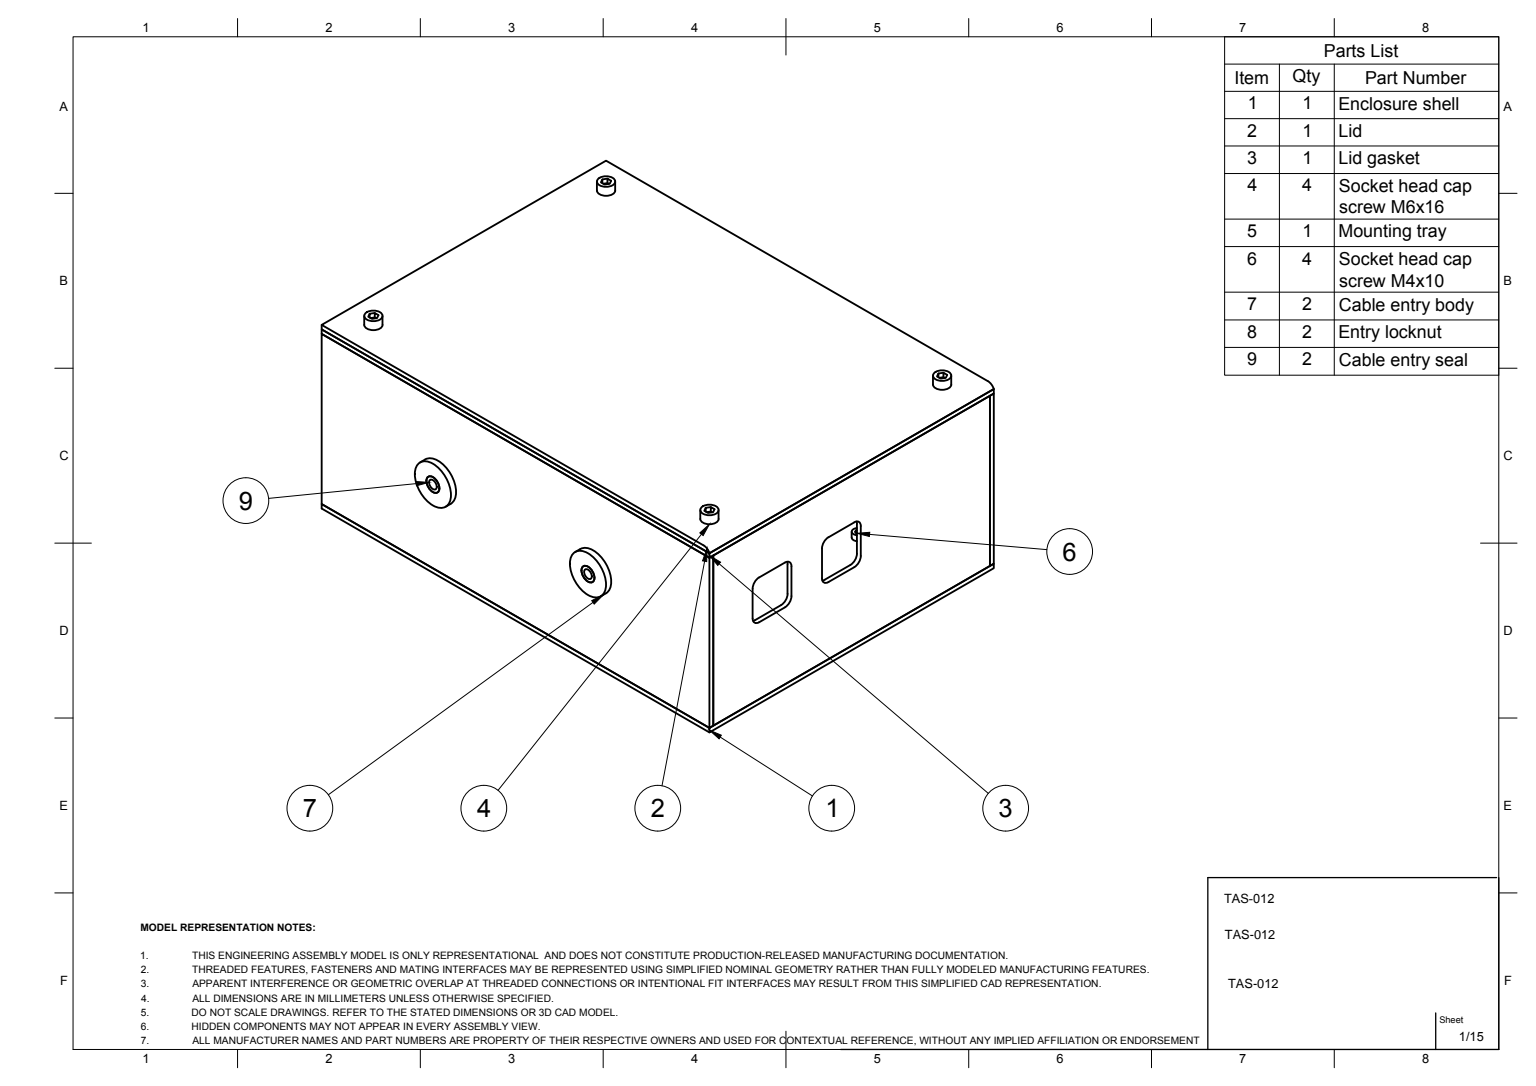
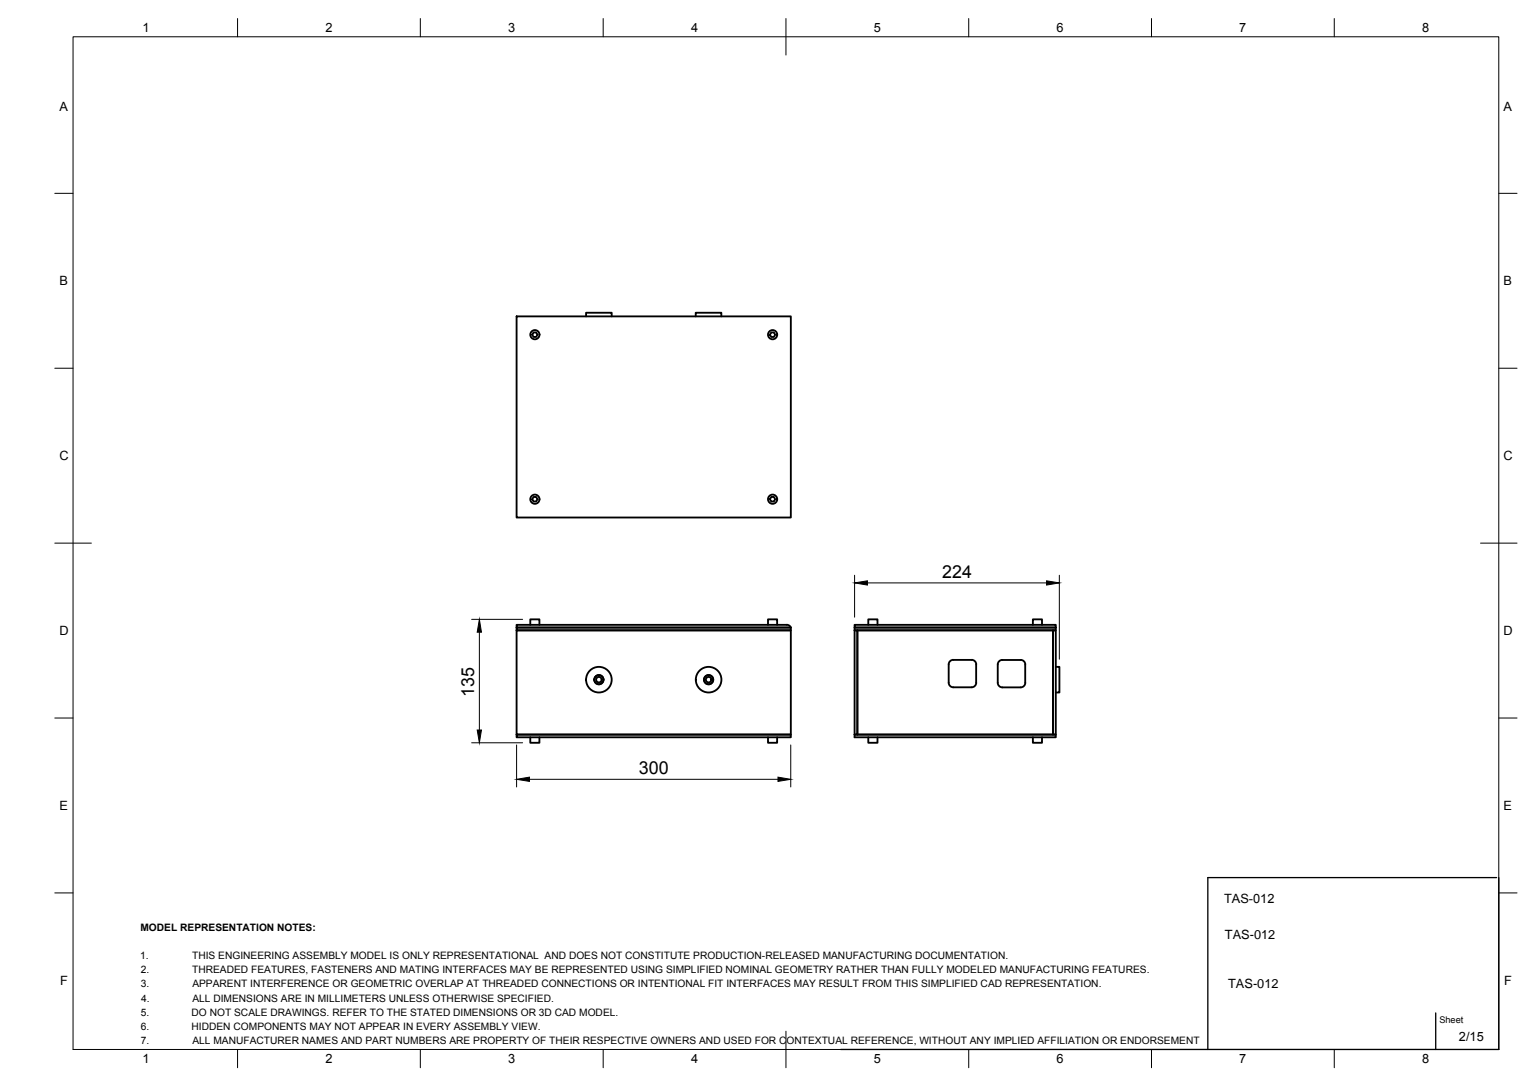
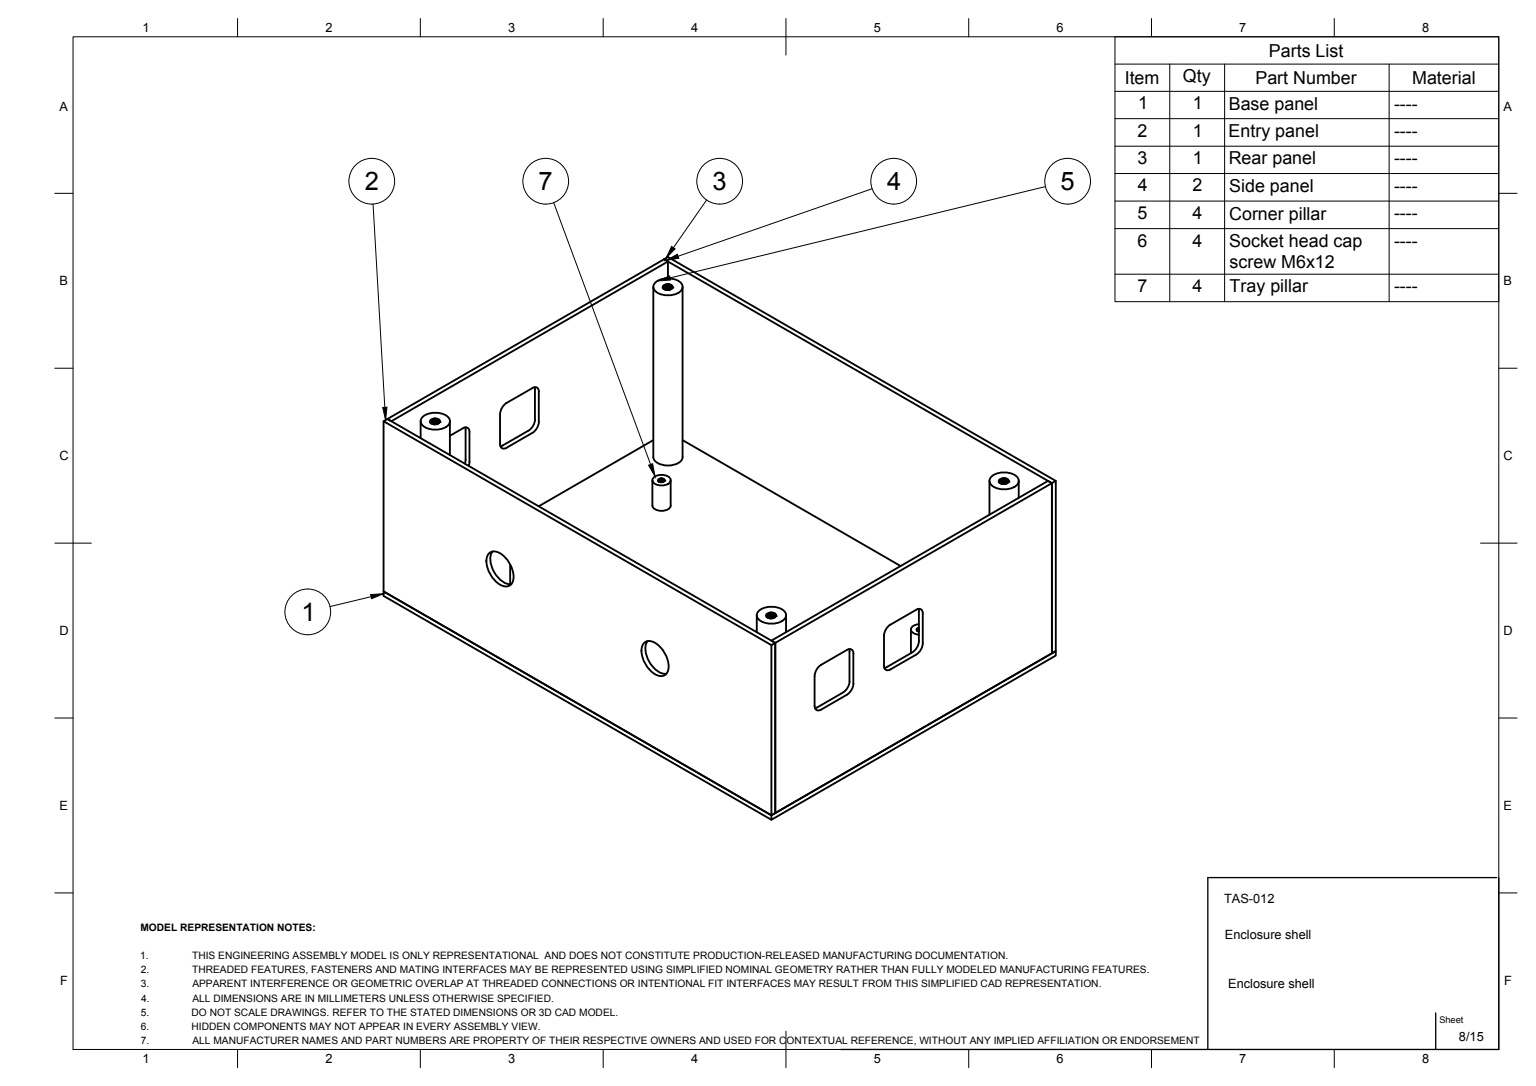
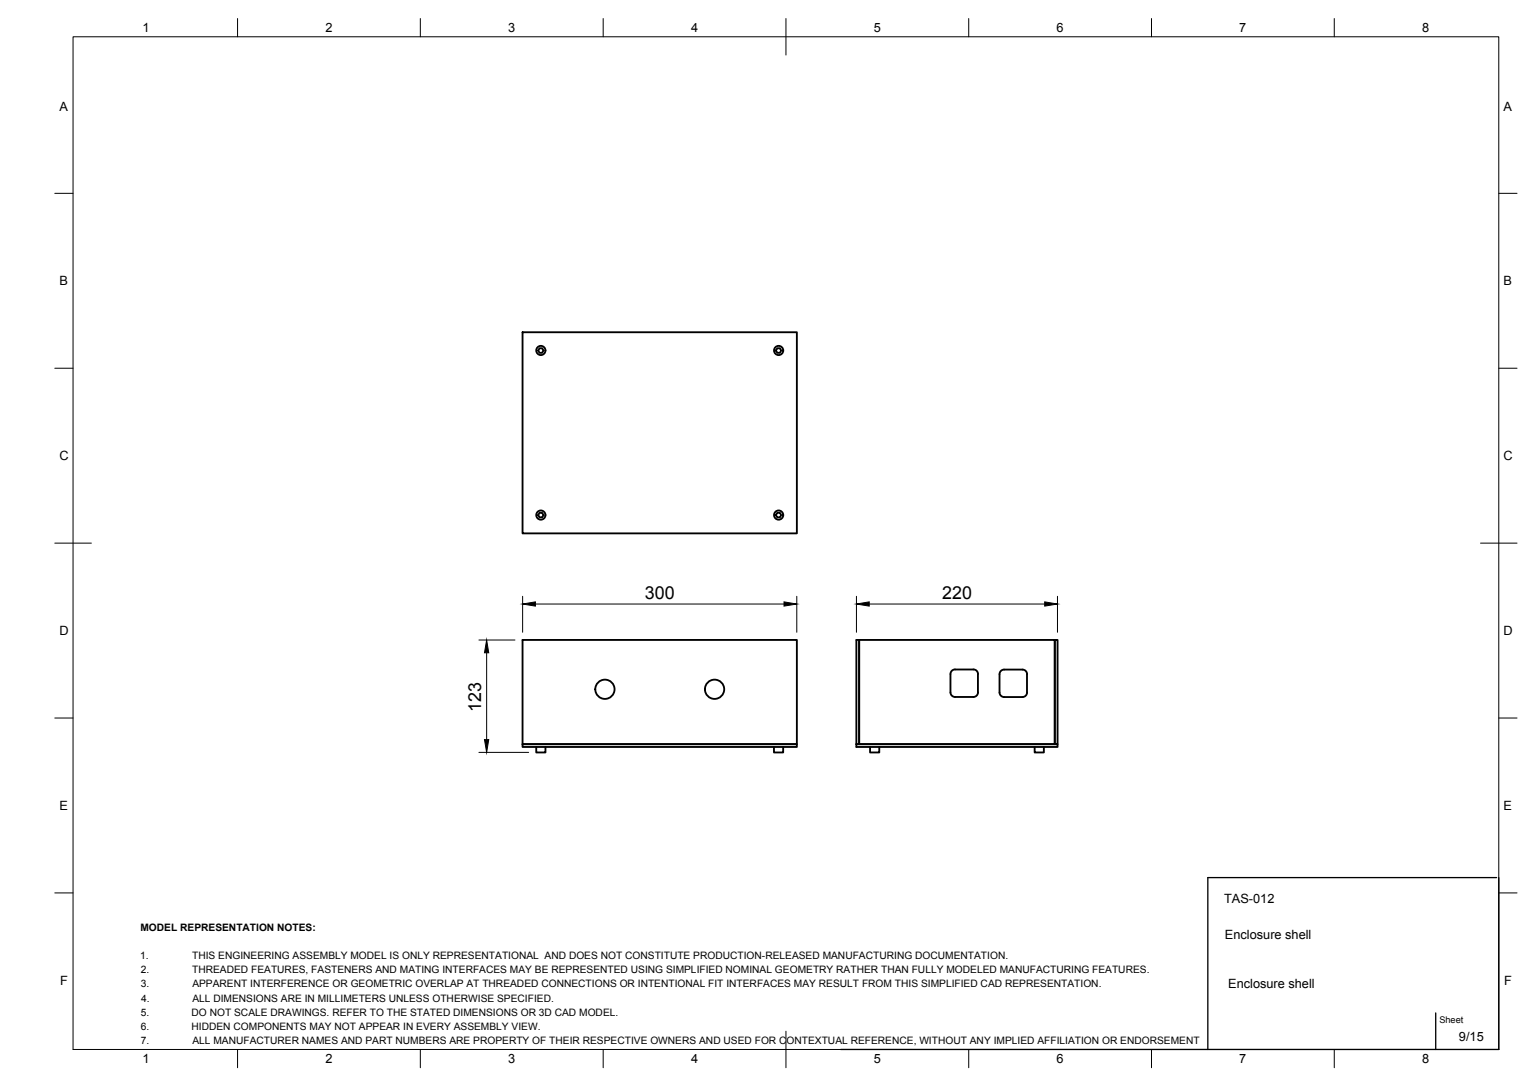
ISO-10303-21;
HEADER;
/* Generated by software containing ST-Developer
 * from STEP Tools, Inc. (www.steptools.com) 
 */

FILE_DESCRIPTION(
/* description */ (
'Independent welded steel electronics enclosure with removable sealed 
lid, internal mounting tray and two threaded cable entries. 300 x 220 
mm body. No ingress or electrical safety rating assigned.'),
/* implementation_level */ '2;1');

FILE_NAME(
/* name */ 'TAS-012.step',
/* time_stamp */ '2026-11-14T09:13:27-08:00',
/* author */ (''),
/* organization */ (''),
/* preprocessor_version */ 'ST-DEVELOPER v20.2',
/* originating_system */ 'Autodesk Translation Framework v15.17.0.0',
/* authorisation */ '');

FILE_SCHEMA (('AUTOMOTIVE_DESIGN { 1 0 10303 214 3 1 1 }'));
ENDSEC;

DATA;
#10=MECHANICAL_DESIGN_GEOMETRIC_PRESENTATION_REPRESENTATION('',(#966,#967,
#968,#969,#970,#971,#972,#973,#974,#975,#976,#977,#978,#979,#980),#94412);
#11=ITEM_DEFINED_TRANSFORMATION($,$,#8434,#8693);
#12=ITEM_DEFINED_TRANSFORMATION($,$,#8453,#8694);
#13=ITEM_DEFINED_TRANSFORMATION($,$,#8466,#8695);
#14=ITEM_DEFINED_TRANSFORMATION($,$,#8473,#8696);
#15=ITEM_DEFINED_TRANSFORMATION($,$,#8512,#8697);
#16=ITEM_DEFINED_TRANSFORMATION($,$,#8614,#8698);
#17=ITEM_DEFINED_TRANSFORMATION($,$,#8647,#8699);
#18=ITEM_DEFINED_TRANSFORMATION($,$,#8473,#8700);
#19=ITEM_DEFINED_TRANSFORMATION($,$,#8512,#8701);
#20=ITEM_DEFINED_TRANSFORMATION($,$,#8512,#8702);
#21=ITEM_DEFINED_TRANSFORMATION($,$,#8512,#8703);
#22=ITEM_DEFINED_TRANSFORMATION($,$,#8614,#8704);
#23=ITEM_DEFINED_TRANSFORMATION($,$,#8614,#8705);
#24=ITEM_DEFINED_TRANSFORMATION($,$,#8614,#8706);
#25=ITEM_DEFINED_TRANSFORMATION($,$,#8647,#8707);
#26=ITEM_DEFINED_TRANSFORMATION($,$,#8647,#8708);
#27=ITEM_DEFINED_TRANSFORMATION($,$,#8647,#8709);
#28=ITEM_DEFINED_TRANSFORMATION($,$,#8433,#8924);
#29=ITEM_DEFINED_TRANSFORMATION($,$,#8710,#8925);
#30=ITEM_DEFINED_TRANSFORMATION($,$,#8731,#8926);
#31=ITEM_DEFINED_TRANSFORMATION($,$,#8773,#8927);
#32=ITEM_DEFINED_TRANSFORMATION($,$,#8754,#8928);
#33=ITEM_DEFINED_TRANSFORMATION($,$,#8810,#8929);
#34=ITEM_DEFINED_TRANSFORMATION($,$,#8845,#8930);
#35=ITEM_DEFINED_TRANSFORMATION($,$,#8889,#8931);
#36=ITEM_DEFINED_TRANSFORMATION($,$,#8915,#8932);
#37=ITEM_DEFINED_TRANSFORMATION($,$,#8773,#8933);
#38=ITEM_DEFINED_TRANSFORMATION($,$,#8773,#8934);
#39=ITEM_DEFINED_TRANSFORMATION($,$,#8773,#8935);
#40=ITEM_DEFINED_TRANSFORMATION($,$,#8810,#8936);
#41=ITEM_DEFINED_TRANSFORMATION($,$,#8810,#8937);
#42=ITEM_DEFINED_TRANSFORMATION($,$,#8810,#8938);
#43=ITEM_DEFINED_TRANSFORMATION($,$,#8845,#8939);
#44=ITEM_DEFINED_TRANSFORMATION($,$,#8889,#8940);
#45=ITEM_DEFINED_TRANSFORMATION($,$,#8915,#8941);
#46=(
REPRESENTATION_RELATIONSHIP($,$,#94488,#94487)
REPRESENTATION_RELATIONSHIP_WITH_TRANSFORMATION(#11)
SHAPE_REPRESENTATION_RELATIONSHIP()
);
#47=(
REPRESENTATION_RELATIONSHIP($,$,#94489,#94487)
REPRESENTATION_RELATIONSHIP_WITH_TRANSFORMATION(#12)
SHAPE_REPRESENTATION_RELATIONSHIP()
);
#48=(
REPRESENTATION_RELATIONSHIP($,$,#94490,#94487)
REPRESENTATION_RELATIONSHIP_WITH_TRANSFORMATION(#13)
SHAPE_REPRESENTATION_RELATIONSHIP()
);
#49=(
REPRESENTATION_RELATIONSHIP($,$,#94491,#94487)
REPRESENTATION_RELATIONSHIP_WITH_TRANSFORMATION(#14)
SHAPE_REPRESENTATION_RELATIONSHIP()
);
#50=(
REPRESENTATION_RELATIONSHIP($,$,#94492,#94487)
REPRESENTATION_RELATIONSHIP_WITH_TRANSFORMATION(#15)
SHAPE_REPRESENTATION_RELATIONSHIP()
);
#51=(
REPRESENTATION_RELATIONSHIP($,$,#94493,#94487)
REPRESENTATION_RELATIONSHIP_WITH_TRANSFORMATION(#16)
SHAPE_REPRESENTATION_RELATIONSHIP()
);
#52=(
REPRESENTATION_RELATIONSHIP($,$,#94494,#94487)
REPRESENTATION_RELATIONSHIP_WITH_TRANSFORMATION(#17)
SHAPE_REPRESENTATION_RELATIONSHIP()
);
#53=(
REPRESENTATION_RELATIONSHIP($,$,#94491,#94487)
REPRESENTATION_RELATIONSHIP_WITH_TRANSFORMATION(#18)
SHAPE_REPRESENTATION_RELATIONSHIP()
);
#54=(
REPRESENTATION_RELATIONSHIP($,$,#94492,#94487)
REPRESENTATION_RELATIONSHIP_WITH_TRANSFORMATION(#19)
SHAPE_REPRESENTATION_RELATIONSHIP()
);
#55=(
REPRESENTATION_RELATIONSHIP($,$,#94492,#94487)
REPRESENTATION_RELATIONSHIP_WITH_TRANSFORMATION(#20)
SHAPE_REPRESENTATION_RELATIONSHIP()
);
#56=(
REPRESENTATION_RELATIONSHIP($,$,#94492,#94487)
REPRESENTATION_RELATIONSHIP_WITH_TRANSFORMATION(#21)
SHAPE_REPRESENTATION_RELATIONSHIP()
);
#57=(
REPRESENTATION_RELATIONSHIP($,$,#94493,#94487)
REPRESENTATION_RELATIONSHIP_WITH_TRANSFORMATION(#22)
SHAPE_REPRESENTATION_RELATIONSHIP()
);
#58=(
REPRESENTATION_RELATIONSHIP($,$,#94493,#94487)
REPRESENTATION_RELATIONSHIP_WITH_TRANSFORMATION(#23)
SHAPE_REPRESENTATION_RELATIONSHIP()
);
#59=(
REPRESENTATION_RELATIONSHIP($,$,#94493,#94487)
REPRESENTATION_RELATIONSHIP_WITH_TRANSFORMATION(#24)
SHAPE_REPRESENTATION_RELATIONSHIP()
);
#60=(
REPRESENTATION_RELATIONSHIP($,$,#94494,#94487)
REPRESENTATION_RELATIONSHIP_WITH_TRANSFORMATION(#25)
SHAPE_REPRESENTATION_RELATIONSHIP()
);
#61=(
REPRESENTATION_RELATIONSHIP($,$,#94494,#94487)
REPRESENTATION_RELATIONSHIP_WITH_TRANSFORMATION(#26)
SHAPE_REPRESENTATION_RELATIONSHIP()
);
#62=(
REPRESENTATION_RELATIONSHIP($,$,#94494,#94487)
REPRESENTATION_RELATIONSHIP_WITH_TRANSFORMATION(#27)
SHAPE_REPRESENTATION_RELATIONSHIP()
);
#63=(
REPRESENTATION_RELATIONSHIP($,$,#94487,#94486)
REPRESENTATION_RELATIONSHIP_WITH_TRANSFORMATION(#28)
SHAPE_REPRESENTATION_RELATIONSHIP()
);
#64=(
REPRESENTATION_RELATIONSHIP($,$,#94495,#94486)
REPRESENTATION_RELATIONSHIP_WITH_TRANSFORMATION(#29)
SHAPE_REPRESENTATION_RELATIONSHIP()
);
#65=(
REPRESENTATION_RELATIONSHIP($,$,#94496,#94486)
REPRESENTATION_RELATIONSHIP_WITH_TRANSFORMATION(#30)
SHAPE_REPRESENTATION_RELATIONSHIP()
);
#66=(
REPRESENTATION_RELATIONSHIP($,$,#94498,#94486)
REPRESENTATION_RELATIONSHIP_WITH_TRANSFORMATION(#31)
SHAPE_REPRESENTATION_RELATIONSHIP()
);
#67=(
REPRESENTATION_RELATIONSHIP($,$,#94497,#94486)
REPRESENTATION_RELATIONSHIP_WITH_TRANSFORMATION(#32)
SHAPE_REPRESENTATION_RELATIONSHIP()
);
#68=(
REPRESENTATION_RELATIONSHIP($,$,#94499,#94486)
REPRESENTATION_RELATIONSHIP_WITH_TRANSFORMATION(#33)
SHAPE_REPRESENTATION_RELATIONSHIP()
);
#69=(
REPRESENTATION_RELATIONSHIP($,$,#94500,#94486)
REPRESENTATION_RELATIONSHIP_WITH_TRANSFORMATION(#34)
SHAPE_REPRESENTATION_RELATIONSHIP()
);
#70=(
REPRESENTATION_RELATIONSHIP($,$,#94501,#94486)
REPRESENTATION_RELATIONSHIP_WITH_TRANSFORMATION(#35)
SHAPE_REPRESENTATION_RELATIONSHIP()
);
#71=(
REPRESENTATION_RELATIONSHIP($,$,#94502,#94486)
REPRESENTATION_RELATIONSHIP_WITH_TRANSFORMATION(#36)
SHAPE_REPRESENTATION_RELATIONSHIP()
);
#72=(
REPRESENTATION_RELATIONSHIP($,$,#94498,#94486)
REPRESENTATION_RELATIONSHIP_WITH_TRANSFORMATION(#37)
SHAPE_REPRESENTATION_RELATIONSHIP()
);
#73=(
REPRESENTATION_RELATIONSHIP($,$,#94498,#94486)
REPRESENTATION_RELATIONSHIP_WITH_TRANSFORMATION(#38)
SHAPE_REPRESENTATION_RELATIONSHIP()
);
#74=(
REPRESENTATION_RELATIONSHIP($,$,#94498,#94486)
REPRESENTATION_RELATIONSHIP_WITH_TRANSFORMATION(#39)
SHAPE_REPRESENTATION_RELATIONSHIP()
);
#75=(
REPRESENTATION_RELATIONSHIP($,$,#94499,#94486)
REPRESENTATION_RELATIONSHIP_WITH_TRANSFORMATION(#40)
SHAPE_REPRESENTATION_RELATIONSHIP()
);
#76=(
REPRESENTATION_RELATIONSHIP($,$,#94499,#94486)
REPRESENTATION_RELATIONSHIP_WITH_TRANSFORMATION(#41)
SHAPE_REPRESENTATION_RELATIONSHIP()
);
#77=(
REPRESENTATION_RELATIONSHIP($,$,#94499,#94486)
REPRESENTATION_RELATIONSHIP_WITH_TRANSFORMATION(#42)
SHAPE_REPRESENTATION_RELATIONSHIP()
);
#78=(
REPRESENTATION_RELATIONSHIP($,$,#94500,#94486)
REPRESENTATION_RELATIONSHIP_WITH_TRANSFORMATION(#43)
SHAPE_REPRESENTATION_RELATIONSHIP()
);
#79=(
REPRESENTATION_RELATIONSHIP($,$,#94501,#94486)
REPRESENTATION_RELATIONSHIP_WITH_TRANSFORMATION(#44)
SHAPE_REPRESENTATION_RELATIONSHIP()
);
#80=(
REPRESENTATION_RELATIONSHIP($,$,#94502,#94486)
REPRESENTATION_RELATIONSHIP_WITH_TRANSFORMATION(#45)
SHAPE_REPRESENTATION_RELATIONSHIP()
);
#81=CONTEXT_DEPENDENT_SHAPE_REPRESENTATION(#46,#94443);
#82=CONTEXT_DEPENDENT_SHAPE_REPRESENTATION(#47,#94444);
#83=CONTEXT_DEPENDENT_SHAPE_REPRESENTATION(#48,#94445);
#84=CONTEXT_DEPENDENT_SHAPE_REPRESENTATION(#49,#94446);
#85=CONTEXT_DEPENDENT_SHAPE_REPRESENTATION(#50,#94447);
#86=CONTEXT_DEPENDENT_SHAPE_REPRESENTATION(#51,#94448);
#87=CONTEXT_DEPENDENT_SHAPE_REPRESENTATION(#52,#94449);
#88=CONTEXT_DEPENDENT_SHAPE_REPRESENTATION(#53,#94450);
#89=CONTEXT_DEPENDENT_SHAPE_REPRESENTATION(#54,#94451);
#90=CONTEXT_DEPENDENT_SHAPE_REPRESENTATION(#55,#94452);
#91=CONTEXT_DEPENDENT_SHAPE_REPRESENTATION(#56,#94453);
#92=CONTEXT_DEPENDENT_SHAPE_REPRESENTATION(#57,#94454);
#93=CONTEXT_DEPENDENT_SHAPE_REPRESENTATION(#58,#94455);
#94=CONTEXT_DEPENDENT_SHAPE_REPRESENTATION(#59,#94456);
#95=CONTEXT_DEPENDENT_SHAPE_REPRESENTATION(#60,#94457);
#96=CONTEXT_DEPENDENT_SHAPE_REPRESENTATION(#61,#94458);
#97=CONTEXT_DEPENDENT_SHAPE_REPRESENTATION(#62,#94459);
#98=CONTEXT_DEPENDENT_SHAPE_REPRESENTATION(#63,#94468);
#99=CONTEXT_DEPENDENT_SHAPE_REPRESENTATION(#64,#94469);
#100=CONTEXT_DEPENDENT_SHAPE_REPRESENTATION(#65,#94470);
#101=CONTEXT_DEPENDENT_SHAPE_REPRESENTATION(#66,#94471);
#102=CONTEXT_DEPENDENT_SHAPE_REPRESENTATION(#67,#94472);
#103=CONTEXT_DEPENDENT_SHAPE_REPRESENTATION(#68,#94473);
#104=CONTEXT_DEPENDENT_SHAPE_REPRESENTATION(#69,#94474);
#105=CONTEXT_DEPENDENT_SHAPE_REPRESENTATION(#70,#94475);
#106=CONTEXT_DEPENDENT_SHAPE_REPRESENTATION(#71,#94476);
#107=CONTEXT_DEPENDENT_SHAPE_REPRESENTATION(#72,#94477);
#108=CONTEXT_DEPENDENT_SHAPE_REPRESENTATION(#73,#94478);
#109=CONTEXT_DEPENDENT_SHAPE_REPRESENTATION(#74,#94479);
#110=CONTEXT_DEPENDENT_SHAPE_REPRESENTATION(#75,#94480);
#111=CONTEXT_DEPENDENT_SHAPE_REPRESENTATION(#76,#94481);
#112=CONTEXT_DEPENDENT_SHAPE_REPRESENTATION(#77,#94482);
#113=CONTEXT_DEPENDENT_SHAPE_REPRESENTATION(#78,#94483);
#114=CONTEXT_DEPENDENT_SHAPE_REPRESENTATION(#79,#94484);
#115=CONTEXT_DEPENDENT_SHAPE_REPRESENTATION(#80,#94485);
#116=NEXT_ASSEMBLY_USAGE_OCCURRENCE('Base panel:1','Base panel:1',
'Base panel:1',#94505,#94506,'Base panel:1');
#117=NEXT_ASSEMBLY_USAGE_OCCURRENCE('Entry panel:1','Entry panel:1',
'Entry panel:1',#94505,#94507,'Entry panel:1');
#118=NEXT_ASSEMBLY_USAGE_OCCURRENCE('Rear panel:1','Rear panel:1',
'Rear panel:1',#94505,#94508,'Rear panel:1');
#119=NEXT_ASSEMBLY_USAGE_OCCURRENCE('Side panel:1','Side panel:1',
'Side panel:1',#94505,#94509,'Side panel:1');
#120=NEXT_ASSEMBLY_USAGE_OCCURRENCE('Corner pillar:1','Corner pillar:1',
'Corner pillar:1',#94505,#94510,'Corner pillar:1');
#121=NEXT_ASSEMBLY_USAGE_OCCURRENCE('Socket head cap screw M6x12:1',
'Socket head cap screw M6x12:1','Socket head cap screw M6x12:1',#94505,
#94511,'Socket head cap screw M6x12:1');
#122=NEXT_ASSEMBLY_USAGE_OCCURRENCE('Tray pillar:1','Tray pillar:1',
'Tray pillar:1',#94505,#94512,'Tray pillar:1');
#123=NEXT_ASSEMBLY_USAGE_OCCURRENCE('Side panel:2','Side panel:2',
'Side panel:2',#94505,#94509,'Side panel:2');
#124=NEXT_ASSEMBLY_USAGE_OCCURRENCE('Corner pillar:2','Corner pillar:2',
'Corner pillar:2',#94505,#94510,'Corner pillar:2');
#125=NEXT_ASSEMBLY_USAGE_OCCURRENCE('Corner pillar:3','Corner pillar:3',
'Corner pillar:3',#94505,#94510,'Corner pillar:3');
#126=NEXT_ASSEMBLY_USAGE_OCCURRENCE('Corner pillar:4','Corner pillar:4',
'Corner pillar:4',#94505,#94510,'Corner pillar:4');
#127=NEXT_ASSEMBLY_USAGE_OCCURRENCE('Socket head cap screw M6x12:2',
'Socket head cap screw M6x12:2','Socket head cap screw M6x12:2',#94505,
#94511,'Socket head cap screw M6x12:2');
#128=NEXT_ASSEMBLY_USAGE_OCCURRENCE('Socket head cap screw M6x12:3',
'Socket head cap screw M6x12:3','Socket head cap screw M6x12:3',#94505,
#94511,'Socket head cap screw M6x12:3');
#129=NEXT_ASSEMBLY_USAGE_OCCURRENCE('Socket head cap screw M6x12:4',
'Socket head cap screw M6x12:4','Socket head cap screw M6x12:4',#94505,
#94511,'Socket head cap screw M6x12:4');
#130=NEXT_ASSEMBLY_USAGE_OCCURRENCE('Tray pillar:2','Tray pillar:2',
'Tray pillar:2',#94505,#94512,'Tray pillar:2');
#131=NEXT_ASSEMBLY_USAGE_OCCURRENCE('Tray pillar:3','Tray pillar:3',
'Tray pillar:3',#94505,#94512,'Tray pillar:3');
#132=NEXT_ASSEMBLY_USAGE_OCCURRENCE('Tray pillar:4','Tray pillar:4',
'Tray pillar:4',#94505,#94512,'Tray pillar:4');
#133=NEXT_ASSEMBLY_USAGE_OCCURRENCE('Enclosure shell:1',
'Enclosure shell:1','Enclosure shell:1',#94504,#94505,
'Enclosure shell:1');
#134=NEXT_ASSEMBLY_USAGE_OCCURRENCE('Lid:1','Lid:1','Lid:1',#94504,#94513,
'Lid:1');
#135=NEXT_ASSEMBLY_USAGE_OCCURRENCE('Lid gasket:1','Lid gasket:1',
'Lid gasket:1',#94504,#94514,'Lid gasket:1');
#136=NEXT_ASSEMBLY_USAGE_OCCURRENCE('Socket head cap screw M6x16:1',
'Socket head cap screw M6x16:1','Socket head cap screw M6x16:1',#94504,
#94516,'Socket head cap screw M6x16:1');
#137=NEXT_ASSEMBLY_USAGE_OCCURRENCE('Mounting tray:1','Mounting tray:1',
'Mounting tray:1',#94504,#94515,'Mounting tray:1');
#138=NEXT_ASSEMBLY_USAGE_OCCURRENCE('Socket head cap screw M4x10:1',
'Socket head cap screw M4x10:1','Socket head cap screw M4x10:1',#94504,
#94517,'Socket head cap screw M4x10:1');
#139=NEXT_ASSEMBLY_USAGE_OCCURRENCE('Cable entry body:1',
'Cable entry body:1','Cable entry body:1',#94504,#94518,
'Cable entry body:1');
#140=NEXT_ASSEMBLY_USAGE_OCCURRENCE('Entry locknut:1','Entry locknut:1',
'Entry locknut:1',#94504,#94519,'Entry locknut:1');
#141=NEXT_ASSEMBLY_USAGE_OCCURRENCE('Cable entry seal:1',
'Cable entry seal:1','Cable entry seal:1',#94504,#94520,
'Cable entry seal:1');
#142=NEXT_ASSEMBLY_USAGE_OCCURRENCE('Socket head cap screw M6x16:2',
'Socket head cap screw M6x16:2','Socket head cap screw M6x16:2',#94504,
#94516,'Socket head cap screw M6x16:2');
#143=NEXT_ASSEMBLY_USAGE_OCCURRENCE('Socket head cap screw M6x16:3',
'Socket head cap screw M6x16:3','Socket head cap screw M6x16:3',#94504,
#94516,'Socket head cap screw M6x16:3');
#144=NEXT_ASSEMBLY_USAGE_OCCURRENCE('Socket head cap screw M6x16:4',
'Socket head cap screw M6x16:4','Socket head cap screw M6x16:4',#94504,
#94516,'Socket head cap screw M6x16:4');
#145=NEXT_ASSEMBLY_USAGE_OCCURRENCE('Socket head cap screw M4x10:2',
'Socket head cap screw M4x10:2','Socket head cap screw M4x10:2',#94504,
#94517,'Socket head cap screw M4x10:2');
#146=NEXT_ASSEMBLY_USAGE_OCCURRENCE('Socket head cap screw M4x10:3',
'Socket head cap screw M4x10:3','Socket head cap screw M4x10:3',#94504,
#94517,'Socket head cap screw M4x10:3');
#147=NEXT_ASSEMBLY_USAGE_OCCURRENCE('Socket head cap screw M4x10:4',
'Socket head cap screw M4x10:4','Socket head cap screw M4x10:4',#94504,
#94517,'Socket head cap screw M4x10:4');
#148=NEXT_ASSEMBLY_USAGE_OCCURRENCE('Cable entry body:2',
'Cable entry body:2','Cable entry body:2',#94504,#94518,
'Cable entry body:2');
#149=NEXT_ASSEMBLY_USAGE_OCCURRENCE('Entry locknut:2','Entry locknut:2',
'Entry locknut:2',#94504,#94519,'Entry locknut:2');
#150=NEXT_ASSEMBLY_USAGE_OCCURRENCE('Cable entry seal:2',
'Cable entry seal:2','Cable entry seal:2',#94504,#94520,
'Cable entry seal:2');
#151=CONICAL_SURFACE('',#8632,2.5,0.785398163397449);
#152=CONICAL_SURFACE('',#8795,2.5,0.785398163397448);
#153=CONICAL_SURFACE('',#8830,1.5,0.785398163397449);
#154=B_SPLINE_SURFACE_WITH_KNOTS('',3,3,((#38427,#38428,#38429,#38430,#38431,
#38432,#38433,#38434,#38435,#38436,#38437,#38438,#38439,#38440,#38441,#38442,
#38443,#38444,#38445,#38446,#38447,#38448,#38449,#38450,#38451,#38452,#38453,
#38454,#38455,#38456,#38457,#38458,#38459,#38460,#38461,#38462,#38463,#38464,
#38465,#38466,#38467,#38468,#38469,#38470,#38471,#38472,#38473,#38474,#38475,
#38476,#38477,#38478,#38479,#38480,#38481,#38482,#38483,#38484,#38485,#38486,
#38487,#38488,#38489,#38490,#38491,#38492,#38493,#38494,#38495,#38496,#38497,
#38498,#38499,#38500,#38501,#38502,#38503,#38504,#38505,#38506,#38507,#38508,
#38509,#38510,#38511,#38512,#38513,#38514,#38515,#38516,#38517,#38518,#38519,
#38520,#38521,#38522,#38523,#38524,#38525,#38526,#38527,#38528,#38529,#38530,
#38531,#38532,#38533,#38534,#38535,#38536,#38537,#38538,#38539,#38540,#38541,
#38542,#38543,#38544,#38545,#38546,#38547,#38548,#38549,#38550,#38551),
(#38552,#38553,#38554,#38555,#38556,#38557,#38558,#38559,#38560,#38561,
#38562,#38563,#38564,#38565,#38566,#38567,#38568,#38569,#38570,#38571,#38572,
#38573,#38574,#38575,#38576,#38577,#38578,#38579,#38580,#38581,#38582,#38583,
#38584,#38585,#38586,#38587,#38588,#38589,#38590,#38591,#38592,#38593,#38594,
#38595,#38596,#38597,#38598,#38599,#38600,#38601,#38602,#38603,#38604,#38605,
#38606,#38607,#38608,#38609,#38610,#38611,#38612,#38613,#38614,#38615,#38616,
#38617,#38618,#38619,#38620,#38621,#38622,#38623,#38624,#38625,#38626,#38627,
#38628,#38629,#38630,#38631,#38632,#38633,#38634,#38635,#38636,#38637,#38638,
#38639,#38640,#38641,#38642,#38643,#38644,#38645,#38646,#38647,#38648,#38649,
#38650,#38651,#38652,#38653,#38654,#38655,#38656,#38657,#38658,#38659,#38660,
#38661,#38662,#38663,#38664,#38665,#38666,#38667,#38668,#38669,#38670,#38671,
#38672,#38673,#38674,#38675,#38676),(#38677,#38678,#38679,#38680,#38681,
#38682,#38683,#38684,#38685,#38686,#38687,#38688,#38689,#38690,#38691,#38692,
#38693,#38694,#38695,#38696,#38697,#38698,#38699,#38700,#38701,#38702,#38703,
#38704,#38705,#38706,#38707,#38708,#38709,#38710,#38711,#38712,#38713,#38714,
#38715,#38716,#38717,#38718,#38719,#38720,#38721,#38722,#38723,#38724,#38725,
#38726,#38727,#38728,#38729,#38730,#38731,#38732,#38733,#38734,#38735,#38736,
#38737,#38738,#38739,#38740,#38741,#38742,#38743,#38744,#38745,#38746,#38747,
#38748,#38749,#38750,#38751,#38752,#38753,#38754,#38755,#38756,#38757,#38758,
#38759,#38760,#38761,#38762,#38763,#38764,#38765,#38766,#38767,#38768,#38769,
#38770,#38771,#38772,#38773,#38774,#38775,#38776,#38777,#38778,#38779,#38780,
#38781,#38782,#38783,#38784,#38785,#38786,#38787,#38788,#38789,#38790,#38791,
#38792,#38793,#38794,#38795,#38796,#38797,#38798,#38799,#38800,#38801),
(#38802,#38803,#38804,#38805,#38806,#38807,#38808,#38809,#38810,#38811,
#38812,#38813,#38814,#38815,#38816,#38817,#38818,#38819,#38820,#38821,#38822,
#38823,#38824,#38825,#38826,#38827,#38828,#38829,#38830,#38831,#38832,#38833,
#38834,#38835,#38836,#38837,#38838,#38839,#38840,#38841,#38842,#38843,#38844,
#38845,#38846,#38847,#38848,#38849,#38850,#38851,#38852,#38853,#38854,#38855,
#38856,#38857,#38858,#38859,#38860,#38861,#38862,#38863,#38864,#38865,#38866,
#38867,#38868,#38869,#38870,#38871,#38872,#38873,#38874,#38875,#38876,#38877,
#38878,#38879,#38880,#38881,#38882,#38883,#38884,#38885,#38886,#38887,#38888,
#38889,#38890,#38891,#38892,#38893,#38894,#38895,#38896,#38897,#38898,#38899,
#38900,#38901,#38902,#38903,#38904,#38905,#38906,#38907,#38908,#38909,#38910,
#38911,#38912,#38913,#38914,#38915,#38916,#38917,#38918,#38919,#38920,#38921,
#38922,#38923,#38924,#38925,#38926)),.UNSPECIFIED.,.F.,.F.,.F.,(4,4),(4,
1,1,1,1,1,1,1,1,1,1,1,1,1,1,1,1,1,1,1,1,1,1,1,1,1,1,1,1,1,1,1,1,1,1,1,1,
1,1,1,1,1,1,1,1,1,1,1,1,1,1,1,1,1,1,1,1,1,1,1,1,1,1,1,1,1,1,1,1,1,1,1,1,
1,1,1,1,1,1,1,1,1,1,1,1,1,1,1,1,1,1,1,1,1,1,1,1,1,1,1,1,1,1,1,1,1,1,1,1,
1,1,1,1,1,1,1,1,1,1,1,1,1,4),(-0.000512721802289974,0.0646569623865103),
(11.8584761405054,12.8540500568113,13.849111251315,14.8441724458186,15.8392336403222,
16.8342948348258,17.8293560293294,18.824417223833,19.8194784183366,20.8145396128402,
21.8096008073438,22.8046620018475,23.7997231963511,24.7947843908547,25.7898455853583,
26.7849067798619,27.7799679743655,28.7750291688691,29.7700903633727,30.7651515578764,
31.76021275238,32.7552739468836,33.7503351413872,34.7453963358908,35.7404575303944,
36.735518724898,37.7305799194016,38.7256411139052,39.7207023084089,40.7157635029125,
41.7108246974161,42.7058858919197,43.7009470864233,44.6960082809269,45.6910694754305,
46.6861306699341,47.6811918644377,48.6762530589414,49.671314253445,50.6663754479486,
51.6614366424522,52.6564978369558,53.6515590314594,54.646620225963,55.6416814204666,
56.6367426149702,57.6318038094739,58.6268650039775,59.6219261984811,60.6169873929847,
61.6120485874883,62.6071097819919,63.6021709764955,64.5972321709991,65.5922933655027,
66.5873545600064,67.58241575451,68.5774769490136,69.5725381435172,70.5675993380208,
71.5626605325244,72.557721727028,73.5527829215316,74.5478441160353,75.5429053105389,
76.5379665050425,77.5330276995461,78.5280888940497,79.5231500885533,80.5182112830569,
81.5132724775605,82.5083336720641,83.5033948665678,84.4984560610714,85.493517255575,
86.4885784500786,87.4836396445822,88.4787008390858,89.4737620335894,90.468823228093,
91.4638844225966,92.4589456171003,93.4540068116039,94.4490680061075,95.4441292006111,
96.4391903951147,97.4342515896183,98.4293127841219,99.4243739786255,100.419435173129,
101.414496367633,102.409557562136,103.40461875664,104.399679951144,105.394741145647,
106.389802340151,107.384863534654,108.379924729158,109.374985923662,110.370047118165,
111.365108312669,112.360169507172,113.355230701676,114.35029189618,115.345353090683,
116.340414285187,117.335475479691,118.330536674194,119.325597868698,120.320659063201,
121.315720257705,122.310781452209,123.305842646712,124.300903841216,125.295965035719,
126.291026230223,127.286087424727,128.28114861923,129.276209813734,130.271271008237,
131.266332202741,132.261393397245,133.256910204201),.UNSPECIFIED.);
#155=B_SPLINE_SURFACE_WITH_KNOTS('',3,3,((#39015,#39016,#39017,#39018,#39019,
#39020,#39021,#39022,#39023,#39024,#39025,#39026,#39027,#39028,#39029,#39030,
#39031,#39032,#39033,#39034,#39035,#39036,#39037,#39038,#39039,#39040,#39041,
#39042,#39043,#39044,#39045,#39046,#39047,#39048,#39049,#39050,#39051,#39052,
#39053,#39054,#39055,#39056,#39057,#39058,#39059,#39060,#39061,#39062,#39063,
#39064,#39065,#39066,#39067,#39068,#39069,#39070,#39071,#39072,#39073,#39074,
#39075,#39076,#39077,#39078,#39079,#39080,#39081,#39082,#39083,#39084,#39085,
#39086,#39087,#39088,#39089,#39090,#39091,#39092,#39093,#39094,#39095,#39096,
#39097,#39098,#39099,#39100,#39101,#39102,#39103,#39104,#39105,#39106,#39107,
#39108,#39109,#39110,#39111,#39112,#39113,#39114,#39115,#39116,#39117,#39118,
#39119,#39120,#39121,#39122,#39123,#39124,#39125,#39126,#39127,#39128,#39129,
#39130,#39131,#39132,#39133,#39134,#39135,#39136,#39137,#39138,#39139),
(#39140,#39141,#39142,#39143,#39144,#39145,#39146,#39147,#39148,#39149,
#39150,#39151,#39152,#39153,#39154,#39155,#39156,#39157,#39158,#39159,#39160,
#39161,#39162,#39163,#39164,#39165,#39166,#39167,#39168,#39169,#39170,#39171,
#39172,#39173,#39174,#39175,#39176,#39177,#39178,#39179,#39180,#39181,#39182,
#39183,#39184,#39185,#39186,#39187,#39188,#39189,#39190,#39191,#39192,#39193,
#39194,#39195,#39196,#39197,#39198,#39199,#39200,#39201,#39202,#39203,#39204,
#39205,#39206,#39207,#39208,#39209,#39210,#39211,#39212,#39213,#39214,#39215,
#39216,#39217,#39218,#39219,#39220,#39221,#39222,#39223,#39224,#39225,#39226,
#39227,#39228,#39229,#39230,#39231,#39232,#39233,#39234,#39235,#39236,#39237,
#39238,#39239,#39240,#39241,#39242,#39243,#39244,#39245,#39246,#39247,#39248,
#39249,#39250,#39251,#39252,#39253,#39254,#39255,#39256,#39257,#39258,#39259,
#39260,#39261,#39262,#39263,#39264),(#39265,#39266,#39267,#39268,#39269,
#39270,#39271,#39272,#39273,#39274,#39275,#39276,#39277,#39278,#39279,#39280,
#39281,#39282,#39283,#39284,#39285,#39286,#39287,#39288,#39289,#39290,#39291,
#39292,#39293,#39294,#39295,#39296,#39297,#39298,#39299,#39300,#39301,#39302,
#39303,#39304,#39305,#39306,#39307,#39308,#39309,#39310,#39311,#39312,#39313,
#39314,#39315,#39316,#39317,#39318,#39319,#39320,#39321,#39322,#39323,#39324,
#39325,#39326,#39327,#39328,#39329,#39330,#39331,#39332,#39333,#39334,#39335,
#39336,#39337,#39338,#39339,#39340,#39341,#39342,#39343,#39344,#39345,#39346,
#39347,#39348,#39349,#39350,#39351,#39352,#39353,#39354,#39355,#39356,#39357,
#39358,#39359,#39360,#39361,#39362,#39363,#39364,#39365,#39366,#39367,#39368,
#39369,#39370,#39371,#39372,#39373,#39374,#39375,#39376,#39377,#39378,#39379,
#39380,#39381,#39382,#39383,#39384,#39385,#39386,#39387,#39388,#39389),
(#39390,#39391,#39392,#39393,#39394,#39395,#39396,#39397,#39398,#39399,
#39400,#39401,#39402,#39403,#39404,#39405,#39406,#39407,#39408,#39409,#39410,
#39411,#39412,#39413,#39414,#39415,#39416,#39417,#39418,#39419,#39420,#39421,
#39422,#39423,#39424,#39425,#39426,#39427,#39428,#39429,#39430,#39431,#39432,
#39433,#39434,#39435,#39436,#39437,#39438,#39439,#39440,#39441,#39442,#39443,
#39444,#39445,#39446,#39447,#39448,#39449,#39450,#39451,#39452,#39453,#39454,
#39455,#39456,#39457,#39458,#39459,#39460,#39461,#39462,#39463,#39464,#39465,
#39466,#39467,#39468,#39469,#39470,#39471,#39472,#39473,#39474,#39475,#39476,
#39477,#39478,#39479,#39480,#39481,#39482,#39483,#39484,#39485,#39486,#39487,
#39488,#39489,#39490,#39491,#39492,#39493,#39494,#39495,#39496,#39497,#39498,
#39499,#39500,#39501,#39502,#39503,#39504,#39505,#39506,#39507,#39508,#39509,
#39510,#39511,#39512,#39513,#39514)),.UNSPECIFIED.,.F.,.F.,.F.,(4,4),(4,
1,1,1,1,1,1,1,1,1,1,1,1,1,1,1,1,1,1,1,1,1,1,1,1,1,1,1,1,1,1,1,1,1,1,1,1,
1,1,1,1,1,1,1,1,1,1,1,1,1,1,1,1,1,1,1,1,1,1,1,1,1,1,1,1,1,1,1,1,1,1,1,1,
1,1,1,1,1,1,1,1,1,1,1,1,1,1,1,1,1,1,1,1,1,1,1,1,1,1,1,1,1,1,1,1,1,1,1,1,
1,1,1,1,1,1,1,1,1,1,1,1,1,4),(-0.000455618124563469,0.0646112265793122),
(14.3984001269718,15.3934613214754,16.388522515979,17.3835837104826,18.3786449049862,
19.3737060994898,20.3687672939934,21.3638284884971,22.3588896830007,23.3539508775043,
24.3490120720079,25.3440732665115,26.3391344610151,27.3341956555187,28.3292568500223,
29.3243180445259,30.3193792390296,31.3144404335332,32.3095016280368,33.3045628225404,
34.299624017044,35.2946852115476,36.2897464060512,37.2848076005548,38.2798687950584,
39.2749299895621,40.2699911840657,41.2650523785693,42.2601135730729,43.2551747675765,
44.2502359620801,45.2452971565837,46.2403583510873,47.235419545591,48.2304807400946,
49.2255419345982,50.2206031291018,51.2156643236054,52.210725518109,53.2057867126126,
54.2008479071162,55.1959091016198,56.1909702961235,57.1860314906271,58.1810926851307,
59.1761538796343,60.1712150741379,61.1662762686415,62.1613374631451,63.1563986576487,
64.1514598521523,65.1465210466559,66.1415822411596,67.1366434356632,68.1317046301668,
69.1267658246704,70.121827019174,71.1168882136776,72.1119494081812,73.1070106026849,
74.1020717971885,75.0971329916921,76.0921941861957,77.0872553806993,78.0823165752029,
79.0773777697065,80.0724389642101,81.0675001587137,82.0625613532173,83.057622547721,
84.0526837422246,85.0477449367282,86.0428061312318,87.0378673257354,88.032928520239,
89.0279897147426,90.0230509092463,91.0181121037498,92.0131732982535,93.0082344927571,
94.0032956872607,94.9983568817643,95.9934180762679,96.9884792707715,97.9835404652751,
98.9786016597787,99.9736628542824,100.968724048786,101.96378524329,102.958846437793,
103.953907632297,104.9489688268,105.944030021304,106.939091215808,107.934152410311,
108.929213604815,109.924274799318,110.919335993822,111.914397188326,112.909458382829,
113.904519577333,114.899580771837,115.89464196634,116.889703160844,117.884764355347,
118.879825549851,119.874886744355,120.869947938858,121.865009133362,122.860070327865,
123.855131522369,124.850192716873,125.845253911376,126.84031510588,127.835376300383,
128.830437494887,129.825498689391,130.820559883894,131.815621078398,132.810682272902,
133.805743467405,134.800804661909,135.795865856412),.UNSPECIFIED.);
#156=B_SPLINE_SURFACE_WITH_KNOTS('',3,3,((#39790,#39791,#39792,#39793,#39794,
#39795,#39796,#39797,#39798,#39799,#39800,#39801,#39802,#39803,#39804,#39805,
#39806,#39807,#39808,#39809,#39810,#39811,#39812,#39813,#39814,#39815,#39816,
#39817,#39818,#39819,#39820,#39821,#39822,#39823,#39824,#39825,#39826,#39827,
#39828,#39829,#39830,#39831,#39832,#39833,#39834,#39835,#39836,#39837,#39838,
#39839,#39840,#39841,#39842,#39843,#39844,#39845,#39846,#39847,#39848,#39849,
#39850,#39851,#39852,#39853,#39854,#39855,#39856,#39857,#39858,#39859,#39860,
#39861,#39862,#39863,#39864,#39865,#39866,#39867,#39868,#39869,#39870,#39871,
#39872,#39873,#39874,#39875,#39876,#39877,#39878,#39879,#39880,#39881,#39882,
#39883,#39884,#39885,#39886,#39887,#39888,#39889,#39890,#39891,#39892,#39893,
#39894,#39895,#39896,#39897,#39898,#39899,#39900,#39901,#39902,#39903,#39904,
#39905,#39906,#39907,#39908,#39909,#39910,#39911,#39912,#39913,#39914),
(#39915,#39916,#39917,#39918,#39919,#39920,#39921,#39922,#39923,#39924,
#39925,#39926,#39927,#39928,#39929,#39930,#39931,#39932,#39933,#39934,#39935,
#39936,#39937,#39938,#39939,#39940,#39941,#39942,#39943,#39944,#39945,#39946,
#39947,#39948,#39949,#39950,#39951,#39952,#39953,#39954,#39955,#39956,#39957,
#39958,#39959,#39960,#39961,#39962,#39963,#39964,#39965,#39966,#39967,#39968,
#39969,#39970,#39971,#39972,#39973,#39974,#39975,#39976,#39977,#39978,#39979,
#39980,#39981,#39982,#39983,#39984,#39985,#39986,#39987,#39988,#39989,#39990,
#39991,#39992,#39993,#39994,#39995,#39996,#39997,#39998,#39999,#40000,#40001,
#40002,#40003,#40004,#40005,#40006,#40007,#40008,#40009,#40010,#40011,#40012,
#40013,#40014,#40015,#40016,#40017,#40018,#40019,#40020,#40021,#40022,#40023,
#40024,#40025,#40026,#40027,#40028,#40029,#40030,#40031,#40032,#40033,#40034,
#40035,#40036,#40037,#40038,#40039),(#40040,#40041,#40042,#40043,#40044,
#40045,#40046,#40047,#40048,#40049,#40050,#40051,#40052,#40053,#40054,#40055,
#40056,#40057,#40058,#40059,#40060,#40061,#40062,#40063,#40064,#40065,#40066,
#40067,#40068,#40069,#40070,#40071,#40072,#40073,#40074,#40075,#40076,#40077,
#40078,#40079,#40080,#40081,#40082,#40083,#40084,#40085,#40086,#40087,#40088,
#40089,#40090,#40091,#40092,#40093,#40094,#40095,#40096,#40097,#40098,#40099,
#40100,#40101,#40102,#40103,#40104,#40105,#40106,#40107,#40108,#40109,#40110,
#40111,#40112,#40113,#40114,#40115,#40116,#40117,#40118,#40119,#40120,#40121,
#40122,#40123,#40124,#40125,#40126,#40127,#40128,#40129,#40130,#40131,#40132,
#40133,#40134,#40135,#40136,#40137,#40138,#40139,#40140,#40141,#40142,#40143,
#40144,#40145,#40146,#40147,#40148,#40149,#40150,#40151,#40152,#40153,#40154,
#40155,#40156,#40157,#40158,#40159,#40160,#40161,#40162,#40163,#40164),
(#40165,#40166,#40167,#40168,#40169,#40170,#40171,#40172,#40173,#40174,
#40175,#40176,#40177,#40178,#40179,#40180,#40181,#40182,#40183,#40184,#40185,
#40186,#40187,#40188,#40189,#40190,#40191,#40192,#40193,#40194,#40195,#40196,
#40197,#40198,#40199,#40200,#40201,#40202,#40203,#40204,#40205,#40206,#40207,
#40208,#40209,#40210,#40211,#40212,#40213,#40214,#40215,#40216,#40217,#40218,
#40219,#40220,#40221,#40222,#40223,#40224,#40225,#40226,#40227,#40228,#40229,
#40230,#40231,#40232,#40233,#40234,#40235,#40236,#40237,#40238,#40239,#40240,
#40241,#40242,#40243,#40244,#40245,#40246,#40247,#40248,#40249,#40250,#40251,
#40252,#40253,#40254,#40255,#40256,#40257,#40258,#40259,#40260,#40261,#40262,
#40263,#40264,#40265,#40266,#40267,#40268,#40269,#40270,#40271,#40272,#40273,
#40274,#40275,#40276,#40277,#40278,#40279,#40280,#40281,#40282,#40283,#40284,
#40285,#40286,#40287,#40288,#40289)),.UNSPECIFIED.,.F.,.F.,.F.,(4,4),(4,
1,1,1,1,1,1,1,1,1,1,1,1,1,1,1,1,1,1,1,1,1,1,1,1,1,1,1,1,1,1,1,1,1,1,1,1,
1,1,1,1,1,1,1,1,1,1,1,1,1,1,1,1,1,1,1,1,1,1,1,1,1,1,1,1,1,1,1,1,1,1,1,1,
1,1,1,1,1,1,1,1,1,1,1,1,1,1,1,1,1,1,1,1,1,1,1,1,1,1,1,1,1,1,1,1,1,1,1,1,
1,1,1,1,1,1,1,1,1,1,1,1,1,4),(-0.000520200608884411,0.0646393933935523),
(11.8584686616988,12.8540500568113,13.8491112513149,14.8441724458185,15.8392336403222,
16.8342948348258,17.8293560293294,18.824417223833,19.8194784183366,20.8145396128402,
21.8096008073438,22.8046620018474,23.799723196351,24.7947843908547,25.7898455853583,
26.7849067798619,27.7799679743655,28.7750291688691,29.7700903633727,30.7651515578763,
31.7602127523799,32.7552739468835,33.7503351413872,34.7453963358908,35.7404575303944,
36.735518724898,37.7305799194016,38.7256411139052,39.7207023084088,40.7157635029124,
41.7108246974161,42.7058858919197,43.7009470864233,44.6960082809269,45.6910694754305,
46.6861306699341,47.6811918644377,48.6762530589413,49.6713142534449,50.6663754479486,
51.6614366424522,52.6564978369558,53.6515590314594,54.646620225963,55.6416814204666,
56.6367426149702,57.6318038094738,58.6268650039775,59.6219261984811,60.6169873929847,
61.6120485874883,62.6071097819919,63.6021709764955,64.5972321709991,65.5922933655027,
66.5873545600063,67.58241575451,68.5774769490136,69.5725381435172,70.5675993380208,
71.5626605325244,72.557721727028,73.5527829215316,74.5478441160352,75.5429053105389,
76.5379665050425,77.5330276995461,78.5280888940497,79.5231500885533,80.5182112830569,
81.5132724775605,82.5083336720641,83.5033948665677,84.4984560610714,85.493517255575,
86.4885784500786,87.4836396445822,88.4787008390858,89.4737620335894,90.468823228093,
91.4638844225966,92.4589456171003,93.4540068116039,94.4490680061075,95.4441292006111,
96.4391903951147,97.4342515896183,98.4293127841219,99.4243739786255,100.419435173129,
101.414496367633,102.409557562136,103.40461875664,104.399679951144,105.394741145647,
106.389802340151,107.384863534654,108.379924729158,109.374985923662,110.370047118165,
111.365108312669,112.360169507172,113.355230701676,114.35029189618,115.345353090683,
116.340414285187,117.335475479691,118.330536674194,119.325597868698,120.320659063201,
121.315720257705,122.310781452209,123.305842646712,124.300903841216,125.295965035719,
126.291026230223,127.286087424727,128.28114861923,129.276209813734,130.271271008237,
131.266332202741,132.261393397245,133.256454591748),.UNSPECIFIED.);
#157=B_SPLINE_SURFACE_WITH_KNOTS('',3,3,((#40378,#40379,#40380,#40381,#40382,
#40383,#40384,#40385,#40386,#40387,#40388,#40389,#40390,#40391,#40392,#40393,
#40394,#40395,#40396,#40397,#40398,#40399,#40400,#40401,#40402,#40403,#40404,
#40405,#40406,#40407,#40408,#40409,#40410,#40411,#40412,#40413,#40414,#40415,
#40416,#40417,#40418,#40419,#40420,#40421,#40422,#40423,#40424,#40425,#40426,
#40427,#40428,#40429,#40430,#40431,#40432,#40433,#40434,#40435,#40436,#40437,
#40438,#40439,#40440,#40441,#40442,#40443,#40444,#40445,#40446,#40447,#40448,
#40449,#40450,#40451,#40452,#40453,#40454,#40455,#40456,#40457,#40458,#40459,
#40460,#40461,#40462,#40463,#40464,#40465,#40466,#40467,#40468,#40469,#40470,
#40471,#40472,#40473,#40474,#40475,#40476,#40477,#40478,#40479,#40480,#40481,
#40482,#40483,#40484,#40485,#40486,#40487,#40488,#40489,#40490,#40491,#40492,
#40493,#40494,#40495,#40496,#40497,#40498,#40499,#40500,#40501,#40502),
(#40503,#40504,#40505,#40506,#40507,#40508,#40509,#40510,#40511,#40512,
#40513,#40514,#40515,#40516,#40517,#40518,#40519,#40520,#40521,#40522,#40523,
#40524,#40525,#40526,#40527,#40528,#40529,#40530,#40531,#40532,#40533,#40534,
#40535,#40536,#40537,#40538,#40539,#40540,#40541,#40542,#40543,#40544,#40545,
#40546,#40547,#40548,#40549,#40550,#40551,#40552,#40553,#40554,#40555,#40556,
#40557,#40558,#40559,#40560,#40561,#40562,#40563,#40564,#40565,#40566,#40567,
#40568,#40569,#40570,#40571,#40572,#40573,#40574,#40575,#40576,#40577,#40578,
#40579,#40580,#40581,#40582,#40583,#40584,#40585,#40586,#40587,#40588,#40589,
#40590,#40591,#40592,#40593,#40594,#40595,#40596,#40597,#40598,#40599,#40600,
#40601,#40602,#40603,#40604,#40605,#40606,#40607,#40608,#40609,#40610,#40611,
#40612,#40613,#40614,#40615,#40616,#40617,#40618,#40619,#40620,#40621,#40622,
#40623,#40624,#40625,#40626,#40627),(#40628,#40629,#40630,#40631,#40632,
#40633,#40634,#40635,#40636,#40637,#40638,#40639,#40640,#40641,#40642,#40643,
#40644,#40645,#40646,#40647,#40648,#40649,#40650,#40651,#40652,#40653,#40654,
#40655,#40656,#40657,#40658,#40659,#40660,#40661,#40662,#40663,#40664,#40665,
#40666,#40667,#40668,#40669,#40670,#40671,#40672,#40673,#40674,#40675,#40676,
#40677,#40678,#40679,#40680,#40681,#40682,#40683,#40684,#40685,#40686,#40687,
#40688,#40689,#40690,#40691,#40692,#40693,#40694,#40695,#40696,#40697,#40698,
#40699,#40700,#40701,#40702,#40703,#40704,#40705,#40706,#40707,#40708,#40709,
#40710,#40711,#40712,#40713,#40714,#40715,#40716,#40717,#40718,#40719,#40720,
#40721,#40722,#40723,#40724,#40725,#40726,#40727,#40728,#40729,#40730,#40731,
#40732,#40733,#40734,#40735,#40736,#40737,#40738,#40739,#40740,#40741,#40742,
#40743,#40744,#40745,#40746,#40747,#40748,#40749,#40750,#40751,#40752),
(#40753,#40754,#40755,#40756,#40757,#40758,#40759,#40760,#40761,#40762,
#40763,#40764,#40765,#40766,#40767,#40768,#40769,#40770,#40771,#40772,#40773,
#40774,#40775,#40776,#40777,#40778,#40779,#40780,#40781,#40782,#40783,#40784,
#40785,#40786,#40787,#40788,#40789,#40790,#40791,#40792,#40793,#40794,#40795,
#40796,#40797,#40798,#40799,#40800,#40801,#40802,#40803,#40804,#40805,#40806,
#40807,#40808,#40809,#40810,#40811,#40812,#40813,#40814,#40815,#40816,#40817,
#40818,#40819,#40820,#40821,#40822,#40823,#40824,#40825,#40826,#40827,#40828,
#40829,#40830,#40831,#40832,#40833,#40834,#40835,#40836,#40837,#40838,#40839,
#40840,#40841,#40842,#40843,#40844,#40845,#40846,#40847,#40848,#40849,#40850,
#40851,#40852,#40853,#40854,#40855,#40856,#40857,#40858,#40859,#40860,#40861,
#40862,#40863,#40864,#40865,#40866,#40867,#40868,#40869,#40870,#40871,#40872,
#40873,#40874,#40875,#40876,#40877)),.UNSPECIFIED.,.F.,.F.,.F.,(4,4),(4,
1,1,1,1,1,1,1,1,1,1,1,1,1,1,1,1,1,1,1,1,1,1,1,1,1,1,1,1,1,1,1,1,1,1,1,1,
1,1,1,1,1,1,1,1,1,1,1,1,1,1,1,1,1,1,1,1,1,1,1,1,1,1,1,1,1,1,1,1,1,1,1,1,
1,1,1,1,1,1,1,1,1,1,1,1,1,1,1,1,1,1,1,1,1,1,1,1,1,1,1,1,1,1,1,1,1,1,1,1,
1,1,1,1,1,1,1,1,1,1,1,1,1,4),(-0.000457317293645526,0.064610822672929),
(14.3984001269718,15.3934613214754,16.388522515979,17.3835837104827,18.3786449049863,
19.3737060994899,20.3687672939935,21.3638284884971,22.3588896830007,23.3539508775043,
24.3490120720079,25.3440732665115,26.3391344610152,27.3341956555188,28.3292568500224,
29.324318044526,30.3193792390296,31.3144404335332,32.3095016280368,33.3045628225404,
34.299624017044,35.2946852115477,36.2897464060513,37.2848076005549,38.2798687950585,
39.2749299895621,40.2699911840657,41.2650523785693,42.2601135730729,43.2551747675765,
44.2502359620802,45.2452971565838,46.2403583510874,47.235419545591,48.2304807400946,
49.2255419345982,50.2206031291018,51.2156643236054,52.2107255181091,53.2057867126127,
54.2008479071163,55.1959091016199,56.1909702961235,57.1860314906271,58.1810926851307,
59.1761538796343,60.1712150741379,61.1662762686416,62.1613374631452,63.1563986576488,
64.1514598521524,65.146521046656,66.1415822411596,67.1366434356632,68.1317046301668,
69.1267658246704,70.121827019174,71.1168882136777,72.1119494081813,73.1070106026849,
74.1020717971885,75.0971329916921,76.0921941861957,77.0872553806993,78.082316575203,
79.0773777697065,80.0724389642102,81.0675001587138,82.0625613532174,83.057622547721,
84.0526837422246,85.0477449367282,86.0428061312318,87.0378673257354,88.0329285202391,
89.0279897147427,90.0230509092463,91.0181121037499,92.0131732982535,93.0082344927571,
94.0032956872607,94.9983568817644,95.9934180762679,96.9884792707716,97.9835404652752,
98.9786016597788,99.9736628542824,100.968724048786,101.96378524329,102.958846437793,
103.953907632297,104.9489688268,105.944030021304,106.939091215808,107.934152410311,
108.929213604815,109.924274799319,110.919335993822,111.914397188326,112.909458382829,
113.904519577333,114.899580771837,115.89464196634,116.889703160844,117.884764355347,
118.879825549851,119.874886744355,120.869947938858,121.865009133362,122.860070327865,
123.855131522369,124.850192716873,125.845253911376,126.84031510588,127.835376300384,
128.830437494887,129.825498689391,130.820559883894,131.815621078398,132.810682272902,
133.805743467405,134.800804661909,135.795865856412),.UNSPECIFIED.);
#158=B_SPLINE_SURFACE_WITH_KNOTS('',3,3,((#47555,#47556,#47557,#47558,#47559,
#47560,#47561,#47562,#47563,#47564,#47565,#47566,#47567,#47568,#47569,#47570,
#47571,#47572,#47573,#47574,#47575,#47576,#47577,#47578,#47579,#47580,#47581,
#47582,#47583,#47584,#47585,#47586,#47587,#47588,#47589,#47590,#47591,#47592,
#47593,#47594,#47595,#47596,#47597,#47598,#47599,#47600,#47601,#47602,#47603,
#47604,#47605,#47606,#47607,#47608,#47609,#47610,#47611,#47612,#47613,#47614,
#47615,#47616,#47617,#47618,#47619,#47620,#47621,#47622,#47623,#47624,#47625,
#47626,#47627,#47628,#47629,#47630,#47631),(#47632,#47633,#47634,#47635,
#47636,#47637,#47638,#47639,#47640,#47641,#47642,#47643,#47644,#47645,#47646,
#47647,#47648,#47649,#47650,#47651,#47652,#47653,#47654,#47655,#47656,#47657,
#47658,#47659,#47660,#47661,#47662,#47663,#47664,#47665,#47666,#47667,#47668,
#47669,#47670,#47671,#47672,#47673,#47674,#47675,#47676,#47677,#47678,#47679,
#47680,#47681,#47682,#47683,#47684,#47685,#47686,#47687,#47688,#47689,#47690,
#47691,#47692,#47693,#47694,#47695,#47696,#47697,#47698,#47699,#47700,#47701,
#47702,#47703,#47704,#47705,#47706,#47707,#47708),(#47709,#47710,#47711,
#47712,#47713,#47714,#47715,#47716,#47717,#47718,#47719,#47720,#47721,#47722,
#47723,#47724,#47725,#47726,#47727,#47728,#47729,#47730,#47731,#47732,#47733,
#47734,#47735,#47736,#47737,#47738,#47739,#47740,#47741,#47742,#47743,#47744,
#47745,#47746,#47747,#47748,#47749,#47750,#47751,#47752,#47753,#47754,#47755,
#47756,#47757,#47758,#47759,#47760,#47761,#47762,#47763,#47764,#47765,#47766,
#47767,#47768,#47769,#47770,#47771,#47772,#47773,#47774,#47775,#47776,#47777,
#47778,#47779,#47780,#47781,#47782,#47783,#47784,#47785),(#47786,#47787,
#47788,#47789,#47790,#47791,#47792,#47793,#47794,#47795,#47796,#47797,#47798,
#47799,#47800,#47801,#47802,#47803,#47804,#47805,#47806,#47807,#47808,#47809,
#47810,#47811,#47812,#47813,#47814,#47815,#47816,#47817,#47818,#47819,#47820,
#47821,#47822,#47823,#47824,#47825,#47826,#47827,#47828,#47829,#47830,#47831,
#47832,#47833,#47834,#47835,#47836,#47837,#47838,#47839,#47840,#47841,#47842,
#47843,#47844,#47845,#47846,#47847,#47848,#47849,#47850,#47851,#47852,#47853,
#47854,#47855,#47856,#47857,#47858,#47859,#47860,#47861,#47862)),
 .UNSPECIFIED.,.F.,.F.,.F.,(4,4),(4,1,1,1,1,1,1,1,1,1,1,1,1,1,1,1,1,1,1,
1,1,1,1,1,1,1,1,1,1,1,1,1,1,1,1,1,1,1,1,1,1,1,1,1,1,1,1,1,1,1,1,1,1,1,1,
1,1,1,1,1,1,1,1,1,1,1,1,1,1,1,1,1,1,1,4),(-0.000421138100199735,0.0663160893162111),
(11.6145651291772,12.6023632471184,13.5896936464185,14.5770240457187,15.5643544450188,
16.551684844319,17.5390152436191,18.5263456429193,19.5136760422194,20.5010064415196,
21.4883368408197,22.4756672401199,23.46299763942,24.4503280387202,25.4376584380203,
26.4249888373205,27.4123192366206,28.3996496359208,29.3869800352209,30.3743104345211,
31.3616408338212,32.3489712331214,33.3363016324215,34.3236320317217,35.3109624310218,
36.298292830322,37.2856232296221,38.2729536289223,39.2602840282224,40.2476144275226,
41.2349448268227,42.2222752261229,43.209605625423,44.1969360247232,45.1842664240233,
46.1715968233235,47.1589272226236,48.1462576219238,49.1335880212239,50.1209184205241,
51.1082488198242,52.0955792191244,53.0829096184245,54.0702400177247,55.0575704170248,
56.0449008163249,57.0322312156251,58.0195616149252,59.0068920142254,59.9942224135255,
60.9815528128257,61.9688832121258,62.956213611426,63.9435440107261,64.9308744100263,
65.9182048093264,66.9055352086266,67.8928656079267,68.8801960072269,69.867526406527,
70.8548568058272,71.8421872051273,72.8295176044275,73.8168480037276,74.8041784030278,
75.7915088023279,76.7788392016281,77.7661696009282,78.7535000002284,79.7408303995285,
80.7281607988287,81.7154911981288,82.702821597429,83.6901519967291,84.6779516871444),
 .UNSPECIFIED.);
#159=B_SPLINE_SURFACE_WITH_KNOTS('',3,3,((#47951,#47952,#47953,#47954,#47955,
#47956,#47957,#47958,#47959,#47960,#47961,#47962,#47963,#47964,#47965,#47966,
#47967,#47968,#47969,#47970,#47971,#47972,#47973,#47974,#47975,#47976,#47977,
#47978,#47979,#47980,#47981,#47982,#47983,#47984,#47985,#47986,#47987,#47988,
#47989,#47990,#47991,#47992,#47993,#47994,#47995,#47996,#47997,#47998,#47999,
#48000,#48001,#48002,#48003,#48004,#48005,#48006,#48007,#48008,#48009,#48010,
#48011,#48012,#48013,#48014,#48015,#48016,#48017,#48018,#48019,#48020,#48021,
#48022,#48023,#48024,#48025,#48026,#48027,#48028,#48029),(#48030,#48031,
#48032,#48033,#48034,#48035,#48036,#48037,#48038,#48039,#48040,#48041,#48042,
#48043,#48044,#48045,#48046,#48047,#48048,#48049,#48050,#48051,#48052,#48053,
#48054,#48055,#48056,#48057,#48058,#48059,#48060,#48061,#48062,#48063,#48064,
#48065,#48066,#48067,#48068,#48069,#48070,#48071,#48072,#48073,#48074,#48075,
#48076,#48077,#48078,#48079,#48080,#48081,#48082,#48083,#48084,#48085,#48086,
#48087,#48088,#48089,#48090,#48091,#48092,#48093,#48094,#48095,#48096,#48097,
#48098,#48099,#48100,#48101,#48102,#48103,#48104,#48105,#48106,#48107,#48108),
(#48109,#48110,#48111,#48112,#48113,#48114,#48115,#48116,#48117,#48118,
#48119,#48120,#48121,#48122,#48123,#48124,#48125,#48126,#48127,#48128,#48129,
#48130,#48131,#48132,#48133,#48134,#48135,#48136,#48137,#48138,#48139,#48140,
#48141,#48142,#48143,#48144,#48145,#48146,#48147,#48148,#48149,#48150,#48151,
#48152,#48153,#48154,#48155,#48156,#48157,#48158,#48159,#48160,#48161,#48162,
#48163,#48164,#48165,#48166,#48167,#48168,#48169,#48170,#48171,#48172,#48173,
#48174,#48175,#48176,#48177,#48178,#48179,#48180,#48181,#48182,#48183,#48184,
#48185,#48186,#48187),(#48188,#48189,#48190,#48191,#48192,#48193,#48194,
#48195,#48196,#48197,#48198,#48199,#48200,#48201,#48202,#48203,#48204,#48205,
#48206,#48207,#48208,#48209,#48210,#48211,#48212,#48213,#48214,#48215,#48216,
#48217,#48218,#48219,#48220,#48221,#48222,#48223,#48224,#48225,#48226,#48227,
#48228,#48229,#48230,#48231,#48232,#48233,#48234,#48235,#48236,#48237,#48238,
#48239,#48240,#48241,#48242,#48243,#48244,#48245,#48246,#48247,#48248,#48249,
#48250,#48251,#48252,#48253,#48254,#48255,#48256,#48257,#48258,#48259,#48260,
#48261,#48262,#48263,#48264,#48265,#48266)),.UNSPECIFIED.,.F.,.F.,.F.,(4,
4),(4,1,1,1,1,1,1,1,1,1,1,1,1,1,1,1,1,1,1,1,1,1,1,1,1,1,1,1,1,1,1,1,1,1,
1,1,1,1,1,1,1,1,1,1,1,1,1,1,1,1,1,1,1,1,1,1,1,1,1,1,1,1,1,1,1,1,1,1,1,1,
1,1,1,1,1,1,4),(-0.000470199680981362,0.066270318112471),(8.30747755240104,
9.2960444961263,10.2846114398516,11.2731783835768,12.2617453273021,13.2503122710274,
14.2388792147526,15.2274461584779,16.2160131022032,17.2045800459284,18.1931469896537,
19.181713933379,20.1702808771042,21.1588478208295,22.1474147645547,23.13598170828,
24.1245486520053,25.1131155957305,26.1016825394558,27.0902494831811,28.0788164269063,
29.0673833706316,30.0559503143569,31.0445172580821,32.0330842018074,33.0216511455327,
34.0102180892579,34.9987850329832,35.9873519767085,36.9759189204337,37.964485864159,
38.9530528078842,39.9416197516095,40.9301866953348,41.91875363906,42.9073205827853,
43.8958875265106,44.8844544702358,45.8730214139611,46.8615883576864,47.8501553014116,
48.8387222451369,49.8272891888622,50.8158561325874,51.8044230763127,52.792990020038,
53.7815569637632,54.7701239074885,55.7586908512138,56.747257794939,57.7358247386643,
58.7243916823895,59.7129586261148,60.7015255698401,61.6900925135653,62.6786594572906,
63.6672264010159,64.6557933447411,65.6443602884664,66.6329272321917,67.6214941759169,
68.6100611196422,69.5986280633675,70.5871950070927,71.575761950818,72.5643288945433,
73.5528958382685,74.5414627819938,75.530029725719,76.5185966694443,77.5071636131696,
78.4957305568948,79.4842975006201,80.4728644443454,81.4614313880706,82.4499983317959,
83.4390354752022),.UNSPECIFIED.);
#160=B_SPLINE_SURFACE_WITH_KNOTS('',3,3,((#58672,#58673,#58674,#58675,#58676,
#58677,#58678,#58679,#58680,#58681,#58682,#58683,#58684,#58685,#58686,#58687,
#58688,#58689,#58690,#58691,#58692,#58693,#58694,#58695,#58696,#58697,#58698,
#58699,#58700,#58701,#58702,#58703,#58704,#58705,#58706,#58707,#58708,#58709,
#58710,#58711,#58712,#58713,#58714,#58715,#58716,#58717,#58718,#58719,#58720,
#58721,#58722,#58723,#58724,#58725,#58726,#58727,#58728,#58729,#58730,#58731,
#58732,#58733,#58734,#58735,#58736,#58737,#58738,#58739,#58740,#58741,#58742,
#58743,#58744,#58745,#58746,#58747,#58748,#58749,#58750,#58751,#58752,#58753,
#58754,#58755,#58756,#58757,#58758,#58759,#58760,#58761,#58762,#58763,#58764,
#58765,#58766,#58767,#58768,#58769,#58770,#58771,#58772,#58773,#58774,#58775),
(#58776,#58777,#58778,#58779,#58780,#58781,#58782,#58783,#58784,#58785,
#58786,#58787,#58788,#58789,#58790,#58791,#58792,#58793,#58794,#58795,#58796,
#58797,#58798,#58799,#58800,#58801,#58802,#58803,#58804,#58805,#58806,#58807,
#58808,#58809,#58810,#58811,#58812,#58813,#58814,#58815,#58816,#58817,#58818,
#58819,#58820,#58821,#58822,#58823,#58824,#58825,#58826,#58827,#58828,#58829,
#58830,#58831,#58832,#58833,#58834,#58835,#58836,#58837,#58838,#58839,#58840,
#58841,#58842,#58843,#58844,#58845,#58846,#58847,#58848,#58849,#58850,#58851,
#58852,#58853,#58854,#58855,#58856,#58857,#58858,#58859,#58860,#58861,#58862,
#58863,#58864,#58865,#58866,#58867,#58868,#58869,#58870,#58871,#58872,#58873,
#58874,#58875,#58876,#58877,#58878,#58879),(#58880,#58881,#58882,#58883,
#58884,#58885,#58886,#58887,#58888,#58889,#58890,#58891,#58892,#58893,#58894,
#58895,#58896,#58897,#58898,#58899,#58900,#58901,#58902,#58903,#58904,#58905,
#58906,#58907,#58908,#58909,#58910,#58911,#58912,#58913,#58914,#58915,#58916,
#58917,#58918,#58919,#58920,#58921,#58922,#58923,#58924,#58925,#58926,#58927,
#58928,#58929,#58930,#58931,#58932,#58933,#58934,#58935,#58936,#58937,#58938,
#58939,#58940,#58941,#58942,#58943,#58944,#58945,#58946,#58947,#58948,#58949,
#58950,#58951,#58952,#58953,#58954,#58955,#58956,#58957,#58958,#58959,#58960,
#58961,#58962,#58963,#58964,#58965,#58966,#58967,#58968,#58969,#58970,#58971,
#58972,#58973,#58974,#58975,#58976,#58977,#58978,#58979,#58980,#58981,#58982,
#58983),(#58984,#58985,#58986,#58987,#58988,#58989,#58990,#58991,#58992,
#58993,#58994,#58995,#58996,#58997,#58998,#58999,#59000,#59001,#59002,#59003,
#59004,#59005,#59006,#59007,#59008,#59009,#59010,#59011,#59012,#59013,#59014,
#59015,#59016,#59017,#59018,#59019,#59020,#59021,#59022,#59023,#59024,#59025,
#59026,#59027,#59028,#59029,#59030,#59031,#59032,#59033,#59034,#59035,#59036,
#59037,#59038,#59039,#59040,#59041,#59042,#59043,#59044,#59045,#59046,#59047,
#59048,#59049,#59050,#59051,#59052,#59053,#59054,#59055,#59056,#59057,#59058,
#59059,#59060,#59061,#59062,#59063,#59064,#59065,#59066,#59067,#59068,#59069,
#59070,#59071,#59072,#59073,#59074,#59075,#59076,#59077,#59078,#59079,#59080,
#59081,#59082,#59083,#59084,#59085,#59086,#59087)),.UNSPECIFIED.,.F.,.F.,
 .F.,(4,4),(4,1,1,1,1,1,1,1,1,1,1,1,1,1,1,1,1,1,1,1,1,1,1,1,1,1,1,1,1,1,
1,1,1,1,1,1,1,1,1,1,1,1,1,1,1,1,1,1,1,1,1,1,1,1,1,1,1,1,1,1,1,1,1,1,1,1,
1,1,1,1,1,1,1,1,1,1,1,1,1,1,1,1,1,1,1,1,1,1,1,1,1,1,1,1,1,1,1,1,1,1,1,4),
(-0.000342905668100493,0.0451832374712266),(11.8612370985886,12.8591085386933,
13.8566370731299,14.8541656075665,15.8516941420031,16.8492226764397,17.8467512108763,
18.8442797453129,19.8418082797495,20.8393368141861,21.8368653486227,22.8343938830593,
23.8319224174959,24.8294509519325,25.8269794863691,26.8245080208057,27.8220365552423,
28.8195650896789,29.8170936241155,30.8146221585521,31.8121506929887,32.8096792274253,
33.8072077618619,34.8047362962985,35.8022648307351,36.7997933651717,37.7973218996083,
38.7948504340449,39.7923789684815,40.7899075029181,41.7874360373547,42.7849645717913,
43.7824931062279,44.7800216406645,45.7775501751011,46.7750787095377,47.7726072439743,
48.7701357784109,49.7676643128475,50.7651928472841,51.7627213817207,52.7602499161573,
53.7577784505939,54.7553069850305,55.7528355194671,56.7503640539037,57.7478925883403,
58.7454211227769,59.7429496572135,60.7404781916501,61.7380067260867,62.7355352605233,
63.7330637949599,64.7305923293965,65.7281208638331,66.7256493982697,67.7231779327063,
68.7207064671429,69.7182350015795,70.7157635360161,71.7132920704527,72.7108206048892,
73.7083491393258,74.7058776737625,75.7034062081991,76.7009347426357,77.6984632770722,
78.6959918115088,79.6935203459455,80.6910488803821,81.6885774148187,82.6861059492552,
83.6836344836918,84.6811630181284,85.678691552565,86.6762200870017,87.6737486214382,
88.6712771558748,89.6688056903114,90.666334224748,91.6638627591846,92.6613912936212,
93.6589198280578,94.6564483624944,95.653976896931,96.6515054313676,97.6490339658042,
98.6465625002408,99.6440910346774,100.641619569114,101.639148103551,102.636676637987,
103.634205172424,104.63173370686,105.629262241297,106.626790775734,107.62431931017,
108.621847844607,109.619376379043,110.61690491348,111.614433447917,112.611961982353),
 .UNSPECIFIED.);
#161=B_SPLINE_SURFACE_WITH_KNOTS('',3,3,((#59170,#59171,#59172,#59173,#59174,
#59175,#59176,#59177,#59178,#59179,#59180,#59181,#59182,#59183,#59184,#59185,
#59186,#59187,#59188,#59189,#59190,#59191,#59192,#59193,#59194,#59195,#59196,
#59197,#59198,#59199,#59200,#59201,#59202,#59203,#59204,#59205,#59206,#59207,
#59208,#59209,#59210,#59211,#59212,#59213,#59214,#59215,#59216,#59217,#59218,
#59219,#59220,#59221,#59222,#59223,#59224,#59225,#59226,#59227,#59228,#59229,
#59230,#59231,#59232,#59233,#59234,#59235,#59236,#59237,#59238,#59239,#59240,
#59241,#59242,#59243,#59244,#59245,#59246,#59247,#59248,#59249,#59250,#59251,
#59252,#59253,#59254,#59255,#59256,#59257,#59258,#59259,#59260,#59261,#59262,
#59263,#59264,#59265,#59266,#59267,#59268,#59269,#59270,#59271,#59272,#59273),
(#59274,#59275,#59276,#59277,#59278,#59279,#59280,#59281,#59282,#59283,
#59284,#59285,#59286,#59287,#59288,#59289,#59290,#59291,#59292,#59293,#59294,
#59295,#59296,#59297,#59298,#59299,#59300,#59301,#59302,#59303,#59304,#59305,
#59306,#59307,#59308,#59309,#59310,#59311,#59312,#59313,#59314,#59315,#59316,
#59317,#59318,#59319,#59320,#59321,#59322,#59323,#59324,#59325,#59326,#59327,
#59328,#59329,#59330,#59331,#59332,#59333,#59334,#59335,#59336,#59337,#59338,
#59339,#59340,#59341,#59342,#59343,#59344,#59345,#59346,#59347,#59348,#59349,
#59350,#59351,#59352,#59353,#59354,#59355,#59356,#59357,#59358,#59359,#59360,
#59361,#59362,#59363,#59364,#59365,#59366,#59367,#59368,#59369,#59370,#59371,
#59372,#59373,#59374,#59375,#59376,#59377),(#59378,#59379,#59380,#59381,
#59382,#59383,#59384,#59385,#59386,#59387,#59388,#59389,#59390,#59391,#59392,
#59393,#59394,#59395,#59396,#59397,#59398,#59399,#59400,#59401,#59402,#59403,
#59404,#59405,#59406,#59407,#59408,#59409,#59410,#59411,#59412,#59413,#59414,
#59415,#59416,#59417,#59418,#59419,#59420,#59421,#59422,#59423,#59424,#59425,
#59426,#59427,#59428,#59429,#59430,#59431,#59432,#59433,#59434,#59435,#59436,
#59437,#59438,#59439,#59440,#59441,#59442,#59443,#59444,#59445,#59446,#59447,
#59448,#59449,#59450,#59451,#59452,#59453,#59454,#59455,#59456,#59457,#59458,
#59459,#59460,#59461,#59462,#59463,#59464,#59465,#59466,#59467,#59468,#59469,
#59470,#59471,#59472,#59473,#59474,#59475,#59476,#59477,#59478,#59479,#59480,
#59481),(#59482,#59483,#59484,#59485,#59486,#59487,#59488,#59489,#59490,
#59491,#59492,#59493,#59494,#59495,#59496,#59497,#59498,#59499,#59500,#59501,
#59502,#59503,#59504,#59505,#59506,#59507,#59508,#59509,#59510,#59511,#59512,
#59513,#59514,#59515,#59516,#59517,#59518,#59519,#59520,#59521,#59522,#59523,
#59524,#59525,#59526,#59527,#59528,#59529,#59530,#59531,#59532,#59533,#59534,
#59535,#59536,#59537,#59538,#59539,#59540,#59541,#59542,#59543,#59544,#59545,
#59546,#59547,#59548,#59549,#59550,#59551,#59552,#59553,#59554,#59555,#59556,
#59557,#59558,#59559,#59560,#59561,#59562,#59563,#59564,#59565,#59566,#59567,
#59568,#59569,#59570,#59571,#59572,#59573,#59574,#59575,#59576,#59577,#59578,
#59579,#59580,#59581,#59582,#59583,#59584,#59585)),.UNSPECIFIED.,.F.,.F.,
 .F.,(4,4),(4,1,1,1,1,1,1,1,1,1,1,1,1,1,1,1,1,1,1,1,1,1,1,1,1,1,1,1,1,1,
1,1,1,1,1,1,1,1,1,1,1,1,1,1,1,1,1,1,1,1,1,1,1,1,1,1,1,1,1,1,1,1,1,1,1,1,
1,1,1,1,1,1,1,1,1,1,1,1,1,1,1,1,1,1,1,1,1,1,1,1,1,1,1,1,1,1,1,1,1,1,1,4),
(-0.000291827121531397,0.0452318691957662),(14.3981410127769,15.3956695472135,
16.3931980816501,17.3907266160867,18.3882551505233,19.3857836849599,20.3833122193965,
21.3808407538331,22.3783692882697,23.3758978227063,24.3734263571429,25.3709548915795,
26.3684834260161,27.3660119604527,28.3635404948893,29.3610690293259,30.3585975637625,
31.3561260981991,32.3536546326357,33.3511831670723,34.3487117015089,35.3462402359455,
36.3437687703821,37.3412973048187,38.3388258392553,39.3363543736919,40.3338829081285,
41.3314114425651,42.3289399770017,43.3264685114383,44.3239970458749,45.3215255803115,
46.3190541147481,47.3165826491847,48.3141111836213,49.3116397180579,50.3091682524945,
51.3066967869311,52.3042253213677,53.3017538558043,54.2992823902409,55.2968109246775,
56.2943394591141,57.2918679935507,58.2893965279873,59.2869250624239,60.2844535968605,
61.2819821312971,62.2795106657337,63.2770392001703,64.2745677346069,65.2720962690435,
66.2696248034801,67.2671533379167,68.2646818723533,69.2622104067899,70.2597389412265,
71.2572674756631,72.2547960100997,73.2523245445363,74.2498530789729,75.2473816134095,
76.2449101478461,77.2424386822827,78.2399672167193,79.2374957511559,80.2350242855925,
81.2325528200291,82.2300813544657,83.2276098889023,84.2251384233389,85.2226669577755,
86.2201954922121,87.2177240266487,88.2152525610853,89.2127810955219,90.2103096299585,
91.2078381643951,92.2053666988317,93.2028952332683,94.2004237677049,95.1979523021415,
96.1954808365781,97.1930093710147,98.1905379054513,99.1880664398879,100.185594974324,
101.183123508761,102.180652043198,103.178180577634,104.175709112071,105.173237646507,
106.170766180944,107.168294715381,108.165823249817,109.163351784254,110.16088031869,
111.158408853127,112.155937387564,113.153465922,114.150994456437,115.148865876639),
 .UNSPECIFIED.);
#162=B_SPLINE_SURFACE_WITH_KNOTS('',3,3,((#69341,#69342,#69343,#69344,#69345,
#69346,#69347,#69348,#69349,#69350,#69351,#69352,#69353,#69354,#69355,#69356,
#69357,#69358,#69359,#69360,#69361,#69362,#69363,#69364,#69365,#69366,#69367,
#69368,#69369,#69370,#69371,#69372,#69373,#69374,#69375,#69376,#69377,#69378,
#69379,#69380,#69381,#69382,#69383,#69384,#69385,#69386,#69387,#69388,#69389,
#69390,#69391,#69392,#69393,#69394,#69395,#69396,#69397,#69398,#69399,#69400,
#69401,#69402,#69403,#69404,#69405,#69406,#69407,#69408,#69409,#69410,#69411,
#69412,#69413,#69414,#69415,#69416,#69417,#69418,#69419,#69420,#69421,#69422,
#69423,#69424,#69425,#69426,#69427,#69428,#69429,#69430,#69431,#69432,#69433,
#69434,#69435,#69436,#69437,#69438,#69439,#69440,#69441,#69442),(#69443,
#69444,#69445,#69446,#69447,#69448,#69449,#69450,#69451,#69452,#69453,#69454,
#69455,#69456,#69457,#69458,#69459,#69460,#69461,#69462,#69463,#69464,#69465,
#69466,#69467,#69468,#69469,#69470,#69471,#69472,#69473,#69474,#69475,#69476,
#69477,#69478,#69479,#69480,#69481,#69482,#69483,#69484,#69485,#69486,#69487,
#69488,#69489,#69490,#69491,#69492,#69493,#69494,#69495,#69496,#69497,#69498,
#69499,#69500,#69501,#69502,#69503,#69504,#69505,#69506,#69507,#69508,#69509,
#69510,#69511,#69512,#69513,#69514,#69515,#69516,#69517,#69518,#69519,#69520,
#69521,#69522,#69523,#69524,#69525,#69526,#69527,#69528,#69529,#69530,#69531,
#69532,#69533,#69534,#69535,#69536,#69537,#69538,#69539,#69540,#69541,#69542,
#69543,#69544),(#69545,#69546,#69547,#69548,#69549,#69550,#69551,#69552,
#69553,#69554,#69555,#69556,#69557,#69558,#69559,#69560,#69561,#69562,#69563,
#69564,#69565,#69566,#69567,#69568,#69569,#69570,#69571,#69572,#69573,#69574,
#69575,#69576,#69577,#69578,#69579,#69580,#69581,#69582,#69583,#69584,#69585,
#69586,#69587,#69588,#69589,#69590,#69591,#69592,#69593,#69594,#69595,#69596,
#69597,#69598,#69599,#69600,#69601,#69602,#69603,#69604,#69605,#69606,#69607,
#69608,#69609,#69610,#69611,#69612,#69613,#69614,#69615,#69616,#69617,#69618,
#69619,#69620,#69621,#69622,#69623,#69624,#69625,#69626,#69627,#69628,#69629,
#69630,#69631,#69632,#69633,#69634,#69635,#69636,#69637,#69638,#69639,#69640,
#69641,#69642,#69643,#69644,#69645,#69646),(#69647,#69648,#69649,#69650,
#69651,#69652,#69653,#69654,#69655,#69656,#69657,#69658,#69659,#69660,#69661,
#69662,#69663,#69664,#69665,#69666,#69667,#69668,#69669,#69670,#69671,#69672,
#69673,#69674,#69675,#69676,#69677,#69678,#69679,#69680,#69681,#69682,#69683,
#69684,#69685,#69686,#69687,#69688,#69689,#69690,#69691,#69692,#69693,#69694,
#69695,#69696,#69697,#69698,#69699,#69700,#69701,#69702,#69703,#69704,#69705,
#69706,#69707,#69708,#69709,#69710,#69711,#69712,#69713,#69714,#69715,#69716,
#69717,#69718,#69719,#69720,#69721,#69722,#69723,#69724,#69725,#69726,#69727,
#69728,#69729,#69730,#69731,#69732,#69733,#69734,#69735,#69736,#69737,#69738,
#69739,#69740,#69741,#69742,#69743,#69744,#69745,#69746,#69747,#69748)),
 .UNSPECIFIED.,.F.,.F.,.F.,(4,4),(4,1,1,1,1,1,1,1,1,1,1,1,1,1,1,1,1,1,1,
1,1,1,1,1,1,1,1,1,1,1,1,1,1,1,1,1,1,1,1,1,1,1,1,1,1,1,1,1,1,1,1,1,1,1,1,
1,1,1,1,1,1,1,1,1,1,1,1,1,1,1,1,1,1,1,1,1,1,1,1,1,1,1,1,1,1,1,1,1,1,1,1,
1,1,1,1,1,1,1,1,4),(-0.000429898909490116,0.0663250612852997),(11.6145561949038,
12.6069034617266,13.598774075635,14.5906446895433,15.5825153034517,16.5743859173601,
17.5662565312685,18.5581271451769,19.5499977590852,20.5418683729936,21.533738986902,
22.5256096008104,23.5174802147187,24.5093508286271,25.5012214425355,26.4930920564439,
27.4849626703523,28.4768332842606,29.468703898169,30.4605745120774,31.4524451259858,
32.4443157398941,33.4361863538025,34.4280569677109,35.4199275816193,36.4117981955277,
37.403668809436,38.3955394233444,39.3874100372528,40.3792806511612,41.3711512650695,
42.3630218789779,43.3548924928863,44.3467631067947,45.3386337207031,46.3305043346114,
47.3223749485198,48.3142455624282,49.3061161763366,50.2979867902449,51.2898574041533,
52.2817280180617,53.2735986319701,54.2654692458785,55.2573398597868,56.2492104736952,
57.2410810876036,58.232951701512,59.2248223154203,60.2166929293287,61.2085635432371,
62.2004341571455,63.1923047710539,64.1841753849622,65.1760459988706,66.167916612779,
67.1597872266874,68.1516578405957,69.1435284545041,70.1353990684125,71.1272696823209,
72.1191402962293,73.1110109101376,74.102881524046,75.0947521379544,76.0866227518628,
77.0784933657711,78.0703639796795,79.0622345935879,80.0541052074963,81.0459758214047,
82.037846435313,83.0297170492214,84.0215876631298,85.0134582770382,86.0053288909465,
86.9971995048549,87.9890701187633,88.9809407326717,89.9728113465801,90.9646819604884,
91.9565525743968,92.9484231883052,93.9402938022136,94.9321644161219,95.9240350300303,
96.9159056439387,97.9077762578471,98.8996468717555,99.8915174856638,100.883388099572,
101.875258713481,102.867129327389,103.858999941297,104.850870555206,105.842741169114,
106.834611783022,107.826482396931,108.818353010839,109.810701887832),
 .UNSPECIFIED.);
#163=B_SPLINE_SURFACE_WITH_KNOTS('',3,3,((#69837,#69838,#69839,#69840,#69841,
#69842,#69843,#69844,#69845,#69846,#69847,#69848,#69849,#69850,#69851,#69852,
#69853,#69854,#69855,#69856,#69857,#69858,#69859,#69860,#69861,#69862,#69863,
#69864,#69865,#69866,#69867,#69868,#69869,#69870,#69871,#69872,#69873,#69874,
#69875,#69876,#69877,#69878,#69879,#69880,#69881,#69882,#69883,#69884,#69885,
#69886,#69887,#69888,#69889,#69890,#69891,#69892,#69893,#69894,#69895,#69896,
#69897,#69898,#69899,#69900,#69901,#69902,#69903,#69904,#69905,#69906,#69907,
#69908,#69909,#69910,#69911,#69912,#69913,#69914,#69915,#69916,#69917,#69918,
#69919,#69920,#69921,#69922,#69923,#69924,#69925,#69926,#69927,#69928,#69929,
#69930,#69931,#69932,#69933,#69934,#69935,#69936,#69937,#69938,#69939,#69940),
(#69941,#69942,#69943,#69944,#69945,#69946,#69947,#69948,#69949,#69950,
#69951,#69952,#69953,#69954,#69955,#69956,#69957,#69958,#69959,#69960,#69961,
#69962,#69963,#69964,#69965,#69966,#69967,#69968,#69969,#69970,#69971,#69972,
#69973,#69974,#69975,#69976,#69977,#69978,#69979,#69980,#69981,#69982,#69983,
#69984,#69985,#69986,#69987,#69988,#69989,#69990,#69991,#69992,#69993,#69994,
#69995,#69996,#69997,#69998,#69999,#70000,#70001,#70002,#70003,#70004,#70005,
#70006,#70007,#70008,#70009,#70010,#70011,#70012,#70013,#70014,#70015,#70016,
#70017,#70018,#70019,#70020,#70021,#70022,#70023,#70024,#70025,#70026,#70027,
#70028,#70029,#70030,#70031,#70032,#70033,#70034,#70035,#70036,#70037,#70038,
#70039,#70040,#70041,#70042,#70043,#70044),(#70045,#70046,#70047,#70048,
#70049,#70050,#70051,#70052,#70053,#70054,#70055,#70056,#70057,#70058,#70059,
#70060,#70061,#70062,#70063,#70064,#70065,#70066,#70067,#70068,#70069,#70070,
#70071,#70072,#70073,#70074,#70075,#70076,#70077,#70078,#70079,#70080,#70081,
#70082,#70083,#70084,#70085,#70086,#70087,#70088,#70089,#70090,#70091,#70092,
#70093,#70094,#70095,#70096,#70097,#70098,#70099,#70100,#70101,#70102,#70103,
#70104,#70105,#70106,#70107,#70108,#70109,#70110,#70111,#70112,#70113,#70114,
#70115,#70116,#70117,#70118,#70119,#70120,#70121,#70122,#70123,#70124,#70125,
#70126,#70127,#70128,#70129,#70130,#70131,#70132,#70133,#70134,#70135,#70136,
#70137,#70138,#70139,#70140,#70141,#70142,#70143,#70144,#70145,#70146,#70147,
#70148),(#70149,#70150,#70151,#70152,#70153,#70154,#70155,#70156,#70157,
#70158,#70159,#70160,#70161,#70162,#70163,#70164,#70165,#70166,#70167,#70168,
#70169,#70170,#70171,#70172,#70173,#70174,#70175,#70176,#70177,#70178,#70179,
#70180,#70181,#70182,#70183,#70184,#70185,#70186,#70187,#70188,#70189,#70190,
#70191,#70192,#70193,#70194,#70195,#70196,#70197,#70198,#70199,#70200,#70201,
#70202,#70203,#70204,#70205,#70206,#70207,#70208,#70209,#70210,#70211,#70212,
#70213,#70214,#70215,#70216,#70217,#70218,#70219,#70220,#70221,#70222,#70223,
#70224,#70225,#70226,#70227,#70228,#70229,#70230,#70231,#70232,#70233,#70234,
#70235,#70236,#70237,#70238,#70239,#70240,#70241,#70242,#70243,#70244,#70245,
#70246,#70247,#70248,#70249,#70250,#70251,#70252)),.UNSPECIFIED.,.F.,.F.,
 .F.,(4,4),(4,1,1,1,1,1,1,1,1,1,1,1,1,1,1,1,1,1,1,1,1,1,1,1,1,1,1,1,1,1,
1,1,1,1,1,1,1,1,1,1,1,1,1,1,1,1,1,1,1,1,1,1,1,1,1,1,1,1,1,1,1,1,1,1,1,1,
1,1,1,1,1,1,1,1,1,1,1,1,1,1,1,1,1,1,1,1,1,1,1,1,1,1,1,1,1,1,1,1,1,1,1,4),
(-0.000478368004393251,0.0662783428032473),(8.30747755240101,9.30018873014199,
10.292899907883,11.2856110856239,12.2783222633649,13.2710334411059,14.2637446188469,
15.2564557965878,16.2491669743288,17.2418781520698,18.2345893298108,19.2273005075518,
20.2200116852927,21.2127228630337,22.2054340407747,23.1981452185157,24.1908563962566,
25.1835675739976,26.1762787517386,27.1689899294796,28.1617011072206,29.1544122849615,
30.1471234627025,31.1398346404435,32.1325458181845,33.1252569959254,34.1179681736664,
35.1106793514074,36.1033905291484,37.0961017068893,38.0888128846303,39.0815240623713,
40.0742352401123,41.0669464178533,42.0596575955942,43.0523687733352,44.0450799510762,
45.0377911288172,46.0305023065581,47.0232134842991,48.0159246620401,49.0086358397811,
50.001347017522,50.994058195263,51.986769373004,52.979480550745,53.972191728486,
54.9649029062269,55.9576140839679,56.9503252617089,57.9430364394499,58.9357476171908,
59.9284587949318,60.9211699726728,61.9138811504138,62.9065923281547,63.8993035058957,
64.8920146836367,65.8847258613777,66.8774370391187,67.8701482168596,68.8628593946006,
69.8555705723416,70.8482817500825,71.8409929278235,72.8337041055645,73.8264152833055,
74.8191264610465,75.8118376387874,76.8045488165284,77.7972599942694,78.7899711720104,
79.7826823497514,80.7753935274923,81.7681047052333,82.7608158829743,83.7535270607153,
84.7462382384562,85.7389494161972,86.7316605939382,87.7243717716792,88.7170829494201,
89.7097941271611,90.7025053049021,91.6952164826431,92.687927660384,93.680638838125,
94.673350015866,95.666061193607,96.658772371348,97.6514835490889,98.6441947268299,
99.6369059045709,100.629617082312,101.622328260053,102.615039437794,103.607750615535,
104.600461793276,105.593172971017,106.585884148758,107.578595326499,108.571784872244),
 .UNSPECIFIED.);
#164=B_SPLINE_SURFACE_WITH_KNOTS('',3,3,((#78223,#78224,#78225,#78226,#78227,
#78228,#78229,#78230,#78231,#78232,#78233,#78234,#78235,#78236,#78237,#78238,
#78239,#78240,#78241,#78242,#78243,#78244,#78245,#78246,#78247,#78248,#78249,
#78250,#78251,#78252,#78253,#78254,#78255,#78256,#78257,#78258,#78259,#78260,
#78261,#78262,#78263,#78264,#78265,#78266,#78267,#78268,#78269,#78270,#78271,
#78272,#78273,#78274,#78275,#78276,#78277,#78278,#78279,#78280,#78281,#78282,
#78283,#78284,#78285,#78286,#78287,#78288,#78289,#78290,#78291,#78292,#78293,
#78294,#78295,#78296,#78297,#78298,#78299,#78300,#78301,#78302,#78303,#78304,
#78305,#78306,#78307,#78308,#78309,#78310),(#78311,#78312,#78313,#78314,
#78315,#78316,#78317,#78318,#78319,#78320,#78321,#78322,#78323,#78324,#78325,
#78326,#78327,#78328,#78329,#78330,#78331,#78332,#78333,#78334,#78335,#78336,
#78337,#78338,#78339,#78340,#78341,#78342,#78343,#78344,#78345,#78346,#78347,
#78348,#78349,#78350,#78351,#78352,#78353,#78354,#78355,#78356,#78357,#78358,
#78359,#78360,#78361,#78362,#78363,#78364,#78365,#78366,#78367,#78368,#78369,
#78370,#78371,#78372,#78373,#78374,#78375,#78376,#78377,#78378,#78379,#78380,
#78381,#78382,#78383,#78384,#78385,#78386,#78387,#78388,#78389,#78390,#78391,
#78392,#78393,#78394,#78395,#78396,#78397,#78398),(#78399,#78400,#78401,
#78402,#78403,#78404,#78405,#78406,#78407,#78408,#78409,#78410,#78411,#78412,
#78413,#78414,#78415,#78416,#78417,#78418,#78419,#78420,#78421,#78422,#78423,
#78424,#78425,#78426,#78427,#78428,#78429,#78430,#78431,#78432,#78433,#78434,
#78435,#78436,#78437,#78438,#78439,#78440,#78441,#78442,#78443,#78444,#78445,
#78446,#78447,#78448,#78449,#78450,#78451,#78452,#78453,#78454,#78455,#78456,
#78457,#78458,#78459,#78460,#78461,#78462,#78463,#78464,#78465,#78466,#78467,
#78468,#78469,#78470,#78471,#78472,#78473,#78474,#78475,#78476,#78477,#78478,
#78479,#78480,#78481,#78482,#78483,#78484,#78485,#78486),(#78487,#78488,
#78489,#78490,#78491,#78492,#78493,#78494,#78495,#78496,#78497,#78498,#78499,
#78500,#78501,#78502,#78503,#78504,#78505,#78506,#78507,#78508,#78509,#78510,
#78511,#78512,#78513,#78514,#78515,#78516,#78517,#78518,#78519,#78520,#78521,
#78522,#78523,#78524,#78525,#78526,#78527,#78528,#78529,#78530,#78531,#78532,
#78533,#78534,#78535,#78536,#78537,#78538,#78539,#78540,#78541,#78542,#78543,
#78544,#78545,#78546,#78547,#78548,#78549,#78550,#78551,#78552,#78553,#78554,
#78555,#78556,#78557,#78558,#78559,#78560,#78561,#78562,#78563,#78564,#78565,
#78566,#78567,#78568,#78569,#78570,#78571,#78572,#78573,#78574)),
 .UNSPECIFIED.,.F.,.F.,.F.,(4,4),(4,1,1,1,1,1,1,1,1,1,1,1,1,1,1,1,1,1,1,
1,1,1,1,1,1,1,1,1,1,1,1,1,1,1,1,1,1,1,1,1,1,1,1,1,1,1,1,1,1,1,1,1,1,1,1,
1,1,1,1,1,1,1,1,1,1,1,1,1,1,1,1,1,1,1,1,1,1,1,1,1,1,1,1,1,1,4),(-0.000292644816034893,
0.0463354841736447),(11.6151020157967,12.6127583869031,13.6100952546957,
14.6074321224883,15.6047689902808,16.6021058580734,17.599442725866,18.5967795936585,
19.5941164614511,20.5914533292437,21.5887901970362,22.5861270648288,23.5834639326213,
24.5808008004139,25.5781376682065,26.575474535999,27.5728114037916,28.5701482715842,
29.5674851393767,30.5648220071693,31.5621588749619,32.5594957427544,33.556832610547,
34.5541694783396,35.5515063461321,36.5488432139247,37.5461800817173,38.5435169495098,
39.5408538173024,40.538190685095,41.5355275528875,42.5328644206801,43.5302012884726,
44.5275381562652,45.5248750240578,46.5222118918503,47.5195487596429,48.5168856274355,
49.514222495228,50.5115593630206,51.5088962308132,52.5062330986057,53.5035699663983,
54.5009068341909,55.4982437019834,56.495580569776,57.4929174375686,58.4902543053611,
59.4875911731537,60.4849280409463,61.4822649087388,62.4796017765314,63.4769386443239,
64.4742755121165,65.4716123799091,66.4689492477016,67.4662861154942,68.4636229832868,
69.4609598510793,70.4582967188719,71.4556335866645,72.452970454457,73.4503073222496,
74.4476441900422,75.4449810578347,76.4423179256273,77.4396547934198,78.4369916612124,
79.434328529005,80.4316653967976,81.4290022645901,82.4263391323827,83.4236760001752,
84.4210128679678,85.4183497357604,86.4156866035529,87.4130234713455,88.4103603391381,
89.4076972069306,90.4050340747232,91.4023709425158,92.3997078103083,93.3970446781009,
94.3943815458935,95.391718413686,96.3893759491978),.UNSPECIFIED.);
#165=B_SPLINE_SURFACE_WITH_KNOTS('',3,3,((#78660,#78661,#78662,#78663,#78664,
#78665,#78666,#78667,#78668,#78669,#78670,#78671,#78672,#78673,#78674,#78675,
#78676,#78677,#78678,#78679,#78680,#78681,#78682,#78683,#78684,#78685,#78686,
#78687,#78688,#78689,#78690,#78691,#78692,#78693,#78694,#78695,#78696,#78697,
#78698,#78699,#78700,#78701,#78702,#78703,#78704,#78705,#78706,#78707,#78708,
#78709,#78710,#78711,#78712,#78713,#78714,#78715,#78716,#78717,#78718,#78719,
#78720,#78721,#78722,#78723,#78724,#78725,#78726,#78727,#78728,#78729,#78730,
#78731,#78732,#78733,#78734,#78735,#78736,#78737,#78738,#78739,#78740,#78741,
#78742,#78743,#78744,#78745,#78746,#78747,#78748,#78749),(#78750,#78751,
#78752,#78753,#78754,#78755,#78756,#78757,#78758,#78759,#78760,#78761,#78762,
#78763,#78764,#78765,#78766,#78767,#78768,#78769,#78770,#78771,#78772,#78773,
#78774,#78775,#78776,#78777,#78778,#78779,#78780,#78781,#78782,#78783,#78784,
#78785,#78786,#78787,#78788,#78789,#78790,#78791,#78792,#78793,#78794,#78795,
#78796,#78797,#78798,#78799,#78800,#78801,#78802,#78803,#78804,#78805,#78806,
#78807,#78808,#78809,#78810,#78811,#78812,#78813,#78814,#78815,#78816,#78817,
#78818,#78819,#78820,#78821,#78822,#78823,#78824,#78825,#78826,#78827,#78828,
#78829,#78830,#78831,#78832,#78833,#78834,#78835,#78836,#78837,#78838,#78839),
(#78840,#78841,#78842,#78843,#78844,#78845,#78846,#78847,#78848,#78849,
#78850,#78851,#78852,#78853,#78854,#78855,#78856,#78857,#78858,#78859,#78860,
#78861,#78862,#78863,#78864,#78865,#78866,#78867,#78868,#78869,#78870,#78871,
#78872,#78873,#78874,#78875,#78876,#78877,#78878,#78879,#78880,#78881,#78882,
#78883,#78884,#78885,#78886,#78887,#78888,#78889,#78890,#78891,#78892,#78893,
#78894,#78895,#78896,#78897,#78898,#78899,#78900,#78901,#78902,#78903,#78904,
#78905,#78906,#78907,#78908,#78909,#78910,#78911,#78912,#78913,#78914,#78915,
#78916,#78917,#78918,#78919,#78920,#78921,#78922,#78923,#78924,#78925,#78926,
#78927,#78928,#78929),(#78930,#78931,#78932,#78933,#78934,#78935,#78936,
#78937,#78938,#78939,#78940,#78941,#78942,#78943,#78944,#78945,#78946,#78947,
#78948,#78949,#78950,#78951,#78952,#78953,#78954,#78955,#78956,#78957,#78958,
#78959,#78960,#78961,#78962,#78963,#78964,#78965,#78966,#78967,#78968,#78969,
#78970,#78971,#78972,#78973,#78974,#78975,#78976,#78977,#78978,#78979,#78980,
#78981,#78982,#78983,#78984,#78985,#78986,#78987,#78988,#78989,#78990,#78991,
#78992,#78993,#78994,#78995,#78996,#78997,#78998,#78999,#79000,#79001,#79002,
#79003,#79004,#79005,#79006,#79007,#79008,#79009,#79010,#79011,#79012,#79013,
#79014,#79015,#79016,#79017,#79018,#79019)),.UNSPECIFIED.,.F.,.F.,.F.,(4,
4),(4,1,1,1,1,1,1,1,1,1,1,1,1,1,1,1,1,1,1,1,1,1,1,1,1,1,1,1,1,1,1,1,1,1,
1,1,1,1,1,1,1,1,1,1,1,1,1,1,1,1,1,1,1,1,1,1,1,1,1,1,1,1,1,1,1,1,1,1,1,1,
1,1,1,1,1,1,1,1,1,1,1,1,1,1,1,1,1,4),(-0.00032060916664835,0.0463085361130159),
(8.3104412613233,9.30873374912645,10.3068805755132,11.3050274018999,12.3031742282867,
13.3013210546734,14.2994678810601,15.2976147074469,16.2957615338336,17.2939083602203,
18.2920551866071,19.2902020129938,20.2883488393806,21.2864956657673,22.284642492154,
23.2827893185408,24.2809361449275,25.2790829713142,26.277229797701,27.2753766240877,
28.2735234504744,29.2716702768612,30.2698171032479,31.2679639296347,32.2661107560214,
33.2642575824081,34.2624044087949,35.2605512351816,36.2586980615683,37.2568448879551,
38.2549917143418,39.2531385407286,40.2512853671153,41.249432193502,42.2475790198888,
43.2457258462755,44.2438726726622,45.242019499049,46.2401663254357,47.2383131518225,
48.2364599782092,49.2346068045959,50.2327536309827,51.2309004573694,52.2290472837561,
53.2271941101429,54.2253409365296,55.2234877629163,56.2216345893031,57.2197814156898,
58.2179282420766,59.2160750684633,60.21422189485,61.2123687212368,62.2105155476235,
63.2086623740102,64.206809200397,65.2049560267837,66.2031028531704,67.2012496795572,
68.1993965059439,69.1975433323307,70.1956901587174,71.1938369851041,72.1919838114909,
73.1901306378776,74.1882774642643,75.1864242906511,76.1845711170378,77.1827179434245,
78.1808647698113,79.179011596198,80.1771584225848,81.1753052489715,82.1734520753582,
83.171598901745,84.1697457281317,85.1678925545184,86.1660393809052,87.1641862072919,
88.1623330336787,89.1604798600654,90.1586266864521,91.1567735128389,92.1549203392256,
93.1530671656123,94.1512139919991,95.1496814275525),.UNSPECIFIED.);
#166=B_SPLINE_SURFACE_WITH_KNOTS('',3,3,((#89566,#89567,#89568,#89569,#89570,
#89571,#89572,#89573,#89574,#89575,#89576,#89577,#89578,#89579,#89580,#89581,
#89582,#89583,#89584,#89585,#89586,#89587,#89588,#89589,#89590,#89591,#89592,
#89593,#89594,#89595,#89596,#89597,#89598,#89599,#89600,#89601,#89602,#89603,
#89604,#89605,#89606,#89607,#89608,#89609,#89610,#89611,#89612,#89613,#89614,
#89615,#89616,#89617,#89618,#89619,#89620,#89621,#89622,#89623,#89624,#89625,
#89626,#89627,#89628,#89629,#89630,#89631,#89632,#89633,#89634,#89635,#89636,
#89637,#89638,#89639,#89640,#89641,#89642,#89643,#89644,#89645,#89646,#89647,
#89648,#89649,#89650,#89651,#89652,#89653,#89654,#89655,#89656,#89657,#89658,
#89659,#89660,#89661,#89662,#89663,#89664,#89665,#89666,#89667,#89668,#89669,
#89670,#89671,#89672,#89673,#89674,#89675,#89676,#89677,#89678,#89679,#89680,
#89681,#89682,#89683,#89684,#89685,#89686,#89687,#89688,#89689,#89690,#89691,
#89692,#89693,#89694,#89695,#89696,#89697,#89698,#89699,#89700,#89701,#89702,
#89703,#89704,#89705,#89706,#89707,#89708,#89709,#89710,#89711,#89712,#89713,
#89714,#89715,#89716,#89717,#89718,#89719,#89720,#89721,#89722,#89723,#89724,
#89725,#89726,#89727,#89728,#89729,#89730,#89731,#89732,#89733,#89734,#89735,
#89736,#89737,#89738,#89739,#89740,#89741,#89742,#89743,#89744,#89745,#89746,
#89747,#89748,#89749,#89750),(#89751,#89752,#89753,#89754,#89755,#89756,
#89757,#89758,#89759,#89760,#89761,#89762,#89763,#89764,#89765,#89766,#89767,
#89768,#89769,#89770,#89771,#89772,#89773,#89774,#89775,#89776,#89777,#89778,
#89779,#89780,#89781,#89782,#89783,#89784,#89785,#89786,#89787,#89788,#89789,
#89790,#89791,#89792,#89793,#89794,#89795,#89796,#89797,#89798,#89799,#89800,
#89801,#89802,#89803,#89804,#89805,#89806,#89807,#89808,#89809,#89810,#89811,
#89812,#89813,#89814,#89815,#89816,#89817,#89818,#89819,#89820,#89821,#89822,
#89823,#89824,#89825,#89826,#89827,#89828,#89829,#89830,#89831,#89832,#89833,
#89834,#89835,#89836,#89837,#89838,#89839,#89840,#89841,#89842,#89843,#89844,
#89845,#89846,#89847,#89848,#89849,#89850,#89851,#89852,#89853,#89854,#89855,
#89856,#89857,#89858,#89859,#89860,#89861,#89862,#89863,#89864,#89865,#89866,
#89867,#89868,#89869,#89870,#89871,#89872,#89873,#89874,#89875,#89876,#89877,
#89878,#89879,#89880,#89881,#89882,#89883,#89884,#89885,#89886,#89887,#89888,
#89889,#89890,#89891,#89892,#89893,#89894,#89895,#89896,#89897,#89898,#89899,
#89900,#89901,#89902,#89903,#89904,#89905,#89906,#89907,#89908,#89909,#89910,
#89911,#89912,#89913,#89914,#89915,#89916,#89917,#89918,#89919,#89920,#89921,
#89922,#89923,#89924,#89925,#89926,#89927,#89928,#89929,#89930,#89931,#89932,
#89933,#89934,#89935),(#89936,#89937,#89938,#89939,#89940,#89941,#89942,
#89943,#89944,#89945,#89946,#89947,#89948,#89949,#89950,#89951,#89952,#89953,
#89954,#89955,#89956,#89957,#89958,#89959,#89960,#89961,#89962,#89963,#89964,
#89965,#89966,#89967,#89968,#89969,#89970,#89971,#89972,#89973,#89974,#89975,
#89976,#89977,#89978,#89979,#89980,#89981,#89982,#89983,#89984,#89985,#89986,
#89987,#89988,#89989,#89990,#89991,#89992,#89993,#89994,#89995,#89996,#89997,
#89998,#89999,#90000,#90001,#90002,#90003,#90004,#90005,#90006,#90007,#90008,
#90009,#90010,#90011,#90012,#90013,#90014,#90015,#90016,#90017,#90018,#90019,
#90020,#90021,#90022,#90023,#90024,#90025,#90026,#90027,#90028,#90029,#90030,
#90031,#90032,#90033,#90034,#90035,#90036,#90037,#90038,#90039,#90040,#90041,
#90042,#90043,#90044,#90045,#90046,#90047,#90048,#90049,#90050,#90051,#90052,
#90053,#90054,#90055,#90056,#90057,#90058,#90059,#90060,#90061,#90062,#90063,
#90064,#90065,#90066,#90067,#90068,#90069,#90070,#90071,#90072,#90073,#90074,
#90075,#90076,#90077,#90078,#90079,#90080,#90081,#90082,#90083,#90084,#90085,
#90086,#90087,#90088,#90089,#90090,#90091,#90092,#90093,#90094,#90095,#90096,
#90097,#90098,#90099,#90100,#90101,#90102,#90103,#90104,#90105,#90106,#90107,
#90108,#90109,#90110,#90111,#90112,#90113,#90114,#90115,#90116,#90117,#90118,
#90119,#90120),(#90121,#90122,#90123,#90124,#90125,#90126,#90127,#90128,
#90129,#90130,#90131,#90132,#90133,#90134,#90135,#90136,#90137,#90138,#90139,
#90140,#90141,#90142,#90143,#90144,#90145,#90146,#90147,#90148,#90149,#90150,
#90151,#90152,#90153,#90154,#90155,#90156,#90157,#90158,#90159,#90160,#90161,
#90162,#90163,#90164,#90165,#90166,#90167,#90168,#90169,#90170,#90171,#90172,
#90173,#90174,#90175,#90176,#90177,#90178,#90179,#90180,#90181,#90182,#90183,
#90184,#90185,#90186,#90187,#90188,#90189,#90190,#90191,#90192,#90193,#90194,
#90195,#90196,#90197,#90198,#90199,#90200,#90201,#90202,#90203,#90204,#90205,
#90206,#90207,#90208,#90209,#90210,#90211,#90212,#90213,#90214,#90215,#90216,
#90217,#90218,#90219,#90220,#90221,#90222,#90223,#90224,#90225,#90226,#90227,
#90228,#90229,#90230,#90231,#90232,#90233,#90234,#90235,#90236,#90237,#90238,
#90239,#90240,#90241,#90242,#90243,#90244,#90245,#90246,#90247,#90248,#90249,
#90250,#90251,#90252,#90253,#90254,#90255,#90256,#90257,#90258,#90259,#90260,
#90261,#90262,#90263,#90264,#90265,#90266,#90267,#90268,#90269,#90270,#90271,
#90272,#90273,#90274,#90275,#90276,#90277,#90278,#90279,#90280,#90281,#90282,
#90283,#90284,#90285,#90286,#90287,#90288,#90289,#90290,#90291,#90292,#90293,
#90294,#90295,#90296,#90297,#90298,#90299,#90300,#90301,#90302,#90303,#90304,
#90305)),.UNSPECIFIED.,.F.,.F.,.F.,(4,4),(4,1,1,1,1,1,1,1,1,1,1,1,1,1,1,
1,1,1,1,1,1,1,1,1,1,1,1,1,1,1,1,1,1,1,1,1,1,1,1,1,1,1,1,1,1,1,1,1,1,1,1,
1,1,1,1,1,1,1,1,1,1,1,1,1,1,1,1,1,1,1,1,1,1,1,1,1,1,1,1,1,1,1,1,1,1,1,1,
1,1,1,1,1,1,1,1,1,1,1,1,1,1,1,1,1,1,1,1,1,1,1,1,1,1,1,1,1,1,1,1,1,1,1,1,
1,1,1,1,1,1,1,1,1,1,1,1,1,1,1,1,1,1,1,1,1,1,1,1,1,1,1,1,1,1,1,1,1,1,1,1,
1,1,1,1,1,1,1,1,1,1,1,1,1,1,1,1,1,1,1,1,1,1,1,4),(-0.000109569828534403,
0.0660914630517642),(8.30203615430833,8.79675414262435,9.29147213094037,
9.78619011925639,10.2809081075724,10.7756260958884,11.2703440842045,11.7650620725205,
12.2597800608365,12.7544980491525,13.2492160374685,13.7439340257846,14.2386520141006,
14.7333700024166,15.2280879907326,15.7228059790487,16.2175239673647,16.7122419556807,
17.2069599439967,17.7016779323128,18.1963959206288,18.6911139089448,19.1858318972608,
19.6805498855768,20.1752678738929,20.6699858622089,21.1647038505249,21.6594218388409,
22.1541398271569,22.648857815473,23.143575803789,23.638293792105,24.133011780421,
24.6277297687371,25.1224477570531,25.6171657453691,26.1118837336851,26.6066017220011,
27.1013197103172,27.5960376986332,28.0907556869492,28.5854736752652,29.0801916635813,
29.5749096518973,30.0696276402133,30.5643456285293,31.0590636168453,31.5537816051614,
32.0484995934774,32.5432175817934,33.0379355701094,33.5326535584255,34.0273715467415,
34.5220895350575,35.0168075233735,35.5115255116895,36.0062435000056,36.5009614883216,
36.9956794766376,37.4903974649536,37.9851154532697,38.4798334415857,38.9745514299017,
39.4692694182177,39.9639874065337,40.4587053948498,40.9534233831658,41.4481413714818,
41.9428593597978,42.4375773481139,42.9322953364299,43.4270133247459,43.9217313130619,
44.416449301378,44.911167289694,45.40588527801,45.900603266326,46.395321254642,
46.8900392429581,47.3847572312741,47.8794752195901,48.3741932079061,48.8689111962221,
49.3636291845382,49.8583471728542,50.3530651611702,50.8477831494862,51.3425011378023,
51.8372191261183,52.3319371144343,52.8266551027503,53.3213730910663,53.8160910793824,
54.3108090676984,54.8055270560144,55.3002450443304,55.7949630326465,56.2896810209625,
56.7843990092785,57.2791169975945,57.7738349859105,58.2685529742266,58.7632709625426,
59.2579889508586,59.7527069391746,60.2474249274907,60.7421429158067,61.2368609041227,
61.7315788924387,62.2262968807547,62.7210148690708,63.2157328573868,63.7104508457028,
64.2051688340188,64.6998868223349,65.1946048106509,65.6893227989669,66.1840407872829,
66.678758775599,67.173476763915,67.668194752231,68.162912740547,68.657630728863,
69.1523487171791,69.6470667054951,70.1417846938111,70.6365026821271,71.1312206704432,
71.6259386587592,72.1206566470752,72.6153746353912,73.1100926237072,73.6048106120233,
74.0995286003393,74.5942465886553,75.0889645769713,75.5836825652873,76.0784005536034,
76.5731185419194,77.0678365302354,77.5625545185514,78.0572725068675,78.5519904951835,
79.0467084834995,79.5414264718155,80.0361444601315,80.5308624484476,81.0255804367636,
81.5202984250796,82.0150164133956,82.5097344017117,83.0044523900277,83.4991703783437,
83.9938883666597,84.4886063549757,84.9833243432918,85.4780423316078,85.9727603199238,
86.4674783082398,86.9621962965559,87.4569142848719,87.9516322731879,88.4463502615039,
88.9410682498199,89.435786238136,89.930504226452,90.425222214768,90.919940203084,
91.4146581914001,91.9093761797161,92.4040941680321,92.8988121563481,93.3935301446641,
93.8882481329802,94.3829661212962,94.8776841096122,95.3724020979282,95.8671200862443,
96.3618380745603,96.8565560628763,97.3512740511923,97.8459920395083,98.3408195976529),
 .UNSPECIFIED.);
#167=B_SPLINE_SURFACE_WITH_KNOTS('',3,3,((#90545,#90546,#90547,#90548,#90549,
#90550,#90551,#90552,#90553,#90554,#90555,#90556,#90557,#90558,#90559,#90560,
#90561,#90562,#90563,#90564,#90565,#90566,#90567,#90568,#90569,#90570,#90571,
#90572,#90573,#90574,#90575,#90576,#90577,#90578,#90579,#90580,#90581,#90582,
#90583,#90584,#90585,#90586,#90587,#90588,#90589,#90590,#90591,#90592,#90593,
#90594,#90595,#90596,#90597,#90598,#90599,#90600,#90601,#90602,#90603,#90604,
#90605,#90606,#90607,#90608,#90609,#90610,#90611,#90612,#90613,#90614,#90615,
#90616,#90617,#90618,#90619,#90620,#90621,#90622,#90623,#90624,#90625,#90626,
#90627,#90628,#90629,#90630,#90631,#90632,#90633,#90634,#90635,#90636,#90637,
#90638,#90639,#90640,#90641,#90642,#90643,#90644,#90645,#90646,#90647,#90648,
#90649,#90650,#90651,#90652,#90653,#90654,#90655,#90656,#90657,#90658,#90659,
#90660,#90661,#90662,#90663,#90664,#90665,#90666,#90667,#90668,#90669,#90670,
#90671,#90672,#90673,#90674,#90675,#90676,#90677,#90678,#90679,#90680,#90681,
#90682,#90683,#90684,#90685,#90686,#90687,#90688,#90689,#90690,#90691,#90692,
#90693,#90694,#90695,#90696,#90697,#90698,#90699,#90700,#90701,#90702,#90703,
#90704,#90705,#90706,#90707,#90708,#90709,#90710,#90711,#90712,#90713,#90714,
#90715,#90716,#90717,#90718,#90719,#90720,#90721,#90722,#90723,#90724,#90725,
#90726,#90727,#90728,#90729),(#90730,#90731,#90732,#90733,#90734,#90735,
#90736,#90737,#90738,#90739,#90740,#90741,#90742,#90743,#90744,#90745,#90746,
#90747,#90748,#90749,#90750,#90751,#90752,#90753,#90754,#90755,#90756,#90757,
#90758,#90759,#90760,#90761,#90762,#90763,#90764,#90765,#90766,#90767,#90768,
#90769,#90770,#90771,#90772,#90773,#90774,#90775,#90776,#90777,#90778,#90779,
#90780,#90781,#90782,#90783,#90784,#90785,#90786,#90787,#90788,#90789,#90790,
#90791,#90792,#90793,#90794,#90795,#90796,#90797,#90798,#90799,#90800,#90801,
#90802,#90803,#90804,#90805,#90806,#90807,#90808,#90809,#90810,#90811,#90812,
#90813,#90814,#90815,#90816,#90817,#90818,#90819,#90820,#90821,#90822,#90823,
#90824,#90825,#90826,#90827,#90828,#90829,#90830,#90831,#90832,#90833,#90834,
#90835,#90836,#90837,#90838,#90839,#90840,#90841,#90842,#90843,#90844,#90845,
#90846,#90847,#90848,#90849,#90850,#90851,#90852,#90853,#90854,#90855,#90856,
#90857,#90858,#90859,#90860,#90861,#90862,#90863,#90864,#90865,#90866,#90867,
#90868,#90869,#90870,#90871,#90872,#90873,#90874,#90875,#90876,#90877,#90878,
#90879,#90880,#90881,#90882,#90883,#90884,#90885,#90886,#90887,#90888,#90889,
#90890,#90891,#90892,#90893,#90894,#90895,#90896,#90897,#90898,#90899,#90900,
#90901,#90902,#90903,#90904,#90905,#90906,#90907,#90908,#90909,#90910,#90911,
#90912,#90913,#90914),(#90915,#90916,#90917,#90918,#90919,#90920,#90921,
#90922,#90923,#90924,#90925,#90926,#90927,#90928,#90929,#90930,#90931,#90932,
#90933,#90934,#90935,#90936,#90937,#90938,#90939,#90940,#90941,#90942,#90943,
#90944,#90945,#90946,#90947,#90948,#90949,#90950,#90951,#90952,#90953,#90954,
#90955,#90956,#90957,#90958,#90959,#90960,#90961,#90962,#90963,#90964,#90965,
#90966,#90967,#90968,#90969,#90970,#90971,#90972,#90973,#90974,#90975,#90976,
#90977,#90978,#90979,#90980,#90981,#90982,#90983,#90984,#90985,#90986,#90987,
#90988,#90989,#90990,#90991,#90992,#90993,#90994,#90995,#90996,#90997,#90998,
#90999,#91000,#91001,#91002,#91003,#91004,#91005,#91006,#91007,#91008,#91009,
#91010,#91011,#91012,#91013,#91014,#91015,#91016,#91017,#91018,#91019,#91020,
#91021,#91022,#91023,#91024,#91025,#91026,#91027,#91028,#91029,#91030,#91031,
#91032,#91033,#91034,#91035,#91036,#91037,#91038,#91039,#91040,#91041,#91042,
#91043,#91044,#91045,#91046,#91047,#91048,#91049,#91050,#91051,#91052,#91053,
#91054,#91055,#91056,#91057,#91058,#91059,#91060,#91061,#91062,#91063,#91064,
#91065,#91066,#91067,#91068,#91069,#91070,#91071,#91072,#91073,#91074,#91075,
#91076,#91077,#91078,#91079,#91080,#91081,#91082,#91083,#91084,#91085,#91086,
#91087,#91088,#91089,#91090,#91091,#91092,#91093,#91094,#91095,#91096,#91097,
#91098,#91099),(#91100,#91101,#91102,#91103,#91104,#91105,#91106,#91107,
#91108,#91109,#91110,#91111,#91112,#91113,#91114,#91115,#91116,#91117,#91118,
#91119,#91120,#91121,#91122,#91123,#91124,#91125,#91126,#91127,#91128,#91129,
#91130,#91131,#91132,#91133,#91134,#91135,#91136,#91137,#91138,#91139,#91140,
#91141,#91142,#91143,#91144,#91145,#91146,#91147,#91148,#91149,#91150,#91151,
#91152,#91153,#91154,#91155,#91156,#91157,#91158,#91159,#91160,#91161,#91162,
#91163,#91164,#91165,#91166,#91167,#91168,#91169,#91170,#91171,#91172,#91173,
#91174,#91175,#91176,#91177,#91178,#91179,#91180,#91181,#91182,#91183,#91184,
#91185,#91186,#91187,#91188,#91189,#91190,#91191,#91192,#91193,#91194,#91195,
#91196,#91197,#91198,#91199,#91200,#91201,#91202,#91203,#91204,#91205,#91206,
#91207,#91208,#91209,#91210,#91211,#91212,#91213,#91214,#91215,#91216,#91217,
#91218,#91219,#91220,#91221,#91222,#91223,#91224,#91225,#91226,#91227,#91228,
#91229,#91230,#91231,#91232,#91233,#91234,#91235,#91236,#91237,#91238,#91239,
#91240,#91241,#91242,#91243,#91244,#91245,#91246,#91247,#91248,#91249,#91250,
#91251,#91252,#91253,#91254,#91255,#91256,#91257,#91258,#91259,#91260,#91261,
#91262,#91263,#91264,#91265,#91266,#91267,#91268,#91269,#91270,#91271,#91272,
#91273,#91274,#91275,#91276,#91277,#91278,#91279,#91280,#91281,#91282,#91283,
#91284)),.UNSPECIFIED.,.F.,.F.,.F.,(4,4),(4,1,1,1,1,1,1,1,1,1,1,1,1,1,1,
1,1,1,1,1,1,1,1,1,1,1,1,1,1,1,1,1,1,1,1,1,1,1,1,1,1,1,1,1,1,1,1,1,1,1,1,
1,1,1,1,1,1,1,1,1,1,1,1,1,1,1,1,1,1,1,1,1,1,1,1,1,1,1,1,1,1,1,1,1,1,1,1,
1,1,1,1,1,1,1,1,1,1,1,1,1,1,1,1,1,1,1,1,1,1,1,1,1,1,1,1,1,1,1,1,1,1,1,1,
1,1,1,1,1,1,1,1,1,1,1,1,1,1,1,1,1,1,1,1,1,1,1,1,1,1,1,1,1,1,1,1,1,1,1,1,
1,1,1,1,1,1,1,1,1,1,1,1,1,1,1,1,1,1,1,1,1,1,1,4),(-7.16819172715052E-5,
0.0661295621106345),(11.6149232889894,12.1097508361343,12.6044688244503,
13.0991868127663,13.5939048010823,14.0886227893984,14.5833407777144,15.0780587660304,
15.5727767543464,16.0674947426624,16.5622127309785,17.0569307192945,17.5516487076105,
18.0463666959265,18.5410846842426,19.0358026725586,19.5305206608746,20.0252386491906,
20.5199566375066,21.0146746258227,21.5093926141387,22.0041106024547,22.4988285907707,
22.9935465790868,23.4882645674028,23.9829825557188,24.4777005440348,24.9724185323508,
25.4671365206669,25.9618545089829,26.4565724972989,26.9512904856149,27.446008473931,
27.940726462247,28.435444450563,28.930162438879,29.424880427195,29.9195984155111,
30.4143164038271,30.9090343921431,31.4037523804591,31.8984703687752,32.3931883570912,
32.8879063454072,33.3826243337232,33.8773423220393,34.3720603103553,34.8667782986713,
35.3614962869873,35.8562142753033,36.3509322636194,36.8456502519354,37.3403682402514,
37.8350862285674,38.3298042168834,38.8245222051995,39.3192401935155,39.8139581818315,
40.3086761701475,40.8033941584636,41.2981121467796,41.7928301350956,42.2875481234116,
42.7822661117277,43.2769841000437,43.7717020883597,44.2664200766757,44.7611380649917,
45.2558560533078,45.7505740416238,46.2452920299398,46.7400100182558,47.2347280065719,
47.7294459948879,48.2241639832039,48.7188819715199,49.2135999598359,49.708317948152,
50.203035936468,50.697753924784,51.1924719131,51.6871899014161,52.1819078897321,
52.6766258780481,53.1713438663641,53.6660618546801,54.1607798429962,54.6554978313122,
55.1502158196282,55.6449338079442,56.1396517962603,56.6343697845763,57.1290877728923,
57.6238057612083,58.1185237495243,58.6132417378404,59.1079597261564,59.6026777144724,
60.0973957027884,60.5921136911045,61.0868316794205,61.5815496677365,62.0762676560525,
62.5709856443685,63.0657036326846,63.5604216210006,64.0551396093166,64.5498575976326,
65.0445755859486,65.5392935742647,66.0340115625807,66.5287295508967,67.0234475392127,
67.5181655275288,68.0128835158448,68.5076015041608,69.0023194924768,69.4970374807929,
69.9917554691089,70.4864734574249,70.9811914457409,71.4759094340569,71.970627422373,
72.465345410689,72.960063399005,73.454781387321,73.9494993756371,74.4442173639531,
74.9389353522691,75.4336533405851,75.9283713289011,76.4230893172172,76.9178073055332,
77.4125252938492,77.9072432821652,78.4019612704813,78.8966792587973,79.3913972471133,
79.8861152354293,80.3808332237453,80.8755512120614,81.3702692003774,81.8649871886934,
82.3597051770094,82.8544231653255,83.3491411536415,83.8438591419575,84.3385771302735,
84.8332951185895,85.3280131069056,85.8227310952216,86.3174490835376,86.8121670718536,
87.3068850601697,87.8016030484857,88.2963210368017,88.7910390251177,89.2857570134337,
89.7804750017498,90.2751929900658,90.7699109783818,91.2646289666978,91.7593469550139,
92.2540649433299,92.7487829316459,93.2435009199619,93.7382189082779,94.232936896594,
94.72765488491,95.222372873226,95.717090861542,96.2118088498581,96.7065268381741,
97.2012448264901,97.6959628148061,98.1906808031221,98.6853987914382,99.1801167797542,
99.6748347680702,100.169552756386,100.664270744702,101.158988733018,101.653706721334),
 .UNSPECIFIED.);
#168=B_SPLINE_SURFACE_WITH_KNOTS('',3,3,((#93399,#93400,#93401,#93402,#93403,
#93404,#93405,#93406,#93407,#93408,#93409,#93410,#93411,#93412,#93413,#93414,
#93415,#93416,#93417,#93418,#93419,#93420,#93421,#93422,#93423,#93424,#93425,
#93426,#93427,#93428,#93429,#93430,#93431,#93432,#93433,#93434,#93435,#93436,
#93437,#93438,#93439,#93440,#93441,#93442,#93443,#93444,#93445,#93446,#93447,
#93448,#93449,#93450,#93451,#93452,#93453,#93454,#93455,#93456,#93457),
(#93458,#93459,#93460,#93461,#93462,#93463,#93464,#93465,#93466,#93467,
#93468,#93469,#93470,#93471,#93472,#93473,#93474,#93475,#93476,#93477,#93478,
#93479,#93480,#93481,#93482,#93483,#93484,#93485,#93486,#93487,#93488,#93489,
#93490,#93491,#93492,#93493,#93494,#93495,#93496,#93497,#93498,#93499,#93500,
#93501,#93502,#93503,#93504,#93505,#93506,#93507,#93508,#93509,#93510,#93511,
#93512,#93513,#93514,#93515,#93516),(#93517,#93518,#93519,#93520,#93521,
#93522,#93523,#93524,#93525,#93526,#93527,#93528,#93529,#93530,#93531,#93532,
#93533,#93534,#93535,#93536,#93537,#93538,#93539,#93540,#93541,#93542,#93543,
#93544,#93545,#93546,#93547,#93548,#93549,#93550,#93551,#93552,#93553,#93554,
#93555,#93556,#93557,#93558,#93559,#93560,#93561,#93562,#93563,#93564,#93565,
#93566,#93567,#93568,#93569,#93570,#93571,#93572,#93573,#93574,#93575),
(#93576,#93577,#93578,#93579,#93580,#93581,#93582,#93583,#93584,#93585,
#93586,#93587,#93588,#93589,#93590,#93591,#93592,#93593,#93594,#93595,#93596,
#93597,#93598,#93599,#93600,#93601,#93602,#93603,#93604,#93605,#93606,#93607,
#93608,#93609,#93610,#93611,#93612,#93613,#93614,#93615,#93616,#93617,#93618,
#93619,#93620,#93621,#93622,#93623,#93624,#93625,#93626,#93627,#93628,#93629,
#93630,#93631,#93632,#93633,#93634)),.UNSPECIFIED.,.F.,.F.,.F.,(4,4),(4,
1,1,1,1,1,1,1,1,1,1,1,1,1,1,1,1,1,1,1,1,1,1,1,1,1,1,1,1,1,1,1,1,1,1,1,1,
1,1,1,1,1,1,1,1,1,1,1,1,1,1,1,1,1,1,1,4),(-0.000103475830100935,0.0645568430532792),
(11.8498163896566,12.3348976354611,12.8198754054355,13.3048531754099,13.7898309453844,
14.2748087153588,14.7597864853332,15.2447642553077,15.7297420252821,16.2147197952565,
16.6996975652309,17.1846753352054,17.6696531051798,18.1546308751542,18.6396086451287,
19.1245864151031,19.6095641850775,20.0945419550519,20.5795197250264,21.0644974950008,
21.5494752649752,22.0344530349496,22.5194308049241,23.0044085748985,23.4893863448729,
23.9743641148474,24.4593418848218,24.9443196547962,25.4292974247706,25.9142751947451,
26.3992529647195,26.8842307346939,27.3692085046684,27.8541862746428,28.3391640446172,
28.8241418145916,29.3091195845661,29.7940973545405,30.2790751245149,30.7640528944893,
31.2490306644638,31.7340084344382,32.2189862044126,32.7039639743871,33.1889417443615,
33.6739195143359,34.1588972843103,34.6438750542848,35.1288528242592,35.6138305942336,
36.0988083642081,36.5837861341825,37.0687639041569,37.5537416741313,38.0387194441058,
38.5236972140802,39.0086749840546),.UNSPECIFIED.);
#169=B_SPLINE_SURFACE_WITH_KNOTS('',3,3,((#93865,#93866,#93867,#93868,#93869,
#93870,#93871,#93872,#93873,#93874,#93875,#93876,#93877,#93878,#93879,#93880,
#93881,#93882,#93883,#93884,#93885,#93886,#93887,#93888,#93889,#93890,#93891,
#93892,#93893,#93894,#93895,#93896,#93897,#93898,#93899,#93900,#93901,#93902,
#93903,#93904,#93905,#93906,#93907,#93908,#93909,#93910,#93911,#93912,#93913,
#93914,#93915,#93916,#93917,#93918,#93919,#93920,#93921,#93922,#93923),
(#93924,#93925,#93926,#93927,#93928,#93929,#93930,#93931,#93932,#93933,
#93934,#93935,#93936,#93937,#93938,#93939,#93940,#93941,#93942,#93943,#93944,
#93945,#93946,#93947,#93948,#93949,#93950,#93951,#93952,#93953,#93954,#93955,
#93956,#93957,#93958,#93959,#93960,#93961,#93962,#93963,#93964,#93965,#93966,
#93967,#93968,#93969,#93970,#93971,#93972,#93973,#93974,#93975,#93976,#93977,
#93978,#93979,#93980,#93981,#93982),(#93983,#93984,#93985,#93986,#93987,
#93988,#93989,#93990,#93991,#93992,#93993,#93994,#93995,#93996,#93997,#93998,
#93999,#94000,#94001,#94002,#94003,#94004,#94005,#94006,#94007,#94008,#94009,
#94010,#94011,#94012,#94013,#94014,#94015,#94016,#94017,#94018,#94019,#94020,
#94021,#94022,#94023,#94024,#94025,#94026,#94027,#94028,#94029,#94030,#94031,
#94032,#94033,#94034,#94035,#94036,#94037,#94038,#94039,#94040,#94041),
(#94042,#94043,#94044,#94045,#94046,#94047,#94048,#94049,#94050,#94051,
#94052,#94053,#94054,#94055,#94056,#94057,#94058,#94059,#94060,#94061,#94062,
#94063,#94064,#94065,#94066,#94067,#94068,#94069,#94070,#94071,#94072,#94073,
#94074,#94075,#94076,#94077,#94078,#94079,#94080,#94081,#94082,#94083,#94084,
#94085,#94086,#94087,#94088,#94089,#94090,#94091,#94092,#94093,#94094,#94095,
#94096,#94097,#94098,#94099,#94100)),.UNSPECIFIED.,.F.,.F.,.F.,(4,4),(4,
1,1,1,1,1,1,1,1,1,1,1,1,1,1,1,1,1,1,1,1,1,1,1,1,1,1,1,1,1,1,1,1,1,1,1,1,
1,1,1,1,1,1,1,1,1,1,1,1,1,1,1,1,1,1,1,4),(-6.74208202416338E-5,0.0645935329637062),
(14.3984001269719,14.8833778969463,15.3683556669207,15.8533334368951,16.3383112068696,
16.823288976844,17.3082667468184,17.7932445167929,18.2782222867673,18.7632000567417,
19.2481778267161,19.7331555966906,20.218133366665,20.7031111366394,21.1880889066139,
21.6730666765883,22.1580444465627,22.6430222165371,23.1279999865116,23.612977756486,
24.0979555264604,24.5829332964348,25.0679110664093,25.5528888363837,26.0378666063581,
26.5228443763326,27.007822146307,27.4927999162814,27.9777776862558,28.4627554562303,
28.9477332262047,29.4327109961791,29.9176887661536,30.402666536128,30.8876443061024,
31.3726220760768,31.8575998460513,32.3425776160257,32.8275553860001,33.3125331559745,
33.797510925949,34.2824886959234,34.7674664658978,35.2524442358723,35.7374220058467,
36.2223997758211,36.7073775457955,37.19235531577,37.6773330857444,38.1623108557188,
38.6472886256933,39.1322663956677,39.6172441656421,40.1022219356165,40.587199705591,
41.0721774755654,41.557258753435),.UNSPECIFIED.);
#170=B_SPLINE_CURVE_WITH_KNOTS('',3,(#10608,#10609,#10610,#10611,#10612,
#10613,#10614,#10615,#10616,#10617,#10618,#10619,#10620,#10621,#10622,#10623,
#10624,#10625,#10626,#10627,#10628,#10629,#10630,#10631,#10632,#10633,#10634,
#10635,#10636,#10637,#10638,#10639,#10640,#10641,#10642,#10643,#10644,#10645,
#10646,#10647,#10648,#10649,#10650,#10651,#10652,#10653,#10654,#10655,#10656,
#10657,#10658,#10659,#10660,#10661,#10662,#10663,#10664,#10665,#10666,#10667,
#10668,#10669,#10670,#10671,#10672,#10673,#10674,#10675,#10676,#10677,#10678,
#10679,#10680,#10681,#10682,#10683),.UNSPECIFIED.,.F.,.F.,(4,3,3,3,3,3,
3,3,3,3,3,3,3,3,3,3,3,3,3,3,3,3,3,3,3,4),(131.030639485952,131.124862922685,
131.219235943061,131.266332202741,131.359553276607,131.452645853409,131.54563967122,
131.638570862278,131.731470852847,131.82436633402,131.917283987168,132.01031659896,
132.103410766158,132.196676516921,132.261393397245,132.358253800053,132.454968934237,
132.555154641426,132.651629546133,132.748037988853,132.844400764937,132.940738621606,
133.037097136043,133.133466654998,133.229897556966,133.256454591748),
 .UNSPECIFIED.);
#171=B_SPLINE_CURVE_WITH_KNOTS('',3,(#10686,#10687,#10688,#10689,#10690,
#10691,#10692,#10693,#10694,#10695,#10696,#10697,#10698,#10699,#10700,#10701,
#10702,#10703,#10704,#10705,#10706,#10707,#10708,#10709,#10710,#10711,#10712,
#10713,#10714,#10715,#10716,#10717,#10718,#10719,#10720,#10721,#10722,#10723,
#10724,#10725,#10726,#10727,#10728,#10729,#10730,#10731,#10732,#10733,#10734,
#10735,#10736,#10737,#10738,#10739,#10740,#10741,#10742,#10743,#10744,#10745,
#10746,#10747,#10748,#10749,#10750,#10751,#10752,#10753,#10754,#10755,#10756,
#10757,#10758,#10759,#10760,#10761,#10762,#10763,#10764,#10765,#10766,#10767,
#10768,#10769,#10770,#10771,#10772,#10773,#10774,#10775,#10776,#10777,#10778,
#10779),.UNSPECIFIED.,.F.,.F.,(4,3,3,3,3,3,3,3,3,3,3,3,3,3,3,3,3,3,3,3,
3,3,3,3,3,3,3,3,3,3,3,4),(131.031745185056,131.129729671724,131.223528237148,
131.317300342785,131.41107178814,131.504868364938,131.598771830413,131.692738307433,
131.78685139804,131.815621078398,131.910038792203,132.004328170091,132.098517526913,
132.192637791453,132.286722645945,132.380797529135,132.474887864195,132.569075924233,
132.663317785296,132.757707314553,132.810682272902,132.904609653633,132.998411531174,
133.095962894,133.189603092652,133.283213322859,133.376819590518,133.470447891049,
133.564178560621,133.657969940107,133.751903898015,133.778822433787),
 .UNSPECIFIED.);
#172=B_SPLINE_CURVE_WITH_KNOTS('',3,(#10785,#10786,#10787,#10788,#10789,
#10790,#10791,#10792,#10793,#10794,#10795,#10796,#10797,#10798,#10799,#10800,
#10801,#10802,#10803,#10804,#10805,#10806,#10807,#10808,#10809,#10810,#10811,
#10812,#10813,#10814,#10815,#10816,#10817,#10818,#10819,#10820,#10821,#10822,
#10823,#10824,#10825,#10826,#10827,#10828,#10829,#10830,#10831,#10832,#10833,
#10834,#10835,#10836,#10837,#10838,#10839,#10840,#10841,#10842,#10843,#10844,
#10845,#10846,#10847,#10848,#10849,#10850,#10851,#10852,#10853,#10854,#10855,
#10856,#10857,#10858,#10859,#10860,#10861,#10862,#10863,#10864,#10865,#10866,
#10867,#10868,#10869,#10870,#10871,#10872,#10873,#10874,#10875,#10876,#10877,
#10878,#10879,#10880,#10881,#10882,#10883,#10884,#10885,#10886,#10887,#10888,
#10889,#10890,#10891,#10892,#10893,#10894,#10895,#10896,#10897,#10898,#10899,
#10900,#10901,#10902,#10903,#10904,#10905,#10906,#10907,#10908,#10909,#10910,
#10911,#10912,#10913,#10914,#10915,#10916,#10917,#10918,#10919,#10920),
 .UNSPECIFIED.,.F.,.F.,(4,3,3,3,3,3,3,3,3,3,3,3,3,3,3,3,3,3,3,3,3,3,3,3,
3,3,3,3,3,3,3,3,3,3,3,3,3,3,3,3,3,3,3,3,3,4),(124.748128028511,124.842034576069,
124.935951918733,125.0299669327,125.124031831941,125.218255583323,125.295965035719,
125.390184105335,125.484275308534,125.578267220964,125.672191936185,125.766082489566,
125.859964553955,125.953863787903,126.047864515545,126.141920902379,126.236129692714,
126.291026230223,126.385285904234,126.479417652453,126.573449997981,126.667414816189,
126.761345254291,126.855266938143,126.949205479067,127.043244801221,127.137339437753,
127.231585558755,127.286087424727,127.380353085992,127.474491224045,127.568530347491,
127.662502487566,127.756440580176,127.850370239497,127.944317065442,128.038365089124,
128.132468674872,128.226724042984,128.28114861923,128.378996644742,128.476673059547,
128.574146032619,128.671497438999,128.768713686957,128.805298797182),
 .UNSPECIFIED.);
#173=B_SPLINE_CURVE_WITH_KNOTS('',3,(#10921,#10922,#10923,#10924,#10925,
#10926,#10927,#10928,#10929,#10930,#10931,#10932,#10933,#10934,#10935,#10936,
#10937,#10938,#10939,#10940,#10941,#10942,#10943,#10944,#10945,#10946,#10947,
#10948,#10949,#10950,#10951,#10952,#10953,#10954,#10955,#10956,#10957,#10958,
#10959,#10960,#10961,#10962,#10963,#10964,#10965,#10966,#10967,#10968,#10969,
#10970,#10971,#10972,#10973,#10974,#10975,#10976,#10977,#10978,#10979,#10980,
#10981,#10982,#10983,#10984,#10985,#10986,#10987,#10988,#10989,#10990,#10991,
#10992,#10993),.UNSPECIFIED.,.F.,.F.,(4,3,3,3,3,3,3,3,3,3,3,3,3,3,3,3,3,
3,3,3,3,3,3,3,4),(128.805298797455,128.904575923864,129.004169174393,129.103925506044,
129.203971261245,129.276209813734,129.370627582079,129.464917013993,129.559106424263,
129.653226741186,129.747311647382,129.84138658154,129.935476966773,130.029665075484,
130.123906984442,130.218296559918,130.271271008237,130.366192067951,130.460422790932,
130.554564192512,130.648641837038,130.744141249266,130.838189532557,130.934414509254,
131.030639485952),.UNSPECIFIED.);
#174=B_SPLINE_CURVE_WITH_KNOTS('',3,(#10995,#10996,#10997,#10998,#10999,
#11000,#11001,#11002,#11003,#11004,#11005,#11006,#11007,#11008,#11009,#11010,
#11011,#11012,#11013,#11014,#11015,#11016,#11017,#11018,#11019,#11020,#11021,
#11022,#11023,#11024,#11025,#11026,#11027,#11028,#11029,#11030,#11031,#11032,
#11033,#11034,#11035,#11036,#11037,#11038,#11039,#11040,#11041,#11042,#11043,
#11044,#11045,#11046,#11047,#11048,#11049,#11050,#11051,#11052,#11053,#11054,
#11055,#11056,#11057,#11058,#11059,#11060,#11061,#11062,#11063,#11064,#11065,
#11066,#11067,#11068,#11069,#11070,#11071,#11072,#11073),.UNSPECIFIED.,
 .F.,.F.,(4,3,3,3,3,3,3,3,3,3,3,3,3,3,3,3,3,3,3,3,3,3,3,3,3,3,4),(128.805298797182,
128.830437494887,128.924697154801,129.018828889054,129.112861220763,129.206826025422,
129.300756450148,129.394678120809,129.488616648745,129.582655958293,129.676750582416,
129.770996691439,129.825498689391,129.919764295011,130.01390237706,130.107941444223,
130.201913527833,130.295851563885,130.389781166627,130.483727936041,130.577775903607,
130.671879433392,130.766134746334,130.820559883894,130.914675364851,131.0086511327,
131.031745185056),.UNSPECIFIED.);
#175=B_SPLINE_CURVE_WITH_KNOTS('',3,(#11074,#11075,#11076,#11077,#11078,
#11079,#11080,#11081),.UNSPECIFIED.,.F.,.F.,(4,1,1,1,1,4),(124.74739205894,
124.850192716873,125.845253911376,126.84031510588,127.835376300383,128.805295331209),
 .UNSPECIFIED.);
#176=B_SPLINE_CURVE_WITH_KNOTS('',3,(#11087,#11088,#11089,#11090,#11091,
#11092,#11093,#11094,#11095,#11096,#11097,#11098,#11099,#11100,#11101,#11102,
#11103,#11104,#11105,#11106,#11107,#11108,#11109,#11110,#11111,#11112,#11113,
#11114,#11115,#11116,#11117,#11118,#11119,#11120,#11121,#11122,#11123,#11124,
#11125,#11126,#11127,#11128,#11129,#11130,#11131,#11132,#11133,#11134,#11135,
#11136,#11137,#11138,#11139,#11140,#11141,#11142,#11143,#11144,#11145,#11146,
#11147,#11148,#11149,#11150,#11151,#11152,#11153,#11154,#11155,#11156,#11157,
#11158,#11159,#11160,#11161,#11162,#11163,#11164,#11165,#11166,#11167,#11168,
#11169,#11170,#11171,#11172,#11173,#11174,#11175,#11176,#11177,#11178,#11179,
#11180,#11181,#11182,#11183,#11184,#11185,#11186,#11187,#11188,#11189,#11190,
#11191,#11192,#11193,#11194,#11195,#11196,#11197,#11198,#11199,#11200,#11201,
#11202,#11203,#11204,#11205,#11206,#11207,#11208,#11209,#11210,#11211,#11212,
#11213,#11214,#11215,#11216,#11217,#11218,#11219),.UNSPECIFIED.,.F.,.F.,
(4,3,3,3,3,3,3,3,3,3,3,3,3,3,3,3,3,3,3,3,3,3,3,3,3,3,3,3,3,3,3,3,3,3,3,
3,3,3,3,3,3,3,3,3,4),(118.465309189798,118.559373810011,118.655151817347,
118.749077565128,118.842980638927,118.936886679199,119.034064476574,119.128108308656,
119.226853088677,119.325597868698,119.419836017092,119.513946331371,119.607957361602,
119.701901126583,119.795810680877,119.889711674647,119.983629743695,120.077649048852,
120.171723895481,120.26595077801,120.320659063201,120.414897817102,120.509008734383,
120.603020364354,120.696964721818,120.790874863903,120.884776440091,120.978695085495,
121.072714954328,121.166790358315,121.261017782786,121.315720257705,121.409959739289,
121.504071392924,121.598083766821,121.69202887633,121.78593977519,121.879842111928,
121.973761520711,122.067782152519,122.16185832038,122.256086502537,122.310781452209,
122.4414864556,122.522113490002),.UNSPECIFIED.);
#177=B_SPLINE_CURVE_WITH_KNOTS('',3,(#11220,#11221,#11222,#11223,#11224,
#11225,#11226,#11227,#11228,#11229,#11230,#11231,#11232,#11233,#11234,#11235,
#11236,#11237,#11238,#11239,#11240,#11241,#11242,#11243,#11244,#11245,#11246,
#11247,#11248,#11249,#11250,#11251,#11252,#11253,#11254,#11255,#11256,#11257,
#11258,#11259,#11260,#11261,#11262,#11263,#11264,#11265,#11266,#11267,#11268,
#11269,#11270,#11271,#11272,#11273,#11274,#11275,#11276,#11277,#11278,#11279,
#11280,#11281,#11282,#11283,#11284,#11285,#11286,#11287,#11288,#11289,#11290,
#11291,#11292,#11293,#11294,#11295),.UNSPECIFIED.,.F.,.F.,(4,3,3,3,3,3,
3,3,3,3,3,3,3,3,3,3,3,3,3,3,3,3,3,3,3,4),(122.522113490206,122.614859586664,
122.707525591219,122.800150201744,122.892760399084,122.985383144327,123.078100878442,
123.170872581003,123.263789214971,123.305842646712,123.400083492223,123.494196487762,
123.588210180099,123.682156568083,123.776068720305,123.869972283944,123.96389289179,
124.057914673282,124.151991964677,124.246221218337,124.300903841216,124.395154214485,
124.489253372224,124.583264788189,124.677212213272,124.748128028511),
 .UNSPECIFIED.);
#178=B_SPLINE_CURVE_WITH_KNOTS('',3,(#11297,#11298,#11299,#11300,#11301,
#11302),.UNSPECIFIED.,.F.,.F.,(4,1,1,4),(122.522113490002,122.860070327865,
123.855131522369,124.74739205894),.UNSPECIFIED.);
#179=B_SPLINE_CURVE_WITH_KNOTS('',3,(#11303,#11304,#11305,#11306,#11307,
#11308,#11309,#11310),.UNSPECIFIED.,.F.,.F.,(4,1,1,1,1,4),(118.464366347269,
118.879825549851,119.874886744355,120.869947938858,121.865009133362,122.522113490002),
 .UNSPECIFIED.);
#180=B_SPLINE_CURVE_WITH_KNOTS('',3,(#11316,#11317,#11318,#11319,#11320,
#11321,#11322,#11323,#11324,#11325,#11326,#11327,#11328,#11329,#11330,#11331,
#11332,#11333,#11334,#11335,#11336,#11337,#11338,#11339,#11340,#11341,#11342,
#11343,#11344,#11345,#11346,#11347,#11348,#11349,#11350,#11351,#11352,#11353,
#11354,#11355,#11356,#11357,#11358,#11359,#11360,#11361,#11362,#11363,#11364,
#11365,#11366,#11367,#11368,#11369,#11370,#11371,#11372,#11373,#11374,#11375,
#11376,#11377,#11378,#11379,#11380,#11381,#11382,#11383,#11384,#11385,#11386,
#11387,#11388,#11389,#11390,#11391,#11392,#11393,#11394,#11395,#11396,#11397,
#11398,#11399,#11400,#11401,#11402,#11403,#11404,#11405,#11406,#11407,#11408,
#11409,#11410,#11411,#11412,#11413,#11414,#11415,#11416,#11417,#11418,#11419,
#11420,#11421,#11422,#11423,#11424,#11425,#11426,#11427,#11428,#11429,#11430,
#11431,#11432,#11433,#11434,#11435,#11436,#11437,#11438,#11439,#11440,#11441,
#11442,#11443,#11444,#11445,#11446,#11447,#11448,#11449,#11450,#11451),
 .UNSPECIFIED.,.F.,.F.,(4,3,3,3,3,3,3,3,3,3,3,3,3,3,3,3,3,3,3,3,3,3,3,3,
3,3,3,3,3,3,3,3,3,3,3,3,3,3,3,3,3,3,3,3,3,4),(112.181027744827,112.275243743586,
112.360169507172,112.454408044935,112.548518748739,112.642530168135,112.736474320159,
112.830384260048,112.924285637504,113.018204087869,113.112223768433,113.20629898769,
113.3005262348,113.355230701676,113.449469228602,113.543579921563,113.637591330125,
113.731535471375,113.825445400529,113.919346767303,114.013265207052,114.107284877163,
114.201360086044,114.295587323002,114.35029189618,114.444530429606,114.538641128994,
114.632652543903,114.726596691355,114.820506626619,114.914407999406,115.008326445062,
115.102346120886,115.196421335378,115.290648577732,115.345353090683,115.438408490029,
115.531337087903,115.624161186544,115.716928481106,115.809665873421,115.90240022995,
115.995209800998,116.088059601802,116.181043570387,116.238928182603),
 .UNSPECIFIED.);
#181=B_SPLINE_CURVE_WITH_KNOTS('',3,(#11452,#11453,#11454,#11455,#11456,
#11457,#11458,#11459,#11460,#11461,#11462,#11463,#11464,#11465,#11466,#11467,
#11468,#11469,#11470,#11471,#11472,#11473,#11474,#11475,#11476,#11477,#11478,
#11479,#11480,#11481,#11482,#11483,#11484,#11485,#11486,#11487,#11488,#11489,
#11490,#11491,#11492,#11493,#11494,#11495,#11496,#11497,#11498,#11499,#11500,
#11501,#11502,#11503,#11504,#11505,#11506,#11507,#11508,#11509,#11510,#11511,
#11512,#11513,#11514,#11515,#11516,#11517,#11518,#11519,#11520,#11521,#11522,
#11523,#11524,#11525,#11526,#11527),.UNSPECIFIED.,.F.,.F.,(4,3,3,3,3,3,
3,3,3,3,3,3,3,3,3,3,3,3,3,3,3,3,3,3,3,4),(116.238928182822,116.340414285187,
116.434652766824,116.528763414508,116.622774777863,116.716718874193,116.810628758621,
116.904530080917,116.998448476488,117.092468103145,117.186543268915,117.280770463729,
117.335475479691,117.429714028249,117.523824742414,117.617836171729,117.711780332983,
117.805690281671,117.899591667489,117.993510125772,118.087529813532,118.18160503959,
118.275832292814,118.330536674194,118.424770353341,118.465309189798),
 .UNSPECIFIED.);
#182=B_SPLINE_CURVE_WITH_KNOTS('',3,(#11529,#11530,#11531,#11532,#11533,
#11534),.UNSPECIFIED.,.F.,.F.,(4,1,1,4),(116.238928182822,116.889703160844,
117.884764355347,118.464366347269),.UNSPECIFIED.);
#183=B_SPLINE_CURVE_WITH_KNOTS('',3,(#11535,#11536,#11537,#11538,#11539,
#11540,#11541,#11542),.UNSPECIFIED.,.F.,.F.,(4,1,1,1,1,4),(112.182488223733,
112.909458382829,113.904519577333,114.899580771837,115.89464196634,116.238928182822),
 .UNSPECIFIED.);
#184=B_SPLINE_CURVE_WITH_KNOTS('',3,(#11548,#11549,#11550,#11551,#11552,
#11553,#11554,#11555,#11556,#11557,#11558,#11559,#11560,#11561,#11562,#11563,
#11564,#11565,#11566,#11567,#11568,#11569,#11570,#11571,#11572,#11573,#11574,
#11575,#11576,#11577,#11578,#11579,#11580,#11581,#11582,#11583,#11584,#11585,
#11586,#11587,#11588,#11589,#11590,#11591,#11592,#11593,#11594,#11595,#11596,
#11597,#11598,#11599,#11600,#11601,#11602,#11603,#11604,#11605,#11606,#11607,
#11608,#11609,#11610,#11611,#11612,#11613,#11614,#11615,#11616,#11617,#11618,
#11619,#11620,#11621,#11622,#11623,#11624,#11625,#11626,#11627,#11628,#11629,
#11630,#11631,#11632,#11633,#11634,#11635,#11636,#11637,#11638,#11639,#11640,
#11641,#11642,#11643,#11644,#11645,#11646,#11647,#11648,#11649,#11650,#11651,
#11652,#11653,#11654,#11655,#11656,#11657,#11658,#11659,#11660,#11661,#11662,
#11663,#11664,#11665,#11666,#11667,#11668,#11669,#11670,#11671,#11672,#11673,
#11674,#11675,#11676,#11677,#11678,#11679,#11680,#11681,#11682,#11683),
 .UNSPECIFIED.,.F.,.F.,(4,3,3,3,3,3,3,3,3,3,3,3,3,3,3,3,3,3,3,3,3,3,3,3,
3,3,3,3,3,3,3,3,3,3,3,3,3,3,3,3,3,3,3,3,3,4),(105.898399443487,105.992303958498,
106.08623467724,106.180271478522,106.274372028075,106.368615159332,106.389802340151,
106.484040874008,106.578151573893,106.672162989362,106.766107137465,106.860017073436,
106.953918446983,107.047836893455,107.141856570169,107.235931785597,107.330159028946,
107.384863534654,107.479102068317,107.573212768008,107.667224183284,107.761168331195,
107.855078266976,107.948979640334,108.042898086619,108.136917763148,108.230992978392,
108.325220221563,108.379924729158,108.474163262819,108.568273962506,108.662285377776,
108.756229525679,108.850139461449,108.944040834797,109.037959281067,109.131978957582,
109.226054172809,109.320281415961,109.374985923662,109.471046274508,109.566961713017,
109.664157003673,109.759830056109,109.857786465876,109.955742875643),
 .UNSPECIFIED.);
#185=B_SPLINE_CURVE_WITH_KNOTS('',3,(#11684,#11685,#11686,#11687,#11688,
#11689,#11690,#11691,#11692,#11693,#11694,#11695,#11696,#11697,#11698,#11699,
#11700,#11701,#11702,#11703,#11704,#11705,#11706,#11707,#11708,#11709,#11710,
#11711,#11712,#11713,#11714,#11715,#11716,#11717,#11718,#11719,#11720,#11721,
#11722,#11723,#11724,#11725,#11726,#11727,#11728,#11729,#11730,#11731,#11732,
#11733,#11734,#11735,#11736,#11737,#11738,#11739,#11740,#11741,#11742,#11743,
#11744,#11745,#11746,#11747,#11748,#11749,#11750,#11751,#11752,#11753,#11754,
#11755,#11756),.UNSPECIFIED.,.F.,.F.,(4,3,3,3,3,3,3,3,3,3,3,3,3,3,3,3,3,
3,3,3,3,3,3,3,4),(109.955742875829,110.059318936413,110.162337101908,110.266192110037,
110.370047118165,110.464285651067,110.558396349998,110.652407764516,110.746351911677,
110.840261846711,110.934163219329,111.028081664878,111.122101340687,111.216176555218,
111.310403797692,111.365108312669,111.459358827616,111.55345200354,111.647455302587,
111.741394476697,111.835295216048,111.929214837184,112.023142266139,112.117153308002,
112.181027744827),.UNSPECIFIED.);
#186=B_SPLINE_CURVE_WITH_KNOTS('',3,(#11758,#11759,#11760,#11761,#11762,
#11763),.UNSPECIFIED.,.F.,.F.,(4,1,1,4),(109.955742875643,110.919335993822,
111.914397188326,112.182488223733),.UNSPECIFIED.);
#187=B_SPLINE_CURVE_WITH_KNOTS('',3,(#11764,#11765,#11766,#11767,#11768,
#11769,#11770,#11771,#11772),.UNSPECIFIED.,.F.,.F.,(4,1,1,1,1,1,4),(105.898136542595,
105.944030021304,106.939091215808,107.934152410311,108.929213604815,109.924274799318,
109.955742875643),.UNSPECIFIED.);
#188=B_SPLINE_CURVE_WITH_KNOTS('',3,(#11778,#11779,#11780,#11781,#11782,
#11783,#11784,#11785,#11786,#11787,#11788,#11789,#11790,#11791,#11792,#11793,
#11794,#11795,#11796,#11797,#11798,#11799,#11800,#11801,#11802,#11803,#11804,
#11805,#11806,#11807,#11808,#11809,#11810,#11811,#11812,#11813,#11814,#11815,
#11816,#11817,#11818,#11819,#11820,#11821,#11822,#11823,#11824,#11825,#11826,
#11827,#11828,#11829,#11830,#11831,#11832,#11833,#11834,#11835,#11836,#11837,
#11838,#11839,#11840,#11841,#11842,#11843,#11844,#11845,#11846,#11847,#11848,
#11849,#11850,#11851,#11852,#11853,#11854,#11855,#11856,#11857,#11858,#11859,
#11860,#11861,#11862,#11863,#11864,#11865,#11866,#11867,#11868,#11869,#11870,
#11871,#11872,#11873,#11874,#11875,#11876,#11877,#11878,#11879,#11880,#11881,
#11882,#11883,#11884,#11885,#11886,#11887,#11888,#11889,#11890,#11891,#11892,
#11893,#11894,#11895,#11896,#11897,#11898,#11899,#11900,#11901,#11902,#11903,
#11904,#11905,#11906,#11907,#11908,#11909,#11910,#11911,#11912,#11913),
 .UNSPECIFIED.,.F.,.F.,(4,3,3,3,3,3,3,3,3,3,3,3,3,3,3,3,3,3,3,3,3,3,3,3,
3,3,3,3,3,3,3,3,3,3,3,3,3,3,3,3,3,3,3,3,3,4),(99.6158155142023,99.7098241487408,
99.8037667638163,99.8976760105222,99.9915775377616,100.085496980766,100.179518115865,
100.273595547336,100.36782410646,100.419435173129,100.513673706899,100.607784406696,
100.701795822077,100.795739970093,100.889649905977,100.983551279438,101.077469725824,
101.171489402453,101.265564617795,101.359791861062,101.414496367633,101.5087349014,
101.602845601194,101.696857016572,101.790801164585,101.884711100466,101.978612473925,
102.072530920308,102.166550596934,102.260625812274,102.354853055537,102.409557562136,
102.5037960959,102.597906795691,102.691918211066,102.785862359076,102.879772294954,
102.97367366841,103.067592114789,103.161611791412,103.255687006749,103.34991425001,
103.40461875664,103.524030082473,103.64134504394,103.672557568263),
 .UNSPECIFIED.);
#189=B_SPLINE_CURVE_WITH_KNOTS('',3,(#11914,#11915,#11916,#11917,#11918,
#11919,#11920,#11921,#11922,#11923,#11924,#11925,#11926,#11927,#11928,#11929,
#11930,#11931,#11932,#11933,#11934,#11935,#11936,#11937,#11938,#11939,#11940,
#11941,#11942,#11943,#11944,#11945,#11946,#11947,#11948,#11949,#11950,#11951,
#11952,#11953,#11954,#11955,#11956,#11957,#11958,#11959,#11960,#11961,#11962,
#11963,#11964,#11965,#11966,#11967,#11968,#11969,#11970,#11971,#11972,#11973,
#11974,#11975,#11976,#11977,#11978,#11979,#11980,#11981,#11982,#11983,#11984,
#11985,#11986,#11987,#11988,#11989),.UNSPECIFIED.,.F.,.F.,(4,3,3,3,3,3,
3,3,3,3,3,3,3,3,3,3,3,3,3,3,3,3,3,3,3,4),(103.672557568463,103.765628528253,
103.858652863662,103.951657206799,104.04466816524,104.137772858376,104.230925480976,
104.324235541602,104.399679951144,104.4939184849,104.588029184684,104.682040600052,
104.775984748054,104.869894683925,104.963796057374,105.057714503746,105.151734180363,
105.245809395693,105.340036638947,105.394741145647,105.488978918377,105.583093547084,
105.677096798483,105.771035902528,105.864939461167,105.898399443487),
 .UNSPECIFIED.);
#190=B_SPLINE_CURVE_WITH_KNOTS('',3,(#11991,#11992,#11993,#11994,#11995,
#11996),.UNSPECIFIED.,.F.,.F.,(4,1,1,4),(103.672557568463,103.953907632297,
104.9489688268,105.898136542595),.UNSPECIFIED.);
#191=B_SPLINE_CURVE_WITH_KNOTS('',3,(#11997,#11998,#11999,#12000,#12001,
#12002,#12003,#12004),.UNSPECIFIED.,.F.,.F.,(4,1,1,1,1,4),(99.6145705654374,
99.9736628542824,100.968724048786,101.96378524329,102.958846437793,103.672557568463),
 .UNSPECIFIED.);
#192=B_SPLINE_CURVE_WITH_KNOTS('',3,(#12010,#12011,#12012,#12013,#12014,
#12015,#12016,#12017,#12018,#12019,#12020,#12021,#12022,#12023,#12024,#12025,
#12026,#12027,#12028,#12029,#12030,#12031,#12032,#12033,#12034,#12035,#12036,
#12037,#12038,#12039,#12040,#12041,#12042,#12043,#12044,#12045,#12046,#12047,
#12048,#12049,#12050,#12051,#12052,#12053,#12054,#12055,#12056,#12057,#12058,
#12059,#12060,#12061,#12062,#12063,#12064,#12065,#12066,#12067,#12068,#12069,
#12070,#12071,#12072,#12073,#12074,#12075,#12076,#12077,#12078,#12079,#12080,
#12081,#12082,#12083,#12084,#12085,#12086,#12087,#12088,#12089,#12090,#12091,
#12092,#12093,#12094,#12095,#12096,#12097,#12098,#12099,#12100,#12101,#12102,
#12103,#12104,#12105,#12106,#12107,#12108,#12109,#12110,#12111,#12112,#12113,
#12114,#12115,#12116,#12117,#12118,#12119,#12120,#12121,#12122,#12123,#12124,
#12125,#12126,#12127,#12128,#12129,#12130,#12131,#12132,#12133,#12134,#12135,
#12136,#12137,#12138,#12139,#12140,#12141,#12142,#12143,#12144,#12145,#12146,
#12147,#12148),.UNSPECIFIED.,.F.,.F.,(4,3,3,3,3,3,3,3,3,3,3,3,3,3,3,3,3,
3,3,3,3,3,3,3,3,3,3,3,3,3,3,3,3,3,3,3,3,3,3,3,3,3,3,3,3,3,4),(93.3315517313818,
93.4257912333858,93.4540068116039,93.548245345372,93.6423560451674,93.7363674605468,
93.8303116085609,93.9242215444431,94.0181229179026,94.1120413642863,94.2060610409137,
94.3001362562545,94.394363499519,94.4490680061075,94.5433065398756,94.6374172396711,
94.7314286550505,94.8253728030646,94.9192827389468,95.0131841124064,95.1071025587901,
95.2011222354176,95.2951974507585,95.389424694023,95.4441292006111,95.5383677343792,
95.6324784341746,95.7264898495538,95.820433997568,95.9143439334501,96.0082453069096,
96.1021637532933,96.1961834299208,96.2902586452616,96.3844858885261,96.4391903951147,
96.5327727036347,96.6262277012863,96.7216207712496,96.8149119236731,96.9081721054003,
97.0014277028664,97.0984138423979,97.1917929587829,97.2852342917175,97.3788110498964,
97.3893722609925),.UNSPECIFIED.);
#193=B_SPLINE_CURVE_WITH_KNOTS('',3,(#12149,#12150,#12151,#12152,#12153,
#12154,#12155,#12156,#12157,#12158,#12159,#12160,#12161,#12162,#12163,#12164,
#12165,#12166,#12167,#12168,#12169,#12170,#12171,#12172,#12173,#12174,#12175,
#12176,#12177,#12178,#12179,#12180,#12181,#12182,#12183,#12184,#12185,#12186,
#12187,#12188,#12189,#12190,#12191,#12192,#12193,#12194,#12195,#12196,#12197,
#12198,#12199,#12200,#12201,#12202,#12203,#12204,#12205,#12206,#12207,#12208,
#12209,#12210,#12211,#12212,#12213,#12214,#12215,#12216,#12217,#12218,#12219,
#12220,#12221,#12222,#12223,#12224),.UNSPECIFIED.,.F.,.F.,(4,3,3,3,3,3,
3,3,3,3,3,3,3,3,3,3,3,3,3,3,3,3,3,3,3,4),(97.3893722612835,97.4342515896183,
97.5284901233866,97.6226008231821,97.7166122385618,97.8105563865762,97.9044663224586,
97.9983676959184,98.0922861423024,98.18630581893,98.280381034271,98.3746082775358,
98.4293127841219,98.5235513178899,98.6176620176852,98.7116734330645,98.8056175810786,
98.8995275169606,98.99342889042,99.0873473368037,99.181367013431,99.2754422287717,
99.3696694720362,99.4243739786255,99.5200947464139,99.6158155142023),
 .UNSPECIFIED.);
#194=B_SPLINE_CURVE_WITH_KNOTS('',3,(#12226,#12227,#12228,#12229,#12230,
#12231),.UNSPECIFIED.,.F.,.F.,(4,1,1,4),(97.3893722612835,97.9835404652751,
98.9786016597787,99.6145705654374),.UNSPECIFIED.);
#195=B_SPLINE_CURVE_WITH_KNOTS('',3,(#12232,#12233,#12234,#12235,#12236,
#12237,#12238,#12239),.UNSPECIFIED.,.F.,.F.,(4,1,1,1,1,4),(93.3328220857922,
94.0032956872607,94.9983568817643,95.9934180762679,96.9884792707715,97.3893722612835),
 .UNSPECIFIED.);
#196=B_SPLINE_CURVE_WITH_KNOTS('',3,(#12245,#12246,#12247,#12248,#12249,
#12250,#12251,#12252,#12253,#12254,#12255,#12256,#12257,#12258,#12259,#12260,
#12261,#12262,#12263,#12264,#12265,#12266,#12267,#12268,#12269,#12270,#12271,
#12272,#12273,#12274,#12275,#12276,#12277,#12278,#12279,#12280,#12281,#12282,
#12283,#12284,#12285,#12286,#12287,#12288,#12289,#12290,#12291,#12292,#12293,
#12294,#12295,#12296,#12297,#12298,#12299,#12300,#12301,#12302,#12303,#12304,
#12305,#12306,#12307,#12308,#12309,#12310,#12311,#12312,#12313,#12314,#12315,
#12316,#12317,#12318,#12319,#12320,#12321,#12322,#12323,#12324,#12325,#12326,
#12327,#12328,#12329,#12330,#12331,#12332,#12333,#12334,#12335,#12336,#12337,
#12338,#12339,#12340,#12341,#12342,#12343,#12344,#12345,#12346,#12347,#12348,
#12349,#12350,#12351,#12352,#12353,#12354,#12355,#12356,#12357,#12358,#12359,
#12360,#12361,#12362,#12363,#12364,#12365,#12366,#12367,#12368,#12369,#12370,
#12371,#12372,#12373,#12374,#12375,#12376,#12377,#12378,#12379,#12380),
 .UNSPECIFIED.,.F.,.F.,(4,3,3,3,3,3,3,3,3,3,3,3,3,3,3,3,3,3,3,3,3,3,3,3,
3,3,3,3,3,3,3,3,3,3,3,3,3,3,3,3,3,3,3,3,3,4),(87.0486737068653,87.1425908968732,
87.2366087113943,87.3306810779644,87.424906653528,87.4836396445822,87.5778781783503,
87.6719888781456,87.7660002935252,87.8599444415393,87.9538543774215,88.0477557508808,
88.1416741972643,88.2356938738917,88.3297690892326,88.4239963324971,88.4787008390858,
88.5729393728539,88.6670500726492,88.7610614880287,88.8550056360428,88.9489155719249,
89.0428169453844,89.1367353917684,89.2307550683958,89.3248302837367,89.4190575270012,
89.4737620335894,89.5680005673576,89.6621112671529,89.7561226825329,89.8500668305469,
89.9439767664291,90.0378781398886,90.1317965862726,90.2258162628999,90.3198914782409,
90.4141187215054,90.468823228093,90.5634949768986,90.6580371372986,90.7524748824258,
90.8468296227406,90.9411345169126,91.0354333352937,91.106186954104),
 .UNSPECIFIED.);
#197=B_SPLINE_CURVE_WITH_KNOTS('',3,(#12381,#12382,#12383,#12384,#12385,
#12386,#12387,#12388,#12389,#12390,#12391,#12392,#12393,#12394,#12395,#12396,
#12397,#12398,#12399,#12400,#12401,#12402,#12403,#12404,#12405,#12406,#12407,
#12408,#12409,#12410,#12411,#12412,#12413,#12414,#12415,#12416,#12417,#12418,
#12419,#12420,#12421,#12422,#12423,#12424,#12425,#12426,#12427,#12428,#12429,
#12430,#12431,#12432,#12433,#12434,#12435,#12436,#12437,#12438,#12439,#12440,
#12441,#12442,#12443,#12444,#12445,#12446,#12447,#12448,#12449,#12450,#12451,
#12452,#12453,#12454,#12455,#12456),.UNSPECIFIED.,.F.,.F.,(4,3,3,3,3,3,
3,3,3,3,3,3,3,3,3,3,3,3,3,3,3,3,3,3,3,4),(91.1061869543323,91.213064427723,
91.3204667481002,91.4284945161649,91.4638844225966,91.5581229563647,91.65223365616,
91.7462450715394,91.8401892195535,91.9340991554356,92.0280005288953,92.121918975279,
92.2159386519064,92.3100138672473,92.4042411105118,92.4589456171003,92.5531921674731,
92.6504871129617,92.7444873978673,92.8384257693604,92.9323279140037,93.0262194804531,
93.1201637235949,93.2141400856374,93.3082154234006,93.3315517313818),
 .UNSPECIFIED.);
#198=B_SPLINE_CURVE_WITH_KNOTS('',3,(#12458,#12459,#12460,#12461,#12462,
#12463),.UNSPECIFIED.,.F.,.F.,(4,1,1,4),(91.106186954104,92.0131732982535,
93.0082344927571,93.3328220857922),.UNSPECIFIED.);
#199=B_SPLINE_CURVE_WITH_KNOTS('',3,(#12464,#12465,#12466,#12467,#12468,
#12469,#12470,#12471),.UNSPECIFIED.,.F.,.F.,(4,1,1,1,1,4),(87.0489316649163,
88.032928520239,89.0279897147426,90.0230509092463,91.0181121037498,91.106186954104),
 .UNSPECIFIED.);
#200=B_SPLINE_CURVE_WITH_KNOTS('',3,(#12477,#12478,#12479,#12480,#12481,
#12482,#12483,#12484,#12485,#12486,#12487,#12488,#12489,#12490,#12491,#12492,
#12493,#12494,#12495,#12496,#12497,#12498,#12499,#12500,#12501,#12502,#12503,
#12504,#12505,#12506,#12507,#12508,#12509,#12510,#12511,#12512,#12513,#12514,
#12515,#12516,#12517,#12518,#12519,#12520,#12521,#12522,#12523,#12524,#12525,
#12526,#12527,#12528,#12529,#12530,#12531,#12532,#12533,#12534,#12535,#12536,
#12537,#12538,#12539,#12540,#12541,#12542,#12543,#12544,#12545,#12546,#12547,
#12548,#12549,#12550,#12551,#12552,#12553,#12554,#12555,#12556,#12557,#12558,
#12559,#12560,#12561,#12562,#12563,#12564,#12565,#12566,#12567,#12568,#12569,
#12570,#12571,#12572,#12573,#12574,#12575,#12576,#12577,#12578,#12579,#12580,
#12581,#12582,#12583,#12584,#12585,#12586,#12587,#12588,#12589,#12590,#12591,
#12592,#12593,#12594,#12595,#12596,#12597,#12598,#12599,#12600,#12601,#12602,
#12603,#12604,#12605,#12606,#12607,#12608,#12609),.UNSPECIFIED.,.F.,.F.,
(4,3,3,3,3,3,3,3,3,3,3,3,3,3,3,3,3,3,3,3,3,3,3,3,3,3,3,3,3,3,3,3,3,3,3,
3,3,3,3,3,3,3,3,3,4),(80.7662489266783,80.8602119699798,80.9541314258835,
81.0480329545828,81.1419421942353,81.2359473431976,81.3299996171077,81.4242143061157,
81.5132724775605,81.6075110113286,81.7016217111242,81.7956331265037,81.8895772745178,
81.9834872103999,82.0773885838594,82.1713070302434,82.2653267068708,82.3594019222119,
82.4536291654764,82.5083336720641,82.6025722058322,82.6966829056277,82.7906943210076,
82.8846384690218,82.9785484049039,83.0724497783636,83.1663682247472,83.2603879013746,
83.3544631167155,83.44869035998,83.5033948665678,83.5976334003359,83.6917441001315,
83.7857555155109,83.879699663525,83.9736095994071,84.0675109728665,84.1614294192497,
84.2554490958772,84.3495243112182,84.4437515544827,84.4984560610714,84.6098153997727,
84.7200586670623,84.8230016467187),.UNSPECIFIED.);
#201=B_SPLINE_CURVE_WITH_KNOTS('',3,(#12610,#12611,#12612,#12613,#12614,
#12615,#12616,#12617,#12618,#12619,#12620,#12621,#12622,#12623,#12624,#12625,
#12626,#12627,#12628,#12629,#12630,#12631,#12632,#12633,#12634,#12635,#12636,
#12637,#12638,#12639,#12640,#12641,#12642,#12643,#12644,#12645,#12646,#12647,
#12648,#12649,#12650,#12651,#12652,#12653,#12654,#12655,#12656,#12657,#12658,
#12659,#12660,#12661,#12662,#12663,#12664,#12665,#12666,#12667,#12668,#12669,
#12670,#12671,#12672,#12673,#12674,#12675,#12676,#12677,#12678,#12679,#12680,
#12681,#12682,#12683,#12684,#12685),.UNSPECIFIED.,.F.,.F.,(4,3,3,3,3,3,
3,3,3,3,3,3,3,3,3,3,3,3,3,3,3,3,3,3,3,4),(84.8230016469244,84.9167396222475,
85.0104582715235,85.1041833778222,85.2015168472604,85.2953896866708,85.3893326790534,
85.4834206132757,85.493517255575,85.5877557893431,85.6818664891383,85.7758779045175,
85.8698220525316,85.9637319884137,86.0576333618732,86.1515518082569,86.2455714848842,
86.3396467002252,86.4338739434898,86.4885784500786,86.5828095671125,86.6769188826881,
86.7709219388292,86.864861379201,86.9587807538247,87.0486737068653),
 .UNSPECIFIED.);
#202=B_SPLINE_CURVE_WITH_KNOTS('',3,(#12687,#12688,#12689,#12690,#12691,
#12692,#12693),.UNSPECIFIED.,.F.,.F.,(4,1,1,1,4),(84.8230016469244,85.0477449367282,
86.0428061312318,87.0378673257354,87.0489316649163),.UNSPECIFIED.);
#203=B_SPLINE_CURVE_WITH_KNOTS('',3,(#12694,#12695,#12696,#12697,#12698,
#12699,#12700,#12701),.UNSPECIFIED.,.F.,.F.,(4,1,1,1,1,4),(80.7648480623333,
81.0675001587137,82.0625613532173,83.057622547721,84.0526837422246,84.8230016469244),
 .UNSPECIFIED.);
#204=B_SPLINE_CURVE_WITH_KNOTS('',3,(#12707,#12708,#12709,#12710,#12711,
#12712,#12713,#12714,#12715),.UNSPECIFIED.,.F.,.F.,(4,1,1,1,1,1,4),(74.4820968515054,
74.5478441160353,75.5429053105389,76.5379665050425,77.5330276995461,78.5280888940497,
78.5398163397448),.UNSPECIFIED.);
#205=B_SPLINE_CURVE_WITH_KNOTS('',3,(#12716,#12717,#12718,#12719,#12720,
#12721,#12722,#12723,#12724,#12725,#12726,#12727,#12728,#12729,#12730,#12731,
#12732,#12733,#12734,#12735,#12736,#12737,#12738,#12739,#12740,#12741,#12742,
#12743,#12744,#12745,#12746,#12747,#12748,#12749,#12750,#12751,#12752,#12753,
#12754,#12755,#12756,#12757,#12758,#12759,#12760,#12761,#12762,#12763,#12764,
#12765,#12766,#12767,#12768,#12769,#12770,#12771,#12772,#12773,#12774,#12775,
#12776,#12777,#12778,#12779,#12780,#12781,#12782,#12783,#12784,#12785,#12786,
#12787,#12788,#12789,#12790,#12791),.UNSPECIFIED.,.F.,.F.,(4,3,3,3,3,3,
3,3,3,3,3,3,3,3,3,3,3,3,3,3,3,3,3,3,3,4),(78.5398163397448,78.6338611328131,
78.7277784183953,78.8215970084241,78.9153494264419,79.0090686503385,79.1027805638895,
79.1965110375713,79.290343065833,79.3842324145137,79.4782706042544,79.5231500885533,
79.6173886223214,79.7114993221167,79.8055107374961,79.8994548855102,79.9933648213923,
80.087266194852,80.1811846412356,80.275204317863,80.3692795332038,80.4635067764684,
80.5182112830569,80.6124499986686,80.7065483033557,80.7662489266783),
 .UNSPECIFIED.);
#206=B_SPLINE_CURVE_WITH_KNOTS('',3,(#12793,#12794,#12795,#12796,#12797,
#12798),.UNSPECIFIED.,.F.,.F.,(4,1,1,4),(78.5398163397448,79.0773777697065,
80.0724389642101,80.7648480623333),.UNSPECIFIED.);
#207=B_SPLINE_CURVE_WITH_KNOTS('',3,(#12799,#12800,#12801,#12802,#12803,
#12804,#12805,#12806),.UNSPECIFIED.,.F.,.F.,(4,1,1,1,1,4),(74.483068094227,
75.0971329916921,76.0921941861957,77.0872553806993,78.0823165752029,78.5398163397448),
 .UNSPECIFIED.);
#208=B_SPLINE_CURVE_WITH_KNOTS('',3,(#12812,#12813,#12814,#12815,#12816,
#12817,#12818,#12819),.UNSPECIFIED.,.F.,.F.,(4,1,1,1,1,4),(68.1987206882195,
68.5774769490136,69.5725381435172,70.5675993380208,71.5626605325244,72.2566310325652),
 .UNSPECIFIED.);
#209=B_SPLINE_CURVE_WITH_KNOTS('',3,(#12820,#12821,#12822,#12823,#12824,
#12825),.UNSPECIFIED.,.F.,.F.,(4,1,1,4),(72.2566310325652,72.557721727028,
73.5527829215316,74.4820968515054),.UNSPECIFIED.);
#210=B_SPLINE_CURVE_WITH_KNOTS('',3,(#12827,#12828,#12829,#12830,#12831,
#12832),.UNSPECIFIED.,.F.,.F.,(4,1,1,4),(72.2566310325652,73.1070106026849,
74.1020717971885,74.483068094227),.UNSPECIFIED.);
#211=B_SPLINE_CURVE_WITH_KNOTS('',3,(#12833,#12834,#12835,#12836,#12837,
#12838,#12839,#12840),.UNSPECIFIED.,.F.,.F.,(4,1,1,1,1,4),(68.1997135830677,
69.1267658246704,70.121827019174,71.1168882136776,72.1119494081812,72.2566310325652),
 .UNSPECIFIED.);
#212=B_SPLINE_CURVE_WITH_KNOTS('',3,(#12846,#12847,#12848,#12849,#12850,
#12851,#12852,#12853),.UNSPECIFIED.,.F.,.F.,(4,1,1,1,1,4),(61.9169450544327,
62.6071097819919,63.6021709764955,64.5972321709991,65.5922933655027,65.9734457253856),
 .UNSPECIFIED.);
#213=B_SPLINE_CURVE_WITH_KNOTS('',3,(#12854,#12855,#12856,#12857,#12858,
#12859),.UNSPECIFIED.,.F.,.F.,(4,1,1,4),(65.9734457253856,66.5873545600064,
67.58241575451,68.1987206882195),.UNSPECIFIED.);
#214=B_SPLINE_CURVE_WITH_KNOTS('',3,(#12861,#12862,#12863,#12864,#12865,
#12866,#12867),.UNSPECIFIED.,.F.,.F.,(4,1,1,1,4),(65.9734457253856,66.1415822411596,
67.1366434356632,68.1317046301668,68.1997135830677),.UNSPECIFIED.);
#215=B_SPLINE_CURVE_WITH_KNOTS('',3,(#12868,#12869,#12870,#12871,#12872,
#12873,#12874,#12875,#12876,#12877,#12878,#12879,#12880,#12881,#12882,#12883,
#12884,#12885,#12886,#12887,#12888,#12889,#12890,#12891,#12892,#12893,#12894,
#12895,#12896,#12897,#12898,#12899,#12900,#12901,#12902,#12903,#12904,#12905,
#12906,#12907,#12908,#12909,#12910,#12911,#12912,#12913,#12914,#12915,#12916,
#12917,#12918,#12919,#12920,#12921,#12922,#12923,#12924,#12925,#12926,#12927,
#12928,#12929,#12930,#12931,#12932,#12933,#12934,#12935,#12936,#12937,#12938,
#12939,#12940,#12941,#12942,#12943,#12944,#12945,#12946,#12947,#12948,#12949,
#12950,#12951,#12952,#12953,#12954,#12955,#12956,#12957,#12958,#12959,#12960,
#12961,#12962,#12963,#12964,#12965,#12966,#12967,#12968,#12969,#12970,#12971,
#12972,#12973,#12974,#12975,#12976,#12977,#12978,#12979,#12980,#12981,#12982,
#12983,#12984,#12985,#12986,#12987,#12988,#12989,#12990,#12991,#12992,#12993,
#12994,#12995,#12996,#12997,#12998,#12999,#13000,#13001,#13002,#13003),
 .UNSPECIFIED.,.F.,.F.,(4,3,3,3,3,3,3,3,3,3,3,3,3,3,3,3,3,3,3,3,3,3,3,3,
3,3,3,3,3,3,3,3,3,3,3,3,3,3,3,3,3,3,3,3,3,4),(61.9155474649507,62.0096207055437,
62.1038467898607,62.1613374631451,62.2555759969132,62.3496866967087,62.443698112088,
62.5376422601021,62.6315521959843,62.7254535694438,62.8193720158276,62.913391692455,
63.0074669077958,63.1016941510604,63.1563986576487,63.2506371914168,63.3447478912122,
63.4387593065916,63.5327034546057,63.6266133904879,63.7205147639474,63.8144332103311,
63.9084528869585,64.0025281022993,64.0967553455639,64.1514598521523,64.2456983859204,
64.3398090857158,64.4338205010951,64.5277646491093,64.6216745849914,64.715575958451,
64.8094944048347,64.903514081462,64.9975892968029,65.0918165400675,65.1465210466559,
65.2393639284444,65.3320574568455,65.4246665115195,65.5172182347161,65.6097397018219,
65.7023016612752,65.7948804375009,65.887574788458,65.9734457253856),
 .UNSPECIFIED.);
#216=B_SPLINE_CURVE_WITH_KNOTS('',3,(#13009,#13010,#13011,#13012,#13013,
#13014,#13015,#13016,#13017),.UNSPECIFIED.,.F.,.F.,(4,1,1,1,1,1,4),(55.63288052974,
55.6416814204666,56.6367426149702,57.6318038094739,58.6268650039775,59.6219261984811,
59.690260418206),.UNSPECIFIED.);
#217=B_SPLINE_CURVE_WITH_KNOTS('',3,(#13018,#13019,#13020,#13021,#13022,
#13023),.UNSPECIFIED.,.F.,.F.,(4,1,1,4),(59.690260418206,60.6169873929847,
61.6120485874883,61.9169450544327),.UNSPECIFIED.);
#218=B_SPLINE_CURVE_WITH_KNOTS('',3,(#13025,#13026,#13027,#13028,#13029,
#13030,#13031,#13032,#13033,#13034,#13035,#13036,#13037,#13038,#13039,#13040,
#13041,#13042,#13043,#13044,#13045,#13046,#13047,#13048,#13049,#13050,#13051,
#13052,#13053,#13054,#13055,#13056,#13057,#13058,#13059,#13060,#13061,#13062,
#13063,#13064,#13065,#13066,#13067,#13068,#13069,#13070,#13071,#13072,#13073,
#13074,#13075,#13076,#13077,#13078,#13079,#13080,#13081,#13082,#13083,#13084,
#13085,#13086,#13087,#13088,#13089,#13090,#13091,#13092,#13093,#13094,#13095,
#13096,#13097),.UNSPECIFIED.,.F.,.F.,(4,3,3,3,3,3,3,3,3,3,3,3,3,3,3,3,3,
3,3,3,3,3,3,3,4),(59.69026041838,59.7892918179424,59.8886169604212,59.9880911992762,
60.0878449487758,60.1712150741379,60.265453607906,60.3595643077015,60.453575723081,
60.5475198710951,60.6414298069773,60.7353311804368,60.8292496268206,60.9232693034479,
61.0173445187888,61.1115717620534,61.1662762686415,61.2604897277826,61.3545858806246,
61.4485905700231,61.5425295525125,61.636449941463,61.7303545167224,61.8243186129422,
61.9155474649507),.UNSPECIFIED.);
#219=B_SPLINE_CURVE_WITH_KNOTS('',3,(#13098,#13099,#13100,#13101,#13102,
#13103,#13104,#13105,#13106,#13107,#13108,#13109,#13110,#13111,#13112,#13113,
#13114,#13115,#13116,#13117,#13118,#13119,#13120,#13121,#13122,#13123,#13124,
#13125,#13126,#13127,#13128,#13129,#13130,#13131,#13132,#13133,#13134,#13135,
#13136,#13137,#13138,#13139,#13140,#13141,#13142,#13143,#13144,#13145,#13146,
#13147,#13148,#13149,#13150,#13151,#13152,#13153,#13154,#13155,#13156,#13157,
#13158,#13159,#13160,#13161,#13162,#13163,#13164,#13165,#13166,#13167,#13168,
#13169,#13170,#13171,#13172,#13173,#13174,#13175,#13176,#13177,#13178,#13179,
#13180,#13181,#13182,#13183,#13184,#13185,#13186,#13187,#13188,#13189,#13190,
#13191,#13192,#13193,#13194,#13195,#13196,#13197,#13198,#13199,#13200,#13201,
#13202,#13203,#13204,#13205,#13206,#13207,#13208,#13209,#13210,#13211,#13212,
#13213,#13214,#13215,#13216,#13217,#13218,#13219,#13220,#13221,#13222,#13223,
#13224,#13225,#13226,#13227,#13228,#13229,#13230,#13231,#13232,#13233),
 .UNSPECIFIED.,.F.,.F.,(4,3,3,3,3,3,3,3,3,3,3,3,3,3,3,3,3,3,3,3,3,3,3,3,
3,3,3,3,3,3,3,3,3,3,3,3,3,3,3,3,3,3,3,3,3,4),(55.6331177742522,55.7270192353002,
55.8209287590395,55.9149343983334,56.0089874786209,56.1032025709014,56.1909702961235,
56.2852088298917,56.3793195296874,56.4733309450668,56.5672750930809,56.661185028963,
56.7550864024225,56.8490048488062,56.9430245254336,57.0370997407745,57.1313269840391,
57.1860314906271,57.2802700243952,57.3743807241905,57.4683921395699,57.562336287584,
57.656246223466,57.7501475969256,57.8440660433095,57.9380857199369,58.0321609352777,
58.1263881785422,58.1810926851307,58.2753312188987,58.3694419186941,58.463453334074,
58.557397482088,58.6513074179702,58.7452087914297,58.8391272378137,58.933146914441,
59.0272221297817,59.1214493730463,59.1761538796343,59.274502750808,59.3726743921946,
59.4706312790708,59.568458264237,59.6661366206854,59.690260418206),
 .UNSPECIFIED.);
#220=B_SPLINE_CURVE_WITH_KNOTS('',3,(#13239,#13240,#13241,#13242,#13243,
#13244,#13245,#13246),.UNSPECIFIED.,.F.,.F.,(4,1,1,1,1,4),(49.3489697493475,
49.671314253445,50.6663754479486,51.6614366424522,52.6564978369558,53.4070751110264),
 .UNSPECIFIED.);
#221=B_SPLINE_CURVE_WITH_KNOTS('',3,(#13247,#13248,#13249,#13250,#13251,
#13252),.UNSPECIFIED.,.F.,.F.,(4,1,1,4),(53.4070751110264,53.6515590314594,
54.646620225963,55.63288052974),.UNSPECIFIED.);
#222=B_SPLINE_CURVE_WITH_KNOTS('',3,(#13254,#13255,#13256,#13257,#13258,
#13259,#13260,#13261,#13262,#13263,#13264,#13265,#13266,#13267,#13268,#13269,
#13270,#13271,#13272,#13273,#13274,#13275,#13276,#13277,#13278,#13279,#13280,
#13281,#13282,#13283,#13284,#13285,#13286,#13287,#13288,#13289,#13290,#13291,
#13292,#13293,#13294,#13295,#13296,#13297,#13298,#13299,#13300,#13301,#13302,
#13303,#13304,#13305,#13306,#13307,#13308,#13309,#13310,#13311,#13312,#13313,
#13314,#13315,#13316,#13317,#13318,#13319,#13320,#13321,#13322,#13323,#13324,
#13325,#13326,#13327,#13328,#13329),.UNSPECIFIED.,.F.,.F.,(4,3,3,3,3,3,
3,3,3,3,3,3,3,3,3,3,3,3,3,3,3,3,3,3,3,4),(53.4070751113289,53.4997993899176,
53.5924384457477,53.685032722364,53.777609233099,53.8701949680628,53.9628735164002,
54.0556031024292,54.1484802212983,54.2008479071162,54.2950864408842,54.3891971406796,
54.483208556059,54.5771527040731,54.6710626399553,54.7649640134149,54.8588824597985,
54.9529021364258,55.0469773517667,55.1412045950313,55.1959091016198,55.2901555279544,
55.3842501725594,55.4782569490822,55.5721977073362,55.6331177742522),
 .UNSPECIFIED.);
#223=B_SPLINE_CURVE_WITH_KNOTS('',3,(#13330,#13331,#13332,#13333,#13334,
#13335,#13336,#13337,#13338,#13339,#13340,#13341,#13342,#13343,#13344,#13345,
#13346,#13347,#13348,#13349,#13350,#13351,#13352,#13353,#13354,#13355,#13356,
#13357,#13358,#13359,#13360,#13361,#13362,#13363,#13364,#13365,#13366,#13367,
#13368,#13369,#13370,#13371,#13372,#13373,#13374,#13375,#13376,#13377,#13378,
#13379,#13380,#13381,#13382,#13383,#13384,#13385,#13386,#13387,#13388,#13389,
#13390,#13391,#13392,#13393,#13394,#13395,#13396,#13397,#13398,#13399,#13400,
#13401,#13402,#13403,#13404,#13405,#13406,#13407,#13408,#13409,#13410,#13411,
#13412,#13413,#13414,#13415,#13416,#13417,#13418,#13419,#13420,#13421,#13422,
#13423,#13424,#13425,#13426,#13427,#13428,#13429,#13430,#13431,#13432,#13433,
#13434,#13435,#13436,#13437,#13438,#13439,#13440,#13441,#13442,#13443,#13444,
#13445,#13446,#13447,#13448,#13449,#13450,#13451,#13452,#13453,#13454,#13455,
#13456,#13457,#13458,#13459,#13460,#13461,#13462,#13463,#13464,#13465),
 .UNSPECIFIED.,.F.,.F.,(4,3,3,3,3,3,3,3,3,3,3,3,3,3,3,3,3,3,3,3,3,3,3,3,
3,3,3,3,3,3,3,3,3,3,3,3,3,3,3,3,3,3,3,3,3,4),(49.3502511000592,49.4443265486276,
49.5413611211869,49.6352901440451,49.7291940914598,49.8230986056186,49.9170293218311,
50.0110661197233,50.1051666643787,50.1994097924107,50.2206031291018,50.3148416628698,
50.4089523626651,50.5029637780443,50.5969079260583,50.6908178619404,50.7847192353998,
50.8786376817835,50.9726573584107,51.0667325737515,51.1609598170159,51.2156643236054,
51.3099028573735,51.4040135571689,51.4980249725482,51.5919691205624,51.6858790564445,
51.779780429904,51.8736988762878,51.9677185529151,52.061793768256,52.1560210115205,
52.210725518109,52.3049640518771,52.3990747516726,52.493086167052,52.5870303150662,
52.6809402509483,52.7748416244079,52.8687600707917,52.9627797474192,53.05685496276,
53.1510822060246,53.2057867126126,53.3395856335401,53.4070751110264),
 .UNSPECIFIED.);
#224=B_SPLINE_CURVE_WITH_KNOTS('',3,(#13471,#13472,#13473,#13474,#13475,
#13476,#13477,#13478),.UNSPECIFIED.,.F.,.F.,(4,1,1,1,1,4),(43.0672191665734,
43.7009470864233,44.6960082809269,45.6910694754305,46.6861306699341,47.1238898038468),
 .UNSPECIFIED.);
#225=B_SPLINE_CURVE_WITH_KNOTS('',3,(#13479,#13480,#13481,#13482,#13483,
#13484),.UNSPECIFIED.,.F.,.F.,(4,1,1,4),(47.1238898038468,47.6811918644377,
48.6762530589414,49.3489697493475),.UNSPECIFIED.);
#226=B_SPLINE_CURVE_WITH_KNOTS('',3,(#13486,#13487,#13488,#13489,#13490,
#13491,#13492,#13493,#13494,#13495,#13496,#13497,#13498,#13499,#13500,#13501,
#13502,#13503,#13504,#13505,#13506,#13507,#13508,#13509,#13510,#13511,#13512,
#13513,#13514,#13515,#13516,#13517,#13518,#13519,#13520,#13521,#13522,#13523,
#13524,#13525,#13526,#13527,#13528,#13529,#13530,#13531,#13532,#13533,#13534,
#13535,#13536,#13537,#13538,#13539,#13540,#13541,#13542,#13543,#13544,#13545,
#13546,#13547,#13548,#13549,#13550,#13551,#13552,#13553,#13554,#13555,#13556,
#13557,#13558,#13559,#13560,#13561),.UNSPECIFIED.,.F.,.F.,(4,3,3,3,3,3,
3,3,3,3,3,3,3,3,3,3,3,3,3,3,3,3,3,3,3,4),(47.1238898038468,47.235419545591,
47.3296580793584,47.4237687791533,47.5177801945321,47.6117243425455,47.7056342784269,
47.7995356518858,47.8934540982688,47.9874737748954,48.0815489902356,48.1757762334995,
48.2304807400946,48.3247192738626,48.418829973658,48.5128413890372,48.6067855370512,
48.7006954729333,48.7945968463928,48.8885152927764,48.9825349694037,49.0766101847445,
49.1708374280089,49.2255419345982,49.3197803055326,49.3502511000592),
 .UNSPECIFIED.);
#227=B_SPLINE_CURVE_WITH_KNOTS('',3,(#13562,#13563,#13564,#13565,#13566,
#13567,#13568,#13569,#13570,#13571,#13572,#13573,#13574,#13575,#13576,#13577,
#13578,#13579,#13580,#13581,#13582,#13583,#13584,#13585,#13586,#13587,#13588,
#13589,#13590,#13591,#13592,#13593,#13594,#13595,#13596,#13597,#13598,#13599,
#13600,#13601,#13602,#13603,#13604,#13605,#13606,#13607,#13608,#13609,#13610,
#13611,#13612,#13613,#13614,#13615,#13616,#13617,#13618,#13619,#13620,#13621,
#13622,#13623,#13624,#13625,#13626,#13627,#13628,#13629,#13630,#13631,#13632,
#13633,#13634,#13635,#13636,#13637,#13638,#13639,#13640,#13641,#13642,#13643,
#13644,#13645,#13646,#13647,#13648,#13649,#13650,#13651,#13652,#13653,#13654,
#13655,#13656,#13657,#13658,#13659,#13660,#13661,#13662,#13663,#13664,#13665,
#13666,#13667,#13668,#13669,#13670,#13671,#13672,#13673,#13674,#13675,#13676,
#13677,#13678,#13679,#13680,#13681,#13682,#13683,#13684,#13685,#13686,#13687,
#13688,#13689,#13690,#13691,#13692,#13693,#13694,#13695,#13696,#13697),
 .UNSPECIFIED.,.F.,.F.,(4,3,3,3,3,3,3,3,3,3,3,3,3,3,3,3,3,3,3,3,3,3,3,3,
3,3,3,3,3,3,3,3,3,3,3,3,3,3,3,3,3,3,3,3,3,4),(43.0659835124591,43.1605791400178,
43.2551747675765,43.3494133013565,43.4435240011641,43.5375354165557,43.6314795645823,
43.725389500477,43.8192908739492,43.9132093203457,44.0072289969859,44.1013042123396,
44.1955314556169,44.2502359620801,44.3444744958442,44.4385851956356,44.5325966110109,
44.6265407590209,44.720450694899,44.8143520683544,44.908270514734,45.0022901913573,
45.0963654066941,45.1905926499546,45.2452971565837,45.3395356903508,45.4336463901451,
45.5276578055234,45.6216019535364,45.7155118894175,45.8094132628759,45.9033317092585,
45.9973513858848,46.0914266012245,46.1856538444878,46.2403583510873,46.333353832454,
46.4262225404454,46.5189866105434,46.6116939361539,46.7043714684796,46.7970461230593,
46.8897940511829,46.9825825279247,47.0754997300084,47.1238898036263),
 .UNSPECIFIED.);
#228=B_SPLINE_CURVE_WITH_KNOTS('',3,(#13703,#13704,#13705,#13706,#13707,
#13708,#13709,#13710),.UNSPECIFIED.,.F.,.F.,(4,1,1,1,1,4),(36.7836747455901,
37.7305799194016,38.7256411139052,39.7207023084089,40.7157635029125,40.8407044966672),
 .UNSPECIFIED.);
#229=B_SPLINE_CURVE_WITH_KNOTS('',3,(#13711,#13712,#13713,#13714,#13715,
#13716),.UNSPECIFIED.,.F.,.F.,(4,1,1,4),(40.8407044966672,41.7108246974161,
42.7058858919197,43.0672191665734),.UNSPECIFIED.);
#230=B_SPLINE_CURVE_WITH_KNOTS('',3,(#13718,#13719,#13720,#13721,#13722,
#13723,#13724,#13725,#13726,#13727,#13728,#13729,#13730,#13731,#13732,#13733,
#13734,#13735,#13736,#13737,#13738,#13739,#13740,#13741,#13742,#13743,#13744,
#13745,#13746,#13747,#13748,#13749,#13750,#13751,#13752,#13753,#13754,#13755,
#13756,#13757,#13758,#13759,#13760,#13761,#13762,#13763,#13764,#13765,#13766,
#13767,#13768,#13769,#13770,#13771,#13772,#13773,#13774,#13775,#13776,#13777,
#13778,#13779,#13780,#13781,#13782,#13783,#13784,#13785,#13786,#13787,#13788,
#13789,#13790),.UNSPECIFIED.,.F.,.F.,(4,3,3,3,3,3,3,3,3,3,3,3,3,3,3,3,3,
3,3,3,3,3,3,3,4),(40.8407044968377,40.9467914672706,41.0491746663428,41.1571135224561,
41.2650523785693,41.3592909123152,41.4534016120883,41.5474130274451,41.6413571754367,
41.7352671112963,41.8291684847333,41.9230869310945,42.0171066076995,42.111181823018,
42.2054090662605,42.2601135730729,42.3543648080943,42.4484583692329,42.5424618160507,
42.6364009011465,42.7303013150761,42.8242184397312,42.9181432776328,43.0121464883181,
43.0659835124591),.UNSPECIFIED.);
#231=B_SPLINE_CURVE_WITH_KNOTS('',3,(#13791,#13792,#13793,#13794,#13795,
#13796,#13797,#13798,#13799,#13800,#13801,#13802,#13803,#13804,#13805,#13806,
#13807,#13808,#13809,#13810,#13811,#13812,#13813,#13814,#13815,#13816,#13817,
#13818,#13819,#13820,#13821,#13822,#13823,#13824,#13825,#13826,#13827,#13828,
#13829,#13830,#13831,#13832,#13833,#13834,#13835,#13836,#13837,#13838,#13839,
#13840,#13841,#13842,#13843,#13844,#13845,#13846,#13847,#13848,#13849,#13850,
#13851,#13852,#13853,#13854,#13855,#13856,#13857,#13858,#13859,#13860,#13861,
#13862,#13863,#13864,#13865,#13866,#13867,#13868,#13869,#13870,#13871,#13872,
#13873,#13874,#13875,#13876,#13877,#13878,#13879,#13880,#13881,#13882,#13883,
#13884,#13885,#13886,#13887,#13888,#13889,#13890,#13891,#13892,#13893,#13894,
#13895,#13896,#13897,#13898,#13899,#13900,#13901,#13902,#13903,#13904,#13905,
#13906,#13907,#13908,#13909,#13910,#13911,#13912,#13913,#13914,#13915,#13916,
#13917,#13918,#13919,#13920,#13921,#13922,#13923,#13924,#13925,#13926),
 .UNSPECIFIED.,.F.,.F.,(4,3,3,3,3,3,3,3,3,3,3,3,3,3,3,3,3,3,3,3,3,3,3,3,
3,3,3,3,3,3,3,3,3,3,3,3,3,3,3,3,3,3,3,3,3,4),(36.7833917266701,36.8772949592417,
36.971221661623,37.0652530285966,37.1593456853982,37.2535836813732,37.2848076005548,
37.3790461348947,37.4731568352694,37.5671682512346,37.6611123998426,37.755022336323,
37.8489237103847,37.9428421573735,38.036861834607,38.1309370505553,38.2251642944236,
38.2798687950584,38.3741073287149,38.4682180283984,38.5622294436654,38.6561735915675,
38.750083527338,38.843984900686,38.9379033469586,39.0319230234764,39.1259982387085,
39.2202254818661,39.2749299895621,39.3691685232372,39.4632792229378,39.5572906382204,
39.6512347861354,39.7451447219173,39.8390460952754,39.932964541557,40.0269842180808,
40.1210594333172,40.2152866764772,40.2699911840657,40.3663474040655,40.4625550535571,
40.5586031869615,40.6545575386078,40.7504306626063,40.8407044966672),
 .UNSPECIFIED.);
#232=B_SPLINE_CURVE_WITH_KNOTS('',3,(#13932,#13933,#13934,#13935,#13936,
#13937,#13938,#13939),.UNSPECIFIED.,.F.,.F.,(4,1,1,1,1,4),(30.4993075292779,
30.7651515578764,31.76021275238,32.7552739468836,33.7503351413872,34.5575191894876),
 .UNSPECIFIED.);
#233=B_SPLINE_CURVE_WITH_KNOTS('',3,(#13940,#13941,#13942,#13943,#13944,
#13945,#13946),.UNSPECIFIED.,.F.,.F.,(4,1,1,1,4),(34.5575191894876,34.7453963358908,
35.7404575303944,36.735518724898,36.7836747455901),.UNSPECIFIED.);
#234=B_SPLINE_CURVE_WITH_KNOTS('',3,(#13948,#13949,#13950,#13951,#13952,
#13953,#13954,#13955,#13956,#13957,#13958,#13959,#13960,#13961,#13962,#13963,
#13964,#13965,#13966,#13967,#13968,#13969,#13970,#13971,#13972,#13973,#13974,
#13975,#13976,#13977,#13978,#13979,#13980,#13981,#13982,#13983,#13984,#13985,
#13986,#13987,#13988,#13989,#13990,#13991,#13992,#13993,#13994,#13995,#13996,
#13997,#13998,#13999,#14000,#14001,#14002,#14003,#14004,#14005,#14006,#14007,
#14008,#14009,#14010,#14011,#14012,#14013,#14014,#14015,#14016,#14017,#14018,
#14019,#14020,#14021,#14022,#14023),.UNSPECIFIED.,.F.,.F.,(4,3,3,3,3,3,
3,3,3,3,3,3,3,3,3,3,3,3,3,3,3,3,3,3,3,4),(34.5575191894876,34.650507384765,
34.7434447378057,34.8363579762665,34.9292737992236,35.0222802874223,35.1153312645007,
35.208542165953,35.2946852115476,35.3889237448561,35.4830344441946,35.5770458591202,
35.6709900066873,35.7648999421268,35.8588013151486,35.9527197611,36.0467394373063,
36.1408146522315,36.2350418950937,36.2897464060512,36.3839854254529,36.4781010625499,
36.572104614555,36.6660439246588,36.7599457437182,36.7833917266701),
 .UNSPECIFIED.);
#235=B_SPLINE_CURVE_WITH_KNOTS('',3,(#14024,#14025,#14026,#14027,#14028,
#14029,#14030,#14031,#14032,#14033,#14034,#14035,#14036,#14037,#14038,#14039,
#14040,#14041,#14042,#14043,#14044,#14045,#14046,#14047,#14048,#14049,#14050,
#14051,#14052,#14053,#14054,#14055,#14056,#14057,#14058,#14059,#14060,#14061,
#14062,#14063,#14064,#14065,#14066,#14067,#14068,#14069,#14070,#14071,#14072,
#14073,#14074,#14075,#14076,#14077,#14078,#14079,#14080,#14081,#14082,#14083,
#14084,#14085,#14086,#14087,#14088,#14089,#14090,#14091,#14092,#14093,#14094,
#14095,#14096,#14097,#14098,#14099,#14100,#14101,#14102,#14103,#14104,#14105,
#14106,#14107,#14108,#14109,#14110,#14111,#14112,#14113,#14114,#14115,#14116,
#14117,#14118,#14119,#14120,#14121,#14122,#14123,#14124,#14125,#14126,#14127,
#14128,#14129,#14130,#14131,#14132,#14133,#14134,#14135,#14136,#14137,#14138,
#14139,#14140,#14141,#14142,#14143,#14144,#14145,#14146,#14147,#14148,#14149,
#14150,#14151,#14152,#14153,#14154,#14155,#14156,#14157,#14158,#14159),
 .UNSPECIFIED.,.F.,.F.,(4,3,3,3,3,3,3,3,3,3,3,3,3,3,3,3,3,3,3,3,3,3,3,3,
3,3,3,3,3,3,3,3,3,3,3,3,3,3,3,3,3,3,3,3,3,4),(30.5007718328711,30.5947895666449,
30.6887372141556,30.7826487508107,30.8765498282776,30.9704660823069,31.0644825169794,
31.1585527858859,31.2527771290475,31.3144404335332,31.408678991978,31.5027897167387,
31.5968011573355,31.6907453308385,31.7846552923679,31.8785566916019,31.9724751638558,
32.0664948663422,32.1605701075741,32.2547973765244,32.3095016280368,32.4037401608989,
32.4978508598401,32.591862274418,32.6858064217136,32.7797163569288,32.8736177297741,
32.9675361755972,33.0615558517501,33.1556310666643,33.2498583095829,33.3045628225404,
33.3988013500615,33.4929120435014,33.5869234524259,33.6808675938635,33.7747775230965,
33.868678889842,33.9625973294547,34.0566169992651,34.1506922077529,34.2449194441747,
34.299624017044,34.4208944647328,34.5397648462028,34.5575191891919),
 .UNSPECIFIED.);
#236=B_SPLINE_CURVE_WITH_KNOTS('',3,(#14165,#14166,#14167,#14168,#14169,
#14170,#14171,#14172),.UNSPECIFIED.,.F.,.F.,(4,1,1,1,1,4),(24.2174208605652,
24.7947843908547,25.7898455853583,26.7849067798619,27.7799679743655,28.274333882308),
 .UNSPECIFIED.);
#237=B_SPLINE_CURVE_WITH_KNOTS('',3,(#14173,#14174,#14175,#14176,#14177,
#14178),.UNSPECIFIED.,.F.,.F.,(4,1,1,4),(28.274333882308,28.7750291688691,
29.7700903633727,30.4993075292779),.UNSPECIFIED.);
#238=B_SPLINE_CURVE_WITH_KNOTS('',3,(#14180,#14181,#14182,#14183,#14184,
#14185,#14186,#14187,#14188,#14189,#14190,#14191,#14192,#14193,#14194,#14195,
#14196,#14197,#14198,#14199,#14200,#14201,#14202,#14203,#14204,#14205,#14206,
#14207,#14208,#14209,#14210,#14211,#14212,#14213,#14214,#14215,#14216,#14217,
#14218,#14219,#14220,#14221,#14222,#14223,#14224,#14225,#14226,#14227,#14228,
#14229,#14230,#14231,#14232,#14233,#14234,#14235,#14236,#14237,#14238,#14239,
#14240,#14241,#14242,#14243,#14244,#14245,#14246,#14247,#14248,#14249,#14250,
#14251,#14252,#14253,#14254,#14255),.UNSPECIFIED.,.F.,.F.,(4,3,3,3,3,3,
3,3,3,3,3,3,3,3,3,3,3,3,3,3,3,3,3,3,3,4),(28.274333882308,28.3292568500223,
28.4234955385194,28.5176063946983,28.6116179678894,28.7055622751876,28.7994723712053,
28.8933739054553,28.9872925130887,29.0813123506841,29.1753877270723,29.2696151299171,
29.3243180445259,29.4185565881387,29.5126672983678,29.6066787247526,29.7006228845845,
29.7945328327832,29.8884342190449,29.9823526787031,30.0763723692509,30.1704475988978,
30.2646748569405,30.3193792390296,30.4135944693525,30.5007718328711),
 .UNSPECIFIED.);
#239=B_SPLINE_CURVE_WITH_KNOTS('',3,(#14256,#14257,#14258,#14259,#14260,
#14261,#14262,#14263,#14264,#14265,#14266,#14267,#14268,#14269,#14270,#14271,
#14272,#14273,#14274,#14275,#14276,#14277,#14278,#14279,#14280,#14281,#14282,
#14283,#14284,#14285,#14286,#14287,#14288,#14289,#14290,#14291,#14292,#14293,
#14294,#14295,#14296,#14297,#14298,#14299,#14300,#14301,#14302,#14303,#14304,
#14305,#14306,#14307,#14308,#14309,#14310,#14311,#14312,#14313,#14314,#14315,
#14316,#14317,#14318,#14319,#14320,#14321,#14322,#14323,#14324,#14325,#14326,
#14327,#14328,#14329,#14330,#14331,#14332,#14333,#14334,#14335,#14336,#14337,
#14338,#14339,#14340,#14341,#14342,#14343,#14344,#14345,#14346,#14347,#14348,
#14349,#14350,#14351,#14352,#14353,#14354,#14355,#14356,#14357,#14358,#14359,
#14360,#14361,#14362,#14363,#14364,#14365,#14366,#14367,#14368,#14369,#14370,
#14371,#14372,#14373,#14374,#14375,#14376,#14377,#14378,#14379,#14380,#14381,
#14382,#14383,#14384,#14385,#14386,#14387,#14388,#14389,#14390,#14391),
 .UNSPECIFIED.,.F.,.F.,(4,3,3,3,3,3,3,3,3,3,3,3,3,3,3,3,3,3,3,3,3,3,3,3,
3,3,3,3,3,3,3,3,3,3,3,3,3,3,3,3,3,3,3,3,3,4),(24.2164936820193,24.3107305689308,
24.3490120720079,24.4432480127433,24.53735608089,24.6313648298541,24.7253062705863,
24.8192134748993,24.9131120958114,25.0070277719615,25.1010446681085,25.1951170930602,
25.2893415577707,25.3440732665115,25.4383127320977,25.5324243724796,25.6264367358588,
25.720381838964,25.8142927339653,25.908195069392,26.0021144794129,26.0961351163385,
26.1902112915144,26.2844394843798,26.3391344610151,26.4333731743329,26.5274840592679,
26.6214956650936,26.7154400107166,26.8093501485702,26.903251728129,26.9971703845084,
27.0911902758432,27.185265708871,27.2794931724116,27.3341956555187,27.4276602318839,
27.5209976121009,27.6151646458553,27.7083392261065,27.8014829430723,27.8946222986052,
27.9895501944879,28.0828111807321,28.1785725314341,28.2743338821362),
 .UNSPECIFIED.);
#240=B_SPLINE_CURVE_WITH_KNOTS('',3,(#14397,#14398,#14399,#14400,#14401,
#14402,#14403,#14404,#14405,#14406,#14407,#14408,#14409,#14410,#14411,#14412,
#14413,#14414,#14415,#14416,#14417,#14418,#14419,#14420,#14421,#14422,#14423,
#14424,#14425,#14426,#14427,#14428,#14429,#14430,#14431,#14432,#14433,#14434,
#14435,#14436,#14437,#14438,#14439,#14440,#14441,#14442,#14443,#14444,#14445,
#14446,#14447,#14448,#14449,#14450,#14451,#14452,#14453,#14454,#14455,#14456,
#14457,#14458,#14459,#14460,#14461,#14462,#14463,#14464,#14465,#14466,#14467,
#14468,#14469,#14470,#14471,#14472),.UNSPECIFIED.,.F.,.F.,(4,3,3,3,3,3,
3,3,3,3,3,3,3,3,3,3,3,3,3,3,3,3,3,3,3,4),(15.7079632679489,15.8007859309492,
15.8935795723414,15.9863709089602,16.0791866498076,16.1721111225518,16.2650994944724,
16.3582389121077,16.388522515979,16.4829033285741,16.5771564891806,16.6713103389117,
16.7653962546427,16.8594474840588,16.9534894914163,17.0475477260245,17.141705019005,
17.2359168213297,17.3302776617067,17.3835837104826,17.4779774291156,17.5722520765761,
17.6664233060793,17.7605330002792,17.854621932,17.9336209525117),
 .UNSPECIFIED.);
#241=B_SPLINE_CURVE_WITH_KNOTS('',3,(#14474,#14475,#14476,#14477,#14478),
 .UNSPECIFIED.,.F.,.F.,(4,1,4),(14.3984001269718,15.3934613214754,15.7079548348344),
 .UNSPECIFIED.);
#242=B_SPLINE_CURVE_WITH_KNOTS('',3,(#14482,#14483,#14484,#14485,#14486,
#14487,#14488,#14489,#14490,#14491,#14492,#14493,#14494,#14495,#14496,#14497,
#14498,#14499,#14500,#14501,#14502,#14503,#14504,#14505,#14506,#14507,#14508,
#14509,#14510,#14511,#14512,#14513,#14514,#14515,#14516,#14517,#14518,#14519,
#14520,#14521,#14522,#14523,#14524,#14525,#14526,#14527,#14528,#14529,#14530,
#14531,#14532,#14533,#14534,#14535,#14536,#14537,#14538,#14539,#14540,#14541,
#14542,#14543,#14544,#14545),.UNSPECIFIED.,.F.,.F.,(4,3,3,3,3,3,3,3,3,3,
3,3,3,3,3,3,3,3,3,3,3,4),(13.8759338288966,13.9698681094706,14.063675502176,
14.1612376201314,14.2548798577636,14.3484908494825,14.4420966018558,14.5357231098688,
14.6294501266586,14.7232367530041,14.8171644342521,14.8441724458186,14.9372022831589,
15.0335474062577,15.1263493200002,15.2190977781909,15.3118197005127,15.4045419742366,
15.4973366037527,15.590174778641,15.6831317332385,15.7079632679489),
 .UNSPECIFIED.);
#243=B_SPLINE_CURVE_WITH_KNOTS('',3,(#14546,#14547,#14548,#14549,#14550,
#14551,#14552),.UNSPECIFIED.,.F.,.F.,(4,1,1,1,4),(15.7079632679489,15.8392336403222,
16.8342948348258,17.8293560293294,17.9344061060102),.UNSPECIFIED.);
#244=B_SPLINE_CURVE_WITH_KNOTS('',3,(#14558,#14559,#14560,#14561,#14562,
#14563,#14564,#14565,#14566,#14567,#14568,#14569),.UNSPECIFIED.,.F.,.F.,
(4,2,2,2,2,4),(-0.0891720069757108,-0.0494869050463887,-0.0101787320937009,
-0.00433426661833915,-0.00195064461630957,0.),.UNSPECIFIED.);
#245=B_SPLINE_CURVE_WITH_KNOTS('',3,(#14577,#14578,#14579,#14580,#14581,
#14582,#14583,#14584,#14585,#14586,#14587,#14588,#14589,#14590,#14591,#14592,
#14593,#14594,#14595,#14596,#14597,#14598,#14599,#14600,#14601,#14602,#14603,
#14604,#14605,#14606,#14607,#14608,#14609,#14610,#14611,#14612,#14613,#14614,
#14615,#14616,#14617,#14618,#14619,#14620,#14621,#14622,#14623,#14624,#14625,
#14626,#14627,#14628,#14629,#14630,#14631,#14632,#14633,#14634,#14635,#14636,
#14637,#14638,#14639,#14640,#14641,#14642,#14643),.UNSPECIFIED.,.F.,.F.,
(4,3,3,3,3,3,3,3,3,3,3,3,3,3,3,3,3,3,3,3,3,3,4),(-119.380510462334,-119.281771177695,
-119.183171276094,-119.084683219952,-118.98625595986,-118.88785925611,-118.789462906781,
-118.690971819416,-118.592433148612,-118.493725456286,-118.41228214593,
-118.313053489152,-118.213961788152,-118.114369183561,-118.015446937852,
-117.916554860053,-117.817663412407,-117.717552797162,-117.618516407178,
-117.517868679302,-117.417220951426,-117.311998815212,-117.299669606592),
 .UNSPECIFIED.);
#246=B_SPLINE_CURVE_WITH_KNOTS('',3,(#14649,#14650,#14651,#14652,#14653,
#14654,#14655,#14656,#14657,#14658,#14659,#14660,#14661,#14662,#14663,#14664,
#14665,#14666,#14667,#14668,#14669,#14670,#14671,#14672,#14673,#14674,#14675,
#14676,#14677,#14678,#14679,#14680,#14681,#14682,#14683,#14684,#14685,#14686,
#14687,#14688,#14689,#14690,#14691,#14692,#14693,#14694,#14695,#14696,#14697,
#14698,#14699,#14700,#14701,#14702,#14703,#14704,#14705,#14706,#14707,#14708,
#14709,#14710,#14711,#14712,#14713,#14714,#14715,#14716,#14717,#14718,#14719,
#14720,#14721,#14722,#14723,#14724,#14725,#14726,#14727,#14728,#14729,#14730,
#14731,#14732,#14733,#14734,#14735,#14736,#14737,#14738,#14739,#14740,#14741,
#14742,#14743,#14744,#14745,#14746,#14747,#14748,#14749,#14750,#14751,#14752,
#14753,#14754,#14755,#14756,#14757,#14758,#14759,#14760,#14761,#14762,#14763,
#14764,#14765,#14766,#14767,#14768,#14769,#14770,#14771,#14772,#14773,#14774,
#14775,#14776,#14777,#14778,#14779,#14780,#14781,#14782,#14783,#14784,#14785,
#14786,#14787,#14788,#14789,#14790,#14791,#14792,#14793,#14794,#14795,#14796,
#14797,#14798,#14799,#14800,#14801,#14802,#14803,#14804,#14805,#14806,#14807,
#14808,#14809,#14810,#14811,#14812,#14813,#14814,#14815,#14816,#14817,#14818,
#14819,#14820,#14821,#14822,#14823,#14824,#14825,#14826,#14827,#14828,#14829,
#14830,#14831,#14832),.UNSPECIFIED.,.F.,.F.,(4,3,3,3,3,3,3,3,3,3,3,3,3,
3,3,3,3,3,3,3,3,3,3,3,3,3,3,3,3,3,3,3,3,3,3,3,3,3,3,3,3,3,3,3,3,3,3,3,3,
3,3,3,3,3,3,3,3,3,3,3,3,4),(114.761330096248,114.860080090372,114.958806946108,
115.057540414678,115.156375577384,115.255263663134,115.354321468029,115.427098562419,
115.526186136662,115.625133609413,115.724761877852,115.823533291856,115.922272394729,
116.021008931117,116.121296637569,116.220174922379,116.321167339651,116.422159756923,
116.521079048506,116.619857573038,116.719527995337,116.818130058757,116.916700027885,
117.015267869772,117.115756140185,117.214468515351,117.315844733388,117.417220951426,
117.516468414644,117.615574873252,117.715163282337,117.814090335468,117.91298347636,
118.011872245612,118.111974720691,118.210999270349,118.311640708139,118.41228214593,
118.51148086908,118.610541479571,118.710141712178,118.809030190265,118.907887549976,
119.006743360195,119.106893355254,119.205892130244,119.306617735339,119.407343340433,
119.505333524646,119.60318256861,119.703085314401,119.800762950198,119.89841208206,
119.996063705263,120.097648912682,120.195465284113,120.293361575936,120.391426373293,
120.402404534937,120.534601350672,120.663480247902,120.690073491388),
 .UNSPECIFIED.);
#247=B_SPLINE_CURVE_WITH_KNOTS('',3,(#14833,#14834,#14835,#14836,#14837,
#14838,#14839,#14840,#14841,#14842,#14843,#14844,#14845,#14846,#14847,#14848,
#14849,#14850,#14851,#14852),.UNSPECIFIED.,.F.,.F.,(4,2,2,2,2,2,2,2,2,4),
(-0.178823947996459,-0.142362827283928,-0.126740729259348,-0.12110726670276,
-0.117062474690017,-0.113022490578283,-0.109070108678785,-0.103377303050124,
-0.0894510093045505,-0.0891720069757108),.UNSPECIFIED.);
#248=B_SPLINE_CURVE_WITH_KNOTS('',3,(#14854,#14855,#14856,#14857,#14858,
#14859,#14860,#14861,#14862,#14863,#14864,#14865,#14866),.UNSPECIFIED.,
 .F.,.F.,(4,3,3,3,4),(-117.299669606592,-117.194805922057,-117.090145972068,
-116.985755035457,-116.946309935109),.UNSPECIFIED.);
#249=B_SPLINE_CURVE_WITH_KNOTS('',3,(#14867,#14868,#14869,#14870,#14871,
#14872,#14873,#14874,#14875,#14876,#14877,#14878,#14879,#14880,#14881,#14882,
#14883,#14884,#14885,#14886,#14887,#14888,#14889,#14890,#14891,#14892,#14893,
#14894,#14895,#14896,#14897,#14898,#14899,#14900,#14901,#14902,#14903,#14904,
#14905,#14906,#14907,#14908,#14909,#14910,#14911,#14912,#14913,#14914,#14915,
#14916,#14917,#14918,#14919,#14920,#14921,#14922,#14923,#14924,#14925,#14926,
#14927,#14928,#14929,#14930,#14931,#14932,#14933,#14934,#14935,#14936,#14937,
#14938,#14939,#14940,#14941,#14942,#14943,#14944,#14945,#14946,#14947,#14948,
#14949,#14950,#14951,#14952,#14953,#14954,#14955,#14956,#14957,#14958,#14959,
#14960,#14961,#14962,#14963,#14964,#14965,#14966,#14967,#14968,#14969,#14970,
#14971,#14972,#14973,#14974,#14975,#14976,#14977,#14978,#14979,#14980,#14981,
#14982,#14983,#14984,#14985,#14986,#14987,#14988,#14989,#14990,#14991,#14992,
#14993,#14994,#14995,#14996,#14997,#14998,#14999,#15000,#15001,#15002,#15003,
#15004,#15005,#15006,#15007,#15008,#15009,#15010,#15011,#15012,#15013,#15014,
#15015,#15016,#15017,#15018,#15019,#15020,#15021,#15022,#15023,#15024,#15025,
#15026,#15027,#15028,#15029,#15030,#15031,#15032,#15033,#15034,#15035,#15036,
#15037,#15038,#15039,#15040,#15041,#15042,#15043,#15044,#15045,#15046,#15047,
#15048,#15049,#15050,#15051,#15052,#15053,#15054,#15055,#15056,#15057,#15058,
#15059,#15060,#15061,#15062,#15063,#15064,#15065,#15066),.UNSPECIFIED.,
 .F.,.F.,(4,2,2,2,2,2,2,2,2,2,2,2,2,2,2,2,2,2,2,2,2,2,2,2,2,2,2,2,2,2,2,
2,2,2,2,2,2,2,2,2,2,2,2,2,2,2,2,2,2,2,2,2,2,2,2,2,2,2,2,2,2,2,2,2,2,2,2,
2,2,2,2,2,2,2,2,2,2,2,2,2,2,2,2,2,2,2,2,2,2,2,2,2,2,2,2,2,2,2,2,4),(-3.17306480281887,
-3.17031484000139,-3.16702949099971,-3.16357845900456,-3.15898974631456,
-3.14908917358974,-3.13871904583365,-3.09338330631132,-3.0497559080526,
-3.04427467983949,-3.04173163639629,-3.03977609528626,-3.03749715605209,
-3.03349583520392,-3.01607623423926,-2.97206449120236,-2.92764725149413,
-2.92031574423137,-2.91629008485033,-2.91286552807971,-2.90879756401509,
-2.9015209743123,-2.85317700352524,-2.81612752193056,-2.80290955054846,
-2.79449102094127,-2.79145426303676,-2.78940447377351,-2.78756203924621,
-2.78502055221003,-2.77854920780034,-2.73999230460291,-2.69688096552749,
-2.67476879138662,-2.66859810618169,-2.66476788008122,-2.6612413129484,
-2.6566883864451,-2.64673342784875,-2.59498225700094,-2.56534414342733,
-2.55179741996168,-2.54323388281634,-2.54018590528232,-2.53814045860138,
-2.53630787075916,-2.53330764179099,-2.52568548954152,-2.47396426601489,
-2.42723505989897,-2.41889428352826,-2.41460669782412,-2.41112133712132,
-2.4070986672778,-2.40021003083625,-2.37040805697371,-2.31979073887641,
-2.30251506025713,-2.29567342382265,-2.29054405344137,-2.28805763546822,
-2.28628746235987,-2.28403114102655,-2.28012678810709,-2.26409276851681,
-2.19920558313719,-2.18168302415323,-2.16947559351126,-2.16448973953458,
-2.16090520542717,-2.15763752132235,-2.15324369428735,-2.14465257285608,
-2.08549010643853,-2.04487905252895,-2.03946046521272,-2.0369158830879,
-2.03495208127562,-2.03265822773036,-2.02858893341875,-2.01006858852172,
-1.95649051486607,-1.9223662483841,-1.91540697721669,-1.91140662811411,
-1.90791571821389,-1.90358913525673,-1.89690266429737,-1.84827039965294,
-1.81100662114177,-1.79781730636118,-1.78941752718114,-1.78639195533164,
-1.78435109299796,-1.78251336957195,-1.77998086993912,-1.77354403440157,
-1.73236136865648,-1.69256242796197,-1.67593543967424),.UNSPECIFIED.);
#250=B_SPLINE_CURVE_WITH_KNOTS('',3,(#15072,#15073,#15074,#15075,#15076,
#15077,#15078,#15079,#15080,#15081,#15082,#15083,#15084,#15085,#15086,#15087,
#15088,#15089,#15090,#15091,#15092,#15093,#15094,#15095,#15096,#15097,#15098,
#15099,#15100,#15101,#15102,#15103,#15104,#15105,#15106,#15107,#15108,#15109,
#15110,#15111,#15112,#15113,#15114,#15115,#15116,#15117,#15118,#15119,#15120,
#15121,#15122,#15123,#15124,#15125,#15126,#15127,#15128,#15129,#15130,#15131,
#15132,#15133,#15134,#15135,#15136,#15137,#15138,#15139,#15140,#15141,#15142,
#15143,#15144,#15145,#15146,#15147,#15148,#15149,#15150,#15151,#15152,#15153,
#15154,#15155,#15156,#15157,#15158,#15159,#15160,#15161,#15162,#15163,#15164,
#15165,#15166,#15167,#15168,#15169,#15170,#15171,#15172,#15173,#15174,#15175,
#15176,#15177,#15178,#15179,#15180,#15181,#15182,#15183,#15184,#15185,#15186,
#15187,#15188,#15189,#15190,#15191,#15192,#15193,#15194,#15195,#15196,#15197,
#15198,#15199,#15200,#15201,#15202,#15203,#15204,#15205,#15206,#15207,#15208,
#15209,#15210,#15211,#15212,#15213,#15214,#15215,#15216,#15217,#15218,#15219,
#15220,#15221,#15222,#15223,#15224,#15225,#15226,#15227,#15228,#15229,#15230,
#15231,#15232,#15233,#15234,#15235,#15236,#15237,#15238,#15239,#15240,#15241,
#15242,#15243,#15244,#15245,#15246,#15247,#15248,#15249,#15250,#15251,#15252),
 .UNSPECIFIED.,.F.,.F.,(4,3,3,3,3,3,3,3,3,3,3,3,3,3,3,3,3,3,3,3,3,3,3,3,
3,3,3,3,3,3,3,3,3,3,3,3,3,3,3,3,3,3,3,3,3,3,3,3,3,3,3,3,3,3,3,3,3,3,3,3,
4),(108.477780689588,108.5768149494,108.675714162024,108.774507135944,108.873242407719,
108.971949794152,109.070659077164,109.169467502809,109.268324650162,109.367357262576,
109.456731395397,109.555791506682,109.654711181245,109.754346357327,109.853089367671,
109.951799904424,110.050507752022,110.150828961492,110.249678553296,110.350735571598,
110.451792589901,110.550848797479,110.649764558671,110.749400711888,110.848139813769,
110.946846452491,111.045550417668,111.145876259352,111.244722046462,111.345787915433,
111.446853784404,111.545915329689,111.644836413925,111.744471234548,111.84321558588,
111.941927435112,112.040636565101,112.140956168553,112.239806956383,112.340860967646,
112.441914978908,112.540979666107,112.639903958053,112.739537984973,112.838285679204,
112.937000914266,113.035713468157,113.136029144471,113.234883413822,113.335929793617,
113.436976173412,113.535600535162,113.634084744862,113.732456535692,113.830767187538,
113.929047085794,114.027326577713,114.125701961597,114.224125092387,114.322720068555,
114.406898669989),.UNSPECIFIED.);
#251=B_SPLINE_CURVE_WITH_KNOTS('',3,(#15253,#15254,#15255,#15256,#15257,
#15258,#15259,#15260,#15261,#15262,#15263,#15264,#15265,#15266,#15267,#15268),
 .UNSPECIFIED.,.F.,.F.,(4,3,3,3,3,4),(114.40689867021,114.432037367915,
114.531100262932,114.630039899472,114.728867567748,114.761330096248),
 .UNSPECIFIED.);
#252=B_SPLINE_CURVE_WITH_KNOTS('',3,(#15269,#15270,#15271,#15272,#15273,
#15274,#15275,#15276,#15277,#15278,#15279,#15280,#15281,#15282,#15283,#15284,
#15285,#15286,#15287,#15288,#15289,#15290,#15291,#15292,#15293,#15294,#15295,
#15296,#15297,#15298,#15299,#15300,#15301,#15302,#15303,#15304,#15305,#15306,
#15307,#15308,#15309,#15310,#15311,#15312,#15313,#15314,#15315,#15316,#15317,
#15318,#15319,#15320,#15321,#15322,#15323,#15324,#15325,#15326,#15327,#15328,
#15329,#15330,#15331,#15332,#15333,#15334,#15335,#15336,#15337,#15338,#15339,
#15340,#15341,#15342,#15343,#15344,#15345,#15346,#15347,#15348,#15349,#15350,
#15351,#15352,#15353,#15354,#15355,#15356,#15357,#15358,#15359,#15360,#15361,
#15362,#15363,#15364,#15365,#15366,#15367,#15368,#15369,#15370,#15371,#15372,
#15373,#15374,#15375,#15376,#15377,#15378,#15379,#15380,#15381,#15382,#15383,
#15384,#15385,#15386,#15387,#15388,#15389,#15390,#15391,#15392,#15393,#15394,
#15395,#15396,#15397,#15398,#15399,#15400,#15401,#15402,#15403,#15404,#15405,
#15406,#15407,#15408,#15409,#15410,#15411,#15412,#15413,#15414,#15415,#15416,
#15417,#15418,#15419,#15420,#15421,#15422,#15423,#15424,#15425,#15426,#15427,
#15428,#15429,#15430,#15431,#15432,#15433,#15434,#15435,#15436,#15437,#15438,
#15439,#15440,#15441,#15442,#15443,#15444,#15445,#15446,#15447,#15448,#15449,
#15450,#15451,#15452,#15453,#15454,#15455,#15456,#15457,#15458,#15459,#15460,
#15461,#15462,#15463,#15464,#15465,#15466,#15467,#15468,#15469,#15470,#15471,
#15472,#15473,#15474,#15475,#15476,#15477,#15478,#15479,#15480,#15481,#15482,
#15483,#15484,#15485,#15486,#15487,#15488,#15489,#15490,#15491,#15492,#15493,
#15494,#15495,#15496,#15497,#15498,#15499,#15500,#15501,#15502,#15503,#15504,
#15505,#15506,#15507,#15508,#15509,#15510,#15511,#15512,#15513,#15514,#15515,
#15516,#15517,#15518,#15519,#15520,#15521,#15522,#15523,#15524,#15525,#15526,
#15527,#15528,#15529,#15530,#15531,#15532,#15533,#15534),.UNSPECIFIED.,
 .F.,.F.,(4,2,2,2,2,2,2,2,2,2,2,2,2,2,2,2,2,2,2,2,2,2,2,2,2,2,2,2,2,2,2,
2,2,2,2,2,2,2,2,2,2,2,2,2,2,2,2,2,2,2,2,2,2,2,2,2,2,2,2,2,2,2,2,2,2,2,2,
2,2,2,2,2,2,2,2,2,2,2,2,2,2,2,2,2,2,2,2,2,2,2,2,2,2,2,2,2,2,2,2,2,2,2,2,
2,2,2,2,2,2,2,2,2,2,2,2,2,2,2,2,2,2,2,2,2,2,2,2,2,2,2,2,2,4),(-1.67593543967424,
-1.66977071673315,-1.66354338195487,-1.65970269687102,-1.6561828918038,
-1.65166153531714,-1.64186898951177,-1.58634824894007,-1.54408962606901,
-1.53768435112349,-1.53515704690784,-1.53332059773318,-1.53127792378963,
-1.52824448468582,-1.51978946372215,-1.5064782730895,-1.46932156034882,
-1.42074022860206,-1.4140535538658,-1.40972678469582,-1.40623565313944,
-1.40223496659467,-1.39527486134847,-1.36113297586233,-1.33008289262082,
-1.311897933727,-1.28951619754529,-1.28561070249212,-1.28314763875336,-1.28119020106764,
-1.27883569814171,-1.274365456639,-1.24122551170778,-1.18894101047551,-1.16756528212953,
-1.16123706487441,-1.15737414235223,-1.15385999665028,-1.14930622145439,
-1.13960488170706,-1.10006900335747,-1.05784774183277,-1.03808274275315,
-1.03394194019783,-1.03163233178748,-1.02986816179068,-1.02745127240965,
-1.02267768203832,-0.980115772537609,-0.921927856483065,-0.912301497716021,
-0.907810551833117,-0.904294918827611,-0.900438921298833,-0.894141611983562,
-0.870516464371559,-0.828011912858863,-0.810533582686724,-0.803829989198249,
-0.786620077210319,-0.782634748517623,-0.780360453081858,-0.778592386597329,
-0.776130388602689,-0.771131501835579,-0.730658552018725,-0.670477574292303,
-0.661027362715015,-0.656520968644825,-0.653013057915604,-0.649126210953403,
-0.642687022142984,-0.617248156183727,-0.587319819794684,-0.538998674496578,
-0.532837592146501,-0.530351753654805,-0.528344334310793,-0.526245201980107,
-0.522947702781798,-0.512354900195278,-0.493979030775597,-0.437748537043523,
-0.414389473105762,-0.407868567874907,-0.403964070590822,-0.400460178951072,
-0.395986550410335,-0.386707768108472,-0.350631073872998,-0.322597152601837,
-0.285219816526485,-0.281097498216689,-0.278570049382816,-0.27660911752628,
-0.276597237604701,-0.276585878671202,-0.276575017380847,-0.276562679594506,
-0.276550465228692,-0.276538372722027,-0.276526400552761,-0.276514547213202,
-0.276502811223774,-0.276491191118132,-0.27647968545302,-0.276468292803317,
-0.276457011765121,-0.276445840955162,-0.276434779009765,-0.276423824572702,
-0.276412976324931,-0.276402232954849,-0.276391593166715,-0.276381055688099,
-0.276370619265946,-0.276360282659443,-0.276350044652056,-0.276339904043702,
-0.276329859643788,-0.276319910288696,-0.276310054812429,-0.273939459509603,
-0.269266499659848,-0.263130102235049,-0.200228930266931,-0.164576114030874,
-0.157409452806997,-0.153322721388574,-0.149872398915665,-0.145672531750551,
-0.137766863027111,-0.0898945060156978),.UNSPECIFIED.);
#253=B_SPLINE_CURVE_WITH_KNOTS('',3,(#15540,#15541,#15542,#15543,#15544,
#15545,#15546,#15547,#15548,#15549,#15550,#15551,#15552,#15553,#15554,#15555,
#15556,#15557,#15558,#15559,#15560,#15561,#15562,#15563,#15564,#15565,#15566,
#15567,#15568,#15569,#15570,#15571,#15572,#15573,#15574,#15575,#15576,#15577,
#15578,#15579,#15580,#15581,#15582,#15583,#15584,#15585,#15586,#15587,#15588,
#15589,#15590,#15591,#15592,#15593,#15594,#15595,#15596,#15597,#15598,#15599,
#15600,#15601,#15602,#15603,#15604,#15605,#15606,#15607,#15608,#15609,#15610,
#15611,#15612,#15613,#15614,#15615,#15616,#15617,#15618,#15619,#15620,#15621,
#15622,#15623,#15624,#15625,#15626,#15627,#15628,#15629,#15630,#15631,#15632,
#15633,#15634,#15635,#15636,#15637,#15638,#15639,#15640,#15641,#15642,#15643,
#15644,#15645,#15646,#15647,#15648,#15649,#15650,#15651,#15652,#15653,#15654,
#15655,#15656,#15657,#15658,#15659,#15660,#15661,#15662,#15663,#15664,#15665,
#15666,#15667,#15668,#15669,#15670,#15671,#15672,#15673,#15674,#15675,#15676,
#15677,#15678,#15679,#15680,#15681,#15682,#15683,#15684,#15685,#15686,#15687,
#15688,#15689,#15690,#15691,#15692,#15693,#15694,#15695,#15696,#15697,#15698,
#15699,#15700,#15701,#15702,#15703,#15704,#15705,#15706,#15707,#15708,#15709,
#15710,#15711,#15712,#15713,#15714,#15715,#15716,#15717,#15718,#15719,#15720),
 .UNSPECIFIED.,.F.,.F.,(4,3,3,3,3,3,3,3,3,3,3,3,3,3,3,3,3,3,3,3,3,3,3,3,
3,3,3,3,3,3,3,3,3,3,3,3,3,3,3,3,3,3,3,3,3,3,3,3,3,3,3,3,3,3,3,3,3,3,3,3,
4),(102.194035073172,102.293066856479,102.392288804316,102.491303033872,
102.590362151105,102.689280824941,102.788916250371,102.88765825113,102.986367777226,
103.085074614465,103.185397017943,103.28424561045,103.385304919413,103.486364228376,
103.585423372849,103.68434207411,103.783977492706,103.88271952114,103.981429074944,
104.080135939883,104.180458310632,104.279306930543,104.380366176711,104.481425422879,
104.580484485822,104.679403105462,104.779038544452,104.877780491632,104.976489964496,
105.075196748918,105.175519216035,105.274367757282,105.375427187332,105.476486617383,
105.575545750516,105.67446443986,105.774099861363,105.872841876573,105.971551416695,
106.070258267518,106.17058065361,106.26942925849,106.370488535188,106.471547811886,
106.570607096495,106.669525938662,106.769161322128,106.867903492302,106.966613187844,
107.06532019433,107.165642397345,107.264491156885,107.365550081638,107.46660900639,
107.565720969537,107.664694591166,107.763559737028,107.862348777346,107.96109209191,
108.059845284113,108.12371336303),.UNSPECIFIED.);
#254=B_SPLINE_CURVE_WITH_KNOTS('',3,(#15721,#15722,#15723,#15724,#15725,
#15726,#15727,#15728,#15729,#15730,#15731,#15732,#15733),.UNSPECIFIED.,
 .F.,.F.,(4,3,3,3,4),(108.123713363395,108.237935126024,108.353261782782,
108.461670200894,108.477780689588),.UNSPECIFIED.);
#255=B_SPLINE_CURVE_WITH_KNOTS('',3,(#15735,#15736,#15737,#15738,#15739,
#15740,#15741,#15742,#15743,#15744,#15745,#15746,#15747,#15748,#15749,#15750,
#15751,#15752,#15753,#15754,#15755,#15756,#15757,#15758),.UNSPECIFIED.,
 .F.,.F.,(4,2,2,2,2,2,2,2,2,2,2,4),(-0.0898945060156978,-0.0877788736441257,
-0.0584159942359854,-0.0420681203200915,-0.0318936166568689,-0.0285276046855637,
-0.0264136235710413,-0.0245613831015139,-0.02256053581784,-0.0198266182957172,
-0.0129848053672012,-0.00073538908808835),.UNSPECIFIED.);
#256=B_SPLINE_CURVE_WITH_KNOTS('',3,(#15759,#15760,#15761,#15762,#15763,
#15764,#15765,#15766,#15767,#15768,#15769,#15770,#15771,#15772,#15773,#15774,
#15775,#15776,#15777,#15778,#15779,#15780,#15781,#15782,#15783,#15784,#15785,
#15786,#15787,#15788,#15789,#15790,#15791,#15792,#15793,#15794,#15795,#15796,
#15797,#15798,#15799,#15800,#15801,#15802,#15803,#15804,#15805,#15806,#15807,
#15808,#15809,#15810,#15811,#15812,#15813,#15814,#15815,#15816,#15817,#15818,
#15819,#15820,#15821,#15822,#15823,#15824,#15825,#15826,#15827,#15828,#15829,
#15830,#15831,#15832,#15833,#15834,#15835,#15836,#15837,#15838,#15839,#15840,
#15841,#15842,#15843,#15844,#15845,#15846,#15847,#15848,#15849,#15850,#15851,
#15852,#15853,#15854,#15855,#15856,#15857,#15858,#15859,#15860,#15861,#15862,
#15863,#15864,#15865,#15866,#15867,#15868,#15869,#15870,#15871,#15872,#15873,
#15874,#15875,#15876,#15877,#15878,#15879,#15880,#15881,#15882,#15883,#15884,
#15885,#15886,#15887,#15888,#15889,#15890,#15891,#15892,#15893,#15894,#15895,
#15896,#15897,#15898,#15899,#15900,#15901,#15902,#15903,#15904,#15905,#15906,
#15907,#15908,#15909,#15910,#15911,#15912,#15913,#15914,#15915,#15916,#15917,
#15918,#15919,#15920,#15921,#15922,#15923,#15924,#15925,#15926,#15927,#15928,
#15929,#15930,#15931,#15932,#15933,#15934,#15935,#15936,#15937,#15938,#15939,
#15940,#15941,#15942,#15943,#15944,#15945,#15946,#15947,#15948,#15949,#15950,
#15951,#15952,#15953,#15954),.UNSPECIFIED.,.F.,.F.,(4,2,2,2,2,2,2,2,2,2,
2,2,2,2,2,2,2,2,2,2,2,2,2,2,2,2,2,2,2,2,2,2,2,2,2,2,2,2,2,2,2,2,2,2,2,2,
2,2,2,2,2,2,2,2,2,2,2,2,2,2,2,2,2,2,2,2,2,2,2,2,2,2,2,2,2,2,2,2,2,2,2,2,
2,2,2,2,2,2,2,2,2,2,2,2,2,2,2,4),(-3.17299869679545,-3.11930868620718,-3.08516340173328,
-3.0782033673962,-3.07420299319222,-3.07071230450638,-3.06638630930797,
-3.05970133226788,-3.01057690666402,-2.97143166652684,-2.95971840779162,
-2.95446075643838,-2.95144690533868,-2.94885196127524,-2.94691465319532,
-2.94475488930145,-2.94118378964679,-2.92926687777781,-2.8733577666771,
-2.83772729522022,-2.82850472930221,-2.82404147000846,-2.82053831344959,
-2.8166269896721,-2.8100763476369,-2.78639181069776,-2.7362217952012,-2.70523489407633,
-2.69984428601455,-2.69730626778358,-2.69534415057137,-2.69304812126027,
-2.68896725915922,-2.67026600134761,-2.61687386102311,-2.58276964344561,
-2.57581212225449,-2.57181256763865,-2.56832222822974,-2.56399619202329,
-2.55731024136613,-2.51013164139134,-2.47613848394035,-2.45215196593302,
-2.44794263153176,-2.44564353797843,-2.44368189528988,-2.44114847131218,
-2.43700648764584,-2.40258751709594,-2.33574739643697,-2.32625748155609,
-2.32174374069557,-2.31823510386827,-2.31435253101593,-2.3079323237752,
-2.28557987932447,-2.22837541068936,-2.20112534521756,-2.19680174369964,
-2.19447838274541,-2.1925193399347,-2.19001909025172,-2.18598847928527,
-2.16008795613757,-2.11364937095877,-2.08032853919854,-2.07340879037839,
-2.06941753445167,-2.06592654366318,-2.06158943649462,-2.05486657409817,
-2.00789996740124,-1.97417154799861,-1.95772113977322,-1.95109781991293,
-1.94609540520812,-1.94363284327397,-1.94186483412151,-1.93959127415406,
-1.93560872631805,-1.91843957669912,-1.87431182369492,-1.8314436777169,
-1.82321565830487,-1.81894926166893,-1.81546293016809,-1.81141865724694,
-1.80444174463076,-1.77305818201536,-1.72333265178782,-1.69868871668601,
-1.69445431188591,-1.69214996679527,-1.69018910419601,-1.68766348217317,
-1.68354749361738,-1.67617331063835),.UNSPECIFIED.);
#257=B_SPLINE_CURVE_WITH_KNOTS('',3,(#15960,#15961,#15962,#15963,#15964,
#15965,#15966,#15967,#15968,#15969,#15970,#15971,#15972,#15973,#15974,#15975,
#15976,#15977,#15978,#15979,#15980,#15981,#15982,#15983,#15984,#15985,#15986,
#15987,#15988,#15989,#15990,#15991,#15992,#15993,#15994,#15995,#15996,#15997,
#15998,#15999,#16000,#16001,#16002,#16003,#16004,#16005,#16006,#16007,#16008,
#16009,#16010,#16011,#16012,#16013,#16014,#16015,#16016,#16017,#16018,#16019,
#16020,#16021,#16022,#16023,#16024,#16025,#16026,#16027,#16028,#16029,#16030,
#16031,#16032,#16033,#16034,#16035,#16036,#16037,#16038,#16039,#16040,#16041,
#16042,#16043,#16044,#16045,#16046,#16047,#16048,#16049,#16050,#16051,#16052,
#16053,#16054,#16055,#16056,#16057,#16058,#16059,#16060,#16061,#16062,#16063,
#16064,#16065,#16066,#16067,#16068,#16069,#16070,#16071,#16072,#16073,#16074,
#16075,#16076,#16077,#16078,#16079,#16080,#16081,#16082,#16083,#16084,#16085,
#16086,#16087,#16088,#16089,#16090,#16091,#16092,#16093,#16094,#16095,#16096,
#16097,#16098,#16099,#16100,#16101,#16102,#16103,#16104,#16105,#16106,#16107,
#16108,#16109,#16110,#16111,#16112,#16113,#16114,#16115,#16116,#16117,#16118,
#16119,#16120,#16121,#16122,#16123,#16124,#16125,#16126,#16127,#16128,#16129,
#16130,#16131,#16132,#16133,#16134,#16135,#16136,#16137,#16138,#16139,#16140),
 .UNSPECIFIED.,.F.,.F.,(4,3,3,3,3,3,3,3,3,3,3,3,3,3,3,3,3,3,3,3,3,3,3,3,
3,3,3,3,3,3,3,3,3,3,3,3,3,3,3,3,3,3,3,3,3,3,3,3,3,3,3,3,3,3,3,3,3,3,3,3,
4),(95.9117879380488,96.0100034795647,96.1082084022929,96.2113902684322,
96.3097261601217,96.4081294765302,96.5066850939811,96.5209358668503,96.6199949843232,
96.7189136584695,96.81854908383,96.9172910850647,97.0160006116976,97.1147074495317,
97.2150298524872,97.3138784457295,97.4149377535417,97.5159970613539,97.6150561795708,
97.7139748544642,97.8136102796383,97.9123522816226,98.0110618090045,98.1097686475857,
98.2100910496536,98.3089396436311,98.4099989497443,98.5110582558575,98.6101173725349,
98.7090360458894,98.8086714714483,98.9074134719061,99.006122997769,99.1048298348414,
99.2051522387213,99.3040008312296,99.4050601407953,99.5061194503611,99.6051785675261,
99.7040972413552,99.8037326667939,99.9024746676917,100.001184193981,100.099891031466,
100.200213434816,100.299062027698,100.400121336281,100.501180644865,100.600239766633,
100.69915844509,100.798793869374,100.897535874927,100.99624540587,101.094952248002,
101.195274645844,101.294123243309,101.395182541339,101.496241839368,101.611067070977,
101.725797563226,101.840528055476),.UNSPECIFIED.);
#258=B_SPLINE_CURVE_WITH_KNOTS('',3,(#16141,#16142,#16143,#16144,#16145,
#16146,#16147,#16148,#16149,#16150,#16151,#16152,#16153),.UNSPECIFIED.,
 .F.,.F.,(4,3,3,3,4),(101.84052805585,101.939398954914,102.038252712471,
102.13715687785,102.194035073172),.UNSPECIFIED.);
#259=B_SPLINE_CURVE_WITH_KNOTS('',3,(#16154,#16155,#16156,#16157,#16158,
#16159,#16160,#16161,#16162,#16163,#16164,#16165,#16166,#16167,#16168,#16169,
#16170,#16171,#16172,#16173,#16174,#16175,#16176,#16177,#16178,#16179,#16180,
#16181,#16182,#16183,#16184,#16185,#16186,#16187,#16188,#16189,#16190,#16191,
#16192,#16193,#16194,#16195,#16196,#16197,#16198,#16199,#16200,#16201,#16202,
#16203,#16204,#16205,#16206,#16207,#16208,#16209,#16210,#16211,#16212,#16213,
#16214,#16215,#16216,#16217,#16218,#16219,#16220,#16221,#16222,#16223,#16224,
#16225,#16226,#16227,#16228,#16229,#16230,#16231,#16232,#16233,#16234,#16235,
#16236,#16237,#16238,#16239,#16240,#16241,#16242,#16243,#16244,#16245,#16246,
#16247,#16248,#16249,#16250,#16251,#16252,#16253,#16254,#16255,#16256,#16257,
#16258,#16259,#16260,#16261,#16262,#16263,#16264,#16265,#16266,#16267,#16268,
#16269,#16270,#16271,#16272,#16273,#16274,#16275,#16276,#16277,#16278,#16279,
#16280,#16281,#16282,#16283,#16284,#16285,#16286,#16287,#16288,#16289,#16290,
#16291,#16292,#16293,#16294,#16295,#16296,#16297,#16298,#16299,#16300,#16301,
#16302,#16303,#16304,#16305,#16306,#16307,#16308,#16309,#16310,#16311,#16312,
#16313,#16314,#16315,#16316,#16317,#16318,#16319,#16320,#16321,#16322,#16323,
#16324,#16325,#16326,#16327,#16328,#16329,#16330,#16331,#16332,#16333,#16334,
#16335,#16336,#16337,#16338,#16339,#16340,#16341,#16342,#16343,#16344,#16345,
#16346,#16347,#16348,#16349,#16350,#16351,#16352,#16353,#16354,#16355),
 .UNSPECIFIED.,.F.,.F.,(4,2,2,2,2,2,2,2,2,2,2,2,2,2,2,2,2,2,2,2,2,2,2,2,
2,2,2,2,2,2,2,2,2,2,2,2,2,2,2,2,2,2,2,2,2,2,2,2,2,2,2,2,2,2,2,2,2,2,2,2,
2,2,2,2,2,2,2,2,2,2,2,2,2,2,2,2,2,2,2,2,2,2,2,2,2,2,2,2,2,2,2,2,2,2,2,2,
2,2,2,2,4),(-1.67617331063835,-1.65240527865461,-1.58687592034162,-1.57442556265288,
-1.56926424535368,-1.56601000523216,-1.56241757877178,-1.55737807047799,
-1.54481344327795,-1.4793696505965,-1.44802118236873,-1.44390266605422,
-1.44137630223774,-1.43941540291114,-1.43711166835483,-1.43287998920887,
-1.40831238849089,-1.37469787011544,-1.3277573326033,-1.32105082638772,
-1.31671879965861,-1.31322833391444,-1.3092337844796,-1.30229826622656,
-1.26864079726897,-1.21935167748512,-1.19652066960891,-1.19259819116766,
-1.19013042844333,-1.18817331943532,-1.18582407860207,-1.181377308325,-1.14936068376642,
-1.14561538752557,-1.08666483299086,-1.07265258302901,-1.06724130086439,
-1.06394192907254,-1.06038726053178,-1.05555970995575,-1.04430782832272,
-1.00383906640406,-0.955902843636391,-0.943964555576926,-0.940391730966087,
-0.938231909977202,-0.936235182236847,-0.933439536542829,-0.926578127566507,
-0.916560121925209,-0.884645511785449,-0.829239768756867,-0.819441950638088,
-0.814920026342847,-0.811400557812437,-0.807561016390277,-0.801337251876116,
-0.778577818170857,-0.738872834052586,-0.697644244322333,-0.691211055000536,
-0.688679419105671,-0.68684210805264,-0.684801515971349,-0.681775846915014,
-0.673372644654906,-0.660172853642147,-0.622915133599126,-0.57429251824916,
-0.567608153363514,-0.563282978348824,-0.559793201584947,-0.555794147350037,
-0.54883710564091,-0.51471845981321,-0.461086219597697,-0.442677525577018,
-0.438616544874642,-0.436325255813899,-0.434362943197346,-0.431819124933974,
-0.426396509729469,-0.381917409217466,-0.327018231694746,-0.317305841914941,
-0.31273167827336,-0.309204618487064,-0.305389709784263,-0.29963636586302,
-0.280325453086069,-0.246025036075861,-0.194715530598949,-0.18918085810934,
-0.186259915204884,-0.1842603314317,-0.182150006312332,-0.178800731731504,
-0.167954900504291,-0.136827243060613,-0.104566733046293,-0.0902712750032826),
 .UNSPECIFIED.);
#260=B_SPLINE_CURVE_WITH_KNOTS('',3,(#16361,#16362,#16363,#16364,#16365,
#16366,#16367,#16368,#16369,#16370,#16371,#16372,#16373,#16374,#16375,#16376,
#16377,#16378,#16379,#16380,#16381,#16382,#16383,#16384,#16385,#16386,#16387,
#16388,#16389,#16390,#16391,#16392,#16393,#16394,#16395,#16396,#16397,#16398,
#16399,#16400,#16401,#16402,#16403,#16404,#16405,#16406,#16407,#16408,#16409,
#16410,#16411,#16412,#16413,#16414,#16415,#16416,#16417,#16418,#16419,#16420,
#16421,#16422,#16423,#16424,#16425,#16426,#16427,#16428,#16429,#16430,#16431,
#16432,#16433,#16434,#16435,#16436,#16437,#16438,#16439,#16440,#16441,#16442,
#16443,#16444,#16445,#16446,#16447,#16448,#16449,#16450,#16451,#16452,#16453,
#16454,#16455,#16456,#16457,#16458,#16459,#16460,#16461,#16462,#16463,#16464,
#16465,#16466,#16467,#16468,#16469,#16470,#16471,#16472,#16473,#16474,#16475,
#16476,#16477,#16478,#16479,#16480,#16481,#16482,#16483,#16484,#16485,#16486,
#16487,#16488,#16489,#16490,#16491,#16492,#16493,#16494,#16495,#16496,#16497,
#16498,#16499,#16500,#16501,#16502,#16503,#16504,#16505,#16506,#16507,#16508,
#16509,#16510,#16511,#16512,#16513,#16514,#16515,#16516,#16517,#16518,#16519,
#16520,#16521,#16522,#16523,#16524,#16525,#16526,#16527,#16528,#16529,#16530,
#16531,#16532,#16533,#16534,#16535,#16536,#16537,#16538,#16539,#16540,#16541,
#16542,#16543,#16544),.UNSPECIFIED.,.F.,.F.,(4,3,3,3,3,3,3,3,3,3,3,3,3,
3,3,3,3,3,3,3,3,3,3,3,3,3,3,3,3,3,3,3,3,3,3,3,3,3,3,3,3,3,3,3,3,3,3,3,3,
3,3,3,3,3,3,3,3,3,3,3,3,4),(89.6284844345084,89.7274368855644,89.8303283623474,
89.929082090238,90.02779646593,90.1265012818364,90.2252263120905,90.3240613148707,
90.4229615017662,90.5220189447325,90.5505686998286,90.6496278174091,90.7485464916642,
90.8481819169977,90.9469239183443,91.04563344509,91.1443402830374,91.2446626858612,
91.3435112792174,91.4445705867748,91.5456298943323,91.6446890119303,91.7436076862031,
91.8432431115322,91.9419851128963,92.0406946396595,92.1394014776244,92.2397238804273,
92.3385724738006,92.4396317813182,92.5406910888358,92.6397502064081,92.7386688806553,
92.8383043059908,92.9370463073297,93.0357558340677,93.1344626720077,93.2347850748407,
93.3336336681899,93.4346929757647,93.5357522833395,93.6348114009011,93.7337300751373,
93.8333655004755,93.9321075018028,94.030817028529,94.129523866457,94.2298462693035,
94.3286948626404,94.4297541702417,94.5308134778431,94.6298725955208,94.7287912698735,
94.8284266951827,94.9271686966265,95.0258782234692,95.1245850615132,95.2249074642216,
95.3237560576724,95.4248153650096,95.5258746723467,95.5573427486709),
 .UNSPECIFIED.);
#261=B_SPLINE_CURVE_WITH_KNOTS('',3,(#16545,#16546,#16547,#16548,#16549,
#16550,#16551,#16552,#16553,#16554,#16555,#16556,#16557),.UNSPECIFIED.,
 .F.,.F.,(4,3,3,3,4),(95.5573427489394,95.6558631085308,95.7542623752097,
95.8525566826487,95.9117879380488),.UNSPECIFIED.);
#262=B_SPLINE_CURVE_WITH_KNOTS('',3,(#16559,#16560,#16561,#16562,#16563,
#16564,#16565,#16566,#16567,#16568,#16569,#16570,#16571,#16572,#16573,#16574,
#16575,#16576),.UNSPECIFIED.,.F.,.F.,(4,2,2,2,2,2,2,2,4),(-0.0902712750032826,
-0.0715222222732456,-0.0644702729272379,-0.0604092697845244,-0.0569242638253706,
-0.0535880866901934,-0.0494330478813112,-0.0431186936204873,-0.000735300760668054),
 .UNSPECIFIED.);
#263=B_SPLINE_CURVE_WITH_KNOTS('',3,(#16577,#16578,#16579,#16580,#16581,
#16582,#16583,#16584,#16585,#16586,#16587,#16588,#16589,#16590,#16591,#16592,
#16593,#16594,#16595,#16596,#16597,#16598,#16599,#16600,#16601,#16602,#16603,
#16604,#16605,#16606,#16607,#16608,#16609,#16610,#16611,#16612,#16613,#16614,
#16615,#16616,#16617,#16618,#16619,#16620,#16621,#16622,#16623,#16624,#16625,
#16626,#16627,#16628,#16629,#16630,#16631,#16632,#16633,#16634,#16635,#16636,
#16637,#16638,#16639,#16640,#16641,#16642,#16643,#16644,#16645,#16646,#16647,
#16648,#16649,#16650,#16651,#16652,#16653,#16654,#16655,#16656,#16657,#16658,
#16659,#16660,#16661,#16662,#16663,#16664,#16665,#16666,#16667,#16668,#16669,
#16670,#16671,#16672,#16673,#16674,#16675,#16676,#16677,#16678,#16679,#16680,
#16681,#16682,#16683,#16684,#16685,#16686,#16687,#16688,#16689,#16690,#16691,
#16692,#16693,#16694,#16695,#16696,#16697,#16698,#16699,#16700,#16701,#16702,
#16703,#16704,#16705,#16706,#16707,#16708,#16709,#16710,#16711,#16712,#16713,
#16714,#16715,#16716,#16717,#16718,#16719,#16720,#16721,#16722,#16723,#16724,
#16725,#16726,#16727,#16728,#16729,#16730,#16731,#16732,#16733,#16734,#16735,
#16736,#16737,#16738,#16739,#16740,#16741,#16742,#16743,#16744,#16745,#16746,
#16747,#16748,#16749,#16750,#16751,#16752,#16753,#16754,#16755,#16756,#16757,
#16758,#16759,#16760,#16761,#16762,#16763,#16764,#16765,#16766,#16767,#16768,
#16769,#16770,#16771,#16772),.UNSPECIFIED.,.F.,.F.,(4,2,2,2,2,2,2,2,2,2,
2,2,2,2,2,2,2,2,2,2,2,2,2,2,2,2,2,2,2,2,2,2,2,2,2,2,2,2,2,2,2,2,2,2,2,2,
2,2,2,2,2,2,2,2,2,2,2,2,2,2,2,2,2,2,2,2,2,2,2,2,2,2,2,2,2,2,2,2,2,2,2,2,
2,2,2,2,2,2,2,2,2,2,2,2,2,2,2,4),(-3.17301486575304,-3.1206283445989,-3.11407337427932,
-3.11056394982659,-3.10753018932838,-3.10548730126036,-3.10365040474306,
-3.10112245888732,-3.0947153741012,-3.05241203064243,-3.01284825003375,
-2.99079619169157,-2.98488514110301,-2.98099007817135,-2.97748268291822,
-2.97298798518856,-2.96360368478635,-2.90144618614788,-2.86327364670942,
-2.85800863157681,-2.85549422419458,-2.85353353619308,-2.85121937078231,
-2.84705977303144,-2.82696252670283,-2.7602873464793,-2.74632465560078,
-2.7360404617071,-2.73137994349378,-2.7278506959479,-2.724036688092,-2.71793424587706,
-2.69861344667929,-2.63812877933858,-2.61935040144618,-2.61212096353624,
-2.60676698599902,-2.60423563489,-2.60227373439065,-2.59997218175929,-2.59586810912478,
-2.57677422610921,-2.51485685331853,-2.48879305540503,-2.48230695477302,
-2.47840940274739,-2.47490297859551,-2.47041398216779,-2.46105822842412,
-2.39996331632049,-2.3609309519789,-2.35551534083815,-2.35297233482591,
-2.35100949683694,-2.34871627676867,-2.34464880324007,-2.3261520343103,
-2.27254313667151,-2.23841063472823,-2.23145093024342,-2.22745050336487,
-2.22395962693813,-2.21963321554159,-2.21294724305685,-2.16432918558983,
-2.12707837980584,-2.11388481409811,-2.10548300889584,-2.10245696381255,
-2.10041584346821,-2.0985778517584,-2.09604499381951,-2.0896072678779,-2.04840130561755,
-2.00862123847753,-1.98583514559368,-1.97960772459686,-1.97576665709208,
-1.97224627618495,-1.96772385759357,-1.95792764197776,-1.90247498967226,
-1.88839175429163,-1.85846943078831,-1.85307884475064,-1.850540663228,-1.8485783394236,
-1.84628197463637,-1.84220029875838,-1.82349073063694,-1.77009891745668,
-1.73599163242005,-1.72903337740783,-1.7250333892754,-1.72154266468868,
-1.71721614218406,-1.7105294228205,-1.67610690530384),.UNSPECIFIED.);
#264=B_SPLINE_CURVE_WITH_KNOTS('',3,(#16778,#16779,#16780,#16781,#16782,
#16783,#16784,#16785,#16786,#16787,#16788,#16789,#16790,#16791,#16792,#16793,
#16794,#16795,#16796,#16797,#16798,#16799,#16800,#16801,#16802,#16803,#16804,
#16805,#16806,#16807,#16808,#16809,#16810,#16811,#16812,#16813,#16814,#16815,
#16816,#16817,#16818,#16819,#16820,#16821,#16822,#16823,#16824,#16825,#16826,
#16827,#16828,#16829,#16830,#16831,#16832,#16833,#16834,#16835,#16836,#16837,
#16838,#16839,#16840,#16841,#16842,#16843,#16844,#16845,#16846,#16847,#16848,
#16849,#16850,#16851,#16852,#16853,#16854,#16855,#16856,#16857,#16858,#16859,
#16860,#16861,#16862,#16863,#16864,#16865,#16866,#16867,#16868,#16869,#16870,
#16871,#16872,#16873,#16874,#16875,#16876,#16877,#16878,#16879,#16880,#16881,
#16882,#16883,#16884,#16885,#16886,#16887,#16888,#16889,#16890,#16891,#16892,
#16893,#16894,#16895,#16896,#16897,#16898,#16899,#16900,#16901,#16902,#16903,
#16904,#16905,#16906,#16907,#16908,#16909,#16910,#16911,#16912,#16913,#16914,
#16915,#16916,#16917,#16918,#16919,#16920,#16921,#16922,#16923,#16924,#16925,
#16926,#16927,#16928,#16929,#16930,#16931,#16932,#16933,#16934,#16935,#16936,
#16937,#16938,#16939,#16940,#16941,#16942,#16943,#16944,#16945,#16946,#16947,
#16948,#16949,#16950,#16951,#16952,#16953,#16954,#16955,#16956,#16957,#16958,
#16959,#16960,#16961),.UNSPECIFIED.,.F.,.F.,(4,3,3,3,3,3,3,3,3,3,3,3,3,
3,3,3,3,3,3,3,3,3,3,3,3,3,3,3,3,3,3,3,3,3,3,3,3,3,3,3,3,3,3,3,3,3,3,3,3,
3,3,3,3,3,3,3,3,3,3,3,3,4),(83.3443379263979,83.4447395826579,83.5453289227515,
83.5851403383034,83.684199455888,83.7831181301475,83.8827535554799,83.9814955568308,
84.0802050835807,84.1789119215326,84.2792343243512,84.3780829177116,84.4791422252593,
84.580201532807,84.6792606503917,84.7781793246507,84.8778147499832,84.9765567513339,
85.0752662780837,85.1739731160353,85.2742955188541,85.3731441122144,85.4742034197625,
85.5752627273106,85.6743218448955,85.7732405191552,85.8728759444876,85.9716179458387,
86.0703274725889,86.1690343105409,86.2693567133593,86.3682053067201,86.4692646142671,
86.5703239218142,86.6693830393988,86.7683017136583,86.8679371389907,86.9666791403415,
87.0653886670914,87.1640955050432,87.2644179078619,87.3632665012222,87.46432580877,
87.5653851163178,87.6644442339017,87.7633629081602,87.8629983334929,87.9617403348428,
88.060449861592,88.159156699543,88.2594791023626,88.3583276957222,88.4593870032718,
88.5604463108214,88.6586782050391,88.7567801508798,88.8547831364389,88.9527180356713,
89.0506354266417,89.1485438993684,89.2465050935619,89.2741574414913),
 .UNSPECIFIED.);
#265=B_SPLINE_CURVE_WITH_KNOTS('',3,(#16962,#16963,#16964,#16965,#16966,
#16967,#16968,#16969,#16970,#16971,#16972,#16973,#16974),.UNSPECIFIED.,
 .F.,.F.,(4,3,3,3,4),(89.2741574417129,89.3952590898568,89.5183032212418,
89.555507505325,89.6284844345084),.UNSPECIFIED.);
#266=B_SPLINE_CURVE_WITH_KNOTS('',3,(#16975,#16976,#16977,#16978,#16979,
#16980,#16981,#16982,#16983,#16984,#16985,#16986,#16987,#16988,#16989,#16990,
#16991,#16992,#16993,#16994,#16995,#16996,#16997,#16998,#16999,#17000,#17001,
#17002,#17003,#17004,#17005,#17006,#17007,#17008,#17009,#17010,#17011,#17012,
#17013,#17014,#17015,#17016,#17017,#17018,#17019,#17020,#17021,#17022,#17023,
#17024,#17025,#17026,#17027,#17028,#17029,#17030,#17031,#17032,#17033,#17034,
#17035,#17036,#17037,#17038,#17039,#17040,#17041,#17042,#17043,#17044,#17045,
#17046,#17047,#17048,#17049,#17050,#17051,#17052,#17053,#17054,#17055,#17056,
#17057,#17058,#17059,#17060,#17061,#17062,#17063,#17064,#17065,#17066,#17067,
#17068,#17069,#17070,#17071,#17072,#17073,#17074,#17075,#17076,#17077,#17078,
#17079,#17080,#17081,#17082,#17083,#17084,#17085,#17086,#17087,#17088,#17089,
#17090,#17091,#17092,#17093,#17094,#17095,#17096,#17097,#17098,#17099,#17100,
#17101,#17102,#17103,#17104,#17105,#17106,#17107,#17108,#17109,#17110,#17111,
#17112,#17113,#17114,#17115,#17116,#17117,#17118,#17119,#17120,#17121,#17122,
#17123,#17124,#17125,#17126,#17127,#17128,#17129,#17130,#17131,#17132,#17133,
#17134,#17135,#17136,#17137,#17138,#17139,#17140,#17141,#17142,#17143,#17144,
#17145,#17146,#17147,#17148,#17149,#17150,#17151,#17152,#17153,#17154,#17155,
#17156,#17157,#17158,#17159,#17160,#17161,#17162,#17163,#17164,#17165,#17166,
#17167,#17168,#17169,#17170,#17171,#17172,#17173,#17174,#17175,#17176,#17177,
#17178,#17179,#17180,#17181,#17182,#17183,#17184,#17185,#17186,#17187,#17188,
#17189,#17190,#17191,#17192,#17193,#17194,#17195,#17196,#17197,#17198,#17199,
#17200,#17201,#17202,#17203,#17204),.UNSPECIFIED.,.F.,.F.,(4,2,2,2,2,2,
2,2,2,2,2,2,2,2,2,2,2,2,2,2,2,2,2,2,2,2,2,2,2,2,2,2,2,2,2,2,2,2,2,2,2,2,
2,2,2,2,2,2,2,2,2,2,2,2,2,2,2,2,2,2,2,2,2,2,2,2,2,2,2,2,2,2,2,2,2,2,2,2,
2,2,2,2,2,2,2,2,2,2,2,2,2,2,2,2,2,2,2,2,2,2,2,2,2,2,2,2,2,2,2,2,2,2,2,2,
4),(-1.67610690530384,-1.6616369887965,-1.62333502436374,-1.61096724728315,
-1.60294978026278,-1.59997780896286,-1.59794773242811,-1.5960994502116,
-1.59352637505502,-1.58683233751666,-1.5768486480398,-1.54513187295802,
-1.48942278688358,-1.47963748100296,-1.47511721859763,-1.47159733351867,
-1.46775561050102,-1.461524424053,-1.43868987089723,-1.39875742273635,-1.3578246093106,
-1.35138663769448,-1.34885387598515,-1.34701600803389,-1.34497511122133,
-1.34194952498888,-1.33355000241599,-1.3203593926047,-1.28308031174571,
-1.23444010741391,-1.22775420407525,-1.22342804097365,-1.21993747175966,
-1.21593751468033,-1.2089789159288,-1.1748529936249,-1.12121280191642,-1.10279567750514,
-1.0987335162647,-1.09644164856244,-1.09447889831456,-1.09193458805955,
-1.08651119289879,-1.04129543346864,-0.987136726983808,-0.978257759967374,
-0.973793857064194,-0.970510122579206,-0.966942804391354,-0.962044746684032,
-0.950371840794784,-0.912877498172957,-0.869045980907529,-0.851501911813965,
-0.847494624944847,-0.845215276346162,-0.843269559894183,-0.840717627740071,
-0.835253506745143,-0.796548696827613,-0.735116849406508,-0.725795186697969,
-0.721313136481602,-0.717808029656794,-0.713907718925966,-0.707406984130386,
-0.681125986141361,-0.617641911449229,-0.600240180318242,-0.59624212837838,
-0.593964878170609,-0.592018837985877,-0.589463724190013,-0.583982715851276,
-0.543041178005608,-0.484272344219113,-0.474814472468086,-0.470289464739249,
-0.466769131731241,-0.462930195873847,-0.456710891376531,-0.434010493816948,
-0.394493357917899,-0.352996728369668,-0.346559228090515,-0.344026660515154,
-0.342188936429314,-0.34014820298669,-0.337122865100116,-0.32872407166341,
-0.315534646011128,-0.259359438239033,-0.22887831113395,-0.221951293100366,
-0.217918225180366,-0.214436322317702,-0.214354968226818,-0.214282117819541,
-0.214216647499058,-0.214157620443795,-0.214104249088067,-0.21405586634476,
-0.214011903269021,-0.213971871545232,-0.213935349618804,-0.21385359452961,
-0.209447266042847,-0.200158986039909,-0.187794132821037,-0.155762060016917,
-0.105580955608446,-0.0963519117470314,-0.0931109279364058,-0.0912314720885978,
-0.0899840747648518),.UNSPECIFIED.);
#267=B_SPLINE_CURVE_WITH_KNOTS('',3,(#17210,#17211,#17212,#17213,#17214,
#17215,#17216,#17217,#17218,#17219,#17220,#17221,#17222,#17223,#17224,#17225,
#17226,#17227,#17228,#17229,#17230,#17231,#17232,#17233,#17234,#17235,#17236,
#17237,#17238,#17239,#17240,#17241,#17242,#17243,#17244,#17245,#17246,#17247,
#17248,#17249,#17250,#17251,#17252,#17253,#17254,#17255,#17256,#17257,#17258,
#17259,#17260,#17261,#17262,#17263,#17264,#17265,#17266,#17267,#17268,#17269,
#17270,#17271,#17272,#17273,#17274,#17275,#17276,#17277,#17278,#17279,#17280,
#17281,#17282,#17283,#17284,#17285,#17286,#17287,#17288,#17289,#17290,#17291,
#17292,#17293,#17294,#17295,#17296,#17297,#17298,#17299,#17300,#17301,#17302,
#17303,#17304,#17305,#17306,#17307,#17308,#17309,#17310,#17311,#17312,#17313,
#17314,#17315,#17316,#17317,#17318,#17319,#17320,#17321,#17322,#17323,#17324,
#17325,#17326,#17327,#17328,#17329,#17330,#17331,#17332,#17333,#17334,#17335,
#17336,#17337,#17338,#17339,#17340,#17341,#17342,#17343,#17344,#17345,#17346,
#17347,#17348,#17349,#17350,#17351,#17352,#17353,#17354,#17355,#17356,#17357,
#17358,#17359,#17360,#17361,#17362,#17363,#17364,#17365,#17366,#17367,#17368,
#17369,#17370,#17371,#17372,#17373,#17374,#17375,#17376,#17377,#17378,#17379,
#17380,#17381,#17382,#17383,#17384,#17385,#17386,#17387,#17388,#17389,#17390),
 .UNSPECIFIED.,.F.,.F.,(4,3,3,3,3,3,3,3,3,3,3,3,3,3,3,3,3,3,3,3,3,3,3,3,
3,3,3,3,3,3,3,3,3,3,3,3,3,3,3,3,3,3,3,3,3,3,3,3,3,3,3,3,3,3,3,3,3,3,3,3,
4),(77.0622289400388,77.1598104900222,77.2573935220109,77.3550721489496,
77.4528016237076,77.5506953978965,77.6147731712817,77.7138322888664,77.8127509631259,
77.9123863884583,78.0111283898092,78.1098379165591,78.2085447545109,78.3088671573295,
78.4077157506899,78.5087750582376,78.6098343657853,78.7088934833699,78.8078121576294,
78.9074475829619,79.0061895843128,79.1048991110627,79.2036059490145,79.3039283518331,
79.4027769451936,79.5038362527413,79.6048955602889,79.7039546778735,79.802873352133,
79.9025087774654,80.0012507788162,80.0999603055661,80.1986671435179,80.2989895463366,
80.397838139697,80.4988974472448,80.5999567547925,80.6990158723771,80.7979345466367,
80.8975699719691,80.99631197332,81.0950215000699,81.1937283380216,81.2940507408402,
81.3928993342007,81.4939586417484,81.5950179492961,81.6940770668806,81.7929957411399,
81.8926311664724,81.9913731678233,82.0900826945732,82.1887895325249,82.2891119353436,
82.3879605287041,82.4890198362519,82.5900791437997,82.699827112012,82.8092455102988,
82.9180995588103,82.990972133969),.UNSPECIFIED.);
#268=B_SPLINE_CURVE_WITH_KNOTS('',3,(#17391,#17392,#17393,#17394,#17395,
#17396,#17397,#17398,#17399,#17400,#17401,#17402,#17403),.UNSPECIFIED.,
 .F.,.F.,(4,3,3,3,4),(82.9909721343117,83.0910899879919,83.1912299242207,
83.2914717628289,83.3443379263979),.UNSPECIFIED.);
#269=B_SPLINE_CURVE_WITH_KNOTS('',3,(#17405,#17406,#17407,#17408,#17409,
#17410,#17411,#17412,#17413,#17414,#17415,#17416),.UNSPECIFIED.,.F.,.F.,
(4,2,2,2,2,4),(-0.0899840747648518,-0.0892272765238516,-0.086389960181531,
-0.0792681453191874,-0.0687374840803309,-0.000736241093440834),
 .UNSPECIFIED.);
#270=B_SPLINE_CURVE_WITH_KNOTS('',3,(#17417,#17418,#17419,#17420,#17421,
#17422,#17423,#17424,#17425,#17426,#17427,#17428,#17429,#17430,#17431,#17432,
#17433,#17434,#17435,#17436,#17437,#17438,#17439,#17440,#17441,#17442,#17443,
#17444,#17445,#17446,#17447,#17448,#17449,#17450,#17451,#17452,#17453,#17454,
#17455,#17456,#17457,#17458,#17459,#17460,#17461,#17462,#17463,#17464,#17465,
#17466,#17467,#17468,#17469,#17470,#17471,#17472,#17473,#17474,#17475,#17476,
#17477,#17478,#17479,#17480,#17481,#17482,#17483,#17484,#17485,#17486,#17487,
#17488,#17489,#17490,#17491,#17492,#17493,#17494,#17495,#17496,#17497,#17498,
#17499,#17500,#17501,#17502,#17503,#17504,#17505,#17506,#17507,#17508,#17509,
#17510,#17511,#17512,#17513,#17514,#17515,#17516,#17517,#17518,#17519,#17520,
#17521,#17522,#17523,#17524,#17525,#17526,#17527,#17528,#17529,#17530,#17531,
#17532,#17533,#17534,#17535,#17536,#17537,#17538,#17539,#17540,#17541,#17542,
#17543,#17544,#17545,#17546,#17547,#17548,#17549,#17550,#17551,#17552,#17553,
#17554,#17555,#17556,#17557,#17558,#17559,#17560,#17561,#17562,#17563,#17564,
#17565,#17566,#17567,#17568,#17569,#17570,#17571,#17572,#17573,#17574,#17575,
#17576,#17577,#17578,#17579,#17580,#17581,#17582,#17583,#17584,#17585,#17586,
#17587,#17588,#17589,#17590,#17591,#17592,#17593,#17594,#17595,#17596,#17597,
#17598,#17599,#17600,#17601,#17602,#17603,#17604,#17605,#17606,#17607,#17608,
#17609,#17610,#17611,#17612,#17613,#17614,#17615,#17616,#17617,#17618,#17619,
#17620,#17621,#17622,#17623,#17624,#17625,#17626,#17627,#17628,#17629,#17630,
#17631,#17632,#17633,#17634,#17635,#17636,#17637,#17638,#17639,#17640,#17641,
#17642,#17643,#17644,#17645,#17646,#17647,#17648,#17649,#17650,#17651,#17652,
#17653,#17654,#17655,#17656),.UNSPECIFIED.,.F.,.F.,(4,2,2,2,2,2,2,2,2,2,
2,2,2,2,2,2,2,2,2,2,2,2,2,2,2,2,2,2,2,2,2,2,2,2,2,2,2,2,2,2,2,2,2,2,2,2,
2,2,2,2,2,2,2,2,2,2,2,2,2,2,2,2,2,2,2,2,2,2,2,2,2,2,2,2,2,2,2,2,2,2,2,2,
2,2,2,2,2,2,2,2,2,2,2,2,2,2,2,2,2,2,2,2,2,2,2,2,2,2,2,2,2,2,2,2,2,2,2,2,
2,4),(-3.17255739968768,-3.1576069634066,-3.14810732836851,-3.1434954008955,
-3.14001384955691,-3.1366931493451,-3.13341536905306,-3.12897456274974,
-3.11789721165226,-3.09383691093029,-3.05431535560038,-3.02234715151782,
-3.01585248463183,-3.0131172296154,-3.0111303830683,-3.00894508086758,-3.00525735952246,
-2.99217804282792,-2.93735433907239,-2.91155966332515,-2.90077694145438,
-2.89242416032427,-2.888175408801,-2.88813682609947,-2.88809592484398,-2.88805255764975,
-2.88800656701802,-2.88795778460018,-2.88790603041391,-2.88785111200833,
-2.8877928235698,-2.88773094498928,-2.88766524088317,-2.88759545956919,
-2.88752133201663,-2.88744257077892,-2.8873916312179,-2.88732376443447,
-2.88383385795497,-2.87950808817963,-2.87282203001381,-2.82425470811119,
-2.78707875500556,-2.77382862793589,-2.76540157604663,-2.76237260180553,
-2.76033129012896,-2.75849452277717,-2.75596512238182,-2.7495456510586,
-2.70805249457556,-2.66848411540881,-2.65343162211825,-2.64254216049128,
-2.63777630490657,-2.63423179872332,-2.6304619102664,-2.62455886316772,
-2.60692581809593,-2.54452914118,-2.52565285485955,-2.51839967740849,-2.51303255352772,
-2.51049922246228,-2.50853776331244,-2.50623903802823,-2.50214536434144,
-2.48321505155067,-2.41545795016458,-2.40141088354109,-2.39108020280365,
-2.38641256868019,-2.38288347968782,-2.37954029889709,-2.37389537766366,
-2.35826974519288,-2.29366213650761,-2.27455594012858,-2.26368070816965,
-2.26035230955456,-2.25824652364475,-2.25624393067389,-2.25377574107253,
-2.24771576250172,-2.19730867504513,-2.15167721387559,-2.14035302513635,
-2.13551344101775,-2.13195685753111,-2.12866062188454,-2.12326571199652,
-2.10935786499212,-2.05034045231045,-2.01466594914582,-2.01015434745451,
-2.00779164049775,-2.00583529778113,-2.00338352628568,-1.99951373709683,
-1.97798602112789,-1.92961929266239,-1.90580901282673,-1.89557754644634,
-1.88750095468426,-1.88326570157758,-1.88011904533669,-1.87617276256836,
-1.86945916271794,-1.84363199615531,-1.78972878497356,-1.77173815772437,
-1.7647101512041,-1.75947235049566,-1.75696389032812,-1.7551908631053,-1.75294907964165,
-1.74910487000024,-1.73376493847121,-1.68831539067684,-1.67587718660285),
 .UNSPECIFIED.);
#271=B_SPLINE_CURVE_WITH_KNOTS('',3,(#17662,#17663,#17664,#17665,#17666,
#17667,#17668,#17669,#17670,#17671,#17672,#17673,#17674,#17675,#17676,#17677,
#17678,#17679,#17680,#17681,#17682,#17683,#17684,#17685,#17686,#17687,#17688,
#17689,#17690,#17691,#17692,#17693,#17694,#17695,#17696,#17697,#17698,#17699,
#17700,#17701,#17702,#17703,#17704,#17705,#17706,#17707,#17708,#17709,#17710,
#17711,#17712,#17713,#17714,#17715,#17716,#17717,#17718,#17719,#17720,#17721,
#17722,#17723,#17724,#17725,#17726,#17727,#17728,#17729,#17730,#17731,#17732,
#17733,#17734,#17735,#17736,#17737,#17738,#17739,#17740,#17741,#17742,#17743,
#17744,#17745,#17746,#17747,#17748,#17749,#17750,#17751,#17752,#17753,#17754,
#17755,#17756,#17757,#17758,#17759,#17760,#17761,#17762,#17763,#17764,#17765,
#17766,#17767,#17768,#17769,#17770,#17771,#17772,#17773,#17774,#17775,#17776,
#17777,#17778,#17779,#17780,#17781,#17782,#17783,#17784,#17785,#17786,#17787,
#17788,#17789,#17790,#17791,#17792,#17793,#17794,#17795,#17796,#17797,#17798,
#17799,#17800,#17801,#17802,#17803,#17804,#17805,#17806,#17807,#17808,#17809,
#17810,#17811,#17812,#17813,#17814,#17815,#17816,#17817,#17818,#17819,#17820,
#17821,#17822,#17823,#17824,#17825,#17826,#17827,#17828,#17829,#17830,#17831,
#17832,#17833,#17834,#17835,#17836,#17837,#17838,#17839,#17840,#17841,#17842),
 .UNSPECIFIED.,.F.,.F.,(4,3,3,3,3,3,3,3,3,3,3,3,3,3,3,3,3,3,3,3,3,3,3,3,
3,3,3,3,3,3,3,3,3,3,3,3,3,3,3,3,3,3,3,3,3,3,3,3,3,3,3,3,3,3,3,3,3,3,3,3,
4),(70.7790859150367,70.8779677866101,70.976750148986,71.0754792147284,
71.1741847940566,71.272896666296,71.3717103894916,71.4705767843822,71.5696140703515,
71.64440600426,71.7434651218447,71.8423837961042,71.9420192214366,72.0407612227875,
72.1394707495375,72.2381775874893,72.3384999903079,72.4373485836684,72.5384078912161,
72.6394671987637,72.7385263163483,72.8374449906077,72.9370804159401,73.0358224172909,
73.1345319440408,73.2332387819926,73.3335611848112,73.4324097781717,73.5334690857194,
73.6345283932672,73.7335875108519,73.8325061851113,73.9321416104438,74.0308836117947,
74.1295931385446,74.2282999764964,74.328622379315,74.4274709726755,74.5285302802232,
74.6295895877709,74.7286487053556,74.827567379615,74.9272028049475,75.0259448062983,
75.1246543330483,75.223361171,75.3236835738186,75.4225321671791,75.5235914747268,
75.6246507822745,75.7237098998592,75.8226285741186,75.9222639994511,76.0210060008019,
76.1197155275518,76.2184223655036,76.3187447683222,76.4175933616826,76.5186526692304,
76.6197119767781,76.7077868271321),.UNSPECIFIED.);
#272=B_SPLINE_CURVE_WITH_KNOTS('',3,(#17843,#17844,#17845,#17846,#17847,
#17848,#17849,#17850,#17851,#17852,#17853,#17854,#17855),.UNSPECIFIED.,
 .F.,.F.,(4,3,3,3,4),(76.7077868273919,76.80563266964,76.9033659598873,
77.0010095015004,77.0622289400388),.UNSPECIFIED.);
#273=B_SPLINE_CURVE_WITH_KNOTS('',3,(#17856,#17857,#17858,#17859,#17860,
#17861,#17862,#17863,#17864,#17865,#17866,#17867,#17868,#17869,#17870,#17871,
#17872,#17873,#17874,#17875,#17876,#17877,#17878,#17879,#17880,#17881,#17882,
#17883,#17884,#17885,#17886,#17887,#17888,#17889,#17890,#17891,#17892,#17893,
#17894,#17895,#17896,#17897,#17898,#17899,#17900,#17901,#17902,#17903,#17904,
#17905,#17906,#17907,#17908,#17909,#17910,#17911,#17912,#17913,#17914,#17915,
#17916,#17917,#17918,#17919,#17920,#17921,#17922,#17923,#17924,#17925,#17926,
#17927,#17928,#17929,#17930,#17931,#17932,#17933,#17934,#17935,#17936,#17937,
#17938,#17939,#17940,#17941,#17942,#17943,#17944,#17945,#17946,#17947,#17948,
#17949,#17950,#17951,#17952,#17953,#17954,#17955,#17956,#17957,#17958,#17959,
#17960,#17961,#17962,#17963,#17964,#17965,#17966,#17967,#17968,#17969,#17970,
#17971,#17972,#17973,#17974,#17975,#17976,#17977,#17978,#17979,#17980,#17981,
#17982,#17983,#17984,#17985,#17986,#17987,#17988,#17989,#17990,#17991,#17992,
#17993,#17994,#17995,#17996,#17997,#17998,#17999,#18000,#18001,#18002,#18003,
#18004,#18005,#18006,#18007,#18008,#18009,#18010,#18011,#18012,#18013,#18014,
#18015,#18016,#18017,#18018,#18019,#18020,#18021,#18022,#18023,#18024,#18025,
#18026,#18027,#18028,#18029,#18030,#18031,#18032,#18033,#18034,#18035,#18036,
#18037,#18038,#18039,#18040,#18041,#18042,#18043,#18044,#18045,#18046,#18047,
#18048,#18049,#18050,#18051,#18052,#18053,#18054,#18055,#18056,#18057,#18058,
#18059,#18060,#18061,#18062,#18063,#18064,#18065,#18066,#18067,#18068,#18069,
#18070,#18071,#18072,#18073,#18074,#18075,#18076,#18077,#18078,#18079,#18080,
#18081,#18082,#18083,#18084,#18085,#18086,#18087,#18088,#18089,#18090,#18091,
#18092,#18093,#18094,#18095,#18096,#18097,#18098,#18099,#18100,#18101,#18102,
#18103,#18104,#18105,#18106,#18107,#18108,#18109,#18110,#18111,#18112,#18113,
#18114,#18115,#18116,#18117,#18118,#18119),.UNSPECIFIED.,.F.,.F.,(4,2,2,
2,2,2,2,2,2,2,2,2,2,2,2,2,2,2,2,2,2,2,2,2,2,2,2,2,2,2,2,2,2,2,2,2,2,2,2,
2,2,2,2,2,2,2,2,2,2,2,2,2,2,2,2,2,2,2,2,2,2,2,2,2,2,2,2,2,2,2,2,2,2,2,2,
2,2,2,2,2,2,2,2,2,2,2,2,2,2,2,2,2,2,2,2,2,2,2,2,2,2,2,2,2,2,2,2,2,2,2,2,
2,2,2,2,2,2,2,2,2,2,2,2,2,2,2,2,2,2,2,2,4),(-1.67587718660285,-1.64470114731754,
-1.63647046963179,-1.63220378597921,-1.62871775902039,-1.62467444600192,
-1.6177007090087,-1.58636809487528,-1.55382222748207,-1.51560561651707,
-1.50915676664446,-1.50662260068978,-1.50478470099826,-1.50274495878806,
-1.4997231097777,-1.49134699995697,-1.47820598339102,-1.44088827611686,
-1.39223653872546,-1.38555236722436,-1.38122735493086,-1.37773773384927,
-1.37373888475572,-1.36678226923295,-1.33266754457923,-1.27905923984327,
-1.26062970521329,-1.25656758957397,-1.25427610557754,-1.25231392102026,
-1.24977065231729,-1.24435057700418,-1.20064947555576,-1.14488351546687,
-1.1351050407246,-1.13058685891227,-1.1270681467531,-1.12322725200407,-1.11699639170761,
-1.09415043676683,-1.05417258885683,-1.01333443966294,-1.0068962700886,
-1.00436392221548,-1.00252652364608,-1.00048635198209,-0.997462188138732,
-0.989068854014529,-0.975890169613667,-0.938614078903735,-0.889984451129513,
-0.883300572107022,-0.878975723789251,-0.875486218612126,-0.871487484358028,
-0.864531022016475,-0.830415817385973,-0.776794804848949,-0.758380451001099,
-0.754319355211467,-0.752028147121937,-0.75006600050795,-0.747522523119937,
-0.742101083048869,-0.697144193570694,-0.64273914651985,-0.633021504888423,
-0.628446534665607,-0.624919573066694,-0.621105483888715,-0.614997317620162,
-0.593529695061223,-0.523171917700296,-0.506923580403083,-0.50300514422664,
-0.500746351216423,-0.498976348647329,-0.496493494002344,-0.491387295857933,
-0.484585700126944,-0.467463706225077,-0.416972038713945,-0.386891587004229,
-0.379985316746016,-0.375957271575916,-0.372470138009076,-0.368183977833826,
-0.359857332809512,-0.308097725810674,-0.259426865680415,-0.253290154277052,
-0.250589983140797,-0.248631522338408,-0.248546394839057,-0.248480095286316,
-0.248434302691515,-0.248401216776203,-0.248356785540407,-0.248314849649355,
-0.248275051527834,-0.24823709904409,-0.248200750116737,-0.248165801610515,
-0.24813208113155,-0.248099440884787,-0.248067752982383,-0.2480369058037,
-0.248006801144657,-0.247977351956688,-0.247948480520079,-0.247920116975015,
-0.247892198115205,-0.247864666392897,-0.247837469092272,-0.247810557626377,
-0.247783886950667,-0.247757415076964,-0.247731102636315,-0.247704912507719,
-0.247678809502094,-0.247652760086345,-0.245124567611522,-0.239610186869502,
-0.194140884841972,-0.140430070911066,-0.131537338139361,-0.127070658394206,
-0.123786806840283,-0.120221209184394,-0.115328872331299,-0.103686018322656,
-0.0900938466068125),.UNSPECIFIED.);
#274=B_SPLINE_CURVE_WITH_KNOTS('',3,(#18125,#18126,#18127,#18128,#18129,
#18130,#18131,#18132,#18133,#18134,#18135,#18136,#18137,#18138,#18139,#18140,
#18141,#18142,#18143,#18144,#18145,#18146,#18147,#18148,#18149,#18150,#18151,
#18152,#18153,#18154,#18155,#18156,#18157,#18158,#18159,#18160,#18161,#18162,
#18163,#18164,#18165,#18166,#18167,#18168,#18169,#18170,#18171,#18172,#18173,
#18174,#18175,#18176,#18177,#18178,#18179,#18180,#18181,#18182,#18183,#18184,
#18185,#18186,#18187,#18188,#18189,#18190,#18191,#18192,#18193,#18194,#18195,
#18196,#18197,#18198,#18199,#18200,#18201,#18202,#18203,#18204,#18205,#18206,
#18207,#18208,#18209,#18210,#18211,#18212,#18213,#18214,#18215,#18216,#18217,
#18218,#18219,#18220,#18221,#18222,#18223,#18224,#18225,#18226,#18227,#18228,
#18229,#18230,#18231,#18232,#18233,#18234,#18235,#18236,#18237,#18238,#18239,
#18240,#18241,#18242,#18243,#18244,#18245,#18246,#18247,#18248,#18249,#18250,
#18251,#18252,#18253,#18254,#18255,#18256,#18257,#18258,#18259,#18260,#18261,
#18262,#18263,#18264,#18265,#18266,#18267,#18268,#18269,#18270,#18271,#18272,
#18273,#18274,#18275,#18276,#18277,#18278,#18279,#18280,#18281,#18282,#18283,
#18284,#18285,#18286,#18287,#18288,#18289,#18290,#18291,#18292,#18293,#18294,
#18295,#18296,#18297,#18298,#18299,#18300,#18301,#18302,#18303,#18304,#18305),
 .UNSPECIFIED.,.F.,.F.,(4,3,3,3,3,3,3,3,3,3,3,3,3,3,3,3,3,3,3,3,3,3,3,3,
3,3,3,3,3,3,3,3,3,3,3,3,3,3,3,3,3,3,3,3,3,3,3,3,3,3,3,3,3,3,3,3,3,3,3,3,
4),(64.494741390819,64.5971431881403,64.6789776427348,64.7780367603194,
64.8769554345788,64.9765908599113,65.0753328612621,65.1740423880121,65.2727492259639,
65.3730716287825,65.471920222143,65.5729795296907,65.6740388372384,65.7730979548231,
65.8720166290825,65.9716520544149,66.0703940557658,66.1691035825159,66.2678104204676,
66.3681328232862,66.4669814166466,66.5680407241943,66.669100031742,66.7681591493267,
66.8670778235862,66.9667132489186,67.0654552502695,67.1641647770195,67.2628716149714,
67.36319401779,67.4620426111503,67.563101918698,67.6641612262456,67.7632203438303,
67.8621390180899,67.9617744434223,68.0605164447731,68.1592259715231,68.257932809475,
68.3582552122935,68.457103805654,68.5581631132016,68.6592224207492,68.7582815383338,
68.8572002125931,68.9568356379256,69.0555776392764,69.1542871660265,69.252994003978,
69.3533164067967,69.4521650001572,69.553224307705,69.6542836152528,69.7520048359883,
69.8496009043765,69.9471033152915,70.0445434457333,70.1419872142467,70.239427096225,
70.3369604616554,70.4246015196188),.UNSPECIFIED.);
#275=B_SPLINE_CURVE_WITH_KNOTS('',3,(#18306,#18307,#18308,#18309,#18310,
#18311,#18312,#18313,#18314,#18315,#18316,#18317,#18318),.UNSPECIFIED.,
 .F.,.F.,(4,3,3,3,4),(70.4246015199525,70.558216925384,70.6493448097564,
70.7484011637564,70.7790859150367),.UNSPECIFIED.);
#276=B_SPLINE_CURVE_WITH_KNOTS('',3,(#18320,#18321,#18322,#18323,#18324,
#18325,#18326,#18327,#18328,#18329,#18330,#18331),.UNSPECIFIED.,.F.,.F.,
(4,2,2,2,2,4),(-0.0900938466068125,-0.0674452343315531,-0.0150635790955834,
-0.00474487467251724,-0.00202527891974473,-0.000735711368292737),
 .UNSPECIFIED.);
#277=B_SPLINE_CURVE_WITH_KNOTS('',3,(#18332,#18333,#18334,#18335,#18336,
#18337,#18338,#18339,#18340,#18341,#18342,#18343,#18344,#18345,#18346,#18347,
#18348,#18349,#18350,#18351,#18352,#18353,#18354,#18355,#18356,#18357,#18358,
#18359,#18360,#18361,#18362,#18363,#18364,#18365,#18366,#18367,#18368,#18369,
#18370,#18371,#18372,#18373,#18374,#18375,#18376,#18377,#18378,#18379,#18380,
#18381,#18382,#18383,#18384,#18385,#18386,#18387,#18388,#18389,#18390,#18391,
#18392,#18393,#18394,#18395,#18396,#18397,#18398,#18399,#18400,#18401,#18402,
#18403,#18404,#18405,#18406,#18407,#18408,#18409,#18410,#18411,#18412,#18413,
#18414,#18415,#18416,#18417,#18418,#18419,#18420,#18421,#18422,#18423,#18424,
#18425,#18426,#18427,#18428,#18429,#18430,#18431,#18432,#18433,#18434,#18435,
#18436,#18437,#18438,#18439,#18440,#18441,#18442,#18443,#18444,#18445,#18446,
#18447,#18448,#18449,#18450,#18451,#18452,#18453,#18454,#18455,#18456,#18457,
#18458,#18459,#18460,#18461,#18462,#18463,#18464,#18465,#18466,#18467,#18468,
#18469,#18470,#18471,#18472,#18473,#18474,#18475,#18476,#18477,#18478,#18479,
#18480,#18481,#18482,#18483,#18484,#18485,#18486,#18487,#18488,#18489,#18490,
#18491,#18492,#18493,#18494,#18495,#18496,#18497,#18498,#18499,#18500,#18501,
#18502,#18503,#18504,#18505,#18506,#18507,#18508,#18509,#18510,#18511,#18512,
#18513,#18514,#18515,#18516,#18517,#18518,#18519,#18520,#18521,#18522,#18523,
#18524,#18525,#18526,#18527,#18528,#18529),.UNSPECIFIED.,.F.,.F.,(4,2,2,
2,2,2,2,2,2,2,2,2,2,2,2,2,2,2,2,2,2,2,2,2,2,2,2,2,2,2,2,2,2,2,2,2,2,2,2,
2,2,2,2,2,2,2,2,2,2,2,2,2,2,2,2,2,2,2,2,2,2,2,2,2,2,2,2,2,2,2,2,2,2,2,2,
2,2,2,2,2,2,2,2,2,2,2,2,2,2,2,2,2,2,2,2,2,2,2,4),(-3.17281145082706,-3.17188027035177,
-3.17011455900862,-3.16814177566368,-3.16536628592734,-3.15874480285747,
-3.15220734656136,-3.10107551468508,-3.06396462670712,-3.05229874038881,
-3.04740198696655,-3.04383505388989,-3.04055129370548,-3.03608676995585,
-3.02720478086407,-2.97321112537944,-2.9403159161049,-2.92508434746351,
-2.9223517896374,-2.91989294767224,-2.91796885123375,-2.91567095303065,
-2.91165945767271,-2.89355018091552,-2.82498478813721,-2.8108738051289,
-2.80050696065795,-2.79583260004176,-2.7923022345682,-2.78849601899172,
-2.78242566322933,-2.76338309446505,-2.69540674641322,-2.68133621198321,
-2.67253820728772,-2.66945904008345,-2.66740713480705,-2.66557876538935,
-2.66308337399262,-2.65686647058534,-2.60936117063643,-2.57254067602311,
-2.55910703345573,-2.54912373534732,-2.54451843205932,-2.54099786332001,
-2.53716081099802,-2.53094935906433,-2.5106642423816,-2.45128072817204,
-2.43258150088448,-2.42186218796596,-2.41855062813285,-2.41644837588608,
-2.41444303680745,-2.41196504279072,-2.40584956329628,-2.35672826458412,
-2.30473691496518,-2.29676401322865,-2.29254987678195,-2.28940496931344,
-2.28544258395633,-2.27865582592454,-2.2517194580498,-2.19877863104351,
-2.18097230430283,-2.17399163084602,-2.16878106314646,-2.16627774498469,
-2.16450522136393,-2.16225978498189,-2.15840015819994,-2.1429358618492,
-2.0975776506416,-2.05401530361326,-2.04578419546068,-2.04151720767012,
-2.03803089221701,-2.03398719957246,-2.02701269506793,-1.99567387081475,
-1.94591795336698,-1.92125799155268,-1.91702303195283,-1.91471858844261,
-1.91275776866927,-1.91023236524179,-1.90611705058611,-1.87501721898451,
-1.82536639610872,-1.79974373585842,-1.79329110579242,-1.78940152535256,
-1.78589457133846,-1.78139417962398,-1.7719744872921,-1.71154169179078,
-1.67612525783103),.UNSPECIFIED.);
#278=B_SPLINE_CURVE_WITH_KNOTS('',3,(#18535,#18536,#18537,#18538,#18539,
#18540,#18541,#18542,#18543,#18544,#18545,#18546,#18547,#18548,#18549,#18550,
#18551,#18552,#18553,#18554,#18555,#18556,#18557,#18558,#18559,#18560,#18561,
#18562,#18563,#18564,#18565,#18566,#18567,#18568,#18569,#18570,#18571,#18572,
#18573,#18574,#18575,#18576,#18577,#18578,#18579,#18580,#18581,#18582,#18583,
#18584,#18585,#18586,#18587,#18588,#18589,#18590,#18591,#18592,#18593,#18594,
#18595,#18596,#18597,#18598,#18599,#18600,#18601,#18602,#18603,#18604,#18605,
#18606,#18607,#18608,#18609,#18610,#18611,#18612,#18613,#18614,#18615,#18616,
#18617,#18618,#18619,#18620,#18621,#18622,#18623,#18624,#18625,#18626,#18627,
#18628,#18629,#18630,#18631,#18632,#18633,#18634,#18635,#18636,#18637,#18638,
#18639,#18640,#18641,#18642,#18643,#18644,#18645,#18646,#18647,#18648,#18649,
#18650,#18651,#18652,#18653,#18654,#18655,#18656,#18657,#18658,#18659,#18660,
#18661,#18662,#18663,#18664,#18665,#18666,#18667,#18668,#18669,#18670,#18671,
#18672,#18673,#18674,#18675,#18676,#18677,#18678,#18679,#18680,#18681,#18682,
#18683,#18684,#18685,#18686,#18687,#18688,#18689,#18690,#18691,#18692,#18693,
#18694,#18695,#18696,#18697,#18698,#18699,#18700,#18701,#18702,#18703,#18704,
#18705,#18706,#18707,#18708,#18709,#18710,#18711,#18712,#18713,#18714,#18715),
 .UNSPECIFIED.,.F.,.F.,(4,3,3,3,3,3,3,3,3,3,3,3,3,3,3,3,3,3,3,3,3,3,3,3,
3,3,3,3,3,3,3,3,3,3,3,3,3,3,3,3,3,3,3,3,3,3,3,3,3,3,3,3,3,3,3,3,3,3,3,3,
4),(58.2125415401659,58.3098255944961,58.4095218148003,58.506928276048,
58.6077693758806,58.7086104757131,58.8076695932977,58.9065882675571,59.0062236928895,
59.1049656942404,59.2036752209903,59.302382058942,59.4027044617607,59.5015530551212,
59.602612362669,59.7036716702167,59.8027307878014,59.901649462061,60.0012848873934,
60.1000268887443,60.1987364154943,60.297443253446,60.3977656562646,60.4966142496251,
60.5976735571727,60.6987328647203,60.7977919823049,60.8967106565642,60.9963460818967,
61.0950880832477,61.1937976099976,61.2925044479492,61.3928268507679,61.4916754441283,
61.5927347516761,61.6937940592239,61.7928531768085,61.891771851068,61.9914072764005,
62.0901492777514,62.1888588045013,62.287565642453,62.3878880452717,62.4867366386322,
62.5877959461799,62.6888552537275,62.787914371312,62.886833045571,62.9864684709035,
63.0852104722542,63.1839199990042,63.2826268369558,63.3829492397746,63.4817978331351,
63.5828571406831,63.6839164482311,63.790091202586,63.8959105065078,64.0015055025796,
64.1067929756919,64.1414162124289),.UNSPECIFIED.);
#279=B_SPLINE_CURVE_WITH_KNOTS('',3,(#18716,#18717,#18718,#18719,#18720,
#18721,#18722,#18723,#18724,#18725,#18726,#18727,#18728),.UNSPECIFIED.,
 .F.,.F.,(4,3,3,3,4),(64.1414162127729,64.2432632342092,64.3451869563365,
64.4472800563271,64.494741390819),.UNSPECIFIED.);
#280=B_SPLINE_CURVE_WITH_KNOTS('',3,(#18729,#18730,#18731,#18732,#18733,
#18734,#18735,#18736,#18737,#18738,#18739,#18740,#18741,#18742,#18743,#18744,
#18745,#18746,#18747,#18748,#18749,#18750,#18751,#18752,#18753,#18754,#18755,
#18756,#18757,#18758,#18759,#18760,#18761,#18762,#18763,#18764,#18765,#18766,
#18767,#18768,#18769,#18770,#18771,#18772,#18773,#18774,#18775,#18776,#18777,
#18778,#18779,#18780,#18781,#18782,#18783,#18784,#18785,#18786,#18787,#18788,
#18789,#18790,#18791,#18792,#18793,#18794,#18795,#18796,#18797,#18798,#18799,
#18800,#18801,#18802,#18803,#18804,#18805,#18806,#18807,#18808,#18809,#18810,
#18811,#18812,#18813,#18814,#18815,#18816,#18817,#18818,#18819,#18820,#18821,
#18822,#18823,#18824,#18825,#18826,#18827,#18828,#18829,#18830,#18831,#18832,
#18833,#18834,#18835,#18836,#18837,#18838,#18839,#18840,#18841,#18842,#18843,
#18844,#18845,#18846,#18847,#18848,#18849,#18850,#18851,#18852,#18853,#18854,
#18855,#18856,#18857,#18858,#18859,#18860,#18861,#18862,#18863,#18864,#18865,
#18866,#18867,#18868,#18869,#18870,#18871,#18872,#18873,#18874,#18875,#18876,
#18877,#18878,#18879,#18880,#18881,#18882,#18883,#18884,#18885,#18886,#18887,
#18888,#18889,#18890,#18891,#18892,#18893,#18894,#18895,#18896,#18897,#18898,
#18899,#18900,#18901,#18902,#18903,#18904,#18905,#18906,#18907,#18908,#18909,
#18910,#18911,#18912,#18913,#18914,#18915,#18916,#18917,#18918,#18919,#18920,
#18921,#18922,#18923,#18924,#18925,#18926,#18927,#18928,#18929,#18930,#18931,
#18932,#18933,#18934,#18935,#18936,#18937,#18938,#18939,#18940,#18941,#18942,
#18943,#18944,#18945,#18946,#18947,#18948,#18949,#18950,#18951,#18952,#18953,
#18954,#18955,#18956,#18957,#18958,#18959,#18960,#18961,#18962),
 .UNSPECIFIED.,.F.,.F.,(4,2,2,2,2,2,2,2,2,2,2,2,2,2,2,2,2,2,2,2,2,2,2,2,
2,2,2,2,2,2,2,2,2,2,2,2,2,2,2,2,2,2,2,2,2,2,2,2,2,2,2,2,2,2,2,2,2,2,2,2,
2,2,2,2,2,2,2,2,2,2,2,2,2,2,2,2,2,2,2,2,2,2,2,2,2,2,2,2,2,2,2,2,2,2,2,2,
2,2,2,2,2,2,2,2,2,2,2,2,2,2,2,2,2,2,2,2,4),(-1.67612525783103,-1.67174155907941,
-1.66648156089626,-1.66396868833182,-1.66200878639615,-1.65969506490472,
-1.65553511836417,-1.63540930721214,-1.62791510237671,-1.58699491302144,
-1.55012914773024,-1.54355213901721,-1.53925941060774,-1.53577151944839,
-1.53174770444095,-1.52467686017826,-1.4879475655404,-1.43011326387354,
-1.41778899611528,-1.41417614708776,-1.41200731945494,-1.41001406766565,
-1.4072399095018,-1.40051159009237,-1.39075243572799,-1.36026795863329,
-1.30278664947792,-1.29310955289729,-1.28860944621497,-1.28509274360082,
-1.28124178547242,-1.27496683694818,-1.25160834000514,-1.20998964578862,
-1.17140470168752,-1.16494154608508,-1.16240479488504,-1.1605660603719,
-1.15852664402118,-1.15550740738203,-1.14715219810917,-1.13405737329597,
-1.09653663451939,-1.04799751253387,-1.04131266115002,-1.03698710189031,
-1.03349697003164,-1.02949745947286,-1.02253949583949,-0.988412944134841,
-0.934735496039016,-0.916364898014789,-0.91230593754306,-0.910014964838313,
-0.908052377271597,-0.905507492527266,-0.900080067987926,-0.892720579479789,
-0.873418276659511,-0.808250294851859,-0.793223255264992,-0.787662671944456,
-0.784335242298483,-0.780797485085342,-0.776074978341524,-0.765435754157361,
-0.750838630810988,-0.708071731289013,-0.669041224697704,-0.662597791203747,
-0.660064384195309,-0.658226564648076,-0.65618634450042,-0.653162822247264,
-0.644775864418675,-0.631611716705835,-0.594313695712995,-0.545669150698194,
-0.538984390849457,-0.534658983050692,-0.531169033245429,-0.527169796921197,
-0.520212480438021,-0.486093596738575,-0.432471748943184,-0.41404901850279,
-0.409987038857585,-0.407695456099797,-0.405733070753092,-0.403189390685247,
-0.397767899600971,-0.353325302359996,-0.298385286632885,-0.288670657109038,
-0.284095927751782,-0.280568643134865,-0.280263529789934,-0.280127193369226,
-0.280024732261122,-0.279947873131842,-0.279890296579403,-0.27981037236961,
-0.279735201254423,-0.275740057189021,-0.27146445934223,-0.264857510107381,
-0.252288982215485,-0.219383292098332,-0.165732596392655,-0.15990316160231,
-0.157505808860149,-0.155521027524159,-0.153383949837367,-0.149913837214301,
-0.137656752234916,-0.114724389595725,-0.0901916154543634),
 .UNSPECIFIED.);
#281=B_SPLINE_CURVE_WITH_KNOTS('',3,(#18968,#18969,#18970,#18971,#18972,
#18973,#18974,#18975,#18976,#18977,#18978,#18979,#18980,#18981,#18982,#18983,
#18984,#18985,#18986,#18987,#18988,#18989,#18990,#18991,#18992,#18993,#18994,
#18995,#18996,#18997,#18998,#18999,#19000,#19001,#19002,#19003,#19004,#19005,
#19006,#19007,#19008,#19009,#19010,#19011,#19012,#19013,#19014,#19015,#19016,
#19017,#19018,#19019,#19020,#19021,#19022,#19023,#19024,#19025,#19026,#19027,
#19028,#19029,#19030,#19031,#19032,#19033,#19034,#19035,#19036,#19037,#19038,
#19039,#19040,#19041,#19042,#19043,#19044,#19045,#19046,#19047,#19048,#19049,
#19050,#19051,#19052,#19053,#19054,#19055,#19056,#19057,#19058,#19059,#19060,
#19061,#19062,#19063,#19064,#19065,#19066,#19067,#19068,#19069,#19070,#19071,
#19072,#19073,#19074,#19075,#19076,#19077,#19078,#19079,#19080,#19081,#19082,
#19083,#19084,#19085,#19086,#19087,#19088,#19089,#19090,#19091,#19092,#19093,
#19094,#19095,#19096,#19097,#19098,#19099,#19100,#19101,#19102,#19103,#19104,
#19105,#19106,#19107,#19108,#19109,#19110,#19111,#19112,#19113,#19114,#19115,
#19116,#19117,#19118,#19119,#19120,#19121,#19122,#19123,#19124,#19125,#19126,
#19127,#19128,#19129,#19130,#19131,#19132,#19133,#19134,#19135,#19136,#19137,
#19138,#19139,#19140,#19141,#19142,#19143,#19144,#19145,#19146,#19147,#19148),
 .UNSPECIFIED.,.F.,.F.,(4,3,3,3,3,3,3,3,3,3,3,3,3,3,3,3,3,3,3,3,3,3,3,3,
3,3,3,3,3,3,3,3,3,3,3,3,3,3,3,3,3,3,3,3,3,3,3,3,3,3,3,3,3,3,3,3,3,3,3,3,
4),(51.9295993767367,52.030679868231,52.1294268781299,52.2281383612316,
52.3268441060956,52.4296939067445,52.5285380981942,52.6274520266398,52.7265185872557,
52.7382433086914,52.8373024262761,52.9362211005355,53.0358565258679,53.1345985272188,
53.2333080539687,53.3320148919204,53.4323372947391,53.5311858880996,53.6322451956473,
53.733304503195,53.8323636207796,53.9312822950391,54.0309177203715,54.1296597217224,
54.2283692484723,54.327076086424,54.4273984892427,54.5262470826031,54.6273063901509,
54.7283656976986,54.8274248152833,54.9263434895427,55.0259789148752,55.1247209162261,
55.223430442976,55.3221372809278,55.4224596837464,55.5213082771069,55.6223675846546,
55.7234268922023,55.822486009787,55.9214046840465,56.0210401093789,56.1197821107298,
56.2184916374798,56.3171984754316,56.4175208782501,56.5163694716106,56.6174287791582,
56.7184880867059,56.8175472042906,56.9164658785501,57.0161013038825,57.1148433052334,
57.2135528319833,57.3122596699351,57.4125820727537,57.5114306661142,57.6124899736618,
57.7135492812095,57.8582309055933),.UNSPECIFIED.);
#282=B_SPLINE_CURVE_WITH_KNOTS('',3,(#19149,#19150,#19151,#19152,#19153,
#19154,#19155,#19156,#19157,#19158,#19159,#19160,#19161),.UNSPECIFIED.,
 .F.,.F.,(4,3,3,3,4),(57.8582309058197,57.9557212700061,58.0531125158964,
58.1504356450135,58.2125415401659),.UNSPECIFIED.);
#283=B_SPLINE_CURVE_WITH_KNOTS('',3,(#19163,#19164,#19165,#19166,#19167,
#19168,#19169,#19170,#19171,#19172,#19173,#19174,#19175,#19176,#19177,#19178,
#19179,#19180,#19181,#19182),.UNSPECIFIED.,.F.,.F.,(4,2,2,2,2,2,2,2,2,4),
(-0.0901916154543634,-0.0674014413990488,-0.0431045913887549,-0.0359174086979867,
-0.031825889082996,-0.0286630733899206,-0.0253644269643822,-0.0213655915020832,
-0.0130902425129321,-0.000734942023342333),.UNSPECIFIED.);
#284=B_SPLINE_CURVE_WITH_KNOTS('',3,(#19183,#19184,#19185,#19186,#19187,
#19188,#19189,#19190,#19191,#19192,#19193,#19194,#19195,#19196,#19197,#19198,
#19199,#19200,#19201,#19202,#19203,#19204,#19205,#19206,#19207,#19208,#19209,
#19210,#19211,#19212,#19213,#19214,#19215,#19216,#19217,#19218,#19219,#19220,
#19221,#19222,#19223,#19224,#19225,#19226,#19227,#19228,#19229,#19230,#19231,
#19232,#19233,#19234,#19235,#19236,#19237,#19238,#19239,#19240,#19241,#19242,
#19243,#19244,#19245,#19246,#19247,#19248,#19249,#19250,#19251,#19252,#19253,
#19254,#19255,#19256,#19257,#19258,#19259,#19260,#19261,#19262,#19263,#19264,
#19265,#19266,#19267,#19268,#19269,#19270,#19271,#19272,#19273,#19274,#19275,
#19276,#19277,#19278,#19279,#19280,#19281,#19282,#19283,#19284,#19285,#19286,
#19287,#19288,#19289,#19290,#19291,#19292,#19293,#19294,#19295,#19296,#19297,
#19298,#19299,#19300,#19301,#19302,#19303,#19304,#19305,#19306,#19307,#19308,
#19309,#19310,#19311,#19312,#19313,#19314,#19315,#19316,#19317,#19318,#19319,
#19320,#19321,#19322,#19323,#19324,#19325,#19326,#19327,#19328,#19329,#19330,
#19331,#19332,#19333,#19334,#19335,#19336,#19337,#19338,#19339,#19340,#19341,
#19342,#19343,#19344,#19345,#19346,#19347,#19348,#19349,#19350,#19351,#19352,
#19353,#19354,#19355,#19356,#19357,#19358,#19359,#19360,#19361,#19362,#19363,
#19364,#19365,#19366,#19367,#19368,#19369,#19370,#19371,#19372,#19373,#19374,
#19375,#19376,#19377,#19378,#19379,#19380,#19381,#19382,#19383,#19384,#19385,
#19386,#19387,#19388),.UNSPECIFIED.,.F.,.F.,(4,2,2,2,2,2,2,2,2,2,2,2,2,
2,2,2,2,2,2,2,2,2,2,2,2,2,2,2,2,2,2,2,2,2,2,2,2,2,2,2,2,2,2,2,2,2,2,2,2,
2,2,2,2,2,2,2,2,2,2,2,2,2,2,2,2,2,2,2,2,2,2,2,2,2,2,2,2,2,2,2,2,2,2,2,2,
2,2,2,2,2,2,2,2,2,2,2,2,2,2,2,2,2,4),(-3.17197906884703,-3.10233466004078,
-3.089202820326,-3.08083016006895,-3.0778087659958,-3.07576908159546,-3.07393104859413,
-3.07139643924237,-3.06494515748726,-3.0250064008028,-2.98434155349365,
-2.969062282852,-2.96149583078054,-2.95522557350808,-2.95145121181416,-2.94795203707633,
-2.94351945030074,-2.93445282117953,-2.87091017572828,-2.83390571702822,
-2.82849433722826,-2.82595265796583,-2.8239905392314,-2.82169780433466,
-2.81763037603098,-2.79911749706469,-2.74554947518647,-2.71143124425603,
-2.70447406319494,-2.70047504552521,-2.69698537465109,-2.69266042605793,
-2.68597665402958,-2.63734724162226,-2.60005378034847,-2.58691715724735,
-2.5785423167163,-2.57552063662163,-2.5734809049158,-2.57164294363849,-2.56910857842963,
-2.56265869954775,-2.52377639203534,-2.48087102576355,-2.45881671916317,
-2.45265493229194,-2.44882903076144,-2.44530566693922,-2.4407557949069,
-2.43080303020682,-2.37959668304745,-2.34968991379883,-2.33608719051898,
-2.32749975612256,-2.32444905958529,-2.32240334456791,-2.32057057596628,
-2.3180567157288,-2.31172952406076,-2.26675882142933,-2.22823420224264,
-2.21444975133346,-2.20426730008706,-2.19962628629593,-2.19610111206187,
-2.19228113815883,-2.18614633315895,-2.16651063085258,-2.10641258449006,
-2.0876653494613,-2.07692801989668,-2.07361479158612,-2.07151237925171,
-2.06950765985588,-2.06703124301668,-2.06092364659599,-2.01164170773385,
-1.98226238920811,-1.95708012101653,-1.95066083152453,-1.94677874952197,
-1.94327051996894,-1.93875725086566,-1.92926807521707,-1.86956606516565,
-1.84058779339195,-1.83111315372105,-1.82453252462884,-1.8217830304196,
-1.81979405219135,-1.81761531280894,-1.81395671970291,-1.8011863593112,
-1.78980566277747,-1.77194431229076,-1.72787970199721,-1.70550815978039,
-1.69931810463794,-1.69548595781237,-1.69196437054264,-1.68742732020908,
-1.67754594539564,-1.67566955000462),.UNSPECIFIED.);
#285=B_SPLINE_CURVE_WITH_KNOTS('',3,(#19394,#19395,#19396,#19397,#19398,
#19399,#19400,#19401,#19402,#19403,#19404,#19405,#19406,#19407,#19408,#19409,
#19410,#19411,#19412,#19413,#19414,#19415,#19416,#19417,#19418,#19419,#19420,
#19421,#19422,#19423,#19424,#19425,#19426,#19427,#19428,#19429,#19430,#19431,
#19432,#19433,#19434,#19435,#19436,#19437,#19438,#19439,#19440,#19441,#19442,
#19443,#19444,#19445,#19446,#19447,#19448,#19449,#19450,#19451,#19452,#19453,
#19454,#19455,#19456,#19457,#19458,#19459,#19460,#19461,#19462,#19463,#19464,
#19465,#19466,#19467,#19468,#19469,#19470,#19471,#19472,#19473,#19474,#19475,
#19476,#19477,#19478,#19479,#19480,#19481,#19482,#19483,#19484,#19485,#19486,
#19487,#19488,#19489,#19490,#19491,#19492,#19493,#19494,#19495,#19496,#19497,
#19498,#19499,#19500,#19501,#19502,#19503,#19504,#19505,#19506,#19507,#19508,
#19509,#19510,#19511,#19512,#19513,#19514,#19515,#19516,#19517,#19518,#19519,
#19520,#19521,#19522,#19523,#19524,#19525,#19526,#19527,#19528,#19529,#19530,
#19531,#19532,#19533,#19534,#19535,#19536,#19537,#19538,#19539,#19540,#19541,
#19542,#19543,#19544,#19545,#19546,#19547,#19548,#19549,#19550,#19551,#19552,
#19553,#19554,#19555,#19556,#19557,#19558,#19559,#19560,#19561,#19562,#19563,
#19564,#19565,#19566,#19567,#19568,#19569,#19570,#19571,#19572,#19573,#19574,
#19575,#19576,#19577),.UNSPECIFIED.,.F.,.F.,(4,3,3,3,3,3,3,3,3,3,3,3,3,
3,3,3,3,3,3,3,3,3,3,3,3,3,3,3,3,3,3,3,3,3,3,3,3,3,3,3,3,3,3,3,3,3,3,3,3,
3,3,3,3,3,3,3,3,3,3,3,3,4),(45.6452617210371,45.7501727111588,45.7728149471661,
45.8718740647507,45.9707927390101,46.0704281643426,46.1691701656934,46.2678796924433,
46.3665865303951,46.4669089332138,46.5657575265742,46.666816834122,46.7678761416697,
46.8669352592544,46.9658539335139,47.0654893588463,47.1642313601972,47.2629408869472,
47.361647724899,47.4619701277176,47.5608187210781,47.6618780286258,47.7629373361734,
47.8619964537581,47.9609151280175,48.0605505533499,48.1592925547008,48.2580020814507,
48.3567089194025,48.4570313222211,48.5558799155816,48.6569392231293,48.757998530677,
48.8570576482616,48.955976322521,49.0556117478535,49.1543537492043,49.2530632759542,
49.351770113906,49.4520925167247,49.5509411100851,49.6520004176329,49.7530597251806,
49.8521188427653,49.9510375170247,50.0506729423571,50.149414943708,50.2481244704579,
50.3468313084097,50.4471537112284,50.5460023045888,50.6470616121365,50.7481209196842,
50.8457129935021,50.9431428324126,51.0404816382021,51.1377609277277,51.2350121400979,
51.3323110164863,51.4296360130142,51.5270774501447,51.5750455980568),
 .UNSPECIFIED.);
#286=B_SPLINE_CURVE_WITH_KNOTS('',3,(#19578,#19579,#19580,#19581,#19582,
#19583,#19584,#19585,#19586,#19587,#19588,#19589,#19590),.UNSPECIFIED.,
 .F.,.F.,(4,3,3,3,4),(51.5750455984137,51.7300295918744,51.7431821141878,
51.842215157546,51.9295993767367),.UNSPECIFIED.);
#287=B_SPLINE_CURVE_WITH_KNOTS('',3,(#19591,#19592,#19593,#19594,#19595,
#19596,#19597,#19598,#19599,#19600,#19601,#19602,#19603,#19604,#19605,#19606,
#19607,#19608,#19609,#19610,#19611,#19612,#19613,#19614,#19615,#19616,#19617,
#19618,#19619,#19620,#19621,#19622,#19623,#19624,#19625,#19626,#19627,#19628,
#19629,#19630,#19631,#19632,#19633,#19634,#19635,#19636,#19637,#19638,#19639,
#19640,#19641,#19642,#19643,#19644,#19645,#19646,#19647,#19648,#19649,#19650,
#19651,#19652,#19653,#19654,#19655,#19656,#19657,#19658,#19659,#19660,#19661,
#19662,#19663,#19664,#19665,#19666,#19667,#19668,#19669,#19670,#19671,#19672,
#19673,#19674,#19675,#19676,#19677,#19678,#19679,#19680,#19681,#19682,#19683,
#19684,#19685,#19686,#19687,#19688,#19689,#19690,#19691,#19692,#19693,#19694,
#19695,#19696,#19697,#19698,#19699,#19700,#19701,#19702,#19703,#19704,#19705,
#19706,#19707,#19708,#19709,#19710,#19711,#19712,#19713,#19714,#19715,#19716,
#19717,#19718,#19719,#19720,#19721,#19722,#19723,#19724,#19725,#19726,#19727,
#19728,#19729,#19730,#19731,#19732,#19733,#19734,#19735,#19736,#19737,#19738,
#19739,#19740,#19741,#19742,#19743,#19744,#19745,#19746,#19747,#19748,#19749,
#19750,#19751,#19752,#19753,#19754,#19755,#19756,#19757,#19758,#19759,#19760,
#19761,#19762,#19763,#19764,#19765,#19766,#19767,#19768,#19769,#19770,#19771,
#19772,#19773,#19774,#19775,#19776,#19777,#19778,#19779,#19780,#19781,#19782,
#19783,#19784,#19785,#19786,#19787,#19788,#19789,#19790,#19791,#19792,#19793,
#19794,#19795,#19796,#19797,#19798,#19799,#19800),.UNSPECIFIED.,.F.,.F.,
(4,2,2,2,2,2,2,2,2,2,2,2,2,2,2,2,2,2,2,2,2,2,2,2,2,2,2,2,2,2,2,2,2,2,2,
2,2,2,2,2,2,2,2,2,2,2,2,2,2,2,2,2,2,2,2,2,2,2,2,2,2,2,2,2,2,2,2,2,2,2,2,
2,2,2,2,2,2,2,2,2,2,2,2,2,2,2,2,2,2,2,2,2,2,2,2,2,2,2,2,2,2,2,2,2,4),(-1.67566955000462,
-1.62411491162083,-1.60674415883351,-1.58623055946249,-1.57503720608005,
-1.57154768364484,-1.56940633036676,-1.56740097292286,-1.56455629235962,
-1.55738628313311,-1.54675921648381,-1.5112589881279,-1.46074593018652,
-1.4507750026778,-1.44622171730574,-1.44269772364112,-1.43887314646134,
-1.43271793382074,-1.41073790447629,-1.3681008033436,-1.3288992828815,-1.32245896173317,
-1.31992615367768,-1.31808855393356,-1.3160483189293,-1.3130243337789,-1.30463325217463,
-1.29145983491177,-1.25417454372432,-1.20553814664101,-1.19885378435457,
-1.19452862728413,-1.19103887555055,-1.18703986156701,-1.18008291986628,
-1.14596555666727,-1.09234301715617,-1.07392508799704,-1.0698635670663,
-1.06757216588501,-1.06560988488886,-1.06306627358454,-1.05764469179629,
-1.01288069432577,-0.958261093183116,-0.948551928914253,-0.943978409472746,
-0.9404514681725,-0.936636312780529,-0.930524050795131,-0.909015149970924,
-0.838288406454097,-0.822399702657275,-0.818507573102457,-0.816254703494791,
-0.814483558449131,-0.811991575260142,-0.806839205561288,-0.79995834299321,
-0.782534985482966,-0.73147080004639,-0.702309511062795,-0.695455624195293,
-0.691439289955971,-0.687950927486531,-0.683648711071536,-0.675243445917033,
-0.62915881384798,-0.578652117622415,-0.569791322604171,-0.566602315316714,
-0.564733098986074,-0.562721715518813,-0.559844891891954,-0.55246797125806,
-0.541425267082822,-0.503271993686869,-0.456142650631887,-0.446146552816527,
-0.441588513029076,-0.438063587498571,-0.43424073841388,-0.428094367904544,
-0.4062162620152,-0.363944647654126,-0.324250480498227,-0.317808583247715,
-0.315275397716622,-0.31343760739642,-0.311397261223514,-0.30837328233016,
-0.299983319833441,-0.286812744540177,-0.230838151453552,-0.21565229953022,
-0.19802124651622,-0.192118292723605,-0.188348355919944,-0.184803732176448,
-0.181320715284496,-0.17349963142948,-0.140472726878903,-0.10990709668926,
-0.0921187839005196,-0.0898458279024645),.UNSPECIFIED.);
#288=B_SPLINE_CURVE_WITH_KNOTS('',3,(#19806,#19807,#19808,#19809,#19810,
#19811,#19812,#19813,#19814,#19815,#19816,#19817,#19818,#19819,#19820,#19821,
#19822,#19823,#19824,#19825,#19826,#19827,#19828,#19829,#19830,#19831,#19832,
#19833,#19834,#19835,#19836,#19837,#19838,#19839,#19840,#19841,#19842,#19843,
#19844,#19845,#19846,#19847,#19848,#19849,#19850,#19851,#19852,#19853,#19854,
#19855,#19856,#19857,#19858,#19859,#19860,#19861,#19862,#19863,#19864,#19865,
#19866,#19867,#19868,#19869,#19870,#19871,#19872,#19873,#19874,#19875,#19876,
#19877,#19878,#19879,#19880,#19881,#19882,#19883,#19884,#19885,#19886,#19887,
#19888,#19889,#19890,#19891,#19892,#19893,#19894,#19895,#19896,#19897,#19898,
#19899,#19900,#19901,#19902,#19903,#19904,#19905,#19906,#19907,#19908,#19909,
#19910,#19911,#19912,#19913,#19914,#19915,#19916,#19917,#19918,#19919,#19920,
#19921,#19922,#19923,#19924,#19925,#19926,#19927,#19928,#19929,#19930,#19931,
#19932,#19933,#19934,#19935,#19936,#19937,#19938,#19939,#19940,#19941,#19942,
#19943,#19944,#19945,#19946,#19947,#19948,#19949,#19950,#19951,#19952,#19953,
#19954,#19955,#19956,#19957,#19958,#19959,#19960,#19961,#19962,#19963,#19964,
#19965,#19966,#19967,#19968,#19969,#19970,#19971,#19972,#19973,#19974,#19975,
#19976,#19977,#19978,#19979,#19980,#19981,#19982,#19983,#19984,#19985,#19986),
 .UNSPECIFIED.,.F.,.F.,(4,3,3,3,3,3,3,3,3,3,3,3,3,3,3,3,3,3,3,3,3,3,3,3,
3,3,3,3,3,3,3,3,3,3,3,3,3,3,3,3,3,3,3,3,3,3,3,3,3,3,3,3,3,3,3,3,3,3,3,3,
4),(39.3627720041259,39.4600899844457,39.5575043562114,39.6549724183856,
39.752599552229,39.8024477801445,39.9015068977291,40.0004255719885,40.1000609973209,
40.1988029986718,40.2975125254217,40.3962193633734,40.4965417661921,40.5953903595525,
40.6964496671003,40.7975089746481,40.8965680922327,40.995486766492,41.0951221918245,
41.1938641931753,41.2925737199253,41.3912805578772,41.4916029606958,41.5904515540563,
41.691510861604,41.7925701691517,41.8916292867364,41.990547960996,42.0901833863284,
42.1889253876793,42.2876349144293,42.3863417523808,42.4866641551994,42.58551274856,
42.6865720561076,42.7876313636553,42.8866904812401,42.9856091554995,43.0852445808319,
43.1839865821829,43.2826961089329,43.3814029468845,43.4817253497031,43.5805739430635,
43.6816332506112,43.7826925581589,43.8817516757435,43.9806703500029,44.0803057753354,
44.1790477766862,44.2777573034362,44.376464141388,44.4767865442066,44.5756351375672,
44.6766944451148,44.7777537526625,44.8811334637464,44.9842446946408,45.0871977961317,
45.1899571772782,45.2918602912341),.UNSPECIFIED.);
#289=B_SPLINE_CURVE_WITH_KNOTS('',3,(#19987,#19988,#19989,#19990,#19991,
#19992,#19993,#19994,#19995,#19996,#19997,#19998,#19999),.UNSPECIFIED.,
 .F.,.F.,(4,3,3,3,4),(45.2918602914992,45.3960300356268,45.5003580442835,
45.6049490187659,45.6452617210371),.UNSPECIFIED.);
#290=B_SPLINE_CURVE_WITH_KNOTS('',3,(#20001,#20002,#20003,#20004,#20005,
#20006,#20007,#20008,#20009,#20010,#20011,#20012,#20013,#20014,#20015,#20016,
#20017,#20018,#20019,#20020),.UNSPECIFIED.,.F.,.F.,(4,2,2,2,2,2,2,2,2,4),
(-0.0898458279024645,-0.0696861600915073,-0.0657796954558397,-0.0633168309216045,
-0.0613600445003724,-0.0590069121563804,-0.0564756214434564,-0.0524233687460561,
-0.044365270485274,-0.000735688467659968),.UNSPECIFIED.);
#291=B_SPLINE_CURVE_WITH_KNOTS('',3,(#20021,#20022,#20023,#20024,#20025,
#20026,#20027,#20028,#20029,#20030,#20031,#20032,#20033,#20034,#20035,#20036,
#20037,#20038,#20039,#20040,#20041,#20042,#20043,#20044,#20045,#20046,#20047,
#20048,#20049,#20050,#20051,#20052,#20053,#20054,#20055,#20056,#20057,#20058,
#20059,#20060,#20061,#20062,#20063,#20064,#20065,#20066,#20067,#20068,#20069,
#20070,#20071,#20072,#20073,#20074,#20075,#20076,#20077,#20078,#20079,#20080,
#20081,#20082,#20083,#20084,#20085,#20086,#20087,#20088,#20089,#20090,#20091,
#20092,#20093,#20094,#20095,#20096,#20097,#20098,#20099,#20100,#20101,#20102,
#20103,#20104,#20105,#20106,#20107,#20108,#20109,#20110,#20111,#20112,#20113,
#20114,#20115,#20116,#20117,#20118,#20119,#20120,#20121,#20122,#20123,#20124,
#20125,#20126,#20127,#20128,#20129,#20130,#20131,#20132,#20133,#20134,#20135,
#20136,#20137,#20138,#20139,#20140,#20141,#20142,#20143,#20144,#20145,#20146,
#20147,#20148,#20149,#20150,#20151,#20152,#20153,#20154,#20155,#20156,#20157,
#20158,#20159,#20160,#20161,#20162,#20163,#20164,#20165,#20166,#20167,#20168,
#20169,#20170,#20171,#20172,#20173,#20174,#20175,#20176,#20177,#20178,#20179,
#20180,#20181,#20182,#20183,#20184,#20185,#20186,#20187,#20188,#20189,#20190,
#20191,#20192,#20193,#20194,#20195,#20196,#20197,#20198,#20199,#20200,#20201,
#20202,#20203,#20204,#20205,#20206,#20207,#20208,#20209,#20210,#20211,#20212,
#20213,#20214,#20215,#20216,#20217,#20218,#20219,#20220,#20221,#20222,#20223,
#20224,#20225,#20226,#20227,#20228,#20229,#20230),.UNSPECIFIED.,.F.,.F.,
(4,2,2,2,2,2,2,2,2,2,2,2,2,2,2,2,2,2,2,2,2,2,2,2,2,2,2,2,2,2,2,2,2,2,2,
2,2,2,2,2,2,2,2,2,2,2,2,2,2,2,2,2,2,2,2,2,2,2,2,2,2,2,2,2,2,2,2,2,2,2,2,
2,2,2,2,2,2,2,2,2,2,2,2,2,2,2,2,2,2,2,2,2,2,2,2,2,2,2,2,2,2,2,2,2,4),(-3.17259999392289,
-3.12496881097331,-3.11836850531031,-3.11409579174395,-3.11002953984388,
-3.10689426367969,-3.10280406102069,-3.09562214452332,-3.05960615618452,
-3.02877649122314,-3.00059430551812,-2.98882473813139,-2.98538225075395,
-2.98325139063015,-2.98126368167241,-2.97885376594607,-2.97270862514894,
-2.92190725684228,-2.88722496237993,-2.87425465035336,-2.86453796234612,
-2.85998224423964,-2.85646882497619,-2.85260892897295,-2.84629076818517,
-2.82498876061778,-2.75953341354037,-2.74562383800142,-2.73689813799119,
-2.73382884353142,-2.73177921139855,-2.7299495445617,-2.72744822390498,
-2.7211251809285,-2.67558398587311,-2.65399673618474,-2.6305432910418,-2.62041360092054,
-2.61240032196748,-2.608178148527,-2.60503280917959,-2.60107718417831,-2.59432029185784,
-2.56783148277945,-2.51451017236128,-2.49663007165224,-2.48963060511916,
-2.48440930915592,-2.48190407937595,-2.47994493067311,-2.47762594694345,
-2.47344187708961,-2.45284748328633,-2.38668621375722,-2.3727707006047,
-2.36251429884992,-2.35786014461553,-2.35433322507059,-2.35051932673315,
-2.34441178492399,-2.32502587302667,-2.26465423624521,-2.24589026394476,
-2.23514667285458,-2.23183287369807,-2.22973041292791,-2.2277259167726,
-2.22525005872627,-2.2191452309043,-2.16980389027994,-2.13419142953018,
-2.12101714495601,-2.11118291204162,-2.1066054820195,-2.10308924688258,
-2.09924010951645,-2.09297109912761,-2.07210282520022,-2.01943346272415,
-1.98615278737952,-1.98168173241009,-1.97932761105158,-1.97737106295488,
-1.97490982246655,-1.97100831342367,-1.94869780021006,-1.93049401466996,
-1.89957831685155,-1.86523602564397,-1.8582685817792,-1.85426741581928,
-1.85077806427195,-1.84645635066849,-1.83978302805478,-1.79122605800795,
-1.75368854772611,-1.74064835924039,-1.73231798451588,-1.72930250868749,
-1.72726408851753,-1.72542504877492,-1.72288632131961,-1.71641036265964,
-1.67799079970043,-1.67605418873215),.UNSPECIFIED.);
#292=B_SPLINE_CURVE_WITH_KNOTS('',3,(#20236,#20237,#20238,#20239,#20240,
#20241,#20242,#20243,#20244,#20245,#20246,#20247,#20248,#20249,#20250,#20251,
#20252,#20253,#20254,#20255,#20256,#20257,#20258,#20259,#20260,#20261,#20262,
#20263,#20264,#20265,#20266,#20267,#20268,#20269,#20270,#20271,#20272,#20273,
#20274,#20275,#20276,#20277,#20278,#20279,#20280,#20281,#20282,#20283,#20284,
#20285,#20286,#20287,#20288,#20289,#20290,#20291,#20292,#20293,#20294,#20295,
#20296,#20297,#20298,#20299,#20300,#20301,#20302,#20303,#20304,#20305,#20306,
#20307,#20308,#20309,#20310,#20311,#20312,#20313,#20314,#20315,#20316,#20317,
#20318,#20319,#20320,#20321,#20322,#20323,#20324,#20325,#20326,#20327,#20328,
#20329,#20330,#20331,#20332,#20333,#20334,#20335,#20336,#20337,#20338,#20339,
#20340,#20341,#20342,#20343,#20344,#20345,#20346,#20347,#20348,#20349,#20350,
#20351,#20352,#20353,#20354,#20355,#20356,#20357,#20358,#20359,#20360,#20361,
#20362,#20363,#20364,#20365,#20366,#20367,#20368,#20369,#20370,#20371,#20372,
#20373,#20374,#20375,#20376,#20377,#20378,#20379,#20380,#20381,#20382,#20383,
#20384,#20385,#20386,#20387,#20388,#20389,#20390,#20391,#20392,#20393,#20394,
#20395,#20396,#20397,#20398,#20399,#20400,#20401,#20402,#20403,#20404,#20405,
#20406,#20407,#20408,#20409,#20410,#20411,#20412,#20413,#20414,#20415,#20416),
 .UNSPECIFIED.,.F.,.F.,(4,3,3,3,3,3,3,3,3,3,3,3,3,3,3,3,3,3,3,3,3,3,3,3,
3,3,3,3,3,3,3,3,3,3,3,3,3,3,3,3,3,3,3,3,3,3,3,3,3,3,3,3,3,3,3,3,3,3,3,3,
4),(33.0800387021028,33.1788114424491,33.2775352322483,33.3762398755367,
33.4749551493895,33.5737748761942,33.672651172472,33.7716939664021,33.8320806131228,
33.9311397307074,34.0300584049669,34.1296938302993,34.2284358316502,34.3271453584,
34.4258521963517,34.5261745991704,34.6250231925307,34.7260825000786,34.8271418076264,
34.9262009252113,35.025119599471,35.1247550248034,35.2234970261545,35.3222065529047,
35.4209133908568,35.5212357936751,35.6200843870359,35.7211436945829,35.82220300213,
35.9212621197145,36.0201807939738,36.1198162193063,36.218558220657,36.3172677474068,
36.4159745853584,36.5162969881772,36.6151455815376,36.7162048890856,36.8172641966336,
36.9163233142183,37.0152419884777,37.1148774138102,37.213619415161,37.312328941911,
37.4110357798628,37.5113581826814,37.6102067760418,37.7112660835895,37.8123253911372,
37.9113845087219,38.0103031829812,38.1099386083137,38.2086806096646,38.3073901364146,
38.4060969743664,38.506419377185,38.6052679705455,38.7063272780932,38.8073865856408,
38.9480297229087,39.0086749840545),.UNSPECIFIED.);
#293=B_SPLINE_CURVE_WITH_KNOTS('',3,(#20417,#20418,#20419,#20420,#20421,
#20422,#20423,#20424,#20425,#20426,#20427,#20428,#20429),.UNSPECIFIED.,
 .F.,.F.,(4,3,3,3,4),(39.0086749844145,39.1061283325211,39.2034999693848,
39.3008301805805,39.3627720041259),.UNSPECIFIED.);
#294=B_SPLINE_CURVE_WITH_KNOTS('',3,(#20430,#20431,#20432,#20433,#20434,
#20435,#20436,#20437,#20438,#20439,#20440,#20441,#20442,#20443,#20444,#20445,
#20446,#20447,#20448,#20449,#20450,#20451,#20452,#20453,#20454,#20455,#20456,
#20457,#20458,#20459,#20460,#20461,#20462,#20463,#20464,#20465,#20466,#20467,
#20468,#20469,#20470,#20471,#20472,#20473,#20474,#20475,#20476,#20477,#20478,
#20479,#20480,#20481,#20482,#20483,#20484,#20485,#20486,#20487,#20488,#20489,
#20490,#20491,#20492,#20493,#20494,#20495,#20496,#20497,#20498,#20499,#20500,
#20501,#20502,#20503,#20504,#20505,#20506,#20507,#20508,#20509,#20510,#20511,
#20512,#20513,#20514,#20515,#20516,#20517,#20518,#20519,#20520,#20521,#20522,
#20523,#20524,#20525,#20526,#20527,#20528,#20529,#20530,#20531,#20532,#20533,
#20534,#20535,#20536,#20537,#20538,#20539,#20540,#20541,#20542,#20543,#20544,
#20545,#20546,#20547,#20548,#20549,#20550,#20551,#20552,#20553,#20554,#20555,
#20556,#20557,#20558,#20559,#20560,#20561,#20562,#20563,#20564,#20565,#20566,
#20567,#20568,#20569,#20570,#20571,#20572,#20573,#20574,#20575,#20576,#20577,
#20578,#20579,#20580,#20581,#20582,#20583,#20584,#20585,#20586,#20587,#20588,
#20589,#20590,#20591,#20592,#20593,#20594,#20595,#20596,#20597,#20598,#20599,
#20600,#20601,#20602,#20603,#20604,#20605,#20606,#20607,#20608,#20609,#20610,
#20611,#20612,#20613,#20614,#20615,#20616,#20617,#20618,#20619,#20620,#20621,
#20622,#20623,#20624,#20625,#20626,#20627,#20628,#20629,#20630,#20631,#20632,
#20633,#20634,#20635,#20636,#20637,#20638,#20639,#20640,#20641,#20642,#20643,
#20644,#20645,#20646,#20647,#20648,#20649,#20650,#20651,#20652,#20653,#20654,
#20655,#20656,#20657,#20658,#20659,#20660,#20661,#20662,#20663,#20664,#20665,
#20666,#20667,#20668,#20669,#20670,#20671,#20672,#20673,#20674,#20675,#20676,
#20677,#20678,#20679,#20680,#20681,#20682,#20683,#20684,#20685,#20686,#20687,
#20688,#20689,#20690,#20691,#20692,#20693,#20694,#20695,#20696,#20697,#20698,
#20699,#20700,#20701,#20702,#20703,#20704,#20705,#20706,#20707,#20708,#20709,
#20710,#20711),.UNSPECIFIED.,.F.,.F.,(4,2,2,2,2,2,2,2,2,2,2,2,2,2,2,2,2,
2,2,2,2,2,2,2,2,2,2,2,2,2,2,2,2,2,2,2,2,2,2,2,2,2,2,2,2,2,2,2,2,2,2,2,2,
2,2,2,2,2,2,2,2,2,2,2,2,2,2,2,2,2,2,2,2,2,2,2,2,2,2,2,2,2,2,2,2,2,2,2,2,
2,2,2,2,2,2,2,2,2,2,2,2,2,2,2,2,2,2,2,2,2,2,2,2,2,2,2,2,2,2,2,2,2,2,2,2,
2,2,2,2,2,2,2,2,2,2,2,2,2,2,2,4),(-1.67605418873215,-1.64446552570341,-1.61379541775656,
-1.60701601277305,-1.60305556305347,-1.59956146742909,-1.59518083036428,
-1.5866652416678,-1.55554836586235,-1.5033602837115,-1.48349741059974,-1.47935214976674,
-1.47704191306747,-1.47508196051158,-1.47256513654394,-1.46728355612929,
-1.46017877962238,-1.44188723341273,-1.38622875021952,-1.36227578346616,
-1.35570970119145,-1.35179569110038,-1.34829420571763,-1.34383866044754,
-1.3346523968148,-1.29929990316282,-1.24450322155425,-1.23144841080082,
-1.22776336141326,-1.22557881180475,-1.22359203767492,-1.22085601540368,
-1.21435562866304,-1.18232067991372,-1.12494103461589,-1.10929772679816,
-1.10365023977041,-1.10030660719022,-1.0967778391588,-1.09211195806968,
-1.0817906749433,-1.06776180082129,-1.00019830630836,-0.981109862488433,
-0.977007476205776,-0.974706853092972,-0.972745751438243,-0.970215414628244,
-0.964863569053112,-0.95763633031546,-0.938861914522575,-0.878450212878529,
-0.85905961949471,-0.8529511941131,-0.849136922517839,-0.845609782394701,
-0.840955519171999,-0.83069956500679,-0.816786713232761,-0.750636562863323,
-0.730066131986696,-0.725883341835163,-0.723564581856462,-0.721605327615493,
-0.719099565054224,-0.713875843771598,-0.706871626704422,-0.688972709089678,
-0.635575059923181,-0.609127613602163,-0.602373012061714,-0.59841781204071,
-0.595272308838384,-0.591049287001067,-0.583032205895378,-0.572897405359785,
-0.549427761675534,-0.502070482124086,-0.4908011501141,-0.477937518753328,
-0.474270282965583,-0.472089614076389,-0.470101324319369,-0.467356181427008,
-0.460801770271742,-0.451376249849108,-0.422654098414317,-0.362494730231977,
-0.35304486090271,-0.348538984343869,-0.345031630484092,-0.341145558191662,
-0.334708025063276,-0.309281319965056,-0.251283129256886,-0.228028623128943,
-0.224087392688026,-0.221614070539676,-0.219656813946372,-0.219638336092407,
-0.219620301519892,-0.219602694229522,-0.219585498971227,-0.219568701210277,
-0.219552287083677,-0.219536243368154,-0.219520557435778,-0.219505217218149,
-0.219490211197498,-0.219475528353639,-0.219461158145889,-0.219447090482153,
-0.219433315699463,-0.219419824552559,-0.219406608180464,-0.219393658073746,
-0.21938096608702,-0.219368524395416,-0.219356325492313,-0.219344362172756,
-0.219332627505137,-0.219321114832145,-0.219309817756675,-0.21929873012358,
-0.21928784600388,-0.219277159697579,-0.219266665729188,-0.219256358809398,
-0.21924623383803,-0.219236285913427,-0.219226510299542,-0.216726955493797,
-0.211587091030562,-0.20456762403992,-0.186609213777033,-0.132898376147193,
-0.10681202752676,-0.100081213120034,-0.0961312667424419,-0.0929852106039781,
-0.0902181295836139),.UNSPECIFIED.);
#295=B_SPLINE_CURVE_WITH_KNOTS('',3,(#20717,#20718,#20719,#20720,#20721,
#20722,#20723,#20724,#20725,#20726,#20727,#20728,#20729,#20730,#20731,#20732,
#20733,#20734,#20735,#20736,#20737,#20738,#20739,#20740,#20741,#20742,#20743,
#20744,#20745,#20746,#20747,#20748,#20749,#20750,#20751,#20752,#20753,#20754,
#20755,#20756,#20757,#20758,#20759,#20760,#20761,#20762,#20763,#20764,#20765,
#20766,#20767,#20768,#20769,#20770,#20771,#20772,#20773,#20774,#20775,#20776,
#20777,#20778,#20779,#20780,#20781,#20782,#20783,#20784,#20785,#20786,#20787,
#20788,#20789,#20790,#20791,#20792,#20793,#20794,#20795,#20796,#20797,#20798,
#20799,#20800,#20801,#20802,#20803,#20804,#20805,#20806,#20807,#20808,#20809,
#20810,#20811,#20812,#20813,#20814,#20815,#20816,#20817,#20818,#20819,#20820,
#20821,#20822,#20823,#20824,#20825,#20826,#20827,#20828,#20829,#20830,#20831,
#20832,#20833,#20834,#20835,#20836,#20837,#20838,#20839,#20840,#20841,#20842,
#20843,#20844,#20845,#20846,#20847,#20848,#20849,#20850,#20851,#20852,#20853,
#20854,#20855,#20856,#20857,#20858,#20859,#20860,#20861,#20862,#20863,#20864,
#20865,#20866,#20867,#20868,#20869,#20870,#20871,#20872,#20873,#20874,#20875,
#20876,#20877,#20878,#20879,#20880,#20881,#20882,#20883,#20884,#20885,#20886,
#20887,#20888,#20889,#20890,#20891,#20892,#20893,#20894,#20895,#20896,#20897),
 .UNSPECIFIED.,.F.,.F.,(4,3,3,3,3,3,3,3,3,3,3,3,3,3,3,3,3,3,3,3,3,3,3,3,
3,3,3,3,3,3,3,3,3,3,3,3,3,3,3,3,3,3,3,3,3,3,3,3,3,3,3,3,3,3,3,3,3,3,3,3,
4),(26.7958998905728,26.8666522515975,26.9657113691588,27.0646300433946,
27.1642654687329,27.2630074700601,27.3617169967863,27.4604238347143,27.560746237561,
27.6595948308979,27.7606541384995,27.8617134461011,27.9607725636749,28.0596912379233,
28.1593266632585,28.2580686645977,28.3567781913358,28.4554850292756,28.5558074321079,
28.654656025456,28.7557153330304,28.8567746406047,28.9558337582019,29.0547524324741,
29.1543878578034,29.2531298591674,29.3518393859305,29.4505462238956,29.5508686266988,
29.6497172200727,29.7507765275905,29.8518358351083,29.9508949526888,30.049813626944,
30.1494490522775,30.2481910536241,30.3469005803698,30.4456074183172,30.5459298211409,
30.6447784144971,30.7458377220545,30.846897029612,30.9459561471956,31.044874821454,
31.1445102467867,31.2432522481365,31.3419617748852,31.4406686128358,31.5409910156558,
31.639839609015,31.7408989165653,31.8419582241156,31.9397107034381,32.037933075085,
32.1354344299592,32.2328770951257,32.3302923655568,32.429091693321,32.5265951482302,
32.6260424124219,32.7254896766136),.UNSPECIFIED.);
#296=B_SPLINE_CURVE_WITH_KNOTS('',3,(#20898,#20899,#20900,#20901,#20902,
#20903,#20904,#20905,#20906,#20907,#20908,#20909,#20910),.UNSPECIFIED.,
 .F.,.F.,(4,3,3,3,4),(32.7254896768749,32.8370194186192,32.936080057733,
33.0349883528382,33.0800387021028),.UNSPECIFIED.);
#297=B_SPLINE_CURVE_WITH_KNOTS('',3,(#20912,#20913,#20914,#20915,#20916,
#20917,#20918,#20919,#20920,#20921,#20922,#20923),.UNSPECIFIED.,.F.,.F.,
(4,2,2,2,2,4),(-0.0902181295836139,-0.0887553371504392,-0.0807045076511089,
-0.0705153572373448,-0.0468548506221579,-0.000736301001977398),
 .UNSPECIFIED.);
#298=B_SPLINE_CURVE_WITH_KNOTS('',3,(#20924,#20925,#20926,#20927,#20928,
#20929,#20930,#20931,#20932,#20933,#20934,#20935,#20936,#20937,#20938,#20939,
#20940,#20941,#20942,#20943,#20944,#20945,#20946,#20947,#20948,#20949,#20950,
#20951,#20952,#20953,#20954,#20955,#20956,#20957,#20958,#20959,#20960,#20961,
#20962,#20963,#20964,#20965,#20966,#20967,#20968,#20969,#20970,#20971,#20972,
#20973,#20974,#20975,#20976,#20977,#20978,#20979,#20980,#20981,#20982,#20983,
#20984,#20985,#20986,#20987,#20988,#20989,#20990,#20991,#20992,#20993,#20994,
#20995,#20996,#20997,#20998,#20999,#21000,#21001,#21002,#21003,#21004,#21005,
#21006,#21007,#21008,#21009,#21010,#21011,#21012,#21013,#21014,#21015,#21016,
#21017,#21018,#21019,#21020,#21021,#21022,#21023,#21024,#21025,#21026,#21027,
#21028,#21029,#21030,#21031,#21032,#21033,#21034,#21035,#21036,#21037,#21038,
#21039,#21040,#21041,#21042,#21043,#21044,#21045,#21046,#21047,#21048,#21049,
#21050,#21051,#21052,#21053,#21054,#21055,#21056,#21057,#21058,#21059,#21060,
#21061,#21062,#21063,#21064,#21065,#21066,#21067,#21068,#21069,#21070,#21071,
#21072,#21073,#21074,#21075,#21076,#21077,#21078,#21079,#21080,#21081,#21082,
#21083,#21084,#21085,#21086,#21087,#21088,#21089,#21090,#21091,#21092,#21093,
#21094,#21095,#21096,#21097,#21098,#21099,#21100,#21101,#21102,#21103,#21104,
#21105,#21106,#21107,#21108,#21109,#21110,#21111,#21112,#21113,#21114,#21115,
#21116,#21117,#21118,#21119,#21120,#21121,#21122,#21123,#21124,#21125),
 .UNSPECIFIED.,.F.,.F.,(4,2,2,2,2,2,2,2,2,2,2,2,2,2,2,2,2,2,2,2,2,2,2,2,
2,2,2,2,2,2,2,2,2,2,2,2,2,2,2,2,2,2,2,2,2,2,2,2,2,2,2,2,2,2,2,2,2,2,2,2,
2,2,2,2,2,2,2,2,2,2,2,2,2,2,2,2,2,2,2,2,2,2,2,2,2,2,2,2,2,2,2,2,2,2,2,2,
2,2,2,2,4),(-3.17338897415504,-3.15145317667747,-3.14756194944923,-3.14509576002276,
-3.14318825463869,-3.14141535638956,-3.13916544226158,-3.13528952983564,
-3.11963491996032,-3.10145196086512,-3.04897341387108,-3.0344935147722,
-3.02391898825236,-3.01920624991346,-3.01566846281435,-3.01187475928096,
-3.00586853141856,-2.98739721949976,-2.93257978086865,-2.90911608726844,
-2.90077838506334,-2.89484499951574,-2.89223441317387,-2.89028827015876,
-2.88809411425886,-2.88436962501802,-2.87091237686426,-2.81629739892998,
-2.78108350996001,-2.77191243662363,-2.76745810105447,-2.76395483749657,
-2.76003600221971,-2.7534549666887,-2.72934498263058,-2.67938776270491,
-2.64990438696998,-2.64365174469296,-2.64095697210415,-2.63897553599654,
-2.63676972479563,-2.63299197959258,-2.61895275076301,-2.55203199647492,
-2.52530058844043,-2.51876657121876,-2.51485828579963,-2.51135354158148,
-2.50688233168194,-2.49762149406868,-2.43563900632499,-2.39733040241475,
-2.39191501264215,-2.38937187009492,-2.38740881571431,-2.3851152135072,
-2.381046765334,-2.3625396277497,-2.30893254648497,-2.27479692368528,-2.26783644213133,
-2.26383555357514,-2.26034426548011,-2.25601733248866,-2.24933053204391,
-2.2006961827,-2.16342015612807,-2.15024469047998,-2.14185091834582,-2.13882576047495,
-2.13678465577309,-2.13494622137547,-2.13241217364397,-2.1259683135347,
-2.08665031358038,-2.04402966533529,-2.02205008673329,-2.01589305528209,
-2.01206703761017,-2.00854151307228,-2.00398596608263,-1.99400882575514,
-1.94371019187171,-1.90805558163563,-1.89740222508034,-1.89021768609199,
-1.88737003247275,-1.88536351595007,-1.88322192583434,-1.879733861959,-1.86856123299659,
-1.81098941514518,-1.78546219930833,-1.77475114567881,-1.76637809000447,
-1.7620815756749,-1.75859260958355,-1.75456977841347,-1.74769053193514,
-1.71811416048442,-1.67634727028989),.UNSPECIFIED.);
#299=B_SPLINE_CURVE_WITH_KNOTS('',3,(#21131,#21132,#21133,#21134,#21135,
#21136,#21137,#21138,#21139,#21140,#21141,#21142,#21143,#21144,#21145,#21146,
#21147,#21148,#21149,#21150,#21151,#21152,#21153,#21154,#21155,#21156,#21157,
#21158,#21159,#21160,#21161,#21162,#21163,#21164,#21165,#21166,#21167,#21168,
#21169,#21170,#21171,#21172,#21173,#21174,#21175,#21176,#21177,#21178,#21179,
#21180,#21181,#21182,#21183,#21184,#21185,#21186,#21187,#21188,#21189,#21190,
#21191,#21192,#21193,#21194,#21195,#21196,#21197,#21198,#21199,#21200,#21201,
#21202,#21203,#21204,#21205,#21206,#21207,#21208,#21209,#21210,#21211,#21212,
#21213,#21214,#21215,#21216,#21217,#21218,#21219,#21220,#21221,#21222,#21223,
#21224,#21225,#21226,#21227,#21228,#21229,#21230,#21231,#21232,#21233,#21234,
#21235,#21236,#21237,#21238,#21239,#21240,#21241,#21242,#21243,#21244,#21245,
#21246,#21247,#21248,#21249,#21250,#21251,#21252,#21253,#21254,#21255,#21256,
#21257,#21258,#21259,#21260,#21261,#21262,#21263,#21264,#21265,#21266,#21267,
#21268,#21269,#21270,#21271,#21272,#21273,#21274,#21275,#21276,#21277,#21278,
#21279,#21280,#21281,#21282,#21283,#21284,#21285,#21286,#21287,#21288,#21289,
#21290,#21291,#21292,#21293,#21294,#21295,#21296,#21297,#21298,#21299,#21300,
#21301,#21302,#21303,#21304,#21305,#21306,#21307,#21308,#21309,#21310,#21311),
 .UNSPECIFIED.,.F.,.F.,(4,3,3,3,3,3,3,3,3,3,3,3,3,3,3,3,3,3,3,3,3,3,3,3,
3,3,3,3,3,3,3,3,3,3,3,3,3,3,3,3,3,3,3,3,3,3,3,3,3,3,3,3,3,3,3,3,3,3,3,3,
4),(20.5129680002155,20.6107259391232,20.7085286089183,20.8065050140131,
20.8962850845758,20.9953442016773,21.0942628754568,21.1938983009096,21.292640301791,
21.3913498280767,21.4900566655699,21.5903790689473,21.6892276618682,21.7902869704738,
21.8913462790794,21.9904053958419,22.0893240692632,22.1889594948032,22.2877014952828,
22.386411021151,22.4851178582115,22.5854402620544,22.6842888545097,22.7853481640464,
22.8864074735831,22.9854665917689,23.0843852666377,23.1840206918188,23.282762693795,
23.3814722211749,23.4801790597604,23.580501461842,23.6793500558389,23.7804093619628,
23.8814686680867,23.9805277855541,24.0794464596959,24.1790818850577,24.2778238862909,
24.3765334129235,24.4752402507583,24.5755626537163,24.6744112469619,24.7754705547761,
24.8765298625903,24.975588980077,25.0745076542362,25.1741430795934,25.27288508084,
25.3715946074844,25.4703014453291,25.5706238482703,25.6694724415217,25.7705317493078,
25.8715910570939,25.9728761869164,26.0739977696392,26.1749480073185,26.2757973957606,
26.3765610499166,26.4423043696953),.UNSPECIFIED.);
#300=B_SPLINE_CURVE_WITH_KNOTS('',3,(#21312,#21313,#21314,#21315,#21316,
#21317,#21318,#21319,#21320,#21321,#21322,#21323,#21324),.UNSPECIFIED.,
 .F.,.F.,(4,3,3,3,4),(26.4423043699728,26.5495705796222,26.6571264780996,
26.765082346119,26.7958998905728),.UNSPECIFIED.);
#301=B_SPLINE_CURVE_WITH_KNOTS('',3,(#21325,#21326,#21327,#21328,#21329,
#21330,#21331,#21332,#21333,#21334,#21335,#21336,#21337,#21338,#21339,#21340,
#21341,#21342,#21343,#21344,#21345,#21346,#21347,#21348,#21349,#21350,#21351,
#21352,#21353,#21354,#21355,#21356,#21357,#21358,#21359,#21360,#21361,#21362,
#21363,#21364,#21365,#21366,#21367,#21368,#21369,#21370,#21371,#21372,#21373,
#21374,#21375,#21376,#21377,#21378,#21379,#21380,#21381,#21382,#21383,#21384,
#21385,#21386,#21387,#21388,#21389,#21390,#21391,#21392,#21393,#21394,#21395,
#21396,#21397,#21398,#21399,#21400,#21401,#21402,#21403,#21404,#21405,#21406,
#21407,#21408,#21409,#21410,#21411,#21412,#21413,#21414,#21415,#21416,#21417,
#21418,#21419,#21420,#21421,#21422,#21423,#21424,#21425,#21426,#21427,#21428,
#21429,#21430,#21431,#21432,#21433,#21434,#21435,#21436,#21437,#21438,#21439,
#21440,#21441,#21442,#21443,#21444,#21445,#21446,#21447,#21448,#21449,#21450,
#21451,#21452,#21453,#21454,#21455,#21456,#21457,#21458,#21459,#21460,#21461,
#21462,#21463,#21464,#21465,#21466,#21467,#21468,#21469,#21470,#21471,#21472,
#21473,#21474,#21475,#21476,#21477,#21478,#21479,#21480,#21481,#21482,#21483,
#21484,#21485,#21486,#21487,#21488,#21489,#21490,#21491,#21492,#21493,#21494,
#21495,#21496,#21497,#21498,#21499,#21500,#21501,#21502,#21503,#21504,#21505,
#21506,#21507,#21508,#21509,#21510,#21511,#21512,#21513,#21514,#21515,#21516,
#21517,#21518,#21519,#21520,#21521,#21522,#21523,#21524,#21525,#21526,#21527,
#21528,#21529,#21530,#21531,#21532,#21533,#21534,#21535,#21536,#21537,#21538,
#21539,#21540,#21541,#21542,#21543,#21544,#21545,#21546,#21547,#21548,#21549,
#21550,#21551,#21552,#21553,#21554,#21555,#21556),.UNSPECIFIED.,.F.,.F.,
(4,2,2,2,2,2,2,2,2,2,2,2,2,2,2,2,2,2,2,2,2,2,2,2,2,2,2,2,2,2,2,2,2,2,2,
2,2,2,2,2,2,2,2,2,2,2,2,2,2,2,2,2,2,2,2,2,2,2,2,2,2,2,2,2,2,2,2,2,2,2,2,
2,2,2,2,2,2,2,2,2,2,2,2,2,2,2,2,2,2,2,2,2,2,2,2,2,2,2,2,2,2,2,2,2,2,2,2,
2,2,2,2,2,2,2,2,4),(-1.67634727028989,-1.66741515781725,-1.65007009753052,
-1.64320884805284,-1.63806717820834,-1.63557685571605,-1.63380546311439,
-1.63155034778241,-1.62765009107774,-1.61166443286676,-1.60273261522532,
-1.58721972708483,-1.52486415310859,-1.51564296736236,-1.51117969066712,
-1.50767621711202,-1.50376422498485,-1.49721170849928,-1.47020172013932,
-1.40068169303466,-1.38914158875836,-1.38561174988993,-1.3834609372194,
-1.38145901503103,-1.3786367864817,-1.37161344401501,-1.36127887301356,
-1.32755292182266,-1.27462480242134,-1.26471717194173,-1.26017426015671,
-1.25665068583042,-1.2528189443509,-1.24663525729233,-1.22435372328808,
-1.18063693076381,-1.16673827571981,-1.15823326743009,-1.13908221184482,
-1.1349751377007,-1.13267294041826,-1.13071118576053,-1.12818089747551,
-1.12283227601954,-1.1156114729253,-1.09686633357667,-1.03698458136081,
-1.01708923153163,-1.01092464452101,-1.00709720834416,-1.00357256756493,
-0.998943121216566,-0.98883068662824,-0.975172844065648,-0.937279909720506,
-0.891402723743196,-0.885089300562871,-0.882588766966048,-0.880758870749702,
-0.878708017677102,-0.875635203490524,-0.866888202350397,-0.852931320846599,
-0.786872125674087,-0.766053683765324,-0.759788706660085,-0.755939624042054,
-0.752421854319723,-0.747840148259659,-0.737987620695772,-0.724784247100402,
-0.68904544589373,-0.639916004034322,-0.633801977568994,-0.631324110062701,
-0.629318670685728,-0.627216094946634,-0.623903612812235,-0.613178048028686,
-0.594461268734392,-0.534944580871909,-0.514733791760564,-0.508533247839354,
-0.504698380367309,-0.501176798729665,-0.496565786413771,-0.486552301820809,
-0.473067577684551,-0.436005111597049,-0.432337303794875,-0.389149229170169,
-0.382756589481615,-0.380231480904177,-0.378395641265319,-0.376352730259696,
-0.37331687277746,-0.364841502733728,-0.35148476677032,-0.322641606957777,
-0.269891760856808,-0.260149903565411,-0.255567057890482,-0.25217184455642,
-0.248905096645079,-0.243525283894319,-0.228601392735488,-0.205469003111721,
-0.174869595024417,-0.157070991986575,-0.134640831473529,-0.130734154595829,
-0.128271092978842,-0.126314108723162,-0.123960689724939,-0.119494270154341,
-0.0901440899991799),.UNSPECIFIED.);
#302=B_SPLINE_CURVE_WITH_KNOTS('',3,(#21562,#21563,#21564,#21565,#21566,
#21567,#21568,#21569,#21570,#21571,#21572,#21573,#21574,#21575,#21576,#21577,
#21578,#21579,#21580,#21581,#21582,#21583,#21584,#21585,#21586,#21587,#21588,
#21589,#21590,#21591,#21592,#21593,#21594,#21595,#21596,#21597,#21598,#21599,
#21600,#21601,#21602,#21603,#21604,#21605,#21606,#21607,#21608,#21609,#21610,
#21611,#21612,#21613,#21614,#21615,#21616,#21617,#21618,#21619,#21620,#21621,
#21622,#21623,#21624,#21625,#21626,#21627,#21628,#21629,#21630,#21631,#21632,
#21633,#21634,#21635,#21636,#21637,#21638,#21639,#21640,#21641,#21642,#21643,
#21644,#21645,#21646,#21647,#21648,#21649,#21650,#21651,#21652,#21653,#21654,
#21655,#21656,#21657,#21658,#21659,#21660,#21661,#21662,#21663,#21664,#21665,
#21666,#21667,#21668,#21669,#21670,#21671,#21672,#21673,#21674,#21675,#21676,
#21677,#21678,#21679,#21680,#21681,#21682,#21683,#21684,#21685,#21686,#21687,
#21688,#21689,#21690,#21691,#21692,#21693,#21694,#21695,#21696,#21697,#21698,
#21699,#21700,#21701,#21702,#21703,#21704,#21705,#21706,#21707,#21708,#21709,
#21710,#21711,#21712,#21713,#21714,#21715,#21716,#21717,#21718,#21719,#21720,
#21721,#21722,#21723,#21724,#21725,#21726,#21727,#21728,#21729,#21730,#21731,
#21732,#21733,#21734,#21735,#21736,#21737,#21738,#21739),.UNSPECIFIED.,
 .F.,.F.,(4,3,3,3,3,3,3,3,3,3,3,3,3,3,3,3,3,3,3,3,3,3,3,3,3,3,3,3,3,3,3,
3,3,3,3,3,3,3,3,3,3,3,3,3,3,3,3,3,3,3,3,3,3,3,3,3,3,3,3,4),(14.2304175189723,
14.3291587597253,14.4278681142516,14.5265753676279,14.6264110051095,14.7252606329009,
14.8255892752276,14.9259179175542,15.0249770454872,15.1238957307452,15.2235311534093,
15.3222731672754,15.4209827070846,15.5196895586242,15.6200119469826,15.7188605551067,
15.8199198335823,15.9209791120578,16.0200381791658,16.1189568020786,16.218592240139,
16.3173341883945,16.4160436615095,16.5147504453582,16.615072910659,16.7139214493074,
16.8149808779344,16.9160403065614,17.0150994500851,17.1140181506013,17.2136535694092,
17.3123955975981,17.4111051513445,17.5098120164147,17.6101343875773,17.7089830080811,
17.8100422545731,17.911101501065,18.0101606176973,18.1090792910617,18.2087147166251,
18.3074567172289,18.4061662432893,18.5048730806102,18.6051954843498,18.7040440772322,
18.8051033864004,18.9061626955686,19.0052218065867,19.1041404741599,19.2037759011489,
19.3025178955699,19.4012274153137,19.4999342461923,19.6002566571623,19.6991052433558,
19.800164566714,19.9012238900722,20.0301714761699,20.1591190622677),
 .UNSPECIFIED.);
#303=B_SPLINE_CURVE_WITH_KNOTS('',3,(#21740,#21741,#21742,#21743,#21744,
#21745,#21746,#21747,#21748,#21749,#21750,#21751,#21752),.UNSPECIFIED.,
 .F.,.F.,(4,3,3,3,4),(20.1591190625158,20.2568630563804,20.3545467790412,
20.4522206776011,20.5129680002155),.UNSPECIFIED.);
#304=B_SPLINE_CURVE_WITH_KNOTS('',3,(#21754,#21755,#21756,#21757,#21758,
#21759,#21760,#21761,#21762,#21763,#21764,#21765,#21766,#21767),
 .UNSPECIFIED.,.F.,.F.,(4,2,2,2,2,2,4),(-0.0901440899991799,-0.0865142020355592,
-0.0179497024792971,-0.00869120363488619,-0.00427521847958375,-0.00207284054739809,
-0.000735550131679377),.UNSPECIFIED.);
#305=B_SPLINE_CURVE_WITH_KNOTS('',3,(#21768,#21769,#21770,#21771,#21772,
#21773,#21774,#21775,#21776,#21777,#21778,#21779,#21780,#21781,#21782,#21783,
#21784,#21785,#21786,#21787,#21788,#21789,#21790,#21791,#21792,#21793,#21794,
#21795,#21796,#21797,#21798,#21799,#21800,#21801,#21802,#21803,#21804,#21805,
#21806,#21807,#21808,#21809,#21810,#21811,#21812,#21813,#21814,#21815,#21816,
#21817,#21818,#21819,#21820,#21821,#21822,#21823,#21824,#21825,#21826,#21827,
#21828,#21829,#21830,#21831,#21832,#21833,#21834,#21835,#21836,#21837,#21838,
#21839,#21840,#21841,#21842,#21843,#21844,#21845,#21846,#21847,#21848,#21849,
#21850,#21851,#21852,#21853,#21854,#21855,#21856,#21857,#21858,#21859,#21860,
#21861,#21862,#21863,#21864,#21865,#21866,#21867,#21868,#21869,#21870,#21871,
#21872,#21873,#21874,#21875,#21876,#21877,#21878,#21879,#21880,#21881,#21882,
#21883,#21884,#21885,#21886,#21887,#21888,#21889,#21890,#21891,#21892,#21893,
#21894,#21895,#21896,#21897,#21898,#21899,#21900,#21901,#21902,#21903,#21904,
#21905,#21906,#21907,#21908,#21909,#21910,#21911,#21912,#21913,#21914,#21915,
#21916,#21917,#21918,#21919,#21920,#21921,#21922,#21923,#21924,#21925,#21926,
#21927,#21928,#21929,#21930,#21931,#21932,#21933,#21934,#21935,#21936,#21937,
#21938,#21939,#21940,#21941,#21942,#21943,#21944,#21945,#21946,#21947,#21948,
#21949,#21950,#21951,#21952,#21953,#21954,#21955,#21956,#21957,#21958,#21959,
#21960,#21961,#21962,#21963,#21964,#21965,#21966,#21967,#21968,#21969,#21970,
#21971),.UNSPECIFIED.,.F.,.F.,(4,2,2,2,2,2,2,2,2,2,2,2,2,2,2,2,2,2,2,2,
2,2,2,2,2,2,2,2,2,2,2,2,2,2,2,2,2,2,2,2,2,2,2,2,2,2,2,2,2,2,2,2,2,2,2,2,
2,2,2,2,2,2,2,2,2,2,2,2,2,2,2,2,2,2,2,2,2,2,2,2,2,2,2,2,2,2,2,2,2,2,2,2,
2,2,2,2,2,2,2,2,2,4),(-3.1722509398096,-3.17060364178562,-3.16756475987777,
-3.16076857491728,-3.13202985013187,-3.08130818076906,-3.06339374770734,
-3.05638483235411,-3.05115778742784,-3.04865107524353,-3.04687793928561,
-3.04463418047412,-3.0407826670575,-3.02542533057891,-3.01857113997389,
-2.95893977948005,-2.9332330746546,-2.92677375012245,-2.92346955050727,
-2.9203213030464,-2.91636991923783,-2.90957452080238,-2.88068670174827,
-2.83632851963011,-2.80674846121586,-2.80048740143094,-2.79779183442152,
-2.79581092189301,-2.79360690004671,-2.78983481507202,-2.77584730469061,
-2.76578292607347,-2.74800166937713,-2.70395026721197,-2.68158065245759,
-2.67539006103701,-2.67155737864756,-2.66803516305312,-2.66349711221027,
-2.65361276970661,-2.600208147281,-2.58280452884286,-2.55529296747341,-2.54924577813284,
-2.54658754310513,-2.54461192544506,-2.54238909799065,-2.538531275098,-2.52355856240514,
-2.5145469624538,-2.46830336670483,-2.43430116973454,-2.42592508108142,
-2.42162858020279,-2.41814038861373,-2.41411929948595,-2.40724512539072,
-2.37773552562209,-2.32699665401711,-2.3096447536604,-2.3027822612045,-2.29764014561524,
-2.29515009680769,-2.29337909812818,-2.29112476577515,-2.28722647397197,
-2.27125846537618,-2.20056490119876,-2.17905603290402,-2.17294358245344,
-2.16912833361109,-2.16560132708545,-2.16102775594893,-2.15131857266118,
-2.09676063498915,-2.05199131310598,-2.04656643728882,-2.04402217086125,
-2.0420597212145,-2.03976847212473,-2.03570822808801,-2.0173176594134,-1.96363422800829,
-1.92950574779454,-1.92254781741689,-1.91854846217572,-1.91505854555955,
-1.91073335040183,-1.90404929937544,-1.85543194457712,-1.81816313581032,
-1.80500257106894,-1.79661667137624,-1.79359340868247,-1.791553324392,-1.78971587244261,
-1.7871829365979,-1.78074074700496,-1.74158616324513,-1.70684684234202,
-1.67788094058519,-1.67566337115906),.UNSPECIFIED.);
#306=B_SPLINE_CURVE_WITH_KNOTS('',3,(#21977,#21978,#21979,#21980,#21981,
#21982,#21983,#21984,#21985,#21986,#21987,#21988,#21989,#21990,#21991,#21992,
#21993,#21994,#21995,#21996,#21997,#21998),.UNSPECIFIED.,.F.,.F.,(4,2,2,
2,2,2,2,2,2,2,4),(-0.0899054331255484,-0.076554022126443,-0.0575923344739192,
-0.0404520211695611,-0.0364869914952116,-0.0342258185213306,-0.0324608490723674,
-0.0305641377237055,-0.0281332474336483,-0.0243291396135012,-0.00076704490792084),
 .UNSPECIFIED.);
#307=B_SPLINE_CURVE_WITH_KNOTS('',3,(#22000,#22001,#22002,#22003,#22004,
#22005,#22006,#22007,#22008,#22009,#22010,#22011,#22012,#22013,#22014,#22015,
#22016,#22017,#22018,#22019,#22020,#22021,#22022,#22023,#22024,#22025,#22026,
#22027,#22028,#22029,#22030,#22031,#22032,#22033,#22034,#22035,#22036,#22037,
#22038,#22039,#22040,#22041,#22042,#22043,#22044,#22045,#22046,#22047,#22048,
#22049,#22050,#22051,#22052,#22053,#22054,#22055,#22056,#22057,#22058,#22059,
#22060,#22061,#22062,#22063,#22064,#22065,#22066,#22067,#22068,#22069,#22070,
#22071,#22072,#22073,#22074,#22075,#22076,#22077,#22078,#22079,#22080,#22081,
#22082,#22083,#22084,#22085,#22086,#22087,#22088,#22089,#22090,#22091,#22092,
#22093,#22094,#22095,#22096,#22097,#22098,#22099,#22100,#22101,#22102,#22103,
#22104,#22105,#22106,#22107,#22108,#22109,#22110,#22111,#22112,#22113,#22114,
#22115,#22116,#22117,#22118,#22119,#22120),.UNSPECIFIED.,.F.,.F.,(4,3,3,
3,3,3,3,3,3,3,3,3,3,3,3,3,3,3,3,3,3,3,3,3,3,3,3,3,3,3,3,3,3,3,3,3,3,3,3,
3,4),(-3.84897440539517,-3.75125824246988,-3.65367165958683,-3.55615640926645,
-3.45868120095872,-3.36121479544941,-3.26366285251732,-3.16606894445241,
-3.06831010828305,-2.98518358351084,-2.88598456951401,-2.78692366642958,
-2.68732350675178,-2.58843473405244,-2.48957707964969,-2.39072097507435,
-2.29057132855757,-2.19157226309705,-2.09084732605214,-1.99012238900722,
-1.89213277745176,-1.7942843081741,-1.69438141896529,-1.59670435988929,
-1.49905580466275,-1.40140475752039,-1.29981886676619,-1.20200306502378,
-1.10410734082398,-1.00604310459973,-0.995061194503613,-0.893246091409371,
-0.791590847240874,-0.690095795641479,-0.588695144143975,-0.487364670179868,
-0.386080230764985,-0.284788586297225,-0.183499496794958,-0.0821381948532282,
-1.10844070079203E-14),.UNSPECIFIED.);
#308=B_SPLINE_CURVE_WITH_KNOTS('',3,(#22124,#22125,#22126,#22127,#22128,
#22129,#22130,#22131,#22132,#22133,#22134,#22135,#22136,#22137,#22138,#22139,
#22140,#22141,#22142,#22143,#22144,#22145,#22146,#22147,#22148,#22149,#22150,
#22151,#22152,#22153,#22154,#22155,#22156,#22157,#22158,#22159,#22160,#22161,
#22162,#22163,#22164,#22165,#22166,#22167,#22168,#22169,#22170,#22171,#22172,
#22173,#22174,#22175,#22176,#22177,#22178,#22179,#22180,#22181,#22182,#22183,
#22184,#22185,#22186,#22187,#22188,#22189,#22190,#22191,#22192,#22193,#22194,
#22195,#22196,#22197,#22198,#22199,#22200,#22201,#22202,#22203,#22204,#22205,
#22206,#22207,#22208,#22209,#22210,#22211,#22212,#22213,#22214,#22215,#22216,
#22217,#22218,#22219,#22220,#22221,#22222,#22223,#22224,#22225,#22226,#22227,
#22228,#22229,#22230,#22231,#22232,#22233,#22234,#22235,#22236,#22237,#22238,
#22239,#22240,#22241,#22242,#22243,#22244,#22245,#22246,#22247,#22248,#22249,
#22250,#22251,#22252,#22253,#22254,#22255,#22256,#22257,#22258,#22259,#22260,
#22261,#22262,#22263,#22264,#22265,#22266,#22267,#22268,#22269,#22270,#22271,
#22272,#22273,#22274,#22275,#22276,#22277,#22278,#22279,#22280,#22281,#22282,
#22283,#22284,#22285,#22286,#22287,#22288,#22289,#22290,#22291,#22292,#22293,
#22294,#22295),.UNSPECIFIED.,.F.,.F.,(4,3,3,3,3,3,3,3,3,3,3,3,3,3,3,3,3,
3,3,3,3,3,3,3,3,3,3,3,3,3,3,3,3,3,3,3,3,3,3,3,3,3,3,3,3,3,3,3,3,3,3,3,3,
3,3,3,3,4),(2.01695526861829,2.11569428289456,2.21429391180832,2.31278169291955,
2.41120867663817,2.50960510300603,2.60800117427649,2.70649198428098,2.80503037766619,
2.90373779545109,2.98518358351083,3.08441219206656,3.18350384345799,3.28309646027754,
3.38201865334366,3.4809106774714,3.57980207048774,3.67991274736941,3.77894908090012,
3.87959692945728,3.98024477801444,4.07917123083895,4.17795538394911,4.27762420752023,
4.37622812463871,4.4747985304458,4.57336539305711,4.67385053792235,4.77255845171639,
4.87393221211723,4.97530597251806,5.0743944712415,5.17334267030362,5.27297073239337,
5.37174238517647,5.47048154357541,5.56921795237523,5.66950525603684,5.76838296393618,
5.86937506547893,5.97036716702167,6.06944598088698,6.16838478747198,6.26801523422864,
6.3667782867615,6.46550916360479,6.56423762247439,6.66453530723711,6.76340597267392,
6.8644171670996,6.96542836152528,7.06514551960968,7.1647175303196,7.2641732783273,
7.36353573611598,7.46284448248297,7.5621384291416,7.59274844815658),
 .UNSPECIFIED.);
#309=B_SPLINE_CURVE_WITH_KNOTS('',3,(#22296,#22297,#22298,#22299,#22300,
#22301,#22302,#22303,#22304,#22305,#22306,#22307,#22308),.UNSPECIFIED.,
 .F.,.F.,(4,3,3,3,4),(7.59274844853383,7.7041721787488,7.81611578899353,
7.92866788548955,7.94663621176237),.UNSPECIFIED.);
#310=B_SPLINE_CURVE_WITH_KNOTS('',3,(#22314,#22315,#22316,#22317,#22318,
#22319),.UNSPECIFIED.,.F.,.F.,(4,1,1,4),(131.030246900353,131.266332202741,
132.261393397245,133.256454591748),.UNSPECIFIED.);
#311=B_SPLINE_CURVE_WITH_KNOTS('',3,(#22322,#22323,#22324,#22325,#22326,
#22327,#22328,#22329,#22330,#22331,#22332,#22333,#22334,#22335,#22336,#22337,
#22338,#22339,#22340,#22341,#22342,#22343,#22344,#22345,#22346,#22347,#22348,
#22349,#22350,#22351,#22352,#22353,#22354,#22355,#22356,#22357,#22358,#22359,
#22360,#22361,#22362,#22363,#22364,#22365,#22366,#22367,#22368,#22369,#22370,
#22371,#22372,#22373,#22374,#22375,#22376,#22377,#22378,#22379,#22380,#22381,
#22382,#22383,#22384,#22385,#22386,#22387,#22388,#22389,#22390,#22391,#22392,
#22393,#22394,#22395,#22396,#22397,#22398,#22399,#22400,#22401,#22402,#22403,
#22404,#22405,#22406,#22407,#22408,#22409,#22410,#22411,#22412,#22413,#22414,
#22415),.UNSPECIFIED.,.F.,.F.,(4,3,3,3,3,3,3,3,3,3,3,3,3,3,3,3,3,3,3,3,
3,3,3,3,3,3,3,3,3,3,3,4),(131.031732990453,131.129719001446,131.223540756003,
131.317335965402,131.411130403081,131.504949834588,131.598875844033,131.69286470379,
131.786999793311,131.815621078398,131.910029099741,132.004308879585,132.098488743851,
132.192599708902,132.286675386837,132.38074122658,132.474822661588,132.569002090768,
132.663235460962,132.757616799081,132.810682272902,132.90455843657,132.998308854135,
133.095869530573,133.189457985588,133.283016460457,133.376571017001,133.470147706645,
133.563827171698,133.657567522566,133.751451095249,133.778794265637),
 .UNSPECIFIED.);
#312=B_SPLINE_CURVE_WITH_KNOTS('',3,(#22421,#22422,#22423,#22424,#22425,
#22426,#22427,#22428,#22429,#22430,#22431,#22432,#22433,#22434,#22435,#22436,
#22437,#22438,#22439,#22440,#22441,#22442,#22443,#22444,#22445,#22446,#22447,
#22448,#22449,#22450,#22451,#22452,#22453,#22454,#22455,#22456,#22457,#22458,
#22459,#22460,#22461,#22462,#22463,#22464,#22465,#22466,#22467,#22468,#22469,
#22470,#22471,#22472,#22473,#22474,#22475,#22476,#22477,#22478,#22479,#22480,
#22481,#22482,#22483,#22484,#22485,#22486,#22487,#22488,#22489,#22490,#22491,
#22492,#22493,#22494,#22495,#22496,#22497,#22498,#22499,#22500,#22501,#22502,
#22503,#22504,#22505,#22506,#22507,#22508,#22509,#22510,#22511,#22512,#22513,
#22514,#22515,#22516,#22517,#22518,#22519,#22520,#22521,#22522,#22523,#22524,
#22525,#22526,#22527,#22528,#22529,#22530,#22531,#22532,#22533,#22534,#22535,
#22536,#22537,#22538,#22539,#22540,#22541,#22542,#22543,#22544,#22545,#22546,
#22547,#22548,#22549,#22550,#22551,#22552,#22553,#22554,#22555,#22556),
 .UNSPECIFIED.,.F.,.F.,(4,3,3,3,3,3,3,3,3,3,3,3,3,3,3,3,3,3,3,3,3,3,3,3,
3,3,3,3,3,3,3,3,3,3,3,3,3,3,3,3,3,3,3,3,3,4),(124.748116942751,124.842021477706,
124.935936809012,125.029949826741,125.124012734743,125.21823452561,125.295965035719,
125.390188901834,125.484284908524,125.578281625117,125.672211126157,125.766106452365,
125.859993270984,125.953897234944,126.047902627316,126.14196364901,126.236176981576,
126.291026230223,126.385283355284,126.479412577247,126.573442422118,126.667404787361,
126.761332802783,126.8552520969,126.949188283725,127.043225319743,127.13731770511,
127.231561651695,127.286087424727,127.380343323035,127.474471636526,127.568500887675,
127.662463125408,127.756391300844,127.85031104033,127.944247955951,128.038286144246,
128.132379922439,128.226625623753,128.28114861923,128.379025264194,128.47673030057,
128.574231689995,128.671611327341,128.768855381404,128.805298797182),
 .UNSPECIFIED.);
#313=B_SPLINE_CURVE_WITH_KNOTS('',3,(#22557,#22558,#22559,#22560,#22561,
#22562),.UNSPECIFIED.,.F.,.F.,(4,1,1,4),(128.80530075582,129.276209813734,
130.271271008237,131.030246900353),.UNSPECIFIED.);
#314=B_SPLINE_CURVE_WITH_KNOTS('',3,(#22564,#22565,#22566,#22567,#22568,
#22569,#22570,#22571,#22572,#22573,#22574,#22575,#22576,#22577,#22578,#22579,
#22580,#22581,#22582,#22583,#22584,#22585,#22586,#22587,#22588,#22589,#22590,
#22591,#22592,#22593,#22594,#22595,#22596,#22597,#22598,#22599,#22600,#22601,
#22602,#22603,#22604,#22605,#22606,#22607,#22608,#22609,#22610,#22611,#22612,
#22613,#22614,#22615,#22616,#22617,#22618,#22619,#22620,#22621,#22622,#22623,
#22624,#22625,#22626,#22627,#22628,#22629,#22630,#22631,#22632,#22633,#22634,
#22635,#22636,#22637,#22638,#22639,#22640,#22641,#22642),.UNSPECIFIED.,
 .F.,.F.,(4,3,3,3,3,3,3,3,3,3,3,3,3,3,3,3,3,3,3,3,3,3,3,3,3,3,4),(128.805298797182,
128.830437494887,128.924694627589,129.018823857126,129.1128537095,129.206816082106,
129.300744104803,129.394663406099,129.488599599999,129.582636642893,129.676729035032,
129.770972988163,129.825498689391,129.919754615869,130.013882957705,130.107912237332,
130.201874503625,130.29580270766,130.389722475749,130.483659419942,130.577697636588,
130.671791443048,130.766037172219,130.820559883894,130.914698557345,131.008697567804,
131.031732990453),.UNSPECIFIED.);
#315=B_SPLINE_CURVE_WITH_KNOTS('',3,(#22643,#22644,#22645,#22646,#22647,
#22648,#22649,#22650),.UNSPECIFIED.,.F.,.F.,(4,1,1,1,1,4),(124.747381147578,
124.850192716873,125.845253911376,126.84031510588,127.835376300384,128.805295307034),
 .UNSPECIFIED.);
#316=B_SPLINE_CURVE_WITH_KNOTS('',3,(#22656,#22657,#22658,#22659,#22660,
#22661,#22662,#22663,#22664,#22665,#22666,#22667,#22668,#22669,#22670,#22671,
#22672,#22673,#22674,#22675,#22676,#22677,#22678,#22679,#22680,#22681,#22682,
#22683,#22684,#22685,#22686,#22687,#22688,#22689,#22690,#22691,#22692,#22693,
#22694,#22695,#22696,#22697,#22698,#22699,#22700,#22701,#22702,#22703,#22704,
#22705,#22706,#22707,#22708,#22709,#22710,#22711,#22712,#22713,#22714,#22715,
#22716,#22717,#22718,#22719,#22720,#22721,#22722,#22723,#22724,#22725,#22726,
#22727,#22728,#22729,#22730,#22731,#22732,#22733,#22734,#22735,#22736,#22737,
#22738,#22739,#22740,#22741,#22742,#22743,#22744,#22745,#22746,#22747,#22748,
#22749,#22750,#22751,#22752,#22753,#22754,#22755,#22756,#22757,#22758,#22759,
#22760,#22761,#22762,#22763,#22764,#22765,#22766,#22767,#22768,#22769,#22770,
#22771,#22772,#22773,#22774,#22775,#22776,#22777,#22778,#22779,#22780,#22781,
#22782,#22783,#22784,#22785,#22786,#22787,#22788),.UNSPECIFIED.,.F.,.F.,
(4,3,3,3,3,3,3,3,3,3,3,3,3,3,3,3,3,3,3,3,3,3,3,3,3,3,3,3,3,3,3,3,3,3,3,
3,3,3,3,3,3,3,3,3,4),(118.465298607546,118.559363166675,118.655142504428,
118.749068183104,118.842971185363,118.936877151751,119.034057330988,119.12810108778,
119.226849478239,119.325597868698,119.419836160087,119.513946617396,119.607957790504,
119.701901697558,119.795811393377,119.889712527958,119.983630736934,120.077650179834,
120.171725163178,120.265952179458,120.320659063201,120.414897776923,120.50900865503,
120.603020246869,120.696964567888,120.790874674582,120.884776216466,120.978694828691,
121.072714666242,121.166790039971,121.261017436083,121.315720257705,121.40995935154,
121.504070615355,121.598082597901,121.692027315394,121.785937821971,121.879839766635,
121.97375878403,122.067779027872,122.161854809123,122.256082610628,122.310781452209,
122.44149000973,122.522113490002),.UNSPECIFIED.);
#317=B_SPLINE_CURVE_WITH_KNOTS('',3,(#22789,#22790,#22791,#22792,#22793,
#22794,#22795,#22796,#22797,#22798,#22799,#22800,#22801,#22802,#22803,#22804,
#22805,#22806,#22807,#22808,#22809,#22810,#22811,#22812,#22813,#22814,#22815,
#22816,#22817,#22818,#22819,#22820,#22821,#22822,#22823,#22824,#22825,#22826,
#22827,#22828,#22829,#22830,#22831,#22832,#22833,#22834,#22835,#22836,#22837,
#22838,#22839,#22840,#22841,#22842,#22843,#22844,#22845,#22846,#22847,#22848,
#22849,#22850,#22851,#22852,#22853,#22854,#22855,#22856,#22857,#22858,#22859,
#22860,#22861,#22862,#22863,#22864),.UNSPECIFIED.,.F.,.F.,(4,3,3,3,3,3,
3,3,3,3,3,3,3,3,3,3,3,3,3,3,3,3,3,3,3,4),(122.522113490219,122.614860375032,
122.707527160722,122.800152547904,122.892763516874,122.98538702816,123.078105516595,
123.170877967855,123.26379533639,123.305842646712,123.400083101606,123.494195711582,
123.58820902383,123.682155041317,123.776066829089,123.869970034715,123.963890291383,
124.057911734141,124.15198869332,124.246217628225,124.300903841216,124.395152233769,
124.489249395523,124.583258807334,124.677204221474,124.748116942751),
 .UNSPECIFIED.);
#318=B_SPLINE_CURVE_WITH_KNOTS('',3,(#22866,#22867,#22868,#22869,#22870,
#22871),.UNSPECIFIED.,.F.,.F.,(4,1,1,4),(122.522120559769,122.860070327865,
123.855131522369,124.747381147578),.UNSPECIFIED.);
#319=B_SPLINE_CURVE_WITH_KNOTS('',3,(#22872,#22873,#22874,#22875,#22876,
#22877,#22878,#22879,#22880,#22881,#22882,#22883,#22884,#22885,#22886,#22887,
#22888,#22889,#22890,#22891,#22892,#22893,#22894,#22895,#22896,#22897,#22898,
#22899,#22900,#22901,#22902,#22903,#22904,#22905,#22906,#22907,#22908,#22909,
#22910,#22911,#22912,#22913,#22914,#22915,#22916,#22917,#22918,#22919,#22920,
#22921,#22922,#22923,#22924,#22925,#22926,#22927,#22928,#22929,#22930,#22931,
#22932,#22933,#22934,#22935,#22936,#22937,#22938,#22939,#22940,#22941,#22942,
#22943,#22944,#22945,#22946,#22947,#22948,#22949,#22950,#22951,#22952,#22953,
#22954,#22955,#22956,#22957,#22958,#22959,#22960,#22961,#22962,#22963,#22964,
#22965,#22966,#22967,#22968,#22969,#22970,#22971,#22972,#22973,#22974,#22975,
#22976,#22977,#22978,#22979,#22980,#22981,#22982,#22983,#22984,#22985,#22986,
#22987,#22988,#22989,#22990,#22991,#22992,#22993,#22994,#22995,#22996,#22997,
#22998,#22999,#23000,#23001,#23002,#23003,#23004,#23005,#23006,#23007),
 .UNSPECIFIED.,.F.,.F.,(4,3,3,3,3,3,3,3,3,3,3,3,3,3,3,3,3,3,3,3,3,3,3,3,
3,3,3,3,3,3,3,3,3,3,3,3,3,3,3,3,3,3,3,3,3,4),(118.464533283335,118.558457081294,
118.652484421599,118.74657114206,118.840805385433,118.879825549851,118.974064053571,
119.068174723327,119.162186108714,119.256130226928,119.35004013314,119.443941477094,
119.537859894174,119.631879541979,119.725954728729,119.820181944045,119.874886744355,
119.969125291968,120.063236005371,120.157247434107,120.251191595053,120.3451015436,
120.439002929444,120.532921387917,120.626941076116,120.721016302753,120.81524355677,
120.869947938858,120.964186560255,121.05829734816,121.152308852005,121.246253088645,
121.340163113221,121.434064575333,121.527983110218,121.622002874577,121.716078177344,
121.810305506689,121.865009133362,121.959298109332,122.053461225864,122.147524199852,
122.24151443669,122.335459191593,122.429414396328,122.522113490002),
 .UNSPECIFIED.);
#320=B_SPLINE_CURVE_WITH_KNOTS('',3,(#23013,#23014,#23015,#23016,#23017,
#23018,#23019,#23020,#23021,#23022,#23023,#23024,#23025,#23026,#23027,#23028,
#23029,#23030,#23031,#23032,#23033,#23034,#23035,#23036,#23037,#23038,#23039,
#23040,#23041,#23042,#23043,#23044,#23045,#23046,#23047,#23048,#23049,#23050,
#23051,#23052,#23053,#23054,#23055,#23056,#23057,#23058,#23059,#23060,#23061,
#23062,#23063,#23064,#23065,#23066,#23067,#23068,#23069,#23070,#23071,#23072,
#23073,#23074,#23075,#23076,#23077,#23078,#23079,#23080,#23081,#23082,#23083,
#23084,#23085,#23086,#23087,#23088,#23089,#23090,#23091,#23092,#23093,#23094,
#23095,#23096,#23097,#23098,#23099,#23100,#23101,#23102,#23103,#23104,#23105,
#23106,#23107,#23108,#23109,#23110,#23111,#23112,#23113,#23114,#23115,#23116,
#23117,#23118,#23119,#23120,#23121,#23122,#23123,#23124,#23125,#23126,#23127,
#23128,#23129,#23130,#23131,#23132,#23133,#23134,#23135,#23136,#23137,#23138,
#23139,#23140,#23141,#23142,#23143,#23144,#23145,#23146,#23147,#23148),
 .UNSPECIFIED.,.F.,.F.,(4,3,3,3,3,3,3,3,3,3,3,3,3,3,3,3,3,3,3,3,3,3,3,3,
3,3,3,3,3,3,3,3,3,3,3,3,3,3,3,3,3,3,3,3,3,4),(112.181017173795,112.275233169463,
112.360169507172,112.454408042794,112.548518744449,112.642530161692,112.736474311568,
112.83038424931,112.924285624625,113.018204072858,113.112223751313,113.206298968473,
113.300526213524,113.355230701676,113.449469231835,113.543579928025,113.637591339807,
113.731535484251,113.825445416582,113.919346786512,114.013265229393,114.107284902579,
114.201360114508,114.295587354442,114.35029189618,114.444530430473,114.53864113076,
114.632652546598,114.72659669502,114.820506631279,114.914408005084,115.008326451781,
115.102346128671,115.196421344247,115.290648587701,115.345353090683,115.438408479076,
115.531337065953,115.624161153566,115.71692843708,115.809665818337,115.902400163806,
115.995209723843,116.088059513646,116.181043471339,116.238928182601),
 .UNSPECIFIED.);
#321=B_SPLINE_CURVE_WITH_KNOTS('',3,(#23149,#23150,#23151,#23152,#23153,
#23154,#23155,#23156,#23157,#23158,#23159,#23160,#23161,#23162,#23163,#23164,
#23165,#23166,#23167,#23168,#23169,#23170,#23171,#23172,#23173,#23174,#23175,
#23176,#23177,#23178,#23179,#23180,#23181,#23182,#23183,#23184,#23185,#23186,
#23187,#23188,#23189,#23190,#23191,#23192,#23193,#23194,#23195,#23196,#23197,
#23198,#23199,#23200,#23201,#23202,#23203,#23204,#23205,#23206,#23207,#23208,
#23209,#23210,#23211,#23212,#23213,#23214,#23215,#23216,#23217,#23218,#23219,
#23220,#23221,#23222,#23223,#23224),.UNSPECIFIED.,.F.,.F.,(4,3,3,3,3,3,
3,3,3,3,3,3,3,3,3,3,3,3,3,3,3,3,3,3,3,4),(116.238928182822,116.340414285187,
116.434652788961,116.528763458769,116.622774844209,116.716718962476,116.810628868741,
116.904530212748,116.998448629879,117.092468277736,117.186543464536,117.280770679902,
117.335475479691,117.429714027298,117.523824740696,117.617836169426,117.711780330368,
117.80569027891,117.899591664751,117.993510123221,118.087529811417,118.181605038051,
118.275832292067,118.330536674194,118.424770286337,118.465298607546),
 .UNSPECIFIED.);
#322=B_SPLINE_CURVE_WITH_KNOTS('',3,(#23226,#23227,#23228,#23229,#23230,
#23231,#23232,#23233,#23234,#23235,#23236,#23237,#23238,#23239,#23240,#23241,
#23242,#23243,#23244,#23245,#23246,#23247,#23248,#23249,#23250,#23251,#23252,
#23253,#23254,#23255,#23256,#23257,#23258,#23259,#23260,#23261,#23262,#23263,
#23264,#23265,#23266,#23267,#23268,#23269,#23270,#23271,#23272,#23273,#23274,
#23275,#23276,#23277,#23278,#23279,#23280,#23281,#23282,#23283,#23284,#23285,
#23286,#23287,#23288,#23289,#23290,#23291,#23292,#23293,#23294,#23295,#23296,
#23297,#23298,#23299,#23300,#23301),.UNSPECIFIED.,.F.,.F.,(4,3,3,3,3,3,
3,3,3,3,3,3,3,3,3,3,3,3,3,3,3,3,3,3,3,4),(116.238928182822,116.332983170984,
116.427030095315,116.521094265264,116.615267370442,116.709495278438,116.803894854092,
116.889703160844,116.983941695136,117.078052395421,117.172063811258,117.266007959679,
117.359917895936,117.453819269739,117.547737716434,117.641757393322,117.735832608897,
117.830059852349,117.884764355347,117.978993315107,118.073100941312,118.170959026818,
118.264897087566,118.358795692125,118.452689035773,118.464533283335),
 .UNSPECIFIED.);
#323=B_SPLINE_CURVE_WITH_KNOTS('',3,(#23302,#23303,#23304,#23305,#23306,
#23307,#23308,#23309,#23310,#23311,#23312,#23313,#23314,#23315,#23316,#23317,
#23318,#23319,#23320,#23321,#23322,#23323,#23324,#23325,#23326,#23327,#23328,
#23329,#23330,#23331,#23332,#23333,#23334,#23335,#23336,#23337,#23338,#23339,
#23340,#23341,#23342,#23343,#23344,#23345,#23346,#23347,#23348,#23349,#23350,
#23351,#23352,#23353,#23354,#23355,#23356,#23357,#23358,#23359,#23360,#23361,
#23362,#23363,#23364,#23365,#23366,#23367,#23368,#23369,#23370,#23371,#23372,
#23373,#23374,#23375,#23376,#23377,#23378,#23379,#23380,#23381,#23382,#23383,
#23384,#23385,#23386,#23387,#23388,#23389,#23390,#23391,#23392,#23393,#23394,
#23395,#23396,#23397,#23398,#23399,#23400,#23401,#23402,#23403,#23404,#23405,
#23406,#23407,#23408,#23409,#23410,#23411,#23412,#23413,#23414,#23415,#23416,
#23417,#23418,#23419,#23420,#23421,#23422,#23423,#23424,#23425,#23426,#23427,
#23428,#23429,#23430,#23431,#23432,#23433,#23434,#23435,#23436,#23437),
 .UNSPECIFIED.,.F.,.F.,(4,3,3,3,3,3,3,3,3,3,3,3,3,3,3,3,3,3,3,3,3,3,3,3,
3,3,3,3,3,3,3,3,3,3,3,3,3,3,3,3,3,3,3,3,3,4),(112.182146568534,112.276098342198,
112.370011913038,112.463912934884,112.557827043936,112.651840160733,112.745905233754,
112.840126670004,112.909458382829,113.003696916176,113.09780761555,113.19181903051,
113.285763178109,113.379673113578,113.473574486628,113.567492932605,113.661512608834,
113.755587823779,113.849815066659,113.904519577333,113.998758111003,114.092868810696,
114.186880225968,114.28082437387,114.374734309636,114.468635682976,114.562554129237,
114.656573805737,114.750649020949,114.844876264081,114.899580771837,114.993819307463,
115.087930009123,115.181941426371,115.275885576251,115.369795513998,115.463696889318,
115.557615337555,115.651635016015,115.745710233179,115.839937478235,115.89464196634,
116.00387938609,116.112620366374,116.220504130663,116.238928182603),
 .UNSPECIFIED.);
#324=B_SPLINE_CURVE_WITH_KNOTS('',3,(#23443,#23444,#23445,#23446,#23447,
#23448,#23449,#23450,#23451,#23452,#23453,#23454,#23455,#23456,#23457,#23458,
#23459,#23460,#23461,#23462,#23463,#23464,#23465,#23466,#23467,#23468,#23469,
#23470,#23471,#23472,#23473,#23474,#23475,#23476,#23477,#23478,#23479,#23480,
#23481,#23482,#23483,#23484,#23485,#23486,#23487,#23488,#23489,#23490,#23491,
#23492,#23493,#23494,#23495,#23496,#23497,#23498,#23499,#23500,#23501,#23502,
#23503,#23504,#23505,#23506,#23507,#23508,#23509,#23510,#23511,#23512,#23513,
#23514,#23515,#23516,#23517,#23518,#23519,#23520,#23521,#23522,#23523,#23524,
#23525,#23526,#23527,#23528,#23529,#23530,#23531,#23532,#23533,#23534,#23535,
#23536,#23537,#23538,#23539,#23540,#23541,#23542,#23543,#23544,#23545,#23546,
#23547,#23548,#23549,#23550,#23551,#23552,#23553,#23554,#23555,#23556,#23557,
#23558,#23559,#23560,#23561,#23562,#23563,#23564,#23565,#23566,#23567,#23568,
#23569,#23570,#23571,#23572,#23573,#23574,#23575,#23576,#23577,#23578),
 .UNSPECIFIED.,.F.,.F.,(4,3,3,3,3,3,3,3,3,3,3,3,3,3,3,3,3,3,3,3,3,3,3,3,
3,3,3,3,3,3,3,3,3,3,3,3,3,3,3,3,3,3,3,3,3,4),(105.898388911918,105.992293425444,
106.086224139824,106.180260935269,106.274361476398,106.368604602101,106.389802340151,
106.484040873954,106.578151573784,106.672162989198,106.766107137247,106.860017073163,
106.953918446657,107.047836893075,107.141856569736,107.235931785111,107.330159028408,
107.384863534654,107.479102068375,107.573212768123,107.667224183456,107.761168331424,
107.85507826726,107.948979640674,108.042898087013,108.136917763597,108.230992978894,
108.325220222116,108.379924729158,108.474163262893,108.568273962654,108.662285377998,
108.756229525977,108.850139461823,108.944040835246,109.037959281593,109.131978958184,
109.226054173488,109.320281416716,109.374985923662,109.471046274231,109.566961712461,
109.664157003256,109.759830055412,109.857786465528,109.955742875643),
 .UNSPECIFIED.);
#325=B_SPLINE_CURVE_WITH_KNOTS('',3,(#23579,#23580,#23581,#23582,#23583,
#23584,#23585,#23586,#23587,#23588,#23589,#23590,#23591,#23592,#23593,#23594,
#23595,#23596,#23597,#23598,#23599,#23600,#23601,#23602,#23603,#23604,#23605,
#23606,#23607,#23608,#23609,#23610,#23611,#23612,#23613,#23614,#23615,#23616,
#23617,#23618,#23619,#23620,#23621,#23622,#23623,#23624,#23625,#23626,#23627,
#23628,#23629,#23630,#23631,#23632,#23633,#23634,#23635,#23636,#23637,#23638,
#23639,#23640,#23641,#23642,#23643,#23644,#23645,#23646,#23647,#23648,#23649,
#23650,#23651),.UNSPECIFIED.,.F.,.F.,(4,3,3,3,3,3,3,3,3,3,3,3,3,3,3,3,3,
3,3,3,3,3,3,3,4),(109.955742875827,110.059318936412,110.162337101285,110.266192109725,
110.370047118165,110.464285651513,110.558396350888,110.652407765849,110.746351913449,
110.840261848919,110.934163221969,111.028081667947,111.122101344177,111.216176559123,
111.310403802003,111.365108312669,111.459358828674,111.553452005303,111.64745530481,
111.741394479135,111.835295218455,111.929214837249,112.023142263765,112.11715329755,
112.181017173795),.UNSPECIFIED.);
#326=B_SPLINE_CURVE_WITH_KNOTS('',3,(#23653,#23654,#23655,#23656,#23657,
#23658,#23659,#23660,#23661,#23662,#23663,#23664,#23665,#23666,#23667,#23668,
#23669,#23670,#23671,#23672,#23673,#23674,#23675,#23676,#23677,#23678,#23679,
#23680,#23681,#23682,#23683,#23684,#23685,#23686,#23687,#23688,#23689,#23690,
#23691,#23692,#23693,#23694,#23695,#23696,#23697,#23698,#23699,#23700,#23701,
#23702,#23703,#23704,#23705,#23706,#23707,#23708,#23709,#23710,#23711,#23712,
#23713,#23714,#23715,#23716,#23717,#23718,#23719,#23720,#23721,#23722,#23723,
#23724,#23725,#23726,#23727,#23728),.UNSPECIFIED.,.F.,.F.,(4,3,3,3,3,3,
3,3,3,3,3,3,3,3,3,3,3,3,3,3,3,3,3,3,3,4),(109.955742875862,110.04949173415,
110.143114524302,110.240142207992,110.333603103301,110.427034076366,110.520461333779,
110.613911072019,110.707463740762,110.801077867967,110.894834565712,110.919335993822,
111.013574527556,111.107685227317,111.201696642662,111.29564079064,111.389550726486,
111.483452099909,111.577370546256,111.671390222847,111.765465438151,111.859692681378,
111.914397188326,112.008631127952,112.102725431347,112.182146568534),
 .UNSPECIFIED.);
#327=B_SPLINE_CURVE_WITH_KNOTS('',3,(#23729,#23730,#23731,#23732,#23733,
#23734,#23735,#23736,#23737,#23738,#23739,#23740,#23741,#23742,#23743,#23744,
#23745,#23746,#23747,#23748,#23749,#23750,#23751,#23752,#23753,#23754,#23755,
#23756,#23757,#23758,#23759,#23760,#23761,#23762,#23763,#23764,#23765,#23766,
#23767,#23768,#23769,#23770,#23771,#23772,#23773,#23774,#23775,#23776,#23777,
#23778,#23779,#23780,#23781,#23782,#23783,#23784,#23785,#23786,#23787,#23788,
#23789,#23790,#23791,#23792,#23793,#23794,#23795,#23796,#23797,#23798,#23799,
#23800,#23801,#23802,#23803,#23804,#23805,#23806,#23807,#23808,#23809,#23810,
#23811,#23812,#23813,#23814,#23815,#23816,#23817,#23818,#23819,#23820,#23821,
#23822,#23823,#23824,#23825,#23826,#23827,#23828,#23829,#23830,#23831,#23832,
#23833,#23834,#23835,#23836,#23837,#23838,#23839,#23840,#23841,#23842,#23843,
#23844,#23845,#23846,#23847,#23848,#23849,#23850,#23851,#23852,#23853,#23854,
#23855,#23856,#23857,#23858,#23859,#23860,#23861,#23862,#23863,#23864,#23865,
#23866,#23867),.UNSPECIFIED.,.F.,.F.,(4,3,3,3,3,3,3,3,3,3,3,3,3,3,3,3,3,
3,3,3,3,3,3,3,3,3,3,3,3,3,3,3,3,3,3,3,3,3,3,3,3,3,3,3,3,3,4),(105.898164363444,
105.944030021304,106.038268555077,106.132379254877,106.226390670261,106.320334818279,
106.414244754166,106.50814612763,106.602064574018,106.69608425065,106.790159465995,
106.884386709264,106.939091215808,107.033329749571,107.127440449361,107.221451864736,
107.315396012745,107.409305948622,107.503207322077,107.597125768456,107.691145445079,
107.785220660415,107.879447903675,107.934152410311,108.028390944072,108.12250164386,
108.216513059233,108.31045720724,108.404367143114,108.498268516567,108.592186962943,
108.686206639563,108.780281854897,108.874509098154,108.929213604815,109.023452138618,
109.117562838448,109.211574253862,109.305518401911,109.399428337828,109.493329711322,
109.58724815774,109.681267834401,109.775343049776,109.869570293073,109.924274799319,
109.955742875643),.UNSPECIFIED.);
#328=B_SPLINE_CURVE_WITH_KNOTS('',3,(#23873,#23874,#23875,#23876,#23877,
#23878,#23879,#23880,#23881,#23882,#23883,#23884,#23885,#23886,#23887,#23888,
#23889,#23890,#23891,#23892,#23893,#23894,#23895,#23896,#23897,#23898,#23899,
#23900,#23901,#23902,#23903,#23904,#23905,#23906,#23907,#23908,#23909,#23910,
#23911,#23912,#23913,#23914,#23915,#23916,#23917,#23918,#23919,#23920,#23921,
#23922,#23923,#23924,#23925,#23926,#23927,#23928,#23929,#23930,#23931,#23932,
#23933,#23934,#23935,#23936,#23937,#23938,#23939,#23940,#23941,#23942,#23943,
#23944,#23945,#23946,#23947,#23948,#23949,#23950,#23951,#23952,#23953,#23954,
#23955,#23956,#23957,#23958,#23959,#23960,#23961,#23962,#23963,#23964,#23965,
#23966,#23967,#23968,#23969,#23970,#23971,#23972,#23973,#23974,#23975,#23976,
#23977,#23978,#23979,#23980,#23981,#23982,#23983,#23984,#23985,#23986,#23987,
#23988,#23989,#23990,#23991,#23992,#23993,#23994,#23995,#23996,#23997,#23998,
#23999,#24000,#24001,#24002,#24003,#24004,#24005,#24006,#24007,#24008),
 .UNSPECIFIED.,.F.,.F.,(4,3,3,3,3,3,3,3,3,3,3,3,3,3,3,3,3,3,3,3,3,3,3,3,
3,3,3,3,3,3,3,3,3,3,3,3,3,3,3,3,3,3,3,3,3,4),(99.6158049460037,99.7098135899942,
99.803756210262,99.8976654592765,99.9915669859436,100.085486425495,100.179507555568,
100.273584979423,100.367813533998,100.419435173129,100.513673706898,100.607784406694,
100.701795822074,100.795739970088,100.889649905971,100.983551279431,101.077469725815,
101.171489402443,101.265564617785,101.35979186105,101.414496367633,101.508734901401,
101.602845601196,101.696857016574,101.790801164588,101.88471110047,101.978612473929,
102.072530920312,102.166550596939,102.260625812279,102.354853055544,102.409557562136,
102.503796095903,102.597906795697,102.691918211075,102.785862359088,102.879772294969,
102.973673668427,103.067592114809,103.161611791436,103.255687006775,103.349914250038,
103.40461875664,103.524030082458,103.641345043911,103.67255756827),
 .UNSPECIFIED.);
#329=B_SPLINE_CURVE_WITH_KNOTS('',3,(#24009,#24010,#24011,#24012,#24013,
#24014,#24015,#24016,#24017,#24018,#24019,#24020,#24021,#24022,#24023,#24024,
#24025,#24026,#24027,#24028,#24029,#24030,#24031,#24032,#24033,#24034,#24035,
#24036,#24037,#24038,#24039,#24040,#24041,#24042,#24043,#24044,#24045,#24046,
#24047,#24048,#24049,#24050,#24051,#24052,#24053,#24054,#24055,#24056,#24057,
#24058,#24059,#24060,#24061,#24062,#24063,#24064,#24065,#24066,#24067,#24068,
#24069,#24070,#24071,#24072,#24073,#24074,#24075,#24076,#24077,#24078,#24079,
#24080,#24081,#24082,#24083,#24084),.UNSPECIFIED.,.F.,.F.,(4,3,3,3,3,3,
3,3,3,3,3,3,3,3,3,3,3,3,3,3,3,3,3,3,3,4),(103.672557568463,103.765628528244,
103.858652863645,103.951657206775,104.044668165207,104.137772858336,104.230925480928,
104.324235541546,104.399679951144,104.493918484907,104.588029184698,104.682040600072,
104.775984748081,104.869894683959,104.963796057413,105.057714503792,105.151734180415,
105.245809395752,105.340036639012,105.394741145647,105.488978919694,105.583093549466,
105.677096801156,105.771035905391,105.864939462047,105.898388911918),
 .UNSPECIFIED.);
#330=B_SPLINE_CURVE_WITH_KNOTS('',3,(#24086,#24087,#24088,#24089,#24090,
#24091,#24092,#24093,#24094,#24095,#24096,#24097,#24098,#24099,#24100,#24101,
#24102,#24103,#24104,#24105,#24106,#24107,#24108,#24109,#24110,#24111,#24112,
#24113,#24114,#24115,#24116,#24117,#24118,#24119,#24120,#24121,#24122,#24123,
#24124,#24125,#24126,#24127,#24128,#24129,#24130,#24131,#24132,#24133,#24134,
#24135,#24136,#24137,#24138,#24139,#24140,#24141,#24142,#24143,#24144,#24145,
#24146,#24147,#24148,#24149,#24150,#24151,#24152,#24153,#24154,#24155,#24156,
#24157,#24158),.UNSPECIFIED.,.F.,.F.,(4,3,3,3,3,3,3,3,3,3,3,3,3,3,3,3,3,
3,3,3,3,3,3,3,4),(103.67255756872,103.787765961805,103.90478701078,103.953907632297,
104.048146166065,104.14225686586,104.236268281238,104.330212429252,104.424122365134,
104.518023738593,104.611942184976,104.705961861603,104.800037076944,104.894264320208,
104.9489688268,105.043210275337,105.137323127687,105.232428282157,105.326369980879,
105.420276687691,105.514174051776,105.610171629693,105.704174610095,105.801169486769,
105.898164363444),.UNSPECIFIED.);
#331=B_SPLINE_CURVE_WITH_KNOTS('',3,(#24159,#24160,#24161,#24162,#24163,
#24164,#24165,#24166,#24167,#24168,#24169,#24170,#24171,#24172,#24173,#24174,
#24175,#24176,#24177,#24178,#24179,#24180,#24181,#24182,#24183,#24184,#24185,
#24186,#24187,#24188,#24189,#24190,#24191,#24192,#24193,#24194,#24195,#24196,
#24197,#24198,#24199,#24200,#24201,#24202,#24203,#24204,#24205,#24206,#24207,
#24208,#24209,#24210,#24211,#24212,#24213,#24214,#24215,#24216,#24217,#24218,
#24219,#24220,#24221,#24222,#24223,#24224,#24225,#24226,#24227,#24228,#24229,
#24230,#24231,#24232,#24233,#24234,#24235,#24236,#24237,#24238,#24239,#24240,
#24241,#24242,#24243,#24244,#24245,#24246,#24247,#24248,#24249,#24250,#24251,
#24252,#24253,#24254,#24255,#24256,#24257,#24258,#24259,#24260,#24261,#24262,
#24263,#24264,#24265,#24266,#24267,#24268,#24269,#24270,#24271,#24272,#24273,
#24274,#24275,#24276,#24277,#24278,#24279,#24280,#24281,#24282,#24283,#24284,
#24285,#24286,#24287,#24288,#24289,#24290,#24291,#24292,#24293,#24294),
 .UNSPECIFIED.,.F.,.F.,(4,3,3,3,3,3,3,3,3,3,3,3,3,3,3,3,3,3,3,3,3,3,3,3,
3,3,3,3,3,3,3,3,3,3,3,3,3,3,3,3,3,3,3,3,3,4),(99.614830573868,99.7088406605666,
99.802900937315,99.8971197623276,99.9736628542824,100.067901388051,100.162012087846,
100.256023503225,100.34996765124,100.443877587122,100.537778960582,100.631697406966,
100.725717083593,100.819792298935,100.914019542199,100.968724048786,101.062962582554,
101.157073282349,101.251084697729,101.345028845743,101.438938781625,101.532840155084,
101.626758601468,101.720778278096,101.814853493436,101.909080736701,101.96378524329,
102.058023777058,102.152134476853,102.246145892232,102.340090040246,102.433999976128,
102.527901349588,102.621819795971,102.715839472598,102.809914687939,102.904141931203,
102.958846437793,103.052298003948,103.145631281771,103.238872954843,103.332049611754,
103.425206679406,103.51835021553,103.611545131343,103.672557568463),
 .UNSPECIFIED.);
#332=B_SPLINE_CURVE_WITH_KNOTS('',3,(#24300,#24301,#24302,#24303,#24304,
#24305,#24306,#24307,#24308,#24309,#24310,#24311,#24312,#24313,#24314,#24315,
#24316,#24317,#24318,#24319,#24320,#24321,#24322,#24323,#24324,#24325,#24326,
#24327,#24328,#24329,#24330,#24331,#24332,#24333,#24334,#24335,#24336,#24337,
#24338,#24339,#24340,#24341,#24342,#24343,#24344,#24345,#24346,#24347,#24348,
#24349,#24350,#24351,#24352,#24353,#24354,#24355,#24356,#24357,#24358,#24359,
#24360,#24361,#24362,#24363,#24364,#24365,#24366,#24367,#24368,#24369,#24370,
#24371,#24372,#24373,#24374,#24375,#24376,#24377,#24378,#24379,#24380,#24381,
#24382,#24383,#24384,#24385,#24386,#24387,#24388,#24389,#24390,#24391,#24392,
#24393,#24394,#24395,#24396,#24397,#24398,#24399,#24400,#24401,#24402,#24403,
#24404,#24405,#24406,#24407,#24408,#24409,#24410,#24411,#24412,#24413,#24414,
#24415,#24416,#24417,#24418,#24419,#24420,#24421,#24422,#24423,#24424,#24425,
#24426,#24427,#24428,#24429,#24430,#24431,#24432,#24433,#24434,#24435,#24436,
#24437,#24438),.UNSPECIFIED.,.F.,.F.,(4,3,3,3,3,3,3,3,3,3,3,3,3,3,3,3,3,
3,3,3,3,3,3,3,3,3,3,3,3,3,3,3,3,3,3,3,3,3,3,3,3,3,3,3,3,3,4),(93.3315411447136,
93.4257806413673,93.4540068116039,93.548245345372,93.6423560451674,93.7363674605467,
93.8303116085608,93.924221544443,94.0181229179025,94.1120413642862,94.2060610409136,
94.3001362562545,94.394363499519,94.4490680061075,94.5433065398756,94.637417239671,
94.7314286550504,94.8253728030645,94.9192827389467,95.0131841124063,95.10710255879,
95.2011222354174,95.2951974507582,95.3894246940228,95.4441292006111,95.5383677343792,
95.6324784341746,95.726489849554,95.8204339975681,95.9143439334503,96.0082453069098,
96.1021637532934,96.1961834299208,96.2902586452616,96.3844858885262,96.4391903951147,
96.5327727036348,96.6262277012867,96.7216207712496,96.8149119236732,96.9081721054004,
97.0014277028667,97.0984138423976,97.1917929587827,97.2852342917173,97.3788110498964,
97.3893722609902),.UNSPECIFIED.);
#333=B_SPLINE_CURVE_WITH_KNOTS('',3,(#24439,#24440,#24441,#24442,#24443,
#24444,#24445,#24446,#24447,#24448,#24449,#24450,#24451,#24452,#24453,#24454,
#24455,#24456,#24457,#24458,#24459,#24460,#24461,#24462,#24463,#24464,#24465,
#24466,#24467,#24468,#24469,#24470,#24471,#24472,#24473,#24474,#24475,#24476,
#24477,#24478,#24479,#24480,#24481,#24482,#24483,#24484,#24485,#24486,#24487,
#24488,#24489,#24490,#24491,#24492,#24493,#24494,#24495,#24496,#24497,#24498,
#24499,#24500,#24501,#24502,#24503,#24504,#24505,#24506,#24507,#24508,#24509,
#24510,#24511,#24512,#24513,#24514),.UNSPECIFIED.,.F.,.F.,(4,3,3,3,3,3,
3,3,3,3,3,3,3,3,3,3,3,3,3,3,3,3,3,3,3,4),(97.3893722612835,97.4342515896183,
97.5284901233865,97.6226008231819,97.7166122385613,97.8105563865755,97.9044663224577,
97.9983676959173,98.0922861423011,98.1863058189285,98.2803810342694,98.3746082775341,
98.4293127841219,98.5235513178899,98.6176620176852,98.7116734330645,98.8056175810786,
98.8995275169606,98.9934288904202,99.0873473368038,99.1813670134312,99.275442228772,
99.3696694720365,99.4243739786255,99.5200894623146,99.6158049460037),
 .UNSPECIFIED.);
#334=B_SPLINE_CURVE_WITH_KNOTS('',3,(#24516,#24517,#24518,#24519,#24520,
#24521,#24522,#24523,#24524,#24525,#24526,#24527,#24528,#24529,#24530,#24531,
#24532,#24533,#24534,#24535,#24536,#24537,#24538,#24539,#24540,#24541,#24542,
#24543,#24544,#24545,#24546,#24547,#24548,#24549,#24550,#24551,#24552,#24553,
#24554,#24555,#24556,#24557,#24558,#24559,#24560,#24561,#24562,#24563,#24564,
#24565,#24566,#24567,#24568,#24569,#24570,#24571,#24572,#24573,#24574,#24575,
#24576,#24577,#24578,#24579,#24580,#24581,#24582,#24583,#24584,#24585,#24586,
#24587,#24588,#24589,#24590,#24591),.UNSPECIFIED.,.F.,.F.,(4,3,3,3,3,3,
3,3,3,3,3,3,3,3,3,3,3,3,3,3,3,3,3,3,3,4),(97.3893722612835,97.4846035291451,
97.5798662932485,97.6751835878792,97.7706423523568,97.8661846756541,97.961893063649,
97.9835404652752,98.0777789990433,98.1718896988386,98.2659011142179,98.359845262232,
98.4537551981142,98.5476565715738,98.6415750179575,98.7355946945849,98.8296699099256,
98.9238971531902,98.9786016597788,99.0728248085171,99.1669279658269,99.2609369867913,
99.3548809239173,99.4487849917754,99.5427012429723,99.614830573868),
 .UNSPECIFIED.);
#335=B_SPLINE_CURVE_WITH_KNOTS('',3,(#24592,#24593,#24594,#24595,#24596,
#24597,#24598,#24599,#24600,#24601,#24602,#24603,#24604,#24605,#24606,#24607,
#24608,#24609,#24610,#24611,#24612,#24613,#24614,#24615,#24616,#24617,#24618,
#24619,#24620,#24621,#24622,#24623,#24624,#24625,#24626,#24627,#24628,#24629,
#24630,#24631,#24632,#24633,#24634,#24635,#24636,#24637,#24638,#24639,#24640,
#24641,#24642,#24643,#24644,#24645,#24646,#24647,#24648,#24649,#24650,#24651,
#24652,#24653,#24654,#24655,#24656,#24657,#24658,#24659,#24660,#24661,#24662,
#24663,#24664,#24665,#24666,#24667,#24668,#24669,#24670,#24671,#24672,#24673,
#24674,#24675,#24676,#24677,#24678,#24679,#24680,#24681,#24682,#24683,#24684,
#24685,#24686,#24687,#24688,#24689,#24690,#24691,#24692,#24693,#24694,#24695,
#24696,#24697,#24698,#24699,#24700,#24701,#24702,#24703,#24704,#24705,#24706,
#24707,#24708,#24709,#24710,#24711,#24712,#24713,#24714,#24715,#24716,#24717,
#24718,#24719,#24720,#24721,#24722,#24723,#24724),.UNSPECIFIED.,.F.,.F.,
(4,3,3,3,3,3,3,3,3,3,3,3,3,3,3,3,3,3,3,3,3,3,3,3,3,3,3,3,3,3,3,3,3,3,3,
3,3,3,3,3,3,3,3,3,4),(93.3325033045339,93.4264290221299,93.520331971357,
93.6142377929244,93.7115022665084,93.8055457879678,93.9044207376143,94.0032956872607,
94.0975342210288,94.191644920824,94.2856563362031,94.3796004842171,94.4735104200992,
94.5674117935589,94.6613302399424,94.7553499165697,94.8494251319105,94.9436523751751,
94.9983568817644,95.0925954155325,95.1867061153279,95.280717530707,95.374661678721,
95.4685716146033,95.5624729880632,95.6563914344467,95.750411111074,95.8444863264147,
95.9387135696792,95.9934180762679,96.0876566100358,96.1817673098313,96.2757787252102,
96.3697228732243,96.4636328091064,96.5575341825662,96.6514526289502,96.7454723055776,
96.8395475209183,96.9337747641829,96.9884792707716,97.0928864960786,97.1969961549413,
97.3005780262804,97.3893722610814),.UNSPECIFIED.);
#336=B_SPLINE_CURVE_WITH_KNOTS('',3,(#24730,#24731,#24732,#24733,#24734,
#24735,#24736,#24737,#24738,#24739,#24740,#24741,#24742,#24743,#24744,#24745,
#24746,#24747,#24748,#24749,#24750,#24751,#24752,#24753,#24754,#24755,#24756,
#24757,#24758,#24759,#24760,#24761,#24762,#24763,#24764,#24765,#24766,#24767,
#24768,#24769,#24770,#24771,#24772,#24773,#24774,#24775,#24776,#24777,#24778,
#24779,#24780,#24781,#24782,#24783,#24784,#24785,#24786,#24787,#24788,#24789,
#24790,#24791,#24792,#24793,#24794,#24795,#24796,#24797,#24798,#24799,#24800,
#24801,#24802,#24803,#24804,#24805,#24806,#24807,#24808,#24809,#24810,#24811,
#24812,#24813,#24814,#24815,#24816,#24817,#24818,#24819,#24820,#24821,#24822,
#24823,#24824,#24825,#24826,#24827,#24828,#24829,#24830,#24831,#24832,#24833,
#24834,#24835,#24836,#24837,#24838,#24839,#24840,#24841,#24842,#24843,#24844,
#24845,#24846,#24847,#24848,#24849,#24850,#24851,#24852,#24853,#24854,#24855,
#24856,#24857,#24858,#24859,#24860,#24861,#24862,#24863,#24864,#24865),
 .UNSPECIFIED.,.F.,.F.,(4,3,3,3,3,3,3,3,3,3,3,3,3,3,3,3,3,3,3,3,3,3,3,3,
3,3,3,3,3,3,3,3,3,3,3,3,3,3,3,3,3,3,3,3,3,4),(87.0486631737809,87.1425803605593,
87.2365981702577,87.3306705294207,87.424896100684,87.4836396445822,87.5778781783503,
87.6719888781456,87.7660002935253,87.8599444415394,87.9538543774217,88.0477557508812,
88.1416741972647,88.2356938738921,88.3297690892331,88.4239963324976,88.4787008390858,
88.5729393728539,88.6670500726492,88.7610614880286,88.8550056360427,88.9489155719248,
89.0428169453843,89.1367353917682,89.2307550683955,89.3248302837365,89.4190575270009,
89.4737620335894,89.5680005673576,89.6621112671533,89.7561226825328,89.8500668305468,
89.9439767664289,90.0378781398886,90.1317965862717,90.2258162628992,90.3198914782399,
90.4141187215044,90.468823228093,90.5634949768987,90.6580371372988,90.7524748824259,
90.8468296227406,90.9411345169124,91.0354333352935,91.106186954104),
 .UNSPECIFIED.);
#337=B_SPLINE_CURVE_WITH_KNOTS('',3,(#24866,#24867,#24868,#24869,#24870,
#24871,#24872,#24873,#24874,#24875,#24876,#24877,#24878,#24879,#24880,#24881,
#24882,#24883,#24884,#24885,#24886,#24887,#24888,#24889,#24890,#24891,#24892,
#24893,#24894,#24895,#24896,#24897,#24898,#24899,#24900,#24901,#24902,#24903,
#24904,#24905,#24906,#24907,#24908,#24909,#24910,#24911,#24912,#24913,#24914,
#24915,#24916,#24917,#24918,#24919,#24920,#24921,#24922,#24923,#24924,#24925,
#24926,#24927,#24928,#24929,#24930,#24931,#24932,#24933,#24934,#24935,#24936,
#24937,#24938,#24939,#24940,#24941),.UNSPECIFIED.,.F.,.F.,(4,3,3,3,3,3,
3,3,3,3,3,3,3,3,3,3,3,3,3,3,3,3,3,3,3,4),(91.1061869543297,91.2130644277206,
91.3204667480979,91.4284945161628,91.4638844225966,91.5581229563647,91.6522336561603,
91.7462450715397,91.8401892195538,91.9340991554359,92.0280005288955,92.1219189752793,
92.2159386519067,92.3100138672475,92.404241110512,92.4589456171003,92.5531921681985,
92.6504857902629,92.744486076237,92.8384244481871,92.9323265926773,93.0262181583636,
93.1201623979588,93.21413875603,93.3082140844942,93.3315411447136),
 .UNSPECIFIED.);
#338=B_SPLINE_CURVE_WITH_KNOTS('',3,(#24943,#24944,#24945,#24946,#24947,
#24948,#24949,#24950,#24951,#24952,#24953,#24954,#24955,#24956,#24957,#24958,
#24959,#24960,#24961,#24962,#24963,#24964,#24965,#24966,#24967,#24968,#24969,
#24970,#24971,#24972,#24973,#24974,#24975,#24976,#24977,#24978,#24979,#24980,
#24981,#24982,#24983,#24984,#24985,#24986,#24987,#24988,#24989,#24990,#24991,
#24992,#24993,#24994,#24995,#24996,#24997,#24998,#24999,#25000,#25001,#25002,
#25003,#25004,#25005,#25006,#25007,#25008,#25009,#25010,#25011,#25012,#25013,
#25014,#25015,#25016,#25017,#25018),.UNSPECIFIED.,.F.,.F.,(4,3,3,3,3,3,
3,3,3,3,3,3,3,3,3,3,3,3,3,3,3,3,3,3,3,4),(91.10618695432,91.1992936832594,
91.29228331494,91.3851832836713,91.4780353414083,91.5708662949906,91.6637029252771,
91.7566310763317,91.8496066804956,91.9427360265074,92.0131732982535,92.1074118320216,
92.2015225318168,92.2955339471963,92.3894780952104,92.4833880310926,92.5772894045521,
92.6712078509361,92.7652275275635,92.8593027429045,92.9535299861691,93.0082344927571,
93.102456462241,93.1965663039992,93.2905714705558,93.3325033045339),
 .UNSPECIFIED.);
#339=B_SPLINE_CURVE_WITH_KNOTS('',3,(#25019,#25020,#25021,#25022,#25023,
#25024,#25025,#25026,#25027,#25028,#25029,#25030,#25031,#25032,#25033,#25034,
#25035,#25036,#25037,#25038,#25039,#25040,#25041,#25042,#25043,#25044,#25045,
#25046,#25047,#25048,#25049,#25050,#25051,#25052,#25053,#25054,#25055,#25056,
#25057,#25058,#25059,#25060,#25061,#25062,#25063,#25064,#25065,#25066,#25067,
#25068,#25069,#25070,#25071,#25072,#25073,#25074,#25075,#25076,#25077,#25078,
#25079,#25080,#25081,#25082,#25083,#25084,#25085,#25086,#25087,#25088,#25089,
#25090,#25091,#25092,#25093,#25094,#25095,#25096,#25097,#25098,#25099,#25100,
#25101,#25102,#25103,#25104,#25105,#25106,#25107,#25108,#25109,#25110,#25111,
#25112,#25113,#25114,#25115,#25116,#25117,#25118,#25119,#25120,#25121,#25122,
#25123,#25124,#25125,#25126,#25127,#25128,#25129,#25130,#25131,#25132,#25133,
#25134,#25135,#25136,#25137,#25138,#25139,#25140,#25141,#25142,#25143,#25144,
#25145,#25146,#25147,#25148,#25149,#25150,#25151,#25152,#25153,#25154),
 .UNSPECIFIED.,.F.,.F.,(4,3,3,3,3,3,3,3,3,3,3,3,3,3,3,3,3,3,3,3,3,3,3,3,
3,3,3,3,3,3,3,3,3,3,3,3,3,3,3,3,3,3,3,3,3,4),(87.0489171655824,87.1431392396,
87.2372368316046,87.3312384766754,87.425177288261,87.5190848946421,87.6129869427592,
87.7069090676515,87.8009340558435,87.8950172831459,87.9892493561579,88.0329285202391,
88.1271670540072,88.2212777538026,88.315289169182,88.4092333171961,88.5031432530783,
88.5970446265378,88.6909630729216,88.784982749549,88.8790579648898,88.9732852081544,
89.0279897147427,89.1222282485108,89.2163389483061,89.3103503636855,89.4042945116996,
89.4982044475817,89.5921058210413,89.6860242674251,89.7800439440525,89.8741191593933,
89.9683464026579,90.0230509092463,90.1172894430144,90.2114001428099,90.3054115581892,
90.3993557062033,90.4932656420854,90.587167015545,90.6810854619286,90.775105138556,
90.8691803538968,90.9634075971614,91.0181121037499,91.106186954104),
 .UNSPECIFIED.);
#340=B_SPLINE_CURVE_WITH_KNOTS('',3,(#25160,#25161,#25162,#25163,#25164,
#25165,#25166,#25167,#25168,#25169,#25170,#25171,#25172,#25173,#25174,#25175,
#25176,#25177,#25178,#25179,#25180,#25181,#25182,#25183,#25184,#25185,#25186,
#25187,#25188,#25189,#25190,#25191,#25192,#25193,#25194,#25195,#25196,#25197,
#25198,#25199,#25200,#25201,#25202,#25203,#25204,#25205,#25206,#25207,#25208,
#25209,#25210,#25211,#25212,#25213,#25214,#25215,#25216,#25217,#25218,#25219,
#25220,#25221,#25222,#25223,#25224,#25225,#25226,#25227,#25228,#25229,#25230,
#25231,#25232,#25233,#25234,#25235,#25236,#25237,#25238,#25239,#25240,#25241,
#25242,#25243,#25244,#25245,#25246,#25247,#25248,#25249,#25250,#25251,#25252,
#25253,#25254,#25255,#25256,#25257,#25258,#25259,#25260,#25261,#25262,#25263,
#25264,#25265,#25266,#25267,#25268,#25269,#25270,#25271,#25272,#25273,#25274,
#25275,#25276,#25277,#25278,#25279,#25280,#25281,#25282,#25283,#25284,#25285,
#25286,#25287,#25288,#25289,#25290,#25291,#25292),.UNSPECIFIED.,.F.,.F.,
(4,3,3,3,3,3,3,3,3,3,3,3,3,3,3,3,3,3,3,3,3,3,3,3,3,3,3,3,3,3,3,3,3,3,3,
3,3,3,3,3,3,3,3,3,4),(80.7662383708046,80.8602014204436,80.954120879801,
81.0480224090736,81.1419316464207,81.2359367913877,81.329989058716,81.4242037444454,
81.5132724775605,81.6075110113286,81.701621711124,81.795633126503,81.8895772745172,
81.9834872103992,82.0773885838586,82.1713070302423,82.2653267068696,82.3594019222105,
82.4536291654751,82.5083336720641,82.6025722058321,82.6966829056277,82.7906943210076,
82.8846384690217,82.9785484049038,83.0724497783633,83.1663682247469,83.2603879013744,
83.3544631167152,83.4486903599797,83.5033948665677,83.5976334003357,83.6917441001312,
83.7857555155109,83.879699663525,83.9736095994071,84.0675109728667,84.1614294192501,
84.2554490958774,84.3495243112181,84.4437515544826,84.4984560610714,84.6098153997746,
84.7200586670639,84.8230016467217),.UNSPECIFIED.);
#341=B_SPLINE_CURVE_WITH_KNOTS('',3,(#25293,#25294,#25295,#25296,#25297,
#25298,#25299,#25300,#25301,#25302,#25303,#25304,#25305,#25306,#25307,#25308,
#25309,#25310,#25311,#25312,#25313,#25314,#25315,#25316,#25317,#25318,#25319,
#25320,#25321,#25322,#25323,#25324,#25325,#25326,#25327,#25328,#25329,#25330,
#25331,#25332,#25333,#25334,#25335,#25336,#25337,#25338,#25339,#25340,#25341,
#25342,#25343,#25344,#25345,#25346,#25347,#25348,#25349,#25350,#25351,#25352,
#25353,#25354,#25355,#25356,#25357,#25358,#25359,#25360,#25361,#25362,#25363,
#25364,#25365,#25366,#25367,#25368),.UNSPECIFIED.,.F.,.F.,(4,3,3,3,3,3,
3,3,3,3,3,3,3,3,3,3,3,3,3,3,3,3,3,3,3,4),(84.8230016469244,84.9167396222475,
85.0104582715234,85.1041833778223,85.2015168472605,85.2953896866708,85.3893326790537,
85.4834206132759,85.493517255575,85.5877557893431,85.6818664891387,85.775877904518,
85.8698220525321,85.9637319884143,86.0576333618738,86.1515518082575,86.2455714848849,
86.3396467002259,86.4338739434905,86.4885784500786,86.5828095682953,86.6769188848032,
86.7709219407424,86.8648613808132,86.9587807515315,87.0486631737809),
 .UNSPECIFIED.);
#342=B_SPLINE_CURVE_WITH_KNOTS('',3,(#25370,#25371,#25372,#25373,#25374,
#25375,#25376,#25377,#25378,#25379,#25380,#25381,#25382,#25383,#25384,#25385,
#25386,#25387,#25388,#25389,#25390,#25391,#25392,#25393,#25394,#25395,#25396,
#25397,#25398,#25399,#25400,#25401,#25402,#25403,#25404,#25405,#25406,#25407,
#25408,#25409,#25410,#25411,#25412,#25413,#25414,#25415,#25416,#25417,#25418,
#25419,#25420,#25421,#25422,#25423,#25424,#25425,#25426,#25427,#25428,#25429,
#25430,#25431,#25432,#25433,#25434,#25435,#25436,#25437,#25438,#25439,#25440,
#25441,#25442,#25443,#25444,#25445),.UNSPECIFIED.,.F.,.F.,(4,3,3,3,3,3,
3,3,3,3,3,3,3,3,3,3,3,3,3,3,3,3,3,3,3,4),(84.8230016469244,84.9501148314948,
85.0477449367282,85.1419834704963,85.2360941702917,85.330105585671,85.4240497336852,
85.5179596695673,85.6118610430269,85.7057794894107,85.7997991660381,85.893874381379,
85.9881016246435,86.0428061312318,86.1370446649999,86.2311553647953,86.3251667801747,
86.4191109281888,86.5130208640709,86.6069222375305,86.7008406839142,86.7948603605416,
86.8889355758824,86.983162819147,87.0378673257354,87.0489171655824),
 .UNSPECIFIED.);
#343=B_SPLINE_CURVE_WITH_KNOTS('',3,(#25446,#25447,#25448,#25449,#25450,
#25451,#25452,#25453,#25454,#25455,#25456,#25457,#25458,#25459,#25460,#25461,
#25462,#25463,#25464,#25465,#25466,#25467,#25468,#25469,#25470,#25471,#25472,
#25473,#25474,#25475,#25476,#25477,#25478,#25479,#25480,#25481,#25482,#25483,
#25484,#25485,#25486,#25487,#25488,#25489,#25490,#25491,#25492,#25493,#25494,
#25495,#25496,#25497,#25498,#25499,#25500,#25501,#25502,#25503,#25504,#25505,
#25506,#25507,#25508,#25509,#25510,#25511,#25512,#25513,#25514,#25515,#25516,
#25517,#25518,#25519,#25520,#25521,#25522,#25523,#25524,#25525,#25526,#25527,
#25528,#25529,#25530,#25531,#25532,#25533,#25534,#25535,#25536,#25537,#25538,
#25539,#25540,#25541,#25542,#25543,#25544,#25545,#25546,#25547,#25548,#25549,
#25550,#25551,#25552,#25553,#25554,#25555,#25556,#25557,#25558,#25559,#25560,
#25561,#25562,#25563,#25564,#25565,#25566,#25567,#25568,#25569,#25570,#25571,
#25572,#25573,#25574,#25575,#25576,#25577,#25578,#25579,#25580,#25581,#25582,
#25583,#25584),.UNSPECIFIED.,.F.,.F.,(4,3,3,3,3,3,3,3,3,3,3,3,3,3,3,3,3,
3,3,3,3,3,3,3,3,3,3,3,3,3,3,3,3,3,3,3,3,3,3,3,3,3,3,3,3,3,4),(80.7651606363239,
80.8591981217149,80.9532996567776,81.047543439675,81.0675001587138,81.161738692482,
81.2558493922774,81.3498608076566,81.4438049556707,81.5377148915528,81.6316162650124,
81.7255347113963,81.8195543880237,81.9136296033645,82.007856846629,82.0625613532174,
82.1567998869855,82.2509105867808,82.34492200216,82.4388661501741,82.5327760860562,
82.6266774595158,82.7205959058996,82.8146155825271,82.908690797868,83.0029180411326,
83.057622547721,83.151861081489,83.2459717812843,83.3399831966636,83.4339273446778,
83.52783728056,83.6217386540197,83.7156571004035,83.8096767770308,83.9037519923715,
83.997979235636,84.0526837422246,84.1489734802914,84.241821690845,84.3345840307345,
84.4272875189037,84.5199591070544,84.6126557703783,84.7053683378321,84.7981603124173,
84.8230016467593),.UNSPECIFIED.);
#344=B_SPLINE_CURVE_WITH_KNOTS('',3,(#25590,#25591,#25592,#25593,#25594,
#25595,#25596,#25597,#25598,#25599,#25600,#25601,#25602,#25603,#25604,#25605,
#25606,#25607,#25608,#25609,#25610,#25611,#25612,#25613,#25614,#25615,#25616,
#25617,#25618,#25619,#25620,#25621,#25622,#25623,#25624,#25625,#25626,#25627,
#25628,#25629,#25630,#25631,#25632,#25633,#25634,#25635,#25636,#25637,#25638,
#25639,#25640,#25641,#25642,#25643,#25644,#25645,#25646,#25647,#25648,#25649,
#25650,#25651,#25652,#25653,#25654,#25655,#25656,#25657,#25658,#25659,#25660,
#25661,#25662,#25663,#25664,#25665,#25666,#25667,#25668,#25669,#25670,#25671,
#25672,#25673,#25674,#25675,#25676,#25677,#25678,#25679,#25680,#25681,#25682,
#25683,#25684,#25685,#25686,#25687,#25688,#25689,#25690,#25691,#25692,#25693,
#25694,#25695,#25696,#25697,#25698,#25699,#25700,#25701,#25702,#25703,#25704,
#25705,#25706,#25707,#25708,#25709,#25710,#25711,#25712,#25713,#25714,#25715,
#25716,#25717,#25718,#25719,#25720,#25721,#25722,#25723,#25724,#25725,#25726,
#25727,#25728),.UNSPECIFIED.,.F.,.F.,(4,3,3,3,3,3,3,3,3,3,3,3,3,3,3,3,3,
3,3,3,3,3,3,3,3,3,3,3,3,3,3,3,3,3,3,3,3,3,3,3,3,3,3,3,3,3,4),(74.4821549297256,
74.5478441160352,74.6420826498033,74.7361933495987,74.8302047649781,74.9241489129923,
75.0180588488744,75.111960222334,75.2058786687177,75.2998983453451,75.393973560686,
75.4882008039505,75.5429053105389,75.637143844307,75.7312545441024,75.8252659594818,
75.9192101074959,76.0131200433781,76.1070214168377,76.2009398632214,76.2949595398488,
76.3890347551896,76.4832619984542,76.5379665050425,76.6322050388106,76.726315738606,
76.8203271539855,76.9142713019996,77.0081812378817,77.1020826113412,77.1960010577249,
77.2900207343523,77.3840959496932,77.4783231929578,77.5330276995461,77.6272662333142,
77.7213769331097,77.815388348489,77.9093324965031,78.0032424323852,78.0971438058448,
78.1910622522284,78.2850819288558,78.3791571441966,78.4733843874612,78.5280888940497,
78.5398163397448),.UNSPECIFIED.);
#345=B_SPLINE_CURVE_WITH_KNOTS('',3,(#25729,#25730,#25731,#25732,#25733,
#25734,#25735,#25736,#25737,#25738,#25739,#25740,#25741,#25742,#25743,#25744,
#25745,#25746,#25747,#25748,#25749,#25750,#25751,#25752,#25753,#25754,#25755,
#25756,#25757,#25758,#25759,#25760,#25761,#25762,#25763,#25764,#25765,#25766,
#25767,#25768,#25769,#25770,#25771,#25772,#25773,#25774,#25775,#25776,#25777,
#25778,#25779,#25780,#25781,#25782,#25783,#25784,#25785,#25786,#25787,#25788,
#25789,#25790,#25791,#25792,#25793,#25794,#25795,#25796,#25797,#25798,#25799,
#25800,#25801,#25802,#25803,#25804),.UNSPECIFIED.,.F.,.F.,(4,3,3,3,3,3,
3,3,3,3,3,3,3,3,3,3,3,3,3,3,3,3,3,3,3,4),(78.5398163399313,78.6338611329994,
78.7277784185812,78.8215970086099,78.9153494266275,79.0090686505241,79.1027805640751,
79.1965110377571,79.2903430660188,79.3842324146997,79.4782706044405,79.5231500885533,
79.6173886223214,79.7114993221168,79.8055107374961,79.8994548855102,79.9933648213924,
80.0872661948518,80.1811846412358,80.2752043178631,80.3692795332041,80.4635067764686,
80.5182112830569,80.6124500013097,80.7065483084735,80.7662383708046),
 .UNSPECIFIED.);
#346=B_SPLINE_CURVE_WITH_KNOTS('',3,(#25806,#25807,#25808,#25809,#25810,
#25811,#25812,#25813,#25814,#25815,#25816,#25817,#25818,#25819,#25820,#25821,
#25822,#25823,#25824,#25825,#25826,#25827,#25828,#25829,#25830,#25831,#25832,
#25833,#25834,#25835,#25836,#25837,#25838,#25839,#25840,#25841,#25842,#25843,
#25844,#25845,#25846,#25847,#25848,#25849,#25850,#25851,#25852,#25853,#25854,
#25855,#25856,#25857,#25858,#25859,#25860,#25861,#25862,#25863,#25864,#25865,
#25866,#25867,#25868,#25869,#25870,#25871,#25872,#25873,#25874,#25875,#25876,
#25877,#25878,#25879,#25880,#25881),.UNSPECIFIED.,.F.,.F.,(4,3,3,3,3,3,
3,3,3,3,3,3,3,3,3,3,3,3,3,3,3,3,3,3,3,4),(78.5398163397448,78.6366735783784,
78.7336184927698,78.8307516518218,78.9279875108045,79.0254289346791,79.0773777697065,
79.1716163034746,79.26572700327,79.3597384186493,79.4536825666634,79.5475925025456,
79.6414938760053,79.7354123223889,79.8294319990163,79.9235072143572,80.0177344576217,
80.0724389642102,80.1666569505644,80.2607562877407,80.3547628245391,80.4487023217272,
80.5426132656405,80.6365078669387,80.7304367289939,80.7651606363239),
 .UNSPECIFIED.);
#347=B_SPLINE_CURVE_WITH_KNOTS('',3,(#25882,#25883,#25884,#25885,#25886,
#25887,#25888,#25889,#25890,#25891,#25892,#25893,#25894,#25895,#25896,#25897,
#25898,#25899,#25900,#25901,#25902,#25903,#25904,#25905,#25906,#25907,#25908,
#25909,#25910,#25911,#25912,#25913,#25914,#25915,#25916,#25917,#25918,#25919,
#25920,#25921,#25922,#25923,#25924,#25925,#25926,#25927,#25928,#25929,#25930,
#25931,#25932,#25933,#25934,#25935,#25936,#25937,#25938,#25939,#25940,#25941,
#25942,#25943,#25944,#25945,#25946,#25947,#25948,#25949,#25950,#25951,#25952,
#25953,#25954,#25955,#25956,#25957,#25958,#25959,#25960,#25961,#25962,#25963,
#25964,#25965,#25966,#25967,#25968,#25969,#25970,#25971,#25972,#25973,#25974,
#25975,#25976,#25977,#25978,#25979,#25980,#25981,#25982,#25983,#25984,#25985,
#25986,#25987,#25988,#25989,#25990,#25991,#25992,#25993,#25994,#25995,#25996,
#25997,#25998,#25999,#26000,#26001,#26002,#26003,#26004,#26005,#26006,#26007,
#26008,#26009,#26010,#26011,#26012,#26013,#26014,#26015,#26016,#26017),
 .UNSPECIFIED.,.F.,.F.,(4,3,3,3,3,3,3,3,3,3,3,3,3,3,3,3,3,3,3,3,3,3,3,3,
3,3,3,3,3,3,3,3,3,3,3,3,3,3,3,3,3,3,3,3,3,4),(74.4828190591072,74.5767280122671,
74.6706296157027,74.7645495046023,74.8585712872853,74.952649698683,75.0468788446621,
75.0971329916921,75.1913715254602,75.2854822252557,75.3794936406352,75.4734377886494,
75.5673477245314,75.6612490979911,75.755167544375,75.8491872210025,75.9432624363433,
76.0374896796078,76.0921941861957,76.1864327199638,76.2805434197591,76.3745548351389,
76.468498983153,76.5624089190352,76.6563102924947,76.7502287388782,76.8442484155056,
76.9383236308464,77.0325508741109,77.0872553806993,77.1814939144675,77.2756046142628,
77.3696160296426,77.4635601776567,77.5574701135388,77.6513714869983,77.7452899333823,
77.8393096100098,77.9333848253505,78.0276120686152,78.082316575203,78.1833244724824,
78.2840046924094,78.3844817302127,78.4846682932388,78.5398163395429),
 .UNSPECIFIED.);
#348=B_SPLINE_CURVE_WITH_KNOTS('',3,(#26023,#26024,#26025,#26026,#26027,
#26028,#26029,#26030,#26031,#26032,#26033,#26034,#26035,#26036,#26037,#26038,
#26039,#26040,#26041,#26042,#26043,#26044,#26045,#26046,#26047,#26048,#26049,
#26050,#26051,#26052,#26053,#26054,#26055,#26056,#26057,#26058,#26059,#26060,
#26061,#26062,#26063,#26064,#26065,#26066,#26067,#26068,#26069,#26070,#26071,
#26072,#26073,#26074,#26075,#26076,#26077,#26078,#26079,#26080,#26081,#26082,
#26083,#26084,#26085,#26086,#26087,#26088,#26089,#26090,#26091,#26092,#26093,
#26094,#26095,#26096,#26097,#26098,#26099,#26100,#26101,#26102,#26103,#26104,
#26105,#26106,#26107,#26108,#26109,#26110,#26111,#26112,#26113,#26114,#26115,
#26116,#26117,#26118,#26119,#26120,#26121,#26122,#26123,#26124,#26125,#26126,
#26127,#26128,#26129,#26130,#26131,#26132,#26133,#26134,#26135,#26136,#26137,
#26138,#26139,#26140,#26141,#26142,#26143,#26144,#26145,#26146,#26147,#26148,
#26149,#26150,#26151,#26152,#26153,#26154,#26155,#26156,#26157,#26158),
 .UNSPECIFIED.,.F.,.F.,(4,3,3,3,3,3,3,3,3,3,3,3,3,3,3,3,3,3,3,3,3,3,3,3,
3,3,3,3,3,3,3,3,3,3,3,3,3,3,3,3,3,3,3,3,3,4),(68.1989521886483,68.2935833787396,
68.3876316115364,68.482554280275,68.5774769490136,68.6717154827817,68.7658261825771,
68.8598375979564,68.9537817459705,69.0476916818527,69.1415930553122,69.2355115016959,
69.3295311783233,69.4236063936641,69.5178336369287,69.5725381435172,69.6667766772854,
69.7608873770811,69.8548987924605,69.9488429404746,70.0427528763567,70.136654249816,
70.2305726961998,70.3245923728273,70.418667588168,70.5128948314325,70.5675993380208,
70.6618378717889,70.7559485715847,70.849959986964,70.943904134978,71.0378140708604,
71.1317154443199,71.2256338907041,71.3196535673314,71.4137287826723,71.5079560259368,
71.5626605325244,71.6563624008107,71.7499437866432,71.8434311143557,71.9368507142558,
72.0302428754377,72.1236189950162,72.2170329468858,72.2566310325651),
 .UNSPECIFIED.);
#349=B_SPLINE_CURVE_WITH_KNOTS('',3,(#26159,#26160,#26161,#26162,#26163,
#26164,#26165,#26166,#26167,#26168,#26169,#26170,#26171,#26172,#26173,#26174,
#26175,#26176,#26177,#26178,#26179,#26180,#26181,#26182,#26183,#26184,#26185,
#26186,#26187,#26188,#26189,#26190,#26191,#26192,#26193,#26194,#26195,#26196,
#26197,#26198,#26199,#26200,#26201,#26202,#26203,#26204,#26205,#26206,#26207,
#26208,#26209,#26210,#26211,#26212,#26213,#26214,#26215,#26216,#26217,#26218,
#26219,#26220,#26221,#26222,#26223,#26224,#26225,#26226,#26227,#26228,#26229,
#26230,#26231),.UNSPECIFIED.,.F.,.F.,(4,3,3,3,3,3,3,3,3,3,3,3,3,3,3,3,3,
3,3,3,3,3,3,3,4),(72.2566310327337,72.3692721053914,72.4833775848208,72.557721727028,
72.6519602607961,72.7460709605916,72.8400823759709,72.934026523985,73.0279364598672,
73.1218378333268,73.2157562797105,73.3097759563379,73.4038511716787,73.4980784149432,
73.5527829215316,73.6470256624285,73.7411394776692,73.8351424981322,73.9290840728993,
74.022989888567,74.1168855945947,74.2108478893634,74.3048420661471,74.3989695987264,
74.4821549297256),.UNSPECIFIED.);
#350=B_SPLINE_CURVE_WITH_KNOTS('',3,(#26233,#26234,#26235,#26236,#26237,
#26238,#26239,#26240,#26241,#26242,#26243,#26244,#26245,#26246,#26247,#26248,
#26249,#26250,#26251,#26252,#26253,#26254,#26255,#26256,#26257,#26258,#26259,
#26260,#26261,#26262,#26263,#26264,#26265,#26266,#26267,#26268,#26269,#26270,
#26271,#26272,#26273,#26274,#26275,#26276,#26277,#26278,#26279,#26280,#26281,
#26282,#26283,#26284,#26285,#26286,#26287,#26288,#26289,#26290,#26291,#26292,
#26293,#26294,#26295,#26296,#26297,#26298,#26299,#26300,#26301,#26302,#26303,
#26304,#26305,#26306,#26307,#26308),.UNSPECIFIED.,.F.,.F.,(4,3,3,3,3,3,
3,3,3,3,3,3,3,3,3,3,3,3,3,3,3,3,3,3,3,4),(72.2566310327574,72.3493964521512,
72.4440982209679,72.5366897572247,72.6292473245243,72.7217979449971,72.8181011094191,
72.9107727200092,73.0035061356872,73.0963757548764,73.1070106026849,73.2012491364529,
73.2953598362483,73.3893712516278,73.4833153996419,73.577225335524,73.6711267089834,
73.7650451553672,73.8590648319946,73.9531400473355,74.0473672906001,74.1020717971885,
74.1972586126682,74.2913585663729,74.3870888127401,74.4828190591072),
 .UNSPECIFIED.);
#351=B_SPLINE_CURVE_WITH_KNOTS('',3,(#26309,#26310,#26311,#26312,#26313,
#26314,#26315,#26316,#26317,#26318,#26319,#26320,#26321,#26322,#26323,#26324,
#26325,#26326,#26327,#26328,#26329,#26330,#26331,#26332,#26333,#26334,#26335,
#26336,#26337,#26338,#26339,#26340,#26341,#26342,#26343,#26344,#26345,#26346,
#26347,#26348,#26349,#26350,#26351,#26352,#26353,#26354,#26355,#26356,#26357,
#26358,#26359,#26360,#26361,#26362,#26363,#26364,#26365,#26366,#26367,#26368,
#26369,#26370,#26371,#26372,#26373,#26374,#26375,#26376,#26377,#26378,#26379,
#26380,#26381,#26382,#26383,#26384,#26385,#26386,#26387,#26388,#26389,#26390,
#26391,#26392,#26393,#26394,#26395,#26396,#26397,#26398,#26399,#26400,#26401,
#26402,#26403,#26404,#26405,#26406,#26407,#26408,#26409,#26410,#26411,#26412,
#26413,#26414,#26415,#26416,#26417,#26418,#26419,#26420,#26421,#26422,#26423,
#26424,#26425,#26426,#26427,#26428,#26429,#26430,#26431,#26432,#26433,#26434,
#26435,#26436,#26437,#26438,#26439,#26440,#26441),.UNSPECIFIED.,.F.,.F.,
(4,3,3,3,3,3,3,3,3,3,3,3,3,3,3,3,3,3,3,3,3,3,3,3,3,3,3,3,3,3,3,3,3,3,3,
3,3,3,3,3,3,3,3,3,4),(68.1996305298463,68.293774062422,68.3878103472842,
68.4817686413498,68.5756855520616,68.6695867368963,68.7634978330989,68.8575061207158,
68.9515635104959,69.0457808101111,69.1267658246704,69.2210043584385,69.3151150582339,
69.4091264736133,69.5030706216274,69.5969805575096,69.6908819309691,69.7848003773529,
69.8788200539803,69.9728952693211,70.0671225125857,70.121827019174,70.2160655529421,
70.3101762527375,70.4041876681169,70.498131816131,70.5920417520132,70.6859431254727,
70.7798615718566,70.8738812484839,70.9679564638248,71.0621837070894,71.1168882136777,
71.2111267474458,71.3052374472412,71.3992488626206,71.4931930106347,71.5871029465169,
71.6810043199765,71.7749227663603,71.8689424429877,71.9630176583286,72.0572449015932,
72.1119494081813,72.2566310325651),.UNSPECIFIED.);
#352=B_SPLINE_CURVE_WITH_KNOTS('',3,(#26447,#26448,#26449,#26450,#26451,
#26452,#26453,#26454,#26455,#26456,#26457,#26458,#26459,#26460,#26461,#26462,
#26463,#26464,#26465,#26466,#26467,#26468,#26469,#26470,#26471,#26472,#26473,
#26474,#26475,#26476,#26477,#26478,#26479,#26480,#26481,#26482,#26483,#26484,
#26485,#26486,#26487,#26488,#26489,#26490,#26491,#26492,#26493,#26494,#26495,
#26496,#26497,#26498,#26499,#26500,#26501,#26502,#26503,#26504,#26505,#26506,
#26507,#26508,#26509,#26510,#26511,#26512,#26513,#26514,#26515,#26516,#26517,
#26518,#26519,#26520,#26521,#26522,#26523,#26524,#26525,#26526,#26527,#26528,
#26529,#26530,#26531,#26532,#26533,#26534,#26535,#26536,#26537,#26538,#26539,
#26540,#26541,#26542,#26543,#26544,#26545,#26546,#26547,#26548,#26549,#26550,
#26551,#26552,#26553,#26554,#26555,#26556,#26557,#26558,#26559,#26560,#26561,
#26562,#26563,#26564,#26565,#26566,#26567,#26568,#26569,#26570,#26571,#26572,
#26573,#26574,#26575,#26576,#26577,#26578,#26579,#26580,#26581,#26582),
 .UNSPECIFIED.,.F.,.F.,(4,3,3,3,3,3,3,3,3,3,3,3,3,3,3,3,3,3,3,3,3,3,3,3,
3,3,3,3,3,3,3,3,3,3,3,3,3,3,3,3,3,3,3,3,3,4),(61.9166125687905,62.0105463165949,
62.1044519156713,62.1983550104404,62.292281235926,62.3863119480559,62.480403645108,
62.5746410275793,62.6071097819919,62.7013483157599,62.7954590155553,62.8894704309345,
62.9834145789486,63.0773245148308,63.1712258882903,63.2651443346738,63.3591640113012,
63.4532392266421,63.5474664699067,63.6021709764955,63.6964095102636,63.7905202100592,
63.8845316254386,63.9784757734527,64.072385709335,64.1662870827944,64.2602055291778,
64.3542252058052,64.4483004211459,64.5425276644105,64.5972321709991,64.6914707047674,
64.7855814045625,64.8795928199422,64.9735369679563,65.0674469038384,65.1613482772981,
65.2552667236817,65.3492864003091,65.44336161565,65.5375888589146,65.5922933655027,
65.6982067190135,65.803770718088,65.9087146730012,65.9734457251659),
 .UNSPECIFIED.);
#353=B_SPLINE_CURVE_WITH_KNOTS('',3,(#26583,#26584,#26585,#26586,#26587,
#26588,#26589,#26590,#26591,#26592,#26593,#26594,#26595,#26596,#26597,#26598,
#26599,#26600,#26601,#26602,#26603,#26604,#26605,#26606,#26607,#26608,#26609,
#26610,#26611,#26612,#26613,#26614,#26615,#26616,#26617,#26618,#26619,#26620,
#26621,#26622,#26623,#26624,#26625,#26626,#26627,#26628,#26629,#26630,#26631,
#26632,#26633,#26634,#26635,#26636,#26637,#26638,#26639,#26640,#26641,#26642,
#26643,#26644,#26645,#26646,#26647,#26648,#26649,#26650,#26651,#26652,#26653,
#26654,#26655,#26656,#26657,#26658),.UNSPECIFIED.,.F.,.F.,(4,3,3,3,3,3,
3,3,3,3,3,3,3,3,3,3,3,3,3,3,3,3,3,3,3,4),(65.9734457253856,66.0682195696543,
66.1630096695599,66.2578400499857,66.3527995240518,66.447831815984,66.5430314924363,
66.5873545600063,66.6815930937744,66.77570379357,66.8697152089495,66.9636593569636,
67.0575692928457,67.1514706663053,67.2453891126893,67.3394087893166,67.4334840046574,
67.527711247922,67.58241575451,67.6766408530215,67.7707454920501,67.8647555289504,
67.9586978558374,68.0526001292267,68.1465074888003,68.1989521886483),
 .UNSPECIFIED.);
#354=B_SPLINE_CURVE_WITH_KNOTS('',3,(#26660,#26661,#26662,#26663,#26664,
#26665,#26666,#26667,#26668,#26669,#26670,#26671,#26672,#26673,#26674,#26675,
#26676,#26677,#26678,#26679,#26680,#26681,#26682,#26683,#26684,#26685,#26686,
#26687,#26688,#26689,#26690,#26691,#26692,#26693,#26694,#26695,#26696,#26697,
#26698,#26699,#26700,#26701,#26702,#26703,#26704,#26705,#26706,#26707,#26708,
#26709,#26710,#26711,#26712,#26713,#26714,#26715,#26716,#26717,#26718,#26719,
#26720,#26721,#26722,#26723,#26724,#26725,#26726,#26727,#26728,#26729,#26730,
#26731,#26732,#26733,#26734,#26735),.UNSPECIFIED.,.F.,.F.,(4,3,3,3,3,3,
3,3,3,3,3,3,3,3,3,3,3,3,3,3,3,3,3,3,3,4),(65.9734457253856,66.1208876232955,
66.1415822411596,66.2358207749277,66.3299314747231,66.4239428901025,66.5178870381166,
66.6117969739988,66.7056983474584,66.7996167938421,66.8936364704694,66.9877116858102,
67.0819389290748,67.1366434356632,67.2308819694313,67.3249926692268,67.4190040846061,
67.5129482326202,67.6068581685024,67.700759541962,67.7946779883457,67.8886976649731,
67.982772880314,68.0770001235786,68.1317046301668,68.1996305298463),
 .UNSPECIFIED.);
#355=B_SPLINE_CURVE_WITH_KNOTS('',3,(#26736,#26737,#26738,#26739,#26740,
#26741,#26742,#26743,#26744,#26745,#26746,#26747,#26748,#26749,#26750,#26751,
#26752,#26753,#26754,#26755,#26756,#26757,#26758,#26759,#26760,#26761,#26762,
#26763,#26764,#26765,#26766,#26767,#26768,#26769,#26770,#26771,#26772,#26773,
#26774,#26775,#26776,#26777,#26778,#26779,#26780,#26781,#26782,#26783,#26784,
#26785,#26786,#26787,#26788,#26789,#26790,#26791,#26792,#26793,#26794,#26795,
#26796,#26797,#26798,#26799,#26800,#26801,#26802,#26803,#26804,#26805,#26806,
#26807,#26808,#26809,#26810,#26811,#26812,#26813,#26814,#26815,#26816,#26817,
#26818,#26819,#26820,#26821,#26822,#26823,#26824,#26825,#26826,#26827,#26828,
#26829,#26830,#26831,#26832,#26833,#26834,#26835,#26836,#26837,#26838,#26839,
#26840,#26841,#26842,#26843,#26844,#26845,#26846,#26847,#26848,#26849,#26850,
#26851,#26852,#26853,#26854,#26855,#26856,#26857,#26858,#26859,#26860,#26861,
#26862,#26863,#26864,#26865,#26866,#26867,#26868,#26869,#26870,#26871),
 .UNSPECIFIED.,.F.,.F.,(4,3,3,3,3,3,3,3,3,3,3,3,3,3,3,3,3,3,3,3,3,3,3,3,
3,3,3,3,3,3,3,3,3,3,3,3,3,3,3,3,3,3,3,3,3,4),(61.915536908638,62.009610141779,
62.1038362217474,62.1613374631452,62.2555759969133,62.3496866967087,62.4436981120881,
62.5376422601022,62.6315521959843,62.7254535694439,62.8193720158276,62.913391692455,
63.0074669077959,63.1016941510604,63.1563986576488,63.2506371914169,63.3447478912123,
63.4387593065916,63.5327034546057,63.6266133904879,63.7205147639474,63.8144332103312,
63.9084528869586,64.0025281022995,64.096755345564,64.1514598521524,64.2456983859205,
64.339809085716,64.4338205010953,64.5277646491094,64.6216745849916,64.7155759584511,
64.8094944048348,64.9035140814622,64.997589296803,65.0918165400676,65.146521046656,
65.2393639284447,65.3320574568457,65.4246665115197,65.5172182347163,65.6097397018221,
65.7023016612755,65.794880437501,65.8875747884578,65.9734457250788),
 .UNSPECIFIED.);
#356=B_SPLINE_CURVE_WITH_KNOTS('',3,(#26877,#26878,#26879,#26880,#26881,
#26882,#26883,#26884,#26885,#26886,#26887,#26888,#26889,#26890,#26891,#26892,
#26893,#26894,#26895,#26896,#26897,#26898,#26899,#26900,#26901,#26902,#26903,
#26904,#26905,#26906,#26907,#26908,#26909,#26910,#26911,#26912,#26913,#26914,
#26915,#26916,#26917,#26918,#26919,#26920,#26921,#26922,#26923,#26924,#26925,
#26926,#26927,#26928,#26929,#26930,#26931,#26932,#26933,#26934,#26935,#26936,
#26937,#26938,#26939,#26940,#26941,#26942,#26943,#26944,#26945,#26946,#26947,
#26948,#26949,#26950,#26951,#26952,#26953,#26954,#26955,#26956,#26957,#26958,
#26959,#26960,#26961,#26962,#26963,#26964,#26965,#26966,#26967,#26968,#26969,
#26970,#26971,#26972,#26973,#26974,#26975,#26976,#26977,#26978,#26979,#26980,
#26981,#26982,#26983,#26984,#26985,#26986,#26987,#26988,#26989,#26990,#26991,
#26992,#26993,#26994,#26995,#26996,#26997,#26998,#26999,#27000,#27001,#27002,
#27003,#27004,#27005,#27006,#27007,#27008,#27009,#27010,#27011,#27012,#27013,
#27014,#27015),.UNSPECIFIED.,.F.,.F.,(4,3,3,3,3,3,3,3,3,3,3,3,3,3,3,3,3,
3,3,3,3,3,3,3,3,3,3,3,3,3,3,3,3,3,3,3,3,3,3,3,3,3,3,3,3,3,4),(55.6328726554313,
55.6416814204666,55.7359199542347,55.8300306540301,55.9240420694095,56.0179862174236,
56.1118961533058,56.2057975267653,56.2997159731491,56.3937356497765,56.4878108651173,
56.5820381083819,56.6367426149702,56.7309811487383,56.8250918485337,56.9191032639131,
57.0130474119272,57.1069573478094,57.200858721269,57.2947771676527,57.3887968442801,
57.482872059621,57.5770993028855,57.6318038094738,57.7260423432419,57.8201530430373,
57.9141644584167,58.0081086064308,58.1020185423129,58.1959199157725,58.2898383621563,
58.3838580387837,58.4779332541246,58.5721604973891,58.6268650039775,58.7211035377456,
58.8152142375411,58.9092256529204,59.0031698009346,59.0970797368167,59.1909811102763,
59.28489955666,59.3789192332874,59.4729944486282,59.5672216918928,59.6219261984811,
59.690260418206),.UNSPECIFIED.);
#357=B_SPLINE_CURVE_WITH_KNOTS('',3,(#27016,#27017,#27018,#27019,#27020,
#27021,#27022,#27023,#27024,#27025,#27026,#27027,#27028,#27029,#27030,#27031,
#27032,#27033,#27034,#27035,#27036,#27037,#27038,#27039,#27040,#27041,#27042,
#27043,#27044,#27045,#27046,#27047,#27048,#27049,#27050,#27051,#27052,#27053,
#27054,#27055,#27056,#27057,#27058,#27059,#27060,#27061,#27062,#27063,#27064,
#27065,#27066,#27067,#27068,#27069,#27070,#27071,#27072,#27073,#27074,#27075,
#27076,#27077,#27078,#27079,#27080,#27081,#27082,#27083,#27084,#27085,#27086,
#27087,#27088,#27089,#27090,#27091),.UNSPECIFIED.,.F.,.F.,(4,3,3,3,3,3,
3,3,3,3,3,3,3,3,3,3,3,3,3,3,3,3,3,3,3,4),(59.6902604184034,59.7835566480732,
59.8767319494283,59.9698120649093,60.0628405197121,60.1558439723099,60.2488490519494,
60.3419437097565,60.4350818947519,60.5283799236479,60.6169873929847,60.7112259267528,
60.8053366265483,60.8993480419277,60.9932921899417,61.0872021258239,61.1811034992834,
61.275021945667,61.3690416222944,61.4631168376352,61.5573440808998,61.6120485874883,
61.7062744396242,61.8003879713356,61.8943961635387,61.9166125687905),
 .UNSPECIFIED.);
#358=B_SPLINE_CURVE_WITH_KNOTS('',3,(#27093,#27094,#27095,#27096,#27097,
#27098,#27099,#27100,#27101,#27102,#27103,#27104,#27105,#27106,#27107,#27108,
#27109,#27110,#27111,#27112,#27113,#27114,#27115,#27116,#27117,#27118,#27119,
#27120,#27121,#27122,#27123,#27124,#27125,#27126,#27127,#27128,#27129,#27130,
#27131,#27132,#27133,#27134,#27135,#27136,#27137,#27138,#27139,#27140,#27141,
#27142,#27143,#27144,#27145,#27146,#27147,#27148,#27149,#27150,#27151,#27152,
#27153,#27154,#27155,#27156,#27157,#27158,#27159,#27160,#27161,#27162,#27163,
#27164,#27165),.UNSPECIFIED.,.F.,.F.,(4,3,3,3,3,3,3,3,3,3,3,3,3,3,3,3,3,
3,3,3,3,3,3,3,4),(59.6902604183787,59.7892918179411,59.8886169604199,59.988091199275,
60.0878449487747,60.1712150741379,60.265453607906,60.3595643077015,60.4535757230808,
60.547519871095,60.6414298069772,60.7353311804367,60.8292496268203,60.9232693034477,
61.0173445187886,61.1115717620532,61.1662762686416,61.260489728568,61.3545858819447,
61.4485905716283,61.5425295541541,61.6364499411022,61.7303545142604,61.8243186029466,
61.915536908638),.UNSPECIFIED.);
#359=B_SPLINE_CURVE_WITH_KNOTS('',3,(#27166,#27167,#27168,#27169,#27170,
#27171,#27172,#27173,#27174,#27175,#27176,#27177,#27178,#27179,#27180,#27181,
#27182,#27183,#27184,#27185,#27186,#27187,#27188,#27189,#27190,#27191,#27192,
#27193,#27194,#27195,#27196,#27197,#27198,#27199,#27200,#27201,#27202,#27203,
#27204,#27205,#27206,#27207,#27208,#27209,#27210,#27211,#27212,#27213,#27214,
#27215,#27216,#27217,#27218,#27219,#27220,#27221,#27222,#27223,#27224,#27225,
#27226,#27227,#27228,#27229,#27230,#27231,#27232,#27233,#27234,#27235,#27236,
#27237,#27238,#27239,#27240,#27241,#27242,#27243,#27244,#27245,#27246,#27247,
#27248,#27249,#27250,#27251,#27252,#27253,#27254,#27255,#27256,#27257,#27258,
#27259,#27260,#27261,#27262,#27263,#27264,#27265,#27266,#27267,#27268,#27269,
#27270,#27271,#27272,#27273,#27274,#27275,#27276,#27277,#27278,#27279,#27280,
#27281,#27282,#27283,#27284,#27285,#27286,#27287,#27288,#27289,#27290,#27291,
#27292,#27293,#27294,#27295,#27296,#27297,#27298,#27299,#27300,#27301),
 .UNSPECIFIED.,.F.,.F.,(4,3,3,3,3,3,3,3,3,3,3,3,3,3,3,3,3,3,3,3,3,3,3,3,
3,3,3,3,3,3,3,3,3,3,3,3,3,3,3,3,3,3,3,3,3,4),(55.6331072412748,55.7270087028561,
55.8209182242538,55.9149238595219,56.0089769332002,56.1031920221626,56.1909702961235,
56.2852088298915,56.3793195296868,56.4733309450663,56.5672750930804,56.6611850289626,
56.7550864024222,56.849004848806,56.9430245254334,57.0370997407743,57.1313269840389,
57.1860314906271,57.2802700243952,57.3743807241906,57.46839213957,57.5623362875841,
57.6562462234663,57.7501475969257,57.8440660433094,57.9380857199368,58.0321609352776,
58.1263881785422,58.1810926851307,58.2753312188987,58.3694419186943,58.4634533340735,
58.5573974820876,58.6513074179696,58.7452087914292,58.8391272378128,58.9331469144401,
59.0272221297808,59.1214493730453,59.1761538796343,59.2745027508079,59.3726743921948,
59.4706312790709,59.5684582642373,59.6661366206867,59.690260418206),
 .UNSPECIFIED.);
#360=B_SPLINE_CURVE_WITH_KNOTS('',3,(#27307,#27308,#27309,#27310,#27311,
#27312,#27313,#27314,#27315,#27316,#27317,#27318,#27319,#27320,#27321,#27322,
#27323,#27324,#27325,#27326,#27327,#27328,#27329,#27330,#27331,#27332,#27333,
#27334,#27335,#27336,#27337,#27338,#27339,#27340,#27341,#27342,#27343,#27344,
#27345,#27346,#27347,#27348,#27349,#27350,#27351,#27352,#27353,#27354,#27355,
#27356,#27357,#27358,#27359,#27360,#27361,#27362,#27363,#27364,#27365,#27366,
#27367,#27368,#27369,#27370,#27371,#27372,#27373,#27374,#27375,#27376,#27377,
#27378,#27379,#27380,#27381,#27382,#27383,#27384,#27385,#27386,#27387,#27388,
#27389,#27390,#27391,#27392,#27393,#27394,#27395,#27396,#27397,#27398,#27399,
#27400,#27401,#27402,#27403,#27404,#27405,#27406,#27407,#27408,#27409,#27410,
#27411,#27412,#27413,#27414,#27415,#27416,#27417,#27418,#27419,#27420,#27421,
#27422,#27423,#27424,#27425,#27426,#27427,#27428,#27429,#27430,#27431,#27432,
#27433,#27434,#27435,#27436,#27437,#27438,#27439,#27440,#27441,#27442),
 .UNSPECIFIED.,.F.,.F.,(4,3,3,3,3,3,3,3,3,3,3,3,3,3,3,3,3,3,3,3,3,3,3,3,
3,3,3,3,3,3,3,3,3,3,3,3,3,3,3,3,3,3,3,3,3,4),(49.3492693022874,49.4432962859874,
49.5373824839442,49.6316163965574,49.6713142534449,49.765552787213,49.8596634870087,
49.9536749023884,50.0476190504025,50.1415289862847,50.2354303597442,50.3293488061279,
50.4233684827553,50.5174436980961,50.6116709413607,50.6663754479486,50.7606139817167,
50.8547246815122,50.9487360968916,51.0426802449057,51.1365901807879,51.2304915542473,
51.3244100006314,51.4184296772588,51.5125048925997,51.6067321358643,51.6614366424522,
51.7556751762202,51.8497858760156,51.9437972913951,52.0377414394091,52.1316513752914,
52.2255527487512,52.3194711951354,52.4134908717627,52.5075660871034,52.601793330368,
52.6564978369558,52.7503199962146,52.8433012289229,52.9361944978272,53.0290267156312,
53.12353881448,53.2163550637721,53.3117150873993,53.4070751110265),
 .UNSPECIFIED.);
#361=B_SPLINE_CURVE_WITH_KNOTS('',3,(#27443,#27444,#27445,#27446,#27447,
#27448,#27449,#27450,#27451,#27452,#27453,#27454,#27455,#27456,#27457,#27458,
#27459,#27460,#27461,#27462,#27463,#27464,#27465,#27466,#27467,#27468,#27469,
#27470,#27471,#27472,#27473,#27474,#27475,#27476,#27477,#27478,#27479,#27480,
#27481,#27482,#27483,#27484,#27485,#27486,#27487,#27488,#27489,#27490,#27491,
#27492,#27493,#27494,#27495,#27496,#27497,#27498,#27499,#27500,#27501,#27502,
#27503,#27504,#27505,#27506,#27507,#27508,#27509,#27510,#27511,#27512,#27513,
#27514,#27515),.UNSPECIFIED.,.F.,.F.,(4,3,3,3,3,3,3,3,3,3,3,3,3,3,3,3,3,
3,3,3,3,3,3,3,4),(53.4070751112921,53.5297330757898,53.6515590314594,53.7457975652275,
53.839908265023,53.9339196804023,54.0278638284164,54.1217737642986,54.2156751377582,
54.309593584142,54.4036132607693,54.4976884761102,54.5919157193747,54.646620225963,
54.7408593113648,54.8349704164143,54.9289820913343,55.0229258433417,55.1168351761681,
55.2107357394637,55.3046531682905,55.3986692222742,55.4927407296692,55.5869583613849,
55.6328726554313),.UNSPECIFIED.);
#362=B_SPLINE_CURVE_WITH_KNOTS('',3,(#27517,#27518,#27519,#27520,#27521,
#27522,#27523,#27524,#27525,#27526,#27527,#27528,#27529,#27530,#27531,#27532,
#27533,#27534,#27535,#27536,#27537,#27538,#27539,#27540,#27541,#27542,#27543,
#27544,#27545,#27546,#27547,#27548,#27549,#27550,#27551,#27552,#27553,#27554,
#27555,#27556,#27557,#27558,#27559,#27560,#27561,#27562,#27563,#27564,#27565,
#27566,#27567,#27568,#27569,#27570,#27571,#27572,#27573,#27574,#27575,#27576,
#27577,#27578,#27579,#27580,#27581,#27582,#27583,#27584,#27585,#27586,#27587,
#27588,#27589,#27590,#27591,#27592),.UNSPECIFIED.,.F.,.F.,(4,3,3,3,3,3,
3,3,3,3,3,3,3,3,3,3,3,3,3,3,3,3,3,3,3,4),(53.407075111341,53.4997993899299,
53.59243844576,53.6850327223763,53.7776092331113,53.8701949680753,53.9628735164128,
54.0556031024416,54.1484802213107,54.2008479071163,54.2950864408844,54.3891971406799,
54.4832085560591,54.5771527040732,54.6710626399553,54.7649640134149,54.8588824597986,
54.9529021364259,55.0469773517668,55.1412045950314,55.1959091016199,55.2901555293964,
55.3842501749379,55.4782569522969,55.5721977094091,55.6331072412748),
 .UNSPECIFIED.);
#363=B_SPLINE_CURVE_WITH_KNOTS('',3,(#27593,#27594,#27595,#27596,#27597,
#27598,#27599,#27600,#27601,#27602,#27603,#27604,#27605,#27606,#27607,#27608,
#27609,#27610,#27611,#27612,#27613,#27614,#27615,#27616,#27617,#27618,#27619,
#27620,#27621,#27622,#27623,#27624,#27625,#27626,#27627,#27628,#27629,#27630,
#27631,#27632,#27633,#27634,#27635,#27636,#27637,#27638,#27639,#27640,#27641,
#27642,#27643,#27644,#27645,#27646,#27647,#27648,#27649,#27650,#27651,#27652,
#27653,#27654,#27655,#27656,#27657,#27658,#27659,#27660,#27661,#27662,#27663,
#27664,#27665,#27666,#27667,#27668,#27669,#27670,#27671,#27672,#27673,#27674,
#27675,#27676,#27677,#27678,#27679,#27680,#27681,#27682,#27683,#27684,#27685,
#27686,#27687,#27688,#27689,#27690,#27691,#27692,#27693,#27694,#27695,#27696,
#27697,#27698,#27699,#27700,#27701,#27702,#27703,#27704,#27705,#27706,#27707,
#27708,#27709,#27710,#27711,#27712,#27713,#27714,#27715,#27716,#27717,#27718,
#27719,#27720,#27721,#27722,#27723,#27724,#27725,#27726,#27727,#27728),
 .UNSPECIFIED.,.F.,.F.,(4,3,3,3,3,3,3,3,3,3,3,3,3,3,3,3,3,3,3,3,3,3,3,3,
3,3,3,3,3,3,3,3,3,3,3,3,3,3,3,3,3,3,3,3,3,4),(49.3502405140517,49.4443159743505,
49.5413518686944,49.6352808952855,49.7291848439067,49.8230893567473,49.9170200691168,
50.0110568618701,50.1051573991158,50.1994005222569,50.2206031291018,50.3148416628699,
50.4089523626653,50.5029637780446,50.5969079260587,50.6908178619408,50.7847192354003,
50.878637681784,50.9726573584114,51.0667325737522,51.1609598170167,51.2156643236054,
51.3099028573735,51.404013557169,51.4980249725484,51.5919691205625,51.6858790564447,
51.7797804299042,51.873698876288,51.9677185529154,52.0617937682562,52.1560210115208,
52.2107255181091,52.3049640518772,52.3990747516726,52.493086167052,52.5870303150661,
52.6809402509483,52.7748416244078,52.8687600707916,52.962779747419,53.0568549627599,
53.1510822060245,53.2057867126127,53.3395856335398,53.4070751110265),
 .UNSPECIFIED.);
#364=B_SPLINE_CURVE_WITH_KNOTS('',3,(#27734,#27735,#27736,#27737,#27738,
#27739,#27740,#27741,#27742,#27743,#27744,#27745,#27746,#27747,#27748,#27749,
#27750,#27751,#27752,#27753,#27754,#27755,#27756,#27757,#27758,#27759,#27760,
#27761,#27762,#27763,#27764,#27765,#27766,#27767,#27768,#27769,#27770,#27771,
#27772,#27773,#27774,#27775,#27776,#27777,#27778,#27779,#27780,#27781,#27782,
#27783,#27784,#27785,#27786,#27787,#27788,#27789,#27790,#27791,#27792,#27793,
#27794,#27795,#27796,#27797,#27798,#27799,#27800,#27801,#27802,#27803,#27804,
#27805,#27806,#27807,#27808,#27809,#27810,#27811,#27812,#27813,#27814,#27815,
#27816,#27817,#27818,#27819,#27820,#27821,#27822,#27823,#27824,#27825,#27826,
#27827,#27828,#27829,#27830,#27831,#27832,#27833,#27834,#27835,#27836,#27837,
#27838,#27839,#27840,#27841,#27842,#27843,#27844,#27845,#27846,#27847,#27848,
#27849,#27850,#27851,#27852,#27853,#27854,#27855,#27856,#27857,#27858,#27859,
#27860,#27861,#27862,#27863,#27864,#27865,#27866,#27867,#27868,#27869),
 .UNSPECIFIED.,.F.,.F.,(4,3,3,3,3,3,3,3,3,3,3,3,3,3,3,3,3,3,3,3,3,3,3,3,
3,3,3,3,3,3,3,3,3,3,3,3,3,3,3,3,3,3,3,3,3,4),(43.0669410879269,43.1608548335968,
43.254755853933,43.3486697851862,43.442682624419,43.5367472614373,43.6309684564177,
43.7009470864233,43.7951856201919,43.889296319988,43.9833077353676,44.0772518833823,
44.1711618192651,44.2650631927253,44.3589816391098,44.4530013157377,44.5470765310791,
44.6413037743443,44.6960082809269,44.7902468146948,44.8843575144902,44.9783689298692,
45.0723130778831,45.1662230137652,45.2601243872245,45.3540428336081,45.4480625102353,
45.5421377255761,45.6363649688403,45.6910694754305,45.7853080091985,45.8794187089939,
45.9734301243732,46.0673742723873,46.1612842082693,46.2551855817288,46.3491040281125,
46.4431237047399,46.5371989200807,46.6314261633452,46.6861306699341,46.7882622974101,
46.890027682399,46.9915575618476,47.0927492023486,47.1238898035594),
 .UNSPECIFIED.);
#365=B_SPLINE_CURVE_WITH_KNOTS('',3,(#27870,#27871,#27872,#27873,#27874,
#27875,#27876,#27877,#27878,#27879,#27880,#27881,#27882,#27883,#27884,#27885,
#27886,#27887,#27888,#27889,#27890,#27891,#27892,#27893,#27894,#27895,#27896,
#27897,#27898,#27899,#27900,#27901,#27902,#27903,#27904,#27905,#27906,#27907,
#27908,#27909,#27910,#27911,#27912,#27913,#27914,#27915,#27916,#27917,#27918,
#27919,#27920,#27921,#27922,#27923,#27924,#27925,#27926,#27927,#27928,#27929,
#27930,#27931,#27932,#27933,#27934,#27935,#27936,#27937,#27938,#27939,#27940,
#27941,#27942,#27943,#27944,#27945),.UNSPECIFIED.,.F.,.F.,(4,3,3,3,3,3,
3,3,3,3,3,3,3,3,3,3,3,3,3,3,3,3,3,3,3,4),(47.1238898038468,47.2201237011967,
47.3164231550396,47.4128894374831,47.5094431103066,47.606199734555,47.6811918644377,
47.7754303982057,47.8695410980011,47.9635525133803,48.0574966613944,48.1514065972766,
48.245307970736,48.3392264171196,48.433246093747,48.5273213090879,48.6215485523525,
48.6762530589413,48.7704727733985,48.864573370564,48.95858070139,49.0562528516144,
49.1501600113785,49.2440515574863,49.3379704500663,49.3492693022874),
 .UNSPECIFIED.);
#366=B_SPLINE_CURVE_WITH_KNOTS('',3,(#27947,#27948,#27949,#27950,#27951,
#27952,#27953,#27954,#27955,#27956,#27957,#27958,#27959,#27960,#27961,#27962,
#27963,#27964,#27965,#27966,#27967,#27968,#27969,#27970,#27971,#27972,#27973,
#27974,#27975,#27976,#27977,#27978,#27979,#27980,#27981,#27982,#27983,#27984,
#27985,#27986,#27987,#27988,#27989,#27990,#27991,#27992,#27993,#27994,#27995,
#27996,#27997,#27998,#27999,#28000,#28001,#28002,#28003,#28004,#28005,#28006,
#28007,#28008,#28009,#28010,#28011,#28012,#28013,#28014,#28015,#28016,#28017,
#28018,#28019,#28020,#28021,#28022),.UNSPECIFIED.,.F.,.F.,(4,3,3,3,3,3,
3,3,3,3,3,3,3,3,3,3,3,3,3,3,3,3,3,3,3,4),(47.1238898038468,47.235419545591,
47.3296580793589,47.4237687791541,47.5177801945334,47.6117243425473,47.7056342784293,
47.7995356518887,47.8934540982721,47.9874737748993,48.08154899024,48.1757762335043,
48.2304807400946,48.3247192738627,48.4188299736581,48.5128413890375,48.6067855370516,
48.7006954729337,48.7945968463932,48.8885152927769,48.9825349694042,49.076610184745,
49.1708374280095,49.2255419345982,49.3197803108064,49.3502405140517),
 .UNSPECIFIED.);
#367=B_SPLINE_CURVE_WITH_KNOTS('',3,(#28023,#28024,#28025,#28026,#28027,
#28028,#28029,#28030,#28031,#28032,#28033,#28034,#28035,#28036,#28037,#28038,
#28039,#28040,#28041,#28042,#28043,#28044,#28045,#28046,#28047,#28048,#28049,
#28050,#28051,#28052,#28053,#28054,#28055,#28056,#28057,#28058,#28059,#28060,
#28061,#28062,#28063,#28064,#28065,#28066,#28067,#28068,#28069,#28070,#28071,
#28072,#28073,#28074,#28075,#28076,#28077,#28078,#28079,#28080,#28081,#28082,
#28083,#28084,#28085,#28086,#28087,#28088,#28089,#28090,#28091,#28092,#28093,
#28094,#28095,#28096,#28097,#28098,#28099,#28100,#28101,#28102,#28103,#28104,
#28105,#28106,#28107,#28108,#28109,#28110,#28111,#28112,#28113,#28114,#28115,
#28116,#28117,#28118,#28119,#28120,#28121,#28122,#28123,#28124,#28125,#28126,
#28127,#28128,#28129,#28130,#28131,#28132,#28133,#28134,#28135,#28136,#28137,
#28138,#28139,#28140,#28141,#28142,#28143,#28144,#28145,#28146,#28147,#28148,
#28149,#28150,#28151,#28152,#28153,#28154,#28155,#28156,#28157,#28158),
 .UNSPECIFIED.,.F.,.F.,(4,3,3,3,3,3,3,3,3,3,3,3,3,3,3,3,3,3,3,3,3,3,3,3,
3,3,3,3,3,3,3,3,3,3,3,3,3,3,3,3,3,3,3,3,3,4),(43.0659729437217,43.1605738556491,
43.2551747675765,43.3494133013489,43.4435240011486,43.5375354165324,43.631479564551,
43.7253895004376,43.8192908739017,43.91320932029,44.007228996922,44.1013042122674,
44.1955314555366,44.2502359620802,44.3444744958471,44.4385851956413,44.5325966110194,
44.6265407590322,44.7204506949132,44.8143520683715,44.9082705147539,45.0022901913801,
45.0963654067197,45.1905926499831,45.2452971565838,45.3395356903515,45.4336463901465,
45.5276578055255,45.6216019535392,45.7155118894209,45.8094132628799,45.9033317092632,
45.9973513858901,46.0914266012305,46.1856538444945,46.2403583510874,46.333353832453,
46.4262225404432,46.51898661054,46.6116939361495,46.7043714684739,46.7970461230525,
46.8897940511749,46.9825825279157,47.0754997299982,47.1238898036239),
 .UNSPECIFIED.);
#368=B_SPLINE_CURVE_WITH_KNOTS('',3,(#28164,#28165,#28166,#28167,#28168,
#28169,#28170,#28171,#28172,#28173,#28174,#28175,#28176,#28177,#28178,#28179,
#28180,#28181,#28182,#28183,#28184,#28185,#28186,#28187,#28188,#28189,#28190,
#28191,#28192,#28193,#28194,#28195,#28196,#28197,#28198,#28199,#28200,#28201,
#28202,#28203,#28204,#28205,#28206,#28207,#28208,#28209,#28210,#28211,#28212,
#28213,#28214,#28215,#28216,#28217,#28218,#28219,#28220,#28221,#28222,#28223,
#28224,#28225,#28226,#28227,#28228,#28229,#28230,#28231,#28232,#28233,#28234,
#28235,#28236,#28237,#28238,#28239,#28240,#28241,#28242,#28243,#28244,#28245,
#28246,#28247,#28248,#28249,#28250,#28251,#28252,#28253,#28254,#28255,#28256,
#28257,#28258,#28259,#28260,#28261,#28262,#28263,#28264,#28265,#28266,#28267,
#28268,#28269,#28270,#28271,#28272,#28273,#28274,#28275,#28276,#28277,#28278,
#28279,#28280,#28281,#28282,#28283,#28284,#28285,#28286,#28287,#28288,#28289,
#28290,#28291,#28292,#28293,#28294,#28295,#28296),.UNSPECIFIED.,.F.,.F.,
(4,3,3,3,3,3,3,3,3,3,3,3,3,3,3,3,3,3,3,3,3,3,3,3,3,3,3,3,3,3,3,3,3,3,3,
3,3,3,3,3,3,3,3,3,4),(36.7836225529413,36.8777922829933,36.9718487623956,
37.0666901570213,37.1606133284242,37.2545156160629,37.3484226595646,37.4439619745238,
37.5380085641333,37.6342942417675,37.7305799194016,37.8248184532023,37.9189291530308,
38.0129405684437,38.1068847164918,38.2007946524082,38.2946960259022,38.3886144723206,
38.4826341489828,38.5767093643585,38.6709366076577,38.7256411139052,38.8198796476661,
38.9139903474544,39.0080017628264,39.1019459108333,39.1958558467081,39.2897572201605,
39.3836756665371,39.4776953431573,39.571770558491,39.6659978017485,39.7207023084088,
39.8149408421724,39.9090515419633,40.0030629573379,40.0970071053473,40.1909170412247,
40.2848184146794,40.3787368610583,40.4727565376808,40.5668317530167,40.6610589962762,
40.7157635029124,40.8407044966672),.UNSPECIFIED.);
#369=B_SPLINE_CURVE_WITH_KNOTS('',3,(#28297,#28298,#28299,#28300,#28301,
#28302,#28303,#28304,#28305,#28306,#28307,#28308,#28309,#28310,#28311,#28312,
#28313,#28314,#28315,#28316,#28317,#28318,#28319,#28320,#28321,#28322,#28323,
#28324,#28325,#28326,#28327,#28328,#28329,#28330,#28331,#28332,#28333,#28334,
#28335,#28336,#28337,#28338,#28339,#28340,#28341,#28342,#28343,#28344,#28345,
#28346,#28347,#28348,#28349,#28350,#28351,#28352,#28353,#28354,#28355,#28356,
#28357,#28358,#28359,#28360,#28361,#28362,#28363,#28364,#28365,#28366,#28367,
#28368,#28369,#28370,#28371,#28372),.UNSPECIFIED.,.F.,.F.,(4,3,3,3,3,3,
3,3,3,3,3,3,3,3,3,3,3,3,3,3,3,3,3,3,3,4),(40.8407044968828,40.9335549962785,
41.0307137089207,41.1233759605245,41.2159998721551,41.3086124205635,41.4012405658138,
41.4939653595684,41.5867468664922,41.6796701952324,41.7108246974161,41.8050632311829,
41.8991739309771,41.993185346355,42.0871294943679,42.1810394302488,42.2749408037072,
42.3688592500896,42.4628789267157,42.5569541420554,42.6511813853187,42.7058858919197,
42.8001014455114,42.894205230012,42.9882080806231,43.0669410879269),
 .UNSPECIFIED.);
#370=B_SPLINE_CURVE_WITH_KNOTS('',3,(#28374,#28375,#28376,#28377,#28378,
#28379,#28380,#28381,#28382,#28383,#28384,#28385,#28386,#28387,#28388,#28389,
#28390,#28391,#28392,#28393,#28394,#28395,#28396,#28397,#28398,#28399,#28400,
#28401,#28402,#28403,#28404,#28405,#28406,#28407,#28408,#28409,#28410,#28411,
#28412,#28413,#28414,#28415,#28416,#28417,#28418,#28419,#28420,#28421,#28422,
#28423,#28424,#28425,#28426,#28427,#28428,#28429,#28430,#28431,#28432,#28433,
#28434,#28435,#28436,#28437,#28438,#28439,#28440,#28441,#28442,#28443,#28444,
#28445,#28446),.UNSPECIFIED.,.F.,.F.,(4,3,3,3,3,3,3,3,3,3,3,3,3,3,3,3,3,
3,3,3,3,3,3,3,4),(40.8407044968363,40.9467914672695,41.0491746662872,41.1571135224282,
41.2650523785693,41.3592909123302,41.4534016121184,41.5474130274904,41.6413571754972,
41.7352671113721,41.8291684848244,41.9230869312007,42.0171066078209,42.1111818231546,
42.205409066412,42.2601135730729,42.3543648088597,42.4484583704197,42.5424618174093,
42.636400902428,42.7303013160319,42.8242184381103,42.9181432733357,43.0121464759615,
43.0659729437217),.UNSPECIFIED.);
#371=B_SPLINE_CURVE_WITH_KNOTS('',3,(#28447,#28448,#28449,#28450,#28451,
#28452,#28453,#28454,#28455,#28456,#28457,#28458,#28459,#28460,#28461,#28462,
#28463,#28464,#28465,#28466,#28467,#28468,#28469,#28470,#28471,#28472,#28473,
#28474,#28475,#28476,#28477,#28478,#28479,#28480,#28481,#28482,#28483,#28484,
#28485,#28486,#28487,#28488,#28489,#28490,#28491,#28492,#28493,#28494,#28495,
#28496,#28497,#28498,#28499,#28500,#28501,#28502,#28503,#28504,#28505,#28506,
#28507,#28508,#28509,#28510,#28511,#28512,#28513,#28514,#28515,#28516,#28517,
#28518,#28519,#28520,#28521,#28522,#28523,#28524,#28525,#28526,#28527,#28528,
#28529,#28530,#28531,#28532,#28533,#28534,#28535,#28536,#28537,#28538,#28539,
#28540,#28541,#28542,#28543,#28544,#28545,#28546,#28547,#28548,#28549,#28550,
#28551,#28552,#28553,#28554,#28555,#28556,#28557,#28558,#28559,#28560,#28561,
#28562,#28563,#28564,#28565,#28566,#28567,#28568,#28569,#28570,#28571,#28572,
#28573,#28574,#28575,#28576,#28577,#28578,#28579,#28580,#28581,#28582),
 .UNSPECIFIED.,.F.,.F.,(4,3,3,3,3,3,3,3,3,3,3,3,3,3,3,3,3,3,3,3,3,3,3,3,
3,3,3,3,3,3,3,3,3,3,3,3,3,3,3,3,3,3,3,3,3,4),(36.7833811949732,36.8772844267835,
36.9712111255313,37.0652424873676,37.1593351364484,37.2535731276351,37.2848076005549,
37.3790461345677,37.473156834611,37.5671682502409,37.6611123985091,37.7550223346473,
37.8489237083645,37.942842155007,38.0368618318937,38.1309370474943,38.2251642910171,
38.2798687950585,38.3741073287897,38.4682180285484,38.562229443891,38.6561735918686,
38.7500835277143,38.8439849011377,38.9379033474859,39.0319230240781,39.1259982393842,
39.2202254826146,39.2749299895621,39.3691685232879,39.46327922304,39.5572906383755,
39.6512347863447,39.7451447221812,39.8390460955947,39.9329645419325,40.0269842185129,
40.1210594338062,40.2152866770234,40.2699911840657,40.3663474040034,40.4625550534326,
40.5586031867734,40.6545575383556,40.7504306622901,40.8407044966672),
 .UNSPECIFIED.);
#372=B_SPLINE_CURVE_WITH_KNOTS('',3,(#28588,#28589,#28590,#28591,#28592,
#28593,#28594,#28595,#28596,#28597,#28598,#28599,#28600,#28601,#28602,#28603,
#28604,#28605,#28606,#28607,#28608,#28609,#28610,#28611,#28612,#28613,#28614,
#28615,#28616,#28617,#28618,#28619,#28620,#28621,#28622,#28623,#28624,#28625,
#28626,#28627,#28628,#28629,#28630,#28631,#28632,#28633,#28634,#28635,#28636,
#28637,#28638,#28639,#28640,#28641,#28642,#28643,#28644,#28645,#28646,#28647,
#28648,#28649,#28650,#28651,#28652,#28653,#28654,#28655,#28656,#28657,#28658,
#28659,#28660,#28661,#28662,#28663,#28664,#28665,#28666,#28667,#28668,#28669,
#28670,#28671,#28672,#28673,#28674,#28675,#28676,#28677,#28678,#28679,#28680,
#28681,#28682,#28683,#28684,#28685,#28686,#28687,#28688,#28689,#28690,#28691,
#28692,#28693,#28694,#28695,#28696,#28697,#28698,#28699,#28700,#28701,#28702,
#28703,#28704,#28705,#28706,#28707,#28708,#28709,#28710,#28711,#28712,#28713,
#28714,#28715,#28716,#28717,#28718,#28719,#28720,#28721,#28722,#28723),
 .UNSPECIFIED.,.F.,.F.,(4,3,3,3,3,3,3,3,3,3,3,3,3,3,3,3,3,3,3,3,3,3,3,3,
3,3,3,3,3,3,3,3,3,3,3,3,3,3,3,3,3,3,3,3,3,4),(30.4996279272502,30.5936877447165,
30.6879063249188,30.7651515578763,30.8593900883337,30.9535007847613,31.0475121967206,
31.141456341251,31.2353662736114,31.3292676435152,31.4231860863138,31.5172057593323,
31.6112809710456,31.7055082106889,31.7602127523799,31.8544512879246,31.9485619895187,
32.0425734067164,32.13651755657,32.2304274943042,32.3243288696259,32.4182473178801,
32.5122669963787,32.606342213594,32.7005694587196,32.7552739468835,32.84951248052,
32.9436231801865,33.0376345954395,33.1315787433317,33.2254886790948,33.3193900524384,
33.4133084987091,33.5073281752292,33.6014033904657,33.6956306336318,33.7503351413872,
33.843198509978,33.9359114578974,34.0285393283358,34.1211092506416,34.2136482865597,
34.3062224486771,34.3988130903768,34.4915064402966,34.5575191892671),
 .UNSPECIFIED.);
#373=B_SPLINE_CURVE_WITH_KNOTS('',3,(#28724,#28725,#28726,#28727,#28728,
#28729,#28730,#28731,#28732,#28733,#28734,#28735,#28736,#28737,#28738,#28739,
#28740,#28741,#28742,#28743,#28744,#28745,#28746,#28747,#28748,#28749,#28750,
#28751,#28752,#28753,#28754,#28755,#28756,#28757,#28758,#28759,#28760,#28761,
#28762,#28763,#28764,#28765,#28766,#28767,#28768,#28769,#28770,#28771,#28772,
#28773,#28774,#28775,#28776,#28777,#28778,#28779,#28780,#28781,#28782,#28783,
#28784,#28785,#28786,#28787,#28788,#28789,#28790,#28791,#28792,#28793,#28794,
#28795,#28796,#28797,#28798,#28799),.UNSPECIFIED.,.F.,.F.,(4,3,3,3,3,3,
3,3,3,3,3,3,3,3,3,3,3,3,3,3,3,3,3,3,3,4),(34.5575191894877,34.6960958089033,
34.7453963358908,34.8396348699029,34.9337455699456,35.0277569855753,35.1217011338427,
35.2156110699801,35.3095124436966,35.4034308903384,35.4974505672243,35.5915257828243,
35.6857530263464,35.7404575303944,35.8346960641258,35.9288067638846,36.0228181792274,
36.1167623272052,36.2106722630512,36.3045736364748,36.3984920828229,36.4925117594152,
36.5865869747213,36.6808142179519,36.735518724898,36.7836225529413),
 .UNSPECIFIED.);
#374=B_SPLINE_CURVE_WITH_KNOTS('',3,(#28801,#28802,#28803,#28804,#28805,
#28806,#28807,#28808,#28809,#28810,#28811,#28812,#28813,#28814,#28815,#28816,
#28817,#28818,#28819,#28820,#28821,#28822,#28823,#28824,#28825,#28826,#28827,
#28828,#28829,#28830,#28831,#28832,#28833,#28834,#28835,#28836,#28837,#28838,
#28839,#28840,#28841,#28842,#28843,#28844,#28845,#28846,#28847,#28848,#28849,
#28850,#28851,#28852,#28853,#28854,#28855,#28856,#28857,#28858,#28859,#28860,
#28861,#28862,#28863,#28864,#28865,#28866,#28867,#28868,#28869,#28870,#28871,
#28872,#28873,#28874,#28875,#28876),.UNSPECIFIED.,.F.,.F.,(4,3,3,3,3,3,
3,3,3,3,3,3,3,3,3,3,3,3,3,3,3,3,3,3,3,4),(34.5575191894877,34.6505073831219,
34.7434447345139,34.8363579713218,34.9292737926231,35.0222802791695,35.1153312545951,
35.2085421544079,35.2946852115477,35.3889237451837,35.4830344448493,35.5770458601016,
35.6709900079932,35.7648999437556,35.8588013170986,35.9527197633688,36.0467394398882,
36.1408146551243,36.2350418982897,36.2897464060513,36.3839854271749,36.4781010657501,
36.57210461853,36.666043929314,36.7599457471408,36.7833811949732),
 .UNSPECIFIED.);
#375=B_SPLINE_CURVE_WITH_KNOTS('',3,(#28877,#28878,#28879,#28880,#28881,
#28882,#28883,#28884,#28885,#28886,#28887,#28888,#28889,#28890,#28891,#28892,
#28893,#28894,#28895,#28896,#28897,#28898,#28899,#28900,#28901,#28902,#28903,
#28904,#28905,#28906,#28907,#28908,#28909,#28910,#28911,#28912,#28913,#28914,
#28915,#28916,#28917,#28918,#28919,#28920,#28921,#28922,#28923,#28924,#28925,
#28926,#28927,#28928,#28929,#28930,#28931,#28932,#28933,#28934,#28935,#28936,
#28937,#28938,#28939,#28940,#28941,#28942,#28943,#28944,#28945,#28946,#28947,
#28948,#28949,#28950,#28951,#28952,#28953,#28954,#28955,#28956,#28957,#28958,
#28959,#28960,#28961,#28962,#28963,#28964,#28965,#28966,#28967,#28968,#28969,
#28970,#28971,#28972,#28973,#28974,#28975,#28976,#28977,#28978,#28979,#28980,
#28981,#28982,#28983,#28984,#28985,#28986,#28987,#28988,#28989,#28990,#28991,
#28992,#28993,#28994,#28995,#28996,#28997,#28998,#28999,#29000,#29001,#29002,
#29003,#29004,#29005,#29006,#29007,#29008,#29009,#29010,#29011,#29012),
 .UNSPECIFIED.,.F.,.F.,(4,3,3,3,3,3,3,3,3,3,3,3,3,3,3,3,3,3,3,3,3,3,3,3,
3,3,3,3,3,3,3,3,3,3,3,3,3,3,3,3,3,3,3,3,3,4),(30.5007612509717,30.5947790154448,
30.6887266897135,30.7826382504506,30.8765393493006,30.9704556219893,31.0644720738379,
31.1585423574244,31.25276671836,31.3144404335332,31.4086789798773,31.5027896923931,
31.5968011206189,31.6907452816136,31.7846552305545,31.8785566171349,31.9724750766856,
32.06649476647,32.1605699949819,32.254797251309,32.3095016280368,32.4037401619858,
32.497850861999,32.5918622776326,32.6858064259543,32.7797163621772,32.8736177360103,
32.9675361827999,33.0615558598808,33.1556310757027,33.2498583194874,33.3045628225404,
33.398801352991,33.4929120494117,33.586923461364,33.6808676058873,33.7747775382403,
33.8686789081369,33.9625973509281,34.0566170239391,34.1506922356449,34.2449194752806,
34.299624017044,34.4208944554796,34.5397648284115,34.557519189206),
 .UNSPECIFIED.);
#376=B_SPLINE_CURVE_WITH_KNOTS('',3,(#29018,#29019,#29020,#29021,#29022,
#29023,#29024,#29025),.UNSPECIFIED.,.F.,.F.,(4,1,1,1,1,4),(24.2174104409543,
24.7947843908547,25.7898455853583,26.7849067798619,27.7799679743655,28.2743336440772),
 .UNSPECIFIED.);
#377=B_SPLINE_CURVE_WITH_KNOTS('',3,(#29026,#29027,#29028,#29029,#29030,
#29031,#29032,#29033,#29034,#29035,#29036,#29037,#29038,#29039,#29040,#29041,
#29042,#29043,#29044,#29045,#29046,#29047,#29048,#29049,#29050,#29051,#29052,
#29053,#29054,#29055,#29056,#29057,#29058,#29059,#29060,#29061,#29062,#29063,
#29064,#29065,#29066,#29067,#29068,#29069,#29070,#29071,#29072,#29073,#29074,
#29075,#29076,#29077,#29078,#29079,#29080,#29081,#29082,#29083,#29084,#29085,
#29086,#29087,#29088,#29089,#29090,#29091,#29092,#29093,#29094,#29095,#29096,
#29097,#29098),.UNSPECIFIED.,.F.,.F.,(4,3,3,3,3,3,3,3,3,3,3,3,3,3,3,3,3,
3,3,3,3,3,3,3,4),(28.2743338823081,28.3725366417317,28.473159773516,28.5717415465316,
28.6733853577003,28.7750291688691,28.8692677151853,28.963378427673,29.0573898558701,
29.151334016836,29.2452439657479,29.3391453522992,29.4330638118205,29.5270835015756,
29.6211587300581,29.7153859863561,29.7700903633727,29.8643053297425,29.9584025213165,
30.0524077829851,30.1463468727215,30.2402636747242,30.3341644786122,30.4281151158429,
30.4996279272502),.UNSPECIFIED.);
#378=B_SPLINE_CURVE_WITH_KNOTS('',3,(#29100,#29101,#29102,#29103,#29104,
#29105,#29106,#29107,#29108,#29109,#29110,#29111,#29112,#29113,#29114,#29115,
#29116,#29117,#29118,#29119,#29120,#29121,#29122,#29123,#29124,#29125,#29126,
#29127,#29128,#29129,#29130,#29131,#29132,#29133,#29134,#29135,#29136,#29137,
#29138,#29139,#29140,#29141,#29142,#29143,#29144,#29145,#29146,#29147,#29148,
#29149,#29150,#29151,#29152,#29153,#29154,#29155,#29156,#29157,#29158,#29159,
#29160,#29161,#29162,#29163,#29164,#29165,#29166,#29167,#29168,#29169,#29170,
#29171,#29172,#29173,#29174,#29175),.UNSPECIFIED.,.F.,.F.,(4,3,3,3,3,3,
3,3,3,3,3,3,3,3,3,3,3,3,3,3,3,3,3,3,3,4),(28.2743338823081,28.3292568500224,
28.423495469431,28.5176062557521,28.6116177584166,28.7055619944834,28.7994720188599,
28.8933734811464,28.9872920165809,29.0813117820562,29.1753870862621,29.2696144175385,
29.324318044526,29.4185565889438,29.5126672998036,29.6066787266445,29.7006228866682,
29.7945328348948,29.8884342210195,29.9823526803752,30.0763723703673,30.1704475993146,
30.2646748564353,30.3193792390296,30.4135944930383,30.5007612509717),
 .UNSPECIFIED.);
#379=B_SPLINE_CURVE_WITH_KNOTS('',3,(#29176,#29177,#29178,#29179,#29180,
#29181,#29182,#29183,#29184,#29185,#29186,#29187,#29188,#29189,#29190,#29191,
#29192,#29193,#29194,#29195,#29196,#29197,#29198,#29199,#29200,#29201,#29202,
#29203,#29204,#29205,#29206,#29207,#29208,#29209,#29210,#29211,#29212,#29213,
#29214,#29215,#29216,#29217,#29218,#29219,#29220,#29221,#29222,#29223,#29224,
#29225,#29226,#29227,#29228,#29229,#29230,#29231,#29232,#29233,#29234,#29235,
#29236,#29237,#29238,#29239,#29240,#29241,#29242,#29243,#29244,#29245,#29246,
#29247,#29248,#29249,#29250,#29251,#29252,#29253,#29254,#29255,#29256,#29257,
#29258,#29259,#29260,#29261,#29262,#29263,#29264,#29265,#29266,#29267,#29268,
#29269,#29270,#29271,#29272,#29273,#29274,#29275,#29276,#29277,#29278,#29279,
#29280,#29281,#29282,#29283,#29284,#29285,#29286,#29287,#29288,#29289,#29290,
#29291,#29292,#29293,#29294,#29295,#29296,#29297,#29298,#29299,#29300,#29301,
#29302,#29303,#29304,#29305,#29306,#29307,#29308,#29309,#29310,#29311),
 .UNSPECIFIED.,.F.,.F.,(4,3,3,3,3,3,3,3,3,3,3,3,3,3,3,3,3,3,3,3,3,3,3,3,
3,3,3,3,3,3,3,3,3,3,3,3,3,3,3,3,3,3,3,3,3,4),(24.216482857356,24.3107193521127,
24.3490120720079,24.4432488148445,24.5373576970504,24.6313672708521,24.72530954913,
24.8192175985477,24.91311707111,25.0070336044477,25.1010513610802,25.1951246496571,
25.2893499744683,25.3440732665115,25.4383123567688,25.5324236179415,25.6264355987757,
25.7203803159484,25.8142908230647,25.9081927691272,26.0021117887765,26.0961320361662,
26.1902078217006,26.2844356286052,26.3391344610152,26.4333731465367,26.5274840022162,
26.6214955773734,26.7154398903322,26.809349994297,26.903251538779,26.9971701589291,
27.0911900124797,27.185265406789,27.2794928305046,27.3341956555188,27.4276603575711,
27.5209978653467,27.6151648674452,27.7083395791818,27.8014834289019,27.894622918338,
27.9895506592872,28.0828117812111,28.178572831673,28.2743338821349),
 .UNSPECIFIED.);
#380=B_SPLINE_CURVE_WITH_KNOTS('',3,(#29317,#29318,#29319,#29320,#29321,
#29322,#29323,#29324,#29325,#29326,#29327,#29328,#29329,#29330,#29331,#29332,
#29333,#29334,#29335,#29336,#29337,#29338,#29339,#29340,#29341,#29342,#29343,
#29344,#29345,#29346,#29347,#29348,#29349,#29350,#29351,#29352,#29353,#29354,
#29355,#29356,#29357,#29358,#29359,#29360,#29361,#29362,#29363,#29364,#29365,
#29366,#29367,#29368,#29369,#29370,#29371,#29372,#29373,#29374,#29375,#29376,
#29377,#29378,#29379,#29380,#29381,#29382,#29383,#29384,#29385,#29386,#29387,
#29388,#29389,#29390,#29391,#29392),.UNSPECIFIED.,.F.,.F.,(4,3,3,3,3,3,
3,3,3,3,3,3,3,3,3,3,3,3,3,3,3,3,3,3,3,4),(15.7079632679489,15.8009022570379,
15.8938127630074,15.9867214110195,16.0796548185911,16.1726969971519,16.2658032398934,
16.3590599897109,16.388522515979,16.482850675556,16.577050577067,16.6711506419944,
16.7651822193176,16.8591787913051,16.9531658921126,17.0471690407496,17.1412713132475,
17.235428054019,17.329734309839,17.3835837104827,17.4779692848255,17.5722355767653,
17.6663981576832,17.7604990407976,17.8545789396576,17.9336096034474),
 .UNSPECIFIED.);
#381=B_SPLINE_CURVE_WITH_KNOTS('',3,(#29394,#29395,#29396,#29397,#29398),
 .UNSPECIFIED.,.F.,.F.,(4,1,4),(14.3984001269718,15.3934613214754,15.7079548718395),
 .UNSPECIFIED.);
#382=B_SPLINE_CURVE_WITH_KNOTS('',3,(#29402,#29403,#29404,#29405,#29406,
#29407,#29408,#29409,#29410,#29411,#29412,#29413,#29414,#29415,#29416,#29417,
#29418,#29419,#29420,#29421,#29422,#29423,#29424,#29425,#29426,#29427,#29428,
#29429,#29430,#29431,#29432,#29433,#29434,#29435,#29436,#29437,#29438,#29439,
#29440,#29441,#29442,#29443,#29444,#29445,#29446,#29447,#29448,#29449,#29450,
#29451,#29452,#29453,#29454,#29455,#29456,#29457,#29458,#29459,#29460,#29461,
#29462,#29463,#29464,#29465),.UNSPECIFIED.,.F.,.F.,(4,3,3,3,3,3,3,3,3,3,
3,3,3,3,3,3,3,3,3,3,3,4),(13.875933913584,13.9698176198018,14.0635739700505,
14.1611487795215,14.2547391272248,14.3482980121981,14.4418514975605,14.5354256347481,
14.6291003941672,14.7228347639158,14.8167105981944,14.8441724458185,14.9372024528207,
15.0335475547118,15.1263491052847,15.2190970034976,15.3118181687131,15.4045394876794,
15.4973328718652,15.5901696304292,15.6831249272467,15.7079632679489),
 .UNSPECIFIED.);
#383=B_SPLINE_CURVE_WITH_KNOTS('',3,(#29466,#29467,#29468,#29469,#29470,
#29471,#29472),.UNSPECIFIED.,.F.,.F.,(4,1,1,1,4),(15.7079632679489,15.8392336403222,
16.8342948348258,17.8293560293294,17.9343967671566),.UNSPECIFIED.);
#384=B_SPLINE_CURVE_WITH_KNOTS('',3,(#29478,#29479,#29480,#29481,#29482,
#29483,#29484,#29485,#29486,#29487,#29488,#29489),.UNSPECIFIED.,.F.,.F.,
(4,2,2,2,2,4),(-0.0891744238985337,-0.0496035464748441,-0.0101627518981445,
-0.0043205186654138,-0.00194322075801571,0.),.UNSPECIFIED.);
#385=B_SPLINE_CURVE_WITH_KNOTS('',3,(#29497,#29498,#29499,#29500,#29501,
#29502,#29503,#29504,#29505,#29506,#29507,#29508,#29509,#29510,#29511,#29512,
#29513,#29514,#29515,#29516,#29517,#29518,#29519,#29520,#29521,#29522,#29523,
#29524,#29525,#29526,#29527,#29528,#29529,#29530,#29531,#29532,#29533,#29534,
#29535,#29536,#29537,#29538,#29539,#29540,#29541,#29542,#29543,#29544,#29545,
#29546,#29547,#29548,#29549,#29550,#29551,#29552,#29553,#29554,#29555,#29556,
#29557,#29558,#29559,#29560,#29561,#29562,#29563),.UNSPECIFIED.,.F.,.F.,
(4,3,3,3,3,3,3,3,3,3,3,3,3,3,3,3,3,3,3,3,3,3,4),(-119.380510126605,-119.281824003816,
-119.183277779352,-119.08484394797,-118.986471229893,-118.88812931942,-118.789787948957,
-118.691351781982,-118.592868088032,-118.494214874655,-118.41228214593,
-118.313062108565,-118.213979277463,-118.114384486708,-118.015471660298,
-117.916589188221,-117.817707520535,-117.717585878258,-117.618559601633,
-117.517890276529,-117.417220951426,-117.311975507606,-117.299671991106),
 .UNSPECIFIED.);
#386=B_SPLINE_CURVE_WITH_KNOTS('',3,(#29569,#29570,#29571,#29572,#29573,
#29574,#29575,#29576,#29577,#29578,#29579,#29580,#29581,#29582,#29583,#29584,
#29585,#29586,#29587,#29588,#29589,#29590,#29591,#29592,#29593,#29594,#29595,
#29596,#29597,#29598,#29599,#29600,#29601,#29602,#29603,#29604,#29605,#29606,
#29607,#29608,#29609,#29610,#29611,#29612,#29613,#29614,#29615,#29616,#29617,
#29618,#29619,#29620,#29621,#29622,#29623,#29624,#29625,#29626,#29627,#29628,
#29629,#29630,#29631,#29632,#29633,#29634,#29635,#29636,#29637,#29638,#29639,
#29640,#29641,#29642,#29643,#29644,#29645,#29646,#29647,#29648,#29649,#29650,
#29651,#29652,#29653,#29654,#29655,#29656,#29657,#29658,#29659,#29660,#29661,
#29662,#29663,#29664,#29665,#29666,#29667,#29668,#29669,#29670,#29671,#29672,
#29673,#29674,#29675,#29676,#29677,#29678,#29679,#29680,#29681,#29682,#29683,
#29684,#29685,#29686,#29687,#29688,#29689,#29690,#29691,#29692,#29693,#29694,
#29695,#29696,#29697,#29698,#29699,#29700,#29701,#29702,#29703,#29704,#29705,
#29706,#29707,#29708,#29709,#29710,#29711,#29712,#29713,#29714,#29715,#29716,
#29717,#29718,#29719,#29720,#29721,#29722,#29723,#29724,#29725,#29726,#29727,
#29728,#29729,#29730,#29731,#29732,#29733,#29734,#29735,#29736,#29737,#29738,
#29739,#29740,#29741,#29742,#29743,#29744,#29745,#29746,#29747,#29748,#29749,
#29750,#29751,#29752),.UNSPECIFIED.,.F.,.F.,(4,3,3,3,3,3,3,3,3,3,3,3,3,
3,3,3,3,3,3,3,3,3,3,3,3,3,3,3,3,3,3,3,3,3,3,3,3,3,3,3,3,3,3,3,3,3,3,3,3,
3,3,3,3,3,3,3,3,3,3,3,3,4),(114.761320057655,114.860067511219,114.958791860699,
115.057522860401,115.156355627907,115.25524135556,115.354296888589,115.427098562419,
115.526175962403,115.625113193801,115.724744014191,115.82350509915,115.922233863131,
116.020960064793,116.121259987825,116.220128053757,116.32114390534,116.422159756923,
116.521103426722,116.619906372427,116.719570694802,116.818197115993,116.916791368532,
117.015383389193,117.115842779751,117.214578838161,117.315899894793,117.417220951426,
117.516458226383,117.615554601375,117.715145544445,117.814062836174,117.912946357322,
118.011825660325,118.111939781727,118.21095533248,118.311618739205,118.41228214593,
118.511423730653,118.610426918485,118.710041471229,118.808872273556,118.907671994955,
119.006470285157,119.106688548976,119.205630694478,119.306487017455,119.407343340433,
119.505449657559,119.603415177681,119.703288847338,119.801083195662,119.898848954802,
119.99661701861,120.098063897692,120.195995241008,120.294006021494,120.392183906562,
120.402404534937,120.533901068514,120.662199975167,120.69007258227),
 .UNSPECIFIED.);
#387=B_SPLINE_CURVE_WITH_KNOTS('',3,(#29753,#29754,#29755,#29756,#29757,
#29758,#29759,#29760,#29761,#29762,#29763,#29764,#29765,#29766,#29767,#29768,
#29769,#29770,#29771,#29772),.UNSPECIFIED.,.F.,.F.,(4,2,2,2,2,2,2,2,2,4),
(-0.178840503134635,-0.141813169590022,-0.126245575166451,-0.120975056350671,
-0.117078626547339,-0.11313785577946,-0.109546939480627,-0.103794973539924,
-0.0894553738401638,-0.0891744238985337),.UNSPECIFIED.);
#388=B_SPLINE_CURVE_WITH_KNOTS('',3,(#29774,#29775,#29776,#29777,#29778,
#29779,#29780,#29781,#29782,#29783,#29784,#29785,#29786),.UNSPECIFIED.,
 .F.,.F.,(4,3,3,3,4),(-117.299671991106,-117.194784025774,-117.090099445131,
-116.985683593692,-116.946309934874),.UNSPECIFIED.);
#389=B_SPLINE_CURVE_WITH_KNOTS('',3,(#29787,#29788,#29789,#29790,#29791,
#29792,#29793,#29794,#29795,#29796),.UNSPECIFIED.,.F.,.F.,(4,1,1,1,1,1,
1,4),(-116.946309934874,-116.422159756923,-115.427098562419,-114.432037367915,
-113.436976173412,-112.441914978908,-111.446853784405,-111.016736858085),
 .UNSPECIFIED.);
#390=B_SPLINE_CURVE_WITH_KNOTS('',3,(#29802,#29803,#29804,#29805,#29806,
#29807,#29808,#29809,#29810,#29811,#29812,#29813,#29814,#29815,#29816,#29817,
#29818,#29819,#29820,#29821,#29822,#29823,#29824,#29825,#29826,#29827,#29828,
#29829,#29830,#29831,#29832,#29833,#29834,#29835,#29836,#29837,#29838,#29839,
#29840,#29841,#29842,#29843,#29844,#29845,#29846,#29847,#29848,#29849,#29850,
#29851,#29852,#29853,#29854,#29855,#29856,#29857,#29858,#29859,#29860,#29861,
#29862,#29863,#29864,#29865,#29866,#29867,#29868,#29869,#29870,#29871,#29872,
#29873,#29874,#29875,#29876,#29877,#29878,#29879,#29880,#29881,#29882,#29883,
#29884,#29885,#29886,#29887,#29888,#29889,#29890,#29891,#29892,#29893,#29894,
#29895,#29896,#29897,#29898,#29899,#29900,#29901,#29902,#29903,#29904,#29905,
#29906,#29907,#29908,#29909,#29910,#29911,#29912,#29913,#29914,#29915,#29916,
#29917,#29918,#29919,#29920,#29921,#29922,#29923,#29924,#29925,#29926,#29927,
#29928,#29929,#29930,#29931,#29932,#29933,#29934,#29935,#29936,#29937,#29938,
#29939,#29940,#29941,#29942,#29943,#29944,#29945,#29946,#29947,#29948,#29949,
#29950,#29951,#29952,#29953,#29954,#29955,#29956,#29957,#29958,#29959,#29960,
#29961,#29962,#29963,#29964,#29965,#29966,#29967,#29968,#29969,#29970,#29971,
#29972,#29973,#29974,#29975,#29976,#29977,#29978,#29979,#29980,#29981,#29982),
 .UNSPECIFIED.,.F.,.F.,(4,3,3,3,3,3,3,3,3,3,3,3,3,3,3,3,3,3,3,3,3,3,3,3,
3,3,3,3,3,3,3,3,3,3,3,3,3,3,3,3,3,3,3,3,3,3,3,3,3,3,3,3,3,3,3,3,3,3,3,3,
4),(108.477770244024,108.576804478106,108.675703662613,108.774496605418,
108.873231844062,108.971939195394,109.070648441376,109.169456830148,109.268313938915,
109.367346518269,109.456731395397,109.555791102734,109.654710371096,109.754345648446,
109.853088250073,109.951798378069,110.050505817417,110.150827510538,110.249676699491,
110.350734644696,110.451792589901,110.550849698287,110.649766361109,110.74940228902,
110.84814228808,110.946849820364,111.045554674319,111.14587945184,111.244726107047,
111.345789945725,111.446853784404,111.545914922601,111.644835605295,111.744470526997,
111.843214492961,111.941925963677,112.040634722456,112.140954786569,112.239805224716,
112.340860101812,112.441914978908,112.540977599963,112.639899812681,112.739534357772,
112.838279956175,112.936993093827,113.035703551551,113.136021707016,113.234873904593,
113.335925039003,113.436976173412,113.535605508397,113.634094697856,113.732471458206,
113.830787072003,113.929071919081,114.027356341127,114.125736595437,114.224164571909,
114.322764300366,114.406898669987),.UNSPECIFIED.);
#391=B_SPLINE_CURVE_WITH_KNOTS('',3,(#29983,#29984,#29985,#29986,#29987,
#29988,#29989,#29990,#29991,#29992,#29993,#29994,#29995,#29996,#29997,#29998),
 .UNSPECIFIED.,.F.,.F.,(4,3,3,3,3,4),(114.40689867021,114.432037367915,
114.531097614611,114.63003462159,114.72885969336,114.761320057655),
 .UNSPECIFIED.);
#392=B_SPLINE_CURVE_WITH_KNOTS('',3,(#30000,#30001,#30002,#30003),
 .UNSPECIFIED.,.F.,.F.,(4,4),(-111.016736858085,-110.663126671174),
 .UNSPECIFIED.);
#393=B_SPLINE_CURVE_WITH_KNOTS('',3,(#30004,#30005,#30006,#30007,#30008,
#30009,#30010,#30011,#30012,#30013,#30014,#30015,#30016,#30017,#30018,#30019,
#30020,#30021,#30022,#30023,#30024,#30025,#30026,#30027,#30028,#30029,#30030,
#30031,#30032,#30033,#30034,#30035,#30036,#30037,#30038,#30039,#30040,#30041,
#30042,#30043,#30044,#30045,#30046,#30047,#30048,#30049,#30050,#30051,#30052,
#30053,#30054,#30055,#30056,#30057,#30058,#30059,#30060,#30061,#30062,#30063,
#30064,#30065,#30066,#30067,#30068,#30069,#30070,#30071,#30072,#30073,#30074,
#30075,#30076,#30077,#30078,#30079,#30080,#30081,#30082,#30083,#30084,#30085,
#30086,#30087,#30088,#30089,#30090,#30091,#30092,#30093,#30094,#30095,#30096,
#30097,#30098,#30099,#30100,#30101,#30102,#30103,#30104,#30105,#30106,#30107,
#30108,#30109,#30110,#30111,#30112,#30113,#30114,#30115,#30116,#30117,#30118,
#30119,#30120,#30121,#30122,#30123,#30124,#30125,#30126,#30127,#30128,#30129,
#30130,#30131,#30132,#30133,#30134,#30135,#30136,#30137,#30138,#30139,#30140,
#30141,#30142,#30143,#30144,#30145,#30146,#30147,#30148,#30149,#30150,#30151,
#30152,#30153,#30154,#30155,#30156,#30157,#30158,#30159,#30160,#30161,#30162,
#30163,#30164,#30165,#30166,#30167,#30168,#30169,#30170,#30171,#30172,#30173,
#30174,#30175,#30176,#30177,#30178,#30179,#30180,#30181,#30182,#30183,#30184,
#30185,#30186,#30187,#30188,#30189,#30190,#30191,#30192,#30193,#30194,#30195,
#30196,#30197,#30198,#30199),.UNSPECIFIED.,.F.,.F.,(4,2,2,2,2,2,2,2,2,2,
2,2,2,2,2,2,2,2,2,2,2,2,2,2,2,2,2,2,2,2,2,2,2,2,2,2,2,2,2,2,2,2,2,2,2,2,
2,2,2,2,2,2,2,2,2,2,2,2,2,2,2,2,2,2,2,2,2,2,2,2,2,2,2,2,2,2,2,2,2,2,2,2,
2,2,2,2,2,2,2,2,2,2,2,2,2,2,2,4),(-3.17357790823559,-3.12979346273682,-3.12593076395734,
-3.12347643776689,-3.1211769410646,-3.119214678798,-3.11668020948361,-3.11253627497692,
-3.07720090000462,-3.04609543198994,-3.00836826368396,-3.00093513976047,
-2.9967042786001,-2.9935565107799,-2.98960312508386,-2.98286326098669,-2.9566808240345,
-2.89669536297659,-2.87623910016699,-2.87228075136747,-2.86995070680013,
-2.86799119315247,-2.86549692111373,-2.86148827761377,-2.83625400853403,
-2.78992482397229,-2.75579095842182,-2.7488298752571,-2.74482858885487,
-2.7413369307013,-2.73700951754869,-2.73032195565072,-2.68310823494367,
-2.64908548782712,-2.62510115459664,-2.62089062446662,-2.61859075072306,
-2.61662837427167,-2.61409394361257,-2.60995021278302,-2.57555402720399,
-2.50879733975849,-2.49919798758817,-2.49466266245402,-2.4911502642112,
-2.48727669215012,-2.48090199051045,-2.45904305875434,-2.40129094881048,
-2.38272990119718,-2.37206266247051,-2.36875609378411,-2.3666544435217,
-2.36464745659887,-2.3621651327232,-2.35602764800739,-2.30725456870824,
-2.27752702082482,-2.25217547315175,-2.24574098049604,-2.2418542696633,
-2.23834477455688,-2.23383396642056,-2.22436550020225,-2.16434426128313,
-2.12446738983707,-2.11899333033687,-2.11643903370558,-2.11449253073795,
-2.11221351407662,-2.10820956447202,-2.09073378455542,-2.02149873611586,
-2.00733261126076,-1.99693387191696,-1.99225281717305,-1.98872044498262,
-1.98491499560063,-1.97885224162176,-1.95988848354198,-1.94872277603346,
-1.89713060891502,-1.87959725169687,-1.87268661520277,-1.86751620560193,
-1.86502022242423,-1.86324811851203,-1.86099667659176,-1.85711269440354,
-1.84134505355604,-1.77041524509253,-1.74887593022735,-1.74275954437367,
-1.73894278031217,-1.73541501400231,-1.73084137269319,-1.72113555474525,
-1.67627843319428),.UNSPECIFIED.);
#394=B_SPLINE_CURVE_WITH_KNOTS('',3,(#30205,#30206,#30207,#30208,#30209,
#30210,#30211,#30212,#30213,#30214,#30215,#30216,#30217,#30218,#30219,#30220,
#30221,#30222,#30223,#30224,#30225,#30226,#30227,#30228,#30229,#30230,#30231,
#30232,#30233,#30234,#30235,#30236,#30237,#30238,#30239,#30240,#30241,#30242,
#30243,#30244,#30245,#30246,#30247,#30248,#30249,#30250,#30251,#30252,#30253,
#30254,#30255,#30256,#30257,#30258,#30259,#30260,#30261,#30262,#30263,#30264,
#30265,#30266,#30267,#30268,#30269,#30270,#30271,#30272,#30273,#30274,#30275,
#30276,#30277,#30278,#30279,#30280,#30281,#30282,#30283,#30284,#30285,#30286,
#30287,#30288,#30289,#30290,#30291,#30292,#30293,#30294,#30295,#30296,#30297,
#30298,#30299,#30300,#30301,#30302,#30303,#30304,#30305,#30306,#30307,#30308,
#30309,#30310,#30311,#30312,#30313,#30314,#30315,#30316,#30317,#30318,#30319,
#30320,#30321,#30322,#30323,#30324,#30325,#30326,#30327,#30328,#30329,#30330,
#30331,#30332,#30333,#30334,#30335,#30336,#30337,#30338,#30339,#30340,#30341,
#30342,#30343,#30344,#30345,#30346,#30347,#30348,#30349,#30350,#30351,#30352,
#30353,#30354,#30355,#30356,#30357,#30358,#30359,#30360,#30361,#30362,#30363,
#30364,#30365,#30366,#30367,#30368,#30369,#30370,#30371,#30372,#30373,#30374,
#30375,#30376,#30377,#30378,#30379,#30380,#30381,#30382,#30383,#30384,#30385),
 .UNSPECIFIED.,.F.,.F.,(4,3,3,3,3,3,3,3,3,3,3,3,3,3,3,3,3,3,3,3,3,3,3,3,
3,3,3,3,3,3,3,3,3,3,3,3,3,3,3,3,3,3,3,3,3,3,3,3,3,3,3,3,3,3,3,3,3,3,3,3,
4),(102.19402465094,102.293056429024,102.392278375189,102.491303033872,
102.590362152007,102.68928082678,102.78891625198,102.887658253753,102.98636778089,
103.085074619194,103.18539702149,103.284245615113,103.385304921744,103.486364228376,
103.585423359634,103.684342047628,103.783977469535,103.88271948467,103.981429025192,
104.080135876886,104.180458263384,104.27930687027,104.380366146575,104.481425422879,
104.580484508879,104.679403151563,104.779038584791,104.877780554818,104.976490050407,
105.075196857402,105.175519297397,105.274367860614,105.375427238998,105.476486617383,
105.575545749521,105.674464438071,105.774099859798,105.872841874706,105.97155141471,
106.070258265596,106.170580652169,106.269429257555,106.370488534721,106.471547811886,
106.570607021582,106.66952578848,106.769161190719,106.867903285305,106.966612905307,
107.065319836401,107.165642128898,107.264490814177,107.365549910283,107.46660900639,
107.565721146446,107.664694944783,107.763560266908,107.86234948203,107.961092970623,
108.059846334627,108.12371336303),.UNSPECIFIED.);
#395=B_SPLINE_CURVE_WITH_KNOTS('',3,(#30386,#30387,#30388,#30389,#30390,
#30391,#30392,#30393,#30394,#30395,#30396,#30397,#30398),.UNSPECIFIED.,
 .F.,.F.,(4,3,3,3,4),(108.12371336339,108.237935255045,108.353262022111,
108.461670200894,108.477770244024),.UNSPECIFIED.);
#396=B_SPLINE_CURVE_WITH_KNOTS('',3,(#30399,#30400,#30401,#30402,#30403,
#30404,#30405,#30406,#30407,#30408,#30409,#30410,#30411,#30412,#30413,#30414,
#30415,#30416,#30417,#30418,#30419,#30420,#30421,#30422,#30423,#30424,#30425,
#30426,#30427,#30428,#30429,#30430,#30431,#30432,#30433,#30434,#30435,#30436,
#30437,#30438,#30439,#30440,#30441,#30442,#30443,#30444,#30445,#30446,#30447,
#30448,#30449,#30450,#30451,#30452,#30453,#30454,#30455,#30456,#30457,#30458,
#30459,#30460,#30461,#30462,#30463,#30464,#30465,#30466,#30467,#30468,#30469,
#30470,#30471,#30472,#30473,#30474,#30475,#30476,#30477,#30478,#30479,#30480,
#30481,#30482,#30483,#30484,#30485,#30486,#30487,#30488,#30489,#30490,#30491,
#30492,#30493,#30494,#30495,#30496,#30497,#30498,#30499,#30500,#30501,#30502,
#30503,#30504,#30505,#30506,#30507,#30508,#30509,#30510,#30511,#30512,#30513,
#30514,#30515,#30516,#30517,#30518,#30519,#30520,#30521,#30522,#30523,#30524,
#30525,#30526,#30527,#30528,#30529,#30530,#30531,#30532,#30533,#30534,#30535,
#30536,#30537,#30538,#30539,#30540,#30541,#30542,#30543,#30544,#30545,#30546,
#30547,#30548,#30549,#30550,#30551,#30552,#30553,#30554,#30555,#30556,#30557,
#30558,#30559,#30560,#30561,#30562,#30563,#30564,#30565,#30566,#30567,#30568,
#30569,#30570,#30571,#30572,#30573,#30574,#30575,#30576,#30577,#30578,#30579,
#30580,#30581,#30582,#30583,#30584,#30585,#30586,#30587,#30588,#30589,#30590,
#30591,#30592,#30593,#30594,#30595,#30596,#30597,#30598,#30599,#30600,#30601,
#30602,#30603,#30604,#30605,#30606,#30607,#30608,#30609,#30610,#30611,#30612,
#30613,#30614,#30615,#30616,#30617,#30618,#30619,#30620,#30621,#30622,#30623,
#30624),.UNSPECIFIED.,.F.,.F.,(4,2,2,2,2,2,2,2,2,2,2,2,2,2,2,2,2,2,2,2,
2,2,2,2,2,2,2,2,2,2,2,2,2,2,2,2,2,2,2,2,2,2,2,2,2,2,2,2,2,2,2,2,2,2,2,2,
2,2,2,2,2,2,2,2,2,2,2,2,2,2,2,2,2,2,2,2,2,2,2,2,2,2,2,2,2,2,2,2,2,2,2,2,
2,2,2,2,2,2,2,2,2,2,2,2,2,2,2,2,2,2,2,2,4),(-1.67627843319428,-1.66639710885997,
-1.62175007372191,-1.61632633228209,-1.61378191144318,-1.61181909335474,
-1.60952721381829,-1.60546516618932,-1.5870545286888,-1.5488705408948,-1.50004385234283,
-1.49335660614414,-1.48902994844544,-1.4855392313552,-1.48153938705054,
-1.47458173804716,-1.44048275966846,-1.38713403887994,-1.36841168351906,
-1.36432944439178,-1.36203298095122,-1.36007074387167,-1.35753289569351,
-1.35214386950049,-1.30767616711323,-1.25263791439702,-1.24281819148523,
-1.23829164261158,-1.23477085926177,-1.23093219358501,-1.22471505248399,
-1.20204426838429,-1.15686220004863,-1.14448152278534,-1.11781581791389,
-1.11375476189054,-1.11124527065836,-1.10928538903317,-1.10696862856517,
-1.10267684680963,-1.07643690716525,-1.02366380264669,-0.996477277876009,
-0.989746221280685,-0.985757497749172,-0.982299187811502,-0.97797384203867,
-0.969455117625521,-0.95850625782231,-0.932100235446576,-0.895789011145295,
-0.86667208461556,-0.862589377129645,-0.86007352901182,-0.858113299618529,
-0.855801561005835,-0.851532940145751,-0.825961943601439,-0.775419296037052,
-0.745604062262852,-0.738711876987958,-0.73468666865785,-0.731198768333297,
-0.726907565002085,-0.718557857908503,-0.667291122726274,-0.618093004951914,
-0.611981572897479,-0.609504260270671,-0.607499069966088,-0.605396527039538,
-0.602083723675056,-0.591353893081907,-0.57262586593982,-0.51296750366228,
-0.492876941554744,-0.486691526098369,-0.482860144684468,-0.479337865418448,
-0.474720272561702,-0.464669518094046,-0.451119228271358,-0.413742392379747,
-0.367121008886682,-0.360855969057173,-0.358352433549508,-0.356522081176278,
-0.354472859369076,-0.351406222596919,-0.342702196891811,-0.328840114076413,
-0.264182848743525,-0.242089245399464,-0.235689991207248,-0.231812179741444,
-0.228450119783473,-0.228393888750984,-0.228342085052784,-0.228294229412539,
-0.228249910148991,-0.228208771500177,-0.223847818883286,-0.218968131988291,
-0.210884133534484,-0.194071607632333,-0.164215288729475,-0.11576510171549,
-0.109613820321097,-0.107129860694167,-0.105123125874876,-0.103023683126422,
-0.0997239845329725,-0.0900473953080078),.UNSPECIFIED.);
#397=B_SPLINE_CURVE_WITH_KNOTS('',3,(#30630,#30631,#30632,#30633,#30634,
#30635,#30636,#30637,#30638,#30639,#30640,#30641,#30642,#30643,#30644,#30645,
#30646,#30647,#30648,#30649,#30650,#30651,#30652,#30653,#30654,#30655,#30656,
#30657,#30658,#30659,#30660,#30661,#30662,#30663,#30664,#30665,#30666,#30667,
#30668,#30669,#30670,#30671,#30672,#30673,#30674,#30675,#30676,#30677,#30678,
#30679,#30680,#30681,#30682,#30683,#30684,#30685,#30686,#30687,#30688,#30689,
#30690,#30691,#30692,#30693,#30694,#30695,#30696,#30697,#30698,#30699,#30700,
#30701,#30702,#30703,#30704,#30705,#30706,#30707,#30708,#30709,#30710,#30711,
#30712,#30713,#30714,#30715,#30716,#30717,#30718,#30719,#30720,#30721,#30722,
#30723,#30724,#30725,#30726,#30727,#30728,#30729,#30730,#30731,#30732,#30733,
#30734,#30735,#30736,#30737,#30738,#30739,#30740,#30741,#30742,#30743,#30744,
#30745,#30746,#30747,#30748,#30749,#30750,#30751,#30752,#30753,#30754,#30755,
#30756,#30757,#30758,#30759,#30760,#30761,#30762,#30763,#30764,#30765,#30766,
#30767,#30768,#30769,#30770,#30771,#30772,#30773,#30774,#30775,#30776,#30777,
#30778,#30779,#30780,#30781,#30782,#30783,#30784,#30785,#30786,#30787,#30788,
#30789,#30790,#30791,#30792,#30793,#30794,#30795,#30796,#30797,#30798,#30799,
#30800,#30801,#30802,#30803,#30804,#30805,#30806,#30807,#30808,#30809,#30810),
 .UNSPECIFIED.,.F.,.F.,(4,3,3,3,3,3,3,3,3,3,3,3,3,3,3,3,3,3,3,3,3,3,3,3,
3,3,3,3,3,3,3,3,3,3,3,3,3,3,3,3,3,3,3,3,3,3,3,3,3,3,3,3,3,3,3,3,3,3,3,3,
4),(95.9117775219804,96.0099930662897,96.1081979885838,96.2113824581504,
96.309718345621,96.4081216556358,96.5066772687822,96.5209358668503,96.6199949843994,
96.7189136586225,96.8185490839639,96.9172910852772,97.0160006119892,97.1147074499024,
97.2150298527653,97.313878446087,97.4149377537205,97.5159970613539,97.615056179209,
97.7139748537395,97.8136102790043,97.9123522806262,98.0110618076464,98.1097686458675,
98.210091048365,98.3089396419895,98.4099989489235,98.5110582558575,98.6101173729991,
98.7090360468166,98.8086714722597,98.9074134731739,99.0061229994903,99.104829837012,
99.2051522403493,99.3040008332928,99.405060141827,99.5061194503612,99.6051785678429,
99.7040972419944,99.8037326673532,99.902474668585,100.001184195212,100.099891033037,
100.200213435994,100.299062029221,100.400121337043,100.501180644865,100.600239764403,
100.699158440622,100.798793865465,100.897535868779,100.996245397488,101.094952237394,
101.195274637887,101.294123233167,101.395182536267,101.496241839368,101.611067080966,
101.725797568223,101.84052805548),.UNSPECIFIED.);
#398=B_SPLINE_CURVE_WITH_KNOTS('',3,(#30811,#30812,#30813,#30814,#30815,
#30816,#30817,#30818,#30819,#30820,#30821,#30822,#30823),.UNSPECIFIED.,
 .F.,.F.,(4,3,3,3,4),(101.84052805585,101.939398955072,102.038252712645,
102.137156873093,102.19402465094),.UNSPECIFIED.);
#399=B_SPLINE_CURVE_WITH_KNOTS('',3,(#30825,#30826,#30827,#30828,#30829,
#30830,#30831,#30832),.UNSPECIFIED.,.F.,.F.,(4,2,2,4),(-0.0900473953080078,
-0.0891091977982808,-0.0706763169128908,-0.000735701929119057),
 .UNSPECIFIED.);
#400=B_SPLINE_CURVE_WITH_KNOTS('',3,(#30833,#30834,#30835,#30836,#30837,
#30838,#30839,#30840,#30841,#30842,#30843,#30844,#30845,#30846,#30847,#30848,
#30849,#30850,#30851,#30852,#30853,#30854,#30855,#30856,#30857,#30858,#30859,
#30860,#30861,#30862,#30863,#30864,#30865,#30866,#30867,#30868,#30869,#30870,
#30871,#30872,#30873,#30874,#30875,#30876,#30877,#30878,#30879,#30880,#30881,
#30882,#30883,#30884,#30885,#30886,#30887,#30888,#30889,#30890,#30891,#30892,
#30893,#30894,#30895,#30896,#30897,#30898,#30899,#30900,#30901,#30902,#30903,
#30904,#30905,#30906,#30907,#30908,#30909,#30910,#30911,#30912,#30913,#30914,
#30915,#30916,#30917,#30918,#30919,#30920,#30921,#30922,#30923,#30924,#30925,
#30926,#30927,#30928,#30929,#30930,#30931,#30932,#30933,#30934,#30935,#30936,
#30937,#30938,#30939,#30940,#30941,#30942,#30943,#30944,#30945,#30946,#30947,
#30948,#30949,#30950,#30951,#30952,#30953,#30954,#30955,#30956,#30957,#30958,
#30959,#30960,#30961,#30962,#30963,#30964,#30965,#30966,#30967,#30968,#30969,
#30970,#30971,#30972,#30973,#30974,#30975,#30976,#30977,#30978,#30979,#30980,
#30981,#30982,#30983,#30984,#30985,#30986,#30987,#30988,#30989,#30990,#30991,
#30992,#30993,#30994,#30995,#30996,#30997,#30998,#30999,#31000,#31001,#31002,
#31003,#31004,#31005,#31006,#31007,#31008,#31009,#31010,#31011,#31012,#31013,
#31014,#31015,#31016,#31017,#31018,#31019,#31020,#31021,#31022,#31023,#31024,
#31025,#31026,#31027,#31028,#31029,#31030,#31031,#31032,#31033,#31034,#31035,
#31036,#31037,#31038,#31039,#31040,#31041,#31042),.UNSPECIFIED.,.F.,.F.,
(4,2,2,2,2,2,2,2,2,2,2,2,2,2,2,2,2,2,2,2,2,2,2,2,2,2,2,2,2,2,2,2,2,2,2,
2,2,2,2,2,2,2,2,2,2,2,2,2,2,2,2,2,2,2,2,2,2,2,2,2,2,2,2,2,2,2,2,2,2,2,2,
2,2,2,2,2,2,2,2,2,2,2,2,2,2,2,2,2,2,2,2,2,2,2,2,2,2,2,2,2,2,2,2,2,4),(-3.17216731230386,
-3.16150091109955,-3.15706135222654,-3.15363950664677,-3.1502747241594,
-3.14646252263513,-3.14036139560858,-3.12101710243409,-3.05783810323741,
-3.04091305881212,-3.0341636521033,-3.02908772453886,-3.02661108861964,
-3.02484204505949,-3.02257972701094,-3.01864471304799,-3.00215905357304,
-2.99408950606481,-2.953475865593,-2.92627126967372,-2.9151120828329,-2.90902930873973,
-2.90496975873134,-2.90112262783562,-2.89780194758751,-2.89347770156811,
-2.88679502367664,-2.83824735383611,-2.80111658919068,-2.78782751153759,
-2.77938305099513,-2.77635209006198,-2.77431067792622,-2.77247480173877,
-2.76945821243725,-2.76173768551373,-2.7101503769379,-2.66333258814837,
-2.65508823582814,-2.65081934424015,-2.64733392916629,-2.64329404828012,
-2.63633306320586,-2.60522340607424,-2.5553195740956,-2.53860089344422,
-2.53190645453539,-2.52686271279235,-2.52439248683972,-2.52262420595838,
-2.52035757281562,-2.51640335833064,-2.49963996646639,-2.43551997335584,
-2.41807375326111,-2.40590910910997,-2.40093334314769,-2.39735360228157,
-2.39408864104896,-2.38969603515127,-2.38110010028033,-2.32202946415757,
-2.28071453761144,-2.2756957484835,-2.27323053107066,-2.27146285698618,
-2.26919286460552,-2.26522358835,-2.24823657897472,-2.19463172011816,-2.17096427140933,
-2.16077442882095,-2.15272423985745,-2.14849527527369,-2.14535015460792,
-2.14140171060477,-2.13467430370914,-2.10861404513114,-2.0549295124778,
-2.02844890262111,-2.02415126045534,-2.02183401788994,-2.0198753759667,
-2.01736956368279,-2.01331842440849,-1.98685232221298,-1.97235854549532,
-1.93550011379477,-1.90722258753614,-1.90058851049009,-1.89666025441831,
-1.89316225987929,-1.8887332258888,-1.87968128872629,-1.81601967290809,
-1.7789972838733,-1.77367015581183,-1.77114491115142,-1.7691846565658,-1.76688144080074,
-1.76276604492914,-1.74343783266141,-1.73496306212675,-1.68973337728938,
-1.67575143484598),.UNSPECIFIED.);
#401=B_SPLINE_CURVE_WITH_KNOTS('',3,(#31048,#31049,#31050,#31051,#31052,
#31053,#31054,#31055,#31056,#31057,#31058,#31059,#31060,#31061,#31062,#31063,
#31064,#31065,#31066,#31067,#31068,#31069,#31070,#31071,#31072,#31073,#31074,
#31075,#31076,#31077,#31078,#31079,#31080,#31081,#31082,#31083,#31084,#31085,
#31086,#31087,#31088,#31089,#31090,#31091,#31092,#31093,#31094,#31095,#31096,
#31097,#31098,#31099,#31100,#31101,#31102,#31103,#31104,#31105,#31106,#31107,
#31108,#31109,#31110,#31111,#31112,#31113,#31114,#31115,#31116,#31117,#31118,
#31119,#31120,#31121,#31122,#31123,#31124,#31125,#31126,#31127,#31128,#31129,
#31130,#31131,#31132,#31133,#31134,#31135,#31136,#31137,#31138,#31139,#31140,
#31141,#31142,#31143,#31144,#31145,#31146,#31147,#31148,#31149,#31150,#31151,
#31152,#31153,#31154,#31155,#31156,#31157,#31158,#31159,#31160,#31161,#31162,
#31163,#31164,#31165,#31166,#31167,#31168,#31169,#31170,#31171,#31172,#31173,
#31174,#31175,#31176,#31177,#31178,#31179,#31180,#31181,#31182,#31183,#31184,
#31185,#31186,#31187,#31188,#31189,#31190,#31191,#31192,#31193,#31194,#31195,
#31196,#31197,#31198,#31199,#31200,#31201,#31202,#31203,#31204,#31205,#31206,
#31207,#31208,#31209,#31210,#31211,#31212,#31213,#31214,#31215,#31216,#31217,
#31218,#31219,#31220,#31221,#31222,#31223,#31224,#31225,#31226,#31227,#31228,
#31229,#31230,#31231),.UNSPECIFIED.,.F.,.F.,(4,3,3,3,3,3,3,3,3,3,3,3,3,
3,3,3,3,3,3,3,3,3,3,3,3,3,3,3,3,3,3,3,3,3,3,3,3,3,3,3,3,3,3,3,3,3,3,3,3,
3,3,3,3,3,3,3,3,3,3,3,3,4),(89.6284739524251,89.7274264175165,89.8303192028056,
89.9290729357282,90.0277873136882,90.1264921291014,90.2252171561015,90.3240521540832,
90.422952333698,90.5220097719534,90.5505686998287,90.649627817412,90.7485464916702,
90.8481819170029,90.9469239183524,91.045633445101,91.1443402830514,91.2446626858716,
91.3435112792307,91.4445705867815,91.5456298943322,91.6446890119216,91.7436076861859,
91.8432431115171,91.9419851128728,92.0406946396275,92.139401477584,92.239723880397,
92.3385724737621,92.439631781299,92.5406910888359,92.6397502064153,92.7386688806695,
92.8383043060033,92.937046307349,93.0357558340939,93.1344626720407,93.2347850748654,
93.3336336682211,93.4346929757803,93.5357522833395,93.6348114009167,93.7337300751687,
93.833365500503,93.9321075018462,94.0308170285885,94.1295238665326,94.2298462693603,
94.3286948627131,94.4297541702781,94.5308134778431,94.6298725954642,94.7287912697602,
94.8284266950835,94.9271686964708,95.025878223257,95.1245850612449,95.2249074640203,
95.3237560574162,95.4248153648815,95.5258746723467,95.5573427486708),
 .UNSPECIFIED.);
#402=B_SPLINE_CURVE_WITH_KNOTS('',3,(#31232,#31233,#31234,#31235,#31236,
#31237,#31238,#31239,#31240,#31241,#31242,#31243,#31244),.UNSPECIFIED.,
 .F.,.F.,(4,3,3,3,4),(95.5573427489414,95.6558631102801,95.7542623785887,
95.8525566861535,95.9117775219804),.UNSPECIFIED.);
#403=B_SPLINE_CURVE_WITH_KNOTS('',3,(#31245,#31246,#31247,#31248,#31249,
#31250,#31251,#31252,#31253,#31254,#31255,#31256,#31257,#31258,#31259,#31260,
#31261,#31262,#31263,#31264,#31265,#31266,#31267,#31268,#31269,#31270,#31271,
#31272,#31273,#31274,#31275,#31276,#31277,#31278,#31279,#31280,#31281,#31282,
#31283,#31284,#31285,#31286,#31287,#31288,#31289,#31290,#31291,#31292,#31293,
#31294,#31295,#31296,#31297,#31298,#31299,#31300,#31301,#31302,#31303,#31304,
#31305,#31306,#31307,#31308,#31309,#31310,#31311,#31312,#31313,#31314,#31315,
#31316,#31317,#31318,#31319,#31320,#31321,#31322,#31323,#31324,#31325,#31326,
#31327,#31328,#31329,#31330,#31331,#31332,#31333,#31334,#31335,#31336,#31337,
#31338,#31339,#31340,#31341,#31342,#31343,#31344,#31345,#31346,#31347,#31348,
#31349,#31350,#31351,#31352,#31353,#31354,#31355,#31356,#31357,#31358,#31359,
#31360,#31361,#31362,#31363,#31364,#31365,#31366,#31367,#31368,#31369,#31370,
#31371,#31372,#31373,#31374,#31375,#31376,#31377,#31378,#31379,#31380,#31381,
#31382,#31383,#31384,#31385,#31386,#31387,#31388,#31389,#31390,#31391,#31392,
#31393,#31394,#31395,#31396,#31397,#31398,#31399,#31400,#31401,#31402,#31403,
#31404,#31405,#31406,#31407,#31408,#31409,#31410,#31411,#31412,#31413,#31414,
#31415,#31416,#31417,#31418,#31419,#31420,#31421,#31422,#31423,#31424,#31425,
#31426,#31427,#31428,#31429,#31430,#31431,#31432,#31433,#31434,#31435,#31436,
#31437,#31438,#31439,#31440,#31441,#31442,#31443,#31444,#31445,#31446,#31447,
#31448,#31449,#31450,#31451,#31452,#31453,#31454,#31455,#31456,#31457,#31458,
#31459,#31460,#31461,#31462,#31463,#31464,#31465,#31466,#31467,#31468),
 .UNSPECIFIED.,.F.,.F.,(4,2,2,2,2,2,2,2,2,2,2,2,2,2,2,2,2,2,2,2,2,2,2,2,
2,2,2,2,2,2,2,2,2,2,2,2,2,2,2,2,2,2,2,2,2,2,2,2,2,2,2,2,2,2,2,2,2,2,2,2,
2,2,2,2,2,2,2,2,2,2,2,2,2,2,2,2,2,2,2,2,2,2,2,2,2,2,2,2,2,2,2,2,2,2,2,2,
2,2,2,2,2,2,2,2,2,2,2,2,2,2,2,4),(-1.67575143484598,-1.65659760087301,-1.64968873704058,
-1.64570073195418,-1.64221080669793,-1.63787271447791,-1.63114388060775,
-1.58622326395788,-1.54071426114126,-1.52550359318917,-1.5216265495086,
-1.51940001325016,-1.51742632422234,-1.51477769681934,-1.50878127891758,
-1.48173292771081,-1.47983099492858,-1.46488570894065,-1.41028476343868,
-1.400576122209,-1.39600327537135,-1.3924770473776,-1.38866286298393,-1.38255261067803,
-1.3610563928036,-1.29043405636996,-1.27444728676971,-1.27054837538144,
-1.26829424495471,-1.2665237858399,-1.26403497073859,-1.25889721131732,
-1.25204112447926,-1.23471087891285,-1.18408446699519,-1.15440822229045,
-1.14752545855638,-1.14350309474887,-1.14001606076846,-1.1357238828875,
-1.12736564754565,-1.11667832001598,-1.09123282933259,-1.03282421715994,
-1.02230211225346,-1.01889285046758,-1.01676943157181,-1.01475474381244,
-1.01185869077247,-1.00435281590645,-0.993047045034347,-0.921226724243941,
-0.901629043921063,-0.895498994096946,-0.891680537389021,-0.88815580386089,
-0.883513966692085,-0.873323885144974,-0.85952679965963,-0.820934356568901,
-0.77612425276344,-0.769792771707386,-0.767278517724604,-0.765445912756933,
-0.763400964174954,-0.760352419423677,-0.751777995489701,-0.738201410154419,
-0.708411151081063,-0.656992866968003,-0.647044412847752,-0.642495912023615,
-0.638973390578904,-0.635148189088157,-0.628987059927146,-0.606928996177307,
-0.564005236263803,-0.525209872388838,-0.518760239326155,-0.516226278789947,
-0.514388705649824,-0.51234955444375,-0.509328995058965,-0.500959168860953,
-0.487830863114414,-0.450355188759478,-0.401848694733782,-0.395166042683844,
-0.390842015027932,-0.387353197742139,-0.383355286908634,-0.376400370451799,
-0.342298167552213,-0.28878119060417,-0.270267835775364,-0.266199440051551,
-0.263906847897739,-0.261983190249551,-0.259522377970279,-0.25678391564395,
-0.252219111522213,-0.242660989339562,-0.213242927003015,-0.154177680014348,
-0.145576792461579,-0.14118282947613,-0.137917405760792,-0.134337693350936,
-0.129362939181372,-0.117205649688445,-0.0997761726508418,-0.0900570484866832),
 .UNSPECIFIED.);
#404=B_SPLINE_CURVE_WITH_KNOTS('',3,(#31474,#31475,#31476,#31477,#31478,
#31479,#31480,#31481,#31482,#31483,#31484,#31485,#31486,#31487,#31488,#31489,
#31490,#31491,#31492,#31493,#31494,#31495,#31496,#31497,#31498,#31499,#31500,
#31501,#31502,#31503,#31504,#31505,#31506,#31507,#31508,#31509,#31510,#31511,
#31512,#31513,#31514,#31515,#31516,#31517,#31518,#31519,#31520,#31521,#31522,
#31523,#31524,#31525,#31526,#31527,#31528,#31529,#31530,#31531,#31532,#31533,
#31534,#31535,#31536,#31537,#31538,#31539,#31540,#31541,#31542,#31543,#31544,
#31545,#31546,#31547,#31548,#31549,#31550,#31551,#31552,#31553,#31554,#31555,
#31556,#31557,#31558,#31559,#31560,#31561,#31562,#31563,#31564,#31565,#31566,
#31567,#31568,#31569,#31570,#31571,#31572,#31573,#31574,#31575,#31576,#31577,
#31578,#31579,#31580,#31581,#31582,#31583,#31584,#31585,#31586,#31587,#31588,
#31589,#31590,#31591,#31592,#31593,#31594,#31595,#31596,#31597,#31598,#31599,
#31600,#31601,#31602,#31603,#31604,#31605,#31606,#31607,#31608,#31609,#31610,
#31611,#31612,#31613,#31614,#31615,#31616,#31617,#31618,#31619,#31620,#31621,
#31622,#31623,#31624,#31625,#31626,#31627,#31628,#31629,#31630,#31631,#31632,
#31633,#31634,#31635,#31636,#31637,#31638,#31639,#31640,#31641,#31642,#31643,
#31644,#31645,#31646,#31647,#31648,#31649,#31650,#31651,#31652,#31653,#31654,
#31655,#31656,#31657),.UNSPECIFIED.,.F.,.F.,(4,3,3,3,3,3,3,3,3,3,3,3,3,
3,3,3,3,3,3,3,3,3,3,3,3,3,3,3,3,3,3,3,3,3,3,3,3,3,3,3,3,3,3,3,3,3,3,3,3,
3,3,3,3,3,3,3,3,3,3,3,3,4),(83.3443274880435,83.4447291342008,83.5453184679384,
83.5851403383034,83.6841994558881,83.7831181301476,83.88275355548,83.9814955568309,
84.0802050835808,84.1789119215326,84.2792343243512,84.3780829177117,84.4791422252593,
84.580201532807,84.6792606503917,84.7781793246512,84.8778147499837,84.9765567513346,
85.0752662780845,85.1739731160364,85.2742955188549,85.3731441122155,85.474203419763,
85.5752627273106,85.6743218448953,85.7732405191548,85.8728759444872,85.9716179458382,
86.0703274725881,86.1690343105399,86.2693567133585,86.3682053067192,86.4692646142667,
86.5703239218142,86.6693830393988,86.7683017136584,86.8679371389908,86.9666791403416,
87.0653886670914,87.1640955050431,87.2644179078617,87.3632665012221,87.4643258087699,
87.5653851163178,87.6644442339022,87.7633629081615,87.862998333494,87.9617403348446,
88.0604498615943,88.1591566995457,88.2594791023646,88.3583276957249,88.4593870032732,
88.5604463108214,88.6586782050377,88.7567801508771,88.8547831364347,88.952718035666,
89.0506354266354,89.1485438993612,89.2465050935532,89.2741574414912),
 .UNSPECIFIED.);
#405=B_SPLINE_CURVE_WITH_KNOTS('',3,(#31658,#31659,#31660,#31661,#31662,
#31663,#31664,#31665,#31666,#31667,#31668,#31669,#31670),.UNSPECIFIED.,
 .F.,.F.,(4,3,3,3,4),(89.2741574417072,89.3952590898502,89.5183032212342,
89.555507505325,89.6284739524251),.UNSPECIFIED.);
#406=B_SPLINE_CURVE_WITH_KNOTS('',3,(#31672,#31673,#31674,#31675,#31676,
#31677,#31678,#31679,#31680,#31681,#31682,#31683,#31684,#31685,#31686,#31687,
#31688,#31689),.UNSPECIFIED.,.F.,.F.,(4,2,2,2,2,2,2,2,4),(-0.0900570484866832,
-0.0300743745962655,-0.0180942513927445,-0.0145216738161618,-0.0123622070809486,
-0.0104875353781127,-0.0085158896592708,-0.00500391853466027,-0.00073464173219576),
 .UNSPECIFIED.);
#407=B_SPLINE_CURVE_WITH_KNOTS('',3,(#31690,#31691,#31692,#31693,#31694,
#31695,#31696,#31697,#31698,#31699,#31700,#31701,#31702,#31703,#31704,#31705,
#31706,#31707,#31708,#31709,#31710,#31711,#31712,#31713,#31714,#31715,#31716,
#31717,#31718,#31719,#31720,#31721,#31722,#31723,#31724,#31725,#31726,#31727,
#31728,#31729,#31730,#31731,#31732,#31733,#31734,#31735,#31736,#31737,#31738,
#31739,#31740,#31741,#31742,#31743,#31744,#31745,#31746,#31747,#31748,#31749,
#31750,#31751,#31752,#31753,#31754,#31755,#31756,#31757,#31758,#31759,#31760,
#31761,#31762,#31763,#31764,#31765,#31766,#31767,#31768,#31769,#31770,#31771,
#31772,#31773,#31774,#31775,#31776,#31777,#31778,#31779,#31780,#31781,#31782,
#31783,#31784,#31785,#31786,#31787,#31788,#31789,#31790,#31791,#31792,#31793,
#31794,#31795,#31796,#31797,#31798,#31799,#31800,#31801,#31802,#31803,#31804,
#31805,#31806,#31807,#31808,#31809,#31810,#31811,#31812,#31813,#31814,#31815,
#31816,#31817,#31818,#31819,#31820,#31821,#31822,#31823,#31824,#31825,#31826,
#31827,#31828,#31829,#31830,#31831,#31832,#31833,#31834,#31835,#31836,#31837,
#31838,#31839,#31840,#31841,#31842,#31843,#31844,#31845,#31846,#31847,#31848,
#31849,#31850,#31851,#31852,#31853,#31854,#31855,#31856,#31857,#31858,#31859,
#31860,#31861,#31862,#31863,#31864,#31865,#31866,#31867,#31868,#31869,#31870,
#31871,#31872,#31873,#31874,#31875,#31876,#31877,#31878,#31879,#31880,#31881,
#31882,#31883,#31884,#31885,#31886,#31887,#31888,#31889,#31890,#31891,#31892,
#31893,#31894,#31895,#31896,#31897,#31898,#31899,#31900,#31901,#31902,#31903,
#31904,#31905,#31906,#31907,#31908,#31909),.UNSPECIFIED.,.F.,.F.,(4,2,2,
2,2,2,2,2,2,2,2,2,2,2,2,2,2,2,2,2,2,2,2,2,2,2,2,2,2,2,2,2,2,2,2,2,2,2,2,
2,2,2,2,2,2,2,2,2,2,2,2,2,2,2,2,2,2,2,2,2,2,2,2,2,2,2,2,2,2,2,2,2,2,2,2,
2,2,2,2,2,2,2,2,2,2,2,2,2,2,2,2,2,2,2,2,2,2,2,2,2,2,2,2,2,2,2,2,2,2,4),
(-3.17296637197709,-3.13078746919988,-3.0925286644018,-3.0695906434777,
-3.06335111484647,-3.0595079607854,-3.05598922374801,-3.05147385451278,
-3.0417129483066,-2.98561694806597,-2.95420895217546,-2.94428148541909,
-2.93959386722636,-2.93680582930531,-2.93435532750786,-2.93434349414453,
-2.93433151630648,-2.93431938943293,-2.93430710881415,-2.93429466956216,
-2.93428206659688,-2.9342692946296,-2.93425634818182,-2.93424322154498,
-2.93422990875741,-2.93421640363605,-2.93420269972696,-2.93418879031003,
-2.93228208241657,-2.92997144626731,-2.92582524274472,-2.90605137058816,
-2.85385911403481,-2.81974157680881,-2.81278384511443,-2.80878448979208,
-2.80529451940085,-2.80096920112055,-2.79428488068219,-2.74575956037338,
-2.70825470123193,-2.6951685751157,-2.68681667134174,-2.68379799411075,
-2.68175875606987,-2.67992004905516,-2.67738315897735,-2.67091881198376,
-2.6322882637127,-2.59602562765379,-2.56796164317022,-2.56133965675876,
-2.55741315550891,-2.55391338865715,-2.54947758509592,-2.54039555090182,
-2.47692937905085,-2.43981823134715,-2.43442438368728,-2.43188589670098,
-2.42992391273856,-2.42762864129485,-2.42355053547913,-2.40489238177681,
-2.35145350166597,-2.31734295794089,-2.31038555351585,-2.30638626893895,
-2.30289629153778,-2.29857087551525,-2.29188623289546,-2.24325844439625,
-2.20598393968121,-2.19281836607498,-2.18442992384185,-2.18140619833199,
-2.17936592317891,-2.17752814189548,-2.17499489180802,-2.16855252078573,
-2.12928902664488,-2.07311645703369,-2.06174160674081,-2.05689341140303,
-2.05333524928393,-2.04959430980873,-2.04382580005754,-2.02725785281374,
-1.97075000790547,-1.93599678355961,-1.93149930624142,-1.92913949463042,
-1.9271829674771,-1.92472774704299,-1.92084669559392,-1.89904951802421,
-1.85287952211509,-1.82784062804831,-1.81726477658645,-1.80897527249778,
-1.80469648362572,-1.80120960724638,-1.79717544842081,-1.79024279660622,
-1.75968796282355,-1.70942068280025,-1.68441845478752,-1.68017082479052,
-1.67786370871181,-1.67616180579166),.UNSPECIFIED.);
#408=B_SPLINE_CURVE_WITH_KNOTS('',3,(#31915,#31916,#31917,#31918,#31919,
#31920,#31921,#31922,#31923,#31924,#31925,#31926,#31927,#31928,#31929,#31930,
#31931,#31932,#31933,#31934,#31935,#31936,#31937,#31938,#31939,#31940,#31941,
#31942,#31943,#31944,#31945,#31946,#31947,#31948,#31949,#31950,#31951,#31952,
#31953,#31954,#31955,#31956,#31957,#31958,#31959,#31960,#31961,#31962,#31963,
#31964,#31965,#31966,#31967,#31968,#31969,#31970,#31971,#31972,#31973,#31974,
#31975,#31976,#31977,#31978,#31979,#31980,#31981,#31982,#31983,#31984,#31985,
#31986,#31987,#31988,#31989,#31990,#31991,#31992,#31993,#31994,#31995,#31996,
#31997,#31998,#31999,#32000,#32001,#32002,#32003,#32004,#32005,#32006,#32007,
#32008,#32009,#32010,#32011,#32012,#32013,#32014,#32015,#32016,#32017,#32018,
#32019,#32020,#32021,#32022,#32023,#32024,#32025,#32026,#32027,#32028,#32029,
#32030,#32031,#32032,#32033,#32034,#32035,#32036,#32037,#32038,#32039,#32040,
#32041,#32042,#32043,#32044,#32045,#32046,#32047,#32048,#32049,#32050,#32051,
#32052,#32053,#32054,#32055,#32056,#32057,#32058,#32059,#32060,#32061,#32062,
#32063,#32064,#32065,#32066,#32067,#32068,#32069,#32070,#32071,#32072,#32073,
#32074,#32075,#32076,#32077,#32078,#32079,#32080,#32081,#32082,#32083,#32084,
#32085,#32086,#32087,#32088,#32089,#32090,#32091,#32092,#32093,#32094,#32095),
 .UNSPECIFIED.,.F.,.F.,(4,3,3,3,3,3,3,3,3,3,3,3,3,3,3,3,3,3,3,3,3,3,3,3,
3,3,3,3,3,3,3,3,3,3,3,3,3,3,3,3,3,3,3,3,3,3,3,3,3,3,3,3,3,3,3,3,3,3,3,3,
4),(77.0622185302826,77.159800081767,77.2573831119389,77.3550617349471,
77.4527912027954,77.5506849731481,77.6147731712817,77.7138322888664,77.8127509631257,
77.9123863884582,78.0111283898091,78.109837916559,78.2085447545109,78.3088671573295,
78.4077157506899,78.5087750582376,78.6098343657853,78.7088934833699,78.8078121576293,
78.9074475829618,79.0061895843126,79.1048991110625,79.2036059490143,79.3039283518329,
79.4027769451934,79.5038362527411,79.6048955602889,79.7039546778735,79.8028733521328,
79.9025087774653,80.0012507788162,80.0999603055662,80.1986671435177,80.2989895463364,
80.3978381396968,80.4988974472446,80.5999567547925,80.6990158723772,80.7979345466366,
80.8975699719691,80.9963119733199,81.0950215000699,81.1937283380219,81.2940507408404,
81.3928993342009,81.4939586417485,81.5950179492961,81.6940770668809,81.79299574114,
81.8926311664725,81.9913731678234,82.0900826945733,82.1887895325252,82.2891119353438,
82.3879605287044,82.4890198362521,82.5900791437998,82.6998271120124,82.8092455102998,
82.9180995588121,82.990972133972),.UNSPECIFIED.);
#409=B_SPLINE_CURVE_WITH_KNOTS('',3,(#32096,#32097,#32098,#32099,#32100,
#32101,#32102,#32103,#32104,#32105,#32106,#32107,#32108),.UNSPECIFIED.,
 .F.,.F.,(4,3,3,3,4),(82.9909721343116,83.0910899849471,83.1912299180565,
83.2914717478673,83.3443274880435),.UNSPECIFIED.);
#410=B_SPLINE_CURVE_WITH_KNOTS('',3,(#32109,#32110,#32111,#32112,#32113,
#32114,#32115,#32116,#32117,#32118,#32119,#32120,#32121,#32122,#32123,#32124,
#32125,#32126,#32127,#32128,#32129,#32130,#32131,#32132,#32133,#32134,#32135,
#32136,#32137,#32138,#32139,#32140,#32141,#32142,#32143,#32144,#32145,#32146,
#32147,#32148,#32149,#32150,#32151,#32152,#32153,#32154,#32155,#32156,#32157,
#32158,#32159,#32160,#32161,#32162,#32163,#32164,#32165,#32166,#32167,#32168,
#32169,#32170,#32171,#32172,#32173,#32174,#32175,#32176,#32177,#32178,#32179,
#32180,#32181,#32182,#32183,#32184,#32185,#32186,#32187,#32188,#32189,#32190,
#32191,#32192,#32193,#32194,#32195,#32196,#32197,#32198,#32199,#32200,#32201,
#32202,#32203,#32204,#32205,#32206,#32207,#32208,#32209,#32210,#32211,#32212,
#32213,#32214,#32215,#32216,#32217,#32218,#32219,#32220,#32221,#32222,#32223,
#32224,#32225,#32226,#32227,#32228,#32229,#32230,#32231,#32232,#32233,#32234,
#32235,#32236,#32237,#32238,#32239,#32240,#32241,#32242,#32243,#32244,#32245,
#32246,#32247,#32248,#32249,#32250,#32251,#32252,#32253,#32254,#32255,#32256,
#32257,#32258,#32259,#32260,#32261,#32262,#32263,#32264,#32265,#32266,#32267,
#32268,#32269,#32270,#32271,#32272,#32273,#32274,#32275,#32276,#32277,#32278,
#32279,#32280,#32281,#32282,#32283,#32284,#32285,#32286,#32287,#32288,#32289,
#32290,#32291,#32292,#32293,#32294,#32295,#32296,#32297,#32298,#32299,#32300,
#32301,#32302,#32303,#32304,#32305,#32306,#32307,#32308,#32309,#32310,#32311,
#32312,#32313,#32314,#32315,#32316,#32317,#32318,#32319,#32320,#32321,#32322,
#32323,#32324,#32325,#32326,#32327,#32328,#32329,#32330,#32331,#32332,#32333,
#32334,#32335,#32336,#32337,#32338,#32339,#32340,#32341,#32342),
 .UNSPECIFIED.,.F.,.F.,(4,2,2,2,2,2,2,2,2,2,2,2,2,2,2,2,2,2,2,2,2,2,2,2,
2,2,2,2,2,2,2,2,2,2,2,2,2,2,2,2,2,2,2,2,2,2,2,2,2,2,2,2,2,2,2,2,2,2,2,2,
2,2,2,2,2,2,2,2,2,2,2,2,2,2,2,2,2,2,2,2,2,2,2,2,2,2,2,2,2,2,2,2,2,2,2,2,
2,2,2,2,2,2,2,2,2,2,2,2,2,2,2,2,2,2,2,2,4),(-1.67616180579166,-1.67590324059147,
-1.67338170220638,-1.66927931773268,-1.63900712545492,-1.58695747241575,
-1.5630710905474,-1.55650970438415,-1.55259648265019,-1.54909445605647,
-1.54463652286485,-1.5354391752262,-1.50000443508411,-1.4450906792585,-1.43219539103183,
-1.42852504090574,-1.42634360912866,-1.42435545860539,-1.42161169852704,
-1.41506611382747,-1.40565769974616,-1.37702624774906,-1.31670134210244,
-1.30726514297897,-1.30276169796662,-1.29925447831602,-1.29536676792491,
-1.28892233960465,-1.26340720815674,-1.20490588541381,-1.18218710761623,
-1.17826903002877,-1.17580260541207,-1.17384558215083,-1.17149529857281,
-1.16704348282125,-1.1347874113362,-1.08477727224885,-1.06070206024459,
-1.05412593336901,-1.05020949460017,-1.0467080581074,-1.04225562170707,
-1.03308691244677,-0.997876251810065,-0.942777711211275,-0.929810669456865,
-0.926133595562848,-0.923950674736683,-0.921963058706431,-0.919222669962956,
-0.912697241400724,-0.880402724237487,-0.82225357056646,-0.807401858428773,
-0.801866291913438,-0.798543681397679,-0.795003477859689,-0.790264614188273,
-0.779531050021669,-0.764763543817644,-0.721045767084842,-0.706929024066574,
-0.680115484606524,-0.676048880761138,-0.673538033476851,-0.671578459373667,
-0.669263673327676,-0.664979672206178,-0.638947608603592,-0.586888922367753,
-0.558886681525968,-0.552107329240199,-0.548108164150461,-0.544618561544081,
-0.540293960443175,-0.531775997788042,-0.520827702395861,-0.494420521592979,
-0.457967415154464,-0.429013006457582,-0.424933936310385,-0.422419463944681,
-0.420459738043952,-0.418147924234948,-0.413877461091165,-0.388232119442468,
-0.337345190076549,-0.307934774758003,-0.301067016493568,-0.297047910273152,
-0.293560378716109,-0.293517093482187,-0.293476237509801,-0.293437665027781,
-0.29340123983713,-0.293366834616729,-0.293334330293681,-0.29330361545272,
-0.293274585787413,-0.293247143603894,-0.29322119736386,-0.29319666124197,
-0.288971835318852,-0.280285996621542,-0.26895192213428,-0.241080750136327,
-0.206362284970749,-0.177891574683012,-0.173820872606083,-0.171308973212394,
-0.169349551514988,-0.167036092461159,-0.162757477725552,-0.136870408833084,
-0.0972604102131988,-0.0902219335216519),.UNSPECIFIED.);
#411=B_SPLINE_CURVE_WITH_KNOTS('',3,(#32348,#32349,#32350,#32351,#32352,
#32353,#32354,#32355,#32356,#32357,#32358,#32359,#32360,#32361,#32362,#32363,
#32364,#32365,#32366,#32367,#32368,#32369,#32370,#32371,#32372,#32373,#32374,
#32375,#32376,#32377,#32378,#32379,#32380,#32381,#32382,#32383,#32384,#32385,
#32386,#32387,#32388,#32389,#32390,#32391,#32392,#32393,#32394,#32395,#32396,
#32397,#32398,#32399,#32400,#32401,#32402,#32403,#32404,#32405,#32406,#32407,
#32408,#32409,#32410,#32411,#32412,#32413,#32414,#32415,#32416,#32417,#32418,
#32419,#32420,#32421,#32422,#32423,#32424,#32425,#32426,#32427,#32428,#32429,
#32430,#32431,#32432,#32433,#32434,#32435,#32436,#32437,#32438,#32439,#32440,
#32441,#32442,#32443,#32444,#32445,#32446,#32447,#32448,#32449,#32450,#32451,
#32452,#32453,#32454,#32455,#32456,#32457,#32458,#32459,#32460,#32461,#32462,
#32463,#32464,#32465,#32466,#32467,#32468,#32469,#32470,#32471,#32472,#32473,
#32474,#32475,#32476,#32477,#32478,#32479,#32480,#32481,#32482,#32483,#32484,
#32485,#32486,#32487,#32488,#32489,#32490,#32491,#32492,#32493,#32494,#32495,
#32496,#32497,#32498,#32499,#32500,#32501,#32502,#32503,#32504,#32505,#32506,
#32507,#32508,#32509,#32510,#32511,#32512,#32513,#32514,#32515,#32516,#32517,
#32518,#32519,#32520,#32521,#32522,#32523,#32524,#32525,#32526,#32527,#32528),
 .UNSPECIFIED.,.F.,.F.,(4,3,3,3,3,3,3,3,3,3,3,3,3,3,3,3,3,3,3,3,3,3,3,3,
3,3,3,3,3,3,3,3,3,3,3,3,3,3,3,3,3,3,3,3,3,3,3,3,3,3,3,3,3,3,3,3,3,3,3,3,
4),(70.779075450487,70.8779573340721,70.976739703664,71.0754687734666,71.174174353704,
71.2728862237033,71.3716999427462,71.4705663306546,71.5696036128791,71.64440600426,
71.7434651218446,71.842383796104,71.9420192214365,72.0407612227874,72.1394707495373,
72.238177587489,72.3384999903077,72.4373485836681,72.5384078912159,72.6394671987636,
72.7385263163483,72.8374449906077,72.9370804159402,73.035822417291,73.134531944041,
73.2332387819928,73.3335611848114,73.4324097781719,73.5334690857196,73.6345283932673,
73.7335875108519,73.8325061851114,73.9321416104438,74.0308836117947,74.1295931385446,
74.2282999764964,74.328622379315,74.4274709726755,74.5285302802232,74.6295895877709,
74.7286487053555,74.827567379615,74.9272028049474,75.0259448062983,75.1246543330482,
75.223361171,75.3236835738186,75.4225321671791,75.5235914747268,75.6246507822745,
75.7237098998592,75.8226285741186,75.9222639994511,76.0210060008019,76.1197155275519,
76.2184223655036,76.3187447683222,76.4175933616827,76.5186526692304,76.6197119767781,
76.707786827132),.UNSPECIFIED.);
#412=B_SPLINE_CURVE_WITH_KNOTS('',3,(#32529,#32530,#32531,#32532,#32533,
#32534,#32535,#32536,#32537,#32538,#32539,#32540,#32541),.UNSPECIFIED.,
 .F.,.F.,(4,3,3,3,4),(76.7077868273942,76.8056326709673,76.9033659624181,
77.0010095032294,77.0622185302826),.UNSPECIFIED.);
#413=B_SPLINE_CURVE_WITH_KNOTS('',3,(#32543,#32544,#32545,#32546,#32547,
#32548,#32549,#32550,#32551,#32552,#32553,#32554,#32555,#32556,#32557,#32558,
#32559,#32560,#32561,#32562),.UNSPECIFIED.,.F.,.F.,(4,2,2,2,2,2,2,2,2,4),
(-0.0902219335216519,-0.0726583194898945,-0.0548807383335625,-0.0489604234752576,
-0.0451871616823215,-0.0416448559837934,-0.0381656831375037,-0.0335591450836605,
-0.0219875622138333,-0.000734571677354467),.UNSPECIFIED.);
#414=B_SPLINE_CURVE_WITH_KNOTS('',3,(#32563,#32564,#32565,#32566,#32567,
#32568,#32569,#32570,#32571,#32572,#32573,#32574,#32575,#32576,#32577,#32578,
#32579,#32580,#32581,#32582,#32583,#32584,#32585,#32586,#32587,#32588,#32589,
#32590,#32591,#32592,#32593,#32594,#32595,#32596,#32597,#32598,#32599,#32600,
#32601,#32602,#32603,#32604,#32605,#32606,#32607,#32608,#32609,#32610,#32611,
#32612,#32613,#32614,#32615,#32616,#32617,#32618,#32619,#32620,#32621,#32622,
#32623,#32624,#32625,#32626,#32627,#32628,#32629,#32630,#32631,#32632,#32633,
#32634,#32635,#32636,#32637,#32638,#32639,#32640,#32641,#32642,#32643,#32644,
#32645,#32646,#32647,#32648,#32649,#32650,#32651,#32652,#32653,#32654,#32655,
#32656,#32657,#32658,#32659,#32660,#32661,#32662,#32663,#32664,#32665,#32666,
#32667,#32668,#32669,#32670,#32671,#32672,#32673,#32674,#32675,#32676,#32677,
#32678,#32679,#32680,#32681,#32682,#32683,#32684,#32685,#32686,#32687,#32688,
#32689,#32690,#32691,#32692,#32693,#32694,#32695,#32696,#32697,#32698,#32699,
#32700,#32701,#32702,#32703,#32704,#32705,#32706,#32707,#32708,#32709,#32710,
#32711,#32712,#32713,#32714,#32715,#32716,#32717,#32718,#32719,#32720,#32721,
#32722,#32723,#32724,#32725,#32726,#32727,#32728,#32729,#32730,#32731,#32732,
#32733,#32734,#32735,#32736,#32737,#32738,#32739,#32740,#32741,#32742,#32743,
#32744,#32745,#32746,#32747,#32748,#32749,#32750,#32751,#32752,#32753,#32754,
#32755,#32756,#32757,#32758,#32759,#32760,#32761,#32762,#32763,#32764,#32765,
#32766,#32767,#32768,#32769,#32770),.UNSPECIFIED.,.F.,.F.,(4,2,2,2,2,2,
2,2,2,2,2,2,2,2,2,2,2,2,2,2,2,2,2,2,2,2,2,2,2,2,2,2,2,2,2,2,2,2,2,2,2,2,
2,2,2,2,2,2,2,2,2,2,2,2,2,2,2,2,2,2,2,2,2,2,2,2,2,2,2,2,2,2,2,2,2,2,2,2,
2,2,2,2,2,2,2,2,2,2,2,2,2,2,2,2,2,2,2,2,2,2,2,2,2,4),(-3.17255687017752,
-3.12637703617202,-3.10731238378642,-3.09645286141489,-3.09312618082806,
-3.09102078364667,-3.08901797848521,-3.08654893600502,-3.08048399926583,
-3.03015395700328,-2.99518292861147,-2.98214811192475,-2.9724776644585,
-2.9680745089668,-2.9647436284611,-2.96100286704291,-2.95523478465193,-2.93866917271469,
-2.87509434693847,-2.85609132604166,-2.84880636641023,-2.84342110699485,
-2.84088437453105,-2.83892268500488,-2.8366265188053,-2.83254396436203,
-2.8138052891689,-2.77081297205662,-2.73093660955173,-2.72119675699531,
-2.71663647969869,-2.71312220255679,-2.70926402702509,-2.7029547969899,
-2.68173202399022,-2.62335191115039,-2.59593027505255,-2.59160157084977,
-2.58927722486086,-2.58731842144972,-2.58481987107659,-2.5807946572808,
-2.55503861369596,-2.54153489467532,-2.49643847865547,-2.4737917097306,
-2.46757733058487,-2.46373972940524,-2.46021950234468,-2.45569308688616,
-2.44587120514403,-2.39099050241885,-2.34647231815942,-2.34106477153636,
-2.33852372765471,-2.33656156666864,-2.33426818511227,-2.33019826053288,
-2.31164778324914,-2.30244987001193,-2.29051103749268,-2.26115855679399,
-2.23661142484505,-2.22617192208892,-2.21796631126521,-2.2137043849023,
-2.21055472614897,-2.20662640323419,-2.19999664637356,-2.17520900703381,
-2.12033477075688,-2.10217056605457,-2.09509763809575,-2.08983378484832,
-2.08732012688649,-2.08536012178259,-2.08304690234235,-2.07888935945493,
-2.05881144511315,-1.99213472436227,-1.97817395567435,-1.9678916226495,
-1.96323242059507,-1.95970436939832,-1.95635822076576,-1.95069862832457,
-1.93496910985383,-1.87042844786639,-1.85135140988253,-1.84404783533786,
-1.83865190141036,-1.8361130709971,-1.83415111741865,-1.83185622657302,
-1.82777959190046,-1.80914482675449,-1.75568531757039,-1.72157350370027,
-1.71461622657685,-1.71061705644185,-1.70712720307786,-1.70280197209477,
-1.6961176756079,-1.67598768218192),.UNSPECIFIED.);
#415=B_SPLINE_CURVE_WITH_KNOTS('',3,(#32776,#32777,#32778,#32779,#32780,
#32781,#32782,#32783,#32784,#32785,#32786,#32787,#32788,#32789,#32790,#32791,
#32792,#32793,#32794,#32795,#32796,#32797,#32798,#32799,#32800,#32801,#32802,
#32803,#32804,#32805,#32806,#32807,#32808,#32809,#32810,#32811,#32812,#32813,
#32814,#32815,#32816,#32817,#32818,#32819,#32820,#32821,#32822,#32823,#32824,
#32825,#32826,#32827,#32828,#32829,#32830,#32831,#32832,#32833,#32834,#32835,
#32836,#32837,#32838,#32839,#32840,#32841,#32842,#32843,#32844,#32845,#32846,
#32847,#32848,#32849,#32850,#32851,#32852,#32853,#32854,#32855,#32856,#32857,
#32858,#32859,#32860,#32861,#32862,#32863,#32864,#32865,#32866,#32867,#32868,
#32869,#32870,#32871,#32872,#32873,#32874,#32875,#32876,#32877,#32878,#32879,
#32880,#32881,#32882,#32883,#32884,#32885,#32886,#32887,#32888,#32889,#32890,
#32891,#32892,#32893,#32894,#32895,#32896,#32897,#32898,#32899,#32900,#32901,
#32902,#32903,#32904,#32905,#32906,#32907,#32908,#32909,#32910,#32911,#32912,
#32913,#32914,#32915,#32916,#32917,#32918,#32919,#32920,#32921,#32922,#32923,
#32924,#32925,#32926,#32927,#32928,#32929,#32930,#32931,#32932,#32933,#32934,
#32935,#32936,#32937,#32938,#32939,#32940,#32941,#32942,#32943,#32944,#32945,
#32946,#32947,#32948,#32949,#32950,#32951,#32952,#32953,#32954,#32955,#32956),
 .UNSPECIFIED.,.F.,.F.,(4,3,3,3,3,3,3,3,3,3,3,3,3,3,3,3,3,3,3,3,3,3,3,3,
3,3,3,3,3,3,3,3,3,3,3,3,3,3,3,3,3,3,3,3,3,3,3,3,3,3,3,3,3,3,3,3,3,3,3,3,
4),(64.4947309352028,64.5971327257698,64.6789776427347,64.7780367603194,
64.8769554345788,64.9765908599112,65.0753328612621,65.1740423880121,65.2727492259639,
65.3730716287825,65.4719202221431,65.5729795296907,65.6740388372384,65.7730979548231,
65.8720166290824,65.9716520544149,66.0703940557658,66.1691035825158,66.2678104204676,
66.3681328232862,66.4669814166466,66.5680407241943,66.669100031742,66.7681591493266,
66.8670778235863,66.9667132489188,67.0654552502696,67.1641647770196,67.2628716149713,
67.3631940177899,67.4620426111503,67.563101918698,67.6641612262456,67.7632203438303,
67.8621390180898,67.9617744434222,68.0605164447731,68.1592259715233,68.2579328094751,
68.3582552122936,68.4571038056543,68.5581631132017,68.6592224207492,68.7582815383338,
68.8572002125931,68.9568356379256,69.0555776392765,69.1542871660265,69.2529940039784,
69.353316406797,69.4521650001575,69.5532243077052,69.6542836152528,69.7520048359883,
69.8496009043764,69.9471033152912,70.0445434457332,70.1419872142465,70.2394270962248,
70.3369604616551,70.4246015195609),.UNSPECIFIED.);
#416=B_SPLINE_CURVE_WITH_KNOTS('',3,(#32957,#32958,#32959,#32960,#32961,
#32962,#32963,#32964,#32965,#32966,#32967,#32968,#32969),.UNSPECIFIED.,
 .F.,.F.,(4,3,3,3,4),(70.4246015199524,70.5582169253846,70.6493448097564,
70.7484011690592,70.779075450487),.UNSPECIFIED.);
#417=B_SPLINE_CURVE_WITH_KNOTS('',3,(#32970,#32971,#32972,#32973,#32974,
#32975,#32976,#32977,#32978,#32979,#32980,#32981,#32982,#32983,#32984,#32985,
#32986,#32987,#32988,#32989,#32990,#32991,#32992,#32993,#32994,#32995,#32996,
#32997,#32998,#32999,#33000,#33001,#33002,#33003,#33004,#33005,#33006,#33007,
#33008,#33009,#33010,#33011,#33012,#33013,#33014,#33015,#33016,#33017,#33018,
#33019,#33020,#33021,#33022,#33023,#33024,#33025,#33026,#33027,#33028,#33029,
#33030,#33031,#33032,#33033,#33034,#33035,#33036,#33037,#33038,#33039,#33040,
#33041,#33042,#33043,#33044,#33045,#33046,#33047,#33048,#33049,#33050,#33051,
#33052,#33053,#33054,#33055,#33056,#33057,#33058,#33059,#33060,#33061,#33062,
#33063,#33064,#33065,#33066,#33067,#33068,#33069,#33070,#33071,#33072,#33073,
#33074,#33075,#33076,#33077,#33078,#33079,#33080,#33081,#33082,#33083,#33084,
#33085,#33086,#33087,#33088,#33089,#33090,#33091,#33092,#33093,#33094,#33095,
#33096,#33097,#33098,#33099,#33100,#33101,#33102,#33103,#33104,#33105,#33106,
#33107,#33108,#33109,#33110,#33111,#33112,#33113,#33114,#33115,#33116,#33117,
#33118,#33119,#33120,#33121,#33122,#33123,#33124,#33125,#33126,#33127,#33128,
#33129,#33130,#33131,#33132,#33133,#33134,#33135,#33136,#33137,#33138,#33139,
#33140,#33141,#33142,#33143,#33144,#33145,#33146,#33147,#33148,#33149,#33150,
#33151,#33152,#33153,#33154,#33155,#33156,#33157,#33158,#33159,#33160,#33161,
#33162,#33163,#33164,#33165,#33166,#33167,#33168,#33169,#33170,#33171,#33172,
#33173,#33174,#33175,#33176,#33177,#33178,#33179,#33180,#33181,#33182,#33183,
#33184,#33185,#33186,#33187,#33188,#33189,#33190,#33191),.UNSPECIFIED.,
 .F.,.F.,(4,2,2,2,2,2,2,2,2,2,2,2,2,2,2,2,2,2,2,2,2,2,2,2,2,2,2,2,2,2,2,
2,2,2,2,2,2,2,2,2,2,2,2,2,2,2,2,2,2,2,2,2,2,2,2,2,2,2,2,2,2,2,2,2,2,2,2,
2,2,2,2,2,2,2,2,2,2,2,2,2,2,2,2,2,2,2,2,2,2,2,2,2,2,2,2,2,2,2,2,2,2,2,2,
2,2,2,2,2,2,2,4),(-1.67598768218192,-1.64781802973257,-1.61129200490768,
-1.59068631767884,-1.58662859151187,-1.58436231468612,-1.58259340344101,
-1.58012109046356,-1.57506885255693,-1.56835983506212,-1.55158797940551,
-1.50156219162751,-1.49928274739267,-1.47034641909263,-1.46350659234859,
-1.45949352857199,-1.4560050068863,-1.45169875058855,-1.44327302165624,
-1.3950818856265,-1.34262895883037,-1.33667164920921,-1.33425237643543,
-1.33226221628564,-1.33013538111098,-1.32671169469097,-1.31492668526521,
-1.293349568365,-1.28016256034407,-1.22378661028309,-1.21403922495425,-1.20952648862046,
-1.20600830713213,-1.20216424306298,-1.19591980341672,-1.17291949412122,
-1.1324594421586,-1.09230875019351,-1.08583460035202,-1.08329609004918,
-1.08145702347058,-1.07941838777931,-1.07640228371058,-1.06806842766069,
-1.05501966955518,-1.01745094942914,-0.968879935990084,-0.962195341532359,
-0.957870079997983,-0.954380282063035,-0.950381263816085,-0.943424463195269,
-0.909314139420925,-0.855795355488474,-0.83726055985558,-0.833191864005302,
-0.830898819053043,-0.828936728818177,-0.82639546768346,-0.820986409217987,
-0.813659033888703,-0.7944853757041,-0.729658190600643,-0.714221158355355,
-0.70860348948435,-0.705265450932967,-0.701733752306944,-0.697048982826981,
-0.686622315631573,-0.672406078420063,-0.602405137493447,-0.58578216499317,
-0.581836951263677,-0.579571959272974,-0.57780281332374,-0.575328571867578,
-0.570266685426739,-0.563541200546925,-0.546707599066957,-0.496554966091625,
-0.484131392750421,-0.464145258862735,-0.457971797803325,-0.454143137060589,
-0.450620235454031,-0.44599726963226,-0.435916220811467,-0.422312523715144,
-0.384676579876693,-0.338425674441042,-0.332156138326956,-0.329651907815647,
-0.327821439567445,-0.32577256727383,-0.322707282051559,-0.314012696228027,
-0.300171376462531,-0.235809667458605,-0.213437476766805,-0.207015727125252,
-0.203133119718856,-0.19962503682749,-0.199583845669812,-0.19954628633179,
-0.199511981429396,-0.195123927313244,-0.18594143980428,-0.173719309919359,
-0.142286043005557,-0.0938487373820991,-0.0899211228894936),
 .UNSPECIFIED.);
#418=B_SPLINE_CURVE_WITH_KNOTS('',3,(#33197,#33198,#33199,#33200,#33201,
#33202,#33203,#33204,#33205,#33206,#33207,#33208,#33209,#33210,#33211,#33212,
#33213,#33214,#33215,#33216,#33217,#33218,#33219,#33220,#33221,#33222,#33223,
#33224,#33225,#33226,#33227,#33228,#33229,#33230,#33231,#33232,#33233,#33234,
#33235,#33236,#33237,#33238,#33239,#33240,#33241,#33242,#33243,#33244,#33245,
#33246,#33247,#33248,#33249,#33250,#33251,#33252,#33253,#33254,#33255,#33256,
#33257,#33258,#33259,#33260,#33261,#33262,#33263,#33264,#33265,#33266,#33267,
#33268,#33269,#33270,#33271,#33272,#33273,#33274,#33275,#33276,#33277,#33278,
#33279,#33280,#33281,#33282,#33283,#33284,#33285,#33286,#33287,#33288,#33289,
#33290,#33291,#33292,#33293,#33294,#33295,#33296,#33297,#33298,#33299,#33300,
#33301,#33302,#33303,#33304,#33305,#33306,#33307,#33308,#33309,#33310,#33311,
#33312,#33313,#33314,#33315,#33316,#33317,#33318,#33319,#33320,#33321,#33322,
#33323,#33324,#33325,#33326,#33327,#33328,#33329,#33330,#33331,#33332,#33333,
#33334,#33335,#33336,#33337,#33338,#33339,#33340,#33341,#33342,#33343,#33344,
#33345,#33346,#33347,#33348,#33349,#33350,#33351,#33352,#33353,#33354,#33355,
#33356,#33357,#33358,#33359,#33360,#33361,#33362,#33363,#33364,#33365,#33366,
#33367,#33368,#33369,#33370,#33371,#33372,#33373,#33374,#33375,#33376,#33377),
 .UNSPECIFIED.,.F.,.F.,(4,3,3,3,3,3,3,3,3,3,3,3,3,3,3,3,3,3,3,3,3,3,3,3,
3,3,3,3,3,3,3,3,3,3,3,3,3,3,3,3,3,3,3,3,3,3,3,3,3,3,3,3,3,3,3,3,3,3,3,3,
4),(58.21253113431,58.3098151884965,58.4095140103006,58.5069204673879,58.6077654715505,
58.7086104757131,58.8076695932978,58.9065882675572,59.0062236928896,59.1049656942405,
59.2036752209904,59.3023820589422,59.4027044617608,59.5015530551214,59.602612362669,
59.7036716702167,59.8027307878014,59.9016494620607,60.0012848873931,60.1000268887439,
60.1987364154939,60.2974432534456,60.3977656562643,60.4966142496248,60.5976735571725,
60.6987328647203,60.7977919823049,60.8967106565645,60.9963460818969,61.0950880832477,
61.1937976099976,61.2925044479495,61.3928268507681,61.4916754441286,61.5927347516762,
61.6937940592239,61.7928531768085,61.8917718510678,61.9914072764003,62.0901492777511,
62.188858804501,62.2875656424526,62.3878880452713,62.4867366386318,62.5877959461796,
62.6888552537275,62.787914371312,62.8868330455714,62.9864684709039,63.0852104722547,
63.1839199990046,63.2826268369563,63.382949239775,63.4817978331354,63.5828571406832,
63.6839164482311,63.7900912025854,63.8959105065072,64.0015055025791,64.1067929756915,
64.1414162124316),.UNSPECIFIED.);
#419=B_SPLINE_CURVE_WITH_KNOTS('',3,(#33378,#33379,#33380,#33381,#33382,
#33383,#33384,#33385,#33386,#33387,#33388,#33389,#33390),.UNSPECIFIED.,
 .F.,.F.,(4,3,3,3,4),(64.1414162127729,64.2432632295712,64.3451869470676,
64.4472800358431,64.4947309352028),.UNSPECIFIED.);
#420=B_SPLINE_CURVE_WITH_KNOTS('',3,(#33392,#33393,#33394,#33395,#33396,
#33397,#33398,#33399,#33400,#33401,#33402,#33403,#33404,#33405,#33406,#33407),
 .UNSPECIFIED.,.F.,.F.,(4,2,2,2,2,2,2,4),(-0.0899211228894936,-0.0825382572484242,
-0.0790353552956432,-0.0768911011408069,-0.0748873442578905,-0.0720511616616847,
-0.0649348746284129,-0.00073565181987095),.UNSPECIFIED.);
#421=B_SPLINE_CURVE_WITH_KNOTS('',3,(#33408,#33409,#33410,#33411,#33412,
#33413,#33414,#33415,#33416,#33417,#33418,#33419,#33420,#33421,#33422,#33423,
#33424,#33425,#33426,#33427,#33428,#33429,#33430,#33431,#33432,#33433,#33434,
#33435,#33436,#33437,#33438,#33439,#33440,#33441,#33442,#33443,#33444,#33445,
#33446,#33447,#33448,#33449,#33450,#33451,#33452,#33453,#33454,#33455,#33456,
#33457,#33458,#33459,#33460,#33461,#33462,#33463,#33464,#33465,#33466,#33467,
#33468,#33469,#33470,#33471,#33472,#33473,#33474,#33475,#33476,#33477,#33478,
#33479,#33480,#33481,#33482,#33483,#33484,#33485,#33486,#33487,#33488,#33489,
#33490,#33491,#33492,#33493,#33494,#33495,#33496,#33497,#33498,#33499,#33500,
#33501,#33502,#33503,#33504,#33505,#33506,#33507,#33508,#33509,#33510,#33511,
#33512,#33513,#33514,#33515,#33516,#33517,#33518,#33519,#33520,#33521,#33522,
#33523,#33524,#33525,#33526,#33527,#33528,#33529,#33530,#33531,#33532,#33533,
#33534,#33535,#33536,#33537,#33538,#33539,#33540,#33541,#33542,#33543,#33544,
#33545,#33546,#33547,#33548,#33549,#33550,#33551,#33552,#33553,#33554,#33555,
#33556,#33557,#33558,#33559,#33560,#33561,#33562,#33563,#33564,#33565,#33566,
#33567,#33568,#33569,#33570,#33571,#33572,#33573,#33574,#33575,#33576,#33577,
#33578,#33579,#33580,#33581,#33582,#33583,#33584,#33585,#33586,#33587,#33588,
#33589,#33590,#33591,#33592,#33593,#33594,#33595,#33596,#33597,#33598,#33599,
#33600,#33601,#33602,#33603,#33604,#33605,#33606,#33607,#33608,#33609,#33610,
#33611,#33612,#33613,#33614,#33615,#33616,#33617,#33618,#33619,#33620,#33621,
#33622,#33623,#33624,#33625,#33626,#33627,#33628,#33629,#33630,#33631,#33632,
#33633,#33634,#33635,#33636,#33637,#33638,#33639,#33640,#33641,#33642,#33643,
#33644,#33645,#33646,#33647,#33648,#33649,#33650,#33651,#33652,#33653,#33654,
#33655,#33656,#33657,#33658,#33659,#33660,#33661),.UNSPECIFIED.,.F.,.F.,
(4,2,2,2,2,2,2,2,2,2,2,2,2,2,2,2,2,2,2,2,2,2,2,2,2,2,2,2,2,2,2,2,2,2,2,
2,2,2,2,2,2,2,2,2,2,2,2,2,2,2,2,2,2,2,2,2,2,2,2,2,2,2,2,2,2,2,2,2,2,2,2,
2,2,2,2,2,2,2,2,2,2,2,2,2,2,2,2,2,2,2,2,2,2,2,2,2,2,2,2,2,2,2,2,2,2,2,2,
2,2,2,2,2,2,2,2,2,2,2,2,2,2,2,2,2,2,2,4),(-3.17295317748813,-3.13881949854016,
-3.13254270590914,-3.12840291351881,-3.12507038797027,-3.12192404985369,
-3.11797162534583,-3.11123133273975,-3.08501080934386,-3.05522340437467,
-3.03074665335081,-3.00497439810983,-3.0006991674959,-2.99838609230363,
-2.99642612004274,-2.99391236753246,-2.9898364238491,-2.9611176016517,-2.92662814993266,
-2.89871982649288,-2.88737551382644,-2.87868711235728,-2.8744600006815,
-2.8744364134477,-2.87441147941909,-2.87438511682015,-2.8743572384032,-2.87432775102356,
-2.87429655520012,-2.8742635446276,-2.87422860563979,-2.87419161662758,
-2.87415244742281,-2.8741109586162,-2.87406700082171,-2.87402041387674,
-2.87397102598451,-2.87391865277373,-2.87386309629366,-2.87380414393727,
-2.87374156727799,-2.87367512083198,-2.87360454074046,-2.87352954338432,
-2.87344982393563,-2.8733929887828,-2.87331706586271,-2.87321562690077,
-2.87308008082605,-2.86957491218778,-2.86509160468945,-2.85576294460097,
-2.79450934558193,-2.75558287221551,-2.75017890530165,-2.74763840595148,
-2.74567613933805,-2.74338202098676,-2.73930937866326,-2.7207181388602,
-2.66720596802176,-2.63308569150018,-2.62612750684263,-2.62212790243688,
-2.61863772129548,-2.61431215038077,-2.60762745597193,-2.55911536298477,
-2.52163446164379,-2.50852108535286,-2.50015649708243,-2.49713595237334,
-2.49509624506778,-2.49325773677067,-2.49072191109271,-2.48426452412769,
-2.44550110633697,-2.40249047862435,-2.38040457173732,-2.37423929543012,
-2.37041226741027,-2.36688856816085,-2.3623392562156,-2.3523918819042,-2.30086983474745,
-2.27116430152585,-2.25760646902335,-2.24903891214524,-2.24599061920154,
-2.24394519611649,-2.24211167596562,-2.23959552548921,-2.23325599985454,
-2.18850062422496,-2.13301145627603,-2.12470306567651,-2.12042041084192,
-2.11693326434142,-2.1129020124388,-2.10598235030052,-2.07566510148396,
-2.02527526430655,-2.00827971161612,-2.00151107708111,-1.99642364881248,
-1.9939443902317,-1.99217469169529,-1.98991322019257,-1.98598337853484,
-1.96958029229012,-1.90508280392682,-1.88759985645926,-1.87541527587832,
-1.87043544890947,-1.86685418031766,-1.86358877407033,-1.85919699769326,
-1.8506070444512,-1.79142675495546,-1.75017420819679,-1.7451558612457,-1.74269029675122,
-1.74092214038338,-1.73865120440277,-1.7346795553971,-1.71766968926413,
-1.67592320998144),.UNSPECIFIED.);
#422=B_SPLINE_CURVE_WITH_KNOTS('',3,(#33667,#33668,#33669,#33670,#33671,
#33672,#33673,#33674,#33675,#33676,#33677,#33678,#33679,#33680,#33681,#33682,
#33683,#33684,#33685,#33686,#33687,#33688,#33689,#33690,#33691,#33692,#33693,
#33694,#33695,#33696,#33697,#33698,#33699,#33700,#33701,#33702,#33703,#33704,
#33705,#33706,#33707,#33708,#33709,#33710,#33711,#33712,#33713,#33714,#33715,
#33716,#33717,#33718,#33719,#33720,#33721,#33722,#33723,#33724,#33725,#33726,
#33727,#33728,#33729,#33730,#33731,#33732,#33733,#33734,#33735,#33736,#33737,
#33738,#33739,#33740,#33741,#33742,#33743,#33744,#33745,#33746,#33747,#33748,
#33749,#33750,#33751,#33752,#33753,#33754,#33755,#33756,#33757,#33758,#33759,
#33760,#33761,#33762,#33763,#33764,#33765,#33766,#33767,#33768,#33769,#33770,
#33771,#33772,#33773,#33774,#33775,#33776,#33777,#33778,#33779,#33780,#33781,
#33782,#33783,#33784,#33785,#33786,#33787,#33788,#33789,#33790,#33791,#33792,
#33793,#33794,#33795,#33796,#33797,#33798,#33799,#33800,#33801,#33802,#33803,
#33804,#33805,#33806,#33807,#33808,#33809,#33810,#33811,#33812,#33813,#33814,
#33815,#33816,#33817,#33818,#33819,#33820,#33821,#33822,#33823,#33824,#33825,
#33826,#33827,#33828,#33829,#33830,#33831,#33832,#33833,#33834,#33835,#33836,
#33837,#33838,#33839,#33840,#33841,#33842,#33843,#33844,#33845,#33846,#33847),
 .UNSPECIFIED.,.F.,.F.,(4,3,3,3,3,3,3,3,3,3,3,3,3,3,3,3,3,3,3,3,3,3,3,3,
3,3,3,3,3,3,3,3,3,3,3,3,3,3,3,3,3,3,3,3,3,3,3,3,3,3,3,3,3,3,3,3,3,3,3,3,
4),(51.9295889271401,52.030670724834,52.1294177394015,52.2281292244128,
52.3268349684299,52.4296870534953,52.5285312410374,52.6274451637171,52.7265117204176,
52.7382433086914,52.8373024262761,52.9362211005355,53.035856525868,53.1345985272188,
53.2333080539688,53.3320148919206,53.4323372947392,53.5311858880997,53.6322451956473,
53.733304503195,53.8323636207797,53.9312822950391,54.0309177203715,54.1296597217224,
54.2283692484724,54.3270760864241,54.4273984892428,54.5262470826032,54.6273063901509,
54.7283656976986,54.8274248152832,54.9263434895427,55.0259789148751,55.124720916226,
55.2234304429759,55.3221372809276,55.4224596837463,55.5213082771068,55.6223675846545,
55.7234268922022,55.8224860097869,55.9214046840463,56.0210401093787,56.1197821107296,
56.2184916374796,56.3171984754314,56.41752087825,56.5163694716105,56.6174287791582,
56.7184880867059,56.8175472042906,56.91646587855,57.0161013038825,57.1148433052334,
57.2135528319833,57.3122596699352,57.4125820727538,57.5114306661142,57.6124899736619,
57.7135492812095,57.8582309055932),.UNSPECIFIED.);
#423=B_SPLINE_CURVE_WITH_KNOTS('',3,(#33848,#33849,#33850,#33851,#33852,
#33853,#33854,#33855,#33856,#33857,#33858,#33859,#33860),.UNSPECIFIED.,
 .F.,.F.,(4,3,3,3,4),(57.8582309058229,57.9557212708262,58.053112517412,
58.150435644654,58.21253113431),.UNSPECIFIED.);
#424=B_SPLINE_CURVE_WITH_KNOTS('',3,(#33861,#33862,#33863,#33864,#33865,
#33866,#33867,#33868,#33869,#33870,#33871,#33872,#33873,#33874,#33875,#33876,
#33877,#33878,#33879,#33880,#33881,#33882,#33883,#33884,#33885,#33886,#33887,
#33888,#33889,#33890,#33891,#33892,#33893,#33894,#33895,#33896,#33897,#33898,
#33899,#33900,#33901,#33902,#33903,#33904,#33905,#33906,#33907,#33908,#33909,
#33910,#33911,#33912,#33913,#33914,#33915,#33916,#33917,#33918,#33919,#33920,
#33921,#33922,#33923,#33924,#33925,#33926,#33927,#33928,#33929,#33930,#33931,
#33932,#33933,#33934,#33935,#33936,#33937,#33938,#33939,#33940,#33941,#33942,
#33943,#33944,#33945,#33946,#33947,#33948,#33949,#33950,#33951,#33952,#33953,
#33954,#33955,#33956,#33957,#33958,#33959,#33960,#33961,#33962,#33963,#33964,
#33965,#33966,#33967,#33968,#33969,#33970,#33971,#33972,#33973,#33974,#33975,
#33976,#33977,#33978,#33979,#33980,#33981,#33982,#33983,#33984,#33985,#33986,
#33987,#33988,#33989,#33990,#33991,#33992,#33993,#33994,#33995,#33996,#33997,
#33998,#33999,#34000,#34001,#34002,#34003,#34004,#34005,#34006,#34007,#34008,
#34009,#34010,#34011,#34012,#34013,#34014,#34015,#34016,#34017,#34018,#34019,
#34020,#34021,#34022,#34023,#34024,#34025,#34026,#34027,#34028,#34029,#34030,
#34031,#34032,#34033,#34034,#34035,#34036,#34037,#34038,#34039,#34040,#34041,
#34042,#34043,#34044,#34045,#34046,#34047,#34048,#34049,#34050,#34051,#34052,
#34053,#34054,#34055,#34056,#34057,#34058,#34059,#34060,#34061,#34062,#34063,
#34064,#34065,#34066,#34067,#34068,#34069,#34070,#34071,#34072,#34073,#34074,
#34075,#34076,#34077,#34078,#34079,#34080,#34081,#34082,#34083,#34084,#34085,
#34086,#34087,#34088,#34089,#34090,#34091,#34092,#34093,#34094,#34095,#34096,
#34097,#34098,#34099,#34100,#34101,#34102,#34103,#34104,#34105,#34106,#34107,
#34108,#34109,#34110,#34111,#34112,#34113,#34114,#34115,#34116,#34117,#34118,
#34119,#34120,#34121,#34122,#34123,#34124,#34125,#34126,#34127,#34128,#34129,
#34130,#34131,#34132,#34133,#34134,#34135,#34136,#34137,#34138,#34139,#34140,
#34141,#34142,#34143,#34144),.UNSPECIFIED.,.F.,.F.,(4,2,2,2,2,2,2,2,2,2,
2,2,2,2,2,2,2,2,2,2,2,2,2,2,2,2,2,2,2,2,2,2,2,2,2,2,2,2,2,2,2,2,2,2,2,2,
2,2,2,2,2,2,2,2,2,2,2,2,2,2,2,2,2,2,2,2,2,2,2,2,2,2,2,2,2,2,2,2,2,2,2,2,
2,2,2,2,2,2,2,2,2,2,2,2,2,2,2,2,2,2,2,2,2,2,2,2,2,2,2,2,2,2,2,2,2,2,2,2,
2,2,2,2,2,2,2,2,2,2,2,2,2,2,2,2,2,2,2,2,2,2,2,4),(-1.67592320998144,-1.64801987356236,
-1.63382763456696,-1.62341555588315,-1.61873363522818,-1.61520263671616,
-1.61140060802024,-1.60534751231179,-1.58644977368995,-1.55255126979351,
-1.50058225176569,-1.49450383036933,-1.49210459370419,-1.49011959022917,
-1.48798398052661,-1.48451948762301,-1.47231678925401,-1.44954183418719,
-1.39715730539802,-1.37591560258209,-1.36960485512921,-1.36574678339733,
-1.36223327665017,-1.35767496110344,-1.34794300656535,-1.30812976654373,
-1.26525775355338,-1.24641153155549,-1.24232347314032,-1.24002631665237,
-1.23806518190785,-1.235530956359,-1.2301573812203,-1.22289180980846,-1.20396354763412,
-1.14057172608681,-1.12375311573915,-1.11795315223345,-1.11420606475655,
-1.11065229109488,-1.10582614633735,-1.09457850972797,-1.05189306089402,
-0.999138571291884,-0.992634191801533,-0.990090867899693,-0.988250830218791,
-0.986214138505041,-0.983206029528501,-0.974926774739709,-0.918371911446345,
-0.875678779087676,-0.868990641786553,-0.864664937209232,-0.861175981087088,
-0.857179241571935,-0.85022980876337,-0.816245099449129,-0.763823548761383,
-0.744201390372336,-0.740069840368587,-0.737762978002056,-0.735803135369725,
-0.733282929926665,-0.727982113991956,-0.697844496036856,-0.684698883442765,
-0.628300630357481,-0.618558241503323,-0.614047196493481,-0.610530073999733,
-0.606686904126458,-0.600443323483241,-0.577438742636601,-0.536955774331928,
-0.496827218990667,-0.490379968424935,-0.487846408578358,-0.486008942353855,
-0.483969688502199,-0.480948600462394,-0.472574889440919,-0.459438111384135,
-0.422120589282921,-0.373470484552808,-0.366787522559929,-0.362463410562818,
-0.358974600626299,-0.354976780873375,-0.348022237096805,-0.313927516957458,
-0.26393248475239,-0.242215310075114,-0.238339088188428,-0.235885712801448,
-0.233993280108135,-0.233974273408042,-0.233955712653511,-0.233937580843393,
-0.233919861832381,-0.233902540274617,-0.23388560157789,-0.233869031867375,
-0.233852817934698,-0.233836947198216,-0.233821407641112,-0.233806187816045,
-0.233791276823863,-0.233776664239748,-0.233762340095032,-0.233748294873074,
-0.233734519460936,-0.233721005171065,-0.233707743668982,-0.233694726943997,
-0.233681947358699,-0.233669397574497,-0.233657070550256,-0.233644959535232,
-0.23363305807667,-0.23362135993261,-0.233609859115898,-0.23359854988632,
-0.233587426734408,-0.233576484351445,-0.233565717605655,-0.233555121573784,
-0.233544691527589,-0.233534422903674,-0.233524311295459,-0.231035451518287,
-0.22823743117379,-0.223523867326237,-0.213515204647212,-0.181647151558495,
-0.126191035270392,-0.116398316434333,-0.11187816708323,-0.108359849878644,
-0.104521338766822,-0.0982987539848973,-0.0902547838960883),
 .UNSPECIFIED.);
#425=B_SPLINE_CURVE_WITH_KNOTS('',3,(#34150,#34151,#34152,#34153,#34154,
#34155,#34156,#34157,#34158,#34159,#34160,#34161,#34162,#34163,#34164,#34165,
#34166,#34167,#34168,#34169,#34170,#34171,#34172,#34173,#34174,#34175,#34176,
#34177,#34178,#34179,#34180,#34181,#34182,#34183,#34184,#34185,#34186,#34187,
#34188,#34189,#34190,#34191,#34192,#34193,#34194,#34195,#34196,#34197,#34198,
#34199,#34200,#34201,#34202,#34203,#34204,#34205,#34206,#34207,#34208,#34209,
#34210,#34211,#34212,#34213,#34214,#34215,#34216,#34217,#34218,#34219,#34220,
#34221,#34222,#34223,#34224,#34225,#34226,#34227,#34228,#34229,#34230,#34231,
#34232,#34233,#34234,#34235,#34236,#34237,#34238,#34239,#34240,#34241,#34242,
#34243,#34244,#34245,#34246,#34247,#34248,#34249,#34250,#34251,#34252,#34253,
#34254,#34255,#34256,#34257,#34258,#34259,#34260,#34261,#34262,#34263,#34264,
#34265,#34266,#34267,#34268,#34269,#34270,#34271,#34272,#34273,#34274,#34275,
#34276,#34277,#34278,#34279,#34280,#34281,#34282,#34283,#34284,#34285,#34286,
#34287,#34288,#34289,#34290,#34291,#34292,#34293,#34294,#34295,#34296,#34297,
#34298,#34299,#34300,#34301,#34302,#34303,#34304,#34305,#34306,#34307,#34308,
#34309,#34310,#34311,#34312,#34313,#34314,#34315,#34316,#34317,#34318,#34319,
#34320,#34321,#34322,#34323,#34324,#34325,#34326,#34327,#34328,#34329,#34330,
#34331,#34332,#34333),.UNSPECIFIED.,.F.,.F.,(4,3,3,3,3,3,3,3,3,3,3,3,3,
3,3,3,3,3,3,3,3,3,3,3,3,3,3,3,3,3,3,3,3,3,3,3,3,3,3,3,3,3,3,3,3,3,3,3,3,
3,3,3,3,3,3,3,3,3,3,3,3,4),(45.6452512469328,45.7501622262758,45.7728149471661,
45.8718740647508,45.9707927390103,46.0704281643427,46.1691701656936,46.2678796924436,
46.3665865303954,46.466908933214,46.5657575265745,46.6668168341221,46.7678761416697,
46.8669352592544,46.9658539335138,47.0654893588463,47.1642313601972,47.2629408869471,
47.3616477248989,47.4619701277175,47.560818721078,47.6618780286257,47.7629373361734,
47.861996453758,47.9609151280175,48.0605505533499,48.1592925547008,48.2580020814507,
48.3567089194025,48.4570313222211,48.5558799155816,48.6569392231293,48.757998530677,
48.8570576482617,48.955976322521,49.0556117478535,49.1543537492043,49.2530632759543,
49.351770113906,49.4520925167247,49.5509411100851,49.6520004176329,49.7530597251806,
49.8521188427653,49.9510375170247,50.0506729423571,50.149414943708,50.248124470458,
50.3468313084098,50.4471537112284,50.5460023045889,50.6470616121365,50.7481209196842,
50.8457129935022,50.9431428324126,51.0404816382021,51.1377609277275,51.2350121400975,
51.3323110164859,51.4296360130139,51.5270774501444,51.5750455980497),
 .UNSPECIFIED.);
#426=B_SPLINE_CURVE_WITH_KNOTS('',3,(#34334,#34335,#34336,#34337,#34338,
#34339,#34340,#34341,#34342,#34343,#34344,#34345,#34346),.UNSPECIFIED.,
 .F.,.F.,(4,3,3,3,4),(51.5750455984136,51.7300295918754,51.7431821141878,
51.8422151608463,51.9295889271401),.UNSPECIFIED.);
#427=B_SPLINE_CURVE_WITH_KNOTS('',3,(#34348,#34349,#34350,#34351,#34352,
#34353),.UNSPECIFIED.,.F.,.F.,(4,2,4),(-0.0902547838960883,-0.0755381864946324,
-0.000735838667914899),.UNSPECIFIED.);
#428=B_SPLINE_CURVE_WITH_KNOTS('',3,(#34354,#34355,#34356,#34357,#34358,
#34359,#34360,#34361,#34362,#34363,#34364,#34365,#34366,#34367,#34368,#34369,
#34370,#34371,#34372,#34373,#34374,#34375,#34376,#34377,#34378,#34379,#34380,
#34381,#34382,#34383,#34384,#34385,#34386,#34387,#34388,#34389,#34390,#34391,
#34392,#34393,#34394,#34395,#34396,#34397,#34398,#34399,#34400,#34401,#34402,
#34403,#34404,#34405,#34406,#34407,#34408,#34409,#34410,#34411,#34412,#34413,
#34414,#34415,#34416,#34417,#34418,#34419,#34420,#34421,#34422,#34423,#34424,
#34425,#34426,#34427,#34428,#34429,#34430,#34431,#34432,#34433,#34434,#34435,
#34436,#34437,#34438,#34439,#34440,#34441,#34442,#34443,#34444,#34445,#34446,
#34447,#34448,#34449,#34450,#34451,#34452,#34453,#34454,#34455,#34456,#34457,
#34458,#34459,#34460,#34461,#34462,#34463,#34464,#34465,#34466,#34467,#34468,
#34469,#34470,#34471,#34472,#34473,#34474,#34475,#34476,#34477,#34478,#34479,
#34480,#34481,#34482,#34483,#34484,#34485,#34486,#34487,#34488,#34489,#34490,
#34491,#34492,#34493,#34494,#34495,#34496,#34497,#34498,#34499,#34500,#34501,
#34502,#34503,#34504,#34505,#34506,#34507,#34508,#34509,#34510,#34511,#34512,
#34513,#34514,#34515,#34516,#34517,#34518,#34519,#34520,#34521,#34522,#34523,
#34524,#34525,#34526,#34527,#34528,#34529,#34530,#34531,#34532,#34533,#34534,
#34535,#34536,#34537,#34538,#34539,#34540,#34541,#34542,#34543,#34544,#34545,
#34546,#34547,#34548,#34549,#34550,#34551,#34552,#34553,#34554,#34555,#34556,
#34557),.UNSPECIFIED.,.F.,.F.,(4,2,2,2,2,2,2,2,2,2,2,2,2,2,2,2,2,2,2,2,
2,2,2,2,2,2,2,2,2,2,2,2,2,2,2,2,2,2,2,2,2,2,2,2,2,2,2,2,2,2,2,2,2,2,2,2,
2,2,2,2,2,2,2,2,2,2,2,2,2,2,2,2,2,2,2,2,2,2,2,2,2,2,2,2,2,2,2,2,2,2,2,2,
2,2,2,2,2,2,2,2,2,4),(-3.17298666581179,-3.16563141916398,-3.16059756997835,
-3.15835235769896,-3.15650595198463,-3.15462878690909,-3.15209114925753,
-3.1479350984291,-3.13236830659073,-3.06800305622745,-3.04166816243616,
-3.03516350889059,-3.03126242370672,-3.02775762557886,-3.02327736620085,
-3.01396460456103,-2.95248174887367,-2.92459997801962,-2.91533808156676,
-2.91087169695868,-2.90817241857315,-2.90574168526152,-2.90381935963668,
-2.90150573483734,-2.8973465919083,-2.87726454855109,-2.81059087786807,
-2.79663008411779,-2.78634765729626,-2.78168834538372,-2.77816018411837,
-2.77481391115882,-2.76915405957496,-2.75342346764264,-2.69613911881825,
-2.6610955226833,-2.65659319807143,-2.65423231370343,-2.65227574303146,
-2.64982153022093,-2.64594399790897,-2.62423560721442,-2.57802327778507,
-2.55294696862275,-2.54236062444264,-2.53406458939325,-2.52978436337409,
-2.526297263886,-2.52226390750591,-2.51533527089136,-2.48485795017648,-2.43454581906813,
-2.41761362011077,-2.41086169515979,-2.40578398538528,-2.40330659278867,
-2.40153705482741,-2.39927416826418,-2.39533830573911,-2.37885141408669,
-2.3086733539788,-2.29444180510874,-2.28400750064803,-2.2793214002882,-2.27578953883554,
-2.27245197735828,-2.26683659806314,-2.2514154710157,-2.18662120967513,
-2.16744718799289,-2.15654586787731,-2.15321460908982,-2.15110818648012,
-2.14910600115559,-2.14663939466139,-2.14058855242489,-2.08999986217308,
-2.0444108637344,-2.0331619659822,-2.0283350017407,-2.02478053842007,-2.021032646738,
-2.01523127308426,-1.99840699957501,-1.94213711660028,-1.91048059898588,
-1.90401588276398,-1.90128582086879,-1.89929993583942,-1.89711264558408,
-1.89341535429896,-1.88023206284989,-1.82539214966138,-1.79014171544812,
-1.78096875465978,-1.77651574521964,-1.77301453179121,-1.76909904415105,
-1.76252619374566,-1.73848491173098,-1.6885199140946,-1.67620980708928),
 .UNSPECIFIED.);
#429=B_SPLINE_CURVE_WITH_KNOTS('',3,(#34563,#34564,#34565,#34566,#34567,
#34568,#34569,#34570,#34571,#34572,#34573,#34574,#34575,#34576,#34577,#34578,
#34579,#34580,#34581,#34582,#34583,#34584,#34585,#34586,#34587,#34588,#34589,
#34590,#34591,#34592,#34593,#34594,#34595,#34596,#34597,#34598,#34599,#34600,
#34601,#34602,#34603,#34604,#34605,#34606,#34607,#34608,#34609,#34610,#34611,
#34612,#34613,#34614,#34615,#34616,#34617,#34618,#34619,#34620,#34621,#34622,
#34623,#34624,#34625,#34626,#34627,#34628,#34629,#34630,#34631,#34632,#34633,
#34634,#34635,#34636,#34637,#34638,#34639,#34640,#34641,#34642,#34643,#34644,
#34645,#34646,#34647,#34648,#34649,#34650,#34651,#34652,#34653,#34654,#34655,
#34656,#34657,#34658,#34659,#34660,#34661,#34662,#34663,#34664,#34665,#34666,
#34667,#34668,#34669,#34670,#34671,#34672,#34673,#34674,#34675,#34676,#34677,
#34678,#34679,#34680,#34681,#34682,#34683,#34684,#34685,#34686,#34687,#34688,
#34689,#34690,#34691,#34692,#34693,#34694,#34695,#34696,#34697,#34698,#34699,
#34700,#34701,#34702,#34703,#34704,#34705,#34706,#34707,#34708,#34709,#34710,
#34711,#34712,#34713,#34714,#34715,#34716,#34717,#34718,#34719,#34720,#34721,
#34722,#34723,#34724,#34725,#34726,#34727,#34728,#34729,#34730,#34731,#34732,
#34733,#34734,#34735,#34736,#34737,#34738,#34739,#34740,#34741,#34742,#34743),
 .UNSPECIFIED.,.F.,.F.,(4,3,3,3,3,3,3,3,3,3,3,3,3,3,3,3,3,3,3,3,3,3,3,3,
3,3,3,3,3,3,3,3,3,3,3,3,3,3,3,3,3,3,3,3,3,3,3,3,3,3,3,3,3,3,3,3,3,3,3,3,
4),(39.3627615986102,39.4600795768122,39.5574939443465,39.6549619992771,
39.7525891288265,39.8024477801445,39.9015068977292,40.0004255719887,40.1000609973211,
40.198802998672,40.2975125254219,40.3962193633735,40.4965417661922,40.5953903595526,
40.6964496671004,40.7975089746481,40.8965680922328,40.9954867664921,41.0951221918246,
41.1938641931755,41.2925737199253,41.391280557877,41.4916029606957,41.5904515540561,
41.6915108616039,41.7925701691517,41.8916292867363,41.9905479609956,42.0901833863281,
42.1889253876789,42.2876349144288,42.3863417523807,42.4866641551993,42.5855127485597,
42.6865720561075,42.7876313636553,42.88669048124,42.9856091554994,43.0852445808319,
43.1839865821828,43.2826961089327,43.3814029468844,43.481725349703,43.5805739430635,
43.6816332506112,43.7826925581589,43.8817516757436,43.9806703500033,44.0803057753357,
44.1790477766866,44.2777573034363,44.3764641413878,44.4767865442065,44.575635137567,
44.6766944451147,44.7777537526625,44.8811334637461,44.9842446946404,45.0871977961312,
45.1899571772778,45.2918602912341),.UNSPECIFIED.);
#430=B_SPLINE_CURVE_WITH_KNOTS('',3,(#34744,#34745,#34746,#34747,#34748,
#34749,#34750,#34751,#34752,#34753,#34754,#34755,#34756),.UNSPECIFIED.,
 .F.,.F.,(4,3,3,3,4),(45.2918602914973,45.3960300286389,45.5003580305241,
45.6049489906218,45.6452512469328),.UNSPECIFIED.);
#431=B_SPLINE_CURVE_WITH_KNOTS('',3,(#34757,#34758,#34759,#34760,#34761,
#34762,#34763,#34764,#34765,#34766,#34767,#34768,#34769,#34770,#34771,#34772,
#34773,#34774,#34775,#34776,#34777,#34778,#34779,#34780,#34781,#34782,#34783,
#34784,#34785,#34786,#34787,#34788,#34789,#34790,#34791,#34792,#34793,#34794,
#34795,#34796,#34797,#34798,#34799,#34800,#34801,#34802,#34803,#34804,#34805,
#34806,#34807,#34808,#34809,#34810,#34811,#34812,#34813,#34814,#34815,#34816,
#34817,#34818,#34819,#34820,#34821,#34822,#34823,#34824,#34825,#34826,#34827,
#34828,#34829,#34830,#34831,#34832,#34833,#34834,#34835,#34836,#34837,#34838,
#34839,#34840,#34841,#34842,#34843,#34844,#34845,#34846,#34847,#34848,#34849,
#34850,#34851,#34852,#34853,#34854,#34855,#34856,#34857,#34858,#34859,#34860,
#34861,#34862,#34863,#34864,#34865,#34866,#34867,#34868,#34869,#34870,#34871,
#34872,#34873,#34874,#34875,#34876,#34877,#34878,#34879,#34880,#34881,#34882,
#34883,#34884,#34885,#34886,#34887,#34888,#34889,#34890,#34891,#34892,#34893,
#34894,#34895,#34896,#34897,#34898,#34899,#34900,#34901,#34902,#34903,#34904,
#34905,#34906,#34907,#34908,#34909,#34910,#34911,#34912,#34913,#34914,#34915,
#34916,#34917,#34918,#34919,#34920,#34921,#34922,#34923,#34924,#34925,#34926,
#34927,#34928,#34929,#34930,#34931,#34932,#34933,#34934,#34935,#34936,#34937,
#34938,#34939,#34940,#34941,#34942,#34943,#34944,#34945,#34946,#34947,#34948,
#34949,#34950,#34951,#34952,#34953,#34954,#34955,#34956,#34957,#34958,#34959,
#34960,#34961,#34962,#34963,#34964,#34965,#34966,#34967,#34968,#34969,#34970,
#34971,#34972,#34973,#34974,#34975,#34976),.UNSPECIFIED.,.F.,.F.,(4,2,2,
2,2,2,2,2,2,2,2,2,2,2,2,2,2,2,2,2,2,2,2,2,2,2,2,2,2,2,2,2,2,2,2,2,2,2,2,
2,2,2,2,2,2,2,2,2,2,2,2,2,2,2,2,2,2,2,2,2,2,2,2,2,2,2,2,2,2,2,2,2,2,2,2,
2,2,2,2,2,2,2,2,2,2,2,2,2,2,2,2,2,2,2,2,2,2,2,2,2,2,2,2,2,2,2,2,2,2,4),
(-1.67620980708928,-1.66640396248898,-1.65442852491712,-1.65098613315536,
-1.64885529433634,-1.64686758732065,-1.64445767447368,-1.63831256449055,
-1.58708365957732,-1.54037389911875,-1.53029087362987,-1.52571772696811,
-1.52219105788161,-1.51837618836454,-1.51226438188968,-1.49075755169447,
-1.42005532763171,-1.40413557489153,-1.40024128409183,-1.39798802132766,
-1.39621711346142,-1.39372619749178,-1.38857873613451,-1.38170622448344,
-1.36431448504218,-1.31340038515004,-1.28405334736977,-1.27718886084294,
-1.2731703025766,-1.26968242211879,-1.26538389909587,-1.25699601434651,
-1.21275366991191,-1.16582932985959,-1.15254605342861,-1.14883941199621,
-1.14665003850391,-1.14466484676266,-1.1419393032769,-1.1355014577652,-1.10412259193519,
-1.04868002323832,-1.03090739425258,-1.02498730949448,-1.02121384829015,
-1.01767111313951,-1.01291550301722,-1.00208462613817,-0.987140444444101,
-0.94240665056427,-0.925877880191999,-0.919080720755033,-0.901983154629366,
-0.898005848074418,-0.895733662995074,-0.893965765407025,-0.891502116813433,
-0.886493201876764,-0.845610100424215,-0.785938569314373,-0.776441463805464,
-0.77192684995559,-0.768418640465444,-0.764537670644353,-0.758122775715849,
-0.732993785994031,-0.703728287952091,-0.654306317631853,-0.648205655514477,
-0.645730575823987,-0.643726325894904,-0.641623699313264,-0.638308892099879,
-0.627555868853611,-0.60876537285979,-0.548097229529708,-0.528933710734291,
-0.52285039706297,-0.519041897927518,-0.515513389284958,-0.510847394425225,
-0.500523998685228,-0.486491083448626,-0.418878452089067,-0.399835748695025,
-0.395736202912422,-0.393436352806003,-0.391475382090186,-0.388944557094879,
-0.383589399826682,-0.376356216443083,-0.357557645879962,-0.296761032303342,
-0.277709131803074,-0.271638333137631,-0.267832487266175,-0.264373154669794,
-0.259895189605234,-0.254907261259269,-0.246554379639805,-0.228921935900892,
-0.162569436010408,-0.148050774553925,-0.144232290987578,-0.142018380918343,
-0.140040963712573,-0.137367023269518,-0.131228439263144,-0.102837806382509,
-0.0901712924560195),.UNSPECIFIED.);
#432=B_SPLINE_CURVE_WITH_KNOTS('',3,(#34982,#34983,#34984,#34985,#34986,
#34987,#34988,#34989,#34990,#34991,#34992,#34993,#34994,#34995,#34996,#34997,
#34998,#34999,#35000,#35001,#35002,#35003,#35004,#35005,#35006,#35007,#35008,
#35009,#35010,#35011,#35012,#35013,#35014,#35015,#35016,#35017,#35018,#35019,
#35020,#35021,#35022,#35023,#35024,#35025,#35026,#35027,#35028,#35029,#35030,
#35031,#35032,#35033,#35034,#35035,#35036,#35037,#35038,#35039,#35040,#35041,
#35042,#35043,#35044,#35045,#35046,#35047,#35048,#35049,#35050,#35051,#35052,
#35053,#35054,#35055,#35056,#35057,#35058,#35059,#35060,#35061,#35062,#35063,
#35064,#35065,#35066,#35067,#35068,#35069,#35070,#35071,#35072,#35073,#35074,
#35075,#35076,#35077,#35078,#35079,#35080,#35081,#35082,#35083,#35084,#35085,
#35086,#35087,#35088,#35089,#35090,#35091,#35092,#35093,#35094,#35095,#35096,
#35097,#35098,#35099,#35100,#35101,#35102,#35103,#35104,#35105,#35106,#35107,
#35108,#35109,#35110,#35111,#35112,#35113,#35114,#35115,#35116,#35117,#35118,
#35119,#35120,#35121,#35122,#35123,#35124,#35125,#35126,#35127,#35128,#35129,
#35130,#35131,#35132,#35133,#35134,#35135,#35136,#35137,#35138,#35139,#35140,
#35141,#35142,#35143,#35144,#35145,#35146,#35147,#35148,#35149,#35150,#35151,
#35152,#35153,#35154,#35155,#35156,#35157,#35158,#35159,#35160,#35161,#35162),
 .UNSPECIFIED.,.F.,.F.,(4,3,3,3,3,3,3,3,3,3,3,3,3,3,3,3,3,3,3,3,3,3,3,3,
3,3,3,3,3,3,3,3,3,3,3,3,3,3,3,3,3,3,3,3,3,3,3,3,3,3,3,3,3,3,3,3,3,3,3,3,
4),(33.0800282649154,33.1788010120089,33.2775248054047,33.3762294491433,
33.4749447203013,33.5737644425482,33.672640731442,33.7716835211257,33.8320806131228,
33.9311397307074,34.0300584049668,34.1296938302993,34.2284358316501,34.3271453584001,
34.4258521963519,34.5261745991705,34.6250231925309,34.7260825000787,34.8271418076264,
34.9262009252112,35.0251195994707,35.1247550248031,35.2234970261541,35.3222065529041,
35.420913390856,35.5212357936745,35.6200843870351,35.7211436945826,35.82220300213,
35.9212621197146,36.020180793974,36.1198162193064,36.2185582206573,36.3172677474071,
36.4159745853588,36.5162969881775,36.615145581538,36.7162048890858,36.8172641966336,
36.9163233142182,37.0152419884777,37.1148774138101,37.213619415161,37.3123289419109,
37.4110357798627,37.5113581826814,37.6102067760418,37.7112660835895,37.8123253911372,
37.9113845087219,38.0103031829814,38.1099386083138,38.2086806096647,38.3073901364147,
38.4060969743665,38.5064193771851,38.6052679705456,38.7063272780932,38.8073865856408,
38.9480297229085,39.0086749840545),.UNSPECIFIED.);
#433=B_SPLINE_CURVE_WITH_KNOTS('',3,(#35163,#35164,#35165,#35166,#35167,
#35168,#35169,#35170,#35171,#35172,#35173,#35174,#35175),.UNSPECIFIED.,
 .F.,.F.,(4,3,3,3,4),(39.0086749844289,39.1061283327374,39.2034999696831,
39.3008301777854,39.3627615986102),.UNSPECIFIED.);
#434=B_SPLINE_CURVE_WITH_KNOTS('',3,(#35177,#35178,#35179,#35180,#35181,
#35182,#35183,#35184,#35185,#35186,#35187,#35188,#35189,#35190,#35191,#35192,
#35193,#35194),.UNSPECIFIED.,.F.,.F.,(4,2,2,2,2,2,2,2,4),(-0.0901712924560195,
-0.0419045892551838,-0.0257637905534428,-0.0200541212030024,-0.0163260946354891,
-0.0130012968151968,-0.00952881353369847,-0.00531895993925087,-0.000734738427498389),
 .UNSPECIFIED.);
#435=B_SPLINE_CURVE_WITH_KNOTS('',3,(#35195,#35196,#35197,#35198,#35199,
#35200,#35201,#35202,#35203,#35204,#35205,#35206,#35207,#35208,#35209,#35210,
#35211,#35212,#35213,#35214,#35215,#35216,#35217,#35218,#35219,#35220,#35221,
#35222,#35223,#35224,#35225,#35226,#35227,#35228,#35229,#35230,#35231,#35232,
#35233,#35234,#35235,#35236,#35237,#35238,#35239,#35240,#35241,#35242,#35243,
#35244,#35245,#35246,#35247,#35248,#35249,#35250,#35251,#35252,#35253,#35254,
#35255,#35256,#35257,#35258,#35259,#35260,#35261,#35262,#35263,#35264,#35265,
#35266,#35267,#35268,#35269,#35270,#35271,#35272,#35273,#35274,#35275,#35276,
#35277,#35278,#35279,#35280,#35281,#35282,#35283,#35284,#35285,#35286,#35287,
#35288,#35289,#35290,#35291,#35292,#35293,#35294,#35295,#35296,#35297,#35298,
#35299,#35300,#35301,#35302,#35303,#35304,#35305,#35306,#35307,#35308,#35309,
#35310,#35311,#35312,#35313,#35314,#35315,#35316,#35317,#35318,#35319,#35320,
#35321,#35322,#35323,#35324,#35325,#35326,#35327,#35328,#35329,#35330,#35331,
#35332,#35333,#35334,#35335,#35336,#35337,#35338,#35339,#35340,#35341,#35342,
#35343,#35344,#35345,#35346,#35347,#35348,#35349,#35350,#35351,#35352,#35353,
#35354,#35355,#35356,#35357,#35358,#35359,#35360,#35361,#35362,#35363,#35364,
#35365,#35366,#35367,#35368,#35369,#35370,#35371,#35372,#35373,#35374,#35375,
#35376,#35377,#35378,#35379,#35380,#35381,#35382,#35383,#35384,#35385,#35386,
#35387,#35388,#35389,#35390,#35391,#35392,#35393,#35394,#35395,#35396,#35397,
#35398,#35399,#35400,#35401,#35402,#35403,#35404,#35405,#35406,#35407,#35408,
#35409,#35410,#35411,#35412,#35413,#35414),.UNSPECIFIED.,.F.,.F.,(4,2,2,
2,2,2,2,2,2,2,2,2,2,2,2,2,2,2,2,2,2,2,2,2,2,2,2,2,2,2,2,2,2,2,2,2,2,2,2,
2,2,2,2,2,2,2,2,2,2,2,2,2,2,2,2,2,2,2,2,2,2,2,2,2,2,2,2,2,2,2,2,2,2,2,2,
2,2,2,2,2,2,2,2,2,2,2,2,2,2,2,2,2,2,2,2,2,2,2,2,2,2,2,2,2,2,2,2,2,2,4),
(-3.17213860495443,-3.1305769562313,-3.1011543313151,-3.07940569487357,
-3.06755913278467,-3.06412937072432,-3.06200121614224,-3.06001183753837,
-3.05759557415168,-3.05141079880141,-3.00074436630835,-2.95610171727953,
-2.94799787544405,-2.94311028336209,-2.9388423190976,-2.93878581376589,
-2.93872617091512,-2.93866302170105,-2.93859593747089,-2.93852441661367,
-2.93844786771765,-2.93836558771644,-2.93827673316758,-2.93818028195483,
-2.93807498135861,-2.93795927634505,-2.93463290382022,-2.93058354075275,
-2.92358311452377,-2.89261504641914,-2.85020348039682,-2.8283124036129,
-2.81641575970837,-2.81298110322945,-2.8108519274099,-2.80886323377176,
-2.80644949850555,-2.80028041505933,-2.74937910858284,-2.69963783857535,
-2.69130680027413,-2.68701988286206,-2.68353288471406,-2.67950584130784,
-2.67260340068405,-2.64258311380944,-2.59209004602213,-2.56675694200023,
-2.56249770513191,-2.56018826617702,-2.55822828324274,-2.55571053571208,
-2.55162043853799,-2.52205241740852,-2.48615474983624,-2.450024113373,-2.44073933772684,
-2.43626485570551,-2.43276121089515,-2.42885794036158,-2.42234136089115,
-2.39902370075791,-2.34278808641017,-2.32441657854521,-2.31382489314394,
-2.31052782164752,-2.30842895870605,-2.30642185025093,-2.30393641996668,
-2.29777657575977,-2.24939876308865,-2.2131415114354,-2.19982771577643,
-2.18991321886205,-2.18532086469977,-2.18180245458665,-2.17796012698621,
-2.17172298777249,-2.15115357121809,-2.09207049766749,-2.07339437663057,
-2.06268427389943,-2.05937400263014,-2.05727221534484,-2.05526703028496,
-2.05278894115209,-2.04667183055632,-1.99759164633159,-1.94556170241649,
-1.93758819768458,-1.93337427330436,-1.93022975370303,-1.92626816563616,
-1.91948356943942,-1.89257179180857,-1.83960741097014,-1.82179683775734,
-1.81481528442673,-1.80960433593195,-1.80710113985355,-1.80514217479726,
-1.80282176944635,-1.79863123416595,-1.77791047766794,-1.72651371559181,
-1.69262381260827,-1.68567753170966,-1.68168099400651,-1.67819127484788,
-1.67563146043802),.UNSPECIFIED.);
#436=B_SPLINE_CURVE_WITH_KNOTS('',3,(#35420,#35421,#35422,#35423,#35424,
#35425,#35426,#35427,#35428,#35429,#35430,#35431,#35432,#35433,#35434,#35435,
#35436,#35437,#35438,#35439,#35440,#35441,#35442,#35443,#35444,#35445,#35446,
#35447,#35448,#35449,#35450,#35451,#35452,#35453,#35454,#35455,#35456,#35457,
#35458,#35459,#35460,#35461,#35462,#35463,#35464,#35465,#35466,#35467,#35468,
#35469,#35470,#35471,#35472,#35473,#35474,#35475,#35476,#35477,#35478,#35479,
#35480,#35481,#35482,#35483,#35484,#35485,#35486,#35487,#35488,#35489,#35490,
#35491,#35492,#35493,#35494,#35495,#35496,#35497,#35498,#35499,#35500,#35501,
#35502,#35503,#35504,#35505,#35506,#35507,#35508,#35509,#35510,#35511,#35512,
#35513,#35514,#35515,#35516,#35517,#35518,#35519,#35520,#35521,#35522,#35523,
#35524,#35525,#35526,#35527,#35528,#35529,#35530,#35531,#35532,#35533,#35534,
#35535,#35536,#35537,#35538,#35539,#35540,#35541,#35542,#35543,#35544,#35545,
#35546,#35547,#35548,#35549,#35550,#35551,#35552,#35553,#35554,#35555,#35556,
#35557,#35558,#35559,#35560,#35561,#35562,#35563,#35564,#35565,#35566,#35567,
#35568,#35569,#35570,#35571,#35572,#35573,#35574,#35575,#35576,#35577,#35578,
#35579,#35580,#35581,#35582,#35583,#35584,#35585,#35586,#35587,#35588,#35589,
#35590,#35591,#35592,#35593,#35594,#35595,#35596,#35597,#35598,#35599,#35600),
 .UNSPECIFIED.,.F.,.F.,(4,3,3,3,3,3,3,3,3,3,3,3,3,3,3,3,3,3,3,3,3,3,3,3,
3,3,3,3,3,3,3,3,3,3,3,3,3,3,3,3,3,3,3,3,3,3,3,3,3,3,3,3,3,3,3,3,3,3,3,3,
4),(26.7958893988467,26.8666522515975,26.9657113691745,27.0646300434264,
27.1642654687607,27.2630074701039,27.3617169968462,27.4604238347903,27.560746237618,
27.659594830971,27.760654138536,27.8617134461011,27.9607725636811,28.0596912379358,
28.1593266632694,28.2580686646153,28.3567781913602,28.4554850293069,28.5558074321313,
28.6546560254866,28.7557153330456,28.8567746406047,28.9558337581938,29.0547524324578,
29.1543878577891,29.2531298591447,29.3518393858993,29.4505462238559,29.550868626669,
29.6497172200342,29.7507765275713,29.8518358351083,29.9508949526917,30.0498136269499,
30.1494490522826,30.2481910536322,30.3469005803809,30.4456074183313,30.5459298211515,
30.6447784145107,30.7458377220613,30.846897029612,30.9459561471962,31.0448748214552,
31.1445102467877,31.2432522481381,31.3419617748876,31.440668612839,31.5409910156581,
31.6398396090181,31.7408989165668,31.8419582241156,31.9397107034369,32.0379330750836,
32.1354344299566,32.2328770951219,32.3302923655519,32.4290916933166,32.5265951482246,
32.6260424124176,32.7254896766106),.UNSPECIFIED.);
#437=B_SPLINE_CURVE_WITH_KNOTS('',3,(#35601,#35602,#35603,#35604,#35605,
#35606,#35607,#35608,#35609,#35610,#35611,#35612,#35613),.UNSPECIFIED.,
 .F.,.F.,(4,3,3,3,4),(32.7254896768748,32.8370194186192,32.9360800605226,
33.034988358453,33.0800282649154),.UNSPECIFIED.);
#438=B_SPLINE_CURVE_WITH_KNOTS('',3,(#35614,#35615,#35616,#35617,#35618,
#35619,#35620,#35621,#35622,#35623,#35624,#35625,#35626,#35627,#35628,#35629,
#35630,#35631,#35632,#35633,#35634,#35635,#35636,#35637,#35638,#35639,#35640,
#35641,#35642,#35643,#35644,#35645,#35646,#35647,#35648,#35649,#35650,#35651,
#35652,#35653,#35654,#35655,#35656,#35657,#35658,#35659,#35660,#35661,#35662,
#35663,#35664,#35665,#35666,#35667,#35668,#35669,#35670,#35671,#35672,#35673,
#35674,#35675,#35676,#35677,#35678,#35679,#35680,#35681,#35682,#35683,#35684,
#35685,#35686,#35687,#35688,#35689,#35690,#35691,#35692,#35693,#35694,#35695,
#35696,#35697,#35698,#35699,#35700,#35701,#35702,#35703,#35704,#35705,#35706,
#35707,#35708,#35709,#35710,#35711,#35712,#35713,#35714,#35715,#35716,#35717,
#35718,#35719,#35720,#35721,#35722,#35723,#35724,#35725,#35726,#35727,#35728,
#35729,#35730,#35731,#35732,#35733,#35734,#35735,#35736,#35737,#35738,#35739,
#35740,#35741,#35742,#35743,#35744,#35745,#35746,#35747,#35748,#35749,#35750,
#35751,#35752,#35753,#35754,#35755,#35756,#35757,#35758,#35759,#35760,#35761,
#35762,#35763,#35764,#35765,#35766,#35767,#35768,#35769,#35770,#35771,#35772,
#35773,#35774,#35775,#35776,#35777,#35778,#35779,#35780,#35781,#35782,#35783,
#35784,#35785,#35786,#35787,#35788,#35789,#35790,#35791,#35792,#35793,#35794,
#35795,#35796,#35797,#35798,#35799,#35800,#35801,#35802,#35803,#35804,#35805,
#35806,#35807,#35808,#35809,#35810,#35811,#35812,#35813,#35814,#35815,#35816,
#35817,#35818,#35819,#35820,#35821,#35822,#35823,#35824,#35825,#35826,#35827),
 .UNSPECIFIED.,.F.,.F.,(4,2,2,2,2,2,2,2,2,2,2,2,2,2,2,2,2,2,2,2,2,2,2,2,
2,2,2,2,2,2,2,2,2,2,2,2,2,2,2,2,2,2,2,2,2,2,2,2,2,2,2,2,2,2,2,2,2,2,2,2,
2,2,2,2,2,2,2,2,2,2,2,2,2,2,2,2,2,2,2,2,2,2,2,2,2,2,2,2,2,2,2,2,2,2,2,2,
2,2,2,2,2,2,2,2,2,2,4),(-1.67563146043802,-1.67386340543512,-1.66716963604788,
-1.62004883247232,-1.58613256227116,-1.57812154314721,-1.56164137422588,
-1.55770653562442,-1.55544409047493,-1.55367482768604,-1.55119769607692,
-1.54612013620645,-1.53936756252354,-1.52243077556491,-1.47211079425904,
-1.44161344681044,-1.43468430113439,-1.43065124715619,-1.4271647674396,
-1.42288575641767,-1.41459350625165,-1.40401381610217,-1.37896072319609,
-1.35009178044402,-1.34249707529684,-1.31153884432721,-1.30742659067437,
-1.30490234200958,-1.30294196663873,-1.30063756072213,-1.29640143650009,
-1.27169965427544,-1.22186607519781,-1.19059645293358,-1.18362628927154,
-1.17958411893583,-1.17609853363485,-1.17183171184376,-1.16359860289831,
-1.11906762448112,-1.07207694077685,-1.05889386108005,-1.05519697111931,
-1.05300993992704,-1.05102431851501,-1.04829464233656,-1.04183100449143,
-1.01017901911471,-0.953933685971024,-0.937056764507021,-0.931249132624984,
-0.927500254438264,-0.923947048010284,-0.91912522029482,-0.90790420809942,
-0.853500325655078,-0.812323806393507,-0.805882857328167,-0.803350148009882,
-0.801512740246387,-0.799472878164731,-0.796449742909075,-0.788062982445321,
-0.774898473240685,-0.737603586528475,-0.688961050274329,-0.682277256365227,
-0.677952588488077,-0.674463318632621,-0.670464959340183,-0.663509444542555,
-0.629409107630959,-0.575942090823529,-0.557366179423912,-0.553295455319311,
-0.551002160769359,-0.549040447091492,-0.546500440077176,-0.541096774914267,
-0.533778536942428,-0.514639994577777,-0.449906076524378,-0.434379647271338,
-0.428744882578528,-0.425403933652341,-0.421874459938085,-0.417201654005583,
-0.406839825564649,-0.392738490504648,-0.324253248694902,-0.3061122984198,
-0.302065712893207,-0.299777868167652,-0.297834089769661,-0.295347737666655,
-0.290212683319745,-0.2832643398259,-0.265580625678848,-0.212103045580461,
-0.185437985291434,-0.178669690013046,-0.174711832992602,-0.171567133299975,
-0.167348948614878,-0.15935377467112,-0.130573393771694,-0.0898485202972664),
 .UNSPECIFIED.);
#439=B_SPLINE_CURVE_WITH_KNOTS('',3,(#35833,#35834,#35835,#35836,#35837,
#35838,#35839,#35840,#35841,#35842,#35843,#35844,#35845,#35846,#35847,#35848,
#35849,#35850,#35851,#35852,#35853,#35854,#35855,#35856,#35857,#35858,#35859,
#35860,#35861,#35862,#35863,#35864,#35865,#35866,#35867,#35868,#35869,#35870,
#35871,#35872,#35873,#35874,#35875,#35876,#35877,#35878,#35879,#35880,#35881,
#35882,#35883,#35884,#35885,#35886,#35887,#35888,#35889,#35890,#35891,#35892,
#35893,#35894,#35895,#35896,#35897,#35898,#35899,#35900,#35901,#35902,#35903,
#35904,#35905,#35906,#35907,#35908,#35909,#35910,#35911,#35912,#35913,#35914,
#35915,#35916,#35917,#35918,#35919,#35920,#35921,#35922,#35923,#35924,#35925,
#35926,#35927,#35928,#35929,#35930,#35931,#35932,#35933,#35934,#35935,#35936,
#35937,#35938,#35939,#35940,#35941,#35942,#35943,#35944,#35945,#35946,#35947,
#35948,#35949,#35950,#35951,#35952,#35953,#35954,#35955,#35956,#35957,#35958,
#35959,#35960,#35961,#35962,#35963,#35964,#35965,#35966,#35967,#35968,#35969,
#35970,#35971,#35972,#35973,#35974,#35975,#35976,#35977,#35978,#35979,#35980,
#35981,#35982,#35983,#35984,#35985,#35986,#35987,#35988,#35989,#35990,#35991,
#35992,#35993,#35994,#35995,#35996,#35997,#35998,#35999,#36000,#36001,#36002,
#36003,#36004,#36005,#36006,#36007,#36008,#36009,#36010,#36011,#36012,#36013),
 .UNSPECIFIED.,.F.,.F.,(4,3,3,3,3,3,3,3,3,3,3,3,3,3,3,3,3,3,3,3,3,3,3,3,
3,3,3,3,3,3,3,3,3,3,3,3,3,3,3,3,3,3,3,3,3,3,3,3,3,3,3,3,3,3,3,3,3,3,3,3,
4),(20.512957591123,20.6107155250157,20.7085181868304,20.8064945872437,
20.8962850845758,20.9953442020216,21.0942628761449,21.1938983015117,21.2926403027342,
21.3913498293589,21.4900566671889,21.5903790701615,21.68922766341,21.7902869712447,
21.8913462790794,21.9904053962616,22.0893240701107,22.1889594955448,22.2877014964694,
22.3864110227881,22.4851178603042,22.5854402636239,22.6842888565421,22.7853481650626,
22.8864074735831,22.985466591425,23.0843852659453,23.1840206912129,23.2827626928314,
23.3814722198508,23.4801790580737,23.580501460577,23.6793500542096,23.7804093611482,
23.8814686680867,23.9805277856326,24.0794464598534,24.1790818851955,24.277823886508,
24.37653341322,24.4752402511339,24.575562653998,24.6744112473215,24.7754705549559,
24.8765298625903,24.9755889801305,25.0745076543444,25.1741430796881,25.2728850809916,
25.3715946076934,25.4703014455965,25.5706238484709,25.669472441782,25.7705317494379,
25.8715910570939,25.9728761868512,26.0739977695077,26.1749480071203,26.2757973954954,
26.376561049584,26.4423043696953),.UNSPECIFIED.);
#440=B_SPLINE_CURVE_WITH_KNOTS('',3,(#36014,#36015,#36016,#36017,#36018,
#36019,#36020,#36021,#36022,#36023,#36024,#36025,#36026),.UNSPECIFIED.,
 .F.,.F.,(4,3,3,3,4),(26.4423043699706,26.5495705688098,26.6571264572063,
26.7650823065106,26.7958893988467),.UNSPECIFIED.);
#441=B_SPLINE_CURVE_WITH_KNOTS('',3,(#36028,#36029,#36030,#36031,#36032,
#36033,#36034,#36035,#36036,#36037,#36038,#36039,#36040,#36041,#36042,#36043,
#36044,#36045,#36046,#36047),.UNSPECIFIED.,.F.,.F.,(4,2,2,2,2,2,2,2,2,4),
(-0.0898485202972664,-0.088519391729811,-0.055828355046822,-0.0516951276582153,
-0.0491646822441494,-0.047203825256235,-0.0449039201267464,-0.0424484392440899,
-0.0385816794505213,-0.000734785208168012),.UNSPECIFIED.);
#442=B_SPLINE_CURVE_WITH_KNOTS('',3,(#36048,#36049,#36050,#36051,#36052,
#36053,#36054,#36055,#36056,#36057,#36058,#36059,#36060,#36061,#36062,#36063,
#36064,#36065,#36066,#36067,#36068,#36069,#36070,#36071,#36072,#36073,#36074,
#36075,#36076,#36077,#36078,#36079,#36080,#36081,#36082,#36083,#36084,#36085,
#36086,#36087,#36088,#36089,#36090,#36091,#36092,#36093,#36094,#36095,#36096,
#36097,#36098,#36099,#36100,#36101,#36102,#36103,#36104,#36105,#36106,#36107,
#36108,#36109,#36110,#36111,#36112,#36113,#36114,#36115,#36116,#36117,#36118,
#36119,#36120,#36121,#36122,#36123,#36124,#36125,#36126,#36127,#36128,#36129,
#36130,#36131,#36132,#36133,#36134,#36135,#36136,#36137,#36138,#36139,#36140,
#36141,#36142,#36143,#36144,#36145,#36146,#36147,#36148,#36149,#36150,#36151,
#36152,#36153,#36154,#36155,#36156,#36157,#36158,#36159,#36160,#36161,#36162,
#36163,#36164,#36165,#36166,#36167,#36168,#36169,#36170,#36171,#36172,#36173,
#36174,#36175,#36176,#36177,#36178,#36179,#36180,#36181,#36182,#36183,#36184,
#36185,#36186,#36187,#36188,#36189,#36190,#36191,#36192,#36193,#36194,#36195,
#36196,#36197,#36198,#36199,#36200,#36201,#36202,#36203,#36204,#36205,#36206,
#36207,#36208,#36209,#36210,#36211,#36212,#36213,#36214,#36215,#36216,#36217,
#36218,#36219,#36220,#36221,#36222,#36223,#36224,#36225,#36226,#36227,#36228,
#36229,#36230,#36231,#36232,#36233,#36234,#36235,#36236,#36237,#36238,#36239),
 .UNSPECIFIED.,.F.,.F.,(4,2,2,2,2,2,2,2,2,2,2,2,2,2,2,2,2,2,2,2,2,2,2,2,
2,2,2,2,2,2,2,2,2,2,2,2,2,2,2,2,2,2,2,2,2,2,2,2,2,2,2,2,2,2,2,2,2,2,2,2,
2,2,2,2,2,2,2,2,2,2,2,2,2,2,2,2,2,2,2,2,2,2,2,2,2,2,2,2,2,2,2,2,2,2,2,4),
(-3.17305528611881,-3.12119598485782,-3.10694997652477,-3.09999708888609,
-3.09599853846014,-3.09250811032236,-3.08818072111211,-3.081490309315,-3.03342159340058,
-2.99274582943489,-2.98132422407236,-2.97385514052582,-2.97101260883616,
-2.96897096893944,-2.96713402424151,-2.96411408264857,-2.95637669928287,
-2.8832775912868,-2.85508809567373,-2.84845826867864,-2.84453020763418,
-2.84103095571322,-2.83659838943983,-2.82753227050961,-2.76396187037434,
-2.72693156883095,-2.72154125280845,-2.71900352543636,-2.71704170994051,
-2.71474614698292,-2.71066639720707,-2.69197707082225,-2.63857324484164,
-2.60446818881316,-2.59751135516865,-2.59351234002292,-2.59002256336977,
-2.58569735161569,-2.57901293907899,-2.53684202504075,-2.47981143701736,
-2.47150581351878,-2.46849361347391,-2.46645574528543,-2.46461590921309,
-2.46157953045154,-2.45373928276605,-2.37990453612947,-2.35250493155654,
-2.34592780132056,-2.34201155910593,-2.33851079216589,-2.33405988214605,
-2.3248967722079,-2.26213151552723,-2.2244837019353,-2.21908248588282,-2.21654290289892,
-2.21458116984241,-2.2122874722992,-2.20821510969055,-2.18961572829298,
-2.13613031711779,-2.10202031010675,-2.09506400109957,-2.09106545166044,
-2.08757617756413,-2.08325171325803,-2.0765686952944,-2.0280387753872,-1.99051817903146,
-1.97745807415392,-1.96911862154623,-1.96610204001727,-1.96406351487456,
-1.96222489682589,-1.95968742708636,-1.95321809107746,-1.91469568611194,
-1.87153696877301,-1.84941278137741,-1.84324518000014,-1.83941828947981,
-1.83589577240727,-1.83134946655419,-1.82141478159157,-1.76954856914802,
-1.74010019936102,-1.72660385128643,-1.71806482397902,-1.71502088900458,
-1.71297673750873,-1.71114307354735,-1.70862510368386,-1.7022724913293,
-1.67601819536357),.UNSPECIFIED.);
#443=B_SPLINE_CURVE_WITH_KNOTS('',3,(#36245,#36246,#36247,#36248,#36249,
#36250,#36251,#36252,#36253,#36254,#36255,#36256,#36257,#36258,#36259,#36260,
#36261,#36262,#36263,#36264,#36265,#36266,#36267,#36268,#36269,#36270,#36271,
#36272,#36273,#36274,#36275,#36276,#36277,#36278,#36279,#36280,#36281,#36282,
#36283,#36284,#36285,#36286,#36287,#36288,#36289,#36290,#36291,#36292,#36293,
#36294,#36295,#36296,#36297,#36298,#36299,#36300,#36301,#36302,#36303,#36304,
#36305,#36306,#36307,#36308,#36309,#36310,#36311,#36312,#36313,#36314,#36315,
#36316,#36317,#36318,#36319,#36320,#36321,#36322,#36323,#36324,#36325,#36326,
#36327,#36328,#36329,#36330,#36331,#36332,#36333,#36334,#36335,#36336,#36337,
#36338,#36339,#36340,#36341,#36342,#36343,#36344,#36345,#36346,#36347,#36348,
#36349,#36350,#36351,#36352,#36353,#36354,#36355,#36356,#36357,#36358,#36359,
#36360,#36361,#36362,#36363,#36364,#36365,#36366,#36367,#36368,#36369,#36370,
#36371,#36372,#36373,#36374,#36375,#36376,#36377,#36378,#36379,#36380,#36381,
#36382,#36383,#36384,#36385,#36386,#36387,#36388,#36389,#36390,#36391,#36392,
#36393,#36394,#36395,#36396,#36397,#36398,#36399,#36400,#36401,#36402,#36403,
#36404,#36405,#36406,#36407,#36408,#36409,#36410,#36411,#36412,#36413,#36414,
#36415,#36416,#36417,#36418,#36419,#36420,#36421,#36422),.UNSPECIFIED.,
 .F.,.F.,(4,3,3,3,3,3,3,3,3,3,3,3,3,3,3,3,3,3,3,3,3,3,3,3,3,3,3,3,3,3,3,
3,3,3,3,3,3,3,3,3,3,3,3,3,3,3,3,3,3,3,3,3,3,3,3,3,3,3,3,4),(14.2304071265534,
14.3291482971637,14.4278575780463,14.5265647543816,14.6264030451747,14.7252525926983,
14.8255852551262,14.9259179175542,15.0249770463333,15.1238957322449,15.2235311547215,
15.3222731687617,15.4209827085634,15.5196895599131,15.6200119479492,15.718860555431,
15.8199198337444,15.9209791120578,16.0200382004424,16.1189568450004,16.2185922776956,
16.3173342483389,16.4160437440714,16.5147505507373,16.6150729896934,16.7139215514226,
16.814980928992,16.9160403065614,17.0150994373653,17.1140181250032,17.2136535470109,
17.312395562029,17.411105102524,17.5098119542802,17.6101343409764,17.7089829481464,
17.8100422246057,17.911101501065,18.0101606188399,18.1090792933301,18.2087147186099,
18.30745672029,18.4061662474056,18.504873085759,18.6051954882114,18.704044082059,
18.8051033888138,18.9061626955686,19.005221809666,19.1041404803751,19.2037759065872,
19.3025179042597,19.4012274272912,19.4999342614895,19.6002566686351,19.6991052581938,
19.800164574133,19.9012238900722,20.0301714761758,20.1591190622793),
 .UNSPECIFIED.);
#444=B_SPLINE_CURVE_WITH_KNOTS('',3,(#36423,#36424,#36425,#36426,#36427,
#36428,#36429,#36430,#36431,#36432,#36433,#36434,#36435),.UNSPECIFIED.,
 .F.,.F.,(4,3,3,3,4),(20.1591190625157,20.2568630541379,20.3545467744327,
20.4522206668084,20.512957591123),.UNSPECIFIED.);
#445=B_SPLINE_CURVE_WITH_KNOTS('',3,(#36436,#36437,#36438,#36439,#36440,
#36441,#36442,#36443,#36444,#36445,#36446,#36447,#36448,#36449,#36450,#36451,
#36452,#36453,#36454,#36455,#36456,#36457,#36458,#36459,#36460,#36461,#36462,
#36463,#36464,#36465,#36466,#36467,#36468,#36469,#36470,#36471,#36472,#36473,
#36474,#36475,#36476,#36477,#36478,#36479,#36480,#36481,#36482,#36483,#36484,
#36485,#36486,#36487,#36488,#36489,#36490,#36491,#36492,#36493,#36494,#36495,
#36496,#36497,#36498,#36499,#36500,#36501,#36502,#36503,#36504,#36505,#36506,
#36507,#36508,#36509,#36510,#36511,#36512,#36513,#36514,#36515,#36516,#36517,
#36518,#36519,#36520,#36521,#36522,#36523,#36524,#36525,#36526,#36527,#36528,
#36529,#36530,#36531,#36532,#36533,#36534,#36535,#36536,#36537,#36538,#36539,
#36540,#36541,#36542,#36543,#36544,#36545,#36546,#36547,#36548,#36549,#36550,
#36551,#36552,#36553,#36554,#36555,#36556,#36557,#36558,#36559,#36560,#36561,
#36562,#36563,#36564,#36565,#36566,#36567,#36568,#36569,#36570,#36571,#36572,
#36573,#36574,#36575,#36576,#36577,#36578,#36579,#36580,#36581,#36582,#36583,
#36584,#36585,#36586,#36587,#36588,#36589,#36590,#36591,#36592,#36593,#36594,
#36595,#36596,#36597,#36598,#36599,#36600,#36601,#36602,#36603,#36604,#36605,
#36606,#36607,#36608,#36609,#36610,#36611,#36612,#36613,#36614,#36615,#36616,
#36617,#36618,#36619,#36620,#36621,#36622,#36623,#36624,#36625,#36626,#36627,
#36628,#36629,#36630,#36631,#36632,#36633,#36634,#36635,#36636,#36637,#36638,
#36639,#36640,#36641,#36642,#36643,#36644,#36645),.UNSPECIFIED.,.F.,.F.,
(4,2,2,2,2,2,2,2,2,2,2,2,2,2,2,2,2,2,2,2,2,2,2,2,2,2,2,2,2,2,2,2,2,2,2,
2,2,2,2,2,2,2,2,2,2,2,2,2,2,2,2,2,2,2,2,2,2,2,2,2,2,2,2,2,2,2,2,2,2,2,2,
2,2,2,2,2,2,2,2,2,2,2,2,2,2,2,2,2,2,2,2,2,2,2,2,2,2,2,2,2,2,2,2,2,4),(-1.67601819536357,
-1.65790025499768,-1.61896284412362,-1.60509562768696,-1.59486655864749,
-1.59021745821083,-1.58669143392088,-1.58287567134888,-1.57675893988783,
-1.55519531241609,-1.48395421543031,-1.46857009413773,-1.4647172953657,
-1.46247364218787,-1.46070116686806,-1.45819612567498,-1.4529754007906,
-1.44597622680274,-1.42809635724663,-1.37479644466355,-1.34823059336616,
-1.34146861434871,-1.33751204574301,-1.33436706400397,-1.33014682113187,
-1.32214207392476,-1.31202687293987,-1.28862509419608,-1.25835229108425,
-1.24086345010961,-1.21824854332673,-1.2143351572252,-1.21187038725554,
-1.20991377772064,-1.20756290828643,-1.20310707712571,-1.17062074321288,
-1.12038416497146,-1.09670656245716,-1.09017793969407,-1.08627230939772,
-1.08276959461745,-1.07830049764668,-1.06904232599539,-1.03312176721833,
-1.00178015394779,-0.967567612180327,-0.963427606838462,-0.960895207831793,
-0.958934267849848,-0.956635946957671,-0.952427836578429,-0.928448821204537,
-0.894431230410167,-0.847246193343973,-0.840556552502571,-0.836230258557596,
-0.832741076230961,-0.828744351174761,-0.821795653901332,-0.787833356059805,
-0.735643723495315,-0.715781079097813,-0.711636231704487,-0.709326296461956,
-0.707366653453092,-0.704850326843802,-0.699570167470669,-0.692467608790283,
-0.674183788867987,-0.618574581215839,-0.594565641896955,-0.587995754370924,
-0.584081261981406,-0.580580464692471,-0.57612733547081,-0.566951714772156,
-0.531678367384627,-0.476953464893904,-0.463757039289214,-0.460058964574486,
-0.457871710637919,-0.455886158413932,-0.453157021728804,-0.446696800430247,
-0.415080292744081,-0.358932806466596,-0.341955533618985,-0.336135123207361,
-0.332383491413861,-0.328831597930515,-0.324017674883814,-0.312843500835583,
-0.258969096150844,-0.217169344008483,-0.210749869566655,-0.208220789721541,
-0.206384342851417,-0.204343743325026,-0.201503213626732,-0.194026652308553,
-0.182594928304509,-0.14240303572949,-0.0938347109390278,-0.0902767619888763),
 .UNSPECIFIED.);
#446=B_SPLINE_CURVE_WITH_KNOTS('',3,(#36651,#36652,#36653,#36654,#36655,
#36656,#36657,#36658,#36659,#36660,#36661,#36662,#36663),.UNSPECIFIED.,
 .F.,.F.,(4,3,3,3,4),(-4.20357826990315,-4.10478695491414,-4.00583745897424,
-3.98024477801445,-3.84897440564112),.UNSPECIFIED.);
#447=B_SPLINE_CURVE_WITH_KNOTS('',3,(#36665,#36666,#36667,#36668,#36669,
#36670,#36671,#36672,#36673,#36674,#36675,#36676,#36677,#36678,#36679,#36680,
#36681,#36682,#36683,#36684,#36685,#36686,#36687,#36688,#36689,#36690,#36691,
#36692,#36693,#36694,#36695,#36696,#36697,#36698,#36699,#36700,#36701,#36702,
#36703,#36704,#36705,#36706,#36707,#36708,#36709,#36710,#36711,#36712,#36713,
#36714,#36715,#36716,#36717,#36718,#36719,#36720,#36721,#36722,#36723,#36724,
#36725,#36726,#36727,#36728,#36729,#36730,#36731,#36732,#36733,#36734,#36735,
#36736,#36737,#36738,#36739,#36740,#36741,#36742,#36743,#36744,#36745,#36746,
#36747,#36748,#36749,#36750,#36751,#36752,#36753,#36754,#36755,#36756,#36757,
#36758,#36759,#36760,#36761,#36762,#36763,#36764,#36765,#36766,#36767,#36768,
#36769,#36770,#36771,#36772,#36773,#36774,#36775,#36776,#36777,#36778,#36779,
#36780,#36781,#36782,#36783,#36784,#36785),.UNSPECIFIED.,.F.,.F.,(4,3,3,
3,3,3,3,3,3,3,3,3,3,3,3,3,3,3,3,3,3,3,3,3,3,3,3,3,3,3,3,3,3,3,3,3,3,3,3,
3,4),(-3.84897440539329,-3.75125999555739,-3.65367480658484,-3.55616073132701,
-3.45868648046565,-3.36122081576358,-3.26366927760976,-3.16607558945825,
-3.06831667010992,-2.98518358351084,-2.88604218773156,-2.78703918957161,
-2.68742458950106,-2.58859397716361,-2.48979444543964,-2.39099634432946,
-2.2907778554989,-2.19183589568085,-2.09097914234403,-1.99012238900722,
-1.89201567343051,-1.79404975393482,-1.69417618400592,-1.59638143615237,
-1.49861527802913,-1.40084681613672,-1.29940041072845,-1.2014686750187,
-1.10345750403516,-1.00527923358739,-0.99506119450361,-0.893332626667933,
-0.791764351772391,-0.690356289583907,-0.58904245229151,-0.487798384630709,
-0.386599710304198,-0.28539210708937,-0.184186082512049,-0.0829053445198521,
-3.08113896577085E-14),.UNSPECIFIED.);
#448=B_SPLINE_CURVE_WITH_KNOTS('',3,(#36789,#36790,#36791,#36792,#36793,
#36794,#36795,#36796,#36797,#36798,#36799,#36800,#36801,#36802,#36803,#36804,
#36805,#36806,#36807,#36808,#36809,#36810,#36811,#36812,#36813,#36814,#36815,
#36816,#36817,#36818,#36819,#36820,#36821,#36822,#36823,#36824,#36825,#36826,
#36827,#36828,#36829,#36830,#36831,#36832,#36833,#36834,#36835,#36836,#36837,
#36838,#36839,#36840,#36841,#36842,#36843,#36844,#36845,#36846,#36847,#36848,
#36849,#36850,#36851,#36852,#36853,#36854,#36855,#36856,#36857,#36858,#36859,
#36860,#36861,#36862,#36863,#36864,#36865,#36866,#36867,#36868,#36869,#36870,
#36871,#36872,#36873,#36874,#36875,#36876,#36877,#36878,#36879,#36880,#36881,
#36882,#36883,#36884,#36885,#36886,#36887,#36888,#36889,#36890,#36891,#36892,
#36893,#36894,#36895,#36896,#36897,#36898,#36899,#36900,#36901,#36902,#36903,
#36904,#36905,#36906,#36907,#36908,#36909,#36910,#36911,#36912,#36913,#36914,
#36915,#36916,#36917,#36918,#36919,#36920,#36921,#36922,#36923,#36924,#36925,
#36926,#36927,#36928,#36929,#36930,#36931,#36932,#36933,#36934,#36935,#36936,
#36937,#36938,#36939,#36940,#36941,#36942,#36943,#36944,#36945,#36946,#36947,
#36948,#36949,#36950,#36951,#36952,#36953,#36954,#36955,#36956,#36957,#36958,
#36959,#36960),.UNSPECIFIED.,.F.,.F.,(4,3,3,3,3,3,3,3,3,3,3,3,3,3,3,3,3,
3,3,3,3,3,3,3,3,3,3,3,3,3,3,3,3,3,3,3,3,3,3,3,3,3,3,3,3,3,3,3,3,3,3,3,3,
3,3,3,3,4),(2.01695560162626,2.11564189726858,2.21418829647648,2.31262230469899,
2.41099520084271,2.50933729039148,2.60767884072445,2.70611518766494,2.80459906192678,
2.9032524542413,2.98518358351084,3.08440364663108,3.18348650423872,3.28308128846069,
3.3819941430274,3.48087664382076,3.57975834074699,3.67987995006385,3.77890625693714,
3.87957551747579,3.98024477801444,4.07919428955199,4.1780018264564,4.27766484471411,
4.37629277757328,4.47488738556402,4.57347860632559,4.67393544787371,4.77266786606485,
4.87398691929145,4.97530597251806,5.07438444725685,5.17332252305007,5.27295310354652,
5.37171446613478,5.47044329472867,5.56916934814539,5.66946880286446,5.76833619817666,
5.86935168259916,5.97036716702167,6.06944373196721,6.16838022720496,6.268011243995,
6.36677184867722,6.46550023158715,6.56422615356924,6.66452670555825,6.76339475286863,
6.86441155719695,6.96542836152528,7.06514996643927,7.16472649372704,7.26418682012562,
7.36355392634545,7.46286736071847,7.56216603022671,7.59274844815647),
 .UNSPECIFIED.);
#449=B_SPLINE_CURVE_WITH_KNOTS('',3,(#36961,#36962,#36963,#36964,#36965,
#36966,#36967,#36968,#36969,#36970,#36971,#36972,#36973),.UNSPECIFIED.,
 .F.,.F.,(4,3,3,3,4),(7.59274844852976,7.7041800085765,7.8161317130083,
7.928691988329,7.9466267193592),.UNSPECIFIED.);
#450=B_SPLINE_CURVE_WITH_KNOTS('',3,(#36976,#36977,#36978,#36979,#36980,
#36981,#36982,#36983,#36984,#36985,#36986,#36987,#36988,#36989,#36990,#36991,
#36992,#36993,#36994,#36995,#36996,#36997,#36998,#36999,#37000,#37001,#37002,
#37003,#37004,#37005,#37006,#37007,#37008,#37009,#37010,#37011,#37012,#37013,
#37014,#37015,#37016,#37017,#37018,#37019,#37020,#37021,#37022,#37023,#37024,
#37025,#37026,#37027,#37028,#37029,#37030,#37031,#37032,#37033,#37034,#37035,
#37036,#37037,#37038,#37039,#37040,#37041,#37042,#37043,#37044,#37045,#37046,
#37047,#37048,#37049,#37050,#37051,#37052,#37053,#37054,#37055,#37056,#37057,
#37058,#37059,#37060,#37061,#37062,#37063,#37064,#37065,#37066,#37067,#37068,
#37069,#37070,#37071,#37072,#37073,#37074,#37075,#37076,#37077,#37078,#37079,
#37080,#37081,#37082,#37083,#37084,#37085,#37086,#37087,#37088,#37089,#37090,
#37091,#37092,#37093,#37094,#37095,#37096,#37097,#37098,#37099,#37100,#37101,
#37102,#37103,#37104,#37105,#37106,#37107,#37108,#37109,#37110,#37111,#37112,
#37113,#37114,#37115,#37116,#37117,#37118,#37119,#37120,#37121,#37122,#37123,
#37124,#37125,#37126,#37127,#37128,#37129,#37130,#37131,#37132,#37133,#37134,
#37135,#37136,#37137,#37138,#37139,#37140,#37141,#37142,#37143,#37144,#37145,
#37146,#37147,#37148,#37149,#37150,#37151,#37152,#37153,#37154,#37155,#37156,
#37157,#37158,#37159),.UNSPECIFIED.,.F.,.F.,(4,3,3,3,3,3,3,3,3,3,3,3,3,
3,3,3,3,3,3,3,3,3,3,3,3,3,3,3,3,3,3,3,3,3,3,3,3,3,3,3,3,3,3,3,3,3,3,3,3,
3,3,3,3,3,3,3,3,3,3,3,3,4),(7.9466267193592,7.96048955602889,8.05955222869409,
8.15847448196122,8.25810901553263,8.35685462726907,8.45556776802807,8.55427821863936,
8.65459635161265,8.75344851699117,8.85449963376183,8.9555507505325,9.05461163472714,
9.15353211785238,9.25316709625034,9.35191099658619,9.450622452008,9.54933124579016,
9.64965142060165,9.74850201721232,9.84955698112422,9.95061194503612,10.0496691800778,
10.148585942413,10.2482218420539,10.3469618738397,10.4456694137526,10.544374250258,
10.6446989725784,10.7435455487723,10.844609344156,10.9456731395397,11.0447328420797,
11.1436521066727,11.243287385094,11.3420299854808,11.4407401131877,11.5394475531969,
11.6397692484085,11.738618440354,11.8396763871987,11.9407343340433,12.039793611144,
12.1387124494771,12.2383478343608,12.3370900097446,12.4357997138898,12.5345067323694,
12.6348289314138,12.7336777112374,12.8347366198922,12.9357955285469,13.0340412306013,
13.1321472235822,13.2301416920862,13.3280762000881,13.4259815616605,13.5238885532223,
13.6218885616932,13.7199390884583,13.8181477780583,13.875933755129),
 .UNSPECIFIED.);
#451=B_SPLINE_CURVE_WITH_KNOTS('',3,(#37160,#37161,#37162,#37163,#37164,
#37165,#37166,#37167,#37168,#37169,#37170,#37171,#37172),.UNSPECIFIED.,
 .F.,.F.,(4,3,3,3,4),(13.8759337553361,13.9308567230506,14.0299036910203,
14.1301554087868,14.2304071265534),.UNSPECIFIED.);
#452=B_SPLINE_CURVE_WITH_KNOTS('',3,(#37174,#37175,#37176,#37177,#37178,
#37179,#37180,#37181,#37182,#37183,#37184,#37185,#37186,#37187,#37188,#37189),
 .UNSPECIFIED.,.F.,.F.,(4,2,2,2,2,2,2,4),(-0.0902767619888763,-0.0871517738827283,
-0.0828276961846434,-0.0793389329993606,-0.0753411934293112,-0.0683868759572198,
-0.0544509421788097,-0.000738945914559194),.UNSPECIFIED.);
#453=B_SPLINE_CURVE_WITH_KNOTS('',3,(#37190,#37191,#37192,#37193,#37194,
#37195,#37196,#37197,#37198,#37199,#37200,#37201,#37202,#37203,#37204,#37205,
#37206,#37207,#37208,#37209,#37210,#37211,#37212,#37213,#37214,#37215,#37216,
#37217,#37218,#37219,#37220,#37221,#37222,#37223,#37224,#37225,#37226,#37227,
#37228,#37229,#37230,#37231,#37232,#37233,#37234,#37235,#37236,#37237,#37238,
#37239,#37240,#37241,#37242,#37243,#37244,#37245,#37246,#37247,#37248,#37249,
#37250,#37251,#37252,#37253,#37254,#37255,#37256,#37257,#37258,#37259,#37260,
#37261,#37262,#37263,#37264,#37265,#37266,#37267,#37268,#37269,#37270,#37271,
#37272,#37273,#37274,#37275,#37276,#37277,#37278,#37279,#37280,#37281,#37282,
#37283,#37284,#37285,#37286,#37287,#37288,#37289,#37290,#37291,#37292,#37293,
#37294,#37295,#37296,#37297,#37298,#37299,#37300,#37301,#37302,#37303,#37304,
#37305,#37306,#37307,#37308,#37309,#37310,#37311,#37312,#37313,#37314,#37315,
#37316,#37317,#37318,#37319,#37320,#37321,#37322,#37323,#37324,#37325,#37326,
#37327,#37328,#37329,#37330,#37331,#37332,#37333,#37334,#37335,#37336,#37337,
#37338,#37339,#37340,#37341,#37342,#37343,#37344,#37345,#37346,#37347,#37348,
#37349,#37350,#37351,#37352,#37353,#37354,#37355,#37356,#37357,#37358,#37359,
#37360,#37361,#37362,#37363,#37364,#37365,#37366,#37367,#37368,#37369,#37370),
 .UNSPECIFIED.,.F.,.F.,(4,3,3,3,3,3,3,3,3,3,3,3,3,3,3,3,3,3,3,3,3,3,3,3,
3,3,3,3,3,3,3,3,3,3,3,3,3,3,3,3,3,3,3,3,3,3,3,3,3,3,3,3,3,3,3,3,3,3,3,3,
4),(-10.1321597128208,-9.98380287347192,-9.95061194503611,-9.85155080805362,
-9.75263012655875,-9.65299520455547,-9.55425123974632,-9.45553977016634,
-9.3568310125024,-9.25651094700993,-9.15766050991737,-9.05660563022494,
-8.95555075053251,-8.85648813509386,-8.75756592802855,-8.6579313815286,
-8.55918578882376,-8.46047265687315,-8.36176220484683,-8.26144404264234,
-8.1625918506966,-8.06154070336275,-7.96048955602889,-7.86144585639168,
-7.76254262764497,-7.66290334438001,-7.56417674344362,-7.46548256638777,
-7.3667910070416,-7.26645034566252,-7.16761670121533,-7.06652253137031,
-6.96542836152528,-6.8663497016468,-6.76741156214399,-6.6677810127537,-6.56901987256432,
-6.47029137085155,-6.37156574645098,-6.27126610159365,-6.1723993736445,
-6.07138327033308,-5.97036716702167,-5.87128979664853,-5.77235259505363,
-5.67272176723669,-5.57396071232545,-5.47523197841698,-5.37650580681207,
-5.27620584823857,-5.17733781201762,-5.07632189226784,-4.97530597251806,
-4.87639029978064,-4.7776031596478,-4.67891439036993,-4.58029393416826,
-4.4816847956452,-4.38308674516142,-4.28441542602605,-4.20357826990315),
 .UNSPECIFIED.);
#454=B_SPLINE_CURVE_WITH_KNOTS('',3,(#37373,#37374,#37375,#37376,#37377,
#37378,#37379,#37380),.UNSPECIFIED.,.F.,.F.,(4,1,1,1,1,4),(17.9343967671566,
18.824417223833,19.8194784183366,20.8145396128402,21.8096008073438,21.9911485751284),
 .UNSPECIFIED.);
#455=B_SPLINE_CURVE_WITH_KNOTS('',3,(#37381,#37382,#37383,#37384,#37385,
#37386),.UNSPECIFIED.,.F.,.F.,(4,1,1,4),(21.9911485751284,22.8046620018474,
23.799723196351,24.2174104409543),.UNSPECIFIED.);
#456=B_SPLINE_CURVE_WITH_KNOTS('',3,(#37388,#37389,#37390,#37391,#37392,
#37393,#37394,#37395,#37396,#37397,#37398,#37399,#37400,#37401,#37402,#37403,
#37404,#37405,#37406,#37407,#37408,#37409,#37410,#37411,#37412,#37413,#37414,
#37415,#37416,#37417,#37418,#37419,#37420,#37421,#37422,#37423,#37424,#37425,
#37426,#37427,#37428,#37429,#37430,#37431,#37432,#37433,#37434,#37435,#37436,
#37437,#37438,#37439,#37440,#37441,#37442,#37443,#37444,#37445,#37446,#37447,
#37448,#37449,#37450,#37451,#37452,#37453,#37454,#37455,#37456,#37457,#37458,
#37459,#37460,#37461,#37462,#37463),.UNSPECIFIED.,.F.,.F.,(4,3,3,3,3,3,
3,3,3,3,3,3,3,3,3,3,3,3,3,3,3,3,3,3,3,4),(21.9911485753542,22.0971791978026,
22.2036796189916,22.3107685681831,22.3588896830007,22.453131598846,22.5472457024974,
22.6412605386286,22.7352081181162,22.8291214907904,22.9230263020776,23.0169481830416,
23.110971268134,23.2050498822345,23.2992804751442,23.3539508775043,23.4481997979404,
23.5442351803674,23.638238265709,23.7321788858051,23.8260827259759,23.9236827588209,
24.0176263675221,24.1116026174092,24.2056723410817,24.216482857356),
 .UNSPECIFIED.);
#457=B_SPLINE_CURVE_WITH_KNOTS('',3,(#37464,#37465,#37466,#37467,#37468,
#37469,#37470,#37471,#37472,#37473,#37474,#37475,#37476,#37477,#37478,#37479,
#37480,#37481,#37482,#37483,#37484,#37485,#37486,#37487,#37488,#37489,#37490,
#37491,#37492,#37493,#37494,#37495,#37496,#37497,#37498,#37499,#37500,#37501,
#37502,#37503,#37504,#37505,#37506,#37507,#37508,#37509,#37510,#37511,#37512,
#37513,#37514,#37515,#37516,#37517,#37518,#37519,#37520,#37521,#37522,#37523,
#37524,#37525,#37526,#37527,#37528,#37529,#37530,#37531,#37532,#37533,#37534,
#37535,#37536,#37537,#37538,#37539,#37540,#37541,#37542,#37543,#37544,#37545,
#37546,#37547,#37548,#37549,#37550,#37551,#37552,#37553,#37554,#37555,#37556,
#37557,#37558,#37559,#37560,#37561,#37562,#37563,#37564,#37565,#37566,#37567,
#37568,#37569,#37570,#37571,#37572,#37573,#37574,#37575,#37576,#37577,#37578,
#37579,#37580,#37581,#37582,#37583,#37584,#37585,#37586,#37587,#37588,#37589,
#37590,#37591,#37592,#37593,#37594,#37595,#37596,#37597,#37598,#37599),
 .UNSPECIFIED.,.F.,.F.,(4,3,3,3,3,3,3,3,3,3,3,3,3,3,3,3,3,3,3,3,3,3,3,3,
3,3,3,3,3,3,3,3,3,3,3,3,3,3,3,3,3,3,3,3,3,4),(17.9336096034474,18.0276908933547,
18.1218726198763,18.2161072832475,18.3104984450518,18.3786449049863,18.4727791665438,
18.566784204418,18.6606887201774,18.7545245606333,18.8483253559992,18.9421168868663,
19.0359249189042,19.1298339751119,19.2237982875258,19.3179152766156,19.3737060994899,
19.4679630484211,19.5620922042144,19.6561220902177,19.7500846514864,19.8440129578934,
19.9379326359175,20.0318692976143,20.1259069400813,20.2200000068637,20.3142447427367,
20.3687672939935,20.4630224260692,20.5571500629404,20.6511787288197,20.7451405242449,
20.8390683466272,20.9329878241461,21.0269245707971,21.1209627371732,21.2150565766248,
21.3093024733283,21.3638284884971,21.4586972705057,21.5534341189419,21.6480638995539,
21.7426049418883,21.8370934443179,21.9315675426925,21.9911485751284),
 .UNSPECIFIED.);
#458=B_SPLINE_CURVE_WITH_KNOTS('',3,(#37602,#37603,#37604,#37605,#37606,
#37607,#37608,#37609,#37610,#37611,#37612,#37613,#37614,#37615,#37616,#37617,
#37618,#37619,#37620,#37621,#37622,#37623,#37624,#37625,#37626,#37627,#37628,
#37629,#37630,#37631,#37632,#37633,#37634,#37635,#37636,#37637,#37638,#37639,
#37640,#37641,#37642,#37643,#37644,#37645,#37646,#37647,#37648,#37649,#37650,
#37651,#37652,#37653,#37654,#37655,#37656,#37657,#37658,#37659,#37660,#37661,
#37662,#37663,#37664,#37665,#37666,#37667,#37668,#37669,#37670,#37671,#37672,
#37673,#37674,#37675,#37676,#37677,#37678,#37679,#37680,#37681,#37682,#37683,
#37684,#37685,#37686,#37687,#37688,#37689,#37690,#37691,#37692,#37693,#37694,
#37695,#37696,#37697,#37698,#37699,#37700,#37701,#37702,#37703,#37704,#37705,
#37706,#37707,#37708,#37709,#37710,#37711,#37712,#37713,#37714,#37715,#37716,
#37717,#37718,#37719,#37720,#37721,#37722,#37723,#37724,#37725,#37726,#37727,
#37728,#37729,#37730,#37731,#37732,#37733,#37734,#37735,#37736,#37737,#37738,
#37739,#37740,#37741,#37742,#37743,#37744,#37745,#37746,#37747,#37748,#37749,
#37750,#37751,#37752,#37753,#37754,#37755,#37756,#37757,#37758,#37759,#37760,
#37761,#37762,#37763,#37764,#37765,#37766,#37767,#37768,#37769,#37770,#37771,
#37772,#37773,#37774,#37775,#37776,#37777,#37778,#37779,#37780,#37781,#37782,
#37783,#37784,#37785),.UNSPECIFIED.,.F.,.F.,(4,3,3,3,3,3,3,3,3,3,3,3,3,
3,3,3,3,3,3,3,3,3,3,3,3,3,3,3,3,3,3,3,3,3,3,3,3,3,3,3,3,3,3,3,3,3,3,3,3,
3,3,3,3,3,3,3,3,3,3,3,3,4),(7.94663621176237,7.96048955602889,8.05955426029293,
8.15847856564649,8.25811258875724,8.35686028739783,8.45557552348595,8.5542880750255,
8.65460374390225,8.75345800260633,8.85450437656942,8.9555507505325,9.05461196409969,
9.15353278770629,9.25316768237252,9.35191194799743,9.45062377725602,9.54933295295884,
9.64965270097816,9.74850369575663,9.84955782039637,9.95061194503612,10.0496683369466,
10.1485842429707,10.2482203550418,10.3469595045535,10.4456661543797,10.5443700941613,
10.6446958555059,10.7435415276227,10.8446073335812,10.9456731395397,11.0447332366077,
11.1436529000012,11.2432880792565,11.3420310859267,11.4407416218237,11.5394494713804,
11.6397706870461,11.738620287719,11.8396773108812,11.9407343340433,12.0397936403621,
12.1387125095246,12.2383478869024,12.3370900968523,12.4357998368967,12.5345068925667,
12.6348290515617,12.7336778714118,12.8347366999794,12.9357955285469,13.0340410984849,
13.1321469572857,13.2301412890246,13.32807565869,13.4259808804952,13.5238877309982,
13.6218875972222,13.7199379808394,13.8181465272218,13.8759337551308),
 .UNSPECIFIED.);
#459=B_SPLINE_CURVE_WITH_KNOTS('',3,(#37786,#37787,#37788,#37789,#37790,
#37791,#37792,#37793,#37794,#37795,#37796,#37797,#37798),.UNSPECIFIED.,
 .F.,.F.,(4,3,3,3,4),(13.8759337553362,13.9308567230506,14.0299037614613,
14.1301606402168,14.2304175189723),.UNSPECIFIED.);
#460=B_SPLINE_CURVE_WITH_KNOTS('',3,(#37799,#37800,#37801,#37802,#37803,
#37804,#37805,#37806,#37807,#37808,#37809,#37810,#37811,#37812,#37813,#37814,
#37815,#37816,#37817,#37818,#37819,#37820,#37821,#37822,#37823,#37824,#37825,
#37826,#37827,#37828,#37829,#37830,#37831,#37832,#37833,#37834,#37835,#37836,
#37837,#37838,#37839,#37840,#37841,#37842,#37843,#37844,#37845,#37846,#37847,
#37848,#37849,#37850,#37851,#37852,#37853,#37854,#37855,#37856,#37857,#37858,
#37859,#37860,#37861,#37862,#37863,#37864,#37865,#37866,#37867,#37868,#37869,
#37870,#37871,#37872,#37873,#37874,#37875,#37876,#37877,#37878,#37879,#37880,
#37881,#37882,#37883,#37884,#37885,#37886,#37887,#37888,#37889,#37890,#37891,
#37892,#37893,#37894,#37895,#37896,#37897,#37898,#37899,#37900,#37901,#37902,
#37903,#37904,#37905,#37906,#37907,#37908,#37909,#37910,#37911,#37912,#37913,
#37914,#37915,#37916,#37917,#37918,#37919,#37920,#37921,#37922,#37923,#37924,
#37925,#37926,#37927,#37928,#37929,#37930,#37931,#37932,#37933,#37934,#37935,
#37936,#37937,#37938,#37939,#37940,#37941,#37942,#37943,#37944,#37945,#37946,
#37947,#37948,#37949,#37950,#37951,#37952,#37953,#37954,#37955,#37956,#37957,
#37958,#37959,#37960,#37961,#37962,#37963,#37964,#37965,#37966,#37967,#37968,
#37969,#37970,#37971,#37972,#37973,#37974,#37975,#37976,#37977,#37978,#37979,
#37980,#37981,#37982,#37983,#37984,#37985,#37986,#37987,#37988,#37989,#37990,
#37991,#37992,#37993,#37994,#37995,#37996,#37997,#37998,#37999,#38000,#38001,
#38002,#38003,#38004,#38005,#38006,#38007,#38008,#38009,#38010,#38011,#38012,
#38013,#38014),.UNSPECIFIED.,.F.,.F.,(4,2,2,2,2,2,2,2,2,2,2,2,2,2,2,2,2,
2,2,2,2,2,2,2,2,2,2,2,2,2,2,2,2,2,2,2,2,2,2,2,2,2,2,2,2,2,2,2,2,2,2,2,2,
2,2,2,2,2,2,2,2,2,2,2,2,2,2,2,2,2,2,2,2,2,2,2,2,2,2,2,2,2,2,2,2,2,2,2,2,
2,2,2,2,2,2,2,2,2,2,2,2,2,2,2,2,2,2,4),(-1.67566337115906,-1.67120280065352,
-1.66726462128888,-1.66376769450309,-1.6593533715074,-1.65037907026849,
-1.58608340457434,-1.54833271630198,-1.54422098019783,-1.54169685999936,
-1.53973643199843,-1.53743177573583,-1.53319487640862,-1.50847890562579,
-1.45861073239527,-1.42736542077124,-1.42039558024787,-1.41635304716419,
-1.41286681818005,-1.4085987839144,-1.40036193884745,-1.35513827352513,
-1.30690664318352,-1.29535139711433,-1.29182033823835,-1.28966953119213,
-1.28766728590246,-1.28484499900533,-1.27782445047594,-1.26749550757044,
-1.2337952532973,-1.18093350517499,-1.17103122946286,-1.16648914127488,
-1.16296548088014,-1.15913288833492,-1.15294607384776,-1.13063081054186,
-1.08678693108625,-1.07049635409441,-1.0596647395255,-1.0448694921111,-1.0410267620009,
-1.0388072323975,-1.03683256472885,-1.03417153449766,-1.02809754080505,
-1.00030329743465,-0.980650030647354,-0.92985854140192,-0.919893440014821,
-0.915343865946071,-0.911823267533509,-0.908002954572419,-0.901856027950359,
-0.87992633456036,-0.837456771983163,-0.79801271437362,-0.791575854261773,
-0.789044804597,-0.787208692572457,-0.785169324595953,-0.782147444534211,
-0.773768467704869,-0.760621899397138,-0.723106531134634,-0.67453467344312,
-0.667845909333403,-0.663518345032452,-0.660026956015257,-0.656026387260442,
-0.649067493270492,-0.614943041357905,-0.583937145289183,-0.565893892558729,
-0.543422439879807,-0.539511130531841,-0.537045046536865,-0.535082597996337,
-0.532717497650554,-0.528224751178082,-0.494449832370743,-0.440408974454265,
-0.421425209527758,-0.415353353066085,-0.411540367366554,-0.407999540220032,
-0.403304853582722,-0.392864074507233,-0.378634910208049,-0.308664620705708,
-0.291943317772405,-0.287990326349166,-0.285723052767593,-0.283785578936228,
-0.281289562982911,-0.276005321504606,-0.268808352370668,-0.250107053490611,
-0.191316020790503,-0.170087279042834,-0.163801700873181,-0.159966627906554,
-0.156479460721741,-0.151963516330361,-0.142356961979044,-0.10337591065964,
-0.0899054331255484),.UNSPECIFIED.);
#461=B_SPLINE_CURVE_WITH_KNOTS('',3,(#38017,#38018,#38019,#38020,#38021,
#38022,#38023,#38024),.UNSPECIFIED.,.F.,.F.,(4,1,1,1,1,4),(17.9344061060102,
18.824417223833,19.8194784183366,20.8145396128402,21.8096008073438,21.9911485751285),
 .UNSPECIFIED.);
#462=B_SPLINE_CURVE_WITH_KNOTS('',3,(#38025,#38026,#38027,#38028,#38029,
#38030),.UNSPECIFIED.,.F.,.F.,(4,1,1,4),(21.9911485751285,22.8046620018475,
23.7997231963511,24.2174208605652),.UNSPECIFIED.);
#463=B_SPLINE_CURVE_WITH_KNOTS('',3,(#38032,#38033,#38034,#38035,#38036,
#38037,#38038,#38039,#38040,#38041,#38042,#38043,#38044,#38045,#38046,#38047,
#38048,#38049,#38050,#38051,#38052,#38053,#38054,#38055,#38056,#38057,#38058,
#38059,#38060,#38061,#38062,#38063,#38064,#38065,#38066,#38067,#38068,#38069,
#38070,#38071,#38072,#38073,#38074,#38075,#38076,#38077,#38078,#38079,#38080,
#38081,#38082,#38083,#38084,#38085,#38086,#38087,#38088,#38089,#38090,#38091,
#38092,#38093,#38094,#38095,#38096,#38097,#38098,#38099,#38100,#38101,#38102,
#38103,#38104,#38105,#38106,#38107),.UNSPECIFIED.,.F.,.F.,(4,3,3,3,3,3,
3,3,3,3,3,3,3,3,3,3,3,3,3,3,3,3,3,3,3,4),(21.9911485753567,22.0971717254703,
22.2036644377552,22.3107455936571,22.3588896830007,22.4531335315797,22.5472495865776,
22.6412663898706,22.7352159519276,22.8291313159636,22.9230381249701,23.0169620075806,
23.1109870881314,23.2050676971499,23.2993002644203,23.3539508775043,23.448200109615,
23.5442368061655,23.6382402270581,23.73218119163,23.8260853847912,23.9236874590982,
24.0176314416696,24.1116080720406,24.2056781869892,24.2164936820193),
 .UNSPECIFIED.);
#464=B_SPLINE_CURVE_WITH_KNOTS('',3,(#38108,#38109,#38110,#38111,#38112,
#38113,#38114,#38115,#38116,#38117,#38118,#38119,#38120,#38121,#38122,#38123,
#38124,#38125,#38126,#38127,#38128,#38129,#38130,#38131,#38132,#38133,#38134,
#38135,#38136,#38137,#38138,#38139,#38140,#38141,#38142,#38143,#38144,#38145,
#38146,#38147,#38148,#38149,#38150,#38151,#38152,#38153,#38154,#38155,#38156,
#38157,#38158,#38159,#38160,#38161,#38162,#38163,#38164,#38165,#38166,#38167,
#38168,#38169,#38170,#38171,#38172,#38173,#38174,#38175,#38176,#38177,#38178,
#38179,#38180,#38181,#38182,#38183,#38184,#38185,#38186,#38187,#38188,#38189,
#38190,#38191,#38192,#38193,#38194,#38195,#38196,#38197,#38198,#38199,#38200,
#38201,#38202,#38203,#38204,#38205,#38206,#38207,#38208,#38209,#38210,#38211,
#38212,#38213,#38214,#38215,#38216,#38217,#38218,#38219,#38220,#38221,#38222,
#38223,#38224,#38225,#38226,#38227,#38228,#38229,#38230,#38231,#38232,#38233,
#38234,#38235,#38236,#38237,#38238,#38239,#38240,#38241,#38242,#38243),
 .UNSPECIFIED.,.F.,.F.,(4,3,3,3,3,3,3,3,3,3,3,3,3,3,3,3,3,3,3,3,3,3,3,3,
3,3,3,3,3,3,3,3,3,3,3,3,3,3,3,3,3,3,3,3,3,4),(17.9336209525117,18.0277115439587,
18.1219027474085,18.2161469932096,18.3105478396887,18.3786449049862,18.4727572299532,
18.5667400362569,18.6606220561052,18.7544350950428,18.8482129069823,18.9419812987881,
19.0357660622794,19.12965178978,19.223592703853,19.3176864139379,19.3737060994898,
19.4679725846016,19.5621113667816,19.6561509555016,19.7501232927928,19.8440614168356,
19.9379909420193,20.0319374683321,20.1259849418975,20.2200878353086,20.3143422937485,
20.3687672939934,20.4630245655481,20.5571543984776,20.6511853137657,20.7451494294165,
20.8390796150494,20.9330014961429,21.0269406840253,21.1209813348621,21.2150776868747,
21.309326116205,21.3638284884971,21.4586930400753,21.5534255947856,21.6480510252089,
21.7425876513507,21.8370717007576,21.9315413125657,21.9911485751285),
 .UNSPECIFIED.);
#465=B_SPLINE_CURVE_WITH_KNOTS('',3,(#38245,#38246,#38247,#38248,#38249,
#38250,#38251,#38252,#38253,#38254,#38255,#38256,#38257,#38258,#38259,#38260,
#38261,#38262,#38263,#38264,#38265,#38266,#38267,#38268,#38269,#38270,#38271,
#38272,#38273,#38274,#38275,#38276,#38277,#38278,#38279,#38280,#38281,#38282,
#38283,#38284,#38285,#38286,#38287,#38288,#38289,#38290,#38291,#38292,#38293,
#38294,#38295,#38296,#38297,#38298,#38299,#38300,#38301,#38302,#38303,#38304,
#38305,#38306,#38307,#38308,#38309,#38310,#38311,#38312,#38313,#38314,#38315,
#38316,#38317,#38318,#38319,#38320,#38321,#38322,#38323,#38324,#38325,#38326,
#38327,#38328,#38329,#38330,#38331,#38332),.UNSPECIFIED.,.F.,.F.,(4,3,3,
3,3,3,3,3,3,3,3,3,3,3,3,3,3,3,3,3,3,3,3,3,3,3,3,3,3,4),(-0.569248610399504,
-0.543620267538966,-0.517275308318863,-0.510365772288032,-0.504797425837249,
-0.476915498166719,-0.449033570496189,-0.44252399619976,-0.414641409554834,
-0.386493730355128,-0.358554115912246,-0.344587775116203,-0.340093641025723,
-0.311161006381323,-0.302297526319618,-0.274516016182276,-0.24600118036232,
-0.234427379674768,-0.228081846962352,-0.199138916344677,-0.169673832321506,
-0.139875499189353,-0.12331359040414,-0.118150586823425,-0.113404796669263,
-0.082855962759546,-0.0522791701779296,-0.0223319110835381,-0.00827276376604753,
-4.5575133329622E-5),.UNSPECIFIED.);
#466=B_SPLINE_CURVE_WITH_KNOTS('',3,(#38333,#38334,#38335,#38336,#38337,
#38338,#38339,#38340,#38341,#38342,#38343,#38344,#38345,#38346,#38347,#38348,
#38349,#38350,#38351,#38352,#38353,#38354,#38355,#38356,#38357,#38358,#38359,
#38360,#38361,#38362,#38363,#38364,#38365,#38366,#38367,#38368,#38369,#38370,
#38371,#38372,#38373,#38374,#38375,#38376,#38377,#38378,#38379,#38380,#38381,
#38382,#38383,#38384,#38385,#38386,#38387,#38388,#38389,#38390,#38391,#38392,
#38393,#38394,#38395,#38396,#38397,#38398,#38399,#38400,#38401,#38402,#38403,
#38404,#38405,#38406,#38407,#38408,#38409,#38410,#38411,#38412,#38413,#38414,
#38415,#38416,#38417,#38418,#38419,#38420,#38421,#38422,#38423,#38424,#38425,
#38426),.UNSPECIFIED.,.F.,.F.,(4,3,3,3,3,3,3,3,3,3,3,3,3,3,3,3,3,3,3,3,
3,3,3,3,3,3,3,3,3,3,3,4),(-0.566847306048012,-0.536671615274114,-0.508620133545833,
-0.497368804130827,-0.489151108516999,-0.459017262376303,-0.429054732234886,
-0.424465688360989,-0.419732324172897,-0.390343746603834,-0.361246162165409,
-0.332930307421861,-0.318054544345632,-0.31168393575571,-0.307251657998185,
-0.279282126811528,-0.273681209148948,-0.244539503877978,-0.215397798607007,
-0.20526406080706,-0.200835933876738,-0.173001262381593,-0.145191835190121,
-0.117980004611901,-0.104040576094789,-0.0999820633207585,-0.0958220791342219,
-0.0691487206705904,-0.0429261084718551,-0.0175178608047413,-0.00680668378120295,
0.),.UNSPECIFIED.);
#467=B_SPLINE_CURVE_WITH_KNOTS('',3,(#38927,#38928,#38929,#38930,#38931,
#38932,#38933,#38934,#38935,#38936,#38937,#38938,#38939,#38940,#38941,#38942,
#38943,#38944,#38945,#38946,#38947,#38948,#38949,#38950,#38951,#38952,#38953,
#38954,#38955,#38956,#38957,#38958,#38959,#38960,#38961,#38962,#38963,#38964,
#38965,#38966,#38967,#38968,#38969,#38970,#38971,#38972,#38973,#38974,#38975,
#38976,#38977,#38978,#38979,#38980,#38981,#38982,#38983,#38984,#38985,#38986,
#38987,#38988,#38989,#38990,#38991,#38992,#38993,#38994,#38995,#38996,#38997,
#38998,#38999,#39000,#39001,#39002,#39003,#39004,#39005,#39006,#39007,#39008,
#39009,#39010,#39011,#39012,#39013,#39014),.UNSPECIFIED.,.F.,.F.,(4,3,3,
3,3,3,3,3,3,3,3,3,3,3,3,3,3,3,3,3,3,3,3,3,3,3,3,3,3,4),(2.82480432200989E-15,
0.0255907113803957,0.0517115692667785,0.0784881552197149,0.0965722362830325,
0.102694013405744,0.130071949357647,0.157822871079344,0.185608274535105,
0.195879267308504,0.202565921639154,0.206307055202583,0.236218131652208,
0.266129208101832,0.294041562878489,0.304150158806137,0.310346957232328,
0.314587143109714,0.342995349661446,0.371961471638149,0.401417288131293,
0.421839549604331,0.426720525203164,0.456769376649525,0.482228947818515,
0.491806157628287,0.499594300990965,0.530091426825922,0.558607661325485,
0.566782725939973),.UNSPECIFIED.);
#468=B_SPLINE_CURVE_WITH_KNOTS('',3,(#39515,#39516,#39517,#39518,#39519,
#39520,#39521,#39522,#39523,#39524,#39525,#39526,#39527,#39528,#39529,#39530,
#39531,#39532,#39533,#39534,#39535,#39536,#39537,#39538,#39539,#39540,#39541,
#39542,#39543,#39544,#39545,#39546,#39547,#39548,#39549,#39550,#39551,#39552,
#39553,#39554,#39555,#39556,#39557,#39558,#39559,#39560,#39561,#39562,#39563,
#39564,#39565,#39566,#39567,#39568,#39569,#39570,#39571,#39572,#39573,#39574,
#39575,#39576,#39577,#39578,#39579,#39580,#39581,#39582,#39583,#39584,#39585,
#39586,#39587,#39588,#39589,#39590,#39591,#39592,#39593,#39594,#39595,#39596,
#39597,#39598,#39599,#39600,#39601,#39602,#39603,#39604,#39605),
 .UNSPECIFIED.,.F.,.F.,(4,3,3,3,3,3,3,3,3,3,3,3,3,3,3,3,3,3,3,3,3,3,3,3,
3,3,3,3,3,3,4),(0.,0.0300171424118715,0.0604767221703259,0.0909614341218146,
0.115102967540566,0.120639952334797,0.150400143466383,0.179964556841017,
0.208757681432093,0.230868013600899,0.235298565007282,0.264095539603867,
0.292892514200451,0.294713444433599,0.323669923579346,0.332474977672906,
0.339298452935022,0.344533949196672,0.37258896016374,0.400766388632645,
0.428518995586946,0.4381296236022,0.44395402827716,0.448920751577058,0.475994417150381,
0.498576104022106,0.507824680125155,0.516910851418298,0.542764323146054,
0.562418700022881,0.569248610399432),.UNSPECIFIED.);
#469=B_SPLINE_CURVE_WITH_KNOTS('',3,(#39608,#39609,#39610,#39611,#39612,
#39613,#39614,#39615,#39616,#39617,#39618,#39619,#39620,#39621,#39622,#39623,
#39624,#39625,#39626,#39627,#39628,#39629,#39630,#39631,#39632,#39633,#39634,
#39635,#39636,#39637,#39638,#39639,#39640,#39641,#39642,#39643,#39644,#39645,
#39646,#39647,#39648,#39649,#39650,#39651,#39652,#39653,#39654,#39655,#39656,
#39657,#39658,#39659,#39660,#39661,#39662,#39663,#39664,#39665,#39666,#39667,
#39668,#39669,#39670,#39671,#39672,#39673,#39674,#39675,#39676,#39677,#39678,
#39679,#39680,#39681,#39682,#39683,#39684,#39685,#39686,#39687,#39688,#39689,
#39690,#39691,#39692,#39693,#39694,#39695),.UNSPECIFIED.,.F.,.F.,(4,3,3,
3,3,3,3,3,3,3,3,3,3,3,3,3,3,3,3,3,3,3,3,3,3,3,3,3,3,4),(-0.569248610399404,
-0.543256008460987,-0.51726340652257,-0.510386891772649,-0.504799190792994,
-0.477751536649517,-0.455804039579998,-0.449084589588299,-0.442520438246206,
-0.414640209544556,-0.386493193867354,-0.358551902567642,-0.344585820477761,
-0.340095051696883,-0.311162205934168,-0.302297526319553,-0.274512659934108,
-0.245995923672874,-0.234411538368291,-0.228082474140717,-0.199101564186637,
-0.169609516621985,-0.139817484612857,-0.118141598597594,-0.113403755408093,
-0.0828544964287721,-0.0522777598708405,-0.0223298996975752,-0.00827276376605614,
-3.66886802170398E-5),.UNSPECIFIED.);
#470=B_SPLINE_CURVE_WITH_KNOTS('',3,(#39696,#39697,#39698,#39699,#39700,
#39701,#39702,#39703,#39704,#39705,#39706,#39707,#39708,#39709,#39710,#39711,
#39712,#39713,#39714,#39715,#39716,#39717,#39718,#39719,#39720,#39721,#39722,
#39723,#39724,#39725,#39726,#39727,#39728,#39729,#39730,#39731,#39732,#39733,
#39734,#39735,#39736,#39737,#39738,#39739,#39740,#39741,#39742,#39743,#39744,
#39745,#39746,#39747,#39748,#39749,#39750,#39751,#39752,#39753,#39754,#39755,
#39756,#39757,#39758,#39759,#39760,#39761,#39762,#39763,#39764,#39765,#39766,
#39767,#39768,#39769,#39770,#39771,#39772,#39773,#39774,#39775,#39776,#39777,
#39778,#39779,#39780,#39781,#39782,#39783,#39784,#39785,#39786,#39787,#39788,
#39789),.UNSPECIFIED.,.F.,.F.,(4,3,3,3,3,3,3,3,3,3,3,3,3,3,3,3,3,3,3,3,
3,3,3,3,3,3,3,3,3,3,3,4),(-0.566847306048046,-0.536423709701718,-0.50605441769512,
-0.496627814140597,-0.490481618468529,-0.460353524838767,-0.430379918137283,
-0.424467116489513,-0.418175703681424,-0.38879497848851,-0.359717952452969,
-0.331422325041021,-0.31805487155635,-0.311685352544617,-0.307252153320408,
-0.279281311857458,-0.273681209148987,-0.244539457621602,-0.215397706094217,
-0.205263802913415,-0.200835700491466,-0.173001176808448,-0.145191581540721,
-0.11797816426377,-0.104038996818512,-0.0999813512410115,-0.0958216236861764,
-0.069100446739826,-0.0431518956349564,-0.0175111779746322,-0.00680668378123909,
0.),.UNSPECIFIED.);
#471=B_SPLINE_CURVE_WITH_KNOTS('',3,(#40290,#40291,#40292,#40293,#40294,
#40295,#40296,#40297,#40298,#40299,#40300,#40301,#40302,#40303,#40304,#40305,
#40306,#40307,#40308,#40309,#40310,#40311,#40312,#40313,#40314,#40315,#40316,
#40317,#40318,#40319,#40320,#40321,#40322,#40323,#40324,#40325,#40326,#40327,
#40328,#40329,#40330,#40331,#40332,#40333,#40334,#40335,#40336,#40337,#40338,
#40339,#40340,#40341,#40342,#40343,#40344,#40345,#40346,#40347,#40348,#40349,
#40350,#40351,#40352,#40353,#40354,#40355,#40356,#40357,#40358,#40359,#40360,
#40361,#40362,#40363,#40364,#40365,#40366,#40367,#40368,#40369,#40370,#40371,
#40372,#40373,#40374,#40375,#40376,#40377),.UNSPECIFIED.,.F.,.F.,(4,3,3,
3,3,3,3,3,3,3,3,3,3,3,3,3,3,3,3,3,3,3,3,3,3,3,3,3,3,4),(7.74627845254649E-15,
0.0255384719591611,0.0516106888482134,0.0783325514691107,0.0899901572052831,
0.0973264106699432,0.102694480428545,0.130069272970533,0.157818590910839,
0.185604967740116,0.195878534404192,0.202565264334309,0.206306310167482,
0.236217759134657,0.266129208101832,0.294113525899595,0.310415969469161,
0.314649901542024,0.34306364441444,0.372033774758409,0.401490366934477,
0.422001683954396,0.426785325677536,0.456835670166022,0.482278667955884,
0.491831076392005,0.499580324142813,0.530077574030736,0.55860766132547,
0.566782993632779),.UNSPECIFIED.);
#472=B_SPLINE_CURVE_WITH_KNOTS('',3,(#40878,#40879,#40880,#40881,#40882,
#40883,#40884,#40885,#40886,#40887,#40888,#40889,#40890,#40891,#40892,#40893,
#40894,#40895,#40896,#40897,#40898,#40899,#40900,#40901,#40902,#40903,#40904,
#40905,#40906,#40907,#40908,#40909,#40910,#40911,#40912,#40913,#40914,#40915,
#40916,#40917,#40918,#40919,#40920,#40921,#40922,#40923,#40924,#40925,#40926,
#40927,#40928,#40929,#40930,#40931,#40932,#40933,#40934,#40935,#40936,#40937,
#40938,#40939,#40940,#40941,#40942,#40943,#40944,#40945,#40946,#40947,#40948,
#40949,#40950,#40951,#40952,#40953,#40954,#40955,#40956,#40957,#40958,#40959,
#40960,#40961,#40962,#40963,#40964,#40965,#40966,#40967,#40968,#40969,#40970,
#40971),.UNSPECIFIED.,.F.,.F.,(4,3,3,3,3,3,3,3,3,3,3,3,3,3,3,3,3,3,3,3,
3,3,3,3,3,3,3,3,3,3,3,4),(5.65216427767104E-15,0.0300138468892199,0.0604718986070861,
0.090957520735419,0.115098416893496,0.120639356618796,0.150402829187302,
0.180004389620233,0.208931385640857,0.22092145313717,0.230873872217119,
0.235299701846774,0.264096922839113,0.292894143831452,0.294713444433604,
0.323669767997715,0.332475376686475,0.339302265504674,0.343483980235969,
0.371527376856032,0.399706760133745,0.427472592753052,0.438139069525203,
0.443961451456035,0.449567836675998,0.476635483291862,0.498576344057142,
0.50782599044979,0.516923305096603,0.54277922365799,0.562418700022943,0.569248610399501),
 .UNSPECIFIED.);
#473=B_SPLINE_CURVE_WITH_KNOTS('',3,(#40987,#40988,#40989,#40990,#40991,
#40992,#40993,#40994,#40995,#40996,#40997,#40998,#40999,#41000,#41001,#41002,
#41003,#41004,#41005,#41006,#41007,#41008,#41009,#41010,#41011,#41012,#41013,
#41014,#41015,#41016,#41017,#41018,#41019,#41020,#41021,#41022,#41023,#41024,
#41025,#41026,#41027,#41028,#41029,#41030,#41031,#41032,#41033,#41034,#41035,
#41036,#41037,#41038,#41039,#41040,#41041,#41042,#41043,#41044,#41045,#41046,
#41047,#41048,#41049,#41050,#41051,#41052,#41053,#41054,#41055,#41056,#41057,
#41058,#41059,#41060,#41061,#41062,#41063,#41064,#41065,#41066,#41067,#41068,
#41069,#41070,#41071,#41072,#41073,#41074,#41075,#41076,#41077,#41078,#41079,
#41080,#41081,#41082,#41083,#41084,#41085,#41086,#41087,#41088,#41089,#41090,
#41091,#41092,#41093,#41094,#41095,#41096,#41097,#41098,#41099,#41100,#41101,
#41102,#41103,#41104,#41105,#41106,#41107,#41108,#41109,#41110,#41111,#41112,
#41113,#41114,#41115,#41116,#41117,#41118,#41119,#41120,#41121,#41122,#41123,
#41124,#41125,#41126,#41127,#41128,#41129,#41130,#41131,#41132,#41133,#41134,
#41135,#41136,#41137,#41138,#41139,#41140,#41141,#41142,#41143,#41144,#41145,
#41146),.UNSPECIFIED.,.F.,.F.,(4,3,3,3,3,3,3,3,3,3,3,3,3,3,3,3,3,3,3,3,
3,3,3,3,3,3,3,3,3,3,3,3,3,3,3,3,3,3,3,3,3,3,3,3,3,3,3,3,3,3,3,3,3,4),(10.3765884621259,
10.476062504193,10.575701989116,10.6749488225681,10.7741470583041,10.8733291136227,
10.9732914311112,11.0725937393473,11.1728860614621,11.2731783835768,11.3739734315995,
11.4746293425727,11.5751758025763,11.675662893882,11.7761214170926,11.8765821358525,
11.9771435293855,12.0777554996725,12.1785433307966,12.2617453273021,12.3622418849439,
12.4625938656695,12.5628296768858,12.6630021764353,12.7631426194066,12.8632822204417,
12.963519970855,13.0638064174393,13.1642692822289,13.2503122710274,13.3509733722753,
13.4514920114239,13.5518968662201,13.6522397819783,13.7525517715489,13.8528638085318,
13.9532741952591,14.0537336534519,14.1543681892404,14.2388792147526,14.3395272139403,
14.4400329912056,14.5404254117544,14.6407561617772,14.7410562727562,14.8413567371902,
14.94175611485,15.0422048581083,15.1428292957157,15.2274461584779,15.3337058424558,
15.4397656277915,15.5455522467424,15.6354744060799),.UNSPECIFIED.);
#474=B_SPLINE_CURVE_WITH_KNOTS('',3,(#41149,#41150,#41151,#41152,#41153,
#41154,#41155,#41156,#41157,#41158,#41159,#41160,#41161,#41162,#41163,#41164,
#41165,#41166,#41167,#41168,#41169,#41170,#41171,#41172,#41173,#41174,#41175,
#41176,#41177,#41178,#41179,#41180,#41181,#41182,#41183,#41184,#41185,#41186,
#41187,#41188,#41189,#41190,#41191,#41192,#41193,#41194,#41195,#41196,#41197,
#41198,#41199,#41200,#41201,#41202,#41203,#41204,#41205,#41206,#41207,#41208,
#41209,#41210,#41211,#41212,#41213,#41214,#41215,#41216,#41217,#41218,#41219,
#41220,#41221,#41222,#41223,#41224,#41225,#41226,#41227,#41228,#41229,#41230,
#41231,#41232,#41233,#41234,#41235,#41236,#41237,#41238,#41239,#41240,#41241,
#41242,#41243,#41244,#41245,#41246,#41247,#41248,#41249,#41250,#41251,#41252,
#41253,#41254,#41255,#41256,#41257,#41258,#41259,#41260,#41261,#41262,#41263,
#41264,#41265,#41266,#41267,#41268,#41269,#41270,#41271,#41272),
 .UNSPECIFIED.,.F.,.F.,(4,3,3,3,3,3,3,3,3,3,3,3,3,3,3,3,3,3,3,3,3,3,3,3,
3,3,3,3,3,3,3,3,3,3,3,3,3,3,3,3,3,4),(11.6150328478182,11.7179803808624,
11.8208668123936,11.923743825148,12.0266196557919,12.1295192791407,12.2324676902163,
12.3355662546403,12.4387454167019,12.542116677988,12.6023632471184,12.7020014773053,
12.8014824096587,12.9008317510654,13.000108664494,13.099345507238,13.1985745856525,
13.2978965799461,13.3972630234654,13.4968082248626,13.5896936464185,13.6904969772465,
13.7911583780746,13.8917060070265,13.9921916408381,14.0926460713056,14.1931000507582,
14.2936502312469,14.394248707087,14.4950184335624,14.5770240457187,14.6778335761568,
14.7785042978673,14.8790659281952,14.979568424407,15.0800425628274,15.1805190830172,
15.2810961053189,15.3817238399707,15.4825265426885,15.5643544450188,15.6355313030285),
 .UNSPECIFIED.);
#475=B_SPLINE_CURVE_WITH_KNOTS('',3,(#41278,#41279,#41280,#41281,#41282,
#41283,#41284,#41285,#41286,#41287,#41288,#41289,#41290,#41291,#41292,#41293,
#41294,#41295,#41296,#41297,#41298,#41299,#41300,#41301,#41302,#41303,#41304,
#41305,#41306,#41307,#41308,#41309,#41310,#41311,#41312,#41313,#41314,#41315,
#41316,#41317,#41318,#41319,#41320,#41321,#41322,#41323,#41324,#41325,#41326,
#41327,#41328,#41329,#41330,#41331,#41332,#41333,#41334,#41335,#41336,#41337,
#41338,#41339,#41340,#41341,#41342,#41343,#41344,#41345,#41346,#41347,#41348,
#41349,#41350,#41351,#41352,#41353,#41354,#41355,#41356,#41357,#41358,#41359,
#41360,#41361,#41362,#41363,#41364,#41365,#41366,#41367,#41368,#41369,#41370,
#41371,#41372,#41373,#41374,#41375,#41376,#41377,#41378,#41379,#41380,#41381,
#41382,#41383,#41384,#41385,#41386,#41387,#41388,#41389,#41390,#41391,#41392,
#41393,#41394,#41395,#41396,#41397,#41398,#41399,#41400,#41401,#41402,#41403,
#41404,#41405,#41406,#41407,#41408,#41409,#41410,#41411,#41412,#41413,#41414,
#41415,#41416,#41417,#41418,#41419,#41420,#41421,#41422,#41423,#41424,#41425,
#41426,#41427,#41428,#41429,#41430,#41431,#41432,#41433,#41434,#41435,#41436,
#41437,#41438,#41439,#41440,#41441,#41442,#41443,#41444,#41445,#41446,#41447,
#41448,#41449,#41450,#41451,#41452,#41453,#41454,#41455,#41456,#41457,#41458,
#41459,#41460,#41461),.UNSPECIFIED.,.F.,.F.,(4,2,2,2,2,2,2,2,2,2,2,2,2,
2,2,2,2,2,2,2,2,2,2,2,2,2,2,2,2,2,2,2,2,2,2,2,2,2,2,2,2,2,2,2,2,2,2,2,2,
2,2,2,2,2,2,2,2,2,2,2,2,2,2,2,2,2,2,2,2,2,2,2,2,2,2,2,2,2,2,2,2,2,2,2,2,
2,2,2,2,2,2,4),(-1.47798032885567,-1.43330105002829,-1.42266852888909,-1.41621704688726,
-1.41027667209523,-1.40235146932106,-1.38344869116994,-1.35396756134988,
-1.3091633574122,-1.30211462050817,-1.29824709869633,-1.29489743491915,
-1.29022623422255,-1.27832883877505,-1.25912318836693,-1.19890762103143,
-1.18784880209941,-1.1813102518222,-1.17539478173152,-1.16765724412668,
-1.14999889591902,-1.1235476371968,-1.08192378164802,-1.06959618943341,
-1.06474023502206,-1.06136355574123,-1.05758671301682,-1.05077554176365,
-1.01806758726353,-0.962977770637023,-0.952336094674094,-0.945882670659189,
-0.939942764890604,-0.93202156547281,-0.9131465496835,-0.88373568893161,
-0.838807211319577,-0.831771220103658,-0.827906481021687,-0.82455656142266,
-0.819881135432661,-0.807951240464271,-0.788664305236778,-0.728660656187504,
-0.717559851953047,-0.711013527078348,-0.705101348091632,-0.697383101725452,
-0.679842868340105,-0.653664381381004,-0.612777103535746,-0.599561789074333,
-0.594580702093023,-0.591217259868671,-0.587506562220662,-0.581007157752874,
-0.572743609204568,-0.553375085000751,-0.493566314178682,-0.482423023175997,
-0.475867857016003,-0.469957418340135,-0.462255416920299,-0.444819551716769,
-0.418879940450158,-0.378623921495441,-0.36464191210661,-0.359556448377355,
-0.356173850391463,-0.352497902133166,-0.346169854884155,-0.338192522185705,
-0.31989959428381,-0.257381885070499,-0.246832400336662,-0.2403970147588,
-0.234449302618064,-0.226480297593191,-0.207281769146584,-0.177040028124113,
-0.133597692724678,-0.126444614393014,-0.122554866839668,-0.119213442765481,
-0.114589088484696,-0.102989423542528,-0.0845016583938039,-0.0329586557572508,
-0.0160821659939653,-0.00847164830242694,-0.00409788643911735,-0.000676582743011211),
 .UNSPECIFIED.);
#476=B_SPLINE_CURVE_WITH_KNOTS('',3,(#41462,#41463,#41464,#41465),
 .UNSPECIFIED.,.F.,.F.,(4,4),(15.6354744060799,15.7079632677027),
 .UNSPECIFIED.);
#477=B_SPLINE_CURVE_WITH_KNOTS('',3,(#41467,#41468,#41469,#41470),
 .UNSPECIFIED.,.F.,.F.,(4,4),(15.6355313030285,15.7079632679489),
 .UNSPECIFIED.);
#478=B_SPLINE_CURVE_WITH_KNOTS('',3,(#41471,#41472,#41473,#41474,#41475,
#41476,#41477,#41478,#41479,#41480,#41481,#41482,#41483,#41484,#41485,#41486,
#41487,#41488,#41489,#41490,#41491,#41492,#41493,#41494,#41495,#41496,#41497,
#41498,#41499,#41500,#41501,#41502,#41503,#41504,#41505,#41506,#41507,#41508,
#41509,#41510,#41511,#41512,#41513,#41514,#41515,#41516,#41517,#41518,#41519,
#41520,#41521,#41522,#41523,#41524,#41525,#41526,#41527,#41528,#41529,#41530,
#41531,#41532,#41533,#41534,#41535,#41536,#41537,#41538,#41539,#41540,#41541,
#41542,#41543,#41544,#41545,#41546,#41547,#41548,#41549,#41550,#41551,#41552,
#41553,#41554,#41555,#41556,#41557,#41558,#41559,#41560,#41561,#41562,#41563,
#41564,#41565,#41566,#41567,#41568,#41569,#41570,#41571,#41572,#41573,#41574,
#41575,#41576,#41577,#41578,#41579,#41580,#41581,#41582,#41583,#41584,#41585,
#41586,#41587,#41588,#41589,#41590,#41591,#41592,#41593,#41594,#41595,#41596,
#41597,#41598,#41599,#41600,#41601,#41602,#41603,#41604,#41605,#41606,#41607,
#41608,#41609,#41610,#41611,#41612,#41613,#41614,#41615,#41616,#41617,#41618,
#41619,#41620,#41621,#41622,#41623,#41624,#41625,#41626,#41627,#41628,#41629,
#41630,#41631,#41632,#41633,#41634,#41635,#41636,#41637,#41638,#41639,#41640,
#41641,#41642,#41643,#41644,#41645,#41646),.UNSPECIFIED.,.F.,.F.,(4,2,2,
2,2,2,2,2,2,2,2,2,2,2,2,2,2,2,2,2,2,2,2,2,2,2,2,2,2,2,2,2,2,2,2,2,2,2,2,
2,2,2,2,2,2,2,2,2,2,2,2,2,2,2,2,2,2,2,2,2,2,2,2,2,2,2,2,2,2,2,2,2,2,2,2,
2,2,2,2,2,2,2,2,2,2,2,2,4),(-2.98914895289037,-2.92873298419057,-2.91557163843783,
-2.90851700668525,-2.90251005083803,-2.89513756844254,-2.88357783616708,
-2.82436448753581,-2.80641267797751,-2.79499011906609,-2.79032938790222,
-2.78690735675631,-2.78283376851302,-2.77514768041812,-2.74274361420564,
-2.712729735914,-2.68565752927767,-2.67659514414619,-2.6703109293323,-2.66390874398197,
-2.65422566793543,-2.62169798390984,-2.58559988663249,-2.56308780984347,
-2.55724497620969,-2.55359428444409,-2.55037600554499,-2.54488793851854,
-2.52828106190174,-2.47617012571485,-2.45094016063448,-2.44207653621755,
-2.43583961700925,-2.42941077081661,-2.41953799437294,-2.38097245010046,
-2.35217056537171,-2.32842811017426,-2.32252209973905,-2.31886943808619,
-2.31567471695582,-2.31028656663783,-2.29455324852778,-2.25152087325597,
-2.22467561339994,-2.21131814894629,-2.20419919317128,-2.19815544289559,
-2.19075783572952,-2.17590297969063,-2.12392107427581,-2.1036799968007,
-2.09131052756701,-2.08649194610422,-2.08304040155196,-2.07903831159411,
-2.07168601841267,-2.0302764061936,-1.9991916879254,-1.9857341978946,-1.97473076940944,
-1.96807318546886,-1.96194506926809,-1.95390177747934,-1.93962735355907,
-1.88876658204379,-1.86882473320778,-1.85657172497545,-1.8517651228926,
-1.8483119790225,-1.84429763895165,-1.83688783626045,-1.78557122892761,
-1.76081295925951,-1.74382015979252,-1.73605165035796,-1.72997662243179,
-1.72311212880431,-1.71138977724004,-1.64550743179752,-1.62384772720852,
-1.61807613133524,-1.61445116995907,-1.61123326167678,-1.6057250927514,
-1.5888725507394,-1.52239112292902,-1.5122482337056),.UNSPECIFIED.);
#479=B_SPLINE_CURVE_WITH_KNOTS('',3,(#41651,#41652,#41653,#41654,#41655,
#41656,#41657,#41658,#41659,#41660,#41661,#41662,#41663,#41664,#41665,#41666,
#41667,#41668,#41669,#41670,#41671,#41672,#41673,#41674,#41675,#41676,#41677,
#41678,#41679,#41680,#41681,#41682,#41683,#41684,#41685,#41686,#41687,#41688,
#41689,#41690,#41691,#41692,#41693,#41694,#41695,#41696,#41697,#41698,#41699,
#41700,#41701,#41702,#41703,#41704,#41705,#41706,#41707,#41708,#41709,#41710,
#41711,#41712,#41713,#41714,#41715,#41716,#41717,#41718,#41719,#41720,#41721,
#41722,#41723,#41724,#41725,#41726,#41727,#41728,#41729,#41730,#41731,#41732,
#41733,#41734,#41735,#41736,#41737,#41738,#41739,#41740,#41741,#41742,#41743,
#41744,#41745,#41746,#41747,#41748,#41749,#41750,#41751,#41752,#41753,#41754,
#41755,#41756,#41757,#41758,#41759,#41760,#41761,#41762,#41763,#41764,#41765,
#41766,#41767,#41768,#41769,#41770,#41771,#41772,#41773,#41774,#41775,#41776,
#41777,#41778,#41779,#41780,#41781,#41782,#41783,#41784,#41785,#41786,#41787,
#41788,#41789,#41790,#41791,#41792,#41793,#41794,#41795,#41796,#41797,#41798,
#41799,#41800,#41801,#41802,#41803,#41804,#41805,#41806,#41807,#41808,#41809,
#41810,#41811,#41812,#41813,#41814,#41815,#41816,#41817,#41818,#41819,#41820,
#41821,#41822,#41823,#41824,#41825,#41826,#41827,#41828,#41829,#41830,#41831,
#41832,#41833,#41834,#41835,#41836,#41837,#41838,#41839,#41840,#41841,#41842,
#41843,#41844),.UNSPECIFIED.,.F.,.F.,(4,2,2,2,2,2,2,2,2,2,2,2,2,2,2,2,2,
2,2,2,2,2,2,2,2,2,2,2,2,2,2,2,2,2,2,2,2,2,2,2,2,2,2,2,2,2,2,2,2,2,2,2,2,
2,2,2,2,2,2,2,2,2,2,2,2,2,2,2,2,2,2,2,2,2,2,2,2,2,2,2,2,2,2,2,2,2,2,2,2,
2,2,2,2,2,2,2,4),(-2.97274808995521,-2.9640236472047,-2.95348427225043,
-2.94901602775192,-2.94571010502777,-2.9423799428634,-2.93840614716746,
-2.93085861552232,-2.90087241224702,-2.86180870102341,-2.84018005884101,
-2.83159264178222,-2.82554402332727,-2.8193129722081,-2.80977031046813,
-2.77679441215418,-2.74252183651167,-2.7258834978171,-2.71507553790633,
-2.71056794796063,-2.70723687863763,-2.70326996368559,-2.69552335076595,
-2.66352120051562,-2.62676763795099,-2.61165712902711,-2.59972363568552,
-2.59300760017189,-2.58712348657146,-2.57969079658784,-2.5675960404565,
-2.51387425148791,-2.49304943582902,-2.48441129141955,-2.4776896882762,
-2.47393129906078,-2.47054696725103,-2.46564674441967,-2.45304579248103,
-2.4066702531642,-2.38334206226959,-2.36708320757952,-2.35957023449622,
-2.35367846775746,-2.34701275133626,-2.33563756635945,-2.29396326529225,
-2.26232848687584,-2.24627499211812,-2.24108783663789,-2.23765216846806,
-2.23399976311814,-2.22777900848114,-2.19251209728969,-2.15620489824737,
-2.13409952585812,-2.12574258082685,-2.11973381380674,-2.11343723379616,
-2.10356944174534,-2.06337947624062,-2.02930305555997,-2.01146750304277,
-2.0061040285687,-2.00263368022068,-1.9994783002486,-1.99396391983363,-1.97599426442391,
-1.91006906850456,-1.89568388821476,-1.88849842755302,-1.88319914011093,
-1.8765164238814,-1.86505879860271,-1.82657694156904,-1.79264819722716,
-1.77599453154855,-1.77074576917699,-1.76729847897115,-1.76366583687039,
-1.75753641811003,-1.72775772653704,-1.68662224085544,-1.66388369827819,
-1.65545058559946,-1.64942935756776,-1.64315651564052,-1.63340388715119,
-1.59433835042962,-1.55815798263997,-1.54095617863748,-1.53565317271213,
-1.53219522158039,-1.52857876487849,-1.52252452838479,-1.49551164359983,
-1.47798032885567),.UNSPECIFIED.);
#480=B_SPLINE_CURVE_WITH_KNOTS('',3,(#41845,#41846,#41847,#41848,#41849,
#41850,#41851,#41852,#41853,#41854,#41855,#41856,#41857,#41858,#41859,#41860,
#41861,#41862,#41863,#41864,#41865,#41866,#41867,#41868,#41869,#41870,#41871,
#41872,#41873,#41874,#41875,#41876,#41877,#41878,#41879,#41880,#41881,#41882,
#41883,#41884,#41885,#41886,#41887,#41888,#41889,#41890,#41891,#41892,#41893,
#41894,#41895,#41896,#41897,#41898,#41899,#41900,#41901,#41902,#41903,#41904,
#41905,#41906,#41907,#41908,#41909,#41910,#41911,#41912,#41913,#41914,#41915,
#41916,#41917,#41918,#41919,#41920,#41921,#41922,#41923,#41924,#41925,#41926,
#41927,#41928,#41929,#41930,#41931,#41932,#41933,#41934,#41935,#41936,#41937,
#41938,#41939,#41940,#41941,#41942,#41943,#41944,#41945,#41946,#41947,#41948,
#41949,#41950,#41951,#41952,#41953,#41954,#41955,#41956,#41957,#41958,#41959,
#41960,#41961,#41962,#41963,#41964,#41965,#41966,#41967,#41968,#41969,#41970,
#41971,#41972,#41973,#41974,#41975,#41976,#41977,#41978,#41979,#41980,#41981,
#41982,#41983,#41984,#41985,#41986,#41987,#41988,#41989,#41990,#41991,#41992,
#41993,#41994,#41995,#41996,#41997,#41998,#41999,#42000,#42001,#42002,#42003,
#42004,#42005,#42006,#42007,#42008,#42009,#42010,#42011,#42012,#42013,#42014,
#42015,#42016,#42017,#42018,#42019,#42020,#42021,#42022,#42023,#42024,#42025,
#42026),.UNSPECIFIED.,.F.,.F.,(4,2,2,2,2,2,2,2,2,2,2,2,2,2,2,2,2,2,2,2,
2,2,2,2,2,2,2,2,2,2,2,2,2,2,2,2,2,2,2,2,2,2,2,2,2,2,2,2,2,2,2,2,2,2,2,2,
2,2,2,2,2,2,2,2,2,2,2,2,2,2,2,2,2,2,2,2,2,2,2,2,2,2,2,2,2,2,2,2,2,2,4),
(-1.5122482337056,-1.50772542513188,-1.50035846230784,-1.49489987394033,
-1.48797405338146,-1.47562536103928,-1.45991055432274,-1.41752610048913,
-1.38983746359247,-1.38365368734325,-1.37994094669798,-1.37635789481356,
-1.37078982936435,-1.35173470670003,-1.3067976258637,-1.27831789422885,
-1.26884624678052,-1.26313112407836,-1.25693462816383,-1.24829850699851,
-1.22510288341081,-1.18252099732315,-1.15508616577586,-1.14891064752082,
-1.14519909407883,-1.14161431561776,-1.13603811019637,-1.11688852049896,
-1.07140854713519,-1.04346491180145,-1.03404764333776,-1.02834218426725,
-1.02213864785108,-1.01345943662038,-0.989893809829303,-0.945832431633345,
-0.9201913339134,-0.914091173173159,-0.910395957622099,-0.906798821014502,
-0.901161874026297,-0.88128153350777,-0.831217203568471,-0.807539369798536,
-0.798640523854862,-0.792460683310774,-0.786057130955777,-0.776305747126482,
-0.739022113301222,-0.687985932876878,-0.680518493001488,-0.676492020185392,
-0.67304305770072,-0.668261655524246,-0.656173077550299,-0.636642848035639,
-0.577749184812847,-0.566384531927911,-0.559655172273088,-0.553550988884097,
-0.545530950763918,-0.526938396743792,-0.498439726677072,-0.452308710537718,
-0.44526763531528,-0.441373227883966,-0.437886630791347,-0.432842424602708,
-0.41880488843608,-0.394015180370477,-0.342646677984083,-0.331454568756659,
-0.324760053346076,-0.318646059672227,-0.31055172393684,-0.29146048132108,
-0.261706745715902,-0.217916538552625,-0.210730749320117,-0.206764377280321,
-0.20330067367785,-0.198408320850292,-0.185532114874522,-0.163984773395862,
-0.106200338112068,-0.0958600959611263,-0.0893383548318248,-0.083157605038447,
-0.0746178047795694,-0.0522232617175424,-0.0181623686306291),
 .UNSPECIFIED.);
#481=B_SPLINE_CURVE_WITH_KNOTS('',3,(#42032,#42033,#42034,#42035,#42036,
#42037,#42038,#42039,#42040,#42041,#42042,#42043,#42044,#42045,#42046,#42047,
#42048,#42049,#42050,#42051,#42052,#42053,#42054,#42055,#42056,#42057,#42058,
#42059,#42060,#42061,#42062,#42063,#42064,#42065,#42066,#42067,#42068,#42069,
#42070,#42071,#42072,#42073,#42074,#42075,#42076,#42077,#42078,#42079,#42080,
#42081,#42082,#42083,#42084,#42085,#42086,#42087,#42088,#42089,#42090,#42091,
#42092,#42093,#42094,#42095,#42096,#42097,#42098,#42099,#42100,#42101,#42102,
#42103,#42104,#42105,#42106,#42107,#42108,#42109,#42110,#42111,#42112,#42113,
#42114,#42115,#42116,#42117,#42118,#42119,#42120,#42121,#42122,#42123,#42124,
#42125,#42126,#42127,#42128,#42129,#42130,#42131,#42132,#42133,#42134,#42135,
#42136,#42137,#42138,#42139,#42140,#42141,#42142,#42143,#42144,#42145,#42146,
#42147,#42148,#42149,#42150,#42151,#42152,#42153,#42154,#42155,#42156,#42157,
#42158,#42159,#42160,#42161,#42162,#42163,#42164,#42165,#42166,#42167,#42168,
#42169,#42170,#42171,#42172,#42173,#42174,#42175,#42176,#42177,#42178,#42179,
#42180,#42181,#42182,#42183,#42184,#42185,#42186,#42187,#42188,#42189,#42190,
#42191,#42192,#42193,#42194,#42195,#42196,#42197,#42198,#42199,#42200,#42201,
#42202,#42203,#42204,#42205,#42206,#42207,#42208,#42209),.UNSPECIFIED.,
 .F.,.F.,(4,2,2,2,2,2,2,2,2,2,2,2,2,2,2,2,2,2,2,2,2,2,2,2,2,2,2,2,2,2,2,
2,2,2,2,2,2,2,2,2,2,2,2,2,2,2,2,2,2,2,2,2,2,2,2,2,2,2,2,2,2,2,2,2,2,2,2,
2,2,2,2,2,2,2,2,2,2,2,2,2,2,2,2,2,2,2,2,2,4),(-1.4777460824475,-1.47573978689171,
-1.46618077890607,-1.42946098154568,-1.37702591149363,-1.36982749058004,
-1.36592864696727,-1.36258738617596,-1.35797547138166,-1.34647594486204,
-1.32823061002263,-1.26670142863415,-1.25556300132005,-1.24900975001786,
-1.24310044149456,-1.23539904509031,-1.21796048791087,-1.19201282697499,
-1.1517362206291,-1.13778908053883,-1.13270933081852,-1.12932894721775,
-1.12565532017276,-1.11932860968657,-1.08139798378654,-1.03185411698654,
-1.0205978945993,-1.0140209026593,-1.00811727050498,-1.00046196495041,-0.983312743943603,
-0.958022872794609,-0.907373812178612,-0.899863490423314,-0.895898763938141,
-0.892569323425368,-0.88806376458844,-0.877259378847734,-0.86062674071379,
-0.826350549151681,-0.793464788560218,-0.7839315132419,-0.777704518404759,
-0.771658292452442,-0.763071631932232,-0.738978265771288,-0.692305104954863,
-0.669320532771877,-0.663427440968239,-0.659846413083829,-0.656364513410194,
-0.650938634201847,-0.632386345995213,-0.589795975442162,-0.558250512578107,
-0.548786776467311,-0.542573453910063,-0.536517178466571,-0.527875507423322,
-0.503280280406226,-0.454232936447933,-0.433908046004194,-0.428186881703376,
-0.424642617772866,-0.421128728299778,-0.415550004391565,-0.395128302092214,
-0.340541670586779,-0.320493766122117,-0.312207870985494,-0.306213243181289,
-0.299898698101786,-0.28993175752408,-0.243536204030134,-0.201674328221789,
-0.194434036500395,-0.190526073901684,-0.187522265175158,-0.183144207166153,
-0.173130113941981,-0.158231371441998,-0.102854711434871,-0.0847466893602929,
-0.0775112901881956,-0.0715235085403913,-0.06531131571646,-0.0558539703595871,
-0.041686806976749,-0.000673344736818981),.UNSPECIFIED.);
#482=B_SPLINE_CURVE_WITH_KNOTS('',3,(#42210,#42211,#42212,#42213),
 .UNSPECIFIED.,.F.,.F.,(4,4),(-2.98989863407752,-2.97274808995521),
 .UNSPECIFIED.);
#483=B_SPLINE_CURVE_WITH_KNOTS('',3,(#42215,#42216,#42217,#42218),
 .UNSPECIFIED.,.F.,.F.,(4,4),(-0.0181623686306291,-0.000670468894133524),
 .UNSPECIFIED.);
#484=B_SPLINE_CURVE_WITH_KNOTS('',3,(#42219,#42220,#42221,#42222,#42223,
#42224,#42225,#42226,#42227,#42228,#42229,#42230,#42231,#42232,#42233,#42234,
#42235,#42236,#42237,#42238,#42239,#42240,#42241,#42242,#42243,#42244,#42245,
#42246,#42247,#42248,#42249,#42250,#42251,#42252,#42253,#42254,#42255,#42256,
#42257,#42258,#42259,#42260,#42261,#42262,#42263,#42264,#42265,#42266,#42267,
#42268,#42269,#42270,#42271,#42272,#42273,#42274,#42275,#42276,#42277,#42278,
#42279,#42280,#42281,#42282,#42283,#42284,#42285,#42286,#42287,#42288,#42289,
#42290,#42291,#42292,#42293,#42294,#42295,#42296,#42297,#42298,#42299,#42300,
#42301,#42302,#42303,#42304,#42305,#42306,#42307,#42308,#42309,#42310,#42311,
#42312,#42313,#42314,#42315,#42316,#42317,#42318,#42319,#42320,#42321,#42322,
#42323,#42324,#42325,#42326,#42327,#42328,#42329,#42330,#42331,#42332,#42333,
#42334,#42335,#42336,#42337,#42338,#42339,#42340,#42341,#42342,#42343,#42344,
#42345,#42346,#42347,#42348,#42349,#42350,#42351,#42352,#42353,#42354,#42355,
#42356,#42357,#42358,#42359,#42360,#42361,#42362,#42363,#42364,#42365,#42366,
#42367,#42368,#42369,#42370,#42371,#42372,#42373,#42374,#42375,#42376,#42377,
#42378,#42379,#42380,#42381,#42382,#42383,#42384,#42385,#42386,#42387,#42388,
#42389,#42390,#42391,#42392,#42393,#42394,#42395,#42396,#42397,#42398,#42399,
#42400,#42401,#42402,#42403,#42404),.UNSPECIFIED.,.F.,.F.,(4,2,2,2,2,2,
2,2,2,2,2,2,2,2,2,2,2,2,2,2,2,2,2,2,2,2,2,2,2,2,2,2,2,2,2,2,2,2,2,2,2,2,
2,2,2,2,2,2,2,2,2,2,2,2,2,2,2,2,2,2,2,2,2,2,2,2,2,2,2,2,2,2,2,2,2,2,2,2,
2,2,2,2,2,2,2,2,2,2,2,2,2,2,4),(-2.98908487091722,-2.96886855829473,-2.96450205707518,
-2.96117612391201,-2.95775733401322,-2.95342242295158,-2.94410224265239,
-2.90147405121839,-2.86461822457242,-2.85165208120246,-2.84460439146685,
-2.83855011127857,-2.83104843045247,-2.81912520641453,-2.76073307004609,
-2.74293070077161,-2.73156074721739,-2.72688652967381,-2.72348020146249,
-2.71940239891614,-2.71169066217723,-2.68008656356456,-2.64341671589513,
-2.62111565549577,-2.61258814368928,-2.60640976797286,-2.59988468845634,
-2.58952636135325,-2.53182902609499,-2.51021838400767,-2.50132651405739,
-2.49441955208431,-2.49055312559073,-2.48709534551545,-2.48201703008245,
-2.46872894727117,-2.41305544126296,-2.38723337185768,-2.37830875503061,
-2.37206189959498,-2.36565047559016,-2.35586078008269,-2.31992548948552,
-2.27044235473586,-2.26109308774307,-2.25675260348975,-2.25333336365217,
-2.24896794365217,-2.23947783105127,-2.19528354486361,-2.1680635499048,
-2.15557724201101,-2.14517925025786,-2.13864572125017,-2.13247051390237,
-2.12396557467725,-2.10341298706472,-2.04979098138973,-2.02941193917131,
-2.0237344600582,-2.02012859466126,-2.01689392977582,-2.01129707047237,
-1.99348520446533,-1.92698093979589,-1.91303898508549,-1.90580451154975,
-1.89975675013751,-1.8924688277342,-1.87868572678518,-1.82567481587226,
-1.80518343015311,-1.79657086485733,-1.78982837142721,-1.78599635911805,
-1.78252406094718,-1.77819267307977,-1.76701723046152,-1.72460308979061,
-1.69802649616672,-1.68023268405016,-1.67233507652708,-1.66624522771497,
-1.65945214727735,-1.64777405605952,-1.59192109787737,-1.57073892565109,
-1.55800167319201,-1.55312817927367,-1.54966703105588,-1.54569058373772,
-1.53845859496727,-1.51233049812282),.UNSPECIFIED.);
#485=B_SPLINE_CURVE_WITH_KNOTS('',3,(#42409,#42410,#42411,#42412,#42413,
#42414,#42415,#42416,#42417,#42418,#42419,#42420,#42421,#42422,#42423,#42424,
#42425,#42426,#42427,#42428,#42429,#42430,#42431,#42432,#42433,#42434,#42435,
#42436,#42437,#42438,#42439,#42440,#42441,#42442,#42443,#42444,#42445,#42446,
#42447,#42448,#42449,#42450,#42451,#42452,#42453,#42454,#42455,#42456,#42457,
#42458,#42459,#42460,#42461,#42462,#42463,#42464,#42465,#42466,#42467,#42468,
#42469,#42470,#42471,#42472,#42473,#42474,#42475,#42476,#42477,#42478,#42479,
#42480,#42481,#42482,#42483,#42484,#42485,#42486,#42487,#42488,#42489,#42490,
#42491,#42492,#42493,#42494,#42495,#42496,#42497,#42498,#42499,#42500,#42501,
#42502,#42503,#42504,#42505,#42506,#42507,#42508,#42509,#42510,#42511,#42512,
#42513,#42514,#42515,#42516,#42517,#42518,#42519,#42520,#42521,#42522,#42523,
#42524,#42525,#42526,#42527,#42528,#42529,#42530,#42531,#42532,#42533,#42534,
#42535,#42536,#42537,#42538,#42539,#42540,#42541,#42542,#42543,#42544,#42545,
#42546,#42547,#42548,#42549,#42550,#42551,#42552,#42553,#42554,#42555,#42556,
#42557,#42558,#42559,#42560,#42561,#42562,#42563,#42564,#42565,#42566,#42567,
#42568,#42569,#42570,#42571,#42572,#42573,#42574,#42575,#42576,#42577,#42578,
#42579,#42580,#42581,#42582,#42583,#42584,#42585,#42586,#42587,#42588,#42589,
#42590),.UNSPECIFIED.,.F.,.F.,(4,2,2,2,2,2,2,2,2,2,2,2,2,2,2,2,2,2,2,2,
2,2,2,2,2,2,2,2,2,2,2,2,2,2,2,2,2,2,2,2,2,2,2,2,2,2,2,2,2,2,2,2,2,2,2,2,
2,2,2,2,2,2,2,2,2,2,2,2,2,2,2,2,2,2,2,2,2,2,2,2,2,2,2,2,2,2,2,2,2,2,4),
(-2.97165059380248,-2.92985561646699,-2.90664980664673,-2.89816571205665,
-2.89213883549381,-2.88662716188596,-2.87761848441644,-2.85112920410734,
-2.79237798509216,-2.7817480326958,-2.77727045252068,-2.7739441805029,-2.76996172162346,
-2.76236468760279,-2.72985809350361,-2.69271539810152,-2.67113811733543,
-2.66285133733886,-2.65685765252881,-2.65130315593011,-2.64205070898714,
-2.61330081692205,-2.56801167805497,-2.54896851637548,-2.5435009653401,
-2.54001099237372,-2.53644152592569,-2.53060022117996,-2.50845534342929,
-2.46109680664917,-2.436860401744,-2.42825947219759,-2.42221157573852,-2.41598988703573,
-2.40647909790062,-2.37406135408483,-2.33942454343257,-2.3226741719821,
-2.31181911125481,-2.30730609971663,-2.3040060171452,-2.30006118022646,
-2.29264344181399,-2.24150833419156,-2.21646408953766,-2.1994241218767,
-2.19178718319025,-2.18588642470474,-2.17930113546562,-2.16800095288249,
-2.11902482674775,-2.08046920919528,-2.07419846877499,-2.07053710606172,
-2.06715096370826,-2.06203779157594,-2.04782997660692,-2.00779869866169,
-1.98194956430747,-1.96455377186536,-1.95685984188138,-1.950952030794,-1.94439617581489,
-1.93324256581522,-1.8735005604764,-1.85410511947647,-1.8421333884692,-1.83745275452307,
-1.8341031134667,-1.83024354880006,-1.82322685980951,-1.77819742072212,
-1.74889265130891,-1.73006196307184,-1.72214971052551,-1.71621323791485,
-1.70976041457717,-1.69911243766783,-1.63698185553424,-1.61850874363784,
-1.60691494836906,-1.60228920226273,-1.5989464888609,-1.59505609596995,
-1.58789650402166,-1.54467737183832,-1.51435025689767,-1.49512204388784,
-1.48794496120307,-1.48197166787465,-1.4777460824475),.UNSPECIFIED.);
#486=B_SPLINE_CURVE_WITH_KNOTS('',3,(#42591,#42592,#42593,#42594,#42595,
#42596,#42597,#42598,#42599,#42600,#42601,#42602,#42603,#42604,#42605,#42606,
#42607,#42608,#42609,#42610,#42611,#42612,#42613,#42614,#42615,#42616,#42617,
#42618,#42619,#42620,#42621,#42622,#42623,#42624,#42625,#42626,#42627,#42628,
#42629,#42630,#42631,#42632,#42633,#42634,#42635,#42636,#42637,#42638,#42639,
#42640,#42641,#42642,#42643,#42644,#42645,#42646,#42647,#42648,#42649,#42650,
#42651,#42652,#42653,#42654,#42655,#42656,#42657,#42658,#42659,#42660,#42661,
#42662,#42663,#42664,#42665,#42666,#42667,#42668,#42669,#42670,#42671,#42672,
#42673,#42674,#42675,#42676,#42677,#42678,#42679,#42680,#42681,#42682,#42683,
#42684,#42685,#42686,#42687,#42688,#42689,#42690,#42691,#42692,#42693,#42694,
#42695,#42696,#42697,#42698,#42699,#42700,#42701,#42702,#42703,#42704,#42705,
#42706,#42707,#42708,#42709,#42710,#42711,#42712,#42713,#42714,#42715,#42716,
#42717,#42718,#42719,#42720,#42721,#42722,#42723,#42724,#42725,#42726,#42727,
#42728,#42729,#42730,#42731,#42732,#42733,#42734,#42735,#42736,#42737,#42738,
#42739,#42740,#42741,#42742,#42743,#42744,#42745,#42746,#42747,#42748,#42749,
#42750,#42751,#42752,#42753,#42754,#42755,#42756,#42757,#42758,#42759,#42760,
#42761,#42762,#42763,#42764,#42765,#42766,#42767,#42768,#42769,#42770,#42771,
#42772,#42773,#42774,#42775,#42776),.UNSPECIFIED.,.F.,.F.,(4,2,2,2,2,2,
2,2,2,2,2,2,2,2,2,2,2,2,2,2,2,2,2,2,2,2,2,2,2,2,2,2,2,2,2,2,2,2,2,2,2,2,
2,2,2,2,2,2,2,2,2,2,2,2,2,2,2,2,2,2,2,2,2,2,2,2,2,2,2,2,2,2,2,2,2,2,2,2,
2,2,2,2,2,2,2,2,2,2,2,2,2,2,4),(-1.51233049812282,-1.49520335693357,-1.45341890982416,
-1.44179633687685,-1.43501448275276,-1.42892221739244,-1.42100365384326,
-1.40307666162952,-1.37618571162187,-1.33293026571111,-1.32266149263571,
-1.31847012783979,-1.31499447906295,-1.31106794433204,-1.30387191976979,
-1.29448320663815,-1.27077863110474,-1.21738804641697,-1.20643332393897,
-1.19978697260604,-1.19365780029338,-1.18545370203068,-1.16560011804255,
-1.13382929713325,-1.09370820494154,-1.08617021238293,-1.08212869115169,
-1.07902932792658,-1.07450155365158,-1.06405705714836,-1.04834628073441,
-1.01910222836283,-0.980492342424274,-0.970617949033637,-0.964189423944362,
-0.957953738999441,-0.949093672426513,-0.923901845062781,-0.872103253505443,
-0.855076986265714,-0.849550864306135,-0.846329101973191,-0.842706965479036,
-0.836951945327968,-0.81553272571764,-0.752350025092124,-0.740119777069768,
-0.732532379017395,-0.726471826127508,-0.71948612745093,-0.706840689927197,
-0.690611628062002,-0.644933748027284,-0.621247171007705,-0.615217829002575,
-0.611537412443848,-0.607927010256222,-0.602227544307099,-0.581557178844596,
-0.525543692297731,-0.507085354766102,-0.4996709517369,-0.493507919090064,
-0.487077773354796,-0.477194564606135,-0.436497505104086,-0.392439880641663,
-0.382774944748766,-0.378378828239623,-0.374959158200164,-0.370647958429207,
-0.361462417670658,-0.348373069524263,-0.30220794346562,-0.274713640483251,
-0.265459003477948,-0.259780921655329,-0.253552134851733,-0.244730887352929,
-0.219902010546971,-0.170050912909116,-0.151014058248076,-0.145300861927663,
-0.142044477138465,-0.138462511690016,-0.132902130437931,-0.113944075677719,
-0.0723202506959316,-0.0405572695984405,-0.0310096331612037,-0.0252806452145648,
-0.0195007169690655,-0.0181291440337079),.UNSPECIFIED.);
#487=B_SPLINE_CURVE_WITH_KNOTS('',3,(#42782,#42783,#42784,#42785,#42786,
#42787,#42788,#42789,#42790,#42791,#42792,#42793,#42794,#42795,#42796,#42797,
#42798,#42799,#42800,#42801,#42802,#42803,#42804,#42805,#42806,#42807,#42808,
#42809,#42810,#42811,#42812,#42813,#42814,#42815,#42816,#42817,#42818,#42819,
#42820,#42821,#42822,#42823,#42824,#42825,#42826,#42827,#42828,#42829,#42830,
#42831,#42832,#42833,#42834,#42835,#42836,#42837,#42838,#42839,#42840,#42841,
#42842,#42843,#42844,#42845,#42846,#42847,#42848,#42849,#42850,#42851,#42852,
#42853,#42854,#42855,#42856,#42857,#42858,#42859,#42860,#42861,#42862,#42863,
#42864,#42865,#42866,#42867,#42868,#42869,#42870,#42871,#42872,#42873,#42874,
#42875,#42876,#42877,#42878,#42879,#42880,#42881,#42882,#42883,#42884,#42885,
#42886,#42887,#42888,#42889,#42890,#42891,#42892,#42893,#42894,#42895,#42896,
#42897,#42898,#42899,#42900,#42901,#42902,#42903,#42904,#42905,#42906,#42907,
#42908,#42909,#42910,#42911,#42912,#42913,#42914,#42915,#42916,#42917,#42918,
#42919,#42920,#42921,#42922,#42923,#42924,#42925,#42926,#42927,#42928,#42929,
#42930,#42931,#42932,#42933,#42934,#42935,#42936,#42937,#42938,#42939,#42940,
#42941,#42942,#42943,#42944,#42945,#42946,#42947,#42948,#42949,#42950,#42951,
#42952,#42953,#42954,#42955,#42956,#42957,#42958,#42959,#42960,#42961,#42962,
#42963,#42964,#42965,#42966,#42967,#42968,#42969,#42970,#42971,#42972,#42973,
#42974,#42975),.UNSPECIFIED.,.F.,.F.,(4,2,2,2,2,2,2,2,2,2,2,2,2,2,2,2,2,
2,2,2,2,2,2,2,2,2,2,2,2,2,2,2,2,2,2,2,2,2,2,2,2,2,2,2,2,2,2,2,2,2,2,2,2,
2,2,2,2,2,2,2,2,2,2,2,2,2,2,2,2,2,2,2,2,2,2,2,2,2,2,2,2,2,2,2,2,2,2,2,2,
2,2,2,2,2,2,2,4),(-1.47740198524613,-1.45419209782398,-1.44032045971751,
-1.4352501292993,-1.43187101371906,-1.42819313379095,-1.42184832287723,
-1.41384206164589,-1.39543862935915,-1.33316152820262,-1.32255035193238,
-1.31610438786692,-1.31016435928457,-1.30223242871395,-1.28327390158397,
-1.25364515757429,-1.20914089113941,-1.20206732243934,-1.19819508434785,
-1.19484766352072,-1.19018811197207,-1.17836578113044,-1.15934145208305,
-1.09869918621491,-1.08773733534814,-1.0812197654682,-1.0753010762563,-1.06752689704047,
-1.04962249895316,-1.02258882149787,-0.979381500558301,-0.968901700613474,
-0.964786742597108,-0.961405132962325,-0.957646011017135,-0.950915371829222,
-0.942261411252994,-0.921365445595675,-0.867317357953329,-0.855520581228181,
-0.848172429018052,-0.8422975477032,-0.835529214059519,-0.823322601153206,
-0.80773920255148,-0.765666384383375,-0.737085149840926,-0.730980303476517,
-0.72735393822743,-0.723904999743672,-0.718642814307026,-0.701838814172476,
-0.66728983497446,-0.626452321077116,-0.616581878607501,-0.61028699035061,
-0.604282158373453,-0.595934562392113,-0.573883613892663,-0.537732734324123,
-0.502256062008874,-0.496026961049312,-0.492373954403145,-0.488941422419189,
-0.483764444369893,-0.4677889554156,-0.436423670465519,-0.394476418726455,
-0.383111768498982,-0.376450408138287,-0.370561372713379,-0.363050357603699,
-0.346789737931292,-0.323449907419803,-0.277011149509601,-0.264466005738296,
-0.259575807388622,-0.256194349316924,-0.252434396578643,-0.245700175762511,
-0.237040224633817,-0.216120757830807,-0.161978125765649,-0.150250295558495,
-0.14292122163854,-0.137047484638825,-0.130264958745839,-0.117987470160476,
-0.102281713933086,-0.060379973287392,-0.0319124698728966,-0.0257839457279635,
-0.0221524351675295,-0.0190288398810346,-0.0155703878589853,-0.00939615265272851,
-0.000672416806236772),.UNSPECIFIED.);
#488=B_SPLINE_CURVE_WITH_KNOTS('',3,(#42976,#42977,#42978,#42979),
 .UNSPECIFIED.,.F.,.F.,(4,4),(-2.9891163108282,-2.97165059380248),
 .UNSPECIFIED.);
#489=B_SPLINE_CURVE_WITH_KNOTS('',3,(#42981,#42982,#42983,#42984,#42985,
#42986),.UNSPECIFIED.,.F.,.F.,(4,2,4),(-0.0181291440337079,-0.0134571638401088,
-0.000668810733621533),.UNSPECIFIED.);
#490=B_SPLINE_CURVE_WITH_KNOTS('',3,(#42987,#42988,#42989,#42990,#42991,
#42992,#42993,#42994,#42995,#42996,#42997,#42998,#42999,#43000,#43001,#43002,
#43003,#43004,#43005,#43006,#43007,#43008,#43009,#43010,#43011,#43012,#43013,
#43014,#43015,#43016,#43017,#43018,#43019,#43020,#43021,#43022,#43023,#43024,
#43025,#43026,#43027,#43028,#43029,#43030,#43031,#43032,#43033,#43034,#43035,
#43036,#43037,#43038,#43039,#43040,#43041,#43042,#43043,#43044,#43045,#43046,
#43047,#43048,#43049,#43050,#43051,#43052,#43053,#43054,#43055,#43056,#43057,
#43058,#43059,#43060,#43061,#43062,#43063,#43064,#43065,#43066,#43067,#43068,
#43069,#43070,#43071,#43072,#43073,#43074,#43075,#43076,#43077,#43078,#43079,
#43080,#43081,#43082,#43083,#43084,#43085,#43086,#43087,#43088,#43089,#43090,
#43091,#43092,#43093,#43094,#43095,#43096,#43097,#43098,#43099,#43100,#43101,
#43102,#43103,#43104,#43105,#43106,#43107,#43108,#43109,#43110,#43111,#43112,
#43113,#43114,#43115,#43116,#43117,#43118,#43119,#43120,#43121,#43122,#43123,
#43124,#43125,#43126,#43127,#43128,#43129,#43130,#43131,#43132,#43133,#43134,
#43135,#43136,#43137,#43138,#43139,#43140,#43141,#43142,#43143,#43144,#43145,
#43146,#43147,#43148,#43149,#43150,#43151,#43152,#43153,#43154,#43155,#43156,
#43157,#43158,#43159,#43160,#43161,#43162,#43163,#43164,#43165,#43166),
 .UNSPECIFIED.,.F.,.F.,(4,2,2,2,2,2,2,2,2,2,2,2,2,2,2,2,2,2,2,2,2,2,2,2,
2,2,2,2,2,2,2,2,2,2,2,2,2,2,2,2,2,2,2,2,2,2,2,2,2,2,2,2,2,2,2,2,2,2,2,2,
2,2,2,2,2,2,2,2,2,2,2,2,2,2,2,2,2,2,2,2,2,2,2,2,2,2,2,2,2,4),(-2.98881938810218,
-2.93439497537859,-2.9145800492518,-2.90614190069954,-2.89950338942194,
-2.89569383111583,-2.89221221432576,-2.88783944062521,-2.87612034321371,
-2.829062810777,-2.80109454743576,-2.7876893881572,-2.78055730618365,-2.77450814625825,
-2.76711070710711,-2.75276469706528,-2.70042708522535,-2.68010482159931,
-2.66770201444379,-2.66287603700549,-2.65942194876788,-2.65542164570109,
-2.64807553758926,-2.60663019871394,-2.57557111169767,-2.56212174080765,
-2.55112457018215,-2.54447037600708,-2.53834529042842,-2.53030610745481,
-2.51247271231874,-2.45761655136665,-2.44235650375148,-2.43212163562672,
-2.42762893439963,-2.42453390605158,-2.42046934605467,-2.41282017713579,
-2.38239946644278,-2.35661588930368,-2.33497759196849,-2.31945630389264,
-2.31193610815551,-2.30588072152425,-2.29884717652222,-2.28631763288667,
-2.23177054917505,-2.21090286647497,-2.19828719256164,-2.19343107434001,
-2.18997276002405,-2.18598823095726,-2.17871673527048,-2.13635825847007,
-2.0909895213314,-2.0808190560409,-2.07433209400389,-2.06820373419418,-2.05960656820613,
-2.03842930636657,-1.97311389950393,-1.96265062722635,-1.95811981327767,
-1.95502021377962,-1.95098091708932,-1.94345322408305,-1.9035001161836,
-1.8716435726131,-1.85175855894381,-1.84355026667493,-1.83742052797324,
-1.83077598431345,-1.81983017266896,-1.76632252253541,-1.74265006321361,
-1.73326821121888,-1.72607672236816,-1.72215114226118,-1.71867513948953,
-1.71448236264089,-1.70420485872274,-1.66098552097911,-1.63411434959317,
-1.61619483341578,-1.60827748096783,-1.60218525173031,-1.59540251917259,
-1.58377621770273,-1.54207743820327,-1.51221321296554),.UNSPECIFIED.);
#491=B_SPLINE_CURVE_WITH_KNOTS('',3,(#43171,#43172,#43173,#43174,#43175,
#43176,#43177,#43178,#43179,#43180,#43181,#43182,#43183,#43184,#43185,#43186,
#43187,#43188,#43189,#43190,#43191,#43192,#43193,#43194,#43195,#43196,#43197,
#43198,#43199,#43200,#43201,#43202,#43203,#43204,#43205,#43206,#43207,#43208,
#43209,#43210,#43211,#43212,#43213,#43214,#43215,#43216,#43217,#43218,#43219,
#43220,#43221,#43222,#43223,#43224,#43225,#43226,#43227,#43228,#43229,#43230,
#43231,#43232,#43233,#43234,#43235,#43236,#43237,#43238,#43239,#43240,#43241,
#43242,#43243,#43244,#43245,#43246,#43247,#43248,#43249,#43250,#43251,#43252,
#43253,#43254,#43255,#43256,#43257,#43258,#43259,#43260,#43261,#43262,#43263,
#43264,#43265,#43266,#43267,#43268,#43269,#43270,#43271,#43272,#43273,#43274,
#43275,#43276,#43277,#43278,#43279,#43280,#43281,#43282,#43283,#43284,#43285,
#43286,#43287,#43288,#43289,#43290,#43291,#43292,#43293,#43294,#43295,#43296,
#43297,#43298,#43299,#43300,#43301,#43302,#43303,#43304,#43305,#43306,#43307,
#43308,#43309,#43310,#43311,#43312,#43313,#43314,#43315,#43316,#43317,#43318,
#43319,#43320,#43321,#43322,#43323,#43324,#43325,#43326,#43327,#43328,#43329,
#43330,#43331,#43332,#43333,#43334,#43335,#43336,#43337,#43338,#43339,#43340,
#43341,#43342,#43343,#43344,#43345,#43346,#43347,#43348,#43349,#43350,#43351,
#43352,#43353,#43354,#43355,#43356),.UNSPECIFIED.,.F.,.F.,(4,2,2,2,2,2,
2,2,2,2,2,2,2,2,2,2,2,2,2,2,2,2,2,2,2,2,2,2,2,2,2,2,2,2,2,2,2,2,2,2,2,2,
2,2,2,2,2,2,2,2,2,2,2,2,2,2,2,2,2,2,2,2,2,2,2,2,2,2,2,2,2,2,2,2,2,2,2,2,
2,2,2,2,2,2,2,2,2,2,2,2,2,2,4),(-2.9716555919461,-2.97154817145025,-2.96562500995768,
-2.96005983868355,-2.95383901635577,-2.94433737881855,-2.91042200232887,
-2.86852541548387,-2.8513991194649,-2.84610485960585,-2.84264957015553,
-2.8390325070509,-2.83297145461849,-2.80573416970697,-2.76262311128696,
-2.73937387006405,-2.73088303932833,-2.72485365470322,-2.71934120629572,
-2.71033477040861,-2.68389380009236,-2.62507751112293,-2.61443080687828,
-2.60994974676855,-2.60662230104157,-2.60264016113958,-2.59504803234435,
-2.56061750264067,-2.52552509769381,-2.51076101299859,-2.49903285782614,
-2.49235964550477,-2.4864721512604,-2.47897955202297,-2.46283025579605,
-2.40289420833313,-2.38185584238939,-2.37623055989595,-2.37270655457017,
-2.36917208392626,-2.36349800441212,-2.34383769818164,-2.29421154679409,
-2.26950356352012,-2.26084938984811,-2.25479028582538,-2.24857898769667,
-2.2391283201122,-2.20782648423084,-2.16496056829367,-2.14635185798616,
-2.14092024430943,-2.13743685635153,-2.13385655909084,-2.12796856647655,
-2.10509538831603,-2.05835465463885,-2.03424771442571,-2.02565895080156,
-2.01961163613887,-2.013383827537,-2.00385000383816,-1.97100922053,-1.9366573715958,
-1.91999726119949,-1.90918084326314,-1.90467288741157,-1.90134276866777,
-1.89737847087723,-1.88964090997174,-1.85773347962173,-1.82092565319927,
-1.79866573414472,-1.79029205047388,-1.78428228818944,-1.77799434293165,
-1.76816076292468,-1.7268722606643,-1.69256122991686,-1.67581401960605,
-1.67055687743046,-1.66710865618302,-1.6634801096047,-1.65736654063487,
-1.62841318210618,-1.58666063730659,-1.56376059691621,-1.55531002587557,
-1.54928716040567,-1.54302197764727,-1.53330094026359,-1.49453840988134,
-1.47740198524613),.UNSPECIFIED.);
#492=B_SPLINE_CURVE_WITH_KNOTS('',3,(#43357,#43358,#43359,#43360,#43361,
#43362,#43363,#43364,#43365,#43366,#43367,#43368,#43369,#43370,#43371,#43372,
#43373,#43374,#43375,#43376,#43377,#43378,#43379,#43380,#43381,#43382,#43383,
#43384,#43385,#43386,#43387,#43388,#43389,#43390,#43391,#43392,#43393,#43394,
#43395,#43396,#43397,#43398,#43399,#43400,#43401,#43402,#43403,#43404,#43405,
#43406,#43407,#43408,#43409,#43410,#43411,#43412,#43413,#43414,#43415,#43416,
#43417,#43418,#43419,#43420,#43421,#43422,#43423,#43424,#43425,#43426,#43427,
#43428,#43429,#43430,#43431,#43432,#43433,#43434,#43435,#43436,#43437,#43438,
#43439,#43440,#43441,#43442,#43443,#43444,#43445,#43446,#43447,#43448,#43449,
#43450,#43451,#43452,#43453,#43454,#43455,#43456,#43457,#43458,#43459,#43460,
#43461,#43462,#43463,#43464,#43465,#43466,#43467,#43468,#43469,#43470,#43471,
#43472,#43473,#43474,#43475,#43476,#43477,#43478,#43479,#43480,#43481,#43482,
#43483,#43484,#43485,#43486,#43487,#43488,#43489,#43490,#43491,#43492,#43493,
#43494,#43495,#43496,#43497,#43498,#43499,#43500,#43501,#43502,#43503,#43504,
#43505,#43506,#43507,#43508,#43509,#43510,#43511,#43512,#43513,#43514,#43515,
#43516,#43517,#43518,#43519,#43520,#43521,#43522,#43523,#43524,#43525,#43526,
#43527,#43528,#43529,#43530,#43531,#43532,#43533,#43534,#43535,#43536,#43537,
#43538,#43539,#43540,#43541,#43542),.UNSPECIFIED.,.F.,.F.,(4,2,2,2,2,2,
2,2,2,2,2,2,2,2,2,2,2,2,2,2,2,2,2,2,2,2,2,2,2,2,2,2,2,2,2,2,2,2,2,2,2,2,
2,2,2,2,2,2,2,2,2,2,2,2,2,2,2,2,2,2,2,2,2,2,2,2,2,2,2,2,2,2,2,2,2,2,2,2,
2,2,2,2,2,2,2,2,2,2,2,2,2,2,4),(-1.51221321296554,-1.51085484546286,-1.49484427234498,
-1.48956990796848,-1.48607821760021,-1.4822859170049,-1.4757319796956,-1.46743687932551,
-1.44817086842178,-1.38861439066354,-1.37738351716336,-1.37068117478839,
-1.3645694920746,-1.35649227251671,-1.3375169891521,-1.30805928939344,-1.26376081573809,
-1.25660526368414,-1.25264542141063,-1.24917991699939,-1.24427476966737,
-1.23130443964399,-1.2095066873353,-1.15225764308533,-1.14183767370461,
-1.13529983490702,-1.12912697543539,-1.12063568008592,-1.09862995947849,
-1.06288856704313,-1.02736365562602,-1.02102341321342,-1.01727665699929,
-1.01371634365497,-1.00826393385117,-0.9904932218741,-0.952110080253169,
-0.916210482773215,-0.906422808865517,-0.900011525037985,-0.893763900962858,
-0.88483664013308,-0.858996623044593,-0.803251455004088,-0.789990848365579,
-0.78491523699523,-0.781423330324444,-0.777541968066019,-0.770564575860217,
-0.761553469633356,-0.739452753531308,-0.682838850924898,-0.672325065863944,
-0.665768099625375,-0.659603789833833,-0.65116703023199,-0.629590554626786,
-0.592731122358163,-0.560392452056923,-0.552624309903082,-0.548534467194944,
-0.545129568803643,-0.540472601588181,-0.529216700190913,-0.511682420954267,
-0.455263475391965,-0.440581766892907,-0.433210612644359,-0.427161116294937,
-0.420003326845187,-0.406468599704118,-0.33913585792777,-0.321417424973873,
-0.315828066139664,-0.312594631019935,-0.3089867166535,-0.303300383466177,
-0.282806771731894,-0.228252557069223,-0.208469866538841,-0.200931991000315,
-0.19473877762972,-0.188350386942891,-0.178680975267564,-0.143101944131677,
-0.0935604393360744,-0.0847617326463241,-0.0804581162290219,-0.0769919585924988,
-0.0731442758265341,-0.066328792090819,-0.0575939795842131,-0.0178393446226998),
 .UNSPECIFIED.);
#493=B_SPLINE_CURVE_WITH_KNOTS('',3,(#43548,#43549,#43550,#43551,#43552,
#43553,#43554,#43555,#43556,#43557,#43558,#43559,#43560,#43561,#43562,#43563,
#43564,#43565,#43566,#43567,#43568,#43569,#43570,#43571,#43572,#43573,#43574,
#43575,#43576,#43577,#43578,#43579,#43580,#43581,#43582,#43583,#43584,#43585,
#43586,#43587,#43588,#43589,#43590,#43591,#43592,#43593,#43594,#43595,#43596,
#43597,#43598,#43599,#43600,#43601,#43602,#43603,#43604,#43605,#43606,#43607,
#43608,#43609,#43610,#43611,#43612,#43613,#43614,#43615,#43616,#43617,#43618,
#43619,#43620,#43621,#43622,#43623,#43624,#43625,#43626,#43627,#43628,#43629,
#43630,#43631,#43632,#43633,#43634,#43635,#43636,#43637,#43638,#43639,#43640,
#43641,#43642,#43643,#43644,#43645,#43646,#43647,#43648,#43649,#43650,#43651,
#43652,#43653,#43654,#43655,#43656,#43657,#43658,#43659,#43660,#43661,#43662,
#43663,#43664,#43665,#43666,#43667,#43668,#43669,#43670,#43671,#43672,#43673,
#43674,#43675,#43676,#43677,#43678,#43679,#43680,#43681,#43682,#43683,#43684,
#43685,#43686,#43687,#43688,#43689,#43690,#43691,#43692,#43693,#43694,#43695,
#43696,#43697,#43698,#43699,#43700,#43701,#43702,#43703,#43704,#43705,#43706,
#43707,#43708,#43709,#43710,#43711,#43712,#43713,#43714,#43715,#43716,#43717,
#43718,#43719,#43720,#43721,#43722,#43723,#43724,#43725),.UNSPECIFIED.,
 .F.,.F.,(4,2,2,2,2,2,2,2,2,2,2,2,2,2,2,2,2,2,2,2,2,2,2,2,2,2,2,2,2,2,2,
2,2,2,2,2,2,2,2,2,2,2,2,2,2,2,2,2,2,2,2,2,2,2,2,2,2,2,2,2,2,2,2,2,2,2,2,
2,2,2,2,2,2,2,2,2,2,2,2,2,2,2,2,2,2,2,2,2,4),(-1.47759266585272,-1.47583902726231,
-1.44357763760892,-1.40282698793516,-1.39145610972514,-1.38479306930802,
-1.37890371782198,-1.37139390483523,-1.35514289943167,-1.33182451894543,
-1.28552002324551,-1.27284185197666,-1.26793124540071,-1.26454620903653,
-1.26079442794825,-1.25410014054262,-1.24550819972451,-1.22486098243887,
-1.17181956373618,-1.15804517865605,-1.15088889585203,-1.14502343023918,
-1.1381019052825,-1.12511555701983,-1.08529653068715,-1.04219353760626,
-1.03502442930169,-1.03113152417172,-1.02778843535297,-1.02316470249161,
-1.01158823444863,-0.99316018795545,-0.930943083829598,-0.920317454469369,
-0.913868291989847,-0.90792886474967,-0.900003118701505,-0.881089033406792,
-0.851574886104677,-0.806854911075443,-0.799800666323608,-0.795932451125106,
-0.792583827677378,-0.787916278389732,-0.776039923746547,-0.756883711320975,
-0.696571545983134,-0.685538991332259,-0.679006748262875,-0.673091380849142,
-0.665345827782787,-0.647628761643719,-0.621037215485704,-0.579029457168609,
-0.567160937681541,-0.562379668855682,-0.559015233292986,-0.555205671877932,
-0.548233251102993,-0.509439276894764,-0.462137164521418,-0.450743910226097,
-0.444138518098801,-0.438239683105726,-0.430633358617338,-0.413792904738116,
-0.389194087090511,-0.336916459752479,-0.329687883995292,-0.325782357178985,
-0.322778032310721,-0.318396075404208,-0.308358989994193,-0.293411418199345,
-0.257639984165958,-0.223524409444837,-0.213959562965366,-0.207725653791638,
-0.201682678058227,-0.19311786264907,-0.16922825281877,-0.123469658836699,
-0.0993831546337505,-0.0934465306990903,-0.0898558423729977,-0.0863806053261936,
-0.080988929077923,-0.0628273352297112,-0.000673664115542865),
 .UNSPECIFIED.);
#494=B_SPLINE_CURVE_WITH_KNOTS('',3,(#43726,#43727,#43728,#43729,#43730,
#43731),.UNSPECIFIED.,.F.,.F.,(4,2,4),(-2.98910690514882,-2.9794000728681,
-2.9716555919461),.UNSPECIFIED.);
#495=B_SPLINE_CURVE_WITH_KNOTS('',3,(#43733,#43734,#43735,#43736),
 .UNSPECIFIED.,.F.,.F.,(4,4),(-0.0178393446226998,-0.000669879165383271),
 .UNSPECIFIED.);
#496=B_SPLINE_CURVE_WITH_KNOTS('',3,(#43737,#43738,#43739,#43740,#43741,
#43742,#43743,#43744,#43745,#43746,#43747,#43748,#43749,#43750,#43751,#43752,
#43753,#43754,#43755,#43756,#43757,#43758,#43759,#43760,#43761,#43762,#43763,
#43764,#43765,#43766,#43767,#43768,#43769,#43770,#43771,#43772,#43773,#43774,
#43775,#43776,#43777,#43778,#43779,#43780,#43781,#43782,#43783,#43784,#43785,
#43786,#43787,#43788,#43789,#43790,#43791,#43792,#43793,#43794,#43795,#43796,
#43797,#43798,#43799,#43800,#43801,#43802,#43803,#43804,#43805,#43806,#43807,
#43808,#43809,#43810,#43811,#43812,#43813,#43814,#43815,#43816,#43817,#43818,
#43819,#43820,#43821,#43822,#43823,#43824,#43825,#43826,#43827,#43828,#43829,
#43830,#43831,#43832,#43833,#43834,#43835,#43836,#43837,#43838,#43839,#43840,
#43841,#43842,#43843,#43844,#43845,#43846,#43847,#43848,#43849,#43850,#43851,
#43852,#43853,#43854,#43855,#43856,#43857,#43858,#43859,#43860,#43861,#43862,
#43863,#43864,#43865,#43866,#43867,#43868,#43869,#43870,#43871,#43872,#43873,
#43874,#43875,#43876,#43877,#43878,#43879,#43880,#43881,#43882,#43883,#43884,
#43885,#43886,#43887,#43888,#43889,#43890,#43891,#43892,#43893,#43894,#43895,
#43896,#43897,#43898,#43899,#43900,#43901,#43902,#43903,#43904,#43905,#43906,
#43907,#43908,#43909,#43910,#43911,#43912,#43913,#43914,#43915,#43916,#43917,
#43918),.UNSPECIFIED.,.F.,.F.,(4,2,2,2,2,2,2,2,2,2,2,2,2,2,2,2,2,2,2,2,
2,2,2,2,2,2,2,2,2,2,2,2,2,2,2,2,2,2,2,2,2,2,2,2,2,2,2,2,2,2,2,2,2,2,2,2,
2,2,2,2,2,2,2,2,2,2,2,2,2,2,2,2,2,2,2,2,2,2,2,2,2,2,2,2,2,2,2,2,2,2,4),
(-2.98894532842057,-2.96679766759181,-2.95895194939698,-2.95299040461239,
-2.94688554234206,-2.94015963035491,-2.92881155233073,-2.88051159025543,
-2.84886443595245,-2.83784551973106,-2.8332256742013,-2.82979396244754,
-2.82566495177523,-2.81745385019771,-2.77198792205609,-2.74433561670034,
-2.72608918694708,-2.71812198458179,-2.71202447485776,-2.70526903091423,
-2.69377513069564,-2.64604539526109,-2.60816966081843,-2.60102031220554,
-2.5971035383971,-2.59362484956453,-2.58863072902918,-2.57593175789617,
-2.51959588682296,-2.49367578698727,-2.48474120277274,-2.47849255209288,
-2.47208360061814,-2.46230643032818,-2.42691896305785,-2.38807462163282,
-2.37020233164769,-2.3647402752484,-2.36117821981831,-2.35743456252897,
-2.35110844570821,-2.31584339009273,-2.27994130921511,-2.26492263576045,
-2.25297939586326,-2.24613340943604,-2.24005431974874,-2.23225222737033,
-2.21572099481243,-2.15832914657657,-2.14326678316657,-2.13312386458711,
-2.12864610895088,-2.12522384127365,-2.12098533011795,-2.11219699852639,
-2.05080030250098,-2.02422687262648,-2.01522738099746,-2.00896703140146,
-2.00257390830332,-1.99287680613008,-1.95992483733062,-1.91899502335571,
-1.90068912626002,-1.89518693704619,-1.89161696413409,-1.88834931939354,
-1.88257538865616,-1.86290446052514,-1.81370721255665,-1.78901287109256,
-1.78020720307339,-1.77398163990907,-1.76830129606733,-1.7590311582901,
-1.73138176545606,-1.68534114535974,-1.66609182213885,-1.66050670321025,
-1.65692009052091,-1.65321108586562,-1.64704707731286,-1.61990304476685,
-1.57711487869409,-1.55386793511717,-1.54522603008742,-1.53902861293514,
-1.53331479880452,-1.52385069073556,-1.51202351089742),.UNSPECIFIED.);
#497=B_SPLINE_CURVE_WITH_KNOTS('',3,(#43923,#43924,#43925,#43926,#43927,
#43928,#43929,#43930,#43931,#43932,#43933,#43934,#43935,#43936,#43937,#43938,
#43939,#43940,#43941,#43942,#43943,#43944,#43945,#43946,#43947,#43948,#43949,
#43950,#43951,#43952,#43953,#43954,#43955,#43956,#43957,#43958,#43959,#43960,
#43961,#43962,#43963,#43964,#43965,#43966,#43967,#43968,#43969,#43970,#43971,
#43972,#43973,#43974,#43975,#43976,#43977,#43978,#43979,#43980,#43981,#43982,
#43983,#43984,#43985,#43986,#43987,#43988,#43989,#43990,#43991,#43992,#43993,
#43994,#43995,#43996,#43997,#43998,#43999,#44000,#44001,#44002,#44003,#44004,
#44005,#44006,#44007,#44008,#44009,#44010,#44011,#44012,#44013,#44014,#44015,
#44016,#44017,#44018,#44019,#44020,#44021,#44022,#44023,#44024,#44025,#44026,
#44027,#44028,#44029,#44030,#44031,#44032,#44033,#44034,#44035,#44036,#44037,
#44038,#44039,#44040,#44041,#44042,#44043,#44044,#44045,#44046,#44047,#44048,
#44049,#44050,#44051,#44052,#44053,#44054,#44055,#44056,#44057,#44058,#44059,
#44060,#44061,#44062,#44063,#44064,#44065,#44066,#44067,#44068,#44069,#44070,
#44071,#44072,#44073,#44074,#44075,#44076,#44077,#44078,#44079,#44080,#44081,
#44082,#44083,#44084,#44085,#44086,#44087,#44088,#44089,#44090,#44091,#44092,
#44093,#44094,#44095,#44096,#44097,#44098,#44099,#44100,#44101,#44102,#44103,
#44104,#44105,#44106,#44107,#44108),.UNSPECIFIED.,.F.,.F.,(4,2,2,2,2,2,
2,2,2,2,2,2,2,2,2,2,2,2,2,2,2,2,2,2,2,2,2,2,2,2,2,2,2,2,2,2,2,2,2,2,2,2,
2,2,2,2,2,2,2,2,2,2,2,2,2,2,2,2,2,2,2,2,2,2,2,2,2,2,2,2,2,2,2,2,2,2,2,2,
2,2,2,2,2,2,2,2,2,2,2,2,2,2,4),(-2.9718798661411,-2.92833422092586,-2.91754480451469,
-2.91304124566946,-2.90974131486556,-2.90578828592925,-2.89833497354585,
-2.84737885793396,-2.82224322820136,-2.80516076667878,-2.79751556758755,
-2.79161238385916,-2.78502841449271,-2.77374097876193,-2.72442391911659,
-2.6863392061329,-2.67996517302808,-2.67628113578022,-2.67290516971136,
-2.66785240361569,-2.65411145792008,-2.60891342949597,-2.58579311774677,
-2.56963426639711,-2.56214003685471,-2.55625224218432,-2.54957971525801,
-2.53816407024515,-2.49932129767375,-2.46563387246433,-2.44904378045224,
-2.44380253340108,-2.44035744773731,-2.43672415821915,-2.43058829529567,
-2.39964548903531,-2.35940066815492,-2.33690977930333,-2.3285081480383,
-2.32249373740921,-2.31621437322995,-2.30642278092401,-2.26575853088833,
-2.23090366431735,-2.2140222697628,-2.2087518173252,-2.20530103728228,-2.20167657954524,
-2.19558186336725,-2.16736205417542,-2.12503467590148,-2.10198455319833,
-2.09351645960803,-2.08749066622084,-2.08197310437768,-2.07293886603976,
-2.04618825963088,-1.9876284293558,-1.97705680568901,-1.97258748370793,
-1.96926086364871,-1.96527005268775,-1.95763720337968,-1.9259235242493,
-1.8889589752926,-1.8666494532543,-1.85826947025256,-1.85225844538663,-1.845972030648,
-1.83614692345946,-1.79663369523838,-1.76150029995517,-1.74394531245887,
-1.73860938034474,-1.73514542677704,-1.7315394766195,-1.7255318735531,-1.69960685868486,
-1.65540848140326,-1.63188891567363,-1.62336613668799,-1.61733049215749,
-1.6110851140738,-1.60146353288126,-1.56605727446876,-1.53231996876569,
-1.51696069078904,-1.50673255100101,-1.5023189224699,-1.49899692535738,
-1.49496616648127,-1.48688770425023,-1.47759266585272),.UNSPECIFIED.);
#498=B_SPLINE_CURVE_WITH_KNOTS('',3,(#44109,#44110,#44111,#44112,#44113,
#44114,#44115,#44116,#44117,#44118,#44119,#44120,#44121,#44122,#44123,#44124,
#44125,#44126,#44127,#44128,#44129,#44130,#44131,#44132,#44133,#44134,#44135,
#44136,#44137,#44138,#44139,#44140,#44141,#44142,#44143,#44144,#44145,#44146,
#44147,#44148,#44149,#44150,#44151,#44152,#44153,#44154,#44155,#44156,#44157,
#44158,#44159,#44160,#44161,#44162,#44163,#44164,#44165,#44166,#44167,#44168,
#44169,#44170,#44171,#44172,#44173,#44174,#44175,#44176,#44177,#44178,#44179,
#44180,#44181,#44182,#44183,#44184,#44185,#44186,#44187,#44188,#44189,#44190,
#44191,#44192,#44193,#44194,#44195,#44196,#44197,#44198,#44199,#44200,#44201,
#44202,#44203,#44204,#44205,#44206,#44207,#44208,#44209,#44210,#44211,#44212,
#44213,#44214,#44215,#44216,#44217,#44218,#44219,#44220,#44221,#44222,#44223,
#44224,#44225,#44226,#44227,#44228,#44229,#44230,#44231,#44232,#44233,#44234,
#44235,#44236,#44237,#44238,#44239,#44240,#44241,#44242,#44243,#44244,#44245,
#44246,#44247,#44248,#44249,#44250,#44251,#44252,#44253,#44254,#44255,#44256,
#44257,#44258,#44259,#44260,#44261,#44262,#44263,#44264,#44265,#44266,#44267,
#44268,#44269,#44270,#44271,#44272,#44273,#44274,#44275,#44276,#44277,#44278,
#44279,#44280,#44281,#44282,#44283,#44284,#44285,#44286,#44287,#44288,#44289,
#44290),.UNSPECIFIED.,.F.,.F.,(4,2,2,2,2,2,2,2,2,2,2,2,2,2,2,2,2,2,2,2,
2,2,2,2,2,2,2,2,2,2,2,2,2,2,2,2,2,2,2,2,2,2,2,2,2,2,2,2,2,2,2,2,2,2,2,2,
2,2,2,2,2,2,2,2,2,2,2,2,2,2,2,2,2,2,2,2,2,2,2,2,2,2,2,2,2,2,2,2,2,2,4),
(-1.51202351089742,-1.49449240811967,-1.45667173300721,-1.43227678108567,
-1.42622370023567,-1.42253844292242,-1.41893281371061,-1.41325518393757,
-1.39286349735994,-1.33909010650591,-1.31869231935832,-1.31021804321852,
-1.30404827134258,-1.29750531163309,-1.28705854709645,-1.27449300749082,
-1.24697289772713,-1.20192620313761,-1.19328075226823,-1.1890690690116,
-1.18598862455779,-1.18167885613466,-1.17249990441517,-1.15942318858956,
-1.11336386847791,-1.08577253446091,-1.07650881157454,-1.07082955720942,
-1.0646029030008,-1.0557913515612,-1.03104693085066,-0.981620263707763,
-0.962138817641369,-0.956388603537074,-0.953125416503227,-0.949550912447172,
-0.944026524766034,-0.925473119625564,-0.883272275422081,-0.851776518799035,
-0.842154500198513,-0.835775928968778,-0.829503648362441,-0.820440033989039,
-0.79320445428282,-0.763440710119895,-0.731148219548661,-0.723384167091417,
-0.719295260506067,-0.715890353808088,-0.711232334437589,-0.699968969113581,
-0.682417090596136,-0.625865676701502,-0.611465296223883,-0.604056643041399,
-0.59800613102232,-0.590881443815959,-0.577519130217075,-0.55077469138695,
-0.50809783953738,-0.491949968254766,-0.486512761700874,-0.483307183798012,
-0.479663483642516,-0.473805488927917,-0.450855961060644,-0.421495425269382,
-0.382785434418195,-0.372902320473972,-0.366472266931216,-0.360238101984609,
-0.351385408219891,-0.326260518998026,-0.27482914644042,-0.257429685626527,
-0.251869123788893,-0.248641189206723,-0.245027282671453,-0.23931102011774,
-0.218418076884369,-0.160464312214743,-0.143113177841032,-0.135285917195027,
-0.129204015954906,-0.122372217698661,-0.110500714053059,-0.0956018553195042,
-0.0455136996519052,-0.0233411546340862,-0.0179078448206664),
 .UNSPECIFIED.);
#499=B_SPLINE_CURVE_WITH_KNOTS('',3,(#44296,#44297,#44298,#44299,#44300,
#44301,#44302,#44303,#44304,#44305,#44306,#44307,#44308,#44309,#44310,#44311,
#44312,#44313,#44314,#44315,#44316,#44317,#44318,#44319,#44320,#44321,#44322,
#44323,#44324,#44325,#44326,#44327,#44328,#44329,#44330,#44331,#44332,#44333,
#44334,#44335,#44336,#44337,#44338,#44339,#44340,#44341,#44342,#44343,#44344,
#44345,#44346,#44347,#44348,#44349,#44350,#44351,#44352,#44353,#44354,#44355,
#44356,#44357,#44358,#44359,#44360,#44361,#44362,#44363,#44364,#44365,#44366,
#44367,#44368,#44369,#44370,#44371,#44372,#44373,#44374,#44375,#44376,#44377,
#44378,#44379,#44380,#44381,#44382,#44383,#44384,#44385,#44386,#44387,#44388,
#44389,#44390,#44391,#44392,#44393,#44394,#44395,#44396,#44397,#44398,#44399,
#44400,#44401,#44402,#44403,#44404,#44405,#44406,#44407,#44408,#44409,#44410,
#44411,#44412,#44413,#44414,#44415,#44416,#44417,#44418,#44419,#44420,#44421,
#44422,#44423,#44424,#44425,#44426,#44427,#44428,#44429,#44430,#44431,#44432,
#44433,#44434,#44435,#44436,#44437,#44438,#44439,#44440,#44441,#44442,#44443,
#44444,#44445,#44446,#44447,#44448,#44449,#44450,#44451,#44452,#44453,#44454,
#44455,#44456,#44457,#44458,#44459,#44460,#44461,#44462,#44463,#44464,#44465,
#44466,#44467,#44468,#44469,#44470,#44471,#44472,#44473,#44474,#44475,#44476,
#44477,#44478,#44479,#44480,#44481,#44482,#44483),.UNSPECIFIED.,.F.,.F.,
(4,2,2,2,2,2,2,2,2,2,2,2,2,2,2,2,2,2,2,2,2,2,2,2,2,2,2,2,2,2,2,2,2,2,2,
2,2,2,2,2,2,2,2,2,2,2,2,2,2,2,2,2,2,2,2,2,2,2,2,2,2,2,2,2,2,2,2,2,2,2,2,
2,2,2,2,2,2,2,2,2,2,2,2,2,2,2,2,2,2,2,2,2,2,4),(-1.47753946869224,-1.46618248352132,
-1.45691851919379,-1.45136133851937,-1.44536781524085,-1.4370870041636,
-1.41556570221468,-1.37860916525036,-1.34325380867798,-1.33703153954625,
-1.3333800194858,-1.32994688395311,-1.3247657300231,-1.30874770913032,-1.2772238021133,
-1.23550219801313,-1.22413729202231,-1.21747637383588,-1.21158808214697,
-1.20407850559651,-1.18782320912539,-1.16449365988635,-1.11810927644965,
-1.10551704404071,-1.10061988830811,-1.09723763413345,-1.09348144488119,
-1.08676374894339,-1.07813152235602,-1.05732120876362,-1.00361841829855,
-0.991564649268644,-0.984145642407389,-0.978265757513395,-0.971547452429796,
-0.959590138548559,-0.944434200786007,-0.907441973027564,-0.875735155161742,
-0.868104334406487,-0.864114602826274,-0.860788807267809,-0.85632061096433,
-0.845751433122958,-0.787224528868138,-0.760505684120399,-0.751476240724885,
-0.74596035248848,-0.73993534232369,-0.731466440891137,-0.708401842201584,
-0.666017075838354,-0.637839663340758,-0.63174657323786,-0.628122923275746,
-0.624672724341686,-0.619402944062406,-0.60251908955384,-0.567641895910534,
-0.527026487599689,-0.517261790184601,-0.510988704370244,-0.504972526134255,
-0.496555407958669,-0.473929093663006,-0.433192562673141,-0.402875551349121,
-0.39674253876911,-0.393110306139631,-0.38966557533869,-0.384424058309238,
-0.367823156862109,-0.334083134923481,-0.295387092282997,-0.283968265791485,
-0.277295805630139,-0.271998076212244,-0.264806017603035,-0.250373220942863,
-0.184319218400211,-0.166526503446687,-0.161028660228815,-0.157877333845171,
-0.154405702471056,-0.149030907458394,-0.131052134028601,-0.103753202124731,
-0.0587944974736545,-0.0480352831879279,-0.0415587955374134,-0.0358769710594849,
-0.0301150406546835,-0.0225717469071839,-0.000673031561821805),
 .UNSPECIFIED.);
#500=B_SPLINE_CURVE_WITH_KNOTS('',3,(#44484,#44485,#44486,#44487),
 .UNSPECIFIED.,.F.,.F.,(4,4),(-2.98904500870718,-2.9718798661411),
 .UNSPECIFIED.);
#501=B_SPLINE_CURVE_WITH_KNOTS('',3,(#44489,#44490,#44491,#44492,#44493,
#44494,#44495,#44496,#44497,#44498,#44499,#44500),.UNSPECIFIED.,.F.,.F.,
(4,2,2,2,2,4),(-0.0179078448206664,-0.0174171828290496,-0.0137593046355443,
-0.0105814554284645,-0.00598018056482628,-0.000668823528435467),
 .UNSPECIFIED.);
#502=B_SPLINE_CURVE_WITH_KNOTS('',3,(#44501,#44502,#44503,#44504,#44505,
#44506,#44507,#44508,#44509,#44510,#44511,#44512,#44513,#44514,#44515,#44516,
#44517,#44518,#44519,#44520,#44521,#44522,#44523,#44524,#44525,#44526,#44527,
#44528,#44529,#44530,#44531,#44532,#44533,#44534,#44535,#44536,#44537,#44538,
#44539,#44540,#44541,#44542,#44543,#44544,#44545,#44546,#44547,#44548,#44549,
#44550,#44551,#44552,#44553,#44554,#44555,#44556,#44557,#44558,#44559,#44560,
#44561,#44562,#44563,#44564,#44565,#44566,#44567,#44568,#44569,#44570,#44571,
#44572,#44573,#44574,#44575,#44576,#44577,#44578,#44579,#44580,#44581,#44582,
#44583,#44584,#44585,#44586,#44587,#44588,#44589,#44590,#44591,#44592,#44593,
#44594,#44595,#44596,#44597,#44598,#44599,#44600,#44601,#44602,#44603,#44604,
#44605,#44606,#44607,#44608,#44609,#44610,#44611,#44612,#44613,#44614,#44615,
#44616,#44617,#44618,#44619,#44620,#44621,#44622,#44623,#44624,#44625,#44626,
#44627,#44628,#44629,#44630,#44631,#44632,#44633,#44634,#44635,#44636,#44637,
#44638,#44639,#44640,#44641,#44642,#44643,#44644,#44645,#44646,#44647,#44648,
#44649,#44650,#44651,#44652,#44653,#44654,#44655,#44656,#44657,#44658,#44659,
#44660,#44661,#44662,#44663,#44664,#44665,#44666,#44667,#44668,#44669,#44670,
#44671,#44672,#44673,#44674,#44675,#44676),.UNSPECIFIED.,.F.,.F.,(4,2,2,
2,2,2,2,2,2,2,2,2,2,2,2,2,2,2,2,2,2,2,2,2,2,2,2,2,2,2,2,2,2,2,2,2,2,2,2,
2,2,2,2,2,2,2,2,2,2,2,2,2,2,2,2,2,2,2,2,2,2,2,2,2,2,2,2,2,2,2,2,2,2,2,2,
2,2,2,2,2,2,2,2,2,2,2,2,4),(-2.9893589500714,-2.95396180238871,-2.92167880417226,
-2.89897537225032,-2.89039827744236,-2.88421156194824,-2.87848314243502,
-2.86893603254614,-2.83859933256492,-2.79528018187012,-2.77651284475504,
-2.77096928492961,-2.76739100976997,-2.76367060426163,-2.75745352729353,
-2.72868485465799,-2.6871891202505,-2.66427774458408,-2.65567556146713,
-2.64948467221613,-2.64376190246831,-2.63424709836998,-2.60415218206783,
-2.56057742482876,-2.54176287545832,-2.5362151629149,-2.53263605008132,
-2.52891679696925,-2.52270508527172,-2.49408539926091,-2.45247093231994,
-2.4295280563586,-2.42092211318199,-2.41473061158603,-2.40900870563828,
-2.39949877201175,-2.36954676781733,-2.32584577114125,-2.30700805930769,
-2.30145832699222,-2.29787881513964,-2.29416013608815,-2.28795107984734,
-2.25943620007469,-2.21773930442969,-2.19477457467764,-2.18616601086925,
-2.17997407065333,-2.17425274676923,-2.16474614980756,-2.13488939141179,
-2.09110428883567,-2.07829060284367,-2.06924513546892,-2.06495945484263,
-2.061880061416,-2.05764571318632,-2.04887942275539,-2.00398066299054,-1.9765176231576,
-1.95834963862161,-1.95039421647341,-1.94429786304221,-1.93753582274803,
-1.92601041527089,-1.87893304191309,-1.8400010618519,-1.83311412112586,
-1.829251753799,-1.82579217605242,-1.82070344413138,-1.8073378147123,-1.76197160465683,
-1.73437690700031,-1.72103900827823,-1.71391878422196,-1.70786769452151,
-1.70045285734424,-1.68884209475638,-1.63453186031581,-1.61372033428905,
-1.60112564720196,-1.59627199375223,-1.59281360746012,-1.58882685126493,
-1.58154657646952,-1.53933447853739,-1.51257715954122),.UNSPECIFIED.);
#503=B_SPLINE_CURVE_WITH_KNOTS('',3,(#44681,#44682,#44683,#44684,#44685,
#44686,#44687,#44688,#44689,#44690,#44691,#44692,#44693,#44694,#44695,#44696,
#44697,#44698,#44699,#44700,#44701,#44702,#44703,#44704,#44705,#44706,#44707,
#44708,#44709,#44710,#44711,#44712,#44713,#44714,#44715,#44716,#44717,#44718,
#44719,#44720,#44721,#44722,#44723,#44724,#44725,#44726,#44727,#44728,#44729,
#44730,#44731,#44732,#44733,#44734,#44735,#44736,#44737,#44738,#44739,#44740,
#44741,#44742,#44743,#44744,#44745,#44746,#44747,#44748,#44749,#44750,#44751,
#44752,#44753,#44754,#44755,#44756,#44757,#44758,#44759,#44760,#44761,#44762,
#44763,#44764,#44765,#44766,#44767,#44768,#44769,#44770,#44771,#44772,#44773,
#44774,#44775,#44776,#44777,#44778,#44779,#44780,#44781,#44782,#44783,#44784,
#44785,#44786,#44787,#44788,#44789,#44790,#44791,#44792,#44793,#44794,#44795,
#44796,#44797,#44798,#44799,#44800,#44801,#44802,#44803,#44804,#44805,#44806,
#44807,#44808,#44809,#44810,#44811,#44812,#44813,#44814,#44815,#44816,#44817,
#44818,#44819,#44820,#44821,#44822,#44823,#44824,#44825,#44826,#44827,#44828,
#44829,#44830,#44831,#44832,#44833,#44834,#44835,#44836,#44837,#44838,#44839,
#44840,#44841,#44842,#44843,#44844,#44845,#44846,#44847,#44848,#44849,#44850,
#44851,#44852,#44853,#44854,#44855,#44856,#44857,#44858,#44859,#44860,#44861,
#44862),.UNSPECIFIED.,.F.,.F.,(4,2,2,2,2,2,2,2,2,2,2,2,2,2,2,2,2,2,2,2,
2,2,2,2,2,2,2,2,2,2,2,2,2,2,2,2,2,2,2,2,2,2,2,2,2,2,2,2,2,2,2,2,2,2,2,2,
2,2,2,2,2,2,2,2,2,2,2,2,2,2,2,2,2,2,2,2,2,2,2,2,2,2,2,2,2,2,2,2,2,2,4),
(-2.97128357771462,-2.96865392351007,-2.94839507124107,-2.89743779778867,
-2.87424675097357,-2.86575034232415,-2.85970887341184,-2.85343553355014,
-2.84372254817052,-2.80512921397255,-2.76888139095612,-2.75167646141285,
-2.74636299393873,-2.74289482553345,-2.73927080171485,-2.73318777092222,
-2.70540183360721,-2.66280405476377,-2.6396957081517,-2.63122186480837,
-2.62519536408187,-2.61967937212161,-2.61065280919548,-2.58399436181157,
-2.52532943588081,-2.51470033019289,-2.51022382573427,-2.50689960110064,
-2.50292240379257,-2.49533992985453,-2.46439673151686,-2.43759652774324,
-2.41661326589724,-2.40149715217623,-2.39418792858843,-2.38832206388745,
-2.38154008369257,-2.36958025763954,-2.31427702486669,-2.29306261007733,
-2.28433149290656,-2.27755752343797,-2.27379214458389,-2.27041571944382,
-2.26555014922623,-2.25315685078844,-2.20659774123285,-2.18324631269954,
-2.16697842734428,-2.15946529237677,-2.15357477231354,-2.14691174631869,
-2.13554374860428,-2.09444098992591,-2.06246445164476,-2.04632417711657,
-2.04112840198186,-2.03769134119473,-2.03404332448252,-2.02783718033924,
-1.99280148943343,-1.95636639207222,-1.93422852071963,-1.92587155874946,
-1.9198660034611,-1.91357562420648,-1.90372367178009,-1.86304824391755,
-1.82830275820345,-1.81144989803916,-1.80618357332534,-1.80273456002231,
-1.79911110429465,-1.79301662424825,-1.76473876971035,-1.72247310490631,
-1.69944253718217,-1.69097893907457,-1.68495576169298,-1.67944023333038,
-1.67040855311391,-1.64365922914048,-1.58512035514045,-1.57455119987541,
-1.57008335592917,-1.56675784628897,-1.56276826608674,-1.55513850805868,
-1.52344861547318,-1.49504695531263,-1.47753946869224),.UNSPECIFIED.);
#504=B_SPLINE_CURVE_WITH_KNOTS('',3,(#44863,#44864,#44865,#44866,#44867,
#44868,#44869,#44870,#44871,#44872,#44873,#44874,#44875,#44876,#44877,#44878,
#44879,#44880,#44881,#44882,#44883,#44884,#44885,#44886,#44887,#44888,#44889,
#44890,#44891,#44892,#44893,#44894,#44895,#44896,#44897,#44898,#44899,#44900,
#44901,#44902,#44903,#44904,#44905,#44906,#44907,#44908,#44909,#44910,#44911,
#44912,#44913,#44914,#44915,#44916,#44917,#44918,#44919,#44920,#44921,#44922,
#44923,#44924,#44925,#44926,#44927,#44928,#44929,#44930,#44931,#44932,#44933,
#44934,#44935,#44936,#44937,#44938,#44939,#44940,#44941,#44942,#44943,#44944,
#44945,#44946,#44947,#44948,#44949,#44950,#44951,#44952,#44953,#44954,#44955,
#44956,#44957,#44958,#44959,#44960,#44961,#44962,#44963,#44964,#44965,#44966,
#44967,#44968,#44969,#44970,#44971,#44972,#44973,#44974,#44975,#44976,#44977,
#44978,#44979,#44980,#44981,#44982,#44983,#44984,#44985,#44986,#44987,#44988,
#44989,#44990,#44991,#44992,#44993,#44994,#44995,#44996,#44997,#44998,#44999,
#45000,#45001,#45002,#45003,#45004,#45005,#45006,#45007,#45008,#45009,#45010,
#45011,#45012,#45013,#45014,#45015,#45016,#45017,#45018,#45019,#45020,#45021,
#45022,#45023,#45024,#45025,#45026,#45027,#45028,#45029,#45030,#45031,#45032,
#45033,#45034,#45035,#45036,#45037,#45038,#45039,#45040,#45041,#45042,#45043,
#45044,#45045,#45046,#45047,#45048,#45049,#45050,#45051,#45052),
 .UNSPECIFIED.,.F.,.F.,(4,2,2,2,2,2,2,2,2,2,2,2,2,2,2,2,2,2,2,2,2,2,2,2,
2,2,2,2,2,2,2,2,2,2,2,2,2,2,2,2,2,2,2,2,2,2,2,2,2,2,2,2,2,2,2,2,2,2,2,2,
2,2,2,2,2,2,2,2,2,2,2,2,2,2,2,2,2,2,2,2,2,2,2,2,2,2,2,2,2,2,2,2,2,2,4),
(-1.51257715954122,-1.50868742133966,-1.49533487415107,-1.48439664682859,
-1.47775337250042,-1.47162264174556,-1.4634097442554,-1.44349605745563,
-1.41156197950073,-1.37163042281252,-1.36412190088113,-1.36008640345056,
-1.35698548095647,-1.35244730746324,-1.34194205458545,-1.27645812943356,
-1.25548021491546,-1.24691136569469,-1.24072542154754,-1.23421220372519,
-1.22391623137693,-1.17835395477159,-1.13641975126835,-1.12911786017158,
-1.12512635660953,-1.12166924981505,-1.11682456796411,-1.10429140385316,
-1.0836392559053,-1.02996126523853,-1.01790672689637,-1.01036825263347,
-1.00431147151791,-0.997291145783022,-0.984467134770748,-0.935729749958118,
-0.9022517156857,-0.894560149693531,-0.890486462769247,-0.88707925026059,
-0.882398395641776,-0.870986077329699,-0.853087660077437,-0.793935948229813,
-0.781406214468887,-0.77437186552303,-0.768315389399056,-0.760793346275567,
-0.745266769469627,-0.723616522503956,-0.697810717945532,-0.667369937506699,
-0.659717484936392,-0.655651421174981,-0.652554121265546,-0.648056854209032,
-0.637807989600492,-0.622522149567441,-0.586094067756851,-0.553599773624756,
-0.543922700212964,-0.537530990548716,-0.531263006261938,-0.522236189919012,
-0.495419122025837,-0.438774520429816,-0.427067279172335,-0.422693862835207,
-0.419211562122838,-0.415404105964945,-0.408768356524173,-0.400334784303282,
-0.380534455343681,-0.322242811813613,-0.310751272000897,-0.303999848558903,
-0.297907870823549,-0.289951107422307,-0.271749399225708,-0.244199026294971,
-0.19902214586421,-0.190474022986768,-0.186282516667828,-0.182891977094015,
-0.178383628957853,-0.168052989178377,-0.152591079151827,-0.0961144860805975,
-0.079151616139969,-0.0713849303718217,-0.065307044284041,-0.0584348018970584,
-0.0512357942656692,-0.0366507069838287,-0.0182409621825525),
 .UNSPECIFIED.);
#505=B_SPLINE_CURVE_WITH_KNOTS('',3,(#45056,#45057,#45058,#45059,#45060,
#45061),.UNSPECIFIED.,.F.,.F.,(4,1,1,4),(-4.09293042013066,-3.9493215972006,
-2.96199119790045,-2.06910254442638),.UNSPECIFIED.);
#506=B_SPLINE_CURVE_WITH_KNOTS('',3,(#45065,#45066,#45067,#45068,#45069),
 .UNSPECIFIED.,.F.,.F.,(4,1,4),(0.,0.988566943725272,1.11730040836823),
 .UNSPECIFIED.);
#507=B_SPLINE_CURVE_WITH_KNOTS('',3,(#45071,#45072,#45073,#45074,#45075,
#45076,#45077,#45078,#45079,#45080,#45081,#45082,#45083,#45084,#45085,#45086,
#45087,#45088,#45089,#45090,#45091,#45092,#45093,#45094,#45095,#45096,#45097,
#45098,#45099,#45100,#45101,#45102,#45103,#45104,#45105,#45106,#45107,#45108,
#45109,#45110,#45111,#45112,#45113,#45114,#45115,#45116,#45117,#45118,#45119,
#45120,#45121,#45122,#45123,#45124,#45125,#45126,#45127,#45128,#45129,#45130,
#45131,#45132,#45133,#45134,#45135,#45136,#45137,#45138,#45139,#45140,#45141,
#45142,#45143,#45144,#45145,#45146,#45147,#45148,#45149,#45150,#45151,#45152,
#45153,#45154,#45155,#45156,#45157,#45158,#45159,#45160,#45161,#45162,#45163,
#45164,#45165,#45166,#45167,#45168,#45169,#45170,#45171,#45172,#45173,#45174,
#45175,#45176,#45177,#45178,#45179,#45180,#45181,#45182,#45183,#45184,#45185,
#45186,#45187,#45188,#45189,#45190,#45191,#45192,#45193,#45194,#45195,#45196,
#45197,#45198,#45199,#45200,#45201,#45202,#45203,#45204,#45205,#45206,#45207,
#45208,#45209,#45210,#45211,#45212,#45213,#45214,#45215,#45216,#45217,#45218,
#45219,#45220,#45221,#45222,#45223,#45224,#45225,#45226,#45227,#45228,#45229,
#45230,#45231,#45232,#45233,#45234,#45235,#45236,#45237,#45238,#45239,#45240,
#45241,#45242,#45243,#45244,#45245,#45246,#45247,#45248,#45249,#45250,#45251,
#45252,#45253,#45254,#45255,#45256,#45257,#45258,#45259,#45260,#45261,#45262,
#45263,#45264,#45265,#45266,#45267,#45268,#45269,#45270,#45271,#45272,#45273,
#45274,#45275,#45276,#45277,#45278,#45279,#45280,#45281),.UNSPECIFIED.,
 .F.,.F.,(4,3,3,3,3,3,3,3,3,3,3,3,3,3,3,3,3,3,3,3,3,3,3,3,3,3,3,3,3,3,3,
3,3,3,3,3,3,3,3,3,3,3,3,3,3,3,3,3,3,3,3,3,3,3,3,3,3,3,3,3,3,3,3,3,3,3,3,
3,3,3,4),(1.11730040836823,1.21037388007188,1.30621888099421,1.39909202481253,
1.49192328569137,1.58474107162718,1.67757377046851,1.77050322392294,1.86349120514412,
1.95661989431377,1.97713388745054,2.07263487628453,2.16800729129127,2.26771898377683,
2.36292314190516,2.45809521423212,2.55326139142238,2.64844785131489,2.74373567178762,
2.83908288421244,2.9345736252384,2.9657008311758,3.0612101519017,3.15659374321842,
3.25630299717875,3.35152542041667,3.44671833584018,3.54190791950783,3.63712033682998,
3.7324378035997,3.82781683687417,3.92334239041227,3.95426777490106,4.04949425818523,
4.14459011568218,4.2443706910502,4.33929523863208,4.43418719540974,4.52907312140792,
4.62397956378642,4.71898930590132,4.81405924567905,4.90927623089053,4.94283471862632,
5.03821711679297,5.13347079444595,5.23321215293416,5.32829814620465,5.42335253563372,
5.51840167611464,5.61347191028934,5.70864539355769,5.80387923767303,5.89925900834736,
5.93140166235159,6.02677164553458,6.12201312336192,6.22175755870129,6.31683198767932,
6.41187507260355,6.50691318440943,6.60197268202006,6.6971359286251,6.79235981409918,
6.88773012583267,6.91996860607685,7.02073121797426,7.12120864243437,7.22151462151028,
7.32158735870522,7.40048571527184),.UNSPECIFIED.);
#508=B_SPLINE_CURVE_WITH_KNOTS('',3,(#45283,#45284,#45285,#45286,#45287,
#45288,#45289,#45290,#45291,#45292,#45293,#45294,#45295,#45296,#45297,#45298,
#45299,#45300,#45301,#45302,#45303,#45304,#45305,#45306,#45307,#45308,#45309,
#45310,#45311,#45312,#45313,#45314,#45315,#45316,#45317,#45318,#45319,#45320,
#45321,#45322,#45323,#45324,#45325,#45326,#45327,#45328,#45329,#45330,#45331,
#45332,#45333,#45334,#45335,#45336,#45337,#45338,#45339,#45340,#45341,#45342,
#45343,#45344,#45345,#45346,#45347,#45348,#45349,#45350,#45351,#45352,#45353,
#45354,#45355,#45356,#45357,#45358,#45359,#45360,#45361,#45362,#45363,#45364,
#45365,#45366,#45367,#45368,#45369,#45370,#45371,#45372,#45373,#45374,#45375,
#45376,#45377,#45378,#45379,#45380,#45381,#45382,#45383,#45384,#45385,#45386,
#45387,#45388,#45389,#45390,#45391,#45392,#45393,#45394,#45395,#45396,#45397,
#45398,#45399,#45400,#45401,#45402,#45403,#45404,#45405,#45406,#45407,#45408,
#45409,#45410,#45411,#45412,#45413,#45414,#45415,#45416,#45417,#45418,#45419,
#45420,#45421,#45422,#45423,#45424,#45425,#45426,#45427,#45428,#45429,#45430,
#45431,#45432,#45433,#45434,#45435,#45436,#45437,#45438,#45439,#45440,#45441,
#45442,#45443,#45444,#45445,#45446,#45447,#45448,#45449,#45450,#45451,#45452,
#45453,#45454,#45455,#45456,#45457,#45458,#45459,#45460,#45461,#45462,#45463,
#45464,#45465,#45466,#45467,#45468,#45469,#45470,#45471,#45472,#45473,#45474,
#45475,#45476,#45477,#45478,#45479,#45480,#45481,#45482,#45483,#45484,#45485,
#45486,#45487,#45488,#45489,#45490),.UNSPECIFIED.,.F.,.F.,(4,3,3,3,3,3,
3,3,3,3,3,3,3,3,3,3,3,3,3,3,3,3,3,3,3,3,3,3,3,3,3,3,3,3,3,3,3,3,3,3,3,3,
3,3,3,3,3,3,3,3,3,3,3,3,3,3,3,3,3,3,3,3,3,3,3,3,3,3,3,4),(7.40048571554782,
7.49937034306215,7.60166164474714,7.70089351874772,7.80471453427491,7.90853554980211,
8.00389380426277,8.09912321670652,8.19887062630912,8.29393223320934,8.38896224533412,
8.48398704975616,8.57903302133985,8.67418248971306,8.76939243491052,8.86474867946115,
8.89710249352738,8.99245676209535,9.08768218520464,9.18743059171064,9.28248823090432,
9.3775142919929,9.47253516730274,9.56757723697213,9.66272286636021,9.75792900460433,
9.85328152193589,9.88566943725264,9.98101947654195,10.0762405859611,10.1759900603382,
10.2710432057759,10.3660647165878,10.4610809908222,10.5561184142973,10.651259355886,
10.7464607767975,10.841808571773,10.8742363809779,10.9695899428316,11.064814624289,
11.1645632118408,11.2596200269402,11.3546452353564,11.4496652304129,11.5447063932207,
11.6398510808652,11.735056256063,11.8304077864152,11.8628033247032,11.9581560172067,
12.0533798239388,12.1531286295,12.2481845629618,12.3432088891243,12.4382280024644,
12.5332682852472,12.6284121003789,12.7236164064074,12.8189670798418,12.8513702684284,
12.9453321463137,13.039144360993,13.1328721337901,13.2265434258128,13.3201861320926,
13.4138735216964,13.5075805203644,13.60140729215,13.6836710227274),
 .UNSPECIFIED.);
#509=B_SPLINE_CURVE_WITH_KNOTS('',3,(#45492,#45493,#45494,#45495,#45496,
#45497,#45498,#45499,#45500,#45501,#45502),.UNSPECIFIED.,.F.,.F.,(4,1,1,
1,1,1,1,1,4),(13.6836710227274,13.8399372121537,14.828504155879,15.8170710996042,
16.8056380433295,17.7942049870548,18.78277193078,19.7713388745053,19.966856329907),
 .UNSPECIFIED.);
#510=B_SPLINE_CURVE_WITH_KNOTS('',3,(#45504,#45505,#45506,#45507,#45508,
#45509,#45510,#45511,#45512,#45513,#45514,#45515,#45516,#45517,#45518,#45519,
#45520,#45521,#45522,#45523,#45524,#45525,#45526,#45527,#45528,#45529,#45530,
#45531,#45532,#45533,#45534,#45535,#45536,#45537,#45538,#45539,#45540,#45541,
#45542,#45543,#45544,#45545,#45546,#45547,#45548,#45549,#45550,#45551,#45552,
#45553,#45554,#45555,#45556,#45557,#45558,#45559,#45560,#45561,#45562,#45563,
#45564,#45565,#45566,#45567,#45568,#45569,#45570,#45571,#45572,#45573,#45574,
#45575,#45576,#45577,#45578,#45579,#45580,#45581,#45582,#45583,#45584,#45585,
#45586,#45587,#45588,#45589,#45590,#45591,#45592,#45593,#45594,#45595,#45596,
#45597,#45598,#45599,#45600,#45601,#45602,#45603,#45604,#45605,#45606,#45607,
#45608,#45609,#45610,#45611,#45612,#45613,#45614,#45615,#45616,#45617,#45618,
#45619,#45620,#45621,#45622,#45623,#45624,#45625,#45626,#45627,#45628,#45629,
#45630,#45631,#45632,#45633,#45634,#45635,#45636,#45637,#45638,#45639,#45640,
#45641,#45642,#45643,#45644,#45645,#45646,#45647,#45648,#45649,#45650,#45651,
#45652,#45653,#45654,#45655,#45656,#45657,#45658,#45659,#45660,#45661,#45662,
#45663,#45664,#45665,#45666,#45667,#45668,#45669,#45670,#45671,#45672,#45673,
#45674,#45675,#45676,#45677,#45678,#45679,#45680,#45681,#45682,#45683,#45684,
#45685,#45686,#45687,#45688,#45689,#45690,#45691,#45692,#45693,#45694,#45695,
#45696,#45697,#45698,#45699,#45700,#45701,#45702,#45703,#45704,#45705,#45706,
#45707,#45708,#45709,#45710,#45711,#45712,#45713,#45714),.UNSPECIFIED.,
 .F.,.F.,(4,3,3,3,3,3,3,3,3,3,3,3,3,3,3,3,3,3,3,3,3,3,3,3,3,3,3,3,3,3,3,
3,3,3,3,3,3,3,3,3,3,3,3,3,3,3,3,3,3,3,3,3,3,3,3,3,3,3,3,3,3,3,3,3,3,3,3,
3,3,3,4),(19.966856329907,20.0606883778646,20.1544324765222,20.2481305658949,
20.3418104960079,20.4355000925652,20.5292828743492,20.6231185270144,20.7170997179296,
20.7599058182306,20.8552583879036,20.9504820669485,21.0502309038244,21.145286698325,
21.2403108816755,21.3353298485237,21.4303699813028,21.5255136419971,21.6207177908408,
21.7160683042774,21.7484727619558,21.8438253317088,21.9390490108222,22.0387978476796,
22.1338536422197,22.2288778255989,22.3238967924648,22.4189369252509,22.5140805859356,
22.60928473476,22.7046352481631,22.7370397056811,22.8323922766482,22.9276159569972,
23.0273647935483,23.1224205893681,23.2174447740405,23.3124637422117,23.4075038763132,
23.5026475383213,23.5978516884751,23.6932022032059,23.7256066494064,23.8209592196533,
23.9161828992727,24.0159317360051,24.110987531078,24.2060117149986,24.3010306824142,
24.3960708157573,24.4912144770068,24.5864186264011,24.6817691403775,24.7141735931316,
24.8095261634606,24.9047498431618,25.0044986798737,25.0995544750262,25.1945786590253,
25.2895976265183,25.3846377599378,25.4797814212618,25.5749855707292,25.6703360847763,
25.7027405368569,25.8008404154051,25.8987825103485,25.9965488931931,26.0942114708792,
26.1917715987827,26.2500416370866),.UNSPECIFIED.);
#511=B_SPLINE_CURVE_WITH_KNOTS('',3,(#45716,#45717,#45718,#45719,#45720,
#45721,#45722,#45723,#45724,#45725,#45726,#45727,#45728,#45729,#45730,#45731,
#45732,#45733,#45734,#45735,#45736,#45737,#45738,#45739,#45740,#45741,#45742,
#45743,#45744,#45745,#45746,#45747,#45748,#45749,#45750,#45751,#45752,#45753,
#45754,#45755,#45756,#45757,#45758,#45759,#45760,#45761,#45762,#45763,#45764,
#45765,#45766,#45767,#45768,#45769,#45770,#45771,#45772,#45773,#45774,#45775,
#45776,#45777,#45778,#45779,#45780,#45781,#45782,#45783,#45784,#45785,#45786,
#45787,#45788,#45789,#45790,#45791,#45792,#45793,#45794,#45795,#45796,#45797,
#45798,#45799,#45800,#45801,#45802,#45803,#45804,#45805,#45806,#45807,#45808,
#45809,#45810,#45811,#45812,#45813,#45814,#45815,#45816,#45817,#45818,#45819,
#45820,#45821,#45822,#45823,#45824,#45825,#45826,#45827,#45828,#45829,#45830,
#45831,#45832,#45833,#45834,#45835,#45836,#45837,#45838,#45839,#45840,#45841,
#45842,#45843,#45844,#45845,#45846,#45847,#45848,#45849,#45850,#45851,#45852,
#45853,#45854,#45855,#45856,#45857,#45858,#45859,#45860,#45861,#45862,#45863,
#45864,#45865,#45866,#45867,#45868,#45869,#45870,#45871,#45872,#45873,#45874,
#45875,#45876,#45877,#45878,#45879,#45880,#45881,#45882,#45883,#45884,#45885,
#45886,#45887,#45888,#45889,#45890,#45891,#45892,#45893,#45894,#45895,#45896,
#45897,#45898,#45899,#45900,#45901,#45902,#45903,#45904,#45905,#45906,#45907,
#45908,#45909,#45910,#45911,#45912,#45913,#45914,#45915,#45916,#45917,#45918,
#45919,#45920,#45921,#45922,#45923,#45924,#45925,#45926),.UNSPECIFIED.,
 .F.,.F.,(4,3,3,3,3,3,3,3,3,3,3,3,3,3,3,3,3,3,3,3,3,3,3,3,3,3,3,3,3,3,3,
3,3,3,3,3,3,3,3,3,3,3,3,3,3,3,3,3,3,3,3,3,3,3,3,3,3,3,3,3,3,3,3,3,3,3,3,
3,3,3,4),(26.2500416373359,26.3519613122933,26.4542712901962,26.5567882928527,
26.6596074482971,26.6913074805822,26.7866600509523,26.8818837306959,26.9816325673974,
27.0766883625954,27.1717125466414,27.2667315141822,27.3617716476502,27.4569153090236,
27.5521194585415,27.6474699726396,27.6798744243074,27.7752269946991,27.8704506744644,
27.9701995111604,28.0652553063801,28.1602794904476,28.25529845801,28.3503385914995,
28.4454822528942,28.5406864024331,28.6360369165519,28.6684413680327,28.7637939384417,
28.8590176182246,28.9587664549163,29.0538222501544,29.1488464342407,29.2438654018219,
29.3389055353305,29.4340491967444,29.5292533463028,29.624603860441,29.6570083117579,
29.752360882151,29.8475845619179,29.9473333986136,30.0423891938351,30.1374133779048,
30.2324323454692,30.3274724789609,30.422616140358,30.5178202898994,30.6131708040208,
30.6455752554832,30.7409278258807,30.8361515056521,30.9359003423466,31.0309561375726,
31.1259803216467,31.2209992892157,31.3160394227119,31.4111830841135,31.5063872336593,
31.6017377477851,31.6341421992085,31.7283920093595,31.822513801464,31.9165313934101,
32.0104926734926,32.1044252862533,32.1983568418308,32.2923673015784,32.386420948748,
32.4806113479254,32.5332269440593),.UNSPECIFIED.);
#512=B_SPLINE_CURVE_WITH_KNOTS('',3,(#45928,#45929,#45930,#45931,#45932,
#45933,#45934,#45935,#45936,#45937,#45938,#45939,#45940,#45941,#45942,#45943,
#45944,#45945,#45946,#45947,#45948,#45949,#45950,#45951,#45952,#45953,#45954,
#45955,#45956,#45957,#45958,#45959,#45960,#45961,#45962,#45963,#45964,#45965,
#45966,#45967,#45968,#45969,#45970,#45971,#45972,#45973,#45974,#45975,#45976,
#45977,#45978,#45979,#45980,#45981,#45982,#45983,#45984,#45985,#45986,#45987,
#45988,#45989,#45990,#45991,#45992,#45993,#45994,#45995,#45996,#45997,#45998,
#45999,#46000,#46001,#46002,#46003,#46004,#46005,#46006,#46007,#46008,#46009,
#46010,#46011,#46012,#46013,#46014,#46015,#46016,#46017,#46018,#46019,#46020,
#46021,#46022,#46023,#46024,#46025,#46026,#46027,#46028,#46029,#46030,#46031,
#46032,#46033,#46034,#46035,#46036,#46037,#46038,#46039,#46040,#46041,#46042,
#46043,#46044,#46045,#46046,#46047,#46048,#46049,#46050,#46051,#46052,#46053,
#46054,#46055,#46056,#46057,#46058,#46059,#46060,#46061,#46062,#46063,#46064,
#46065,#46066,#46067,#46068,#46069,#46070,#46071,#46072,#46073,#46074,#46075,
#46076,#46077,#46078,#46079,#46080,#46081,#46082,#46083,#46084,#46085,#46086,
#46087,#46088,#46089,#46090,#46091,#46092,#46093,#46094,#46095,#46096,#46097,
#46098,#46099,#46100,#46101,#46102,#46103,#46104,#46105,#46106,#46107,#46108,
#46109,#46110,#46111,#46112,#46113,#46114,#46115,#46116,#46117,#46118,#46119,
#46120,#46121,#46122,#46123,#46124,#46125,#46126,#46127,#46128,#46129,#46130,
#46131,#46132,#46133,#46134,#46135,#46136,#46137,#46138),.UNSPECIFIED.,
 .F.,.F.,(4,3,3,3,3,3,3,3,3,3,3,3,3,3,3,3,3,3,3,3,3,3,3,3,3,3,3,3,3,3,3,
3,3,3,3,3,3,3,3,3,3,3,3,3,3,3,3,3,3,3,3,3,3,3,3,3,3,3,3,3,3,3,3,3,3,3,3,
3,3,3,4),(32.5332269442662,32.6227091429337,32.7180617133311,32.8132853931022,
32.9130342297968,33.0080900250228,33.1031142090968,33.1981331766657,33.2931733101617,
33.3883169715633,33.4835211211092,33.578871635235,33.611276086659,33.7066286570568,
33.8018523368284,33.9016011735229,33.9966569687493,34.0916811528238,34.1867001203931,
34.2817402538897,34.3768839152916,34.4720880648378,34.567438578964,34.5998430303843,
34.6951956007822,34.790419280554,34.8901681172485,34.985223912475,35.0802480965497,
35.1752670641192,35.270307197616,35.3654508590182,35.4606550085646,35.556005522691,
35.5884099741095,35.6837625445072,35.7789862242788,35.8787350609733,35.9737908561996,
36.068815040274,36.1638340078432,36.2588741413398,36.3540178027417,36.4492219522878,
36.544572466414,36.5769769178348,36.6723294882327,36.7675531680045,36.8673020046989,
36.9623577999254,37.057381984,37.1524009515694,37.247441085066,37.3425847464681,
37.4377888960145,37.5331394101408,37.5655438615601,37.660896431958,37.7561201117295,
37.855868948424,37.9509247436504,38.0459489277249,38.1409678952943,38.2360080287909,
38.3311516901928,38.4263558397392,38.5217063538654,38.5541108052853,38.6750958169878,
38.7939679214662,38.8164120719258),.UNSPECIFIED.);
#513=B_SPLINE_CURVE_WITH_KNOTS('',3,(#46140,#46141,#46142,#46143,#46144,
#46145,#46146,#46147,#46148,#46149),.UNSPECIFIED.,.F.,.F.,(4,1,1,1,1,1,
1,4),(38.8164122514458,39.5426777490106,40.5312446927359,41.5198116364611,
42.5083785801864,43.4969455239117,44.4855124676369,45.0995975586253),
 .UNSPECIFIED.);
#514=B_SPLINE_CURVE_WITH_KNOTS('',3,(#46151,#46152,#46153,#46154,#46155,
#46156,#46157,#46158,#46159,#46160),.UNSPECIFIED.,.F.,.F.,(4,1,1,1,1,1,
1,4),(45.0995975586253,45.4740794113622,46.4626463550875,47.4512132988127,
48.439780242538,49.4283471862633,50.4169141299885,51.3827800491886),
 .UNSPECIFIED.);
#515=B_SPLINE_CURVE_WITH_KNOTS('',3,(#46162,#46163,#46164,#46165,#46166,
#46167,#46168,#46169,#46170,#46171,#46172,#46173,#46174,#46175,#46176,#46177,
#46178,#46179,#46180,#46181,#46182,#46183,#46184,#46185,#46186,#46187,#46188,
#46189,#46190,#46191,#46192,#46193,#46194,#46195,#46196,#46197,#46198,#46199,
#46200,#46201,#46202,#46203,#46204,#46205,#46206,#46207,#46208,#46209,#46210,
#46211,#46212,#46213,#46214,#46215,#46216,#46217,#46218,#46219,#46220,#46221,
#46222,#46223,#46224,#46225,#46226,#46227,#46228,#46229,#46230,#46231,#46232,
#46233,#46234,#46235,#46236,#46237,#46238,#46239,#46240,#46241,#46242,#46243,
#46244,#46245,#46246,#46247,#46248,#46249,#46250,#46251,#46252,#46253,#46254,
#46255,#46256,#46257,#46258,#46259,#46260,#46261,#46262,#46263,#46264,#46265,
#46266,#46267,#46268,#46269,#46270,#46271,#46272,#46273,#46274,#46275,#46276,
#46277,#46278,#46279,#46280,#46281,#46282,#46283,#46284,#46285,#46286,#46287,
#46288,#46289,#46290,#46291,#46292,#46293,#46294,#46295,#46296,#46297,#46298,
#46299,#46300,#46301,#46302,#46303,#46304,#46305,#46306,#46307,#46308,#46309,
#46310,#46311,#46312,#46313,#46314,#46315,#46316,#46317,#46318,#46319,#46320,
#46321,#46322,#46323,#46324,#46325,#46326,#46327,#46328,#46329,#46330,#46331,
#46332,#46333,#46334,#46335,#46336,#46337,#46338,#46339,#46340,#46341,#46342,
#46343,#46344,#46345,#46346,#46347,#46348,#46349,#46350,#46351,#46352,#46353,
#46354,#46355,#46356,#46357,#46358,#46359,#46360,#46361,#46362,#46363,#46364,
#46365,#46366,#46367,#46368,#46369,#46370,#46371,#46372),.UNSPECIFIED.,
 .F.,.F.,(4,3,3,3,3,3,3,3,3,3,3,3,3,3,3,3,3,3,3,3,3,3,3,3,3,3,3,3,3,3,3,
3,3,3,3,3,3,3,3,3,3,3,3,3,3,3,3,3,3,3,3,3,3,3,3,3,3,3,3,3,3,3,3,3,3,3,3,
3,3,3,4),(51.3827828658049,51.4054810737138,51.5008336447139,51.5960573250891,
51.6958061616329,51.7908619574615,51.8858861421364,51.9809051103038,52.075945244395,
52.1710889063835,52.2662930565123,52.36164357121,52.394048017439,52.4894005871162,
52.5846242661698,52.6843731030441,52.7794288975638,52.8744530809372,52.969472047812,
53.0645121806213,53.1596558413507,53.2548599902323,53.3502105037107,53.3826149611643,
53.4779675308754,53.5731912099506,53.672940046818,53.7679958413289,53.8630200246824,
53.9580389915263,54.053079124294,54.148222784966,54.2434269337809,54.3387774471797,
54.3711819048896,54.4665344793659,54.5617581632274,54.6615069989008,54.7565627982158,
54.8515869863696,54.946605958004,55.0416460955462,55.136789760942,55.2319939144568,
55.327344432481,55.3597488486148,55.4551014129466,55.5503250866643,55.6500739248737,
55.7451297141187,55.8401538922509,55.9351728539245,56.0302129815792,56.1253566372516,
56.2205607811269,56.3159112897158,56.3483157923401,56.4436683605826,56.5388920381325,
56.6386408753741,56.7336966682308,56.828720849887,56.9237398149926,57.0187799459837,
57.1139236048325,57.2091277517951,57.3044782633144,57.3368827360654,57.4485132464071,
57.5591246734767,57.6659679604612),.UNSPECIFIED.);
#516=B_SPLINE_CURVE_WITH_KNOTS('',3,(#46374,#46375,#46376,#46377,#46378,
#46379,#46380,#46381,#46382,#46383),.UNSPECIFIED.,.F.,.F.,(4,1,1,1,1,1,
1,4),(57.6659681729845,58.3254496797906,59.3140166235159,60.3025835672412,
61.2911505109664,62.2797174546917,63.268284398417,63.9491534801641),
 .UNSPECIFIED.);
#517=B_SPLINE_CURVE_WITH_KNOTS('',3,(#46385,#46386,#46387,#46388,#46389,
#46390,#46391,#46392,#46393,#46394),.UNSPECIFIED.,.F.,.F.,(4,1,1,1,1,1,
1,4),(63.9491534801641,64.2568513421422,65.2454182858675,66.2339852295928,
67.222552173318,68.2111191170433,69.1996860607685,69.4794631267919),
 .UNSPECIFIED.);
#518=B_SPLINE_CURVE_WITH_KNOTS('',3,(#46398,#46399,#46400,#46401,#46402,
#46403,#46404,#46405,#46406,#46407,#46408,#46409,#46410,#46411,#46412,#46413,
#46414,#46415,#46416,#46417,#46418,#46419,#46420,#46421,#46422,#46423,#46424,
#46425,#46426,#46427,#46428,#46429,#46430,#46431,#46432,#46433,#46434,#46435,
#46436,#46437,#46438,#46439,#46440,#46441,#46442,#46443,#46444,#46445,#46446,
#46447,#46448,#46449,#46450,#46451,#46452,#46453,#46454,#46455,#46456,#46457,
#46458,#46459,#46460,#46461,#46462,#46463,#46464,#46465,#46466,#46467,#46468,
#46469,#46470,#46471,#46472,#46473,#46474,#46475,#46476,#46477,#46478,#46479,
#46480,#46481,#46482,#46483,#46484,#46485,#46486,#46487,#46488,#46489,#46490,
#46491,#46492,#46493,#46494,#46495,#46496,#46497,#46498,#46499,#46500,#46501,
#46502,#46503,#46504,#46505,#46506,#46507,#46508,#46509,#46510,#46511,#46512,
#46513,#46514,#46515,#46516,#46517,#46518,#46519,#46520,#46521,#46522,#46523,
#46524,#46525,#46526,#46527,#46528,#46529,#46530,#46531,#46532,#46533,#46534,
#46535,#46536,#46537,#46538,#46539,#46540,#46541,#46542,#46543,#46544,#46545,
#46546,#46547,#46548,#46549,#46550,#46551),.UNSPECIFIED.,.F.,.F.,(4,3,3,
3,3,3,3,3,3,3,3,3,3,3,3,3,3,3,3,3,3,3,3,3,3,3,3,3,3,3,3,3,3,3,3,3,3,3,3,
3,3,3,3,3,3,3,3,3,3,3,3,4),(-71.5480958397728,-71.4478687915014,-71.3473161830486,
-71.2465915735931,-71.1455739445365,-71.0877887496107,-70.9922715804326,
-70.8968826481691,-70.7973296109368,-70.702108211632,-70.6069187283835,
-70.5117349944208,-70.4165308556829,-70.3212255530631,-70.2258607810251,
-70.1303531882947,-70.1004583503106,-70.004935306632,-69.9095376969293,
-69.8099864786894,-69.7147494053626,-69.6195416955273,-69.5243371935969,
-69.4291097545351,-69.3337774799512,-69.2383835718144,-69.142843853146,
-69.1131279510104,-69.0178865528629,-68.922775479434,-68.8231532384685,
-68.7282128188874,-68.633304840629,-68.5384027636419,-68.4434800606417,
-68.3484542673785,-68.2533682026849,-68.1581358107866,-68.1257975517103,
-68.0303999276791,-67.9351307097886,-67.8355477651162,-67.7404455532529,
-67.6453747884525,-67.5503091374064,-67.4552222789518,-67.360032376824,
-67.2647820395354,-67.1693864892511,-67.1384671524101,-67.0084331297282,
-66.9247834919266),.UNSPECIFIED.);
#519=B_SPLINE_CURVE_WITH_KNOTS('',3,(#46553,#46554,#46555,#46556,#46557,
#46558,#46559,#46560,#46561,#46562),.UNSPECIFIED.,.F.,.F.,(4,1,1,1,1,1,
1,4),(-66.9247821671427,-66.15113675311,-65.1638063538098,-64.1764759545097,
-63.1891455552095,-62.2018151559094,-61.2144847566092,-60.641598184747),
 .UNSPECIFIED.);
#520=B_SPLINE_CURVE_WITH_KNOTS('',3,(#46564,#46565,#46566,#46567,#46568,
#46569,#46570,#46571,#46572,#46573),.UNSPECIFIED.,.F.,.F.,(4,1,1,1,1,1,
1,4),(-60.641598184747,-60.2271543573091,-59.2398239580089,-58.2524935587088,
-57.2651631594086,-56.2778327601085,-55.2905023608083,-54.3584128775674),
 .UNSPECIFIED.);
#521=B_SPLINE_CURVE_WITH_KNOTS('',3,(#46575,#46576,#46577,#46578,#46579,
#46580,#46581,#46582,#46583,#46584,#46585),.UNSPECIFIED.,.F.,.F.,(4,1,1,
1,1,1,1,1,4),(-54.3584128775674,-54.3031719615082,-53.315841562208,-52.3285111629079,
-51.3411807636077,-50.3538503643076,-49.3665199650074,-48.3791895657073,
-48.0752275703878),.UNSPECIFIED.);
#522=B_SPLINE_CURVE_WITH_KNOTS('',3,(#46587,#46588,#46589,#46590,#46591,
#46592,#46593,#46594,#46595,#46596),.UNSPECIFIED.,.F.,.F.,(4,1,1,1,1,1,
1,4),(-48.0752275703878,-47.3918591664071,-46.404528767107,-45.4171983678069,
-44.4298679685067,-43.4425375692066,-42.4552071699064,-41.7920422632082),
 .UNSPECIFIED.);
#523=B_SPLINE_CURVE_WITH_KNOTS('',3,(#46598,#46599,#46600,#46601,#46602,
#46603,#46604,#46605,#46606,#46607,#46608),.UNSPECIFIED.,.F.,.F.,(4,1,1,
1,1,1,1,1,4),(-41.7920422632082,-41.4678767706063,-40.4805463713061,-39.4932159720059,
-38.5058855727058,-37.5185551734057,-36.5312247741055,-35.5438943748054,
-35.5088569560286),.UNSPECIFIED.);
#524=B_SPLINE_CURVE_WITH_KNOTS('',3,(#46610,#46611,#46612,#46613,#46614,
#46615,#46616,#46617,#46618,#46619),.UNSPECIFIED.,.F.,.F.,(4,1,1,1,1,1,
1,4),(-35.5088569560286,-34.5565639755052,-33.5692335762051,-32.5819031769049,
-31.5945727776048,-30.6072423783046,-29.6199119790045,-29.225671648849),
 .UNSPECIFIED.);
#525=B_SPLINE_CURVE_WITH_KNOTS('',3,(#46621,#46622,#46623,#46624,#46625,
#46626,#46627,#46628,#46629,#46630),.UNSPECIFIED.,.F.,.F.,(4,1,1,1,1,1,
1,4),(-29.225671648849,-28.6325815797043,-27.6452511804042,-26.657920781104,
-25.6705903818039,-24.6832599825037,-23.6959295832036,-22.9424863416694),
 .UNSPECIFIED.);
#526=B_SPLINE_CURVE_WITH_KNOTS('',3,(#46632,#46633,#46634,#46635,#46636,
#46637,#46638,#46639,#46640,#46641,#46642),.UNSPECIFIED.,.F.,.F.,(4,1,1,
1,1,1,1,1,4),(-22.9424863416694,-22.7085991839034,-21.7212687846033,-20.7339383853031,
-19.746607986003,-18.7592775867028,-17.7719471874027,-16.7846167881025,
-16.6593010344898),.UNSPECIFIED.);
#527=B_SPLINE_CURVE_WITH_KNOTS('',3,(#46644,#46645,#46646,#46647,#46648,
#46649,#46650,#46651,#46652,#46653,#46654,#46655,#46656,#46657,#46658,#46659,
#46660,#46661,#46662,#46663,#46664,#46665,#46666,#46667,#46668,#46669,#46670,
#46671,#46672,#46673,#46674,#46675,#46676,#46677,#46678,#46679,#46680,#46681,
#46682,#46683,#46684,#46685,#46686,#46687,#46688,#46689,#46690,#46691,#46692,
#46693,#46694,#46695,#46696,#46697,#46698,#46699,#46700,#46701,#46702,#46703,
#46704,#46705,#46706,#46707,#46708,#46709,#46710,#46711,#46712,#46713,#46714,
#46715,#46716,#46717,#46718,#46719,#46720,#46721,#46722,#46723,#46724,#46725,
#46726,#46727,#46728,#46729,#46730,#46731,#46732,#46733,#46734,#46735,#46736,
#46737,#46738,#46739,#46740,#46741,#46742,#46743,#46744,#46745,#46746,#46747,
#46748,#46749,#46750,#46751,#46752,#46753,#46754,#46755,#46756,#46757,#46758,
#46759,#46760,#46761,#46762,#46763,#46764,#46765,#46766,#46767,#46768,#46769,
#46770,#46771,#46772,#46773,#46774,#46775,#46776,#46777,#46778,#46779,#46780,
#46781,#46782,#46783,#46784,#46785,#46786,#46787,#46788,#46789,#46790,#46791,
#46792,#46793,#46794,#46795,#46796,#46797,#46798,#46799,#46800,#46801,#46802,
#46803,#46804,#46805,#46806,#46807,#46808,#46809,#46810,#46811,#46812,#46813,
#46814,#46815,#46816,#46817,#46818,#46819,#46820,#46821,#46822,#46823,#46824,
#46825,#46826,#46827,#46828,#46829,#46830,#46831,#46832,#46833,#46834,#46835,
#46836,#46837,#46838,#46839,#46840,#46841,#46842,#46843,#46844,#46845,#46846,
#46847,#46848,#46849,#46850,#46851,#46852,#46853,#46854),.UNSPECIFIED.,
 .F.,.F.,(4,3,3,3,3,3,3,3,3,3,3,3,3,3,3,3,3,3,3,3,3,3,3,3,3,3,3,3,3,3,3,
3,3,3,3,3,3,3,3,3,3,3,3,3,3,3,3,3,3,3,3,3,3,3,3,3,3,3,3,3,3,3,3,3,3,3,3,
3,3,3,4),(-16.6593010344898,-16.5653248924565,-16.4693200794998,-16.3755301668361,
-16.281777908926,-16.1880355175729,-16.0903482353803,-15.9964879999612,
-15.9025665271193,-15.8085079323049,-15.7972863888024,-15.7019189811482,
-15.6066801580444,-15.5070896369767,-15.4120180367218,-15.316977895839,
-15.2219428405017,-15.1268865089978,-15.0317268581315,-14.9365066464886,
-14.8411407847332,-14.8099559895022,-14.7145884131069,-14.6193494200575,
-14.5197589413256,-14.4246871693757,-14.3296468565278,-14.2346116291798,
-14.1395551258434,-14.0443953043764,-13.9491749226522,-13.8538088929973,
-13.8226255902021,-13.727258549964,-13.6320200938329,-13.5324294809666,
-13.4373582439689,-13.3423184642153,-13.2472837674279,-13.1522277914397,
-13.0570684896125,-12.9618486236562,-12.8664830997774,-12.8352951909019,
-12.7399276379914,-12.6446886719872,-12.5450981869391,-12.4500264506047,
-12.3549861764143,-12.2599509906954,-12.1648945318917,-12.0697347589848,
-11.9745144282059,-11.8791484525789,-11.8479647916018,-11.7525963589307,
-11.6573565044856,-11.5577662404626,-11.4626936006782,-11.3676524195072,
-11.2726163244718,-11.1775589552082,-11.0823982752983,-10.9871770384881,
-10.8918101658113,-10.8606343923016,-10.7600650610283,-10.6597728389421,
-10.5596465466219,-10.4597437159183,-10.3761157274923),.UNSPECIFIED.);
#528=B_SPLINE_CURVE_WITH_KNOTS('',3,(#46855,#46856,#46857,#46858,#46859,
#46860,#46861,#46862,#46863,#46864,#46865,#46866,#46867,#46868,#46869,#46870,
#46871,#46872,#46873,#46874,#46875,#46876,#46877,#46878,#46879,#46880,#46881,
#46882,#46883,#46884,#46885,#46886,#46887,#46888,#46889,#46890,#46891,#46892,
#46893,#46894,#46895,#46896,#46897,#46898,#46899,#46900,#46901,#46902,#46903,
#46904,#46905,#46906,#46907,#46908,#46909,#46910,#46911,#46912,#46913,#46914,
#46915,#46916,#46917,#46918,#46919,#46920,#46921,#46922,#46923,#46924,#46925,
#46926,#46927,#46928,#46929,#46930,#46931,#46932,#46933,#46934,#46935,#46936,
#46937,#46938,#46939,#46940,#46941,#46942,#46943,#46944,#46945,#46946,#46947,
#46948,#46949,#46950,#46951,#46952,#46953,#46954,#46955,#46956,#46957,#46958,
#46959,#46960,#46961,#46962,#46963,#46964,#46965,#46966,#46967,#46968,#46969,
#46970,#46971,#46972,#46973,#46974,#46975,#46976,#46977,#46978,#46979,#46980,
#46981,#46982,#46983,#46984,#46985,#46986,#46987,#46988,#46989,#46990,#46991,
#46992,#46993,#46994,#46995,#46996,#46997,#46998,#46999,#47000,#47001,#47002,
#47003,#47004,#47005,#47006,#47007,#47008,#47009,#47010,#47011,#47012,#47013,
#47014,#47015,#47016,#47017,#47018,#47019,#47020,#47021,#47022,#47023,#47024,
#47025,#47026,#47027,#47028,#47029,#47030,#47031,#47032,#47033,#47034,#47035,
#47036,#47037,#47038,#47039,#47040,#47041,#47042,#47043,#47044,#47045,#47046,
#47047,#47048,#47049,#47050,#47051,#47052,#47053,#47054,#47055,#47056,#47057,
#47058,#47059,#47060,#47061,#47062),.UNSPECIFIED.,.F.,.F.,(4,3,3,3,3,3,
3,3,3,3,3,3,3,3,3,3,3,3,3,3,3,3,3,3,3,3,3,3,3,3,3,3,3,3,3,3,3,3,3,3,3,3,
3,3,3,3,3,3,3,3,3,3,3,3,3,3,3,3,3,3,3,3,3,3,3,3,3,3,3,4),(-10.3761157273102,
-10.277030159422,-10.1760986178168,-10.0766550971632,-9.97497954508236,
-9.87330399300149,-9.77793465170269,-9.68269391144577,-9.58310387172771,
-9.48803040862856,-9.39298842864118,-9.29795156015412,-9.20289344369246,
-9.10773205948534,-9.01251014240612,-8.91714263045597,-8.88597359370134,
-8.7906003941096,-8.69535573499435,-8.5957666674202,-8.50068916445218,-8.40564310920763,
-8.31060213558218,-8.21553988958314,-8.12037436320737,-8.02514829195954,
-7.92977664283056,-7.89864319440119,-7.80329505616397,-7.70807553182495,
-7.60848018973446,-7.51342782279223,-7.41840685045479,-7.32339087466709,
-7.22835350940553,-7.13321255084905,-7.03801089429927,-6.94266323112823,
-6.91131279510104,-6.81592594731719,-6.7206677800099,-6.62108210698378,
-6.52599153730943,-6.43093260402686,-6.33587895645016,-6.24080425618366,
-6.14562666958989,-6.05038875257428,-5.9550056715846,-5.92398239580089,
-5.82858542316081,-5.73331672119191,-5.63373363060551,-5.5386315937293,
-5.44356087860388,-5.34849515201683,-5.25340809279504,-5.15821780479437,
-5.06296697390101,-4.96757077445709,-4.93665199650074,-4.84277093189022,
-4.7490388889567,-4.65539094679393,-4.56179908829439,-4.46823536276442,
-4.37440912710598,-4.28077696275078,-4.18685369144072,-4.09293042013066),
 .UNSPECIFIED.);
#529=B_SPLINE_CURVE_WITH_KNOTS('',3,(#47065,#47066,#47067,#47068),
 .UNSPECIFIED.,.F.,.F.,(4,4),(-0.0182409621825525,-0.000698701667614549),
 .UNSPECIFIED.);
#530=B_SPLINE_CURVE_WITH_KNOTS('',3,(#47070,#47071,#47072,#47073,#47074,
#47075,#47076,#47077,#47078,#47079,#47080,#47081,#47082,#47083,#47084,#47085,
#47086,#47087,#47088,#47089,#47090,#47091,#47092,#47093,#47094,#47095,#47096,
#47097,#47098,#47099,#47100,#47101,#47102,#47103,#47104,#47105,#47106,#47107,
#47108,#47109,#47110,#47111,#47112,#47113,#47114,#47115,#47116,#47117,#47118,
#47119,#47120,#47121,#47122,#47123,#47124,#47125,#47126,#47127,#47128,#47129,
#47130,#47131,#47132,#47133,#47134,#47135,#47136,#47137,#47138,#47139,#47140,
#47141,#47142,#47143,#47144,#47145,#47146,#47147,#47148,#47149,#47150,#47151,
#47152,#47153,#47154,#47155,#47156,#47157,#47158,#47159,#47160,#47161,#47162,
#47163,#47164,#47165,#47166,#47167,#47168,#47169,#47170,#47171,#47172,#47173,
#47174,#47175,#47176,#47177,#47178,#47179,#47180,#47181,#47182,#47183,#47184,
#47185,#47186,#47187,#47188,#47189,#47190,#47191,#47192,#47193,#47194,#47195,
#47196,#47197,#47198,#47199,#47200,#47201,#47202,#47203,#47204,#47205,#47206,
#47207,#47208,#47209,#47210,#47211,#47212,#47213,#47214,#47215,#47216,#47217,
#47218,#47219,#47220,#47221,#47222,#47223,#47224,#47225,#47226,#47227,#47228,
#47229,#47230,#47231,#47232,#47233,#47234,#47235,#47236,#47237,#47238,#47239,
#47240,#47241,#47242,#47243,#47244,#47245,#47246,#47247,#47248,#47249,#47250,
#47251,#47252,#47253,#47254,#47255,#47256),.UNSPECIFIED.,.F.,.F.,(4,3,3,
3,3,3,3,3,3,3,3,3,3,3,3,3,3,3,3,3,3,3,3,3,3,3,3,3,3,3,3,3,3,3,3,3,3,3,3,
3,3,3,3,3,3,3,3,3,3,3,3,3,3,3,3,3,3,3,3,3,3,3,4),(78.5398163397448,78.677046774016,
78.7535000002284,78.8541764825381,78.9547110029923,79.0551323551228,79.1554921585444,
79.2558214002717,79.3561510284159,79.4565790619252,79.5570564320356,79.6577081753727,
79.7408303995285,79.8413353461935,79.9416976613493,80.0419466171441,80.1421339931493,
80.2422910182837,80.342448882667,80.4427070395265,80.5430153144406,80.6435011743321,
80.7281607988287,80.8289888931789,80.9296740991317,81.0302440428158,81.1307510764058,
81.2312259823438,81.3316995027274,81.4322676917544,81.5328833565173,81.6336687762747,
81.7154911981288,81.8162854342717,81.9169397387056,82.0174832941154,82.1179667039081,
82.2184207568815,82.318876204121,82.4194307102225,82.5200350970089,82.6208132889057,
82.702821597429,82.8023943022322,82.9018239519552,83.0011436471454,83.1004040721794,
83.1996375603753,83.2988764084443,83.3982287259881,83.4976367746819,83.5972422198623,
83.6901519967291,83.7935465522308,83.8967794207781,83.9998522816575,84.1028308874541,
84.2057403662952,84.3086057649522,84.4114805456595,84.5143560839271,84.6173011712591,
84.6774823960293),.UNSPECIFIED.);
#531=B_SPLINE_CURVE_WITH_KNOTS('',3,(#47260,#47261,#47262,#47263,#47264,
#47265,#47266,#47267,#47268,#47269,#47270,#47271,#47272,#47273,#47274,#47275,
#47276,#47277,#47278,#47279,#47280,#47281,#47282,#47283,#47284,#47285,#47286,
#47287,#47288,#47289,#47290,#47291,#47292,#47293,#47294,#47295,#47296,#47297,
#47298,#47299,#47300,#47301,#47302,#47303,#47304,#47305,#47306,#47307,#47308,
#47309,#47310,#47311,#47312,#47313,#47314,#47315,#47316,#47317,#47318,#47319,
#47320,#47321,#47322,#47323,#47324,#47325,#47326,#47327,#47328,#47329,#47330,
#47331,#47332,#47333,#47334,#47335,#47336,#47337,#47338,#47339,#47340,#47341,
#47342,#47343,#47344,#47345,#47346,#47347,#47348,#47349,#47350,#47351,#47352,
#47353,#47354,#47355,#47356,#47357,#47358,#47359,#47360,#47361,#47362,#47363,
#47364,#47365,#47366,#47367,#47368,#47369,#47370,#47371,#47372,#47373,#47374,
#47375,#47376,#47377,#47378,#47379,#47380,#47381,#47382,#47383,#47384,#47385,
#47386,#47387,#47388,#47389,#47390,#47391,#47392,#47393,#47394,#47395,#47396,
#47397,#47398,#47399,#47400,#47401,#47402,#47403,#47404,#47405,#47406,#47407,
#47408,#47409,#47410),.UNSPECIFIED.,.F.,.F.,(4,3,3,3,3,3,3,3,3,3,3,3,3,
3,3,3,3,3,3,3,3,3,3,3,3,3,3,3,3,3,3,3,3,3,3,3,3,3,3,3,3,3,3,3,3,3,3,3,3,
3,4),(78.5398163400955,78.6396051546265,78.7392548410145,78.8387975186506,
78.9382836159524,79.0377452469571,79.1372144915425,79.2367866223946,79.3364166299699,
79.4362117134907,79.4842975006201,79.5851111912929,79.6857816535804,79.7863364727349,
79.8868281365189,79.9872874516924,80.0877451844647,80.1882977346122,80.2888976157929,
80.3896681150517,80.4728644443454,80.5736414351339,80.6742781542139,80.7748037594743,
80.8752689834692,80.9757046432654,81.0761415180248,81.1766776525678,81.277263544666,
81.3780241833049,81.4614313880706,81.5609873162485,81.6603998580491,81.7597020774321,
81.8589447763137,81.9581603063024,82.0573809821283,82.1567152897885,82.2561051556921,
82.3556933778849,82.4499983317959,82.5533841966888,82.6566079229631,82.7596710669683,
82.8626396280425,82.9655387682385,83.0683935679595,83.1712576539379,83.2741223179695,
83.3770569248603,83.4385652755212),.UNSPECIFIED.);
#532=B_SPLINE_CURVE_WITH_KNOTS('',3,(#47411,#47412,#47413,#47414,#47415,
#47416,#47417,#47418,#47419,#47420,#47421,#47422),.UNSPECIFIED.,.F.,.F.,
(4,2,2,2,2,4),(-2.98855656026776,-2.98466939185962,-2.98096825215168,-2.9778891399808,
-2.97434988120648,-2.97128357771462),.UNSPECIFIED.);
#533=B_SPLINE_CURVE_WITH_KNOTS('',3,(#47425,#47426,#47427,#47428,#47429,
#47430,#47431,#47432,#47433,#47434,#47435,#47436,#47437,#47438,#47439,#47440,
#47441,#47442,#47443,#47444,#47445,#47446,#47447,#47448,#47449,#47450,#47451,
#47452,#47453,#47454,#47455,#47456),.UNSPECIFIED.,.F.,.F.,(4,2,2,2,2,2,
2,2,2,2,2,2,2,2,2,4),(-2.19429233995567,-2.08491574472027,-1.96884002433686,
-1.79513299643777,-1.58607354155283,-1.34152662368927,-1.12750671314745,
-1.05017184774955,-0.892675460524429,-0.709583783276434,-0.553226716657333,
-0.367073680837577,-0.242877737203899,-0.136980729082507,-0.0715905781283026,
-7.46082012014841E-5),.UNSPECIFIED.);
#534=B_SPLINE_CURVE_WITH_KNOTS('',3,(#47457,#47458,#47459,#47460,#47461,
#47462,#47463,#47464,#47465,#47466,#47467,#47468,#47469,#47470,#47471,#47472,
#47473,#47474,#47475,#47476,#47477,#47478,#47479,#47480,#47481,#47482,#47483,
#47484,#47485,#47486,#47487,#47488,#47489,#47490,#47491,#47492,#47493,#47494,
#47495,#47496,#47497,#47498,#47499,#47500,#47501,#47502,#47503,#47504,#47505,
#47506,#47507,#47508,#47509,#47510,#47511,#47512,#47513,#47514,#47515,#47516,
#47517),.UNSPECIFIED.,.F.,.F.,(4,3,3,3,3,3,3,3,3,3,3,3,3,3,3,3,3,3,3,3,
4),(-0.410648750432938,-0.381294613665594,-0.352267124576947,-0.328792823836752,
-0.311187098281605,-0.306018425011984,-0.301691296836585,-0.274143229574461,
-0.258369921616165,-0.230117472373342,-0.201352788326674,-0.195525900786732,
-0.16833922287309,-0.141249160586392,-0.114615533759621,-0.100282139063474,
-0.0960342097686789,-0.0702554174629941,-0.0448546715641945,-0.0201984500449382,
0.),.UNSPECIFIED.);
#535=B_SPLINE_CURVE_WITH_KNOTS('',3,(#47518,#47519,#47520,#47521,#47522,
#47523,#47524,#47525,#47526,#47527,#47528,#47529,#47530,#47531,#47532,#47533,
#47534,#47535,#47536,#47537,#47538,#47539,#47540,#47541,#47542,#47543,#47544,
#47545,#47546,#47547,#47548,#47549,#47550,#47551),.UNSPECIFIED.,.F.,.F.,
(4,3,3,3,3,3,3,3,3,3,3,4),(-0.219677966288006,-0.206985183547511,-0.179985476037348,
-0.178213580556878,-0.148819200354015,-0.130216800309763,-0.118450459252591,
-0.113866160083042,-0.0841488051349767,-0.0540951018364117,-0.0242019686830237,
0.),.UNSPECIFIED.);
#536=B_SPLINE_CURVE_WITH_KNOTS('',3,(#47863,#47864,#47865,#47866,#47867,
#47868,#47869,#47870,#47871,#47872,#47873,#47874,#47875,#47876,#47877,#47878,
#47879,#47880,#47881,#47882,#47883,#47884,#47885,#47886,#47887,#47888,#47889,
#47890,#47891,#47892,#47893,#47894,#47895,#47896,#47897,#47898,#47899,#47900,
#47901,#47902,#47903,#47904,#47905,#47906,#47907,#47908,#47909,#47910,#47911,
#47912,#47913,#47914,#47915,#47916,#47917,#47918,#47919,#47920,#47921,#47922,
#47923,#47924,#47925,#47926,#47927,#47928,#47929,#47930,#47931,#47932,#47933,
#47934,#47935,#47936,#47937,#47938,#47939,#47940,#47941,#47942,#47943,#47944,
#47945,#47946,#47947,#47948,#47949,#47950),.UNSPECIFIED.,.F.,.F.,(4,3,3,
3,3,3,3,3,3,3,3,3,3,3,3,3,3,3,3,3,3,3,3,3,3,3,3,3,3,4),(-0.55274537837504,
-0.525174630400016,-0.495956305234574,-0.483208430614118,-0.476222765985277,
-0.469631349081844,-0.440661555816212,-0.411705679997849,-0.408301329738247,
-0.401969450637142,-0.397429868442983,-0.369148459214845,-0.341142139849232,
-0.313940382864803,-0.29772704364586,-0.291366968188088,-0.26455959815265,
-0.249599392264211,-0.222018910858968,-0.194438429453726,-0.189292991414398,
-0.162671573252089,-0.136033750846249,-0.109916719326503,-0.0950850259724172,
-0.09115324392662,-0.0655931049064447,-0.0404250325731723,-0.0160423336426468,
0.),.UNSPECIFIED.);
#537=B_SPLINE_CURVE_WITH_KNOTS('',3,(#48267,#48268,#48269,#48270,#48271,
#48272,#48273,#48274,#48275,#48276,#48277,#48278,#48279,#48280,#48281,#48282,
#48283,#48284,#48285,#48286,#48287,#48288,#48289,#48290,#48291,#48292,#48293,
#48294,#48295,#48296,#48297,#48298,#48299,#48300,#48301,#48302,#48303,#48304,
#48305,#48306,#48307,#48308,#48309,#48310,#48311,#48312,#48313,#48314,#48315,
#48316,#48317,#48318,#48319,#48320,#48321,#48322,#48323,#48324,#48325,#48326,
#48327,#48328,#48329,#48330,#48331,#48332,#48333,#48334,#48335,#48336,#48337,
#48338,#48339,#48340,#48341,#48342,#48343,#48344,#48345,#48346,#48347,#48348,
#48349,#48350,#48351),.UNSPECIFIED.,.F.,.F.,(4,3,3,3,3,3,3,3,3,3,3,3,3,
3,3,3,3,3,3,3,3,3,3,3,3,3,3,3,4),(-0.555272788399385,-0.533197712400843,
-0.50828572908666,-0.492097097422296,-0.487698425831477,-0.462241873724153,
-0.43610473287827,-0.427671428401512,-0.42202191869945,-0.395298681472729,
-0.368236505229611,-0.341280288641109,-0.32517826205158,-0.321068892319616,
-0.293156561265571,-0.279892116585652,-0.252647806442289,-0.225403496298925,
-0.220542492202756,-0.216708298034074,-0.188804183704433,-0.160414457473374,
-0.131690244065431,-0.114355289595352,-0.109564750157472,-0.0800994390250807,
-0.0505572378463981,-0.021577624140468,-4.47678306657353E-15),
 .UNSPECIFIED.);
#538=B_SPLINE_CURVE_WITH_KNOTS('',3,(#48404,#48405,#48406,#48407),
 .UNSPECIFIED.,.F.,.F.,(4,4),(112.182457130247,112.611961982353),
 .UNSPECIFIED.);
#539=B_SPLINE_CURVE_WITH_KNOTS('',3,(#48410,#48411,#48412,#48413,#48414,
#48415,#48416,#48417,#48418,#48419,#48420,#48421,#48422,#48423,#48424,#48425,
#48426,#48427,#48428,#48429,#48430,#48431,#48432,#48433,#48434,#48435,#48436,
#48437,#48438,#48439,#48440),.UNSPECIFIED.,.F.,.F.,(4,3,3,3,3,3,3,3,3,3,
4),(112.181990371131,112.285911257127,112.391911114027,112.495583234741,
112.599202596607,112.702804270412,112.81058073089,112.914317775615,113.018127482769,
113.122103490096,113.133910112327),.UNSPECIFIED.);
#540=B_SPLINE_CURVE_WITH_KNOTS('',3,(#48446,#48447,#48448,#48449,#48450,
#48451,#48452,#48453,#48454,#48455,#48456,#48457,#48458,#48459,#48460,#48461,
#48462,#48463,#48464,#48465,#48466,#48467,#48468,#48469,#48470,#48471,#48472,
#48473,#48474,#48475,#48476,#48477,#48478,#48479,#48480,#48481,#48482,#48483,
#48484,#48485,#48486,#48487,#48488,#48489,#48490,#48491,#48492,#48493,#48494,
#48495,#48496,#48497,#48498,#48499,#48500,#48501,#48502,#48503,#48504,#48505,
#48506,#48507,#48508,#48509,#48510,#48511,#48512,#48513,#48514,#48515,#48516,
#48517,#48518,#48519,#48520,#48521,#48522,#48523,#48524,#48525,#48526,#48527,
#48528,#48529,#48530,#48531,#48532,#48533,#48534,#48535,#48536,#48537,#48538,
#48539,#48540,#48541,#48542,#48543,#48544,#48545,#48546,#48547,#48548,#48549,
#48550,#48551,#48552,#48553,#48554,#48555,#48556,#48557,#48558,#48559,#48560,
#48561,#48562,#48563,#48564,#48565,#48566),.UNSPECIFIED.,.F.,.F.,(4,3,3,
3,3,3,3,3,3,3,3,3,3,3,3,3,3,3,3,3,3,3,3,3,3,3,3,3,3,3,3,3,3,3,3,3,3,3,3,
3,4),(105.899155442176,106.00304508501,106.1068896956,106.210723989893,
106.314740686353,106.41871988312,106.522893881941,106.626790775734,106.731006157979,
106.835066684879,106.939005596441,107.042879290909,107.146722500751,107.250569915224,
107.354526007897,107.45854099524,107.562737655316,107.62431931017,107.728358547242,
107.832242196635,107.936003986749,108.03970049976,108.143366723004,108.247037600669,
108.350819047469,108.454660186161,108.558686145832,108.621847844607,108.726235019868,
108.830466334637,108.934573735116,109.038614403188,109.14262283246,109.246633471616,
109.350748646957,109.45492061008,109.559269251373,109.619376379043,109.74022388422,
109.860008885434,109.955742675385),.UNSPECIFIED.);
#541=B_SPLINE_CURVE_WITH_KNOTS('',3,(#48567,#48568,#48569,#48570,#48571,
#48572),.UNSPECIFIED.,.F.,.F.,(4,1,1,4),(109.955742875643,110.61690491348,
111.614433447917,112.182457130247),.UNSPECIFIED.);
#542=B_SPLINE_CURVE_WITH_KNOTS('',3,(#48574,#48575,#48576,#48577,#48578,
#48579,#48580,#48581,#48582,#48583,#48584,#48585,#48586,#48587,#48588,#48589,
#48590,#48591,#48592,#48593,#48594,#48595,#48596,#48597,#48598,#48599,#48600,
#48601,#48602,#48603,#48604,#48605,#48606,#48607,#48608,#48609,#48610,#48611,
#48612,#48613,#48614,#48615,#48616,#48617,#48618,#48619,#48620,#48621,#48622,
#48623,#48624,#48625,#48626,#48627,#48628,#48629,#48630,#48631,#48632,#48633,
#48634,#48635,#48636,#48637,#48638,#48639,#48640,#48641,#48642,#48643),
 .UNSPECIFIED.,.F.,.F.,(4,3,3,3,3,3,3,3,3,3,3,3,3,3,3,3,3,3,3,3,3,3,3,4),
(109.955742875643,110.103561930893,110.16088031869,110.264919435449,110.368802964289,
110.472564634045,110.576261026872,110.679927130268,110.783597888585,110.887379217594,
110.991220239184,111.095246084109,111.158408853127,111.262796080625,111.367027447102,
111.471134898278,111.575175616393,111.679184094987,111.783194782677,111.887310005039,
111.991482014394,112.0958307002,112.155937387564,112.181990371131),
 .UNSPECIFIED.);
#543=B_SPLINE_CURVE_WITH_KNOTS('',3,(#48644,#48645,#48646,#48647,#48648,
#48649,#48650,#48651),.UNSPECIFIED.,.F.,.F.,(4,1,1,1,1,4),(105.897706904075,
106.170766180944,107.168294715381,108.165823249817,109.163351784254,109.955739920457),
 .UNSPECIFIED.);
#544=B_SPLINE_CURVE_WITH_KNOTS('',3,(#48657,#48658,#48659,#48660,#48661,
#48662,#48663,#48664,#48665,#48666,#48667,#48668,#48669,#48670,#48671,#48672,
#48673,#48674,#48675,#48676,#48677,#48678,#48679,#48680,#48681,#48682,#48683,
#48684,#48685,#48686,#48687,#48688,#48689,#48690,#48691,#48692,#48693,#48694,
#48695,#48696,#48697,#48698,#48699,#48700,#48701,#48702,#48703,#48704,#48705,
#48706,#48707,#48708,#48709,#48710,#48711,#48712,#48713,#48714,#48715,#48716,
#48717,#48718,#48719,#48720,#48721,#48722,#48723,#48724,#48725,#48726,#48727,
#48728,#48729,#48730,#48731,#48732,#48733,#48734,#48735,#48736,#48737,#48738,
#48739,#48740,#48741,#48742,#48743,#48744,#48745,#48746,#48747,#48748,#48749,
#48750,#48751,#48752,#48753,#48754,#48755,#48756,#48757,#48758,#48759,#48760,
#48761,#48762,#48763,#48764,#48765,#48766,#48767,#48768,#48769,#48770,#48771,
#48772,#48773,#48774,#48775,#48776,#48777,#48778,#48779,#48780,#48781,#48782,
#48783),.UNSPECIFIED.,.F.,.F.,(4,3,3,3,3,3,3,3,3,3,3,3,3,3,3,3,3,3,3,3,
3,3,3,3,3,3,3,3,3,3,3,3,3,3,3,3,3,3,3,3,3,3,4),(99.6152477845043,99.6440910346774,
99.7482777229514,99.8523091754732,99.9562185935285,100.060062552649,100.163875831174,
100.267693164011,100.371619156583,100.475603988335,100.57977073543,100.641619569114,
100.745806998585,100.849839202802,100.95374938437,101.057594113864,101.161408168437,
101.265226281812,101.369153056302,101.473138671925,101.577306197386,101.639148103551,
101.743331447498,101.847359555346,101.951265644064,102.055106285069,102.158916261446,
102.262730312857,102.366653077886,102.470634707604,102.574798327491,102.636676637987,
102.740865744067,102.844899598207,102.94881138278,103.052657685547,103.156473281631,
103.260292902696,103.364221123497,103.468208153012,103.572377026272,103.634205172424,
103.672557568463),.UNSPECIFIED.);
#545=B_SPLINE_CURVE_WITH_KNOTS('',3,(#48784,#48785,#48786,#48787,#48788,
#48789,#48790,#48791,#48792,#48793,#48794,#48795,#48796,#48797,#48798,#48799,
#48800,#48801,#48802,#48803,#48804,#48805,#48806,#48807,#48808,#48809,#48810,
#48811,#48812,#48813,#48814,#48815,#48816,#48817,#48818,#48819,#48820,#48821,
#48822,#48823,#48824,#48825,#48826,#48827,#48828,#48829,#48830,#48831,#48832,
#48833,#48834,#48835,#48836,#48837,#48838,#48839,#48840,#48841,#48842,#48843,
#48844,#48845,#48846,#48847,#48848,#48849,#48850,#48851,#48852,#48853),
 .UNSPECIFIED.,.F.,.F.,(4,3,3,3,3,3,3,3,3,3,3,3,3,3,3,3,3,3,3,3,3,3,3,4),
(103.672557568731,103.776102954499,103.883056798544,103.98633119127,104.089546016561,
104.192736914806,104.295939489046,104.399253774652,104.502635390832,104.606186629628,
104.63173370686,104.735898602296,104.839908226138,104.943795866233,105.047618090183,
105.151409707593,105.255205484688,105.359110229006,105.463073953701,105.567220044936,
105.629262241297,105.733467137487,105.837506123452,105.899155442176),
 .UNSPECIFIED.);
#546=B_SPLINE_CURVE_WITH_KNOTS('',3,(#48855,#48856,#48857,#48858,#48859,
#48860),.UNSPECIFIED.,.F.,.F.,(4,1,1,4),(103.672557568463,104.175709112071,
105.173237646507,105.897706904075),.UNSPECIFIED.);
#547=B_SPLINE_CURVE_WITH_KNOTS('',3,(#48861,#48862,#48863,#48864,#48865,
#48866,#48867,#48868),.UNSPECIFIED.,.F.,.F.,(4,1,1,1,1,4),(99.6157845049343,
100.185594974324,101.183123508761,102.180652043198,103.178180577634,103.672557568463),
 .UNSPECIFIED.);
#548=B_SPLINE_CURVE_WITH_KNOTS('',3,(#48874,#48875,#48876,#48877,#48878,
#48879,#48880,#48881,#48882,#48883,#48884,#48885,#48886,#48887,#48888,#48889,
#48890,#48891,#48892,#48893,#48894,#48895,#48896,#48897,#48898,#48899,#48900,
#48901,#48902,#48903,#48904,#48905,#48906,#48907,#48908,#48909,#48910,#48911,
#48912,#48913,#48914,#48915,#48916,#48917,#48918,#48919,#48920,#48921,#48922,
#48923,#48924,#48925,#48926,#48927,#48928,#48929,#48930,#48931,#48932,#48933,
#48934,#48935,#48936,#48937,#48938,#48939,#48940,#48941,#48942,#48943,#48944,
#48945,#48946,#48947,#48948,#48949,#48950,#48951,#48952,#48953,#48954,#48955,
#48956,#48957,#48958,#48959,#48960,#48961,#48962,#48963,#48964,#48965,#48966,
#48967,#48968,#48969,#48970,#48971,#48972,#48973,#48974,#48975,#48976,#48977,
#48978,#48979,#48980,#48981,#48982,#48983,#48984,#48985,#48986,#48987,#48988,
#48989,#48990,#48991,#48992,#48993,#48994,#48995,#48996,#48997,#48998,#48999,
#49000),.UNSPECIFIED.,.F.,.F.,(4,3,3,3,3,3,3,3,3,3,3,3,3,3,3,3,3,3,3,3,
3,3,3,3,3,3,3,3,3,3,3,3,3,3,3,3,3,3,3,3,3,3,4),(93.3317577724807,93.4357061372678,
93.5397274007927,93.6439169172147,93.6589198280578,93.7631062477657,93.8671374348272,
93.9710465932312,94.0748902964138,94.178703323056,94.2825204084065,94.3864461618292,
94.4904307587697,94.5945972803976,94.6564483624944,94.7606348092475,94.8646660235604,
94.9685752093887,95.0724189400873,95.1762319942962,95.2800491072232,95.3839748880465,
95.4879595123299,95.5921260609117,95.653976896931,95.7581632576346,95.862194385787,
95.9661034856999,96.0699471306798,96.1737600994903,96.2775771274626,96.3815028245876,
96.4854873657548,96.5896538330368,96.6515054313676,96.7545601552911,96.8574737962598,
96.9602827783287,97.0675551490674,97.1702895580433,97.2730250439425,97.3758312784415,
97.3893722612836),.UNSPECIFIED.);
#549=B_SPLINE_CURVE_WITH_KNOTS('',3,(#49001,#49002,#49003,#49004,#49005,
#49006,#49007,#49008,#49009,#49010,#49011,#49012,#49013,#49014,#49015,#49016,
#49017,#49018,#49019,#49020,#49021,#49022,#49023,#49024,#49025,#49026,#49027,
#49028,#49029,#49030,#49031,#49032,#49033,#49034,#49035,#49036,#49037,#49038,
#49039,#49040,#49041,#49042,#49043,#49044,#49045,#49046,#49047,#49048,#49049,
#49050,#49051,#49052,#49053,#49054,#49055,#49056,#49057,#49058,#49059,#49060,
#49061,#49062,#49063,#49064,#49065,#49066,#49067),.UNSPECIFIED.,.F.,.F.,
(4,3,3,3,3,3,3,3,3,3,3,3,3,3,3,3,3,3,3,3,3,3,4),(97.3893722615972,97.522113023048,
97.6490339658042,97.753220555222,97.8572519130545,97.9611612429749,98.0650051180403,
98.1688183166771,98.2726355738801,98.3765614977545,98.4805462646138,98.5847129534722,
98.6465625002408,98.7507505133837,98.8588126722738,98.9627174078728,99.0665572074508,
99.1703668484503,99.274181065115,99.3780952818548,99.482069213541,99.5862024944616,
99.6152477845043),.UNSPECIFIED.);
#550=B_SPLINE_CURVE_WITH_KNOTS('',3,(#49069,#49070,#49071,#49072,#49073,
#49074),.UNSPECIFIED.,.F.,.F.,(4,1,1,4),(97.3893756995033,98.1905379054513,
99.1880664398879,99.6157845049343),.UNSPECIFIED.);
#551=B_SPLINE_CURVE_WITH_KNOTS('',3,(#49075,#49076,#49077,#49078,#49079,
#49080,#49081,#49082,#49083,#49084,#49085,#49086,#49087,#49088,#49089,#49090,
#49091,#49092,#49093,#49094,#49095,#49096,#49097,#49098,#49099,#49100,#49101,
#49102,#49103,#49104,#49105,#49106,#49107,#49108,#49109,#49110,#49111,#49112,
#49113,#49114,#49115,#49116,#49117,#49118,#49119,#49120,#49121,#49122,#49123,
#49124,#49125,#49126,#49127,#49128,#49129,#49130,#49131,#49132,#49133,#49134,
#49135,#49136,#49137,#49138,#49139,#49140,#49141,#49142,#49143,#49144,#49145,
#49146,#49147,#49148,#49149,#49150,#49151,#49152,#49153,#49154,#49155,#49156,
#49157,#49158,#49159,#49160,#49161,#49162,#49163,#49164,#49165,#49166,#49167,
#49168,#49169,#49170,#49171,#49172,#49173,#49174,#49175,#49176,#49177,#49178,
#49179,#49180,#49181,#49182,#49183,#49184,#49185,#49186,#49187,#49188,#49189,
#49190,#49191,#49192,#49193,#49194,#49195,#49196,#49197,#49198),
 .UNSPECIFIED.,.F.,.F.,(4,3,3,3,3,3,3,3,3,3,3,3,3,3,3,3,3,3,3,3,3,3,3,3,
3,3,3,3,3,3,3,3,3,3,3,3,3,3,3,3,3,4),(93.3327430891432,93.4412031739634,
93.5450898018628,93.6489210495062,93.7527316794015,93.856556420739,93.9604959875624,
94.0645034316264,94.1686838441858,94.2004237677049,94.304610191284,94.4086413823106,
94.5125505447987,94.6163942521362,94.7202072829974,94.8240243726246,94.9279501303813,
95.0319347316947,95.1361012577082,95.1979523021415,95.3021387136097,95.4061698925181,
95.5100790429346,95.6139227382356,95.7177357571129,95.8215528348257,95.9254785808556,
96.02946317053,96.1336296851692,96.1954808365781,96.2996672562813,96.403698443338,
96.507607601737,96.6114513049142,96.7152643315507,96.8190814168954,96.9230071703122,
97.0269917672468,97.1311582888685,97.1930093710147,97.3433995313053,97.3893722612836),
 .UNSPECIFIED.);
#552=B_SPLINE_CURVE_WITH_KNOTS('',3,(#49204,#49205,#49206,#49207,#49208,
#49209,#49210,#49211),.UNSPECIFIED.,.F.,.F.,(4,1,1,1,1,4),(87.0496595016183,
87.6737486214382,88.6712771558748,89.6688056903114,90.666334224748,91.1061824133145),
 .UNSPECIFIED.);
#553=B_SPLINE_CURVE_WITH_KNOTS('',3,(#49212,#49213,#49214,#49215,#49216,
#49217,#49218,#49219,#49220,#49221,#49222,#49223,#49224,#49225,#49226,#49227,
#49228,#49229,#49230,#49231,#49232,#49233,#49234,#49235,#49236,#49237,#49238,
#49239,#49240,#49241,#49242,#49243,#49244,#49245,#49246,#49247,#49248,#49249,
#49250,#49251,#49252,#49253,#49254,#49255,#49256,#49257,#49258,#49259,#49260,
#49261,#49262,#49263,#49264,#49265,#49266,#49267,#49268,#49269,#49270,#49271,
#49272,#49273,#49274,#49275,#49276,#49277,#49278,#49279,#49280,#49281),
 .UNSPECIFIED.,.F.,.F.,(4,3,3,3,3,3,3,3,3,3,3,3,3,3,3,3,3,3,3,3,3,3,3,4),
(91.106186954104,91.2126211244869,91.3191385189971,91.4258526613343,91.5326811144277,
91.6397297919096,91.6638627591846,91.7680491827495,91.872080373762,91.9759895362358,
92.0798332435591,92.1836462744062,92.2874633640191,92.3913891217618,92.4953737230612,
92.5995402490611,92.6613912936212,92.7655571697299,92.8695782280914,92.9734894823971,
93.0773351303294,93.1811423577143,93.2849756902826,93.3317577724807),
 .UNSPECIFIED.);
#554=B_SPLINE_CURVE_WITH_KNOTS('',3,(#49283,#49284,#49285,#49286,#49287,
#49288,#49289,#49290,#49291,#49292,#49293,#49294,#49295,#49296,#49297,#49298,
#49299,#49300,#49301,#49302,#49303,#49304,#49305,#49306,#49307,#49308,#49309,
#49310,#49311,#49312,#49313,#49314,#49315,#49316,#49317,#49318,#49319,#49320,
#49321,#49322,#49323,#49324,#49325,#49326,#49327,#49328,#49329,#49330,#49331,
#49332,#49333,#49334,#49335,#49336,#49337,#49338,#49339,#49340,#49341,#49342,
#49343,#49344,#49345,#49346,#49347,#49348,#49349,#49350,#49351,#49352),
 .UNSPECIFIED.,.F.,.F.,(4,3,3,3,3,3,3,3,3,3,3,3,3,3,3,3,3,3,3,3,3,3,3,4),
(91.106186954104,91.2078381643951,91.3120245843195,91.4160557716771,91.5199649304926,
91.6238086341573,91.7276216613509,91.8314387473207,91.9353645014613,92.0393490991763,
92.1435156216584,92.2053666988317,92.3095531170952,92.4135843027923,92.5174934599552,
92.6213371619734,92.7251501875286,92.8289672718709,92.9328930244111,93.0368776205386,
93.1410441414708,93.2028952332683,93.3070788384004,93.3327430891432),
 .UNSPECIFIED.);
#555=B_SPLINE_CURVE_WITH_KNOTS('',3,(#49353,#49354,#49355,#49356,#49357,
#49358,#49359,#49360,#49361,#49362,#49363,#49364,#49365,#49366,#49367,#49368,
#49369,#49370,#49371,#49372,#49373,#49374,#49375,#49376,#49377,#49378,#49379,
#49380,#49381,#49382,#49383,#49384,#49385,#49386,#49387,#49388,#49389,#49390,
#49391,#49392,#49393,#49394,#49395,#49396,#49397,#49398,#49399,#49400,#49401,
#49402,#49403,#49404,#49405,#49406,#49407,#49408,#49409,#49410,#49411,#49412,
#49413,#49414,#49415,#49416,#49417,#49418,#49419,#49420,#49421,#49422,#49423,
#49424,#49425,#49426,#49427,#49428,#49429,#49430,#49431,#49432,#49433,#49434,
#49435,#49436,#49437,#49438,#49439,#49440,#49441,#49442,#49443,#49444,#49445,
#49446,#49447,#49448,#49449,#49450,#49451,#49452,#49453,#49454,#49455,#49456,
#49457,#49458,#49459,#49460,#49461,#49462,#49463,#49464,#49465,#49466,#49467,
#49468,#49469,#49470,#49471,#49472,#49473,#49474,#49475,#49476),
 .UNSPECIFIED.,.F.,.F.,(4,3,3,3,3,3,3,3,3,3,3,3,3,3,3,3,3,3,3,3,3,3,3,3,
3,3,3,3,3,3,3,3,3,3,3,3,3,3,3,3,3,4),(87.0484659949012,87.1526312129392,
87.2177240266487,87.3219104458962,87.4259416325748,87.5298507907112,87.6336944936971,
87.7375075202133,87.8413246055082,87.9452503589819,88.0492349560335,88.1534014778652,
88.2152525610853,88.3194389804513,88.4234701672489,88.5273793255043,88.6312230286093,
88.7350360552444,88.8388531406578,88.9427788942487,89.0467634914171,89.1509300133632,
89.2127810955219,89.3169675146659,89.4209987012417,89.5249078592767,89.6287515621622,
89.7325645885791,89.8363816737758,89.940307427154,90.0442920241114,90.1484585458519,
90.2103096299585,90.3131827202774,90.4158805806228,90.5184806859093,90.6210195308692,
90.7235335246182,90.8261208446082,90.9287446851267,91.0315305432363,91.1061869536522),
 .UNSPECIFIED.);
#556=B_SPLINE_CURVE_WITH_KNOTS('',3,(#49482,#49483,#49484,#49485,#49486,
#49487,#49488,#49489,#49490,#49491,#49492,#49493,#49494,#49495,#49496,#49497,
#49498,#49499,#49500,#49501,#49502,#49503,#49504,#49505,#49506,#49507,#49508,
#49509,#49510,#49511,#49512,#49513,#49514,#49515,#49516,#49517,#49518,#49519,
#49520,#49521,#49522,#49523,#49524,#49525,#49526,#49527,#49528,#49529,#49530,
#49531,#49532,#49533,#49534,#49535,#49536,#49537,#49538,#49539,#49540,#49541,
#49542,#49543,#49544,#49545,#49546,#49547,#49548,#49549,#49550,#49551,#49552,
#49553,#49554,#49555,#49556,#49557,#49558,#49559,#49560,#49561,#49562,#49563,
#49564,#49565,#49566,#49567,#49568,#49569,#49570,#49571,#49572,#49573,#49574,
#49575,#49576,#49577,#49578,#49579,#49580,#49581,#49582,#49583,#49584,#49585,
#49586,#49587,#49588,#49589,#49590,#49591,#49592,#49593,#49594,#49595,#49596,
#49597,#49598,#49599,#49600,#49601,#49602),.UNSPECIFIED.,.F.,.F.,(4,3,3,
3,3,3,3,3,3,3,3,3,3,3,3,3,3,3,3,3,3,3,3,3,3,3,3,3,3,3,3,3,3,3,3,3,3,3,3,
3,4),(80.7662207640143,80.8702913123123,80.9742249190925,81.0780833656369,
81.1819014489876,81.2857139129852,81.3896288357873,81.4935939089057,81.5977500997127,
81.6885774148187,81.7927638340834,81.8967950207793,82.0007041789332,82.1045478819369,
82.2083609084708,82.3121779937836,82.4161037472752,82.5200883443447,82.6242548661941,
82.6861059492552,82.7902923685379,82.8943235552519,82.9982327134239,83.1020764164457,
83.2058894429977,83.3097065283284,83.4136322818377,83.517616878925,83.6217834007917,
83.6836344836918,83.7878209029459,83.8918520896312,83.9957612477749,84.0996049507683,
84.2034179772922,84.3072350625951,84.4111608160771,84.5151454131373,84.6193119349777,
84.6811630181284,84.8230016469244),.UNSPECIFIED.);
#557=B_SPLINE_CURVE_WITH_KNOTS('',3,(#49603,#49604,#49605,#49606,#49607,
#49608),.UNSPECIFIED.,.F.,.F.,(4,1,1,4),(84.8230094328245,85.678691552565,
86.6762200870017,87.0496595016183),.UNSPECIFIED.);
#558=B_SPLINE_CURVE_WITH_KNOTS('',3,(#49610,#49611,#49612,#49613,#49614,
#49615,#49616,#49617,#49618,#49619,#49620,#49621,#49622,#49623,#49624,#49625,
#49626,#49627,#49628,#49629,#49630,#49631,#49632,#49633,#49634,#49635,#49636,
#49637,#49638,#49639,#49640,#49641,#49642,#49643,#49644,#49645,#49646,#49647,
#49648,#49649,#49650,#49651,#49652,#49653,#49654,#49655,#49656,#49657,#49658,
#49659,#49660,#49661,#49662,#49663,#49664,#49665,#49666,#49667,#49668,#49669,
#49670,#49671,#49672,#49673,#49674,#49675,#49676),.UNSPECIFIED.,.F.,.F.,
(4,3,3,3,3,3,3,3,3,3,3,3,3,3,3,3,3,3,3,3,3,3,4),(84.8230020854923,84.9377584637952,
85.0529305011137,85.1686597771981,85.2226669577755,85.3268533770583,85.4308845637724,
85.5347937219446,85.6386374249663,85.7424504515183,85.8462675368491,85.9501932903585,
86.0541778874458,86.1583444093125,86.2201954922121,86.3243482544069,86.4283607931299,
86.5322681004129,86.6361050454483,86.7399459750719,86.843781441697,86.947723926167,
87.0484659949012),.UNSPECIFIED.);
#559=B_SPLINE_CURVE_WITH_KNOTS('',3,(#49677,#49678,#49679,#49680,#49681,
#49682,#49683,#49684),.UNSPECIFIED.,.F.,.F.,(4,1,1,1,1,4),(80.7656839778309,
81.2325528200291,82.2300813544657,83.2276098889023,84.2251384233389,84.8230016469244),
 .UNSPECIFIED.);
#560=B_SPLINE_CURVE_WITH_KNOTS('',3,(#49690,#49691,#49692,#49693,#49694,
#49695,#49696,#49697,#49698,#49699,#49700,#49701,#49702,#49703,#49704,#49705,
#49706,#49707,#49708,#49709,#49710,#49711,#49712,#49713,#49714,#49715,#49716,
#49717,#49718,#49719,#49720,#49721,#49722,#49723,#49724,#49725,#49726,#49727,
#49728,#49729,#49730,#49731,#49732,#49733,#49734,#49735,#49736,#49737,#49738,
#49739,#49740,#49741,#49742,#49743,#49744,#49745,#49746,#49747,#49748,#49749,
#49750,#49751,#49752,#49753,#49754,#49755,#49756,#49757,#49758,#49759,#49760,
#49761,#49762,#49763,#49764,#49765,#49766,#49767,#49768,#49769,#49770,#49771,
#49772,#49773,#49774,#49775,#49776,#49777,#49778,#49779,#49780,#49781,#49782,
#49783,#49784,#49785,#49786,#49787,#49788,#49789,#49790,#49791,#49792,#49793,
#49794,#49795,#49796,#49797,#49798,#49799,#49800,#49801,#49802,#49803,#49804,
#49805,#49806,#49807,#49808,#49809,#49810,#49811,#49812,#49813,#49814,#49815,
#49816),.UNSPECIFIED.,.F.,.F.,(4,3,3,3,3,3,3,3,3,3,3,3,3,3,3,3,3,3,3,3,
3,3,3,3,3,3,3,3,3,3,3,3,3,3,3,3,3,3,3,3,3,3,4),(74.4820777272201,74.5860984994285,
74.6902876866266,74.7058776737625,74.8100640930311,74.9140952797311,75.0180044378891,
75.1218481408968,75.2256611674348,75.3294782527517,75.4334040062473,75.5373886033209,
75.6415551251743,75.7034062081991,75.8075926274676,75.9116238141675,76.0155329723254,
76.1193766753329,76.2231897018708,76.3270067871875,76.430932540683,76.5349171377565,
76.6390836596097,76.7009347426357,76.8051211619046,76.9091523486048,77.0130615067631,
77.1169052097711,77.2207182363094,77.3245353216266,77.4284610751225,77.5324456721964,
77.63661219405,77.6984632770722,77.8036324098624,77.9060965907556,78.0084634414074,
78.1107696824831,78.2180313467107,78.3203753326952,78.4227592903825,78.5252692707006,
78.5398163393936),.UNSPECIFIED.);
#561=B_SPLINE_CURVE_WITH_KNOTS('',3,(#49817,#49818,#49819,#49820,#49821,
#49822,#49823,#49824,#49825,#49826,#49827,#49828,#49829,#49830,#49831,#49832,
#49833,#49834,#49835,#49836,#49837,#49838,#49839,#49840,#49841,#49842,#49843,
#49844,#49845,#49846,#49847,#49848,#49849,#49850,#49851,#49852,#49853,#49854,
#49855,#49856,#49857,#49858,#49859,#49860,#49861,#49862,#49863,#49864,#49865,
#49866,#49867,#49868,#49869,#49870,#49871,#49872,#49873,#49874,#49875,#49876,
#49877,#49878,#49879,#49880,#49881,#49882,#49883),.UNSPECIFIED.,.F.,.F.,
(4,3,3,3,3,3,3,3,3,3,3,3,3,3,3,3,3,3,3,3,3,3,4),(78.5398163397448,78.6959918115088,
78.8001782307767,78.904209417476,79.0081185756333,79.1119622786403,79.2157753051776,
79.3195923904937,79.4235181439887,79.5275027410616,79.6316692629143,79.6935203459455,
79.7977067652162,79.9017379519181,80.0056471100781,80.1094908130878,80.2133038396278,
80.3171209249467,80.4210466784442,80.5250312755198,80.629197797375,80.6910488803821,
80.7662207640143),.UNSPECIFIED.);
#562=B_SPLINE_CURVE_WITH_KNOTS('',3,(#49885,#49886,#49887,#49888,#49889,
#49890),.UNSPECIFIED.,.F.,.F.,(4,1,1,4),(78.5398163397448,79.2374957511559,
80.2350242855925,80.7656839778309),.UNSPECIFIED.);
#563=B_SPLINE_CURVE_WITH_KNOTS('',3,(#49891,#49892,#49893,#49894,#49895,
#49896,#49897,#49898,#49899,#49900,#49901,#49902,#49903,#49904,#49905,#49906,
#49907,#49908,#49909,#49910,#49911,#49912,#49913,#49914,#49915,#49916,#49917,
#49918,#49919,#49920,#49921,#49922,#49923,#49924,#49925,#49926,#49927,#49928,
#49929,#49930,#49931,#49932,#49933,#49934,#49935,#49936,#49937,#49938,#49939,
#49940,#49941,#49942,#49943,#49944,#49945,#49946,#49947,#49948,#49949,#49950,
#49951,#49952,#49953,#49954,#49955,#49956,#49957,#49958,#49959,#49960,#49961,
#49962,#49963,#49964,#49965,#49966,#49967,#49968,#49969,#49970,#49971,#49972,
#49973,#49974,#49975,#49976,#49977,#49978,#49979,#49980,#49981,#49982,#49983,
#49984,#49985,#49986,#49987,#49988,#49989,#49990,#49991,#49992,#49993,#49994,
#49995,#49996,#49997,#49998,#49999,#50000,#50001,#50002,#50003,#50004,#50005,
#50006,#50007,#50008,#50009,#50010,#50011,#50012,#50013,#50014),
 .UNSPECIFIED.,.F.,.F.,(4,3,3,3,3,3,3,3,3,3,3,3,3,3,3,3,3,3,3,3,3,3,3,3,
3,3,3,3,3,3,3,3,3,3,3,3,3,3,3,3,3,4),(74.483258856194,74.58714895619,74.6909820348205,
74.7947928570274,74.8986161527883,75.0025532911364,75.1065568345892,75.2107347646363,
75.2473816134095,75.3515680326781,75.4555992193779,75.5595083775358,75.6633520805436,
75.7671651070816,75.8709821923984,75.974907945894,76.0788925429675,76.1830590648209,
76.2449101478461,76.3490965671147,76.4531277538146,76.5570369119727,76.6608806149803,
76.7646936415184,76.8685107268353,76.9724364803309,77.0764210774048,77.1805875992581,
77.2424386822827,77.3466251015512,77.4506562882509,77.5545654464089,77.6584091494165,
77.7622221759546,77.8660392612716,77.9699650147671,78.0739496118409,78.1781161336942,
78.2399672167193,78.3667743019381,78.4918646593798,78.5398161595682),
 .UNSPECIFIED.);
#564=B_SPLINE_CURVE_WITH_KNOTS('',3,(#50020,#50021,#50022,#50023,#50024,
#50025,#50026,#50027),.UNSPECIFIED.,.F.,.F.,(4,1,1,1,1,4),(68.1996051490179,
68.7207064671429,69.7182350015795,70.7157635360161,71.7132920704527,72.2566310325652),
 .UNSPECIFIED.);
#565=B_SPLINE_CURVE_WITH_KNOTS('',3,(#50028,#50029,#50030,#50031,#50032,
#50033,#50034,#50035,#50036,#50037,#50038,#50039,#50040,#50041,#50042,#50043,
#50044,#50045,#50046,#50047,#50048,#50049,#50050,#50051,#50052,#50053,#50054,
#50055,#50056,#50057,#50058,#50059,#50060,#50061,#50062,#50063,#50064,#50065,
#50066,#50067,#50068,#50069,#50070,#50071,#50072,#50073,#50074,#50075,#50076,
#50077,#50078,#50079,#50080,#50081,#50082,#50083,#50084,#50085,#50086,#50087,
#50088,#50089,#50090,#50091,#50092,#50093,#50094),.UNSPECIFIED.,.F.,.F.,
(4,3,3,3,3,3,3,3,3,3,3,3,3,3,3,3,3,3,3,3,3,3,4),(72.2566312677228,72.3701786020144,
72.4815875706104,72.5962040877498,72.7108206048892,72.8150070241578,72.9190382108577,
73.0229473690157,73.1267910720234,73.2306040985615,73.3344211838783,73.438346937374,
73.5423315344476,73.646498056301,73.7083491393258,73.8125058078903,73.9165206668431,
74.0204287152825,74.1242648270253,74.228091613986,74.3319123109939,74.4358068237418,
74.4820777272201),.UNSPECIFIED.);
#566=B_SPLINE_CURVE_WITH_KNOTS('',3,(#50096,#50097,#50098,#50099,#50100,
#50101,#50102,#50103,#50104,#50105,#50106,#50107,#50108,#50109,#50110,#50111,
#50112,#50113,#50114,#50115,#50116,#50117,#50118,#50119,#50120,#50121,#50122,
#50123,#50124,#50125,#50126,#50127,#50128,#50129,#50130,#50131,#50132,#50133,
#50134,#50135,#50136,#50137,#50138,#50139,#50140,#50141,#50142,#50143,#50144,
#50145,#50146,#50147,#50148,#50149,#50150,#50151,#50152,#50153,#50154,#50155,
#50156,#50157,#50158,#50159,#50160,#50161,#50162,#50163,#50164,#50165),
 .UNSPECIFIED.,.F.,.F.,(4,3,3,3,3,3,3,3,3,3,3,3,3,3,3,3,3,3,3,3,3,3,3,4),
(72.2566310325652,72.3607828828408,72.4647795326403,72.5686542861374,72.6724637223968,
72.7762426721719,72.8800259229371,72.983917905017,73.0878690474533,73.1920015684938,
73.2523245445363,73.356510963805,73.4605421505049,73.564451308663,73.6682950116707,
73.7721080382088,73.8759251235256,73.9798508770212,74.0838354740948,74.1880019959481,
74.2498530789729,74.3540440432939,74.4580688811934,74.483258856194),
 .UNSPECIFIED.);
#567=B_SPLINE_CURVE_WITH_KNOTS('',3,(#50166,#50167,#50168,#50169,#50170,
#50171,#50172,#50173,#50174,#50175,#50176,#50177,#50178,#50179,#50180,#50181,
#50182,#50183,#50184,#50185,#50186,#50187,#50188,#50189,#50190,#50191,#50192,
#50193,#50194,#50195,#50196,#50197,#50198,#50199,#50200,#50201,#50202,#50203,
#50204,#50205,#50206,#50207,#50208,#50209,#50210,#50211,#50212,#50213,#50214,
#50215,#50216,#50217,#50218,#50219,#50220,#50221,#50222,#50223,#50224,#50225,
#50226,#50227,#50228,#50229,#50230,#50231,#50232,#50233,#50234,#50235,#50236,
#50237,#50238,#50239,#50240,#50241,#50242,#50243,#50244,#50245,#50246,#50247,
#50248,#50249,#50250,#50251,#50252,#50253,#50254,#50255,#50256,#50257,#50258,
#50259,#50260,#50261,#50262,#50263,#50264,#50265,#50266,#50267,#50268,#50269,
#50270,#50271,#50272,#50273,#50274,#50275,#50276,#50277,#50278,#50279,#50280,
#50281,#50282,#50283,#50284,#50285,#50286,#50287,#50288,#50289,#50290,#50291,
#50292),.UNSPECIFIED.,.F.,.F.,(4,3,3,3,3,3,3,3,3,3,3,3,3,3,3,3,3,3,3,3,
3,3,3,3,3,3,3,3,3,3,3,3,3,3,3,3,3,3,3,3,3,3,4),(68.1991556033306,68.2646818723533,
68.3688682916219,68.4728994783219,68.5768086364799,68.6806523394876,68.7844653660256,
68.8882824513425,68.9922082048381,69.0961928019117,69.2003593237651,69.2622104067899,
69.3663968260585,69.4704280127585,69.5743371709165,69.6781808739242,69.7819939004622,
69.885810985779,69.9897367392747,70.0937213363483,70.1978878582017,70.2597389412265,
70.3639253604952,70.4679565471951,70.5718657053531,70.6757094083608,70.7795224348989,
70.8833395202158,70.9872652737114,71.091249870785,71.1954163926384,71.2572674756631,
71.3614538949318,71.4654850816318,71.5693942397898,71.6732379427974,71.7770509693354,
71.8808680546522,71.9847938081478,72.0887784052214,72.1929449270748,72.2547960100997,
72.2566310321323),.UNSPECIFIED.);
#568=B_SPLINE_CURVE_WITH_KNOTS('',3,(#50298,#50299,#50300,#50301,#50302,
#50303,#50304,#50305,#50306,#50307,#50308,#50309,#50310,#50311,#50312,#50313,
#50314,#50315,#50316,#50317,#50318,#50319,#50320,#50321,#50322,#50323,#50324,
#50325,#50326,#50327,#50328,#50329,#50330,#50331,#50332,#50333,#50334,#50335,
#50336,#50337,#50338,#50339,#50340,#50341,#50342,#50343,#50344,#50345,#50346,
#50347,#50348,#50349,#50350,#50351,#50352,#50353,#50354,#50355,#50356,#50357,
#50358,#50359,#50360,#50361,#50362,#50363,#50364,#50365,#50366,#50367,#50368,
#50369,#50370,#50371,#50372,#50373,#50374,#50375,#50376,#50377,#50378,#50379,
#50380,#50381,#50382,#50383,#50384,#50385,#50386,#50387,#50388,#50389,#50390,
#50391,#50392,#50393,#50394,#50395,#50396,#50397,#50398,#50399,#50400,#50401,
#50402,#50403,#50404,#50405,#50406,#50407,#50408,#50409,#50410,#50411,#50412,
#50413,#50414,#50415,#50416,#50417,#50418),.UNSPECIFIED.,.F.,.F.,(4,3,3,
3,3,3,3,3,3,3,3,3,3,3,3,3,3,3,3,3,3,3,3,3,3,3,3,3,3,3,3,3,3,3,3,3,3,3,3,
3,4),(61.9168822289229,62.0208161626315,62.1246748131786,62.2284929778564,
62.3323054006316,62.4362202018145,62.5401850432597,62.6443411223858,62.7355352605233,
62.8397216797919,62.9437528664919,63.0476620246499,63.1515057276576,63.2553187541956,
63.3591358395125,63.4630615930081,63.5670461900817,63.6712127119351,63.7330637949599,
63.8372502142285,63.9412814009285,64.0451905590865,64.1490342620942,64.2528472886323,
64.356664373949,64.4605901274447,64.5645747245183,64.6687412463717,64.7305923293965,
64.8347787486652,64.9388099353651,65.0427190935231,65.1465627965308,65.2503758230688,
65.3541929083857,65.4581186618813,65.5621032589549,65.6662697808083,65.7281208638331,
65.8639211032556,65.9734456460794),.UNSPECIFIED.);
#569=B_SPLINE_CURVE_WITH_KNOTS('',3,(#50419,#50420,#50421,#50422,#50423,
#50424),.UNSPECIFIED.,.F.,.F.,(4,1,1,4),(65.9734457253856,66.7256493982697,
67.7231779327063,68.1996051490179),.UNSPECIFIED.);
#570=B_SPLINE_CURVE_WITH_KNOTS('',3,(#50426,#50427,#50428,#50429,#50430,
#50431,#50432,#50433,#50434,#50435,#50436,#50437,#50438,#50439,#50440,#50441,
#50442,#50443,#50444,#50445,#50446,#50447,#50448,#50449,#50450,#50451,#50452,
#50453,#50454,#50455,#50456,#50457,#50458,#50459,#50460,#50461,#50462,#50463,
#50464,#50465,#50466,#50467,#50468,#50469,#50470,#50471,#50472,#50473,#50474,
#50475,#50476,#50477,#50478,#50479,#50480,#50481,#50482,#50483,#50484,#50485,
#50486,#50487,#50488,#50489,#50490,#50491,#50492),.UNSPECIFIED.,.F.,.F.,
(4,3,3,3,3,3,3,3,3,3,3,3,3,3,3,3,3,3,3,3,3,3,4),(65.973445898234,66.098877789982,
66.2261301221736,66.2696248034801,66.3738112227488,66.4778424094487,66.5817515676067,
66.6855952706144,66.7894082971524,66.8932253824693,66.9971511359649,67.1011357330385,
67.2053022548919,67.2671533379167,67.371344420459,67.4753543177416,67.5792620003784,
67.6831023298771,67.7869100863057,67.8907809338262,67.9946786755476,68.0987368797689,
68.1991556033306),.UNSPECIFIED.);
#571=B_SPLINE_CURVE_WITH_KNOTS('',3,(#50493,#50494,#50495,#50496,#50497,
#50498,#50499,#50500),.UNSPECIFIED.,.F.,.F.,(4,1,1,1,1,4),(61.91564316731,
62.2795106657337,63.2770392001703,64.2745677346069,65.2720962690435,65.9734457253856),
 .UNSPECIFIED.);
#572=B_SPLINE_CURVE_WITH_KNOTS('',3,(#50506,#50507,#50508,#50509,#50510,
#50511,#50512,#50513,#50514,#50515,#50516,#50517,#50518,#50519,#50520,#50521,
#50522,#50523,#50524,#50525,#50526,#50527,#50528,#50529,#50530,#50531,#50532,
#50533,#50534,#50535,#50536,#50537,#50538,#50539,#50540,#50541,#50542,#50543,
#50544,#50545,#50546,#50547,#50548,#50549,#50550,#50551,#50552,#50553,#50554,
#50555,#50556,#50557,#50558,#50559,#50560,#50561,#50562,#50563,#50564,#50565,
#50566,#50567,#50568,#50569,#50570,#50571,#50572,#50573,#50574,#50575,#50576,
#50577,#50578,#50579,#50580,#50581,#50582,#50583,#50584,#50585,#50586,#50587,
#50588,#50589,#50590,#50591,#50592,#50593,#50594,#50595,#50596,#50597,#50598,
#50599,#50600,#50601,#50602,#50603,#50604,#50605,#50606,#50607,#50608,#50609,
#50610,#50611,#50612,#50613,#50614,#50615,#50616,#50617,#50618,#50619,#50620,
#50621,#50622,#50623,#50624,#50625,#50626,#50627,#50628,#50629,#50630,#50631,
#50632),.UNSPECIFIED.,.F.,.F.,(4,3,3,3,3,3,3,3,3,3,3,3,3,3,3,3,3,3,3,3,
3,3,3,3,3,3,3,3,3,3,3,3,3,3,3,3,3,3,3,3,3,3,4),(55.6326174533268,55.73680638972,
55.7528355194671,55.8570219387357,55.9610531254357,56.0649622835937,56.1688059866014,
56.2726190131394,56.3764360984563,56.4803618519519,56.5843464490255,56.6885129708789,
56.7503640539037,56.8545504731723,56.9585816598723,57.0624908180303,57.166334521038,
57.270147547576,57.3739646328929,57.4778903863885,57.5818749834621,57.6860415053155,
57.7478925883403,57.8520790076089,57.9561101943089,58.0600193524669,58.1638630554746,
58.2676760820126,58.3714931673294,58.475418920825,58.5794035178986,58.683570039752,
58.7454211227769,58.8487780338705,58.9539633318708,59.0570447634811,59.1600643665938,
59.2630580262842,59.3698586241814,59.4729706208906,59.5761501528133,59.6794897442538,
59.690260417873),.UNSPECIFIED.);
#573=B_SPLINE_CURVE_WITH_KNOTS('',3,(#50633,#50634,#50635,#50636,#50637,
#50638,#50639,#50640,#50641,#50642,#50643,#50644,#50645,#50646,#50647,#50648,
#50649,#50650,#50651,#50652,#50653,#50654,#50655,#50656,#50657,#50658,#50659,
#50660,#50661,#50662,#50663,#50664,#50665,#50666,#50667,#50668,#50669,#50670,
#50671,#50672,#50673,#50674,#50675,#50676,#50677,#50678,#50679,#50680,#50681,
#50682,#50683,#50684,#50685,#50686,#50687,#50688,#50689,#50690,#50691,#50692,
#50693,#50694,#50695,#50696,#50697,#50698,#50699,#50700,#50701,#50702),
 .UNSPECIFIED.,.F.,.F.,(4,3,3,3,3,3,3,3,3,3,3,3,3,3,3,3,3,3,3,3,3,3,3,4),
(59.690260418206,59.7429496572135,59.8471360764821,59.9511672631822,60.0550764213402,
60.1589201243479,60.2627331508859,60.3665502362027,60.4704759896983,60.574460586772,
60.6786271086253,60.7404781916501,60.8446646109187,60.9486957976187,61.0526049557767,
61.1564486587844,61.2602616853224,61.3640787706392,61.4680045241349,61.5719891212085,
61.6761556430618,61.7380067260867,61.842168294112,61.9168822289229),
 .UNSPECIFIED.);
#574=B_SPLINE_CURVE_WITH_KNOTS('',3,(#50704,#50705,#50706,#50707,#50708,
#50709),.UNSPECIFIED.,.F.,.F.,(4,1,1,4),(59.690260418206,60.2844535968605,
61.2819821312971,61.91564316731),.UNSPECIFIED.);
#575=B_SPLINE_CURVE_WITH_KNOTS('',3,(#50710,#50711,#50712,#50713,#50714,
#50715,#50716,#50717,#50718,#50719,#50720,#50721,#50722,#50723,#50724,#50725,
#50726,#50727,#50728,#50729,#50730,#50731,#50732,#50733,#50734,#50735,#50736,
#50737,#50738,#50739,#50740,#50741,#50742,#50743,#50744,#50745,#50746,#50747,
#50748,#50749,#50750,#50751,#50752,#50753,#50754,#50755,#50756,#50757,#50758,
#50759,#50760,#50761,#50762,#50763,#50764,#50765,#50766,#50767,#50768,#50769,
#50770,#50771,#50772,#50773,#50774,#50775,#50776,#50777,#50778,#50779,#50780,
#50781,#50782,#50783,#50784,#50785,#50786,#50787,#50788,#50789,#50790,#50791,
#50792,#50793,#50794,#50795,#50796,#50797,#50798,#50799,#50800,#50801,#50802,
#50803,#50804,#50805,#50806,#50807,#50808,#50809,#50810,#50811,#50812,#50813,
#50814,#50815,#50816,#50817,#50818,#50819,#50820,#50821,#50822,#50823,#50824,
#50825,#50826,#50827,#50828,#50829,#50830,#50831,#50832,#50833),
 .UNSPECIFIED.,.F.,.F.,(4,3,3,3,3,3,3,3,3,3,3,3,3,3,3,3,3,3,3,3,3,3,3,3,
3,3,3,3,3,3,3,3,3,3,3,3,3,3,3,3,3,4),(55.6335626494765,55.7373959362262,
55.8412067845232,55.9450299244374,56.0489667972699,56.1529699116885,56.2571475712116,
56.2943394591141,56.3985258783827,56.5025570650826,56.6064662232406,56.7103099262482,
56.8141229527862,56.9179400381028,57.0218657915985,57.1258503886722,57.2300169105256,
57.2918679935507,57.3960544128194,57.5000855995192,57.6039947576773,57.7078384606848,
57.8116514872228,57.9154685725394,58.019394326035,58.1233789231088,58.2275454449622,
58.2893965279873,58.3935829472557,58.4976141339561,58.6015232921141,58.7053669951219,
58.8091800216598,58.9129971069768,59.0169228604724,59.120907457546,59.2250739793994,
59.2869250624239,59.4023023751458,59.5173142795046,59.631721429585,59.6902599887701),
 .UNSPECIFIED.);
#576=B_SPLINE_CURVE_WITH_KNOTS('',3,(#50839,#50840,#50841,#50842,#50843,
#50844,#50845,#50846),.UNSPECIFIED.,.F.,.F.,(4,1,1,1,1,4),(49.3495089121257,
49.7676643128475,50.7651928472841,51.7627213817207,52.7602499161573,53.4070751110264),
 .UNSPECIFIED.);
#577=B_SPLINE_CURVE_WITH_KNOTS('',3,(#50847,#50848,#50849,#50850,#50851,
#50852,#50853,#50854,#50855,#50856,#50857,#50858,#50859,#50860,#50861,#50862,
#50863,#50864,#50865,#50866,#50867,#50868,#50869,#50870,#50871,#50872,#50873,
#50874,#50875,#50876,#50877,#50878,#50879,#50880,#50881,#50882,#50883,#50884,
#50885,#50886,#50887,#50888,#50889,#50890,#50891,#50892,#50893,#50894,#50895,
#50896,#50897,#50898,#50899,#50900,#50901,#50902,#50903,#50904,#50905,#50906,
#50907,#50908,#50909,#50910,#50911,#50912,#50913),.UNSPECIFIED.,.F.,.F.,
(4,3,3,3,3,3,3,3,3,3,3,3,3,3,3,3,3,3,3,3,3,3,4),(53.4070753517635,53.5260748736241,
53.6461598280863,53.7577784505939,53.8619648698625,53.9659960565623,54.0699052147203,
54.173748917728,54.277561944266,54.3813790295829,54.4853047830786,54.5892893801522,
54.6934559020056,54.7553069850305,54.8649707935675,54.9689754329642,55.0728781103241,
55.1767136856929,55.2805169373318,55.3843685433793,55.4882480448386,55.5922481426596,
55.6326174533268),.UNSPECIFIED.);
#578=B_SPLINE_CURVE_WITH_KNOTS('',3,(#50915,#50916,#50917,#50918,#50919,
#50920,#50921,#50922,#50923,#50924,#50925,#50926,#50927,#50928,#50929,#50930,
#50931,#50932,#50933,#50934,#50935,#50936,#50937,#50938,#50939,#50940,#50941,
#50942,#50943,#50944,#50945,#50946,#50947,#50948,#50949,#50950,#50951,#50952,
#50953,#50954,#50955,#50956,#50957,#50958,#50959,#50960,#50961,#50962,#50963,
#50964,#50965,#50966,#50967,#50968,#50969,#50970,#50971,#50972,#50973,#50974,
#50975,#50976,#50977,#50978,#50979,#50980,#50981,#50982,#50983,#50984),
 .UNSPECIFIED.,.F.,.F.,(4,3,3,3,3,3,3,3,3,3,3,3,3,3,3,3,3,3,3,3,3,3,3,4),
(53.4070751114733,53.5098558320602,53.612486311178,53.7150344153122,53.8175366234368,
53.920029348614,54.0226180274639,54.1252565130453,54.2280753277646,54.2992823902409,
54.4034688095096,54.5074999962095,54.6114091543675,54.7152528573752,54.8190658839133,
54.9228829692301,55.0268087227257,55.1307933197992,55.2349598416526,55.2968109246775,
55.4009764939796,55.505005930678,55.6089152639628,55.6335626494765),
 .UNSPECIFIED.);
#579=B_SPLINE_CURVE_WITH_KNOTS('',3,(#50985,#50986,#50987,#50988,#50989,
#50990,#50991,#50992,#50993,#50994,#50995,#50996,#50997,#50998,#50999,#51000,
#51001,#51002,#51003,#51004,#51005,#51006,#51007,#51008,#51009,#51010,#51011,
#51012,#51013,#51014,#51015,#51016,#51017,#51018,#51019,#51020,#51021,#51022,
#51023,#51024,#51025,#51026,#51027,#51028,#51029,#51030,#51031,#51032,#51033,
#51034,#51035,#51036,#51037,#51038,#51039,#51040,#51041,#51042,#51043,#51044,
#51045,#51046,#51047,#51048,#51049,#51050,#51051,#51052,#51053,#51054,#51055,
#51056,#51057,#51058,#51059,#51060,#51061,#51062,#51063,#51064,#51065,#51066,
#51067,#51068,#51069,#51070,#51071,#51072,#51073,#51074,#51075,#51076,#51077,
#51078,#51079,#51080,#51081,#51082,#51083,#51084,#51085,#51086,#51087,#51088,
#51089,#51090,#51091,#51092,#51093,#51094,#51095,#51096,#51097,#51098,#51099,
#51100,#51101,#51102,#51103,#51104,#51105,#51106,#51107,#51108),
 .UNSPECIFIED.,.F.,.F.,(4,3,3,3,3,3,3,3,3,3,3,3,3,3,3,3,3,3,3,3,3,3,3,3,
3,3,3,3,3,3,3,3,3,3,3,3,3,3,3,3,3,4),(49.3501402663156,49.4542648365893,
49.5611277635774,49.6650067633435,49.7688341253606,49.8726446068756,49.9817755182803,
50.0857237633826,50.1897448377912,50.2939342287898,50.3091682524945,50.413354671763,
50.5173858584629,50.6212950166208,50.7251387196283,50.8289517461662,50.932768831483,
51.0366945849785,51.140679182052,51.2448457039053,51.3066967869311,51.4108832061997,
51.5149143928997,51.6188235510577,51.7226672540654,51.8264802806034,51.9302973659203,
52.0342231194159,52.1382077164896,52.2423742383429,52.3042253213677,52.4084117406364,
52.5124429273364,52.6163520854945,52.7201957885022,52.8240088150403,52.9278259003571,
53.0317516538528,53.1357362509265,53.2399027727799,53.3017538558043,53.4070751110264),
 .UNSPECIFIED.);
#580=B_SPLINE_CURVE_WITH_KNOTS('',3,(#51114,#51115,#51116,#51117,#51118,
#51119,#51120,#51121,#51122,#51123,#51124,#51125,#51126,#51127,#51128,#51129,
#51130,#51131,#51132,#51133,#51134,#51135,#51136,#51137,#51138,#51139,#51140,
#51141,#51142,#51143,#51144,#51145,#51146,#51147,#51148,#51149,#51150,#51151,
#51152,#51153,#51154,#51155,#51156,#51157,#51158,#51159,#51160,#51161,#51162,
#51163,#51164,#51165,#51166,#51167,#51168,#51169,#51170,#51171,#51172,#51173,
#51174,#51175,#51176,#51177,#51178,#51179,#51180,#51181,#51182,#51183,#51184,
#51185,#51186,#51187,#51188,#51189,#51190,#51191,#51192,#51193,#51194,#51195,
#51196,#51197,#51198,#51199,#51200,#51201,#51202,#51203,#51204,#51205,#51206,
#51207,#51208,#51209,#51210,#51211,#51212,#51213,#51214,#51215,#51216,#51217,
#51218,#51219,#51220,#51221,#51222,#51223,#51224,#51225,#51226,#51227,#51228,
#51229,#51230,#51231,#51232,#51233,#51234),.UNSPECIFIED.,.F.,.F.,(4,3,3,
3,3,3,3,3,3,3,3,3,3,3,3,3,3,3,3,3,3,3,3,3,3,3,3,3,3,3,3,3,3,3,3,3,3,3,3,
3,4),(43.0672872443465,43.1711461664278,43.274964439754,43.3787768084601,
43.4826914487572,43.5866559831908,43.690811914766,43.7824931062279,43.8866795254984,
43.9907107122005,44.0946198703604,44.1984635733701,44.3022765999102,44.4060936852289,
44.5100194387266,44.6140040358023,44.7181705576576,44.7800216406645,44.8842080599324,
44.9882392466315,45.0921484047887,45.1959921077957,45.2998051343331,45.4036222196496,
45.5075479731445,45.6115325702172,45.7156990920699,45.7775501751011,45.8817365943696,
45.9857677810689,46.0896769392268,46.1935206422343,46.2973336687722,46.4011507540888,
46.5050765075843,46.6090611046576,46.7132276265108,46.7750787095377,46.8955468169138,
47.0149579018511,47.1238895638475),.UNSPECIFIED.);
#581=B_SPLINE_CURVE_WITH_KNOTS('',3,(#51235,#51236,#51237,#51238,#51239,
#51240),.UNSPECIFIED.,.F.,.F.,(4,1,1,4),(47.1238898038468,47.7726072439743,
48.7701357784109,49.3495089121257),.UNSPECIFIED.);
#582=B_SPLINE_CURVE_WITH_KNOTS('',3,(#51242,#51243,#51244,#51245,#51246,
#51247,#51248,#51249,#51250,#51251,#51252,#51253,#51254,#51255,#51256,#51257,
#51258,#51259,#51260,#51261,#51262,#51263,#51264,#51265,#51266,#51267,#51268,
#51269,#51270,#51271,#51272,#51273,#51274,#51275,#51276,#51277,#51278,#51279,
#51280,#51281,#51282,#51283,#51284,#51285,#51286,#51287,#51288,#51289,#51290,
#51291,#51292,#51293,#51294,#51295,#51296,#51297,#51298,#51299,#51300,#51301,
#51302,#51303,#51304,#51305,#51306,#51307,#51308,#51309,#51310,#51311),
 .UNSPECIFIED.,.F.,.F.,(4,3,3,3,3,3,3,3,3,3,3,3,3,3,3,3,3,3,3,3,3,3,3,4),
(47.1238898038468,47.2757519674286,47.3165826491847,47.4207690684526,47.524800255152,
47.6287094133093,47.7325531163163,47.8363661428537,47.9401832281699,48.0441089816649,
48.1480935787378,48.2522601005905,48.3141111836213,48.4182976028898,48.5223287895896,
48.6262379477475,48.7300816507551,48.8338946772929,48.9377117626097,49.0416375161052,
49.1456221131786,49.2497886350318,49.3116397180579,49.3501402663156),
 .UNSPECIFIED.);
#583=B_SPLINE_CURVE_WITH_KNOTS('',3,(#51312,#51313,#51314,#51315,#51316,
#51317,#51318,#51319),.UNSPECIFIED.,.F.,.F.,(4,1,1,1,1,4),(43.0658398005562,
43.3264685114383,44.3239970458749,45.3215255803115,46.3190541147481,47.1238860295235),
 .UNSPECIFIED.);
#584=B_SPLINE_CURVE_WITH_KNOTS('',3,(#51325,#51326,#51327,#51328,#51329,
#51330,#51331,#51332,#51333,#51334,#51335,#51336,#51337,#51338,#51339,#51340,
#51341,#51342,#51343,#51344,#51345,#51346,#51347,#51348,#51349,#51350,#51351,
#51352,#51353,#51354,#51355,#51356,#51357,#51358,#51359,#51360,#51361,#51362,
#51363,#51364,#51365,#51366,#51367,#51368,#51369,#51370,#51371,#51372,#51373,
#51374,#51375,#51376,#51377,#51378,#51379,#51380,#51381,#51382,#51383,#51384,
#51385,#51386,#51387,#51388,#51389,#51390,#51391,#51392,#51393,#51394,#51395,
#51396,#51397,#51398,#51399,#51400,#51401,#51402,#51403,#51404,#51405,#51406,
#51407,#51408,#51409,#51410,#51411,#51412,#51413,#51414,#51415,#51416,#51417,
#51418,#51419,#51420,#51421,#51422,#51423,#51424,#51425,#51426,#51427,#51428,
#51429,#51430,#51431,#51432,#51433,#51434,#51435,#51436,#51437,#51438,#51439,
#51440,#51441,#51442,#51443,#51444,#51445,#51446,#51447,#51448,#51449,#51450,
#51451),.UNSPECIFIED.,.F.,.F.,(4,3,3,3,3,3,3,3,3,3,3,3,3,3,3,3,3,3,3,3,
3,3,3,3,3,3,3,3,3,3,3,3,3,3,3,3,3,3,3,3,3,3,4),(36.7834620528982,36.7997933651717,
36.9039797843287,37.0080109709146,37.1119201289555,37.2157638318444,37.3195768582619,
37.4233939434569,37.5273196968292,37.6313042937785,37.7354708155074,37.7973218996083,
37.9015083189688,38.0055395057619,38.1094486640147,38.2132923671181,38.3171053937527,
38.4209224791667,38.5248482327598,38.6288328299312,38.7329993518819,38.7948504340449,
38.899036853292,39.0030680399703,39.1069771981065,39.2108209010924,39.3146339276087,
39.4184510129037,39.5223767663778,39.6263613634299,39.7305278852622,39.7923789684815,
39.8965653877372,40.0005965744239,40.1045057325683,40.2083494355621,40.3121624620861,
40.4159795473886,40.5199053008698,40.6238898979288,40.7280564197675,40.7899075029181,
40.8407044966672),.UNSPECIFIED.);
#585=B_SPLINE_CURVE_WITH_KNOTS('',3,(#51452,#51453,#51454,#51455,#51456,
#51457,#51458,#51459,#51460,#51461,#51462,#51463,#51464,#51465,#51466,#51467,
#51468,#51469,#51470,#51471,#51472,#51473,#51474,#51475,#51476,#51477,#51478,
#51479,#51480,#51481,#51482,#51483,#51484,#51485,#51486,#51487,#51488,#51489,
#51490,#51491,#51492,#51493,#51494,#51495,#51496,#51497,#51498,#51499,#51500,
#51501,#51502,#51503,#51504,#51505,#51506,#51507,#51508,#51509,#51510,#51511,
#51512,#51513,#51514,#51515,#51516,#51517,#51518,#51519,#51520,#51521),
 .UNSPECIFIED.,.F.,.F.,(4,3,3,3,3,3,3,3,3,3,3,3,3,3,3,3,3,3,3,3,3,3,3,4),
(40.8407044969988,40.9440672893101,41.0494883828156,41.1525861150597,41.2556259852456,
41.3586438439961,41.4658418923358,41.5689883265775,41.6722057013573,41.7755885097806,
41.7874360373547,41.8916224566194,41.9956536433155,42.0995628014695,42.2034065044732,
42.3072195310072,42.4110366163199,42.5149623698115,42.6189469668809,42.7231134887303,
42.7849645717913,42.8891423345831,42.9931552794839,43.0672872443465),
 .UNSPECIFIED.);
#586=B_SPLINE_CURVE_WITH_KNOTS('',3,(#51523,#51524,#51525,#51526,#51527,
#51528),.UNSPECIFIED.,.F.,.F.,(4,1,1,4),(40.8407051184979,41.3314114425651,
42.3289399770017,43.0658398005562),.UNSPECIFIED.);
#587=B_SPLINE_CURVE_WITH_KNOTS('',3,(#51529,#51530,#51531,#51532,#51533,
#51534,#51535,#51536,#51537,#51538,#51539,#51540,#51541,#51542,#51543,#51544,
#51545,#51546,#51547,#51548,#51549,#51550,#51551,#51552,#51553,#51554,#51555,
#51556,#51557,#51558,#51559,#51560,#51561,#51562,#51563,#51564,#51565,#51566,
#51567,#51568,#51569,#51570,#51571,#51572,#51573,#51574,#51575,#51576,#51577,
#51578,#51579,#51580,#51581,#51582,#51583,#51584,#51585,#51586,#51587,#51588,
#51589,#51590,#51591,#51592,#51593,#51594,#51595,#51596,#51597,#51598,#51599,
#51600,#51601,#51602,#51603,#51604,#51605,#51606,#51607,#51608,#51609,#51610,
#51611,#51612,#51613,#51614,#51615,#51616,#51617,#51618,#51619,#51620,#51621,
#51622,#51623,#51624,#51625,#51626,#51627,#51628,#51629,#51630,#51631,#51632,
#51633,#51634,#51635,#51636,#51637,#51638,#51639,#51640,#51641,#51642,#51643,
#51644,#51645,#51646,#51647,#51648,#51649,#51650,#51651,#51652),
 .UNSPECIFIED.,.F.,.F.,(4,3,3,3,3,3,3,3,3,3,3,3,3,3,3,3,3,3,3,3,3,3,3,3,
3,3,3,3,3,3,3,3,3,3,3,3,3,3,3,3,3,4),(36.7837376627694,36.887548540786,
36.9913715043335,37.0953080764532,37.1993107049402,37.303488058312,37.3412973048187,
37.4454837247122,37.5495149120458,37.6534240708478,37.7572677745056,37.8610808016985,
37.9648978876741,38.0688236418301,38.172808239566,38.2769747620775,38.3388258392553,
38.4430122584196,38.547043445015,38.6509526030691,38.7547963059732,38.8586093324081,
38.9624264176225,39.0663521710174,39.1703367679912,39.2745032897469,39.3363543736919,
39.4405407928485,39.544571979434,39.6484811374745,39.7523248403629,39.85613786678,
39.9599549519746,40.0638807053465,40.1678653022953,40.2720318240237,40.3338829081285,
40.4430298278223,40.5518710897036,40.6605292202185,40.7689635853024,40.8407044966672),
 .UNSPECIFIED.);
#588=B_SPLINE_CURVE_WITH_KNOTS('',3,(#51658,#51659,#51660,#51661,#51662,
#51663,#51664,#51665),.UNSPECIFIED.,.F.,.F.,(4,1,1,1,1,4),(30.4995607225879,
30.8146221585521,31.8121506929887,32.8096792274253,33.8072077618619,34.5575191894876),
 .UNSPECIFIED.);
#589=B_SPLINE_CURVE_WITH_KNOTS('',3,(#51666,#51667,#51668,#51669,#51670,
#51671,#51672,#51673,#51674,#51675,#51676,#51677,#51678,#51679,#51680,#51681,
#51682,#51683,#51684,#51685,#51686,#51687,#51688,#51689,#51690,#51691,#51692,
#51693,#51694,#51695,#51696,#51697,#51698,#51699,#51700,#51701,#51702,#51703,
#51704,#51705,#51706,#51707,#51708,#51709,#51710,#51711,#51712,#51713,#51714,
#51715,#51716,#51717,#51718,#51719,#51720,#51721,#51722,#51723,#51724,#51725,
#51726,#51727,#51728,#51729,#51730,#51731,#51732),.UNSPECIFIED.,.F.,.F.,
(4,3,3,3,3,3,3,3,3,3,3,3,3,3,3,3,3,3,3,3,3,3,4),(34.5575192801504,34.6928923433788,
34.8047362962985,34.9089227161898,35.0129539035213,35.116863062321,35.2207067659762,
35.3245197931666,35.4283368791399,35.5322626332934,35.6362472310269,35.7404137535359,
35.8022648307351,35.9064523898748,36.0104843838919,36.1143930799466,36.2182358499137,
36.3220474727609,36.4258626833867,36.5297810949895,36.6337581570599,36.7379046758095,
36.7834620528982),.UNSPECIFIED.);
#590=B_SPLINE_CURVE_WITH_KNOTS('',3,(#51734,#51735,#51736,#51737,#51738,
#51739,#51740,#51741,#51742,#51743,#51744,#51745,#51746,#51747,#51748,#51749,
#51750,#51751,#51752,#51753,#51754,#51755,#51756,#51757,#51758,#51759,#51760,
#51761,#51762,#51763,#51764,#51765,#51766,#51767,#51768,#51769,#51770,#51771,
#51772,#51773,#51774,#51775,#51776,#51777,#51778,#51779,#51780,#51781,#51782,
#51783,#51784,#51785,#51786,#51787,#51788,#51789,#51790,#51791,#51792,#51793,
#51794,#51795,#51796,#51797,#51798,#51799,#51800,#51801,#51802,#51803),
 .UNSPECIFIED.,.F.,.F.,(4,3,3,3,3,3,3,3,3,3,3,3,3,3,3,3,3,3,3,3,3,3,3,4),
(34.5575191899647,34.6600276259523,34.7624524502431,34.8648302680991,34.9671976162021,
35.0696598730461,35.1721712758146,35.2748625475711,35.3462402359455,35.4504266548286,
35.5544578411485,35.658366998936,35.7622107015796,35.8660237277603,35.9698408127272,
36.0737665658867,36.1777511626315,36.2819176841713,36.3437687703821,36.4479637269223,
36.5519784416308,36.6558896246249,36.75972644537,36.7837376627694),
 .UNSPECIFIED.);
#591=B_SPLINE_CURVE_WITH_KNOTS('',3,(#51804,#51805,#51806,#51807,#51808,
#51809,#51810,#51811,#51812,#51813,#51814,#51815,#51816,#51817,#51818,#51819,
#51820,#51821,#51822,#51823,#51824,#51825,#51826,#51827,#51828,#51829,#51830,
#51831,#51832,#51833,#51834,#51835,#51836,#51837,#51838,#51839,#51840,#51841,
#51842,#51843,#51844,#51845,#51846,#51847,#51848,#51849,#51850,#51851,#51852,
#51853,#51854,#51855,#51856,#51857,#51858,#51859,#51860,#51861,#51862,#51863,
#51864,#51865,#51866,#51867,#51868,#51869,#51870,#51871,#51872,#51873,#51874,
#51875,#51876,#51877,#51878,#51879,#51880,#51881,#51882,#51883,#51884,#51885,
#51886,#51887,#51888,#51889,#51890,#51891,#51892,#51893,#51894,#51895,#51896,
#51897,#51898,#51899,#51900,#51901,#51902,#51903,#51904,#51905,#51906,#51907,
#51908,#51909,#51910,#51911,#51912,#51913,#51914,#51915,#51916,#51917,#51918,
#51919,#51920,#51921,#51922,#51923,#51924,#51925,#51926,#51927),
 .UNSPECIFIED.,.F.,.F.,(4,3,3,3,3,3,3,3,3,3,3,3,3,3,3,3,3,3,3,3,3,3,3,3,
3,3,3,3,3,3,3,3,3,3,3,3,3,3,3,3,3,4),(30.5009126726331,30.6078143508288,
30.7116934740814,30.815520868173,30.9193312905574,31.0285299924679,31.1324780670269,
31.2364989095826,31.3406881250854,31.3561260981991,31.4603125441236,31.5643437578127,
31.6682529433233,31.7720966738931,31.8759097281617,31.9797268413366,32.0836526226934,
32.1876372476719,32.2918037971965,32.3536546326357,32.4578410516562,32.5618722381836,
32.6657813962831,32.769625099303,32.8734381259239,32.9772552113946,33.0811809651525,
33.1851655625499,33.2893320848217,33.3511831670723,33.4553695791772,33.5594007585792,
33.6633099092749,33.7671536047227,33.8709666236145,33.9747837012098,34.0787094469216,
34.1826940361645,34.2868605501974,34.3487117015089,34.4945927786811,34.5575191894876),
 .UNSPECIFIED.);
#592=B_SPLINE_CURVE_WITH_KNOTS('',3,(#51933,#51934,#51935,#51936,#51937,
#51938,#51939,#51940),.UNSPECIFIED.,.F.,.F.,(4,1,1,1,1,4),(24.2177548267501,
24.8294509519325,25.8269794863691,26.8245080208057,27.8220365552423,28.274333882308),
 .UNSPECIFIED.);
#593=B_SPLINE_CURVE_WITH_KNOTS('',3,(#51941,#51942,#51943,#51944,#51945,
#51946),.UNSPECIFIED.,.F.,.F.,(4,1,1,4),(28.274333882308,28.8195650896789,
29.8170936241155,30.4995607225879),.UNSPECIFIED.);
#594=B_SPLINE_CURVE_WITH_KNOTS('',3,(#51948,#51949,#51950,#51951,#51952,
#51953,#51954,#51955,#51956,#51957,#51958,#51959,#51960,#51961,#51962,#51963,
#51964,#51965,#51966,#51967,#51968,#51969,#51970,#51971,#51972,#51973,#51974,
#51975,#51976,#51977,#51978,#51979,#51980,#51981,#51982,#51983,#51984,#51985,
#51986,#51987,#51988,#51989,#51990,#51991,#51992,#51993,#51994,#51995,#51996,
#51997,#51998,#51999,#52000,#52001,#52002,#52003,#52004,#52005,#52006,#52007,
#52008,#52009,#52010,#52011,#52012,#52013,#52014,#52015,#52016,#52017),
 .UNSPECIFIED.,.F.,.F.,(4,3,3,3,3,3,3,3,3,3,3,3,3,3,3,3,3,3,3,3,3,3,3,4),
(28.2743338823081,28.3635404948893,28.4677270806907,28.5717584358195,28.6756677644013,
28.779511638971,28.883324837953,28.9871420963408,29.0910680226713,29.1950527927073,
29.2992194858461,29.3610690293259,29.4652554639064,29.569286666705,29.6731958420586,
29.777039562931,29.8808526079774,29.984669712422,30.0885954858662,30.1925801033819,
30.2967466462425,30.3585975637625,30.4627747018241,30.5009126726331),
 .UNSPECIFIED.);
#595=B_SPLINE_CURVE_WITH_KNOTS('',3,(#52018,#52019,#52020,#52021,#52022,
#52023,#52024,#52025),.UNSPECIFIED.,.F.,.F.,(4,1,1,1,1,4),(24.2163931842857,
24.3734263571429,25.3709548915795,26.3684834260161,27.3660119604527,28.2743252313376),
 .UNSPECIFIED.);
#596=B_SPLINE_CURVE_WITH_KNOTS('',3,(#52031,#52032,#52033,#52034,#52035,
#52036),.UNSPECIFIED.,.F.,.F.,(4,1,1,4),(15.7079632679489,16.3931980816501,
17.3907266160867,17.9337012577548),.UNSPECIFIED.);
#597=B_SPLINE_CURVE_WITH_KNOTS('',3,(#52038,#52039,#52040,#52041,#52042),
 .UNSPECIFIED.,.F.,.F.,(4,1,4),(14.3981410127769,15.3956695472135,15.7079632679489),
 .UNSPECIFIED.);
#598=B_SPLINE_CURVE_WITH_KNOTS('',3,(#52046,#52047,#52048,#52049,#52050,
#52051,#52052,#52053,#52054,#52055,#52056,#52057,#52058,#52059,#52060,#52061,
#52062,#52063,#52064,#52065,#52066,#52067,#52068,#52069,#52070,#52071,#52072,
#52073,#52074,#52075,#52076,#52077,#52078,#52079,#52080,#52081,#52082,#52083,
#52084,#52085,#52086,#52087,#52088,#52089,#52090,#52091,#52092,#52093,#52094,
#52095,#52096,#52097,#52098,#52099,#52100,#52101,#52102,#52103),
 .UNSPECIFIED.,.F.,.F.,(4,3,3,3,3,3,3,3,3,3,3,3,3,3,3,3,3,3,3,4),(13.8761928828999,
13.9801649720632,14.0894150515011,14.1931072386484,14.296736927948,14.4003392051333,
14.5039491154842,14.6076671378982,14.7114479052023,14.8153999666522,14.8541656075665,
14.9608903151143,15.0635176111712,15.1660512775799,15.2685278719585,15.3709838699761,
15.4735074808561,15.5760720021476,15.6787728795733,15.7079632679489),
 .UNSPECIFIED.);
#599=B_SPLINE_CURVE_WITH_KNOTS('',3,(#52104,#52105,#52106,#52107,#52108,
#52109,#52110),.UNSPECIFIED.,.F.,.F.,(4,1,1,1,4),(15.7079632679489,15.8516941420031,
16.8492226764397,17.8467512108763,17.9345079337947),.UNSPECIFIED.);
#600=B_SPLINE_CURVE_WITH_KNOTS('',3,(#52116,#52117,#52118,#52119,#52120,
#52121,#52122,#52123,#52124,#52125,#52126,#52127,#52128,#52129,#52130,#52131,
#52132,#52133,#52134,#52135,#52136,#52137,#52138,#52139,#52140,#52141,#52142,
#52143,#52144,#52145,#52146,#52147,#52148,#52149,#52150,#52151,#52152,#52153,
#52154,#52155,#52156,#52157,#52158,#52159,#52160,#52161,#52162,#52163,#52164,
#52165,#52166,#52167,#52168,#52169,#52170,#52171,#52172,#52173,#52174,#52175,
#52176,#52177,#52178,#52179,#52180,#52181,#52182,#52183,#52184,#52185,#52186,
#52187,#52188,#52189,#52190,#52191,#52192,#52193,#52194,#52195,#52196,#52197,
#52198,#52199,#52200,#52201,#52202,#52203,#52204,#52205,#52206,#52207,#52208,
#52209,#52210,#52211,#52212,#52213,#52214,#52215,#52216,#52217,#52218,#52219,
#52220,#52221,#52222,#52223,#52224,#52225,#52226,#52227,#52228,#52229,#52230,
#52231,#52232,#52233,#52234,#52235,#52236,#52237,#52238,#52239,#52240,#52241,
#52242,#52243,#52244,#52245,#52246,#52247,#52248,#52249,#52250,#52251),
 .UNSPECIFIED.,.F.,.F.,(4,3,3,3,3,3,3,3,3,3,3,3,3,3,3,3,3,3,3,3,3,3,3,3,
3,3,3,3,3,3,3,3,3,3,3,3,3,3,3,3,3,3,3,3,3,4),(95.9108836822778,96.0202873100601,
96.1295970836597,96.2388539961436,96.3480989644021,96.4574524049631,96.5668605200234,
96.6764760888946,96.7602678403501,96.870274343827,96.981214597697,97.0909160403511,
97.2005489408146,97.3101536583972,97.4220643374946,97.5318017309419,97.6447990528643,
97.7577963747867,97.8677427759327,97.978690542594,98.088340801476,98.1979259593122,
98.3074864207066,98.4194460428358,98.529148157587,98.6422365334051,98.7553249092233,
98.863931659696,98.9750468826915,99.0833537633358,99.1915974508863,99.2998202680834,
99.4130785619775,99.5214671674737,99.6299441469002,99.7386243094718,99.7528534436599,
99.8657192639262,99.9783447484258,100.090828298591,100.203203130945,100.315502311895,
100.42779296924,100.54006917202,100.652430269464,100.750381978097),
 .UNSPECIFIED.);
#601=B_SPLINE_CURVE_WITH_KNOTS('',3,(#52255,#52256,#52257,#52258,#52259,
#52260,#52261,#52262,#52263,#52264),.UNSPECIFIED.,.F.,.F.,(4,3,3,4),(-98.7357640758916,
-98.6263458761001,-98.5171144442792,-98.4464074264151),.UNSPECIFIED.);
#602=B_SPLINE_CURVE_WITH_KNOTS('',3,(#52269,#52270,#52271,#52272,#52273,
#52274,#52275,#52276,#52277,#52278,#52279,#52280,#52281),.UNSPECIFIED.,
 .F.,.F.,(4,3,3,3,4),(-98.4464074264151,-98.3373449196508,-98.228335758133,
-98.1193172715618,-98.094162871386),.UNSPECIFIED.);
#603=B_SPLINE_CURVE_WITH_KNOTS('',3,(#52282,#52283,#52284,#52285,#52286,
#52287,#52288,#52289,#52290,#52291,#52292,#52293,#52294,#52295,#52296,#52297,
#52298,#52299,#52300,#52301,#52302,#52303,#52304,#52305,#52306,#52307,#52308,
#52309,#52310,#52311,#52312,#52313,#52314,#52315,#52316,#52317,#52318,#52319,
#52320,#52321,#52322,#52323,#52324,#52325,#52326,#52327,#52328,#52329,#52330,
#52331,#52332,#52333,#52334,#52335,#52336,#52337,#52338,#52339,#52340,#52341,
#52342,#52343,#52344,#52345,#52346,#52347,#52348,#52349,#52350,#52351,#52352,
#52353,#52354,#52355,#52356,#52357,#52358,#52359,#52360,#52361,#52362,#52363,
#52364,#52365,#52366,#52367,#52368,#52369,#52370,#52371,#52372,#52373,#52374,
#52375,#52376,#52377,#52378,#52379,#52380,#52381,#52382,#52383,#52384,#52385,
#52386,#52387,#52388,#52389,#52390,#52391,#52392,#52393,#52394,#52395,#52396,
#52397,#52398,#52399,#52400,#52401,#52402,#52403,#52404,#52405,#52406,#52407,
#52408,#52409,#52410,#52411,#52412,#52413,#52414,#52415,#52416,#52417,#52418,
#52419,#52420,#52421,#52422,#52423,#52424,#52425,#52426,#52427,#52428,#52429,
#52430,#52431,#52432,#52433,#52434,#52435,#52436,#52437,#52438,#52439,#52440,
#52441,#52442,#52443,#52444),.UNSPECIFIED.,.F.,.F.,(4,3,3,3,3,3,3,3,3,3,
3,3,3,3,3,3,3,3,3,3,3,3,3,3,3,3,3,3,3,3,3,3,3,3,3,3,3,3,3,3,3,3,3,3,3,3,
3,3,3,3,3,3,3,3,4),(-98.0941628710682,-97.96814081787,-97.8409325597495,
-97.7577963747867,-97.6478110000828,-97.5368681051162,-97.4271754338014,
-97.3175466708406,-97.2079414641239,-97.0960230581805,-96.9862737960981,
-96.8732708182241,-96.7602678403501,-96.6506201762776,-96.5396350674821,
-96.4302948044108,-96.3210229586511,-96.2117785902267,-96.0995187691484,
-95.9901358924464,-95.8764375991799,-95.7627393059135,-95.6529127814426,
-95.5419500301969,-95.4324257238689,-95.3229684069732,-95.2135374400353,
-95.1014557728957,-94.991885638747,-94.8785482051119,-94.7652107714769,
-94.6553934240873,-94.5444295257064,-94.4349133954284,-94.3254638552065,
-94.2160402511401,-94.1039507476152,-93.9943868569596,-93.881034547,-93.7676822370403,
-93.6579087468788,-93.5469393663444,-93.4374690990798,-93.3280660442032,
-93.2186894719818,-93.1065555296373,-92.9970394857318,-92.8835965941678,
-92.7701537026037,-92.6610396721199,-92.5520859975439,-92.4432521481903,
-92.3344888111749,-92.2257252315868,-92.1641970933112),.UNSPECIFIED.);
#604=B_SPLINE_CURVE_WITH_KNOTS('',3,(#52450,#52451,#52452,#52453,#52454,
#52455,#52456,#52457,#52458,#52459,#52460,#52461,#52462,#52463,#52464,#52465,
#52466,#52467,#52468,#52469,#52470,#52471,#52472,#52473,#52474,#52475,#52476,
#52477,#52478,#52479,#52480,#52481,#52482,#52483,#52484,#52485,#52486,#52487,
#52488,#52489,#52490,#52491,#52492,#52493,#52494,#52495,#52496,#52497,#52498,
#52499,#52500,#52501,#52502,#52503,#52504,#52505,#52506,#52507,#52508,#52509,
#52510,#52511,#52512,#52513,#52514,#52515,#52516,#52517,#52518,#52519,#52520,
#52521,#52522,#52523,#52524,#52525,#52526,#52527,#52528,#52529,#52530,#52531,
#52532,#52533,#52534,#52535,#52536,#52537,#52538,#52539,#52540,#52541,#52542,
#52543,#52544,#52545,#52546,#52547,#52548,#52549,#52550,#52551,#52552,#52553,
#52554,#52555,#52556,#52557,#52558,#52559,#52560,#52561,#52562,#52563,#52564,
#52565,#52566,#52567,#52568,#52569,#52570,#52571,#52572,#52573,#52574,#52575,
#52576,#52577,#52578,#52579,#52580,#52581,#52582,#52583,#52584,#52585,#52586,
#52587,#52588,#52589,#52590,#52591,#52592,#52593,#52594,#52595,#52596,#52597,
#52598,#52599,#52600,#52601,#52602,#52603,#52604,#52605,#52606,#52607,#52608,
#52609,#52610,#52611,#52612,#52613,#52614,#52615),.UNSPECIFIED.,.F.,.F.,
(4,3,3,3,3,3,3,3,3,3,3,3,3,3,3,3,3,3,3,3,3,3,3,3,3,3,3,3,3,3,3,3,3,3,3,
3,3,3,3,3,3,3,3,3,3,3,3,3,3,3,3,3,3,3,3,4),(89.6265168405702,89.7416999786078,
89.7775680992939,89.8873597387442,89.9983268506175,90.1078160365984,90.2172382449346,
90.326634173892,90.4387497888516,90.5482854700897,90.6616910519101,90.7750966337305,
90.8848943530555,90.9958607049444,91.1053559024537,91.2147840805338,91.3241859281211,
91.4362957381326,91.5458371451358,91.6592311566515,91.7726251681671,91.8824260289159,
91.9933919881269,92.1028905104742,92.2123220720462,92.3217273557269,92.4338339424461,
92.5433788739247,92.6567662882642,92.7701537026037,92.8799258782005,92.9908954230555,
93.1003651299235,93.2097679068537,93.3191444831736,93.4312789216403,93.5407956652934,
93.6542389511669,93.7676822370403,93.8775024156856,93.9884659601595,94.0979832706209,
94.2074333726056,94.3168569209728,94.4289453835988,94.538507696895,94.651859234186,
94.7652107714769,94.8734085310505,94.9814556744687,95.089395275171,95.1972702333879,
95.305166435024,95.4130758431646,95.5210990899593,95.5576018624958),
 .UNSPECIFIED.);
#605=B_SPLINE_CURVE_WITH_KNOTS('',3,(#52616,#52617,#52618,#52619,#52620,
#52621,#52622,#52623,#52624,#52625,#52626,#52627,#52628),.UNSPECIFIED.,
 .F.,.F.,(4,3,3,3,4),(95.5576018628657,95.7133781757262,95.7627393059135,
95.8723662565049,95.9108836822778),.UNSPECIFIED.);
#606=B_SPLINE_CURVE_WITH_KNOTS('',3,(#52630,#52631,#52632,#52633,#52634,
#52635,#52636,#52637,#52638,#52639,#52640,#52641,#52642),.UNSPECIFIED.,
 .F.,.F.,(4,3,3,3,4),(-92.1641970933112,-92.0553357947036,-91.9464069945238,
-91.8372961626777,-91.8109778956704),.UNSPECIFIED.);
#607=B_SPLINE_CURVE_WITH_KNOTS('',3,(#52643,#52644,#52645,#52646,#52647,
#52648,#52649,#52650,#52651,#52652),.UNSPECIFIED.,.F.,.F.,(4,1,1,1,1,1,
1,4),(-91.8109775642065,-91.7726251681671,-90.7750966337305,-89.7775680992939,
-88.7800395648573,-87.7825110304207,-86.7849824959841,-85.8810642303289),
 .UNSPECIFIED.);
#608=B_SPLINE_CURVE_WITH_KNOTS('',3,(#52658,#52659,#52660,#52661,#52662,
#52663,#52664,#52665,#52666,#52667,#52668,#52669,#52670,#52671,#52672,#52673,
#52674,#52675,#52676,#52677,#52678,#52679,#52680,#52681,#52682,#52683,#52684,
#52685,#52686,#52687,#52688,#52689,#52690,#52691,#52692,#52693,#52694,#52695,
#52696,#52697,#52698,#52699,#52700,#52701,#52702,#52703,#52704,#52705,#52706,
#52707,#52708,#52709,#52710,#52711,#52712,#52713,#52714,#52715,#52716,#52717,
#52718,#52719,#52720,#52721,#52722,#52723,#52724,#52725,#52726,#52727,#52728,
#52729,#52730,#52731,#52732,#52733,#52734,#52735,#52736,#52737,#52738,#52739,
#52740,#52741,#52742,#52743,#52744,#52745,#52746,#52747,#52748,#52749,#52750,
#52751,#52752,#52753,#52754,#52755,#52756,#52757,#52758,#52759,#52760,#52761,
#52762,#52763,#52764,#52765,#52766,#52767,#52768,#52769,#52770,#52771,#52772,
#52773,#52774,#52775,#52776,#52777,#52778,#52779,#52780,#52781,#52782,#52783,
#52784,#52785,#52786,#52787,#52788,#52789,#52790,#52791,#52792,#52793,#52794,
#52795,#52796,#52797,#52798,#52799,#52800,#52801,#52802,#52803,#52804,#52805,
#52806,#52807,#52808,#52809,#52810,#52811,#52812,#52813,#52814,#52815,#52816,
#52817,#52818,#52819,#52820,#52821,#52822,#52823,#52824,#52825,#52826,#52827,
#52828,#52829,#52830,#52831,#52832,#52833,#52834,#52835,#52836,#52837,#52838,
#52839,#52840,#52841,#52842,#52843,#52844,#52845,#52846,#52847,#52848,#52849,
#52850,#52851,#52852,#52853),.UNSPECIFIED.,.F.,.F.,(4,2,2,2,2,2,2,2,2,2,
2,2,2,2,2,2,2,2,2,2,2,2,2,2,2,2,2,2,2,2,2,2,2,2,2,2,2,2,2,2,2,2,2,2,2,2,
2,2,2,2,2,2,2,2,2,2,2,2,2,2,2,2,2,2,2,2,2,2,2,2,2,2,2,2,2,2,2,2,2,2,2,2,
2,2,2,2,2,2,2,2,2,2,2,2,2,2,2,4),(-0.991236153398999,-0.990017865976998,
-0.964607879434727,-0.943939536477733,-0.922340595067815,-0.91885741669439,
-0.916924820957,-0.915292113581256,-0.913130929280484,-0.908382445715242,
-0.886866887530864,-0.847302037237583,-0.838963004043493,-0.835172705929818,
-0.83222782939185,-0.829008582358732,-0.823744300259359,-0.802366888533965,
-0.781707146913141,-0.775200231778021,-0.755609484870657,-0.752164588709421,
-0.750240610566901,-0.748606734880102,-0.746432954453861,-0.741614150301461,
-0.734848095536509,-0.714847540287023,-0.678606366608066,-0.672285034585661,
-0.668505018026553,-0.665561651923485,-0.662337497142246,-0.657050020559074,
-0.635291539871278,-0.604902387260126,-0.588774647522847,-0.585428344628336,
-0.583526493905173,-0.582038967196741,-0.579918876560076,-0.575393286400109,
-0.556033025010661,-0.522722974749949,-0.508051222584194,-0.503202641130385,
-0.500072158908907,-0.497092601997238,-0.493012007878406,-0.483182245670826,
-0.468851008500812,-0.448369897731706,-0.442067401786093,-0.42232462769962,
-0.418875902185947,-0.41695111693077,-0.41531747189453,-0.413145182831603,
-0.408334228069118,-0.401582738643682,-0.381657016717515,-0.345307233686974,
-0.338992396615969,-0.335214346322189,-0.332271413861628,-0.329046622193269,
-0.323755526239595,-0.301932589169151,-0.271249539362225,-0.255458224900243,
-0.252129948707979,-0.25023224562982,-0.248744110519532,-0.246618113211251,
-0.242060270886421,-0.222397340509815,-0.188245937030999,-0.174547669159655,
-0.169803535366404,-0.166695138592338,-0.163918924956194,-0.160999925688576,
-0.153812070139955,-0.144424563473928,-0.119742431598706,-0.0909134879582886,
-0.0862462850030538,-0.0841228543318537,-0.0824756176659709,-0.0805358393016943,
-0.0769189482045256,-0.0722721498534541,-0.0613630431171712,-0.0268129717864068,
-0.00882475856751817,-0.00411511755648563,-0.00192617516552268,-0.000492596523146994),
 .UNSPECIFIED.);
#609=B_SPLINE_CURVE_WITH_KNOTS('',3,(#52854,#52855,#52856,#52857,#52858,
#52859,#52860,#52861,#52862,#52863),.UNSPECIFIED.,.F.,.F.,(4,3,3,4),(89.2744165556861,
89.3888571977691,89.5076870191697,89.6265168405702),.UNSPECIFIED.);
#610=B_SPLINE_CURVE_WITH_KNOTS('',3,(#52865,#52866,#52867,#52868,#52869),
 .UNSPECIFIED.,.F.,.F.,(4,1,4),(-85.8810642303289,-85.7874539615475,-85.5277947543664),
 .UNSPECIFIED.);
#611=B_SPLINE_CURVE_WITH_KNOTS('',3,(#52870,#52871,#52872,#52873,#52874,
#52875,#52876,#52877,#52878,#52879,#52880,#52881,#52882,#52883,#52884,#52885,
#52886,#52887,#52888,#52889,#52890,#52891,#52892,#52893,#52894,#52895,#52896,
#52897,#52898,#52899,#52900,#52901,#52902,#52903,#52904,#52905,#52906,#52907,
#52908,#52909,#52910,#52911,#52912,#52913,#52914,#52915,#52916,#52917,#52918,
#52919,#52920,#52921,#52922,#52923,#52924,#52925,#52926,#52927,#52928,#52929,
#52930,#52931,#52932,#52933,#52934,#52935,#52936,#52937,#52938,#52939,#52940,
#52941,#52942,#52943,#52944,#52945,#52946,#52947,#52948,#52949,#52950,#52951,
#52952,#52953,#52954,#52955,#52956,#52957,#52958,#52959,#52960,#52961,#52962,
#52963,#52964,#52965,#52966,#52967,#52968,#52969,#52970,#52971,#52972,#52973,
#52974,#52975,#52976,#52977,#52978,#52979,#52980,#52981,#52982,#52983,#52984,
#52985,#52986,#52987,#52988,#52989,#52990,#52991,#52992,#52993,#52994,#52995,
#52996,#52997,#52998,#52999,#53000,#53001,#53002,#53003,#53004,#53005,#53006,
#53007,#53008,#53009,#53010,#53011,#53012,#53013,#53014,#53015,#53016,#53017,
#53018,#53019,#53020,#53021,#53022,#53023,#53024,#53025,#53026,#53027,#53028,
#53029,#53030,#53031,#53032,#53033,#53034,#53035,#53036,#53037,#53038,#53039,
#53040,#53041,#53042,#53043,#53044,#53045,#53046,#53047,#53048,#53049,#53050,
#53051,#53052,#53053,#53054,#53055,#53056,#53057,#53058,#53059,#53060,#53061,
#53062,#53063,#53064,#53065,#53066,#53067),.UNSPECIFIED.,.F.,.F.,(4,2,2,
2,2,2,2,2,2,2,2,2,2,2,2,2,2,2,2,2,2,2,2,2,2,2,2,2,2,2,2,2,2,2,2,2,2,2,2,
2,2,2,2,2,2,2,2,2,2,2,2,2,2,2,2,2,2,2,2,2,2,2,2,2,2,2,2,2,2,2,2,2,2,2,2,
2,2,2,2,2,2,2,2,2,2,2,2,2,2,2,2,2,2,2,2,2,2,2,4),(-2.10007152061629,-2.0785364363192,
-2.06876879443929,-2.06502723271782,-2.06215732255702,-2.05921404607757,
-2.05598824670138,-2.05069402147021,-2.03118054673824,-2.00235696093729,
-1.98395474968524,-1.97974526720886,-1.97762987828826,-1.97614281246107,
-1.97423760999817,-1.97087673633506,-1.95440479701274,-1.92475158618459,
-1.91005468091917,-1.90004862616664,-1.89594033809507,-1.89295588930762,
-1.88983397620689,-1.88502666320277,-1.87074353320602,-1.83712252901638,
-1.81765266149352,-1.81311512035469,-1.81099274588001,-1.80950487068175,
-1.80760434937467,-1.80426421072928,-1.78830678225958,-1.75774075509178,
-1.73594359349288,-1.73065335347535,-1.7274285024067,-1.72448514336714,
-1.72070602457934,-1.71438825398602,-1.67812384382059,-1.65816570442503,
-1.65140813162939,-1.64659340759779,-1.64442030513839,-1.64278642186039,
-1.64086183814362,-1.63741442463673,-1.61774086211831,-1.61091935796612,
-1.58934289314332,-1.57589480595146,-1.56650337691086,-1.56249273044517,
-1.55952460204975,-1.55636969220717,-1.55140653185989,-1.53567471638681,
-1.50330150153963,-1.48428216903819,-1.47979338804293,-1.47768013943784,
-1.47619333302005,-1.47428671986486,-1.47091952137281,-1.45431269890522,
-1.42472988080548,-1.40267757024358,-1.39737216894697,-1.39414406265657,
-1.3912015888965,-1.38742894494581,-1.38113410054262,-1.34447867491172,
-1.32477939660341,-1.31807187240799,-1.3132839097142,-1.31111561939044,
-1.30946745101539,-1.30753341744949,-1.30404363491216,-1.28090286767243,
-1.26369671357128,-1.23877829312778,-1.23190785859255,-1.22835316959585,
-1.22571934640295,-1.22241412492548,-1.21674873049364,-1.18586948899327,
-1.16100699126578,-1.15264414030638,-1.14700762821841,-1.14469491349508,
-1.14302837901843,-1.14117530047933,-1.13796378017104,-1.12482076840509,
-1.10917023491673),.UNSPECIFIED.);
#612=B_SPLINE_CURVE_WITH_KNOTS('',3,(#53072,#53073,#53074,#53075,#53076,
#53077,#53078,#53079,#53080,#53081,#53082,#53083,#53084,#53085,#53086,#53087,
#53088,#53089,#53090,#53091,#53092,#53093,#53094,#53095,#53096,#53097,#53098,
#53099,#53100,#53101,#53102,#53103,#53104,#53105,#53106,#53107,#53108,#53109,
#53110,#53111,#53112,#53113,#53114,#53115,#53116,#53117,#53118,#53119,#53120,
#53121,#53122,#53123,#53124,#53125,#53126,#53127,#53128,#53129,#53130,#53131,
#53132,#53133,#53134,#53135,#53136,#53137,#53138,#53139,#53140,#53141,#53142,
#53143,#53144,#53145,#53146,#53147,#53148,#53149,#53150,#53151,#53152,#53153,
#53154,#53155,#53156,#53157,#53158,#53159,#53160,#53161,#53162,#53163,#53164,
#53165,#53166,#53167,#53168,#53169,#53170,#53171,#53172,#53173,#53174,#53175,
#53176,#53177,#53178,#53179,#53180,#53181,#53182,#53183,#53184,#53185,#53186,
#53187,#53188,#53189,#53190,#53191,#53192,#53193,#53194,#53195,#53196,#53197,
#53198,#53199,#53200,#53201,#53202,#53203,#53204,#53205,#53206,#53207,#53208,
#53209,#53210,#53211,#53212,#53213,#53214,#53215,#53216,#53217,#53218,#53219,
#53220,#53221,#53222,#53223,#53224,#53225,#53226,#53227,#53228,#53229,#53230,
#53231,#53232,#53233,#53234,#53235,#53236,#53237,#53238,#53239,#53240,#53241,
#53242,#53243,#53244,#53245,#53246,#53247,#53248,#53249,#53250,#53251,#53252,
#53253,#53254,#53255,#53256,#53257,#53258,#53259,#53260,#53261,#53262,#53263,
#53264,#53265,#53266,#53267,#53268,#53269,#53270,#53271,#53272,#53273,#53274,
#53275,#53276,#53277),.UNSPECIFIED.,.F.,.F.,(4,2,2,2,2,2,2,2,2,2,2,2,2,
2,2,2,2,2,2,2,2,2,2,2,2,2,2,2,2,2,2,2,2,2,2,2,2,2,2,2,2,2,2,2,2,2,2,2,2,
2,2,2,2,2,2,2,2,2,2,2,2,2,2,2,2,2,2,2,2,2,2,2,2,2,2,2,2,2,2,2,2,2,2,2,2,
2,2,2,2,2,2,2,2,2,2,2,2,2,2,2,2,2,4),(-2.04110855067476,-2.03076381586652,
-2.0089897584076,-2.00370085006763,-2.00047627473838,-1.99753282492654,
-1.99375311899073,-1.98743331218493,-1.95119882772989,-1.9227955618766,
-1.91903491361895,-1.91706514786033,-1.91542090533246,-1.91330183013505,
-1.9087821044297,-1.87733516721823,-1.84328564492068,-1.8374611115415,-1.83412207505555,
-1.83120008618467,-1.82755386181497,-1.82045488802992,-1.79003848636111,
-1.76583945065451,-1.75833314785634,-1.75312652038043,-1.75088491962852,
-1.74922852743731,-1.74733944422112,-1.74404971753485,-1.72886487565409,
-1.69991045873406,-1.68066422640008,-1.67235630589557,-1.66853045390329,
-1.66558949205946,-1.66235617697529,-1.65702615309848,-1.63683232564857,
-1.59348012562206,-1.58694185735254,-1.5844926639368,-1.58280268163173,
-1.5810039402212,-1.57804075298967,-1.56789594052795,-1.5614471595886,-1.53077701651864,
-1.50895423388436,-1.50366243583937,-1.50043725944239,-1.49749401035757,
-1.49371560151973,-1.48740032500443,-1.45108553155655,-1.43115839232335,
-1.42440671967328,-1.41959513566273,-1.41742260217782,-1.41578878496851,
-1.41386385492518,-1.41041487609998,-1.39068210556499,-1.3843349556325,
-1.36377373663007,-1.34226063994424,-1.33698756646965,-1.33376636446422,
-1.33082192576004,-1.32703529271342,-1.31871741782793,-1.27915109257104,
-1.25763989993403,-1.25289175908312,-1.25073061963213,-1.24909788341911,
-1.24716521061065,-1.24368172671001,-1.22210948972152,-1.21796305475088,
-1.19793272430067,-1.18314095768735,-1.1730891574056,-1.16897367766887,
-1.16598788307167,-1.16323883382283,-1.15948784036015,-1.15190960686635,
-1.1124401334353,-1.09095944765144,-1.08621421578381,-1.08405354553322,
-1.0824207897418,-1.08048764160776,-1.07700226613155,-1.05522095651838,
-1.05034361097503,-1.01159072374133,-1.00545858411251,-1.00169182335993,
-0.998757891544168,-0.99549323853491,-0.991236153398999),.UNSPECIFIED.);
#613=B_SPLINE_CURVE_WITH_KNOTS('',3,(#53278,#53279,#53280,#53281,#53282,
#53283,#53284,#53285,#53286,#53287,#53288,#53289,#53290,#53291,#53292,#53293,
#53294,#53295,#53296,#53297,#53298,#53299,#53300,#53301,#53302,#53303,#53304,
#53305,#53306,#53307,#53308,#53309,#53310,#53311,#53312,#53313,#53314,#53315,
#53316,#53317,#53318,#53319,#53320,#53321,#53322,#53323,#53324,#53325,#53326,
#53327,#53328,#53329,#53330,#53331,#53332,#53333,#53334,#53335,#53336,#53337,
#53338,#53339,#53340,#53341,#53342,#53343,#53344,#53345,#53346,#53347,#53348,
#53349,#53350,#53351,#53352,#53353,#53354,#53355,#53356,#53357,#53358,#53359,
#53360,#53361,#53362,#53363,#53364,#53365,#53366,#53367,#53368,#53369,#53370,
#53371,#53372,#53373,#53374,#53375,#53376,#53377,#53378,#53379,#53380,#53381,
#53382,#53383,#53384,#53385,#53386,#53387,#53388,#53389,#53390,#53391,#53392,
#53393,#53394,#53395,#53396,#53397,#53398,#53399,#53400,#53401,#53402,#53403,
#53404,#53405,#53406,#53407,#53408,#53409,#53410,#53411,#53412,#53413,#53414,
#53415,#53416,#53417,#53418,#53419,#53420,#53421,#53422,#53423,#53424,#53425,
#53426,#53427,#53428,#53429,#53430,#53431,#53432,#53433,#53434,#53435,#53436,
#53437,#53438,#53439,#53440,#53441,#53442,#53443,#53444,#53445,#53446,#53447,
#53448,#53449,#53450,#53451,#53452,#53453,#53454,#53455,#53456,#53457,#53458,
#53459,#53460,#53461,#53462,#53463,#53464,#53465,#53466,#53467,#53468,#53469,
#53470,#53471,#53472,#53473,#53474,#53475,#53476,#53477,#53478,#53479,#53480,
#53481,#53482,#53483,#53484,#53485),.UNSPECIFIED.,.F.,.F.,(4,2,2,2,2,2,
2,2,2,2,2,2,2,2,2,2,2,2,2,2,2,2,2,2,2,2,2,2,2,2,2,2,2,2,2,2,2,2,2,2,2,2,
2,2,2,2,2,2,2,2,2,2,2,2,2,2,2,2,2,2,2,2,2,2,2,2,2,2,2,2,2,2,2,2,2,2,2,2,
2,2,2,2,2,2,2,2,2,2,2,2,2,2,2,2,2,2,2,2,2,2,2,2,2,4),(-1.10917023491673,
-1.09780314118422,-1.07225908258597,-1.06530958502227,-1.06173924456896,
-1.05910391043913,-1.05580982384355,-1.05019632888415,-1.02079744724882,
-0.991284433603716,-0.981650882393839,-0.978739801476121,-0.976952504346429,
-0.975255931018385,-0.972771926128064,-0.965985524808992,-0.955132329620842,
-0.933346313864944,-0.903406464592416,-0.89773614042774,-0.89442984961194,
-0.891796144927973,-0.888242899319584,-0.881379711288852,-0.856519376055898,
-0.839293624574117,-0.816141745348745,-0.812652454382971,-0.810718532503337,
-0.809070373076671,-0.806901949031408,-0.80211321737921,-0.795403477182408,
-0.775694480284611,-0.739015888895629,-0.73272011790953,-0.728947250626557,
-0.726004774124995,-0.722776837720733,-0.717472097304373,-0.695425227256277,
-0.66590515143579,-0.656794159610615,-0.648140599938779,-0.645338199308374,
-0.643574731727522,-0.641861932312708,-0.63929625790687,-0.631894661130396,
-0.619577769341614,-0.582592117112216,-0.568401254974707,-0.56360377197765,
-0.560484046483025,-0.557498655147684,-0.553384158147427,-0.543336734996394,
-0.528555263686441,-0.508544994584828,-0.504278305999244,-0.482840000822797,
-0.479358804460191,-0.477426768689665,-0.475794169803756,-0.47363264486231,
-0.46888156102796,-0.447336716776784,-0.407675194317095,-0.399431332731411,
-0.395658018203836,-0.392715731836914,-0.38948855191263,-0.3841863293089,
-0.36217520988874,-0.332095131052859,-0.315950488554445,-0.312603752403881,
-0.310701885660114,-0.309214500928508,-0.307094799918483,-0.302570723735803,
-0.283222458346412,-0.249943173278937,-0.235241836313093,-0.230390355519392,
-0.227259427235587,-0.22428046285279,-0.220202299774329,-0.210386694139145,
-0.19608391261695,-0.175665101246482,-0.151511714522243,-0.146768846520951,
-0.144631870956978,-0.142983443199958,-0.141215798394648,-0.138114853869353,
-0.134124858945641,-0.12544065447551,-0.0954286080090174,-0.0700939486962987,
-0.064493435702309,-0.0612024694929878,-0.0595374781479462),
 .UNSPECIFIED.);
#614=B_SPLINE_CURVE_WITH_KNOTS('',3,(#53491,#53492,#53493,#53494,#53495,
#53496,#53497,#53498,#53499,#53500,#53501,#53502,#53503,#53504,#53505,#53506,
#53507,#53508,#53509,#53510,#53511,#53512,#53513,#53514,#53515,#53516,#53517,
#53518,#53519,#53520,#53521,#53522,#53523,#53524,#53525,#53526,#53527,#53528,
#53529,#53530,#53531,#53532,#53533,#53534,#53535,#53536,#53537,#53538,#53539,
#53540,#53541,#53542,#53543,#53544,#53545,#53546,#53547,#53548,#53549,#53550,
#53551,#53552,#53553,#53554,#53555,#53556,#53557,#53558,#53559,#53560,#53561,
#53562,#53563,#53564,#53565,#53566,#53567,#53568,#53569,#53570,#53571,#53572,
#53573,#53574,#53575,#53576,#53577,#53578,#53579,#53580,#53581,#53582,#53583,
#53584,#53585,#53586,#53587,#53588,#53589,#53590,#53591,#53592,#53593,#53594,
#53595,#53596,#53597,#53598,#53599,#53600,#53601,#53602,#53603,#53604,#53605,
#53606,#53607,#53608,#53609,#53610,#53611,#53612,#53613,#53614,#53615,#53616,
#53617,#53618,#53619,#53620,#53621,#53622,#53623,#53624,#53625,#53626,#53627,
#53628,#53629,#53630,#53631,#53632,#53633,#53634,#53635,#53636,#53637,#53638,
#53639,#53640,#53641,#53642,#53643,#53644,#53645,#53646,#53647,#53648,#53649,
#53650,#53651,#53652,#53653,#53654,#53655,#53656,#53657,#53658,#53659,#53660,
#53661,#53662,#53663,#53664,#53665,#53666,#53667,#53668,#53669,#53670,#53671,
#53672,#53673,#53674,#53675,#53676,#53677,#53678,#53679,#53680,#53681,#53682,
#53683,#53684,#53685,#53686,#53687,#53688,#53689,#53690,#53691,#53692,#53693,
#53694,#53695,#53696,#53697,#53698,#53699,#53700),.UNSPECIFIED.,.F.,.F.,
(4,2,2,2,2,2,2,2,2,2,2,2,2,2,2,2,2,2,2,2,2,2,2,2,2,2,2,2,2,2,2,2,2,2,2,
2,2,2,2,2,2,2,2,2,2,2,2,2,2,2,2,2,2,2,2,2,2,2,2,2,2,2,2,2,2,2,2,2,2,2,2,
2,2,2,2,2,2,2,2,2,2,2,2,2,2,2,2,2,2,2,2,2,2,2,2,2,2,2,2,2,2,2,2,2,4),(-0.991340061094534,
-0.98920246580239,-0.985892070943082,-0.983998417543123,-0.9823432842587,
-0.980110386246792,-0.974953970657174,-0.967544151433446,-0.943937354432828,
-0.912714269366428,-0.905623704154458,-0.90197943989973,-0.899057888336441,
-0.895718120940077,-0.889889042822999,-0.855667907249648,-0.824460926690277,
-0.819932370416947,-0.817811816006102,-0.816167668474606,-0.814199530731012,
-0.81044599135912,-0.782161991903423,-0.745755684101324,-0.739444483520501,
-0.735667531524847,-0.732724835093212,-0.729499672142621,-0.724206501792553,
-0.702346267814432,-0.671566076484301,-0.655890806045303,-0.652577464861746,
-0.650683172186911,-0.649028228394813,-0.646796586869404,-0.641647315516918,
-0.634251286145616,-0.61072709880859,-0.579397105721552,-0.572307765744901,
-0.568663805211868,-0.565742339225463,-0.562402497996578,-0.55657283896063,
-0.522141438871249,-0.491184089837036,-0.486631504524908,-0.48450650002899,
-0.482862087066209,-0.480897454163308,-0.477160737336082,-0.472314058866212,
-0.460681236454466,-0.439388367291313,-0.410256793518379,-0.404609510813054,
-0.401276691124032,-0.398382162433067,-0.394741678270005,-0.387432190858959,
-0.377835793013308,-0.352143498200701,-0.324794333482777,-0.320082217557296,
-0.31795072339367,-0.316302806272113,-0.314369013785592,-0.31078001980745,
-0.282230708124701,-0.245814300630239,-0.239504047872713,-0.23572745066662,
-0.232784908843778,-0.229559791713426,-0.224266409621652,-0.202399707202107,
-0.171610172324106,-0.155971765936306,-0.152648983812978,-0.150752608621542,
-0.149153715295316,-0.149134145752116,-0.149114703943759,-0.149095383505877,
-0.149076178237325,-0.149057082091785,-0.149038089174465,-0.149019193737152,
-0.14900039015904,-0.148981672947616,-0.148963036725475,-0.146845365989864,
-0.144331827442144,-0.139921370409683,-0.1298384769529,-0.0943091076171302,
-0.0760052498260046,-0.0708057193007756,-0.0676007636255934,-0.0646523535893921,
-0.060768233202206,-0.0521261683564409,-0.0242665367690054,-0.000492710661275274),
 .UNSPECIFIED.);
#615=B_SPLINE_CURVE_WITH_KNOTS('',3,(#53701,#53702,#53703,#53704,#53705,
#53706,#53707,#53708,#53709,#53710,#53711,#53712,#53713,#53714,#53715,#53716,
#53717,#53718,#53719,#53720),.UNSPECIFIED.,.F.,.F.,(4,2,2,2,2,2,2,2,2,4),
(-2.09993882802925,-2.08869886965324,-2.08628696029132,-2.08456699226199,
-2.083031835045,-2.08149453819177,-2.07937193789139,-2.07393091411062,-2.05926295066118,
-2.04110855067476),.UNSPECIFIED.);
#616=B_SPLINE_CURVE_WITH_KNOTS('',3,(#53722,#53723,#53724,#53725,#53726,
#53727,#53728,#53729,#53730,#53731,#53732,#53733),.UNSPECIFIED.,.F.,.F.,
(4,2,2,2,2,4),(-0.0595374781479462,-0.0582743076702352,-0.0545553048994626,
-0.0468312306777383,-0.0365100484917665,-0.000492659668756888),
 .UNSPECIFIED.);
#617=B_SPLINE_CURVE_WITH_KNOTS('',3,(#53734,#53735,#53736,#53737,#53738,
#53739,#53740,#53741,#53742,#53743,#53744,#53745,#53746,#53747,#53748,#53749,
#53750,#53751,#53752,#53753,#53754,#53755,#53756,#53757,#53758,#53759,#53760,
#53761,#53762,#53763,#53764,#53765,#53766,#53767,#53768,#53769,#53770,#53771,
#53772,#53773,#53774,#53775,#53776,#53777,#53778,#53779,#53780,#53781,#53782,
#53783,#53784,#53785,#53786,#53787,#53788,#53789,#53790,#53791,#53792,#53793,
#53794,#53795,#53796,#53797,#53798,#53799,#53800,#53801,#53802,#53803,#53804,
#53805,#53806,#53807,#53808,#53809,#53810,#53811,#53812,#53813,#53814,#53815,
#53816,#53817,#53818,#53819,#53820,#53821,#53822,#53823,#53824,#53825,#53826,
#53827,#53828,#53829,#53830,#53831,#53832,#53833,#53834,#53835,#53836,#53837,
#53838,#53839,#53840,#53841,#53842,#53843,#53844,#53845,#53846,#53847,#53848,
#53849,#53850,#53851,#53852,#53853,#53854,#53855,#53856,#53857,#53858,#53859,
#53860,#53861,#53862,#53863,#53864,#53865,#53866,#53867,#53868,#53869,#53870,
#53871,#53872,#53873,#53874,#53875,#53876,#53877,#53878,#53879,#53880,#53881,
#53882,#53883,#53884,#53885,#53886,#53887,#53888,#53889,#53890,#53891,#53892,
#53893,#53894,#53895,#53896,#53897,#53898,#53899,#53900,#53901,#53902,#53903,
#53904,#53905,#53906,#53907,#53908,#53909,#53910,#53911,#53912,#53913,#53914,
#53915,#53916,#53917,#53918,#53919,#53920,#53921,#53922,#53923,#53924,#53925,
#53926,#53927),.UNSPECIFIED.,.F.,.F.,(4,2,2,2,2,2,2,2,2,2,2,2,2,2,2,2,2,
2,2,2,2,2,2,2,2,2,2,2,2,2,2,2,2,2,2,2,2,2,2,2,2,2,2,2,2,2,2,2,2,2,2,2,2,
2,2,2,2,2,2,2,2,2,2,2,2,2,2,2,2,2,2,2,2,2,2,2,2,2,2,2,2,2,2,2,2,2,2,2,2,
2,2,2,2,2,2,2,4),(-2.10000173286267,-2.08784529945252,-2.0818241350934,
-2.07949850599191,-2.0778111684359,-2.07613401143259,-2.07430816150208,
-2.07122208891968,-2.05973632205585,-2.0406965402433,-2.02426558874489,
-2.00238112718897,-1.99708503033397,-1.99385859131561,-1.99091506206345,
-1.98713749800015,-1.98082635373945,-1.94442082373072,-1.91584332378824,
-1.91227305338482,-1.91034281151202,-1.90869375455209,-1.90655549055158,
-1.90180801965512,-1.87801516213019,-1.85810522698771,-1.84324566348585,
-1.83316100065038,-1.82904006134694,-1.82605296058888,-1.82293408717729,
-1.81814324970362,-1.8040214362917,-1.77025181881292,-1.75072729195109,
-1.74618340308607,-1.74405958903847,-1.74257129557485,-1.74067106548965,
-1.73733322421561,-1.72144948256797,-1.69101286710652,-1.66901622816419,
-1.66371331839731,-1.66048533576287,-1.65754207797673,-1.65376718790769,
-1.64746578413458,-1.61088989558763,-1.58249500163516,-1.57890531012757,
-1.57697093211146,-1.57532239559003,-1.57318990373664,-1.56847489950099,
-1.54107916896174,-1.51538017288048,-1.50578041664814,-1.49846906384927,
-1.49482743453616,-1.49193191133557,-1.48859784864288,-1.48294820288119,
-1.45382101360991,-1.43252740890118,-1.42090686924639,-1.4160628922804,
-1.41232721597242,-1.41036238500471,-1.40871736604499,-1.40659097788066,
-1.40203333348044,-1.37106994167086,-1.33659729825625,-1.33076479108221,
-1.3274236643598,-1.32450128086828,-1.32085644192214,-1.31376619512649,
-1.28248779203966,-1.25894019818624,-1.25154000611395,-1.2463877398711,
-1.2441551699199,-1.24249966160833,-1.24060489505375,-1.23729101618844,
-1.22162033473911,-1.19087605209644,-1.16892862033792,-1.16362881542626,
-1.16040159976283,-1.15745831756361,-1.15368239412195,-1.14737699328768,
-1.11087458577517,-1.10913982844865),.UNSPECIFIED.);
#618=B_SPLINE_CURVE_WITH_KNOTS('',3,(#53932,#53933,#53934,#53935,#53936,
#53937,#53938,#53939,#53940,#53941,#53942,#53943,#53944,#53945,#53946,#53947,
#53948,#53949,#53950,#53951,#53952,#53953,#53954,#53955,#53956,#53957,#53958,
#53959,#53960,#53961,#53962,#53963,#53964,#53965,#53966,#53967,#53968,#53969,
#53970,#53971,#53972,#53973,#53974,#53975,#53976,#53977,#53978,#53979,#53980,
#53981,#53982,#53983,#53984,#53985,#53986,#53987,#53988,#53989,#53990,#53991,
#53992,#53993,#53994,#53995,#53996,#53997,#53998,#53999,#54000,#54001,#54002,
#54003,#54004,#54005,#54006,#54007,#54008,#54009,#54010,#54011,#54012,#54013,
#54014,#54015,#54016,#54017,#54018,#54019,#54020,#54021,#54022,#54023,#54024,
#54025,#54026,#54027,#54028,#54029,#54030,#54031,#54032,#54033,#54034,#54035,
#54036,#54037,#54038,#54039,#54040,#54041,#54042,#54043,#54044,#54045,#54046,
#54047,#54048,#54049,#54050,#54051,#54052,#54053,#54054,#54055,#54056,#54057,
#54058,#54059,#54060,#54061,#54062,#54063,#54064,#54065,#54066,#54067,#54068,
#54069,#54070,#54071,#54072,#54073,#54074,#54075,#54076,#54077,#54078,#54079,
#54080,#54081,#54082,#54083,#54084,#54085,#54086,#54087,#54088,#54089,#54090,
#54091,#54092,#54093,#54094,#54095,#54096,#54097,#54098,#54099,#54100,#54101,
#54102,#54103,#54104,#54105,#54106,#54107,#54108,#54109,#54110,#54111,#54112,
#54113,#54114,#54115,#54116,#54117,#54118,#54119,#54120,#54121,#54122,#54123,
#54124,#54125,#54126,#54127,#54128,#54129,#54130,#54131),.UNSPECIFIED.,
 .F.,.F.,(4,2,2,2,2,2,2,2,2,2,2,2,2,2,2,2,2,2,2,2,2,2,2,2,2,2,2,2,2,2,2,
2,2,2,2,2,2,2,2,2,2,2,2,2,2,2,2,2,2,2,2,2,2,2,2,2,2,2,2,2,2,2,2,2,2,2,2,
2,2,2,2,2,2,2,2,2,2,2,2,2,2,2,2,2,2,2,2,2,2,2,2,2,2,2,2,2,2,2,2,4),(-2.04097989592064,
-2.01643454881326,-1.99867457066985,-1.98823495665113,-1.98533631711536,
-1.98355188807003,-1.98187373456921,-1.97979424848172,-1.97461318682226,
-1.93094583053922,-1.90926005730472,-1.90397737789773,-1.90075461085136,
-1.89781152551908,-1.89403050179105,-1.88574139544896,-1.84615706595855,
-1.82463996225972,-1.81989185650961,-1.81773103186237,-1.81609866344362,
-1.81416658211516,-1.81068452397676,-1.78917818454528,-1.78496385128544,
-1.76502065433151,-1.75018716651009,-1.7401160856542,-1.73599824120865,
-1.73301257318057,-1.72989447874049,-1.72510339229687,-1.71096730234241,
-1.67395778297624,-1.66164165710378,-1.65661185068838,-1.65276631331365,
-1.65077934945949,-1.64913666607856,-1.64703984197957,-1.64263691113105,
-1.60940824133699,-1.58149842274345,-1.57286227549758,-1.56897911009622,
-1.56603078727429,-1.56282530839965,-1.55762350900728,-1.53928147727738,
-1.5039076559364,-1.49377807312749,-1.48731153633058,-1.48487291656532,
-1.48318514643127,-1.48160694366644,-1.47885640457167,-1.47063158883834,
-1.46097793927844,-1.43144234155053,-1.4093908147684,-1.40408622499255,
-1.40085871152601,-1.39791684553085,-1.39414507832638,-1.38785193178936,
-1.35119126814421,-1.33150154608391,-1.32479638229279,-1.3200099074253,
-1.31784214574603,-1.31619431841227,-1.31426062354715,-1.3107713203957,
-1.28759459939239,-1.27033585626588,-1.24787614812831,-1.23948837808926,
-1.23564870486035,-1.23270630613491,-1.22948053264786,-1.22418418485653,
-1.20461265651106,-1.16085419733883,-1.1562515897723,-1.15266118188117,
-1.15072706590745,-1.14907916860977,-1.14694803739181,-1.14223810389979,
-1.11470911711937,-1.08911525072692,-1.07480794059978,-1.07013750571097,
-1.06704446230174,-1.06407714097964,-1.05989566405639,-1.05017299558284,
-1.03563134770873,-1.00482702409126,-0.991340061094534),.UNSPECIFIED.);
#619=B_SPLINE_CURVE_WITH_KNOTS('',3,(#54132,#54133,#54134,#54135,#54136,
#54137,#54138,#54139,#54140,#54141,#54142,#54143,#54144,#54145,#54146,#54147,
#54148,#54149,#54150,#54151,#54152,#54153,#54154,#54155,#54156,#54157,#54158,
#54159,#54160,#54161,#54162,#54163,#54164,#54165,#54166,#54167,#54168,#54169,
#54170,#54171,#54172,#54173,#54174,#54175,#54176,#54177,#54178,#54179,#54180,
#54181,#54182,#54183,#54184,#54185,#54186,#54187,#54188,#54189,#54190,#54191,
#54192,#54193,#54194,#54195,#54196,#54197,#54198,#54199,#54200,#54201,#54202,
#54203,#54204,#54205,#54206,#54207,#54208,#54209,#54210,#54211,#54212,#54213,
#54214,#54215,#54216,#54217,#54218,#54219,#54220,#54221,#54222,#54223,#54224,
#54225,#54226,#54227,#54228,#54229,#54230,#54231,#54232,#54233,#54234,#54235,
#54236,#54237,#54238,#54239,#54240,#54241,#54242,#54243,#54244,#54245,#54246,
#54247,#54248,#54249,#54250,#54251,#54252,#54253,#54254,#54255,#54256,#54257,
#54258,#54259,#54260,#54261,#54262,#54263,#54264,#54265,#54266,#54267,#54268,
#54269,#54270,#54271,#54272,#54273,#54274,#54275,#54276,#54277,#54278,#54279,
#54280,#54281,#54282,#54283,#54284,#54285,#54286,#54287,#54288,#54289,#54290,
#54291,#54292,#54293,#54294,#54295,#54296,#54297,#54298,#54299,#54300,#54301,
#54302,#54303,#54304,#54305,#54306,#54307,#54308,#54309,#54310,#54311,#54312,
#54313,#54314,#54315,#54316,#54317,#54318,#54319,#54320,#54321,#54322,#54323,
#54324,#54325,#54326,#54327,#54328,#54329,#54330,#54331,#54332,#54333,#54334,
#54335,#54336,#54337,#54338,#54339,#54340,#54341,#54342,#54343,#54344,#54345,
#54346,#54347,#54348,#54349,#54350,#54351,#54352,#54353,#54354,#54355,#54356,
#54357),.UNSPECIFIED.,.F.,.F.,(4,2,2,2,2,2,2,2,2,2,2,2,2,2,2,2,2,2,2,2,
2,2,2,2,2,2,2,2,2,2,2,2,2,2,2,2,2,2,2,2,2,2,2,2,2,2,2,2,2,2,2,2,2,2,2,2,
2,2,2,2,2,2,2,2,2,2,2,2,2,2,2,2,2,2,2,2,2,2,2,2,2,2,2,2,2,2,2,2,2,2,2,2,
2,2,2,2,2,2,2,2,2,2,2,2,2,2,2,2,2,2,2,2,4),(-1.10913982844865,-1.09106795055996,
-1.084339173503,-1.07953965907219,-1.0773690951644,-1.075735260039,-1.07380849983863,
-1.07035212401128,-1.05034070711872,-1.00500181410813,-0.998796004615634,
-0.995048507963371,-0.992109253737245,-0.988867863748533,-0.983501070336844,
-0.960350817368616,-0.930304611090647,-0.915259285440901,-0.911976323597886,
-0.910088670522428,-0.90843177836852,-0.906187085717017,-0.900962974022094,
-0.893421857911931,-0.869012640474297,-0.838843482889157,-0.831733018178526,
-0.828084257752818,-0.825161867104849,-0.821824138487046,-0.816006486673927,
-0.779593122733005,-0.750755265648821,-0.746087432986437,-0.743963636303344,
-0.742316129337228,-0.740376097056809,-0.736758660438702,-0.70720974270184,
-0.671929604503066,-0.665562772728414,-0.6617697733166,-0.65882439883221,
-0.655606218072681,-0.650347376521122,-0.629059517547184,-0.608319980153307,
-0.601733200781957,-0.582200106433717,-0.578756636158879,-0.576832920459043,
-0.575198902864116,-0.573024444829927,-0.568202222356984,-0.561429840172035,
-0.541396630496964,-0.50520549265272,-0.49888142881401,-0.495100549399652,
-0.492156947280929,-0.488932972074349,-0.483646795348441,-0.461912400671883,
-0.431660848866696,-0.415380230393842,-0.412027905528294,-0.41012464830468,
-0.408637300633719,-0.406519119590564,-0.40200395121782,-0.38274076947758,
-0.34969940393548,-0.334719566271866,-0.329835559107048,-0.326697510677828,
-0.323721627064164,-0.319663319304236,-0.309975102200079,-0.295932772271624,
-0.27521813333345,-0.268188939960367,-0.248899798409811,-0.245463052959539,
-0.243540896974316,-0.242056603922087,-0.239965790128632,-0.235595186403043,
-0.217633463249286,-0.185672870046334,-0.168553711526254,-0.163442706653727,
-0.160256378829578,-0.157506521636873,-0.157347050096386,-0.1571997612204,
-0.157060874279407,-0.156927548981441,-0.156797526364973,-0.156668907090355,
-0.156540004483214,-0.156409239524296,-0.153312770234407,-0.148952569479307,
-0.141429206504758,-0.124370185405663,-0.105014574945038,-0.0823638306380467,
-0.0788764371682638,-0.0769430257481847,-0.0753106291282405,-0.0731511473577938,
-0.0684113095755912,-0.0594010420905767),.UNSPECIFIED.);
#620=B_SPLINE_CURVE_WITH_KNOTS('',3,(#54363,#54364,#54365,#54366,#54367,
#54368,#54369,#54370,#54371,#54372,#54373,#54374,#54375,#54376,#54377,#54378,
#54379,#54380,#54381,#54382,#54383,#54384,#54385,#54386,#54387,#54388,#54389,
#54390,#54391,#54392,#54393,#54394,#54395,#54396,#54397,#54398,#54399,#54400,
#54401,#54402,#54403,#54404,#54405,#54406,#54407,#54408,#54409,#54410,#54411,
#54412,#54413,#54414,#54415,#54416,#54417,#54418,#54419,#54420,#54421,#54422,
#54423,#54424,#54425,#54426,#54427,#54428,#54429,#54430,#54431,#54432,#54433,
#54434,#54435,#54436,#54437,#54438,#54439,#54440,#54441,#54442,#54443,#54444,
#54445,#54446,#54447,#54448,#54449,#54450,#54451,#54452,#54453,#54454,#54455,
#54456,#54457,#54458,#54459,#54460,#54461,#54462,#54463,#54464,#54465,#54466,
#54467,#54468,#54469,#54470,#54471,#54472,#54473,#54474,#54475,#54476,#54477,
#54478,#54479,#54480,#54481,#54482,#54483,#54484,#54485,#54486,#54487,#54488,
#54489,#54490,#54491,#54492,#54493,#54494,#54495,#54496,#54497,#54498,#54499,
#54500,#54501,#54502,#54503,#54504,#54505,#54506,#54507,#54508,#54509,#54510,
#54511,#54512,#54513,#54514,#54515,#54516,#54517,#54518,#54519,#54520,#54521,
#54522,#54523,#54524,#54525,#54526,#54527,#54528,#54529,#54530,#54531,#54532,
#54533,#54534,#54535,#54536,#54537,#54538,#54539,#54540,#54541,#54542,#54543,
#54544,#54545,#54546,#54547,#54548,#54549,#54550,#54551,#54552,#54553,#54554,
#54555,#54556,#54557,#54558,#54559,#54560),.UNSPECIFIED.,.F.,.F.,(4,2,2,
2,2,2,2,2,2,2,2,2,2,2,2,2,2,2,2,2,2,2,2,2,2,2,2,2,2,2,2,2,2,2,2,2,2,2,2,
2,2,2,2,2,2,2,2,2,2,2,2,2,2,2,2,2,2,2,2,2,2,2,2,2,2,2,2,2,2,2,2,2,2,2,2,
2,2,2,2,2,2,2,2,2,2,2,2,2,2,2,2,2,2,2,2,2,2,2,4),(-0.991324874888266,-0.976739863257293,
-0.97132404534437,-0.9680718997956,-0.965134788555649,-0.961343670438805,
-0.953231687803036,-0.925996969295892,-0.892901263883769,-0.88755141755747,
-0.885443544004503,-0.883757626556907,-0.881984258502916,-0.879137521470844,
-0.869182132443042,-0.84949895295485,-0.812767132215365,-0.806473074275067,
-0.802700394931127,-0.799757587866313,-0.796528806945328,-0.791221566304062,
-0.769142814089731,-0.740242030405451,-0.723060592501381,-0.719663886134979,
-0.717750497905008,-0.716264597104834,-0.714160638432258,-0.709721983734,
-0.691159604463721,-0.645942161180393,-0.639709908564875,-0.635954908158763,
-0.633014682940957,-0.629777267565902,-0.624428950938107,-0.601620481290346,
-0.570022012622387,-0.556046124880154,-0.552779930235178,-0.55091489918402,
-0.549251997097842,-0.546963887581918,-0.541479622435086,-0.533423736025437,
-0.505566285595962,-0.477117657240083,-0.471450133161718,-0.468144343035572,
-0.465510431747339,-0.46195612249418,-0.455088109869861,-0.430191779750625,
-0.41298779477031,-0.389850134986449,-0.38636068152024,-0.384426670059028,
-0.382778438811334,-0.3806099374494,-0.375821114883758,-0.369111337072889,
-0.349403208019381,-0.312716183273986,-0.306420196159932,-0.302647173907626,
-0.299704566828113,-0.296476480729612,-0.291171488673828,-0.269124112555203,
-0.239561566097529,-0.229557653630966,-0.22164623104683,-0.21893474500181,
-0.217363954288633,-0.215669937024994,-0.213199481235841,-0.206511008517992,
-0.162846542597495,-0.143110644288626,-0.137789571447329,-0.134558234162309,
-0.131616865973127,-0.131487372485602,-0.131362803029669,-0.131242428153373,
-0.131125605603381,-0.131011764075998,-0.127489392331951,-0.118715462853635,
-0.106353615936504,-0.0804420554854634,-0.0565122364423548,-0.0530177863972708,
-0.0510828083351631,-0.0494349514420726,-0.0472685080778907,-0.0424901910055939,
-0.000492539812704547),.UNSPECIFIED.);
#621=B_SPLINE_CURVE_WITH_KNOTS('',3,(#54561,#54562,#54563,#54564,#54565,
#54566,#54567,#54568,#54569,#54570,#54571,#54572,#54573,#54574,#54575,#54576,
#54577,#54578,#54579,#54580),.UNSPECIFIED.,.F.,.F.,(4,2,2,2,2,2,2,2,2,4),
(-2.10003377121719,-2.08459930780237,-2.0760706583423,-2.07213879347443,
-2.06920340574752,-2.06622732444713,-2.0630905739407,-2.05821171241528,
-2.04326789181161,-2.04097989592064),.UNSPECIFIED.);
#622=B_SPLINE_CURVE_WITH_KNOTS('',3,(#54582,#54583,#54584,#54585,#54586,
#54587,#54588,#54589),.UNSPECIFIED.,.F.,.F.,(4,2,2,4),(-0.0594010420905767,
-0.0469797452701944,-0.00923093699204744,-0.000492411924495984),
 .UNSPECIFIED.);
#623=B_SPLINE_CURVE_WITH_KNOTS('',3,(#54590,#54591,#54592,#54593,#54594,
#54595,#54596,#54597,#54598,#54599,#54600,#54601,#54602,#54603,#54604,#54605,
#54606,#54607,#54608,#54609,#54610,#54611,#54612,#54613,#54614,#54615,#54616,
#54617,#54618,#54619,#54620,#54621,#54622,#54623,#54624,#54625,#54626,#54627,
#54628,#54629,#54630,#54631,#54632,#54633,#54634,#54635,#54636,#54637,#54638,
#54639,#54640,#54641,#54642,#54643,#54644,#54645,#54646,#54647,#54648,#54649,
#54650,#54651,#54652,#54653,#54654,#54655,#54656,#54657,#54658,#54659,#54660,
#54661,#54662,#54663,#54664,#54665,#54666,#54667,#54668,#54669,#54670,#54671,
#54672,#54673,#54674,#54675,#54676,#54677,#54678,#54679,#54680,#54681,#54682,
#54683,#54684,#54685,#54686,#54687,#54688,#54689,#54690,#54691,#54692,#54693,
#54694,#54695,#54696,#54697,#54698,#54699,#54700,#54701,#54702,#54703,#54704,
#54705,#54706,#54707,#54708,#54709,#54710,#54711,#54712,#54713,#54714,#54715,
#54716,#54717,#54718,#54719,#54720,#54721,#54722,#54723,#54724,#54725,#54726,
#54727,#54728,#54729,#54730,#54731,#54732,#54733,#54734,#54735,#54736,#54737,
#54738,#54739,#54740,#54741,#54742,#54743,#54744,#54745,#54746,#54747,#54748,
#54749,#54750,#54751,#54752,#54753,#54754,#54755,#54756,#54757,#54758,#54759,
#54760,#54761,#54762,#54763,#54764,#54765,#54766,#54767,#54768,#54769,#54770,
#54771,#54772,#54773,#54774,#54775,#54776,#54777,#54778,#54779,#54780,#54781,
#54782,#54783,#54784,#54785),.UNSPECIFIED.,.F.,.F.,(4,2,2,2,2,2,2,2,2,2,
2,2,2,2,2,2,2,2,2,2,2,2,2,2,2,2,2,2,2,2,2,2,2,2,2,2,2,2,2,2,2,2,2,2,2,2,
2,2,2,2,2,2,2,2,2,2,2,2,2,2,2,2,2,2,2,2,2,2,2,2,2,2,2,2,2,2,2,2,2,2,2,2,
2,2,2,2,2,2,2,2,2,2,2,2,2,2,2,4),(-2.09968458105429,-2.09731412985729,-2.09467903382393,
-2.0919058211916,-2.08880466245833,-2.0840951227781,-2.07059180368999,-2.02615847253882,
-2.01796616203498,-2.01241383089942,-2.0101148004495,-2.0084504287947,-2.0065910758917,
-2.00335035789764,-1.98977461733642,-1.96306696649972,-1.93767331476089,
-1.93074293448994,-1.92717651869468,-1.92454172588388,-1.92124527557621,
-1.91562011309231,-1.88635358662017,-1.8651031661546,-1.85345166798431,
-1.84632420712183,-1.84379431072544,-1.842088833935,-1.8403156444537,-1.83746834126897,
-1.82842234805155,-1.82065795448036,-1.78998778027071,-1.76816706326629,
-1.76287584474351,-1.75965101225839,-1.75670806738825,-1.75293003141391,
-1.74661532366266,-1.71031196095746,-1.69038451391682,-1.6836331638887,
-1.67882189485682,-1.67664955647517,-1.67501590571389,-1.6730911851793,
-1.6696426018293,-1.64991166355826,-1.64356689621778,-1.62300825172028,
-1.60871963610255,-1.59891174835192,-1.59483466261056,-1.59185578800477,
-1.58872432854165,-1.5838707204169,-1.56914958775325,-1.53591074285196,
-1.51657963151166,-1.51205726580885,-1.50993785558262,-1.50845045998029,
-1.50654832081517,-1.50320046929565,-1.48703645491905,-1.45694693675365,
-1.43492761107478,-1.42962457074456,-1.42639719018042,-1.42345492024717,
-1.41968190443652,-1.41338500525859,-1.37677741883421,-1.34843042423717,
-1.3448410194355,-1.34290705708564,-1.34125904080504,-1.33912743065624,
-1.3344151773375,-1.30704854662197,-1.28134086087788,-1.27174066592667,
-1.26442958450656,-1.26078867996609,-1.25789399819178,-1.25456119740361,
-1.24891440363802,-1.21980895362846,-1.19855495402512,-1.18690664084724,
-1.18205561883779,-1.17831599836515,-1.17635071084594,-1.17470628252862,
-1.1725819091216,-1.16803301826951,-1.13701033063592,-1.10891213746094),
 .UNSPECIFIED.);
#624=B_SPLINE_CURVE_WITH_KNOTS('',3,(#54790,#54791,#54792,#54793,#54794,
#54795,#54796,#54797,#54798,#54799,#54800,#54801,#54802,#54803,#54804,#54805,
#54806,#54807,#54808,#54809,#54810,#54811,#54812,#54813,#54814,#54815,#54816,
#54817,#54818,#54819,#54820,#54821,#54822,#54823,#54824,#54825,#54826,#54827,
#54828,#54829,#54830,#54831,#54832,#54833,#54834,#54835,#54836,#54837,#54838,
#54839,#54840,#54841,#54842,#54843,#54844,#54845,#54846,#54847,#54848,#54849,
#54850,#54851,#54852,#54853,#54854,#54855,#54856,#54857,#54858,#54859,#54860,
#54861,#54862,#54863,#54864,#54865,#54866,#54867,#54868,#54869,#54870,#54871,
#54872,#54873,#54874,#54875,#54876,#54877,#54878,#54879,#54880,#54881,#54882,
#54883,#54884,#54885,#54886,#54887,#54888,#54889,#54890,#54891,#54892,#54893,
#54894,#54895,#54896,#54897,#54898,#54899,#54900,#54901,#54902,#54903,#54904,
#54905,#54906,#54907,#54908,#54909,#54910,#54911,#54912,#54913,#54914,#54915,
#54916,#54917,#54918,#54919,#54920,#54921,#54922,#54923,#54924,#54925,#54926,
#54927,#54928,#54929,#54930,#54931,#54932,#54933,#54934,#54935,#54936,#54937,
#54938,#54939,#54940,#54941,#54942,#54943,#54944,#54945,#54946,#54947,#54948,
#54949,#54950,#54951,#54952,#54953,#54954,#54955,#54956,#54957,#54958,#54959,
#54960,#54961,#54962,#54963,#54964,#54965,#54966,#54967,#54968,#54969,#54970,
#54971,#54972,#54973,#54974,#54975,#54976,#54977,#54978,#54979,#54980,#54981,
#54982,#54983,#54984,#54985,#54986,#54987,#54988,#54989,#54990,#54991),
 .UNSPECIFIED.,.F.,.F.,(4,2,2,2,2,2,2,2,2,2,2,2,2,2,2,2,2,2,2,2,2,2,2,2,
2,2,2,2,2,2,2,2,2,2,2,2,2,2,2,2,2,2,2,2,2,2,2,2,2,2,2,2,2,2,2,2,2,2,2,2,
2,2,2,2,2,2,2,2,2,2,2,2,2,2,2,2,2,2,2,2,2,2,2,2,2,2,2,2,2,2,2,2,2,2,2,2,
2,2,2,2,4),(-2.04133053968484,-2.00942223267799,-1.98795143919906,-1.97509604920505,
-1.97112329979462,-1.96807677610341,-1.96512522884565,-1.96129213452401,
-1.95303791682513,-1.91351867964898,-1.89201084448789,-1.8872625944005,
-1.88510121523301,-1.88346821490706,-1.88153512918655,-1.8780506710343,
-1.85643322193555,-1.85233311422696,-1.83213734321064,-1.81743756213607,
-1.80742944091667,-1.8033202825645,-1.80033520078978,-1.79721262807208,
-1.79240431156436,-1.77811853012929,-1.74448730218503,-1.72501198332002,
-1.72047330597303,-1.71835044768818,-1.7168622551832,-1.71496137023007,
-1.71162068632634,-1.69566475339045,-1.66508540409417,-1.64328136065559,
-1.63798983732462,-1.63476427433656,-1.63182031474892,-1.62804049768809,
-1.62172174024913,-1.58543742188698,-1.56548051770844,-1.55872249340508,
-1.55390725974498,-1.55173379183105,-1.5500995775605,-1.5481745458862,-1.54472621542136,
-1.52504269730513,-1.5182229436901,-1.49663901712644,-1.48318900479111,
-1.4737960033512,-1.46978457248824,-1.46681582961828,-1.46366023857543,
-1.45869595479566,-1.44296031706477,-1.4105781386192,-1.39155354968455,
-1.3870636548549,-1.38494992787545,-1.38346280514221,-1.38155582439192,
-1.37818807047584,-1.36158153196709,-1.33198545659644,-1.30992730332048,
-1.30462067555095,-1.30139186559733,-1.29844878149714,-1.29467540227027,
-1.28837945222244,-1.25170717386403,-1.23200708220547,-1.2252987191653,
-1.22051003932177,-1.21834134355003,-1.21669283455972,-1.2147583733192,
-1.21126776474198,-1.18811478769983,-1.17089578437679,-1.14598239922988,
-1.13911178210425,-1.13555659528586,-1.13292224432861,-1.12961615727611,
-1.12394877422018,-1.09320784447763,-1.06947528105522,-1.06034051730432,
-1.05433192601215,-1.05196062056218,-1.05028432022268,-1.04845608644409,
-1.04535946854249,-1.0322681027794,-0.998255818184011,-0.991324874888266),
 .UNSPECIFIED.);
#625=B_SPLINE_CURVE_WITH_KNOTS('',3,(#54992,#54993,#54994,#54995,#54996,
#54997,#54998,#54999,#55000,#55001,#55002,#55003,#55004,#55005,#55006,#55007,
#55008,#55009,#55010,#55011,#55012,#55013,#55014,#55015,#55016,#55017,#55018,
#55019,#55020,#55021,#55022,#55023,#55024,#55025,#55026,#55027,#55028,#55029,
#55030,#55031,#55032,#55033,#55034,#55035,#55036,#55037,#55038,#55039,#55040,
#55041,#55042,#55043,#55044,#55045,#55046,#55047,#55048,#55049,#55050,#55051,
#55052,#55053,#55054,#55055,#55056,#55057,#55058,#55059,#55060,#55061,#55062,
#55063,#55064,#55065,#55066,#55067,#55068,#55069,#55070,#55071,#55072,#55073,
#55074,#55075,#55076,#55077,#55078,#55079,#55080,#55081,#55082,#55083,#55084,
#55085,#55086,#55087,#55088,#55089,#55090,#55091,#55092,#55093,#55094,#55095,
#55096,#55097,#55098,#55099,#55100,#55101,#55102,#55103,#55104,#55105,#55106,
#55107,#55108,#55109,#55110,#55111,#55112,#55113,#55114,#55115,#55116,#55117,
#55118,#55119,#55120,#55121,#55122,#55123,#55124,#55125,#55126,#55127,#55128,
#55129,#55130,#55131,#55132,#55133,#55134,#55135,#55136,#55137,#55138,#55139,
#55140,#55141,#55142,#55143,#55144,#55145,#55146,#55147,#55148,#55149,#55150,
#55151,#55152,#55153,#55154,#55155,#55156,#55157,#55158,#55159,#55160,#55161,
#55162,#55163,#55164,#55165,#55166,#55167,#55168,#55169,#55170,#55171,#55172,
#55173,#55174,#55175,#55176,#55177,#55178,#55179,#55180,#55181,#55182,#55183,
#55184,#55185,#55186,#55187,#55188,#55189,#55190,#55191,#55192,#55193,#55194,
#55195,#55196,#55197,#55198,#55199,#55200,#55201),.UNSPECIFIED.,.F.,.F.,
(4,2,2,2,2,2,2,2,2,2,2,2,2,2,2,2,2,2,2,2,2,2,2,2,2,2,2,2,2,2,2,2,2,2,2,
2,2,2,2,2,2,2,2,2,2,2,2,2,2,2,2,2,2,2,2,2,2,2,2,2,2,2,2,2,2,2,2,2,2,2,2,
2,2,2,2,2,2,2,2,2,2,2,2,2,2,2,2,2,2,2,2,2,2,2,2,2,2,2,2,2,2,2,2,2,4),(-1.10891213746094,
-1.1025633642418,-1.09675596498821,-1.09342079918388,-1.09049873079705,
-1.08684784268661,-1.07972500987875,-1.04984946772662,-1.01641280378912,
-1.01203215014507,-1.00993950979549,-1.00829694968953,-1.00630630431078,
-1.00244296863831,-0.997382484187126,-0.984949815622372,-0.947137552229913,
-0.933764272117823,-0.92905725596907,-0.925956683426332,-0.922960333752754,
-0.918782528297241,-0.908315985064879,-0.892645539132459,-0.863007997155038,
-0.848033052976157,-0.844754056027536,-0.842867547764913,-0.841210837261998,
-0.838965284184677,-0.833734379988036,-0.826179421124063,-0.801678757061201,
-0.77165171134716,-0.764535389508557,-0.76088589450098,-0.757964011777495,
-0.754628051859136,-0.748816601694433,-0.741684943745739,-0.725990412548922,
-0.696612974909208,-0.68143520548209,-0.678146421345032,-0.676257694871797,
-0.67460150521706,-0.672359971784562,-0.667152730616636,-0.659643961682607,
-0.635430963657303,-0.605008980703444,-0.597909140214804,-0.594263036266875,
-0.591341421426077,-0.588003111309202,-0.582180588827743,-0.547717074415929,
-0.516788018608673,-0.512232779815384,-0.510107292827893,-0.508462856755302,
-0.506498606252927,-0.502763688836621,-0.497920003563948,-0.486298037287833,
-0.464995829294303,-0.435862159743072,-0.430214682084528,-0.426881836216722,
-0.423987334639317,-0.420346945837214,-0.413037846239776,-0.403442054520717,
-0.377751919203769,-0.350404162156482,-0.345692216817802,-0.343560764867445,
-0.341912862038218,-0.339979054060065,-0.33638993902098,-0.307783451178721,
-0.271435876720952,-0.265122102020854,-0.261344529032147,-0.25840187089686,
-0.255177276220613,-0.249886250283688,-0.228057817584104,-0.197351102087575,
-0.181589326238876,-0.178268193931256,-0.176372201113465,-0.174717731899929,
-0.172489337486825,-0.167358551905306,-0.159998141976578,-0.136685618662079,
-0.105083823888635,-0.0979982857234888,-0.0943552260900261,-0.0914339671919788,
-0.0880937989132507,-0.0822620718678626,-0.0750984618859152,-0.0593641111093442),
 .UNSPECIFIED.);
#626=B_SPLINE_CURVE_WITH_KNOTS('',3,(#55207,#55208,#55209,#55210,#55211,
#55212,#55213,#55214,#55215,#55216,#55217,#55218,#55219,#55220,#55221,#55222,
#55223,#55224,#55225,#55226,#55227,#55228,#55229,#55230,#55231,#55232,#55233,
#55234,#55235,#55236,#55237,#55238,#55239,#55240,#55241,#55242,#55243,#55244,
#55245,#55246,#55247,#55248,#55249,#55250,#55251,#55252,#55253,#55254,#55255,
#55256,#55257,#55258,#55259,#55260,#55261,#55262,#55263,#55264,#55265,#55266,
#55267,#55268,#55269,#55270,#55271,#55272,#55273,#55274,#55275,#55276,#55277,
#55278,#55279,#55280,#55281,#55282,#55283,#55284,#55285,#55286,#55287,#55288,
#55289,#55290,#55291,#55292,#55293,#55294,#55295,#55296,#55297,#55298,#55299,
#55300,#55301,#55302,#55303,#55304,#55305,#55306,#55307,#55308,#55309,#55310,
#55311,#55312,#55313,#55314,#55315,#55316,#55317,#55318,#55319,#55320,#55321,
#55322,#55323,#55324,#55325,#55326,#55327,#55328,#55329,#55330,#55331,#55332,
#55333,#55334,#55335,#55336,#55337,#55338,#55339,#55340,#55341,#55342,#55343,
#55344,#55345,#55346,#55347,#55348,#55349,#55350,#55351,#55352,#55353,#55354,
#55355,#55356,#55357,#55358,#55359,#55360,#55361,#55362,#55363,#55364,#55365,
#55366,#55367,#55368,#55369,#55370,#55371,#55372),.UNSPECIFIED.,.F.,.F.,
(4,3,3,3,3,3,3,3,3,3,3,3,3,3,3,3,3,3,3,3,3,3,3,3,3,3,3,3,3,3,3,3,3,3,3,
3,3,3,3,3,3,3,3,3,3,3,3,3,3,3,3,3,3,3,3,4),(45.6442294067315,45.755562043948,
45.8671127049469,45.8863125840836,45.9961074696102,46.107074175724,46.2165666038188,
46.3259920438982,46.4353911890671,46.5475036714304,46.6570424939021,46.7704418062112,
46.8838411185202,46.9936360040466,47.1046027101604,47.2140951382552,47.3235205783346,
47.4329197235036,47.5450322058669,47.6545710283387,47.7679703406478,47.8813696529568,
47.9911645384834,48.1021312445971,48.211623672692,48.3210491127715,48.4304482579405,
48.5425607403037,48.6520995627755,48.7654988750845,48.8788981873934,48.9886930729199,
49.0996597790337,49.2091522071285,49.3185776472081,49.4279767923771,49.5400892747403,
49.649628097212,49.763027409521,49.87642672183,49.9862216073565,50.0971883134703,
50.2066807415652,50.3161061816448,50.4255053268137,50.5376178091769,50.6471566316488,
50.7605559439577,50.8739552562666,50.9830326905725,51.0919496345074,51.2007480886016,
51.3094873290939,51.418191872754,51.5269441665217,51.5753047126086),
 .UNSPECIFIED.);
#627=B_SPLINE_CURVE_WITH_KNOTS('',3,(#55373,#55374,#55375,#55376,#55377,
#55378,#55379,#55380,#55381,#55382,#55383,#55384,#55385,#55386,#55387,#55388,
#55389,#55390),.UNSPECIFIED.,.F.,.F.,(4,2,2,2,2,2,2,2,4),(-2.10014213462196,
-2.06257558601288,-2.05743286849352,-2.05352065982169,-2.05151969222044,
-2.04987707829303,-2.04779506593583,-2.04347211109637,-2.04133053968484),
 .UNSPECIFIED.);
#628=B_SPLINE_CURVE_WITH_KNOTS('',3,(#55392,#55393,#55394,#55395,#55396,
#55397,#55398,#55399,#55400,#55401,#55402,#55403,#55404,#55405,#55406,#55407,
#55408,#55409,#55410,#55411),.UNSPECIFIED.,.F.,.F.,(4,2,2,2,2,2,2,2,2,4),
(-0.0593641111093442,-0.0592945763534438,-0.0244898707930381,-0.014250358420362,
-0.0112791011793178,-0.00947879736946485,-0.00791757388433898,-0.00623963099242318,
-0.00362518939908151,-0.000491822792723786),.UNSPECIFIED.);
#629=B_SPLINE_CURVE_WITH_KNOTS('',3,(#55412,#55413,#55414,#55415,#55416,
#55417,#55418,#55419,#55420,#55421,#55422,#55423,#55424,#55425,#55426,#55427,
#55428,#55429,#55430,#55431,#55432,#55433,#55434,#55435,#55436,#55437,#55438,
#55439,#55440,#55441,#55442,#55443,#55444,#55445,#55446,#55447,#55448,#55449,
#55450,#55451,#55452,#55453,#55454,#55455,#55456,#55457,#55458,#55459,#55460,
#55461,#55462,#55463,#55464,#55465,#55466,#55467,#55468,#55469,#55470,#55471,
#55472,#55473,#55474,#55475,#55476,#55477,#55478,#55479,#55480,#55481,#55482,
#55483,#55484,#55485,#55486,#55487,#55488,#55489,#55490,#55491,#55492,#55493,
#55494,#55495,#55496,#55497,#55498,#55499,#55500,#55501,#55502,#55503,#55504,
#55505,#55506,#55507,#55508,#55509,#55510,#55511,#55512,#55513,#55514,#55515,
#55516,#55517,#55518,#55519,#55520,#55521,#55522,#55523,#55524,#55525,#55526,
#55527,#55528,#55529,#55530,#55531,#55532,#55533,#55534,#55535,#55536,#55537,
#55538,#55539,#55540,#55541,#55542,#55543,#55544,#55545,#55546,#55547,#55548,
#55549,#55550,#55551,#55552,#55553,#55554,#55555,#55556,#55557,#55558,#55559,
#55560,#55561,#55562,#55563,#55564,#55565,#55566,#55567,#55568,#55569,#55570,
#55571,#55572,#55573,#55574,#55575,#55576,#55577,#55578,#55579,#55580,#55581,
#55582,#55583,#55584,#55585,#55586,#55587,#55588,#55589,#55590,#55591,#55592,
#55593,#55594,#55595,#55596,#55597,#55598,#55599,#55600,#55601,#55602,#55603,
#55604,#55605,#55606,#55607,#55608,#55609,#55610,#55611,#55612,#55613,#55614,
#55615,#55616,#55617,#55618,#55619,#55620,#55621,#55622,#55623,#55624,#55625,
#55626,#55627,#55628,#55629,#55630,#55631,#55632,#55633,#55634,#55635,#55636,
#55637,#55638,#55639,#55640,#55641,#55642,#55643,#55644,#55645,#55646,#55647,
#55648,#55649,#55650,#55651,#55652,#55653,#55654,#55655,#55656,#55657,#55658,
#55659,#55660,#55661,#55662,#55663,#55664,#55665,#55666,#55667,#55668,#55669,
#55670,#55671),.UNSPECIFIED.,.F.,.F.,(4,2,2,2,2,2,2,2,2,2,2,2,2,2,2,2,2,
2,2,2,2,2,2,2,2,2,2,2,2,2,2,2,2,2,2,2,2,2,2,2,2,2,2,2,2,2,2,2,2,2,2,2,2,
2,2,2,2,2,2,2,2,2,2,2,2,2,2,2,2,2,2,2,2,2,2,2,2,2,2,2,2,2,2,2,2,2,2,2,2,
2,2,2,2,2,2,2,2,2,2,2,2,2,2,2,2,2,2,2,2,2,2,2,2,2,2,2,2,2,2,2,2,2,2,2,2,
2,2,2,2,4),(-2.10006909147699,-2.06042698248811,-2.03980647629323,-2.03146648594754,
-2.02763510315893,-2.02469359950251,-2.02146337858658,-2.01614706804224,
-1.9962000499577,-1.95269366760667,-1.94816988454401,-1.9456127155445,-1.94345601991161,
-1.94343583567694,-1.94341562285936,-1.94339537552586,-1.94337508765153,
-1.94335475310606,-1.94333436565094,-1.94332346393289,-1.94331229026595,
-1.94330083104297,-1.94328907174349,-1.94327699684956,-1.94326458976273,
-1.94325183269404,-1.94323870656951,-1.94322519089653,-1.94321126362617,
-1.94319690099945,-1.94318207737893,-1.94316676504375,-1.94315093398021,
-1.94313455162251,-1.94311758257521,-1.94309998828557,-1.94308172667756,
-1.94306275172435,-1.94304301296563,-1.94302245494273,-1.94300101655145,
-1.94297863027483,-1.94295522130587,-1.94293070650797,-1.9429049931827,
-1.94287797761661,-1.94284954334717,-1.94281955908304,-1.94278787619298,
-1.94275432565812,-1.94271871433806,-1.94268082036658,-1.9426509704841,
-1.94106261086972,-1.93892177710552,-1.93415824915268,-1.90981690568386,
-1.88889157001418,-1.86796294276235,-1.86272692591118,-1.85951375564633,
-1.85656712836847,-1.85276434150927,-1.8443535857145,-1.80489322408999,
-1.7834167699023,-1.7786722163301,-1.77651177960524,-1.77487916580743,-1.77294613552,
-1.76946084057255,-1.74764142224433,-1.72666562914355,-1.70171666859176,
-1.69626138724263,-1.69300111494656,-1.69006638979896,-1.68629198979989,
-1.68013322697073,-1.64170984436539,-1.61505485131496,-1.61138390437407,
-1.60943272697357,-1.60778665110324,-1.6056782471193,-1.60109476798526,
-1.57036777474382,-1.53571154464025,-1.52987941141069,-1.52653873141973,
-1.52361687344045,-1.5199728666579,-1.51288480756635,-1.48151926610307,
-1.45804627885887,-1.45065909735514,-1.44551377912789,-1.4432826365378,
-1.44162754666876,-1.4397325201904,-1.43641660695055,-1.42071035358183,
-1.38992362895068,-1.36806146041605,-1.36276742635263,-1.35954181364691,
-1.35659876059069,-1.35282142280912,-1.34650978290014,-1.31013975697264,
-1.2815396563814,-1.27797123007123,-1.27604159322631,-1.27439280202657,
-1.27225456611438,-1.26750592928128,-1.24199245658235,-1.21960968147045,
-1.20721341351749,-1.19836180926394,-1.19444110580818,-1.19148686272814,
-1.18829666656338,-1.18316827059753,-1.16617833419779,-1.13421088682827,
-1.11620325570252,-1.11182720358427,-1.10973528143656,-1.10915292416611),
 .UNSPECIFIED.);
#630=B_SPLINE_CURVE_WITH_KNOTS('',3,(#55677,#55678,#55679,#55680,#55681,
#55682,#55683,#55684,#55685,#55686,#55687,#55688,#55689,#55690,#55691,#55692,
#55693,#55694,#55695,#55696,#55697,#55698,#55699,#55700,#55701,#55702,#55703,
#55704,#55705,#55706,#55707,#55708,#55709,#55710,#55711,#55712,#55713,#55714,
#55715,#55716,#55717,#55718,#55719,#55720,#55721,#55722,#55723,#55724,#55725,
#55726,#55727,#55728,#55729,#55730,#55731,#55732,#55733,#55734,#55735,#55736,
#55737,#55738,#55739,#55740,#55741,#55742,#55743,#55744,#55745,#55746,#55747,
#55748,#55749,#55750,#55751,#55752,#55753,#55754,#55755,#55756,#55757,#55758,
#55759,#55760,#55761,#55762,#55763,#55764,#55765,#55766,#55767,#55768,#55769,
#55770,#55771,#55772,#55773,#55774,#55775,#55776,#55777,#55778,#55779,#55780,
#55781,#55782,#55783,#55784,#55785,#55786,#55787,#55788,#55789,#55790,#55791,
#55792,#55793,#55794,#55795,#55796,#55797,#55798,#55799,#55800,#55801,#55802,
#55803,#55804,#55805,#55806,#55807,#55808,#55809,#55810,#55811,#55812,#55813,
#55814,#55815,#55816,#55817,#55818,#55819,#55820,#55821,#55822,#55823,#55824,
#55825,#55826,#55827,#55828,#55829,#55830,#55831,#55832,#55833,#55834,#55835,
#55836,#55837,#55838,#55839,#55840,#55841,#55842,#55843,#55844,#55845,#55846,
#55847,#55848,#55849,#55850,#55851,#55852,#55853,#55854,#55855,#55856,#55857,
#55858,#55859,#55860,#55861,#55862,#55863,#55864,#55865,#55866,#55867,#55868,
#55869,#55870,#55871,#55872,#55873,#55874),.UNSPECIFIED.,.F.,.F.,(4,2,2,
2,2,2,2,2,2,2,2,2,2,2,2,2,2,2,2,2,2,2,2,2,2,2,2,2,2,2,2,2,2,2,2,2,2,2,2,
2,2,2,2,2,2,2,2,2,2,2,2,2,2,2,2,2,2,2,2,2,2,2,2,2,2,2,2,2,2,2,2,2,2,2,2,
2,2,2,2,2,2,2,2,2,2,2,2,2,2,2,2,2,2,2,2,2,2,2,4),(-0.991222341842758,-0.988736115830365,
-0.985429716872542,-0.982795938841155,-0.979242614379858,-0.97237936274641,
-0.947519773672175,-0.930290479672997,-0.907134999625649,-0.903645530734768,
-0.901711534824292,-0.900063332870706,-0.897894891023519,-0.893106279894226,
-0.886396860354405,-0.866690331178903,-0.830001964819376,-0.823706201888839,
-0.819933275710456,-0.816990721566128,-0.813762671172812,-0.808457685745978,
-0.786409302719088,-0.756874383810196,-0.747473952614986,-0.739061707527578,
-0.736287968513925,-0.734704989278039,-0.733019983597198,-0.730597830420924,
-0.724247191690939,-0.714373236978621,-0.692675034975813,-0.661142621969833,
-0.655506115389764,-0.652175401548015,-0.649280127069679,-0.645635326646925,
-0.638305155457721,-0.62867351816379,-0.602809969022405,-0.57570419916963,
-0.570981310248147,-0.568847690715342,-0.567199351129337,-0.565266535647471,
-0.561683013099233,-0.55709150769755,-0.513350292512699,-0.493703961778137,
-0.488402931426541,-0.485175984463718,-0.482233604856421,-0.478395525181586,
-0.47001767855272,-0.447878611317424,-0.40878714859733,-0.404208972333476,
-0.402079171605349,-0.400434372151114,-0.398473261013458,-0.394753734461102,
-0.389935915374499,-0.378409162882555,-0.357003699504285,-0.327747189498164,
-0.322071754712161,-0.318764586794498,-0.316131316457517,-0.31258013407555,
-0.305726186973548,-0.280935442020369,-0.263662120324144,-0.240476898439039,
-0.236987752763299,-0.235053980647722,-0.233405999141088,-0.231237886185148,
-0.226450149586381,-0.219742070273756,-0.200040491879911,-0.163350076492882,
-0.15705717722147,-0.153285322170092,-0.150426831357105,-0.147370968562231,
-0.143046309003511,-0.137612748193346,-0.127188487944933,-0.10056308469208,
-0.0980535496024327,-0.0738493315394838,-0.0703514591928269,-0.0684157770337268,
-0.0667681107699831,-0.0646029501361435,-0.0598313828507849,-0.0380777263262519,
-0.000492602108507802),.UNSPECIFIED.);
#631=B_SPLINE_CURVE_WITH_KNOTS('',3,(#55875,#55876,#55877,#55878,#55879,
#55880,#55881,#55882,#55883,#55884,#55885,#55886,#55887),.UNSPECIFIED.,
 .F.,.F.,(4,3,3,3,4),(45.292119405429,45.4031325580051,45.5141760165917,
45.6253344673629,45.6442294067315),.UNSPECIFIED.);
#632=B_SPLINE_CURVE_WITH_KNOTS('',3,(#55888,#55889,#55890,#55891,#55892,
#55893,#55894,#55895,#55896,#55897,#55898,#55899,#55900,#55901,#55902,#55903,
#55904,#55905,#55906,#55907,#55908,#55909,#55910,#55911,#55912,#55913,#55914,
#55915,#55916,#55917,#55918,#55919,#55920,#55921,#55922,#55923,#55924,#55925,
#55926,#55927,#55928,#55929,#55930,#55931,#55932,#55933,#55934,#55935,#55936,
#55937,#55938,#55939,#55940,#55941,#55942,#55943,#55944,#55945,#55946,#55947,
#55948,#55949,#55950,#55951,#55952,#55953,#55954,#55955,#55956,#55957,#55958,
#55959,#55960,#55961,#55962,#55963,#55964,#55965,#55966,#55967,#55968,#55969,
#55970,#55971,#55972,#55973,#55974,#55975,#55976,#55977,#55978,#55979,#55980,
#55981,#55982,#55983,#55984,#55985,#55986,#55987,#55988,#55989,#55990,#55991,
#55992,#55993,#55994,#55995,#55996,#55997,#55998,#55999,#56000,#56001,#56002,
#56003,#56004,#56005,#56006,#56007,#56008,#56009,#56010,#56011,#56012,#56013,
#56014,#56015,#56016,#56017,#56018,#56019,#56020,#56021,#56022,#56023,#56024,
#56025,#56026,#56027,#56028,#56029,#56030,#56031,#56032,#56033,#56034,#56035,
#56036,#56037,#56038,#56039,#56040,#56041,#56042,#56043,#56044,#56045,#56046,
#56047,#56048,#56049,#56050,#56051,#56052,#56053,#56054,#56055,#56056,#56057,
#56058,#56059,#56060,#56061,#56062,#56063,#56064,#56065,#56066,#56067,#56068,
#56069,#56070,#56071,#56072,#56073,#56074,#56075,#56076,#56077,#56078,#56079,
#56080,#56081,#56082,#56083,#56084,#56085,#56086,#56087,#56088,#56089,#56090,
#56091,#56092,#56093),.UNSPECIFIED.,.F.,.F.,(4,2,2,2,2,2,2,2,2,2,2,2,2,
2,2,2,2,2,2,2,2,2,2,2,2,2,2,2,2,2,2,2,2,2,2,2,2,2,2,2,2,2,2,2,2,2,2,2,2,
2,2,2,2,2,2,2,2,2,2,2,2,2,2,2,2,2,2,2,2,2,2,2,2,2,2,2,2,2,2,2,2,2,2,2,2,
2,2,2,2,2,2,2,2,2,2,2,2,2,2,2,2,2,4),(-1.10915292416611,-1.10825079081598,
-1.1063292457688,-1.10289549192893,-1.08373122537149,-1.05032496968337,
-1.034182926507,-1.02917413652272,-1.02600957642963,-1.02304572664456,-1.0190614413913,
-1.00983003115074,-0.996699510755589,-0.974812585359114,-0.969892933399924,
-0.948188552366218,-0.944704778830646,-0.942772132535236,-0.941139560443809,
-0.938978777311095,-0.934232014918134,-0.912731628609526,-0.873210557968264,
-0.86494358154075,-0.861108709719495,-0.85815753172259,-0.854959575707928,
-0.849793919947537,-0.8299010179121,-0.808108115825579,-0.80243886498364,
-0.781526984439174,-0.778053098808981,-0.776122729579546,-0.77448995192073,
-0.772326122139348,-0.767562066886004,-0.745884970981147,-0.705803009331144,
-0.697938340202351,-0.694193146788012,-0.691262126798466,-0.687986381573837,
-0.682457315225892,-0.655683597708827,-0.616535719565333,-0.611970389837679,
-0.609843019397428,-0.608198443177589,-0.606235604667619,-0.602507540321231,
-0.597675354062329,-0.586095646882868,-0.564748692695435,-0.53552226810327,
-0.529847010859261,-0.526539953097078,-0.523906770614772,-0.52035570345531,
-0.513501949899647,-0.488711339626953,-0.471441110104947,-0.448259215918448,
-0.444770263564931,-0.442836574476547,-0.441188643516863,-0.43902055935761,
-0.434232728108947,-0.427524365655815,-0.407820441283542,-0.371143199941577,
-0.364848511758308,-0.361076221795289,-0.358134154423512,-0.354906625022364,
-0.34960245615806,-0.327556027713085,-0.29809201700578,-0.290151711519928,
-0.280500342728967,-0.277587680632365,-0.275800206820813,-0.274104153945243,
-0.27162191162735,-0.264846607656808,-0.254018215977439,-0.232211835145648,
-0.204762088487403,-0.197717886763157,-0.194083215877829,-0.191162420136257,
-0.187815947342846,-0.181955129649531,-0.148651351729641,-0.116513062467537,
-0.112089796990142,-0.109981402893426,-0.108335548915263,-0.106384922637174,
-0.102715710338574,-0.0979818938659247,-0.086760354592038,-0.0595119917279155),
 .UNSPECIFIED.);
#633=B_SPLINE_CURVE_WITH_KNOTS('',3,(#56098,#56099,#56100,#56101,#56102,
#56103,#56104,#56105,#56106,#56107,#56108,#56109,#56110,#56111,#56112,#56113,
#56114,#56115,#56116,#56117,#56118,#56119,#56120,#56121,#56122,#56123,#56124,
#56125,#56126,#56127,#56128,#56129,#56130,#56131,#56132,#56133,#56134,#56135,
#56136,#56137,#56138,#56139,#56140,#56141,#56142,#56143,#56144,#56145,#56146,
#56147,#56148,#56149,#56150,#56151,#56152,#56153,#56154,#56155,#56156,#56157,
#56158,#56159,#56160,#56161,#56162,#56163,#56164,#56165,#56166,#56167,#56168,
#56169,#56170,#56171,#56172,#56173,#56174,#56175,#56176,#56177,#56178,#56179,
#56180,#56181,#56182,#56183,#56184,#56185,#56186,#56187,#56188,#56189,#56190,
#56191,#56192,#56193,#56194,#56195,#56196,#56197,#56198,#56199,#56200,#56201,
#56202,#56203,#56204,#56205,#56206,#56207,#56208,#56209,#56210,#56211,#56212,
#56213,#56214,#56215,#56216,#56217,#56218,#56219,#56220,#56221,#56222,#56223,
#56224,#56225,#56226,#56227,#56228,#56229,#56230,#56231,#56232,#56233,#56234,
#56235,#56236,#56237,#56238,#56239,#56240,#56241,#56242,#56243,#56244,#56245,
#56246,#56247,#56248,#56249,#56250,#56251,#56252,#56253,#56254,#56255,#56256,
#56257,#56258,#56259,#56260,#56261,#56262,#56263,#56264,#56265,#56266,#56267,
#56268,#56269,#56270,#56271,#56272,#56273,#56274,#56275,#56276,#56277,#56278,
#56279,#56280,#56281,#56282,#56283,#56284,#56285,#56286,#56287,#56288,#56289,
#56290,#56291,#56292,#56293,#56294,#56295),.UNSPECIFIED.,.F.,.F.,(4,2,2,
2,2,2,2,2,2,2,2,2,2,2,2,2,2,2,2,2,2,2,2,2,2,2,2,2,2,2,2,2,2,2,2,2,2,2,2,
2,2,2,2,2,2,2,2,2,2,2,2,2,2,2,2,2,2,2,2,2,2,2,2,2,2,2,2,2,2,2,2,2,2,2,2,
2,2,2,2,2,2,2,2,2,2,2,2,2,2,2,2,2,2,2,2,2,2,2,4),(-2.04125292518874,-2.03894385906771,
-2.0086167602156,-1.9987512842822,-1.99063901794145,-1.98680858232649,-1.98386672724615,
-1.98063505013605,-1.97531385257718,-1.95529170396841,-1.91182131686073,
-1.90522195471023,-1.90276389947667,-1.90107210296551,-1.89949808281679,
-1.89677059908336,-1.88873496970261,-1.87884691711931,-1.84929135617849,
-1.82723320617522,-1.82192692860413,-1.81869837618869,-1.8157555554526,
-1.81198255346591,-1.805687322463,-1.76901551993487,-1.74931893601361,-1.7426115061407,
-1.73782343040583,-1.735654957439,-1.73400659546301,-1.73207228034356,-1.72858187445159,
-1.70540462604948,-1.68815013902088,-1.66329142738332,-1.65642812632849,
-1.65287458858188,-1.6502405978268,-1.64693384168821,-1.64126246351765,
-1.61146634867061,-1.58996633424274,-1.57885772947006,-1.57415475056505,
-1.57050358363136,-1.56855643539007,-1.56690974422363,-1.56479554535921,
-1.56018091462033,-1.5212275442612,-1.49428882348829,-1.48875217555391,
-1.48547435892506,-1.48254298373868,-1.47879940539059,-1.47094602709401,
-1.43086114350963,-1.40918592963673,-1.40442145407425,-1.40225729315876,
-1.4006241911428,-1.39869339030437,-1.39521856928128,-1.37431388654119,
-1.3693983096508,-1.35200433253846,-1.32741732477023,-1.32197815909426,
-1.31872113395761,-1.3157853426765,-1.31200397973758,-1.30582179682574,
-1.2603921976727,-1.24195914797297,-1.23753472188651,-1.23543340192903,
-1.23394771856894,-1.23203233495851,-1.22862692917518,-1.2105229577108,
-1.16505843700595,-1.15697142647289,-1.15318503265454,-1.15024872501543,
-1.14699457244317,-1.14156845026328,-1.11988391122826,-1.08606896867069,
-1.07728730461913,-1.07144720620063,-1.0691021411999,-1.0674303954053,-1.06559159566497,
-1.06244592629941,-1.05027315976444,-1.0243561927847,-0.994406655279623,
-0.991222341842758),.UNSPECIFIED.);
#634=B_SPLINE_CURVE_WITH_KNOTS('',3,(#56297,#56298,#56299,#56300,#56301,
#56302,#56303,#56304,#56305,#56306,#56307,#56308,#56309,#56310,#56311,#56312,
#56313,#56314,#56315,#56316),.UNSPECIFIED.,.F.,.F.,(4,2,2,2,2,2,2,2,2,4),
(-0.0595119917279155,-0.0586930344537183,-0.0373482121527803,-0.0313487865350335,
-0.0276208962624948,-0.0246916304183028,-0.0219520084146087,-0.0187213524838508,
-0.0116698606299128,-0.000491772399311334),.UNSPECIFIED.);
#635=B_SPLINE_CURVE_WITH_KNOTS('',3,(#56317,#56318,#56319,#56320,#56321,
#56322,#56323,#56324,#56325,#56326,#56327,#56328,#56329,#56330,#56331,#56332,
#56333,#56334,#56335,#56336,#56337,#56338,#56339,#56340,#56341,#56342,#56343,
#56344,#56345,#56346,#56347,#56348,#56349,#56350,#56351,#56352,#56353,#56354,
#56355,#56356,#56357,#56358,#56359,#56360,#56361,#56362,#56363,#56364,#56365,
#56366,#56367,#56368,#56369,#56370,#56371,#56372,#56373,#56374,#56375,#56376,
#56377,#56378,#56379,#56380,#56381,#56382,#56383,#56384,#56385,#56386,#56387,
#56388,#56389,#56390,#56391,#56392,#56393,#56394,#56395,#56396,#56397,#56398,
#56399,#56400,#56401,#56402,#56403,#56404,#56405,#56406,#56407,#56408,#56409,
#56410,#56411,#56412,#56413,#56414,#56415,#56416,#56417,#56418,#56419,#56420,
#56421,#56422,#56423,#56424,#56425,#56426,#56427,#56428,#56429,#56430,#56431,
#56432,#56433,#56434,#56435,#56436,#56437,#56438,#56439,#56440,#56441,#56442,
#56443,#56444,#56445,#56446,#56447,#56448,#56449,#56450,#56451,#56452,#56453,
#56454,#56455,#56456,#56457,#56458,#56459,#56460,#56461,#56462,#56463,#56464,
#56465,#56466,#56467,#56468,#56469,#56470,#56471,#56472,#56473,#56474,#56475,
#56476,#56477,#56478,#56479,#56480,#56481,#56482,#56483,#56484,#56485,#56486,
#56487,#56488,#56489,#56490,#56491,#56492,#56493,#56494,#56495,#56496,#56497,
#56498,#56499,#56500,#56501,#56502,#56503,#56504,#56505,#56506,#56507,#56508),
 .UNSPECIFIED.,.F.,.F.,(4,2,2,2,2,2,2,2,2,2,2,2,2,2,2,2,2,2,2,2,2,2,2,2,
2,2,2,2,2,2,2,2,2,2,2,2,2,2,2,2,2,2,2,2,2,2,2,2,2,2,2,2,2,2,2,2,2,2,2,2,
2,2,2,2,2,2,2,2,2,2,2,2,2,2,2,2,2,2,2,2,2,2,2,2,2,2,2,2,2,2,2,2,2,2,2,4),
(-2.09985264300038,-2.07634126040968,-2.0477689920784,-2.04419976479163,
-2.04226962137628,-2.04062035027246,-2.03848143268273,-2.03390404652844,
-2.00367752407994,-1.97990014181989,-1.97070510626822,-1.96369652470103,
-1.96018700760897,-1.95731214266405,-1.95400536132066,-1.94833536546717,
-1.91899508832036,-1.89188103455156,-1.88393026275446,-1.87849779140609,
-1.87621791806677,-1.87455590342492,-1.87268611498573,-1.86939907698012,
-1.8550482065297,-1.82377445548619,-1.80100035802833,-1.79565283567918,
-1.79241516797978,-1.78947425041419,-1.78571772784181,-1.77948155930131,
-1.7419519284354,-1.71468113426106,-1.71091699538094,-1.70894621044565,
-1.70730159572318,-1.70518264378745,-1.70066528096452,-1.66924956737454,
-1.63516145693111,-1.62932990872132,-1.62598885726903,-1.62306626476174,
-1.61942080460461,-1.61232818849689,-1.58125977909918,-1.55754893325383,
-1.55012152043423,-1.54495513727622,-1.54272006680958,-1.54106416116889,
-1.53917061969497,-1.53586246591984,-1.52030333385083,-1.491369123967,-1.47561549844014,
-1.46846572503323,-1.46264273169486,-1.45930353940011,-1.45638080715795,
-1.45273285379155,-1.44562790888823,-1.41536663362571,-1.39104426208925,
-1.38351736472024,-1.37829988427577,-1.37605612779594,-1.37439914198933,
-1.37251052066494,-1.36922399137595,-1.35411744860148,-1.32460582471591,
-1.30890549408723,-1.30177142889655,-1.29595846626567,-1.29262145640245,
-1.2896985584405,-1.28604766821214,-1.27892817879026,-1.24896296684978,
-1.22442902039424,-1.21318670327752,-1.21022695482445,-1.20842874223766,
-1.20675744247451,-1.20470659342738,-1.20067066639486,-1.16834932325329,
-1.13513191413727,-1.12928549372802,-1.12594145994443,-1.12301946258418,
-1.11937894018971,-1.11230940815688,-1.10892217029559),.UNSPECIFIED.);
#636=B_SPLINE_CURVE_WITH_KNOTS('',3,(#56514,#56515,#56516,#56517,#56518,
#56519,#56520,#56521,#56522,#56523,#56524,#56525,#56526,#56527,#56528,#56529,
#56530,#56531,#56532,#56533,#56534,#56535,#56536,#56537,#56538,#56539,#56540,
#56541,#56542,#56543,#56544,#56545,#56546,#56547,#56548,#56549,#56550,#56551,
#56552,#56553,#56554,#56555,#56556,#56557,#56558,#56559,#56560,#56561,#56562,
#56563,#56564,#56565,#56566,#56567,#56568,#56569,#56570,#56571,#56572,#56573,
#56574,#56575,#56576,#56577,#56578,#56579,#56580,#56581,#56582,#56583,#56584,
#56585,#56586,#56587,#56588,#56589,#56590,#56591,#56592,#56593,#56594,#56595,
#56596,#56597,#56598,#56599,#56600,#56601,#56602,#56603,#56604,#56605,#56606,
#56607,#56608,#56609,#56610,#56611,#56612,#56613,#56614,#56615,#56616,#56617,
#56618,#56619,#56620,#56621,#56622,#56623,#56624,#56625,#56626,#56627,#56628,
#56629,#56630,#56631,#56632,#56633,#56634,#56635,#56636,#56637,#56638,#56639,
#56640,#56641,#56642,#56643,#56644,#56645,#56646,#56647,#56648,#56649,#56650,
#56651,#56652,#56653,#56654,#56655,#56656,#56657,#56658,#56659,#56660,#56661,
#56662,#56663,#56664,#56665,#56666,#56667,#56668,#56669,#56670,#56671,#56672,
#56673,#56674,#56675,#56676,#56677,#56678,#56679,#56680,#56681,#56682,#56683,
#56684,#56685,#56686,#56687,#56688,#56689,#56690,#56691,#56692,#56693,#56694,
#56695,#56696,#56697,#56698,#56699,#56700,#56701,#56702,#56703,#56704,#56705,
#56706,#56707,#56708,#56709,#56710,#56711),.UNSPECIFIED.,.F.,.F.,(4,2,2,
2,2,2,2,2,2,2,2,2,2,2,2,2,2,2,2,2,2,2,2,2,2,2,2,2,2,2,2,2,2,2,2,2,2,2,2,
2,2,2,2,2,2,2,2,2,2,2,2,2,2,2,2,2,2,2,2,2,2,2,2,2,2,2,2,2,2,2,2,2,2,2,2,
2,2,2,2,2,2,2,2,2,2,2,2,2,2,2,2,2,2,2,2,2,2,2,4),(-0.991342359623623,-0.975835741061672,
-0.971794971303946,-0.969743212814923,-0.968072009170711,-0.966275028603975,
-0.963319374625724,-0.952121241183367,-0.927768063492579,-0.897528344122859,
-0.890422007491915,-0.88677445412746,-0.883852594659744,-0.880515003648459,
-0.874696371383313,-0.841004067262,-0.809194504970679,-0.80475635347989,
-0.802644998649867,-0.800998853951234,-0.799050350652882,-0.795391476131473,
-0.790674925746254,-0.779515916321856,-0.758056026301051,-0.728274550313147,
-0.722603026298116,-0.71929668125776,-0.716663283719795,-0.713110911863436,
-0.706251058904969,-0.681414394153353,-0.664173309890699,-0.641010840331872,
-0.637521770485119,-0.635588009058922,-0.633940015803678,-0.631771860119216,
-0.626983925141381,-0.620275487243704,-0.600572143853975,-0.563887321355189,
-0.557592417685907,-0.553819985285405,-0.550877804085015,-0.547650150454212,
-0.542345788290194,-0.52029942361843,-0.490783397563295,-0.481730749060472,
-0.473028532839146,-0.470220605273364,-0.468456040720251,-0.466744374073428,
-0.464183686712158,-0.456819858487764,-0.444595292746979,-0.408196906789883,
-0.393413768926188,-0.388553455325311,-0.385420683702292,-0.382442721578806,
-0.378370326822386,-0.368591201930815,-0.354363130366284,-0.333746464794258,
-0.327283429937007,-0.307663483050674,-0.304218190638545,-0.302294269442552,
-0.300660627497915,-0.298487399945628,-0.293670763739243,-0.286908483169456,
-0.266925607332375,-0.230666924039089,-0.224347649236332,-0.22056846853901,
-0.217625527026843,-0.214401607785031,-0.209113985222482,-0.187344644158807,
-0.167058649673325,-0.143036928693502,-0.138294097017229,-0.136157184391538,
-0.134508828517522,-0.132953913036267,-0.130112873812364,-0.118903817561915,
-0.0944770245339817,-0.0643468468871919,-0.057236613713599,-0.0535885291722072,
-0.0506669537412706,-0.0473304568577627,-0.0415157530421755,-0.0343788544218471,
-0.00049243862796517),.UNSPECIFIED.);
#637=B_SPLINE_CURVE_WITH_KNOTS('',3,(#56712,#56713,#56714,#56715,#56716,
#56717,#56718,#56719,#56720,#56721,#56722,#56723,#56724,#56725,#56726,#56727,
#56728,#56729),.UNSPECIFIED.,.F.,.F.,(4,2,2,2,2,2,2,2,4),(-2.10003863830129,
-2.07623146422239,-2.07278785006591,-2.07065464050834,-2.0690363565175,
-2.0674037107728,-2.06546955883118,-2.06197975505772,-2.04125292518874),
 .UNSPECIFIED.);
#638=B_SPLINE_CURVE_WITH_KNOTS('',3,(#56730,#56731,#56732,#56733,#56734,
#56735,#56736,#56737,#56738,#56739,#56740,#56741,#56742,#56743,#56744,#56745,
#56746,#56747,#56748,#56749,#56750,#56751,#56752,#56753,#56754,#56755,#56756,
#56757,#56758,#56759,#56760,#56761,#56762,#56763,#56764,#56765,#56766,#56767,
#56768,#56769,#56770,#56771,#56772,#56773,#56774,#56775,#56776,#56777,#56778,
#56779,#56780,#56781,#56782,#56783,#56784,#56785,#56786,#56787,#56788,#56789,
#56790,#56791,#56792,#56793,#56794,#56795,#56796,#56797,#56798,#56799,#56800,
#56801,#56802,#56803,#56804,#56805,#56806,#56807,#56808,#56809,#56810,#56811,
#56812,#56813,#56814,#56815,#56816,#56817,#56818,#56819,#56820,#56821,#56822,
#56823,#56824,#56825,#56826,#56827,#56828,#56829,#56830,#56831,#56832,#56833,
#56834,#56835,#56836,#56837,#56838,#56839,#56840,#56841,#56842,#56843,#56844,
#56845,#56846,#56847,#56848,#56849,#56850,#56851,#56852,#56853,#56854,#56855,
#56856,#56857,#56858,#56859,#56860,#56861,#56862,#56863,#56864,#56865,#56866,
#56867,#56868,#56869,#56870,#56871,#56872,#56873,#56874,#56875,#56876,#56877,
#56878,#56879,#56880,#56881,#56882,#56883,#56884,#56885,#56886,#56887,#56888,
#56889,#56890,#56891,#56892,#56893,#56894,#56895,#56896,#56897,#56898,#56899,
#56900,#56901,#56902,#56903,#56904,#56905,#56906,#56907,#56908,#56909,#56910,
#56911,#56912,#56913,#56914,#56915,#56916,#56917,#56918,#56919,#56920,#56921,
#56922,#56923,#56924,#56925,#56926,#56927,#56928,#56929,#56930,#56931),
 .UNSPECIFIED.,.F.,.F.,(4,2,2,2,2,2,2,2,2,2,2,2,2,2,2,2,2,2,2,2,2,2,2,2,
2,2,2,2,2,2,2,2,2,2,2,2,2,2,2,2,2,2,2,2,2,2,2,2,2,2,2,2,2,2,2,2,2,2,2,2,
2,2,2,2,2,2,2,2,2,2,2,2,2,2,2,2,2,2,2,2,2,2,2,2,2,2,2,2,2,2,2,2,2,2,2,2,
2,2,2,2,4),(-1.10892217029559,-1.07977061052498,-1.05716920039812,-1.04992924047292,
-1.04486002851235,-1.04266549991244,-1.04100992873101,-1.03911560203961,
-1.03571400353351,-1.01627636280745,-0.984411849646787,-0.967153296080242,
-0.961999934824887,-0.958804169550778,-0.955851415031561,-0.951942584082718,
-0.943161785897095,-0.930902592489248,-0.909029488294242,-0.882809097489435,
-0.878053163624821,-0.875913518789525,-0.87426444993826,-0.87233549498649,
-0.868770758403794,-0.864210344046972,-0.820568312949517,-0.800799331652675,
-0.795476441022647,-0.792244627651719,-0.789303225026949,-0.785474199084657,
-0.777148459163312,-0.757063927222483,-0.736613062583773,-0.714189528100988,
-0.710702658399633,-0.70876932791681,-0.70713686119596,-0.704977106573372,
-0.700235985337598,-0.678792316347286,-0.63944817301007,-0.630911625566706,
-0.627087149890059,-0.624137522882779,-0.620934841114427,-0.61574710587523,
-0.595536204111023,-0.573963587623792,-0.567249067055552,-0.547481566526644,
-0.544032326559917,-0.542107459018176,-0.540473853577796,-0.538301761381941,
-0.533491848869111,-0.526742255744353,-0.50682574584309,-0.470468009964309,
-0.464154122883258,-0.460376354461172,-0.457433470609105,-0.454208554046077,
-0.448916827016657,-0.427082142033797,-0.396359823121102,-0.380611628413457,
-0.377291981024385,-0.375396229468092,-0.373741538414354,-0.371512267349576,
-0.366377026296749,-0.35900820694939,-0.335647175203267,-0.304104335968121,
-0.297017436280988,-0.293373916451746,-0.290452404761072,-0.287112073825418,
-0.281280395793052,-0.274117027901466,-0.258314683090749,-0.229447591516495,
-0.213959816265293,-0.210656215495483,-0.20876409421353,-0.207108606424764,
-0.204872950091473,-0.199700445513516,-0.19225937055201,-0.16846260644167,
-0.137546108323334,-0.130419868389251,-0.126768253711598,-0.123846104205907,
-0.12051138894092,-0.114927369485567,-0.0925606574938055,-0.0692245969056221,
-0.0592684060220813),.UNSPECIFIED.);
#639=B_SPLINE_CURVE_WITH_KNOTS('',3,(#56936,#56937,#56938,#56939,#56940,
#56941,#56942,#56943,#56944,#56945,#56946,#56947,#56948,#56949,#56950,#56951,
#56952,#56953,#56954,#56955,#56956,#56957,#56958,#56959,#56960,#56961,#56962,
#56963,#56964,#56965,#56966,#56967,#56968,#56969,#56970,#56971,#56972,#56973,
#56974,#56975,#56976,#56977,#56978,#56979,#56980,#56981,#56982,#56983,#56984,
#56985,#56986,#56987,#56988,#56989,#56990,#56991,#56992,#56993,#56994,#56995,
#56996,#56997,#56998,#56999,#57000,#57001,#57002,#57003,#57004,#57005,#57006,
#57007,#57008,#57009,#57010,#57011,#57012,#57013,#57014,#57015,#57016,#57017,
#57018,#57019,#57020,#57021,#57022,#57023,#57024,#57025,#57026,#57027,#57028,
#57029,#57030,#57031,#57032,#57033,#57034,#57035,#57036,#57037,#57038,#57039,
#57040,#57041,#57042,#57043,#57044,#57045,#57046,#57047,#57048,#57049,#57050,
#57051,#57052,#57053,#57054,#57055,#57056,#57057,#57058,#57059,#57060,#57061,
#57062,#57063,#57064,#57065,#57066,#57067,#57068,#57069,#57070,#57071,#57072,
#57073,#57074,#57075,#57076,#57077,#57078,#57079,#57080,#57081,#57082,#57083,
#57084,#57085,#57086,#57087,#57088,#57089,#57090,#57091,#57092,#57093,#57094,
#57095,#57096,#57097,#57098,#57099,#57100,#57101,#57102,#57103,#57104,#57105,
#57106,#57107,#57108,#57109,#57110,#57111,#57112,#57113,#57114,#57115,#57116,
#57117,#57118,#57119,#57120,#57121,#57122,#57123,#57124,#57125,#57126,#57127,
#57128,#57129,#57130,#57131,#57132,#57133,#57134,#57135,#57136,#57137,#57138,
#57139,#57140,#57141,#57142,#57143,#57144,#57145,#57146,#57147,#57148,#57149,
#57150,#57151,#57152,#57153,#57154,#57155),.UNSPECIFIED.,.F.,.F.,(4,2,2,
2,2,2,2,2,2,2,2,2,2,2,2,2,2,2,2,2,2,2,2,2,2,2,2,2,2,2,2,2,2,2,2,2,2,2,2,
2,2,2,2,2,2,2,2,2,2,2,2,2,2,2,2,2,2,2,2,2,2,2,2,2,2,2,2,2,2,2,2,2,2,2,2,
2,2,2,2,2,2,2,2,2,2,2,2,2,2,2,2,2,2,2,2,2,2,2,2,2,2,2,2,2,2,2,2,2,2,4),
(-2.04107968292539,-2.03912981917729,-2.0048225815275,-1.98351435642058,
-1.97650461157569,-1.97166709581427,-1.96954725840733,-1.9695285662276,
-1.96950978091368,-1.96949089720669,-1.9694719097205,-1.96945281294638,
-1.96943360124378,-1.96941426883361,-1.96939480978555,-1.96937521801775,
-1.96935548728387,-1.96933561116716,-1.96931558306975,-1.96768229331185,
-1.96575619541819,-1.9623010616684,-1.94230173381455,-1.9363019019545,-1.91613618146969,
-1.89421833913387,-1.88892149847947,-1.88569557019274,-1.88275313205163,
-1.87897783864951,-1.87267247716432,-1.83620825638503,-1.81638736440693,
-1.80965665605659,-1.80485646689005,-1.80268618791043,-1.80105282377578,
-1.79912693680099,-1.79567286095932,-1.77571946601929,-1.76913999928947,
-1.74748708344607,-1.72736324038356,-1.72218144260936,-1.71898014772262,
-1.71603030302744,-1.71220343282242,-1.70365209525522,-1.66434714192865,
-1.64292097543161,-1.63818169056154,-1.63602236387148,-1.63439002904643,
-1.63245666470425,-1.62896924848144,-1.6064982183182,-1.58606343303989,
-1.56597522035059,-1.55764800827625,-1.55381889592321,-1.55087769236065,
-1.54764636768968,-1.54232490151658,-1.52256891253161,-1.47895025392957,
-1.47439047428474,-1.47082595849344,-1.46889720594573,-1.46724838536718,
-1.46510913243169,-1.46035444640193,-1.43408802627636,-1.39878650370007,
-1.39078641298447,-1.38701616642852,-1.38408211823684,-1.38081999444658,
-1.37535530481451,-1.35304886052624,-1.3198322720283,-1.31111597266874,
-1.30530757804627,-1.30296768369608,-1.30129696484661,-1.2994563381938,
-1.29630154351432,-1.28399906419146,-1.25639063979944,-1.22812636576549,
-1.22254554291355,-1.21925860776149,-1.21632945573473,-1.21260294499472,
-1.20660840436975,-1.16655994392253,-1.14140035187514,-1.13762737104125,
-1.13565516393516,-1.134011272871,-1.13189571311841,-1.12739418954014,-1.09573079631599,
-1.0624488105668,-1.05630214962849,-1.05289547679305,-1.05027172928781,
-1.04684103859437,-1.0405789325978,-1.00799398371958,-0.991342359623623),
 .UNSPECIFIED.);
#640=B_SPLINE_CURVE_WITH_KNOTS('',3,(#57157,#57158,#57159,#57160,#57161,
#57162,#57163,#57164,#57165,#57166,#57167,#57168,#57169,#57170,#57171,#57172,
#57173,#57174),.UNSPECIFIED.,.F.,.F.,(4,2,2,2,2,2,2,2,4),(-0.0592684060220813,
-0.0476535235343102,-0.0441711697069289,-0.0422389384242401,-0.0406064702951486,
-0.0384455037053382,-0.0360426986767971,-0.0291414406123908,-0.000492293290300633),
 .UNSPECIFIED.);
#641=B_SPLINE_CURVE_WITH_KNOTS('',3,(#57175,#57176,#57177,#57178,#57179,
#57180,#57181,#57182,#57183,#57184,#57185,#57186,#57187,#57188,#57189,#57190,
#57191,#57192,#57193,#57194,#57195,#57196,#57197,#57198,#57199,#57200,#57201,
#57202,#57203,#57204,#57205,#57206,#57207,#57208,#57209,#57210,#57211,#57212,
#57213,#57214,#57215,#57216,#57217,#57218,#57219,#57220,#57221,#57222,#57223,
#57224,#57225,#57226,#57227,#57228,#57229,#57230,#57231,#57232,#57233,#57234,
#57235,#57236,#57237,#57238,#57239,#57240,#57241,#57242,#57243,#57244,#57245,
#57246,#57247,#57248,#57249,#57250,#57251,#57252,#57253,#57254,#57255,#57256,
#57257,#57258,#57259,#57260,#57261,#57262,#57263,#57264,#57265,#57266,#57267,
#57268,#57269,#57270,#57271,#57272,#57273,#57274,#57275,#57276,#57277,#57278,
#57279,#57280,#57281,#57282,#57283,#57284,#57285,#57286,#57287,#57288,#57289,
#57290,#57291,#57292,#57293,#57294,#57295,#57296,#57297,#57298,#57299,#57300,
#57301,#57302,#57303,#57304,#57305,#57306,#57307,#57308,#57309,#57310,#57311,
#57312,#57313,#57314,#57315,#57316,#57317,#57318,#57319,#57320,#57321,#57322,
#57323,#57324,#57325,#57326,#57327,#57328,#57329,#57330,#57331,#57332,#57333,
#57334,#57335,#57336,#57337,#57338,#57339,#57340,#57341,#57342,#57343,#57344,
#57345,#57346,#57347,#57348,#57349,#57350,#57351,#57352,#57353,#57354,#57355,
#57356,#57357,#57358,#57359,#57360,#57361,#57362,#57363,#57364,#57365,#57366),
 .UNSPECIFIED.,.F.,.F.,(4,2,2,2,2,2,2,2,2,2,2,2,2,2,2,2,2,2,2,2,2,2,2,2,
2,2,2,2,2,2,2,2,2,2,2,2,2,2,2,2,2,2,2,2,2,2,2,2,2,2,2,2,2,2,2,2,2,2,2,2,
2,2,2,2,2,2,2,2,2,2,2,2,2,2,2,2,2,2,2,2,2,2,2,2,2,2,2,2,2,2,2,2,2,2,2,4),
(-2.10024321870136,-2.07707792275481,-2.06711782544992,-2.06329783132158,
-2.05972750725702,-2.05709217806112,-2.05379808839827,-2.04818456503473,
-2.02230314793019,-1.99230694904503,-1.98355151667432,-1.97831015024971,
-1.97601402809443,-1.97435004430234,-1.97248918633476,-1.96924172354253,
-1.95559655504945,-1.92250708278932,-1.90068718550792,-1.89539582732966,
-1.89217086591551,-1.88922777510974,-1.88544951258308,-1.87913433710995,
-1.84270016161805,-1.81418127696254,-1.81060830863966,-1.80867775764828,
-1.80702917180144,-1.80489244488389,-1.80015197634527,-1.77433796645994,
-1.75215349924101,-1.73980992255565,-1.73098599752092,-1.7270701043728,
-1.72411665625155,-1.72092460280781,-1.71578717108399,-1.69869766620876,
-1.66678662080639,-1.64883354501731,-1.64446379018397,-1.64237311605805,
-1.64088880077462,-1.63896648074959,-1.6355290666056,-1.61622713407328,
-1.60917179549341,-1.59223406547781,-1.56767410822126,-1.56223672969039,
-1.55898031957867,-1.55604479404011,-1.55226336367259,-1.54608017128318,
-1.50066732507311,-1.48223264758986,-1.47780833117923,-1.47570717308704,
-1.47422164579736,-1.47230651246261,-1.46890164978239,-1.4510590234456,
-1.40576998535077,-1.3974001136669,-1.39356326812386,-1.39062088277286,
-1.38739298356253,-1.38208815819019,-1.3623654816402,-1.31870481884646,
-1.31413282570107,-1.31056085255604,-1.30863044521136,-1.30698172807918,
-1.30484451165599,-1.30010172423279,-1.27420809119123,-1.25207771052209,
-1.23974817930593,-1.23093148578801,-1.22701669035783,-1.22406326691605,
-1.22087046843874,-1.21573011602368,-1.1986107891338,-1.16671382283516,
-1.14877524470587,-1.1444070115815,-1.14231655680953,-1.14083219336127,
-1.13890952443559,-1.1354708287498,-1.11612762531855,-1.10923588654368),
 .UNSPECIFIED.);
#642=B_SPLINE_CURVE_WITH_KNOTS('',3,(#57372,#57373,#57374,#57375,#57376,
#57377,#57378,#57379,#57380,#57381,#57382,#57383,#57384,#57385,#57386,#57387,
#57388,#57389,#57390,#57391,#57392,#57393,#57394,#57395,#57396,#57397,#57398,
#57399,#57400,#57401,#57402,#57403,#57404,#57405,#57406,#57407,#57408,#57409,
#57410,#57411,#57412,#57413,#57414,#57415,#57416,#57417,#57418,#57419,#57420,
#57421,#57422,#57423,#57424,#57425,#57426,#57427,#57428,#57429,#57430,#57431,
#57432,#57433,#57434,#57435,#57436,#57437,#57438,#57439,#57440,#57441,#57442,
#57443,#57444,#57445,#57446,#57447,#57448,#57449,#57450,#57451,#57452,#57453,
#57454,#57455,#57456,#57457,#57458,#57459,#57460,#57461,#57462,#57463,#57464,
#57465,#57466,#57467,#57468,#57469,#57470,#57471,#57472,#57473,#57474,#57475,
#57476,#57477,#57478,#57479,#57480,#57481,#57482,#57483,#57484,#57485,#57486,
#57487,#57488,#57489,#57490,#57491,#57492,#57493,#57494,#57495,#57496,#57497,
#57498,#57499,#57500,#57501,#57502,#57503,#57504,#57505,#57506,#57507,#57508,
#57509,#57510,#57511,#57512,#57513,#57514,#57515,#57516,#57517,#57518,#57519,
#57520,#57521,#57522,#57523,#57524,#57525,#57526,#57527,#57528,#57529,#57530,
#57531,#57532,#57533,#57534,#57535,#57536,#57537,#57538,#57539,#57540,#57541,
#57542,#57543,#57544,#57545,#57546,#57547,#57548,#57549,#57550,#57551,#57552,
#57553,#57554,#57555,#57556,#57557,#57558,#57559,#57560,#57561),
 .UNSPECIFIED.,.F.,.F.,(4,2,2,2,2,2,2,2,2,2,2,2,2,2,2,2,2,2,2,2,2,2,2,2,
2,2,2,2,2,2,2,2,2,2,2,2,2,2,2,2,2,2,2,2,2,2,2,2,2,2,2,2,2,2,2,2,2,2,2,2,
2,2,2,2,2,2,2,2,2,2,2,2,2,2,2,2,2,2,2,2,2,2,2,2,2,2,2,2,2,2,2,2,2,2,4),
(-0.991267371540882,-0.981097406136092,-0.961289637880318,-0.955963818240538,
-0.952730934488633,-0.949789014332813,-0.945959973544135,-0.937636954346978,
-0.917741432724483,-0.899079532049941,-0.874679746066063,-0.871177710298744,
-0.869240758346818,-0.86759270846697,-0.865427943897829,-0.860660623001553,
-0.838957771522791,-0.79880290397272,-0.790989179326245,-0.787252812944483,
-0.784322095269493,-0.781039835244787,-0.775482867469908,-0.747961936710415,
-0.721701316292262,-0.707512672722365,-0.704234828931467,-0.702367217000256,
-0.700704961506073,-0.698421757030807,-0.692967771532784,-0.68497266253003,
-0.657551018852252,-0.628614552485425,-0.622983204284046,-0.619653476414371,
-0.616757809401868,-0.613110873353384,-0.605770555596228,-0.596121644487729,
-0.570173960882816,-0.543192066135581,-0.538460341580936,-0.536325031335904,
-0.534676403898006,-0.532744477392873,-0.529165651271156,-0.524582011701536,
-0.480864614772306,-0.461176484442266,-0.455872907032115,-0.452645234750042,
-0.449702725036517,-0.445865241338196,-0.437491895333081,-0.415543915585245,
-0.376154006902127,-0.371637296527056,-0.369518833154948,-0.367874677932461,
-0.365904570733226,-0.362142035717488,-0.335352594349984,-0.297235673647581,
-0.291046981012426,-0.287264091086249,-0.284328531102157,-0.281073205365896,
-0.275640321869276,-0.251163953398819,-0.235940471739304,-0.209866033016854,
-0.205097771000572,-0.202956161961828,-0.201307155286976,-0.199380178941985,
-0.195823792956285,-0.167698745841791,-0.130677556443954,-0.124434073669649,
-0.120676282483605,-0.117736173207668,-0.114501241627693,-0.110357857457294,
-0.0954997269774895,-0.0680120021072093,-0.0665756166986164,-0.0431806880535247,
-0.0384358331732864,-0.0362985123773095,-0.0346500636920598,-0.0327204332147608,
-0.0306502677252412,-0.027362718736346,-0.000492130215965281),
 .UNSPECIFIED.);
#643=B_SPLINE_CURVE_WITH_KNOTS('',3,(#57562,#57563,#57564,#57565,#57566,
#57567,#57568,#57569,#57570,#57571,#57572,#57573,#57574,#57575,#57576,#57577),
 .UNSPECIFIED.,.F.,.F.,(4,2,2,2,2,2,2,4),(-2.10016741640826,-2.06493740655749,
-2.05955177493146,-2.05604419942285,-2.05269364711443,-2.04977344098074,
-2.04614491118763,-2.04107968292539),.UNSPECIFIED.);
#644=B_SPLINE_CURVE_WITH_KNOTS('',3,(#57578,#57579,#57580,#57581,#57582,
#57583,#57584,#57585,#57586,#57587,#57588,#57589,#57590,#57591,#57592,#57593,
#57594,#57595,#57596,#57597,#57598,#57599,#57600,#57601,#57602,#57603,#57604,
#57605,#57606,#57607,#57608,#57609,#57610,#57611,#57612,#57613,#57614,#57615,
#57616,#57617,#57618,#57619,#57620,#57621,#57622,#57623,#57624,#57625,#57626,
#57627,#57628,#57629,#57630,#57631,#57632,#57633,#57634,#57635,#57636,#57637,
#57638,#57639,#57640,#57641,#57642,#57643,#57644,#57645,#57646,#57647,#57648,
#57649,#57650,#57651,#57652,#57653,#57654,#57655,#57656,#57657,#57658,#57659,
#57660,#57661,#57662,#57663,#57664,#57665,#57666,#57667,#57668,#57669,#57670,
#57671,#57672,#57673,#57674,#57675,#57676,#57677,#57678,#57679,#57680,#57681,
#57682,#57683,#57684,#57685,#57686,#57687,#57688,#57689,#57690,#57691,#57692,
#57693,#57694,#57695,#57696,#57697,#57698,#57699,#57700,#57701,#57702,#57703,
#57704,#57705,#57706,#57707,#57708,#57709,#57710,#57711,#57712,#57713,#57714,
#57715,#57716,#57717,#57718,#57719,#57720,#57721,#57722,#57723,#57724,#57725,
#57726,#57727,#57728,#57729,#57730,#57731,#57732,#57733,#57734,#57735,#57736,
#57737,#57738,#57739,#57740,#57741,#57742,#57743,#57744,#57745,#57746,#57747,
#57748,#57749,#57750,#57751,#57752,#57753,#57754,#57755,#57756,#57757,#57758,
#57759,#57760,#57761,#57762,#57763,#57764,#57765,#57766,#57767,#57768,#57769,
#57770,#57771,#57772,#57773,#57774,#57775,#57776,#57777,#57778,#57779,#57780,
#57781,#57782,#57783,#57784,#57785,#57786,#57787,#57788,#57789,#57790,#57791),
 .UNSPECIFIED.,.F.,.F.,(4,2,2,2,2,2,2,2,2,2,2,2,2,2,2,2,2,2,2,2,2,2,2,2,
2,2,2,2,2,2,2,2,2,2,2,2,2,2,2,2,2,2,2,2,2,2,2,2,2,2,2,2,2,2,2,2,2,2,2,2,
2,2,2,2,2,2,2,2,2,2,2,2,2,2,2,2,2,2,2,2,2,2,2,2,2,2,2,2,2,2,2,2,2,2,2,2,
2,2,2,2,2,2,2,2,2,2,4),(-1.10923588654368,-1.10907489650741,-1.08811016372412,
-1.0742351092368,-1.064630297109,-1.06058510884969,-1.05761126720607,-1.05484576592113,
-1.05027687983568,-1.0368672406629,-1.0139618145347,-0.982338813730652,
-0.977836583040976,-0.975720782895241,-0.974076736880993,-0.97210439253702,
-0.968331230092938,-0.943182445645729,-0.903080754354083,-0.897088202095896,
-0.893362148587139,-0.890432858589156,-0.887145247687724,-0.881561944909125,
-0.853209100684674,-0.825443254516931,-0.813394637755911,-0.810258547377462,
-0.80842192441521,-0.806749511416559,-0.804399805379745,-0.798529409980879,
-0.789683242550104,-0.755268601597045,-0.734188241135488,-0.728801347940153,
-0.725555796140642,-0.722617826945827,-0.718815949577427,-0.710641946634318,
-0.68706843989935,-0.660144754735399,-0.646899933302174,-0.643683003100304,
-0.641828772518293,-0.640162724308558,-0.63785269387803,-0.632232526221822,
-0.623901805757191,-0.597859235588111,-0.568080476315045,-0.562408813783103,
-0.559102368203098,-0.55646887779565,-0.552916361888428,-0.546056153431242,
-0.521217451267762,-0.503977855429484,-0.480816552076902,-0.477327416086255,
-0.475393603404864,-0.473745555206681,-0.471577308491671,-0.466789096983762,
-0.460080209879909,-0.440374969823515,-0.403691347393369,-0.397396071909866,
-0.393623437094854,-0.390681107057097,-0.387453296630241,-0.38214868304125,
-0.360100628016921,-0.330638238472297,-0.322750972856152,-0.313051057321137,
-0.310133127459941,-0.308344368223593,-0.306648647781612,-0.304169277322039,
-0.297416795480203,-0.253609349296573,-0.234068468048544,-0.228773062820673,
-0.225547285533778,-0.222604507906213,-0.218763783217159,-0.210371186849552,
-0.187685857503641,-0.161867181656076,-0.147127221360853,-0.14385974154063,
-0.141975822633647,-0.140318648031415,-0.140299661724828,-0.140280785134233,
-0.140262012701252,-0.14024333899365,-0.140224758702261,-0.138112029931578,
-0.133231174375814,-0.12618494866544,-0.10467721515721,-0.0706109688986338,
-0.0635859596188316,-0.0599556336597502,-0.059542488620295),
 .UNSPECIFIED.);
#645=B_SPLINE_CURVE_WITH_KNOTS('',3,(#57797,#57798,#57799,#57800,#57801,
#57802,#57803,#57804,#57805,#57806),.UNSPECIFIED.,.F.,.F.,(4,3,3,4),(-4.19977379117109,
-4.09016305838479,-3.9901141377464,-3.84638326369218),.UNSPECIFIED.);
#646=B_SPLINE_CURVE_WITH_KNOTS('',3,(#57808,#57809,#57810,#57811,#57812,
#57813,#57814,#57815,#57816,#57817,#57818,#57819,#57820,#57821,#57822,#57823,
#57824,#57825,#57826,#57827,#57828,#57829,#57830,#57831,#57832,#57833,#57834,
#57835,#57836,#57837,#57838,#57839,#57840,#57841,#57842,#57843,#57844,#57845,
#57846,#57847,#57848,#57849,#57850,#57851,#57852,#57853,#57854,#57855,#57856,
#57857,#57858,#57859,#57860,#57861,#57862,#57863,#57864,#57865,#57866,#57867,
#57868,#57869,#57870,#57871,#57872,#57873,#57874,#57875,#57876,#57877,#57878,
#57879,#57880,#57881,#57882,#57883,#57884,#57885,#57886,#57887,#57888,#57889,
#57890,#57891,#57892,#57893,#57894,#57895,#57896,#57897,#57898,#57899,#57900,
#57901,#57902,#57903,#57904,#57905,#57906,#57907,#57908,#57909,#57910,#57911,
#57912,#57913,#57914,#57915,#57916),.UNSPECIFIED.,.F.,.F.,(4,3,3,3,3,3,
3,3,3,3,3,3,3,3,3,3,3,3,3,3,3,3,3,3,3,3,3,3,3,3,3,3,3,3,3,3,4),(-3.84638326322552,
-3.73817105610137,-3.63007941822935,-3.52206551072006,-3.41408661602619,
-3.30602494476234,-3.19792576134903,-3.08962895712806,-2.9925856033098,
-2.88263947138076,-2.77169167106731,-2.66204168456622,-2.55245679950798,
-2.44289661082298,-2.33093672533553,-2.22123487990582,-2.10814597438951,
-1.9950570688732,-1.88644978490181,-1.77533462859366,-1.66702721094067,
-1.55878298609703,-1.45055963187852,-1.33730185751804,-1.22891272071361,
-1.12043521194772,-1.0117545264651,-0.997528534436599,-0.884663102669983,
-0.77203800889968,-0.659554849770297,-0.547180407463164,-0.434881614271142,
-0.322591337129412,-0.210315510204404,-0.0979547765619886,0.),
 .UNSPECIFIED.);
#647=B_SPLINE_CURVE_WITH_KNOTS('',3,(#57920,#57921,#57922,#57923,#57924,
#57925,#57926,#57927,#57928,#57929,#57930,#57931,#57932,#57933,#57934,#57935,
#57936,#57937,#57938,#57939,#57940,#57941,#57942,#57943,#57944,#57945,#57946,
#57947,#57948,#57949,#57950,#57951,#57952,#57953,#57954,#57955,#57956,#57957,
#57958,#57959,#57960,#57961,#57962,#57963,#57964,#57965,#57966,#57967,#57968,
#57969,#57970,#57971,#57972,#57973,#57974,#57975,#57976,#57977,#57978,#57979,
#57980,#57981,#57982,#57983,#57984,#57985,#57986,#57987,#57988,#57989,#57990,
#57991,#57992,#57993,#57994,#57995,#57996,#57997,#57998,#57999,#58000,#58001,
#58002,#58003,#58004,#58005,#58006,#58007,#58008,#58009,#58010,#58011,#58012,
#58013,#58014,#58015,#58016,#58017,#58018,#58019,#58020,#58021,#58022,#58023,
#58024,#58025,#58026,#58027,#58028,#58029,#58030,#58031,#58032,#58033,#58034,
#58035,#58036,#58037,#58038,#58039,#58040,#58041,#58042,#58043,#58044,#58045,
#58046,#58047,#58048,#58049,#58050,#58051,#58052,#58053,#58054,#58055,#58056,
#58057,#58058,#58059,#58060,#58061,#58062,#58063,#58064,#58065,#58066,#58067,
#58068,#58069,#58070,#58071,#58072,#58073),.UNSPECIFIED.,.F.,.F.,(4,3,3,
3,3,3,3,3,3,3,3,3,3,3,3,3,3,3,3,3,3,3,3,3,3,3,3,3,3,3,3,3,3,3,3,3,3,3,3,
3,3,3,3,3,3,3,3,3,3,3,3,4),(2.01461790129682,2.12418716397154,2.23356422085981,
2.34283392492382,2.4520374248202,2.56121577723765,2.67048870477471,2.77980488942863,
2.889327464259,2.9925856033098,3.10257102449589,3.2135139136522,3.3232066348227,
3.43283544876539,3.54244070750851,3.65435906506798,3.76410838117625,3.87711125946132,
3.9901141377464,4.09976168164098,4.21074680545873,4.32008694433128,4.42935866471988,
4.53860290679355,4.65086284814091,4.76024559746015,4.87394413482158,4.987642672183,
5.09746924953473,5.20843199417034,5.31795635452642,5.42741372572691,5.53684474715618,
5.64892636202204,5.75849655049291,5.87183387855625,5.9851712066196,6.09498856633222,
6.20595246317272,6.31546860664133,6.42491816034262,6.53434177815616,6.64643126888117,
6.75599517379492,6.86934745742556,6.98269974105619,7.09372976479652,7.20457605112106,
7.31525682042945,7.42584067486135,7.5363740838632,7.59300756235147),
 .UNSPECIFIED.);
#648=B_SPLINE_CURVE_WITH_KNOTS('',3,(#58074,#58075,#58076,#58077,#58078,
#58079,#58080,#58081,#58082,#58083),.UNSPECIFIED.,.F.,.F.,(4,2,2,2,4),(-2.10021521608555,
-2.08977397566189,-2.04619577452829,-2.04163297633637,-2.04133728664231),
 .UNSPECIFIED.);
#649=B_SPLINE_CURVE_WITH_KNOTS('',3,(#58085,#58086,#58087,#58088,#58089,
#58090,#58091,#58092,#58093,#58094,#58095,#58096,#58097,#58098,#58099,#58100,
#58101,#58102,#58103,#58104,#58105,#58106,#58107,#58108,#58109,#58110,#58111,
#58112,#58113,#58114,#58115,#58116,#58117,#58118,#58119,#58120,#58121,#58122,
#58123,#58124,#58125,#58126,#58127,#58128,#58129,#58130,#58131,#58132,#58133,
#58134,#58135,#58136,#58137,#58138,#58139,#58140,#58141,#58142,#58143,#58144,
#58145,#58146,#58147,#58148,#58149,#58150,#58151,#58152,#58153,#58154,#58155,
#58156,#58157,#58158,#58159,#58160,#58161,#58162,#58163,#58164,#58165,#58166,
#58167,#58168,#58169,#58170,#58171,#58172,#58173,#58174,#58175,#58176,#58177,
#58178,#58179,#58180,#58181,#58182,#58183,#58184,#58185,#58186,#58187,#58188,
#58189,#58190,#58191,#58192,#58193,#58194,#58195,#58196,#58197,#58198,#58199,
#58200,#58201,#58202,#58203,#58204,#58205,#58206,#58207,#58208,#58209,#58210,
#58211,#58212,#58213,#58214,#58215,#58216,#58217,#58218,#58219,#58220,#58221,
#58222,#58223,#58224,#58225,#58226,#58227,#58228,#58229,#58230,#58231,#58232,
#58233,#58234,#58235,#58236,#58237,#58238,#58239,#58240,#58241,#58242,#58243,
#58244,#58245,#58246,#58247,#58248,#58249,#58250,#58251,#58252,#58253,#58254,
#58255,#58256,#58257,#58258,#58259,#58260,#58261,#58262,#58263,#58264,#58265,
#58266,#58267,#58268,#58269,#58270,#58271,#58272,#58273,#58274,#58275,#58276,
#58277,#58278,#58279,#58280,#58281,#58282,#58283,#58284,#58285,#58286,#58287,
#58288,#58289,#58290),.UNSPECIFIED.,.F.,.F.,(4,2,2,2,2,2,2,2,2,2,2,2,2,
2,2,2,2,2,2,2,2,2,2,2,2,2,2,2,2,2,2,2,2,2,2,2,2,2,2,2,2,2,2,2,2,2,2,2,2,
2,2,2,2,2,2,2,2,2,2,2,2,2,2,2,2,2,2,2,2,2,2,2,2,2,2,2,2,2,2,2,2,2,2,2,2,
2,2,2,2,2,2,2,2,2,2,2,2,2,2,2,2,2,4),(-2.04133728664231,-2.03806711232071,
-2.03613907650113,-2.03449055238448,-2.03235217524117,-2.02760496330045,
-2.00202283253427,-1.97591246252407,-1.96559219509398,-1.96019425817351,
-1.95593710094107,-1.95287443123683,-1.94992358151013,-1.94610252245451,
-1.93759501511552,-1.89825821024276,-1.87681852679445,-1.87207606932991,
-1.8699148703817,-1.8682811787169,-1.86634641277876,-1.8628553805761,-1.83968413016769,
-1.82243749714789,-1.79756842834387,-1.79070352001133,-1.78714940531321,
-1.78451508752835,-1.78120805003946,-1.77553653065459,-1.74564750693976,
-1.72396566567071,-1.71301873243646,-1.70619061438184,-1.70370068664817,
-1.70200282576786,-1.70043652798863,-1.69774825086984,-1.69001707168038,
-1.68012220978552,-1.64983524325786,-1.62808615729811,-1.62279842835429,
-1.61957399019187,-1.61663030034402,-1.61284979232203,-1.60456738736788,
-1.56495150346657,-1.54342226860357,-1.53867210557083,-1.53651054213067,
-1.53487761097175,-1.53294478498958,-1.52946168918287,-1.50799234015133,
-1.48675521374221,-1.46170057201891,-1.45623931075393,-1.45297715685123,
-1.4500417908405,-1.44626803601958,-1.43825317764822,-1.39834539656004,
-1.37672504194426,-1.37196540548511,-1.36980178070214,-1.36816840109125,
-1.36623647588984,-1.36275755849242,-1.34162583446689,-1.33696943245491,
-1.316926136774,-1.30217031603712,-1.29213517037851,-1.28802172545601,-1.28503580743141,
-1.2819143899054,-1.27711198179445,-1.26288326346744,-1.22919925276079,
-1.20970439702231,-1.20516353826991,-1.20304024190205,-1.20155196837831,
-1.19965130151577,-1.19631170686557,-1.18038607711524,-1.14977864296839,
-1.12796756740681,-1.12267550373085,-1.11944977035899,-1.1165057593254,
-1.11272602219167,-1.10640773541409,-1.07010882937329,-1.05015950680568,
-1.04028702126582,-1.03735074321361,-1.03555761652194,-1.03386376621982,
-1.03139575260707,-1.02472742835449,-0.991267371540882),.UNSPECIFIED.);
#650=B_SPLINE_CURVE_WITH_KNOTS('',3,(#58292,#58293,#58294,#58295,#58296,
#58297,#58298,#58299,#58300,#58301,#58302,#58303),.UNSPECIFIED.,.F.,.F.,
(4,2,2,2,2,4),(-0.059542488620295,-0.0570356295461016,-0.0536871209915682,
-0.0478149555195779,-0.0135375548234137,-0.000495262918588897),
 .UNSPECIFIED.);
#651=B_SPLINE_CURVE_WITH_KNOTS('',3,(#58304,#58305,#58306,#58307,#58308,
#58309,#58310,#58311,#58312,#58313,#58314,#58315,#58316,#58317,#58318,#58319,
#58320,#58321,#58322,#58323,#58324,#58325,#58326,#58327,#58328,#58329,#58330,
#58331,#58332,#58333,#58334,#58335,#58336,#58337,#58338,#58339,#58340,#58341,
#58342,#58343,#58344,#58345,#58346,#58347,#58348,#58349,#58350,#58351,#58352,
#58353,#58354,#58355,#58356,#58357,#58358,#58359,#58360,#58361,#58362,#58363,
#58364,#58365,#58366,#58367,#58368,#58369,#58370,#58371,#58372,#58373,#58374,
#58375,#58376,#58377,#58378,#58379,#58380,#58381,#58382,#58383,#58384,#58385,
#58386,#58387,#58388,#58389,#58390,#58391,#58392,#58393,#58394,#58395,#58396,
#58397,#58398,#58399,#58400,#58401,#58402,#58403,#58404,#58405,#58406,#58407,
#58408,#58409,#58410,#58411,#58412,#58413,#58414,#58415,#58416,#58417,#58418,
#58419,#58420,#58421,#58422,#58423,#58424,#58425,#58426,#58427,#58428,#58429,
#58430,#58431,#58432,#58433,#58434,#58435,#58436,#58437,#58438,#58439,#58440,
#58441,#58442,#58443,#58444,#58445,#58446,#58447,#58448,#58449,#58450,#58451,
#58452,#58453,#58454,#58455,#58456,#58457,#58458,#58459,#58460,#58461,#58462,
#58463,#58464,#58465,#58466),.UNSPECIFIED.,.F.,.F.,(4,3,3,3,3,3,3,3,3,3,
3,3,3,3,3,3,3,3,3,3,3,3,3,3,3,3,3,3,3,3,3,3,3,3,3,3,3,3,3,3,3,3,3,3,3,3,
3,3,3,3,3,3,3,3,4),(-10.1295685708718,-9.97528534436599,-9.86548762739471,
-9.75452127521155,-9.64502607996208,-9.53559790410113,-9.42619605868901,
-9.31408624649911,-9.20454484153936,-9.09115082573437,-8.97775680992939,
-8.86795596066623,-8.75699000001955,-8.64749148931064,-8.53805993940168,
-8.42865466738962,-8.31654806941542,-8.2070031494851,-8.09361571248895,
-7.9802282754928,-7.87045607245003,-7.7594865310258,-7.65001679670524,-7.54061399239432,
-7.43123738880844,-7.31910297687038,-7.20958620654151,-7.09614297379885,
-6.9826997410562,-6.87287957692727,-6.76191603063881,-6.65239873427587,
-6.54294864619697,-6.43352511152299,-6.32143663529715,-6.21187433502042,
-6.09852277082001,-5.9851712066196,-5.87534579900835,-5.76438290815518,
-5.65485906417595,-5.54540196447979,-5.43597096998016,-5.32388889553087,
-5.21431813074235,-5.10098040146268,-4.987642672183,-4.87803538336313,-4.76858440184659,
-4.65924852673594,-4.54437984284473,-4.43511949060869,-4.32585491445155,
-4.21650483607428,-4.19977379117109),.UNSPECIFIED.);
#652=B_SPLINE_CURVE_WITH_KNOTS('',3,(#58469,#58470,#58471,#58472,#58473,
#58474,#58475,#58476),.UNSPECIFIED.,.F.,.F.,(4,1,1,1,1,4),(17.9345079337947,
18.8442797453129,19.8418082797495,20.8393368141861,21.8368653486227,21.9911485751285),
 .UNSPECIFIED.);
#653=B_SPLINE_CURVE_WITH_KNOTS('',3,(#58477,#58478,#58479,#58480,#58481,
#58482),.UNSPECIFIED.,.F.,.F.,(4,1,1,4),(21.9911485751285,22.8343938830593,
23.8319224174959,24.2177548267501),.UNSPECIFIED.);
#654=B_SPLINE_CURVE_WITH_KNOTS('',3,(#58484,#58485,#58486,#58487,#58488,
#58489),.UNSPECIFIED.,.F.,.F.,(4,1,1,4),(21.9911485751285,22.3783692882697,
23.3758978227063,24.2163931842857),.UNSPECIFIED.);
#655=B_SPLINE_CURVE_WITH_KNOTS('',3,(#58490,#58491,#58492,#58493,#58494,
#58495,#58496,#58497),.UNSPECIFIED.,.F.,.F.,(4,1,1,1,1,4),(17.9337012577548,
18.3882551505233,19.3857836849599,20.3833122193965,21.3808407538331,21.9911485751285),
 .UNSPECIFIED.);
#656=B_SPLINE_CURVE_WITH_KNOTS('',3,(#58499,#58500,#58501,#58502,#58503,
#58504,#58505,#58506,#58507,#58508,#58509,#58510,#58511,#58512,#58513,#58514,
#58515,#58516,#58517,#58518,#58519,#58520,#58521,#58522,#58523,#58524,#58525,
#58526,#58527,#58528,#58529,#58530,#58531,#58532,#58533,#58534,#58535,#58536,
#58537,#58538,#58539,#58540,#58541,#58542,#58543,#58544,#58545,#58546,#58547,
#58548,#58549,#58550,#58551,#58552,#58553,#58554,#58555,#58556,#58557,#58558,
#58559,#58560,#58561,#58562,#58563,#58564,#58565,#58566,#58567,#58568,#58569,
#58570,#58571,#58572,#58573,#58574,#58575,#58576,#58577,#58578,#58579,#58580,
#58581,#58582,#58583,#58584,#58585,#58586),.UNSPECIFIED.,.F.,.F.,(4,3,3,
3,3,3,3,3,3,3,3,3,3,3,3,3,3,3,3,3,3,3,3,3,3,3,3,3,3,4),(-0.378621596831436,
-0.359663577262707,-0.347848706298584,-0.340612126761629,-0.335326919244971,
-0.315444091624407,-0.301124382400315,-0.297137489673917,-0.293208696506955,
-0.272699616571317,-0.251996264868775,-0.231506732846842,-0.228782241774587,
-0.224183786203168,-0.203193217736025,-0.200837552551342,-0.180373385774626,
-0.159349797507194,-0.154347721681245,-0.15081253799708,-0.12949386489982,
-0.107562916419308,-0.085631967938795,-0.0802146534577825,-0.0759481457753231,
-0.0534010597619021,-0.0308288102439276,-0.00877074246183405,-0.00403427920390156,
-4.65348914561155E-5),.UNSPECIFIED.);
#657=B_SPLINE_CURVE_WITH_KNOTS('',3,(#58587,#58588,#58589,#58590,#58591,
#58592,#58593,#58594,#58595,#58596,#58597,#58598,#58599,#58600,#58601,#58602,
#58603,#58604,#58605,#58606,#58607,#58608,#58609,#58610,#58611,#58612,#58613,
#58614,#58615,#58616,#58617,#58618,#58619,#58620,#58621,#58622,#58623,#58624,
#58625,#58626,#58627,#58628,#58629,#58630,#58631,#58632,#58633,#58634,#58635,
#58636,#58637,#58638,#58639,#58640,#58641,#58642,#58643,#58644,#58645,#58646,
#58647,#58648,#58649,#58650,#58651,#58652,#58653,#58654,#58655,#58656,#58657,
#58658,#58659,#58660,#58661,#58662,#58663,#58664,#58665,#58666,#58667,#58668,
#58669,#58670,#58671),.UNSPECIFIED.,.F.,.F.,(4,3,3,3,3,3,3,3,3,3,3,3,3,
3,3,3,3,3,3,3,3,3,3,3,3,3,3,3,4),(-0.376940817211628,-0.354431931598271,
-0.33291050214917,-0.328061832757599,-0.305813770680128,-0.290194499089435,
-0.284255854807366,-0.277973785325902,-0.256315628127061,-0.235159936382763,
-0.214950283336026,-0.208195454784792,-0.204402290359773,-0.183827312742316,
-0.180862865680239,-0.159776092357818,-0.140305803166316,-0.136023358723937,
-0.132589553322146,-0.112137183595652,-0.0919021865118393,-0.0718392599446326,
-0.0676313463151555,-0.0636633141776788,-0.044090905576146,-0.0251703687379681,
-0.00636244806541706,-0.00328482218945705,0.),.UNSPECIFIED.);
#658=B_SPLINE_CURVE_WITH_KNOTS('',3,(#59088,#59089,#59090,#59091,#59092,
#59093,#59094,#59095,#59096,#59097,#59098,#59099,#59100,#59101,#59102,#59103,
#59104,#59105,#59106,#59107,#59108,#59109,#59110,#59111,#59112,#59113,#59114,
#59115,#59116,#59117,#59118,#59119,#59120,#59121,#59122,#59123,#59124,#59125,
#59126,#59127,#59128,#59129,#59130,#59131,#59132,#59133,#59134,#59135,#59136,
#59137,#59138,#59139,#59140,#59141,#59142,#59143,#59144,#59145,#59146,#59147,
#59148,#59149,#59150,#59151,#59152,#59153,#59154,#59155,#59156,#59157,#59158,
#59159,#59160,#59161,#59162,#59163,#59164,#59165,#59166,#59167,#59168,#59169),
 .UNSPECIFIED.,.F.,.F.,(4,3,3,3,3,3,3,3,3,3,3,3,3,3,3,3,3,3,3,3,3,3,3,3,
3,3,3,4),(0.,0.0186931777979472,0.038069582663444,0.0557727123654966,0.0644773333531983,
0.0684521454610112,0.0885308791156241,0.108995971082426,0.125989856347167,
0.133855323484509,0.137288340283486,0.158362746619097,0.177197233492055,
0.197771878148169,0.205648382326712,0.209124428921397,0.22992781965306,
0.251270152758872,0.269193970891297,0.278737264184526,0.284782300229465,
0.307041766598089,0.322965425288574,0.328171269586608,0.333183333893234,
0.355704745759864,0.37292316965919,0.376894465478604),.UNSPECIFIED.);
#659=B_SPLINE_CURVE_WITH_KNOTS('',3,(#59586,#59587,#59588,#59589,#59590,
#59591,#59592,#59593,#59594,#59595,#59596,#59597,#59598,#59599,#59600,#59601,
#59602,#59603,#59604,#59605,#59606,#59607,#59608,#59609,#59610,#59611,#59612,
#59613,#59614,#59615,#59616,#59617,#59618,#59619,#59620,#59621,#59622,#59623,
#59624,#59625,#59626,#59627,#59628,#59629,#59630,#59631,#59632,#59633,#59634,
#59635,#59636,#59637,#59638,#59639,#59640,#59641,#59642,#59643,#59644,#59645,
#59646,#59647,#59648,#59649,#59650,#59651,#59652,#59653,#59654,#59655,#59656,
#59657,#59658,#59659,#59660,#59661,#59662,#59663,#59664,#59665,#59666,#59667,
#59668,#59669,#59670),.UNSPECIFIED.,.F.,.F.,(4,3,3,3,3,3,3,3,3,3,3,3,3,
3,3,3,3,3,3,3,3,3,3,3,3,3,3,3,4),(1.30794053536005E-15,0.0222065049803711,
0.0447372655622252,0.062893202204516,0.0719711705256613,0.0777843945802568,
0.0810491388468067,0.102995977799722,0.124600763208028,0.142866962546818,
0.150422887918052,0.153918794618638,0.157566976032779,0.17833659004605,
0.197155519647457,0.218478442759019,0.224327897336195,0.229401225301518,
0.250048769456985,0.270748189563912,0.291016884823382,0.296885783013855,
0.300621344353643,0.320441444472329,0.334296858333292,0.338763771301729,
0.357786582134865,0.375324744080583,0.378621596831427),.UNSPECIFIED.);
#660=B_SPLINE_CURVE_WITH_KNOTS('',3,(#59880,#59881,#59882,#59883,#59884,
#59885,#59886,#59887,#59888,#59889,#59890,#59891,#59892,#59893,#59894,#59895,
#59896,#59897,#59898,#59899,#59900,#59901,#59902,#59903,#59904,#59905,#59906,
#59907,#59908,#59909,#59910,#59911,#59912,#59913,#59914,#59915,#59916,#59917,
#59918,#59919,#59920,#59921,#59922,#59923,#59924,#59925,#59926,#59927,#59928,
#59929,#59930,#59931,#59932,#59933,#59934,#59935,#59936,#59937,#59938,#59939,
#59940,#59941,#59942,#59943,#59944,#59945,#59946,#59947,#59948,#59949,#59950,
#59951,#59952,#59953,#59954,#59955,#59956,#59957,#59958,#59959,#59960,#59961,
#59962,#59963,#59964,#59965,#59966,#59967,#59968,#59969,#59970,#59971,#59972,
#59973,#59974,#59975,#59976,#59977,#59978,#59979,#59980,#59981,#59982,#59983,
#59984,#59985,#59986,#59987,#59988,#59989,#59990,#59991,#59992,#59993,#59994,
#59995,#59996,#59997,#59998,#59999,#60000,#60001,#60002,#60003,#60004,#60005,
#60006,#60007,#60008,#60009,#60010,#60011,#60012,#60013,#60014,#60015,#60016,
#60017,#60018,#60019,#60020,#60021,#60022,#60023,#60024,#60025,#60026,#60027,
#60028,#60029,#60030,#60031,#60032,#60033,#60034,#60035,#60036,#60037,#60038,
#60039,#60040,#60041,#60042,#60043,#60044,#60045,#60046,#60047,#60048,#60049,
#60050,#60051,#60052,#60053,#60054,#60055,#60056,#60057,#60058,#60059,#60060,
#60061,#60062,#60063,#60064,#60065,#60066,#60067,#60068,#60069,#60070,#60071,
#60072,#60073,#60074,#60075,#60076,#60077,#60078,#60079,#60080,#60081,#60082,
#60083,#60084,#60085,#60086,#60087,#60088,#60089,#60090,#60091,#60092,#60093,
#60094,#60095,#60096,#60097,#60098,#60099),.UNSPECIFIED.,.F.,.F.,(4,2,2,
2,2,2,2,2,2,2,2,2,2,2,2,2,2,2,2,2,2,2,2,2,2,2,2,2,2,2,2,2,2,2,2,2,2,2,2,
2,2,2,2,2,2,2,2,2,2,2,2,2,2,2,2,2,2,2,2,2,2,2,2,2,2,2,2,2,2,2,2,2,2,2,2,
2,2,2,2,2,2,2,2,2,2,2,2,2,2,2,2,2,2,2,2,2,2,2,2,2,2,2,2,2,2,2,2,2,2,4),
(-1.25131977917524,-1.23656241881066,-1.20701295486785,-1.19935871676255,
-1.16998794161902,-1.16491791364363,-1.16206861960701,-1.15985345132094,
-1.15669994958711,-1.14996749086125,-1.12074390449838,-1.0680149534151,
-1.05340619187006,-1.04716889055948,-1.04274260344209,-1.03812375910127,
-1.03112895839771,-1.00928158984193,-0.968195495489653,-0.933932853647884,
-0.92881700987865,-0.925953556630634,-0.923730250269325,-0.920569233340291,
-0.913843744006523,-0.884771920553245,-0.832301822404733,-0.817786153245362,
-0.811551968163211,-0.807118490998376,-0.802483582653689,-0.795446646811962,
-0.773291417064023,-0.731159554570256,-0.698108987017462,-0.693006864744909,
-0.690148059879696,-0.687721451057466,-0.684473160784883,-0.677133693698043,
-0.666683646671541,-0.634103674058093,-0.589030563247094,-0.579716218945477,
-0.574137223679013,-0.569781993080877,-0.564995877635212,-0.557099295630797,
-0.522644451837198,-0.498367101298772,-0.491757393674209,-0.461620048853493,
-0.45655361502068,-0.453713766588345,-0.451501624306616,-0.448354019829487,
-0.441665163028119,-0.412925065500677,-0.361710023544992,-0.345200197292985,
-0.338660560506218,-0.334572225302417,-0.330068155759284,-0.323731329808694,
-0.307418910181425,-0.282201113022025,-0.22776757811646,-0.221258922839231,
-0.218103105280213,-0.215673498636336,-0.215595324444493,-0.215532309095076,
-0.215481049666447,-0.215439050839442,-0.215404439133561,-0.215346195470749,
-0.215290095264256,-0.215235966328501,-0.215183653324741,-0.215133015668737,
-0.215083925738375,-0.215036267342248,-0.214989934391034,-0.214944829751753,
-0.214900864254929,-0.214857955826897,-0.214816028731415,-0.214775012905456,
-0.214734843373777,-0.21469545973249,-0.214656805689996,-0.214618828661828,
-0.214581479411155,-0.214544711722475,-0.214508482116246,-0.214472749586117,
-0.214437475364664,-0.214402622713177,-0.211017314188223,-0.202128083903168,
-0.188616362646853,-0.128692901795126,-0.112341255688242,-0.105779734258138,
-0.10123828105323,-0.0965920861369307,-0.0897300410221464,-0.0697341073430826,
-0.0351736997662141,-0.00354544123312327),.UNSPECIFIED.);
#661=B_SPLINE_CURVE_WITH_KNOTS('',3,(#60102,#60103,#60104,#60105,#60106,
#60107,#60108,#60109,#60110,#60111,#60112,#60113,#60114,#60115,#60116,#60117,
#60118,#60119,#60120,#60121,#60122,#60123,#60124,#60125,#60126,#60127,#60128,
#60129,#60130,#60131,#60132,#60133,#60134,#60135,#60136,#60137,#60138,#60139,
#60140,#60141,#60142,#60143,#60144,#60145,#60146,#60147,#60148,#60149,#60150,
#60151,#60152,#60153,#60154,#60155,#60156,#60157,#60158,#60159,#60160,#60161,
#60162,#60163,#60164,#60165,#60166,#60167,#60168,#60169,#60170,#60171,#60172,
#60173,#60174,#60175,#60176,#60177,#60178,#60179,#60180,#60181,#60182,#60183,
#60184,#60185,#60186,#60187,#60188,#60189,#60190,#60191,#60192,#60193,#60194,
#60195,#60196,#60197,#60198,#60199,#60200,#60201,#60202,#60203,#60204,#60205,
#60206,#60207,#60208,#60209,#60210,#60211,#60212,#60213,#60214,#60215,#60216,
#60217,#60218,#60219,#60220,#60221,#60222,#60223,#60224,#60225),
 .UNSPECIFIED.,.F.,.F.,(4,3,3,3,3,3,3,3,3,3,3,3,3,3,3,3,3,3,3,3,3,3,3,3,
3,3,3,3,3,3,3,3,3,3,3,3,3,3,3,3,3,4),(11.6150328478182,11.7179446012586,
11.8207946212876,11.923634938576,12.0264737944964,12.1293362764885,12.2322474918762,
12.335310488753,12.4384541798223,12.5417938440493,12.6069034617266,12.706476373012,
12.8058907630902,12.9051721677229,13.0043802300127,13.103547378039,13.2027059877237,
13.3019580568064,13.4012539542961,13.5007320275801,13.598774075635,13.6995165720154,
13.8001157862556,13.9005997135967,14.0010206760435,14.1014095657536,14.2017972346013,
14.3022816451625,14.4028137969415,14.5035204650583,14.5906446895433,14.691401271234,
14.7920178477645,14.8925240235074,14.9929702101377,15.0933872721949,15.1938060367443,
15.2943259460171,15.3948960718821,15.4956444670245,15.5825153034517,15.63538085578),
 .UNSPECIFIED.);
#662=B_SPLINE_CURVE_WITH_KNOTS('',3,(#60230,#60231,#60232,#60233,#60234,
#60235,#60236,#60237,#60238,#60239,#60240,#60241,#60242,#60243,#60244,#60245,
#60246,#60247,#60248,#60249,#60250,#60251,#60252,#60253,#60254,#60255,#60256,
#60257,#60258,#60259,#60260,#60261,#60262,#60263,#60264,#60265,#60266,#60267,
#60268,#60269,#60270,#60271,#60272,#60273,#60274,#60275,#60276,#60277,#60278,
#60279,#60280,#60281,#60282,#60283,#60284,#60285,#60286,#60287,#60288,#60289,
#60290,#60291,#60292,#60293,#60294,#60295,#60296,#60297,#60298,#60299,#60300,
#60301,#60302,#60303,#60304,#60305,#60306,#60307,#60308,#60309,#60310,#60311,
#60312,#60313,#60314,#60315,#60316,#60317,#60318,#60319,#60320,#60321,#60322,
#60323,#60324,#60325,#60326,#60327,#60328,#60329,#60330,#60331,#60332,#60333,
#60334,#60335,#60336,#60337,#60338,#60339,#60340,#60341,#60342,#60343,#60344,
#60345,#60346,#60347,#60348,#60349,#60350,#60351,#60352,#60353,#60354,#60355,
#60356,#60357,#60358,#60359,#60360,#60361,#60362,#60363,#60364,#60365,#60366,
#60367,#60368,#60369,#60370,#60371,#60372,#60373,#60374,#60375,#60376,#60377,
#60378,#60379,#60380,#60381,#60382,#60383,#60384,#60385,#60386,#60387,#60388,
#60389,#60390,#60391,#60392,#60393,#60394,#60395,#60396,#60397,#60398,#60399,
#60400,#60401,#60402,#60403,#60404,#60405,#60406,#60407,#60408,#60409,#60410,
#60411,#60412,#60413,#60414,#60415,#60416,#60417,#60418,#60419,#60420,#60421,
#60422,#60423,#60424,#60425,#60426,#60427,#60428,#60429,#60430,#60431,#60432,
#60433,#60434,#60435,#60436,#60437),.UNSPECIFIED.,.F.,.F.,(4,2,2,2,2,2,
2,2,2,2,2,2,2,2,2,2,2,2,2,2,2,2,2,2,2,2,2,2,2,2,2,2,2,2,2,2,2,2,2,2,2,2,
2,2,2,2,2,2,2,2,2,2,2,2,2,2,2,2,2,2,2,2,2,2,2,2,2,2,2,2,2,2,2,2,2,2,2,2,
2,2,2,2,2,2,2,2,2,2,2,2,2,2,2,2,2,2,2,2,2,2,2,2,2,4),(-2.74540210132995,
-2.71148878064438,-2.70502039877798,-2.69915538242511,-2.69474829232318,
-2.68999575073976,-2.68235751778743,-2.65577199448838,-2.61843778059984,
-2.58646854578538,-2.58146128272585,-2.57906790744654,-2.57685167660375,
-2.5740019528062,-2.56893555598404,-2.53982230770332,-2.53176532679166,
-2.50196619744075,-2.48265943784217,-2.46910514556952,-2.46320930388327,
-2.45879747327701,-2.45405728408279,-2.44647752147774,-2.42140337771276,
-2.37665569015157,-2.35859977029646,-2.35122810245577,-2.3455848945712,
-2.34264415389782,-2.34019248203058,-2.33702027417077,-2.33042982937092,
-2.288215565947,-2.27425605039392,-2.24993867509917,-2.23401637799999,-2.22775355936165,
-2.22327975268266,-2.21920417986974,-2.21265335612755,-2.19593832494037,
-2.14529820496415,-2.11679946167232,-2.11014329207341,-2.10700360387211,
-2.1047891237258,-2.10192724727491,-2.09680631926088,-2.0620156496777,-2.03518318405526,
-2.01273978387739,-2.00245242345074,-1.99402362209504,-1.98910255041698,
-1.98473739185936,-1.97920515005959,-1.97033142881071,-1.91601554106387,
-1.87897954341978,-1.87342601186145,-1.87050375095237,-1.86805047724644,
-1.86490727860569,-1.85805079628739,-1.82035089359626,-1.78375010644519,
-1.76321164751351,-1.75635960175413,-1.7517712136186,-1.74732686040429,
-1.74098224081769,-1.72559708094449,-1.6736629840931,-1.64471559334932,
-1.63801146479455,-1.63486230392345,-1.63264573452409,-1.62978691323599,
-1.62468688200851,-1.59180961546464,-1.56425704241657,-1.52943407360889,
-1.52148361789708,-1.51666231162885,-1.51227240238779,-1.50664404484596,
-1.49723139443558,-1.45555750097605,-1.42076350483367,-1.40468769956954,
-1.40034876208145,-1.39768636854869,-1.39518354337576,-1.39147126710944,
-1.38196612464931,-1.31695904095716,-1.29241366120115,-1.28488616538071,
-1.28015964555661,-1.27574774387445,-1.26983247445604,-1.25614345626771,
-1.25131977917524),.UNSPECIFIED.);
#663=B_SPLINE_CURVE_WITH_KNOTS('',3,(#60439,#60440,#60441,#60442),
 .UNSPECIFIED.,.F.,.F.,(4,4),(15.63538085578,15.7079632679489),
 .UNSPECIFIED.);
#664=B_SPLINE_CURVE_WITH_KNOTS('',3,(#60443,#60444,#60445,#60446,#60447,
#60448,#60449,#60450,#60451,#60452,#60453,#60454,#60455,#60456,#60457,#60458,
#60459,#60460,#60461,#60462,#60463,#60464,#60465,#60466,#60467,#60468,#60469,
#60470,#60471,#60472,#60473,#60474,#60475,#60476,#60477,#60478,#60479,#60480,
#60481,#60482,#60483,#60484,#60485,#60486,#60487,#60488,#60489,#60490,#60491,
#60492,#60493,#60494,#60495,#60496,#60497,#60498,#60499,#60500,#60501,#60502,
#60503,#60504,#60505,#60506,#60507,#60508,#60509,#60510,#60511,#60512,#60513,
#60514,#60515,#60516,#60517,#60518,#60519,#60520,#60521,#60522,#60523,#60524,
#60525,#60526,#60527,#60528,#60529,#60530,#60531,#60532,#60533,#60534,#60535,
#60536,#60537,#60538,#60539,#60540,#60541,#60542,#60543,#60544,#60545,#60546,
#60547,#60548,#60549,#60550,#60551,#60552,#60553,#60554,#60555,#60556,#60557,
#60558,#60559,#60560,#60561,#60562,#60563,#60564,#60565,#60566,#60567,#60568,
#60569,#60570,#60571,#60572,#60573,#60574,#60575,#60576,#60577,#60578,#60579,
#60580,#60581,#60582,#60583,#60584,#60585,#60586,#60587,#60588,#60589,#60590,
#60591,#60592,#60593,#60594,#60595,#60596,#60597,#60598,#60599,#60600,#60601,
#60602,#60603,#60604,#60605,#60606,#60607,#60608,#60609,#60610,#60611,#60612,
#60613,#60614,#60615,#60616,#60617,#60618,#60619,#60620,#60621,#60622,#60623,
#60624,#60625,#60626,#60627,#60628,#60629,#60630,#60631,#60632,#60633,#60634,
#60635,#60636,#60637,#60638,#60639,#60640,#60641,#60642,#60643,#60644),
 .UNSPECIFIED.,.F.,.F.,(4,2,2,2,2,2,2,2,2,2,2,2,2,2,2,2,2,2,2,2,2,2,2,2,
2,2,2,2,2,2,2,2,2,2,2,2,2,2,2,2,2,2,2,2,2,2,2,2,2,2,2,2,2,2,2,2,2,2,2,2,
2,2,2,2,2,2,2,2,2,2,2,2,2,2,2,2,2,2,2,2,2,2,2,2,2,2,2,2,2,2,2,2,2,2,2,2,
2,2,2,2,4),(-2.98988513948328,-2.9890416521686,-2.92263169910402,-2.91052211338097,
-2.9048225881356,-2.90037948007852,-2.89542472032189,-2.88706812245068,
-2.84498674133361,-2.81330044732805,-2.79856800781766,-2.79208647956025,
-2.78714431285256,-2.78427320418269,-2.78176278084892,-2.77848125081889,
-2.77109437620559,-2.71703359952672,-2.69214521419253,-2.68109477778924,
-2.67214054105368,-2.66702812690655,-2.66255677049176,-2.65697043445206,
-2.64565031060122,-2.5895185263064,-2.56698077938366,-2.55846505756579,
-2.55213377816661,-2.54900629168709,-2.54649376766983,-2.54335120435105,
-2.53691296744397,-2.49073918797809,-2.44466978940957,-2.43626015740604,
-2.43127026806654,-2.42679216377246,-2.42104160876643,-2.40879222669042,
-2.3407514312561,-2.32660208625429,-2.31740882957647,-2.31379753759757,
-2.31124456163607,-2.30844073832737,-2.30362363718131,-2.28399700056034,
-2.24687156102182,-2.21489833999116,-2.20269571671468,-2.19695802201051,
-2.19248628526751,-2.18749989640427,-2.1790879421364,-2.13842309363864,
-2.1083431943885,-2.09199254371572,-2.08182672658222,-2.07807663020203,
-2.07549982550455,-2.07308939971531,-2.06886808333821,-2.05594812003229,
-2.00914412269069,-1.98453734522703,-1.97357278556821,-1.96467723026801,
-1.95958411605605,-1.95512177504329,-1.94953678494926,-1.94071360967437,
-1.87646035777905,-1.85749363828203,-1.84984564474205,-1.84401589113536,
-1.84099521807015,-1.83848503844687,-1.83523888030372,-1.82848788858546,
-1.78966867805449,-1.76999982516351,-1.74742136431683,-1.73703879719564,
-1.7285131056941,-1.72349915266241,-1.71902672977988,-1.71332117265768,
-1.70408025654224,-1.65409075944999,-1.62557319984512,-1.61580239479506,
-1.60878389507161,-1.60553432523165,-1.60326403243555,-1.60035323528149,
-1.59518844543772,-1.56351406666289,-1.55856664877721,-1.52619751615928,
-1.51264578802335),.UNSPECIFIED.);
#665=B_SPLINE_CURVE_WITH_KNOTS('',3,(#60650,#60651,#60652,#60653,#60654,
#60655,#60656,#60657,#60658,#60659,#60660),.UNSPECIFIED.,.F.,.F.,(4,1,1,
1,1,1,1,1,4),(21.9911485751285,22.2054340407747,23.1981452185157,24.1908563962566,
25.1835675739976,26.1762787517386,27.1689899294796,28.1617011072206,28.2016224877447),
 .UNSPECIFIED.);
#666=B_SPLINE_CURVE_WITH_KNOTS('',3,(#60661,#60662,#60663,#60664),
 .UNSPECIFIED.,.F.,.F.,(4,4),(-2.762961044583,-2.74540210132995),
 .UNSPECIFIED.);
#667=B_SPLINE_CURVE_WITH_KNOTS('',3,(#60665,#60666,#60667,#60668,#60669,
#60670,#60671,#60672,#60673,#60674,#60675,#60676,#60677,#60678,#60679,#60680,
#60681,#60682,#60683,#60684,#60685,#60686,#60687,#60688,#60689,#60690,#60691,
#60692,#60693,#60694,#60695,#60696,#60697,#60698,#60699,#60700,#60701,#60702,
#60703,#60704,#60705,#60706,#60707,#60708,#60709,#60710,#60711,#60712,#60713,
#60714,#60715,#60716,#60717,#60718,#60719,#60720,#60721,#60722,#60723,#60724,
#60725,#60726,#60727,#60728,#60729,#60730,#60731,#60732,#60733,#60734,#60735,
#60736,#60737,#60738,#60739,#60740,#60741,#60742,#60743,#60744,#60745,#60746,
#60747,#60748,#60749,#60750,#60751,#60752,#60753,#60754,#60755,#60756,#60757,
#60758,#60759,#60760,#60761,#60762,#60763,#60764,#60765,#60766,#60767,#60768,
#60769,#60770,#60771,#60772,#60773,#60774,#60775,#60776,#60777,#60778,#60779,
#60780,#60781,#60782,#60783,#60784,#60785,#60786,#60787,#60788,#60789,#60790,
#60791,#60792,#60793,#60794,#60795,#60796,#60797,#60798,#60799,#60800,#60801,
#60802,#60803,#60804,#60805,#60806,#60807,#60808,#60809,#60810,#60811,#60812,
#60813,#60814,#60815,#60816,#60817,#60818,#60819,#60820,#60821,#60822,#60823,
#60824,#60825,#60826,#60827,#60828,#60829,#60830,#60831,#60832,#60833,#60834,
#60835,#60836,#60837,#60838,#60839,#60840,#60841,#60842,#60843,#60844,#60845,
#60846,#60847,#60848,#60849,#60850,#60851,#60852,#60853,#60854,#60855,#60856,
#60857,#60858,#60859,#60860,#60861,#60862,#60863,#60864,#60865,#60866,#60867,
#60868,#60869,#60870,#60871,#60872,#60873,#60874,#60875,#60876,#60877,#60878,
#60879,#60880),.UNSPECIFIED.,.F.,.F.,(4,2,2,2,2,2,2,2,2,2,2,2,2,2,2,2,2,
2,2,2,2,2,2,2,2,2,2,2,2,2,2,2,2,2,2,2,2,2,2,2,2,2,2,2,2,2,2,2,2,2,2,2,2,
2,2,2,2,2,2,2,2,2,2,2,2,2,2,2,2,2,2,2,2,2,2,2,2,2,2,2,2,2,2,2,2,2,2,2,2,
2,2,2,2,2,2,2,2,2,2,2,2,2,2,2,2,2,2,4),(-1.51264578802335,-1.50824742685751,
-1.49533761970036,-1.48953443554317,-1.48503835802918,-1.48012834175573,
-1.47208960266296,-1.43768348666959,-1.41207448473708,-1.37709072636435,
-1.3718917214899,-1.36897323675787,-1.36670395455006,-1.36346509250798,
-1.35650637519991,-1.32565656373753,-1.26655813435419,-1.25736763246281,
-1.25215959838171,-1.24775061296511,-1.24234006042237,-1.2318878269114,
-1.21836221161977,-1.18325177190705,-1.1436904093263,-1.13694585630377,
-1.13370104690605,-1.13119171527509,-1.12817229721059,-1.12234305813237,
-1.09805717878198,-1.04539492736767,-1.02620490939015,-1.0192124889966,
-1.01499050691231,-1.01045185975469,-1.00426957108446,-0.989441746128937,
-0.967641506053302,-0.924403025948637,-0.904505636141447,-0.899659065410351,
-0.896847146869314,-0.894294815974935,-0.890693927051407,-0.881574126068692,
-0.867585440150397,-0.802323655848105,-0.78841984888466,-0.782832153608177,
-0.778671699346145,-0.774083128238035,-0.767614388424231,-0.750847631532854,
-0.724715793534429,-0.686591942583678,-0.668354451969255,-0.663623739851483,
-0.660837131401936,-0.658274547699032,-0.654612485700317,-0.645081672151302,
-0.580326066405161,-0.555678940085506,-0.548037582743291,-0.543212133210271,
-0.538686221769879,-0.532580758242613,-0.51823649151297,-0.497442371630394,
-0.469183815947758,-0.436055784894154,-0.429142947436221,-0.425912986079974,
-0.423405037435553,-0.420375001722253,-0.414491988616732,-0.374626674798603,
-0.324495723259461,-0.315268308078574,-0.309567249806176,-0.305096086043443,
-0.300081178282735,-0.29154798623774,-0.281152175522218,-0.258526113875507,
-0.218170322377199,-0.196907800629956,-0.191989462241814,-0.189162234580494,
-0.186615972927455,-0.186594270579785,-0.18657307999466,-0.186552377311534,
-0.186532140083982,-0.186512347162349,-0.183227486755542,-0.175322346189646,
-0.163544859603235,-0.122545419456931,-0.0852549480989891,-0.0769461251879338,
-0.0719788213987705,-0.0674979115811748,-0.0617113107814555,-0.0553956176738501,
-0.0447410390484928,-0.0182464691462297),.UNSPECIFIED.);
#668=B_SPLINE_CURVE_WITH_KNOTS('',3,(#60886,#60887,#60888,#60889,#60890,
#60891,#60892,#60893,#60894,#60895,#60896,#60897,#60898,#60899,#60900,#60901,
#60902,#60903,#60904,#60905,#60906,#60907,#60908,#60909,#60910,#60911,#60912,
#60913,#60914,#60915,#60916,#60917,#60918,#60919,#60920,#60921,#60922,#60923,
#60924,#60925,#60926,#60927,#60928,#60929,#60930,#60931,#60932,#60933,#60934,
#60935,#60936,#60937,#60938,#60939,#60940,#60941,#60942,#60943,#60944,#60945,
#60946,#60947,#60948,#60949,#60950,#60951,#60952,#60953,#60954,#60955,#60956,
#60957,#60958,#60959,#60960,#60961,#60962,#60963,#60964,#60965,#60966,#60967,
#60968,#60969,#60970,#60971,#60972,#60973,#60974,#60975,#60976,#60977,#60978,
#60979,#60980,#60981,#60982,#60983,#60984,#60985,#60986,#60987,#60988,#60989,
#60990,#60991,#60992,#60993,#60994,#60995,#60996,#60997,#60998,#60999,#61000,
#61001,#61002,#61003,#61004,#61005,#61006,#61007,#61008,#61009,#61010,#61011,
#61012,#61013,#61014,#61015,#61016,#61017,#61018,#61019,#61020,#61021,#61022,
#61023,#61024,#61025,#61026,#61027,#61028,#61029,#61030,#61031,#61032,#61033,
#61034,#61035,#61036,#61037,#61038,#61039,#61040,#61041,#61042,#61043,#61044,
#61045,#61046,#61047,#61048,#61049,#61050,#61051,#61052,#61053,#61054,#61055,
#61056,#61057,#61058,#61059,#61060,#61061,#61062,#61063,#61064,#61065,#61066,
#61067,#61068,#61069,#61070,#61071,#61072,#61073,#61074,#61075),
 .UNSPECIFIED.,.F.,.F.,(4,3,3,3,3,3,3,3,3,3,3,3,3,3,3,3,3,3,3,3,3,3,3,3,
3,3,3,3,3,3,3,3,3,3,3,3,3,3,3,3,3,3,3,3,3,3,3,3,3,3,3,3,3,3,3,3,3,3,3,3,
3,3,3,4),(28.2743341515405,28.373510423933,28.4725496186461,28.5715132139937,
28.6704339425324,28.7693444802945,28.8683439593539,28.9673864432613,29.0666027207686,
29.1544122849615,29.2549893084417,29.3554225402566,29.4557405947623,29.555995827914,
29.6562193813565,29.7564423567437,29.8567645084394,29.9571353509374,30.0576848454224,
30.1471234627025,30.2477004859965,30.348133717608,30.4484517718857,30.5487070047943,
30.6489305579792,30.7491535330941,30.8494756844967,30.9498465266896,31.0503960208528,
31.1398346404435,31.240411665129,31.3408448981566,31.441162953881,31.5414181882544,
31.6416417429197,31.741864719529,31.8421868724372,31.9425577161444,32.0431072118187,
32.1325458181845,32.2331228421251,32.3335560743984,32.4338741293577,32.5341293629598,
32.6343529168488,32.7345758926779,32.8348980448052,32.9352688877297,33.0358183826278,
33.1252569959254,33.2258340199109,33.3262672522277,33.4265853072283,33.5268405408702,
33.6270640947977,33.7272870706639,33.8276092228255,33.9279800657829,34.028529560711,
34.1179681736664,34.2266510107969,34.3350816319526,34.4431465276488,34.4851594650687),
 .UNSPECIFIED.);
#669=B_SPLINE_CURVE_WITH_KNOTS('',3,(#61076,#61077,#61078,#61079),
 .UNSPECIFIED.,.F.,.F.,(4,4),(28.2016224877447,28.2743338823081),
 .UNSPECIFIED.);
#670=B_SPLINE_CURVE_WITH_KNOTS('',3,(#61081,#61082,#61083,#61084),
 .UNSPECIFIED.,.F.,.F.,(4,4),(-0.0182464691462297,-0.000683907669467373),
 .UNSPECIFIED.);
#671=B_SPLINE_CURVE_WITH_KNOTS('',3,(#61085,#61086,#61087,#61088,#61089,
#61090,#61091,#61092,#61093,#61094,#61095,#61096,#61097,#61098,#61099,#61100,
#61101,#61102,#61103,#61104,#61105,#61106,#61107,#61108,#61109,#61110,#61111,
#61112,#61113,#61114,#61115,#61116,#61117,#61118,#61119,#61120,#61121,#61122,
#61123,#61124,#61125,#61126,#61127,#61128,#61129,#61130,#61131,#61132,#61133,
#61134,#61135,#61136,#61137,#61138,#61139,#61140,#61141,#61142,#61143,#61144,
#61145,#61146,#61147,#61148,#61149,#61150,#61151,#61152,#61153,#61154,#61155,
#61156,#61157,#61158,#61159,#61160,#61161,#61162,#61163,#61164,#61165,#61166,
#61167,#61168,#61169,#61170,#61171,#61172,#61173,#61174,#61175,#61176,#61177,
#61178,#61179,#61180,#61181,#61182,#61183,#61184,#61185,#61186,#61187,#61188,
#61189,#61190,#61191,#61192,#61193,#61194,#61195,#61196,#61197,#61198,#61199,
#61200,#61201,#61202,#61203,#61204,#61205,#61206,#61207,#61208,#61209,#61210,
#61211,#61212,#61213,#61214,#61215,#61216,#61217,#61218,#61219,#61220,#61221,
#61222,#61223,#61224,#61225,#61226,#61227,#61228,#61229,#61230,#61231,#61232,
#61233,#61234,#61235,#61236,#61237,#61238,#61239,#61240,#61241,#61242,#61243,
#61244,#61245,#61246,#61247,#61248,#61249,#61250,#61251,#61252,#61253,#61254,
#61255,#61256,#61257,#61258,#61259,#61260,#61261,#61262,#61263,#61264,#61265,
#61266,#61267,#61268,#61269,#61270,#61271,#61272,#61273,#61274,#61275,#61276),
 .UNSPECIFIED.,.F.,.F.,(4,2,2,2,2,2,2,2,2,2,2,2,2,2,2,2,2,2,2,2,2,2,2,2,
2,2,2,2,2,2,2,2,2,2,2,2,2,2,2,2,2,2,2,2,2,2,2,2,2,2,2,2,2,2,2,2,2,2,2,2,
2,2,2,2,2,2,2,2,2,2,2,2,2,2,2,2,2,2,2,2,2,2,2,2,2,2,2,2,2,2,2,2,2,2,2,4),
(-2.98929371686741,-2.95942260090057,-2.94908673202952,-2.94568016859995,
-2.94316029079119,-2.94062978415982,-2.93775045959017,-2.93272485907433,
-2.90843250200678,-2.87437961387487,-2.83806022771823,-2.82988827047787,
-2.82487872151955,-2.82040690508782,-2.81469754036461,-2.80544058838125,
-2.75593338036318,-2.7158543386228,-2.70972363013292,-2.70664396034991,
-2.70413863945052,-2.70096718609043,-2.69436491288393,-2.65053170443754,
-2.60255764740952,-2.59401548864488,-2.58899881337042,-2.58452817192148,
-2.5788306642466,-2.56961506201767,-2.51918854198363,-2.47993569648334,
-2.47381344470312,-2.47073541619546,-2.46822998609407,-2.46505657156555,
-2.45844424087166,-2.41492993222893,-2.36663326561542,-2.35809988403435,
-2.35308499392165,-2.34861390609176,-2.34291303084164,-2.33368600588134,
-2.28348667391634,-2.24385299524389,-2.23783757590937,-2.23478083512784,
-2.2322744837398,-2.22907669904788,-2.22233593505826,-2.17997121825981,
-2.13055414439691,-2.12210950622387,-2.11711337269429,-2.11263862408216,
-2.1069048595422,-2.09756380269823,-2.05062964505076,-2.00816461292868,
-2.0020088171623,-1.99892404087715,-1.99641868753577,-1.99325238957545,
-1.98667783099717,-1.94278275659959,-1.89622751751532,-1.88690136356124,
-1.88171981654142,-1.87726777759646,-1.87180809826288,-1.86340471640823,
-1.80448355847513,-1.77349374584792,-1.76652174530783,-1.76328075195105,
-1.7610114383161,-1.7580947528467,-1.75290379581136,-1.71823848535071,-1.6913656798286,
-1.66908442485546,-1.6540291179165,-1.64781178677845,-1.64326744954752,
-1.63848103257163,-1.63102546613321,-1.60757504267856,-1.55338306018242,
-1.54017386336012,-1.53141974456107,-1.52787527070329,-1.52533191440914,
-1.52249470265252,-1.51753139877423,-1.51249653208003),.UNSPECIFIED.);
#672=B_SPLINE_CURVE_WITH_KNOTS('',3,(#61282,#61283,#61284,#61285,#61286,
#61287,#61288,#61289,#61290,#61291,#61292,#61293,#61294,#61295,#61296,#61297,
#61298,#61299,#61300,#61301,#61302,#61303,#61304,#61305,#61306,#61307,#61308,
#61309,#61310,#61311,#61312,#61313,#61314,#61315,#61316,#61317,#61318,#61319,
#61320,#61321,#61322,#61323,#61324,#61325,#61326,#61327,#61328,#61329,#61330,
#61331,#61332,#61333,#61334,#61335,#61336,#61337,#61338,#61339,#61340,#61341,
#61342,#61343,#61344,#61345,#61346,#61347,#61348,#61349,#61350,#61351,#61352,
#61353,#61354,#61355,#61356,#61357,#61358,#61359,#61360,#61361,#61362,#61363,
#61364,#61365,#61366,#61367,#61368,#61369,#61370,#61371,#61372,#61373,#61374,
#61375,#61376,#61377,#61378,#61379,#61380,#61381,#61382,#61383,#61384,#61385,
#61386,#61387,#61388,#61389,#61390,#61391,#61392,#61393,#61394,#61395,#61396,
#61397,#61398,#61399,#61400,#61401,#61402,#61403,#61404,#61405,#61406,#61407,
#61408,#61409,#61410,#61411,#61412,#61413,#61414,#61415,#61416,#61417,#61418,
#61419,#61420,#61421,#61422,#61423,#61424,#61425,#61426,#61427,#61428,#61429,
#61430,#61431,#61432,#61433,#61434,#61435,#61436,#61437,#61438,#61439,#61440,
#61441,#61442,#61443,#61444,#61445,#61446,#61447,#61448,#61449,#61450,#61451,
#61452,#61453,#61454,#61455,#61456,#61457,#61458,#61459,#61460,#61461,#61462,
#61463,#61464,#61465,#61466,#61467,#61468,#61469,#61470,#61471,#61472,#61473,
#61474,#61475,#61476,#61477,#61478,#61479,#61480,#61481,#61482,#61483,#61484,
#61485,#61486,#61487,#61488,#61489,#61490,#61491,#61492,#61493),
 .UNSPECIFIED.,.F.,.F.,(4,2,2,2,2,2,2,2,2,2,2,2,2,2,2,2,2,2,2,2,2,2,2,2,
2,2,2,2,2,2,2,2,2,2,2,2,2,2,2,2,2,2,2,2,2,2,2,2,2,2,2,2,2,2,2,2,2,2,2,2,
2,2,2,2,2,2,2,2,2,2,2,2,2,2,2,2,2,2,2,2,2,2,2,2,2,2,2,2,2,2,2,2,2,2,2,2,
2,2,2,2,2,2,2,2,2,4),(-1.47764986309498,-1.44881698295396,-1.43952935990818,
-1.43393724919047,-1.42955351574726,-1.42471638787349,-1.41668651112816,
-1.38010143774755,-1.36673596052301,-1.3238902221451,-1.3173053247027,-1.31413388159894,
-1.31168179412128,-1.30873929395105,-1.30308979745928,-1.29570878360394,
-1.27762005080888,-1.23287911256112,-1.20786267104714,-1.20028680944599,
-1.19554653131156,-1.19113289607351,-1.18523203237493,-1.17165416714221,
-1.15230025713113,-1.12244653776663,-1.11456732622048,-1.0853317294815,
-1.08026094845732,-1.07740969601219,-1.07519282195167,-1.0720358270436,
-1.06528879051481,-1.03592788138144,-0.982763616052192,-0.96867115490706,
-0.963124607704263,-0.959037394949743,-0.954572856963394,-0.948364471522385,
-0.932819019168934,-0.909343910254935,-0.88178178658113,-0.849287754897747,
-0.844189428715838,-0.841332067872399,-0.839116256016836,-0.835968326961959,
-0.829269658035917,-0.80037308628289,-0.748574614133139,-0.73307883344986,
-0.72671348772298,-0.722265155154821,-0.717681504132227,-0.710853651652471,
-0.690533097450211,-0.654617291282131,-0.615826663941689,-0.609030837664496,
-0.605864859041756,-0.603413243436209,-0.600466773694076,-0.594797424277209,
-0.587382541278495,-0.569163338586325,-0.524253167997968,-0.499551149716652,
-0.492004393270059,-0.487270472516489,-0.482854716063843,-0.476938764594269,
-0.463268157125065,-0.443729201528938,-0.41412128665872,-0.406489302572081,
-0.377089580736931,-0.372015853250601,-0.369164033033085,-0.366947395512771,
-0.36379162035778,-0.357050598854746,-0.327745978010035,-0.27474717456546,
-0.260494257252249,-0.254924401431048,-0.250831639655306,-0.246372204598149,
-0.240191700280601,-0.224832490828784,-0.201766456536337,-0.175008249335334,
-0.141068520831317,-0.135961156695513,-0.13310186622085,-0.13088649291921,
-0.127741700869035,-0.121059297816463,-0.0923160942520134,-0.0460591495953894,
-0.0261999556201138,-0.0192392761083748,-0.0150892407283716,-0.0109091130635428,
-0.0059084454421249,-0.00068537780707878),.UNSPECIFIED.);
#673=B_SPLINE_CURVE_WITH_KNOTS('',3,(#61494,#61495,#61496,#61497),
 .UNSPECIFIED.,.F.,.F.,(4,4),(34.4851594650687,34.557519189258),
 .UNSPECIFIED.);
#674=B_SPLINE_CURVE_WITH_KNOTS('',3,(#61498,#61499,#61500,#61501,#61502,
#61503,#61504,#61505,#61506,#61507,#61508,#61509,#61510,#61511,#61512,#61513,
#61514,#61515,#61516,#61517,#61518,#61519,#61520,#61521,#61522,#61523,#61524,
#61525,#61526,#61527,#61528,#61529,#61530,#61531,#61532,#61533,#61534,#61535,
#61536,#61537,#61538,#61539,#61540,#61541,#61542,#61543,#61544,#61545,#61546,
#61547,#61548,#61549,#61550,#61551,#61552,#61553,#61554,#61555,#61556,#61557,
#61558,#61559,#61560,#61561,#61562,#61563,#61564,#61565,#61566,#61567,#61568,
#61569,#61570,#61571,#61572,#61573,#61574,#61575,#61576,#61577,#61578,#61579,
#61580,#61581,#61582,#61583,#61584,#61585,#61586,#61587,#61588,#61589,#61590,
#61591,#61592,#61593,#61594,#61595,#61596,#61597,#61598,#61599,#61600,#61601,
#61602,#61603,#61604,#61605,#61606,#61607,#61608,#61609,#61610,#61611,#61612,
#61613,#61614,#61615,#61616,#61617,#61618,#61619,#61620,#61621,#61622,#61623,
#61624,#61625,#61626,#61627,#61628,#61629,#61630,#61631,#61632,#61633,#61634,
#61635,#61636,#61637,#61638,#61639,#61640,#61641,#61642,#61643,#61644,#61645,
#61646,#61647,#61648,#61649,#61650,#61651,#61652,#61653,#61654,#61655,#61656,
#61657,#61658,#61659,#61660,#61661,#61662,#61663,#61664,#61665,#61666,#61667,
#61668,#61669,#61670,#61671,#61672,#61673,#61674,#61675,#61676,#61677,#61678,
#61679,#61680,#61681,#61682,#61683,#61684,#61685),.UNSPECIFIED.,.F.,.F.,
(4,2,2,2,2,2,2,2,2,2,2,2,2,2,2,2,2,2,2,2,2,2,2,2,2,2,2,2,2,2,2,2,2,2,2,
2,2,2,2,2,2,2,2,2,2,2,2,2,2,2,2,2,2,2,2,2,2,2,2,2,2,2,2,2,2,2,2,2,2,2,2,
2,2,2,2,2,2,2,2,2,2,2,2,2,2,2,2,2,2,2,2,2,2,4),(-1.51249653208003,-1.49532235228339,
-1.46458408338178,-1.42271694013379,-1.41433716581086,-1.4093543853258,
-1.40487617875404,-1.39911645151077,-1.38681096003889,-1.35206241795467,
-1.31023612226106,-1.29707975235174,-1.29283106324752,-1.2901496382989,
-1.28752206697662,-1.2835244523702,-1.27144029660535,-1.25023835607663,
-1.19930033730217,-1.18307841925596,-1.17650573344924,-1.17194350696784,
-1.16726573912676,-1.16033721323982,-1.13994895294347,-1.10402802489318,
-1.06568240683567,-1.05880163461925,-1.05557740777576,-1.05306950387456,
-1.05003415764808,-1.04412606768488,-1.01231876880348,-0.956134751789516,
-0.944651118225109,-0.93904235943167,-0.93457966203583,-0.92950623864646,
-0.920698109854971,-0.875213513816718,-0.829062597455482,-0.822617541309217,
-0.819475930441066,-0.816970753190448,-0.813862126005212,-0.807586417741081,
-0.799163071815572,-0.777007837465092,-0.722531516718579,-0.709667997760202,
-0.703783173293315,-0.699274966223604,-0.694402196525816,-0.686539012550412,
-0.655275588327369,-0.627014132778495,-0.593882809767509,-0.586969370135155,
-0.583739154616511,-0.581231009634986,-0.578200736404825,-0.572317327458206,
-0.532551298529391,-0.48230275119364,-0.473079938289183,-0.467379937167282,
-0.46290854034125,-0.457892265062286,-0.449353968788562,-0.401310764105049,
-0.357438847579887,-0.350857567516843,-0.347689830387979,-0.345184251086645,
-0.342100310645394,-0.335949489212392,-0.293906824364619,-0.246666962872415,
-0.23728011121668,-0.231532871480163,-0.227232089831868,-0.22247592499597,
-0.217439405894266,-0.199883383200268,-0.171834221934627,-0.128940005275336,
-0.117149301677165,-0.113066575360789,-0.110683308995864,-0.108081841643167,
-0.104212107675829,-0.0931671729726866,-0.0746899741359773,-0.0180297629229655),
 .UNSPECIFIED.);
#675=B_SPLINE_CURVE_WITH_KNOTS('',3,(#61690,#61691,#61692,#61693,#61694,
#61695,#61696,#61697,#61698,#61699,#61700,#61701,#61702,#61703,#61704,#61705,
#61706,#61707,#61708,#61709,#61710,#61711,#61712,#61713,#61714,#61715,#61716,
#61717,#61718,#61719,#61720,#61721,#61722,#61723,#61724,#61725,#61726,#61727,
#61728,#61729,#61730,#61731,#61732,#61733,#61734,#61735,#61736,#61737,#61738,
#61739,#61740,#61741,#61742,#61743,#61744,#61745,#61746,#61747,#61748,#61749,
#61750,#61751,#61752,#61753,#61754,#61755,#61756,#61757,#61758,#61759,#61760,
#61761,#61762,#61763,#61764,#61765,#61766,#61767,#61768,#61769,#61770,#61771,
#61772,#61773,#61774,#61775,#61776,#61777,#61778,#61779,#61780,#61781,#61782,
#61783,#61784,#61785,#61786,#61787,#61788,#61789,#61790,#61791,#61792,#61793,
#61794,#61795,#61796,#61797,#61798,#61799,#61800,#61801,#61802,#61803,#61804,
#61805,#61806,#61807,#61808,#61809,#61810,#61811,#61812,#61813,#61814,#61815,
#61816,#61817,#61818,#61819,#61820,#61821,#61822,#61823,#61824,#61825,#61826,
#61827,#61828,#61829,#61830,#61831,#61832,#61833,#61834,#61835,#61836,#61837,
#61838,#61839,#61840,#61841,#61842,#61843,#61844,#61845,#61846,#61847,#61848,
#61849,#61850,#61851,#61852,#61853,#61854,#61855,#61856,#61857,#61858,#61859,
#61860,#61861,#61862,#61863,#61864,#61865,#61866,#61867,#61868,#61869,#61870,
#61871,#61872,#61873,#61874,#61875,#61876,#61877,#61878,#61879,#61880,#61881,
#61882,#61883,#61884,#61885,#61886,#61887,#61888,#61889,#61890,#61891),
 .UNSPECIFIED.,.F.,.F.,(4,2,2,2,2,2,2,2,2,2,2,2,2,2,2,2,2,2,2,2,2,2,2,2,
2,2,2,2,2,2,2,2,2,2,2,2,2,2,2,2,2,2,2,2,2,2,2,2,2,2,2,2,2,2,2,2,2,2,2,2,
2,2,2,2,2,2,2,2,2,2,2,2,2,2,2,2,2,2,2,2,2,2,2,2,2,2,2,2,2,2,2,2,2,2,2,2,
2,2,2,2,4),(-2.97190100113565,-2.97131175839763,-2.96845623843134,-2.96614107326616,
-2.96368022360977,-2.96045676381779,-2.95314821990278,-2.9310116849298,
-2.8994834220475,-2.8741892507486,-2.85784077341721,-2.8515174500756,-2.84703296917863,
-2.84296937776516,-2.83648537192792,-2.82021859310396,-2.7691538133824,
-2.74783173551207,-2.73964661187022,-2.73353245624978,-2.73049709068879,
-2.72804986538015,-2.72498731645274,-2.71873425796821,-2.67134910166512,
-2.62584286662948,-2.61755510053169,-2.61266388972297,-2.60829333690894,
-2.60271046178093,-2.59366244347109,-2.53047808995372,-2.51090300052764,
-2.50314293653978,-2.4972728276138,-2.49428592775775,-2.4918372626154,-2.4887214702138,
-2.48219178918329,-2.43821677823288,-2.39005253042042,-2.38158662294442,
-2.37665736844077,-2.372292967894,-2.36677250990311,-2.35794023223671,-2.30319488462053,
-2.26702351366726,-2.26116128265609,-2.25817590582041,-2.2557270818585,
-2.25260930181604,-2.24606947775557,-2.20219743268914,-2.15388707018597,
-2.14545093407467,-2.14052788955146,-2.13616234341669,-2.13063143780608,
-2.12176362860523,-2.06738242309581,-2.03039970235347,-2.02484735762898,
-2.02192509490361,-2.01947146370955,-2.01632727476398,-2.00946641205748,
-1.97242088651315,-1.95327364695403,-1.92913718080272,-1.9132943332153,
-1.90704270160636,-1.90257066044696,-1.89849250452637,-1.89192825028888,
-1.87512632282246,-1.82456092977286,-1.79608646698237,-1.78943242359899,
-1.78629291450267,-1.78407810670438,-1.78121503164371,-1.77609084830558,
-1.74120126708856,-1.71422341379356,-1.69192515350075,-1.68167972891799,
-1.67327725702302,-1.66836091218807,-1.66399354090812,-1.65844976348067,
-1.6495391375974,-1.59560011757762,-1.55825787324151,-1.55269382525663,
-1.54976889499946,-1.54731514883066,-1.54417345713816,-1.53756924516136,
-1.49521188663987,-1.47764986309498),.UNSPECIFIED.);
#676=B_SPLINE_CURVE_WITH_KNOTS('',3,(#61893,#61894,#61895,#61896,#61897,
#61898,#61899,#61900),.UNSPECIFIED.,.F.,.F.,(4,2,2,4),(-0.0180297629229655,
-0.0117363126142654,-0.00498186049605689,-0.000717196793377947),
 .UNSPECIFIED.);
#677=B_SPLINE_CURVE_WITH_KNOTS('',3,(#61901,#61902,#61903,#61904,#61905,
#61906,#61907,#61908,#61909,#61910),.UNSPECIFIED.,.F.,.F.,(4,1,1,1,1,1,
1,4),(40.8407044966673,41.3711512650695,42.3630218789779,43.3548924928863,
44.3467631067947,45.3386337207031,46.3305043346114,47.0500693632372),
 .UNSPECIFIED.);
#678=B_SPLINE_CURVE_WITH_KNOTS('',3,(#61916,#61917,#61918,#61919,#61920,
#61921,#61922,#61923,#61924,#61925),.UNSPECIFIED.,.F.,.F.,(4,1,1,1,1,1,
1,4),(47.1238982701508,48.0159246620401,49.0086358397811,50.001347017522,
50.994058195263,51.986769373004,52.979480550745,53.334785281413),
 .UNSPECIFIED.);
#679=B_SPLINE_CURVE_WITH_KNOTS('',3,(#61926,#61927,#61928,#61929,#61930,
#61931),.UNSPECIFIED.,.F.,.F.,(4,2,4),(-2.98912319920029,-2.97800245941442,
-2.97190100113565),.UNSPECIFIED.);
#680=B_SPLINE_CURVE_WITH_KNOTS('',3,(#61933,#61934,#61935,#61936),
 .UNSPECIFIED.,.F.,.F.,(4,4),(47.0500693632372,47.1238868231314),
 .UNSPECIFIED.);
#681=B_SPLINE_CURVE_WITH_KNOTS('',3,(#61937,#61938,#61939,#61940,#61941,
#61942,#61943,#61944,#61945,#61946,#61947,#61948,#61949,#61950,#61951,#61952,
#61953,#61954,#61955,#61956,#61957,#61958,#61959,#61960,#61961,#61962,#61963,
#61964,#61965,#61966,#61967,#61968,#61969,#61970,#61971,#61972,#61973,#61974,
#61975,#61976,#61977,#61978,#61979,#61980,#61981,#61982,#61983,#61984,#61985,
#61986,#61987,#61988,#61989,#61990,#61991,#61992,#61993,#61994,#61995,#61996,
#61997,#61998,#61999,#62000,#62001,#62002,#62003,#62004,#62005,#62006,#62007,
#62008,#62009,#62010,#62011,#62012,#62013,#62014,#62015,#62016,#62017,#62018,
#62019,#62020,#62021,#62022,#62023,#62024,#62025,#62026,#62027,#62028,#62029,
#62030,#62031,#62032,#62033,#62034,#62035,#62036,#62037,#62038,#62039,#62040,
#62041,#62042,#62043,#62044,#62045,#62046,#62047,#62048,#62049,#62050,#62051,
#62052,#62053,#62054,#62055,#62056,#62057,#62058,#62059,#62060,#62061,#62062,
#62063,#62064,#62065,#62066,#62067,#62068,#62069,#62070,#62071,#62072,#62073,
#62074,#62075,#62076,#62077,#62078,#62079,#62080,#62081,#62082,#62083,#62084,
#62085,#62086,#62087,#62088,#62089,#62090,#62091,#62092,#62093,#62094,#62095,
#62096,#62097,#62098,#62099,#62100,#62101,#62102,#62103,#62104,#62105,#62106,
#62107,#62108,#62109,#62110,#62111,#62112,#62113,#62114,#62115,#62116,#62117,
#62118,#62119,#62120,#62121,#62122,#62123,#62124,#62125,#62126,#62127,#62128,
#62129,#62130,#62131,#62132),.UNSPECIFIED.,.F.,.F.,(4,2,2,2,2,2,2,2,2,2,
2,2,2,2,2,2,2,2,2,2,2,2,2,2,2,2,2,2,2,2,2,2,2,2,2,2,2,2,2,2,2,2,2,2,2,2,
2,2,2,2,2,2,2,2,2,2,2,2,2,2,2,2,2,2,2,2,2,2,2,2,2,2,2,2,2,2,2,2,2,2,2,2,
2,2,2,2,2,2,2,2,2,2,2,2,2,2,2,4),(-2.98909564641531,-2.96016523086049,-2.94987452961653,
-2.94645872464972,-2.94393562506273,-2.94140386423417,-2.93853047506777,
-2.93353056391019,-2.9097072416286,-2.87574585450262,-2.83957868726566,
-2.83099748365331,-2.82590079067047,-2.82144224541615,-2.81587122359658,
-2.80708918644641,-2.75168571123234,-2.71653949738635,-2.71046049087622,
-2.70739124745004,-2.70488575083645,-2.70170311196662,-2.69504130183218,
-2.65219393568004,-2.60317763100082,-2.59471946091289,-2.58972083401277,
-2.58524722022996,-2.57951958099087,-2.5701985894611,-2.5225942068571,-2.48058541046492,
-2.47454829458135,-2.47148738179386,-2.46898147804595,-2.46578917294243,
-2.45907649892798,-2.4163849241686,-2.36743409430002,-2.35889744843827,
-2.35388208983118,-2.34941146072798,-2.3437123742855,-2.33449081491071,
-2.28419526214826,-2.25591530249727,-2.2461917115635,-2.23919903320737,
-2.23595455218833,-2.23368514586778,-2.23077164283522,-2.22559364226457,
-2.19158596652003,-2.18795264412711,-2.14966417018502,-2.12854639265802,
-2.12153709128879,-2.11684371734355,-2.11229536734441,-2.10579395675903,
-2.08996220026183,-2.03860744878683,-2.01728738733133,-2.00906080850749,
-2.00289778220183,-1.9998117494116,-1.99730667387238,-1.99414236314651,
-1.9875772571877,-1.94357760116908,-1.89584018740329,-1.88723032427049,
-1.88219937517131,-1.87773130277114,-1.87205793923073,-1.86292562612946,
-1.80012982619518,-1.7736545022907,-1.76715992439133,-1.76400902932515,
-1.76150407853096,-1.75840518126524,-1.7521776128705,-1.70393705597441,
-1.66620796990811,-1.65375655302756,-1.64797126848625,-1.64349058091613,
-1.63852271118832,-1.63021101707353,-1.59282358972378,-1.54079007272048,
-1.53221975494757,-1.52870455191223,-1.52616578910238,-1.52331499820292,
-1.51828796833696,-1.51241459518593),.UNSPECIFIED.);
#682=B_SPLINE_CURVE_WITH_KNOTS('',3,(#62138,#62139,#62140,#62141,#62142,
#62143,#62144,#62145,#62146,#62147,#62148,#62149,#62150,#62151,#62152,#62153,
#62154,#62155,#62156,#62157,#62158,#62159,#62160,#62161,#62162,#62163,#62164,
#62165,#62166,#62167,#62168,#62169,#62170,#62171,#62172,#62173,#62174,#62175,
#62176,#62177,#62178,#62179,#62180,#62181,#62182,#62183,#62184,#62185,#62186,
#62187,#62188,#62189,#62190,#62191,#62192,#62193,#62194,#62195,#62196,#62197,
#62198,#62199,#62200,#62201,#62202,#62203,#62204,#62205,#62206,#62207,#62208,
#62209,#62210,#62211,#62212,#62213,#62214,#62215,#62216,#62217,#62218,#62219,
#62220,#62221,#62222,#62223,#62224,#62225,#62226,#62227,#62228,#62229,#62230,
#62231,#62232,#62233,#62234,#62235,#62236,#62237,#62238,#62239,#62240,#62241,
#62242,#62243,#62244,#62245,#62246,#62247,#62248,#62249,#62250,#62251,#62252,
#62253,#62254,#62255,#62256,#62257,#62258,#62259,#62260,#62261,#62262,#62263,
#62264,#62265,#62266,#62267,#62268,#62269,#62270,#62271,#62272,#62273,#62274,
#62275,#62276,#62277,#62278,#62279,#62280,#62281,#62282,#62283,#62284,#62285,
#62286,#62287,#62288,#62289,#62290,#62291,#62292,#62293,#62294,#62295,#62296,
#62297,#62298,#62299,#62300,#62301,#62302,#62303,#62304,#62305,#62306,#62307,
#62308,#62309,#62310,#62311,#62312,#62313,#62314,#62315,#62316,#62317,#62318,
#62319,#62320,#62321,#62322,#62323,#62324,#62325,#62326,#62327),
 .UNSPECIFIED.,.F.,.F.,(4,3,3,3,3,3,3,3,3,3,3,3,3,3,3,3,3,3,3,3,3,3,3,3,
3,3,3,3,3,3,3,3,3,3,3,3,3,3,3,3,3,3,3,3,3,3,3,3,3,3,3,3,3,3,3,3,3,3,3,3,
3,3,3,4),(53.4070751110264,53.5094895370782,53.611968539674,53.7146203178466,
53.8173674042498,53.9203240275781,53.972191728486,54.0727687525615,54.1732019849704,
54.2735200400656,54.3737752738037,54.4739988278287,54.5742218037934,54.6745439560551,
54.7749147991135,54.8754642941431,54.9649029062269,55.0654799303024,55.165913162711,
55.2662312178063,55.3664864515444,55.4667100055694,55.5669329815341,55.6672551337958,
55.7676259768542,55.8681754718837,55.9576140839679,56.0581911080434,56.1586243404524,
56.2589423955477,56.3591976292858,56.4594211833108,56.5596441592756,56.6599663115373,
56.7603371545958,56.8608866496254,56.9503252617089,57.0509022857844,57.1513355181932,
57.2516535732885,57.3519088070266,57.4521323610516,57.5523553370163,57.6526774892779,
57.7530483323363,57.8535978273659,57.9430364394499,58.0436134635254,58.1440466959342,
58.2443647510295,58.3446199847677,58.4448435387926,58.5450665147576,58.6453886670194,
58.7457595100778,58.8463090051074,58.9357476171908,59.0350728526044,59.1342668431611,
59.2333624091373,59.3324091722181,59.4314232994544,59.5304864406886,59.6164740057542),
 .UNSPECIFIED.);
#683=B_SPLINE_CURVE_WITH_KNOTS('',3,(#62328,#62329,#62330,#62331),
 .UNSPECIFIED.,.F.,.F.,(4,4),(53.334785281413,53.4070701237542),
 .UNSPECIFIED.);
#684=B_SPLINE_CURVE_WITH_KNOTS('',3,(#62332,#62333,#62334,#62335,#62336,
#62337,#62338,#62339,#62340,#62341,#62342,#62343,#62344,#62345,#62346,#62347,
#62348,#62349,#62350,#62351,#62352,#62353,#62354,#62355,#62356,#62357,#62358,
#62359,#62360,#62361,#62362,#62363,#62364,#62365,#62366,#62367,#62368,#62369,
#62370,#62371,#62372,#62373,#62374,#62375,#62376,#62377,#62378,#62379,#62380,
#62381,#62382,#62383,#62384,#62385,#62386,#62387,#62388,#62389,#62390,#62391,
#62392,#62393,#62394,#62395,#62396,#62397,#62398,#62399,#62400,#62401,#62402,
#62403,#62404,#62405,#62406,#62407,#62408,#62409,#62410,#62411,#62412,#62413,
#62414,#62415,#62416,#62417,#62418,#62419,#62420,#62421,#62422,#62423,#62424,
#62425,#62426,#62427,#62428,#62429,#62430,#62431,#62432,#62433,#62434,#62435,
#62436,#62437,#62438,#62439,#62440,#62441,#62442,#62443,#62444,#62445,#62446,
#62447,#62448,#62449,#62450,#62451,#62452,#62453,#62454,#62455,#62456,#62457,
#62458,#62459,#62460,#62461,#62462,#62463,#62464,#62465,#62466,#62467,#62468,
#62469,#62470,#62471,#62472,#62473,#62474,#62475,#62476,#62477,#62478,#62479,
#62480,#62481,#62482,#62483,#62484,#62485,#62486,#62487,#62488,#62489,#62490,
#62491,#62492,#62493,#62494,#62495,#62496,#62497,#62498,#62499,#62500,#62501,
#62502,#62503,#62504,#62505,#62506,#62507,#62508,#62509,#62510,#62511,#62512,
#62513,#62514,#62515,#62516,#62517),.UNSPECIFIED.,.F.,.F.,(4,2,2,2,2,2,
2,2,2,2,2,2,2,2,2,2,2,2,2,2,2,2,2,2,2,2,2,2,2,2,2,2,2,2,2,2,2,2,2,2,2,2,
2,2,2,2,2,2,2,2,2,2,2,2,2,2,2,2,2,2,2,2,2,2,2,2,2,2,2,2,2,2,2,2,2,2,2,2,
2,2,2,2,2,2,2,2,2,2,2,2,2,2,4),(-1.51241459518593,-1.49524509246308,-1.46505511337229,
-1.42360606407568,-1.41522311013593,-1.41023995122281,-1.40576233768265,
-1.40000467888127,-1.38770887107532,-1.35318820490325,-1.3117549439869,
-1.29808955902646,-1.29378382502586,-1.29109013811061,-1.28847284228217,
-1.28452410408607,-1.27284615938273,-1.25273662743795,-1.20569110063573,
-1.18525163153861,-1.17811502024508,-1.17339514153084,-1.16881191855104,
-1.16237214340507,-1.14581063957843,-1.12016133266688,-1.09611557475652,
-1.06394850766189,-1.05878169525847,-1.05587045934723,-1.05360024374072,
-1.05035130867201,-1.04333585878254,-1.03357148537055,-1.00508041225542,
-0.955137735674959,-0.945900910309668,-0.940196955583426,-0.935725252867187,
-0.930711542384892,-0.922184902475477,-0.873835482265823,-0.830306263634118,
-0.823689576972656,-0.820515143933244,-0.818009453206771,-0.81493175935616,
-0.808812116937569,-0.769760127189184,-0.719147160121579,-0.709943008732649,
-0.704248427502345,-0.699777641969742,-0.694758257362915,-0.686205127832704,
-0.637702076993659,-0.594420233382172,-0.58777320939651,-0.584592975690829,
-0.582087066564602,-0.579014465404662,-0.572920562333852,-0.536349612376319,
-0.48282439921669,-0.473828365994832,-0.468194089672247,-0.463729205340216,
-0.458672599772318,-0.449943755976233,-0.401925510290071,-0.35844253953196,
-0.351820136631256,-0.348644566767666,-0.346138781236953,-0.343061958930788,
-0.336946936495131,-0.298352707192188,-0.24724089508629,-0.238053169451893,
-0.232363258103448,-0.228092179612958,-0.223252127632017,-0.218161637497641,
-0.199900841164055,-0.170049856811425,-0.121938455918974,-0.115690262250876,
-0.112587085718642,-0.110081899281292,-0.106934758984033,-0.100460824792478,
-0.0741727939511685,-0.0180007184006807),.UNSPECIFIED.);
#685=B_SPLINE_CURVE_WITH_KNOTS('',3,(#62523,#62524,#62525,#62526,#62527,
#62528,#62529,#62530,#62531,#62532,#62533,#62534,#62535,#62536,#62537,#62538,
#62539,#62540,#62541,#62542,#62543,#62544,#62545,#62546,#62547,#62548,#62549,
#62550,#62551,#62552,#62553,#62554,#62555,#62556,#62557,#62558,#62559,#62560,
#62561,#62562,#62563,#62564,#62565,#62566,#62567,#62568,#62569,#62570,#62571,
#62572,#62573,#62574,#62575,#62576,#62577,#62578,#62579,#62580,#62581,#62582,
#62583,#62584,#62585,#62586,#62587,#62588,#62589,#62590,#62591,#62592,#62593,
#62594,#62595,#62596,#62597,#62598,#62599,#62600,#62601,#62602,#62603,#62604,
#62605,#62606,#62607,#62608,#62609,#62610,#62611,#62612,#62613,#62614,#62615,
#62616,#62617,#62618,#62619,#62620,#62621,#62622,#62623,#62624,#62625,#62626,
#62627,#62628,#62629,#62630,#62631,#62632,#62633,#62634,#62635,#62636,#62637,
#62638,#62639,#62640,#62641,#62642,#62643,#62644,#62645,#62646,#62647,#62648,
#62649,#62650,#62651,#62652,#62653,#62654,#62655,#62656,#62657,#62658,#62659,
#62660,#62661,#62662,#62663,#62664,#62665,#62666,#62667,#62668,#62669,#62670,
#62671,#62672,#62673,#62674,#62675,#62676,#62677,#62678,#62679,#62680,#62681,
#62682,#62683,#62684,#62685,#62686,#62687,#62688,#62689,#62690,#62691,#62692,
#62693,#62694,#62695,#62696,#62697,#62698,#62699,#62700,#62701,#62702,#62703,
#62704,#62705,#62706,#62707,#62708,#62709,#62710,#62711,#62712,#62713,#62714,
#62715,#62716,#62717,#62718,#62719,#62720,#62721,#62722,#62723,#62724,#62725,
#62726,#62727,#62728),.UNSPECIFIED.,.F.,.F.,(4,2,2,2,2,2,2,2,2,2,2,2,2,
2,2,2,2,2,2,2,2,2,2,2,2,2,2,2,2,2,2,2,2,2,2,2,2,2,2,2,2,2,2,2,2,2,2,2,2,
2,2,2,2,2,2,2,2,2,2,2,2,2,2,2,2,2,2,2,2,2,2,2,2,2,2,2,2,2,2,2,2,2,2,2,2,
2,2,2,2,2,2,2,2,2,2,2,2,2,2,2,2,2,4),(-1.47756856596777,-1.47667518010056,
-1.47402767376772,-1.47148251209158,-1.46769128329404,-1.4568569678724,
-1.43879538213463,-1.39408829884182,-1.36900200688479,-1.36141950416248,
-1.35667758649383,-1.35226412399069,-1.34636607086331,-1.3328068075458,
-1.31349037355033,-1.28358727468684,-1.27565553739564,-1.24644897713212,
-1.24137845605213,-1.23852713753658,-1.23631007987131,-1.23315265124239,
-1.22640402224165,-1.19703029445297,-1.14383034860837,-1.1297679363977,
-1.12422576203256,-1.1201394154692,-1.11567355010628,-1.10945906303664,
-1.09387420491701,-1.07031265089973,-1.04315932934328,-1.01039061091018,
-1.00529095439064,-1.00243317233192,-1.00021723432547,-0.997069386712347,
-0.990371887374177,-0.961489030219941,-0.909732843962621,-0.894191467386958,
-0.88781729693775,-0.883367104204696,-0.878785147064071,-0.871966779059083,
-0.851732597209932,-0.816087272756875,-0.776882310149309,-0.770104851823568,
-0.76694213732142,-0.764490561249494,-0.761541129569988,-0.755857930867351,
-0.748419638422406,-0.730111089011565,-0.670366855268694,-0.657149882358595,
-0.651745696304398,-0.647287261691925,-0.64271634239969,-0.635951725103874,
-0.616181514229606,-0.581942003030305,-0.540629896265991,-0.533934140365763,
-0.530786727433254,-0.52833615314165,-0.525374738656974,-0.519632322484477,
-0.512092865096358,-0.493391591500168,-0.429962513770676,-0.419414811119862,
-0.413991023162881,-0.409634379042546,-0.404639474259673,-0.395864875451135,
-0.348284159340901,-0.304211584097677,-0.297685142273985,-0.294569675055742,
-0.292120673318311,-0.289132619720033,-0.283258159864416,-0.275491752606876,
-0.255893014993365,-0.19283578273377,-0.183755819193247,-0.178163213947666,
-0.173790991041131,-0.168904058046772,-0.160966872435302,-0.128065793818931,
-0.0940482035040311,-0.0657814238749686,-0.0607335324943708,-0.0578875980400268,
-0.0556701326240175,-0.0525061282772593,-0.0490024008786595,-0.0389255836744063,
-0.000685810379229455),.UNSPECIFIED.);
#686=B_SPLINE_CURVE_WITH_KNOTS('',3,(#62729,#62730,#62731,#62732),
 .UNSPECIFIED.,.F.,.F.,(4,4),(59.6164740057542,59.690260418206),
 .UNSPECIFIED.);
#687=B_SPLINE_CURVE_WITH_KNOTS('',3,(#62734,#62735,#62736,#62737,#62738,
#62739,#62740,#62741),.UNSPECIFIED.,.F.,.F.,(4,2,2,4),(-0.0180007184006807,
-0.0122274356288746,-0.00513494177923378,-0.000683356472381724),
 .UNSPECIFIED.);
#688=B_SPLINE_CURVE_WITH_KNOTS('',3,(#62742,#62743,#62744,#62745,#62746,
#62747,#62748,#62749,#62750,#62751,#62752,#62753,#62754,#62755,#62756,#62757,
#62758,#62759,#62760,#62761,#62762,#62763,#62764,#62765,#62766,#62767,#62768,
#62769,#62770,#62771,#62772,#62773,#62774,#62775,#62776,#62777,#62778,#62779,
#62780,#62781,#62782,#62783,#62784,#62785,#62786,#62787,#62788,#62789,#62790,
#62791,#62792,#62793,#62794,#62795,#62796,#62797,#62798,#62799,#62800,#62801,
#62802,#62803,#62804,#62805,#62806,#62807,#62808,#62809,#62810,#62811,#62812,
#62813,#62814,#62815,#62816,#62817,#62818,#62819,#62820,#62821,#62822,#62823,
#62824,#62825,#62826,#62827,#62828,#62829,#62830,#62831,#62832,#62833,#62834,
#62835,#62836,#62837,#62838,#62839,#62840,#62841,#62842,#62843,#62844,#62845,
#62846,#62847,#62848,#62849,#62850,#62851,#62852,#62853,#62854,#62855,#62856,
#62857,#62858,#62859,#62860,#62861,#62862,#62863,#62864,#62865,#62866,#62867,
#62868,#62869,#62870,#62871,#62872,#62873,#62874,#62875,#62876,#62877,#62878,
#62879,#62880,#62881,#62882,#62883,#62884,#62885,#62886,#62887,#62888,#62889,
#62890,#62891,#62892,#62893,#62894,#62895,#62896,#62897,#62898,#62899,#62900,
#62901,#62902,#62903,#62904,#62905,#62906,#62907,#62908,#62909,#62910,#62911,
#62912,#62913,#62914,#62915,#62916,#62917,#62918,#62919,#62920,#62921,#62922,
#62923,#62924,#62925,#62926,#62927,#62928,#62929,#62930,#62931,#62932,#62933,
#62934,#62935,#62936,#62937,#62938,#62939,#62940,#62941,#62942,#62943,#62944,
#62945,#62946,#62947),.UNSPECIFIED.,.F.,.F.,(4,2,2,2,2,2,2,2,2,2,2,2,2,
2,2,2,2,2,2,2,2,2,2,2,2,2,2,2,2,2,2,2,2,2,2,2,2,2,2,2,2,2,2,2,2,2,2,2,2,
2,2,2,2,2,2,2,2,2,2,2,2,2,2,2,2,2,2,2,2,2,2,2,2,2,2,2,2,2,2,2,2,2,2,2,2,
2,2,2,2,2,2,2,2,2,2,2,2,2,2,2,2,2,4),(-2.98838788646982,-2.98528829418108,
-2.98146659002245,-2.97698691775857,-2.97081660209869,-2.95622861621512,
-2.94199447241219,-2.90215992325245,-2.88154888698576,-2.8734939388036,
-2.86742976418027,-2.86436410567773,-2.86185935104928,-2.85867488688888,
-2.8520000353513,-2.80903100507921,-2.7602925067911,-2.7517825329484,-2.74677398413034,
-2.74230405660114,-2.73659847599713,-2.7273506004005,-2.67725560329362,
-2.64889106712198,-2.63915262817281,-2.63215259343949,-2.62890746399829,
-2.62663866234702,-2.62372742221094,-2.61855671960823,-2.5850262691835,
-2.55849687775771,-2.53532586746911,-2.51986167747301,-2.5135841501213,
-2.50903140221415,-2.50483499055254,-2.49797458944606,-2.47973438304461,
-2.42604023861142,-2.40847775111068,-2.39780500766514,-2.39398502459098,
-2.39139427283262,-2.38866508409898,-2.38419332343814,-2.36890733353992,
-2.32348241613457,-2.29984068542966,-2.28416264700806,-2.27785303069014,
-2.27329462940184,-2.26910511197311,-2.26228360239454,-2.24431833420245,
-2.19031822096395,-2.17271683158259,-2.16202805560938,-2.15820588586896,
-2.15561466131597,-2.15288605412615,-2.14841716375823,-2.1331631205036,
-2.08771965115224,-2.06406438951804,-2.05337176105262,-2.04464970313674,
-2.03959597537389,-2.03513299238843,-2.02950025852013,-2.02050481739934,
-1.95707037668424,-1.93776486726977,-1.93003288892616,-1.92415534085002,
-1.92112698118282,-1.91861975919638,-1.91538991616257,-1.90847433297581,
-1.87503247989781,-1.84639674010233,-1.81583133899907,-1.80801480599274,
-1.8031531778308,-1.79864340372126,-1.79273940388295,-1.77922388291805,
-1.72525466950789,-1.70322992144778,-1.69483799623768,-1.68858116350246,
-1.68547694434599,-1.68297266310022,-1.67982885004434,-1.67336872111006,
-1.62750489725578,-1.58185642475913,-1.5730452000715,-1.56797224927187,
-1.56351126538561,-1.55790639166416,-1.54900779818947,-1.5120028941296),
 .UNSPECIFIED.);
#689=B_SPLINE_CURVE_WITH_KNOTS('',3,(#62952,#62953,#62954,#62955,#62956,
#62957,#62958,#62959,#62960,#62961,#62962,#62963,#62964,#62965,#62966,#62967,
#62968,#62969,#62970,#62971,#62972,#62973,#62974,#62975,#62976,#62977,#62978,
#62979,#62980,#62981,#62982,#62983,#62984,#62985,#62986,#62987,#62988,#62989,
#62990,#62991,#62992,#62993,#62994,#62995,#62996,#62997,#62998,#62999,#63000,
#63001,#63002,#63003,#63004,#63005,#63006,#63007,#63008,#63009,#63010,#63011,
#63012,#63013,#63014,#63015,#63016,#63017,#63018,#63019,#63020,#63021,#63022,
#63023,#63024,#63025,#63026,#63027,#63028,#63029,#63030,#63031,#63032,#63033,
#63034,#63035,#63036,#63037,#63038,#63039,#63040,#63041,#63042,#63043,#63044,
#63045,#63046,#63047,#63048,#63049,#63050,#63051,#63052,#63053,#63054,#63055,
#63056,#63057,#63058,#63059,#63060,#63061,#63062,#63063,#63064,#63065,#63066,
#63067,#63068,#63069,#63070,#63071,#63072,#63073,#63074,#63075,#63076,#63077,
#63078,#63079,#63080,#63081,#63082,#63083,#63084,#63085,#63086,#63087,#63088,
#63089,#63090,#63091,#63092,#63093,#63094,#63095,#63096,#63097,#63098,#63099,
#63100,#63101,#63102,#63103,#63104,#63105,#63106,#63107,#63108,#63109,#63110,
#63111,#63112,#63113,#63114,#63115,#63116,#63117,#63118,#63119,#63120,#63121,
#63122,#63123,#63124,#63125,#63126,#63127,#63128,#63129,#63130,#63131,#63132,
#63133,#63134,#63135,#63136,#63137,#63138,#63139,#63140,#63141,#63142,#63143,
#63144,#63145,#63146,#63147,#63148,#63149,#63150,#63151,#63152,#63153,#63154,
#63155,#63156,#63157,#63158,#63159,#63160,#63161,#63162,#63163,#63164,#63165,
#63166,#63167,#63168,#63169,#63170,#63171,#63172,#63173,#63174,#63175),
 .UNSPECIFIED.,.F.,.F.,(4,2,2,2,2,2,2,2,2,2,2,2,2,2,2,2,2,2,2,2,2,2,2,2,
2,2,2,2,2,2,2,2,2,2,2,2,2,2,2,2,2,2,2,2,2,2,2,2,2,2,2,2,2,2,2,2,2,2,2,2,
2,2,2,2,2,2,2,2,2,2,2,2,2,2,2,2,2,2,2,2,2,2,2,2,2,2,2,2,2,2,2,2,2,2,2,2,
2,2,2,2,2,2,2,2,2,2,2,2,2,2,2,4),(-2.97196931891727,-2.91428574589538,-2.89770718111958,
-2.89332752620021,-2.89065668856314,-2.8881571917411,-2.88506034809745,
-2.87733615891202,-2.83080695999882,-2.80140723545357,-2.78924401518633,
-2.78239363240096,-2.77683289895904,-2.77675093910441,-2.77666503218692,
-2.77657439665546,-2.77647809242424,-2.77637497071679,-2.77626360401267,
-2.77614218585477,-2.77600838367988,-2.77585911584778,-2.77569020139731,
-2.77151261174643,-2.76677917299566,-2.75923275586235,-2.73403288392933,
-2.68930540982225,-2.67126639267519,-2.66389889500036,-2.65825802425226,
-2.65531760896332,-2.65286580560208,-2.64969289432205,-2.64309896224071,
-2.60041906988531,-2.58694267669041,-2.56260522765195,-2.54667350710196,
-2.54040916226628,-2.53593496955431,-2.53131623922925,-2.52431587657374,
-2.50426004130823,-2.45668716948417,-2.43634704095623,-2.42839779910167,
-2.42241840095309,-2.41940947627274,-2.41696141396609,-2.4138698835983,
-2.40746814786311,-2.36129838918073,-2.35101771342128,-2.32659359258713,
-2.31062344486255,-2.3043534254354,-2.29987810058965,-2.29580359007659,
-2.28925989618402,-2.27259386323244,-2.22189897772901,-2.19337950611251,
-2.18672074475212,-2.18358037378002,-2.18136549643623,-2.1785030912631,
-2.17338182004744,-2.13861537134678,-2.11263585630217,-2.089649271752,-2.07432504692235,
-2.0681497711038,-2.06369119347227,-2.05959719771755,-2.05402254107939,
-2.04276512924811,-1.98170695539743,-1.96324744653309,-1.9557701536014,
-1.95006453590518,-1.94711055600451,-1.94465935321661,-1.94150247240344,
-1.93475626206012,-1.89437742870489,-1.85957041175885,-1.83960993084124,
-1.83282307632219,-1.82824748064158,-1.82379229001105,-1.81739122276488,
-1.80170578259206,-1.75006355372384,-1.72857959653916,-1.72035516172327,
-1.7142181717278,-1.71117772595403,-1.7087297468675,-1.70567042821201,-1.69943700442974,
-1.65149482931027,-1.60646578565236,-1.59818389317943,-1.59329293009228,
-1.588920634794,-1.58333282259018,-1.57427100609585,-1.5222212838022,-1.49481084704842,
-1.48094622016344,-1.47756856596777),.UNSPECIFIED.);
#690=B_SPLINE_CURVE_WITH_KNOTS('',3,(#63176,#63177,#63178,#63179,#63180,
#63181,#63182,#63183,#63184,#63185,#63186,#63187,#63188,#63189,#63190,#63191,
#63192,#63193,#63194,#63195,#63196,#63197,#63198,#63199,#63200,#63201,#63202,
#63203,#63204,#63205,#63206,#63207,#63208,#63209,#63210,#63211,#63212,#63213,
#63214,#63215,#63216,#63217,#63218,#63219,#63220,#63221,#63222,#63223,#63224,
#63225,#63226,#63227,#63228,#63229,#63230,#63231,#63232,#63233,#63234,#63235,
#63236,#63237,#63238,#63239,#63240,#63241,#63242,#63243,#63244,#63245,#63246,
#63247,#63248,#63249,#63250,#63251,#63252,#63253,#63254,#63255,#63256,#63257,
#63258,#63259,#63260,#63261,#63262,#63263,#63264,#63265,#63266,#63267,#63268,
#63269,#63270,#63271,#63272,#63273,#63274,#63275,#63276,#63277,#63278,#63279,
#63280,#63281,#63282,#63283,#63284,#63285,#63286,#63287,#63288,#63289,#63290,
#63291,#63292,#63293,#63294,#63295,#63296,#63297,#63298,#63299,#63300,#63301,
#63302,#63303,#63304,#63305,#63306,#63307,#63308,#63309,#63310,#63311,#63312,
#63313,#63314,#63315,#63316,#63317,#63318,#63319,#63320,#63321,#63322,#63323,
#63324,#63325,#63326,#63327,#63328,#63329,#63330,#63331,#63332,#63333,#63334,
#63335,#63336,#63337,#63338,#63339,#63340,#63341,#63342,#63343,#63344,#63345,
#63346,#63347,#63348,#63349,#63350,#63351,#63352,#63353,#63354,#63355,#63356,
#63357,#63358,#63359,#63360,#63361,#63362,#63363,#63364,#63365,#63366,#63367,
#63368,#63369,#63370,#63371,#63372,#63373,#63374,#63375,#63376,#63377,#63378,
#63379),.UNSPECIFIED.,.F.,.F.,(4,2,2,2,2,2,2,2,2,2,2,2,2,2,2,2,2,2,2,2,
2,2,2,2,2,2,2,2,2,2,2,2,2,2,2,2,2,2,2,2,2,2,2,2,2,2,2,2,2,2,2,2,2,2,2,2,
2,2,2,2,2,2,2,2,2,2,2,2,2,2,2,2,2,2,2,2,2,2,2,2,2,2,2,2,2,2,2,2,2,2,2,2,
2,2,2,2,2,2,2,2,2,4),(-1.5120028941296,-1.49444504748298,-1.48728459445354,
-1.45724761769968,-1.45209467100208,-1.4491869789942,-1.44691683246572,
-1.44366447210436,-1.43662765579084,-1.42682267054302,-1.39811444349937,
-1.34851334425224,-1.33926454099114,-1.33355789785115,-1.32908688024209,
-1.32407683922482,-1.31556370112943,-1.26712239155253,-1.22370563941062,
-1.21707857541056,-1.21390264893852,-1.21139751980532,-1.20832265762709,
-1.20221489895544,-1.16416629342023,-1.1124282396071,-1.10329512972379,
-1.09762185695204,-1.0931542402523,-1.08812420456324,-1.07951697127604,
-1.03267877083928,-0.987655116524005,-0.981141842507781,-0.977987636574164,
-0.975482995647184,-0.972388122203787,-0.966179543090284,-0.957873677743406,
-0.936216969035032,-0.883605726750471,-0.869115066171862,-0.863435418991197,
-0.859253556753791,-0.854686904773009,-0.848334975518078,-0.832377054725447,
-0.808109829651744,-0.761758703975713,-0.748010228477541,-0.743695910328262,
-0.741000695311787,-0.738385488167906,-0.734445219280618,-0.722832593392474,
-0.70289333577784,-0.656441201509723,-0.63532751128321,-0.628121469429759,
-0.6233878902741,-0.618815212573951,-0.612430104171281,-0.596245082914192,
-0.571463117374698,-0.517978298974142,-0.510303021561183,-0.507174599073968,
-0.50462776690422,-0.50187130991816,-0.497277351391218,-0.478702815592633,
-0.431620935217259,-0.401101540546551,-0.393087553320132,-0.388183410694565,
-0.383686678799748,-0.377774027577873,-0.364590799483157,-0.298543914095754,
-0.277389452300924,-0.272476340623328,-0.269650200824313,-0.267103474300365,
-0.263536057283984,-0.254632889000594,-0.241108764369719,-0.182931385201981,
-0.163200816634732,-0.156143039607164,-0.151909514214553,-0.147379338457002,
-0.141245807342578,-0.126724135291483,-0.0825275835693964,-0.0545755851130164,
-0.0404434800717171,-0.036087373177055,-0.0333827955054112,-0.0310247821076836,
-0.0284248721535145,-0.0248021682944244,-0.0178498417920879),
 .UNSPECIFIED.);
#691=B_SPLINE_CURVE_WITH_KNOTS('',3,(#63385,#63386,#63387,#63388,#63389,
#63390,#63391,#63392,#63393,#63394),.UNSPECIFIED.,.F.,.F.,(4,1,1,1,1,1,
1,4),(72.2566310325652,72.8337041055645,73.8264152833055,74.8191264610465,
75.8118376387874,76.8045488165284,77.7972599942694,78.4660953116528),
 .UNSPECIFIED.);
#692=B_SPLINE_CURVE_WITH_KNOTS('',3,(#63395,#63396,#63397,#63398),
 .UNSPECIFIED.,.F.,.F.,(4,4),(-2.98921828163543,-2.97196931891727),
 .UNSPECIFIED.);
#693=B_SPLINE_CURVE_WITH_KNOTS('',3,(#63400,#63401,#63402,#63403),
 .UNSPECIFIED.,.F.,.F.,(4,4),(-0.0178498417920879,-0.000682550733952316),
 .UNSPECIFIED.);
#694=B_SPLINE_CURVE_WITH_KNOTS('',3,(#63404,#63405,#63406,#63407,#63408,
#63409,#63410,#63411,#63412,#63413,#63414,#63415,#63416,#63417,#63418,#63419,
#63420,#63421,#63422,#63423,#63424,#63425,#63426,#63427,#63428,#63429,#63430,
#63431,#63432,#63433,#63434,#63435,#63436,#63437,#63438,#63439,#63440,#63441,
#63442,#63443,#63444,#63445,#63446,#63447,#63448,#63449,#63450,#63451,#63452,
#63453,#63454,#63455,#63456,#63457,#63458,#63459,#63460,#63461,#63462,#63463,
#63464,#63465,#63466,#63467,#63468,#63469,#63470,#63471,#63472,#63473,#63474,
#63475,#63476,#63477,#63478,#63479,#63480,#63481,#63482,#63483,#63484,#63485,
#63486,#63487,#63488,#63489,#63490,#63491,#63492,#63493,#63494,#63495,#63496,
#63497,#63498,#63499,#63500,#63501,#63502,#63503,#63504,#63505,#63506,#63507,
#63508,#63509,#63510,#63511,#63512,#63513,#63514,#63515,#63516,#63517,#63518,
#63519,#63520,#63521,#63522,#63523,#63524,#63525,#63526,#63527,#63528,#63529,
#63530,#63531,#63532,#63533,#63534,#63535,#63536,#63537,#63538,#63539,#63540,
#63541,#63542,#63543,#63544,#63545,#63546,#63547,#63548,#63549,#63550,#63551,
#63552,#63553,#63554,#63555,#63556,#63557,#63558,#63559,#63560,#63561,#63562,
#63563,#63564,#63565,#63566,#63567,#63568,#63569,#63570,#63571,#63572,#63573,
#63574,#63575,#63576,#63577,#63578,#63579,#63580,#63581,#63582,#63583,#63584,
#63585,#63586,#63587,#63588,#63589,#63590,#63591,#63592,#63593,#63594,#63595),
 .UNSPECIFIED.,.F.,.F.,(4,2,2,2,2,2,2,2,2,2,2,2,2,2,2,2,2,2,2,2,2,2,2,2,
2,2,2,2,2,2,2,2,2,2,2,2,2,2,2,2,2,2,2,2,2,2,2,2,2,2,2,2,2,2,2,2,2,2,2,2,
2,2,2,2,2,2,2,2,2,2,2,2,2,2,2,2,2,2,2,2,2,2,2,2,2,2,2,2,2,2,2,2,2,2,2,4),
(-2.98961608686735,-2.92955913902989,-2.91434706881341,-2.90810641341164,
-2.90355878245489,-2.89878126957801,-2.89136529818291,-2.86828728786766,
-2.81952199490476,-2.80265574864177,-2.79556266327165,-2.7902365920153,
-2.78738327906901,-2.78487795006288,-2.78170355459493,-2.77508552931107,
-2.73176464316543,-2.68325779438362,-2.67474161328496,-2.66973054623383,
-2.6652590592707,-2.65955243548637,-2.65030489731358,-2.60057345985161,
-2.57191013064851,-2.56211255982198,-2.55508008937664,-2.55182827136203,
-2.54955797523332,-2.54664928170565,-2.54149290374496,-2.51116381551174,
-2.50419149324638,-2.46562836721085,-2.44442895495745,-2.43741060940826,
-2.4327153431829,-2.42816825824175,-2.42167408142716,-2.40588093378539,
-2.35448508388209,-2.33315361186218,-2.32492426680635,-2.31875963743648,
-2.31567325629579,-2.31316814710835,-2.31000410779275,-2.30344058556475,
-2.25941788879275,-2.21217626815809,-2.20330445866743,-2.19821813770763,
-2.19375787644256,-2.18817045447724,-2.17933346841292,-2.12413724305368,
-2.08887880164089,-2.08279807846928,-2.07972831250716,-2.07722258152124,
-2.07403988823319,-2.06737877282502,-2.02426117147748,-1.97561129597601,
-1.96709475401779,-1.96208342366462,-1.95761167086137,-1.95190466527456,
-1.94265641734554,-1.89292608283016,-1.86425834913199,-1.85445968316169,
-1.847426521533,-1.84417446243856,-1.8419040278866,-1.8389951989531,-1.83383867288096,
-1.80352186809264,-1.79692428835465,-1.76704386674269,-1.74784768075342,
-1.73429599963488,-1.72832061537338,-1.72381459720499,-1.71893741187965,
-1.71105181699964,-1.68269328521487,-1.6335070501788,-1.61459848585955,
-1.60998049580903,-1.60721855136846,-1.60467387721262,-1.60096911118102,
-1.59390153680279,-1.54740719322482,-1.51254166440623),.UNSPECIFIED.);
#695=B_SPLINE_CURVE_WITH_KNOTS('',3,(#63601,#63602,#63603,#63604,#63605,
#63606,#63607,#63608,#63609,#63610,#63611,#63612,#63613,#63614,#63615,#63616,
#63617,#63618,#63619,#63620,#63621,#63622,#63623,#63624,#63625,#63626,#63627,
#63628,#63629,#63630,#63631,#63632,#63633,#63634,#63635,#63636,#63637,#63638,
#63639,#63640,#63641,#63642,#63643,#63644,#63645,#63646,#63647,#63648,#63649,
#63650,#63651,#63652,#63653,#63654,#63655,#63656,#63657,#63658,#63659,#63660,
#63661,#63662,#63663,#63664,#63665,#63666,#63667,#63668,#63669,#63670,#63671,
#63672,#63673,#63674,#63675,#63676,#63677,#63678,#63679,#63680,#63681,#63682,
#63683,#63684,#63685,#63686,#63687,#63688,#63689,#63690,#63691,#63692,#63693,
#63694,#63695,#63696,#63697,#63698,#63699,#63700,#63701,#63702,#63703,#63704,
#63705,#63706,#63707,#63708,#63709,#63710,#63711,#63712,#63713,#63714,#63715,
#63716,#63717,#63718,#63719,#63720,#63721,#63722,#63723,#63724,#63725,#63726,
#63727,#63728,#63729,#63730,#63731,#63732,#63733,#63734,#63735,#63736,#63737,
#63738,#63739,#63740,#63741,#63742,#63743,#63744,#63745,#63746,#63747,#63748,
#63749,#63750,#63751,#63752,#63753,#63754,#63755,#63756,#63757,#63758,#63759,
#63760,#63761,#63762,#63763,#63764,#63765,#63766,#63767,#63768,#63769,#63770,
#63771,#63772,#63773,#63774,#63775,#63776,#63777,#63778,#63779,#63780,#63781,
#63782,#63783,#63784,#63785,#63786,#63787,#63788,#63789,#63790),
 .UNSPECIFIED.,.F.,.F.,(4,3,3,3,3,3,3,3,3,3,3,3,3,3,3,3,3,3,3,3,3,3,3,3,
3,3,3,3,3,3,3,3,3,3,3,3,3,3,3,3,3,3,3,3,3,3,3,3,3,3,3,3,3,3,3,3,3,3,3,3,
3,3,3,4),(78.5398163397448,78.669184564488,78.7899711720104,78.8905481960992,
78.9909814285215,79.09129948363,79.1915547173813,79.2917782714196,79.3920012473976,
79.4923233996722,79.5926942427436,79.6932437377857,79.7826823497514,79.8832593738159,
79.9836926062141,80.0840106612987,80.1842658950263,80.2844894490409,80.3847124249955,
80.4850345772472,80.5854054202958,80.6859549153159,80.7753935274923,80.8759705515419,
80.9764037839248,81.0767218389937,81.1769770727055,81.277200626704,81.3774236026423,
81.4777457548775,81.5781165979097,81.6786660929132,81.7681047052333,81.8686817294026,
81.9691149619056,82.0694330170946,82.1696882509264,82.2699118050448,82.3701347811025,
82.4704569334559,82.5708277766054,82.6713772717241,82.7608158829743,82.8613929069483,
82.9618261392563,83.0621441942518,83.1623994278909,83.2626229818178,83.3628459576855,
83.4631681098523,83.563538952817,83.6640884477557,83.7535270607153,83.8541040846601,
83.9545373169367,84.0548553718979,84.1551106055011,84.2553341593904,84.3555571352188,
84.4558792873442,84.5562501302661,84.6567996251603,84.7462382384562,84.7500696323053),
 .UNSPECIFIED.);
#696=B_SPLINE_CURVE_WITH_KNOTS('',3,(#63791,#63792,#63793,#63794),
 .UNSPECIFIED.,.F.,.F.,(4,4),(78.4660953116528,78.5398163397448),
 .UNSPECIFIED.);
#697=B_SPLINE_CURVE_WITH_KNOTS('',3,(#63795,#63796,#63797,#63798,#63799,
#63800,#63801,#63802,#63803,#63804,#63805,#63806,#63807,#63808,#63809,#63810,
#63811,#63812,#63813,#63814,#63815,#63816,#63817,#63818,#63819,#63820,#63821,
#63822,#63823,#63824,#63825,#63826,#63827,#63828,#63829,#63830,#63831,#63832,
#63833,#63834,#63835,#63836,#63837,#63838,#63839,#63840,#63841,#63842,#63843,
#63844,#63845,#63846,#63847,#63848,#63849,#63850,#63851,#63852,#63853,#63854,
#63855,#63856,#63857,#63858,#63859,#63860,#63861,#63862,#63863,#63864,#63865,
#63866,#63867,#63868,#63869,#63870,#63871,#63872,#63873,#63874,#63875,#63876,
#63877,#63878,#63879,#63880,#63881,#63882,#63883,#63884,#63885,#63886,#63887,
#63888,#63889,#63890,#63891,#63892,#63893,#63894,#63895,#63896,#63897,#63898,
#63899,#63900,#63901,#63902,#63903,#63904,#63905,#63906,#63907,#63908,#63909,
#63910,#63911,#63912,#63913,#63914,#63915,#63916,#63917,#63918,#63919,#63920,
#63921,#63922,#63923,#63924,#63925,#63926,#63927,#63928,#63929,#63930,#63931,
#63932,#63933,#63934,#63935,#63936,#63937,#63938,#63939,#63940,#63941,#63942,
#63943,#63944,#63945,#63946,#63947,#63948,#63949,#63950,#63951,#63952,#63953,
#63954,#63955,#63956,#63957,#63958,#63959,#63960,#63961,#63962,#63963,#63964,
#63965,#63966,#63967,#63968,#63969,#63970,#63971,#63972,#63973,#63974,#63975,
#63976,#63977,#63978,#63979,#63980,#63981,#63982,#63983,#63984,#63985,#63986,
#63987,#63988,#63989,#63990,#63991,#63992,#63993,#63994,#63995,#63996,#63997,
#63998,#63999,#64000,#64001,#64002,#64003,#64004,#64005,#64006,#64007,#64008,
#64009,#64010,#64011,#64012,#64013,#64014,#64015,#64016,#64017,#64018,#64019,
#64020,#64021,#64022,#64023,#64024,#64025,#64026,#64027,#64028,#64029,#64030,
#64031,#64032,#64033,#64034,#64035,#64036,#64037,#64038,#64039,#64040,#64041,
#64042,#64043,#64044,#64045,#64046,#64047,#64048,#64049,#64050,#64051,#64052,
#64053,#64054,#64055,#64056,#64057,#64058,#64059,#64060),.UNSPECIFIED.,
 .F.,.F.,(4,2,2,2,2,2,2,2,2,2,2,2,2,2,2,2,2,2,2,2,2,2,2,2,2,2,2,2,2,2,2,
2,2,2,2,2,2,2,2,2,2,2,2,2,2,2,2,2,2,2,2,2,2,2,2,2,2,2,2,2,2,2,2,2,2,2,2,
2,2,2,2,2,2,2,2,2,2,2,2,2,2,2,2,2,2,2,2,2,2,2,2,2,2,2,2,2,2,2,2,2,2,2,2,
2,2,2,2,2,2,2,2,2,2,2,2,2,2,2,2,2,2,2,2,2,2,2,2,2,2,2,2,2,4),(-1.51254166440623,
-1.50358687733872,-1.49521768662821,-1.49023743753114,-1.48575918136067,
-1.47999613363582,-1.46767039141004,-1.43238520659278,-1.38960746151934,
-1.37767405555367,-1.3735732534584,-1.37118657045784,-1.36858843453146,
-1.36473510723931,-1.35381633081085,-1.33565393081433,-1.27696212473058,
-1.26307088832274,-1.25748537385371,-1.25332555565174,-1.24873671272699,
-1.24226571564178,-1.22548154805426,-1.19930777629856,-1.16107507700933,
-1.14299695310182,-1.1382776414061,-1.13549359618687,-1.13293007873679,
-1.12926199883559,-1.11968899045097,-1.05483920518293,-1.03021664517121,
-1.02264111850684,-1.01782981551288,-1.01329818103851,-1.0071553853881,
-0.992574997544352,-0.971291801131024,-0.928899172051115,-0.907462969713808,
-0.902536198441425,-0.899707147346546,-0.897161522018309,-0.893600777255911,
-0.884740280170151,-0.871306797053486,-0.81431481812923,-0.793507373232208,
-0.786332615335024,-0.78160518115067,-0.777027760574175,-0.77061818250404,
-0.754265956675427,-0.729101403556005,-0.674411365757629,-0.667761866795157,
-0.664581318302855,-0.662075593307231,-0.659003749268963,-0.652912891037507,
-0.616590240131492,-0.562768921474694,-0.553800789239317,-0.548174885242987,
-0.543711091212179,-0.538649814232322,-0.529897606858921,-0.481156763813978,
-0.438618535914785,-0.431885478227617,-0.428689115376463,-0.426182796879897,
-0.423124751072955,-0.417102966785914,-0.409123661148039,-0.388828131798958,
-0.341126501054896,-0.321439833701956,-0.314386989202548,-0.310154259528849,
-0.30562332056504,-0.299485886361556,-0.284940522597808,-0.263730620661781,
-0.236097740513245,-0.203010952122292,-0.196119542944986,-0.192893608593384,
-0.190385934214598,-0.190331662082248,-0.190279979933743,-0.190230688356025,
-0.190183607911403,-0.190138576699426,-0.190095448269347,-0.190054089815314,
-0.190014380625071,-0.189976210726914,-0.18993947971519,-0.189904095729544,
-0.189869974564239,-0.189837038875559,-0.189805217494056,-0.189774444819543,
-0.189744660278097,-0.189715807843964,-0.189687835624076,-0.189660695471361,
-0.189634342651879,-0.189608735545615,-0.189583835371524,-0.189559605951785,
-0.189536013493062,-0.189513026385609,-0.189490615029967,-0.189468751676441,
-0.189447410277488,-0.189426566364043,-0.189406196915075,-0.189386280251627,
-0.186109378997095,-0.178221264837677,-0.16649512808658,-0.125880405963827,
-0.0881332296270172,-0.0798166726120481,-0.0748477520311481,-0.0703672557747848,
-0.0645838298938687,-0.0582726373553926,-0.0476295332544095,-0.018241527118741),
 .UNSPECIFIED.);
#698=B_SPLINE_CURVE_WITH_KNOTS('',3,(#64066,#64067,#64068,#64069,#64070,
#64071,#64072,#64073,#64074,#64075,#64076,#64077,#64078,#64079,#64080,#64081,
#64082,#64083,#64084,#64085,#64086,#64087,#64088,#64089,#64090,#64091,#64092,
#64093,#64094,#64095,#64096,#64097,#64098,#64099,#64100,#64101,#64102,#64103,
#64104,#64105,#64106,#64107,#64108,#64109,#64110,#64111,#64112,#64113,#64114,
#64115,#64116,#64117,#64118,#64119,#64120,#64121,#64122,#64123,#64124,#64125,
#64126,#64127,#64128,#64129,#64130,#64131,#64132,#64133,#64134,#64135,#64136,
#64137,#64138,#64139,#64140,#64141,#64142,#64143,#64144,#64145,#64146,#64147,
#64148,#64149,#64150,#64151,#64152,#64153,#64154,#64155,#64156,#64157,#64158,
#64159,#64160,#64161,#64162,#64163,#64164,#64165,#64166,#64167,#64168,#64169,
#64170,#64171,#64172,#64173,#64174,#64175,#64176,#64177,#64178,#64179,#64180,
#64181,#64182,#64183,#64184,#64185,#64186,#64187,#64188,#64189,#64190,#64191,
#64192,#64193,#64194,#64195,#64196,#64197,#64198,#64199,#64200,#64201,#64202,
#64203,#64204,#64205,#64206,#64207,#64208,#64209,#64210,#64211,#64212,#64213,
#64214,#64215,#64216,#64217,#64218,#64219,#64220,#64221,#64222,#64223,#64224,
#64225,#64226,#64227,#64228,#64229,#64230,#64231,#64232,#64233,#64234,#64235,
#64236,#64237,#64238,#64239,#64240,#64241,#64242,#64243,#64244,#64245,#64246,
#64247,#64248,#64249,#64250,#64251,#64252,#64253,#64254,#64255,#64256,#64257,
#64258,#64259,#64260,#64261,#64262,#64263,#64264,#64265,#64266,#64267,#64268,
#64269,#64270,#64271,#64272,#64273,#64274,#64275,#64276,#64277,#64278,#64279,
#64280,#64281,#64282,#64283,#64284,#64285,#64286,#64287,#64288,#64289,#64290,
#64291,#64292,#64293,#64294,#64295,#64296,#64297,#64298,#64299,#64300,#64301,
#64302,#64303,#64304,#64305,#64306,#64307,#64308,#64309,#64310,#64311,#64312,
#64313,#64314,#64315,#64316,#64317,#64318,#64319,#64320,#64321,#64322,#64323,
#64324,#64325,#64326,#64327,#64328,#64329,#64330,#64331,#64332,#64333,#64334,
#64335,#64336,#64337,#64338,#64339),.UNSPECIFIED.,.F.,.F.,(4,2,2,2,2,2,
2,2,2,2,2,2,2,2,2,2,2,2,2,2,2,2,2,2,2,2,2,2,2,2,2,2,2,2,2,2,2,2,2,2,2,2,
2,2,2,2,2,2,2,2,2,2,2,2,2,2,2,2,2,2,2,2,2,2,2,2,2,2,2,2,2,2,2,2,2,2,2,2,
2,2,2,2,2,2,2,2,2,2,2,2,2,2,2,2,2,2,2,2,2,2,2,2,2,2,2,2,2,2,2,2,2,2,2,2,
2,2,2,2,2,2,2,2,2,2,2,2,2,2,2,2,2,2,2,2,2,2,4),(-1.47758203553868,-1.42899975050051,
-1.40713396065841,-1.40225440817748,-1.39947453781305,-1.3969931931183,
-1.39355802552855,-1.38519875808859,-1.37273993155273,-1.32570381463777,
-1.29475606810944,-1.28681911537627,-1.28200235399692,-1.27761433094251,
-1.27188949146447,-1.2593428096774,-1.2227452640396,-1.17694041345732,-1.16840489189888,
-1.16484135947674,-1.16236394737657,-1.15964851340514,-1.15506554840041,
-1.13569936181252,-1.08283230436195,-1.05794342324226,-1.05038012635333,
-1.04564311339815,-1.04122940714009,-1.03532371679027,-1.02171241288969,
-1.00229058451556,-0.972532735680228,-0.964753332609068,-0.93546001536075,
-0.930388941922798,-0.927537948770019,-0.925321539766668,-0.922165550488369,
-0.915421990420157,-0.886087943674784,-0.832997115617142,-0.818845009136248,
-0.813290140658679,-0.809201415034091,-0.804739670631151,-0.798543469926555,
-0.783075299601176,-0.759768673717856,-0.731919319327381,-0.699458372272132,
-0.694361092433451,-0.691504288722078,-0.689288891172297,-0.686141527371202,
-0.67944397083235,-0.650551410103965,-0.598758518977501,-0.583269703219454,
-0.576906316715529,-0.57245896232353,-0.567875990948625,-0.561048516978307,
-0.540723772421731,-0.504789693549326,-0.466042391789734,-0.459247212219221,
-0.456081713271364,-0.453630552682631,-0.450684730797207,-0.445016901202972,
-0.437604183251857,-0.419391363518556,-0.374493515410956,-0.349789149628837,
-0.342243162330127,-0.337509995168157,-0.333095125730737,-0.327180643448004,
-0.313514765506184,-0.293983788171101,-0.26437545984912,-0.230141940365606,
-0.223269271662711,-0.220123160218621,-0.217765263502421,-0.217724439695203,
-0.217668032038743,-0.217614643452261,-0.217564008431681,-0.21751589221921,
-0.217470086422374,-0.217426405360392,-0.217384683009115,-0.217344770432778,
-0.217306533610085,-0.217269851581783,-0.217234614873007,-0.217200724139939,
-0.217168089011508,-0.217136627076906,-0.217106263010309,-0.217076927817307,
-0.217048558167393,-0.217021095815192,-0.21699448709232,-0.216968682453933,
-0.216943636077767,-0.216919305522286,-0.216895651408788,-0.216872637143664,
-0.216850228665975,-0.216828394236927,-0.216807104224317,-0.216786330941784,
-0.216766048473687,-0.216746232539398,-0.216726860360167,-0.216707910535952,
-0.21668936293948,-0.216671198627902,-0.216653399739507,-0.216635949424207,
-0.21661883176486,-0.213409431385154,-0.209564823591307,-0.202719038906595,
-0.186615837149335,-0.156725257244662,-0.115182717864199,-0.106906053210041,
-0.102017091908541,-0.0976459234138118,-0.0920586358523389,-0.0802794519782047,
-0.0133182801247358,-0.000686390217275949),.UNSPECIFIED.);
#699=B_SPLINE_CURVE_WITH_KNOTS('',3,(#64340,#64341,#64342,#64343),
 .UNSPECIFIED.,.F.,.F.,(4,4),(84.7500696323053,84.8230016469244),
 .UNSPECIFIED.);
#700=B_SPLINE_CURVE_WITH_KNOTS('',3,(#64345,#64346,#64347,#64348),
 .UNSPECIFIED.,.F.,.F.,(4,4),(-0.018241527118741,-0.00068348472876189),
 .UNSPECIFIED.);
#701=B_SPLINE_CURVE_WITH_KNOTS('',3,(#64349,#64350,#64351,#64352,#64353,
#64354,#64355,#64356,#64357,#64358,#64359,#64360,#64361,#64362,#64363,#64364,
#64365,#64366,#64367,#64368,#64369,#64370,#64371,#64372,#64373,#64374,#64375,
#64376,#64377,#64378,#64379,#64380,#64381,#64382,#64383,#64384,#64385,#64386,
#64387,#64388,#64389,#64390,#64391,#64392,#64393,#64394,#64395,#64396,#64397,
#64398,#64399,#64400,#64401,#64402,#64403,#64404,#64405,#64406,#64407,#64408,
#64409,#64410,#64411,#64412,#64413,#64414,#64415,#64416,#64417,#64418,#64419,
#64420,#64421,#64422,#64423,#64424,#64425,#64426,#64427,#64428,#64429,#64430,
#64431,#64432,#64433,#64434,#64435,#64436,#64437,#64438,#64439,#64440,#64441,
#64442,#64443,#64444,#64445,#64446,#64447,#64448,#64449,#64450,#64451,#64452,
#64453,#64454,#64455,#64456,#64457,#64458,#64459,#64460,#64461,#64462,#64463,
#64464,#64465,#64466,#64467,#64468,#64469,#64470,#64471,#64472,#64473,#64474,
#64475,#64476,#64477,#64478,#64479,#64480,#64481,#64482,#64483,#64484,#64485,
#64486,#64487,#64488,#64489,#64490,#64491,#64492,#64493,#64494,#64495,#64496,
#64497,#64498,#64499,#64500,#64501,#64502,#64503,#64504,#64505,#64506,#64507,
#64508,#64509,#64510,#64511,#64512,#64513,#64514,#64515,#64516,#64517,#64518,
#64519,#64520,#64521,#64522,#64523,#64524,#64525,#64526,#64527,#64528,#64529,
#64530,#64531,#64532,#64533,#64534,#64535,#64536,#64537,#64538,#64539,#64540,
#64541,#64542,#64543,#64544,#64545,#64546,#64547,#64548,#64549,#64550,#64551,
#64552,#64553,#64554),.UNSPECIFIED.,.F.,.F.,(4,2,2,2,2,2,2,2,2,2,2,2,2,
2,2,2,2,2,2,2,2,2,2,2,2,2,2,2,2,2,2,2,2,2,2,2,2,2,2,2,2,2,2,2,2,2,2,2,2,
2,2,2,2,2,2,2,2,2,2,2,2,2,2,2,2,2,2,2,2,2,2,2,2,2,2,2,2,2,2,2,2,2,2,2,2,
2,2,2,2,2,2,2,2,2,2,2,2,2,2,2,2,2,4),(-2.98941746380008,-2.96248487704949,
-2.95231218207499,-2.94882509966526,-2.94627588425307,-2.94373207430651,
-2.94089801440436,-2.93594791514604,-2.91432438045648,-2.8836342351491,
-2.85719872258917,-2.85385350591768,-2.84108214507179,-2.83289489716619,
-2.82788178193595,-2.82341030018426,-2.81770620487656,-2.80846815849808,
-2.75850278040354,-2.7299945269286,-2.72022646336742,-2.71320971940145,
-2.70996065224898,-2.70769055209363,-2.70477968793288,-2.69961414476861,
-2.66748843187319,-2.62506845358489,-2.60279592023616,-2.59566308670309,
-2.59094421025465,-2.58641306322525,-2.58000852807909,-2.56478878050303,
-2.5128242690168,-2.49133668963146,-2.48307011798251,-2.47688417195004,
-2.47379346268617,-2.47128830746959,-2.46812857314816,-2.4615881171433,
-2.41718024451569,-2.3710766057594,-2.3617565374957,-2.35657631550999,-2.35212428603858,
-2.34666319032082,-2.33825485350738,-2.2793750251368,-2.24835956015106,
-2.24138509149896,-2.2381436810177,-2.23587435621901,-2.2329580516155,-2.22776864658227,
-2.19316842332354,-2.16639978102874,-2.1440154174088,-2.13369023897457,
-2.12520137845459,-2.12019559056495,-2.11572225121708,-2.11000420519358,
-2.10071871235496,-2.05192667878566,-2.01107833642564,-2.00500291545911,
-2.00193397183937,-1.99942787532982,-1.99624340477556,-1.98957420302857,
-1.94650761390652,-1.89783660757977,-1.88930258607995,-1.88428713949085,
-1.87981544634602,-1.87411364917727,-1.86488481127286,-1.81469155770055,
-1.78633021881076,-1.77659001368226,-1.76958804112824,-1.7663414572083,
-1.76407142606589,-1.76115830980542,-1.75598361612362,-1.72232344586827,
-1.68106494468326,-1.65910026878054,-1.65199894354638,-1.64728615091001,
-1.6427500366689,-1.63631989534542,-1.6209137889279,-1.55749218930709,-1.54360611773456,
-1.53453442609139,-1.53094071300473,-1.52838945582394,-1.52557417449396,
-1.52071262104022,-1.5126288124337),.UNSPECIFIED.);
#702=B_SPLINE_CURVE_WITH_KNOTS('',3,(#64559,#64560,#64561,#64562,#64563,
#64564,#64565,#64566,#64567,#64568,#64569,#64570,#64571,#64572,#64573,#64574,
#64575,#64576,#64577,#64578,#64579,#64580,#64581,#64582,#64583,#64584,#64585,
#64586,#64587,#64588,#64589,#64590,#64591,#64592,#64593,#64594,#64595,#64596,
#64597,#64598,#64599,#64600,#64601,#64602,#64603,#64604,#64605,#64606,#64607,
#64608,#64609,#64610,#64611,#64612,#64613,#64614,#64615,#64616,#64617,#64618,
#64619,#64620,#64621,#64622,#64623,#64624,#64625,#64626,#64627,#64628,#64629,
#64630,#64631,#64632,#64633,#64634,#64635,#64636,#64637,#64638,#64639,#64640,
#64641,#64642,#64643,#64644,#64645,#64646,#64647,#64648,#64649,#64650,#64651,
#64652,#64653,#64654,#64655,#64656,#64657,#64658,#64659,#64660,#64661,#64662,
#64663,#64664,#64665,#64666,#64667,#64668,#64669,#64670,#64671,#64672,#64673,
#64674,#64675,#64676,#64677,#64678,#64679,#64680,#64681,#64682,#64683,#64684,
#64685,#64686,#64687,#64688,#64689,#64690,#64691,#64692,#64693,#64694,#64695,
#64696,#64697,#64698,#64699,#64700,#64701,#64702,#64703,#64704,#64705,#64706,
#64707,#64708,#64709,#64710,#64711,#64712,#64713,#64714,#64715,#64716,#64717,
#64718,#64719,#64720,#64721,#64722,#64723,#64724,#64725,#64726,#64727,#64728,
#64729,#64730,#64731,#64732,#64733,#64734,#64735,#64736,#64737,#64738,#64739,
#64740,#64741,#64742,#64743,#64744,#64745,#64746,#64747,#64748,#64749,#64750,
#64751,#64752,#64753,#64754,#64755,#64756,#64757,#64758,#64759,#64760,#64761,
#64762,#64763,#64764,#64765,#64766,#64767,#64768,#64769,#64770),
 .UNSPECIFIED.,.F.,.F.,(4,2,2,2,2,2,2,2,2,2,2,2,2,2,2,2,2,2,2,2,2,2,2,2,
2,2,2,2,2,2,2,2,2,2,2,2,2,2,2,2,2,2,2,2,2,2,2,2,2,2,2,2,2,2,2,2,2,2,2,2,
2,2,2,2,2,2,2,2,2,2,2,2,2,2,2,2,2,2,2,2,2,2,2,2,2,2,2,2,2,2,2,2,2,2,2,2,
2,2,2,2,2,2,2,2,2,4),(-2.97123293200389,-2.96018209535889,-2.94653467953259,
-2.94079549607278,-2.93646395987323,-2.93205085822967,-2.92731797038154,
-2.91976888812843,-2.89452044756518,-2.85305399826597,-2.83095702050522,
-2.82093864347159,-2.81719917840001,-2.81466532553443,-2.81200479945457,
-2.80766912760509,-2.79316376233238,-2.74654337121384,-2.72285941677932,
-2.70722156330017,-2.70100199176108,-2.6965374885075,-2.69245577118526,
-2.68692507089546,-2.6729220767887,-2.61967055034795,-2.59028083733551,
-2.58353308211964,-2.58037710025521,-2.57816148795362,-2.57531257791512,
-2.57024769457214,-2.54114604092698,-2.53307565643954,-2.50305994527748,
-2.47424683310716,-2.46665470925122,-2.46191282517589,-2.45750347458752,
-2.45171891303322,-2.43844732353472,-2.37841434063925,-2.36007289003813,
-2.35262755738223,-2.34694137947838,-2.34399231281459,-2.34154212281015,
-2.33838262903737,-2.33161714927247,-2.29182937796836,-2.27299017606512,
-2.25029265179837,-2.23993149663796,-2.23145590628294,-2.22652531930293,
-2.22216229783813,-2.21664703612831,-2.20783025530979,-2.15296321683991,
-2.11638120526222,-2.11084257064889,-2.10792360009756,-2.10547035317752,
-2.1023236770765,-2.09544626523312,-2.05969758416929,-2.02174087186709,
-2.00078955048243,-1.99389317820185,-1.98929664490684,-1.98486034402827,
-1.97855490257305,-1.96340147311525,-1.9112460583597,-1.88222542586457,
-1.87551505987632,-1.87236556510723,-1.87015021318367,-1.86729558461131,
-1.86220703159483,-1.83158661124563,-1.82167068961519,-1.7851724584713,
-1.76466958750591,-1.7578226795325,-1.75323610498249,-1.74879229022575,
-1.74244630831792,-1.72704898276516,-1.67513483577027,-1.646196369831,-1.63949441442758,
-1.63634640075441,-1.63413112420566,-1.63127522924421,-1.62618137293291,
-1.59446744729977,-1.5896706765963,-1.56069768784271,-1.53039679859945,
-1.52270284543596,-1.51793834871118,-1.5135352569642,-1.50779809362037,
-1.49481626177982,-1.47758203553868),.UNSPECIFIED.);
#703=B_SPLINE_CURVE_WITH_KNOTS('',3,(#64771,#64772,#64773,#64774,#64775,
#64776,#64777,#64778,#64779,#64780,#64781,#64782,#64783,#64784,#64785,#64786,
#64787,#64788,#64789,#64790,#64791,#64792,#64793,#64794,#64795,#64796,#64797,
#64798,#64799,#64800,#64801,#64802,#64803,#64804,#64805,#64806,#64807,#64808,
#64809,#64810,#64811,#64812,#64813,#64814,#64815,#64816,#64817,#64818,#64819,
#64820,#64821,#64822,#64823,#64824,#64825,#64826,#64827,#64828,#64829,#64830,
#64831,#64832,#64833,#64834,#64835,#64836,#64837,#64838,#64839,#64840,#64841,
#64842,#64843,#64844,#64845,#64846,#64847,#64848,#64849,#64850,#64851,#64852,
#64853,#64854,#64855,#64856,#64857,#64858,#64859,#64860,#64861,#64862,#64863,
#64864,#64865,#64866,#64867,#64868,#64869,#64870,#64871,#64872,#64873,#64874,
#64875,#64876,#64877,#64878,#64879,#64880,#64881,#64882,#64883,#64884,#64885,
#64886,#64887,#64888,#64889,#64890,#64891,#64892,#64893,#64894,#64895,#64896,
#64897,#64898,#64899,#64900,#64901,#64902,#64903,#64904,#64905,#64906,#64907,
#64908,#64909,#64910,#64911,#64912,#64913,#64914,#64915,#64916,#64917,#64918,
#64919,#64920,#64921,#64922,#64923,#64924,#64925,#64926,#64927,#64928,#64929,
#64930,#64931,#64932,#64933,#64934,#64935,#64936,#64937,#64938,#64939,#64940,
#64941,#64942,#64943,#64944,#64945,#64946,#64947,#64948,#64949,#64950,#64951,
#64952,#64953,#64954,#64955,#64956,#64957,#64958,#64959,#64960,#64961,#64962,
#64963,#64964,#64965,#64966,#64967,#64968),.UNSPECIFIED.,.F.,.F.,(4,2,2,
2,2,2,2,2,2,2,2,2,2,2,2,2,2,2,2,2,2,2,2,2,2,2,2,2,2,2,2,2,2,2,2,2,2,2,2,
2,2,2,2,2,2,2,2,2,2,2,2,2,2,2,2,2,2,2,2,2,2,2,2,2,2,2,2,2,2,2,2,2,2,2,2,
2,2,2,2,2,2,2,2,2,2,2,2,2,2,2,2,2,2,2,2,2,2,2,4),(-1.5126288124337,-1.50038114054109,
-1.49546479199589,-1.44606412386808,-1.42366624092399,-1.41631822307126,
-1.4115541165769,-1.40699740606741,-1.40070895674774,-1.38518831930661,
-1.36189724087179,-1.33558914890058,-1.30191823245816,-1.2967426740572,
-1.29382928014378,-1.29155911992285,-1.28831253492428,-1.28131112506051,
-1.27157323930674,-1.24322194045223,-1.19306223892939,-1.18383415560942,
-1.17813236805072,-1.17366044373705,-1.16864448607963,-1.16010901161033,
-1.11197953383842,-1.06819237216739,-1.06160211412162,-1.05843249665659,
-1.05592666101242,-1.05284392336975,-1.046699957856,-1.00536760922362,-0.957249337814812,
-0.947943166028995,-0.942218832374047,-0.937744412304101,-0.93274138091446,
-0.924267106080874,-0.875232155528154,-0.832413316551177,-0.825706622371078,
-0.82251486321443,-0.820008271450277,-0.816945132400755,-0.810899680953753,
-0.802879772017047,-0.782420659953794,-0.734145338154514,-0.71508205717588,
-0.708106128584507,-0.703886922727287,-0.699345825018686,-0.693150408393322,
-0.678240186779483,-0.656266216843191,-0.612830331704289,-0.593349426309233,
-0.588537752568741,-0.585733238735222,-0.583177617711738,-0.579558131695105,
-0.570316762160553,-0.556064258954025,-0.485626409173881,-0.476148484033475,
-0.470375057600833,-0.465895201878667,-0.460919756707715,-0.452574728771954,
-0.409888181588814,-0.365730445953171,-0.355471964610801,-0.351597197392485,
-0.349252732260916,-0.346607310085745,-0.342525237517454,-0.329701962106306,
-0.306408896864487,-0.247724994857589,-0.239296265007748,-0.233828769446615,
-0.229375971070713,-0.227916074284677,-0.227172544964561,-0.22641533902017,
-0.219485513050008,-0.199084759498255,-0.163124337587808,-0.124902246056914,
-0.117977158098232,-0.11474477389471,-0.112236499212788,-0.109207970221842,
-0.103333172622581,-0.0956076681871372,-0.0763324108419592,-0.0180105444581843),
 .UNSPECIFIED.);
#704=B_SPLINE_CURVE_WITH_KNOTS('',3,(#64974,#64975,#64976,#64977,#64978,
#64979,#64980,#64981,#64982,#64983),.UNSPECIFIED.,.F.,.F.,(4,1,1,1,1,1,
1,4),(97.3893749664237,97.6514835490889,98.6441947268299,99.6369059045709,
100.629617082312,101.622328260053,102.615039437794,103.599566372989),
 .UNSPECIFIED.);
#705=B_SPLINE_CURVE_WITH_KNOTS('',3,(#64984,#64985,#64986,#64987),
 .UNSPECIFIED.,.F.,.F.,(4,4),(-2.98877382828685,-2.97123293200389),
 .UNSPECIFIED.);
#706=B_SPLINE_CURVE_WITH_KNOTS('',3,(#64989,#64990,#64991,#64992,#64993,
#64994,#64995,#64996),.UNSPECIFIED.,.F.,.F.,(4,2,2,4),(-0.0180105444581843,
-0.0141561210882267,-0.00572761886439141,-0.000683821560827492),
 .UNSPECIFIED.);
#707=B_SPLINE_CURVE_WITH_KNOTS('',3,(#64997,#64998,#64999,#65000,#65001,
#65002,#65003,#65004,#65005,#65006,#65007,#65008,#65009,#65010,#65011,#65012,
#65013,#65014,#65015,#65016,#65017,#65018,#65019,#65020,#65021,#65022,#65023,
#65024,#65025,#65026,#65027,#65028,#65029,#65030,#65031,#65032,#65033,#65034,
#65035,#65036,#65037,#65038,#65039,#65040,#65041,#65042,#65043,#65044,#65045,
#65046,#65047,#65048,#65049,#65050,#65051,#65052,#65053,#65054,#65055,#65056,
#65057,#65058,#65059,#65060,#65061,#65062,#65063,#65064,#65065,#65066,#65067,
#65068,#65069,#65070,#65071,#65072,#65073,#65074,#65075,#65076,#65077,#65078,
#65079,#65080,#65081,#65082,#65083,#65084,#65085,#65086,#65087,#65088,#65089,
#65090,#65091,#65092,#65093,#65094,#65095,#65096,#65097,#65098,#65099,#65100,
#65101,#65102,#65103,#65104,#65105,#65106,#65107,#65108,#65109,#65110,#65111,
#65112,#65113,#65114,#65115,#65116,#65117,#65118,#65119,#65120,#65121,#65122,
#65123,#65124,#65125,#65126,#65127,#65128,#65129,#65130,#65131,#65132,#65133,
#65134,#65135,#65136,#65137,#65138,#65139,#65140,#65141,#65142,#65143,#65144,
#65145,#65146,#65147,#65148,#65149,#65150,#65151,#65152,#65153,#65154,#65155,
#65156,#65157,#65158,#65159,#65160,#65161,#65162,#65163,#65164,#65165,#65166,
#65167,#65168,#65169,#65170,#65171,#65172,#65173,#65174,#65175,#65176,#65177,
#65178,#65179,#65180,#65181,#65182,#65183,#65184,#65185,#65186),
 .UNSPECIFIED.,.F.,.F.,(4,3,3,3,3,3,3,3,3,3,3,3,3,3,3,3,3,3,3,3,3,3,3,3,
3,3,3,3,3,3,3,3,3,3,3,3,3,3,3,3,3,3,3,3,3,3,3,3,3,3,3,3,3,3,3,3,3,3,3,3,
3,3,3,4),(97.3893722612836,97.493384673513,97.5976334276354,97.7019998579112,
97.8066354474768,97.9077762578471,98.0083650106068,98.1088102098943,98.2091404938834,
98.3094081259277,98.4096442296323,98.5098798887576,98.6102146041844,98.7105981065155,
98.8111596237581,98.8996468717555,99.000231660288,99.1006728858691,99.2009992006014,
99.301262868009,99.4014950171848,99.5017267373846,99.6020575655355,99.7024372028987,
99.8029949370643,99.8915174856638,99.9921074860471,100.092553907656,100.192885370718,
100.293154154975,100.393391382668,100.493628136167,100.593963892524,100.694348408067,
100.794910880808,100.883388099572,100.983981673788,101.08443173694,101.184766925044,
101.285039483294,101.385280528212,101.485521136495,101.585860778769,101.686249203348,
101.786815578012,101.875258713481,101.975825805746,102.076249303367,102.176557925544,
102.27680393036,102.377018471189,102.477232661605,102.57754620383,102.677908662145,
102.778449594122,102.867129327389,102.96625050879,103.065243338486,103.164140823337,
103.262975843551,103.361809067418,103.4606412558,103.559547384382,103.598719667128),
 .UNSPECIFIED.);
#708=B_SPLINE_CURVE_WITH_KNOTS('',3,(#65190,#65191,#65192,#65193,#65194,
#65195),.UNSPECIFIED.,.F.,.F.,(4,1,1,4),(-4.09293042013066,-3.96748245563351,
-2.97561184172513,-2.06906822660971),.UNSPECIFIED.);
#709=B_SPLINE_CURVE_WITH_KNOTS('',3,(#65199,#65200,#65201,#65202,#65203),
 .UNSPECIFIED.,.F.,.F.,(4,1,4),(0.,0.992711177740983,1.1173004083682),
 .UNSPECIFIED.);
#710=B_SPLINE_CURVE_WITH_KNOTS('',3,(#65205,#65206,#65207,#65208,#65209,
#65210,#65211,#65212,#65213,#65214,#65215,#65216,#65217,#65218,#65219,#65220,
#65221,#65222,#65223,#65224,#65225,#65226,#65227,#65228,#65229,#65230,#65231,
#65232,#65233,#65234,#65235,#65236,#65237,#65238,#65239,#65240,#65241,#65242,
#65243,#65244,#65245,#65246,#65247,#65248,#65249,#65250,#65251,#65252,#65253,
#65254,#65255,#65256,#65257,#65258,#65259,#65260,#65261,#65262,#65263,#65264,
#65265,#65266,#65267,#65268,#65269,#65270,#65271,#65272,#65273,#65274,#65275,
#65276,#65277,#65278,#65279,#65280,#65281,#65282,#65283,#65284,#65285,#65286,
#65287,#65288,#65289,#65290,#65291,#65292,#65293,#65294,#65295,#65296,#65297,
#65298,#65299,#65300,#65301,#65302,#65303,#65304,#65305,#65306,#65307,#65308,
#65309,#65310,#65311,#65312,#65313,#65314,#65315,#65316,#65317,#65318,#65319,
#65320,#65321,#65322,#65323,#65324,#65325,#65326,#65327,#65328,#65329,#65330,
#65331,#65332,#65333,#65334,#65335,#65336,#65337,#65338,#65339,#65340,#65341,
#65342,#65343,#65344,#65345,#65346,#65347,#65348,#65349,#65350,#65351,#65352,
#65353,#65354,#65355,#65356,#65357,#65358,#65359,#65360,#65361,#65362,#65363,
#65364,#65365,#65366,#65367,#65368,#65369,#65370,#65371,#65372,#65373,#65374,
#65375,#65376,#65377,#65378,#65379,#65380,#65381,#65382,#65383,#65384,#65385,
#65386,#65387,#65388,#65389,#65390,#65391,#65392,#65393,#65394,#65395,#65396,
#65397,#65398,#65399,#65400,#65401,#65402,#65403,#65404,#65405,#65406,#65407,
#65408,#65409,#65410,#65411,#65412,#65413,#65414,#65415),.UNSPECIFIED.,
 .F.,.F.,(4,3,3,3,3,3,3,3,3,3,3,3,3,3,3,3,3,3,3,3,3,3,3,3,3,3,3,3,3,3,3,
3,3,3,3,3,3,3,3,3,3,3,3,3,3,3,3,3,3,3,3,3,3,3,3,3,3,3,3,3,3,3,3,3,3,3,3,
3,3,3,4),(1.1173004083682,1.21032980834395,1.3072163767362,1.4000398708129,
1.49281995955612,1.58558508021891,1.6783636479266,1.77123897043941,1.8641715077765,
1.95724799133377,1.98542235548196,2.08087078878419,2.17618953906202,2.27140784073711,
2.3665583879355,2.46167490015914,2.55678364613916,2.65191088024338,2.74713937184165,
2.84242574410779,2.93785940901966,2.97813353322293,3.07359703316209,3.16893382142426,
3.26917268261672,3.36434619530356,3.45948972117081,3.55462950391444,3.64979177626171,
3.74505982279029,3.84038921166125,3.93586752489477,3.97084471096391,4.06602029899652,
4.16106424190066,4.25600618469319,4.35087925914523,4.44571772712217,4.54054821730625,
4.63539734391196,4.73034964786798,4.82536054310032,4.92052244082011,4.96355588870488,
5.05888749329321,5.15408932749402,5.24919080357482,5.3442251834698,5.43922599598654,
5.53421966847994,5.62923261450247,5.72434871738995,5.81952363603612,5.91484834628159,
5.95626706644586,6.05158819173318,6.14677979675512,6.24187130762467,6.33689615981954,
6.43188772174665,6.52687243390915,6.62187672325866,6.71698468340639,6.81215174233597,
6.90746910348022,6.94897824418683,7.05133621204183,7.1533540140597,7.25515818809801,
7.35665992559863,7.40048571532638),.UNSPECIFIED.);
#711=B_SPLINE_CURVE_WITH_KNOTS('',3,(#65417,#65418,#65419,#65420,#65421,
#65422,#65423,#65424,#65425,#65426,#65427,#65428,#65429,#65430,#65431,#65432,
#65433,#65434,#65435,#65436,#65437,#65438,#65439,#65440,#65441,#65442,#65443,
#65444,#65445,#65446,#65447,#65448,#65449,#65450,#65451,#65452,#65453,#65454,
#65455,#65456,#65457,#65458,#65459,#65460,#65461,#65462,#65463,#65464,#65465,
#65466,#65467,#65468,#65469,#65470,#65471,#65472,#65473,#65474,#65475,#65476,
#65477,#65478,#65479,#65480,#65481,#65482,#65483,#65484,#65485,#65486,#65487,
#65488,#65489,#65490,#65491,#65492,#65493,#65494,#65495,#65496,#65497,#65498,
#65499,#65500,#65501,#65502,#65503,#65504,#65505,#65506,#65507,#65508,#65509,
#65510,#65511,#65512,#65513,#65514,#65515,#65516,#65517,#65518,#65519,#65520,
#65521,#65522,#65523,#65524,#65525,#65526,#65527,#65528,#65529,#65530,#65531,
#65532,#65533,#65534,#65535,#65536,#65537,#65538,#65539,#65540,#65541,#65542,
#65543,#65544,#65545,#65546,#65547,#65548,#65549,#65550,#65551,#65552,#65553,
#65554,#65555,#65556,#65557,#65558,#65559,#65560,#65561,#65562,#65563,#65564,
#65565,#65566,#65567,#65568,#65569,#65570,#65571,#65572,#65573,#65574,#65575,
#65576,#65577,#65578,#65579,#65580,#65581,#65582,#65583,#65584,#65585,#65586,
#65587,#65588,#65589,#65590,#65591,#65592,#65593,#65594,#65595,#65596,#65597,
#65598,#65599,#65600,#65601,#65602,#65603,#65604,#65605,#65606,#65607,#65608,
#65609,#65610,#65611,#65612,#65613,#65614,#65615,#65616,#65617,#65618,#65619,
#65620,#65621,#65622,#65623,#65624,#65625,#65626,#65627),.UNSPECIFIED.,
 .F.,.F.,(4,3,3,3,3,3,3,3,3,3,3,3,3,3,3,3,3,3,3,3,3,3,3,3,3,3,3,3,3,3,3,
3,3,3,3,3,3,3,3,3,3,3,3,3,3,3,3,3,3,3,3,3,3,3,3,3,3,3,3,3,3,3,3,3,3,3,3,
3,3,3,4),(7.40048571554779,7.49824612985645,7.59608965728392,7.69411743523722,
7.79224606749592,7.89057934795509,7.94168942192781,8.03699764920788,8.13217600279553,
8.22725392955767,8.32226475962273,8.41724203232331,8.51221220555734,8.60720172346273,
8.7022946487693,8.79744650061537,8.89274853363321,8.93440059966879,9.02970523102217,
9.12487999259607,9.21995433644279,9.31496161266825,9.40993535119827,9.50490201456794,
9.59988805157463,9.69497756112813,9.79012602969033,9.8854247615887,9.92711177740977,
10.0224119143356,10.1175820941002,10.212651775755,10.3076542898582,10.4026232059893,
10.4975849926482,10.5925661045524,10.6876506453834,10.7827941131637,10.8780878423386,
10.9198229551507,11.015126647672,11.1103004319231,11.2053737615344,11.3003799727728,
11.3953526151215,11.4903181524017,11.5853030346704,11.680391352975,11.7755386076768,
11.870836102385,11.9125341328917,12.0078370228027,12.1030100004079,12.1980825205225,
12.2930879215015,12.3880597534642,12.4830244812746,12.5780085560348,12.6730960747126,
12.7682425331656,12.8635392443914,12.9052453106327,13.0025485246029,13.0963989586797,
13.1901630945498,13.2838688632371,13.3775441272426,13.4712489108769,13.5649722634797,
13.6587806403493,13.6836710223941),.UNSPECIFIED.);
#712=B_SPLINE_CURVE_WITH_KNOTS('',3,(#65629,#65630,#65631,#65632,#65633,
#65634,#65635,#65636,#65637,#65638,#65639,#65640,#65641,#65642,#65643,#65644,
#65645,#65646,#65647,#65648,#65649,#65650,#65651,#65652,#65653,#65654,#65655,
#65656,#65657,#65658,#65659,#65660,#65661,#65662,#65663,#65664,#65665,#65666,
#65667,#65668,#65669,#65670,#65671,#65672,#65673,#65674,#65675,#65676,#65677,
#65678,#65679,#65680,#65681,#65682,#65683,#65684,#65685,#65686,#65687,#65688,
#65689,#65690,#65691,#65692,#65693,#65694,#65695,#65696,#65697,#65698,#65699,
#65700,#65701,#65702,#65703,#65704,#65705,#65706,#65707,#65708,#65709,#65710,
#65711,#65712,#65713,#65714,#65715,#65716,#65717,#65718,#65719,#65720,#65721,
#65722,#65723,#65724,#65725,#65726,#65727,#65728,#65729,#65730,#65731,#65732,
#65733,#65734,#65735,#65736,#65737,#65738,#65739,#65740,#65741,#65742,#65743,
#65744,#65745,#65746,#65747,#65748,#65749,#65750,#65751,#65752,#65753,#65754,
#65755,#65756,#65757,#65758,#65759,#65760,#65761,#65762,#65763,#65764,#65765,
#65766,#65767,#65768,#65769,#65770,#65771,#65772,#65773,#65774,#65775,#65776,
#65777,#65778,#65779,#65780,#65781,#65782,#65783,#65784,#65785,#65786,#65787,
#65788,#65789,#65790,#65791,#65792,#65793,#65794,#65795,#65796,#65797,#65798,
#65799,#65800,#65801,#65802,#65803,#65804,#65805,#65806,#65807,#65808,#65809,
#65810,#65811,#65812,#65813,#65814,#65815,#65816,#65817,#65818,#65819,#65820,
#65821,#65822,#65823,#65824,#65825,#65826,#65827,#65828,#65829,#65830,#65831,
#65832,#65833,#65834,#65835,#65836),.UNSPECIFIED.,.F.,.F.,(4,3,3,3,3,3,
3,3,3,3,3,3,3,3,3,3,3,3,3,3,3,3,3,3,3,3,3,3,3,3,3,3,3,3,3,3,3,3,3,3,3,3,
3,3,3,3,3,3,3,3,3,3,3,3,3,3,3,3,3,3,3,3,3,3,3,3,3,3,3,4),(13.6836710227274,
13.8145638300528,13.8979564883737,13.9932593777273,14.0884323511339,14.1835048634302,
14.2785102512182,14.3734820666447,14.4684467745816,14.5634308261355,14.6585183166849,
14.7536647441496,14.8489614202729,14.8906676661147,14.9859704022949,15.0811432213058,
15.1762155782123,15.2712208097971,15.3661924685803,15.4611570196336,15.5561409142636,
15.6512282487803,15.7463745205009,15.8416710428038,15.8833788438556,15.9786815267226,
16.0738542910791,16.1689265920748,16.2639317661137,16.3589033663558,16.4538678579444,
16.5488516922565,16.6439389655255,16.7390851753785,16.8343816354455,16.8760900215966,
16.971392776919,17.0665656148329,17.1616379903769,17.2566432401223,17.3516149167606,
17.4465794853395,17.5415633971411,17.6366507481872,17.7317970360928,17.8270935738962,
17.8688011993376,17.9641039278211,18.0592767386331,18.1543490868526,18.249354309059,
18.3443259580365,18.4392904988676,18.5342743828697,18.6293617062065,18.7245079664151,
18.8198044768031,18.8615123770786,18.9568151010649,19.0519879072284,19.1470602506551,
19.2420654678741,19.337037111745,19.4320016473566,19.5269855260317,19.6220728439113,
19.7172190985804,19.8125156033542,19.8542235548195,19.966856329907),
 .UNSPECIFIED.);
#713=B_SPLINE_CURVE_WITH_KNOTS('',3,(#65838,#65839,#65840,#65841,#65842,
#65843,#65844,#65845,#65846,#65847),.UNSPECIFIED.,.F.,.F.,(4,1,1,1,1,1,
1,4),(19.9668647663903,20.8469347325605,21.8396459103015,22.8323570880425,
23.8250682657834,24.8177794435244,25.8104906212654,26.2500416370865),
 .UNSPECIFIED.);
#714=B_SPLINE_CURVE_WITH_KNOTS('',3,(#65849,#65850,#65851,#65852,#65853,
#65854,#65855,#65856,#65857,#65858),.UNSPECIFIED.,.F.,.F.,(4,1,1,1,1,1,
1,4),(26.2500416370865,26.8032017990064,27.7959129767474,28.7886241544883,
29.7813353322293,30.7740465099703,31.7667576877113,32.5332265095628),
 .UNSPECIFIED.);
#715=B_SPLINE_CURVE_WITH_KNOTS('',3,(#65860,#65861,#65862,#65863,#65864,
#65865,#65866,#65867,#65868,#65869,#65870,#65871,#65872,#65873,#65874,#65875,
#65876,#65877,#65878,#65879,#65880,#65881,#65882,#65883,#65884,#65885,#65886,
#65887,#65888,#65889,#65890,#65891,#65892,#65893,#65894,#65895,#65896,#65897,
#65898,#65899,#65900,#65901,#65902,#65903,#65904,#65905,#65906,#65907,#65908,
#65909,#65910,#65911,#65912,#65913,#65914,#65915,#65916,#65917,#65918,#65919,
#65920,#65921,#65922,#65923,#65924,#65925,#65926,#65927,#65928,#65929,#65930,
#65931,#65932,#65933,#65934,#65935,#65936,#65937,#65938,#65939,#65940,#65941,
#65942,#65943,#65944,#65945,#65946,#65947,#65948,#65949,#65950,#65951,#65952,
#65953,#65954,#65955,#65956,#65957,#65958,#65959,#65960,#65961,#65962,#65963,
#65964,#65965,#65966,#65967,#65968,#65969,#65970,#65971,#65972,#65973,#65974,
#65975,#65976,#65977,#65978,#65979,#65980,#65981,#65982,#65983,#65984,#65985,
#65986,#65987,#65988,#65989,#65990,#65991,#65992,#65993,#65994,#65995,#65996,
#65997,#65998,#65999,#66000,#66001,#66002,#66003,#66004,#66005,#66006,#66007,
#66008,#66009,#66010,#66011,#66012,#66013,#66014,#66015,#66016,#66017,#66018,
#66019,#66020,#66021,#66022,#66023,#66024,#66025,#66026,#66027,#66028,#66029,
#66030,#66031,#66032,#66033,#66034,#66035,#66036,#66037,#66038,#66039,#66040,
#66041,#66042,#66043,#66044,#66045,#66046,#66047,#66048,#66049,#66050,#66051,
#66052,#66053,#66054,#66055,#66056,#66057,#66058,#66059,#66060,#66061,#66062,
#66063,#66064,#66065,#66066,#66067),.UNSPECIFIED.,.F.,.F.,(4,3,3,3,3,3,
3,3,3,3,3,3,3,3,3,3,3,3,3,3,3,3,3,3,3,3,3,3,3,3,3,3,3,3,3,3,3,3,3,3,3,3,
3,3,3,3,3,3,3,3,3,3,3,3,3,3,3,3,3,3,3,3,3,3,3,3,3,3,3,4),(32.5332269442661,
32.6610063604515,32.7594688654522,32.8547715954818,32.9499444077968,33.0450167574743,
33.140021981065,33.2349936313803,33.329958173501,33.4249420587423,33.5200293832342,
33.6151756445514,33.7104721559659,33.7521800431932,33.8474827732234,33.9426555855391,
34.0377279352173,34.1327331588088,34.2277048091247,34.3226693512461,34.417653236488,
34.5127405609806,34.6078868222985,34.7031833337137,34.7448912209342,34.8401939509647,
34.9353667632806,35.030439112959,35.1254443365508,35.220415986867,35.3153805289887,
35.4103644142309,35.5054517387237,35.6005980000419,35.6958945114574,35.7376023986752,
35.8329051287053,35.9280779410209,36.0231502906989,36.1181555142903,36.2131271646062,
36.3080917067275,36.4030755919693,36.4981629164617,36.5933091777795,36.6886056891946,
36.7303135764161,36.8256163064463,36.920789118762,37.0158614684403,37.1108666920318,
37.2058383423478,37.3008028844693,37.3957867697112,37.4908740942038,37.5860203555218,
37.681316866937,37.7230247541571,37.8183274841874,37.9135002965031,38.0085726461813,
38.1035778697729,38.198549520089,38.2935140622104,38.3884979474524,38.483585271945,
38.5787315332631,38.6740280446784,38.7157359318981,38.8164122514457),
 .UNSPECIFIED.);
#716=B_SPLINE_CURVE_WITH_KNOTS('',3,(#66069,#66070,#66071,#66072,#66073,
#66074,#66075,#66076,#66077,#66078,#66079,#66080,#66081,#66082,#66083,#66084,
#66085,#66086,#66087,#66088,#66089,#66090,#66091,#66092,#66093,#66094,#66095,
#66096,#66097,#66098,#66099,#66100,#66101,#66102,#66103,#66104,#66105,#66106,
#66107,#66108,#66109,#66110,#66111,#66112,#66113,#66114,#66115,#66116,#66117,
#66118,#66119,#66120,#66121,#66122,#66123,#66124,#66125,#66126,#66127,#66128,
#66129,#66130,#66131,#66132,#66133,#66134,#66135,#66136,#66137,#66138,#66139,
#66140,#66141,#66142,#66143,#66144,#66145,#66146,#66147,#66148,#66149,#66150,
#66151,#66152,#66153,#66154,#66155,#66156,#66157,#66158,#66159,#66160,#66161,
#66162,#66163,#66164,#66165,#66166,#66167,#66168,#66169,#66170,#66171,#66172,
#66173,#66174,#66175,#66176,#66177,#66178,#66179,#66180,#66181,#66182,#66183,
#66184,#66185,#66186,#66187,#66188,#66189,#66190,#66191,#66192,#66193,#66194,
#66195,#66196,#66197,#66198,#66199,#66200,#66201,#66202,#66203,#66204,#66205,
#66206,#66207,#66208,#66209,#66210,#66211,#66212,#66213,#66214,#66215,#66216,
#66217,#66218,#66219,#66220,#66221,#66222,#66223,#66224,#66225,#66226,#66227,
#66228,#66229,#66230,#66231,#66232,#66233,#66234,#66235,#66236,#66237,#66238,
#66239,#66240,#66241,#66242,#66243,#66244,#66245,#66246,#66247,#66248,#66249,
#66250,#66251,#66252,#66253,#66254,#66255,#66256,#66257,#66258,#66259,#66260,
#66261,#66262,#66263,#66264,#66265,#66266,#66267,#66268,#66269,#66270,#66271,
#66272,#66273,#66274,#66275,#66276,#66277,#66278,#66279),.UNSPECIFIED.,
 .F.,.F.,(4,3,3,3,3,3,3,3,3,3,3,3,3,3,3,3,3,3,3,3,3,3,3,3,3,3,3,3,3,3,3,
3,3,3,3,3,3,3,3,3,3,3,3,3,3,3,3,3,3,3,3,3,3,3,3,3,3,3,3,3,3,3,3,3,3,3,3,
3,3,3,4),(38.8164122516606,38.9104710740768,39.0044137650042,39.0982701591792,
39.1920814649995,39.2858754296552,39.3796797770884,39.4735791389773,39.5675317808481,
39.6616329706406,39.7084471096391,39.8037498396694,39.8989226519849,39.993995001663,
40.0890002252545,40.1839718755706,40.2789364176921,40.3739203029341,40.4690076274267,
40.5641538887446,40.6594504001598,40.7011582873801,40.7964610174103,40.8916338297258,
40.9867061794043,41.0817114029959,41.1766830533118,41.2716475954333,41.3666314806755,
41.4617188051681,41.5568650664861,41.6521615779013,41.693869465121,41.7891721951512,
41.8843450074669,41.9794173571453,42.0744225807369,42.1693942310528,42.2643587731741,
42.3593426584158,42.4544299829083,42.5495762442263,42.6448727556416,42.686580642862,
42.7818833728922,42.8770561852078,42.972128534886,43.0671337584776,43.1621054087936,
43.2570699509149,43.3520538361566,43.4471411606493,43.542287421967,43.6375839333822,
43.679291820603,43.7745945506333,43.8697673629495,43.9648397126277,44.0598449362192,
44.1548165865352,44.2497811286566,44.3447650138982,44.4398523383908,44.5349985997084,
44.6302951111235,44.672002998344,44.778901555894,44.8823115123222,44.985464121309,
45.0882552304087,45.099597228544),.UNSPECIFIED.);
#717=B_SPLINE_CURVE_WITH_KNOTS('',3,(#66281,#66282,#66283,#66284,#66285,
#66286,#66287,#66288,#66289,#66290),.UNSPECIFIED.,.F.,.F.,(4,1,1,1,1,1,
1,4),(45.0995975586253,45.6647141760849,46.6574253538259,47.6501365315669,
48.6428477093079,49.6355588870488,50.6282700647898,51.3827828658049),
 .UNSPECIFIED.);
#718=B_SPLINE_CURVE_WITH_KNOTS('',3,(#66292,#66293,#66294,#66295,#66296,
#66297,#66298,#66299,#66300,#66301,#66302),.UNSPECIFIED.,.F.,.F.,(4,1,1,
1,1,1,1,1,4),(51.3827828658049,51.6209812425308,52.6136924202718,53.6064035980127,
54.5991147757537,55.5918259534947,56.5845371312357,57.5772483089767,57.6659681729845),
 .UNSPECIFIED.);
#719=B_SPLINE_CURVE_WITH_KNOTS('',3,(#66304,#66305,#66306,#66307,#66308,
#66309,#66310,#66311,#66312,#66313,#66314,#66315,#66316,#66317,#66318,#66319,
#66320,#66321,#66322,#66323,#66324,#66325,#66326,#66327,#66328,#66329,#66330,
#66331,#66332,#66333,#66334,#66335,#66336,#66337,#66338,#66339,#66340,#66341,
#66342,#66343,#66344,#66345,#66346,#66347,#66348,#66349,#66350,#66351,#66352,
#66353,#66354,#66355,#66356,#66357,#66358,#66359,#66360,#66361,#66362,#66363,
#66364,#66365,#66366,#66367,#66368,#66369,#66370,#66371,#66372,#66373,#66374,
#66375,#66376,#66377,#66378,#66379,#66380,#66381,#66382,#66383,#66384,#66385,
#66386,#66387,#66388,#66389,#66390,#66391,#66392,#66393,#66394,#66395,#66396,
#66397,#66398,#66399,#66400,#66401,#66402,#66403,#66404,#66405,#66406,#66407,
#66408,#66409,#66410,#66411,#66412,#66413,#66414,#66415,#66416,#66417,#66418,
#66419,#66420,#66421,#66422,#66423,#66424,#66425,#66426,#66427,#66428,#66429,
#66430,#66431,#66432,#66433,#66434,#66435,#66436,#66437,#66438,#66439,#66440,
#66441,#66442,#66443,#66444,#66445,#66446,#66447,#66448,#66449,#66450,#66451,
#66452,#66453,#66454,#66455,#66456,#66457,#66458,#66459,#66460,#66461,#66462,
#66463,#66464,#66465,#66466,#66467,#66468,#66469,#66470,#66471,#66472,#66473,
#66474,#66475,#66476,#66477,#66478,#66479,#66480,#66481,#66482,#66483,#66484,
#66485,#66486,#66487,#66488,#66489,#66490,#66491,#66492,#66493,#66494,#66495,
#66496,#66497,#66498,#66499,#66500,#66501,#66502,#66503,#66504,#66505,#66506,
#66507,#66508,#66509,#66510,#66511),.UNSPECIFIED.,.F.,.F.,(4,3,3,3,3,3,
3,3,3,3,3,3,3,3,3,3,3,3,3,3,3,3,3,3,3,3,3,3,3,3,3,3,3,3,3,3,3,3,3,3,3,3,
3,3,3,3,3,3,3,3,3,3,3,3,3,3,3,3,3,3,3,3,3,3,3,3,3,3,3,4),(57.6659681729845,
57.7601239022619,57.8541607955583,57.9481076140006,58.0420067651304,58.1358859245011,
58.229772741962,58.3237532139684,58.4177843761107,58.5119675653933,58.5699594867177,
58.665262216748,58.7604350290637,58.8555073787417,58.9505126023331,59.0454842526491,
59.1404487947705,59.2354326800123,59.330520004505,59.425666265823,59.5209627772383,
59.5626706644586,59.6579733944888,59.7531462068047,59.8482185564831,59.9432237800747,
60.0381954303908,60.133159972512,60.2281438577538,60.3232311822464,60.4183774435642,
60.5136739549794,60.5553818421996,60.6506845722298,60.7458573845455,60.8409297342235,
60.935934957815,61.0309066081311,61.1258711502524,61.2208550354948,61.3159423599874,
61.4110886213055,61.5063851327206,61.5480930199406,61.6433957499709,61.7385685622864,
61.833640911965,61.9286461355565,62.0236177858725,62.118582327994,62.2135662132359,
62.3086535377286,62.4037997990464,62.4990963104617,62.5408041976816,62.6361069277118,
62.7312797400277,62.826352089706,62.9213573132975,63.0163289636135,63.111293505735,
63.206277390977,63.3013647154696,63.3965109767875,63.4918074882025,63.5335153754225,
63.6379533631389,63.7421227640998,63.8458245660772,63.9491534799855),
 .UNSPECIFIED.);
#720=B_SPLINE_CURVE_WITH_KNOTS('',3,(#66513,#66514,#66515,#66516,#66517,
#66518,#66519,#66520,#66521,#66522,#66523,#66524,#66525,#66526,#66527,#66528,
#66529,#66530,#66531,#66532,#66533,#66534,#66535,#66536,#66537,#66538,#66539,
#66540,#66541,#66542,#66543,#66544,#66545,#66546,#66547,#66548,#66549,#66550,
#66551,#66552,#66553,#66554,#66555,#66556,#66557,#66558,#66559,#66560,#66561,
#66562,#66563,#66564,#66565,#66566,#66567,#66568,#66569,#66570,#66571,#66572,
#66573,#66574,#66575,#66576,#66577,#66578,#66579,#66580,#66581,#66582,#66583,
#66584,#66585,#66586,#66587,#66588,#66589,#66590,#66591,#66592,#66593,#66594,
#66595,#66596,#66597,#66598,#66599,#66600,#66601,#66602,#66603,#66604,#66605,
#66606,#66607,#66608,#66609,#66610,#66611,#66612,#66613,#66614,#66615,#66616,
#66617,#66618,#66619,#66620,#66621,#66622,#66623,#66624,#66625,#66626,#66627,
#66628,#66629,#66630,#66631,#66632,#66633,#66634,#66635,#66636,#66637,#66638,
#66639,#66640,#66641,#66642,#66643,#66644,#66645,#66646,#66647,#66648,#66649,
#66650,#66651,#66652,#66653,#66654,#66655,#66656,#66657,#66658,#66659,#66660,
#66661,#66662,#66663,#66664,#66665,#66666,#66667,#66668,#66669,#66670,#66671,
#66672,#66673,#66674,#66675,#66676,#66677,#66678,#66679,#66680,#66681,#66682,
#66683,#66684,#66685,#66686,#66687,#66688,#66689,#66690,#66691,#66692,#66693,
#66694,#66695,#66696,#66697,#66698,#66699,#66700,#66701,#66702,#66703,#66704,
#66705,#66706,#66707,#66708,#66709,#66710,#66711,#66712,#66713,#66714,#66715,
#66716,#66717,#66718,#66719,#66720),.UNSPECIFIED.,.F.,.F.,(4,3,3,3,3,3,
3,3,3,3,3,3,3,3,3,3,3,3,3,3,3,3,3,3,3,3,3,3,3,3,3,3,3,3,3,3,3,3,3,3,3,3,
3,3,3,3,3,3,3,3,3,3,3,3,3,3,3,3,3,3,3,3,3,3,3,3,3,3,3,4),(63.9491534801641,
64.0458634592205,64.1426193688178,64.2395234686266,64.3365021408146,64.4336819362929,
64.5262265531635,64.6215292831939,64.7167020955097,64.811774445188,64.9067796687797,
65.0017513190958,65.0967158612177,65.1916997464599,65.2867870709527,65.3819333322708,
65.4772298436862,65.5189377309045,65.6142404609347,65.7094132732503,65.8044856229284,
65.8994908465199,65.9944624968358,66.0894270389571,66.1844109241988,66.2794982486914,
66.3746445100095,66.4699410214246,66.5116489086455,66.6069516386749,66.70212445099,
66.797196800667,66.8922020242578,66.987173674573,67.0821382166934,67.1771221019346,
67.2722094264265,67.3673556877436,67.4626521991581,67.5043600863864,67.5996628164186,
67.694835628736,67.789907978416,67.8849132020092,67.979884852327,68.07484939445,
68.1698332796939,68.2649206041882,68.3600668655079,68.4553633769248,68.4970712641274,
68.5923739941569,68.6875468064717,68.7826191561489,68.8776243797395,68.9725960300548,
69.0675605721757,69.1625444574167,69.2576317819083,69.3527780432254,69.4480745546398,
69.4897824418684,69.5839866200001,69.6780732484959,69.7720701604336,69.8660050891807,
69.9599324042788,70.0538503457583,70.1478411652905,70.2323387873437),
 .UNSPECIFIED.);
#721=B_SPLINE_CURVE_WITH_KNOTS('',3,(#66722,#66723,#66724,#66725,#66726,
#66727,#66728,#66729,#66730,#66731,#66732),.UNSPECIFIED.,.F.,.F.,(4,1,1,
1,1,1,1,1,4),(70.2323404852416,70.4824936196094,71.4752047973503,72.4679159750913,
73.4606271528323,74.4533383305733,75.4460495083142,76.4387606860552,76.5155240945233),
 .UNSPECIFIED.);
#722=B_SPLINE_CURVE_WITH_KNOTS('',3,(#66734,#66735,#66736,#66737,#66738,
#66739,#66740,#66741,#66742,#66743),.UNSPECIFIED.,.F.,.F.,(4,1,1,1,1,1,
1,4),(76.5155240945233,77.4314718637962,78.4241830415372,79.4168942192782,
80.4096053970191,81.4023165747601,82.3950277525011,82.7987030501078),
 .UNSPECIFIED.);
#723=B_SPLINE_CURVE_WITH_KNOTS('',3,(#66745,#66746,#66747,#66748,#66749,
#66750,#66751,#66752,#66753,#66754,#66755,#66756,#66757,#66758,#66759,#66760,
#66761,#66762,#66763,#66764,#66765,#66766,#66767,#66768,#66769,#66770,#66771,
#66772,#66773,#66774,#66775,#66776,#66777,#66778,#66779,#66780,#66781,#66782,
#66783,#66784,#66785,#66786,#66787,#66788,#66789,#66790,#66791,#66792,#66793,
#66794,#66795,#66796,#66797,#66798,#66799,#66800,#66801,#66802,#66803,#66804,
#66805,#66806,#66807,#66808,#66809,#66810,#66811,#66812,#66813,#66814,#66815,
#66816,#66817,#66818,#66819,#66820,#66821,#66822,#66823,#66824,#66825,#66826,
#66827,#66828,#66829,#66830,#66831,#66832,#66833,#66834,#66835,#66836,#66837,
#66838,#66839,#66840,#66841,#66842,#66843,#66844,#66845,#66846,#66847,#66848,
#66849,#66850,#66851,#66852,#66853,#66854,#66855,#66856,#66857,#66858,#66859,
#66860,#66861,#66862,#66863,#66864,#66865,#66866,#66867,#66868,#66869,#66870,
#66871,#66872,#66873,#66874,#66875,#66876,#66877,#66878,#66879,#66880,#66881,
#66882,#66883,#66884,#66885,#66886,#66887,#66888,#66889,#66890,#66891,#66892,
#66893,#66894,#66895,#66896,#66897,#66898,#66899,#66900,#66901,#66902,#66903,
#66904,#66905,#66906,#66907,#66908,#66909,#66910,#66911,#66912,#66913,#66914,
#66915,#66916,#66917,#66918,#66919,#66920,#66921,#66922,#66923,#66924,#66925,
#66926,#66927,#66928,#66929,#66930,#66931,#66932,#66933,#66934,#66935,#66936,
#66937,#66938,#66939,#66940,#66941,#66942,#66943,#66944,#66945,#66946,#66947,
#66948,#66949,#66950,#66951,#66952),.UNSPECIFIED.,.F.,.F.,(4,3,3,3,3,3,
3,3,3,3,3,3,3,3,3,3,3,3,3,3,3,3,3,3,3,3,3,3,3,3,3,3,3,3,3,3,3,3,3,3,3,3,
3,3,3,3,3,3,3,3,3,3,3,3,3,3,3,3,3,3,3,3,3,3,3,3,3,3,3,4),(82.7987094017029,
82.895106815508,82.9915395652103,83.0905894064683,83.1872287620549,83.2874838461485,
83.3877389302421,83.4830416091242,83.5782143703192,83.6732866689735,83.7682918418933,
83.863263441777,83.9582279337673,84.0532117692414,84.148299044809,84.2434452576144,
84.338741721605,84.380450107983,84.4757528488978,84.5709256716648,84.6659980313535,
84.7610032642682,84.8559749234772,84.9509394740533,85.0459233673026,85.1410106990881,
85.2361569673007,85.3314534849416,85.373161285724,85.468464179738,85.5636371568421,
85.6587096718769,85.7537150609738,85.8486868768196,85.9436515842866,86.0386356344819,
86.1337231223428,86.2288695463545,86.324166217889,86.365872463465,86.4611748113714,
86.5563472414657,86.6514192093459,86.7464240533369,86.841395325572,86.9363594915972,
87.031343003194,87.126429959959,87.2215758564116,87.3168720107783,87.358583641206,
87.4538865705107,87.5490595793686,87.6441321226302,87.7391375346734,87.8341093701794,
87.9290740940189,88.0240581572941,88.1191456532476,88.2142920825123,88.3095887549497,
88.351294818947,88.4456074585947,88.5398015981657,88.6339049701896,88.7279452082351,
88.8219735339946,88.9159914878525,89.0100736649993,89.0818947088825),
 .UNSPECIFIED.);
#724=B_SPLINE_CURVE_WITH_KNOTS('',3,(#66954,#66955,#66956,#66957,#66958,
#66959,#66960,#66961,#66962,#66963,#66964,#66965,#66966,#66967,#66968,#66969,
#66970,#66971,#66972,#66973,#66974,#66975,#66976,#66977,#66978,#66979,#66980,
#66981,#66982,#66983,#66984,#66985,#66986,#66987,#66988,#66989,#66990,#66991,
#66992,#66993,#66994,#66995,#66996,#66997,#66998,#66999,#67000,#67001,#67002,
#67003,#67004,#67005,#67006,#67007,#67008,#67009,#67010,#67011,#67012,#67013,
#67014,#67015,#67016,#67017,#67018,#67019,#67020,#67021,#67022,#67023,#67024,
#67025,#67026,#67027,#67028,#67029,#67030,#67031,#67032,#67033,#67034,#67035,
#67036,#67037,#67038,#67039,#67040,#67041,#67042,#67043,#67044,#67045,#67046,
#67047,#67048,#67049,#67050,#67051,#67052,#67053,#67054,#67055,#67056,#67057,
#67058,#67059,#67060,#67061,#67062,#67063,#67064,#67065,#67066,#67067,#67068,
#67069,#67070,#67071,#67072,#67073,#67074,#67075,#67076,#67077,#67078,#67079,
#67080,#67081,#67082,#67083,#67084,#67085,#67086,#67087,#67088,#67089,#67090,
#67091,#67092,#67093,#67094,#67095,#67096,#67097,#67098,#67099,#67100,#67101,
#67102,#67103,#67104,#67105,#67106,#67107,#67108,#67109,#67110,#67111,#67112,
#67113,#67114,#67115,#67116,#67117,#67118,#67119,#67120,#67121,#67122,#67123,
#67124,#67125,#67126,#67127,#67128,#67129,#67130,#67131,#67132,#67133,#67134,
#67135,#67136,#67137),.UNSPECIFIED.,.F.,.F.,(4,3,3,3,3,3,3,3,3,3,3,3,3,
3,3,3,3,3,3,3,3,3,3,3,3,3,3,3,3,3,3,3,3,3,3,3,3,3,3,3,3,3,3,3,3,3,3,3,3,
3,3,3,3,3,3,3,3,3,3,3,3,4),(89.0818947090523,89.2010772987298,89.3225086931315,
89.3440059966879,89.4393059557034,89.5344759943235,89.6295455714376,89.72454803557,
89.819516935694,89.9144787402817,90.0094599040507,90.1045445475032,90.1996881470965,
90.2949820514435,90.3367171744289,90.4320221177038,90.5271971267366,90.622271653863,
90.7172790176911,90.8122527842734,90.9072194161947,91.0022053622507,91.0972946918649,
91.1924429293055,91.287741354068,91.3294283521699,91.4247365779264,91.5199149303054,
91.6149928561725,91.7100036858097,91.8049809583734,91.899951131761,91.9949406501105,
92.0900335762961,92.1851854292711,92.2804874637891,92.3221395299109,92.4174227169089,
92.5125759541894,92.607628723862,92.702614440878,92.7975666381309,92.8925118047009,
92.9874764159754,93.0825447346589,93.1776721164449,93.2729501198545,93.3148507076518,
93.4101742137088,93.505367707397,93.6004606169913,93.6954861375727,93.7904779132753,
93.8854623849804,93.9804659796295,94.0755725658572,94.1707378601395,94.266052876599,
94.3075618853928,94.4222874520932,94.5356827162139,94.6122043555102),
 .UNSPECIFIED.);
#725=B_SPLINE_CURVE_WITH_KNOTS('',3,(#67141,#67142,#67143,#67144,#67145,
#67146,#67147,#67148,#67149,#67150,#67151,#67152,#67153,#67154,#67155,#67156,
#67157,#67158,#67159,#67160,#67161,#67162,#67163,#67164,#67165,#67166,#67167,
#67168,#67169,#67170,#67171,#67172,#67173,#67174,#67175,#67176,#67177,#67178,
#67179,#67180,#67181,#67182,#67183,#67184,#67185,#67186,#67187,#67188,#67189,
#67190,#67191,#67192,#67193,#67194,#67195,#67196,#67197,#67198,#67199,#67200,
#67201,#67202,#67203,#67204,#67205,#67206,#67207,#67208,#67209,#67210,#67211,
#67212,#67213,#67214,#67215,#67216,#67217,#67218,#67219,#67220,#67221,#67222,
#67223,#67224,#67225,#67226,#67227,#67228,#67229,#67230,#67231,#67232,#67233,
#67234,#67235,#67236,#67237,#67238,#67239,#67240,#67241,#67242,#67243,#67244,
#67245,#67246,#67247,#67248,#67249,#67250,#67251,#67252,#67253,#67254,#67255,
#67256,#67257,#67258,#67259,#67260,#67261,#67262,#67263,#67264,#67265,#67266,
#67267,#67268,#67269,#67270,#67271,#67272,#67273,#67274,#67275,#67276,#67277,
#67278,#67279,#67280,#67281,#67282,#67283,#67284,#67285,#67286,#67287,#67288,
#67289,#67290,#67291,#67292,#67293,#67294),.UNSPECIFIED.,.F.,.F.,(4,3,3,
3,3,3,3,3,3,3,3,3,3,3,3,3,3,3,3,3,3,3,3,3,3,3,3,3,3,3,3,3,3,3,3,3,3,3,3,
3,3,3,3,3,3,3,3,3,3,3,3,4),(-96.6808311787084,-96.5809449266008,-96.480745285623,
-96.3803817017057,-96.2797248066616,-96.2114495491126,-96.1159900242025,
-96.0206599529141,-95.9205248257004,-95.8253649156292,-95.730237536908,
-95.6351164381511,-95.5399753811037,-95.4447324428179,-95.3494303233826,
-95.2539827866144,-95.2195789352043,-95.1241060636225,-95.0287597025951,
-94.9286282799327,-94.8334447617397,-94.7382911316415,-94.6431411596734,
-94.5479686267728,-94.452690465454,-94.357350914987,-94.2618629298127,-94.2277083212959,
-94.1325225818946,-94.03746828344,-93.9425157966575,-93.8476319848257,-93.7527826436286,
-93.6579411577424,-93.5630809262139,-93.4681176414075,-93.3730956835252,
-93.2779232583095,-93.2358377073875,-93.140495698385,-93.0452832460174,
-92.9501709549859,-92.8551255574552,-92.7601135863588,-92.665108628832,
-92.5700842857123,-92.4749569070836,-92.3797706305332,-92.2844350940134,
-92.2439670934791,-92.1042237372444,-92.0575247206449),.UNSPECIFIED.);
#726=B_SPLINE_CURVE_WITH_KNOTS('',3,(#67296,#67297,#67298,#67299,#67300,
#67301,#67302,#67303,#67304,#67305),.UNSPECIFIED.,.F.,.F.,(4,1,1,1,1,1,
1,4),(-92.0575206890591,-91.2520964795708,-90.2602258656624,-89.268355251754,
-88.2764846378456,-87.2846140239373,-86.2927434100289,-85.7743394134653),
 .UNSPECIFIED.);
#727=B_SPLINE_CURVE_WITH_KNOTS('',3,(#67307,#67308,#67309,#67310,#67311,
#67312,#67313,#67314,#67315,#67316,#67317,#67318,#67319,#67320,#67321,#67322,
#67323,#67324,#67325,#67326,#67327,#67328,#67329,#67330,#67331,#67332,#67333,
#67334,#67335,#67336,#67337,#67338,#67339,#67340,#67341,#67342,#67343,#67344,
#67345,#67346,#67347,#67348,#67349,#67350,#67351,#67352,#67353,#67354,#67355,
#67356,#67357,#67358,#67359,#67360,#67361,#67362,#67363,#67364,#67365,#67366,
#67367,#67368,#67369,#67370,#67371,#67372,#67373,#67374,#67375,#67376,#67377,
#67378,#67379,#67380,#67381,#67382,#67383,#67384,#67385,#67386,#67387,#67388,
#67389,#67390,#67391,#67392,#67393,#67394,#67395,#67396,#67397,#67398,#67399,
#67400,#67401,#67402,#67403,#67404,#67405,#67406,#67407,#67408,#67409,#67410,
#67411,#67412,#67413,#67414,#67415,#67416,#67417,#67418,#67419,#67420,#67421,
#67422,#67423,#67424,#67425,#67426,#67427,#67428,#67429,#67430,#67431,#67432,
#67433,#67434,#67435,#67436,#67437,#67438,#67439,#67440,#67441,#67442,#67443,
#67444,#67445,#67446,#67447,#67448,#67449,#67450,#67451,#67452,#67453,#67454,
#67455,#67456,#67457,#67458,#67459,#67460,#67461,#67462,#67463,#67464,#67465,
#67466,#67467,#67468,#67469,#67470,#67471,#67472,#67473,#67474,#67475,#67476,
#67477,#67478,#67479,#67480,#67481,#67482,#67483,#67484,#67485,#67486,#67487,
#67488,#67489,#67490,#67491,#67492,#67493,#67494,#67495,#67496,#67497,#67498,
#67499,#67500,#67501,#67502,#67503,#67504,#67505,#67506,#67507,#67508,#67509,
#67510,#67511,#67512,#67513,#67514),.UNSPECIFIED.,.F.,.F.,(4,3,3,3,3,3,
3,3,3,3,3,3,3,3,3,3,3,3,3,3,3,3,3,3,3,3,3,3,3,3,3,3,3,3,3,3,3,3,3,3,3,3,
3,3,3,3,3,3,3,3,3,3,3,3,3,3,3,3,3,3,3,3,3,3,3,3,3,3,3,4),(-85.7743392960028,
-85.6739374733394,-85.5732262312564,-85.472355561626,-85.371202429377,-85.3008727961205,
-85.2055602958256,-85.1103775106317,-85.0152950012911,-84.9202794272017,
-84.8252972923522,-84.7303221451598,-84.635327547713,-84.5402296359904,
-84.4450727078759,-84.3497660603351,-84.3090021822121,-84.2136891674468,
-84.1185058602982,-84.023422822308,-83.9284067118599,-83.8334240360757,
-83.7384483440533,-83.6434531985585,-83.5483547372275,-83.4531972578332,
-83.3578900616534,-83.3171315683037,-83.2218187096071,-83.1266355598024,
-83.0315526801975,-82.9365367290044,-82.8415542129483,-82.7465786809226,
-82.6515836954888,-82.5564853933454,-82.4613280728628,-82.3660210336682,
-82.3252609543953,-82.2299481472722,-82.1347650503614,-82.0396822248883,
-81.9446663294413,-81.8496838701141,-81.754708395731,-81.6597134687846,
-81.5646152260565,-81.4694579656052,-81.3741509868217,-81.333390340487,
-81.2380774610597,-81.1428942907392,-81.0478113908618,-80.9527954198476,
-80.8578128842607,-80.7628373330209,-80.6678423287162,-80.5727440083377,
-80.4775866699588,-80.382279613558,-80.3415197265786,-80.2475783950597,
-80.1530253589629,-80.0593194743372,-79.9656701712186,-79.8720495386157,
-79.7768256805332,-79.6831364418205,-79.5871452740531,-79.4911541062857),
 .UNSPECIFIED.);
#728=B_SPLINE_CURVE_WITH_KNOTS('',3,(#67516,#67517,#67518,#67519,#67520,
#67521,#67522,#67523,#67524,#67525,#67526),.UNSPECIFIED.,.F.,.F.,(4,1,1,
1,1,1,1,1,4),(-79.4911541062857,-79.3496491126702,-78.3577784987618,-77.3659078848535,
-76.3740372709451,-75.3821666570367,-74.3902960431283,-73.3984254292199,
-73.2079687991062),.UNSPECIFIED.);
#729=B_SPLINE_CURVE_WITH_KNOTS('',3,(#67528,#67529,#67530,#67531,#67532,
#67533,#67534,#67535,#67536,#67537,#67538,#67539,#67540,#67541,#67542,#67543,
#67544,#67545,#67546,#67547,#67548,#67549,#67550,#67551,#67552,#67553,#67554,
#67555,#67556,#67557,#67558,#67559,#67560,#67561,#67562,#67563,#67564,#67565,
#67566,#67567,#67568,#67569,#67570,#67571,#67572,#67573,#67574,#67575,#67576,
#67577,#67578,#67579,#67580,#67581,#67582,#67583,#67584,#67585,#67586,#67587,
#67588,#67589,#67590,#67591,#67592,#67593,#67594,#67595,#67596,#67597,#67598,
#67599,#67600,#67601,#67602,#67603,#67604,#67605,#67606,#67607,#67608,#67609,
#67610,#67611,#67612,#67613,#67614,#67615,#67616,#67617,#67618,#67619,#67620,
#67621,#67622,#67623,#67624,#67625,#67626,#67627,#67628,#67629,#67630,#67631,
#67632,#67633,#67634,#67635,#67636,#67637,#67638,#67639,#67640,#67641,#67642,
#67643,#67644,#67645,#67646,#67647,#67648,#67649,#67650,#67651,#67652,#67653,
#67654,#67655,#67656,#67657,#67658,#67659,#67660,#67661,#67662,#67663,#67664,
#67665,#67666,#67667,#67668,#67669,#67670,#67671,#67672,#67673,#67674,#67675,
#67676,#67677,#67678,#67679,#67680,#67681,#67682,#67683,#67684,#67685,#67686,
#67687,#67688,#67689,#67690,#67691,#67692,#67693,#67694,#67695,#67696,#67697,
#67698,#67699,#67700,#67701,#67702,#67703,#67704,#67705,#67706,#67707,#67708,
#67709,#67710,#67711,#67712,#67713,#67714,#67715,#67716,#67717,#67718,#67719,
#67720,#67721,#67722,#67723,#67724,#67725,#67726,#67727,#67728,#67729,#67730,
#67731,#67732,#67733,#67734,#67735,#67736,#67737,#67738),.UNSPECIFIED.,
 .F.,.F.,(4,3,3,3,3,3,3,3,3,3,3,3,3,3,3,3,3,3,3,3,3,3,3,3,3,3,3,3,3,3,3,
3,3,3,3,3,3,3,3,3,3,3,3,3,3,3,3,3,3,3,3,3,3,3,3,3,3,3,3,3,3,3,3,3,3,3,3,
3,3,3,4),(-73.2079687991062,-73.1141930383266,-73.0205086469885,-72.9268725476114,
-72.8332568363415,-72.7396336360451,-72.6459179993694,-72.5521513863378,
-72.4582359235161,-72.4065548153116,-72.3112419613016,-72.2160588167084,
-72.1209759428295,-72.0259599981062,-71.9309774889811,-71.8360019643406,
-71.7410069867394,-71.6459086930605,-71.5507513814166,-71.4554443515525,
-71.4146842014032,-71.3193713475026,-71.2241882030198,-71.1291053292529,
-71.0340893846429,-70.9391068756322,-70.8441313511065,-70.7491363736211,
-70.6540380800576,-70.5588807685294,-70.4635737387803,-70.4228135874948,
-70.3275007335772,-70.2323175890775,-70.1372347152933,-70.0422187706665,
-69.9472362616387,-69.8522607370961,-69.7572657595937,-69.662167466014,
-69.5670101544696,-69.4717031247048,-69.4309429735864,-69.3356301196485,
-69.2404469751282,-69.145364101323,-69.0503481566748,-68.9553656476253,
-68.8603901230612,-68.7653951455369,-68.670296851935,-68.5751395403683,
-68.4798325105811,-68.4390723596781,-68.3437595057564,-68.2485763612523,
-68.1534934874637,-68.0584775428324,-67.9634950338001,-67.8685195092529,
-67.7735245317458,-67.678426238161,-67.5832689266113,-67.4879618968412,
-67.4472017457697,-67.3481553896538,-67.249282246638,-67.1506135548848,
-67.0520677119532,-66.9536573933733,-66.9247834919266),.UNSPECIFIED.);
#730=B_SPLINE_CURVE_WITH_KNOTS('',3,(#67740,#67741,#67742,#67743,#67744,
#67745,#67746,#67747,#67748,#67749,#67750,#67751,#67752,#67753,#67754,#67755,
#67756,#67757,#67758,#67759,#67760,#67761,#67762,#67763,#67764,#67765,#67766,
#67767,#67768,#67769,#67770,#67771,#67772,#67773,#67774,#67775,#67776,#67777,
#67778,#67779,#67780,#67781,#67782,#67783,#67784,#67785,#67786,#67787,#67788,
#67789,#67790,#67791,#67792,#67793,#67794,#67795,#67796,#67797,#67798,#67799,
#67800,#67801,#67802,#67803,#67804,#67805,#67806,#67807,#67808,#67809,#67810,
#67811,#67812,#67813,#67814,#67815,#67816,#67817,#67818,#67819,#67820,#67821,
#67822,#67823,#67824,#67825,#67826,#67827,#67828,#67829,#67830,#67831,#67832,
#67833,#67834,#67835,#67836,#67837,#67838,#67839,#67840,#67841,#67842,#67843,
#67844,#67845,#67846,#67847,#67848,#67849,#67850,#67851,#67852,#67853,#67854,
#67855,#67856,#67857,#67858,#67859,#67860,#67861,#67862,#67863,#67864,#67865,
#67866,#67867,#67868,#67869,#67870,#67871,#67872,#67873,#67874,#67875,#67876,
#67877,#67878,#67879,#67880,#67881,#67882,#67883,#67884,#67885,#67886,#67887,
#67888,#67889,#67890,#67891,#67892,#67893,#67894,#67895,#67896,#67897,#67898,
#67899,#67900,#67901,#67902,#67903,#67904,#67905,#67906,#67907,#67908,#67909,
#67910,#67911,#67912,#67913,#67914,#67915,#67916,#67917,#67918,#67919,#67920,
#67921,#67922,#67923,#67924,#67925,#67926,#67927,#67928,#67929,#67930,#67931,
#67932,#67933,#67934,#67935,#67936,#67937,#67938,#67939,#67940,#67941,#67942,
#67943,#67944,#67945,#67946,#67947),.UNSPECIFIED.,.F.,.F.,(4,3,3,3,3,3,
3,3,3,3,3,3,3,3,3,3,3,3,3,3,3,3,3,3,3,3,3,3,3,3,3,3,3,3,3,3,3,3,3,3,3,3,
3,3,3,3,3,3,3,3,3,3,3,3,3,3,3,3,3,3,3,3,3,3,3,3,3,3,3,4),(-66.9247834916582,
-66.8241972479502,-66.7232917051859,-66.6222208880497,-66.5208647849073,
-66.4553311318613,-66.3600182779336,-66.2648351334237,-66.1697522596294,
-66.0747363149919,-65.9797538059533,-65.8847782813999,-65.7897833038863,
-65.6946850102952,-65.5995276987392,-65.5042206689629,-65.4634605179529,
-65.3681476640275,-65.2729645195198,-65.1778816457278,-65.0828657010926,
-64.9878831920564,-64.8929076675055,-64.7979126899944,-64.7028143964057,
-64.6076570848523,-64.5123500550785,-64.4715899040445,-64.3762770501184,
-64.2810939056101,-64.1860110318173,-64.0909950871814,-63.9960125781445,
-63.9010370535929,-63.8060420760811,-63.7109437824917,-63.6157864709376,
-63.5204794411631,-63.4797192901362,-63.3844064362099,-63.2892232917013,
-63.1941404179083,-63.0991244732721,-63.004141964235,-62.9091664396831,
-62.8141714621711,-62.7190731685814,-62.623915857027,-62.5286088272522,
-62.4878486762278,-62.3925358223018,-62.2973526777935,-62.2022698040008,
-62.107253859365,-62.0122713503281,-61.9172958257766,-61.8223008482649,
-61.7272025546755,-61.6320452431215,-61.5367382133469,-61.4959780623194,
-61.4020258640311,-61.3069724041206,-61.2132558463476,-61.1195956834216,
-61.0259640136845,-60.9298725564501,-60.8361708089317,-60.7388844968393,
-60.641598184747),.UNSPECIFIED.);
#731=B_SPLINE_CURVE_WITH_KNOTS('',3,(#67949,#67950,#67951,#67952,#67953,
#67954,#67955,#67956,#67957,#67958,#67959),.UNSPECIFIED.,.F.,.F.,(4,1,1,
1,1,1,1,1,4),(-60.641598184747,-60.5041074484111,-59.5122368345027,-58.5203662205943,
-57.5284956066859,-56.5366249927775,-55.5447543788692,-54.5528837649608,
-54.3584128775674),.UNSPECIFIED.);
#732=B_SPLINE_CURVE_WITH_KNOTS('',3,(#67961,#67962,#67963,#67964,#67965,
#67966,#67967,#67968,#67969,#67970,#67971,#67972,#67973,#67974,#67975,#67976,
#67977,#67978,#67979,#67980,#67981,#67982,#67983,#67984,#67985,#67986,#67987,
#67988,#67989,#67990,#67991,#67992,#67993,#67994,#67995,#67996,#67997,#67998,
#67999,#68000,#68001,#68002,#68003,#68004,#68005,#68006,#68007,#68008,#68009,
#68010,#68011,#68012,#68013,#68014,#68015,#68016,#68017,#68018,#68019,#68020,
#68021,#68022,#68023,#68024,#68025,#68026,#68027,#68028,#68029,#68030,#68031,
#68032,#68033,#68034,#68035,#68036,#68037,#68038,#68039,#68040,#68041,#68042,
#68043,#68044,#68045,#68046,#68047,#68048,#68049,#68050,#68051,#68052,#68053,
#68054,#68055,#68056,#68057,#68058,#68059,#68060,#68061,#68062,#68063,#68064,
#68065,#68066,#68067,#68068,#68069,#68070,#68071,#68072,#68073,#68074,#68075,
#68076,#68077,#68078,#68079,#68080,#68081,#68082,#68083,#68084,#68085,#68086,
#68087,#68088,#68089,#68090,#68091,#68092,#68093,#68094,#68095,#68096,#68097,
#68098,#68099,#68100,#68101,#68102,#68103,#68104,#68105,#68106,#68107,#68108,
#68109,#68110,#68111,#68112,#68113,#68114,#68115,#68116,#68117,#68118,#68119,
#68120,#68121,#68122,#68123,#68124,#68125,#68126,#68127,#68128,#68129,#68130,
#68131,#68132,#68133,#68134,#68135,#68136,#68137,#68138,#68139,#68140,#68141,
#68142,#68143,#68144,#68145,#68146,#68147,#68148,#68149,#68150,#68151,#68152,
#68153,#68154,#68155,#68156,#68157,#68158,#68159,#68160,#68161,#68162,#68163,
#68164,#68165,#68166,#68167,#68168,#68169,#68170,#68171),.UNSPECIFIED.,
 .F.,.F.,(4,3,3,3,3,3,3,3,3,3,3,3,3,3,3,3,3,3,3,3,3,3,3,3,3,3,3,3,3,3,3,
3,3,3,3,3,3,3,3,3,3,3,3,3,3,3,3,3,3,3,3,3,3,3,3,3,3,3,3,3,3,3,3,3,3,3,3,
3,3,3,4),(-54.3584128775674,-54.2646323366795,-54.1709411722708,-54.0772969876914,
-53.9836718890636,-53.8900380078539,-53.7963108600296,-53.7025315890191,
-53.6086045466861,-53.5610131510524,-53.4657002971262,-53.3705171526179,
-53.2754342788251,-53.1804183341892,-53.0854358251522,-52.9904603006004,
-52.8954653230883,-52.8003670294989,-52.7052097179446,-52.60990268817,-52.569142537144,
-52.4738296832179,-52.3786465387095,-52.2835636649166,-52.1885477202807,
-52.0935652112438,-51.9985896866921,-51.9035947091802,-51.8084964155908,
-51.7133391040365,-51.6180320742619,-51.5772719232356,-51.4819590693095,
-51.3867759248012,-51.2916930510088,-51.1966771063729,-51.101694597336,
-51.0067190727841,-50.9117240952724,-50.8166258016831,-50.7214684901288,
-50.6261614603543,-50.5854013093273,-50.4900884554012,-50.394905310893,
-50.2998224371,-50.2048064924641,-50.1098239834272,-50.0148484588757,-49.9198534813636,
-49.8247551877742,-49.7295978762199,-49.6342908464453,-49.5935306954189,
-49.4982178414929,-49.4030346969844,-49.3079518231912,-49.2129358785552,
-49.1179533695183,-49.0229778449664,-48.9279828674541,-48.8328845738646,
-48.7377272623104,-48.6424202325358,-48.6016600815105,-48.5027680424292,
-48.4040468426938,-48.3055256886538,-48.2071242950924,-48.1088534778964,
-48.0752275703878),.UNSPECIFIED.);
#733=B_SPLINE_CURVE_WITH_KNOTS('',3,(#68173,#68174,#68175,#68176,#68177,
#68178,#68179,#68180,#68181,#68182,#68183,#68184,#68185,#68186,#68187,#68188,
#68189,#68190,#68191,#68192,#68193,#68194,#68195,#68196,#68197,#68198,#68199,
#68200,#68201,#68202,#68203,#68204,#68205,#68206,#68207,#68208,#68209,#68210,
#68211,#68212,#68213,#68214,#68215,#68216,#68217,#68218,#68219,#68220,#68221,
#68222,#68223,#68224,#68225,#68226,#68227,#68228,#68229,#68230,#68231,#68232,
#68233,#68234,#68235,#68236,#68237,#68238,#68239,#68240,#68241,#68242,#68243,
#68244,#68245,#68246,#68247,#68248,#68249,#68250,#68251,#68252,#68253,#68254,
#68255,#68256,#68257,#68258,#68259,#68260,#68261,#68262,#68263,#68264,#68265,
#68266,#68267,#68268,#68269,#68270,#68271,#68272,#68273,#68274,#68275,#68276,
#68277,#68278,#68279,#68280,#68281,#68282,#68283,#68284,#68285,#68286,#68287,
#68288,#68289,#68290,#68291,#68292,#68293,#68294,#68295,#68296,#68297,#68298,
#68299,#68300,#68301,#68302,#68303,#68304,#68305,#68306,#68307,#68308,#68309,
#68310,#68311,#68312,#68313,#68314,#68315,#68316,#68317,#68318,#68319,#68320,
#68321,#68322,#68323,#68324,#68325,#68326,#68327,#68328,#68329,#68330,#68331,
#68332,#68333,#68334,#68335,#68336,#68337,#68338,#68339,#68340,#68341,#68342,
#68343,#68344,#68345,#68346,#68347,#68348,#68349,#68350,#68351,#68352,#68353,
#68354,#68355,#68356,#68357,#68358,#68359,#68360,#68361,#68362,#68363,#68364,
#68365,#68366,#68367,#68368,#68369,#68370,#68371,#68372,#68373,#68374,#68375,
#68376,#68377,#68378,#68379,#68380),.UNSPECIFIED.,.F.,.F.,(4,3,3,3,3,3,
3,3,3,3,3,3,3,3,3,3,3,3,3,3,3,3,3,3,3,3,3,3,3,3,3,3,3,3,3,3,3,3,3,3,3,3,
3,3,3,3,3,3,3,3,3,3,3,3,3,3,3,3,3,3,3,3,3,3,3,3,3,3,3,4),(-48.0752275700803,
-47.9744522344853,-47.8733473108059,-47.772071053497,-47.6705065609339,
-47.6097894676021,-47.5144766136761,-47.4192934691677,-47.3242105953751,
-47.2291946507392,-47.1342121417024,-47.0392366171508,-46.944241639639,
-46.8491433460497,-46.7539860344955,-46.6586790047209,-46.6179188536938,
-46.5226059997677,-46.4274228552593,-46.3323399814666,-46.2373240368307,
-46.1423415277937,-46.0473660032421,-45.9523710257302,-45.8572727321408,
-45.7621154205866,-45.666808390812,-45.6260482397854,-45.5307353858593,
-45.4355522413509,-45.3404693675581,-45.2454534229221,-45.1504709138852,
-45.0554953893335,-44.9605004118216,-44.8654021182322,-44.770244806678,
-44.6749377769034,-44.634177625877,-44.5388647719509,-44.4436816274425,
-44.3485987536498,-44.2535828090139,-44.1586002999769,-44.0636247754252,
-43.9686297979134,-43.873531504324,-43.7783741927699,-43.6830671629953,
-43.6423070119686,-43.5469941580425,-43.4518110135341,-43.3567281397412,
-43.2617121951052,-43.1667296860683,-43.0717541615167,-42.9767591840048,
-42.8816608904153,-42.7865035788611,-42.6911965490865,-42.6504363980602,
-42.5564717447825,-42.4609180595857,-42.3671892541391,-42.2735166658413,
-42.1798724036703,-42.0829148685548,-41.9891990816263,-41.8906206724173,
-41.7920422632082),.UNSPECIFIED.);
#734=B_SPLINE_CURVE_WITH_KNOTS('',3,(#68382,#68383,#68384,#68385,#68386,
#68387,#68388,#68389,#68390,#68391,#68392),.UNSPECIFIED.,.F.,.F.,(4,1,1,
1,1,1,1,1,4),(-41.7920422632082,-41.6585657841519,-40.6666951702435,-39.6748245563351,
-38.6829539424267,-37.6910833285184,-36.69921271461,-35.7073421007016,-35.5088569560286),
 .UNSPECIFIED.);
#735=B_SPLINE_CURVE_WITH_KNOTS('',3,(#68394,#68395,#68396,#68397,#68398,
#68399,#68400,#68401,#68402,#68403,#68404,#68405,#68406,#68407,#68408,#68409,
#68410,#68411,#68412,#68413,#68414,#68415,#68416,#68417,#68418,#68419,#68420,
#68421,#68422,#68423,#68424,#68425,#68426,#68427,#68428,#68429,#68430,#68431,
#68432,#68433,#68434,#68435,#68436,#68437,#68438,#68439,#68440,#68441,#68442,
#68443,#68444,#68445,#68446,#68447,#68448,#68449,#68450,#68451,#68452,#68453,
#68454,#68455,#68456,#68457,#68458,#68459,#68460,#68461,#68462,#68463,#68464,
#68465,#68466,#68467,#68468,#68469,#68470,#68471,#68472,#68473,#68474,#68475,
#68476,#68477,#68478,#68479,#68480,#68481,#68482,#68483,#68484,#68485,#68486,
#68487,#68488,#68489,#68490,#68491,#68492,#68493,#68494,#68495,#68496,#68497,
#68498,#68499,#68500,#68501,#68502,#68503,#68504,#68505,#68506,#68507,#68508,
#68509,#68510,#68511,#68512,#68513,#68514,#68515,#68516,#68517,#68518,#68519,
#68520,#68521,#68522,#68523,#68524,#68525,#68526,#68527,#68528,#68529,#68530,
#68531,#68532,#68533,#68534,#68535,#68536,#68537,#68538,#68539,#68540,#68541,
#68542,#68543,#68544,#68545,#68546,#68547,#68548,#68549,#68550,#68551,#68552,
#68553,#68554,#68555,#68556,#68557,#68558,#68559,#68560,#68561,#68562,#68563,
#68564,#68565,#68566,#68567,#68568,#68569,#68570,#68571,#68572,#68573,#68574,
#68575,#68576,#68577,#68578,#68579,#68580,#68581,#68582,#68583,#68584,#68585,
#68586,#68587,#68588,#68589,#68590,#68591,#68592,#68593,#68594,#68595,#68596,
#68597,#68598,#68599,#68600,#68601,#68602,#68603,#68604),.UNSPECIFIED.,
 .F.,.F.,(4,3,3,3,3,3,3,3,3,3,3,3,3,3,3,3,3,3,3,3,3,3,3,3,3,3,3,3,3,3,3,
3,3,3,3,3,3,3,3,3,3,3,3,3,3,3,3,3,3,3,3,3,3,3,3,3,3,3,3,3,3,3,3,3,3,3,3,
3,3,3,4),(-35.5088569560286,-35.4150700759351,-35.321370554688,-35.2277166821189,
-35.1340805756398,-35.0404343766173,-34.9466940692927,-34.8529004798333,
-34.758960180959,-34.7154714867932,-34.6201586328671,-34.5249754883587,
-34.429892614566,-34.3348766699301,-34.2398941608932,-34.1449186363415,
-34.0499236588296,-33.9548253652401,-33.859668053686,-33.7643610239114,
-33.7236008728848,-33.6282880189595,-33.5331048744518,-33.4380220006598,
-33.3430060560246,-33.2480235469885,-33.1530480224376,-33.0580530449264,
-32.9629547513378,-32.8677974397844,-32.7724904100105,-32.7317302589765,
-32.6364174050486,-32.5412342605387,-32.4461513867441,-32.3511354421064,
-32.2561529330677,-32.1611774085145,-32.0661824310004,-31.9710841374094,
-31.8759268258537,-31.7806197960775,-31.7398596450681,-31.6445467911428,
-31.5493636466353,-31.4542807728439,-31.3592648282087,-31.2642823191725,
-31.1693067946216,-31.0743118171102,-30.9792135235215,-30.8840562119678,
-30.7887491821939,-30.7479890311597,-30.6526761772381,-30.5574930327345,
-30.4624101589461,-30.3673942143148,-30.2724117052827,-30.1774361807356,
-30.0824412032285,-29.9873429096436,-29.8921855980939,-29.7968785683237,
-29.7561184172513,-29.6573775631943,-29.5588052664884,-29.4604287441025,
-29.3621690345465,-29.2640350167219,-29.225671648849),.UNSPECIFIED.);
#736=B_SPLINE_CURVE_WITH_KNOTS('',3,(#68606,#68607,#68608,#68609,#68610,
#68611,#68612,#68613,#68614,#68615),.UNSPECIFIED.,.F.,.F.,(4,1,1,1,1,1,
1,4),(-29.2256689641518,-28.764247803343,-27.7723771894346,-26.7805065755262,
-25.7886359616178,-24.7967653477094,-23.8048947338011,-22.9424863416694),
 .UNSPECIFIED.);
#737=B_SPLINE_CURVE_WITH_KNOTS('',3,(#68617,#68618,#68619,#68620,#68621,
#68622,#68623,#68624,#68625,#68626,#68627),.UNSPECIFIED.,.F.,.F.,(4,1,1,
1,1,1,1,1,4),(-22.9424863416694,-22.8130241198927,-21.8211535059843,-20.8292828920759,
-19.8374122781676,-18.8455416642592,-17.8536710503508,-16.8618004364424,
-16.6593010344898),.UNSPECIFIED.);
#738=B_SPLINE_CURVE_WITH_KNOTS('',3,(#68629,#68630,#68631,#68632,#68633,
#68634,#68635,#68636,#68637,#68638,#68639,#68640,#68641,#68642,#68643,#68644,
#68645,#68646,#68647,#68648,#68649,#68650,#68651,#68652,#68653,#68654,#68655,
#68656,#68657,#68658,#68659,#68660,#68661,#68662,#68663,#68664,#68665,#68666,
#68667,#68668,#68669,#68670,#68671,#68672,#68673,#68674,#68675,#68676,#68677,
#68678,#68679,#68680,#68681,#68682,#68683,#68684,#68685,#68686,#68687,#68688,
#68689,#68690,#68691,#68692,#68693,#68694,#68695,#68696,#68697,#68698,#68699,
#68700,#68701,#68702,#68703,#68704,#68705,#68706,#68707,#68708,#68709,#68710,
#68711,#68712,#68713,#68714,#68715,#68716,#68717,#68718,#68719,#68720,#68721,
#68722,#68723,#68724,#68725,#68726,#68727,#68728,#68729,#68730,#68731,#68732,
#68733,#68734,#68735,#68736,#68737,#68738,#68739,#68740,#68741,#68742,#68743,
#68744,#68745,#68746,#68747,#68748,#68749,#68750,#68751,#68752,#68753,#68754,
#68755,#68756,#68757,#68758,#68759,#68760,#68761,#68762,#68763,#68764,#68765,
#68766,#68767,#68768,#68769,#68770,#68771,#68772,#68773,#68774,#68775,#68776,
#68777,#68778,#68779,#68780,#68781,#68782,#68783,#68784,#68785,#68786,#68787,
#68788,#68789,#68790,#68791,#68792,#68793,#68794,#68795,#68796,#68797,#68798,
#68799,#68800,#68801,#68802,#68803,#68804,#68805,#68806,#68807,#68808,#68809,
#68810,#68811,#68812,#68813,#68814,#68815,#68816,#68817,#68818,#68819,#68820,
#68821,#68822,#68823,#68824,#68825,#68826,#68827,#68828,#68829,#68830,#68831,
#68832,#68833,#68834,#68835,#68836,#68837,#68838,#68839),.UNSPECIFIED.,
 .F.,.F.,(4,3,3,3,3,3,3,3,3,3,3,3,3,3,3,3,3,3,3,3,3,3,3,3,3,3,3,3,3,3,3,
3,3,3,3,3,3,3,3,3,3,3,3,3,3,3,3,3,3,3,3,3,3,3,3,3,3,3,3,3,3,3,3,3,3,3,3,
3,3,3,4),(-16.6593010344898,-16.5606296329953,-16.4669232014932,-16.3732596170644,
-16.2796110115953,-16.1859495380336,-16.0921922443136,-15.9983791947975,
-15.9044217971492,-15.869929822534,-15.774616959187,-15.6794338056938,-15.5843509233581,
-15.4893349708615,-15.3943524543906,-15.2993769228379,-15.2043819387649,
-15.1092836393092,-15.0141263222782,-14.9188192876671,-14.8780592086257,
-14.7827461890252,-14.6875628780416,-14.592479837212,-14.4974637254086,
-14.402481049193,-14.3075053576623,-14.2125102135824,-14.1174117550459,
-14.0222542792401,-13.9269470878258,-13.8861885947173,-13.7908761215009,
-13.6956933577844,-13.6006108643442,-13.5055952978454,-13.4106131654119,
-13.3156380154653,-13.2206434100938,-13.1255454827213,-13.0303885345095,
-12.9350818602807,-12.8943179808089,-12.7990049356622,-12.7038216026842,
-12.6087385433885,-12.5137224183594,-12.4187397321764,-12.3237640339271,
-12.2287688863699,-12.1336704292036,-12.0385129575439,-11.9432057744304,
-11.9024473669005,-11.8071335232423,-11.7119493829509,-11.6168655087749,
-11.5218485611603,-11.4268650479544,-11.3318885193192,-11.2368925390841,
-11.1417932508704,-11.046634947928,-10.9513269410766,-10.9105767529922,
-10.8119870552616,-10.7135637207956,-10.6153319956712,-10.5172142509035,
-10.4192173278538,-10.3761157273102),.UNSPECIFIED.);
#739=B_SPLINE_CURVE_WITH_KNOTS('',3,(#68840,#68841,#68842,#68843,#68844,
#68845,#68846,#68847,#68848,#68849),.UNSPECIFIED.,.F.,.F.,(4,1,1,1,1,1,
1,4),(-10.3761127482158,-9.91870613908378,-8.9268355251754,-7.93496491126702,
-6.94309429735864,-5.95122368345026,-4.95935306954189,-4.09293042013066),
 .UNSPECIFIED.);
#740=B_SPLINE_CURVE_WITH_KNOTS('',3,(#68852,#68853,#68854,#68855),
 .UNSPECIFIED.,.F.,.F.,(4,4),(103.598719667128,103.672557568218),
 .UNSPECIFIED.);
#741=B_SPLINE_CURVE_WITH_KNOTS('',3,(#68857,#68858,#68859,#68860,#68861,
#68862,#68863,#68864,#68865,#68866,#68867,#68868,#68869,#68870,#68871,#68872,
#68873,#68874,#68875,#68876,#68877,#68878,#68879,#68880,#68881,#68882,#68883,
#68884,#68885,#68886,#68887,#68888,#68889,#68890,#68891,#68892,#68893,#68894,
#68895,#68896,#68897,#68898,#68899,#68900,#68901,#68902,#68903,#68904,#68905,
#68906,#68907,#68908,#68909,#68910,#68911,#68912,#68913,#68914,#68915,#68916,
#68917,#68918,#68919,#68920,#68921,#68922,#68923,#68924,#68925,#68926,#68927,
#68928,#68929,#68930,#68931,#68932,#68933,#68934,#68935,#68936,#68937,#68938,
#68939,#68940,#68941,#68942,#68943,#68944,#68945,#68946,#68947,#68948,#68949,
#68950,#68951,#68952,#68953,#68954,#68955,#68956,#68957,#68958,#68959,#68960,
#68961,#68962,#68963,#68964,#68965,#68966,#68967,#68968,#68969,#68970,#68971,
#68972,#68973,#68974,#68975,#68976,#68977,#68978,#68979,#68980,#68981,#68982,
#68983,#68984,#68985,#68986,#68987,#68988,#68989,#68990,#68991,#68992,#68993,
#68994,#68995,#68996,#68997,#68998,#68999,#69000,#69001,#69002,#69003,#69004,
#69005,#69006,#69007,#69008,#69009,#69010,#69011,#69012,#69013,#69014,#69015,
#69016,#69017,#69018,#69019,#69020,#69021,#69022,#69023,#69024,#69025,#69026,
#69027,#69028,#69029,#69030,#69031,#69032,#69033,#69034,#69035,#69036,#69037,
#69038,#69039,#69040,#69041,#69042,#69043),.UNSPECIFIED.,.F.,.F.,(4,3,3,
3,3,3,3,3,3,3,3,3,3,3,3,3,3,3,3,3,3,3,3,3,3,3,3,3,3,3,3,3,3,3,3,3,3,3,3,
3,3,3,3,3,3,3,3,3,3,3,3,3,3,3,3,3,3,3,3,3,3,3,4),(103.672557568463,103.820034675392,
103.858999941297,103.959617585576,104.060092020312,104.160451913393,104.260749367129,
104.361015461365,104.461281236281,104.561646050319,104.662059688377,104.762651052579,
104.850870555206,104.951316799698,105.051619155889,105.151806756723,105.251931866953,
105.352025803237,105.452119842625,105.552314769,105.652559264494,105.752984690398,
105.842741169114,105.943516664012,106.044148018232,106.144662702836,106.245113571047,
106.34553149369,106.44594730048,106.546458311783,106.647016259314,106.747747136848,
106.834611783022,106.935344605953,107.035936261338,107.136415835605,107.236834401933,
107.337222849264,107.437612028115,107.538100986795,107.638639364,107.739354989191,
107.826482396931,107.925989483572,108.025352284445,108.124603771469,108.223795063832,
108.322958565098,108.422126641208,108.521408812288,108.620746084475,108.720284355729,
108.818353010839,108.921718483103,109.024920625112,109.127960648325,109.230905205988,
109.333779542361,109.436608819253,109.539447067769,109.642285379207,109.745194616777,
109.810223624748),.UNSPECIFIED.);
#742=B_SPLINE_CURVE_WITH_KNOTS('',3,(#69047,#69048,#69049,#69050,#69051,
#69052,#69053,#69054,#69055,#69056,#69057,#69058,#69059,#69060,#69061,#69062,
#69063,#69064,#69065,#69066,#69067,#69068,#69069,#69070,#69071,#69072,#69073,
#69074,#69075,#69076,#69077,#69078,#69079,#69080,#69081,#69082,#69083,#69084,
#69085,#69086,#69087,#69088,#69089,#69090,#69091,#69092,#69093,#69094,#69095,
#69096,#69097,#69098,#69099,#69100,#69101,#69102,#69103,#69104,#69105,#69106,
#69107,#69108,#69109,#69110,#69111,#69112,#69113,#69114,#69115,#69116,#69117,
#69118,#69119,#69120,#69121,#69122,#69123,#69124,#69125,#69126,#69127,#69128,
#69129,#69130,#69131,#69132,#69133,#69134,#69135,#69136,#69137,#69138,#69139,
#69140,#69141,#69142,#69143,#69144,#69145,#69146,#69147,#69148,#69149,#69150,
#69151,#69152,#69153,#69154,#69155,#69156,#69157,#69158,#69159,#69160,#69161,
#69162,#69163,#69164,#69165,#69166,#69167,#69168,#69169,#69170,#69171,#69172,
#69173,#69174,#69175,#69176,#69177,#69178,#69179,#69180,#69181,#69182,#69183,
#69184,#69185,#69186,#69187,#69188,#69189,#69190,#69191,#69192,#69193,#69194,
#69195,#69196,#69197),.UNSPECIFIED.,.F.,.F.,(4,3,3,3,3,3,3,3,3,3,3,3,3,
3,3,3,3,3,3,3,3,3,3,3,3,3,3,3,3,3,3,3,3,3,3,3,3,3,3,3,3,3,3,3,3,3,3,3,3,
3,4),(103.67255780872,103.772028396805,103.875582571364,103.974810689988,
104.073986558126,104.173142610607,104.272311252423,104.371585990288,104.47092364339,
104.570421796513,104.600461793276,104.701227449666,104.8018487344,104.902353090162,
105.002793462484,105.103200738506,105.203605764118,105.304106096047,105.404653264734,
105.50537395965,105.593172971017,105.693893970835,105.794473571861,105.894940843091,
105.995346945599,106.095722787311,106.196099237591,106.296575605139,106.397101306063,
106.497804905763,106.585884148758,106.685379877789,106.784731096122,106.883970749977,
106.98315003858,107.082301377603,107.181457144904,107.280741690303,107.380066654784,
107.47959327395,107.578595326499,107.681954817579,107.785150670333,107.888184011499,
107.991121663445,108.093988893523,108.196810886437,108.299641785865,108.402472625654,
108.505374666306,108.57130650424),.UNSPECIFIED.);
#743=B_SPLINE_CURVE_WITH_KNOTS('',3,(#69198,#69199,#69200,#69201,#69202),
 .UNSPECIFIED.,.F.,.F.,(4,1,4),(103.599566372989,103.607750615535,103.672557568463),
 .UNSPECIFIED.);
#744=B_SPLINE_CURVE_WITH_KNOTS('',3,(#69205,#69206,#69207,#69208,#69209,
#69210,#69211,#69212,#69213,#69214,#69215,#69216,#69217,#69218,#69219,#69220,
#69221,#69222,#69223,#69224,#69225,#69226,#69227,#69228,#69229,#69230,#69231,
#69232,#69233,#69234),.UNSPECIFIED.,.F.,.F.,(4,2,2,2,2,2,2,2,2,2,2,2,2,
2,4),(-2.23305280487553,-1.97896579953537,-1.73577232135028,-1.53430986639811,
-1.37974696990534,-1.21783860833472,-1.04897899044366,-0.891695760805949,
-0.708676356012324,-0.554482474707368,-0.368500908541818,-0.241956806614549,
-0.138087935175818,-0.0732023944895521,-0.00018678784649391),
 .UNSPECIFIED.);
#745=B_SPLINE_CURVE_WITH_KNOTS('',3,(#69235,#69236,#69237,#69238,#69239,
#69240,#69241,#69242,#69243,#69244,#69245,#69246,#69247,#69248,#69249,#69250,
#69251,#69252,#69253,#69254,#69255,#69256,#69257,#69258,#69259,#69260,#69261,
#69262,#69263,#69264,#69265,#69266,#69267,#69268,#69269,#69270,#69271,#69272,
#69273,#69274,#69275,#69276,#69277,#69278,#69279,#69280,#69281,#69282,#69283,
#69284,#69285,#69286,#69287,#69288,#69289,#69290,#69291,#69292,#69293,#69294,
#69295,#69296,#69297,#69298),.UNSPECIFIED.,.F.,.F.,(4,3,3,3,3,3,3,3,3,3,
3,3,3,3,3,3,3,3,3,3,3,4),(-0.410648750433038,-0.381296088292737,-0.350882391849445,
-0.328072119516976,-0.310964415267624,-0.305842993500878,-0.301661871504881,
-0.274116258800685,-0.259641302519569,-0.231392457082299,-0.202468399947011,
-0.198019208917011,-0.170841895434807,-0.143725312403613,-0.117042212888725,
-0.102411936277635,-0.097195049751494,-0.0935363835720784,-0.0677899334604712,
-0.0424347820407558,-0.0178142542830924,0.),.UNSPECIFIED.);
#746=B_SPLINE_CURVE_WITH_KNOTS('',3,(#69300,#69301,#69302,#69303,#69304,
#69305,#69306,#69307,#69308,#69309,#69310,#69311,#69312,#69313,#69314,#69315,
#69316,#69317,#69318,#69319,#69320,#69321,#69322,#69323,#69324,#69325,#69326,
#69327,#69328,#69329,#69330,#69331,#69332,#69333),.UNSPECIFIED.,.F.,.F.,
(4,3,3,3,3,3,3,3,3,3,3,4),(-0.219677966288016,-0.201006229477425,-0.173906949584204,
-0.172158028090248,-0.142713390739092,-0.124874216896705,-0.114789665948937,
-0.110082687886506,-0.0803547102951982,-0.0502957032480209,-0.0203907630638487,
0.),.UNSPECIFIED.);
#747=B_SPLINE_CURVE_WITH_KNOTS('',3,(#69334,#69335,#69336,#69337),
 .UNSPECIFIED.,.F.,.F.,(4,4),(-0.00018678784649391,-7.03322184060005E-5),
 .UNSPECIFIED.);
#748=B_SPLINE_CURVE_WITH_KNOTS('',3,(#69749,#69750,#69751,#69752,#69753,
#69754,#69755,#69756,#69757,#69758,#69759,#69760,#69761,#69762,#69763,#69764,
#69765,#69766,#69767,#69768,#69769,#69770,#69771,#69772,#69773,#69774,#69775,
#69776,#69777,#69778,#69779,#69780,#69781,#69782,#69783,#69784,#69785,#69786,
#69787,#69788,#69789,#69790,#69791,#69792,#69793,#69794,#69795,#69796,#69797,
#69798,#69799,#69800,#69801,#69802,#69803,#69804,#69805,#69806,#69807,#69808,
#69809,#69810,#69811,#69812,#69813,#69814,#69815,#69816,#69817,#69818,#69819,
#69820,#69821,#69822,#69823,#69824,#69825,#69826,#69827,#69828,#69829,#69830,
#69831,#69832,#69833,#69834,#69835,#69836),.UNSPECIFIED.,.F.,.F.,(4,3,3,
3,3,3,3,3,3,3,3,3,3,3,3,3,3,3,3,3,3,3,3,3,3,3,3,3,3,4),(-0.552745378375041,
-0.527830263536694,-0.499859837592608,-0.485874624620565,-0.477192997531472,
-0.471889411648522,-0.442927810370459,-0.413963015571315,-0.408336266644177,
-0.40114435110069,-0.397446251891128,-0.369166582261538,-0.341169387622816,
-0.31397908943666,-0.298150853306366,-0.293754274173184,-0.266922432865955,
-0.250809444272419,-0.223156811908825,-0.19550417954523,-0.19139998392206,
-0.16479071965233,-0.138164593557966,-0.111921701546741,-0.097931488853398,
-0.091170251499608,-0.0656115897288642,-0.0404467470576775,-0.0160684028764294,
0.),.UNSPECIFIED.);
#749=B_SPLINE_CURVE_WITH_KNOTS('',3,(#70254,#70255,#70256,#70257,#70258,
#70259,#70260,#70261,#70262,#70263,#70264,#70265,#70266,#70267,#70268,#70269,
#70270,#70271,#70272,#70273,#70274,#70275,#70276,#70277,#70278,#70279,#70280,
#70281,#70282,#70283,#70284,#70285,#70286,#70287,#70288,#70289,#70290,#70291,
#70292,#70293,#70294,#70295,#70296,#70297,#70298,#70299,#70300,#70301,#70302,
#70303,#70304,#70305,#70306,#70307,#70308,#70309,#70310,#70311,#70312,#70313,
#70314,#70315,#70316,#70317,#70318,#70319,#70320,#70321,#70322,#70323,#70324,
#70325,#70326,#70327,#70328,#70329,#70330,#70331,#70332,#70333,#70334,#70335,
#70336,#70337,#70338,#70339,#70340,#70341,#70342,#70343,#70344),
 .UNSPECIFIED.,.F.,.F.,(4,3,3,3,3,3,3,3,3,3,3,3,3,3,3,3,3,3,3,3,3,3,3,3,
3,3,3,3,3,3,4),(-0.555272788399392,-0.535208229286056,-0.510357943747353,
-0.495927663091087,-0.490771565699598,-0.465394215383921,-0.439311463621092,
-0.431518091480653,-0.425427657470475,-0.415445052851753,-0.3887274389215,
-0.361614454556187,-0.341463747205989,-0.332379220304646,-0.326285899706679,
-0.321326754662703,-0.293412801441296,-0.281011625155395,-0.25378286604002,
-0.226554106924644,-0.220947145848259,-0.216688100237889,-0.188776530116757,
-0.160380134586806,-0.131653127387196,-0.114279480489655,-0.109581292141837,
-0.0801117384511105,-0.0505679692699675,-0.0215915474950309,-5.6663350074274E-15),
 .UNSPECIFIED.);
#750=B_SPLINE_CURVE_WITH_KNOTS('',3,(#70345,#70346,#70347,#70348),
 .UNSPECIFIED.,.F.,.F.,(4,4),(-0.0122626075766948,0.),.UNSPECIFIED.);
#751=B_SPLINE_CURVE_WITH_KNOTS('',3,(#70401,#70402,#70403,#70404,#70405,
#70406,#70407,#70408,#70409,#70410,#70411,#70412,#70413,#70414,#70415,#70416,
#70417,#70418,#70419,#70420,#70421,#70422,#70423,#70424,#70425,#70426,#70427,
#70428,#70429,#70430,#70431,#70432,#70433,#70434,#70435,#70436,#70437,#70438,
#70439,#70440,#70441,#70442,#70443,#70444,#70445,#70446,#70447,#70448,#70449,
#70450,#70451,#70452,#70453,#70454,#70455,#70456,#70457,#70458,#70459,#70460,
#70461,#70462,#70463,#70464,#70465,#70466,#70467,#70468,#70469,#70470,#70471,
#70472,#70473,#70474,#70475,#70476,#70477,#70478,#70479,#70480,#70481,#70482,
#70483,#70484,#70485,#70486,#70487,#70488,#70489,#70490,#70491,#70492,#70493,
#70494,#70495,#70496,#70497,#70498,#70499,#70500,#70501,#70502,#70503,#70504,
#70505,#70506,#70507,#70508,#70509,#70510,#70511,#70512,#70513,#70514,#70515,
#70516,#70517,#70518,#70519,#70520,#70521,#70522,#70523,#70524,#70525,#70526,
#70527,#70528,#70529,#70530,#70531,#70532,#70533,#70534,#70535,#70536,#70537,
#70538,#70539,#70540,#70541,#70542,#70543,#70544,#70545,#70546,#70547,#70548,
#70549,#70550,#70551,#70552),.UNSPECIFIED.,.F.,.F.,(4,2,2,2,2,2,2,2,2,2,
2,2,2,2,2,2,2,2,2,2,2,2,2,2,2,2,2,2,2,2,2,2,2,2,2,2,2,2,2,2,2,2,2,2,2,2,
2,2,2,2,2,2,2,2,2,2,2,2,2,2,2,2,2,2,2,2,2,2,2,2,2,2,2,2,2,4),(-0.832439720450299,
-0.826869617590163,-0.808861481405132,-0.780833499987269,-0.773067704421429,
-0.770108009538214,-0.768116382574119,-0.765959909741239,-0.762312705606626,
-0.745384908804739,-0.710099303019498,-0.698437745806221,-0.693536562115759,
-0.690028044113998,-0.686321672851416,-0.680574311193837,-0.659513503810848,
-0.641702968844016,-0.619034945456304,-0.615199849331523,-0.613000754903716,
-0.610993910382176,-0.608099115151558,-0.600283250865247,-0.587338578003027,
-0.547496595729687,-0.540453152200995,-0.53643269261139,-0.532958434968226,
-0.528651633463663,-0.519936259154898,-0.496482419123063,-0.466547506714132,
-0.460791187104995,-0.458246606971097,-0.456292094196737,-0.453959155317699,
-0.449413634630061,-0.432138088304667,-0.391101350064625,-0.384215720243609,
-0.380253477545728,-0.376813274772498,-0.372529386569256,-0.363797509627219,
-0.340555173373787,-0.310851867363394,-0.304874719620947,-0.302302699397911,
-0.300345282932302,-0.298021463020673,-0.293587363299895,-0.266670733512251,
-0.235518952311434,-0.228315190518444,-0.224253817045827,-0.220772909219321,
-0.216494292647445,-0.207963661830024,-0.187274992636306,-0.162167397931397,
-0.150746811951765,-0.147346959752381,-0.145436952164745,-0.143356908199464,
-0.140258588566548,-0.131161889402246,-0.114680445555956,-0.0814104958311417,
-0.0745199702012672,-0.0704979001465721,-0.0673189880139064,-0.0630357511075485,
-0.054645733886394,-0.0361759680233267,-0.0023879060453043),
 .UNSPECIFIED.);
#752=B_SPLINE_CURVE_WITH_KNOTS('',3,(#70555,#70556,#70557,#70558,#70559,
#70560,#70561,#70562,#70563,#70564,#70565,#70566,#70567,#70568,#70569,#70570,
#70571,#70572,#70573,#70574,#70575,#70576,#70577,#70578,#70579,#70580,#70581,
#70582,#70583,#70584,#70585,#70586,#70587,#70588,#70589,#70590,#70591,#70592,
#70593,#70594,#70595,#70596,#70597,#70598,#70599,#70600,#70601,#70602,#70603,
#70604,#70605,#70606,#70607,#70608,#70609,#70610,#70611,#70612,#70613,#70614,
#70615,#70616,#70617,#70618,#70619,#70620,#70621,#70622,#70623,#70624,#70625,
#70626,#70627,#70628,#70629,#70630,#70631,#70632,#70633,#70634,#70635,#70636,
#70637,#70638,#70639,#70640,#70641,#70642,#70643,#70644,#70645,#70646,#70647,
#70648,#70649,#70650,#70651,#70652,#70653,#70654,#70655,#70656,#70657,#70658,
#70659,#70660,#70661,#70662,#70663,#70664,#70665,#70666),.UNSPECIFIED.,
 .F.,.F.,(4,3,3,3,3,3,3,3,3,3,3,3,3,3,3,3,3,3,3,3,3,3,3,3,3,3,3,3,3,3,3,
3,3,3,3,3,3,4),(11.6154215191106,11.7297367073171,11.8439967914085,11.9582288133417,
12.0724673659051,12.1867470405937,12.3011995048193,12.4157406678187,12.530525337464,
12.6127583869031,12.7233097241135,12.8341579154363,12.9443596551425,13.0544807973123,
13.1645659360347,13.2759482656999,13.3861659307822,13.4981305927389,13.6100952546957,
13.7219645675355,13.833635115484,13.9451945236061,14.0566854135963,14.1681503097769,
14.2797130483556,14.3913205741359,14.5031410552373,14.6074321224883,14.7193243877964,
14.8310242929563,14.9426169352525,15.0541448818272,15.165650607069,15.2772598312806,
15.3889170097142,15.5007919240759,15.6047689902808,15.7079632679489),
 .UNSPECIFIED.);
#753=B_SPLINE_CURVE_WITH_KNOTS('',3,(#70671,#70672,#70673,#70674,#70675,
#70676,#70677,#70678,#70679,#70680,#70681,#70682,#70683,#70684,#70685,#70686,
#70687,#70688,#70689,#70690,#70691,#70692,#70693,#70694,#70695,#70696,#70697,
#70698,#70699,#70700,#70701,#70702,#70703,#70704,#70705,#70706,#70707,#70708,
#70709,#70710,#70711,#70712,#70713,#70714,#70715,#70716,#70717,#70718,#70719,
#70720,#70721,#70722,#70723,#70724,#70725,#70726,#70727,#70728,#70729,#70730,
#70731,#70732,#70733,#70734,#70735,#70736,#70737,#70738,#70739,#70740,#70741,
#70742,#70743,#70744,#70745,#70746,#70747,#70748,#70749,#70750,#70751,#70752,
#70753,#70754,#70755,#70756,#70757,#70758,#70759,#70760,#70761,#70762,#70763,
#70764,#70765,#70766,#70767,#70768,#70769,#70770,#70771,#70772,#70773,#70774,
#70775,#70776,#70777,#70778,#70779,#70780,#70781,#70782,#70783,#70784,#70785,
#70786,#70787,#70788,#70789,#70790,#70791,#70792,#70793,#70794,#70795,#70796,
#70797,#70798,#70799,#70800,#70801,#70802,#70803,#70804,#70805,#70806,#70807,
#70808,#70809,#70810,#70811,#70812,#70813,#70814,#70815,#70816,#70817,#70818,
#70819,#70820,#70821,#70822,#70823,#70824,#70825,#70826,#70827,#70828,#70829,
#70830,#70831,#70832,#70833,#70834,#70835,#70836,#70837,#70838,#70839,#70840,
#70841,#70842,#70843,#70844,#70845,#70846,#70847,#70848,#70849,#70850,#70851,
#70852,#70853,#70854,#70855,#70856,#70857,#70858,#70859,#70860,#70861,#70862,
#70863,#70864,#70865,#70866),.UNSPECIFIED.,.F.,.F.,(4,2,2,2,2,2,2,2,2,2,
2,2,2,2,2,2,2,2,2,2,2,2,2,2,2,2,2,2,2,2,2,2,2,2,2,2,2,2,2,2,2,2,2,2,2,2,
2,2,2,2,2,2,2,2,2,2,2,2,2,2,2,2,2,2,2,2,2,2,2,2,2,2,2,2,2,2,2,2,2,2,2,2,
2,2,2,2,2,2,2,2,2,2,2,2,2,2,2,4),(-1.81266124409322,-1.79276733540908,-1.78774245874958,
-1.78413545154694,-1.78088602738699,-1.77736034007158,-1.77313278625767,
-1.7628751938338,-1.7323430897624,-1.71481907485556,-1.70722121063355,-1.70434762990126,
-1.7023504852535,-1.70015348315893,-1.69631767835098,-1.67351815566529,
-1.65541173314562,-1.64160753480484,-1.63183242889914,-1.62734498751931,
-1.62386335554168,-1.61997943666278,-1.61337001706326,-1.57553292977467,
-1.55521461552979,-1.55031952255415,-1.5479061712476,-1.54614597725326,
-1.54373626788022,-1.53886064333773,-1.51624503464281,-1.49171518082637,
-1.48221880177508,-1.47477499011064,-1.47072014374758,-1.46725832855774,
-1.46302087718533,-1.45646202949209,-1.42673369885665,-1.40664731369372,
-1.39972586861402,-1.39469439482473,-1.39225491704881,-1.39049374067723,
-1.38810922361249,-1.38350809718788,-1.35550847596574,-1.33447172786105,
-1.32160487271448,-1.31664992147481,-1.31309896675601,-1.30940398565582,
-1.30370368758022,-1.28496422757591,-1.25377074519704,-1.2452465080184,
-1.23938766061273,-1.23679901624852,-1.23483900918868,-1.23248535635403,
-1.22803136628759,-1.19791152225578,-1.17811930534118,-1.16966889416318,
-1.16285427057515,-1.1589275445767,-1.1554530653352,-1.15103746979047,-1.14167963972413,
-1.10345299130861,-1.08597266242713,-1.08230006165834,-1.08013759385632,
-1.07814544078735,-1.07519412185959,-1.0675132415997,-1.03577012209783,
-1.01674010447895,-1.00827217657733,-1.00401716030596,-1.00055292200238,
-0.996508697051606,-0.989330113494435,-0.958829720251869,-0.939285289971974,
-0.929240270944908,-0.926087449720401,-0.924036862450091,-0.921932934084776,
-0.918522952283085,-0.906720319599159,-0.879123388800726,-0.856559613760745,
-0.850608065480583,-0.846863204477219,-0.843342368646973,-0.838554784676353,
-0.832439720450299),.UNSPECIFIED.);
#754=B_SPLINE_CURVE_WITH_KNOTS('',3,(#70867,#70868,#70869,#70870,#70871,
#70872,#70873,#70874,#70875,#70876,#70877,#70878,#70879,#70880,#70881,#70882,
#70883,#70884,#70885,#70886,#70887,#70888,#70889,#70890,#70891,#70892,#70893,
#70894,#70895,#70896,#70897,#70898,#70899,#70900,#70901,#70902,#70903,#70904,
#70905,#70906,#70907,#70908,#70909,#70910,#70911,#70912,#70913,#70914,#70915,
#70916,#70917,#70918,#70919,#70920,#70921,#70922,#70923,#70924,#70925,#70926,
#70927,#70928,#70929,#70930,#70931,#70932,#70933,#70934,#70935,#70936,#70937,
#70938,#70939,#70940,#70941,#70942,#70943,#70944,#70945,#70946,#70947,#70948,
#70949,#70950,#70951,#70952,#70953,#70954,#70955,#70956,#70957,#70958,#70959,
#70960,#70961,#70962,#70963,#70964,#70965,#70966,#70967,#70968,#70969,#70970,
#70971,#70972,#70973,#70974,#70975,#70976,#70977,#70978,#70979,#70980,#70981,
#70982,#70983,#70984,#70985,#70986,#70987,#70988,#70989,#70990,#70991,#70992,
#70993,#70994,#70995,#70996,#70997,#70998,#70999,#71000,#71001,#71002,#71003,
#71004,#71005,#71006,#71007,#71008,#71009,#71010,#71011,#71012,#71013,#71014,
#71015,#71016,#71017,#71018,#71019,#71020,#71021,#71022,#71023,#71024,#71025,
#71026,#71027,#71028,#71029,#71030,#71031,#71032,#71033,#71034,#71035,#71036,
#71037,#71038,#71039,#71040,#71041,#71042,#71043,#71044,#71045,#71046,#71047,
#71048),.UNSPECIFIED.,.F.,.F.,(4,2,2,2,2,2,2,2,2,2,2,2,2,2,2,2,2,2,2,2,
2,2,2,2,2,2,2,2,2,2,2,2,2,2,2,2,2,2,2,2,2,2,2,2,2,2,2,2,2,2,2,2,2,2,2,2,
2,2,2,2,2,2,2,2,2,2,2,2,2,2,2,2,2,2,2,2,2,2,2,2,2,2,2,2,2,2,2,2,2,2,4),
(-1.96102087353794,-1.9210778220991,-1.90768908845313,-1.90261212238301,
-1.89899015149673,-1.89523318959838,-1.88945687161051,-1.87049428660702,
-1.83951008342334,-1.83097501089664,-1.82509143330846,-1.82247247770524,
-1.82048980956498,-1.81806425199519,-1.81343965417973,-1.78516880189389,
-1.76443962673408,-1.75162769858289,-1.74659723188267,-1.74295525739004,
-1.73912896791266,-1.73313981744852,-1.71180491373212,-1.68359856445809,
-1.67539295566126,-1.66966423271282,-1.66705279884891,-1.66523129778753,
-1.66284792368806,-1.65842885407551,-1.62771414722485,-1.61961046122069,
-1.60534611178343,-1.59530372652048,-1.59070105366264,-1.58712704584553,
-1.58313340890746,-1.57630917514173,-1.5346589707257,-1.51655478492516,
-1.51279866884452,-1.51058411870794,-1.50853877336182,-1.50548920668655,
-1.4973716571128,-1.46972231222516,-1.44787597417284,-1.43901825751871,
-1.43462845050102,-1.43107726977685,-1.42695364633554,-1.41968164444321,
-1.39470015102531,-1.37120756793841,-1.36008734388033,-1.35678146074471,
-1.35466499630122,-1.35251672689708,-1.34907010977359,-1.33745151397172,
-1.29225652359672,-1.28337842663391,-1.27898131374437,-1.27542515951872,
-1.27129654480343,-1.26401681150532,-1.23627793034829,-1.21497380005684,
-1.20779765089936,-1.20260594018093,-1.20009827410376,-1.19828959709471,
-1.19583459759449,-1.19091409455555,-1.16913219523892,-1.14959138748375,
-1.1371471825431,-1.12802558112617,-1.12358507365322,-1.12002743601037,
-1.11593420152398,-1.10881552061661,-1.07570747800498,-1.05034180750753,
-1.04630214323217,-1.0440267864096,-1.04198301226627,-1.0390664807431,-1.03185902089032,
-1.00344831019565,-0.980904423115737),.UNSPECIFIED.);
#755=B_SPLINE_CURVE_WITH_KNOTS('',3,(#71054,#71055,#71056,#71057,#71058,
#71059,#71060,#71061,#71062,#71063,#71064,#71065,#71066,#71067,#71068,#71069,
#71070,#71071,#71072,#71073,#71074,#71075,#71076,#71077,#71078,#71079,#71080,
#71081,#71082,#71083,#71084,#71085,#71086,#71087,#71088,#71089,#71090,#71091,
#71092,#71093,#71094,#71095,#71096,#71097,#71098,#71099,#71100,#71101,#71102,
#71103,#71104,#71105,#71106,#71107,#71108,#71109,#71110,#71111,#71112,#71113,
#71114,#71115,#71116,#71117,#71118,#71119,#71120,#71121,#71122,#71123,#71124,
#71125,#71126,#71127,#71128,#71129,#71130,#71131,#71132,#71133,#71134,#71135,
#71136,#71137,#71138,#71139,#71140,#71141,#71142,#71143,#71144,#71145,#71146,
#71147,#71148,#71149,#71150,#71151,#71152,#71153,#71154,#71155,#71156,#71157,
#71158,#71159,#71160,#71161,#71162,#71163,#71164,#71165,#71166,#71167,#71168,
#71169,#71170,#71171,#71172,#71173,#71174,#71175,#71176,#71177,#71178,#71179,
#71180,#71181,#71182,#71183,#71184,#71185,#71186,#71187,#71188,#71189,#71190,
#71191,#71192,#71193,#71194,#71195,#71196,#71197,#71198,#71199,#71200,#71201,
#71202,#71203,#71204,#71205,#71206,#71207,#71208,#71209,#71210,#71211,#71212,
#71213,#71214,#71215,#71216,#71217,#71218,#71219,#71220,#71221,#71222,#71223,
#71224,#71225,#71226,#71227,#71228,#71229,#71230,#71231,#71232,#71233,#71234,
#71235,#71236,#71237,#71238,#71239,#71240,#71241,#71242,#71243,#71244,#71245,
#71246,#71247,#71248,#71249,#71250,#71251,#71252,#71253,#71254,#71255),
 .UNSPECIFIED.,.F.,.F.,(4,2,2,2,2,2,2,2,2,2,2,2,2,2,2,2,2,2,2,2,2,2,2,2,
2,2,2,2,2,2,2,2,2,2,2,2,2,2,2,2,2,2,2,2,2,2,2,2,2,2,2,2,2,2,2,2,2,2,2,2,
2,2,2,2,2,2,2,2,2,2,2,2,2,2,2,2,2,2,2,2,2,2,2,2,2,2,2,2,2,2,2,2,2,2,2,2,
2,2,2,2,4),(-0.980716191876809,-0.978672414235096,-0.975552940822149,-0.9658198544226,
-0.947332372975558,-0.915346301054667,-0.908220296565291,-0.904188294608421,
-0.900724825447165,-0.896458506346105,-0.887925166365051,-0.867229831789358,
-0.851433104800938,-0.831211436196844,-0.827406101660201,-0.825215264582828,
-0.823214725473008,-0.820323686055612,-0.812482189011151,-0.799467606998332,
-0.759486841028773,-0.752420392631451,-0.748401240518977,-0.744937024328307,
-0.740654684353247,-0.732034741535917,-0.709515640088466,-0.681414125596727,
-0.673741943135579,-0.670792836053422,-0.668801940592265,-0.666639961731244,
-0.662968627902431,-0.645501182592887,-0.607320550303155,-0.597940841755656,
-0.593521418931444,-0.590046548917378,-0.586122134330912,-0.579318836840885,
-0.570885681008858,-0.551164226425078,-0.520884723318463,-0.516443766903541,
-0.514092675065296,-0.512131947584437,-0.50953863252289,-0.50365430091602,
-0.495080015106225,-0.46340479176953,-0.445223537395943,-0.439544557874311,
-0.435853383142865,-0.432298818044017,-0.427326658916701,-0.414336065217353,
-0.392957897996095,-0.365563030778318,-0.360817628661323,-0.358433238305253,
-0.356671732192621,-0.354231240731384,-0.349195017611983,-0.342265819072556,
-0.322135019265096,-0.292499944231819,-0.285940715682199,-0.281703032443595,
-0.278241069661093,-0.274186109587776,-0.266742437072289,-0.25724536044257,
-0.232720451109095,-0.210047820755655,-0.205170490036375,-0.202760397462087,
-0.201000066178924,-0.198586752943693,-0.19369283147691,-0.173388659758249,
-0.135538027557963,-0.128941334878982,-0.125059671368355,-0.121576885851969,
-0.121418326610126,-0.121105132131795,-0.120818138703037,-0.120549361318739,
-0.120292763115349,-0.12004352354332,-0.114702401092651,-0.10833759547208,
-0.095859929684811,-0.0672894665218258,-0.0521997457773358,-0.048558064801975,
-0.0464025343649477,-0.0443849164773167,-0.0413984264305185,-0.0379008712970157,
-0.000461226072117141),.UNSPECIFIED.);
#756=B_SPLINE_CURVE_WITH_KNOTS('',3,(#71256,#71257,#71258,#71259),
 .UNSPECIFIED.,.F.,.F.,(4,4),(-1.81279307941281,-1.81266124409322),
 .UNSPECIFIED.);
#757=B_SPLINE_CURVE_WITH_KNOTS('',3,(#71260,#71261,#71262,#71263,#71264,
#71265,#71266,#71267,#71268,#71269,#71270,#71271,#71272,#71273,#71274,#71275,
#71276,#71277,#71278,#71279,#71280,#71281,#71282,#71283,#71284,#71285,#71286,
#71287,#71288,#71289,#71290,#71291,#71292,#71293,#71294,#71295,#71296,#71297,
#71298,#71299,#71300,#71301,#71302,#71303,#71304,#71305,#71306,#71307,#71308,
#71309,#71310,#71311,#71312,#71313,#71314,#71315,#71316,#71317,#71318,#71319,
#71320,#71321,#71322,#71323,#71324,#71325,#71326,#71327,#71328,#71329,#71330,
#71331,#71332,#71333,#71334,#71335,#71336,#71337,#71338,#71339,#71340,#71341,
#71342,#71343,#71344,#71345,#71346,#71347,#71348,#71349,#71350,#71351,#71352,
#71353,#71354,#71355,#71356,#71357,#71358,#71359,#71360,#71361,#71362,#71363,
#71364,#71365,#71366,#71367,#71368,#71369,#71370,#71371,#71372,#71373,#71374,
#71375,#71376,#71377,#71378,#71379,#71380,#71381,#71382,#71383,#71384,#71385,
#71386,#71387,#71388,#71389,#71390,#71391,#71392,#71393,#71394,#71395,#71396,
#71397,#71398,#71399,#71400,#71401,#71402,#71403,#71404,#71405,#71406,#71407,
#71408,#71409,#71410,#71411,#71412,#71413,#71414,#71415,#71416,#71417,#71418,
#71419,#71420,#71421,#71422,#71423,#71424,#71425,#71426,#71427,#71428,#71429,
#71430,#71431,#71432,#71433,#71434,#71435,#71436,#71437,#71438,#71439,#71440,
#71441,#71442,#71443,#71444,#71445,#71446,#71447,#71448,#71449,#71450,#71451),
 .UNSPECIFIED.,.F.,.F.,(4,2,2,2,2,2,2,2,2,2,2,2,2,2,2,2,2,2,2,2,2,2,2,2,
2,2,2,2,2,2,2,2,2,2,2,2,2,2,2,2,2,2,2,2,2,2,2,2,2,2,2,2,2,2,2,2,2,2,2,2,
2,2,2,2,2,2,2,2,2,2,2,2,2,2,2,2,2,2,2,2,2,2,2,2,2,2,2,2,2,2,2,2,2,2,2,4),
(-0.980904423115737,-0.972309092665265,-0.967911239980157,-0.964356670061167,
-0.96023244197007,-0.952761930816234,-0.943276463222857,-0.90475584504256,
-0.893569305804469,-0.890160546322017,-0.888020726753385,-0.885894250088703,
-0.882548861917824,-0.871021927181748,-0.845746410962784,-0.820760652838631,
-0.814660219619431,-0.810817202357983,-0.807197220895649,-0.802258543788371,
-0.790053692382802,-0.770883527908946,-0.739872021250145,-0.735481255138904,
-0.733105515086185,-0.731289433760281,-0.728684994697651,-0.722959927762331,
-0.714757572972524,-0.686593909683455,-0.664982129833851,-0.658982708344533,
-0.655160576120025,-0.651530644986104,-0.646530683504691,-0.633888634654308,
-0.613587865561554,-0.584603538494515,-0.580024773159365,-0.577609051934373,
-0.575595831675303,-0.572925510782955,-0.566819246973655,-0.557846581828862,
-0.522421297807217,-0.508032661170162,-0.502665909260056,-0.499339314808945,
-0.495678356795963,-0.490499572828544,-0.476486923011896,-0.439072799233891,
-0.42696797794444,-0.423469899586423,-0.421310447275918,-0.419200546260371,
-0.41593476390406,-0.405257096551555,-0.383548484379536,-0.35632540096174,
-0.349042137014981,-0.344912979061732,-0.341357276543842,-0.336961999290346,
-0.328092887858217,-0.30640436039894,-0.279004868602742,-0.270548502866671,
-0.267450027899942,-0.265394080363657,-0.263193208916502,-0.259503681376291,
-0.242900379794272,-0.20897487711414,-0.196292724032656,-0.191152695594487,
-0.18753475804462,-0.183762378235801,-0.178007648640162,-0.15806775532313,
-0.139471274744065,-0.116531584014577,-0.112631590709609,-0.110385528703995,
-0.108328879096892,-0.105338770352972,-0.0971946734452351,-0.0803228132367113,
-0.0490461816621293,-0.0392202172345926,-0.0346546877443938,-0.0310851311254527,
-0.0277462493411522,-0.0237922304117463,-0.0153089648461796,-0.000597831378872224),
 .UNSPECIFIED.);
#758=B_SPLINE_CURVE_WITH_KNOTS('',3,(#71456,#71457,#71458,#71459,#71460,
#71461,#71462,#71463,#71464,#71465,#71466,#71467,#71468,#71469,#71470,#71471,
#71472,#71473,#71474,#71475,#71476,#71477,#71478,#71479,#71480,#71481,#71482,
#71483,#71484,#71485,#71486,#71487,#71488,#71489,#71490,#71491,#71492,#71493,
#71494,#71495,#71496,#71497,#71498,#71499,#71500,#71501,#71502,#71503,#71504,
#71505,#71506,#71507,#71508,#71509,#71510,#71511,#71512,#71513,#71514,#71515,
#71516,#71517,#71518,#71519,#71520,#71521,#71522,#71523,#71524,#71525,#71526,
#71527,#71528,#71529,#71530,#71531,#71532,#71533,#71534,#71535,#71536,#71537,
#71538,#71539,#71540,#71541,#71542,#71543,#71544,#71545,#71546,#71547,#71548,
#71549,#71550,#71551,#71552,#71553,#71554,#71555,#71556,#71557,#71558,#71559,
#71560,#71561,#71562,#71563,#71564,#71565,#71566,#71567,#71568,#71569,#71570,
#71571,#71572,#71573,#71574,#71575,#71576,#71577,#71578,#71579,#71580,#71581,
#71582,#71583,#71584,#71585,#71586,#71587,#71588,#71589,#71590,#71591,#71592,
#71593,#71594,#71595,#71596,#71597,#71598,#71599,#71600,#71601,#71602,#71603,
#71604,#71605,#71606,#71607,#71608,#71609,#71610,#71611,#71612,#71613,#71614,
#71615,#71616,#71617,#71618,#71619,#71620,#71621,#71622,#71623,#71624,#71625,
#71626,#71627,#71628,#71629,#71630,#71631,#71632,#71633,#71634,#71635,#71636,
#71637,#71638,#71639,#71640,#71641,#71642,#71643,#71644,#71645,#71646,#71647,
#71648,#71649),.UNSPECIFIED.,.F.,.F.,(4,2,2,2,2,2,2,2,2,2,2,2,2,2,2,2,2,
2,2,2,2,2,2,2,2,2,2,2,2,2,2,2,2,2,2,2,2,2,2,2,2,2,2,2,2,2,2,2,2,2,2,2,2,
2,2,2,2,2,2,2,2,2,2,2,2,2,2,2,2,2,2,2,2,2,2,2,2,2,2,2,2,2,2,2,2,2,2,2,2,
2,2,2,2,2,2,2,4),(-1.96077830518356,-1.92303894553549,-1.9195585575685,
-1.91658380744085,-1.9145687419356,-1.91240997604103,-1.90875175203967,
-1.89321851940835,-1.86415749453336,-1.8522439460463,-1.84606658036546,
-1.84085238143544,-1.84059957515371,-1.8403367951535,-1.836767361395,-1.83353101195692,
-1.82916628937187,-1.81800094255874,-1.78514103559423,-1.76697589556691,
-1.76231414430016,-1.75994658742278,-1.75798800408095,-1.75546118351887,
-1.74980269346822,-1.71982555162952,-1.69641729695568,-1.68769612473125,
-1.683395728164,-1.6799311672285,-1.67592743936131,-1.66893016253422,-1.63503008075999,
-1.61774316276034,-1.60838458051561,-1.60530687648307,-1.60327189209518,
-1.6014080574858,-1.5981679426452,-1.58817764278762,-1.56193844426803,-1.54462594126031,
-1.53323266176232,-1.52848627646465,-1.52496963953694,-1.52120487833068,
-1.51516720654675,-1.48955336042955,-1.46455211737487,-1.45681757544216,
-1.4513574615147,-1.44883891487086,-1.44688311432965,-1.4444736878445,-1.4395981081522,
-1.41745863509723,-1.39735585152558,-1.3852885529307,-1.37640520956997,
-1.37207497037054,-1.36860820717853,-1.36462587699,-1.3577284847528,-1.31693071867146,
-1.30423768142103,-1.29652465936375,-1.29365133925854,-1.2916540969872,
-1.28945666156045,-1.28561942663399,-1.2627869355318,-1.24465266536888,
-1.23088331404665,-1.22112532142519,-1.21664059111359,-1.21315904218343,
-1.20927314628933,-1.20265510938848,-1.16487163089148,-1.14451539340036,
-1.13961622560703,-1.13720201432049,-1.13544178047744,-1.13303291572945,
-1.1281614471451,-1.1065266821292,-1.08766959324548,-1.06813449892399,-1.06249601517894,
-1.05881313566057,-1.05529383379258,-1.05032143653054,-1.03824005750755,
-0.999864443733036,-0.986286956218584,-0.982831507346819,-0.980716191876809),
 .UNSPECIFIED.);
#759=B_SPLINE_CURVE_WITH_KNOTS('',3,(#71651,#71652,#71653,#71654),
 .UNSPECIFIED.,.F.,.F.,(4,4),(-0.000597831378872224,-0.000459283554306568),
 .UNSPECIFIED.);
#760=B_SPLINE_CURVE_WITH_KNOTS('',3,(#71655,#71656,#71657,#71658,#71659,
#71660,#71661,#71662,#71663,#71664,#71665,#71666,#71667,#71668,#71669,#71670,
#71671,#71672,#71673,#71674,#71675,#71676,#71677,#71678,#71679,#71680,#71681,
#71682,#71683,#71684,#71685,#71686,#71687,#71688,#71689,#71690,#71691,#71692,
#71693,#71694,#71695,#71696,#71697,#71698,#71699,#71700,#71701,#71702,#71703,
#71704,#71705,#71706,#71707,#71708,#71709,#71710,#71711,#71712,#71713,#71714,
#71715,#71716,#71717,#71718,#71719,#71720,#71721,#71722,#71723,#71724,#71725,
#71726,#71727,#71728,#71729,#71730,#71731,#71732,#71733,#71734,#71735,#71736,
#71737,#71738,#71739,#71740,#71741,#71742,#71743,#71744,#71745,#71746,#71747,
#71748,#71749,#71750,#71751,#71752,#71753,#71754,#71755,#71756,#71757,#71758,
#71759,#71760,#71761,#71762,#71763,#71764,#71765,#71766,#71767,#71768,#71769,
#71770,#71771,#71772,#71773,#71774,#71775,#71776,#71777,#71778,#71779,#71780,
#71781,#71782,#71783,#71784,#71785,#71786,#71787,#71788,#71789,#71790,#71791,
#71792,#71793,#71794,#71795,#71796,#71797,#71798,#71799,#71800,#71801,#71802,
#71803,#71804,#71805,#71806,#71807,#71808,#71809,#71810,#71811,#71812,#71813,
#71814,#71815,#71816,#71817,#71818,#71819,#71820,#71821,#71822,#71823,#71824,
#71825,#71826,#71827,#71828,#71829,#71830,#71831,#71832,#71833,#71834,#71835,
#71836,#71837,#71838,#71839,#71840,#71841,#71842),.UNSPECIFIED.,.F.,.F.,
(4,2,2,2,2,2,2,2,2,2,2,2,2,2,2,2,2,2,2,2,2,2,2,2,2,2,2,2,2,2,2,2,2,2,2,
2,2,2,2,2,2,2,2,2,2,2,2,2,2,2,2,2,2,2,2,2,2,2,2,2,2,2,2,2,2,2,2,2,2,2,2,
2,2,2,2,2,2,2,2,2,2,2,2,2,2,2,2,2,2,2,2,2,2,4),(-1.96074712009502,-1.92330424369733,
-1.91964900608186,-1.9165439369243,-1.91446667464182,-1.91226232233701,
-1.90855451791569,-1.89319835882291,-1.86270909330847,-1.85157888718564,
-1.84325044659449,-1.83909365930445,-1.83553748075556,-1.83143088685372,
-1.82424920041514,-1.79201810489301,-1.7660358722662,-1.76192199699911,
-1.75963086648069,-1.75759221883059,-1.75470944996851,-1.74774631995332,
-1.71913240192821,-1.70099305695676,-1.692916777697,-1.68630278654894,-1.68235370328846,
-1.67877137455857,-1.67416767598951,-1.66381511017221,-1.62321974667725,
-1.61385009927947,-1.60755407687908,-1.60485220579725,-1.60283635909023,
-1.60044296819685,-1.59596875323513,-1.56575238006591,-1.54618049028869,
-1.53381754508987,-1.52885686033675,-1.52523362303198,-1.5213988312098,
-1.51533697940125,-1.49203488962347,-1.45787684641395,-1.45184851036184,
-1.44919146734801,-1.44717937984815,-1.44475410711998,-1.44012978729441,
-1.40504022982573,-1.38246919686681,-1.37544078819509,-1.37140591104813,
-1.36784042477756,-1.36331120523256,-1.35369281373714,-1.31590449233759,
-1.30413128628005,-1.29905106068833,-1.29504853712373,-1.29278070371425,
-1.2907332666829,-1.28779703409595,-1.28047076918301,-1.2521577912366,-1.23412924260284,
-1.22238684520311,-1.2175154038011,-1.21390593321297,-1.21003814889031,
-1.20381827504736,-1.17635519627127,-1.1531758249164,-1.14568426713791,
-1.14032563253653,-1.13778740111077,-1.13578019987408,-1.13325293777625,
-1.12795342809861,-1.09766149812672,-1.07893185758297,-1.07070186369002,
-1.06399169130368,-1.06002215112043,-1.05644384244576,-1.05187637399718,
-1.04174797824096,-1.00458373023303,-0.992891559070608,-0.985555656151887,
-0.982692227419022,-0.98065608999199),.UNSPECIFIED.);
#761=B_SPLINE_CURVE_WITH_KNOTS('',3,(#71847,#71848,#71849,#71850,#71851,
#71852,#71853,#71854,#71855,#71856,#71857,#71858,#71859,#71860,#71861,#71862,
#71863,#71864,#71865,#71866,#71867,#71868,#71869,#71870,#71871,#71872,#71873,
#71874,#71875,#71876,#71877,#71878,#71879,#71880,#71881,#71882,#71883,#71884,
#71885,#71886,#71887,#71888,#71889,#71890,#71891,#71892,#71893,#71894,#71895,
#71896,#71897,#71898,#71899,#71900,#71901,#71902,#71903,#71904,#71905,#71906,
#71907,#71908,#71909,#71910,#71911,#71912,#71913,#71914,#71915,#71916,#71917,
#71918,#71919,#71920,#71921,#71922,#71923,#71924,#71925,#71926,#71927,#71928,
#71929,#71930,#71931,#71932,#71933,#71934,#71935,#71936,#71937,#71938,#71939,
#71940,#71941,#71942,#71943,#71944,#71945,#71946,#71947,#71948,#71949,#71950,
#71951,#71952,#71953,#71954,#71955,#71956,#71957,#71958,#71959,#71960,#71961,
#71962,#71963,#71964,#71965,#71966,#71967,#71968,#71969,#71970,#71971,#71972,
#71973,#71974,#71975,#71976,#71977,#71978,#71979,#71980,#71981,#71982,#71983,
#71984,#71985,#71986,#71987,#71988,#71989,#71990,#71991,#71992,#71993,#71994,
#71995,#71996,#71997,#71998,#71999,#72000,#72001,#72002,#72003,#72004,#72005,
#72006,#72007,#72008,#72009,#72010,#72011,#72012,#72013,#72014,#72015,#72016,
#72017,#72018,#72019,#72020,#72021),.UNSPECIFIED.,.F.,.F.,(4,3,3,3,3,3,
3,3,3,3,3,3,3,3,3,3,3,3,3,3,3,3,3,3,3,3,3,3,3,3,3,3,3,3,3,3,3,3,3,3,3,3,
3,3,3,3,3,3,3,3,3,3,3,3,3,3,3,3,4),(34.5575191894876,34.6681294449895,34.7786939471955,
34.8892566164147,34.9999369681898,35.1106862346866,35.2216338987612,35.2605512351816,
35.37223736211,35.4837245346131,35.59510057765,35.7064084453262,35.8176909943029,
35.9290742355253,36.0405033729067,36.1521504834875,36.2586980615683,36.370384188506,
36.4818713610179,36.5932474040636,36.7045552717483,36.8158378207331,36.9272210619631,
37.0386501993518,37.1502973099394,37.2568448879551,37.3685310149238,37.4800181874678,
37.591394230546,37.7027020982637,37.8139846472819,37.9253678885457,38.0367970259687,
38.1484441365904,38.2549917143418,38.3666778412903,38.4781650138137,38.5895410568709,
38.7008489245676,38.8121314735645,38.923514714807,39.0349438522084,39.1465909628088,
39.2531385407286,39.3648246676801,39.4763118402064,39.5876878832665,39.6989957509661,
39.810278299966,39.9216615412113,40.0330906786155,40.1447377892186,40.2512853671153,
40.3649135742225,40.4838613048337,40.5970963231696,40.7102234970804,40.8232764462415,
40.8407044966673),.UNSPECIFIED.);
#762=B_SPLINE_CURVE_WITH_KNOTS('',3,(#72023,#72024,#72025,#72026,#72027,
#72028,#72029,#72030,#72031,#72032,#72033,#72034,#72035,#72036,#72037,#72038,
#72039,#72040,#72041,#72042,#72043,#72044,#72045,#72046,#72047,#72048,#72049,
#72050,#72051,#72052,#72053,#72054,#72055,#72056,#72057,#72058,#72059,#72060,
#72061,#72062,#72063,#72064,#72065,#72066,#72067,#72068,#72069,#72070,#72071,
#72072,#72073,#72074,#72075,#72076,#72077,#72078,#72079,#72080,#72081,#72082,
#72083,#72084,#72085,#72086,#72087,#72088,#72089,#72090,#72091,#72092,#72093,
#72094,#72095,#72096,#72097,#72098,#72099,#72100,#72101,#72102,#72103,#72104,
#72105,#72106,#72107,#72108,#72109,#72110,#72111,#72112,#72113,#72114,#72115,
#72116,#72117,#72118,#72119,#72120,#72121,#72122,#72123,#72124,#72125,#72126,
#72127,#72128,#72129,#72130,#72131,#72132,#72133,#72134,#72135,#72136,#72137,
#72138,#72139,#72140,#72141,#72142,#72143,#72144,#72145,#72146,#72147,#72148,
#72149,#72150,#72151,#72152,#72153,#72154,#72155,#72156,#72157,#72158,#72159,
#72160,#72161,#72162,#72163,#72164,#72165,#72166,#72167,#72168,#72169,#72170,
#72171,#72172,#72173,#72174,#72175,#72176,#72177,#72178,#72179,#72180,#72181,
#72182,#72183,#72184,#72185,#72186,#72187,#72188,#72189,#72190,#72191,#72192,
#72193,#72194,#72195,#72196,#72197,#72198,#72199,#72200,#72201,#72202,#72203,
#72204,#72205,#72206,#72207,#72208,#72209,#72210),.UNSPECIFIED.,.F.,.F.,
(4,2,2,2,2,2,2,2,2,2,2,2,2,2,2,2,2,2,2,2,2,2,2,2,2,2,2,2,2,2,2,2,2,2,2,
2,2,2,2,2,2,2,2,2,2,2,2,2,2,2,2,2,2,2,2,2,2,2,2,2,2,2,2,2,2,2,2,2,2,2,2,
2,2,2,2,2,2,2,2,2,2,2,2,2,2,2,2,2,2,2,2,2,2,4),(-0.98065608999199,-0.978354702906265,
-0.974193919631416,-0.949387547585181,-0.915908231415091,-0.908821162648226,
-0.904734130968147,-0.901174921302342,-0.896723296316679,-0.887544075129815,
-0.874989860281017,-0.855663936812527,-0.833802167380706,-0.828878787362181,
-0.826423081130071,-0.82461481632714,-0.822109099220653,-0.816924570097771,
-0.809762571184661,-0.788538410753232,-0.76067583807875,-0.75339538298205,
-0.74926700149047,-0.745711510526034,-0.741315910330264,-0.732444019185328,
-0.710902281581362,-0.683737513180867,-0.674991815107569,-0.671854897333428,
-0.669977362296841,-0.667842635552226,-0.664459261541117,-0.652499968117858,
-0.625142869306548,-0.602615314358564,-0.596577586739665,-0.592747420525063,
-0.589121192518809,-0.584144603645494,-0.571672275053566,-0.551817993592194,
-0.522063864325581,-0.517540737473104,-0.51513669383677,-0.513121874948797,
-0.510434546710223,-0.504227734429962,-0.49504679898894,-0.457076872418203,
-0.444858001434442,-0.439797534295136,-0.436193291229638,-0.432398455631287,
-0.426533013505774,-0.40497061089671,-0.396478025091819,-0.366393612079883,
-0.361901695905956,-0.359504295286125,-0.357488593866831,-0.354791605270093,
-0.348526688220211,-0.339224200642259,-0.299582270111105,-0.28869705123921,
-0.284334487053402,-0.2807101963141,-0.276947551747818,-0.271240817672782,
-0.251930638356581,-0.222204132934795,-0.209058317342049,-0.20547891517917,
-0.20330189090496,-0.201205602423778,-0.198006186347572,-0.187976053693093,
-0.168623959617772,-0.138280502160977,-0.130982680625002,-0.126850506466004,
-0.123295148575431,-0.119161910226838,-0.110979038605763,-0.100108977707732,
-0.0691474134185848,-0.0537121579076861,-0.0499997589962834,-0.0477939540241356,
-0.0457163929279189,-0.0426124913361034,-0.0389597549555495,-0.000459537643221521),
 .UNSPECIFIED.);
#763=B_SPLINE_CURVE_WITH_KNOTS('',3,(#72211,#72212,#72213,#72214),
 .UNSPECIFIED.,.F.,.F.,(4,4),(-1.96107617980448,-1.96094824870565),
 .UNSPECIFIED.);
#764=B_SPLINE_CURVE_WITH_KNOTS('',3,(#72219,#72220,#72221,#72222,#72223,
#72224,#72225,#72226,#72227,#72228,#72229,#72230,#72231,#72232,#72233,#72234,
#72235,#72236,#72237,#72238,#72239,#72240,#72241,#72242,#72243,#72244,#72245,
#72246,#72247,#72248,#72249,#72250,#72251,#72252,#72253,#72254,#72255,#72256,
#72257,#72258,#72259,#72260,#72261,#72262,#72263,#72264,#72265,#72266,#72267,
#72268,#72269,#72270,#72271,#72272,#72273,#72274,#72275,#72276,#72277,#72278,
#72279,#72280,#72281,#72282,#72283,#72284,#72285,#72286,#72287,#72288,#72289,
#72290,#72291,#72292,#72293,#72294,#72295,#72296,#72297,#72298,#72299,#72300,
#72301,#72302,#72303,#72304,#72305,#72306,#72307,#72308,#72309,#72310,#72311,
#72312,#72313,#72314,#72315,#72316,#72317,#72318,#72319,#72320,#72321,#72322,
#72323,#72324,#72325,#72326,#72327,#72328,#72329,#72330,#72331,#72332,#72333,
#72334,#72335,#72336,#72337,#72338,#72339,#72340,#72341,#72342,#72343,#72344,
#72345,#72346,#72347,#72348,#72349,#72350,#72351,#72352,#72353,#72354,#72355,
#72356,#72357,#72358,#72359,#72360,#72361,#72362,#72363,#72364,#72365,#72366,
#72367,#72368,#72369,#72370,#72371,#72372,#72373,#72374,#72375,#72376,#72377,
#72378,#72379,#72380,#72381,#72382,#72383,#72384,#72385,#72386,#72387,#72388,
#72389,#72390,#72391,#72392,#72393,#72394,#72395,#72396,#72397,#72398,#72399,
#72400),.UNSPECIFIED.,.F.,.F.,(4,2,2,2,2,2,2,2,2,2,2,2,2,2,2,2,2,2,2,2,
2,2,2,2,2,2,2,2,2,2,2,2,2,2,2,2,2,2,2,2,2,2,2,2,2,2,2,2,2,2,2,2,2,2,2,2,
2,2,2,2,2,2,2,2,2,2,2,2,2,2,2,2,2,2,2,2,2,2,2,2,2,2,2,2,2,2,2,2,2,2,4),
(-0.980843112000428,-0.951920574072764,-0.93097803249815,-0.925099911148539,
-0.921367497327225,-0.91783491128297,-0.912993712403994,-0.900959549939245,
-0.882102504874166,-0.851692751608264,-0.846500859890778,-0.843996323995269,
-0.842040399321844,-0.839617112311938,-0.834672024400599,-0.82791130780217,
-0.808676648352998,-0.777776377591259,-0.770611187344655,-0.766570667561399,
-0.763107510018653,-0.758851260513236,-0.750372561968623,-0.7311477990017,
-0.698670106784975,-0.691619400082618,-0.688768213516583,-0.686774255122743,
-0.684566624811173,-0.680683350602813,-0.654745732793106,-0.621847824984893,
-0.614772571925623,-0.610751308994798,-0.607286912467112,-0.603006452561707,
-0.594397921901346,-0.572089128443636,-0.544372433545687,-0.536220949894704,
-0.533208722537171,-0.531206090741462,-0.529065140719352,-0.525491672187407,
-0.510019644546239,-0.490440197595961,-0.464169367786274,-0.458064434101782,
-0.454284899439612,-0.450772458330907,-0.446059429260661,-0.434893145343032,
-0.418105823058623,-0.40231999448564,-0.382063445330295,-0.378257749039759,
-0.376066771552237,-0.374066157652966,-0.371175085181421,-0.363333968365896,
-0.350320666080443,-0.31033364904223,-0.303267813120982,-0.299248678097146,
-0.295784288883258,-0.29150149383613,-0.282879758802574,-0.26033630380799,
-0.232190580316864,-0.224570131660876,-0.221628142527779,-0.219638453710298,
-0.2174737853687,-0.213790256587188,-0.196037542778051,-0.15627237749183,
-0.148909068258633,-0.144442515297959,-0.140962687612453,-0.137065955198825,
-0.130396844528511,-0.122181170805865,-0.1033298746528,-0.0729347737568217,
-0.0677325559330417,-0.0652261680387528,-0.0632703974100668,-0.060849291775129,
-0.0559147129440345,-0.0352129286778182,-0.000461241006961862),
 .UNSPECIFIED.);
#765=B_SPLINE_CURVE_WITH_KNOTS('',3,(#72401,#72402,#72403,#72404,#72405,
#72406,#72407,#72408,#72409,#72410,#72411,#72412,#72413,#72414,#72415,#72416,
#72417,#72418,#72419,#72420,#72421,#72422,#72423,#72424,#72425,#72426,#72427,
#72428,#72429,#72430,#72431,#72432,#72433,#72434,#72435,#72436,#72437,#72438,
#72439,#72440,#72441,#72442,#72443,#72444,#72445,#72446,#72447,#72448,#72449,
#72450,#72451,#72452,#72453,#72454,#72455,#72456,#72457,#72458,#72459,#72460,
#72461,#72462,#72463,#72464,#72465,#72466,#72467,#72468,#72469,#72470,#72471,
#72472,#72473,#72474,#72475,#72476,#72477,#72478,#72479,#72480,#72481,#72482,
#72483,#72484,#72485,#72486,#72487,#72488,#72489,#72490,#72491,#72492,#72493,
#72494,#72495,#72496,#72497,#72498,#72499,#72500,#72501,#72502,#72503,#72504,
#72505,#72506,#72507,#72508,#72509,#72510,#72511,#72512,#72513,#72514,#72515,
#72516,#72517,#72518,#72519,#72520,#72521,#72522,#72523,#72524,#72525,#72526,
#72527,#72528,#72529,#72530,#72531,#72532,#72533,#72534,#72535,#72536,#72537,
#72538,#72539,#72540,#72541,#72542,#72543,#72544,#72545,#72546,#72547,#72548,
#72549,#72550,#72551,#72552,#72553,#72554,#72555,#72556,#72557,#72558,#72559,
#72560,#72561,#72562,#72563,#72564,#72565,#72566,#72567,#72568,#72569,#72570,
#72571,#72572,#72573,#72574,#72575,#72576,#72577,#72578,#72579,#72580,#72581,
#72582,#72583,#72584,#72585,#72586,#72587,#72588,#72589,#72590,#72591,#72592,
#72593,#72594,#72595,#72596),.UNSPECIFIED.,.F.,.F.,(4,2,2,2,2,2,2,2,2,2,
2,2,2,2,2,2,2,2,2,2,2,2,2,2,2,2,2,2,2,2,2,2,2,2,2,2,2,2,2,2,2,2,2,2,2,2,
2,2,2,2,2,2,2,2,2,2,2,2,2,2,2,2,2,2,2,2,2,2,2,2,2,2,2,2,2,2,2,2,2,2,2,2,
2,2,2,2,2,2,2,2,2,2,2,2,2,2,2,4),(-1.96094824870565,-1.94267634822966,-1.93757453855741,
-1.93389463107528,-1.93055551091535,-1.9269214938182,-1.92251663056985,
-1.91154006639502,-1.87350459780632,-1.85864331623043,-1.85496703801708,
-1.85276935269738,-1.85071229151882,-1.84760615733215,-1.83908925293603,
-1.81176687156231,-1.79012862831546,-1.78126315531497,-1.77686916771891,
-1.77331423489394,-1.76918566440406,-1.76190268610234,-1.7343598368956,
-1.71287409363393,-1.70566593266085,-1.70045741216294,-1.69794737952514,
-1.69613912756977,-1.69368799836249,-1.6887871031636,-1.66477914100608,
-1.64186978462822,-1.62779393690583,-1.62260782452132,-1.61894576998243,
-1.61562084588853,-1.6111258986462,-1.59938454147771,-1.56082000852686,
-1.55159161358485,-1.54536280668352,-1.54267198467194,-1.54065707216635,
-1.53825592832371,-1.53374570314146,-1.50389074900865,-1.48411910081444,
-1.47167854009571,-1.46670677666156,-1.46308157573251,-1.45925023965997,
-1.45320583801524,-1.43049911488401,-1.40327188396087,-1.39133703508837,
-1.38795574999922,-1.38582158762654,-1.38394390962964,-1.38080570146556,
-1.37204859339793,-1.34491635319189,-1.32339648253723,-1.31452753071019,
-1.31013264948267,-1.30657736343626,-1.3024487962458,-1.29516694059518,
-1.26727687454462,-1.2460478462039,-1.23888422228237,-1.23369935126642,
-1.23119363198083,-1.22938545045483,-1.22692995124973,-1.22200731257903,
-1.20005947164307,-1.18040185363748,-1.16810231749209,-1.15905619361396,
-1.15462879402588,-1.15107139437516,-1.14696713959246,-1.13979947207659,
-1.10741709051519,-1.08935693558775,-1.07971427928637,-1.07655697035418,
-1.07446917337377,-1.07255135964997,-1.06919749202155,-1.05860448862994,
-1.03288755325588,-1.00939408982909,-1.00224172321199,-0.998181261802422,
-0.994619040136678,-0.990128788067818,-0.980733160320695),.UNSPECIFIED.);
#766=B_SPLINE_CURVE_WITH_KNOTS('',3,(#72602,#72603,#72604,#72605),
 .UNSPECIFIED.,.F.,.F.,(4,4),(-0.00059011187237714,-0.000461155693138806),
 .UNSPECIFIED.);
#767=B_SPLINE_CURVE_WITH_KNOTS('',3,(#72606,#72607,#72608,#72609,#72610,
#72611,#72612,#72613,#72614,#72615,#72616,#72617,#72618,#72619,#72620,#72621,
#72622,#72623,#72624,#72625,#72626,#72627,#72628,#72629,#72630,#72631,#72632,
#72633,#72634,#72635,#72636,#72637,#72638,#72639,#72640,#72641,#72642,#72643,
#72644,#72645,#72646,#72647,#72648,#72649,#72650,#72651,#72652,#72653,#72654,
#72655,#72656,#72657,#72658,#72659,#72660,#72661,#72662,#72663,#72664,#72665,
#72666,#72667,#72668,#72669,#72670,#72671,#72672,#72673,#72674,#72675,#72676,
#72677,#72678,#72679,#72680,#72681,#72682,#72683,#72684,#72685,#72686,#72687,
#72688,#72689,#72690,#72691,#72692,#72693,#72694,#72695,#72696,#72697,#72698,
#72699,#72700,#72701,#72702,#72703,#72704,#72705,#72706,#72707,#72708,#72709,
#72710,#72711,#72712,#72713,#72714,#72715,#72716,#72717,#72718,#72719,#72720,
#72721,#72722,#72723,#72724,#72725,#72726,#72727,#72728,#72729,#72730,#72731,
#72732,#72733,#72734,#72735,#72736,#72737,#72738,#72739,#72740,#72741,#72742,
#72743,#72744,#72745,#72746,#72747,#72748,#72749,#72750,#72751,#72752,#72753,
#72754,#72755,#72756,#72757,#72758,#72759,#72760,#72761,#72762,#72763,#72764,
#72765,#72766,#72767,#72768,#72769,#72770,#72771,#72772,#72773,#72774,#72775,
#72776,#72777,#72778,#72779,#72780,#72781,#72782,#72783,#72784,#72785,#72786,
#72787,#72788,#72789,#72790,#72791,#72792,#72793,#72794,#72795,#72796,#72797,
#72798,#72799,#72800,#72801),.UNSPECIFIED.,.F.,.F.,(4,2,2,2,2,2,2,2,2,2,
2,2,2,2,2,2,2,2,2,2,2,2,2,2,2,2,2,2,2,2,2,2,2,2,2,2,2,2,2,2,2,2,2,2,2,2,
2,2,2,2,2,2,2,2,2,2,2,2,2,2,2,2,2,2,2,2,2,2,2,2,2,2,2,2,2,2,2,2,2,2,2,2,
2,2,2,2,2,2,2,2,2,2,2,2,2,2,2,4),(-1.96127857229901,-1.93985522552035,-1.93700892692586,
-1.93497772268674,-1.93297545631679,-1.9307879581078,-1.92699884857685,
-1.90790234968511,-1.87940921983079,-1.87195841343185,-1.86239540273868,
-1.85790757498593,-1.85442493793339,-1.85053917484657,-1.84392478290888,
-1.80609446922914,-1.78575694549569,-1.78085901044206,-1.77844467143018,
-1.77668401697316,-1.77427409324974,-1.76939903078909,-1.74652197923517,
-1.72215977722551,-1.71269518625917,-1.70526957307602,-1.70121772876528,
-1.69775484887694,-1.69351154078721,-1.68693455370028,-1.65825100925579,
-1.63739223770426,-1.62698053371964,-1.6237901417199,-1.62173153125583,
-1.61963407206586,-1.61626223470719,-1.60492755997675,-1.57965943749913,
-1.55876354021825,-1.55022265238004,-1.54595450920383,-1.54249039986191,
-1.53845859622391,-1.5313355561556,-1.49920527951765,-1.48078140345377,
-1.47106678260229,-1.46794885087909,-1.46590515583363,-1.46404846154953,
-1.46084862882604,-1.45121968388429,-1.42140637127894,-1.40285859854245,
-1.39440415322682,-1.39015220588884,-1.38668890395976,-1.38264408512937,
-1.37546006126579,-1.34522146269267,-1.32548750285831,-1.31863081097612,
-1.31363393132335,-1.31120058178205,-1.30943908130048,-1.30704709829179,
-1.30226459374186,-1.26775643081585,-1.24719481008332,-1.23866762891304,
-1.23440207498481,-1.23093813475068,-1.22690435255795,-1.21977193102939,
-1.18784730529338,-1.16928634353494,-1.15953032900894,-1.15640795109055,
-1.15436336841416,-1.15224834363795,-1.14879534229973,-1.1366500323816,
-1.09134295434657,-1.08283722572539,-1.07857598041775,-1.07511261894959,
-1.07107621795231,-1.06393023611763,-1.03236525183324,-1.01356487762936,
-1.00373761011916,-1.00060782109162,-0.998561885635286,-0.996449192684477,
-0.993006259241398,-0.980949239411572,-0.980843112000428),.UNSPECIFIED.);
#768=B_SPLINE_CURVE_WITH_KNOTS('',3,(#72802,#72803,#72804,#72805,#72806,
#72807,#72808,#72809,#72810,#72811,#72812,#72813,#72814,#72815,#72816,#72817,
#72818,#72819,#72820,#72821,#72822,#72823,#72824,#72825,#72826,#72827,#72828,
#72829,#72830,#72831,#72832,#72833,#72834,#72835,#72836,#72837,#72838,#72839,
#72840,#72841,#72842,#72843,#72844,#72845,#72846,#72847,#72848,#72849,#72850,
#72851,#72852,#72853,#72854,#72855,#72856,#72857,#72858,#72859,#72860,#72861,
#72862,#72863,#72864,#72865,#72866,#72867,#72868,#72869,#72870,#72871,#72872,
#72873,#72874,#72875,#72876,#72877,#72878,#72879,#72880,#72881,#72882,#72883,
#72884,#72885,#72886,#72887,#72888,#72889,#72890,#72891,#72892,#72893,#72894,
#72895,#72896,#72897,#72898,#72899,#72900,#72901,#72902,#72903,#72904,#72905,
#72906,#72907,#72908,#72909,#72910,#72911,#72912,#72913,#72914,#72915,#72916,
#72917,#72918,#72919,#72920,#72921,#72922,#72923,#72924,#72925,#72926,#72927,
#72928,#72929,#72930,#72931,#72932,#72933,#72934,#72935,#72936,#72937,#72938,
#72939,#72940,#72941,#72942,#72943,#72944,#72945,#72946,#72947,#72948,#72949,
#72950,#72951,#72952,#72953,#72954,#72955,#72956,#72957,#72958,#72959,#72960,
#72961,#72962,#72963,#72964,#72965,#72966,#72967,#72968,#72969,#72970,#72971,
#72972,#72973,#72974,#72975,#72976,#72977,#72978,#72979,#72980,#72981,#72982,
#72983,#72984,#72985,#72986,#72987),.UNSPECIFIED.,.F.,.F.,(4,2,2,2,2,2,
2,2,2,2,2,2,2,2,2,2,2,2,2,2,2,2,2,2,2,2,2,2,2,2,2,2,2,2,2,2,2,2,2,2,2,2,
2,2,2,2,2,2,2,2,2,2,2,2,2,2,2,2,2,2,2,2,2,2,2,2,2,2,2,2,2,2,2,2,2,2,2,2,
2,2,2,2,2,2,2,2,2,2,2,2,2,2,4),(-0.980733160320695,-0.967761504262221,-0.948816939040578,
-0.925615934930639,-0.921704656449749,-0.919456247566718,-0.917400783658444,
-0.914417073381265,-0.906210218868975,-0.892340202238349,-0.857447780109865,
-0.84805983114872,-0.84357098931083,-0.84000888947004,-0.83594749315517,
-0.828790636149438,-0.805263320242643,-0.779487937654314,-0.768944693925615,
-0.765595495593097,-0.763678570539921,-0.761589899403417,-0.758428350507042,
-0.748746862897344,-0.730560785329596,-0.69840951887371,-0.691231455176459,
-0.68712493722333,-0.683567663126316,-0.679143139684937,-0.670113361242895,
-0.657843241635455,-0.638007028562777,-0.616141147498622,-0.611217759662292,
-0.608762059977652,-0.606953805240607,-0.604448108809262,-0.599263646035777,
-0.592101757689801,-0.570878122232942,-0.543015147146856,-0.535734734621049,
-0.531606375940406,-0.528050903872007,-0.523655326072108,-0.514783476570161,
-0.493242124790231,-0.466077933963418,-0.457331743442727,-0.454194771661292,
-0.452317234082736,-0.450182537319255,-0.446799267891242,-0.434841052809533,
-0.407489250081597,-0.384955897295301,-0.378917993806803,-0.375087805123129,
-0.371461617414524,-0.366485182889639,-0.354013835852142,-0.334162041423826,
-0.304403816341197,-0.299881093357489,-0.297477143201675,-0.295462324625449,
-0.292774894446566,-0.286567418615831,-0.277385079455814,-0.239396270312896,
-0.227191933947655,-0.222134383304945,-0.218530646968789,-0.214734972591239,
-0.208865350260263,-0.187235817964272,-0.178898893781169,-0.148678529994814,
-0.144220005801542,-0.141829740753544,-0.139813034845904,-0.137105467137435,
-0.130776404475948,-0.121338809078955,-0.079629984705879,-0.070119736786701,
-0.0656092752384031,-0.0620452669038608,-0.0579979519653199,-0.050910013176525,
-0.0279014211884546,-0.000459681452164959),.UNSPECIFIED.);
#769=B_SPLINE_CURVE_WITH_KNOTS('',3,(#72992,#72993,#72994,#72995,#72996,
#72997,#72998,#72999,#73000,#73001,#73002,#73003,#73004,#73005,#73006,#73007,
#73008,#73009,#73010,#73011,#73012,#73013,#73014,#73015,#73016,#73017,#73018,
#73019,#73020,#73021,#73022,#73023,#73024,#73025,#73026,#73027,#73028,#73029,
#73030,#73031,#73032,#73033,#73034,#73035,#73036,#73037,#73038,#73039,#73040,
#73041,#73042,#73043,#73044,#73045,#73046,#73047,#73048,#73049,#73050,#73051,
#73052,#73053,#73054,#73055,#73056,#73057,#73058,#73059,#73060,#73061,#73062,
#73063,#73064,#73065,#73066,#73067,#73068,#73069,#73070,#73071,#73072,#73073,
#73074,#73075,#73076,#73077,#73078,#73079,#73080,#73081,#73082,#73083,#73084,
#73085,#73086,#73087,#73088,#73089,#73090,#73091,#73092,#73093,#73094,#73095,
#73096,#73097,#73098,#73099,#73100,#73101,#73102,#73103,#73104,#73105,#73106,
#73107,#73108,#73109,#73110,#73111,#73112,#73113,#73114,#73115,#73116,#73117,
#73118,#73119,#73120,#73121,#73122,#73123,#73124,#73125,#73126,#73127,#73128,
#73129,#73130,#73131,#73132,#73133,#73134,#73135,#73136,#73137,#73138,#73139,
#73140,#73141,#73142,#73143,#73144,#73145,#73146,#73147,#73148,#73149,#73150,
#73151,#73152,#73153,#73154,#73155,#73156,#73157,#73158,#73159,#73160,#73161,
#73162,#73163,#73164,#73165,#73166,#73167,#73168,#73169,#73170,#73171,#73172,
#73173,#73174,#73175,#73176,#73177,#73178,#73179,#73180,#73181,#73182,#73183,
#73184,#73185,#73186,#73187,#73188,#73189,#73190,#73191,#73192,#73193),
 .UNSPECIFIED.,.F.,.F.,(4,2,2,2,2,2,2,2,2,2,2,2,2,2,2,2,2,2,2,2,2,2,2,2,
2,2,2,2,2,2,2,2,2,2,2,2,2,2,2,2,2,2,2,2,2,2,2,2,2,2,2,2,2,2,2,2,2,2,2,2,
2,2,2,2,2,2,2,2,2,2,2,2,2,2,2,2,2,2,2,2,2,2,2,2,2,2,2,2,2,2,2,2,2,2,2,2,
2,2,2,2,4),(-0.980958235625572,-0.975406899605016,-0.956980154301351,-0.937231546846887,
-0.915150637366387,-0.910272526204308,-0.907862091967822,-0.906101545886403,
-0.903687986300938,-0.898793683562232,-0.878489188932872,-0.840649420634971,
-0.834041349898184,-0.830157017775664,-0.82667426539394,-0.822184329765441,
-0.812399541060252,-0.79857560561528,-0.780471253032548,-0.757646123466051,
-0.753808693670861,-0.751610917625146,-0.749613154731316,-0.746738837912992,
-0.739021188337069,-0.726319242544386,-0.685568997510446,-0.678664072793847,
-0.67467954056057,-0.67121208938256,-0.666882607455337,-0.658007148872636,
-0.645954181051805,-0.625705485140268,-0.603629163034814,-0.598751555046212,
-0.596341365080416,-0.594580995264852,-0.592167674597972,-0.587273847306234,
-0.566971242905889,-0.529135492171083,-0.52252805126537,-0.518644101583167,
-0.515161699457701,-0.510672225720102,-0.500888488324427,-0.487066081313597,
-0.468963384765506,-0.446140456083161,-0.442303407652579,-0.440105851115569,
-0.438108288613477,-0.435234261312038,-0.427517396431934,-0.414816752040312,
-0.374070516828562,-0.367166299282084,-0.363182169535609,-0.359715065365717,
-0.355386012453588,-0.346511417249682,-0.334459608486693,-0.314212928270044,
-0.292138917556691,-0.287261798795247,-0.284851850388718,-0.283091656914107,
-0.280678577880857,-0.275785240201533,-0.255484663542433,-0.217652712589653,
-0.211045932227278,-0.207162371337938,-0.203680318120044,-0.199191294627028,
-0.189408540320903,-0.175587524035446,-0.157482387143983,-0.134673379179808,
-0.130832621134821,-0.128634409119919,-0.126637404924991,-0.126596649745598,
-0.126556227922343,-0.126516094302381,-0.126476205440239,-0.12643651938905,
-0.126396995504326,-0.126357594267301,-0.12367729715794,-0.115989709383476,
-0.10318508505241,-0.0716022958255544,-0.0588240534330478,-0.0537446451827897,
-0.0502066078269937,-0.0465521100214381,-0.0410533708285637,-0.0321694988875906,
-0.00059011187237714),.UNSPECIFIED.);
#770=B_SPLINE_CURVE_WITH_KNOTS('',3,(#73194,#73195,#73196,#73197,#73198,
#73199,#73200,#73201,#73202,#73203,#73204),.UNSPECIFIED.,.F.,.F.,(4,1,1,
1,1,1,1,1,4),(53.4070751110265,53.5035699663983,54.5009068341909,55.4982437019834,
56.495580569776,57.4929174375686,58.4902543053611,59.4875911731537,59.690260418206),
 .UNSPECIFIED.);
#771=B_SPLINE_CURVE_WITH_KNOTS('',3,(#73209,#73210,#73211,#73212,#73213,
#73214,#73215,#73216,#73217,#73218,#73219,#73220,#73221,#73222,#73223,#73224,
#73225,#73226,#73227,#73228,#73229,#73230,#73231,#73232,#73233,#73234,#73235,
#73236,#73237,#73238,#73239,#73240,#73241,#73242,#73243,#73244,#73245,#73246,
#73247,#73248,#73249,#73250,#73251,#73252,#73253,#73254,#73255,#73256,#73257,
#73258,#73259,#73260,#73261,#73262,#73263,#73264,#73265,#73266,#73267,#73268,
#73269,#73270,#73271,#73272,#73273,#73274,#73275,#73276,#73277,#73278,#73279,
#73280,#73281,#73282,#73283,#73284,#73285,#73286,#73287,#73288,#73289,#73290,
#73291,#73292,#73293,#73294,#73295,#73296,#73297,#73298,#73299,#73300,#73301,
#73302,#73303,#73304,#73305,#73306,#73307,#73308,#73309,#73310,#73311,#73312,
#73313,#73314,#73315,#73316,#73317,#73318,#73319,#73320,#73321,#73322,#73323,
#73324,#73325,#73326,#73327,#73328,#73329,#73330,#73331,#73332,#73333,#73334,
#73335,#73336,#73337,#73338,#73339,#73340,#73341,#73342,#73343,#73344,#73345,
#73346,#73347,#73348,#73349,#73350,#73351,#73352,#73353,#73354,#73355,#73356,
#73357,#73358,#73359,#73360,#73361,#73362,#73363,#73364,#73365,#73366,#73367,
#73368,#73369,#73370,#73371,#73372,#73373,#73374,#73375,#73376,#73377,#73378,
#73379,#73380,#73381,#73382,#73383,#73384,#73385,#73386,#73387,#73388,#73389,
#73390,#73391,#73392,#73393,#73394,#73395,#73396,#73397,#73398,#73399,#73400,
#73401,#73402,#73403,#73404,#73405,#73406,#73407,#73408,#73409,#73410,#73411,
#73412,#73413,#73414),.UNSPECIFIED.,.F.,.F.,(4,2,2,2,2,2,2,2,2,2,2,2,2,
2,2,2,2,2,2,2,2,2,2,2,2,2,2,2,2,2,2,2,2,2,2,2,2,2,2,2,2,2,2,2,2,2,2,2,2,
2,2,2,2,2,2,2,2,2,2,2,2,2,2,2,2,2,2,2,2,2,2,2,2,2,2,2,2,2,2,2,2,2,2,2,2,
2,2,2,2,2,2,2,2,2,2,2,2,2,2,2,2,2,4),(-1.96126727528156,-1.93105273007122,
-1.92614954479132,-1.9225878868318,-1.9190141682557,-1.91578186639374,-1.91060622751215,
-1.8971310223569,-1.86633677311141,-1.85360048447955,-1.84595726088857,
-1.84327343451982,-1.84323393550042,-1.84319431115929,-1.84315452198443,
-1.84311452734102,-1.84307428529263,-1.84303375240652,-1.84299288354599,
-1.84099577856314,-1.83879891828285,-1.83496354364745,-1.81217175410611,
-1.7940741447777,-1.78026355404499,-1.77048549291687,-1.76599770443607,
-1.76251619351848,-1.75863280749374,-1.75202530252767,-1.714178197679,-1.69386802818047,
-1.68897397016179,-1.68656093249807,-1.6848009550598,-1.68239155645483,
-1.67751634973343,-1.65547438286872,-1.6352431033575,-1.62319130938956,
-1.61431613734523,-1.60998730604795,-1.60652055169849,-1.60253700940801,
-1.59563434610147,-1.55485900302106,-1.5421561108588,-1.53443907116245,
-1.53156514719995,-1.52956775785536,-1.52737046975683,-1.52353411615729,
-1.50072836385892,-1.48264311429537,-1.46882789384559,-1.45904707339614,
-1.45455836707444,-1.45107628042242,-1.44719239157592,-1.44058438424282,
-1.40272741777444,-1.38241646894521,-1.37752188648585,-1.37510851450253,
-1.37334825943277,-1.37093843086255,-1.36606220420035,-1.34397497225194,
-1.32386963099932,-1.31176816100545,-1.30286619566858,-1.2985320530226,
-1.29506440608076,-1.29108350664864,-1.28419492750851,-1.24334228229088,
-1.23066571853421,-1.22295878625003,-1.22008595558023,-1.21808850931274,
-1.21589023180595,-1.2120502790455,-1.18916021826107,-1.17093210297243,
-1.15724498181596,-1.14752731350888,-1.14304894156047,-1.13956753873734,
-1.13567689041728,-1.12903824464905,-1.09138538062198,-1.07093762712603,
-1.06602852102047,-1.06361211869405,-1.06185149136653,-1.05944386438801,
-1.05458021903962,-1.03062461239784,-1.00701771470968,-0.993266430473634,
-0.988196433148869,-0.984623917390367,-0.980958235625572),.UNSPECIFIED.);
#772=B_SPLINE_CURVE_WITH_KNOTS('',3,(#73415,#73416,#73417,#73418,#73419,
#73420,#73421,#73422,#73423,#73424,#73425,#73426,#73427,#73428,#73429,#73430,
#73431,#73432,#73433,#73434,#73435,#73436,#73437,#73438,#73439,#73440,#73441,
#73442,#73443,#73444,#73445,#73446,#73447,#73448,#73449,#73450,#73451,#73452,
#73453,#73454,#73455,#73456,#73457,#73458,#73459,#73460,#73461,#73462,#73463,
#73464,#73465,#73466,#73467,#73468,#73469,#73470,#73471,#73472,#73473,#73474,
#73475,#73476,#73477,#73478,#73479,#73480,#73481,#73482,#73483,#73484,#73485,
#73486,#73487,#73488,#73489,#73490,#73491,#73492,#73493,#73494,#73495,#73496,
#73497,#73498,#73499,#73500,#73501,#73502,#73503,#73504,#73505,#73506,#73507,
#73508,#73509,#73510,#73511,#73512,#73513,#73514,#73515,#73516,#73517,#73518,
#73519,#73520,#73521,#73522,#73523,#73524,#73525,#73526,#73527,#73528,#73529,
#73530,#73531,#73532,#73533,#73534,#73535,#73536,#73537,#73538,#73539,#73540,
#73541,#73542,#73543,#73544,#73545,#73546,#73547,#73548,#73549,#73550,#73551,
#73552,#73553,#73554,#73555,#73556,#73557,#73558,#73559,#73560,#73561,#73562,
#73563,#73564,#73565,#73566,#73567,#73568,#73569,#73570,#73571,#73572,#73573,
#73574,#73575,#73576,#73577,#73578,#73579,#73580,#73581,#73582,#73583,#73584,
#73585,#73586,#73587,#73588,#73589,#73590,#73591,#73592,#73593,#73594,#73595,
#73596,#73597,#73598,#73599,#73600,#73601,#73602,#73603,#73604,#73605,#73606,
#73607,#73608,#73609,#73610,#73611,#73612,#73613,#73614,#73615,#73616,#73617,
#73618,#73619,#73620,#73621,#73622,#73623,#73624,#73625,#73626,#73627,#73628,
#73629,#73630,#73631,#73632,#73633,#73634,#73635,#73636,#73637,#73638,#73639,
#73640,#73641,#73642),.UNSPECIFIED.,.F.,.F.,(4,2,2,2,2,2,2,2,2,2,2,2,2,
2,2,2,2,2,2,2,2,2,2,2,2,2,2,2,2,2,2,2,2,2,2,2,2,2,2,2,2,2,2,2,2,2,2,2,2,
2,2,2,2,2,2,2,2,2,2,2,2,2,2,2,2,2,2,2,2,2,2,2,2,2,2,2,2,2,2,2,2,2,2,2,2,
2,2,2,2,2,2,2,2,2,2,2,2,2,2,2,2,2,2,2,2,2,2,2,2,2,2,2,2,4),(-1.96131520446786,
-1.92943788095853,-1.92355672830733,-1.91837460556017,-1.91471296339964,
-1.91138682424772,-1.90688779805298,-1.89510294268181,-1.86372161370852,
-1.84999153718589,-1.84190809620745,-1.83915186119982,-1.83910758411492,
-1.83906325091772,-1.83901881608251,-1.83897423305584,-1.83892945405349,
-1.83888442984455,-1.83883910951657,-1.83879344021992,-1.83874736689821,
-1.83870083198413,-1.83865377506573,-1.83860613252695,-1.83855783714504,
-1.83853547678861,-1.8385110017733,-1.83848414646628,-1.83845459947384,
-1.83842199313684,-1.83838588992743,-1.83834576463254,-1.83635435198796,
-1.83391150945114,-1.82905403662827,-1.80453896845411,-1.78146948874141,
-1.76784738566127,-1.76271755252238,-1.75906519874492,-1.75528189243785,
-1.74947292118165,-1.73076361478782,-1.69983068591383,-1.69129819113837,
-1.68540827473551,-1.68277488549388,-1.68078271735008,-1.67834796852817,
-1.6735319106261,-1.64664242592921,-1.62516055964462,-1.61208483775083,
-1.60702606446256,-1.6033860227435,-1.59958199752634,-1.59367168168661,
-1.5735367041001,-1.54396919897841,-1.53559271686923,-1.52978051426087,
-1.52716063798383,-1.525342894526,-1.52297802099035,-1.51863753168265,-1.48721048630946,
-1.46827175016755,-1.4561578629458,-1.45123214649465,-1.44761411998053,
-1.44376628162906,-1.43764310130131,-1.41208793139349,-1.38726369023038,
-1.37583450283323,-1.3724975502077,-1.37037274843329,-1.36848817139706,
-1.36531206127979,-1.3562621341192,-1.32936021908511,-1.30803579769229,
-1.29912998301075,-1.29472808674067,-1.29117211718057,-1.28704832559484,
-1.27978989045142,-1.25015983649447,-1.23019949219605,-1.22326526031531,
-1.21820366844893,-1.21572123541111,-1.21371292489881,-1.21112617790703,
-1.20550117193668,-1.15935381865111,-1.14548612303428,-1.14032552970299,
-1.13666786901576,-1.13333789054813,-1.12795141043088,-1.11338299794338,
-1.0781257168,-1.06916468951207,-1.06306458668341,-1.06039527187634,-1.05838212573782,
-1.05596560285485,-1.05138316117734,-1.02250725217986,-1.00216615844222,
-0.989508566415736,-0.984506513065352,-0.980876168428268),.UNSPECIFIED.);
#773=B_SPLINE_CURVE_WITH_KNOTS('',3,(#73648,#73649,#73650,#73651,#73652,
#73653,#73654,#73655,#73656,#73657,#73658,#73659,#73660,#73661,#73662,#73663,
#73664,#73665,#73666,#73667,#73668,#73669,#73670,#73671,#73672,#73673,#73674,
#73675,#73676,#73677,#73678,#73679,#73680,#73681,#73682,#73683,#73684,#73685,
#73686,#73687,#73688,#73689,#73690,#73691,#73692,#73693,#73694,#73695,#73696,
#73697,#73698,#73699,#73700,#73701,#73702,#73703,#73704,#73705,#73706,#73707,
#73708,#73709,#73710,#73711,#73712,#73713,#73714,#73715,#73716,#73717,#73718,
#73719,#73720,#73721,#73722,#73723,#73724,#73725,#73726,#73727,#73728,#73729,
#73730,#73731,#73732,#73733,#73734,#73735,#73736,#73737,#73738,#73739,#73740,
#73741,#73742,#73743,#73744,#73745,#73746,#73747,#73748,#73749,#73750,#73751,
#73752,#73753,#73754,#73755,#73756,#73757,#73758,#73759,#73760,#73761,#73762,
#73763,#73764,#73765,#73766,#73767,#73768,#73769,#73770,#73771,#73772,#73773,
#73774,#73775,#73776,#73777,#73778,#73779,#73780,#73781,#73782,#73783,#73784,
#73785,#73786,#73787,#73788,#73789,#73790,#73791,#73792,#73793,#73794,#73795,
#73796,#73797,#73798,#73799,#73800,#73801,#73802,#73803,#73804,#73805,#73806,
#73807,#73808,#73809,#73810,#73811,#73812,#73813,#73814,#73815,#73816,#73817,
#73818,#73819,#73820,#73821,#73822,#73823,#73824,#73825,#73826,#73827,#73828,
#73829,#73830,#73831,#73832,#73833,#73834,#73835,#73836,#73837,#73838,#73839,
#73840,#73841,#73842,#73843),.UNSPECIFIED.,.F.,.F.,(4,2,2,2,2,2,2,2,2,2,
2,2,2,2,2,2,2,2,2,2,2,2,2,2,2,2,2,2,2,2,2,2,2,2,2,2,2,2,2,2,2,2,2,2,2,2,
2,2,2,2,2,2,2,2,2,2,2,2,2,2,2,2,2,2,2,2,2,2,2,2,2,2,2,2,2,2,2,2,2,2,2,2,
2,2,2,2,2,2,2,2,2,2,2,2,2,2,2,4),(-0.980645665338926,-0.974666323535037,
-0.97223769601446,-0.970257683639558,-0.968071541575421,-0.964288528935635,
-0.943592129360979,-0.908089213287009,-0.899205389329285,-0.894874388002916,
-0.891406785570255,-0.887423241042882,-0.880333304964163,-0.85676840480011,
-0.831089529238214,-0.820300547249837,-0.816977775915276,-0.814891115931844,
-0.812823437358398,-0.809589205111678,-0.798722729599752,-0.776101980797758,
-0.74984617806715,-0.743234039859205,-0.738980812807193,-0.735517896332518,
-0.73147514494383,-0.724093278070161,-0.714701125806817,-0.690700662497402,
-0.66726349693708,-0.662401068154134,-0.659993746122316,-0.658233185691063,
-0.655816696659856,-0.650906776451215,-0.630449032200712,-0.592853965402241,
-0.586212115740881,-0.58232090418751,-0.578839760015425,-0.574362793964848,
-0.564653076170167,-0.550979972651322,-0.532716106511657,-0.509798427376246,
-0.505957740907556,-0.50375933952987,-0.501761982408931,-0.498889608050369,
-0.491185464030826,-0.478516946050841,-0.437686937697177,-0.430799919361101,
-0.42681938163587,-0.423351716855175,-0.419017117386274,-0.410112784871566,
-0.39800523574692,-0.377884853016302,-0.35578324384419,-0.350905737624942,
-0.348495644493398,-0.34673536829787,-0.3443222050675,-0.339428793451435,
-0.319128790248061,-0.281292609047425,-0.274685858405628,-0.270802184187558,
-0.267319950605578,-0.262830583825892,-0.253046602453103,-0.239223390495474,
-0.221123327188658,-0.19830251176959,-0.194465697669086,-0.192268263689428,
-0.190270803426278,-0.187396910440489,-0.17968032809377,-0.166980042977409,
-0.126237977392895,-0.119333261613625,-0.115349155606177,-0.111882252861876,
-0.107553688668094,-0.0989119825103673,-0.0871418306658754,-0.0577696942921653,
-0.0422319173104418,-0.0385724939397159,-0.0364132232087641,-0.0343978211934399,
-0.0323424207994555,-0.0294317383989918,-0.0243303419455859,-0.000460869334322469),
 .UNSPECIFIED.);
#774=B_SPLINE_CURVE_WITH_KNOTS('',3,(#73844,#73845,#73846,#73847),
 .UNSPECIFIED.,.F.,.F.,(4,4),(-1.96141007892017,-1.96126727528156),
 .UNSPECIFIED.);
#775=B_SPLINE_CURVE_WITH_KNOTS('',3,(#73848,#73849,#73850,#73851,#73852,
#73853,#73854,#73855,#73856,#73857,#73858,#73859,#73860,#73861,#73862,#73863,
#73864,#73865,#73866,#73867,#73868,#73869,#73870,#73871,#73872,#73873,#73874,
#73875,#73876,#73877,#73878,#73879,#73880,#73881,#73882,#73883,#73884,#73885,
#73886,#73887,#73888,#73889,#73890,#73891,#73892,#73893,#73894,#73895,#73896,
#73897,#73898,#73899,#73900,#73901,#73902,#73903,#73904,#73905,#73906,#73907,
#73908,#73909,#73910,#73911,#73912,#73913,#73914,#73915,#73916,#73917,#73918,
#73919,#73920,#73921,#73922,#73923,#73924,#73925,#73926,#73927,#73928,#73929,
#73930,#73931,#73932,#73933,#73934,#73935,#73936,#73937,#73938,#73939,#73940,
#73941,#73942,#73943,#73944,#73945,#73946,#73947,#73948,#73949,#73950,#73951,
#73952,#73953,#73954,#73955,#73956,#73957,#73958,#73959,#73960,#73961,#73962,
#73963,#73964,#73965,#73966,#73967,#73968,#73969,#73970,#73971,#73972,#73973,
#73974,#73975,#73976,#73977,#73978,#73979,#73980,#73981,#73982,#73983,#73984,
#73985,#73986,#73987,#73988,#73989,#73990,#73991,#73992,#73993,#73994,#73995,
#73996,#73997,#73998,#73999,#74000,#74001,#74002,#74003,#74004,#74005,#74006,
#74007,#74008,#74009,#74010,#74011,#74012,#74013,#74014,#74015,#74016,#74017,
#74018,#74019,#74020,#74021,#74022,#74023,#74024,#74025,#74026,#74027,#74028,
#74029,#74030,#74031,#74032,#74033,#74034,#74035),.UNSPECIFIED.,.F.,.F.,
(4,2,2,2,2,2,2,2,2,2,2,2,2,2,2,2,2,2,2,2,2,2,2,2,2,2,2,2,2,2,2,2,2,2,2,
2,2,2,2,2,2,2,2,2,2,2,2,2,2,2,2,2,2,2,2,2,2,2,2,2,2,2,2,2,2,2,2,2,2,2,2,
2,2,2,2,2,2,2,2,2,2,2,2,2,2,2,2,2,2,2,2,2,2,4),(-0.980876168428268,-0.977054577333388,
-0.971058136352527,-0.947128510180332,-0.913627961840072,-0.907482535791466,
-0.904833905222632,-0.902818455338693,-0.900419719119447,-0.895784983276597,
-0.878273227041829,-0.83826909371721,-0.831190969785972,-0.827105983365669,
-0.823580675930354,-0.819143780139889,-0.81004528608956,-0.797644721499304,
-0.778040914206429,-0.756182211256192,-0.751259083678782,-0.748803498409371,
-0.746995320137182,-0.744489719700661,-0.739305420901276,-0.732143731276741,
-0.710920394724917,-0.683059416039829,-0.675779308071825,-0.671651124032574,
-0.668095803463219,-0.663700414361992,-0.654828950867061,-0.633288137205705,
-0.606124496814735,-0.597379435812432,-0.594242696942268,-0.592365256933383,
-0.59023062496181,-0.586847378039513,-0.574888246676247,-0.547530371600936,
-0.525006295033887,-0.51896894127087,-0.515138976049794,-0.511512913338456,
-0.506536511101398,-0.494064408776799,-0.474210112073718,-0.44445913581959,
-0.439936071794941,-0.43753211068626,-0.435517392602543,-0.432830240312782,
-0.426624007951772,-0.417444101433213,-0.379483725265717,-0.367259580537071,
-0.362198184110808,-0.358593915911576,-0.354799609725716,-0.348936152852545,
-0.327401860553773,-0.318880499806321,-0.288795859276366,-0.284304324023758,
-0.281907073605292,-0.279891463930923,-0.277194552678228,-0.270929622593811,
-0.261626923386461,-0.221977407363355,-0.211100078830289,-0.206738840858881,
-0.20311499433603,-0.199352136194739,-0.193643715993576,-0.174309406808942,
-0.144190326869769,-0.131417655661919,-0.127864249414894,-0.125692908616759,
-0.123592591542536,-0.120838162179996,-0.112761670237951,-0.0990543182056354,
-0.0674553159482955,-0.0558526492312413,-0.0513687559118857,-0.0480461738853702,
-0.044381004067567,-0.0391794224292523,-0.0332689907290768,-0.000593869235482755),
 .UNSPECIFIED.);
#776=B_SPLINE_CURVE_WITH_KNOTS('',3,(#74041,#74042,#74043,#74044),
 .UNSPECIFIED.,.F.,.F.,(4,4),(-0.000575552145866446,-0.000460828836829869),
 .UNSPECIFIED.);
#777=B_SPLINE_CURVE_WITH_KNOTS('',3,(#74045,#74046,#74047,#74048,#74049,
#74050,#74051,#74052,#74053,#74054,#74055,#74056,#74057,#74058,#74059,#74060,
#74061,#74062,#74063,#74064,#74065,#74066,#74067,#74068,#74069,#74070,#74071,
#74072,#74073,#74074,#74075,#74076,#74077,#74078,#74079,#74080,#74081,#74082,
#74083,#74084,#74085,#74086,#74087,#74088,#74089,#74090,#74091,#74092,#74093,
#74094,#74095,#74096,#74097,#74098,#74099,#74100,#74101,#74102,#74103,#74104,
#74105,#74106,#74107,#74108,#74109,#74110,#74111,#74112,#74113,#74114,#74115,
#74116,#74117,#74118,#74119,#74120,#74121,#74122,#74123,#74124,#74125,#74126,
#74127,#74128,#74129,#74130,#74131,#74132,#74133,#74134,#74135,#74136,#74137,
#74138,#74139,#74140,#74141,#74142,#74143,#74144,#74145,#74146,#74147,#74148,
#74149,#74150,#74151,#74152,#74153,#74154,#74155,#74156,#74157,#74158,#74159,
#74160,#74161,#74162,#74163,#74164,#74165,#74166,#74167,#74168,#74169,#74170,
#74171,#74172,#74173,#74174,#74175,#74176,#74177,#74178,#74179,#74180,#74181,
#74182,#74183,#74184,#74185,#74186,#74187,#74188,#74189,#74190,#74191,#74192,
#74193,#74194,#74195,#74196,#74197,#74198,#74199,#74200,#74201,#74202,#74203,
#74204,#74205,#74206,#74207,#74208,#74209,#74210,#74211,#74212,#74213,#74214,
#74215,#74216,#74217,#74218,#74219,#74220,#74221,#74222,#74223,#74224,#74225,
#74226,#74227,#74228,#74229,#74230,#74231,#74232,#74233,#74234,#74235,#74236,
#74237,#74238,#74239,#74240,#74241,#74242,#74243,#74244,#74245,#74246),
 .UNSPECIFIED.,.F.,.F.,(4,2,2,2,2,2,2,2,2,2,2,2,2,2,2,2,2,2,2,2,2,2,2,2,
2,2,2,2,2,2,2,2,2,2,2,2,2,2,2,2,2,2,2,2,2,2,2,2,2,2,2,2,2,2,2,2,2,2,2,2,
2,2,2,2,2,2,2,2,2,2,2,2,2,2,2,2,2,2,2,2,2,2,2,2,2,2,2,2,2,2,2,2,2,2,2,2,
2,2,2,2,4),(-1.961075810873,-1.91899853770295,-1.90998182103901,-1.90694299155077,
-1.90491534220976,-1.90304236077713,-1.8997563454517,-1.8893489139275,-1.86341553042212,
-1.84622210656141,-1.83844349395447,-1.83215983190748,-1.83188418037971,
-1.83161731506151,-1.83135527090537,-1.83109406229579,-1.8308294449826,
-1.83055660950542,-1.83026974685407,-1.82996137869829,-1.82986837677026,
-1.82968979753097,-1.82929230164806,-1.82582900399034,-1.82179662391704,
-1.81466844992312,-1.78236237688157,-1.76408344162407,-1.75441378202244,
-1.75130115434868,-1.7492588257632,-1.7471417152126,-1.74367783445721,-1.73139069868062,
-1.68623717362766,-1.67774757120391,-1.67348987226925,-1.67002732821849,
-1.6659895482079,-1.65883478865551,-1.62757226213126,-1.60857171259333,
-1.59868595244813,-1.59555035007265,-1.59350350518122,-1.59165102702241,
-1.58847137800807,-1.57900844240478,-1.55236121576361,-1.5283076110314,
-1.5211548559745,-1.51715893867982,-1.51369317433401,-1.50938093191052,
-1.50256268998503,-1.46193662360606,-1.44402953233452,-1.44033945560061,
-1.43817346777158,-1.4361845989699,-1.43324681038929,-1.42565416635324,
-1.39750794326695,-1.37496776301316,-1.36634819298059,-1.36206593053318,
-1.35860168529218,-1.35458239461893,-1.34751548241122,-1.30750617965681,
-1.29448563991458,-1.28664220003162,-1.28375081202092,-1.28175019362452,
-1.27955941510628,-1.27575453902151,-1.25548477657915,-1.23972014239311,
-1.22295403440966,-1.21179633566403,-1.20708473601124,-1.20357254405719,
-1.19979250101891,-1.1936850302796,-1.1673764481476,-1.14772300672639,-1.13232057046893,
-1.12875071981942,-1.12661057406961,-1.12460748037476,-1.12159283019553,
-1.11342327548466,-1.07482374194821,-1.05772822712093,-1.05229567064237,
-1.04865398905507,-1.04510515845138,-1.0399686208525,-1.02678462238953,
-0.989724130567848,-0.980645665338926),.UNSPECIFIED.);
#778=B_SPLINE_CURVE_WITH_KNOTS('',3,(#74248,#74249,#74250,#74251),
 .UNSPECIFIED.,.F.,.F.,(4,4),(-0.000593869235482755,-0.000459408681297817),
 .UNSPECIFIED.);
#779=B_SPLINE_CURVE_WITH_KNOTS('',3,(#74252,#74253,#74254,#74255,#74256,
#74257,#74258,#74259,#74260,#74261,#74262,#74263,#74264,#74265,#74266,#74267,
#74268,#74269,#74270,#74271,#74272,#74273,#74274,#74275,#74276,#74277,#74278,
#74279,#74280,#74281,#74282,#74283,#74284,#74285,#74286,#74287,#74288,#74289,
#74290,#74291,#74292,#74293,#74294,#74295,#74296,#74297,#74298,#74299,#74300,
#74301,#74302,#74303,#74304,#74305,#74306,#74307,#74308,#74309,#74310,#74311,
#74312,#74313,#74314,#74315,#74316,#74317,#74318,#74319,#74320,#74321,#74322,
#74323,#74324,#74325,#74326,#74327,#74328,#74329,#74330,#74331,#74332,#74333,
#74334,#74335,#74336,#74337,#74338,#74339,#74340,#74341,#74342,#74343,#74344,
#74345,#74346,#74347,#74348,#74349,#74350,#74351,#74352,#74353,#74354,#74355,
#74356,#74357,#74358,#74359,#74360,#74361,#74362,#74363,#74364,#74365,#74366,
#74367,#74368,#74369,#74370,#74371,#74372,#74373,#74374,#74375,#74376,#74377,
#74378,#74379,#74380,#74381,#74382,#74383,#74384,#74385,#74386,#74387,#74388,
#74389,#74390,#74391,#74392,#74393,#74394,#74395,#74396,#74397,#74398,#74399,
#74400,#74401,#74402,#74403,#74404,#74405,#74406,#74407,#74408,#74409,#74410,
#74411,#74412,#74413,#74414,#74415,#74416,#74417,#74418,#74419,#74420,#74421,
#74422,#74423,#74424,#74425,#74426,#74427,#74428,#74429,#74430,#74431,#74432,
#74433,#74434,#74435,#74436,#74437,#74438,#74439,#74440,#74441,#74442,#74443,
#74444,#74445,#74446,#74447),.UNSPECIFIED.,.F.,.F.,(4,2,2,2,2,2,2,2,2,2,
2,2,2,2,2,2,2,2,2,2,2,2,2,2,2,2,2,2,2,2,2,2,2,2,2,2,2,2,2,2,2,2,2,2,2,2,
2,2,2,2,2,2,2,2,2,2,2,2,2,2,2,2,2,2,2,2,2,2,2,2,2,2,2,2,2,2,2,2,2,2,2,2,
2,2,2,2,2,2,2,2,2,2,2,2,2,2,2,4),(-1.96095646099311,-1.93797621015352,-1.9347460978949,
-1.93254341532058,-1.93041904654259,-1.92827638974903,-1.92485595093305,
-1.91354033516731,-1.88921053153627,-1.86780065348812,-1.8591642713876,
-1.85476922440857,-1.85121379045361,-1.84708503604146,-1.83980280839497,
-1.81192126711676,-1.79068411128328,-1.78351891530459,-1.77833314729868,
-1.77582719487037,-1.77401893116401,-1.77156344685772,-1.76664120722514,
-1.74478166349544,-1.72518210094038,-1.71279999533315,-1.70371020745299,
-1.69927475738958,-1.69571666817842,-1.69161797086906,-1.68447675942516,
-1.65166771350105,-1.62594442589702,-1.62195617052201,-1.61969121517274,
-1.61764235909756,-1.61469844374575,-1.60732581056317,-1.57534812098983,
-1.55177478391219,-1.5457960189052,-1.54197781464795,-1.53834516078742,
-1.53333095064799,-1.52138774635452,-1.4830397119817,-1.4738260797527,-1.46760396261687,
-1.46491391257529,-1.46289870369644,-1.46049614633478,-1.45598067874288,
-1.42616602642821,-1.40636450065013,-1.39391143065581,-1.38893724766454,
-1.38531106842197,-1.38147940727529,-1.37543602554564,-1.35279227623871,
-1.325500776513,-1.3135518393757,-1.31016886069965,-1.30803404276792,-1.30615612044012,
-1.30301807546051,-1.29426535540527,-1.26712253259344,-1.24559510288315,
-1.23672438290905,-1.2323286050034,-1.22877258450223,-1.22464315431967,
-1.21735974942338,-1.18946990832735,-1.16823199635046,-1.16106610088098,
-1.15587973537714,-1.15337341850365,-1.15156485961709,-1.14910892750324,
-1.1441856525028,-1.12229264185881,-1.10245524418662,-1.09021670995437,
-1.08120233489742,-1.07678014582888,-1.07322241907951,-1.06911280232661,
-1.06192255250942,-1.02993008681522,-1.01160663459219,-1.00188219983893,
-0.998715416197789,-0.996625442669738,-0.994709137080463,-0.991364475530684,
-0.980870200702631),.UNSPECIFIED.);
#780=B_SPLINE_CURVE_WITH_KNOTS('',3,(#74452,#74453,#74454,#74455,#74456,
#74457,#74458,#74459,#74460,#74461,#74462,#74463,#74464,#74465,#74466,#74467,
#74468,#74469,#74470,#74471,#74472,#74473,#74474,#74475,#74476,#74477,#74478,
#74479,#74480,#74481,#74482,#74483,#74484,#74485,#74486,#74487,#74488,#74489,
#74490,#74491,#74492,#74493,#74494,#74495,#74496,#74497,#74498,#74499,#74500,
#74501,#74502,#74503,#74504,#74505,#74506,#74507,#74508,#74509,#74510,#74511,
#74512,#74513,#74514,#74515,#74516,#74517,#74518,#74519,#74520,#74521,#74522,
#74523,#74524,#74525,#74526,#74527,#74528,#74529,#74530,#74531,#74532,#74533,
#74534,#74535,#74536,#74537,#74538,#74539,#74540,#74541,#74542,#74543,#74544,
#74545,#74546,#74547,#74548,#74549,#74550,#74551,#74552,#74553,#74554,#74555,
#74556,#74557,#74558,#74559,#74560,#74561,#74562,#74563,#74564,#74565,#74566,
#74567,#74568,#74569,#74570,#74571,#74572,#74573,#74574,#74575,#74576,#74577,
#74578,#74579,#74580,#74581,#74582,#74583,#74584,#74585,#74586,#74587,#74588,
#74589,#74590,#74591,#74592,#74593,#74594,#74595,#74596,#74597,#74598,#74599,
#74600,#74601,#74602,#74603,#74604,#74605,#74606,#74607,#74608,#74609,#74610,
#74611,#74612,#74613,#74614,#74615,#74616,#74617,#74618,#74619,#74620,#74621,
#74622,#74623,#74624,#74625,#74626,#74627,#74628,#74629,#74630,#74631,#74632,
#74633,#74634,#74635,#74636,#74637,#74638,#74639,#74640,#74641,#74642,#74643,
#74644,#74645,#74646,#74647,#74648,#74649),.UNSPECIFIED.,.F.,.F.,(4,2,2,
2,2,2,2,2,2,2,2,2,2,2,2,2,2,2,2,2,2,2,2,2,2,2,2,2,2,2,2,2,2,2,2,2,2,2,2,
2,2,2,2,2,2,2,2,2,2,2,2,2,2,2,2,2,2,2,2,2,2,2,2,2,2,2,2,2,2,2,2,2,2,2,2,
2,2,2,2,2,2,2,2,2,2,2,2,2,2,2,2,2,2,2,2,2,2,2,4),(-0.980863317691536,-0.965867117327354,
-0.960509977420319,-0.957246005987621,-0.953700602037113,-0.948778820150156,
-0.936160706365215,-0.915796960466177,-0.886633299232025,-0.882101790965228,
-0.879731730871915,-0.877791687500907,-0.875235281143686,-0.869564325728112,
-0.861418051207541,-0.833411462878822,-0.811346039029316,-0.805410731783076,
-0.801666513767412,-0.798139560333822,-0.793332781792027,-0.781537061532407,
-0.763266075494988,-0.734529140602185,-0.727602164655597,-0.724769359783965,
-0.722778449107396,-0.720563024669574,-0.716642471906693,-0.711668238966146,
-0.700170469933032,-0.664625105612122,-0.653268497146771,-0.648885013568821,
-0.64564373405902,-0.642077590800852,-0.637040066926753,-0.623543900163697,
-0.600708867265467,-0.575511695663898,-0.570716949960351,-0.568322971638379,
-0.566562074793609,-0.564132239351519,-0.559151679267259,-0.552325315706278,
-0.53274413159117,-0.502342724765227,-0.495166210540832,-0.491123668033165,
-0.487661210975058,-0.483408908339107,-0.474949025075862,-0.456241589004391,
-0.425830697244409,-0.416794217648005,-0.413666201389874,-0.411823256843222,
-0.409765135979663,-0.406575817981292,-0.39616940360447,-0.375325037058781,
-0.346670459095679,-0.340096333282019,-0.335854279904117,-0.332392069852111,
-0.328340602631258,-0.3209145732756,-0.311447462031061,-0.287073273178223,
-0.264187156199857,-0.259311646353736,-0.256901878484548,-0.25514152450932,
-0.252727849594165,-0.247832003799856,-0.227509167754953,-0.189707310226555,
-0.183095414116581,-0.179210607710657,-0.175728497822314,-0.171240891875978,
-0.161467671206921,-0.147666351322913,-0.129541294107978,-0.106706335594181,
-0.10286893895474,-0.100671349009583,-0.0986738861195674,-0.0958001874210858,
-0.0880853442082756,-0.0557117277541239,-0.0327323384169256,-0.0267749109151,
-0.0230263763554905,-0.0197066597234133,-0.0162728494754162,-0.00976563376091629,
-0.000575552145866446),.UNSPECIFIED.);
#781=B_SPLINE_CURVE_WITH_KNOTS('',3,(#74650,#74651,#74652,#74653,#74654,
#74655,#74656,#74657,#74658,#74659,#74660,#74661,#74662,#74663,#74664,#74665,
#74666,#74667,#74668,#74669,#74670,#74671,#74672,#74673,#74674,#74675,#74676,
#74677,#74678,#74679,#74680,#74681,#74682,#74683,#74684,#74685,#74686,#74687,
#74688,#74689,#74690,#74691,#74692,#74693,#74694,#74695,#74696,#74697,#74698,
#74699,#74700,#74701,#74702,#74703,#74704,#74705,#74706,#74707,#74708,#74709,
#74710,#74711,#74712,#74713,#74714,#74715,#74716,#74717,#74718,#74719,#74720,
#74721,#74722,#74723,#74724,#74725,#74726,#74727,#74728,#74729,#74730,#74731,
#74732,#74733,#74734,#74735,#74736,#74737,#74738,#74739,#74740,#74741,#74742,
#74743,#74744,#74745,#74746,#74747,#74748,#74749,#74750,#74751,#74752,#74753,
#74754,#74755,#74756,#74757,#74758,#74759,#74760,#74761,#74762,#74763,#74764,
#74765,#74766,#74767,#74768,#74769,#74770,#74771,#74772,#74773,#74774,#74775,
#74776,#74777,#74778,#74779,#74780,#74781,#74782,#74783,#74784,#74785,#74786,
#74787,#74788,#74789,#74790,#74791,#74792,#74793,#74794,#74795,#74796,#74797,
#74798,#74799,#74800,#74801,#74802,#74803,#74804,#74805,#74806,#74807,#74808,
#74809,#74810,#74811,#74812,#74813,#74814,#74815,#74816,#74817,#74818,#74819,
#74820,#74821,#74822,#74823,#74824,#74825,#74826,#74827,#74828,#74829,#74830,
#74831,#74832,#74833),.UNSPECIFIED.,.F.,.F.,(4,2,2,2,2,2,2,2,2,2,2,2,2,
2,2,2,2,2,2,2,2,2,2,2,2,2,2,2,2,2,2,2,2,2,2,2,2,2,2,2,2,2,2,2,2,2,2,2,2,
2,2,2,2,2,2,2,2,2,2,2,2,2,2,2,2,2,2,2,2,2,2,2,2,2,2,2,2,2,2,2,2,2,2,2,2,
2,2,2,2,2,2,4),(-0.980870200702631,-0.959233141018411,-0.93190896443026,
-0.924624978851224,-0.920495370274395,-0.916939257898618,-0.91254344802788,
-0.903673180419709,-0.881982256206798,-0.854580117112285,-0.846121338780522,
-0.843022317621479,-0.840966102919178,-0.838765037533061,-0.835075393420603,
-0.818476808473076,-0.784580675202224,-0.771866281982843,-0.766721228358717,
-0.763102076304601,-0.759330410068892,-0.753580809435499,-0.733717236154346,
-0.715126304519363,-0.692092080343054,-0.688187746217947,-0.685940577943202,
-0.683884040587284,-0.680895671239572,-0.672655764602268,-0.658699668096323,
-0.623474250443168,-0.61437873329379,-0.609941876992769,-0.606383262467072,
-0.602284622260668,-0.594946843738724,-0.570014243225577,-0.54140189445304,
-0.534395639274989,-0.531506733698327,-0.529466550543011,-0.52717683878325,
-0.523072437473335,-0.517823279884699,-0.505421432498898,-0.46416692731791,
-0.457272884855933,-0.453265143176066,-0.449694296194633,-0.445117747607311,
-0.435228549961263,-0.42127824178971,-0.403401120909165,-0.380802589911048,
-0.376914723694649,-0.374671180476488,-0.372613267552639,-0.369616253580438,
-0.361308613811237,-0.347171414597535,-0.311227236971825,-0.302865741900337,
-0.298513455877025,-0.294959963192897,-0.290796418098491,-0.283134262465949,
-0.273323743896622,-0.247400704669714,-0.226926391642494,-0.222011856884129,
-0.219557785889306,-0.217749322902074,-0.215241546837998,-0.210046558937141,
-0.202865165695763,-0.181531973896022,-0.1538286593312,-0.146535290734253,
-0.142403965070233,-0.13884840128958,-0.134455871016647,-0.125601745092855,
-0.103360060575001,-0.0750737990044077,-0.0676887033980364,-0.0647427232674537,
-0.0626934621791439,-0.0604290573631328,-0.0564441447427007,-0.0309181846902309,
-0.000459946153919901),.UNSPECIFIED.);
#782=B_SPLINE_CURVE_WITH_KNOTS('',3,(#74838,#74839,#74840,#74841,#74842,
#74843,#74844,#74845,#74846,#74847,#74848,#74849,#74850,#74851,#74852,#74853,
#74854,#74855,#74856,#74857,#74858,#74859,#74860,#74861,#74862,#74863,#74864,
#74865,#74866,#74867,#74868,#74869,#74870,#74871,#74872,#74873,#74874,#74875,
#74876,#74877,#74878,#74879,#74880,#74881,#74882,#74883,#74884,#74885,#74886,
#74887,#74888,#74889,#74890,#74891,#74892,#74893,#74894,#74895,#74896,#74897,
#74898,#74899,#74900,#74901,#74902,#74903,#74904,#74905,#74906,#74907,#74908,
#74909,#74910,#74911,#74912,#74913,#74914,#74915,#74916,#74917,#74918,#74919,
#74920,#74921,#74922,#74923,#74924,#74925,#74926,#74927,#74928,#74929,#74930,
#74931,#74932,#74933,#74934,#74935,#74936,#74937,#74938,#74939,#74940,#74941,
#74942,#74943,#74944,#74945,#74946,#74947,#74948,#74949,#74950,#74951,#74952,
#74953,#74954,#74955,#74956,#74957,#74958,#74959,#74960,#74961,#74962,#74963,
#74964,#74965,#74966,#74967,#74968,#74969,#74970,#74971,#74972,#74973,#74974,
#74975,#74976,#74977,#74978,#74979,#74980,#74981,#74982,#74983,#74984,#74985,
#74986,#74987,#74988,#74989,#74990,#74991,#74992,#74993,#74994,#74995,#74996,
#74997,#74998,#74999,#75000,#75001,#75002,#75003,#75004,#75005,#75006,#75007,
#75008,#75009,#75010,#75011,#75012,#75013,#75014,#75015,#75016,#75017,#75018,
#75019,#75020,#75021,#75022,#75023),.UNSPECIFIED.,.F.,.F.,(4,2,2,2,2,2,
2,2,2,2,2,2,2,2,2,2,2,2,2,2,2,2,2,2,2,2,2,2,2,2,2,2,2,2,2,2,2,2,2,2,2,2,
2,2,2,2,2,2,2,2,2,2,2,2,2,2,2,2,2,2,2,2,2,2,2,2,2,2,2,2,2,2,2,2,2,2,2,2,
2,2,2,2,2,2,2,2,2,2,2,2,2,2,4),(-1.96110176712048,-1.93829452872204,-1.9186414530334,
-1.9006083574055,-1.89511660925849,-1.89148282314228,-1.8879775752466,-1.88296957684836,
-1.8705452485945,-1.83871994755745,-1.82085867669616,-1.81624560361653,
-1.8138996090342,-1.81194724276637,-1.80942122989633,-1.8037698646084,-1.77377296835817,
-1.75031288736422,-1.74158015519043,-1.73727086618697,-1.73379725776558,
-1.72978049298282,-1.72275139326327,-1.68282918403212,-1.66990776228069,
-1.66210217842162,-1.65920917062187,-1.65720301166931,-1.65500399323105,
-1.65116775426461,-1.62844641714766,-1.61049576819412,-1.5965862356164,
-1.5867598494002,-1.5822626255474,-1.57877859390135,-1.57489724205419,-1.5683054359448,
-1.53026405657233,-1.51002820173751,-1.50514152785202,-1.5027302127129,
-1.50097133141034,-1.49856354659451,-1.49368966976771,-1.47157101569616,
-1.45146416591831,-1.43938269548927,-1.43049338145184,-1.42616464337538,
-1.42273291481658,-1.41876854997284,-1.41194303965079,-1.37078896027392,
-1.35822156490455,-1.3505599610277,-1.3476955096223,-1.34570092152039,-1.34350102237631,
-1.33965322447287,-1.31655626217935,-1.29810095462964,-1.28467235989981,
-1.27508348352818,-1.27062655032077,-1.26714662126167,-1.26324183739805,
-1.25653819528689,-1.21940199925403,-1.19865761267728,-1.19371779055523,
-1.19129475812602,-1.18953338640535,-1.18713056761634,-1.18229177995356,
-1.15869262558282,-1.13481850835135,-1.12098292052455,-1.11590301804018,
-1.1123290773621,-1.10909528462873,-1.10474409925921,-1.09369781525337,
-1.06070327618473,-1.04725096680036,-1.03923958507351,-1.0363260922519,
-1.03432190919966,-1.03214053542194,-1.02837803395873,-1.0101859617264,
-0.980971677752746,-0.980863317691536),.UNSPECIFIED.);
#783=B_SPLINE_CURVE_WITH_KNOTS('',3,(#75024,#75025,#75026,#75027,#75028,
#75029,#75030,#75031,#75032,#75033,#75034,#75035,#75036,#75037,#75038,#75039,
#75040,#75041,#75042,#75043,#75044,#75045,#75046,#75047,#75048,#75049,#75050,
#75051,#75052,#75053,#75054,#75055,#75056,#75057,#75058,#75059,#75060,#75061,
#75062,#75063,#75064,#75065,#75066,#75067,#75068,#75069,#75070,#75071,#75072,
#75073,#75074,#75075,#75076,#75077,#75078,#75079,#75080,#75081,#75082,#75083,
#75084,#75085,#75086,#75087,#75088,#75089,#75090,#75091,#75092,#75093,#75094,
#75095,#75096,#75097,#75098,#75099,#75100,#75101,#75102,#75103,#75104,#75105,
#75106,#75107,#75108,#75109,#75110,#75111,#75112,#75113,#75114,#75115,#75116,
#75117,#75118,#75119,#75120,#75121,#75122,#75123,#75124,#75125,#75126,#75127,
#75128,#75129,#75130,#75131,#75132,#75133,#75134,#75135,#75136,#75137,#75138,
#75139,#75140,#75141,#75142,#75143,#75144,#75145,#75146,#75147,#75148,#75149,
#75150,#75151,#75152,#75153,#75154,#75155,#75156,#75157,#75158,#75159,#75160,
#75161,#75162,#75163,#75164,#75165,#75166,#75167,#75168,#75169,#75170,#75171,
#75172,#75173,#75174,#75175,#75176,#75177,#75178,#75179,#75180,#75181,#75182,
#75183,#75184,#75185,#75186,#75187,#75188,#75189,#75190,#75191,#75192,#75193,
#75194,#75195,#75196,#75197,#75198),.UNSPECIFIED.,.F.,.F.,(4,3,3,3,3,3,
3,3,3,3,3,3,3,3,3,3,3,3,3,3,3,3,3,3,3,3,3,3,3,3,3,3,3,3,3,3,3,3,3,3,3,3,
3,3,3,3,3,3,3,3,3,3,3,3,3,3,3,3,4),(84.8230016469244,84.9358865834066,85.0488192149489,
85.161925902012,85.2751347285546,85.3885713550513,85.4183497357604,85.5300439425675,
85.6415395478339,85.7529242433787,85.8642409672866,85.9755325604619,86.0869248023224,
86.198363088933,86.3100187360176,86.4156866035529,86.5273871490937,86.638889046833,
86.7502800027488,86.8616029448844,86.9729007040699,87.0842989814853,87.1957432424682,
87.307404682471,87.4130234713455,87.5247274427104,87.636232886227,87.7476274581574,
87.8589540796684,87.9702555748027,88.0816576457093,88.1931057379006,88.3047710215193,
88.4103603391381,88.5220342594052,88.6335095720259,88.7448739843744,88.856170468079,
88.9674418975776,89.0788142562456,89.1902327795706,89.3018691256319,89.4076972069306,
89.5194208240826,89.6309455635425,89.7423592069936,89.8537046463937,89.9650246763212,
90.0764446943708,90.187910442542,90.2995926613635,90.4050340747232,90.5159923259385,
90.6267854997885,90.7374578203841,90.8480714967823,90.9586521781964,91.0692819971788,
91.106186954104),.UNSPECIFIED.);
#784=B_SPLINE_CURVE_WITH_KNOTS('',3,(#75202,#75203,#75204,#75205,#75206,
#75207,#75208,#75209,#75210,#75211,#75212,#75213,#75214,#75215,#75216,#75217,
#75218,#75219,#75220,#75221,#75222,#75223,#75224,#75225,#75226,#75227,#75228,
#75229,#75230,#75231,#75232,#75233,#75234,#75235,#75236,#75237,#75238,#75239,
#75240,#75241,#75242,#75243,#75244,#75245,#75246,#75247,#75248,#75249,#75250,
#75251,#75252,#75253,#75254,#75255,#75256,#75257,#75258,#75259,#75260,#75261,
#75262),.UNSPECIFIED.,.F.,.F.,(4,3,3,3,3,3,3,3,3,3,3,3,3,3,3,3,3,3,3,3,
4),(-4.09254174883832,-3.98934747117026,-3.88363643282297,-3.77808492915444,
-3.6726592602599,-3.56730087600952,-3.46197396509548,-3.35664276205073,
-3.25120381048226,-3.14570400968359,-3.04002763980351,-2.99201060337769,
-2.88747517765022,-2.78311496418647,-2.67885241980798,-2.57465006492938,
-2.47047050196767,-2.36620671122195,-2.26190327247319,-2.15741710786687,
-2.06549325648379),.UNSPECIFIED.);
#785=B_SPLINE_CURVE_WITH_KNOTS('',3,(#75266,#75267,#75268,#75269,#75270,
#75271,#75272,#75273,#75274,#75275,#75276,#75277,#75278,#75279,#75280,#75281,
#75282,#75283,#75284,#75285,#75286,#75287,#75288,#75289,#75290,#75291,#75292,
#75293,#75294,#75295,#75296,#75297,#75298,#75299),.UNSPECIFIED.,.F.,.F.,
(4,3,3,3,3,3,3,3,3,3,3,4),(0.,0.107971890026954,0.219243757071925,0.327137813760554,
0.435034263883378,0.542962282944035,0.650951076303133,0.759107773599422,
0.867362596774567,0.975816836522539,0.998146826386724,1.11419103802952),
 .UNSPECIFIED.);
#786=B_SPLINE_CURVE_WITH_KNOTS('',3,(#75301,#75302,#75303,#75304,#75305,
#75306,#75307,#75308,#75309,#75310,#75311,#75312,#75313,#75314,#75315,#75316,
#75317,#75318,#75319,#75320,#75321,#75322,#75323,#75324,#75325,#75326,#75327,
#75328,#75329,#75330,#75331,#75332,#75333,#75334,#75335,#75336,#75337,#75338,
#75339,#75340,#75341,#75342,#75343,#75344,#75345,#75346,#75347,#75348,#75349,
#75350,#75351,#75352,#75353,#75354,#75355,#75356,#75357,#75358,#75359,#75360,
#75361,#75362,#75363,#75364,#75365,#75366,#75367,#75368,#75369,#75370,#75371,
#75372,#75373,#75374,#75375,#75376,#75377,#75378,#75379,#75380,#75381,#75382,
#75383,#75384,#75385,#75386,#75387,#75388,#75389,#75390,#75391,#75392,#75393,
#75394,#75395,#75396,#75397,#75398,#75399,#75400,#75401,#75402,#75403,#75404,
#75405,#75406,#75407,#75408,#75409,#75410,#75411,#75412,#75413,#75414,#75415,
#75416,#75417,#75418,#75419,#75420,#75421,#75422,#75423,#75424,#75425,#75426,
#75427,#75428,#75429,#75430,#75431,#75432,#75433,#75434,#75435,#75436,#75437,
#75438,#75439,#75440,#75441,#75442,#75443,#75444,#75445,#75446,#75447,#75448,
#75449,#75450,#75451,#75452,#75453,#75454,#75455,#75456,#75457,#75458,#75459,
#75460,#75461,#75462,#75463,#75464,#75465,#75466,#75467,#75468,#75469,#75470,
#75471,#75472,#75473,#75474,#75475,#75476,#75477,#75478,#75479,#75480,#75481,
#75482,#75483,#75484,#75485,#75486,#75487,#75488,#75489,#75490),
 .UNSPECIFIED.,.F.,.F.,(4,3,3,3,3,3,3,3,3,3,3,3,3,3,3,3,3,3,3,3,3,3,3,3,
3,3,3,3,3,3,3,3,3,3,3,3,3,3,3,3,3,3,3,3,3,3,3,3,3,3,3,3,3,3,3,3,3,3,3,3,
3,3,3,4),(1.11419103844362,1.21719178712621,1.32003180936696,1.42278371743724,
1.52548628532692,1.62817819909424,1.7309676550256,1.83380962645345,1.93683300941319,
1.99629365277347,2.10195062249824,2.20744865406854,2.31282196833917,2.41812869905107,
2.52340471398939,2.62868583588416,2.73407645641426,2.83952870871035,2.94515978418996,
2.9944404791602,3.10012104081475,3.20564648920596,3.31105278134987,3.41639592985287,
3.52171175683583,3.62703604294105,3.7324746359267,3.83797767810928,3.94366338405182,
3.99258730554694,4.09793916383869,4.20312978186129,4.30819381927125,4.41319030347723,
4.51815558391299,4.62312596419388,4.72820798570695,4.83335241117602,4.93868011359328,
4.99073413193368,5.09626132963981,5.20162955424616,5.30687369011875,5.4120517192167,
5.51719971962021,5.62235372499639,5.72761949265099,5.83294800853446,5.93845839412689,
5.98888095832042,6.09439886020279,6.19975815061375,6.30499393635141,6.41016398359831,
6.51530438389174,6.62045118475443,6.72571040049498,6.83103272751,6.93653755417126,
6.98702778470716,7.10330090801871,7.21921658035719,7.33454806250759,7.39737593147595),
 .UNSPECIFIED.);
#787=B_SPLINE_CURVE_WITH_KNOTS('',3,(#75492,#75493,#75494,#75495,#75496,
#75497,#75498,#75499,#75500,#75501),.UNSPECIFIED.,.F.,.F.,(4,1,1,1,1,1,
1,4),(7.39737634520911,7.9851746110939,8.98332143748063,9.98146826386737,
10.9796150902541,11.9777619166408,12.9759087430276,13.6805616523887),
 .UNSPECIFIED.);
#788=B_SPLINE_CURVE_WITH_KNOTS('',3,(#75503,#75504,#75505,#75506,#75507,
#75508,#75509,#75510,#75511,#75512,#75513,#75514,#75515,#75516,#75517,#75518,
#75519,#75520,#75521,#75522,#75523,#75524,#75525,#75526,#75527,#75528,#75529,
#75530,#75531,#75532,#75533,#75534,#75535,#75536,#75537,#75538,#75539,#75540,
#75541,#75542,#75543,#75544,#75545,#75546,#75547,#75548,#75549,#75550,#75551,
#75552,#75553,#75554,#75555,#75556,#75557,#75558,#75559,#75560,#75561,#75562,
#75563,#75564,#75565,#75566,#75567,#75568,#75569,#75570,#75571,#75572,#75573,
#75574,#75575,#75576,#75577,#75578,#75579,#75580,#75581,#75582,#75583,#75584,
#75585,#75586,#75587,#75588,#75589,#75590,#75591,#75592,#75593,#75594,#75595,
#75596,#75597,#75598,#75599,#75600,#75601,#75602,#75603,#75604,#75605,#75606,
#75607,#75608,#75609,#75610,#75611,#75612,#75613,#75614,#75615,#75616,#75617,
#75618,#75619,#75620,#75621,#75622,#75623,#75624,#75625,#75626,#75627,#75628,
#75629,#75630,#75631,#75632,#75633,#75634,#75635,#75636,#75637,#75638,#75639,
#75640,#75641,#75642,#75643,#75644,#75645,#75646,#75647,#75648,#75649,#75650,
#75651,#75652,#75653,#75654,#75655,#75656,#75657,#75658,#75659,#75660,#75661,
#75662,#75663,#75664,#75665,#75666,#75667,#75668,#75669,#75670,#75671,#75672,
#75673,#75674,#75675,#75676,#75677,#75678,#75679,#75680,#75681,#75682,#75683,
#75684,#75685,#75686,#75687,#75688,#75689,#75690,#75691,#75692),
 .UNSPECIFIED.,.F.,.F.,(4,3,3,3,3,3,3,3,3,3,3,3,3,3,3,3,3,3,3,3,3,3,3,3,
3,3,3,3,3,3,3,3,3,3,3,3,3,3,3,3,3,3,3,3,3,3,3,3,3,3,3,3,3,3,3,3,3,3,3,3,
3,3,3,4),(13.6805618202843,13.8080138554844,13.9373859483242,13.9740555694143,
14.0795516490623,14.1848886090792,14.2901014205325,14.3952481069312,14.5003647949379,
14.6054875668125,14.7107224370753,14.8160202021566,14.9215003896649,14.972202395801,
15.0776983156651,15.1830351147283,15.2882477642988,15.3933942883333,15.4985108137438,
15.6036334230391,15.7088681318705,15.8141657359377,15.9196457647817,15.9703492221878,
16.0758450672949,16.181181789708,16.2863943601952,16.3915408036808,16.4966572471969,
16.6017797733711,16.707014397786,16.8123119165726,16.9177918596926,16.9684960485745,
17.0739919802754,17.179328790682,17.2845414508035,17.38968798489,17.4948045198368,
17.5999271381349,17.7051618550945,17.8104594668023,17.915939502448,17.9666428749613,
18.0721387779979,18.1774755594657,18.2826881903856,18.3878346951245,18.4929512006224,
18.5980737894155,18.7033084769877,18.8086060593322,18.9140860659618,18.964789701348,
19.0703011871416,19.1756535393357,19.2808816837827,19.3860436404998,19.4911755122156,
19.596313357183,19.7015632702855,19.8068759332889,19.9123712558797,19.9637469595683),
 .UNSPECIFIED.);
#789=B_SPLINE_CURVE_WITH_KNOTS('',3,(#75694,#75695,#75696,#75697,#75698,
#75699,#75700,#75701,#75702,#75703,#75704,#75705,#75706,#75707,#75708,#75709,
#75710,#75711,#75712,#75713,#75714,#75715,#75716,#75717,#75718,#75719,#75720,
#75721,#75722,#75723,#75724,#75725,#75726,#75727,#75728,#75729,#75730,#75731,
#75732,#75733,#75734,#75735,#75736,#75737,#75738,#75739,#75740,#75741,#75742,
#75743,#75744,#75745,#75746,#75747,#75748,#75749,#75750,#75751,#75752,#75753,
#75754,#75755,#75756,#75757,#75758,#75759,#75760,#75761,#75762,#75763,#75764,
#75765,#75766,#75767,#75768,#75769,#75770,#75771,#75772,#75773,#75774,#75775,
#75776,#75777,#75778,#75779,#75780,#75781,#75782,#75783,#75784,#75785,#75786,
#75787,#75788,#75789,#75790,#75791,#75792,#75793,#75794,#75795,#75796,#75797,
#75798,#75799,#75800,#75801,#75802,#75803,#75804,#75805,#75806,#75807,#75808,
#75809,#75810,#75811,#75812,#75813,#75814,#75815,#75816,#75817,#75818,#75819,
#75820,#75821,#75822,#75823,#75824,#75825,#75826,#75827,#75828,#75829,#75830,
#75831,#75832,#75833,#75834,#75835,#75836,#75837,#75838,#75839,#75840,#75841,
#75842,#75843,#75844,#75845,#75846,#75847,#75848,#75849,#75850,#75851,#75852,
#75853,#75854,#75855,#75856,#75857,#75858,#75859,#75860,#75861,#75862,#75863,
#75864,#75865,#75866,#75867,#75868,#75869,#75870,#75871,#75872,#75873,#75874,
#75875,#75876,#75877,#75878,#75879,#75880,#75881,#75882,#75883),
 .UNSPECIFIED.,.F.,.F.,(4,3,3,3,3,3,3,3,3,3,3,3,3,3,3,3,3,3,3,3,3,3,3,3,
3,3,3,3,3,3,3,3,3,3,3,3,3,3,3,3,3,3,3,3,3,3,3,3,3,3,3,3,3,3,3,3,3,3,3,3,
3,3,3,4),(19.9637469598682,20.0692273547104,20.1745486411723,20.279745835274,
20.3848769652241,20.4899781819352,20.5950855919875,20.7003051304565,20.8055877081546,
20.911052473179,20.9610833541215,21.0665792569406,21.1719160381134,21.2771286686244,
21.382275172884,21.4873916778326,21.5925142660069,21.6977489528586,21.8030465344233,
21.9085265401897,21.9592301805082,22.0647260827278,22.170062863275,22.2752754931247,
22.3804219967011,22.4855385009456,22.5906610883958,22.6958957744983,22.8011933552983,
22.9066733602838,22.9573770068949,23.0628729107958,23.1682096930542,23.2734223246508,
23.3785688299953,23.4836853360264,23.5888079252789,23.6940426131956,23.7993401958192,
23.9048202026235,23.9555238332817,24.0610197363911,24.1663565178484,24.2715691486333,
24.3767156531599,24.4818321583686,24.5869547467952,24.6921894338859,24.7974870156826,
24.9029670216672,24.9536706596684,25.0591665627647,25.1645033442062,25.2697159749714,
25.374862479476,25.4799789846599,25.5851015730596,25.6903362601201,25.7956338418846,
25.9011138478342,25.9518174860552,26.0810388351796,26.2084013336569,26.2469320954389),
 .UNSPECIFIED.);
#790=B_SPLINE_CURVE_WITH_KNOTS('',3,(#75885,#75886,#75887,#75888,#75889,
#75890,#75891,#75892,#75893,#75894),.UNSPECIFIED.,.F.,.F.,(4,1,1,1,1,1,
1,4),(26.2469322667479,26.9499643124419,27.9481111388286,28.9462579652154,
29.9444047916021,30.9425516179888,31.9406984443756,32.5301175739274),
 .UNSPECIFIED.);
#791=B_SPLINE_CURVE_WITH_KNOTS('',3,(#75896,#75897,#75898,#75899,#75900,
#75901,#75902,#75903,#75904,#75905,#75906,#75907,#75908,#75909,#75910,#75911,
#75912,#75913,#75914,#75915,#75916,#75917,#75918,#75919,#75920,#75921,#75922,
#75923,#75924,#75925,#75926,#75927,#75928,#75929,#75930,#75931,#75932,#75933,
#75934,#75935,#75936,#75937,#75938,#75939,#75940,#75941,#75942,#75943,#75944,
#75945,#75946,#75947,#75948,#75949,#75950,#75951,#75952,#75953,#75954,#75955,
#75956,#75957,#75958,#75959,#75960,#75961,#75962,#75963,#75964,#75965,#75966,
#75967,#75968,#75969,#75970,#75971,#75972,#75973,#75974,#75975,#75976,#75977,
#75978,#75979,#75980,#75981,#75982,#75983,#75984,#75985,#75986,#75987,#75988,
#75989,#75990,#75991,#75992,#75993,#75994,#75995,#75996,#75997,#75998,#75999,
#76000,#76001,#76002,#76003,#76004,#76005,#76006,#76007,#76008,#76009,#76010,
#76011,#76012,#76013,#76014,#76015,#76016,#76017,#76018,#76019,#76020,#76021,
#76022,#76023,#76024,#76025,#76026,#76027,#76028,#76029,#76030,#76031,#76032,
#76033,#76034,#76035,#76036,#76037,#76038,#76039,#76040,#76041,#76042,#76043,
#76044,#76045,#76046,#76047,#76048,#76049,#76050,#76051,#76052,#76053,#76054,
#76055,#76056,#76057,#76058,#76059,#76060,#76061,#76062,#76063,#76064,#76065,
#76066,#76067,#76068,#76069,#76070,#76071,#76072,#76073,#76074,#76075,#76076,
#76077,#76078,#76079,#76080,#76081,#76082,#76083,#76084,#76085),
 .UNSPECIFIED.,.F.,.F.,(4,3,3,3,3,3,3,3,3,3,3,3,3,3,3,3,3,3,3,3,3,3,3,3,
3,3,3,3,3,3,3,3,3,3,3,3,3,3,3,3,3,3,3,3,3,3,3,3,3,3,3,3,3,3,3,3,3,3,3,3,
3,3,3,4),(32.5301179915019,32.6456707590869,32.7616131287804,32.8780966879654,
32.9388452707623,33.0443411739821,33.1496779555496,33.2548905864443,33.3600370910804,
33.4651535963978,33.5702761849327,33.6755108721297,33.7808084540318,33.8862884601192,
33.9369920971491,34.0424880003695,34.1478247819377,34.253037412833,34.3581839174697,
34.4633004227878,34.5684230113232,34.6736576985209,34.7789552804236,34.8844352865115,
34.9351389235358,35.0406348267566,35.1459716083252,35.251184239221,35.3563307438581,
35.4614472491767,35.5665698377125,35.6718045249107,35.7771021068139,35.8825821129023,
35.9332857499225,36.038781653143,36.1441184347112,36.2493310656066,36.3544775702434,
36.4595940755615,36.564716664097,36.6699513512947,36.7752489331975,36.8807289392856,
36.9314325763093,37.0369284795299,37.1422652610982,37.2474778919937,37.3526243966306,
37.4577409019488,37.5628634904844,37.6680981776822,37.7733957595852,37.8788757656733,
37.929579402696,38.0336606369063,38.1375625429156,38.2413648015755,38.3451054038156,
38.4488222501643,38.552612207333,38.6564423147378,38.7604271016251,38.813302881107),
 .UNSPECIFIED.);
#792=B_SPLINE_CURVE_WITH_KNOTS('',3,(#76087,#76088,#76089,#76090,#76091,
#76092,#76093,#76094,#76095,#76096,#76097),.UNSPECIFIED.,.F.,.F.,(4,1,1,
1,1,1,1,1,4),(38.813302881107,38.9277262290827,39.9258730554695,40.9240198818562,
41.9221667082429,42.9203135346297,43.9184603610164,44.9166071874032,45.0964881882866),
 .UNSPECIFIED.);
#793=B_SPLINE_CURVE_WITH_KNOTS('',3,(#76099,#76100,#76101,#76102,#76103,
#76104,#76105,#76106,#76107,#76108),.UNSPECIFIED.,.F.,.F.,(4,1,1,1,1,1,
1,4),(45.0964881882866,45.9147540137899,46.9129008401766,47.9110476665634,
48.9091944929501,49.9073413193368,50.9054881457236,51.3796715846493),
 .UNSPECIFIED.);
#794=B_SPLINE_CURVE_WITH_KNOTS('',3,(#76110,#76111,#76112,#76113,#76114,
#76115,#76116,#76117,#76118,#76119,#76120,#76121,#76122,#76123,#76124,#76125,
#76126,#76127,#76128,#76129,#76130,#76131,#76132,#76133,#76134,#76135,#76136,
#76137,#76138,#76139,#76140,#76141,#76142,#76143,#76144,#76145,#76146,#76147,
#76148,#76149,#76150,#76151,#76152,#76153,#76154,#76155,#76156,#76157,#76158,
#76159,#76160,#76161,#76162,#76163,#76164,#76165,#76166,#76167,#76168,#76169,
#76170,#76171,#76172,#76173,#76174,#76175,#76176,#76177,#76178,#76179,#76180,
#76181,#76182,#76183,#76184,#76185,#76186,#76187,#76188,#76189,#76190,#76191,
#76192,#76193,#76194,#76195,#76196,#76197,#76198,#76199,#76200,#76201,#76202,
#76203,#76204,#76205,#76206,#76207,#76208,#76209,#76210,#76211,#76212,#76213,
#76214,#76215,#76216,#76217,#76218,#76219,#76220,#76221,#76222,#76223,#76224,
#76225,#76226,#76227,#76228,#76229,#76230,#76231,#76232,#76233,#76234,#76235,
#76236,#76237,#76238,#76239,#76240,#76241,#76242,#76243,#76244,#76245,#76246,
#76247,#76248,#76249,#76250,#76251,#76252,#76253,#76254,#76255,#76256,#76257,
#76258,#76259,#76260,#76261,#76262,#76263,#76264,#76265,#76266,#76267,#76268,
#76269,#76270,#76271,#76272,#76273,#76274,#76275,#76276,#76277,#76278,#76279,
#76280,#76281,#76282,#76283,#76284,#76285,#76286,#76287,#76288,#76289,#76290,
#76291,#76292,#76293,#76294,#76295,#76296,#76297,#76298,#76299),
 .UNSPECIFIED.,.F.,.F.,(4,3,3,3,3,3,3,3,3,3,3,3,3,3,3,3,3,3,3,3,3,3,3,3,
3,3,3,3,3,3,3,3,3,3,3,3,3,3,3,3,3,3,3,3,3,3,3,3,3,3,3,3,3,3,3,3,3,3,3,3,
3,3,3,4),(51.3796734954662,51.4887071556465,51.5979949885878,51.7074131825927,
51.8171173718269,51.9036349721103,52.0091308753307,52.1144676568988,52.2196802877941,
52.3248267924308,52.4299432977489,52.5350658862844,52.640300573482,52.7455981553849,
52.8510781614729,52.901781798497,53.0072777017168,53.1126144832843,53.217827114179,
53.3229736188151,53.4280901241326,53.5332127126676,53.6384473998648,53.743744981767,
53.8492249878544,53.8999286248838,54.0054245281066,54.1107613096772,54.2159739405749,
54.3211204452141,54.4262369505345,54.5313595390723,54.6365942262723,54.7418918081774,
54.8473718142677,54.8980754512705,55.0035713544892,55.1089081360556,55.2141207669493,
55.3192672715845,55.4243837769011,55.529506365435,55.6347410526312,55.7400386345324,
55.8455186406191,55.8962222776573,56.0017181808736,56.1070549624377,56.2122675933288,
56.3174140979613,56.422530603275,56.5276531918063,56.6328878789998,56.7381854608983,
56.843665466982,56.894369104044,56.9984595657844,57.1024080693009,57.2062527224879,
57.3100314827545,57.413817463461,57.5176075792081,57.6214910298516,57.6628588026458),
 .UNSPECIFIED.);
#795=B_SPLINE_CURVE_WITH_KNOTS('',3,(#76301,#76302,#76303,#76304,#76305,
#76306,#76307,#76308,#76309,#76310,#76311),.UNSPECIFIED.,.F.,.F.,(4,1,1,
1,1,1,1,1,4),(57.6628588026458,57.8925159304307,58.8906627568175,59.8888095832042,
60.8869564095909,61.8851032359777,62.8832500623644,63.8813968887512,63.9460441098254),
 .UNSPECIFIED.);
#796=B_SPLINE_CURVE_WITH_KNOTS('',3,(#76313,#76314,#76315,#76316,#76317,
#76318,#76319,#76320,#76321,#76322,#76323,#76324,#76325,#76326,#76327,#76328,
#76329,#76330,#76331,#76332,#76333,#76334,#76335,#76336,#76337,#76338,#76339,
#76340,#76341,#76342,#76343,#76344,#76345,#76346,#76347,#76348,#76349,#76350,
#76351,#76352,#76353,#76354,#76355,#76356,#76357,#76358,#76359,#76360,#76361,
#76362,#76363,#76364,#76365,#76366,#76367,#76368,#76369,#76370,#76371,#76372,
#76373,#76374,#76375,#76376,#76377,#76378,#76379,#76380,#76381,#76382,#76383,
#76384,#76385,#76386,#76387,#76388,#76389,#76390,#76391,#76392,#76393,#76394,
#76395,#76396,#76397,#76398,#76399,#76400,#76401,#76402,#76403,#76404,#76405,
#76406,#76407,#76408,#76409,#76410,#76411,#76412,#76413,#76414,#76415,#76416,
#76417,#76418,#76419,#76420,#76421,#76422,#76423,#76424,#76425,#76426,#76427,
#76428,#76429,#76430,#76431,#76432,#76433,#76434,#76435,#76436,#76437,#76438,
#76439,#76440,#76441,#76442,#76443,#76444,#76445,#76446,#76447,#76448,#76449,
#76450,#76451,#76452,#76453,#76454,#76455,#76456,#76457,#76458,#76459,#76460,
#76461,#76462,#76463,#76464,#76465,#76466,#76467,#76468,#76469,#76470,#76471,
#76472,#76473,#76474,#76475,#76476,#76477,#76478,#76479,#76480,#76481,#76482,
#76483,#76484,#76485,#76486,#76487,#76488,#76489,#76490,#76491,#76492,#76493,
#76494,#76495,#76496,#76497,#76498,#76499),.UNSPECIFIED.,.F.,.F.,(4,3,3,
3,3,3,3,3,3,3,3,3,3,3,3,3,3,3,3,3,3,3,3,3,3,3,3,3,3,3,3,3,3,3,3,3,3,3,3,
3,3,3,3,3,3,3,3,3,3,3,3,3,3,3,3,3,3,3,3,3,3,3,4),(63.9460441098254,64.050525963831,
64.1548391807715,64.2590586452409,64.3632218680578,64.4673662827088,64.5716035009599,
64.6758837527691,64.7803585946505,64.8795437151379,64.9850396180399,65.0903763992768,
65.1955890298238,65.3007355341018,65.4058520390515,65.5109746272094,65.6162093140186,
65.721506895526,65.8269869012125,65.8776905415246,65.9831864493903,66.0885232356215,
66.1937358711839,66.2988823804876,66.4039988904652,66.509121483646,66.6143561754361,
66.7196537619078,66.8251337724805,66.8758373679114,66.9813332627005,67.0866700358464,
67.1918826583736,67.2970291546803,67.4021456517187,67.507268232037,67.6125029111667,
67.7178004850744,67.823280483364,67.8739841942981,67.979480098073,68.0848168801108,
68.1900295113507,68.2951760162542,68.4002925217617,68.5054151104092,68.610649797603,
68.7159473794359,68.8214273853541,68.8721310206848,68.9776269533426,69.0829637644887,
69.1881764250249,69.2933229593248,69.398439494284,69.5035621123933,69.6087968288627,
69.7140944399076,69.8195744746314,69.8702778470716,69.9912176372233,70.1111669584549,
70.2292291731328),.UNSPECIFIED.);
#797=B_SPLINE_CURVE_WITH_KNOTS('',3,(#76501,#76502,#76503,#76504,#76505,
#76506,#76507,#76508,#76509,#76510),.UNSPECIFIED.,.F.,.F.,(4,1,1,1,1,1,
1,4),(70.229229417005,70.8684246734583,71.8665714998451,72.8647183262318,
73.8628651526185,74.8610119790053,75.859158805392,76.5124147241846),
 .UNSPECIFIED.);
#798=B_SPLINE_CURVE_WITH_KNOTS('',3,(#76512,#76513,#76514,#76515,#76516,
#76517,#76518,#76519,#76520,#76521,#76522,#76523,#76524,#76525,#76526,#76527,
#76528,#76529,#76530,#76531,#76532,#76533,#76534,#76535,#76536,#76537,#76538,
#76539,#76540,#76541,#76542,#76543,#76544,#76545,#76546,#76547,#76548,#76549,
#76550,#76551,#76552,#76553,#76554,#76555,#76556,#76557,#76558,#76559,#76560,
#76561,#76562,#76563,#76564,#76565,#76566,#76567,#76568,#76569,#76570,#76571,
#76572,#76573,#76574,#76575,#76576,#76577,#76578,#76579,#76580,#76581,#76582,
#76583,#76584,#76585,#76586,#76587,#76588,#76589,#76590,#76591,#76592,#76593,
#76594,#76595,#76596,#76597,#76598,#76599,#76600,#76601,#76602,#76603,#76604,
#76605,#76606,#76607,#76608,#76609,#76610,#76611,#76612,#76613,#76614,#76615,
#76616,#76617,#76618,#76619,#76620,#76621,#76622,#76623,#76624,#76625,#76626,
#76627,#76628,#76629,#76630,#76631,#76632,#76633,#76634,#76635,#76636,#76637,
#76638,#76639,#76640,#76641,#76642,#76643,#76644,#76645,#76646,#76647,#76648,
#76649,#76650),.UNSPECIFIED.,.F.,.F.,(4,3,3,3,3,3,3,3,3,3,3,3,3,3,3,3,3,
3,3,3,3,3,3,3,3,3,3,3,3,3,3,3,3,3,3,3,3,3,3,3,3,3,3,3,3,3,4),(76.5124149635497,
76.6335427431329,76.755837417112,76.8573056317787,76.9628043403963,77.0681439068555,
77.1733592794405,77.2785084974948,77.3836276841624,77.488752918151,77.5939901791019,
77.6992902976895,77.8047727570283,77.8554524581655,77.9609542845702,78.0662970454053,
78.17151570875,78.276668275278,78.3817908625963,78.4869195439332,78.5921602982041,
78.6974639414213,78.8029499357427,78.8535992845522,78.9590728007151,79.0643871541541,
79.1695774039509,79.2747015691714,79.3797958096304,79.4848962408019,79.5901090829246,
79.6953849654392,79.8008437246019,79.8517461109389,79.9572667741261,80.0626281974763,
80.1678651799042,80.2730358426097,80.3781762780868,80.4833225342001,80.5885803347549,
80.6939007480483,80.7994029135444,80.8498929373257,80.972024192404,81.0930688950015,
81.1967061267808),.UNSPECIFIED.);
#799=B_SPLINE_CURVE_WITH_KNOTS('',3,(#76654,#76655,#76656,#76657,#76658,
#76659,#76660,#76661,#76662,#76663,#76664,#76665,#76666,#76667,#76668,#76669,
#76670,#76671,#76672,#76673,#76674,#76675,#76676,#76677,#76678,#76679,#76680,
#76681,#76682,#76683,#76684,#76685,#76686,#76687,#76688,#76689,#76690,#76691,
#76692,#76693,#76694,#76695,#76696,#76697,#76698,#76699,#76700,#76701,#76702,
#76703,#76704,#76705,#76706,#76707,#76708,#76709,#76710,#76711,#76712,#76713,
#76714,#76715,#76716,#76717,#76718,#76719,#76720,#76721,#76722,#76723,#76724,
#76725,#76726,#76727,#76728,#76729,#76730,#76731,#76732,#76733,#76734,#76735,
#76736,#76737,#76738,#76739,#76740,#76741,#76742,#76743,#76744,#76745,#76746,
#76747,#76748,#76749,#76750,#76751,#76752,#76753,#76754,#76755,#76756,#76757,
#76758,#76759,#76760,#76761,#76762,#76763,#76764,#76765,#76766,#76767,#76768),
 .UNSPECIFIED.,.F.,.F.,(4,3,3,3,3,3,3,3,3,3,3,3,3,3,3,3,3,3,3,3,3,3,3,3,
3,3,3,3,3,3,3,3,3,3,3,3,3,3,4),(-83.261823785886,-83.1517588372496,-83.0413517915619,
-82.930757367669,-82.8198433883014,-82.7789600267829,-82.6732910907865,
-82.5677808221992,-82.4623949729488,-82.3570755146399,-82.2517866003674,
-82.1464924281016,-82.0410888596141,-81.9356235523786,-81.8299800036617,
-81.7816231589903,-81.6759325426703,-81.5703968024453,-81.4649799626522,
-81.3596260975942,-81.2542994029756,-81.1489641158244,-81.0435146406177,
-80.938000619518,-80.8323045173012,-80.7842862911978,-80.6789235796683,
-80.5737218686868,-80.4686464770282,-80.3636384661016,-80.2586615036662,
-80.1536793031293,-80.0485855762287,-79.9434293428101,-79.8380904225242,
-79.7869494234052,-79.6576514134494,-79.5302108335803,-79.4907655987199),
 .UNSPECIFIED.);
#800=B_SPLINE_CURVE_WITH_KNOTS('',3,(#76770,#76771,#76772,#76773,#76774,
#76775,#76776,#76777,#76778,#76779),.UNSPECIFIED.,.F.,.F.,(4,1,1,1,1,1,
1,4),(-79.4907654349934,-78.7896125556126,-77.7922756878201,-76.7949388200275,
-75.7976019522349,-74.8002650844424,-73.8029282166498,-73.2075801278138),
 .UNSPECIFIED.);
#801=B_SPLINE_CURVE_WITH_KNOTS('',3,(#76781,#76782,#76783,#76784,#76785,
#76786,#76787,#76788,#76789,#76790,#76791,#76792,#76793,#76794,#76795,#76796,
#76797,#76798,#76799,#76800,#76801,#76802,#76803,#76804,#76805,#76806,#76807,
#76808,#76809,#76810,#76811,#76812,#76813,#76814,#76815,#76816,#76817,#76818,
#76819,#76820,#76821,#76822,#76823,#76824,#76825,#76826,#76827,#76828,#76829,
#76830,#76831,#76832,#76833,#76834,#76835,#76836,#76837,#76838,#76839,#76840,
#76841,#76842,#76843,#76844,#76845,#76846,#76847,#76848,#76849,#76850,#76851,
#76852,#76853,#76854,#76855,#76856,#76857,#76858,#76859,#76860,#76861,#76862,
#76863,#76864,#76865,#76866,#76867,#76868,#76869,#76870,#76871,#76872,#76873,
#76874,#76875,#76876,#76877,#76878,#76879,#76880,#76881,#76882,#76883,#76884,
#76885,#76886,#76887,#76888,#76889,#76890,#76891,#76892,#76893,#76894,#76895,
#76896,#76897,#76898,#76899,#76900,#76901,#76902,#76903,#76904,#76905,#76906,
#76907,#76908,#76909,#76910,#76911,#76912,#76913,#76914,#76915,#76916,#76917,
#76918,#76919,#76920,#76921,#76922,#76923,#76924,#76925,#76926,#76927,#76928,
#76929,#76930,#76931,#76932,#76933,#76934,#76935,#76936,#76937,#76938,#76939,
#76940,#76941,#76942,#76943,#76944,#76945,#76946,#76947,#76948,#76949,#76950,
#76951,#76952,#76953,#76954,#76955,#76956,#76957,#76958,#76959,#76960,#76961,
#76962,#76963,#76964,#76965,#76966,#76967,#76968,#76969,#76970),
 .UNSPECIFIED.,.F.,.F.,(4,3,3,3,3,3,3,3,3,3,3,3,3,3,3,3,3,3,3,3,3,3,3,3,
3,3,3,3,3,3,3,3,3,3,3,3,3,3,3,3,3,3,3,3,3,3,3,3,3,3,3,3,3,3,3,3,3,3,3,3,
3,3,3,4),(-73.2075796958808,-73.091556451448,-72.9751182134163,-72.8581229582674,
-72.8055913488572,-72.7000843592375,-72.594736238552,-72.4895119913637,
-72.38435368872,-72.2792252221004,-72.1740905272145,-72.0688438405957,-71.963534153129,
-71.8580426246082,-71.8082544810647,-71.7027481426044,-71.5974006878884,
-71.4921771253551,-71.3870195185762,-71.2818917579841,-71.1767577782527,
-71.071511815753,-70.9662028585869,-70.8607120622803,-70.8109176132721,
-70.7054106731065,-70.6000626073486,-70.4948384229603,-70.3896801879757,
-70.284551793783,-70.1794171760054,-70.0741705730911,-69.9688609732197,
-69.8633695374144,-69.8135807454795,-69.7080739686073,-69.602726067379,
-69.4975020485289,-69.39234397961,-69.2872157517546,-69.1820813003305,-69.076834862647,
-68.971525427607,-68.8660341542782,-68.816243877687,-68.7107371737072,-68.605389347242,
-68.5001654055624,-68.3950074152649,-68.289879267364,-68.1847448971112,
-68.079498541892,-67.9741891901756,-67.868698000628,-67.8189070098944,-67.7147383019953,
-67.6107484692928,-67.506858120488,-67.4030293549668,-67.2992243609191,
-67.1953437258928,-67.0914232330471,-66.9873412561956,-66.9243948210849),
 .UNSPECIFIED.);
#802=B_SPLINE_CURVE_WITH_KNOTS('',3,(#76972,#76973,#76974,#76975,#76976,
#76977,#76978,#76979,#76980,#76981,#76982,#76983,#76984,#76985,#76986,#76987,
#76988,#76989,#76990,#76991,#76992,#76993,#76994,#76995,#76996,#76997,#76998,
#76999,#77000,#77001,#77002,#77003,#77004,#77005,#77006,#77007,#77008,#77009,
#77010,#77011,#77012,#77013,#77014,#77015,#77016,#77017,#77018,#77019,#77020,
#77021,#77022,#77023,#77024,#77025,#77026,#77027,#77028,#77029,#77030,#77031,
#77032,#77033,#77034,#77035,#77036,#77037,#77038,#77039,#77040,#77041,#77042,
#77043,#77044,#77045,#77046,#77047,#77048,#77049,#77050,#77051,#77052,#77053,
#77054,#77055,#77056,#77057,#77058,#77059,#77060,#77061,#77062,#77063,#77064,
#77065,#77066,#77067,#77068,#77069,#77070,#77071,#77072,#77073,#77074,#77075,
#77076,#77077,#77078,#77079,#77080,#77081,#77082,#77083,#77084,#77085,#77086,
#77087,#77088,#77089,#77090,#77091,#77092,#77093,#77094,#77095,#77096,#77097,
#77098,#77099,#77100,#77101,#77102,#77103,#77104,#77105,#77106,#77107,#77108,
#77109,#77110,#77111,#77112,#77113,#77114,#77115,#77116,#77117,#77118,#77119,
#77120,#77121,#77122,#77123,#77124,#77125,#77126,#77127,#77128,#77129,#77130,
#77131,#77132,#77133,#77134,#77135,#77136,#77137,#77138,#77139,#77140,#77141,
#77142,#77143,#77144,#77145,#77146,#77147,#77148,#77149,#77150,#77151,#77152,
#77153,#77154,#77155,#77156,#77157,#77158,#77159,#77160,#77161),
 .UNSPECIFIED.,.F.,.F.,(4,3,3,3,3,3,3,3,3,3,3,3,3,3,3,3,3,3,3,3,3,3,3,3,
3,3,3,3,3,3,3,3,3,3,3,3,3,3,3,3,3,3,3,3,3,3,3,3,3,3,3,3,3,3,3,3,3,3,3,3,
3,3,3,4),(-66.9243948206342,-66.8215701421018,-66.7160633807799,-66.6107154958515,
-66.505491494335,-66.4003334433823,-66.2952052340995,-66.1900708018291,
-66.084824384052,-65.9795149693774,-65.8740237169125,-65.8242332743093,
-65.7187265202069,-65.6133786427231,-65.5081546489489,-65.4029966059188,
-65.2978684047274,-65.1927339807054,-65.0874875713589,-64.9821781652316,
-64.8766869214049,-64.8268964065167,-64.7213896402397,-64.6160417503741,
-64.5108177439724,-64.4056596881695,-64.3005314740794,-64.1953970370521,
-64.0901506146277,-63.9848411953617,-63.8793499384404,-63.8295595387242,
-63.7240527773937,-63.6187048925305,-63.5134808911892,-63.4083228404798,
-63.3031946315083,-63.1980601996171,-63.0928137823199,-62.9875043681835,
-62.8820131163417,-62.8322226709316,-62.72671591014,-62.621368025841,-62.5161440250985,
-62.4109859750092,-62.3058577666781,-62.2007233354468,-62.0954769188346,
-61.9901675053986,-61.8846762542736,-61.834885803139,-61.7293790406761,
-61.624031154676,-61.5188071521967,-61.4136491003493,-61.3085208902418,
-61.203386457218,-61.0981400388015,-60.9928306235517,-60.8873393706174,
-60.8375489353465,-60.6852937514664,-60.6412095134546),.UNSPECIFIED.);
#803=B_SPLINE_CURVE_WITH_KNOTS('',3,(#77163,#77164,#77165,#77166,#77167,
#77168,#77169,#77170,#77171,#77172),.UNSPECIFIED.,.F.,.F.,(4,1,1,1,1,1,
1,4),(-60.6412060917588,-59.8402120675539,-58.8428751997613,-57.8455383319688,
-56.8482014641762,-55.8508645963836,-54.8535277285911,-54.358024206275),
 .UNSPECIFIED.);
#804=B_SPLINE_CURVE_WITH_KNOTS('',3,(#77174,#77175,#77176,#77177,#77178,
#77179,#77180,#77181,#77182,#77183),.UNSPECIFIED.,.F.,.F.,(4,1,1,1,1,1,
1,4),(-54.358024206275,-53.8561908607985,-52.8588539930059,-51.8615171252134,
-50.8641802574208,-49.8668433896283,-48.8695065218357,-48.0748417313677),
 .UNSPECIFIED.);
#805=B_SPLINE_CURVE_WITH_KNOTS('',3,(#77185,#77186,#77187,#77188,#77189,
#77190,#77191,#77192,#77193,#77194,#77195,#77196,#77197,#77198,#77199,#77200,
#77201,#77202,#77203,#77204,#77205,#77206,#77207,#77208,#77209,#77210,#77211,
#77212,#77213,#77214,#77215,#77216,#77217,#77218,#77219,#77220,#77221,#77222,
#77223,#77224,#77225,#77226,#77227,#77228,#77229,#77230,#77231,#77232,#77233,
#77234,#77235,#77236,#77237,#77238,#77239,#77240,#77241,#77242,#77243,#77244,
#77245,#77246,#77247,#77248,#77249,#77250,#77251,#77252,#77253,#77254,#77255,
#77256,#77257,#77258,#77259,#77260,#77261,#77262,#77263,#77264,#77265,#77266,
#77267,#77268,#77269,#77270,#77271,#77272,#77273,#77274,#77275,#77276,#77277,
#77278,#77279,#77280,#77281,#77282,#77283,#77284,#77285,#77286,#77287,#77288,
#77289,#77290,#77291,#77292,#77293,#77294,#77295,#77296,#77297,#77298,#77299,
#77300,#77301,#77302,#77303,#77304,#77305,#77306,#77307,#77308,#77309,#77310,
#77311,#77312,#77313,#77314,#77315,#77316,#77317,#77318,#77319,#77320,#77321,
#77322,#77323,#77324,#77325,#77326,#77327,#77328,#77329,#77330,#77331,#77332,
#77333,#77334,#77335,#77336,#77337,#77338,#77339,#77340,#77341,#77342,#77343,
#77344,#77345,#77346,#77347,#77348,#77349,#77350,#77351,#77352,#77353,#77354,
#77355,#77356,#77357,#77358,#77359,#77360,#77361,#77362,#77363,#77364,#77365,
#77366,#77367,#77368,#77369,#77370,#77371,#77372,#77373,#77374),
 .UNSPECIFIED.,.F.,.F.,(4,3,3,3,3,3,3,3,3,3,3,3,3,3,3,3,3,3,3,3,3,3,3,3,
3,3,3,3,3,3,3,3,3,3,3,3,3,3,3,3,3,3,3,3,3,3,3,3,3,3,3,3,3,3,3,3,3,3,3,3,
3,3,3,4),(-48.0748388990954,-47.9249917028415,-47.8721696540431,-47.7666628922655,
-47.6613150069605,-47.5560910051876,-47.4509329540531,-47.3458047446638,
-47.2406703123627,-47.1354238946705,-47.0301144801472,-46.9246232279348,
-46.8748327862506,-46.7693260244729,-46.6639781391679,-46.5587541373949,
-46.4535960862603,-46.3484678768709,-46.2433334445698,-46.1380870268776,
-46.0327776123541,-45.9272863601416,-45.877495918458,-45.7719891566803,
-45.6666412713754,-45.5614172696023,-45.4562592184678,-45.3511310090785,
-45.2459965767774,-45.1407501590852,-45.0354407445618,-44.9299494923494,
-44.8801590506654,-44.7746522888878,-44.6693044035828,-44.5640804018098,
-44.4589223506753,-44.353794141286,-44.248659708985,-44.1434132912928,-44.0381038767694,
-43.932612624557,-43.8828221828729,-43.7773154210952,-43.6719675357902,
-43.5667435340172,-43.4615854828827,-43.3564572734934,-43.2513228411923,
-43.1460764235,-43.0407670089766,-42.9352757567642,-42.8854853150803,-42.7799785533026,
-42.6746306679976,-42.5694066662245,-42.46424861509,-42.3591204057007,-42.2539859733997,
-42.1487395557075,-42.043430141184,-41.9379388889716,-41.8881484472877,
-41.7916535919158),.UNSPECIFIED.);
#806=B_SPLINE_CURVE_WITH_KNOTS('',3,(#77376,#77377,#77378,#77379,#77380,
#77381,#77382,#77383,#77384,#77385),.UNSPECIFIED.,.F.,.F.,(4,1,1,1,1,1,
1,4),(-41.7916448301768,-40.8908115794952,-39.8934747117026,-38.89613784391,
-37.8988009761175,-36.9014641083249,-35.9041272405323,-35.5084682847363),
 .UNSPECIFIED.);
#807=B_SPLINE_CURVE_WITH_KNOTS('',3,(#77387,#77388,#77389,#77390,#77391,
#77392,#77393,#77394,#77395,#77396),.UNSPECIFIED.,.F.,.F.,(4,1,1,1,1,1,
1,4),(-35.5084682847363,-34.9067903727398,-33.9094535049472,-32.9121166371546,
-31.9147797693621,-30.9174429015695,-29.9201060337769,-29.2252829775567),
 .UNSPECIFIED.);
#808=B_SPLINE_CURVE_WITH_KNOTS('',3,(#77398,#77399,#77400,#77401,#77402,
#77403,#77404,#77405,#77406,#77407,#77408,#77409,#77410,#77411,#77412,#77413,
#77414,#77415,#77416,#77417,#77418,#77419,#77420,#77421,#77422,#77423,#77424,
#77425,#77426,#77427,#77428,#77429,#77430,#77431,#77432,#77433,#77434,#77435,
#77436,#77437,#77438,#77439,#77440,#77441,#77442,#77443,#77444,#77445,#77446,
#77447,#77448,#77449,#77450,#77451,#77452,#77453,#77454,#77455,#77456,#77457,
#77458,#77459,#77460,#77461,#77462,#77463,#77464,#77465,#77466,#77467,#77468,
#77469,#77470,#77471,#77472,#77473,#77474,#77475,#77476,#77477,#77478,#77479,
#77480,#77481,#77482,#77483,#77484,#77485,#77486,#77487,#77488,#77489,#77490,
#77491,#77492,#77493,#77494,#77495,#77496,#77497,#77498,#77499,#77500,#77501,
#77502,#77503,#77504,#77505,#77506,#77507,#77508,#77509,#77510,#77511,#77512,
#77513,#77514,#77515,#77516,#77517,#77518,#77519,#77520,#77521,#77522,#77523,
#77524,#77525,#77526,#77527,#77528,#77529,#77530,#77531,#77532,#77533,#77534,
#77535,#77536,#77537,#77538,#77539,#77540,#77541,#77542,#77543,#77544,#77545,
#77546,#77547,#77548,#77549,#77550,#77551,#77552,#77553,#77554,#77555,#77556,
#77557,#77558,#77559,#77560,#77561,#77562,#77563,#77564,#77565,#77566,#77567,
#77568,#77569,#77570,#77571,#77572,#77573,#77574,#77575,#77576,#77577,#77578,
#77579,#77580,#77581,#77582,#77583,#77584,#77585,#77586,#77587),
 .UNSPECIFIED.,.F.,.F.,(4,3,3,3,3,3,3,3,3,3,3,3,3,3,3,3,3,3,3,3,3,3,3,3,
3,3,3,3,3,3,3,3,3,3,3,3,3,3,3,3,3,3,3,3,3,3,3,3,3,3,3,3,3,3,3,3,3,3,3,3,
3,3,3,4),(-29.2252827922655,-29.0991589622948,-28.9713058339057,-28.9227691659844,
-28.8172624042227,-28.7119145189336,-28.6066905171762,-28.5015324660573,
-28.3964042566833,-28.2912698243975,-28.1860234067202,-28.0807139922114,
-27.9752227400132,-27.9254322981918,-27.8199255364382,-27.7145776511576,
-27.6093536494092,-27.5041955982994,-27.399067388935,-27.2939329566588,
-27.1886865389915,-27.083377124493,-26.9778858723053,-26.9280954303993,
-26.822588668514,-26.7172407831012,-26.6120167812205,-26.5068587299785,
-26.4017305204819,-26.2965960880741,-26.1913496702766,-26.0860402556486,
-25.9805490033337,-25.9307585626067,-25.8252518009642,-25.7199039157939,
-25.6146799141543,-25.5095218631522,-25.4043936538942,-25.2992592217232,
-25.1940128041582,-25.0887033897605,-24.9832121376703,-24.9334216948141,
-24.8279149331472,-24.7225670479549,-24.6173430462968,-24.5121849952785,
-24.4070567860065,-24.3019223538238,-24.1966759362505,-24.0913665218466,
-23.985875269753,-23.9360848270216,-23.8306415847865,-23.7253571698249,
-23.6201964101123,-23.5151013526131,-23.4100357905481,-23.3049635610877,
-23.1997792451331,-23.0945313462189,-22.989102608445,-22.9420976708651),
 .UNSPECIFIED.);
#809=B_SPLINE_CURVE_WITH_KNOTS('',3,(#77589,#77590,#77591,#77592,#77593,
#77594,#77595,#77596,#77597,#77598,#77599,#77600,#77601,#77602,#77603,#77604,
#77605,#77606,#77607,#77608,#77609,#77610,#77611,#77612,#77613,#77614,#77615,
#77616,#77617,#77618,#77619,#77620,#77621,#77622,#77623,#77624,#77625,#77626,
#77627,#77628,#77629,#77630,#77631,#77632,#77633,#77634,#77635,#77636,#77637,
#77638,#77639,#77640,#77641,#77642,#77643,#77644,#77645,#77646,#77647,#77648,
#77649,#77650,#77651,#77652,#77653,#77654,#77655,#77656,#77657,#77658,#77659,
#77660,#77661,#77662,#77663,#77664,#77665,#77666,#77667,#77668,#77669,#77670,
#77671,#77672,#77673,#77674,#77675,#77676,#77677,#77678,#77679,#77680,#77681,
#77682,#77683,#77684,#77685,#77686,#77687,#77688,#77689,#77690,#77691,#77692,
#77693,#77694,#77695,#77696,#77697,#77698,#77699,#77700,#77701,#77702,#77703,
#77704,#77705,#77706,#77707,#77708,#77709,#77710,#77711,#77712,#77713,#77714,
#77715,#77716,#77717,#77718,#77719,#77720,#77721,#77722,#77723,#77724,#77725,
#77726,#77727,#77728,#77729,#77730,#77731,#77732,#77733,#77734,#77735,#77736,
#77737,#77738,#77739,#77740,#77741,#77742,#77743,#77744,#77745,#77746,#77747,
#77748,#77749,#77750,#77751,#77752,#77753,#77754,#77755,#77756,#77757,#77758,
#77759,#77760,#77761,#77762,#77763,#77764,#77765,#77766,#77767,#77768,#77769,
#77770,#77771,#77772,#77773,#77774,#77775,#77776,#77777,#77778,#77779,#77780,
#77781),.UNSPECIFIED.,.F.,.F.,(4,3,3,3,3,3,3,3,3,3,3,3,3,3,3,3,3,3,3,3,
3,3,3,3,3,3,3,3,3,3,3,3,3,3,3,3,3,3,3,3,3,3,3,3,3,3,3,3,3,3,3,3,3,3,3,3,
3,3,3,3,3,3,3,3,4),(-22.9420976703771,-22.938747959229,-22.8332411985356,
-22.7278933143125,-22.6226693136126,-22.5175112635451,-22.4123830552153,
-22.3072486239646,-22.202002207302,-22.0966927937979,-21.9912015425781,
-21.9414110914364,-21.8359043300259,-21.7305564451011,-21.6253324437251,
-21.5201743929979,-21.4150461840255,-21.3099117521501,-21.2046653348939,
-21.099355920813,-20.9938646690483,-20.9440742236439,-20.8385674571758,
-20.7332195671627,-20.6279955606782,-20.5228375048328,-20.4177092907404,
-20.312574853751,-20.2073284314246,-20.1020190122912,-19.9965277555541,
-19.9467373558513,-19.8412306024336,-19.7358827254785,-19.6306587320008,
-19.5255006891231,-19.42037248794,-19.3152380637825,-19.2099916540847,-19.1046822474822,
-18.9991910029953,-18.9494004880587,-18.843893726015,-18.738545840529,-18.6333218386999,
-18.5281637875865,-18.4230355782947,-18.3179011461671,-18.2126547287602,
-18.1073453145864,-18.0018540628175,-17.9520636202662,-17.8465568287251,
-17.7412089135173,-17.6359848817813,-17.5308268006639,-17.425698561317,
-17.3205640991286,-17.2153176518591,-17.1100082078919,-17.0045169267502,
-16.9547267524736,-16.8256995639624,-16.6984996556285,-16.6589125353624),
 .UNSPECIFIED.);
#810=B_SPLINE_CURVE_WITH_KNOTS('',3,(#77783,#77784,#77785,#77786,#77787,
#77788,#77789,#77790,#77791,#77792),.UNSPECIFIED.,.F.,.F.,(4,1,1,1,1,1,
1,4),(-16.6589123631975,-15.957389884681,-14.9600530168885,-13.9627161490959,
-12.9653792813033,-11.9680424135108,-10.9707055457182,-10.3757270560179),
 .UNSPECIFIED.);
#811=B_SPLINE_CURVE_WITH_KNOTS('',3,(#77793,#77794,#77795,#77796,#77797,
#77798,#77799,#77800,#77801,#77802),.UNSPECIFIED.,.F.,.F.,(4,1,1,1,1,1,
1,4),(-10.3757270560179,-9.97336867792565,-8.97603181013308,-7.97869494234052,
-6.98135807454796,-5.98402120675539,-4.98668433896283,-4.09255056086263),
 .UNSPECIFIED.);
#812=B_SPLINE_CURVE_WITH_KNOTS('',3,(#77805,#77806,#77807,#77808,#77809,
#77810,#77811,#77812,#77813,#77814,#77815,#77816,#77817,#77818,#77819,#77820,
#77821,#77822,#77823,#77824,#77825,#77826,#77827,#77828,#77829,#77830,#77831,
#77832,#77833,#77834,#77835,#77836,#77837,#77838,#77839,#77840,#77841,#77842,
#77843,#77844,#77845,#77846,#77847,#77848,#77849,#77850,#77851,#77852,#77853,
#77854,#77855,#77856,#77857,#77858,#77859,#77860,#77861,#77862,#77863,#77864,
#77865,#77866,#77867,#77868,#77869,#77870,#77871,#77872,#77873,#77874,#77875,
#77876,#77877,#77878,#77879,#77880,#77881,#77882,#77883,#77884,#77885,#77886,
#77887,#77888,#77889,#77890,#77891,#77892,#77893,#77894,#77895,#77896,#77897,
#77898,#77899,#77900,#77901,#77902,#77903,#77904,#77905,#77906,#77907,#77908,
#77909,#77910,#77911,#77912,#77913,#77914,#77915,#77916,#77917,#77918,#77919,
#77920,#77921,#77922,#77923,#77924,#77925,#77926,#77927,#77928,#77929,#77930,
#77931,#77932,#77933,#77934,#77935,#77936,#77937,#77938,#77939,#77940,#77941,
#77942,#77943,#77944,#77945,#77946,#77947,#77948,#77949),.UNSPECIFIED.,
 .F.,.F.,(4,3,3,3,3,3,3,3,3,3,3,3,3,3,3,3,3,3,3,3,3,3,3,3,3,3,3,3,3,3,3,
3,3,3,3,3,3,3,3,3,3,3,3,3,3,3,3,3,4),(91.1061869546275,91.240949975046,
91.377756011333,91.4023709425158,91.5139078873181,91.6252460499158,91.736473290312,
91.8476328030592,91.9587676852827,92.0700052418336,92.1812896847161,92.2927949344866,
92.3997078103083,92.5116216959549,92.6233352578315,92.7349367134751,92.8464686433293,
92.9579735293104,93.0695743704088,93.1812190271,93.2930745898801,93.3970446781009,
93.508902541041,93.6205658556783,93.7321205945633,93.8436093723387,93.9550747093353,
94.0666418835812,94.1782560360033,94.2900867617897,94.3943815458935,94.5048591627506,
94.6157165691175,94.7258879039597,94.8359949135827,94.9460821633185,95.0574912259104,
95.167750747137,95.2797345804115,95.391718413686,95.5065472606386,95.6211289936563,
95.7355648062727,95.849889628328,95.9641382305635,96.0783796323015,96.1926089700896,
96.3069226046808,96.3890552814785),.UNSPECIFIED.);
#813=B_SPLINE_CURVE_WITH_KNOTS('',3,(#77952,#77953,#77954,#77955,#77956,
#77957,#77958,#77959,#77960,#77961,#77962,#77963,#77964,#77965,#77966,#77967,
#77968,#77969,#77970,#77971,#77972,#77973,#77974,#77975,#77976,#77977,#77978,
#77979,#77980,#77981,#77982,#77983,#77984,#77985,#77986,#77987,#77988,#77989,
#77990,#77991,#77992,#77993,#77994,#77995,#77996,#77997,#77998,#77999,#78000,
#78001,#78002,#78003,#78004,#78005,#78006,#78007,#78008,#78009,#78010,#78011,
#78012,#78013,#78014,#78015,#78016,#78017,#78018,#78019,#78020,#78021,#78022,
#78023,#78024,#78025,#78026,#78027,#78028,#78029,#78030,#78031,#78032,#78033,
#78034,#78035,#78036,#78037,#78038,#78039,#78040,#78041,#78042,#78043,#78044,
#78045,#78046,#78047,#78048,#78049,#78050,#78051,#78052,#78053,#78054,#78055,
#78056,#78057,#78058,#78059,#78060,#78061,#78062,#78063),.UNSPECIFIED.,
 .F.,.F.,(4,3,3,3,3,3,3,3,3,3,3,3,3,3,3,3,3,3,3,3,3,3,3,3,3,3,3,3,3,3,3,
3,3,3,3,3,3,4),(91.106186954104,91.1567735128389,91.2686768073151,91.380379426595,
91.4919697243224,91.603490302343,91.7149836637296,91.8265730643033,91.938206154167,
92.0500508175322,92.1549203392256,92.2667654043467,92.3784155768566,92.4899569626954,
92.6014322014353,92.712883838097,92.824437435839,92.9360379010216,93.0478556711412,
93.1530671656123,93.2635326749248,93.3744928395591,93.4846514236711,93.5947455296085,
93.7048197379926,93.8164183014942,93.9266649332374,94.0389394626183,94.1512139919991,
94.2660363471297,94.3806110684729,94.4950395788434,94.6093568388985,94.7235976498901,
94.8378311521221,94.9520524352461,95.066358323657,95.1493608183857),
 .UNSPECIFIED.);
#814=B_SPLINE_CURVE_WITH_KNOTS('',3,(#78066,#78067,#78068,#78069,#78070,
#78071,#78072,#78073,#78074,#78075,#78076,#78077,#78078,#78079,#78080,#78081,
#78082,#78083,#78084,#78085,#78086,#78087,#78088,#78089,#78090,#78091),
 .UNSPECIFIED.,.F.,.F.,(4,2,2,2,2,2,2,2,2,2,2,2,4),(-0.913628530073302,
-0.835954964095443,-0.751212961809997,-0.639956110136178,-0.529437845948086,
-0.428568674976155,-0.345923223199362,-0.279967532511881,-0.210201642795373,
-0.152537234598984,-0.0832286370344242,-0.0398354201531648,-4.96018234762577E-5),
 .UNSPECIFIED.);
#815=B_SPLINE_CURVE_WITH_KNOTS('',3,(#78092,#78093,#78094,#78095,#78096,
#78097,#78098,#78099,#78100,#78101,#78102,#78103,#78104,#78105,#78106,#78107,
#78108,#78109,#78110,#78111,#78112,#78113,#78114,#78115,#78116,#78117,#78118,
#78119,#78120,#78121,#78122,#78123,#78124,#78125,#78126,#78127,#78128,#78129,
#78130,#78131,#78132,#78133,#78134,#78135,#78136,#78137,#78138,#78139,#78140,
#78141,#78142,#78143,#78144,#78145,#78146,#78147,#78148,#78149,#78150,#78151,
#78152),.UNSPECIFIED.,.F.,.F.,(4,3,3,3,3,3,3,3,3,3,3,3,3,3,3,3,3,3,3,3,
4),(-0.271362855059931,-0.249815153611103,-0.228817936840513,-0.21475709335129,
-0.20269615019584,-0.199258579296682,-0.179079219908023,-0.172574562883619,
-0.151002742523167,-0.132127399707771,-0.128545224966699,-0.108660381316369,
-0.088904641890274,-0.0695673848931777,-0.0643977176859483,-0.0611873514593056,
-0.0424333152675423,-0.0240015440670001,-0.00742689876696626,-0.00610711498195276,
-1.33929388601358E-14),.UNSPECIFIED.);
#816=B_SPLINE_CURVE_WITH_KNOTS('',3,(#78153,#78154,#78155,#78156,#78157,
#78158,#78159,#78160,#78161,#78162,#78163,#78164,#78165,#78166,#78167,#78168,
#78169,#78170,#78171,#78172,#78173,#78174,#78175,#78176,#78177,#78178,#78179,
#78180,#78181,#78182,#78183,#78184,#78185,#78186,#78187,#78188,#78189,#78190,
#78191,#78192,#78193,#78194,#78195,#78196,#78197,#78198,#78199,#78200,#78201,
#78202,#78203,#78204,#78205,#78206,#78207,#78208,#78209,#78210,#78211,#78212,
#78213,#78214,#78215,#78216,#78217,#78218,#78219),.UNSPECIFIED.,.F.,.F.,
(4,3,3,3,3,3,3,3,3,3,3,3,3,3,3,3,3,3,3,3,3,3,4),(-0.304888653691309,-0.297138437894475,
-0.27579526247451,-0.25452115728438,-0.238505141940676,-0.229387728747905,
-0.225368790891129,-0.221917825979367,-0.200380627888395,-0.178797401191701,
-0.157590348312134,-0.15077543359462,-0.1472283770012,-0.12639303453475,
-0.106224887749054,-0.105100297430208,-0.083375892217648,-0.0782531846850942,
-0.0733795998480499,-0.0515968866484263,-0.0295071888683422,-0.00749310652115608,
-5.77388764150222E-6),.UNSPECIFIED.);
#817=B_SPLINE_CURVE_WITH_KNOTS('',3,(#78575,#78576,#78577,#78578,#78579,
#78580,#78581,#78582,#78583,#78584,#78585,#78586,#78587,#78588,#78589,#78590,
#78591,#78592,#78593,#78594,#78595,#78596,#78597,#78598,#78599,#78600,#78601,
#78602,#78603,#78604,#78605,#78606,#78607,#78608,#78609,#78610,#78611,#78612,
#78613,#78614,#78615,#78616,#78617,#78618,#78619,#78620,#78621,#78622,#78623,
#78624,#78625,#78626,#78627,#78628,#78629,#78630,#78631,#78632,#78633,#78634,
#78635,#78636,#78637,#78638,#78639,#78640,#78641,#78642,#78643,#78644,#78645,
#78646,#78647,#78648,#78649,#78650,#78651,#78652,#78653,#78654,#78655,#78656,
#78657,#78658,#78659),.UNSPECIFIED.,.F.,.F.,(4,3,3,3,3,3,3,3,3,3,3,3,3,
3,3,3,3,3,3,3,3,3,3,3,3,3,3,3,4),(-0.364629307890664,-0.350886157932352,
-0.32922367190401,-0.318978960138819,-0.313744359949613,-0.309365983727222,
-0.288066930719578,-0.266904292681073,-0.264007580396482,-0.260298494201204,
-0.239603026511185,-0.219189259610856,-0.199417582510638,-0.194877404256716,
-0.191399198693004,-0.171813503246808,-0.166173778995206,-0.146078326122423,
-0.126707179806039,-0.123380359543154,-0.103933540649634,-0.0846710840002831,
-0.0655680939453014,-0.062174737667072,-0.0589393440631834,-0.0403289038697169,
-0.0223014018348129,-0.00442011167346308,0.),.UNSPECIFIED.);
#818=B_SPLINE_CURVE_WITH_KNOTS('',3,(#79021,#79022,#79023,#79024,#79025,
#79026,#79027,#79028,#79029,#79030,#79031,#79032,#79033,#79034,#79035,#79036,
#79037,#79038,#79039,#79040,#79041,#79042,#79043,#79044,#79045,#79046,#79047,
#79048,#79049,#79050,#79051,#79052,#79053,#79054,#79055,#79056,#79057,#79058,
#79059,#79060,#79061,#79062,#79063,#79064,#79065,#79066,#79067,#79068,#79069,
#79070,#79071,#79072,#79073,#79074,#79075,#79076,#79077,#79078,#79079,#79080,
#79081,#79082,#79083,#79084,#79085,#79086,#79087,#79088,#79089,#79090,#79091,
#79092,#79093,#79094,#79095,#79096,#79097,#79098,#79099,#79100,#79101,#79102),
 .UNSPECIFIED.,.F.,.F.,(4,3,3,3,3,3,3,3,3,3,3,3,3,3,3,3,3,3,3,3,3,3,3,3,
3,3,3,4),(-0.366397579005846,-0.355505695503922,-0.337427534487906,-0.327287439123245,
-0.321639660907082,-0.302932980904847,-0.290487499977824,-0.283637563200549,
-0.278450433971176,-0.258630766453179,-0.238832793368305,-0.226847110991912,
-0.218285448981465,-0.214861428615519,-0.194431505887542,-0.187234374154516,
-0.16731282220457,-0.147391270254625,-0.143955108128756,-0.123548173224516,
-0.102525007863438,-0.0815018425023604,-0.0762248591763458,-0.071232862628432,
-0.0495803100067464,-0.0278917785029102,-0.0066769277724615,-3.86019020422907E-15),
 .UNSPECIFIED.);
#819=B_SPLINE_CURVE_WITH_KNOTS('',3,(#79103,#79104,#79105,#79106),
 .UNSPECIFIED.,.F.,.F.,(4,4),(-0.0125583369336329,0.),.UNSPECIFIED.);
#820=B_SPLINE_CURVE_WITH_KNOTS('',3,(#79159,#79160,#79161,#79162,#79163,
#79164,#79165,#79166,#79167,#79168,#79169,#79170,#79171,#79172,#79173,#79174,
#79175,#79176,#79177,#79178,#79179,#79180,#79181,#79182,#79183,#79184,#79185,
#79186,#79187,#79188,#79189,#79190,#79191,#79192,#79193,#79194,#79195,#79196,
#79197,#79198,#79199,#79200,#79201,#79202,#79203,#79204,#79205,#79206,#79207,
#79208,#79209,#79210,#79211,#79212,#79213,#79214,#79215,#79216,#79217,#79218,
#79219,#79220,#79221,#79222,#79223,#79224,#79225,#79226,#79227,#79228,#79229,
#79230,#79231,#79232,#79233,#79234,#79235,#79236,#79237,#79238,#79239,#79240,
#79241,#79242,#79243,#79244,#79245,#79246,#79247,#79248,#79249,#79250,#79251,
#79252,#79253,#79254,#79255,#79256,#79257,#79258,#79259,#79260,#79261,#79262,
#79263,#79264,#79265,#79266,#79267,#79268,#79269,#79270,#79271,#79272,#79273,
#79274,#79275,#79276,#79277,#79278,#79279,#79280,#79281,#79282,#79283,#79284,
#79285,#79286,#79287,#79288,#79289,#79290,#79291,#79292,#79293,#79294,#79295,
#79296,#79297,#79298,#79299,#79300),.UNSPECIFIED.,.F.,.F.,(4,3,3,3,3,3,
3,3,3,3,3,3,3,3,3,3,3,3,3,3,3,3,3,3,3,3,3,3,3,3,3,3,3,3,3,3,3,3,3,3,3,3,
3,3,3,3,3,4),(10.3761157660455,10.4506267934108,10.5251285903801,10.5996351081557,
10.6741416414348,10.7486637991409,10.7756260958884,10.8504232250368,10.9252072529087,
10.9999831359438,11.074764867993,11.1495458255052,11.224342920955,11.2703440842045,
11.345139615213,11.4199219903501,11.494696171193,11.5694761383234,11.6442552982486,
11.719050557087,11.7650620725205,11.8398643668488,11.9146536010829,11.9894347157191,
12.064221679377,12.1390078597512,12.2138101295199,12.2597800608365,12.3345766451278,
12.409360096945,12.4841353745425,12.5589164609149,12.6336967509814,12.7084931494411,
12.7544980491525,12.8292980165575,12.9040848916852,12.9788636222862,13.0536481814959,
13.1284319498564,13.2032318119081,13.2492160374685,13.3240137948197,13.3987981794526,
13.4735800434188,13.5483567240136,13.6231416482335,13.6614849715988),
 .UNSPECIFIED.);
#821=B_SPLINE_CURVE_WITH_KNOTS('',3,(#79303,#79304,#79305,#79306,#79307,
#79308,#79309,#79310,#79311,#79312,#79313,#79314,#79315,#79316,#79317,#79318,
#79319,#79320,#79321,#79322,#79323,#79324,#79325,#79326,#79327,#79328,#79329,
#79330,#79331,#79332,#79333,#79334,#79335,#79336,#79337,#79338,#79339,#79340,
#79341,#79342,#79343,#79344,#79345,#79346,#79347,#79348,#79349,#79350,#79351,
#79352,#79353,#79354,#79355,#79356,#79357,#79358,#79359,#79360,#79361,#79362,
#79363,#79364,#79365,#79366,#79367,#79368,#79369,#79370,#79371,#79372,#79373,
#79374,#79375,#79376,#79377,#79378,#79379,#79380,#79381,#79382,#79383,#79384,
#79385,#79386,#79387,#79388,#79389,#79390),.UNSPECIFIED.,.F.,.F.,(4,3,3,
3,3,3,3,3,3,3,3,3,3,3,3,3,3,3,3,3,3,3,3,3,3,3,3,3,3,4),(11.6150328478182,
11.6902644851111,11.765490800086,11.8407152603781,11.915951572411,11.9911896602386,
12.0664446325848,12.1097508361343,12.1843206348914,12.2588742437492,12.3334173056347,
12.4079642286108,12.4825096216488,12.5570715231469,12.6044688244503,12.6793948372725,
12.7543093202956,12.8292168206913,12.9041309543681,12.9790445298975,13.0539736854477,
13.0991868127663,13.1739291377348,13.2486577313256,13.3233777185475,13.3981032598866,
13.4728279518355,13.5475690389764,13.5939048010823,13.6615138258512),
 .UNSPECIFIED.);
#822=B_SPLINE_CURVE_WITH_KNOTS('',3,(#79396,#79397,#79398,#79399,#79400,
#79401,#79402,#79403,#79404,#79405,#79406,#79407,#79408,#79409,#79410,#79411,
#79412,#79413,#79414,#79415,#79416,#79417,#79418,#79419,#79420,#79421,#79422,
#79423,#79424,#79425,#79426,#79427,#79428,#79429,#79430,#79431,#79432,#79433,
#79434,#79435,#79436,#79437,#79438,#79439,#79440,#79441,#79442,#79443,#79444,
#79445,#79446,#79447,#79448,#79449,#79450,#79451,#79452,#79453,#79454,#79455,
#79456,#79457,#79458,#79459,#79460,#79461,#79462,#79463,#79464,#79465,#79466,
#79467,#79468,#79469,#79470,#79471,#79472,#79473,#79474,#79475,#79476,#79477,
#79478,#79479,#79480,#79481,#79482,#79483,#79484,#79485,#79486,#79487,#79488,
#79489,#79490,#79491,#79492,#79493,#79494,#79495,#79496,#79497,#79498,#79499,
#79500,#79501,#79502,#79503,#79504,#79505,#79506,#79507,#79508,#79509,#79510,
#79511,#79512,#79513,#79514,#79515,#79516,#79517,#79518,#79519,#79520,#79521,
#79522,#79523,#79524,#79525,#79526,#79527,#79528,#79529,#79530,#79531,#79532,
#79533,#79534,#79535,#79536,#79537,#79538,#79539,#79540,#79541,#79542,#79543,
#79544,#79545,#79546,#79547,#79548,#79549,#79550,#79551,#79552,#79553,#79554,
#79555,#79556,#79557,#79558,#79559,#79560,#79561,#79562,#79563,#79564,#79565,
#79566,#79567,#79568,#79569,#79570,#79571,#79572,#79573,#79574,#79575,#79576,
#79577,#79578,#79579,#79580,#79581,#79582,#79583,#79584,#79585,#79586,#79587,
#79588,#79589,#79590,#79591,#79592,#79593,#79594,#79595,#79596,#79597),
 .UNSPECIFIED.,.F.,.F.,(4,2,2,2,2,2,2,2,2,2,2,2,2,2,2,2,2,2,2,2,2,2,2,2,
2,2,2,2,2,2,2,2,2,2,2,2,2,2,2,2,2,2,2,2,2,2,2,2,2,2,2,2,2,2,2,2,2,2,2,2,
2,2,2,2,2,2,2,2,2,2,2,2,2,2,2,2,2,2,2,2,2,2,2,2,2,2,2,2,2,2,2,2,2,2,2,2,
2,2,2,2,4),(-3.97109063192392,-3.9649584214025,-3.94125537962466,-3.91058322495257,
-3.89203316749827,-3.84035677009342,-3.74824131557227,-3.73197860427002,
-3.71922584434786,-3.7030726518714,-3.65804376908474,-3.52982073441756,
-3.50151446932462,-3.47782076935689,-3.4473215548278,-3.41239070554766,
-3.33572477575311,-3.28181642319089,-3.26520322651505,-3.25253604022651,
-3.23404990159059,-3.16534005368315,-3.07245755536263,-3.04222784660332,
-3.01852003999537,-2.99040223435899,-2.92206615278128,-2.82216886043237,
-2.80355774413339,-2.79088364704611,-2.77406349559966,-2.71944855650011,
-2.60247397040471,-2.57415598977363,-2.55046311454246,-2.51997956828078,
-2.4850754427358,-2.40855380420268,-2.35454076431744,-2.33788289742667,
-2.3252186833505,-2.30679093405412,-2.23683808586572,-2.14563298851787,
-2.11519033019849,-2.09146875015941,-2.0635047653402,-1.99725335964054,
-1.92544579474782,-1.88783821260595,-1.87222481097903,-1.85935818272856,
-1.83875150547172,-1.81194280557731,-1.73607218751607,-1.67481226399478,
-1.64659832981041,-1.62289804626951,-1.5922742192944,-1.57376850668018,
-1.52228771650205,-1.42937494715888,-1.41329236281721,-1.40056336817996,
-1.38425485370735,-1.33736129887648,-1.23960749036547,-1.19865388794307,
-1.17365645574888,-1.14883914487401,-1.10910255959279,-1.05646920957979,
-0.965000054988304,-0.949200763425442,-0.936504180056433,-0.919932085860634,
-0.869443816545504,-0.752738157034909,-0.722675470641795,-0.699000369934617,
-0.673666991491305,-0.664833626055923,-0.649423893463878,-0.601283018334735,
-0.502106716811277,-0.484581341103242,-0.47641641941256,-0.464785993756397,
-0.449891830642469,-0.436902619345004,-0.358101489383389,-0.286795121484024,
-0.257554411525978,-0.233892389125443,-0.211223048857578,-0.156660280482908,
-0.0839224513368464,-0.0354159956040736,-0.0191828792016435,-0.00973861638456724,
-0.000140069715062154),.UNSPECIFIED.);
#823=B_SPLINE_CURVE_WITH_KNOTS('',3,(#79598,#79599,#79600,#79601,#79602,
#79603,#79604,#79605,#79606,#79607,#79608,#79609,#79610,#79611,#79612,#79613,
#79614,#79615,#79616,#79617,#79618,#79619,#79620,#79621,#79622,#79623,#79624,
#79625,#79626,#79627,#79628,#79629,#79630,#79631,#79632,#79633,#79634,#79635,
#79636,#79637,#79638,#79639,#79640,#79641,#79642,#79643,#79644,#79645,#79646,
#79647,#79648,#79649,#79650,#79651,#79652,#79653,#79654,#79655,#79656,#79657,
#79658,#79659,#79660,#79661,#79662,#79663,#79664,#79665,#79666,#79667,#79668,
#79669,#79670,#79671,#79672,#79673,#79674,#79675,#79676,#79677,#79678,#79679,
#79680,#79681,#79682,#79683,#79684,#79685,#79686,#79687,#79688),
 .UNSPECIFIED.,.F.,.F.,(4,3,3,3,3,3,3,3,3,3,3,3,3,3,3,3,3,3,3,3,3,3,3,3,
3,3,3,3,3,3,4),(13.6614849715988,13.7362826754358,13.7439340257846,13.8187329504215,
13.8935187704987,13.9682964370049,14.0430799261714,14.1178626229009,14.1926614179982,
14.2386520141006,14.3134508885949,14.3882366586011,14.4630142752602,14.5377977152858,
14.6125803633574,14.6873791108762,14.7333700024166,14.8081687869976,14.882954465705,
14.9577319899606,15.0325153365808,15.1072978908342,15.1820965445166,15.2280879907326,
15.302789587196,15.3774777760568,15.4521578013161,15.5268433257792,15.6015287495532,
15.6762295160124,15.7079632678645),.UNSPECIFIED.);
#824=B_SPLINE_CURVE_WITH_KNOTS('',3,(#79690,#79691,#79692,#79693,#79694,
#79695,#79696,#79697,#79698,#79699,#79700,#79701,#79702,#79703,#79704,#79705,
#79706,#79707,#79708,#79709,#79710,#79711,#79712,#79713,#79714,#79715,#79716,
#79717,#79718,#79719,#79720,#79721,#79722,#79723,#79724,#79725,#79726,#79727,
#79728,#79729,#79730,#79731,#79732,#79733,#79734,#79735,#79736,#79737,#79738,
#79739,#79740,#79741,#79742,#79743,#79744,#79745,#79746,#79747,#79748,#79749,
#79750,#79751,#79752,#79753,#79754,#79755,#79756,#79757,#79758,#79759,#79760,
#79761,#79762,#79763,#79764,#79765,#79766,#79767,#79768,#79769,#79770,#79771,
#79772,#79773,#79774,#79775,#79776,#79777),.UNSPECIFIED.,.F.,.F.,(4,3,3,
3,3,3,3,3,3,3,3,3,3,3,3,3,3,3,3,3,3,3,3,3,3,3,3,3,3,4),(13.6615138258512,
13.7363191624509,13.8111159963363,13.8859184780869,13.9607196890201,14.0355373534483,
14.0886227893984,14.1634199053517,14.2382039199167,14.3129797895736,14.3877615082347,
14.4625424523753,14.5373395345686,14.5833407777144,14.6581363061753,14.7329186787134,
14.8076928569137,14.8824728213545,14.9572519785678,15.0320472346775,15.0780587660304,
15.1528610671284,15.2276503082195,15.302431429779,15.3772184004102,15.4520045877747,
15.5268068645131,15.5727767543464,15.650970727164,15.7079632679489),
 .UNSPECIFIED.);
#825=B_SPLINE_CURVE_WITH_KNOTS('',3,(#79778,#79779,#79780,#79781,#79782,
#79783,#79784,#79785,#79786,#79787,#79788,#79789),.UNSPECIFIED.,.F.,.F.,
(4,1,1,1,1,1,1,1,1,4),(15.7079632679489,16.0674947426624,16.5622127309785,
17.0569307192945,17.5516487076105,18.0463666959265,18.5410846842426,19.0358026725586,
19.5305206608746,19.9446639604968),.UNSPECIFIED.);
#826=B_SPLINE_CURVE_WITH_KNOTS('',3,(#79794,#79795,#79796,#79797,#79798,
#79799,#79800,#79801,#79802,#79803,#79804,#79805,#79806,#79807,#79808,#79809,
#79810,#79811,#79812,#79813,#79814,#79815,#79816,#79817,#79818,#79819,#79820,
#79821,#79822,#79823,#79824,#79825,#79826,#79827,#79828,#79829,#79830,#79831,
#79832,#79833,#79834,#79835,#79836,#79837,#79838,#79839,#79840,#79841,#79842,
#79843,#79844,#79845,#79846,#79847,#79848,#79849,#79850,#79851,#79852,#79853,
#79854,#79855,#79856,#79857,#79858,#79859,#79860,#79861,#79862,#79863,#79864,
#79865,#79866,#79867,#79868,#79869,#79870,#79871,#79872,#79873,#79874,#79875,
#79876,#79877,#79878,#79879,#79880,#79881,#79882,#79883,#79884,#79885,#79886,
#79887,#79888,#79889,#79890,#79891,#79892,#79893,#79894,#79895,#79896,#79897,
#79898,#79899,#79900,#79901,#79902,#79903,#79904,#79905,#79906,#79907,#79908,
#79909,#79910,#79911,#79912,#79913,#79914,#79915,#79916,#79917,#79918,#79919,
#79920,#79921,#79922,#79923,#79924,#79925,#79926,#79927,#79928,#79929,#79930,
#79931,#79932,#79933,#79934,#79935,#79936,#79937,#79938,#79939,#79940,#79941,
#79942,#79943,#79944,#79945,#79946,#79947,#79948,#79949,#79950,#79951,#79952,
#79953,#79954,#79955,#79956,#79957,#79958,#79959,#79960,#79961,#79962,#79963,
#79964,#79965,#79966,#79967,#79968,#79969,#79970,#79971,#79972,#79973,#79974,
#79975,#79976,#79977,#79978,#79979,#79980,#79981,#79982,#79983,#79984,#79985,
#79986,#79987,#79988,#79989,#79990,#79991,#79992,#79993,#79994,#79995,#79996,
#79997,#79998,#79999,#80000,#80001,#80002,#80003,#80004,#80005,#80006,#80007,
#80008,#80009,#80010,#80011,#80012,#80013,#80014,#80015,#80016,#80017,#80018,
#80019,#80020,#80021,#80022,#80023,#80024,#80025,#80026,#80027,#80028,#80029,
#80030,#80031,#80032,#80033,#80034,#80035,#80036,#80037,#80038,#80039,#80040,
#80041,#80042,#80043,#80044,#80045,#80046,#80047,#80048,#80049,#80050,#80051,
#80052,#80053,#80054,#80055,#80056,#80057,#80058,#80059,#80060,#80061,#80062,
#80063,#80064,#80065,#80066,#80067,#80068,#80069,#80070,#80071,#80072,#80073,
#80074,#80075,#80076,#80077,#80078,#80079,#80080,#80081,#80082,#80083,#80084,
#80085,#80086,#80087,#80088,#80089,#80090,#80091,#80092,#80093,#80094,#80095,
#80096,#80097,#80098,#80099,#80100,#80101),.UNSPECIFIED.,.F.,.F.,(4,2,2,
2,2,2,2,2,2,2,2,2,2,2,2,2,2,2,2,2,2,2,2,2,2,2,2,2,2,2,2,2,2,2,2,2,2,2,2,
2,2,2,2,2,2,2,2,2,2,2,2,2,2,2,2,2,2,2,2,2,2,2,2,2,2,2,2,2,2,2,2,2,2,2,2,
2,2,2,2,2,2,2,2,2,2,2,2,2,2,2,2,2,2,2,2,2,2,2,2,2,2,2,2,2,2,2,2,2,2,2,2,
2,2,2,2,2,2,2,2,2,2,2,2,2,2,2,2,2,2,2,2,2,2,2,2,2,2,2,2,2,2,2,2,2,2,2,2,
2,2,2,2,2,2,4),(-9.86013605182866,-9.85775592310744,-9.80120571927038,-9.78509274360098,
-9.76249470244743,-9.74934425532136,-9.73451575923864,-9.70134415794215,
-9.62845209064997,-9.55767673893976,-9.52939672097626,-9.50570105156311,
-9.47568485969833,-9.38097537979839,-9.33321054321053,-9.31169702354504,
-9.29405595272518,-9.28265001569269,-9.26623359882227,-9.21661344277033,
-9.13666290115609,-9.10114259414212,-9.07029916734766,-9.04658601691335,
-9.01852858927522,-8.89654998353862,-8.84560378324243,-8.8290011938466,
-8.81630761709997,-8.8005391354648,-8.70955394869662,-8.65661582770117,
-8.61674042232065,-8.59190236775481,-8.56692658301866,-8.52612083856455,
-8.42830549826841,-8.38123731803778,-8.3649147337912,-8.35218752366493,
-8.33612032199704,-8.24313778883039,-8.16742303449248,-8.13887189008925,
-8.11519192950506,-8.08500583940029,-7.98521965495371,-7.92449884912506,
-7.90501076512387,-7.8922684876077,-7.87604877900771,-7.83693885180086,
-7.7655751863258,-7.72118503160559,-7.68545871628982,-7.6612173431972,-7.63535576288555,
-7.58841906612945,-7.49441766873105,-7.47359980156074,-7.44683028829438,
-7.43298830831523,-7.41914254335625,-7.39235073028266,-7.28964779422958,
-7.25087949922825,-7.21818171589099,-7.19431121702325,-7.16732570321357,
-7.11144587243985,-7.02819044901947,-6.98844486983763,-6.97280647748618,
-6.95994613294143,-6.93939078254868,-6.88412961052176,-6.85306375000533,
-6.77649597594078,-6.74790554766224,-6.72422736167339,-6.69408941231124,
-6.59384716829753,-6.54927633205444,-6.52053385070342,-6.50636651372026,
-6.49448858324354,-6.47179765676272,-6.36363430158537,-6.32427069852211,
-6.29124106043262,-6.26733515011524,-6.24050357706787,-6.18597660025094,
-6.16949424205874,-6.09754507421765,-6.07916661576279,-6.06729844499258,
-6.0490075016292,-6.03634929855385,-6.01958334460289,-5.96547711678565,
-5.88919331281921,-5.84055104036619,-5.81445688424311,-5.79031754994828,
-5.75535671470574,-5.71242984849447,-5.64152711550889,-5.59920056388999,
-5.58285392158756,-5.5701300056767,-5.55084368472898,-5.53804144574276,
-5.45977517752814,-5.38672804378348,-5.35770365462632,-5.33403881488783,
-5.30440026965166,-5.27092874007404,-5.2016691711656,-5.19262313337488,
-5.13721349899873,-5.12033590631651,-5.10768281194952,-5.08952855945553,
-5.07778672957253,-5.05969028240922,-4.98987066092593,-4.96996673442988,
-4.91648815815063,-4.88953017159539,-4.86565349808146,-4.83289749484037,
-4.75387142711427,-4.67736449371335,-4.65855758971717,-4.64587098151835,
-4.62919627952934,-4.57711505794881,-4.45671660136064,-4.4285728621856,
-4.4048668683294,-4.37414531940268,-4.35554992977496,-4.30367308439143,
-4.28314416449104,-4.26293236475343,-4.21358916027192,-4.19482286021633,
-4.18213903445771,-4.16543487941048,-4.1128678875124,-3.99313738636478,
-3.97109063192392),.UNSPECIFIED.);
#827=B_SPLINE_CURVE_WITH_KNOTS('',3,(#80103,#80104,#80105,#80106,#80107,
#80108,#80109,#80110),.UNSPECIFIED.,.F.,.F.,(4,1,1,1,1,4),(19.9446639604968,
20.0252386491906,20.5199566375066,21.0146746258227,21.5093926141387,21.9911485575199),
 .UNSPECIFIED.);
#828=B_SPLINE_CURVE_WITH_KNOTS('',3,(#80111,#80112,#80113,#80114,#80115,
#80116,#80117,#80118,#80119,#80120,#80121,#80122,#80123,#80124,#80125,#80126,
#80127,#80128,#80129,#80130,#80131,#80132,#80133,#80134,#80135,#80136,#80137,
#80138,#80139,#80140,#80141,#80142,#80143,#80144,#80145,#80146,#80147,#80148,
#80149,#80150,#80151,#80152,#80153,#80154,#80155,#80156,#80157,#80158,#80159,
#80160,#80161,#80162,#80163,#80164,#80165,#80166,#80167,#80168,#80169,#80170,
#80171,#80172,#80173,#80174,#80175,#80176,#80177,#80178,#80179,#80180,#80181,
#80182,#80183,#80184,#80185,#80186,#80187,#80188,#80189,#80190,#80191,#80192,
#80193,#80194,#80195,#80196,#80197,#80198,#80199,#80200,#80201,#80202,#80203,
#80204,#80205,#80206,#80207,#80208,#80209,#80210,#80211,#80212,#80213,#80214,
#80215,#80216,#80217,#80218,#80219,#80220,#80221,#80222,#80223,#80224,#80225,
#80226,#80227,#80228,#80229,#80230,#80231,#80232,#80233,#80234,#80235,#80236,
#80237,#80238,#80239,#80240,#80241,#80242,#80243,#80244,#80245,#80246,#80247,
#80248,#80249,#80250,#80251,#80252,#80253,#80254,#80255,#80256,#80257,#80258,
#80259,#80260,#80261,#80262,#80263,#80264,#80265,#80266,#80267,#80268,#80269,
#80270,#80271,#80272,#80273,#80274,#80275,#80276,#80277,#80278,#80279,#80280,
#80281,#80282,#80283,#80284,#80285,#80286,#80287,#80288,#80289,#80290,#80291,
#80292,#80293,#80294,#80295,#80296,#80297,#80298,#80299,#80300,#80301,#80302,
#80303,#80304,#80305,#80306,#80307,#80308,#80309,#80310),.UNSPECIFIED.,
 .F.,.F.,(4,2,2,2,2,2,2,2,2,2,2,2,2,2,2,2,2,2,2,2,2,2,2,2,2,2,2,2,2,2,2,
2,2,2,2,2,2,2,2,2,2,2,2,2,2,2,2,2,2,2,2,2,2,2,2,2,2,2,2,2,2,2,2,2,2,2,2,
2,2,2,2,2,2,2,2,2,2,2,2,2,2,2,2,2,2,2,2,2,2,2,2,2,2,2,2,2,2,2,2,4),(-11.7781659429298,
-11.7695015011355,-11.7608648717293,-11.7446191234857,-11.6961485739992,
-11.6253310868354,-11.5693010683801,-11.546580909873,-11.5229169989328,
-11.4938896650299,-11.4207905883937,-11.3425572214838,-11.3297661630289,
-11.3149993089201,-11.3033988389499,-11.2945967762062,-11.27631395539,-11.1983463453215,
-11.13949459,-11.1168460665849,-11.1068983920934,-11.0813894076414,-11.0577201330965,
-11.0278361945305,-10.9092863261089,-10.8599661768067,-10.8434748824404,
-10.830769568392,-10.8117030092558,-10.757330661835,-10.6843363809635,-10.6501063763627,
-10.6200191075797,-10.5965648779771,-10.5680452639929,-10.4555779698413,
-10.3974659494186,-10.3804778821854,-10.3678152467337,-10.3494180968824,
-10.2636130824389,-10.1884160541029,-10.1575629366113,-10.1338495789973,
-10.1057997660604,-9.98369695884995,-9.93284204766808,-9.91624569593284,
-9.90355173584416,-9.88463638359643,-9.81037554518269,-9.7497025044728,
-9.7292453368533,-9.6965321207523,-9.6726603626042,-9.64568293025807,-9.58987219510691,
-9.50654307814477,-9.47869354785551,-9.45753575641754,-9.44459690261661,
-9.42923247726541,-9.39657756671605,-9.3238580101053,-9.2537602354624,-9.22552374854818,
-9.20182540347174,-9.17175387252392,-9.07754270399396,-9.00960384726125,
-8.99118342280821,-8.97851965180629,-8.96185630990279,-8.90783600130185,
-8.83133154849194,-8.79643098946603,-8.76594954274167,-8.74225692517295,
-8.71393769160619,-8.59699032178751,-8.54235438486408,-8.52553317220681,
-8.51285924140121,-8.49424976045908,-8.39900512355604,-8.3496835568728,
-8.31149720599506,-8.28690780339787,-8.26465669098099,-8.22564678861382,
-8.12025152888348,-8.07671557608262,-8.06069651088904,-8.04792037962756,
-8.03149393709917,-7.92656790738476,-7.86153813609482,-7.83367099818519,
-7.80993962364222,-7.80726529325742),.UNSPECIFIED.);
#829=B_SPLINE_CURVE_WITH_KNOTS('',3,(#80316,#80317,#80318,#80319,#80320,
#80321,#80322,#80323,#80324,#80325,#80326,#80327),.UNSPECIFIED.,.F.,.F.,
(4,1,1,1,1,1,1,1,1,4),(28.2743338823081,28.5854736752652,29.0801916635813,
29.5749096518973,30.0696276402133,30.5643456285293,31.0590636168453,31.5537816051614,
32.0484995934774,32.5110459440461),.UNSPECIFIED.);
#830=B_SPLINE_CURVE_WITH_KNOTS('',3,(#80328,#80329,#80330,#80331,#80332,
#80333,#80334,#80335,#80336,#80337,#80338,#80339,#80340,#80341,#80342,#80343,
#80344,#80345,#80346,#80347,#80348,#80349,#80350,#80351,#80352,#80353,#80354,
#80355,#80356,#80357,#80358,#80359,#80360,#80361,#80362,#80363,#80364,#80365,
#80366,#80367,#80368,#80369,#80370,#80371,#80372,#80373,#80374,#80375,#80376,
#80377,#80378,#80379,#80380,#80381,#80382,#80383,#80384,#80385,#80386,#80387,
#80388,#80389,#80390,#80391,#80392,#80393,#80394,#80395,#80396,#80397,#80398,
#80399,#80400,#80401,#80402,#80403,#80404,#80405,#80406,#80407,#80408,#80409,
#80410,#80411,#80412,#80413,#80414,#80415,#80416,#80417,#80418,#80419,#80420,
#80421,#80422,#80423,#80424,#80425,#80426,#80427,#80428,#80429,#80430,#80431,
#80432,#80433,#80434,#80435),.UNSPECIFIED.,.F.,.F.,(4,2,2,2,2,2,2,2,2,2,
2,2,2,2,2,2,2,2,2,2,2,2,2,2,2,2,2,2,2,2,2,2,2,2,2,2,2,2,2,2,2,2,2,2,2,2,
2,2,2,2,2,2,2,4),(-11.778252564853,-11.6406709475873,-11.6235349277419,
-11.6112523485181,-11.598568535928,-11.5798024599838,-11.5304636051125,
-11.5206877207964,-11.5075055668975,-11.445472516879,-11.4136118290732,
-11.3858150712362,-11.3629328315184,-11.3338397533264,-11.2579743756513,
-11.1949532381769,-11.1702611569884,-11.152796955343,-11.152515566578,-11.1520536549756,
-11.1513315226703,-11.150268370153,-11.1496141462943,-11.1369542046494,
-11.1202217431636,-11.0691368366197,-10.9907289590674,-10.9554812177169,
-10.924796590793,-10.9010927554962,-10.8729225884066,-10.7530181607851,
-10.7005758873345,-10.6838791394854,-10.6711945775082,-10.6555200921164,
-10.5636129805667,-10.4860973636492,-10.4574659762096,-10.4361630462076,
-10.4073916427012,-10.3366881833582,-10.2569399767523,-10.2293878667224,
-10.2154146117674,-10.2034293258265,-10.1800043676687,-10.0728753989478,
-10.0336200014843,-10.0006505217454,-9.97675121384317,-9.94989254594728,
-9.89513072885096,-9.86013605182866),.UNSPECIFIED.);
#831=B_SPLINE_CURVE_WITH_KNOTS('',3,(#80436,#80437,#80438,#80439,#80440,
#80441,#80442,#80443,#80444,#80445,#80446,#80447,#80448,#80449,#80450,#80451,
#80452,#80453,#80454,#80455,#80456,#80457,#80458,#80459,#80460,#80461,#80462,
#80463,#80464,#80465,#80466,#80467,#80468,#80469,#80470,#80471,#80472,#80473,
#80474,#80475,#80476,#80477,#80478,#80479,#80480,#80481,#80482,#80483,#80484,
#80485,#80486,#80487,#80488,#80489,#80490,#80491,#80492,#80493,#80494,#80495,
#80496,#80497,#80498,#80499,#80500,#80501,#80502,#80503,#80504,#80505,#80506,
#80507,#80508,#80509,#80510,#80511,#80512,#80513,#80514,#80515,#80516,#80517,
#80518,#80519,#80520,#80521,#80522,#80523,#80524,#80525,#80526,#80527,#80528,
#80529,#80530,#80531,#80532,#80533,#80534,#80535,#80536,#80537,#80538,#80539,
#80540,#80541,#80542,#80543,#80544,#80545,#80546,#80547,#80548,#80549,#80550,
#80551,#80552,#80553,#80554,#80555,#80556,#80557,#80558,#80559,#80560,#80561,
#80562,#80563,#80564,#80565,#80566,#80567,#80568,#80569,#80570,#80571,#80572,
#80573,#80574,#80575,#80576,#80577,#80578,#80579,#80580,#80581,#80582,#80583,
#80584,#80585,#80586,#80587,#80588,#80589,#80590,#80591,#80592,#80593,#80594,
#80595,#80596,#80597,#80598,#80599,#80600,#80601,#80602,#80603,#80604,#80605,
#80606,#80607,#80608,#80609,#80610,#80611,#80612,#80613,#80614,#80615,#80616,
#80617,#80618,#80619,#80620,#80621,#80622,#80623,#80624,#80625,#80626,#80627,
#80628,#80629,#80630,#80631,#80632,#80633,#80634,#80635,#80636,#80637,#80638,
#80639,#80640,#80641,#80642,#80643,#80644,#80645,#80646,#80647,#80648,#80649,
#80650,#80651,#80652,#80653,#80654,#80655,#80656,#80657,#80658,#80659,#80660,
#80661,#80662,#80663,#80664,#80665,#80666,#80667,#80668,#80669,#80670,#80671,
#80672,#80673,#80674,#80675,#80676,#80677,#80678,#80679,#80680,#80681,#80682,
#80683,#80684,#80685,#80686,#80687,#80688,#80689,#80690,#80691,#80692,#80693,
#80694,#80695,#80696,#80697,#80698,#80699,#80700,#80701,#80702,#80703,#80704,
#80705,#80706,#80707,#80708,#80709,#80710,#80711,#80712,#80713,#80714,#80715,
#80716,#80717,#80718,#80719,#80720,#80721,#80722,#80723,#80724,#80725,#80726,
#80727,#80728,#80729,#80730,#80731,#80732,#80733,#80734,#80735),
 .UNSPECIFIED.,.F.,.F.,(4,2,2,2,2,2,2,2,2,2,2,2,2,2,2,2,2,2,2,2,2,2,2,2,
2,2,2,2,2,2,2,2,2,2,2,2,2,2,2,2,2,2,2,2,2,2,2,2,2,2,2,2,2,2,2,2,2,2,2,2,
2,2,2,2,2,2,2,2,2,2,2,2,2,2,2,2,2,2,2,2,2,2,2,2,2,2,2,2,2,2,2,2,2,2,2,2,
2,2,2,2,2,2,2,2,2,2,2,2,2,2,2,2,2,2,2,2,2,2,2,2,2,2,2,2,2,2,2,2,2,2,2,2,
2,2,2,2,2,2,2,2,2,2,2,2,2,2,2,2,2,4),(-7.80726529325742,-7.77935749609294,
-7.67305087886337,-7.61532396084259,-7.59835246544215,-7.58568871944003,
-7.56727066738562,-7.47118503282339,-7.42209034280295,-7.38401311193093,
-7.35943952478874,-7.33717305143281,-7.29804852312495,-7.19964982003832,
-7.15047690409958,-7.13399591078041,-7.12128917107599,-7.10220677162885,
-7.04762646706141,-7.01303062849308,-6.96101782570722,-6.94239188993943,
-6.91163719378434,-6.88792947523917,-6.85980982007647,-6.73896706821418,
-6.68720740777731,-6.67055278508652,-6.65786440302101,-6.63903011343649,
-6.56284146877764,-6.48357197730743,-6.45081089598387,-6.42693388028032,
-6.39997866352125,-6.34652087598751,-6.32989519195407,-6.25758324449705,
-6.23131673594426,-6.21100128453345,-6.19817022235686,-6.18241309711473,
-6.14686954960281,-6.11611080039932,-6.04600090885001,-6.02380754583908,
-5.98930233089118,-5.96522178535301,-5.93897523237577,-5.88918110525131,
-5.80898148854834,-5.75967792345171,-5.74327726051686,-5.73187018921226,
-5.71420974715616,-5.6926632020871,-5.64475803048892,-5.55036136288458,
-5.52031075793103,-5.49661326915974,-5.46835998403671,-5.39800749783332,
-5.32522198340407,-5.29281571825591,-5.27749425283985,-5.26454117835684,
-5.24328084015127,-5.21523579186608,-5.13040125871549,-5.0759326908419,
-5.0491080994601,-5.02520070541903,-4.99215618326773,-4.95276549104083,
-4.84434110764955,-4.82183199912996,-4.80998016703858,-4.79576089979521,
-4.76669207336761,-4.6887629815646,-4.65102056503018,-4.60678762499012,
-4.58130911634682,-4.55685806621619,-4.51963156128297,-4.49466563782946,
-4.40554657926642,-4.36686138093599,-4.3510076779813,-4.33949694543313,
-4.32066136354435,-4.29707312666952,-4.23980418042955,-4.1963896853928,
-4.14646511054971,-4.12020136732982,-4.09612672528735,-4.06166971512036,
-4.0395240005844,-3.9696941780766,-3.92927284834963,-3.89911281573639,-3.8847234296745,
-3.87132508166856,-3.84718798128298,-3.723868174573,-3.67950966880563,-3.65401301968522,
-3.62957324258816,-3.59242578765454,-3.56754300871115,-3.47909488615639,
-3.44000695207153,-3.42395354489741,-3.41130481685074,-3.39166051011915,
-3.3295062352493,-3.23111223937331,-3.20106004713098,-3.17738496280548,
-3.14872381429807,-3.07048034386312,-2.97957200166355,-2.96382341457031,
-2.95113180129177,-2.93450944732577,-2.88325837040146,-2.76170931335911,
-2.73362826711275,-2.70991711376523,-2.67910727891974,-2.64364459968794,
-2.56402503823103,-2.51397747236937,-2.49754039088955,-2.48613588695837,
-2.46852001598447,-2.44704958953221,-2.3994666130595,-2.30436443440703,
-2.27439122337597,-2.2506977762483,-2.22238404925131,-2.15106455046269,
-2.05533442705832,-2.03644540328393,-2.02375314844008,-2.00713760892109,
-1.95599150686342,-1.91824501396425),.UNSPECIFIED.);
#832=B_SPLINE_CURVE_WITH_KNOTS('',3,(#80741,#80742,#80743,#80744,#80745,
#80746,#80747,#80748,#80749,#80750,#80751,#80752,#80753,#80754,#80755,#80756,
#80757,#80758,#80759,#80760,#80761,#80762,#80763,#80764,#80765,#80766,#80767,
#80768,#80769,#80770,#80771,#80772,#80773,#80774,#80775,#80776,#80777,#80778,
#80779,#80780,#80781,#80782,#80783,#80784,#80785,#80786,#80787,#80788,#80789,
#80790,#80791,#80792,#80793,#80794,#80795,#80796,#80797,#80798,#80799,#80800,
#80801,#80802,#80803,#80804,#80805,#80806,#80807,#80808,#80809,#80810,#80811,
#80812,#80813,#80814,#80815,#80816,#80817,#80818,#80819,#80820,#80821,#80822,
#80823,#80824,#80825,#80826,#80827,#80828,#80829,#80830,#80831,#80832,#80833,
#80834,#80835,#80836,#80837,#80838,#80839,#80840,#80841,#80842,#80843,#80844,
#80845,#80846,#80847,#80848,#80849,#80850,#80851,#80852,#80853,#80854,#80855,
#80856,#80857,#80858,#80859,#80860,#80861,#80862,#80863,#80864,#80865,#80866,
#80867,#80868,#80869,#80870,#80871,#80872,#80873,#80874,#80875,#80876,#80877,
#80878,#80879,#80880,#80881,#80882,#80883,#80884,#80885,#80886,#80887,#80888,
#80889,#80890,#80891,#80892,#80893,#80894,#80895,#80896,#80897,#80898,#80899,
#80900,#80901,#80902,#80903,#80904,#80905,#80906,#80907,#80908,#80909,#80910,
#80911,#80912,#80913,#80914,#80915,#80916,#80917,#80918,#80919,#80920,#80921,
#80922,#80923,#80924,#80925,#80926,#80927,#80928,#80929,#80930,#80931,#80932,
#80933,#80934),.UNSPECIFIED.,.F.,.F.,(4,2,2,2,2,2,2,2,2,2,2,2,2,2,2,2,2,
2,2,2,2,2,2,2,2,2,2,2,2,2,2,2,2,2,2,2,2,2,2,2,2,2,2,2,2,2,2,2,2,2,2,2,2,
2,2,2,2,2,2,2,2,2,2,2,2,2,2,2,2,2,2,2,2,2,2,2,2,2,2,2,2,2,2,2,2,2,2,2,2,
2,2,2,2,2,2,2,4),(-3.97117590885512,-3.94669210599682,-3.91832163603527,
-3.89463165039578,-3.86421585636958,-3.8294276465923,-3.7535305641743,-3.70095786973156,
-3.68480102203414,-3.67206237742609,-3.65581860712673,-3.60972342272422,
-3.48546404062927,-3.45625278551107,-3.43259021326658,-3.40314936400795,
-3.37001008928841,-3.30231304465889,-3.25471306968969,-3.22710654390848,
-3.21312430909366,-3.19941166328336,-3.17340453068049,-3.09590210320283,
-3.02140843908474,-2.99233187439596,-2.96866796824151,-2.93908586509719,
-2.85571691487168,-2.77465612436432,-2.75627897603085,-2.74361703761271,
-2.72661210030565,-2.66810690159166,-2.55612981204258,-2.52758977816173,
-2.50413606401613,-2.47407252071042,-2.38836528380176,-2.3118553058605,
-2.29304889556372,-2.28036241622853,-2.26368760924573,-2.21160285508002,
-2.09121087589847,-2.06306707946917,-2.03936130748535,-2.00864042433467,
-1.99004556608244,-1.93817082040966,-1.91785217331093,-1.89587697902556,
-1.84473820161903,-1.82916976320421,-1.81649459529526,-1.7996884101607,
-1.74533279986831,-1.62801440519616,-1.59971318465083,-1.576019203503,-1.54551343126094,
-1.45913347520987,-1.38469760991913,-1.365779818563,-1.35308564020557,-1.33649089694924,
-1.28566093199827,-1.16352397162026,-1.13547607916695,-1.11176242983227,
-1.08090624861425,-1.00568594923737,-0.919885438748811,-0.901498384786369,
-0.888836175204954,-0.871839799565827,-0.8135330797845,-0.701310851708188,
-0.672781243510081,-0.649327404532392,-0.62189163869072,-0.589287260920047,
-0.524022535056337,-0.457700442076925,-0.438593440647315,-0.426817530209833,
-0.411870657074917,-0.393914572892701,-0.375874474294829,-0.306470523602214,
-0.286747545038346,-0.232123890928064,-0.205281683836191,-0.182245325000184,
-0.158840728001359,-0.126585532836681,-0.000142354813690746),
 .UNSPECIFIED.);
#833=B_SPLINE_CURVE_WITH_KNOTS('',3,(#80935,#80936,#80937,#80938,#80939,
#80940,#80941,#80942,#80943),.UNSPECIFIED.,.F.,.F.,(4,1,1,1,1,1,4),(32.5110459440461,
32.5432175817934,33.0379355701094,33.5326535584255,34.0273715467415,34.5220895350575,
34.5575191894876),.UNSPECIFIED.);
#834=B_SPLINE_CURVE_WITH_KNOTS('',3,(#80945,#80946,#80947,#80948,#80949,
#80950,#80951,#80952,#80953,#80954,#80955,#80956,#80957,#80958,#80959,#80960,
#80961,#80962,#80963,#80964,#80965,#80966,#80967,#80968,#80969,#80970,#80971,
#80972,#80973,#80974,#80975,#80976,#80977,#80978,#80979,#80980,#80981,#80982,
#80983,#80984,#80985,#80986,#80987,#80988,#80989,#80990,#80991,#80992,#80993,
#80994,#80995,#80996,#80997,#80998,#80999,#81000,#81001,#81002,#81003,#81004,
#81005,#81006,#81007,#81008,#81009,#81010,#81011,#81012,#81013,#81014,#81015,
#81016,#81017,#81018,#81019,#81020,#81021,#81022,#81023,#81024,#81025,#81026,
#81027,#81028,#81029,#81030,#81031,#81032,#81033,#81034,#81035,#81036,#81037,
#81038,#81039,#81040,#81041,#81042,#81043,#81044,#81045,#81046,#81047,#81048,
#81049,#81050,#81051,#81052,#81053,#81054),.UNSPECIFIED.,.F.,.F.,(4,2,2,
2,2,2,2,2,2,2,2,2,2,2,2,2,2,2,2,2,2,2,2,2,2,2,2,2,2,2,2,2,2,2,2,2,2,2,2,
2,2,2,2,2,2,2,2,2,2,2,2,2,2,2,4),(-1.91824501396425,-1.8342962072515,-1.8062233370852,
-1.78251154726549,-1.75169024170491,-1.64528869417893,-1.59185174083218,
-1.572850276496,-1.5601497685894,-1.5436131796231,-1.49364886915071,-1.39509152131626,
-1.35654326121122,-1.33435343049951,-1.3096967027995,-1.27105115822649,
-1.24456381956939,-1.14148313179044,-1.11499221548568,-1.1011975431422,
-1.0873036587019,-1.06022641471589,-0.98116527554644,-0.909790542086502,
-0.88076198567875,-0.857097422887064,-0.827463893622975,-0.794000655713836,
-0.724779681140215,-0.716059543688041,-0.660156861263222,-0.64332592836881,
-0.630670960003319,-0.629780525361832,-0.628733844006517,-0.62803050250851,
-0.627587692028264,-0.627323204165017,-0.609917659297998,-0.585254988701595,
-0.522393448448096,-0.446313546842396,-0.417219738677862,-0.394335955943159,
-0.36653663262421,-0.334674406927403,-0.272634956591863,-0.259378025635748,
-0.23422814172291,-0.196144838492948,-0.179462759142269,-0.166799940165386,
-0.153984094128512,-0.135253108926845,-0.000139984804832171),
 .UNSPECIFIED.);
#835=B_SPLINE_CURVE_WITH_KNOTS('',3,(#81055,#81056,#81057,#81058,#81059,
#81060,#81061,#81062,#81063,#81064,#81065,#81066),.UNSPECIFIED.,.F.,.F.,
(4,1,1,1,1,1,1,1,1,4),(34.5575191894876,34.8667782986713,35.3614962869873,
35.8562142753033,36.3509322636194,36.8456502519354,37.3403682402514,37.8350862285674,
38.3298042168834,38.7942318298859),.UNSPECIFIED.);
#836=B_SPLINE_CURVE_WITH_KNOTS('',3,(#81071,#81072,#81073,#81074,#81075,
#81076,#81077,#81078,#81079,#81080,#81081,#81082,#81083,#81084,#81085,#81086,
#81087,#81088,#81089,#81090,#81091,#81092,#81093,#81094,#81095,#81096,#81097,
#81098,#81099,#81100,#81101,#81102,#81103,#81104,#81105,#81106,#81107,#81108,
#81109,#81110,#81111,#81112,#81113,#81114,#81115,#81116,#81117,#81118,#81119,
#81120,#81121,#81122,#81123,#81124,#81125,#81126,#81127,#81128,#81129,#81130,
#81131,#81132,#81133,#81134,#81135,#81136,#81137,#81138,#81139,#81140,#81141,
#81142,#81143,#81144,#81145,#81146,#81147,#81148,#81149,#81150,#81151,#81152,
#81153,#81154,#81155,#81156,#81157,#81158,#81159,#81160,#81161,#81162,#81163,
#81164,#81165,#81166,#81167,#81168,#81169,#81170,#81171,#81172,#81173,#81174,
#81175,#81176,#81177,#81178,#81179,#81180,#81181,#81182,#81183,#81184,#81185,
#81186,#81187,#81188,#81189,#81190,#81191,#81192,#81193,#81194,#81195,#81196,
#81197,#81198,#81199,#81200,#81201,#81202,#81203,#81204,#81205,#81206,#81207,
#81208,#81209,#81210,#81211,#81212,#81213,#81214,#81215,#81216,#81217,#81218,
#81219,#81220,#81221,#81222,#81223,#81224,#81225,#81226,#81227,#81228,#81229,
#81230,#81231,#81232,#81233,#81234,#81235,#81236,#81237,#81238,#81239,#81240,
#81241,#81242,#81243,#81244,#81245,#81246,#81247,#81248,#81249,#81250,#81251,
#81252,#81253,#81254,#81255,#81256,#81257,#81258,#81259,#81260,#81261,#81262,
#81263,#81264,#81265,#81266,#81267,#81268,#81269,#81270,#81271,#81272,#81273,
#81274,#81275,#81276,#81277,#81278,#81279,#81280,#81281,#81282,#81283,#81284,
#81285,#81286,#81287,#81288,#81289,#81290,#81291,#81292,#81293,#81294,#81295,
#81296,#81297,#81298,#81299,#81300,#81301,#81302,#81303,#81304,#81305,#81306,
#81307,#81308,#81309,#81310,#81311,#81312,#81313,#81314,#81315,#81316,#81317,
#81318,#81319,#81320,#81321,#81322,#81323,#81324,#81325,#81326,#81327,#81328,
#81329,#81330,#81331,#81332,#81333,#81334,#81335,#81336,#81337,#81338,#81339,
#81340,#81341,#81342,#81343,#81344,#81345,#81346,#81347,#81348,#81349,#81350,
#81351,#81352,#81353,#81354,#81355,#81356,#81357,#81358,#81359,#81360,#81361,
#81362,#81363,#81364,#81365,#81366,#81367,#81368),.UNSPECIFIED.,.F.,.F.,
(4,2,2,2,2,2,2,2,2,2,2,2,2,2,2,2,2,2,2,2,2,2,2,2,2,2,2,2,2,2,2,2,2,2,2,
2,2,2,2,2,2,2,2,2,2,2,2,2,2,2,2,2,2,2,2,2,2,2,2,2,2,2,2,2,2,2,2,2,2,2,2,
2,2,2,2,2,2,2,2,2,2,2,2,2,2,2,2,2,2,2,2,2,2,2,2,2,2,2,2,2,2,2,2,2,2,2,2,
2,2,2,2,2,2,2,2,2,2,2,2,2,2,2,2,2,2,2,2,2,2,2,2,2,2,2,2,2,2,2,2,2,2,2,2,
2,2,2,2,2,4),(-9.86033244913055,-9.77739253699707,-9.72608805652884,-9.70946221456373,
-9.69677094322151,-9.67789630566169,-9.58370404394948,-9.53411900141677,
-9.4958060569039,-9.47119783710931,-9.44896361531342,-9.41008279524055,
-9.31161175459176,-9.26210699274753,-9.24560223454247,-9.2328980318875,
-9.21384994916835,-9.15973800623508,-9.0865412548556,-9.05227082661466,
-9.02215941597697,-8.99870349725517,-8.97020186124062,-8.91993015267223,
-8.83613964537186,-8.80822929074451,-8.78703944730677,-8.77409598781925,
-8.75874466618789,-8.72616719264965,-8.71460591101003,-8.64361178224165,
-8.58131395590594,-8.55368052872497,-8.52992100104272,-8.49898199278193,
-8.41371278870625,-8.36129776720617,-8.33872740203133,-8.32047261013326,
-8.30781587696831,-8.29102083704401,-8.23690113026724,-8.22576947493894,
-8.15689905032915,-8.12350961599345,-8.09391980192682,-8.07025570510155,
-8.04118613511597,-7.96727658597128,-7.91431314121214,-7.87005969786478,
-7.85397490925657,-7.84121039815357,-7.82486478496651,-7.73961184116769,
-7.66314229947051,-7.63230474640208,-7.60859179350799,-7.58052989993121,
-7.45862679723594,-7.40762576420864,-7.39101949292255,-7.37832618291459,
-7.36256119343595,-7.27146810243856,-7.21858318283746,-7.17873180614436,
-7.15389716371441,-7.12891735908514,-7.08808541847225,-6.99027954696925,
-6.94324135847825,-6.92692105665543,-6.91419341668011,-6.89812340003582,
-6.80515230070911,-6.75368581940515,-6.73518324516962,-6.70456260377428,
-6.6808620763586,-6.65264484757364,-6.53363498250119,-6.48053465728852,
-6.463798708702,-6.45111745010716,-6.4354809092715,-6.34385213485923,-6.27122998973946,
-6.2407010657508,-6.21700532389978,-6.1887201022444,-6.07105406488286,-6.01695397039558,
-6.00016133534451,-5.98748472432999,-5.96883638058315,-5.88932349350522,
-5.85688907718263,-5.7996625413613,-5.77186850167902,-5.74835431386524,
-5.71726481319648,-5.64013499651377,-5.5561899478352,-5.53983783589433,
-5.52707224812301,-5.51099234058698,-5.46679473976078,-5.40816786213515,
-5.39720969879808,-5.33637019363306,-5.30845410012555,-5.28472697569694,
-5.25367452506697,-5.23477430860724,-5.18153367420624,-5.09224079483206,
-5.07600190110426,-5.06325217333186,-5.04707826682177,-5.00181284160679,
-4.87419332313879,-4.84578181499333,-4.82209415948423,-4.79173118246769,
-4.7570330918028,-4.68161596568595,-4.62656862638144,-4.6096571361798,-4.59700524646752,
-4.57889121193606,-4.56718649646222,-4.54917257720713,-4.47996380352212,
-4.46032468063247,-4.40545256047621,-4.37858099181817,-4.35468437146394,
-4.3217420755776,-4.30106674047401,-4.23928386116105,-4.22927950101439,
-4.16785287070975,-4.14845555875556,-4.13572163212356,-4.11944533935889,
-4.07295488621113,-3.97117590885512),.UNSPECIFIED.);
#837=B_SPLINE_CURVE_WITH_KNOTS('',3,(#81370,#81371,#81372,#81373,#81374,
#81375,#81376,#81377,#81378),.UNSPECIFIED.,.F.,.F.,(4,1,1,1,1,1,4),(38.7942318298859,
38.8245222051995,39.3192401935155,39.8139581818315,40.3086761701475,40.8033941584636,
40.8407044966672),.UNSPECIFIED.);
#838=B_SPLINE_CURVE_WITH_KNOTS('',3,(#81379,#81380,#81381,#81382,#81383,
#81384,#81385,#81386,#81387,#81388,#81389,#81390,#81391,#81392,#81393,#81394,
#81395,#81396,#81397,#81398,#81399,#81400,#81401,#81402,#81403,#81404,#81405,
#81406,#81407,#81408,#81409,#81410,#81411,#81412,#81413,#81414,#81415,#81416,
#81417,#81418,#81419,#81420,#81421,#81422,#81423,#81424,#81425,#81426,#81427,
#81428,#81429,#81430,#81431,#81432,#81433,#81434,#81435,#81436,#81437,#81438,
#81439,#81440,#81441,#81442,#81443,#81444,#81445,#81446,#81447,#81448,#81449,
#81450,#81451,#81452,#81453,#81454,#81455,#81456,#81457,#81458,#81459,#81460,
#81461,#81462,#81463,#81464,#81465,#81466,#81467,#81468,#81469,#81470,#81471,
#81472,#81473,#81474,#81475,#81476,#81477,#81478,#81479,#81480,#81481,#81482,
#81483,#81484,#81485,#81486,#81487,#81488,#81489,#81490,#81491,#81492,#81493,
#81494,#81495,#81496,#81497,#81498,#81499,#81500,#81501,#81502,#81503,#81504,
#81505,#81506,#81507,#81508,#81509,#81510,#81511,#81512,#81513,#81514,#81515,
#81516,#81517,#81518,#81519,#81520,#81521,#81522,#81523,#81524,#81525,#81526,
#81527,#81528,#81529,#81530,#81531,#81532,#81533,#81534,#81535,#81536,#81537,
#81538,#81539,#81540,#81541,#81542,#81543,#81544,#81545,#81546,#81547,#81548,
#81549,#81550,#81551,#81552,#81553,#81554,#81555,#81556,#81557,#81558,#81559,
#81560,#81561,#81562,#81563,#81564,#81565,#81566,#81567,#81568,#81569,#81570,
#81571,#81572,#81573,#81574,#81575,#81576,#81577,#81578,#81579,#81580,#81581,
#81582,#81583,#81584),.UNSPECIFIED.,.F.,.F.,(4,2,2,2,2,2,2,2,2,2,2,2,2,
2,2,2,2,2,2,2,2,2,2,2,2,2,2,2,2,2,2,2,2,2,2,2,2,2,2,2,2,2,2,2,2,2,2,2,2,
2,2,2,2,2,2,2,2,2,2,2,2,2,2,2,2,2,2,2,2,2,2,2,2,2,2,2,2,2,2,2,2,2,2,2,2,
2,2,2,2,2,2,2,2,2,2,2,2,2,2,2,2,2,4),(-11.7781831743828,-11.6260661591714,
-11.6017687512626,-11.5793373662868,-11.5539682497423,-11.5104874491002,
-11.4117913943339,-11.3821460219622,-11.365635591246,-11.3568105796511,
-11.3448291022619,-11.3284934608432,-11.2832616135781,-11.2097913377315,
-11.1693775682343,-11.1378568324822,-11.1343972580855,-11.1114130120227,
-11.0846875885037,-11.0310599347158,-11.0142787233368,-10.9415863014961,
-10.9152604997613,-10.8949131518813,-10.8820784311998,-10.8663378351426,
-10.8303263626715,-10.7390074721489,-10.7137762171665,-10.6762987149449,
-10.6518120688465,-10.6294573281325,-10.5896720157373,-10.4914848761713,
-10.4431744763155,-10.4267566561111,-10.4140423728019,-10.3948660301994,
-10.3303755979629,-10.2640571819278,-10.2312187377213,-10.2019574387005,
-10.1782955211556,-10.1489069072841,-10.025056066204,-9.97904025569186,
-9.96280326709271,-9.9500638566959,-9.93389977234738,-9.84134158836594,
-9.78977879127754,-9.77125454352334,-9.74061054432852,-9.71690924558964,
-9.68871022344481,-9.56202468271073,-9.51544944811176,-9.49916648734847,
-9.48643380623231,-9.47032222349466,-9.37754625099469,-9.32603165477186,
-9.30751829735652,-9.27688610265486,-9.25318533589026,-9.22497743715288,
-9.16377067687952,-9.08784253829277,-9.06102515672551,-9.04041388539968,
-9.02754667261904,-9.0119354141544,-8.97443421784928,-8.90261099926778,
-8.83628479849076,-8.80831510907377,-8.78459403637256,-8.75415933515382,
-8.66289066274043,-8.59341019005958,-8.57477704409865,-8.56328836775181,
-8.54730785134841,-8.5062499668104,-8.43507091744583,-8.39124270955568,
-8.35580860507305,-8.33160692971632,-8.30566037143869,-8.25810507985645,
-8.21190747541639,-8.15402958371029,-8.13031948200305,-8.11141517262278,
-8.09989680431939,-8.08408519176954,-8.04553184658872,-7.97394355569426,
-7.90868877073898,-7.88080345692803,-7.85707400606071,-7.8265184254936,
-7.80724139219308),.UNSPECIFIED.);
#839=B_SPLINE_CURVE_WITH_KNOTS('',3,(#81590,#81591,#81592,#81593,#81594,
#81595,#81596,#81597,#81598,#81599,#81600,#81601,#81602),.UNSPECIFIED.,
 .F.,.F.,(4,1,1,1,1,1,1,1,1,1,4),(47.1238898038468,47.3847572312741,47.8794752195901,
48.3741932079061,48.8689111962221,49.3636291845382,49.8583471728542,50.3530651611702,
50.8477831494862,51.3425011378023,51.3606186663471),.UNSPECIFIED.);
#840=B_SPLINE_CURVE_WITH_KNOTS('',3,(#81603,#81604,#81605,#81606,#81607,
#81608,#81609,#81610,#81611,#81612,#81613,#81614,#81615,#81616,#81617,#81618,
#81619,#81620,#81621,#81622,#81623,#81624,#81625,#81626,#81627,#81628,#81629,
#81630,#81631,#81632,#81633,#81634,#81635,#81636,#81637,#81638,#81639,#81640,
#81641,#81642,#81643,#81644,#81645,#81646,#81647,#81648,#81649,#81650,#81651,
#81652,#81653,#81654,#81655,#81656,#81657,#81658,#81659,#81660,#81661,#81662,
#81663,#81664,#81665,#81666,#81667,#81668,#81669,#81670,#81671,#81672,#81673,
#81674,#81675,#81676,#81677,#81678,#81679,#81680,#81681,#81682,#81683,#81684,
#81685,#81686,#81687,#81688,#81689,#81690,#81691,#81692,#81693,#81694,#81695,
#81696,#81697,#81698,#81699,#81700,#81701,#81702),.UNSPECIFIED.,.F.,.F.,
(4,2,2,2,2,2,2,2,2,2,2,2,2,2,2,2,2,2,2,2,2,2,2,2,2,2,2,2,2,2,2,2,2,2,2,
2,2,2,2,2,2,2,2,2,2,2,2,2,2,4),(-11.7784366611071,-11.7628329720818,-11.7438991398111,
-11.6731931297632,-11.5857198879355,-11.5712330140719,-11.5596933549217,
-11.5477413454121,-11.5245409275816,-11.429055081479,-11.3974403810343,
-11.3770429577357,-11.3465365156196,-11.3239349171576,-11.2987398156749,
-11.2552837584844,-11.157740113712,-11.1282150063576,-11.1117428477294,
-11.0996706976597,-11.0868939480905,-11.0704638980195,-10.9731801343212,
-10.9019065435147,-10.8735957935129,-10.8499022671194,-10.8199255897818,
-10.724853489267,-10.6772553015051,-10.6557812424994,-10.6381633068063,
-10.6267587391384,-10.6103235151704,-10.5603129861121,-10.4806667080049,
-10.4451996306652,-10.4143872066649,-10.3906759963909,-10.362597003124,
-10.2410084683321,-10.1897840972919,-10.1731634678615,-10.1604717404985,
-10.1415899762254,-10.0660389719386,-9.98146986987404,-9.95066607423389,
-9.92695529116087,-9.89887002508965,-9.86033244913055),.UNSPECIFIED.);
#841=B_SPLINE_CURVE_WITH_KNOTS('',3,(#81703,#81704,#81705,#81706,#81707,
#81708,#81709,#81710,#81711,#81712,#81713,#81714,#81715,#81716,#81717,#81718,
#81719,#81720,#81721,#81722,#81723,#81724,#81725,#81726,#81727,#81728,#81729,
#81730,#81731,#81732,#81733,#81734,#81735,#81736,#81737,#81738,#81739,#81740,
#81741,#81742,#81743,#81744,#81745,#81746,#81747,#81748,#81749,#81750,#81751,
#81752,#81753,#81754,#81755,#81756,#81757,#81758,#81759,#81760,#81761,#81762,
#81763,#81764,#81765,#81766,#81767,#81768,#81769,#81770,#81771,#81772,#81773,
#81774,#81775,#81776,#81777,#81778,#81779,#81780,#81781,#81782,#81783,#81784,
#81785,#81786,#81787,#81788,#81789,#81790,#81791,#81792,#81793,#81794,#81795,
#81796,#81797,#81798,#81799,#81800,#81801,#81802,#81803,#81804,#81805,#81806,
#81807,#81808,#81809,#81810,#81811,#81812,#81813,#81814,#81815,#81816,#81817,
#81818,#81819,#81820,#81821,#81822,#81823,#81824,#81825,#81826,#81827,#81828,
#81829,#81830,#81831,#81832,#81833,#81834,#81835,#81836,#81837,#81838,#81839,
#81840,#81841,#81842,#81843,#81844,#81845,#81846,#81847,#81848,#81849,#81850,
#81851,#81852,#81853,#81854,#81855,#81856,#81857,#81858,#81859,#81860,#81861,
#81862,#81863,#81864,#81865,#81866,#81867,#81868,#81869,#81870,#81871,#81872,
#81873,#81874,#81875,#81876,#81877,#81878,#81879,#81880,#81881,#81882,#81883,
#81884,#81885,#81886,#81887,#81888,#81889,#81890,#81891,#81892,#81893,#81894,
#81895,#81896,#81897,#81898,#81899,#81900,#81901,#81902,#81903,#81904,#81905,
#81906,#81907,#81908,#81909,#81910,#81911,#81912,#81913,#81914,#81915,#81916,
#81917,#81918,#81919,#81920,#81921,#81922,#81923,#81924,#81925,#81926,#81927,
#81928,#81929,#81930,#81931,#81932,#81933,#81934,#81935,#81936,#81937,#81938,
#81939,#81940,#81941,#81942,#81943,#81944,#81945,#81946,#81947,#81948,#81949,
#81950,#81951,#81952,#81953,#81954,#81955,#81956,#81957,#81958,#81959,#81960,
#81961,#81962,#81963,#81964,#81965,#81966,#81967,#81968,#81969,#81970,#81971,
#81972,#81973,#81974,#81975,#81976,#81977,#81978,#81979,#81980,#81981,#81982,
#81983,#81984,#81985,#81986,#81987,#81988,#81989,#81990,#81991,#81992,#81993,
#81994),.UNSPECIFIED.,.F.,.F.,(4,2,2,2,2,2,2,2,2,2,2,2,2,2,2,2,2,2,2,2,
2,2,2,2,2,2,2,2,2,2,2,2,2,2,2,2,2,2,2,2,2,2,2,2,2,2,2,2,2,2,2,2,2,2,2,2,
2,2,2,2,2,2,2,2,2,2,2,2,2,2,2,2,2,2,2,2,2,2,2,2,2,2,2,2,2,2,2,2,2,2,2,2,
2,2,2,2,2,2,2,2,2,2,2,2,2,2,2,2,2,2,2,2,2,2,2,2,2,2,2,2,2,2,2,2,2,2,2,2,
2,2,2,2,2,2,2,2,2,2,2,2,2,2,2,2,2,4),(-7.80724139219308,-7.71981411584434,
-7.66238540670509,-7.64542715140195,-7.63276260216355,-7.61432806879973,
-7.51902370635884,-7.46954082116731,-7.43127702730007,-7.40667626901852,
-7.38443574036619,-7.34550564743403,-7.24705048558355,-7.19761483203255,
-7.18111515690178,-7.16841058865532,-7.14935567740324,-7.09514549910357,
-7.06013174301192,-7.00811444826017,-6.98948750202281,-6.95873170878801,
-6.93502392881301,-6.90690505996573,-6.78604788650302,-6.73429865586456,
-6.71764468902357,-6.7049562462725,-6.68612105310803,-6.60994322166724,
-6.52663647899754,-6.49554504837585,-6.4718157252893,-6.44392648958552,
-6.38310357438839,-6.30610461156731,-6.28709356693267,-6.26185675755588,
-6.248274504511,-6.23413839171721,-6.20558963652288,-6.08739629825127,-6.06691649875384,
-6.03417942648747,-6.01030504049926,-5.9833386803844,-5.92762805862817,
-5.9085270784957,-5.88912162087633,-5.8114649031761,-5.79277306680576,-5.78009411540398,
-5.76333503166283,-5.70982622853529,-5.59289502256792,-5.56414726593092,
-5.54284402610689,-5.51418991434288,-5.43611253566099,-5.34507201881703,
-5.32930315830641,-5.31660970274705,-5.30000788713656,-5.24906994341387,
-5.12708537128809,-5.09902902657562,-5.07531612920752,-5.04447208400203,
-5.02576378834927,-4.97338409018216,-4.88079830608383,-4.86525974655114,
-4.85258707442919,-4.83574942302132,-4.78080134286866,-4.66426854438349,
-4.63592963200015,-4.61223831586623,-4.58178290849773,-4.54692666753449,
-4.47066198081675,-4.41655177900153,-4.39977664938611,-4.38711922061191,
-4.36884058323063,-4.34622863933131,-4.29362138147143,-4.20868051162857,
-4.17772831554607,-4.153968166327,-4.12634409390635,-4.06414485520939,-3.99316939908279,
-3.9512880072954,-3.9350046218929,-3.9222721619858,-3.90288743283804,-3.82514334413091,
-3.79455919053801,-3.73524112807164,-3.70744511817718,-3.68393208073028,
-3.65284815981533,-3.57575833230207,-3.49175970537597,-3.47541175515693,
-3.46264712666091,-3.44656482193475,-3.40233582021728,-3.34944051758646,
-3.27544666702614,-3.24637554499574,-3.22271196292625,-3.1931250345579,
-3.0666442707149,-3.02358198437376,-3.00743616719612,-2.99468229505708,
-2.97507273668637,-2.9619614306192,-2.92136634805748,-2.81027466971957,
-2.7817001388985,-2.75824833629441,-2.7282273842617,-2.64473239184088,-2.56664748201972,
-2.54747680819553,-2.53476292974152,-2.51834114956905,-2.46997835697277,
-2.37177799286476,-2.33203424036561,-2.30968496589827,-2.28519289835624,
-2.24767871416892,-2.22240866395265,-2.13076386697722,-2.09522623310789,
-2.07946916398594,-2.06663819593896,-2.0463229812227,-2.0200569220251,-1.94774618660062,
-1.93112068746492,-1.91819499630147),.UNSPECIFIED.);
#842=B_SPLINE_CURVE_WITH_KNOTS('',3,(#82000,#82001,#82002,#82003,#82004,
#82005,#82006,#82007,#82008,#82009,#82010,#82011,#82012,#82013,#82014,#82015,
#82016,#82017,#82018,#82019,#82020,#82021,#82022,#82023,#82024,#82025,#82026,
#82027,#82028,#82029,#82030,#82031,#82032,#82033,#82034,#82035,#82036,#82037,
#82038,#82039,#82040,#82041,#82042,#82043,#82044,#82045,#82046,#82047,#82048,
#82049,#82050,#82051,#82052,#82053,#82054,#82055,#82056,#82057,#82058,#82059,
#82060,#82061,#82062,#82063,#82064,#82065,#82066,#82067,#82068,#82069,#82070,
#82071,#82072,#82073,#82074,#82075,#82076,#82077,#82078,#82079,#82080,#82081,
#82082,#82083,#82084,#82085,#82086,#82087,#82088,#82089,#82090,#82091,#82092,
#82093,#82094,#82095,#82096,#82097,#82098,#82099,#82100,#82101,#82102,#82103,
#82104,#82105,#82106,#82107,#82108,#82109,#82110,#82111,#82112,#82113,#82114,
#82115,#82116,#82117,#82118,#82119,#82120,#82121,#82122,#82123,#82124,#82125,
#82126,#82127,#82128,#82129,#82130,#82131,#82132,#82133,#82134,#82135,#82136,
#82137,#82138,#82139,#82140,#82141,#82142,#82143,#82144,#82145,#82146,#82147,
#82148,#82149,#82150,#82151,#82152,#82153,#82154,#82155,#82156,#82157,#82158,
#82159,#82160,#82161,#82162,#82163,#82164,#82165,#82166,#82167,#82168,#82169,
#82170,#82171,#82172,#82173,#82174,#82175,#82176,#82177,#82178,#82179,#82180,
#82181,#82182,#82183,#82184,#82185,#82186,#82187,#82188,#82189,#82190,#82191,
#82192,#82193,#82194,#82195,#82196,#82197,#82198,#82199,#82200,#82201,#82202,
#82203,#82204,#82205,#82206,#82207,#82208,#82209,#82210,#82211,#82212,#82213,
#82214,#82215,#82216,#82217,#82218,#82219,#82220,#82221,#82222,#82223,#82224,
#82225,#82226,#82227,#82228,#82229,#82230,#82231,#82232,#82233,#82234,#82235,
#82236,#82237,#82238,#82239,#82240,#82241,#82242,#82243,#82244,#82245,#82246,
#82247,#82248,#82249,#82250,#82251,#82252,#82253,#82254,#82255,#82256,#82257,
#82258,#82259,#82260,#82261),.UNSPECIFIED.,.F.,.F.,(4,2,2,2,2,2,2,2,2,2,
2,2,2,2,2,2,2,2,2,2,2,2,2,2,2,2,2,2,2,2,2,2,2,2,2,2,2,2,2,2,2,2,2,2,2,2,
2,2,2,2,2,2,2,2,2,2,2,2,2,2,2,2,2,2,2,2,2,2,2,2,2,2,2,2,2,2,2,2,2,2,2,2,
2,2,2,2,2,2,2,2,2,2,2,2,2,2,2,2,2,2,2,2,2,2,2,2,2,2,2,2,2,2,2,2,2,2,2,2,
2,2,2,2,2,2,2,2,2,2,2,2,4),(-3.97106902784548,-3.92763702759207,-3.88658726948169,
-3.86157564296453,-3.83677143377912,-3.79712325142066,-3.74468343813467,
-3.71930870986453,-3.67855003444377,-3.64596163986994,-3.63121485673307,
-3.61802438814193,-3.59516984522404,-3.57878598034135,-3.52057697670576,
-3.47447712698077,-3.42716169972195,-3.40124808422559,-3.3770314632448,
-3.34148628585702,-3.29655584204512,-3.22516500407385,-3.18603234543882,
-3.16989907684228,-3.15714308560228,-3.13751237530974,-3.07548303671522,
-2.97699289886706,-2.94692082160117,-2.92324532436927,-2.89460137822684,
-2.81677771574109,-2.72646537129329,-2.71028098076275,-2.69753885782243,
-2.68131928490212,-2.63551235245105,-2.51274633614994,-2.48287398686597,
-2.45920466084796,-2.43039101748281,-2.34751381213038,-2.26309873669759,
-2.2467721866917,-2.23401058227639,-2.21791067086075,-2.17348570310189,
-2.1200220147858,-2.04674442946513,-2.0177048269426,-1.99404069618889,-1.96441975132728,
-1.93097753686296,-1.86185582314895,-1.85352372285057,-1.79693737035706,
-1.78016703054182,-1.76750929180927,-1.74922452449514,-1.68025602220506,
-1.58712567071024,-1.55692645471647,-1.53322060704891,-1.50508041606367,
-1.4364223163488,-1.36405595990008,-1.32992978739223,-1.31433086946165,
-1.3014604671143,-1.28082355616448,-1.2539582281551,-1.17770366320611,-1.11698099230666,
-1.08875463234774,-1.06505534980239,-1.03444869698213,-1.01595871852822,
-0.964547150835598,-0.871350335210757,-0.855331785850333,-0.842610685524731,
-0.841971808595246,-0.841598533267113,-0.841016873017116,-0.840476030622721,
-0.839967576677204,-0.839484904299374,-0.839022702077622,-0.838576597640662,
-0.838142908864513,-0.837718465167538,-0.837300475579303,-0.836886428710489,
-0.83647401478626,-0.83606106307723,-0.835645490086229,-0.835225255142268,
-0.8347983209602,-0.834362617250619,-0.833916005886004,-0.83345624637869,
-0.83298096054626,-0.832487595370593,-0.831973383073842,-0.831435297421812,
-0.830870005246937,-0.830273812123175,-0.829642601008122,-0.828971762612169,
-0.811325756352297,-0.778014452110565,-0.656225603591129,-0.627005057000953,
-0.60526296837011,-0.578223232538482,-0.513942971878402,-0.408329105522501,
-0.392024514695536,-0.37945768711879,-0.372205583438089,-0.368508017567174,
-0.364538771885888,-0.35870535677802,-0.336516659750203,-0.28582242840502,
-0.19456591449315,-0.164613128014372,-0.140941586881161,-0.118416890036587,
-0.0893764328265369,-0.000139981276188635),.UNSPECIFIED.);
#843=B_SPLINE_CURVE_WITH_KNOTS('',3,(#82262,#82263,#82264,#82265,#82266,
#82267,#82268,#82269),.UNSPECIFIED.,.F.,.F.,(4,1,1,1,1,4),(51.3606186663471,
51.8372191261183,52.3319371144343,52.8266551027503,53.3213730910663,53.4070751110264),
 .UNSPECIFIED.);
#844=B_SPLINE_CURVE_WITH_KNOTS('',3,(#82271,#82272,#82273,#82274,#82275,
#82276,#82277,#82278,#82279,#82280,#82281,#82282,#82283,#82284,#82285,#82286,
#82287,#82288,#82289,#82290,#82291,#82292,#82293,#82294,#82295,#82296,#82297,
#82298,#82299,#82300,#82301,#82302,#82303,#82304,#82305,#82306,#82307,#82308,
#82309,#82310,#82311,#82312,#82313,#82314,#82315,#82316,#82317,#82318,#82319,
#82320,#82321,#82322,#82323,#82324,#82325,#82326,#82327,#82328,#82329,#82330,
#82331,#82332,#82333,#82334,#82335,#82336,#82337,#82338,#82339,#82340,#82341,
#82342,#82343,#82344,#82345,#82346,#82347,#82348,#82349,#82350,#82351,#82352,
#82353,#82354,#82355,#82356,#82357,#82358,#82359,#82360,#82361,#82362,#82363,
#82364,#82365,#82366,#82367,#82368,#82369,#82370,#82371,#82372,#82373,#82374,
#82375,#82376),.UNSPECIFIED.,.F.,.F.,(4,2,2,2,2,2,2,2,2,2,2,2,2,2,2,2,2,
2,2,2,2,2,2,2,2,2,2,2,2,2,2,2,2,2,2,2,2,2,2,2,2,2,2,2,2,2,2,2,2,2,2,2,4),
(-1.91819499630147,-1.87766457283462,-1.85070973980333,-1.82683283538219,
-1.79407155318896,-1.71482950507396,-1.63860667925558,-1.61977518415059,
-1.6070870775522,-1.59043063343498,-1.53863980797281,-1.41784389016388,
-1.38972214811814,-1.36601476848303,-1.33526346641363,-1.31664055887158,
-1.26464110781738,-1.23166413753118,-1.22234416155914,-1.17083002724642,
-1.15404420940821,-1.1413872571699,-1.12312171934314,-1.10053258824019,
-1.0480302443296,-0.96291390268036,-0.931969030139395,-0.908209396563523,
-0.880580497888131,-0.818328981072665,-0.747343504341567,-0.740218637105036,
-0.70416063323493,-0.688422966350614,-0.675998044370477,-0.662701351071325,
-0.642577968887252,-0.600420092881105,-0.493624541301765,-0.464976406255507,
-0.443133510839089,-0.420702987473508,-0.368555841706777,-0.279372293480822,
-0.24073541960509,-0.224897825626572,-0.212422821125956,-0.199161181862277,
-0.179138713400343,-0.100949134524616,-0.0341860253130483,-0.0155898498183682,
-0.000147296708047949),.UNSPECIFIED.);
#845=B_SPLINE_CURVE_WITH_KNOTS('',3,(#82377,#82378,#82379,#82380,#82381,
#82382,#82383,#82384,#82385,#82386,#82387,#82388,#82389),.UNSPECIFIED.,
 .F.,.F.,(4,1,1,1,1,1,1,1,1,1,4),(53.4070751110264,53.6660618546801,54.1607798429962,
54.6554978313122,55.1502158196282,55.6449338079442,56.1396517962603,56.6343697845763,
57.1290877728923,57.6238057612083,57.6438045939519),.UNSPECIFIED.);
#846=B_SPLINE_CURVE_WITH_KNOTS('',3,(#82394,#82395,#82396,#82397,#82398,
#82399,#82400,#82401,#82402,#82403,#82404,#82405,#82406,#82407,#82408,#82409,
#82410,#82411,#82412,#82413,#82414,#82415,#82416,#82417,#82418,#82419,#82420,
#82421,#82422,#82423,#82424,#82425,#82426,#82427,#82428,#82429,#82430,#82431,
#82432,#82433,#82434,#82435,#82436,#82437,#82438,#82439,#82440,#82441,#82442,
#82443,#82444,#82445,#82446,#82447,#82448,#82449,#82450,#82451,#82452,#82453,
#82454,#82455,#82456,#82457,#82458,#82459,#82460,#82461,#82462,#82463,#82464,
#82465,#82466,#82467,#82468,#82469,#82470,#82471,#82472,#82473,#82474,#82475,
#82476,#82477,#82478,#82479,#82480,#82481,#82482,#82483,#82484,#82485,#82486,
#82487,#82488,#82489,#82490,#82491,#82492,#82493,#82494,#82495,#82496,#82497,
#82498,#82499,#82500,#82501,#82502,#82503,#82504,#82505,#82506,#82507,#82508,
#82509,#82510,#82511,#82512,#82513,#82514,#82515,#82516,#82517,#82518,#82519,
#82520,#82521,#82522,#82523,#82524,#82525,#82526,#82527,#82528,#82529,#82530,
#82531,#82532,#82533,#82534,#82535,#82536,#82537,#82538,#82539,#82540,#82541,
#82542,#82543,#82544,#82545,#82546,#82547,#82548,#82549,#82550,#82551,#82552,
#82553,#82554,#82555,#82556,#82557,#82558,#82559,#82560,#82561,#82562,#82563,
#82564,#82565,#82566,#82567,#82568,#82569,#82570,#82571,#82572,#82573,#82574,
#82575,#82576,#82577,#82578,#82579,#82580,#82581,#82582,#82583,#82584,#82585,
#82586,#82587,#82588,#82589,#82590,#82591,#82592,#82593,#82594,#82595,#82596,
#82597,#82598,#82599,#82600,#82601,#82602,#82603,#82604,#82605,#82606,#82607,
#82608,#82609,#82610,#82611,#82612,#82613,#82614,#82615,#82616,#82617,#82618,
#82619,#82620,#82621,#82622,#82623,#82624,#82625,#82626,#82627,#82628,#82629,
#82630,#82631,#82632,#82633,#82634,#82635,#82636,#82637,#82638,#82639,#82640,
#82641,#82642,#82643,#82644,#82645,#82646,#82647,#82648,#82649,#82650,#82651,
#82652,#82653,#82654,#82655,#82656,#82657,#82658,#82659,#82660,#82661,#82662,
#82663,#82664,#82665,#82666,#82667,#82668,#82669,#82670,#82671,#82672,#82673,
#82674,#82675,#82676,#82677,#82678,#82679,#82680,#82681,#82682,#82683,#82684,
#82685),.UNSPECIFIED.,.F.,.F.,(4,2,2,2,2,2,2,2,2,2,2,2,2,2,2,2,2,2,2,2,
2,2,2,2,2,2,2,2,2,2,2,2,2,2,2,2,2,2,2,2,2,2,2,2,2,2,2,2,2,2,2,2,2,2,2,2,
2,2,2,2,2,2,2,2,2,2,2,2,2,2,2,2,2,2,2,2,2,2,2,2,2,2,2,2,2,2,2,2,2,2,2,2,
2,2,2,2,2,2,2,2,2,2,2,2,2,2,2,2,2,2,2,2,2,2,2,2,2,2,2,2,2,2,2,2,2,2,2,2,
2,2,2,2,2,2,2,2,2,2,2,2,2,2,2,2,2,4),(-9.86015336115856,-9.85112107665557,
-9.73234097774461,-9.67907491002362,-9.66232973585665,-9.64964966553001,
-9.63093939286098,-9.55346161428105,-9.46848977915582,-9.43844076773081,
-9.41498789206796,-9.38643655715724,-9.2747466562768,-9.21601068168618,
-9.19899630765461,-9.18633504712259,-9.16796991697759,-9.11662958873329,
-9.04061738726003,-9.00580818792979,-8.97538018470112,-8.95168998360197,
-8.92332970768221,-8.80723506060394,-8.75194962552062,-8.73509428103419,
-8.7224227714209,-8.70385735242706,-8.62502559433194,-8.54105198095022,
-8.51102185785259,-8.48756957904827,-8.45900234775354,-8.3477111488377,
-8.3072202899935,-8.28012563495795,-8.26622884022644,-8.25243701797931,
-8.22596286234655,-8.12286278334457,-8.09637382329746,-8.05772678593365,
-8.03306987492616,-8.01088026991953,-7.97233364650726,-7.87377414164528,
-7.82380622701391,-7.80726935678347,-7.79456889389346,-7.77556793543447,
-7.72280811588031,-7.6863040883554,-7.63424773593838,-7.59477525556185,
-7.56999679569308,-7.54790772441784,-7.51012282186554,-7.40273633132772,
-7.35891725706706,-7.34287192003409,-7.33010040689837,-7.31370626843554,
-7.2282247323264,-7.22215939427984,-7.170348323014,-7.13098885485114,-7.10622698907692,
-7.0811671137208,-7.03979329316824,-7.00574600627153,-6.93141886167929,
-6.90484124158917,-6.88435831391051,-6.87150695686912,-6.85583337717617,
-6.82117650596712,-6.72870682155704,-6.70334030097632,-6.66573504471784,
-6.64122963123573,-6.61889390092359,-6.57925290940474,-6.48101497679801,
-6.43251820348115,-6.41608627558843,-6.40337347458836,-6.38421758849865,
-6.31915745810591,-6.25316707945606,-6.23169953994733,-6.19793527587825,
-6.17394561104494,-6.147424039819,-6.0954754239936,-6.0546002044583,-5.99766332840923,
-5.97414202140216,-5.9553443672419,-5.9438378775019,-5.92796091797475,-5.88921018058492,
-5.80738331403327,-5.751789343871,-5.72419275012434,-5.702808400446,-5.67277371661147,
-5.58763036529654,-5.5103155132909,-5.49158776523044,-5.47890645502993,
-5.46217389855026,-5.409127062288,-5.29005024509407,-5.26183725705596,-5.23813683574541,
-5.20751153712327,-5.18900449860782,-5.13751794380597,-5.04462723108378,
-5.02853972464975,-5.01581007563393,-4.99950581333244,-4.95266601441447,
-4.85493067453439,-4.81393048047088,-4.78892608679856,-4.76411500771177,
-4.72442103281901,-4.67188119314957,-4.57984323469745,-4.56420311164501,
-4.55152179124098,-4.53479024155588,-4.48175935887976,-4.36266193486768,
-4.33445019780762,-4.31074982326731,-4.28012318965012,-4.26161487334029,
-4.21012252237014,-4.1172562378652,-4.10116362116595,-4.0884333873929,-4.0721338186792,
-4.02535174248445,-3.97106902784548),.UNSPECIFIED.);
#847=B_SPLINE_CURVE_WITH_KNOTS('',3,(#82687,#82688,#82689,#82690,#82691,
#82692,#82693,#82694),.UNSPECIFIED.,.F.,.F.,(4,1,1,1,1,4),(57.6438045939519,
58.1185237495243,58.6132417378404,59.1079597261564,59.6026777144724,59.690260418206),
 .UNSPECIFIED.);
#848=B_SPLINE_CURVE_WITH_KNOTS('',3,(#82695,#82696,#82697,#82698,#82699,
#82700,#82701,#82702,#82703,#82704,#82705,#82706,#82707,#82708,#82709,#82710,
#82711,#82712,#82713,#82714,#82715,#82716,#82717,#82718,#82719,#82720,#82721,
#82722,#82723,#82724,#82725,#82726,#82727,#82728,#82729,#82730,#82731,#82732,
#82733,#82734,#82735,#82736,#82737,#82738,#82739,#82740,#82741,#82742,#82743,
#82744,#82745,#82746,#82747,#82748,#82749,#82750,#82751,#82752,#82753,#82754,
#82755,#82756,#82757,#82758,#82759,#82760,#82761,#82762,#82763,#82764,#82765,
#82766,#82767,#82768,#82769,#82770,#82771,#82772,#82773,#82774,#82775,#82776,
#82777,#82778,#82779,#82780,#82781,#82782,#82783,#82784,#82785,#82786,#82787,
#82788,#82789,#82790,#82791,#82792,#82793,#82794,#82795,#82796,#82797,#82798,
#82799,#82800,#82801,#82802,#82803,#82804,#82805,#82806,#82807,#82808,#82809,
#82810,#82811,#82812,#82813,#82814,#82815,#82816,#82817,#82818,#82819,#82820,
#82821,#82822,#82823,#82824,#82825,#82826,#82827,#82828,#82829,#82830,#82831,
#82832,#82833,#82834,#82835,#82836,#82837,#82838,#82839,#82840,#82841,#82842,
#82843,#82844,#82845,#82846,#82847,#82848,#82849,#82850,#82851,#82852,#82853,
#82854,#82855,#82856,#82857,#82858,#82859,#82860,#82861,#82862,#82863,#82864,
#82865,#82866,#82867,#82868,#82869,#82870,#82871,#82872,#82873,#82874,#82875,
#82876,#82877,#82878,#82879,#82880,#82881,#82882,#82883,#82884,#82885,#82886,
#82887,#82888,#82889,#82890,#82891,#82892,#82893,#82894,#82895,#82896,#82897,
#82898,#82899,#82900,#82901,#82902,#82903,#82904,#82905,#82906,#82907,#82908,
#82909,#82910,#82911,#82912,#82913,#82914,#82915,#82916,#82917,#82918,#82919,
#82920,#82921,#82922,#82923,#82924,#82925,#82926,#82927,#82928,#82929,#82930,
#82931,#82932,#82933,#82934,#82935,#82936,#82937,#82938),.UNSPECIFIED.,
 .F.,.F.,(4,2,2,2,2,2,2,2,2,2,2,2,2,2,2,2,2,2,2,2,2,2,2,2,2,2,2,2,2,2,2,
2,2,2,2,2,2,2,2,2,2,2,2,2,2,2,2,2,2,2,2,2,2,2,2,2,2,2,2,2,2,2,2,2,2,2,2,
2,2,2,2,2,2,2,2,2,2,2,2,2,2,2,2,2,2,2,2,2,2,2,2,2,2,2,2,2,2,2,2,2,2,2,2,
2,2,2,2,2,2,2,2,2,2,2,2,2,2,2,2,2,2,4),(-11.7782433813122,-11.671195119626,
-11.6473056010272,-11.6246665597352,-11.598752315003,-11.5514323970964,
-11.5051023112653,-11.4470576971769,-11.4233144249748,-11.4167649936174,
-11.412514330664,-11.408934675872,-11.4013304508867,-11.3888355709107,-11.3698816668961,
-11.2712794337868,-11.2029058896194,-11.1753604768282,-11.1537618919276,
-11.1248693547153,-11.0009641587299,-10.9682950672716,-10.9508432664319,
-10.9501945134906,-10.9495829148123,-10.9490041309768,-10.9484542778668,
-10.9479298614948,-10.9474277204746,-10.946944974927,-10.9464789807197,
-10.9460272879692,-10.9455876028475,-10.9451577517098,-10.9447356465859,
-10.9443192509673,-10.9439065447685,-10.9434954871308,-10.9430839754008,
-10.9426697982165,-10.942250579915,-10.9293947922388,-10.9137394347937,
-10.876819551278,-10.8455121371138,-10.7764745552988,-10.7430501617321,
-10.7134397120378,-10.6897756517681,-10.6607260850306,-10.550848274455,
-10.5103612654862,-10.4972729434807,-10.4776873479655,-10.4649358198072,
-10.4487756267148,-10.4096435430698,-10.3214283543408,-10.2965750221025,
-10.2594557512361,-10.2350202376197,-10.2126083449402,-10.1723981475647,
-10.0688810548932,-10.0256192830561,-10.0096257475398,-9.99684474971968,
-9.98038599542834,-9.8835911299728,-9.82680570880455,-9.79262003133798,
-9.76857950739939,-9.7422188362255,-9.69154298124339,-9.60225585210072,
-9.56134555490115,-9.54558388244023,-9.53275390079849,-9.5124474570374,
-9.45661100564261,-9.38619139679131,-9.36394538057102,-9.329386850422,-9.30529951752727,
-9.27907138823502,-9.22941808939449,-9.18566307231222,-9.12834348619326,
-9.10474506181329,-9.08590380981178,-9.07439252219019,-9.05854250537307,
-9.01986837505997,-8.94831148201065,-8.88320511691128,-8.85533163827514,
-8.83160077915512,-8.80102750444044,-8.69458410696588,-8.63695913221868,
-8.61999204731709,-8.60732795400351,-8.5889041838377,-8.49284378594965,
-8.44374158551736,-8.40566064934577,-8.38108641082387,-8.35579106529998,
-8.31281680921966,-8.21339842953975,-8.17076238758113,-8.15482828655533,
-8.1420355796061,-8.12550048789552,-8.04370013019104,-7.96980156264351,
-7.936648225396,-7.91272887766949,-7.88595269996078,-7.83189839505448,-7.81526137055862,
-7.8073037175468),.UNSPECIFIED.);
#849=B_SPLINE_CURVE_WITH_KNOTS('',3,(#82944,#82945,#82946,#82947,#82948,
#82949,#82950,#82951,#82952,#82953,#82954,#82955,#82956,#82957,#82958,#82959,
#82960,#82961,#82962,#82963,#82964,#82965,#82966,#82967,#82968,#82969,#82970,
#82971,#82972,#82973,#82974,#82975,#82976,#82977,#82978,#82979,#82980,#82981,
#82982,#82983,#82984,#82985,#82986,#82987,#82988,#82989,#82990,#82991,#82992,
#82993,#82994,#82995,#82996,#82997,#82998,#82999,#83000,#83001,#83002,#83003,
#83004,#83005,#83006,#83007,#83008,#83009,#83010,#83011,#83012,#83013,#83014,
#83015,#83016,#83017,#83018,#83019,#83020,#83021,#83022,#83023,#83024,#83025,
#83026,#83027,#83028,#83029,#83030,#83031,#83032,#83033,#83034,#83035,#83036,
#83037,#83038,#83039,#83040,#83041,#83042,#83043,#83044,#83045,#83046,#83047,
#83048,#83049,#83050,#83051,#83052,#83053,#83054,#83055,#83056,#83057,#83058,
#83059,#83060,#83061,#83062,#83063,#83064,#83065,#83066,#83067,#83068,#83069,
#83070,#83071,#83072,#83073,#83074,#83075,#83076,#83077,#83078,#83079,#83080,
#83081,#83082,#83083,#83084,#83085,#83086,#83087,#83088,#83089,#83090,#83091,
#83092,#83093,#83094,#83095,#83096,#83097,#83098,#83099,#83100,#83101,#83102,
#83103,#83104,#83105,#83106,#83107,#83108,#83109,#83110,#83111,#83112,#83113,
#83114,#83115,#83116,#83117,#83118,#83119,#83120,#83121,#83122,#83123,#83124,
#83125,#83126,#83127,#83128,#83129,#83130,#83131,#83132,#83133,#83134,#83135,
#83136,#83137,#83138,#83139,#83140,#83141,#83142,#83143,#83144,#83145,#83146,
#83147,#83148,#83149),.UNSPECIFIED.,.F.,.F.,(4,2,2,2,2,2,2,2,2,2,2,2,2,
2,2,2,2,2,2,2,2,2,2,2,2,2,2,2,2,2,2,2,2,2,2,2,2,2,2,2,2,2,2,2,2,2,2,2,2,
2,2,2,2,2,2,2,2,2,2,2,2,2,2,2,2,2,2,2,2,2,2,2,2,2,2,2,2,2,2,2,2,2,2,2,2,
2,2,2,2,2,2,2,2,2,2,2,2,2,2,2,2,2,4),(-3.97106360210015,-3.93154941246759,
-3.91534326741906,-3.90259826317977,-3.88639738128753,-3.84081185867932,
-3.71951182690687,-3.68931028839893,-3.66560431106409,-3.63746587323261,
-3.56883288056332,-3.49647260530372,-3.46232003672252,-3.44671727956274,
-3.4338479046664,-3.41321909845903,-3.38636894111882,-3.31021733843855,
-3.24969937392289,-3.22136309713559,-3.19767141447138,-3.16721203280993,
-3.13234915561305,-3.05604983167387,-3.00194770542473,-2.98518978414246,
-2.97253136466594,-2.95423098475025,-2.93158130477272,-2.87880094740292,
-2.7941439040794,-2.76318007271603,-2.73941878842122,-2.71180168845739,
-2.6496813948042,-2.57872010813792,-2.53681247685938,-2.52049133638009,
-2.50776412338351,-2.48843866028749,-2.47559908004031,-2.39722618196737,
-2.3243639623351,-2.29535416049886,-2.27168940342283,-2.24203587860026,
-2.22441494897889,-2.19927707050256,-2.1087441126888,-2.07134810063568,
-2.05573238847377,-2.04286631347507,-2.02226430252417,-1.99546437139115,
-1.9196533220304,-1.85833069935911,-1.83011171892852,-1.80641172640206,
-1.77579456936414,-1.7572950110357,-1.70584144049654,-1.6128177573806,-1.59675964194115,
-1.58403364622509,-1.56770317870616,-1.52053350097482,-1.42268634605136,
-1.38196842104908,-1.35700580281315,-1.33215568560653,-1.29219779257155,
-1.23907726405921,-1.14832949305187,-1.13259936320152,-1.11990966706137,
-1.10326930029612,-1.05173452906981,-0.936637390580611,-0.906425310718271,
-0.882744613850218,-0.854215098157555,-0.778946988843379,-0.684767816069046,
-0.668980502577175,-0.656285143818308,-0.644039947635034,-0.627019610541083,
-0.59575401550241,-0.479312122330603,-0.447076554926775,-0.423615884180066,
-0.399483243967795,-0.372125365902695,-0.34827155072839,-0.267531186387864,
-0.218913608109173,-0.202548666952636,-0.191138962330041,-0.178542598726127,
-0.160457842190778,-0.125671030034368,-0.025411561791965,-0.000144225401985139),
 .UNSPECIFIED.);
#850=B_SPLINE_CURVE_WITH_KNOTS('',3,(#83150,#83151,#83152,#83153,#83154,
#83155,#83156,#83157,#83158,#83159,#83160,#83161,#83162,#83163,#83164,#83165,
#83166,#83167,#83168,#83169,#83170,#83171,#83172,#83173,#83174,#83175,#83176,
#83177,#83178,#83179,#83180,#83181,#83182,#83183,#83184,#83185,#83186,#83187,
#83188,#83189,#83190,#83191,#83192,#83193,#83194,#83195,#83196,#83197,#83198,
#83199,#83200,#83201,#83202,#83203,#83204,#83205,#83206,#83207,#83208,#83209,
#83210,#83211,#83212,#83213,#83214,#83215,#83216,#83217,#83218,#83219,#83220,
#83221,#83222,#83223,#83224,#83225,#83226,#83227,#83228,#83229,#83230,#83231,
#83232,#83233,#83234,#83235,#83236,#83237,#83238,#83239,#83240,#83241,#83242,
#83243,#83244,#83245,#83246,#83247,#83248,#83249,#83250,#83251,#83252,#83253,
#83254,#83255,#83256,#83257,#83258,#83259,#83260,#83261,#83262,#83263,#83264,
#83265,#83266,#83267,#83268,#83269,#83270,#83271,#83272,#83273,#83274,#83275,
#83276,#83277,#83278,#83279,#83280,#83281,#83282,#83283),.UNSPECIFIED.,
 .F.,.F.,(4,2,2,2,2,2,2,2,2,2,2,2,2,2,2,2,2,2,2,2,2,2,2,2,2,2,2,2,2,2,2,
2,2,2,2,2,2,2,2,2,2,2,2,2,2,2,2,2,2,2,2,2,2,2,2,2,2,2,2,2,2,2,2,2,2,2,4),
(-11.7782575909705,-11.7575540749702,-11.7369611070762,-11.7099771235911,
-11.6568567564943,-11.5552551067953,-11.5282812880275,-11.516182296382,
-11.5034219449728,-11.4871032548703,-11.4023154228092,-11.3197716048351,
-11.2964182480323,-11.2787602779056,-11.2535336455908,-11.212763532941,
-11.1112177793469,-11.0812833824136,-11.0776916759057,-11.0756434608909,
-11.073407044803,-11.071605746434,-11.0701524098604,-11.0689762136385,-11.0680206179461,
-11.0672409400877,-11.0666020329901,-11.0660762717131,-11.0656419014181,
-11.0652817257151,-11.0649820852044,-11.0647320703852,-11.0645229180375,
-11.0637768884411,-11.0630779539183,-11.0624209159605,-11.0618010465555,
-11.0533233711773,-11.0406372792275,-11.0249428765762,-10.9303725641988,
-10.8792717018237,-10.8608525571439,-10.8303232403025,-10.8066283466347,
-10.7783454237913,-10.6606599979269,-10.6065800181202,-10.5897890331692,
-10.5771128407755,-10.5584639193114,-10.4804095028337,-10.3930812579989,
-10.3640423659618,-10.3403784154605,-10.3107571883045,-10.1896140519374,
-10.1418789080586,-10.1255045955927,-10.1127846910637,-10.0967756194634,
-10.0035404674789,-9.95213954384135,-9.93365204672542,-9.90304812855436,
-9.87934913223944,-9.86015336115856),.UNSPECIFIED.);
#851=B_SPLINE_CURVE_WITH_KNOTS('',3,(#83284,#83285,#83286,#83287,#83288,
#83289,#83290,#83291,#83292,#83293,#83294,#83295,#83296,#83297,#83298,#83299,
#83300,#83301,#83302,#83303,#83304,#83305,#83306,#83307,#83308,#83309,#83310,
#83311,#83312,#83313,#83314,#83315,#83316,#83317,#83318,#83319,#83320,#83321,
#83322,#83323,#83324,#83325,#83326,#83327,#83328,#83329,#83330,#83331,#83332,
#83333,#83334,#83335,#83336,#83337,#83338,#83339,#83340,#83341,#83342,#83343,
#83344,#83345,#83346,#83347,#83348,#83349,#83350,#83351,#83352,#83353,#83354,
#83355,#83356,#83357,#83358,#83359,#83360,#83361,#83362,#83363,#83364,#83365,
#83366,#83367,#83368,#83369,#83370,#83371,#83372,#83373,#83374,#83375,#83376,
#83377,#83378,#83379,#83380,#83381,#83382,#83383,#83384,#83385,#83386,#83387,
#83388,#83389,#83390,#83391,#83392,#83393,#83394,#83395,#83396,#83397,#83398,
#83399,#83400,#83401,#83402,#83403,#83404,#83405,#83406,#83407,#83408,#83409,
#83410,#83411,#83412,#83413,#83414,#83415,#83416,#83417,#83418,#83419,#83420,
#83421,#83422,#83423,#83424,#83425,#83426,#83427,#83428,#83429,#83430,#83431,
#83432,#83433,#83434,#83435,#83436,#83437,#83438,#83439,#83440,#83441,#83442,
#83443,#83444,#83445,#83446,#83447,#83448,#83449,#83450,#83451,#83452,#83453,
#83454,#83455,#83456,#83457,#83458,#83459,#83460,#83461,#83462,#83463,#83464,
#83465,#83466,#83467,#83468,#83469,#83470,#83471,#83472,#83473,#83474,#83475,
#83476,#83477,#83478,#83479,#83480,#83481,#83482,#83483,#83484,#83485,#83486,
#83487,#83488,#83489,#83490,#83491,#83492,#83493,#83494,#83495,#83496,#83497,
#83498,#83499,#83500,#83501,#83502,#83503,#83504,#83505,#83506,#83507,#83508,
#83509,#83510,#83511,#83512,#83513,#83514,#83515,#83516,#83517,#83518,#83519,
#83520,#83521,#83522,#83523,#83524,#83525,#83526,#83527,#83528,#83529,#83530,
#83531,#83532,#83533,#83534,#83535,#83536,#83537,#83538,#83539,#83540,#83541,
#83542,#83543,#83544,#83545,#83546,#83547,#83548,#83549,#83550,#83551,#83552,
#83553,#83554,#83555,#83556,#83557,#83558,#83559,#83560,#83561,#83562,#83563,
#83564,#83565,#83566,#83567,#83568,#83569,#83570,#83571,#83572,#83573,#83574,
#83575),.UNSPECIFIED.,.F.,.F.,(4,2,2,2,2,2,2,2,2,2,2,2,2,2,2,2,2,2,2,2,
2,2,2,2,2,2,2,2,2,2,2,2,2,2,2,2,2,2,2,2,2,2,2,2,2,2,2,2,2,2,2,2,2,2,2,2,
2,2,2,2,2,2,2,2,2,2,2,2,2,2,2,2,2,2,2,2,2,2,2,2,2,2,2,2,2,2,2,2,2,2,2,2,
2,2,2,2,2,2,2,2,2,2,2,2,2,2,2,2,2,2,2,2,2,2,2,2,2,2,2,2,2,2,2,2,2,2,2,2,
2,2,2,2,2,2,2,2,2,2,2,2,2,2,2,2,2,4),(-7.8073037175468,-7.74292118198365,
-7.72449205042442,-7.71260130911684,-7.69428604059757,-7.68162690632006,
-7.66488060267763,-7.61367995023372,-7.59095399533706,-7.52745080722082,
-7.50644536633783,-7.47315903063662,-7.44922483001077,-7.42250653484181,
-7.36894106007636,-7.34884172523891,-7.27858411274764,-7.26042892551343,
-7.24866073428695,-7.23047799738935,-7.21782404205162,-7.20097033190753,
-7.14531212426787,-7.07022069676661,-7.03558484160617,-7.00525851864319,
-6.98157288953722,-6.95313368063236,-6.82423245389675,-6.7800873275622,
-6.76401234746762,-6.75124615385068,-6.73488860646261,-6.64579612220412,
-6.59260484784879,-6.55261484140024,-6.52775983008803,-6.50280191517561,
-6.4621168874173,-6.36425471880772,-6.31704451025778,-6.30071072326953,
-6.28798505209198,-6.27193033623732,-6.17889231185864,-6.12744299971697,
-6.10894438036917,-6.07832812733441,-6.0546279934244,-6.02640789041755,
-5.9648222721677,-5.88921276289147,-5.85155812821751,-5.83593747359763,
-5.82307248216422,-5.80248010435335,-5.7756983179467,-5.70001064467656,
-5.63853809686397,-5.61031499222469,-5.58661499050462,-5.55600259843744,
-5.53750752466101,-5.48607402915805,-5.39296460190005,-5.37692548423314,
-5.36420168938903,-5.34785376741974,-5.30046325973471,-5.20254393802874,
-5.16201099553745,-5.13707554200837,-5.11219868402656,-5.0720616089203,
-5.01854408903397,-4.93091528972588,-4.91241031564853,-4.89974197024353,
-4.88283908428359,-4.82660225763457,-4.71828360346469,-4.68784014166486,
-4.66411818976943,-4.63615403090008,-4.56990446544818,-4.49809651958925,
-4.46048584326041,-4.44487184088536,-4.43200512455116,-4.411398905625,-4.38459121790057,
-4.30872876916115,-4.24745901609728,-4.21924384248143,-4.19554328001026,
-4.16492013479057,-4.14641518012815,-4.09493811802865,-4.00200708452449,
-3.9859280708723,-3.97319935991522,-3.95688717489712,-3.90994985184454,
-3.81218014182191,-3.77126329230043,-3.74627101771131,-3.72144820066655,
-3.68167629419756,-3.62896589164102,-3.53876932865768,-3.52250366458213,
-3.5097504086274,-3.49359941899154,-3.44859693966417,-3.32031140685774,
-3.29201449886223,-3.26831995178768,-3.23780768369129,-3.16531250903986,
-3.07345863005895,-3.05784470727535,-3.04516560990965,-3.02840673795051,
-2.97490384846812,-2.85796307568887,-2.82921547333254,-2.80791202717228,
-2.77925723658052,-2.70116875374401,-2.61014015700233,-2.5943707035695,
-2.58167708720648,-2.56507556253835,-2.51414391047934,-2.39214873923174,
-2.36409266784384,-2.34037950757043,-2.30953442163685,-2.23440519405854,
-2.14857693793214,-2.13014579159411,-2.1174813608415,-2.10052024235325,
-2.04302775384782,-1.9364103796757,-1.91819812389623),.UNSPECIFIED.);
#852=B_SPLINE_CURVE_WITH_KNOTS('',3,(#83580,#83581,#83582,#83583,#83584,
#83585,#83586,#83587,#83588,#83589,#83590,#83591,#83592,#83593,#83594,#83595,
#83596,#83597,#83598,#83599,#83600,#83601,#83602,#83603,#83604,#83605,#83606,
#83607,#83608,#83609,#83610,#83611,#83612,#83613,#83614,#83615,#83616,#83617,
#83618,#83619,#83620,#83621,#83622,#83623,#83624,#83625,#83626,#83627,#83628,
#83629,#83630,#83631,#83632,#83633,#83634,#83635,#83636,#83637,#83638,#83639,
#83640,#83641,#83642,#83643,#83644,#83645,#83646,#83647,#83648,#83649,#83650,
#83651,#83652,#83653,#83654,#83655,#83656,#83657,#83658,#83659,#83660,#83661,
#83662,#83663,#83664,#83665,#83666,#83667,#83668,#83669,#83670,#83671,#83672,
#83673,#83674,#83675,#83676,#83677,#83678,#83679,#83680,#83681,#83682,#83683,
#83684,#83685,#83686,#83687,#83688,#83689,#83690,#83691,#83692,#83693,#83694,
#83695,#83696,#83697,#83698,#83699,#83700,#83701,#83702,#83703,#83704,#83705,
#83706,#83707,#83708,#83709,#83710,#83711,#83712,#83713,#83714,#83715,#83716,
#83717,#83718,#83719,#83720,#83721,#83722,#83723,#83724,#83725,#83726,#83727,
#83728,#83729,#83730,#83731,#83732,#83733,#83734,#83735,#83736,#83737,#83738,
#83739,#83740,#83741,#83742,#83743,#83744,#83745,#83746,#83747,#83748,#83749,
#83750,#83751,#83752,#83753,#83754,#83755,#83756,#83757,#83758,#83759,#83760,
#83761,#83762,#83763,#83764,#83765,#83766,#83767,#83768,#83769,#83770,#83771,
#83772,#83773,#83774,#83775,#83776,#83777,#83778,#83779,#83780,#83781,#83782,
#83783,#83784,#83785,#83786,#83787,#83788,#83789,#83790,#83791,#83792,#83793,
#83794,#83795,#83796,#83797,#83798,#83799,#83800,#83801,#83802,#83803,#83804,
#83805,#83806,#83807,#83808,#83809,#83810,#83811,#83812,#83813,#83814,#83815,
#83816,#83817,#83818,#83819,#83820,#83821,#83822,#83823,#83824,#83825,#83826,
#83827,#83828,#83829,#83830,#83831,#83832,#83833,#83834,#83835,#83836,#83837,
#83838,#83839,#83840,#83841,#83842,#83843,#83844,#83845,#83846,#83847,#83848,
#83849,#83850,#83851,#83852,#83853,#83854,#83855,#83856,#83857,#83858,#83859,
#83860,#83861,#83862,#83863,#83864,#83865,#83866,#83867,#83868,#83869,#83870,
#83871),.UNSPECIFIED.,.F.,.F.,(4,2,2,2,2,2,2,2,2,2,2,2,2,2,2,2,2,2,2,2,
2,2,2,2,2,2,2,2,2,2,2,2,2,2,2,2,2,2,2,2,2,2,2,2,2,2,2,2,2,2,2,2,2,2,2,2,
2,2,2,2,2,2,2,2,2,2,2,2,2,2,2,2,2,2,2,2,2,2,2,2,2,2,2,2,2,2,2,2,2,2,2,2,
2,2,2,2,2,2,2,2,2,2,2,2,2,2,2,2,2,2,2,2,2,2,2,2,2,2,2,2,2,2,2,2,2,2,2,2,
2,2,2,2,2,2,2,2,2,2,2,2,2,2,2,2,2,4),(-9.86012475374465,-9.81805694591507,
-9.76638317281649,-9.7478337986043,-9.71716245642267,-9.69345967754844,
-9.66528061631865,-9.54555410367724,-9.49298378056098,-9.47627951278026,
-9.46359582714404,-9.44792917678455,-9.35599498939593,-9.27848877374205,
-9.2498581365546,-9.22618212653158,-9.19609412078237,-9.09756635372558,
-9.03560090988958,-9.01597708359595,-9.00333063785702,-8.98726567364478,
-8.94583519820819,-8.85912738720152,-8.83446527295588,-8.797528558207,-8.77311903712428,
-8.74757353706966,-8.70287391096224,-8.60587561757498,-8.56362781215548,
-8.54773149448201,-8.5349311880803,-8.51488175645492,-8.41798442006454,
-8.34957371320675,-8.32145076090209,-8.29774339591059,-8.26752068805409,
-8.17457810077457,-8.10400393729673,-8.08639603827367,-8.07499209212843,
-8.05854877960523,-8.00836498502534,-7.92885360126043,-7.89341029095786,
-7.86261175139507,-7.83890147756646,-7.81081295402954,-7.6894002479943,
-7.63805055333626,-7.62142192899553,-7.6087310591234,-7.58986068890172,
-7.49565365602257,-7.43545002996782,-7.40226368727481,-7.3783407408959,
-7.35157920361877,-7.29764869517202,-7.28097034323694,-7.2085273413631,
-7.18224031306595,-7.1619138010534,-7.14908145427972,-7.13333004864614,
-7.09800147018681,-7.00618995472378,-6.98090040037943,-6.94336774212854,
-6.9188729496194,-6.89652639576043,-6.85680356230483,-6.75859380374859,
-6.71020258763505,-6.69377859603814,-6.68106493058263,-6.66189746374913,
-6.59716168654103,-6.53098402851683,-6.49817641346088,-6.46893341864697,
-6.44527117415028,-6.41586328678028,-6.31097887003897,-6.26806098370764,
-6.23997186839252,-6.22591030662268,-6.21397617601239,-6.19089758677078,
-6.08328545867654,-6.04397954033149,-6.01098207459441,-5.98707990649186,
-5.96023430116837,-5.90558409960236,-5.88914154606991,-5.81713829752032,
-5.78112854424425,-5.76538747743229,-5.75255264710922,-5.73220558493534,
-5.70588056727411,-5.63319361589111,-5.61641489390075,-5.56278034871493,
-5.53605385922234,-5.51212180327659,-5.47885455286815,-5.41720906178363,
-5.32477741280231,-5.30583278021585,-5.29313653306905,-5.27656039918392,
-5.22601295040308,-5.10939772673686,-5.07932617848319,-5.05565063942082,
-5.02700611151578,-4.94916988681424,-4.85843366697098,-4.84243004761189,
-4.82971068321558,-4.81333104316248,-4.76552781880852,-4.64449837592189,
-4.61486517093543,-4.59120076920861,-4.56217230790328,-4.54511589829703,
-4.52119248885457,-4.43996218829928,-4.39195915984871,-4.37562787348718,
-4.3642154411799,-4.34646832220976,-4.3350999553969,-4.30221744949254,-4.20427050082486,
-4.16381437130908,-4.13889058125131,-4.1140030748158,-4.07379210163428,
-4.02010945622261,-3.97106360210015),.UNSPECIFIED.);
#853=B_SPLINE_CURVE_WITH_KNOTS('',3,(#83873,#83874,#83875,#83876,#83877,
#83878,#83879,#83880,#83881,#83882,#83883,#83884,#83885,#83886,#83887,#83888,
#83889,#83890,#83891,#83892,#83893,#83894,#83895,#83896,#83897,#83898,#83899,
#83900,#83901,#83902,#83903,#83904,#83905,#83906,#83907,#83908,#83909,#83910,
#83911,#83912,#83913,#83914,#83915,#83916,#83917,#83918,#83919,#83920,#83921,
#83922,#83923,#83924,#83925,#83926,#83927,#83928,#83929,#83930,#83931,#83932,
#83933,#83934,#83935,#83936,#83937,#83938,#83939,#83940,#83941,#83942,#83943,
#83944,#83945,#83946,#83947,#83948,#83949,#83950,#83951,#83952,#83953,#83954,
#83955,#83956,#83957,#83958,#83959,#83960,#83961,#83962,#83963,#83964,#83965,
#83966,#83967,#83968,#83969,#83970,#83971,#83972,#83973,#83974,#83975,#83976,
#83977,#83978,#83979,#83980,#83981,#83982,#83983,#83984,#83985,#83986,#83987,
#83988,#83989,#83990,#83991,#83992,#83993,#83994,#83995,#83996,#83997,#83998,
#83999,#84000,#84001,#84002,#84003,#84004,#84005,#84006,#84007,#84008,#84009,
#84010,#84011,#84012,#84013,#84014,#84015,#84016,#84017,#84018),
 .UNSPECIFIED.,.F.,.F.,(4,2,2,2,2,2,2,2,2,2,2,2,2,2,2,2,2,2,2,2,2,2,2,2,
2,2,2,2,2,2,2,2,2,2,2,2,2,2,2,2,2,2,2,2,2,2,2,2,2,2,2,2,2,2,2,2,2,2,2,2,
2,2,2,2,2,2,2,2,2,2,2,2,4),(-1.91819812389623,-1.9058490804987,-1.88211911746911,
-1.8542374965745,-1.78903080278789,-1.71745145019472,-1.67885684990661,
-1.66303268597609,-1.65151661409857,-1.632632900303,-1.60895940878541,-1.55126479817968,
-1.50557186200159,-1.45752823120374,-1.43151501950158,-1.40734235008991,
-1.37212664127907,-1.32871571446535,-1.22425509209492,-1.20433294426275,
-1.19154660427064,-1.17558047072642,-1.13260917932051,-1.03102427025317,
-0.989537169418201,-0.964460755422503,-0.939713715787689,-0.900453552421356,
-0.848856656785603,-0.756458768016186,-0.740252681795145,-0.727507654282451,
-0.719301269264677,-0.71873817849579,-0.718145823758188,-0.717520203283071,
-0.716856944383347,-0.716151248054843,-0.715397830381653,-0.7151825000816,
-0.714925079174424,-0.714616512330017,-0.714245513008139,-0.713797931162959,
-0.713255927242603,-0.712596898445036,-0.711792097955374,-0.710804894237682,
-0.709588649502659,-0.708084278206175,-0.706217712918539,-0.705744296785534,
-0.704892428077784,-0.703365751696435,-0.70065560504686,-0.672629558219046,
-0.587941888667891,-0.534793224722198,-0.507542293239183,-0.489843497568673,
-0.4673732733938,-0.438828689271821,-0.389528553450192,-0.294195689020745,
-0.275606447982955,-0.262933621783939,-0.250609911718129,-0.218573040534112,
-0.146182347082779,-0.0746323275261985,-0.0468036259155507,-0.0233663524740781,
-0.000143848792500651),.UNSPECIFIED.);
#854=B_SPLINE_CURVE_WITH_KNOTS('',3,(#84019,#84020,#84021,#84022,#84023,
#84024,#84025,#84026,#84027,#84028,#84029,#84030,#84031,#84032,#84033,#84034,
#84035,#84036,#84037,#84038,#84039,#84040,#84041,#84042,#84043,#84044,#84045,
#84046,#84047,#84048,#84049,#84050,#84051,#84052,#84053,#84054,#84055,#84056,
#84057,#84058,#84059,#84060,#84061,#84062,#84063,#84064,#84065,#84066,#84067,
#84068,#84069,#84070,#84071,#84072,#84073,#84074,#84075,#84076,#84077,#84078,
#84079,#84080,#84081,#84082,#84083,#84084,#84085,#84086,#84087,#84088,#84089,
#84090,#84091,#84092,#84093,#84094,#84095,#84096,#84097,#84098,#84099,#84100,
#84101,#84102,#84103,#84104,#84105,#84106,#84107,#84108,#84109,#84110,#84111,
#84112,#84113,#84114,#84115,#84116,#84117,#84118,#84119,#84120,#84121,#84122,
#84123,#84124,#84125,#84126,#84127,#84128,#84129,#84130,#84131,#84132,#84133,
#84134,#84135,#84136,#84137,#84138,#84139,#84140,#84141,#84142,#84143,#84144,
#84145,#84146,#84147,#84148,#84149,#84150,#84151,#84152,#84153,#84154,#84155,
#84156,#84157,#84158,#84159,#84160,#84161,#84162,#84163,#84164,#84165,#84166,
#84167,#84168,#84169,#84170,#84171,#84172,#84173,#84174,#84175,#84176,#84177,
#84178,#84179,#84180,#84181,#84182,#84183,#84184,#84185,#84186,#84187,#84188,
#84189,#84190,#84191,#84192,#84193,#84194,#84195,#84196,#84197,#84198,#84199,
#84200,#84201,#84202,#84203,#84204,#84205,#84206,#84207,#84208,#84209,#84210,
#84211,#84212,#84213,#84214,#84215,#84216,#84217,#84218,#84219,#84220,#84221,
#84222),.UNSPECIFIED.,.F.,.F.,(4,2,2,2,2,2,2,2,2,2,2,2,2,2,2,2,2,2,2,2,
2,2,2,2,2,2,2,2,2,2,2,2,2,2,2,2,2,2,2,2,2,2,2,2,2,2,2,2,2,2,2,2,2,2,2,2,
2,2,2,2,2,2,2,2,2,2,2,2,2,2,2,2,2,2,2,2,2,2,2,2,2,2,2,2,2,2,2,2,2,2,2,2,
2,2,2,2,2,2,2,2,2,4),(-11.7783190292283,-11.7492162270637,-11.6675692593062,
-11.6250943656212,-11.6048886037439,-11.5915631425151,-11.5791772908065,
-11.5635179196079,-11.525627476028,-11.4538809289882,-11.3879040295678,
-11.3609520810337,-11.3392014628929,-11.3107537491765,-11.2008946537563,
-11.1602437590013,-11.14051677233,-11.1273575764358,-11.1232389866094,-11.1104767599408,
-11.0941474555619,-11.0097935177337,-10.9268645008013,-10.8980490731557,
-10.8743792632854,-10.8445075675873,-10.7258181191681,-10.6765803703627,
-10.660094455377,-10.6473879660322,-10.6283118597966,-10.5738190323731,
-10.5009125332178,-10.4666990779374,-10.4366211984448,-10.4131665256044,
-10.3846372850365,-10.2723753449478,-10.2140939986964,-10.1970981782366,
-10.1844354813104,-10.1660464241347,-10.0850851367844,-10.0039359258322,
-9.97350105142926,-9.94980993292345,-9.92145352610052,-9.80525892818735,
-9.75004641150789,-9.73319446332854,-9.72052233655845,-9.70195142450754,
-9.62316445555718,-9.53811863693912,-9.50846790629941,-9.48480253204695,
-9.45578853103084,-9.38288293308005,-9.30453061291114,-9.29169887196127,
-9.27238150622478,-9.25965469807577,-9.24332753729619,-9.19800023294773,
-9.11456874202166,-9.06388283604925,-9.03752038408268,-9.01347958822037,
-8.98482051548703,-8.93972627840673,-8.93224317711163,-8.85712997391759,
-8.83043356948044,-8.80988686941316,-8.79702747752518,-8.7813845630056,
-8.74433414612589,-8.65359593667067,-8.62843334346072,-8.61080096401444,
-8.581134549036,-8.5574690611916,-8.52846982546471,-8.41722914928883,-8.3592803577413,
-8.34229878682887,-8.32963526726845,-8.31122863279196,-8.2233421871445,
-8.16985239876153,-8.1508972069372,-8.11978528243707,-8.09605412315632,
-8.06817744717281,-8.00405001307945,-7.9295594695943,-7.90295688921793,
-7.88246048809213,-7.86960732914023,-7.85393996722258,-7.81713156719808,
-7.80730129127322),.UNSPECIFIED.);
#855=B_SPLINE_CURVE_WITH_KNOTS('',3,(#84228,#84229,#84230,#84231,#84232,
#84233,#84234,#84235,#84236,#84237,#84238,#84239,#84240,#84241,#84242,#84243,
#84244,#84245,#84246,#84247,#84248,#84249,#84250,#84251,#84252,#84253,#84254,
#84255,#84256,#84257,#84258,#84259,#84260,#84261,#84262,#84263,#84264,#84265,
#84266,#84267,#84268,#84269,#84270,#84271,#84272,#84273,#84274,#84275,#84276,
#84277,#84278,#84279,#84280,#84281,#84282,#84283,#84284,#84285,#84286,#84287,
#84288,#84289,#84290,#84291,#84292,#84293,#84294,#84295,#84296,#84297,#84298,
#84299,#84300,#84301,#84302,#84303,#84304,#84305,#84306,#84307,#84308,#84309,
#84310,#84311,#84312,#84313,#84314,#84315,#84316,#84317,#84318,#84319,#84320,
#84321,#84322,#84323,#84324,#84325,#84326,#84327,#84328,#84329,#84330,#84331,
#84332,#84333,#84334,#84335,#84336,#84337,#84338,#84339,#84340,#84341,#84342,
#84343,#84344,#84345,#84346,#84347,#84348,#84349,#84350,#84351,#84352,#84353,
#84354,#84355,#84356,#84357,#84358,#84359,#84360,#84361,#84362,#84363,#84364,
#84365,#84366,#84367,#84368,#84369,#84370,#84371,#84372,#84373,#84374,#84375,
#84376,#84377,#84378,#84379,#84380,#84381,#84382,#84383,#84384,#84385,#84386,
#84387,#84388,#84389,#84390,#84391,#84392,#84393,#84394,#84395,#84396,#84397,
#84398,#84399,#84400,#84401,#84402,#84403,#84404,#84405,#84406,#84407,#84408,
#84409,#84410,#84411,#84412,#84413,#84414,#84415,#84416,#84417,#84418,#84419,
#84420,#84421,#84422,#84423,#84424,#84425,#84426,#84427,#84428,#84429,#84430,
#84431,#84432,#84433,#84434,#84435),.UNSPECIFIED.,.F.,.F.,(4,2,2,2,2,2,
2,2,2,2,2,2,2,2,2,2,2,2,2,2,2,2,2,2,2,2,2,2,2,2,2,2,2,2,2,2,2,2,2,2,2,2,
2,2,2,2,2,2,2,2,2,2,2,2,2,2,2,2,2,2,2,2,2,2,2,2,2,2,2,2,2,2,2,2,2,2,2,2,
2,2,2,2,2,2,2,2,2,2,2,2,2,2,2,2,2,2,2,2,2,2,2,2,2,4),(-3.97107570014323,
-3.95473179825932,-3.93020570680576,-3.89245600578724,-3.86693551442944,
-3.77312373637299,-3.73891431794088,-3.72373572613475,-3.71073286783546,
-3.68911897534789,-3.66039358571638,-3.5700233681002,-3.5202329848614,-3.49398699035555,
-3.46990632381394,-3.435399829625,-3.41320515749296,-3.34308808260247,-3.31458177455716,
-3.27658819463,-3.26091007323842,-3.24805997714065,-3.22758670622655,-3.20102707365061,
-3.12681642009985,-3.11318670439561,-3.05874838764347,-3.0319273757567,
-3.00801922012637,-2.97496708060967,-2.93556261129145,-2.82700389684559,
-2.80458806588298,-2.79274951820068,-2.77850296973325,-2.74926141772127,
-2.6715669437198,-2.6012429510694,-2.57252089631481,-2.55121669997346,-2.52253624128907,
-2.4437933480278,-2.35348830357128,-2.33772156953117,-2.32502823325172,
-2.30842407283542,-2.25745220623051,-2.13551300270738,-2.10745377660231,
-2.08374091170392,-2.05290041843001,-1.97974715544867,-1.89197199852887,
-1.87352118462463,-1.86085578434366,-1.8439104376255,-1.78676740370546,
-1.67968103479866,-1.64915145851153,-1.62542377696657,-1.59752035123772,
-1.53204166259927,-1.46040373978181,-1.4220408298139,-1.40628173318693,
-1.39345118573078,-1.3731398189934,-1.34688094275814,-1.27461648875262,
-1.25800982781872,-1.20449761438769,-1.17753565025881,-1.15366022090385,
-1.12091370672339,-1.10042492291373,-1.03959272848015,-0.965578501506255,
-0.94667038583358,-0.933976851013923,-0.917375117779512,-0.866439678260105,
-0.744449990918004,-0.716393696059684,-0.692680660979183,-0.665114002403756,
-0.652555049898491,-0.609840083087632,-0.538690221656287,-0.495670496848202,
-0.479810627250529,-0.471533796712322,-0.459537431588819,-0.429186928283623,
-0.40372805506196,-0.305148315625417,-0.266691316274866,-0.244513739481454,
-0.222150760767069,-0.197667044314299,-0.108830485409659,-0.0392328373056414,
-0.0201720577622807,-0.00991112195934663,-0.000147043797163775),
 .UNSPECIFIED.);
#856=B_SPLINE_CURVE_WITH_KNOTS('',3,(#84436,#84437,#84438,#84439,#84440,
#84441,#84442,#84443,#84444,#84445,#84446,#84447,#84448,#84449,#84450,#84451,
#84452,#84453,#84454,#84455,#84456,#84457,#84458,#84459,#84460,#84461,#84462,
#84463,#84464,#84465,#84466,#84467,#84468,#84469,#84470,#84471,#84472,#84473,
#84474,#84475,#84476,#84477,#84478,#84479,#84480,#84481,#84482,#84483,#84484,
#84485,#84486,#84487,#84488,#84489,#84490,#84491,#84492,#84493,#84494,#84495,
#84496,#84497,#84498,#84499,#84500,#84501,#84502,#84503,#84504,#84505,#84506,
#84507,#84508,#84509,#84510,#84511,#84512,#84513,#84514,#84515,#84516,#84517,
#84518,#84519,#84520,#84521,#84522,#84523,#84524,#84525,#84526,#84527,#84528,
#84529,#84530,#84531,#84532,#84533,#84534,#84535,#84536,#84537,#84538,#84539,
#84540,#84541,#84542,#84543,#84544,#84545),.UNSPECIFIED.,.F.,.F.,(4,2,2,
2,2,2,2,2,2,2,2,2,2,2,2,2,2,2,2,2,2,2,2,2,2,2,2,2,2,2,2,2,2,2,2,2,2,2,2,
2,2,2,2,2,2,2,2,2,2,2,2,2,2,2,4),(-11.7781571887288,-11.7684257903246,-11.7554890562485,
-11.6940865751676,-11.6184770809455,-11.5900780734401,-11.567636756316,
-11.5439447904632,-11.5139922544665,-11.4186973918007,-11.3712036358175,
-11.349754490077,-11.3335855379709,-11.3300998060477,-11.3175519573378,
-11.2987524687992,-11.2329152060424,-11.1673992444472,-11.1347387363269,
-11.1112175349723,-11.0882967914464,-11.0617153499735,-11.0092792105663,
-10.9690171151081,-10.9121529858805,-10.8886466206752,-10.869857523657,
-10.8583521437458,-10.8424703702003,-10.8037065509359,-10.7749688230159,
-10.7058418005106,-10.6723987048533,-10.6427772116743,-10.6191131712757,
-10.5900743152024,-10.5145386260965,-10.5015478941132,-10.4473075308457,
-10.4243447954512,-10.4058650551817,-10.3931983270468,-10.3765805758244,
-10.3226581850168,-10.2460126486708,-10.2110859833837,-10.1805892538587,
-10.1568959033466,-10.128588281631,-10.0003736155827,-9.95534136766762,
-9.93918797693893,-9.92643540149527,-9.91017329198182,-9.86012475374465),
 .UNSPECIFIED.);
#857=B_SPLINE_CURVE_WITH_KNOTS('',3,(#84546,#84547,#84548,#84549,#84550,
#84551,#84552,#84553,#84554,#84555,#84556,#84557,#84558,#84559,#84560,#84561,
#84562,#84563,#84564,#84565,#84566,#84567,#84568,#84569,#84570,#84571,#84572,
#84573,#84574,#84575,#84576,#84577,#84578,#84579,#84580,#84581,#84582,#84583,
#84584,#84585,#84586,#84587,#84588,#84589,#84590,#84591,#84592,#84593,#84594,
#84595,#84596,#84597,#84598,#84599,#84600,#84601,#84602,#84603,#84604,#84605,
#84606,#84607,#84608,#84609,#84610,#84611,#84612,#84613,#84614,#84615,#84616,
#84617,#84618,#84619,#84620,#84621,#84622,#84623,#84624,#84625,#84626,#84627,
#84628,#84629,#84630,#84631,#84632,#84633,#84634,#84635,#84636,#84637,#84638,
#84639,#84640,#84641,#84642,#84643,#84644,#84645,#84646,#84647,#84648,#84649,
#84650,#84651,#84652,#84653,#84654,#84655,#84656,#84657,#84658,#84659,#84660,
#84661,#84662,#84663,#84664,#84665,#84666,#84667,#84668,#84669,#84670,#84671,
#84672,#84673,#84674,#84675,#84676,#84677,#84678,#84679,#84680,#84681,#84682,
#84683,#84684,#84685,#84686,#84687,#84688,#84689,#84690,#84691,#84692,#84693,
#84694,#84695,#84696,#84697,#84698,#84699,#84700,#84701,#84702,#84703,#84704,
#84705,#84706,#84707,#84708,#84709,#84710,#84711,#84712,#84713,#84714,#84715,
#84716,#84717,#84718,#84719,#84720,#84721,#84722,#84723,#84724,#84725,#84726,
#84727,#84728,#84729,#84730,#84731,#84732,#84733,#84734,#84735,#84736,#84737,
#84738,#84739,#84740,#84741,#84742,#84743,#84744,#84745,#84746,#84747,#84748,
#84749,#84750,#84751,#84752,#84753,#84754,#84755,#84756,#84757,#84758,#84759,
#84760,#84761,#84762,#84763,#84764,#84765,#84766,#84767,#84768,#84769,#84770,
#84771,#84772,#84773,#84774,#84775,#84776,#84777,#84778,#84779,#84780,#84781,
#84782,#84783,#84784,#84785,#84786,#84787,#84788,#84789,#84790,#84791,#84792,
#84793,#84794,#84795,#84796,#84797,#84798,#84799,#84800,#84801,#84802,#84803,
#84804,#84805,#84806,#84807,#84808,#84809,#84810,#84811,#84812,#84813,#84814,
#84815,#84816,#84817,#84818,#84819,#84820,#84821,#84822,#84823,#84824,#84825,
#84826,#84827,#84828,#84829,#84830,#84831,#84832,#84833,#84834,#84835,#84836,
#84837,#84838,#84839,#84840,#84841),.UNSPECIFIED.,.F.,.F.,(4,2,2,2,2,2,
2,2,2,2,2,2,2,2,2,2,2,2,2,2,2,2,2,2,2,2,2,2,2,2,2,2,2,2,2,2,2,2,2,2,2,2,
2,2,2,2,2,2,2,2,2,2,2,2,2,2,2,2,2,2,2,2,2,2,2,2,2,2,2,2,2,2,2,2,2,2,2,2,
2,2,2,2,2,2,2,2,2,2,2,2,2,2,2,2,2,2,2,2,2,2,2,2,2,2,2,2,2,2,2,2,2,2,2,2,
2,2,2,2,2,2,2,2,2,2,2,2,2,2,2,2,2,2,2,2,2,2,2,2,2,2,2,2,2,2,2,2,2,4),(-7.80730129127322,
-7.72626070803151,-7.7010822693862,-7.68344262614194,-7.65376820880232,
-7.63010261009414,-7.60111076828799,-7.48968140974421,-7.43188466833877,
-7.41490973134245,-7.40224583193526,-7.38383101509938,-7.28772569745943,
-7.23863452479943,-7.20055861038576,-7.17598471389478,-7.15371732777224,
-7.1145893216891,-7.01618875752558,-6.98220030310816,-6.95799161114217,
-6.94458131688635,-6.93020955348779,-6.90016498701403,-6.78420541842453,
-6.76372608325726,-6.73098929393947,-6.70711456424249,-6.68014729356618,
-6.6244319247151,-6.54099330071706,-6.51312896722129,-6.49196324499553,
-6.47902305637814,-6.46366139852171,-6.43102404018116,-6.3921140042867,
-6.3828728016361,-6.30179277408867,-6.26829252794629,-6.24433370615216,
-6.21770519992345,-6.16488740897721,-6.14781873464011,-6.07445189168421,
-6.04802116493502,-6.02761715835029,-6.01477537602664,-5.99906261136243,
-5.96089838110735,-5.88921372726034,-5.87222516816054,-5.82413357039492,
-5.79601889169422,-5.77231047110769,-5.74154799098932,-5.72291497052435,
-5.67087114022673,-5.63446608085268,-5.58157199415807,-5.56257499411121,
-5.54987477891329,-5.533334978487,-5.48332472992724,-5.38475873854658,-5.34624272353777,
-5.32405710250212,-5.29939539128026,-5.26071639208904,-5.23419256346272,
-5.13073009081111,-5.10454072761013,-5.09079717233722,-5.0768488704392,
-5.0494467043246,-5.00821659146785,-4.8983025910283,-4.86968351672077,-4.84623348659058,
-4.81626545227133,-4.7355749325088,-4.65241000009572,-4.63600142053206,
-4.6232278169302,-4.60719412831721,-4.56350114418109,-4.45700660607494,
-4.41867979288013,-4.39651931476581,-4.37182872781416,-4.33295255148146,
-4.28217884332469,-4.19043276846567,-4.17146627557357,-4.15876841884557,
-4.14220758361283,-4.0918874399943,-3.99326890603292,-3.95497042562246,
-3.93281373032131,-3.90811878823828,-3.86921273373862,-3.81837530397846,
-3.72385475547863,-3.70793706089702,-3.69522766568379,-3.67876860681528,
-3.62990008463346,-3.53157225065714,-3.49221893819145,-3.46992183369893,
-3.44537909090425,-3.40751491414312,-3.38187216716478,-3.28697109242537,
-3.25457842163597,-3.23925935398732,-3.22630551638532,-3.20503953442129,
-3.17698367024549,-3.09206456882485,-3.03767070147343,-3.01085483748964,
-2.98694536507005,-2.95388153121467,-2.91445600178413,-2.80569186649304,
-2.78341806290467,-2.7715995416598,-2.75731036407457,-2.72779742144896,
-2.68121261314395,-2.58403220313755,-2.55393779383181,-2.53026137975239,
-2.501635595418,-2.42425151436333,-2.33196494646441,-2.31638248565394,-2.3037060794182,
-2.28691440657283,-2.23282568172364,-2.11515125868408,-2.08686739980335,
-2.06317206648552,-2.03264264600147,-1.96001370979526,-1.91821254494555),
 .UNSPECIFIED.);
#858=B_SPLINE_CURVE_WITH_KNOTS('',3,(#84846,#84847,#84848,#84849,#84850,
#84851,#84852,#84853,#84854,#84855,#84856,#84857,#84858,#84859,#84860,#84861,
#84862,#84863,#84864,#84865,#84866,#84867,#84868,#84869,#84870,#84871,#84872,
#84873,#84874,#84875,#84876,#84877,#84878,#84879,#84880,#84881,#84882,#84883,
#84884,#84885,#84886,#84887,#84888,#84889,#84890,#84891,#84892,#84893,#84894,
#84895,#84896,#84897,#84898,#84899,#84900,#84901,#84902,#84903,#84904,#84905,
#84906,#84907,#84908,#84909,#84910,#84911,#84912,#84913,#84914,#84915,#84916,
#84917,#84918,#84919,#84920,#84921,#84922,#84923,#84924,#84925,#84926,#84927,
#84928,#84929,#84930,#84931,#84932,#84933,#84934,#84935,#84936,#84937,#84938,
#84939,#84940,#84941,#84942,#84943,#84944,#84945,#84946,#84947,#84948,#84949,
#84950,#84951,#84952,#84953,#84954,#84955,#84956,#84957,#84958,#84959,#84960,
#84961,#84962,#84963,#84964,#84965,#84966,#84967,#84968,#84969,#84970,#84971,
#84972,#84973,#84974,#84975,#84976,#84977,#84978,#84979,#84980,#84981,#84982,
#84983,#84984,#84985,#84986,#84987,#84988,#84989,#84990,#84991,#84992,#84993,
#84994,#84995,#84996,#84997,#84998,#84999,#85000,#85001,#85002,#85003,#85004,
#85005,#85006,#85007,#85008,#85009,#85010,#85011,#85012,#85013,#85014,#85015,
#85016,#85017,#85018,#85019,#85020,#85021,#85022,#85023,#85024,#85025,#85026,
#85027,#85028,#85029,#85030,#85031,#85032,#85033,#85034,#85035,#85036,#85037,
#85038,#85039,#85040,#85041,#85042,#85043,#85044,#85045,#85046,#85047,#85048,
#85049,#85050,#85051,#85052,#85053,#85054,#85055,#85056,#85057,#85058,#85059,
#85060,#85061,#85062,#85063,#85064,#85065,#85066,#85067,#85068,#85069,#85070,
#85071,#85072,#85073,#85074,#85075,#85076,#85077,#85078,#85079,#85080,#85081,
#85082,#85083,#85084,#85085,#85086,#85087,#85088,#85089,#85090,#85091,#85092,
#85093,#85094,#85095,#85096,#85097,#85098,#85099,#85100,#85101,#85102,#85103,
#85104,#85105,#85106,#85107,#85108,#85109,#85110,#85111,#85112,#85113,#85114,
#85115,#85116,#85117,#85118,#85119,#85120,#85121,#85122,#85123,#85124,#85125,
#85126,#85127,#85128,#85129,#85130,#85131,#85132,#85133,#85134,#85135,#85136,
#85137,#85138,#85139,#85140,#85141,#85142,#85143,#85144,#85145),
 .UNSPECIFIED.,.F.,.F.,(4,2,2,2,2,2,2,2,2,2,2,2,2,2,2,2,2,2,2,2,2,2,2,2,
2,2,2,2,2,2,2,2,2,2,2,2,2,2,2,2,2,2,2,2,2,2,2,2,2,2,2,2,2,2,2,2,2,2,2,2,
2,2,2,2,2,2,2,2,2,2,2,2,2,2,2,2,2,2,2,2,2,2,2,2,2,2,2,2,2,2,2,2,2,2,2,2,
2,2,2,2,2,2,2,2,2,2,2,2,2,2,2,2,2,2,2,2,2,2,2,2,2,2,2,2,2,2,2,2,2,2,2,2,
2,2,2,2,2,2,2,2,2,2,2,2,2,2,2,2,2,4),(-9.8600466769179,-9.84206584295104,
-9.79430053056243,-9.77278706780202,-9.75514611306556,-9.74374035233858,
-9.72732434117913,-9.67770771118887,-9.59775640398324,-9.5622363248628,
-9.53139320116547,-9.50768043446348,-9.47962362525768,-9.35764431995831,
-9.30670089523282,-9.29009870977196,-9.27740533364911,-9.26163699141251,
-9.1706516862146,-9.09252639283127,-9.06387052371785,-9.04019569192078,
-9.01013840244186,-8.91243686329657,-8.84726702784952,-8.82876592470117,
-8.81609803268091,-8.79949637671837,-8.74632813309397,-8.73373247455104,
-8.66489886320464,-8.63151756204156,-8.60193276709316,-8.57826917693296,
-8.54919598653495,-8.47445370961755,-8.382795493253,-8.36466988482914,-8.35201795540257,
-8.33511703818709,-8.28095016071714,-8.20492567263585,-8.1701142663127,
-8.13968501214976,-8.1159948466224,-8.08763574886608,-7.95968375768151,
-7.91456398152732,-7.89840293084959,-7.88565151964558,-7.86939832085296,
-7.77721892949442,-7.72556684497607,-7.70702233864676,-7.67635623416614,
-7.65265361993511,-7.62447047066011,-7.56248924296279,-7.48709766992981,
-7.46035999964738,-7.43979135923156,-7.42692949892786,-7.4112978538634,
-7.37357186022674,-7.2833181460758,-7.25821413681925,-7.24060880799932,
-7.21097249982408,-7.1873080957152,-7.15828261302411,-7.08521608330629,
-7.03157243862825,-6.98708575100017,-6.97098029202599,-6.95821961452808,
-6.94189975247792,-6.85702473987766,-6.85210149800976,-6.799249349395,-6.75941316163392,
-6.73458112984575,-6.70959952742261,-6.66875298260193,-6.57095507150738,
-6.52393579735874,-6.50761723821256,-6.49488964383261,-6.47556007015856,
-6.4185636006122,-6.34764494607684,-6.32531467145704,-6.29067099213656,
-6.26657284584925,-6.24037397369317,-6.19094286150453,-6.14691162042031,
-6.089548533163,-6.06594136975729,-6.04709518216505,-6.03451899219249,-6.01824476240093,
-5.97111573519495,-5.88917195261918,-5.83889056476543,-5.81258073154367,
-5.78852284640933,-5.75419725231639,-5.73218081449458,-5.66310093541642,
-5.65472823129876,-5.59811080858734,-5.58134289117328,-5.56868497150465,
-5.55039702061101,-5.48146309781162,-5.38829079710632,-5.35809650215912,
-5.334390859045,-5.30624678933474,-5.2375340976441,-5.16515432719394,-5.13108510646865,
-5.11549448602193,-5.1026217984588,-5.081967154605,-5.05506865657269,-4.97858870805779,
-4.91773408247829,-4.88964365055376,-4.86593346613737,-4.83513744712718,
-4.76040354563755,-4.67441673901827,-4.65581324173366,-4.64313956778014,
-4.62631353331931,-4.57158857672458,-4.454759122508,-4.42643406752544,-4.40274161142435,
-4.37226730420765,-4.27753378678927,-4.21180739773302,-4.19267462735229,
-4.17996384509378,-4.16351678919367,-4.11481223648704,-4.01652416287867,
-3.97704559273293,-3.97107570014323),.UNSPECIFIED.);
#859=B_SPLINE_CURVE_WITH_KNOTS('',3,(#85147,#85148,#85149,#85150,#85151,
#85152,#85153,#85154,#85155,#85156,#85157,#85158,#85159,#85160,#85161,#85162,
#85163,#85164,#85165,#85166,#85167,#85168,#85169,#85170,#85171,#85172,#85173,
#85174,#85175,#85176,#85177,#85178,#85179,#85180,#85181,#85182,#85183,#85184,
#85185,#85186,#85187,#85188,#85189,#85190,#85191,#85192,#85193,#85194,#85195,
#85196,#85197,#85198,#85199,#85200,#85201,#85202,#85203,#85204,#85205,#85206,
#85207,#85208,#85209,#85210,#85211,#85212,#85213,#85214,#85215,#85216,#85217,
#85218,#85219,#85220,#85221,#85222,#85223,#85224,#85225,#85226,#85227,#85228,
#85229,#85230,#85231,#85232,#85233,#85234,#85235,#85236,#85237,#85238,#85239,
#85240,#85241,#85242,#85243,#85244,#85245,#85246,#85247,#85248),
 .UNSPECIFIED.,.F.,.F.,(4,2,2,2,2,2,2,2,2,2,2,2,2,2,2,2,2,2,2,2,2,2,2,2,
2,2,2,2,2,2,2,2,2,2,2,2,2,2,2,2,2,2,2,2,2,2,2,2,2,2,4),(-1.91821254494555,
-1.86839903619994,-1.85276133308806,-1.84008019964067,-1.82334605577424,
-1.77027108258705,-1.6512336036067,-1.62301874449097,-1.59931853966615,
-1.56869598641094,-1.55019143328576,-1.49871569663207,-1.40578377547403,
-1.389705496664,-1.37697703585121,-1.36066464945206,-1.3137224669229,-1.21595229946101,
-1.17504082588153,-1.15004962676499,-1.12522652147238,-1.08545077294208,
-1.03273142049454,-0.941827689680017,-0.925862908919356,-0.913148172761548,
-0.89673304559461,-0.848459661708831,-0.75028302974387,-0.710468741360725,
-0.688109987795645,-0.665657646085728,-0.641409806040928,-0.606317324509801,
-0.5287690856591,-0.476739578401613,-0.460004654608429,-0.448135954610373,
-0.437461668385129,-0.40482392682485,-0.349255322368366,-0.322063337722082,
-0.260137630910478,-0.231948035731113,-0.208246000535885,-0.185278800870477,
-0.154617101514796,-0.0828852558936575,-0.0228474886777043,-0.00990135018824966,
-0.000147253532549841),.UNSPECIFIED.);
#860=B_SPLINE_CURVE_WITH_KNOTS('',3,(#85249,#85250,#85251,#85252,#85253,
#85254,#85255,#85256,#85257,#85258,#85259,#85260,#85261,#85262,#85263,#85264,
#85265,#85266,#85267,#85268,#85269,#85270,#85271,#85272,#85273,#85274,#85275,
#85276,#85277,#85278,#85279,#85280,#85281,#85282,#85283,#85284,#85285,#85286,
#85287,#85288,#85289,#85290,#85291,#85292,#85293,#85294,#85295,#85296,#85297,
#85298,#85299,#85300,#85301,#85302,#85303,#85304,#85305,#85306,#85307,#85308,
#85309,#85310,#85311,#85312,#85313,#85314,#85315,#85316,#85317,#85318,#85319,
#85320,#85321,#85322,#85323,#85324,#85325,#85326,#85327,#85328,#85329,#85330,
#85331,#85332,#85333,#85334,#85335,#85336,#85337,#85338,#85339,#85340,#85341,
#85342,#85343,#85344,#85345,#85346,#85347,#85348,#85349,#85350,#85351,#85352,
#85353,#85354,#85355,#85356,#85357,#85358,#85359,#85360,#85361,#85362,#85363,
#85364,#85365,#85366,#85367,#85368,#85369,#85370,#85371,#85372,#85373,#85374,
#85375,#85376,#85377,#85378,#85379,#85380,#85381,#85382,#85383,#85384,#85385,
#85386,#85387,#85388,#85389,#85390,#85391,#85392,#85393,#85394,#85395,#85396,
#85397,#85398,#85399,#85400,#85401,#85402,#85403,#85404,#85405,#85406,#85407,
#85408,#85409,#85410,#85411,#85412,#85413,#85414,#85415,#85416,#85417,#85418,
#85419,#85420,#85421,#85422,#85423,#85424,#85425,#85426,#85427,#85428,#85429,
#85430,#85431,#85432),.UNSPECIFIED.,.F.,.F.,(4,3,3,3,3,3,3,3,3,3,3,3,3,
3,3,3,3,3,3,3,3,3,3,3,3,3,3,3,3,3,3,3,3,3,3,3,3,3,3,3,3,3,3,3,3,3,3,3,3,
3,3,3,3,3,3,3,3,3,3,3,3,4),(84.8230016469244,84.8332951185895,84.9080939578295,
84.9828796919349,85.0576572721575,85.1324406751991,85.2072232860376,85.2820219961831,
85.3280131069056,85.4028119461453,85.4775976802505,85.5523752604729,85.6271586635142,
85.7019412743525,85.7767399844978,85.8227310952216,85.8975299344615,85.972315668567,
86.0470932487896,86.1218766518312,86.1966592626696,86.271457972815,86.3174490835376,
86.3922479227778,86.4670336568836,86.5418112371066,86.6165946401485,86.6913772509873,
86.766175961133,86.8121670718536,86.886965911092,86.9617516451959,87.036529225417,
87.111312628457,87.186095239294,87.2608939494379,87.3068850601697,87.3816838994136,
87.4564696335229,87.5312472137495,87.606030616795,87.6808132276374,87.7556119377866,
87.8016030484857,87.8764018877177,87.9511876218152,88.0259652020298,88.1007486050634,
88.1755312158941,88.2503299260317,88.2963210368017,88.3711198760534,88.4459056101707,
88.5206831904052,88.5954665934584,88.6702492043086,88.7450479144654,88.7910390251177,
88.8658384445578,88.9406237466334,89.0154044721172,89.0597207272658),
 .UNSPECIFIED.);
#861=B_SPLINE_CURVE_WITH_KNOTS('',3,(#85438,#85439,#85440,#85441,#85442,
#85443,#85444,#85445,#85446,#85447,#85448,#85449),.UNSPECIFIED.,.F.,.F.,
(4,1,1,1,1,1,1,1,1,4),(91.106186954104,91.4146581914001,91.9093761797161,
92.4040941680321,92.8988121563481,93.3935301446641,93.8882481329802,94.3829661212962,
94.8776841096122,95.3428995923426),.UNSPECIFIED.);
#862=B_SPLINE_CURVE_WITH_KNOTS('',3,(#85450,#85451,#85452,#85453,#85454,
#85455,#85456,#85457,#85458,#85459,#85460,#85461,#85462,#85463,#85464,#85465,
#85466,#85467,#85468,#85469,#85470,#85471,#85472,#85473,#85474,#85475,#85476,
#85477,#85478,#85479,#85480,#85481,#85482,#85483,#85484,#85485,#85486,#85487,
#85488,#85489,#85490,#85491,#85492,#85493,#85494,#85495,#85496,#85497,#85498,
#85499,#85500,#85501,#85502,#85503,#85504,#85505,#85506,#85507,#85508,#85509,
#85510,#85511,#85512,#85513,#85514,#85515,#85516,#85517,#85518,#85519,#85520,
#85521,#85522,#85523,#85524,#85525,#85526,#85527,#85528,#85529,#85530,#85531,
#85532,#85533,#85534,#85535,#85536,#85537,#85538,#85539,#85540,#85541,#85542,
#85543,#85544,#85545,#85546,#85547,#85548,#85549,#85550,#85551),
 .UNSPECIFIED.,.F.,.F.,(4,2,2,2,2,2,2,2,2,2,2,2,2,2,2,2,2,2,2,2,2,2,2,2,
2,2,2,2,2,2,2,2,2,2,2,2,2,2,2,2,2,2,2,2,2,2,2,2,2,2,4),(-11.7781008861112,
-11.6373344995044,-11.6204440228226,-11.6082405011693,-11.5955300900881,
-11.5764003055972,-11.521236726541,-11.448850777203,-11.4147410879726,-11.3853834696144,
-11.3650025297003,-11.3380786473167,-11.2870480504116,-11.1997437417241,
-11.1713879083436,-11.1552922460493,-11.1423547247261,-11.1294614398261,
-11.1077194521551,-10.9981785551021,-10.9586748743302,-10.9255678000331,
-10.901653876741,-10.8748578918298,-10.8226435275272,-10.7359207671394,
-10.6954923810874,-10.679781165207,-10.6669393575842,-10.6465333506768,
-10.5875984842728,-10.5771417319825,-10.5153295996795,-10.4946488797552,
-10.4617012485059,-10.4378046521462,-10.4109367477416,-10.356091672179,
-10.3188209767005,-10.2622824118571,-10.2461714752425,-10.223575498489,
-10.2104255409795,-10.1955967608558,-10.1624218729707,-10.0895319682909,
-10.0187614880707,-9.99048216776105,-9.96678687148919,-9.93677087038606,
-9.8600466769179),.UNSPECIFIED.);
#863=B_SPLINE_CURVE_WITH_KNOTS('',3,(#85553,#85554,#85555,#85556,#85557,
#85558,#85559,#85560,#85561,#85562,#85563,#85564,#85565,#85566,#85567,#85568,
#85569,#85570,#85571,#85572,#85573,#85574,#85575,#85576,#85577,#85578,#85579,
#85580,#85581,#85582,#85583,#85584,#85585,#85586,#85587,#85588,#85589,#85590,
#85591,#85592,#85593,#85594,#85595,#85596,#85597,#85598,#85599,#85600,#85601,
#85602,#85603,#85604,#85605,#85606,#85607,#85608,#85609,#85610,#85611,#85612,
#85613,#85614,#85615,#85616,#85617,#85618,#85619,#85620,#85621,#85622,#85623,
#85624,#85625,#85626,#85627,#85628,#85629,#85630,#85631,#85632,#85633,#85634,
#85635,#85636,#85637,#85638,#85639,#85640),.UNSPECIFIED.,.F.,.F.,(4,3,3,
3,3,3,3,3,3,3,3,3,3,3,3,3,3,3,3,3,3,3,3,3,3,3,3,3,3,4),(89.0597207272658,
89.1345030603627,89.2101300368982,89.2857570134337,89.3605558526666,89.4353415867648,
89.51011916698,89.5849025700143,89.6596851808455,89.7344838909835,89.7804750017498,
89.8552738410552,89.9300595752263,90.0048371555148,90.0796205586221,90.1544031695262,
90.2292018797362,90.2751929900658,90.3499918291084,90.4247775630155,90.4995551430398,
90.574338545884,90.6491211565263,90.7239198664782,90.7699109783818,90.844662845243,
90.9194034691721,90.9941340614828,91.0688657268607,91.106186954104),
 .UNSPECIFIED.);
#864=B_SPLINE_CURVE_WITH_KNOTS('',3,(#85641,#85642,#85643,#85644,#85645,
#85646,#85647,#85648,#85649,#85650,#85651,#85652,#85653,#85654,#85655,#85656,
#85657,#85658,#85659,#85660,#85661,#85662,#85663,#85664,#85665,#85666,#85667,
#85668,#85669,#85670,#85671,#85672,#85673,#85674,#85675,#85676,#85677,#85678,
#85679,#85680,#85681,#85682,#85683,#85684,#85685,#85686,#85687,#85688,#85689,
#85690,#85691,#85692,#85693,#85694,#85695,#85696,#85697,#85698,#85699,#85700,
#85701,#85702,#85703,#85704,#85705,#85706,#85707,#85708,#85709,#85710,#85711,
#85712,#85713,#85714,#85715,#85716,#85717,#85718,#85719,#85720,#85721,#85722,
#85723,#85724,#85725,#85726,#85727,#85728,#85729,#85730,#85731,#85732,#85733,
#85734,#85735,#85736,#85737,#85738,#85739,#85740,#85741,#85742,#85743,#85744,
#85745,#85746,#85747,#85748,#85749,#85750,#85751,#85752,#85753,#85754,#85755,
#85756,#85757,#85758,#85759,#85760,#85761,#85762,#85763,#85764,#85765,#85766,
#85767,#85768,#85769,#85770,#85771,#85772,#85773,#85774,#85775,#85776,#85777,
#85778,#85779,#85780,#85781,#85782,#85783,#85784,#85785,#85786,#85787,#85788,
#85789,#85790,#85791,#85792,#85793,#85794,#85795,#85796,#85797,#85798,#85799,
#85800,#85801,#85802,#85803,#85804,#85805,#85806,#85807,#85808,#85809,#85810,
#85811,#85812,#85813,#85814,#85815,#85816,#85817,#85818,#85819,#85820,#85821,
#85822,#85823,#85824,#85825,#85826,#85827,#85828,#85829,#85830,#85831,#85832,
#85833,#85834,#85835,#85836,#85837,#85838,#85839,#85840,#85841,#85842,#85843,
#85844,#85845,#85846),.UNSPECIFIED.,.F.,.F.,(4,2,2,2,2,2,2,2,2,2,2,2,2,
2,2,2,2,2,2,2,2,2,2,2,2,2,2,2,2,2,2,2,2,2,2,2,2,2,2,2,2,2,2,2,2,2,2,2,2,
2,2,2,2,2,2,2,2,2,2,2,2,2,2,2,2,2,2,2,2,2,2,2,2,2,2,2,2,2,2,2,2,2,2,2,2,
2,2,2,2,2,2,2,2,2,2,2,2,2,2,2,2,2,4),(3.97111550692216,3.97113291895875,
4.05886938220161,4.0753469959609,4.08813073331088,4.10410901890245,4.14720834959645,
4.24963595295934,4.29056238122401,4.31555593643396,4.34037718712831,4.38013965713478,
4.43282973021619,4.52464759682786,4.54026339947647,4.55294268108289,4.56969968345249,
4.62316945547823,4.74015577297554,4.76890125462364,4.7902047242648,4.8188615406612,
4.89700492592713,4.98797494789984,5.00374183230533,5.01643515394136,5.03303905472039,
5.08400744818666,5.20595262076944,5.2340115200502,5.25772426301847,5.28856482758201,
5.36213873326477,5.45026796838605,5.4666165203696,5.47938127320626,5.49546317426482,
5.53968671564407,5.59825383041793,5.60908745337636,5.66994420194613,5.69790110751523,
5.72162340382834,5.75261292456542,5.82892088851126,5.91398669658113,5.93031406258297,
5.94307581000045,5.9591751323507,6.00359319168067,6.0570361280124,6.13034059755623,
6.15938195459454,6.18304606453259,6.21266514967658,6.31223090855942,6.35175081649339,
6.38420996516903,6.39954059264249,6.41249050247763,6.4337284912338,6.46173099130339,
6.54623412483111,6.60099653493925,6.62785504108533,6.6517540685518,6.68472296091405,
6.72397753991101,6.83110222091231,6.85452882225789,6.86651426093276,6.88048691393189,
6.90803603368656,6.9877793691155,7.05848750832287,7.08725928390142,7.10856196329304,
7.11361305138611,7.11757744323573,7.12180840095472,7.12584174217891,7.13010887615431,
7.15838277076461,7.20673642095831,7.27959302486014,7.31290626717513,7.3277542678025,
7.33388097037029,7.34868294758195,7.36666252185189,7.40109222177752,7.52017794390152,
7.54964610547424,7.57248418053326,7.5997657930554,7.63094270208009,7.69014620826772,
7.76724077614046,7.78599033757201,7.79867295753841,7.81095914821328,7.82810653147107,
7.94206718808575),.UNSPECIFIED.);
#865=B_SPLINE_CURVE_WITH_KNOTS('',3,(#85852,#85853,#85854,#85855,#85856,
#85857,#85858,#85859,#85860,#85861,#85862,#85863,#85864,#85865,#85866,#85867,
#85868,#85869,#85870,#85871,#85872,#85873,#85874,#85875,#85876,#85877,#85878,
#85879,#85880,#85881,#85882,#85883,#85884,#85885,#85886,#85887,#85888,#85889,
#85890,#85891,#85892,#85893,#85894,#85895,#85896,#85897,#85898,#85899,#85900,
#85901,#85902,#85903,#85904,#85905,#85906,#85907,#85908,#85909,#85910,#85911,
#85912,#85913,#85914,#85915,#85916,#85917,#85918,#85919,#85920,#85921,#85922,
#85923,#85924,#85925,#85926,#85927,#85928,#85929,#85930,#85931,#85932,#85933,
#85934,#85935,#85936,#85937,#85938,#85939),.UNSPECIFIED.,.F.,.F.,(4,3,3,
3,3,3,3,3,3,3,3,3,3,3,3,3,3,3,3,3,3,3,3,3,3,3,3,3,3,4),(-4.09293042005646,
-4.0158857439365,-3.95774390652818,-3.88404094726653,-3.81035073834264,
-3.7366685538583,-3.66298068070267,-3.58929384691513,-3.51559086689293,
-3.46302591821216,-3.38932987780264,-3.3156465955138,-3.24197132533718,
-3.16829029817759,-3.09461026130577,-3.02091395433786,-2.96830792989613,
-2.89461009057983,-2.82092503805656,-2.74724803112181,-2.67356533033049,
-2.59988365776423,-2.52618578604003,-2.47358994158011,-2.4001630892653,
-2.326749936501,-2.25333914533707,-2.17993256163102,-2.10651636312689,-2.07410208625457),
 .UNSPECIFIED.);
#866=B_SPLINE_CURVE_WITH_KNOTS('',3,(#85942,#85943,#85944,#85945,#85946,
#85947),.UNSPECIFIED.,.F.,.F.,(4,1,1,4),(0.,0.494717988316024,0.989435976632052,
1.12274180646091),.UNSPECIFIED.);
#867=B_SPLINE_CURVE_WITH_KNOTS('',3,(#85952,#85953,#85954,#85955,#85956,
#85957,#85958,#85959,#85960,#85961,#85962,#85963,#85964,#85965,#85966,#85967,
#85968,#85969,#85970,#85971,#85972,#85973,#85974,#85975,#85976,#85977,#85978,
#85979,#85980,#85981,#85982,#85983,#85984,#85985,#85986,#85987,#85988,#85989,
#85990,#85991,#85992,#85993,#85994,#85995,#85996,#85997,#85998,#85999,#86000,
#86001,#86002,#86003,#86004,#86005,#86006,#86007,#86008,#86009,#86010,#86011,
#86012,#86013,#86014,#86015,#86016,#86017,#86018,#86019,#86020,#86021,#86022,
#86023,#86024,#86025,#86026,#86027,#86028,#86029,#86030,#86031,#86032,#86033,
#86034,#86035,#86036,#86037,#86038,#86039,#86040,#86041,#86042,#86043,#86044,
#86045,#86046,#86047,#86048,#86049,#86050,#86051,#86052,#86053,#86054,#86055,
#86056,#86057,#86058,#86059,#86060,#86061,#86062,#86063,#86064,#86065,#86066,
#86067,#86068,#86069,#86070,#86071,#86072,#86073,#86074,#86075,#86076,#86077,
#86078,#86079,#86080,#86081,#86082,#86083,#86084,#86085,#86086,#86087,#86088,
#86089,#86090,#86091,#86092,#86093,#86094,#86095,#86096,#86097,#86098,#86099,
#86100,#86101,#86102,#86103,#86104,#86105,#86106,#86107,#86108,#86109,#86110,
#86111,#86112,#86113,#86114,#86115,#86116,#86117,#86118,#86119,#86120,#86121,
#86122,#86123,#86124,#86125,#86126,#86127,#86128,#86129,#86130,#86131,#86132,
#86133,#86134,#86135,#86136,#86137,#86138,#86139,#86140,#86141,#86142,#86143,
#86144,#86145,#86146,#86147,#86148,#86149,#86150,#86151,#86152,#86153,#86154,
#86155,#86156,#86157,#86158,#86159,#86160,#86161,#86162,#86163,#86164,#86165,
#86166,#86167,#86168,#86169,#86170,#86171,#86172,#86173,#86174,#86175,#86176,
#86177,#86178,#86179,#86180,#86181,#86182,#86183,#86184,#86185,#86186,#86187,
#86188,#86189,#86190,#86191,#86192,#86193,#86194,#86195,#86196,#86197,#86198,
#86199,#86200,#86201,#86202,#86203,#86204,#86205,#86206,#86207,#86208,#86209,
#86210,#86211,#86212,#86213,#86214,#86215,#86216,#86217,#86218,#86219),
 .UNSPECIFIED.,.F.,.F.,(4,3,3,3,3,3,3,3,3,3,3,3,3,3,3,3,3,3,3,3,3,3,3,3,
3,3,3,3,3,3,3,3,3,3,3,3,3,3,3,3,3,3,3,3,3,3,3,3,3,3,3,3,3,3,3,3,3,3,3,3,
3,3,3,3,3,3,3,3,3,3,3,3,3,3,3,3,3,3,3,3,3,3,3,3,3,3,3,3,3,4),(-10.3761157273102,
-10.3025013652053,-10.2288999145983,-10.1553063912111,-10.0817072749245,
-10.0081084996647,-9.93449407177046,-9.89435976632045,-9.82066032120756,
-9.7469736341422,-9.67329496895587,-9.59961058593755,-9.52592722042616,
-9.45222765048504,-9.39964177800442,-9.32594233388247,-9.25225564780493,
-9.17857698360052,-9.10489260154891,-9.03120923699388,-8.95750966798643,
-8.9049237896884,-8.83122434794995,-8.75753766427595,-8.6838590024869,-8.61017462285223,
-8.53649126071152,-8.46279169409683,-8.41020580137238,-8.33650634776591,
-8.26281965216746,-8.18914097843315,-8.11545658690664,-8.04177321292283,
-7.96807363462363,-7.91548781305636,-7.8417883910061,-7.76810172708217,
-7.69442308504722,-7.62073872503153,-7.54705538240238,-7.4733558349973,
-7.42076982474033,-7.34707033959855,-7.27338361239049,-7.1997049070654,
-7.12602048420316,-7.05233707907581,-6.97863747014909,-6.92605183642431,
-6.85235244796297,-6.77866581764632,-6.70498720914059,-6.63130288229327,
-6.55761957257925,-6.48392005746314,-6.43133384810829,-6.35763436695287,
-6.28394764394594,-6.21026894302116,-6.13658452482969,-6.06290112451683,
-5.98920152059817,-5.93661585979227,-5.8629163313047,-5.7892295601607,-5.71555081044249,
-5.6418663428139,-5.56818289278328,-5.49448323904549,-5.44189787147625,
-5.36819885346765,-5.29451259553663,-5.22083436025188,-5.14715040521026,
-5.07346746591818,-4.99976831650723,-4.94717988316022,-4.87347930006267,
-4.79979147073412,-4.72611166235466,-4.65242614294801,-4.57874164666216,
-4.50504096253567,-4.4524618948442,-4.37893940144604,-4.30542631917865,
-4.23192289045638,-4.15841395294959,-4.09293042013065),.UNSPECIFIED.);
#868=B_SPLINE_CURVE_WITH_KNOTS('',3,(#86220,#86221,#86222,#86223,#86224,
#86225,#86226,#86227,#86228,#86229,#86230,#86231,#86232,#86233,#86234,#86235),
 .UNSPECIFIED.,.F.,.F.,(4,1,1,1,1,1,1,1,1,1,1,1,1,4),(1.12274180646091,
1.48415396494807,1.97887195326409,2.47358994158012,2.96830792989614,3.46302591821216,
3.95774390652818,4.4524618948442,4.94717988316022,5.44189787147624,5.93661585979226,
6.43133384810828,6.9260518364243,7.4059271136405),.UNSPECIFIED.);
#869=B_SPLINE_CURVE_WITH_KNOTS('',3,(#86240,#86241,#86242,#86243,#86244,
#86245,#86246,#86247,#86248,#86249,#86250,#86251,#86252,#86253,#86254,#86255,
#86256),.UNSPECIFIED.,.F.,.F.,(4,1,1,1,1,1,1,1,1,1,1,1,1,1,4),(-16.6593010344898,
-16.3256936144287,-15.8309756261127,-15.3362576377967,-14.8415396494807,
-14.3468216611646,-13.8521036728486,-13.3573856845326,-12.8626676962166,
-12.3679497079006,-11.8732317195845,-11.3785137312685,-10.8837957429525,
-10.3890777546365,-10.3761157273102),.UNSPECIFIED.);
#870=B_SPLINE_CURVE_WITH_KNOTS('',3,(#86257,#86258,#86259,#86260,#86261,
#86262,#86263,#86264,#86265,#86266,#86267,#86268,#86269,#86270,#86271,#86272,
#86273),.UNSPECIFIED.,.F.,.F.,(4,1,1,1,1,1,1,1,1,1,1,1,1,1,4),(7.4059271136405,
7.42076982474033,7.91548781305635,8.41020580137237,8.90492378968839,9.39964177800441,
9.89435976632044,10.3890777546365,10.8837957429525,11.3785137312685,11.8732317195845,
12.3679497079006,12.8626676962166,13.3573856845326,13.6891124208201),
 .UNSPECIFIED.);
#871=B_SPLINE_CURVE_WITH_KNOTS('',3,(#86278,#86279,#86280,#86281,#86282,
#86283,#86284,#86285,#86286,#86287,#86288,#86289,#86290,#86291,#86292,#86293,
#86294),.UNSPECIFIED.,.F.,.F.,(4,1,1,1,1,1,1,1,1,1,1,1,1,1,4),(-22.9424863074193,
-22.757027462537,-22.262309474221,-21.767591485905,-21.272873497589,-20.7781555092729,
-20.2834375209569,-19.7887195326409,-19.2940015443249,-18.7992835560088,
-18.3045655676928,-17.8098475793768,-17.3151295910608,-16.8204116027448,
-16.6593010344898),.UNSPECIFIED.);
#872=B_SPLINE_CURVE_WITH_KNOTS('',3,(#86295,#86296,#86297,#86298,#86299,
#86300,#86301,#86302,#86303,#86304,#86305,#86306,#86307,#86308,#86309,#86310,
#86311),.UNSPECIFIED.,.F.,.F.,(4,1,1,1,1,1,1,1,1,1,1,1,1,1,4),(13.6891124208201,
13.8521036728486,14.3468216611646,14.8415396494807,15.3362576377967,15.8309756261127,
16.3256936144287,16.8204116027448,17.3151295910608,17.8098475793768,18.3045655676928,
18.7992835560088,19.2940015443249,19.7887195326409,19.9722976935382),
 .UNSPECIFIED.);
#873=B_SPLINE_CURVE_WITH_KNOTS('',3,(#86316,#86317,#86318,#86319,#86320,
#86321,#86322,#86323,#86324,#86325,#86326,#86327,#86328,#86329,#86330,#86331,
#86332,#86333,#86334,#86335,#86336,#86337,#86338,#86339,#86340,#86341,#86342,
#86343,#86344,#86345,#86346,#86347,#86348,#86349,#86350,#86351,#86352,#86353,
#86354,#86355,#86356,#86357,#86358,#86359,#86360,#86361,#86362,#86363,#86364,
#86365,#86366,#86367,#86368,#86369,#86370,#86371,#86372,#86373,#86374,#86375,
#86376,#86377,#86378,#86379,#86380,#86381,#86382,#86383,#86384,#86385,#86386,
#86387,#86388,#86389,#86390,#86391,#86392,#86393,#86394,#86395,#86396,#86397,
#86398,#86399,#86400,#86401,#86402,#86403,#86404,#86405,#86406,#86407,#86408,
#86409,#86410,#86411,#86412,#86413,#86414,#86415,#86416,#86417,#86418,#86419,
#86420,#86421,#86422,#86423,#86424,#86425,#86426,#86427,#86428,#86429,#86430,
#86431,#86432,#86433,#86434,#86435,#86436,#86437,#86438,#86439,#86440,#86441,
#86442,#86443,#86444,#86445,#86446,#86447,#86448,#86449,#86450,#86451,#86452,
#86453,#86454,#86455,#86456,#86457,#86458,#86459,#86460,#86461,#86462,#86463,
#86464,#86465,#86466,#86467,#86468,#86469,#86470,#86471,#86472,#86473,#86474,
#86475,#86476,#86477,#86478,#86479,#86480,#86481,#86482,#86483,#86484,#86485,
#86486,#86487,#86488,#86489,#86490,#86491,#86492,#86493,#86494,#86495,#86496,
#86497,#86498,#86499,#86500,#86501,#86502,#86503,#86504,#86505,#86506,#86507,
#86508,#86509,#86510,#86511,#86512,#86513,#86514,#86515,#86516,#86517,#86518,
#86519,#86520,#86521,#86522,#86523,#86524,#86525,#86526,#86527,#86528,#86529,
#86530,#86531,#86532,#86533,#86534,#86535,#86536,#86537,#86538,#86539,#86540,
#86541,#86542,#86543,#86544,#86545,#86546,#86547,#86548,#86549,#86550,#86551,
#86552,#86553,#86554,#86555,#86556,#86557,#86558,#86559,#86560,#86561,#86562,
#86563,#86564,#86565,#86566,#86567,#86568,#86569,#86570,#86571,#86572,#86573,
#86574,#86575,#86576,#86577,#86578,#86579,#86580,#86581,#86582,#86583,#86584,
#86585,#86586),.UNSPECIFIED.,.F.,.F.,(4,3,3,3,3,3,3,3,3,3,3,3,3,3,3,3,3,
3,3,3,3,3,3,3,3,3,3,3,3,3,3,3,3,3,3,3,3,3,3,3,3,3,3,3,3,3,3,3,3,3,3,3,3,
3,3,3,3,3,3,3,3,3,3,3,3,3,3,3,3,3,3,3,3,3,3,3,3,3,3,3,3,3,3,3,3,3,3,3,3,
3,4),(-29.225671648849,-29.1883613106453,-29.1146618663602,-29.0409751801236,
-28.9672965157639,-28.8936121335643,-28.8199287688656,-28.7462291997225,
-28.6936433223293,-28.6199438780423,-28.5462571918037,-28.4725785274421,
-28.3988941452407,-28.3252107805401,-28.2515112113951,-28.1989253340133,
-28.125225889727,-28.051539203489,-27.9778605391277,-27.9041761569269,-27.830492792227,
-27.7567932230827,-27.7042073456973,-27.6305079014107,-27.5568212151724,
-27.4831425508109,-27.4094581686098,-27.3357748039096,-27.262075234765,
-27.2094893573812,-27.1357899130947,-27.0621032268566,-26.9884245624954,
-26.9147401802944,-26.8410568155944,-26.7673572464499,-26.7147713690652,
-26.6410719247788,-26.5673852385407,-26.4937065741796,-26.4200221919787,
-26.3463388272787,-26.2726392581342,-26.2200533807492,-26.1463539364628,
-26.0726672502246,-25.9989885858634,-25.9253042036624,-25.8516208389624,
-25.7779212698179,-25.7253353924332,-25.6516359481466,-25.5779492619084,
-25.5042705975471,-25.430586215346,-25.3569028506459,-25.2832032815013,
-25.2306174041171,-25.1569179598307,-25.0832312735925,-25.0095526092314,
-24.9358682270305,-24.8621848623305,-24.788485293186,-24.7358994158011,
-24.6621999715146,-24.5885132852765,-24.5148346209152,-24.4411502387143,
-24.3674668740142,-24.2937673048697,-24.2411814274851,-24.1674819831987,
-24.0937952969606,-24.0201166325994,-23.9464322503984,-23.8727488856986,
-23.7990493165541,-23.7464634391691,-23.6727639948825,-23.5990773086443,
-23.525398644283,-23.4517142620819,-23.3780308973818,-23.3043313282371,
-23.251745450853,-23.1744306735571,-23.1005806216386,-23.0267406498906,
-22.9529038759223,-22.9424863416694),.UNSPECIFIED.);
#874=B_SPLINE_CURVE_WITH_KNOTS('',3,(#86587,#86588,#86589,#86590,#86591,
#86592,#86593,#86594,#86595,#86596,#86597,#86598,#86599,#86600,#86601,#86602,
#86603,#86604,#86605,#86606,#86607,#86608,#86609,#86610,#86611,#86612,#86613,
#86614,#86615,#86616,#86617,#86618,#86619,#86620,#86621,#86622,#86623,#86624,
#86625,#86626,#86627,#86628,#86629,#86630,#86631,#86632,#86633,#86634,#86635,
#86636,#86637,#86638,#86639,#86640,#86641,#86642,#86643,#86644,#86645,#86646,
#86647,#86648,#86649,#86650,#86651,#86652,#86653,#86654,#86655,#86656,#86657,
#86658,#86659,#86660,#86661,#86662,#86663,#86664,#86665,#86666,#86667,#86668,
#86669,#86670,#86671,#86672,#86673,#86674,#86675,#86676,#86677,#86678,#86679,
#86680,#86681,#86682,#86683,#86684,#86685,#86686,#86687,#86688,#86689,#86690,
#86691,#86692,#86693,#86694,#86695,#86696,#86697,#86698,#86699,#86700,#86701,
#86702,#86703,#86704,#86705,#86706,#86707,#86708,#86709,#86710,#86711,#86712,
#86713,#86714,#86715,#86716,#86717,#86718,#86719,#86720,#86721,#86722,#86723,
#86724,#86725,#86726,#86727,#86728,#86729,#86730,#86731,#86732,#86733,#86734,
#86735,#86736,#86737,#86738,#86739,#86740,#86741,#86742,#86743,#86744,#86745,
#86746,#86747,#86748,#86749,#86750,#86751,#86752,#86753,#86754,#86755,#86756,
#86757,#86758,#86759,#86760,#86761,#86762,#86763,#86764,#86765,#86766,#86767,
#86768,#86769,#86770,#86771,#86772,#86773,#86774,#86775,#86776,#86777,#86778,
#86779,#86780,#86781,#86782,#86783,#86784,#86785,#86786,#86787,#86788,#86789,
#86790,#86791,#86792,#86793,#86794,#86795,#86796,#86797,#86798,#86799,#86800,
#86801,#86802,#86803,#86804,#86805,#86806,#86807,#86808,#86809,#86810,#86811,
#86812,#86813,#86814,#86815,#86816,#86817,#86818,#86819,#86820,#86821,#86822,
#86823,#86824,#86825,#86826,#86827,#86828,#86829,#86830,#86831,#86832,#86833,
#86834,#86835,#86836,#86837,#86838,#86839,#86840,#86841,#86842,#86843,#86844,
#86845,#86846,#86847,#86848,#86849,#86850,#86851,#86852,#86853,#86854,#86855,
#86856,#86857),.UNSPECIFIED.,.F.,.F.,(4,3,3,3,3,3,3,3,3,3,3,3,3,3,3,3,3,
3,3,3,3,3,3,3,3,3,3,3,3,3,3,3,3,3,3,3,3,3,3,3,3,3,3,3,3,3,3,3,3,3,3,3,3,
3,3,3,3,3,3,3,3,3,3,3,3,3,3,3,3,3,3,3,3,3,3,3,3,3,3,3,3,3,3,3,3,3,3,3,3,
3,4),(19.9722977279997,20.0461173438319,20.1199461706305,20.1937774306606,
20.2676235799437,20.2834375209569,20.3571369652434,20.4308236514814,20.5045023158425,
20.5781866980435,20.6518700627436,20.7255696318881,20.7781555092729,20.8518549535596,
20.925541639798,20.9992203041592,21.0729046863603,21.1465880510605,21.2202876202051,
21.272873497589,21.3465729418755,21.4202596281136,21.4939382924747,21.5676226746756,
21.6413060393754,21.7150056085199,21.767591485905,21.8412909301915,21.9149776164295,
21.9886562807907,22.0623406629917,22.1360240276917,22.2097235968362,22.262309474221,
22.3360089185075,22.4096956047458,22.4833742691071,22.557058651308,22.6307420160076,
22.7044415851521,22.757027462537,22.8307269068236,22.9044135930619,22.9780922574236,
23.0517766396246,23.1254600043248,23.1991595734695,23.2517454508531,23.3254448951396,
23.3991315813778,23.4728102457384,23.5464946279395,23.6201779926391,23.6938775617836,
23.7464634391691,23.8201628834554,23.8938495696935,23.9675282340557,24.0412126162567,
24.1148959809567,24.188595550101,24.2411814274851,24.3148808717717,24.3885675580098,
24.4622462223718,24.5359306045729,24.609613969273,24.6833135384175,24.7358994158011,
24.8095988600875,24.8832855463251,24.9569642106865,25.0306485928871,25.1043319575873,
25.1780315267316,25.2306174041171,25.3043168484037,25.3780035346426,25.4516821990037,
25.5253665812046,25.5990499459048,25.6727495150494,25.7253353924332,25.7990348367194,
25.8727215229571,25.9464001873184,26.0200845695193,26.09376793422,26.1674675033644,
26.2200533807492,26.2554830351793),.UNSPECIFIED.);
#875=B_SPLINE_CURVE_WITH_KNOTS('',3,(#86862,#86863,#86864,#86865,#86866,
#86867,#86868,#86869,#86870,#86871,#86872,#86873,#86874,#86875,#86876,#86877),
 .UNSPECIFIED.,.F.,.F.,(4,1,1,1,1,1,1,1,1,1,1,1,1,4),(-35.5088569560286,
-35.1249771704376,-34.6302591821216,-34.1355411938056,-33.6408232054895,
-33.1461052171735,-32.6513872288575,-32.1566692405415,-31.6619512522254,
-31.1672332639094,-30.6725152755934,-30.1777972872774,-29.6830792989613,
-29.2256716823632),.UNSPECIFIED.);
#876=B_SPLINE_CURVE_WITH_KNOTS('',3,(#86878,#86879,#86880,#86881,#86882,
#86883,#86884,#86885,#86886,#86887,#86888,#86889,#86890,#86891,#86892,#86893),
 .UNSPECIFIED.,.F.,.F.,(4,1,1,1,1,1,1,1,1,1,1,1,1,4),(26.2554830679407,
26.7147713690652,27.2094893573812,27.7042073456972,28.1989253340133,28.6936433223293,
29.1883613106453,29.6830792989613,30.1777972872774,30.6725152755934,31.1672332639094,
31.6619512522254,32.1566692405414,32.5386683423589),.UNSPECIFIED.);
#877=B_SPLINE_CURVE_WITH_KNOTS('',3,(#86898,#86899,#86900,#86901,#86902,
#86903,#86904,#86905,#86906,#86907,#86908,#86909,#86910,#86911,#86912,#86913,
#86914),.UNSPECIFIED.,.F.,.F.,(4,1,1,1,1,1,1,1,1,1,1,1,1,1,4),(-41.7920422544505,
-41.5563110185459,-41.0615930302299,-40.5668750419138,-40.0721570535978,
-39.5774390652818,-39.0827210769658,-38.5880030886497,-38.0932851003337,
-37.5985671120177,-37.1038491237017,-36.6091311353857,-36.1144131470696,
-35.6196951587536,-35.5088569560286),.UNSPECIFIED.);
#878=B_SPLINE_CURVE_WITH_KNOTS('',3,(#86915,#86916,#86917,#86918,#86919,
#86920,#86921,#86922,#86923,#86924,#86925,#86926,#86927,#86928,#86929,#86930,
#86931),.UNSPECIFIED.,.F.,.F.,(4,1,1,1,1,1,1,1,1,1,1,1,1,1,4),(32.5386683423589,
32.6513872288575,33.1461052171735,33.6408232054895,34.1355411938055,34.6302591821215,
35.1249771704376,35.6196951587536,36.1144131470696,36.6091311353856,37.1038491237017,
37.5985671120177,38.0932851003337,38.5880030886497,38.8218536394787),
 .UNSPECIFIED.);
#879=B_SPLINE_CURVE_WITH_KNOTS('',3,(#86936,#86937,#86938,#86939,#86940,
#86941,#86942,#86943,#86944,#86945,#86946,#86947,#86948,#86949,#86950,#86951,
#86952,#86953,#86954,#86955,#86956,#86957,#86958,#86959,#86960,#86961,#86962,
#86963,#86964,#86965,#86966,#86967,#86968,#86969,#86970,#86971,#86972,#86973,
#86974,#86975,#86976,#86977,#86978,#86979,#86980,#86981,#86982,#86983,#86984,
#86985,#86986,#86987,#86988,#86989,#86990,#86991,#86992,#86993,#86994,#86995,
#86996,#86997,#86998,#86999,#87000,#87001,#87002,#87003,#87004,#87005,#87006,
#87007,#87008,#87009,#87010,#87011,#87012,#87013,#87014,#87015,#87016,#87017,
#87018,#87019,#87020,#87021,#87022,#87023,#87024,#87025,#87026,#87027,#87028,
#87029,#87030,#87031,#87032,#87033,#87034,#87035,#87036,#87037,#87038,#87039,
#87040,#87041,#87042,#87043,#87044,#87045,#87046,#87047,#87048,#87049,#87050,
#87051,#87052,#87053,#87054,#87055,#87056,#87057,#87058,#87059,#87060,#87061,
#87062,#87063,#87064,#87065,#87066,#87067,#87068,#87069,#87070,#87071,#87072,
#87073,#87074,#87075,#87076,#87077,#87078,#87079,#87080,#87081,#87082,#87083,
#87084,#87085,#87086,#87087,#87088,#87089,#87090,#87091,#87092,#87093,#87094,
#87095,#87096,#87097,#87098,#87099,#87100,#87101,#87102,#87103,#87104,#87105,
#87106,#87107,#87108,#87109,#87110,#87111,#87112,#87113,#87114,#87115,#87116,
#87117,#87118,#87119,#87120,#87121,#87122,#87123,#87124,#87125,#87126,#87127,
#87128,#87129,#87130,#87131,#87132,#87133,#87134,#87135,#87136,#87137,#87138,
#87139,#87140,#87141,#87142,#87143,#87144,#87145,#87146,#87147,#87148,#87149,
#87150,#87151,#87152,#87153,#87154,#87155,#87156,#87157,#87158,#87159,#87160,
#87161,#87162,#87163,#87164,#87165,#87166,#87167,#87168,#87169,#87170,#87171,
#87172,#87173,#87174,#87175,#87176,#87177,#87178,#87179,#87180,#87181,#87182,
#87183,#87184,#87185,#87186,#87187,#87188,#87189,#87190,#87191,#87192,#87193,
#87194,#87195,#87196,#87197,#87198,#87199,#87200,#87201,#87202,#87203,#87204,
#87205,#87206),.UNSPECIFIED.,.F.,.F.,(4,3,3,3,3,3,3,3,3,3,3,3,3,3,3,3,3,
3,3,3,3,3,3,3,3,3,3,3,3,3,3,3,3,3,3,3,3,3,3,3,3,3,3,3,3,3,3,3,3,3,3,3,3,
3,3,3,3,3,3,3,3,3,3,3,3,3,3,3,3,3,3,3,3,3,3,3,3,3,3,3,3,3,3,3,3,3,3,3,3,
3,4),(-48.0752275703878,-47.9965820207153,-47.9876448666542,-47.9139454223674,
-47.840258736129,-47.7665800717675,-47.6928956895662,-47.6192123248658,
-47.545512755721,-47.4929268783381,-47.4192274340518,-47.3455407478136,
-47.2718620834526,-47.1981777012517,-47.1244943365519,-47.0507947674075,
-46.9982088900221,-46.9245094457356,-46.8508227594974,-46.7771440951362,
-46.7034597129352,-46.6297763482352,-46.5560767790907,-46.5034909017061,
-46.4297914574196,-46.3561047711814,-46.2824261068201,-46.2087417246192,
-46.1350583599191,-46.0613587907746,-46.0087729133901,-45.9350734691036,
-45.8613867828655,-45.7877081185043,-45.7140237363033,-45.6403403716033,
-45.5666408024589,-45.5140549250741,-45.4403554807875,-45.3666687945493,
-45.292990130188,-45.2193057479869,-45.1456223832868,-45.0719228141422,
-45.019336936758,-44.9456374924716,-44.8719508062334,-44.7982721418722,
-44.7245877596713,-44.6509043949712,-44.5772048258267,-44.524618948442,
-44.4509195041556,-44.3772328179174,-44.3035541535563,-44.2298697713553,
-44.1561864066553,-44.0824868375109,-44.029900960126,-43.9562015158396,
-43.8825148296014,-43.8088361652403,-43.7351517830394,-43.6614684183394,
-43.5877688491949,-43.53518297181,-43.4614835275234,-43.3877968412851,-43.3141181769239,
-43.2404337947228,-43.1667504300226,-43.093050860878,-43.0404649834939,
-42.9667655392075,-42.8930788529692,-42.819400188608,-42.7457158064071,
-42.6720324417071,-42.5983328725626,-42.5457469951779,-42.4720475508914,
-42.3983608646531,-42.3246822002922,-42.2509978180912,-42.177314453391,
-42.1036148842465,-42.0510290068619,-41.9765921073299,-41.9021699654454,
-41.8277591073817,-41.7920422632082),.UNSPECIFIED.);
#880=B_SPLINE_CURVE_WITH_KNOTS('',3,(#87207,#87208,#87209,#87210,#87211,
#87212,#87213,#87214,#87215,#87216,#87217,#87218,#87219,#87220,#87221,#87222,
#87223,#87224,#87225,#87226,#87227,#87228,#87229,#87230,#87231,#87232,#87233,
#87234,#87235,#87236,#87237,#87238,#87239,#87240,#87241,#87242,#87243,#87244,
#87245,#87246,#87247,#87248,#87249,#87250,#87251,#87252,#87253,#87254,#87255,
#87256,#87257,#87258,#87259,#87260,#87261,#87262,#87263,#87264,#87265,#87266,
#87267,#87268,#87269,#87270,#87271,#87272,#87273,#87274,#87275,#87276,#87277,
#87278,#87279,#87280,#87281,#87282,#87283,#87284,#87285,#87286,#87287,#87288,
#87289,#87290,#87291,#87292,#87293,#87294,#87295,#87296,#87297,#87298,#87299,
#87300,#87301,#87302,#87303,#87304,#87305,#87306,#87307,#87308,#87309,#87310,
#87311,#87312,#87313,#87314,#87315,#87316,#87317,#87318,#87319,#87320,#87321,
#87322,#87323,#87324,#87325,#87326,#87327,#87328,#87329,#87330,#87331,#87332,
#87333,#87334,#87335,#87336,#87337,#87338,#87339,#87340,#87341,#87342,#87343,
#87344,#87345,#87346,#87347,#87348,#87349,#87350,#87351,#87352,#87353,#87354,
#87355,#87356,#87357,#87358,#87359,#87360,#87361,#87362,#87363,#87364,#87365,
#87366,#87367,#87368,#87369,#87370,#87371,#87372,#87373,#87374,#87375,#87376,
#87377,#87378,#87379,#87380,#87381,#87382,#87383,#87384,#87385,#87386,#87387,
#87388,#87389,#87390,#87391,#87392,#87393,#87394,#87395,#87396,#87397,#87398,
#87399,#87400,#87401,#87402,#87403,#87404,#87405,#87406,#87407,#87408,#87409,
#87410,#87411,#87412,#87413,#87414,#87415,#87416,#87417,#87418,#87419,#87420,
#87421,#87422,#87423,#87424,#87425,#87426,#87427,#87428,#87429,#87430,#87431,
#87432,#87433,#87434,#87435,#87436,#87437,#87438,#87439,#87440,#87441,#87442,
#87443,#87444,#87445,#87446,#87447,#87448,#87449,#87450,#87451,#87452,#87453,
#87454,#87455,#87456,#87457,#87458,#87459,#87460,#87461,#87462,#87463,#87464,
#87465,#87466,#87467,#87468,#87469,#87470,#87471,#87472,#87473,#87474,#87475,
#87476,#87477),.UNSPECIFIED.,.F.,.F.,(4,3,3,3,3,3,3,3,3,3,3,3,3,3,3,3,3,
3,3,3,3,3,3,3,3,3,3,3,3,3,3,3,3,3,3,3,3,3,3,3,3,3,3,3,3,3,3,3,3,3,3,3,3,
3,3,3,3,3,3,3,3,3,3,3,3,3,3,3,3,3,3,3,3,3,3,3,3,3,3,3,3,3,3,3,3,3,3,3,3,
3,4),(38.8218536495384,38.8962424641098,38.9706355075857,39.0450460704514,
39.0827210769657,39.1564205212523,39.2301072074908,39.3037858718524,39.3774702540536,
39.4511536187539,39.5248531878985,39.5774390652818,39.6511385095681,39.7248251958061,
39.7985038601673,39.8721882423682,39.9458716070683,40.0195711762127,40.0721570535978,
40.1458564978843,40.2195431841225,40.2932218484837,40.3669062306847,40.4405895953846,
40.5142891645291,40.5668750419138,40.6405744862003,40.7142611724381,40.7879398367993,
40.8616242190003,40.9353075837005,41.009007152845,41.0615930302298,41.1352924745163,
41.2089791607543,41.2826578251155,41.3563422073166,41.4300255720167,41.5037251411614,
41.5563110185459,41.6300104628323,41.7036971490704,41.7773758134322,41.8510601956332,
41.924743560333,41.9984431294775,42.0510290068619,42.1247284511482,42.1984151373863,
42.2720938017479,42.3457781839489,42.419461548649,42.4931611177934,42.5457469951779,
42.6194464394643,42.6931331257019,42.7668117900624,42.8404961722633,42.9141795369633,
42.9878791061077,43.0404649834939,43.1141644277804,43.1878511140188,43.2615297783803,
43.3352141605814,43.4088975252817,43.4825970944261,43.53518297181,43.6088824160963,
43.6825691023342,43.7562477666954,43.8299321488965,43.9036155135963,43.9773150827406,
44.029900960126,44.1036004044123,44.1772870906506,44.2509657550119,44.3246501372129,
44.3983335019129,44.4720330710574,44.524618948442,44.5983183927284,44.6720050789663,
44.7456837433274,44.8193681255284,44.8930514902286,44.9667510593729,45.019336936758,
45.0980543814215,45.105038956718),.UNSPECIFIED.);
#881=B_SPLINE_CURVE_WITH_KNOTS('',3,(#87482,#87483,#87484,#87485,#87486,
#87487,#87488,#87489,#87490,#87491,#87492,#87493,#87494,#87495,#87496,#87497,
#87498,#87499,#87500,#87501,#87502,#87503,#87504,#87505,#87506,#87507,#87508,
#87509,#87510,#87511,#87512,#87513,#87514,#87515,#87516,#87517,#87518,#87519,
#87520,#87521,#87522,#87523,#87524,#87525,#87526,#87527,#87528,#87529,#87530,
#87531,#87532,#87533,#87534,#87535,#87536,#87537,#87538,#87539,#87540,#87541,
#87542,#87543,#87544,#87545,#87546,#87547,#87548,#87549,#87550,#87551,#87552,
#87553,#87554,#87555,#87556,#87557,#87558,#87559,#87560,#87561,#87562,#87563,
#87564,#87565,#87566,#87567,#87568,#87569,#87570,#87571,#87572,#87573,#87574,
#87575,#87576,#87577,#87578,#87579,#87580,#87581,#87582,#87583,#87584,#87585,
#87586,#87587,#87588,#87589,#87590,#87591,#87592,#87593,#87594,#87595,#87596,
#87597,#87598,#87599,#87600,#87601,#87602,#87603,#87604,#87605,#87606,#87607,
#87608,#87609,#87610,#87611,#87612,#87613,#87614,#87615,#87616,#87617,#87618,
#87619,#87620,#87621,#87622,#87623,#87624,#87625,#87626,#87627,#87628,#87629,
#87630,#87631,#87632,#87633,#87634,#87635,#87636,#87637,#87638,#87639,#87640,
#87641,#87642,#87643,#87644,#87645,#87646,#87647,#87648,#87649,#87650,#87651,
#87652,#87653,#87654,#87655,#87656,#87657,#87658,#87659,#87660,#87661,#87662,
#87663,#87664,#87665,#87666,#87667,#87668,#87669,#87670,#87671,#87672,#87673,
#87674,#87675,#87676,#87677,#87678,#87679,#87680,#87681,#87682,#87683,#87684,
#87685,#87686,#87687,#87688,#87689,#87690,#87691,#87692,#87693,#87694,#87695,
#87696,#87697,#87698,#87699,#87700,#87701,#87702,#87703,#87704,#87705,#87706,
#87707,#87708,#87709,#87710,#87711,#87712,#87713,#87714,#87715,#87716,#87717,
#87718,#87719,#87720,#87721,#87722,#87723,#87724,#87725,#87726,#87727,#87728,
#87729,#87730,#87731,#87732,#87733,#87734,#87735,#87736,#87737,#87738,#87739,
#87740,#87741,#87742,#87743,#87744,#87745,#87746,#87747,#87748,#87749),
 .UNSPECIFIED.,.F.,.F.,(4,3,3,3,3,3,3,3,3,3,3,3,3,3,3,3,3,3,3,3,3,3,3,3,
3,3,3,3,3,3,3,3,3,3,3,3,3,3,3,3,3,3,3,3,3,3,3,3,3,3,3,3,3,3,3,3,3,3,3,3,
3,3,3,3,3,3,3,3,3,3,3,3,3,3,3,3,3,3,3,3,3,3,3,3,3,3,3,3,3,4),(-54.3584128775674,
-54.2849899685177,-54.2115785832115,-54.1381640530566,-54.0647521810993,
-53.9913225211834,-53.9242607264464,-53.85056128216,-53.7768745959221,-53.703195931561,
-53.62951154936,-53.5558281846599,-53.4821286155154,-53.4295427381304,-53.355843293844,
-53.282156607606,-53.2084779432451,-53.1347935610442,-53.0611101963441,
-52.9874106271997,-52.9348247498144,-52.8611253055281,-52.7874386192901,
-52.7137599549282,-52.6400755727273,-52.5663922080273,-52.4926926388828,
-52.4401067614984,-52.3664073172119,-52.2927206309733,-52.2190419666122,
-52.1453575844111,-52.0716742197112,-51.9979746505666,-51.9453887731823,
-51.871689328896,-51.7980026426579,-51.7243239782976,-51.6506395960966,
-51.5769562313966,-51.5032566622521,-51.4506707848663,-51.3769713405799,
-51.3032846543415,-51.2296059899809,-51.1559216077799,-51.0822382430798,
-51.0085386739351,-50.9559527965503,-50.882253352264,-50.8085666660261,
-50.7348880016648,-50.6612036194638,-50.587520254764,-50.5138206856195,
-50.4612348082343,-50.3875353639481,-50.3138486777102,-50.2401700133499,
-50.1664856311489,-50.092802266449,-50.0191026973044,-49.9665168199183,
-49.8928173756317,-49.8191306893936,-49.7454520250325,-49.6717676428314,
-49.5980842781316,-49.5243847089868,-49.4717988316022,-49.3980993873157,
-49.3244127010775,-49.2507340367163,-49.1770496545154,-49.1033662898151,
-49.0296667206704,-48.9770808432862,-48.9033813989998,-48.8296947127613,
-48.7560160484013,-48.6823316662005,-48.6086483015005,-48.5349487323562,
-48.4823628549702,-48.4089545042359,-48.3355599148838,-48.262167220395,
-48.1887787589612,-48.115379492763,-48.0752275704749),.UNSPECIFIED.);
#882=B_SPLINE_CURVE_WITH_KNOTS('',3,(#87750,#87751,#87752,#87753,#87754,
#87755,#87756,#87757,#87758,#87759,#87760,#87761,#87762,#87763,#87764,#87765,
#87766,#87767,#87768,#87769,#87770,#87771,#87772,#87773,#87774,#87775,#87776,
#87777,#87778,#87779,#87780,#87781,#87782,#87783,#87784,#87785,#87786,#87787,
#87788,#87789,#87790,#87791,#87792,#87793,#87794,#87795,#87796,#87797,#87798,
#87799,#87800,#87801,#87802,#87803,#87804,#87805,#87806,#87807,#87808,#87809,
#87810,#87811,#87812,#87813,#87814,#87815,#87816,#87817,#87818,#87819,#87820,
#87821,#87822,#87823,#87824,#87825,#87826,#87827,#87828,#87829,#87830,#87831,
#87832,#87833,#87834,#87835,#87836,#87837,#87838,#87839,#87840,#87841,#87842,
#87843,#87844,#87845,#87846,#87847,#87848,#87849,#87850,#87851,#87852,#87853,
#87854,#87855,#87856,#87857,#87858,#87859,#87860,#87861,#87862,#87863,#87864,
#87865,#87866,#87867,#87868,#87869,#87870,#87871,#87872,#87873,#87874,#87875,
#87876,#87877,#87878,#87879,#87880,#87881,#87882,#87883,#87884,#87885,#87886,
#87887,#87888,#87889,#87890,#87891,#87892,#87893,#87894,#87895,#87896,#87897,
#87898,#87899,#87900,#87901,#87902,#87903,#87904,#87905,#87906,#87907,#87908,
#87909,#87910,#87911,#87912,#87913,#87914,#87915,#87916,#87917,#87918,#87919,
#87920,#87921,#87922,#87923,#87924,#87925,#87926,#87927,#87928,#87929,#87930,
#87931,#87932,#87933,#87934,#87935,#87936,#87937,#87938,#87939,#87940,#87941,
#87942,#87943,#87944,#87945,#87946,#87947,#87948,#87949,#87950,#87951,#87952,
#87953,#87954,#87955,#87956,#87957,#87958,#87959,#87960,#87961,#87962,#87963,
#87964,#87965,#87966,#87967,#87968,#87969,#87970,#87971,#87972,#87973,#87974,
#87975,#87976,#87977,#87978,#87979,#87980,#87981,#87982,#87983,#87984,#87985,
#87986,#87987,#87988,#87989,#87990,#87991,#87992,#87993,#87994,#87995,#87996,
#87997,#87998,#87999,#88000,#88001,#88002,#88003,#88004,#88005,#88006,#88007,
#88008,#88009,#88010,#88011,#88012,#88013,#88014,#88015,#88016,#88017),
 .UNSPECIFIED.,.F.,.F.,(4,3,3,3,3,3,3,3,3,3,3,3,3,3,3,3,3,3,3,3,3,3,3,3,
3,3,3,3,3,3,3,3,3,3,3,3,3,3,3,3,3,3,3,3,3,3,3,3,3,3,3,3,3,3,3,3,3,3,3,3,
3,3,3,3,3,3,3,3,3,3,3,3,3,3,3,3,3,3,3,3,3,3,3,3,3,3,3,3,3,4),(45.1050389568105,
45.1784373110113,45.2518258373623,45.3252185210999,45.3986103264318,45.4720183448909,
45.514054925074,45.5877543693606,45.661441055599,45.7351197199599,45.808804102161,
45.8824874668611,45.9561870360059,46.0087729133901,46.0824723576764,46.1561590439145,
46.2298377082755,46.3035220904764,46.3772054551767,46.4509050243212,46.5034909017061,
46.5771903459926,46.6508770322308,46.7245556965918,46.7982400787927,46.8719234434926,
46.9456230126372,46.9982088900221,47.0719083343085,47.1455950205465,47.2192736849076,
47.2929580671085,47.3666414318084,47.4403410009529,47.4929268783381,47.5666263226245,
47.6403130088627,47.7139916732241,47.7876760554253,47.8613594201254,47.9350589892702,
47.9876448666542,48.0613443109406,48.1350309971786,48.2087096615394,48.2823940437402,
48.3560774084403,48.4297769775848,48.4823628549702,48.5560622992565,48.6297489854944,
48.703427649855,48.7771120320559,48.8507953967557,48.9244949659001,48.9770808432862,
49.0507802875726,49.1244669738108,49.1981456381717,49.2718300203727,49.3455133850727,
49.4192129542173,49.4717988316022,49.5454982758885,49.6191849621266,49.6928636264875,
49.7665480086884,49.8402313733884,49.9139309425329,49.9665168199182,50.0402162642048,
50.1139029504433,50.1875816148053,50.2612659970064,50.334949361707,50.4086489308515,
50.4612348082343,50.5349342525207,50.6086209387594,50.6822996031205,50.7559839853216,
50.8296673500208,50.9033669191653,50.9559527965503,51.0293775994402,51.1027887792278,
51.1761997331969,51.2496062660259,51.3230273800014,51.3882242638976),
 .UNSPECIFIED.);
#883=B_SPLINE_CURVE_WITH_KNOTS('',3,(#88022,#88023,#88024,#88025,#88026,
#88027,#88028,#88029,#88030,#88031,#88032,#88033,#88034,#88035,#88036,#88037,
#88038),.UNSPECIFIED.,.F.,.F.,(4,1,1,1,1,1,1,1,1,1,1,1,1,1,4),(-60.641598184747,
-60.3555945745547,-59.8608765862387,-59.3661585979227,-58.8714406096067,
-58.3767226212906,-57.8820046329746,-57.3872866446586,-56.8925686563426,
-56.3978506680265,-55.9031326797105,-55.4084146913945,-54.9136967030785,
-54.4189787147625,-54.3584128775674),.UNSPECIFIED.);
#884=B_SPLINE_CURVE_WITH_KNOTS('',3,(#88039,#88040,#88041,#88042,#88043,
#88044,#88045,#88046,#88047,#88048,#88049,#88050,#88051,#88052,#88053,#88054,
#88055),.UNSPECIFIED.,.F.,.F.,(4,1,1,1,1,1,1,1,1,1,1,1,1,1,4),(51.3882242638976,
51.4506707848663,51.9453887731823,52.4401067614984,52.9348247498144,53.4295427381304,
53.9242607264464,54.4189787147624,54.9136967030785,55.4084146913945,55.9031326797105,
56.3978506680265,56.8925686563425,57.3872866446586,57.6714095710772),
 .UNSPECIFIED.);
#885=B_SPLINE_CURVE_WITH_KNOTS('',3,(#88060,#88061,#88062,#88063,#88064,
#88065,#88066,#88067,#88068,#88069,#88070,#88071,#88072,#88073,#88074,#88075,
#88076,#88077,#88078,#88079,#88080,#88081,#88082,#88083,#88084,#88085,#88086,
#88087,#88088,#88089,#88090,#88091,#88092,#88093,#88094,#88095,#88096,#88097,
#88098,#88099,#88100,#88101,#88102,#88103,#88104,#88105,#88106,#88107,#88108,
#88109,#88110,#88111,#88112,#88113,#88114,#88115,#88116,#88117,#88118,#88119,
#88120,#88121,#88122,#88123,#88124,#88125,#88126,#88127,#88128,#88129,#88130,
#88131,#88132,#88133,#88134,#88135,#88136,#88137,#88138,#88139,#88140,#88141,
#88142,#88143,#88144,#88145,#88146,#88147,#88148,#88149,#88150,#88151,#88152,
#88153,#88154,#88155,#88156,#88157,#88158,#88159,#88160,#88161,#88162,#88163,
#88164,#88165,#88166,#88167,#88168,#88169,#88170,#88171,#88172,#88173,#88174,
#88175,#88176,#88177,#88178,#88179,#88180,#88181,#88182,#88183,#88184,#88185,
#88186,#88187,#88188,#88189,#88190,#88191,#88192,#88193,#88194,#88195,#88196,
#88197,#88198,#88199,#88200,#88201,#88202,#88203,#88204,#88205,#88206,#88207,
#88208,#88209,#88210,#88211,#88212,#88213,#88214,#88215,#88216,#88217,#88218,
#88219,#88220,#88221,#88222,#88223,#88224,#88225,#88226,#88227,#88228,#88229,
#88230,#88231,#88232,#88233,#88234,#88235,#88236,#88237,#88238,#88239,#88240,
#88241,#88242,#88243,#88244,#88245,#88246,#88247,#88248,#88249,#88250,#88251,
#88252,#88253,#88254,#88255,#88256,#88257,#88258,#88259,#88260,#88261,#88262,
#88263,#88264,#88265,#88266,#88267,#88268,#88269,#88270,#88271,#88272,#88273,
#88274,#88275,#88276,#88277,#88278,#88279,#88280,#88281,#88282,#88283,#88284,
#88285,#88286,#88287,#88288,#88289,#88290,#88291,#88292,#88293,#88294,#88295,
#88296,#88297,#88298,#88299,#88300,#88301,#88302,#88303,#88304,#88305,#88306,
#88307,#88308,#88309,#88310,#88311,#88312,#88313,#88314,#88315,#88316,#88317,
#88318,#88319,#88320,#88321,#88322,#88323,#88324,#88325,#88326,#88327),
 .UNSPECIFIED.,.F.,.F.,(4,3,3,3,3,3,3,3,3,3,3,3,3,3,3,3,3,3,3,3,3,3,3,3,
3,3,3,3,3,3,3,3,3,3,3,3,3,3,3,3,3,3,3,3,3,3,3,3,3,3,3,3,3,3,3,3,3,3,3,3,
3,3,3,3,3,3,3,3,3,3,3,3,3,3,3,3,3,3,3,3,3,3,3,3,3,3,3,3,3,4),(-66.9247834918443,
-66.8478145143248,-66.786928422663,-66.7132289783763,-66.639542292138,-66.5658636277763,
-66.4921792455751,-66.4184958808748,-66.3447963117301,-66.292210434347,
-66.2185109900607,-66.1448243038226,-66.0711456394617,-65.9974612572609,
-65.923777892561,-65.8500783234165,-65.797492446031,-65.7237930017444,-65.650106315506,
-65.5764276511447,-65.5027432689435,-65.4290599042433,-65.3553603350986,
-65.3027744577149,-65.2290750134285,-65.1553883271904,-65.0817096628292,
-65.0080252806283,-64.9343419159282,-64.8606423467837,-64.8080564693989,
-64.7343570251125,-64.6606703388743,-64.5869916745131,-64.5133072923122,
-64.4396239276122,-64.3659243584678,-64.3133384810829,-64.2396390367964,
-64.1659523505581,-64.0922736861969,-64.0185893039959,-63.9449059392958,
-63.8712063701512,-63.8186204927669,-63.7449210484805,-63.6712343622425,
-63.5975556978814,-63.5238713156805,-63.4501879509805,-63.3764883818361,
-63.3239025044509,-63.2502030601643,-63.176516373926,-63.1028377095646,
-63.0291533273635,-62.9554699626634,-62.8817703935188,-62.8291845161348,
-62.7554850718484,-62.6817983856102,-62.608119721249,-62.5344353390481,
-62.4607519743481,-62.3870524052036,-62.3344665278188,-62.2607670835324,
-62.1870803972943,-62.1134017329332,-62.0397173507323,-61.9660339860323,
-61.8923344168878,-61.8397485395028,-61.7660490952164,-61.6923624089782,
-61.6186837446169,-61.5449993624159,-61.4713159977159,-61.3976164285713,
-61.3450305511868,-61.2713311069004,-61.1976444206621,-61.1239657563008,
-61.0502813740998,-60.9765980093998,-60.9028984402553,-60.8503125628708,
-60.7750416493584,-60.6997883345464,-60.6415981883296),.UNSPECIFIED.);
#886=B_SPLINE_CURVE_WITH_KNOTS('',3,(#88328,#88329,#88330,#88331,#88332,
#88333,#88334,#88335,#88336,#88337,#88338,#88339,#88340,#88341,#88342,#88343,
#88344,#88345,#88346,#88347,#88348,#88349,#88350,#88351,#88352,#88353,#88354,
#88355,#88356,#88357,#88358,#88359,#88360,#88361,#88362,#88363,#88364,#88365,
#88366,#88367,#88368,#88369,#88370,#88371,#88372,#88373,#88374,#88375,#88376,
#88377,#88378,#88379,#88380,#88381,#88382,#88383,#88384,#88385,#88386,#88387,
#88388,#88389,#88390,#88391,#88392,#88393,#88394,#88395,#88396,#88397,#88398,
#88399,#88400,#88401,#88402,#88403,#88404,#88405,#88406,#88407,#88408,#88409,
#88410,#88411,#88412,#88413,#88414,#88415,#88416,#88417,#88418,#88419,#88420,
#88421,#88422,#88423,#88424,#88425,#88426,#88427,#88428,#88429,#88430,#88431,
#88432,#88433,#88434,#88435,#88436,#88437,#88438,#88439,#88440,#88441,#88442,
#88443,#88444,#88445,#88446,#88447,#88448,#88449,#88450,#88451,#88452,#88453,
#88454,#88455,#88456,#88457,#88458,#88459,#88460,#88461,#88462,#88463,#88464,
#88465,#88466,#88467,#88468,#88469,#88470,#88471,#88472,#88473,#88474,#88475,
#88476,#88477,#88478,#88479,#88480,#88481,#88482,#88483,#88484,#88485,#88486,
#88487,#88488,#88489,#88490,#88491,#88492,#88493,#88494,#88495,#88496,#88497,
#88498,#88499,#88500,#88501,#88502,#88503,#88504,#88505,#88506,#88507,#88508,
#88509,#88510,#88511,#88512,#88513,#88514,#88515,#88516,#88517,#88518,#88519,
#88520,#88521,#88522,#88523,#88524,#88525,#88526,#88527,#88528,#88529,#88530,
#88531,#88532,#88533,#88534,#88535,#88536,#88537,#88538,#88539,#88540,#88541,
#88542,#88543,#88544,#88545,#88546,#88547,#88548,#88549,#88550,#88551,#88552,
#88553,#88554,#88555,#88556,#88557,#88558,#88559,#88560,#88561,#88562,#88563,
#88564,#88565,#88566,#88567,#88568,#88569,#88570,#88571,#88572,#88573,#88574,
#88575,#88576,#88577,#88578,#88579,#88580,#88581,#88582,#88583,#88584,#88585,
#88586,#88587,#88588,#88589,#88590,#88591,#88592,#88593,#88594,#88595),
 .UNSPECIFIED.,.F.,.F.,(4,3,3,3,3,3,3,3,3,3,3,3,3,3,3,3,3,3,3,3,3,3,3,3,
3,3,3,3,3,3,3,3,3,3,3,3,3,3,3,3,3,3,3,3,3,3,3,3,3,3,3,3,3,3,3,3,3,3,3,3,
3,3,3,3,3,3,3,3,3,3,3,3,3,3,3,3,3,3,3,3,3,3,3,3,3,3,3,3,3,4),(57.6714095742863,
57.7466199377083,57.8218544415793,57.8820046329746,57.9557040772608,58.0293907634987,
58.1030694278597,58.1767538100604,58.2504371747602,58.3241367439045,58.3767226212906,
58.4504220655772,58.5241087518157,58.5977874161769,58.671471798378,58.7451551630782,
58.8188547322229,58.8714406096067,58.9451400538932,59.0188267401314,59.0925054044924,
59.1661897866933,59.2398731513933,59.3135727205378,59.3661585979227,59.4398580422092,
59.5135447284473,59.5872233928085,59.6609077750095,59.7345911397095,59.808290708854,
59.8608765862387,59.9345760305252,60.0082627167634,60.0819413811247,60.1556257633256,
60.2293091280257,60.3030086971702,60.3555945745547,60.4292940188412,60.5029807050793,
60.5766593694405,60.6503437516414,60.7240271163415,60.797726685486,60.8503125628707,
60.9240120071571,60.9976986933953,61.0713773577564,61.1450617399574,61.2187451046574,
61.2924446738019,61.3450305511867,61.4187299954732,61.4924166817115,61.5660953460727,
61.6397797282737,61.7134630929739,61.7871626621185,61.8397485395028,61.9134479837892,
61.9871346700274,62.0608133343884,62.1344977165894,62.2081810812892,62.2818806504337,
62.3344665278188,62.4081659721052,62.4818526583434,62.5555313227047,62.6292157049056,
62.7028990696057,62.7765986387502,62.8291845161348,62.9028839604212,62.9765706466592,
63.0502493110202,63.1239336932211,63.1976170579211,63.2713166270657,63.3239025044508,
63.3976019487374,63.4712886349756,63.5449672993371,63.6186516815382,63.6923350462384,
63.7660346153831,63.8186204927669,63.8956443550278,63.9545948781802),
 .UNSPECIFIED.);
#887=B_SPLINE_CURVE_WITH_KNOTS('',3,(#88600,#88601,#88602,#88603,#88604,
#88605,#88606,#88607,#88608,#88609,#88610,#88611,#88612,#88613,#88614,#88615,
#88616,#88617,#88618,#88619,#88620,#88621,#88622,#88623,#88624,#88625,#88626,
#88627,#88628,#88629,#88630,#88631,#88632,#88633,#88634,#88635,#88636,#88637,
#88638,#88639,#88640,#88641,#88642,#88643,#88644,#88645,#88646,#88647,#88648,
#88649,#88650,#88651,#88652,#88653,#88654,#88655,#88656,#88657,#88658,#88659,
#88660,#88661,#88662,#88663,#88664,#88665,#88666,#88667,#88668,#88669,#88670,
#88671,#88672,#88673,#88674,#88675,#88676,#88677,#88678,#88679,#88680,#88681,
#88682,#88683,#88684,#88685,#88686,#88687,#88688,#88689,#88690,#88691,#88692,
#88693,#88694,#88695,#88696,#88697,#88698,#88699,#88700,#88701,#88702,#88703,
#88704,#88705,#88706,#88707,#88708,#88709,#88710,#88711,#88712,#88713,#88714,
#88715,#88716,#88717,#88718,#88719,#88720,#88721,#88722,#88723,#88724,#88725,
#88726,#88727,#88728,#88729,#88730,#88731,#88732,#88733,#88734,#88735,#88736,
#88737,#88738,#88739,#88740,#88741,#88742,#88743,#88744,#88745,#88746,#88747,
#88748,#88749,#88750,#88751,#88752,#88753,#88754,#88755,#88756,#88757,#88758,
#88759,#88760,#88761,#88762,#88763,#88764,#88765,#88766,#88767,#88768,#88769,
#88770,#88771,#88772,#88773,#88774,#88775,#88776,#88777,#88778,#88779,#88780,
#88781,#88782,#88783,#88784,#88785,#88786,#88787,#88788,#88789,#88790,#88791,
#88792,#88793,#88794,#88795,#88796,#88797,#88798,#88799,#88800,#88801,#88802,
#88803,#88804,#88805,#88806,#88807,#88808,#88809,#88810,#88811,#88812,#88813,
#88814,#88815,#88816,#88817,#88818,#88819,#88820,#88821,#88822,#88823,#88824,
#88825,#88826,#88827,#88828,#88829,#88830,#88831,#88832,#88833,#88834,#88835,
#88836,#88837,#88838,#88839,#88840,#88841,#88842,#88843,#88844,#88845,#88846,
#88847,#88848,#88849,#88850,#88851,#88852,#88853,#88854,#88855,#88856,#88857,
#88858,#88859,#88860,#88861,#88862,#88863,#88864,#88865,#88866,#88867),
 .UNSPECIFIED.,.F.,.F.,(4,3,3,3,3,3,3,3,3,3,3,3,3,3,3,3,3,3,3,3,3,3,3,3,
3,3,3,3,3,3,3,3,3,3,3,3,3,3,3,3,3,3,3,3,3,3,3,3,3,3,3,3,3,3,3,3,3,3,3,3,
3,3,3,3,3,3,3,3,3,3,3,3,3,3,3,3,3,3,3,3,3,3,3,3,3,3,3,3,3,4),(-73.2079687991061,
-73.1343380786446,-73.0607202596719,-72.9871104049237,-72.9134949479314,
-72.8398799780221,-72.7662492451856,-72.7235442824553,-72.6498448381687,
-72.5761581519305,-72.502479487569,-72.4287951053677,-72.3551117406675,
-72.2814121715227,-72.2288262941392,-72.1551268498529,-72.081440163615,
-72.0077614992544,-71.9340771170534,-71.8603937523532,-71.7866941832088,
-71.7341083058232,-71.6604088615369,-71.5867221752989,-71.5130435109382,
-71.4393591287373,-71.3656757640373,-71.2919761948928,-71.2393903175072,
-71.1656908732209,-71.0920041869828,-71.0183255226214,-70.9446411404204,
-70.8709577757201,-70.7972582065759,-70.7446723291912,-70.6709728849046,
-70.5972861986664,-70.5236075343048,-70.4499231521037,-70.3762397874038,
-70.3025402182592,-70.2499543408751,-70.1762548965886,-70.1025682103503,
-70.028889545989,-69.9552051637882,-69.8815217990882,-69.8078222299438,
-69.7552363525591,-69.6815369082727,-69.6078502220346,-69.534171557674,
-69.4604871754731,-69.3868038107734,-69.3131042416287,-69.2605183642431,
-69.1868189199567,-69.1131322337188,-69.039453569357,-68.9657691871559,
-68.8920858224556,-68.8183862533109,-68.7658003759271,-68.6921009316406,
-68.6184142454021,-68.544735581041,-68.4710511988402,-68.3973678341401,
-68.3236682649954,-68.2710823876111,-68.1973829433246,-68.1236962570865,
-68.0500175927256,-67.9763332105245,-67.9026498458241,-67.8289502766797,
-67.7763643992951,-67.7026649550085,-67.62897826877,-67.5552996044088,-67.4816152222079,
-67.4079318575082,-67.3342322883634,-67.281646410979,-67.2081092887614,
-67.134581747801,-67.0610638753131,-66.987541017849,-66.9247834919265),
 .UNSPECIFIED.);
#888=B_SPLINE_CURVE_WITH_KNOTS('',3,(#88868,#88869,#88870,#88871,#88872,
#88873,#88874,#88875,#88876,#88877,#88878,#88879,#88880,#88881,#88882,#88883,
#88884,#88885,#88886,#88887,#88888,#88889,#88890,#88891,#88892,#88893,#88894,
#88895,#88896,#88897,#88898,#88899,#88900,#88901,#88902,#88903,#88904,#88905,
#88906,#88907,#88908,#88909,#88910,#88911,#88912,#88913,#88914,#88915,#88916,
#88917,#88918,#88919,#88920,#88921,#88922,#88923,#88924,#88925,#88926,#88927,
#88928,#88929,#88930,#88931,#88932,#88933,#88934,#88935,#88936,#88937,#88938,
#88939,#88940,#88941,#88942,#88943,#88944,#88945,#88946,#88947,#88948,#88949,
#88950,#88951,#88952,#88953,#88954,#88955,#88956,#88957,#88958,#88959,#88960,
#88961,#88962,#88963,#88964,#88965,#88966,#88967,#88968,#88969,#88970,#88971,
#88972,#88973,#88974,#88975,#88976,#88977,#88978,#88979,#88980,#88981,#88982,
#88983,#88984,#88985,#88986,#88987,#88988,#88989,#88990,#88991,#88992,#88993,
#88994,#88995,#88996,#88997,#88998,#88999,#89000,#89001,#89002,#89003,#89004,
#89005,#89006,#89007,#89008,#89009,#89010,#89011,#89012,#89013,#89014,#89015,
#89016,#89017,#89018,#89019,#89020,#89021,#89022,#89023,#89024,#89025,#89026,
#89027,#89028,#89029,#89030,#89031,#89032,#89033,#89034,#89035,#89036,#89037,
#89038,#89039,#89040,#89041,#89042,#89043,#89044,#89045,#89046,#89047,#89048,
#89049,#89050,#89051,#89052,#89053,#89054,#89055,#89056,#89057,#89058,#89059,
#89060,#89061,#89062,#89063,#89064,#89065,#89066,#89067,#89068,#89069,#89070,
#89071,#89072,#89073,#89074,#89075,#89076,#89077,#89078,#89079,#89080,#89081,
#89082,#89083,#89084,#89085,#89086,#89087,#89088,#89089,#89090,#89091,#89092,
#89093,#89094,#89095,#89096,#89097,#89098,#89099,#89100,#89101,#89102,#89103,
#89104,#89105,#89106,#89107,#89108,#89109,#89110,#89111,#89112,#89113,#89114,
#89115,#89116,#89117,#89118,#89119,#89120,#89121,#89122,#89123,#89124,#89125,
#89126,#89127,#89128,#89129,#89130,#89131,#89132,#89133,#89134,#89135),
 .UNSPECIFIED.,.F.,.F.,(4,3,3,3,3,3,3,3,3,3,3,3,3,3,3,3,3,3,3,3,3,3,3,3,
3,3,3,3,3,3,3,3,3,3,3,3,3,3,3,3,3,3,3,3,3,3,3,3,3,3,3,3,3,3,3,3,3,3,3,3,
3,3,3,3,3,3,3,3,3,3,3,3,3,3,3,3,3,3,3,3,3,3,3,3,3,3,3,3,3,4),(63.9545948782568,
64.0281047268907,64.1016188939417,64.1751309958523,64.2486607942513,64.3133384810829,
64.3870379253694,64.4607246116078,64.5344032759691,64.6080876581701,64.6817710228699,
64.7554705920144,64.8080564693989,64.8817559136852,64.9554425999232,65.0291212642843,
65.1028056464851,65.176489011185,65.2501885803294,65.3027744577149,65.3764739020017,
65.4501605882402,65.5238392526012,65.5975236348023,65.6712069995025,65.7449065686472,
65.797492446031,65.8711918903174,65.9448785765557,66.0185572409169,66.0922416231179,
66.165924987818,66.2396245569625,66.292210434347,66.3659098786334,66.4395965648714,
66.5132752292325,66.5869596114334,66.6606429761336,66.7343425452781,66.786928422663,
66.8606278669494,66.9343145531879,67.0079932175491,67.08167759975,67.15536096445,
67.2290605335945,67.281646410979,67.3553458552654,67.4290325415035,67.5027112058644,
67.5763955880654,67.6500789527652,67.7237785219097,67.776364399295,67.8500638435817,
67.9237505298202,67.9974291941811,68.0711135763821,68.1447969410826,68.2184965102273,
68.2710823876111,68.3447818318976,68.4184685181356,68.492147182497,68.565831564698,
68.6395149293978,68.7132144985424,68.7658003759271,68.8394998202134,68.9131865064515,
68.9868651708136,69.0605495530148,69.1342329177144,69.2079324868591,69.2605183642431,
69.3342178085296,69.4079044947675,69.4815831591289,69.5552675413299,69.6289509060304,
69.7026504751748,69.7552363525591,69.828855753,69.902462147405,69.9760605064764,
70.0496643152218,70.1232676569756,70.1968865583481,70.2377801854364),
 .UNSPECIFIED.);
#889=B_SPLINE_CURVE_WITH_KNOTS('',3,(#89140,#89141,#89142,#89143,#89144,
#89145,#89146,#89147,#89148,#89149,#89150,#89151,#89152,#89153,#89154,#89155,
#89156),.UNSPECIFIED.,.F.,.F.,(4,1,1,1,1,1,1,1,1,1,1,1,1,1,4),(-79.4911541062857,
-79.1548781305636,-78.6601601422475,-78.1654421539315,-77.6707241656155,
-77.1760061772995,-76.6812881889835,-76.1865702006674,-75.6918522123514,
-75.1971342240354,-74.7024162357194,-74.2076982474033,-73.7129802590873,
-73.2182622707713,-73.2079687991061),.UNSPECIFIED.);
#890=B_SPLINE_CURVE_WITH_KNOTS('',3,(#89157,#89158,#89159,#89160,#89161,
#89162,#89163,#89164,#89165,#89166,#89167,#89168,#89169,#89170,#89171,#89172,
#89173,#89174),.UNSPECIFIED.,.F.,.F.,(4,2,1,1,1,1,1,1,1,1,1,1,1,1,4),(70.2377801854364,
70.2499543408751,70.7446723291912,71.2393903175072,71.7341083058232,72.2288262941392,
72.7235442824553,73.2182622707713,73.7129802590873,74.2076982474033,74.7024162357194,
75.1971342240354,75.6918522123514,76.1865702006674,76.520965492616),
 .UNSPECIFIED.);
#891=B_SPLINE_CURVE_WITH_KNOTS('',3,(#89179,#89180,#89181,#89182,#89183,
#89184,#89185,#89186,#89187,#89188,#89189,#89190,#89191,#89192,#89193,#89194,
#89195),.UNSPECIFIED.,.F.,.F.,(4,1,1,1,1,1,1,1,1,1,1,1,1,1,4),(-85.7743394134653,
-85.5862119786719,-85.0914939903558,-84.5967760020398,-84.1020580137238,
-83.6073400254078,-83.1126220370918,-82.6179040487757,-82.1231860604597,
-81.6284680721437,-81.1337500838277,-80.6390320955116,-80.1443141071956,
-79.6495961188796,-79.4911541062857),.UNSPECIFIED.);
#892=B_SPLINE_CURVE_WITH_KNOTS('',3,(#89196,#89197,#89198,#89199,#89200,
#89201,#89202,#89203,#89204,#89205,#89206,#89207,#89208,#89209,#89210,#89211,
#89212),.UNSPECIFIED.,.F.,.F.,(4,1,1,1,1,1,1,1,1,1,1,1,1,1,4),(76.520965492616,
76.6812881889834,77.1760061772995,77.6707241656155,78.1654421539315,78.6601601422475,
79.1548781305636,79.6495961188796,80.1443141071956,80.6390320955116,81.1337500838276,
81.6284680721437,82.1231860604597,82.6179040487757,82.8041507997956),
 .UNSPECIFIED.);
#893=B_SPLINE_CURVE_WITH_KNOTS('',3,(#89215,#89216,#89217,#89218,#89219,
#89220,#89221,#89222,#89223,#89224,#89225,#89226,#89227,#89228),
 .UNSPECIFIED.,.F.,.F.,(4,1,1,1,1,1,1,1,1,1,1,4),(82.8041507997956,83.1126220370917,
83.6073400254078,84.1020580137238,84.5967760020398,85.0914939903558,85.5862119786719,
86.0809299669879,86.5756479553039,87.0703659436199,87.5650839319359,87.9645943005142),
 .UNSPECIFIED.);
#894=B_SPLINE_CURVE_WITH_KNOTS('',3,(#89231,#89232,#89233,#89234,#89235,
#89236,#89237,#89238,#89239,#89240,#89241,#89242),.UNSPECIFIED.,.F.,.F.,
(4,1,1,1,1,1,1,1,1,4),(-90.0386738735161,-89.5439558852,-89.049237896884,
-88.554519908568,-88.059801920252,-87.565083931936,-87.0703659436199,-86.5756479553039,
-86.0809299669879,-85.7743394134653),.UNSPECIFIED.);
#895=B_SPLINE_CURVE_WITH_KNOTS('',3,(#89245,#89246,#89247,#89248,#89249,
#89250,#89251,#89252,#89253,#89254,#89255,#89256,#89257,#89258,#89259,#89260,
#89261,#89262,#89263,#89264,#89265,#89266,#89267,#89268,#89269,#89270,#89271,
#89272,#89273,#89274,#89275,#89276,#89277,#89278,#89279,#89280,#89281,#89282,
#89283,#89284,#89285,#89286,#89287,#89288,#89289,#89290,#89291,#89292,#89293,
#89294,#89295,#89296,#89297,#89298,#89299,#89300,#89301,#89302,#89303,#89304,
#89305,#89306,#89307,#89308,#89309,#89310,#89311,#89312,#89313,#89314,#89315,
#89316,#89317,#89318,#89319,#89320,#89321,#89322,#89323,#89324,#89325,#89326,
#89327,#89328,#89329,#89330,#89331,#89332,#89333,#89334,#89335,#89336,#89337,
#89338,#89339,#89340,#89341,#89342,#89343,#89344,#89345,#89346,#89347,#89348,
#89349,#89350,#89351,#89352,#89353,#89354,#89355,#89356,#89357,#89358,#89359,
#89360,#89361,#89362,#89363,#89364,#89365,#89366,#89367,#89368,#89369,#89370,
#89371,#89372,#89373,#89374,#89375,#89376,#89377,#89378,#89379,#89380,#89381,
#89382,#89383,#89384,#89385,#89386,#89387,#89388,#89389,#89390,#89391,#89392,
#89393,#89394,#89395,#89396,#89397,#89398,#89399,#89400,#89401,#89402,#89403,
#89404,#89405,#89406,#89407,#89408,#89409,#89410,#89411,#89412,#89413,#89414,
#89415,#89416,#89417,#89418,#89419,#89420,#89421,#89422,#89423,#89424,#89425,
#89426,#89427,#89428,#89429,#89430,#89431,#89432,#89433,#89434,#89435,#89436,
#89437,#89438,#89439,#89440,#89441,#89442,#89443,#89444,#89445,#89446,#89447,
#89448,#89449,#89450,#89451,#89452,#89453,#89454,#89455,#89456,#89457,#89458,
#89459,#89460,#89461,#89462,#89463,#89464,#89465,#89466,#89467,#89468,#89469,
#89470,#89471,#89472,#89473,#89474,#89475,#89476,#89477,#89478,#89479,#89480,
#89481,#89482,#89483,#89484,#89485,#89486,#89487,#89488,#89489,#89490,#89491,
#89492,#89493,#89494,#89495,#89496,#89497,#89498,#89499,#89500,#89501,#89502,
#89503,#89504,#89505,#89506,#89507,#89508,#89509,#89510),.UNSPECIFIED.,
 .F.,.F.,(4,2,2,2,2,2,2,2,2,2,2,2,2,2,2,2,2,2,2,2,2,2,2,2,2,2,2,2,2,2,2,
2,2,2,2,2,2,2,2,2,2,2,2,2,2,2,2,2,2,2,2,2,2,2,2,2,2,2,2,2,2,2,2,2,2,2,2,
2,2,2,2,2,2,2,2,2,2,2,2,2,2,2,2,2,2,2,2,2,2,2,2,2,2,2,2,2,2,2,2,2,2,2,2,
2,2,2,2,2,2,2,2,2,2,2,2,2,2,2,2,2,2,2,2,2,2,2,2,2,2,2,2,2,4),(0.000806536570366526,
0.0978003361637292,0.122342092926343,0.144799418030591,0.170108313118547,
0.212755320991058,0.311961287499786,0.341649545444072,0.350237546985673,
0.352689178741491,0.357656528872034,0.361646872304124,0.369787679675562,
0.382333782200091,0.401478017557775,0.456766923535376,0.507133058620796,
0.550622939497385,0.584005853074657,0.602887593835211,0.615707664529721,
0.64389890831545,0.768159170579458,0.802030575372541,0.819832498734995,
0.820510466711981,0.821147232581718,0.821747546569198,0.822315640753646,
0.822855301407632,0.823369932496131,0.823862611612536,0.824336139550256,
0.824793084584511,0.825235822466177,0.82566657306378,0.826087434577109,
0.826500416210535,0.826907470256461,0.827310524617655,0.827711516934067,
0.828112431733179,0.828515342373826,0.828922460087897,0.82933619324368,
0.829759221158954,0.830194588654903,0.830645830450056,0.831117139099606,
0.831613597758712,0.832141511881989,0.832708896547149,0.832988407388964,
0.833454442338801,0.834298637669974,0.834887291990056,0.837917198917195,
0.849841924882182,0.872904700728933,0.980586037635136,1.01991034241355,
1.05292365511241,1.07683603606502,1.1036947511368,1.15842606998003,1.17857090524075,
1.23687903608412,1.2815776031101,1.2977091084122,1.31047768007438,1.32680346737593,
1.41501023402502,1.46871813436071,1.508939195608,1.53382891132972,1.55875272082743,
1.59920151456328,1.69718527454096,1.7446997449492,1.76105644238005,1.77377592145688,
1.7897964777256,1.88298181221335,1.9343978888977,1.95288847865006,1.98349465481415,
2.00719076852861,2.03540940789467,2.09694696682855,2.17258861480466,2.19936264635097,
2.21995029942446,2.23281393268813,2.24843594844663,2.28271950079373,2.35505383464592,
2.42356416928124,2.45169641598032,2.47540641013983,2.5056264398898,2.59858526291233,
2.66907531156463,2.68671086066504,2.69811732658436,2.71454126798159,2.76432041916046,
2.84414567412818,2.87964328691644,2.91047271917343,2.93418332506308,2.96224620540681,
3.0841214683408,3.13514871107225,3.15175565772508,3.16444780888165,3.18334490460585,
3.27745398936972,3.32706045035602,3.36538391255637,3.38999416386613,3.41222778470923,
3.45110120676371,3.55670717924409,3.6002730318699,3.616295430426,3.62907171901554,
3.64549628961051,3.75045023678176,3.81546463042191,3.84333064507004,3.8670621649,
3.89764589794579,3.97111550692216),.UNSPECIFIED.);
#896=B_SPLINE_CURVE_WITH_KNOTS('',3,(#89514,#89515,#89516,#89517,#89518,
#89519,#89520,#89521,#89522,#89523,#89524,#89525,#89526,#89527,#89528,#89529,
#89530,#89531,#89532,#89533,#89534,#89535,#89536,#89537,#89538,#89539,#89540,
#89541,#89542,#89543,#89544,#89545,#89546,#89547,#89548,#89549,#89550,#89551,
#89552,#89553,#89554,#89555,#89556),.UNSPECIFIED.,.F.,.F.,(4,3,3,3,3,3,
3,3,3,3,3,3,3,3,4),(97.3893722664106,97.463731471798,97.5380780115012,97.615056518503,
97.6894051268309,97.76375727863,97.8381276809787,97.8459920395083,97.9212470945102,
97.9964884789106,98.0717196667722,98.1469501062026,98.2221751739854,98.2974062174588,
98.3407100278244),.UNSPECIFIED.);
#897=B_SPLINE_CURVE_WITH_KNOTS('',3,(#89557,#89558,#89559,#89560,#89561,
#89562,#89563,#89564,#89565),.UNSPECIFIED.,.F.,.F.,(4,1,1,1,1,1,4),(95.3428995923426,
95.3724020979282,95.8671200862443,96.3618380745603,96.8565560628763,97.3512740511923,
97.3893722612836),.UNSPECIFIED.);
#898=B_SPLINE_CURVE_WITH_KNOTS('',3,(#90306,#90307,#90308,#90309,#90310,
#90311,#90312,#90313,#90314,#90315,#90316,#90317,#90318,#90319,#90320,#90321,
#90322,#90323,#90324,#90325,#90326,#90327,#90328,#90329,#90330,#90331,#90332,
#90333,#90334,#90335,#90336,#90337,#90338,#90339,#90340,#90341,#90342,#90343,
#90344,#90345,#90346,#90347,#90348,#90349,#90350,#90351,#90352,#90353,#90354,
#90355,#90356,#90357,#90358,#90359,#90360,#90361,#90362,#90363,#90364,#90365,
#90366,#90367,#90368,#90369,#90370,#90371,#90372,#90373,#90374,#90375,#90376,
#90377,#90378,#90379,#90380,#90381,#90382,#90383,#90384,#90385,#90386,#90387,
#90388,#90389,#90390,#90391,#90392,#90393,#90394,#90395,#90396,#90397,#90398,
#90399,#90400,#90401,#90402,#90403,#90404,#90405,#90406,#90407,#90408,#90409,
#90410,#90411,#90412,#90413,#90414,#90415,#90416,#90417,#90418,#90419,#90420,
#90421,#90422,#90423),.UNSPECIFIED.,.F.,.F.,(4,3,3,3,3,3,3,3,3,3,3,3,3,
3,3,3,3,3,3,3,3,3,3,3,3,3,3,3,3,3,3,3,3,3,3,3,3,3,3,4),(3.9627874635238E-7,
0.0743187604012306,0.0947553987316233,0.168865895081324,0.24331753745554,
0.317543543810035,0.384132560472308,0.394183661157522,0.467915452531873,
0.541515418454756,0.583899610459125,0.657733552016035,0.731321143746018,
0.752263425776805,0.765228983131914,0.775235303088961,0.848353720857463,
0.921585303941482,0.99412411295158,1.06639765623861,1.12291086999283,1.13978254049866,
1.15333692391085,1.22526683640984,1.29857596887547,1.37106752217119,1.44478544422177,
1.51850336627235,1.52634774495678,1.54198813411966,1.6136839676136,1.68574649957796,
1.72631299944046,1.74783827110233,1.76349445406413,1.77572612606673,1.84737189178447,
1.91878510437671,1.9892523021272,2.01027849847794),.UNSPECIFIED.);
#899=B_SPLINE_CURVE_WITH_KNOTS('',3,(#90424,#90425,#90426,#90427,#90428,
#90429,#90430,#90431,#90432,#90433,#90434,#90435,#90436,#90437,#90438,#90439,
#90440,#90441,#90442,#90443,#90444,#90445,#90446,#90447,#90448,#90449,#90450,
#90451,#90452,#90453,#90454,#90455,#90456,#90457,#90458,#90459,#90460,#90461,
#90462,#90463,#90464,#90465,#90466,#90467,#90468,#90469,#90470,#90471,#90472,
#90473,#90474,#90475,#90476,#90477,#90478,#90479,#90480,#90481,#90482,#90483,
#90484,#90485,#90486,#90487,#90488,#90489,#90490,#90491,#90492,#90493,#90494,
#90495,#90496,#90497,#90498,#90499,#90500,#90501,#90502,#90503,#90504,#90505,
#90506,#90507,#90508,#90509,#90510,#90511,#90512,#90513,#90514,#90515,#90516,
#90517,#90518,#90519,#90520,#90521,#90522,#90523,#90524,#90525,#90526,#90527,
#90528,#90529,#90530,#90531,#90532,#90533,#90534,#90535,#90536,#90537,#90538,
#90539,#90540,#90541,#90542,#90543,#90544),.UNSPECIFIED.,.F.,.F.,(4,3,3,
3,3,3,3,3,3,3,3,3,3,3,3,3,3,3,3,3,3,3,3,3,3,3,3,3,3,3,3,3,3,3,3,3,3,3,3,
3,4),(-2.01027849847796,-1.93864883240901,-1.92070302042893,-1.84940600763368,
-1.79961994695732,-1.77688322270267,-1.7655613495308,-1.73844370067774,
-1.66642770916695,-1.59440274213944,-1.55318604449898,-1.52608655166908,
-1.51248154317586,-1.4511175222228,-1.37975752627662,-1.30728555503059,
-1.23463428834696,-1.16242067546908,-1.1463119704265,-1.09560707621285,
-1.02237008042034,-0.973988125444813,-0.901002560842819,-0.82780347338264,
-0.785600895008091,-0.772328125694967,-0.76155408296478,-0.688117520641271,
-0.614297719065266,-0.540711111505799,-0.490182846386249,-0.430056172450728,
-0.403750752603938,-0.389451921142354,-0.379313437087383,-0.306096966484562,
-0.231747457148313,-0.157301211215449,-0.0832353330587671,-0.00916945490208512,
-5.46117353640499E-15),.UNSPECIFIED.);
#900=B_SPLINE_CURVE_WITH_KNOTS('',3,(#91286,#91287,#91288,#91289,#91290,
#91291,#91292,#91293,#91294,#91295,#91296,#91297,#91298,#91299,#91300,#91301,
#91302,#91303,#91304,#91305,#91306,#91307,#91308,#91309,#91310,#91311,#91312,
#91313,#91314,#91315,#91316,#91317,#91318,#91319,#91320,#91321,#91322,#91323,
#91324,#91325,#91326,#91327,#91328,#91329,#91330,#91331,#91332,#91333,#91334,
#91335,#91336,#91337,#91338,#91339,#91340,#91341,#91342,#91343,#91344,#91345,
#91346,#91347,#91348,#91349,#91350,#91351,#91352,#91353,#91354,#91355,#91356,
#91357,#91358,#91359,#91360,#91361,#91362,#91363,#91364,#91365,#91366,#91367,
#91368,#91369,#91370,#91371,#91372,#91373,#91374,#91375,#91376,#91377,#91378,
#91379,#91380,#91381,#91382,#91383,#91384,#91385,#91386,#91387,#91388,#91389,
#91390,#91391,#91392,#91393,#91394,#91395,#91396,#91397,#91398,#91399,#91400,
#91401,#91402,#91403,#91404,#91405,#91406),.UNSPECIFIED.,.F.,.F.,(4,3,3,
3,3,3,3,3,3,3,3,3,3,3,3,3,3,3,3,3,3,3,3,3,3,3,3,3,3,3,3,3,3,3,3,3,3,3,3,
3,4),(0.,0.0716146571298102,0.0895455174761734,0.161056667463161,0.232704853117562,
0.304147485270842,0.339868801347482,0.357918124505382,0.366825163752922,
0.375590117424122,0.447629242845613,0.519979645211168,0.559487114576289,
0.63157350721065,0.703843799735493,0.73770758688256,0.745512094209105,0.818142982850016,
0.8910726172438,0.96376737166813,1.03603564877275,1.10887280851242,1.11368092827931,
1.12160931061262,1.19382320400099,1.26874221162545,1.34231143819719,1.41790533634802,
1.49349923449884,1.50227960552724,1.51891527711939,1.59200292456703,1.66575726114028,
1.70851112764835,1.73020926256932,1.74764381613927,1.76035480684199,1.78416451981067,
1.85850190150601,1.93314504735542,2.00778819320483),.UNSPECIFIED.);
#901=B_SPLINE_CURVE_WITH_KNOTS('',3,(#91407,#91408,#91409,#91410),
 .UNSPECIFIED.,.F.,.F.,(4,4),(0.,0.000711284740995393),.UNSPECIFIED.);
#902=B_SPLINE_CURVE_WITH_KNOTS('',3,(#91411,#91412,#91413,#91414,#91415,
#91416,#91417,#91418,#91419,#91420,#91421,#91422,#91423,#91424,#91425,#91426,
#91427,#91428,#91429,#91430,#91431,#91432,#91433,#91434,#91435,#91436,#91437,
#91438,#91439,#91440,#91441,#91442,#91443,#91444,#91445,#91446,#91447,#91448,
#91449,#91450,#91451,#91452,#91453,#91454,#91455,#91456,#91457,#91458,#91459,
#91460,#91461,#91462,#91463,#91464,#91465,#91466,#91467,#91468,#91469,#91470,
#91471,#91472,#91473,#91474,#91475,#91476,#91477,#91478,#91479,#91480,#91481,
#91482,#91483,#91484,#91485,#91486,#91487,#91488,#91489,#91490,#91491,#91492,
#91493,#91494,#91495,#91496,#91497,#91498,#91499,#91500,#91501,#91502,#91503,
#91504,#91505,#91506,#91507,#91508,#91509,#91510,#91511,#91512,#91513,#91514,
#91515,#91516,#91517,#91518,#91519,#91520,#91521,#91522,#91523,#91524,#91525,
#91526,#91527,#91528,#91529,#91530,#91531),.UNSPECIFIED.,.F.,.F.,(4,3,3,
3,3,3,3,3,3,3,3,3,3,3,3,3,3,3,3,3,3,3,3,3,3,3,3,3,3,3,3,3,3,3,3,3,3,3,3,
3,4),(-2.00778819320479,-1.93363330609131,-1.91321255832737,-1.83897355307137,
-1.76467605789325,-1.75162085734409,-1.74164675852145,-1.67739297918314,
-1.60348492023008,-1.53028776793595,-1.49971429773937,-1.49060173162983,
-1.42561568789313,-1.35278602352358,-1.27922221004438,-1.20576872343774,
-1.13312878374067,-1.11692732896057,-1.10856339625353,-1.03571490313795,
-0.96298798677832,-0.943739908687974,-0.870803091850739,-0.797994780817984,
-0.756800525433452,-0.743508832763832,-0.732449565606889,-0.660202669875926,
-0.58787384738682,-0.516205504225887,-0.468440737741721,-0.410352915438056,
-0.384939493180202,-0.37128601545293,-0.360693101664746,-0.28954884186388,
-0.217764646472875,-0.146189250061888,-0.0749637046871438,-0.00373815931239996,
0.),.UNSPECIFIED.);
#903=B_SPLINE_CURVE_WITH_KNOTS('',3,(#91553,#91554,#91555,#91556,#91557,
#91558,#91559,#91560),.UNSPECIFIED.,.F.,.F.,(4,1,1,1,1,4),(36.7831101328767,
37.0687639041569,37.5537416741313,38.0387194441058,38.5236972140802,39.0086749840546),
 .UNSPECIFIED.);
#904=B_SPLINE_CURVE_WITH_KNOTS('',3,(#91563,#91564,#91565,#91566,#91567,
#91568,#91569,#91570,#91571),.UNSPECIFIED.,.F.,.F.,(4,1,1,1,1,1,4),(36.7831178657995,
37.19235531577,37.6773330857444,38.1623108557188,38.6472886256933,39.1322663956677,
39.5311215742981),.UNSPECIFIED.);
#905=B_SPLINE_CURVE_WITH_KNOTS('',3,(#91577,#91578,#91579,#91580,#91581,
#91582,#91583,#91584,#91585,#91586,#91587,#91588,#91589,#91590,#91591,#91592,
#91593,#91594,#91595,#91596,#91597,#91598,#91599,#91600,#91601,#91602,#91603,
#91604,#91605,#91606,#91607,#91608,#91609,#91610,#91611,#91612,#91613,#91614,
#91615,#91616,#91617,#91618,#91619,#91620,#91621,#91622,#91623,#91624,#91625,
#91626,#91627,#91628,#91629,#91630,#91631,#91632,#91633,#91634,#91635,#91636,
#91637,#91638,#91639,#91640,#91641,#91642,#91643,#91644,#91645,#91646,#91647,
#91648,#91649,#91650,#91651,#91652,#91653,#91654,#91655,#91656,#91657,#91658,
#91659,#91660,#91661,#91662,#91663,#91664,#91665,#91666,#91667,#91668,#91669,
#91670,#91671,#91672,#91673,#91674,#91675,#91676,#91677,#91678,#91679,#91680,
#91681,#91682,#91683,#91684,#91685,#91686,#91687,#91688,#91689,#91690,#91691,
#91692,#91693,#91694,#91695,#91696,#91697,#91698,#91699,#91700,#91701,#91702,
#91703,#91704,#91705,#91706,#91707,#91708,#91709,#91710,#91711,#91712,#91713,
#91714,#91715,#91716,#91717,#91718,#91719,#91720,#91721,#91722,#91723,#91724,
#91725,#91726,#91727,#91728,#91729,#91730,#91731,#91732,#91733,#91734,#91735,
#91736,#91737,#91738,#91739,#91740,#91741,#91742,#91743,#91744,#91745,#91746,
#91747,#91748,#91749,#91750,#91751,#91752,#91753,#91754),.UNSPECIFIED.,
 .F.,.F.,(4,3,3,3,3,3,3,3,3,3,3,3,3,3,3,3,3,3,3,3,3,3,3,3,3,3,3,3,3,3,3,
3,3,3,3,3,3,3,3,3,3,3,3,3,3,3,3,3,3,3,3,3,3,3,3,3,3,3,3,4),(30.4999165270005,
30.5734012599987,30.6468852042545,30.7203838367086,30.7640528944893,30.8375517166681,
30.9110384964528,30.9845177829552,31.0580025409672,31.1314864866202,31.2049851437445,
31.2490306644638,31.3225294639419,31.3960162209481,31.4694954846612,31.5429802200288,
31.6164641431568,31.6899627780857,31.7340084344382,31.8075072776668,31.8809940785443,
31.9544733861202,32.0279581650285,32.1014421314428,32.1749408089864,32.2189862044126,
32.2924849833025,32.3659717197231,32.4394509629135,32.5129356779971,32.5864195810097,
32.6599181962126,32.7039639743871,32.7774628074511,32.8509495979873,32.9244288950775,
32.9979136633574,33.0713976190805,33.1448962859055,33.1889417443615,33.2624406390856,
33.3359274919474,33.4094068518393,33.4828916831912,33.5563757020343,33.6298744316436,
33.6739195143359,33.7474179822581,33.8209044062208,33.8943833363914,33.9678677398215,
34.04135133247,34.1148496413041,34.1588972843103,34.2321178175882,34.3053253639141,
34.3785312054903,34.4517331639191,34.5249449085031,34.5575191894877),
 .UNSPECIFIED.);
#906=B_SPLINE_CURVE_WITH_KNOTS('',3,(#91755,#91756,#91757,#91758,#91759,
#91760,#91761,#91762,#91763),.UNSPECIFIED.,.F.,.F.,(4,1,1,1,1,1,4),(34.5575191894877,
34.6438750542848,35.1288528242592,35.6138305942336,36.0988083642081,36.5837861341825,
36.7831101328767),.UNSPECIFIED.);
#907=B_SPLINE_CURVE_WITH_KNOTS('',3,(#91765,#91766,#91767,#91768,#91769,
#91770,#91771,#91772,#91773),.UNSPECIFIED.,.F.,.F.,(4,1,1,1,1,1,4),(34.5575191894877,
34.7674664658978,35.2524442358723,35.7374220058467,36.2223997758211,36.7073775457955,
36.7831178657995),.UNSPECIFIED.);
#908=B_SPLINE_CURVE_WITH_KNOTS('',3,(#91774,#91775,#91776,#91777,#91778,
#91779,#91780,#91781,#91782,#91783,#91784,#91785),.UNSPECIFIED.,.F.,.F.,
(4,1,1,1,1,1,1,1,1,4),(30.4999349764196,30.8876443061024,31.3726220760768,
31.8575998460513,32.3425776160257,32.8275553860001,33.3125331559745,33.797510925949,
34.2824886959234,34.5575191894877),.UNSPECIFIED.);
#909=B_SPLINE_CURVE_WITH_KNOTS('',3,(#91791,#91792,#91793,#91794,#91795,
#91796,#91797,#91798,#91799,#91800,#91801,#91802),.UNSPECIFIED.,.F.,.F.,
(4,1,1,1,1,1,1,1,1,4),(24.2167278608201,24.4593418848218,24.9443196547962,
25.4292974247706,25.9142751947451,26.3992529647195,26.8842307346939,27.3692085046684,
27.8541862746428,28.2743338538108),.UNSPECIFIED.);
#910=B_SPLINE_CURVE_WITH_KNOTS('',3,(#91803,#91804,#91805,#91806,#91807,
#91808,#91809,#91810,#91811,#91812,#91813,#91814,#91815,#91816,#91817,#91818,
#91819,#91820,#91821,#91822,#91823,#91824,#91825,#91826,#91827,#91828,#91829,
#91830,#91831,#91832,#91833,#91834,#91835,#91836,#91837,#91838,#91839,#91840,
#91841,#91842,#91843,#91844,#91845,#91846,#91847,#91848,#91849,#91850,#91851,
#91852,#91853,#91854,#91855,#91856,#91857,#91858,#91859,#91860,#91861,#91862,
#91863,#91864,#91865,#91866,#91867,#91868,#91869,#91870,#91871,#91872,#91873,
#91874,#91875,#91876,#91877,#91878,#91879,#91880,#91881,#91882,#91883,#91884,
#91885,#91886,#91887,#91888,#91889,#91890,#91891,#91892,#91893,#91894,#91895,
#91896,#91897,#91898,#91899),.UNSPECIFIED.,.F.,.F.,(4,3,3,3,3,3,3,3,3,3,
3,3,3,3,3,3,3,3,3,3,3,3,3,3,3,3,3,3,3,3,3,3,4),(28.2743338823081,28.3391640446172,
28.4126628601145,28.4861496331911,28.5596289129786,28.6331136643131,28.7065976033206,
28.780096253892,28.8241418145916,28.8976406294224,28.9711274018309,29.0446066809508,
29.118091431623,29.1915753699723,29.2650740198958,29.3091195845661,29.382618400207,
29.4561051734266,29.5295844533558,29.6030692048292,29.6765531439741,29.7500517946789,
29.7940973545405,29.86759616995,29.9410829429414,30.0145622226464,30.0880469739032,
30.1615309128359,30.2350295633372,30.2790751245149,30.3525735089709,30.4262450179857,
30.4999165270005),.UNSPECIFIED.);
#911=B_SPLINE_CURVE_WITH_KNOTS('',3,(#91901,#91902,#91903,#91904,#91905,
#91906,#91907,#91908,#91909),.UNSPECIFIED.,.F.,.F.,(4,1,1,1,1,1,4),(28.2743338823081,
28.4627554562303,28.9477332262047,29.4327109961791,29.9176887661536,30.402666536128,
30.4999349764196),.UNSPECIFIED.);
#912=B_SPLINE_CURVE_WITH_KNOTS('',3,(#91910,#91911,#91912,#91913,#91914,
#91915,#91916,#91917,#91918,#91919,#91920,#91921),.UNSPECIFIED.,.F.,.F.,
(4,1,1,1,1,1,1,1,1,4),(24.2167503458098,24.5829332964348,25.0679110664093,
25.5528888363837,26.0378666063581,26.5228443763326,27.007822146307,27.4927999162814,
27.9777776862558,28.2743338823081),.UNSPECIFIED.);
#913=B_SPLINE_CURVE_WITH_KNOTS('',3,(#91927,#91928,#91929,#91930,#91931,
#91932,#91933,#91934,#91935,#91936,#91937,#91938,#91939,#91940,#91941,#91942,
#91943,#91944,#91945,#91946,#91947,#91948,#91949,#91950,#91951,#91952,#91953,
#91954,#91955,#91956,#91957,#91958,#91959,#91960,#91961,#91962,#91963,#91964,
#91965,#91966,#91967,#91968,#91969,#91970,#91971,#91972,#91973,#91974,#91975,
#91976,#91977,#91978,#91979,#91980,#91981,#91982,#91983,#91984,#91985,#91986,
#91987,#91988,#91989,#91990,#91991,#91992,#91993,#91994,#91995,#91996,#91997,
#91998,#91999,#92000,#92001,#92002,#92003,#92004,#92005,#92006,#92007,#92008,
#92009,#92010,#92011,#92012,#92013,#92014,#92015,#92016,#92017,#92018,#92019,
#92020,#92021,#92022,#92023),.UNSPECIFIED.,.F.,.F.,(4,3,3,3,3,3,3,3,3,3,
3,3,3,3,3,3,3,3,3,3,3,3,3,3,3,3,3,3,3,3,3,3,4),(15.707963270772,15.7844208965149,
15.8533334368951,15.926784338244,16.0002226755263,16.0736531423664,16.1470888545948,
16.2205237063183,16.2939735101588,16.3383112068696,16.4118254124913,16.4853277239607,
16.5588226436237,16.6323230769943,16.7058226958758,16.7793369216993,16.823288976844,
16.8967862501396,16.9702714821782,17.0437492266874,17.1172324624461,17.1907148995946,
17.2642120793322,17.3082667468184,17.3817630095345,17.455247191035,17.5287238482588,
17.6022059487071,17.6756872251217,17.7491832120583,17.7932445167929,17.8667471690964,
17.9335555972082),.UNSPECIFIED.);
#914=B_SPLINE_CURVE_WITH_KNOTS('',3,(#92025,#92026,#92027,#92028,#92029,
#92030),.UNSPECIFIED.,.F.,.F.,(4,1,1,4),(14.3984001269719,14.8833778969463,
15.3683556669207,15.707963267949),.UNSPECIFIED.);
#915=B_SPLINE_CURVE_WITH_KNOTS('',3,(#92034,#92035,#92036,#92037,#92038,
#92039,#92040),.UNSPECIFIED.,.F.,.F.,(4,1,1,1,4),(13.8759337553363,14.2748087153588,
14.7597864853332,15.2447642553077,15.707963267949),.UNSPECIFIED.);
#916=B_SPLINE_CURVE_WITH_KNOTS('',3,(#92041,#92042,#92043,#92044,#92045,
#92046,#92047,#92048,#92049),.UNSPECIFIED.,.F.,.F.,(4,1,1,1,1,1,4),(15.707963267949,
15.7297420252821,16.2147197952565,16.6996975652309,17.1846753352054,17.6696531051798,
17.9335366650258),.UNSPECIFIED.);
#917=B_SPLINE_CURVE_WITH_KNOTS('',3,(#92055,#92056,#92057,#92058,#92059,
#92060,#92061,#92062,#92063,#92064,#92065,#92066,#92067,#92068,#92069,#92070,
#92071,#92072,#92073,#92074,#92075,#92076,#92077,#92078,#92079,#92080,#92081,
#92082,#92083,#92084,#92085),.UNSPECIFIED.,.F.,.F.,(4,3,3,3,3,3,3,3,3,3,
4),(26.4423043696954,26.5177281543605,26.595752751477,26.6737773485935,
26.7487609216721,26.8237315844015,26.8986926879938,26.9736532318385,27.0486088408042,
27.1235698163438,27.158755118568),.UNSPECIFIED.);
#918=B_SPLINE_CURVE_WITH_KNOTS('',3,(#92088,#92089,#92090,#92091,#92092,
#92093,#92094,#92095,#92096,#92097,#92098,#92099,#92100,#92101,#92102,#92103,
#92104,#92105,#92106,#92107,#92108,#92109,#92110,#92111,#92112,#92113,#92114,
#92115,#92116,#92117,#92118,#92119,#92120,#92121,#92122,#92123,#92124,#92125,
#92126,#92127,#92128,#92129,#92130,#92131,#92132,#92133,#92134,#92135,#92136,
#92137,#92138,#92139,#92140,#92141,#92142,#92143,#92144,#92145,#92146,#92147,
#92148,#92149,#92150,#92151,#92152,#92153,#92154,#92155,#92156,#92157,#92158,
#92159,#92160,#92161,#92162,#92163,#92164,#92165,#92166,#92167,#92168,#92169,
#92170,#92171,#92172,#92173,#92174,#92175,#92176,#92177,#92178,#92179,#92180,
#92181,#92182,#92183,#92184,#92185,#92186,#92187,#92188,#92189,#92190,#92191,
#92192,#92193,#92194,#92195,#92196),.UNSPECIFIED.,.F.,.F.,(4,3,3,3,3,3,
3,3,3,3,3,3,3,3,3,3,3,3,3,3,3,3,3,3,3,3,3,3,3,3,3,3,3,3,3,3,4),(-25.1327214822589,
-25.0584480753609,-24.9841839577683,-24.9099156896555,-24.8356478285455,
-24.7613652784986,-24.7338662686958,-24.6593137477544,-24.584773583022,
-24.5102410217215,-24.4357028715999,-24.3611653050792,-24.2866130834149,
-24.2488884987214,-24.1743369699811,-24.0997978383104,-24.0252663476834,
-23.9507293171368,-23.8761928963057,-23.8016418528938,-23.763910728747,
-23.6893538742066,-23.6148093411984,-23.5402723904301,-23.4657298505343,
-23.3911879016937,-23.3166313367843,-23.2789329587725,-23.2043806207413,
-23.1298406614389,-23.055308327415,-22.9807704358101,-22.9062331452823,
-22.8316812245033,-22.7939551887981,-22.7146359699226,-22.7075993240011),
 .UNSPECIFIED.);
#919=B_SPLINE_CURVE_WITH_KNOTS('',3,(#92201,#92202,#92203,#92204,#92205,
#92206,#92207,#92208,#92209,#92210,#92211,#92212,#92213,#92214,#92215,#92216,
#92217),.UNSPECIFIED.,.F.,.F.,(4,1,1,1,1,1,1,1,1,1,1,1,1,1,4),(20.1591190804798,
20.369066338926,20.8540441089004,21.3390218788748,21.8239996488493,22.3089774188237,
22.7939551887981,23.2789329587725,23.763910728747,24.2488884987214,24.7338662686958,
25.2188440386703,25.7038218086447,26.1887995786191,26.4423043696954),
 .UNSPECIFIED.);
#920=B_SPLINE_CURVE_WITH_KNOTS('',3,(#92218,#92219,#92220,#92221,#92222,
#92223,#92224,#92225,#92226,#92227,#92228,#92229,#92230,#92231,#92232,#92233,
#92234),.UNSPECIFIED.,.F.,.F.,(4,1,1,1,1,1,1,1,1,1,1,1,1,1,4),(-22.7075993038896,
-22.3089774188237,-21.8239996488493,-21.3390218788748,-20.8540441089004,
-20.369066338926,-19.8840885689515,-19.3991107989771,-18.9141330290027,
-18.4291552590283,-17.9441774890538,-17.4591997190794,-16.974221949105,
-16.4892441791305,-16.4244140168215),.UNSPECIFIED.);
#921=B_SPLINE_CURVE_WITH_KNOTS('',3,(#92239,#92240,#92241,#92242,#92243,
#92244,#92245,#92246,#92247,#92248,#92249,#92250,#92251,#92252,#92253,#92254,
#92255,#92256,#92257,#92258,#92259,#92260,#92261,#92262,#92263,#92264,#92265,
#92266,#92267,#92268,#92269,#92270,#92271,#92272,#92273,#92274,#92275,#92276,
#92277,#92278,#92279,#92280,#92281,#92282,#92283,#92284,#92285,#92286,#92287,
#92288,#92289,#92290,#92291,#92292,#92293,#92294,#92295,#92296,#92297,#92298,
#92299,#92300,#92301,#92302,#92303,#92304,#92305,#92306,#92307,#92308,#92309,
#92310,#92311,#92312,#92313,#92314,#92315,#92316,#92317,#92318,#92319,#92320,
#92321,#92322,#92323,#92324,#92325,#92326,#92327,#92328,#92329,#92330,#92331,
#92332,#92333,#92334,#92335,#92336,#92337,#92338,#92339,#92340,#92341,#92342,
#92343,#92344,#92345,#92346,#92347,#92348,#92349,#92350,#92351,#92352,#92353,
#92354,#92355,#92356,#92357,#92358,#92359,#92360,#92361,#92362,#92363,#92364,
#92365,#92366,#92367,#92368,#92369,#92370,#92371,#92372,#92373,#92374,#92375,
#92376,#92377,#92378,#92379,#92380,#92381,#92382,#92383,#92384,#92385,#92386,
#92387,#92388,#92389,#92390,#92391,#92392,#92393,#92394,#92395,#92396,#92397,
#92398,#92399,#92400,#92401,#92402,#92403,#92404,#92405,#92406,#92407,#92408,
#92409,#92410,#92411,#92412,#92413,#92414,#92415,#92416,#92417,#92418,#92419,
#92420,#92421,#92422,#92423,#92424,#92425,#92426,#92427,#92428,#92429,#92430,
#92431,#92432,#92433,#92434,#92435,#92436,#92437,#92438,#92439,#92440,#92441,
#92442,#92443,#92444,#92445,#92446,#92447,#92448,#92449,#92450,#92451,#92452,
#92453,#92454,#92455,#92456,#92457,#92458,#92459,#92460,#92461,#92462,#92463,
#92464,#92465,#92466,#92467,#92468,#92469,#92470,#92471,#92472,#92473,#92474,
#92475,#92476,#92477,#92478,#92479,#92480,#92481,#92482,#92483,#92484,#92485,
#92486,#92487,#92488,#92489,#92490,#92491,#92492,#92493,#92494,#92495,#92496,
#92497,#92498,#92499,#92500,#92501,#92502,#92503,#92504,#92505,#92506,#92507,
#92508,#92509,#92510,#92511,#92512),.UNSPECIFIED.,.F.,.F.,(4,3,3,3,3,3,
3,3,3,3,3,3,3,3,3,3,3,3,3,3,3,3,3,3,3,3,3,3,3,3,3,3,3,3,3,3,3,3,3,3,3,3,
3,3,3,3,3,3,3,3,3,3,3,3,3,3,3,3,3,3,3,3,3,3,3,3,3,3,3,3,3,3,3,3,3,3,3,3,
3,3,3,3,3,3,3,3,3,3,3,3,3,4),(13.875933755441,13.9523182994839,14.0287249568119,
14.0643553292584,14.1389094507212,14.2134512150667,14.2879853701618,14.3625250938589,
14.4370642196202,14.5116179688183,14.5493330992328,14.6238872206886,14.6984289850271,
14.7729631401157,14.847502863806,14.9220419895609,14.9965957387525,15.0343108692073,
15.1088649906549,15.1834067549852,15.2579409100652,15.3324806337471,15.4070197594934,
15.4815735086768,15.5192886391817,15.5938427606885,15.6683845250781,15.7429186802175,
15.8174584039587,15.8919975297641,15.9665512790057,16.0042664091561,16.0788205304861,
16.1533622946982,16.2278964496601,16.3024361732247,16.3769752988544,16.4515290479228,
16.4892441791306,16.5637983008486,16.63834006545,16.7128742208012,16.7874139447523,
16.8619530707664,16.9365068202134,16.974221949105,17.0487760701572,17.1233178340913,
17.1978519887755,17.2723917120651,17.3469308374218,17.421484586222,17.4591997190794,
17.5337538409431,17.6082956056894,17.6828297611844,17.7573694852764,17.8319086114295,
17.9064623610119,17.9441774890538,18.0187316106808,18.0932733751937,18.1678075304591,
18.2423472543295,18.3168863802656,18.3914401296395,18.4291552590283,18.5037093783136,
18.5782511404699,18.652785293371,18.7273250148823,18.8018641384667,18.8764178855145,
18.9141330290027,18.9886871574017,19.0632289287109,19.1377630907763,19.2123028214034,
19.2868419540601,19.361395710057,19.3991107989771,19.4736649046515,19.5482066531576,
19.6227407924106,19.6972805003736,19.7718196104903,19.8463733442772,19.8840885689515,
19.9590919762986,20.0340811182084,20.1090627868793,20.1591190625159),
 .UNSPECIFIED.);
#922=B_SPLINE_CURVE_WITH_KNOTS('',3,(#92513,#92514,#92515,#92516,#92517,
#92518,#92519,#92520,#92521,#92522,#92523,#92524,#92525,#92526,#92527,#92528,
#92529,#92530,#92531,#92532,#92533,#92534,#92535,#92536,#92537,#92538,#92539,
#92540,#92541,#92542,#92543,#92544,#92545,#92546,#92547,#92548,#92549,#92550,
#92551,#92552,#92553,#92554,#92555,#92556,#92557,#92558,#92559,#92560,#92561,
#92562,#92563,#92564,#92565,#92566,#92567,#92568,#92569,#92570,#92571,#92572,
#92573,#92574,#92575,#92576,#92577,#92578,#92579,#92580,#92581,#92582,#92583,
#92584,#92585,#92586,#92587,#92588,#92589,#92590,#92591,#92592,#92593,#92594,
#92595,#92596,#92597,#92598,#92599,#92600,#92601,#92602,#92603,#92604,#92605,
#92606,#92607,#92608,#92609,#92610,#92611,#92612,#92613,#92614,#92615,#92616,
#92617,#92618,#92619,#92620,#92621,#92622,#92623,#92624,#92625,#92626,#92627,
#92628,#92629,#92630,#92631,#92632,#92633,#92634,#92635,#92636,#92637,#92638,
#92639,#92640,#92641,#92642,#92643,#92644,#92645,#92646),.UNSPECIFIED.,
 .F.,.F.,(4,2,2,2,2,2,2,2,2,2,2,2,2,2,2,2,2,2,2,2,2,2,2,2,2,2,2,2,2,2,2,
2,2,2,2,2,2,2,2,2,2,2,2,2,2,2,2,2,2,2,2,2,2,2,2,2,2,2,2,2,2,2,2,2,2,2,4),
(-11.9638822364953,-11.8246083790295,-11.7850044251456,-11.6666270333911,
-11.5743370158719,-11.5215522030845,-11.4158180763237,-11.3232843333124,
-11.2057648180386,-11.1128389478311,-11.0601758544271,-10.9543628118302,
-10.8617403001231,-10.7431358111963,-10.6510075779731,-10.5981889032602,
-10.4924721527717,-10.3999587256611,-10.2827338271333,-10.1895841942765,
-10.1369613809018,-10.0311187869314,-9.93846355365529,-9.81949932331109,
-9.72762965184425,-9.67475748844462,-9.56907034488649,-9.47659094888344,
-9.35985373725229,-9.26633560082532,-9.21377938322884,-9.10789030268266,
-9.01518304757671,-8.89564575967799,-8.80418932594369,-8.75123141475238,
-8.64559381869177,-8.553170722345,-8.43726518248948,-8.34311795190573,-8.29067395121869,
-8.18470869086248,-8.09191538508498,-7.97144842696542,-7.88066151373026,
-7.82756201475512,-7.72200805187734,-7.62967907343574,-7.51531308141315,
-7.4216169743245,-7.37052605180074,-7.26053897090964,-7.16810461835174,
-7.05208466657828,-6.95801620826587,-6.90555528047204,-6.79959525914511,
-6.70680909004534,-6.58645618078307,-6.49557951578119,-6.44249606341095,
-6.33692658741559,-6.24458135416368,-6.12999569275972,-6.03483388751013,
-5.98256195553799,-5.98255038595961),.UNSPECIFIED.);
#923=B_SPLINE_CURVE_WITH_KNOTS('',3,(#92652,#92653,#92654,#92655,#92656,
#92657,#92658,#92659,#92660,#92661,#92662,#92663,#92664,#92665,#92666,#92667,
#92668,#92669,#92670,#92671,#92672,#92673,#92674,#92675,#92676,#92677,#92678,
#92679,#92680,#92681,#92682,#92683,#92684,#92685,#92686,#92687,#92688,#92689,
#92690,#92691,#92692,#92693,#92694,#92695,#92696,#92697,#92698,#92699,#92700,
#92701,#92702,#92703,#92704,#92705,#92706,#92707,#92708,#92709,#92710,#92711,
#92712,#92713,#92714,#92715,#92716,#92717,#92718,#92719,#92720,#92721,#92722,
#92723,#92724,#92725,#92726,#92727,#92728,#92729,#92730,#92731,#92732,#92733,
#92734,#92735,#92736,#92737,#92738,#92739,#92740,#92741,#92742,#92743,#92744,
#92745,#92746,#92747,#92748,#92749,#92750,#92751,#92752,#92753,#92754,#92755,
#92756,#92757,#92758,#92759,#92760,#92761,#92762,#92763,#92764,#92765,#92766,
#92767,#92768,#92769,#92770,#92771,#92772,#92773,#92774,#92775,#92776,#92777,
#92778,#92779,#92780,#92781,#92782,#92783,#92784,#92785,#92786,#92787,#92788,
#92789,#92790,#92791,#92792,#92793,#92794,#92795,#92796,#92797,#92798,#92799,
#92800,#92801,#92802,#92803,#92804,#92805,#92806,#92807,#92808,#92809,#92810,
#92811,#92812,#92813,#92814,#92815,#92816,#92817,#92818,#92819,#92820),
 .UNSPECIFIED.,.F.,.F.,(4,3,3,3,3,3,3,3,3,3,3,3,3,3,3,3,3,3,3,3,3,3,3,3,
3,3,3,3,3,3,3,3,3,3,3,3,3,3,3,3,3,3,3,3,3,3,3,3,3,3,3,3,3,3,3,3,4),(-3.85804340235828,
-3.78362003001371,-3.70920911636523,-3.63480552147699,-3.56039643756462,
-3.48598674990222,-3.41156317849099,-3.394844389821,-3.32029297434401,-3.24575391528527,
-3.17122245665661,-3.09668539716685,-3.02214891259346,-2.94759775312034,
-2.90986661984657,-2.83531402775715,-2.76077381741281,-2.68624123601308,
-2.61170310407322,-2.53716557759435,-2.46261342883627,-2.42488884987214,
-2.35031879820004,-2.27576102010989,-2.2012108168873,-2.12665510830727,
-2.05210006164846,-1.97753058928639,-1.93991107989771,-1.86540678926133,
-1.79091504818262,-1.71643095751296,-1.64194100546716,-1.56745139902857,
-1.49294647488379,-1.45493330992328,-1.38026437631378,-1.30560745184444,
-1.23095814532789,-1.15630411372744,-1.08165136647512,-1.00698575704174,
-0.969955539948856,-0.895616091376641,-0.821289274965453,-0.746969710952536,
-0.672642549632695,-0.598314479491087,-0.523968178294443,-0.484977769974428,
-0.409993929498993,-0.335022998273941,-0.260061626001027,-0.185100815258932,
-0.110144940981982,-0.0351837042315546,-1.28400083291566E-15),
 .UNSPECIFIED.);
#924=B_SPLINE_CURVE_WITH_KNOTS('',3,(#92823,#92824,#92825,#92826,#92827,
#92828,#92829,#92830,#92831,#92832,#92833,#92834,#92835,#92836,#92837,#92838,
#92839,#92840,#92841,#92842,#92843,#92844,#92845,#92846,#92847,#92848,#92849,
#92850,#92851,#92852,#92853,#92854,#92855,#92856,#92857,#92858,#92859,#92860,
#92861,#92862,#92863,#92864,#92865,#92866,#92867,#92868,#92869,#92870,#92871,
#92872,#92873,#92874,#92875,#92876,#92877,#92878,#92879,#92880,#92881,#92882,
#92883,#92884,#92885,#92886,#92887,#92888,#92889,#92890,#92891,#92892,#92893,
#92894,#92895,#92896,#92897,#92898,#92899,#92900,#92901,#92902,#92903,#92904,
#92905,#92906,#92907,#92908,#92909,#92910,#92911,#92912,#92913,#92914,#92915,
#92916,#92917,#92918,#92919,#92920,#92921,#92922,#92923,#92924,#92925,#92926,
#92927,#92928,#92929,#92930,#92931,#92932,#92933,#92934,#92935,#92936),
 .UNSPECIFIED.,.F.,.F.,(4,2,2,2,2,2,2,2,2,2,2,2,2,2,2,2,2,2,2,2,2,2,2,2,
2,2,2,2,2,2,2,2,2,2,2,2,2,2,2,2,2,2,2,2,2,2,2,2,2,2,2,2,2,2,2,2,4),(-11.2826168307778,
-11.1762469541903,-11.125251757876,-11.0024781283703,-10.913262956463,-10.8603484703286,
-10.7551997075349,-10.6630450538886,-10.5459538031153,-10.4526792588227,
-10.4002938827596,-10.2941831409333,-10.2013817166273,-10.0822414864162,
-9.99048362981615,-9.93747996123894,-9.83187816625984,-9.73943941398009,
-9.6233884934606,-9.52931042843913,-9.4768674967077,-9.37088092946969,-9.2780814777363,
-9.15745351747334,-9.06676588322009,-9.01363578521839,-8.90807491228135,
-8.86523714088575,-8.7827607709068,-8.65107318309677,-8.59051603867521,
-8.49516414937743,-8.3776343569781,-8.28788852307351,-8.18483687985127,
-8.12709756418481,-8.01873894340126,-7.9048736756614,-7.738383419085,-7.68875444778559,
-7.63979152259541,-7.5167676520058,-7.47512511439043,-7.39235876813903,
-7.26177739136488,-7.20372069393057,-7.09423898142508,-6.98111650500347,
-6.81154393892334,-6.74566579468266,-6.64203139701929,-6.52111251348614,
-6.34946821939356,-6.28376743197177,-6.18037248448461,-6.05975907348889,
-5.98309645076391),.UNSPECIFIED.);
#925=B_SPLINE_CURVE_WITH_KNOTS('',3,(#92938,#92939,#92940,#92941,#92942,
#92943,#92944,#92945,#92946,#92947,#92948,#92949,#92950,#92951,#92952,#92953,
#92954,#92955,#92956,#92957,#92958,#92959,#92960,#92961,#92962,#92963,#92964,
#92965,#92966,#92967,#92968,#92969,#92970,#92971,#92972,#92973,#92974,#92975,
#92976,#92977,#92978,#92979,#92980,#92981,#92982,#92983,#92984,#92985,#92986,
#92987,#92988,#92989,#92990,#92991,#92992,#92993,#92994,#92995,#92996,#92997,
#92998,#92999,#93000,#93001,#93002,#93003,#93004,#93005,#93006,#93007,#93008,
#93009,#93010,#93011,#93012,#93013,#93014,#93015,#93016,#93017,#93018,#93019,
#93020,#93021,#93022,#93023,#93024,#93025,#93026,#93027,#93028,#93029,#93030,
#93031,#93032,#93033,#93034,#93035,#93036,#93037,#93038,#93039,#93040,#93041,
#93042,#93043,#93044,#93045,#93046,#93047,#93048,#93049,#93050,#93051,#93052,
#93053),.UNSPECIFIED.,.F.,.F.,(4,2,2,2,2,2,2,2,2,2,2,2,2,2,2,2,2,2,2,2,
2,2,2,2,2,2,2,2,2,2,2,2,2,2,2,2,2,2,2,2,2,2,2,2,2,2,2,2,2,2,2,2,2,2,2,2,
2,4),(-5.98309645076391,-5.96179369819221,-5.87096264149203,-5.8159836647812,
-5.7322865699612,-5.64206252030099,-5.55924398589808,-5.51771648526159,
-5.39571852179474,-5.34633766037634,-5.22017712755589,-5.12476205799574,
-5.00448193589412,-4.90358088052579,-4.83962638261926,-4.66429586956545,
-4.54360496937077,-4.44139652900391,-4.37654387058763,-4.20314070678402,
-4.08320416938816,-3.97905656025761,-3.9127972674704,-3.74229346245245,
-3.62029939866371,-3.51762452494512,-3.45244184022386,-3.27973147588721,
-3.15905809947262,-3.05558871364941,-2.98983174029597,-2.81830834359997,
-2.69742813409663,-2.59369687418265,-2.52774726666072,-2.35661682998401,
-2.23138451959968,-2.13347087231659,-2.07142227037775,-1.89177931761666,
-1.77501663505352,-1.67613549123449,-1.62112530578369,-1.53015943268023,
-1.43230303448501,-1.31210058664763,-1.20826608339593,-1.14224024437481,
-0.97125966403786,-0.847074837591189,-0.747627482567506,-0.684625096025565,
-0.507174670272276,-0.387108301925727,-0.285075944693684,-0.220346759625927,
-0.0744964973377189,-0.0001310575238002),.UNSPECIFIED.);
#926=B_SPLINE_CURVE_WITH_KNOTS('',3,(#93054,#93055,#93056,#93057,#93058,
#93059,#93060,#93061,#93062,#93063,#93064,#93065,#93066,#93067,#93068,#93069,
#93070,#93071,#93072,#93073,#93074,#93075,#93076,#93077,#93078,#93079,#93080,
#93081,#93082,#93083,#93084,#93085,#93086,#93087,#93088,#93089,#93090,#93091,
#93092,#93093,#93094,#93095,#93096,#93097,#93098,#93099,#93100,#93101,#93102,
#93103,#93104,#93105,#93106,#93107,#93108,#93109,#93110,#93111,#93112,#93113,
#93114,#93115,#93116,#93117,#93118,#93119,#93120,#93121,#93122,#93123,#93124,
#93125,#93126,#93127,#93128,#93129,#93130,#93131,#93132,#93133,#93134,#93135,
#93136,#93137,#93138,#93139,#93140,#93141,#93142,#93143,#93144,#93145,#93146,
#93147,#93148,#93149,#93150,#93151,#93152,#93153,#93154,#93155,#93156,#93157,
#93158,#93159,#93160,#93161,#93162,#93163,#93164,#93165,#93166,#93167,#93168,
#93169,#93170,#93171,#93172,#93173,#93174,#93175),.UNSPECIFIED.,.F.,.F.,
(4,2,2,2,2,2,2,2,2,2,2,2,2,2,2,2,2,2,2,2,2,2,2,2,2,2,2,2,2,2,2,2,2,2,2,
2,2,2,2,2,2,2,2,2,2,2,2,2,2,2,2,2,2,2,2,2,2,2,2,2,4),(-5.98255038595961,
-5.90311477667104,-5.80173701362555,-5.70830267876734,-5.60178531374225,
-5.55015212437345,-5.41169735934466,-5.32015103300485,-5.20817938309062,
-5.10826992870272,-5.05297087285603,-4.96075345802036,-4.86390438307122,
-4.74332112600621,-4.64111274998532,-4.5762623599312,-4.40286879072047,
-4.28277227534319,-4.17885092835326,-4.11276209785121,-3.94192825741033,
-3.81850957491799,-3.71795461265881,-3.65423326151255,-3.47840649608167,
-3.35992304227894,-3.26149860727525,-3.20661906968306,-3.11620539458233,
-3.01790489144965,-2.89723410425966,-2.79358318138824,-2.72769335289786,
-2.55815918652112,-2.4450887916942,-2.33554639484681,-2.27747578243195,
-2.14689175849319,-2.06413358293121,-2.02248679724396,-1.89940786726995,
-1.85047156732237,-1.71740925151478,-1.62591851574838,-1.51377348428522,
-1.41419276829883,-1.35899612404205,-1.26721981099963,-1.17002106870236,
-1.05004144920438,-0.94659983994607,-0.880841108726548,-0.709318050707547,
-0.580922441173507,-0.490518786270498,-0.435174627672907,-0.342764808991137,
-0.246067136066954,-0.170663750263522,-0.032663736953733,-0.000134629797728273),
 .UNSPECIFIED.);
#927=B_SPLINE_CURVE_WITH_KNOTS('',3,(#93178,#93179,#93180,#93181,#93182,
#93183,#93184,#93185,#93186,#93187,#93188,#93189),.UNSPECIFIED.,.F.,.F.,
(4,1,1,1,1,1,1,1,1,4),(17.9335366650258,18.1546308751542,18.6396086451287,
19.1245864151031,19.6095641850775,20.0945419550519,20.5795197250264,21.0644974950008,
21.5494752649752,21.9911485751285),.UNSPECIFIED.);
#928=B_SPLINE_CURVE_WITH_KNOTS('',3,(#93190,#93191,#93192,#93193,#93194,
#93195,#93196,#93197,#93198),.UNSPECIFIED.,.F.,.F.,(4,1,1,1,1,1,4),(21.9911485751285,
22.0344530349496,22.5194308049241,23.0044085748985,23.4893863448729,23.9743641148474,
24.2167278608201),.UNSPECIFIED.);
#929=B_SPLINE_CURVE_WITH_KNOTS('',3,(#93200,#93201,#93202,#93203,#93204,
#93205,#93206,#93207,#93208),.UNSPECIFIED.,.F.,.F.,(4,1,1,1,1,1,4),(21.9911486045731,
22.1580444465627,22.6430222165371,23.1279999865116,23.612977756486,24.0979555264604,
24.2167503458098),.UNSPECIFIED.);
#930=B_SPLINE_CURVE_WITH_KNOTS('',3,(#93209,#93210,#93211,#93212,#93213,
#93214,#93215,#93216,#93217,#93218,#93219,#93220,#93221,#93222,#93223,#93224,
#93225,#93226,#93227,#93228,#93229,#93230,#93231,#93232,#93233,#93234,#93235,
#93236,#93237,#93238,#93239,#93240,#93241,#93242,#93243,#93244,#93245,#93246,
#93247,#93248,#93249,#93250,#93251,#93252,#93253,#93254,#93255,#93256,#93257,
#93258,#93259,#93260,#93261,#93262,#93263,#93264,#93265,#93266,#93267,#93268,
#93269,#93270,#93271,#93272,#93273,#93274,#93275,#93276,#93277,#93278,#93279,
#93280,#93281,#93282,#93283,#93284,#93285,#93286,#93287,#93288,#93289,#93290,
#93291,#93292,#93293,#93294,#93295,#93296,#93297,#93298,#93299,#93300,#93301,
#93302,#93303,#93304,#93305,#93306,#93307,#93308,#93309,#93310,#93311,#93312,
#93313,#93314,#93315,#93316,#93317,#93318,#93319,#93320,#93321,#93322,#93323,
#93324,#93325,#93326,#93327,#93328,#93329,#93330,#93331,#93332,#93333,#93334,
#93335,#93336,#93337,#93338,#93339,#93340,#93341,#93342,#93343,#93344,#93345,
#93346,#93347,#93348,#93349,#93350,#93351,#93352,#93353,#93354,#93355,#93356,
#93357,#93358,#93359,#93360,#93361,#93362,#93363,#93364,#93365,#93366,#93367,
#93368,#93369,#93370,#93371,#93372,#93373,#93374,#93375,#93376,#93377,#93378,
#93379,#93380,#93381,#93382,#93383,#93384,#93385,#93386),.UNSPECIFIED.,
 .F.,.F.,(4,3,3,3,3,3,3,3,3,3,3,3,3,3,3,3,3,3,3,3,3,3,3,3,3,3,3,3,3,3,3,
3,3,3,3,3,3,3,3,3,3,3,3,3,3,3,3,3,3,3,3,3,3,3,3,3,3,3,3,4),(17.9335555972082,
18.007038108634,18.0805259216794,18.1540125117814,18.2275142346009,18.2782222867673,
18.3517193566403,18.4252043632004,18.498681860891,18.5721648191973,18.6456469619359,
18.7191438227812,18.7632000567417,18.836699748599,18.9101874079279,18.9836675811948,
19.0571532306,19.1306380687981,19.2041376145015,19.2481778267161,19.3216763040303,
19.395162735418,19.4686416710373,19.5421260768971,19.6156096702605,19.6891079771531,
19.7331555966906,19.8066544900448,19.8801413415835,19.9536207002029,20.0271055303679,
20.1005895480742,20.1740882766318,20.218133366665,20.291632198477,20.3651189882224,
20.4385982849825,20.5120830536293,20.5855670101137,20.659065678305,20.7031111366394,
20.7766099170402,20.8500966545468,20.9235758983977,20.9970606134957,21.0705445161567,
21.1440431304441,21.1880889066139,21.2615877487943,21.3350745488855,21.4085538559384,
21.4820386347234,21.5555226012415,21.629021279239,21.6730666765883,21.7466012061225,
21.8201249209659,21.893639208639,21.9671526510914,21.9911485751285),
 .UNSPECIFIED.);
#931=B_SPLINE_CURVE_WITH_KNOTS('',3,(#93635,#93636,#93637,#93638,#93639,
#93640,#93641,#93642,#93643,#93644,#93645,#93646,#93647,#93648,#93649,#93650,
#93651,#93652,#93653,#93654,#93655,#93656,#93657,#93658,#93659,#93660,#93661,
#93662,#93663,#93664,#93665,#93666,#93667,#93668,#93669,#93670,#93671,#93672,
#93673,#93674,#93675,#93676,#93677,#93678,#93679,#93680,#93681,#93682,#93683,
#93684,#93685,#93686,#93687,#93688,#93689,#93690,#93691,#93692,#93693,#93694,
#93695,#93696,#93697,#93698,#93699,#93700,#93701,#93702,#93703,#93704,#93705,
#93706,#93707,#93708,#93709,#93710,#93711,#93712,#93713,#93714,#93715,#93716,
#93717,#93718,#93719,#93720,#93721,#93722,#93723,#93724,#93725,#93726,#93727,
#93728,#93729,#93730,#93731,#93732,#93733,#93734,#93735,#93736,#93737,#93738,
#93739,#93740,#93741,#93742,#93743,#93744,#93745,#93746,#93747,#93748,#93749),
 .UNSPECIFIED.,.F.,.F.,(4,3,3,3,3,3,3,3,3,3,3,3,3,3,3,3,3,3,3,3,3,3,3,3,
3,3,3,3,3,3,3,3,3,3,3,3,3,3,4),(0.,0.0739126635462495,0.150740513686272,
0.225935951919889,0.303580008013115,0.381224064106341,0.389885207948467,
0.400073548669132,0.474555444274402,0.487104039232364,0.561377161816764,
0.635987840137627,0.710367183555496,0.774793244282009,0.786415201228137,
0.860297905292171,0.934077532582566,0.968071426461548,1.04206547690771,
1.1158601918424,1.15671189269083,1.16870781265367,1.24198330165962,1.31537204770392,
1.38812719592645,1.4426737986298,1.50108005437742,1.52663279126701,1.54012983179738,
1.55002299318499,1.57202511761386,1.6448077654029,1.71108678520487,1.76079605005635,
1.77610764545378,1.84829504017901,1.9099238446108,1.98235653582154,1.99217144768675),
 .UNSPECIFIED.);
#932=B_SPLINE_CURVE_WITH_KNOTS('',3,(#93750,#93751,#93752,#93753,#93754,
#93755,#93756,#93757,#93758,#93759,#93760,#93761,#93762,#93763,#93764,#93765,
#93766,#93767,#93768,#93769,#93770,#93771,#93772,#93773,#93774,#93775,#93776,
#93777,#93778,#93779,#93780,#93781,#93782,#93783,#93784,#93785,#93786,#93787,
#93788,#93789,#93790,#93791,#93792,#93793,#93794,#93795,#93796,#93797,#93798,
#93799,#93800,#93801,#93802,#93803,#93804,#93805,#93806,#93807,#93808,#93809,
#93810,#93811,#93812,#93813,#93814,#93815,#93816,#93817,#93818,#93819,#93820,
#93821,#93822,#93823,#93824,#93825,#93826,#93827,#93828,#93829,#93830,#93831,
#93832,#93833,#93834,#93835,#93836,#93837,#93838,#93839,#93840,#93841,#93842,
#93843,#93844,#93845,#93846,#93847,#93848,#93849,#93850,#93851,#93852,#93853,
#93854,#93855,#93856,#93857,#93858,#93859,#93860,#93861,#93862,#93863,#93864),
 .UNSPECIFIED.,.F.,.F.,(4,3,3,3,3,3,3,3,3,3,3,3,3,3,3,3,3,3,3,3,3,3,3,3,
3,3,3,3,3,3,3,3,3,3,3,3,3,3,4),(0.,0.0709761209897443,0.142931446040141,
0.21545925542993,0.287856627714121,0.332469159572249,0.365928558465845,
0.375861814980538,0.448916300094163,0.466306755146632,0.538880173574122,
0.611947284117477,0.684979149532332,0.748511465508852,0.756781309220838,
0.830210843243463,0.903989318076003,0.939195971997139,1.01278289101164,
1.08650672760772,1.12800034646411,1.14013519160853,1.21408946536429,1.28844299347222,
1.36258786411151,1.41845567845884,1.47903742889201,1.50554194470653,1.51621439279437,
1.52551173241115,1.59979138412183,1.67562095857243,1.73249313941038,1.74983333918112,
1.76344979329115,1.83852338945091,1.90310968192423,1.97800052830964,1.98979055697635),
 .UNSPECIFIED.);
#933=B_SPLINE_CURVE_WITH_KNOTS('',3,(#94101,#94102,#94103,#94104,#94105,
#94106,#94107,#94108,#94109,#94110,#94111,#94112,#94113,#94114,#94115,#94116,
#94117,#94118,#94119,#94120,#94121,#94122,#94123,#94124,#94125,#94126,#94127,
#94128,#94129,#94130,#94131,#94132,#94133,#94134,#94135,#94136,#94137,#94138,
#94139,#94140,#94141,#94142,#94143,#94144,#94145,#94146,#94147,#94148,#94149,
#94150,#94151,#94152,#94153,#94154,#94155,#94156,#94157,#94158,#94159,#94160,
#94161,#94162,#94163,#94164,#94165,#94166,#94167,#94168,#94169,#94170,#94171,
#94172,#94173,#94174,#94175,#94176,#94177,#94178,#94179,#94180,#94181,#94182,
#94183,#94184,#94185,#94186,#94187,#94188,#94189,#94190,#94191,#94192,#94193,
#94194,#94195,#94196,#94197,#94198,#94199,#94200,#94201,#94202,#94203,#94204,
#94205,#94206,#94207,#94208,#94209,#94210,#94211,#94212),.UNSPECIFIED.,
 .F.,.F.,(4,3,3,3,3,3,3,3,3,3,3,3,3,3,3,3,3,3,3,3,3,3,3,3,3,3,3,3,3,3,3,
3,3,3,3,3,3,4),(0.,0.0707412612887614,0.144538066072586,0.217130768668796,
0.291529624546427,0.365928480424058,0.374378535179976,0.447428921852669,
0.466306755146633,0.538735411390327,0.611788295327192,0.684950044616232,
0.748511526461462,0.757906047956915,0.831343763816251,0.905121500651129,
0.939195971997151,1.01278287709315,1.08650671046459,1.12800033146387,1.14013518859003,
1.21408944402746,1.28844296470764,1.36258783663024,1.41845567845885,1.47903742889203,
1.50554194470654,1.51621439199532,1.52551173161284,1.5997913820326,1.67562095700551,
1.7324931382352,1.74983333999573,1.76344979518143,1.83852339153841,1.90310968192426,
1.97800053497444,1.98979104577926),.UNSPECIFIED.);
#934=B_SPLINE_CURVE_WITH_KNOTS('',3,(#94214,#94215,#94216,#94217),
 .UNSPECIFIED.,.F.,.F.,(4,4),(0.,0.000891519205898623),.UNSPECIFIED.);
#935=B_SPLINE_CURVE_WITH_KNOTS('',3,(#94218,#94219,#94220,#94221,#94222,
#94223,#94224,#94225,#94226,#94227,#94228,#94229,#94230,#94231,#94232,#94233,
#94234,#94235,#94236,#94237,#94238,#94239,#94240,#94241,#94242,#94243,#94244,
#94245,#94246,#94247,#94248,#94249,#94250,#94251,#94252,#94253,#94254,#94255,
#94256,#94257,#94258,#94259,#94260,#94261,#94262,#94263,#94264,#94265,#94266,
#94267,#94268,#94269,#94270,#94271,#94272,#94273,#94274,#94275,#94276,#94277,
#94278,#94279,#94280,#94281,#94282,#94283,#94284,#94285,#94286,#94287,#94288,
#94289,#94290,#94291,#94292,#94293,#94294,#94295,#94296,#94297,#94298,#94299,
#94300,#94301,#94302,#94303,#94304,#94305,#94306,#94307,#94308,#94309,#94310,
#94311,#94312,#94313,#94314,#94315,#94316,#94317,#94318,#94319,#94320,#94321,
#94322,#94323,#94324,#94325,#94326,#94327,#94328,#94329,#94330,#94331,#94332,
#94333,#94334,#94335),.UNSPECIFIED.,.F.,.F.,(4,3,3,3,3,3,3,3,3,3,3,3,3,
3,3,3,3,3,3,3,3,3,3,3,3,3,3,3,3,3,3,3,3,3,3,3,3,3,3,4),(0.,0.0741261668227613,
0.149049466564394,0.224263098602536,0.298872907613775,0.34593069051842,
0.381224027696904,0.391900396664017,0.403121243662082,0.477602560183117,
0.487104039232354,0.561377195983551,0.635987882023318,0.710367213466364,
0.774793266715159,0.786415222382851,0.860297938446043,0.934077552859576,
0.968071426461543,1.04206547223162,1.11586018693168,1.15671188839394,1.16870781125156,
1.2419832929878,1.31537203776292,1.38812718419361,1.4426737986298,1.50108005437742,
1.52663279126701,1.54012983204117,1.55002299328553,1.57202512135779,1.64480776723829,
1.71108678658141,1.76079605108876,1.77610764643868,1.84829504471514,1.90992384461079,
1.98235653831781,1.99217144768673),.UNSPECIFIED.);
#936=SHAPE_REPRESENTATION_RELATIONSHIP('SRR','None',#94488,#951);
#937=SHAPE_REPRESENTATION_RELATIONSHIP('SRR','None',#94489,#952);
#938=SHAPE_REPRESENTATION_RELATIONSHIP('SRR','None',#94490,#953);
#939=SHAPE_REPRESENTATION_RELATIONSHIP('SRR','None',#94491,#954);
#940=SHAPE_REPRESENTATION_RELATIONSHIP('SRR','None',#94492,#955);
#941=SHAPE_REPRESENTATION_RELATIONSHIP('SRR','None',#94493,#956);
#942=SHAPE_REPRESENTATION_RELATIONSHIP('SRR','None',#94494,#957);
#943=SHAPE_REPRESENTATION_RELATIONSHIP('SRR','None',#94495,#958);
#944=SHAPE_REPRESENTATION_RELATIONSHIP('SRR','None',#94496,#959);
#945=SHAPE_REPRESENTATION_RELATIONSHIP('SRR','None',#94497,#960);
#946=SHAPE_REPRESENTATION_RELATIONSHIP('SRR','None',#94498,#961);
#947=SHAPE_REPRESENTATION_RELATIONSHIP('SRR','None',#94499,#962);
#948=SHAPE_REPRESENTATION_RELATIONSHIP('SRR','None',#94500,#963);
#949=SHAPE_REPRESENTATION_RELATIONSHIP('SRR','None',#94501,#964);
#950=SHAPE_REPRESENTATION_RELATIONSHIP('SRR','None',#94502,#965);
#951=ADVANCED_BREP_SHAPE_REPRESENTATION('',(#981),#94397);
#952=ADVANCED_BREP_SHAPE_REPRESENTATION('',(#982),#94398);
#953=ADVANCED_BREP_SHAPE_REPRESENTATION('',(#983),#94399);
#954=ADVANCED_BREP_SHAPE_REPRESENTATION('',(#984),#94400);
#955=ADVANCED_BREP_SHAPE_REPRESENTATION('',(#985),#94401);
#956=ADVANCED_BREP_SHAPE_REPRESENTATION('',(#986),#94402);
#957=ADVANCED_BREP_SHAPE_REPRESENTATION('',(#987),#94403);
#958=ADVANCED_BREP_SHAPE_REPRESENTATION('',(#988),#94404);
#959=ADVANCED_BREP_SHAPE_REPRESENTATION('',(#989),#94405);
#960=ADVANCED_BREP_SHAPE_REPRESENTATION('',(#990),#94406);
#961=ADVANCED_BREP_SHAPE_REPRESENTATION('',(#991),#94407);
#962=ADVANCED_BREP_SHAPE_REPRESENTATION('',(#992),#94408);
#963=ADVANCED_BREP_SHAPE_REPRESENTATION('',(#993),#94409);
#964=ADVANCED_BREP_SHAPE_REPRESENTATION('',(#994),#94410);
#965=ADVANCED_BREP_SHAPE_REPRESENTATION('',(#995),#94411);
#966=STYLED_ITEM('',(#94576),#981);
#967=STYLED_ITEM('',(#94576),#982);
#968=STYLED_ITEM('',(#94576),#983);
#969=STYLED_ITEM('',(#94576),#984);
#970=STYLED_ITEM('',(#94577),#985);
#971=STYLED_ITEM('',(#94578),#986);
#972=STYLED_ITEM('',(#94577),#987);
#973=STYLED_ITEM('',(#94579),#988);
#974=STYLED_ITEM('',(#94578),#989);
#975=STYLED_ITEM('',(#94580),#990);
#976=STYLED_ITEM('',(#94578),#991);
#977=STYLED_ITEM('',(#94578),#992);
#978=STYLED_ITEM('',(#94577),#993);
#979=STYLED_ITEM('',(#94581),#994);
#980=STYLED_ITEM('',(#94578),#995);
#981=MANIFOLD_SOLID_BREP('Body1',#8251);
#982=MANIFOLD_SOLID_BREP('Body1',#8252);
#983=MANIFOLD_SOLID_BREP('Body1',#8253);
#984=MANIFOLD_SOLID_BREP('Body1',#8254);
#985=MANIFOLD_SOLID_BREP('Body1',#8255);
#986=MANIFOLD_SOLID_BREP('Body1',#8256);
#987=MANIFOLD_SOLID_BREP('Body1',#8257);
#988=MANIFOLD_SOLID_BREP('Body1',#8258);
#989=MANIFOLD_SOLID_BREP('Body1',#8259);
#990=MANIFOLD_SOLID_BREP('Body1',#8260);
#991=MANIFOLD_SOLID_BREP('Body1',#8261);
#992=MANIFOLD_SOLID_BREP('Body1',#8262);
#993=MANIFOLD_SOLID_BREP('Body1',#8263);
#994=MANIFOLD_SOLID_BREP('Body1',#8264);
#995=MANIFOLD_SOLID_BREP('Body1',#8265);
#996=FACE_BOUND('',#1523,.T.);
#997=FACE_BOUND('',#1524,.T.);
#998=FACE_BOUND('',#1525,.T.);
#999=FACE_BOUND('',#1526,.T.);
#1000=FACE_BOUND('',#1528,.T.);
#1001=FACE_BOUND('',#1529,.T.);
#1002=FACE_BOUND('',#1530,.T.);
#1003=FACE_BOUND('',#1531,.T.);
#1004=FACE_BOUND('',#1535,.T.);
#1005=FACE_BOUND('',#1536,.T.);
#1006=FACE_BOUND('',#1539,.T.);
#1007=FACE_BOUND('',#1540,.T.);
#1008=FACE_BOUND('',#1568,.T.);
#1009=FACE_BOUND('',#1569,.T.);
#1010=FACE_BOUND('',#1572,.T.);
#1011=FACE_BOUND('',#1573,.T.);
#1012=FACE_BOUND('',#1666,.T.);
#1013=FACE_BOUND('',#1668,.T.);
#1014=FACE_BOUND('',#1693,.T.);
#1015=FACE_BOUND('',#1696,.T.);
#1016=FACE_BOUND('',#1737,.T.);
#1017=FACE_BOUND('',#1741,.T.);
#1018=FACE_BOUND('',#1742,.T.);
#1019=FACE_BOUND('',#1743,.T.);
#1020=FACE_BOUND('',#1744,.T.);
#1021=FACE_BOUND('',#1753,.T.);
#1022=FACE_BOUND('',#1754,.T.);
#1023=FACE_BOUND('',#1755,.T.);
#1024=FACE_BOUND('',#1756,.T.);
#1025=FACE_BOUND('',#1770,.T.);
#1026=FACE_BOUND('',#1771,.T.);
#1027=FACE_BOUND('',#1772,.T.);
#1028=FACE_BOUND('',#1773,.T.);
#1029=FACE_BOUND('',#1774,.T.);
#1030=FACE_BOUND('',#1776,.T.);
#1031=FACE_BOUND('',#1777,.T.);
#1032=FACE_BOUND('',#1778,.T.);
#1033=FACE_BOUND('',#1779,.T.);
#1034=FACE_BOUND('',#1780,.T.);
#1035=FACE_BOUND('',#1790,.T.);
#1036=FACE_BOUND('',#1791,.T.);
#1037=FACE_BOUND('',#1792,.T.);
#1038=FACE_BOUND('',#1793,.T.);
#1039=FACE_BOUND('',#1795,.T.);
#1040=FACE_BOUND('',#1796,.T.);
#1041=FACE_BOUND('',#1797,.T.);
#1042=FACE_BOUND('',#1798,.T.);
#1043=FACE_BOUND('',#1827,.T.);
#1044=FACE_BOUND('',#1830,.T.);
#1045=FACE_BOUND('',#1858,.T.);
#1046=FACE_BOUND('',#1861,.T.);
#1047=FACE_BOUND('',#1896,.T.);
#1048=FACE_BOUND('',#1900,.T.);
#1049=FACE_BOUND('',#1902,.T.);
#1050=FACE_BOUND('',#1918,.T.);
#1051=FACE_BOUND('',#1919,.T.);
#1052=FACE_BOUND('',#1920,.T.);
#1053=FACE_BOUND('',#1923,.T.);
#1054=FACE_BOUND('',#1924,.T.);
#1055=FACE_BOUND('',#1925,.T.);
#1056=FACE_BOUND('',#1929,.T.);
#1057=FACE_BOUND('',#1931,.T.);
#1058=PLANE('',#8447);
#1059=PLANE('',#8448);
#1060=PLANE('',#8449);
#1061=PLANE('',#8450);
#1062=PLANE('',#8451);
#1063=PLANE('',#8452);
#1064=PLANE('',#8460);
#1065=PLANE('',#8461);
#1066=PLANE('',#8462);
#1067=PLANE('',#8463);
#1068=PLANE('',#8464);
#1069=PLANE('',#8465);
#1070=PLANE('',#8467);
#1071=PLANE('',#8468);
#1072=PLANE('',#8469);
#1073=PLANE('',#8470);
#1074=PLANE('',#8471);
#1075=PLANE('',#8472);
#1076=PLANE('',#8477);
#1077=PLANE('',#8481);
#1078=PLANE('',#8485);
#1079=PLANE('',#8489);
#1080=PLANE('',#8493);
#1081=PLANE('',#8497);
#1082=PLANE('',#8501);
#1083=PLANE('',#8505);
#1084=PLANE('',#8506);
#1085=PLANE('',#8507);
#1086=PLANE('',#8508);
#1087=PLANE('',#8509);
#1088=PLANE('',#8510);
#1089=PLANE('',#8511);
#1090=PLANE('',#8605);
#1091=PLANE('',#8606);
#1092=PLANE('',#8607);
#1093=PLANE('',#8608);
#1094=PLANE('',#8612);
#1095=PLANE('',#8613);
#1096=PLANE('',#8634);
#1097=PLANE('',#8635);
#1098=PLANE('',#8636);
#1099=PLANE('',#8637);
#1100=PLANE('',#8638);
#1101=PLANE('',#8639);
#1102=PLANE('',#8640);
#1103=PLANE('',#8641);
#1104=PLANE('',#8645);
#1105=PLANE('',#8646);
#1106=PLANE('',#8686);
#1107=PLANE('',#8687);
#1108=PLANE('',#8691);
#1109=PLANE('',#8692);
#1110=PLANE('',#8714);
#1111=PLANE('',#8719);
#1112=PLANE('',#8728);
#1113=PLANE('',#8729);
#1114=PLANE('',#8730);
#1115=PLANE('',#8744);
#1116=PLANE('',#8745);
#1117=PLANE('',#8746);
#1118=PLANE('',#8747);
#1119=PLANE('',#8748);
#1120=PLANE('',#8749);
#1121=PLANE('',#8750);
#1122=PLANE('',#8751);
#1123=PLANE('',#8752);
#1124=PLANE('',#8753);
#1125=PLANE('',#8767);
#1126=PLANE('',#8768);
#1127=PLANE('',#8769);
#1128=PLANE('',#8770);
#1129=PLANE('',#8771);
#1130=PLANE('',#8772);
#1131=PLANE('',#8797);
#1132=PLANE('',#8798);
#1133=PLANE('',#8799);
#1134=PLANE('',#8800);
#1135=PLANE('',#8801);
#1136=PLANE('',#8802);
#1137=PLANE('',#8803);
#1138=PLANE('',#8804);
#1139=PLANE('',#8808);
#1140=PLANE('',#8809);
#1141=PLANE('',#8832);
#1142=PLANE('',#8833);
#1143=PLANE('',#8834);
#1144=PLANE('',#8835);
#1145=PLANE('',#8836);
#1146=PLANE('',#8837);
#1147=PLANE('',#8838);
#1148=PLANE('',#8839);
#1149=PLANE('',#8843);
#1150=PLANE('',#8844);
#1151=PLANE('',#8880);
#1152=PLANE('',#8887);
#1153=PLANE('',#8888);
#1154=PLANE('',#8910);
#1155=PLANE('',#8914);
#1156=PLANE('',#8922);
#1157=PLANE('',#8923);
#1158=FACE_OUTER_BOUND('',#1514,.T.);
#1159=FACE_OUTER_BOUND('',#1515,.T.);
#1160=FACE_OUTER_BOUND('',#1516,.T.);
#1161=FACE_OUTER_BOUND('',#1517,.T.);
#1162=FACE_OUTER_BOUND('',#1518,.T.);
#1163=FACE_OUTER_BOUND('',#1519,.T.);
#1164=FACE_OUTER_BOUND('',#1520,.T.);
#1165=FACE_OUTER_BOUND('',#1521,.T.);
#1166=FACE_OUTER_BOUND('',#1522,.T.);
#1167=FACE_OUTER_BOUND('',#1527,.T.);
#1168=FACE_OUTER_BOUND('',#1532,.T.);
#1169=FACE_OUTER_BOUND('',#1533,.T.);
#1170=FACE_OUTER_BOUND('',#1534,.T.);
#1171=FACE_OUTER_BOUND('',#1537,.T.);
#1172=FACE_OUTER_BOUND('',#1538,.T.);
#1173=FACE_OUTER_BOUND('',#1541,.T.);
#1174=FACE_OUTER_BOUND('',#1542,.T.);
#1175=FACE_OUTER_BOUND('',#1543,.T.);
#1176=FACE_OUTER_BOUND('',#1544,.T.);
#1177=FACE_OUTER_BOUND('',#1545,.T.);
#1178=FACE_OUTER_BOUND('',#1546,.T.);
#1179=FACE_OUTER_BOUND('',#1547,.T.);
#1180=FACE_OUTER_BOUND('',#1548,.T.);
#1181=FACE_OUTER_BOUND('',#1549,.T.);
#1182=FACE_OUTER_BOUND('',#1550,.T.);
#1183=FACE_OUTER_BOUND('',#1551,.T.);
#1184=FACE_OUTER_BOUND('',#1552,.T.);
#1185=FACE_OUTER_BOUND('',#1553,.T.);
#1186=FACE_OUTER_BOUND('',#1554,.T.);
#1187=FACE_OUTER_BOUND('',#1555,.T.);
#1188=FACE_OUTER_BOUND('',#1556,.T.);
#1189=FACE_OUTER_BOUND('',#1557,.T.);
#1190=FACE_OUTER_BOUND('',#1558,.T.);
#1191=FACE_OUTER_BOUND('',#1559,.T.);
#1192=FACE_OUTER_BOUND('',#1560,.T.);
#1193=FACE_OUTER_BOUND('',#1561,.T.);
#1194=FACE_OUTER_BOUND('',#1562,.T.);
#1195=FACE_OUTER_BOUND('',#1563,.T.);
#1196=FACE_OUTER_BOUND('',#1564,.T.);
#1197=FACE_OUTER_BOUND('',#1565,.T.);
#1198=FACE_OUTER_BOUND('',#1566,.T.);
#1199=FACE_OUTER_BOUND('',#1567,.T.);
#1200=FACE_OUTER_BOUND('',#1570,.T.);
#1201=FACE_OUTER_BOUND('',#1571,.T.);
#1202=FACE_OUTER_BOUND('',#1574,.T.);
#1203=FACE_OUTER_BOUND('',#1575,.T.);
#1204=FACE_OUTER_BOUND('',#1576,.T.);
#1205=FACE_OUTER_BOUND('',#1577,.T.);
#1206=FACE_OUTER_BOUND('',#1578,.T.);
#1207=FACE_OUTER_BOUND('',#1579,.T.);
#1208=FACE_OUTER_BOUND('',#1580,.T.);
#1209=FACE_OUTER_BOUND('',#1581,.T.);
#1210=FACE_OUTER_BOUND('',#1582,.T.);
#1211=FACE_OUTER_BOUND('',#1583,.T.);
#1212=FACE_OUTER_BOUND('',#1584,.T.);
#1213=FACE_OUTER_BOUND('',#1585,.T.);
#1214=FACE_OUTER_BOUND('',#1586,.T.);
#1215=FACE_OUTER_BOUND('',#1587,.T.);
#1216=FACE_OUTER_BOUND('',#1588,.T.);
#1217=FACE_OUTER_BOUND('',#1589,.T.);
#1218=FACE_OUTER_BOUND('',#1590,.T.);
#1219=FACE_OUTER_BOUND('',#1591,.T.);
#1220=FACE_OUTER_BOUND('',#1592,.T.);
#1221=FACE_OUTER_BOUND('',#1593,.T.);
#1222=FACE_OUTER_BOUND('',#1594,.T.);
#1223=FACE_OUTER_BOUND('',#1595,.T.);
#1224=FACE_OUTER_BOUND('',#1596,.T.);
#1225=FACE_OUTER_BOUND('',#1597,.T.);
#1226=FACE_OUTER_BOUND('',#1598,.T.);
#1227=FACE_OUTER_BOUND('',#1599,.T.);
#1228=FACE_OUTER_BOUND('',#1600,.T.);
#1229=FACE_OUTER_BOUND('',#1601,.T.);
#1230=FACE_OUTER_BOUND('',#1602,.T.);
#1231=FACE_OUTER_BOUND('',#1603,.T.);
#1232=FACE_OUTER_BOUND('',#1604,.T.);
#1233=FACE_OUTER_BOUND('',#1605,.T.);
#1234=FACE_OUTER_BOUND('',#1606,.T.);
#1235=FACE_OUTER_BOUND('',#1607,.T.);
#1236=FACE_OUTER_BOUND('',#1608,.T.);
#1237=FACE_OUTER_BOUND('',#1609,.T.);
#1238=FACE_OUTER_BOUND('',#1610,.T.);
#1239=FACE_OUTER_BOUND('',#1611,.T.);
#1240=FACE_OUTER_BOUND('',#1612,.T.);
#1241=FACE_OUTER_BOUND('',#1613,.T.);
#1242=FACE_OUTER_BOUND('',#1614,.T.);
#1243=FACE_OUTER_BOUND('',#1615,.T.);
#1244=FACE_OUTER_BOUND('',#1616,.T.);
#1245=FACE_OUTER_BOUND('',#1617,.T.);
#1246=FACE_OUTER_BOUND('',#1618,.T.);
#1247=FACE_OUTER_BOUND('',#1619,.T.);
#1248=FACE_OUTER_BOUND('',#1620,.T.);
#1249=FACE_OUTER_BOUND('',#1621,.T.);
#1250=FACE_OUTER_BOUND('',#1622,.T.);
#1251=FACE_OUTER_BOUND('',#1623,.T.);
#1252=FACE_OUTER_BOUND('',#1624,.T.);
#1253=FACE_OUTER_BOUND('',#1625,.T.);
#1254=FACE_OUTER_BOUND('',#1626,.T.);
#1255=FACE_OUTER_BOUND('',#1627,.T.);
#1256=FACE_OUTER_BOUND('',#1628,.T.);
#1257=FACE_OUTER_BOUND('',#1629,.T.);
#1258=FACE_OUTER_BOUND('',#1630,.T.);
#1259=FACE_OUTER_BOUND('',#1631,.T.);
#1260=FACE_OUTER_BOUND('',#1632,.T.);
#1261=FACE_OUTER_BOUND('',#1633,.T.);
#1262=FACE_OUTER_BOUND('',#1634,.T.);
#1263=FACE_OUTER_BOUND('',#1635,.T.);
#1264=FACE_OUTER_BOUND('',#1636,.T.);
#1265=FACE_OUTER_BOUND('',#1637,.T.);
#1266=FACE_OUTER_BOUND('',#1638,.T.);
#1267=FACE_OUTER_BOUND('',#1639,.T.);
#1268=FACE_OUTER_BOUND('',#1640,.T.);
#1269=FACE_OUTER_BOUND('',#1641,.T.);
#1270=FACE_OUTER_BOUND('',#1642,.T.);
#1271=FACE_OUTER_BOUND('',#1643,.T.);
#1272=FACE_OUTER_BOUND('',#1644,.T.);
#1273=FACE_OUTER_BOUND('',#1645,.T.);
#1274=FACE_OUTER_BOUND('',#1646,.T.);
#1275=FACE_OUTER_BOUND('',#1647,.T.);
#1276=FACE_OUTER_BOUND('',#1648,.T.);
#1277=FACE_OUTER_BOUND('',#1649,.T.);
#1278=FACE_OUTER_BOUND('',#1650,.T.);
#1279=FACE_OUTER_BOUND('',#1651,.T.);
#1280=FACE_OUTER_BOUND('',#1652,.T.);
#1281=FACE_OUTER_BOUND('',#1653,.T.);
#1282=FACE_OUTER_BOUND('',#1654,.T.);
#1283=FACE_OUTER_BOUND('',#1655,.T.);
#1284=FACE_OUTER_BOUND('',#1656,.T.);
#1285=FACE_OUTER_BOUND('',#1657,.T.);
#1286=FACE_OUTER_BOUND('',#1658,.T.);
#1287=FACE_OUTER_BOUND('',#1659,.T.);
#1288=FACE_OUTER_BOUND('',#1660,.T.);
#1289=FACE_OUTER_BOUND('',#1661,.T.);
#1290=FACE_OUTER_BOUND('',#1662,.T.);
#1291=FACE_OUTER_BOUND('',#1663,.T.);
#1292=FACE_OUTER_BOUND('',#1664,.T.);
#1293=FACE_OUTER_BOUND('',#1665,.T.);
#1294=FACE_OUTER_BOUND('',#1667,.T.);
#1295=FACE_OUTER_BOUND('',#1669,.T.);
#1296=FACE_OUTER_BOUND('',#1670,.T.);
#1297=FACE_OUTER_BOUND('',#1671,.T.);
#1298=FACE_OUTER_BOUND('',#1672,.T.);
#1299=FACE_OUTER_BOUND('',#1673,.T.);
#1300=FACE_OUTER_BOUND('',#1674,.T.);
#1301=FACE_OUTER_BOUND('',#1675,.T.);
#1302=FACE_OUTER_BOUND('',#1676,.T.);
#1303=FACE_OUTER_BOUND('',#1677,.T.);
#1304=FACE_OUTER_BOUND('',#1678,.T.);
#1305=FACE_OUTER_BOUND('',#1679,.T.);
#1306=FACE_OUTER_BOUND('',#1680,.T.);
#1307=FACE_OUTER_BOUND('',#1681,.T.);
#1308=FACE_OUTER_BOUND('',#1682,.T.);
#1309=FACE_OUTER_BOUND('',#1683,.T.);
#1310=FACE_OUTER_BOUND('',#1684,.T.);
#1311=FACE_OUTER_BOUND('',#1685,.T.);
#1312=FACE_OUTER_BOUND('',#1686,.T.);
#1313=FACE_OUTER_BOUND('',#1687,.T.);
#1314=FACE_OUTER_BOUND('',#1688,.T.);
#1315=FACE_OUTER_BOUND('',#1689,.T.);
#1316=FACE_OUTER_BOUND('',#1690,.T.);
#1317=FACE_OUTER_BOUND('',#1691,.T.);
#1318=FACE_OUTER_BOUND('',#1692,.T.);
#1319=FACE_OUTER_BOUND('',#1694,.T.);
#1320=FACE_OUTER_BOUND('',#1695,.T.);
#1321=FACE_OUTER_BOUND('',#1697,.T.);
#1322=FACE_OUTER_BOUND('',#1698,.T.);
#1323=FACE_OUTER_BOUND('',#1699,.T.);
#1324=FACE_OUTER_BOUND('',#1700,.T.);
#1325=FACE_OUTER_BOUND('',#1701,.T.);
#1326=FACE_OUTER_BOUND('',#1702,.T.);
#1327=FACE_OUTER_BOUND('',#1703,.T.);
#1328=FACE_OUTER_BOUND('',#1704,.T.);
#1329=FACE_OUTER_BOUND('',#1705,.T.);
#1330=FACE_OUTER_BOUND('',#1706,.T.);
#1331=FACE_OUTER_BOUND('',#1707,.T.);
#1332=FACE_OUTER_BOUND('',#1708,.T.);
#1333=FACE_OUTER_BOUND('',#1709,.T.);
#1334=FACE_OUTER_BOUND('',#1710,.T.);
#1335=FACE_OUTER_BOUND('',#1711,.T.);
#1336=FACE_OUTER_BOUND('',#1712,.T.);
#1337=FACE_OUTER_BOUND('',#1713,.T.);
#1338=FACE_OUTER_BOUND('',#1714,.T.);
#1339=FACE_OUTER_BOUND('',#1715,.T.);
#1340=FACE_OUTER_BOUND('',#1716,.T.);
#1341=FACE_OUTER_BOUND('',#1717,.T.);
#1342=FACE_OUTER_BOUND('',#1718,.T.);
#1343=FACE_OUTER_BOUND('',#1719,.T.);
#1344=FACE_OUTER_BOUND('',#1720,.T.);
#1345=FACE_OUTER_BOUND('',#1721,.T.);
#1346=FACE_OUTER_BOUND('',#1722,.T.);
#1347=FACE_OUTER_BOUND('',#1723,.T.);
#1348=FACE_OUTER_BOUND('',#1724,.T.);
#1349=FACE_OUTER_BOUND('',#1725,.T.);
#1350=FACE_OUTER_BOUND('',#1726,.T.);
#1351=FACE_OUTER_BOUND('',#1727,.T.);
#1352=FACE_OUTER_BOUND('',#1728,.T.);
#1353=FACE_OUTER_BOUND('',#1729,.T.);
#1354=FACE_OUTER_BOUND('',#1730,.T.);
#1355=FACE_OUTER_BOUND('',#1731,.T.);
#1356=FACE_OUTER_BOUND('',#1732,.T.);
#1357=FACE_OUTER_BOUND('',#1733,.T.);
#1358=FACE_OUTER_BOUND('',#1734,.T.);
#1359=FACE_OUTER_BOUND('',#1735,.T.);
#1360=FACE_OUTER_BOUND('',#1736,.T.);
#1361=FACE_OUTER_BOUND('',#1738,.T.);
#1362=FACE_OUTER_BOUND('',#1739,.T.);
#1363=FACE_OUTER_BOUND('',#1740,.T.);
#1364=FACE_OUTER_BOUND('',#1745,.T.);
#1365=FACE_OUTER_BOUND('',#1746,.T.);
#1366=FACE_OUTER_BOUND('',#1747,.T.);
#1367=FACE_OUTER_BOUND('',#1748,.T.);
#1368=FACE_OUTER_BOUND('',#1749,.T.);
#1369=FACE_OUTER_BOUND('',#1750,.T.);
#1370=FACE_OUTER_BOUND('',#1751,.T.);
#1371=FACE_OUTER_BOUND('',#1752,.T.);
#1372=FACE_OUTER_BOUND('',#1757,.T.);
#1373=FACE_OUTER_BOUND('',#1758,.T.);
#1374=FACE_OUTER_BOUND('',#1759,.T.);
#1375=FACE_OUTER_BOUND('',#1760,.T.);
#1376=FACE_OUTER_BOUND('',#1761,.T.);
#1377=FACE_OUTER_BOUND('',#1762,.T.);
#1378=FACE_OUTER_BOUND('',#1763,.T.);
#1379=FACE_OUTER_BOUND('',#1764,.T.);
#1380=FACE_OUTER_BOUND('',#1765,.T.);
#1381=FACE_OUTER_BOUND('',#1766,.T.);
#1382=FACE_OUTER_BOUND('',#1767,.T.);
#1383=FACE_OUTER_BOUND('',#1768,.T.);
#1384=FACE_OUTER_BOUND('',#1769,.T.);
#1385=FACE_OUTER_BOUND('',#1775,.T.);
#1386=FACE_OUTER_BOUND('',#1781,.T.);
#1387=FACE_OUTER_BOUND('',#1782,.T.);
#1388=FACE_OUTER_BOUND('',#1783,.T.);
#1389=FACE_OUTER_BOUND('',#1784,.T.);
#1390=FACE_OUTER_BOUND('',#1785,.T.);
#1391=FACE_OUTER_BOUND('',#1786,.T.);
#1392=FACE_OUTER_BOUND('',#1787,.T.);
#1393=FACE_OUTER_BOUND('',#1788,.T.);
#1394=FACE_OUTER_BOUND('',#1789,.T.);
#1395=FACE_OUTER_BOUND('',#1794,.T.);
#1396=FACE_OUTER_BOUND('',#1799,.T.);
#1397=FACE_OUTER_BOUND('',#1800,.T.);
#1398=FACE_OUTER_BOUND('',#1801,.T.);
#1399=FACE_OUTER_BOUND('',#1802,.T.);
#1400=FACE_OUTER_BOUND('',#1803,.T.);
#1401=FACE_OUTER_BOUND('',#1804,.T.);
#1402=FACE_OUTER_BOUND('',#1805,.T.);
#1403=FACE_OUTER_BOUND('',#1806,.T.);
#1404=FACE_OUTER_BOUND('',#1807,.T.);
#1405=FACE_OUTER_BOUND('',#1808,.T.);
#1406=FACE_OUTER_BOUND('',#1809,.T.);
#1407=FACE_OUTER_BOUND('',#1810,.T.);
#1408=FACE_OUTER_BOUND('',#1811,.T.);
#1409=FACE_OUTER_BOUND('',#1812,.T.);
#1410=FACE_OUTER_BOUND('',#1813,.T.);
#1411=FACE_OUTER_BOUND('',#1814,.T.);
#1412=FACE_OUTER_BOUND('',#1815,.T.);
#1413=FACE_OUTER_BOUND('',#1816,.T.);
#1414=FACE_OUTER_BOUND('',#1817,.T.);
#1415=FACE_OUTER_BOUND('',#1818,.T.);
#1416=FACE_OUTER_BOUND('',#1819,.T.);
#1417=FACE_OUTER_BOUND('',#1820,.T.);
#1418=FACE_OUTER_BOUND('',#1821,.T.);
#1419=FACE_OUTER_BOUND('',#1822,.T.);
#1420=FACE_OUTER_BOUND('',#1823,.T.);
#1421=FACE_OUTER_BOUND('',#1824,.T.);
#1422=FACE_OUTER_BOUND('',#1825,.T.);
#1423=FACE_OUTER_BOUND('',#1826,.T.);
#1424=FACE_OUTER_BOUND('',#1828,.T.);
#1425=FACE_OUTER_BOUND('',#1829,.T.);
#1426=FACE_OUTER_BOUND('',#1831,.T.);
#1427=FACE_OUTER_BOUND('',#1832,.T.);
#1428=FACE_OUTER_BOUND('',#1833,.T.);
#1429=FACE_OUTER_BOUND('',#1834,.T.);
#1430=FACE_OUTER_BOUND('',#1835,.T.);
#1431=FACE_OUTER_BOUND('',#1836,.T.);
#1432=FACE_OUTER_BOUND('',#1837,.T.);
#1433=FACE_OUTER_BOUND('',#1838,.T.);
#1434=FACE_OUTER_BOUND('',#1839,.T.);
#1435=FACE_OUTER_BOUND('',#1840,.T.);
#1436=FACE_OUTER_BOUND('',#1841,.T.);
#1437=FACE_OUTER_BOUND('',#1842,.T.);
#1438=FACE_OUTER_BOUND('',#1843,.T.);
#1439=FACE_OUTER_BOUND('',#1844,.T.);
#1440=FACE_OUTER_BOUND('',#1845,.T.);
#1441=FACE_OUTER_BOUND('',#1846,.T.);
#1442=FACE_OUTER_BOUND('',#1847,.T.);
#1443=FACE_OUTER_BOUND('',#1848,.T.);
#1444=FACE_OUTER_BOUND('',#1849,.T.);
#1445=FACE_OUTER_BOUND('',#1850,.T.);
#1446=FACE_OUTER_BOUND('',#1851,.T.);
#1447=FACE_OUTER_BOUND('',#1852,.T.);
#1448=FACE_OUTER_BOUND('',#1853,.T.);
#1449=FACE_OUTER_BOUND('',#1854,.T.);
#1450=FACE_OUTER_BOUND('',#1855,.T.);
#1451=FACE_OUTER_BOUND('',#1856,.T.);
#1452=FACE_OUTER_BOUND('',#1857,.T.);
#1453=FACE_OUTER_BOUND('',#1859,.T.);
#1454=FACE_OUTER_BOUND('',#1860,.T.);
#1455=FACE_OUTER_BOUND('',#1862,.T.);
#1456=FACE_OUTER_BOUND('',#1863,.T.);
#1457=FACE_OUTER_BOUND('',#1864,.T.);
#1458=FACE_OUTER_BOUND('',#1865,.T.);
#1459=FACE_OUTER_BOUND('',#1866,.T.);
#1460=FACE_OUTER_BOUND('',#1867,.T.);
#1461=FACE_OUTER_BOUND('',#1868,.T.);
#1462=FACE_OUTER_BOUND('',#1869,.T.);
#1463=FACE_OUTER_BOUND('',#1870,.T.);
#1464=FACE_OUTER_BOUND('',#1871,.T.);
#1465=FACE_OUTER_BOUND('',#1872,.T.);
#1466=FACE_OUTER_BOUND('',#1873,.T.);
#1467=FACE_OUTER_BOUND('',#1874,.T.);
#1468=FACE_OUTER_BOUND('',#1875,.T.);
#1469=FACE_OUTER_BOUND('',#1876,.T.);
#1470=FACE_OUTER_BOUND('',#1877,.T.);
#1471=FACE_OUTER_BOUND('',#1878,.T.);
#1472=FACE_OUTER_BOUND('',#1879,.T.);
#1473=FACE_OUTER_BOUND('',#1880,.T.);
#1474=FACE_OUTER_BOUND('',#1881,.T.);
#1475=FACE_OUTER_BOUND('',#1882,.T.);
#1476=FACE_OUTER_BOUND('',#1883,.T.);
#1477=FACE_OUTER_BOUND('',#1884,.T.);
#1478=FACE_OUTER_BOUND('',#1885,.T.);
#1479=FACE_OUTER_BOUND('',#1886,.T.);
#1480=FACE_OUTER_BOUND('',#1887,.T.);
#1481=FACE_OUTER_BOUND('',#1888,.T.);
#1482=FACE_OUTER_BOUND('',#1889,.T.);
#1483=FACE_OUTER_BOUND('',#1890,.T.);
#1484=FACE_OUTER_BOUND('',#1891,.T.);
#1485=FACE_OUTER_BOUND('',#1892,.T.);
#1486=FACE_OUTER_BOUND('',#1893,.T.);
#1487=FACE_OUTER_BOUND('',#1894,.T.);
#1488=FACE_OUTER_BOUND('',#1895,.T.);
#1489=FACE_OUTER_BOUND('',#1897,.T.);
#1490=FACE_OUTER_BOUND('',#1898,.T.);
#1491=FACE_OUTER_BOUND('',#1899,.T.);
#1492=FACE_OUTER_BOUND('',#1901,.T.);
#1493=FACE_OUTER_BOUND('',#1903,.T.);
#1494=FACE_OUTER_BOUND('',#1904,.T.);
#1495=FACE_OUTER_BOUND('',#1905,.T.);
#1496=FACE_OUTER_BOUND('',#1906,.T.);
#1497=FACE_OUTER_BOUND('',#1907,.T.);
#1498=FACE_OUTER_BOUND('',#1908,.T.);
#1499=FACE_OUTER_BOUND('',#1909,.T.);
#1500=FACE_OUTER_BOUND('',#1910,.T.);
#1501=FACE_OUTER_BOUND('',#1911,.T.);
#1502=FACE_OUTER_BOUND('',#1912,.T.);
#1503=FACE_OUTER_BOUND('',#1913,.T.);
#1504=FACE_OUTER_BOUND('',#1914,.T.);
#1505=FACE_OUTER_BOUND('',#1915,.T.);
#1506=FACE_OUTER_BOUND('',#1916,.T.);
#1507=FACE_OUTER_BOUND('',#1917,.T.);
#1508=FACE_OUTER_BOUND('',#1921,.T.);
#1509=FACE_OUTER_BOUND('',#1922,.T.);
#1510=FACE_OUTER_BOUND('',#1926,.T.);
#1511=FACE_OUTER_BOUND('',#1927,.T.);
#1512=FACE_OUTER_BOUND('',#1928,.T.);
#1513=FACE_OUTER_BOUND('',#1930,.T.);
#1514=EDGE_LOOP('',(#5094,#5095,#5096,#5097));
#1515=EDGE_LOOP('',(#5098,#5099,#5100,#5101));
#1516=EDGE_LOOP('',(#5102,#5103,#5104,#5105));
#1517=EDGE_LOOP('',(#5106,#5107,#5108,#5109));
#1518=EDGE_LOOP('',(#5110,#5111,#5112,#5113));
#1519=EDGE_LOOP('',(#5114,#5115,#5116,#5117));
#1520=EDGE_LOOP('',(#5118,#5119,#5120,#5121));
#1521=EDGE_LOOP('',(#5122,#5123,#5124,#5125));
#1522=EDGE_LOOP('',(#5126,#5127,#5128,#5129));
#1523=EDGE_LOOP('',(#5130));
#1524=EDGE_LOOP('',(#5131));
#1525=EDGE_LOOP('',(#5132));
#1526=EDGE_LOOP('',(#5133));
#1527=EDGE_LOOP('',(#5134,#5135,#5136,#5137));
#1528=EDGE_LOOP('',(#5138));
#1529=EDGE_LOOP('',(#5139));
#1530=EDGE_LOOP('',(#5140));
#1531=EDGE_LOOP('',(#5141));
#1532=EDGE_LOOP('',(#5142,#5143,#5144,#5145));
#1533=EDGE_LOOP('',(#5146,#5147,#5148,#5149));
#1534=EDGE_LOOP('',(#5150,#5151,#5152,#5153));
#1535=EDGE_LOOP('',(#5154));
#1536=EDGE_LOOP('',(#5155));
#1537=EDGE_LOOP('',(#5156,#5157,#5158,#5159));
#1538=EDGE_LOOP('',(#5160,#5161,#5162,#5163));
#1539=EDGE_LOOP('',(#5164));
#1540=EDGE_LOOP('',(#5165));
#1541=EDGE_LOOP('',(#5166,#5167,#5168,#5169));
#1542=EDGE_LOOP('',(#5170,#5171,#5172,#5173));
#1543=EDGE_LOOP('',(#5174,#5175,#5176,#5177));
#1544=EDGE_LOOP('',(#5178,#5179,#5180,#5181));
#1545=EDGE_LOOP('',(#5182,#5183,#5184,#5185));
#1546=EDGE_LOOP('',(#5186,#5187,#5188,#5189));
#1547=EDGE_LOOP('',(#5190,#5191,#5192,#5193));
#1548=EDGE_LOOP('',(#5194,#5195,#5196,#5197));
#1549=EDGE_LOOP('',(#5198,#5199,#5200,#5201));
#1550=EDGE_LOOP('',(#5202,#5203,#5204,#5205));
#1551=EDGE_LOOP('',(#5206,#5207,#5208,#5209));
#1552=EDGE_LOOP('',(#5210,#5211,#5212,#5213));
#1553=EDGE_LOOP('',(#5214,#5215,#5216,#5217));
#1554=EDGE_LOOP('',(#5218,#5219,#5220,#5221));
#1555=EDGE_LOOP('',(#5222,#5223,#5224,#5225));
#1556=EDGE_LOOP('',(#5226,#5227,#5228,#5229));
#1557=EDGE_LOOP('',(#5230,#5231,#5232,#5233));
#1558=EDGE_LOOP('',(#5234,#5235,#5236,#5237));
#1559=EDGE_LOOP('',(#5238,#5239,#5240,#5241));
#1560=EDGE_LOOP('',(#5242,#5243,#5244,#5245));
#1561=EDGE_LOOP('',(#5246,#5247,#5248,#5249));
#1562=EDGE_LOOP('',(#5250,#5251,#5252,#5253));
#1563=EDGE_LOOP('',(#5254,#5255,#5256,#5257));
#1564=EDGE_LOOP('',(#5258,#5259,#5260,#5261));
#1565=EDGE_LOOP('',(#5262,#5263,#5264,#5265));
#1566=EDGE_LOOP('',(#5266,#5267,#5268,#5269));
#1567=EDGE_LOOP('',(#5270,#5271,#5272,#5273));
#1568=EDGE_LOOP('',(#5274,#5275,#5276,#5277,#5278,#5279,#5280,#5281));
#1569=EDGE_LOOP('',(#5282,#5283,#5284,#5285,#5286,#5287,#5288,#5289));
#1570=EDGE_LOOP('',(#5290,#5291,#5292,#5293));
#1571=EDGE_LOOP('',(#5294,#5295,#5296,#5297));
#1572=EDGE_LOOP('',(#5298,#5299,#5300,#5301,#5302,#5303,#5304,#5305));
#1573=EDGE_LOOP('',(#5306,#5307,#5308,#5309,#5310,#5311,#5312,#5313));
#1574=EDGE_LOOP('',(#5314,#5315,#5316,#5317));
#1575=EDGE_LOOP('',(#5318,#5319,#5320,#5321));
#1576=EDGE_LOOP('',(#5322,#5323,#5324,#5325));
#1577=EDGE_LOOP('',(#5326,#5327,#5328,#5329,#5330,#5331));
#1578=EDGE_LOOP('',(#5332,#5333,#5334,#5335,#5336,#5337));
#1579=EDGE_LOOP('',(#5338,#5339,#5340,#5341,#5342,#5343));
#1580=EDGE_LOOP('',(#5344,#5345,#5346,#5347,#5348,#5349));
#1581=EDGE_LOOP('',(#5350,#5351,#5352,#5353,#5354,#5355));
#1582=EDGE_LOOP('',(#5356,#5357,#5358,#5359,#5360,#5361));
#1583=EDGE_LOOP('',(#5362,#5363,#5364,#5365,#5366,#5367));
#1584=EDGE_LOOP('',(#5368,#5369,#5370,#5371,#5372,#5373));
#1585=EDGE_LOOP('',(#5374,#5375,#5376,#5377,#5378,#5379));
#1586=EDGE_LOOP('',(#5380,#5381,#5382,#5383,#5384,#5385));
#1587=EDGE_LOOP('',(#5386,#5387,#5388,#5389,#5390,#5391));
#1588=EDGE_LOOP('',(#5392,#5393,#5394,#5395,#5396,#5397));
#1589=EDGE_LOOP('',(#5398,#5399,#5400,#5401,#5402,#5403));
#1590=EDGE_LOOP('',(#5404,#5405,#5406,#5407,#5408,#5409));
#1591=EDGE_LOOP('',(#5410,#5411,#5412,#5413,#5414,#5415));
#1592=EDGE_LOOP('',(#5416,#5417,#5418,#5419,#5420,#5421));
#1593=EDGE_LOOP('',(#5422,#5423,#5424,#5425,#5426,#5427));
#1594=EDGE_LOOP('',(#5428,#5429,#5430,#5431,#5432,#5433));
#1595=EDGE_LOOP('',(#5434,#5435,#5436,#5437,#5438,#5439,#5440,#5441));
#1596=EDGE_LOOP('',(#5442,#5443,#5444,#5445,#5446,#5447));
#1597=EDGE_LOOP('',(#5448,#5449,#5450,#5451,#5452));
#1598=EDGE_LOOP('',(#5453,#5454,#5455,#5456,#5457,#5458));
#1599=EDGE_LOOP('',(#5459,#5460,#5461,#5462,#5463));
#1600=EDGE_LOOP('',(#5464,#5465,#5466,#5467,#5468,#5469));
#1601=EDGE_LOOP('',(#5470,#5471,#5472,#5473,#5474));
#1602=EDGE_LOOP('',(#5475,#5476,#5477,#5478,#5479,#5480));
#1603=EDGE_LOOP('',(#5481,#5482,#5483,#5484,#5485));
#1604=EDGE_LOOP('',(#5486,#5487,#5488,#5489,#5490,#5491));
#1605=EDGE_LOOP('',(#5492,#5493,#5494,#5495,#5496));
#1606=EDGE_LOOP('',(#5497,#5498,#5499,#5500,#5501,#5502));
#1607=EDGE_LOOP('',(#5503,#5504,#5505,#5506,#5507));
#1608=EDGE_LOOP('',(#5508,#5509,#5510,#5511,#5512,#5513));
#1609=EDGE_LOOP('',(#5514,#5515,#5516,#5517,#5518));
#1610=EDGE_LOOP('',(#5519,#5520,#5521,#5522,#5523,#5524));
#1611=EDGE_LOOP('',(#5525,#5526,#5527,#5528,#5529));
#1612=EDGE_LOOP('',(#5530,#5531,#5532,#5533,#5534,#5535));
#1613=EDGE_LOOP('',(#5536,#5537,#5538,#5539,#5540,#5541));
#1614=EDGE_LOOP('',(#5542,#5543,#5544,#5545));
#1615=EDGE_LOOP('',(#5546,#5547,#5548,#5549,#5550,#5551));
#1616=EDGE_LOOP('',(#5552,#5553,#5554,#5555,#5556,#5557));
#1617=EDGE_LOOP('',(#5558,#5559,#5560,#5561,#5562,#5563));
#1618=EDGE_LOOP('',(#5564,#5565,#5566,#5567,#5568,#5569));
#1619=EDGE_LOOP('',(#5570,#5571,#5572,#5573,#5574,#5575));
#1620=EDGE_LOOP('',(#5576,#5577,#5578,#5579,#5580,#5581));
#1621=EDGE_LOOP('',(#5582,#5583,#5584,#5585,#5586,#5587));
#1622=EDGE_LOOP('',(#5588,#5589,#5590,#5591,#5592,#5593));
#1623=EDGE_LOOP('',(#5594,#5595,#5596,#5597,#5598,#5599));
#1624=EDGE_LOOP('',(#5600,#5601,#5602,#5603,#5604,#5605));
#1625=EDGE_LOOP('',(#5606,#5607,#5608,#5609,#5610,#5611));
#1626=EDGE_LOOP('',(#5612,#5613,#5614,#5615,#5616,#5617));
#1627=EDGE_LOOP('',(#5618,#5619,#5620,#5621,#5622,#5623));
#1628=EDGE_LOOP('',(#5624,#5625,#5626,#5627,#5628,#5629));
#1629=EDGE_LOOP('',(#5630,#5631,#5632,#5633,#5634,#5635));
#1630=EDGE_LOOP('',(#5636,#5637,#5638,#5639,#5640,#5641));
#1631=EDGE_LOOP('',(#5642,#5643,#5644,#5645,#5646,#5647));
#1632=EDGE_LOOP('',(#5648,#5649,#5650,#5651,#5652,#5653));
#1633=EDGE_LOOP('',(#5654,#5655,#5656,#5657,#5658,#5659,#5660,#5661));
#1634=EDGE_LOOP('',(#5662,#5663,#5664,#5665,#5666,#5667));
#1635=EDGE_LOOP('',(#5668,#5669,#5670,#5671,#5672,#5673));
#1636=EDGE_LOOP('',(#5674,#5675,#5676,#5677,#5678));
#1637=EDGE_LOOP('',(#5679,#5680,#5681,#5682,#5683,#5684));
#1638=EDGE_LOOP('',(#5685,#5686,#5687,#5688,#5689));
#1639=EDGE_LOOP('',(#5690,#5691,#5692,#5693,#5694,#5695));
#1640=EDGE_LOOP('',(#5696,#5697,#5698,#5699,#5700));
#1641=EDGE_LOOP('',(#5701,#5702,#5703,#5704,#5705,#5706));
#1642=EDGE_LOOP('',(#5707,#5708,#5709,#5710,#5711));
#1643=EDGE_LOOP('',(#5712,#5713,#5714,#5715,#5716,#5717));
#1644=EDGE_LOOP('',(#5718,#5719,#5720,#5721,#5722));
#1645=EDGE_LOOP('',(#5723,#5724,#5725,#5726,#5727,#5728));
#1646=EDGE_LOOP('',(#5729,#5730,#5731,#5732,#5733));
#1647=EDGE_LOOP('',(#5734,#5735,#5736,#5737,#5738,#5739));
#1648=EDGE_LOOP('',(#5740,#5741,#5742,#5743,#5744));
#1649=EDGE_LOOP('',(#5745,#5746,#5747,#5748,#5749,#5750));
#1650=EDGE_LOOP('',(#5751,#5752,#5753,#5754,#5755));
#1651=EDGE_LOOP('',(#5756,#5757,#5758,#5759,#5760,#5761));
#1652=EDGE_LOOP('',(#5762,#5763,#5764,#5765,#5766,#5767));
#1653=EDGE_LOOP('',(#5768,#5769,#5770,#5771,#5772,#5773));
#1654=EDGE_LOOP('',(#5774,#5775,#5776,#5777,#5778));
#1655=EDGE_LOOP('',(#5779,#5780,#5781,#5782,#5783,#5784));
#1656=EDGE_LOOP('',(#5785,#5786,#5787,#5788,#5789));
#1657=EDGE_LOOP('',(#5790,#5791,#5792,#5793,#5794,#5795,#5796,#5797,#5798,
#5799,#5800,#5801,#5802,#5803,#5804,#5805,#5806,#5807,#5808,#5809,#5810,
#5811,#5812,#5813,#5814,#5815,#5816,#5817,#5818,#5819,#5820,#5821,#5822,
#5823,#5824,#5825,#5826,#5827,#5828,#5829,#5830,#5831,#5832,#5833,#5834,
#5835,#5836,#5837,#5838,#5839,#5840,#5841,#5842,#5843,#5844,#5845,#5846,
#5847,#5848,#5849,#5850,#5851,#5852,#5853,#5854,#5855,#5856,#5857,#5858,
#5859,#5860));
#1658=EDGE_LOOP('',(#5861,#5862,#5863,#5864,#5865,#5866,#5867,#5868,#5869,
#5870,#5871,#5872,#5873,#5874,#5875,#5876,#5877,#5878,#5879,#5880,#5881,
#5882,#5883,#5884,#5885,#5886,#5887,#5888,#5889,#5890,#5891,#5892,#5893,
#5894,#5895,#5896,#5897,#5898,#5899,#5900,#5901,#5902,#5903,#5904,#5905,
#5906,#5907,#5908,#5909,#5910,#5911,#5912,#5913,#5914,#5915,#5916,#5917,
#5918,#5919,#5920,#5921,#5922,#5923,#5924,#5925,#5926,#5927,#5928,#5929,
#5930,#5931,#5932,#5933,#5934,#5935,#5936,#5937,#5938,#5939,#5940));
#1659=EDGE_LOOP('',(#5941));
#1660=EDGE_LOOP('',(#5942,#5943,#5944,#5945,#5946));
#1661=EDGE_LOOP('',(#5947,#5948,#5949,#5950,#5951,#5952,#5953,#5954,#5955,
#5956,#5957,#5958,#5959,#5960,#5961,#5962,#5963,#5964,#5965,#5966,#5967,
#5968,#5969,#5970,#5971,#5972,#5973,#5974,#5975,#5976,#5977,#5978,#5979,
#5980,#5981,#5982,#5983,#5984,#5985,#5986,#5987,#5988,#5989,#5990,#5991,
#5992,#5993,#5994,#5995,#5996,#5997,#5998,#5999,#6000,#6001,#6002,#6003,
#6004,#6005,#6006,#6007,#6008,#6009,#6010,#6011,#6012,#6013,#6014,#6015,
#6016,#6017,#6018));
#1662=EDGE_LOOP('',(#6019,#6020,#6021,#6022,#6023,#6024,#6025,#6026,#6027,
#6028,#6029,#6030,#6031,#6032,#6033,#6034,#6035,#6036,#6037,#6038,#6039,
#6040,#6041,#6042,#6043,#6044,#6045,#6046,#6047,#6048,#6049,#6050,#6051,
#6052,#6053,#6054,#6055,#6056,#6057,#6058,#6059,#6060,#6061,#6062,#6063,
#6064,#6065,#6066,#6067,#6068,#6069,#6070,#6071,#6072,#6073,#6074,#6075,
#6076,#6077,#6078,#6079,#6080,#6081,#6082,#6083,#6084,#6085,#6086,#6087,
#6088,#6089,#6090,#6091,#6092,#6093,#6094,#6095,#6096,#6097,#6098));
#1663=EDGE_LOOP('',(#6099));
#1664=EDGE_LOOP('',(#6100,#6101,#6102,#6103));
#1665=EDGE_LOOP('',(#6104));
#1666=EDGE_LOOP('',(#6105,#6106,#6107,#6108));
#1667=EDGE_LOOP('',(#6109));
#1668=EDGE_LOOP('',(#6110,#6111,#6112,#6113));
#1669=EDGE_LOOP('',(#6114,#6115,#6116,#6117));
#1670=EDGE_LOOP('',(#6118,#6119,#6120,#6121,#6122,#6123));
#1671=EDGE_LOOP('',(#6124,#6125,#6126,#6127));
#1672=EDGE_LOOP('',(#6128,#6129,#6130,#6131,#6132,#6133));
#1673=EDGE_LOOP('',(#6134,#6135,#6136,#6137));
#1674=EDGE_LOOP('',(#6138,#6139,#6140,#6141,#6142,#6143));
#1675=EDGE_LOOP('',(#6144,#6145,#6146,#6147));
#1676=EDGE_LOOP('',(#6148,#6149,#6150,#6151,#6152,#6153));
#1677=EDGE_LOOP('',(#6154,#6155,#6156,#6157));
#1678=EDGE_LOOP('',(#6158,#6159,#6160,#6161,#6162,#6163));
#1679=EDGE_LOOP('',(#6164,#6165,#6166,#6167));
#1680=EDGE_LOOP('',(#6168,#6169,#6170,#6171,#6172,#6173,#6174,#6175,#6176,
#6177,#6178,#6179,#6180,#6181,#6182,#6183,#6184,#6185,#6186,#6187,#6188,
#6189,#6190,#6191,#6192,#6193));
#1681=EDGE_LOOP('',(#6194,#6195,#6196,#6197,#6198,#6199));
#1682=EDGE_LOOP('',(#6200,#6201,#6202,#6203,#6204,#6205,#6206,#6207));
#1683=EDGE_LOOP('',(#6208,#6209,#6210,#6211,#6212,#6213,#6214,#6215,#6216,
#6217,#6218,#6219,#6220,#6221,#6222,#6223,#6224,#6225,#6226,#6227,#6228,
#6229,#6230,#6231,#6232,#6233,#6234,#6235,#6236,#6237,#6238,#6239));
#1684=EDGE_LOOP('',(#6240,#6241,#6242,#6243,#6244,#6245,#6246,#6247,#6248,
#6249,#6250,#6251,#6252,#6253,#6254,#6255,#6256,#6257,#6258,#6259,#6260,
#6261,#6262,#6263,#6264,#6265,#6266,#6267,#6268,#6269,#6270,#6271,#6272));
#1685=EDGE_LOOP('',(#6273,#6274,#6275,#6276));
#1686=EDGE_LOOP('',(#6277,#6278,#6279,#6280));
#1687=EDGE_LOOP('',(#6281,#6282,#6283,#6284));
#1688=EDGE_LOOP('',(#6285,#6286,#6287,#6288));
#1689=EDGE_LOOP('',(#6289,#6290,#6291,#6292));
#1690=EDGE_LOOP('',(#6293,#6294,#6295,#6296));
#1691=EDGE_LOOP('',(#6297,#6298,#6299,#6300,#6301,#6302));
#1692=EDGE_LOOP('',(#6303));
#1693=EDGE_LOOP('',(#6304,#6305,#6306,#6307));
#1694=EDGE_LOOP('',(#6308,#6309,#6310,#6311));
#1695=EDGE_LOOP('',(#6312));
#1696=EDGE_LOOP('',(#6313,#6314,#6315,#6316,#6317,#6318));
#1697=EDGE_LOOP('',(#6319));
#1698=EDGE_LOOP('',(#6320,#6321,#6322,#6323));
#1699=EDGE_LOOP('',(#6324,#6325,#6326,#6327,#6328,#6329));
#1700=EDGE_LOOP('',(#6330,#6331,#6332,#6333,#6334,#6335));
#1701=EDGE_LOOP('',(#6336,#6337,#6338,#6339,#6340,#6341));
#1702=EDGE_LOOP('',(#6342,#6343,#6344,#6345,#6346,#6347));
#1703=EDGE_LOOP('',(#6348,#6349,#6350,#6351,#6352,#6353));
#1704=EDGE_LOOP('',(#6354,#6355,#6356,#6357,#6358,#6359));
#1705=EDGE_LOOP('',(#6360,#6361,#6362,#6363,#6364,#6365));
#1706=EDGE_LOOP('',(#6366,#6367,#6368,#6369,#6370,#6371));
#1707=EDGE_LOOP('',(#6372,#6373,#6374,#6375,#6376,#6377));
#1708=EDGE_LOOP('',(#6378,#6379,#6380,#6381,#6382,#6383));
#1709=EDGE_LOOP('',(#6384,#6385,#6386,#6387,#6388,#6389));
#1710=EDGE_LOOP('',(#6390,#6391,#6392,#6393,#6394,#6395));
#1711=EDGE_LOOP('',(#6396,#6397,#6398,#6399,#6400,#6401));
#1712=EDGE_LOOP('',(#6402,#6403,#6404,#6405,#6406,#6407));
#1713=EDGE_LOOP('',(#6408,#6409,#6410,#6411,#6412,#6413));
#1714=EDGE_LOOP('',(#6414,#6415,#6416,#6417,#6418,#6419,#6420,#6421,#6422));
#1715=EDGE_LOOP('',(#6423,#6424,#6425,#6426,#6427,#6428));
#1716=EDGE_LOOP('',(#6429,#6430,#6431,#6432,#6433,#6434));
#1717=EDGE_LOOP('',(#6435,#6436,#6437,#6438));
#1718=EDGE_LOOP('',(#6439,#6440,#6441,#6442,#6443,#6444));
#1719=EDGE_LOOP('',(#6445,#6446,#6447,#6448));
#1720=EDGE_LOOP('',(#6449,#6450,#6451,#6452,#6453,#6454));
#1721=EDGE_LOOP('',(#6455,#6456,#6457,#6458));
#1722=EDGE_LOOP('',(#6459,#6460,#6461,#6462,#6463,#6464));
#1723=EDGE_LOOP('',(#6465,#6466,#6467,#6468,#6469));
#1724=EDGE_LOOP('',(#6470,#6471,#6472,#6473,#6474));
#1725=EDGE_LOOP('',(#6475,#6476,#6477,#6478,#6479));
#1726=EDGE_LOOP('',(#6480,#6481,#6482,#6483,#6484));
#1727=EDGE_LOOP('',(#6485,#6486,#6487,#6488,#6489));
#1728=EDGE_LOOP('',(#6490,#6491,#6492,#6493,#6494,#6495));
#1729=EDGE_LOOP('',(#6496,#6497,#6498,#6499,#6500));
#1730=EDGE_LOOP('',(#6501,#6502,#6503,#6504,#6505,#6506));
#1731=EDGE_LOOP('',(#6507,#6508,#6509,#6510));
#1732=EDGE_LOOP('',(#6511,#6512,#6513,#6514,#6515,#6516,#6517,#6518,#6519,
#6520,#6521,#6522,#6523,#6524,#6525,#6526,#6527,#6528,#6529,#6530,#6531,
#6532,#6533,#6534,#6535,#6536,#6537,#6538,#6539,#6540,#6541,#6542,#6543,
#6544,#6545,#6546,#6547,#6548,#6549,#6550,#6551,#6552,#6553,#6554,#6555,
#6556,#6557,#6558,#6559,#6560,#6561,#6562,#6563,#6564,#6565,#6566,#6567,
#6568,#6569,#6570,#6571,#6572));
#1733=EDGE_LOOP('',(#6573,#6574,#6575,#6576,#6577,#6578,#6579,#6580,#6581,
#6582,#6583,#6584,#6585,#6586,#6587,#6588,#6589,#6590,#6591,#6592,#6593,
#6594,#6595,#6596,#6597,#6598,#6599,#6600,#6601,#6602,#6603,#6604,#6605,
#6606,#6607,#6608,#6609,#6610,#6611,#6612,#6613,#6614,#6615,#6616,#6617,
#6618,#6619,#6620,#6621,#6622,#6623,#6624,#6625,#6626,#6627,#6628,#6629,
#6630,#6631,#6632));
#1734=EDGE_LOOP('',(#6633));
#1735=EDGE_LOOP('',(#6634,#6635,#6636,#6637));
#1736=EDGE_LOOP('',(#6638));
#1737=EDGE_LOOP('',(#6639,#6640,#6641,#6642));
#1738=EDGE_LOOP('',(#6643));
#1739=EDGE_LOOP('',(#6644,#6645,#6646,#6647));
#1740=EDGE_LOOP('',(#6648,#6649,#6650,#6651));
#1741=EDGE_LOOP('',(#6652));
#1742=EDGE_LOOP('',(#6653));
#1743=EDGE_LOOP('',(#6654));
#1744=EDGE_LOOP('',(#6655));
#1745=EDGE_LOOP('',(#6656,#6657,#6658,#6659));
#1746=EDGE_LOOP('',(#6660,#6661,#6662,#6663));
#1747=EDGE_LOOP('',(#6664,#6665,#6666,#6667));
#1748=EDGE_LOOP('',(#6668,#6669,#6670,#6671));
#1749=EDGE_LOOP('',(#6672,#6673,#6674,#6675));
#1750=EDGE_LOOP('',(#6676,#6677,#6678,#6679));
#1751=EDGE_LOOP('',(#6680,#6681,#6682,#6683));
#1752=EDGE_LOOP('',(#6684,#6685,#6686,#6687));
#1753=EDGE_LOOP('',(#6688));
#1754=EDGE_LOOP('',(#6689));
#1755=EDGE_LOOP('',(#6690));
#1756=EDGE_LOOP('',(#6691));
#1757=EDGE_LOOP('',(#6692,#6693,#6694,#6695));
#1758=EDGE_LOOP('',(#6696,#6697,#6698,#6699));
#1759=EDGE_LOOP('',(#6700,#6701,#6702,#6703));
#1760=EDGE_LOOP('',(#6704,#6705,#6706,#6707));
#1761=EDGE_LOOP('',(#6708,#6709,#6710,#6711));
#1762=EDGE_LOOP('',(#6712,#6713,#6714,#6715));
#1763=EDGE_LOOP('',(#6716,#6717,#6718,#6719));
#1764=EDGE_LOOP('',(#6720,#6721,#6722,#6723));
#1765=EDGE_LOOP('',(#6724,#6725,#6726,#6727));
#1766=EDGE_LOOP('',(#6728,#6729,#6730,#6731));
#1767=EDGE_LOOP('',(#6732,#6733,#6734,#6735));
#1768=EDGE_LOOP('',(#6736,#6737,#6738,#6739));
#1769=EDGE_LOOP('',(#6740,#6741,#6742,#6743));
#1770=EDGE_LOOP('',(#6744,#6745,#6746,#6747));
#1771=EDGE_LOOP('',(#6748));
#1772=EDGE_LOOP('',(#6749));
#1773=EDGE_LOOP('',(#6750));
#1774=EDGE_LOOP('',(#6751));
#1775=EDGE_LOOP('',(#6752,#6753,#6754,#6755));
#1776=EDGE_LOOP('',(#6756,#6757,#6758,#6759));
#1777=EDGE_LOOP('',(#6760));
#1778=EDGE_LOOP('',(#6761));
#1779=EDGE_LOOP('',(#6762));
#1780=EDGE_LOOP('',(#6763));
#1781=EDGE_LOOP('',(#6764,#6765,#6766,#6767));
#1782=EDGE_LOOP('',(#6768,#6769,#6770,#6771));
#1783=EDGE_LOOP('',(#6772,#6773,#6774,#6775));
#1784=EDGE_LOOP('',(#6776,#6777,#6778,#6779));
#1785=EDGE_LOOP('',(#6780,#6781,#6782,#6783));
#1786=EDGE_LOOP('',(#6784,#6785,#6786,#6787));
#1787=EDGE_LOOP('',(#6788,#6789,#6790,#6791));
#1788=EDGE_LOOP('',(#6792,#6793,#6794,#6795));
#1789=EDGE_LOOP('',(#6796,#6797,#6798,#6799));
#1790=EDGE_LOOP('',(#6800));
#1791=EDGE_LOOP('',(#6801));
#1792=EDGE_LOOP('',(#6802));
#1793=EDGE_LOOP('',(#6803));
#1794=EDGE_LOOP('',(#6804,#6805,#6806,#6807));
#1795=EDGE_LOOP('',(#6808));
#1796=EDGE_LOOP('',(#6809));
#1797=EDGE_LOOP('',(#6810));
#1798=EDGE_LOOP('',(#6811));
#1799=EDGE_LOOP('',(#6812,#6813,#6814,#6815));
#1800=EDGE_LOOP('',(#6816,#6817,#6818,#6819,#6820));
#1801=EDGE_LOOP('',(#6821,#6822,#6823,#6824,#6825));
#1802=EDGE_LOOP('',(#6826,#6827,#6828,#6829,#6830,#6831));
#1803=EDGE_LOOP('',(#6832,#6833,#6834,#6835,#6836));
#1804=EDGE_LOOP('',(#6837,#6838,#6839,#6840,#6841));
#1805=EDGE_LOOP('',(#6842,#6843,#6844,#6845,#6846,#6847));
#1806=EDGE_LOOP('',(#6848,#6849,#6850,#6851,#6852));
#1807=EDGE_LOOP('',(#6853,#6854,#6855,#6856,#6857,#6858));
#1808=EDGE_LOOP('',(#6859,#6860,#6861,#6862));
#1809=EDGE_LOOP('',(#6863,#6864,#6865,#6866,#6867,#6868));
#1810=EDGE_LOOP('',(#6869,#6870,#6871,#6872,#6873));
#1811=EDGE_LOOP('',(#6874,#6875,#6876,#6877,#6878,#6879));
#1812=EDGE_LOOP('',(#6880,#6881,#6882,#6883));
#1813=EDGE_LOOP('',(#6884,#6885,#6886,#6887,#6888,#6889));
#1814=EDGE_LOOP('',(#6890,#6891,#6892,#6893,#6894,#6895,#6896,#6897,#6898,
#6899,#6900,#6901,#6902,#6903,#6904,#6905,#6906,#6907,#6908,#6909,#6910,
#6911,#6912,#6913,#6914,#6915,#6916,#6917,#6918,#6919,#6920,#6921,#6922,
#6923));
#1815=EDGE_LOOP('',(#6924,#6925,#6926,#6927,#6928,#6929));
#1816=EDGE_LOOP('',(#6930,#6931,#6932,#6933,#6934,#6935,#6936,#6937,#6938));
#1817=EDGE_LOOP('',(#6939,#6940,#6941,#6942,#6943,#6944,#6945,#6946,#6947,
#6948,#6949,#6950,#6951,#6952,#6953,#6954,#6955,#6956,#6957,#6958,#6959,
#6960,#6961,#6962,#6963,#6964,#6965,#6966,#6967,#6968,#6969,#6970,#6971,
#6972,#6973,#6974,#6975,#6976,#6977,#6978,#6979,#6980,#6981));
#1818=EDGE_LOOP('',(#6982,#6983,#6984,#6985,#6986,#6987,#6988,#6989,#6990,
#6991,#6992,#6993,#6994,#6995,#6996,#6997,#6998,#6999,#7000,#7001,#7002,
#7003,#7004,#7005,#7006,#7007,#7008,#7009,#7010,#7011,#7012,#7013,#7014,
#7015,#7016,#7017,#7018,#7019,#7020,#7021,#7022,#7023,#7024,#7025,#7026,
#7027,#7028,#7029));
#1819=EDGE_LOOP('',(#7030,#7031,#7032,#7033));
#1820=EDGE_LOOP('',(#7034,#7035,#7036,#7037));
#1821=EDGE_LOOP('',(#7038,#7039,#7040,#7041));
#1822=EDGE_LOOP('',(#7042,#7043,#7044,#7045));
#1823=EDGE_LOOP('',(#7046,#7047,#7048,#7049));
#1824=EDGE_LOOP('',(#7050,#7051,#7052,#7053));
#1825=EDGE_LOOP('',(#7054,#7055,#7056,#7057,#7058,#7059));
#1826=EDGE_LOOP('',(#7060));
#1827=EDGE_LOOP('',(#7061,#7062,#7063,#7064,#7065));
#1828=EDGE_LOOP('',(#7066,#7067,#7068,#7069));
#1829=EDGE_LOOP('',(#7070));
#1830=EDGE_LOOP('',(#7071,#7072,#7073,#7074,#7075,#7076));
#1831=EDGE_LOOP('',(#7077));
#1832=EDGE_LOOP('',(#7078,#7079,#7080,#7081));
#1833=EDGE_LOOP('',(#7082,#7083,#7084,#7085));
#1834=EDGE_LOOP('',(#7086,#7087,#7088,#7089,#7090));
#1835=EDGE_LOOP('',(#7091,#7092,#7093,#7094,#7095));
#1836=EDGE_LOOP('',(#7096,#7097,#7098,#7099,#7100));
#1837=EDGE_LOOP('',(#7101,#7102,#7103,#7104));
#1838=EDGE_LOOP('',(#7105,#7106,#7107,#7108,#7109));
#1839=EDGE_LOOP('',(#7110,#7111,#7112,#7113));
#1840=EDGE_LOOP('',(#7114,#7115,#7116,#7117));
#1841=EDGE_LOOP('',(#7118,#7119,#7120,#7121,#7122));
#1842=EDGE_LOOP('',(#7123,#7124,#7125,#7126,#7127,#7128));
#1843=EDGE_LOOP('',(#7129,#7130,#7131,#7132));
#1844=EDGE_LOOP('',(#7133,#7134,#7135,#7136));
#1845=EDGE_LOOP('',(#7137,#7138,#7139,#7140,#7141,#7142,#7143,#7144,#7145,
#7146,#7147,#7148,#7149,#7150,#7151,#7152,#7153,#7154,#7155,#7156,#7157,
#7158,#7159,#7160,#7161,#7162,#7163,#7164,#7165,#7166));
#1846=EDGE_LOOP('',(#7167,#7168,#7169,#7170));
#1847=EDGE_LOOP('',(#7171,#7172,#7173,#7174,#7175,#7176,#7177,#7178));
#1848=EDGE_LOOP('',(#7179,#7180,#7181,#7182,#7183,#7184,#7185,#7186,#7187,
#7188,#7189,#7190,#7191,#7192,#7193,#7194,#7195,#7196,#7197,#7198,#7199,
#7200,#7201,#7202,#7203,#7204,#7205,#7206,#7207,#7208,#7209,#7210,#7211));
#1849=EDGE_LOOP('',(#7212,#7213,#7214,#7215,#7216,#7217,#7218,#7219,#7220,
#7221,#7222,#7223,#7224,#7225,#7226,#7227,#7228,#7229,#7230,#7231,#7232,
#7233,#7234,#7235,#7236,#7237,#7238,#7239,#7240,#7241,#7242,#7243,#7244,
#7245,#7246,#7247));
#1850=EDGE_LOOP('',(#7248,#7249,#7250,#7251));
#1851=EDGE_LOOP('',(#7252,#7253,#7254,#7255));
#1852=EDGE_LOOP('',(#7256,#7257,#7258,#7259));
#1853=EDGE_LOOP('',(#7260,#7261,#7262,#7263));
#1854=EDGE_LOOP('',(#7264,#7265,#7266,#7267));
#1855=EDGE_LOOP('',(#7268,#7269,#7270,#7271));
#1856=EDGE_LOOP('',(#7272,#7273,#7274,#7275,#7276,#7277));
#1857=EDGE_LOOP('',(#7278));
#1858=EDGE_LOOP('',(#7279,#7280,#7281,#7282,#7283));
#1859=EDGE_LOOP('',(#7284,#7285,#7286,#7287));
#1860=EDGE_LOOP('',(#7288));
#1861=EDGE_LOOP('',(#7289,#7290,#7291,#7292,#7293,#7294));
#1862=EDGE_LOOP('',(#7295));
#1863=EDGE_LOOP('',(#7296,#7297,#7298,#7299));
#1864=EDGE_LOOP('',(#7300,#7301,#7302,#7303,#7304,#7305));
#1865=EDGE_LOOP('',(#7306,#7307,#7308,#7309,#7310));
#1866=EDGE_LOOP('',(#7311,#7312,#7313,#7314,#7315));
#1867=EDGE_LOOP('',(#7316,#7317,#7318,#7319,#7320,#7321));
#1868=EDGE_LOOP('',(#7322,#7323,#7324,#7325,#7326));
#1869=EDGE_LOOP('',(#7327,#7328,#7329,#7330,#7331));
#1870=EDGE_LOOP('',(#7332,#7333,#7334,#7335,#7336,#7337));
#1871=EDGE_LOOP('',(#7338,#7339,#7340,#7341,#7342));
#1872=EDGE_LOOP('',(#7343,#7344,#7345,#7346,#7347));
#1873=EDGE_LOOP('',(#7348,#7349,#7350,#7351,#7352));
#1874=EDGE_LOOP('',(#7353,#7354,#7355,#7356,#7357));
#1875=EDGE_LOOP('',(#7358,#7359,#7360,#7361,#7362));
#1876=EDGE_LOOP('',(#7363,#7364,#7365,#7366,#7367,#7368));
#1877=EDGE_LOOP('',(#7369,#7370,#7371,#7372));
#1878=EDGE_LOOP('',(#7373,#7374,#7375,#7376));
#1879=EDGE_LOOP('',(#7377,#7378,#7379,#7380));
#1880=EDGE_LOOP('',(#7381,#7382,#7383,#7384));
#1881=EDGE_LOOP('',(#7385,#7386,#7387,#7388));
#1882=EDGE_LOOP('',(#7389,#7390,#7391,#7392));
#1883=EDGE_LOOP('',(#7393,#7394,#7395,#7396));
#1884=EDGE_LOOP('',(#7397,#7398,#7399,#7400));
#1885=EDGE_LOOP('',(#7401,#7402,#7403,#7404));
#1886=EDGE_LOOP('',(#7405,#7406,#7407,#7408));
#1887=EDGE_LOOP('',(#7409,#7410,#7411,#7412));
#1888=EDGE_LOOP('',(#7413,#7414,#7415,#7416));
#1889=EDGE_LOOP('',(#7417,#7418,#7419,#7420));
#1890=EDGE_LOOP('',(#7421,#7422,#7423,#7424));
#1891=EDGE_LOOP('',(#7425,#7426,#7427,#7428));
#1892=EDGE_LOOP('',(#7429,#7430,#7431,#7432,#7433));
#1893=EDGE_LOOP('',(#7434,#7435,#7436,#7437,#7438,#7439,#7440,#7441,#7442,
#7443,#7444,#7445,#7446,#7447,#7448,#7449,#7450,#7451,#7452,#7453,#7454,
#7455,#7456,#7457,#7458,#7459,#7460,#7461,#7462,#7463,#7464,#7465,#7466,
#7467,#7468,#7469,#7470,#7471,#7472,#7473,#7474));
#1894=EDGE_LOOP('',(#7475,#7476,#7477,#7478,#7479,#7480,#7481,#7482,#7483,
#7484,#7485,#7486,#7487,#7488,#7489,#7490,#7491,#7492,#7493,#7494,#7495,
#7496,#7497,#7498,#7499,#7500,#7501,#7502,#7503,#7504,#7505,#7506,#7507,
#7508,#7509,#7510,#7511,#7512,#7513,#7514,#7515,#7516));
#1895=EDGE_LOOP('',(#7517));
#1896=EDGE_LOOP('',(#7518,#7519,#7520,#7521));
#1897=EDGE_LOOP('',(#7522,#7523,#7524,#7525));
#1898=EDGE_LOOP('',(#7526,#7527,#7528,#7529));
#1899=EDGE_LOOP('',(#7530,#7531,#7532,#7533,#7534));
#1900=EDGE_LOOP('',(#7535));
#1901=EDGE_LOOP('',(#7536));
#1902=EDGE_LOOP('',(#7537));
#1903=EDGE_LOOP('',(#7538,#7539,#7540,#7541));
#1904=EDGE_LOOP('',(#7542,#7543,#7544,#7545,#7546,#7547));
#1905=EDGE_LOOP('',(#7548,#7549,#7550,#7551,#7552,#7553));
#1906=EDGE_LOOP('',(#7554,#7555,#7556,#7557,#7558,#7559));
#1907=EDGE_LOOP('',(#7560,#7561,#7562,#7563));
#1908=EDGE_LOOP('',(#7564,#7565,#7566,#7567));
#1909=EDGE_LOOP('',(#7568,#7569,#7570,#7571));
#1910=EDGE_LOOP('',(#7572,#7573,#7574,#7575));
#1911=EDGE_LOOP('',(#7576,#7577,#7578,#7579));
#1912=EDGE_LOOP('',(#7580,#7581,#7582,#7583,#7584,#7585));
#1913=EDGE_LOOP('',(#7586,#7587,#7588,#7589));
#1914=EDGE_LOOP('',(#7590,#7591,#7592,#7593));
#1915=EDGE_LOOP('',(#7594,#7595,#7596,#7597,#7598,#7599,#7600,#7601,#7602,
#7603,#7604,#7605,#7606,#7607,#7608,#7609));
#1916=EDGE_LOOP('',(#7610,#7611,#7612,#7613,#7614,#7615,#7616,#7617,#7618,
#7619,#7620,#7621,#7622,#7623,#7624,#7625,#7626));
#1917=EDGE_LOOP('',(#7627));
#1918=EDGE_LOOP('',(#7628));
#1919=EDGE_LOOP('',(#7629));
#1920=EDGE_LOOP('',(#7630,#7631,#7632,#7633));
#1921=EDGE_LOOP('',(#7634,#7635,#7636,#7637));
#1922=EDGE_LOOP('',(#7638));
#1923=EDGE_LOOP('',(#7639));
#1924=EDGE_LOOP('',(#7640));
#1925=EDGE_LOOP('',(#7641,#7642,#7643,#7644,#7645));
#1926=EDGE_LOOP('',(#7646,#7647,#7648,#7649));
#1927=EDGE_LOOP('',(#7650,#7651,#7652,#7653));
#1928=EDGE_LOOP('',(#7654));
#1929=EDGE_LOOP('',(#7655));
#1930=EDGE_LOOP('',(#7656));
#1931=EDGE_LOOP('',(#7657));
#1932=LINE('',#10367,#2330);
#1933=LINE('',#10373,#2331);
#1934=LINE('',#10379,#2332);
#1935=LINE('',#10385,#2333);
#1936=LINE('',#10390,#2334);
#1937=LINE('',#10392,#2335);
#1938=LINE('',#10394,#2336);
#1939=LINE('',#10395,#2337);
#1940=LINE('',#10398,#2338);
#1941=LINE('',#10400,#2339);
#1942=LINE('',#10401,#2340);
#1943=LINE('',#10404,#2341);
#1944=LINE('',#10406,#2342);
#1945=LINE('',#10407,#2343);
#1946=LINE('',#10409,#2344);
#1947=LINE('',#10410,#2345);
#1948=LINE('',#10418,#2346);
#1949=LINE('',#10424,#2347);
#1950=LINE('',#10429,#2348);
#1951=LINE('',#10431,#2349);
#1952=LINE('',#10433,#2350);
#1953=LINE('',#10434,#2351);
#1954=LINE('',#10437,#2352);
#1955=LINE('',#10439,#2353);
#1956=LINE('',#10440,#2354);
#1957=LINE('',#10443,#2355);
#1958=LINE('',#10445,#2356);
#1959=LINE('',#10446,#2357);
#1960=LINE('',#10448,#2358);
#1961=LINE('',#10449,#2359);
#1962=LINE('',#10456,#2360);
#1963=LINE('',#10458,#2361);
#1964=LINE('',#10460,#2362);
#1965=LINE('',#10461,#2363);
#1966=LINE('',#10464,#2364);
#1967=LINE('',#10466,#2365);
#1968=LINE('',#10467,#2366);
#1969=LINE('',#10470,#2367);
#1970=LINE('',#10472,#2368);
#1971=LINE('',#10473,#2369);
#1972=LINE('',#10475,#2370);
#1973=LINE('',#10476,#2371);
#1974=LINE('',#10485,#2372);
#1975=LINE('',#10488,#2373);
#1976=LINE('',#10491,#2374);
#1977=LINE('',#10493,#2375);
#1978=LINE('',#10494,#2376);
#1979=LINE('',#10499,#2377);
#1980=LINE('',#10503,#2378);
#1981=LINE('',#10505,#2379);
#1982=LINE('',#10506,#2380);
#1983=LINE('',#10512,#2381);
#1984=LINE('',#10515,#2382);
#1985=LINE('',#10517,#2383);
#1986=LINE('',#10518,#2384);
#1987=LINE('',#10523,#2385);
#1988=LINE('',#10526,#2386);
#1989=LINE('',#10527,#2387);
#1990=LINE('',#10533,#2388);
#1991=LINE('',#10536,#2389);
#1992=LINE('',#10539,#2390);
#1993=LINE('',#10541,#2391);
#1994=LINE('',#10542,#2392);
#1995=LINE('',#10548,#2393);
#1996=LINE('',#10551,#2394);
#1997=LINE('',#10553,#2395);
#1998=LINE('',#10554,#2396);
#1999=LINE('',#10559,#2397);
#2000=LINE('',#10563,#2398);
#2001=LINE('',#10565,#2399);
#2002=LINE('',#10566,#2400);
#2003=LINE('',#10571,#2401);
#2004=LINE('',#10574,#2402);
#2005=LINE('',#10575,#2403);
#2006=LINE('',#10579,#2404);
#2007=LINE('',#10581,#2405);
#2008=LINE('',#10583,#2406);
#2009=LINE('',#10584,#2407);
#2010=LINE('',#10587,#2408);
#2011=LINE('',#10589,#2409);
#2012=LINE('',#10590,#2410);
#2013=LINE('',#10593,#2411);
#2014=LINE('',#10595,#2412);
#2015=LINE('',#10596,#2413);
#2016=LINE('',#10598,#2414);
#2017=LINE('',#10599,#2415);
#2018=LINE('',#10606,#2416);
#2019=LINE('',#10783,#2417);
#2020=LINE('',#11085,#2418);
#2021=LINE('',#11314,#2419);
#2022=LINE('',#11546,#2420);
#2023=LINE('',#11776,#2421);
#2024=LINE('',#12008,#2422);
#2025=LINE('',#12243,#2423);
#2026=LINE('',#12475,#2424);
#2027=LINE('',#12705,#2425);
#2028=LINE('',#12810,#2426);
#2029=LINE('',#12844,#2427);
#2030=LINE('',#13007,#2428);
#2031=LINE('',#13237,#2429);
#2032=LINE('',#13469,#2430);
#2033=LINE('',#13701,#2431);
#2034=LINE('',#13930,#2432);
#2035=LINE('',#14163,#2433);
#2036=LINE('',#14395,#2434);
#2037=LINE('',#14556,#2435);
#2038=LINE('',#14573,#2436);
#2039=LINE('',#14647,#2437);
#2040=LINE('',#15070,#2438);
#2041=LINE('',#15538,#2439);
#2042=LINE('',#15958,#2440);
#2043=LINE('',#16359,#2441);
#2044=LINE('',#16776,#2442);
#2045=LINE('',#17208,#2443);
#2046=LINE('',#17660,#2444);
#2047=LINE('',#18123,#2445);
#2048=LINE('',#18533,#2446);
#2049=LINE('',#18966,#2447);
#2050=LINE('',#19392,#2448);
#2051=LINE('',#19804,#2449);
#2052=LINE('',#20234,#2450);
#2053=LINE('',#20715,#2451);
#2054=LINE('',#21129,#2452);
#2055=LINE('',#21560,#2453);
#2056=LINE('',#21975,#2454);
#2057=LINE('',#22312,#2455);
#2058=LINE('',#22419,#2456);
#2059=LINE('',#22654,#2457);
#2060=LINE('',#23011,#2458);
#2061=LINE('',#23441,#2459);
#2062=LINE('',#23871,#2460);
#2063=LINE('',#24298,#2461);
#2064=LINE('',#24728,#2462);
#2065=LINE('',#25158,#2463);
#2066=LINE('',#25588,#2464);
#2067=LINE('',#26021,#2465);
#2068=LINE('',#26445,#2466);
#2069=LINE('',#26875,#2467);
#2070=LINE('',#27305,#2468);
#2071=LINE('',#27732,#2469);
#2072=LINE('',#28162,#2470);
#2073=LINE('',#28586,#2471);
#2074=LINE('',#29016,#2472);
#2075=LINE('',#29315,#2473);
#2076=LINE('',#29476,#2474);
#2077=LINE('',#29493,#2475);
#2078=LINE('',#29567,#2476);
#2079=LINE('',#29800,#2477);
#2080=LINE('',#30203,#2478);
#2081=LINE('',#30628,#2479);
#2082=LINE('',#31046,#2480);
#2083=LINE('',#31472,#2481);
#2084=LINE('',#31913,#2482);
#2085=LINE('',#32346,#2483);
#2086=LINE('',#32774,#2484);
#2087=LINE('',#33195,#2485);
#2088=LINE('',#33665,#2486);
#2089=LINE('',#34148,#2487);
#2090=LINE('',#34561,#2488);
#2091=LINE('',#34980,#2489);
#2092=LINE('',#35418,#2490);
#2093=LINE('',#35831,#2491);
#2094=LINE('',#36243,#2492);
#2095=LINE('',#36649,#2493);
#2096=LINE('',#40977,#2494);
#2097=LINE('',#40985,#2495);
#2098=LINE('',#41276,#2496);
#2099=LINE('',#41650,#2497);
#2100=LINE('',#42030,#2498);
#2101=LINE('',#42408,#2499);
#2102=LINE('',#42780,#2500);
#2103=LINE('',#43170,#2501);
#2104=LINE('',#43546,#2502);
#2105=LINE('',#43922,#2503);
#2106=LINE('',#44294,#2504);
#2107=LINE('',#44680,#2505);
#2108=LINE('',#47553,#2506);
#2109=LINE('',#48355,#2507);
#2110=LINE('',#48357,#2508);
#2111=LINE('',#48359,#2509);
#2112=LINE('',#48360,#2510);
#2113=LINE('',#48363,#2511);
#2114=LINE('',#48365,#2512);
#2115=LINE('',#48366,#2513);
#2116=LINE('',#48369,#2514);
#2117=LINE('',#48371,#2515);
#2118=LINE('',#48372,#2516);
#2119=LINE('',#48375,#2517);
#2120=LINE('',#48377,#2518);
#2121=LINE('',#48378,#2519);
#2122=LINE('',#48381,#2520);
#2123=LINE('',#48383,#2521);
#2124=LINE('',#48384,#2522);
#2125=LINE('',#48386,#2523);
#2126=LINE('',#48387,#2524);
#2127=LINE('',#48394,#2525);
#2128=LINE('',#48402,#2526);
#2129=LINE('',#48444,#2527);
#2130=LINE('',#48655,#2528);
#2131=LINE('',#48872,#2529);
#2132=LINE('',#49202,#2530);
#2133=LINE('',#49480,#2531);
#2134=LINE('',#49688,#2532);
#2135=LINE('',#50018,#2533);
#2136=LINE('',#50296,#2534);
#2137=LINE('',#50504,#2535);
#2138=LINE('',#50837,#2536);
#2139=LINE('',#51112,#2537);
#2140=LINE('',#51323,#2538);
#2141=LINE('',#51656,#2539);
#2142=LINE('',#51931,#2540);
#2143=LINE('',#52029,#2541);
#2144=LINE('',#52114,#2542);
#2145=LINE('',#52266,#2543);
#2146=LINE('',#52448,#2544);
#2147=LINE('',#52656,#2545);
#2148=LINE('',#53071,#2546);
#2149=LINE('',#53489,#2547);
#2150=LINE('',#53931,#2548);
#2151=LINE('',#54361,#2549);
#2152=LINE('',#54789,#2550);
#2153=LINE('',#55205,#2551);
#2154=LINE('',#55675,#2552);
#2155=LINE('',#56097,#2553);
#2156=LINE('',#56512,#2554);
#2157=LINE('',#56935,#2555);
#2158=LINE('',#57370,#2556);
#2159=LINE('',#57795,#2557);
#2160=LINE('',#59676,#2558);
#2161=LINE('',#59703,#2559);
#2162=LINE('',#59706,#2560);
#2163=LINE('',#59709,#2561);
#2164=LINE('',#59711,#2562);
#2165=LINE('',#59712,#2563);
#2166=LINE('',#59723,#2564);
#2167=LINE('',#59724,#2565);
#2168=LINE('',#59727,#2566);
#2169=LINE('',#59731,#2567);
#2170=LINE('',#59735,#2568);
#2171=LINE('',#59739,#2569);
#2172=LINE('',#59743,#2570);
#2173=LINE('',#59744,#2571);
#2174=LINE('',#59746,#2572);
#2175=LINE('',#59753,#2573);
#2176=LINE('',#59759,#2574);
#2177=LINE('',#59765,#2575);
#2178=LINE('',#59771,#2576);
#2179=LINE('',#59776,#2577);
#2180=LINE('',#59778,#2578);
#2181=LINE('',#59780,#2579);
#2182=LINE('',#59781,#2580);
#2183=LINE('',#59784,#2581);
#2184=LINE('',#59786,#2582);
#2185=LINE('',#59787,#2583);
#2186=LINE('',#59790,#2584);
#2187=LINE('',#59792,#2585);
#2188=LINE('',#59793,#2586);
#2189=LINE('',#59795,#2587);
#2190=LINE('',#59796,#2588);
#2191=LINE('',#59800,#2589);
#2192=LINE('',#59802,#2590);
#2193=LINE('',#59804,#2591);
#2194=LINE('',#59805,#2592);
#2195=LINE('',#59808,#2593);
#2196=LINE('',#59810,#2594);
#2197=LINE('',#59811,#2595);
#2198=LINE('',#59814,#2596);
#2199=LINE('',#59816,#2597);
#2200=LINE('',#59817,#2598);
#2201=LINE('',#59819,#2599);
#2202=LINE('',#59820,#2600);
#2203=LINE('',#59828,#2601);
#2204=LINE('',#59834,#2602);
#2205=LINE('',#59840,#2603);
#2206=LINE('',#59846,#2604);
#2207=LINE('',#59851,#2605);
#2208=LINE('',#59853,#2606);
#2209=LINE('',#59855,#2607);
#2210=LINE('',#59856,#2608);
#2211=LINE('',#59859,#2609);
#2212=LINE('',#59861,#2610);
#2213=LINE('',#59862,#2611);
#2214=LINE('',#59865,#2612);
#2215=LINE('',#59867,#2613);
#2216=LINE('',#59868,#2614);
#2217=LINE('',#59870,#2615);
#2218=LINE('',#59871,#2616);
#2219=LINE('',#59878,#2617);
#2220=LINE('',#60229,#2618);
#2221=LINE('',#60648,#2619);
#2222=LINE('',#60884,#2620);
#2223=LINE('',#61280,#2621);
#2224=LINE('',#61689,#2622);
#2225=LINE('',#61914,#2623);
#2226=LINE('',#62136,#2624);
#2227=LINE('',#62521,#2625);
#2228=LINE('',#62951,#2626);
#2229=LINE('',#63383,#2627);
#2230=LINE('',#63599,#2628);
#2231=LINE('',#64064,#2629);
#2232=LINE('',#64558,#2630);
#2233=LINE('',#64972,#2631);
#2234=LINE('',#69339,#2632);
#2235=LINE('',#70352,#2633);
#2236=LINE('',#70354,#2634);
#2237=LINE('',#70356,#2635);
#2238=LINE('',#70357,#2636);
#2239=LINE('',#70360,#2637);
#2240=LINE('',#70362,#2638);
#2241=LINE('',#70363,#2639);
#2242=LINE('',#70366,#2640);
#2243=LINE('',#70368,#2641);
#2244=LINE('',#70369,#2642);
#2245=LINE('',#70372,#2643);
#2246=LINE('',#70374,#2644);
#2247=LINE('',#70375,#2645);
#2248=LINE('',#70378,#2646);
#2249=LINE('',#70380,#2647);
#2250=LINE('',#70381,#2648);
#2251=LINE('',#70383,#2649);
#2252=LINE('',#70384,#2650);
#2253=LINE('',#70391,#2651);
#2254=LINE('',#70399,#2652);
#2255=LINE('',#70670,#2653);
#2256=LINE('',#71052,#2654);
#2257=LINE('',#71455,#2655);
#2258=LINE('',#71846,#2656);
#2259=LINE('',#72218,#2657);
#2260=LINE('',#72600,#2658);
#2261=LINE('',#72991,#2659);
#2262=LINE('',#73208,#2660);
#2263=LINE('',#73646,#2661);
#2264=LINE('',#74039,#2662);
#2265=LINE('',#74451,#2663);
#2266=LINE('',#74837,#2664);
#2267=LINE('',#78221,#2665);
#2268=LINE('',#79110,#2666);
#2269=LINE('',#79112,#2667);
#2270=LINE('',#79114,#2668);
#2271=LINE('',#79115,#2669);
#2272=LINE('',#79118,#2670);
#2273=LINE('',#79120,#2671);
#2274=LINE('',#79121,#2672);
#2275=LINE('',#79124,#2673);
#2276=LINE('',#79126,#2674);
#2277=LINE('',#79127,#2675);
#2278=LINE('',#79130,#2676);
#2279=LINE('',#79132,#2677);
#2280=LINE('',#79133,#2678);
#2281=LINE('',#79136,#2679);
#2282=LINE('',#79138,#2680);
#2283=LINE('',#79139,#2681);
#2284=LINE('',#79141,#2682);
#2285=LINE('',#79142,#2683);
#2286=LINE('',#79149,#2684);
#2287=LINE('',#79157,#2685);
#2288=LINE('',#79394,#2686);
#2289=LINE('',#79793,#2687);
#2290=LINE('',#80314,#2688);
#2291=LINE('',#80739,#2689);
#2292=LINE('',#81070,#2690);
#2293=LINE('',#81588,#2691);
#2294=LINE('',#81998,#2692);
#2295=LINE('',#82393,#2693);
#2296=LINE('',#82942,#2694);
#2297=LINE('',#83579,#2695);
#2298=LINE('',#84226,#2696);
#2299=LINE('',#84845,#2697);
#2300=LINE('',#85436,#2698);
#2301=LINE('',#85850,#2699);
#2302=LINE('',#85951,#2700);
#2303=LINE('',#86239,#2701);
#2304=LINE('',#86277,#2702);
#2305=LINE('',#86315,#2703);
#2306=LINE('',#86861,#2704);
#2307=LINE('',#86897,#2705);
#2308=LINE('',#86935,#2706);
#2309=LINE('',#87481,#2707);
#2310=LINE('',#88021,#2708);
#2311=LINE('',#88059,#2709);
#2312=LINE('',#88599,#2710);
#2313=LINE('',#89139,#2711);
#2314=LINE('',#89178,#2712);
#2315=LINE('',#91537,#2713);
#2316=LINE('',#91543,#2714);
#2317=LINE('',#91551,#2715);
#2318=LINE('',#91575,#2716);
#2319=LINE('',#91789,#2717);
#2320=LINE('',#91925,#2718);
#2321=LINE('',#92053,#2719);
#2322=LINE('',#92200,#2720);
#2323=LINE('',#92238,#2721);
#2324=LINE('',#92650,#2722);
#2325=LINE('',#93391,#2723);
#2326=LINE('',#93397,#2724);
#2327=LINE('',#94341,#2725);
#2328=LINE('',#94349,#2726);
#2329=LINE('',#94355,#2727);
#2330=VECTOR('',#8952,3.5);
#2331=VECTOR('',#8959,3.5);
#2332=VECTOR('',#8966,3.5);
#2333=VECTOR('',#8973,3.5);
#2334=VECTOR('',#8978,10.);
#2335=VECTOR('',#8979,10.);
#2336=VECTOR('',#8980,10.);
#2337=VECTOR('',#8981,10.);
#2338=VECTOR('',#8984,10.);
#2339=VECTOR('',#8985,10.);
#2340=VECTOR('',#8986,10.);
#2341=VECTOR('',#8989,10.);
#2342=VECTOR('',#8990,10.);
#2343=VECTOR('',#8991,10.);
#2344=VECTOR('',#8994,10.);
#2345=VECTOR('',#8995,10.);
#2346=VECTOR('',#9006,10.5);
#2347=VECTOR('',#9013,10.5);
#2348=VECTOR('',#9018,10.);
#2349=VECTOR('',#9019,10.);
#2350=VECTOR('',#9020,10.);
#2351=VECTOR('',#9021,10.);
#2352=VECTOR('',#9024,10.);
#2353=VECTOR('',#9025,10.);
#2354=VECTOR('',#9026,10.);
#2355=VECTOR('',#9029,10.);
#2356=VECTOR('',#9030,10.);
#2357=VECTOR('',#9031,10.);
#2358=VECTOR('',#9034,10.);
#2359=VECTOR('',#9035,10.);
#2360=VECTOR('',#9044,10.);
#2361=VECTOR('',#9045,10.);
#2362=VECTOR('',#9046,10.);
#2363=VECTOR('',#9047,10.);
#2364=VECTOR('',#9050,10.);
#2365=VECTOR('',#9051,10.);
#2366=VECTOR('',#9052,10.);
#2367=VECTOR('',#9055,10.);
#2368=VECTOR('',#9056,10.);
#2369=VECTOR('',#9057,10.);
#2370=VECTOR('',#9060,10.);
#2371=VECTOR('',#9061,10.);
#2372=VECTOR('',#9072,10.);
#2373=VECTOR('',#9075,10.);
#2374=VECTOR('',#9078,10.);
#2375=VECTOR('',#9079,10.);
#2376=VECTOR('',#9080,10.);
#2377=VECTOR('',#9085,10.);
#2378=VECTOR('',#9090,10.);
#2379=VECTOR('',#9091,10.);
#2380=VECTOR('',#9092,10.);
#2381=VECTOR('',#9097,10.);
#2382=VECTOR('',#9100,10.);
#2383=VECTOR('',#9103,10.);
#2384=VECTOR('',#9104,10.);
#2385=VECTOR('',#9109,10.);
#2386=VECTOR('',#9114,10.);
#2387=VECTOR('',#9115,10.);
#2388=VECTOR('',#9120,10.);
#2389=VECTOR('',#9123,10.);
#2390=VECTOR('',#9126,10.);
#2391=VECTOR('',#9127,10.);
#2392=VECTOR('',#9128,10.);
#2393=VECTOR('',#9133,10.);
#2394=VECTOR('',#9136,10.);
#2395=VECTOR('',#9139,10.);
#2396=VECTOR('',#9140,10.);
#2397=VECTOR('',#9145,10.);
#2398=VECTOR('',#9150,10.);
#2399=VECTOR('',#9151,10.);
#2400=VECTOR('',#9152,10.);
#2401=VECTOR('',#9157,10.);
#2402=VECTOR('',#9162,10.);
#2403=VECTOR('',#9163,10.);
#2404=VECTOR('',#9166,10.);
#2405=VECTOR('',#9167,10.);
#2406=VECTOR('',#9168,10.);
#2407=VECTOR('',#9169,10.);
#2408=VECTOR('',#9172,10.);
#2409=VECTOR('',#9173,10.);
#2410=VECTOR('',#9174,10.);
#2411=VECTOR('',#9177,10.);
#2412=VECTOR('',#9178,10.);
#2413=VECTOR('',#9179,10.);
#2414=VECTOR('',#9182,10.);
#2415=VECTOR('',#9183,10.);
#2416=VECTOR('',#9192,3.0735);
#2417=VECTOR('',#9197,3.0735);
#2418=VECTOR('',#9200,3.0735);
#2419=VECTOR('',#9203,3.0735);
#2420=VECTOR('',#9206,3.0735);
#2421=VECTOR('',#9209,3.0735);
#2422=VECTOR('',#9212,3.0735);
#2423=VECTOR('',#9215,3.0735);
#2424=VECTOR('',#9218,3.0735);
#2425=VECTOR('',#9221,3.0735);
#2426=VECTOR('',#9224,3.0735);
#2427=VECTOR('',#9227,3.0735);
#2428=VECTOR('',#9230,3.0735);
#2429=VECTOR('',#9233,3.0735);
#2430=VECTOR('',#9236,3.0735);
#2431=VECTOR('',#9239,3.0735);
#2432=VECTOR('',#9242,3.0735);
#2433=VECTOR('',#9245,3.0735);
#2434=VECTOR('',#9248,3.0735);
#2435=VECTOR('',#9253,2.5175);
#2436=VECTOR('',#9256,2.5175);
#2437=VECTOR('',#9263,2.5175);
#2438=VECTOR('',#9266,2.5175);
#2439=VECTOR('',#9269,2.5175);
#2440=VECTOR('',#9272,2.5175);
#2441=VECTOR('',#9275,2.5175);
#2442=VECTOR('',#9278,2.5175);
#2443=VECTOR('',#9281,2.5175);
#2444=VECTOR('',#9284,2.5175);
#2445=VECTOR('',#9287,2.5175);
#2446=VECTOR('',#9290,2.5175);
#2447=VECTOR('',#9293,2.5175);
#2448=VECTOR('',#9296,2.5175);
#2449=VECTOR('',#9299,2.5175);
#2450=VECTOR('',#9302,2.5175);
#2451=VECTOR('',#9305,2.5175);
#2452=VECTOR('',#9308,2.5175);
#2453=VECTOR('',#9311,2.5175);
#2454=VECTOR('',#9314,2.5175);
#2455=VECTOR('',#9319,3.0735);
#2456=VECTOR('',#9324,3.0735);
#2457=VECTOR('',#9327,3.0735);
#2458=VECTOR('',#9330,3.0735);
#2459=VECTOR('',#9333,3.0735);
#2460=VECTOR('',#9336,3.0735);
#2461=VECTOR('',#9339,3.0735);
#2462=VECTOR('',#9342,3.0735);
#2463=VECTOR('',#9345,3.0735);
#2464=VECTOR('',#9348,3.0735);
#2465=VECTOR('',#9351,3.0735);
#2466=VECTOR('',#9354,3.0735);
#2467=VECTOR('',#9357,3.0735);
#2468=VECTOR('',#9360,3.0735);
#2469=VECTOR('',#9363,3.0735);
#2470=VECTOR('',#9366,3.0735);
#2471=VECTOR('',#9369,3.0735);
#2472=VECTOR('',#9372,3.0735);
#2473=VECTOR('',#9375,3.0735);
#2474=VECTOR('',#9380,2.5175);
#2475=VECTOR('',#9383,2.5175);
#2476=VECTOR('',#9390,2.5175);
#2477=VECTOR('',#9393,2.5175);
#2478=VECTOR('',#9396,2.5175);
#2479=VECTOR('',#9399,2.5175);
#2480=VECTOR('',#9402,2.5175);
#2481=VECTOR('',#9405,2.5175);
#2482=VECTOR('',#9408,2.5175);
#2483=VECTOR('',#9411,2.5175);
#2484=VECTOR('',#9414,2.5175);
#2485=VECTOR('',#9417,2.5175);
#2486=VECTOR('',#9420,2.5175);
#2487=VECTOR('',#9423,2.5175);
#2488=VECTOR('',#9426,2.5175);
#2489=VECTOR('',#9429,2.5175);
#2490=VECTOR('',#9432,2.5175);
#2491=VECTOR('',#9435,2.5175);
#2492=VECTOR('',#9438,2.5175);
#2493=VECTOR('',#9441,2.5175);
#2494=VECTOR('',#9464,8.);
#2495=VECTOR('',#9475,2.37175);
#2496=VECTOR('',#9480,2.37175);
#2497=VECTOR('',#9483,2.37175);
#2498=VECTOR('',#9486,2.37175);
#2499=VECTOR('',#9489,2.37175);
#2500=VECTOR('',#9492,2.37175);
#2501=VECTOR('',#9495,2.37175);
#2502=VECTOR('',#9498,2.37175);
#2503=VECTOR('',#9501,2.37175);
#2504=VECTOR('',#9504,2.37175);
#2505=VECTOR('',#9507,2.37175);
#2506=VECTOR('',#9520,2.5);
#2507=VECTOR('',#9525,10.);
#2508=VECTOR('',#9526,10.);
#2509=VECTOR('',#9527,10.);
#2510=VECTOR('',#9528,10.);
#2511=VECTOR('',#9531,10.);
#2512=VECTOR('',#9532,10.);
#2513=VECTOR('',#9533,10.);
#2514=VECTOR('',#9536,9.99999999999999);
#2515=VECTOR('',#9537,10.);
#2516=VECTOR('',#9538,10.);
#2517=VECTOR('',#9541,10.);
#2518=VECTOR('',#9542,10.);
#2519=VECTOR('',#9543,10.);
#2520=VECTOR('',#9546,10.);
#2521=VECTOR('',#9547,10.);
#2522=VECTOR('',#9548,10.);
#2523=VECTOR('',#9551,10.);
#2524=VECTOR('',#9552,10.);
#2525=VECTOR('',#9561,5.);
#2526=VECTOR('',#9572,2.05475);
#2527=VECTOR('',#9577,2.05475);
#2528=VECTOR('',#9580,2.05475);
#2529=VECTOR('',#9583,2.05475);
#2530=VECTOR('',#9586,2.05475);
#2531=VECTOR('',#9589,2.05475);
#2532=VECTOR('',#9592,2.05475);
#2533=VECTOR('',#9595,2.05475);
#2534=VECTOR('',#9598,2.05475);
#2535=VECTOR('',#9601,2.05475);
#2536=VECTOR('',#9604,2.05475);
#2537=VECTOR('',#9607,2.05475);
#2538=VECTOR('',#9610,2.05475);
#2539=VECTOR('',#9613,2.05475);
#2540=VECTOR('',#9616,2.05475);
#2541=VECTOR('',#9619,2.05475);
#2542=VECTOR('',#9624,1.666);
#2543=VECTOR('',#9627,1.666);
#2544=VECTOR('',#9632,1.666);
#2545=VECTOR('',#9635,1.666);
#2546=VECTOR('',#9638,1.666);
#2547=VECTOR('',#9641,1.666);
#2548=VECTOR('',#9644,1.666);
#2549=VECTOR('',#9647,1.666);
#2550=VECTOR('',#9650,1.666);
#2551=VECTOR('',#9653,1.666);
#2552=VECTOR('',#9656,1.666);
#2553=VECTOR('',#9659,1.666);
#2554=VECTOR('',#9662,1.666);
#2555=VECTOR('',#9665,1.666);
#2556=VECTOR('',#9668,1.666);
#2557=VECTOR('',#9671,1.666);
#2558=VECTOR('',#9686,5.);
#2559=VECTOR('',#9733,5.);
#2560=VECTOR('',#9736,10.);
#2561=VECTOR('',#9739,10.);
#2562=VECTOR('',#9740,10.);
#2563=VECTOR('',#9741,10.);
#2564=VECTOR('',#9752,10.);
#2565=VECTOR('',#9753,10.);
#2566=VECTOR('',#9756,3.5);
#2567=VECTOR('',#9761,3.5);
#2568=VECTOR('',#9766,3.5);
#2569=VECTOR('',#9771,3.5);
#2570=VECTOR('',#9776,10.);
#2571=VECTOR('',#9777,10.);
#2572=VECTOR('',#9780,10.);
#2573=VECTOR('',#9789,3.5);
#2574=VECTOR('',#9796,3.5);
#2575=VECTOR('',#9803,3.5);
#2576=VECTOR('',#9810,3.5);
#2577=VECTOR('',#9815,10.);
#2578=VECTOR('',#9816,10.);
#2579=VECTOR('',#9817,10.);
#2580=VECTOR('',#9818,10.);
#2581=VECTOR('',#9821,10.);
#2582=VECTOR('',#9822,10.);
#2583=VECTOR('',#9823,10.);
#2584=VECTOR('',#9826,10.);
#2585=VECTOR('',#9827,10.);
#2586=VECTOR('',#9828,10.);
#2587=VECTOR('',#9831,10.);
#2588=VECTOR('',#9832,10.);
#2589=VECTOR('',#9835,10.);
#2590=VECTOR('',#9836,10.);
#2591=VECTOR('',#9837,10.);
#2592=VECTOR('',#9838,10.);
#2593=VECTOR('',#9841,10.);
#2594=VECTOR('',#9842,10.);
#2595=VECTOR('',#9843,10.);
#2596=VECTOR('',#9846,10.);
#2597=VECTOR('',#9847,10.);
#2598=VECTOR('',#9848,10.);
#2599=VECTOR('',#9851,10.);
#2600=VECTOR('',#9852,10.);
#2601=VECTOR('',#9863,2.5);
#2602=VECTOR('',#9870,2.5);
#2603=VECTOR('',#9877,2.5);
#2604=VECTOR('',#9884,2.5);
#2605=VECTOR('',#9889,10.);
#2606=VECTOR('',#9890,10.);
#2607=VECTOR('',#9891,10.);
#2608=VECTOR('',#9892,10.);
#2609=VECTOR('',#9895,10.);
#2610=VECTOR('',#9896,10.);
#2611=VECTOR('',#9897,10.);
#2612=VECTOR('',#9900,10.);
#2613=VECTOR('',#9901,10.);
#2614=VECTOR('',#9902,10.);
#2615=VECTOR('',#9905,10.);
#2616=VECTOR('',#9906,10.);
#2617=VECTOR('',#9915,2.37175);
#2618=VECTOR('',#9920,2.37175);
#2619=VECTOR('',#9923,2.37175);
#2620=VECTOR('',#9926,2.37175);
#2621=VECTOR('',#9929,2.37175);
#2622=VECTOR('',#9932,2.37175);
#2623=VECTOR('',#9935,2.37175);
#2624=VECTOR('',#9938,2.37175);
#2625=VECTOR('',#9941,2.37175);
#2626=VECTOR('',#9944,2.37175);
#2627=VECTOR('',#9947,2.37175);
#2628=VECTOR('',#9950,2.37175);
#2629=VECTOR('',#9953,2.37175);
#2630=VECTOR('',#9956,2.37175);
#2631=VECTOR('',#9959,2.37175);
#2632=VECTOR('',#9972,2.5);
#2633=VECTOR('',#9977,10.);
#2634=VECTOR('',#9978,10.);
#2635=VECTOR('',#9979,10.);
#2636=VECTOR('',#9980,10.);
#2637=VECTOR('',#9983,10.);
#2638=VECTOR('',#9984,10.);
#2639=VECTOR('',#9985,10.);
#2640=VECTOR('',#9988,9.99999999999999);
#2641=VECTOR('',#9989,10.);
#2642=VECTOR('',#9990,10.);
#2643=VECTOR('',#9993,10.);
#2644=VECTOR('',#9994,10.);
#2645=VECTOR('',#9995,10.);
#2646=VECTOR('',#9998,10.);
#2647=VECTOR('',#9999,10.);
#2648=VECTOR('',#10000,10.);
#2649=VECTOR('',#10003,10.);
#2650=VECTOR('',#10004,10.);
#2651=VECTOR('',#10013,5.);
#2652=VECTOR('',#10024,1.5555);
#2653=VECTOR('',#10029,1.5555);
#2654=VECTOR('',#10032,1.5555);
#2655=VECTOR('',#10035,1.5555);
#2656=VECTOR('',#10038,1.5555);
#2657=VECTOR('',#10041,1.5555);
#2658=VECTOR('',#10044,1.5555);
#2659=VECTOR('',#10047,1.5555);
#2660=VECTOR('',#10050,1.5555);
#2661=VECTOR('',#10053,1.5555);
#2662=VECTOR('',#10056,1.5555);
#2663=VECTOR('',#10059,1.5555);
#2664=VECTOR('',#10062,1.5555);
#2665=VECTOR('',#10075,1.5);
#2666=VECTOR('',#10080,10.);
#2667=VECTOR('',#10081,10.);
#2668=VECTOR('',#10082,10.);
#2669=VECTOR('',#10083,10.);
#2670=VECTOR('',#10086,10.);
#2671=VECTOR('',#10087,10.);
#2672=VECTOR('',#10088,10.);
#2673=VECTOR('',#10091,10.);
#2674=VECTOR('',#10092,10.);
#2675=VECTOR('',#10093,10.);
#2676=VECTOR('',#10096,10.);
#2677=VECTOR('',#10097,10.);
#2678=VECTOR('',#10098,10.);
#2679=VECTOR('',#10101,10.);
#2680=VECTOR('',#10102,10.);
#2681=VECTOR('',#10103,10.);
#2682=VECTOR('',#10106,10.);
#2683=VECTOR('',#10107,10.);
#2684=VECTOR('',#10116,3.5);
#2685=VECTOR('',#10127,9.37025);
#2686=VECTOR('',#10132,9.37025);
#2687=VECTOR('',#10135,9.37025);
#2688=VECTOR('',#10138,9.37025);
#2689=VECTOR('',#10141,9.37025);
#2690=VECTOR('',#10144,9.37025);
#2691=VECTOR('',#10147,9.37025);
#2692=VECTOR('',#10150,9.37025);
#2693=VECTOR('',#10153,9.37025);
#2694=VECTOR('',#10156,9.37025);
#2695=VECTOR('',#10159,9.37025);
#2696=VECTOR('',#10162,9.37025);
#2697=VECTOR('',#10165,9.37025);
#2698=VECTOR('',#10168,9.37025);
#2699=VECTOR('',#10171,9.942);
#2700=VECTOR('',#10176,9.942);
#2701=VECTOR('',#10179,9.942);
#2702=VECTOR('',#10182,9.942);
#2703=VECTOR('',#10185,9.942);
#2704=VECTOR('',#10188,9.942);
#2705=VECTOR('',#10191,9.942);
#2706=VECTOR('',#10194,9.942);
#2707=VECTOR('',#10197,9.942);
#2708=VECTOR('',#10200,9.942);
#2709=VECTOR('',#10203,9.942);
#2710=VECTOR('',#10206,9.942);
#2711=VECTOR('',#10209,9.942);
#2712=VECTOR('',#10212,9.942);
#2713=VECTOR('',#10227,14.);
#2714=VECTOR('',#10234,5.);
#2715=VECTOR('',#10245,10.076);
#2716=VECTOR('',#10250,10.076);
#2717=VECTOR('',#10253,10.076);
#2718=VECTOR('',#10256,10.076);
#2719=VECTOR('',#10261,9.5175);
#2720=VECTOR('',#10266,9.5175);
#2721=VECTOR('',#10269,9.5175);
#2722=VECTOR('',#10272,9.5175);
#2723=VECTOR('',#10283,1.);
#2724=VECTOR('',#10290,1.);
#2725=VECTOR('',#10299,14.);
#2726=VECTOR('',#10310,3.);
#2727=VECTOR('',#10317,5.);
#2728=CIRCLE('',#8436,3.5);
#2729=CIRCLE('',#8437,3.5);
#2730=CIRCLE('',#8439,3.5);
#2731=CIRCLE('',#8440,3.5);
#2732=CIRCLE('',#8442,3.5);
#2733=CIRCLE('',#8443,3.5);
#2734=CIRCLE('',#8445,3.5);
#2735=CIRCLE('',#8446,3.5);
#2736=CIRCLE('',#8455,10.5);
#2737=CIRCLE('',#8456,10.5);
#2738=CIRCLE('',#8458,10.5);
#2739=CIRCLE('',#8459,10.5);
#2740=CIRCLE('',#8475,5.);
#2741=CIRCLE('',#8476,5.);
#2742=CIRCLE('',#8479,5.);
#2743=CIRCLE('',#8480,5.);
#2744=CIRCLE('',#8483,5.);
#2745=CIRCLE('',#8484,5.);
#2746=CIRCLE('',#8487,5.);
#2747=CIRCLE('',#8488,5.);
#2748=CIRCLE('',#8491,5.);
#2749=CIRCLE('',#8492,5.);
#2750=CIRCLE('',#8495,5.);
#2751=CIRCLE('',#8496,5.);
#2752=CIRCLE('',#8499,5.);
#2753=CIRCLE('',#8500,5.);
#2754=CIRCLE('',#8503,5.);
#2755=CIRCLE('',#8504,5.);
#2756=CIRCLE('',#8514,3.0735);
#2757=CIRCLE('',#8533,3.0735);
#2758=CIRCLE('',#8535,2.5175);
#2759=CIRCLE('',#8536,2.5175);
#2760=CIRCLE('',#8537,2.5175);
#2761=CIRCLE('',#8556,2.5175);
#2762=CIRCLE('',#8558,3.0735);
#2763=CIRCLE('',#8577,3.0735);
#2764=CIRCLE('',#8579,2.5175);
#2765=CIRCLE('',#8580,2.5175);
#2766=CIRCLE('',#8581,2.5175);
#2767=CIRCLE('',#8600,2.5175);
#2768=CIRCLE('',#8610,8.);
#2769=CIRCLE('',#8611,8.);
#2770=CIRCLE('',#8616,2.37175);
#2771=CIRCLE('',#8628,2.942);
#2772=CIRCLE('',#8629,2.942);
#2773=CIRCLE('',#8631,2.37175);
#2774=CIRCLE('',#8633,2.);
#2775=CIRCLE('',#8642,5.);
#2776=CIRCLE('',#8644,5.);
#2777=CIRCLE('',#8649,2.05475);
#2778=CIRCLE('',#8665,2.05475);
#2779=CIRCLE('',#8667,1.666);
#2780=CIRCLE('',#8668,1.666);
#2781=CIRCLE('',#8683,1.666);
#2782=CIRCLE('',#8689,5.);
#2783=CIRCLE('',#8690,5.);
#2784=CIRCLE('',#8712,5.00000000000001);
#2785=CIRCLE('',#8713,5.00000000000001);
#2786=CIRCLE('',#8715,3.5);
#2787=CIRCLE('',#8716,3.5);
#2788=CIRCLE('',#8717,3.5);
#2789=CIRCLE('',#8718,3.5);
#2790=CIRCLE('',#8721,3.5);
#2791=CIRCLE('',#8723,3.5);
#2792=CIRCLE('',#8725,3.5);
#2793=CIRCLE('',#8727,3.5);
#2794=CIRCLE('',#8733,3.5);
#2795=CIRCLE('',#8734,3.5);
#2796=CIRCLE('',#8736,3.5);
#2797=CIRCLE('',#8737,3.5);
#2798=CIRCLE('',#8739,3.5);
#2799=CIRCLE('',#8740,3.5);
#2800=CIRCLE('',#8742,3.5);
#2801=CIRCLE('',#8743,3.5);
#2802=CIRCLE('',#8756,2.5);
#2803=CIRCLE('',#8757,2.5);
#2804=CIRCLE('',#8759,2.5);
#2805=CIRCLE('',#8760,2.5);
#2806=CIRCLE('',#8762,2.5);
#2807=CIRCLE('',#8763,2.5);
#2808=CIRCLE('',#8765,2.5);
#2809=CIRCLE('',#8766,2.5);
#2810=CIRCLE('',#8775,2.37175);
#2811=CIRCLE('',#8791,2.942);
#2812=CIRCLE('',#8792,2.942);
#2813=CIRCLE('',#8794,2.37175);
#2814=CIRCLE('',#8796,2.);
#2815=CIRCLE('',#8805,5.);
#2816=CIRCLE('',#8807,5.);
#2817=CIRCLE('',#8812,1.5555);
#2818=CIRCLE('',#8826,1.954);
#2819=CIRCLE('',#8827,1.954);
#2820=CIRCLE('',#8829,1.5555);
#2821=CIRCLE('',#8831,1.);
#2822=CIRCLE('',#8840,3.5);
#2823=CIRCLE('',#8842,3.5);
#2824=CIRCLE('',#8847,9.37025);
#2825=CIRCLE('',#8862,9.942);
#2826=CIRCLE('',#8877,9.942);
#2827=CIRCLE('',#8879,9.37025);
#2828=CIRCLE('',#8881,14.);
#2829=CIRCLE('',#8883,14.);
#2830=CIRCLE('',#8885,5.);
#2831=CIRCLE('',#8886,5.);
#2832=CIRCLE('',#8891,10.076);
#2833=CIRCLE('',#8895,10.076);
#2834=CIRCLE('',#8897,9.5175);
#2835=CIRCLE('',#8901,9.5175);
#2836=CIRCLE('',#8905,1.);
#2837=CIRCLE('',#8906,1.);
#2838=CIRCLE('',#8908,1.);
#2839=CIRCLE('',#8909,1.);
#2840=CIRCLE('',#8911,14.);
#2841=CIRCLE('',#8913,14.);
#2842=CIRCLE('',#8917,3.);
#2843=CIRCLE('',#8918,3.);
#2844=CIRCLE('',#8920,5.);
#2845=CIRCLE('',#8921,5.);
#2846=VERTEX_POINT('',#10364);
#2847=VERTEX_POINT('',#10366);
#2848=VERTEX_POINT('',#10370);
#2849=VERTEX_POINT('',#10372);
#2850=VERTEX_POINT('',#10376);
#2851=VERTEX_POINT('',#10378);
#2852=VERTEX_POINT('',#10382);
#2853=VERTEX_POINT('',#10384);
#2854=VERTEX_POINT('',#10388);
#2855=VERTEX_POINT('',#10389);
#2856=VERTEX_POINT('',#10391);
#2857=VERTEX_POINT('',#10393);
#2858=VERTEX_POINT('',#10397);
#2859=VERTEX_POINT('',#10399);
#2860=VERTEX_POINT('',#10403);
#2861=VERTEX_POINT('',#10405);
#2862=VERTEX_POINT('',#10415);
#2863=VERTEX_POINT('',#10417);
#2864=VERTEX_POINT('',#10421);
#2865=VERTEX_POINT('',#10423);
#2866=VERTEX_POINT('',#10427);
#2867=VERTEX_POINT('',#10428);
#2868=VERTEX_POINT('',#10430);
#2869=VERTEX_POINT('',#10432);
#2870=VERTEX_POINT('',#10436);
#2871=VERTEX_POINT('',#10438);
#2872=VERTEX_POINT('',#10442);
#2873=VERTEX_POINT('',#10444);
#2874=VERTEX_POINT('',#10454);
#2875=VERTEX_POINT('',#10455);
#2876=VERTEX_POINT('',#10457);
#2877=VERTEX_POINT('',#10459);
#2878=VERTEX_POINT('',#10463);
#2879=VERTEX_POINT('',#10465);
#2880=VERTEX_POINT('',#10469);
#2881=VERTEX_POINT('',#10471);
#2882=VERTEX_POINT('',#10481);
#2883=VERTEX_POINT('',#10482);
#2884=VERTEX_POINT('',#10484);
#2885=VERTEX_POINT('',#10486);
#2886=VERTEX_POINT('',#10490);
#2887=VERTEX_POINT('',#10492);
#2888=VERTEX_POINT('',#10496);
#2889=VERTEX_POINT('',#10498);
#2890=VERTEX_POINT('',#10502);
#2891=VERTEX_POINT('',#10504);
#2892=VERTEX_POINT('',#10508);
#2893=VERTEX_POINT('',#10509);
#2894=VERTEX_POINT('',#10511);
#2895=VERTEX_POINT('',#10513);
#2896=VERTEX_POINT('',#10520);
#2897=VERTEX_POINT('',#10522);
#2898=VERTEX_POINT('',#10529);
#2899=VERTEX_POINT('',#10530);
#2900=VERTEX_POINT('',#10532);
#2901=VERTEX_POINT('',#10534);
#2902=VERTEX_POINT('',#10538);
#2903=VERTEX_POINT('',#10540);
#2904=VERTEX_POINT('',#10544);
#2905=VERTEX_POINT('',#10545);
#2906=VERTEX_POINT('',#10547);
#2907=VERTEX_POINT('',#10549);
#2908=VERTEX_POINT('',#10556);
#2909=VERTEX_POINT('',#10558);
#2910=VERTEX_POINT('',#10562);
#2911=VERTEX_POINT('',#10564);
#2912=VERTEX_POINT('',#10568);
#2913=VERTEX_POINT('',#10570);
#2914=VERTEX_POINT('',#10577);
#2915=VERTEX_POINT('',#10578);
#2916=VERTEX_POINT('',#10580);
#2917=VERTEX_POINT('',#10582);
#2918=VERTEX_POINT('',#10586);
#2919=VERTEX_POINT('',#10588);
#2920=VERTEX_POINT('',#10592);
#2921=VERTEX_POINT('',#10594);
#2922=VERTEX_POINT('',#10604);
#2923=VERTEX_POINT('',#10605);
#2924=VERTEX_POINT('',#10607);
#2925=VERTEX_POINT('',#10684);
#2926=VERTEX_POINT('',#10781);
#2927=VERTEX_POINT('',#10782);
#2928=VERTEX_POINT('',#10784);
#2929=VERTEX_POINT('',#10994);
#2930=VERTEX_POINT('',#11083);
#2931=VERTEX_POINT('',#11084);
#2932=VERTEX_POINT('',#11086);
#2933=VERTEX_POINT('',#11296);
#2934=VERTEX_POINT('',#11312);
#2935=VERTEX_POINT('',#11313);
#2936=VERTEX_POINT('',#11315);
#2937=VERTEX_POINT('',#11528);
#2938=VERTEX_POINT('',#11544);
#2939=VERTEX_POINT('',#11545);
#2940=VERTEX_POINT('',#11547);
#2941=VERTEX_POINT('',#11757);
#2942=VERTEX_POINT('',#11774);
#2943=VERTEX_POINT('',#11775);
#2944=VERTEX_POINT('',#11777);
#2945=VERTEX_POINT('',#11990);
#2946=VERTEX_POINT('',#12006);
#2947=VERTEX_POINT('',#12007);
#2948=VERTEX_POINT('',#12009);
#2949=VERTEX_POINT('',#12225);
#2950=VERTEX_POINT('',#12241);
#2951=VERTEX_POINT('',#12242);
#2952=VERTEX_POINT('',#12244);
#2953=VERTEX_POINT('',#12457);
#2954=VERTEX_POINT('',#12473);
#2955=VERTEX_POINT('',#12474);
#2956=VERTEX_POINT('',#12476);
#2957=VERTEX_POINT('',#12686);
#2958=VERTEX_POINT('',#12703);
#2959=VERTEX_POINT('',#12704);
#2960=VERTEX_POINT('',#12706);
#2961=VERTEX_POINT('',#12792);
#2962=VERTEX_POINT('',#12808);
#2963=VERTEX_POINT('',#12809);
#2964=VERTEX_POINT('',#12811);
#2965=VERTEX_POINT('',#12826);
#2966=VERTEX_POINT('',#12842);
#2967=VERTEX_POINT('',#12843);
#2968=VERTEX_POINT('',#12845);
#2969=VERTEX_POINT('',#12860);
#2970=VERTEX_POINT('',#13005);
#2971=VERTEX_POINT('',#13006);
#2972=VERTEX_POINT('',#13008);
#2973=VERTEX_POINT('',#13024);
#2974=VERTEX_POINT('',#13235);
#2975=VERTEX_POINT('',#13236);
#2976=VERTEX_POINT('',#13238);
#2977=VERTEX_POINT('',#13253);
#2978=VERTEX_POINT('',#13467);
#2979=VERTEX_POINT('',#13468);
#2980=VERTEX_POINT('',#13470);
#2981=VERTEX_POINT('',#13485);
#2982=VERTEX_POINT('',#13699);
#2983=VERTEX_POINT('',#13700);
#2984=VERTEX_POINT('',#13702);
#2985=VERTEX_POINT('',#13717);
#2986=VERTEX_POINT('',#13928);
#2987=VERTEX_POINT('',#13929);
#2988=VERTEX_POINT('',#13931);
#2989=VERTEX_POINT('',#13947);
#2990=VERTEX_POINT('',#14161);
#2991=VERTEX_POINT('',#14162);
#2992=VERTEX_POINT('',#14164);
#2993=VERTEX_POINT('',#14179);
#2994=VERTEX_POINT('',#14393);
#2995=VERTEX_POINT('',#14394);
#2996=VERTEX_POINT('',#14396);
#2997=VERTEX_POINT('',#14473);
#2998=VERTEX_POINT('',#14479);
#2999=VERTEX_POINT('',#14481);
#3000=VERTEX_POINT('',#14554);
#3001=VERTEX_POINT('',#14555);
#3002=VERTEX_POINT('',#14557);
#3003=VERTEX_POINT('',#14570);
#3004=VERTEX_POINT('',#14572);
#3005=VERTEX_POINT('',#14575);
#3006=VERTEX_POINT('',#14645);
#3007=VERTEX_POINT('',#14646);
#3008=VERTEX_POINT('',#14648);
#3009=VERTEX_POINT('',#14853);
#3010=VERTEX_POINT('',#15068);
#3011=VERTEX_POINT('',#15069);
#3012=VERTEX_POINT('',#15071);
#3013=VERTEX_POINT('',#15536);
#3014=VERTEX_POINT('',#15537);
#3015=VERTEX_POINT('',#15539);
#3016=VERTEX_POINT('',#15734);
#3017=VERTEX_POINT('',#15956);
#3018=VERTEX_POINT('',#15957);
#3019=VERTEX_POINT('',#15959);
#3020=VERTEX_POINT('',#16357);
#3021=VERTEX_POINT('',#16358);
#3022=VERTEX_POINT('',#16360);
#3023=VERTEX_POINT('',#16558);
#3024=VERTEX_POINT('',#16774);
#3025=VERTEX_POINT('',#16775);
#3026=VERTEX_POINT('',#16777);
#3027=VERTEX_POINT('',#17206);
#3028=VERTEX_POINT('',#17207);
#3029=VERTEX_POINT('',#17209);
#3030=VERTEX_POINT('',#17404);
#3031=VERTEX_POINT('',#17658);
#3032=VERTEX_POINT('',#17659);
#3033=VERTEX_POINT('',#17661);
#3034=VERTEX_POINT('',#18121);
#3035=VERTEX_POINT('',#18122);
#3036=VERTEX_POINT('',#18124);
#3037=VERTEX_POINT('',#18319);
#3038=VERTEX_POINT('',#18531);
#3039=VERTEX_POINT('',#18532);
#3040=VERTEX_POINT('',#18534);
#3041=VERTEX_POINT('',#18964);
#3042=VERTEX_POINT('',#18965);
#3043=VERTEX_POINT('',#18967);
#3044=VERTEX_POINT('',#19162);
#3045=VERTEX_POINT('',#19390);
#3046=VERTEX_POINT('',#19391);
#3047=VERTEX_POINT('',#19393);
#3048=VERTEX_POINT('',#19802);
#3049=VERTEX_POINT('',#19803);
#3050=VERTEX_POINT('',#19805);
#3051=VERTEX_POINT('',#20000);
#3052=VERTEX_POINT('',#20232);
#3053=VERTEX_POINT('',#20233);
#3054=VERTEX_POINT('',#20235);
#3055=VERTEX_POINT('',#20713);
#3056=VERTEX_POINT('',#20714);
#3057=VERTEX_POINT('',#20716);
#3058=VERTEX_POINT('',#20911);
#3059=VERTEX_POINT('',#21127);
#3060=VERTEX_POINT('',#21128);
#3061=VERTEX_POINT('',#21130);
#3062=VERTEX_POINT('',#21558);
#3063=VERTEX_POINT('',#21559);
#3064=VERTEX_POINT('',#21561);
#3065=VERTEX_POINT('',#21753);
#3066=VERTEX_POINT('',#21973);
#3067=VERTEX_POINT('',#21974);
#3068=VERTEX_POINT('',#21976);
#3069=VERTEX_POINT('',#21999);
#3070=VERTEX_POINT('',#22121);
#3071=VERTEX_POINT('',#22123);
#3072=VERTEX_POINT('',#22310);
#3073=VERTEX_POINT('',#22311);
#3074=VERTEX_POINT('',#22313);
#3075=VERTEX_POINT('',#22320);
#3076=VERTEX_POINT('',#22417);
#3077=VERTEX_POINT('',#22418);
#3078=VERTEX_POINT('',#22420);
#3079=VERTEX_POINT('',#22563);
#3080=VERTEX_POINT('',#22652);
#3081=VERTEX_POINT('',#22653);
#3082=VERTEX_POINT('',#22655);
#3083=VERTEX_POINT('',#22865);
#3084=VERTEX_POINT('',#23009);
#3085=VERTEX_POINT('',#23010);
#3086=VERTEX_POINT('',#23012);
#3087=VERTEX_POINT('',#23225);
#3088=VERTEX_POINT('',#23439);
#3089=VERTEX_POINT('',#23440);
#3090=VERTEX_POINT('',#23442);
#3091=VERTEX_POINT('',#23652);
#3092=VERTEX_POINT('',#23869);
#3093=VERTEX_POINT('',#23870);
#3094=VERTEX_POINT('',#23872);
#3095=VERTEX_POINT('',#24085);
#3096=VERTEX_POINT('',#24296);
#3097=VERTEX_POINT('',#24297);
#3098=VERTEX_POINT('',#24299);
#3099=VERTEX_POINT('',#24515);
#3100=VERTEX_POINT('',#24726);
#3101=VERTEX_POINT('',#24727);
#3102=VERTEX_POINT('',#24729);
#3103=VERTEX_POINT('',#24942);
#3104=VERTEX_POINT('',#25156);
#3105=VERTEX_POINT('',#25157);
#3106=VERTEX_POINT('',#25159);
#3107=VERTEX_POINT('',#25369);
#3108=VERTEX_POINT('',#25586);
#3109=VERTEX_POINT('',#25587);
#3110=VERTEX_POINT('',#25589);
#3111=VERTEX_POINT('',#25805);
#3112=VERTEX_POINT('',#26019);
#3113=VERTEX_POINT('',#26020);
#3114=VERTEX_POINT('',#26022);
#3115=VERTEX_POINT('',#26232);
#3116=VERTEX_POINT('',#26443);
#3117=VERTEX_POINT('',#26444);
#3118=VERTEX_POINT('',#26446);
#3119=VERTEX_POINT('',#26659);
#3120=VERTEX_POINT('',#26873);
#3121=VERTEX_POINT('',#26874);
#3122=VERTEX_POINT('',#26876);
#3123=VERTEX_POINT('',#27092);
#3124=VERTEX_POINT('',#27303);
#3125=VERTEX_POINT('',#27304);
#3126=VERTEX_POINT('',#27306);
#3127=VERTEX_POINT('',#27516);
#3128=VERTEX_POINT('',#27730);
#3129=VERTEX_POINT('',#27731);
#3130=VERTEX_POINT('',#27733);
#3131=VERTEX_POINT('',#27946);
#3132=VERTEX_POINT('',#28160);
#3133=VERTEX_POINT('',#28161);
#3134=VERTEX_POINT('',#28163);
#3135=VERTEX_POINT('',#28373);
#3136=VERTEX_POINT('',#28584);
#3137=VERTEX_POINT('',#28585);
#3138=VERTEX_POINT('',#28587);
#3139=VERTEX_POINT('',#28800);
#3140=VERTEX_POINT('',#29014);
#3141=VERTEX_POINT('',#29015);
#3142=VERTEX_POINT('',#29017);
#3143=VERTEX_POINT('',#29099);
#3144=VERTEX_POINT('',#29313);
#3145=VERTEX_POINT('',#29314);
#3146=VERTEX_POINT('',#29316);
#3147=VERTEX_POINT('',#29393);
#3148=VERTEX_POINT('',#29399);
#3149=VERTEX_POINT('',#29401);
#3150=VERTEX_POINT('',#29474);
#3151=VERTEX_POINT('',#29475);
#3152=VERTEX_POINT('',#29477);
#3153=VERTEX_POINT('',#29490);
#3154=VERTEX_POINT('',#29492);
#3155=VERTEX_POINT('',#29495);
#3156=VERTEX_POINT('',#29565);
#3157=VERTEX_POINT('',#29566);
#3158=VERTEX_POINT('',#29568);
#3159=VERTEX_POINT('',#29773);
#3160=VERTEX_POINT('',#29798);
#3161=VERTEX_POINT('',#29799);
#3162=VERTEX_POINT('',#29801);
#3163=VERTEX_POINT('',#29999);
#3164=VERTEX_POINT('',#30201);
#3165=VERTEX_POINT('',#30202);
#3166=VERTEX_POINT('',#30204);
#3167=VERTEX_POINT('',#30626);
#3168=VERTEX_POINT('',#30627);
#3169=VERTEX_POINT('',#30629);
#3170=VERTEX_POINT('',#30824);
#3171=VERTEX_POINT('',#31044);
#3172=VERTEX_POINT('',#31045);
#3173=VERTEX_POINT('',#31047);
#3174=VERTEX_POINT('',#31470);
#3175=VERTEX_POINT('',#31471);
#3176=VERTEX_POINT('',#31473);
#3177=VERTEX_POINT('',#31671);
#3178=VERTEX_POINT('',#31911);
#3179=VERTEX_POINT('',#31912);
#3180=VERTEX_POINT('',#31914);
#3181=VERTEX_POINT('',#32344);
#3182=VERTEX_POINT('',#32345);
#3183=VERTEX_POINT('',#32347);
#3184=VERTEX_POINT('',#32542);
#3185=VERTEX_POINT('',#32772);
#3186=VERTEX_POINT('',#32773);
#3187=VERTEX_POINT('',#32775);
#3188=VERTEX_POINT('',#33193);
#3189=VERTEX_POINT('',#33194);
#3190=VERTEX_POINT('',#33196);
#3191=VERTEX_POINT('',#33391);
#3192=VERTEX_POINT('',#33663);
#3193=VERTEX_POINT('',#33664);
#3194=VERTEX_POINT('',#33666);
#3195=VERTEX_POINT('',#34146);
#3196=VERTEX_POINT('',#34147);
#3197=VERTEX_POINT('',#34149);
#3198=VERTEX_POINT('',#34347);
#3199=VERTEX_POINT('',#34559);
#3200=VERTEX_POINT('',#34560);
#3201=VERTEX_POINT('',#34562);
#3202=VERTEX_POINT('',#34978);
#3203=VERTEX_POINT('',#34979);
#3204=VERTEX_POINT('',#34981);
#3205=VERTEX_POINT('',#35176);
#3206=VERTEX_POINT('',#35416);
#3207=VERTEX_POINT('',#35417);
#3208=VERTEX_POINT('',#35419);
#3209=VERTEX_POINT('',#35829);
#3210=VERTEX_POINT('',#35830);
#3211=VERTEX_POINT('',#35832);
#3212=VERTEX_POINT('',#36027);
#3213=VERTEX_POINT('',#36241);
#3214=VERTEX_POINT('',#36242);
#3215=VERTEX_POINT('',#36244);
#3216=VERTEX_POINT('',#36647);
#3217=VERTEX_POINT('',#36648);
#3218=VERTEX_POINT('',#36650);
#3219=VERTEX_POINT('',#36664);
#3220=VERTEX_POINT('',#36786);
#3221=VERTEX_POINT('',#36788);
#3222=VERTEX_POINT('',#36975);
#3223=VERTEX_POINT('',#37173);
#3224=VERTEX_POINT('',#37372);
#3225=VERTEX_POINT('',#37387);
#3226=VERTEX_POINT('',#37601);
#3227=VERTEX_POINT('',#38016);
#3228=VERTEX_POINT('',#38031);
#3229=VERTEX_POINT('',#40974);
#3230=VERTEX_POINT('',#40976);
#3231=VERTEX_POINT('',#40983);
#3232=VERTEX_POINT('',#40984);
#3233=VERTEX_POINT('',#40986);
#3234=VERTEX_POINT('',#41147);
#3235=VERTEX_POINT('',#41274);
#3236=VERTEX_POINT('',#41275);
#3237=VERTEX_POINT('',#41277);
#3238=VERTEX_POINT('',#41466);
#3239=VERTEX_POINT('',#41648);
#3240=VERTEX_POINT('',#41649);
#3241=VERTEX_POINT('',#42028);
#3242=VERTEX_POINT('',#42029);
#3243=VERTEX_POINT('',#42031);
#3244=VERTEX_POINT('',#42214);
#3245=VERTEX_POINT('',#42406);
#3246=VERTEX_POINT('',#42407);
#3247=VERTEX_POINT('',#42778);
#3248=VERTEX_POINT('',#42779);
#3249=VERTEX_POINT('',#42781);
#3250=VERTEX_POINT('',#42980);
#3251=VERTEX_POINT('',#43168);
#3252=VERTEX_POINT('',#43169);
#3253=VERTEX_POINT('',#43544);
#3254=VERTEX_POINT('',#43545);
#3255=VERTEX_POINT('',#43547);
#3256=VERTEX_POINT('',#43732);
#3257=VERTEX_POINT('',#43920);
#3258=VERTEX_POINT('',#43921);
#3259=VERTEX_POINT('',#44292);
#3260=VERTEX_POINT('',#44293);
#3261=VERTEX_POINT('',#44295);
#3262=VERTEX_POINT('',#44488);
#3263=VERTEX_POINT('',#44678);
#3264=VERTEX_POINT('',#44679);
#3265=VERTEX_POINT('',#45054);
#3266=VERTEX_POINT('',#45055);
#3267=VERTEX_POINT('',#45062);
#3268=VERTEX_POINT('',#45064);
#3269=VERTEX_POINT('',#45070);
#3270=VERTEX_POINT('',#45282);
#3271=VERTEX_POINT('',#45491);
#3272=VERTEX_POINT('',#45503);
#3273=VERTEX_POINT('',#45715);
#3274=VERTEX_POINT('',#45927);
#3275=VERTEX_POINT('',#46139);
#3276=VERTEX_POINT('',#46150);
#3277=VERTEX_POINT('',#46161);
#3278=VERTEX_POINT('',#46373);
#3279=VERTEX_POINT('',#46384);
#3280=VERTEX_POINT('',#46395);
#3281=VERTEX_POINT('',#46397);
#3282=VERTEX_POINT('',#46552);
#3283=VERTEX_POINT('',#46563);
#3284=VERTEX_POINT('',#46574);
#3285=VERTEX_POINT('',#46586);
#3286=VERTEX_POINT('',#46597);
#3287=VERTEX_POINT('',#46609);
#3288=VERTEX_POINT('',#46620);
#3289=VERTEX_POINT('',#46631);
#3290=VERTEX_POINT('',#46643);
#3291=VERTEX_POINT('',#47064);
#3292=VERTEX_POINT('',#47069);
#3293=VERTEX_POINT('',#47257);
#3294=VERTEX_POINT('',#47259);
#3295=VERTEX_POINT('',#47424);
#3296=VERTEX_POINT('',#47552);
#3297=VERTEX_POINT('',#48353);
#3298=VERTEX_POINT('',#48354);
#3299=VERTEX_POINT('',#48356);
#3300=VERTEX_POINT('',#48358);
#3301=VERTEX_POINT('',#48362);
#3302=VERTEX_POINT('',#48364);
#3303=VERTEX_POINT('',#48368);
#3304=VERTEX_POINT('',#48370);
#3305=VERTEX_POINT('',#48374);
#3306=VERTEX_POINT('',#48376);
#3307=VERTEX_POINT('',#48380);
#3308=VERTEX_POINT('',#48382);
#3309=VERTEX_POINT('',#48390);
#3310=VERTEX_POINT('',#48393);
#3311=VERTEX_POINT('',#48400);
#3312=VERTEX_POINT('',#48401);
#3313=VERTEX_POINT('',#48403);
#3314=VERTEX_POINT('',#48408);
#3315=VERTEX_POINT('',#48442);
#3316=VERTEX_POINT('',#48443);
#3317=VERTEX_POINT('',#48445);
#3318=VERTEX_POINT('',#48573);
#3319=VERTEX_POINT('',#48653);
#3320=VERTEX_POINT('',#48654);
#3321=VERTEX_POINT('',#48656);
#3322=VERTEX_POINT('',#48854);
#3323=VERTEX_POINT('',#48870);
#3324=VERTEX_POINT('',#48871);
#3325=VERTEX_POINT('',#48873);
#3326=VERTEX_POINT('',#49068);
#3327=VERTEX_POINT('',#49200);
#3328=VERTEX_POINT('',#49201);
#3329=VERTEX_POINT('',#49203);
#3330=VERTEX_POINT('',#49282);
#3331=VERTEX_POINT('',#49478);
#3332=VERTEX_POINT('',#49479);
#3333=VERTEX_POINT('',#49481);
#3334=VERTEX_POINT('',#49609);
#3335=VERTEX_POINT('',#49686);
#3336=VERTEX_POINT('',#49687);
#3337=VERTEX_POINT('',#49689);
#3338=VERTEX_POINT('',#49884);
#3339=VERTEX_POINT('',#50016);
#3340=VERTEX_POINT('',#50017);
#3341=VERTEX_POINT('',#50019);
#3342=VERTEX_POINT('',#50095);
#3343=VERTEX_POINT('',#50294);
#3344=VERTEX_POINT('',#50295);
#3345=VERTEX_POINT('',#50297);
#3346=VERTEX_POINT('',#50425);
#3347=VERTEX_POINT('',#50502);
#3348=VERTEX_POINT('',#50503);
#3349=VERTEX_POINT('',#50505);
#3350=VERTEX_POINT('',#50703);
#3351=VERTEX_POINT('',#50835);
#3352=VERTEX_POINT('',#50836);
#3353=VERTEX_POINT('',#50838);
#3354=VERTEX_POINT('',#50914);
#3355=VERTEX_POINT('',#51110);
#3356=VERTEX_POINT('',#51111);
#3357=VERTEX_POINT('',#51113);
#3358=VERTEX_POINT('',#51241);
#3359=VERTEX_POINT('',#51321);
#3360=VERTEX_POINT('',#51322);
#3361=VERTEX_POINT('',#51324);
#3362=VERTEX_POINT('',#51522);
#3363=VERTEX_POINT('',#51654);
#3364=VERTEX_POINT('',#51655);
#3365=VERTEX_POINT('',#51657);
#3366=VERTEX_POINT('',#51733);
#3367=VERTEX_POINT('',#51929);
#3368=VERTEX_POINT('',#51930);
#3369=VERTEX_POINT('',#51932);
#3370=VERTEX_POINT('',#51947);
#3371=VERTEX_POINT('',#52027);
#3372=VERTEX_POINT('',#52028);
#3373=VERTEX_POINT('',#52030);
#3374=VERTEX_POINT('',#52037);
#3375=VERTEX_POINT('',#52043);
#3376=VERTEX_POINT('',#52045);
#3377=VERTEX_POINT('',#52112);
#3378=VERTEX_POINT('',#52113);
#3379=VERTEX_POINT('',#52115);
#3380=VERTEX_POINT('',#52252);
#3381=VERTEX_POINT('',#52254);
#3382=VERTEX_POINT('',#52265);
#3383=VERTEX_POINT('',#52268);
#3384=VERTEX_POINT('',#52446);
#3385=VERTEX_POINT('',#52447);
#3386=VERTEX_POINT('',#52449);
#3387=VERTEX_POINT('',#52629);
#3388=VERTEX_POINT('',#52654);
#3389=VERTEX_POINT('',#52655);
#3390=VERTEX_POINT('',#52657);
#3391=VERTEX_POINT('',#52864);
#3392=VERTEX_POINT('',#53069);
#3393=VERTEX_POINT('',#53070);
#3394=VERTEX_POINT('',#53487);
#3395=VERTEX_POINT('',#53488);
#3396=VERTEX_POINT('',#53490);
#3397=VERTEX_POINT('',#53721);
#3398=VERTEX_POINT('',#53929);
#3399=VERTEX_POINT('',#53930);
#3400=VERTEX_POINT('',#54359);
#3401=VERTEX_POINT('',#54360);
#3402=VERTEX_POINT('',#54362);
#3403=VERTEX_POINT('',#54581);
#3404=VERTEX_POINT('',#54787);
#3405=VERTEX_POINT('',#54788);
#3406=VERTEX_POINT('',#55203);
#3407=VERTEX_POINT('',#55204);
#3408=VERTEX_POINT('',#55206);
#3409=VERTEX_POINT('',#55391);
#3410=VERTEX_POINT('',#55673);
#3411=VERTEX_POINT('',#55674);
#3412=VERTEX_POINT('',#55676);
#3413=VERTEX_POINT('',#56095);
#3414=VERTEX_POINT('',#56096);
#3415=VERTEX_POINT('',#56296);
#3416=VERTEX_POINT('',#56510);
#3417=VERTEX_POINT('',#56511);
#3418=VERTEX_POINT('',#56513);
#3419=VERTEX_POINT('',#56933);
#3420=VERTEX_POINT('',#56934);
#3421=VERTEX_POINT('',#57156);
#3422=VERTEX_POINT('',#57368);
#3423=VERTEX_POINT('',#57369);
#3424=VERTEX_POINT('',#57371);
#3425=VERTEX_POINT('',#57793);
#3426=VERTEX_POINT('',#57794);
#3427=VERTEX_POINT('',#57796);
#3428=VERTEX_POINT('',#57807);
#3429=VERTEX_POINT('',#57917);
#3430=VERTEX_POINT('',#57919);
#3431=VERTEX_POINT('',#58291);
#3432=VERTEX_POINT('',#58468);
#3433=VERTEX_POINT('',#58483);
#3434=VERTEX_POINT('',#59673);
#3435=VERTEX_POINT('',#59675);
#3436=VERTEX_POINT('',#59699);
#3437=VERTEX_POINT('',#59700);
#3438=VERTEX_POINT('',#59702);
#3439=VERTEX_POINT('',#59704);
#3440=VERTEX_POINT('',#59708);
#3441=VERTEX_POINT('',#59710);
#3442=VERTEX_POINT('',#59713);
#3443=VERTEX_POINT('',#59715);
#3444=VERTEX_POINT('',#59717);
#3445=VERTEX_POINT('',#59719);
#3446=VERTEX_POINT('',#59722);
#3447=VERTEX_POINT('',#59726);
#3448=VERTEX_POINT('',#59730);
#3449=VERTEX_POINT('',#59734);
#3450=VERTEX_POINT('',#59738);
#3451=VERTEX_POINT('',#59742);
#3452=VERTEX_POINT('',#59750);
#3453=VERTEX_POINT('',#59752);
#3454=VERTEX_POINT('',#59756);
#3455=VERTEX_POINT('',#59758);
#3456=VERTEX_POINT('',#59762);
#3457=VERTEX_POINT('',#59764);
#3458=VERTEX_POINT('',#59768);
#3459=VERTEX_POINT('',#59770);
#3460=VERTEX_POINT('',#59774);
#3461=VERTEX_POINT('',#59775);
#3462=VERTEX_POINT('',#59777);
#3463=VERTEX_POINT('',#59779);
#3464=VERTEX_POINT('',#59783);
#3465=VERTEX_POINT('',#59785);
#3466=VERTEX_POINT('',#59789);
#3467=VERTEX_POINT('',#59791);
#3468=VERTEX_POINT('',#59798);
#3469=VERTEX_POINT('',#59799);
#3470=VERTEX_POINT('',#59801);
#3471=VERTEX_POINT('',#59803);
#3472=VERTEX_POINT('',#59807);
#3473=VERTEX_POINT('',#59809);
#3474=VERTEX_POINT('',#59813);
#3475=VERTEX_POINT('',#59815);
#3476=VERTEX_POINT('',#59825);
#3477=VERTEX_POINT('',#59827);
#3478=VERTEX_POINT('',#59831);
#3479=VERTEX_POINT('',#59833);
#3480=VERTEX_POINT('',#59837);
#3481=VERTEX_POINT('',#59839);
#3482=VERTEX_POINT('',#59843);
#3483=VERTEX_POINT('',#59845);
#3484=VERTEX_POINT('',#59849);
#3485=VERTEX_POINT('',#59850);
#3486=VERTEX_POINT('',#59852);
#3487=VERTEX_POINT('',#59854);
#3488=VERTEX_POINT('',#59858);
#3489=VERTEX_POINT('',#59860);
#3490=VERTEX_POINT('',#59864);
#3491=VERTEX_POINT('',#59866);
#3492=VERTEX_POINT('',#59876);
#3493=VERTEX_POINT('',#59877);
#3494=VERTEX_POINT('',#59879);
#3495=VERTEX_POINT('',#60100);
#3496=VERTEX_POINT('',#60227);
#3497=VERTEX_POINT('',#60228);
#3498=VERTEX_POINT('',#60438);
#3499=VERTEX_POINT('',#60646);
#3500=VERTEX_POINT('',#60647);
#3501=VERTEX_POINT('',#60649);
#3502=VERTEX_POINT('',#60882);
#3503=VERTEX_POINT('',#60883);
#3504=VERTEX_POINT('',#60885);
#3505=VERTEX_POINT('',#61080);
#3506=VERTEX_POINT('',#61278);
#3507=VERTEX_POINT('',#61279);
#3508=VERTEX_POINT('',#61281);
#3509=VERTEX_POINT('',#61687);
#3510=VERTEX_POINT('',#61688);
#3511=VERTEX_POINT('',#61892);
#3512=VERTEX_POINT('',#61912);
#3513=VERTEX_POINT('',#61913);
#3514=VERTEX_POINT('',#61915);
#3515=VERTEX_POINT('',#61932);
#3516=VERTEX_POINT('',#62134);
#3517=VERTEX_POINT('',#62135);
#3518=VERTEX_POINT('',#62137);
#3519=VERTEX_POINT('',#62519);
#3520=VERTEX_POINT('',#62520);
#3521=VERTEX_POINT('',#62522);
#3522=VERTEX_POINT('',#62733);
#3523=VERTEX_POINT('',#62949);
#3524=VERTEX_POINT('',#62950);
#3525=VERTEX_POINT('',#63381);
#3526=VERTEX_POINT('',#63382);
#3527=VERTEX_POINT('',#63384);
#3528=VERTEX_POINT('',#63399);
#3529=VERTEX_POINT('',#63597);
#3530=VERTEX_POINT('',#63598);
#3531=VERTEX_POINT('',#63600);
#3532=VERTEX_POINT('',#64062);
#3533=VERTEX_POINT('',#64063);
#3534=VERTEX_POINT('',#64065);
#3535=VERTEX_POINT('',#64344);
#3536=VERTEX_POINT('',#64556);
#3537=VERTEX_POINT('',#64557);
#3538=VERTEX_POINT('',#64970);
#3539=VERTEX_POINT('',#64971);
#3540=VERTEX_POINT('',#64973);
#3541=VERTEX_POINT('',#64988);
#3542=VERTEX_POINT('',#65188);
#3543=VERTEX_POINT('',#65189);
#3544=VERTEX_POINT('',#65196);
#3545=VERTEX_POINT('',#65198);
#3546=VERTEX_POINT('',#65204);
#3547=VERTEX_POINT('',#65416);
#3548=VERTEX_POINT('',#65628);
#3549=VERTEX_POINT('',#65837);
#3550=VERTEX_POINT('',#65848);
#3551=VERTEX_POINT('',#65859);
#3552=VERTEX_POINT('',#66068);
#3553=VERTEX_POINT('',#66280);
#3554=VERTEX_POINT('',#66291);
#3555=VERTEX_POINT('',#66303);
#3556=VERTEX_POINT('',#66512);
#3557=VERTEX_POINT('',#66721);
#3558=VERTEX_POINT('',#66733);
#3559=VERTEX_POINT('',#66744);
#3560=VERTEX_POINT('',#66953);
#3561=VERTEX_POINT('',#67138);
#3562=VERTEX_POINT('',#67140);
#3563=VERTEX_POINT('',#67295);
#3564=VERTEX_POINT('',#67306);
#3565=VERTEX_POINT('',#67515);
#3566=VERTEX_POINT('',#67527);
#3567=VERTEX_POINT('',#67739);
#3568=VERTEX_POINT('',#67948);
#3569=VERTEX_POINT('',#67960);
#3570=VERTEX_POINT('',#68172);
#3571=VERTEX_POINT('',#68381);
#3572=VERTEX_POINT('',#68393);
#3573=VERTEX_POINT('',#68605);
#3574=VERTEX_POINT('',#68616);
#3575=VERTEX_POINT('',#68628);
#3576=VERTEX_POINT('',#68851);
#3577=VERTEX_POINT('',#68856);
#3578=VERTEX_POINT('',#69044);
#3579=VERTEX_POINT('',#69046);
#3580=VERTEX_POINT('',#69204);
#3581=VERTEX_POINT('',#69299);
#3582=VERTEX_POINT('',#69338);
#3583=VERTEX_POINT('',#70253);
#3584=VERTEX_POINT('',#70350);
#3585=VERTEX_POINT('',#70351);
#3586=VERTEX_POINT('',#70353);
#3587=VERTEX_POINT('',#70355);
#3588=VERTEX_POINT('',#70359);
#3589=VERTEX_POINT('',#70361);
#3590=VERTEX_POINT('',#70365);
#3591=VERTEX_POINT('',#70367);
#3592=VERTEX_POINT('',#70371);
#3593=VERTEX_POINT('',#70373);
#3594=VERTEX_POINT('',#70377);
#3595=VERTEX_POINT('',#70379);
#3596=VERTEX_POINT('',#70387);
#3597=VERTEX_POINT('',#70390);
#3598=VERTEX_POINT('',#70397);
#3599=VERTEX_POINT('',#70398);
#3600=VERTEX_POINT('',#70400);
#3601=VERTEX_POINT('',#70553);
#3602=VERTEX_POINT('',#70668);
#3603=VERTEX_POINT('',#70669);
#3604=VERTEX_POINT('',#71050);
#3605=VERTEX_POINT('',#71051);
#3606=VERTEX_POINT('',#71053);
#3607=VERTEX_POINT('',#71453);
#3608=VERTEX_POINT('',#71454);
#3609=VERTEX_POINT('',#71650);
#3610=VERTEX_POINT('',#71844);
#3611=VERTEX_POINT('',#71845);
#3612=VERTEX_POINT('',#72022);
#3613=VERTEX_POINT('',#72216);
#3614=VERTEX_POINT('',#72217);
#3615=VERTEX_POINT('',#72598);
#3616=VERTEX_POINT('',#72599);
#3617=VERTEX_POINT('',#72601);
#3618=VERTEX_POINT('',#72989);
#3619=VERTEX_POINT('',#72990);
#3620=VERTEX_POINT('',#73206);
#3621=VERTEX_POINT('',#73207);
#3622=VERTEX_POINT('',#73644);
#3623=VERTEX_POINT('',#73645);
#3624=VERTEX_POINT('',#73647);
#3625=VERTEX_POINT('',#74037);
#3626=VERTEX_POINT('',#74038);
#3627=VERTEX_POINT('',#74040);
#3628=VERTEX_POINT('',#74247);
#3629=VERTEX_POINT('',#74449);
#3630=VERTEX_POINT('',#74450);
#3631=VERTEX_POINT('',#74835);
#3632=VERTEX_POINT('',#74836);
#3633=VERTEX_POINT('',#75200);
#3634=VERTEX_POINT('',#75201);
#3635=VERTEX_POINT('',#75263);
#3636=VERTEX_POINT('',#75265);
#3637=VERTEX_POINT('',#75300);
#3638=VERTEX_POINT('',#75491);
#3639=VERTEX_POINT('',#75502);
#3640=VERTEX_POINT('',#75693);
#3641=VERTEX_POINT('',#75884);
#3642=VERTEX_POINT('',#75895);
#3643=VERTEX_POINT('',#76086);
#3644=VERTEX_POINT('',#76098);
#3645=VERTEX_POINT('',#76109);
#3646=VERTEX_POINT('',#76300);
#3647=VERTEX_POINT('',#76312);
#3648=VERTEX_POINT('',#76500);
#3649=VERTEX_POINT('',#76511);
#3650=VERTEX_POINT('',#76651);
#3651=VERTEX_POINT('',#76653);
#3652=VERTEX_POINT('',#76769);
#3653=VERTEX_POINT('',#76780);
#3654=VERTEX_POINT('',#76971);
#3655=VERTEX_POINT('',#77162);
#3656=VERTEX_POINT('',#77173);
#3657=VERTEX_POINT('',#77184);
#3658=VERTEX_POINT('',#77375);
#3659=VERTEX_POINT('',#77386);
#3660=VERTEX_POINT('',#77397);
#3661=VERTEX_POINT('',#77588);
#3662=VERTEX_POINT('',#77782);
#3663=VERTEX_POINT('',#77804);
#3664=VERTEX_POINT('',#77950);
#3665=VERTEX_POINT('',#78065);
#3666=VERTEX_POINT('',#78220);
#3667=VERTEX_POINT('',#79020);
#3668=VERTEX_POINT('',#79108);
#3669=VERTEX_POINT('',#79109);
#3670=VERTEX_POINT('',#79111);
#3671=VERTEX_POINT('',#79113);
#3672=VERTEX_POINT('',#79117);
#3673=VERTEX_POINT('',#79119);
#3674=VERTEX_POINT('',#79123);
#3675=VERTEX_POINT('',#79125);
#3676=VERTEX_POINT('',#79129);
#3677=VERTEX_POINT('',#79131);
#3678=VERTEX_POINT('',#79135);
#3679=VERTEX_POINT('',#79137);
#3680=VERTEX_POINT('',#79145);
#3681=VERTEX_POINT('',#79148);
#3682=VERTEX_POINT('',#79155);
#3683=VERTEX_POINT('',#79156);
#3684=VERTEX_POINT('',#79158);
#3685=VERTEX_POINT('',#79301);
#3686=VERTEX_POINT('',#79392);
#3687=VERTEX_POINT('',#79393);
#3688=VERTEX_POINT('',#79395);
#3689=VERTEX_POINT('',#79689);
#3690=VERTEX_POINT('',#79791);
#3691=VERTEX_POINT('',#79792);
#3692=VERTEX_POINT('',#80102);
#3693=VERTEX_POINT('',#80312);
#3694=VERTEX_POINT('',#80313);
#3695=VERTEX_POINT('',#80315);
#3696=VERTEX_POINT('',#80737);
#3697=VERTEX_POINT('',#80738);
#3698=VERTEX_POINT('',#80740);
#3699=VERTEX_POINT('',#80944);
#3700=VERTEX_POINT('',#81068);
#3701=VERTEX_POINT('',#81069);
#3702=VERTEX_POINT('',#81369);
#3703=VERTEX_POINT('',#81586);
#3704=VERTEX_POINT('',#81587);
#3705=VERTEX_POINT('',#81589);
#3706=VERTEX_POINT('',#81996);
#3707=VERTEX_POINT('',#81997);
#3708=VERTEX_POINT('',#81999);
#3709=VERTEX_POINT('',#82270);
#3710=VERTEX_POINT('',#82391);
#3711=VERTEX_POINT('',#82392);
#3712=VERTEX_POINT('',#82686);
#3713=VERTEX_POINT('',#82940);
#3714=VERTEX_POINT('',#82941);
#3715=VERTEX_POINT('',#82943);
#3716=VERTEX_POINT('',#83577);
#3717=VERTEX_POINT('',#83578);
#3718=VERTEX_POINT('',#83872);
#3719=VERTEX_POINT('',#84224);
#3720=VERTEX_POINT('',#84225);
#3721=VERTEX_POINT('',#84227);
#3722=VERTEX_POINT('',#84843);
#3723=VERTEX_POINT('',#84844);
#3724=VERTEX_POINT('',#85146);
#3725=VERTEX_POINT('',#85434);
#3726=VERTEX_POINT('',#85435);
#3727=VERTEX_POINT('',#85437);
#3728=VERTEX_POINT('',#85552);
#3729=VERTEX_POINT('',#85848);
#3730=VERTEX_POINT('',#85849);
#3731=VERTEX_POINT('',#85851);
#3732=VERTEX_POINT('',#85940);
#3733=VERTEX_POINT('',#85949);
#3734=VERTEX_POINT('',#85950);
#3735=VERTEX_POINT('',#86237);
#3736=VERTEX_POINT('',#86238);
#3737=VERTEX_POINT('',#86275);
#3738=VERTEX_POINT('',#86276);
#3739=VERTEX_POINT('',#86313);
#3740=VERTEX_POINT('',#86314);
#3741=VERTEX_POINT('',#86859);
#3742=VERTEX_POINT('',#86860);
#3743=VERTEX_POINT('',#86895);
#3744=VERTEX_POINT('',#86896);
#3745=VERTEX_POINT('',#86933);
#3746=VERTEX_POINT('',#86934);
#3747=VERTEX_POINT('',#87479);
#3748=VERTEX_POINT('',#87480);
#3749=VERTEX_POINT('',#88019);
#3750=VERTEX_POINT('',#88020);
#3751=VERTEX_POINT('',#88057);
#3752=VERTEX_POINT('',#88058);
#3753=VERTEX_POINT('',#88597);
#3754=VERTEX_POINT('',#88598);
#3755=VERTEX_POINT('',#89137);
#3756=VERTEX_POINT('',#89138);
#3757=VERTEX_POINT('',#89176);
#3758=VERTEX_POINT('',#89177);
#3759=VERTEX_POINT('',#89214);
#3760=VERTEX_POINT('',#89229);
#3761=VERTEX_POINT('',#89244);
#3762=VERTEX_POINT('',#89511);
#3763=VERTEX_POINT('',#89513);
#3764=VERTEX_POINT('',#91285);
#3765=VERTEX_POINT('',#91533);
#3766=VERTEX_POINT('',#91536);
#3767=VERTEX_POINT('',#91540);
#3768=VERTEX_POINT('',#91542);
#3769=VERTEX_POINT('',#91549);
#3770=VERTEX_POINT('',#91550);
#3771=VERTEX_POINT('',#91552);
#3772=VERTEX_POINT('',#91561);
#3773=VERTEX_POINT('',#91573);
#3774=VERTEX_POINT('',#91574);
#3775=VERTEX_POINT('',#91576);
#3776=VERTEX_POINT('',#91764);
#3777=VERTEX_POINT('',#91787);
#3778=VERTEX_POINT('',#91788);
#3779=VERTEX_POINT('',#91790);
#3780=VERTEX_POINT('',#91900);
#3781=VERTEX_POINT('',#91923);
#3782=VERTEX_POINT('',#91924);
#3783=VERTEX_POINT('',#91926);
#3784=VERTEX_POINT('',#92024);
#3785=VERTEX_POINT('',#92031);
#3786=VERTEX_POINT('',#92033);
#3787=VERTEX_POINT('',#92051);
#3788=VERTEX_POINT('',#92052);
#3789=VERTEX_POINT('',#92054);
#3790=VERTEX_POINT('',#92086);
#3791=VERTEX_POINT('',#92198);
#3792=VERTEX_POINT('',#92199);
#3793=VERTEX_POINT('',#92236);
#3794=VERTEX_POINT('',#92237);
#3795=VERTEX_POINT('',#92648);
#3796=VERTEX_POINT('',#92649);
#3797=VERTEX_POINT('',#92651);
#3798=VERTEX_POINT('',#92821);
#3799=VERTEX_POINT('',#93177);
#3800=VERTEX_POINT('',#93199);
#3801=VERTEX_POINT('',#93388);
#3802=VERTEX_POINT('',#93390);
#3803=VERTEX_POINT('',#93394);
#3804=VERTEX_POINT('',#93396);
#3805=VERTEX_POINT('',#94213);
#3806=VERTEX_POINT('',#94337);
#3807=VERTEX_POINT('',#94340);
#3808=VERTEX_POINT('',#94346);
#3809=VERTEX_POINT('',#94348);
#3810=VERTEX_POINT('',#94352);
#3811=VERTEX_POINT('',#94354);
#3812=EDGE_CURVE('',#2846,#2846,#2728,.T.);
#3813=EDGE_CURVE('',#2846,#2847,#1932,.T.);
#3814=EDGE_CURVE('',#2847,#2847,#2729,.T.);
#3815=EDGE_CURVE('',#2848,#2848,#2730,.T.);
#3816=EDGE_CURVE('',#2848,#2849,#1933,.T.);
#3817=EDGE_CURVE('',#2849,#2849,#2731,.T.);
#3818=EDGE_CURVE('',#2850,#2850,#2732,.T.);
#3819=EDGE_CURVE('',#2850,#2851,#1934,.T.);
#3820=EDGE_CURVE('',#2851,#2851,#2733,.T.);
#3821=EDGE_CURVE('',#2852,#2852,#2734,.T.);
#3822=EDGE_CURVE('',#2852,#2853,#1935,.T.);
#3823=EDGE_CURVE('',#2853,#2853,#2735,.T.);
#3824=EDGE_CURVE('',#2854,#2855,#1936,.T.);
#3825=EDGE_CURVE('',#2855,#2856,#1937,.T.);
#3826=EDGE_CURVE('',#2857,#2856,#1938,.T.);
#3827=EDGE_CURVE('',#2854,#2857,#1939,.T.);
#3828=EDGE_CURVE('',#2858,#2854,#1940,.T.);
#3829=EDGE_CURVE('',#2859,#2857,#1941,.T.);
#3830=EDGE_CURVE('',#2858,#2859,#1942,.T.);
#3831=EDGE_CURVE('',#2860,#2858,#1943,.T.);
#3832=EDGE_CURVE('',#2861,#2859,#1944,.T.);
#3833=EDGE_CURVE('',#2860,#2861,#1945,.T.);
#3834=EDGE_CURVE('',#2855,#2860,#1946,.T.);
#3835=EDGE_CURVE('',#2856,#2861,#1947,.T.);
#3836=EDGE_CURVE('',#2862,#2862,#2736,.T.);
#3837=EDGE_CURVE('',#2862,#2863,#1948,.T.);
#3838=EDGE_CURVE('',#2863,#2863,#2737,.T.);
#3839=EDGE_CURVE('',#2864,#2864,#2738,.T.);
#3840=EDGE_CURVE('',#2864,#2865,#1949,.T.);
#3841=EDGE_CURVE('',#2865,#2865,#2739,.T.);
#3842=EDGE_CURVE('',#2866,#2867,#1950,.T.);
#3843=EDGE_CURVE('',#2867,#2868,#1951,.T.);
#3844=EDGE_CURVE('',#2869,#2868,#1952,.T.);
#3845=EDGE_CURVE('',#2866,#2869,#1953,.T.);
#3846=EDGE_CURVE('',#2870,#2866,#1954,.T.);
#3847=EDGE_CURVE('',#2871,#2869,#1955,.T.);
#3848=EDGE_CURVE('',#2870,#2871,#1956,.T.);
#3849=EDGE_CURVE('',#2872,#2870,#1957,.T.);
#3850=EDGE_CURVE('',#2873,#2871,#1958,.T.);
#3851=EDGE_CURVE('',#2872,#2873,#1959,.T.);
#3852=EDGE_CURVE('',#2867,#2872,#1960,.T.);
#3853=EDGE_CURVE('',#2868,#2873,#1961,.T.);
#3854=EDGE_CURVE('',#2874,#2875,#1962,.T.);
#3855=EDGE_CURVE('',#2875,#2876,#1963,.T.);
#3856=EDGE_CURVE('',#2877,#2876,#1964,.T.);
#3857=EDGE_CURVE('',#2874,#2877,#1965,.T.);
#3858=EDGE_CURVE('',#2878,#2874,#1966,.T.);
#3859=EDGE_CURVE('',#2879,#2877,#1967,.T.);
#3860=EDGE_CURVE('',#2878,#2879,#1968,.T.);
#3861=EDGE_CURVE('',#2880,#2878,#1969,.T.);
#3862=EDGE_CURVE('',#2881,#2879,#1970,.T.);
#3863=EDGE_CURVE('',#2880,#2881,#1971,.T.);
#3864=EDGE_CURVE('',#2875,#2880,#1972,.T.);
#3865=EDGE_CURVE('',#2876,#2881,#1973,.T.);
#3866=EDGE_CURVE('',#2882,#2883,#2740,.T.);
#3867=EDGE_CURVE('',#2883,#2884,#1974,.T.);
#3868=EDGE_CURVE('',#2884,#2885,#2741,.T.);
#3869=EDGE_CURVE('',#2885,#2882,#1975,.T.);
#3870=EDGE_CURVE('',#2886,#2883,#1976,.T.);
#3871=EDGE_CURVE('',#2887,#2886,#1977,.T.);
#3872=EDGE_CURVE('',#2884,#2887,#1978,.T.);
#3873=EDGE_CURVE('',#2886,#2888,#2742,.T.);
#3874=EDGE_CURVE('',#2888,#2889,#1979,.T.);
#3875=EDGE_CURVE('',#2889,#2887,#2743,.T.);
#3876=EDGE_CURVE('',#2890,#2888,#1980,.T.);
#3877=EDGE_CURVE('',#2891,#2890,#1981,.T.);
#3878=EDGE_CURVE('',#2889,#2891,#1982,.T.);
#3879=EDGE_CURVE('',#2892,#2893,#2744,.T.);
#3880=EDGE_CURVE('',#2893,#2894,#1983,.T.);
#3881=EDGE_CURVE('',#2894,#2895,#2745,.T.);
#3882=EDGE_CURVE('',#2895,#2892,#1984,.T.);
#3883=EDGE_CURVE('',#2894,#2885,#1985,.T.);
#3884=EDGE_CURVE('',#2882,#2893,#1986,.T.);
#3885=EDGE_CURVE('',#2890,#2896,#2746,.T.);
#3886=EDGE_CURVE('',#2896,#2897,#1987,.T.);
#3887=EDGE_CURVE('',#2897,#2891,#2747,.T.);
#3888=EDGE_CURVE('',#2897,#2895,#1988,.T.);
#3889=EDGE_CURVE('',#2892,#2896,#1989,.T.);
#3890=EDGE_CURVE('',#2898,#2899,#2748,.T.);
#3891=EDGE_CURVE('',#2899,#2900,#1990,.T.);
#3892=EDGE_CURVE('',#2900,#2901,#2749,.T.);
#3893=EDGE_CURVE('',#2901,#2898,#1991,.T.);
#3894=EDGE_CURVE('',#2902,#2899,#1992,.T.);
#3895=EDGE_CURVE('',#2903,#2902,#1993,.T.);
#3896=EDGE_CURVE('',#2900,#2903,#1994,.T.);
#3897=EDGE_CURVE('',#2904,#2905,#2750,.T.);
#3898=EDGE_CURVE('',#2905,#2906,#1995,.T.);
#3899=EDGE_CURVE('',#2906,#2907,#2751,.T.);
#3900=EDGE_CURVE('',#2907,#2904,#1996,.T.);
#3901=EDGE_CURVE('',#2906,#2901,#1997,.T.);
#3902=EDGE_CURVE('',#2898,#2905,#1998,.T.);
#3903=EDGE_CURVE('',#2902,#2908,#2752,.T.);
#3904=EDGE_CURVE('',#2908,#2909,#1999,.T.);
#3905=EDGE_CURVE('',#2909,#2903,#2753,.T.);
#3906=EDGE_CURVE('',#2910,#2908,#2000,.T.);
#3907=EDGE_CURVE('',#2911,#2910,#2001,.T.);
#3908=EDGE_CURVE('',#2909,#2911,#2002,.T.);
#3909=EDGE_CURVE('',#2910,#2912,#2754,.T.);
#3910=EDGE_CURVE('',#2912,#2913,#2003,.T.);
#3911=EDGE_CURVE('',#2913,#2911,#2755,.T.);
#3912=EDGE_CURVE('',#2913,#2907,#2004,.T.);
#3913=EDGE_CURVE('',#2904,#2912,#2005,.T.);
#3914=EDGE_CURVE('',#2914,#2915,#2006,.T.);
#3915=EDGE_CURVE('',#2915,#2916,#2007,.T.);
#3916=EDGE_CURVE('',#2917,#2916,#2008,.T.);
#3917=EDGE_CURVE('',#2914,#2917,#2009,.T.);
#3918=EDGE_CURVE('',#2918,#2914,#2010,.T.);
#3919=EDGE_CURVE('',#2919,#2917,#2011,.T.);
#3920=EDGE_CURVE('',#2918,#2919,#2012,.T.);
#3921=EDGE_CURVE('',#2920,#2918,#2013,.T.);
#3922=EDGE_CURVE('',#2921,#2919,#2014,.T.);
#3923=EDGE_CURVE('',#2920,#2921,#2015,.T.);
#3924=EDGE_CURVE('',#2915,#2920,#2016,.T.);
#3925=EDGE_CURVE('',#2916,#2921,#2017,.T.);
#3926=EDGE_CURVE('',#2922,#2923,#2018,.T.);
#3927=EDGE_CURVE('',#2923,#2924,#170,.T.);
#3928=EDGE_CURVE('',#2925,#2924,#2756,.T.);
#3929=EDGE_CURVE('',#2922,#2925,#171,.T.);
#3930=EDGE_CURVE('',#2926,#2927,#2019,.T.);
#3931=EDGE_CURVE('',#2927,#2928,#172,.T.);
#3932=EDGE_CURVE('',#2928,#2923,#173,.T.);
#3933=EDGE_CURVE('',#2929,#2922,#174,.T.);
#3934=EDGE_CURVE('',#2926,#2929,#175,.T.);
#3935=EDGE_CURVE('',#2930,#2931,#2020,.T.);
#3936=EDGE_CURVE('',#2931,#2932,#176,.T.);
#3937=EDGE_CURVE('',#2932,#2927,#177,.T.);
#3938=EDGE_CURVE('',#2933,#2926,#178,.T.);
#3939=EDGE_CURVE('',#2930,#2933,#179,.T.);
#3940=EDGE_CURVE('',#2934,#2935,#2021,.T.);
#3941=EDGE_CURVE('',#2935,#2936,#180,.T.);
#3942=EDGE_CURVE('',#2936,#2931,#181,.T.);
#3943=EDGE_CURVE('',#2937,#2930,#182,.T.);
#3944=EDGE_CURVE('',#2934,#2937,#183,.T.);
#3945=EDGE_CURVE('',#2938,#2939,#2022,.T.);
#3946=EDGE_CURVE('',#2939,#2940,#184,.T.);
#3947=EDGE_CURVE('',#2940,#2935,#185,.T.);
#3948=EDGE_CURVE('',#2941,#2934,#186,.T.);
#3949=EDGE_CURVE('',#2938,#2941,#187,.T.);
#3950=EDGE_CURVE('',#2942,#2943,#2023,.T.);
#3951=EDGE_CURVE('',#2943,#2944,#188,.T.);
#3952=EDGE_CURVE('',#2944,#2939,#189,.T.);
#3953=EDGE_CURVE('',#2945,#2938,#190,.T.);
#3954=EDGE_CURVE('',#2942,#2945,#191,.T.);
#3955=EDGE_CURVE('',#2946,#2947,#2024,.T.);
#3956=EDGE_CURVE('',#2947,#2948,#192,.T.);
#3957=EDGE_CURVE('',#2948,#2943,#193,.T.);
#3958=EDGE_CURVE('',#2949,#2942,#194,.T.);
#3959=EDGE_CURVE('',#2946,#2949,#195,.T.);
#3960=EDGE_CURVE('',#2950,#2951,#2025,.T.);
#3961=EDGE_CURVE('',#2951,#2952,#196,.T.);
#3962=EDGE_CURVE('',#2952,#2947,#197,.T.);
#3963=EDGE_CURVE('',#2953,#2946,#198,.T.);
#3964=EDGE_CURVE('',#2950,#2953,#199,.T.);
#3965=EDGE_CURVE('',#2954,#2955,#2026,.T.);
#3966=EDGE_CURVE('',#2955,#2956,#200,.T.);
#3967=EDGE_CURVE('',#2956,#2951,#201,.T.);
#3968=EDGE_CURVE('',#2957,#2950,#202,.T.);
#3969=EDGE_CURVE('',#2954,#2957,#203,.T.);
#3970=EDGE_CURVE('',#2958,#2959,#2027,.T.);
#3971=EDGE_CURVE('',#2959,#2960,#204,.T.);
#3972=EDGE_CURVE('',#2960,#2955,#205,.T.);
#3973=EDGE_CURVE('',#2961,#2954,#206,.T.);
#3974=EDGE_CURVE('',#2958,#2961,#207,.T.);
#3975=EDGE_CURVE('',#2962,#2963,#2028,.T.);
#3976=EDGE_CURVE('',#2963,#2964,#208,.T.);
#3977=EDGE_CURVE('',#2964,#2959,#209,.T.);
#3978=EDGE_CURVE('',#2965,#2958,#210,.T.);
#3979=EDGE_CURVE('',#2962,#2965,#211,.T.);
#3980=EDGE_CURVE('',#2966,#2967,#2029,.T.);
#3981=EDGE_CURVE('',#2967,#2968,#212,.T.);
#3982=EDGE_CURVE('',#2968,#2963,#213,.T.);
#3983=EDGE_CURVE('',#2969,#2962,#214,.T.);
#3984=EDGE_CURVE('',#2966,#2969,#215,.T.);
#3985=EDGE_CURVE('',#2970,#2971,#2030,.T.);
#3986=EDGE_CURVE('',#2971,#2972,#216,.T.);
#3987=EDGE_CURVE('',#2972,#2967,#217,.T.);
#3988=EDGE_CURVE('',#2973,#2966,#218,.T.);
#3989=EDGE_CURVE('',#2970,#2973,#219,.T.);
#3990=EDGE_CURVE('',#2974,#2975,#2031,.T.);
#3991=EDGE_CURVE('',#2975,#2976,#220,.T.);
#3992=EDGE_CURVE('',#2976,#2971,#221,.T.);
#3993=EDGE_CURVE('',#2977,#2970,#222,.T.);
#3994=EDGE_CURVE('',#2974,#2977,#223,.T.);
#3995=EDGE_CURVE('',#2978,#2979,#2032,.T.);
#3996=EDGE_CURVE('',#2979,#2980,#224,.T.);
#3997=EDGE_CURVE('',#2980,#2975,#225,.T.);
#3998=EDGE_CURVE('',#2981,#2974,#226,.T.);
#3999=EDGE_CURVE('',#2978,#2981,#227,.T.);
#4000=EDGE_CURVE('',#2982,#2983,#2033,.T.);
#4001=EDGE_CURVE('',#2983,#2984,#228,.T.);
#4002=EDGE_CURVE('',#2984,#2979,#229,.T.);
#4003=EDGE_CURVE('',#2985,#2978,#230,.T.);
#4004=EDGE_CURVE('',#2982,#2985,#231,.T.);
#4005=EDGE_CURVE('',#2986,#2987,#2034,.T.);
#4006=EDGE_CURVE('',#2987,#2988,#232,.T.);
#4007=EDGE_CURVE('',#2988,#2983,#233,.T.);
#4008=EDGE_CURVE('',#2989,#2982,#234,.T.);
#4009=EDGE_CURVE('',#2986,#2989,#235,.T.);
#4010=EDGE_CURVE('',#2990,#2991,#2035,.T.);
#4011=EDGE_CURVE('',#2991,#2992,#236,.T.);
#4012=EDGE_CURVE('',#2992,#2987,#237,.T.);
#4013=EDGE_CURVE('',#2993,#2986,#238,.T.);
#4014=EDGE_CURVE('',#2990,#2993,#239,.T.);
#4015=EDGE_CURVE('',#2994,#2995,#2036,.T.);
#4016=EDGE_CURVE('',#2996,#2994,#240,.T.);
#4017=EDGE_CURVE('',#2997,#2996,#241,.T.);
#4018=EDGE_CURVE('',#2998,#2997,#2757,.T.);
#4019=EDGE_CURVE('',#2998,#2999,#242,.T.);
#4020=EDGE_CURVE('',#2999,#2995,#243,.T.);
#4021=EDGE_CURVE('',#3000,#3001,#2037,.T.);
#4022=EDGE_CURVE('',#3001,#3002,#244,.T.);
#4023=EDGE_CURVE('',#3002,#3003,#2758,.T.);
#4024=EDGE_CURVE('',#3003,#3004,#2038,.T.);
#4025=EDGE_CURVE('',#3004,#3004,#2759,.F.);
#4026=EDGE_CURVE('',#3003,#3005,#2760,.T.);
#4027=EDGE_CURVE('',#3005,#3000,#245,.T.);
#4028=EDGE_CURVE('',#3006,#3007,#2039,.T.);
#4029=EDGE_CURVE('',#3007,#3008,#246,.T.);
#4030=EDGE_CURVE('',#3008,#3001,#247,.T.);
#4031=EDGE_CURVE('',#3000,#3009,#248,.T.);
#4032=EDGE_CURVE('',#3009,#3006,#249,.T.);
#4033=EDGE_CURVE('',#3010,#3011,#2040,.T.);
#4034=EDGE_CURVE('',#3011,#3012,#250,.T.);
#4035=EDGE_CURVE('',#3012,#3007,#251,.T.);
#4036=EDGE_CURVE('',#3006,#3010,#252,.T.);
#4037=EDGE_CURVE('',#3013,#3014,#2041,.T.);
#4038=EDGE_CURVE('',#3014,#3015,#253,.T.);
#4039=EDGE_CURVE('',#3015,#3011,#254,.T.);
#4040=EDGE_CURVE('',#3010,#3016,#255,.T.);
#4041=EDGE_CURVE('',#3016,#3013,#256,.T.);
#4042=EDGE_CURVE('',#3017,#3018,#2042,.T.);
#4043=EDGE_CURVE('',#3018,#3019,#257,.T.);
#4044=EDGE_CURVE('',#3019,#3014,#258,.T.);
#4045=EDGE_CURVE('',#3013,#3017,#259,.T.);
#4046=EDGE_CURVE('',#3020,#3021,#2043,.T.);
#4047=EDGE_CURVE('',#3021,#3022,#260,.T.);
#4048=EDGE_CURVE('',#3022,#3018,#261,.T.);
#4049=EDGE_CURVE('',#3017,#3023,#262,.T.);
#4050=EDGE_CURVE('',#3023,#3020,#263,.T.);
#4051=EDGE_CURVE('',#3024,#3025,#2044,.T.);
#4052=EDGE_CURVE('',#3025,#3026,#264,.T.);
#4053=EDGE_CURVE('',#3026,#3021,#265,.T.);
#4054=EDGE_CURVE('',#3020,#3024,#266,.T.);
#4055=EDGE_CURVE('',#3027,#3028,#2045,.T.);
#4056=EDGE_CURVE('',#3028,#3029,#267,.T.);
#4057=EDGE_CURVE('',#3029,#3025,#268,.T.);
#4058=EDGE_CURVE('',#3024,#3030,#269,.T.);
#4059=EDGE_CURVE('',#3030,#3027,#270,.T.);
#4060=EDGE_CURVE('',#3031,#3032,#2046,.T.);
#4061=EDGE_CURVE('',#3032,#3033,#271,.T.);
#4062=EDGE_CURVE('',#3033,#3028,#272,.T.);
#4063=EDGE_CURVE('',#3027,#3031,#273,.T.);
#4064=EDGE_CURVE('',#3034,#3035,#2047,.T.);
#4065=EDGE_CURVE('',#3035,#3036,#274,.T.);
#4066=EDGE_CURVE('',#3036,#3032,#275,.T.);
#4067=EDGE_CURVE('',#3031,#3037,#276,.T.);
#4068=EDGE_CURVE('',#3037,#3034,#277,.T.);
#4069=EDGE_CURVE('',#3038,#3039,#2048,.T.);
#4070=EDGE_CURVE('',#3039,#3040,#278,.T.);
#4071=EDGE_CURVE('',#3040,#3035,#279,.T.);
#4072=EDGE_CURVE('',#3034,#3038,#280,.T.);
#4073=EDGE_CURVE('',#3041,#3042,#2049,.T.);
#4074=EDGE_CURVE('',#3042,#3043,#281,.T.);
#4075=EDGE_CURVE('',#3043,#3039,#282,.T.);
#4076=EDGE_CURVE('',#3038,#3044,#283,.T.);
#4077=EDGE_CURVE('',#3044,#3041,#284,.T.);
#4078=EDGE_CURVE('',#3045,#3046,#2050,.T.);
#4079=EDGE_CURVE('',#3046,#3047,#285,.T.);
#4080=EDGE_CURVE('',#3047,#3042,#286,.T.);
#4081=EDGE_CURVE('',#3041,#3045,#287,.T.);
#4082=EDGE_CURVE('',#3048,#3049,#2051,.T.);
#4083=EDGE_CURVE('',#3049,#3050,#288,.T.);
#4084=EDGE_CURVE('',#3050,#3046,#289,.T.);
#4085=EDGE_CURVE('',#3045,#3051,#290,.T.);
#4086=EDGE_CURVE('',#3051,#3048,#291,.T.);
#4087=EDGE_CURVE('',#3052,#3053,#2052,.T.);
#4088=EDGE_CURVE('',#3053,#3054,#292,.T.);
#4089=EDGE_CURVE('',#3054,#3049,#293,.T.);
#4090=EDGE_CURVE('',#3048,#3052,#294,.T.);
#4091=EDGE_CURVE('',#3055,#3056,#2053,.T.);
#4092=EDGE_CURVE('',#3056,#3057,#295,.T.);
#4093=EDGE_CURVE('',#3057,#3053,#296,.T.);
#4094=EDGE_CURVE('',#3052,#3058,#297,.T.);
#4095=EDGE_CURVE('',#3058,#3055,#298,.T.);
#4096=EDGE_CURVE('',#3059,#3060,#2054,.T.);
#4097=EDGE_CURVE('',#3060,#3061,#299,.T.);
#4098=EDGE_CURVE('',#3061,#3056,#300,.T.);
#4099=EDGE_CURVE('',#3055,#3059,#301,.T.);
#4100=EDGE_CURVE('',#3062,#3063,#2055,.T.);
#4101=EDGE_CURVE('',#3063,#3064,#302,.T.);
#4102=EDGE_CURVE('',#3064,#3060,#303,.T.);
#4103=EDGE_CURVE('',#3059,#3065,#304,.T.);
#4104=EDGE_CURVE('',#3065,#3062,#305,.T.);
#4105=EDGE_CURVE('',#3066,#3067,#2056,.T.);
#4106=EDGE_CURVE('',#3066,#3068,#306,.T.);
#4107=EDGE_CURVE('',#3068,#3069,#307,.T.);
#4108=EDGE_CURVE('',#3070,#3069,#2761,.F.);
#4109=EDGE_CURVE('',#3070,#3071,#308,.T.);
#4110=EDGE_CURVE('',#3071,#3067,#309,.T.);
#4111=EDGE_CURVE('',#3072,#3073,#2057,.T.);
#4112=EDGE_CURVE('',#3073,#3074,#310,.T.);
#4113=EDGE_CURVE('',#3075,#3074,#2762,.T.);
#4114=EDGE_CURVE('',#3072,#3075,#311,.T.);
#4115=EDGE_CURVE('',#3076,#3077,#2058,.T.);
#4116=EDGE_CURVE('',#3077,#3078,#312,.T.);
#4117=EDGE_CURVE('',#3078,#3073,#313,.T.);
#4118=EDGE_CURVE('',#3079,#3072,#314,.T.);
#4119=EDGE_CURVE('',#3076,#3079,#315,.T.);
#4120=EDGE_CURVE('',#3080,#3081,#2059,.T.);
#4121=EDGE_CURVE('',#3081,#3082,#316,.T.);
#4122=EDGE_CURVE('',#3082,#3077,#317,.T.);
#4123=EDGE_CURVE('',#3083,#3076,#318,.T.);
#4124=EDGE_CURVE('',#3080,#3083,#319,.T.);
#4125=EDGE_CURVE('',#3084,#3085,#2060,.T.);
#4126=EDGE_CURVE('',#3085,#3086,#320,.T.);
#4127=EDGE_CURVE('',#3086,#3081,#321,.T.);
#4128=EDGE_CURVE('',#3087,#3080,#322,.T.);
#4129=EDGE_CURVE('',#3084,#3087,#323,.T.);
#4130=EDGE_CURVE('',#3088,#3089,#2061,.T.);
#4131=EDGE_CURVE('',#3089,#3090,#324,.T.);
#4132=EDGE_CURVE('',#3090,#3085,#325,.T.);
#4133=EDGE_CURVE('',#3091,#3084,#326,.T.);
#4134=EDGE_CURVE('',#3088,#3091,#327,.T.);
#4135=EDGE_CURVE('',#3092,#3093,#2062,.T.);
#4136=EDGE_CURVE('',#3093,#3094,#328,.T.);
#4137=EDGE_CURVE('',#3094,#3089,#329,.T.);
#4138=EDGE_CURVE('',#3095,#3088,#330,.T.);
#4139=EDGE_CURVE('',#3092,#3095,#331,.T.);
#4140=EDGE_CURVE('',#3096,#3097,#2063,.T.);
#4141=EDGE_CURVE('',#3097,#3098,#332,.T.);
#4142=EDGE_CURVE('',#3098,#3093,#333,.T.);
#4143=EDGE_CURVE('',#3099,#3092,#334,.T.);
#4144=EDGE_CURVE('',#3096,#3099,#335,.T.);
#4145=EDGE_CURVE('',#3100,#3101,#2064,.T.);
#4146=EDGE_CURVE('',#3101,#3102,#336,.T.);
#4147=EDGE_CURVE('',#3102,#3097,#337,.T.);
#4148=EDGE_CURVE('',#3103,#3096,#338,.T.);
#4149=EDGE_CURVE('',#3100,#3103,#339,.T.);
#4150=EDGE_CURVE('',#3104,#3105,#2065,.T.);
#4151=EDGE_CURVE('',#3105,#3106,#340,.T.);
#4152=EDGE_CURVE('',#3106,#3101,#341,.T.);
#4153=EDGE_CURVE('',#3107,#3100,#342,.T.);
#4154=EDGE_CURVE('',#3104,#3107,#343,.T.);
#4155=EDGE_CURVE('',#3108,#3109,#2066,.T.);
#4156=EDGE_CURVE('',#3109,#3110,#344,.T.);
#4157=EDGE_CURVE('',#3110,#3105,#345,.T.);
#4158=EDGE_CURVE('',#3111,#3104,#346,.T.);
#4159=EDGE_CURVE('',#3108,#3111,#347,.T.);
#4160=EDGE_CURVE('',#3112,#3113,#2067,.T.);
#4161=EDGE_CURVE('',#3113,#3114,#348,.T.);
#4162=EDGE_CURVE('',#3114,#3109,#349,.T.);
#4163=EDGE_CURVE('',#3115,#3108,#350,.T.);
#4164=EDGE_CURVE('',#3112,#3115,#351,.T.);
#4165=EDGE_CURVE('',#3116,#3117,#2068,.T.);
#4166=EDGE_CURVE('',#3117,#3118,#352,.T.);
#4167=EDGE_CURVE('',#3118,#3113,#353,.T.);
#4168=EDGE_CURVE('',#3119,#3112,#354,.T.);
#4169=EDGE_CURVE('',#3116,#3119,#355,.T.);
#4170=EDGE_CURVE('',#3120,#3121,#2069,.T.);
#4171=EDGE_CURVE('',#3121,#3122,#356,.T.);
#4172=EDGE_CURVE('',#3122,#3117,#357,.T.);
#4173=EDGE_CURVE('',#3123,#3116,#358,.T.);
#4174=EDGE_CURVE('',#3120,#3123,#359,.T.);
#4175=EDGE_CURVE('',#3124,#3125,#2070,.T.);
#4176=EDGE_CURVE('',#3125,#3126,#360,.T.);
#4177=EDGE_CURVE('',#3126,#3121,#361,.T.);
#4178=EDGE_CURVE('',#3127,#3120,#362,.T.);
#4179=EDGE_CURVE('',#3124,#3127,#363,.T.);
#4180=EDGE_CURVE('',#3128,#3129,#2071,.T.);
#4181=EDGE_CURVE('',#3129,#3130,#364,.T.);
#4182=EDGE_CURVE('',#3130,#3125,#365,.T.);
#4183=EDGE_CURVE('',#3131,#3124,#366,.T.);
#4184=EDGE_CURVE('',#3128,#3131,#367,.T.);
#4185=EDGE_CURVE('',#3132,#3133,#2072,.T.);
#4186=EDGE_CURVE('',#3133,#3134,#368,.T.);
#4187=EDGE_CURVE('',#3134,#3129,#369,.T.);
#4188=EDGE_CURVE('',#3135,#3128,#370,.T.);
#4189=EDGE_CURVE('',#3132,#3135,#371,.T.);
#4190=EDGE_CURVE('',#3136,#3137,#2073,.T.);
#4191=EDGE_CURVE('',#3137,#3138,#372,.T.);
#4192=EDGE_CURVE('',#3138,#3133,#373,.T.);
#4193=EDGE_CURVE('',#3139,#3132,#374,.T.);
#4194=EDGE_CURVE('',#3136,#3139,#375,.T.);
#4195=EDGE_CURVE('',#3140,#3141,#2074,.T.);
#4196=EDGE_CURVE('',#3141,#3142,#376,.T.);
#4197=EDGE_CURVE('',#3142,#3137,#377,.T.);
#4198=EDGE_CURVE('',#3143,#3136,#378,.T.);
#4199=EDGE_CURVE('',#3140,#3143,#379,.T.);
#4200=EDGE_CURVE('',#3144,#3145,#2075,.T.);
#4201=EDGE_CURVE('',#3146,#3144,#380,.T.);
#4202=EDGE_CURVE('',#3147,#3146,#381,.T.);
#4203=EDGE_CURVE('',#3148,#3147,#2763,.T.);
#4204=EDGE_CURVE('',#3148,#3149,#382,.T.);
#4205=EDGE_CURVE('',#3149,#3145,#383,.T.);
#4206=EDGE_CURVE('',#3150,#3151,#2076,.T.);
#4207=EDGE_CURVE('',#3151,#3152,#384,.T.);
#4208=EDGE_CURVE('',#3152,#3153,#2764,.T.);
#4209=EDGE_CURVE('',#3153,#3154,#2077,.T.);
#4210=EDGE_CURVE('',#3154,#3154,#2765,.F.);
#4211=EDGE_CURVE('',#3153,#3155,#2766,.T.);
#4212=EDGE_CURVE('',#3155,#3150,#385,.T.);
#4213=EDGE_CURVE('',#3156,#3157,#2078,.T.);
#4214=EDGE_CURVE('',#3157,#3158,#386,.T.);
#4215=EDGE_CURVE('',#3158,#3151,#387,.T.);
#4216=EDGE_CURVE('',#3150,#3159,#388,.T.);
#4217=EDGE_CURVE('',#3159,#3156,#389,.T.);
#4218=EDGE_CURVE('',#3160,#3161,#2079,.T.);
#4219=EDGE_CURVE('',#3161,#3162,#390,.T.);
#4220=EDGE_CURVE('',#3162,#3157,#391,.T.);
#4221=EDGE_CURVE('',#3156,#3163,#392,.T.);
#4222=EDGE_CURVE('',#3163,#3160,#393,.T.);
#4223=EDGE_CURVE('',#3164,#3165,#2080,.T.);
#4224=EDGE_CURVE('',#3165,#3166,#394,.T.);
#4225=EDGE_CURVE('',#3166,#3161,#395,.T.);
#4226=EDGE_CURVE('',#3160,#3164,#396,.T.);
#4227=EDGE_CURVE('',#3167,#3168,#2081,.T.);
#4228=EDGE_CURVE('',#3168,#3169,#397,.T.);
#4229=EDGE_CURVE('',#3169,#3165,#398,.T.);
#4230=EDGE_CURVE('',#3164,#3170,#399,.T.);
#4231=EDGE_CURVE('',#3170,#3167,#400,.T.);
#4232=EDGE_CURVE('',#3171,#3172,#2082,.T.);
#4233=EDGE_CURVE('',#3172,#3173,#401,.T.);
#4234=EDGE_CURVE('',#3173,#3168,#402,.T.);
#4235=EDGE_CURVE('',#3167,#3171,#403,.T.);
#4236=EDGE_CURVE('',#3174,#3175,#2083,.T.);
#4237=EDGE_CURVE('',#3175,#3176,#404,.T.);
#4238=EDGE_CURVE('',#3176,#3172,#405,.T.);
#4239=EDGE_CURVE('',#3171,#3177,#406,.T.);
#4240=EDGE_CURVE('',#3177,#3174,#407,.T.);
#4241=EDGE_CURVE('',#3178,#3179,#2084,.T.);
#4242=EDGE_CURVE('',#3179,#3180,#408,.T.);
#4243=EDGE_CURVE('',#3180,#3175,#409,.T.);
#4244=EDGE_CURVE('',#3174,#3178,#410,.T.);
#4245=EDGE_CURVE('',#3181,#3182,#2085,.T.);
#4246=EDGE_CURVE('',#3182,#3183,#411,.T.);
#4247=EDGE_CURVE('',#3183,#3179,#412,.T.);
#4248=EDGE_CURVE('',#3178,#3184,#413,.T.);
#4249=EDGE_CURVE('',#3184,#3181,#414,.T.);
#4250=EDGE_CURVE('',#3185,#3186,#2086,.T.);
#4251=EDGE_CURVE('',#3186,#3187,#415,.T.);
#4252=EDGE_CURVE('',#3187,#3182,#416,.T.);
#4253=EDGE_CURVE('',#3181,#3185,#417,.T.);
#4254=EDGE_CURVE('',#3188,#3189,#2087,.T.);
#4255=EDGE_CURVE('',#3189,#3190,#418,.T.);
#4256=EDGE_CURVE('',#3190,#3186,#419,.T.);
#4257=EDGE_CURVE('',#3185,#3191,#420,.T.);
#4258=EDGE_CURVE('',#3191,#3188,#421,.T.);
#4259=EDGE_CURVE('',#3192,#3193,#2088,.T.);
#4260=EDGE_CURVE('',#3193,#3194,#422,.T.);
#4261=EDGE_CURVE('',#3194,#3189,#423,.T.);
#4262=EDGE_CURVE('',#3188,#3192,#424,.T.);
#4263=EDGE_CURVE('',#3195,#3196,#2089,.T.);
#4264=EDGE_CURVE('',#3196,#3197,#425,.T.);
#4265=EDGE_CURVE('',#3197,#3193,#426,.T.);
#4266=EDGE_CURVE('',#3192,#3198,#427,.T.);
#4267=EDGE_CURVE('',#3198,#3195,#428,.T.);
#4268=EDGE_CURVE('',#3199,#3200,#2090,.T.);
#4269=EDGE_CURVE('',#3200,#3201,#429,.T.);
#4270=EDGE_CURVE('',#3201,#3196,#430,.T.);
#4271=EDGE_CURVE('',#3195,#3199,#431,.T.);
#4272=EDGE_CURVE('',#3202,#3203,#2091,.T.);
#4273=EDGE_CURVE('',#3203,#3204,#432,.T.);
#4274=EDGE_CURVE('',#3204,#3200,#433,.T.);
#4275=EDGE_CURVE('',#3199,#3205,#434,.T.);
#4276=EDGE_CURVE('',#3205,#3202,#435,.T.);
#4277=EDGE_CURVE('',#3206,#3207,#2092,.T.);
#4278=EDGE_CURVE('',#3207,#3208,#436,.T.);
#4279=EDGE_CURVE('',#3208,#3203,#437,.T.);
#4280=EDGE_CURVE('',#3202,#3206,#438,.T.);
#4281=EDGE_CURVE('',#3209,#3210,#2093,.T.);
#4282=EDGE_CURVE('',#3210,#3211,#439,.T.);
#4283=EDGE_CURVE('',#3211,#3207,#440,.T.);
#4284=EDGE_CURVE('',#3206,#3212,#441,.T.);
#4285=EDGE_CURVE('',#3212,#3209,#442,.T.);
#4286=EDGE_CURVE('',#3213,#3214,#2094,.T.);
#4287=EDGE_CURVE('',#3214,#3215,#443,.T.);
#4288=EDGE_CURVE('',#3215,#3210,#444,.T.);
#4289=EDGE_CURVE('',#3209,#3213,#445,.T.);
#4290=EDGE_CURVE('',#3216,#3217,#2095,.T.);
#4291=EDGE_CURVE('',#3216,#3218,#446,.T.);
#4292=EDGE_CURVE('',#3218,#3219,#447,.T.);
#4293=EDGE_CURVE('',#3220,#3219,#2767,.T.);
#4294=EDGE_CURVE('',#3220,#3221,#448,.T.);
#4295=EDGE_CURVE('',#3221,#3217,#449,.T.);
#4296=EDGE_CURVE('',#3217,#3222,#450,.T.);
#4297=EDGE_CURVE('',#3222,#3214,#451,.T.);
#4298=EDGE_CURVE('',#3213,#3223,#452,.T.);
#4299=EDGE_CURVE('',#3223,#3216,#453,.T.);
#4300=EDGE_CURVE('',#3145,#3224,#454,.T.);
#4301=EDGE_CURVE('',#3224,#3141,#455,.T.);
#4302=EDGE_CURVE('',#3225,#3140,#456,.T.);
#4303=EDGE_CURVE('',#3144,#3225,#457,.T.);
#4304=EDGE_CURVE('',#3067,#3226,#458,.T.);
#4305=EDGE_CURVE('',#3226,#3063,#459,.T.);
#4306=EDGE_CURVE('',#3062,#3066,#460,.T.);
#4307=EDGE_CURVE('',#2995,#3227,#461,.T.);
#4308=EDGE_CURVE('',#3227,#2991,#462,.T.);
#4309=EDGE_CURVE('',#3228,#2990,#463,.T.);
#4310=EDGE_CURVE('',#2994,#3228,#464,.T.);
#4311=EDGE_CURVE('',#3002,#2925,#465,.T.);
#4312=EDGE_CURVE('',#2924,#3005,#466,.T.);
#4313=EDGE_CURVE('',#3069,#2998,#467,.T.);
#4314=EDGE_CURVE('',#2997,#3070,#468,.T.);
#4315=EDGE_CURVE('',#3152,#3075,#469,.T.);
#4316=EDGE_CURVE('',#3074,#3155,#470,.T.);
#4317=EDGE_CURVE('',#3219,#3148,#471,.T.);
#4318=EDGE_CURVE('',#3147,#3220,#472,.T.);
#4319=EDGE_CURVE('',#3229,#3229,#2768,.T.);
#4320=EDGE_CURVE('',#3229,#3230,#2096,.T.);
#4321=EDGE_CURVE('',#3230,#3230,#2769,.T.);
#4322=EDGE_CURVE('',#3231,#3232,#2097,.T.);
#4323=EDGE_CURVE('',#3233,#3231,#473,.T.);
#4324=EDGE_CURVE('',#3234,#3233,#2770,.T.);
#4325=EDGE_CURVE('',#3234,#3232,#474,.T.);
#4326=EDGE_CURVE('',#3235,#3236,#2098,.T.);
#4327=EDGE_CURVE('',#3237,#3235,#475,.F.);
#4328=EDGE_CURVE('',#3231,#3237,#476,.T.);
#4329=EDGE_CURVE('',#3232,#3238,#477,.T.);
#4330=EDGE_CURVE('',#3238,#3236,#478,.T.);
#4331=EDGE_CURVE('',#3239,#3240,#2099,.T.);
#4332=EDGE_CURVE('',#3235,#3239,#479,.F.);
#4333=EDGE_CURVE('',#3236,#3240,#480,.T.);
#4334=EDGE_CURVE('',#3241,#3242,#2100,.T.);
#4335=EDGE_CURVE('',#3243,#3241,#481,.F.);
#4336=EDGE_CURVE('',#3239,#3243,#482,.F.);
#4337=EDGE_CURVE('',#3240,#3244,#483,.T.);
#4338=EDGE_CURVE('',#3244,#3242,#484,.T.);
#4339=EDGE_CURVE('',#3245,#3246,#2101,.T.);
#4340=EDGE_CURVE('',#3241,#3245,#485,.F.);
#4341=EDGE_CURVE('',#3242,#3246,#486,.T.);
#4342=EDGE_CURVE('',#3247,#3248,#2102,.T.);
#4343=EDGE_CURVE('',#3249,#3247,#487,.F.);
#4344=EDGE_CURVE('',#3245,#3249,#488,.F.);
#4345=EDGE_CURVE('',#3246,#3250,#489,.T.);
#4346=EDGE_CURVE('',#3250,#3248,#490,.T.);
#4347=EDGE_CURVE('',#3251,#3252,#2103,.T.);
#4348=EDGE_CURVE('',#3247,#3251,#491,.F.);
#4349=EDGE_CURVE('',#3248,#3252,#492,.T.);
#4350=EDGE_CURVE('',#3253,#3254,#2104,.T.);
#4351=EDGE_CURVE('',#3255,#3253,#493,.F.);
#4352=EDGE_CURVE('',#3251,#3255,#494,.F.);
#4353=EDGE_CURVE('',#3252,#3256,#495,.T.);
#4354=EDGE_CURVE('',#3256,#3254,#496,.T.);
#4355=EDGE_CURVE('',#3257,#3258,#2105,.T.);
#4356=EDGE_CURVE('',#3253,#3257,#497,.F.);
#4357=EDGE_CURVE('',#3254,#3258,#498,.T.);
#4358=EDGE_CURVE('',#3259,#3260,#2106,.T.);
#4359=EDGE_CURVE('',#3261,#3259,#499,.F.);
#4360=EDGE_CURVE('',#3257,#3261,#500,.F.);
#4361=EDGE_CURVE('',#3258,#3262,#501,.T.);
#4362=EDGE_CURVE('',#3262,#3260,#502,.T.);
#4363=EDGE_CURVE('',#3263,#3264,#2107,.T.);
#4364=EDGE_CURVE('',#3259,#3263,#503,.F.);
#4365=EDGE_CURVE('',#3260,#3264,#504,.T.);
#4366=EDGE_CURVE('',#3265,#3266,#505,.T.);
#4367=EDGE_CURVE('',#3266,#3267,#2771,.F.);
#4368=EDGE_CURVE('',#3267,#3268,#506,.T.);
#4369=EDGE_CURVE('',#3268,#3269,#507,.T.);
#4370=EDGE_CURVE('',#3269,#3270,#508,.T.);
#4371=EDGE_CURVE('',#3270,#3271,#509,.T.);
#4372=EDGE_CURVE('',#3271,#3272,#510,.T.);
#4373=EDGE_CURVE('',#3272,#3273,#511,.T.);
#4374=EDGE_CURVE('',#3273,#3274,#512,.T.);
#4375=EDGE_CURVE('',#3274,#3275,#513,.T.);
#4376=EDGE_CURVE('',#3275,#3276,#514,.T.);
#4377=EDGE_CURVE('',#3276,#3277,#515,.T.);
#4378=EDGE_CURVE('',#3277,#3278,#516,.T.);
#4379=EDGE_CURVE('',#3278,#3279,#517,.T.);
#4380=EDGE_CURVE('',#3279,#3280,#2772,.T.);
#4381=EDGE_CURVE('',#3280,#3281,#518,.T.);
#4382=EDGE_CURVE('',#3281,#3282,#519,.T.);
#4383=EDGE_CURVE('',#3282,#3283,#520,.T.);
#4384=EDGE_CURVE('',#3283,#3284,#521,.T.);
#4385=EDGE_CURVE('',#3284,#3285,#522,.T.);
#4386=EDGE_CURVE('',#3285,#3286,#523,.T.);
#4387=EDGE_CURVE('',#3286,#3287,#524,.T.);
#4388=EDGE_CURVE('',#3287,#3288,#525,.T.);
#4389=EDGE_CURVE('',#3288,#3289,#526,.T.);
#4390=EDGE_CURVE('',#3289,#3290,#527,.T.);
#4391=EDGE_CURVE('',#3290,#3265,#528,.T.);
#4392=EDGE_CURVE('',#3264,#3291,#529,.T.);
#4393=EDGE_CURVE('',#3291,#3292,#530,.T.);
#4394=EDGE_CURVE('',#3292,#3293,#2773,.T.);
#4395=EDGE_CURVE('',#3294,#3293,#531,.T.);
#4396=EDGE_CURVE('',#3263,#3294,#532,.F.);
#4397=EDGE_CURVE('',#3293,#3295,#533,.T.);
#4398=EDGE_CURVE('',#3280,#3292,#534,.T.);
#4399=EDGE_CURVE('',#3295,#3279,#535,.T.);
#4400=EDGE_CURVE('',#3295,#3296,#2108,.T.);
#4401=EDGE_CURVE('',#3296,#3296,#2774,.T.);
#4402=EDGE_CURVE('',#3266,#3234,#536,.T.);
#4403=EDGE_CURVE('',#3233,#3267,#537,.T.);
#4404=EDGE_CURVE('',#3297,#3298,#2109,.T.);
#4405=EDGE_CURVE('',#3297,#3299,#2110,.T.);
#4406=EDGE_CURVE('',#3299,#3300,#2111,.T.);
#4407=EDGE_CURVE('',#3298,#3300,#2112,.T.);
#4408=EDGE_CURVE('',#3301,#3297,#2113,.T.);
#4409=EDGE_CURVE('',#3301,#3302,#2114,.T.);
#4410=EDGE_CURVE('',#3302,#3299,#2115,.T.);
#4411=EDGE_CURVE('',#3303,#3301,#2116,.T.);
#4412=EDGE_CURVE('',#3303,#3304,#2117,.T.);
#4413=EDGE_CURVE('',#3304,#3302,#2118,.T.);
#4414=EDGE_CURVE('',#3305,#3303,#2119,.T.);
#4415=EDGE_CURVE('',#3305,#3306,#2120,.T.);
#4416=EDGE_CURVE('',#3306,#3304,#2121,.T.);
#4417=EDGE_CURVE('',#3307,#3305,#2122,.T.);
#4418=EDGE_CURVE('',#3307,#3308,#2123,.T.);
#4419=EDGE_CURVE('',#3308,#3306,#2124,.T.);
#4420=EDGE_CURVE('',#3298,#3307,#2125,.T.);
#4421=EDGE_CURVE('',#3300,#3308,#2126,.T.);
#4422=EDGE_CURVE('',#3309,#3309,#2775,.T.);
#4423=EDGE_CURVE('',#3309,#3310,#2127,.T.);
#4424=EDGE_CURVE('',#3310,#3310,#2776,.T.);
#4425=EDGE_CURVE('',#3311,#3312,#2128,.T.);
#4426=EDGE_CURVE('',#3312,#3313,#538,.T.);
#4427=EDGE_CURVE('',#3314,#3313,#2777,.T.);
#4428=EDGE_CURVE('',#3311,#3314,#539,.T.);
#4429=EDGE_CURVE('',#3315,#3316,#2129,.T.);
#4430=EDGE_CURVE('',#3316,#3317,#540,.T.);
#4431=EDGE_CURVE('',#3317,#3312,#541,.T.);
#4432=EDGE_CURVE('',#3318,#3311,#542,.T.);
#4433=EDGE_CURVE('',#3315,#3318,#543,.T.);
#4434=EDGE_CURVE('',#3319,#3320,#2130,.T.);
#4435=EDGE_CURVE('',#3320,#3321,#544,.T.);
#4436=EDGE_CURVE('',#3321,#3316,#545,.T.);
#4437=EDGE_CURVE('',#3322,#3315,#546,.T.);
#4438=EDGE_CURVE('',#3319,#3322,#547,.T.);
#4439=EDGE_CURVE('',#3323,#3324,#2131,.T.);
#4440=EDGE_CURVE('',#3324,#3325,#548,.T.);
#4441=EDGE_CURVE('',#3325,#3320,#549,.T.);
#4442=EDGE_CURVE('',#3326,#3319,#550,.T.);
#4443=EDGE_CURVE('',#3323,#3326,#551,.T.);
#4444=EDGE_CURVE('',#3327,#3328,#2132,.T.);
#4445=EDGE_CURVE('',#3328,#3329,#552,.T.);
#4446=EDGE_CURVE('',#3329,#3324,#553,.T.);
#4447=EDGE_CURVE('',#3330,#3323,#554,.T.);
#4448=EDGE_CURVE('',#3327,#3330,#555,.T.);
#4449=EDGE_CURVE('',#3331,#3332,#2133,.T.);
#4450=EDGE_CURVE('',#3332,#3333,#556,.T.);
#4451=EDGE_CURVE('',#3333,#3328,#557,.T.);
#4452=EDGE_CURVE('',#3334,#3327,#558,.T.);
#4453=EDGE_CURVE('',#3331,#3334,#559,.T.);
#4454=EDGE_CURVE('',#3335,#3336,#2134,.T.);
#4455=EDGE_CURVE('',#3336,#3337,#560,.T.);
#4456=EDGE_CURVE('',#3337,#3332,#561,.T.);
#4457=EDGE_CURVE('',#3338,#3331,#562,.T.);
#4458=EDGE_CURVE('',#3335,#3338,#563,.T.);
#4459=EDGE_CURVE('',#3339,#3340,#2135,.T.);
#4460=EDGE_CURVE('',#3340,#3341,#564,.T.);
#4461=EDGE_CURVE('',#3341,#3336,#565,.T.);
#4462=EDGE_CURVE('',#3342,#3335,#566,.T.);
#4463=EDGE_CURVE('',#3339,#3342,#567,.T.);
#4464=EDGE_CURVE('',#3343,#3344,#2136,.T.);
#4465=EDGE_CURVE('',#3344,#3345,#568,.T.);
#4466=EDGE_CURVE('',#3345,#3340,#569,.T.);
#4467=EDGE_CURVE('',#3346,#3339,#570,.T.);
#4468=EDGE_CURVE('',#3343,#3346,#571,.T.);
#4469=EDGE_CURVE('',#3347,#3348,#2137,.T.);
#4470=EDGE_CURVE('',#3348,#3349,#572,.T.);
#4471=EDGE_CURVE('',#3349,#3344,#573,.T.);
#4472=EDGE_CURVE('',#3350,#3343,#574,.T.);
#4473=EDGE_CURVE('',#3347,#3350,#575,.T.);
#4474=EDGE_CURVE('',#3351,#3352,#2138,.T.);
#4475=EDGE_CURVE('',#3352,#3353,#576,.T.);
#4476=EDGE_CURVE('',#3353,#3348,#577,.T.);
#4477=EDGE_CURVE('',#3354,#3347,#578,.T.);
#4478=EDGE_CURVE('',#3351,#3354,#579,.T.);
#4479=EDGE_CURVE('',#3355,#3356,#2139,.T.);
#4480=EDGE_CURVE('',#3356,#3357,#580,.T.);
#4481=EDGE_CURVE('',#3357,#3352,#581,.T.);
#4482=EDGE_CURVE('',#3358,#3351,#582,.T.);
#4483=EDGE_CURVE('',#3355,#3358,#583,.T.);
#4484=EDGE_CURVE('',#3359,#3360,#2140,.T.);
#4485=EDGE_CURVE('',#3360,#3361,#584,.T.);
#4486=EDGE_CURVE('',#3361,#3356,#585,.T.);
#4487=EDGE_CURVE('',#3362,#3355,#586,.T.);
#4488=EDGE_CURVE('',#3359,#3362,#587,.T.);
#4489=EDGE_CURVE('',#3363,#3364,#2141,.T.);
#4490=EDGE_CURVE('',#3364,#3365,#588,.T.);
#4491=EDGE_CURVE('',#3365,#3360,#589,.T.);
#4492=EDGE_CURVE('',#3366,#3359,#590,.T.);
#4493=EDGE_CURVE('',#3363,#3366,#591,.T.);
#4494=EDGE_CURVE('',#3367,#3368,#2142,.T.);
#4495=EDGE_CURVE('',#3368,#3369,#592,.T.);
#4496=EDGE_CURVE('',#3369,#3364,#593,.T.);
#4497=EDGE_CURVE('',#3370,#3363,#594,.T.);
#4498=EDGE_CURVE('',#3367,#3370,#595,.T.);
#4499=EDGE_CURVE('',#3371,#3372,#2143,.T.);
#4500=EDGE_CURVE('',#3373,#3371,#596,.T.);
#4501=EDGE_CURVE('',#3374,#3373,#597,.T.);
#4502=EDGE_CURVE('',#3375,#3374,#2778,.T.);
#4503=EDGE_CURVE('',#3375,#3376,#598,.T.);
#4504=EDGE_CURVE('',#3376,#3372,#599,.T.);
#4505=EDGE_CURVE('',#3377,#3378,#2144,.T.);
#4506=EDGE_CURVE('',#3378,#3379,#600,.T.);
#4507=EDGE_CURVE('',#3379,#3380,#2779,.T.);
#4508=EDGE_CURVE('',#3380,#3381,#601,.T.);
#4509=EDGE_CURVE('',#3381,#3382,#2145,.T.);
#4510=EDGE_CURVE('',#3382,#3382,#2780,.F.);
#4511=EDGE_CURVE('',#3381,#3383,#602,.T.);
#4512=EDGE_CURVE('',#3383,#3377,#603,.T.);
#4513=EDGE_CURVE('',#3384,#3385,#2146,.T.);
#4514=EDGE_CURVE('',#3385,#3386,#604,.T.);
#4515=EDGE_CURVE('',#3386,#3378,#605,.T.);
#4516=EDGE_CURVE('',#3377,#3387,#606,.T.);
#4517=EDGE_CURVE('',#3387,#3384,#607,.T.);
#4518=EDGE_CURVE('',#3388,#3389,#2147,.T.);
#4519=EDGE_CURVE('',#3389,#3390,#608,.T.);
#4520=EDGE_CURVE('',#3390,#3385,#609,.T.);
#4521=EDGE_CURVE('',#3384,#3391,#610,.T.);
#4522=EDGE_CURVE('',#3391,#3388,#611,.T.);
#4523=EDGE_CURVE('',#3392,#3393,#2148,.T.);
#4524=EDGE_CURVE('',#3393,#3389,#612,.T.);
#4525=EDGE_CURVE('',#3388,#3392,#613,.T.);
#4526=EDGE_CURVE('',#3394,#3395,#2149,.T.);
#4527=EDGE_CURVE('',#3395,#3396,#614,.T.);
#4528=EDGE_CURVE('',#3396,#3393,#615,.T.);
#4529=EDGE_CURVE('',#3392,#3397,#616,.T.);
#4530=EDGE_CURVE('',#3397,#3394,#617,.T.);
#4531=EDGE_CURVE('',#3398,#3399,#2150,.T.);
#4532=EDGE_CURVE('',#3399,#3395,#618,.T.);
#4533=EDGE_CURVE('',#3394,#3398,#619,.T.);
#4534=EDGE_CURVE('',#3400,#3401,#2151,.T.);
#4535=EDGE_CURVE('',#3401,#3402,#620,.T.);
#4536=EDGE_CURVE('',#3402,#3399,#621,.T.);
#4537=EDGE_CURVE('',#3398,#3403,#622,.T.);
#4538=EDGE_CURVE('',#3403,#3400,#623,.T.);
#4539=EDGE_CURVE('',#3404,#3405,#2152,.T.);
#4540=EDGE_CURVE('',#3405,#3401,#624,.T.);
#4541=EDGE_CURVE('',#3400,#3404,#625,.T.);
#4542=EDGE_CURVE('',#3406,#3407,#2153,.T.);
#4543=EDGE_CURVE('',#3407,#3408,#626,.T.);
#4544=EDGE_CURVE('',#3408,#3405,#627,.T.);
#4545=EDGE_CURVE('',#3404,#3409,#628,.T.);
#4546=EDGE_CURVE('',#3409,#3406,#629,.T.);
#4547=EDGE_CURVE('',#3410,#3411,#2154,.T.);
#4548=EDGE_CURVE('',#3411,#3412,#630,.T.);
#4549=EDGE_CURVE('',#3412,#3407,#631,.T.);
#4550=EDGE_CURVE('',#3406,#3410,#632,.T.);
#4551=EDGE_CURVE('',#3413,#3414,#2155,.T.);
#4552=EDGE_CURVE('',#3414,#3411,#633,.T.);
#4553=EDGE_CURVE('',#3410,#3415,#634,.T.);
#4554=EDGE_CURVE('',#3415,#3413,#635,.T.);
#4555=EDGE_CURVE('',#3416,#3417,#2156,.T.);
#4556=EDGE_CURVE('',#3417,#3418,#636,.T.);
#4557=EDGE_CURVE('',#3418,#3414,#637,.T.);
#4558=EDGE_CURVE('',#3413,#3416,#638,.T.);
#4559=EDGE_CURVE('',#3419,#3420,#2157,.T.);
#4560=EDGE_CURVE('',#3420,#3417,#639,.T.);
#4561=EDGE_CURVE('',#3416,#3421,#640,.T.);
#4562=EDGE_CURVE('',#3421,#3419,#641,.T.);
#4563=EDGE_CURVE('',#3422,#3423,#2158,.T.);
#4564=EDGE_CURVE('',#3423,#3424,#642,.T.);
#4565=EDGE_CURVE('',#3424,#3420,#643,.T.);
#4566=EDGE_CURVE('',#3419,#3422,#644,.T.);
#4567=EDGE_CURVE('',#3425,#3426,#2159,.T.);
#4568=EDGE_CURVE('',#3425,#3427,#645,.T.);
#4569=EDGE_CURVE('',#3427,#3428,#646,.T.);
#4570=EDGE_CURVE('',#3429,#3428,#2781,.T.);
#4571=EDGE_CURVE('',#3429,#3430,#647,.T.);
#4572=EDGE_CURVE('',#3430,#3426,#648,.T.);
#4573=EDGE_CURVE('',#3426,#3423,#649,.T.);
#4574=EDGE_CURVE('',#3422,#3431,#650,.T.);
#4575=EDGE_CURVE('',#3431,#3425,#651,.T.);
#4576=EDGE_CURVE('',#3372,#3432,#652,.T.);
#4577=EDGE_CURVE('',#3432,#3368,#653,.T.);
#4578=EDGE_CURVE('',#3433,#3367,#654,.T.);
#4579=EDGE_CURVE('',#3371,#3433,#655,.T.);
#4580=EDGE_CURVE('',#3379,#3314,#656,.T.);
#4581=EDGE_CURVE('',#3313,#3380,#657,.T.);
#4582=EDGE_CURVE('',#3428,#3375,#658,.T.);
#4583=EDGE_CURVE('',#3374,#3429,#659,.T.);
#4584=EDGE_CURVE('',#3434,#3434,#2782,.T.);
#4585=EDGE_CURVE('',#3434,#3435,#2160,.T.);
#4586=EDGE_CURVE('',#3435,#3435,#2783,.T.);
#4587=EDGE_CURVE('',#3436,#3437,#2784,.T.);
#4588=EDGE_CURVE('',#3437,#3438,#2161,.T.);
#4589=EDGE_CURVE('',#3438,#3439,#2785,.T.);
#4590=EDGE_CURVE('',#3439,#3436,#2162,.T.);
#4591=EDGE_CURVE('',#3437,#3440,#2163,.T.);
#4592=EDGE_CURVE('',#3440,#3441,#2164,.T.);
#4593=EDGE_CURVE('',#3441,#3438,#2165,.T.);
#4594=EDGE_CURVE('',#3442,#3442,#2786,.T.);
#4595=EDGE_CURVE('',#3443,#3443,#2787,.T.);
#4596=EDGE_CURVE('',#3444,#3444,#2788,.T.);
#4597=EDGE_CURVE('',#3445,#3445,#2789,.T.);
#4598=EDGE_CURVE('',#3436,#3446,#2166,.T.);
#4599=EDGE_CURVE('',#3446,#3440,#2167,.T.);
#4600=EDGE_CURVE('',#3445,#3447,#2168,.T.);
#4601=EDGE_CURVE('',#3447,#3447,#2790,.T.);
#4602=EDGE_CURVE('',#3444,#3448,#2169,.T.);
#4603=EDGE_CURVE('',#3448,#3448,#2791,.T.);
#4604=EDGE_CURVE('',#3443,#3449,#2170,.T.);
#4605=EDGE_CURVE('',#3449,#3449,#2792,.T.);
#4606=EDGE_CURVE('',#3442,#3450,#2171,.T.);
#4607=EDGE_CURVE('',#3450,#3450,#2793,.T.);
#4608=EDGE_CURVE('',#3451,#3441,#2172,.T.);
#4609=EDGE_CURVE('',#3451,#3439,#2173,.T.);
#4610=EDGE_CURVE('',#3446,#3451,#2174,.T.);
#4611=EDGE_CURVE('',#3452,#3452,#2794,.T.);
#4612=EDGE_CURVE('',#3452,#3453,#2175,.T.);
#4613=EDGE_CURVE('',#3453,#3453,#2795,.T.);
#4614=EDGE_CURVE('',#3454,#3454,#2796,.T.);
#4615=EDGE_CURVE('',#3454,#3455,#2176,.T.);
#4616=EDGE_CURVE('',#3455,#3455,#2797,.T.);
#4617=EDGE_CURVE('',#3456,#3456,#2798,.T.);
#4618=EDGE_CURVE('',#3456,#3457,#2177,.T.);
#4619=EDGE_CURVE('',#3457,#3457,#2799,.T.);
#4620=EDGE_CURVE('',#3458,#3458,#2800,.T.);
#4621=EDGE_CURVE('',#3458,#3459,#2178,.T.);
#4622=EDGE_CURVE('',#3459,#3459,#2801,.T.);
#4623=EDGE_CURVE('',#3460,#3461,#2179,.T.);
#4624=EDGE_CURVE('',#3461,#3462,#2180,.T.);
#4625=EDGE_CURVE('',#3463,#3462,#2181,.T.);
#4626=EDGE_CURVE('',#3460,#3463,#2182,.T.);
#4627=EDGE_CURVE('',#3464,#3460,#2183,.T.);
#4628=EDGE_CURVE('',#3465,#3463,#2184,.T.);
#4629=EDGE_CURVE('',#3464,#3465,#2185,.T.);
#4630=EDGE_CURVE('',#3466,#3464,#2186,.T.);
#4631=EDGE_CURVE('',#3467,#3465,#2187,.T.);
#4632=EDGE_CURVE('',#3466,#3467,#2188,.T.);
#4633=EDGE_CURVE('',#3461,#3466,#2189,.T.);
#4634=EDGE_CURVE('',#3462,#3467,#2190,.T.);
#4635=EDGE_CURVE('',#3468,#3469,#2191,.T.);
#4636=EDGE_CURVE('',#3469,#3470,#2192,.T.);
#4637=EDGE_CURVE('',#3471,#3470,#2193,.T.);
#4638=EDGE_CURVE('',#3468,#3471,#2194,.T.);
#4639=EDGE_CURVE('',#3472,#3468,#2195,.T.);
#4640=EDGE_CURVE('',#3473,#3471,#2196,.T.);
#4641=EDGE_CURVE('',#3472,#3473,#2197,.T.);
#4642=EDGE_CURVE('',#3474,#3472,#2198,.T.);
#4643=EDGE_CURVE('',#3475,#3473,#2199,.T.);
#4644=EDGE_CURVE('',#3474,#3475,#2200,.T.);
#4645=EDGE_CURVE('',#3469,#3474,#2201,.T.);
#4646=EDGE_CURVE('',#3470,#3475,#2202,.T.);
#4647=EDGE_CURVE('',#3476,#3476,#2802,.T.);
#4648=EDGE_CURVE('',#3476,#3477,#2203,.T.);
#4649=EDGE_CURVE('',#3477,#3477,#2803,.T.);
#4650=EDGE_CURVE('',#3478,#3478,#2804,.T.);
#4651=EDGE_CURVE('',#3478,#3479,#2204,.T.);
#4652=EDGE_CURVE('',#3479,#3479,#2805,.T.);
#4653=EDGE_CURVE('',#3480,#3480,#2806,.T.);
#4654=EDGE_CURVE('',#3480,#3481,#2205,.T.);
#4655=EDGE_CURVE('',#3481,#3481,#2807,.T.);
#4656=EDGE_CURVE('',#3482,#3482,#2808,.T.);
#4657=EDGE_CURVE('',#3482,#3483,#2206,.T.);
#4658=EDGE_CURVE('',#3483,#3483,#2809,.T.);
#4659=EDGE_CURVE('',#3484,#3485,#2207,.T.);
#4660=EDGE_CURVE('',#3485,#3486,#2208,.T.);
#4661=EDGE_CURVE('',#3487,#3486,#2209,.T.);
#4662=EDGE_CURVE('',#3484,#3487,#2210,.T.);
#4663=EDGE_CURVE('',#3488,#3484,#2211,.T.);
#4664=EDGE_CURVE('',#3489,#3487,#2212,.T.);
#4665=EDGE_CURVE('',#3488,#3489,#2213,.T.);
#4666=EDGE_CURVE('',#3490,#3488,#2214,.T.);
#4667=EDGE_CURVE('',#3491,#3489,#2215,.T.);
#4668=EDGE_CURVE('',#3490,#3491,#2216,.T.);
#4669=EDGE_CURVE('',#3485,#3490,#2217,.T.);
#4670=EDGE_CURVE('',#3486,#3491,#2218,.T.);
#4671=EDGE_CURVE('',#3492,#3493,#2219,.T.);
#4672=EDGE_CURVE('',#3494,#3492,#660,.F.);
#4673=EDGE_CURVE('',#3495,#3494,#2810,.T.);
#4674=EDGE_CURVE('',#3495,#3493,#661,.T.);
#4675=EDGE_CURVE('',#3496,#3497,#2220,.T.);
#4676=EDGE_CURVE('',#3492,#3496,#662,.F.);
#4677=EDGE_CURVE('',#3493,#3498,#663,.T.);
#4678=EDGE_CURVE('',#3498,#3497,#664,.T.);
#4679=EDGE_CURVE('',#3499,#3500,#2221,.T.);
#4680=EDGE_CURVE('',#3501,#3499,#665,.T.);
#4681=EDGE_CURVE('',#3496,#3501,#666,.F.);
#4682=EDGE_CURVE('',#3497,#3500,#667,.T.);
#4683=EDGE_CURVE('',#3502,#3503,#2222,.T.);
#4684=EDGE_CURVE('',#3504,#3502,#668,.T.);
#4685=EDGE_CURVE('',#3499,#3504,#669,.T.);
#4686=EDGE_CURVE('',#3500,#3505,#670,.T.);
#4687=EDGE_CURVE('',#3505,#3503,#671,.T.);
#4688=EDGE_CURVE('',#3506,#3507,#2223,.T.);
#4689=EDGE_CURVE('',#3508,#3506,#672,.F.);
#4690=EDGE_CURVE('',#3502,#3508,#673,.T.);
#4691=EDGE_CURVE('',#3503,#3507,#674,.T.);
#4692=EDGE_CURVE('',#3509,#3510,#2224,.T.);
#4693=EDGE_CURVE('',#3506,#3509,#675,.F.);
#4694=EDGE_CURVE('',#3507,#3511,#676,.T.);
#4695=EDGE_CURVE('',#3511,#3510,#677,.T.);
#4696=EDGE_CURVE('',#3512,#3513,#2225,.T.);
#4697=EDGE_CURVE('',#3514,#3512,#678,.T.);
#4698=EDGE_CURVE('',#3509,#3514,#679,.F.);
#4699=EDGE_CURVE('',#3510,#3515,#680,.T.);
#4700=EDGE_CURVE('',#3515,#3513,#681,.T.);
#4701=EDGE_CURVE('',#3516,#3517,#2226,.T.);
#4702=EDGE_CURVE('',#3518,#3516,#682,.T.);
#4703=EDGE_CURVE('',#3512,#3518,#683,.T.);
#4704=EDGE_CURVE('',#3513,#3517,#684,.T.);
#4705=EDGE_CURVE('',#3519,#3520,#2227,.T.);
#4706=EDGE_CURVE('',#3521,#3519,#685,.F.);
#4707=EDGE_CURVE('',#3516,#3521,#686,.T.);
#4708=EDGE_CURVE('',#3517,#3522,#687,.T.);
#4709=EDGE_CURVE('',#3522,#3520,#688,.T.);
#4710=EDGE_CURVE('',#3523,#3524,#2228,.T.);
#4711=EDGE_CURVE('',#3519,#3523,#689,.F.);
#4712=EDGE_CURVE('',#3520,#3524,#690,.T.);
#4713=EDGE_CURVE('',#3525,#3526,#2229,.T.);
#4714=EDGE_CURVE('',#3527,#3525,#691,.T.);
#4715=EDGE_CURVE('',#3523,#3527,#692,.F.);
#4716=EDGE_CURVE('',#3524,#3528,#693,.T.);
#4717=EDGE_CURVE('',#3528,#3526,#694,.T.);
#4718=EDGE_CURVE('',#3529,#3530,#2230,.T.);
#4719=EDGE_CURVE('',#3531,#3529,#695,.T.);
#4720=EDGE_CURVE('',#3525,#3531,#696,.T.);
#4721=EDGE_CURVE('',#3526,#3530,#697,.T.);
#4722=EDGE_CURVE('',#3532,#3533,#2231,.T.);
#4723=EDGE_CURVE('',#3534,#3532,#698,.F.);
#4724=EDGE_CURVE('',#3529,#3534,#699,.T.);
#4725=EDGE_CURVE('',#3530,#3535,#700,.T.);
#4726=EDGE_CURVE('',#3535,#3533,#701,.T.);
#4727=EDGE_CURVE('',#3536,#3537,#2232,.T.);
#4728=EDGE_CURVE('',#3532,#3536,#702,.F.);
#4729=EDGE_CURVE('',#3533,#3537,#703,.T.);
#4730=EDGE_CURVE('',#3538,#3539,#2233,.T.);
#4731=EDGE_CURVE('',#3540,#3538,#704,.T.);
#4732=EDGE_CURVE('',#3536,#3540,#705,.F.);
#4733=EDGE_CURVE('',#3537,#3541,#706,.T.);
#4734=EDGE_CURVE('',#3541,#3539,#707,.T.);
#4735=EDGE_CURVE('',#3542,#3543,#708,.T.);
#4736=EDGE_CURVE('',#3543,#3544,#2811,.F.);
#4737=EDGE_CURVE('',#3544,#3545,#709,.T.);
#4738=EDGE_CURVE('',#3545,#3546,#710,.T.);
#4739=EDGE_CURVE('',#3546,#3547,#711,.T.);
#4740=EDGE_CURVE('',#3547,#3548,#712,.T.);
#4741=EDGE_CURVE('',#3548,#3549,#713,.T.);
#4742=EDGE_CURVE('',#3549,#3550,#714,.T.);
#4743=EDGE_CURVE('',#3550,#3551,#715,.T.);
#4744=EDGE_CURVE('',#3551,#3552,#716,.T.);
#4745=EDGE_CURVE('',#3552,#3553,#717,.T.);
#4746=EDGE_CURVE('',#3553,#3554,#718,.T.);
#4747=EDGE_CURVE('',#3554,#3555,#719,.T.);
#4748=EDGE_CURVE('',#3555,#3556,#720,.T.);
#4749=EDGE_CURVE('',#3556,#3557,#721,.T.);
#4750=EDGE_CURVE('',#3557,#3558,#722,.T.);
#4751=EDGE_CURVE('',#3558,#3559,#723,.T.);
#4752=EDGE_CURVE('',#3559,#3560,#724,.T.);
#4753=EDGE_CURVE('',#3560,#3561,#2812,.T.);
#4754=EDGE_CURVE('',#3561,#3562,#725,.T.);
#4755=EDGE_CURVE('',#3562,#3563,#726,.T.);
#4756=EDGE_CURVE('',#3563,#3564,#727,.T.);
#4757=EDGE_CURVE('',#3564,#3565,#728,.T.);
#4758=EDGE_CURVE('',#3565,#3566,#729,.T.);
#4759=EDGE_CURVE('',#3566,#3567,#730,.T.);
#4760=EDGE_CURVE('',#3567,#3568,#731,.T.);
#4761=EDGE_CURVE('',#3568,#3569,#732,.T.);
#4762=EDGE_CURVE('',#3569,#3570,#733,.T.);
#4763=EDGE_CURVE('',#3570,#3571,#734,.T.);
#4764=EDGE_CURVE('',#3571,#3572,#735,.T.);
#4765=EDGE_CURVE('',#3572,#3573,#736,.T.);
#4766=EDGE_CURVE('',#3573,#3574,#737,.T.);
#4767=EDGE_CURVE('',#3574,#3575,#738,.T.);
#4768=EDGE_CURVE('',#3575,#3542,#739,.T.);
#4769=EDGE_CURVE('',#3539,#3576,#740,.T.);
#4770=EDGE_CURVE('',#3576,#3577,#741,.T.);
#4771=EDGE_CURVE('',#3577,#3578,#2813,.T.);
#4772=EDGE_CURVE('',#3579,#3578,#742,.T.);
#4773=EDGE_CURVE('',#3538,#3579,#743,.T.);
#4774=EDGE_CURVE('',#3578,#3580,#744,.T.);
#4775=EDGE_CURVE('',#3561,#3577,#745,.T.);
#4776=EDGE_CURVE('',#3581,#3560,#746,.T.);
#4777=EDGE_CURVE('',#3580,#3581,#747,.T.);
#4778=EDGE_CURVE('',#3580,#3582,#2234,.T.);
#4779=EDGE_CURVE('',#3582,#3582,#2814,.T.);
#4780=EDGE_CURVE('',#3543,#3495,#748,.T.);
#4781=EDGE_CURVE('',#3583,#3544,#749,.T.);
#4782=EDGE_CURVE('',#3583,#3494,#750,.T.);
#4783=EDGE_CURVE('',#3584,#3585,#2235,.T.);
#4784=EDGE_CURVE('',#3584,#3586,#2236,.T.);
#4785=EDGE_CURVE('',#3586,#3587,#2237,.T.);
#4786=EDGE_CURVE('',#3585,#3587,#2238,.T.);
#4787=EDGE_CURVE('',#3588,#3584,#2239,.T.);
#4788=EDGE_CURVE('',#3588,#3589,#2240,.T.);
#4789=EDGE_CURVE('',#3589,#3586,#2241,.T.);
#4790=EDGE_CURVE('',#3590,#3588,#2242,.T.);
#4791=EDGE_CURVE('',#3590,#3591,#2243,.T.);
#4792=EDGE_CURVE('',#3591,#3589,#2244,.T.);
#4793=EDGE_CURVE('',#3592,#3590,#2245,.T.);
#4794=EDGE_CURVE('',#3592,#3593,#2246,.T.);
#4795=EDGE_CURVE('',#3593,#3591,#2247,.T.);
#4796=EDGE_CURVE('',#3594,#3592,#2248,.T.);
#4797=EDGE_CURVE('',#3594,#3595,#2249,.T.);
#4798=EDGE_CURVE('',#3595,#3593,#2250,.T.);
#4799=EDGE_CURVE('',#3585,#3594,#2251,.T.);
#4800=EDGE_CURVE('',#3587,#3595,#2252,.T.);
#4801=EDGE_CURVE('',#3596,#3596,#2815,.T.);
#4802=EDGE_CURVE('',#3596,#3597,#2253,.T.);
#4803=EDGE_CURVE('',#3597,#3597,#2816,.T.);
#4804=EDGE_CURVE('',#3598,#3599,#2254,.T.);
#4805=EDGE_CURVE('',#3600,#3598,#751,.F.);
#4806=EDGE_CURVE('',#3601,#3600,#2817,.T.);
#4807=EDGE_CURVE('',#3601,#3599,#752,.T.);
#4808=EDGE_CURVE('',#3602,#3603,#2255,.T.);
#4809=EDGE_CURVE('',#3598,#3602,#753,.F.);
#4810=EDGE_CURVE('',#3599,#3603,#754,.T.);
#4811=EDGE_CURVE('',#3604,#3605,#2256,.T.);
#4812=EDGE_CURVE('',#3606,#3604,#755,.F.);
#4813=EDGE_CURVE('',#3602,#3606,#756,.F.);
#4814=EDGE_CURVE('',#3603,#3605,#757,.T.);
#4815=EDGE_CURVE('',#3607,#3608,#2257,.T.);
#4816=EDGE_CURVE('',#3604,#3607,#758,.F.);
#4817=EDGE_CURVE('',#3605,#3609,#759,.T.);
#4818=EDGE_CURVE('',#3609,#3608,#760,.T.);
#4819=EDGE_CURVE('',#3610,#3611,#2258,.T.);
#4820=EDGE_CURVE('',#3607,#3610,#761,.T.);
#4821=EDGE_CURVE('',#3608,#3612,#762,.T.);
#4822=EDGE_CURVE('',#3612,#3611,#763,.T.);
#4823=EDGE_CURVE('',#3613,#3614,#2259,.T.);
#4824=EDGE_CURVE('',#3610,#3613,#764,.F.);
#4825=EDGE_CURVE('',#3611,#3614,#765,.T.);
#4826=EDGE_CURVE('',#3615,#3616,#2260,.T.);
#4827=EDGE_CURVE('',#3617,#3615,#766,.F.);
#4828=EDGE_CURVE('',#3613,#3617,#767,.F.);
#4829=EDGE_CURVE('',#3614,#3616,#768,.T.);
#4830=EDGE_CURVE('',#3618,#3619,#2261,.T.);
#4831=EDGE_CURVE('',#3615,#3618,#769,.F.);
#4832=EDGE_CURVE('',#3616,#3619,#770,.T.);
#4833=EDGE_CURVE('',#3620,#3621,#2262,.T.);
#4834=EDGE_CURVE('',#3618,#3620,#771,.F.);
#4835=EDGE_CURVE('',#3619,#3621,#772,.T.);
#4836=EDGE_CURVE('',#3622,#3623,#2263,.T.);
#4837=EDGE_CURVE('',#3624,#3622,#773,.F.);
#4838=EDGE_CURVE('',#3620,#3624,#774,.F.);
#4839=EDGE_CURVE('',#3621,#3623,#775,.T.);
#4840=EDGE_CURVE('',#3625,#3626,#2264,.T.);
#4841=EDGE_CURVE('',#3627,#3625,#776,.F.);
#4842=EDGE_CURVE('',#3622,#3627,#777,.F.);
#4843=EDGE_CURVE('',#3623,#3628,#778,.T.);
#4844=EDGE_CURVE('',#3628,#3626,#779,.T.);
#4845=EDGE_CURVE('',#3629,#3630,#2265,.T.);
#4846=EDGE_CURVE('',#3625,#3629,#780,.F.);
#4847=EDGE_CURVE('',#3626,#3630,#781,.T.);
#4848=EDGE_CURVE('',#3631,#3632,#2266,.T.);
#4849=EDGE_CURVE('',#3629,#3631,#782,.F.);
#4850=EDGE_CURVE('',#3630,#3632,#783,.T.);
#4851=EDGE_CURVE('',#3633,#3634,#784,.T.);
#4852=EDGE_CURVE('',#3634,#3635,#2818,.F.);
#4853=EDGE_CURVE('',#3635,#3636,#785,.T.);
#4854=EDGE_CURVE('',#3636,#3637,#786,.T.);
#4855=EDGE_CURVE('',#3637,#3638,#787,.T.);
#4856=EDGE_CURVE('',#3638,#3639,#788,.T.);
#4857=EDGE_CURVE('',#3639,#3640,#789,.T.);
#4858=EDGE_CURVE('',#3640,#3641,#790,.T.);
#4859=EDGE_CURVE('',#3641,#3642,#791,.T.);
#4860=EDGE_CURVE('',#3642,#3643,#792,.T.);
#4861=EDGE_CURVE('',#3643,#3644,#793,.T.);
#4862=EDGE_CURVE('',#3644,#3645,#794,.T.);
#4863=EDGE_CURVE('',#3645,#3646,#795,.T.);
#4864=EDGE_CURVE('',#3646,#3647,#796,.T.);
#4865=EDGE_CURVE('',#3647,#3648,#797,.T.);
#4866=EDGE_CURVE('',#3648,#3649,#798,.T.);
#4867=EDGE_CURVE('',#3649,#3650,#2819,.T.);
#4868=EDGE_CURVE('',#3650,#3651,#799,.T.);
#4869=EDGE_CURVE('',#3651,#3652,#800,.T.);
#4870=EDGE_CURVE('',#3652,#3653,#801,.T.);
#4871=EDGE_CURVE('',#3653,#3654,#802,.T.);
#4872=EDGE_CURVE('',#3654,#3655,#803,.T.);
#4873=EDGE_CURVE('',#3655,#3656,#804,.T.);
#4874=EDGE_CURVE('',#3656,#3657,#805,.T.);
#4875=EDGE_CURVE('',#3657,#3658,#806,.T.);
#4876=EDGE_CURVE('',#3658,#3659,#807,.T.);
#4877=EDGE_CURVE('',#3659,#3660,#808,.T.);
#4878=EDGE_CURVE('',#3660,#3661,#809,.T.);
#4879=EDGE_CURVE('',#3661,#3662,#810,.T.);
#4880=EDGE_CURVE('',#3662,#3633,#811,.T.);
#4881=EDGE_CURVE('',#3632,#3663,#812,.T.);
#4882=EDGE_CURVE('',#3663,#3664,#2820,.T.);
#4883=EDGE_CURVE('',#3631,#3664,#813,.T.);
#4884=EDGE_CURVE('',#3664,#3665,#814,.T.);
#4885=EDGE_CURVE('',#3650,#3663,#815,.T.);
#4886=EDGE_CURVE('',#3665,#3649,#816,.T.);
#4887=EDGE_CURVE('',#3665,#3666,#2267,.T.);
#4888=EDGE_CURVE('',#3666,#3666,#2821,.T.);
#4889=EDGE_CURVE('',#3634,#3601,#817,.T.);
#4890=EDGE_CURVE('',#3667,#3635,#818,.T.);
#4891=EDGE_CURVE('',#3667,#3600,#819,.T.);
#4892=EDGE_CURVE('',#3668,#3669,#2268,.T.);
#4893=EDGE_CURVE('',#3668,#3670,#2269,.T.);
#4894=EDGE_CURVE('',#3670,#3671,#2270,.T.);
#4895=EDGE_CURVE('',#3669,#3671,#2271,.T.);
#4896=EDGE_CURVE('',#3672,#3668,#2272,.T.);
#4897=EDGE_CURVE('',#3672,#3673,#2273,.T.);
#4898=EDGE_CURVE('',#3673,#3670,#2274,.T.);
#4899=EDGE_CURVE('',#3674,#3672,#2275,.T.);
#4900=EDGE_CURVE('',#3674,#3675,#2276,.T.);
#4901=EDGE_CURVE('',#3675,#3673,#2277,.T.);
#4902=EDGE_CURVE('',#3676,#3674,#2278,.T.);
#4903=EDGE_CURVE('',#3676,#3677,#2279,.T.);
#4904=EDGE_CURVE('',#3677,#3675,#2280,.T.);
#4905=EDGE_CURVE('',#3678,#3676,#2281,.T.);
#4906=EDGE_CURVE('',#3678,#3679,#2282,.T.);
#4907=EDGE_CURVE('',#3679,#3677,#2283,.T.);
#4908=EDGE_CURVE('',#3669,#3678,#2284,.T.);
#4909=EDGE_CURVE('',#3671,#3679,#2285,.T.);
#4910=EDGE_CURVE('',#3680,#3680,#2822,.T.);
#4911=EDGE_CURVE('',#3680,#3681,#2286,.T.);
#4912=EDGE_CURVE('',#3681,#3681,#2823,.T.);
#4913=EDGE_CURVE('',#3682,#3683,#2287,.T.);
#4914=EDGE_CURVE('',#3684,#3682,#820,.T.);
#4915=EDGE_CURVE('',#3685,#3684,#2824,.T.);
#4916=EDGE_CURVE('',#3685,#3683,#821,.T.);
#4917=EDGE_CURVE('',#3686,#3687,#2288,.T.);
#4918=EDGE_CURVE('',#3688,#3686,#822,.F.);
#4919=EDGE_CURVE('',#3682,#3688,#823,.T.);
#4920=EDGE_CURVE('',#3683,#3689,#824,.T.);
#4921=EDGE_CURVE('',#3689,#3687,#825,.T.);
#4922=EDGE_CURVE('',#3690,#3691,#2289,.T.);
#4923=EDGE_CURVE('',#3686,#3690,#826,.F.);
#4924=EDGE_CURVE('',#3687,#3692,#827,.T.);
#4925=EDGE_CURVE('',#3692,#3691,#828,.T.);
#4926=EDGE_CURVE('',#3693,#3694,#2290,.T.);
#4927=EDGE_CURVE('',#3695,#3693,#829,.T.);
#4928=EDGE_CURVE('',#3690,#3695,#830,.F.);
#4929=EDGE_CURVE('',#3691,#3694,#831,.T.);
#4930=EDGE_CURVE('',#3696,#3697,#2291,.T.);
#4931=EDGE_CURVE('',#3698,#3696,#832,.F.);
#4932=EDGE_CURVE('',#3693,#3698,#833,.T.);
#4933=EDGE_CURVE('',#3694,#3699,#834,.T.);
#4934=EDGE_CURVE('',#3699,#3697,#835,.T.);
#4935=EDGE_CURVE('',#3700,#3701,#2292,.T.);
#4936=EDGE_CURVE('',#3696,#3700,#836,.F.);
#4937=EDGE_CURVE('',#3697,#3702,#837,.T.);
#4938=EDGE_CURVE('',#3702,#3701,#838,.T.);
#4939=EDGE_CURVE('',#3703,#3704,#2293,.T.);
#4940=EDGE_CURVE('',#3705,#3703,#839,.T.);
#4941=EDGE_CURVE('',#3700,#3705,#840,.F.);
#4942=EDGE_CURVE('',#3701,#3704,#841,.T.);
#4943=EDGE_CURVE('',#3706,#3707,#2294,.T.);
#4944=EDGE_CURVE('',#3708,#3706,#842,.F.);
#4945=EDGE_CURVE('',#3703,#3708,#843,.T.);
#4946=EDGE_CURVE('',#3704,#3709,#844,.T.);
#4947=EDGE_CURVE('',#3709,#3707,#845,.T.);
#4948=EDGE_CURVE('',#3710,#3711,#2295,.T.);
#4949=EDGE_CURVE('',#3706,#3710,#846,.F.);
#4950=EDGE_CURVE('',#3707,#3712,#847,.T.);
#4951=EDGE_CURVE('',#3712,#3711,#848,.T.);
#4952=EDGE_CURVE('',#3713,#3714,#2296,.T.);
#4953=EDGE_CURVE('',#3715,#3713,#849,.F.);
#4954=EDGE_CURVE('',#3710,#3715,#850,.F.);
#4955=EDGE_CURVE('',#3711,#3714,#851,.T.);
#4956=EDGE_CURVE('',#3716,#3717,#2297,.T.);
#4957=EDGE_CURVE('',#3713,#3716,#852,.F.);
#4958=EDGE_CURVE('',#3714,#3718,#853,.T.);
#4959=EDGE_CURVE('',#3718,#3717,#854,.T.);
#4960=EDGE_CURVE('',#3719,#3720,#2298,.T.);
#4961=EDGE_CURVE('',#3721,#3719,#855,.F.);
#4962=EDGE_CURVE('',#3716,#3721,#856,.F.);
#4963=EDGE_CURVE('',#3717,#3720,#857,.T.);
#4964=EDGE_CURVE('',#3722,#3723,#2299,.T.);
#4965=EDGE_CURVE('',#3719,#3722,#858,.F.);
#4966=EDGE_CURVE('',#3720,#3724,#859,.T.);
#4967=EDGE_CURVE('',#3724,#3723,#860,.T.);
#4968=EDGE_CURVE('',#3725,#3726,#2300,.T.);
#4969=EDGE_CURVE('',#3727,#3725,#861,.T.);
#4970=EDGE_CURVE('',#3722,#3727,#862,.F.);
#4971=EDGE_CURVE('',#3723,#3728,#863,.T.);
#4972=EDGE_CURVE('',#3728,#3726,#864,.F.);
#4973=EDGE_CURVE('',#3729,#3730,#2301,.T.);
#4974=EDGE_CURVE('',#3729,#3731,#865,.T.);
#4975=EDGE_CURVE('',#3731,#3732,#2825,.F.);
#4976=EDGE_CURVE('',#3732,#3730,#866,.T.);
#4977=EDGE_CURVE('',#3733,#3734,#2302,.T.);
#4978=EDGE_CURVE('',#3733,#3729,#867,.T.);
#4979=EDGE_CURVE('',#3730,#3734,#868,.T.);
#4980=EDGE_CURVE('',#3735,#3736,#2303,.T.);
#4981=EDGE_CURVE('',#3735,#3733,#869,.T.);
#4982=EDGE_CURVE('',#3734,#3736,#870,.T.);
#4983=EDGE_CURVE('',#3737,#3738,#2304,.T.);
#4984=EDGE_CURVE('',#3737,#3735,#871,.T.);
#4985=EDGE_CURVE('',#3736,#3738,#872,.T.);
#4986=EDGE_CURVE('',#3739,#3740,#2305,.T.);
#4987=EDGE_CURVE('',#3739,#3737,#873,.T.);
#4988=EDGE_CURVE('',#3738,#3740,#874,.T.);
#4989=EDGE_CURVE('',#3741,#3742,#2306,.T.);
#4990=EDGE_CURVE('',#3741,#3739,#875,.T.);
#4991=EDGE_CURVE('',#3740,#3742,#876,.T.);
#4992=EDGE_CURVE('',#3743,#3744,#2307,.T.);
#4993=EDGE_CURVE('',#3743,#3741,#877,.T.);
#4994=EDGE_CURVE('',#3742,#3744,#878,.T.);
#4995=EDGE_CURVE('',#3745,#3746,#2308,.T.);
#4996=EDGE_CURVE('',#3745,#3743,#879,.T.);
#4997=EDGE_CURVE('',#3744,#3746,#880,.T.);
#4998=EDGE_CURVE('',#3747,#3748,#2309,.T.);
#4999=EDGE_CURVE('',#3747,#3745,#881,.T.);
#5000=EDGE_CURVE('',#3746,#3748,#882,.T.);
#5001=EDGE_CURVE('',#3749,#3750,#2310,.T.);
#5002=EDGE_CURVE('',#3749,#3747,#883,.T.);
#5003=EDGE_CURVE('',#3748,#3750,#884,.T.);
#5004=EDGE_CURVE('',#3751,#3752,#2311,.T.);
#5005=EDGE_CURVE('',#3751,#3749,#885,.T.);
#5006=EDGE_CURVE('',#3750,#3752,#886,.T.);
#5007=EDGE_CURVE('',#3753,#3754,#2312,.T.);
#5008=EDGE_CURVE('',#3753,#3751,#887,.T.);
#5009=EDGE_CURVE('',#3752,#3754,#888,.T.);
#5010=EDGE_CURVE('',#3755,#3756,#2313,.T.);
#5011=EDGE_CURVE('',#3755,#3753,#889,.T.);
#5012=EDGE_CURVE('',#3754,#3756,#890,.T.);
#5013=EDGE_CURVE('',#3757,#3758,#2314,.T.);
#5014=EDGE_CURVE('',#3757,#3755,#891,.T.);
#5015=EDGE_CURVE('',#3756,#3758,#892,.T.);
#5016=EDGE_CURVE('',#3758,#3759,#893,.T.);
#5017=EDGE_CURVE('',#3760,#3759,#2826,.F.);
#5018=EDGE_CURVE('',#3760,#3757,#894,.T.);
#5019=EDGE_CURVE('',#3726,#3761,#895,.F.);
#5020=EDGE_CURVE('',#3762,#3761,#2827,.T.);
#5021=EDGE_CURVE('',#3763,#3762,#896,.T.);
#5022=EDGE_CURVE('',#3725,#3763,#897,.T.);
#5023=EDGE_CURVE('',#3759,#3762,#898,.T.);
#5024=EDGE_CURVE('',#3684,#3732,#899,.T.);
#5025=EDGE_CURVE('',#3764,#3760,#900,.T.);
#5026=EDGE_CURVE('',#3761,#3764,#901,.T.);
#5027=EDGE_CURVE('',#3731,#3685,#902,.T.);
#5028=EDGE_CURVE('',#3765,#3765,#2828,.T.);
#5029=EDGE_CURVE('',#3765,#3766,#2315,.T.);
#5030=EDGE_CURVE('',#3766,#3766,#2829,.T.);
#5031=EDGE_CURVE('',#3767,#3767,#2830,.T.);
#5032=EDGE_CURVE('',#3767,#3768,#2316,.T.);
#5033=EDGE_CURVE('',#3768,#3768,#2831,.T.);
#5034=EDGE_CURVE('',#3769,#3770,#2317,.T.);
#5035=EDGE_CURVE('',#3770,#3771,#903,.T.);
#5036=EDGE_CURVE('',#3772,#3771,#2832,.T.);
#5037=EDGE_CURVE('',#3769,#3772,#904,.T.);
#5038=EDGE_CURVE('',#3773,#3774,#2318,.T.);
#5039=EDGE_CURVE('',#3774,#3775,#905,.T.);
#5040=EDGE_CURVE('',#3775,#3770,#906,.T.);
#5041=EDGE_CURVE('',#3776,#3769,#907,.T.);
#5042=EDGE_CURVE('',#3773,#3776,#908,.T.);
#5043=EDGE_CURVE('',#3777,#3778,#2319,.T.);
#5044=EDGE_CURVE('',#3778,#3779,#909,.T.);
#5045=EDGE_CURVE('',#3779,#3774,#910,.T.);
#5046=EDGE_CURVE('',#3780,#3773,#911,.T.);
#5047=EDGE_CURVE('',#3777,#3780,#912,.T.);
#5048=EDGE_CURVE('',#3781,#3782,#2320,.T.);
#5049=EDGE_CURVE('',#3783,#3781,#913,.T.);
#5050=EDGE_CURVE('',#3784,#3783,#914,.T.);
#5051=EDGE_CURVE('',#3785,#3784,#2833,.T.);
#5052=EDGE_CURVE('',#3785,#3786,#915,.T.);
#5053=EDGE_CURVE('',#3786,#3782,#916,.T.);
#5054=EDGE_CURVE('',#3787,#3788,#2321,.T.);
#5055=EDGE_CURVE('',#3788,#3789,#917,.T.);
#5056=EDGE_CURVE('',#3790,#3789,#2834,.F.);
#5057=EDGE_CURVE('',#3790,#3787,#918,.T.);
#5058=EDGE_CURVE('',#3791,#3792,#2322,.T.);
#5059=EDGE_CURVE('',#3792,#3788,#919,.T.);
#5060=EDGE_CURVE('',#3787,#3791,#920,.T.);
#5061=EDGE_CURVE('',#3793,#3794,#2323,.T.);
#5062=EDGE_CURVE('',#3794,#3792,#921,.T.);
#5063=EDGE_CURVE('',#3791,#3793,#922,.T.);
#5064=EDGE_CURVE('',#3795,#3796,#2324,.T.);
#5065=EDGE_CURVE('',#3795,#3797,#923,.T.);
#5066=EDGE_CURVE('',#3797,#3798,#2835,.F.);
#5067=EDGE_CURVE('',#3798,#3796,#924,.T.);
#5068=EDGE_CURVE('',#3796,#3794,#925,.T.);
#5069=EDGE_CURVE('',#3793,#3795,#926,.T.);
#5070=EDGE_CURVE('',#3782,#3799,#927,.T.);
#5071=EDGE_CURVE('',#3799,#3778,#928,.T.);
#5072=EDGE_CURVE('',#3800,#3777,#929,.T.);
#5073=EDGE_CURVE('',#3781,#3800,#930,.T.);
#5074=EDGE_CURVE('',#3801,#3801,#2836,.T.);
#5075=EDGE_CURVE('',#3801,#3802,#2325,.T.);
#5076=EDGE_CURVE('',#3802,#3802,#2837,.T.);
#5077=EDGE_CURVE('',#3803,#3803,#2838,.T.);
#5078=EDGE_CURVE('',#3803,#3804,#2326,.T.);
#5079=EDGE_CURVE('',#3804,#3804,#2839,.T.);
#5080=EDGE_CURVE('',#3771,#3790,#931,.T.);
#5081=EDGE_CURVE('',#3797,#3785,#932,.T.);
#5082=EDGE_CURVE('',#3789,#3772,#933,.T.);
#5083=EDGE_CURVE('',#3798,#3805,#934,.T.);
#5084=EDGE_CURVE('',#3784,#3805,#935,.T.);
#5085=EDGE_CURVE('',#3806,#3806,#2840,.T.);
#5086=EDGE_CURVE('',#3806,#3807,#2327,.T.);
#5087=EDGE_CURVE('',#3807,#3807,#2841,.T.);
#5088=EDGE_CURVE('',#3808,#3808,#2842,.T.);
#5089=EDGE_CURVE('',#3808,#3809,#2328,.T.);
#5090=EDGE_CURVE('',#3809,#3809,#2843,.T.);
#5091=EDGE_CURVE('',#3810,#3810,#2844,.T.);
#5092=EDGE_CURVE('',#3810,#3811,#2329,.T.);
#5093=EDGE_CURVE('',#3811,#3811,#2845,.T.);
#5094=ORIENTED_EDGE('',*,*,#3812,.F.);
#5095=ORIENTED_EDGE('',*,*,#3813,.T.);
#5096=ORIENTED_EDGE('',*,*,#3814,.F.);
#5097=ORIENTED_EDGE('',*,*,#3813,.F.);
#5098=ORIENTED_EDGE('',*,*,#3815,.F.);
#5099=ORIENTED_EDGE('',*,*,#3816,.T.);
#5100=ORIENTED_EDGE('',*,*,#3817,.F.);
#5101=ORIENTED_EDGE('',*,*,#3816,.F.);
#5102=ORIENTED_EDGE('',*,*,#3818,.F.);
#5103=ORIENTED_EDGE('',*,*,#3819,.T.);
#5104=ORIENTED_EDGE('',*,*,#3820,.F.);
#5105=ORIENTED_EDGE('',*,*,#3819,.F.);
#5106=ORIENTED_EDGE('',*,*,#3821,.F.);
#5107=ORIENTED_EDGE('',*,*,#3822,.T.);
#5108=ORIENTED_EDGE('',*,*,#3823,.F.);
#5109=ORIENTED_EDGE('',*,*,#3822,.F.);
#5110=ORIENTED_EDGE('',*,*,#3824,.T.);
#5111=ORIENTED_EDGE('',*,*,#3825,.T.);
#5112=ORIENTED_EDGE('',*,*,#3826,.F.);
#5113=ORIENTED_EDGE('',*,*,#3827,.F.);
#5114=ORIENTED_EDGE('',*,*,#3828,.T.);
#5115=ORIENTED_EDGE('',*,*,#3827,.T.);
#5116=ORIENTED_EDGE('',*,*,#3829,.F.);
#5117=ORIENTED_EDGE('',*,*,#3830,.F.);
#5118=ORIENTED_EDGE('',*,*,#3831,.T.);
#5119=ORIENTED_EDGE('',*,*,#3830,.T.);
#5120=ORIENTED_EDGE('',*,*,#3832,.F.);
#5121=ORIENTED_EDGE('',*,*,#3833,.F.);
#5122=ORIENTED_EDGE('',*,*,#3834,.T.);
#5123=ORIENTED_EDGE('',*,*,#3833,.T.);
#5124=ORIENTED_EDGE('',*,*,#3835,.F.);
#5125=ORIENTED_EDGE('',*,*,#3825,.F.);
#5126=ORIENTED_EDGE('',*,*,#3835,.T.);
#5127=ORIENTED_EDGE('',*,*,#3832,.T.);
#5128=ORIENTED_EDGE('',*,*,#3829,.T.);
#5129=ORIENTED_EDGE('',*,*,#3826,.T.);
#5130=ORIENTED_EDGE('',*,*,#3812,.T.);
#5131=ORIENTED_EDGE('',*,*,#3815,.T.);
#5132=ORIENTED_EDGE('',*,*,#3818,.T.);
#5133=ORIENTED_EDGE('',*,*,#3821,.T.);
#5134=ORIENTED_EDGE('',*,*,#3834,.F.);
#5135=ORIENTED_EDGE('',*,*,#3824,.F.);
#5136=ORIENTED_EDGE('',*,*,#3828,.F.);
#5137=ORIENTED_EDGE('',*,*,#3831,.F.);
#5138=ORIENTED_EDGE('',*,*,#3814,.T.);
#5139=ORIENTED_EDGE('',*,*,#3817,.T.);
#5140=ORIENTED_EDGE('',*,*,#3820,.T.);
#5141=ORIENTED_EDGE('',*,*,#3823,.T.);
#5142=ORIENTED_EDGE('',*,*,#3836,.F.);
#5143=ORIENTED_EDGE('',*,*,#3837,.T.);
#5144=ORIENTED_EDGE('',*,*,#3838,.F.);
#5145=ORIENTED_EDGE('',*,*,#3837,.F.);
#5146=ORIENTED_EDGE('',*,*,#3839,.F.);
#5147=ORIENTED_EDGE('',*,*,#3840,.T.);
#5148=ORIENTED_EDGE('',*,*,#3841,.F.);
#5149=ORIENTED_EDGE('',*,*,#3840,.F.);
#5150=ORIENTED_EDGE('',*,*,#3842,.T.);
#5151=ORIENTED_EDGE('',*,*,#3843,.T.);
#5152=ORIENTED_EDGE('',*,*,#3844,.F.);
#5153=ORIENTED_EDGE('',*,*,#3845,.F.);
#5154=ORIENTED_EDGE('',*,*,#3836,.T.);
#5155=ORIENTED_EDGE('',*,*,#3839,.T.);
#5156=ORIENTED_EDGE('',*,*,#3846,.T.);
#5157=ORIENTED_EDGE('',*,*,#3845,.T.);
#5158=ORIENTED_EDGE('',*,*,#3847,.F.);
#5159=ORIENTED_EDGE('',*,*,#3848,.F.);
#5160=ORIENTED_EDGE('',*,*,#3849,.T.);
#5161=ORIENTED_EDGE('',*,*,#3848,.T.);
#5162=ORIENTED_EDGE('',*,*,#3850,.F.);
#5163=ORIENTED_EDGE('',*,*,#3851,.F.);
#5164=ORIENTED_EDGE('',*,*,#3838,.T.);
#5165=ORIENTED_EDGE('',*,*,#3841,.T.);
#5166=ORIENTED_EDGE('',*,*,#3852,.T.);
#5167=ORIENTED_EDGE('',*,*,#3851,.T.);
#5168=ORIENTED_EDGE('',*,*,#3853,.F.);
#5169=ORIENTED_EDGE('',*,*,#3843,.F.);
#5170=ORIENTED_EDGE('',*,*,#3853,.T.);
#5171=ORIENTED_EDGE('',*,*,#3850,.T.);
#5172=ORIENTED_EDGE('',*,*,#3847,.T.);
#5173=ORIENTED_EDGE('',*,*,#3844,.T.);
#5174=ORIENTED_EDGE('',*,*,#3852,.F.);
#5175=ORIENTED_EDGE('',*,*,#3842,.F.);
#5176=ORIENTED_EDGE('',*,*,#3846,.F.);
#5177=ORIENTED_EDGE('',*,*,#3849,.F.);
#5178=ORIENTED_EDGE('',*,*,#3854,.T.);
#5179=ORIENTED_EDGE('',*,*,#3855,.T.);
#5180=ORIENTED_EDGE('',*,*,#3856,.F.);
#5181=ORIENTED_EDGE('',*,*,#3857,.F.);
#5182=ORIENTED_EDGE('',*,*,#3858,.T.);
#5183=ORIENTED_EDGE('',*,*,#3857,.T.);
#5184=ORIENTED_EDGE('',*,*,#3859,.F.);
#5185=ORIENTED_EDGE('',*,*,#3860,.F.);
#5186=ORIENTED_EDGE('',*,*,#3861,.T.);
#5187=ORIENTED_EDGE('',*,*,#3860,.T.);
#5188=ORIENTED_EDGE('',*,*,#3862,.F.);
#5189=ORIENTED_EDGE('',*,*,#3863,.F.);
#5190=ORIENTED_EDGE('',*,*,#3864,.T.);
#5191=ORIENTED_EDGE('',*,*,#3863,.T.);
#5192=ORIENTED_EDGE('',*,*,#3865,.F.);
#5193=ORIENTED_EDGE('',*,*,#3855,.F.);
#5194=ORIENTED_EDGE('',*,*,#3865,.T.);
#5195=ORIENTED_EDGE('',*,*,#3862,.T.);
#5196=ORIENTED_EDGE('',*,*,#3859,.T.);
#5197=ORIENTED_EDGE('',*,*,#3856,.T.);
#5198=ORIENTED_EDGE('',*,*,#3864,.F.);
#5199=ORIENTED_EDGE('',*,*,#3854,.F.);
#5200=ORIENTED_EDGE('',*,*,#3858,.F.);
#5201=ORIENTED_EDGE('',*,*,#3861,.F.);
#5202=ORIENTED_EDGE('',*,*,#3866,.T.);
#5203=ORIENTED_EDGE('',*,*,#3867,.T.);
#5204=ORIENTED_EDGE('',*,*,#3868,.T.);
#5205=ORIENTED_EDGE('',*,*,#3869,.T.);
#5206=ORIENTED_EDGE('',*,*,#3867,.F.);
#5207=ORIENTED_EDGE('',*,*,#3870,.F.);
#5208=ORIENTED_EDGE('',*,*,#3871,.F.);
#5209=ORIENTED_EDGE('',*,*,#3872,.F.);
#5210=ORIENTED_EDGE('',*,*,#3873,.T.);
#5211=ORIENTED_EDGE('',*,*,#3874,.T.);
#5212=ORIENTED_EDGE('',*,*,#3875,.T.);
#5213=ORIENTED_EDGE('',*,*,#3871,.T.);
#5214=ORIENTED_EDGE('',*,*,#3874,.F.);
#5215=ORIENTED_EDGE('',*,*,#3876,.F.);
#5216=ORIENTED_EDGE('',*,*,#3877,.F.);
#5217=ORIENTED_EDGE('',*,*,#3878,.F.);
#5218=ORIENTED_EDGE('',*,*,#3879,.T.);
#5219=ORIENTED_EDGE('',*,*,#3880,.T.);
#5220=ORIENTED_EDGE('',*,*,#3881,.T.);
#5221=ORIENTED_EDGE('',*,*,#3882,.T.);
#5222=ORIENTED_EDGE('',*,*,#3869,.F.);
#5223=ORIENTED_EDGE('',*,*,#3883,.F.);
#5224=ORIENTED_EDGE('',*,*,#3880,.F.);
#5225=ORIENTED_EDGE('',*,*,#3884,.F.);
#5226=ORIENTED_EDGE('',*,*,#3885,.T.);
#5227=ORIENTED_EDGE('',*,*,#3886,.T.);
#5228=ORIENTED_EDGE('',*,*,#3887,.T.);
#5229=ORIENTED_EDGE('',*,*,#3877,.T.);
#5230=ORIENTED_EDGE('',*,*,#3882,.F.);
#5231=ORIENTED_EDGE('',*,*,#3888,.F.);
#5232=ORIENTED_EDGE('',*,*,#3886,.F.);
#5233=ORIENTED_EDGE('',*,*,#3889,.F.);
#5234=ORIENTED_EDGE('',*,*,#3890,.T.);
#5235=ORIENTED_EDGE('',*,*,#3891,.T.);
#5236=ORIENTED_EDGE('',*,*,#3892,.T.);
#5237=ORIENTED_EDGE('',*,*,#3893,.T.);
#5238=ORIENTED_EDGE('',*,*,#3891,.F.);
#5239=ORIENTED_EDGE('',*,*,#3894,.F.);
#5240=ORIENTED_EDGE('',*,*,#3895,.F.);
#5241=ORIENTED_EDGE('',*,*,#3896,.F.);
#5242=ORIENTED_EDGE('',*,*,#3897,.T.);
#5243=ORIENTED_EDGE('',*,*,#3898,.T.);
#5244=ORIENTED_EDGE('',*,*,#3899,.T.);
#5245=ORIENTED_EDGE('',*,*,#3900,.T.);
#5246=ORIENTED_EDGE('',*,*,#3893,.F.);
#5247=ORIENTED_EDGE('',*,*,#3901,.F.);
#5248=ORIENTED_EDGE('',*,*,#3898,.F.);
#5249=ORIENTED_EDGE('',*,*,#3902,.F.);
#5250=ORIENTED_EDGE('',*,*,#3903,.T.);
#5251=ORIENTED_EDGE('',*,*,#3904,.T.);
#5252=ORIENTED_EDGE('',*,*,#3905,.T.);
#5253=ORIENTED_EDGE('',*,*,#3895,.T.);
#5254=ORIENTED_EDGE('',*,*,#3904,.F.);
#5255=ORIENTED_EDGE('',*,*,#3906,.F.);
#5256=ORIENTED_EDGE('',*,*,#3907,.F.);
#5257=ORIENTED_EDGE('',*,*,#3908,.F.);
#5258=ORIENTED_EDGE('',*,*,#3909,.T.);
#5259=ORIENTED_EDGE('',*,*,#3910,.T.);
#5260=ORIENTED_EDGE('',*,*,#3911,.T.);
#5261=ORIENTED_EDGE('',*,*,#3907,.T.);
#5262=ORIENTED_EDGE('',*,*,#3900,.F.);
#5263=ORIENTED_EDGE('',*,*,#3912,.F.);
#5264=ORIENTED_EDGE('',*,*,#3910,.F.);
#5265=ORIENTED_EDGE('',*,*,#3913,.F.);
#5266=ORIENTED_EDGE('',*,*,#3914,.T.);
#5267=ORIENTED_EDGE('',*,*,#3915,.T.);
#5268=ORIENTED_EDGE('',*,*,#3916,.F.);
#5269=ORIENTED_EDGE('',*,*,#3917,.F.);
#5270=ORIENTED_EDGE('',*,*,#3918,.T.);
#5271=ORIENTED_EDGE('',*,*,#3917,.T.);
#5272=ORIENTED_EDGE('',*,*,#3919,.F.);
#5273=ORIENTED_EDGE('',*,*,#3920,.F.);
#5274=ORIENTED_EDGE('',*,*,#3906,.T.);
#5275=ORIENTED_EDGE('',*,*,#3903,.F.);
#5276=ORIENTED_EDGE('',*,*,#3894,.T.);
#5277=ORIENTED_EDGE('',*,*,#3890,.F.);
#5278=ORIENTED_EDGE('',*,*,#3902,.T.);
#5279=ORIENTED_EDGE('',*,*,#3897,.F.);
#5280=ORIENTED_EDGE('',*,*,#3913,.T.);
#5281=ORIENTED_EDGE('',*,*,#3909,.F.);
#5282=ORIENTED_EDGE('',*,*,#3870,.T.);
#5283=ORIENTED_EDGE('',*,*,#3866,.F.);
#5284=ORIENTED_EDGE('',*,*,#3884,.T.);
#5285=ORIENTED_EDGE('',*,*,#3879,.F.);
#5286=ORIENTED_EDGE('',*,*,#3889,.T.);
#5287=ORIENTED_EDGE('',*,*,#3885,.F.);
#5288=ORIENTED_EDGE('',*,*,#3876,.T.);
#5289=ORIENTED_EDGE('',*,*,#3873,.F.);
#5290=ORIENTED_EDGE('',*,*,#3921,.T.);
#5291=ORIENTED_EDGE('',*,*,#3920,.T.);
#5292=ORIENTED_EDGE('',*,*,#3922,.F.);
#5293=ORIENTED_EDGE('',*,*,#3923,.F.);
#5294=ORIENTED_EDGE('',*,*,#3924,.T.);
#5295=ORIENTED_EDGE('',*,*,#3923,.T.);
#5296=ORIENTED_EDGE('',*,*,#3925,.F.);
#5297=ORIENTED_EDGE('',*,*,#3915,.F.);
#5298=ORIENTED_EDGE('',*,*,#3908,.T.);
#5299=ORIENTED_EDGE('',*,*,#3911,.F.);
#5300=ORIENTED_EDGE('',*,*,#3912,.T.);
#5301=ORIENTED_EDGE('',*,*,#3899,.F.);
#5302=ORIENTED_EDGE('',*,*,#3901,.T.);
#5303=ORIENTED_EDGE('',*,*,#3892,.F.);
#5304=ORIENTED_EDGE('',*,*,#3896,.T.);
#5305=ORIENTED_EDGE('',*,*,#3905,.F.);
#5306=ORIENTED_EDGE('',*,*,#3872,.T.);
#5307=ORIENTED_EDGE('',*,*,#3875,.F.);
#5308=ORIENTED_EDGE('',*,*,#3878,.T.);
#5309=ORIENTED_EDGE('',*,*,#3887,.F.);
#5310=ORIENTED_EDGE('',*,*,#3888,.T.);
#5311=ORIENTED_EDGE('',*,*,#3881,.F.);
#5312=ORIENTED_EDGE('',*,*,#3883,.T.);
#5313=ORIENTED_EDGE('',*,*,#3868,.F.);
#5314=ORIENTED_EDGE('',*,*,#3925,.T.);
#5315=ORIENTED_EDGE('',*,*,#3922,.T.);
#5316=ORIENTED_EDGE('',*,*,#3919,.T.);
#5317=ORIENTED_EDGE('',*,*,#3916,.T.);
#5318=ORIENTED_EDGE('',*,*,#3924,.F.);
#5319=ORIENTED_EDGE('',*,*,#3914,.F.);
#5320=ORIENTED_EDGE('',*,*,#3918,.F.);
#5321=ORIENTED_EDGE('',*,*,#3921,.F.);
#5322=ORIENTED_EDGE('',*,*,#3926,.T.);
#5323=ORIENTED_EDGE('',*,*,#3927,.T.);
#5324=ORIENTED_EDGE('',*,*,#3928,.F.);
#5325=ORIENTED_EDGE('',*,*,#3929,.F.);
#5326=ORIENTED_EDGE('',*,*,#3930,.T.);
#5327=ORIENTED_EDGE('',*,*,#3931,.T.);
#5328=ORIENTED_EDGE('',*,*,#3932,.T.);
#5329=ORIENTED_EDGE('',*,*,#3926,.F.);
#5330=ORIENTED_EDGE('',*,*,#3933,.F.);
#5331=ORIENTED_EDGE('',*,*,#3934,.F.);
#5332=ORIENTED_EDGE('',*,*,#3935,.T.);
#5333=ORIENTED_EDGE('',*,*,#3936,.T.);
#5334=ORIENTED_EDGE('',*,*,#3937,.T.);
#5335=ORIENTED_EDGE('',*,*,#3930,.F.);
#5336=ORIENTED_EDGE('',*,*,#3938,.F.);
#5337=ORIENTED_EDGE('',*,*,#3939,.F.);
#5338=ORIENTED_EDGE('',*,*,#3940,.T.);
#5339=ORIENTED_EDGE('',*,*,#3941,.T.);
#5340=ORIENTED_EDGE('',*,*,#3942,.T.);
#5341=ORIENTED_EDGE('',*,*,#3935,.F.);
#5342=ORIENTED_EDGE('',*,*,#3943,.F.);
#5343=ORIENTED_EDGE('',*,*,#3944,.F.);
#5344=ORIENTED_EDGE('',*,*,#3945,.T.);
#5345=ORIENTED_EDGE('',*,*,#3946,.T.);
#5346=ORIENTED_EDGE('',*,*,#3947,.T.);
#5347=ORIENTED_EDGE('',*,*,#3940,.F.);
#5348=ORIENTED_EDGE('',*,*,#3948,.F.);
#5349=ORIENTED_EDGE('',*,*,#3949,.F.);
#5350=ORIENTED_EDGE('',*,*,#3950,.T.);
#5351=ORIENTED_EDGE('',*,*,#3951,.T.);
#5352=ORIENTED_EDGE('',*,*,#3952,.T.);
#5353=ORIENTED_EDGE('',*,*,#3945,.F.);
#5354=ORIENTED_EDGE('',*,*,#3953,.F.);
#5355=ORIENTED_EDGE('',*,*,#3954,.F.);
#5356=ORIENTED_EDGE('',*,*,#3955,.T.);
#5357=ORIENTED_EDGE('',*,*,#3956,.T.);
#5358=ORIENTED_EDGE('',*,*,#3957,.T.);
#5359=ORIENTED_EDGE('',*,*,#3950,.F.);
#5360=ORIENTED_EDGE('',*,*,#3958,.F.);
#5361=ORIENTED_EDGE('',*,*,#3959,.F.);
#5362=ORIENTED_EDGE('',*,*,#3960,.T.);
#5363=ORIENTED_EDGE('',*,*,#3961,.T.);
#5364=ORIENTED_EDGE('',*,*,#3962,.T.);
#5365=ORIENTED_EDGE('',*,*,#3955,.F.);
#5366=ORIENTED_EDGE('',*,*,#3963,.F.);
#5367=ORIENTED_EDGE('',*,*,#3964,.F.);
#5368=ORIENTED_EDGE('',*,*,#3965,.T.);
#5369=ORIENTED_EDGE('',*,*,#3966,.T.);
#5370=ORIENTED_EDGE('',*,*,#3967,.T.);
#5371=ORIENTED_EDGE('',*,*,#3960,.F.);
#5372=ORIENTED_EDGE('',*,*,#3968,.F.);
#5373=ORIENTED_EDGE('',*,*,#3969,.F.);
#5374=ORIENTED_EDGE('',*,*,#3970,.T.);
#5375=ORIENTED_EDGE('',*,*,#3971,.T.);
#5376=ORIENTED_EDGE('',*,*,#3972,.T.);
#5377=ORIENTED_EDGE('',*,*,#3965,.F.);
#5378=ORIENTED_EDGE('',*,*,#3973,.F.);
#5379=ORIENTED_EDGE('',*,*,#3974,.F.);
#5380=ORIENTED_EDGE('',*,*,#3975,.T.);
#5381=ORIENTED_EDGE('',*,*,#3976,.T.);
#5382=ORIENTED_EDGE('',*,*,#3977,.T.);
#5383=ORIENTED_EDGE('',*,*,#3970,.F.);
#5384=ORIENTED_EDGE('',*,*,#3978,.F.);
#5385=ORIENTED_EDGE('',*,*,#3979,.F.);
#5386=ORIENTED_EDGE('',*,*,#3980,.T.);
#5387=ORIENTED_EDGE('',*,*,#3981,.T.);
#5388=ORIENTED_EDGE('',*,*,#3982,.T.);
#5389=ORIENTED_EDGE('',*,*,#3975,.F.);
#5390=ORIENTED_EDGE('',*,*,#3983,.F.);
#5391=ORIENTED_EDGE('',*,*,#3984,.F.);
#5392=ORIENTED_EDGE('',*,*,#3985,.T.);
#5393=ORIENTED_EDGE('',*,*,#3986,.T.);
#5394=ORIENTED_EDGE('',*,*,#3987,.T.);
#5395=ORIENTED_EDGE('',*,*,#3980,.F.);
#5396=ORIENTED_EDGE('',*,*,#3988,.F.);
#5397=ORIENTED_EDGE('',*,*,#3989,.F.);
#5398=ORIENTED_EDGE('',*,*,#3990,.T.);
#5399=ORIENTED_EDGE('',*,*,#3991,.T.);
#5400=ORIENTED_EDGE('',*,*,#3992,.T.);
#5401=ORIENTED_EDGE('',*,*,#3985,.F.);
#5402=ORIENTED_EDGE('',*,*,#3993,.F.);
#5403=ORIENTED_EDGE('',*,*,#3994,.F.);
#5404=ORIENTED_EDGE('',*,*,#3995,.T.);
#5405=ORIENTED_EDGE('',*,*,#3996,.T.);
#5406=ORIENTED_EDGE('',*,*,#3997,.T.);
#5407=ORIENTED_EDGE('',*,*,#3990,.F.);
#5408=ORIENTED_EDGE('',*,*,#3998,.F.);
#5409=ORIENTED_EDGE('',*,*,#3999,.F.);
#5410=ORIENTED_EDGE('',*,*,#4000,.T.);
#5411=ORIENTED_EDGE('',*,*,#4001,.T.);
#5412=ORIENTED_EDGE('',*,*,#4002,.T.);
#5413=ORIENTED_EDGE('',*,*,#3995,.F.);
#5414=ORIENTED_EDGE('',*,*,#4003,.F.);
#5415=ORIENTED_EDGE('',*,*,#4004,.F.);
#5416=ORIENTED_EDGE('',*,*,#4005,.T.);
#5417=ORIENTED_EDGE('',*,*,#4006,.T.);
#5418=ORIENTED_EDGE('',*,*,#4007,.T.);
#5419=ORIENTED_EDGE('',*,*,#4000,.F.);
#5420=ORIENTED_EDGE('',*,*,#4008,.F.);
#5421=ORIENTED_EDGE('',*,*,#4009,.F.);
#5422=ORIENTED_EDGE('',*,*,#4010,.T.);
#5423=ORIENTED_EDGE('',*,*,#4011,.T.);
#5424=ORIENTED_EDGE('',*,*,#4012,.T.);
#5425=ORIENTED_EDGE('',*,*,#4005,.F.);
#5426=ORIENTED_EDGE('',*,*,#4013,.F.);
#5427=ORIENTED_EDGE('',*,*,#4014,.F.);
#5428=ORIENTED_EDGE('',*,*,#4015,.F.);
#5429=ORIENTED_EDGE('',*,*,#4016,.F.);
#5430=ORIENTED_EDGE('',*,*,#4017,.F.);
#5431=ORIENTED_EDGE('',*,*,#4018,.F.);
#5432=ORIENTED_EDGE('',*,*,#4019,.T.);
#5433=ORIENTED_EDGE('',*,*,#4020,.T.);
#5434=ORIENTED_EDGE('',*,*,#4021,.T.);
#5435=ORIENTED_EDGE('',*,*,#4022,.T.);
#5436=ORIENTED_EDGE('',*,*,#4023,.T.);
#5437=ORIENTED_EDGE('',*,*,#4024,.T.);
#5438=ORIENTED_EDGE('',*,*,#4025,.T.);
#5439=ORIENTED_EDGE('',*,*,#4024,.F.);
#5440=ORIENTED_EDGE('',*,*,#4026,.T.);
#5441=ORIENTED_EDGE('',*,*,#4027,.T.);
#5442=ORIENTED_EDGE('',*,*,#4028,.T.);
#5443=ORIENTED_EDGE('',*,*,#4029,.T.);
#5444=ORIENTED_EDGE('',*,*,#4030,.T.);
#5445=ORIENTED_EDGE('',*,*,#4021,.F.);
#5446=ORIENTED_EDGE('',*,*,#4031,.T.);
#5447=ORIENTED_EDGE('',*,*,#4032,.T.);
#5448=ORIENTED_EDGE('',*,*,#4033,.T.);
#5449=ORIENTED_EDGE('',*,*,#4034,.T.);
#5450=ORIENTED_EDGE('',*,*,#4035,.T.);
#5451=ORIENTED_EDGE('',*,*,#4028,.F.);
#5452=ORIENTED_EDGE('',*,*,#4036,.T.);
#5453=ORIENTED_EDGE('',*,*,#4037,.T.);
#5454=ORIENTED_EDGE('',*,*,#4038,.T.);
#5455=ORIENTED_EDGE('',*,*,#4039,.T.);
#5456=ORIENTED_EDGE('',*,*,#4033,.F.);
#5457=ORIENTED_EDGE('',*,*,#4040,.T.);
#5458=ORIENTED_EDGE('',*,*,#4041,.T.);
#5459=ORIENTED_EDGE('',*,*,#4042,.T.);
#5460=ORIENTED_EDGE('',*,*,#4043,.T.);
#5461=ORIENTED_EDGE('',*,*,#4044,.T.);
#5462=ORIENTED_EDGE('',*,*,#4037,.F.);
#5463=ORIENTED_EDGE('',*,*,#4045,.T.);
#5464=ORIENTED_EDGE('',*,*,#4046,.T.);
#5465=ORIENTED_EDGE('',*,*,#4047,.T.);
#5466=ORIENTED_EDGE('',*,*,#4048,.T.);
#5467=ORIENTED_EDGE('',*,*,#4042,.F.);
#5468=ORIENTED_EDGE('',*,*,#4049,.T.);
#5469=ORIENTED_EDGE('',*,*,#4050,.T.);
#5470=ORIENTED_EDGE('',*,*,#4051,.T.);
#5471=ORIENTED_EDGE('',*,*,#4052,.T.);
#5472=ORIENTED_EDGE('',*,*,#4053,.T.);
#5473=ORIENTED_EDGE('',*,*,#4046,.F.);
#5474=ORIENTED_EDGE('',*,*,#4054,.T.);
#5475=ORIENTED_EDGE('',*,*,#4055,.T.);
#5476=ORIENTED_EDGE('',*,*,#4056,.T.);
#5477=ORIENTED_EDGE('',*,*,#4057,.T.);
#5478=ORIENTED_EDGE('',*,*,#4051,.F.);
#5479=ORIENTED_EDGE('',*,*,#4058,.T.);
#5480=ORIENTED_EDGE('',*,*,#4059,.T.);
#5481=ORIENTED_EDGE('',*,*,#4060,.T.);
#5482=ORIENTED_EDGE('',*,*,#4061,.T.);
#5483=ORIENTED_EDGE('',*,*,#4062,.T.);
#5484=ORIENTED_EDGE('',*,*,#4055,.F.);
#5485=ORIENTED_EDGE('',*,*,#4063,.T.);
#5486=ORIENTED_EDGE('',*,*,#4064,.T.);
#5487=ORIENTED_EDGE('',*,*,#4065,.T.);
#5488=ORIENTED_EDGE('',*,*,#4066,.T.);
#5489=ORIENTED_EDGE('',*,*,#4060,.F.);
#5490=ORIENTED_EDGE('',*,*,#4067,.T.);
#5491=ORIENTED_EDGE('',*,*,#4068,.T.);
#5492=ORIENTED_EDGE('',*,*,#4069,.T.);
#5493=ORIENTED_EDGE('',*,*,#4070,.T.);
#5494=ORIENTED_EDGE('',*,*,#4071,.T.);
#5495=ORIENTED_EDGE('',*,*,#4064,.F.);
#5496=ORIENTED_EDGE('',*,*,#4072,.T.);
#5497=ORIENTED_EDGE('',*,*,#4073,.T.);
#5498=ORIENTED_EDGE('',*,*,#4074,.T.);
#5499=ORIENTED_EDGE('',*,*,#4075,.T.);
#5500=ORIENTED_EDGE('',*,*,#4069,.F.);
#5501=ORIENTED_EDGE('',*,*,#4076,.T.);
#5502=ORIENTED_EDGE('',*,*,#4077,.T.);
#5503=ORIENTED_EDGE('',*,*,#4078,.T.);
#5504=ORIENTED_EDGE('',*,*,#4079,.T.);
#5505=ORIENTED_EDGE('',*,*,#4080,.T.);
#5506=ORIENTED_EDGE('',*,*,#4073,.F.);
#5507=ORIENTED_EDGE('',*,*,#4081,.T.);
#5508=ORIENTED_EDGE('',*,*,#4082,.T.);
#5509=ORIENTED_EDGE('',*,*,#4083,.T.);
#5510=ORIENTED_EDGE('',*,*,#4084,.T.);
#5511=ORIENTED_EDGE('',*,*,#4078,.F.);
#5512=ORIENTED_EDGE('',*,*,#4085,.T.);
#5513=ORIENTED_EDGE('',*,*,#4086,.T.);
#5514=ORIENTED_EDGE('',*,*,#4087,.T.);
#5515=ORIENTED_EDGE('',*,*,#4088,.T.);
#5516=ORIENTED_EDGE('',*,*,#4089,.T.);
#5517=ORIENTED_EDGE('',*,*,#4082,.F.);
#5518=ORIENTED_EDGE('',*,*,#4090,.T.);
#5519=ORIENTED_EDGE('',*,*,#4091,.T.);
#5520=ORIENTED_EDGE('',*,*,#4092,.T.);
#5521=ORIENTED_EDGE('',*,*,#4093,.T.);
#5522=ORIENTED_EDGE('',*,*,#4087,.F.);
#5523=ORIENTED_EDGE('',*,*,#4094,.T.);
#5524=ORIENTED_EDGE('',*,*,#4095,.T.);
#5525=ORIENTED_EDGE('',*,*,#4096,.T.);
#5526=ORIENTED_EDGE('',*,*,#4097,.T.);
#5527=ORIENTED_EDGE('',*,*,#4098,.T.);
#5528=ORIENTED_EDGE('',*,*,#4091,.F.);
#5529=ORIENTED_EDGE('',*,*,#4099,.T.);
#5530=ORIENTED_EDGE('',*,*,#4100,.T.);
#5531=ORIENTED_EDGE('',*,*,#4101,.T.);
#5532=ORIENTED_EDGE('',*,*,#4102,.T.);
#5533=ORIENTED_EDGE('',*,*,#4096,.F.);
#5534=ORIENTED_EDGE('',*,*,#4103,.T.);
#5535=ORIENTED_EDGE('',*,*,#4104,.T.);
#5536=ORIENTED_EDGE('',*,*,#4105,.F.);
#5537=ORIENTED_EDGE('',*,*,#4106,.T.);
#5538=ORIENTED_EDGE('',*,*,#4107,.T.);
#5539=ORIENTED_EDGE('',*,*,#4108,.F.);
#5540=ORIENTED_EDGE('',*,*,#4109,.T.);
#5541=ORIENTED_EDGE('',*,*,#4110,.T.);
#5542=ORIENTED_EDGE('',*,*,#4111,.T.);
#5543=ORIENTED_EDGE('',*,*,#4112,.T.);
#5544=ORIENTED_EDGE('',*,*,#4113,.F.);
#5545=ORIENTED_EDGE('',*,*,#4114,.F.);
#5546=ORIENTED_EDGE('',*,*,#4115,.T.);
#5547=ORIENTED_EDGE('',*,*,#4116,.T.);
#5548=ORIENTED_EDGE('',*,*,#4117,.T.);
#5549=ORIENTED_EDGE('',*,*,#4111,.F.);
#5550=ORIENTED_EDGE('',*,*,#4118,.F.);
#5551=ORIENTED_EDGE('',*,*,#4119,.F.);
#5552=ORIENTED_EDGE('',*,*,#4120,.T.);
#5553=ORIENTED_EDGE('',*,*,#4121,.T.);
#5554=ORIENTED_EDGE('',*,*,#4122,.T.);
#5555=ORIENTED_EDGE('',*,*,#4115,.F.);
#5556=ORIENTED_EDGE('',*,*,#4123,.F.);
#5557=ORIENTED_EDGE('',*,*,#4124,.F.);
#5558=ORIENTED_EDGE('',*,*,#4125,.T.);
#5559=ORIENTED_EDGE('',*,*,#4126,.T.);
#5560=ORIENTED_EDGE('',*,*,#4127,.T.);
#5561=ORIENTED_EDGE('',*,*,#4120,.F.);
#5562=ORIENTED_EDGE('',*,*,#4128,.F.);
#5563=ORIENTED_EDGE('',*,*,#4129,.F.);
#5564=ORIENTED_EDGE('',*,*,#4130,.T.);
#5565=ORIENTED_EDGE('',*,*,#4131,.T.);
#5566=ORIENTED_EDGE('',*,*,#4132,.T.);
#5567=ORIENTED_EDGE('',*,*,#4125,.F.);
#5568=ORIENTED_EDGE('',*,*,#4133,.F.);
#5569=ORIENTED_EDGE('',*,*,#4134,.F.);
#5570=ORIENTED_EDGE('',*,*,#4135,.T.);
#5571=ORIENTED_EDGE('',*,*,#4136,.T.);
#5572=ORIENTED_EDGE('',*,*,#4137,.T.);
#5573=ORIENTED_EDGE('',*,*,#4130,.F.);
#5574=ORIENTED_EDGE('',*,*,#4138,.F.);
#5575=ORIENTED_EDGE('',*,*,#4139,.F.);
#5576=ORIENTED_EDGE('',*,*,#4140,.T.);
#5577=ORIENTED_EDGE('',*,*,#4141,.T.);
#5578=ORIENTED_EDGE('',*,*,#4142,.T.);
#5579=ORIENTED_EDGE('',*,*,#4135,.F.);
#5580=ORIENTED_EDGE('',*,*,#4143,.F.);
#5581=ORIENTED_EDGE('',*,*,#4144,.F.);
#5582=ORIENTED_EDGE('',*,*,#4145,.T.);
#5583=ORIENTED_EDGE('',*,*,#4146,.T.);
#5584=ORIENTED_EDGE('',*,*,#4147,.T.);
#5585=ORIENTED_EDGE('',*,*,#4140,.F.);
#5586=ORIENTED_EDGE('',*,*,#4148,.F.);
#5587=ORIENTED_EDGE('',*,*,#4149,.F.);
#5588=ORIENTED_EDGE('',*,*,#4150,.T.);
#5589=ORIENTED_EDGE('',*,*,#4151,.T.);
#5590=ORIENTED_EDGE('',*,*,#4152,.T.);
#5591=ORIENTED_EDGE('',*,*,#4145,.F.);
#5592=ORIENTED_EDGE('',*,*,#4153,.F.);
#5593=ORIENTED_EDGE('',*,*,#4154,.F.);
#5594=ORIENTED_EDGE('',*,*,#4155,.T.);
#5595=ORIENTED_EDGE('',*,*,#4156,.T.);
#5596=ORIENTED_EDGE('',*,*,#4157,.T.);
#5597=ORIENTED_EDGE('',*,*,#4150,.F.);
#5598=ORIENTED_EDGE('',*,*,#4158,.F.);
#5599=ORIENTED_EDGE('',*,*,#4159,.F.);
#5600=ORIENTED_EDGE('',*,*,#4160,.T.);
#5601=ORIENTED_EDGE('',*,*,#4161,.T.);
#5602=ORIENTED_EDGE('',*,*,#4162,.T.);
#5603=ORIENTED_EDGE('',*,*,#4155,.F.);
#5604=ORIENTED_EDGE('',*,*,#4163,.F.);
#5605=ORIENTED_EDGE('',*,*,#4164,.F.);
#5606=ORIENTED_EDGE('',*,*,#4165,.T.);
#5607=ORIENTED_EDGE('',*,*,#4166,.T.);
#5608=ORIENTED_EDGE('',*,*,#4167,.T.);
#5609=ORIENTED_EDGE('',*,*,#4160,.F.);
#5610=ORIENTED_EDGE('',*,*,#4168,.F.);
#5611=ORIENTED_EDGE('',*,*,#4169,.F.);
#5612=ORIENTED_EDGE('',*,*,#4170,.T.);
#5613=ORIENTED_EDGE('',*,*,#4171,.T.);
#5614=ORIENTED_EDGE('',*,*,#4172,.T.);
#5615=ORIENTED_EDGE('',*,*,#4165,.F.);
#5616=ORIENTED_EDGE('',*,*,#4173,.F.);
#5617=ORIENTED_EDGE('',*,*,#4174,.F.);
#5618=ORIENTED_EDGE('',*,*,#4175,.T.);
#5619=ORIENTED_EDGE('',*,*,#4176,.T.);
#5620=ORIENTED_EDGE('',*,*,#4177,.T.);
#5621=ORIENTED_EDGE('',*,*,#4170,.F.);
#5622=ORIENTED_EDGE('',*,*,#4178,.F.);
#5623=ORIENTED_EDGE('',*,*,#4179,.F.);
#5624=ORIENTED_EDGE('',*,*,#4180,.T.);
#5625=ORIENTED_EDGE('',*,*,#4181,.T.);
#5626=ORIENTED_EDGE('',*,*,#4182,.T.);
#5627=ORIENTED_EDGE('',*,*,#4175,.F.);
#5628=ORIENTED_EDGE('',*,*,#4183,.F.);
#5629=ORIENTED_EDGE('',*,*,#4184,.F.);
#5630=ORIENTED_EDGE('',*,*,#4185,.T.);
#5631=ORIENTED_EDGE('',*,*,#4186,.T.);
#5632=ORIENTED_EDGE('',*,*,#4187,.T.);
#5633=ORIENTED_EDGE('',*,*,#4180,.F.);
#5634=ORIENTED_EDGE('',*,*,#4188,.F.);
#5635=ORIENTED_EDGE('',*,*,#4189,.F.);
#5636=ORIENTED_EDGE('',*,*,#4190,.T.);
#5637=ORIENTED_EDGE('',*,*,#4191,.T.);
#5638=ORIENTED_EDGE('',*,*,#4192,.T.);
#5639=ORIENTED_EDGE('',*,*,#4185,.F.);
#5640=ORIENTED_EDGE('',*,*,#4193,.F.);
#5641=ORIENTED_EDGE('',*,*,#4194,.F.);
#5642=ORIENTED_EDGE('',*,*,#4195,.T.);
#5643=ORIENTED_EDGE('',*,*,#4196,.T.);
#5644=ORIENTED_EDGE('',*,*,#4197,.T.);
#5645=ORIENTED_EDGE('',*,*,#4190,.F.);
#5646=ORIENTED_EDGE('',*,*,#4198,.F.);
#5647=ORIENTED_EDGE('',*,*,#4199,.F.);
#5648=ORIENTED_EDGE('',*,*,#4200,.F.);
#5649=ORIENTED_EDGE('',*,*,#4201,.F.);
#5650=ORIENTED_EDGE('',*,*,#4202,.F.);
#5651=ORIENTED_EDGE('',*,*,#4203,.F.);
#5652=ORIENTED_EDGE('',*,*,#4204,.T.);
#5653=ORIENTED_EDGE('',*,*,#4205,.T.);
#5654=ORIENTED_EDGE('',*,*,#4206,.T.);
#5655=ORIENTED_EDGE('',*,*,#4207,.T.);
#5656=ORIENTED_EDGE('',*,*,#4208,.T.);
#5657=ORIENTED_EDGE('',*,*,#4209,.T.);
#5658=ORIENTED_EDGE('',*,*,#4210,.T.);
#5659=ORIENTED_EDGE('',*,*,#4209,.F.);
#5660=ORIENTED_EDGE('',*,*,#4211,.T.);
#5661=ORIENTED_EDGE('',*,*,#4212,.T.);
#5662=ORIENTED_EDGE('',*,*,#4213,.T.);
#5663=ORIENTED_EDGE('',*,*,#4214,.T.);
#5664=ORIENTED_EDGE('',*,*,#4215,.T.);
#5665=ORIENTED_EDGE('',*,*,#4206,.F.);
#5666=ORIENTED_EDGE('',*,*,#4216,.T.);
#5667=ORIENTED_EDGE('',*,*,#4217,.T.);
#5668=ORIENTED_EDGE('',*,*,#4218,.T.);
#5669=ORIENTED_EDGE('',*,*,#4219,.T.);
#5670=ORIENTED_EDGE('',*,*,#4220,.T.);
#5671=ORIENTED_EDGE('',*,*,#4213,.F.);
#5672=ORIENTED_EDGE('',*,*,#4221,.T.);
#5673=ORIENTED_EDGE('',*,*,#4222,.T.);
#5674=ORIENTED_EDGE('',*,*,#4223,.T.);
#5675=ORIENTED_EDGE('',*,*,#4224,.T.);
#5676=ORIENTED_EDGE('',*,*,#4225,.T.);
#5677=ORIENTED_EDGE('',*,*,#4218,.F.);
#5678=ORIENTED_EDGE('',*,*,#4226,.T.);
#5679=ORIENTED_EDGE('',*,*,#4227,.T.);
#5680=ORIENTED_EDGE('',*,*,#4228,.T.);
#5681=ORIENTED_EDGE('',*,*,#4229,.T.);
#5682=ORIENTED_EDGE('',*,*,#4223,.F.);
#5683=ORIENTED_EDGE('',*,*,#4230,.T.);
#5684=ORIENTED_EDGE('',*,*,#4231,.T.);
#5685=ORIENTED_EDGE('',*,*,#4232,.T.);
#5686=ORIENTED_EDGE('',*,*,#4233,.T.);
#5687=ORIENTED_EDGE('',*,*,#4234,.T.);
#5688=ORIENTED_EDGE('',*,*,#4227,.F.);
#5689=ORIENTED_EDGE('',*,*,#4235,.T.);
#5690=ORIENTED_EDGE('',*,*,#4236,.T.);
#5691=ORIENTED_EDGE('',*,*,#4237,.T.);
#5692=ORIENTED_EDGE('',*,*,#4238,.T.);
#5693=ORIENTED_EDGE('',*,*,#4232,.F.);
#5694=ORIENTED_EDGE('',*,*,#4239,.T.);
#5695=ORIENTED_EDGE('',*,*,#4240,.T.);
#5696=ORIENTED_EDGE('',*,*,#4241,.T.);
#5697=ORIENTED_EDGE('',*,*,#4242,.T.);
#5698=ORIENTED_EDGE('',*,*,#4243,.T.);
#5699=ORIENTED_EDGE('',*,*,#4236,.F.);
#5700=ORIENTED_EDGE('',*,*,#4244,.T.);
#5701=ORIENTED_EDGE('',*,*,#4245,.T.);
#5702=ORIENTED_EDGE('',*,*,#4246,.T.);
#5703=ORIENTED_EDGE('',*,*,#4247,.T.);
#5704=ORIENTED_EDGE('',*,*,#4241,.F.);
#5705=ORIENTED_EDGE('',*,*,#4248,.T.);
#5706=ORIENTED_EDGE('',*,*,#4249,.T.);
#5707=ORIENTED_EDGE('',*,*,#4250,.T.);
#5708=ORIENTED_EDGE('',*,*,#4251,.T.);
#5709=ORIENTED_EDGE('',*,*,#4252,.T.);
#5710=ORIENTED_EDGE('',*,*,#4245,.F.);
#5711=ORIENTED_EDGE('',*,*,#4253,.T.);
#5712=ORIENTED_EDGE('',*,*,#4254,.T.);
#5713=ORIENTED_EDGE('',*,*,#4255,.T.);
#5714=ORIENTED_EDGE('',*,*,#4256,.T.);
#5715=ORIENTED_EDGE('',*,*,#4250,.F.);
#5716=ORIENTED_EDGE('',*,*,#4257,.T.);
#5717=ORIENTED_EDGE('',*,*,#4258,.T.);
#5718=ORIENTED_EDGE('',*,*,#4259,.T.);
#5719=ORIENTED_EDGE('',*,*,#4260,.T.);
#5720=ORIENTED_EDGE('',*,*,#4261,.T.);
#5721=ORIENTED_EDGE('',*,*,#4254,.F.);
#5722=ORIENTED_EDGE('',*,*,#4262,.T.);
#5723=ORIENTED_EDGE('',*,*,#4263,.T.);
#5724=ORIENTED_EDGE('',*,*,#4264,.T.);
#5725=ORIENTED_EDGE('',*,*,#4265,.T.);
#5726=ORIENTED_EDGE('',*,*,#4259,.F.);
#5727=ORIENTED_EDGE('',*,*,#4266,.T.);
#5728=ORIENTED_EDGE('',*,*,#4267,.T.);
#5729=ORIENTED_EDGE('',*,*,#4268,.T.);
#5730=ORIENTED_EDGE('',*,*,#4269,.T.);
#5731=ORIENTED_EDGE('',*,*,#4270,.T.);
#5732=ORIENTED_EDGE('',*,*,#4263,.F.);
#5733=ORIENTED_EDGE('',*,*,#4271,.T.);
#5734=ORIENTED_EDGE('',*,*,#4272,.T.);
#5735=ORIENTED_EDGE('',*,*,#4273,.T.);
#5736=ORIENTED_EDGE('',*,*,#4274,.T.);
#5737=ORIENTED_EDGE('',*,*,#4268,.F.);
#5738=ORIENTED_EDGE('',*,*,#4275,.T.);
#5739=ORIENTED_EDGE('',*,*,#4276,.T.);
#5740=ORIENTED_EDGE('',*,*,#4277,.T.);
#5741=ORIENTED_EDGE('',*,*,#4278,.T.);
#5742=ORIENTED_EDGE('',*,*,#4279,.T.);
#5743=ORIENTED_EDGE('',*,*,#4272,.F.);
#5744=ORIENTED_EDGE('',*,*,#4280,.T.);
#5745=ORIENTED_EDGE('',*,*,#4281,.T.);
#5746=ORIENTED_EDGE('',*,*,#4282,.T.);
#5747=ORIENTED_EDGE('',*,*,#4283,.T.);
#5748=ORIENTED_EDGE('',*,*,#4277,.F.);
#5749=ORIENTED_EDGE('',*,*,#4284,.T.);
#5750=ORIENTED_EDGE('',*,*,#4285,.T.);
#5751=ORIENTED_EDGE('',*,*,#4286,.T.);
#5752=ORIENTED_EDGE('',*,*,#4287,.T.);
#5753=ORIENTED_EDGE('',*,*,#4288,.T.);
#5754=ORIENTED_EDGE('',*,*,#4281,.F.);
#5755=ORIENTED_EDGE('',*,*,#4289,.T.);
#5756=ORIENTED_EDGE('',*,*,#4290,.F.);
#5757=ORIENTED_EDGE('',*,*,#4291,.T.);
#5758=ORIENTED_EDGE('',*,*,#4292,.T.);
#5759=ORIENTED_EDGE('',*,*,#4293,.F.);
#5760=ORIENTED_EDGE('',*,*,#4294,.T.);
#5761=ORIENTED_EDGE('',*,*,#4295,.T.);
#5762=ORIENTED_EDGE('',*,*,#4290,.T.);
#5763=ORIENTED_EDGE('',*,*,#4296,.T.);
#5764=ORIENTED_EDGE('',*,*,#4297,.T.);
#5765=ORIENTED_EDGE('',*,*,#4286,.F.);
#5766=ORIENTED_EDGE('',*,*,#4298,.T.);
#5767=ORIENTED_EDGE('',*,*,#4299,.T.);
#5768=ORIENTED_EDGE('',*,*,#4200,.T.);
#5769=ORIENTED_EDGE('',*,*,#4300,.T.);
#5770=ORIENTED_EDGE('',*,*,#4301,.T.);
#5771=ORIENTED_EDGE('',*,*,#4195,.F.);
#5772=ORIENTED_EDGE('',*,*,#4302,.F.);
#5773=ORIENTED_EDGE('',*,*,#4303,.F.);
#5774=ORIENTED_EDGE('',*,*,#4105,.T.);
#5775=ORIENTED_EDGE('',*,*,#4304,.T.);
#5776=ORIENTED_EDGE('',*,*,#4305,.T.);
#5777=ORIENTED_EDGE('',*,*,#4100,.F.);
#5778=ORIENTED_EDGE('',*,*,#4306,.T.);
#5779=ORIENTED_EDGE('',*,*,#4015,.T.);
#5780=ORIENTED_EDGE('',*,*,#4307,.T.);
#5781=ORIENTED_EDGE('',*,*,#4308,.T.);
#5782=ORIENTED_EDGE('',*,*,#4010,.F.);
#5783=ORIENTED_EDGE('',*,*,#4309,.F.);
#5784=ORIENTED_EDGE('',*,*,#4310,.F.);
#5785=ORIENTED_EDGE('',*,*,#4023,.F.);
#5786=ORIENTED_EDGE('',*,*,#4311,.T.);
#5787=ORIENTED_EDGE('',*,*,#3928,.T.);
#5788=ORIENTED_EDGE('',*,*,#4312,.T.);
#5789=ORIENTED_EDGE('',*,*,#4026,.F.);
#5790=ORIENTED_EDGE('',*,*,#4312,.F.);
#5791=ORIENTED_EDGE('',*,*,#3927,.F.);
#5792=ORIENTED_EDGE('',*,*,#3932,.F.);
#5793=ORIENTED_EDGE('',*,*,#3931,.F.);
#5794=ORIENTED_EDGE('',*,*,#3937,.F.);
#5795=ORIENTED_EDGE('',*,*,#3936,.F.);
#5796=ORIENTED_EDGE('',*,*,#3942,.F.);
#5797=ORIENTED_EDGE('',*,*,#3941,.F.);
#5798=ORIENTED_EDGE('',*,*,#3947,.F.);
#5799=ORIENTED_EDGE('',*,*,#3946,.F.);
#5800=ORIENTED_EDGE('',*,*,#3952,.F.);
#5801=ORIENTED_EDGE('',*,*,#3951,.F.);
#5802=ORIENTED_EDGE('',*,*,#3957,.F.);
#5803=ORIENTED_EDGE('',*,*,#3956,.F.);
#5804=ORIENTED_EDGE('',*,*,#3962,.F.);
#5805=ORIENTED_EDGE('',*,*,#3961,.F.);
#5806=ORIENTED_EDGE('',*,*,#3967,.F.);
#5807=ORIENTED_EDGE('',*,*,#3966,.F.);
#5808=ORIENTED_EDGE('',*,*,#3972,.F.);
#5809=ORIENTED_EDGE('',*,*,#3971,.F.);
#5810=ORIENTED_EDGE('',*,*,#3977,.F.);
#5811=ORIENTED_EDGE('',*,*,#3976,.F.);
#5812=ORIENTED_EDGE('',*,*,#3982,.F.);
#5813=ORIENTED_EDGE('',*,*,#3981,.F.);
#5814=ORIENTED_EDGE('',*,*,#3987,.F.);
#5815=ORIENTED_EDGE('',*,*,#3986,.F.);
#5816=ORIENTED_EDGE('',*,*,#3992,.F.);
#5817=ORIENTED_EDGE('',*,*,#3991,.F.);
#5818=ORIENTED_EDGE('',*,*,#3997,.F.);
#5819=ORIENTED_EDGE('',*,*,#3996,.F.);
#5820=ORIENTED_EDGE('',*,*,#4002,.F.);
#5821=ORIENTED_EDGE('',*,*,#4001,.F.);
#5822=ORIENTED_EDGE('',*,*,#4007,.F.);
#5823=ORIENTED_EDGE('',*,*,#4006,.F.);
#5824=ORIENTED_EDGE('',*,*,#4012,.F.);
#5825=ORIENTED_EDGE('',*,*,#4011,.F.);
#5826=ORIENTED_EDGE('',*,*,#4308,.F.);
#5827=ORIENTED_EDGE('',*,*,#4307,.F.);
#5828=ORIENTED_EDGE('',*,*,#4020,.F.);
#5829=ORIENTED_EDGE('',*,*,#4019,.F.);
#5830=ORIENTED_EDGE('',*,*,#4313,.F.);
#5831=ORIENTED_EDGE('',*,*,#4107,.F.);
#5832=ORIENTED_EDGE('',*,*,#4106,.F.);
#5833=ORIENTED_EDGE('',*,*,#4306,.F.);
#5834=ORIENTED_EDGE('',*,*,#4104,.F.);
#5835=ORIENTED_EDGE('',*,*,#4103,.F.);
#5836=ORIENTED_EDGE('',*,*,#4099,.F.);
#5837=ORIENTED_EDGE('',*,*,#4095,.F.);
#5838=ORIENTED_EDGE('',*,*,#4094,.F.);
#5839=ORIENTED_EDGE('',*,*,#4090,.F.);
#5840=ORIENTED_EDGE('',*,*,#4086,.F.);
#5841=ORIENTED_EDGE('',*,*,#4085,.F.);
#5842=ORIENTED_EDGE('',*,*,#4081,.F.);
#5843=ORIENTED_EDGE('',*,*,#4077,.F.);
#5844=ORIENTED_EDGE('',*,*,#4076,.F.);
#5845=ORIENTED_EDGE('',*,*,#4072,.F.);
#5846=ORIENTED_EDGE('',*,*,#4068,.F.);
#5847=ORIENTED_EDGE('',*,*,#4067,.F.);
#5848=ORIENTED_EDGE('',*,*,#4063,.F.);
#5849=ORIENTED_EDGE('',*,*,#4059,.F.);
#5850=ORIENTED_EDGE('',*,*,#4058,.F.);
#5851=ORIENTED_EDGE('',*,*,#4054,.F.);
#5852=ORIENTED_EDGE('',*,*,#4050,.F.);
#5853=ORIENTED_EDGE('',*,*,#4049,.F.);
#5854=ORIENTED_EDGE('',*,*,#4045,.F.);
#5855=ORIENTED_EDGE('',*,*,#4041,.F.);
#5856=ORIENTED_EDGE('',*,*,#4040,.F.);
#5857=ORIENTED_EDGE('',*,*,#4036,.F.);
#5858=ORIENTED_EDGE('',*,*,#4032,.F.);
#5859=ORIENTED_EDGE('',*,*,#4031,.F.);
#5860=ORIENTED_EDGE('',*,*,#4027,.F.);
#5861=ORIENTED_EDGE('',*,*,#4311,.F.);
#5862=ORIENTED_EDGE('',*,*,#4022,.F.);
#5863=ORIENTED_EDGE('',*,*,#4030,.F.);
#5864=ORIENTED_EDGE('',*,*,#4029,.F.);
#5865=ORIENTED_EDGE('',*,*,#4035,.F.);
#5866=ORIENTED_EDGE('',*,*,#4034,.F.);
#5867=ORIENTED_EDGE('',*,*,#4039,.F.);
#5868=ORIENTED_EDGE('',*,*,#4038,.F.);
#5869=ORIENTED_EDGE('',*,*,#4044,.F.);
#5870=ORIENTED_EDGE('',*,*,#4043,.F.);
#5871=ORIENTED_EDGE('',*,*,#4048,.F.);
#5872=ORIENTED_EDGE('',*,*,#4047,.F.);
#5873=ORIENTED_EDGE('',*,*,#4053,.F.);
#5874=ORIENTED_EDGE('',*,*,#4052,.F.);
#5875=ORIENTED_EDGE('',*,*,#4057,.F.);
#5876=ORIENTED_EDGE('',*,*,#4056,.F.);
#5877=ORIENTED_EDGE('',*,*,#4062,.F.);
#5878=ORIENTED_EDGE('',*,*,#4061,.F.);
#5879=ORIENTED_EDGE('',*,*,#4066,.F.);
#5880=ORIENTED_EDGE('',*,*,#4065,.F.);
#5881=ORIENTED_EDGE('',*,*,#4071,.F.);
#5882=ORIENTED_EDGE('',*,*,#4070,.F.);
#5883=ORIENTED_EDGE('',*,*,#4075,.F.);
#5884=ORIENTED_EDGE('',*,*,#4074,.F.);
#5885=ORIENTED_EDGE('',*,*,#4080,.F.);
#5886=ORIENTED_EDGE('',*,*,#4079,.F.);
#5887=ORIENTED_EDGE('',*,*,#4084,.F.);
#5888=ORIENTED_EDGE('',*,*,#4083,.F.);
#5889=ORIENTED_EDGE('',*,*,#4089,.F.);
#5890=ORIENTED_EDGE('',*,*,#4088,.F.);
#5891=ORIENTED_EDGE('',*,*,#4093,.F.);
#5892=ORIENTED_EDGE('',*,*,#4092,.F.);
#5893=ORIENTED_EDGE('',*,*,#4098,.F.);
#5894=ORIENTED_EDGE('',*,*,#4097,.F.);
#5895=ORIENTED_EDGE('',*,*,#4102,.F.);
#5896=ORIENTED_EDGE('',*,*,#4101,.F.);
#5897=ORIENTED_EDGE('',*,*,#4305,.F.);
#5898=ORIENTED_EDGE('',*,*,#4304,.F.);
#5899=ORIENTED_EDGE('',*,*,#4110,.F.);
#5900=ORIENTED_EDGE('',*,*,#4109,.F.);
#5901=ORIENTED_EDGE('',*,*,#4314,.F.);
#5902=ORIENTED_EDGE('',*,*,#4017,.T.);
#5903=ORIENTED_EDGE('',*,*,#4016,.T.);
#5904=ORIENTED_EDGE('',*,*,#4310,.T.);
#5905=ORIENTED_EDGE('',*,*,#4309,.T.);
#5906=ORIENTED_EDGE('',*,*,#4014,.T.);
#5907=ORIENTED_EDGE('',*,*,#4013,.T.);
#5908=ORIENTED_EDGE('',*,*,#4009,.T.);
#5909=ORIENTED_EDGE('',*,*,#4008,.T.);
#5910=ORIENTED_EDGE('',*,*,#4004,.T.);
#5911=ORIENTED_EDGE('',*,*,#4003,.T.);
#5912=ORIENTED_EDGE('',*,*,#3999,.T.);
#5913=ORIENTED_EDGE('',*,*,#3998,.T.);
#5914=ORIENTED_EDGE('',*,*,#3994,.T.);
#5915=ORIENTED_EDGE('',*,*,#3993,.T.);
#5916=ORIENTED_EDGE('',*,*,#3989,.T.);
#5917=ORIENTED_EDGE('',*,*,#3988,.T.);
#5918=ORIENTED_EDGE('',*,*,#3984,.T.);
#5919=ORIENTED_EDGE('',*,*,#3983,.T.);
#5920=ORIENTED_EDGE('',*,*,#3979,.T.);
#5921=ORIENTED_EDGE('',*,*,#3978,.T.);
#5922=ORIENTED_EDGE('',*,*,#3974,.T.);
#5923=ORIENTED_EDGE('',*,*,#3973,.T.);
#5924=ORIENTED_EDGE('',*,*,#3969,.T.);
#5925=ORIENTED_EDGE('',*,*,#3968,.T.);
#5926=ORIENTED_EDGE('',*,*,#3964,.T.);
#5927=ORIENTED_EDGE('',*,*,#3963,.T.);
#5928=ORIENTED_EDGE('',*,*,#3959,.T.);
#5929=ORIENTED_EDGE('',*,*,#3958,.T.);
#5930=ORIENTED_EDGE('',*,*,#3954,.T.);
#5931=ORIENTED_EDGE('',*,*,#3953,.T.);
#5932=ORIENTED_EDGE('',*,*,#3949,.T.);
#5933=ORIENTED_EDGE('',*,*,#3948,.T.);
#5934=ORIENTED_EDGE('',*,*,#3944,.T.);
#5935=ORIENTED_EDGE('',*,*,#3943,.T.);
#5936=ORIENTED_EDGE('',*,*,#3939,.T.);
#5937=ORIENTED_EDGE('',*,*,#3938,.T.);
#5938=ORIENTED_EDGE('',*,*,#3934,.T.);
#5939=ORIENTED_EDGE('',*,*,#3933,.T.);
#5940=ORIENTED_EDGE('',*,*,#3929,.T.);
#5941=ORIENTED_EDGE('',*,*,#4025,.F.);
#5942=ORIENTED_EDGE('',*,*,#4208,.F.);
#5943=ORIENTED_EDGE('',*,*,#4315,.T.);
#5944=ORIENTED_EDGE('',*,*,#4113,.T.);
#5945=ORIENTED_EDGE('',*,*,#4316,.T.);
#5946=ORIENTED_EDGE('',*,*,#4211,.F.);
#5947=ORIENTED_EDGE('',*,*,#4316,.F.);
#5948=ORIENTED_EDGE('',*,*,#4112,.F.);
#5949=ORIENTED_EDGE('',*,*,#4117,.F.);
#5950=ORIENTED_EDGE('',*,*,#4116,.F.);
#5951=ORIENTED_EDGE('',*,*,#4122,.F.);
#5952=ORIENTED_EDGE('',*,*,#4121,.F.);
#5953=ORIENTED_EDGE('',*,*,#4127,.F.);
#5954=ORIENTED_EDGE('',*,*,#4126,.F.);
#5955=ORIENTED_EDGE('',*,*,#4132,.F.);
#5956=ORIENTED_EDGE('',*,*,#4131,.F.);
#5957=ORIENTED_EDGE('',*,*,#4137,.F.);
#5958=ORIENTED_EDGE('',*,*,#4136,.F.);
#5959=ORIENTED_EDGE('',*,*,#4142,.F.);
#5960=ORIENTED_EDGE('',*,*,#4141,.F.);
#5961=ORIENTED_EDGE('',*,*,#4147,.F.);
#5962=ORIENTED_EDGE('',*,*,#4146,.F.);
#5963=ORIENTED_EDGE('',*,*,#4152,.F.);
#5964=ORIENTED_EDGE('',*,*,#4151,.F.);
#5965=ORIENTED_EDGE('',*,*,#4157,.F.);
#5966=ORIENTED_EDGE('',*,*,#4156,.F.);
#5967=ORIENTED_EDGE('',*,*,#4162,.F.);
#5968=ORIENTED_EDGE('',*,*,#4161,.F.);
#5969=ORIENTED_EDGE('',*,*,#4167,.F.);
#5970=ORIENTED_EDGE('',*,*,#4166,.F.);
#5971=ORIENTED_EDGE('',*,*,#4172,.F.);
#5972=ORIENTED_EDGE('',*,*,#4171,.F.);
#5973=ORIENTED_EDGE('',*,*,#4177,.F.);
#5974=ORIENTED_EDGE('',*,*,#4176,.F.);
#5975=ORIENTED_EDGE('',*,*,#4182,.F.);
#5976=ORIENTED_EDGE('',*,*,#4181,.F.);
#5977=ORIENTED_EDGE('',*,*,#4187,.F.);
#5978=ORIENTED_EDGE('',*,*,#4186,.F.);
#5979=ORIENTED_EDGE('',*,*,#4192,.F.);
#5980=ORIENTED_EDGE('',*,*,#4191,.F.);
#5981=ORIENTED_EDGE('',*,*,#4197,.F.);
#5982=ORIENTED_EDGE('',*,*,#4196,.F.);
#5983=ORIENTED_EDGE('',*,*,#4301,.F.);
#5984=ORIENTED_EDGE('',*,*,#4300,.F.);
#5985=ORIENTED_EDGE('',*,*,#4205,.F.);
#5986=ORIENTED_EDGE('',*,*,#4204,.F.);
#5987=ORIENTED_EDGE('',*,*,#4317,.F.);
#5988=ORIENTED_EDGE('',*,*,#4292,.F.);
#5989=ORIENTED_EDGE('',*,*,#4291,.F.);
#5990=ORIENTED_EDGE('',*,*,#4299,.F.);
#5991=ORIENTED_EDGE('',*,*,#4298,.F.);
#5992=ORIENTED_EDGE('',*,*,#4289,.F.);
#5993=ORIENTED_EDGE('',*,*,#4285,.F.);
#5994=ORIENTED_EDGE('',*,*,#4284,.F.);
#5995=ORIENTED_EDGE('',*,*,#4280,.F.);
#5996=ORIENTED_EDGE('',*,*,#4276,.F.);
#5997=ORIENTED_EDGE('',*,*,#4275,.F.);
#5998=ORIENTED_EDGE('',*,*,#4271,.F.);
#5999=ORIENTED_EDGE('',*,*,#4267,.F.);
#6000=ORIENTED_EDGE('',*,*,#4266,.F.);
#6001=ORIENTED_EDGE('',*,*,#4262,.F.);
#6002=ORIENTED_EDGE('',*,*,#4258,.F.);
#6003=ORIENTED_EDGE('',*,*,#4257,.F.);
#6004=ORIENTED_EDGE('',*,*,#4253,.F.);
#6005=ORIENTED_EDGE('',*,*,#4249,.F.);
#6006=ORIENTED_EDGE('',*,*,#4248,.F.);
#6007=ORIENTED_EDGE('',*,*,#4244,.F.);
#6008=ORIENTED_EDGE('',*,*,#4240,.F.);
#6009=ORIENTED_EDGE('',*,*,#4239,.F.);
#6010=ORIENTED_EDGE('',*,*,#4235,.F.);
#6011=ORIENTED_EDGE('',*,*,#4231,.F.);
#6012=ORIENTED_EDGE('',*,*,#4230,.F.);
#6013=ORIENTED_EDGE('',*,*,#4226,.F.);
#6014=ORIENTED_EDGE('',*,*,#4222,.F.);
#6015=ORIENTED_EDGE('',*,*,#4221,.F.);
#6016=ORIENTED_EDGE('',*,*,#4217,.F.);
#6017=ORIENTED_EDGE('',*,*,#4216,.F.);
#6018=ORIENTED_EDGE('',*,*,#4212,.F.);
#6019=ORIENTED_EDGE('',*,*,#4315,.F.);
#6020=ORIENTED_EDGE('',*,*,#4207,.F.);
#6021=ORIENTED_EDGE('',*,*,#4215,.F.);
#6022=ORIENTED_EDGE('',*,*,#4214,.F.);
#6023=ORIENTED_EDGE('',*,*,#4220,.F.);
#6024=ORIENTED_EDGE('',*,*,#4219,.F.);
#6025=ORIENTED_EDGE('',*,*,#4225,.F.);
#6026=ORIENTED_EDGE('',*,*,#4224,.F.);
#6027=ORIENTED_EDGE('',*,*,#4229,.F.);
#6028=ORIENTED_EDGE('',*,*,#4228,.F.);
#6029=ORIENTED_EDGE('',*,*,#4234,.F.);
#6030=ORIENTED_EDGE('',*,*,#4233,.F.);
#6031=ORIENTED_EDGE('',*,*,#4238,.F.);
#6032=ORIENTED_EDGE('',*,*,#4237,.F.);
#6033=ORIENTED_EDGE('',*,*,#4243,.F.);
#6034=ORIENTED_EDGE('',*,*,#4242,.F.);
#6035=ORIENTED_EDGE('',*,*,#4247,.F.);
#6036=ORIENTED_EDGE('',*,*,#4246,.F.);
#6037=ORIENTED_EDGE('',*,*,#4252,.F.);
#6038=ORIENTED_EDGE('',*,*,#4251,.F.);
#6039=ORIENTED_EDGE('',*,*,#4256,.F.);
#6040=ORIENTED_EDGE('',*,*,#4255,.F.);
#6041=ORIENTED_EDGE('',*,*,#4261,.F.);
#6042=ORIENTED_EDGE('',*,*,#4260,.F.);
#6043=ORIENTED_EDGE('',*,*,#4265,.F.);
#6044=ORIENTED_EDGE('',*,*,#4264,.F.);
#6045=ORIENTED_EDGE('',*,*,#4270,.F.);
#6046=ORIENTED_EDGE('',*,*,#4269,.F.);
#6047=ORIENTED_EDGE('',*,*,#4274,.F.);
#6048=ORIENTED_EDGE('',*,*,#4273,.F.);
#6049=ORIENTED_EDGE('',*,*,#4279,.F.);
#6050=ORIENTED_EDGE('',*,*,#4278,.F.);
#6051=ORIENTED_EDGE('',*,*,#4283,.F.);
#6052=ORIENTED_EDGE('',*,*,#4282,.F.);
#6053=ORIENTED_EDGE('',*,*,#4288,.F.);
#6054=ORIENTED_EDGE('',*,*,#4287,.F.);
#6055=ORIENTED_EDGE('',*,*,#4297,.F.);
#6056=ORIENTED_EDGE('',*,*,#4296,.F.);
#6057=ORIENTED_EDGE('',*,*,#4295,.F.);
#6058=ORIENTED_EDGE('',*,*,#4294,.F.);
#6059=ORIENTED_EDGE('',*,*,#4318,.F.);
#6060=ORIENTED_EDGE('',*,*,#4202,.T.);
#6061=ORIENTED_EDGE('',*,*,#4201,.T.);
#6062=ORIENTED_EDGE('',*,*,#4303,.T.);
#6063=ORIENTED_EDGE('',*,*,#4302,.T.);
#6064=ORIENTED_EDGE('',*,*,#4199,.T.);
#6065=ORIENTED_EDGE('',*,*,#4198,.T.);
#6066=ORIENTED_EDGE('',*,*,#4194,.T.);
#6067=ORIENTED_EDGE('',*,*,#4193,.T.);
#6068=ORIENTED_EDGE('',*,*,#4189,.T.);
#6069=ORIENTED_EDGE('',*,*,#4188,.T.);
#6070=ORIENTED_EDGE('',*,*,#4184,.T.);
#6071=ORIENTED_EDGE('',*,*,#4183,.T.);
#6072=ORIENTED_EDGE('',*,*,#4179,.T.);
#6073=ORIENTED_EDGE('',*,*,#4178,.T.);
#6074=ORIENTED_EDGE('',*,*,#4174,.T.);
#6075=ORIENTED_EDGE('',*,*,#4173,.T.);
#6076=ORIENTED_EDGE('',*,*,#4169,.T.);
#6077=ORIENTED_EDGE('',*,*,#4168,.T.);
#6078=ORIENTED_EDGE('',*,*,#4164,.T.);
#6079=ORIENTED_EDGE('',*,*,#4163,.T.);
#6080=ORIENTED_EDGE('',*,*,#4159,.T.);
#6081=ORIENTED_EDGE('',*,*,#4158,.T.);
#6082=ORIENTED_EDGE('',*,*,#4154,.T.);
#6083=ORIENTED_EDGE('',*,*,#4153,.T.);
#6084=ORIENTED_EDGE('',*,*,#4149,.T.);
#6085=ORIENTED_EDGE('',*,*,#4148,.T.);
#6086=ORIENTED_EDGE('',*,*,#4144,.T.);
#6087=ORIENTED_EDGE('',*,*,#4143,.T.);
#6088=ORIENTED_EDGE('',*,*,#4139,.T.);
#6089=ORIENTED_EDGE('',*,*,#4138,.T.);
#6090=ORIENTED_EDGE('',*,*,#4134,.T.);
#6091=ORIENTED_EDGE('',*,*,#4133,.T.);
#6092=ORIENTED_EDGE('',*,*,#4129,.T.);
#6093=ORIENTED_EDGE('',*,*,#4128,.T.);
#6094=ORIENTED_EDGE('',*,*,#4124,.T.);
#6095=ORIENTED_EDGE('',*,*,#4123,.T.);
#6096=ORIENTED_EDGE('',*,*,#4119,.T.);
#6097=ORIENTED_EDGE('',*,*,#4118,.T.);
#6098=ORIENTED_EDGE('',*,*,#4114,.T.);
#6099=ORIENTED_EDGE('',*,*,#4210,.F.);
#6100=ORIENTED_EDGE('',*,*,#4319,.F.);
#6101=ORIENTED_EDGE('',*,*,#4320,.T.);
#6102=ORIENTED_EDGE('',*,*,#4321,.T.);
#6103=ORIENTED_EDGE('',*,*,#4320,.F.);
#6104=ORIENTED_EDGE('',*,*,#4319,.T.);
#6105=ORIENTED_EDGE('',*,*,#4318,.T.);
#6106=ORIENTED_EDGE('',*,*,#4293,.T.);
#6107=ORIENTED_EDGE('',*,*,#4317,.T.);
#6108=ORIENTED_EDGE('',*,*,#4203,.T.);
#6109=ORIENTED_EDGE('',*,*,#4321,.F.);
#6110=ORIENTED_EDGE('',*,*,#4314,.T.);
#6111=ORIENTED_EDGE('',*,*,#4108,.T.);
#6112=ORIENTED_EDGE('',*,*,#4313,.T.);
#6113=ORIENTED_EDGE('',*,*,#4018,.T.);
#6114=ORIENTED_EDGE('',*,*,#4322,.F.);
#6115=ORIENTED_EDGE('',*,*,#4323,.F.);
#6116=ORIENTED_EDGE('',*,*,#4324,.F.);
#6117=ORIENTED_EDGE('',*,*,#4325,.T.);
#6118=ORIENTED_EDGE('',*,*,#4326,.F.);
#6119=ORIENTED_EDGE('',*,*,#4327,.F.);
#6120=ORIENTED_EDGE('',*,*,#4328,.F.);
#6121=ORIENTED_EDGE('',*,*,#4322,.T.);
#6122=ORIENTED_EDGE('',*,*,#4329,.T.);
#6123=ORIENTED_EDGE('',*,*,#4330,.T.);
#6124=ORIENTED_EDGE('',*,*,#4331,.F.);
#6125=ORIENTED_EDGE('',*,*,#4332,.F.);
#6126=ORIENTED_EDGE('',*,*,#4326,.T.);
#6127=ORIENTED_EDGE('',*,*,#4333,.T.);
#6128=ORIENTED_EDGE('',*,*,#4334,.F.);
#6129=ORIENTED_EDGE('',*,*,#4335,.F.);
#6130=ORIENTED_EDGE('',*,*,#4336,.F.);
#6131=ORIENTED_EDGE('',*,*,#4331,.T.);
#6132=ORIENTED_EDGE('',*,*,#4337,.T.);
#6133=ORIENTED_EDGE('',*,*,#4338,.T.);
#6134=ORIENTED_EDGE('',*,*,#4339,.F.);
#6135=ORIENTED_EDGE('',*,*,#4340,.F.);
#6136=ORIENTED_EDGE('',*,*,#4334,.T.);
#6137=ORIENTED_EDGE('',*,*,#4341,.T.);
#6138=ORIENTED_EDGE('',*,*,#4342,.F.);
#6139=ORIENTED_EDGE('',*,*,#4343,.F.);
#6140=ORIENTED_EDGE('',*,*,#4344,.F.);
#6141=ORIENTED_EDGE('',*,*,#4339,.T.);
#6142=ORIENTED_EDGE('',*,*,#4345,.T.);
#6143=ORIENTED_EDGE('',*,*,#4346,.T.);
#6144=ORIENTED_EDGE('',*,*,#4347,.F.);
#6145=ORIENTED_EDGE('',*,*,#4348,.F.);
#6146=ORIENTED_EDGE('',*,*,#4342,.T.);
#6147=ORIENTED_EDGE('',*,*,#4349,.T.);
#6148=ORIENTED_EDGE('',*,*,#4350,.F.);
#6149=ORIENTED_EDGE('',*,*,#4351,.F.);
#6150=ORIENTED_EDGE('',*,*,#4352,.F.);
#6151=ORIENTED_EDGE('',*,*,#4347,.T.);
#6152=ORIENTED_EDGE('',*,*,#4353,.T.);
#6153=ORIENTED_EDGE('',*,*,#4354,.T.);
#6154=ORIENTED_EDGE('',*,*,#4355,.F.);
#6155=ORIENTED_EDGE('',*,*,#4356,.F.);
#6156=ORIENTED_EDGE('',*,*,#4350,.T.);
#6157=ORIENTED_EDGE('',*,*,#4357,.T.);
#6158=ORIENTED_EDGE('',*,*,#4358,.F.);
#6159=ORIENTED_EDGE('',*,*,#4359,.F.);
#6160=ORIENTED_EDGE('',*,*,#4360,.F.);
#6161=ORIENTED_EDGE('',*,*,#4355,.T.);
#6162=ORIENTED_EDGE('',*,*,#4361,.T.);
#6163=ORIENTED_EDGE('',*,*,#4362,.T.);
#6164=ORIENTED_EDGE('',*,*,#4363,.F.);
#6165=ORIENTED_EDGE('',*,*,#4364,.F.);
#6166=ORIENTED_EDGE('',*,*,#4358,.T.);
#6167=ORIENTED_EDGE('',*,*,#4365,.T.);
#6168=ORIENTED_EDGE('',*,*,#4366,.T.);
#6169=ORIENTED_EDGE('',*,*,#4367,.T.);
#6170=ORIENTED_EDGE('',*,*,#4368,.T.);
#6171=ORIENTED_EDGE('',*,*,#4369,.T.);
#6172=ORIENTED_EDGE('',*,*,#4370,.T.);
#6173=ORIENTED_EDGE('',*,*,#4371,.T.);
#6174=ORIENTED_EDGE('',*,*,#4372,.T.);
#6175=ORIENTED_EDGE('',*,*,#4373,.T.);
#6176=ORIENTED_EDGE('',*,*,#4374,.T.);
#6177=ORIENTED_EDGE('',*,*,#4375,.T.);
#6178=ORIENTED_EDGE('',*,*,#4376,.T.);
#6179=ORIENTED_EDGE('',*,*,#4377,.T.);
#6180=ORIENTED_EDGE('',*,*,#4378,.T.);
#6181=ORIENTED_EDGE('',*,*,#4379,.T.);
#6182=ORIENTED_EDGE('',*,*,#4380,.T.);
#6183=ORIENTED_EDGE('',*,*,#4381,.T.);
#6184=ORIENTED_EDGE('',*,*,#4382,.T.);
#6185=ORIENTED_EDGE('',*,*,#4383,.T.);
#6186=ORIENTED_EDGE('',*,*,#4384,.T.);
#6187=ORIENTED_EDGE('',*,*,#4385,.T.);
#6188=ORIENTED_EDGE('',*,*,#4386,.T.);
#6189=ORIENTED_EDGE('',*,*,#4387,.T.);
#6190=ORIENTED_EDGE('',*,*,#4388,.T.);
#6191=ORIENTED_EDGE('',*,*,#4389,.T.);
#6192=ORIENTED_EDGE('',*,*,#4390,.T.);
#6193=ORIENTED_EDGE('',*,*,#4391,.T.);
#6194=ORIENTED_EDGE('',*,*,#4363,.T.);
#6195=ORIENTED_EDGE('',*,*,#4392,.T.);
#6196=ORIENTED_EDGE('',*,*,#4393,.T.);
#6197=ORIENTED_EDGE('',*,*,#4394,.T.);
#6198=ORIENTED_EDGE('',*,*,#4395,.F.);
#6199=ORIENTED_EDGE('',*,*,#4396,.F.);
#6200=ORIENTED_EDGE('',*,*,#4397,.F.);
#6201=ORIENTED_EDGE('',*,*,#4394,.F.);
#6202=ORIENTED_EDGE('',*,*,#4398,.F.);
#6203=ORIENTED_EDGE('',*,*,#4380,.F.);
#6204=ORIENTED_EDGE('',*,*,#4399,.F.);
#6205=ORIENTED_EDGE('',*,*,#4400,.T.);
#6206=ORIENTED_EDGE('',*,*,#4401,.F.);
#6207=ORIENTED_EDGE('',*,*,#4400,.F.);
#6208=ORIENTED_EDGE('',*,*,#4398,.T.);
#6209=ORIENTED_EDGE('',*,*,#4393,.F.);
#6210=ORIENTED_EDGE('',*,*,#4392,.F.);
#6211=ORIENTED_EDGE('',*,*,#4365,.F.);
#6212=ORIENTED_EDGE('',*,*,#4362,.F.);
#6213=ORIENTED_EDGE('',*,*,#4361,.F.);
#6214=ORIENTED_EDGE('',*,*,#4357,.F.);
#6215=ORIENTED_EDGE('',*,*,#4354,.F.);
#6216=ORIENTED_EDGE('',*,*,#4353,.F.);
#6217=ORIENTED_EDGE('',*,*,#4349,.F.);
#6218=ORIENTED_EDGE('',*,*,#4346,.F.);
#6219=ORIENTED_EDGE('',*,*,#4345,.F.);
#6220=ORIENTED_EDGE('',*,*,#4341,.F.);
#6221=ORIENTED_EDGE('',*,*,#4338,.F.);
#6222=ORIENTED_EDGE('',*,*,#4337,.F.);
#6223=ORIENTED_EDGE('',*,*,#4333,.F.);
#6224=ORIENTED_EDGE('',*,*,#4330,.F.);
#6225=ORIENTED_EDGE('',*,*,#4329,.F.);
#6226=ORIENTED_EDGE('',*,*,#4325,.F.);
#6227=ORIENTED_EDGE('',*,*,#4402,.F.);
#6228=ORIENTED_EDGE('',*,*,#4366,.F.);
#6229=ORIENTED_EDGE('',*,*,#4391,.F.);
#6230=ORIENTED_EDGE('',*,*,#4390,.F.);
#6231=ORIENTED_EDGE('',*,*,#4389,.F.);
#6232=ORIENTED_EDGE('',*,*,#4388,.F.);
#6233=ORIENTED_EDGE('',*,*,#4387,.F.);
#6234=ORIENTED_EDGE('',*,*,#4386,.F.);
#6235=ORIENTED_EDGE('',*,*,#4385,.F.);
#6236=ORIENTED_EDGE('',*,*,#4384,.F.);
#6237=ORIENTED_EDGE('',*,*,#4383,.F.);
#6238=ORIENTED_EDGE('',*,*,#4382,.F.);
#6239=ORIENTED_EDGE('',*,*,#4381,.F.);
#6240=ORIENTED_EDGE('',*,*,#4397,.T.);
#6241=ORIENTED_EDGE('',*,*,#4399,.T.);
#6242=ORIENTED_EDGE('',*,*,#4379,.F.);
#6243=ORIENTED_EDGE('',*,*,#4378,.F.);
#6244=ORIENTED_EDGE('',*,*,#4377,.F.);
#6245=ORIENTED_EDGE('',*,*,#4376,.F.);
#6246=ORIENTED_EDGE('',*,*,#4375,.F.);
#6247=ORIENTED_EDGE('',*,*,#4374,.F.);
#6248=ORIENTED_EDGE('',*,*,#4373,.F.);
#6249=ORIENTED_EDGE('',*,*,#4372,.F.);
#6250=ORIENTED_EDGE('',*,*,#4371,.F.);
#6251=ORIENTED_EDGE('',*,*,#4370,.F.);
#6252=ORIENTED_EDGE('',*,*,#4369,.F.);
#6253=ORIENTED_EDGE('',*,*,#4368,.F.);
#6254=ORIENTED_EDGE('',*,*,#4403,.F.);
#6255=ORIENTED_EDGE('',*,*,#4323,.T.);
#6256=ORIENTED_EDGE('',*,*,#4328,.T.);
#6257=ORIENTED_EDGE('',*,*,#4327,.T.);
#6258=ORIENTED_EDGE('',*,*,#4332,.T.);
#6259=ORIENTED_EDGE('',*,*,#4336,.T.);
#6260=ORIENTED_EDGE('',*,*,#4335,.T.);
#6261=ORIENTED_EDGE('',*,*,#4340,.T.);
#6262=ORIENTED_EDGE('',*,*,#4344,.T.);
#6263=ORIENTED_EDGE('',*,*,#4343,.T.);
#6264=ORIENTED_EDGE('',*,*,#4348,.T.);
#6265=ORIENTED_EDGE('',*,*,#4352,.T.);
#6266=ORIENTED_EDGE('',*,*,#4351,.T.);
#6267=ORIENTED_EDGE('',*,*,#4356,.T.);
#6268=ORIENTED_EDGE('',*,*,#4360,.T.);
#6269=ORIENTED_EDGE('',*,*,#4359,.T.);
#6270=ORIENTED_EDGE('',*,*,#4364,.T.);
#6271=ORIENTED_EDGE('',*,*,#4396,.T.);
#6272=ORIENTED_EDGE('',*,*,#4395,.T.);
#6273=ORIENTED_EDGE('',*,*,#4404,.F.);
#6274=ORIENTED_EDGE('',*,*,#4405,.T.);
#6275=ORIENTED_EDGE('',*,*,#4406,.T.);
#6276=ORIENTED_EDGE('',*,*,#4407,.F.);
#6277=ORIENTED_EDGE('',*,*,#4408,.F.);
#6278=ORIENTED_EDGE('',*,*,#4409,.T.);
#6279=ORIENTED_EDGE('',*,*,#4410,.T.);
#6280=ORIENTED_EDGE('',*,*,#4405,.F.);
#6281=ORIENTED_EDGE('',*,*,#4411,.F.);
#6282=ORIENTED_EDGE('',*,*,#4412,.T.);
#6283=ORIENTED_EDGE('',*,*,#4413,.T.);
#6284=ORIENTED_EDGE('',*,*,#4409,.F.);
#6285=ORIENTED_EDGE('',*,*,#4414,.F.);
#6286=ORIENTED_EDGE('',*,*,#4415,.T.);
#6287=ORIENTED_EDGE('',*,*,#4416,.T.);
#6288=ORIENTED_EDGE('',*,*,#4412,.F.);
#6289=ORIENTED_EDGE('',*,*,#4417,.F.);
#6290=ORIENTED_EDGE('',*,*,#4418,.T.);
#6291=ORIENTED_EDGE('',*,*,#4419,.T.);
#6292=ORIENTED_EDGE('',*,*,#4415,.F.);
#6293=ORIENTED_EDGE('',*,*,#4420,.F.);
#6294=ORIENTED_EDGE('',*,*,#4407,.T.);
#6295=ORIENTED_EDGE('',*,*,#4421,.T.);
#6296=ORIENTED_EDGE('',*,*,#4418,.F.);
#6297=ORIENTED_EDGE('',*,*,#4421,.F.);
#6298=ORIENTED_EDGE('',*,*,#4406,.F.);
#6299=ORIENTED_EDGE('',*,*,#4410,.F.);
#6300=ORIENTED_EDGE('',*,*,#4413,.F.);
#6301=ORIENTED_EDGE('',*,*,#4416,.F.);
#6302=ORIENTED_EDGE('',*,*,#4419,.F.);
#6303=ORIENTED_EDGE('',*,*,#4422,.T.);
#6304=ORIENTED_EDGE('',*,*,#4402,.T.);
#6305=ORIENTED_EDGE('',*,*,#4324,.T.);
#6306=ORIENTED_EDGE('',*,*,#4403,.T.);
#6307=ORIENTED_EDGE('',*,*,#4367,.F.);
#6308=ORIENTED_EDGE('',*,*,#4422,.F.);
#6309=ORIENTED_EDGE('',*,*,#4423,.T.);
#6310=ORIENTED_EDGE('',*,*,#4424,.T.);
#6311=ORIENTED_EDGE('',*,*,#4423,.F.);
#6312=ORIENTED_EDGE('',*,*,#4424,.F.);
#6313=ORIENTED_EDGE('',*,*,#4404,.T.);
#6314=ORIENTED_EDGE('',*,*,#4420,.T.);
#6315=ORIENTED_EDGE('',*,*,#4417,.T.);
#6316=ORIENTED_EDGE('',*,*,#4414,.T.);
#6317=ORIENTED_EDGE('',*,*,#4411,.T.);
#6318=ORIENTED_EDGE('',*,*,#4408,.T.);
#6319=ORIENTED_EDGE('',*,*,#4401,.T.);
#6320=ORIENTED_EDGE('',*,*,#4425,.T.);
#6321=ORIENTED_EDGE('',*,*,#4426,.T.);
#6322=ORIENTED_EDGE('',*,*,#4427,.F.);
#6323=ORIENTED_EDGE('',*,*,#4428,.F.);
#6324=ORIENTED_EDGE('',*,*,#4429,.T.);
#6325=ORIENTED_EDGE('',*,*,#4430,.T.);
#6326=ORIENTED_EDGE('',*,*,#4431,.T.);
#6327=ORIENTED_EDGE('',*,*,#4425,.F.);
#6328=ORIENTED_EDGE('',*,*,#4432,.F.);
#6329=ORIENTED_EDGE('',*,*,#4433,.F.);
#6330=ORIENTED_EDGE('',*,*,#4434,.T.);
#6331=ORIENTED_EDGE('',*,*,#4435,.T.);
#6332=ORIENTED_EDGE('',*,*,#4436,.T.);
#6333=ORIENTED_EDGE('',*,*,#4429,.F.);
#6334=ORIENTED_EDGE('',*,*,#4437,.F.);
#6335=ORIENTED_EDGE('',*,*,#4438,.F.);
#6336=ORIENTED_EDGE('',*,*,#4439,.T.);
#6337=ORIENTED_EDGE('',*,*,#4440,.T.);
#6338=ORIENTED_EDGE('',*,*,#4441,.T.);
#6339=ORIENTED_EDGE('',*,*,#4434,.F.);
#6340=ORIENTED_EDGE('',*,*,#4442,.F.);
#6341=ORIENTED_EDGE('',*,*,#4443,.F.);
#6342=ORIENTED_EDGE('',*,*,#4444,.T.);
#6343=ORIENTED_EDGE('',*,*,#4445,.T.);
#6344=ORIENTED_EDGE('',*,*,#4446,.T.);
#6345=ORIENTED_EDGE('',*,*,#4439,.F.);
#6346=ORIENTED_EDGE('',*,*,#4447,.F.);
#6347=ORIENTED_EDGE('',*,*,#4448,.F.);
#6348=ORIENTED_EDGE('',*,*,#4449,.T.);
#6349=ORIENTED_EDGE('',*,*,#4450,.T.);
#6350=ORIENTED_EDGE('',*,*,#4451,.T.);
#6351=ORIENTED_EDGE('',*,*,#4444,.F.);
#6352=ORIENTED_EDGE('',*,*,#4452,.F.);
#6353=ORIENTED_EDGE('',*,*,#4453,.F.);
#6354=ORIENTED_EDGE('',*,*,#4454,.T.);
#6355=ORIENTED_EDGE('',*,*,#4455,.T.);
#6356=ORIENTED_EDGE('',*,*,#4456,.T.);
#6357=ORIENTED_EDGE('',*,*,#4449,.F.);
#6358=ORIENTED_EDGE('',*,*,#4457,.F.);
#6359=ORIENTED_EDGE('',*,*,#4458,.F.);
#6360=ORIENTED_EDGE('',*,*,#4459,.T.);
#6361=ORIENTED_EDGE('',*,*,#4460,.T.);
#6362=ORIENTED_EDGE('',*,*,#4461,.T.);
#6363=ORIENTED_EDGE('',*,*,#4454,.F.);
#6364=ORIENTED_EDGE('',*,*,#4462,.F.);
#6365=ORIENTED_EDGE('',*,*,#4463,.F.);
#6366=ORIENTED_EDGE('',*,*,#4464,.T.);
#6367=ORIENTED_EDGE('',*,*,#4465,.T.);
#6368=ORIENTED_EDGE('',*,*,#4466,.T.);
#6369=ORIENTED_EDGE('',*,*,#4459,.F.);
#6370=ORIENTED_EDGE('',*,*,#4467,.F.);
#6371=ORIENTED_EDGE('',*,*,#4468,.F.);
#6372=ORIENTED_EDGE('',*,*,#4469,.T.);
#6373=ORIENTED_EDGE('',*,*,#4470,.T.);
#6374=ORIENTED_EDGE('',*,*,#4471,.T.);
#6375=ORIENTED_EDGE('',*,*,#4464,.F.);
#6376=ORIENTED_EDGE('',*,*,#4472,.F.);
#6377=ORIENTED_EDGE('',*,*,#4473,.F.);
#6378=ORIENTED_EDGE('',*,*,#4474,.T.);
#6379=ORIENTED_EDGE('',*,*,#4475,.T.);
#6380=ORIENTED_EDGE('',*,*,#4476,.T.);
#6381=ORIENTED_EDGE('',*,*,#4469,.F.);
#6382=ORIENTED_EDGE('',*,*,#4477,.F.);
#6383=ORIENTED_EDGE('',*,*,#4478,.F.);
#6384=ORIENTED_EDGE('',*,*,#4479,.T.);
#6385=ORIENTED_EDGE('',*,*,#4480,.T.);
#6386=ORIENTED_EDGE('',*,*,#4481,.T.);
#6387=ORIENTED_EDGE('',*,*,#4474,.F.);
#6388=ORIENTED_EDGE('',*,*,#4482,.F.);
#6389=ORIENTED_EDGE('',*,*,#4483,.F.);
#6390=ORIENTED_EDGE('',*,*,#4484,.T.);
#6391=ORIENTED_EDGE('',*,*,#4485,.T.);
#6392=ORIENTED_EDGE('',*,*,#4486,.T.);
#6393=ORIENTED_EDGE('',*,*,#4479,.F.);
#6394=ORIENTED_EDGE('',*,*,#4487,.F.);
#6395=ORIENTED_EDGE('',*,*,#4488,.F.);
#6396=ORIENTED_EDGE('',*,*,#4489,.T.);
#6397=ORIENTED_EDGE('',*,*,#4490,.T.);
#6398=ORIENTED_EDGE('',*,*,#4491,.T.);
#6399=ORIENTED_EDGE('',*,*,#4484,.F.);
#6400=ORIENTED_EDGE('',*,*,#4492,.F.);
#6401=ORIENTED_EDGE('',*,*,#4493,.F.);
#6402=ORIENTED_EDGE('',*,*,#4494,.T.);
#6403=ORIENTED_EDGE('',*,*,#4495,.T.);
#6404=ORIENTED_EDGE('',*,*,#4496,.T.);
#6405=ORIENTED_EDGE('',*,*,#4489,.F.);
#6406=ORIENTED_EDGE('',*,*,#4497,.F.);
#6407=ORIENTED_EDGE('',*,*,#4498,.F.);
#6408=ORIENTED_EDGE('',*,*,#4499,.F.);
#6409=ORIENTED_EDGE('',*,*,#4500,.F.);
#6410=ORIENTED_EDGE('',*,*,#4501,.F.);
#6411=ORIENTED_EDGE('',*,*,#4502,.F.);
#6412=ORIENTED_EDGE('',*,*,#4503,.T.);
#6413=ORIENTED_EDGE('',*,*,#4504,.T.);
#6414=ORIENTED_EDGE('',*,*,#4505,.T.);
#6415=ORIENTED_EDGE('',*,*,#4506,.T.);
#6416=ORIENTED_EDGE('',*,*,#4507,.T.);
#6417=ORIENTED_EDGE('',*,*,#4508,.T.);
#6418=ORIENTED_EDGE('',*,*,#4509,.T.);
#6419=ORIENTED_EDGE('',*,*,#4510,.T.);
#6420=ORIENTED_EDGE('',*,*,#4509,.F.);
#6421=ORIENTED_EDGE('',*,*,#4511,.T.);
#6422=ORIENTED_EDGE('',*,*,#4512,.T.);
#6423=ORIENTED_EDGE('',*,*,#4513,.T.);
#6424=ORIENTED_EDGE('',*,*,#4514,.T.);
#6425=ORIENTED_EDGE('',*,*,#4515,.T.);
#6426=ORIENTED_EDGE('',*,*,#4505,.F.);
#6427=ORIENTED_EDGE('',*,*,#4516,.T.);
#6428=ORIENTED_EDGE('',*,*,#4517,.T.);
#6429=ORIENTED_EDGE('',*,*,#4518,.T.);
#6430=ORIENTED_EDGE('',*,*,#4519,.T.);
#6431=ORIENTED_EDGE('',*,*,#4520,.T.);
#6432=ORIENTED_EDGE('',*,*,#4513,.F.);
#6433=ORIENTED_EDGE('',*,*,#4521,.T.);
#6434=ORIENTED_EDGE('',*,*,#4522,.T.);
#6435=ORIENTED_EDGE('',*,*,#4523,.T.);
#6436=ORIENTED_EDGE('',*,*,#4524,.T.);
#6437=ORIENTED_EDGE('',*,*,#4518,.F.);
#6438=ORIENTED_EDGE('',*,*,#4525,.T.);
#6439=ORIENTED_EDGE('',*,*,#4526,.T.);
#6440=ORIENTED_EDGE('',*,*,#4527,.T.);
#6441=ORIENTED_EDGE('',*,*,#4528,.T.);
#6442=ORIENTED_EDGE('',*,*,#4523,.F.);
#6443=ORIENTED_EDGE('',*,*,#4529,.T.);
#6444=ORIENTED_EDGE('',*,*,#4530,.T.);
#6445=ORIENTED_EDGE('',*,*,#4531,.T.);
#6446=ORIENTED_EDGE('',*,*,#4532,.T.);
#6447=ORIENTED_EDGE('',*,*,#4526,.F.);
#6448=ORIENTED_EDGE('',*,*,#4533,.T.);
#6449=ORIENTED_EDGE('',*,*,#4534,.T.);
#6450=ORIENTED_EDGE('',*,*,#4535,.T.);
#6451=ORIENTED_EDGE('',*,*,#4536,.T.);
#6452=ORIENTED_EDGE('',*,*,#4531,.F.);
#6453=ORIENTED_EDGE('',*,*,#4537,.T.);
#6454=ORIENTED_EDGE('',*,*,#4538,.T.);
#6455=ORIENTED_EDGE('',*,*,#4539,.T.);
#6456=ORIENTED_EDGE('',*,*,#4540,.T.);
#6457=ORIENTED_EDGE('',*,*,#4534,.F.);
#6458=ORIENTED_EDGE('',*,*,#4541,.T.);
#6459=ORIENTED_EDGE('',*,*,#4542,.T.);
#6460=ORIENTED_EDGE('',*,*,#4543,.T.);
#6461=ORIENTED_EDGE('',*,*,#4544,.T.);
#6462=ORIENTED_EDGE('',*,*,#4539,.F.);
#6463=ORIENTED_EDGE('',*,*,#4545,.T.);
#6464=ORIENTED_EDGE('',*,*,#4546,.T.);
#6465=ORIENTED_EDGE('',*,*,#4547,.T.);
#6466=ORIENTED_EDGE('',*,*,#4548,.T.);
#6467=ORIENTED_EDGE('',*,*,#4549,.T.);
#6468=ORIENTED_EDGE('',*,*,#4542,.F.);
#6469=ORIENTED_EDGE('',*,*,#4550,.T.);
#6470=ORIENTED_EDGE('',*,*,#4551,.T.);
#6471=ORIENTED_EDGE('',*,*,#4552,.T.);
#6472=ORIENTED_EDGE('',*,*,#4547,.F.);
#6473=ORIENTED_EDGE('',*,*,#4553,.T.);
#6474=ORIENTED_EDGE('',*,*,#4554,.T.);
#6475=ORIENTED_EDGE('',*,*,#4555,.T.);
#6476=ORIENTED_EDGE('',*,*,#4556,.T.);
#6477=ORIENTED_EDGE('',*,*,#4557,.T.);
#6478=ORIENTED_EDGE('',*,*,#4551,.F.);
#6479=ORIENTED_EDGE('',*,*,#4558,.T.);
#6480=ORIENTED_EDGE('',*,*,#4559,.T.);
#6481=ORIENTED_EDGE('',*,*,#4560,.T.);
#6482=ORIENTED_EDGE('',*,*,#4555,.F.);
#6483=ORIENTED_EDGE('',*,*,#4561,.T.);
#6484=ORIENTED_EDGE('',*,*,#4562,.T.);
#6485=ORIENTED_EDGE('',*,*,#4563,.T.);
#6486=ORIENTED_EDGE('',*,*,#4564,.T.);
#6487=ORIENTED_EDGE('',*,*,#4565,.T.);
#6488=ORIENTED_EDGE('',*,*,#4559,.F.);
#6489=ORIENTED_EDGE('',*,*,#4566,.T.);
#6490=ORIENTED_EDGE('',*,*,#4567,.F.);
#6491=ORIENTED_EDGE('',*,*,#4568,.T.);
#6492=ORIENTED_EDGE('',*,*,#4569,.T.);
#6493=ORIENTED_EDGE('',*,*,#4570,.F.);
#6494=ORIENTED_EDGE('',*,*,#4571,.T.);
#6495=ORIENTED_EDGE('',*,*,#4572,.T.);
#6496=ORIENTED_EDGE('',*,*,#4567,.T.);
#6497=ORIENTED_EDGE('',*,*,#4573,.T.);
#6498=ORIENTED_EDGE('',*,*,#4563,.F.);
#6499=ORIENTED_EDGE('',*,*,#4574,.T.);
#6500=ORIENTED_EDGE('',*,*,#4575,.T.);
#6501=ORIENTED_EDGE('',*,*,#4499,.T.);
#6502=ORIENTED_EDGE('',*,*,#4576,.T.);
#6503=ORIENTED_EDGE('',*,*,#4577,.T.);
#6504=ORIENTED_EDGE('',*,*,#4494,.F.);
#6505=ORIENTED_EDGE('',*,*,#4578,.F.);
#6506=ORIENTED_EDGE('',*,*,#4579,.F.);
#6507=ORIENTED_EDGE('',*,*,#4507,.F.);
#6508=ORIENTED_EDGE('',*,*,#4580,.T.);
#6509=ORIENTED_EDGE('',*,*,#4427,.T.);
#6510=ORIENTED_EDGE('',*,*,#4581,.T.);
#6511=ORIENTED_EDGE('',*,*,#4581,.F.);
#6512=ORIENTED_EDGE('',*,*,#4426,.F.);
#6513=ORIENTED_EDGE('',*,*,#4431,.F.);
#6514=ORIENTED_EDGE('',*,*,#4430,.F.);
#6515=ORIENTED_EDGE('',*,*,#4436,.F.);
#6516=ORIENTED_EDGE('',*,*,#4435,.F.);
#6517=ORIENTED_EDGE('',*,*,#4441,.F.);
#6518=ORIENTED_EDGE('',*,*,#4440,.F.);
#6519=ORIENTED_EDGE('',*,*,#4446,.F.);
#6520=ORIENTED_EDGE('',*,*,#4445,.F.);
#6521=ORIENTED_EDGE('',*,*,#4451,.F.);
#6522=ORIENTED_EDGE('',*,*,#4450,.F.);
#6523=ORIENTED_EDGE('',*,*,#4456,.F.);
#6524=ORIENTED_EDGE('',*,*,#4455,.F.);
#6525=ORIENTED_EDGE('',*,*,#4461,.F.);
#6526=ORIENTED_EDGE('',*,*,#4460,.F.);
#6527=ORIENTED_EDGE('',*,*,#4466,.F.);
#6528=ORIENTED_EDGE('',*,*,#4465,.F.);
#6529=ORIENTED_EDGE('',*,*,#4471,.F.);
#6530=ORIENTED_EDGE('',*,*,#4470,.F.);
#6531=ORIENTED_EDGE('',*,*,#4476,.F.);
#6532=ORIENTED_EDGE('',*,*,#4475,.F.);
#6533=ORIENTED_EDGE('',*,*,#4481,.F.);
#6534=ORIENTED_EDGE('',*,*,#4480,.F.);
#6535=ORIENTED_EDGE('',*,*,#4486,.F.);
#6536=ORIENTED_EDGE('',*,*,#4485,.F.);
#6537=ORIENTED_EDGE('',*,*,#4491,.F.);
#6538=ORIENTED_EDGE('',*,*,#4490,.F.);
#6539=ORIENTED_EDGE('',*,*,#4496,.F.);
#6540=ORIENTED_EDGE('',*,*,#4495,.F.);
#6541=ORIENTED_EDGE('',*,*,#4577,.F.);
#6542=ORIENTED_EDGE('',*,*,#4576,.F.);
#6543=ORIENTED_EDGE('',*,*,#4504,.F.);
#6544=ORIENTED_EDGE('',*,*,#4503,.F.);
#6545=ORIENTED_EDGE('',*,*,#4582,.F.);
#6546=ORIENTED_EDGE('',*,*,#4569,.F.);
#6547=ORIENTED_EDGE('',*,*,#4568,.F.);
#6548=ORIENTED_EDGE('',*,*,#4575,.F.);
#6549=ORIENTED_EDGE('',*,*,#4574,.F.);
#6550=ORIENTED_EDGE('',*,*,#4566,.F.);
#6551=ORIENTED_EDGE('',*,*,#4562,.F.);
#6552=ORIENTED_EDGE('',*,*,#4561,.F.);
#6553=ORIENTED_EDGE('',*,*,#4558,.F.);
#6554=ORIENTED_EDGE('',*,*,#4554,.F.);
#6555=ORIENTED_EDGE('',*,*,#4553,.F.);
#6556=ORIENTED_EDGE('',*,*,#4550,.F.);
#6557=ORIENTED_EDGE('',*,*,#4546,.F.);
#6558=ORIENTED_EDGE('',*,*,#4545,.F.);
#6559=ORIENTED_EDGE('',*,*,#4541,.F.);
#6560=ORIENTED_EDGE('',*,*,#4538,.F.);
#6561=ORIENTED_EDGE('',*,*,#4537,.F.);
#6562=ORIENTED_EDGE('',*,*,#4533,.F.);
#6563=ORIENTED_EDGE('',*,*,#4530,.F.);
#6564=ORIENTED_EDGE('',*,*,#4529,.F.);
#6565=ORIENTED_EDGE('',*,*,#4525,.F.);
#6566=ORIENTED_EDGE('',*,*,#4522,.F.);
#6567=ORIENTED_EDGE('',*,*,#4521,.F.);
#6568=ORIENTED_EDGE('',*,*,#4517,.F.);
#6569=ORIENTED_EDGE('',*,*,#4516,.F.);
#6570=ORIENTED_EDGE('',*,*,#4512,.F.);
#6571=ORIENTED_EDGE('',*,*,#4511,.F.);
#6572=ORIENTED_EDGE('',*,*,#4508,.F.);
#6573=ORIENTED_EDGE('',*,*,#4580,.F.);
#6574=ORIENTED_EDGE('',*,*,#4506,.F.);
#6575=ORIENTED_EDGE('',*,*,#4515,.F.);
#6576=ORIENTED_EDGE('',*,*,#4514,.F.);
#6577=ORIENTED_EDGE('',*,*,#4520,.F.);
#6578=ORIENTED_EDGE('',*,*,#4519,.F.);
#6579=ORIENTED_EDGE('',*,*,#4524,.F.);
#6580=ORIENTED_EDGE('',*,*,#4528,.F.);
#6581=ORIENTED_EDGE('',*,*,#4527,.F.);
#6582=ORIENTED_EDGE('',*,*,#4532,.F.);
#6583=ORIENTED_EDGE('',*,*,#4536,.F.);
#6584=ORIENTED_EDGE('',*,*,#4535,.F.);
#6585=ORIENTED_EDGE('',*,*,#4540,.F.);
#6586=ORIENTED_EDGE('',*,*,#4544,.F.);
#6587=ORIENTED_EDGE('',*,*,#4543,.F.);
#6588=ORIENTED_EDGE('',*,*,#4549,.F.);
#6589=ORIENTED_EDGE('',*,*,#4548,.F.);
#6590=ORIENTED_EDGE('',*,*,#4552,.F.);
#6591=ORIENTED_EDGE('',*,*,#4557,.F.);
#6592=ORIENTED_EDGE('',*,*,#4556,.F.);
#6593=ORIENTED_EDGE('',*,*,#4560,.F.);
#6594=ORIENTED_EDGE('',*,*,#4565,.F.);
#6595=ORIENTED_EDGE('',*,*,#4564,.F.);
#6596=ORIENTED_EDGE('',*,*,#4573,.F.);
#6597=ORIENTED_EDGE('',*,*,#4572,.F.);
#6598=ORIENTED_EDGE('',*,*,#4571,.F.);
#6599=ORIENTED_EDGE('',*,*,#4583,.F.);
#6600=ORIENTED_EDGE('',*,*,#4501,.T.);
#6601=ORIENTED_EDGE('',*,*,#4500,.T.);
#6602=ORIENTED_EDGE('',*,*,#4579,.T.);
#6603=ORIENTED_EDGE('',*,*,#4578,.T.);
#6604=ORIENTED_EDGE('',*,*,#4498,.T.);
#6605=ORIENTED_EDGE('',*,*,#4497,.T.);
#6606=ORIENTED_EDGE('',*,*,#4493,.T.);
#6607=ORIENTED_EDGE('',*,*,#4492,.T.);
#6608=ORIENTED_EDGE('',*,*,#4488,.T.);
#6609=ORIENTED_EDGE('',*,*,#4487,.T.);
#6610=ORIENTED_EDGE('',*,*,#4483,.T.);
#6611=ORIENTED_EDGE('',*,*,#4482,.T.);
#6612=ORIENTED_EDGE('',*,*,#4478,.T.);
#6613=ORIENTED_EDGE('',*,*,#4477,.T.);
#6614=ORIENTED_EDGE('',*,*,#4473,.T.);
#6615=ORIENTED_EDGE('',*,*,#4472,.T.);
#6616=ORIENTED_EDGE('',*,*,#4468,.T.);
#6617=ORIENTED_EDGE('',*,*,#4467,.T.);
#6618=ORIENTED_EDGE('',*,*,#4463,.T.);
#6619=ORIENTED_EDGE('',*,*,#4462,.T.);
#6620=ORIENTED_EDGE('',*,*,#4458,.T.);
#6621=ORIENTED_EDGE('',*,*,#4457,.T.);
#6622=ORIENTED_EDGE('',*,*,#4453,.T.);
#6623=ORIENTED_EDGE('',*,*,#4452,.T.);
#6624=ORIENTED_EDGE('',*,*,#4448,.T.);
#6625=ORIENTED_EDGE('',*,*,#4447,.T.);
#6626=ORIENTED_EDGE('',*,*,#4443,.T.);
#6627=ORIENTED_EDGE('',*,*,#4442,.T.);
#6628=ORIENTED_EDGE('',*,*,#4438,.T.);
#6629=ORIENTED_EDGE('',*,*,#4437,.T.);
#6630=ORIENTED_EDGE('',*,*,#4433,.T.);
#6631=ORIENTED_EDGE('',*,*,#4432,.T.);
#6632=ORIENTED_EDGE('',*,*,#4428,.T.);
#6633=ORIENTED_EDGE('',*,*,#4510,.F.);
#6634=ORIENTED_EDGE('',*,*,#4584,.F.);
#6635=ORIENTED_EDGE('',*,*,#4585,.T.);
#6636=ORIENTED_EDGE('',*,*,#4586,.T.);
#6637=ORIENTED_EDGE('',*,*,#4585,.F.);
#6638=ORIENTED_EDGE('',*,*,#4584,.T.);
#6639=ORIENTED_EDGE('',*,*,#4583,.T.);
#6640=ORIENTED_EDGE('',*,*,#4570,.T.);
#6641=ORIENTED_EDGE('',*,*,#4582,.T.);
#6642=ORIENTED_EDGE('',*,*,#4502,.T.);
#6643=ORIENTED_EDGE('',*,*,#4586,.F.);
#6644=ORIENTED_EDGE('',*,*,#4587,.T.);
#6645=ORIENTED_EDGE('',*,*,#4588,.T.);
#6646=ORIENTED_EDGE('',*,*,#4589,.T.);
#6647=ORIENTED_EDGE('',*,*,#4590,.T.);
#6648=ORIENTED_EDGE('',*,*,#4588,.F.);
#6649=ORIENTED_EDGE('',*,*,#4591,.T.);
#6650=ORIENTED_EDGE('',*,*,#4592,.T.);
#6651=ORIENTED_EDGE('',*,*,#4593,.T.);
#6652=ORIENTED_EDGE('',*,*,#4594,.T.);
#6653=ORIENTED_EDGE('',*,*,#4595,.T.);
#6654=ORIENTED_EDGE('',*,*,#4596,.T.);
#6655=ORIENTED_EDGE('',*,*,#4597,.T.);
#6656=ORIENTED_EDGE('',*,*,#4587,.F.);
#6657=ORIENTED_EDGE('',*,*,#4598,.T.);
#6658=ORIENTED_EDGE('',*,*,#4599,.T.);
#6659=ORIENTED_EDGE('',*,*,#4591,.F.);
#6660=ORIENTED_EDGE('',*,*,#4597,.F.);
#6661=ORIENTED_EDGE('',*,*,#4600,.T.);
#6662=ORIENTED_EDGE('',*,*,#4601,.F.);
#6663=ORIENTED_EDGE('',*,*,#4600,.F.);
#6664=ORIENTED_EDGE('',*,*,#4596,.F.);
#6665=ORIENTED_EDGE('',*,*,#4602,.T.);
#6666=ORIENTED_EDGE('',*,*,#4603,.F.);
#6667=ORIENTED_EDGE('',*,*,#4602,.F.);
#6668=ORIENTED_EDGE('',*,*,#4595,.F.);
#6669=ORIENTED_EDGE('',*,*,#4604,.T.);
#6670=ORIENTED_EDGE('',*,*,#4605,.F.);
#6671=ORIENTED_EDGE('',*,*,#4604,.F.);
#6672=ORIENTED_EDGE('',*,*,#4594,.F.);
#6673=ORIENTED_EDGE('',*,*,#4606,.T.);
#6674=ORIENTED_EDGE('',*,*,#4607,.F.);
#6675=ORIENTED_EDGE('',*,*,#4606,.F.);
#6676=ORIENTED_EDGE('',*,*,#4589,.F.);
#6677=ORIENTED_EDGE('',*,*,#4593,.F.);
#6678=ORIENTED_EDGE('',*,*,#4608,.F.);
#6679=ORIENTED_EDGE('',*,*,#4609,.T.);
#6680=ORIENTED_EDGE('',*,*,#4610,.T.);
#6681=ORIENTED_EDGE('',*,*,#4608,.T.);
#6682=ORIENTED_EDGE('',*,*,#4592,.F.);
#6683=ORIENTED_EDGE('',*,*,#4599,.F.);
#6684=ORIENTED_EDGE('',*,*,#4610,.F.);
#6685=ORIENTED_EDGE('',*,*,#4598,.F.);
#6686=ORIENTED_EDGE('',*,*,#4590,.F.);
#6687=ORIENTED_EDGE('',*,*,#4609,.F.);
#6688=ORIENTED_EDGE('',*,*,#4601,.T.);
#6689=ORIENTED_EDGE('',*,*,#4603,.T.);
#6690=ORIENTED_EDGE('',*,*,#4605,.T.);
#6691=ORIENTED_EDGE('',*,*,#4607,.T.);
#6692=ORIENTED_EDGE('',*,*,#4611,.F.);
#6693=ORIENTED_EDGE('',*,*,#4612,.T.);
#6694=ORIENTED_EDGE('',*,*,#4613,.F.);
#6695=ORIENTED_EDGE('',*,*,#4612,.F.);
#6696=ORIENTED_EDGE('',*,*,#4614,.F.);
#6697=ORIENTED_EDGE('',*,*,#4615,.T.);
#6698=ORIENTED_EDGE('',*,*,#4616,.F.);
#6699=ORIENTED_EDGE('',*,*,#4615,.F.);
#6700=ORIENTED_EDGE('',*,*,#4617,.F.);
#6701=ORIENTED_EDGE('',*,*,#4618,.T.);
#6702=ORIENTED_EDGE('',*,*,#4619,.F.);
#6703=ORIENTED_EDGE('',*,*,#4618,.F.);
#6704=ORIENTED_EDGE('',*,*,#4620,.F.);
#6705=ORIENTED_EDGE('',*,*,#4621,.T.);
#6706=ORIENTED_EDGE('',*,*,#4622,.F.);
#6707=ORIENTED_EDGE('',*,*,#4621,.F.);
#6708=ORIENTED_EDGE('',*,*,#4623,.T.);
#6709=ORIENTED_EDGE('',*,*,#4624,.T.);
#6710=ORIENTED_EDGE('',*,*,#4625,.F.);
#6711=ORIENTED_EDGE('',*,*,#4626,.F.);
#6712=ORIENTED_EDGE('',*,*,#4627,.T.);
#6713=ORIENTED_EDGE('',*,*,#4626,.T.);
#6714=ORIENTED_EDGE('',*,*,#4628,.F.);
#6715=ORIENTED_EDGE('',*,*,#4629,.F.);
#6716=ORIENTED_EDGE('',*,*,#4630,.T.);
#6717=ORIENTED_EDGE('',*,*,#4629,.T.);
#6718=ORIENTED_EDGE('',*,*,#4631,.F.);
#6719=ORIENTED_EDGE('',*,*,#4632,.F.);
#6720=ORIENTED_EDGE('',*,*,#4633,.T.);
#6721=ORIENTED_EDGE('',*,*,#4632,.T.);
#6722=ORIENTED_EDGE('',*,*,#4634,.F.);
#6723=ORIENTED_EDGE('',*,*,#4624,.F.);
#6724=ORIENTED_EDGE('',*,*,#4635,.T.);
#6725=ORIENTED_EDGE('',*,*,#4636,.T.);
#6726=ORIENTED_EDGE('',*,*,#4637,.F.);
#6727=ORIENTED_EDGE('',*,*,#4638,.F.);
#6728=ORIENTED_EDGE('',*,*,#4639,.T.);
#6729=ORIENTED_EDGE('',*,*,#4638,.T.);
#6730=ORIENTED_EDGE('',*,*,#4640,.F.);
#6731=ORIENTED_EDGE('',*,*,#4641,.F.);
#6732=ORIENTED_EDGE('',*,*,#4642,.T.);
#6733=ORIENTED_EDGE('',*,*,#4641,.T.);
#6734=ORIENTED_EDGE('',*,*,#4643,.F.);
#6735=ORIENTED_EDGE('',*,*,#4644,.F.);
#6736=ORIENTED_EDGE('',*,*,#4645,.T.);
#6737=ORIENTED_EDGE('',*,*,#4644,.T.);
#6738=ORIENTED_EDGE('',*,*,#4646,.F.);
#6739=ORIENTED_EDGE('',*,*,#4636,.F.);
#6740=ORIENTED_EDGE('',*,*,#4646,.T.);
#6741=ORIENTED_EDGE('',*,*,#4643,.T.);
#6742=ORIENTED_EDGE('',*,*,#4640,.T.);
#6743=ORIENTED_EDGE('',*,*,#4637,.T.);
#6744=ORIENTED_EDGE('',*,*,#4634,.T.);
#6745=ORIENTED_EDGE('',*,*,#4631,.T.);
#6746=ORIENTED_EDGE('',*,*,#4628,.T.);
#6747=ORIENTED_EDGE('',*,*,#4625,.T.);
#6748=ORIENTED_EDGE('',*,*,#4620,.T.);
#6749=ORIENTED_EDGE('',*,*,#4617,.T.);
#6750=ORIENTED_EDGE('',*,*,#4614,.T.);
#6751=ORIENTED_EDGE('',*,*,#4611,.T.);
#6752=ORIENTED_EDGE('',*,*,#4645,.F.);
#6753=ORIENTED_EDGE('',*,*,#4635,.F.);
#6754=ORIENTED_EDGE('',*,*,#4639,.F.);
#6755=ORIENTED_EDGE('',*,*,#4642,.F.);
#6756=ORIENTED_EDGE('',*,*,#4633,.F.);
#6757=ORIENTED_EDGE('',*,*,#4623,.F.);
#6758=ORIENTED_EDGE('',*,*,#4627,.F.);
#6759=ORIENTED_EDGE('',*,*,#4630,.F.);
#6760=ORIENTED_EDGE('',*,*,#4622,.T.);
#6761=ORIENTED_EDGE('',*,*,#4619,.T.);
#6762=ORIENTED_EDGE('',*,*,#4616,.T.);
#6763=ORIENTED_EDGE('',*,*,#4613,.T.);
#6764=ORIENTED_EDGE('',*,*,#4647,.F.);
#6765=ORIENTED_EDGE('',*,*,#4648,.T.);
#6766=ORIENTED_EDGE('',*,*,#4649,.F.);
#6767=ORIENTED_EDGE('',*,*,#4648,.F.);
#6768=ORIENTED_EDGE('',*,*,#4650,.F.);
#6769=ORIENTED_EDGE('',*,*,#4651,.T.);
#6770=ORIENTED_EDGE('',*,*,#4652,.F.);
#6771=ORIENTED_EDGE('',*,*,#4651,.F.);
#6772=ORIENTED_EDGE('',*,*,#4653,.F.);
#6773=ORIENTED_EDGE('',*,*,#4654,.T.);
#6774=ORIENTED_EDGE('',*,*,#4655,.F.);
#6775=ORIENTED_EDGE('',*,*,#4654,.F.);
#6776=ORIENTED_EDGE('',*,*,#4656,.F.);
#6777=ORIENTED_EDGE('',*,*,#4657,.T.);
#6778=ORIENTED_EDGE('',*,*,#4658,.F.);
#6779=ORIENTED_EDGE('',*,*,#4657,.F.);
#6780=ORIENTED_EDGE('',*,*,#4659,.T.);
#6781=ORIENTED_EDGE('',*,*,#4660,.T.);
#6782=ORIENTED_EDGE('',*,*,#4661,.F.);
#6783=ORIENTED_EDGE('',*,*,#4662,.F.);
#6784=ORIENTED_EDGE('',*,*,#4663,.T.);
#6785=ORIENTED_EDGE('',*,*,#4662,.T.);
#6786=ORIENTED_EDGE('',*,*,#4664,.F.);
#6787=ORIENTED_EDGE('',*,*,#4665,.F.);
#6788=ORIENTED_EDGE('',*,*,#4666,.T.);
#6789=ORIENTED_EDGE('',*,*,#4665,.T.);
#6790=ORIENTED_EDGE('',*,*,#4667,.F.);
#6791=ORIENTED_EDGE('',*,*,#4668,.F.);
#6792=ORIENTED_EDGE('',*,*,#4669,.T.);
#6793=ORIENTED_EDGE('',*,*,#4668,.T.);
#6794=ORIENTED_EDGE('',*,*,#4670,.F.);
#6795=ORIENTED_EDGE('',*,*,#4660,.F.);
#6796=ORIENTED_EDGE('',*,*,#4670,.T.);
#6797=ORIENTED_EDGE('',*,*,#4667,.T.);
#6798=ORIENTED_EDGE('',*,*,#4664,.T.);
#6799=ORIENTED_EDGE('',*,*,#4661,.T.);
#6800=ORIENTED_EDGE('',*,*,#4647,.T.);
#6801=ORIENTED_EDGE('',*,*,#4650,.T.);
#6802=ORIENTED_EDGE('',*,*,#4653,.T.);
#6803=ORIENTED_EDGE('',*,*,#4656,.T.);
#6804=ORIENTED_EDGE('',*,*,#4669,.F.);
#6805=ORIENTED_EDGE('',*,*,#4659,.F.);
#6806=ORIENTED_EDGE('',*,*,#4663,.F.);
#6807=ORIENTED_EDGE('',*,*,#4666,.F.);
#6808=ORIENTED_EDGE('',*,*,#4649,.T.);
#6809=ORIENTED_EDGE('',*,*,#4652,.T.);
#6810=ORIENTED_EDGE('',*,*,#4655,.T.);
#6811=ORIENTED_EDGE('',*,*,#4658,.T.);
#6812=ORIENTED_EDGE('',*,*,#4671,.F.);
#6813=ORIENTED_EDGE('',*,*,#4672,.F.);
#6814=ORIENTED_EDGE('',*,*,#4673,.F.);
#6815=ORIENTED_EDGE('',*,*,#4674,.T.);
#6816=ORIENTED_EDGE('',*,*,#4675,.F.);
#6817=ORIENTED_EDGE('',*,*,#4676,.F.);
#6818=ORIENTED_EDGE('',*,*,#4671,.T.);
#6819=ORIENTED_EDGE('',*,*,#4677,.T.);
#6820=ORIENTED_EDGE('',*,*,#4678,.T.);
#6821=ORIENTED_EDGE('',*,*,#4679,.F.);
#6822=ORIENTED_EDGE('',*,*,#4680,.F.);
#6823=ORIENTED_EDGE('',*,*,#4681,.F.);
#6824=ORIENTED_EDGE('',*,*,#4675,.T.);
#6825=ORIENTED_EDGE('',*,*,#4682,.T.);
#6826=ORIENTED_EDGE('',*,*,#4683,.F.);
#6827=ORIENTED_EDGE('',*,*,#4684,.F.);
#6828=ORIENTED_EDGE('',*,*,#4685,.F.);
#6829=ORIENTED_EDGE('',*,*,#4679,.T.);
#6830=ORIENTED_EDGE('',*,*,#4686,.T.);
#6831=ORIENTED_EDGE('',*,*,#4687,.T.);
#6832=ORIENTED_EDGE('',*,*,#4688,.F.);
#6833=ORIENTED_EDGE('',*,*,#4689,.F.);
#6834=ORIENTED_EDGE('',*,*,#4690,.F.);
#6835=ORIENTED_EDGE('',*,*,#4683,.T.);
#6836=ORIENTED_EDGE('',*,*,#4691,.T.);
#6837=ORIENTED_EDGE('',*,*,#4692,.F.);
#6838=ORIENTED_EDGE('',*,*,#4693,.F.);
#6839=ORIENTED_EDGE('',*,*,#4688,.T.);
#6840=ORIENTED_EDGE('',*,*,#4694,.T.);
#6841=ORIENTED_EDGE('',*,*,#4695,.T.);
#6842=ORIENTED_EDGE('',*,*,#4696,.F.);
#6843=ORIENTED_EDGE('',*,*,#4697,.F.);
#6844=ORIENTED_EDGE('',*,*,#4698,.F.);
#6845=ORIENTED_EDGE('',*,*,#4692,.T.);
#6846=ORIENTED_EDGE('',*,*,#4699,.T.);
#6847=ORIENTED_EDGE('',*,*,#4700,.T.);
#6848=ORIENTED_EDGE('',*,*,#4701,.F.);
#6849=ORIENTED_EDGE('',*,*,#4702,.F.);
#6850=ORIENTED_EDGE('',*,*,#4703,.F.);
#6851=ORIENTED_EDGE('',*,*,#4696,.T.);
#6852=ORIENTED_EDGE('',*,*,#4704,.T.);
#6853=ORIENTED_EDGE('',*,*,#4705,.F.);
#6854=ORIENTED_EDGE('',*,*,#4706,.F.);
#6855=ORIENTED_EDGE('',*,*,#4707,.F.);
#6856=ORIENTED_EDGE('',*,*,#4701,.T.);
#6857=ORIENTED_EDGE('',*,*,#4708,.T.);
#6858=ORIENTED_EDGE('',*,*,#4709,.T.);
#6859=ORIENTED_EDGE('',*,*,#4710,.F.);
#6860=ORIENTED_EDGE('',*,*,#4711,.F.);
#6861=ORIENTED_EDGE('',*,*,#4705,.T.);
#6862=ORIENTED_EDGE('',*,*,#4712,.T.);
#6863=ORIENTED_EDGE('',*,*,#4713,.F.);
#6864=ORIENTED_EDGE('',*,*,#4714,.F.);
#6865=ORIENTED_EDGE('',*,*,#4715,.F.);
#6866=ORIENTED_EDGE('',*,*,#4710,.T.);
#6867=ORIENTED_EDGE('',*,*,#4716,.T.);
#6868=ORIENTED_EDGE('',*,*,#4717,.T.);
#6869=ORIENTED_EDGE('',*,*,#4718,.F.);
#6870=ORIENTED_EDGE('',*,*,#4719,.F.);
#6871=ORIENTED_EDGE('',*,*,#4720,.F.);
#6872=ORIENTED_EDGE('',*,*,#4713,.T.);
#6873=ORIENTED_EDGE('',*,*,#4721,.T.);
#6874=ORIENTED_EDGE('',*,*,#4722,.F.);
#6875=ORIENTED_EDGE('',*,*,#4723,.F.);
#6876=ORIENTED_EDGE('',*,*,#4724,.F.);
#6877=ORIENTED_EDGE('',*,*,#4718,.T.);
#6878=ORIENTED_EDGE('',*,*,#4725,.T.);
#6879=ORIENTED_EDGE('',*,*,#4726,.T.);
#6880=ORIENTED_EDGE('',*,*,#4727,.F.);
#6881=ORIENTED_EDGE('',*,*,#4728,.F.);
#6882=ORIENTED_EDGE('',*,*,#4722,.T.);
#6883=ORIENTED_EDGE('',*,*,#4729,.T.);
#6884=ORIENTED_EDGE('',*,*,#4730,.F.);
#6885=ORIENTED_EDGE('',*,*,#4731,.F.);
#6886=ORIENTED_EDGE('',*,*,#4732,.F.);
#6887=ORIENTED_EDGE('',*,*,#4727,.T.);
#6888=ORIENTED_EDGE('',*,*,#4733,.T.);
#6889=ORIENTED_EDGE('',*,*,#4734,.T.);
#6890=ORIENTED_EDGE('',*,*,#4735,.T.);
#6891=ORIENTED_EDGE('',*,*,#4736,.T.);
#6892=ORIENTED_EDGE('',*,*,#4737,.T.);
#6893=ORIENTED_EDGE('',*,*,#4738,.T.);
#6894=ORIENTED_EDGE('',*,*,#4739,.T.);
#6895=ORIENTED_EDGE('',*,*,#4740,.T.);
#6896=ORIENTED_EDGE('',*,*,#4741,.T.);
#6897=ORIENTED_EDGE('',*,*,#4742,.T.);
#6898=ORIENTED_EDGE('',*,*,#4743,.T.);
#6899=ORIENTED_EDGE('',*,*,#4744,.T.);
#6900=ORIENTED_EDGE('',*,*,#4745,.T.);
#6901=ORIENTED_EDGE('',*,*,#4746,.T.);
#6902=ORIENTED_EDGE('',*,*,#4747,.T.);
#6903=ORIENTED_EDGE('',*,*,#4748,.T.);
#6904=ORIENTED_EDGE('',*,*,#4749,.T.);
#6905=ORIENTED_EDGE('',*,*,#4750,.T.);
#6906=ORIENTED_EDGE('',*,*,#4751,.T.);
#6907=ORIENTED_EDGE('',*,*,#4752,.T.);
#6908=ORIENTED_EDGE('',*,*,#4753,.T.);
#6909=ORIENTED_EDGE('',*,*,#4754,.T.);
#6910=ORIENTED_EDGE('',*,*,#4755,.T.);
#6911=ORIENTED_EDGE('',*,*,#4756,.T.);
#6912=ORIENTED_EDGE('',*,*,#4757,.T.);
#6913=ORIENTED_EDGE('',*,*,#4758,.T.);
#6914=ORIENTED_EDGE('',*,*,#4759,.T.);
#6915=ORIENTED_EDGE('',*,*,#4760,.T.);
#6916=ORIENTED_EDGE('',*,*,#4761,.T.);
#6917=ORIENTED_EDGE('',*,*,#4762,.T.);
#6918=ORIENTED_EDGE('',*,*,#4763,.T.);
#6919=ORIENTED_EDGE('',*,*,#4764,.T.);
#6920=ORIENTED_EDGE('',*,*,#4765,.T.);
#6921=ORIENTED_EDGE('',*,*,#4766,.T.);
#6922=ORIENTED_EDGE('',*,*,#4767,.T.);
#6923=ORIENTED_EDGE('',*,*,#4768,.T.);
#6924=ORIENTED_EDGE('',*,*,#4730,.T.);
#6925=ORIENTED_EDGE('',*,*,#4769,.T.);
#6926=ORIENTED_EDGE('',*,*,#4770,.T.);
#6927=ORIENTED_EDGE('',*,*,#4771,.T.);
#6928=ORIENTED_EDGE('',*,*,#4772,.F.);
#6929=ORIENTED_EDGE('',*,*,#4773,.F.);
#6930=ORIENTED_EDGE('',*,*,#4774,.F.);
#6931=ORIENTED_EDGE('',*,*,#4771,.F.);
#6932=ORIENTED_EDGE('',*,*,#4775,.F.);
#6933=ORIENTED_EDGE('',*,*,#4753,.F.);
#6934=ORIENTED_EDGE('',*,*,#4776,.F.);
#6935=ORIENTED_EDGE('',*,*,#4777,.F.);
#6936=ORIENTED_EDGE('',*,*,#4778,.T.);
#6937=ORIENTED_EDGE('',*,*,#4779,.F.);
#6938=ORIENTED_EDGE('',*,*,#4778,.F.);
#6939=ORIENTED_EDGE('',*,*,#4775,.T.);
#6940=ORIENTED_EDGE('',*,*,#4770,.F.);
#6941=ORIENTED_EDGE('',*,*,#4769,.F.);
#6942=ORIENTED_EDGE('',*,*,#4734,.F.);
#6943=ORIENTED_EDGE('',*,*,#4733,.F.);
#6944=ORIENTED_EDGE('',*,*,#4729,.F.);
#6945=ORIENTED_EDGE('',*,*,#4726,.F.);
#6946=ORIENTED_EDGE('',*,*,#4725,.F.);
#6947=ORIENTED_EDGE('',*,*,#4721,.F.);
#6948=ORIENTED_EDGE('',*,*,#4717,.F.);
#6949=ORIENTED_EDGE('',*,*,#4716,.F.);
#6950=ORIENTED_EDGE('',*,*,#4712,.F.);
#6951=ORIENTED_EDGE('',*,*,#4709,.F.);
#6952=ORIENTED_EDGE('',*,*,#4708,.F.);
#6953=ORIENTED_EDGE('',*,*,#4704,.F.);
#6954=ORIENTED_EDGE('',*,*,#4700,.F.);
#6955=ORIENTED_EDGE('',*,*,#4699,.F.);
#6956=ORIENTED_EDGE('',*,*,#4695,.F.);
#6957=ORIENTED_EDGE('',*,*,#4694,.F.);
#6958=ORIENTED_EDGE('',*,*,#4691,.F.);
#6959=ORIENTED_EDGE('',*,*,#4687,.F.);
#6960=ORIENTED_EDGE('',*,*,#4686,.F.);
#6961=ORIENTED_EDGE('',*,*,#4682,.F.);
#6962=ORIENTED_EDGE('',*,*,#4678,.F.);
#6963=ORIENTED_EDGE('',*,*,#4677,.F.);
#6964=ORIENTED_EDGE('',*,*,#4674,.F.);
#6965=ORIENTED_EDGE('',*,*,#4780,.F.);
#6966=ORIENTED_EDGE('',*,*,#4735,.F.);
#6967=ORIENTED_EDGE('',*,*,#4768,.F.);
#6968=ORIENTED_EDGE('',*,*,#4767,.F.);
#6969=ORIENTED_EDGE('',*,*,#4766,.F.);
#6970=ORIENTED_EDGE('',*,*,#4765,.F.);
#6971=ORIENTED_EDGE('',*,*,#4764,.F.);
#6972=ORIENTED_EDGE('',*,*,#4763,.F.);
#6973=ORIENTED_EDGE('',*,*,#4762,.F.);
#6974=ORIENTED_EDGE('',*,*,#4761,.F.);
#6975=ORIENTED_EDGE('',*,*,#4760,.F.);
#6976=ORIENTED_EDGE('',*,*,#4759,.F.);
#6977=ORIENTED_EDGE('',*,*,#4758,.F.);
#6978=ORIENTED_EDGE('',*,*,#4757,.F.);
#6979=ORIENTED_EDGE('',*,*,#4756,.F.);
#6980=ORIENTED_EDGE('',*,*,#4755,.F.);
#6981=ORIENTED_EDGE('',*,*,#4754,.F.);
#6982=ORIENTED_EDGE('',*,*,#4774,.T.);
#6983=ORIENTED_EDGE('',*,*,#4777,.T.);
#6984=ORIENTED_EDGE('',*,*,#4776,.T.);
#6985=ORIENTED_EDGE('',*,*,#4752,.F.);
#6986=ORIENTED_EDGE('',*,*,#4751,.F.);
#6987=ORIENTED_EDGE('',*,*,#4750,.F.);
#6988=ORIENTED_EDGE('',*,*,#4749,.F.);
#6989=ORIENTED_EDGE('',*,*,#4748,.F.);
#6990=ORIENTED_EDGE('',*,*,#4747,.F.);
#6991=ORIENTED_EDGE('',*,*,#4746,.F.);
#6992=ORIENTED_EDGE('',*,*,#4745,.F.);
#6993=ORIENTED_EDGE('',*,*,#4744,.F.);
#6994=ORIENTED_EDGE('',*,*,#4743,.F.);
#6995=ORIENTED_EDGE('',*,*,#4742,.F.);
#6996=ORIENTED_EDGE('',*,*,#4741,.F.);
#6997=ORIENTED_EDGE('',*,*,#4740,.F.);
#6998=ORIENTED_EDGE('',*,*,#4739,.F.);
#6999=ORIENTED_EDGE('',*,*,#4738,.F.);
#7000=ORIENTED_EDGE('',*,*,#4737,.F.);
#7001=ORIENTED_EDGE('',*,*,#4781,.F.);
#7002=ORIENTED_EDGE('',*,*,#4782,.T.);
#7003=ORIENTED_EDGE('',*,*,#4672,.T.);
#7004=ORIENTED_EDGE('',*,*,#4676,.T.);
#7005=ORIENTED_EDGE('',*,*,#4681,.T.);
#7006=ORIENTED_EDGE('',*,*,#4680,.T.);
#7007=ORIENTED_EDGE('',*,*,#4685,.T.);
#7008=ORIENTED_EDGE('',*,*,#4684,.T.);
#7009=ORIENTED_EDGE('',*,*,#4690,.T.);
#7010=ORIENTED_EDGE('',*,*,#4689,.T.);
#7011=ORIENTED_EDGE('',*,*,#4693,.T.);
#7012=ORIENTED_EDGE('',*,*,#4698,.T.);
#7013=ORIENTED_EDGE('',*,*,#4697,.T.);
#7014=ORIENTED_EDGE('',*,*,#4703,.T.);
#7015=ORIENTED_EDGE('',*,*,#4702,.T.);
#7016=ORIENTED_EDGE('',*,*,#4707,.T.);
#7017=ORIENTED_EDGE('',*,*,#4706,.T.);
#7018=ORIENTED_EDGE('',*,*,#4711,.T.);
#7019=ORIENTED_EDGE('',*,*,#4715,.T.);
#7020=ORIENTED_EDGE('',*,*,#4714,.T.);
#7021=ORIENTED_EDGE('',*,*,#4720,.T.);
#7022=ORIENTED_EDGE('',*,*,#4719,.T.);
#7023=ORIENTED_EDGE('',*,*,#4724,.T.);
#7024=ORIENTED_EDGE('',*,*,#4723,.T.);
#7025=ORIENTED_EDGE('',*,*,#4728,.T.);
#7026=ORIENTED_EDGE('',*,*,#4732,.T.);
#7027=ORIENTED_EDGE('',*,*,#4731,.T.);
#7028=ORIENTED_EDGE('',*,*,#4773,.T.);
#7029=ORIENTED_EDGE('',*,*,#4772,.T.);
#7030=ORIENTED_EDGE('',*,*,#4783,.F.);
#7031=ORIENTED_EDGE('',*,*,#4784,.T.);
#7032=ORIENTED_EDGE('',*,*,#4785,.T.);
#7033=ORIENTED_EDGE('',*,*,#4786,.F.);
#7034=ORIENTED_EDGE('',*,*,#4787,.F.);
#7035=ORIENTED_EDGE('',*,*,#4788,.T.);
#7036=ORIENTED_EDGE('',*,*,#4789,.T.);
#7037=ORIENTED_EDGE('',*,*,#4784,.F.);
#7038=ORIENTED_EDGE('',*,*,#4790,.F.);
#7039=ORIENTED_EDGE('',*,*,#4791,.T.);
#7040=ORIENTED_EDGE('',*,*,#4792,.T.);
#7041=ORIENTED_EDGE('',*,*,#4788,.F.);
#7042=ORIENTED_EDGE('',*,*,#4793,.F.);
#7043=ORIENTED_EDGE('',*,*,#4794,.T.);
#7044=ORIENTED_EDGE('',*,*,#4795,.T.);
#7045=ORIENTED_EDGE('',*,*,#4791,.F.);
#7046=ORIENTED_EDGE('',*,*,#4796,.F.);
#7047=ORIENTED_EDGE('',*,*,#4797,.T.);
#7048=ORIENTED_EDGE('',*,*,#4798,.T.);
#7049=ORIENTED_EDGE('',*,*,#4794,.F.);
#7050=ORIENTED_EDGE('',*,*,#4799,.F.);
#7051=ORIENTED_EDGE('',*,*,#4786,.T.);
#7052=ORIENTED_EDGE('',*,*,#4800,.T.);
#7053=ORIENTED_EDGE('',*,*,#4797,.F.);
#7054=ORIENTED_EDGE('',*,*,#4800,.F.);
#7055=ORIENTED_EDGE('',*,*,#4785,.F.);
#7056=ORIENTED_EDGE('',*,*,#4789,.F.);
#7057=ORIENTED_EDGE('',*,*,#4792,.F.);
#7058=ORIENTED_EDGE('',*,*,#4795,.F.);
#7059=ORIENTED_EDGE('',*,*,#4798,.F.);
#7060=ORIENTED_EDGE('',*,*,#4801,.T.);
#7061=ORIENTED_EDGE('',*,*,#4780,.T.);
#7062=ORIENTED_EDGE('',*,*,#4673,.T.);
#7063=ORIENTED_EDGE('',*,*,#4782,.F.);
#7064=ORIENTED_EDGE('',*,*,#4781,.T.);
#7065=ORIENTED_EDGE('',*,*,#4736,.F.);
#7066=ORIENTED_EDGE('',*,*,#4801,.F.);
#7067=ORIENTED_EDGE('',*,*,#4802,.T.);
#7068=ORIENTED_EDGE('',*,*,#4803,.T.);
#7069=ORIENTED_EDGE('',*,*,#4802,.F.);
#7070=ORIENTED_EDGE('',*,*,#4803,.F.);
#7071=ORIENTED_EDGE('',*,*,#4783,.T.);
#7072=ORIENTED_EDGE('',*,*,#4799,.T.);
#7073=ORIENTED_EDGE('',*,*,#4796,.T.);
#7074=ORIENTED_EDGE('',*,*,#4793,.T.);
#7075=ORIENTED_EDGE('',*,*,#4790,.T.);
#7076=ORIENTED_EDGE('',*,*,#4787,.T.);
#7077=ORIENTED_EDGE('',*,*,#4779,.T.);
#7078=ORIENTED_EDGE('',*,*,#4804,.F.);
#7079=ORIENTED_EDGE('',*,*,#4805,.F.);
#7080=ORIENTED_EDGE('',*,*,#4806,.F.);
#7081=ORIENTED_EDGE('',*,*,#4807,.T.);
#7082=ORIENTED_EDGE('',*,*,#4808,.F.);
#7083=ORIENTED_EDGE('',*,*,#4809,.F.);
#7084=ORIENTED_EDGE('',*,*,#4804,.T.);
#7085=ORIENTED_EDGE('',*,*,#4810,.T.);
#7086=ORIENTED_EDGE('',*,*,#4811,.F.);
#7087=ORIENTED_EDGE('',*,*,#4812,.F.);
#7088=ORIENTED_EDGE('',*,*,#4813,.F.);
#7089=ORIENTED_EDGE('',*,*,#4808,.T.);
#7090=ORIENTED_EDGE('',*,*,#4814,.T.);
#7091=ORIENTED_EDGE('',*,*,#4815,.F.);
#7092=ORIENTED_EDGE('',*,*,#4816,.F.);
#7093=ORIENTED_EDGE('',*,*,#4811,.T.);
#7094=ORIENTED_EDGE('',*,*,#4817,.T.);
#7095=ORIENTED_EDGE('',*,*,#4818,.T.);
#7096=ORIENTED_EDGE('',*,*,#4819,.F.);
#7097=ORIENTED_EDGE('',*,*,#4820,.F.);
#7098=ORIENTED_EDGE('',*,*,#4815,.T.);
#7099=ORIENTED_EDGE('',*,*,#4821,.T.);
#7100=ORIENTED_EDGE('',*,*,#4822,.T.);
#7101=ORIENTED_EDGE('',*,*,#4823,.F.);
#7102=ORIENTED_EDGE('',*,*,#4824,.F.);
#7103=ORIENTED_EDGE('',*,*,#4819,.T.);
#7104=ORIENTED_EDGE('',*,*,#4825,.T.);
#7105=ORIENTED_EDGE('',*,*,#4826,.F.);
#7106=ORIENTED_EDGE('',*,*,#4827,.F.);
#7107=ORIENTED_EDGE('',*,*,#4828,.F.);
#7108=ORIENTED_EDGE('',*,*,#4823,.T.);
#7109=ORIENTED_EDGE('',*,*,#4829,.T.);
#7110=ORIENTED_EDGE('',*,*,#4830,.F.);
#7111=ORIENTED_EDGE('',*,*,#4831,.F.);
#7112=ORIENTED_EDGE('',*,*,#4826,.T.);
#7113=ORIENTED_EDGE('',*,*,#4832,.T.);
#7114=ORIENTED_EDGE('',*,*,#4833,.F.);
#7115=ORIENTED_EDGE('',*,*,#4834,.F.);
#7116=ORIENTED_EDGE('',*,*,#4830,.T.);
#7117=ORIENTED_EDGE('',*,*,#4835,.T.);
#7118=ORIENTED_EDGE('',*,*,#4836,.F.);
#7119=ORIENTED_EDGE('',*,*,#4837,.F.);
#7120=ORIENTED_EDGE('',*,*,#4838,.F.);
#7121=ORIENTED_EDGE('',*,*,#4833,.T.);
#7122=ORIENTED_EDGE('',*,*,#4839,.T.);
#7123=ORIENTED_EDGE('',*,*,#4840,.F.);
#7124=ORIENTED_EDGE('',*,*,#4841,.F.);
#7125=ORIENTED_EDGE('',*,*,#4842,.F.);
#7126=ORIENTED_EDGE('',*,*,#4836,.T.);
#7127=ORIENTED_EDGE('',*,*,#4843,.T.);
#7128=ORIENTED_EDGE('',*,*,#4844,.T.);
#7129=ORIENTED_EDGE('',*,*,#4845,.F.);
#7130=ORIENTED_EDGE('',*,*,#4846,.F.);
#7131=ORIENTED_EDGE('',*,*,#4840,.T.);
#7132=ORIENTED_EDGE('',*,*,#4847,.T.);
#7133=ORIENTED_EDGE('',*,*,#4848,.F.);
#7134=ORIENTED_EDGE('',*,*,#4849,.F.);
#7135=ORIENTED_EDGE('',*,*,#4845,.T.);
#7136=ORIENTED_EDGE('',*,*,#4850,.T.);
#7137=ORIENTED_EDGE('',*,*,#4851,.T.);
#7138=ORIENTED_EDGE('',*,*,#4852,.T.);
#7139=ORIENTED_EDGE('',*,*,#4853,.T.);
#7140=ORIENTED_EDGE('',*,*,#4854,.T.);
#7141=ORIENTED_EDGE('',*,*,#4855,.T.);
#7142=ORIENTED_EDGE('',*,*,#4856,.T.);
#7143=ORIENTED_EDGE('',*,*,#4857,.T.);
#7144=ORIENTED_EDGE('',*,*,#4858,.T.);
#7145=ORIENTED_EDGE('',*,*,#4859,.T.);
#7146=ORIENTED_EDGE('',*,*,#4860,.T.);
#7147=ORIENTED_EDGE('',*,*,#4861,.T.);
#7148=ORIENTED_EDGE('',*,*,#4862,.T.);
#7149=ORIENTED_EDGE('',*,*,#4863,.T.);
#7150=ORIENTED_EDGE('',*,*,#4864,.T.);
#7151=ORIENTED_EDGE('',*,*,#4865,.T.);
#7152=ORIENTED_EDGE('',*,*,#4866,.T.);
#7153=ORIENTED_EDGE('',*,*,#4867,.T.);
#7154=ORIENTED_EDGE('',*,*,#4868,.T.);
#7155=ORIENTED_EDGE('',*,*,#4869,.T.);
#7156=ORIENTED_EDGE('',*,*,#4870,.T.);
#7157=ORIENTED_EDGE('',*,*,#4871,.T.);
#7158=ORIENTED_EDGE('',*,*,#4872,.T.);
#7159=ORIENTED_EDGE('',*,*,#4873,.T.);
#7160=ORIENTED_EDGE('',*,*,#4874,.T.);
#7161=ORIENTED_EDGE('',*,*,#4875,.T.);
#7162=ORIENTED_EDGE('',*,*,#4876,.T.);
#7163=ORIENTED_EDGE('',*,*,#4877,.T.);
#7164=ORIENTED_EDGE('',*,*,#4878,.T.);
#7165=ORIENTED_EDGE('',*,*,#4879,.T.);
#7166=ORIENTED_EDGE('',*,*,#4880,.T.);
#7167=ORIENTED_EDGE('',*,*,#4848,.T.);
#7168=ORIENTED_EDGE('',*,*,#4881,.T.);
#7169=ORIENTED_EDGE('',*,*,#4882,.T.);
#7170=ORIENTED_EDGE('',*,*,#4883,.F.);
#7171=ORIENTED_EDGE('',*,*,#4884,.F.);
#7172=ORIENTED_EDGE('',*,*,#4882,.F.);
#7173=ORIENTED_EDGE('',*,*,#4885,.F.);
#7174=ORIENTED_EDGE('',*,*,#4867,.F.);
#7175=ORIENTED_EDGE('',*,*,#4886,.F.);
#7176=ORIENTED_EDGE('',*,*,#4887,.T.);
#7177=ORIENTED_EDGE('',*,*,#4888,.F.);
#7178=ORIENTED_EDGE('',*,*,#4887,.F.);
#7179=ORIENTED_EDGE('',*,*,#4885,.T.);
#7180=ORIENTED_EDGE('',*,*,#4881,.F.);
#7181=ORIENTED_EDGE('',*,*,#4850,.F.);
#7182=ORIENTED_EDGE('',*,*,#4847,.F.);
#7183=ORIENTED_EDGE('',*,*,#4844,.F.);
#7184=ORIENTED_EDGE('',*,*,#4843,.F.);
#7185=ORIENTED_EDGE('',*,*,#4839,.F.);
#7186=ORIENTED_EDGE('',*,*,#4835,.F.);
#7187=ORIENTED_EDGE('',*,*,#4832,.F.);
#7188=ORIENTED_EDGE('',*,*,#4829,.F.);
#7189=ORIENTED_EDGE('',*,*,#4825,.F.);
#7190=ORIENTED_EDGE('',*,*,#4822,.F.);
#7191=ORIENTED_EDGE('',*,*,#4821,.F.);
#7192=ORIENTED_EDGE('',*,*,#4818,.F.);
#7193=ORIENTED_EDGE('',*,*,#4817,.F.);
#7194=ORIENTED_EDGE('',*,*,#4814,.F.);
#7195=ORIENTED_EDGE('',*,*,#4810,.F.);
#7196=ORIENTED_EDGE('',*,*,#4807,.F.);
#7197=ORIENTED_EDGE('',*,*,#4889,.F.);
#7198=ORIENTED_EDGE('',*,*,#4851,.F.);
#7199=ORIENTED_EDGE('',*,*,#4880,.F.);
#7200=ORIENTED_EDGE('',*,*,#4879,.F.);
#7201=ORIENTED_EDGE('',*,*,#4878,.F.);
#7202=ORIENTED_EDGE('',*,*,#4877,.F.);
#7203=ORIENTED_EDGE('',*,*,#4876,.F.);
#7204=ORIENTED_EDGE('',*,*,#4875,.F.);
#7205=ORIENTED_EDGE('',*,*,#4874,.F.);
#7206=ORIENTED_EDGE('',*,*,#4873,.F.);
#7207=ORIENTED_EDGE('',*,*,#4872,.F.);
#7208=ORIENTED_EDGE('',*,*,#4871,.F.);
#7209=ORIENTED_EDGE('',*,*,#4870,.F.);
#7210=ORIENTED_EDGE('',*,*,#4869,.F.);
#7211=ORIENTED_EDGE('',*,*,#4868,.F.);
#7212=ORIENTED_EDGE('',*,*,#4886,.T.);
#7213=ORIENTED_EDGE('',*,*,#4866,.F.);
#7214=ORIENTED_EDGE('',*,*,#4865,.F.);
#7215=ORIENTED_EDGE('',*,*,#4864,.F.);
#7216=ORIENTED_EDGE('',*,*,#4863,.F.);
#7217=ORIENTED_EDGE('',*,*,#4862,.F.);
#7218=ORIENTED_EDGE('',*,*,#4861,.F.);
#7219=ORIENTED_EDGE('',*,*,#4860,.F.);
#7220=ORIENTED_EDGE('',*,*,#4859,.F.);
#7221=ORIENTED_EDGE('',*,*,#4858,.F.);
#7222=ORIENTED_EDGE('',*,*,#4857,.F.);
#7223=ORIENTED_EDGE('',*,*,#4856,.F.);
#7224=ORIENTED_EDGE('',*,*,#4855,.F.);
#7225=ORIENTED_EDGE('',*,*,#4854,.F.);
#7226=ORIENTED_EDGE('',*,*,#4853,.F.);
#7227=ORIENTED_EDGE('',*,*,#4890,.F.);
#7228=ORIENTED_EDGE('',*,*,#4891,.T.);
#7229=ORIENTED_EDGE('',*,*,#4805,.T.);
#7230=ORIENTED_EDGE('',*,*,#4809,.T.);
#7231=ORIENTED_EDGE('',*,*,#4813,.T.);
#7232=ORIENTED_EDGE('',*,*,#4812,.T.);
#7233=ORIENTED_EDGE('',*,*,#4816,.T.);
#7234=ORIENTED_EDGE('',*,*,#4820,.T.);
#7235=ORIENTED_EDGE('',*,*,#4824,.T.);
#7236=ORIENTED_EDGE('',*,*,#4828,.T.);
#7237=ORIENTED_EDGE('',*,*,#4827,.T.);
#7238=ORIENTED_EDGE('',*,*,#4831,.T.);
#7239=ORIENTED_EDGE('',*,*,#4834,.T.);
#7240=ORIENTED_EDGE('',*,*,#4838,.T.);
#7241=ORIENTED_EDGE('',*,*,#4837,.T.);
#7242=ORIENTED_EDGE('',*,*,#4842,.T.);
#7243=ORIENTED_EDGE('',*,*,#4841,.T.);
#7244=ORIENTED_EDGE('',*,*,#4846,.T.);
#7245=ORIENTED_EDGE('',*,*,#4849,.T.);
#7246=ORIENTED_EDGE('',*,*,#4883,.T.);
#7247=ORIENTED_EDGE('',*,*,#4884,.T.);
#7248=ORIENTED_EDGE('',*,*,#4892,.F.);
#7249=ORIENTED_EDGE('',*,*,#4893,.T.);
#7250=ORIENTED_EDGE('',*,*,#4894,.T.);
#7251=ORIENTED_EDGE('',*,*,#4895,.F.);
#7252=ORIENTED_EDGE('',*,*,#4896,.F.);
#7253=ORIENTED_EDGE('',*,*,#4897,.T.);
#7254=ORIENTED_EDGE('',*,*,#4898,.T.);
#7255=ORIENTED_EDGE('',*,*,#4893,.F.);
#7256=ORIENTED_EDGE('',*,*,#4899,.F.);
#7257=ORIENTED_EDGE('',*,*,#4900,.T.);
#7258=ORIENTED_EDGE('',*,*,#4901,.T.);
#7259=ORIENTED_EDGE('',*,*,#4897,.F.);
#7260=ORIENTED_EDGE('',*,*,#4902,.F.);
#7261=ORIENTED_EDGE('',*,*,#4903,.T.);
#7262=ORIENTED_EDGE('',*,*,#4904,.T.);
#7263=ORIENTED_EDGE('',*,*,#4900,.F.);
#7264=ORIENTED_EDGE('',*,*,#4905,.F.);
#7265=ORIENTED_EDGE('',*,*,#4906,.T.);
#7266=ORIENTED_EDGE('',*,*,#4907,.T.);
#7267=ORIENTED_EDGE('',*,*,#4903,.F.);
#7268=ORIENTED_EDGE('',*,*,#4908,.F.);
#7269=ORIENTED_EDGE('',*,*,#4895,.T.);
#7270=ORIENTED_EDGE('',*,*,#4909,.T.);
#7271=ORIENTED_EDGE('',*,*,#4906,.F.);
#7272=ORIENTED_EDGE('',*,*,#4909,.F.);
#7273=ORIENTED_EDGE('',*,*,#4894,.F.);
#7274=ORIENTED_EDGE('',*,*,#4898,.F.);
#7275=ORIENTED_EDGE('',*,*,#4901,.F.);
#7276=ORIENTED_EDGE('',*,*,#4904,.F.);
#7277=ORIENTED_EDGE('',*,*,#4907,.F.);
#7278=ORIENTED_EDGE('',*,*,#4910,.T.);
#7279=ORIENTED_EDGE('',*,*,#4889,.T.);
#7280=ORIENTED_EDGE('',*,*,#4806,.T.);
#7281=ORIENTED_EDGE('',*,*,#4891,.F.);
#7282=ORIENTED_EDGE('',*,*,#4890,.T.);
#7283=ORIENTED_EDGE('',*,*,#4852,.F.);
#7284=ORIENTED_EDGE('',*,*,#4910,.F.);
#7285=ORIENTED_EDGE('',*,*,#4911,.T.);
#7286=ORIENTED_EDGE('',*,*,#4912,.T.);
#7287=ORIENTED_EDGE('',*,*,#4911,.F.);
#7288=ORIENTED_EDGE('',*,*,#4912,.F.);
#7289=ORIENTED_EDGE('',*,*,#4892,.T.);
#7290=ORIENTED_EDGE('',*,*,#4908,.T.);
#7291=ORIENTED_EDGE('',*,*,#4905,.T.);
#7292=ORIENTED_EDGE('',*,*,#4902,.T.);
#7293=ORIENTED_EDGE('',*,*,#4899,.T.);
#7294=ORIENTED_EDGE('',*,*,#4896,.T.);
#7295=ORIENTED_EDGE('',*,*,#4888,.T.);
#7296=ORIENTED_EDGE('',*,*,#4913,.F.);
#7297=ORIENTED_EDGE('',*,*,#4914,.F.);
#7298=ORIENTED_EDGE('',*,*,#4915,.F.);
#7299=ORIENTED_EDGE('',*,*,#4916,.T.);
#7300=ORIENTED_EDGE('',*,*,#4917,.F.);
#7301=ORIENTED_EDGE('',*,*,#4918,.F.);
#7302=ORIENTED_EDGE('',*,*,#4919,.F.);
#7303=ORIENTED_EDGE('',*,*,#4913,.T.);
#7304=ORIENTED_EDGE('',*,*,#4920,.T.);
#7305=ORIENTED_EDGE('',*,*,#4921,.T.);
#7306=ORIENTED_EDGE('',*,*,#4922,.F.);
#7307=ORIENTED_EDGE('',*,*,#4923,.F.);
#7308=ORIENTED_EDGE('',*,*,#4917,.T.);
#7309=ORIENTED_EDGE('',*,*,#4924,.T.);
#7310=ORIENTED_EDGE('',*,*,#4925,.T.);
#7311=ORIENTED_EDGE('',*,*,#4926,.F.);
#7312=ORIENTED_EDGE('',*,*,#4927,.F.);
#7313=ORIENTED_EDGE('',*,*,#4928,.F.);
#7314=ORIENTED_EDGE('',*,*,#4922,.T.);
#7315=ORIENTED_EDGE('',*,*,#4929,.T.);
#7316=ORIENTED_EDGE('',*,*,#4930,.F.);
#7317=ORIENTED_EDGE('',*,*,#4931,.F.);
#7318=ORIENTED_EDGE('',*,*,#4932,.F.);
#7319=ORIENTED_EDGE('',*,*,#4926,.T.);
#7320=ORIENTED_EDGE('',*,*,#4933,.T.);
#7321=ORIENTED_EDGE('',*,*,#4934,.T.);
#7322=ORIENTED_EDGE('',*,*,#4935,.F.);
#7323=ORIENTED_EDGE('',*,*,#4936,.F.);
#7324=ORIENTED_EDGE('',*,*,#4930,.T.);
#7325=ORIENTED_EDGE('',*,*,#4937,.T.);
#7326=ORIENTED_EDGE('',*,*,#4938,.T.);
#7327=ORIENTED_EDGE('',*,*,#4939,.F.);
#7328=ORIENTED_EDGE('',*,*,#4940,.F.);
#7329=ORIENTED_EDGE('',*,*,#4941,.F.);
#7330=ORIENTED_EDGE('',*,*,#4935,.T.);
#7331=ORIENTED_EDGE('',*,*,#4942,.T.);
#7332=ORIENTED_EDGE('',*,*,#4943,.F.);
#7333=ORIENTED_EDGE('',*,*,#4944,.F.);
#7334=ORIENTED_EDGE('',*,*,#4945,.F.);
#7335=ORIENTED_EDGE('',*,*,#4939,.T.);
#7336=ORIENTED_EDGE('',*,*,#4946,.T.);
#7337=ORIENTED_EDGE('',*,*,#4947,.T.);
#7338=ORIENTED_EDGE('',*,*,#4948,.F.);
#7339=ORIENTED_EDGE('',*,*,#4949,.F.);
#7340=ORIENTED_EDGE('',*,*,#4943,.T.);
#7341=ORIENTED_EDGE('',*,*,#4950,.T.);
#7342=ORIENTED_EDGE('',*,*,#4951,.T.);
#7343=ORIENTED_EDGE('',*,*,#4952,.F.);
#7344=ORIENTED_EDGE('',*,*,#4953,.F.);
#7345=ORIENTED_EDGE('',*,*,#4954,.F.);
#7346=ORIENTED_EDGE('',*,*,#4948,.T.);
#7347=ORIENTED_EDGE('',*,*,#4955,.T.);
#7348=ORIENTED_EDGE('',*,*,#4956,.F.);
#7349=ORIENTED_EDGE('',*,*,#4957,.F.);
#7350=ORIENTED_EDGE('',*,*,#4952,.T.);
#7351=ORIENTED_EDGE('',*,*,#4958,.T.);
#7352=ORIENTED_EDGE('',*,*,#4959,.T.);
#7353=ORIENTED_EDGE('',*,*,#4960,.F.);
#7354=ORIENTED_EDGE('',*,*,#4961,.F.);
#7355=ORIENTED_EDGE('',*,*,#4962,.F.);
#7356=ORIENTED_EDGE('',*,*,#4956,.T.);
#7357=ORIENTED_EDGE('',*,*,#4963,.T.);
#7358=ORIENTED_EDGE('',*,*,#4964,.F.);
#7359=ORIENTED_EDGE('',*,*,#4965,.F.);
#7360=ORIENTED_EDGE('',*,*,#4960,.T.);
#7361=ORIENTED_EDGE('',*,*,#4966,.T.);
#7362=ORIENTED_EDGE('',*,*,#4967,.T.);
#7363=ORIENTED_EDGE('',*,*,#4968,.F.);
#7364=ORIENTED_EDGE('',*,*,#4969,.F.);
#7365=ORIENTED_EDGE('',*,*,#4970,.F.);
#7366=ORIENTED_EDGE('',*,*,#4964,.T.);
#7367=ORIENTED_EDGE('',*,*,#4971,.T.);
#7368=ORIENTED_EDGE('',*,*,#4972,.T.);
#7369=ORIENTED_EDGE('',*,*,#4973,.F.);
#7370=ORIENTED_EDGE('',*,*,#4974,.T.);
#7371=ORIENTED_EDGE('',*,*,#4975,.T.);
#7372=ORIENTED_EDGE('',*,*,#4976,.T.);
#7373=ORIENTED_EDGE('',*,*,#4977,.F.);
#7374=ORIENTED_EDGE('',*,*,#4978,.T.);
#7375=ORIENTED_EDGE('',*,*,#4973,.T.);
#7376=ORIENTED_EDGE('',*,*,#4979,.T.);
#7377=ORIENTED_EDGE('',*,*,#4980,.F.);
#7378=ORIENTED_EDGE('',*,*,#4981,.T.);
#7379=ORIENTED_EDGE('',*,*,#4977,.T.);
#7380=ORIENTED_EDGE('',*,*,#4982,.T.);
#7381=ORIENTED_EDGE('',*,*,#4983,.F.);
#7382=ORIENTED_EDGE('',*,*,#4984,.T.);
#7383=ORIENTED_EDGE('',*,*,#4980,.T.);
#7384=ORIENTED_EDGE('',*,*,#4985,.T.);
#7385=ORIENTED_EDGE('',*,*,#4986,.F.);
#7386=ORIENTED_EDGE('',*,*,#4987,.T.);
#7387=ORIENTED_EDGE('',*,*,#4983,.T.);
#7388=ORIENTED_EDGE('',*,*,#4988,.T.);
#7389=ORIENTED_EDGE('',*,*,#4989,.F.);
#7390=ORIENTED_EDGE('',*,*,#4990,.T.);
#7391=ORIENTED_EDGE('',*,*,#4986,.T.);
#7392=ORIENTED_EDGE('',*,*,#4991,.T.);
#7393=ORIENTED_EDGE('',*,*,#4992,.F.);
#7394=ORIENTED_EDGE('',*,*,#4993,.T.);
#7395=ORIENTED_EDGE('',*,*,#4989,.T.);
#7396=ORIENTED_EDGE('',*,*,#4994,.T.);
#7397=ORIENTED_EDGE('',*,*,#4995,.F.);
#7398=ORIENTED_EDGE('',*,*,#4996,.T.);
#7399=ORIENTED_EDGE('',*,*,#4992,.T.);
#7400=ORIENTED_EDGE('',*,*,#4997,.T.);
#7401=ORIENTED_EDGE('',*,*,#4998,.F.);
#7402=ORIENTED_EDGE('',*,*,#4999,.T.);
#7403=ORIENTED_EDGE('',*,*,#4995,.T.);
#7404=ORIENTED_EDGE('',*,*,#5000,.T.);
#7405=ORIENTED_EDGE('',*,*,#5001,.F.);
#7406=ORIENTED_EDGE('',*,*,#5002,.T.);
#7407=ORIENTED_EDGE('',*,*,#4998,.T.);
#7408=ORIENTED_EDGE('',*,*,#5003,.T.);
#7409=ORIENTED_EDGE('',*,*,#5004,.F.);
#7410=ORIENTED_EDGE('',*,*,#5005,.T.);
#7411=ORIENTED_EDGE('',*,*,#5001,.T.);
#7412=ORIENTED_EDGE('',*,*,#5006,.T.);
#7413=ORIENTED_EDGE('',*,*,#5007,.F.);
#7414=ORIENTED_EDGE('',*,*,#5008,.T.);
#7415=ORIENTED_EDGE('',*,*,#5004,.T.);
#7416=ORIENTED_EDGE('',*,*,#5009,.T.);
#7417=ORIENTED_EDGE('',*,*,#5010,.F.);
#7418=ORIENTED_EDGE('',*,*,#5011,.T.);
#7419=ORIENTED_EDGE('',*,*,#5007,.T.);
#7420=ORIENTED_EDGE('',*,*,#5012,.T.);
#7421=ORIENTED_EDGE('',*,*,#5013,.F.);
#7422=ORIENTED_EDGE('',*,*,#5014,.T.);
#7423=ORIENTED_EDGE('',*,*,#5010,.T.);
#7424=ORIENTED_EDGE('',*,*,#5015,.T.);
#7425=ORIENTED_EDGE('',*,*,#5013,.T.);
#7426=ORIENTED_EDGE('',*,*,#5016,.T.);
#7427=ORIENTED_EDGE('',*,*,#5017,.F.);
#7428=ORIENTED_EDGE('',*,*,#5018,.T.);
#7429=ORIENTED_EDGE('',*,*,#4968,.T.);
#7430=ORIENTED_EDGE('',*,*,#5019,.T.);
#7431=ORIENTED_EDGE('',*,*,#5020,.F.);
#7432=ORIENTED_EDGE('',*,*,#5021,.F.);
#7433=ORIENTED_EDGE('',*,*,#5022,.F.);
#7434=ORIENTED_EDGE('',*,*,#5023,.F.);
#7435=ORIENTED_EDGE('',*,*,#5016,.F.);
#7436=ORIENTED_EDGE('',*,*,#5015,.F.);
#7437=ORIENTED_EDGE('',*,*,#5012,.F.);
#7438=ORIENTED_EDGE('',*,*,#5009,.F.);
#7439=ORIENTED_EDGE('',*,*,#5006,.F.);
#7440=ORIENTED_EDGE('',*,*,#5003,.F.);
#7441=ORIENTED_EDGE('',*,*,#5000,.F.);
#7442=ORIENTED_EDGE('',*,*,#4997,.F.);
#7443=ORIENTED_EDGE('',*,*,#4994,.F.);
#7444=ORIENTED_EDGE('',*,*,#4991,.F.);
#7445=ORIENTED_EDGE('',*,*,#4988,.F.);
#7446=ORIENTED_EDGE('',*,*,#4985,.F.);
#7447=ORIENTED_EDGE('',*,*,#4982,.F.);
#7448=ORIENTED_EDGE('',*,*,#4979,.F.);
#7449=ORIENTED_EDGE('',*,*,#4976,.F.);
#7450=ORIENTED_EDGE('',*,*,#5024,.F.);
#7451=ORIENTED_EDGE('',*,*,#4914,.T.);
#7452=ORIENTED_EDGE('',*,*,#4919,.T.);
#7453=ORIENTED_EDGE('',*,*,#4918,.T.);
#7454=ORIENTED_EDGE('',*,*,#4923,.T.);
#7455=ORIENTED_EDGE('',*,*,#4928,.T.);
#7456=ORIENTED_EDGE('',*,*,#4927,.T.);
#7457=ORIENTED_EDGE('',*,*,#4932,.T.);
#7458=ORIENTED_EDGE('',*,*,#4931,.T.);
#7459=ORIENTED_EDGE('',*,*,#4936,.T.);
#7460=ORIENTED_EDGE('',*,*,#4941,.T.);
#7461=ORIENTED_EDGE('',*,*,#4940,.T.);
#7462=ORIENTED_EDGE('',*,*,#4945,.T.);
#7463=ORIENTED_EDGE('',*,*,#4944,.T.);
#7464=ORIENTED_EDGE('',*,*,#4949,.T.);
#7465=ORIENTED_EDGE('',*,*,#4954,.T.);
#7466=ORIENTED_EDGE('',*,*,#4953,.T.);
#7467=ORIENTED_EDGE('',*,*,#4957,.T.);
#7468=ORIENTED_EDGE('',*,*,#4962,.T.);
#7469=ORIENTED_EDGE('',*,*,#4961,.T.);
#7470=ORIENTED_EDGE('',*,*,#4965,.T.);
#7471=ORIENTED_EDGE('',*,*,#4970,.T.);
#7472=ORIENTED_EDGE('',*,*,#4969,.T.);
#7473=ORIENTED_EDGE('',*,*,#5022,.T.);
#7474=ORIENTED_EDGE('',*,*,#5021,.T.);
#7475=ORIENTED_EDGE('',*,*,#5025,.F.);
#7476=ORIENTED_EDGE('',*,*,#5026,.F.);
#7477=ORIENTED_EDGE('',*,*,#5019,.F.);
#7478=ORIENTED_EDGE('',*,*,#4972,.F.);
#7479=ORIENTED_EDGE('',*,*,#4971,.F.);
#7480=ORIENTED_EDGE('',*,*,#4967,.F.);
#7481=ORIENTED_EDGE('',*,*,#4966,.F.);
#7482=ORIENTED_EDGE('',*,*,#4963,.F.);
#7483=ORIENTED_EDGE('',*,*,#4959,.F.);
#7484=ORIENTED_EDGE('',*,*,#4958,.F.);
#7485=ORIENTED_EDGE('',*,*,#4955,.F.);
#7486=ORIENTED_EDGE('',*,*,#4951,.F.);
#7487=ORIENTED_EDGE('',*,*,#4950,.F.);
#7488=ORIENTED_EDGE('',*,*,#4947,.F.);
#7489=ORIENTED_EDGE('',*,*,#4946,.F.);
#7490=ORIENTED_EDGE('',*,*,#4942,.F.);
#7491=ORIENTED_EDGE('',*,*,#4938,.F.);
#7492=ORIENTED_EDGE('',*,*,#4937,.F.);
#7493=ORIENTED_EDGE('',*,*,#4934,.F.);
#7494=ORIENTED_EDGE('',*,*,#4933,.F.);
#7495=ORIENTED_EDGE('',*,*,#4929,.F.);
#7496=ORIENTED_EDGE('',*,*,#4925,.F.);
#7497=ORIENTED_EDGE('',*,*,#4924,.F.);
#7498=ORIENTED_EDGE('',*,*,#4921,.F.);
#7499=ORIENTED_EDGE('',*,*,#4920,.F.);
#7500=ORIENTED_EDGE('',*,*,#4916,.F.);
#7501=ORIENTED_EDGE('',*,*,#5027,.F.);
#7502=ORIENTED_EDGE('',*,*,#4974,.F.);
#7503=ORIENTED_EDGE('',*,*,#4978,.F.);
#7504=ORIENTED_EDGE('',*,*,#4981,.F.);
#7505=ORIENTED_EDGE('',*,*,#4984,.F.);
#7506=ORIENTED_EDGE('',*,*,#4987,.F.);
#7507=ORIENTED_EDGE('',*,*,#4990,.F.);
#7508=ORIENTED_EDGE('',*,*,#4993,.F.);
#7509=ORIENTED_EDGE('',*,*,#4996,.F.);
#7510=ORIENTED_EDGE('',*,*,#4999,.F.);
#7511=ORIENTED_EDGE('',*,*,#5002,.F.);
#7512=ORIENTED_EDGE('',*,*,#5005,.F.);
#7513=ORIENTED_EDGE('',*,*,#5008,.F.);
#7514=ORIENTED_EDGE('',*,*,#5011,.F.);
#7515=ORIENTED_EDGE('',*,*,#5014,.F.);
#7516=ORIENTED_EDGE('',*,*,#5018,.F.);
#7517=ORIENTED_EDGE('',*,*,#5028,.T.);
#7518=ORIENTED_EDGE('',*,*,#5027,.T.);
#7519=ORIENTED_EDGE('',*,*,#4915,.T.);
#7520=ORIENTED_EDGE('',*,*,#5024,.T.);
#7521=ORIENTED_EDGE('',*,*,#4975,.F.);
#7522=ORIENTED_EDGE('',*,*,#5028,.F.);
#7523=ORIENTED_EDGE('',*,*,#5029,.T.);
#7524=ORIENTED_EDGE('',*,*,#5030,.T.);
#7525=ORIENTED_EDGE('',*,*,#5029,.F.);
#7526=ORIENTED_EDGE('',*,*,#5031,.T.);
#7527=ORIENTED_EDGE('',*,*,#5032,.T.);
#7528=ORIENTED_EDGE('',*,*,#5033,.F.);
#7529=ORIENTED_EDGE('',*,*,#5032,.F.);
#7530=ORIENTED_EDGE('',*,*,#5025,.T.);
#7531=ORIENTED_EDGE('',*,*,#5017,.T.);
#7532=ORIENTED_EDGE('',*,*,#5023,.T.);
#7533=ORIENTED_EDGE('',*,*,#5020,.T.);
#7534=ORIENTED_EDGE('',*,*,#5026,.T.);
#7535=ORIENTED_EDGE('',*,*,#5033,.T.);
#7536=ORIENTED_EDGE('',*,*,#5030,.F.);
#7537=ORIENTED_EDGE('',*,*,#5031,.F.);
#7538=ORIENTED_EDGE('',*,*,#5034,.T.);
#7539=ORIENTED_EDGE('',*,*,#5035,.T.);
#7540=ORIENTED_EDGE('',*,*,#5036,.F.);
#7541=ORIENTED_EDGE('',*,*,#5037,.F.);
#7542=ORIENTED_EDGE('',*,*,#5038,.T.);
#7543=ORIENTED_EDGE('',*,*,#5039,.T.);
#7544=ORIENTED_EDGE('',*,*,#5040,.T.);
#7545=ORIENTED_EDGE('',*,*,#5034,.F.);
#7546=ORIENTED_EDGE('',*,*,#5041,.F.);
#7547=ORIENTED_EDGE('',*,*,#5042,.F.);
#7548=ORIENTED_EDGE('',*,*,#5043,.T.);
#7549=ORIENTED_EDGE('',*,*,#5044,.T.);
#7550=ORIENTED_EDGE('',*,*,#5045,.T.);
#7551=ORIENTED_EDGE('',*,*,#5038,.F.);
#7552=ORIENTED_EDGE('',*,*,#5046,.F.);
#7553=ORIENTED_EDGE('',*,*,#5047,.F.);
#7554=ORIENTED_EDGE('',*,*,#5048,.F.);
#7555=ORIENTED_EDGE('',*,*,#5049,.F.);
#7556=ORIENTED_EDGE('',*,*,#5050,.F.);
#7557=ORIENTED_EDGE('',*,*,#5051,.F.);
#7558=ORIENTED_EDGE('',*,*,#5052,.T.);
#7559=ORIENTED_EDGE('',*,*,#5053,.T.);
#7560=ORIENTED_EDGE('',*,*,#5054,.T.);
#7561=ORIENTED_EDGE('',*,*,#5055,.T.);
#7562=ORIENTED_EDGE('',*,*,#5056,.F.);
#7563=ORIENTED_EDGE('',*,*,#5057,.T.);
#7564=ORIENTED_EDGE('',*,*,#5058,.T.);
#7565=ORIENTED_EDGE('',*,*,#5059,.T.);
#7566=ORIENTED_EDGE('',*,*,#5054,.F.);
#7567=ORIENTED_EDGE('',*,*,#5060,.T.);
#7568=ORIENTED_EDGE('',*,*,#5061,.T.);
#7569=ORIENTED_EDGE('',*,*,#5062,.T.);
#7570=ORIENTED_EDGE('',*,*,#5058,.F.);
#7571=ORIENTED_EDGE('',*,*,#5063,.T.);
#7572=ORIENTED_EDGE('',*,*,#5064,.F.);
#7573=ORIENTED_EDGE('',*,*,#5065,.T.);
#7574=ORIENTED_EDGE('',*,*,#5066,.T.);
#7575=ORIENTED_EDGE('',*,*,#5067,.T.);
#7576=ORIENTED_EDGE('',*,*,#5064,.T.);
#7577=ORIENTED_EDGE('',*,*,#5068,.T.);
#7578=ORIENTED_EDGE('',*,*,#5061,.F.);
#7579=ORIENTED_EDGE('',*,*,#5069,.T.);
#7580=ORIENTED_EDGE('',*,*,#5048,.T.);
#7581=ORIENTED_EDGE('',*,*,#5070,.T.);
#7582=ORIENTED_EDGE('',*,*,#5071,.T.);
#7583=ORIENTED_EDGE('',*,*,#5043,.F.);
#7584=ORIENTED_EDGE('',*,*,#5072,.F.);
#7585=ORIENTED_EDGE('',*,*,#5073,.F.);
#7586=ORIENTED_EDGE('',*,*,#5074,.F.);
#7587=ORIENTED_EDGE('',*,*,#5075,.T.);
#7588=ORIENTED_EDGE('',*,*,#5076,.F.);
#7589=ORIENTED_EDGE('',*,*,#5075,.F.);
#7590=ORIENTED_EDGE('',*,*,#5077,.F.);
#7591=ORIENTED_EDGE('',*,*,#5078,.T.);
#7592=ORIENTED_EDGE('',*,*,#5079,.F.);
#7593=ORIENTED_EDGE('',*,*,#5078,.F.);
#7594=ORIENTED_EDGE('',*,*,#5080,.F.);
#7595=ORIENTED_EDGE('',*,*,#5035,.F.);
#7596=ORIENTED_EDGE('',*,*,#5040,.F.);
#7597=ORIENTED_EDGE('',*,*,#5039,.F.);
#7598=ORIENTED_EDGE('',*,*,#5045,.F.);
#7599=ORIENTED_EDGE('',*,*,#5044,.F.);
#7600=ORIENTED_EDGE('',*,*,#5071,.F.);
#7601=ORIENTED_EDGE('',*,*,#5070,.F.);
#7602=ORIENTED_EDGE('',*,*,#5053,.F.);
#7603=ORIENTED_EDGE('',*,*,#5052,.F.);
#7604=ORIENTED_EDGE('',*,*,#5081,.F.);
#7605=ORIENTED_EDGE('',*,*,#5065,.F.);
#7606=ORIENTED_EDGE('',*,*,#5069,.F.);
#7607=ORIENTED_EDGE('',*,*,#5063,.F.);
#7608=ORIENTED_EDGE('',*,*,#5060,.F.);
#7609=ORIENTED_EDGE('',*,*,#5057,.F.);
#7610=ORIENTED_EDGE('',*,*,#5082,.F.);
#7611=ORIENTED_EDGE('',*,*,#5055,.F.);
#7612=ORIENTED_EDGE('',*,*,#5059,.F.);
#7613=ORIENTED_EDGE('',*,*,#5062,.F.);
#7614=ORIENTED_EDGE('',*,*,#5068,.F.);
#7615=ORIENTED_EDGE('',*,*,#5067,.F.);
#7616=ORIENTED_EDGE('',*,*,#5083,.T.);
#7617=ORIENTED_EDGE('',*,*,#5084,.F.);
#7618=ORIENTED_EDGE('',*,*,#5050,.T.);
#7619=ORIENTED_EDGE('',*,*,#5049,.T.);
#7620=ORIENTED_EDGE('',*,*,#5073,.T.);
#7621=ORIENTED_EDGE('',*,*,#5072,.T.);
#7622=ORIENTED_EDGE('',*,*,#5047,.T.);
#7623=ORIENTED_EDGE('',*,*,#5046,.T.);
#7624=ORIENTED_EDGE('',*,*,#5042,.T.);
#7625=ORIENTED_EDGE('',*,*,#5041,.T.);
#7626=ORIENTED_EDGE('',*,*,#5037,.T.);
#7627=ORIENTED_EDGE('',*,*,#5085,.T.);
#7628=ORIENTED_EDGE('',*,*,#5074,.T.);
#7629=ORIENTED_EDGE('',*,*,#5077,.T.);
#7630=ORIENTED_EDGE('',*,*,#5082,.T.);
#7631=ORIENTED_EDGE('',*,*,#5036,.T.);
#7632=ORIENTED_EDGE('',*,*,#5080,.T.);
#7633=ORIENTED_EDGE('',*,*,#5056,.T.);
#7634=ORIENTED_EDGE('',*,*,#5085,.F.);
#7635=ORIENTED_EDGE('',*,*,#5086,.T.);
#7636=ORIENTED_EDGE('',*,*,#5087,.T.);
#7637=ORIENTED_EDGE('',*,*,#5086,.F.);
#7638=ORIENTED_EDGE('',*,*,#5087,.F.);
#7639=ORIENTED_EDGE('',*,*,#5076,.T.);
#7640=ORIENTED_EDGE('',*,*,#5079,.T.);
#7641=ORIENTED_EDGE('',*,*,#5084,.T.);
#7642=ORIENTED_EDGE('',*,*,#5083,.F.);
#7643=ORIENTED_EDGE('',*,*,#5066,.F.);
#7644=ORIENTED_EDGE('',*,*,#5081,.T.);
#7645=ORIENTED_EDGE('',*,*,#5051,.T.);
#7646=ORIENTED_EDGE('',*,*,#5088,.T.);
#7647=ORIENTED_EDGE('',*,*,#5089,.T.);
#7648=ORIENTED_EDGE('',*,*,#5090,.F.);
#7649=ORIENTED_EDGE('',*,*,#5089,.F.);
#7650=ORIENTED_EDGE('',*,*,#5091,.F.);
#7651=ORIENTED_EDGE('',*,*,#5092,.T.);
#7652=ORIENTED_EDGE('',*,*,#5093,.T.);
#7653=ORIENTED_EDGE('',*,*,#5092,.F.);
#7654=ORIENTED_EDGE('',*,*,#5091,.T.);
#7655=ORIENTED_EDGE('',*,*,#5090,.T.);
#7656=ORIENTED_EDGE('',*,*,#5093,.F.);
#7657=ORIENTED_EDGE('',*,*,#5088,.F.);
#7658=CYLINDRICAL_SURFACE('',#8435,3.5);
#7659=CYLINDRICAL_SURFACE('',#8438,3.5);
#7660=CYLINDRICAL_SURFACE('',#8441,3.5);
#7661=CYLINDRICAL_SURFACE('',#8444,3.5);
#7662=CYLINDRICAL_SURFACE('',#8454,10.5);
#7663=CYLINDRICAL_SURFACE('',#8457,10.5);
#7664=CYLINDRICAL_SURFACE('',#8474,5.);
#7665=CYLINDRICAL_SURFACE('',#8478,5.);
#7666=CYLINDRICAL_SURFACE('',#8482,5.);
#7667=CYLINDRICAL_SURFACE('',#8486,5.);
#7668=CYLINDRICAL_SURFACE('',#8490,5.);
#7669=CYLINDRICAL_SURFACE('',#8494,5.);
#7670=CYLINDRICAL_SURFACE('',#8498,5.);
#7671=CYLINDRICAL_SURFACE('',#8502,5.);
#7672=CYLINDRICAL_SURFACE('',#8513,3.0735);
#7673=CYLINDRICAL_SURFACE('',#8515,3.0735);
#7674=CYLINDRICAL_SURFACE('',#8516,3.0735);
#7675=CYLINDRICAL_SURFACE('',#8517,3.0735);
#7676=CYLINDRICAL_SURFACE('',#8518,3.0735);
#7677=CYLINDRICAL_SURFACE('',#8519,3.0735);
#7678=CYLINDRICAL_SURFACE('',#8520,3.0735);
#7679=CYLINDRICAL_SURFACE('',#8521,3.0735);
#7680=CYLINDRICAL_SURFACE('',#8522,3.0735);
#7681=CYLINDRICAL_SURFACE('',#8523,3.0735);
#7682=CYLINDRICAL_SURFACE('',#8524,3.0735);
#7683=CYLINDRICAL_SURFACE('',#8525,3.0735);
#7684=CYLINDRICAL_SURFACE('',#8526,3.0735);
#7685=CYLINDRICAL_SURFACE('',#8527,3.0735);
#7686=CYLINDRICAL_SURFACE('',#8528,3.0735);
#7687=CYLINDRICAL_SURFACE('',#8529,3.0735);
#7688=CYLINDRICAL_SURFACE('',#8530,3.0735);
#7689=CYLINDRICAL_SURFACE('',#8531,3.0735);
#7690=CYLINDRICAL_SURFACE('',#8532,3.0735);
#7691=CYLINDRICAL_SURFACE('',#8534,2.5175);
#7692=CYLINDRICAL_SURFACE('',#8538,2.5175);
#7693=CYLINDRICAL_SURFACE('',#8539,2.5175);
#7694=CYLINDRICAL_SURFACE('',#8540,2.5175);
#7695=CYLINDRICAL_SURFACE('',#8541,2.5175);
#7696=CYLINDRICAL_SURFACE('',#8542,2.5175);
#7697=CYLINDRICAL_SURFACE('',#8543,2.5175);
#7698=CYLINDRICAL_SURFACE('',#8544,2.5175);
#7699=CYLINDRICAL_SURFACE('',#8545,2.5175);
#7700=CYLINDRICAL_SURFACE('',#8546,2.5175);
#7701=CYLINDRICAL_SURFACE('',#8547,2.5175);
#7702=CYLINDRICAL_SURFACE('',#8548,2.5175);
#7703=CYLINDRICAL_SURFACE('',#8549,2.5175);
#7704=CYLINDRICAL_SURFACE('',#8550,2.5175);
#7705=CYLINDRICAL_SURFACE('',#8551,2.5175);
#7706=CYLINDRICAL_SURFACE('',#8552,2.5175);
#7707=CYLINDRICAL_SURFACE('',#8553,2.5175);
#7708=CYLINDRICAL_SURFACE('',#8554,2.5175);
#7709=CYLINDRICAL_SURFACE('',#8555,2.5175);
#7710=CYLINDRICAL_SURFACE('',#8557,3.0735);
#7711=CYLINDRICAL_SURFACE('',#8559,3.0735);
#7712=CYLINDRICAL_SURFACE('',#8560,3.0735);
#7713=CYLINDRICAL_SURFACE('',#8561,3.0735);
#7714=CYLINDRICAL_SURFACE('',#8562,3.0735);
#7715=CYLINDRICAL_SURFACE('',#8563,3.0735);
#7716=CYLINDRICAL_SURFACE('',#8564,3.0735);
#7717=CYLINDRICAL_SURFACE('',#8565,3.0735);
#7718=CYLINDRICAL_SURFACE('',#8566,3.0735);
#7719=CYLINDRICAL_SURFACE('',#8567,3.0735);
#7720=CYLINDRICAL_SURFACE('',#8568,3.0735);
#7721=CYLINDRICAL_SURFACE('',#8569,3.0735);
#7722=CYLINDRICAL_SURFACE('',#8570,3.0735);
#7723=CYLINDRICAL_SURFACE('',#8571,3.0735);
#7724=CYLINDRICAL_SURFACE('',#8572,3.0735);
#7725=CYLINDRICAL_SURFACE('',#8573,3.0735);
#7726=CYLINDRICAL_SURFACE('',#8574,3.0735);
#7727=CYLINDRICAL_SURFACE('',#8575,3.0735);
#7728=CYLINDRICAL_SURFACE('',#8576,3.0735);
#7729=CYLINDRICAL_SURFACE('',#8578,2.5175);
#7730=CYLINDRICAL_SURFACE('',#8582,2.5175);
#7731=CYLINDRICAL_SURFACE('',#8583,2.5175);
#7732=CYLINDRICAL_SURFACE('',#8584,2.5175);
#7733=CYLINDRICAL_SURFACE('',#8585,2.5175);
#7734=CYLINDRICAL_SURFACE('',#8586,2.5175);
#7735=CYLINDRICAL_SURFACE('',#8587,2.5175);
#7736=CYLINDRICAL_SURFACE('',#8588,2.5175);
#7737=CYLINDRICAL_SURFACE('',#8589,2.5175);
#7738=CYLINDRICAL_SURFACE('',#8590,2.5175);
#7739=CYLINDRICAL_SURFACE('',#8591,2.5175);
#7740=CYLINDRICAL_SURFACE('',#8592,2.5175);
#7741=CYLINDRICAL_SURFACE('',#8593,2.5175);
#7742=CYLINDRICAL_SURFACE('',#8594,2.5175);
#7743=CYLINDRICAL_SURFACE('',#8595,2.5175);
#7744=CYLINDRICAL_SURFACE('',#8596,2.5175);
#7745=CYLINDRICAL_SURFACE('',#8597,2.5175);
#7746=CYLINDRICAL_SURFACE('',#8598,2.5175);
#7747=CYLINDRICAL_SURFACE('',#8599,2.5175);
#7748=CYLINDRICAL_SURFACE('',#8601,2.5175);
#7749=CYLINDRICAL_SURFACE('',#8602,3.0735);
#7750=CYLINDRICAL_SURFACE('',#8603,2.5175);
#7751=CYLINDRICAL_SURFACE('',#8604,3.0735);
#7752=CYLINDRICAL_SURFACE('',#8609,8.);
#7753=CYLINDRICAL_SURFACE('',#8615,2.37175);
#7754=CYLINDRICAL_SURFACE('',#8617,2.37175);
#7755=CYLINDRICAL_SURFACE('',#8618,2.37175);
#7756=CYLINDRICAL_SURFACE('',#8619,2.37175);
#7757=CYLINDRICAL_SURFACE('',#8620,2.37175);
#7758=CYLINDRICAL_SURFACE('',#8621,2.37175);
#7759=CYLINDRICAL_SURFACE('',#8622,2.37175);
#7760=CYLINDRICAL_SURFACE('',#8623,2.37175);
#7761=CYLINDRICAL_SURFACE('',#8624,2.37175);
#7762=CYLINDRICAL_SURFACE('',#8625,2.37175);
#7763=CYLINDRICAL_SURFACE('',#8626,2.37175);
#7764=CYLINDRICAL_SURFACE('',#8627,2.942);
#7765=CYLINDRICAL_SURFACE('',#8630,2.37175);
#7766=CYLINDRICAL_SURFACE('',#8643,5.);
#7767=CYLINDRICAL_SURFACE('',#8648,2.05475);
#7768=CYLINDRICAL_SURFACE('',#8650,2.05475);
#7769=CYLINDRICAL_SURFACE('',#8651,2.05475);
#7770=CYLINDRICAL_SURFACE('',#8652,2.05475);
#7771=CYLINDRICAL_SURFACE('',#8653,2.05475);
#7772=CYLINDRICAL_SURFACE('',#8654,2.05475);
#7773=CYLINDRICAL_SURFACE('',#8655,2.05475);
#7774=CYLINDRICAL_SURFACE('',#8656,2.05475);
#7775=CYLINDRICAL_SURFACE('',#8657,2.05475);
#7776=CYLINDRICAL_SURFACE('',#8658,2.05475);
#7777=CYLINDRICAL_SURFACE('',#8659,2.05475);
#7778=CYLINDRICAL_SURFACE('',#8660,2.05475);
#7779=CYLINDRICAL_SURFACE('',#8661,2.05475);
#7780=CYLINDRICAL_SURFACE('',#8662,2.05475);
#7781=CYLINDRICAL_SURFACE('',#8663,2.05475);
#7782=CYLINDRICAL_SURFACE('',#8664,2.05475);
#7783=CYLINDRICAL_SURFACE('',#8666,1.666);
#7784=CYLINDRICAL_SURFACE('',#8669,1.666);
#7785=CYLINDRICAL_SURFACE('',#8670,1.666);
#7786=CYLINDRICAL_SURFACE('',#8671,1.666);
#7787=CYLINDRICAL_SURFACE('',#8672,1.666);
#7788=CYLINDRICAL_SURFACE('',#8673,1.666);
#7789=CYLINDRICAL_SURFACE('',#8674,1.666);
#7790=CYLINDRICAL_SURFACE('',#8675,1.666);
#7791=CYLINDRICAL_SURFACE('',#8676,1.666);
#7792=CYLINDRICAL_SURFACE('',#8677,1.666);
#7793=CYLINDRICAL_SURFACE('',#8678,1.666);
#7794=CYLINDRICAL_SURFACE('',#8679,1.666);
#7795=CYLINDRICAL_SURFACE('',#8680,1.666);
#7796=CYLINDRICAL_SURFACE('',#8681,1.666);
#7797=CYLINDRICAL_SURFACE('',#8682,1.666);
#7798=CYLINDRICAL_SURFACE('',#8684,1.666);
#7799=CYLINDRICAL_SURFACE('',#8685,2.05475);
#7800=CYLINDRICAL_SURFACE('',#8688,5.);
#7801=CYLINDRICAL_SURFACE('',#8711,5.00000000000001);
#7802=CYLINDRICAL_SURFACE('',#8720,3.5);
#7803=CYLINDRICAL_SURFACE('',#8722,3.5);
#7804=CYLINDRICAL_SURFACE('',#8724,3.5);
#7805=CYLINDRICAL_SURFACE('',#8726,3.5);
#7806=CYLINDRICAL_SURFACE('',#8732,3.5);
#7807=CYLINDRICAL_SURFACE('',#8735,3.5);
#7808=CYLINDRICAL_SURFACE('',#8738,3.5);
#7809=CYLINDRICAL_SURFACE('',#8741,3.5);
#7810=CYLINDRICAL_SURFACE('',#8755,2.5);
#7811=CYLINDRICAL_SURFACE('',#8758,2.5);
#7812=CYLINDRICAL_SURFACE('',#8761,2.5);
#7813=CYLINDRICAL_SURFACE('',#8764,2.5);
#7814=CYLINDRICAL_SURFACE('',#8774,2.37175);
#7815=CYLINDRICAL_SURFACE('',#8776,2.37175);
#7816=CYLINDRICAL_SURFACE('',#8777,2.37175);
#7817=CYLINDRICAL_SURFACE('',#8778,2.37175);
#7818=CYLINDRICAL_SURFACE('',#8779,2.37175);
#7819=CYLINDRICAL_SURFACE('',#8780,2.37175);
#7820=CYLINDRICAL_SURFACE('',#8781,2.37175);
#7821=CYLINDRICAL_SURFACE('',#8782,2.37175);
#7822=CYLINDRICAL_SURFACE('',#8783,2.37175);
#7823=CYLINDRICAL_SURFACE('',#8784,2.37175);
#7824=CYLINDRICAL_SURFACE('',#8785,2.37175);
#7825=CYLINDRICAL_SURFACE('',#8786,2.37175);
#7826=CYLINDRICAL_SURFACE('',#8787,2.37175);
#7827=CYLINDRICAL_SURFACE('',#8788,2.37175);
#7828=CYLINDRICAL_SURFACE('',#8789,2.37175);
#7829=CYLINDRICAL_SURFACE('',#8790,2.942);
#7830=CYLINDRICAL_SURFACE('',#8793,2.37175);
#7831=CYLINDRICAL_SURFACE('',#8806,5.);
#7832=CYLINDRICAL_SURFACE('',#8811,1.5555);
#7833=CYLINDRICAL_SURFACE('',#8813,1.5555);
#7834=CYLINDRICAL_SURFACE('',#8814,1.5555);
#7835=CYLINDRICAL_SURFACE('',#8815,1.5555);
#7836=CYLINDRICAL_SURFACE('',#8816,1.5555);
#7837=CYLINDRICAL_SURFACE('',#8817,1.5555);
#7838=CYLINDRICAL_SURFACE('',#8818,1.5555);
#7839=CYLINDRICAL_SURFACE('',#8819,1.5555);
#7840=CYLINDRICAL_SURFACE('',#8820,1.5555);
#7841=CYLINDRICAL_SURFACE('',#8821,1.5555);
#7842=CYLINDRICAL_SURFACE('',#8822,1.5555);
#7843=CYLINDRICAL_SURFACE('',#8823,1.5555);
#7844=CYLINDRICAL_SURFACE('',#8824,1.5555);
#7845=CYLINDRICAL_SURFACE('',#8825,1.954);
#7846=CYLINDRICAL_SURFACE('',#8828,1.5555);
#7847=CYLINDRICAL_SURFACE('',#8841,3.5);
#7848=CYLINDRICAL_SURFACE('',#8846,9.37025);
#7849=CYLINDRICAL_SURFACE('',#8848,9.37025);
#7850=CYLINDRICAL_SURFACE('',#8849,9.37025);
#7851=CYLINDRICAL_SURFACE('',#8850,9.37025);
#7852=CYLINDRICAL_SURFACE('',#8851,9.37025);
#7853=CYLINDRICAL_SURFACE('',#8852,9.37025);
#7854=CYLINDRICAL_SURFACE('',#8853,9.37025);
#7855=CYLINDRICAL_SURFACE('',#8854,9.37025);
#7856=CYLINDRICAL_SURFACE('',#8855,9.37025);
#7857=CYLINDRICAL_SURFACE('',#8856,9.37025);
#7858=CYLINDRICAL_SURFACE('',#8857,9.37025);
#7859=CYLINDRICAL_SURFACE('',#8858,9.37025);
#7860=CYLINDRICAL_SURFACE('',#8859,9.37025);
#7861=CYLINDRICAL_SURFACE('',#8860,9.37025);
#7862=CYLINDRICAL_SURFACE('',#8861,9.942);
#7863=CYLINDRICAL_SURFACE('',#8863,9.942);
#7864=CYLINDRICAL_SURFACE('',#8864,9.942);
#7865=CYLINDRICAL_SURFACE('',#8865,9.942);
#7866=CYLINDRICAL_SURFACE('',#8866,9.942);
#7867=CYLINDRICAL_SURFACE('',#8867,9.942);
#7868=CYLINDRICAL_SURFACE('',#8868,9.942);
#7869=CYLINDRICAL_SURFACE('',#8869,9.942);
#7870=CYLINDRICAL_SURFACE('',#8870,9.942);
#7871=CYLINDRICAL_SURFACE('',#8871,9.942);
#7872=CYLINDRICAL_SURFACE('',#8872,9.942);
#7873=CYLINDRICAL_SURFACE('',#8873,9.942);
#7874=CYLINDRICAL_SURFACE('',#8874,9.942);
#7875=CYLINDRICAL_SURFACE('',#8875,9.942);
#7876=CYLINDRICAL_SURFACE('',#8876,9.942);
#7877=CYLINDRICAL_SURFACE('',#8878,9.37025);
#7878=CYLINDRICAL_SURFACE('',#8882,14.);
#7879=CYLINDRICAL_SURFACE('',#8884,5.);
#7880=CYLINDRICAL_SURFACE('',#8890,10.076);
#7881=CYLINDRICAL_SURFACE('',#8892,10.076);
#7882=CYLINDRICAL_SURFACE('',#8893,10.076);
#7883=CYLINDRICAL_SURFACE('',#8894,10.076);
#7884=CYLINDRICAL_SURFACE('',#8896,9.5175);
#7885=CYLINDRICAL_SURFACE('',#8898,9.5175);
#7886=CYLINDRICAL_SURFACE('',#8899,9.5175);
#7887=CYLINDRICAL_SURFACE('',#8900,9.5175);
#7888=CYLINDRICAL_SURFACE('',#8902,9.5175);
#7889=CYLINDRICAL_SURFACE('',#8903,10.076);
#7890=CYLINDRICAL_SURFACE('',#8904,1.);
#7891=CYLINDRICAL_SURFACE('',#8907,1.);
#7892=CYLINDRICAL_SURFACE('',#8912,14.);
#7893=CYLINDRICAL_SURFACE('',#8916,3.);
#7894=CYLINDRICAL_SURFACE('',#8919,5.);
#7895=ADVANCED_FACE('',(#1158),#7658,.F.);
#7896=ADVANCED_FACE('',(#1159),#7659,.F.);
#7897=ADVANCED_FACE('',(#1160),#7660,.F.);
#7898=ADVANCED_FACE('',(#1161),#7661,.F.);
#7899=ADVANCED_FACE('',(#1162),#1058,.T.);
#7900=ADVANCED_FACE('',(#1163),#1059,.T.);
#7901=ADVANCED_FACE('',(#1164),#1060,.T.);
#7902=ADVANCED_FACE('',(#1165),#1061,.T.);
#7903=ADVANCED_FACE('',(#1166,#996,#997,#998,#999),#1062,.T.);
#7904=ADVANCED_FACE('',(#1167,#1000,#1001,#1002,#1003),#1063,.F.);
#7905=ADVANCED_FACE('',(#1168),#7662,.F.);
#7906=ADVANCED_FACE('',(#1169),#7663,.F.);
#7907=ADVANCED_FACE('',(#1170,#1004,#1005),#1064,.T.);
#7908=ADVANCED_FACE('',(#1171),#1065,.T.);
#7909=ADVANCED_FACE('',(#1172,#1006,#1007),#1066,.T.);
#7910=ADVANCED_FACE('',(#1173),#1067,.T.);
#7911=ADVANCED_FACE('',(#1174),#1068,.T.);
#7912=ADVANCED_FACE('',(#1175),#1069,.F.);
#7913=ADVANCED_FACE('',(#1176),#1070,.T.);
#7914=ADVANCED_FACE('',(#1177),#1071,.T.);
#7915=ADVANCED_FACE('',(#1178),#1072,.T.);
#7916=ADVANCED_FACE('',(#1179),#1073,.T.);
#7917=ADVANCED_FACE('',(#1180),#1074,.T.);
#7918=ADVANCED_FACE('',(#1181),#1075,.F.);
#7919=ADVANCED_FACE('',(#1182),#7664,.F.);
#7920=ADVANCED_FACE('',(#1183),#1076,.F.);
#7921=ADVANCED_FACE('',(#1184),#7665,.F.);
#7922=ADVANCED_FACE('',(#1185),#1077,.F.);
#7923=ADVANCED_FACE('',(#1186),#7666,.F.);
#7924=ADVANCED_FACE('',(#1187),#1078,.F.);
#7925=ADVANCED_FACE('',(#1188),#7667,.F.);
#7926=ADVANCED_FACE('',(#1189),#1079,.F.);
#7927=ADVANCED_FACE('',(#1190),#7668,.F.);
#7928=ADVANCED_FACE('',(#1191),#1080,.F.);
#7929=ADVANCED_FACE('',(#1192),#7669,.F.);
#7930=ADVANCED_FACE('',(#1193),#1081,.F.);
#7931=ADVANCED_FACE('',(#1194),#7670,.F.);
#7932=ADVANCED_FACE('',(#1195),#1082,.F.);
#7933=ADVANCED_FACE('',(#1196),#7671,.F.);
#7934=ADVANCED_FACE('',(#1197),#1083,.F.);
#7935=ADVANCED_FACE('',(#1198),#1084,.T.);
#7936=ADVANCED_FACE('',(#1199,#1008,#1009),#1085,.T.);
#7937=ADVANCED_FACE('',(#1200),#1086,.T.);
#7938=ADVANCED_FACE('',(#1201,#1010,#1011),#1087,.T.);
#7939=ADVANCED_FACE('',(#1202),#1088,.T.);
#7940=ADVANCED_FACE('',(#1203),#1089,.F.);
#7941=ADVANCED_FACE('',(#1204),#7672,.F.);
#7942=ADVANCED_FACE('',(#1205),#7673,.F.);
#7943=ADVANCED_FACE('',(#1206),#7674,.F.);
#7944=ADVANCED_FACE('',(#1207),#7675,.F.);
#7945=ADVANCED_FACE('',(#1208),#7676,.F.);
#7946=ADVANCED_FACE('',(#1209),#7677,.F.);
#7947=ADVANCED_FACE('',(#1210),#7678,.F.);
#7948=ADVANCED_FACE('',(#1211),#7679,.F.);
#7949=ADVANCED_FACE('',(#1212),#7680,.F.);
#7950=ADVANCED_FACE('',(#1213),#7681,.F.);
#7951=ADVANCED_FACE('',(#1214),#7682,.F.);
#7952=ADVANCED_FACE('',(#1215),#7683,.F.);
#7953=ADVANCED_FACE('',(#1216),#7684,.F.);
#7954=ADVANCED_FACE('',(#1217),#7685,.F.);
#7955=ADVANCED_FACE('',(#1218),#7686,.F.);
#7956=ADVANCED_FACE('',(#1219),#7687,.F.);
#7957=ADVANCED_FACE('',(#1220),#7688,.F.);
#7958=ADVANCED_FACE('',(#1221),#7689,.F.);
#7959=ADVANCED_FACE('',(#1222),#7690,.F.);
#7960=ADVANCED_FACE('',(#1223),#7691,.F.);
#7961=ADVANCED_FACE('',(#1224),#7692,.F.);
#7962=ADVANCED_FACE('',(#1225),#7693,.F.);
#7963=ADVANCED_FACE('',(#1226),#7694,.F.);
#7964=ADVANCED_FACE('',(#1227),#7695,.F.);
#7965=ADVANCED_FACE('',(#1228),#7696,.F.);
#7966=ADVANCED_FACE('',(#1229),#7697,.F.);
#7967=ADVANCED_FACE('',(#1230),#7698,.F.);
#7968=ADVANCED_FACE('',(#1231),#7699,.F.);
#7969=ADVANCED_FACE('',(#1232),#7700,.F.);
#7970=ADVANCED_FACE('',(#1233),#7701,.F.);
#7971=ADVANCED_FACE('',(#1234),#7702,.F.);
#7972=ADVANCED_FACE('',(#1235),#7703,.F.);
#7973=ADVANCED_FACE('',(#1236),#7704,.F.);
#7974=ADVANCED_FACE('',(#1237),#7705,.F.);
#7975=ADVANCED_FACE('',(#1238),#7706,.F.);
#7976=ADVANCED_FACE('',(#1239),#7707,.F.);
#7977=ADVANCED_FACE('',(#1240),#7708,.F.);
#7978=ADVANCED_FACE('',(#1241),#7709,.F.);
#7979=ADVANCED_FACE('',(#1242),#7710,.F.);
#7980=ADVANCED_FACE('',(#1243),#7711,.F.);
#7981=ADVANCED_FACE('',(#1244),#7712,.F.);
#7982=ADVANCED_FACE('',(#1245),#7713,.F.);
#7983=ADVANCED_FACE('',(#1246),#7714,.F.);
#7984=ADVANCED_FACE('',(#1247),#7715,.F.);
#7985=ADVANCED_FACE('',(#1248),#7716,.F.);
#7986=ADVANCED_FACE('',(#1249),#7717,.F.);
#7987=ADVANCED_FACE('',(#1250),#7718,.F.);
#7988=ADVANCED_FACE('',(#1251),#7719,.F.);
#7989=ADVANCED_FACE('',(#1252),#7720,.F.);
#7990=ADVANCED_FACE('',(#1253),#7721,.F.);
#7991=ADVANCED_FACE('',(#1254),#7722,.F.);
#7992=ADVANCED_FACE('',(#1255),#7723,.F.);
#7993=ADVANCED_FACE('',(#1256),#7724,.F.);
#7994=ADVANCED_FACE('',(#1257),#7725,.F.);
#7995=ADVANCED_FACE('',(#1258),#7726,.F.);
#7996=ADVANCED_FACE('',(#1259),#7727,.F.);
#7997=ADVANCED_FACE('',(#1260),#7728,.F.);
#7998=ADVANCED_FACE('',(#1261),#7729,.F.);
#7999=ADVANCED_FACE('',(#1262),#7730,.F.);
#8000=ADVANCED_FACE('',(#1263),#7731,.F.);
#8001=ADVANCED_FACE('',(#1264),#7732,.F.);
#8002=ADVANCED_FACE('',(#1265),#7733,.F.);
#8003=ADVANCED_FACE('',(#1266),#7734,.F.);
#8004=ADVANCED_FACE('',(#1267),#7735,.F.);
#8005=ADVANCED_FACE('',(#1268),#7736,.F.);
#8006=ADVANCED_FACE('',(#1269),#7737,.F.);
#8007=ADVANCED_FACE('',(#1270),#7738,.F.);
#8008=ADVANCED_FACE('',(#1271),#7739,.F.);
#8009=ADVANCED_FACE('',(#1272),#7740,.F.);
#8010=ADVANCED_FACE('',(#1273),#7741,.F.);
#8011=ADVANCED_FACE('',(#1274),#7742,.F.);
#8012=ADVANCED_FACE('',(#1275),#7743,.F.);
#8013=ADVANCED_FACE('',(#1276),#7744,.F.);
#8014=ADVANCED_FACE('',(#1277),#7745,.F.);
#8015=ADVANCED_FACE('',(#1278),#7746,.F.);
#8016=ADVANCED_FACE('',(#1279),#7747,.F.);
#8017=ADVANCED_FACE('',(#1280),#7748,.F.);
#8018=ADVANCED_FACE('',(#1281),#7749,.F.);
#8019=ADVANCED_FACE('',(#1282),#7750,.F.);
#8020=ADVANCED_FACE('',(#1283),#7751,.F.);
#8021=ADVANCED_FACE('',(#1284),#1090,.F.);
#8022=ADVANCED_FACE('',(#1285),#154,.F.);
#8023=ADVANCED_FACE('',(#1286),#155,.F.);
#8024=ADVANCED_FACE('',(#1287),#1091,.F.);
#8025=ADVANCED_FACE('',(#1288),#1092,.T.);
#8026=ADVANCED_FACE('',(#1289),#156,.F.);
#8027=ADVANCED_FACE('',(#1290),#157,.F.);
#8028=ADVANCED_FACE('',(#1291),#1093,.F.);
#8029=ADVANCED_FACE('',(#1292),#7752,.T.);
#8030=ADVANCED_FACE('',(#1293,#1012),#1094,.T.);
#8031=ADVANCED_FACE('',(#1294,#1013),#1095,.F.);
#8032=ADVANCED_FACE('',(#1295),#7753,.T.);
#8033=ADVANCED_FACE('',(#1296),#7754,.T.);
#8034=ADVANCED_FACE('',(#1297),#7755,.T.);
#8035=ADVANCED_FACE('',(#1298),#7756,.T.);
#8036=ADVANCED_FACE('',(#1299),#7757,.T.);
#8037=ADVANCED_FACE('',(#1300),#7758,.T.);
#8038=ADVANCED_FACE('',(#1301),#7759,.T.);
#8039=ADVANCED_FACE('',(#1302),#7760,.T.);
#8040=ADVANCED_FACE('',(#1303),#7761,.T.);
#8041=ADVANCED_FACE('',(#1304),#7762,.T.);
#8042=ADVANCED_FACE('',(#1305),#7763,.T.);
#8043=ADVANCED_FACE('',(#1306),#7764,.T.);
#8044=ADVANCED_FACE('',(#1307),#7765,.T.);
#8045=ADVANCED_FACE('',(#1308),#151,.T.);
#8046=ADVANCED_FACE('',(#1309),#158,.F.);
#8047=ADVANCED_FACE('',(#1310),#159,.F.);
#8048=ADVANCED_FACE('',(#1311),#1096,.F.);
#8049=ADVANCED_FACE('',(#1312),#1097,.F.);
#8050=ADVANCED_FACE('',(#1313),#1098,.F.);
#8051=ADVANCED_FACE('',(#1314),#1099,.F.);
#8052=ADVANCED_FACE('',(#1315),#1100,.F.);
#8053=ADVANCED_FACE('',(#1316),#1101,.F.);
#8054=ADVANCED_FACE('',(#1317),#1102,.F.);
#8055=ADVANCED_FACE('',(#1318,#1014),#1103,.T.);
#8056=ADVANCED_FACE('',(#1319),#7766,.T.);
#8057=ADVANCED_FACE('',(#1320,#1015),#1104,.F.);
#8058=ADVANCED_FACE('',(#1321),#1105,.T.);
#8059=ADVANCED_FACE('',(#1322),#7767,.F.);
#8060=ADVANCED_FACE('',(#1323),#7768,.F.);
#8061=ADVANCED_FACE('',(#1324),#7769,.F.);
#8062=ADVANCED_FACE('',(#1325),#7770,.F.);
#8063=ADVANCED_FACE('',(#1326),#7771,.F.);
#8064=ADVANCED_FACE('',(#1327),#7772,.F.);
#8065=ADVANCED_FACE('',(#1328),#7773,.F.);
#8066=ADVANCED_FACE('',(#1329),#7774,.F.);
#8067=ADVANCED_FACE('',(#1330),#7775,.F.);
#8068=ADVANCED_FACE('',(#1331),#7776,.F.);
#8069=ADVANCED_FACE('',(#1332),#7777,.F.);
#8070=ADVANCED_FACE('',(#1333),#7778,.F.);
#8071=ADVANCED_FACE('',(#1334),#7779,.F.);
#8072=ADVANCED_FACE('',(#1335),#7780,.F.);
#8073=ADVANCED_FACE('',(#1336),#7781,.F.);
#8074=ADVANCED_FACE('',(#1337),#7782,.F.);
#8075=ADVANCED_FACE('',(#1338),#7783,.F.);
#8076=ADVANCED_FACE('',(#1339),#7784,.F.);
#8077=ADVANCED_FACE('',(#1340),#7785,.F.);
#8078=ADVANCED_FACE('',(#1341),#7786,.F.);
#8079=ADVANCED_FACE('',(#1342),#7787,.F.);
#8080=ADVANCED_FACE('',(#1343),#7788,.F.);
#8081=ADVANCED_FACE('',(#1344),#7789,.F.);
#8082=ADVANCED_FACE('',(#1345),#7790,.F.);
#8083=ADVANCED_FACE('',(#1346),#7791,.F.);
#8084=ADVANCED_FACE('',(#1347),#7792,.F.);
#8085=ADVANCED_FACE('',(#1348),#7793,.F.);
#8086=ADVANCED_FACE('',(#1349),#7794,.F.);
#8087=ADVANCED_FACE('',(#1350),#7795,.F.);
#8088=ADVANCED_FACE('',(#1351),#7796,.F.);
#8089=ADVANCED_FACE('',(#1352),#7797,.F.);
#8090=ADVANCED_FACE('',(#1353),#7798,.F.);
#8091=ADVANCED_FACE('',(#1354),#7799,.F.);
#8092=ADVANCED_FACE('',(#1355),#1106,.T.);
#8093=ADVANCED_FACE('',(#1356),#160,.F.);
#8094=ADVANCED_FACE('',(#1357),#161,.F.);
#8095=ADVANCED_FACE('',(#1358),#1107,.F.);
#8096=ADVANCED_FACE('',(#1359),#7800,.T.);
#8097=ADVANCED_FACE('',(#1360,#1016),#1108,.T.);
#8098=ADVANCED_FACE('',(#1361),#1109,.F.);
#8099=ADVANCED_FACE('',(#1362),#7801,.T.);
#8100=ADVANCED_FACE('',(#1363,#1017,#1018,#1019,#1020),#1110,.T.);
#8101=ADVANCED_FACE('',(#1364),#1111,.T.);
#8102=ADVANCED_FACE('',(#1365),#7802,.F.);
#8103=ADVANCED_FACE('',(#1366),#7803,.F.);
#8104=ADVANCED_FACE('',(#1367),#7804,.F.);
#8105=ADVANCED_FACE('',(#1368),#7805,.F.);
#8106=ADVANCED_FACE('',(#1369),#1112,.T.);
#8107=ADVANCED_FACE('',(#1370),#1113,.T.);
#8108=ADVANCED_FACE('',(#1371,#1021,#1022,#1023,#1024),#1114,.F.);
#8109=ADVANCED_FACE('',(#1372),#7806,.F.);
#8110=ADVANCED_FACE('',(#1373),#7807,.F.);
#8111=ADVANCED_FACE('',(#1374),#7808,.F.);
#8112=ADVANCED_FACE('',(#1375),#7809,.F.);
#8113=ADVANCED_FACE('',(#1376),#1115,.T.);
#8114=ADVANCED_FACE('',(#1377),#1116,.T.);
#8115=ADVANCED_FACE('',(#1378),#1117,.T.);
#8116=ADVANCED_FACE('',(#1379),#1118,.T.);
#8117=ADVANCED_FACE('',(#1380),#1119,.T.);
#8118=ADVANCED_FACE('',(#1381),#1120,.T.);
#8119=ADVANCED_FACE('',(#1382),#1121,.T.);
#8120=ADVANCED_FACE('',(#1383),#1122,.T.);
#8121=ADVANCED_FACE('',(#1384,#1025,#1026,#1027,#1028,#1029),#1123,.T.);
#8122=ADVANCED_FACE('',(#1385,#1030,#1031,#1032,#1033,#1034),#1124,.F.);
#8123=ADVANCED_FACE('',(#1386),#7810,.F.);
#8124=ADVANCED_FACE('',(#1387),#7811,.F.);
#8125=ADVANCED_FACE('',(#1388),#7812,.F.);
#8126=ADVANCED_FACE('',(#1389),#7813,.F.);
#8127=ADVANCED_FACE('',(#1390),#1125,.T.);
#8128=ADVANCED_FACE('',(#1391),#1126,.T.);
#8129=ADVANCED_FACE('',(#1392),#1127,.T.);
#8130=ADVANCED_FACE('',(#1393),#1128,.T.);
#8131=ADVANCED_FACE('',(#1394,#1035,#1036,#1037,#1038),#1129,.T.);
#8132=ADVANCED_FACE('',(#1395,#1039,#1040,#1041,#1042),#1130,.F.);
#8133=ADVANCED_FACE('',(#1396),#7814,.T.);
#8134=ADVANCED_FACE('',(#1397),#7815,.T.);
#8135=ADVANCED_FACE('',(#1398),#7816,.T.);
#8136=ADVANCED_FACE('',(#1399),#7817,.T.);
#8137=ADVANCED_FACE('',(#1400),#7818,.T.);
#8138=ADVANCED_FACE('',(#1401),#7819,.T.);
#8139=ADVANCED_FACE('',(#1402),#7820,.T.);
#8140=ADVANCED_FACE('',(#1403),#7821,.T.);
#8141=ADVANCED_FACE('',(#1404),#7822,.T.);
#8142=ADVANCED_FACE('',(#1405),#7823,.T.);
#8143=ADVANCED_FACE('',(#1406),#7824,.T.);
#8144=ADVANCED_FACE('',(#1407),#7825,.T.);
#8145=ADVANCED_FACE('',(#1408),#7826,.T.);
#8146=ADVANCED_FACE('',(#1409),#7827,.T.);
#8147=ADVANCED_FACE('',(#1410),#7828,.T.);
#8148=ADVANCED_FACE('',(#1411),#7829,.T.);
#8149=ADVANCED_FACE('',(#1412),#7830,.T.);
#8150=ADVANCED_FACE('',(#1413),#152,.T.);
#8151=ADVANCED_FACE('',(#1414),#162,.F.);
#8152=ADVANCED_FACE('',(#1415),#163,.F.);
#8153=ADVANCED_FACE('',(#1416),#1131,.F.);
#8154=ADVANCED_FACE('',(#1417),#1132,.F.);
#8155=ADVANCED_FACE('',(#1418),#1133,.F.);
#8156=ADVANCED_FACE('',(#1419),#1134,.F.);
#8157=ADVANCED_FACE('',(#1420),#1135,.F.);
#8158=ADVANCED_FACE('',(#1421),#1136,.F.);
#8159=ADVANCED_FACE('',(#1422),#1137,.F.);
#8160=ADVANCED_FACE('',(#1423,#1043),#1138,.T.);
#8161=ADVANCED_FACE('',(#1424),#7831,.T.);
#8162=ADVANCED_FACE('',(#1425,#1044),#1139,.F.);
#8163=ADVANCED_FACE('',(#1426),#1140,.T.);
#8164=ADVANCED_FACE('',(#1427),#7832,.T.);
#8165=ADVANCED_FACE('',(#1428),#7833,.T.);
#8166=ADVANCED_FACE('',(#1429),#7834,.T.);
#8167=ADVANCED_FACE('',(#1430),#7835,.T.);
#8168=ADVANCED_FACE('',(#1431),#7836,.T.);
#8169=ADVANCED_FACE('',(#1432),#7837,.T.);
#8170=ADVANCED_FACE('',(#1433),#7838,.T.);
#8171=ADVANCED_FACE('',(#1434),#7839,.T.);
#8172=ADVANCED_FACE('',(#1435),#7840,.T.);
#8173=ADVANCED_FACE('',(#1436),#7841,.T.);
#8174=ADVANCED_FACE('',(#1437),#7842,.T.);
#8175=ADVANCED_FACE('',(#1438),#7843,.T.);
#8176=ADVANCED_FACE('',(#1439),#7844,.T.);
#8177=ADVANCED_FACE('',(#1440),#7845,.T.);
#8178=ADVANCED_FACE('',(#1441),#7846,.T.);
#8179=ADVANCED_FACE('',(#1442),#153,.T.);
#8180=ADVANCED_FACE('',(#1443),#164,.F.);
#8181=ADVANCED_FACE('',(#1444),#165,.F.);
#8182=ADVANCED_FACE('',(#1445),#1141,.F.);
#8183=ADVANCED_FACE('',(#1446),#1142,.F.);
#8184=ADVANCED_FACE('',(#1447),#1143,.F.);
#8185=ADVANCED_FACE('',(#1448),#1144,.F.);
#8186=ADVANCED_FACE('',(#1449),#1145,.F.);
#8187=ADVANCED_FACE('',(#1450),#1146,.F.);
#8188=ADVANCED_FACE('',(#1451),#1147,.F.);
#8189=ADVANCED_FACE('',(#1452,#1045),#1148,.T.);
#8190=ADVANCED_FACE('',(#1453),#7847,.T.);
#8191=ADVANCED_FACE('',(#1454,#1046),#1149,.F.);
#8192=ADVANCED_FACE('',(#1455),#1150,.T.);
#8193=ADVANCED_FACE('',(#1456),#7848,.T.);
#8194=ADVANCED_FACE('',(#1457),#7849,.T.);
#8195=ADVANCED_FACE('',(#1458),#7850,.T.);
#8196=ADVANCED_FACE('',(#1459),#7851,.T.);
#8197=ADVANCED_FACE('',(#1460),#7852,.T.);
#8198=ADVANCED_FACE('',(#1461),#7853,.T.);
#8199=ADVANCED_FACE('',(#1462),#7854,.T.);
#8200=ADVANCED_FACE('',(#1463),#7855,.T.);
#8201=ADVANCED_FACE('',(#1464),#7856,.T.);
#8202=ADVANCED_FACE('',(#1465),#7857,.T.);
#8203=ADVANCED_FACE('',(#1466),#7858,.T.);
#8204=ADVANCED_FACE('',(#1467),#7859,.T.);
#8205=ADVANCED_FACE('',(#1468),#7860,.T.);
#8206=ADVANCED_FACE('',(#1469),#7861,.T.);
#8207=ADVANCED_FACE('',(#1470),#7862,.T.);
#8208=ADVANCED_FACE('',(#1471),#7863,.T.);
#8209=ADVANCED_FACE('',(#1472),#7864,.T.);
#8210=ADVANCED_FACE('',(#1473),#7865,.T.);
#8211=ADVANCED_FACE('',(#1474),#7866,.T.);
#8212=ADVANCED_FACE('',(#1475),#7867,.T.);
#8213=ADVANCED_FACE('',(#1476),#7868,.T.);
#8214=ADVANCED_FACE('',(#1477),#7869,.T.);
#8215=ADVANCED_FACE('',(#1478),#7870,.T.);
#8216=ADVANCED_FACE('',(#1479),#7871,.T.);
#8217=ADVANCED_FACE('',(#1480),#7872,.T.);
#8218=ADVANCED_FACE('',(#1481),#7873,.T.);
#8219=ADVANCED_FACE('',(#1482),#7874,.T.);
#8220=ADVANCED_FACE('',(#1483),#7875,.T.);
#8221=ADVANCED_FACE('',(#1484),#7876,.T.);
#8222=ADVANCED_FACE('',(#1485),#7877,.T.);
#8223=ADVANCED_FACE('',(#1486),#166,.F.);
#8224=ADVANCED_FACE('',(#1487),#167,.F.);
#8225=ADVANCED_FACE('',(#1488,#1047),#1151,.T.);
#8226=ADVANCED_FACE('',(#1489),#7878,.T.);
#8227=ADVANCED_FACE('',(#1490),#7879,.F.);
#8228=ADVANCED_FACE('',(#1491,#1048),#1152,.T.);
#8229=ADVANCED_FACE('',(#1492,#1049),#1153,.F.);
#8230=ADVANCED_FACE('',(#1493),#7880,.F.);
#8231=ADVANCED_FACE('',(#1494),#7881,.F.);
#8232=ADVANCED_FACE('',(#1495),#7882,.F.);
#8233=ADVANCED_FACE('',(#1496),#7883,.F.);
#8234=ADVANCED_FACE('',(#1497),#7884,.F.);
#8235=ADVANCED_FACE('',(#1498),#7885,.F.);
#8236=ADVANCED_FACE('',(#1499),#7886,.F.);
#8237=ADVANCED_FACE('',(#1500),#7887,.F.);
#8238=ADVANCED_FACE('',(#1501),#7888,.F.);
#8239=ADVANCED_FACE('',(#1502),#7889,.F.);
#8240=ADVANCED_FACE('',(#1503),#7890,.F.);
#8241=ADVANCED_FACE('',(#1504),#7891,.F.);
#8242=ADVANCED_FACE('',(#1505),#168,.F.);
#8243=ADVANCED_FACE('',(#1506),#169,.F.);
#8244=ADVANCED_FACE('',(#1507,#1050,#1051,#1052),#1154,.T.);
#8245=ADVANCED_FACE('',(#1508),#7892,.T.);
#8246=ADVANCED_FACE('',(#1509,#1053,#1054,#1055),#1155,.F.);
#8247=ADVANCED_FACE('',(#1510),#7893,.F.);
#8248=ADVANCED_FACE('',(#1511),#7894,.T.);
#8249=ADVANCED_FACE('',(#1512,#1056),#1156,.T.);
#8250=ADVANCED_FACE('',(#1513,#1057),#1157,.F.);
#8251=CLOSED_SHELL('',(#7895,#7896,#7897,#7898,#7899,#7900,#7901,#7902,
#7903,#7904));
#8252=CLOSED_SHELL('',(#7905,#7906,#7907,#7908,#7909,#7910,#7911,#7912));
#8253=CLOSED_SHELL('',(#7913,#7914,#7915,#7916,#7917,#7918));
#8254=CLOSED_SHELL('',(#7919,#7920,#7921,#7922,#7923,#7924,#7925,#7926,
#7927,#7928,#7929,#7930,#7931,#7932,#7933,#7934,#7935,#7936,#7937,#7938,
#7939,#7940));
#8255=CLOSED_SHELL('',(#7941,#7942,#7943,#7944,#7945,#7946,#7947,#7948,
#7949,#7950,#7951,#7952,#7953,#7954,#7955,#7956,#7957,#7958,#7959,#7960,
#7961,#7962,#7963,#7964,#7965,#7966,#7967,#7968,#7969,#7970,#7971,#7972,
#7973,#7974,#7975,#7976,#7977,#7978,#7979,#7980,#7981,#7982,#7983,#7984,
#7985,#7986,#7987,#7988,#7989,#7990,#7991,#7992,#7993,#7994,#7995,#7996,
#7997,#7998,#7999,#8000,#8001,#8002,#8003,#8004,#8005,#8006,#8007,#8008,
#8009,#8010,#8011,#8012,#8013,#8014,#8015,#8016,#8017,#8018,#8019,#8020,
#8021,#8022,#8023,#8024,#8025,#8026,#8027,#8028,#8029,#8030,#8031));
#8256=CLOSED_SHELL('',(#8032,#8033,#8034,#8035,#8036,#8037,#8038,#8039,
#8040,#8041,#8042,#8043,#8044,#8045,#8046,#8047,#8048,#8049,#8050,#8051,
#8052,#8053,#8054,#8055,#8056,#8057,#8058));
#8257=CLOSED_SHELL('',(#8059,#8060,#8061,#8062,#8063,#8064,#8065,#8066,
#8067,#8068,#8069,#8070,#8071,#8072,#8073,#8074,#8075,#8076,#8077,#8078,
#8079,#8080,#8081,#8082,#8083,#8084,#8085,#8086,#8087,#8088,#8089,#8090,
#8091,#8092,#8093,#8094,#8095,#8096,#8097,#8098));
#8258=CLOSED_SHELL('',(#8099,#8100,#8101,#8102,#8103,#8104,#8105,#8106,
#8107,#8108));
#8259=CLOSED_SHELL('',(#8109,#8110,#8111,#8112,#8113,#8114,#8115,#8116,
#8117,#8118,#8119,#8120,#8121,#8122));
#8260=CLOSED_SHELL('',(#8123,#8124,#8125,#8126,#8127,#8128,#8129,#8130,
#8131,#8132));
#8261=CLOSED_SHELL('',(#8133,#8134,#8135,#8136,#8137,#8138,#8139,#8140,
#8141,#8142,#8143,#8144,#8145,#8146,#8147,#8148,#8149,#8150,#8151,#8152,
#8153,#8154,#8155,#8156,#8157,#8158,#8159,#8160,#8161,#8162,#8163));
#8262=CLOSED_SHELL('',(#8164,#8165,#8166,#8167,#8168,#8169,#8170,#8171,
#8172,#8173,#8174,#8175,#8176,#8177,#8178,#8179,#8180,#8181,#8182,#8183,
#8184,#8185,#8186,#8187,#8188,#8189,#8190,#8191,#8192));
#8263=CLOSED_SHELL('',(#8193,#8194,#8195,#8196,#8197,#8198,#8199,#8200,
#8201,#8202,#8203,#8204,#8205,#8206,#8207,#8208,#8209,#8210,#8211,#8212,
#8213,#8214,#8215,#8216,#8217,#8218,#8219,#8220,#8221,#8222,#8223,#8224,
#8225,#8226,#8227,#8228,#8229));
#8264=CLOSED_SHELL('',(#8230,#8231,#8232,#8233,#8234,#8235,#8236,#8237,
#8238,#8239,#8240,#8241,#8242,#8243,#8244,#8245,#8246));
#8265=CLOSED_SHELL('',(#8247,#8248,#8249,#8250));
#8266=DERIVED_UNIT_ELEMENT(#8296,1.);
#8267=DERIVED_UNIT_ELEMENT(#94414,-3.);
#8268=DERIVED_UNIT_ELEMENT(#8296,1.);
#8269=DERIVED_UNIT_ELEMENT(#94414,-3.);
#8270=DERIVED_UNIT_ELEMENT(#8296,1.);
#8271=DERIVED_UNIT_ELEMENT(#94414,-3.);
#8272=DERIVED_UNIT_ELEMENT(#8296,1.);
#8273=DERIVED_UNIT_ELEMENT(#94414,-3.);
#8274=DERIVED_UNIT_ELEMENT(#8296,1.);
#8275=DERIVED_UNIT_ELEMENT(#94414,-3.);
#8276=DERIVED_UNIT_ELEMENT(#8296,1.);
#8277=DERIVED_UNIT_ELEMENT(#94414,-3.);
#8278=DERIVED_UNIT_ELEMENT(#8296,1.);
#8279=DERIVED_UNIT_ELEMENT(#94414,-3.);
#8280=DERIVED_UNIT_ELEMENT(#8296,1.);
#8281=DERIVED_UNIT_ELEMENT(#94414,-3.);
#8282=DERIVED_UNIT_ELEMENT(#8296,1.);
#8283=DERIVED_UNIT_ELEMENT(#94414,-3.);
#8284=DERIVED_UNIT_ELEMENT(#8296,1.);
#8285=DERIVED_UNIT_ELEMENT(#94414,-3.);
#8286=DERIVED_UNIT_ELEMENT(#8296,1.);
#8287=DERIVED_UNIT_ELEMENT(#94414,-3.);
#8288=DERIVED_UNIT_ELEMENT(#8296,1.);
#8289=DERIVED_UNIT_ELEMENT(#94414,-3.);
#8290=DERIVED_UNIT_ELEMENT(#8296,1.);
#8291=DERIVED_UNIT_ELEMENT(#94414,-3.);
#8292=DERIVED_UNIT_ELEMENT(#8296,1.);
#8293=DERIVED_UNIT_ELEMENT(#94414,-3.);
#8294=DERIVED_UNIT_ELEMENT(#8296,1.);
#8295=DERIVED_UNIT_ELEMENT(#94414,-3.);
#8296=(
MASS_UNIT()
NAMED_UNIT(*)
SI_UNIT(.KILO.,.GRAM.)
);
#8297=DERIVED_UNIT((#8266,#8267));
#8298=DERIVED_UNIT((#8268,#8269));
#8299=DERIVED_UNIT((#8270,#8271));
#8300=DERIVED_UNIT((#8272,#8273));
#8301=DERIVED_UNIT((#8274,#8275));
#8302=DERIVED_UNIT((#8276,#8277));
#8303=DERIVED_UNIT((#8278,#8279));
#8304=DERIVED_UNIT((#8280,#8281));
#8305=DERIVED_UNIT((#8282,#8283));
#8306=DERIVED_UNIT((#8284,#8285));
#8307=DERIVED_UNIT((#8286,#8287));
#8308=DERIVED_UNIT((#8288,#8289));
#8309=DERIVED_UNIT((#8290,#8291));
#8310=DERIVED_UNIT((#8292,#8293));
#8311=DERIVED_UNIT((#8294,#8295));
#8312=MEASURE_REPRESENTATION_ITEM('density measure',
POSITIVE_RATIO_MEASURE(7850.),#8297);
#8313=MEASURE_REPRESENTATION_ITEM('density measure',
POSITIVE_RATIO_MEASURE(7850.),#8298);
#8314=MEASURE_REPRESENTATION_ITEM('density measure',
POSITIVE_RATIO_MEASURE(7850.),#8299);
#8315=MEASURE_REPRESENTATION_ITEM('density measure',
POSITIVE_RATIO_MEASURE(7850.),#8300);
#8316=MEASURE_REPRESENTATION_ITEM('density measure',
POSITIVE_RATIO_MEASURE(7850.),#8301);
#8317=MEASURE_REPRESENTATION_ITEM('density measure',
POSITIVE_RATIO_MEASURE(7850.),#8302);
#8318=MEASURE_REPRESENTATION_ITEM('density measure',
POSITIVE_RATIO_MEASURE(7850.),#8303);
#8319=MEASURE_REPRESENTATION_ITEM('density measure',
POSITIVE_RATIO_MEASURE(7850.),#8304);
#8320=MEASURE_REPRESENTATION_ITEM('density measure',
POSITIVE_RATIO_MEASURE(1250.),#8305);
#8321=MEASURE_REPRESENTATION_ITEM('density measure',
POSITIVE_RATIO_MEASURE(7850.),#8306);
#8322=MEASURE_REPRESENTATION_ITEM('density measure',
POSITIVE_RATIO_MEASURE(7850.),#8307);
#8323=MEASURE_REPRESENTATION_ITEM('density measure',
POSITIVE_RATIO_MEASURE(7850.),#8308);
#8324=MEASURE_REPRESENTATION_ITEM('density measure',
POSITIVE_RATIO_MEASURE(7850.),#8309);
#8325=MEASURE_REPRESENTATION_ITEM('density measure',
POSITIVE_RATIO_MEASURE(7850.),#8310);
#8326=MEASURE_REPRESENTATION_ITEM('density measure',
POSITIVE_RATIO_MEASURE(1200.),#8311);
#8327=PROPERTY_DEFINITION_REPRESENTATION(#8402,#8357);
#8328=PROPERTY_DEFINITION_REPRESENTATION(#8403,#8358);
#8329=PROPERTY_DEFINITION_REPRESENTATION(#8404,#8359);
#8330=PROPERTY_DEFINITION_REPRESENTATION(#8405,#8360);
#8331=PROPERTY_DEFINITION_REPRESENTATION(#8406,#8361);
#8332=PROPERTY_DEFINITION_REPRESENTATION(#8407,#8362);
#8333=PROPERTY_DEFINITION_REPRESENTATION(#8408,#8363);
#8334=PROPERTY_DEFINITION_REPRESENTATION(#8409,#8364);
#8335=PROPERTY_DEFINITION_REPRESENTATION(#8410,#8365);
#8336=PROPERTY_DEFINITION_REPRESENTATION(#8411,#8366);
#8337=PROPERTY_DEFINITION_REPRESENTATION(#8412,#8367);
#8338=PROPERTY_DEFINITION_REPRESENTATION(#8413,#8368);
#8339=PROPERTY_DEFINITION_REPRESENTATION(#8414,#8369);
#8340=PROPERTY_DEFINITION_REPRESENTATION(#8415,#8370);
#8341=PROPERTY_DEFINITION_REPRESENTATION(#8416,#8371);
#8342=PROPERTY_DEFINITION_REPRESENTATION(#8417,#8372);
#8343=PROPERTY_DEFINITION_REPRESENTATION(#8418,#8373);
#8344=PROPERTY_DEFINITION_REPRESENTATION(#8419,#8374);
#8345=PROPERTY_DEFINITION_REPRESENTATION(#8420,#8375);
#8346=PROPERTY_DEFINITION_REPRESENTATION(#8421,#8376);
#8347=PROPERTY_DEFINITION_REPRESENTATION(#8422,#8377);
#8348=PROPERTY_DEFINITION_REPRESENTATION(#8423,#8378);
#8349=PROPERTY_DEFINITION_REPRESENTATION(#8424,#8379);
#8350=PROPERTY_DEFINITION_REPRESENTATION(#8425,#8380);
#8351=PROPERTY_DEFINITION_REPRESENTATION(#8426,#8381);
#8352=PROPERTY_DEFINITION_REPRESENTATION(#8427,#8382);
#8353=PROPERTY_DEFINITION_REPRESENTATION(#8428,#8383);
#8354=PROPERTY_DEFINITION_REPRESENTATION(#8429,#8384);
#8355=PROPERTY_DEFINITION_REPRESENTATION(#8430,#8385);
#8356=PROPERTY_DEFINITION_REPRESENTATION(#8431,#8386);
#8357=REPRESENTATION('material name',(#8387),#94397);
#8358=REPRESENTATION('density',(#8312),#94397);
#8359=REPRESENTATION('material name',(#8388),#94398);
#8360=REPRESENTATION('density',(#8313),#94398);
#8361=REPRESENTATION('material name',(#8389),#94399);
#8362=REPRESENTATION('density',(#8314),#94399);
#8363=REPRESENTATION('material name',(#8390),#94400);
#8364=REPRESENTATION('density',(#8315),#94400);
#8365=REPRESENTATION('material name',(#8391),#94401);
#8366=REPRESENTATION('density',(#8316),#94401);
#8367=REPRESENTATION('material name',(#8392),#94402);
#8368=REPRESENTATION('density',(#8317),#94402);
#8369=REPRESENTATION('material name',(#8393),#94403);
#8370=REPRESENTATION('density',(#8318),#94403);
#8371=REPRESENTATION('material name',(#8394),#94404);
#8372=REPRESENTATION('density',(#8319),#94404);
#8373=REPRESENTATION('material name',(#8395),#94405);
#8374=REPRESENTATION('density',(#8320),#94405);
#8375=REPRESENTATION('material name',(#8396),#94406);
#8376=REPRESENTATION('density',(#8321),#94406);
#8377=REPRESENTATION('material name',(#8397),#94407);
#8378=REPRESENTATION('density',(#8322),#94407);
#8379=REPRESENTATION('material name',(#8398),#94408);
#8380=REPRESENTATION('density',(#8323),#94408);
#8381=REPRESENTATION('material name',(#8399),#94409);
#8382=REPRESENTATION('density',(#8324),#94409);
#8383=REPRESENTATION('material name',(#8400),#94410);
#8384=REPRESENTATION('density',(#8325),#94410);
#8385=REPRESENTATION('material name',(#8401),#94411);
#8386=REPRESENTATION('density',(#8326),#94411);
#8387=DESCRIPTIVE_REPRESENTATION_ITEM('Steel','Steel');
#8388=DESCRIPTIVE_REPRESENTATION_ITEM('Steel','Steel');
#8389=DESCRIPTIVE_REPRESENTATION_ITEM('Steel','Steel');
#8390=DESCRIPTIVE_REPRESENTATION_ITEM('Steel','Steel');
#8391=DESCRIPTIVE_REPRESENTATION_ITEM('Steel','Steel');
#8392=DESCRIPTIVE_REPRESENTATION_ITEM('Steel','Steel');
#8393=DESCRIPTIVE_REPRESENTATION_ITEM('Steel','Steel');
#8394=DESCRIPTIVE_REPRESENTATION_ITEM('Steel','Steel');
#8395=DESCRIPTIVE_REPRESENTATION_ITEM('Rubber, Silicone',
'Rubber, Silicone');
#8396=DESCRIPTIVE_REPRESENTATION_ITEM('Steel','Steel');
#8397=DESCRIPTIVE_REPRESENTATION_ITEM('Steel','Steel');
#8398=DESCRIPTIVE_REPRESENTATION_ITEM('Steel','Steel');
#8399=DESCRIPTIVE_REPRESENTATION_ITEM('Steel','Steel');
#8400=DESCRIPTIVE_REPRESENTATION_ITEM('Steel','Steel');
#8401=DESCRIPTIVE_REPRESENTATION_ITEM('Rubber, Nitrile',
'Rubber, Nitrile');
#8402=PROPERTY_DEFINITION('material property','material name',#94506);
#8403=PROPERTY_DEFINITION('material property','density of part',#94506);
#8404=PROPERTY_DEFINITION('material property','material name',#94507);
#8405=PROPERTY_DEFINITION('material property','density of part',#94507);
#8406=PROPERTY_DEFINITION('material property','material name',#94508);
#8407=PROPERTY_DEFINITION('material property','density of part',#94508);
#8408=PROPERTY_DEFINITION('material property','material name',#94509);
#8409=PROPERTY_DEFINITION('material property','density of part',#94509);
#8410=PROPERTY_DEFINITION('material property','material name',#94510);
#8411=PROPERTY_DEFINITION('material property','density of part',#94510);
#8412=PROPERTY_DEFINITION('material property','material name',#94511);
#8413=PROPERTY_DEFINITION('material property','density of part',#94511);
#8414=PROPERTY_DEFINITION('material property','material name',#94512);
#8415=PROPERTY_DEFINITION('material property','density of part',#94512);
#8416=PROPERTY_DEFINITION('material property','material name',#94513);
#8417=PROPERTY_DEFINITION('material property','density of part',#94513);
#8418=PROPERTY_DEFINITION('material property','material name',#94514);
#8419=PROPERTY_DEFINITION('material property','density of part',#94514);
#8420=PROPERTY_DEFINITION('material property','material name',#94515);
#8421=PROPERTY_DEFINITION('material property','density of part',#94515);
#8422=PROPERTY_DEFINITION('material property','material name',#94516);
#8423=PROPERTY_DEFINITION('material property','density of part',#94516);
#8424=PROPERTY_DEFINITION('material property','material name',#94517);
#8425=PROPERTY_DEFINITION('material property','density of part',#94517);
#8426=PROPERTY_DEFINITION('material property','material name',#94518);
#8427=PROPERTY_DEFINITION('material property','density of part',#94518);
#8428=PROPERTY_DEFINITION('material property','material name',#94519);
#8429=PROPERTY_DEFINITION('material property','density of part',#94519);
#8430=PROPERTY_DEFINITION('material property','material name',#94520);
#8431=PROPERTY_DEFINITION('material property','density of part',#94520);
#8432=AXIS2_PLACEMENT_3D('',#10360,#8942,#8943);
#8433=AXIS2_PLACEMENT_3D('',#10361,#8944,#8945);
#8434=AXIS2_PLACEMENT_3D('',#10362,#8946,#8947);
#8435=AXIS2_PLACEMENT_3D('',#10363,#8948,#8949);
#8436=AXIS2_PLACEMENT_3D('',#10365,#8950,#8951);
#8437=AXIS2_PLACEMENT_3D('',#10368,#8953,#8954);
#8438=AXIS2_PLACEMENT_3D('',#10369,#8955,#8956);
#8439=AXIS2_PLACEMENT_3D('',#10371,#8957,#8958);
#8440=AXIS2_PLACEMENT_3D('',#10374,#8960,#8961);
#8441=AXIS2_PLACEMENT_3D('',#10375,#8962,#8963);
#8442=AXIS2_PLACEMENT_3D('',#10377,#8964,#8965);
#8443=AXIS2_PLACEMENT_3D('',#10380,#8967,#8968);
#8444=AXIS2_PLACEMENT_3D('',#10381,#8969,#8970);
#8445=AXIS2_PLACEMENT_3D('',#10383,#8971,#8972);
#8446=AXIS2_PLACEMENT_3D('',#10386,#8974,#8975);
#8447=AXIS2_PLACEMENT_3D('',#10387,#8976,#8977);
#8448=AXIS2_PLACEMENT_3D('',#10396,#8982,#8983);
#8449=AXIS2_PLACEMENT_3D('',#10402,#8987,#8988);
#8450=AXIS2_PLACEMENT_3D('',#10408,#8992,#8993);
#8451=AXIS2_PLACEMENT_3D('',#10411,#8996,#8997);
#8452=AXIS2_PLACEMENT_3D('',#10412,#8998,#8999);
#8453=AXIS2_PLACEMENT_3D('',#10413,#9000,#9001);
#8454=AXIS2_PLACEMENT_3D('',#10414,#9002,#9003);
#8455=AXIS2_PLACEMENT_3D('',#10416,#9004,#9005);
#8456=AXIS2_PLACEMENT_3D('',#10419,#9007,#9008);
#8457=AXIS2_PLACEMENT_3D('',#10420,#9009,#9010);
#8458=AXIS2_PLACEMENT_3D('',#10422,#9011,#9012);
#8459=AXIS2_PLACEMENT_3D('',#10425,#9014,#9015);
#8460=AXIS2_PLACEMENT_3D('',#10426,#9016,#9017);
#8461=AXIS2_PLACEMENT_3D('',#10435,#9022,#9023);
#8462=AXIS2_PLACEMENT_3D('',#10441,#9027,#9028);
#8463=AXIS2_PLACEMENT_3D('',#10447,#9032,#9033);
#8464=AXIS2_PLACEMENT_3D('',#10450,#9036,#9037);
#8465=AXIS2_PLACEMENT_3D('',#10451,#9038,#9039);
#8466=AXIS2_PLACEMENT_3D('',#10452,#9040,#9041);
#8467=AXIS2_PLACEMENT_3D('',#10453,#9042,#9043);
#8468=AXIS2_PLACEMENT_3D('',#10462,#9048,#9049);
#8469=AXIS2_PLACEMENT_3D('',#10468,#9053,#9054);
#8470=AXIS2_PLACEMENT_3D('',#10474,#9058,#9059);
#8471=AXIS2_PLACEMENT_3D('',#10477,#9062,#9063);
#8472=AXIS2_PLACEMENT_3D('',#10478,#9064,#9065);
#8473=AXIS2_PLACEMENT_3D('',#10479,#9066,#9067);
#8474=AXIS2_PLACEMENT_3D('',#10480,#9068,#9069);
#8475=AXIS2_PLACEMENT_3D('',#10483,#9070,#9071);
#8476=AXIS2_PLACEMENT_3D('',#10487,#9073,#9074);
#8477=AXIS2_PLACEMENT_3D('',#10489,#9076,#9077);
#8478=AXIS2_PLACEMENT_3D('',#10495,#9081,#9082);
#8479=AXIS2_PLACEMENT_3D('',#10497,#9083,#9084);
#8480=AXIS2_PLACEMENT_3D('',#10500,#9086,#9087);
#8481=AXIS2_PLACEMENT_3D('',#10501,#9088,#9089);
#8482=AXIS2_PLACEMENT_3D('',#10507,#9093,#9094);
#8483=AXIS2_PLACEMENT_3D('',#10510,#9095,#9096);
#8484=AXIS2_PLACEMENT_3D('',#10514,#9098,#9099);
#8485=AXIS2_PLACEMENT_3D('',#10516,#9101,#9102);
#8486=AXIS2_PLACEMENT_3D('',#10519,#9105,#9106);
#8487=AXIS2_PLACEMENT_3D('',#10521,#9107,#9108);
#8488=AXIS2_PLACEMENT_3D('',#10524,#9110,#9111);
#8489=AXIS2_PLACEMENT_3D('',#10525,#9112,#9113);
#8490=AXIS2_PLACEMENT_3D('',#10528,#9116,#9117);
#8491=AXIS2_PLACEMENT_3D('',#10531,#9118,#9119);
#8492=AXIS2_PLACEMENT_3D('',#10535,#9121,#9122);
#8493=AXIS2_PLACEMENT_3D('',#10537,#9124,#9125);
#8494=AXIS2_PLACEMENT_3D('',#10543,#9129,#9130);
#8495=AXIS2_PLACEMENT_3D('',#10546,#9131,#9132);
#8496=AXIS2_PLACEMENT_3D('',#10550,#9134,#9135);
#8497=AXIS2_PLACEMENT_3D('',#10552,#9137,#9138);
#8498=AXIS2_PLACEMENT_3D('',#10555,#9141,#9142);
#8499=AXIS2_PLACEMENT_3D('',#10557,#9143,#9144);
#8500=AXIS2_PLACEMENT_3D('',#10560,#9146,#9147);
#8501=AXIS2_PLACEMENT_3D('',#10561,#9148,#9149);
#8502=AXIS2_PLACEMENT_3D('',#10567,#9153,#9154);
#8503=AXIS2_PLACEMENT_3D('',#10569,#9155,#9156);
#8504=AXIS2_PLACEMENT_3D('',#10572,#9158,#9159);
#8505=AXIS2_PLACEMENT_3D('',#10573,#9160,#9161);
#8506=AXIS2_PLACEMENT_3D('',#10576,#9164,#9165);
#8507=AXIS2_PLACEMENT_3D('',#10585,#9170,#9171);
#8508=AXIS2_PLACEMENT_3D('',#10591,#9175,#9176);
#8509=AXIS2_PLACEMENT_3D('',#10597,#9180,#9181);
#8510=AXIS2_PLACEMENT_3D('',#10600,#9184,#9185);
#8511=AXIS2_PLACEMENT_3D('',#10601,#9186,#9187);
#8512=AXIS2_PLACEMENT_3D('',#10602,#9188,#9189);
#8513=AXIS2_PLACEMENT_3D('',#10603,#9190,#9191);
#8514=AXIS2_PLACEMENT_3D('',#10685,#9193,#9194);
#8515=AXIS2_PLACEMENT_3D('',#10780,#9195,#9196);
#8516=AXIS2_PLACEMENT_3D('',#11082,#9198,#9199);
#8517=AXIS2_PLACEMENT_3D('',#11311,#9201,#9202);
#8518=AXIS2_PLACEMENT_3D('',#11543,#9204,#9205);
#8519=AXIS2_PLACEMENT_3D('',#11773,#9207,#9208);
#8520=AXIS2_PLACEMENT_3D('',#12005,#9210,#9211);
#8521=AXIS2_PLACEMENT_3D('',#12240,#9213,#9214);
#8522=AXIS2_PLACEMENT_3D('',#12472,#9216,#9217);
#8523=AXIS2_PLACEMENT_3D('',#12702,#9219,#9220);
#8524=AXIS2_PLACEMENT_3D('',#12807,#9222,#9223);
#8525=AXIS2_PLACEMENT_3D('',#12841,#9225,#9226);
#8526=AXIS2_PLACEMENT_3D('',#13004,#9228,#9229);
#8527=AXIS2_PLACEMENT_3D('',#13234,#9231,#9232);
#8528=AXIS2_PLACEMENT_3D('',#13466,#9234,#9235);
#8529=AXIS2_PLACEMENT_3D('',#13698,#9237,#9238);
#8530=AXIS2_PLACEMENT_3D('',#13927,#9240,#9241);
#8531=AXIS2_PLACEMENT_3D('',#14160,#9243,#9244);
#8532=AXIS2_PLACEMENT_3D('',#14392,#9246,#9247);
#8533=AXIS2_PLACEMENT_3D('',#14480,#9249,#9250);
#8534=AXIS2_PLACEMENT_3D('',#14553,#9251,#9252);
#8535=AXIS2_PLACEMENT_3D('',#14571,#9254,#9255);
#8536=AXIS2_PLACEMENT_3D('',#14574,#9257,#9258);
#8537=AXIS2_PLACEMENT_3D('',#14576,#9259,#9260);
#8538=AXIS2_PLACEMENT_3D('',#14644,#9261,#9262);
#8539=AXIS2_PLACEMENT_3D('',#15067,#9264,#9265);
#8540=AXIS2_PLACEMENT_3D('',#15535,#9267,#9268);
#8541=AXIS2_PLACEMENT_3D('',#15955,#9270,#9271);
#8542=AXIS2_PLACEMENT_3D('',#16356,#9273,#9274);
#8543=AXIS2_PLACEMENT_3D('',#16773,#9276,#9277);
#8544=AXIS2_PLACEMENT_3D('',#17205,#9279,#9280);
#8545=AXIS2_PLACEMENT_3D('',#17657,#9282,#9283);
#8546=AXIS2_PLACEMENT_3D('',#18120,#9285,#9286);
#8547=AXIS2_PLACEMENT_3D('',#18530,#9288,#9289);
#8548=AXIS2_PLACEMENT_3D('',#18963,#9291,#9292);
#8549=AXIS2_PLACEMENT_3D('',#19389,#9294,#9295);
#8550=AXIS2_PLACEMENT_3D('',#19801,#9297,#9298);
#8551=AXIS2_PLACEMENT_3D('',#20231,#9300,#9301);
#8552=AXIS2_PLACEMENT_3D('',#20712,#9303,#9304);
#8553=AXIS2_PLACEMENT_3D('',#21126,#9306,#9307);
#8554=AXIS2_PLACEMENT_3D('',#21557,#9309,#9310);
#8555=AXIS2_PLACEMENT_3D('',#21972,#9312,#9313);
#8556=AXIS2_PLACEMENT_3D('',#22122,#9315,#9316);
#8557=AXIS2_PLACEMENT_3D('',#22309,#9317,#9318);
#8558=AXIS2_PLACEMENT_3D('',#22321,#9320,#9321);
#8559=AXIS2_PLACEMENT_3D('',#22416,#9322,#9323);
#8560=AXIS2_PLACEMENT_3D('',#22651,#9325,#9326);
#8561=AXIS2_PLACEMENT_3D('',#23008,#9328,#9329);
#8562=AXIS2_PLACEMENT_3D('',#23438,#9331,#9332);
#8563=AXIS2_PLACEMENT_3D('',#23868,#9334,#9335);
#8564=AXIS2_PLACEMENT_3D('',#24295,#9337,#9338);
#8565=AXIS2_PLACEMENT_3D('',#24725,#9340,#9341);
#8566=AXIS2_PLACEMENT_3D('',#25155,#9343,#9344);
#8567=AXIS2_PLACEMENT_3D('',#25585,#9346,#9347);
#8568=AXIS2_PLACEMENT_3D('',#26018,#9349,#9350);
#8569=AXIS2_PLACEMENT_3D('',#26442,#9352,#9353);
#8570=AXIS2_PLACEMENT_3D('',#26872,#9355,#9356);
#8571=AXIS2_PLACEMENT_3D('',#27302,#9358,#9359);
#8572=AXIS2_PLACEMENT_3D('',#27729,#9361,#9362);
#8573=AXIS2_PLACEMENT_3D('',#28159,#9364,#9365);
#8574=AXIS2_PLACEMENT_3D('',#28583,#9367,#9368);
#8575=AXIS2_PLACEMENT_3D('',#29013,#9370,#9371);
#8576=AXIS2_PLACEMENT_3D('',#29312,#9373,#9374);
#8577=AXIS2_PLACEMENT_3D('',#29400,#9376,#9377);
#8578=AXIS2_PLACEMENT_3D('',#29473,#9378,#9379);
#8579=AXIS2_PLACEMENT_3D('',#29491,#9381,#9382);
#8580=AXIS2_PLACEMENT_3D('',#29494,#9384,#9385);
#8581=AXIS2_PLACEMENT_3D('',#29496,#9386,#9387);
#8582=AXIS2_PLACEMENT_3D('',#29564,#9388,#9389);
#8583=AXIS2_PLACEMENT_3D('',#29797,#9391,#9392);
#8584=AXIS2_PLACEMENT_3D('',#30200,#9394,#9395);
#8585=AXIS2_PLACEMENT_3D('',#30625,#9397,#9398);
#8586=AXIS2_PLACEMENT_3D('',#31043,#9400,#9401);
#8587=AXIS2_PLACEMENT_3D('',#31469,#9403,#9404);
#8588=AXIS2_PLACEMENT_3D('',#31910,#9406,#9407);
#8589=AXIS2_PLACEMENT_3D('',#32343,#9409,#9410);
#8590=AXIS2_PLACEMENT_3D('',#32771,#9412,#9413);
#8591=AXIS2_PLACEMENT_3D('',#33192,#9415,#9416);
#8592=AXIS2_PLACEMENT_3D('',#33662,#9418,#9419);
#8593=AXIS2_PLACEMENT_3D('',#34145,#9421,#9422);
#8594=AXIS2_PLACEMENT_3D('',#34558,#9424,#9425);
#8595=AXIS2_PLACEMENT_3D('',#34977,#9427,#9428);
#8596=AXIS2_PLACEMENT_3D('',#35415,#9430,#9431);
#8597=AXIS2_PLACEMENT_3D('',#35828,#9433,#9434);
#8598=AXIS2_PLACEMENT_3D('',#36240,#9436,#9437);
#8599=AXIS2_PLACEMENT_3D('',#36646,#9439,#9440);
#8600=AXIS2_PLACEMENT_3D('',#36787,#9442,#9443);
#8601=AXIS2_PLACEMENT_3D('',#36974,#9444,#9445);
#8602=AXIS2_PLACEMENT_3D('',#37371,#9446,#9447);
#8603=AXIS2_PLACEMENT_3D('',#37600,#9448,#9449);
#8604=AXIS2_PLACEMENT_3D('',#38015,#9450,#9451);
#8605=AXIS2_PLACEMENT_3D('',#38244,#9452,#9453);
#8606=AXIS2_PLACEMENT_3D('',#39606,#9454,#9455);
#8607=AXIS2_PLACEMENT_3D('',#39607,#9456,#9457);
#8608=AXIS2_PLACEMENT_3D('',#40972,#9458,#9459);
#8609=AXIS2_PLACEMENT_3D('',#40973,#9460,#9461);
#8610=AXIS2_PLACEMENT_3D('',#40975,#9462,#9463);
#8611=AXIS2_PLACEMENT_3D('',#40978,#9465,#9466);
#8612=AXIS2_PLACEMENT_3D('',#40979,#9467,#9468);
#8613=AXIS2_PLACEMENT_3D('',#40980,#9469,#9470);
#8614=AXIS2_PLACEMENT_3D('',#40981,#9471,#9472);
#8615=AXIS2_PLACEMENT_3D('',#40982,#9473,#9474);
#8616=AXIS2_PLACEMENT_3D('',#41148,#9476,#9477);
#8617=AXIS2_PLACEMENT_3D('',#41273,#9478,#9479);
#8618=AXIS2_PLACEMENT_3D('',#41647,#9481,#9482);
#8619=AXIS2_PLACEMENT_3D('',#42027,#9484,#9485);
#8620=AXIS2_PLACEMENT_3D('',#42405,#9487,#9488);
#8621=AXIS2_PLACEMENT_3D('',#42777,#9490,#9491);
#8622=AXIS2_PLACEMENT_3D('',#43167,#9493,#9494);
#8623=AXIS2_PLACEMENT_3D('',#43543,#9496,#9497);
#8624=AXIS2_PLACEMENT_3D('',#43919,#9499,#9500);
#8625=AXIS2_PLACEMENT_3D('',#44291,#9502,#9503);
#8626=AXIS2_PLACEMENT_3D('',#44677,#9505,#9506);
#8627=AXIS2_PLACEMENT_3D('',#45053,#9508,#9509);
#8628=AXIS2_PLACEMENT_3D('',#45063,#9510,#9511);
#8629=AXIS2_PLACEMENT_3D('',#46396,#9512,#9513);
#8630=AXIS2_PLACEMENT_3D('',#47063,#9514,#9515);
#8631=AXIS2_PLACEMENT_3D('',#47258,#9516,#9517);
#8632=AXIS2_PLACEMENT_3D('',#47423,#9518,#9519);
#8633=AXIS2_PLACEMENT_3D('',#47554,#9521,#9522);
#8634=AXIS2_PLACEMENT_3D('',#48352,#9523,#9524);
#8635=AXIS2_PLACEMENT_3D('',#48361,#9529,#9530);
#8636=AXIS2_PLACEMENT_3D('',#48367,#9534,#9535);
#8637=AXIS2_PLACEMENT_3D('',#48373,#9539,#9540);
#8638=AXIS2_PLACEMENT_3D('',#48379,#9544,#9545);
#8639=AXIS2_PLACEMENT_3D('',#48385,#9549,#9550);
#8640=AXIS2_PLACEMENT_3D('',#48388,#9553,#9554);
#8641=AXIS2_PLACEMENT_3D('',#48389,#9555,#9556);
#8642=AXIS2_PLACEMENT_3D('',#48391,#9557,#9558);
#8643=AXIS2_PLACEMENT_3D('',#48392,#9559,#9560);
#8644=AXIS2_PLACEMENT_3D('',#48395,#9562,#9563);
#8645=AXIS2_PLACEMENT_3D('',#48396,#9564,#9565);
#8646=AXIS2_PLACEMENT_3D('',#48397,#9566,#9567);
#8647=AXIS2_PLACEMENT_3D('',#48398,#9568,#9569);
#8648=AXIS2_PLACEMENT_3D('',#48399,#9570,#9571);
#8649=AXIS2_PLACEMENT_3D('',#48409,#9573,#9574);
#8650=AXIS2_PLACEMENT_3D('',#48441,#9575,#9576);
#8651=AXIS2_PLACEMENT_3D('',#48652,#9578,#9579);
#8652=AXIS2_PLACEMENT_3D('',#48869,#9581,#9582);
#8653=AXIS2_PLACEMENT_3D('',#49199,#9584,#9585);
#8654=AXIS2_PLACEMENT_3D('',#49477,#9587,#9588);
#8655=AXIS2_PLACEMENT_3D('',#49685,#9590,#9591);
#8656=AXIS2_PLACEMENT_3D('',#50015,#9593,#9594);
#8657=AXIS2_PLACEMENT_3D('',#50293,#9596,#9597);
#8658=AXIS2_PLACEMENT_3D('',#50501,#9599,#9600);
#8659=AXIS2_PLACEMENT_3D('',#50834,#9602,#9603);
#8660=AXIS2_PLACEMENT_3D('',#51109,#9605,#9606);
#8661=AXIS2_PLACEMENT_3D('',#51320,#9608,#9609);
#8662=AXIS2_PLACEMENT_3D('',#51653,#9611,#9612);
#8663=AXIS2_PLACEMENT_3D('',#51928,#9614,#9615);
#8664=AXIS2_PLACEMENT_3D('',#52026,#9617,#9618);
#8665=AXIS2_PLACEMENT_3D('',#52044,#9620,#9621);
#8666=AXIS2_PLACEMENT_3D('',#52111,#9622,#9623);
#8667=AXIS2_PLACEMENT_3D('',#52253,#9625,#9626);
#8668=AXIS2_PLACEMENT_3D('',#52267,#9628,#9629);
#8669=AXIS2_PLACEMENT_3D('',#52445,#9630,#9631);
#8670=AXIS2_PLACEMENT_3D('',#52653,#9633,#9634);
#8671=AXIS2_PLACEMENT_3D('',#53068,#9636,#9637);
#8672=AXIS2_PLACEMENT_3D('',#53486,#9639,#9640);
#8673=AXIS2_PLACEMENT_3D('',#53928,#9642,#9643);
#8674=AXIS2_PLACEMENT_3D('',#54358,#9645,#9646);
#8675=AXIS2_PLACEMENT_3D('',#54786,#9648,#9649);
#8676=AXIS2_PLACEMENT_3D('',#55202,#9651,#9652);
#8677=AXIS2_PLACEMENT_3D('',#55672,#9654,#9655);
#8678=AXIS2_PLACEMENT_3D('',#56094,#9657,#9658);
#8679=AXIS2_PLACEMENT_3D('',#56509,#9660,#9661);
#8680=AXIS2_PLACEMENT_3D('',#56932,#9663,#9664);
#8681=AXIS2_PLACEMENT_3D('',#57367,#9666,#9667);
#8682=AXIS2_PLACEMENT_3D('',#57792,#9669,#9670);
#8683=AXIS2_PLACEMENT_3D('',#57918,#9672,#9673);
#8684=AXIS2_PLACEMENT_3D('',#58084,#9674,#9675);
#8685=AXIS2_PLACEMENT_3D('',#58467,#9676,#9677);
#8686=AXIS2_PLACEMENT_3D('',#58498,#9678,#9679);
#8687=AXIS2_PLACEMENT_3D('',#59671,#9680,#9681);
#8688=AXIS2_PLACEMENT_3D('',#59672,#9682,#9683);
#8689=AXIS2_PLACEMENT_3D('',#59674,#9684,#9685);
#8690=AXIS2_PLACEMENT_3D('',#59677,#9687,#9688);
#8691=AXIS2_PLACEMENT_3D('',#59678,#9689,#9690);
#8692=AXIS2_PLACEMENT_3D('',#59679,#9691,#9692);
#8693=AXIS2_PLACEMENT_3D('',#59680,#9693,#9694);
#8694=AXIS2_PLACEMENT_3D('',#59681,#9695,#9696);
#8695=AXIS2_PLACEMENT_3D('',#59682,#9697,#9698);
#8696=AXIS2_PLACEMENT_3D('',#59683,#9699,#9700);
#8697=AXIS2_PLACEMENT_3D('',#59684,#9701,#9702);
#8698=AXIS2_PLACEMENT_3D('',#59685,#9703,#9704);
#8699=AXIS2_PLACEMENT_3D('',#59686,#9705,#9706);
#8700=AXIS2_PLACEMENT_3D('',#59687,#9707,#9708);
#8701=AXIS2_PLACEMENT_3D('',#59688,#9709,#9710);
#8702=AXIS2_PLACEMENT_3D('',#59689,#9711,#9712);
#8703=AXIS2_PLACEMENT_3D('',#59690,#9713,#9714);
#8704=AXIS2_PLACEMENT_3D('',#59691,#9715,#9716);
#8705=AXIS2_PLACEMENT_3D('',#59692,#9717,#9718);
#8706=AXIS2_PLACEMENT_3D('',#59693,#9719,#9720);
#8707=AXIS2_PLACEMENT_3D('',#59694,#9721,#9722);
#8708=AXIS2_PLACEMENT_3D('',#59695,#9723,#9724);
#8709=AXIS2_PLACEMENT_3D('',#59696,#9725,#9726);
#8710=AXIS2_PLACEMENT_3D('',#59697,#9727,#9728);
#8711=AXIS2_PLACEMENT_3D('',#59698,#9729,#9730);
#8712=AXIS2_PLACEMENT_3D('',#59701,#9731,#9732);
#8713=AXIS2_PLACEMENT_3D('',#59705,#9734,#9735);
#8714=AXIS2_PLACEMENT_3D('',#59707,#9737,#9738);
#8715=AXIS2_PLACEMENT_3D('',#59714,#9742,#9743);
#8716=AXIS2_PLACEMENT_3D('',#59716,#9744,#9745);
#8717=AXIS2_PLACEMENT_3D('',#59718,#9746,#9747);
#8718=AXIS2_PLACEMENT_3D('',#59720,#9748,#9749);
#8719=AXIS2_PLACEMENT_3D('',#59721,#9750,#9751);
#8720=AXIS2_PLACEMENT_3D('',#59725,#9754,#9755);
#8721=AXIS2_PLACEMENT_3D('',#59728,#9757,#9758);
#8722=AXIS2_PLACEMENT_3D('',#59729,#9759,#9760);
#8723=AXIS2_PLACEMENT_3D('',#59732,#9762,#9763);
#8724=AXIS2_PLACEMENT_3D('',#59733,#9764,#9765);
#8725=AXIS2_PLACEMENT_3D('',#59736,#9767,#9768);
#8726=AXIS2_PLACEMENT_3D('',#59737,#9769,#9770);
#8727=AXIS2_PLACEMENT_3D('',#59740,#9772,#9773);
#8728=AXIS2_PLACEMENT_3D('',#59741,#9774,#9775);
#8729=AXIS2_PLACEMENT_3D('',#59745,#9778,#9779);
#8730=AXIS2_PLACEMENT_3D('',#59747,#9781,#9782);
#8731=AXIS2_PLACEMENT_3D('',#59748,#9783,#9784);
#8732=AXIS2_PLACEMENT_3D('',#59749,#9785,#9786);
#8733=AXIS2_PLACEMENT_3D('',#59751,#9787,#9788);
#8734=AXIS2_PLACEMENT_3D('',#59754,#9790,#9791);
#8735=AXIS2_PLACEMENT_3D('',#59755,#9792,#9793);
#8736=AXIS2_PLACEMENT_3D('',#59757,#9794,#9795);
#8737=AXIS2_PLACEMENT_3D('',#59760,#9797,#9798);
#8738=AXIS2_PLACEMENT_3D('',#59761,#9799,#9800);
#8739=AXIS2_PLACEMENT_3D('',#59763,#9801,#9802);
#8740=AXIS2_PLACEMENT_3D('',#59766,#9804,#9805);
#8741=AXIS2_PLACEMENT_3D('',#59767,#9806,#9807);
#8742=AXIS2_PLACEMENT_3D('',#59769,#9808,#9809);
#8743=AXIS2_PLACEMENT_3D('',#59772,#9811,#9812);
#8744=AXIS2_PLACEMENT_3D('',#59773,#9813,#9814);
#8745=AXIS2_PLACEMENT_3D('',#59782,#9819,#9820);
#8746=AXIS2_PLACEMENT_3D('',#59788,#9824,#9825);
#8747=AXIS2_PLACEMENT_3D('',#59794,#9829,#9830);
#8748=AXIS2_PLACEMENT_3D('',#59797,#9833,#9834);
#8749=AXIS2_PLACEMENT_3D('',#59806,#9839,#9840);
#8750=AXIS2_PLACEMENT_3D('',#59812,#9844,#9845);
#8751=AXIS2_PLACEMENT_3D('',#59818,#9849,#9850);
#8752=AXIS2_PLACEMENT_3D('',#59821,#9853,#9854);
#8753=AXIS2_PLACEMENT_3D('',#59822,#9855,#9856);
#8754=AXIS2_PLACEMENT_3D('',#59823,#9857,#9858);
#8755=AXIS2_PLACEMENT_3D('',#59824,#9859,#9860);
#8756=AXIS2_PLACEMENT_3D('',#59826,#9861,#9862);
#8757=AXIS2_PLACEMENT_3D('',#59829,#9864,#9865);
#8758=AXIS2_PLACEMENT_3D('',#59830,#9866,#9867);
#8759=AXIS2_PLACEMENT_3D('',#59832,#9868,#9869);
#8760=AXIS2_PLACEMENT_3D('',#59835,#9871,#9872);
#8761=AXIS2_PLACEMENT_3D('',#59836,#9873,#9874);
#8762=AXIS2_PLACEMENT_3D('',#59838,#9875,#9876);
#8763=AXIS2_PLACEMENT_3D('',#59841,#9878,#9879);
#8764=AXIS2_PLACEMENT_3D('',#59842,#9880,#9881);
#8765=AXIS2_PLACEMENT_3D('',#59844,#9882,#9883);
#8766=AXIS2_PLACEMENT_3D('',#59847,#9885,#9886);
#8767=AXIS2_PLACEMENT_3D('',#59848,#9887,#9888);
#8768=AXIS2_PLACEMENT_3D('',#59857,#9893,#9894);
#8769=AXIS2_PLACEMENT_3D('',#59863,#9898,#9899);
#8770=AXIS2_PLACEMENT_3D('',#59869,#9903,#9904);
#8771=AXIS2_PLACEMENT_3D('',#59872,#9907,#9908);
#8772=AXIS2_PLACEMENT_3D('',#59873,#9909,#9910);
#8773=AXIS2_PLACEMENT_3D('',#59874,#9911,#9912);
#8774=AXIS2_PLACEMENT_3D('',#59875,#9913,#9914);
#8775=AXIS2_PLACEMENT_3D('',#60101,#9916,#9917);
#8776=AXIS2_PLACEMENT_3D('',#60226,#9918,#9919);
#8777=AXIS2_PLACEMENT_3D('',#60645,#9921,#9922);
#8778=AXIS2_PLACEMENT_3D('',#60881,#9924,#9925);
#8779=AXIS2_PLACEMENT_3D('',#61277,#9927,#9928);
#8780=AXIS2_PLACEMENT_3D('',#61686,#9930,#9931);
#8781=AXIS2_PLACEMENT_3D('',#61911,#9933,#9934);
#8782=AXIS2_PLACEMENT_3D('',#62133,#9936,#9937);
#8783=AXIS2_PLACEMENT_3D('',#62518,#9939,#9940);
#8784=AXIS2_PLACEMENT_3D('',#62948,#9942,#9943);
#8785=AXIS2_PLACEMENT_3D('',#63380,#9945,#9946);
#8786=AXIS2_PLACEMENT_3D('',#63596,#9948,#9949);
#8787=AXIS2_PLACEMENT_3D('',#64061,#9951,#9952);
#8788=AXIS2_PLACEMENT_3D('',#64555,#9954,#9955);
#8789=AXIS2_PLACEMENT_3D('',#64969,#9957,#9958);
#8790=AXIS2_PLACEMENT_3D('',#65187,#9960,#9961);
#8791=AXIS2_PLACEMENT_3D('',#65197,#9962,#9963);
#8792=AXIS2_PLACEMENT_3D('',#67139,#9964,#9965);
#8793=AXIS2_PLACEMENT_3D('',#68850,#9966,#9967);
#8794=AXIS2_PLACEMENT_3D('',#69045,#9968,#9969);
#8795=AXIS2_PLACEMENT_3D('',#69203,#9970,#9971);
#8796=AXIS2_PLACEMENT_3D('',#69340,#9973,#9974);
#8797=AXIS2_PLACEMENT_3D('',#70349,#9975,#9976);
#8798=AXIS2_PLACEMENT_3D('',#70358,#9981,#9982);
#8799=AXIS2_PLACEMENT_3D('',#70364,#9986,#9987);
#8800=AXIS2_PLACEMENT_3D('',#70370,#9991,#9992);
#8801=AXIS2_PLACEMENT_3D('',#70376,#9996,#9997);
#8802=AXIS2_PLACEMENT_3D('',#70382,#10001,#10002);
#8803=AXIS2_PLACEMENT_3D('',#70385,#10005,#10006);
#8804=AXIS2_PLACEMENT_3D('',#70386,#10007,#10008);
#8805=AXIS2_PLACEMENT_3D('',#70388,#10009,#10010);
#8806=AXIS2_PLACEMENT_3D('',#70389,#10011,#10012);
#8807=AXIS2_PLACEMENT_3D('',#70392,#10014,#10015);
#8808=AXIS2_PLACEMENT_3D('',#70393,#10016,#10017);
#8809=AXIS2_PLACEMENT_3D('',#70394,#10018,#10019);
#8810=AXIS2_PLACEMENT_3D('',#70395,#10020,#10021);
#8811=AXIS2_PLACEMENT_3D('',#70396,#10022,#10023);
#8812=AXIS2_PLACEMENT_3D('',#70554,#10025,#10026);
#8813=AXIS2_PLACEMENT_3D('',#70667,#10027,#10028);
#8814=AXIS2_PLACEMENT_3D('',#71049,#10030,#10031);
#8815=AXIS2_PLACEMENT_3D('',#71452,#10033,#10034);
#8816=AXIS2_PLACEMENT_3D('',#71843,#10036,#10037);
#8817=AXIS2_PLACEMENT_3D('',#72215,#10039,#10040);
#8818=AXIS2_PLACEMENT_3D('',#72597,#10042,#10043);
#8819=AXIS2_PLACEMENT_3D('',#72988,#10045,#10046);
#8820=AXIS2_PLACEMENT_3D('',#73205,#10048,#10049);
#8821=AXIS2_PLACEMENT_3D('',#73643,#10051,#10052);
#8822=AXIS2_PLACEMENT_3D('',#74036,#10054,#10055);
#8823=AXIS2_PLACEMENT_3D('',#74448,#10057,#10058);
#8824=AXIS2_PLACEMENT_3D('',#74834,#10060,#10061);
#8825=AXIS2_PLACEMENT_3D('',#75199,#10063,#10064);
#8826=AXIS2_PLACEMENT_3D('',#75264,#10065,#10066);
#8827=AXIS2_PLACEMENT_3D('',#76652,#10067,#10068);
#8828=AXIS2_PLACEMENT_3D('',#77803,#10069,#10070);
#8829=AXIS2_PLACEMENT_3D('',#77951,#10071,#10072);
#8830=AXIS2_PLACEMENT_3D('',#78064,#10073,#10074);
#8831=AXIS2_PLACEMENT_3D('',#78222,#10076,#10077);
#8832=AXIS2_PLACEMENT_3D('',#79107,#10078,#10079);
#8833=AXIS2_PLACEMENT_3D('',#79116,#10084,#10085);
#8834=AXIS2_PLACEMENT_3D('',#79122,#10089,#10090);
#8835=AXIS2_PLACEMENT_3D('',#79128,#10094,#10095);
#8836=AXIS2_PLACEMENT_3D('',#79134,#10099,#10100);
#8837=AXIS2_PLACEMENT_3D('',#79140,#10104,#10105);
#8838=AXIS2_PLACEMENT_3D('',#79143,#10108,#10109);
#8839=AXIS2_PLACEMENT_3D('',#79144,#10110,#10111);
#8840=AXIS2_PLACEMENT_3D('',#79146,#10112,#10113);
#8841=AXIS2_PLACEMENT_3D('',#79147,#10114,#10115);
#8842=AXIS2_PLACEMENT_3D('',#79150,#10117,#10118);
#8843=AXIS2_PLACEMENT_3D('',#79151,#10119,#10120);
#8844=AXIS2_PLACEMENT_3D('',#79152,#10121,#10122);
#8845=AXIS2_PLACEMENT_3D('',#79153,#10123,#10124);
#8846=AXIS2_PLACEMENT_3D('',#79154,#10125,#10126);
#8847=AXIS2_PLACEMENT_3D('',#79302,#10128,#10129);
#8848=AXIS2_PLACEMENT_3D('',#79391,#10130,#10131);
#8849=AXIS2_PLACEMENT_3D('',#79790,#10133,#10134);
#8850=AXIS2_PLACEMENT_3D('',#80311,#10136,#10137);
#8851=AXIS2_PLACEMENT_3D('',#80736,#10139,#10140);
#8852=AXIS2_PLACEMENT_3D('',#81067,#10142,#10143);
#8853=AXIS2_PLACEMENT_3D('',#81585,#10145,#10146);
#8854=AXIS2_PLACEMENT_3D('',#81995,#10148,#10149);
#8855=AXIS2_PLACEMENT_3D('',#82390,#10151,#10152);
#8856=AXIS2_PLACEMENT_3D('',#82939,#10154,#10155);
#8857=AXIS2_PLACEMENT_3D('',#83576,#10157,#10158);
#8858=AXIS2_PLACEMENT_3D('',#84223,#10160,#10161);
#8859=AXIS2_PLACEMENT_3D('',#84842,#10163,#10164);
#8860=AXIS2_PLACEMENT_3D('',#85433,#10166,#10167);
#8861=AXIS2_PLACEMENT_3D('',#85847,#10169,#10170);
#8862=AXIS2_PLACEMENT_3D('',#85941,#10172,#10173);
#8863=AXIS2_PLACEMENT_3D('',#85948,#10174,#10175);
#8864=AXIS2_PLACEMENT_3D('',#86236,#10177,#10178);
#8865=AXIS2_PLACEMENT_3D('',#86274,#10180,#10181);
#8866=AXIS2_PLACEMENT_3D('',#86312,#10183,#10184);
#8867=AXIS2_PLACEMENT_3D('',#86858,#10186,#10187);
#8868=AXIS2_PLACEMENT_3D('',#86894,#10189,#10190);
#8869=AXIS2_PLACEMENT_3D('',#86932,#10192,#10193);
#8870=AXIS2_PLACEMENT_3D('',#87478,#10195,#10196);
#8871=AXIS2_PLACEMENT_3D('',#88018,#10198,#10199);
#8872=AXIS2_PLACEMENT_3D('',#88056,#10201,#10202);
#8873=AXIS2_PLACEMENT_3D('',#88596,#10204,#10205);
#8874=AXIS2_PLACEMENT_3D('',#89136,#10207,#10208);
#8875=AXIS2_PLACEMENT_3D('',#89175,#10210,#10211);
#8876=AXIS2_PLACEMENT_3D('',#89213,#10213,#10214);
#8877=AXIS2_PLACEMENT_3D('',#89230,#10215,#10216);
#8878=AXIS2_PLACEMENT_3D('',#89243,#10217,#10218);
#8879=AXIS2_PLACEMENT_3D('',#89512,#10219,#10220);
#8880=AXIS2_PLACEMENT_3D('',#91532,#10221,#10222);
#8881=AXIS2_PLACEMENT_3D('',#91534,#10223,#10224);
#8882=AXIS2_PLACEMENT_3D('',#91535,#10225,#10226);
#8883=AXIS2_PLACEMENT_3D('',#91538,#10228,#10229);
#8884=AXIS2_PLACEMENT_3D('',#91539,#10230,#10231);
#8885=AXIS2_PLACEMENT_3D('',#91541,#10232,#10233);
#8886=AXIS2_PLACEMENT_3D('',#91544,#10235,#10236);
#8887=AXIS2_PLACEMENT_3D('',#91545,#10237,#10238);
#8888=AXIS2_PLACEMENT_3D('',#91546,#10239,#10240);
#8889=AXIS2_PLACEMENT_3D('',#91547,#10241,#10242);
#8890=AXIS2_PLACEMENT_3D('',#91548,#10243,#10244);
#8891=AXIS2_PLACEMENT_3D('',#91562,#10246,#10247);
#8892=AXIS2_PLACEMENT_3D('',#91572,#10248,#10249);
#8893=AXIS2_PLACEMENT_3D('',#91786,#10251,#10252);
#8894=AXIS2_PLACEMENT_3D('',#91922,#10254,#10255);
#8895=AXIS2_PLACEMENT_3D('',#92032,#10257,#10258);
#8896=AXIS2_PLACEMENT_3D('',#92050,#10259,#10260);
#8897=AXIS2_PLACEMENT_3D('',#92087,#10262,#10263);
#8898=AXIS2_PLACEMENT_3D('',#92197,#10264,#10265);
#8899=AXIS2_PLACEMENT_3D('',#92235,#10267,#10268);
#8900=AXIS2_PLACEMENT_3D('',#92647,#10270,#10271);
#8901=AXIS2_PLACEMENT_3D('',#92822,#10273,#10274);
#8902=AXIS2_PLACEMENT_3D('',#92937,#10275,#10276);
#8903=AXIS2_PLACEMENT_3D('',#93176,#10277,#10278);
#8904=AXIS2_PLACEMENT_3D('',#93387,#10279,#10280);
#8905=AXIS2_PLACEMENT_3D('',#93389,#10281,#10282);
#8906=AXIS2_PLACEMENT_3D('',#93392,#10284,#10285);
#8907=AXIS2_PLACEMENT_3D('',#93393,#10286,#10287);
#8908=AXIS2_PLACEMENT_3D('',#93395,#10288,#10289);
#8909=AXIS2_PLACEMENT_3D('',#93398,#10291,#10292);
#8910=AXIS2_PLACEMENT_3D('',#94336,#10293,#10294);
#8911=AXIS2_PLACEMENT_3D('',#94338,#10295,#10296);
#8912=AXIS2_PLACEMENT_3D('',#94339,#10297,#10298);
#8913=AXIS2_PLACEMENT_3D('',#94342,#10300,#10301);
#8914=AXIS2_PLACEMENT_3D('',#94343,#10302,#10303);
#8915=AXIS2_PLACEMENT_3D('',#94344,#10304,#10305);
#8916=AXIS2_PLACEMENT_3D('',#94345,#10306,#10307);
#8917=AXIS2_PLACEMENT_3D('',#94347,#10308,#10309);
#8918=AXIS2_PLACEMENT_3D('',#94350,#10311,#10312);
#8919=AXIS2_PLACEMENT_3D('',#94351,#10313,#10314);
#8920=AXIS2_PLACEMENT_3D('',#94353,#10315,#10316);
#8921=AXIS2_PLACEMENT_3D('',#94356,#10318,#10319);
#8922=AXIS2_PLACEMENT_3D('',#94357,#10320,#10321);
#8923=AXIS2_PLACEMENT_3D('',#94358,#10322,#10323);
#8924=AXIS2_PLACEMENT_3D('',#94359,#10324,#10325);
#8925=AXIS2_PLACEMENT_3D('',#94360,#10326,#10327);
#8926=AXIS2_PLACEMENT_3D('',#94361,#10328,#10329);
#8927=AXIS2_PLACEMENT_3D('',#94362,#10330,#10331);
#8928=AXIS2_PLACEMENT_3D('',#94363,#10332,#10333);
#8929=AXIS2_PLACEMENT_3D('',#94364,#10334,#10335);
#8930=AXIS2_PLACEMENT_3D('',#94365,#10336,#10337);
#8931=AXIS2_PLACEMENT_3D('',#94366,#10338,#10339);
#8932=AXIS2_PLACEMENT_3D('',#94367,#10340,#10341);
#8933=AXIS2_PLACEMENT_3D('',#94368,#10342,#10343);
#8934=AXIS2_PLACEMENT_3D('',#94369,#10344,#10345);
#8935=AXIS2_PLACEMENT_3D('',#94370,#10346,#10347);
#8936=AXIS2_PLACEMENT_3D('',#94371,#10348,#10349);
#8937=AXIS2_PLACEMENT_3D('',#94372,#10350,#10351);
#8938=AXIS2_PLACEMENT_3D('',#94373,#10352,#10353);
#8939=AXIS2_PLACEMENT_3D('',#94374,#10354,#10355);
#8940=AXIS2_PLACEMENT_3D('',#94375,#10356,#10357);
#8941=AXIS2_PLACEMENT_3D('',#94376,#10358,#10359);
#8942=DIRECTION('axis',(0.,0.,1.));
#8943=DIRECTION('refdir',(1.,0.,0.));
#8944=DIRECTION('axis',(0.,0.,1.));
#8945=DIRECTION('refdir',(1.,0.,0.));
#8946=DIRECTION('axis',(0.,0.,1.));
#8947=DIRECTION('refdir',(1.,0.,0.));
#8948=DIRECTION('center_axis',(0.,0.,-1.));
#8949=DIRECTION('ref_axis',(1.,0.,0.));
#8950=DIRECTION('center_axis',(0.,0.,-1.));
#8951=DIRECTION('ref_axis',(1.,0.,0.));
#8952=DIRECTION('',(0.,0.,-1.));
#8953=DIRECTION('center_axis',(0.,0.,1.));
#8954=DIRECTION('ref_axis',(1.,0.,0.));
#8955=DIRECTION('center_axis',(0.,0.,-1.));
#8956=DIRECTION('ref_axis',(1.,0.,0.));
#8957=DIRECTION('center_axis',(0.,0.,-1.));
#8958=DIRECTION('ref_axis',(1.,0.,0.));
#8959=DIRECTION('',(0.,0.,-1.));
#8960=DIRECTION('center_axis',(0.,0.,1.));
#8961=DIRECTION('ref_axis',(1.,0.,0.));
#8962=DIRECTION('center_axis',(0.,0.,-1.));
#8963=DIRECTION('ref_axis',(1.,0.,0.));
#8964=DIRECTION('center_axis',(0.,0.,-1.));
#8965=DIRECTION('ref_axis',(1.,0.,0.));
#8966=DIRECTION('',(0.,0.,-1.));
#8967=DIRECTION('center_axis',(0.,0.,1.));
#8968=DIRECTION('ref_axis',(1.,0.,0.));
#8969=DIRECTION('center_axis',(0.,0.,-1.));
#8970=DIRECTION('ref_axis',(1.,0.,0.));
#8971=DIRECTION('center_axis',(0.,0.,-1.));
#8972=DIRECTION('ref_axis',(1.,0.,0.));
#8973=DIRECTION('',(0.,0.,-1.));
#8974=DIRECTION('center_axis',(0.,0.,1.));
#8975=DIRECTION('ref_axis',(1.,0.,0.));
#8976=DIRECTION('center_axis',(0.,1.,0.));
#8977=DIRECTION('ref_axis',(-1.,0.,0.));
#8978=DIRECTION('',(-1.,0.,0.));
#8979=DIRECTION('',(0.,0.,1.));
#8980=DIRECTION('',(-1.,0.,0.));
#8981=DIRECTION('',(0.,0.,1.));
#8982=DIRECTION('center_axis',(1.,0.,0.));
#8983=DIRECTION('ref_axis',(0.,1.,0.));
#8984=DIRECTION('',(0.,1.,0.));
#8985=DIRECTION('',(0.,1.,0.));
#8986=DIRECTION('',(0.,0.,1.));
#8987=DIRECTION('center_axis',(0.,-1.,0.));
#8988=DIRECTION('ref_axis',(1.,0.,0.));
#8989=DIRECTION('',(1.,0.,0.));
#8990=DIRECTION('',(1.,0.,0.));
#8991=DIRECTION('',(0.,0.,1.));
#8992=DIRECTION('center_axis',(-1.,0.,0.));
#8993=DIRECTION('ref_axis',(0.,-1.,0.));
#8994=DIRECTION('',(0.,-1.,0.));
#8995=DIRECTION('',(0.,-1.,0.));
#8996=DIRECTION('center_axis',(0.,0.,1.));
#8997=DIRECTION('ref_axis',(1.,0.,0.));
#8998=DIRECTION('center_axis',(0.,0.,1.));
#8999=DIRECTION('ref_axis',(1.,0.,0.));
#9000=DIRECTION('axis',(0.,0.,1.));
#9001=DIRECTION('refdir',(1.,0.,0.));
#9002=DIRECTION('center_axis',(0.,-1.,0.));
#9003=DIRECTION('ref_axis',(0.,0.,1.));
#9004=DIRECTION('center_axis',(0.,-1.,0.));
#9005=DIRECTION('ref_axis',(0.,0.,1.));
#9006=DIRECTION('',(0.,-1.,0.));
#9007=DIRECTION('center_axis',(0.,1.,0.));
#9008=DIRECTION('ref_axis',(0.,0.,1.));
#9009=DIRECTION('center_axis',(0.,-1.,0.));
#9010=DIRECTION('ref_axis',(0.,0.,1.));
#9011=DIRECTION('center_axis',(0.,-1.,0.));
#9012=DIRECTION('ref_axis',(0.,0.,1.));
#9013=DIRECTION('',(0.,-1.,0.));
#9014=DIRECTION('center_axis',(0.,1.,0.));
#9015=DIRECTION('ref_axis',(0.,0.,1.));
#9016=DIRECTION('center_axis',(0.,1.,0.));
#9017=DIRECTION('ref_axis',(-1.,0.,0.));
#9018=DIRECTION('',(-1.,0.,0.));
#9019=DIRECTION('',(0.,0.,1.));
#9020=DIRECTION('',(-1.,0.,0.));
#9021=DIRECTION('',(0.,0.,1.));
#9022=DIRECTION('center_axis',(1.,0.,0.));
#9023=DIRECTION('ref_axis',(0.,1.,0.));
#9024=DIRECTION('',(0.,1.,0.));
#9025=DIRECTION('',(0.,1.,0.));
#9026=DIRECTION('',(0.,0.,1.));
#9027=DIRECTION('center_axis',(0.,-1.,0.));
#9028=DIRECTION('ref_axis',(1.,0.,0.));
#9029=DIRECTION('',(1.,0.,0.));
#9030=DIRECTION('',(1.,0.,0.));
#9031=DIRECTION('',(0.,0.,1.));
#9032=DIRECTION('center_axis',(-1.,0.,0.));
#9033=DIRECTION('ref_axis',(0.,-1.,0.));
#9034=DIRECTION('',(0.,-1.,0.));
#9035=DIRECTION('',(0.,-1.,0.));
#9036=DIRECTION('center_axis',(0.,0.,1.));
#9037=DIRECTION('ref_axis',(1.,0.,0.));
#9038=DIRECTION('center_axis',(0.,0.,1.));
#9039=DIRECTION('ref_axis',(1.,0.,0.));
#9040=DIRECTION('axis',(0.,0.,1.));
#9041=DIRECTION('refdir',(1.,0.,0.));
#9042=DIRECTION('center_axis',(0.,1.,0.));
#9043=DIRECTION('ref_axis',(-1.,0.,0.));
#9044=DIRECTION('',(-1.,0.,0.));
#9045=DIRECTION('',(0.,0.,1.));
#9046=DIRECTION('',(-1.,0.,0.));
#9047=DIRECTION('',(0.,0.,1.));
#9048=DIRECTION('center_axis',(1.,0.,0.));
#9049=DIRECTION('ref_axis',(0.,1.,0.));
#9050=DIRECTION('',(0.,1.,0.));
#9051=DIRECTION('',(0.,1.,0.));
#9052=DIRECTION('',(0.,0.,1.));
#9053=DIRECTION('center_axis',(0.,-1.,0.));
#9054=DIRECTION('ref_axis',(1.,0.,0.));
#9055=DIRECTION('',(1.,0.,0.));
#9056=DIRECTION('',(1.,0.,0.));
#9057=DIRECTION('',(0.,0.,1.));
#9058=DIRECTION('center_axis',(-1.,0.,0.));
#9059=DIRECTION('ref_axis',(0.,-1.,0.));
#9060=DIRECTION('',(0.,-1.,0.));
#9061=DIRECTION('',(0.,-1.,0.));
#9062=DIRECTION('center_axis',(0.,0.,1.));
#9063=DIRECTION('ref_axis',(1.,0.,0.));
#9064=DIRECTION('center_axis',(0.,0.,1.));
#9065=DIRECTION('ref_axis',(1.,0.,0.));
#9066=DIRECTION('axis',(0.,0.,1.));
#9067=DIRECTION('refdir',(1.,0.,0.));
#9068=DIRECTION('center_axis',(-1.,0.,0.));
#9069=DIRECTION('ref_axis',(0.,-0.707106781186548,0.707106781186548));
#9070=DIRECTION('center_axis',(1.,0.,0.));
#9071=DIRECTION('ref_axis',(0.,-0.707106781186548,0.707106781186548));
#9072=DIRECTION('',(-1.,0.,0.));
#9073=DIRECTION('center_axis',(-1.,0.,0.));
#9074=DIRECTION('ref_axis',(0.,-0.707106781186548,0.707106781186548));
#9075=DIRECTION('',(1.,0.,0.));
#9076=DIRECTION('center_axis',(0.,-1.,0.));
#9077=DIRECTION('ref_axis',(0.,0.,1.));
#9078=DIRECTION('',(0.,0.,1.));
#9079=DIRECTION('',(1.,0.,0.));
#9080=DIRECTION('',(0.,0.,-1.));
#9081=DIRECTION('center_axis',(-1.,0.,0.));
#9082=DIRECTION('ref_axis',(0.,-0.707106781186548,-0.707106781186548));
#9083=DIRECTION('center_axis',(1.,0.,0.));
#9084=DIRECTION('ref_axis',(0.,-0.707106781186548,-0.707106781186548));
#9085=DIRECTION('',(-1.,0.,0.));
#9086=DIRECTION('center_axis',(-1.,0.,0.));
#9087=DIRECTION('ref_axis',(0.,-0.707106781186548,-0.707106781186548));
#9088=DIRECTION('center_axis',(0.,0.,-1.));
#9089=DIRECTION('ref_axis',(0.,-1.,0.));
#9090=DIRECTION('',(0.,-1.,0.));
#9091=DIRECTION('',(1.,0.,0.));
#9092=DIRECTION('',(0.,1.,0.));
#9093=DIRECTION('center_axis',(-1.,0.,0.));
#9094=DIRECTION('ref_axis',(0.,0.707106781186548,0.707106781186548));
#9095=DIRECTION('center_axis',(1.,0.,0.));
#9096=DIRECTION('ref_axis',(0.,0.707106781186548,0.707106781186548));
#9097=DIRECTION('',(-1.,0.,0.));
#9098=DIRECTION('center_axis',(-1.,0.,0.));
#9099=DIRECTION('ref_axis',(0.,0.707106781186548,0.707106781186548));
#9100=DIRECTION('',(1.,0.,0.));
#9101=DIRECTION('center_axis',(0.,0.,1.));
#9102=DIRECTION('ref_axis',(0.,1.,0.));
#9103=DIRECTION('',(0.,-1.,0.));
#9104=DIRECTION('',(0.,1.,0.));
#9105=DIRECTION('center_axis',(-1.,0.,0.));
#9106=DIRECTION('ref_axis',(0.,0.707106781186548,-0.707106781186548));
#9107=DIRECTION('center_axis',(1.,0.,0.));
#9108=DIRECTION('ref_axis',(0.,0.707106781186548,-0.707106781186548));
#9109=DIRECTION('',(-1.,0.,0.));
#9110=DIRECTION('center_axis',(-1.,0.,0.));
#9111=DIRECTION('ref_axis',(0.,0.707106781186548,-0.707106781186548));
#9112=DIRECTION('center_axis',(0.,1.,0.));
#9113=DIRECTION('ref_axis',(0.,0.,-1.));
#9114=DIRECTION('',(0.,0.,1.));
#9115=DIRECTION('',(0.,0.,-1.));
#9116=DIRECTION('center_axis',(-1.,0.,0.));
#9117=DIRECTION('ref_axis',(0.,0.707106781186548,0.707106781186548));
#9118=DIRECTION('center_axis',(1.,0.,0.));
#9119=DIRECTION('ref_axis',(0.,0.707106781186548,0.707106781186548));
#9120=DIRECTION('',(-1.,0.,0.));
#9121=DIRECTION('center_axis',(-1.,0.,0.));
#9122=DIRECTION('ref_axis',(0.,0.707106781186548,0.707106781186548));
#9123=DIRECTION('',(1.,0.,0.));
#9124=DIRECTION('center_axis',(0.,0.,1.));
#9125=DIRECTION('ref_axis',(0.,1.,0.));
#9126=DIRECTION('',(0.,1.,0.));
#9127=DIRECTION('',(1.,0.,0.));
#9128=DIRECTION('',(0.,-1.,0.));
#9129=DIRECTION('center_axis',(-1.,0.,0.));
#9130=DIRECTION('ref_axis',(0.,0.707106781186548,-0.707106781186548));
#9131=DIRECTION('center_axis',(1.,0.,0.));
#9132=DIRECTION('ref_axis',(0.,0.707106781186548,-0.707106781186548));
#9133=DIRECTION('',(-1.,0.,0.));
#9134=DIRECTION('center_axis',(-1.,0.,0.));
#9135=DIRECTION('ref_axis',(0.,0.707106781186548,-0.707106781186548));
#9136=DIRECTION('',(1.,0.,0.));
#9137=DIRECTION('center_axis',(0.,1.,0.));
#9138=DIRECTION('ref_axis',(0.,0.,-1.));
#9139=DIRECTION('',(0.,0.,1.));
#9140=DIRECTION('',(0.,0.,-1.));
#9141=DIRECTION('center_axis',(-1.,0.,0.));
#9142=DIRECTION('ref_axis',(0.,-0.707106781186548,0.707106781186548));
#9143=DIRECTION('center_axis',(1.,0.,0.));
#9144=DIRECTION('ref_axis',(0.,-0.707106781186548,0.707106781186548));
#9145=DIRECTION('',(-1.,0.,0.));
#9146=DIRECTION('center_axis',(-1.,0.,0.));
#9147=DIRECTION('ref_axis',(0.,-0.707106781186548,0.707106781186548));
#9148=DIRECTION('center_axis',(0.,-1.,0.));
#9149=DIRECTION('ref_axis',(0.,0.,1.));
#9150=DIRECTION('',(0.,0.,1.));
#9151=DIRECTION('',(1.,0.,0.));
#9152=DIRECTION('',(0.,0.,-1.));
#9153=DIRECTION('center_axis',(-1.,0.,0.));
#9154=DIRECTION('ref_axis',(0.,-0.707106781186548,-0.707106781186548));
#9155=DIRECTION('center_axis',(1.,0.,0.));
#9156=DIRECTION('ref_axis',(0.,-0.707106781186548,-0.707106781186548));
#9157=DIRECTION('',(-1.,0.,0.));
#9158=DIRECTION('center_axis',(-1.,0.,0.));
#9159=DIRECTION('ref_axis',(0.,-0.707106781186548,-0.707106781186548));
#9160=DIRECTION('center_axis',(0.,0.,-1.));
#9161=DIRECTION('ref_axis',(0.,-1.,0.));
#9162=DIRECTION('',(0.,1.,0.));
#9163=DIRECTION('',(0.,-1.,0.));
#9164=DIRECTION('center_axis',(0.,1.,0.));
#9165=DIRECTION('ref_axis',(-1.,0.,0.));
#9166=DIRECTION('',(-1.,0.,0.));
#9167=DIRECTION('',(0.,0.,1.));
#9168=DIRECTION('',(-1.,0.,0.));
#9169=DIRECTION('',(0.,0.,1.));
#9170=DIRECTION('center_axis',(1.,0.,0.));
#9171=DIRECTION('ref_axis',(0.,1.,0.));
#9172=DIRECTION('',(0.,1.,0.));
#9173=DIRECTION('',(0.,1.,0.));
#9174=DIRECTION('',(0.,0.,1.));
#9175=DIRECTION('center_axis',(0.,-1.,0.));
#9176=DIRECTION('ref_axis',(1.,0.,0.));
#9177=DIRECTION('',(1.,0.,0.));
#9178=DIRECTION('',(1.,0.,0.));
#9179=DIRECTION('',(0.,0.,1.));
#9180=DIRECTION('center_axis',(-1.,0.,0.));
#9181=DIRECTION('ref_axis',(0.,-1.,0.));
#9182=DIRECTION('',(0.,-1.,0.));
#9183=DIRECTION('',(0.,-1.,0.));
#9184=DIRECTION('center_axis',(0.,0.,1.));
#9185=DIRECTION('ref_axis',(1.,0.,0.));
#9186=DIRECTION('center_axis',(0.,0.,1.));
#9187=DIRECTION('ref_axis',(1.,0.,0.));
#9188=DIRECTION('axis',(0.,0.,1.));
#9189=DIRECTION('refdir',(1.,0.,0.));
#9190=DIRECTION('center_axis',(0.,0.,1.));
#9191=DIRECTION('ref_axis',(0.60921024449365,-0.793008750269496,0.));
#9192=DIRECTION('',(0.,0.,1.));
#9193=DIRECTION('center_axis',(0.,0.,-1.));
#9194=DIRECTION('ref_axis',(-1.,-8.91852360097567E-14,0.));
#9195=DIRECTION('center_axis',(0.,0.,1.));
#9196=DIRECTION('ref_axis',(0.60921024449365,-0.793008750269496,0.));
#9197=DIRECTION('',(0.,0.,1.));
#9198=DIRECTION('center_axis',(0.,0.,1.));
#9199=DIRECTION('ref_axis',(0.60921024449365,-0.793008750269496,0.));
#9200=DIRECTION('',(0.,0.,1.));
#9201=DIRECTION('center_axis',(0.,0.,1.));
#9202=DIRECTION('ref_axis',(0.60921024449365,-0.793008750269496,0.));
#9203=DIRECTION('',(0.,0.,1.));
#9204=DIRECTION('center_axis',(0.,0.,1.));
#9205=DIRECTION('ref_axis',(0.60921024449365,-0.793008750269496,0.));
#9206=DIRECTION('',(0.,0.,1.));
#9207=DIRECTION('center_axis',(0.,0.,1.));
#9208=DIRECTION('ref_axis',(0.60921024449365,-0.793008750269496,0.));
#9209=DIRECTION('',(0.,0.,1.));
#9210=DIRECTION('center_axis',(0.,0.,1.));
#9211=DIRECTION('ref_axis',(0.60921024449365,-0.793008750269496,0.));
#9212=DIRECTION('',(0.,0.,1.));
#9213=DIRECTION('center_axis',(0.,0.,1.));
#9214=DIRECTION('ref_axis',(0.60921024449365,-0.793008750269496,0.));
#9215=DIRECTION('',(0.,0.,1.));
#9216=DIRECTION('center_axis',(0.,0.,1.));
#9217=DIRECTION('ref_axis',(0.60921024449365,-0.793008750269496,0.));
#9218=DIRECTION('',(0.,0.,1.));
#9219=DIRECTION('center_axis',(0.,0.,1.));
#9220=DIRECTION('ref_axis',(0.60921024449365,-0.793008750269496,0.));
#9221=DIRECTION('',(0.,0.,1.));
#9222=DIRECTION('center_axis',(0.,0.,1.));
#9223=DIRECTION('ref_axis',(0.60921024449365,-0.793008750269496,0.));
#9224=DIRECTION('',(0.,0.,1.));
#9225=DIRECTION('center_axis',(0.,0.,1.));
#9226=DIRECTION('ref_axis',(0.60921024449365,-0.793008750269496,0.));
#9227=DIRECTION('',(0.,0.,1.));
#9228=DIRECTION('center_axis',(0.,0.,1.));
#9229=DIRECTION('ref_axis',(0.60921024449365,-0.793008750269496,0.));
#9230=DIRECTION('',(0.,0.,1.));
#9231=DIRECTION('center_axis',(0.,0.,1.));
#9232=DIRECTION('ref_axis',(0.60921024449365,-0.793008750269496,0.));
#9233=DIRECTION('',(0.,0.,1.));
#9234=DIRECTION('center_axis',(0.,0.,1.));
#9235=DIRECTION('ref_axis',(0.60921024449365,-0.793008750269496,0.));
#9236=DIRECTION('',(0.,0.,1.));
#9237=DIRECTION('center_axis',(0.,0.,1.));
#9238=DIRECTION('ref_axis',(0.60921024449365,-0.793008750269496,0.));
#9239=DIRECTION('',(0.,0.,1.));
#9240=DIRECTION('center_axis',(0.,0.,1.));
#9241=DIRECTION('ref_axis',(0.60921024449365,-0.793008750269496,0.));
#9242=DIRECTION('',(0.,0.,1.));
#9243=DIRECTION('center_axis',(0.,0.,1.));
#9244=DIRECTION('ref_axis',(0.60921024449365,-0.793008750269496,0.));
#9245=DIRECTION('',(0.,0.,1.));
#9246=DIRECTION('center_axis',(0.,0.,1.));
#9247=DIRECTION('ref_axis',(0.60921024449365,-0.793008750269496,0.));
#9248=DIRECTION('',(0.,0.,1.));
#9249=DIRECTION('center_axis',(0.,0.,1.));
#9250=DIRECTION('ref_axis',(-1.,-8.91852360097567E-14,0.));
#9251=DIRECTION('center_axis',(0.,0.,1.));
#9252=DIRECTION('ref_axis',(-0.938002783430529,-0.346627722890971,0.));
#9253=DIRECTION('',(0.,0.,1.));
#9254=DIRECTION('center_axis',(0.,0.,-1.));
#9255=DIRECTION('ref_axis',(-1.,0.,0.));
#9256=DIRECTION('',(0.,0.,1.));
#9257=DIRECTION('center_axis',(0.,0.,-1.));
#9258=DIRECTION('ref_axis',(-1.,0.,0.));
#9259=DIRECTION('center_axis',(0.,0.,-1.));
#9260=DIRECTION('ref_axis',(-1.,0.,0.));
#9261=DIRECTION('center_axis',(0.,0.,1.));
#9262=DIRECTION('ref_axis',(-0.938002783430529,-0.346627722890971,0.));
#9263=DIRECTION('',(0.,0.,1.));
#9264=DIRECTION('center_axis',(0.,0.,1.));
#9265=DIRECTION('ref_axis',(-0.938002783430529,-0.346627722890971,0.));
#9266=DIRECTION('',(0.,0.,1.));
#9267=DIRECTION('center_axis',(0.,0.,1.));
#9268=DIRECTION('ref_axis',(-0.938002783430529,-0.346627722890971,0.));
#9269=DIRECTION('',(0.,0.,1.));
#9270=DIRECTION('center_axis',(0.,0.,1.));
#9271=DIRECTION('ref_axis',(-0.938002783430529,-0.346627722890971,0.));
#9272=DIRECTION('',(0.,0.,1.));
#9273=DIRECTION('center_axis',(0.,0.,1.));
#9274=DIRECTION('ref_axis',(-0.938002783430529,-0.346627722890971,0.));
#9275=DIRECTION('',(0.,0.,1.));
#9276=DIRECTION('center_axis',(0.,0.,1.));
#9277=DIRECTION('ref_axis',(-0.938002783430529,-0.346627722890971,0.));
#9278=DIRECTION('',(0.,0.,1.));
#9279=DIRECTION('center_axis',(0.,0.,1.));
#9280=DIRECTION('ref_axis',(-0.938002783430529,-0.346627722890971,0.));
#9281=DIRECTION('',(0.,0.,1.));
#9282=DIRECTION('center_axis',(0.,0.,1.));
#9283=DIRECTION('ref_axis',(-0.938002783430529,-0.346627722890971,0.));
#9284=DIRECTION('',(0.,0.,1.));
#9285=DIRECTION('center_axis',(0.,0.,1.));
#9286=DIRECTION('ref_axis',(-0.938002783430529,-0.346627722890971,0.));
#9287=DIRECTION('',(0.,0.,1.));
#9288=DIRECTION('center_axis',(0.,0.,1.));
#9289=DIRECTION('ref_axis',(-0.938002783430529,-0.346627722890971,0.));
#9290=DIRECTION('',(0.,0.,1.));
#9291=DIRECTION('center_axis',(0.,0.,1.));
#9292=DIRECTION('ref_axis',(-0.938002783430529,-0.346627722890971,0.));
#9293=DIRECTION('',(0.,0.,1.));
#9294=DIRECTION('center_axis',(0.,0.,1.));
#9295=DIRECTION('ref_axis',(-0.938002783430529,-0.346627722890971,0.));
#9296=DIRECTION('',(0.,0.,1.));
#9297=DIRECTION('center_axis',(0.,0.,1.));
#9298=DIRECTION('ref_axis',(-0.938002783430529,-0.346627722890971,0.));
#9299=DIRECTION('',(0.,0.,1.));
#9300=DIRECTION('center_axis',(0.,0.,1.));
#9301=DIRECTION('ref_axis',(-0.938002783430529,-0.346627722890971,0.));
#9302=DIRECTION('',(0.,0.,1.));
#9303=DIRECTION('center_axis',(0.,0.,1.));
#9304=DIRECTION('ref_axis',(-0.938002783430529,-0.346627722890971,0.));
#9305=DIRECTION('',(0.,0.,1.));
#9306=DIRECTION('center_axis',(0.,0.,1.));
#9307=DIRECTION('ref_axis',(-0.938002783430529,-0.346627722890971,0.));
#9308=DIRECTION('',(0.,0.,1.));
#9309=DIRECTION('center_axis',(0.,0.,1.));
#9310=DIRECTION('ref_axis',(-0.938002783430529,-0.346627722890971,0.));
#9311=DIRECTION('',(0.,0.,1.));
#9312=DIRECTION('center_axis',(0.,0.,1.));
#9313=DIRECTION('ref_axis',(-0.938002783430529,-0.346627722890971,0.));
#9314=DIRECTION('',(0.,0.,1.));
#9315=DIRECTION('center_axis',(0.,0.,-1.));
#9316=DIRECTION('ref_axis',(-1.,0.,0.));
#9317=DIRECTION('center_axis',(0.,0.,-1.));
#9318=DIRECTION('ref_axis',(-0.609201867263802,-0.793015185808126,0.));
#9319=DIRECTION('',(0.,0.,-1.));
#9320=DIRECTION('center_axis',(0.,0.,1.));
#9321=DIRECTION('ref_axis',(1.,-1.05172447564359E-13,0.));
#9322=DIRECTION('center_axis',(0.,0.,-1.));
#9323=DIRECTION('ref_axis',(-0.609201867263802,-0.793015185808126,0.));
#9324=DIRECTION('',(0.,0.,-1.));
#9325=DIRECTION('center_axis',(0.,0.,-1.));
#9326=DIRECTION('ref_axis',(-0.609201867263802,-0.793015185808126,0.));
#9327=DIRECTION('',(0.,0.,-1.));
#9328=DIRECTION('center_axis',(0.,0.,-1.));
#9329=DIRECTION('ref_axis',(-0.609201867263802,-0.793015185808126,0.));
#9330=DIRECTION('',(0.,0.,-1.));
#9331=DIRECTION('center_axis',(0.,0.,-1.));
#9332=DIRECTION('ref_axis',(-0.609201867263802,-0.793015185808126,0.));
#9333=DIRECTION('',(0.,0.,-1.));
#9334=DIRECTION('center_axis',(0.,0.,-1.));
#9335=DIRECTION('ref_axis',(-0.609201867263802,-0.793015185808126,0.));
#9336=DIRECTION('',(0.,0.,-1.));
#9337=DIRECTION('center_axis',(0.,0.,-1.));
#9338=DIRECTION('ref_axis',(-0.609201867263802,-0.793015185808126,0.));
#9339=DIRECTION('',(0.,0.,-1.));
#9340=DIRECTION('center_axis',(0.,0.,-1.));
#9341=DIRECTION('ref_axis',(-0.609201867263802,-0.793015185808126,0.));
#9342=DIRECTION('',(0.,0.,-1.));
#9343=DIRECTION('center_axis',(0.,0.,-1.));
#9344=DIRECTION('ref_axis',(-0.609201867263802,-0.793015185808126,0.));
#9345=DIRECTION('',(0.,0.,-1.));
#9346=DIRECTION('center_axis',(0.,0.,-1.));
#9347=DIRECTION('ref_axis',(-0.609201867263802,-0.793015185808126,0.));
#9348=DIRECTION('',(0.,0.,-1.));
#9349=DIRECTION('center_axis',(0.,0.,-1.));
#9350=DIRECTION('ref_axis',(-0.609201867263802,-0.793015185808126,0.));
#9351=DIRECTION('',(0.,0.,-1.));
#9352=DIRECTION('center_axis',(0.,0.,-1.));
#9353=DIRECTION('ref_axis',(-0.609201867263802,-0.793015185808126,0.));
#9354=DIRECTION('',(0.,0.,-1.));
#9355=DIRECTION('center_axis',(0.,0.,-1.));
#9356=DIRECTION('ref_axis',(-0.609201867263802,-0.793015185808126,0.));
#9357=DIRECTION('',(0.,0.,-1.));
#9358=DIRECTION('center_axis',(0.,0.,-1.));
#9359=DIRECTION('ref_axis',(-0.609201867263802,-0.793015185808126,0.));
#9360=DIRECTION('',(0.,0.,-1.));
#9361=DIRECTION('center_axis',(0.,0.,-1.));
#9362=DIRECTION('ref_axis',(-0.609201867263802,-0.793015185808126,0.));
#9363=DIRECTION('',(0.,0.,-1.));
#9364=DIRECTION('center_axis',(0.,0.,-1.));
#9365=DIRECTION('ref_axis',(-0.609201867263802,-0.793015185808126,0.));
#9366=DIRECTION('',(0.,0.,-1.));
#9367=DIRECTION('center_axis',(0.,0.,-1.));
#9368=DIRECTION('ref_axis',(-0.609201867263802,-0.793015185808126,0.));
#9369=DIRECTION('',(0.,0.,-1.));
#9370=DIRECTION('center_axis',(0.,0.,-1.));
#9371=DIRECTION('ref_axis',(-0.609201867263802,-0.793015185808126,0.));
#9372=DIRECTION('',(0.,0.,-1.));
#9373=DIRECTION('center_axis',(0.,0.,-1.));
#9374=DIRECTION('ref_axis',(-0.609201867263802,-0.793015185808126,0.));
#9375=DIRECTION('',(0.,0.,-1.));
#9376=DIRECTION('center_axis',(0.,0.,-1.));
#9377=DIRECTION('ref_axis',(1.,-1.05172447564359E-13,0.));
#9378=DIRECTION('center_axis',(0.,0.,-1.));
#9379=DIRECTION('ref_axis',(0.938006403579049,-0.346617926317579,0.));
#9380=DIRECTION('',(0.,0.,-1.));
#9381=DIRECTION('center_axis',(0.,0.,1.));
#9382=DIRECTION('ref_axis',(1.,0.,0.));
#9383=DIRECTION('',(0.,0.,-1.));
#9384=DIRECTION('center_axis',(0.,0.,1.));
#9385=DIRECTION('ref_axis',(1.,0.,0.));
#9386=DIRECTION('center_axis',(0.,0.,1.));
#9387=DIRECTION('ref_axis',(1.,0.,0.));
#9388=DIRECTION('center_axis',(0.,0.,-1.));
#9389=DIRECTION('ref_axis',(0.938006403579049,-0.346617926317579,0.));
#9390=DIRECTION('',(0.,0.,-1.));
#9391=DIRECTION('center_axis',(0.,0.,-1.));
#9392=DIRECTION('ref_axis',(0.938006403579049,-0.346617926317579,0.));
#9393=DIRECTION('',(0.,0.,-1.));
#9394=DIRECTION('center_axis',(0.,0.,-1.));
#9395=DIRECTION('ref_axis',(0.938006403579049,-0.346617926317579,0.));
#9396=DIRECTION('',(0.,0.,-1.));
#9397=DIRECTION('center_axis',(0.,0.,-1.));
#9398=DIRECTION('ref_axis',(0.938006403579049,-0.346617926317579,0.));
#9399=DIRECTION('',(0.,0.,-1.));
#9400=DIRECTION('center_axis',(0.,0.,-1.));
#9401=DIRECTION('ref_axis',(0.938006403579049,-0.346617926317579,0.));
#9402=DIRECTION('',(0.,0.,-1.));
#9403=DIRECTION('center_axis',(0.,0.,-1.));
#9404=DIRECTION('ref_axis',(0.938006403579049,-0.346617926317579,0.));
#9405=DIRECTION('',(0.,0.,-1.));
#9406=DIRECTION('center_axis',(0.,0.,-1.));
#9407=DIRECTION('ref_axis',(0.938006403579049,-0.346617926317579,0.));
#9408=DIRECTION('',(0.,0.,-1.));
#9409=DIRECTION('center_axis',(0.,0.,-1.));
#9410=DIRECTION('ref_axis',(0.938006403579049,-0.346617926317579,0.));
#9411=DIRECTION('',(0.,0.,-1.));
#9412=DIRECTION('center_axis',(0.,0.,-1.));
#9413=DIRECTION('ref_axis',(0.938006403579049,-0.346617926317579,0.));
#9414=DIRECTION('',(0.,0.,-1.));
#9415=DIRECTION('center_axis',(0.,0.,-1.));
#9416=DIRECTION('ref_axis',(0.938006403579049,-0.346617926317579,0.));
#9417=DIRECTION('',(0.,0.,-1.));
#9418=DIRECTION('center_axis',(0.,0.,-1.));
#9419=DIRECTION('ref_axis',(0.938006403579049,-0.346617926317579,0.));
#9420=DIRECTION('',(0.,0.,-1.));
#9421=DIRECTION('center_axis',(0.,0.,-1.));
#9422=DIRECTION('ref_axis',(0.938006403579049,-0.346617926317579,0.));
#9423=DIRECTION('',(0.,0.,-1.));
#9424=DIRECTION('center_axis',(0.,0.,-1.));
#9425=DIRECTION('ref_axis',(0.938006403579049,-0.346617926317579,0.));
#9426=DIRECTION('',(0.,0.,-1.));
#9427=DIRECTION('center_axis',(0.,0.,-1.));
#9428=DIRECTION('ref_axis',(0.938006403579049,-0.346617926317579,0.));
#9429=DIRECTION('',(0.,0.,-1.));
#9430=DIRECTION('center_axis',(0.,0.,-1.));
#9431=DIRECTION('ref_axis',(0.938006403579049,-0.346617926317579,0.));
#9432=DIRECTION('',(0.,0.,-1.));
#9433=DIRECTION('center_axis',(0.,0.,-1.));
#9434=DIRECTION('ref_axis',(0.938006403579049,-0.346617926317579,0.));
#9435=DIRECTION('',(0.,0.,-1.));
#9436=DIRECTION('center_axis',(0.,0.,-1.));
#9437=DIRECTION('ref_axis',(0.938006403579049,-0.346617926317579,0.));
#9438=DIRECTION('',(0.,0.,-1.));
#9439=DIRECTION('center_axis',(0.,0.,-1.));
#9440=DIRECTION('ref_axis',(0.938006403579049,-0.346617926317579,0.));
#9441=DIRECTION('',(0.,0.,-1.));
#9442=DIRECTION('center_axis',(0.,0.,-1.));
#9443=DIRECTION('ref_axis',(1.,0.,0.));
#9444=DIRECTION('center_axis',(0.,0.,-1.));
#9445=DIRECTION('ref_axis',(0.938006403579049,-0.346617926317579,0.));
#9446=DIRECTION('center_axis',(0.,0.,-1.));
#9447=DIRECTION('ref_axis',(-0.609201867263802,-0.793015185808126,0.));
#9448=DIRECTION('center_axis',(0.,0.,1.));
#9449=DIRECTION('ref_axis',(-0.938002783430529,-0.346627722890971,0.));
#9450=DIRECTION('center_axis',(0.,0.,1.));
#9451=DIRECTION('ref_axis',(0.60921024449365,-0.793008750269496,0.));
#9452=DIRECTION('center_axis',(0.,0.,1.));
#9453=DIRECTION('ref_axis',(1.,0.,0.));
#9454=DIRECTION('center_axis',(0.,0.,1.));
#9455=DIRECTION('ref_axis',(-1.,0.,0.));
#9456=DIRECTION('center_axis',(0.,0.,1.));
#9457=DIRECTION('ref_axis',(1.,0.,0.));
#9458=DIRECTION('center_axis',(0.,0.,-1.));
#9459=DIRECTION('ref_axis',(1.,0.,0.));
#9460=DIRECTION('center_axis',(0.,0.,1.));
#9461=DIRECTION('ref_axis',(1.,0.,0.));
#9462=DIRECTION('center_axis',(0.,0.,1.));
#9463=DIRECTION('ref_axis',(1.,0.,0.));
#9464=DIRECTION('',(0.,0.,-1.));
#9465=DIRECTION('center_axis',(0.,0.,1.));
#9466=DIRECTION('ref_axis',(1.,0.,0.));
#9467=DIRECTION('center_axis',(0.,0.,1.));
#9468=DIRECTION('ref_axis',(1.,0.,0.));
#9469=DIRECTION('center_axis',(0.,0.,1.));
#9470=DIRECTION('ref_axis',(1.,0.,0.));
#9471=DIRECTION('axis',(0.,0.,1.));
#9472=DIRECTION('refdir',(1.,0.,0.));
#9473=DIRECTION('center_axis',(0.,0.,1.));
#9474=DIRECTION('ref_axis',(0.997344302588954,-0.0728309144069492,0.));
#9475=DIRECTION('',(0.,0.,-1.));
#9476=DIRECTION('center_axis',(0.,0.,-1.));
#9477=DIRECTION('ref_axis',(1.,7.52212518638754E-14,0.));
#9478=DIRECTION('center_axis',(0.,0.,1.));
#9479=DIRECTION('ref_axis',(0.997344302588954,-0.0728309144069492,0.));
#9480=DIRECTION('',(0.,0.,-1.));
#9481=DIRECTION('center_axis',(0.,0.,1.));
#9482=DIRECTION('ref_axis',(0.997344302588954,-0.0728309144069492,0.));
#9483=DIRECTION('',(0.,0.,-1.));
#9484=DIRECTION('center_axis',(0.,0.,1.));
#9485=DIRECTION('ref_axis',(0.997344302588954,-0.0728309144069492,0.));
#9486=DIRECTION('',(0.,0.,-1.));
#9487=DIRECTION('center_axis',(0.,0.,1.));
#9488=DIRECTION('ref_axis',(0.997344302588954,-0.0728309144069492,0.));
#9489=DIRECTION('',(0.,0.,-1.));
#9490=DIRECTION('center_axis',(0.,0.,1.));
#9491=DIRECTION('ref_axis',(0.997344302588954,-0.0728309144069492,0.));
#9492=DIRECTION('',(0.,0.,-1.));
#9493=DIRECTION('center_axis',(0.,0.,1.));
#9494=DIRECTION('ref_axis',(0.997344302588954,-0.0728309144069492,0.));
#9495=DIRECTION('',(0.,0.,-1.));
#9496=DIRECTION('center_axis',(0.,0.,1.));
#9497=DIRECTION('ref_axis',(0.997344302588954,-0.0728309144069492,0.));
#9498=DIRECTION('',(0.,0.,-1.));
#9499=DIRECTION('center_axis',(0.,0.,1.));
#9500=DIRECTION('ref_axis',(0.997344302588954,-0.0728309144069492,0.));
#9501=DIRECTION('',(0.,0.,-1.));
#9502=DIRECTION('center_axis',(0.,0.,1.));
#9503=DIRECTION('ref_axis',(0.997344302588954,-0.0728309144069492,0.));
#9504=DIRECTION('',(0.,0.,-1.));
#9505=DIRECTION('center_axis',(0.,0.,1.));
#9506=DIRECTION('ref_axis',(0.997344302588954,-0.0728309144069492,0.));
#9507=DIRECTION('',(0.,0.,-1.));
#9508=DIRECTION('center_axis',(0.,0.,1.));
#9509=DIRECTION('ref_axis',(1.,0.,0.));
#9510=DIRECTION('center_axis',(0.,0.,-1.));
#9511=DIRECTION('ref_axis',(1.,0.,0.));
#9512=DIRECTION('center_axis',(0.,0.,-1.));
#9513=DIRECTION('ref_axis',(1.,0.,0.));
#9514=DIRECTION('center_axis',(0.,0.,1.));
#9515=DIRECTION('ref_axis',(0.997344302588954,-0.0728309144069492,0.));
#9516=DIRECTION('center_axis',(0.,0.,-1.));
#9517=DIRECTION('ref_axis',(1.,7.52212518638754E-14,0.));
#9518=DIRECTION('center_axis',(0.,0.,-1.));
#9519=DIRECTION('ref_axis',(1.,0.,0.));
#9520=DIRECTION('',(0.707106781186548,-8.65956056235494E-17,0.707106781186547));
#9521=DIRECTION('center_axis',(0.,0.,1.));
#9522=DIRECTION('ref_axis',(1.,0.,0.));
#9523=DIRECTION('center_axis',(-1.92296268638356E-16,-1.,0.));
#9524=DIRECTION('ref_axis',(1.,-1.92296268638356E-16,0.));
#9525=DIRECTION('',(1.,-1.92296268638356E-16,0.));
#9526=DIRECTION('',(0.,0.,1.));
#9527=DIRECTION('',(1.,-1.92296268638356E-16,0.));
#9528=DIRECTION('',(0.,0.,1.));
#9529=DIRECTION('center_axis',(-0.866025403784439,-0.5,0.));
#9530=DIRECTION('ref_axis',(0.5,-0.866025403784439,0.));
#9531=DIRECTION('',(0.5,-0.866025403784439,0.));
#9532=DIRECTION('',(0.,0.,1.));
#9533=DIRECTION('',(0.5,-0.866025403784439,0.));
#9534=DIRECTION('center_axis',(-0.866025403784439,0.5,0.));
#9535=DIRECTION('ref_axis',(-0.5,-0.866025403784439,0.));
#9536=DIRECTION('',(-0.5,-0.866025403784439,0.));
#9537=DIRECTION('',(0.,0.,1.));
#9538=DIRECTION('',(-0.5,-0.866025403784439,0.));
#9539=DIRECTION('center_axis',(1.92296268638356E-16,1.,0.));
#9540=DIRECTION('ref_axis',(-1.,1.92296268638356E-16,0.));
#9541=DIRECTION('',(-1.,1.92296268638356E-16,0.));
#9542=DIRECTION('',(0.,0.,1.));
#9543=DIRECTION('',(-1.,1.92296268638356E-16,0.));
#9544=DIRECTION('center_axis',(0.866025403784439,0.5,0.));
#9545=DIRECTION('ref_axis',(-0.5,0.866025403784439,0.));
#9546=DIRECTION('',(-0.5,0.866025403784439,0.));
#9547=DIRECTION('',(0.,0.,1.));
#9548=DIRECTION('',(-0.5,0.866025403784439,0.));
#9549=DIRECTION('center_axis',(0.866025403784439,-0.5,0.));
#9550=DIRECTION('ref_axis',(0.5,0.866025403784439,0.));
#9551=DIRECTION('',(0.5,0.866025403784439,0.));
#9552=DIRECTION('',(0.5,0.866025403784439,0.));
#9553=DIRECTION('center_axis',(0.,0.,1.));
#9554=DIRECTION('ref_axis',(1.,0.,0.));
#9555=DIRECTION('center_axis',(0.,0.,1.));
#9556=DIRECTION('ref_axis',(1.,0.,0.));
#9557=DIRECTION('center_axis',(0.,0.,1.));
#9558=DIRECTION('ref_axis',(1.,0.,0.));
#9559=DIRECTION('center_axis',(0.,0.,1.));
#9560=DIRECTION('ref_axis',(1.,0.,0.));
#9561=DIRECTION('',(0.,0.,-1.));
#9562=DIRECTION('center_axis',(0.,0.,1.));
#9563=DIRECTION('ref_axis',(1.,0.,0.));
#9564=DIRECTION('center_axis',(0.,0.,1.));
#9565=DIRECTION('ref_axis',(1.,0.,0.));
#9566=DIRECTION('center_axis',(0.,0.,1.));
#9567=DIRECTION('ref_axis',(1.,0.,0.));
#9568=DIRECTION('axis',(0.,0.,1.));
#9569=DIRECTION('refdir',(1.,0.,0.));
#9570=DIRECTION('center_axis',(0.,0.,-1.));
#9571=DIRECTION('ref_axis',(-0.609351707504989,-0.792900054584911,0.));
#9572=DIRECTION('',(0.,0.,-1.));
#9573=DIRECTION('center_axis',(0.,0.,1.));
#9574=DIRECTION('ref_axis',(1.,-8.20798086521558E-14,0.));
#9575=DIRECTION('center_axis',(0.,0.,-1.));
#9576=DIRECTION('ref_axis',(-0.609351707504989,-0.792900054584911,0.));
#9577=DIRECTION('',(0.,0.,-1.));
#9578=DIRECTION('center_axis',(0.,0.,-1.));
#9579=DIRECTION('ref_axis',(-0.609351707504989,-0.792900054584911,0.));
#9580=DIRECTION('',(0.,0.,-1.));
#9581=DIRECTION('center_axis',(0.,0.,-1.));
#9582=DIRECTION('ref_axis',(-0.609351707504989,-0.792900054584911,0.));
#9583=DIRECTION('',(0.,0.,-1.));
#9584=DIRECTION('center_axis',(0.,0.,-1.));
#9585=DIRECTION('ref_axis',(-0.609351707504989,-0.792900054584911,0.));
#9586=DIRECTION('',(0.,0.,-1.));
#9587=DIRECTION('center_axis',(0.,0.,-1.));
#9588=DIRECTION('ref_axis',(-0.609351707504989,-0.792900054584911,0.));
#9589=DIRECTION('',(0.,0.,-1.));
#9590=DIRECTION('center_axis',(0.,0.,-1.));
#9591=DIRECTION('ref_axis',(-0.609351707504989,-0.792900054584911,0.));
#9592=DIRECTION('',(0.,0.,-1.));
#9593=DIRECTION('center_axis',(0.,0.,-1.));
#9594=DIRECTION('ref_axis',(-0.609351707504989,-0.792900054584911,0.));
#9595=DIRECTION('',(0.,0.,-1.));
#9596=DIRECTION('center_axis',(0.,0.,-1.));
#9597=DIRECTION('ref_axis',(-0.609351707504989,-0.792900054584911,0.));
#9598=DIRECTION('',(0.,0.,-1.));
#9599=DIRECTION('center_axis',(0.,0.,-1.));
#9600=DIRECTION('ref_axis',(-0.609351707504989,-0.792900054584911,0.));
#9601=DIRECTION('',(0.,0.,-1.));
#9602=DIRECTION('center_axis',(0.,0.,-1.));
#9603=DIRECTION('ref_axis',(-0.609351707504989,-0.792900054584911,0.));
#9604=DIRECTION('',(0.,0.,-1.));
#9605=DIRECTION('center_axis',(0.,0.,-1.));
#9606=DIRECTION('ref_axis',(-0.609351707504989,-0.792900054584911,0.));
#9607=DIRECTION('',(0.,0.,-1.));
#9608=DIRECTION('center_axis',(0.,0.,-1.));
#9609=DIRECTION('ref_axis',(-0.609351707504989,-0.792900054584911,0.));
#9610=DIRECTION('',(0.,0.,-1.));
#9611=DIRECTION('center_axis',(0.,0.,-1.));
#9612=DIRECTION('ref_axis',(-0.609351707504989,-0.792900054584911,0.));
#9613=DIRECTION('',(0.,0.,-1.));
#9614=DIRECTION('center_axis',(0.,0.,-1.));
#9615=DIRECTION('ref_axis',(-0.609351707504989,-0.792900054584911,0.));
#9616=DIRECTION('',(0.,0.,-1.));
#9617=DIRECTION('center_axis',(0.,0.,-1.));
#9618=DIRECTION('ref_axis',(-0.609351707504989,-0.792900054584911,0.));
#9619=DIRECTION('',(0.,0.,-1.));
#9620=DIRECTION('center_axis',(0.,0.,-1.));
#9621=DIRECTION('ref_axis',(1.,-8.20798086521558E-14,0.));
#9622=DIRECTION('center_axis',(0.,0.,-1.));
#9623=DIRECTION('ref_axis',(0.938434153860821,-0.345458157911382,0.));
#9624=DIRECTION('',(0.,0.,-1.));
#9625=DIRECTION('center_axis',(0.,0.,1.));
#9626=DIRECTION('ref_axis',(1.,0.,0.));
#9627=DIRECTION('',(0.,0.,-1.));
#9628=DIRECTION('center_axis',(0.,0.,1.));
#9629=DIRECTION('ref_axis',(1.,0.,0.));
#9630=DIRECTION('center_axis',(0.,0.,-1.));
#9631=DIRECTION('ref_axis',(0.938434153860821,-0.345458157911382,0.));
#9632=DIRECTION('',(0.,0.,-1.));
#9633=DIRECTION('center_axis',(0.,0.,-1.));
#9634=DIRECTION('ref_axis',(0.938434153860821,-0.345458157911382,0.));
#9635=DIRECTION('',(0.,0.,-1.));
#9636=DIRECTION('center_axis',(0.,0.,-1.));
#9637=DIRECTION('ref_axis',(0.938434153860821,-0.345458157911382,0.));
#9638=DIRECTION('',(0.,0.,-1.));
#9639=DIRECTION('center_axis',(0.,0.,-1.));
#9640=DIRECTION('ref_axis',(0.938434153860821,-0.345458157911382,0.));
#9641=DIRECTION('',(0.,0.,-1.));
#9642=DIRECTION('center_axis',(0.,0.,-1.));
#9643=DIRECTION('ref_axis',(0.938434153860821,-0.345458157911382,0.));
#9644=DIRECTION('',(0.,0.,-1.));
#9645=DIRECTION('center_axis',(0.,0.,-1.));
#9646=DIRECTION('ref_axis',(0.938434153860821,-0.345458157911382,0.));
#9647=DIRECTION('',(0.,0.,-1.));
#9648=DIRECTION('center_axis',(0.,0.,-1.));
#9649=DIRECTION('ref_axis',(0.938434153860821,-0.345458157911382,0.));
#9650=DIRECTION('',(0.,0.,-1.));
#9651=DIRECTION('center_axis',(0.,0.,-1.));
#9652=DIRECTION('ref_axis',(0.938434153860821,-0.345458157911382,0.));
#9653=DIRECTION('',(0.,0.,-1.));
#9654=DIRECTION('center_axis',(0.,0.,-1.));
#9655=DIRECTION('ref_axis',(0.938434153860821,-0.345458157911382,0.));
#9656=DIRECTION('',(0.,0.,-1.));
#9657=DIRECTION('center_axis',(0.,0.,-1.));
#9658=DIRECTION('ref_axis',(0.938434153860821,-0.345458157911382,0.));
#9659=DIRECTION('',(0.,0.,-1.));
#9660=DIRECTION('center_axis',(0.,0.,-1.));
#9661=DIRECTION('ref_axis',(0.938434153860821,-0.345458157911382,0.));
#9662=DIRECTION('',(0.,0.,-1.));
#9663=DIRECTION('center_axis',(0.,0.,-1.));
#9664=DIRECTION('ref_axis',(0.938434153860821,-0.345458157911382,0.));
#9665=DIRECTION('',(0.,0.,-1.));
#9666=DIRECTION('center_axis',(0.,0.,-1.));
#9667=DIRECTION('ref_axis',(0.938434153860821,-0.345458157911382,0.));
#9668=DIRECTION('',(0.,0.,-1.));
#9669=DIRECTION('center_axis',(0.,0.,-1.));
#9670=DIRECTION('ref_axis',(0.938434153860821,-0.345458157911382,0.));
#9671=DIRECTION('',(0.,0.,-1.));
#9672=DIRECTION('center_axis',(0.,0.,-1.));
#9673=DIRECTION('ref_axis',(1.,0.,0.));
#9674=DIRECTION('center_axis',(0.,0.,-1.));
#9675=DIRECTION('ref_axis',(0.938434153860821,-0.345458157911382,0.));
#9676=DIRECTION('center_axis',(0.,0.,-1.));
#9677=DIRECTION('ref_axis',(-0.609351707504989,-0.792900054584911,0.));
#9678=DIRECTION('center_axis',(0.,0.,1.));
#9679=DIRECTION('ref_axis',(1.,0.,0.));
#9680=DIRECTION('center_axis',(0.,0.,-1.));
#9681=DIRECTION('ref_axis',(1.,0.,0.));
#9682=DIRECTION('center_axis',(0.,0.,1.));
#9683=DIRECTION('ref_axis',(1.,0.,0.));
#9684=DIRECTION('center_axis',(0.,0.,1.));
#9685=DIRECTION('ref_axis',(1.,0.,0.));
#9686=DIRECTION('',(0.,0.,-1.));
#9687=DIRECTION('center_axis',(0.,0.,1.));
#9688=DIRECTION('ref_axis',(1.,0.,0.));
#9689=DIRECTION('center_axis',(0.,0.,1.));
#9690=DIRECTION('ref_axis',(1.,0.,0.));
#9691=DIRECTION('center_axis',(0.,0.,1.));
#9692=DIRECTION('ref_axis',(1.,0.,0.));
#9693=DIRECTION('',(0.,0.,1.));
#9694=DIRECTION('',(1.,0.,0.));
#9695=DIRECTION('',(0.,0.,1.));
#9696=DIRECTION('',(1.,0.,0.));
#9697=DIRECTION('',(0.,0.,1.));
#9698=DIRECTION('',(1.,0.,0.));
#9699=DIRECTION('',(0.,0.,1.));
#9700=DIRECTION('',(1.,0.,0.));
#9701=DIRECTION('',(0.,0.,1.));
#9702=DIRECTION('',(1.,0.,0.));
#9703=DIRECTION('',(0.,0.,1.));
#9704=DIRECTION('',(-1.,1.22464679914735E-16,0.));
#9705=DIRECTION('',(0.,0.,1.));
#9706=DIRECTION('',(1.,0.,0.));
#9707=DIRECTION('',(0.,0.,1.));
#9708=DIRECTION('',(1.,0.,0.));
#9709=DIRECTION('',(0.,0.,1.));
#9710=DIRECTION('',(1.,0.,0.));
#9711=DIRECTION('',(0.,0.,1.));
#9712=DIRECTION('',(1.,0.,0.));
#9713=DIRECTION('',(0.,0.,1.));
#9714=DIRECTION('',(1.,0.,0.));
#9715=DIRECTION('',(0.,0.,1.));
#9716=DIRECTION('',(-1.,1.22464679914735E-16,0.));
#9717=DIRECTION('',(0.,0.,1.));
#9718=DIRECTION('',(-1.,1.22464679914735E-16,0.));
#9719=DIRECTION('',(0.,0.,1.));
#9720=DIRECTION('',(-1.,1.22464679914735E-16,0.));
#9721=DIRECTION('',(0.,0.,1.));
#9722=DIRECTION('',(1.,0.,0.));
#9723=DIRECTION('',(0.,0.,1.));
#9724=DIRECTION('',(1.,0.,0.));
#9725=DIRECTION('',(0.,0.,1.));
#9726=DIRECTION('',(1.,0.,0.));
#9727=DIRECTION('axis',(0.,0.,1.));
#9728=DIRECTION('refdir',(1.,0.,0.));
#9729=DIRECTION('center_axis',(0.,-1.,0.));
#9730=DIRECTION('ref_axis',(0.916515138991168,0.,0.399999999999999));
#9731=DIRECTION('center_axis',(0.,-1.,0.));
#9732=DIRECTION('ref_axis',(0.916515138991168,0.,0.399999999999999));
#9733=DIRECTION('',(0.,-1.,0.));
#9734=DIRECTION('center_axis',(0.,1.,0.));
#9735=DIRECTION('ref_axis',(0.916515138991168,0.,0.399999999999999));
#9736=DIRECTION('',(0.,1.,0.));
#9737=DIRECTION('center_axis',(0.,0.,1.));
#9738=DIRECTION('ref_axis',(1.,0.,0.));
#9739=DIRECTION('',(-1.,0.,0.));
#9740=DIRECTION('',(0.,-1.,0.));
#9741=DIRECTION('',(1.,0.,0.));
#9742=DIRECTION('center_axis',(0.,0.,-1.));
#9743=DIRECTION('ref_axis',(1.,0.,0.));
#9744=DIRECTION('center_axis',(0.,0.,-1.));
#9745=DIRECTION('ref_axis',(1.,0.,0.));
#9746=DIRECTION('center_axis',(0.,0.,-1.));
#9747=DIRECTION('ref_axis',(1.,0.,0.));
#9748=DIRECTION('center_axis',(0.,0.,-1.));
#9749=DIRECTION('ref_axis',(1.,0.,0.));
#9750=DIRECTION('center_axis',(0.,1.,0.));
#9751=DIRECTION('ref_axis',(-1.,0.,0.));
#9752=DIRECTION('',(-1.,0.,0.));
#9753=DIRECTION('',(0.,0.,1.));
#9754=DIRECTION('center_axis',(0.,0.,-1.));
#9755=DIRECTION('ref_axis',(1.,0.,0.));
#9756=DIRECTION('',(0.,0.,-1.));
#9757=DIRECTION('center_axis',(0.,0.,1.));
#9758=DIRECTION('ref_axis',(1.,0.,0.));
#9759=DIRECTION('center_axis',(0.,0.,-1.));
#9760=DIRECTION('ref_axis',(1.,0.,0.));
#9761=DIRECTION('',(0.,0.,-1.));
#9762=DIRECTION('center_axis',(0.,0.,1.));
#9763=DIRECTION('ref_axis',(1.,0.,0.));
#9764=DIRECTION('center_axis',(0.,0.,-1.));
#9765=DIRECTION('ref_axis',(1.,0.,0.));
#9766=DIRECTION('',(0.,0.,-1.));
#9767=DIRECTION('center_axis',(0.,0.,1.));
#9768=DIRECTION('ref_axis',(1.,0.,0.));
#9769=DIRECTION('center_axis',(0.,0.,-1.));
#9770=DIRECTION('ref_axis',(1.,0.,0.));
#9771=DIRECTION('',(0.,0.,-1.));
#9772=DIRECTION('center_axis',(0.,0.,1.));
#9773=DIRECTION('ref_axis',(1.,0.,0.));
#9774=DIRECTION('center_axis',(0.,-1.,0.));
#9775=DIRECTION('ref_axis',(1.,0.,0.));
#9776=DIRECTION('',(0.,0.,1.));
#9777=DIRECTION('',(1.,0.,0.));
#9778=DIRECTION('center_axis',(-1.,0.,0.));
#9779=DIRECTION('ref_axis',(0.,-1.,0.));
#9780=DIRECTION('',(0.,-1.,0.));
#9781=DIRECTION('center_axis',(0.,0.,1.));
#9782=DIRECTION('ref_axis',(1.,0.,0.));
#9783=DIRECTION('axis',(0.,0.,1.));
#9784=DIRECTION('refdir',(1.,0.,0.));
#9785=DIRECTION('center_axis',(0.,0.,-1.));
#9786=DIRECTION('ref_axis',(1.,0.,0.));
#9787=DIRECTION('center_axis',(0.,0.,-1.));
#9788=DIRECTION('ref_axis',(1.,0.,0.));
#9789=DIRECTION('',(0.,0.,-1.));
#9790=DIRECTION('center_axis',(0.,0.,1.));
#9791=DIRECTION('ref_axis',(1.,0.,0.));
#9792=DIRECTION('center_axis',(0.,0.,-1.));
#9793=DIRECTION('ref_axis',(1.,0.,0.));
#9794=DIRECTION('center_axis',(0.,0.,-1.));
#9795=DIRECTION('ref_axis',(1.,0.,0.));
#9796=DIRECTION('',(0.,0.,-1.));
#9797=DIRECTION('center_axis',(0.,0.,1.));
#9798=DIRECTION('ref_axis',(1.,0.,0.));
#9799=DIRECTION('center_axis',(0.,0.,-1.));
#9800=DIRECTION('ref_axis',(1.,0.,0.));
#9801=DIRECTION('center_axis',(0.,0.,-1.));
#9802=DIRECTION('ref_axis',(1.,0.,0.));
#9803=DIRECTION('',(0.,0.,-1.));
#9804=DIRECTION('center_axis',(0.,0.,1.));
#9805=DIRECTION('ref_axis',(1.,0.,0.));
#9806=DIRECTION('center_axis',(0.,0.,-1.));
#9807=DIRECTION('ref_axis',(1.,0.,0.));
#9808=DIRECTION('center_axis',(0.,0.,-1.));
#9809=DIRECTION('ref_axis',(1.,0.,0.));
#9810=DIRECTION('',(0.,0.,-1.));
#9811=DIRECTION('center_axis',(0.,0.,1.));
#9812=DIRECTION('ref_axis',(1.,0.,0.));
#9813=DIRECTION('center_axis',(0.,1.,0.));
#9814=DIRECTION('ref_axis',(-1.,0.,0.));
#9815=DIRECTION('',(-1.,0.,0.));
#9816=DIRECTION('',(0.,0.,1.));
#9817=DIRECTION('',(-1.,0.,0.));
#9818=DIRECTION('',(0.,0.,1.));
#9819=DIRECTION('center_axis',(-1.,0.,0.));
#9820=DIRECTION('ref_axis',(0.,-1.,0.));
#9821=DIRECTION('',(0.,-1.,0.));
#9822=DIRECTION('',(0.,-1.,0.));
#9823=DIRECTION('',(0.,0.,1.));
#9824=DIRECTION('center_axis',(0.,-1.,0.));
#9825=DIRECTION('ref_axis',(1.,0.,0.));
#9826=DIRECTION('',(1.,0.,0.));
#9827=DIRECTION('',(1.,0.,0.));
#9828=DIRECTION('',(0.,0.,1.));
#9829=DIRECTION('center_axis',(1.,0.,0.));
#9830=DIRECTION('ref_axis',(0.,1.,0.));
#9831=DIRECTION('',(0.,1.,0.));
#9832=DIRECTION('',(0.,1.,0.));
#9833=DIRECTION('center_axis',(0.,1.,0.));
#9834=DIRECTION('ref_axis',(-1.,0.,0.));
#9835=DIRECTION('',(-1.,0.,0.));
#9836=DIRECTION('',(0.,0.,1.));
#9837=DIRECTION('',(-1.,0.,0.));
#9838=DIRECTION('',(0.,0.,1.));
#9839=DIRECTION('center_axis',(1.,0.,0.));
#9840=DIRECTION('ref_axis',(0.,1.,0.));
#9841=DIRECTION('',(0.,1.,0.));
#9842=DIRECTION('',(0.,1.,0.));
#9843=DIRECTION('',(0.,0.,1.));
#9844=DIRECTION('center_axis',(0.,-1.,0.));
#9845=DIRECTION('ref_axis',(1.,0.,0.));
#9846=DIRECTION('',(1.,0.,0.));
#9847=DIRECTION('',(1.,0.,0.));
#9848=DIRECTION('',(0.,0.,1.));
#9849=DIRECTION('center_axis',(-1.,0.,0.));
#9850=DIRECTION('ref_axis',(0.,-1.,0.));
#9851=DIRECTION('',(0.,-1.,0.));
#9852=DIRECTION('',(0.,-1.,0.));
#9853=DIRECTION('center_axis',(0.,0.,1.));
#9854=DIRECTION('ref_axis',(1.,0.,0.));
#9855=DIRECTION('center_axis',(0.,0.,1.));
#9856=DIRECTION('ref_axis',(1.,0.,0.));
#9857=DIRECTION('axis',(0.,0.,1.));
#9858=DIRECTION('refdir',(1.,0.,0.));
#9859=DIRECTION('center_axis',(0.,0.,-1.));
#9860=DIRECTION('ref_axis',(1.,0.,0.));
#9861=DIRECTION('center_axis',(0.,0.,-1.));
#9862=DIRECTION('ref_axis',(1.,0.,0.));
#9863=DIRECTION('',(0.,0.,-1.));
#9864=DIRECTION('center_axis',(0.,0.,1.));
#9865=DIRECTION('ref_axis',(1.,0.,0.));
#9866=DIRECTION('center_axis',(0.,0.,-1.));
#9867=DIRECTION('ref_axis',(1.,0.,0.));
#9868=DIRECTION('center_axis',(0.,0.,-1.));
#9869=DIRECTION('ref_axis',(1.,0.,0.));
#9870=DIRECTION('',(0.,0.,-1.));
#9871=DIRECTION('center_axis',(0.,0.,1.));
#9872=DIRECTION('ref_axis',(1.,0.,0.));
#9873=DIRECTION('center_axis',(0.,0.,-1.));
#9874=DIRECTION('ref_axis',(1.,0.,0.));
#9875=DIRECTION('center_axis',(0.,0.,-1.));
#9876=DIRECTION('ref_axis',(1.,0.,0.));
#9877=DIRECTION('',(0.,0.,-1.));
#9878=DIRECTION('center_axis',(0.,0.,1.));
#9879=DIRECTION('ref_axis',(1.,0.,0.));
#9880=DIRECTION('center_axis',(0.,0.,-1.));
#9881=DIRECTION('ref_axis',(1.,0.,0.));
#9882=DIRECTION('center_axis',(0.,0.,-1.));
#9883=DIRECTION('ref_axis',(1.,0.,0.));
#9884=DIRECTION('',(0.,0.,-1.));
#9885=DIRECTION('center_axis',(0.,0.,1.));
#9886=DIRECTION('ref_axis',(1.,0.,0.));
#9887=DIRECTION('center_axis',(0.,1.,0.));
#9888=DIRECTION('ref_axis',(-1.,0.,0.));
#9889=DIRECTION('',(-1.,0.,0.));
#9890=DIRECTION('',(0.,0.,1.));
#9891=DIRECTION('',(-1.,0.,0.));
#9892=DIRECTION('',(0.,0.,1.));
#9893=DIRECTION('center_axis',(1.,0.,0.));
#9894=DIRECTION('ref_axis',(0.,1.,0.));
#9895=DIRECTION('',(0.,1.,0.));
#9896=DIRECTION('',(0.,1.,0.));
#9897=DIRECTION('',(0.,0.,1.));
#9898=DIRECTION('center_axis',(0.,-1.,0.));
#9899=DIRECTION('ref_axis',(1.,0.,0.));
#9900=DIRECTION('',(1.,0.,0.));
#9901=DIRECTION('',(1.,0.,0.));
#9902=DIRECTION('',(0.,0.,1.));
#9903=DIRECTION('center_axis',(-1.,0.,0.));
#9904=DIRECTION('ref_axis',(0.,-1.,0.));
#9905=DIRECTION('',(0.,-1.,0.));
#9906=DIRECTION('',(0.,-1.,0.));
#9907=DIRECTION('center_axis',(0.,0.,1.));
#9908=DIRECTION('ref_axis',(1.,0.,0.));
#9909=DIRECTION('center_axis',(0.,0.,1.));
#9910=DIRECTION('ref_axis',(1.,0.,0.));
#9911=DIRECTION('axis',(0.,0.,1.));
#9912=DIRECTION('refdir',(1.,0.,0.));
#9913=DIRECTION('center_axis',(0.,0.,1.));
#9914=DIRECTION('ref_axis',(0.997339946684471,-0.0728905394918792,0.));
#9915=DIRECTION('',(0.,0.,-1.));
#9916=DIRECTION('center_axis',(0.,0.,-1.));
#9917=DIRECTION('ref_axis',(1.,1.10476514494527E-13,0.));
#9918=DIRECTION('center_axis',(0.,0.,1.));
#9919=DIRECTION('ref_axis',(0.997339946684471,-0.0728905394918792,0.));
#9920=DIRECTION('',(0.,0.,-1.));
#9921=DIRECTION('center_axis',(0.,0.,1.));
#9922=DIRECTION('ref_axis',(0.997339946684471,-0.0728905394918792,0.));
#9923=DIRECTION('',(0.,0.,-1.));
#9924=DIRECTION('center_axis',(0.,0.,1.));
#9925=DIRECTION('ref_axis',(0.997339946684471,-0.0728905394918792,0.));
#9926=DIRECTION('',(0.,0.,-1.));
#9927=DIRECTION('center_axis',(0.,0.,1.));
#9928=DIRECTION('ref_axis',(0.997339946684471,-0.0728905394918792,0.));
#9929=DIRECTION('',(0.,0.,-1.));
#9930=DIRECTION('center_axis',(0.,0.,1.));
#9931=DIRECTION('ref_axis',(0.997339946684471,-0.0728905394918792,0.));
#9932=DIRECTION('',(0.,0.,-1.));
#9933=DIRECTION('center_axis',(0.,0.,1.));
#9934=DIRECTION('ref_axis',(0.997339946684471,-0.0728905394918792,0.));
#9935=DIRECTION('',(0.,0.,-1.));
#9936=DIRECTION('center_axis',(0.,0.,1.));
#9937=DIRECTION('ref_axis',(0.997339946684471,-0.0728905394918792,0.));
#9938=DIRECTION('',(0.,0.,-1.));
#9939=DIRECTION('center_axis',(0.,0.,1.));
#9940=DIRECTION('ref_axis',(0.997339946684471,-0.0728905394918792,0.));
#9941=DIRECTION('',(0.,0.,-1.));
#9942=DIRECTION('center_axis',(0.,0.,1.));
#9943=DIRECTION('ref_axis',(0.997339946684471,-0.0728905394918792,0.));
#9944=DIRECTION('',(0.,0.,-1.));
#9945=DIRECTION('center_axis',(0.,0.,1.));
#9946=DIRECTION('ref_axis',(0.997339946684471,-0.0728905394918792,0.));
#9947=DIRECTION('',(0.,0.,-1.));
#9948=DIRECTION('center_axis',(0.,0.,1.));
#9949=DIRECTION('ref_axis',(0.997339946684471,-0.0728905394918792,0.));
#9950=DIRECTION('',(0.,0.,-1.));
#9951=DIRECTION('center_axis',(0.,0.,1.));
#9952=DIRECTION('ref_axis',(0.997339946684471,-0.0728905394918792,0.));
#9953=DIRECTION('',(0.,0.,-1.));
#9954=DIRECTION('center_axis',(0.,0.,1.));
#9955=DIRECTION('ref_axis',(0.997339946684471,-0.0728905394918792,0.));
#9956=DIRECTION('',(0.,0.,-1.));
#9957=DIRECTION('center_axis',(0.,0.,1.));
#9958=DIRECTION('ref_axis',(0.997339946684471,-0.0728905394918792,0.));
#9959=DIRECTION('',(0.,0.,-1.));
#9960=DIRECTION('center_axis',(0.,0.,1.));
#9961=DIRECTION('ref_axis',(1.,0.,0.));
#9962=DIRECTION('center_axis',(0.,0.,-1.));
#9963=DIRECTION('ref_axis',(1.,0.,0.));
#9964=DIRECTION('center_axis',(0.,0.,-1.));
#9965=DIRECTION('ref_axis',(1.,0.,0.));
#9966=DIRECTION('center_axis',(0.,0.,1.));
#9967=DIRECTION('ref_axis',(0.997339946684471,-0.0728905394918792,0.));
#9968=DIRECTION('center_axis',(0.,0.,-1.));
#9969=DIRECTION('ref_axis',(1.,1.10476514494527E-13,0.));
#9970=DIRECTION('center_axis',(0.,0.,-1.));
#9971=DIRECTION('ref_axis',(1.,0.,0.));
#9972=DIRECTION('',(0.707106781186547,-8.65956056235493E-17,0.707106781186548));
#9973=DIRECTION('center_axis',(0.,0.,1.));
#9974=DIRECTION('ref_axis',(1.,0.,0.));
#9975=DIRECTION('center_axis',(-1.92296268638356E-16,-1.,0.));
#9976=DIRECTION('ref_axis',(1.,-1.92296268638356E-16,0.));
#9977=DIRECTION('',(1.,-1.92296268638356E-16,0.));
#9978=DIRECTION('',(0.,0.,1.));
#9979=DIRECTION('',(1.,-1.92296268638356E-16,0.));
#9980=DIRECTION('',(0.,0.,1.));
#9981=DIRECTION('center_axis',(-0.866025403784439,-0.5,0.));
#9982=DIRECTION('ref_axis',(0.5,-0.866025403784439,0.));
#9983=DIRECTION('',(0.5,-0.866025403784439,0.));
#9984=DIRECTION('',(0.,0.,1.));
#9985=DIRECTION('',(0.5,-0.866025403784439,0.));
#9986=DIRECTION('center_axis',(-0.866025403784439,0.5,0.));
#9987=DIRECTION('ref_axis',(-0.5,-0.866025403784439,0.));
#9988=DIRECTION('',(-0.5,-0.866025403784439,0.));
#9989=DIRECTION('',(0.,0.,1.));
#9990=DIRECTION('',(-0.5,-0.866025403784439,0.));
#9991=DIRECTION('center_axis',(1.92296268638356E-16,1.,0.));
#9992=DIRECTION('ref_axis',(-1.,1.92296268638356E-16,0.));
#9993=DIRECTION('',(-1.,1.92296268638356E-16,0.));
#9994=DIRECTION('',(0.,0.,1.));
#9995=DIRECTION('',(-1.,1.92296268638356E-16,0.));
#9996=DIRECTION('center_axis',(0.866025403784439,0.5,0.));
#9997=DIRECTION('ref_axis',(-0.5,0.866025403784439,0.));
#9998=DIRECTION('',(-0.5,0.866025403784439,0.));
#9999=DIRECTION('',(0.,0.,1.));
#10000=DIRECTION('',(-0.5,0.866025403784439,0.));
#10001=DIRECTION('center_axis',(0.866025403784439,-0.5,0.));
#10002=DIRECTION('ref_axis',(0.5,0.866025403784439,0.));
#10003=DIRECTION('',(0.5,0.866025403784439,0.));
#10004=DIRECTION('',(0.5,0.866025403784439,0.));
#10005=DIRECTION('center_axis',(0.,0.,1.));
#10006=DIRECTION('ref_axis',(1.,0.,0.));
#10007=DIRECTION('center_axis',(0.,0.,1.));
#10008=DIRECTION('ref_axis',(1.,0.,0.));
#10009=DIRECTION('center_axis',(0.,0.,1.));
#10010=DIRECTION('ref_axis',(1.,0.,0.));
#10011=DIRECTION('center_axis',(0.,0.,1.));
#10012=DIRECTION('ref_axis',(1.,0.,0.));
#10013=DIRECTION('',(0.,0.,-1.));
#10014=DIRECTION('center_axis',(0.,0.,1.));
#10015=DIRECTION('ref_axis',(1.,0.,0.));
#10016=DIRECTION('center_axis',(0.,0.,1.));
#10017=DIRECTION('ref_axis',(1.,0.,0.));
#10018=DIRECTION('center_axis',(0.,0.,1.));
#10019=DIRECTION('ref_axis',(1.,0.,0.));
#10020=DIRECTION('axis',(0.,0.,1.));
#10021=DIRECTION('refdir',(1.,0.,0.));
#10022=DIRECTION('center_axis',(0.,0.,1.));
#10023=DIRECTION('ref_axis',(1.,9.40280585438808E-14,0.));
#10024=DIRECTION('',(0.,0.,-1.));
#10025=DIRECTION('center_axis',(0.,0.,-1.));
#10026=DIRECTION('ref_axis',(1.,9.40280585438808E-14,0.));
#10027=DIRECTION('center_axis',(0.,0.,1.));
#10028=DIRECTION('ref_axis',(1.,9.40280585438808E-14,0.));
#10029=DIRECTION('',(0.,0.,-1.));
#10030=DIRECTION('center_axis',(0.,0.,1.));
#10031=DIRECTION('ref_axis',(1.,9.40280585438808E-14,0.));
#10032=DIRECTION('',(0.,0.,-1.));
#10033=DIRECTION('center_axis',(0.,0.,1.));
#10034=DIRECTION('ref_axis',(1.,9.40280585438808E-14,0.));
#10035=DIRECTION('',(0.,0.,-1.));
#10036=DIRECTION('center_axis',(0.,0.,1.));
#10037=DIRECTION('ref_axis',(1.,9.40280585438808E-14,0.));
#10038=DIRECTION('',(0.,0.,-1.));
#10039=DIRECTION('center_axis',(0.,0.,1.));
#10040=DIRECTION('ref_axis',(1.,9.40280585438808E-14,0.));
#10041=DIRECTION('',(0.,0.,-1.));
#10042=DIRECTION('center_axis',(0.,0.,1.));
#10043=DIRECTION('ref_axis',(1.,9.40280585438808E-14,0.));
#10044=DIRECTION('',(0.,0.,-1.));
#10045=DIRECTION('center_axis',(0.,0.,1.));
#10046=DIRECTION('ref_axis',(1.,9.40280585438808E-14,0.));
#10047=DIRECTION('',(0.,0.,-1.));
#10048=DIRECTION('center_axis',(0.,0.,1.));
#10049=DIRECTION('ref_axis',(1.,9.40280585438808E-14,0.));
#10050=DIRECTION('',(0.,0.,-1.));
#10051=DIRECTION('center_axis',(0.,0.,1.));
#10052=DIRECTION('ref_axis',(1.,9.40280585438808E-14,0.));
#10053=DIRECTION('',(0.,0.,-1.));
#10054=DIRECTION('center_axis',(0.,0.,1.));
#10055=DIRECTION('ref_axis',(1.,9.40280585438808E-14,0.));
#10056=DIRECTION('',(0.,0.,-1.));
#10057=DIRECTION('center_axis',(0.,0.,1.));
#10058=DIRECTION('ref_axis',(1.,9.40280585438808E-14,0.));
#10059=DIRECTION('',(0.,0.,-1.));
#10060=DIRECTION('center_axis',(0.,0.,1.));
#10061=DIRECTION('ref_axis',(1.,9.40280585438808E-14,0.));
#10062=DIRECTION('',(0.,0.,-1.));
#10063=DIRECTION('center_axis',(0.,0.,1.));
#10064=DIRECTION('ref_axis',(1.,0.,0.));
#10065=DIRECTION('center_axis',(0.,0.,-1.));
#10066=DIRECTION('ref_axis',(1.,0.,0.));
#10067=DIRECTION('center_axis',(0.,0.,-1.));
#10068=DIRECTION('ref_axis',(1.,0.,0.));
#10069=DIRECTION('center_axis',(0.,0.,1.));
#10070=DIRECTION('ref_axis',(1.,9.40280585438808E-14,0.));
#10071=DIRECTION('center_axis',(0.,0.,-1.));
#10072=DIRECTION('ref_axis',(1.,9.40280585438808E-14,0.));
#10073=DIRECTION('center_axis',(0.,0.,-1.));
#10074=DIRECTION('ref_axis',(1.,0.,0.));
#10075=DIRECTION('',(0.707106781186548,-8.65956056235494E-17,0.707106781186547));
#10076=DIRECTION('center_axis',(0.,0.,1.));
#10077=DIRECTION('ref_axis',(1.,0.,0.));
#10078=DIRECTION('center_axis',(-1.60246890531964E-16,-1.,0.));
#10079=DIRECTION('ref_axis',(1.,-1.60246890531964E-16,0.));
#10080=DIRECTION('',(1.,-1.60246890531964E-16,0.));
#10081=DIRECTION('',(0.,0.,1.));
#10082=DIRECTION('',(1.,-1.60246890531964E-16,0.));
#10083=DIRECTION('',(0.,0.,1.));
#10084=DIRECTION('center_axis',(-0.866025403784439,-0.5,0.));
#10085=DIRECTION('ref_axis',(0.5,-0.866025403784439,0.));
#10086=DIRECTION('',(0.5,-0.866025403784439,0.));
#10087=DIRECTION('',(0.,0.,1.));
#10088=DIRECTION('',(0.5,-0.866025403784439,0.));
#10089=DIRECTION('center_axis',(-0.866025403784439,0.5,0.));
#10090=DIRECTION('ref_axis',(-0.5,-0.866025403784439,0.));
#10091=DIRECTION('',(-0.5,-0.866025403784439,0.));
#10092=DIRECTION('',(0.,0.,1.));
#10093=DIRECTION('',(-0.5,-0.866025403784439,0.));
#10094=DIRECTION('center_axis',(1.60246890531964E-16,1.,0.));
#10095=DIRECTION('ref_axis',(-1.,1.60246890531964E-16,0.));
#10096=DIRECTION('',(-1.,1.60246890531964E-16,0.));
#10097=DIRECTION('',(0.,0.,1.));
#10098=DIRECTION('',(-1.,1.60246890531964E-16,0.));
#10099=DIRECTION('center_axis',(0.866025403784439,0.5,0.));
#10100=DIRECTION('ref_axis',(-0.5,0.866025403784439,0.));
#10101=DIRECTION('',(-0.5,0.866025403784439,0.));
#10102=DIRECTION('',(0.,0.,1.));
#10103=DIRECTION('',(-0.5,0.866025403784439,0.));
#10104=DIRECTION('center_axis',(0.866025403784439,-0.5,0.));
#10105=DIRECTION('ref_axis',(0.5,0.866025403784439,0.));
#10106=DIRECTION('',(0.5,0.866025403784439,0.));
#10107=DIRECTION('',(0.5,0.866025403784439,0.));
#10108=DIRECTION('center_axis',(0.,0.,1.));
#10109=DIRECTION('ref_axis',(1.,0.,0.));
#10110=DIRECTION('center_axis',(0.,0.,1.));
#10111=DIRECTION('ref_axis',(1.,0.,0.));
#10112=DIRECTION('center_axis',(0.,0.,1.));
#10113=DIRECTION('ref_axis',(1.,0.,0.));
#10114=DIRECTION('center_axis',(0.,0.,1.));
#10115=DIRECTION('ref_axis',(1.,0.,0.));
#10116=DIRECTION('',(0.,0.,-1.));
#10117=DIRECTION('center_axis',(0.,0.,1.));
#10118=DIRECTION('ref_axis',(1.,0.,0.));
#10119=DIRECTION('center_axis',(0.,0.,1.));
#10120=DIRECTION('ref_axis',(1.,0.,0.));
#10121=DIRECTION('center_axis',(0.,0.,1.));
#10122=DIRECTION('ref_axis',(1.,0.,0.));
#10123=DIRECTION('axis',(0.,0.,1.));
#10124=DIRECTION('refdir',(1.,0.,0.));
#10125=DIRECTION('center_axis',(0.,0.,1.));
#10126=DIRECTION('ref_axis',(-0.457930858638424,-0.888987811337521,0.));
#10127=DIRECTION('',(0.,0.,-1.));
#10128=DIRECTION('center_axis',(0.,0.,-1.));
#10129=DIRECTION('ref_axis',(1.,7.94191995926203E-14,0.));
#10130=DIRECTION('center_axis',(0.,0.,1.));
#10131=DIRECTION('ref_axis',(-0.457930858638424,-0.888987811337521,0.));
#10132=DIRECTION('',(0.,0.,-1.));
#10133=DIRECTION('center_axis',(0.,0.,1.));
#10134=DIRECTION('ref_axis',(-0.457930858638424,-0.888987811337521,0.));
#10135=DIRECTION('',(0.,0.,-1.));
#10136=DIRECTION('center_axis',(0.,0.,1.));
#10137=DIRECTION('ref_axis',(-0.457930858638424,-0.888987811337521,0.));
#10138=DIRECTION('',(0.,0.,-1.));
#10139=DIRECTION('center_axis',(0.,0.,1.));
#10140=DIRECTION('ref_axis',(-0.457930858638424,-0.888987811337521,0.));
#10141=DIRECTION('',(0.,0.,-1.));
#10142=DIRECTION('center_axis',(0.,0.,1.));
#10143=DIRECTION('ref_axis',(-0.457930858638424,-0.888987811337521,0.));
#10144=DIRECTION('',(0.,0.,-1.));
#10145=DIRECTION('center_axis',(0.,0.,1.));
#10146=DIRECTION('ref_axis',(-0.457930858638424,-0.888987811337521,0.));
#10147=DIRECTION('',(0.,0.,-1.));
#10148=DIRECTION('center_axis',(0.,0.,1.));
#10149=DIRECTION('ref_axis',(-0.457930858638424,-0.888987811337521,0.));
#10150=DIRECTION('',(0.,0.,-1.));
#10151=DIRECTION('center_axis',(0.,0.,1.));
#10152=DIRECTION('ref_axis',(-0.457930858638424,-0.888987811337521,0.));
#10153=DIRECTION('',(0.,0.,-1.));
#10154=DIRECTION('center_axis',(0.,0.,1.));
#10155=DIRECTION('ref_axis',(-0.457930858638424,-0.888987811337521,0.));
#10156=DIRECTION('',(0.,0.,-1.));
#10157=DIRECTION('center_axis',(0.,0.,1.));
#10158=DIRECTION('ref_axis',(-0.457930858638424,-0.888987811337521,0.));
#10159=DIRECTION('',(0.,0.,-1.));
#10160=DIRECTION('center_axis',(0.,0.,1.));
#10161=DIRECTION('ref_axis',(-0.457930858638424,-0.888987811337521,0.));
#10162=DIRECTION('',(0.,0.,-1.));
#10163=DIRECTION('center_axis',(0.,0.,1.));
#10164=DIRECTION('ref_axis',(-0.457930858638424,-0.888987811337521,0.));
#10165=DIRECTION('',(0.,0.,-1.));
#10166=DIRECTION('center_axis',(0.,0.,1.));
#10167=DIRECTION('ref_axis',(-0.457930858638424,-0.888987811337521,0.));
#10168=DIRECTION('',(0.,0.,-1.));
#10169=DIRECTION('center_axis',(0.,0.,1.));
#10170=DIRECTION('ref_axis',(1.,0.,0.));
#10171=DIRECTION('',(0.,0.,-1.));
#10172=DIRECTION('center_axis',(0.,0.,-1.));
#10173=DIRECTION('ref_axis',(1.,0.,0.));
#10174=DIRECTION('center_axis',(0.,0.,1.));
#10175=DIRECTION('ref_axis',(1.,0.,0.));
#10176=DIRECTION('',(0.,0.,-1.));
#10177=DIRECTION('center_axis',(0.,0.,1.));
#10178=DIRECTION('ref_axis',(1.,0.,0.));
#10179=DIRECTION('',(0.,0.,-1.));
#10180=DIRECTION('center_axis',(0.,0.,1.));
#10181=DIRECTION('ref_axis',(1.,0.,0.));
#10182=DIRECTION('',(0.,0.,-1.));
#10183=DIRECTION('center_axis',(0.,0.,1.));
#10184=DIRECTION('ref_axis',(1.,0.,0.));
#10185=DIRECTION('',(0.,0.,-1.));
#10186=DIRECTION('center_axis',(0.,0.,1.));
#10187=DIRECTION('ref_axis',(1.,0.,0.));
#10188=DIRECTION('',(0.,0.,-1.));
#10189=DIRECTION('center_axis',(0.,0.,1.));
#10190=DIRECTION('ref_axis',(1.,0.,0.));
#10191=DIRECTION('',(0.,0.,-1.));
#10192=DIRECTION('center_axis',(0.,0.,1.));
#10193=DIRECTION('ref_axis',(1.,0.,0.));
#10194=DIRECTION('',(0.,0.,-1.));
#10195=DIRECTION('center_axis',(0.,0.,1.));
#10196=DIRECTION('ref_axis',(1.,0.,0.));
#10197=DIRECTION('',(0.,0.,-1.));
#10198=DIRECTION('center_axis',(0.,0.,1.));
#10199=DIRECTION('ref_axis',(1.,0.,0.));
#10200=DIRECTION('',(0.,0.,-1.));
#10201=DIRECTION('center_axis',(0.,0.,1.));
#10202=DIRECTION('ref_axis',(1.,0.,0.));
#10203=DIRECTION('',(0.,0.,-1.));
#10204=DIRECTION('center_axis',(0.,0.,1.));
#10205=DIRECTION('ref_axis',(1.,0.,0.));
#10206=DIRECTION('',(0.,0.,-1.));
#10207=DIRECTION('center_axis',(0.,0.,1.));
#10208=DIRECTION('ref_axis',(1.,0.,0.));
#10209=DIRECTION('',(0.,0.,-1.));
#10210=DIRECTION('center_axis',(0.,0.,1.));
#10211=DIRECTION('ref_axis',(1.,0.,0.));
#10212=DIRECTION('',(0.,0.,-1.));
#10213=DIRECTION('center_axis',(0.,0.,1.));
#10214=DIRECTION('ref_axis',(1.,0.,0.));
#10215=DIRECTION('center_axis',(0.,0.,-1.));
#10216=DIRECTION('ref_axis',(1.,0.,0.));
#10217=DIRECTION('center_axis',(0.,0.,1.));
#10218=DIRECTION('ref_axis',(-0.457930858638424,-0.888987811337521,0.));
#10219=DIRECTION('center_axis',(0.,0.,1.));
#10220=DIRECTION('ref_axis',(1.,7.94191995926203E-14,0.));
#10221=DIRECTION('center_axis',(0.,0.,1.));
#10222=DIRECTION('ref_axis',(1.,0.,0.));
#10223=DIRECTION('center_axis',(0.,0.,1.));
#10224=DIRECTION('ref_axis',(1.,0.,0.));
#10225=DIRECTION('center_axis',(0.,0.,1.));
#10226=DIRECTION('ref_axis',(1.,0.,0.));
#10227=DIRECTION('',(0.,0.,-1.));
#10228=DIRECTION('center_axis',(0.,0.,1.));
#10229=DIRECTION('ref_axis',(1.,0.,0.));
#10230=DIRECTION('center_axis',(0.,0.,1.));
#10231=DIRECTION('ref_axis',(1.,0.,0.));
#10232=DIRECTION('center_axis',(0.,0.,-1.));
#10233=DIRECTION('ref_axis',(1.,0.,0.));
#10234=DIRECTION('',(0.,0.,1.));
#10235=DIRECTION('center_axis',(0.,0.,-1.));
#10236=DIRECTION('ref_axis',(1.,0.,0.));
#10237=DIRECTION('center_axis',(0.,0.,1.));
#10238=DIRECTION('ref_axis',(1.,0.,0.));
#10239=DIRECTION('center_axis',(0.,0.,1.));
#10240=DIRECTION('ref_axis',(1.,0.,0.));
#10241=DIRECTION('axis',(0.,0.,1.));
#10242=DIRECTION('refdir',(1.,0.,0.));
#10243=DIRECTION('center_axis',(0.,0.,1.));
#10244=DIRECTION('ref_axis',(-0.608987077531584,0.793180143094581,0.));
#10245=DIRECTION('',(0.,0.,1.));
#10246=DIRECTION('center_axis',(0.,0.,-1.));
#10247=DIRECTION('ref_axis',(1.,3.67286437305492E-16,0.));
#10248=DIRECTION('center_axis',(0.,0.,1.));
#10249=DIRECTION('ref_axis',(-0.608987077531584,0.793180143094581,0.));
#10250=DIRECTION('',(0.,0.,1.));
#10251=DIRECTION('center_axis',(0.,0.,1.));
#10252=DIRECTION('ref_axis',(-0.608987077531584,0.793180143094581,0.));
#10253=DIRECTION('',(0.,0.,1.));
#10254=DIRECTION('center_axis',(0.,0.,1.));
#10255=DIRECTION('ref_axis',(-0.608987077531584,0.793180143094581,0.));
#10256=DIRECTION('',(0.,0.,1.));
#10257=DIRECTION('center_axis',(0.,0.,1.));
#10258=DIRECTION('ref_axis',(1.,3.67286437305492E-16,0.));
#10259=DIRECTION('center_axis',(0.,0.,1.));
#10260=DIRECTION('ref_axis',(1.,0.,0.));
#10261=DIRECTION('',(0.,0.,1.));
#10262=DIRECTION('center_axis',(0.,0.,1.));
#10263=DIRECTION('ref_axis',(1.,0.,0.));
#10264=DIRECTION('center_axis',(0.,0.,1.));
#10265=DIRECTION('ref_axis',(1.,0.,0.));
#10266=DIRECTION('',(0.,0.,1.));
#10267=DIRECTION('center_axis',(0.,0.,1.));
#10268=DIRECTION('ref_axis',(1.,0.,0.));
#10269=DIRECTION('',(0.,0.,1.));
#10270=DIRECTION('center_axis',(0.,0.,1.));
#10271=DIRECTION('ref_axis',(1.,0.,0.));
#10272=DIRECTION('',(0.,0.,1.));
#10273=DIRECTION('center_axis',(0.,0.,1.));
#10274=DIRECTION('ref_axis',(1.,0.,0.));
#10275=DIRECTION('center_axis',(0.,0.,1.));
#10276=DIRECTION('ref_axis',(1.,0.,0.));
#10277=DIRECTION('center_axis',(0.,0.,1.));
#10278=DIRECTION('ref_axis',(-0.608987077531584,0.793180143094581,0.));
#10279=DIRECTION('center_axis',(0.,0.,-1.));
#10280=DIRECTION('ref_axis',(1.,0.,0.));
#10281=DIRECTION('center_axis',(0.,0.,-1.));
#10282=DIRECTION('ref_axis',(1.,0.,0.));
#10283=DIRECTION('',(0.,0.,-1.));
#10284=DIRECTION('center_axis',(0.,0.,1.));
#10285=DIRECTION('ref_axis',(1.,0.,0.));
#10286=DIRECTION('center_axis',(0.,0.,-1.));
#10287=DIRECTION('ref_axis',(1.,0.,0.));
#10288=DIRECTION('center_axis',(0.,0.,-1.));
#10289=DIRECTION('ref_axis',(1.,0.,0.));
#10290=DIRECTION('',(0.,0.,-1.));
#10291=DIRECTION('center_axis',(0.,0.,1.));
#10292=DIRECTION('ref_axis',(1.,0.,0.));
#10293=DIRECTION('center_axis',(0.,0.,1.));
#10294=DIRECTION('ref_axis',(1.,0.,0.));
#10295=DIRECTION('center_axis',(0.,0.,1.));
#10296=DIRECTION('ref_axis',(1.,0.,0.));
#10297=DIRECTION('center_axis',(0.,0.,1.));
#10298=DIRECTION('ref_axis',(1.,0.,0.));
#10299=DIRECTION('',(0.,0.,-1.));
#10300=DIRECTION('center_axis',(0.,0.,1.));
#10301=DIRECTION('ref_axis',(1.,0.,0.));
#10302=DIRECTION('center_axis',(0.,0.,1.));
#10303=DIRECTION('ref_axis',(1.,0.,0.));
#10304=DIRECTION('axis',(0.,0.,1.));
#10305=DIRECTION('refdir',(1.,0.,0.));
#10306=DIRECTION('center_axis',(0.,0.,1.));
#10307=DIRECTION('ref_axis',(1.,0.,0.));
#10308=DIRECTION('center_axis',(0.,0.,-1.));
#10309=DIRECTION('ref_axis',(1.,0.,0.));
#10310=DIRECTION('',(0.,0.,1.));
#10311=DIRECTION('center_axis',(0.,0.,-1.));
#10312=DIRECTION('ref_axis',(1.,0.,0.));
#10313=DIRECTION('center_axis',(0.,0.,1.));
#10314=DIRECTION('ref_axis',(1.,0.,0.));
#10315=DIRECTION('center_axis',(0.,0.,1.));
#10316=DIRECTION('ref_axis',(1.,0.,0.));
#10317=DIRECTION('',(0.,0.,-1.));
#10318=DIRECTION('center_axis',(0.,0.,1.));
#10319=DIRECTION('ref_axis',(1.,0.,0.));
#10320=DIRECTION('center_axis',(0.,0.,1.));
#10321=DIRECTION('ref_axis',(1.,0.,0.));
#10322=DIRECTION('center_axis',(0.,0.,1.));
#10323=DIRECTION('ref_axis',(1.,0.,0.));
#10324=DIRECTION('',(0.,0.,1.));
#10325=DIRECTION('',(1.,0.,0.));
#10326=DIRECTION('',(0.,0.,1.));
#10327=DIRECTION('',(1.,0.,0.));
#10328=DIRECTION('',(0.,0.,1.));
#10329=DIRECTION('',(1.,0.,0.));
#10330=DIRECTION('',(0.,-1.22464679914735E-16,-1.));
#10331=DIRECTION('',(1.,0.,0.));
#10332=DIRECTION('',(0.,0.,1.));
#10333=DIRECTION('',(1.,0.,0.));
#10334=DIRECTION('',(-5.87255029570814E-33,-1.22464679914735E-16,-1.));
#10335=DIRECTION('',(-0.342020143325668,0.939692620785909,-1.15079156022785E-16));
#10336=DIRECTION('',(0.,1.,2.22044604925031E-16));
#10337=DIRECTION('',(1.,0.,0.));
#10338=DIRECTION('',(0.,1.,2.22044604925031E-16));
#10339=DIRECTION('',(1.,0.,0.));
#10340=DIRECTION('',(0.,1.,2.22044604925031E-16));
#10341=DIRECTION('',(1.,0.,0.));
#10342=DIRECTION('',(0.,-1.22464679914735E-16,-1.));
#10343=DIRECTION('',(1.,0.,0.));
#10344=DIRECTION('',(0.,-1.22464679914735E-16,-1.));
#10345=DIRECTION('',(1.,0.,0.));
#10346=DIRECTION('',(0.,-1.22464679914735E-16,-1.));
#10347=DIRECTION('',(1.,0.,0.));
#10348=DIRECTION('',(-1.16638531977603E-32,-1.22464679914735E-16,-1.));
#10349=DIRECTION('',(-0.342020143325668,0.939692620785909,-1.15079156022785E-16));
#10350=DIRECTION('',(-1.16638531977603E-32,-1.22464679914735E-16,-1.));
#10351=DIRECTION('',(-0.342020143325668,0.939692620785909,-1.15079156022785E-16));
#10352=DIRECTION('',(-1.16638531977603E-32,-1.22464679914735E-16,-1.));
#10353=DIRECTION('',(-0.342020143325668,0.939692620785909,-1.15079156022785E-16));
#10354=DIRECTION('',(0.,1.,2.22044604925031E-16));
#10355=DIRECTION('',(1.,0.,0.));
#10356=DIRECTION('',(0.,1.,2.22044604925031E-16));
#10357=DIRECTION('',(1.,0.,0.));
#10358=DIRECTION('',(0.,1.,2.22044604925031E-16));
#10359=DIRECTION('',(1.,0.,0.));
#10360=CARTESIAN_POINT('',(0.,0.,0.));
#10361=CARTESIAN_POINT('',(0.,0.,0.));
#10362=CARTESIAN_POINT('',(0.,0.,0.));
#10363=CARTESIAN_POINT('Origin',(130.,-90.,1.5));
#10364=CARTESIAN_POINT('',(126.5,-90.,3.));
#10365=CARTESIAN_POINT('Origin',(130.,-90.,3.));
#10366=CARTESIAN_POINT('',(126.5,-90.,0.));
#10367=CARTESIAN_POINT('',(126.5,-90.,1.5));
#10368=CARTESIAN_POINT('Origin',(130.,-90.,0.));
#10369=CARTESIAN_POINT('Origin',(-130.,-90.,1.5));
#10370=CARTESIAN_POINT('',(-133.5,-90.,3.));
#10371=CARTESIAN_POINT('Origin',(-130.,-90.,3.));
#10372=CARTESIAN_POINT('',(-133.5,-90.,0.));
#10373=CARTESIAN_POINT('',(-133.5,-90.,1.5));
#10374=CARTESIAN_POINT('Origin',(-130.,-90.,0.));
#10375=CARTESIAN_POINT('Origin',(-130.,90.,1.5));
#10376=CARTESIAN_POINT('',(-133.5,90.,3.));
#10377=CARTESIAN_POINT('Origin',(-130.,90.,3.));
#10378=CARTESIAN_POINT('',(-133.5,90.,0.));
#10379=CARTESIAN_POINT('',(-133.5,90.,1.5));
#10380=CARTESIAN_POINT('Origin',(-130.,90.,0.));
#10381=CARTESIAN_POINT('Origin',(130.,90.,1.5));
#10382=CARTESIAN_POINT('',(126.5,90.,3.));
#10383=CARTESIAN_POINT('Origin',(130.,90.,3.));
#10384=CARTESIAN_POINT('',(126.5,90.,0.));
#10385=CARTESIAN_POINT('',(126.5,90.,1.5));
#10386=CARTESIAN_POINT('Origin',(130.,90.,0.));
#10387=CARTESIAN_POINT('Origin',(150.,110.,0.));
#10388=CARTESIAN_POINT('',(150.,110.,0.));
#10389=CARTESIAN_POINT('',(-150.,110.,0.));
#10390=CARTESIAN_POINT('',(150.,110.,0.));
#10391=CARTESIAN_POINT('',(-150.,110.,3.));
#10392=CARTESIAN_POINT('',(-150.,110.,0.));
#10393=CARTESIAN_POINT('',(150.,110.,3.));
#10394=CARTESIAN_POINT('',(150.,110.,3.));
#10395=CARTESIAN_POINT('',(150.,110.,0.));
#10396=CARTESIAN_POINT('Origin',(150.,-110.,0.));
#10397=CARTESIAN_POINT('',(150.,-110.,0.));
#10398=CARTESIAN_POINT('',(150.,-110.,0.));
#10399=CARTESIAN_POINT('',(150.,-110.,3.));
#10400=CARTESIAN_POINT('',(150.,-110.,3.));
#10401=CARTESIAN_POINT('',(150.,-110.,0.));
#10402=CARTESIAN_POINT('Origin',(-150.,-110.,0.));
#10403=CARTESIAN_POINT('',(-150.,-110.,0.));
#10404=CARTESIAN_POINT('',(-150.,-110.,0.));
#10405=CARTESIAN_POINT('',(-150.,-110.,3.));
#10406=CARTESIAN_POINT('',(-150.,-110.,3.));
#10407=CARTESIAN_POINT('',(-150.,-110.,0.));
#10408=CARTESIAN_POINT('Origin',(-150.,110.,0.));
#10409=CARTESIAN_POINT('',(-150.,110.,0.));
#10410=CARTESIAN_POINT('',(-150.,110.,3.));
#10411=CARTESIAN_POINT('Origin',(0.,0.,3.));
#10412=CARTESIAN_POINT('Origin',(0.,0.,0.));
#10413=CARTESIAN_POINT('',(0.,0.,0.));
#10414=CARTESIAN_POINT('Origin',(-60.,-2.77555756156289E-16,60.));
#10415=CARTESIAN_POINT('',(-60.,1.5,49.5));
#10416=CARTESIAN_POINT('Origin',(-60.,1.5,60.));
#10417=CARTESIAN_POINT('',(-60.,-1.5,49.5));
#10418=CARTESIAN_POINT('',(-60.,-2.77555756156289E-16,49.5));
#10419=CARTESIAN_POINT('Origin',(-60.,-1.5,60.));
#10420=CARTESIAN_POINT('Origin',(60.,-2.77555756156289E-16,60.));
#10421=CARTESIAN_POINT('',(60.,1.5,49.5));
#10422=CARTESIAN_POINT('Origin',(60.,1.5,60.));
#10423=CARTESIAN_POINT('',(60.,-1.5,49.5));
#10424=CARTESIAN_POINT('',(60.,-2.77555756156289E-16,49.5));
#10425=CARTESIAN_POINT('Origin',(60.,-1.5,60.));
#10426=CARTESIAN_POINT('Origin',(150.,1.5,0.));
#10427=CARTESIAN_POINT('',(150.,1.5,0.));
#10428=CARTESIAN_POINT('',(-150.,1.5,0.));
#10429=CARTESIAN_POINT('',(150.,1.5,0.));
#10430=CARTESIAN_POINT('',(-150.,1.5,114.));
#10431=CARTESIAN_POINT('',(-150.,1.5,0.));
#10432=CARTESIAN_POINT('',(150.,1.5,114.));
#10433=CARTESIAN_POINT('',(150.,1.5,114.));
#10434=CARTESIAN_POINT('',(150.,1.5,0.));
#10435=CARTESIAN_POINT('Origin',(150.,-1.5,0.));
#10436=CARTESIAN_POINT('',(150.,-1.5,0.));
#10437=CARTESIAN_POINT('',(150.,-1.5,0.));
#10438=CARTESIAN_POINT('',(150.,-1.5,114.));
#10439=CARTESIAN_POINT('',(150.,-1.5,114.));
#10440=CARTESIAN_POINT('',(150.,-1.5,0.));
#10441=CARTESIAN_POINT('Origin',(-150.,-1.5,0.));
#10442=CARTESIAN_POINT('',(-150.,-1.5,0.));
#10443=CARTESIAN_POINT('',(-150.,-1.5,0.));
#10444=CARTESIAN_POINT('',(-150.,-1.5,114.));
#10445=CARTESIAN_POINT('',(-150.,-1.5,114.));
#10446=CARTESIAN_POINT('',(-150.,-1.5,0.));
#10447=CARTESIAN_POINT('Origin',(-150.,1.5,0.));
#10448=CARTESIAN_POINT('',(-150.,1.5,0.));
#10449=CARTESIAN_POINT('',(-150.,1.5,114.));
#10450=CARTESIAN_POINT('Origin',(0.,0.,114.));
#10451=CARTESIAN_POINT('Origin',(0.,0.,0.));
#10452=CARTESIAN_POINT('',(0.,0.,0.));
#10453=CARTESIAN_POINT('Origin',(150.,1.5,0.));
#10454=CARTESIAN_POINT('',(150.,1.5,0.));
#10455=CARTESIAN_POINT('',(-150.,1.5,0.));
#10456=CARTESIAN_POINT('',(150.,1.5,0.));
#10457=CARTESIAN_POINT('',(-150.,1.5,114.));
#10458=CARTESIAN_POINT('',(-150.,1.5,0.));
#10459=CARTESIAN_POINT('',(150.,1.5,114.));
#10460=CARTESIAN_POINT('',(150.,1.5,114.));
#10461=CARTESIAN_POINT('',(150.,1.5,0.));
#10462=CARTESIAN_POINT('Origin',(150.,-1.5,0.));
#10463=CARTESIAN_POINT('',(150.,-1.5,0.));
#10464=CARTESIAN_POINT('',(150.,-1.5,0.));
#10465=CARTESIAN_POINT('',(150.,-1.5,114.));
#10466=CARTESIAN_POINT('',(150.,-1.5,114.));
#10467=CARTESIAN_POINT('',(150.,-1.5,0.));
#10468=CARTESIAN_POINT('Origin',(-150.,-1.5,0.));
#10469=CARTESIAN_POINT('',(-150.,-1.5,0.));
#10470=CARTESIAN_POINT('',(-150.,-1.5,0.));
#10471=CARTESIAN_POINT('',(-150.,-1.5,114.));
#10472=CARTESIAN_POINT('',(-150.,-1.5,114.));
#10473=CARTESIAN_POINT('',(-150.,-1.5,0.));
#10474=CARTESIAN_POINT('Origin',(-150.,1.5,0.));
#10475=CARTESIAN_POINT('',(-150.,1.5,0.));
#10476=CARTESIAN_POINT('',(-150.,1.5,114.));
#10477=CARTESIAN_POINT('Origin',(0.,0.,114.));
#10478=CARTESIAN_POINT('Origin',(0.,0.,0.));
#10479=CARTESIAN_POINT('',(0.,0.,0.));
#10480=CARTESIAN_POINT('Origin',(298.5,-17.9108928257202,76.6590099406496));
#10481=CARTESIAN_POINT('',(1.5,-17.9108928257202,81.6590099406496));
#10482=CARTESIAN_POINT('',(1.5,-22.9108928257202,76.6590099406496));
#10483=CARTESIAN_POINT('Origin',(1.49999999999999,-17.9108928257202,76.6590099406496));
#10484=CARTESIAN_POINT('',(-1.5,-22.9108928257202,76.6590099406496));
#10485=CARTESIAN_POINT('',(298.5,-22.9108928257202,76.6590099406496));
#10486=CARTESIAN_POINT('',(-1.5,-17.9108928257202,81.6590099406496));
#10487=CARTESIAN_POINT('Origin',(-1.49999999999999,-17.9108928257202,76.6590099406496));
#10488=CARTESIAN_POINT('',(298.5,-17.9108928257202,81.6590099406496));
#10489=CARTESIAN_POINT('Origin',(298.5,-22.9108928257202,51.6590099406496));
#10490=CARTESIAN_POINT('',(1.5,-22.9108928257202,56.6590099406496));
#10491=CARTESIAN_POINT('',(1.5,-22.9108928257202,25.8295049703248));
#10492=CARTESIAN_POINT('',(-1.5,-22.9108928257202,56.6590099406496));
#10493=CARTESIAN_POINT('',(298.5,-22.9108928257202,56.6590099406496));
#10494=CARTESIAN_POINT('',(-1.5,-22.9108928257202,25.8295049703248));
#10495=CARTESIAN_POINT('Origin',(298.5,-17.9108928257202,56.6590099406496));
#10496=CARTESIAN_POINT('',(1.5,-17.9108928257202,51.6590099406496));
#10497=CARTESIAN_POINT('Origin',(1.49999999999999,-17.9108928257202,56.6590099406496));
#10498=CARTESIAN_POINT('',(-1.5,-17.9108928257202,51.6590099406496));
#10499=CARTESIAN_POINT('',(298.5,-17.9108928257202,51.6590099406496));
#10500=CARTESIAN_POINT('Origin',(-1.49999999999999,-17.9108928257202,56.6590099406496));
#10501=CARTESIAN_POINT('Origin',(298.5,7.0891071742798,51.6590099406496));
#10502=CARTESIAN_POINT('',(1.5,2.0891071742798,51.6590099406496));
#10503=CARTESIAN_POINT('',(1.5,-49.9554464128601,51.6590099406496));
#10504=CARTESIAN_POINT('',(-1.5,2.0891071742798,51.6590099406496));
#10505=CARTESIAN_POINT('',(298.5,2.0891071742798,51.6590099406496));
#10506=CARTESIAN_POINT('',(-1.5,57.0445535871399,51.6590099406496));
#10507=CARTESIAN_POINT('Origin',(298.5,2.0891071742798,76.6590099406496));
#10508=CARTESIAN_POINT('',(1.5,7.0891071742798,76.6590099406496));
#10509=CARTESIAN_POINT('',(1.5,2.0891071742798,81.6590099406496));
#10510=CARTESIAN_POINT('Origin',(1.49999999999999,2.0891071742798,76.6590099406496));
#10511=CARTESIAN_POINT('',(-1.5,2.0891071742798,81.6590099406496));
#10512=CARTESIAN_POINT('',(298.5,2.0891071742798,81.6590099406496));
#10513=CARTESIAN_POINT('',(-1.5,7.0891071742798,76.6590099406496));
#10514=CARTESIAN_POINT('Origin',(-1.49999999999999,2.0891071742798,76.6590099406496));
#10515=CARTESIAN_POINT('',(298.5,7.0891071742798,76.6590099406496));
#10516=CARTESIAN_POINT('Origin',(298.5,-22.9108928257202,81.6590099406496));
#10517=CARTESIAN_POINT('',(-1.5,42.0445535871399,81.6590099406496));
#10518=CARTESIAN_POINT('',(1.5,-64.9554464128601,81.6590099406496));
#10519=CARTESIAN_POINT('Origin',(298.5,2.0891071742798,56.6590099406496));
#10520=CARTESIAN_POINT('',(1.5,7.0891071742798,56.6590099406496));
#10521=CARTESIAN_POINT('Origin',(1.49999999999999,2.0891071742798,56.6590099406496));
#10522=CARTESIAN_POINT('',(-1.5,7.0891071742798,56.6590099406496));
#10523=CARTESIAN_POINT('',(298.5,7.0891071742798,56.6590099406496));
#10524=CARTESIAN_POINT('Origin',(-1.49999999999999,2.0891071742798,56.6590099406496));
#10525=CARTESIAN_POINT('Origin',(298.5,7.0891071742798,81.6590099406496));
#10526=CARTESIAN_POINT('',(-1.5,7.0891071742798,40.8295049703248));
#10527=CARTESIAN_POINT('',(1.5,7.0891071742798,40.8295049703248));
#10528=CARTESIAN_POINT('Origin',(298.5,-51.5734387277091,76.5706645852841));
#10529=CARTESIAN_POINT('',(1.5,-46.5734387277091,76.5706645852841));
#10530=CARTESIAN_POINT('',(1.5,-51.5734387277091,81.5706645852841));
#10531=CARTESIAN_POINT('Origin',(1.49999999999999,-51.5734387277091,76.5706645852841));
#10532=CARTESIAN_POINT('',(-1.5,-51.5734387277091,81.5706645852841));
#10533=CARTESIAN_POINT('',(298.5,-51.5734387277091,81.5706645852841));
#10534=CARTESIAN_POINT('',(-1.5,-46.5734387277091,76.5706645852841));
#10535=CARTESIAN_POINT('Origin',(-1.49999999999999,-51.5734387277091,76.5706645852841));
#10536=CARTESIAN_POINT('',(298.5,-46.5734387277091,76.5706645852841));
#10537=CARTESIAN_POINT('Origin',(298.5,-76.5734387277091,81.5706645852841));
#10538=CARTESIAN_POINT('',(1.5,-71.5734387277091,81.5706645852841));
#10539=CARTESIAN_POINT('',(1.5,-91.7867193638546,81.5706645852841));
#10540=CARTESIAN_POINT('',(-1.5,-71.5734387277091,81.5706645852841));
#10541=CARTESIAN_POINT('',(298.5,-71.5734387277091,81.5706645852841));
#10542=CARTESIAN_POINT('',(-1.5,15.2132806361454,81.5706645852841));
#10543=CARTESIAN_POINT('Origin',(298.5,-51.5734387277091,56.5706645852841));
#10544=CARTESIAN_POINT('',(1.5,-51.5734387277091,51.5706645852841));
#10545=CARTESIAN_POINT('',(1.5,-46.5734387277091,56.5706645852841));
#10546=CARTESIAN_POINT('Origin',(1.49999999999999,-51.5734387277091,56.5706645852841));
#10547=CARTESIAN_POINT('',(-1.5,-46.5734387277091,56.5706645852841));
#10548=CARTESIAN_POINT('',(298.5,-46.5734387277091,56.5706645852841));
#10549=CARTESIAN_POINT('',(-1.5,-51.5734387277091,51.5706645852841));
#10550=CARTESIAN_POINT('Origin',(-1.49999999999999,-51.5734387277091,56.5706645852841));
#10551=CARTESIAN_POINT('',(298.5,-51.5734387277091,51.5706645852841));
#10552=CARTESIAN_POINT('Origin',(298.5,-46.5734387277091,81.5706645852841));
#10553=CARTESIAN_POINT('',(-1.5,-46.5734387277091,40.785332292642));
#10554=CARTESIAN_POINT('',(1.5,-46.5734387277091,40.785332292642));
#10555=CARTESIAN_POINT('Origin',(298.5,-71.5734387277091,76.5706645852841));
#10556=CARTESIAN_POINT('',(1.5,-76.5734387277091,76.5706645852841));
#10557=CARTESIAN_POINT('Origin',(1.49999999999999,-71.5734387277091,76.5706645852841));
#10558=CARTESIAN_POINT('',(-1.5,-76.5734387277091,76.5706645852841));
#10559=CARTESIAN_POINT('',(298.5,-76.5734387277091,76.5706645852841));
#10560=CARTESIAN_POINT('Origin',(-1.49999999999999,-71.5734387277091,76.5706645852841));
#10561=CARTESIAN_POINT('Origin',(298.5,-76.5734387277091,51.5706645852841));
#10562=CARTESIAN_POINT('',(1.5,-76.5734387277091,56.5706645852841));
#10563=CARTESIAN_POINT('',(1.5,-76.5734387277091,25.785332292642));
#10564=CARTESIAN_POINT('',(-1.5,-76.5734387277091,56.5706645852841));
#10565=CARTESIAN_POINT('',(298.5,-76.5734387277091,56.5706645852841));
#10566=CARTESIAN_POINT('',(-1.5,-76.5734387277091,25.785332292642));
#10567=CARTESIAN_POINT('Origin',(298.5,-71.5734387277091,56.5706645852841));
#10568=CARTESIAN_POINT('',(1.5,-71.5734387277091,51.5706645852841));
#10569=CARTESIAN_POINT('Origin',(1.49999999999999,-71.5734387277091,56.5706645852841));
#10570=CARTESIAN_POINT('',(-1.5,-71.5734387277091,51.5706645852841));
#10571=CARTESIAN_POINT('',(298.5,-71.5734387277091,51.5706645852841));
#10572=CARTESIAN_POINT('Origin',(-1.49999999999999,-71.5734387277091,56.5706645852841));
#10573=CARTESIAN_POINT('Origin',(298.5,-46.5734387277091,51.5706645852841));
#10574=CARTESIAN_POINT('',(-1.5,30.2132806361454,51.5706645852841));
#10575=CARTESIAN_POINT('',(1.5,-76.7867193638546,51.5706645852841));
#10576=CARTESIAN_POINT('Origin',(1.5,107.,0.));
#10577=CARTESIAN_POINT('',(1.5,107.,0.));
#10578=CARTESIAN_POINT('',(-1.5,107.,0.));
#10579=CARTESIAN_POINT('',(1.5,107.,0.));
#10580=CARTESIAN_POINT('',(-1.5,107.,114.));
#10581=CARTESIAN_POINT('',(-1.5,107.,0.));
#10582=CARTESIAN_POINT('',(1.5,107.,114.));
#10583=CARTESIAN_POINT('',(1.5,107.,114.));
#10584=CARTESIAN_POINT('',(1.5,107.,0.));
#10585=CARTESIAN_POINT('Origin',(1.5,-107.,0.));
#10586=CARTESIAN_POINT('',(1.5,-107.,0.));
#10587=CARTESIAN_POINT('',(1.5,-107.,0.));
#10588=CARTESIAN_POINT('',(1.5,-107.,114.));
#10589=CARTESIAN_POINT('',(1.5,-107.,114.));
#10590=CARTESIAN_POINT('',(1.5,-107.,0.));
#10591=CARTESIAN_POINT('Origin',(-1.5,-107.,0.));
#10592=CARTESIAN_POINT('',(-1.5,-107.,0.));
#10593=CARTESIAN_POINT('',(-1.5,-107.,0.));
#10594=CARTESIAN_POINT('',(-1.5,-107.,114.));
#10595=CARTESIAN_POINT('',(-1.5,-107.,114.));
#10596=CARTESIAN_POINT('',(-1.5,-107.,0.));
#10597=CARTESIAN_POINT('Origin',(-1.5,107.,0.));
#10598=CARTESIAN_POINT('',(-1.5,107.,0.));
#10599=CARTESIAN_POINT('',(-1.5,107.,114.));
#10600=CARTESIAN_POINT('Origin',(0.,0.,114.));
#10601=CARTESIAN_POINT('Origin',(0.,0.,0.));
#10602=CARTESIAN_POINT('',(0.,0.,0.));
#10603=CARTESIAN_POINT('Origin',(0.,0.,-2.20842344717744));
#10604=CARTESIAN_POINT('',(-1.87240768645123,2.4373123939533,18.5627733953368));
#10605=CARTESIAN_POINT('',(-1.87240768645124,2.43731239395329,18.6457505235039));
#10606=CARTESIAN_POINT('',(-1.87240768645123,2.4373123939533,-2.20842344717744));
#10607=CARTESIAN_POINT('',(-0.793799282532847,-2.9692229537457,19.));
#10608=CARTESIAN_POINT('Ctrl Pts',(-1.87240768645124,2.43731239395329,18.6457505235039));
#10609=CARTESIAN_POINT('Ctrl Pts',(-1.94899259408632,2.37847784731174,18.6507492320743));
#10610=CARTESIAN_POINT('Ctrl Pts',(-2.02273224209293,2.31608369066104,18.6557479406448));
#10611=CARTESIAN_POINT('Ctrl Pts',(-2.09329518872703,2.25044828930866,18.6607466492152));
#10612=CARTESIAN_POINT('Ctrl Pts',(-2.16397015698635,2.18470868901501,18.6657532934443));
#10613=CARTESIAN_POINT('Ctrl Pts',(-2.23145804949518,2.11571788291669,18.6707599376733));
#10614=CARTESIAN_POINT('Ctrl Pts',(-2.29546581565982,2.04382947897744,18.6757665819024));
#10615=CARTESIAN_POINT('Ctrl Pts',(-2.32740848703842,2.00795402509804,18.6782651160788));
#10616=CARTESIAN_POINT('Ctrl Pts',(-2.35848510104462,1.97135743377959,18.6807636502553));
#10617=CARTESIAN_POINT('Ctrl Pts',(-2.38866325982295,1.93408636859164,18.6832621844317));
#10618=CARTESIAN_POINT('Ctrl Pts',(-2.44839709830004,1.86031302131227,18.6882077160004));
#10619=CARTESIAN_POINT('Ctrl Pts',(-2.5048278901498,1.78362392824008,18.6931532475691));
#10620=CARTESIAN_POINT('Ctrl Pts',(-2.55765354176341,1.7043504951462,18.6980987791378));
#10621=CARTESIAN_POINT('Ctrl Pts',(-2.61040637785506,1.62518633351858,18.7030374937256));
#10622=CARTESIAN_POINT('Ctrl Pts',(-2.65956369759587,1.5434452776277,18.7079762083133));
#10623=CARTESIAN_POINT('Ctrl Pts',(-2.70486310812873,1.45949231456839,18.712914922901));
#10624=CARTESIAN_POINT('Ctrl Pts',(-2.75011446193948,1.37562841457122,18.7178483981616));
#10625=CARTESIAN_POINT('Ctrl Pts',(-2.79151582599366,1.28955766248506,18.7227818734221));
#10626=CARTESIAN_POINT('Ctrl Pts',(-2.8288483148355,1.20167360861939,18.7277153486826));
#10627=CARTESIAN_POINT('Ctrl Pts',(-2.86615566208602,1.11384874033268,18.7326455014907));
#10628=CARTESIAN_POINT('Ctrl Pts',(-2.89939940145408,1.02421340789372,18.7375756542988));
#10629=CARTESIAN_POINT('Ctrl Pts',(-2.92840727959673,0.933184362709153,
18.7425058071068));
#10630=CARTESIAN_POINT('Ctrl Pts',(-2.95740541870615,0.842185879390947,
18.7474343046776));
#10631=CARTESIAN_POINT('Ctrl Pts',(-2.98217038382058,0.749795039982814,
18.7523628022484));
#10632=CARTESIAN_POINT('Ctrl Pts',(-3.00257903406844,0.656446032947613,
18.7572912998191));
#10633=CARTESIAN_POINT('Ctrl Pts',(-3.02298669367368,0.563101557104024,
18.762219558159));
#10634=CARTESIAN_POINT('Ctrl Pts',(-3.03903836267948,0.46879944501066,18.7671478164989));
#10635=CARTESIAN_POINT('Ctrl Pts',(-3.05066178046823,0.373985228572495,
18.7720760748388));
#10636=CARTESIAN_POINT('Ctrl Pts',(-3.06228797249442,0.279148382202736,
18.7770055094384));
#10637=CARTESIAN_POINT('Ctrl Pts',(-3.06948376034883,0.183799634724477,
18.7819349440381));
#10638=CARTESIAN_POINT('Ctrl Pts',(-3.07222875606254,0.0883895945368608,
18.7868643786377));
#10639=CARTESIAN_POINT('Ctrl Pts',(-3.07497714791223,-0.00713848790058853,
18.7917999119828));
#10640=CARTESIAN_POINT('Ctrl Pts',(-3.07326374320136,-0.10272756458361,
18.796735445328));
#10641=CARTESIAN_POINT('Ctrl Pts',(-3.06712031399051,-0.197927333905002,
18.8016709786731));
#10642=CARTESIAN_POINT('Ctrl Pts',(-3.06097281995468,-0.293190092541926,
18.806609777634));
#10643=CARTESIAN_POINT('Ctrl Pts',(-3.05038952050478,-0.388062585579013,
18.8115485765948));
#10644=CARTESIAN_POINT('Ctrl Pts',(-3.03545377308445,-0.482102314314468,
18.8164873755557));
#10645=CARTESIAN_POINT('Ctrl Pts',(-3.02049049731446,-0.576315369396592,
18.8214352773074));
#10646=CARTESIAN_POINT('Ctrl Pts',(-3.00115884957716,-0.669692156824441,
18.8263831790592));
#10647=CARTESIAN_POINT('Ctrl Pts',(-2.97759271814336,-0.761803028912078,
18.8313310808109));
#10648=CARTESIAN_POINT('Ctrl Pts',(-2.96124023617427,-0.825718541697934,
18.8347644179459));
#10649=CARTESIAN_POINT('Ctrl Pts',(-2.94284992820392,-0.889024842653302,
18.8381977550809));
#10650=CARTESIAN_POINT('Ctrl Pts',(-2.92248003136601,-0.95158431905266,
18.8416310922159));
#10651=CARTESIAN_POINT('Ctrl Pts',(-2.89199283230741,-1.04521578047666,
18.8467696961815));
#10652=CARTESIAN_POINT('Ctrl Pts',(-2.85695819522448,-1.13751478481036,
18.851908300147));
#10653=CARTESIAN_POINT('Ctrl Pts',(-2.8175101424337,-1.22802233175267,18.8570469041126));
#10654=CARTESIAN_POINT('Ctrl Pts',(-2.77812125277038,-1.31839413791291,
18.8621778013383));
#10655=CARTESIAN_POINT('Ctrl Pts',(-2.73433228100744,-1.40697946042347,
18.867308698564));
#10656=CARTESIAN_POINT('Ctrl Pts',(-2.68632654671846,-1.49333584112739,
18.8724395957898));
#10657=CARTESIAN_POINT('Ctrl Pts',(-2.63659815126665,-1.58279107627869,
18.8777546126318));
#10658=CARTESIAN_POINT('Ctrl Pts',(-2.5823447794107,-1.66985396060582,18.8830696294739));
#10659=CARTESIAN_POINT('Ctrl Pts',(-2.5238245897669,-1.75405578306049,18.888384646316));
#10660=CARTESIAN_POINT('Ctrl Pts',(-2.46747194348866,-1.83513883398108,
18.8935027989722));
#10661=CARTESIAN_POINT('Ctrl Pts',(-2.40716320133204,-1.91356862756652,
18.8986209516284));
#10662=CARTESIAN_POINT('Ctrl Pts',(-2.34317480499982,-1.98895301181654,
18.9037391042846));
#10663=CARTESIAN_POINT('Ctrl Pts',(-2.27923049055607,-2.06428546343174,
18.9088537310228));
#10664=CARTESIAN_POINT('Ctrl Pts',(-2.21161183051787,-2.1365763693934,18.913968357761));
#10665=CARTESIAN_POINT('Ctrl Pts',(-2.14063640845943,-2.20546548755085,
18.9190829844993));
#10666=CARTESIAN_POINT('Ctrl Pts',(-2.06969460595462,-2.27432197439262,
18.9241951885472));
#10667=CARTESIAN_POINT('Ctrl Pts',(-1.99539949979887,-2.33977959626579,
18.9293073925951));
#10668=CARTESIAN_POINT('Ctrl Pts',(-1.91810601416181,-2.40151443227732,
18.934419596643));
#10669=CARTESIAN_POINT('Ctrl Pts',(-1.84083251662006,-2.46323330366033,
18.939530478675));
#10670=CARTESIAN_POINT('Ctrl Pts',(-1.7605625036411,-2.52123105148741,18.9446413607069));
#10671=CARTESIAN_POINT('Ctrl Pts',(-1.67768396001371,-2.57522402526707,
18.9497522427389));
#10672=CARTESIAN_POINT('Ctrl Pts',(-1.59478764470598,-2.62922857678238,
18.9548642206994));
#10673=CARTESIAN_POINT('Ctrl Pts',(-1.50928202221776,-2.67922641180854,
18.9599761986599));
#10674=CARTESIAN_POINT('Ctrl Pts',(-1.4215837615457,-2.72497740521084,18.9650881766204));
#10675=CARTESIAN_POINT('Ctrl Pts',(-1.33387548538877,-2.77073362355578,
18.9702007383888));
#10676=CARTESIAN_POINT('Ctrl Pts',(-1.24397443858875,-2.81224185129505,
18.9753133001572));
#10677=CARTESIAN_POINT('Ctrl Pts',(-1.15232053332067,-2.84930862464696,
18.9804258619256));
#10678=CARTESIAN_POINT('Ctrl Pts',(-1.06060824867288,-2.88639900785194,
18.9855416801639));
#10679=CARTESIAN_POINT('Ctrl Pts',(-0.967141258677279,-2.91904214160113,
18.9906574984022));
#10680=CARTESIAN_POINT('Ctrl Pts',(-0.872377774838882,-2.94709335922145,
18.9957733166406));
#10681=CARTESIAN_POINT('Ctrl Pts',(-0.846279946393651,-2.95481865419249,
18.9971822110937));
#10682=CARTESIAN_POINT('Ctrl Pts',(-0.820083868285662,-2.96219596869362,
18.9985911055469));
#10683=CARTESIAN_POINT('Ctrl Pts',(-0.793799282532847,-2.9692229537457,
19.));
#10684=CARTESIAN_POINT('',(0.793800071764984,-2.96922274275035,18.9999843185276));
#10685=CARTESIAN_POINT('Origin',(0.,0.,19.));
#10686=CARTESIAN_POINT('Ctrl Pts',(-1.87240768645123,2.4373123939533,18.5627733953368));
#10687=CARTESIAN_POINT('Ctrl Pts',(-1.95202497174946,2.37614829478545,18.5679716338033));
#10688=CARTESIAN_POINT('Ctrl Pts',(-2.02872648937363,2.31101413800602,18.5731698722698));
#10689=CARTESIAN_POINT('Ctrl Pts',(-2.10209926441082,2.24222677991399,18.5783681107363));
#10690=CARTESIAN_POINT('Ctrl Pts',(-2.17233753654655,2.17637803458964,18.5833442791837));
#10691=CARTESIAN_POINT('Ctrl Pts',(-2.23952528158551,2.10718214798762,18.5883204476311));
#10692=CARTESIAN_POINT('Ctrl Pts',(-2.30333394996718,2.03495822191233,18.5932966160784));
#10693=CARTESIAN_POINT('Ctrl Pts',(-2.36712461846038,1.9627546695989,18.5982713807906));
#10694=CARTESIAN_POINT('Ctrl Pts',(-2.42753781287959,1.88752510479804,18.6032461455027));
#10695=CARTESIAN_POINT('Ctrl Pts',(-2.48428317614486,1.8096240909989,18.6082209102148));
#10696=CARTESIAN_POINT('Ctrl Pts',(-2.54102813984596,1.73172362572836,18.6131956398978));
#10697=CARTESIAN_POINT('Ctrl Pts',(-2.59410506502922,1.65115210523789,18.6181703695809));
#10698=CARTESIAN_POINT('Ctrl Pts',(-2.64326574704364,1.5682947556202,18.6231450992639));
#10699=CARTESIAN_POINT('Ctrl Pts',(-2.69243960448518,1.48541519961873,18.6281211622114));
#10700=CARTESIAN_POINT('Ctrl Pts',(-2.7376949094152,1.40024897630273,18.6330972251589));
#10701=CARTESIAN_POINT('Ctrl Pts',(-2.77882895177474,1.31320672659657,18.6380732881063));
#10702=CARTESIAN_POINT('Ctrl Pts',(-2.82000986965535,1.22606528530661,18.6430550216743));
#10703=CARTESIAN_POINT('Ctrl Pts',(-2.85705996437771,1.13704394986257,18.6480367552422));
#10704=CARTESIAN_POINT('Ctrl Pts',(-2.88982443219444,1.04657393484267,18.6530184888102));
#10705=CARTESIAN_POINT('Ctrl Pts',(-2.92261088577821,0.95604321220851,18.6580035652444));
#10706=CARTESIAN_POINT('Ctrl Pts',(-2.9511058585197,0.864062295027149,18.6629886416786));
#10707=CARTESIAN_POINT('Ctrl Pts',(-2.975204841963,0.771076130067551,18.6679737181128));
#10708=CARTESIAN_POINT('Ctrl Pts',(-2.99934142645839,0.677944881078109,
18.6729665726394));
#10709=CARTESIAN_POINT('Ctrl Pts',(-3.01906824474975,0.583805684132802,
18.6779594271659));
#10710=CARTESIAN_POINT('Ctrl Pts',(-3.03433217735862,0.489111937542002,
18.6829522816925));
#10711=CARTESIAN_POINT('Ctrl Pts',(-3.03899824941449,0.46016475491518,18.6844785606392));
#10712=CARTESIAN_POINT('Ctrl Pts',(-3.04324764171201,0.431165770154121,
18.686004839586));
#10713=CARTESIAN_POINT('Ctrl Pts',(-3.04707980808541,0.402127956200752,
18.6875311185327));
#10714=CARTESIAN_POINT('Ctrl Pts',(-3.05965639508212,0.30683026873236,18.6925401338219));
#10715=CARTESIAN_POINT('Ctrl Pts',(-3.06777977856026,0.210777340040537,
18.697549149111));
#10716=CARTESIAN_POINT('Ctrl Pts',(-3.07136944940218,0.114420082498388,
18.7025581644002));
#10717=CARTESIAN_POINT('Ctrl Pts',(-3.07495424103575,0.018193797169766,
18.7075603712575));
#10718=CARTESIAN_POINT('Ctrl Pts',(-3.07401755234348,-0.0783355616180718,
18.7125625781148));
#10719=CARTESIAN_POINT('Ctrl Pts',(-3.06853038122612,-0.174709900956579,
18.7175647849721));
#10720=CARTESIAN_POINT('Ctrl Pts',(-3.0630490308355,-0.270982007526868,
18.7225616855471));
#10721=CARTESIAN_POINT('Ctrl Pts',(-3.05302681956203,-0.367098987402478,
18.7275585861221));
#10722=CARTESIAN_POINT('Ctrl Pts',(-3.03848678339903,-0.462601682994587,
18.732555486697));
#10723=CARTESIAN_POINT('Ctrl Pts',(-3.02395741303011,-0.558034322909119,
18.7375487218126));
#10724=CARTESIAN_POINT('Ctrl Pts',(-3.00491687262805,-0.652853143524043,
18.7425419569282));
#10725=CARTESIAN_POINT('Ctrl Pts',(-2.98144003620813,-0.746604018536794,
18.7475351920437));
#10726=CARTESIAN_POINT('Ctrl Pts',(-2.95797203227419,-0.840319622473202,
18.7525265485979));
#10727=CARTESIAN_POINT('Ctrl Pts',(-2.93007115499145,-0.932967655586887,
18.757517905152));
#10728=CARTESIAN_POINT('Ctrl Pts',(-2.89786320815082,-1.02410501260654,
18.7625092617061));
#10729=CARTESIAN_POINT('Ctrl Pts',(-2.86565867477284,-1.11523271070675,
18.7675000892663));
#10730=CARTESIAN_POINT('Ctrl Pts',(-2.82914812531306,-1.20484963895358,
18.7724909168265));
#10731=CARTESIAN_POINT('Ctrl Pts',(-2.78850664465149,-1.29252966802874,
18.7774817443867));
#10732=CARTESIAN_POINT('Ctrl Pts',(-2.74785848859646,-1.38022409861397,
18.782473391694));
#10733=CARTESIAN_POINT('Ctrl Pts',(-2.70307823772816,-1.4659806016047,18.7874650390013));
#10734=CARTESIAN_POINT('Ctrl Pts',(-2.65438789732525,-1.54939573399866,
18.7924566863087));
#10735=CARTESIAN_POINT('Ctrl Pts',(-2.60564698570869,-1.6328975037923,18.7974535180871));
#10736=CARTESIAN_POINT('Ctrl Pts',(-2.55298809732327,-1.71405266973642,
18.8024503498655));
#10737=CARTESIAN_POINT('Ctrl Pts',(-2.49667761527606,-1.79248518414503,
18.8074471816439));
#10738=CARTESIAN_POINT('Ctrl Pts',(-2.44033496820012,-1.87096249987637,
18.8124468676554));
#10739=CARTESIAN_POINT('Ctrl Pts',(-2.38033684479047,-1.94671372420204,
18.8174465536668));
#10740=CARTESIAN_POINT('Ctrl Pts',(-2.31698981315392,-2.01939606212871,
18.8224462396782));
#10741=CARTESIAN_POINT('Ctrl Pts',(-2.25354352263576,-2.09219228648999,
18.8274537597307));
#10742=CARTESIAN_POINT('Ctrl Pts',(-2.18673814776625,-2.16190970667863,
18.8324612797831));
#10743=CARTESIAN_POINT('Ctrl Pts',(-2.11691691042164,-2.2282425910055,18.8374687998355));
#10744=CARTESIAN_POINT('Ctrl Pts',(-2.07773060268851,-2.26547110366031,
18.8402792086627));
#10745=CARTESIAN_POINT('Ctrl Pts',(-2.03759494160999,-2.30163425068253,
18.8430896174898));
#10746=CARTESIAN_POINT('Ctrl Pts',(-1.99657483514119,-2.33668379925075,
18.8459000263169));
#10747=CARTESIAN_POINT('Ctrl Pts',(-1.92384403406119,-2.39882848789992,
18.8508830286286));
#10748=CARTESIAN_POINT('Ctrl Pts',(-1.84807908471453,-2.45768521307757,
18.8558660309403));
#10749=CARTESIAN_POINT('Ctrl Pts',(-1.76961069950184,-2.51294254256013,
18.860849033252));
#10750=CARTESIAN_POINT('Ctrl Pts',(-1.69124716159385,-2.56812603871422,
18.8658253774126));
#10751=CARTESIAN_POINT('Ctrl Pts',(-1.61018772438855,-2.61971944386175,
18.8708017215732));
#10752=CARTESIAN_POINT('Ctrl Pts',(-1.52679728102083,-2.6674505267516,18.8757780657338));
#10753=CARTESIAN_POINT('Ctrl Pts',(-1.44007352228023,-2.7170895351295,18.8809533262669));
#10754=CARTESIAN_POINT('Ctrl Pts',(-1.35082886036575,-2.76255065514993,
18.8861285868));
#10755=CARTESIAN_POINT('Ctrl Pts',(-1.25950866889961,-2.80357631659399,
18.8913038473331));
#10756=CARTESIAN_POINT('Ctrl Pts',(-1.1718498128674,-2.84295712047113,18.8962716141622));
#10757=CARTESIAN_POINT('Ctrl Pts',(-1.08227910453418,-2.87825109438257,
18.9012393809914));
#10758=CARTESIAN_POINT('Ctrl Pts',(-0.991215645650244,-2.90927719439351,
18.9062071478205));
#10759=CARTESIAN_POINT('Ctrl Pts',(-0.900181330555704,-2.94029336486591,
18.9111733247743));
#10760=CARTESIAN_POINT('Ctrl Pts',(-0.807655632238675,-2.96704423262761,
18.9161395017281));
#10761=CARTESIAN_POINT('Ctrl Pts',(-0.71407584706654,-2.98939758724667,
18.9211056786819));
#10762=CARTESIAN_POINT('Ctrl Pts',(-0.620500023152401,-3.01174999564209,
18.9260716454161));
#10763=CARTESIAN_POINT('Ctrl Pts',(-0.525870631315329,-3.02970515889201,
18.9310376121502));
#10764=CARTESIAN_POINT('Ctrl Pts',(-0.43063719198603,-3.04318153564298,
18.9360035788844));
#10765=CARTESIAN_POINT('Ctrl Pts',(-0.335381336785275,-3.05666108443869,
18.9409707144986));
#10766=CARTESIAN_POINT('Ctrl Pts',(-0.239521589473096,-3.06565969150054,
18.9459378501129));
#10767=CARTESIAN_POINT('Ctrl Pts',(-0.143513543742,-3.07014757182169,18.9509049857271));
#10768=CARTESIAN_POINT('Ctrl Pts',(-0.047400527061884,-3.0746403589926,
18.9558775521877));
#10769=CARTESIAN_POINT('Ctrl Pts',(0.0488606694604206,-3.07461255735108,
18.9608501186482));
#10770=CARTESIAN_POINT('Ctrl Pts',(0.144813823536495,-3.07008651449967,
18.9658226851088));
#10771=CARTESIAN_POINT('Ctrl Pts',(0.240829127043579,-3.06555754010328,
18.9707984723303));
#10772=CARTESIAN_POINT('Ctrl Pts',(0.336535551564223,-3.05652456728976,
18.9757742595519));
#10773=CARTESIAN_POINT('Ctrl Pts',(0.431483474223454,-3.04306165916369,
18.9807500467734));
#10774=CARTESIAN_POINT('Ctrl Pts',(0.526575733441245,-3.02957828518883,
18.9857333980152));
#10775=CARTESIAN_POINT('Ctrl Pts',(0.620906757112716,-3.01165162134643,
18.9907167492569));
#10776=CARTESIAN_POINT('Ctrl Pts',(0.714038869693054,-2.9894064197709,18.9957001004986));
#10777=CARTESIAN_POINT('Ctrl Pts',(0.740727621661937,-2.98303164042897,
18.997128173175));
#10778=CARTESIAN_POINT('Ctrl Pts',(0.767318026974863,-2.97630252452361,
18.9985562458513));
#10779=CARTESIAN_POINT('Ctrl Pts',(0.793800071764984,-2.96922274275035,
18.9999843185276));
#10780=CARTESIAN_POINT('Origin',(0.,0.,-2.20842344717744));
#10781=CARTESIAN_POINT('',(-1.8746299318936,2.44024828799233,17.5625875311804));
#10782=CARTESIAN_POINT('',(-1.87240768645122,2.4373123939533,17.6458577700207));
#10783=CARTESIAN_POINT('',(-1.87240768645123,2.4373123939533,-2.20842344717744));
#10784=CARTESIAN_POINT('',(3.07349994772162,0.000566881991104972,18.2915765528661));
#10785=CARTESIAN_POINT('Ctrl Pts',(-1.87240768645122,2.4373123939533,17.6458577700207));
#10786=CARTESIAN_POINT('Ctrl Pts',(-1.94892700937515,2.37852823121723,17.6508396670982));
#10787=CARTESIAN_POINT('Ctrl Pts',(-2.0226886447178,2.31612696413998,17.6558215641758));
#10788=CARTESIAN_POINT('Ctrl Pts',(-2.09334166204538,2.25040506041581,17.6608034612533));
#10789=CARTESIAN_POINT('Ctrl Pts',(-2.16400280134918,2.18467560157567,17.665785931029));
#10790=CARTESIAN_POINT('Ctrl Pts',(-2.23155429177968,2.11562504719635,17.6707684008046));
#10791=CARTESIAN_POINT('Ctrl Pts',(-2.29568115259007,2.04358760410282,17.6757508705803));
#10792=CARTESIAN_POINT('Ctrl Pts',(-2.35987470346979,1.97147524416458,17.6807385219795));
#10793=CARTESIAN_POINT('Ctrl Pts',(-2.4206362195532,1.89637012043201,17.6857261733787));
#10794=CARTESIAN_POINT('Ctrl Pts',(-2.47769035766569,1.81864035519133,17.690713824778));
#10795=CARTESIAN_POINT('Ctrl Pts',(-2.53477476925467,1.74086934578681,17.6957041226732));
#10796=CARTESIAN_POINT('Ctrl Pts',(-2.5881476418964,1.66047128685132,17.7006944205684));
#10797=CARTESIAN_POINT('Ctrl Pts',(-2.63757762074887,1.57784236998654,17.7056847184636));
#10798=CARTESIAN_POINT('Ctrl Pts',(-2.68709107450033,1.49507391350127,17.7106834437267));
#10799=CARTESIAN_POINT('Ctrl Pts',(-2.73264812472186,1.41006746009895,17.7156821689897));
#10800=CARTESIAN_POINT('Ctrl Pts',(-2.77406388216768,1.32324292087764,17.7206808942527));
#10801=CARTESIAN_POINT('Ctrl Pts',(-2.80822083075527,1.25163584412182,17.724803508744));
#10802=CARTESIAN_POINT('Ctrl Pts',(-2.83956177706021,1.17879263909227,17.7289261232353));
#10803=CARTESIAN_POINT('Ctrl Pts',(-2.86800843670303,1.1049569480302,17.7330487377265));
#10804=CARTESIAN_POINT('Ctrl Pts',(-2.90249867852821,1.01543463250934,17.7380472146142));
#10805=CARTESIAN_POINT('Ctrl Pts',(-2.9328540880347,0.924138278697285,17.7430456915019));
#10806=CARTESIAN_POINT('Ctrl Pts',(-2.95889064443608,0.831485660891783,
17.7480441683895));
#10807=CARTESIAN_POINT('Ctrl Pts',(-2.98489186615198,0.738958783643437,
17.7530358617531));
#10808=CARTESIAN_POINT('Ctrl Pts',(-3.00658576558368,0.645079719611513,
17.7580275551166));
#10809=CARTESIAN_POINT('Ctrl Pts',(-3.02383667694098,0.550285381585332,
17.7630192484801));
#10810=CARTESIAN_POINT('Ctrl Pts',(-3.04106938408581,0.45559107631888,17.7680056743047));
#10811=CARTESIAN_POINT('Ctrl Pts',(-3.05386834532723,0.359983846857202,
17.7729921001294));
#10812=CARTESIAN_POINT('Ctrl Pts',(-3.06214821691609,0.263913901940749,
17.777978525954));
#10813=CARTESIAN_POINT('Ctrl Pts',(-3.07042216901413,0.167912639871801,
17.782961386856));
#10814=CARTESIAN_POINT('Ctrl Pts',(-3.07418341646149,0.0714497562502933,
17.7879442477579));
#10815=CARTESIAN_POINT('Ctrl Pts',(-3.07339818251466,-0.0250172283751209,
17.7929271086599));
#10816=CARTESIAN_POINT('Ctrl Pts',(-3.0726132341693,-0.121449126499266,
17.79790815722));
#10817=CARTESIAN_POINT('Ctrl Pts',(-3.0672850935275,-0.217884683964007,
17.8028892057801));
#10818=CARTESIAN_POINT('Ctrl Pts',(-3.05743207966062,-0.313865143432855,
17.8078702543401));
#10819=CARTESIAN_POINT('Ctrl Pts',(-3.04757995664121,-0.409836924952933,
17.8128508525452));
#10820=CARTESIAN_POINT('Ctrl Pts',(-3.03320381880281,-0.505353253435056,
17.8178314507502));
#10821=CARTESIAN_POINT('Ctrl Pts',(-3.01437387261111,-0.599960337121987,
17.8228120489553));
#10822=CARTESIAN_POINT('Ctrl Pts',(-2.99554048271711,-0.694584722963035,
17.8277935580337));
#10823=CARTESIAN_POINT('Ctrl Pts',(-2.97225175257638,-0.78829910306216,
17.8327750671122));
#10824=CARTESIAN_POINT('Ctrl Pts',(-2.94462881146846,-0.880660781839319,
17.8377565761907));
#10825=CARTESIAN_POINT('Ctrl Pts',(-2.91697601330841,-0.973122292399328,
17.8427434696768));
#10826=CARTESIAN_POINT('Ctrl Pts',(-2.88497977756987,-1.06422776123953,
17.847730363163));
#10827=CARTESIAN_POINT('Ctrl Pts',(-2.8488107845463,-1.15355076344854,17.8527172566491));
#10828=CARTESIAN_POINT('Ctrl Pts',(-2.81262037533797,-1.2429266551012,17.8577071029471));
#10829=CARTESIAN_POINT('Ctrl Pts',(-2.77225247299561,-1.33051757998906,
17.8626969492451));
#10830=CARTESIAN_POINT('Ctrl Pts',(-2.72792457571076,-1.41592011046997,
17.8676867955432));
#10831=CARTESIAN_POINT('Ctrl Pts',(-2.6835248520789,-1.50146102224493,17.872684727098));
#10832=CARTESIAN_POINT('Ctrl Pts',(-2.63515254142937,-1.58480607960722,
17.8776826586528));
#10833=CARTESIAN_POINT('Ctrl Pts',(-2.58306941612667,-1.66557937111116,
17.8826805902075));
#10834=CARTESIAN_POINT('Ctrl Pts',(-2.55271998449031,-1.71264689008769,
17.8855929419753));
#10835=CARTESIAN_POINT('Ctrl Pts',(-2.52111132603805,-1.75884173985027,
17.888505293743));
#10836=CARTESIAN_POINT('Ctrl Pts',(-2.48830142754434,-1.80409485772806,
17.8914176455108));
#10837=CARTESIAN_POINT('Ctrl Pts',(-2.43196544577463,-1.88179637284473,
17.8964182765285));
#10838=CARTESIAN_POINT('Ctrl Pts',(-2.37188764610327,-1.95699282588048,
17.9014189075462));
#10839=CARTESIAN_POINT('Ctrl Pts',(-2.30831858452725,-2.02930223533265,
17.9064195385639));
#10840=CARTESIAN_POINT('Ctrl Pts',(-2.24483579656334,-2.10151350909133,
17.9114133829075));
#10841=CARTESIAN_POINT('Ctrl Pts',(-2.17787145089707,-2.17084519978337,
17.9164072272512));
#10842=CARTESIAN_POINT('Ctrl Pts',(-2.10771847124951,-2.23694548345587,
17.9214010715948));
#10843=CARTESIAN_POINT('Ctrl Pts',(-2.03763957282423,-2.30297596553431,
17.9263896424619));
#10844=CARTESIAN_POINT('Ctrl Pts',(-1.96437905187812,-2.36578152492138,
17.931378213329));
#10845=CARTESIAN_POINT('Ctrl Pts',(-1.88826837164119,-2.42504532053724,
17.9363667841961));
#10846=CARTESIAN_POINT('Ctrl Pts',(-1.81221234866321,-2.4842665571244,17.9413517726276));
#10847=CARTESIAN_POINT('Ctrl Pts',(-1.73331058057633,-2.53995081750557,
17.9463367610591));
#10848=CARTESIAN_POINT('Ctrl Pts',(-1.65192872920764,-2.59182054232511,
17.9513217494906));
#10849=CARTESIAN_POINT('Ctrl Pts',(-1.57057665405401,-2.64367128890743,
17.9563049140009));
#10850=CARTESIAN_POINT('Ctrl Pts',(-1.48674666820128,-2.69171003744208,
17.9612880785111));
#10851=CARTESIAN_POINT('Ctrl Pts',(-1.40083382973748,-2.73570225563072,
17.9662712430214));
#10852=CARTESIAN_POINT('Ctrl Pts',(-1.31492899828999,-2.77969037377547,
17.9712539431042));
#10853=CARTESIAN_POINT('Ctrl Pts',(-1.22694209079712,-2.81963251158411,
17.976236643187));
#10854=CARTESIAN_POINT('Ctrl Pts',(-1.13729225024013,-2.85534036281907,
17.9812193432699));
#10855=CARTESIAN_POINT('Ctrl Pts',(-1.0476263193209,-2.8910546229027,17.9862029376482));
#10856=CARTESIAN_POINT('Ctrl Pts',(-0.956297270211579,-2.92253292479704,
17.9911865320265));
#10857=CARTESIAN_POINT('Ctrl Pts',(-0.863742668553909,-2.94963571522305,
17.9961701264049));
#10858=CARTESIAN_POINT('Ctrl Pts',(-0.771088770415735,-2.97676758266578,
18.0011590673934));
#10859=CARTESIAN_POINT('Ctrl Pts',(-0.677207116561666,-2.99951444348679,
18.006148008382));
#10860=CARTESIAN_POINT('Ctrl Pts',(-0.582548608831353,-3.01778716418979,
18.0111369493706));
#10861=CARTESIAN_POINT('Ctrl Pts',(-0.487834422514082,-3.0360706329945,
18.0161288248781));
#10862=CARTESIAN_POINT('Ctrl Pts',(-0.392342906487234,-3.0498746586468,
18.0211207003856));
#10863=CARTESIAN_POINT('Ctrl Pts',(-0.296531179966286,-3.05916189655072,
18.0261125758932));
#10864=CARTESIAN_POINT('Ctrl Pts',(-0.200565204604544,-3.06846408612843,
18.0311124879014));
#10865=CARTESIAN_POINT('Ctrl Pts',(-0.104278427312059,-3.0732349463007,
18.0361123999097));
#10866=CARTESIAN_POINT('Ctrl Pts',(-0.00812900767658515,-3.07348924989729,
18.0411123119179));
#10867=CARTESIAN_POINT('Ctrl Pts',(0.0474735224485313,-3.07363631187066,
18.0440037257103));
#10868=CARTESIAN_POINT('Ctrl Pts',(0.103030173947787,-3.07227390587906,
18.0468951395027));
#10869=CARTESIAN_POINT('Ctrl Pts',(0.158453394787989,-3.06941277310175,
18.049786553295));
#10870=CARTESIAN_POINT('Ctrl Pts',(0.254312618482903,-3.06446419806834,
18.0547875019464));
#10871=CARTESIAN_POINT('Ctrl Pts',(0.350107281262537,-3.05501208153653,
18.0597884505978));
#10872=CARTESIAN_POINT('Ctrl Pts',(0.4453804778901,-3.0410587761361,18.0647893992492));
#10873=CARTESIAN_POINT('Ctrl Pts',(0.540524788304321,-3.02712434685991,
18.0697835825841));
#10874=CARTESIAN_POINT('Ctrl Pts',(0.635148604263144,-3.00870089391408,
18.0747777659189));
#10875=CARTESIAN_POINT('Ctrl Pts',(0.728797270700946,-2.9858427266383,18.0797719492538));
#10876=CARTESIAN_POINT('Ctrl Pts',(0.822347437359301,-2.96300860161023,
18.0847608797006));
#10877=CARTESIAN_POINT('Ctrl Pts',(0.914924069585438,-2.93574913850191,
18.0897498101474));
#10878=CARTESIAN_POINT('Ctrl Pts',(1.00608089271511,-2.90417001694349,18.0947387405942));
#10879=CARTESIAN_POINT('Ctrl Pts',(1.09717278551479,-2.87261338895948,18.0997241174629));
#10880=CARTESIAN_POINT('Ctrl Pts',(1.18684646638078,-2.83674336243439,18.1047094943315));
#10881=CARTESIAN_POINT('Ctrl Pts',(1.27467000622693,-2.79671568544703,18.1096948712001));
#10882=CARTESIAN_POINT('Ctrl Pts',(1.36246172633447,-2.75670251106593,18.1146784417946));
#10883=CARTESIAN_POINT('Ctrl Pts',(1.44840423857149,-2.71253486102905,18.1196620123891));
#10884=CARTESIAN_POINT('Ctrl Pts',(1.53208571652399,-2.66441656037925,18.1246455829836));
#10885=CARTESIAN_POINT('Ctrl Pts',(1.61575968197491,-2.6163025795481,18.1296287061782));
#10886=CARTESIAN_POINT('Ctrl Pts',(1.6971726365371,-2.56423887209535,18.1346118293728));
#10887=CARTESIAN_POINT('Ctrl Pts',(1.77593842944867,-2.50847462510733,18.1395949525674));
#10888=CARTESIAN_POINT('Ctrl Pts',(1.85471861763025,-2.45270018662168,18.1445789864798));
#10889=CARTESIAN_POINT('Ctrl Pts',(1.93085032532406,-2.39322411890687,18.1495630203921));
#10890=CARTESIAN_POINT('Ctrl Pts',(2.00397827758716,-2.33033759634925,18.1545470543045));
#10891=CARTESIAN_POINT('Ctrl Pts',(2.07718500189069,-2.26738333362465,18.1595364569234));
#10892=CARTESIAN_POINT('Ctrl Pts',(2.14738117805299,-2.2010115683744,18.1645258595424));
#10893=CARTESIAN_POINT('Ctrl Pts',(2.21424657112028,-2.1315521040505,18.1695152621613));
#10894=CARTESIAN_POINT('Ctrl Pts',(2.28115146719131,-2.06205160418707,18.1745076124395));
#10895=CARTESIAN_POINT('Ctrl Pts',(2.34472137306829,-1.98946010282752,18.1794999627176));
#10896=CARTESIAN_POINT('Ctrl Pts',(2.40467611751276,-1.91414080460758,18.1844923129958));
#10897=CARTESIAN_POINT('Ctrl Pts',(2.46472756467901,-1.83870002173771,18.1894927155784));
#10898=CARTESIAN_POINT('Ctrl Pts',(2.5211519506014,-1.76052301211704,18.1944931181611));
#10899=CARTESIAN_POINT('Ctrl Pts',(2.57371225948025,-1.68000221886791,18.1994935207438));
#10900=CARTESIAN_POINT('Ctrl Pts',(2.6040614331707,-1.63350820861306,18.2023808341889));
#10901=CARTESIAN_POINT('Ctrl Pts',(2.63312313152376,-1.58623323858147,18.205268147634));
#10902=CARTESIAN_POINT('Ctrl Pts',(2.6608588761498,-1.53825625017903,18.208155461079));
#10903=CARTESIAN_POINT('Ctrl Pts',(2.71072399288484,-1.45200011537753,18.2133464600564));
#10904=CARTESIAN_POINT('Ctrl Pts',(2.75646487212837,-1.36318966043797,18.2185374590337));
#10905=CARTESIAN_POINT('Ctrl Pts',(2.79782224151893,-1.27223934653115,18.2237284580111));
#10906=CARTESIAN_POINT('Ctrl Pts',(2.83910707630913,-1.1814485457841,18.2289103527576));
#10907=CARTESIAN_POINT('Ctrl Pts',(2.87602354093142,-1.08852570938133,18.2340922475042));
#10908=CARTESIAN_POINT('Ctrl Pts',(2.90835739213462,-0.993911228237162,
18.2392741422507));
#10909=CARTESIAN_POINT('Ctrl Pts',(2.94062389796345,-0.899493811389925,
18.2444452440782));
#10910=CARTESIAN_POINT('Ctrl Pts',(2.96832668061917,-0.803392138253361,
18.2496163459056));
#10911=CARTESIAN_POINT('Ctrl Pts',(2.99129936445153,-0.706066825613475,
18.254787447733));
#10912=CARTESIAN_POINT('Ctrl Pts',(3.01424339712983,-0.608862895505413,
18.2599521002471));
#10913=CARTESIAN_POINT('Ctrl Pts',(3.0324689794172,-0.510438741737216,18.2651167527612));
#10914=CARTESIAN_POINT('Ctrl Pts',(3.0458592447649,-0.411270848809141,18.2702814052753));
#10915=CARTESIAN_POINT('Ctrl Pts',(3.05923091965564,-0.312240636232969,
18.2754388874125));
#10916=CARTESIAN_POINT('Ctrl Pts',(3.06778059797625,-0.212469128371478,
18.2805963695496));
#10917=CARTESIAN_POINT('Ctrl Pts',(3.0714424736794,-0.112442789356175,18.2857538516868));
#10918=CARTESIAN_POINT('Ctrl Pts',(3.07282053680199,-0.0748001656682735,
18.2876947520654));
#10919=CARTESIAN_POINT('Ctrl Pts',(3.07350689903397,-0.0371215440459636,
18.289635652444));
#10920=CARTESIAN_POINT('Ctrl Pts',(3.07349994772178,0.000566881145854129,
18.2915765528226));
#10921=CARTESIAN_POINT('Ctrl Pts',(3.07349994772162,0.000566881991102313,
18.2915765528661));
#10922=CARTESIAN_POINT('Ctrl Pts',(3.07348108465619,0.102837956996753,18.2968433680007));
#10923=CARTESIAN_POINT('Ctrl Pts',(3.06835333742015,0.204987653606154,18.3021101831354));
#10924=CARTESIAN_POINT('Ctrl Pts',(3.05817840423343,0.306507908348619,18.30737699827));
#10925=CARTESIAN_POINT('Ctrl Pts',(3.04797107142034,0.408351429913868,18.3126605843101));
#10926=CARTESIAN_POINT('Ctrl Pts',(3.03268444834494,0.509561143595813,18.3179441703501));
#10927=CARTESIAN_POINT('Ctrl Pts',(3.01243181314503,0.609636630421547,18.3232277563902));
#10928=CARTESIAN_POINT('Ctrl Pts',(2.99214601482956,0.709875988017733,18.3285199941525));
#10929=CARTESIAN_POINT('Ctrl Pts',(2.96687806690077,0.808977066377082,18.3338122319149));
#10930=CARTESIAN_POINT('Ctrl Pts',(2.93679113505847,0.906454675668872,18.3391044696772));
#10931=CARTESIAN_POINT('Ctrl Pts',(2.90661691184847,1.0042150972421,18.3444120618357));
#10932=CARTESIAN_POINT('Ctrl Pts',(2.87159586571238,1.10034229232758,18.3497196539942));
#10933=CARTESIAN_POINT('Ctrl Pts',(2.83193989422544,1.19436957659444,18.3550272461528));
#10934=CARTESIAN_POINT('Ctrl Pts',(2.80330609589967,1.26226246116806,18.3588596203896));
#10935=CARTESIAN_POINT('Ctrl Pts',(2.77225681532059,1.32906099180651,18.3626919946264));
#10936=CARTESIAN_POINT('Ctrl Pts',(2.73888628269538,1.3945982147067,18.3665243688633));
#10937=CARTESIAN_POINT('Ctrl Pts',(2.69527008178349,1.48025716157833,18.3715333870459));
#10938=CARTESIAN_POINT('Ctrl Pts',(2.64755618379696,1.56401602255294,18.3765424052285));
#10939=CARTESIAN_POINT('Ctrl Pts',(2.59593365674044,1.64545759586876,18.3815514234111));
#10940=CARTESIAN_POINT('Ctrl Pts',(2.54438129710067,1.72678847051985,18.3865536331346));
#10941=CARTESIAN_POINT('Ctrl Pts',(2.48893110021215,1.8058079518594,18.3915558428581));
#10942=CARTESIAN_POINT('Ctrl Pts',(2.42981864846207,1.88212209635452,18.3965580525815));
#10943=CARTESIAN_POINT('Ctrl Pts',(2.37076890283357,1.95835528727927,18.401554955992));
#10944=CARTESIAN_POINT('Ctrl Pts',(2.30806489226961,2.03188850305573,18.4065518594025));
#10945=CARTESIAN_POINT('Ctrl Pts',(2.24198568692741,2.10235639928453,18.411548762813));
#10946=CARTESIAN_POINT('Ctrl Pts',(2.17595495448098,2.17277260326051,18.4165420007075));
#10947=CARTESIAN_POINT('Ctrl Pts',(2.10655424822711,2.24012764054148,18.4215352386021));
#10948=CARTESIAN_POINT('Ctrl Pts',(2.03410250820549,2.30408967623054,18.4265284764967));
#10949=CARTESIAN_POINT('Ctrl Pts',(1.96167802657922,2.36802764759131,18.4315198357938));
#10950=CARTESIAN_POINT('Ctrl Pts',(1.88620511956672,2.42857486500866,18.4365111950909));
#10951=CARTESIAN_POINT('Ctrl Pts',(1.80803845577153,2.4854374247708,18.4415025543881));
#10952=CARTESIAN_POINT('Ctrl Pts',(1.72988007684324,2.54229395768317,18.4464933846522));
#10953=CARTESIAN_POINT('Ctrl Pts',(1.64902886245486,2.59546635246374,18.4514842149163));
#10954=CARTESIAN_POINT('Ctrl Pts',(1.56587047797939,2.64470261016104,18.4564750451804));
#10955=CARTESIAN_POINT('Ctrl Pts',(1.48269843538775,2.69394695452971,18.4614666951494));
#10956=CARTESIAN_POINT('Ctrl Pts',(1.39721884635418,2.73925365523797,18.4664583451185));
#10957=CARTESIAN_POINT('Ctrl Pts',(1.30984319299196,2.78041598682151,18.4714499950875));
#10958=CARTESIAN_POINT('Ctrl Pts',(1.22237679015729,2.82162107012973,18.4764468294482));
#10959=CARTESIAN_POINT('Ctrl Pts',(1.13301078749947,2.85867300405083,18.4814436638088));
#10960=CARTESIAN_POINT('Ctrl Pts',(1.04217772116053,2.89141277708954,18.4864404981694));
#10961=CARTESIAN_POINT('Ctrl Pts',(0.951292770975532,2.92417125108609,18.4914401867218));
#10962=CARTESIAN_POINT('Ctrl Pts',(0.858939505900463,2.95261253015875,18.4964398752741));
#10963=CARTESIAN_POINT('Ctrl Pts',(0.765564742944816,2.97662776886191,18.5014395638265));
#10964=CARTESIAN_POINT('Ctrl Pts',(0.672043672190903,3.0006806367551,18.5064470863309));
#10965=CARTESIAN_POINT('Ctrl Pts',(0.577498335266228,3.02029352699308,18.5114546088354));
#10966=CARTESIAN_POINT('Ctrl Pts',(0.482384761461372,3.03540890028178,18.5164621313399));
#10967=CARTESIAN_POINT('Ctrl Pts',(0.429003982127228,3.0438921311583,18.5192725131091));
#10968=CARTESIAN_POINT('Ctrl Pts',(0.37544430968187,3.05095966618729,18.5220828948782));
#10969=CARTESIAN_POINT('Ctrl Pts',(0.321786553589066,3.05660852317226,18.5248932766474));
#10970=CARTESIAN_POINT('Ctrl Pts',(0.225641124389739,3.0667302990133,18.5299289952664));
#10971=CARTESIAN_POINT('Ctrl Pts',(0.128852929442827,3.0723286581662,18.5349647138855));
#10972=CARTESIAN_POINT('Ctrl Pts',(0.0318828348761874,3.073334627866,18.5400004325045));
#10973=CARTESIAN_POINT('Ctrl Pts',(-0.0643820208470067,3.07433328140395,
18.5449995276223));
#10974=CARTESIAN_POINT('Ctrl Pts',(-0.16082569776443,3.07080608065001,18.5499986227401));
#10975=CARTESIAN_POINT('Ctrl Pts',(-0.256989783873565,3.06273709302392,
18.5549977178579));
#10976=CARTESIAN_POINT('Ctrl Pts',(-0.353062715945296,3.05467575399961,
18.5599920743283));
#10977=CARTESIAN_POINT('Ctrl Pts',(-0.448856150415055,3.04208121920463,
18.5649864307986));
#10978=CARTESIAN_POINT('Ctrl Pts',(-0.543911997377421,3.02498958495875,
18.569980787269));
#10979=CARTESIAN_POINT('Ctrl Pts',(-0.638903467979729,3.00790952598399,
18.5749717613226));
#10980=CARTESIAN_POINT('Ctrl Pts',(-0.733157914833171,2.98633849890491,
18.5799627353762));
#10981=CARTESIAN_POINT('Ctrl Pts',(-0.826223737422982,2.96036426571441,
18.5849537094297));
#10982=CARTESIAN_POINT('Ctrl Pts',(-0.92069603634875,2.93399749159631,18.5900201106026));
#10983=CARTESIAN_POINT('Ctrl Pts',(-1.01394303112386,2.90309338515365,18.5950865117754));
#10984=CARTESIAN_POINT('Ctrl Pts',(-1.1055050498395,2.86779720949361,18.6001529129483));
#10985=CARTESIAN_POINT('Ctrl Pts',(-1.19567576894536,2.83303736490308,18.60514232934));
#10986=CARTESIAN_POINT('Ctrl Pts',(-1.28421195811642,2.79401819649673,18.6101317457316));
#10987=CARTESIAN_POINT('Ctrl Pts',(-1.37069309330137,2.75092760609507,18.6151211621233));
#10988=CARTESIAN_POINT('Ctrl Pts',(-1.45917578460393,2.70683970877039,18.6202260556867));
#10989=CARTESIAN_POINT('Ctrl Pts',(-1.54550667851344,2.65848978448217,18.6253309492502));
#10990=CARTESIAN_POINT('Ctrl Pts',(-1.62926181217111,2.60612896791408,18.6304358428136));
#10991=CARTESIAN_POINT('Ctrl Pts',(-1.71301694582878,2.55376815134599,18.635540736377));
#10992=CARTESIAN_POINT('Ctrl Pts',(-1.79419592504642,2.49739673258324,18.6406456299405));
#10993=CARTESIAN_POINT('Ctrl Pts',(-1.87240768645124,2.43731239395329,18.6457505235039));
#10994=CARTESIAN_POINT('',(3.07396038371946,0.000496328078016796,18.2084233953208));
#10995=CARTESIAN_POINT('Ctrl Pts',(3.07349995977581,0.000497250552599549,
18.2084234471775));
#10996=CARTESIAN_POINT('Ctrl Pts',(3.07349581818499,0.0260963758433496,
18.2097570965117));
#10997=CARTESIAN_POINT('Ctrl Pts',(3.07317186094799,0.0516926665754111,
18.2110907458459));
#10998=CARTESIAN_POINT('Ctrl Pts',(3.07252826222747,0.0772808372976627,
18.2124243951801));
#10999=CARTESIAN_POINT('Ctrl Pts',(3.07011503473139,0.173225834067707,18.21742502545));
#11000=CARTESIAN_POINT('Ctrl Pts',(3.06319919775923,0.269225925428171,18.2224256557198));
#11001=CARTESIAN_POINT('Ctrl Pts',(3.05177086479431,0.364824394459287,18.2274262859897));
#11002=CARTESIAN_POINT('Ctrl Pts',(3.04035804193262,0.460293120847487,18.2324201295924));
#11003=CARTESIAN_POINT('Ctrl Pts',(3.02444494626311,0.555360876268122,18.2374139731951));
#11004=CARTESIAN_POINT('Ctrl Pts',(3.00407368908106,0.64957179785678,18.2424078167978));
#11005=CARTESIAN_POINT('Ctrl Pts',(2.9837239438239,0.743683233279711,18.2473963869318));
#11006=CARTESIAN_POINT('Ctrl Pts',(2.95892548819042,0.836939207032645,18.2523849570657));
#11007=CARTESIAN_POINT('Ctrl Pts',(2.92977200971182,0.928890855326471,18.2573735271997));
#11008=CARTESIAN_POINT('Ctrl Pts',(2.90063946710002,1.02077647076384,18.2623585149124));
#11009=CARTESIAN_POINT('Ctrl Pts',(2.86715825122914,1.11135920580007,18.2673435026252));
#11010=CARTESIAN_POINT('Ctrl Pts',(2.82947248356031,1.2002031972858,18.2723284903379));
#11011=CARTESIAN_POINT('Ctrl Pts',(2.79180050439657,1.28901468244607,18.2773116541385));
#11012=CARTESIAN_POINT('Ctrl Pts',(2.74992720120223,1.37608828457834,18.2822948179391));
#11013=CARTESIAN_POINT('Ctrl Pts',(2.70404529326473,1.46100694795502,18.2872779817398));
#11014=CARTESIAN_POINT('Ctrl Pts',(2.6581676613985,1.54591769713911,18.2922606811228));
#11015=CARTESIAN_POINT('Ctrl Pts',(2.60828237629102,1.6286735209441,18.2972433805059));
#11016=CARTESIAN_POINT('Ctrl Pts',(2.55462818999486,1.7088818159497,18.3022260798889));
#11017=CARTESIAN_POINT('Ctrl Pts',(2.50096437372331,1.78910450692254,18.3072096735782));
#11018=CARTESIAN_POINT('Ctrl Pts',(2.44353055681198,1.86677839636644,18.3121932672675));
#11019=CARTESIAN_POINT('Ctrl Pts',(2.38260828915974,1.94154062291452,18.3171768609568));
#11020=CARTESIAN_POINT('Ctrl Pts',(2.32162066127232,2.01638305784778,18.3221658012766));
#11021=CARTESIAN_POINT('Ctrl Pts',(2.25713738853279,2.08830725285345,18.3271547415964));
#11022=CARTESIAN_POINT('Ctrl Pts',(2.18947957108095,2.15698434343395,18.3321436819162));
#11023=CARTESIAN_POINT('Ctrl Pts',(2.12178195683039,2.22570183035671,18.3371355567654));
#11024=CARTESIAN_POINT('Ctrl Pts',(2.05090640186082,2.291168112132,18.3421274316146));
#11025=CARTESIAN_POINT('Ctrl Pts',(1.97720846543889,2.35309348182277,18.3471193064637));
#11026=CARTESIAN_POINT('Ctrl Pts',(1.90339188117032,2.41511854645919,18.3521192178365));
#11027=CARTESIAN_POINT('Ctrl Pts',(1.82674419102255,2.47359105018672,18.3571191292092));
#11028=CARTESIAN_POINT('Ctrl Pts',(1.74765133310118,2.52826364683545,18.362119040582));
#11029=CARTESIAN_POINT('Ctrl Pts',(1.7019123755448,2.5598805038227,18.3650104613761));
#11030=CARTESIAN_POINT('Ctrl Pts',(1.65535619738727,2.59022741164452,18.3679018821703));
#11031=CARTESIAN_POINT('Ctrl Pts',(1.60806103526927,2.61926362874162,18.3707933029644));
#11032=CARTESIAN_POINT('Ctrl Pts',(1.52626023406071,2.66948411041971,18.3757942486638));
#11033=CARTESIAN_POINT('Ctrl Pts',(1.44196164653047,2.71595665020612,18.3807951943631));
#11034=CARTESIAN_POINT('Ctrl Pts',(1.355543141196,2.75842437676955,18.3857961400624));
#11035=CARTESIAN_POINT('Ctrl Pts',(1.26924154378735,2.80083465251492,18.3907903204262));
#11036=CARTESIAN_POINT('Ctrl Pts',(1.18082611868765,2.83925069083241,18.39578450079));
#11037=CARTESIAN_POINT('Ctrl Pts',(1.09070231052193,2.87345971258031,18.4007786811537));
#11038=CARTESIAN_POINT('Ctrl Pts',(1.00067329500927,2.9076327531153,18.4057676086146));
#11039=CARTESIAN_POINT('Ctrl Pts',(0.908939876541152,2.9376074189381,18.4107565360755));
#11040=CARTESIAN_POINT('Ctrl Pts',(0.815929691739153,2.96321801225263,18.4157454635365));
#11041=CARTESIAN_POINT('Ctrl Pts',(0.722985757623182,2.98881036327058,18.4207308374095));
#11042=CARTESIAN_POINT('Ctrl Pts',(0.628767286827081,3.01004470529546,18.4257162112825));
#11043=CARTESIAN_POINT('Ctrl Pts',(0.533718454632727,3.02680472795727,18.4307015851556));
#11044=CARTESIAN_POINT('Ctrl Pts',(0.438704060118033,3.04355867820052,18.4356851527496));
#11045=CARTESIAN_POINT('Ctrl Pts',(0.342860333539901,3.05584145402598,18.4406687203437));
#11046=CARTESIAN_POINT('Ctrl Pts',(0.246642116342153,3.06358775236589,18.4456522879377));
#11047=CARTESIAN_POINT('Ctrl Pts',(0.150432537159386,3.07133335527989,18.4506354081307));
#11048=CARTESIAN_POINT('Ctrl Pts',(0.0538489714644777,3.07454325542527,
18.4556185283237));
#11049=CARTESIAN_POINT('Ctrl Pts',(-0.0426492036916367,3.07320407643626,
18.4606016485167));
#11050=CARTESIAN_POINT('Ctrl Pts',(-0.139165014954978,3.0718646526975,18.4655856794299));
#11051=CARTESIAN_POINT('Ctrl Pts',(-0.235594966070892,3.06597450475753,
18.4705697103432));
#11052=CARTESIAN_POINT('Ctrl Pts',(-0.331481341451637,3.05557234741209,
18.4755537412564));
#11053=CARTESIAN_POINT('Ctrl Pts',(-0.427471004300964,3.04515898500758,
18.4805431408984));
#11054=CARTESIAN_POINT('Ctrl Pts',(-0.522915485626964,3.03022395747985,
18.4855325405403));
#11055=CARTESIAN_POINT('Ctrl Pts',(-0.617364065253234,3.01085766201825,
18.4905219401823));
#11056=CARTESIAN_POINT('Ctrl Pts',(-0.711868443774845,2.99147992522108,
18.4955142874915));
#11057=CARTESIAN_POINT('Ctrl Pts',(-0.805375324145514,2.96766581587002,
18.5005066348007));
#11058=CARTESIAN_POINT('Ctrl Pts',(-0.89744808296427,2.93955595088506,18.50549898211));
#11059=CARTESIAN_POINT('Ctrl Pts',(-0.989669349432891,2.91140074643117,
18.5104993817658));
#11060=CARTESIAN_POINT('Ctrl Pts',(-1.08045146271283,2.87893609864151,18.5154997814216));
#11061=CARTESIAN_POINT('Ctrl Pts',(-1.16937680199829,2.84235116495978,18.5205001810775));
#11062=CARTESIAN_POINT('Ctrl Pts',(-1.2207242928934,2.82122620143178,18.5233875243012));
#11063=CARTESIAN_POINT('Ctrl Pts',(-1.27145312842869,2.79872833948767,18.5262748675248));
#11064=CARTESIAN_POINT('Ctrl Pts',(-1.32148688040794,2.77490084055443,18.5291622107485));
#11065=CARTESIAN_POINT('Ctrl Pts',(-1.40800849234638,2.7336967826013,18.5341551920871));
#11066=CARTESIAN_POINT('Ctrl Pts',(-1.49275570937198,2.68836859676869,18.5391481734257));
#11067=CARTESIAN_POINT('Ctrl Pts',(-1.5753080589408,2.63909203504466,18.5441411547643));
#11068=CARTESIAN_POINT('Ctrl Pts',(-1.65773786070718,2.5898886236838,18.5491267240923));
#11069=CARTESIAN_POINT('Ctrl Pts',(-1.73797889834575,2.53674871403438,18.5541122934203));
#11070=CARTESIAN_POINT('Ctrl Pts',(-1.81563271272675,2.47989517973573,18.5590978627483));
#11071=CARTESIAN_POINT('Ctrl Pts',(-1.83471573057289,2.465923721691,18.5603230402778));
#11072=CARTESIAN_POINT('Ctrl Pts',(-1.85364261641151,2.45172821585054,18.5615482178073));
#11073=CARTESIAN_POINT('Ctrl Pts',(-1.87240768645123,2.4373123939533,18.5627733953368));
#11074=CARTESIAN_POINT('Ctrl Pts',(-1.8746299318936,2.44024828799233,17.5625875311804));
#11075=CARTESIAN_POINT('Ctrl Pts',(-1.95834209400996,2.37692452213389,17.5680412754681));
#11076=CARTESIAN_POINT('Ctrl Pts',(-2.81517875351248,1.65341120062326,17.6262846556839));
#11077=CARTESIAN_POINT('Ctrl Pts',(-3.56999562230916,-0.655354264402703,
17.7373176718277));
#11078=CARTESIAN_POINT('Ctrl Pts',(-1.39399312869632,-3.35125860275677,
17.8956865796119));
#11079=CARTESIAN_POINT('Ctrl Pts',(2.02304254293428,-2.99694469112536,18.0527216541862));
#11080=CARTESIAN_POINT('Ctrl Pts',(3.07627241680049,-0.988770447851309,
18.1569670928325));
#11081=CARTESIAN_POINT('Ctrl Pts',(3.0783977291544,0.000487437709835295,
18.2084228955508));
#11082=CARTESIAN_POINT('Origin',(0.,0.,-2.20842344717744));
#11083=CARTESIAN_POINT('',(-1.86972588535603,2.43378780274861,16.5626129315945));
#11084=CARTESIAN_POINT('',(-1.87240768645125,2.43731239395329,16.6459160952886));
#11085=CARTESIAN_POINT('',(-1.87240768645123,2.4373123939533,-2.20842344717744));
#11086=CARTESIAN_POINT('',(3.07349878900434,-0.00272836743798955,17.2915765528552));
#11087=CARTESIAN_POINT('Ctrl Pts',(-1.87240768645125,2.43731239395329,16.6459160952886));
#11088=CARTESIAN_POINT('Ctrl Pts',(-1.94869008435301,2.3787102432702,16.650906378381));
#11089=CARTESIAN_POINT('Ctrl Pts',(-2.02231571227431,2.31644890824351,16.6558966614733));
#11090=CARTESIAN_POINT('Ctrl Pts',(-2.09291629670881,2.25080066309095,16.6608869445657));
#11091=CARTESIAN_POINT('Ctrl Pts',(-2.16480287083741,2.18395663510773,16.665968125668));
#11092=CARTESIAN_POINT('Ctrl Pts',(-2.23355271443631,2.11360133218143,16.6710493067703));
#11093=CARTESIAN_POINT('Ctrl Pts',(-2.29881105051213,2.04006617638824,16.6761304878727));
#11094=CARTESIAN_POINT('Ctrl Pts',(-2.36280734971843,1.96795312363041,16.6811134035536));
#11095=CARTESIAN_POINT('Ctrl Pts',(-2.42344567718209,1.89278245461709,16.6860963192346));
#11096=CARTESIAN_POINT('Ctrl Pts',(-2.4804285996563,1.81490391261,16.6910792349156));
#11097=CARTESIAN_POINT('Ctrl Pts',(-2.53739776626703,1.73704417073715,16.6960609477044));
#11098=CARTESIAN_POINT('Ctrl Pts',(-2.59071302240877,1.65647820902671,16.7010426604933));
#11099=CARTESIAN_POINT('Ctrl Pts',(-2.64011835287779,1.57358740869322,16.7060243732821));
#11100=CARTESIAN_POINT('Ctrl Pts',(-2.68952524410106,1.4906939897725,16.7110062434473));
#11101=CARTESIAN_POINT('Ctrl Pts',(-2.7350217401748,1.40547596383643,16.7159881136125));
#11102=CARTESIAN_POINT('Ctrl Pts',(-2.77639671341757,1.31834120762575,16.7209699837777));
#11103=CARTESIAN_POINT('Ctrl Pts',(-2.81921322186053,1.22817061094453,16.726125426048));
#11104=CARTESIAN_POINT('Ctrl Pts',(-2.8576155186533,1.13594772403954,16.7312808683183));
#11105=CARTESIAN_POINT('Ctrl Pts',(-2.8914236036249,1.04214768358462,16.7364363105887));
#11106=CARTESIAN_POINT('Ctrl Pts',(-2.92414138435231,0.951372676410906,
16.7414254908364));
#11107=CARTESIAN_POINT('Ctrl Pts',(-2.95255666769649,0.859121130163589,
16.7464146710841));
#11108=CARTESIAN_POINT('Ctrl Pts',(-2.97655742563126,0.765838195651939,
16.7514038513318));
#11109=CARTESIAN_POINT('Ctrl Pts',(-3.00175790406929,0.6678923480172,16.7566424246134));
#11110=CARTESIAN_POINT('Ctrl Pts',(-3.02209094743006,0.56880986948559,16.761880997895));
#11111=CARTESIAN_POINT('Ctrl Pts',(-3.03748798446673,0.469115118302798,
16.7671195711767));
#11112=CARTESIAN_POINT('Ctrl Pts',(-3.0528850215034,0.369420367120006,16.7723581444583));
#11113=CARTESIAN_POINT('Ctrl Pts',(-3.06334606838429,0.269113900212103,
16.7775967177399));
#11114=CARTESIAN_POINT('Ctrl Pts',(-3.0688654966124,0.168721112199794,16.7828352910216));
#11115=CARTESIAN_POINT('Ctrl Pts',(-3.07413302261529,0.0729101695618671,
16.7878347800698));
#11116=CARTESIAN_POINT('Ctrl Pts',(-3.07491862900344,-0.02331598262082,
16.7928342691181));
#11117=CARTESIAN_POINT('Ctrl Pts',(-3.07117587759827,-0.119503049578297,
16.7978337581663));
#11118=CARTESIAN_POINT('Ctrl Pts',(-3.06743820323802,-0.215559638711458,
16.8028264654041));
#11119=CARTESIAN_POINT('Ctrl Pts',(-3.05918439625417,-0.311576813109383,
16.8078191726419));
#11120=CARTESIAN_POINT('Ctrl Pts',(-3.04641991747264,-0.407096961946395,
16.8128118798798));
#11121=CARTESIAN_POINT('Ctrl Pts',(-3.03366890489975,-0.502516339394628,
16.8177993199352));
#11122=CARTESIAN_POINT('Ctrl Pts',(-3.01641673826346,-0.597439300872269,
16.8227867599907));
#11123=CARTESIAN_POINT('Ctrl Pts',(-2.99472084953958,-0.69141108129167,
16.8277742000462));
#11124=CARTESIAN_POINT('Ctrl Pts',(-2.97304048430665,-0.785315624544578,
16.8327580715693));
#11125=CARTESIAN_POINT('Ctrl Pts',(-2.9469228161462,-0.878269913198738,
16.8377419430925));
#11126=CARTESIAN_POINT('Ctrl Pts',(-2.91647659018144,-0.9698281027706,16.8427258146156));
#11127=CARTESIAN_POINT('Ctrl Pts',(-2.8860414515551,-1.06135295038955,16.8477078712054));
#11128=CARTESIAN_POINT('Ctrl Pts',(-2.85128102541957,-1.15148229295804,
16.8526899277952));
#11129=CARTESIAN_POINT('Ctrl Pts',(-2.812354003565,-1.23978514615714,16.857671984385));
#11130=CARTESIAN_POINT('Ctrl Pts',(-2.77343053018542,-1.32807994992298,
16.8626535868249));
#11131=CARTESIAN_POINT('Ctrl Pts',(-2.73034139346628,-1.41454819375258,
16.8676351892648));
#11132=CARTESIAN_POINT('Ctrl Pts',(-2.68329312531964,-1.49877958806903,
16.8726167917047));
#11133=CARTESIAN_POINT('Ctrl Pts',(-2.63623630175471,-1.58302629931083,
16.8775993000163));
#11134=CARTESIAN_POINT('Ctrl Pts',(-2.58521913104524,-1.66503497000622,
16.8825818083278));
#11135=CARTESIAN_POINT('Ctrl Pts',(-2.53049318192716,-1.74442153914131,
16.8875643166394));
#11136=CARTESIAN_POINT('Ctrl Pts',(-2.47570824264697,-1.82389368059919,
16.8925521956933));
#11137=CARTESIAN_POINT('Ctrl Pts',(-2.41720679334826,-1.90073771581067,
16.8975400747472));
#11138=CARTESIAN_POINT('Ctrl Pts',(-2.35528254233724,-1.97460031291435,
16.9025279538011));
#11139=CARTESIAN_POINT('Ctrl Pts',(-2.29332170985965,-2.04850654400765,
16.9075187794217));
#11140=CARTESIAN_POINT('Ctrl Pts',(-2.22793434694105,-2.11942750743609,
16.9125096050422));
#11141=CARTESIAN_POINT('Ctrl Pts',(-2.15945163440285,-2.18704615604584,
16.9175004306627));
#11142=CARTESIAN_POINT('Ctrl Pts',(-2.09085824583123,-2.25477408426114,
16.9224993220383));
#11143=CARTESIAN_POINT('Ctrl Pts',(-2.01915984518205,-2.31918874783033,
16.9274982134139));
#11144=CARTESIAN_POINT('Ctrl Pts',(-1.94472127489543,-2.3800129018493,16.9324971047894));
#11145=CARTESIAN_POINT('Ctrl Pts',(-1.90150211680463,-2.41532750714279,
16.9353994694615));
#11146=CARTESIAN_POINT('Ctrl Pts',(-1.857359822824,-2.44943255052934,16.9383018341336));
#11147=CARTESIAN_POINT('Ctrl Pts',(-1.81237000627372,-2.48228064697757,
16.9412041988057));
#11148=CARTESIAN_POINT('Ctrl Pts',(-1.73487197768212,-2.5388637342831,16.946203719977));
#11149=CARTESIAN_POINT('Ctrl Pts',(-1.65458546237634,-2.59191343652079,
16.9512032411484));
#11150=CARTESIAN_POINT('Ctrl Pts',(-1.57186624083407,-2.64114345898253,
16.9562027623198));
#11151=CARTESIAN_POINT('Ctrl Pts',(-1.48925922945181,-2.69030670000465,
16.9611955015478));
#11152=CARTESIAN_POINT('Ctrl Pts',(-1.40422644437154,-2.73566033649841,
16.9661882407759));
#11153=CARTESIAN_POINT('Ctrl Pts',(-1.31715470384538,-2.77695980095823,
16.971180980004));
#11154=CARTESIAN_POINT('Ctrl Pts',(-1.23017482427609,-2.8182156943547,16.9761684518766));
#11155=CARTESIAN_POINT('Ctrl Pts',(-1.14116066002593,-2.85542573134479,
16.9811559237493));
#11156=CARTESIAN_POINT('Ctrl Pts',(-1.05052493798665,-2.88839048687468,
16.986143395622));
#11157=CARTESIAN_POINT('Ctrl Pts',(-0.959954072733928,-2.92133165360244,
16.9911272985773));
#11158=CARTESIAN_POINT('Ctrl Pts',(-0.86776436775069,-2.95003342831423,
16.9961112015327));
#11159=CARTESIAN_POINT('Ctrl Pts',(-0.774389004784814,-2.97434428391677,
17.001095104488));
#11160=CARTESIAN_POINT('Ctrl Pts',(-0.681047649964934,-2.99864628528732,
17.0060771922611));
#11161=CARTESIAN_POINT('Ctrl Pts',(-0.586521919521054,-3.01856043452411,
17.0110592800342));
#11162=CARTESIAN_POINT('Ctrl Pts',(-0.491259724133798,-3.03398519005021,
17.0160413678073));
#11163=CARTESIAN_POINT('Ctrl Pts',(-0.396006217970347,-3.04940853862623,
17.0210230011454));
#11164=CARTESIAN_POINT('Ctrl Pts',(-0.300016813767278,-3.06034323766132,
17.0260046344836));
#11165=CARTESIAN_POINT('Ctrl Pts',(-0.203748110307505,-3.06673914077251,
17.0309862678217));
#11166=CARTESIAN_POINT('Ctrl Pts',(-0.107461907339179,-3.0731362065166,
17.0359688067099));
#11167=CARTESIAN_POINT('Ctrl Pts',(-0.0108967422766421,-3.07499280871843,
17.0409513455981));
#11168=CARTESIAN_POINT('Ctrl Pts',(0.0854882658993729,-3.0723108577085,
17.0459338844863));
#11169=CARTESIAN_POINT('Ctrl Pts',(0.181977155694252,-3.06962601615139,
17.0509217934442));
#11170=CARTESIAN_POINT('Ctrl Pts',(0.2782850614439,-3.06239286808041,17.0559097024021));
#11171=CARTESIAN_POINT('Ctrl Pts',(0.373955696445788,-3.05066540071109,
17.0608976113599));
#11172=CARTESIAN_POINT('Ctrl Pts',(0.469682841667079,-3.03893100622402,
17.0658884665492));
#11173=CARTESIAN_POINT('Ctrl Pts',(0.564771534129519,-3.02269708037209,
17.0708793217385));
#11174=CARTESIAN_POINT('Ctrl Pts',(0.658775520175408,-3.00206879734919,
17.0758701769277));
#11175=CARTESIAN_POINT('Ctrl Pts',(0.752931411299467,-2.98140718019785,
17.0808690970542));
#11176=CARTESIAN_POINT('Ctrl Pts',(0.845998672439075,-2.95633714078435,
17.0858680171808));
#11177=CARTESIAN_POINT('Ctrl Pts',(0.937546108359654,-2.92701375888459,
17.0908669373073));
#11178=CARTESIAN_POINT('Ctrl Pts',(0.990692751657682,-2.90999046049892,
17.0937689937348));
#11179=CARTESIAN_POINT('Ctrl Pts',(1.04332753340845,-2.89153459877591,17.0966710501624));
#11180=CARTESIAN_POINT('Ctrl Pts',(1.09536956551501,-2.87168378568105,17.0995731065899));
#11181=CARTESIAN_POINT('Ctrl Pts',(1.18502573068125,-2.83748550968229,17.1045726663661));
#11182=CARTESIAN_POINT('Ctrl Pts',(1.27323626739536,-2.79902445047461,17.1095722261422));
#11183=CARTESIAN_POINT('Ctrl Pts',(1.35956732428756,-2.75644316842005,17.1145717859184));
#11184=CARTESIAN_POINT('Ctrl Pts',(1.44578128034576,-2.71391964430129,17.1195645642113));
#11185=CARTESIAN_POINT('Ctrl Pts',(1.53012043295859,-2.66728719709655,17.1245573425042));
#11186=CARTESIAN_POINT('Ctrl Pts',(1.61216903342187,-2.61673713958349,17.129550120797));
#11187=CARTESIAN_POINT('Ctrl Pts',(1.69413107963522,-2.5662404080539,17.1345376321362));
#11188=CARTESIAN_POINT('Ctrl Pts',(1.77380700550127,-2.5118345108883,17.1395251434754));
#11189=CARTESIAN_POINT('Ctrl Pts',(1.8508048220962,-2.45375707039337,17.1445126548146));
#11190=CARTESIAN_POINT('Ctrl Pts',(1.92774754795333,-2.39572118340201,17.1494965976671));
#11191=CARTESIAN_POINT('Ctrl Pts',(2.00201562431126,-2.33401923887228,17.1544805405196));
#11192=CARTESIAN_POINT('Ctrl Pts',(2.07324610249455,-2.26893209428823,17.1594644833722));
#11193=CARTESIAN_POINT('Ctrl Pts',(2.1444506416915,-2.20386865156042,17.1644466112934));
#11194=CARTESIAN_POINT('Ctrl Pts',(2.21261945681859,-2.13542275389542,17.1694287392146));
#11195=CARTESIAN_POINT('Ctrl Pts',(2.27742350786363,-2.06391482765887,17.1744108671358));
#11196=CARTESIAN_POINT('Ctrl Pts',(2.34222165054095,-1.99241342100119,17.1793925408224));
#11197=CARTESIAN_POINT('Ctrl Pts',(2.40365534443321,-1.91785086620241,17.184374214509));
#11198=CARTESIAN_POINT('Ctrl Pts',(2.46143392943952,-1.84058285904328,17.1893558881956));
#11199=CARTESIAN_POINT('Ctrl Pts',(2.51922301896186,-1.76330080406661,17.1943384675824));
#11200=CARTESIAN_POINT('Ctrl Pts',(2.57335541701767,-1.68331267143298,17.1993210469691));
#11201=CARTESIAN_POINT('Ctrl Pts',(2.62358275631767,-1.60100461297042,17.2043036263558));
#11202=CARTESIAN_POINT('Ctrl Pts',(2.6738642288716,-1.51860784578685,17.2092915757907));
#11203=CARTESIAN_POINT('Ctrl Pts',(2.72023201128706,-1.43388653640455,17.2142795252257));
#11204=CARTESIAN_POINT('Ctrl Pts',(2.76248296010173,-1.34725281411753,17.2192674746606));
#11205=CARTESIAN_POINT('Ctrl Pts',(2.80475886568258,-1.26056791907319,17.2242583703747));
#11206=CARTESIAN_POINT('Ctrl Pts',(2.84291292215504,-1.17196876482895,17.2292492660888));
#11207=CARTESIAN_POINT('Ctrl Pts',(2.87679038382587,-1.08188693379992,17.2342401618028));
#11208=CARTESIAN_POINT('Ctrl Pts',(2.91072258686855,-0.9916595427801,17.2392391221258));
#11209=CARTESIAN_POINT('Ctrl Pts',(2.94036426167294,-0.899945108481694,
17.2442380824487));
#11210=CARTESIAN_POINT('Ctrl Pts',(2.96561072154697,-0.807189753555912,
17.2492370427717));
#11211=CARTESIAN_POINT('Ctrl Pts',(2.98026508312541,-0.753349709597235,
17.2521386999725));
#11212=CARTESIAN_POINT('Ctrl Pts',(2.99343954445976,-0.699159152140327,
17.2550403571733));
#11213=CARTESIAN_POINT('Ctrl Pts',(3.00512161925494,-0.644706369975154,
17.2579420143741));
#11214=CARTESIAN_POINT('Ctrl Pts',(3.03303837637569,-0.514580076409504,
17.2648761301663));
#11215=CARTESIAN_POINT('Ctrl Pts',(3.05251132490793,-0.382583461353266,
17.2718102459585));
#11216=CARTESIAN_POINT('Ctrl Pts',(3.06334550588529,-0.249632853551782,
17.2787443617507));
#11217=CARTESIAN_POINT('Ctrl Pts',(3.07002870744382,-0.167620589669179,
17.2830217587747));
#11218=CARTESIAN_POINT('Ctrl Pts',(3.073425537775,-0.0852456668693086,17.2872991557986));
#11219=CARTESIAN_POINT('Ctrl Pts',(3.07349878900378,-0.0027283680658539,
17.2915765528226));
#11220=CARTESIAN_POINT('Ctrl Pts',(3.07349878900434,-0.00272836743798955,
17.2915765528551));
#11221=CARTESIAN_POINT('Ctrl Pts',(3.07358305061729,0.0921921193577995,
17.2964968860897));
#11222=CARTESIAN_POINT('Ctrl Pts',(3.06926587962942,0.187247177514582,17.3014172193243));
#11223=CARTESIAN_POINT('Ctrl Pts',(3.06053658859495,0.281989432198457,17.3063375525589));
#11224=CARTESIAN_POINT('Ctrl Pts',(3.05181483583495,0.376649871174996,17.311253636786));
#11225=CARTESIAN_POINT('Ctrl Pts',(3.03868857510245,0.470997594766093,17.3161697210132));
#11226=CARTESIAN_POINT('Ctrl Pts',(3.02119917645395,0.564586385058986,17.3210858052403));
#11227=CARTESIAN_POINT('Ctrl Pts',(3.00371759034355,0.658133369112316,17.325999693446));
#11228=CARTESIAN_POINT('Ctrl Pts',(2.9818768187115,0.7509216489512,17.3309135816516));
#11229=CARTESIAN_POINT('Ctrl Pts',(2.95576980972152,0.842512363077729,17.3358274698573));
#11230=CARTESIAN_POINT('Ctrl Pts',(2.92966686320602,0.934088824903684,17.3407405934198));
#11231=CARTESIAN_POINT('Ctrl Pts',(2.89929912243473,1.02446765630521,17.3456537169823));
#11232=CARTESIAN_POINT('Ctrl Pts',(2.8648098432871,1.11322361266969,17.3505668405448));
#11233=CARTESIAN_POINT('Ctrl Pts',(2.8303158911327,1.2019915947185,17.3554806297942));
#11234=CARTESIAN_POINT('Ctrl Pts',(2.79169945727649,1.28913584410698,17.3603944190435));
#11235=CARTESIAN_POINT('Ctrl Pts',(2.74915205689293,1.37425078427534,17.3653082082929));
#11236=CARTESIAN_POINT('Ctrl Pts',(2.70656102219928,1.45945301371776,17.3702270368584));
#11237=CARTESIAN_POINT('Ctrl Pts',(2.66003117857506,1.54262137562882,17.375145865424));
#11238=CARTESIAN_POINT('Ctrl Pts',(2.60979994620126,1.62337503085637,17.3800646939895));
#11239=CARTESIAN_POINT('Ctrl Pts',(2.55953947560667,1.70417569056875,17.3849863856701));
#11240=CARTESIAN_POINT('Ctrl Pts',(2.50557358689705,1.78255847568588,17.3899080773507));
#11241=CARTESIAN_POINT('Ctrl Pts',(2.44818165604469,1.85817351961713,17.3948297690312));
#11242=CARTESIAN_POINT('Ctrl Pts',(2.39070006538224,1.93390669218384,17.3997591495617));
#11243=CARTESIAN_POINT('Ctrl Pts',(2.32978204222512,2.00686314975054,17.4046885300922));
#11244=CARTESIAN_POINT('Ctrl Pts',(2.26574540435209,2.07672819903265,17.4096179106226));
#11245=CARTESIAN_POINT('Ctrl Pts',(2.23676286091777,2.10834864152643,17.4118489144678));
#11246=CARTESIAN_POINT('Ctrl Pts',(2.20714197249847,2.13933636676563,17.414079918313));
#11247=CARTESIAN_POINT('Ctrl Pts',(2.17691441210261,2.16966492629161,17.4163109221582));
#11248=CARTESIAN_POINT('Ctrl Pts',(2.10917509258733,2.2376305827079,17.421310554293));
#11249=CARTESIAN_POINT('Ctrl Pts',(2.03813081623026,2.30254021499092,17.4263101864277));
#11250=CARTESIAN_POINT('Ctrl Pts',(1.96408843828732,2.36405559507091,17.4313098185624));
#11251=CARTESIAN_POINT('Ctrl Pts',(1.89014650846582,2.42548752153231,17.4363026680455));
#11252=CARTESIAN_POINT('Ctrl Pts',(1.81321489532017,2.48353406932517,17.4412955175286));
#11253=CARTESIAN_POINT('Ctrl Pts',(1.73363761247245,2.53789339386445,17.4462883670117));
#11254=CARTESIAN_POINT('Ctrl Pts',(1.65414429548935,2.59219536123443,17.4512759482963));
#11255=CARTESIAN_POINT('Ctrl Pts',(1.57201121881274,2.6428175933025,17.4562635295809));
#11256=CARTESIAN_POINT('Ctrl Pts',(1.48761502005967,2.68949880128117,17.4612511108654));
#11257=CARTESIAN_POINT('Ctrl Pts',(1.40327924050138,2.73614659020735,17.4662351215432));
#11258=CARTESIAN_POINT('Ctrl Pts',(1.31668394268969,2.77885875197917,17.4712191322209));
#11259=CARTESIAN_POINT('Ctrl Pts',(1.22823343028284,2.81741812493915,17.4762031428986));
#11260=CARTESIAN_POINT('Ctrl Pts',(1.13981515084028,2.85596344616718,17.4811853373129));
#11261=CARTESIAN_POINT('Ctrl Pts',(1.049543402046,2.89035881022278,17.4861675317271));
#11262=CARTESIAN_POINT('Ctrl Pts',(0.957844823162484,2.920434136347,17.4911497261413));
#11263=CARTESIAN_POINT('Ctrl Pts',(0.866154630424322,2.95050671198086,17.496131464917));
#11264=CARTESIAN_POINT('Ctrl Pts',(0.773038284169241,2.9762598985608,17.5011132036927));
#11265=CARTESIAN_POINT('Ctrl Pts',(0.678939012032467,2.99757302962586,17.5060949424683));
#11266=CARTESIAN_POINT('Ctrl Pts',(0.584822660166249,3.01889002918538,17.5110775854673));
#11267=CARTESIAN_POINT('Ctrl Pts',(0.489723456199211,3.0357652757786,17.5160602284662));
#11268=CARTESIAN_POINT('Ctrl Pts',(0.394095226857328,3.04812913147857,17.5210428714652));
#11269=CARTESIAN_POINT('Ctrl Pts',(0.298363984376298,3.06050630583554,17.5260308818927));
#11270=CARTESIAN_POINT('Ctrl Pts',(0.202103014846611,3.06836233080819,17.5310188923203));
#11271=CARTESIAN_POINT('Ctrl Pts',(0.105771460058256,3.07167945076259,17.5360069027479));
#11272=CARTESIAN_POINT('Ctrl Pts',(0.0093830316901561,3.07499852912497,
17.5409978580673));
#11273=CARTESIAN_POINT('Ctrl Pts',(-0.0870756262138116,3.07377337222112,
17.5459888133867));
#11274=CARTESIAN_POINT('Ctrl Pts',(-0.183147307629121,3.06803834945201,
17.5509797687061));
#11275=CARTESIAN_POINT('Ctrl Pts',(-0.2793741728314,3.06229406294837,17.5559787858741));
#11276=CARTESIAN_POINT('Ctrl Pts',(-0.375212377248489,3.0520254112681,17.5609778030421));
#11277=CARTESIAN_POINT('Ctrl Pts',(-0.470211814422976,3.0373184060248,17.5659768202101));
#11278=CARTESIAN_POINT('Ctrl Pts',(-0.525341386131542,3.02878371440669,
17.5688778234542));
#11279=CARTESIAN_POINT('Ctrl Pts',(-0.580188698312286,3.01875529372928,
17.5717788266983));
#11280=CARTESIAN_POINT('Ctrl Pts',(-0.63466808551724,3.00725766625108,17.5746798299425));
#11281=CARTESIAN_POINT('Ctrl Pts',(-0.72856816399157,2.98744048074548,17.5796799675404));
#11282=CARTESIAN_POINT('Ctrl Pts',(-0.821703970702003,2.96318632888084,
17.5846801051384));
#11283=CARTESIAN_POINT('Ctrl Pts',(-0.91362461730408,2.93456850467935,17.5896802427364));
#11284=CARTESIAN_POINT('Ctrl Pts',(-1.00539778619647,2.90599659498482,17.5946723581014));
#11285=CARTESIAN_POINT('Ctrl Pts',(-1.09595925769914,2.87307506905623,17.5996644734665));
#11286=CARTESIAN_POINT('Ctrl Pts',(-1.18486876550315,2.8359281123708,17.6046565888315));
#11287=CARTESIAN_POINT('Ctrl Pts',(-1.27369537056722,2.79881579297632,17.6096440493508));
#11288=CARTESIAN_POINT('Ctrl Pts',(-1.36087266910783,2.75748603727323,17.6146315098701));
#11289=CARTESIAN_POINT('Ctrl Pts',(-1.44597648784965,2.71211250625522,17.6196189703894));
#11290=CARTESIAN_POINT('Ctrl Pts',(-1.53102237885595,2.66676985970214,17.6246030360869));
#11291=CARTESIAN_POINT('Ctrl Pts',(-1.61399720877885,2.61738911376037,17.6295871017845));
#11292=CARTESIAN_POINT('Ctrl Pts',(-1.6944987107767,2.56419117250959,17.6345711674821));
#11293=CARTESIAN_POINT('Ctrl Pts',(-1.75526492802091,2.52403493225613,17.6383333683283));
#11294=CARTESIAN_POINT('Ctrl Pts',(-1.81462225713076,2.48170468535302,17.6420955691745));
#11295=CARTESIAN_POINT('Ctrl Pts',(-1.87240768645122,2.4373123939533,17.6458577700207));
#11296=CARTESIAN_POINT('',(3.07052265917054,0.00228167610776854,17.2084234471775));
#11297=CARTESIAN_POINT('Ctrl Pts',(3.07052265917054,0.00228167610776854,
17.2084234471775));
#11298=CARTESIAN_POINT('Ctrl Pts',(3.07292892970749,0.349269622054914,17.2263526142767));
#11299=CARTESIAN_POINT('Ctrl Pts',(2.85875296905493,1.71502694578071,17.297071417304));
#11300=CARTESIAN_POINT('Ctrl Pts',(0.943423291082137,3.4474838904957,17.4151261119716));
#11301=CARTESIAN_POINT('Ctrl Pts',(-1.14804840810742,2.98986828496906,17.51525163954));
#11302=CARTESIAN_POINT('Ctrl Pts',(-1.8746299318936,2.44024828799233,17.5625875311804));
#11303=CARTESIAN_POINT('Ctrl Pts',(-1.869725885356,2.43378780274863,16.5626129315945));
#11304=CARTESIAN_POINT('Ctrl Pts',(-2.20951416667467,2.1750721455896,16.5846537268424));
#11305=CARTESIAN_POINT('Ctrl Pts',(-3.18623258927536,1.06968771491757,16.6594841580185));
#11306=CARTESIAN_POINT('Ctrl Pts',(-3.19506800687155,-1.72217162700502,
16.7871042251226));
#11307=CARTESIAN_POINT('Ctrl Pts',(-0.295015685898992,-3.61763670826351,
16.9454731329068));
#11308=CARTESIAN_POINT('Ctrl Pts',(2.51507553838982,-2.37564449952294,17.0859128735917));
#11309=CARTESIAN_POINT('Ctrl Pts',(3.06584404144206,-0.672382261526633,
17.1735629783486));
#11310=CARTESIAN_POINT('Ctrl Pts',(3.07052265917054,0.00228167610776854,
17.2084234471775));
#11311=CARTESIAN_POINT('Origin',(0.,0.,-2.20842344717744));
#11312=CARTESIAN_POINT('',(-1.87172893090613,2.4364505825814,15.5628209763329));
#11313=CARTESIAN_POINT('',(-1.87240768645122,2.43731239395331,15.6457416395408));
#11314=CARTESIAN_POINT('',(-1.87240768645123,2.4373123939533,-2.20842344717744));
#11315=CARTESIAN_POINT('',(3.07349950431729,0.00174555474377873,16.2915765527877));
#11316=CARTESIAN_POINT('Ctrl Pts',(-1.87240768645122,2.4373123939533,15.6457416395408));
#11317=CARTESIAN_POINT('Ctrl Pts',(-1.94889871322255,2.37854996906821,15.6507399535145));
#11318=CARTESIAN_POINT('Ctrl Pts',(-2.02253509863369,2.31624920628633,15.6557382674881));
#11319=CARTESIAN_POINT('Ctrl Pts',(-2.09298992423544,2.25073219798557,15.6607365814617));
#11320=CARTESIAN_POINT('Ctrl Pts',(-2.15649750194303,2.19167554061267,15.6652420331519));
#11321=CARTESIAN_POINT('Ctrl Pts',(-2.21742035531678,2.13000631152701,15.6697474848421));
#11322=CARTESIAN_POINT('Ctrl Pts',(-2.27554719717683,2.06598335022833,15.6742529365322));
#11323=CARTESIAN_POINT('Ctrl Pts',(-2.3400481018543,1.9949397705025,15.6792524462372));
#11324=CARTESIAN_POINT('Ctrl Pts',(-2.40133209132135,1.92074789302041,15.6842519559421));
#11325=CARTESIAN_POINT('Ctrl Pts',(-2.45907667225312,1.84373104599899,15.689251465647));
#11326=CARTESIAN_POINT('Ctrl Pts',(-2.51674292303881,1.76681867182645,15.6942441935498));
#11327=CARTESIAN_POINT('Ctrl Pts',(-2.57087904625347,1.68708929227079,15.6992369214525));
#11328=CARTESIAN_POINT('Ctrl Pts',(-2.62120073979498,1.60490153333414,15.7042296493553));
#11329=CARTESIAN_POINT('Ctrl Pts',(-2.67146934522459,1.52280048040112,15.7092171100566));
#11330=CARTESIAN_POINT('Ctrl Pts',(-2.71793129270596,1.43824657623757,15.7142045707578));
#11331=CARTESIAN_POINT('Ctrl Pts',(-2.7603444125331,1.35162900760427,15.7191920314591));
#11332=CARTESIAN_POINT('Ctrl Pts',(-2.8027271847805,1.26507341586823,15.7241759235156));
#11333=CARTESIAN_POINT('Ctrl Pts',(-2.84106669604593,1.17645748818041,15.729159815572));
#11334=CARTESIAN_POINT('Ctrl Pts',(-2.87516622868607,1.0861958421128,15.7341437076285));
#11335=CARTESIAN_POINT('Ctrl Pts',(-2.9092533431198,0.995967067104246,15.7391257846747));
#11336=CARTESIAN_POINT('Ctrl Pts',(-2.9391033919043,0.904094174735669,15.7441078617209));
#11337=CARTESIAN_POINT('Ctrl Pts',(-2.96456779391088,0.811011741780841,
15.7490899387671));
#11338=CARTESIAN_POINT('Ctrl Pts',(-2.99002987414817,0.717937795808494,
15.7540715615622));
#11339=CARTESIAN_POINT('Ctrl Pts',(-3.0111069869707,0.623654951964332,15.7590531843573));
#11340=CARTESIAN_POINT('Ctrl Pts',(-3.0277007316326,0.528611889453358,15.7640348071524));
#11341=CARTESIAN_POINT('Ctrl Pts',(-3.04429749332698,0.433551546454296,
15.7690173356935));
#11342=CARTESIAN_POINT('Ctrl Pts',(-3.05640919250096,0.337731142704052,
15.7739998642346));
#11343=CARTESIAN_POINT('Ctrl Pts',(-3.06398892224302,0.241607397179938,
15.7789823927757));
#11344=CARTESIAN_POINT('Ctrl Pts',(-3.07157682181259,0.145380044476267,
15.7839702917455));
#11345=CARTESIAN_POINT('Ctrl Pts',(-3.0746229653488,0.0488491355876539,
15.7889581907154));
#11346=CARTESIAN_POINT('Ctrl Pts',(-3.07313252882311,-0.0475258907255083,
15.7939460896852));
#11347=CARTESIAN_POINT('Ctrl Pts',(-3.07164121187647,-0.143957847066444,
15.7989369350743));
#11348=CARTESIAN_POINT('Ctrl Pts',(-3.0656080063516,-0.240233299583437,
15.8039277804633));
#11349=CARTESIAN_POINT('Ctrl Pts',(-3.05509005170745,-0.335897344374959,
15.8089186258524));
#11350=CARTESIAN_POINT('Ctrl Pts',(-3.04455509979157,-0.431715984600633,
15.8139175365696));
#11351=CARTESIAN_POINT('Ctrl Pts',(-3.02952099559556,-0.526920810886396,
15.8189164472867));
#11352=CARTESIAN_POINT('Ctrl Pts',(-3.01009610214631,-0.621066587286403,
15.8239153580039));
#11353=CARTESIAN_POINT('Ctrl Pts',(-2.99881880738429,-0.675723755617151,
15.8268175201081));
#11354=CARTESIAN_POINT('Ctrl Pts',(-2.98606254577936,-0.730024228112748,
15.8297196822123));
#11355=CARTESIAN_POINT('Ctrl Pts',(-2.9718561208065,-0.783883567390549,
15.8326218443165));
#11356=CARTESIAN_POINT('Ctrl Pts',(-2.94738293536546,-0.876666206259633,
15.8376213534465));
#11357=CARTESIAN_POINT('Ctrl Pts',(-2.91851752846084,-0.968464617543111,
15.8426208625764));
#11358=CARTESIAN_POINT('Ctrl Pts',(-2.88535552324197,-1.05883225984905,
15.8476203717064));
#11359=CARTESIAN_POINT('Ctrl Pts',(-2.85223850207296,-1.14907731902107,
15.8526130990339));
#11360=CARTESIAN_POINT('Ctrl Pts',(-2.81483661589741,-1.23789505791854,
15.8576058263614));
#11361=CARTESIAN_POINT('Ctrl Pts',(-2.77329588864699,-1.32485175171175,
15.862598553689));
#11362=CARTESIAN_POINT('Ctrl Pts',(-2.73179898581234,-1.41171670839406,
15.8675860138155));
#11363=CARTESIAN_POINT('Ctrl Pts',(-2.68617211019909,-1.49672412902359,
15.8725734739421));
#11364=CARTESIAN_POINT('Ctrl Pts',(-2.63660985891815,-1.57945899024179,
15.8775609340687));
#11365=CARTESIAN_POINT('Ctrl Pts',(-2.58708307056109,-1.66213465277532,
15.8825448255535));
#11366=CARTESIAN_POINT('Ctrl Pts',(-2.53362672924973,-1.74254061295899,
15.8875287170383));
#11367=CARTESIAN_POINT('Ctrl Pts',(-2.47648150971177,-1.82028612642511,
15.8925126085232));
#11368=CARTESIAN_POINT('Ctrl Pts',(-2.41935710102748,-1.89800332692791,
15.8974946849999));
#11369=CARTESIAN_POINT('Ctrl Pts',(-2.35854674301075,-1.97306165241466,
15.9024767614766));
#11370=CARTESIAN_POINT('Ctrl Pts',(-2.29433406001567,-2.04509986823431,
15.9074588379533));
#11371=CARTESIAN_POINT('Ctrl Pts',(-2.2301272317088,-2.117131515861,15.9124404601817));
#11372=CARTESIAN_POINT('Ctrl Pts',(-2.16251898740404,-2.18614327373474,
15.9174220824101));
#11373=CARTESIAN_POINT('Ctrl Pts',(-2.09183210125438,-2.25180832003119,
15.9224037046385));
#11374=CARTESIAN_POINT('Ctrl Pts',(-2.02113236294399,-2.31748530542661,
15.9273862326164));
#11375=CARTESIAN_POINT('Ctrl Pts',(-1.94735319274614,-2.37981407204683,
15.9323687605942));
#11376=CARTESIAN_POINT('Ctrl Pts',(-1.87085214441084,-2.43850661343236,
15.9373512885721));
#11377=CARTESIAN_POINT('Ctrl Pts',(-1.79426863911818,-2.49726241680564,
15.9423391869874));
#11378=CARTESIAN_POINT('Ctrl Pts',(-1.71495774750215,-2.5523739027431,15.9473270854027));
#11379=CARTESIAN_POINT('Ctrl Pts',(-1.63330766125205,-2.60359527071612,
15.9523149838181));
#11380=CARTESIAN_POINT('Ctrl Pts',(-1.55160934312264,-2.65484689588729,
15.9573058286567));
#11381=CARTESIAN_POINT('Ctrl Pts',(-1.46756946122401,-2.70220361210594,
15.9622966734953));
#11382=CARTESIAN_POINT('Ctrl Pts',(-1.38160069503937,-2.74546567442879,
15.9672875183339));
#11383=CARTESIAN_POINT('Ctrl Pts',(-1.29549300100815,-2.78879764941206,
15.9722864285125));
#11384=CARTESIAN_POINT('Ctrl Pts',(-1.20745059917281,-2.82802157915426,
15.9772853386911));
#11385=CARTESIAN_POINT('Ctrl Pts',(-1.11790594835827,-2.86298594838068,
15.9822842488697));
#11386=CARTESIAN_POINT('Ctrl Pts',(-1.06591989781353,-2.88328486572901,
15.9851864166133));
#11387=CARTESIAN_POINT('Ctrl Pts',(-1.0134278131718,-2.90214902794488,15.988088584357));
#11388=CARTESIAN_POINT('Ctrl Pts',(-0.960516202473417,-2.91955662297994,
15.9909907521007));
#11389=CARTESIAN_POINT('Ctrl Pts',(-0.869366371595686,-2.94954435766598,
15.9959902615755));
#11390=CARTESIAN_POINT('Ctrl Pts',(-0.776650751275227,-2.97531206614178,
16.0009897710503));
#11391=CARTESIAN_POINT('Ctrl Pts',(-0.68279595920373,-2.99669683620066,
16.0059892805251));
#11392=CARTESIAN_POINT('Ctrl Pts',(-0.589068480626812,-3.01805259793991,
16.0109820081936));
#11393=CARTESIAN_POINT('Ctrl Pts',(-0.494205325772783,-3.03503714072928,
16.0159747358621));
#11394=CARTESIAN_POINT('Ctrl Pts',(-0.398649802683796,-3.04753680614692,
16.0209674635306));
#11395=CARTESIAN_POINT('Ctrl Pts',(-0.303195088327821,-3.06002328472414,
16.0259549239939));
#11396=CARTESIAN_POINT('Ctrl Pts',(-0.207049890730401,-3.06803423510474,
16.0309423844572));
#11397=CARTESIAN_POINT('Ctrl Pts',(-0.110668277027359,-3.07150692371998,
16.0359298449204));
#11398=CARTESIAN_POINT('Ctrl Pts',(-0.0143556267159142,-3.07497712754196,
16.0409137367343));
#11399=CARTESIAN_POINT('Ctrl Pts',(0.0821926659962651,-3.07391550919141,
16.0458976285481));
#11400=CARTESIAN_POINT('Ctrl Pts',(0.17851781197312,-3.06831120338344,16.050881520362));
#11401=CARTESIAN_POINT('Ctrl Pts',(0.274807878659714,-3.06270893852821,
16.0558635971629));
#11402=CARTESIAN_POINT('Ctrl Pts',(0.370874522301607,-3.05256729867365,
16.0608456739638));
#11403=CARTESIAN_POINT('Ctrl Pts',(0.466260322292488,-3.03792751096133,
16.0658277507647));
#11404=CARTESIAN_POINT('Ctrl Pts',(0.561637425239996,-3.02328905806896,
16.0708093733121));
#11405=CARTESIAN_POINT('Ctrl Pts',(0.656333374104444,-3.00415333950665,
16.0757909958594));
#11406=CARTESIAN_POINT('Ctrl Pts',(0.749898298321378,-2.98061315708273,
16.0807726184068));
#11407=CARTESIAN_POINT('Ctrl Pts',(0.843480234236463,-2.95706869465238,
16.0857551466981));
#11408=CARTESIAN_POINT('Ctrl Pts',(0.935930311420518,-2.9291182850923,16.0907376749893));
#11409=CARTESIAN_POINT('Ctrl Pts',(1.02681228152849,-2.89690503615535,16.0957202032806));
#11410=CARTESIAN_POINT('Ctrl Pts',(1.11779220893244,-2.86465706610974,16.100708101999));
#11411=CARTESIAN_POINT('Ctrl Pts',(1.20720024053117,-2.82813723066903,16.1056960007174));
#11412=CARTESIAN_POINT('Ctrl Pts',(1.29461884911216,-2.7875373155392,16.1106838994358));
#11413=CARTESIAN_POINT('Ctrl Pts',(1.38208909702406,-2.74691341750132,16.115674744572));
#11414=CARTESIAN_POINT('Ctrl Pts',(1.46756719315786,-2.70220484410954,16.1206655897083));
#11415=CARTESIAN_POINT('Ctrl Pts',(1.55066090894839,-2.65364899628028,16.1256564348446));
#11416=CARTESIAN_POINT('Ctrl Pts',(1.63388890622909,-2.60501468100567,16.1306553453095));
#11417=CARTESIAN_POINT('Ctrl Pts',(1.71472446124332,-2.55252091564937,16.1356542557744));
#11418=CARTESIAN_POINT('Ctrl Pts',(1.79280503120254,-2.49644795060799,16.1406531662393));
#11419=CARTESIAN_POINT('Ctrl Pts',(1.8381354414299,-2.46389426267619,16.1435553307878));
#11420=CARTESIAN_POINT('Ctrl Pts',(1.88253790320472,-2.43013496521521,16.1464574953363));
#11421=CARTESIAN_POINT('Ctrl Pts',(1.925947021523,-2.39523074468551,16.1493596598848));
#11422=CARTESIAN_POINT('Ctrl Pts',(1.99978833044786,-2.33585673685569,16.1542964021472));
#11423=CARTESIAN_POINT('Ctrl Pts',(2.07102705737978,-2.27294757807149,16.1592331444097));
#11424=CARTESIAN_POINT('Ctrl Pts',(2.13929911914238,-2.20676268067879,16.1641698866721));
#11425=CARTESIAN_POINT('Ctrl Pts',(2.20747815032313,-2.1406679698039,16.1690999019075));
#11426=CARTESIAN_POINT('Ctrl Pts',(2.27269822491405,-2.07130669737316,16.1740299171429));
#11427=CARTESIAN_POINT('Ctrl Pts',(2.3346270297246,-1.99897946014443,16.1789599323783));
#11428=CARTESIAN_POINT('Ctrl Pts',(2.39648619491134,-1.9267335556914,16.1838844037573));
#11429=CARTESIAN_POINT('Ctrl Pts',(2.45506115559679,-1.85152865704026,16.1888088751362));
#11430=CARTESIAN_POINT('Ctrl Pts',(2.51005623275266,-1.77370233083783,16.1937333465151));
#11431=CARTESIAN_POINT('Ctrl Pts',(2.56501765545072,-1.69592363076753,16.198654804344));
#11432=CARTESIAN_POINT('Ctrl Pts',(2.61640328445328,-1.61552705540436,16.203576262173));
#11433=CARTESIAN_POINT('Ctrl Pts',(2.66395815262426,-1.53288264751961,16.2084977200019));
#11434=CARTESIAN_POINT('Ctrl Pts',(2.71149769214496,-1.4502648789102,16.2134175914673));
#11435=CARTESIAN_POINT('Ctrl Pts',(2.75520869880651,-1.36540110770887,16.2183374629328));
#11436=CARTESIAN_POINT('Ctrl Pts',(2.79488060015965,-1.27868865673049,16.2232573343982));
#11437=CARTESIAN_POINT('Ctrl Pts',(2.83455120284155,-1.19197904430946,16.2281770448103));
#11438=CARTESIAN_POINT('Ctrl Pts',(2.87018277699916,-1.10342128335657,16.2330967552223));
#11439=CARTESIAN_POINT('Ctrl Pts',(2.90161214691215,-1.01343435845241,16.2380164656343));
#11440=CARTESIAN_POINT('Ctrl Pts',(2.93306700840162,-0.923374447402365,
16.2429401663005));
#11441=CARTESIAN_POINT('Ctrl Pts',(2.96031271082498,-0.831883484354772,
16.2478638669667));
#11442=CARTESIAN_POINT('Ctrl Pts',(2.98323557337827,-0.739396891885824,
16.2527875676329));
#11443=CARTESIAN_POINT('Ctrl Pts',(3.00616837220371,-0.646870209661507,
16.2577134025539));
#11444=CARTESIAN_POINT('Ctrl Pts',(3.02477451242689,-0.553347481295938,
16.2626392374749));
#11445=CARTESIAN_POINT('Ctrl Pts',(3.03899162259589,-0.459273521762331,
16.2675650723959));
#11446=CARTESIAN_POINT('Ctrl Pts',(3.05322927646138,-0.365063625540591,
16.2724980251388));
#11447=CARTESIAN_POINT('Ctrl Pts',(3.06306519115917,-0.270301356403268,
16.2774309778817));
#11448=CARTESIAN_POINT('Ctrl Pts',(3.06848897953641,-0.175435550740501,
16.2823639306246));
#11449=CARTESIAN_POINT('Ctrl Pts',(3.07186540981505,-0.116379452609501,
16.2854348046789));
#11450=CARTESIAN_POINT('Ctrl Pts',(3.07353302896985,-0.0572832459287992,
16.2885056787333));
#11451=CARTESIAN_POINT('Ctrl Pts',(3.07349950431729,0.00174555474379678,
16.2915765527877));
#11452=CARTESIAN_POINT('Ctrl Pts',(3.07349950431691,0.00174555541427581,
16.2915765528226));
#11453=CARTESIAN_POINT('Ctrl Pts',(3.07344072725167,0.105237704331132,16.2969605577714));
#11454=CARTESIAN_POINT('Ctrl Pts',(3.06815507646861,0.208578371493949,16.3023445627202));
#11455=CARTESIAN_POINT('Ctrl Pts',(3.05768593610749,0.311382347172158,16.3077285676691));
#11456=CARTESIAN_POINT('Ctrl Pts',(3.04796444844869,0.406844586320621,16.3127280743964));
#11457=CARTESIAN_POINT('Ctrl Pts',(3.03375104390199,0.502018799209545,16.3177275811238));
#11458=CARTESIAN_POINT('Ctrl Pts',(3.01507061941287,0.596449000295305,16.3227270878511));
#11459=CARTESIAN_POINT('Ctrl Pts',(2.99641553481127,0.690751107360806,16.3277198127766));
#11460=CARTESIAN_POINT('Ctrl Pts',(2.97330555755281,0.784310781501738,16.3327125377021));
#11461=CARTESIAN_POINT('Ctrl Pts',(2.94581736658922,0.876676846221759,16.3377052626275));
#11462=CARTESIAN_POINT('Ctrl Pts',(2.91835817496481,0.968945467103353,16.3426927203558));
#11463=CARTESIAN_POINT('Ctrl Pts',(2.88653007627914,1.06002256334226,16.347680178084));
#11464=CARTESIAN_POINT('Ctrl Pts',(2.85046064290332,1.14946786525731,16.3526676358122));
#11465=CARTESIAN_POINT('Ctrl Pts',(2.8144170179336,1.23884916725721,16.357651524914));
#11466=CARTESIAN_POINT('Ctrl Pts',(2.77413825493212,1.32660059008976,16.3626354140157));
#11467=CARTESIAN_POINT('Ctrl Pts',(2.72980122341365,1.41229866906733,16.3676193031175));
#11468=CARTESIAN_POINT('Ctrl Pts',(2.68548033824461,1.49796553911905,16.3726013772215));
#11469=CARTESIAN_POINT('Ctrl Pts',(2.63710432250965,1.58158016158151,16.3775834513254));
#11470=CARTESIAN_POINT('Ctrl Pts',(2.58489706785975,1.6627415308971,16.3825655254294));
#11471=CARTESIAN_POINT('Ctrl Pts',(2.53269457314998,1.74389550041242,16.3875471452981));
#11472=CARTESIAN_POINT('Ctrl Pts',(2.47666177164626,1.82259629240314,16.3925287651669));
#11473=CARTESIAN_POINT('Ctrl Pts',(2.41706658745815,1.89847079561246,16.3975103850356));
#11474=CARTESIAN_POINT('Ctrl Pts',(2.35746056758654,1.97435909443486,16.4024929106697));
#11475=CARTESIAN_POINT('Ctrl Pts',(2.2942911498305,2.04741973872511,16.4074754363039));
#11476=CARTESIAN_POINT('Ctrl Pts',(2.22786665969213,2.11731254108416,16.412457961938));
#11477=CARTESIAN_POINT('Ctrl Pts',(2.1613705731089,2.18728067825058,16.417445858048));
#11478=CARTESIAN_POINT('Ctrl Pts',(2.09161271260839,2.25407383804249,16.422433754158));
#11479=CARTESIAN_POINT('Ctrl Pts',(2.01893824213935,2.31738875125156,16.4274216502681));
#11480=CARTESIAN_POINT('Ctrl Pts',(1.94622084153036,2.38074106573879,16.4324124928196));
#11481=CARTESIAN_POINT('Ctrl Pts',(1.87058374441533,2.44061077016044,16.4374033353712));
#11482=CARTESIAN_POINT('Ctrl Pts',(1.79240347777767,2.49673627418887,16.4423941779227));
#11483=CARTESIAN_POINT('Ctrl Pts',(1.71409686885811,2.5529524791647,16.4473930858655));
#11484=CARTESIAN_POINT('Ctrl Pts',(1.63323925193748,2.60541216294122,16.4523919938082));
#11485=CARTESIAN_POINT('Ctrl Pts',(1.55023420471965,2.65389829505903,16.457390901751));
#11486=CARTESIAN_POINT('Ctrl Pts',(1.5020443754255,2.68204764872133,16.4602930929851));
#11487=CARTESIAN_POINT('Ctrl Pts',(1.45313118248957,2.70885856575204,16.4631952842192));
#11488=CARTESIAN_POINT('Ctrl Pts',(1.40357668229841,2.73429602400841,16.4660974754532));
#11489=CARTESIAN_POINT('Ctrl Pts',(1.31821075943991,2.77811630452486,16.4710969857309));
#11490=CARTESIAN_POINT('Ctrl Pts',(1.23064079775987,2.81801197819068,16.4760964960085));
#11491=CARTESIAN_POINT('Ctrl Pts',(1.14126283010773,2.85375566624308,16.4810960062861));
#11492=CARTESIAN_POINT('Ctrl Pts',(1.05200610348146,2.88945086805752,16.4860887347386));
#11493=CARTESIAN_POINT('Ctrl Pts',(0.960946649267999,2.92100511620065,16.491081463191));
#11494=CARTESIAN_POINT('Ctrl Pts',(0.868504659300871,2.94823708455963,16.4960741916434));
#11495=CARTESIAN_POINT('Ctrl Pts',(0.776160193714096,2.97544032375732,16.5010616528709));
#11496=CARTESIAN_POINT('Ctrl Pts',(0.682436510708975,2.99833022462567,16.5060491140985));
#11497=CARTESIAN_POINT('Ctrl Pts',(0.587772362556805,3.01677408829604,16.511036575326));
#11498=CARTESIAN_POINT('Ctrl Pts',(0.493175949506328,3.03520475481621,16.5160204678721));
#11499=CARTESIAN_POINT('Ctrl Pts',(0.397640838690288,3.04919562465904,16.5210043604181));
#11500=CARTESIAN_POINT('Ctrl Pts',(0.301618526377949,3.05866449852637,16.5259882529642));
#11501=CARTESIAN_POINT('Ctrl Pts',(0.205631183452242,3.06812992402111,16.5309703304772));
#11502=CARTESIAN_POINT('Ctrl Pts',(0.109157427959209,3.07307658255847,16.5359524079903));
#11503=CARTESIAN_POINT('Ctrl Pts',(0.0126555189035832,3.0734739445522,16.5409344855033));
#11504=CARTESIAN_POINT('Ctrl Pts',(-0.0838375909435241,3.07387127031379,
16.545916108742));
#11505=CARTESIAN_POINT('Ctrl Pts',(-0.180358410290221,3.06972012263184,
16.5508977319808));
#11506=CARTESIAN_POINT('Ctrl Pts',(-0.276448104101494,3.06104209310141,
16.5558793552195));
#11507=CARTESIAN_POINT('Ctrl Pts',(-0.372555268239498,3.052362485795,16.5608618841806));
#11508=CARTESIAN_POINT('Ctrl Pts',(-0.468230713995893,3.03915440158997,
16.5658444131417));
#11509=CARTESIAN_POINT('Ctrl Pts',(-0.563021225989915,3.02149124590571,
16.5708269421029));
#11510=CARTESIAN_POINT('Ctrl Pts',(-0.65791390739893,3.0038090520894,16.5758148414545));
#11511=CARTESIAN_POINT('Ctrl Pts',(-0.751919318580594,2.98166228084182,
16.5808027408062));
#11512=CARTESIAN_POINT('Ctrl Pts',(-0.844595154077178,2.95517533755771,
16.5857906401578));
#11513=CARTESIAN_POINT('Ctrl Pts',(-0.937325734045256,2.92867274819172,
16.5907814859077));
#11514=CARTESIAN_POINT('Ctrl Pts',(-1.0287247587648,2.89782502219214,16.5957723316575));
#11515=CARTESIAN_POINT('Ctrl Pts',(-1.11836780700864,2.86280556417069,16.6007631774073));
#11516=CARTESIAN_POINT('Ctrl Pts',(-1.20815571994477,2.82772951410882,16.6057620884489));
#11517=CARTESIAN_POINT('Ctrl Pts',(-1.29618158954533,2.78846844924509,16.6107609994904));
#11518=CARTESIAN_POINT('Ctrl Pts',(-1.38204364321624,2.74524272483247,16.615759910532));
#11519=CARTESIAN_POINT('Ctrl Pts',(-1.43189154145502,2.72014768669051,16.6186620681004));
#11520=CARTESIAN_POINT('Ctrl Pts',(-1.48101062256676,2.69371721369591,16.6215642256689));
#11521=CARTESIAN_POINT('Ctrl Pts',(-1.52932683708478,2.66600106439819,16.6244663832373));
#11522=CARTESIAN_POINT('Ctrl Pts',(-1.61255627029755,2.6182572703137,16.6294656351847));
#11523=CARTESIAN_POINT('Ctrl Pts',(-1.69369397800676,2.5665284006922,16.634464887132));
#11524=CARTESIAN_POINT('Ctrl Pts',(-1.77233367960811,2.51102281513466,16.6394641390793));
#11525=CARTESIAN_POINT('Ctrl Pts',(-1.80616406839357,2.4871446022099,16.6416147911491));
#11526=CARTESIAN_POINT('Ctrl Pts',(-1.83953241787483,2.46256804264623,16.6437654432188));
#11527=CARTESIAN_POINT('Ctrl Pts',(-1.87240768645125,2.43731239395329,16.6459160952886));
#11528=CARTESIAN_POINT('',(3.07037524043715,-0.00221840733777449,16.2084234471775));
#11529=CARTESIAN_POINT('Ctrl Pts',(3.07037524043715,-0.00221840733777449,
16.2084234471775));
#11530=CARTESIAN_POINT('Ctrl Pts',(3.06588334332531,0.666027613145282,16.2429481320417));
#11531=CARTESIAN_POINT('Ctrl Pts',(2.52336161388572,2.36268932502765,16.3302624528339));
#11532=CARTESIAN_POINT('Ctrl Pts',(0.167664259077209,3.42172443700271,16.4483256143063));
#11533=CARTESIAN_POINT('Ctrl Pts',(-1.39569145920811,2.79471881426235,16.5318640909144));
#11534=CARTESIAN_POINT('Ctrl Pts',(-1.869725885356,2.43378780274863,16.5626129315945));
#11535=CARTESIAN_POINT('Ctrl Pts',(-1.87172893090644,2.43645058258115,15.5628209763329));
#11536=CARTESIAN_POINT('Ctrl Pts',(-2.45835653554609,1.9767821845083,15.6013879410997));
#11537=CARTESIAN_POINT('Ctrl Pts',(-3.47096169057706,0.381579628323511,
15.6927445417946));
#11538=CARTESIAN_POINT('Ctrl Pts',(-2.51002850343834,-2.62184868499999,
15.8368907784176));
#11539=CARTESIAN_POINT('Ctrl Pts',(0.832597508902196,-3.53286213886185,
15.9952596862017));
#11540=CARTESIAN_POINT('Ctrl Pts',(2.85331955098111,-1.72819282485178,16.1191039091217));
#11541=CARTESIAN_POINT('Ctrl Pts',(3.07275163521828,-0.355747510086772,
16.1901584961136));
#11542=CARTESIAN_POINT('Ctrl Pts',(3.07037524043715,-0.00221840733777449,
16.2084234471775));
#11543=CARTESIAN_POINT('Origin',(0.,0.,-2.20842344717744));
#11544=CARTESIAN_POINT('',(-1.87525415797411,2.44104769786763,14.562635342152));
#11545=CARTESIAN_POINT('',(-1.87240768645123,2.43731239395329,14.6458302897736));
#11546=CARTESIAN_POINT('',(-1.87240768645123,2.4373123939533,-2.20842344717744));
#11547=CARTESIAN_POINT('',(3.07349970959544,0.00133608261959707,15.2915765528521));
#11548=CARTESIAN_POINT('Ctrl Pts',(-1.87240768645123,2.43731239395329,14.6458302897736));
#11549=CARTESIAN_POINT('Ctrl Pts',(-1.94893277448196,2.37852380231007,14.6508120790211));
#11550=CARTESIAN_POINT('Ctrl Pts',(-2.02268470075316,2.31612913500427,14.6557938682687));
#11551=CARTESIAN_POINT('Ctrl Pts',(-2.09331608143157,2.25042885540067,14.6607756575162));
#11552=CARTESIAN_POINT('Ctrl Pts',(-2.16396717155315,2.18471024236065,14.6657588369149));
#11553=CARTESIAN_POINT('Ctrl Pts',(-2.23149566505041,2.11568448362781,14.6707420163135));
#11554=CARTESIAN_POINT('Ctrl Pts',(-2.29559068105625,2.04368923152413,14.6757251957122));
#11555=CARTESIAN_POINT('Ctrl Pts',(-2.35975808405306,1.97161267013951,14.6807140029644));
#11556=CARTESIAN_POINT('Ctrl Pts',(-2.42048397971851,1.89656025150382,14.6857028102166));
#11557=CARTESIAN_POINT('Ctrl Pts',(-2.47749766809196,1.81890284363924,14.6906916174688));
#11558=CARTESIAN_POINT('Ctrl Pts',(-2.53455000648345,1.74119279122033,14.6956838066718));
#11559=CARTESIAN_POINT('Ctrl Pts',(-2.5878848860152,1.66087459943201,14.7006759958748));
#11560=CARTESIAN_POINT('Ctrl Pts',(-2.63727597990184,1.57834649422514,14.7056681850778));
#11561=CARTESIAN_POINT('Ctrl Pts',(-2.68674191146347,1.49569334194947,14.7106679384751));
#11562=CARTESIAN_POINT('Ctrl Pts',(-2.7322519277768,1.41082398076427,14.7156676918725));
#11563=CARTESIAN_POINT('Ctrl Pts',(-2.77362663010867,1.32415919237531,14.7206674452698));
#11564=CARTESIAN_POINT('Ctrl Pts',(-2.78292824485698,1.30467572957304,14.7217914601223));
#11565=CARTESIAN_POINT('Ctrl Pts',(-2.79202105216519,1.2851015921285,14.7229154749748));
#11566=CARTESIAN_POINT('Ctrl Pts',(-2.8009033586599,1.26544167208436,14.7240394898273));
#11567=CARTESIAN_POINT('Ctrl Pts',(-2.84041100002516,1.17799624663823,14.729038999325));
#11568=CARTESIAN_POINT('Ctrl Pts',(-2.87588898212958,1.08854528756348,14.7340385088227));
#11569=CARTESIAN_POINT('Ctrl Pts',(-2.90712996363765,0.997495676441848,
14.7390380183204));
#11570=CARTESIAN_POINT('Ctrl Pts',(-2.9383285669528,0.906569573539159,14.7440307460152));
#11571=CARTESIAN_POINT('Ctrl Pts',(-2.96530145113131,0.814049540111176,
14.7490234737101));
#11572=CARTESIAN_POINT('Ctrl Pts',(-2.98788847522648,0.720364289515247,
14.7540162014049));
#11573=CARTESIAN_POINT('Ctrl Pts',(-3.01045167058067,0.626777874496728,
14.7590036618979));
#11574=CARTESIAN_POINT('Ctrl Pts',(-3.02863810165544,0.532029110500205,
14.7639911223909));
#11575=CARTESIAN_POINT('Ctrl Pts',(-3.04233712002355,0.436562822657639,
14.7689785828838));
#11576=CARTESIAN_POINT('Ctrl Pts',(-3.05602633642372,0.341164843176166,
14.7739624747322));
#11577=CARTESIAN_POINT('Ctrl Pts',(-3.06523446096093,0.245050793739427,
14.7789463665806));
#11578=CARTESIAN_POINT('Ctrl Pts',(-3.06990191759497,0.148675708663856,
14.783930258429));
#11579=CARTESIAN_POINT('Ctrl Pts',(-3.0745676744569,0.0523357210075346,
14.7889123352674));
#11580=CARTESIAN_POINT('Ctrl Pts',(-3.07469602772451,-0.044264675407972,
14.7938944121058));
#11581=CARTESIAN_POINT('Ctrl Pts',(-3.0702793440808,-0.140666269271646,
14.7988764889442));
#11582=CARTESIAN_POINT('Ctrl Pts',(-3.06586306313689,-0.237059073530537,
14.8038581115319));
#11583=CARTESIAN_POINT('Ctrl Pts',(-3.0569025894642,-0.333252672781994,
14.8088397341197));
#11584=CARTESIAN_POINT('Ctrl Pts',(-3.04344237477877,-0.4287898802455,14.8138213567075));
#11585=CARTESIAN_POINT('Ctrl Pts',(-3.02997971278918,-0.524344458056383,
14.818803885042));
#11586=CARTESIAN_POINT('Ctrl Pts',(-3.01201574625005,-0.619241972402748,
14.8237864133764));
#11587=CARTESIAN_POINT('Ctrl Pts',(-2.98964639589013,-0.713033433676944,
14.8287689417109));
#11588=CARTESIAN_POINT('Ctrl Pts',(-2.96725293466763,-0.806925988322121,
14.8337568404766));
#11589=CARTESIAN_POINT('Ctrl Pts',(-2.94044471197877,-0.899709682159225,
14.8387447392422));
#11590=CARTESIAN_POINT('Ctrl Pts',(-2.90936804084717,-0.990948965838843,
14.8437326380079));
#11591=CARTESIAN_POINT('Ctrl Pts',(-2.8782730122995,-1.08224214581533,14.8487234831938));
#11592=CARTESIAN_POINT('Ctrl Pts',(-2.84290467559671,-1.17198869088507,
14.8537143283797));
#11593=CARTESIAN_POINT('Ctrl Pts',(-2.80345738990325,-1.25977335778975,
14.8587051735656));
#11594=CARTESIAN_POINT('Ctrl Pts',(-2.76394635640081,-1.34769988693106,
14.8637040840832));
#11595=CARTESIAN_POINT('Ctrl Pts',(-2.7203434102168,-1.43365781601732,14.8687029946009));
#11596=CARTESIAN_POINT('Ctrl Pts',(-2.67288867297959,-1.51725686416552,
14.8737019051185));
#11597=CARTESIAN_POINT('Ctrl Pts',(-2.64533838230143,-1.56579107193887,
14.8766040692828));
#11598=CARTESIAN_POINT('Ctrl Pts',(-2.61649066707091,-1.61353075410667,
14.8795062334471));
#11599=CARTESIAN_POINT('Ctrl Pts',(-2.58639891791687,-1.66040443488881,
14.8824083976114));
#11600=CARTESIAN_POINT('Ctrl Pts',(-2.53456036679689,-1.74115293790765,
14.8874079070988));
#11601=CARTESIAN_POINT('Ctrl Pts',(-2.47884563527945,-1.81961330975353,
14.8924074165862));
#11602=CARTESIAN_POINT('Ctrl Pts',(-2.41948312518099,-1.8953901068024,14.8974069260736));
#11603=CARTESIAN_POINT('Ctrl Pts',(-2.36020113995041,-1.97106411310741,
14.9023996537582));
#11604=CARTESIAN_POINT('Ctrl Pts',(-2.29728147872303,-2.04406143677695,
14.9073923814427));
#11605=CARTESIAN_POINT('Ctrl Pts',(-2.23099655396568,-2.11401433916453,
14.9123851091273));
#11606=CARTESIAN_POINT('Ctrl Pts',(-2.16478155813299,-2.18389344300352,
14.91737256961));
#11607=CARTESIAN_POINT('Ctrl Pts',(-2.09520865681056,-2.2507341934602,14.9223600300927));
#11608=CARTESIAN_POINT('Ctrl Pts',(-2.02259072317702,-2.3142015937507,14.9273474905754));
#11609=CARTESIAN_POINT('Ctrl Pts',(-1.95002474937136,-2.37762358163368,
14.9323313824136));
#11610=CARTESIAN_POINT('Ctrl Pts',(-1.87441840416002,-2.43767672965214,
14.9373152742519));
#11611=CARTESIAN_POINT('Ctrl Pts',(-1.79612093054769,-2.49406332173995,
14.9422991660901));
#11612=CARTESIAN_POINT('Ctrl Pts',(-1.71785197093536,-2.55042937922794,
14.9472812429184));
#11613=CARTESIAN_POINT('Ctrl Pts',(-1.63689418600184,-2.60313127755666,
14.9522633197467));
#11614=CARTESIAN_POINT('Ctrl Pts',(-1.55362860267938,-2.65191259564423,
14.957245396575));
#11615=CARTESIAN_POINT('Ctrl Pts',(-1.4703706112591,-2.70068946599985,14.9622270191527));
#11616=CARTESIAN_POINT('Ctrl Pts',(-1.38480561864298,-2.74554624509045,
14.9672086417304));
#11617=CARTESIAN_POINT('Ctrl Pts',(-1.29734131138029,-2.78627130261683,
14.9721902643081));
#11618=CARTESIAN_POINT('Ctrl Pts',(-1.20986110156398,-2.8270037646769,14.9771727926327));
#11619=CARTESIAN_POINT('Ctrl Pts',(-1.12048128922809,-2.86360282799463,
14.9821553209572));
#11620=CARTESIAN_POINT('Ctrl Pts',(-1.02963070758082,-2.8959044970452,14.9871378492818));
#11621=CARTESIAN_POINT('Ctrl Pts',(-0.938682202394371,-2.928240982535,14.9921257480376));
#11622=CARTESIAN_POINT('Ctrl Pts',(-0.846260177329899,-2.95627067918442,
14.9971136467935));
#11623=CARTESIAN_POINT('Ctrl Pts',(-0.752809628174246,-2.9798791777064,
15.0021015455494));
#11624=CARTESIAN_POINT('Ctrl Pts',(-0.659303876495205,-3.00350162209283,
15.0070923907256));
#11625=CARTESIAN_POINT('Ctrl Pts',(-0.564768820949472,-3.02269758079422,
15.0120832359017));
#11626=CARTESIAN_POINT('Ctrl Pts',(-0.469658583527638,-3.03740400093876,
15.0170740810779));
#11627=CARTESIAN_POINT('Ctrl Pts',(-0.374394645557665,-3.05213418703005,
15.0220729915861));
#11628=CARTESIAN_POINT('Ctrl Pts',(-0.278554105879261,-3.0623603009767,
15.0270719020943));
#11629=CARTESIAN_POINT('Ctrl Pts',(-0.182595063680014,-3.06807126591279,
15.0320708126024));
#11630=CARTESIAN_POINT('Ctrl Pts',(-0.126885143956322,-3.07138682003716,
15.0349729768668));
#11631=CARTESIAN_POINT('Ctrl Pts',(-0.0711352813546049,-3.07318152364552,
15.0378751411312));
#11632=CARTESIAN_POINT('Ctrl Pts',(-0.0154344978284385,-3.0734612452863,
15.0407773053956));
#11633=CARTESIAN_POINT('Ctrl Pts',(0.0805203035956334,-3.07394311704455,
15.0457768148829));
#11634=CARTESIAN_POINT('Ctrl Pts',(0.176666230714479,-3.06992790200305,
15.0507763243702));
#11635=CARTESIAN_POINT('Ctrl Pts',(0.272547234741744,-3.06139188194433,
15.0557758338575));
#11636=CARTESIAN_POINT('Ctrl Pts',(0.368298176794052,-3.05286744094277,
15.0607685615419));
#11637=CARTESIAN_POINT('Ctrl Pts',(0.463784476478959,-3.039834421342,15.0657612892262));
#11638=CARTESIAN_POINT('Ctrl Pts',(0.558549362064147,-3.02232110473684,
15.0707540169105));
#11639=CARTESIAN_POINT('Ctrl Pts',(0.653214273082363,-3.00482626423951,
15.075741477393));
#11640=CARTESIAN_POINT('Ctrl Pts',(0.747158853611802,-2.98286060228277,
15.0807289378754));
#11641=CARTESIAN_POINT('Ctrl Pts',(0.839931766644163,-2.95650416495259,
15.0857163983578));
#11642=CARTESIAN_POINT('Ctrl Pts',(0.932638298487297,-2.93016658626979,
15.0907002901956));
#11643=CARTESIAN_POINT('Ctrl Pts',(1.0241744084024,-2.89944459738611,15.0956841820333));
#11644=CARTESIAN_POINT('Ctrl Pts',(1.11410022855096,-2.86446904866202,15.1006680738711));
#11645=CARTESIAN_POINT('Ctrl Pts',(1.20399329994227,-2.82950623716682,15.1056501506989));
#11646=CARTESIAN_POINT('Ctrl Pts',(1.29227683804504,-2.79029310256283,15.1106322275266));
#11647=CARTESIAN_POINT('Ctrl Pts',(1.37852830812589,-2.74700963844242,15.1156143043544));
#11648=CARTESIAN_POINT('Ctrl Pts',(1.4647719140591,-2.7037301207771,15.1205959269315));
#11649=CARTESIAN_POINT('Ctrl Pts',(1.54898342808684,-2.65638120849873,15.1255775495086));
#11650=CARTESIAN_POINT('Ctrl Pts',(1.63076337076852,-2.60518964349233,15.1305591720857));
#11651=CARTESIAN_POINT('Ctrl Pts',(1.7125581824843,-2.55398877095769,15.1355417004095));
#11652=CARTESIAN_POINT('Ctrl Pts',(1.79192017278298,-2.4989440910873,15.1405242287334));
#11653=CARTESIAN_POINT('Ctrl Pts',(1.86847830457372,-2.44032601824784,15.1455067570572));
#11654=CARTESIAN_POINT('Ctrl Pts',(1.94511895474752,-2.38164476376488,15.1504946558123));
#11655=CARTESIAN_POINT('Ctrl Pts',(2.01894936386824,-2.31938269426886,15.1554825545673));
#11656=CARTESIAN_POINT('Ctrl Pts',(2.0896312876575,-2.25385077847733,15.1604704533224));
#11657=CARTESIAN_POINT('Ctrl Pts',(2.16035496422921,-2.18828015208375,15.1654612984977));
#11658=CARTESIAN_POINT('Ctrl Pts',(2.22792614485703,-2.1194361465061,15.170452143673));
#11659=CARTESIAN_POINT('Ctrl Pts',(2.29204469385155,-2.04766534653174,15.1754429888483));
#11660=CARTESIAN_POINT('Ctrl Pts',(2.35626686004106,-1.97577856313149,15.1804418993555));
#11661=CARTESIAN_POINT('Ctrl Pts',(2.41702497696603,-1.90095588155568,15.1854408098626));
#11662=CARTESIAN_POINT('Ctrl Pts',(2.47406034061865,-1.82357552105141,15.1904397203698));
#11663=CARTESIAN_POINT('Ctrl Pts',(2.50717275466987,-1.77865162870884,15.1933418846398));
#11664=CARTESIAN_POINT('Ctrl Pts',(2.53903123799888,-1.73286620314677,15.1962440489098));
#11665=CARTESIAN_POINT('Ctrl Pts',(2.56959224495687,-1.68629711043384,15.1991462131798));
#11666=CARTESIAN_POINT('Ctrl Pts',(2.62325694598382,-1.60452243458724,15.2042423730706));
#11667=CARTESIAN_POINT('Ctrl Pts',(2.67310143634579,-1.52005111486671,15.2093385329613));
#11668=CARTESIAN_POINT('Ctrl Pts',(2.71885041980543,-1.43326712259921,15.2144346928521));
#11669=CARTESIAN_POINT('Ctrl Pts',(2.76453038840025,-1.34661404877059,15.2195231649046));
#11670=CARTESIAN_POINT('Ctrl Pts',(2.80612694416417,-1.25765560565154,15.2246116369571));
#11671=CARTESIAN_POINT('Ctrl Pts',(2.84340806580197,-1.16680453432968,15.2297001090096));
#11672=CARTESIAN_POINT('Ctrl Pts',(2.88118664983322,-1.07474118748064,15.2348564793273));
#11673=CARTESIAN_POINT('Ctrl Pts',(2.91453352909174,-0.98073468158956,15.2400128496451));
#11674=CARTESIAN_POINT('Ctrl Pts',(2.94325508575896,-0.885241068949039,
15.2451692199628));
#11675=CARTESIAN_POINT('Ctrl Pts',(2.97152681557719,-0.79124304345131,15.2502448330347));
#11676=CARTESIAN_POINT('Ctrl Pts',(2.99531692206572,-0.695804568008259,
15.2553204461067));
#11677=CARTESIAN_POINT('Ctrl Pts',(3.0144892537006,-0.599380337785263,15.2603960591786));
#11678=CARTESIAN_POINT('Ctrl Pts',(3.03411915706434,-0.500654822430843,
15.2655928081193));
#11679=CARTESIAN_POINT('Ctrl Pts',(3.0489078940216,-0.400896314881121,15.2707895570599));
#11680=CARTESIAN_POINT('Ctrl Pts',(3.05876400975235,-0.300607688929764,
15.2759863060006));
#11681=CARTESIAN_POINT('Ctrl Pts',(3.06862012548311,-0.200319062978392,
15.2811830549413));
#11682=CARTESIAN_POINT('Ctrl Pts',(3.07354354442197,-0.0995007836552704,
15.2863798038819));
#11683=CARTESIAN_POINT('Ctrl Pts',(3.07349970959569,0.00133608204624416,
15.2915765528226));
#11684=CARTESIAN_POINT('Ctrl Pts',(3.07349970959544,0.00133608261957393,
15.2915765528522));
#11685=CARTESIAN_POINT('Ctrl Pts',(3.07345335999379,0.107957847706477,15.2970714335281));
#11686=CARTESIAN_POINT('Ctrl Pts',(3.06785451556908,0.214401037215095,15.3025663142041));
#11687=CARTESIAN_POINT('Ctrl Pts',(3.05678458082994,0.320109788042046,15.3080611948801));
#11688=CARTESIAN_POINT('Ctrl Pts',(3.04577427243867,0.425249156402119,15.3135264783024));
#11689=CARTESIAN_POINT('Ctrl Pts',(3.0293518421405,0.529661713023204,15.3189917617247));
#11690=CARTESIAN_POINT('Ctrl Pts',(3.00764794714884,0.632815989061115,15.324457045147));
#11691=CARTESIAN_POINT('Ctrl Pts',(2.98576774592482,0.736808213391975,15.3299667244498));
#11692=CARTESIAN_POINT('Ctrl Pts',(2.95852002176638,0.839521339723275,15.3354764037526));
#11693=CARTESIAN_POINT('Ctrl Pts',(2.92608819114021,0.940430830880104,15.3409860830555));
#11694=CARTESIAN_POINT('Ctrl Pts',(2.89365636051403,1.04134032203693,15.3464957623583));
#11695=CARTESIAN_POINT('Ctrl Pts',(2.85604060194039,1.14044592833878,15.3520054416611));
#11696=CARTESIAN_POINT('Ctrl Pts',(2.81347151615592,1.23724705608028,15.3575151209639));
#11697=CARTESIAN_POINT('Ctrl Pts',(2.77484412337439,1.32508486405897,15.3625146304109));
#11698=CARTESIAN_POINT('Ctrl Pts',(2.73203143966757,1.4112662729297,15.367514139858));
#11699=CARTESIAN_POINT('Ctrl Pts',(2.68519747965701,1.49536508761026,15.372513649305));
#11700=CARTESIAN_POINT('Ctrl Pts',(2.63842704961544,1.5793498227834,15.3775063769492));
#11701=CARTESIAN_POINT('Ctrl Pts',(2.58764639613873,1.66125719809427,15.3824991045934));
#11702=CARTESIAN_POINT('Ctrl Pts',(2.53306732292495,1.74068152961126,15.3874918322377));
#11703=CARTESIAN_POINT('Ctrl Pts',(2.47854582925639,1.82002207046238,15.3924792926802));
#11704=CARTESIAN_POINT('Ctrl Pts',(2.42023412928086,1.89688441517076,15.3974667531228));
#11705=CARTESIAN_POINT('Ctrl Pts',(2.35838909377463,1.97088891933687,15.4024542135653));
#11706=CARTESIAN_POINT('Ctrl Pts',(2.29658830983209,2.04484047155619,15.4074381053637));
#11707=CARTESIAN_POINT('Ctrl Pts',(2.23125949694744,2.11593791243814,15.4124219971621));
#11708=CARTESIAN_POINT('Ctrl Pts',(2.16270125905387,2.18383275781064,15.4174058889605));
#11709=CARTESIAN_POINT('Ctrl Pts',(2.0941679883689,2.25170287756562,15.4223879657492));
#11710=CARTESIAN_POINT('Ctrl Pts',(2.022407940991,2.31637241056922,15.4273700425379));
#11711=CARTESIAN_POINT('Ctrl Pts',(1.94775754940253,2.37752871249654,15.4323521193266));
#11712=CARTESIAN_POINT('Ctrl Pts',(1.87311396420502,2.43867943838209,15.437333741865));
#11713=CARTESIAN_POINT('Ctrl Pts',(1.79558089842724,2.49631729201769,15.4423153644034));
#11714=CARTESIAN_POINT('Ctrl Pts',(1.71552809589033,2.55016972027567,15.4472969869419));
#11715=CARTESIAN_POINT('Ctrl Pts',(1.63546073833702,2.60403193985828,15.4522795152274));
#11716=CARTESIAN_POINT('Ctrl Pts',(1.55287309840775,2.65410712220057,15.457262043513));
#11717=CARTESIAN_POINT('Ctrl Pts',(1.46816322861558,2.70016647341254,15.4622445717985));
#11718=CARTESIAN_POINT('Ctrl Pts',(1.38336205405292,2.74627546982525,15.4672324705162));
#11719=CARTESIAN_POINT('Ctrl Pts',(1.29643446922358,2.78835978367424,15.4722203692338));
#11720=CARTESIAN_POINT('Ctrl Pts',(1.20780221607635,2.82623708432981,15.4772082679515));
#11721=CARTESIAN_POINT('Ctrl Pts',(1.11911760663284,2.8641367596301,15.4821991130898));
#11722=CARTESIAN_POINT('Ctrl Pts',(1.02872673496034,2.89782432019123,15.4871899582281));
#11723=CARTESIAN_POINT('Ctrl Pts',(0.937068357705508,2.92716674328387,15.4921808033664));
#11724=CARTESIAN_POINT('Ctrl Pts',(0.845261858177207,2.95655658447999,15.4971797138376));
#11725=CARTESIAN_POINT('Ctrl Pts',(0.752184186637816,2.98158715319984,15.5021786243089));
#11726=CARTESIAN_POINT('Ctrl Pts',(0.658286124793895,3.00217614871344,15.5071775347801));
#11727=CARTESIAN_POINT('Ctrl Pts',(0.6037727187388,3.01412928438694,15.5100796994361));
#11728=CARTESIAN_POINT('Ctrl Pts',(0.548982951197105,3.02458635612461,15.5129818640921));
#11729=CARTESIAN_POINT('Ctrl Pts',(0.494005671626,3.03353929369661,15.5158840287482));
#11730=CARTESIAN_POINT('Ctrl Pts',(0.39928521003126,3.04896432720255,15.5208841738624));
#11731=CARTESIAN_POINT('Ctrl Pts',(0.303675208612645,3.05997581872414,15.5258843189766));
#11732=CARTESIAN_POINT('Ctrl Pts',(0.207622625814003,3.06647926705042,15.5308844640909));
#11733=CARTESIAN_POINT('Ctrl Pts',(0.111730390356419,3.0729718587124,15.5358762621107));
#11734=CARTESIAN_POINT('Ctrl Pts',(0.0153974777927567,3.07497135057233,
15.5408680601306));
#11735=CARTESIAN_POINT('Ctrl Pts',(-0.0809207646067817,3.07243455257479,
15.5458598581505));
#11736=CARTESIAN_POINT('Ctrl Pts',(-0.177147004766832,3.06990017770179,
15.5508468880539));
#11737=CARTESIAN_POINT('Ctrl Pts',(-0.273358166450199,3.0628381328422,15.5558339179573));
#11738=CARTESIAN_POINT('Ctrl Pts',(-0.369096071907349,3.05125717364213,
15.5608209478607));
#11739=CARTESIAN_POINT('Ctrl Pts',(-0.464768669155436,3.03968411446558,
15.5658045758305));
#11740=CARTESIAN_POINT('Ctrl Pts',(-0.559968217377031,3.02359831967842,
15.5707882038004));
#11741=CARTESIAN_POINT('Ctrl Pts',(-0.65423990659825,3.00306050465426,15.5757718317703));
#11742=CARTESIAN_POINT('Ctrl Pts',(-0.74847302501317,2.98253109257792,15.5807534207128));
#11743=CARTESIAN_POINT('Ctrl Pts',(-0.84177861100914,2.95755337559329,15.5857350096554));
#11744=CARTESIAN_POINT('Ctrl Pts',(-0.93371137753408,2.92823928555427,15.5907165985979));
#11745=CARTESIAN_POINT('Ctrl Pts',(-1.02566263012013,2.89891930096775,15.5956991892503));
#11746=CARTESIAN_POINT('Ctrl Pts',(-1.11624009047942,2.86526132574961,15.6006817799027));
#11747=CARTESIAN_POINT('Ctrl Pts',(-1.20501358122756,2.82742719076144,15.6056643705551));
#11748=CARTESIAN_POINT('Ctrl Pts',(-1.29379445198079,2.78958991050877,15.6106473754252));
#11749=CARTESIAN_POINT('Ctrl Pts',(-1.38077065412379,2.74757595989212,15.6156303802952));
#11750=CARTESIAN_POINT('Ctrl Pts',(-1.46553343822706,2.70159471265369,15.6206133851652));
#11751=CARTESIAN_POINT('Ctrl Pts',(-1.55037167699749,2.65557253354,15.6256008258378));
#11752=CARTESIAN_POINT('Ctrl Pts',(-1.63299218083952,2.60557622236346,15.6305882665103));
#11753=CARTESIAN_POINT('Ctrl Pts',(-1.7130124979475,2.55186019050333,15.6355757071829));
#11754=CARTESIAN_POINT('Ctrl Pts',(-1.76738114006162,2.51536361291474,15.6389643513022));
#11755=CARTESIAN_POINT('Ctrl Pts',(-1.82055002616516,2.47715081678408,15.6423529954215));
#11756=CARTESIAN_POINT('Ctrl Pts',(-1.87240768645122,2.4373123939533,15.6457416395408));
#11757=CARTESIAN_POINT('',(3.07834638629682,-0.000587882647548141,15.2084234471775));
#11758=CARTESIAN_POINT('Ctrl Pts',(3.07834638629682,-0.000587882647548141,
15.2084234471775));
#11759=CARTESIAN_POINT('Ctrl Pts',(3.07575445609013,0.982278794615726,15.2595436498067));
#11760=CARTESIAN_POINT('Ctrl Pts',(2.03467585423313,2.98483364549918,15.3634534883639));
#11761=CARTESIAN_POINT('Ctrl Pts',(-0.534116492601284,3.26769481122963,
15.4815859980824));
#11762=CARTESIAN_POINT('Ctrl Pts',(-1.65539322584549,2.60596644955508,15.5485983051717));
#11763=CARTESIAN_POINT('Ctrl Pts',(-1.87172893090644,2.43645058258115,15.5628209763329));
#11764=CARTESIAN_POINT('Ctrl Pts',(-1.87525415797411,2.44104769786763,14.562635342152));
#11765=CARTESIAN_POINT('Ctrl Pts',(-1.91249396820152,2.41267325486651,14.5650700668161));
#11766=CARTESIAN_POINT('Ctrl Pts',(-2.74116781123522,1.74852114079692,14.6202944274082));
#11767=CARTESIAN_POINT('Ctrl Pts',(-3.60135346758601,-0.452312705771215,
14.7283084239283));
#11768=CARTESIAN_POINT('Ctrl Pts',(-1.58136610914474,-3.26704986372211,
14.8866773317125));
#11769=CARTESIAN_POINT('Ctrl Pts',(1.87939897421738,-3.10518809039125,15.0450462394967));
#11770=CARTESIAN_POINT('Ctrl Pts',(3.06346382418965,-1.07966618593221,15.1522949446517));
#11771=CARTESIAN_POINT('Ctrl Pts',(3.07843103100426,-0.0326853759081321,
15.2067540138786));
#11772=CARTESIAN_POINT('Ctrl Pts',(3.07834638629682,-0.000587882647548141,
15.2084234471775));
#11773=CARTESIAN_POINT('Origin',(0.,0.,-2.20842344717744));
#11774=CARTESIAN_POINT('',(-1.87032611617503,2.43456032588387,13.5625747566432));
#11775=CARTESIAN_POINT('',(-1.87240768645124,2.43731239395329,13.6459260020382));
#11776=CARTESIAN_POINT('',(-1.87240768645123,2.4373123939533,-2.20842344717744));
#11777=CARTESIAN_POINT('',(3.07349878502588,-0.00273284548775181,14.2915765527908));
#11778=CARTESIAN_POINT('Ctrl Pts',(-1.87240768645124,2.43731239395329,13.6459260020382));
#11779=CARTESIAN_POINT('Ctrl Pts',(-1.9487521347337,2.37866257453064,13.6509133149982));
#11780=CARTESIAN_POINT('Ctrl Pts',(-2.02242004960628,2.31635947729713,13.6559006279582));
#11781=CARTESIAN_POINT('Ctrl Pts',(-2.09304608808842,2.25067996906218,13.6608879409183));
#11782=CARTESIAN_POINT('Ctrl Pts',(-2.1636225280082,2.18504658558881,13.665871751437));
#11783=CARTESIAN_POINT('Ctrl Pts',(-2.2311610176019,2.11604180284899,13.6708555619558));
#11784=CARTESIAN_POINT('Ctrl Pts',(-2.29532957011213,2.0439824888117,13.6758393724745));
#11785=CARTESIAN_POINT('Ctrl Pts',(-2.35947532998472,1.97194877020658,13.6808214127463));
#11786=CARTESIAN_POINT('Ctrl Pts',(-2.42025323946719,1.89686300354484,13.685803453018));
#11787=CARTESIAN_POINT('Ctrl Pts',(-2.47736913516805,1.81907790325668,13.6907854932898));
#11788=CARTESIAN_POINT('Ctrl Pts',(-2.53448033586542,1.74129919700844,13.6957671240311));
#11789=CARTESIAN_POINT('Ctrl Pts',(-2.58792986166185,1.66082195226451,13.7007487547725));
#11790=CARTESIAN_POINT('Ctrl Pts',(-2.63746537424263,1.57802999010512,13.7057303855138));
#11791=CARTESIAN_POINT('Ctrl Pts',(-2.68701033785819,1.49522223180933,13.710712966716));
#11792=CARTESIAN_POINT('Ctrl Pts',(-2.73263957979876,1.41009925568748,13.7156955479182));
#11793=CARTESIAN_POINT('Ctrl Pts',(-2.77414597988313,1.32307079640443,13.7206781291204));
#11794=CARTESIAN_POINT('Ctrl Pts',(-2.81569732138376,1.23594810629897,13.7256661052558));
#11795=CARTESIAN_POINT('Ctrl Pts',(-2.85311672012191,1.14691621111724,13.7306540813912));
#11796=CARTESIAN_POINT('Ctrl Pts',(-2.88624472676201,1.05640599545746,13.7356420575266));
#11797=CARTESIAN_POINT('Ctrl Pts',(-2.91939256922463,0.965841585635226,
13.7406330202772));
#11798=CARTESIAN_POINT('Ctrl Pts',(-2.94824377220229,0.873797511510271,
13.7456239830279));
#11799=CARTESIAN_POINT('Ctrl Pts',(-2.97268903577202,0.780718993364979,
13.7506149457785));
#11800=CARTESIAN_POINT('Ctrl Pts',(-2.9971735686465,0.687490952238094,13.7556139261001));
#11801=CARTESIAN_POINT('Ctrl Pts',(-3.01723793901163,0.593225578119903,
13.7606129064218));
#11802=CARTESIAN_POINT('Ctrl Pts',(-3.03282414139059,0.498377344387172,
13.7656118867435));
#11803=CARTESIAN_POINT('Ctrl Pts',(-3.04136104928331,0.446426868223962,
13.7683499388697));
#11804=CARTESIAN_POINT('Ctrl Pts',(-3.04855542185305,0.394301620162721,
13.7710879909959));
#11805=CARTESIAN_POINT('Ctrl Pts',(-3.05440435245989,0.34207645588974,13.7738260431222));
#11806=CARTESIAN_POINT('Ctrl Pts',(-3.06508412871873,0.246716618851419,
13.7788255526152));
#11807=CARTESIAN_POINT('Ctrl Pts',(-3.07131261933319,0.150688668848877,
13.7838250621083));
#11808=CARTESIAN_POINT('Ctrl Pts',(-3.07301775946229,0.054443549014884,
13.7888245716014));
#11809=CARTESIAN_POINT('Ctrl Pts',(-3.07472058657965,-0.0416710149252134,
13.7938172992916));
#11810=CARTESIAN_POINT('Ctrl Pts',(-3.07191225019003,-0.138001728080463,
13.7988100269818));
#11811=CARTESIAN_POINT('Ctrl Pts',(-3.06457231374823,-0.23409140054223,
13.803802754672));
#11812=CARTESIAN_POINT('Ctrl Pts',(-3.05724012075436,-0.330079700821654,
13.8087902151603));
#11813=CARTESIAN_POINT('Ctrl Pts',(-3.04538586475401,-0.425827030564542,
13.8137776756486));
#11814=CARTESIAN_POINT('Ctrl Pts',(-3.02904115811137,-0.520876100879417,
13.8187651361369));
#11815=CARTESIAN_POINT('Ctrl Pts',(-3.01270814648839,-0.615857161362664,
13.8237490279807));
#11816=CARTESIAN_POINT('Ctrl Pts',(-2.99189114573891,-0.710140524268516,
13.8287329198245));
#11817=CARTESIAN_POINT('Ctrl Pts',(-2.96667350386284,-0.803274904051028,
13.8337168116682));
#11818=CARTESIAN_POINT('Ctrl Pts',(-2.94146504562736,-0.89637536659911,
13.838698888502));
#11819=CARTESIAN_POINT('Ctrl Pts',(-2.91185924507421,-0.988327254129027,
13.8436809653358));
#11820=CARTESIAN_POINT('Ctrl Pts',(-2.87799015758435,-1.07869129172697,
13.8486630421696));
#11821=CARTESIAN_POINT('Ctrl Pts',(-2.84412415817497,-1.16904709020655,
13.8536446647528));
#11822=CARTESIAN_POINT('Ctrl Pts',(-2.80599579889547,-1.25781491561944,
13.8586262873359));
#11823=CARTESIAN_POINT('Ctrl Pts',(-2.76378806944643,-1.34457344804423,
13.8636079099191));
#11824=CARTESIAN_POINT('Ctrl Pts',(-2.72157266588854,-1.4313477546988,13.868590438249));
#11825=CARTESIAN_POINT('Ctrl Pts',(-2.67527661120517,-1.51611164812035,
13.8735729665789));
#11826=CARTESIAN_POINT('Ctrl Pts',(-2.62512934371512,-1.59846744688962,
13.8785554949088));
#11827=CARTESIAN_POINT('Ctrl Pts',(-2.57492802486133,-1.68091201307252,
13.88354339367));
#11828=CARTESIAN_POINT('Ctrl Pts',(-2.52086743470754,-1.76094292723813,
13.8885312924311));
#11829=CARTESIAN_POINT('Ctrl Pts',(-2.46322082221231,-1.83819080375779,
13.8935191911923));
#11830=CARTESIAN_POINT('Ctrl Pts',(-2.40554015707186,-1.91548431165837,
13.8985100363737));
#11831=CARTESIAN_POINT('Ctrl Pts',(-2.34426953036604,-1.98999116959674,
13.9035008815551));
#11832=CARTESIAN_POINT('Ctrl Pts',(-2.27972165649791,-2.0613760983611,13.9084917267365));
#11833=CARTESIAN_POINT('Ctrl Pts',(-2.21506947163559,-2.13287638697302,
13.9134906372497));
#11834=CARTESIAN_POINT('Ctrl Pts',(-2.1471297736494,-2.20124436127135,13.918489547763));
#11835=CARTESIAN_POINT('Ctrl Pts',(-2.07625113660596,-2.26618257599481,
13.9234884582762));
#11836=CARTESIAN_POINT('Ctrl Pts',(-2.035101881555,-2.30388306335847,13.9263906224863));
#11837=CARTESIAN_POINT('Ctrl Pts',(-1.99296267410306,-2.34042831230664,
13.9292927866964));
#11838=CARTESIAN_POINT('Ctrl Pts',(-1.9499063098848,-2.3757667462677,13.9321949509065));
#11839=CARTESIAN_POINT('Ctrl Pts',(-1.87573383511858,-2.43664367233532,
13.9371944603994));
#11840=CARTESIAN_POINT('Ctrl Pts',(-1.79857744293475,-2.49415064949183,
13.9421939698923));
#11841=CARTESIAN_POINT('Ctrl Pts',(-1.71877614513896,-2.54798171361202,
13.9471934793852));
#11842=CARTESIAN_POINT('Ctrl Pts',(-1.6390830972969,-2.60173975623556,13.9521862070752));
#11843=CARTESIAN_POINT('Ctrl Pts',(-1.55675263514735,-2.6518315524901,13.9571789347653));
#11844=CARTESIAN_POINT('Ctrl Pts',(-1.47215711934958,-2.69799104259972,
13.9621716624553));
#11845=CARTESIAN_POINT('Ctrl Pts',(-1.38765084968853,-2.74410183561085,
13.9671591229435));
#11846=CARTESIAN_POINT('Ctrl Pts',(-1.30088465999158,-2.78628836027448,
13.9721465834316));
#11847=CARTESIAN_POINT('Ctrl Pts',(-1.21225933205399,-2.824328161147,13.9771340439198));
#11848=CARTESIAN_POINT('Ctrl Pts',(-1.12369741761024,-2.86234074365278,
13.9821179357634));
#11849=CARTESIAN_POINT('Ctrl Pts',(-1.03327941163226,-2.8962123281375,13.987101827607));
#11850=CARTESIAN_POINT('Ctrl Pts',(-0.941429227903033,-2.92576712314051,
13.9920857194506));
#11851=CARTESIAN_POINT('Ctrl Pts',(-0.849612493735829,-2.95531115501917,
13.9970677962843));
#11852=CARTESIAN_POINT('Ctrl Pts',(-0.756365035543576,-2.9805413866251,
14.0020498731179));
#11853=CARTESIAN_POINT('Ctrl Pts',(-0.66212830039646,-3.00133109866507,
14.0070319499515));
#11854=CARTESIAN_POINT('Ctrl Pts',(-0.56790015746843,-3.02211891516229,
14.0120135725345));
#11855=CARTESIAN_POINT('Ctrl Pts',(-0.472683345612832,-3.03846692266898,
14.0169951951176));
#11856=CARTESIAN_POINT('Ctrl Pts',(-0.376930893757469,-3.05029922324535,
14.0219768177006));
#11857=CARTESIAN_POINT('Ctrl Pts',(-0.281161032419288,-3.06213367514244,
14.0269593460303));
#11858=CARTESIAN_POINT('Ctrl Pts',(-0.184855773315668,-3.06945073573416,
14.0319418743601));
#11859=CARTESIAN_POINT('Ctrl Pts',(-0.0884736066038495,-3.07222633784272,
14.0369244026899));
#11860=CARTESIAN_POINT('Ctrl Pts',(0.00801244587907222,-3.07500493164129,
14.0419123014509));
#11861=CARTESIAN_POINT('Ctrl Pts',(0.10457513195456,-3.07323228183864,14.0469002002119));
#11862=CARTESIAN_POINT('Ctrl Pts',(0.200755842985021,-3.06693647497097,
14.0518880989729));
#11863=CARTESIAN_POINT('Ctrl Pts',(0.296993369281649,-3.06063694908377,
14.0568789441541));
#11864=CARTESIAN_POINT('Ctrl Pts',(0.392848035266852,-3.0498089952097,14.0618697893354));
#11865=CARTESIAN_POINT('Ctrl Pts',(0.487868353479512,-3.03453237248727,
14.0668606345166));
#11866=CARTESIAN_POINT('Ctrl Pts',(0.583042226926029,-3.01923106235672,
14.0718595450297));
#11867=CARTESIAN_POINT('Ctrl Pts',(0.677378630943842,-2.99946681816297,
14.0768584555428));
#11868=CARTESIAN_POINT('Ctrl Pts',(0.770438289047837,-2.97537007660712,
14.0818573660559));
#11869=CARTESIAN_POINT('Ctrl Pts',(0.824464943171497,-2.96138048812087,
14.0847595302675));
#11870=CARTESIAN_POINT('Ctrl Pts',(0.878061573354344,-2.94593156383784,
14.087661694479));
#11871=CARTESIAN_POINT('Ctrl Pts',(0.931145283868948,-2.92905628322991,
14.0905638586905));
#11872=CARTESIAN_POINT('Ctrl Pts',(1.02259169946942,-2.89998552105282,14.0955633681833));
#11873=CARTESIAN_POINT('Ctrl Pts',(1.11283602641801,-2.86657709802122,14.100562877676));
#11874=CARTESIAN_POINT('Ctrl Pts',(1.20143704886018,-2.82894879197665,14.1055623871688));
#11875=CARTESIAN_POINT('Ctrl Pts',(1.28991788457799,-2.7913715284903,14.1105551148587));
#11876=CARTESIAN_POINT('Ctrl Pts',(1.37675944546292,-2.7495859286715,14.1155478425485));
#11877=CARTESIAN_POINT('Ctrl Pts',(1.46153583028535,-2.70375946910817,14.1205405702384));
#11878=CARTESIAN_POINT('Ctrl Pts',(1.54622277815864,-2.6579813553046,14.1255280307264));
#11879=CARTESIAN_POINT('Ctrl Pts',(1.62884849700867,-2.60817106398228,14.1305154912144));
#11880=CARTESIAN_POINT('Ctrl Pts',(1.70900818665148,-2.55454365160555,14.1355029517024));
#11881=CARTESIAN_POINT('Ctrl Pts',(1.78911052016263,-2.50095461089591,14.1404868435459));
#11882=CARTESIAN_POINT('Ctrl Pts',(1.86674996841423,-2.44355412209013,14.1454707353893));
#11883=CARTESIAN_POINT('Ctrl Pts',(1.94154827836441,-2.38260205086376,14.1504546272328));
#11884=CARTESIAN_POINT('Ctrl Pts',(2.01631934862266,-2.32167217687211,14.1554367040662));
#11885=CARTESIAN_POINT('Ctrl Pts',(2.08825099642142,-2.25719356731368,14.1604187808997));
#11886=CARTESIAN_POINT('Ctrl Pts',(2.1569965840487,-2.18946751206823,14.1654008577332));
#11887=CARTESIAN_POINT('Ctrl Pts',(2.22573590366212,-2.12174763187877,14.170382480316));
#11888=CARTESIAN_POINT('Ctrl Pts',(2.29128942808784,-2.05078120288479,14.1753641028989));
#11889=CARTESIAN_POINT('Ctrl Pts',(2.35334684241256,-1.97690689950408,14.1803457254817));
#11890=CARTESIAN_POINT('Ctrl Pts',(2.41541553986862,-1.9030191644734,14.1853282538113));
#11891=CARTESIAN_POINT('Ctrl Pts',(2.47398658249804,-1.82622284117964,14.1903107821409));
#11892=CARTESIAN_POINT('Ctrl Pts',(2.52879015725592,-1.74688940421699,14.1952933104705));
#11893=CARTESIAN_POINT('Ctrl Pts',(2.58365280219058,-1.66747045750125,14.2002812092313));
#11894=CARTESIAN_POINT('Ctrl Pts',(2.63473962238392,-1.58550929943602,14.2052691079922));
#11895=CARTESIAN_POINT('Ctrl Pts',(2.68182448641721,-1.50140589916687,14.210257006753));
#11896=CARTESIAN_POINT('Ctrl Pts',(2.72893716412597,-1.41725281786477,14.2152478519341));
#11897=CARTESIAN_POINT('Ctrl Pts',(2.77204298248141,-1.33095536715174,14.2202386971152));
#11898=CARTESIAN_POINT('Ctrl Pts',(2.81096302978059,-1.24293567621448,14.2252295422963));
#11899=CARTESIAN_POINT('Ctrl Pts',(2.84994597285909,-1.1547737432338,14.2302284528092));
#11900=CARTESIAN_POINT('Ctrl Pts',(2.88472947973862,-1.0648844217315,14.2352273633222));
#11901=CARTESIAN_POINT('Ctrl Pts',(2.9151837949497,-0.973707189899856,14.2402262738351));
#11902=CARTESIAN_POINT('Ctrl Pts',(2.93286433224172,-0.920773395906811,
14.2431284380483));
#11903=CARTESIAN_POINT('Ctrl Pts',(2.94908666271836,-0.867405765024594,
14.2460306022615));
#11904=CARTESIAN_POINT('Ctrl Pts',(2.96383331659796,-0.813691785274952,
14.2489327664748));
#11905=CARTESIAN_POINT('Ctrl Pts',(2.99602294044835,-0.696442623684468,
14.2552677340639));
#11906=CARTESIAN_POINT('Ctrl Pts',(3.0212702832211,-0.577211563723087,14.261602701653));
#11907=CARTESIAN_POINT('Ctrl Pts',(3.03937583013342,-0.456724001121871,
14.2679376692422));
#11908=CARTESIAN_POINT('Ctrl Pts',(3.0571635192287,-0.338351697110416,14.2741614212476));
#11909=CARTESIAN_POINT('Ctrl Pts',(3.06805797242532,-0.218766467335917,
14.280385173253));
#11910=CARTESIAN_POINT('Ctrl Pts',(3.07191552615637,-0.0986775058431663,
14.2866089252584));
#11911=CARTESIAN_POINT('Ctrl Pts',(3.07294185722405,-0.0667269380329351,
14.2882648011025));
#11912=CARTESIAN_POINT('Ctrl Pts',(3.07347032466018,-0.0347408385475268,
14.2899206769466));
#11913=CARTESIAN_POINT('Ctrl Pts',(3.07349878502588,-0.00273284548777434,
14.2915765527908));
#11914=CARTESIAN_POINT('Ctrl Pts',(3.07349878502642,-0.00273284487212046,
14.2915765528226));
#11915=CARTESIAN_POINT('Ctrl Pts',(3.07358364945225,0.092710080672881,14.2965141205922));
#11916=CARTESIAN_POINT('Ctrl Pts',(3.069218504179,0.188253195776559,14.3014516883618));
#11917=CARTESIAN_POINT('Ctrl Pts',(3.06040211108299,0.283445177201534,14.3063892561314));
#11918=CARTESIAN_POINT('Ctrl Pts',(3.05159013460488,0.378589471709134,14.3113243504008));
#11919=CARTESIAN_POINT('Ctrl Pts',(3.03833137922742,0.473382536333788,14.3162594446702));
#11920=CARTESIAN_POINT('Ctrl Pts',(3.02067664916565,0.567375388244305,14.3211945389396));
#11921=CARTESIAN_POINT('Ctrl Pts',(3.00302571336008,0.661348039734878,14.326128572586));
#11922=CARTESIAN_POINT('Ctrl Pts',(2.98098076245997,0.75452037973125,14.3310626062324));
#11923=CARTESIAN_POINT('Ctrl Pts',(2.95464399796869,0.846452063183483,14.3359966398788));
#11924=CARTESIAN_POINT('Ctrl Pts',(2.9283053601704,0.938390285641968,14.340931024478));
#11925=CARTESIAN_POINT('Ctrl Pts',(2.89767442723464,1.02908724567049,14.3458654090772));
#11926=CARTESIAN_POINT('Ctrl Pts',(2.86290337237835,1.11811740457999,14.3507997936764));
#11927=CARTESIAN_POINT('Ctrl Pts',(2.82809727590647,1.20723728641037,14.3557391510556));
#11928=CARTESIAN_POINT('Ctrl Pts',(2.78914288932616,1.29468659443031,14.3606785084349));
#11929=CARTESIAN_POINT('Ctrl Pts',(2.74624057947654,1.38005975582087,14.3656178658141));
#11930=CARTESIAN_POINT('Ctrl Pts',(2.70331618390134,1.46547686655169,14.3705597659304));
#11931=CARTESIAN_POINT('Ctrl Pts',(2.6564400393954,1.54881531245498,14.3755016660467));
#11932=CARTESIAN_POINT('Ctrl Pts',(2.60585741194769,1.62969610621038,14.3804435661629));
#11933=CARTESIAN_POINT('Ctrl Pts',(2.55518929437882,1.71071359727091,14.3853938186259));
#11934=CARTESIAN_POINT('Ctrl Pts',(2.50080243806243,1.78926477176493,14.3903440710888));
#11935=CARTESIAN_POINT('Ctrl Pts',(2.44298415864097,1.8650015149134,14.3952943235517));
#11936=CARTESIAN_POINT('Ctrl Pts',(2.39623608107655,1.92623728980343,14.3992967737875));
#11937=CARTESIAN_POINT('Ctrl Pts',(2.34724563426181,1.98563375217512,14.4032992240232));
#11938=CARTESIAN_POINT('Ctrl Pts',(2.29618206790021,2.04302475781708,14.407301674259));
#11939=CARTESIAN_POINT('Ctrl Pts',(2.2323979432512,2.11471256418133,14.4123011837513));
#11940=CARTESIAN_POINT('Ctrl Pts',(2.165141381716,2.18353636969329,14.4173006932437));
#11941=CARTESIAN_POINT('Ctrl Pts',(2.09469959610768,2.24914113653775,14.422300202736));
#11942=CARTESIAN_POINT('Ctrl Pts',(2.02435336433424,2.31465691093257,14.4272929304255));
#11943=CARTESIAN_POINT('Ctrl Pts',(1.95083081414323,2.37696202838997,14.432285658115));
#11944=CARTESIAN_POINT('Ctrl Pts',(1.87445831609767,2.43573567351063,14.4372783858044));
#11945=CARTESIAN_POINT('Ctrl Pts',(1.79816638911234,2.49444731391726,14.4422658462921));
#11946=CARTESIAN_POINT('Ctrl Pts',(1.71903083728364,2.54963462199363,14.4472533067797));
#11947=CARTESIAN_POINT('Ctrl Pts',(1.63741289771372,2.60101542717469,14.4522407672673));
#11948=CARTESIAN_POINT('Ctrl Pts',(1.55585335768723,2.65235946818872,14.4572246591103));
#11949=CARTESIAN_POINT('Ctrl Pts',(1.47181533135017,2.69990218759118,14.4622085509534));
#11950=CARTESIAN_POINT('Ctrl Pts',(1.38569017436835,2.74340390585474,14.4671924427965));
#11951=CARTESIAN_POINT('Ctrl Pts',(1.29959638203551,2.78688978186998,14.4721745196296));
#11952=CARTESIAN_POINT('Ctrl Pts',(1.21141736067392,2.82633738301604,14.4771565964627));
#11953=CARTESIAN_POINT('Ctrl Pts',(1.12156942928375,2.86155277171261,14.4821386732958));
#11954=CARTESIAN_POINT('Ctrl Pts',(1.03172968995484,2.89676494957709,14.4871202958782));
#11955=CARTESIAN_POINT('Ctrl Pts',(0.940221751890307,2.92774552217978,14.4921019184607));
#11956=CARTESIAN_POINT('Ctrl Pts',(0.847481291118539,2.95434894878788,14.4970835410432));
#11957=CARTESIAN_POINT('Ctrl Pts',(0.754723968496831,2.98095721236771,14.5020660693724));
#11958=CARTESIAN_POINT('Ctrl Pts',(0.660734100066584,3.00318662840565,14.5070485977017));
#11959=CARTESIAN_POINT('Ctrl Pts',(0.56596083020831,3.02094200352637,14.5120311260309));
#11960=CARTESIAN_POINT('Ctrl Pts',(0.471085408732499,3.03871651632474,14.5170190247914));
#11961=CARTESIAN_POINT('Ctrl Pts',(0.375425332250775,3.05200727985058,14.5220069235519));
#11962=CARTESIAN_POINT('Ctrl Pts',(0.279437986272481,3.06077059934716,14.5269948223123));
#11963=CARTESIAN_POINT('Ctrl Pts',(0.183393939251215,3.06953909545687,14.5319856674931));
#11964=CARTESIAN_POINT('Ctrl Pts',(0.0870226761306488,3.07377480305766,
14.5369765126738));
#11965=CARTESIAN_POINT('Ctrl Pts',(-0.0092174026773135,3.07348617850933,
14.5419673578546));
#11966=CARTESIAN_POINT('Ctrl Pts',(-0.105613007883394,3.07319708753644,
14.5469662683672));
#11967=CARTESIAN_POINT('Ctrl Pts',(-0.201876567349512,3.06836908706779,
14.5519651788798));
#11968=CARTESIAN_POINT('Ctrl Pts',(-0.297553848429102,3.0590625945353,14.5569640893924));
#11969=CARTESIAN_POINT('Ctrl Pts',(-0.353100188140001,3.053659623319,14.5598662536093));
#11970=CARTESIAN_POINT('Ctrl Pts',(-0.408449077039367,3.04674814464449,
14.5627684178262));
#11971=CARTESIAN_POINT('Ctrl Pts',(-0.463513494023612,3.03834782256048,
14.5656705820431));
#11972=CARTESIAN_POINT('Ctrl Pts',(-0.558371273141645,3.02387684583167,
14.5706700511617));
#11973=CARTESIAN_POINT('Ctrl Pts',(-0.652717332392701,3.00493397839403,
14.5756695202804));
#11974=CARTESIAN_POINT('Ctrl Pts',(-0.746097506323219,2.98156682988295,
14.580668989399));
#11975=CARTESIAN_POINT('Ctrl Pts',(-0.839355656886615,2.95823021609912,
14.5856619255243));
#11976=CARTESIAN_POINT('Ctrl Pts',(-0.931650007815505,2.9304809143819,14.5906548616496));
#11977=CARTESIAN_POINT('Ctrl Pts',(-1.02253371283178,2.89841802646245,14.5956477977749));
#11978=CARTESIAN_POINT('Ctrl Pts',(-1.11330986408678,2.86639308246476,14.6006348251506));
#11979=CARTESIAN_POINT('Ctrl Pts',(-1.20267827845999,2.83006485205293,14.6056218525262));
#11980=CARTESIAN_POINT('Ctrl Pts',(-1.29020571006753,2.78958267052782,14.6106088799019));
#11981=CARTESIAN_POINT('Ctrl Pts',(-1.37767341338736,2.74912811384376,14.6155925041547));
#11982=CARTESIAN_POINT('Ctrl Pts',(-1.46330223346942,2.70452542312112,14.6205761284074));
#11983=CARTESIAN_POINT('Ctrl Pts',(-1.54667811974368,2.65597233492861,14.6255597526602));
#11984=CARTESIAN_POINT('Ctrl Pts',(-1.63002245760475,2.60743761862943,14.6305414911706));
#11985=CARTESIAN_POINT('Ctrl Pts',(-1.71111517708098,2.55495569623841,14.6355232296811));
#11986=CARTESIAN_POINT('Ctrl Pts',(-1.78956701475662,2.4987701274217,14.6405049681915));
#11987=CARTESIAN_POINT('Ctrl Pts',(-1.81752119604303,2.47874992620123,14.6422800753855));
#11988=CARTESIAN_POINT('Ctrl Pts',(-1.8451403277701,2.45825989830704,14.6440551825796));
#11989=CARTESIAN_POINT('Ctrl Pts',(-1.87240768645123,2.43731239395329,14.6458302897736));
#11990=CARTESIAN_POINT('',(3.07201600109834,0.00268254658689539,14.2084234471775));
#11991=CARTESIAN_POINT('Ctrl Pts',(3.07201600109834,0.00268254658689539,
14.2084234471775));
#11992=CARTESIAN_POINT('Ctrl Pts',(3.07445542476385,0.291196008346456,14.2233495316436));
#11993=CARTESIAN_POINT('Ctrl Pts',(2.90505334785583,1.59729724456565,14.2910652520378));
#11994=CARTESIAN_POINT('Ctrl Pts',(1.09056355056046,3.43559442656078,14.4091358836959));
#11995=CARTESIAN_POINT('Ctrl Pts',(-1.10506138538983,3.0278871793826,14.512280430888));
#11996=CARTESIAN_POINT('Ctrl Pts',(-1.87525415797411,2.44104769786763,14.562635342152));
#11997=CARTESIAN_POINT('Ctrl Pts',(-1.87032611617489,2.43456032588397,13.5625747566432));
#11998=CARTESIAN_POINT('Ctrl Pts',(-2.16435218332819,2.21187124699417,13.5816251942419));
#11999=CARTESIAN_POINT('Ctrl Pts',(-3.12451768131251,1.18293877132523,13.6534652677685));
#12000=CARTESIAN_POINT('Ctrl Pts',(-3.28738484392744,-1.53864696090213,
13.7780949772233));
#12001=CARTESIAN_POINT('Ctrl Pts',(-0.499216609585515,-3.59515178526775,
13.9364638850075));
#12002=CARTESIAN_POINT('Ctrl Pts',(2.43813708336016,-2.49101688819496,14.0799067083255));
#12003=CARTESIAN_POINT('Ctrl Pts',(3.0658278247078,-0.729200240998579,14.1705598957155));
#12004=CARTESIAN_POINT('Ctrl Pts',(3.07201600109834,0.00268254658689539,
14.2084234471775));
#12005=CARTESIAN_POINT('Origin',(0.,0.,-2.20842344717744));
#12006=CARTESIAN_POINT('',(-1.87077372492537,2.43522501013495,12.5628034348477));
#12007=CARTESIAN_POINT('',(-1.87240768645123,2.43731239395329,12.6457543573089));
#12008=CARTESIAN_POINT('',(-1.87240768645123,2.4373123939533,-2.20842344717744));
#12009=CARTESIAN_POINT('',(3.0734998880982,0.000829373473843992,13.2915765527763));
#12010=CARTESIAN_POINT('Ctrl Pts',(-1.87240768645123,2.43731239395329,12.6457543573089));
#12011=CARTESIAN_POINT('Ctrl Pts',(-1.94880608375446,2.37862112946951,12.6507539181684));
#12012=CARTESIAN_POINT('Ctrl Pts',(-2.02234126144047,2.31641200752082,12.6557534790279));
#12013=CARTESIAN_POINT('Ctrl Pts',(-2.09269109792243,2.25101004410825,12.6607530398874));
#12014=CARTESIAN_POINT('Ctrl Pts',(-2.11375404150425,2.23142850796846,12.6622499228026));
#12015=CARTESIAN_POINT('Ctrl Pts',(-2.1345317118694,2.21156099226433,12.6637468057178));
#12016=CARTESIAN_POINT('Ctrl Pts',(-2.15501616577206,2.19141679633544,12.665243688633));
#12017=CARTESIAN_POINT('Ctrl Pts',(-2.22343315463912,2.12413625104231,12.670243198126));
#12018=CARTESIAN_POINT('Ctrl Pts',(-2.28881650109085,2.05353044898989,12.675242707619));
#12019=CARTESIAN_POINT('Ctrl Pts',(-2.35082593556614,1.97990395491033,12.6802422171119));
#12020=CARTESIAN_POINT('Ctrl Pts',(-2.41275125463733,1.90637733470246,12.685234944802));
#12021=CARTESIAN_POINT('Ctrl Pts',(-2.47131147724655,1.82983849895282,12.6902276724921));
#12022=CARTESIAN_POINT('Ctrl Pts',(-2.52620246685423,1.75062941437062,12.6952204001822));
#12023=CARTESIAN_POINT('Ctrl Pts',(-2.5810355478515,1.67150389337603,12.7002078606704));
#12024=CARTESIAN_POINT('Ctrl Pts',(-2.63220684236038,1.58971408254247,12.7051953211587));
#12025=CARTESIAN_POINT('Ctrl Pts',(-2.67945254972863,1.50563484409492,12.7101827816469));
#12026=CARTESIAN_POINT('Ctrl Pts',(-2.72666445168885,1.4216157663079,12.7151666734906));
#12027=CARTESIAN_POINT('Ctrl Pts',(-2.7699561359476,1.33531089903631,12.7201505653342));
#12028=CARTESIAN_POINT('Ctrl Pts',(-2.80910774232458,1.24712306610539,12.7251344571779));
#12029=CARTESIAN_POINT('Ctrl Pts',(-2.84824509065619,1.15896734899905,12.7301165340116));
#12030=CARTESIAN_POINT('Ctrl Pts',(-2.88324517883553,1.06893042949471,12.7350986108453));
#12031=CARTESIAN_POINT('Ctrl Pts',(-2.91393507687166,0.977437782049056,
12.740080687679));
#12032=CARTESIAN_POINT('Ctrl Pts',(-2.94462217669613,0.885953476624977,
12.7450623102621));
#12033=CARTESIAN_POINT('Ctrl Pts',(-2.97099972828891,0.793014123380326,
12.7500439328451));
#12034=CARTESIAN_POINT('Ctrl Pts',(-2.99294410379904,0.699062115648202,
12.7550255554282));
#12035=CARTESIAN_POINT('Ctrl Pts',(-3.01489246918329,0.605093025785723,
12.760008083758));
#12036=CARTESIAN_POINT('Ctrl Pts',(-3.03240595790341,0.510111343237154,
12.7649906120879));
#12037=CARTESIAN_POINT('Ctrl Pts',(-3.04541189860072,0.414570401573901,
12.7699731404177));
#12038=CARTESIAN_POINT('Ctrl Pts',(-3.05843185778531,0.318926480856186,
12.7749610391787));
#12039=CARTESIAN_POINT('Ctrl Pts',(-3.06693451014778,0.2227225332634,12.7799489379398));
#12040=CARTESIAN_POINT('Ctrl Pts',(-3.07089902991347,0.126417554463398,
12.7849368367008));
#12041=CARTESIAN_POINT('Ctrl Pts',(-3.07486589157541,0.0300556869905675,
12.7899276818821));
#12042=CARTESIAN_POINT('Ctrl Pts',(-3.07428928547725,-0.0664068917736713,
12.7949185270634));
#12043=CARTESIAN_POINT('Ctrl Pts',(-3.06920052266675,-0.162512773842922,
12.7999093722448));
#12044=CARTESIAN_POINT('Ctrl Pts',(-3.06410353628705,-0.258773965444591,
12.8049082827579));
#12045=CARTESIAN_POINT('Ctrl Pts',(-3.05447987696272,-0.354676872871751,
12.8099071932711));
#12046=CARTESIAN_POINT('Ctrl Pts',(-3.04041254424232,-0.449770842556444,
12.8149061037842));
#12047=CARTESIAN_POINT('Ctrl Pts',(-3.0322456227786,-0.504978535267283,
12.8178082679952));
#12048=CARTESIAN_POINT('Ctrl Pts',(-3.02258192059223,-0.559913777938567,
12.8207104322062));
#12049=CARTESIAN_POINT('Ctrl Pts',(-3.01144541790488,-0.614490638642867,
12.8236125964172));
#12050=CARTESIAN_POINT('Ctrl Pts',(-2.99226075196033,-0.708509278992453,
12.8286121059102));
#12051=CARTESIAN_POINT('Ctrl Pts',(-2.96863521495116,-0.801793764721497,
12.8336116154031));
#12052=CARTESIAN_POINT('Ctrl Pts',(-2.94063901313134,-0.893892859603408,
12.8386111248961));
#12053=CARTESIAN_POINT('Ctrl Pts',(-2.91268078798151,-0.985867022647913,
12.8436038525862));
#12054=CARTESIAN_POINT('Ctrl Pts',(-2.88036380765218,-1.07665857419513,
12.8485965802763));
#12055=CARTESIAN_POINT('Ctrl Pts',(-2.84380932356707,-1.16582622255336,
12.8535893079664));
#12056=CARTESIAN_POINT('Ctrl Pts',(-2.80729340354125,-1.25489980129017,
12.8585767684546));
#12057=CARTESIAN_POINT('Ctrl Pts',(-2.76654903238322,-1.34235247853241,
12.8635642289429));
#12058=CARTESIAN_POINT('Ctrl Pts',(-2.72174701495838,-1.42775888600462,
12.8685516894311));
#12059=CARTESIAN_POINT('Ctrl Pts',(-2.67697705442427,-1.51310418319588,
12.8735355812748));
#12060=CARTESIAN_POINT('Ctrl Pts',(-2.62815542265776,-1.59640573367598,
12.8785194731184));
#12061=CARTESIAN_POINT('Ctrl Pts',(-2.57550030195739,-1.6772598023614,12.8835033649621));
#12062=CARTESIAN_POINT('Ctrl Pts',(-2.52286435694783,-1.75808442599756,
12.8884854417958));
#12063=CARTESIAN_POINT('Ctrl Pts',(-2.46639793613164,-1.83646297131842,
12.8934675186295));
#12064=CARTESIAN_POINT('Ctrl Pts',(-2.40636377219709,-1.91201873574957,
12.8984495954632));
#12065=CARTESIAN_POINT('Ctrl Pts',(-2.34633508199521,-1.98756761123568,
12.9034312180463));
#12066=CARTESIAN_POINT('Ctrl Pts',(-2.28273956864474,-2.0602938739697,12.9084128406293));
#12067=CARTESIAN_POINT('Ctrl Pts',(-2.21588099888406,-2.12985296412324,
12.9133944632124));
#12068=CARTESIAN_POINT('Ctrl Pts',(-2.14901027305742,-2.19942470134495,
12.9183769915422));
#12069=CARTESIAN_POINT('Ctrl Pts',(-2.07887561677486,-2.26582780590368,
12.923359519872));
#12070=CARTESIAN_POINT('Ctrl Pts',(-2.005817716704,-2.3287545034538,12.9283420482019));
#12071=CARTESIAN_POINT('Ctrl Pts',(-1.93268107098398,-2.39174902670988,
12.9333299469629));
#12072=CARTESIAN_POINT('Ctrl Pts',(-1.85661522429066,-2.4512593753601,12.938317845724));
#12073=CARTESIAN_POINT('Ctrl Pts',(-1.77799384002364,-2.5070181799975,12.943305744485));
#12074=CARTESIAN_POINT('Ctrl Pts',(-1.6993260130258,-2.56280992212613,12.9482965896663));
#12075=CARTESIAN_POINT('Ctrl Pts',(-1.61810001205918,-2.61484547096943,
12.9532874348476));
#12076=CARTESIAN_POINT('Ctrl Pts',(-1.53471655476278,-2.66290205350048,
12.958278280029));
#12077=CARTESIAN_POINT('Ctrl Pts',(-1.4511983476937,-2.71103629668247,12.9632771905421));
#12078=CARTESIAN_POINT('Ctrl Pts',(-1.36551611247509,-2.75517853314285,
12.9682761010553));
#12079=CARTESIAN_POINT('Ctrl Pts',(-1.27809304307681,-2.79515302322407,
12.9732750115684));
#12080=CARTESIAN_POINT('Ctrl Pts',(-1.22733876320876,-2.81836058698418,
12.9761771757794));
#12081=CARTESIAN_POINT('Ctrl Pts',(-1.17599808773102,-2.8401643267722,12.9790793399904));
#12082=CARTESIAN_POINT('Ctrl Pts',(-1.12415615175048,-2.86053757124103,
12.9819815042013));
#12083=CARTESIAN_POINT('Ctrl Pts',(-1.03484892024039,-2.89563421695799,
12.9869810136943));
#12084=CARTESIAN_POINT('Ctrl Pts',(-0.943739652778633,-2.92660618265725,
12.9919805231873));
#12085=CARTESIAN_POINT('Ctrl Pts',(-0.851245066735443,-2.95326668053506,
12.9969800326802));
#12086=CARTESIAN_POINT('Ctrl Pts',(-0.75887594901092,-2.97989101361678,
13.0019727603703));
#12087=CARTESIAN_POINT('Ctrl Pts',(-0.665125665625023,-3.00221538180513,
13.0069654880604));
#12088=CARTESIAN_POINT('Ctrl Pts',(-0.570430384171196,-3.02010122790848,
13.0119582157505));
#12089=CARTESIAN_POINT('Ctrl Pts',(-0.47583500385242,-3.03796820489502,
13.0169456762387));
#12090=CARTESIAN_POINT('Ctrl Pts',(-0.380297036382623,-3.05140588734459,
13.021933136727));
#12091=CARTESIAN_POINT('Ctrl Pts',(-0.284266272365235,-3.06032595263896,
13.0269205972152));
#12092=CARTESIAN_POINT('Ctrl Pts',(-0.188304220604123,-3.06923963541812,
13.0319044890589));
#12093=CARTESIAN_POINT('Ctrl Pts',(-0.0918505090899103,-3.0736420865382,
13.0368883809025));
#12094=CARTESIAN_POINT('Ctrl Pts',(0.00463742261106573,-3.07349650143148,
13.0418722727462));
#12095=CARTESIAN_POINT('Ctrl Pts',(0.101090215797046,-3.07335096934325,
13.0468543495799));
#12096=CARTESIAN_POINT('Ctrl Pts',(0.197576765895643,-3.06866069254264,
13.0518364264136));
#12097=CARTESIAN_POINT('Ctrl Pts',(0.293638052471368,-3.05944095287698,
13.0568185032473));
#12098=CARTESIAN_POINT('Ctrl Pts',(0.389690580470852,-3.05022205383917,
13.0618001258304));
#12099=CARTESIAN_POINT('Ctrl Pts',(0.485317485101032,-3.03647455514263,
13.0667817484134));
#12100=CARTESIAN_POINT('Ctrl Pts',(0.580064365961156,-3.01826565784758,
13.0717633709965));
#12101=CARTESIAN_POINT('Ctrl Pts',(0.674828473473575,-3.00005344985418,
13.0767458993263));
#12102=CARTESIAN_POINT('Ctrl Pts',(0.768711808385569,-2.97737831517527,
13.0817284276561));
#12103=CARTESIAN_POINT('Ctrl Pts',(0.861270724562416,-2.95035845093638,
13.086710955986));
#12104=CARTESIAN_POINT('Ctrl Pts',(0.953929405609807,-2.92330946326597,
13.091698854747));
#12105=CARTESIAN_POINT('Ctrl Pts',(1.04526039592009,-2.89190652011431,13.0966867535081));
#12106=CARTESIAN_POINT('Ctrl Pts',(1.13483598647618,-2.85631747776725,13.1016746522691));
#12107=CARTESIAN_POINT('Ctrl Pts',(1.22446449056301,-2.82070741248442,13.1066654974504));
#12108=CARTESIAN_POINT('Ctrl Pts',(1.31233513051117,-2.78090650531467,13.1116563426317));
#12109=CARTESIAN_POINT('Ctrl Pts',(1.39804287468024,-2.73712958599987,13.116647187813));
#12110=CARTESIAN_POINT('Ctrl Pts',(1.48388912472832,-2.69328192207792,13.1216460983262));
#12111=CARTESIAN_POINT('Ctrl Pts',(1.56756511884007,-2.64544563374796,13.1266450088394));
#12112=CARTESIAN_POINT('Ctrl Pts',(1.64869303932901,-2.59388001111618,13.1316439193525));
#12113=CARTESIAN_POINT('Ctrl Pts',(1.6957926116729,-2.56394310703967,13.1345460835635));
#12114=CARTESIAN_POINT('Ctrl Pts',(1.74203393130432,-2.53275002469665,13.1374482477745));
#12115=CARTESIAN_POINT('Ctrl Pts',(1.78734827456124,-2.50035765350139,13.1403504119855));
#12116=CARTESIAN_POINT('Ctrl Pts',(1.86486694926461,-2.44494443320335,13.1453151076478));
#12117=CARTESIAN_POINT('Ctrl Pts',(1.93995177014087,-2.38581864905354,13.1502798033101));
#12118=CARTESIAN_POINT('Ctrl Pts',(2.01222215380273,-2.32322281620715,13.1552444989724));
#12119=CARTESIAN_POINT('Ctrl Pts',(2.08439421967946,-2.26071213973233,13.1602024405834));
#12120=CARTESIAN_POINT('Ctrl Pts',(2.1537591213376,-2.19474108272853,13.1651603821943));
#12121=CARTESIAN_POINT('Ctrl Pts',(2.21996586382998,-2.12559493164375,13.1701183238053));
#12122=CARTESIAN_POINT('Ctrl Pts',(2.2875456035691,-2.05501482577601,13.1751790833458));
#12123=CARTESIAN_POINT('Ctrl Pts',(2.35183433745504,-1.98112672110611,13.1802398428862));
#12124=CARTESIAN_POINT('Ctrl Pts',(2.41249487126627,-1.90427696150374,13.1853006024267));
#12125=CARTESIAN_POINT('Ctrl Pts',(2.47181879393753,-1.82912053096289,13.1902498517783));
#12126=CARTESIAN_POINT('Ctrl Pts',(2.52767247112209,-1.75113198889143,13.19519910113));
#12127=CARTESIAN_POINT('Ctrl Pts',(2.57977928200115,-1.67067085512306,13.2001483504816));
#12128=CARTESIAN_POINT('Ctrl Pts',(2.63186879451725,-1.59023643275524,13.2050959567868));
#12129=CARTESIAN_POINT('Ctrl Pts',(2.68021366949812,-1.50733142313621,13.210043563092));
#12130=CARTESIAN_POINT('Ctrl Pts',(2.72458015982682,-1.42234496613096,13.2149911693972));
#12131=CARTESIAN_POINT('Ctrl Pts',(2.76894446929367,-1.33736268668675,13.2199385324997));
#12132=CARTESIAN_POINT('Ctrl Pts',(2.80933057728359,-1.25029955885806,13.2248858956023));
#12133=CARTESIAN_POINT('Ctrl Pts',(2.84555087825037,-1.16156896019503,13.2298332587049));
#12134=CARTESIAN_POINT('Ctrl Pts',(2.88322011483118,-1.06928883485702,13.2349785332108));
#12135=CARTESIAN_POINT('Ctrl Pts',(2.91638305279126,-0.975205509233901,
13.2401238077168));
#12136=CARTESIAN_POINT('Ctrl Pts',(2.94488468889668,-0.879804761922721,
13.2452690822227));
#12137=CARTESIAN_POINT('Ctrl Pts',(2.97232631723561,-0.787952075245871,
13.2502229982075));
#12138=CARTESIAN_POINT('Ctrl Pts',(2.99544715264295,-0.694878677984494,
13.2551769141922));
#12139=CARTESIAN_POINT('Ctrl Pts',(3.01416077415891,-0.601030013827718,
13.260130830177));
#12140=CARTESIAN_POINT('Ctrl Pts',(3.03288686416896,-0.50711882027153,13.2650880468522));
#12141=CARTESIAN_POINT('Ctrl Pts',(3.04719983161365,-0.412431771857661,
13.2700452635274));
#12142=CARTESIAN_POINT('Ctrl Pts',(3.05706504618851,-0.317420152750973,
13.2750024802026));
#12143=CARTESIAN_POINT('Ctrl Pts',(3.06694455849492,-0.222270832572119,
13.2799668814102));
#12144=CARTESIAN_POINT('Ctrl Pts',(3.0723634378255,-0.12679644661346,13.2849312826177));
#12145=CARTESIAN_POINT('Ctrl Pts',(3.0733391029767,-0.0314484993978609,
13.2898956838253));
#12146=CARTESIAN_POINT('Ctrl Pts',(3.07344921798625,-0.0206873892918313,
13.2904559734756));
#12147=CARTESIAN_POINT('Ctrl Pts',(3.07350279090741,-0.00992788374214916,
13.291016263126));
#12148=CARTESIAN_POINT('Ctrl Pts',(3.0734998880982,0.000829373473862042,
13.2915765527763));
#12149=CARTESIAN_POINT('Ctrl Pts',(3.07349988809796,0.000829374363056769,
13.2915765528226));
#12150=CARTESIAN_POINT('Ctrl Pts',(3.07348755274492,0.0465417906928214,
13.2939574751383));
#12151=CARTESIAN_POINT('Ctrl Pts',(3.07245544142313,0.0922390841768832,
13.296338397454));
#12152=CARTESIAN_POINT('Ctrl Pts',(3.07040526815993,0.137890316033319,13.2987193197697));
#12153=CARTESIAN_POINT('Ctrl Pts',(3.06610027230851,0.233749708642161,13.3037188292627));
#12154=CARTESIAN_POINT('Ctrl Pts',(3.05729425420337,0.329575672356923,13.3087183387557));
#12155=CARTESIAN_POINT('Ctrl Pts',(3.04398627306693,0.424911543006448,13.3137178482487));
#12156=CARTESIAN_POINT('Ctrl Pts',(3.03069634412241,0.520118091152705,13.3187105759387));
#12157=CARTESIAN_POINT('Ctrl Pts',(3.01291664934233,0.614835436467569,13.3237033036288));
#12158=CARTESIAN_POINT('Ctrl Pts',(2.99069821909271,0.708608786507531,13.3286960313189));
#12159=CARTESIAN_POINT('Ctrl Pts',(2.96850322872691,0.802283208027114,13.3336834918072));
#12160=CARTESIAN_POINT('Ctrl Pts',(2.94187891259022,0.895015189178195,13.3386709522954));
#12161=CARTESIAN_POINT('Ctrl Pts',(2.91092773001671,0.986357947511824,13.3436584127837));
#12162=CARTESIAN_POINT('Ctrl Pts',(2.87999869373785,1.07763534796666,13.3486423046273));
#12163=CARTESIAN_POINT('Ctrl Pts',(2.84474908614169,1.16752508712019,13.353626196471));
#12164=CARTESIAN_POINT('Ctrl Pts',(2.80533153550818,1.25559437155609,13.3586100883147));
#12165=CARTESIAN_POINT('Ctrl Pts',(2.76592833977033,1.34363158333984,13.3635921651484));
#12166=CARTESIAN_POINT('Ctrl Pts',(2.72236039596414,1.42984925739188,13.3685742419821));
#12167=CARTESIAN_POINT('Ctrl Pts',(2.6748285498448,1.51383436311082,13.3735563188158));
#12168=CARTESIAN_POINT('Ctrl Pts',(2.62730103753478,1.597811811323,13.3785379413989));
#12169=CARTESIAN_POINT('Ctrl Pts',(2.57581055784248,1.67955671398161,13.383519563982));
#12170=CARTESIAN_POINT('Ctrl Pts',(2.52060349661509,1.75868139890425,13.3885011865651));
#12171=CARTESIAN_POINT('Ctrl Pts',(2.46538639777125,1.83782047008873,13.3934837148949));
#12172=CARTESIAN_POINT('Ctrl Pts',(2.40645162657592,1.91433801742991,13.3984662432247));
#12173=CARTESIAN_POINT('Ctrl Pts',(2.34408776827732,1.98787695409264,13.4034487715546));
#12174=CARTESIAN_POINT('Ctrl Pts',(2.28165669093055,2.06149515489106,13.4084366703156));
#12175=CARTESIAN_POINT('Ctrl Pts',(2.21578943203965,2.13212800019607,13.4134245690767));
#12176=CARTESIAN_POINT('Ctrl Pts',(2.14681344500153,2.19945317803327,13.4184124678378));
#12177=CARTESIAN_POINT('Ctrl Pts',(2.07779671290118,2.26681812577705,13.4234033130191));
#12178=CARTESIAN_POINT('Ctrl Pts',(2.00566792421392,2.33087122421097,13.4283941582004));
#12179=CARTESIAN_POINT('Ctrl Pts',(1.93078820319821,2.39132999905714,13.4333850033817));
#12180=CARTESIAN_POINT('Ctrl Pts',(1.85578747466234,2.45188647681028,13.4383839138949));
#12181=CARTESIAN_POINT('Ctrl Pts',(1.77802729086811,2.50883677345668,13.4433828244081));
#12182=CARTESIAN_POINT('Ctrl Pts',(1.69789830452451,2.56194137276652,13.4483817349212));
#12183=CARTESIAN_POINT('Ctrl Pts',(1.65137867273552,2.59277174413303,13.4512838991321));
#12184=CARTESIAN_POINT('Ctrl Pts',(1.60406112681724,2.6223067720711,13.454186063343));
#12185=CARTESIAN_POINT('Ctrl Pts',(1.55602560798144,2.65050684913395,13.4570882275538));
#12186=CARTESIAN_POINT('Ctrl Pts',(1.47327562728747,2.69908664777204,13.4620877370468));
#12187=CARTESIAN_POINT('Ctrl Pts',(1.38810309789964,2.74387282325471,13.4670872465398));
#12188=CARTESIAN_POINT('Ctrl Pts',(1.30089055399384,2.78461595494416,13.4720867560327));
#12189=CARTESIAN_POINT('Ctrl Pts',(1.21379631335012,2.82530381883416,13.4770794837228));
#12190=CARTESIAN_POINT('Ctrl Pts',(1.12466795224939,2.86195935453381,13.4820722114129));
#12191=CARTESIAN_POINT('Ctrl Pts',(1.03391473064707,2.89437775346464,13.487064939103));
#12192=CARTESIAN_POINT('Ctrl Pts',(0.943257251405859,2.92676195180178,13.4920523995912));
#12193=CARTESIAN_POINT('Ctrl Pts',(0.85097873054469,2.95491775272395,13.4970398600794));
#12194=CARTESIAN_POINT('Ctrl Pts',(0.757509709879273,2.97868784692835,13.5020273205677));
#12195=CARTESIAN_POINT('Ctrl Pts',(0.66410756848307,3.00244093307468,13.5070112124113));
#12196=CARTESIAN_POINT('Ctrl Pts',(0.56951704488257,3.02181444297084,13.511995104255));
#12197=CARTESIAN_POINT('Ctrl Pts',(0.474184261561738,3.03670076498939,13.5169789960987));
#12198=CARTESIAN_POINT('Ctrl Pts',(0.378886196079456,3.05158166577816,13.5219610729324));
#12199=CARTESIAN_POINT('Ctrl Pts',(0.282846841222,3.06197855785909,13.526943149766));
#12200=CARTESIAN_POINT('Ctrl Pts',(0.186521994656292,3.06783503394649,13.5319252265997));
#12201=CARTESIAN_POINT('Ctrl Pts',(0.0902059306974106,3.07369097605819,
13.5369068491828));
#12202=CARTESIAN_POINT('Ctrl Pts',(-0.00639513505244603,3.07500729879151,
13.5418884717659));
#12203=CARTESIAN_POINT('Ctrl Pts',(-0.102821880998386,3.07177959996937,
13.5468700943489));
#12204=CARTESIAN_POINT('Ctrl Pts',(-0.199266159025749,3.0685513142947,13.5518526226787));
#12205=CARTESIAN_POINT('Ctrl Pts',(-0.295535615593142,3.060777380984,13.5568351510086));
#12206=CARTESIAN_POINT('Ctrl Pts',(-0.391173608329201,3.04850544663229,
13.5618176793384));
#12207=CARTESIAN_POINT('Ctrl Pts',(-0.486914684726433,3.03622028494396,
13.5668055780994));
#12208=CARTESIAN_POINT('Ctrl Pts',(-0.582022502372989,3.01942749922731,
13.5717934768605));
#12209=CARTESIAN_POINT('Ctrl Pts',(-0.676048425958196,2.99822627160784,
13.5767813756215));
#12210=CARTESIAN_POINT('Ctrl Pts',(-0.770129891947036,2.97701252013221,
13.5817722208028));
#12211=CARTESIAN_POINT('Ctrl Pts',(-0.863127768351872,2.95138525807377,
13.5867630659841));
#12212=CARTESIAN_POINT('Ctrl Pts',(-0.954608503261393,2.92149360011297,
13.5917539111654));
#12213=CARTESIAN_POINT('Ctrl Pts',(-1.04623707334875,2.89155363647804,13.5967528216786));
#12214=CARTESIAN_POINT('Ctrl Pts',(-1.13634319626783,2.85733567212815,13.6017517321918));
#12215=CARTESIAN_POINT('Ctrl Pts',(-1.22451327617568,2.81903697855659,13.6067506427049));
#12216=CARTESIAN_POINT('Ctrl Pts',(-1.27570123997674,2.79680231411921,13.6096528069159));
#12217=CARTESIAN_POINT('Ctrl Pts',(-1.32623710529655,2.77319311371407,13.612554971127));
#12218=CARTESIAN_POINT('Ctrl Pts',(-1.37604412559677,2.74825486707667,13.615457135338));
#12219=CARTESIAN_POINT('Ctrl Pts',(-1.46319537732426,2.70461846005538,13.620535279788));
#12220=CARTESIAN_POINT('Ctrl Pts',(-1.54842440768503,2.65675455361347,13.6256134242381));
#12221=CARTESIAN_POINT('Ctrl Pts',(-1.63129387777118,2.60485748829879,13.6306915686881));
#12222=CARTESIAN_POINT('Ctrl Pts',(-1.71416334785733,2.55296042298411,13.6357697131381));
#12223=CARTESIAN_POINT('Ctrl Pts',(-1.79467281409763,2.49703037383199,13.6408478575881));
#12224=CARTESIAN_POINT('Ctrl Pts',(-1.87240768645124,2.43731239395329,13.6459260020382));
#12225=CARTESIAN_POINT('',(3.06928040870884,-0.00152685987410479,13.2084234471775));
#12226=CARTESIAN_POINT('Ctrl Pts',(3.06928040870884,-0.00152685987410479,
13.2084234471775));
#12227=CARTESIAN_POINT('Ctrl Pts',(3.06652007425599,0.609139336840024,13.2399450494086));
#12228=CARTESIAN_POINT('Ctrl Pts',(2.59469260810837,2.24642660009674,13.3242562875677));
#12229=CARTESIAN_POINT('Ctrl Pts',(0.302932054135814,3.43691440433902,13.4423067240563));
#12230=CARTESIAN_POINT('Ctrl Pts',(-1.34959247200755,2.82895289348612,13.5288355583138));
#12231=CARTESIAN_POINT('Ctrl Pts',(-1.87032611617489,2.43456032588397,13.5625747566432));
#12232=CARTESIAN_POINT('Ctrl Pts',(-1.87077372492565,2.43522501013474,12.5628034348477));
#12233=CARTESIAN_POINT('Ctrl Pts',(-2.41311427435265,2.01152685162279,12.5983731641431));
#12234=CARTESIAN_POINT('Ctrl Pts',(-3.42739819600353,0.513862713512807,
12.6867325293666));
#12235=CARTESIAN_POINT('Ctrl Pts',(-2.65434324796239,-2.47564042307807,
12.8278815305183));
#12236=CARTESIAN_POINT('Ctrl Pts',(0.631386762879294,-3.57430893153388,
12.9862504383024));
#12237=CARTESIAN_POINT('Ctrl Pts',(2.80237170594808,-1.84593683533756,13.1130977438555));
#12238=CARTESIAN_POINT('Ctrl Pts',(3.07114284215139,-0.413551259969408,
13.1871554134805));
#12239=CARTESIAN_POINT('Ctrl Pts',(3.06928040870884,-0.00152685987410479,
13.2084234471775));
#12240=CARTESIAN_POINT('Origin',(0.,0.,-2.20842344717744));
#12241=CARTESIAN_POINT('',(-1.87543872716782,2.44124936891338,11.5626912125175));
#12242=CARTESIAN_POINT('',(-1.87240768645122,2.43731239395331,11.6458032628636));
#12243=CARTESIAN_POINT('',(-1.87240768645123,2.4373123939533,-2.20842344717744));
#12244=CARTESIAN_POINT('',(3.0734992979985,0.00207730660589298,12.2915765528589));
#12245=CARTESIAN_POINT('Ctrl Pts',(-1.87240768645122,2.43731239395331,11.6458032628637));
#12246=CARTESIAN_POINT('Ctrl Pts',(-1.94893212434008,2.37852430176621,11.6507857245407));
#12247=CARTESIAN_POINT('Ctrl Pts',(-2.02266837301939,2.31614178282391,11.6557681862177));
#12248=CARTESIAN_POINT('Ctrl Pts',(-2.09327268938354,2.25046921727025,11.6607506478947));
#12249=CARTESIAN_POINT('Ctrl Pts',(-2.16395265244197,2.18472628898603,11.665738447868));
#12250=CARTESIAN_POINT('Ctrl Pts',(-2.23149366165016,2.1156865757866,11.6707262478412));
#12251=CARTESIAN_POINT('Ctrl Pts',(-2.29558845112282,2.04369173631239,11.6757140478144));
#12252=CARTESIAN_POINT('Ctrl Pts',(-2.35972043037824,1.97165512320162,11.6807047418638));
#12253=CARTESIAN_POINT('Ctrl Pts',(-2.42040193214456,1.89666031063711,11.6856954359131));
#12254=CARTESIAN_POINT('Ctrl Pts',(-2.47736699806578,1.81908081373383,11.6906861299624));
#12255=CARTESIAN_POINT('Ctrl Pts',(-2.53442483895091,1.74137496860452,11.6956849520013));
#12256=CARTESIAN_POINT('Ctrl Pts',(-2.58775391427102,1.66107639850951,11.7006837740402));
#12257=CARTESIAN_POINT('Ctrl Pts',(-2.63713249157206,1.5785862256763,11.7056825960791));
#12258=CARTESIAN_POINT('Ctrl Pts',(-2.66791130636354,1.52716818387506,11.7087984780287));
#12259=CARTESIAN_POINT('Ctrl Pts',(-2.69715614419527,1.47489912502561,11.7119143599783));
#12260=CARTESIAN_POINT('Ctrl Pts',(-2.72482273064765,1.42188021174286,11.7150302419279));
#12261=CARTESIAN_POINT('Ctrl Pts',(-2.76921445146487,1.33681005679142,11.7200297514209));
#12262=CARTESIAN_POINT('Ctrl Pts',(-2.80969643364756,1.24950959633874,11.7250292609139));
#12263=CARTESIAN_POINT('Ctrl Pts',(-2.84603864801091,1.16037332959193,11.7300287704068));
#12264=CARTESIAN_POINT('Ctrl Pts',(-2.88233156439122,1.071357975625,11.7350214980969));
#12265=CARTESIAN_POINT('Ctrl Pts',(-2.91449570921462,0.980512167588973,
11.740014225787));
#12266=CARTESIAN_POINT('Ctrl Pts',(-2.94234694291603,0.888254871932991,
11.7450069534771));
#12267=CARTESIAN_POINT('Ctrl Pts',(-2.97016879426799,0.79609490539819,11.7499944139653));
#12268=CARTESIAN_POINT('Ctrl Pts',(-2.99368665346054,0.702526829448481,
11.7549818744536));
#12269=CARTESIAN_POINT('Ctrl Pts',(-3.01276488262554,0.607988496616754,
11.7599693349418));
#12270=CARTESIAN_POINT('Ctrl Pts',(-3.03182946087159,0.513517808172177,
11.7649532267855));
#12271=CARTESIAN_POINT('Ctrl Pts',(-3.04646063755331,0.418078672019116,
11.7699371186292));
#12272=CARTESIAN_POINT('Ctrl Pts',(-3.05657318778469,0.322122023021898,
11.7749210104728));
#12273=CARTESIAN_POINT('Ctrl Pts',(-3.06668205527574,0.226200319059687,
11.7799030873065));
#12274=CARTESIAN_POINT('Ctrl Pts',(-3.07227551993004,0.129761912812199,
11.7848851641402));
#12275=CARTESIAN_POINT('Ctrl Pts',(-3.07331998006635,0.033264848187884,
11.7898672409739));
#12276=CARTESIAN_POINT('Ctrl Pts',(-3.07436434497196,-0.0632234181271112,
11.794848863557));
#12277=CARTESIAN_POINT('Ctrl Pts',(-3.0708605254204,-0.15976989324702,11.79983048614));
#12278=CARTESIAN_POINT('Ctrl Pts',(-3.06282703587796,-0.255915607759755,
11.8048121087231));
#12279=CARTESIAN_POINT('Ctrl Pts',(-3.05479208570558,-0.352078803257317,
11.8097946370529));
#12280=CARTESIAN_POINT('Ctrl Pts',(-3.04222586650875,-0.447840656006502,
11.8147771653827));
#12281=CARTESIAN_POINT('Ctrl Pts',(-3.02519874309449,-0.542747468699325,
11.8197596937125));
#12282=CARTESIAN_POINT('Ctrl Pts',(-3.00815326695057,-0.637756576949281,
11.8247475924736));
#12283=CARTESIAN_POINT('Ctrl Pts',(-2.98663736511198,-0.731908372459006,
11.8297354912346));
#12284=CARTESIAN_POINT('Ctrl Pts',(-2.96077247436889,-0.824759725628947,
11.8347233899957));
#12285=CARTESIAN_POINT('Ctrl Pts',(-2.93489230487979,-0.917665927367752,
11.839714235177));
#12286=CARTESIAN_POINT('Ctrl Pts',(-2.90465816868911,-1.00926974052672,
11.8447050803583));
#12287=CARTESIAN_POINT('Ctrl Pts',(-2.87024062061914,-1.09914559078762,
11.8496959255396));
#12288=CARTESIAN_POINT('Ctrl Pts',(-2.83576745292237,-1.18916668269209,
11.8546948360528));
#12289=CARTESIAN_POINT('Ctrl Pts',(-2.79709755011834,-1.27745383401603,
11.859693746566));
#12290=CARTESIAN_POINT('Ctrl Pts',(-2.75444856847886,-1.3636038037512,11.8646926570791));
#12291=CARTESIAN_POINT('Ctrl Pts',(-2.72968830365239,-1.41361897371392,
11.8675948212901));
#12292=CARTESIAN_POINT('Ctrl Pts',(-2.70358774084556,-1.46291429447049,
11.8704969855011));
#12293=CARTESIAN_POINT('Ctrl Pts',(-2.67619614131917,-1.51141538406501,
11.8733991497121));
#12294=CARTESIAN_POINT('Ctrl Pts',(-2.62900909334269,-1.59496739567366,
11.8783986592051));
#12295=CARTESIAN_POINT('Ctrl Pts',(-2.57782261901533,-1.67645424199032,
11.8833981686981));
#12296=CARTESIAN_POINT('Ctrl Pts',(-2.52284238147979,-1.75546819060027,
11.888397678191));
#12297=CARTESIAN_POINT('Ctrl Pts',(-2.46793672428747,-1.83437495729047,
11.8933904058811));
#12298=CARTESIAN_POINT('Ctrl Pts',(-2.40924778022429,-1.91081513582678,
11.8983831335712));
#12299=CARTESIAN_POINT('Ctrl Pts',(-2.34702672004189,-1.98440616442537,
11.9033758612613));
#12300=CARTESIAN_POINT('Ctrl Pts',(-2.28487130150936,-2.05791955634404,
11.9083633217495));
#12301=CARTESIAN_POINT('Ctrl Pts',(-2.21919145641302,-2.12858944021296,
11.9133507822378));
#12302=CARTESIAN_POINT('Ctrl Pts',(-2.15028060383048,-2.19606365453974,
11.918338242726));
#12303=CARTESIAN_POINT('Ctrl Pts',(-2.08141905857388,-2.26348958948883,
11.9233221345697));
#12304=CARTESIAN_POINT('Ctrl Pts',(-2.00933141444839,-2.3277240942753,11.9283060264133));
#12305=CARTESIAN_POINT('Ctrl Pts',(-1.93434951131711,-2.38845017073149,
11.933289918257));
#12306=CARTESIAN_POINT('Ctrl Pts',(-1.85939491473789,-2.44915413225461,
11.9382719950907));
#12307=CARTESIAN_POINT('Ctrl Pts',(-1.78154849414485,-2.5063519280796,11.9432540719244));
#12308=CARTESIAN_POINT('Ctrl Pts',(-1.70117615874688,-2.55976599065446,
11.9482361487581));
#12309=CARTESIAN_POINT('Ctrl Pts',(-1.62081115145419,-2.61317518309744,
11.9532177713412));
#12310=CARTESIAN_POINT('Ctrl Pts',(-1.53792105293739,-2.66280108538084,
11.9581993939242));
#12311=CARTESIAN_POINT('Ctrl Pts',(-1.45290092342857,-2.70840934068328,
11.9631810165073));
#12312=CARTESIAN_POINT('Ctrl Pts',(-1.36786533576198,-2.75402588837023,
11.9681635448371));
#12313=CARTESIAN_POINT('Ctrl Pts',(-1.28069933480257,-2.79562313087148,
11.973146073167));
#12314=CARTESIAN_POINT('Ctrl Pts',(-1.19182178858111,-2.83301307343671,
11.9781286014968));
#12315=CARTESIAN_POINT('Ctrl Pts',(-1.10284844546368,-2.87044331684947,
11.9831165002579));
#12316=CARTESIAN_POINT('Ctrl Pts',(-1.01216027941078,-2.90365703641834,
11.9881043990189));
#12317=CARTESIAN_POINT('Ctrl Pts',(-0.920195100561816,-2.93251482978382,
11.99309229778));
#12318=CARTESIAN_POINT('Ctrl Pts',(-0.828175596619435,-2.96138966984393,
11.9980831429613));
#12319=CARTESIAN_POINT('Ctrl Pts',(-0.734878002202757,-2.98590334872945,
12.0030739881426));
#12320=CARTESIAN_POINT('Ctrl Pts',(-0.640752144605902,-3.00596722190761,
12.0080648333239));
#12321=CARTESIAN_POINT('Ctrl Pts',(-0.546474177246193,-3.0260635188115,
12.0130637438371));
#12322=CARTESIAN_POINT('Ctrl Pts',(-0.451365706887995,-3.04169558002864,
12.0180626543502));
#12323=CARTESIAN_POINT('Ctrl Pts',(-0.355883472275034,-3.05282642876425,
12.0230615648634));
#12324=CARTESIAN_POINT('Ctrl Pts',(-0.300450368732202,-3.05928854701045,
12.0259637290744));
#12325=CARTESIAN_POINT('Ctrl Pts',(-0.244891341822311,-3.0642345106269,
12.0288658932853));
#12326=CARTESIAN_POINT('Ctrl Pts',(-0.189295602926492,-3.06766514220713,
12.0317680574963));
#12327=CARTESIAN_POINT('Ctrl Pts',(-0.0935217582459796,-3.07357503355216,
12.0367675669893));
#12328=CARTESIAN_POINT('Ctrl Pts',(0.00269733563998463,-3.07500585446188,
12.0417670764823));
#12329=CARTESIAN_POINT('Ctrl Pts',(0.098907702308422,-3.07190812304406,
12.0467665859752));
#12330=CARTESIAN_POINT('Ctrl Pts',(0.194987560225207,-3.06881459367924,
12.0517593136653));
#12331=CARTESIAN_POINT('Ctrl Pts',(0.291058279470483,-3.06120473470366,
12.0567520413554));
#12332=CARTESIAN_POINT('Ctrl Pts',(0.386662219863552,-3.04908093984568,
12.0617447690455));
#12333=CARTESIAN_POINT('Ctrl Pts',(0.482165300510072,-3.03696993528557,
12.0667322295338));
#12334=CARTESIAN_POINT('Ctrl Pts',(0.577202148086028,-3.0203545165175,12.071719690022));
#12335=CARTESIAN_POINT('Ctrl Pts',(0.671317619773631,-2.9992890663258,12.0767071505103));
#12336=CARTESIAN_POINT('Ctrl Pts',(0.765365749640577,-2.97823868895627,
12.081691042354));
#12337=CARTESIAN_POINT('Ctrl Pts',(0.858493387073661,-2.95274470561031,
12.0866749341976));
#12338=CARTESIAN_POINT('Ctrl Pts',(0.950253965723925,-2.92291287085776,
12.0916588260413));
#12339=CARTESIAN_POINT('Ctrl Pts',(1.04198112744419,-2.89309190012054,12.096640902875));
#12340=CARTESIAN_POINT('Ctrl Pts',(1.13234180252484,-2.85893635232281,12.1016229797087));
#12341=CARTESIAN_POINT('Ctrl Pts',(1.2209039496047,-2.8206020271991,12.1066050565424));
#12342=CARTESIAN_POINT('Ctrl Pts',(1.30945802185707,-2.78227119728267,12.1115866791254));
#12343=CARTESIAN_POINT('Ctrl Pts',(1.39621348936971,-2.73976252209484,12.1165683017085));
#12344=CARTESIAN_POINT('Ctrl Pts',(1.48075868428879,-2.69327977917322,12.1215499242916));
#12345=CARTESIAN_POINT('Ctrl Pts',(1.56531925101419,-2.6467885848698,12.1265324526214));
#12346=CARTESIAN_POINT('Ctrl Pts',(1.64766836240094,-2.59632209934946,12.1315149809513));
#12347=CARTESIAN_POINT('Ctrl Pts',(1.72742027654962,-2.54212931184966,12.1364975092811));
#12348=CARTESIAN_POINT('Ctrl Pts',(1.8072581515078,-2.48787811251195,12.1414854080421));
#12349=CARTESIAN_POINT('Ctrl Pts',(1.88449287681957,-2.42989283993656,12.1464733068032));
#12350=CARTESIAN_POINT('Ctrl Pts',(1.95876915644739,-2.36846482805855,12.1514612055642));
#12351=CARTESIAN_POINT('Ctrl Pts',(2.03308931209322,-2.30700052981066,12.1564520507456));
#12352=CARTESIAN_POINT('Ctrl Pts',(2.10444721774524,-2.2420897381237,12.1614428959269));
#12353=CARTESIAN_POINT('Ctrl Pts',(2.17252360988074,-2.17406150200742,12.1664337411082));
#12354=CARTESIAN_POINT('Ctrl Pts',(2.24071001518497,-2.10592333054375,12.1714326516213));
#12355=CARTESIAN_POINT('Ctrl Pts',(2.30560402268989,-2.03465797948364,12.1764315621345));
#12356=CARTESIAN_POINT('Ctrl Pts',(2.3669259444233,-1.96062842568802,12.1814304726477));
#12357=CARTESIAN_POINT('Ctrl Pts',(2.40252695911084,-1.91764987645977,12.1843326368586));
#12358=CARTESIAN_POINT('Ctrl Pts',(2.4369247941656,-1.87374023092778,12.1872348010695));
#12359=CARTESIAN_POINT('Ctrl Pts',(2.47007156829696,-1.82897476677263,12.1901369652805));
#12360=CARTESIAN_POINT('Ctrl Pts',(2.52743545420019,-1.75150354836614,12.195159457545));
#12361=CARTESIAN_POINT('Ctrl Pts',(2.58125253037603,-1.67119415335723,12.2001819498095));
#12362=CARTESIAN_POINT('Ctrl Pts',(2.63123135768053,-1.58840290617925,12.205204442074));
#12363=CARTESIAN_POINT('Ctrl Pts',(2.68114177306038,-1.50572498516095,12.2102200594601));
#12364=CARTESIAN_POINT('Ctrl Pts',(2.72722415798716,-1.4205723301429,12.2152356768462));
#12365=CARTESIAN_POINT('Ctrl Pts',(2.7692284194762,-1.33333274570354,12.2202512942323));
#12366=CARTESIAN_POINT('Ctrl Pts',(2.81118629016555,-1.24618951134734,12.2252613722161));
#12367=CARTESIAN_POINT('Ctrl Pts',(2.84907480323787,-1.1569643170881,12.2302714501999));
#12368=CARTESIAN_POINT('Ctrl Pts',(2.88268867979679,-1.06607139787701,12.2352815281837));
#12369=CARTESIAN_POINT('Ctrl Pts',(2.91627301188162,-0.97525836780017,12.2402872026255));
#12370=CARTESIAN_POINT('Ctrl Pts',(2.94559003048152,-0.8827809332977,12.2452928770672));
#12371=CARTESIAN_POINT('Ctrl Pts',(2.97048212200562,-0.789074275873315,
12.250298551509));
#12372=CARTESIAN_POINT('Ctrl Pts',(2.99536106342463,-0.695417122219682,
12.2553015815307));
#12373=CARTESIAN_POINT('Ctrl Pts',(3.01581961525063,-0.6005324551105,12.2603046115525));
#12374=CARTESIAN_POINT('Ctrl Pts',(3.03174994754583,-0.504870781047844,
12.2653076415742));
#12375=CARTESIAN_POINT('Ctrl Pts',(3.04767925349592,-0.409215270189403,
12.2703103492652));
#12376=CARTESIAN_POINT('Ctrl Pts',(3.05908083949576,-0.312783277793277,
12.2753130569563));
#12377=CARTESIAN_POINT('Ctrl Pts',(3.06589809758784,-0.216034962927947,
12.2803157646473));
#12378=CARTESIAN_POINT('Ctrl Pts',(3.07101317419918,-0.14344345533498,12.2840693607057));
#12379=CARTESIAN_POINT('Ctrl Pts',(3.07354846896932,-0.0706741086629879,
12.2878229567642));
#12380=CARTESIAN_POINT('Ctrl Pts',(3.07349929799898,0.00207730590177175,
12.2915765528226));
#12381=CARTESIAN_POINT('Ctrl Pts',(3.0734992979985,0.00207730660587326,
12.2915765528589));
#12382=CARTESIAN_POINT('Ctrl Pts',(3.07342502235092,0.1119725671587,12.297246578924));
#12383=CARTESIAN_POINT('Ctrl Pts',(3.06745263996488,0.221638779441771,12.3029166049891));
#12384=CARTESIAN_POINT('Ctrl Pts',(3.05567972599531,0.330490033346267,12.3085866310542));
#12385=CARTESIAN_POINT('Ctrl Pts',(3.04384899836097,0.439875826951024,12.3142845011167));
#12386=CARTESIAN_POINT('Ctrl Pts',(3.02616075202313,0.548438458326586,12.3199823711792));
#12387=CARTESIAN_POINT('Ctrl Pts',(3.00276350587142,0.6556016914307,12.3256802412417));
#12388=CARTESIAN_POINT('Ctrl Pts',(2.97923000797536,0.76338897991921,12.3314112923346));
#12389=CARTESIAN_POINT('Ctrl Pts',(2.94992093138339,0.869760348844745,12.3371423434275));
#12390=CARTESIAN_POINT('Ctrl Pts',(2.91503564058203,0.974150637292065,12.3428733945204));
#12391=CARTESIAN_POINT('Ctrl Pts',(2.90360721621096,1.00834890507739,12.3447508873685));
#12392=CARTESIAN_POINT('Ctrl Pts',(2.89158071887444,1.04233473933266,12.3466283802165));
#12393=CARTESIAN_POINT('Ctrl Pts',(2.87896424539992,1.07608880846745,12.3485058730646));
#12394=CARTESIAN_POINT('Ctrl Pts',(2.84536828312017,1.16597132878745,12.3535053825576));
#12395=CARTESIAN_POINT('Ctrl Pts',(2.8075000202345,1.25443689238546,12.3585048920505));
#12396=CARTESIAN_POINT('Ctrl Pts',(2.76549909601537,1.34105070744479,12.3635044015435));
#12397=CARTESIAN_POINT('Ctrl Pts',(2.72355514578328,1.4275470314139,12.3684971292336));
#12398=CARTESIAN_POINT('Ctrl Pts',(2.67748986552302,1.51219620745523,12.3734898569237));
#12399=CARTESIAN_POINT('Ctrl Pts',(2.62749176748801,1.59458121830867,12.3784825846138));
#12400=CARTESIAN_POINT('Ctrl Pts',(2.57754641618609,1.67687931505238,12.383470045102));
#12401=CARTESIAN_POINT('Ctrl Pts',(2.52367672164747,1.75691762180739,12.3884575055903));
#12402=CARTESIAN_POINT('Ctrl Pts',(2.4661176642449,1.83430256939777,12.3934449660785));
#12403=CARTESIAN_POINT('Ctrl Pts',(2.40859979169336,1.91163214624927,12.3984288579222));
#12404=CARTESIAN_POINT('Ctrl Pts',(2.34739806535293,1.98631178693987,12.4034127497658));
#12405=CARTESIAN_POINT('Ctrl Pts',(2.28279089484576,2.05797667149297,12.4083966416095));
#12406=CARTESIAN_POINT('Ctrl Pts',(2.21820725266996,2.12961545747004,12.4133787184432));
#12407=CARTESIAN_POINT('Ctrl Pts',(2.15022092405051,2.19824134301797,12.4183607952769));
#12408=CARTESIAN_POINT('Ctrl Pts',(2.07915011426217,2.26352315039268,12.4233428721106));
#12409=CARTESIAN_POINT('Ctrl Pts',(2.00808578449422,2.32879900557064,12.4283244946937));
#12410=CARTESIAN_POINT('Ctrl Pts',(1.93393785610592,2.3907310919662,12.4333061172767));
#12411=CARTESIAN_POINT('Ctrl Pts',(1.85706006057644,2.44902637417645,12.4382877398598));
#12412=CARTESIAN_POINT('Ctrl Pts',(1.78016828730922,2.50733225549611,12.4432702681896));
#12413=CARTESIAN_POINT('Ctrl Pts',(1.70054601096471,2.56199975421922,12.4482527965195));
#12414=CARTESIAN_POINT('Ctrl Pts',(1.61857770211763,2.61277792248167,12.4532353248493));
#12415=CARTESIAN_POINT('Ctrl Pts',(1.53652104351402,2.66361082212586,12.4582232236103));
#12416=CARTESIAN_POINT('Ctrl Pts',(1.4521136779172,2.71054579056773,12.4632111223714));
#12417=CARTESIAN_POINT('Ctrl Pts',(1.36576635612441,2.75337692851499,12.4681990211324));
#12418=CARTESIAN_POINT('Ctrl Pts',(1.27936802778348,2.79623336740332,12.4731898663138));
#12419=CARTESIAN_POINT('Ctrl Pts',(1.19102786326098,2.83498097260127,12.4781807114951));
#12420=CARTESIAN_POINT('Ctrl Pts',(1.10117639047012,2.8694621111057,12.4831715566764));
#12421=CARTESIAN_POINT('Ctrl Pts',(1.01117971543017,2.90399897200073,12.4881704671895));
#12422=CARTESIAN_POINT('Ctrl Pts',(0.919667271856441,2.93425546127061,12.4931693777027));
#12423=CARTESIAN_POINT('Ctrl Pts',(0.827084463137039,2.96012390633185,12.4981682882159));
#12424=CARTESIAN_POINT('Ctrl Pts',(0.773334648390229,2.97514207384115,12.5010704524268));
#12425=CARTESIAN_POINT('Ctrl Pts',(0.719224272795122,2.98868220974375,12.5039726166378));
#12426=CARTESIAN_POINT('Ctrl Pts',(0.664841586868226,3.00073122994555,12.5068747808488));
#12427=CARTESIAN_POINT('Ctrl Pts',(0.571149478699316,3.02148964017917,12.5118747156359));
#12428=CARTESIAN_POINT('Ctrl Pts',(0.476319648394481,3.03789227164926,12.5168746504229));
#12429=CARTESIAN_POINT('Ctrl Pts',(0.38079293596222,3.04981950120352,12.52187458521));
#12430=CARTESIAN_POINT('Ctrl Pts',(0.282176421702118,3.06213251578836,12.5270362423808));
#12431=CARTESIAN_POINT('Ctrl Pts',(0.182817606641743,3.06967548974739,12.5321978995516));
#12432=CARTESIAN_POINT('Ctrl Pts',(0.0832165932657832,3.07237322742619,
12.5373595567224));
#12433=CARTESIAN_POINT('Ctrl Pts',(-0.0130116700547539,3.07497961267195,
12.5423464267206));
#12434=CARTESIAN_POINT('Ctrl Pts',(-0.109465510670845,3.07306357916795,
12.5473332967189));
#12435=CARTESIAN_POINT('Ctrl Pts',(-0.205686907854918,3.06660971529425,
12.5523201667172));
#12436=CARTESIAN_POINT('Ctrl Pts',(-0.30184492868777,3.06016010226657,12.5573037521069));
#12437=CARTESIAN_POINT('Ctrl Pts',(-0.397770373701489,3.04917862723745,
12.5622873374966));
#12438=CARTESIAN_POINT('Ctrl Pts',(-0.49300583624215,3.03370194571437,12.5672709228863));
#12439=CARTESIAN_POINT('Ctrl Pts',(-0.588204571716693,3.01823123269389,
12.5722525863819));
#12440=CARTESIAN_POINT('Ctrl Pts',(-0.682713420992185,2.99826882989282,
12.5772342498776));
#12441=CARTESIAN_POINT('Ctrl Pts',(-0.776081777843846,2.97390304551085,
12.5822159133732));
#12442=CARTESIAN_POINT('Ctrl Pts',(-0.869439616633389,2.94954000596496,
12.5871970156782));
#12443=CARTESIAN_POINT('Ctrl Pts',(-0.96165679443306,2.92077468393078,12.5921781179832));
#12444=CARTESIAN_POINT('Ctrl Pts',(-1.05229559545297,2.88774587347818,12.5971592202883));
#12445=CARTESIAN_POINT('Ctrl Pts',(-1.14298524824181,2.85469853262339,12.6021431171786));
#12446=CARTESIAN_POINT('Ctrl Pts',(-1.23209434306856,2.81738307702337,12.607127014069));
#12447=CARTESIAN_POINT('Ctrl Pts',(-1.31920345658343,2.77598711995181,12.6121109109593));
#12448=CARTESIAN_POINT('Ctrl Pts',(-1.4063423521144,2.73457700988281,12.6170965118103));
#12449=CARTESIAN_POINT('Ctrl Pts',(-1.49147951532831,2.68908382281959,12.6220821126612));
#12450=CARTESIAN_POINT('Ctrl Pts',(-1.57422008596841,2.639741156048,12.6270677135122));
#12451=CARTESIAN_POINT('Ctrl Pts',(-1.65704779881578,2.59034652167621,12.6320585651882));
#12452=CARTESIAN_POINT('Ctrl Pts',(-1.7374735140984,2.53709455552647,12.6370494168642));
#12453=CARTESIAN_POINT('Ctrl Pts',(-1.81513171210194,2.48026190506605,12.6420402685402));
#12454=CARTESIAN_POINT('Ctrl Pts',(-1.83439558793767,2.46616401005907,12.6432782981298));
#12455=CARTESIAN_POINT('Ctrl Pts',(-1.85348932959634,2.45184597482623,12.6445163277194));
#12456=CARTESIAN_POINT('Ctrl Pts',(-1.87240768645123,2.43731239395329,12.6457543573089));
#12457=CARTESIAN_POINT('',(3.07749897857868,-0.00155006825877461,12.2084234471775));
#12458=CARTESIAN_POINT('Ctrl Pts',(3.07749897857868,-0.00155006825877461,
12.2084234471775));
#12459=CARTESIAN_POINT('Ctrl Pts',(3.07177196381206,0.924255192727474,12.2565405671735));
#12460=CARTESIAN_POINT('Ctrl Pts',(2.13549779090968,2.87581154197502,12.3574473230977));
#12461=CARTESIAN_POINT('Ctrl Pts',(-0.413050570340105,3.30353187187741,
12.4755739856545));
#12462=CARTESIAN_POINT('Ctrl Pts',(-1.60821750621956,2.64034444383588,12.5455835282151));
#12463=CARTESIAN_POINT('Ctrl Pts',(-1.87077372492565,2.43522501013474,12.5628034348477));
#12464=CARTESIAN_POINT('Ctrl Pts',(-1.87543872716782,2.44124936891338,11.5626912125175));
#12465=CARTESIAN_POINT('Ctrl Pts',(-2.67063619912824,1.82902599129973,11.6148938670213));
#12466=CARTESIAN_POINT('Ctrl Pts',(-3.61429065672828,-0.258675541093378,
11.7198861574532));
#12467=CARTESIAN_POINT('Ctrl Pts',(-1.76367158133378,-3.17234867812122,
11.8776680838132));
#12468=CARTESIAN_POINT('Ctrl Pts',(1.70070785150167,-3.20654430598149,12.0360369915973));
#12469=CARTESIAN_POINT('Ctrl Pts',(3.03378404611734,-1.1965068427,12.1462887793855));
#12470=CARTESIAN_POINT('Ctrl Pts',(3.07805511260628,-0.0914523698142579,
12.2037509312455));
#12471=CARTESIAN_POINT('Ctrl Pts',(3.07749897857868,-0.00155006825877461,
12.2084234471775));
#12472=CARTESIAN_POINT('Origin',(0.,0.,-2.20842344717744));
#12473=CARTESIAN_POINT('',(-1.87115843792479,2.43565187781327,10.5625482443637));
#12474=CARTESIAN_POINT('',(-1.87240768645123,2.4373123939533,10.6459243044939));
#12475=CARTESIAN_POINT('',(-1.87240768645123,2.4373123939533,-2.20842344717744));
#12476=CARTESIAN_POINT('',(3.07349905914928,-0.00240487182579642,11.2915765527899));
#12477=CARTESIAN_POINT('Ctrl Pts',(-1.87240768645123,2.4373123939533,10.6459243044939));
#12478=CARTESIAN_POINT('Ctrl Pts',(-1.94880420429965,2.37862257331628,10.6509091987637));
#12479=CARTESIAN_POINT('Ctrl Pts',(-2.02250521179709,2.3162862646041,10.6558940930335));
#12480=CARTESIAN_POINT('Ctrl Pts',(-2.09314840489398,2.2505848140183,10.6608789873033));
#12481=CARTESIAN_POINT('Ctrl Pts',(-2.16375882816078,2.18491384089648,10.6658615691898));
#12482=CARTESIAN_POINT('Ctrl Pts',(-2.23131393414587,2.11588112560119,10.6708441510764));
#12483=CARTESIAN_POINT('Ctrl Pts',(-2.2954853084557,2.04380758601783,10.6758267329629));
#12484=CARTESIAN_POINT('Ctrl Pts',(-2.35964443383017,1.97174780372324,10.6808083637817));
#12485=CARTESIAN_POINT('Ctrl Pts',(-2.42042081939891,1.89664867850762,10.6857899946005));
#12486=CARTESIAN_POINT('Ctrl Pts',(-2.47752441800935,1.81886640745478,10.6907716254193));
#12487=CARTESIAN_POINT('Ctrl Pts',(-2.53463270582119,1.74107774912086,10.6957536653168));
#12488=CARTESIAN_POINT('Ctrl Pts',(-2.58806734829466,1.6606058615445,10.7007357052144));
#12489=CARTESIAN_POINT('Ctrl Pts',(-2.63758058586237,1.57783741338641,10.705717745112));
#12490=CARTESIAN_POINT('Ctrl Pts',(-2.6871443911959,1.49498443398558,10.7107048731564));
#12491=CARTESIAN_POINT('Ctrl Pts',(-2.73277856605105,1.40983058652907,10.7156920012009));
#12492=CARTESIAN_POINT('Ctrl Pts',(-2.77428055371357,1.32278859206101,10.7206791292454));
#12493=CARTESIAN_POINT('Ctrl Pts',(-2.81580334639611,1.23570296328675,10.725668757346));
#12494=CARTESIAN_POINT('Ctrl Pts',(-2.85318965513954,1.14672770694656,10.7306583854466));
#12495=CARTESIAN_POINT('Ctrl Pts',(-2.88628533694828,1.05629503630253,10.7356480135472));
#12496=CARTESIAN_POINT('Ctrl Pts',(-2.91943817036192,0.96570620110831,10.7406462580364));
#12497=CARTESIAN_POINT('Ctrl Pts',(-2.94828543995732,0.873655342310838,
10.7456445025256));
#12498=CARTESIAN_POINT('Ctrl Pts',(-2.97272303537711,0.780589523974215,
10.7506427470147));
#12499=CARTESIAN_POINT('Ctrl Pts',(-2.99582312290602,0.692617343708724,
10.7553674297508));
#12500=CARTESIAN_POINT('Ctrl Pts',(-3.0149834079316,0.603738674301219,10.7600921124868));
#12501=CARTESIAN_POINT('Ctrl Pts',(-3.03015849914791,0.51433619359491,10.7648167952229));
#12502=CARTESIAN_POINT('Ctrl Pts',(-3.04621629960373,0.419733322681323,
10.7698163047159));
#12503=CARTESIAN_POINT('Ctrl Pts',(-3.05786774372333,0.324211570568965,
10.7748158142088));
#12504=CARTESIAN_POINT('Ctrl Pts',(-3.06501536928884,0.228217080918975,
10.7798153237018));
#12505=CARTESIAN_POINT('Ctrl Pts',(-3.07215329914568,0.132352807184427,
10.7848080513919));
#12506=CARTESIAN_POINT('Ctrl Pts',(-3.07479952016354,0.0360175043909558,
10.789800779082));
#12507=CARTESIAN_POINT('Ctrl Pts',(-3.07290776230443,-0.0603335260793813,
10.7947935067721));
#12508=CARTESIAN_POINT('Ctrl Pts',(-3.07101800020218,-0.156582908641232,
10.7997809672603));
#12509=CARTESIAN_POINT('Ctrl Pts',(-3.06459978496209,-0.252847549351398,
10.8047684277486));
#12510=CARTESIAN_POINT('Ctrl Pts',(-3.05365880648686,-0.348669103255899,
10.8097558882368));
#12511=CARTESIAN_POINT('Ctrl Pts',(-3.04272565653749,-0.444422094598561,
10.8147397800805));
#12512=CARTESIAN_POINT('Ctrl Pts',(-3.02727622630673,-0.53973219451599,
10.8197236719241));
#12513=CARTESIAN_POINT('Ctrl Pts',(-3.00736819811476,-0.6341441247603,10.8247075637678));
#12514=CARTESIAN_POINT('Ctrl Pts',(-2.98746741993359,-0.728521672517914,
10.8296896406015));
#12515=CARTESIAN_POINT('Ctrl Pts',(-2.9631113604055,-0.822001271418687,
10.8346717174352));
#12516=CARTESIAN_POINT('Ctrl Pts',(-2.93440900753201,-0.914136765760458,
10.8396537942689));
#12517=CARTESIAN_POINT('Ctrl Pts',(-2.90570927165185,-1.0062638594678,10.8446354168519));
#12518=CARTESIAN_POINT('Ctrl Pts',(-2.87266416104143,-1.09704667322843,
10.849617039435));
#12519=CARTESIAN_POINT('Ctrl Pts',(-2.83543253547355,-1.18605420903854,
10.8545986620181));
#12520=CARTESIAN_POINT('Ctrl Pts',(-2.79819414053999,-1.27507792798728,
10.8595811903479));
#12521=CARTESIAN_POINT('Ctrl Pts',(-2.75676788836516,-1.36232532300698,
10.8645637186778));
#12522=CARTESIAN_POINT('Ctrl Pts',(-2.71136035032648,-1.44738636883089,
10.8695462470076));
#12523=CARTESIAN_POINT('Ctrl Pts',(-2.66590386965403,-1.53253909792575,
10.8745341457687));
#12524=CARTESIAN_POINT('Ctrl Pts',(-2.61645774311551,-1.615500385283,10.8795220445297));
#12525=CARTESIAN_POINT('Ctrl Pts',(-2.56327388343319,-1.69588597744935,
10.8845099432908));
#12526=CARTESIAN_POINT('Ctrl Pts',(-2.51005860731485,-1.77631905448852,
10.8895007884721));
#12527=CARTESIAN_POINT('Ctrl Pts',(-2.45310146076598,-1.85417305267419,
10.8944916336534));
#12528=CARTESIAN_POINT('Ctrl Pts',(-2.39269568836348,-1.92909553752187,
10.8994824788347));
#12529=CARTESIAN_POINT('Ctrl Pts',(-2.33219229870749,-2.00413909899692,
10.9044813893479));
#12530=CARTESIAN_POINT('Ctrl Pts',(-2.26822944612432,-2.07624135944133,
10.909480299861));
#12531=CARTESIAN_POINT('Ctrl Pts',(-2.20113831793107,-2.14508562890519,
10.9144792103742));
#12532=CARTESIAN_POINT('Ctrl Pts',(-2.16218793652258,-2.18505381286063,
10.9173813745851));
#12533=CARTESIAN_POINT('Ctrl Pts',(-2.12218382895313,-2.22392461687581,
10.9202835387961));
#12534=CARTESIAN_POINT('Ctrl Pts',(-2.08119575623373,-2.26164242846537,
10.923185703007));
#12535=CARTESIAN_POINT('Ctrl Pts',(-2.01058629248023,-2.32661826835241,
10.9281852125));
#12536=CARTESIAN_POINT('Ctrl Pts',(-1.93680703068045,-2.38839837684194,
10.933184721993));
#12537=CARTESIAN_POINT('Ctrl Pts',(-1.86017912923878,-2.44665809976475,
10.9381842314859));
#12538=CARTESIAN_POINT('Ctrl Pts',(-1.78365517305884,-2.50483879374337,
10.943176959176));
#12539=CARTESIAN_POINT('Ctrl Pts',(-1.70429060344906,-2.559508329507,10.9481696868661));
#12540=CARTESIAN_POINT('Ctrl Pts',(-1.62244213190176,-2.61038000655653,
10.9531624145562));
#12541=CARTESIAN_POINT('Ctrl Pts',(-1.54068000842828,-2.66119801526942,
10.9581498750445));
#12542=CARTESIAN_POINT('Ctrl Pts',(-1.45643956315769,-2.7082258997491,10.9631373355327));
#12543=CARTESIAN_POINT('Ctrl Pts',(-1.37010835017776,-2.75121888601637,
10.968124796021));
#12544=CARTESIAN_POINT('Ctrl Pts',(-1.28383890919933,-2.79418110979671,
10.9731086878647));
#12545=CARTESIAN_POINT('Ctrl Pts',(-1.19548206628226,-2.83311397959144,
10.9780925797083));
#12546=CARTESIAN_POINT('Ctrl Pts',(-1.10545111053776,-2.86781800193297,
10.983076471552));
#12547=CARTESIAN_POINT('Ctrl Pts',(-1.01545294183751,-2.9025093859291,10.9880585483857));
#12548=CARTESIAN_POINT('Ctrl Pts',(-0.923782280826665,-2.93297482464626,
10.9930406252194));
#12549=CARTESIAN_POINT('Ctrl Pts',(-0.83087269815376,-2.95906282621081,
10.9980227020531));
#12550=CARTESIAN_POINT('Ctrl Pts',(-0.737971586694155,-2.98514844915068,
11.0030043246362));
#12551=CARTESIAN_POINT('Ctrl Pts',(-0.643832200827791,-3.0068573099751,
11.0079859472193));
#12552=CARTESIAN_POINT('Ctrl Pts',(-0.54890254980647,-3.02408800149995,
11.0129675698023));
#12553=CARTESIAN_POINT('Ctrl Pts',(-0.45395563890225,-3.04132182586806,
11.0179500981321));
#12554=CARTESIAN_POINT('Ctrl Pts',(-0.358218609393281,-3.05407578555472,
11.022932626462));
#12555=CARTESIAN_POINT('Ctrl Pts',(-0.262147855418949,-3.06229991214108,
11.0279151547918));
#12556=CARTESIAN_POINT('Ctrl Pts',(-0.165973551330405,-3.07053290312386,
11.0329030535528));
#12557=CARTESIAN_POINT('Ctrl Pts',(-0.069465242745026,-3.07422627605858,
11.0378909523139));
#12558=CARTESIAN_POINT('Ctrl Pts',(0.0269176072301352,-3.07338212600077,
11.042878851075));
#12559=CARTESIAN_POINT('Ctrl Pts',(0.123357391877683,-3.07253747729193,
11.0478696962563));
#12560=CARTESIAN_POINT('Ctrl Pts',(0.219671132277135,-3.06714999302599,
11.0528605414376));
#12561=CARTESIAN_POINT('Ctrl Pts',(0.315403551634229,-3.0572737609865,11.0578513866189));
#12562=CARTESIAN_POINT('Ctrl Pts',(0.411290676998466,-3.04738156870663,
11.062850297132));
#12563=CARTESIAN_POINT('Ctrl Pts',(0.506594171740867,-3.03298620967495,
11.0678492076452));
#12564=CARTESIAN_POINT('Ctrl Pts',(0.600868083322849,-3.0141930589204,11.0728481181584));
#12565=CARTESIAN_POINT('Ctrl Pts',(0.655599683638426,-3.00328251963643,
11.0757502823693));
#12566=CARTESIAN_POINT('Ctrl Pts',(0.709984512979423,-2.99089065275642,
11.0786524465803));
#12567=CARTESIAN_POINT('Ctrl Pts',(0.763937942530848,-2.97704569497375,
11.0815546107912));
#12568=CARTESIAN_POINT('Ctrl Pts',(0.85688260851611,-2.9531952189727,11.0865541202842));
#12569=CARTESIAN_POINT('Ctrl Pts',(0.948872521154095,-2.92494601987679,
11.0915536297772));
#12570=CARTESIAN_POINT('Ctrl Pts',(1.03946050783772,-2.89239072440875,11.0965531392701));
#12571=CARTESIAN_POINT('Ctrl Pts',(1.12992561249269,-2.85987958999226,11.1015458669602));
#12572=CARTESIAN_POINT('Ctrl Pts',(1.21899216114105,-2.82307411537443,11.1065385946503));
#12573=CARTESIAN_POINT('Ctrl Pts',(1.30622545948717,-2.78211741286875,11.1115313223404));
#12574=CARTESIAN_POINT('Ctrl Pts',(1.39336672890235,-2.74120391865186,11.1165187828287));
#12575=CARTESIAN_POINT('Ctrl Pts',(1.47867819752203,-2.6961480881761,11.1215062433169));
#12576=CARTESIAN_POINT('Ctrl Pts',(1.5617435463928,-2.64714173124531,11.1264937038051));
#12577=CARTESIAN_POINT('Ctrl Pts',(1.64474946006468,-2.59817043950851,11.1314775956488));
#12578=CARTESIAN_POINT('Ctrl Pts',(1.72551207194317,-2.54525446306206,11.1364614874925));
#12579=CARTESIAN_POINT('Ctrl Pts',(1.80363903254495,-2.48863185109415,11.1414453793361));
#12580=CARTESIAN_POINT('Ctrl Pts',(1.88173754124274,-2.43202985967909,11.1464274561698));
#12581=CARTESIAN_POINT('Ctrl Pts',(1.95720195069225,-2.37172417211289,11.1514095330035));
#12582=CARTESIAN_POINT('Ctrl Pts',(2.02966913246219,-2.3079959841235,11.1563916098372));
#12583=CARTESIAN_POINT('Ctrl Pts',(2.10212970689451,-2.24427360667681,11.1613732324203));
#12584=CARTESIAN_POINT('Ctrl Pts',(2.17159326746409,-2.17712963924476,11.1663548550033));
#12585=CARTESIAN_POINT('Ctrl Pts',(2.23773083527072,-2.10688465723176,11.1713364775864));
#12586=CARTESIAN_POINT('Ctrl Pts',(2.30388042805232,-2.03662690344354,11.1763190059162));
#12587=CARTESIAN_POINT('Ctrl Pts',(2.36670252620823,-1.96326733494622,11.181301534246));
#12588=CARTESIAN_POINT('Ctrl Pts',(2.4259067321126,-1.8871615662393,11.1862840625758));
#12589=CARTESIAN_POINT('Ctrl Pts',(2.48517475142586,-1.81097376672962,11.1912719613369));
#12590=CARTESIAN_POINT('Ctrl Pts',(2.54081682341243,-1.73203420469199,11.1962598600979));
#12591=CARTESIAN_POINT('Ctrl Pts',(2.59258454998284,-1.65072941489217,11.201247758859));
#12592=CARTESIAN_POINT('Ctrl Pts',(2.6443828564599,-1.56937659723704,11.2062386040403));
#12593=CARTESIAN_POINT('Ctrl Pts',(2.69230204253117,-1.48565615061418,11.2112294492216));
#12594=CARTESIAN_POINT('Ctrl Pts',(2.73613960045087,-1.39997940586444,11.2162202944029));
#12595=CARTESIAN_POINT('Ctrl Pts',(2.78004800097113,-1.31416420533171,11.2212192049161));
#12596=CARTESIAN_POINT('Ctrl Pts',(2.81986142135796,-1.22638679349434,11.2262181154292));
#12597=CARTESIAN_POINT('Ctrl Pts',(2.85542544981688,-1.13707860350023,11.2312170259424));
#12598=CARTESIAN_POINT('Ctrl Pts',(2.87607247886868,-1.08522989925399,11.2341191901534));
#12599=CARTESIAN_POINT('Ctrl Pts',(2.89528818176261,-1.03286555270386,11.2370213543644));
#12600=CARTESIAN_POINT('Ctrl Pts',(2.9130501669288,-0.980071923358748,11.2399235185754));
#12601=CARTESIAN_POINT('Ctrl Pts',(2.94920738770405,-0.872602465756003,
11.24583131498));
#12602=CARTESIAN_POINT('Ctrl Pts',(2.97944169451371,-0.763046477916852,
11.2517391113846));
#12603=CARTESIAN_POINT('Ctrl Pts',(3.00354581196166,-0.652008286333519,
11.2576469077892));
#12604=CARTESIAN_POINT('Ctrl Pts',(3.02740835185802,-0.542082947544464,
11.2634954947664));
#12605=CARTESIAN_POINT('Ctrl Pts',(3.04526290787206,-0.430705059009903,
11.2693440817437));
#12606=CARTESIAN_POINT('Ctrl Pts',(3.05695463632113,-0.318481712936139,
11.2751926687209));
#12607=CARTESIAN_POINT('Ctrl Pts',(3.0678721407953,-0.213689774925965,11.2806539634106));
#12608=CARTESIAN_POINT('Ctrl Pts',(3.07341630993048,-0.108160880684027,
11.2861152581002));
#12609=CARTESIAN_POINT('Ctrl Pts',(3.07349905914928,-0.00240487182581181,
11.2915765527899));
#12610=CARTESIAN_POINT('Ctrl Pts',(3.07349905914977,-0.00240487119193424,
11.2915765528226));
#12611=CARTESIAN_POINT('Ctrl Pts',(3.07357440903969,0.0938945965502631,
11.2965495068653));
#12612=CARTESIAN_POINT('Ctrl Pts',(3.06911954638383,0.19025278966347,11.301522460908));
#12613=CARTESIAN_POINT('Ctrl Pts',(3.0601446217697,0.286211711594748,11.3064954149507));
#12614=CARTESIAN_POINT('Ctrl Pts',(3.05117154752427,0.382150849584164,11.3114673437147));
#12615=CARTESIAN_POINT('Ctrl Pts',(3.03768030403397,0.477690441648078,11.3164392724788));
#12616=CARTESIAN_POINT('Ctrl Pts',(3.01973301736176,0.572376409240685,11.3214112012428));
#12617=CARTESIAN_POINT('Ctrl Pts',(3.0017844941583,0.667068900502275,11.3263834725626));
#12618=CARTESIAN_POINT('Ctrl Pts',(2.97937940044349,0.760907217840555,11.3313557438823));
#12619=CARTESIAN_POINT('Ctrl Pts',(2.95263100332818,0.853447366968359,11.3363280152021));
#12620=CARTESIAN_POINT('Ctrl Pts',(2.92485280817899,0.949550259060418,11.3414917161319));
#12621=CARTESIAN_POINT('Ctrl Pts',(2.89239026140698,1.04425251028761,11.3466554170616));
#12622=CARTESIAN_POINT('Ctrl Pts',(2.85542656316388,1.1370758076655,11.3518191179914));
#12623=CARTESIAN_POINT('Ctrl Pts',(2.81977708586466,1.22659883133449,11.3567992267962));
#12624=CARTESIAN_POINT('Ctrl Pts',(2.77994134730084,1.31437386440542,11.3617793356009));
#12625=CARTESIAN_POINT('Ctrl Pts',(2.73613155296547,1.39999513387254,11.3667594444057));
#12626=CARTESIAN_POINT('Ctrl Pts',(2.69228901873109,1.48568038975541,11.3717432749412));
#12627=CARTESIAN_POINT('Ctrl Pts',(2.64446673693219,1.56920829804497,11.3767271054767));
#12628=CARTESIAN_POINT('Ctrl Pts',(2.59292101568734,1.65020085335298,11.3817109360122));
#12629=CARTESIAN_POINT('Ctrl Pts',(2.5412957660873,1.73131836965778,11.3867024559512));
#12630=CARTESIAN_POINT('Ctrl Pts',(2.4859358713261,1.80989237280952,11.3916939758901));
#12631=CARTESIAN_POINT('Ctrl Pts',(2.42713849798068,1.885577089811,11.396685495829));
#12632=CARTESIAN_POINT('Ctrl Pts',(2.42082891055362,1.89369886994575,11.3972211393392));
#12633=CARTESIAN_POINT('Ctrl Pts',(2.41447977355891,1.90178741316436,11.3977567828494));
#12634=CARTESIAN_POINT('Ctrl Pts',(2.40809147900629,1.90984231776796,11.3982924263596));
#12635=CARTESIAN_POINT('Ctrl Pts',(2.34846536825864,1.98502398479978,11.4032919358526));
#12636=CARTESIAN_POINT('Ctrl Pts',(2.28521034726906,2.05754269684224,11.4082914453455));
#12637=CARTESIAN_POINT('Ctrl Pts',(2.21859308199777,2.12702773524739,11.4132909548385));
#12638=CARTESIAN_POINT('Ctrl Pts',(2.15206618262392,2.19641851763906,11.4182836825286));
#12639=CARTESIAN_POINT('Ctrl Pts',(2.08218640456877,2.26278349084693,11.4232764102187));
#12640=CARTESIAN_POINT('Ctrl Pts',(2.00926144500829,2.32578388841337,11.4282691379088));
#12641=CARTESIAN_POINT('Ctrl Pts',(1.93641341944198,2.38871782214838,11.433256598397));
#12642=CARTESIAN_POINT('Ctrl Pts',(1.86052692921064,2.4482939510779,11.4382440588852));
#12643=CARTESIAN_POINT('Ctrl Pts',(1.78194666857371,2.50421011905133,11.4432315193734));
#12644=CARTESIAN_POINT('Ctrl Pts',(1.70342263394998,2.5600862776996,11.4482154112171));
#12645=CARTESIAN_POINT('Ctrl Pts',(1.62220901724139,2.61230742764699,11.4531993030607));
#12646=CARTESIAN_POINT('Ctrl Pts',(1.53868298702528,2.66061213171687,11.4581831949044));
#12647=CARTESIAN_POINT('Ctrl Pts',(1.45518737492063,2.7088992444099,11.4631652717381));
#12648=CARTESIAN_POINT('Ctrl Pts',(1.36938140212152,2.75327252554152,11.4681473485718));
#12649=CARTESIAN_POINT('Ctrl Pts',(1.28166974847641,2.79351479427628,11.4731294254055));
#12650=CARTESIAN_POINT('Ctrl Pts',(1.19396609211332,2.83375339384326,11.4781110479886));
#12651=CARTESIAN_POINT('Ctrl Pts',(1.10435749941049,2.86986154698606,11.4830926705716));
#12652=CARTESIAN_POINT('Ctrl Pts',(1.01327071436631,2.90166929704396,11.4880742931547));
#12653=CARTESIAN_POINT('Ctrl Pts',(0.922167368139779,2.93348283031123,11.4930568214845));
#12654=CARTESIAN_POINT('Ctrl Pts',(0.829585710239929,2.96099426297874,11.4980393498143));
#12655=CARTESIAN_POINT('Ctrl Pts',(0.735968779924244,2.98408314310725,11.5030218781442));
#12656=CARTESIAN_POINT('Ctrl Pts',(0.642250944354815,3.00719690964572,11.5080097769052));
#12657=CARTESIAN_POINT('Ctrl Pts',(0.547496035534339,3.02587850176322,11.5129976756662));
#12658=CARTESIAN_POINT('Ctrl Pts',(0.452158234263065,3.04005841739729,11.5179855744273));
#12659=CARTESIAN_POINT('Ctrl Pts',(0.35676411564386,3.05424670930218,11.5229764196086));
#12660=CARTESIAN_POINT('Ctrl Pts',(0.260786855513396,3.0639279857834,11.5279672647899));
#12661=CARTESIAN_POINT('Ctrl Pts',(0.16468459847902,3.06908475494304,11.5329581099712));
#12662=CARTESIAN_POINT('Ctrl Pts',(0.068427037770403,3.07424985757188,11.5379570204844));
#12663=CARTESIAN_POINT('Ctrl Pts',(-0.0279554845304961,3.074875850145,11.5429559309975));
#12664=CARTESIAN_POINT('Ctrl Pts',(-0.124006045127911,3.0709973544065,11.5479548415107));
#12665=CARTESIAN_POINT('Ctrl Pts',(-0.179769095632414,3.0687456574627,11.5508570057217));
#12666=CARTESIAN_POINT('Ctrl Pts',(-0.235420357734087,3.06497669821172,
11.5537591699327));
#12667=CARTESIAN_POINT('Ctrl Pts',(-0.290871837190708,3.05970518585195,
11.5566613341437));
#12668=CARTESIAN_POINT('Ctrl Pts',(-0.386389650552053,3.05062475484006,
11.5616604501667));
#12669=CARTESIAN_POINT('Ctrl Pts',(-0.481649604251123,3.03705127990046,
11.5666595661897));
#12670=CARTESIAN_POINT('Ctrl Pts',(-0.576195663337729,3.01900659282997,
11.5716586822127));
#12671=CARTESIAN_POINT('Ctrl Pts',(-0.670619513877616,3.00098522999957,
11.5766513364677));
#12672=CARTESIAN_POINT('Ctrl Pts',(-0.764330875845443,2.97850421941971,
11.5816439907226));
#12673=CARTESIAN_POINT('Ctrl Pts',(-0.856878087759706,2.95163720547043,
11.5866366449776));
#12674=CARTESIAN_POINT('Ctrl Pts',(-0.949320804020787,2.92480052723968,
11.5916236619945));
#12675=CARTESIAN_POINT('Ctrl Pts',(-1.04060156506698,2.89358781598924,11.5966106790113));
#12676=CARTESIAN_POINT('Ctrl Pts',(-1.13027937124325,2.85812364899456,11.6015976960282));
#12677=CARTESIAN_POINT('Ctrl Pts',(-1.21989648872633,2.82268348207349,11.6065813381237));
#12678=CARTESIAN_POINT('Ctrl Pts',(-1.30791240017554,2.78299773785967,11.6115649802192));
#12679=CARTESIAN_POINT('Ctrl Pts',(-1.39390252402616,2.73924040630126,11.6165486223146));
#12680=CARTESIAN_POINT('Ctrl Pts',(-1.47987428012675,2.69549242144097,11.6215311998891));
#12681=CARTESIAN_POINT('Ctrl Pts',(-1.56382071308338,2.64767476729304,11.6265137774636));
#12682=CARTESIAN_POINT('Ctrl Pts',(-1.64533919886181,2.59600870004104,11.6314963550381));
#12683=CARTESIAN_POINT('Ctrl Pts',(-1.72336290210065,2.54655761099916,11.6362653243133));
#12684=CARTESIAN_POINT('Ctrl Pts',(-1.79916222732898,2.49358148814015,11.6410342935885));
#12685=CARTESIAN_POINT('Ctrl Pts',(-1.87240768645122,2.43731239395331,11.6458032628637));
#12686=CARTESIAN_POINT('',(3.07371628270923,0.00276101913198965,11.2084234471775));
#12687=CARTESIAN_POINT('Ctrl Pts',(3.07371628270923,0.00276101913198965,
11.2084234471775));
#12688=CARTESIAN_POINT('Ctrl Pts',(3.07581988160793,0.232901496003139,11.2203464490105));
#12689=CARTESIAN_POINT('Ctrl Pts',(2.94733814809347,1.47967347839142,11.2850590867715));
#12690=CARTESIAN_POINT('Ctrl Pts',(1.2479789847658,3.4083547403351,11.4025613604607));
#12691=CARTESIAN_POINT('Ctrl Pts',(-1.04966881457196,3.06922939603839,11.508727613741));
#12692=CARTESIAN_POINT('Ctrl Pts',(-1.86649730169686,2.4481333818731,11.5621042310933));
#12693=CARTESIAN_POINT('Ctrl Pts',(-1.87543872716782,2.44124936891338,11.5626912125175));
#12694=CARTESIAN_POINT('Ctrl Pts',(-1.87115843792448,2.43565187781351,10.5625482443637));
#12695=CARTESIAN_POINT('Ctrl Pts',(-2.11905849301121,2.24865376720641,10.5786044367557));
#12696=CARTESIAN_POINT('Ctrl Pts',(-3.0601924156055,1.29275809429756,10.6474502650758));
#12697=CARTESIAN_POINT('Ctrl Pts',(-3.36917065569085,-1.35019356953496,
10.7690857293239));
#12698=CARTESIAN_POINT('Ctrl Pts',(-0.701818273267178,-3.56114935009612,
10.9274546371081));
#12699=CARTESIAN_POINT('Ctrl Pts',(2.35600370687118,-2.60536866769977,11.0739005430593));
#12700=CARTESIAN_POINT('Ctrl Pts',(3.06650610127338,-0.786055991087847,
11.1675568130824));
#12701=CARTESIAN_POINT('Ctrl Pts',(3.07371628270923,0.00276101913198965,
11.2084234471775));
#12702=CARTESIAN_POINT('Origin',(0.,0.,-2.20842344717744));
#12703=CARTESIAN_POINT('',(-1.87002230068587,2.43424832114153,9.56277191102392));
#12704=CARTESIAN_POINT('',(-1.87507731191802,2.44082532704937,9.64577043858893));
#12705=CARTESIAN_POINT('',(-1.87240768645123,2.4373123939533,-2.20842344717744));
#12706=CARTESIAN_POINT('',(3.0739867692329,-0.000220521378201549,10.2915765528225));
#12707=CARTESIAN_POINT('Ctrl Pts',(-1.87507731191802,2.44082532704937,9.64577043858893));
#12708=CARTESIAN_POINT('Ctrl Pts',(-1.92849728325354,2.40024009778082,9.64925843930383));
#12709=CARTESIAN_POINT('Ctrl Pts',(-2.76718558415343,1.71569386742277,9.70553607594679));
#12710=CARTESIAN_POINT('Ctrl Pts',(-3.59172323438899,-0.523312921182784,
9.81460334851782));
#12711=CARTESIAN_POINT('Ctrl Pts',(-1.51656848075747,-3.29762827636767,
9.97297225630197));
#12712=CARTESIAN_POINT('Ctrl Pts',(1.9403270808479,-3.06748480440487,10.1313411640862));
#12713=CARTESIAN_POINT('Ctrl Pts',(3.07300908756268,-1.0389883880359,10.2375425962597));
#12714=CARTESIAN_POINT('Ctrl Pts',(3.0784786722727,-0.0121816033650862,
10.2909543925051));
#12715=CARTESIAN_POINT('Ctrl Pts',(3.07846623440684,-0.000220842725659706,
10.2915765528225));
#12716=CARTESIAN_POINT('Ctrl Pts',(3.07349999209138,-0.000220486457828013,
10.2915765528225));
#12717=CARTESIAN_POINT('Ctrl Pts',(3.0735068617889,0.0955405661343771,10.2965657840521));
#12718=CARTESIAN_POINT('Ctrl Pts',(3.06903399635637,0.191473368380318,10.3015550152818));
#12719=CARTESIAN_POINT('Ctrl Pts',(3.06005921740527,0.287123381097861,10.3065442465114));
#12720=CARTESIAN_POINT('Ctrl Pts',(3.05109660660792,0.382643709945966,10.3115267132588));
#12721=CARTESIAN_POINT('Ctrl Pts',(3.03764425277441,0.477881575931341,10.3165091800062));
#12722=CARTESIAN_POINT('Ctrl Pts',(3.019731980344,0.572381880292938,10.3214916467536));
#12723=CARTESIAN_POINT('Ctrl Pts',(3.00183853151596,0.666782876419912,10.3264688775392));
#12724=CARTESIAN_POINT('Ctrl Pts',(2.97949456205797,0.760447420636118,10.3314461083249));
#12725=CARTESIAN_POINT('Ctrl Pts',(2.95278164157565,0.852926038513187,10.3364233391106));
#12726=CARTESIAN_POINT('Ctrl Pts',(2.92608756221715,0.945339429486644,10.341397059362));
#12727=CARTESIAN_POINT('Ctrl Pts',(2.8950307790698,1.03656813428827,10.3463707796135));
#12728=CARTESIAN_POINT('Ctrl Pts',(2.8597436192445,1.12617435692275,10.3513444998649));
#12729=CARTESIAN_POINT('Ctrl Pts',(2.82446895324371,1.21574885344421,10.3563164591136));
#12730=CARTESIAN_POINT('Ctrl Pts',(2.78496704774315,1.30370159915195,10.3612884183622));
#12731=CARTESIAN_POINT('Ctrl Pts',(2.74141929078964,1.38961236396573,10.3662603776108));
#12732=CARTESIAN_POINT('Ctrl Pts',(2.69787493067551,1.47551642751427,10.3712319490336));
#12733=CARTESIAN_POINT('Ctrl Pts',(2.65028554620233,1.55937843360771,10.3762035204563));
#12734=CARTESIAN_POINT('Ctrl Pts',(2.59887915089251,1.640801453271,10.3811750918791));
#12735=CARTESIAN_POINT('Ctrl Pts',(2.54746257427934,1.72224059918585,10.3861476479473));
#12736=CARTESIAN_POINT('Ctrl Pts',(2.49222772110145,1.80123942658639,10.3911202040156));
#12737=CARTESIAN_POINT('Ctrl Pts',(2.43344610969157,1.87742970074168,10.3960927600839));
#12738=CARTESIAN_POINT('Ctrl Pts',(2.37460080990357,1.95370252511756,10.4010707037899));
#12739=CARTESIAN_POINT('Ctrl Pts',(2.31220135119068,2.02716037259249,10.406048647496));
#12740=CARTESIAN_POINT('Ctrl Pts',(2.24655957909046,2.09746807069783,10.4110265912021));
#12741=CARTESIAN_POINT('Ctrl Pts',(2.18087770752789,2.16781871860181,10.4160075758508));
#12742=CARTESIAN_POINT('Ctrl Pts',(2.11194989512604,2.23501507871381,10.4209885604995));
#12743=CARTESIAN_POINT('Ctrl Pts',(2.04012333288603,2.29876032604837,10.4259695451483));
#12744=CARTESIAN_POINT('Ctrl Pts',(1.96818290531611,2.36260662755274,10.4309584260605));
#12745=CARTESIAN_POINT('Ctrl Pts',(1.89333489730439,2.42299061854258,10.4359473069727));
#12746=CARTESIAN_POINT('Ctrl Pts',(1.8159577522221,2.47965717230113,10.4409361878849));
#12747=CARTESIAN_POINT('Ctrl Pts',(1.77902970865396,2.50670113940314,10.4433171184748));
#12748=CARTESIAN_POINT('Ctrl Pts',(1.74152601497156,2.53289905876088,10.4456980490646));
#12749=CARTESIAN_POINT('Ctrl Pts',(1.70348979365072,2.5582268806593,10.4480789796545));
#12750=CARTESIAN_POINT('Ctrl Pts',(1.62362083384983,2.61141057553755,10.4530784891475));
#12751=CARTESIAN_POINT('Ctrl Pts',(1.54111857553602,2.66094378308378,10.4580779986405));
#12752=CARTESIAN_POINT('Ctrl Pts',(1.45635082880792,2.70655583970301,10.4630775081334));
#12753=CARTESIAN_POINT('Ctrl Pts',(1.37169806899008,2.75210602385703,10.4680702358235));
#12754=CARTESIAN_POINT('Ctrl Pts',(1.28478631163001,2.79374542205774,10.4730629635136));
#12755=CARTESIAN_POINT('Ctrl Pts',(1.19601257379454,2.83124639926047,10.4780556912037));
#12756=CARTESIAN_POINT('Ctrl Pts',(1.10733249001466,2.86870781387757,10.4830431516919));
#12757=CARTESIAN_POINT('Ctrl Pts',(1.01679473296664,2.90203931679327,10.4880306121802));
#12758=CARTESIAN_POINT('Ctrl Pts',(0.924820254834722,2.93105949210306,10.4930180726684));
#12759=CARTESIAN_POINT('Ctrl Pts',(0.832911586591927,2.96005890279903,10.4980019645121));
#12760=CARTESIAN_POINT('Ctrl Pts',(0.739568658314046,2.98475298673081,10.5029858563557));
#12761=CARTESIAN_POINT('Ctrl Pts',(0.645230789620373,3.00500906456634,10.5079697481994));
#12762=CARTESIAN_POINT('Ctrl Pts',(0.550927276441999,3.02525776564001,10.5129518250331));
#12763=CARTESIAN_POINT('Ctrl Pts',(0.455629971505204,3.04107157979621,10.5179339018668));
#12764=CARTESIAN_POINT('Ctrl Pts',(0.359790751080044,3.05236840264036,10.5229159787005));
#12765=CARTESIAN_POINT('Ctrl Pts',(0.263960268983606,3.06366419547455,10.5278976012836));
#12766=CARTESIAN_POINT('Ctrl Pts',(0.167588405601096,3.070443764618,10.5328792238666));
#12767=CARTESIAN_POINT('Ctrl Pts',(0.0711334977556424,3.0726767281146,10.5378608464497));
#12768=CARTESIAN_POINT('Ctrl Pts',(-0.0253389472913298,3.07491009760331,
10.5428433747795));
#12769=CARTESIAN_POINT('Ctrl Pts',(-0.121894027946735,3.0725952095872,10.5478259031094));
#12770=CARTESIAN_POINT('Ctrl Pts',(-0.218073137579717,3.06575379909512,
10.5528084314392));
#12771=CARTESIAN_POINT('Ctrl Pts',(-0.314355914118239,3.05890501457079,
10.5577963302002));
#12772=CARTESIAN_POINT('Ctrl Pts',(-0.41026147202538,3.04751999844631,10.5627842289613));
#12773=CARTESIAN_POINT('Ctrl Pts',(-0.505336283203386,3.03167239174654,
10.5677721277223));
#12774=CARTESIAN_POINT('Ctrl Pts',(-0.600467256377221,3.01581542364799,
10.5727629729036));
#12775=CARTESIAN_POINT('Ctrl Pts',(-0.694766076783461,2.99549070848603,
10.5777538180849));
#12776=CARTESIAN_POINT('Ctrl Pts',(-0.787791450552504,2.97082259322841,
10.5827446632662));
#12777=CARTESIAN_POINT('Ctrl Pts',(-0.880967155674901,2.94611461367354,
10.5877435737794));
#12778=CARTESIAN_POINT('Ctrl Pts',(-0.972864886698754,2.91704935082506,
10.5927424842926));
#12779=CARTESIAN_POINT('Ctrl Pts',(-1.06306054931225,2.88380036037447,10.5977413948057));
#12780=CARTESIAN_POINT('Ctrl Pts',(-1.11542448408048,2.8644973482715,10.6006435590167));
#12781=CARTESIAN_POINT('Ctrl Pts',(-1.16721513135671,2.84378510836322,10.6035457232277));
#12782=CARTESIAN_POINT('Ctrl Pts',(-1.21835329387807,2.82170471546837,10.6064478874387));
#12783=CARTESIAN_POINT('Ctrl Pts',(-1.30644831667027,2.7836671204625,10.6114474065788));
#12784=CARTESIAN_POINT('Ctrl Pts',(-1.39291503604813,2.74143320524252,10.6164469257189));
#12785=CARTESIAN_POINT('Ctrl Pts',(-1.47732616423593,2.69516412384552,10.6214464448589));
#12786=CARTESIAN_POINT('Ctrl Pts',(-1.56161152410786,2.6489639810419,10.6264385149681));
#12787=CARTESIAN_POINT('Ctrl Pts',(-1.64384700138803,2.59874083633503,10.6314305850773));
#12788=CARTESIAN_POINT('Ctrl Pts',(-1.72362566041007,2.5447036827057,10.6364226551865));
#12789=CARTESIAN_POINT('Ctrl Pts',(-1.77424119155379,2.51041983705109,10.6395898716223));
#12790=CARTESIAN_POINT('Ctrl Pts',(-1.82386818012003,2.47460172337064,10.6427570880581));
#12791=CARTESIAN_POINT('Ctrl Pts',(-1.87240768645123,2.4373123939533,10.6459243044939));
#12792=CARTESIAN_POINT('',(3.06865031396352,-0.000662305851861743,10.2084234471775));
#12793=CARTESIAN_POINT('Ctrl Pts',(3.06865031396352,-0.000662305851861743,
10.2084234471775));
#12794=CARTESIAN_POINT('Ctrl Pts',(3.0675799278391,0.552109147929758,10.2369419667754));
#12795=CARTESIAN_POINT('Ctrl Pts',(2.66113839896666,2.12956437036722,10.3182501223015));
#12796=CARTESIAN_POINT('Ctrl Pts',(0.440568577236155,3.44770654288841,10.4362917213636));
#12797=CARTESIAN_POINT('Ctrl Pts',(-1.30401135511826,2.86346716363096,10.5258148008277));
#12798=CARTESIAN_POINT('Ctrl Pts',(-1.87115843792448,2.43565187781351,10.5625482443637));
#12799=CARTESIAN_POINT('Ctrl Pts',(-1.87002230068597,2.43424832114145,9.56277191102393));
#12800=CARTESIAN_POINT('Ctrl Pts',(-2.36808575988716,2.04690839709662,9.59534906562752));
#12801=CARTESIAN_POINT('Ctrl Pts',(-3.38005807385769,0.642742195174603,
9.68071585615918));
#12802=CARTESIAN_POINT('Ctrl Pts',(-2.79015488039725,-2.32150152396616,
9.81887228261889));
#12803=CARTESIAN_POINT('Ctrl Pts',(0.428153388171217,-3.60430551682002,
9.97724119040307));
#12804=CARTESIAN_POINT('Ctrl Pts',(2.74707663572839,-1.96358325211724,10.1070915785893));
#12805=CARTESIAN_POINT('Ctrl Pts',(3.0695612822224,-0.471106790621865,10.1841523308474));
#12806=CARTESIAN_POINT('Ctrl Pts',(3.06865031396352,-0.000662305851861743,
10.2084234471775));
#12807=CARTESIAN_POINT('Origin',(0.,0.,-2.20842344717744));
#12808=CARTESIAN_POINT('',(-1.87509145403828,2.44076729861451,8.56274498137416));
#12809=CARTESIAN_POINT('',(-1.87008710121024,2.4342504331012,8.6457400628962));
#12810=CARTESIAN_POINT('',(-1.87240768645123,2.4373123939533,-2.20842344717744));
#12811=CARTESIAN_POINT('',(3.07146331992749,0.00257687728019439,9.29157655282255));
#12812=CARTESIAN_POINT('Ctrl Pts',(-1.87008710121014,2.43425043310128,8.64574006289619));
#12813=CARTESIAN_POINT('Ctrl Pts',(-2.18011611706346,2.19903440513027,8.66583370660699));
#12814=CARTESIAN_POINT('Ctrl Pts',(-3.14634585166812,1.14383563916985,8.73871698624584));
#12815=CARTESIAN_POINT('Ctrl Pts',(-3.25637227139195,-1.60323792246698,
8.86438990181277));
#12816=CARTESIAN_POINT('Ctrl Pts',(-0.428153365804491,-3.60430532853098,
9.02275880959692));
#12817=CARTESIAN_POINT('Ctrl Pts',(2.46555070482014,-2.45088718888649,9.16515435993354));
#12818=CARTESIAN_POINT('Ctrl Pts',(3.06576103701022,-0.709387139347176,
9.25476027434207));
#12819=CARTESIAN_POINT('Ctrl Pts',(3.07146331992749,0.00257687728019439,
9.29157655282255));
#12820=CARTESIAN_POINT('Ctrl Pts',(3.07146331992749,0.00257687728019439,
9.29157655282255));
#12821=CARTESIAN_POINT('Ctrl Pts',(3.07393735062978,0.311474359502131,9.30754991027013));
#12822=CARTESIAN_POINT('Ctrl Pts',(2.88937061009456,1.63834518503067,9.37631290364576));
#12823=CARTESIAN_POINT('Ctrl Pts',(1.03904173686729,3.44037562732375,9.49437753223457));
#12824=CARTESIAN_POINT('Ctrl Pts',(-1.1200052362076,3.01448294124964,9.59646880337577));
#12825=CARTESIAN_POINT('Ctrl Pts',(-1.87507731191802,2.44082532704937,9.64577043858893));
#12826=CARTESIAN_POINT('',(3.07611314785335,-0.00227856489099164,9.20842344717746));
#12827=CARTESIAN_POINT('Ctrl Pts',(3.07611314785335,-0.00227856489099164,
9.20842344717746));
#12828=CARTESIAN_POINT('Ctrl Pts',(3.06889864904703,0.866771338679833,9.25353748454042));
#12829=CARTESIAN_POINT('Ctrl Pts',(2.23070911990389,2.7649081202533,9.35144115783146));
#12830=CARTESIAN_POINT('Ctrl Pts',(-0.289334010845272,3.33608061026952,
9.46955731244694));
#12831=CARTESIAN_POINT('Ctrl Pts',(-1.56099904527893,2.67457320759152,9.54255942969946));
#12832=CARTESIAN_POINT('Ctrl Pts',(-1.87002230068597,2.43424832114145,9.56277191102393));
#12833=CARTESIAN_POINT('Ctrl Pts',(-1.87509145403828,2.44076729861451,8.56274498137416));
#12834=CARTESIAN_POINT('Ctrl Pts',(-2.62208853077648,1.86033637000951,8.61192663029266));
#12835=CARTESIAN_POINT('Ctrl Pts',(-3.59091621734738,-0.111479728561327,
8.71389791513923));
#12836=CARTESIAN_POINT('Ctrl Pts',(-1.94032718221066,-3.06748496465039,
8.86865883591383));
#12837=CARTESIAN_POINT('Ctrl Pts',(1.51656855998305,-3.29762844863588,9.02702774369802));
#12838=CARTESIAN_POINT('Ctrl Pts',(3.0005807836722,-1.31362321131185,9.14028261411922));
#12839=CARTESIAN_POINT('Ctrl Pts',(3.07734060608858,-0.150136716870874,
9.20074784861237));
#12840=CARTESIAN_POINT('Ctrl Pts',(3.07611314785335,-0.00227856489099164,
9.20842344717746));
#12841=CARTESIAN_POINT('Origin',(0.,0.,-2.20842344717744));
#12842=CARTESIAN_POINT('',(-1.87240768645123,2.4373123939533,7.56258888046525));
#12843=CARTESIAN_POINT('',(-1.87108789359224,2.43562943220425,7.64596441938478));
#12844=CARTESIAN_POINT('',(-1.87240768645123,2.4373123939533,-2.20842344717744));
#12845=CARTESIAN_POINT('',(3.06961342576491,-0.00179236055451414,8.29157655282255));
#12846=CARTESIAN_POINT('Ctrl Pts',(-1.87108789359255,2.43562943220401,7.6459644193848));
#12847=CARTESIAN_POINT('Ctrl Pts',(-2.4288603418159,1.99933281172997,7.68257879536437));
#12848=CARTESIAN_POINT('Ctrl Pts',(-3.44303055876561,0.468116087731995,
7.77198280727201));
#12849=CARTESIAN_POINT('Ctrl Pts',(-2.60495841071609,-2.52755294392938,
7.9141764551077));
#12850=CARTESIAN_POINT('Ctrl Pts',(0.701818236604134,-3.56114916406156,
8.07254536289188));
#12851=CARTESIAN_POINT('Ctrl Pts',(2.8206242810132,-1.80488084996747,8.19834539546349));
#12852=CARTESIAN_POINT('Ctrl Pts',(3.07170577833404,-0.393421405353705,
8.27135579210705));
#12853=CARTESIAN_POINT('Ctrl Pts',(3.06961342576491,-0.00179236055451414,
8.29157655282255));
#12854=CARTESIAN_POINT('Ctrl Pts',(3.06961342576491,-0.00179236055451414,
8.29157655282255));
#12855=CARTESIAN_POINT('Ctrl Pts',(3.06624334633598,0.628990905670613,8.32414542803511));
#12856=CARTESIAN_POINT('Ctrl Pts',(2.57037956950142,2.28704841286455,8.40950393917573));
#12857=CARTESIAN_POINT('Ctrl Pts',(0.2554864632756,3.43210578860563,8.52755844253362));
#12858=CARTESIAN_POINT('Ctrl Pts',(-1.36561382421955,2.81698944901127,8.61304407067893));
#12859=CARTESIAN_POINT('Ctrl Pts',(-1.87008710121014,2.43425043310128,8.64574006289619));
#12860=CARTESIAN_POINT('',(3.07349899192449,0.00248930494810733,8.20842344717746));
#12861=CARTESIAN_POINT('Ctrl Pts',(3.07544103263855,0.00249087785624028,
8.20842344717746));
#12862=CARTESIAN_POINT('Ctrl Pts',(3.07695265662786,0.174416482836779,8.21734336637735));
#12863=CARTESIAN_POINT('Ctrl Pts',(2.98575884214701,1.36222404473923,8.2790529215053));
#12864=CARTESIAN_POINT('Ctrl Pts',(1.43881299711621,3.33228911436436,8.3935521125613));
#12865=CARTESIAN_POINT('Ctrl Pts',(-0.940162896586096,3.11776444662607,
8.50273937142698));
#12866=CARTESIAN_POINT('Ctrl Pts',(-1.82029142580991,2.48334796226457,8.5591369943646));
#12867=CARTESIAN_POINT('Ctrl Pts',(-1.87509145403828,2.44076729861451,8.56274498137416));
#12868=CARTESIAN_POINT('Ctrl Pts',(-1.87240768645123,2.4373123939533,7.56258888046525));
#12869=CARTESIAN_POINT('Ctrl Pts',(-1.94889060415999,2.37855619866402,7.56757962088293));
#12870=CARTESIAN_POINT('Ctrl Pts',(-2.02253758922204,2.31624850330128,7.57257036130061));
#12871=CARTESIAN_POINT('Ctrl Pts',(-2.09301755323034,2.25070650504895,7.57756110171829));
#12872=CARTESIAN_POINT('Ctrl Pts',(-2.16361202823142,2.18505801867062,7.58255995074737));
#12873=CARTESIAN_POINT('Ctrl Pts',(-2.23102890013812,2.11616504953983,7.58755879977645));
#12874=CARTESIAN_POINT('Ctrl Pts',(-2.29497537334076,2.04438017153353,7.59255764880554));
#12875=CARTESIAN_POINT('Ctrl Pts',(-2.33399138281656,2.00058167350474,7.5956076237505));
#12876=CARTESIAN_POINT('Ctrl Pts',(-2.37171628177913,1.95570725733652,7.59865759869547));
#12877=CARTESIAN_POINT('Ctrl Pts',(-2.4080914790063,1.90984231776795,7.60170757364043));
#12878=CARTESIAN_POINT('Ctrl Pts',(-2.46771758975397,1.83466065073611,7.60670708313341));
#12879=CARTESIAN_POINT('Ctrl Pts',(-2.52392424819064,1.75655192635735,7.61170659262638));
#12880=CARTESIAN_POINT('Ctrl Pts',(-2.57641121104058,1.67586023332031,7.61670610211936));
#12881=CARTESIAN_POINT('Ctrl Pts',(-2.62882697565872,1.59527799805247,7.62169882980945));
#12882=CARTESIAN_POINT('Ctrl Pts',(-2.67753283546951,1.51212012247806,7.62669155749954));
#12883=CARTESIAN_POINT('Ctrl Pts',(-2.722269004492,1.42676337112436,7.63168428518964));
#12884=CARTESIAN_POINT('Ctrl Pts',(-2.7669579779838,1.3414966689918,7.63667174567787));
#12885=CARTESIAN_POINT('Ctrl Pts',(-2.80768538333751,1.25403608935131,7.6416592061661));
#12886=CARTESIAN_POINT('Ctrl Pts',(-2.84423550879916,1.16478608357327,7.64664666665433));
#12887=CARTESIAN_POINT('Ctrl Pts',(-2.88075948179167,1.07559993826063,7.651630558498));
#12888=CARTESIAN_POINT('Ctrl Pts',(-2.91311195088674,0.984627317191547,
7.65661445034167));
#12889=CARTESIAN_POINT('Ctrl Pts',(-2.94112424919369,0.892295018928627,
7.66159834218534));
#12890=CARTESIAN_POINT('Ctrl Pts',(-2.9691263461154,0.799996345801906,7.66658041901903));
#12891=CARTESIAN_POINT('Ctrl Pts',(-2.99279128538638,0.706339398938925,
7.67156249585273));
#12892=CARTESIAN_POINT('Ctrl Pts',(-3.01199975905624,0.611767685845843,
7.67654457268643));
#12893=CARTESIAN_POINT('Ctrl Pts',(-3.03120648135583,0.51720459551419,7.6815261952695));
#12894=CARTESIAN_POINT('Ctrl Pts',(-3.04595745871357,0.421727334993386,
7.68650781785256));
#12895=CARTESIAN_POINT('Ctrl Pts',(-3.05618439138251,0.325790140842137,
7.69148944043563));
#12896=CARTESIAN_POINT('Ctrl Pts',(-3.066413183488,0.229835503618643,7.69647196876546));
#12897=CARTESIAN_POINT('Ctrl Pts',(-3.07211625082295,0.133421203175779,
7.70145449709529));
#12898=CARTESIAN_POINT('Ctrl Pts',(-3.07327720859963,0.0370060684490644,
7.70643702542512));
#12899=CARTESIAN_POINT('Ctrl Pts',(-3.0744394177177,-0.0595129875833837,
7.71142492418617));
#12900=CARTESIAN_POINT('Ctrl Pts',(-3.07104973812129,-0.156032440036607,
7.71641282294722));
#12901=CARTESIAN_POINT('Ctrl Pts',(-3.06314393340569,-0.252094215006905,
7.72140072170827));
#12902=CARTESIAN_POINT('Ctrl Pts',(-3.05523345862272,-0.348212734986198,
7.72639156688958));
#12903=CARTESIAN_POINT('Ctrl Pts',(-3.04280160336488,-0.443872604060398,
7.73138241207089));
#12904=CARTESIAN_POINT('Ctrl Pts',(-3.02593567731295,-0.538623733941082,
7.7363732572522));
#12905=CARTESIAN_POINT('Ctrl Pts',(-3.0090424954986,-0.633527984040422,
7.74137216776536));
#12906=CARTESIAN_POINT('Ctrl Pts',(-2.98770103195924,-0.727520134807251,
7.74637107827852));
#12907=CARTESIAN_POINT('Ctrl Pts',(-2.9620490623146,-0.820163155988626,
7.75136998879168));
#12908=CARTESIAN_POINT('Ctrl Pts',(-2.94715657163131,-0.873947927642711,
7.75427215300265));
#12909=CARTESIAN_POINT('Ctrl Pts',(-2.93081215209485,-0.927278294014041,
7.75717431721363));
#12910=CARTESIAN_POINT('Ctrl Pts',(-2.91305016692879,-0.98007192335876,
7.76007648142461));
#12911=CARTESIAN_POINT('Ctrl Pts',(-2.88245189371052,-1.07101862102636,
7.76507599091758));
#12912=CARTESIAN_POINT('Ctrl Pts',(-2.84753670122274,-1.16069074941773,
7.77007550041056));
#12913=CARTESIAN_POINT('Ctrl Pts',(-2.80842974048275,-1.24864912716583,
7.77507500990354));
#12914=CARTESIAN_POINT('Ctrl Pts',(-2.76937582808669,-1.33648818993301,
7.78006773759363));
#12915=CARTESIAN_POINT('Ctrl Pts',(-2.72614162500842,-1.42261772455461,
7.78506046528372));
#12916=CARTESIAN_POINT('Ctrl Pts',(-2.67890171754387,-1.50661469451898,
7.79005319297381));
#12917=CARTESIAN_POINT('Ctrl Pts',(-2.6317116469909,-1.59052304979738,7.79504065346204));
#12918=CARTESIAN_POINT('Ctrl Pts',(-2.58052448695269,-1.67230293231824,
7.80002811395028));
#12919=CARTESIAN_POINT('Ctrl Pts',(-2.52556204351728,-1.75155320054654,
7.80501557443851));
#12920=CARTESIAN_POINT('Ctrl Pts',(-2.47063892699494,-1.83074676335538,
7.80999946628218));
#12921=CARTESIAN_POINT('Ctrl Pts',(-2.41194614658159,-1.90741395039178,
7.81498335812585));
#12922=CARTESIAN_POINT('Ctrl Pts',(-2.34974986666695,-1.98118091402544,
7.81996724996951));
#12923=CARTESIAN_POINT('Ctrl Pts',(-2.28757623709701,-2.05492101355795,
7.82494932680321));
#12924=CARTESIAN_POINT('Ctrl Pts',(-2.22190192574253,-2.12576265296946,
7.8299314036369));
#12925=CARTESIAN_POINT('Ctrl Pts',(-2.15303398587823,-2.1933642893175,7.8349134804706));
#12926=CARTESIAN_POINT('Ctrl Pts',(-2.08417232518345,-2.26095976195375,
7.83989510305366));
#12927=CARTESIAN_POINT('Ctrl Pts',(-2.01211792829748,-2.32531551149458,
7.84487672563673));
#12928=CARTESIAN_POINT('Ctrl Pts',(-1.93721461943757,-2.38612693883568,
7.8498583482198));
#12929=CARTESIAN_POINT('Ctrl Pts',(-1.86229769183637,-2.44694942276573,
7.85484087654963));
#12930=CARTESIAN_POINT('Ctrl Pts',(-1.78453116435683,-2.50422602803074,
7.85982340487945));
#12931=CARTESIAN_POINT('Ctrl Pts',(-1.70429097844702,-2.55769320106695,
7.86480593320928));
#12932=CARTESIAN_POINT('Ctrl Pts',(-1.62396430544244,-2.61121800383581,
7.86979383197033));
#12933=CARTESIAN_POINT('Ctrl Pts',(-1.54115901700692,-2.66092493329987,
7.87478173073138));
#12934=CARTESIAN_POINT('Ctrl Pts',(-1.45627881354217,-2.70659458863499,
7.87976962949243));
#12935=CARTESIAN_POINT('Ctrl Pts',(-1.37134847017622,-2.75229122166235,
7.88476047467374));
#12936=CARTESIAN_POINT('Ctrl Pts',(-1.28434116699347,-2.79394564242777,
7.88975131985505));
#12937=CARTESIAN_POINT('Ctrl Pts',(-1.19568197046988,-2.83138603434665,
7.89474216503636));
#12938=CARTESIAN_POINT('Ctrl Pts',(-1.10687949844573,-2.86888693088439,
7.89974107554952));
#12939=CARTESIAN_POINT('Ctrl Pts',(-1.0164202143759,-2.90216004912347,7.90473998606268));
#12940=CARTESIAN_POINT('Ctrl Pts',(-0.924745708016164,-2.93108301238735,
7.90973889657584));
#12941=CARTESIAN_POINT('Ctrl Pts',(-0.871523216692048,-2.94787450898226,
7.91264106078682));
#12942=CARTESIAN_POINT('Ctrl Pts',(-0.817891372082817,-2.96320073719094,
7.9155432249978));
#12943=CARTESIAN_POINT('Ctrl Pts',(-0.763937942530774,-2.97704569497377,
7.91844538920878));
#12944=CARTESIAN_POINT('Ctrl Pts',(-0.670993276545539,-3.00089617097481,
7.92344489870176));
#12945=CARTESIAN_POINT('Ctrl Pts',(-0.576767356000975,-3.02043170716473,
7.92844440819473));
#12946=CARTESIAN_POINT('Ctrl Pts',(-0.481696701506282,-3.03551816627046,
7.93344391768771));
#12947=CARTESIAN_POINT('Ctrl Pts',(-0.386755009750755,-3.0505841606902,
7.9384366453778));
#12948=CARTESIAN_POINT('Ctrl Pts',(-0.290971291227511,-3.06121300426838,
7.94342937306789));
#12949=CARTESIAN_POINT('Ctrl Pts',(-0.194795439480239,-3.06732081575399,
7.94842210075799));
#12950=CARTESIAN_POINT('Ctrl Pts',(-0.0987210508323314,-3.07342218365243,
7.95340956124622));
#12951=CARTESIAN_POINT('Ctrl Pts',(-0.00225578710280942,-3.075011973412,
7.95839702173445));
#12952=CARTESIAN_POINT('Ctrl Pts',(0.0941431146125853,-3.07205783213322,
7.96338448222268));
#12953=CARTESIAN_POINT('Ctrl Pts',(0.190473040660504,-3.06910580461157,
7.96836837406634));
#12954=CARTESIAN_POINT('Ctrl Pts',(0.286736261591087,-3.06161632286734,
7.97335226591001));
#12955=CARTESIAN_POINT('Ctrl Pts',(0.382474283278711,-3.04960910161129,
7.97833615775367));
#12956=CARTESIAN_POINT('Ctrl Pts',(0.478177439550023,-3.03760625308784,
7.98331823458737));
#12957=CARTESIAN_POINT('Ctrl Pts',(0.57335534149521,-3.02108898855313,7.98830031142107));
#12958=CARTESIAN_POINT('Ctrl Pts',(0.667554329894348,-3.00012890833699,
7.99328238825476));
#12959=CARTESIAN_POINT('Ctrl Pts',(0.761744729515948,-2.97917073919728,
7.99826401083783));
#12960=CARTESIAN_POINT('Ctrl Pts',(0.854955964602248,-2.95377065527513,
8.0032456334209));
#12961=CARTESIAN_POINT('Ctrl Pts',(0.946745344142695,-2.92405121421362,
8.00822725600397));
#12962=CARTESIAN_POINT('Ctrl Pts',(1.03855141260955,-2.8943263696341,8.0132097843338));
#12963=CARTESIAN_POINT('Ctrl Pts',(1.12893469451006,-2.86028074348634,8.01819231266362));
#12964=CARTESIAN_POINT('Ctrl Pts',(1.21746944123998,-2.82208618040747,8.02317484099344));
#12965=CARTESIAN_POINT('Ctrl Pts',(1.30609961537883,-2.78385044921862,8.02816273975449));
#12966=CARTESIAN_POINT('Ctrl Pts',(1.39287687288442,-2.7414570274477,8.03315063851555));
#12967=CARTESIAN_POINT('Ctrl Pts',(1.47739738672416,-2.69512508275602,8.0381385372766));
#12968=CARTESIAN_POINT('Ctrl Pts',(1.56196782799152,-2.64876576914867,8.04312938245791));
#12969=CARTESIAN_POINT('Ctrl Pts',(1.64427849681297,-2.59846352889428,8.04812022763922));
#12970=CARTESIAN_POINT('Ctrl Pts',(1.7239538466565,-2.5444813586659,8.05311107282053));
#12971=CARTESIAN_POINT('Ctrl Pts',(1.80375795387742,-2.49041195188721,8.05810998333369));
#12972=CARTESIAN_POINT('Ctrl Pts',(1.88091788718259,-2.43265100345217,8.06310889384685));
#12973=CARTESIAN_POINT('Ctrl Pts',(1.95509057372796,-2.37150228726858,8.06810780436));
#12974=CARTESIAN_POINT('Ctrl Pts',(1.99815222001228,-2.33600182868093,8.07100996857099));
#12975=CARTESIAN_POINT('Ctrl Pts',(2.0402076835136,-2.2993602400556,8.07391213278197));
#12976=CARTESIAN_POINT('Ctrl Pts',(2.08119575623356,-2.26164242846552,8.07681429699296));
#12977=CARTESIAN_POINT('Ctrl Pts',(2.15075950934274,-2.19762886649112,8.0817397648488));
#12978=CARTESIAN_POINT('Ctrl Pts',(2.2175068160232,-2.13027396279288,8.08666523270465));
#12979=CARTESIAN_POINT('Ctrl Pts',(2.28109244639392,-2.05985909736676,8.0915907005605));
#12980=CARTESIAN_POINT('Ctrl Pts',(2.3445757885859,-1.98955750609235,8.09650824497305));
#12981=CARTESIAN_POINT('Ctrl Pts',(2.40490726497235,-1.91620607231197,8.1014257893856));
#12982=CARTESIAN_POINT('Ctrl Pts',(2.46177625232316,-1.84012497768432,8.10634333379815));
#12983=CARTESIAN_POINT('Ctrl Pts',(2.51859341366845,-1.76411321749385,8.1112563967403));
#12984=CARTESIAN_POINT('Ctrl Pts',(2.57195407934571,-1.68537709464414,8.11616945968244));
#12985=CARTESIAN_POINT('Ctrl Pts',(2.62158640063749,-1.60427148388063,8.12108252262459));
#12986=CARTESIAN_POINT('Ctrl Pts',(2.67118799605355,-1.52321608315874,8.1259925440374));
#12987=CARTESIAN_POINT('Ctrl Pts',(2.71706559402599,-1.43979449251527,8.1309025654502));
#12988=CARTESIAN_POINT('Ctrl Pts',(2.75899012028254,-1.35439128990973,8.13581258686301));
#12989=CARTESIAN_POINT('Ctrl Pts',(2.800900940989,-1.26901600647168,8.14072100314034));
#12990=CARTESIAN_POINT('Ctrl Pts',(2.83886105818273,-1.18166080472173,8.14562941941766));
#12991=CARTESIAN_POINT('Ctrl Pts',(2.87268751225075,-1.09273450890808,8.15053783569499));
#12992=CARTESIAN_POINT('Ctrl Pts',(2.90652877058616,-1.00376929418623,8.15544840015809));
#12993=CARTESIAN_POINT('Ctrl Pts',(2.9362325826473,-0.913232033076059,8.16035896462118));
#12994=CARTESIAN_POINT('Ctrl Pts',(2.96166455066029,-0.821550570179439,
8.16526952908427));
#12995=CARTESIAN_POINT('Ctrl Pts',(2.98710113918497,-0.729852450480216,
8.17018098570484));
#12996=CARTESIAN_POINT('Ctrl Pts',(3.0082642306464,-0.637010155946488,8.17509244232541));
#12997=CARTESIAN_POINT('Ctrl Pts',(3.02507014949394,-0.543463743630365,
8.18000389894599));
#12998=CARTESIAN_POINT('Ctrl Pts',(3.04189704873931,-0.449800548592386,
8.18492148699649));
#12999=CARTESIAN_POINT('Ctrl Pts',(3.05435584318727,-0.355431929188367,
8.189839075047));
#13000=CARTESIAN_POINT('Ctrl Pts',(3.0624145814086,-0.260804872607883,8.1947566630975));
#13001=CARTESIAN_POINT('Ctrl Pts',(3.0698801000122,-0.173143500330372,8.19931225779082));
#13002=CARTESIAN_POINT('Ctrl Pts',(3.07357006286123,-0.0852606722414295,
8.20386785248414));
#13003=CARTESIAN_POINT('Ctrl Pts',(3.07349899192449,0.00248930494810733,
8.20842344717746));
#13004=CARTESIAN_POINT('Origin',(0.,0.,-2.20842344717744));
#13005=CARTESIAN_POINT('',(-1.87240768645124,2.43731239395329,6.5627091405633));
#13006=CARTESIAN_POINT('',(-1.87543519516197,2.44126013959499,6.6458244875715));
#13007=CARTESIAN_POINT('',(-1.87240768645123,2.4373123939533,-2.20842344717744));
#13008=CARTESIAN_POINT('',(3.07786885453234,-0.00123528292102317,7.29157655282255));
#13009=CARTESIAN_POINT('Ctrl Pts',(-1.87543519516259,2.44126013959451,6.64582448757154));
#13010=CARTESIAN_POINT('Ctrl Pts',(-1.88255777719139,2.43579791465536,6.64629138932579));
#13011=CARTESIAN_POINT('Ctrl Pts',(-2.69199670149138,1.80887592431544,6.6995479270081));
#13012=CARTESIAN_POINT('Ctrl Pts',(-3.61557748169771,-0.319267411063196,
6.80559410061847));
#13013=CARTESIAN_POINT('Ctrl Pts',(-1.70070776265665,-3.20654413847151,
6.96396300840265));
#13014=CARTESIAN_POINT('Ctrl Pts',(1.76367148919952,-3.17234851239761,7.12233191618683));
#13015=CARTESIAN_POINT('Ctrl Pts',(3.0445276197161,-1.15572815572695,7.23153643099346));
#13016=CARTESIAN_POINT('Ctrl Pts',(3.07822572016116,-0.070965146153975,
7.28795130987203));
#13017=CARTESIAN_POINT('Ctrl Pts',(3.07786885453234,-0.00123528292102317,
7.29157655282255));
#13018=CARTESIAN_POINT('Ctrl Pts',(3.07786885453234,-0.00123528292102317,
7.29157655282255));
#13019=CARTESIAN_POINT('Ctrl Pts',(3.0730291562681,0.944418965649178,7.34074094580009));
#13020=CARTESIAN_POINT('Ctrl Pts',(2.10098001424261,2.9140591129136,7.44269497470569));
#13021=CARTESIAN_POINT('Ctrl Pts',(-0.455571413424762,3.29139779091718,
7.56082426355977));
#13022=CARTESIAN_POINT('Ctrl Pts',(-1.62467882336431,2.62837370441962,7.62978915943631));
#13023=CARTESIAN_POINT('Ctrl Pts',(-1.87108789359255,2.43562943220401,7.6459644193848));
#13024=CARTESIAN_POINT('',(3.07349998753216,0.000276838914890879,7.20842344720515));
#13025=CARTESIAN_POINT('Ctrl Pts',(3.07349998753216,0.000276838914890267,
7.20842344720515));
#13026=CARTESIAN_POINT('Ctrl Pts',(3.0734907994524,0.102284040624626,7.21367722612571));
#13027=CARTESIAN_POINT('Ctrl Pts',(3.06839901409326,0.20417997742157,7.21893100504626));
#13028=CARTESIAN_POINT('Ctrl Pts',(3.05828337165217,0.305458783923172,7.22418478396682));
#13029=CARTESIAN_POINT('Ctrl Pts',(3.0481377246032,0.407037999508376,7.22945414643309));
#13030=CARTESIAN_POINT('Ctrl Pts',(3.03293845951892,0.507996061934451,7.23472350889935));
#13031=CARTESIAN_POINT('Ctrl Pts',(3.01279594210165,0.607834567341986,7.23999287136562));
#13032=CARTESIAN_POINT('Ctrl Pts',(2.99262318887218,0.707822939731749,7.24527014364032));
#13033=CARTESIAN_POINT('Ctrl Pts',(2.96749246796263,0.806688050722019,7.25054741591501));
#13034=CARTESIAN_POINT('Ctrl Pts',(2.93756412736932,0.903946484916509,7.25582468818971));
#13035=CARTESIAN_POINT('Ctrl Pts',(2.90755169173929,1.00147820361103,7.26111678896464));
#13036=CARTESIAN_POINT('Ctrl Pts',(2.87271479946082,1.09739387420792,7.26640888973958));
#13037=CARTESIAN_POINT('Ctrl Pts',(2.83326264746001,1.1912283662287,7.27170099051452));
#13038=CARTESIAN_POINT('Ctrl Pts',(2.80029014392393,1.26965141701431,7.2761239130337));
#13039=CARTESIAN_POINT('Ctrl Pts',(2.76409481162759,1.34662108790793,7.28054683555289));
#13040=CARTESIAN_POINT('Ctrl Pts',(2.72482273064765,1.42188021174286,7.28496975807208));
#13041=CARTESIAN_POINT('Ctrl Pts',(2.68043100983039,1.50695036669435,7.28996926756506));
#13042=CARTESIAN_POINT('Ctrl Pts',(2.63197360866318,1.59008905533462,7.29496877705804));
#13043=CARTESIAN_POINT('Ctrl Pts',(2.57964256266099,1.6708819524155,7.29996828655102));
#13044=CARTESIAN_POINT('Ctrl Pts',(2.52738250339041,1.75156525444452,7.30496101424111));
#13045=CARTESIAN_POINT('Ctrl Pts',(2.47125947900092,1.82990872375334,7.30995374193121));
#13046=CARTESIAN_POINT('Ctrl Pts',(2.41151184191219,1.9055216835075,7.31494646962131));
#13047=CARTESIAN_POINT('Ctrl Pts',(2.35182723707454,1.9810548734951,7.31993393010954));
#13048=CARTESIAN_POINT('Ctrl Pts',(2.28852589187282,2.05386293783942,7.32492139059777));
#13049=CARTESIAN_POINT('Ctrl Pts',(2.22188939148064,2.12358418293832,7.32990885108601));
#13050=CARTESIAN_POINT('Ctrl Pts',(2.15530057106218,2.19325554085654,7.33489274292968));
#13051=CARTESIAN_POINT('Ctrl Pts',(2.08538164189108,2.25984415387933,7.33987663477335));
#13052=CARTESIAN_POINT('Ctrl Pts',(2.01245375433213,2.32302219891987,7.34486052661702));
#13053=CARTESIAN_POINT('Ctrl Pts',(1.9395524253036,2.38617723608115,7.34984260345071));
#13054=CARTESIAN_POINT('Ctrl Pts',(1.86364464653801,2.44592388593928,7.35482468028441));
#13055=CARTESIAN_POINT('Ctrl Pts',(1.78508692598543,2.501972605101,7.35980675711811));
#13056=CARTESIAN_POINT('Ctrl Pts',(1.70653636808716,2.55801621391078,7.36478837970118));
#13057=CARTESIAN_POINT('Ctrl Pts',(1.6253367062168,2.61036230757298,7.36977000228424));
#13058=CARTESIAN_POINT('Ctrl Pts',(1.54187501558459,2.6587635634475,7.37475162486731));
#13059=CARTESIAN_POINT('Ctrl Pts',(1.45839815014636,2.70717361952319,7.37973415319714));
#13060=CARTESIAN_POINT('Ctrl Pts',(1.37265881889303,2.75163719318927,7.38471668152697));
#13061=CARTESIAN_POINT('Ctrl Pts',(1.28506942846019,2.79195250927321,7.3896992098568));
#13062=CARTESIAN_POINT('Ctrl Pts',(1.19738562957334,2.83231127932625,7.39468710861785));
#13063=CARTESIAN_POINT('Ctrl Pts',(1.10784818990066,2.86851268159868,7.3996750073789));
#13064=CARTESIAN_POINT('Ctrl Pts',(1.01689005841237,2.90040287875703,7.40466290613995));
#13065=CARTESIAN_POINT('Ctrl Pts',(0.925878196707301,2.93231191389258,7.40965375132126));
#13066=CARTESIAN_POINT('Ctrl Pts',(0.833444392583186,2.95990454753982,7.41464459650257));
#13067=CARTESIAN_POINT('Ctrl Pts',(0.74003528797117,2.9830772739836,7.41963544168388));
#13068=CARTESIAN_POINT('Ctrl Pts',(0.646475231887209,3.0062874481385,7.42463435219704));
#13069=CARTESIAN_POINT('Ctrl Pts',(0.55193715843439,3.02506336728004,7.4296332627102));
#13070=CARTESIAN_POINT('Ctrl Pts',(0.456876329764853,3.03935293595538,7.43463217322336));
#13071=CARTESIAN_POINT('Ctrl Pts',(0.401687877380416,3.04764887857939,7.43753433743433));
#13072=CARTESIAN_POINT('Ctrl Pts',(0.346323316646573,3.05443367349224,7.44043650164529));
#13073=CARTESIAN_POINT('Ctrl Pts',(0.290871837190702,3.05970518585195,7.44333866585626));
#13074=CARTESIAN_POINT('Ctrl Pts',(0.195371922835088,3.06878391528922,7.44833684509896));
#13075=CARTESIAN_POINT('Ctrl Pts',(0.0992788577162925,3.07340316990389,
7.45333502434166));
#13076=CARTESIAN_POINT('Ctrl Pts',(0.00304436661068013,3.07349849224494,
7.45833320358435));
#13077=CARTESIAN_POINT('Ctrl Pts',(-0.0930703017848441,3.07359369589902,
7.4633251595346));
#13078=CARTESIAN_POINT('Ctrl Pts',(-0.189325611690144,3.06917615571992,
7.46831711548484));
#13079=CARTESIAN_POINT('Ctrl Pts',(-0.285264308459432,3.06023308333192,
7.47330907143509));
#13080=CARTESIAN_POINT('Ctrl Pts',(-0.381109750793669,3.05129870379874,
7.47829617509895));
#13081=CARTESIAN_POINT('Ctrl Pts',(-0.476638757002943,3.03784757285239,
7.48328327876281));
#13082=CARTESIAN_POINT('Ctrl Pts',(-0.571394728592988,3.01991892509321,
7.48827038242667));
#13083=CARTESIAN_POINT('Ctrl Pts',(-0.666084468146671,3.00200280900703,
7.49325400023074));
#13084=CARTESIAN_POINT('Ctrl Pts',(-0.760001817139245,2.97961547816257,
7.49823761803481));
#13085=CARTESIAN_POINT('Ctrl Pts',(-0.852697018688738,2.95284778549781,
7.50322123583888));
#13086=CARTESIAN_POINT('Ctrl Pts',(-0.94537387288352,2.92608539101834,7.50820386722508));
#13087=CARTESIAN_POINT('Ctrl Pts',(-1.03682863594406,2.89494446852317,7.51318649861128));
#13088=CARTESIAN_POINT('Ctrl Pts',(-1.12662418623037,2.85956643444435,7.51816912999748));
#13089=CARTESIAN_POINT('Ctrl Pts',(-1.21640461733843,2.82419435708389,7.5231509224413));
#13090=CARTESIAN_POINT('Ctrl Pts',(-1.30452598436501,2.78458675206373,7.52813271488512));
#13091=CARTESIAN_POINT('Ctrl Pts',(-1.39057003939577,2.74093363938911,7.53311450732895));
#13092=CARTESIAN_POINT('Ctrl Pts',(-1.47666863303423,2.69725285740037,7.53809945745779));
#13093=CARTESIAN_POINT('Ctrl Pts',(-1.56068689183067,2.64952164364708,7.54308440758664));
#13094=CARTESIAN_POINT('Ctrl Pts',(-1.64223045413458,2.59797640203158,7.54806935771549));
#13095=CARTESIAN_POINT('Ctrl Pts',(-1.72140032727714,2.54793161462588,7.55290919863207));
#13096=CARTESIAN_POINT('Ctrl Pts',(-1.79823729817869,2.49429204311649,7.55774903954866));
#13097=CARTESIAN_POINT('Ctrl Pts',(-1.87240768645123,2.4373123939533,7.56258888046525));
#13098=CARTESIAN_POINT('Ctrl Pts',(-1.87240768645124,2.43731239395329,6.5627091405633));
#13099=CARTESIAN_POINT('Ctrl Pts',(-1.94892008865579,2.37853354789643,6.56769076779308));
#13100=CARTESIAN_POINT('Ctrl Pts',(-2.02267799124896,2.31613618435552,6.57267239502285));
#13101=CARTESIAN_POINT('Ctrl Pts',(-2.09332988527124,2.25041601519148,6.57765402225263));
#13102=CARTESIAN_POINT('Ctrl Pts',(-2.16398784569987,2.18469020307537,6.58263607722147));
#13103=CARTESIAN_POINT('Ctrl Pts',(-2.23153894679076,2.11564131807246,6.58761813219031));
#13104=CARTESIAN_POINT('Ctrl Pts',(-2.29566752976676,2.04360290731212,6.59260018715915));
#13105=CARTESIAN_POINT('Ctrl Pts',(-2.35986174777179,1.97149076588504,6.59758734121653));
#13106=CARTESIAN_POINT('Ctrl Pts',(-2.42062615831467,1.89638331565215,6.60257449527391));
#13107=CARTESIAN_POINT('Ctrl Pts',(-2.47768464333418,1.81864814029157,6.60756164933129));
#13108=CARTESIAN_POINT('Ctrl Pts',(-2.53477192355408,1.74087373500838,6.61255132021154));
#13109=CARTESIAN_POINT('Ctrl Pts',(-2.58814930967629,1.66046932891588,6.6175409910918));
#13110=CARTESIAN_POINT('Ctrl Pts',(-2.63758460280537,1.57783069847308,6.62253066197205));
#13111=CARTESIAN_POINT('Ctrl Pts',(-2.68710505115045,1.49504971810212,6.62752892785549));
#13112=CARTESIAN_POINT('Ctrl Pts',(-2.73266963029805,1.41002721092648,6.63252719373892));
#13113=CARTESIAN_POINT('Ctrl Pts',(-2.77409252163596,1.32318287904713,6.63752545962236));
#13114=CARTESIAN_POINT('Ctrl Pts',(-2.81268074414734,1.24228151523177,6.64218168206004));
#13115=CARTESIAN_POINT('Ctrl Pts',(-2.84767512121639,1.15979962218973,6.64683790449771));
#13116=CARTESIAN_POINT('Ctrl Pts',(-2.87896424539989,1.07608880846751,6.65149412693539));
#13117=CARTESIAN_POINT('Ctrl Pts',(-2.91256020767968,0.9862062881474,6.65649363642837));
#13118=CARTESIAN_POINT('Ctrl Pts',(-2.9420018871256,0.894591066769512,6.66149314592135));
#13119=CARTESIAN_POINT('Ctrl Pts',(-2.96710950151727,0.801662931665151,
6.66649265541433));
#13120=CARTESIAN_POINT('Ctrl Pts',(-2.99218305758949,0.70886085298577,6.67148538310444));
#13121=CARTESIAN_POINT('Ctrl Pts',(-3.01293411947718,0.614749820260872,
6.67647811079455));
#13122=CARTESIAN_POINT('Ctrl Pts',(-3.02923145456872,0.519768260527229,
6.68147083848466));
#13123=CARTESIAN_POINT('Ctrl Pts',(-3.04551159638247,0.424886903945295,
6.68645829897289));
#13124=CARTESIAN_POINT('Ctrl Pts',(-3.05734727803301,0.329137276385941,
6.69144575946111));
#13125=CARTESIAN_POINT('Ctrl Pts',(-3.0646577226007,0.232970584632222,6.69643321994934));
#13126=CARTESIAN_POINT('Ctrl Pts',(-3.07196293637442,0.136872702394353,
6.70141711179301));
#13127=CARTESIAN_POINT('Ctrl Pts',(-3.07474931670532,0.0403587856497919,
6.70640100363668));
#13128=CARTESIAN_POINT('Ctrl Pts',(-3.07298772560657,-0.0561131737775446,
6.71138489548034));
#13129=CARTESIAN_POINT('Ctrl Pts',(-3.07122677603566,-0.152550000506614,
6.71636697231404));
#13130=CARTESIAN_POINT('Ctrl Pts',(-3.06492115384698,-0.248944461837164,
6.72134904914773));
#13131=CARTESIAN_POINT('Ctrl Pts',(-3.05409382663993,-0.344837857666258,
6.72633112598143));
#13132=CARTESIAN_POINT('Ctrl Pts',(-3.04326748663569,-0.440722510226871,
6.7313127485645));
#13133=CARTESIAN_POINT('Ctrl Pts',(-3.02792031072521,-0.536105751947464,
6.73629437114756));
#13134=CARTESIAN_POINT('Ctrl Pts',(-3.00812710105978,-0.630534371679836,
6.74127599373063));
#13135=CARTESIAN_POINT('Ctrl Pts',(-2.98833029264009,-0.724980160199006,
6.74625852206045));
#13136=CARTESIAN_POINT('Ctrl Pts',(-2.96408593513457,-0.818470552411485,
6.75124105039028));
#13137=CARTESIAN_POINT('Ctrl Pts',(-2.93551963948915,-0.910563944033318,
6.7562235787201));
#13138=CARTESIAN_POINT('Ctrl Pts',(-2.90692255358704,-1.00275659875887,
6.76121147748115));
#13139=CARTESIAN_POINT('Ctrl Pts',(-2.8739943597189,-1.0935488268306,6.7661993762422));
#13140=CARTESIAN_POINT('Ctrl Pts',(-2.83691005410301,-1.18251579056233,
6.77118727500326));
#13141=CARTESIAN_POINT('Ctrl Pts',(-2.79980384227881,-1.2715353083006,6.77617812018457));
#13142=CARTESIAN_POINT('Ctrl Pts',(-2.75853681795526,-1.35872701822717,
6.78116896536588));
#13143=CARTESIAN_POINT('Ctrl Pts',(-2.71333056440624,-1.44368954358578,
6.78615981054719));
#13144=CARTESIAN_POINT('Ctrl Pts',(-2.66805125640985,-1.52878937053099,
6.79115872106035));
#13145=CARTESIAN_POINT('Ctrl Pts',(-2.61882023196557,-1.61165244254711,
6.79615763157351));
#13146=CARTESIAN_POINT('Ctrl Pts',(-2.5659030726829,-1.69190533765825,6.80115654208667));
#13147=CARTESIAN_POINT('Ctrl Pts',(-2.53518152137452,-1.73849690584187,
6.80405870629763));
#13148=CARTESIAN_POINT('Ctrl Pts',(-2.50321834242866,-1.78420930261702,
6.8069608705086));
#13149=CARTESIAN_POINT('Ctrl Pts',(-2.47007156829701,-1.82897476677256,
6.80986303471956));
#13150=CARTESIAN_POINT('Ctrl Pts',(-2.41297017778761,-1.90609147924443,
6.81486254421253));
#13151=CARTESIAN_POINT('Ctrl Pts',(-2.35215360522452,-1.9806669831205,6.81986205370551));
#13152=CARTESIAN_POINT('Ctrl Pts',(-2.28787608227214,-2.05232192459348,
6.82486156319848));
#13153=CARTESIAN_POINT('Ctrl Pts',(-2.22368575137151,-2.12387966659332,
6.82985429088857));
#13154=CARTESIAN_POINT('Ctrl Pts',(-2.15604409120953,-2.19252439589185,
6.83484701857866));
#13155=CARTESIAN_POINT('Ctrl Pts',(-2.08524740120198,-2.25790733330232,
6.83983974626875));
#13156=CARTESIAN_POINT('Ctrl Pts',(-2.01452539991779,-2.32322129336195,
6.84482720675698));
#13157=CARTESIAN_POINT('Ctrl Pts',(-1.94065530636246,-2.38528000601394,
6.84981466724521));
#13158=CARTESIAN_POINT('Ctrl Pts',(-1.86397161018464,-2.44377005596388,
6.85480212773344));
#13159=CARTESIAN_POINT('Ctrl Pts',(-1.78734278298395,-2.50221825491584,
6.85978601957711));
#13160=CARTESIAN_POINT('Ctrl Pts',(-1.70790470332665,-2.55710260187456,
6.86476991142077));
#13161=CARTESIAN_POINT('Ctrl Pts',(-1.62602566699892,-2.608149301758,6.86975380326444));
#13162=CARTESIAN_POINT('Ctrl Pts',(-1.54417644898836,-2.65917741169758,
6.87473588009813));
#13163=CARTESIAN_POINT('Ctrl Pts',(-1.45988841264609,-2.70637041939934,
6.87971795693182));
#13164=CARTESIAN_POINT('Ctrl Pts',(-1.373558816825,-2.74949784992138,6.88470003376551));
#13165=CARTESIAN_POINT('Ctrl Pts',(-1.28723709227403,-2.79262134821541,
6.88968165634858));
#13166=CARTESIAN_POINT('Ctrl Pts',(-1.19887457110102,-2.83167981031415,
6.89466327893165));
#13167=CARTESIAN_POINT('Ctrl Pts',(-1.10889212946868,-2.86648922816787,
6.89964490151472));
#13168=CARTESIAN_POINT('Ctrl Pts',(-1.01889332744293,-2.9013049749871,6.90462742984456));
#13169=CARTESIAN_POINT('Ctrl Pts',(-0.927274429425946,-2.93186998493455,
6.90960995817438));
#13170=CARTESIAN_POINT('Ctrl Pts',(-0.834474238759799,-2.95804918736086,
6.91459248650422));
#13171=CARTESIAN_POINT('Ctrl Pts',(-0.741574023164949,-2.98425660710911,
6.91958038526527));
#13172=CARTESIAN_POINT('Ctrl Pts',(-0.647490396150168,-3.00606866243137,
6.92456828402632));
#13173=CARTESIAN_POINT('Ctrl Pts',(-0.552674985253281,-3.02340083526404,
6.92955618278737));
#13174=CARTESIAN_POINT('Ctrl Pts',(-0.457803565591813,-3.04074324644908,
6.93454702796868));
#13175=CARTESIAN_POINT('Ctrl Pts',(-0.362199936161134,-3.05360044739323,
6.93953787314999));
#13176=CARTESIAN_POINT('Ctrl Pts',(-0.266321410047212,-3.0619397702356,
6.9445287183313));
#13177=CARTESIAN_POINT('Ctrl Pts',(-0.170287941813808,-3.07029256963429,
6.94952762884446));
#13178=CARTESIAN_POINT('Ctrl Pts',(-0.073979128169933,-3.07411289505045,
6.95452653935761));
#13179=CARTESIAN_POINT('Ctrl Pts',(0.0221472110900531,-3.07342020411153,
6.95952544987077));
#13180=CARTESIAN_POINT('Ctrl Pts',(0.0779542556048634,-3.07301805591405,
6.96242761408176));
#13181=CARTESIAN_POINT('Ctrl Pts',(0.133699864030344,-3.07109577378738,
6.96532977829275));
#13182=CARTESIAN_POINT('Ctrl Pts',(0.189295602926454,-3.06766514220713,
6.96823194250373));
#13183=CARTESIAN_POINT('Ctrl Pts',(0.285069447606795,-3.06175525086211,
6.9732314519967));
#13184=CARTESIAN_POINT('Ctrl Pts',(0.380734482790612,-3.05134552848551,
6.97823096148967));
#13185=CARTESIAN_POINT('Ctrl Pts',(0.475834092604456,-3.0364426828635,6.98323047098264));
#13186=CARTESIAN_POINT('Ctrl Pts',(0.5708047004015,-3.02156005285694,6.98822319867273));
#13187=CARTESIAN_POINT('Ctrl Pts',(0.665210977222059,-3.00219648017976,
6.99321592636282));
#13188=CARTESIAN_POINT('Ctrl Pts',(0.758599049095575,-2.97841060512336,
6.99820865405291));
#13189=CARTESIAN_POINT('Ctrl Pts',(0.851888598907804,-2.95464982356544,
7.00319611454117));
#13190=CARTESIAN_POINT('Ctrl Pts',(0.944161656059448,-2.92647612196475,
7.00818357502943));
#13191=CARTESIAN_POINT('Ctrl Pts',(1.03497321680813,-2.89399942821173,7.01317103551769));
#13192=CARTESIAN_POINT('Ctrl Pts',(1.12571979976179,-2.86154597229245,7.01815492736135));
#13193=CARTESIAN_POINT('Ctrl Pts',(1.21500655304333,-2.82479579230441,7.02313881920501));
#13194=CARTESIAN_POINT('Ctrl Pts',(1.30240330023451,-2.78390874375189,7.02812271104868));
#13195=CARTESIAN_POINT('Ctrl Pts',(1.3897682196951,-2.74303658524973,7.03310478788238));
#13196=CARTESIAN_POINT('Ctrl Pts',(1.4752441034335,-2.69803073734582,7.03808686471607));
#13197=CARTESIAN_POINT('Ctrl Pts',(1.55842134264391,-2.6490989352593,7.04306894154977));
#13198=CARTESIAN_POINT('Ctrl Pts',(1.64159099800624,-2.60017159462591,7.04805056413284));
#13199=CARTESIAN_POINT('Ctrl Pts',(1.7224620472756,-2.54731923422812,7.0530321867159));
#13200=CARTESIAN_POINT('Ctrl Pts',(1.80065099923568,-2.49079469827434,7.05801380929897));
#13201=CARTESIAN_POINT('Ctrl Pts',(1.87885416732519,-2.43425988516376,7.06299633762881));
#13202=CARTESIAN_POINT('Ctrl Pts',(1.95437391391174,-2.37405182770905,7.06797886595865));
#13203=CARTESIAN_POINT('Ctrl Pts',(2.02685803561213,-2.31046505134237,7.07296139428849));
#13204=CARTESIAN_POINT('Ctrl Pts',(2.09942028451285,-2.24680973780234,7.07794929304953));
#13205=CARTESIAN_POINT('Ctrl Pts',(2.16894004583742,-2.17976872487001,7.08293719181058));
#13206=CARTESIAN_POINT('Ctrl Pts',(2.23510053716814,-2.10967481824823,7.08792509057163));
#13207=CARTESIAN_POINT('Ctrl Pts',(2.3013001104092,-2.03953950619371,7.09291593575293));
#13208=CARTESIAN_POINT('Ctrl Pts',(2.36413617665463,-1.9663480425164,7.09790678093424));
#13209=CARTESIAN_POINT('Ctrl Pts',(2.42333234953121,-1.89046623183688,7.10289762611554));
#13210=CARTESIAN_POINT('Ctrl Pts',(2.48262418491815,-1.81446179423493,7.10789653662871));
#13211=CARTESIAN_POINT('Ctrl Pts',(2.5382641283343,-1.73575868649176,7.11289544714187));
#13212=CARTESIAN_POINT('Ctrl Pts',(2.59001923998573,-1.65475151805452,7.11789435765503));
#13213=CARTESIAN_POINT('Ctrl Pts',(2.62006615368293,-1.60772204944317,7.12079652186599));
#13214=CARTESIAN_POINT('Ctrl Pts',(2.64880454179316,-1.55991647365887,7.12369868607694));
#13215=CARTESIAN_POINT('Ctrl Pts',(2.67619614131918,-1.511415384065,7.1266008502879));
#13216=CARTESIAN_POINT('Ctrl Pts',(2.72544131435982,-1.42421914174841,7.13181841995284));
#13217=CARTESIAN_POINT('Ctrl Pts',(2.77049117203043,-1.33449006635658,7.13703598961777));
#13218=CARTESIAN_POINT('Ctrl Pts',(2.81108935767531,-1.24264993991252,7.14225355928271));
#13219=CARTESIAN_POINT('Ctrl Pts',(2.8516143832756,-1.15097531415871,7.14746172661541));
#13220=CARTESIAN_POINT('Ctrl Pts',(2.88770355110386,-1.05719755939824,7.15266989394812));
#13221=CARTESIAN_POINT('Ctrl Pts',(2.91914588564439,-0.961763769501352,
7.15787806128082));
#13222=CARTESIAN_POINT('Ctrl Pts',(2.95051943878262,-0.866538744951909,
7.1630748355329));
#13223=CARTESIAN_POINT('Ctrl Pts',(2.97726629363165,-0.769665267033125,
7.16827160978499));
#13224=CARTESIAN_POINT('Ctrl Pts',(2.9992236063298,-0.671610012755951,7.17346838403706));
#13225=CARTESIAN_POINT('Ctrl Pts',(3.021151801193,-0.573684790634829,7.17865826678939));
#13226=CARTESIAN_POINT('Ctrl Pts',(3.03830301001047,-0.474581284233719,
7.18384814954172));
#13227=CARTESIAN_POINT('Ctrl Pts',(3.05056405627979,-0.37478152106769,7.18903803229404));
#13228=CARTESIAN_POINT('Ctrl Pts',(3.06280647431905,-0.275133383864656,
7.194220030048));
#13229=CARTESIAN_POINT('Ctrl Pts',(3.07017348425874,-0.174791477733736,
7.19940202780196));
#13230=CARTESIAN_POINT('Ctrl Pts',(3.07260306387723,-0.0742473019864619,
7.20458402555591));
#13231=CARTESIAN_POINT('Ctrl Pts',(3.07320310147929,-0.049415727973635,
7.2058638327631));
#13232=CARTESIAN_POINT('Ctrl Pts',(3.07350222572077,-0.0245718569918277,
7.20714363997028));
#13233=CARTESIAN_POINT('Ctrl Pts',(3.07349998753221,0.000276838377213211,
7.20842344717746));
#13234=CARTESIAN_POINT('Origin',(0.,0.,-2.20842344717744));
#13235=CARTESIAN_POINT('',(-1.87240768645123,2.4373123939533,5.56275985257814));
#13236=CARTESIAN_POINT('',(-1.87084604423464,2.43524047469653,5.64570902492364));
#13237=CARTESIAN_POINT('',(-1.87240768645123,2.4373123939533,-2.20842344717744));
#13238=CARTESIAN_POINT('',(3.07311034755939,0.00277269570115833,6.29157655282255));
#13239=CARTESIAN_POINT('Ctrl Pts',(-1.87084604423436,2.43524047469674,5.64570902492362));
#13240=CARTESIAN_POINT('Ctrl Pts',(-2.13486897241354,2.23583486155222,5.66280993199216));
#13241=CARTESIAN_POINT('Ctrl Pts',(-3.08290902783559,1.25484794830019,5.73270047498876));
#13242=CARTESIAN_POINT('Ctrl Pts',(-3.34186209072106,-1.41643565774369,
5.85538065391343));
#13243=CARTESIAN_POINT('Ctrl Pts',(-0.631386729895664,-3.57430874481187,
6.01374956169758));
#13244=CARTESIAN_POINT('Ctrl Pts',(2.38524471380796,-2.56562027744576,6.15914819466731));
#13245=CARTESIAN_POINT('Ctrl Pts',(3.06618249768684,-0.76621717896174,6.25175719170896));
#13246=CARTESIAN_POINT('Ctrl Pts',(3.07311034755939,0.00277269570115833,
6.29157655282255));
#13247=CARTESIAN_POINT('Ctrl Pts',(3.07311034755939,0.00277269570115833,
6.29157655282255));
#13248=CARTESIAN_POINT('Ctrl Pts',(3.07536694119141,0.253254112905881,6.30454682763701));
#13249=CARTESIAN_POINT('Ctrl Pts',(2.93303834198825,1.5206760271736,6.37030673837954));
#13250=CARTESIAN_POINT('Ctrl Pts',(1.1873595229057,3.42479583189181,6.48838938329588));
#13251=CARTESIAN_POINT('Ctrl Pts',(-1.07725235962685,3.053377230368,6.59350175339774));
#13252=CARTESIAN_POINT('Ctrl Pts',(-1.87543519516259,2.44126013959451,6.64582448757154));
#13253=CARTESIAN_POINT('',(3.07349882217906,-0.00269073669219618,6.2084234472256));
#13254=CARTESIAN_POINT('Ctrl Pts',(3.07349882217906,-0.00269073669218799,
6.2084234472256));
#13255=CARTESIAN_POINT('Ctrl Pts',(3.07358187200714,0.0921730786858093,
6.21334262298627));
#13256=CARTESIAN_POINT('Ctrl Pts',(3.06926874327925,0.187176666180301,6.21826179874695));
#13257=CARTESIAN_POINT('Ctrl Pts',(3.06054730741738,0.281873072605769,6.22318097450763));
#13258=CARTESIAN_POINT('Ctrl Pts',(3.05183388741538,0.376482443692495,6.22809562906053));
#13259=CARTESIAN_POINT('Ctrl Pts',(3.03872025259062,0.470784745903885,6.23301028361344));
#13260=CARTESIAN_POINT('Ctrl Pts',(3.02124633040207,0.564333997763762,6.23792493816634));
#13261=CARTESIAN_POINT('Ctrl Pts',(3.00378085463484,0.657838030445783,6.24283721710818));
#13262=CARTESIAN_POINT('Ctrl Pts',(2.98195935854854,0.750589291198084,6.24774949605002));
#13263=CARTESIAN_POINT('Ctrl Pts',(2.95587337233148,0.842148951636062,6.25266177499185));
#13264=CARTESIAN_POINT('Ctrl Pts',(2.92979239118119,0.933691044702462,6.25757311142441));
#13265=CARTESIAN_POINT('Ctrl Pts',(2.89944866936247,1.02404155634354,6.26248444785697));
#13266=CARTESIAN_POINT('Ctrl Pts',(2.86498409548813,1.11277508176634,6.26739578428952));
#13267=CARTESIAN_POINT('Ctrl Pts',(2.8305160875989,1.20151744850685,6.27230761008262));
#13268=CARTESIAN_POINT('Ctrl Pts',(2.79192657793376,1.28864208772415,6.27721943587571));
#13269=CARTESIAN_POINT('Ctrl Pts',(2.74940578904599,1.37374308266152,6.28213126166881));
#13270=CARTESIAN_POINT('Ctrl Pts',(2.70684237482433,1.45892938782994,6.2870480113643));
#13271=CARTESIAN_POINT('Ctrl Pts',(2.66034001807517,1.54208759401821,6.2919647610598));
#13272=CARTESIAN_POINT('Ctrl Pts',(2.61013494932703,1.62283634304312,6.2968815107553));
#13273=CARTESIAN_POINT('Ctrl Pts',(2.55990223285614,1.70362956006859,6.30180096808442));
#13274=CARTESIAN_POINT('Ctrl Pts',(2.50596300435945,1.78201030765024,6.30672042541354));
#13275=CARTESIAN_POINT('Ctrl Pts',(2.44859557063384,1.85762805251007,6.31163988274266));
#13276=CARTESIAN_POINT('Ctrl Pts',(2.39113686527861,1.93336610525806,6.31656716693205));
#13277=CARTESIAN_POINT('Ctrl Pts',(2.33023935842095,2.00633203472531,6.32149445112143));
#13278=CARTESIAN_POINT('Ctrl Pts',(2.26621999104809,2.0762102981572,6.32642173531081));
#13279=CARTESIAN_POINT('Ctrl Pts',(2.23012341357383,2.11561034619337,6.32919992732955));
#13280=CARTESIAN_POINT('Ctrl Pts',(2.1930350019566,2.15402947379665,6.33197811934829));
#13281=CARTESIAN_POINT('Ctrl Pts',(2.15501616577207,2.19141679633543,6.33475631136702));
#13282=CARTESIAN_POINT('Ctrl Pts',(2.08659917690504,2.25869734162852,6.33975582085999));
#13283=CARTESIAN_POINT('Ctrl Pts',(2.01490820660427,2.32288897701831,6.34475533035296));
#13284=CARTESIAN_POINT('Ctrl Pts',(1.94025347588063,2.38365658166883,6.34975483984593));
#13285=CARTESIAN_POINT('Ctrl Pts',(1.86570001382517,2.44434175544952,6.35474756753602));
#13286=CARTESIAN_POINT('Ctrl Pts',(1.78819111899676,2.50161185473718,6.35974029522612));
#13287=CARTESIAN_POINT('Ctrl Pts',(1.70807380396387,2.55516851307549,6.36473302291621));
#13288=CARTESIAN_POINT('Ctrl Pts',(1.62804101067879,2.60866867048928,6.36972048340444));
#13289=CARTESIAN_POINT('Ctrl Pts',(1.54540563062918,2.65846293222649,6.37470794389267));
#13290=CARTESIAN_POINT('Ctrl Pts',(1.46054689172026,2.70429381301039,6.3796954043809));
#13291=CARTESIAN_POINT('Ctrl Pts',(1.37574887122264,2.75009190072778,6.38467929622457));
#13292=CARTESIAN_POINT('Ctrl Pts',(1.28873103955486,2.791932037111,6.38966318806824));
#13293=CARTESIAN_POINT('Ctrl Pts',(1.19989984636415,2.82960113950629,6.3946470799119));
#13294=CARTESIAN_POINT('Ctrl Pts',(1.11110100329383,2.86725652374747,6.3996291567456));
#13295=CARTESIAN_POINT('Ctrl Pts',(1.02049051452189,2.90074372086693,6.4046112335793));
#13296=CARTESIAN_POINT('Ctrl Pts',(0.928496691140445,2.92989695118126,6.409593310413));
#13297=CARTESIAN_POINT('Ctrl Pts',(0.836511255476272,2.95904752339264,6.41457493299607));
#13298=CARTESIAN_POINT('Ctrl Pts',(0.743143154476896,2.98386478201134,6.41955655557915));
#13299=CARTESIAN_POINT('Ctrl Pts',(0.648836790001681,3.00423252594407,6.42453817816222));
#13300=CARTESIAN_POINT('Ctrl Pts',(0.554513278968048,3.02460397309147,6.42952070649203));
#13301=CARTESIAN_POINT('Ctrl Pts',(0.459251594733455,3.04052420624505,6.43450323482185));
#13302=CARTESIAN_POINT('Ctrl Pts',(0.363506224417138,3.05192815688869,6.43948576315167));
#13303=CARTESIAN_POINT('Ctrl Pts',(0.267657654702218,3.06334439931046,6.44447366191272));
#13304=CARTESIAN_POINT('Ctrl Pts',(0.171324794697949,3.07023458893296,6.44946156067377));
#13305=CARTESIAN_POINT('Ctrl Pts',(0.074966924490973,3.07258559038351,6.45444945943482));
#13306=CARTESIAN_POINT('Ctrl Pts',(-0.021447865632527,3.07493798060288,
6.45944030461614));
#13307=CARTESIAN_POINT('Ctrl Pts',(-0.11788725673191,3.07274585359341,6.46443114979745));
#13308=CARTESIAN_POINT('Ctrl Pts',(-0.213894429391949,3.06604817690053,
6.46942199497876));
#13309=CARTESIAN_POINT('Ctrl Pts',(-0.310056752067485,3.05933967659299,
6.47442090549192));
#13310=CARTESIAN_POINT('Ctrl Pts',(-0.405785025921967,3.04811113899375,
6.47941981600508));
#13311=CARTESIAN_POINT('Ctrl Pts',(-0.50063005071512,3.03245309977269,6.48441872651824));
#13312=CARTESIAN_POINT('Ctrl Pts',(-0.555693216142961,3.02336267878555,
6.48732089072923));
#13313=CARTESIAN_POINT('Ctrl Pts',(-0.610458900941248,3.01278025014737,
6.49022305494021));
#13314=CARTESIAN_POINT('Ctrl Pts',(-0.664841586868172,3.00073122994556,
6.4931252191512));
#13315=CARTESIAN_POINT('Ctrl Pts',(-0.758533571728651,2.97997284703214,
6.49812514735784));
#13316=CARTESIAN_POINT('Ctrl Pts',(-0.8514169915867,2.95478576948772,6.50312507556447));
#13317=CARTESIAN_POINT('Ctrl Pts',(-0.943041736551915,2.92524777294525,
6.50812500377111));
#13318=CARTESIAN_POINT('Ctrl Pts',(-1.03451892194578,2.89575734667553,6.51311687970689));
#13319=CARTESIAN_POINT('Ctrl Pts',(-1.12474105055002,2.86193007375763,6.51810875564268));
#13320=CARTESIAN_POINT('Ctrl Pts',(-1.21326914801803,2.82389451369339,6.52310063157846));
#13321=CARTESIAN_POINT('Ctrl Pts',(-1.30171457559361,2.78589447224695,6.5280878459677));
#13322=CARTESIAN_POINT('Ctrl Pts',(-1.38846871344482,2.74369412203258,6.53307506035695));
#13323=CARTESIAN_POINT('Ctrl Pts',(-1.47310917413638,2.69747133646962,6.53806227474619));
#13324=CARTESIAN_POINT('Ctrl Pts',(-1.55769019425479,2.65128101184608,6.5430459867575));
#13325=CARTESIAN_POINT('Ctrl Pts',(-1.64016010366088,2.60107407660144,6.54802969876881));
#13326=CARTESIAN_POINT('Ctrl Pts',(-1.72011891763209,2.54707541294015,6.55301341078012));
#13327=CARTESIAN_POINT('Ctrl Pts',(-1.77197177030419,2.51205757547788,6.55624532070785));
#13328=CARTESIAN_POINT('Ctrl Pts',(-1.82276904813623,2.4754461055598,6.55947723063557));
#13329=CARTESIAN_POINT('Ctrl Pts',(-1.87240768645124,2.43731239395329,6.5627091405633));
#13330=CARTESIAN_POINT('Ctrl Pts',(-1.87240768645123,2.4373123939533,5.56275985257814));
#13331=CARTESIAN_POINT('Ctrl Pts',(-1.94867787076473,2.37871962607096,5.56775071013256));
#13332=CARTESIAN_POINT('Ctrl Pts',(-2.02229488902666,2.31646673029867,5.57274156768697));
#13333=CARTESIAN_POINT('Ctrl Pts',(-2.09288995973404,2.25082515234845,5.57773242524139));
#13334=CARTESIAN_POINT('Ctrl Pts',(-2.16570558394975,2.18311883199131,5.58288026919926));
#13335=CARTESIAN_POINT('Ctrl Pts',(-2.23530558256172,2.1118073480244,5.58802811315714));
#13336=CARTESIAN_POINT('Ctrl Pts',(-2.30132069780014,2.03723471791462,5.59317595711501));
#13337=CARTESIAN_POINT('Ctrl Pts',(-2.36522302770871,1.96504875271235,5.59815904654424));
#13338=CARTESIAN_POINT('Ctrl Pts',(-2.42576613994928,1.88980756866498,5.60314213597346));
#13339=CARTESIAN_POINT('Ctrl Pts',(-2.48265241930305,1.81186070516713,5.60812522540269));
#13340=CARTESIAN_POINT('Ctrl Pts',(-2.53952351220385,1.73393465048978,5.61310698453832));
#13341=CARTESIAN_POINT('Ctrl Pts',(-2.5927394535247,1.65330470610248,5.61808874367394));
#13342=CARTESIAN_POINT('Ctrl Pts',(-2.64204400985501,1.57035209427353,5.62307050280957));
#13343=CARTESIAN_POINT('Ctrl Pts',(-2.69134886375604,1.48739898179575,5.62805229201191));
#13344=CARTESIAN_POINT('Ctrl Pts',(-2.73674206215645,1.40212355182324,5.63303408121425));
#13345=CARTESIAN_POINT('Ctrl Pts',(-2.7780122302168,1.31493357199741,5.63801587041658));
#13346=CARTESIAN_POINT('Ctrl Pts',(-2.8192939138382,1.22771926366548,5.64299904968105));
#13347=CARTESIAN_POINT('Ctrl Pts',(-2.85645009413505,1.13858974097728,5.64798222894551));
#13348=CARTESIAN_POINT('Ctrl Pts',(-2.88931707809965,1.04797379366171,5.65296540820997));
#13349=CARTESIAN_POINT('Ctrl Pts',(-2.92222118075134,0.957255508236955,
5.65795421528233));
#13350=CARTESIAN_POINT('Ctrl Pts',(-2.95082627120404,0.865047861450858,
5.66294302235469));
#13351=CARTESIAN_POINT('Ctrl Pts',(-2.97501828281642,0.771795612133184,
5.66793182942705));
#13352=CARTESIAN_POINT('Ctrl Pts',(-2.99922669399225,0.678480147891317,
5.67292401837023));
#13353=CARTESIAN_POINT('Ctrl Pts',(-3.01901598159721,0.584119100388228,
5.67791620731341));
#13354=CARTESIAN_POINT('Ctrl Pts',(-3.03432342957772,0.489166203570661,
5.68290839625659));
#13355=CARTESIAN_POINT('Ctrl Pts',(-3.04965407176638,0.394069431872271,
5.68790814948283));
#13356=CARTESIAN_POINT('Ctrl Pts',(-3.06048927543287,0.298379456239109,
5.69290790270908));
#13357=CARTESIAN_POINT('Ctrl Pts',(-3.06681826942858,0.202553578835506,
5.69790765593532));
#13358=CARTESIAN_POINT('Ctrl Pts',(-3.06824152970727,0.181004314438745,
5.69903199736699));
#13359=CARTESIAN_POINT('Ctrl Pts',(-3.06943711614308,0.159448168233771,
5.70015633879866));
#13360=CARTESIAN_POINT('Ctrl Pts',(-3.07040526815993,0.137890316033282,
5.70128068023033));
#13361=CARTESIAN_POINT('Ctrl Pts',(-3.07471026401133,0.0420309234247481,
5.7062801897233));
#13362=CARTESIAN_POINT('Ctrl Pts',(-3.07452936043882,-0.0541986383043321,
5.71127969921626));
#13363=CARTESIAN_POINT('Ctrl Pts',(-3.06982068590684,-0.150343627661687,
5.71627920870923));
#13364=CARTESIAN_POINT('Ctrl Pts',(-3.06511839866196,-0.246358196951463,
5.72127193639932));
#13365=CARTESIAN_POINT('Ctrl Pts',(-3.05590056835119,-0.342287987185201,
5.72626466408941));
#13366=CARTESIAN_POINT('Ctrl Pts',(-3.04217725314556,-0.437675462464726,
5.7312573917795));
#13367=CARTESIAN_POINT('Ctrl Pts',(-3.02846841569156,-0.532962306362232,
5.73624485226772));
#13368=CARTESIAN_POINT('Ctrl Pts',(-3.01026360454062,-0.627707540484224,
5.74123231275594));
#13369=CARTESIAN_POINT('Ctrl Pts',(-2.98762481780047,-0.721456996682917,
5.74621977324417));
#13370=CARTESIAN_POINT('Ctrl Pts',(-2.96500222964141,-0.815139372954289,
5.75120366508783));
#13371=CARTESIAN_POINT('Ctrl Pts',(-2.93795207564248,-0.907826962249409,
5.75618755693149));
#13372=CARTESIAN_POINT('Ctrl Pts',(-2.90658757484834,-0.999075032085795,
5.76117144877515));
#13373=CARTESIAN_POINT('Ctrl Pts',(-2.87523449622858,-1.09028987163512,
5.76615352560884));
#13374=CARTESIAN_POINT('Ctrl Pts',(-2.83957033511789,-1.18006581862899,
5.77113560244253));
#13375=CARTESIAN_POINT('Ctrl Pts',(-2.79975810543453,-1.26797350171589,
5.77611767927622));
#13376=CARTESIAN_POINT('Ctrl Pts',(-2.75994950570929,-1.35587316964736,
5.78109930185929));
#13377=CARTESIAN_POINT('Ctrl Pts',(-2.71599377062049,-1.44190451255417,
5.78608092444235));
#13378=CARTESIAN_POINT('Ctrl Pts',(-2.66810154393448,-1.52565933328985,
5.79106254702541));
#13379=CARTESIAN_POINT('Ctrl Pts',(-2.62020060959783,-1.60942938212764,
5.79604507535524));
#13380=CARTESIAN_POINT('Ctrl Pts',(-2.56836198016167,-1.69092170572364,
5.80102760368506));
#13381=CARTESIAN_POINT('Ctrl Pts',(-2.51284107053017,-1.76975478647658,
5.80601013201488));
#13382=CARTESIAN_POINT('Ctrl Pts',(-2.45726031754067,-1.84867283767229,
5.81099803077592));
#13383=CARTESIAN_POINT('Ctrl Pts',(-2.39798961388144,-1.92492556429473,
5.81598592953697));
#13384=CARTESIAN_POINT('Ctrl Pts',(-2.33532620329277,-1.99816259954343,
5.82097382829801));
#13385=CARTESIAN_POINT('Ctrl Pts',(-2.27262577656736,-2.0714428969141,5.82596467347932));
#13386=CARTESIAN_POINT('Ctrl Pts',(-2.20652895301908,-2.14170363625871,
5.83095551866062));
#13387=CARTESIAN_POINT('Ctrl Pts',(-2.13737008268281,-2.20863110990778,
5.83594636384193));
#13388=CARTESIAN_POINT('Ctrl Pts',(-2.06809944986559,-2.27566674004441,
5.84094527435508));
#13389=CARTESIAN_POINT('Ctrl Pts',(-1.99575721875399,-2.33935805868011,
5.84594418486824));
#13390=CARTESIAN_POINT('Ctrl Pts',(-1.9207109996448,-2.39943149638482,5.85094309538139));
#13391=CARTESIAN_POINT('Ctrl Pts',(-1.87714221586694,-2.43430769200422,
5.85384525959243));
#13392=CARTESIAN_POINT('Ctrl Pts',(-1.83266261781887,-2.46796528230561,
5.85674742380347));
#13393=CARTESIAN_POINT('Ctrl Pts',(-1.78734827456123,-2.50035765350139,
5.85964958801451));
#13394=CARTESIAN_POINT('Ctrl Pts',(-1.70928601729032,-2.5561594467553,5.86464909750748));
#13395=CARTESIAN_POINT('Ctrl Pts',(-1.62847091007287,-2.60840004133584,
5.86964860700046));
#13396=CARTESIAN_POINT('Ctrl Pts',(-1.54526158954145,-2.65679673100669,
5.87464811649343));
#13397=CARTESIAN_POINT('Ctrl Pts',(-1.46216514192501,-2.70512777087528,
5.87964084418353));
#13398=CARTESIAN_POINT('Ctrl Pts',(-1.37668131185556,-2.74962504996738,
5.88463357187361));
#13399=CARTESIAN_POINT('Ctrl Pts',(-1.2891993531016,-2.79004789886525,5.8896262995637));
#13400=CARTESIAN_POINT('Ctrl Pts',(-1.20180968560897,-2.83042810267648,
5.89461376005193));
#13401=CARTESIAN_POINT('Ctrl Pts',(-1.11242647631994,-2.86674223814857,
5.89960122054016));
#13402=CARTESIAN_POINT('Ctrl Pts',(-1.02146443293957,-2.89879503625894,
5.90458868102839));
#13403=CARTESIAN_POINT('Ctrl Pts',(-0.930567475027476,-2.93082489984302,
5.90957257287206));
#13404=CARTESIAN_POINT('Ctrl Pts',(-0.838094341623338,-2.95859934203635,
5.91455646471573));
#13405=CARTESIAN_POINT('Ctrl Pts',(-0.744479713188049,-2.98197119480578,
5.9195403565594));
#13406=CARTESIAN_POINT('Ctrl Pts',(-0.650899176881863,-3.0053345361253,
5.92452243339309));
#13407=CARTESIAN_POINT('Ctrl Pts',(-0.55617839695845,-3.02429836741265,
5.92950451022679));
#13408=CARTESIAN_POINT('Ctrl Pts',(-0.460766279977206,-3.03876565158223,
5.93448658706048));
#13409=CARTESIAN_POINT('Ctrl Pts',(-0.365362862382894,-3.05323161666879,
5.93946820964355));
#13410=CARTESIAN_POINT('Ctrl Pts',(-0.269268667082945,-3.06320178413059,
5.94444983222662));
#13411=CARTESIAN_POINT('Ctrl Pts',(-0.172940772022078,-3.06863059676013,
5.94943145480969));
#13412=CARTESIAN_POINT('Ctrl Pts',(-0.0765953628526493,-3.07406039644346,
5.95441398313951));
#13413=CARTESIAN_POINT('Ctrl Pts',(0.0199833922000153,-3.07494717679239,
5.95939651146934));
#13414=CARTESIAN_POINT('Ctrl Pts',(0.116336418072036,-3.07129746000451,
5.96437903979916));
#13415=CARTESIAN_POINT('Ctrl Pts',(0.21279329830562,-3.06764380935982,5.96936693856021));
#13416=CARTESIAN_POINT('Ctrl Pts',(0.309023524251918,-3.05944391643605,
5.97435483732126));
#13417=CARTESIAN_POINT('Ctrl Pts',(0.404571376123319,-3.04675634923794,
5.97934273608231));
#13418=CARTESIAN_POINT('Ctrl Pts',(0.500175669422252,-3.03406128731974,
5.98433358126362));
#13419=CARTESIAN_POINT('Ctrl Pts',(0.595096354296386,-3.01687335086815,
5.98932442644493));
#13420=CARTESIAN_POINT('Ctrl Pts',(0.688888257774321,-2.99530219148263,
5.99431527162624));
#13421=CARTESIAN_POINT('Ctrl Pts',(0.782831731336869,-2.9736961725588,5.9993141821394));
#13422=CARTESIAN_POINT('Ctrl Pts',(0.875642358699442,-2.94769290506517,
6.00431309265256));
#13423=CARTESIAN_POINT('Ctrl Pts',(0.966890525934692,-2.91745179237939,
6.00931200316572));
#13424=CARTESIAN_POINT('Ctrl Pts',(1.0198655020962,-2.89989503182007,6.0122141673767));
#13425=CARTESIAN_POINT('Ctrl Pts',(1.07231421576954,-2.88091081571002,6.01511633158769));
#13426=CARTESIAN_POINT('Ctrl Pts',(1.12415615175047,-2.86053757124104,6.01801849579868));
#13427=CARTESIAN_POINT('Ctrl Pts',(1.21346338326062,-2.82544092552406,6.02301800529165));
#13428=CARTESIAN_POINT('Ctrl Pts',(1.30128230224825,-2.78609631033278,6.02801751478463));
#13429=CARTESIAN_POINT('Ctrl Pts',(1.38718051662889,-2.74265062745607,6.03301702427761));
#13430=CARTESIAN_POINT('Ctrl Pts',(1.47296221062716,-2.69926387837233,6.0380097519677));
#13431=CARTESIAN_POINT('Ctrl Pts',(1.55682798976621,-2.65178731426579,6.0430024796578));
#13432=CARTESIAN_POINT('Ctrl Pts',(1.63836405257326,-2.60041640535429,6.0479952073479));
#13433=CARTESIAN_POINT('Ctrl Pts',(1.71981409688929,-2.54909969145681,6.05298266783613));
#13434=CARTESIAN_POINT('Ctrl Pts',(1.79893894139447,-2.49389703282577,6.05797012832436));
#13435=CARTESIAN_POINT('Ctrl Pts',(1.87534900768173,-2.43504996856064,6.06295758881259));
#13436=CARTESIAN_POINT('Ctrl Pts',(1.95170440078042,-2.37624501074557,6.06794148065626));
#13437=CARTESIAN_POINT('Ctrl Pts',(2.02534853045345,-2.3138010982686,6.07292537249993));
#13438=CARTESIAN_POINT('Ctrl Pts',(2.09592129083453,-2.24800271188149,6.0779092643436));
#13439=CARTESIAN_POINT('Ctrl Pts',(2.1664683503642,-2.18222828763702,6.0828913411773));
#13440=CARTESIAN_POINT('Ctrl Pts',(2.23394594223766,-2.11310211573837,6.08787341801099));
#13441=CARTESIAN_POINT('Ctrl Pts',(2.29802826461911,-2.0409479035516,6.09285549484469));
#13442=CARTESIAN_POINT('Ctrl Pts',(2.36210474416911,-1.96880027016666,6.09783711742776));
#13443=CARTESIAN_POINT('Ctrl Pts',(2.42278627835587,-1.89362547373654,6.10281874001084));
#13444=CARTESIAN_POINT('Ctrl Pts',(2.47978579734471,-1.81578210402225,6.10780036259391));
#13445=CARTESIAN_POINT('Ctrl Pts',(2.53679567985041,-1.73792458101177,6.11278289092374));
#13446=CARTESIAN_POINT('Ctrl Pts',(2.59012195831738,-1.6573978753062,6.11776541925357));
#13447=CARTESIAN_POINT('Ctrl Pts',(2.63952015937944,-1.57459060654811,6.1227479475834));
#13448=CARTESIAN_POINT('Ctrl Pts',(2.68897160442201,-1.49169408375831,6.12773584634445));
#13449=CARTESIAN_POINT('Ctrl Pts',(2.73448629423379,-1.40651246813039,6.1327237451055));
#13450=CARTESIAN_POINT('Ctrl Pts',(2.77586523785553,-1.31945990134799,6.13771164386656));
#13451=CARTESIAN_POINT('Ctrl Pts',(2.8172686245872,-1.23235591141961,6.14270248904787));
#13452=CARTESIAN_POINT('Ctrl Pts',(2.85453123114794,-1.14337917441077,6.14769333422918));
#13453=CARTESIAN_POINT('Ctrl Pts',(2.88750265733424,-1.05296279795998,6.15268417941049));
#13454=CARTESIAN_POINT('Ctrl Pts',(2.9205273661779,-0.962400306361512,6.15768308992365));
#13455=CARTESIAN_POINT('Ctrl Pts',(2.94924691696318,-0.870393948567786,
6.16268200043681));
#13456=CARTESIAN_POINT('Ctrl Pts',(2.97356111204012,-0.777390868844463,
6.16768091094997));
#13457=CARTESIAN_POINT('Ctrl Pts',(2.98767694519714,-0.723397061839546,
6.17058307516093));
#13458=CARTESIAN_POINT('Ctrl Pts',(3.0003089152176,-0.669067499346793,6.1734852393719));
#13459=CARTESIAN_POINT('Ctrl Pts',(3.01144541790487,-0.61449063864291,6.17638740358286));
#13460=CARTESIAN_POINT('Ctrl Pts',(3.03868361335526,-0.481003920176007,
6.18348565679818));
#13461=CARTESIAN_POINT('Ctrl Pts',(3.05705350500806,-0.345651342796243,
6.1905839100135));
#13462=CARTESIAN_POINT('Ctrl Pts',(3.06635784075604,-0.209408315102262,
6.19768216322882));
#13463=CARTESIAN_POINT('Ctrl Pts',(3.07105103823204,-0.140686006383418,
6.2012625912117));
#13464=CARTESIAN_POINT('Ctrl Pts',(3.07343837424032,-0.0717374795267619,
6.20484301919458));
#13465=CARTESIAN_POINT('Ctrl Pts',(3.07349882217824,-0.00269073762051493,
6.20842344717746));
#13466=CARTESIAN_POINT('Origin',(0.,0.,-2.20842344717744));
#13467=CARTESIAN_POINT('',(-1.87240768645123,2.4373123939533,4.56258760229939));
#13468=CARTESIAN_POINT('',(-1.87025628839741,2.4345543755422,4.64593736840472));
#13469=CARTESIAN_POINT('',(-1.87240768645123,2.4373123939533,-2.20842344717744));
#13470=CARTESIAN_POINT('',(3.06881272651402,-0.000977486742642815,5.29157655282255));
#13471=CARTESIAN_POINT('Ctrl Pts',(-1.87025628839757,2.43455437554208,4.64593736840473));
#13472=CARTESIAN_POINT('Ctrl Pts',(-2.38377235667202,2.03450370412233,4.67955767874455));
#13473=CARTESIAN_POINT('Ctrl Pts',(-3.39698165770904,0.598186149263013,
4.76596762501243));
#13474=CARTESIAN_POINT('Ctrl Pts',(-2.74378617582191,-2.37612491828059,
4.90516720720836));
#13475=CARTESIAN_POINT('Ctrl Pts',(0.499216583506413,-3.59515159745691,
5.06353611499254));
#13476=CARTESIAN_POINT('Ctrl Pts',(2.76686331140346,-1.92257446296493,5.19233923019727));
#13477=CARTESIAN_POINT('Ctrl Pts',(3.0701031042517,-0.451063181367307,5.26835270947394));
#13478=CARTESIAN_POINT('Ctrl Pts',(3.06881272651402,-0.000977486742642815,
5.29157655282255));
#13479=CARTESIAN_POINT('Ctrl Pts',(3.06881272651402,-0.000977486742642815,
5.29157655282255));
#13480=CARTESIAN_POINT('Ctrl Pts',(3.0671699734189,0.572017262252944,5.32114234540199));
#13481=CARTESIAN_POINT('Ctrl Pts',(2.6385116023052,2.17037498979142,5.4034977739095));
#13482=CARTESIAN_POINT('Ctrl Pts',(0.392306605071205,3.44445527983356,5.52154193127653));
#13483=CARTESIAN_POINT('Ctrl Pts',(-1.31984353549509,2.85138991238784,5.61002029606411));
#13484=CARTESIAN_POINT('Ctrl Pts',(-1.87084604423436,2.43524047469674,5.64570902492362));
#13485=CARTESIAN_POINT('',(3.07349942256352,0.00188401212730468,5.20842344714237));
#13486=CARTESIAN_POINT('Ctrl Pts',(3.07349942256311,0.00188401280199884,
5.20842344717746));
#13487=CARTESIAN_POINT('Ctrl Pts',(3.07342968576285,0.11564970223751,5.21434028374424));
#13488=CARTESIAN_POINT('Ctrl Pts',(3.06704369053517,0.229219670324171,5.22025712031102));
#13489=CARTESIAN_POINT('Ctrl Pts',(3.05440435245992,0.342076455889465,5.22617395687781));
#13490=CARTESIAN_POINT('Ctrl Pts',(3.04372457620137,0.437436292925306,5.23117346637075));
#13491=CARTESIAN_POINT('Ctrl Pts',(3.02855599778435,0.532463002356707,5.23617297586368));
#13492=CARTESIAN_POINT('Ctrl Pts',(3.00892809284608,0.626700871294788,5.24117248535662));
#13493=CARTESIAN_POINT('Ctrl Pts',(2.98932681303621,0.720810907162142,5.24616521304668));
#13494=CARTESIAN_POINT('Ctrl Pts',(2.96527831752864,0.814133803139797,5.25115794073675));
#13495=CARTESIAN_POINT('Ctrl Pts',(2.93686381305271,0.906219175244882,5.25615066842681));
#13496=CARTESIAN_POINT('Ctrl Pts',(2.90847928516275,0.998207399603617,5.26113812891501));
#13497=CARTESIAN_POINT('Ctrl Pts',(2.87573803355213,1.08896027823987,5.26612558940321));
#13498=CARTESIAN_POINT('Ctrl Pts',(2.83877204625539,1.17803884460529,5.27111304989142));
#13499=CARTESIAN_POINT('Ctrl Pts',(2.80183250898673,1.26705367317406,5.27609694173504));
#13500=CARTESIAN_POINT('Ctrl Pts',(2.76067441317566,1.35439616678284,5.28108083357867));
#13501=CARTESIAN_POINT('Ctrl Pts',(2.71547887272697,1.43964465816169,5.2860647254223));
#13502=CARTESIAN_POINT('Ctrl Pts',(2.67029979137473,1.52486210415137,5.29104680225596));
#13503=CARTESIAN_POINT('Ctrl Pts',(2.62108639218778,1.6079866756494,5.29602887908962));
#13504=CARTESIAN_POINT('Ctrl Pts',(2.56806658326335,1.68861963565692,5.30101095592328));
#13505=CARTESIAN_POINT('Ctrl Pts',(2.51505160852398,1.76924524379617,5.30599257850631));
#13506=CARTESIAN_POINT('Ctrl Pts',(2.45823115538501,1.84737932544126,5.31097420108934));
#13507=CARTESIAN_POINT('Ctrl Pts',(2.39787688202416,1.92265147872777,5.31595582367237));
#13508=CARTESIAN_POINT('Ctrl Pts',(2.33751163519306,1.99793731781794,5.32093835200216));
#13509=CARTESIAN_POINT('Ctrl Pts',(2.2736115667338,2.07035985269263,5.32592088033194));
#13510=CARTESIAN_POINT('Ctrl Pts',(2.20648840351205,2.13958200945111,5.33090340866173));
#13511=CARTESIAN_POINT('Ctrl Pts',(2.1392928914128,2.20887877749277,5.33589130742274));
#13512=CARTESIAN_POINT('Ctrl Pts',(2.06886765507404,2.27496796508148,5.34087920618375));
#13513=CARTESIAN_POINT('Ctrl Pts',(1.9955608871673,2.33754978462664,5.34586710494477));
#13514=CARTESIAN_POINT('Ctrl Pts',(1.92221081594657,2.40016857211159,5.35085795012604));
#13515=CARTESIAN_POINT('Ctrl Pts',(1.84597617062353,2.45927559731828,5.35584879530731));
#13516=CARTESIAN_POINT('Ctrl Pts',(1.7672360867378,2.51461306441601,5.36083964048859));
#13517=CARTESIAN_POINT('Ctrl Pts',(1.68836875688804,2.57003995825803,5.36583855100171));
#13518=CARTESIAN_POINT('Ctrl Pts',(1.60698827419281,2.62168489516321,5.37083746151483));
#13519=CARTESIAN_POINT('Ctrl Pts',(1.52350037602741,2.66933490859509,5.37583637202795));
#13520=CARTESIAN_POINT('Ctrl Pts',(1.47503069658438,2.69699856916447,5.37873853623929));
#13521=CARTESIAN_POINT('Ctrl Pts',(1.42585114590227,2.72331662043663,5.38164070045063));
#13522=CARTESIAN_POINT('Ctrl Pts',(1.37604412559674,2.74825486707669,5.38454286466197));
#13523=CARTESIAN_POINT('Ctrl Pts',(1.29024240911866,2.79121556527837,5.38954237415494));
#13524=CARTESIAN_POINT('Ctrl Pts',(1.20227618216278,2.83022971901549,5.39454188364791));
#13525=CARTESIAN_POINT('Ctrl Pts',(1.11254374124125,2.86507393863141,5.39954139314088));
#13526=CARTESIAN_POINT('Ctrl Pts',(1.02293302180603,2.89987089228469,5.40453412083097));
#13527=CARTESIAN_POINT('Ctrl Pts',(0.931561255708756,2.93050899617844,5.40952684852107));
#13528=CARTESIAN_POINT('Ctrl Pts',(0.838850434690195,2.95681115362819,5.41451957621116));
#13529=CARTESIAN_POINT('Ctrl Pts',(0.746237421251002,2.98308556296478,5.41950703669938));
#13530=CARTESIAN_POINT('Ctrl Pts',(0.652288581242648,3.00503300014876,5.4244944971876));
#13531=CARTESIAN_POINT('Ctrl Pts',(0.557443977510773,3.02252517970272,5.42948195767582));
#13532=CARTESIAN_POINT('Ctrl Pts',(0.462667237309793,3.04000484319334,5.43446584951948));
#13533=CARTESIAN_POINT('Ctrl Pts',(0.36699643798775,3.0530355069444,5.43944974136315));
#13534=CARTESIAN_POINT('Ctrl Pts',(0.270883878545778,3.0615395104986,5.44443363320681));
#13535=CARTESIAN_POINT('Ctrl Pts',(0.174806320917514,3.07004041710532,5.4494157100405));
#13536=CARTESIAN_POINT('Ctrl Pts',(0.0782877596238715,3.07401790025223,
5.45439778687419));
#13537=CARTESIAN_POINT('Ctrl Pts',(-0.018213262897366,3.07344603451153,
5.45937986370788));
#13538=CARTESIAN_POINT('Ctrl Pts',(-0.114705486748633,3.0728742209118,5.46436148629095));
#13539=CARTESIAN_POINT('Ctrl Pts',(-0.211179736053418,3.06775388589988,
5.46934310887402));
#13540=CARTESIAN_POINT('Ctrl Pts',(-0.307177415866493,3.05811122838617,
5.47432473145708));
#13541=CARTESIAN_POINT('Ctrl Pts',(-0.40319254974915,3.04846681766743,5.47930725978691));
#13542=CARTESIAN_POINT('Ctrl Pts',(-0.49873050529916,3.03429849538759,5.48428978811673));
#13543=CARTESIAN_POINT('Ctrl Pts',(-0.593338827350413,3.0156842152252,5.48927231644655));
#13544=CARTESIAN_POINT('Ctrl Pts',(-0.688049123229613,2.99704987161215,
5.4942602152076));
#13545=CARTESIAN_POINT('Ctrl Pts',(-0.781827353774678,2.9739600880389,5.49924811396864));
#13546=CARTESIAN_POINT('Ctrl Pts',(-0.874232485423852,2.94654370601042,
5.50423601272969));
#13547=CARTESIAN_POINT('Ctrl Pts',(-0.966692202052608,2.91911112874878,
5.509226857911));
#13548=CARTESIAN_POINT('Ctrl Pts',(-1.05777679044786,2.88734700852964,5.5142177030923));
#13549=CARTESIAN_POINT('Ctrl Pts',(-1.14706359251928,2.85142900397621,5.51920854827361));
#13550=CARTESIAN_POINT('Ctrl Pts',(-1.23649468431763,2.81545295502038,5.52420745878676));
#13551=CARTESIAN_POINT('Ctrl Pts',(-1.32412178980427,2.77530980048819,5.52920636929992));
#13552=CARTESIAN_POINT('Ctrl Pts',(-1.40954536994406,2.73122391979663,5.53420527981307));
#13553=CARTESIAN_POINT('Ctrl Pts',(-1.45913882763995,2.70562944979801,5.5371074440241));
#13554=CARTESIAN_POINT('Ctrl Pts',(-1.50799008914286,2.67870692619843,5.54000960823512));
#13555=CARTESIAN_POINT('Ctrl Pts',(-1.55602560798146,2.65050684913394,5.54291177244615));
#13556=CARTESIAN_POINT('Ctrl Pts',(-1.63877544569276,2.60192713443629,5.54791127330053));
#13557=CARTESIAN_POINT('Ctrl Pts',(-1.71939343083612,2.54938315646748,5.55291077415492));
#13558=CARTESIAN_POINT('Ctrl Pts',(-1.79747533480956,2.49308737727968,5.5579102750093));
#13559=CARTESIAN_POINT('Ctrl Pts',(-1.82272213851202,2.47488484360536,5.55952680086558));
#13560=CARTESIAN_POINT('Ctrl Pts',(-1.8477039709751,2.45629043995846,5.56114332672186));
#13561=CARTESIAN_POINT('Ctrl Pts',(-1.87240768645123,2.4373123939533,5.56275985257814));
#13562=CARTESIAN_POINT('Ctrl Pts',(-1.87240768645123,2.4373123939533,4.56258760229939));
#13563=CARTESIAN_POINT('Ctrl Pts',(-1.94922488799432,2.37829939300283,4.56760605620634));
#13564=CARTESIAN_POINT('Ctrl Pts',(-2.02316578639418,2.315715664159,4.57262451011329));
#13565=CARTESIAN_POINT('Ctrl Pts',(-2.09389869348013,2.24988677747175,4.57764296402024));
#13566=CARTESIAN_POINT('Ctrl Pts',(-2.16463160056609,2.18405789078449,4.5826614179272));
#13567=CARTESIAN_POINT('Ctrl Pts',(-2.23215624896084,2.11498420753435,4.58767987183415));
#13568=CARTESIAN_POINT('Ctrl Pts',(-2.29618206790087,2.04302475781634,4.5926983257411));
#13569=CARTESIAN_POINT('Ctrl Pts',(-2.35996619256591,1.97133695143401,4.59769783523471));
#13570=CARTESIAN_POINT('Ctrl Pts',(-2.42050194477723,1.89653331526934,4.60269734472831));
#13571=CARTESIAN_POINT('Ctrl Pts',(-2.47747009481934,1.81894040014396,4.60769685422192));
#13572=CARTESIAN_POINT('Ctrl Pts',(-2.53436096792775,1.7414527393151,4.61268958191266));
#13573=CARTESIAN_POINT('Ctrl Pts',(-2.58769359935125,1.66118367006765,4.61768230960339));
#13574=CARTESIAN_POINT('Ctrl Pts',(-2.63718730318107,1.5784946556579,4.62267503729413));
#13575=CARTESIAN_POINT('Ctrl Pts',(-2.68662879240102,1.49589287607388,4.62766249778301));
#13576=CARTESIAN_POINT('Ctrl Pts',(-2.73223918088222,1.41087660114449,4.63264995827189));
#13577=CARTESIAN_POINT('Ctrl Pts',(-2.77378021992166,1.32383743018974,4.63763741876078));
#13578=CARTESIAN_POINT('Ctrl Pts',(-2.81529153537671,1.2368605377962,4.6426213106051));
#13579=CARTESIAN_POINT('Ctrl Pts',(-2.85273910121061,1.1478640218185,4.64760520244944));
#13580=CARTESIAN_POINT('Ctrl Pts',(-2.88593037390322,1.05726445461048,4.65258909429376));
#13581=CARTESIAN_POINT('Ctrl Pts',(-2.91910955915642,0.966697881520837,
4.65757117112813));
#13582=CARTESIAN_POINT('Ctrl Pts',(-2.94803538017669,0.8745298288834,4.66255324796249));
#13583=CARTESIAN_POINT('Ctrl Pts',(-2.97256362798983,0.781196343790704,
4.66753532479685));
#13584=CARTESIAN_POINT('Ctrl Pts',(-2.99708963939189,0.687871368561476,
4.67251694738059));
#13585=CARTESIAN_POINT('Ctrl Pts',(-3.01721876336985,0.593381596735652,
4.67749856996433));
#13586=CARTESIAN_POINT('Ctrl Pts',(-3.03285711043859,0.498176673141256,
4.68248019254807));
#13587=CARTESIAN_POINT('Ctrl Pts',(-3.04849830083437,0.402954439614213,
4.68746272087858));
#13588=CARTESIAN_POINT('Ctrl Pts',(-3.0596470216313,0.307017229243321,4.69244524920908));
#13589=CARTESIAN_POINT('Ctrl Pts',(-3.06626095532859,0.210822209046808,
4.69742777753958));
#13590=CARTESIAN_POINT('Ctrl Pts',(-3.07288201787166,0.114523504795564,
4.70241567630131));
#13591=CARTESIAN_POINT('Ctrl Pts',(-3.07495850504973,0.0179668746095363,
4.70740357506304));
#13592=CARTESIAN_POINT('Ctrl Pts',(-3.07250020693417,-0.0783883179400242,
4.71239147382477));
#13593=CARTESIAN_POINT('Ctrl Pts',(-3.07004045666818,-0.174800428824401,
4.71738231900676));
#13594=CARTESIAN_POINT('Ctrl Pts',(-3.06304061909772,-0.271010427539188,
4.72237316418875));
#13595=CARTESIAN_POINT('Ctrl Pts',(-3.05156239961503,-0.366564007038006,
4.72736400937074));
#13596=CARTESIAN_POINT('Ctrl Pts',(-3.0400656310398,-0.462272003534262,
4.73236291988458));
#13597=CARTESIAN_POINT('Ctrl Pts',(-3.02407610227852,-0.557321030063018,
4.73736183039841));
#13598=CARTESIAN_POINT('Ctrl Pts',(-3.00370664260785,-0.651266961509247,
4.74236074091225));
#13599=CARTESIAN_POINT('Ctrl Pts',(-2.99188096248128,-0.705808149760561,
4.74526290511659));
#13600=CARTESIAN_POINT('Ctrl Pts',(-2.97857997043236,-0.759977805689979,
4.74816506932093));
#13601=CARTESIAN_POINT('Ctrl Pts',(-2.96383331659785,-0.813691785275364,
4.75106723352527));
#13602=CARTESIAN_POINT('Ctrl Pts',(-2.93842950391147,-0.90622395503668,
4.75606674301803));
#13603=CARTESIAN_POINT('Ctrl Pts',(-2.90864357578993,-0.997727833434325,
4.76106625251079));
#13604=CARTESIAN_POINT('Ctrl Pts',(-2.87457563542604,-1.08775786194123,
4.76606576200356));
#13605=CARTESIAN_POINT('Ctrl Pts',(-2.84055390800695,-1.17766576528609,
4.77105848969344));
#13606=CARTESIAN_POINT('Ctrl Pts',(-2.80226186642582,-1.2661033851133,4.77605121738332));
#13607=CARTESIAN_POINT('Ctrl Pts',(-2.75984988339205,-1.35263848501397,
4.7810439450732));
#13608=CARTESIAN_POINT('Ctrl Pts',(-2.71748264393132,-1.43908229256549,
4.78603140556121));
#13609=CARTESIAN_POINT('Ctrl Pts',(-2.67100429562576,-1.52362717813468,
4.79101886604923));
#13610=CARTESIAN_POINT('Ctrl Pts',(-2.62061359408541,-1.60586009368648,
4.79600632653724));
#13611=CARTESIAN_POINT('Ctrl Pts',(-2.57025894826994,-1.68803416966495,
4.80099021838069));
#13612=CARTESIAN_POINT('Ctrl Pts',(-2.5159977429492,-1.76789919102667,4.80597411022414));
#13613=CARTESIAN_POINT('Ctrl Pts',(-2.45807456517958,-1.84506685028408,
4.8109580020676));
#13614=CARTESIAN_POINT('Ctrl Pts',(-2.4001724815967,-1.92220640699123,4.81594007890107));
#13615=CARTESIAN_POINT('Ctrl Pts',(-2.33861133852885,-1.99665020263482,
4.82092215573455));
#13616=CARTESIAN_POINT('Ctrl Pts',(-2.27367837411193,-2.06803986931967,
4.82590423256803));
#13617=CARTESIAN_POINT('Ctrl Pts',(-2.20875133008542,-2.13942302691163,
4.83088585515088));
#13618=CARTESIAN_POINT('Ctrl Pts',(-2.14045337143884,-2.20775228458013,
4.83586747773373));
#13619=CARTESIAN_POINT('Ctrl Pts',(-2.06911053850813,-2.27270407872089,
4.84084910031658));
#13620=CARTESIAN_POINT('Ctrl Pts',(-1.99775473419338,-2.33766768224224,
4.84583162864619));
#13621=CARTESIAN_POINT('Ctrl Pts',(-1.92335328073249,-2.39925230718283,
4.8508141569758));
#13622=CARTESIAN_POINT('Ctrl Pts',(-1.84626660646391,-2.45717355265277,
4.85579668530541));
#13623=CARTESIAN_POINT('Ctrl Pts',(-1.76909684412133,-2.51515722868902,
4.86078458406624));
#13624=CARTESIAN_POINT('Ctrl Pts',(-1.68923643434323,-2.56946937814897,
4.86577248282708));
#13625=CARTESIAN_POINT('Ctrl Pts',(-1.60707601796877,-2.61986811165556,
4.87076038158791));
#13626=CARTESIAN_POINT('Ctrl Pts',(-1.52486706830866,-2.67029661638577,
4.875751226769));
#13627=CARTESIAN_POINT('Ctrl Pts',(-1.44035579115729,-2.71680689062622,
4.88074207195009));
#13628=CARTESIAN_POINT('Ctrl Pts',(-1.35395685135728,-2.7592033442033,4.88573291713119));
#13629=CARTESIAN_POINT('Ctrl Pts',(-1.26741828868862,-2.80166831152005,
4.89073182764413));
#13630=CARTESIAN_POINT('Ctrl Pts',(-1.17898637464839,-2.84000600902761,
4.89573073815708));
#13631=CARTESIAN_POINT('Ctrl Pts',(-1.08909506803239,-2.87406927244065,
4.90072964867002));
#13632=CARTESIAN_POINT('Ctrl Pts',(-1.03690782994163,-2.89384501833651,
4.90363181288317));
#13633=CARTESIAN_POINT('Ctrl Pts',(-0.984228994413888,-2.91218100261231,
4.90653397709631));
#13634=CARTESIAN_POINT('Ctrl Pts',(-0.931145283869829,-2.92905628322963,
4.90943614130945));
#13635=CARTESIAN_POINT('Ctrl Pts',(-0.839698868266351,-2.95812704540771,
4.91443565080237));
#13636=CARTESIAN_POINT('Ctrl Pts',(-0.74672912593629,-2.98296226812754,
4.91943516029529));
#13637=CARTESIAN_POINT('Ctrl Pts',(-0.652664289274368,-3.00340333213939,
4.92443466978821));
#13638=CARTESIAN_POINT('Ctrl Pts',(-0.558727050966137,-3.02381666797769,
4.92942739747825));
#13639=CARTESIAN_POINT('Ctrl Pts',(-0.463698095917904,-3.03984759908492,
4.93442012516828));
#13640=CARTESIAN_POINT('Ctrl Pts',(-0.36802185135121,-3.05138692514208,
4.93941285285832));
#13641=CARTESIAN_POINT('Ctrl Pts',(-0.272446542810913,-3.06291407750111,
4.94440031334649));
#13642=CARTESIAN_POINT('Ctrl Pts',(-0.176225735751422,-3.06995899243969,
4.94938777383466));
#13643=CARTESIAN_POINT('Ctrl Pts',(-0.0798141044801399,-3.07246349998271,
4.95437523432283));
#13644=CARTESIAN_POINT('Ctrl Pts',(0.0165285420153408,-3.07496621549205,
4.95935912616644));
#13645=CARTESIAN_POINT('Ctrl Pts',(0.113061303733088,-3.07293497063588,
4.96434301801005));
#13646=CARTESIAN_POINT('Ctrl Pts',(0.209325305543598,-3.06636350853239,
4.96932690985366));
#13647=CARTESIAN_POINT('Ctrl Pts',(0.305554250388853,-3.05979443959265,
4.97430898668729));
#13648=CARTESIAN_POINT('Ctrl Pts',(0.401514192299747,-3.04868846846636,
4.97929106352093));
#13649=CARTESIAN_POINT('Ctrl Pts',(0.496748147799032,-3.03309141432602,
4.98427314035457));
#13650=CARTESIAN_POINT('Ctrl Pts',(0.591973420155595,-3.01749578227769,
4.98925476293758));
#13651=CARTESIAN_POINT('Ctrl Pts',(0.68647240454356,-2.9974099524712,4.99423638552059));
#13652=CARTESIAN_POINT('Ctrl Pts',(0.779796185138011,-2.97293124031556,
4.99921800810359));
#13653=CARTESIAN_POINT('Ctrl Pts',(0.873136933640147,-2.94844807749873,
5.00420053643336));
#13654=CARTESIAN_POINT('Ctrl Pts',(0.965301629408796,-2.91957055751148,
5.00918306476313));
#13655=CARTESIAN_POINT('Ctrl Pts',(1.0558554834001,-2.886446162355,5.0141655930929));
#13656=CARTESIAN_POINT('Ctrl Pts',(1.14650694110024,-2.85328606398241,5.01915349185389));
#13657=CARTESIAN_POINT('Ctrl Pts',(1.23554367782967,-2.81587010292265,5.02414139061488));
#13658=CARTESIAN_POINT('Ctrl Pts',(1.3225501136303,-2.77439424864897,5.02912928937587));
#13659=CARTESIAN_POINT('Ctrl Pts',(1.4096079453268,-2.73289389401888,5.03412013455712));
#13660=CARTESIAN_POINT('Ctrl Pts',(1.49463270131337,-2.68732907814428,5.03911097973837));
#13661=CARTESIAN_POINT('Ctrl Pts',(1.57723455714045,-2.63794112932074,5.04410182491962));
#13662=CARTESIAN_POINT('Ctrl Pts',(1.65996989965248,-2.58847336832471,5.04910073543271));
#13663=CARTESIAN_POINT('Ctrl Pts',(1.74027415819936,-2.53517038031442,5.05409964594581));
#13664=CARTESIAN_POINT('Ctrl Pts',(1.81778762297006,-2.47831604275501,5.0590985564589));
#13665=CARTESIAN_POINT('Ctrl Pts',(1.8627887892808,-2.44530872579961,5.06200072067047));
#13666=CARTESIAN_POINT('Ctrl Pts',(1.9068499456451,-2.41110518024639,5.06490288488204));
#13667=CARTESIAN_POINT('Ctrl Pts',(1.94990630988549,-2.37576674626714,5.06780504909361));
#13668=CARTESIAN_POINT('Ctrl Pts',(2.02310041339419,-2.31569281666009,5.07273861260852));
#13669=CARTESIAN_POINT('Ctrl Pts',(2.0936608174452,-2.25211385751832,5.07767217612343));
#13670=CARTESIAN_POINT('Ctrl Pts',(2.16122630734251,-2.18529245146975,5.08260573963834));
#13671=CARTESIAN_POINT('Ctrl Pts',(2.22869969055807,-2.11856213775234,5.0875325776168));
#13672=CARTESIAN_POINT('Ctrl Pts',(2.29318595058021,-2.04859847115308,5.09245941559526));
#13673=CARTESIAN_POINT('Ctrl Pts',(2.35435603556388,-1.97570491415189,5.09738625357373));
#13674=CARTESIAN_POINT('Ctrl Pts',(2.41545719842112,-1.90289348845643,5.10230754033953));
#13675=CARTESIAN_POINT('Ctrl Pts',(2.47324932477958,-1.82715907853083,5.10722882710534));
#13676=CARTESIAN_POINT('Ctrl Pts',(2.52744035697135,-1.74884175726466,5.11215011387114));
#13677=CARTESIAN_POINT('Ctrl Pts',(2.58159824009642,-1.67057234329976,5.11706839024839));
#13678=CARTESIAN_POINT('Ctrl Pts',(2.63215914616383,-1.58972352520295,5.12198666662564));
#13679=CARTESIAN_POINT('Ctrl Pts',(2.678872048634,-1.50666744739757,5.12690494300289));
#13680=CARTESIAN_POINT('Ctrl Pts',(2.72556993901313,-1.42363806126268,5.13182163879729));
#13681=CARTESIAN_POINT('Ctrl Pts',(2.76842206103465,-1.33840321787111,5.13673833459168));
#13682=CARTESIAN_POINT('Ctrl Pts',(2.8072220542146,-1.25136189343097,5.14165503038608));
#13683=CARTESIAN_POINT('Ctrl Pts',(2.84602084260932,-1.16432327172591,5.14657157351131));
#13684=CARTESIAN_POINT('Ctrl Pts',(2.88076757018275,-1.07547869382835,5.15148811663654));
#13685=CARTESIAN_POINT('Ctrl Pts',(2.91130349058757,-0.985248311692343,
5.15640465976177));
#13686=CARTESIAN_POINT('Ctrl Pts',(2.94186355432602,-0.8949465885851,5.16132509016924));
#13687=CARTESIAN_POINT('Ctrl Pts',(2.96820601883254,-0.803257302184073,
5.16624552057671));
#13688=CARTESIAN_POINT('Ctrl Pts',(2.99022180531888,-0.710616496427913,
5.17116595098418));
#13689=CARTESIAN_POINT('Ctrl Pts',(3.01224721692289,-0.617935188886504,
5.17608853256265));
#13690=CARTESIAN_POINT('Ctrl Pts',(3.02994210090488,-0.52430197766384,5.18101111414113));
#13691=CARTESIAN_POINT('Ctrl Pts',(3.04324877593432,-0.430161757684539,
5.18593369571961));
#13692=CARTESIAN_POINT('Ctrl Pts',(3.05657391129798,-0.335890937091645,
5.19086310638957));
#13693=CARTESIAN_POINT('Ctrl Pts',(3.06549864354479,-0.241112153047857,
5.19579251705953));
#13694=CARTESIAN_POINT('Ctrl Pts',(3.0700173061377,-0.146273681894655,5.2007219277295));
#13695=CARTESIAN_POINT('Ctrl Pts',(3.0723705670046,-0.0968830362660627,
5.20328910086712));
#13696=CARTESIAN_POINT('Ctrl Pts',(3.07352967967375,-0.0474761854391445,
5.20585627400474));
#13697=CARTESIAN_POINT('Ctrl Pts',(3.07349942256352,0.00188401212731454,
5.20842344714237));
#13698=CARTESIAN_POINT('Origin',(0.,0.,-2.20842344717744));
#13699=CARTESIAN_POINT('',(-1.87240768645123,2.4373123939533,3.56268206416256));
#13700=CARTESIAN_POINT('',(-1.87526655020737,2.4410026577968,3.64588021366773));
#13701=CARTESIAN_POINT('',(-1.87240768645123,2.4373123939533,-2.20842344717744));
#13702=CARTESIAN_POINT('',(3.0766413087884,-0.00205726601264529,4.29157655282254));
#13703=CARTESIAN_POINT('Ctrl Pts',(-1.87526655020737,2.4410026577968,3.64588021366773));
#13704=CARTESIAN_POINT('Ctrl Pts',(-2.6388745207397,1.84934209790722,3.69611509335153));
#13705=CARTESIAN_POINT('Ctrl Pts',(-3.59964389029708,-0.162448805822295,
3.7991396089634));
#13706=CARTESIAN_POINT('Ctrl Pts',(-1.87939887603769,-3.10518792817496,
3.9549537605033));
#13707=CARTESIAN_POINT('Ctrl Pts',(1.58136602653418,-3.26704969305195,4.11332266828749));
#13708=CARTESIAN_POINT('Ctrl Pts',(3.01256814619275,-1.2727511792973,4.22553026572723));
#13709=CARTESIAN_POINT('Ctrl Pts',(3.07762631741651,-0.129684115097173,
4.28494822723892));
#13710=CARTESIAN_POINT('Ctrl Pts',(3.0766413087884,-0.00205726601264529,
4.29157655282254));
#13711=CARTESIAN_POINT('Ctrl Pts',(3.0766413087884,-0.00205726601264529,
4.29157655282254));
#13712=CARTESIAN_POINT('Ctrl Pts',(3.06978146335676,0.886767900244137,4.33773786316697));
#13713=CARTESIAN_POINT('Ctrl Pts',(2.19813638014636,2.80377976238209,4.43668880943947));
#13714=CARTESIAN_POINT('Ctrl Pts',(-0.332778404768295,3.3251151002074,4.55480908130019));
#13715=CARTESIAN_POINT('Ctrl Pts',(-1.57746432401505,2.66265166241204,4.62676804281649));
#13716=CARTESIAN_POINT('Ctrl Pts',(-1.87025628839757,2.43455437554208,4.64593736840473));
#13717=CARTESIAN_POINT('',(3.07349977118744,0.00118596406329618,4.20842344720459));
#13718=CARTESIAN_POINT('Ctrl Pts',(3.07349977118744,0.0011859640632942,
4.20842344720459));
#13719=CARTESIAN_POINT('Ctrl Pts',(3.07345762577915,0.110408415858429,4.21405153578527));
#13720=CARTESIAN_POINT('Ctrl Pts',(3.06758844717546,0.219451566274083,4.21967962436595));
#13721=CARTESIAN_POINT('Ctrl Pts',(3.05597865567641,0.32771436656059,4.22530771294663));
#13722=CARTESIAN_POINT('Ctrl Pts',(3.04477419211802,0.432197431621468,4.23073931035393));
#13723=CARTESIAN_POINT('Ctrl Pts',(3.02822341389494,0.535953470165536,4.23617090776124));
#13724=CARTESIAN_POINT('Ctrl Pts',(3.00645543745351,0.638457479090209,4.24160250516854));
#13725=CARTESIAN_POINT('Ctrl Pts',(2.9835062573314,0.74652370060515,4.24732883933591));
#13726=CARTESIAN_POINT('Ctrl Pts',(2.95475800374141,0.853197801579446,4.25305517350328));
#13727=CARTESIAN_POINT('Ctrl Pts',(2.9204200294079,0.957887833638757,4.25878150767065));
#13728=CARTESIAN_POINT('Ctrl Pts',(2.8860820550744,1.06257786569806,4.26450784183801));
#13729=CARTESIAN_POINT('Ctrl Pts',(2.84615458915048,1.16528350102013,4.27023417600538));
#13730=CARTESIAN_POINT('Ctrl Pts',(2.80090335865945,1.26544167208537,4.27596051017275));
#13731=CARTESIAN_POINT('Ctrl Pts',(2.76139571734074,1.3528870974284,4.28096001966454));
#13732=CARTESIAN_POINT('Ctrl Pts',(2.71771963212303,1.43863417231869,4.28595952915634));
#13733=CARTESIAN_POINT('Ctrl Pts',(2.67004338983875,1.52225837044123,4.29095903864814));
#13734=CARTESIAN_POINT('Ctrl Pts',(2.62243182007454,1.60576913286978,4.29595176633705));
#13735=CARTESIAN_POINT('Ctrl Pts',(2.57083109298431,1.68716236360383,4.30094449402595));
#13736=CARTESIAN_POINT('Ctrl Pts',(2.51545707606337,1.76603452641298,4.30593722171486));
#13737=CARTESIAN_POINT('Ctrl Pts',(2.46014147733459,1.84482348107832,4.31092468220189));
#13738=CARTESIAN_POINT('Ctrl Pts',(2.40106075310402,1.92109629771701,4.31591214268892));
#13739=CARTESIAN_POINT('Ctrl Pts',(2.33847557414465,1.99447593094748,4.32089960317596));
#13740=CARTESIAN_POINT('Ctrl Pts',(2.27593517634376,2.06780305933514,4.32588349501843));
#13741=CARTESIAN_POINT('Ctrl Pts',(2.20989559268149,2.13824078662851,4.3308673868609));
#13742=CARTESIAN_POINT('Ctrl Pts',(2.14065891202591,2.20544364524783,4.33585127870338));
#13743=CARTESIAN_POINT('Ctrl Pts',(2.07144744565466,2.27262203025043,4.34083335553588));
#13744=CARTESIAN_POINT('Ctrl Pts',(1.99904151029799,2.33656758183441,4.34581543236837));
#13745=CARTESIAN_POINT('Ctrl Pts',(1.92378066150868,2.39697105038948,4.35079750920087));
#13746=CARTESIAN_POINT('Ctrl Pts',(1.84852667477487,2.45736901153983,4.35577913178275));
#13747=CARTESIAN_POINT('Ctrl Pts',(1.77041863459167,2.51422525714381,4.36076075436462));
#13748=CARTESIAN_POINT('Ctrl Pts',(1.68982900351582,2.56727096132775,4.36574237694649));
#13749=CARTESIAN_POINT('Ctrl Pts',(1.60922471982507,2.62032631015537,4.37072490527512));
#13750=CARTESIAN_POINT('Ctrl Pts',(1.52613831584143,2.66956950030223,4.37570743360376));
#13751=CARTESIAN_POINT('Ctrl Pts',(1.44097012189121,2.71477574724264,4.38068996193239));
#13752=CARTESIAN_POINT('Ctrl Pts',(1.35571012917975,2.76003071985489,4.38567786069225));
#13753=CARTESIAN_POINT('Ctrl Pts',(1.26836425520858,2.80123985628929,4.39066575945211));
#13754=CARTESIAN_POINT('Ctrl Pts',(1.17935605189272,2.83822507086102,4.39565365821197));
#13755=CARTESIAN_POINT('Ctrl Pts',(1.09029527020938,2.87523213310667,4.4006445033921));
#13756=CARTESIAN_POINT('Ctrl Pts',(0.999570616588127,2.9080101561935,4.40563534857222));
#13757=CARTESIAN_POINT('Ctrl Pts',(0.907622161561579,2.93643053073664,4.41062619375235));
#13758=CARTESIAN_POINT('Ctrl Pts',(0.815525115509369,2.96489683332286,4.41562510426434));
#13759=CARTESIAN_POINT('Ctrl Pts',(0.722200743773071,2.98899131624859,4.42062401477633));
#13760=CARTESIAN_POINT('Ctrl Pts',(0.628100631914152,3.00863621034332,4.42562292528832));
#13761=CARTESIAN_POINT('Ctrl Pts',(0.573469932414809,3.02004123723208,4.42852508951118));
#13762=CARTESIAN_POINT('Ctrl Pts',(0.518577911122112,3.02994750045903,4.43142725373405));
#13763=CARTESIAN_POINT('Ctrl Pts',(0.463513494024363,3.03834782256037,4.43432941795692));
#13764=CARTESIAN_POINT('Ctrl Pts',(0.368642164044329,3.05282086653356,4.4393296012723));
#13765=CARTESIAN_POINT('Ctrl Pts',(0.272925653470679,3.06287158941055,4.44432978458769));
#13766=CARTESIAN_POINT('Ctrl Pts',(0.176811857637761,3.06840998189595,4.44932996790308));
#13767=CARTESIAN_POINT('Ctrl Pts',(0.0808588515851836,3.07393910914628,
4.45432178635919));
#13768=CARTESIAN_POINT('Ctrl Pts',(-0.0154896827983501,3.07497089992487,
4.4593136048153));
#13769=CARTESIAN_POINT('Ctrl Pts',(-0.111777981769336,3.0714667396525,4.46430542327141));
#13770=CARTESIAN_POINT('Ctrl Pts',(-0.207974064497727,3.06796593534859,
4.46929246101432));
#13771=CARTESIAN_POINT('Ctrl Pts',(-0.304109590402857,3.05993782645941,
4.47427949875723));
#13772=CARTESIAN_POINT('Ctrl Pts',(-0.399726490619734,3.04739577060428,
4.47926653650014));
#13773=CARTESIAN_POINT('Ctrl Pts',(-0.495277924424917,3.0348623019695,4.48425015974765));
#13774=CARTESIAN_POINT('Ctrl Pts',(-0.590311004409107,3.01782108546238,
4.48923378299516));
#13775=CARTESIAN_POINT('Ctrl Pts',(-0.6843715547045,2.99633740174757,4.49421740624267));
#13776=CARTESIAN_POINT('Ctrl Pts',(-0.778393383831029,2.97486256205229,
4.4991989779211));
#13777=CARTESIAN_POINT('Ctrl Pts',(-0.871443052055211,2.94894898937803,
4.50418054959952));
#13778=CARTESIAN_POINT('Ctrl Pts',(-0.963076423723207,2.91871308149131,
4.50916212127795));
#13779=CARTESIAN_POINT('Ctrl Pts',(-1.05472610266889,2.8884717927555,4.51414457948789));
#13780=CARTESIAN_POINT('Ctrl Pts',(-1.14495856171286,2.85390676117679,4.51912703769784));
#13781=CARTESIAN_POINT('Ctrl Pts',(-1.23334530459458,2.81518411647169,4.52410949590779));
#13782=CARTESIAN_POINT('Ctrl Pts',(-1.32173930652233,2.77645829154464,4.52909236331817));
#13783=CARTESIAN_POINT('Ctrl Pts',(-1.40828689198012,2.7335743583164,4.53407523072855));
#13784=CARTESIAN_POINT('Ctrl Pts',(-1.4925814678542,2.68674576613013,4.53905809813893));
#13785=CARTESIAN_POINT('Ctrl Pts',(-1.57694638082662,2.63987809921979,4.54404512335462));
#13786=CARTESIAN_POINT('Ctrl Pts',(-1.65905415102559,2.58905942264468,4.54903214857031));
#13787=CARTESIAN_POINT('Ctrl Pts',(-1.73852499335928,2.5345479079049,4.554019173786));
#13788=CARTESIAN_POINT('Ctrl Pts',(-1.78403911597311,2.50332836004464,4.5568753166238));
#13789=CARTESIAN_POINT('Ctrl Pts',(-1.82868886306956,2.47089834754116,4.5597314594616));
#13790=CARTESIAN_POINT('Ctrl Pts',(-1.87240768645123,2.4373123939533,4.56258760229939));
#13791=CARTESIAN_POINT('Ctrl Pts',(-1.87240768645123,2.4373123939533,3.56268206416256));
#13792=CARTESIAN_POINT('Ctrl Pts',(-1.94893179304657,2.37852455627463,3.56766378537458));
#13793=CARTESIAN_POINT('Ctrl Pts',(-2.02268548271812,2.31612868029567,3.5726455065866));
#13794=CARTESIAN_POINT('Ctrl Pts',(-2.09332073888429,2.25042452309713,3.57762722779863));
#13795=CARTESIAN_POINT('Ctrl Pts',(-2.16397364935239,2.18470394405639,3.58261019412273));
#13796=CARTESIAN_POINT('Ctrl Pts',(-2.23150625682829,2.1156737403338,3.58759316044683));
#13797=CARTESIAN_POINT('Ctrl Pts',(-2.29560695052068,2.04367095656838,3.59257612677093));
#13798=CARTESIAN_POINT('Ctrl Pts',(-2.35977907302726,1.97158793851585,3.59756464572411));
#13799=CARTESIAN_POINT('Ctrl Pts',(-2.42051135734872,1.89652605799303,3.60255316467729));
#13800=CARTESIAN_POINT('Ctrl Pts',(-2.47753227791021,1.81885570123445,3.60754168363046));
#13801=CARTESIAN_POINT('Ctrl Pts',(-2.53459036481876,1.74113471878608,3.61253345411001));
#13802=CARTESIAN_POINT('Ctrl Pts',(-2.58793202987521,1.66080224067301,3.61752522458955));
#13803=CARTESIAN_POINT('Ctrl Pts',(-2.63733005394467,1.578256137818,3.6225169950691));
#13804=CARTESIAN_POINT('Ctrl Pts',(-2.68680438012126,1.49558253104556,3.62751647603126));
#13805=CARTESIAN_POINT('Ctrl Pts',(-2.73232270149939,1.41068886153324,3.63251595699342));
#13806=CARTESIAN_POINT('Ctrl Pts',(-2.7737046480908,1.32399576100512,3.63751543795558));
#13807=CARTESIAN_POINT('Ctrl Pts',(-2.78741574776541,1.29527169555264,3.63917191831574));
#13808=CARTESIAN_POINT('Ctrl Pts',(-2.80067315699813,1.26635023217343,3.64082839867589));
#13809=CARTESIAN_POINT('Ctrl Pts',(-2.81347151615409,1.23724705608444,3.64248487903604));
#13810=CARTESIAN_POINT('Ctrl Pts',(-2.85209890952511,1.14940924676559,3.64748438855936));
#13811=CARTESIAN_POINT('Ctrl Pts',(-2.88667670430598,1.05960647673055,3.65248389808267));
#13812=CARTESIAN_POINT('Ctrl Pts',(-2.91700165612439,0.968247689471843,
3.65748340760598));
#13813=CARTESIAN_POINT('Ctrl Pts',(-2.94728547234083,0.877012829820052,
3.6624761353268));
#13814=CARTESIAN_POINT('Ctrl Pts',(-2.97332777390544,0.784226560922798,
3.66746886304762));
#13815=CARTESIAN_POINT('Ctrl Pts',(-2.99497273372111,0.690319182890849,
3.67246159076844));
#13816=CARTESIAN_POINT('Ctrl Pts',(-3.01659485865146,0.596510874768349,
3.67744905128776));
#13817=CARTESIAN_POINT('Ctrl Pts',(-3.03382876598409,0.501584234202811,
3.68243651180707));
#13818=CARTESIAN_POINT('Ctrl Pts',(-3.04656828046346,0.405985175189797,
3.68742397232638));
#13819=CARTESIAN_POINT('Ctrl Pts',(-3.05929867952357,0.3104545195297,3.69240786420155));
#13820=CARTESIAN_POINT('Ctrl Pts',(-3.06754102085665,0.214252835756214,
3.69739175607672));
#13821=CARTESIAN_POINT('Ctrl Pts',(-3.07124030155397,0.117835733589989,
3.70237564795189));
#13822=CARTESIAN_POINT('Ctrl Pts',(-3.07493823506507,0.0214537441395582,
3.70735772481733));
#13823=CARTESIAN_POINT('Ctrl Pts',(-3.07409637838022,-0.0751430696406089,
3.71233980168276));
#13824=CARTESIAN_POINT('Ctrl Pts',(-3.06871171064564,-0.171495442931594,
3.7173218785482));
#13825=CARTESIAN_POINT('Ctrl Pts',(-3.06332753386848,-0.267839031109949,
3.72230350116321));
#13826=CARTESIAN_POINT('Ctrl Pts',(-3.0534013942232,-0.363937784842323,
3.72728512377822));
#13827=CARTESIAN_POINT('Ctrl Pts',(-3.03898233292869,-0.459334986853035,
3.73226674639323));
#13828=CARTESIAN_POINT('Ctrl Pts',(-3.02456064999435,-0.554749533758849,
3.73724927475516));
#13829=CARTESIAN_POINT('Ctrl Pts',(-3.0056444886985,-0.649461841596929,
3.74223180311709));
#13830=CARTESIAN_POINT('Ctrl Pts',(-2.98233427434873,-0.743023906778798,
3.74721433147902));
#13831=CARTESIAN_POINT('Ctrl Pts',(-2.95899893502323,-0.836686818078247,
3.75220223027223));
#13832=CARTESIAN_POINT('Ctrl Pts',(-2.93126019367038,-0.929196584942988,
3.75719012906543));
#13833=CARTESIAN_POINT('Ctrl Pts',(-2.89926873036408,-1.02011914947866,
3.76217802785864));
#13834=CARTESIAN_POINT('Ctrl Pts',(-2.86725836926098,-1.11109542322207,
3.76716887307217));
#13835=CARTESIAN_POINT('Ctrl Pts',(-2.83099044908122,-1.20048222119091,
3.77215971828571));
#13836=CARTESIAN_POINT('Ctrl Pts',(-2.79066348967254,-1.28786627310785,
3.77715056349924));
#13837=CARTESIAN_POINT('Ctrl Pts',(-2.75027136088101,-1.3753915398552,3.78214947404443));
#13838=CARTESIAN_POINT('Ctrl Pts',(-2.70580729733472,-1.46090720879924,
3.78714838458962));
#13839=CARTESIAN_POINT('Ctrl Pts',(-2.65751532832826,-1.54402543039301,
3.79214729513482));
#13840=CARTESIAN_POINT('Ctrl Pts',(-2.62947897768579,-1.59228048508068,
3.79504945902995));
#13841=CARTESIAN_POINT('Ctrl Pts',(-2.60015324796666,-1.63972802373726,
3.79795162292508));
#13842=CARTESIAN_POINT('Ctrl Pts',(-2.56959224495613,-1.68629711043497,
3.80085378682021));
#13843=CARTESIAN_POINT('Ctrl Pts',(-2.51694531321621,-1.76652090177191,
3.80585329630727));
#13844=CARTESIAN_POINT('Ctrl Pts',(-2.46044537736041,-1.84441774704064,
3.81085280579432));
#13845=CARTESIAN_POINT('Ctrl Pts',(-2.40032479931129,-1.91959451650894,
3.81585231528138));
#13846=CARTESIAN_POINT('Ctrl Pts',(-2.34028577444489,-1.9946693091664,3.82084504296553));
#13847=CARTESIAN_POINT('Ctrl Pts',(-2.2766361402387,-2.06703101930238,3.82583777064968));
#13848=CARTESIAN_POINT('Ctrl Pts',(-2.20965198879184,-2.13631466278455,
3.83083049833384));
#13849=CARTESIAN_POINT('Ctrl Pts',(-2.14273850393668,-2.20552521376887,
3.8358179588161));
#13850=CARTESIAN_POINT('Ctrl Pts',(-2.07249779856724,-2.27166383959328,
3.84080541929837));
#13851=CARTESIAN_POINT('Ctrl Pts',(-1.99924609461182,-2.33439870270256,
3.84579287978064));
#13852=CARTESIAN_POINT('Ctrl Pts',(-1.92604680396258,-2.39708867755108,
3.85077677161837));
#13853=CARTESIAN_POINT('Ctrl Pts',(-1.8498411300987,-2.4563794465704,3.8557606634561));
#13854=CARTESIAN_POINT('Ctrl Pts',(-1.77098128851237,-2.51197681632197,
3.86074455529383));
#13855=CARTESIAN_POINT('Ctrl Pts',(-1.69215016572705,-2.56755393888859,
3.8657266321216));
#13856=CARTESIAN_POINT('Ctrl Pts',(-1.61066715411105,-2.61944008196891,
3.87070870894937));
#13857=CARTESIAN_POINT('Ctrl Pts',(-1.52691583673615,-2.6673826642468,3.87569078577714));
#13858=CARTESIAN_POINT('Ctrl Pts',(-1.44317215555176,-2.71532087526578,
3.88067240835429));
#13859=CARTESIAN_POINT('Ctrl Pts',(-1.35716096085037,-2.75931602244041,
3.88565403093144));
#13860=CARTESIAN_POINT('Ctrl Pts',(-1.26929204412124,-2.79916058073318,
3.89063565350859));
#13861=CARTESIAN_POINT('Ctrl Pts',(-1.18140715127442,-2.83901238346888,
3.89561818183252));
#13862=CARTESIAN_POINT('Ctrl Pts',(-1.0916642653861,-2.87471191733804,3.90060071015645));
#13863=CARTESIAN_POINT('Ctrl Pts',(-1.00049384511949,-2.9060995020608,3.90558323848038));
#13864=CARTESIAN_POINT('Ctrl Pts',(-0.909225156574733,-2.9375209179746,
3.91057113723562));
#13865=CARTESIAN_POINT('Ctrl Pts',(-0.816526277577877,-2.9646209630174,
3.91555903599086));
#13866=CARTESIAN_POINT('Ctrl Pts',(-0.722843330537677,-2.98728970297445,
3.9205469347461));
#13867=CARTESIAN_POINT('Ctrl Pts',(-0.62910504369396,-3.00997183366755,
3.92553777992164));
#13868=CARTESIAN_POINT('Ctrl Pts',(-0.534381962176159,-3.02821736415241,
3.93052862509718));
#13869=CARTESIAN_POINT('Ctrl Pts',(-0.439128818339874,-3.04196780569805,
3.93551947027272));
#13870=CARTESIAN_POINT('Ctrl Pts',(-0.343721743015635,-3.05574046830478,
3.94051838078021));
#13871=CARTESIAN_POINT('Ctrl Pts',(-0.247783331579856,-3.06500349485755,
3.94551729128769));
#13872=CARTESIAN_POINT('Ctrl Pts',(-0.151771771365071,-3.06975040995464,
3.95051620179518));
#13873=CARTESIAN_POINT('Ctrl Pts',(-0.0960313617058057,-3.07250627593097,
3.95341836606492));
#13874=CARTESIAN_POINT('Ctrl Pts',(-0.0402662857999868,-3.07374096692759,
3.95632053033466));
#13875=CARTESIAN_POINT('Ctrl Pts',(0.015434497828892,-3.07346124528629,
3.9592226946044));
#13876=CARTESIAN_POINT('Ctrl Pts',(0.111389299267059,-3.07297937352795,
3.96422220409244));
#13877=CARTESIAN_POINT('Ctrl Pts',(0.207490050402046,-3.06799872222247,
3.96922171358048));
#13878=CARTESIAN_POINT('Ctrl Pts',(0.303280487235858,-3.0585001546611,3.97422122306852));
#13879=CARTESIAN_POINT('Ctrl Pts',(0.398940984948382,-3.04901447184651,
3.97921395075358));
#13880=CARTESIAN_POINT('Ctrl Pts',(0.494291571865417,-3.03502309575796,
3.98420667843864));
#13881=CARTESIAN_POINT('Ctrl Pts',(0.588875783338042,-3.01655889413716,
3.9891994061237));
#13882=CARTESIAN_POINT('Ctrl Pts',(0.683360210849682,-2.99811417178405,
3.9941868666068));
#13883=CARTESIAN_POINT('Ctrl Pts',(0.777079441640563,-2.9752060880826,3.99917432708989));
#13884=CARTESIAN_POINT('Ctrl Pts',(0.869582965406786,-2.94791921807134,
4.00416178757299));
#13885=CARTESIAN_POINT('Ctrl Pts',(0.96202030073714,-2.92065187245409,4.0091456794114));
#13886=CARTESIAN_POINT('Ctrl Pts',(1.05324323847752,-2.88901209286882,4.01412957124982));
#13887=CARTESIAN_POINT('Ctrl Pts',(1.14281324716655,-2.85313514087585,4.01911346308823));
#13888=CARTESIAN_POINT('Ctrl Pts',(1.23235063667565,-2.81727125438069,4.02409553991661));
#13889=CARTESIAN_POINT('Ctrl Pts',(1.32023588608128,-2.7771734244486,4.02907761674499));
#13890=CARTESIAN_POINT('Ctrl Pts',(1.4060482897216,-2.73302587930868,4.03405969357336));
#13891=CARTESIAN_POINT('Ctrl Pts',(1.49185286924658,-2.68888235940835,4.03904131615105));
#13892=CARTESIAN_POINT('Ctrl Pts',(1.57558458851359,-2.64069005939631,4.04402293872873));
#13893=CARTESIAN_POINT('Ctrl Pts',(1.65684626550578,-2.58867972188132,4.04900456130642));
#13894=CARTESIAN_POINT('Ctrl Pts',(1.73812271730209,-2.53665992797093,4.05398708963083));
#13895=CARTESIAN_POINT('Ctrl Pts',(1.81692786521932,-2.48082095456316,4.05896961795524));
#13896=CARTESIAN_POINT('Ctrl Pts',(1.89289340677911,-2.42143692888586,4.06395214627965));
#13897=CARTESIAN_POINT('Ctrl Pts',(1.96894082799592,-2.36198889598166,4.06894004503521));
#13898=CARTESIAN_POINT('Ctrl Pts',(2.04214218608905,-2.29898845324128,4.07392794379076));
#13899=CARTESIAN_POINT('Ctrl Pts',(2.11216237704504,-2.23274995084435,4.07891584254631));
#13900=CARTESIAN_POINT('Ctrl Pts',(2.18222392988828,-2.16647232045547,4.08390668772208));
#13901=CARTESIAN_POINT('Ctrl Pts',(2.24910026970181,-2.09695313798019,4.08889753289785));
#13902=CARTESIAN_POINT('Ctrl Pts',(2.31249475684799,-2.02454198512912,4.09388837807362));
#13903=CARTESIAN_POINT('Ctrl Pts',(2.37599169108638,-1.95201381402635,4.09888728858123));
#13904=CARTESIAN_POINT('Ctrl Pts',(2.43599526416855,-1.87658468390078,4.10388619908884));
#13905=CARTESIAN_POINT('Ctrl Pts',(2.49225058376852,-1.79863539320938,4.10888510959645));
#13906=CARTESIAN_POINT('Ctrl Pts',(2.52491013587622,-1.75338120321994,4.11178727386049));
#13907=CARTESIAN_POINT('Ctrl Pts',(2.55630716772764,-1.70727811728341,4.11468943812453));
#13908=CARTESIAN_POINT('Ctrl Pts',(2.58639891791606,-1.66040443489008,4.11759160238857));
#13909=CARTESIAN_POINT('Ctrl Pts',(2.6394023618579,-1.57784138749249,4.12270345862544));
#13910=CARTESIAN_POINT('Ctrl Pts',(2.68853322222333,-1.49260657023215,4.12781531486231));
#13911=CARTESIAN_POINT('Ctrl Pts',(2.73351906799659,-1.40508923378519,4.13292717109918));
#13912=CARTESIAN_POINT('Ctrl Pts',(2.77843555063002,-1.317706839277,4.1380311454258));
#13913=CARTESIAN_POINT('Ctrl Pts',(2.81921954333956,-1.22804928936143,4.14313511975242));
#13914=CARTESIAN_POINT('Ctrl Pts',(2.8556422189893,-1.1365341029313,4.14823909407904));
#13915=CARTESIAN_POINT('Ctrl Pts',(2.89200450440251,-1.04517065229916,4.15333460581439));
#13916=CARTESIAN_POINT('Ctrl Pts',(2.924019720944,-0.951956079566954,4.15843011754974));
#13917=CARTESIAN_POINT('Ctrl Pts',(2.95150578656232,-0.857330649101683,
4.1635256292851));
#13918=CARTESIAN_POINT('Ctrl Pts',(2.97896501468297,-0.762797611262038,
4.16861616574366));
#13919=CARTESIAN_POINT('Ctrl Pts',(3.00190377200421,-0.666856849596358,
4.17370670220221));
#13920=CARTESIAN_POINT('Ctrl Pts',(3.02018879138804,-0.569966590577061,
4.17879723866078));
#13921=CARTESIAN_POINT('Ctrl Pts',(3.03845833206675,-0.47315835147345,4.18388346585878));
#13922=CARTESIAN_POINT('Ctrl Pts',(3.05208189916622,-0.375402619071065,
4.1889696930568));
#13923=CARTESIAN_POINT('Ctrl Pts',(3.06097682471455,-0.277169855071588,
4.1940559202548));
#13924=CARTESIAN_POINT('Ctrl Pts',(3.06935225882419,-0.184674191356969,
4.19884509589569));
#13925=CARTESIAN_POINT('Ctrl Pts',(3.07353563445991,-0.0917559825750235,
4.20363427153658));
#13926=CARTESIAN_POINT('Ctrl Pts',(3.07349977118764,0.00118596353673709,
4.20842344717746));
#13927=CARTESIAN_POINT('Origin',(0.,0.,-2.20842344717744));
#13928=CARTESIAN_POINT('',(-1.87240768645123,2.4373123939533,2.56277205249695));
#13929=CARTESIAN_POINT('',(-1.87178979188679,2.43648733431069,2.64569210698702));
#13930=CARTESIAN_POINT('',(-1.87240768645123,2.4373123939533,-2.20842344717744));
#13931=CARTESIAN_POINT('',(3.07484942901424,0.00262471338485415,3.29157655282254));
#13932=CARTESIAN_POINT('Ctrl Pts',(-1.87178979188648,2.43648733431093,2.645692106987));
#13933=CARTESIAN_POINT('Ctrl Pts',(-2.0894887030698,2.27255165391444,2.65979557073464));
#13934=CARTESIAN_POINT('Ctrl Pts',(-3.01698552853461,1.36245345030385,2.72668867041033));
#13935=CARTESIAN_POINT('Ctrl Pts',(-3.41664634935444,-1.2250959035962,2.84637140601408));
#13936=CARTESIAN_POINT('Ctrl Pts',(-0.832597465415741,-3.53286195426117,
3.00474031379826));
#13937=CARTESIAN_POINT('Ctrl Pts',(2.2996550447433,-2.6791845859618,3.15314202940108));
#13938=CARTESIAN_POINT('Ctrl Pts',(3.06738194658167,-0.823160515664817,
3.24875410907584));
#13939=CARTESIAN_POINT('Ctrl Pts',(3.07484942901424,0.00262471338485415,
3.29157655282254));
#13940=CARTESIAN_POINT('Ctrl Pts',(3.07484942901424,0.00262471338485415,
3.29157655282254));
#13941=CARTESIAN_POINT('Ctrl Pts',(3.07658753235455,0.194831401241035,3.3015437450039));
#13942=CARTESIAN_POINT('Ctrl Pts',(2.97278968204648,1.40315899371448,3.36430057311331));
#13943=CARTESIAN_POINT('Ctrl Pts',(1.37275537107956,3.36004090547696,3.47984703715079));
#13944=CARTESIAN_POINT('Ctrl Pts',(-0.978619792012921,3.10112051414917,
3.58798106525116));
#13945=CARTESIAN_POINT('Ctrl Pts',(-1.83643233296303,2.47109227917888,3.64332545742347));
#13946=CARTESIAN_POINT('Ctrl Pts',(-1.87526655020737,2.4410026577968,3.64588021366773));
#13947=CARTESIAN_POINT('',(3.07349876324234,-0.00275723554104452,3.2084234471304));
#13948=CARTESIAN_POINT('Ctrl Pts',(3.07349876324315,-0.00275723463170688,
3.20842344717746));
#13949=CARTESIAN_POINT('Ctrl Pts',(3.0735842794169,0.0925679332825739,3.21335662415332));
#13950=CARTESIAN_POINT('Ctrl Pts',(3.06923075795488,0.187999949967112,3.21828980112919));
#13951=CARTESIAN_POINT('Ctrl Pts',(3.0604351335259,0.283088402235619,3.22322297810505));
#13952=CARTESIAN_POINT('Ctrl Pts',(3.05164431819358,0.378124863930588,3.22815345781648));
#13953=CARTESIAN_POINT('Ctrl Pts',(3.03841626328675,0.472817687881733,3.23308393752792));
#13954=CARTESIAN_POINT('Ctrl Pts',(3.02079995091825,0.566718542604943,3.23801441723935));
#13955=CARTESIAN_POINT('Ctrl Pts',(3.00318820947799,0.660595032747312,3.24294361763259));
#13956=CARTESIAN_POINT('Ctrl Pts',(2.98119055500706,0.75367952049474,3.24787281802583));
#13957=CARTESIAN_POINT('Ctrl Pts',(2.95490740437485,0.845532070101819,3.25280201841907));
#13958=CARTESIAN_POINT('Ctrl Pts',(2.92862352264444,0.937387174700717,3.25773135592409));
#13959=CARTESIAN_POINT('Ctrl Pts',(2.89805403289688,1.0280098414945,3.26266069342911));
#13960=CARTESIAN_POINT('Ctrl Pts',(2.86334938943221,1.11697471951615,3.26759003093413));
#13961=CARTESIAN_POINT('Ctrl Pts',(2.82861088193035,1.20602640753317,3.27252417837961));
#13962=CARTESIAN_POINT('Ctrl Pts',(2.78972932530905,1.29341665643582,3.27745832582509));
#13963=CARTESIAN_POINT('Ctrl Pts',(2.74690346004834,1.37873987074229,3.28239247327057));
#13964=CARTESIAN_POINT('Ctrl Pts',(2.70405710939133,1.46410389869835,3.28732898092442));
#13965=CARTESIAN_POINT('Ctrl Pts',(2.65726291414173,1.54739853173953,3.29226548857827));
#13966=CARTESIAN_POINT('Ctrl Pts',(2.60676462830897,1.62824458316224,3.29720199623213));
#13967=CARTESIAN_POINT('Ctrl Pts',(2.55617955234244,1.70922958266015,3.30214698813752));
#13968=CARTESIAN_POINT('Ctrl Pts',(2.50187792443551,1.7877572238769,3.30709198004292));
#13969=CARTESIAN_POINT('Ctrl Pts',(2.44414572994418,1.86347897782498,3.31203697194832));
#13970=CARTESIAN_POINT('Ctrl Pts',(2.39079116535085,1.93345901665323,3.31660700245478));
#13971=CARTESIAN_POINT('Ctrl Pts',(2.33450719914795,2.00104271688985,3.32117703296123));
#13972=CARTESIAN_POINT('Ctrl Pts',(2.27554719717419,2.06598335023124,3.32574706346769));
#13973=CARTESIAN_POINT('Ctrl Pts',(2.21104629554571,2.13702692659862,3.33074657293629));
#13974=CARTESIAN_POINT('Ctrl Pts',(2.14310189670449,2.20517177128013,3.33574608240488));
#13975=CARTESIAN_POINT('Ctrl Pts',(2.07200476478582,2.27006574898281,3.34074559187347));
#13976=CARTESIAN_POINT('Ctrl Pts',(2.00100407567367,2.33487169841813,3.34573831953932));
#13977=CARTESIAN_POINT('Ctrl Pts',(1.92685947450858,2.39643525162542,3.35073104720517));
#13978=CARTESIAN_POINT('Ctrl Pts',(1.84990053748908,2.45443888728108,3.35572377487102));
#13979=CARTESIAN_POINT('Ctrl Pts',(1.77302279020602,2.51238133056491,3.36071123533518));
#13980=CARTESIAN_POINT('Ctrl Pts',(1.69333695805015,2.56677105944817,3.36569869579933));
#13981=CARTESIAN_POINT('Ctrl Pts',(1.61120709387242,2.61732954567345,3.37068615626349));
#13982=CARTESIAN_POINT('Ctrl Pts',(1.52913599552668,2.66785185612348,3.37567004808345));
#13983=CARTESIAN_POINT('Ctrl Pts',(1.44462471435453,2.71454814412126,3.3806539399034));
#13984=CARTESIAN_POINT('Ctrl Pts',(1.35806699349407,2.75718267279881,3.38563783172335));
#13985=CARTESIAN_POINT('Ctrl Pts',(1.27154079480793,2.79980167503883,3.39061990853357));
#13986=CARTESIAN_POINT('Ctrl Pts',(1.18297003057217,2.83836166318928,3.39560198534378));
#13987=CARTESIAN_POINT('Ctrl Pts',(1.09277294659231,2.8726728907406,3.40058406215399));
#13988=CARTESIAN_POINT('Ctrl Pts',(1.00258408650373,2.90698098990026,3.40556568471384));
#13989=CARTESIAN_POINT('Ctrl Pts',(0.910769611829694,2.93704094276129,3.41054730727369));
#13990=CARTESIAN_POINT('Ctrl Pts',(0.817766638355192,2.96271159163244,3.41552892983354));
#13991=CARTESIAN_POINT('Ctrl Pts',(0.724746755296085,2.98838690788134,3.42051145814043));
#13992=CARTESIAN_POINT('Ctrl Pts',(0.630538367425689,3.00967121844639,3.42549398644732));
#13993=CARTESIAN_POINT('Ctrl Pts',(0.535591552539519,3.02647384572349,3.43047651475421));
#13994=CARTESIAN_POINT('Ctrl Pts',(0.440542398968198,3.04329458375853,3.43546441349292));
#13995=CARTESIAN_POINT('Ctrl Pts',(0.34475366237185,3.05562391804869,3.44045231223163));
#13996=CARTESIAN_POINT('Ctrl Pts',(0.248683144034158,3.06342274978059,3.44544021097033));
#13997=CARTESIAN_POINT('Ctrl Pts',(0.152555875516732,3.07122618838992,3.4504310561296));
#13998=CARTESIAN_POINT('Ctrl Pts',(0.0561469323296408,3.0744937807667,3.45542190128886));
#13999=CARTESIAN_POINT('Ctrl Pts',(-0.0400853931705421,3.07323858677688,
3.46041274644812));
#14000=CARTESIAN_POINT('Ctrl Pts',(-0.13647323255312,3.0719813643617,3.46541165693994));
#14001=CARTESIAN_POINT('Ctrl Pts',(-0.232683446457692,3.06618678761908,
3.47041056743175));
#14002=CARTESIAN_POINT('Ctrl Pts',(-0.328262431952541,3.0559198330075,3.47540947792356));
#14003=CARTESIAN_POINT('Ctrl Pts',(-0.383751709792868,3.04995925606618,
3.47831164236633));
#14004=CARTESIAN_POINT('Ctrl Pts',(-0.439028396098693,3.04249223061018,
3.4812138068091));
#14005=CARTESIAN_POINT('Ctrl Pts',(-0.494005671630389,3.0335392936959,3.48411597125187));
#14006=CARTESIAN_POINT('Ctrl Pts',(-0.588714580362088,3.01811614154995,
3.48911550650851));
#14007=CARTESIAN_POINT('Ctrl Pts',(-0.682866867034428,2.9982263454016,3.49411504176514));
#14008=CARTESIAN_POINT('Ctrl Pts',(-0.77600884927957,2.97392207628912,3.49911457702178));
#14009=CARTESIAN_POINT('Ctrl Pts',(-0.869028885514338,2.94964962750709,
3.50410756664386));
#14010=CARTESIAN_POINT('Ctrl Pts',(-0.96104082446848,2.92097429983823,3.50910055626593));
#14011=CARTESIAN_POINT('Ctrl Pts',(-1.0515988235673,2.88799968218001,3.514093545888));
#14012=CARTESIAN_POINT('Ctrl Pts',(-1.14204897447052,2.85506433496782,3.51908058921128));
#14013=CARTESIAN_POINT('Ctrl Pts',(-1.23104821975664,2.81784003257502,3.52406763253455));
#14014=CARTESIAN_POINT('Ctrl Pts',(-1.31816483149295,2.77648045680411,3.52905467585783));
#14015=CARTESIAN_POINT('Ctrl Pts',(-1.40522190785358,2.73514914611184,3.53403831104238));
#14016=CARTESIAN_POINT('Ctrl Pts',(-1.4903985123169,2.68968836607186,3.53902194622693));
#14017=CARTESIAN_POINT('Ctrl Pts',(-1.5732825990588,2.64030000445003,3.54400558141149));
#14018=CARTESIAN_POINT('Ctrl Pts',(-1.65613360688019,2.5909313536527,3.54898722763436));
#14019=CARTESIAN_POINT('Ctrl Pts',(-1.7366935394388,2.53763846205762,3.55396887385724));
#14020=CARTESIAN_POINT('Ctrl Pts',(-1.81457562117796,2.48066877374361,3.55895052008011));
#14021=CARTESIAN_POINT('Ctrl Pts',(-1.83402169771838,2.46644423204288,3.56019436810759));
#14022=CARTESIAN_POINT('Ctrl Pts',(-1.85330096510086,2.45199068140142,3.56143821613508));
#14023=CARTESIAN_POINT('Ctrl Pts',(-1.87240768645123,2.4373123939533,3.56268206416256));
#14024=CARTESIAN_POINT('Ctrl Pts',(-1.87240768645123,2.4373123939533,2.56277205249695));
#14025=CARTESIAN_POINT('Ctrl Pts',(-1.94874179693929,2.37867051629705,2.56775984818642));
#14026=CARTESIAN_POINT('Ctrl Pts',(-2.02240282813516,2.31637425317476,2.57274764387588));
#14027=CARTESIAN_POINT('Ctrl Pts',(-2.09302490950143,2.25069966415035,2.57773543956535));
#14028=CARTESIAN_POINT('Ctrl Pts',(-2.16359434507864,2.18507403276772,2.58271951706308));
#14029=CARTESIAN_POINT('Ctrl Pts',(-2.23112901408335,2.11607538019443,2.58770359456081));
#14030=CARTESIAN_POINT('Ctrl Pts',(-2.29529630712004,2.04401984151845,2.59268767205853));
#14031=CARTESIAN_POINT('Ctrl Pts',(-2.35943893603888,1.97199199898195,2.59766983381587));
#14032=CARTESIAN_POINT('Ctrl Pts',(-2.42021646901576,1.89690993229495,2.60265199557321));
#14033=CARTESIAN_POINT('Ctrl Pts',(-2.47733402183739,1.81912572249611,2.60763415733055));
#14034=CARTESIAN_POINT('Ctrl Pts',(-2.53444521331875,1.74135017574043,2.61261576421072));
#14035=CARTESIAN_POINT('Ctrl Pts',(-2.5878969753007,1.66087343803078,2.61759737109089));
#14036=CARTESIAN_POINT('Ctrl Pts',(-2.63743616477765,1.57807880878078,2.62257897797106));
#14037=CARTESIAN_POINT('Ctrl Pts',(-2.686983360921,1.49527079802449,2.62756138999287));
#14038=CARTESIAN_POINT('Ctrl Pts',(-2.73261650341584,1.41014452848584,2.63254380201468));
#14039=CARTESIAN_POINT('Ctrl Pts',(-2.77412759930302,1.32310933515915,2.63752621403649));
#14040=CARTESIAN_POINT('Ctrl Pts',(-2.81568297515355,1.23598130122951,2.64251394080649));
#14041=CARTESIAN_POINT('Ctrl Pts',(-2.85310733598039,1.14694067481163,2.6475016675765));
#14042=CARTESIAN_POINT('Ctrl Pts',(-2.88624030085153,1.05641808756783,2.6524893943465));
#14043=CARTESIAN_POINT('Ctrl Pts',(-2.91939223780762,0.965843666682782,
2.65747997711132));
#14044=CARTESIAN_POINT('Ctrl Pts',(-2.94824775430845,0.87378601396475,2.66247055987614));
#14045=CARTESIAN_POINT('Ctrl Pts',(-2.97269658770118,0.780690237847104,
2.66746114264096));
#14046=CARTESIAN_POINT('Ctrl Pts',(-2.99718546494448,0.687441983560535,
2.67245989929888));
#14047=CARTESIAN_POINT('Ctrl Pts',(-3.01725315369669,0.593152639522881,
2.6774586559568));
#14048=CARTESIAN_POINT('Ctrl Pts',(-3.03284066354309,0.498276790107153,
2.68245741261471));
#14049=CARTESIAN_POINT('Ctrl Pts',(-3.04304160879334,0.436187119916245,
2.68572875252014));
#14050=CARTESIAN_POINT('Ctrl Pts',(-3.051324850439,0.373846396131847,2.68900009242556));
#14051=CARTESIAN_POINT('Ctrl Pts',(-3.05768593609462,0.311382347298604,
2.69227143233099));
#14052=CARTESIAN_POINT('Ctrl Pts',(-3.06740743167987,0.215920030353821,
2.69727094313311));
#14053=CARTESIAN_POINT('Ctrl Pts',(-3.07267115330314,0.11983434104367,2.70227045393522));
#14054=CARTESIAN_POINT('Ctrl Pts',(-3.07340956897462,0.02357692378719,2.70726996473734));
#14055=CARTESIAN_POINT('Ctrl Pts',(-3.07414698299245,-0.0725499212228172,
2.71226269375188));
#14056=CARTESIAN_POINT('Ctrl Pts',(-3.07037128764889,-0.168847596017427,
2.71725542276642));
#14057=CARTESIAN_POINT('Ctrl Pts',(-3.06206663938885,-0.264858728272064,
2.72224815178096));
#14058=CARTESIAN_POINT('Ctrl Pts',(-3.05377075229881,-0.360768571486514,
2.72723561360701));
#14059=CARTESIAN_POINT('Ctrl Pts',(-3.04095544813071,-0.456392038100134,
2.73222307543307));
#14060=CARTESIAN_POINT('Ctrl Pts',(-3.02365693060796,-0.551272179586862,
2.73721053725913));
#14061=CARTESIAN_POINT('Ctrl Pts',(-3.0063707905256,-0.646084432406635,
2.74219443045503));
#14062=CARTESIAN_POINT('Ctrl Pts',(-2.98460789261121,-0.740153986815278,
2.74717832365092));
#14063=CARTESIAN_POINT('Ctrl Pts',(-2.95845611331786,-0.833030416954972,
2.75216221684681));
#14064=CARTESIAN_POINT('Ctrl Pts',(-2.93231385780814,-0.925873023964895,
2.75714429504114));
#14065=CARTESIAN_POINT('Ctrl Pts',(-2.90178601544909,-1.017522947919,2.76212637323547));
#14066=CARTESIAN_POINT('Ctrl Pts',(-2.86701104688474,-1.10754228228129,
2.76710845142979));
#14067=CARTESIAN_POINT('Ctrl Pts',(-2.83223924894844,-1.19755340907826,
2.77209007538023));
#14068=CARTESIAN_POINT('Ctrl Pts',(-2.79322125305204,-1.28593383246197,
2.77707169933068));
#14069=CARTESIAN_POINT('Ctrl Pts',(-2.75014427135568,-1.37226409146692,
2.78205332328112));
#14070=CARTESIAN_POINT('Ctrl Pts',(-2.70705945746326,-1.45861004691781,
2.7870358529834));
#14071=CARTESIAN_POINT('Ctrl Pts',(-2.65991438812218,-1.54290470493198,
2.79201838268568));
#14072=CARTESIAN_POINT('Ctrl Pts',(-2.60894248435051,-1.62475270836856,
2.79700091238796));
#14073=CARTESIAN_POINT('Ctrl Pts',(-2.55791564039992,-1.7066889318562,2.80198881252088));
#14074=CARTESIAN_POINT('Ctrl Pts',(-2.50305395974698,-1.78617286274464,
2.80697671265379));
#14075=CARTESIAN_POINT('Ctrl Pts',(-2.4446343876474,-1.86283787827385,2.8119646127867));
#14076=CARTESIAN_POINT('Ctrl Pts',(-2.38618030629432,-1.93954818089368,
2.81695545934158));
#14077=CARTESIAN_POINT('Ctrl Pts',(-2.32416443074657,-2.01343591645363,
2.82194630589645));
#14078=CARTESIAN_POINT('Ctrl Pts',(-2.25890282716458,-2.08416896326278,
2.82693715245132));
#14079=CARTESIAN_POINT('Ctrl Pts',(-2.19353575935452,-2.15501631627606,
2.83193606432716));
#14080=CARTESIAN_POINT('Ctrl Pts',(-2.12491280238239,-2.22269849282685,
2.83693497620299));
#14081=CARTESIAN_POINT('Ctrl Pts',(-2.0533855002772,-2.28692156342349,2.84193388807883));
#14082=CARTESIAN_POINT('Ctrl Pts',(-2.01185986159587,-2.32420668317651,
2.8448360387576));
#14083=CARTESIAN_POINT('Ctrl Pts',(-1.96935593236938,-2.3603266909794,2.84773818943638));
#14084=CARTESIAN_POINT('Ctrl Pts',(-1.9259470215076,-2.39523074469789,2.85064034011516));
#14085=CARTESIAN_POINT('Ctrl Pts',(-1.85116687262225,-2.4553596509974,2.85563984956007));
#14086=CARTESIAN_POINT('Ctrl Pts',(-1.77343680286138,-2.51208880948381,
2.86063935900498));
#14087=CARTESIAN_POINT('Ctrl Pts',(-1.69309887987733,-2.56511567633082,
2.86563886844989));
#14088=CARTESIAN_POINT('Ctrl Pts',(-1.61286993473259,-2.6180706125981,2.87063159609466));
#14089=CARTESIAN_POINT('Ctrl Pts',(-1.53004053020147,-2.6673329986404,2.87562432373944));
#14090=CARTESIAN_POINT('Ctrl Pts',(-1.44498568032854,-2.71264052790735,
2.88061705138421));
#14091=CARTESIAN_POINT('Ctrl Pts',(-1.36002056113136,-2.75790025889797,
2.88560451182993));
#14092=CARTESIAN_POINT('Ctrl Pts',(-1.27283504921582,-2.79921322206013,
2.89059197227564));
#14093=CARTESIAN_POINT('Ctrl Pts',(-1.18383214038874,-2.83636099842432,
2.89557943272135));
#14094=CARTESIAN_POINT('Ctrl Pts',(-1.09489291514546,-2.87348219471871,
2.9005633245269));
#14095=CARTESIAN_POINT('Ctrl Pts',(-1.00413928203352,-2.90644396028856,
2.90554721633245));
#14096=CARTESIAN_POINT('Ctrl Pts',(-0.911996899011164,-2.93507477011984,
2.910531108138));
#14097=CARTESIAN_POINT('Ctrl Pts',(-0.819888071912237,-2.96369515333493,
2.91551318493631));
#14098=CARTESIAN_POINT('Ctrl Pts',(-0.726391918532192,-2.98798758446537,
2.92049526173463));
#14099=CARTESIAN_POINT('Ctrl Pts',(-0.631951136375388,-3.00782978428532,
2.92547733853294));
#14100=CARTESIAN_POINT('Ctrl Pts',(-0.537518964989268,-3.02767017496488,
2.93045896108342));
#14101=CARTESIAN_POINT('Ctrl Pts',(-0.442142765685321,-3.04306105097527,
2.9354405836339));
#14102=CARTESIAN_POINT('Ctrl Pts',(-0.346276306816527,-3.05393106820333,
2.94042220618437));
#14103=CARTESIAN_POINT('Ctrl Pts',(-0.250392417681477,-3.06480306179826,
2.94540473448446));
#14104=CARTESIAN_POINT('Ctrl Pts',(-0.154018528120127,-3.07115251474852,
2.95038726278454));
#14105=CARTESIAN_POINT('Ctrl Pts',(-0.0576133468764672,-3.07295996593865,
2.95536979108463));
#14106=CARTESIAN_POINT('Ctrl Pts',(0.0388957450335715,-3.07476936529646,
2.96035768982051));
#14107=CARTESIAN_POINT('Ctrl Pts',(0.13543575634752,-3.07202698101351,2.96534558855638));
#14108=CARTESIAN_POINT('Ctrl Pts',(0.231548383653232,-3.06476550424785,
2.97033348729226));
#14109=CARTESIAN_POINT('Ctrl Pts',(0.327717786056384,-3.05749973802447,
2.97532433245094));
#14110=CARTESIAN_POINT('Ctrl Pts',(0.423458866290721,-3.04570961754902,
2.98031517760962));
#14111=CARTESIAN_POINT('Ctrl Pts',(0.518320960736258,-3.02947943245394,
2.9853060227683));
#14112=CARTESIAN_POINT('Ctrl Pts',(0.61333635480394,-3.01322301895586,2.99030493326311));
#14113=CARTESIAN_POINT('Ctrl Pts',(0.707469498310246,-2.99251230768777,
2.99530384375791));
#14114=CARTESIAN_POINT('Ctrl Pts',(0.800282446976151,-2.9674821406475,3.00030275425271));
#14115=CARTESIAN_POINT('Ctrl Pts',(0.854165878090701,-2.95295064153141,
3.00320491880159));
#14116=CARTESIAN_POINT('Ctrl Pts',(0.907604650046743,-2.9369641988445,3.00610708335046));
#14117=CARTESIAN_POINT('Ctrl Pts',(0.960516202499753,-2.91955662297128,
3.00900924789933));
#14118=CARTESIAN_POINT('Ctrl Pts',(1.05166602766874,-2.88956889016248,3.0140087570609));
#14119=CARTESIAN_POINT('Ctrl Pts',(1.14157026009048,-2.85525578898929,3.01900826622246));
#14120=CARTESIAN_POINT('Ctrl Pts',(1.22978888909977,-2.8167395226124,3.02400777538403));
#14121=CARTESIAN_POINT('Ctrl Pts',(1.3178878499894,-2.77827550335413,3.02900050273695));
#14122=CARTESIAN_POINT('Ctrl Pts',(1.40430535290841,-2.73561982452741,3.03399323008987));
#14123=CARTESIAN_POINT('Ctrl Pts',(1.48861720018372,-2.68894423172315,3.03898595744279));
#14124=CARTESIAN_POINT('Ctrl Pts',(1.57284010049035,-2.64231788054536,3.04397341758858));
#14125=CARTESIAN_POINT('Ctrl Pts',(1.65496137919667,-2.59168025754403,3.04896087773436));
#14126=CARTESIAN_POINT('Ctrl Pts',(1.73457841647093,-2.53725047386205,3.05394833788015));
#14127=CARTESIAN_POINT('Ctrl Pts',(1.81413848578713,-2.48285963603564,3.05893222937493));
#14128=CARTESIAN_POINT('Ctrl Pts',(1.89119751444243,-2.4246822786342,3.0639161208697));
#14129=CARTESIAN_POINT('Ctrl Pts',(1.9653798784427,-2.36298205312959,3.06890001236448));
#14130=CARTESIAN_POINT('Ctrl Pts',(2.03953522700394,-2.30130429736834,3.07388208884543));
#14131=CARTESIAN_POINT('Ctrl Pts',(2.11081565526192,-2.23610650298653,3.07886416532637));
#14132=CARTESIAN_POINT('Ctrl Pts',(2.17887756899577,-2.16769342604693,3.08384624180731));
#14133=CARTESIAN_POINT('Ctrl Pts',(2.24693327700375,-2.09928658685144,3.0888278640342));
#14134=CARTESIAN_POINT('Ctrl Pts',(2.3117707444701,-2.02766535927851,3.09380948626107));
#14135=CARTESIAN_POINT('Ctrl Pts',(2.37308307360751,-1.95317151723998,3.09879110848796));
#14136=CARTESIAN_POINT('Ctrl Pts',(2.43440655037017,-1.87866413095274,3.10377363645857));
#14137=CARTESIAN_POINT('Ctrl Pts',(2.49220333699067,-1.80128343187748,3.10875616442918));
#14138=CARTESIAN_POINT('Ctrl Pts',(2.54620736493229,-1.72140358567205,3.11373869239979));
#14139=CARTESIAN_POINT('Ctrl Pts',(2.60026960123481,-1.6414376407978,3.11872659079919));
#14140=CARTESIAN_POINT('Ctrl Pts',(2.65053067121611,-1.55896753530423,3.12371448919859));
#14141=CARTESIAN_POINT('Ctrl Pts',(2.6967684719449,-1.47439548925109,3.12870238759799));
#14142=CARTESIAN_POINT('Ctrl Pts',(2.74303358596144,-1.38977348535843,3.13369323241573));
#14143=CARTESIAN_POINT('Ctrl Pts',(2.78527050641838,-1.30304746305312,3.13868407723347));
#14144=CARTESIAN_POINT('Ctrl Pts',(2.82330457028139,-1.21464132707076,3.14367492205122));
#14145=CARTESIAN_POINT('Ctrl Pts',(2.86140009816075,-1.12609232451997,3.14867383220135));
#14146=CARTESIAN_POINT('Ctrl Pts',(2.89527905328596,-1.0358581974992,3.15367274235149));
#14147=CARTESIAN_POINT('Ctrl Pts',(2.92481610062052,-0.9443797051774,3.15867165250163));
#14148=CARTESIAN_POINT('Ctrl Pts',(2.94196413148312,-0.891270943430509,
3.16157382022893));
#14149=CARTESIAN_POINT('Ctrl Pts',(2.9576496683022,-0.837743011043862,3.16447598795622));
#14150=CARTESIAN_POINT('Ctrl Pts',(2.97185612080094,-0.783883567411629,
3.16737815568352));
#14151=CARTESIAN_POINT('Ctrl Pts',(3.0033493354305,-0.664486623080219,3.1738117527504));
#14152=CARTESIAN_POINT('Ctrl Pts',(3.0276611199019,-0.543122418651518,3.18024534981728));
#14153=CARTESIAN_POINT('Ctrl Pts',(3.04459242610206,-0.420546321969373,
3.18667894688416));
#14154=CARTESIAN_POINT('Ctrl Pts',(3.06118864443189,-0.300396131635276,
3.19298521648355));
#14155=CARTESIAN_POINT('Ctrl Pts',(3.0706936399446,-0.179081323696639,3.19929148608295));
#14156=CARTESIAN_POINT('Ctrl Pts',(3.0729651698961,-0.0573351079655099,
3.20559775568234));
#14157=CARTESIAN_POINT('Ctrl Pts',(3.07330444298811,-0.0391512336901752,
3.2065396528317));
#14158=CARTESIAN_POINT('Ctrl Pts',(3.07348243553562,-0.020957779401148,
3.20748154998105));
#14159=CARTESIAN_POINT('Ctrl Pts',(3.07349876324234,-0.00275723554103428,
3.2084234471304));
#14160=CARTESIAN_POINT('Origin',(0.,0.,-2.20842344717744));
#14161=CARTESIAN_POINT('',(-1.87240768645123,2.4373123939533,1.56259812102449));
#14162=CARTESIAN_POINT('',(-1.86967516139564,2.4337884984361,1.64589879171829));
#14163=CARTESIAN_POINT('',(-1.87240768645123,2.4373123939533,-2.20842344717744));
#14164=CARTESIAN_POINT('',(3.06851769484666,-5.29070161844891E-5,2.29157655282254));
#14165=CARTESIAN_POINT('Ctrl Pts',(-1.86967516139566,2.43378849843609,1.64589879171829));
#14166=CARTESIAN_POINT('Ctrl Pts',(-2.33881678074012,2.07024255782115,1.67652887832048));
#14167=CARTESIAN_POINT('Ctrl Pts',(-3.347303037218,0.724834725607579,1.75994860085072));
#14168=CARTESIAN_POINT('Ctrl Pts',(-2.87382423513241,-2.21708609137177,
1.89615795930903));
#14169=CARTESIAN_POINT('Ctrl Pts',(0.295015670113215,-3.61763651773389,
2.0545268670932));
#14170=CARTESIAN_POINT('Ctrl Pts',(2.70865137306433,-2.04009181137399,2.18633306493104));
#14171=CARTESIAN_POINT('Ctrl Pts',(3.06859605637346,-0.508461450263827,
2.26534962684082));
#14172=CARTESIAN_POINT('Ctrl Pts',(3.06851769484666,-5.29070161844891E-5,
2.29157655282254));
#14173=CARTESIAN_POINT('Ctrl Pts',(3.06851769484666,-5.29070161844891E-5,
2.29157655282254));
#14174=CARTESIAN_POINT('Ctrl Pts',(3.06843833005534,0.514864803047814,2.31813926276888));
#14175=CARTESIAN_POINT('Ctrl Pts',(2.70185886612363,2.05321498844667,2.39749160864328));
#14176=CARTESIAN_POINT('Ctrl Pts',(0.531438462838955,3.45227005220736,2.51553012669809));
#14177=CARTESIAN_POINT('Ctrl Pts',(-1.27463594994892,2.88616721946652,2.60700593480658));
#14178=CARTESIAN_POINT('Ctrl Pts',(-1.87178979188648,2.43648733431093,2.645692106987));
#14179=CARTESIAN_POINT('',(3.0734998353151,0.00100614018965784,2.20842344715011));
#14180=CARTESIAN_POINT('Ctrl Pts',(3.07349983531492,0.00100614071472882,
2.20842344717745));
#14181=CARTESIAN_POINT('Ctrl Pts',(3.07348151913187,0.0569573459386727,
2.21133720111112));
#14182=CARTESIAN_POINT('Ctrl Pts',(3.0719354652809,0.112881503038161,2.21425095504479));
#14183=CARTESIAN_POINT('Ctrl Pts',(3.06886549665176,0.168721111483932,2.21716470897846));
#14184=CARTESIAN_POINT('Ctrl Pts',(3.06359794048394,0.264532603198921,2.22216422668006));
#14185=CARTESIAN_POINT('Ctrl Pts',(3.05382990902008,0.360265456024861,2.22716374438167));
#14186=CARTESIAN_POINT('Ctrl Pts',(3.03956504934842,0.455463018015246,2.23216326208327));
#14187=CARTESIAN_POINT('Ctrl Pts',(3.02531953958613,0.550531447000532,2.23715599806976));
#14188=CARTESIAN_POINT('Ctrl Pts',(3.00658938911884,0.64506559784126,2.24214873405625));
#14189=CARTESIAN_POINT('Ctrl Pts',(2.98343019475376,0.738611212365163,2.24714147004275));
#14190=CARTESIAN_POINT('Ctrl Pts',(2.96029543236287,0.832058140207496,2.25212893890315));
#14191=CARTESIAN_POINT('Ctrl Pts',(2.93274101956111,0.924518181053002,2.25711640776356));
#14192=CARTESIAN_POINT('Ctrl Pts',(2.90087389905939,1.01554560299179,2.26210387662396));
#14193=CARTESIAN_POINT('Ctrl Pts',(2.86902957968994,1.10650789421733,2.26708777691791));
#14194=CARTESIAN_POINT('Ctrl Pts',(2.83287883161229,1.19603919116548,2.27207167721187));
#14195=CARTESIAN_POINT('Ctrl Pts',(2.7925786234219,1.28370825424121,2.27705557750582));
#14196=CARTESIAN_POINT('Ctrl Pts',(2.75229309117913,1.3713453912641,2.28203766283497));
#14197=CARTESIAN_POINT('Ctrl Pts',(2.70786128434982,1.45712124341626,2.28701974816412));
#14198=CARTESIAN_POINT('Ctrl Pts',(2.65948818804544,1.54062481728901,2.29200183349326));
#14199=CARTESIAN_POINT('Ctrl Pts',(2.61111950190808,1.62412077815503,2.29698346460653));
#14200=CARTESIAN_POINT('Ctrl Pts',(2.55881046089606,1.70534449288149,2.3019650957198));
#14201=CARTESIAN_POINT('Ctrl Pts',(2.50281133318863,1.78391078265214,2.30694672683307));
#14202=CARTESIAN_POINT('Ctrl Pts',(2.44680202359668,1.86249135751833,2.31192926371746));
#14203=CARTESIAN_POINT('Ctrl Pts',(2.38710154962829,1.93841319040467,2.31691180060185));
#14204=CARTESIAN_POINT('Ctrl Pts',(2.3240020695165,2.01132211017605,2.32189433748624));
#14205=CARTESIAN_POINT('Ctrl Pts',(2.26083457777066,2.08430961466415,2.3268822447869));
#14206=CARTESIAN_POINT('Ctrl Pts',(2.19426105355551,2.15427739031301,2.33187015208757));
#14207=CARTESIAN_POINT('Ctrl Pts',(2.12461217200144,2.2209064294975,2.33685805938824));
#14208=CARTESIAN_POINT('Ctrl Pts',(2.05492214790873,2.28757482735879,2.34184891311338));
#14209=CARTESIAN_POINT('Ctrl Pts',(1.98215348019765,2.35090027368193,2.34683976683852));
#14210=CARTESIAN_POINT('Ctrl Pts',(1.90667011304086,2.41060393470946,2.35183062056366));
#14211=CARTESIAN_POINT('Ctrl Pts',(1.83106476424255,2.47040407726467,2.35682953954281));
#14212=CARTESIAN_POINT('Ctrl Pts',(1.75273631267024,2.52657049209211,2.36182845852196));
#14213=CARTESIAN_POINT('Ctrl Pts',(1.67207779799985,2.57886759788788,2.36682737750111));
#14214=CARTESIAN_POINT('Ctrl Pts',(1.62525218562726,2.60922823636737,2.36972945725495));
#14215=CARTESIAN_POINT('Ctrl Pts',(1.57764175605759,2.6382856582793,2.37263153700879));
#14216=CARTESIAN_POINT('Ctrl Pts',(1.52932683703008,2.66600106442957,2.37553361676263));
#14217=CARTESIAN_POINT('Ctrl Pts',(1.44609310741097,2.71374732310551,2.38053312677789));
#14218=CARTESIAN_POINT('Ctrl Pts',(1.36047505246342,2.75767581755783,2.38553263679314));
#14219=CARTESIAN_POINT('Ctrl Pts',(1.27285769233677,2.79754098183728,2.39053214680839));
#14220=CARTESIAN_POINT('Ctrl Pts',(1.18535918404278,2.83735206952933,2.39552487505201));
#14221=CARTESIAN_POINT('Ctrl Pts',(1.09586715668542,2.87311060126025,2.40051760329563));
#14222=CARTESIAN_POINT('Ctrl Pts',(1.00479290675893,2.90461588932632,2.40551033153924));
#14223=CARTESIAN_POINT('Ctrl Pts',(0.913814737306463,2.93608794030273,2.41049779261133));
#14224=CARTESIAN_POINT('Ctrl Pts',(0.821258076180029,2.96331552483282,2.41548525368342));
#14225=CARTESIAN_POINT('Ctrl Pts',(0.727555023575959,2.9861456658491,2.42047271475551));
#14226=CARTESIAN_POINT('Ctrl Pts',(0.633919016878905,3.008959471565,2.42545660722612));
#14227=CARTESIAN_POINT('Ctrl Pts',(0.539138674605391,3.02738198511897,2.43044049969674));
#14228=CARTESIAN_POINT('Ctrl Pts',(0.443661177673654,3.04131008110407,2.43542439216736));
#14229=CARTESIAN_POINT('Ctrl Pts',(0.348218450770178,3.05523310489617,2.44040646965447));
#14230=CARTESIAN_POINT('Ctrl Pts',(0.252079507566787,3.06466489982751,2.44538854714158));
#14231=CARTESIAN_POINT('Ctrl Pts',(0.155700689380518,3.06955363942812,2.4503706246287));
#14232=CARTESIAN_POINT('Ctrl Pts',(0.0593306582226456,3.07444193331365,
2.45535224789094));
#14233=CARTESIAN_POINT('Ctrl Pts',(-0.0372787660290401,3.07478797331731,
2.46033387115318));
#14234=CARTESIAN_POINT('Ctrl Pts',(-0.133668240644852,3.07059197084909,
2.46531549441542));
#14235=CARTESIAN_POINT('Ctrl Pts',(-0.230075241047957,3.06639520545269,
2.47029802344947));
#14236=CARTESIAN_POINT('Ctrl Pts',(-0.326261773850551,3.05765477657871,
2.47528055248353));
#14237=CARTESIAN_POINT('Ctrl Pts',(-0.42177169818593,3.04442291487391,2.48026308151759));
#14238=CARTESIAN_POINT('Ctrl Pts',(-0.517384568786063,3.03117679108328,
2.48525098101714));
#14239=CARTESIAN_POINT('Ctrl Pts',(-0.612318939430988,3.01342962992525,
2.4902388805167));
#14240=CARTESIAN_POINT('Ctrl Pts',(-0.706127193526199,2.99128511455575,
2.49522678001625));
#14241=CARTESIAN_POINT('Ctrl Pts',(-0.799990861821142,2.9691275180282,2.50021762595652));
#14242=CARTESIAN_POINT('Ctrl Pts',(-0.892726667212065,2.94256751585795,
2.50520847189678));
#14243=CARTESIAN_POINT('Ctrl Pts',(-0.983902577260418,2.91175856974103,
2.51019931783705));
#14244=CARTESIAN_POINT('Ctrl Pts',(-1.07522583031713,2.88089983544209,2.51519822913422));
#14245=CARTESIAN_POINT('Ctrl Pts',(-1.16498374596833,2.84577860631539,2.52019714043138));
#14246=CARTESIAN_POINT('Ctrl Pts',(-1.25276473051643,2.80659629800477,2.52519605172855));
#14247=CARTESIAN_POINT('Ctrl Pts',(-1.3037266773949,2.78384869811191,2.52809820933464));
#14248=CARTESIAN_POINT('Ctrl Pts',(-1.35402275645602,2.75973318744216,2.53100036694073));
#14249=CARTESIAN_POINT('Ctrl Pts',(-1.40357668246183,2.73429602392452,2.53390252454682));
#14250=CARTESIAN_POINT('Ctrl Pts',(-1.48892148252625,2.6904865862149,2.53890079775363));
#14251=CARTESIAN_POINT('Ctrl Pts',(-1.57236306688953,2.64260062643993,2.54389907096044));
#14252=CARTESIAN_POINT('Ctrl Pts',(-1.65348613732799,2.59082725083402,2.54889734416725));
#14253=CARTESIAN_POINT('Ctrl Pts',(-1.72854932379068,2.54292134039566,2.55352224694382));
#14254=CARTESIAN_POINT('Ctrl Pts',(-1.8016273535101,2.49168771316857,2.55814714972038));
#14255=CARTESIAN_POINT('Ctrl Pts',(-1.87240768645123,2.4373123939533,2.56277205249695));
#14256=CARTESIAN_POINT('Ctrl Pts',(-1.87240768645123,2.4373123939533,1.56259812102449));
#14257=CARTESIAN_POINT('Ctrl Pts',(-1.94882482793984,2.37860672969176,1.56759754314901));
#14258=CARTESIAN_POINT('Ctrl Pts',(-2.02238011400756,2.31637935109213,1.57259696527352));
#14259=CARTESIAN_POINT('Ctrl Pts',(-2.09275054956073,2.25095477238288,1.57759638739804));
#14260=CARTESIAN_POINT('Ctrl Pts',(-2.12133687210871,2.22437758702305,1.57962728421261));
#14261=CARTESIAN_POINT('Ctrl Pts',(-2.14939807886449,2.19727319978244,1.58165818102718));
#14262=CARTESIAN_POINT('Ctrl Pts',(-2.17691441706924,2.16966492130838,1.58368907784175));
#14263=CARTESIAN_POINT('Ctrl Pts',(-2.24465021132717,2.1017028016172,1.58868844977007));
#14264=CARTESIAN_POINT('Ctrl Pts',(-2.30931938227318,2.0304461905262,1.59368782169838));
#14265=CARTESIAN_POINT('Ctrl Pts',(-2.37058473659246,1.95620302030103,1.5986871936267));
#14266=CARTESIAN_POINT('Ctrl Pts',(-2.43176695745554,1.88206059365938,1.60367978170349));
#14267=CARTESIAN_POINT('Ctrl Pts',(-2.48955426417674,1.80493999780551,1.60867236978029));
#14268=CARTESIAN_POINT('Ctrl Pts',(-2.54364596787284,1.72518620447888,1.61366495785708));
#14269=CARTESIAN_POINT('Ctrl Pts',(-2.59768058460601,1.64551658121035,1.61865227688759));
#14270=CARTESIAN_POINT('Ctrl Pts',(-2.6480271066488,1.56321964633603,1.62363959591809));
#14271=CARTESIAN_POINT('Ctrl Pts',(-2.69442550748228,1.47867286261325,1.6286269149486));
#14272=CARTESIAN_POINT('Ctrl Pts',(-2.74079068806385,1.39418661255978,1.6336106631665));
#14273=CARTESIAN_POINT('Ctrl Pts',(-2.7832131563224,1.30745409967807,1.63859441138441));
#14274=CARTESIAN_POINT('Ctrl Pts',(-2.82147710351386,1.21888030763773,1.64357815960231));
#14275=CARTESIAN_POINT('Ctrl Pts',(-2.85972710562926,1.13033879580782,1.64856009152176));
#14276=CARTESIAN_POINT('Ctrl Pts',(-2.89382142398838,1.03995774068917,1.65354202344122));
#14277=CARTESIAN_POINT('Ctrl Pts',(-2.92359140418526,0.948164306106309,
1.65852395536067));
#14278=CARTESIAN_POINT('Ctrl Pts',(-2.95335866331643,0.856379261719421,
1.66350543191656));
#14279=CARTESIAN_POINT('Ctrl Pts',(-2.97880223487575,0.763182512169141,
1.66848690847245));
#14280=CARTESIAN_POINT('Ctrl Pts',(-2.99980293344201,0.669017645890376,
1.67346838502835));
#14281=CARTESIAN_POINT('Ctrl Pts',(-3.02080744646165,0.574835676014279,
1.67845076639272));
#14282=CARTESIAN_POINT('Ctrl Pts',(-3.03736738830957,0.479685668652976,
1.68343314775708));
#14283=CARTESIAN_POINT('Ctrl Pts',(-3.04941463707283,0.384021641585425,
1.68841552912145));
#14284=CARTESIAN_POINT('Ctrl Pts',(-3.06147487006335,0.288254510191585,
1.69340328037343));
#14285=CARTESIAN_POINT('Ctrl Pts',(-3.06901264516244,0.191972689359046,
1.69839103162542));
#14286=CARTESIAN_POINT('Ctrl Pts',(-3.07201174019826,0.095635339096251,
1.7033787828774));
#14287=CARTESIAN_POINT('Ctrl Pts',(-3.075012606577,-0.000758910491449369,
1.70836948002397));
#14288=CARTESIAN_POINT('Ctrl Pts',(-3.07346946228496,-0.0972083160843792,
1.71336017717054));
#14289=CARTESIAN_POINT('Ctrl Pts',(-3.06741820345264,-0.193255828184808,
1.71835087431711));
#14290=CARTESIAN_POINT('Ctrl Pts',(-3.06135716458187,-0.289458572177848,
1.7233496374234));
#14291=CARTESIAN_POINT('Ctrl Pts',(-3.05077351079541,-0.385257689649415,
1.72834840052969));
#14292=CARTESIAN_POINT('Ctrl Pts',(-3.03575475640733,-0.480203403726241,
1.73334716363598));
#14293=CARTESIAN_POINT('Ctrl Pts',(-3.02703088524136,-0.535354061095335,
1.73625077096596));
#14294=CARTESIAN_POINT('Ctrl Pts',(-3.01681154598786,-0.59021698782647,
1.73915437829595));
#14295=CARTESIAN_POINT('Ctrl Pts',(-3.00512162006299,-0.644706366208652,
1.74205798562594));
#14296=CARTESIAN_POINT('Ctrl Pts',(-2.98499339097518,-0.738528576715243,
1.7470575445534));
#14297=CARTESIAN_POINT('Ctrl Pts',(-2.96043180028799,-0.831572020007051,
1.75205710348086));
#14298=CARTESIAN_POINT('Ctrl Pts',(-2.93151159147554,-0.923386180882382,
1.75705666240832));
#14299=CARTESIAN_POINT('Ctrl Pts',(-2.90263060966395,-1.01507580620574,
1.76204943999807));
#14300=CARTESIAN_POINT('Ctrl Pts',(-2.86940289013932,-1.10553904783446,
1.76704221758783));
#14301=CARTESIAN_POINT('Ctrl Pts',(-2.8319541189141,-1.19433584822924,1.77203499517759));
#14302=CARTESIAN_POINT('Ctrl Pts',(-2.79454485185385,-1.28303897816871,
1.77702250595877));
#14303=CARTESIAN_POINT('Ctrl Pts',(-2.75292355451497,-1.37007875917954,
1.78201001673995));
#14304=CARTESIAN_POINT('Ctrl Pts',(-2.70726530367091,-1.45503155482609,
1.78699752752113));
#14305=CARTESIAN_POINT('Ctrl Pts',(-2.66163971859919,-1.53992357178246,
1.79198147003395));
#14306=CARTESIAN_POINT('Ctrl Pts',(-2.61198312884155,-1.62273118607782,
1.79696541254677));
#14307=CARTESIAN_POINT('Ctrl Pts',(-2.55851776865546,-1.70305286984119,
1.8019493550596));
#14308=CARTESIAN_POINT('Ctrl Pts',(-2.50507187673896,-1.78334530617803,
1.80693148277614));
#14309=CARTESIAN_POINT('Ctrl Pts',(-2.44782021295935,-1.86115324548523,
1.81191361049269));
#14310=CARTESIAN_POINT('Ctrl Pts',(-2.38702928791256,-1.93610263897544,
1.81689573820924));
#14311=CARTESIAN_POINT('Ctrl Pts',(-2.32624390369737,-2.01104520115048,
1.82187741182625));
#14312=CARTESIAN_POINT('Ctrl Pts',(-2.26192017623445,-2.0831293947229,1.82685908544326));
#14313=CARTESIAN_POINT('Ctrl Pts',(-2.19436532499682,-2.15201372450355,
1.83184075906028));
#14314=CARTESIAN_POINT('Ctrl Pts',(-2.12679819002139,-2.22091057976577,
1.83682333851264));
#14315=CARTESIAN_POINT('Ctrl Pts',(-2.05599907181081,-2.28660610232763,
1.84180591796501));
#14316=CARTESIAN_POINT('Ctrl Pts',(-1.98231173822915,-2.34879595164819,
1.84678849741737));
#14317=CARTESIAN_POINT('Ctrl Pts',(-1.90854498399631,-2.41105282956226,
1.85177644712383));
#14318=CARTESIAN_POINT('Ctrl Pts',(-1.83188413571029,-2.46979620735661,
1.85676439683028));
#14319=CARTESIAN_POINT('Ctrl Pts',(-1.75270553031896,-2.52476247872732,
1.86175234653674));
#14320=CARTESIAN_POINT('Ctrl Pts',(-1.6734801539065,-2.57976121882652,1.86674324263888));
#14321=CARTESIAN_POINT('Ctrl Pts',(-1.59173443083607,-2.63097817697288,
1.87173413874102));
#14322=CARTESIAN_POINT('Ctrl Pts',(-1.50787130299238,-2.6781946127218,1.87672503484316));
#14323=CARTESIAN_POINT('Ctrl Pts',(-1.42387266072209,-2.72548734550829,
1.88172399573421));
#14324=CARTESIAN_POINT('Ctrl Pts',(-1.33775017361861,-2.76876645086329,
1.88672295662526));
#14325=CARTESIAN_POINT('Ctrl Pts',(-1.24992878636426,-2.80786044507521,
1.89172191751631));
#14326=CARTESIAN_POINT('Ctrl Pts',(-1.19895265514617,-2.83055264615619,
1.89462357614757));
#14327=CARTESIAN_POINT('Ctrl Pts',(-1.1474044639194,-2.85183569365316,1.89752523477884));
#14328=CARTESIAN_POINT('Ctrl Pts',(-1.09536956545426,-2.87168378570422,
1.90042689341011));
#14329=CARTESIAN_POINT('Ctrl Pts',(-1.00571413125093,-2.90588178288372,
1.90542641242849));
#14330=CARTESIAN_POINT('Ctrl Pts',(-0.914298179497828,-2.93593718597948,
1.91042593144687));
#14331=CARTESIAN_POINT('Ctrl Pts',(-0.821540285226743,-2.96166740363424,
1.91542545046525));
#14332=CARTESIAN_POINT('Ctrl Pts',(-0.72890821070842,-2.98736272000485,
1.9204181879773));
#14333=CARTESIAN_POINT('Ctrl Pts',(-0.634938230676253,-3.00874439452058,
1.92541092548935));
#14334=CARTESIAN_POINT('Ctrl Pts',(-0.540067884674282,-3.02567825948885,
1.93040366300141));
#14335=CARTESIAN_POINT('Ctrl Pts',(-0.445297618949502,-3.04259426064643,
1.93539113359313));
#14336=CARTESIAN_POINT('Ctrl Pts',(-0.34962930525442,-3.05507170308052,
1.94037860418486));
#14337=CARTESIAN_POINT('Ctrl Pts',(-0.253513600610845,-3.06302678804893,
1.94536607477658));
#14338=CARTESIAN_POINT('Ctrl Pts',(-0.157466661538478,-3.0709761815857,
1.95034997710373));
#14339=CARTESIAN_POINT('Ctrl Pts',(-0.0609734040397047,-3.07440961357692,
1.95533387943087));
#14340=CARTESIAN_POINT('Ctrl Pts',(0.0355083839726203,-3.0732948775976,
1.96031778175802));
#14341=CARTESIAN_POINT('Ctrl Pts',(0.13195504026161,-3.0721805475249,1.96529986930663));
#14342=CARTESIAN_POINT('Ctrl Pts',(0.228389796879552,-3.06652134506973,
1.97028195685525));
#14343=CARTESIAN_POINT('Ctrl Pts',(0.324353808531808,-3.05633716348359,
1.97526404440386));
#14344=CARTESIAN_POINT('Ctrl Pts',(0.42030907471396,-3.04615391001054,1.98024567792084));
#14345=CARTESIAN_POINT('Ctrl Pts',(0.515793244734481,-3.03144654378952,
1.98522731143781));
#14346=CARTESIAN_POINT('Ctrl Pts',(0.610352614800831,-3.01228682824292,
1.99020894495478));
#14347=CARTESIAN_POINT('Ctrl Pts',(0.704929181312647,-2.99312362833508,
1.99519148442522));
#14348=CARTESIAN_POINT('Ctrl Pts',(0.798580183652301,-2.96950655824357,
2.00017402389566));
#14349=CARTESIAN_POINT('Ctrl Pts',(0.890863184148258,-2.94155826682546,
2.0051565633661));
#14350=CARTESIAN_POINT('Ctrl Pts',(0.983245656525631,-2.91357984993338,
2.01014447351774));
#14351=CARTESIAN_POINT('Ctrl Pts',(1.07425676240429,-2.88126101868106,2.01513238366937));
#14352=CARTESIAN_POINT('Ctrl Pts',(1.16347049934951,-2.84477391845879,2.020120293821));
#14353=CARTESIAN_POINT('Ctrl Pts',(1.25273693878055,-2.80826526369854,2.02511115055097));
#14354=CARTESIAN_POINT('Ctrl Pts',(1.34020349726109,-2.76758362200166,2.03010200728093));
#14355=CARTESIAN_POINT('Ctrl Pts',(1.42546732052527,-2.72294788200482,2.0350928640109));
#14356=CARTESIAN_POINT('Ctrl Pts',(1.51086893430869,-2.67824000846346,2.04009178621006));
#14357=CARTESIAN_POINT('Ctrl Pts',(1.59406032626629,-2.62956549869764,2.04509070840922));
#14358=CARTESIAN_POINT('Ctrl Pts',(1.67466630137768,-2.57718742605772,2.05008963060838));
#14359=CARTESIAN_POINT('Ctrl Pts',(1.72146101309108,-2.54678004241276,2.05299168747035));
#14360=CARTESIAN_POINT('Ctrl Pts',(1.7673849620253,-2.51512525908508,2.05589374433232));
#14361=CARTESIAN_POINT('Ctrl Pts',(1.81237000721957,-2.48228064628699,2.05879580119428));
#14362=CARTESIAN_POINT('Ctrl Pts',(1.8892313844923,-2.4261623926596,2.06375425097179));
#14363=CARTESIAN_POINT('Ctrl Pts',(1.96362979729519,-2.36636412933964,2.0687127007493));
#14364=CARTESIAN_POINT('Ctrl Pts',(2.0351876424133,-2.30313124032657,2.0736711505268));
#14365=CARTESIAN_POINT('Ctrl Pts',(2.10664810430205,-2.23998440509172,2.07862285233906));
#14366=CARTESIAN_POINT('Ctrl Pts',(2.1752753464389,-2.17341252342043,2.08357455415132));
#14367=CARTESIAN_POINT('Ctrl Pts',(2.24072173531615,-2.10370348549451,2.08852625596358));
#14368=CARTESIAN_POINT('Ctrl Pts',(2.30674986141293,-2.03337482068628,2.09352197226302));
#14369=CARTESIAN_POINT('Ctrl Pts',(2.36953992237088,-1.95985320948171,2.09851768856246));
#14370=CARTESIAN_POINT('Ctrl Pts',(2.42876994344176,-1.88347519543899,2.1035134048619));
#14371=CARTESIAN_POINT('Ctrl Pts',(2.48737572225326,-1.8079021512948,2.10845646986773));
#14372=CARTESIAN_POINT('Ctrl Pts',(2.54249586388351,-1.72953298782537,2.11339953487355));
#14373=CARTESIAN_POINT('Ctrl Pts',(2.59385731432301,-1.64872874753035,2.11834259987938));
#14374=CARTESIAN_POINT('Ctrl Pts',(2.6452017517199,-1.56795127295109,2.12328402753707));
#14375=CARTESIAN_POINT('Ctrl Pts',(2.69278973145011,-1.48474070068797,2.12822545519475));
#14376=CARTESIAN_POINT('Ctrl Pts',(2.73639132183341,-1.39948732891541,2.13316688285244));
#14377=CARTESIAN_POINT('Ctrl Pts',(2.77999087058241,-1.31423794911211,2.13810807912892));
#14378=CARTESIAN_POINT('Ctrl Pts',(2.81960419835934,-1.2269463583883,2.14304927540541));
#14379=CARTESIAN_POINT('Ctrl Pts',(2.85504772508441,-1.13802668575493,2.1479904716819));
#14380=CARTESIAN_POINT('Ctrl Pts',(2.89117186826129,-1.04739950267674,2.15302655297091));
#14381=CARTESIAN_POINT('Ctrl Pts',(2.92296420655424,-0.955081501042653,
2.15806263425993));
#14382=CARTESIAN_POINT('Ctrl Pts',(2.95028273665268,-0.861530048117416,
2.16309871554895));
#14383=CARTESIAN_POINT('Ctrl Pts',(2.97712156033067,-0.769621334843533,
2.16804636453508));
#14384=CARTESIAN_POINT('Ctrl Pts',(2.99964237774386,-0.676522593922476,
2.1729940135212));
#14385=CARTESIAN_POINT('Ctrl Pts',(3.0177620145246,-0.582678876991815,2.17794166250733));
#14386=CARTESIAN_POINT('Ctrl Pts',(3.0363674460371,-0.486319172359758,2.18302195994779));
#14387=CARTESIAN_POINT('Ctrl Pts',(3.05033226418924,-0.389174478221524,
2.18810225738826));
#14388=CARTESIAN_POINT('Ctrl Pts',(3.05962333423175,-0.291731559185131,
2.19318255482872));
#14389=CARTESIAN_POINT('Ctrl Pts',(3.06891440427426,-0.194288640148734,
2.19826285226918));
#14390=CARTESIAN_POINT('Ctrl Pts',(3.07353177061625,-0.0965480017052525,
2.20334314970964));
#14391=CARTESIAN_POINT('Ctrl Pts',(3.0734998353151,0.00100614018966156,
2.2084234471501));
#14392=CARTESIAN_POINT('Origin',(0.,0.,-2.20842344717744));
#14393=CARTESIAN_POINT('',(-1.87240768645124,2.43731239395329,0.562647869306095));
#14394=CARTESIAN_POINT('',(-1.87460960294492,2.44013607231272,0.645925936011554));
#14395=CARTESIAN_POINT('',(-1.87240768645123,2.4373123939533,-2.20842344717744));
#14396=CARTESIAN_POINT('',(3.07312700507994,-0.003721818839033,0.20842328729948));
#14397=CARTESIAN_POINT('Ctrl Pts',(3.07349774975442,-0.00371917390008725,
0.208423447177455));
#14398=CARTESIAN_POINT('Ctrl Pts',(3.07361316870223,0.0916621892469147,
0.213347842393274));
#14399=CARTESIAN_POINT('Ctrl Pts',(3.06928430893304,0.187123126142624,0.218272237609092));
#14400=CARTESIAN_POINT('Ctrl Pts',(3.06051597387791,0.282213081975554,0.22319663282491));
#14401=CARTESIAN_POINT('Ctrl Pts',(3.05175038029966,0.377273307316475,0.228119488396596));
#14402=CARTESIAN_POINT('Ctrl Pts',(3.03854810894313,0.471962334451556,0.233042343968281));
#14403=CARTESIAN_POINT('Ctrl Pts',(3.02096597683338,0.565832852364695,0.237965199539966));
#14404=CARTESIAN_POINT('Ctrl Pts',(3.00338428142197,0.659701038757444,0.242887932839628));
#14405=CARTESIAN_POINT('Ctrl Pts',(2.98142302492759,0.752750314370692,0.24781066613929));
#14406=CARTESIAN_POINT('Ctrl Pts',(2.9551902667484,0.844542916207064,0.252733399438952));
#14407=CARTESIAN_POINT('Ctrl Pts',(2.92895060932353,0.936359659603639,0.257657427423152));
#14408=CARTESIAN_POINT('Ctrl Pts',(2.89843734394202,1.02691864090875,0.262581455407353));
#14409=CARTESIAN_POINT('Ctrl Pts',(2.86380821853239,1.11579780312849,0.267505483391553));
#14410=CARTESIAN_POINT('Ctrl Pts',(2.82913852575285,1.20478108561716,0.272435279782038));
#14411=CARTESIAN_POINT('Ctrl Pts',(2.79034351655396,1.29208020342226,0.277365076172523));
#14412=CARTESIAN_POINT('Ctrl Pts',(2.7476287120519,1.37729398122116,0.282294872563008));
#14413=CARTESIAN_POINT('Ctrl Pts',(2.7048845348696,1.462566355965,0.287228058910085));
#14414=CARTESIAN_POINT('Ctrl Pts',(2.65821542095587,1.54575014745966,0.292161245257162));
#14415=CARTESIAN_POINT('Ctrl Pts',(2.60787122855021,1.62647161220232,0.297094431604238));
#14416=CARTESIAN_POINT('Ctrl Pts',(2.55744525952703,1.70732419690207,0.302035631175359));
#14417=CARTESIAN_POINT('Ctrl Pts',(2.50333255845057,1.78570610794303,0.306976830746478));
#14418=CARTESIAN_POINT('Ctrl Pts',(2.4458241421049,1.86127550778944,0.311918030317599));
#14419=CARTESIAN_POINT('Ctrl Pts',(2.42712569901718,1.88584634823316,0.313524625401182));
#14420=CARTESIAN_POINT('Ctrl Pts',(2.40806856342506,1.91012014284281,0.315131220484766));
#14421=CARTESIAN_POINT('Ctrl Pts',(2.38866356117224,1.93408599641483,0.31673781556835));
#14422=CARTESIAN_POINT('Ctrl Pts',(2.32818661500641,2.00877713107227,0.32174487318753));
#14423=CARTESIAN_POINT('Ctrl Pts',(2.26409871749897,2.08075782097448,0.326751930806709));
#14424=CARTESIAN_POINT('Ctrl Pts',(2.19667160266441,2.14965953584464,0.331758988425889));
#14425=CARTESIAN_POINT('Ctrl Pts',(2.12933568438833,2.21846805972945,0.33675927389674));
#14426=CARTESIAN_POINT('Ctrl Pts',(2.05866982887286,2.28420557567377,0.341759559367591));
#14427=CARTESIAN_POINT('Ctrl Pts',(1.98498641726937,2.34653599445142,0.346759844838442));
#14428=CARTESIAN_POINT('Ctrl Pts',(1.91138064299977,2.40880073810045,0.351754861703726));
#14429=CARTESIAN_POINT('Ctrl Pts',(1.83476396597669,2.46766524067924,0.356749878569008));
#14430=CARTESIAN_POINT('Ctrl Pts',(1.75548533902005,2.52283044901667,0.361744895434291));
#14431=CARTESIAN_POINT('Ctrl Pts',(1.67626391327478,2.57795585448587,0.366736308288929));
#14432=CARTESIAN_POINT('Ctrl Pts',(1.59438471424826,2.62938702330613,0.371727721143567));
#14433=CARTESIAN_POINT('Ctrl Pts',(1.51022870707359,2.67686598512717,0.376719133998204));
#14434=CARTESIAN_POINT('Ctrl Pts',(1.42610372539023,2.72432744305077,0.381708706686686));
#14435=CARTESIAN_POINT('Ctrl Pts',(1.33970398406318,2.76783937455939,0.386698279375168));
#14436=CARTESIAN_POINT('Ctrl Pts',(1.25143748023826,2.80718835902668,0.39168785206365));
#14437=CARTESIAN_POINT('Ctrl Pts',(1.16317963125899,2.84653348518564,0.396676935506727));
#14438=CARTESIAN_POINT('Ctrl Pts',(1.07305578331699,2.88171629801509,0.401666018949803));
#14439=CARTESIAN_POINT('Ctrl Pts',(0.98149550589776,2.91257082693323,0.406655102392879));
#14440=CARTESIAN_POINT('Ctrl Pts',(0.889919429458282,2.94343067989953,0.411645046718343));
#14441=CARTESIAN_POINT('Ctrl Pts',(0.796906845792688,2.96996062600182,0.416634991043808));
#14442=CARTESIAN_POINT('Ctrl Pts',(0.702903124588431,2.99204435920389,0.421624935369272));
#14443=CARTESIAN_POINT('Ctrl Pts',(0.608800402423276,3.01415135011086,0.426620134904602));
#14444=CARTESIAN_POINT('Ctrl Pts',(0.513704885280354,3.03180267934536,0.431615334439933));
#14445=CARTESIAN_POINT('Ctrl Pts',(0.418072580235202,3.04493309740222,0.436610533975263));
#14446=CARTESIAN_POINT('Ctrl Pts',(0.322384911934895,3.0580711168934,0.441608625321119));
#14447=CARTESIAN_POINT('Ctrl Pts',(0.226160272395216,3.06668297410534,0.446606716666975));
#14448=CARTESIAN_POINT('Ctrl Pts',(0.129858157580303,3.07075546224538,0.451604808012832));
#14449=CARTESIAN_POINT('Ctrl Pts',(0.0334036979499793,3.07483439284471,
0.456610806072938));
#14450=CARTESIAN_POINT('Ctrl Pts',(-0.0631280445224013,3.07435961705346,
0.461616804133045));
#14451=CARTESIAN_POINT('Ctrl Pts',(-0.15927927418525,3.06937002702754,0.466622802193152));
#14452=CARTESIAN_POINT('Ctrl Pts',(-0.213596744417433,3.06655132248622,
0.469450775912943));
#14453=CARTESIAN_POINT('Ctrl Pts',(-0.267792888430964,3.06229274258228,
0.472278749632735));
#14454=CARTESIAN_POINT('Ctrl Pts',(-0.32178651822468,3.05660852689526,0.475106723352527));
#14455=CARTESIAN_POINT('Ctrl Pts',(-0.417397797165186,3.04654298520664,
0.480114465658285));
#14456=CARTESIAN_POINT('Ctrl Pts',(-0.51269765553892,3.0319700686472,0.485122207964043));
#14457=CARTESIAN_POINT('Ctrl Pts',(-0.607228892070632,3.01291807433171,
0.490129950269802));
#14458=CARTESIAN_POINT('Ctrl Pts',(-0.701640883960441,2.9938901127944,0.495131375653663));
#14459=CARTESIAN_POINT('Ctrl Pts',(-0.795285755605436,2.97039438641494,
0.500132801037524));
#14460=CARTESIAN_POINT('Ctrl Pts',(-0.887711441776127,2.94251094239932,
0.505134226421385));
#14461=CARTESIAN_POINT('Ctrl Pts',(-0.980035738273924,2.91465808612814,
0.510130165312208));
#14462=CARTESIAN_POINT('Ctrl Pts',(-1.07114309297848,2.88242721119824,0.515126104203032));
#14463=CARTESIAN_POINT('Ctrl Pts',(-1.16059282370576,2.84594914704439,0.520122043093856));
#14464=CARTESIAN_POINT('Ctrl Pts',(-1.2499841043487,2.8094949191381,0.525114717435451));
#14465=CARTESIAN_POINT('Ctrl Pts',(-1.33771951023168,2.76879918260247,0.530107391777045));
#14466=CARTESIAN_POINT('Ctrl Pts',(-1.4233754604941,2.72404195056964,0.53510006611864));
#14467=CARTESIAN_POINT('Ctrl Pts',(-1.50901251334216,2.6792945928766,0.540091638976503));
#14468=CARTESIAN_POINT('Ctrl Pts',(-1.59257063149162,2.63048771559511,0.545083211834367));
#14469=CARTESIAN_POINT('Ctrl Pts',(-1.67364885409248,2.57784828164788,0.550074784692231));
#14470=CARTESIAN_POINT('Ctrl Pts',(-1.74172381310375,2.53365112002564,0.554265812896852));
#14471=CARTESIAN_POINT('Ctrl Pts',(-1.80805081637324,2.48675303952213,0.558456841101473));
#14472=CARTESIAN_POINT('Ctrl Pts',(-1.87240768645124,2.43731239395329,0.562647869306095));
#14473=CARTESIAN_POINT('',(0.793799282532869,-2.96922295374569,0.));
#14474=CARTESIAN_POINT('Ctrl Pts',(0.793799282532864,-2.9692229537457,-2.77555756156289E-16));
#14475=CARTESIAN_POINT('Ctrl Pts',(1.77865212890011,-2.70592999965461,0.0527896359280583));
#14476=CARTESIAN_POINT('Ctrl Pts',(2.87781245894031,-1.66713001938774,0.122263670929926));
#14477=CARTESIAN_POINT('Ctrl Pts',(3.07278338813921,-0.326580109130746,
0.191737705931794));
#14478=CARTESIAN_POINT('Ctrl Pts',(3.07038535690584,-0.00374137810051507,
0.208422105005604));
#14479=CARTESIAN_POINT('',(-0.794090168544026,-2.96914517230494,1.17075019123725E-8));
#14480=CARTESIAN_POINT('Origin',(0.,0.,0.));
#14481=CARTESIAN_POINT('',(3.07349932342359,0.00203934174087983,0.291576552822545));
#14482=CARTESIAN_POINT('Ctrl Pts',(-0.794090168544026,-2.96914517230494,
1.17075020789059E-8));
#14483=CARTESIAN_POINT('Ctrl Pts',(-0.701681804640572,-2.99385954934229,
0.00498338006721378));
#14484=CARTESIAN_POINT('Ctrl Pts',(-0.607952002928877,-3.01430028785914,
0.00996674842692535));
#14485=CARTESIAN_POINT('Ctrl Pts',(-0.513333254559353,-3.0303285663049,
0.014950116786637));
#14486=CARTESIAN_POINT('Ctrl Pts',(-0.418842318648037,-3.04633519350601,
0.0199267535358467));
#14487=CARTESIAN_POINT('Ctrl Pts',(-0.323465254399358,-3.05794113166517,
0.0249033902850561));
#14488=CARTESIAN_POINT('Ctrl Pts',(-0.22764855061392,-3.06505764830017,
0.0298800270342658));
#14489=CARTESIAN_POINT('Ctrl Pts',(-0.127996697095714,-3.07245900991306,
0.0350558581446337));
#14490=CARTESIAN_POINT('Ctrl Pts',(-0.0278697350491978,-3.07500388554417,
0.0402316892550016));
#14491=CARTESIAN_POINT('Ctrl Pts',(0.0722193954406267,-3.0726513972337,
0.0454075203653694));
#14492=CARTESIAN_POINT('Ctrl Pts',(0.16828711453244,-3.07039342791104,0.0503753953658225));
#14493=CARTESIAN_POINT('Ctrl Pts',(0.264319494128326,-3.06362406015239,
0.0553432703662757));
#14494=CARTESIAN_POINT('Ctrl Pts',(0.359860335496799,-3.05236019973661,
0.0603111453667289));
#14495=CARTESIAN_POINT('Ctrl Pts',(0.455369297438528,-3.04110009777018,
0.0652773627199928));
#14496=CARTESIAN_POINT('Ctrl Pts',(0.550386608294095,-3.02534853439546,
0.070243580073257));
#14497=CARTESIAN_POINT('Ctrl Pts',(0.644460645377193,-3.00517432548596,
0.0752097974265209));
#14498=CARTESIAN_POINT('Ctrl Pts',(0.738529417198413,-2.98500124571365,
0.0801757368238713));
#14499=CARTESIAN_POINT('Ctrl Pts',(0.831654588017938,-2.96040610585117,
0.0851416762212218));
#14500=CARTESIAN_POINT('Ctrl Pts',(0.92339529074792,-2.93150872197655,0.0901076156185723));
#14501=CARTESIAN_POINT('Ctrl Pts',(1.01515633557142,-2.90260493055034,0.0950746561368062));
#14502=CARTESIAN_POINT('Ctrl Pts',(1.10553188114381,-2.86939713383231,0.10004169665504));
#14503=CARTESIAN_POINT('Ctrl Pts',(1.19409783655646,-2.83205448512757,0.105008737173274));
#14504=CARTESIAN_POINT('Ctrl Pts',(1.28275886820376,-2.79467174880209,0.109981109847725));
#14505=CARTESIAN_POINT('Ctrl Pts',(1.36960602534491,-2.75314547478082,0.114953482522177));
#14506=CARTESIAN_POINT('Ctrl Pts',(1.45423707810273,-2.70769214843033,0.119925855196628));
#14507=CARTESIAN_POINT('Ctrl Pts',(1.53892195546335,-2.66220991416533,0.124901390256227));
#14508=CARTESIAN_POINT('Ctrl Pts',(1.62138754456656,-2.61279588348197,0.129876925315825));
#14509=CARTESIAN_POINT('Ctrl Pts',(1.70125981259282,-2.55971039378611,0.134852460375423));
#14510=CARTESIAN_POINT('Ctrl Pts',(1.78125220835393,-2.5065450636176,0.139835478630018));
#14511=CARTESIAN_POINT('Ctrl Pts',(1.85864314528324,-2.44969751742716,0.144818496884613));
#14512=CARTESIAN_POINT('Ctrl Pts',(1.93309117950554,-2.38946871536705,0.149801515139208));
#14513=CARTESIAN_POINT('Ctrl Pts',(1.95449800380548,-2.37215049606194,0.151234334653837));
#14514=CARTESIAN_POINT('Ctrl Pts',(1.97566174365417,-2.35455294918859,0.152667154168466));
#14515=CARTESIAN_POINT('Ctrl Pts',(1.99657486217591,-2.33668377615099,0.154099973683096));
#14516=CARTESIAN_POINT('Ctrl Pts',(2.06861067308952,-2.27513291902838,0.159035359839011));
#14517=CARTESIAN_POINT('Ctrl Pts',(2.13793692587052,-2.21012849622858,0.163970745994926));
#14518=CARTESIAN_POINT('Ctrl Pts',(2.20419808661067,-2.14194141959622,0.168906132150841));
#14519=CARTESIAN_POINT('Ctrl Pts',(2.27282058312028,-2.07132437371387,0.174017399678828));
#14520=CARTESIAN_POINT('Ctrl Pts',(2.33815500896462,-1.99729382004998,0.179128667206816));
#14521=CARTESIAN_POINT('Ctrl Pts',(2.39984250587212,-1.92019743698648,0.184239934734803));
#14522=CARTESIAN_POINT('Ctrl Pts',(2.45926136987769,-1.84593636739824,0.189163229168309));
#14523=CARTESIAN_POINT('Ctrl Pts',(2.51529650561875,-1.76883138580461,0.194086523601816));
#14524=CARTESIAN_POINT('Ctrl Pts',(2.56766478650435,-1.68923053315572,0.199009818035321));
#14525=CARTESIAN_POINT('Ctrl Pts',(2.62000290232932,-1.60967553201286,0.203930276563723));
#14526=CARTESIAN_POINT('Ctrl Pts',(2.66867810976985,-1.52762789052164,0.208850735092124));
#14527=CARTESIAN_POINT('Ctrl Pts',(2.71344918565114,-1.44346657976178,0.213771193620525));
#14528=CARTESIAN_POINT('Ctrl Pts',(2.75820745226931,-1.35932934803849,0.218690244377353));
#14529=CARTESIAN_POINT('Ctrl Pts',(2.79906359485162,-1.2730800467947,0.223609295134181));
#14530=CARTESIAN_POINT('Ctrl Pts',(2.83582177726882,-1.18512324151031,0.228528345891009));
#14531=CARTESIAN_POINT('Ctrl Pts',(2.87258009899405,-1.09716610288277,0.233447415290305));
#14532=CARTESIAN_POINT('Ctrl Pts',(2.90524025808181,-1.00750186476344,0.238366484689601));
#14533=CARTESIAN_POINT('Ctrl Pts',(2.93365459175633,-0.916554955399307,
0.243285554088897));
#14534=CARTESIAN_POINT('Ctrl Pts',(2.96209109854565,-0.825537075648002,
0.248208462082184));
#14535=CARTESIAN_POINT('Ctrl Pts',(2.98627503311865,-0.733234958457678,
0.253131370075472));
#14536=CARTESIAN_POINT('Ctrl Pts',(3.00610882031872,-0.640087502144834,
0.258054278068759));
#14537=CARTESIAN_POINT('Ctrl Pts',(3.02595191484239,-0.546896334890099,
0.262979496215793));
#14538=CARTESIAN_POINT('Ctrl Pts',(3.04144072570293,-0.452859483996052,
0.267904714362827));
#14539=CARTESIAN_POINT('Ctrl Pts',(3.05252927802725,-0.35842329275095,0.272829932509862));
#14540=CARTESIAN_POINT('Ctrl Pts',(3.06363201734979,-0.263866277250587,
0.277761452116186));
#14541=CARTESIAN_POINT('Ctrl Pts',(3.07032323534061,-0.168909351265706,
0.282692971722511));
#14542=CARTESIAN_POINT('Ctrl Pts',(3.07260901440491,-0.0740006391709276,
0.287624491328835));
#14543=CARTESIAN_POINT('Ctrl Pts',(3.07321961317529,-0.0486477326681363,
0.288941845160071));
#14544=CARTESIAN_POINT('Ctrl Pts',(3.07351613553083,-0.0232982459732372,
0.290259198991308));
#14545=CARTESIAN_POINT('Ctrl Pts',(3.07349932342359,0.00203934174087994,
0.291576552822545));
#14546=CARTESIAN_POINT('Ctrl Pts',(3.07648182967171,0.00204132070649662,
0.291576552822545));
#14547=CARTESIAN_POINT('Ctrl Pts',(3.07754652659738,0.136117656503392,0.298540662370786));
#14548=CARTESIAN_POINT('Ctrl Pts',(3.00879647423619,1.28547432247006,0.358294407847086));
#14549=CARTESIAN_POINT('Ctrl Pts',(1.56063394451812,3.27734706691301,0.470837789251445));
#14550=CARTESIAN_POINT('Ctrl Pts',(-0.867537302958989,3.14799344447871,
0.581990140766207));
#14551=CARTESIAN_POINT('Ctrl Pts',(-1.79004208889524,2.50612566616128,0.64035285635291));
#14552=CARTESIAN_POINT('Ctrl Pts',(-1.87460960294492,2.44013607231272,0.645925936011554));
#14553=CARTESIAN_POINT('Origin',(0.,0.,10.));
#14554=CARTESIAN_POINT('',(2.36142200728635,0.872635292378032,18.6688222409353));
#14555=CARTESIAN_POINT('',(2.36142200730535,0.872635292326632,18.9466764589532));
#14556=CARTESIAN_POINT('',(2.36142200728636,0.87263529237802,10.));
#14557=CARTESIAN_POINT('',(1.91346599666504,1.63598720337497,19.));
#14558=CARTESIAN_POINT('Ctrl Pts',(2.36142200732435,0.872635292275214,18.9466764589532));
#14559=CARTESIAN_POINT('Ctrl Pts',(2.31565239500422,0.99649158224678,18.9546790697769));
#14560=CARTESIAN_POINT('Ctrl Pts',(2.26020795009562,1.11655953327844,18.9624334565676));
#14561=CARTESIAN_POINT('Ctrl Pts',(2.13159976529488,1.34580753201374,18.9779049061883));
#14562=CARTESIAN_POINT('Ctrl Pts',(2.05881463877152,1.45471361970388,18.985602132961));
#14563=CARTESIAN_POINT('Ctrl Pts',(1.96587805277887,1.57273895687923,18.9948599363643));
#14564=CARTESIAN_POINT('Ctrl Pts',(1.95367226283063,1.58787562286953,18.9960660351914));
#14565=CARTESIAN_POINT('Ctrl Pts',(1.93624377484013,1.60898389621206,18.9977767766616));
#14566=CARTESIAN_POINT('Ctrl Pts',(1.93116605552455,1.61507485795793,18.9982738626392));
#14567=CARTESIAN_POINT('Ctrl Pts',(1.92188090786595,1.62610643482651,18.9991806156347));
#14568=CARTESIAN_POINT('Ctrl Pts',(1.91768297315338,1.63105498807247,18.9995897567832));
#14569=CARTESIAN_POINT('Ctrl Pts',(1.91346599666504,1.63598720337497,19.));
#14570=CARTESIAN_POINT('',(2.36142200728636,0.87263529237802,19.));
#14571=CARTESIAN_POINT('Origin',(0.,0.,19.));
#14572=CARTESIAN_POINT('',(2.36142200728636,0.87263529237802,20.));
#14573=CARTESIAN_POINT('',(2.36142200728636,0.87263529237802,10.));
#14574=CARTESIAN_POINT('Origin',(0.,0.,20.));
#14575=CARTESIAN_POINT('',(-1.91360951419324,1.63581932901806,18.9999983489143));
#14576=CARTESIAN_POINT('Origin',(0.,0.,19.));
#14577=CARTESIAN_POINT('Ctrl Pts',(-1.91360951419324,1.63581932901806,18.9999983489143));
#14578=CARTESIAN_POINT('Ctrl Pts',(-1.8600938132237,1.6984229140946,18.9947600671717));
#14579=CARTESIAN_POINT('Ctrl Pts',(-1.80340132000449,1.75851618901605,18.9895217854291));
#14580=CARTESIAN_POINT('Ctrl Pts',(-1.74379734202027,1.81575799047204,18.9842835036865));
#14581=CARTESIAN_POINT('Ctrl Pts',(-1.68427750262003,1.87291898785618,18.9790526164438));
#14582=CARTESIAN_POINT('Ctrl Pts',(-1.62185467307349,1.92723618657456,18.9738217292011));
#14583=CARTESIAN_POINT('Ctrl Pts',(-1.55683385998117,1.97840202750001,18.9685908419584));
#14584=CARTESIAN_POINT('Ctrl Pts',(-1.4918868023647,2.02950982914902,18.9633658883015));
#14585=CARTESIAN_POINT('Ctrl Pts',(-1.42434798122953,2.0774730912236,18.9581409346447));
#14586=CARTESIAN_POINT('Ctrl Pts',(-1.35455755196941,2.12202264087889,18.9529159809879));
#14587=CARTESIAN_POINT('Ctrl Pts',(-1.28481020389697,2.1665446903808,18.9476942526617));
#14588=CARTESIAN_POINT('Ctrl Pts',(-1.21281439735469,2.20765696094641,18.9424725243355));
#14589=CARTESIAN_POINT('Ctrl Pts',(-1.13894057102776,2.24513265213149,18.9372507960092));
#14590=CARTESIAN_POINT('Ctrl Pts',(-1.06508967852922,2.28259670914092,18.9320306887473));
#14591=CARTESIAN_POINT('Ctrl Pts',(-0.989362338275737,2.31642621871755,
18.9268105814854));
#14592=CARTESIAN_POINT('Ctrl Pts',(-0.912153717615124,2.34644024970612,
18.9215904742235));
#14593=CARTESIAN_POINT('Ctrl Pts',(-0.834945375056506,2.37645417258549,
18.9163703857641));
#14594=CARTESIAN_POINT('Ctrl Pts',(-0.756256196450567,2.402652477312,18.9111502973048));
#14595=CARTESIAN_POINT('Ctrl Pts',(-0.676500116885295,2.42490285204463,
18.9059302088455));
#14596=CARTESIAN_POINT('Ctrl Pts',(-0.596667246521566,2.44717464989699,
18.9007050943773));
#14597=CARTESIAN_POINT('Ctrl Pts',(-0.515765872187058,2.46549080080498,
18.8954799799091));
#14598=CARTESIAN_POINT('Ctrl Pts',(-0.434223277835914,2.47976942375404,
18.890254865441));
#14599=CARTESIAN_POINT('Ctrl Pts',(-0.352641288274004,2.49405494505316,
18.8850272265929));
#14600=CARTESIAN_POINT('Ctrl Pts',(-0.270417923313533,2.50429899596022,
18.8797995877449));
#14601=CARTESIAN_POINT('Ctrl Pts',(-0.187986351410114,2.5104715456829,18.8745719488968));
#14602=CARTESIAN_POINT('Ctrl Pts',(-0.105413386187175,2.51665468306364,
18.8693353431785));
#14603=CARTESIAN_POINT('Ctrl Pts',(-0.0226319659163586,2.51875235648336,
18.8640987374602));
#14604=CARTESIAN_POINT('Ctrl Pts',(0.0599242294916328,2.51678670862666,
18.8588621317418));
#14605=CARTESIAN_POINT('Ctrl Pts',(0.128041006268894,2.51516486067672,18.8545414299336));
#14606=CARTESIAN_POINT('Ctrl Pts',(0.196004367846044,2.51077775312145,18.8502207281253));
#14607=CARTESIAN_POINT('Ctrl Pts',(0.263574962959677,2.50366421248953,18.845900026317));
#14608=CARTESIAN_POINT('Ctrl Pts',(0.345901422450609,2.49499723813942,18.8406357825761));
#14609=CARTESIAN_POINT('Ctrl Pts',(0.427945987928208,2.48224996490047,18.8353715388353));
#14610=CARTESIAN_POINT('Ctrl Pts',(0.509273644888992,2.4654505885581,18.8301072950944));
#14611=CARTESIAN_POINT('Ctrl Pts',(0.590489053101737,2.44867439878021,18.8248503170832));
#14612=CARTESIAN_POINT('Ctrl Pts',(0.670989071903334,2.4278573082844,18.819593339072));
#14613=CARTESIAN_POINT('Ctrl Pts',(0.750344228463646,2.40307923065622,18.8143363610608));
#14614=CARTESIAN_POINT('Ctrl Pts',(0.830100521369724,2.37817590108544,18.8090528092888));
#14615=CARTESIAN_POINT('Ctrl Pts',(0.908699876890739,2.34927147444271,18.8037692575168));
#14616=CARTESIAN_POINT('Ctrl Pts',(0.985717073963406,2.31649910427287,18.7984857057448));
#14617=CARTESIAN_POINT('Ctrl Pts',(1.06221586746298,2.2839473252754,18.793237717616));
#14618=CARTESIAN_POINT('Ctrl Pts',(1.13715330866122,2.24757969720965,18.7879897294872));
#14619=CARTESIAN_POINT('Ctrl Pts',(1.21012998151385,2.20757597328864,18.7827417413584));
#14620=CARTESIAN_POINT('Ctrl Pts',(1.28308439897037,2.16758444913896,18.777495353687));
#14621=CARTESIAN_POINT('Ctrl Pts',(1.35407883312648,2.12395925246732,18.7722489660156));
#14622=CARTESIAN_POINT('Ctrl Pts',(1.42273781237011,2.07692642316773,18.7670025783441));
#14623=CARTESIAN_POINT('Ctrl Pts',(1.49139635411015,2.02989389356721,18.7617562241033));
#14624=CARTESIAN_POINT('Ctrl Pts',(1.55771909206239,1.97945403520153,18.7565098698626));
#14625=CARTESIAN_POINT('Ctrl Pts',(1.6213600736698,1.92587584270364,18.7512635156218));
#14626=CARTESIAN_POINT('Ctrl Pts',(1.68578564307139,1.87163711991841,18.745952482531));
#14627=CARTESIAN_POINT('Ctrl Pts',(1.74746249947729,1.81418244866758,18.7406414494403));
#14628=CARTESIAN_POINT('Ctrl Pts',(1.80606817423016,1.75383123476374,18.7353304163495));
#14629=CARTESIAN_POINT('Ctrl Pts',(1.86404498763655,1.69412761251034,18.7300763726789));
#14630=CARTESIAN_POINT('Ctrl Pts',(1.91901595311641,1.63158970209983,18.7248223290083));
#14631=CARTESIAN_POINT('Ctrl Pts',(1.97070894874087,1.56656071996991,18.7195682853376));
#14632=CARTESIAN_POINT('Ctrl Pts',(2.02324299766552,1.50047370590806,18.7142287575368));
#14633=CARTESIAN_POINT('Ctrl Pts',(2.07239117086506,1.43181423934472,18.708889229736));
#14634=CARTESIAN_POINT('Ctrl Pts',(2.11791422955211,1.36097228710239,18.7035497019352));
#14635=CARTESIAN_POINT('Ctrl Pts',(2.16343728823915,1.29013033486007,18.6982101741343));
#14636=CARTESIAN_POINT('Ctrl Pts',(2.20533504378927,1.21710635501938,18.6928706463335));
#14637=CARTESIAN_POINT('Ctrl Pts',(2.24341832330765,1.14231365073149,18.6875311185327));
#14638=CARTESIAN_POINT('Ctrl Pts',(2.2832324761903,1.06412164099167,18.6819489108323));
#14639=CARTESIAN_POINT('Ctrl Pts',(2.31901070827217,0.98373642613171,18.6763667031319));
#14640=CARTESIAN_POINT('Ctrl Pts',(2.3505213598588,0.901585041384082,18.6707844954316));
#14641=CARTESIAN_POINT('Ctrl Pts',(2.35421356200506,0.891959105270082,18.6701304105995));
#14642=CARTESIAN_POINT('Ctrl Pts',(2.3578472220091,0.882308951807992,18.6694763257674));
#14643=CARTESIAN_POINT('Ctrl Pts',(2.36142200728635,0.872635292378032,18.6688222409353));
#14644=CARTESIAN_POINT('Origin',(0.,0.,10.));
#14645=CARTESIAN_POINT('',(2.36142200245778,0.872635305444532,17.6666805052528));
#14646=CARTESIAN_POINT('',(2.36142200728635,0.872635292378034,17.9438262109491));
#14647=CARTESIAN_POINT('',(2.36142200728636,0.87263529237802,10.));
#14648=CARTESIAN_POINT('',(2.51749787287094,-0.00327262742782446,18.8874150286091));
#14649=CARTESIAN_POINT('Ctrl Pts',(2.36142200728635,0.872635292378034,17.9438262109491));
#14650=CARTESIAN_POINT('Ctrl Pts',(2.33264089115126,0.950519331253507,17.9490650608475));
#14651=CARTESIAN_POINT('Ctrl Pts',(2.2999848229152,1.02702598391504,17.9543039107459));
#14652=CARTESIAN_POINT('Ctrl Pts',(2.26361541332485,1.10174929569216,17.9595427606443));
#14653=CARTESIAN_POINT('Ctrl Pts',(2.22725452555323,1.17645509883978,17.9647803830131));
#14654=CARTESIAN_POINT('Ctrl Pts',(2.18718222668459,1.24937797670333,17.9700180053818));
#14655=CARTESIAN_POINT('Ctrl Pts',(2.14360739219153,1.32013393189548,17.9752556277506));
#14656=CARTESIAN_POINT('Ctrl Pts',(2.10002963900747,1.39089462640042,17.9804936009411));
#14657=CARTESIAN_POINT('Ctrl Pts',(2.05294912741505,1.45948771806852,17.9857315741316));
#14658=CARTESIAN_POINT('Ctrl Pts',(2.00261888863162,1.52555689402128,17.9909695473222));
#14659=CARTESIAN_POINT('Ctrl Pts',(1.95223681038431,1.59169412032992,17.9962129155541));
#14660=CARTESIAN_POINT('Ctrl Pts',(1.89859860128339,1.65530187235901,18.0014562837861));
#14661=CARTESIAN_POINT('Ctrl Pts',(1.84199822589728,1.71605617209673,18.006699652018));
#14662=CARTESIAN_POINT('Ctrl Pts',(1.78536754283389,1.77684300380438,18.0119458279047));
#14663=CARTESIAN_POINT('Ctrl Pts',(1.72577186567806,1.83477301881369,18.0171920037913));
#14664=CARTESIAN_POINT('Ctrl Pts',(1.66354099252487,1.88956016474453,18.022438179678));
#14665=CARTESIAN_POINT('Ctrl Pts',(1.60120331408269,1.94444134048175,18.027693359445));
#14666=CARTESIAN_POINT('Ctrl Pts',(1.53622176737099,1.99616858588041,18.0329485392119));
#14667=CARTESIAN_POINT('Ctrl Pts',(1.46895787176047,2.04449725384823,18.0382037189789));
#14668=CARTESIAN_POINT('Ctrl Pts',(1.41953954591432,2.08000399694817,18.0420646637509));
#14669=CARTESIAN_POINT('Ctrl Pts',(1.36888992101459,2.11367715937145,18.0459256085229));
#14670=CARTESIAN_POINT('Ctrl Pts',(1.31716077966232,2.14543555729818,18.049786553295));
#14671=CARTESIAN_POINT('Ctrl Pts',(1.24673044471657,2.18867529692748,18.0550433123749));
#14672=CARTESIAN_POINT('Ctrl Pts',(1.17403926396638,2.22852266631261,18.0603000714548));
#14673=CARTESIAN_POINT('Ctrl Pts',(1.09944747821751,2.26473430950325,18.0655568305348));
#14674=CARTESIAN_POINT('Ctrl Pts',(1.02496115897755,2.30089475247726,18.0708061569997));
#14675=CARTESIAN_POINT('Ctrl Pts',(0.948579983971734,2.33342948049938,18.0760554834646));
#14676=CARTESIAN_POINT('Ctrl Pts',(0.87069149526328,2.36213940530109,18.0813048099295));
#14677=CARTESIAN_POINT('Ctrl Pts',(0.79226710456764,2.39104686514307,18.0865902537274));
#14678=CARTESIAN_POINT('Ctrl Pts',(0.712314978667257,2.41607643120506,18.0918756975253));
#14679=CARTESIAN_POINT('Ctrl Pts',(0.631254210649159,2.43707291059125,18.0971611413232));
#14680=CARTESIAN_POINT('Ctrl Pts',(0.550890606996052,2.45788880943798,18.1024011275815));
#14681=CARTESIAN_POINT('Ctrl Pts',(0.469437811902277,2.47474061061156,18.1076411138399));
#14682=CARTESIAN_POINT('Ctrl Pts',(0.387320725466731,2.48752666430411,18.1128811000982));
#14683=CARTESIAN_POINT('Ctrl Pts',(0.305230502026731,2.50030853528976,18.1181193721978));
#14684=CARTESIAN_POINT('Ctrl Pts',(0.222476874103383,2.50902722947594,18.1233576442973));
#14685=CARTESIAN_POINT('Ctrl Pts',(0.139494101629973,2.51363236086951,18.1285959163968));
#14686=CARTESIAN_POINT('Ctrl Pts',(0.0565134860927702,2.51823737256385,
18.1338340523401));
#14687=CARTESIAN_POINT('Ctrl Pts',(-0.0266958016974763,2.51872900954754,
18.1390721882835));
#14688=CARTESIAN_POINT('Ctrl Pts',(-0.109696611036355,2.5151089247838,18.1443103242268));
#14689=CARTESIAN_POINT('Ctrl Pts',(-0.194001379126069,2.51143196778901,
18.1496307522978));
#14690=CARTESIAN_POINT('Ctrl Pts',(-0.278090571199433,2.5035129838956,18.1549511803689));
#14691=CARTESIAN_POINT('Ctrl Pts',(-0.36151034579989,2.49140854134356,18.1602716084399));
#14692=CARTESIAN_POINT('Ctrl Pts',(-0.443757757009223,2.47947421199772,
18.1655172643705));
#14693=CARTESIAN_POINT('Ctrl Pts',(-0.525354000224621,2.4634714718566,18.1707629203012));
#14694=CARTESIAN_POINT('Ctrl Pts',(-0.605875105640386,2.44350600702459,
18.1760085762319));
#14695=CARTESIAN_POINT('Ctrl Pts',(-0.688117845721868,2.42311365738773,
18.1813663903731));
#14696=CARTESIAN_POINT('Ctrl Pts',(-0.769238453549124,2.39858731570485,
18.1867242045143));
#14697=CARTESIAN_POINT('Ctrl Pts',(-0.848804130873332,2.37009236052361,
18.1920820186555));
#14698=CARTESIAN_POINT('Ctrl Pts',(-0.928369808197552,2.34159740534236,
18.1974398327967));
#14699=CARTESIAN_POINT('Ctrl Pts',(-1.00638011389758,2.30913409197741,18.2027976469379));
#14700=CARTESIAN_POINT('Ctrl Pts',(-1.08242824839124,2.27291780253591,18.2081554610792));
#14701=CARTESIAN_POINT('Ctrl Pts',(-1.15691530191002,2.23744494435415,18.2134032924867));
#14702=CARTESIAN_POINT('Ctrl Pts',(-1.22979665503187,2.19823998620112,18.2186511238942));
#14703=CARTESIAN_POINT('Ctrl Pts',(-1.30067285720552,2.15547126367503,18.2238989553018));
#14704=CARTESIAN_POINT('Ctrl Pts',(-1.3714481990332,2.1127634031593,18.2291393187853));
#14705=CARTESIAN_POINT('Ctrl Pts',(-1.44022366427724,2.06650208784539,18.2343796822688));
#14706=CARTESIAN_POINT('Ctrl Pts',(-1.50662195862707,2.01690270558169,18.2396200457524));
#14707=CARTESIAN_POINT('Ctrl Pts',(-1.57361978096847,1.96685547720503,18.244907725882));
#14708=CARTESIAN_POINT('Ctrl Pts',(-1.63819684952987,1.91340979165176,18.2501954060116));
#14709=CARTESIAN_POINT('Ctrl Pts',(-1.69999317353582,1.85683318042618,18.2554830861412));
#14710=CARTESIAN_POINT('Ctrl Pts',(-1.76112710793961,1.80086300914027,18.260714088072));
#14711=CARTESIAN_POINT('Ctrl Pts',(-1.81953927606449,1.74182903057646,18.2659450900029));
#14712=CARTESIAN_POINT('Ctrl Pts',(-1.87491370595946,1.68003120364039,18.2711760919337));
#14713=CARTESIAN_POINT('Ctrl Pts',(-1.93027011185859,1.61825349147168,18.2764053912094));
#14714=CARTESIAN_POINT('Ctrl Pts',(-1.98259043442758,1.55371406188586,18.281634690485));
#14715=CARTESIAN_POINT('Ctrl Pts',(-2.03159657928035,1.48674866371434,18.2868639897607));
#14716=CARTESIAN_POINT('Ctrl Pts',(-2.08060166653038,1.41978471072462,18.2920931761828));
#14717=CARTESIAN_POINT('Ctrl Pts',(-2.12629244576203,1.35039526739066,18.2973223626048));
#14718=CARTESIAN_POINT('Ctrl Pts',(-2.16843289020646,1.27894685216816,18.3025515490269));
#14719=CARTESIAN_POINT('Ctrl Pts',(-2.21139437029597,1.20610638481011,18.3078826173466));
#14720=CARTESIAN_POINT('Ctrl Pts',(-2.25066543593152,1.13112628537219,18.3132136856663));
#14721=CARTESIAN_POINT('Ctrl Pts',(-2.28604494139125,1.05442153617018,18.318544753986));
#14722=CARTESIAN_POINT('Ctrl Pts',(-2.32079919680567,0.979072364082393,
18.3237816081366));
#14723=CARTESIAN_POINT('Ctrl Pts',(-2.35179821306474,0.902059468043717,
18.3290184622873));
#14724=CARTESIAN_POINT('Ctrl Pts',(-2.37890060185484,0.823794984504448,
18.3342553164379));
#14725=CARTESIAN_POINT('Ctrl Pts',(-2.40673437315984,0.743418462973202,
18.3396334918421));
#14726=CARTESIAN_POINT('Ctrl Pts',(-2.4304580292705,0.661722333881856,18.3450116672464));
#14727=CARTESIAN_POINT('Ctrl Pts',(-2.44997408672011,0.579165973102676,
18.3503898426506));
#14728=CARTESIAN_POINT('Ctrl Pts',(-2.46949014416972,0.496609612323496,
18.3557680180548));
#14729=CARTESIAN_POINT('Ctrl Pts',(-2.48479857801772,0.413193544991591,
18.361146193459));
#14730=CARTESIAN_POINT('Ctrl Pts',(-2.49585925389778,0.329382505201515,
18.3665243688632));
#14731=CARTESIAN_POINT('Ctrl Pts',(-2.50668767148743,0.247331376743258,
18.3717896103167));
#14732=CARTESIAN_POINT('Ctrl Pts',(-2.51348535610504,0.164596633023612,
18.3770548517702));
#14733=CARTESIAN_POINT('Ctrl Pts',(-2.51617695364797,0.0816075237390802,
18.3823200932237));
#14734=CARTESIAN_POINT('Ctrl Pts',(-2.51886472713688,-0.00126367979163271,
18.3875778541503));
#14735=CARTESIAN_POINT('Ctrl Pts',(-2.51745798731002,-0.0843880754561358,
18.3928356150769));
#14736=CARTESIAN_POINT('Ctrl Pts',(-2.51193293504969,-0.167329554510471,
18.3980933760035));
#14737=CARTESIAN_POINT('Ctrl Pts',(-2.50638101469612,-0.250674374435956,
18.403376705197));
#14738=CARTESIAN_POINT('Ctrl Pts',(-2.49667055461409,-0.333834027997151,
18.4086600343905));
#14739=CARTESIAN_POINT('Ctrl Pts',(-2.48283047278443,-0.416364135598939,
18.413943363584));
#14740=CARTESIAN_POINT('Ctrl Pts',(-2.46908230145528,-0.498346169599006,
18.4191916067544));
#14741=CARTESIAN_POINT('Ctrl Pts',(-2.45125926710657,-0.579706534825325,
18.4244398499249));
#14742=CARTESIAN_POINT('Ctrl Pts',(-2.42944167002257,-0.660014713440488,
18.4296880930953));
#14743=CARTESIAN_POINT('Ctrl Pts',(-2.40763155202069,-0.740295362375832,
18.4349345371656));
#14744=CARTESIAN_POINT('Ctrl Pts',(-2.38182971157803,-0.81952409805105,
18.4401809812359));
#14745=CARTESIAN_POINT('Ctrl Pts',(-2.35216708556151,-0.897282704392028,
18.4454274253062));
#14746=CARTESIAN_POINT('Ctrl Pts',(-2.322505770802,-0.975037873359741,18.4506736374538));
#14747=CARTESIAN_POINT('Ctrl Pts',(-2.28898417448708,-1.05132261320712,
18.4559198496013));
#14748=CARTESIAN_POINT('Ctrl Pts',(-2.2517819549871,-1.12573721498157,18.4611660617489));
#14749=CARTESIAN_POINT('Ctrl Pts',(-2.21412313610845,-1.20106514024561,
18.4664766629905));
#14750=CARTESIAN_POINT('Ctrl Pts',(-2.17269292696622,-1.27447626811301,
18.471787264232));
#14751=CARTESIAN_POINT('Ctrl Pts',(-2.12772552152618,-1.34558179054495,
18.4770978654736));
#14752=CARTESIAN_POINT('Ctrl Pts',(-2.08324233497737,-1.41592163310507,
18.4823512809954));
#14753=CARTESIAN_POINT('Ctrl Pts',(-2.03529808117403,-1.48400493984633,
18.4876046965172));
#14754=CARTESIAN_POINT('Ctrl Pts',(-1.98416200106852,-1.54948617403182,
18.492858112039));
#14755=CARTESIAN_POINT('Ctrl Pts',(-1.93219096315314,-1.61603659591747,
18.4981973061404));
#14756=CARTESIAN_POINT('Ctrl Pts',(-1.87692325468778,-1.67989883468787,
18.5035365002418));
#14757=CARTESIAN_POINT('Ctrl Pts',(-1.81868142999892,-1.74074814553314,
18.5088756943432));
#14758=CARTESIAN_POINT('Ctrl Pts',(-1.76043960531006,-1.80159745637843,
18.5142148884447));
#14759=CARTESIAN_POINT('Ctrl Pts',(-1.69922406428985,-1.85943354653535,
18.5195540825461));
#14760=CARTESIAN_POINT('Ctrl Pts',(-1.63539194646763,-1.91397477293428,
18.5248932766475));
#14761=CARTESIAN_POINT('Ctrl Pts',(-1.5724748745046,-1.96773414021472,18.5301559323601));
#14762=CARTESIAN_POINT('Ctrl Pts',(-1.50679150832135,-2.01848415799354,
18.5354185880727));
#14763=CARTESIAN_POINT('Ctrl Pts',(-1.43866120240419,-2.06592840986733,
18.5406812437853));
#14764=CARTESIAN_POINT('Ctrl Pts',(-1.37062575312898,-2.11330660593302,
18.5459365723937));
#14765=CARTESIAN_POINT('Ctrl Pts',(-1.30015050609536,-2.15738791838507,
18.5511919010021));
#14766=CARTESIAN_POINT('Ctrl Pts',(-1.22758857361836,-2.19791549972278,
18.5564472296105));
#14767=CARTESIAN_POINT('Ctrl Pts',(-1.15463136774808,-2.23866385074027,
18.5617311860614));
#14768=CARTESIAN_POINT('Ctrl Pts',(-1.07956502959159,-2.27581932701635,
18.5670151425123));
#14769=CARTESIAN_POINT('Ctrl Pts',(-1.00277889174594,-2.30916451217075,
18.5722990989632));
#14770=CARTESIAN_POINT('Ctrl Pts',(-0.926541476321039,-2.34227140886279,
18.577545295664));
#14771=CARTESIAN_POINT('Ctrl Pts',(-0.848609189515541,-2.3716221112681,
18.5827914923648));
#14772=CARTESIAN_POINT('Ctrl Pts',(-0.769387001676135,-2.39705024804484,
18.5880376890656));
#14773=CARTESIAN_POINT('Ctrl Pts',(-0.690189743594728,-2.42247038305699,
18.5932822348852));
#14774=CARTESIAN_POINT('Ctrl Pts',(-0.609703828204644,-2.44397026379184,
18.5985267807049));
#14775=CARTESIAN_POINT('Ctrl Pts',(-0.528351380128789,-2.46143272691252,
18.6037713265246));
#14776=CARTESIAN_POINT('Ctrl Pts',(-0.447000207173294,-2.4788949163261,
18.6090157901411));
#14777=CARTESIAN_POINT('Ctrl Pts',(-0.364782978333853,-2.49231971854964,
18.6142602537577));
#14778=CARTESIAN_POINT('Ctrl Pts',(-0.282132717401159,-2.50164093741924,
18.6195047173742));
#14779=CARTESIAN_POINT('Ctrl Pts',(-0.198400428870973,-2.51108418634593,
18.624817839629));
#14780=CARTESIAN_POINT('Ctrl Pts',(-0.114224166418886,-2.51631555418445,
18.6301309618838));
#14781=CARTESIAN_POINT('Ctrl Pts',(-0.0300584464804562,-2.51732054768462,
18.6354440841385));
#14782=CARTESIAN_POINT('Ctrl Pts',(0.0531397919727716,-2.51831398882588,
18.6406961322718));
#14783=CARTESIAN_POINT('Ctrl Pts',(0.136327266117714,-2.51517779919644,
18.645948180405));
#14784=CARTESIAN_POINT('Ctrl Pts',(0.219067828737113,-2.50795046530278,
18.6512002285383));
#14785=CARTESIAN_POINT('Ctrl Pts',(0.303251630370289,-2.50059706542755,
18.6565438878538));
#14786=CARTESIAN_POINT('Ctrl Pts',(0.386972287484825,-2.48900850579982,
18.6618875471694));
#14787=CARTESIAN_POINT('Ctrl Pts',(0.469780780888515,-2.4732796582489,18.6672312064849));
#14788=CARTESIAN_POINT('Ctrl Pts',(0.552589274292217,-2.45755081069797,
18.6725748658005));
#14789=CARTESIAN_POINT('Ctrl Pts',(0.634485138727603,-2.43768185432414,
18.6779185251161));
#14790=CARTESIAN_POINT('Ctrl Pts',(0.715036925982957,-2.4138203007848,18.6832621844316));
#14791=CARTESIAN_POINT('Ctrl Pts',(0.793401155857259,-2.39060675915616,
18.6884607251623));
#14792=CARTESIAN_POINT('Ctrl Pts',(0.870796489168577,-2.36352475954149,
18.693659265893));
#14793=CARTESIAN_POINT('Ctrl Pts',(0.946807723733528,-2.33267258402857,
18.6988578066236));
#14794=CARTESIAN_POINT('Ctrl Pts',(1.02270947544916,-2.3018648464741,18.7040488596315));
#14795=CARTESIAN_POINT('Ctrl Pts',(1.0972306524512,-2.2672978882898,18.7092399126394));
#14796=CARTESIAN_POINT('Ctrl Pts',(1.16997007122369,-2.22912006909472,18.7144309656473));
#14797=CARTESIAN_POINT('Ctrl Pts',(1.24423617918151,-2.19014095584659,18.719730970921));
#14798=CARTESIAN_POINT('Ctrl Pts',(1.31664440076205,-2.14739780935237,18.7250309761947));
#14799=CARTESIAN_POINT('Ctrl Pts',(1.38678828785133,-2.1011007816567,18.7303309814684));
#14800=CARTESIAN_POINT('Ctrl Pts',(1.45536987689799,-2.05583491660041,18.7355129409906));
#14801=CARTESIAN_POINT('Ctrl Pts',(1.52178654142308,-2.00717212042383,18.7406949005128));
#14802=CARTESIAN_POINT('Ctrl Pts',(1.58568414928241,-1.95535470662346,18.745876860035));
#14803=CARTESIAN_POINT('Ctrl Pts',(1.64956311077339,-1.90355241399299,18.7510573073765));
#14804=CARTESIAN_POINT('Ctrl Pts',(1.71092410785923,-1.84859762784992,18.756237754718));
#14805=CARTESIAN_POINT('Ctrl Pts',(1.76944477290446,-1.79077397949632,18.7614182020596));
#14806=CARTESIAN_POINT('Ctrl Pts',(1.82796693099788,-1.73294885587763,18.7665987815708));
#14807=CARTESIAN_POINT('Ctrl Pts',(1.88364827803949,-1.67225505749713,18.771779361082));
#14808=CARTESIAN_POINT('Ctrl Pts',(1.93620323103858,-1.60901314417122,18.7769599405932));
#14809=CARTESIAN_POINT('Ctrl Pts',(1.99087519271403,-1.54322373205442,18.7823492032284));
#14810=CARTESIAN_POINT('Ctrl Pts',(2.04216318445828,-1.47467698774535,18.7877384658637));
#14811=CARTESIAN_POINT('Ctrl Pts',(2.08979333702531,-1.403769945014,18.7931277284989));
#14812=CARTESIAN_POINT('Ctrl Pts',(2.135656399308,-1.33549357087281,18.7983170481751));
#14813=CARTESIAN_POINT('Ctrl Pts',(2.17812806476868,-1.26502939632748,18.8035063678513));
#14814=CARTESIAN_POINT('Ctrl Pts',(2.21701030897764,-1.19275795528132,18.8086956875275));
#14815=CARTESIAN_POINT('Ctrl Pts',(2.25592432173553,-1.12042746520499,18.8138892471122));
#14816=CARTESIAN_POINT('Ctrl Pts',(2.29124288223879,-1.04628719853895,18.8190828066968));
#14817=CARTESIAN_POINT('Ctrl Pts',(2.32281609350656,-0.970737681223372,
18.8242763662815));
#14818=CARTESIAN_POINT('Ctrl Pts',(2.35444365066132,-0.895058123111655,
18.8294788653624));
#14819=CARTESIAN_POINT('Ctrl Pts',(2.38231285023912,-0.817964920789799,
18.8346813644433));
#14820=CARTESIAN_POINT('Ctrl Pts',(2.40632380071148,-0.739872972968649,
18.8398838635241));
#14821=CARTESIAN_POINT('Ctrl Pts',(2.4090117795033,-0.731130732639723,18.840466273088));
#14822=CARTESIAN_POINT('Ctrl Pts',(2.41165145841306,-0.722375984062057,
18.841048682652));
#14823=CARTESIAN_POINT('Ctrl Pts',(2.41424273752183,-0.713609314907739,
18.8416310922159));
#14824=CARTESIAN_POINT('Ctrl Pts',(2.44544639966121,-0.608042847191675,
18.848644351111));
#14825=CARTESIAN_POINT('Ctrl Pts',(2.46972564711354,-0.50041571271031,18.855657610006));
#14826=CARTESIAN_POINT('Ctrl Pts',(2.48687075747628,-0.391510007036009,
18.8626708689011));
#14827=CARTESIAN_POINT('Ctrl Pts',(2.50358555430506,-0.285337652042246,
18.8695081067526));
#14828=CARTESIAN_POINT('Ctrl Pts',(2.51351991815498,-0.177949699224724,
18.876345344604));
#14829=CARTESIAN_POINT('Ctrl Pts',(2.51652405256726,-0.0700923879638654,
18.8831825824554));
#14830=CARTESIAN_POINT('Ctrl Pts',(2.51714393432919,-0.0478367991762561,
18.88459339784));
#14831=CARTESIAN_POINT('Ctrl Pts',(2.51746889864049,-0.0255613129373036,
18.8860042132245));
#14832=CARTESIAN_POINT('Ctrl Pts',(2.51749787287094,-0.00327262742782446,
18.8874150286091));
#14833=CARTESIAN_POINT('Ctrl Pts',(2.5174977918681,-0.00333435739759424,
18.8883467778039));
#14834=CARTESIAN_POINT('Ctrl Pts',(2.51765838212971,0.117914081443941,18.8967380675264));
#14835=CARTESIAN_POINT('Ctrl Pts',(2.50905949712985,0.239027813720937,18.9050106031213));
#14836=CARTESIAN_POINT('Ctrl Pts',(2.4843513699158,0.410492998213102,18.916492485084));
#14837=CARTESIAN_POINT('Ctrl Pts',(2.4753494131927,0.461684008912046,18.9198922662718));
#14838=CARTESIAN_POINT('Ctrl Pts',(2.46095346766611,0.530910030959187,18.9244560997678));
#14839=CARTESIAN_POINT('Ctrl Pts',(2.45693322385993,0.549214523906593,18.9256596523586));
#14840=CARTESIAN_POINT('Ctrl Pts',(2.44967583322526,0.58058213555707,18.9277171463199));
#14841=CARTESIAN_POINT('Ctrl Pts',(2.44653768751871,0.593667127329751,18.9285739324056));
#14842=CARTESIAN_POINT('Ctrl Pts',(2.44005564336439,0.619770394269378,18.9302804135346));
#14843=CARTESIAN_POINT('Ctrl Pts',(2.43671210086245,0.632788299594441,18.9311300876594));
#14844=CARTESIAN_POINT('Ctrl Pts',(2.4298915001758,0.658487997445961,18.9328051096885));
#14845=CARTESIAN_POINT('Ctrl Pts',(2.42641901716019,0.671170550557235,18.9336305591408));
#14846=CARTESIAN_POINT('Ctrl Pts',(2.4177027392349,0.702053006102434,18.9356381287255));
#14847=CARTESIAN_POINT('Ctrl Pts',(2.41235257431326,0.720222217601793,18.9368171788481));
#14848=CARTESIAN_POINT('Ctrl Pts',(2.39320910069792,0.782625872440048,18.9408614814428));
#14849=CARTESIAN_POINT('Ctrl Pts',(2.37839963254998,0.826540131713007,18.9436981953647));
#14850=CARTESIAN_POINT('Ctrl Pts',(2.36206508692986,0.870893585294821,18.9465639241001));
#14851=CARTESIAN_POINT('Ctrl Pts',(2.3617437862239,0.871764532426716,18.9466201973601));
#14852=CARTESIAN_POINT('Ctrl Pts',(2.36142200732435,0.872635292275211,18.9466764589532));
#14853=CARTESIAN_POINT('',(2.51749995481779,0.000475351647371232,18.6124102744318));
#14854=CARTESIAN_POINT('Ctrl Pts',(2.36142200728635,0.872635292378032,18.6688222409353));
#14855=CARTESIAN_POINT('Ctrl Pts',(2.39182664777468,0.790357864682992,18.6632590496871));
#14856=CARTESIAN_POINT('Ctrl Pts',(2.41796845445713,0.706378112618749,18.6576958584389));
#14857=CARTESIAN_POINT('Ctrl Pts',(2.43966855119106,0.621147011849314,18.6521326671906));
#14858=CARTESIAN_POINT('Ctrl Pts',(2.46132648786374,0.53608150243519,18.6465802843958));
#14859=CARTESIAN_POINT('Ctrl Pts',(2.47855979566509,0.449769843114856,18.6410279016009));
#14860=CARTESIAN_POINT('Ctrl Pts',(2.49123848450133,0.362680387310241,18.6354755188061));
#14861=CARTESIAN_POINT('Ctrl Pts',(2.50388458458775,0.2758147824514,18.6299374076143));
#14862=CARTESIAN_POINT('Ctrl Pts',(2.51199933246258,0.188175732793444,18.6243992964224));
#14863=CARTESIAN_POINT('Ctrl Pts',(2.51550346002756,0.10024266850695,18.6188611852306));
#14864=CARTESIAN_POINT('Ctrl Pts',(2.51682752769016,0.0670163304993951,
18.6167685576635));
#14865=CARTESIAN_POINT('Ctrl Pts',(2.51749381825413,0.0337481357832397,
18.6146759300965));
#14866=CARTESIAN_POINT('Ctrl Pts',(2.51749995717886,0.000464332231146367,
18.6125833025294));
#14867=CARTESIAN_POINT('Ctrl Pts',(2.5174999250055,0.000614489468989278,
18.6102255169021));
#14868=CARTESIAN_POINT('Ctrl Pts',(2.51750215682766,-0.00852905554551879,
18.6096432037694));
#14869=CARTESIAN_POINT('Ctrl Pts',(2.51745457472059,-0.0176726609456453,
18.6090624523556));
#14870=CARTESIAN_POINT('Ctrl Pts',(2.51724081692323,-0.0377392730921901,
18.6077912985835));
#14871=CARTESIAN_POINT('Ctrl Pts',(2.51705335857769,-0.0486618879025092,
18.6071015767941));
#14872=CARTESIAN_POINT('Ctrl Pts',(2.51652321895366,-0.0710550350449813,
18.6056918967218));
#14873=CARTESIAN_POINT('Ctrl Pts',(2.51617319279684,-0.0825251503035088,
18.6049721848102));
#14874=CARTESIAN_POINT('Ctrl Pts',(2.51517505996313,-0.1092405163893,18.6033011595809));
#14875=CARTESIAN_POINT('Ctrl Pts',(2.51446674850497,-0.124483169890081,
18.6023517496857));
#14876=CARTESIAN_POINT('Ctrl Pts',(2.51179270181138,-0.172590805891551,
18.5993672322175));
#14877=CARTESIAN_POINT('Ctrl Pts',(2.50932080267067,-0.205424990720745,
18.5973479059267));
#14878=CARTESIAN_POINT('Ctrl Pts',(2.50294237901877,-0.272534459338966,
18.5932509609013));
#14879=CARTESIAN_POINT('Ctrl Pts',(2.49897407636564,-0.306796851110074,
18.5911755754704));
#14880=CARTESIAN_POINT('Ctrl Pts',(2.47388169562043,-0.49035655441772,18.5801220371626));
#14881=CARTESIAN_POINT('Ctrl Pts',(2.44008132633024,-0.637610747818397,
18.5715104264123));
#14882=CARTESIAN_POINT('Ctrl Pts',(2.34828874984688,-0.918914003074701,
18.554520694451));
#14883=CARTESIAN_POINT('Ctrl Pts',(2.29143671601587,-1.05269615862231,18.5461696239991));
#14884=CARTESIAN_POINT('Ctrl Pts',(2.21484386812655,-1.19691481828407,18.5360963819896));
#14885=CARTESIAN_POINT('Ctrl Pts',(2.20612073906994,-1.21291783819977,18.5349627942739));
#14886=CARTESIAN_POINT('Ctrl Pts',(2.19309766363557,-1.23620402197328,18.5332879029808));
#14887=CARTESIAN_POINT('Ctrl Pts',(2.18893332199568,-1.24356288667622,18.5327548497083));
#14888=CARTESIAN_POINT('Ctrl Pts',(2.18150138742202,-1.25654296434937,18.5318076962865));
#14889=CARTESIAN_POINT('Ctrl Pts',(2.17824898891568,-1.2621726763102,18.5313945655384));
#14890=CARTESIAN_POINT('Ctrl Pts',(2.17115908911866,-1.27433585449356,18.5304968911937));
#14891=CARTESIAN_POINT('Ctrl Pts',(2.16731392855611,-1.28086454857782,18.5300118764737));
#14892=CARTESIAN_POINT('Ctrl Pts',(2.15663661342312,-1.29880781465307,18.5286703027629));
#14893=CARTESIAN_POINT('Ctrl Pts',(2.14974347720989,-1.3101855539294,18.5278100006524));
#14894=CARTESIAN_POINT('Ctrl Pts',(2.11236129470614,-1.37079894464956,18.5231773356763));
#14895=CARTESIAN_POINT('Ctrl Pts',(2.08027262538127,-1.41902242933382,18.5193157565869));
#14896=CARTESIAN_POINT('Ctrl Pts',(1.96135817837331,-1.58501790711836,18.5055018677823));
#14897=CARTESIAN_POINT('Ctrl Pts',(1.86596150603354,-1.69628845843337,18.4952931815981));
#14898=CARTESIAN_POINT('Ctrl Pts',(1.65596353148766,-1.90194316928332,18.4751138802844));
#14899=CARTESIAN_POINT('Ctrl Pts',(1.54158667528325,-1.99577722167655,18.46518817903));
#14900=CARTESIAN_POINT('Ctrl Pts',(1.3994938472954,-2.09280133522046,18.4540948901075));
#14901=CARTESIAN_POINT('Ctrl Pts',(1.37916369961352,-2.10625449912207,18.4525341443093));
#14902=CARTESIAN_POINT('Ctrl Pts',(1.34737181736315,-2.12663457366111,18.4501333128665));
#14903=CARTESIAN_POINT('Ctrl Pts',(1.33604526466212,-2.13376861119355,18.4492856397384));
#14904=CARTESIAN_POINT('Ctrl Pts',(1.31497877597158,-2.14680384247007,18.4477229673254));
#14905=CARTESIAN_POINT('Ctrl Pts',(1.30525471416179,-2.15272990811629,18.4470070751909));
#14906=CARTESIAN_POINT('Ctrl Pts',(1.28389210564039,-2.165550805658,18.4454459824142));
#14907=CARTESIAN_POINT('Ctrl Pts',(1.27223747322,-2.17241825020526,18.4446017842655));
#14908=CARTESIAN_POINT('Ctrl Pts',(1.23958226989907,-2.19130727091362,18.4422567395579));
#14909=CARTESIAN_POINT('Ctrl Pts',(1.21846254718342,-2.20312070543127,18.4407633018467));
#14910=CARTESIAN_POINT('Ctrl Pts',(1.05574709208051,-2.291080804161,18.4294252073927));
#14911=CARTESIAN_POINT('Ctrl Pts',(0.907314559160761,-2.35381450550131,
18.4200773793681));
#14912=CARTESIAN_POINT('Ctrl Pts',(0.63631902210136,-2.43887071743909,18.4037250874671));
#14913=CARTESIAN_POINT('Ctrl Pts',(0.516198619736816,-2.46708894810063,
18.3966955322491));
#14914=CARTESIAN_POINT('Ctrl Pts',(0.351086272340018,-2.49328641539471,
18.3868073814731));
#14915=CARTESIAN_POINT('Ctrl Pts',(0.307498870734705,-2.49903636165727,
18.3841752962588));
#14916=CARTESIAN_POINT('Ctrl Pts',(0.235944972828393,-2.50657534043136,
18.3797870180712));
#14917=CARTESIAN_POINT('Ctrl Pts',(0.208058453146061,-2.50904394094888,
18.3780601133164));
#14918=CARTESIAN_POINT('Ctrl Pts',(0.170066351849919,-2.51176942506044,
18.3756777559617));
#14919=CARTESIAN_POINT('Ctrl Pts',(0.15999071874977,-2.51243132652685,18.3750431142095));
#14920=CARTESIAN_POINT('Ctrl Pts',(0.143108231205909,-2.51343842860559,
18.3739745751576));
#14921=CARTESIAN_POINT('Ctrl Pts',(0.136303352677024,-2.51381663887619,
18.3735424756562));
#14922=CARTESIAN_POINT('Ctrl Pts',(0.123379379834958,-2.51448231342796,
18.3727190237121));
#14923=CARTESIAN_POINT('Ctrl Pts',(0.117260598476626,-2.51477508458086,
18.3723279758135));
#14924=CARTESIAN_POINT('Ctrl Pts',(0.102699251475504,-2.51541855645151,
18.3713946362235));
#14925=CARTESIAN_POINT('Ctrl Pts',(0.0942559322292057,-2.51574908621491,
18.3708512598506));
#14926=CARTESIAN_POINT('Ctrl Pts',(0.0643087139798407,-2.51677045761506,
18.3689166154294));
#14927=CARTESIAN_POINT('Ctrl Pts',(0.0427984857373781,-2.51722811127943,
18.3675135515741));
#14928=CARTESIAN_POINT('Ctrl Pts',(-0.106888217363795,-2.51849378338224,
18.3576681227493));
#14929=CARTESIAN_POINT('Ctrl Pts',(-0.234946055302919,-2.5097868758584,
18.3488381640748));
#14930=CARTESIAN_POINT('Ctrl Pts',(-0.503575502989314,-2.47077936348239,
18.3300900861767));
#14931=CARTESIAN_POINT('Ctrl Pts',(-0.643378209288076,-2.43811636455717,
18.3202072137338));
#14932=CARTESIAN_POINT('Ctrl Pts',(-0.849548430825008,-2.37096551133567,
18.3057367769633));
#14933=CARTESIAN_POINT('Ctrl Pts',(-0.918419064808094,-2.34514780102968,
18.3009172323515));
#14934=CARTESIAN_POINT('Ctrl Pts',(-1.00494494794857,-2.30831385722584,
18.2948785592409));
#14935=CARTESIAN_POINT('Ctrl Pts',(-1.02372444467275,-2.30004685037655,
18.2935688292029));
#14936=CARTESIAN_POINT('Ctrl Pts',(-1.0539941776916,-2.28627748301375,18.2914587031916));
#14937=CARTESIAN_POINT('Ctrl Pts',(-1.06554709736118,-2.28091601093088,
18.290653568122));
#14938=CARTESIAN_POINT('Ctrl Pts',(-1.0876582576966,-2.27045001681488,18.2891128712107));
#14939=CARTESIAN_POINT('Ctrl Pts',(-1.09822246495921,-2.26535895374548,
18.2883768732966));
#14940=CARTESIAN_POINT('Ctrl Pts',(-1.12234339922585,-2.25352629498757,
18.2866964456641));
#14941=CARTESIAN_POINT('Ctrl Pts',(-1.13587573993024,-2.24673580716248,
18.2857537318026));
#14942=CARTESIAN_POINT('Ctrl Pts',(-1.1787994319751,-2.22470988276268,18.2827629298786));
#14943=CARTESIAN_POINT('Ctrl Pts',(-1.20795263313733,-2.20901624153878,
18.2807308004649));
#14944=CARTESIAN_POINT('Ctrl Pts',(-1.38669512353555,-2.10819919986852,
18.2682485152041));
#14945=CARTESIAN_POINT('Ctrl Pts',(-1.52754018283228,-2.00849614696838,
18.2583523836813));
#14946=CARTESIAN_POINT('Ctrl Pts',(-1.73133497450843,-1.83030151883563,
18.2427990255119));
#14947=CARTESIAN_POINT('Ctrl Pts',(-1.8016680470265,-1.76111177525823,18.2371410928996));
#14948=CARTESIAN_POINT('Ctrl Pts',(-1.89796815155397,-1.65455522497619,
18.2286576468602));
#14949=CARTESIAN_POINT('Ctrl Pts',(-1.92727228067405,-1.62032626177155,
18.2259632270064));
#14950=CARTESIAN_POINT('Ctrl Pts',(-1.97357354142685,-1.56320974065637,
18.221481791625));
#14951=CARTESIAN_POINT('Ctrl Pts',(-1.99112899057248,-1.54078629321933,
18.2197259042988));
#14952=CARTESIAN_POINT('Ctrl Pts',(-2.01441083786353,-1.50998607333527,
18.2173113740732));
#14953=CARTESIAN_POINT('Ctrl Pts',(-2.02047323228907,-1.50186446617077,
18.2166744459023));
#14954=CARTESIAN_POINT('Ctrl Pts',(-2.03052157048186,-1.48823205725804,
18.2156045152353));
#14955=CARTESIAN_POINT('Ctrl Pts',(-2.03453459191065,-1.48274121026991,
18.2151733485443));
#14956=CARTESIAN_POINT('Ctrl Pts',(-2.04210065786843,-1.47230033616332,
18.2143529248706));
#14957=CARTESIAN_POINT('Ctrl Pts',(-2.04565807661919,-1.46735353899278,
18.2139639825756));
#14958=CARTESIAN_POINT('Ctrl Pts',(-2.05499196665383,-1.45427431102632,
18.2129351218001));
#14959=CARTESIAN_POINT('Ctrl Pts',(-2.06073805160998,-1.44612047541567,
18.2122931984065));
#14960=CARTESIAN_POINT('Ctrl Pts',(-2.08090968685881,-1.41713206975643,
18.2100098541999));
#14961=CARTESIAN_POINT('Ctrl Pts',(-2.09506842391018,-1.39611482742013,
18.2083522321623));
#14962=CARTESIAN_POINT('Ctrl Pts',(-2.20280946246587,-1.23085355228727,
18.1953233523252));
#14963=CARTESIAN_POINT('Ctrl Pts',(-2.28170313318702,-1.07758730895573,
18.183305322428));
#14964=CARTESIAN_POINT('Ctrl Pts',(-2.40096807913243,-0.772842550326007,
18.16077654559));
#14965=CARTESIAN_POINT('Ctrl Pts',(-2.44407672341112,-0.623247284441368,
18.1502789325224));
#14966=CARTESIAN_POINT('Ctrl Pts',(-2.47830648694301,-0.44336480746625,
18.1384347767445));
#14967=CARTESIAN_POINT('Ctrl Pts',(-2.48304045724959,-0.41603555603686,
18.1366549545893));
#14968=CARTESIAN_POINT('Ctrl Pts',(-2.48952296639736,-0.374546288205229,
18.1339816503384));
#14969=CARTESIAN_POINT('Ctrl Pts',(-2.49160424266433,-0.360441165509516,
18.1330777936971));
#14970=CARTESIAN_POINT('Ctrl Pts',(-2.49516000834397,-0.334838937390025,
18.1314460033085));
#14971=CARTESIAN_POINT('Ctrl Pts',(-2.49667512519751,-0.323347966905891,
18.1307168153441));
#14972=CARTESIAN_POINT('Ctrl Pts',(-2.49976791433957,-0.298572562846173,
18.1291513500969));
#14973=CARTESIAN_POINT('Ctrl Pts',(-2.50131917156891,-0.285285144660354,
18.1283159196029));
#14974=CARTESIAN_POINT('Ctrl Pts',(-2.50523947138852,-0.249211248167154,
18.1260586744285));
#14975=CARTESIAN_POINT('Ctrl Pts',(-2.50740355604969,-0.226403435474002,
18.124643263406));
#14976=CARTESIAN_POINT('Ctrl Pts',(-2.51727053576669,-0.104779714195217,
18.1171533110186));
#14977=CARTESIAN_POINT('Ctrl Pts',(-2.51944471725618,-0.00559727014803007,
18.1112529460383));
#14978=CARTESIAN_POINT('Ctrl Pts',(-2.50951361894324,0.261716261458144,
18.0956166396101));
#14979=CARTESIAN_POINT('Ctrl Pts',(-2.48640071093977,0.428908180040172,
18.0861402634124));
#14980=CARTESIAN_POINT('Ctrl Pts',(-2.4332504101922,0.648382920894336,18.0729323896871));
#14981=CARTESIAN_POINT('Ctrl Pts',(-2.41781887649505,0.703746411155615,
18.0695291981744));
#14982=CARTESIAN_POINT('Ctrl Pts',(-2.39365247952273,0.780225453935727,
18.0646673341947));
#14983=CARTESIAN_POINT('Ctrl Pts',(-2.38650335343618,0.801826428148148,
18.0632758613125));
#14984=CARTESIAN_POINT('Ctrl Pts',(-2.37348422768559,0.839446142002436,
18.0608155720463));
#14985=CARTESIAN_POINT('Ctrl Pts',(-2.36774225033013,0.855507921418181,
18.0597532270337));
#14986=CARTESIAN_POINT('Ctrl Pts',(-2.35897550264946,0.879266277089992,
18.0581623230088));
#14987=CARTESIAN_POINT('Ctrl Pts',(-2.35607517117383,0.887008676011476,
18.0576407800213));
#14988=CARTESIAN_POINT('Ctrl Pts',(-2.35104486999594,0.900238254329221,
18.0567440697138));
#14989=CARTESIAN_POINT('Ctrl Pts',(-2.34893371664179,0.905732459996498,
18.0563700177828));
#14990=CARTESIAN_POINT('Ctrl Pts',(-2.34408774918382,0.918213025561536,
18.0555165174362));
#14991=CARTESIAN_POINT('Ctrl Pts',(-2.3413410133645,0.925194461628468,18.0550363783652));
#14992=CARTESIAN_POINT('Ctrl Pts',(-2.33375633283213,0.944222514339445,
18.0537205576419));
#14993=CARTESIAN_POINT('Ctrl Pts',(-2.32885642554597,0.956243959366076,
18.0528813549417));
#14994=CARTESIAN_POINT('Ctrl Pts',(-2.30336102467174,1.01743607856899,18.0485710949978));
#14995=CARTESIAN_POINT('Ctrl Pts',(-2.28130184340732,1.0659780358445,18.0450245042719));
#14996=CARTESIAN_POINT('Ctrl Pts',(-2.16229088158447,1.307222895608,18.0268732345917));
#14997=CARTESIAN_POINT('Ctrl Pts',(-2.04239454666965,1.4876065921646,18.0116674768687));
#14998=CARTESIAN_POINT('Ctrl Pts',(-1.86275853591999,1.69450022495305,17.9932464886632));
#14999=CARTESIAN_POINT('Ctrl Pts',(-1.82304533522172,1.73715483612866,17.989379074569));
#15000=CARTESIAN_POINT('Ctrl Pts',(-1.75321018681335,1.80712701078356,17.9829169698991));
#15001=CARTESIAN_POINT('Ctrl Pts',(-1.72384321403486,1.83516181250431,17.9802928554026));
#15002=CARTESIAN_POINT('Ctrl Pts',(-1.68154310476118,1.87363122150665,17.9766394603273));
#15003=CARTESIAN_POINT('Ctrl Pts',(-1.66916641951126,1.88466566074717,17.9755851193295));
#15004=CARTESIAN_POINT('Ctrl Pts',(-1.64770536912818,1.90342201726563,17.97378148613));
#15005=CARTESIAN_POINT('Ctrl Pts',(-1.63867363253257,1.91120304866168,17.973029766383));
#15006=CARTESIAN_POINT('Ctrl Pts',(-1.6213032622306,1.92595433096631,17.9715977739447));
#15007=CARTESIAN_POINT('Ctrl Pts',(-1.61297411930702,1.93293529365318,17.9709170746223));
#15008=CARTESIAN_POINT('Ctrl Pts',(-1.59333973553138,1.94917630856568,17.9693261455656));
#15009=CARTESIAN_POINT('Ctrl Pts',(-1.58199847862048,1.95839235661377,17.9684176916708));
#15010=CARTESIAN_POINT('Ctrl Pts',(-1.54824618255078,1.98533535237214,17.9657442862546));
#15011=CARTESIAN_POINT('Ctrl Pts',(-1.52561241840828,2.00278045533442,17.9639903776879));
#15012=CARTESIAN_POINT('Ctrl Pts',(-1.3448027711089,2.13729630868681,17.9502668259166));
#15013=CARTESIAN_POINT('Ctrl Pts',(-1.17369340217554,2.23584047429716,17.9390565443938));
#15014=CARTESIAN_POINT('Ctrl Pts',(-0.868694022597619,2.36673347575912,
17.9199538483269));
#15015=CARTESIAN_POINT('Ctrl Pts',(-0.740478007227817,2.40992517383426,
17.9121320784809));
#15016=CARTESIAN_POINT('Ctrl Pts',(-0.59195237903389,2.44698250183437,17.9026836557075));
#15017=CARTESIAN_POINT('Ctrl Pts',(-0.57442225536348,2.45115687235571,17.9015624038222));
#15018=CARTESIAN_POINT('Ctrl Pts',(-0.548597167432117,2.45701424511822,
17.89989966211));
#15019=CARTESIAN_POINT('Ctrl Pts',(-0.54033567518004,2.45884428259756,17.8993661115137));
#15020=CARTESIAN_POINT('Ctrl Pts',(-0.525682492459146,2.46201275618266,
17.8984166181944));
#15021=CARTESIAN_POINT('Ctrl Pts',(-0.519294610278079,2.46336801978397,
17.898001630626));
#15022=CARTESIAN_POINT('Ctrl Pts',(-0.505433697216426,2.46625246260113,
17.897098779707));
#15023=CARTESIAN_POINT('Ctrl Pts',(-0.497959087383205,2.46777251285386,
17.8966104371215));
#15024=CARTESIAN_POINT('Ctrl Pts',(-0.477206012533261,2.47189477157104,
17.8952507019427));
#15025=CARTESIAN_POINT('Ctrl Pts',(-0.463913527443257,2.47442388446784,
17.8943754034019));
#15026=CARTESIAN_POINT('Ctrl Pts',(-0.390016087292666,2.48786772124458,
17.8894874567727));
#15027=CARTESIAN_POINT('Ctrl Pts',(-0.329051614929678,2.49666218118155,
17.8853738880233));
#15028=CARTESIAN_POINT('Ctrl Pts',(-0.0907274039402323,2.52216174314133,
17.8691277088495));
#15029=CARTESIAN_POINT('Ctrl Pts',(0.0878890297624799,2.52226318313915,
17.8566408237309));
#15030=CARTESIAN_POINT('Ctrl Pts',(0.37784878674303,2.49156733109126,17.8368264141302));
#15031=CARTESIAN_POINT('Ctrl Pts',(0.489745303522463,2.47200996762349,17.8292830768543));
#15032=CARTESIAN_POINT('Ctrl Pts',(0.622430834440168,2.43945110547026,17.820485205456));
#15033=CARTESIAN_POINT('Ctrl Pts',(0.644830326647705,2.43362604931074,17.81900476532));
#15034=CARTESIAN_POINT('Ctrl Pts',(0.679975037906846,2.42396724141288,17.8166888698142));
#15035=CARTESIAN_POINT('Ctrl Pts',(0.692775186326517,2.42034001575675,17.8158468428201));
#15036=CARTESIAN_POINT('Ctrl Pts',(0.716690810139699,2.41335768634948,17.8142761340494));
#15037=CARTESIAN_POINT('Ctrl Pts',(0.727812942920345,2.41002683947314,17.8135466926743));
#15038=CARTESIAN_POINT('Ctrl Pts',(0.752667534497244,2.40239565658569,17.8119187306687));
#15039=CARTESIAN_POINT('Ctrl Pts',(0.766387037348629,2.39805425936081,17.8110215675678));
#15040=CARTESIAN_POINT('Ctrl Pts',(0.801213112165103,2.38670449902357,17.8087474211037));
#15041=CARTESIAN_POINT('Ctrl Pts',(0.822265691116809,2.3795335673898,17.8073757456373));
#15042=CARTESIAN_POINT('Ctrl Pts',(0.995633971855635,2.31790516357311,17.796098633377));
#15043=CARTESIAN_POINT('Ctrl Pts',(1.14247782094492,2.24916100652835,17.786700276714));
#15044=CARTESIAN_POINT('Ctrl Pts',(1.38842169511592,2.10367748891348,17.7702622177524));
#15045=CARTESIAN_POINT('Ctrl Pts',(1.49030434171812,2.03277231051378,17.7631969895323));
#15046=CARTESIAN_POINT('Ctrl Pts',(1.62060746778923,1.92700867776693,17.7532734308492));
#15047=CARTESIAN_POINT('Ctrl Pts',(1.65394055401943,1.89847602683982,17.7506470757152));
#15048=CARTESIAN_POINT('Ctrl Pts',(1.70725102104016,1.85037312391305,17.746268079972));
#15049=CARTESIAN_POINT('Ctrl Pts',(1.72767883130065,1.83131440570978,17.7445448003496));
#15050=CARTESIAN_POINT('Ctrl Pts',(1.75502617637599,1.80493507186594,17.7421682616341));
#15051=CARTESIAN_POINT('Ctrl Pts',(1.762225996684,1.797906288429,17.7415358440357));
#15052=CARTESIAN_POINT('Ctrl Pts',(1.77421124589107,1.78606460329909,17.7404713325206));
#15053=CARTESIAN_POINT('Ctrl Pts',(1.77901978727859,1.78127507893163,17.7400410328778));
#15054=CARTESIAN_POINT('Ctrl Pts',(1.78812124143953,1.77213600586748,17.7392203078144));
#15055=CARTESIAN_POINT('Ctrl Pts',(1.79241778971287,1.76779016361785,17.7388301856064));
#15056=CARTESIAN_POINT('Ctrl Pts',(1.80259739227062,1.75741850810234,17.737899587598));
#15057=CARTESIAN_POINT('Ctrl Pts',(1.80846607340502,1.75137877907153,17.7373580349747));
#15058=CARTESIAN_POINT('Ctrl Pts',(1.829143066152,1.7298843972971,17.7354323911853));
#15059=CARTESIAN_POINT('Ctrl Pts',(1.843783994868,1.71427095094739,17.7340366112429));
#15060=CARTESIAN_POINT('Ctrl Pts',(1.95060687708032,1.59740082862512,17.72362332876));
#15061=CARTESIAN_POINT('Ctrl Pts',(2.03458155198715,1.48896864539858,17.7141630399245));
#15062=CARTESIAN_POINT('Ctrl Pts',(2.18154057222212,1.26340494733854,17.6955637949297));
#15063=CARTESIAN_POINT('Ctrl Pts',(2.24491992639096,1.14701884207999,17.6864546519252));
#15064=CARTESIAN_POINT('Ctrl Pts',(2.3213954756214,0.975697529016985,17.6739183267136));
#15065=CARTESIAN_POINT('Ctrl Pts',(2.3422604104862,0.924488129415224,17.6702722055998));
#15066=CARTESIAN_POINT('Ctrl Pts',(2.36142200245778,0.872635305444532,17.6666805052528));
#15067=CARTESIAN_POINT('Origin',(0.,0.,10.));
#15068=CARTESIAN_POINT('',(2.36142200368728,0.872635302117405,16.6687517122259));
#15069=CARTESIAN_POINT('',(2.36142200728636,0.872635292378013,16.9437682627171));
#15070=CARTESIAN_POINT('',(2.36142200728636,0.87263529237802,10.));
#15071=CARTESIAN_POINT('',(2.5174999670525,0.000407296750592275,17.8874166974728));
#15072=CARTESIAN_POINT('Ctrl Pts',(2.36142200728636,0.872635292378013,16.9437682627171));
#15073=CARTESIAN_POINT('Ctrl Pts',(2.33277467475577,0.950157301949081,16.9490221933786));
#15074=CARTESIAN_POINT('Ctrl Pts',(2.30025475204426,1.02640554539073,16.9542761240401));
#15075=CARTESIAN_POINT('Ctrl Pts',(2.26399624137994,1.10096651584755,16.9595300547015));
#15076=CARTESIAN_POINT('Ctrl Pts',(2.22778717431102,1.17542581190054,16.9647768208872));
#15077=CARTESIAN_POINT('Ctrl Pts',(2.18784984627795,1.2482019935627,16.9700235870729));
#15078=CARTESIAN_POINT('Ctrl Pts',(2.14436702227656,1.31889966402785,16.9752703532586));
#15079=CARTESIAN_POINT('Ctrl Pts',(2.10093090803895,1.38952139021929,16.980511483306));
#15080=CARTESIAN_POINT('Ctrl Pts',(2.0539571081917,1.45806865172029,16.9857526133534));
#15081=CARTESIAN_POINT('Ctrl Pts',(2.00367452828408,1.52417014624535,16.9909937434007));
#15082=CARTESIAN_POINT('Ctrl Pts',(1.95342131699091,1.59023303278111,16.9962318122542));
#15083=CARTESIAN_POINT('Ctrl Pts',(1.89986344117179,1.65385262204952,17.0014698811077));
#15084=CARTESIAN_POINT('Ctrl Pts',(1.84327274321826,1.71468709801778,17.0067079499612));
#15085=CARTESIAN_POINT('Ctrl Pts',(1.78669802791096,1.77550439278942,17.0119445394513));
#15086=CARTESIAN_POINT('Ctrl Pts',(1.72709250588652,1.83353779898866,17.0171811289415));
#15087=CARTESIAN_POINT('Ctrl Pts',(1.66476695867383,1.88848013579913,17.0224177184317));
#15088=CARTESIAN_POINT('Ctrl Pts',(1.60244021392815,1.9434235282804,17.0276544085385));
#15089=CARTESIAN_POINT('Ctrl Pts',(1.53739368726397,1.9952754293427,17.0328910986454));
#15090=CARTESIAN_POINT('Ctrl Pts',(1.46997247333479,2.04376788741726,17.0381277887522));
#15091=CARTESIAN_POINT('Ctrl Pts',(1.40248354220258,2.09230905083896,17.043369738539));
#15092=CARTESIAN_POINT('Ctrl Pts',(1.33261553516941,2.13748376155191,17.0486116883258));
#15093=CARTESIAN_POINT('Ctrl Pts',(1.26074345964852,2.1790668137883,17.0538536381126));
#15094=CARTESIAN_POINT('Ctrl Pts',(1.18883594453469,2.22067037032254,17.0590981726663));
#15095=CARTESIAN_POINT('Ctrl Pts',(1.11492280324316,2.25867852924783,17.0643427072201));
#15096=CARTESIAN_POINT('Ctrl Pts',(1.03940244297438,2.29291273526467,17.0695872417738));
#15097=CARTESIAN_POINT('Ctrl Pts',(0.963748038937281,2.32720770478903,17.0748410850381));
#15098=CARTESIAN_POINT('Ctrl Pts',(0.886481146144829,2.35771516755753,17.0800949283025));
#15099=CARTESIAN_POINT('Ctrl Pts',(0.808018755863324,2.38430533702651,17.0853487715668));
#15100=CARTESIAN_POINT('Ctrl Pts',(0.737208666948436,2.40830221320636,17.0900902165744));
#15101=CARTESIAN_POINT('Ctrl Pts',(0.665425344416089,2.42910922742866,17.0948316615821));
#15102=CARTESIAN_POINT('Ctrl Pts',(0.592982195154382,2.44666678692255,17.0995731065898));
#15103=CARTESIAN_POINT('Ctrl Pts',(0.512687973536151,2.46612715808869,17.1048284087145));
#15104=CARTESIAN_POINT('Ctrl Pts',(0.431286506734991,2.48166665495804,17.1100837108393));
#15105=CARTESIAN_POINT('Ctrl Pts',(0.349195168056678,2.49316445197782,17.115339012964));
#15106=CARTESIAN_POINT('Ctrl Pts',(0.267220209607418,2.50464594866346,17.1205868646893));
#15107=CARTESIAN_POINT('Ctrl Pts',(0.18455777506545,2.5120970632641,17.1258347164146));
#15108=CARTESIAN_POINT('Ctrl Pts',(0.101637619020051,2.51544748392805,17.1310825681398));
#15109=CARTESIAN_POINT('Ctrl Pts',(0.0181176884826902,2.51882213871006,
17.1363683783996));
#15110=CARTESIAN_POINT('Ctrl Pts',(-0.0656632470085882,2.51803641614374,
17.1416541886594));
#15111=CARTESIAN_POINT('Ctrl Pts',(-0.149258427858184,2.51307146172036,
17.1469399989191));
#15112=CARTESIAN_POINT('Ctrl Pts',(-0.232105070298294,2.50815096511201,
17.1521784783164));
#15113=CARTESIAN_POINT('Ctrl Pts',(-0.314768802335826,2.49912580955793,
17.1574169577138));
#15114=CARTESIAN_POINT('Ctrl Pts',(-0.39681426657695,2.48602990485654,17.1626554371111));
#15115=CARTESIAN_POINT('Ctrl Pts',(-0.4788327485456,2.47293830700224,17.1678921937309));
#15116=CARTESIAN_POINT('Ctrl Pts',(-0.560232911258984,2.45577869149736,
17.1731289503508));
#15117=CARTESIAN_POINT('Ctrl Pts',(-0.640586253136465,2.43463662633515,
17.1783657069706));
#15118=CARTESIAN_POINT('Ctrl Pts',(-0.720937405960774,2.41349513714282,
17.1836023209264));
#15119=CARTESIAN_POINT('Ctrl Pts',(-0.800241348690656,2.38837153241022,
17.1888389348821));
#15120=CARTESIAN_POINT('Ctrl Pts',(-0.878082833579531,2.35940178591374,
17.1940755488378));
#15121=CARTESIAN_POINT('Ctrl Pts',(-0.957196623425065,2.32995853416343,
17.1993977542992));
#15122=CARTESIAN_POINT('Ctrl Pts',(-1.03479925207399,2.29654243797504,17.2047199597605));
#15123=CARTESIAN_POINT('Ctrl Pts',(-1.11047572288176,2.25934723291712,17.2100421652219));
#15124=CARTESIAN_POINT('Ctrl Pts',(-1.18504209113089,2.22269764648891,17.2152862989413));
#15125=CARTESIAN_POINT('Ctrl Pts',(-1.25773805734807,2.18237936896989,17.2205304326607));
#15126=CARTESIAN_POINT('Ctrl Pts',(-1.32819293953474,2.13862333414981,17.2257745663801));
#15127=CARTESIAN_POINT('Ctrl Pts',(-1.40022116128764,2.09389017611688,17.2311358077125));
#15128=CARTESIAN_POINT('Ctrl Pts',(-1.46990658020088,2.04556416416079,17.2364970490448));
#15129=CARTESIAN_POINT('Ctrl Pts',(-1.5368875120115,1.99393656504491,17.2418582903771));
#15130=CARTESIAN_POINT('Ctrl Pts',(-1.60386844382214,1.94230896592902,17.2472195317095));
#15131=CARTESIAN_POINT('Ctrl Pts',(-1.6681445457099,1.8873801604566,17.2525807730418));
#15132=CARTESIAN_POINT('Ctrl Pts',(-1.72939442071244,1.8294811252398,17.2579420143741));
#15133=CARTESIAN_POINT('Ctrl Pts',(-1.78943161985282,1.77272842317791,17.2631971094008));
#15134=CARTESIAN_POINT('Ctrl Pts',(-1.84678312947741,1.71291243033947,17.2684522044274));
#15135=CARTESIAN_POINT('Ctrl Pts',(-1.90112037151567,1.65031741886466,17.2737072994541));
#15136=CARTESIAN_POINT('Ctrl Pts',(-1.95538057174684,1.58781115743711,17.2789549435686));
#15137=CARTESIAN_POINT('Ctrl Pts',(-2.00663469334919,1.52253404934597,17.284202587683));
#15138=CARTESIAN_POINT('Ctrl Pts',(-2.05458978583795,1.45480825607032,17.2894502317975));
#15139=CARTESIAN_POINT('Ctrl Pts',(-2.1028941297072,1.38658922369182,17.2947360938959));
#15140=CARTESIAN_POINT('Ctrl Pts',(-2.14785084336907,1.31588601347509,17.3000219559943));
#15141=CARTESIAN_POINT('Ctrl Pts',(-2.18920084141125,1.2430631222767,17.3053078180926));
#15142=CARTESIAN_POINT('Ctrl Pts',(-2.23017855419591,1.17089587533675,17.3105460901396));
#15143=CARTESIAN_POINT('Ctrl Pts',(-2.26761400262287,1.0966473707698,17.3157843621865));
#15144=CARTESIAN_POINT('Ctrl Pts',(-2.30129860612775,1.02070121751396,17.3210226342335));
#15145=CARTESIAN_POINT('Ctrl Pts',(-2.33497213490514,0.944780033616912,
17.3262591840564));
#15146=CARTESIAN_POINT('Ctrl Pts',(-2.36489708099854,0.867162731030279,
17.3314957338792));
#15147=CARTESIAN_POINT('Ctrl Pts',(-2.39091192672311,0.788255294085104,
17.3367322837021));
#15148=CARTESIAN_POINT('Ctrl Pts',(-2.41692606781552,0.709349994408706,
17.341968691689));
#15149=CARTESIAN_POINT('Ctrl Pts',(-2.43903017560629,0.629155068422387,
17.3472050996759));
#15150=CARTESIAN_POINT('Ctrl Pts',(-2.45711222843626,0.548092826872433,
17.3524415076628));
#15151=CARTESIAN_POINT('Ctrl Pts',(-2.47549140060318,0.465698592783337,
17.3577639588707));
#15152=CARTESIAN_POINT('Ctrl Pts',(-2.48971502236485,0.382408759267712,
17.3630864100787));
#15153=CARTESIAN_POINT('Ctrl Pts',(-2.49971964547033,0.298676989488158,
17.3684088612866));
#15154=CARTESIAN_POINT('Ctrl Pts',(-2.50957667561334,0.21618047063444,17.3736527931608));
#15155=CARTESIAN_POINT('Ctrl Pts',(-2.51533838730665,0.133255439081672,
17.3788967250349));
#15156=CARTESIAN_POINT('Ctrl Pts',(-2.51699667917541,0.0503385242130254,
17.384140656909));
#15157=CARTESIAN_POINT('Ctrl Pts',(-2.51869221637152,-0.0344407091621792,
17.3895023677839));
#15158=CARTESIAN_POINT('Ctrl Pts',(-2.51609779009976,-0.119210944760911,
17.3948640786588));
#15159=CARTESIAN_POINT('Ctrl Pts',(-2.5092608266804,-0.203510082519756,
17.4002257895336));
#15160=CARTESIAN_POINT('Ctrl Pts',(-2.50242386326104,-0.287809220278612,
17.4055875004085));
#15161=CARTESIAN_POINT('Ctrl Pts',(-2.4913444955995,-0.371636764972206,
17.4109492112834));
#15162=CARTESIAN_POINT('Ctrl Pts',(-2.47612541957012,-0.454542799479524,
17.4163109221582));
#15163=CARTESIAN_POINT('Ctrl Pts',(-2.46120816605392,-0.535804653509427,
17.421566300359));
#15164=CARTESIAN_POINT('Ctrl Pts',(-2.44225883457613,-0.616481443158024,
17.4268216785598));
#15165=CARTESIAN_POINT('Ctrl Pts',(-2.41933699953252,-0.696142753099517,
17.4320770567606));
#15166=CARTESIAN_POINT('Ctrl Pts',(-2.39644766574833,-0.775691109915955,
17.4373249832713));
#15167=CARTESIAN_POINT('Ctrl Pts',(-2.36959714308071,-0.854226407314903,
17.4425729097821));
#15168=CARTESIAN_POINT('Ctrl Pts',(-2.33889618428474,-0.931327487588705,
17.4478208362928));
#15169=CARTESIAN_POINT('Ctrl Pts',(-2.30797371162681,-1.0089848683405,17.4531066276949));
#15170=CARTESIAN_POINT('Ctrl Pts',(-2.27314509150085,-1.08518678259642,
17.4583924190969));
#15171=CARTESIAN_POINT('Ctrl Pts',(-2.23457499040448,-1.15951751270035,
17.463678210499));
#15172=CARTESIAN_POINT('Ctrl Pts',(-2.19634960303706,-1.23318392452612,
17.468916761038));
#15173=CARTESIAN_POINT('Ctrl Pts',(-2.15444956181177,-1.30501204838975,
17.474155311577));
#15174=CARTESIAN_POINT('Ctrl Pts',(-2.10908309225795,-1.37461804147611,
17.479393862116));
#15175=CARTESIAN_POINT('Ctrl Pts',(-2.06373155526043,-1.44420112346933,
17.484630688365));
#15176=CARTESIAN_POINT('Ctrl Pts',(-2.01491610773994,-1.51156314109537,
17.4898675146139));
#15177=CARTESIAN_POINT('Ctrl Pts',(-1.96288936701981,-1.57634754506757,
17.4951043408629));
#15178=CARTESIAN_POINT('Ctrl Pts',(-1.91086405949419,-1.6411301644065,17.5003410228516));
#15179=CARTESIAN_POINT('Ctrl Pts',(-1.85562792436406,-1.70333495216445,
17.5055777048404));
#15180=CARTESIAN_POINT('Ctrl Pts',(-1.79747422211945,-1.76263798631939,
17.5108143868291));
#15181=CARTESIAN_POINT('Ctrl Pts',(-1.7383717221883,-1.82290856990695,17.5161365070885));
#15182=CARTESIAN_POINT('Ctrl Pts',(-1.67625593135551,-1.88018150174497,
17.521458627348));
#15183=CARTESIAN_POINT('Ctrl Pts',(-1.6114727360507,-1.93415663041163,17.5267807476074));
#15184=CARTESIAN_POINT('Ctrl Pts',(-1.54763805495449,-1.98734148968497,
17.532024944778));
#15185=CARTESIAN_POINT('Ctrl Pts',(-1.48121397244005,-2.03732424332915,
17.5372691419485));
#15186=CARTESIAN_POINT('Ctrl Pts',(-1.4125623381495,-2.08386033381358,17.5425133391191));
#15187=CARTESIAN_POINT('Ctrl Pts',(-1.34238057048667,-2.13143363813568,
17.547874420923));
#15188=CARTESIAN_POINT('Ctrl Pts',(-1.26987119731387,-2.17540452485945,
17.5532355027269));
#15189=CARTESIAN_POINT('Ctrl Pts',(-1.19544746063087,-2.21556124241042,
17.5585965845308));
#15190=CARTESIAN_POINT('Ctrl Pts',(-1.12102372394787,-2.25571795996139,
17.5639576663347));
#15191=CARTESIAN_POINT('Ctrl Pts',(-1.04468611101973,-2.29206035026829,
17.5693187481386));
#15192=CARTESIAN_POINT('Ctrl Pts',(-0.966867730000397,-2.3244296166337,
17.5746798299424));
#15193=CARTESIAN_POINT('Ctrl Pts',(-0.890581262222371,-2.35616166969414,
17.579935374827));
#15194=CARTESIAN_POINT('Ctrl Pts',(-0.812590244233387,-2.38419277371056,
17.5851909197115));
#15195=CARTESIAN_POINT('Ctrl Pts',(-0.733288179464249,-2.40833857583563,
17.590446464596));
#15196=CARTESIAN_POINT('Ctrl Pts',(-0.654098502204564,-2.43245015834017,
17.595694561281));
#15197=CARTESIAN_POINT('Ctrl Pts',(-0.573601906437922,-2.45268724280885,
17.600942657966));
#15198=CARTESIAN_POINT('Ctrl Pts',(-0.492211990480921,-2.46891344652396,
17.606190754651));
#15199=CARTESIAN_POINT('Ctrl Pts',(-0.410238140398427,-2.48525606557093,
17.6114765039458));
#15200=CARTESIAN_POINT('Ctrl Pts',(-0.327358535705637,-2.49752982911297,
17.6167622532406));
#15201=CARTESIAN_POINT('Ctrl Pts',(-0.244011507871158,-2.50564655009968,
17.6220480025355));
#15202=CARTESIAN_POINT('Ctrl Pts',(-0.161405925479705,-2.51369106568274,
17.6272867304207));
#15203=CARTESIAN_POINT('Ctrl Pts',(-0.0783416707482684,-2.51765216040642,
17.6325254583061));
#15204=CARTESIAN_POINT('Ctrl Pts',(0.00474589535283771,-2.51749552660522,
17.6377641861914));
#15205=CARTESIAN_POINT('Ctrl Pts',(0.0878061498949002,-2.51733894429083,
17.6430011920642));
#15206=CARTESIAN_POINT('Ctrl Pts',(0.170889239592013,-2.51306732251811,
17.648238197937));
#15207=CARTESIAN_POINT('Ctrl Pts',(0.253558530604507,-2.50469844922651,
17.6534752038098));
#15208=CARTESIAN_POINT('Ctrl Pts',(0.33622557626592,-2.49632980323889,17.6587120674422));
#15209=CARTESIAN_POINT('Ctrl Pts',(0.418478386678491,-2.48386417448843,
17.6639489310745));
#15210=CARTESIAN_POINT('Ctrl Pts',(0.499885569466697,-2.4673712058462,17.6691857947069));
#15211=CARTESIAN_POINT('Ctrl Pts',(0.582614830094737,-2.4506103862895,17.6745077066252));
#15212=CARTESIAN_POINT('Ctrl Pts',(0.664470266354718,-2.42969032947554,
17.6798296185435));
#15213=CARTESIAN_POINT('Ctrl Pts',(0.745011870101685,-2.40473773276996,
17.6851515304618));
#15214=CARTESIAN_POINT('Ctrl Pts',(0.824380137189749,-2.38014864753034,
17.6903959123328));
#15215=CARTESIAN_POINT('Ctrl Pts',(0.902472181408065,-2.35164396016609,
17.6956402942038));
#15216=CARTESIAN_POINT('Ctrl Pts',(0.978885838437445,-2.31939405132173,
17.7008846760748));
#15217=CARTESIAN_POINT('Ctrl Pts',(1.0569939814684,-2.28642899519594,17.7062453530168));
#15218=CARTESIAN_POINT('Ctrl Pts',(1.13334794865923,-2.24955084994424,17.7116060299587));
#15219=CARTESIAN_POINT('Ctrl Pts',(1.20754524343109,-2.20899088614393,17.7169667069007));
#15220=CARTESIAN_POINT('Ctrl Pts',(1.28174253820295,-2.16843092234362,17.7223273838426));
#15221=CARTESIAN_POINT('Ctrl Pts',(1.35378276292312,-2.12418946243883,17.7276880607846));
#15222=CARTESIAN_POINT('Ctrl Pts',(1.42329700739684,-2.07654325231506,17.7330487377266));
#15223=CARTESIAN_POINT('Ctrl Pts',(1.49114503923816,-2.03003909182148,17.7382809226205));
#15224=CARTESIAN_POINT('Ctrl Pts',(1.55684230741931,-1.98011643527403,17.7435131075144));
#15225=CARTESIAN_POINT('Ctrl Pts',(1.62002178070411,-1.92700173327485,17.7487452924084));
#15226=CARTESIAN_POINT('Ctrl Pts',(1.68311147158066,-1.8739625109467,17.7539700420051));
#15227=CARTESIAN_POINT('Ctrl Pts',(1.74369011917883,-1.81774054837828,17.7591947916019));
#15228=CARTESIAN_POINT('Ctrl Pts',(1.80141980490829,-1.75860539533011,17.7644195411987));
#15229=CARTESIAN_POINT('Ctrl Pts',(1.85908359270269,-1.69953774454575,17.7696383267891));
#15230=CARTESIAN_POINT('Ctrl Pts',(1.91390455729977,-1.63756384313869,17.7748571123796));
#15231=CARTESIAN_POINT('Ctrl Pts',(1.96557915130772,-1.57299232354911,17.78007589797));
#15232=CARTESIAN_POINT('Ctrl Pts',(2.0172216290745,-1.50846093575999,17.7852914400366));
#15233=CARTESIAN_POINT('Ctrl Pts',(2.06572132715847,-1.44133549699604,17.7905069821033));
#15234=CARTESIAN_POINT('Ctrl Pts',(2.11081356801578,-1.37195930372606,17.7957225241699));
#15235=CARTESIAN_POINT('Ctrl Pts',(2.15589170309462,-1.3026048127533,17.8009364347079));
#15236=CARTESIAN_POINT('Ctrl Pts',(2.19756424383842,-1.23100135583603,17.8061503452459));
#15237=CARTESIAN_POINT('Ctrl Pts',(2.23560946646314,-1.15752173347216,17.811364255784));
#15238=CARTESIAN_POINT('Ctrl Pts',(2.27365453179013,-1.08404241490932,17.8165781447651));
#15239=CARTESIAN_POINT('Ctrl Pts',(2.30807209595416,-1.00868736085614,17.8217920337462));
#15240=CARTESIAN_POINT('Ctrl Pts',(2.33868677023716,-0.931853229171688,
17.8270059227274));
#15241=CARTESIAN_POINT('Ctrl Pts',(2.36933131546493,-0.854944129905247,
17.8322248989353));
#15242=CARTESIAN_POINT('Ctrl Pts',(2.39616538709405,-0.776553504509373,
17.8374438751432));
#15243=CARTESIAN_POINT('Ctrl Pts',(2.41906231446636,-0.697096671006736,
17.842662851351));
#15244=CARTESIAN_POINT('Ctrl Pts',(2.44197035495879,-0.61760127279533,17.847884360611));
#15245=CARTESIAN_POINT('Ctrl Pts',(2.46093733889407,-0.53703908994231,17.853105869871));
#15246=CARTESIAN_POINT('Ctrl Pts',(2.47588753009016,-0.455836800120435,
17.8583273791309));
#15247=CARTESIAN_POINT('Ctrl Pts',(2.49086382410593,-0.374492732263679,
17.8635580050713));
#15248=CARTESIAN_POINT('Ctrl Pts',(2.50180925357153,-0.292506787464058,
17.8687886310116));
#15249=CARTESIAN_POINT('Ctrl Pts',(2.50869990928057,-0.210311709554351,
17.874019256952));
#15250=CARTESIAN_POINT('Ctrl Pts',(2.51458302607921,-0.140135043641119,
17.8784850704589));
#15251=CARTESIAN_POINT('Ctrl Pts',(2.51751132661983,-0.0698061540768173,
17.8829508839658));
#15252=CARTESIAN_POINT('Ctrl Pts',(2.5174999670525,0.000407296750591967,
17.8874166974728));
#15253=CARTESIAN_POINT('Ctrl Pts',(2.51749996705241,0.000407297304472808,
17.887416697508));
#15254=CARTESIAN_POINT('Ctrl Pts',(2.51749657468057,0.0213755087636416,
17.8887503468423));
#15255=CARTESIAN_POINT('Ctrl Pts',(2.51723122171354,0.0423413984397853,
17.8900839961765));
#15256=CARTESIAN_POINT('Ctrl Pts',(2.51670405080776,0.0633006370255141,
17.8914176455107));
#15257=CARTESIAN_POINT('Ctrl Pts',(2.5146266529764,0.145893732181795,17.896673095317));
#15258=CARTESIAN_POINT('Ctrl Pts',(2.50847531607989,0.228536699531577,17.9019285451234));
#15259=CARTESIAN_POINT('Ctrl Pts',(2.49824190001089,0.310795204322675,17.9071839949297));
#15260=CARTESIAN_POINT('Ctrl Pts',(2.48802121681506,0.392951359409476,17.9124329056707));
#15261=CARTESIAN_POINT('Ctrl Pts',(2.47372859023847,0.474723547684112,17.9176818164117));
#15262=CARTESIAN_POINT('Ctrl Pts',(2.45540786448767,0.555678386310031,17.9229307271527));
#15263=CARTESIAN_POINT('Ctrl Pts',(2.43710787198325,0.63654160975444,17.9281736977929));
#15264=CARTESIAN_POINT('Ctrl Pts',(2.41478894139686,0.716588874401286,17.933416668433));
#15265=CARTESIAN_POINT('Ctrl Pts',(2.38854638991777,0.795394489049787,17.9386596390731));
#15266=CARTESIAN_POINT('Ctrl Pts',(2.37992633856821,0.821280251165781,17.9403818296984));
#15267=CARTESIAN_POINT('Ctrl Pts',(2.37088335268766,0.847032122939052,17.9421040203238));
#15268=CARTESIAN_POINT('Ctrl Pts',(2.36142200728635,0.872635292378034,17.9438262109491));
#15269=CARTESIAN_POINT('Ctrl Pts',(2.36142200245778,0.872635305444532,17.6666805052528));
#15270=CARTESIAN_POINT('Ctrl Pts',(2.36852647042101,0.853410038188607,17.6653488246657));
#15271=CARTESIAN_POINT('Ctrl Pts',(2.37539678106655,0.834096324145541,17.664024563499));
#15272=CARTESIAN_POINT('Ctrl Pts',(2.38873305764868,0.795103455874879,17.6613777297893));
#15273=CARTESIAN_POINT('Ctrl Pts',(2.39519300344129,0.775426105040596,17.66005555027));
#15274=CARTESIAN_POINT('Ctrl Pts',(2.40524360830356,0.743486775147538,17.6579307055959));
#15275=CARTESIAN_POINT('Ctrl Pts',(2.40898492362142,0.731273579197981,17.6571231700799));
#15276=CARTESIAN_POINT('Ctrl Pts',(2.41597663677348,0.707813659158462,17.6555813333287));
#15277=CARTESIAN_POINT('Ctrl Pts',(2.41924184681766,0.696571733251215,17.6548465694267));
#15278=CARTESIAN_POINT('Ctrl Pts',(2.42652206522257,0.670837570782211,17.6531737039883));
#15279=CARTESIAN_POINT('Ctrl Pts',(2.43048590078596,0.656331228056072,17.6522372708427));
#15280=CARTESIAN_POINT('Ctrl Pts',(2.44262275397272,0.610295951665459,17.64928557178));
#15281=CARTESIAN_POINT('Ctrl Pts',(2.4503142302106,0.578642712636493,17.6472856822565));
#15282=CARTESIAN_POINT('Ctrl Pts',(2.4975046369567,0.366581558053989,17.6340659710036));
#15283=CARTESIAN_POINT('Ctrl Pts',(2.51766433186062,0.182446283241399,17.6234981640375));
#15284=CARTESIAN_POINT('Ctrl Pts',(2.51737314526642,-0.142834673721351,
17.6047994949253));
#15285=CARTESIAN_POINT('Ctrl Pts',(2.50547210456535,-0.283140984149819,
17.5967034201887));
#15286=CARTESIAN_POINT('Ctrl Pts',(2.47836124638302,-0.442702605875776,
17.586762917611));
#15287=CARTESIAN_POINT('Ctrl Pts',(2.47452654459574,-0.463657606306495,
17.5854424349002));
#15288=CARTESIAN_POINT('Ctrl Pts',(2.46880880944116,-0.492808231115945,
17.5835813541932));
#15289=CARTESIAN_POINT('Ctrl Pts',(2.46714981917896,-0.501047557853925,
17.5830526232002));
#15290=CARTESIAN_POINT('Ctrl Pts',(2.46421419884374,-0.515259088736036,
17.5821357333558));
#15291=CARTESIAN_POINT('Ctrl Pts',(2.46295702464022,-0.52123530116268,17.5817486602479));
#15292=CARTESIAN_POINT('Ctrl Pts',(2.46025563017538,-0.533848878301397,
17.5809283994724));
#15293=CARTESIAN_POINT('Ctrl Pts',(2.45880627580423,-0.540485046418643,
17.5804949144544));
#15294=CARTESIAN_POINT('Ctrl Pts',(2.45513795121516,-0.556961074306295,
17.5794139983031));
#15295=CARTESIAN_POINT('Ctrl Pts',(2.45288668210509,-0.566793537660574,
17.5787647830077));
#15296=CARTESIAN_POINT('Ctrl Pts',(2.44413713215133,-0.603978751760093,
17.5762944641234));
#15297=CARTESIAN_POINT('Ctrl Pts',(2.43724017005016,-0.631234386566123,
17.5744528644979));
#15298=CARTESIAN_POINT('Ctrl Pts',(2.41831461962658,-0.701084408853424,
17.5696631146307));
#15299=CARTESIAN_POINT('Ctrl Pts',(2.40561685005594,-0.743486432645809,
17.566687766892));
#15300=CARTESIAN_POINT('Ctrl Pts',(2.35326574772843,-0.902887038657014,
17.5552960553576));
#15301=CARTESIAN_POINT('Ctrl Pts',(2.30613835098239,-1.01724605370534,17.5467044586598));
#15302=CARTESIAN_POINT('Ctrl Pts',(2.1784670537797,-1.27207300962614,17.5270809238036));
#15303=CARTESIAN_POINT('Ctrl Pts',(2.09238842307821,-1.40918985266541,17.5161731667699));
#15304=CARTESIAN_POINT('Ctrl Pts',(1.98017136880731,-1.55474178976035,17.5043194883343));
#15305=CARTESIAN_POINT('Ctrl Pts',(1.96636158319714,-1.57217138333776,17.5028944245018));
#15306=CARTESIAN_POINT('Ctrl Pts',(1.9432378780257,-1.60057484736021,17.5005622258075));
#15307=CARTESIAN_POINT('Ctrl Pts',(1.93405779151004,-1.61165559772919,17.4996498425999));
#15308=CARTESIAN_POINT('Ctrl Pts',(1.91729955697565,-1.63153408181015,17.4980081898046));
#15309=CARTESIAN_POINT('Ctrl Pts',(1.90975464670018,-1.64035918261111,17.4972776066568));
#15310=CARTESIAN_POINT('Ctrl Pts',(1.89343293617127,-1.65918504066857,17.4957151231963));
#15311=CARTESIAN_POINT('Ctrl Pts',(1.88463733026128,-1.66916908284766,17.4948840246181));
#15312=CARTESIAN_POINT('Ctrl Pts',(1.86032366647938,-1.69633073303629,17.4926158484728));
#15313=CARTESIAN_POINT('Ctrl Pts',(1.84464695245412,-1.71336504447413,17.4911854083391));
#15314=CARTESIAN_POINT('Ctrl Pts',(1.75069344833865,-1.81267040253474,17.4827934073785));
#15315=CARTESIAN_POINT('Ctrl Pts',(1.66715297498732,-1.88979022795572,17.4760660046176));
#15316=CARTESIAN_POINT('Ctrl Pts',(1.49822145318466,-2.02578578548784,17.4634503421306));
#15317=CARTESIAN_POINT('Ctrl Pts',(1.41385019477008,-2.08554635922527,17.4575516252619));
#15318=CARTESIAN_POINT('Ctrl Pts',(1.2746231586498,-2.17181993181033,17.4481173036935));
#15319=CARTESIAN_POINT('Ctrl Pts',(1.22206953903167,-2.20182005116195,17.4446172366581));
#15320=CARTESIAN_POINT('Ctrl Pts',(1.10254187341139,-2.26445375093377,17.436685062568));
#15321=CARTESIAN_POINT('Ctrl Pts',(1.03510107053155,-2.29606466647722,17.4322283108932));
#15322=CARTESIAN_POINT('Ctrl Pts',(0.954372317157444,-2.32962409901796,
17.4268033747336));
#15323=CARTESIAN_POINT('Ctrl Pts',(0.942340328305685,-2.3345170060709,17.4259925276703));
#15324=CARTESIAN_POINT('Ctrl Pts',(0.92265979136514,-2.34234332592722,17.4246616525941));
#15325=CARTESIAN_POINT('Ctrl Pts',(0.915033669660928,-2.34533296698862,
17.4241448293723));
#15326=CARTESIAN_POINT('Ctrl Pts',(0.90132122913042,-2.35063154618716,17.4232133058139));
#15327=CARTESIAN_POINT('Ctrl Pts',(0.895240384186967,-2.35295415948832,
17.4227994217957));
#15328=CARTESIAN_POINT('Ctrl Pts',(0.881825309052589,-2.3580185920181,17.4218845545394));
#15329=CARTESIAN_POINT('Ctrl Pts',(0.87448736370691,-2.36074975436955,17.4213829782638));
#15330=CARTESIAN_POINT('Ctrl Pts',(0.853181412280496,-2.36856680301356,
17.4199235527773));
#15331=CARTESIAN_POINT('Ctrl Pts',(0.83918122564888,-2.37356315861529,17.4189607341301));
#15332=CARTESIAN_POINT('Ctrl Pts',(0.721029303889196,-2.41455298544116,
17.4108079374253));
#15333=CARTESIAN_POINT('Ctrl Pts',(0.614672686949972,-2.44379241553572,
17.4032962562693));
#15334=CARTESIAN_POINT('Ctrl Pts',(0.336499328528819,-2.50095706370979,
17.3837385649846));
#15335=CARTESIAN_POINT('Ctrl Pts',(0.163053289205865,-2.5182225300802,17.3716617216909));
#15336=CARTESIAN_POINT('Ctrl Pts',(-0.0818745105656113,-2.51717197942581,
17.3553260338495));
#15337=CARTESIAN_POINT('Ctrl Pts',(-0.152911277046764,-2.51385719079346,
17.3506665708687));
#15338=CARTESIAN_POINT('Ctrl Pts',(-0.244680875857199,-2.50566965780357,
17.3447468227948));
#15339=CARTESIAN_POINT('Ctrl Pts',(-0.265619383338332,-2.50353660891511,
17.3434027949171));
#15340=CARTESIAN_POINT('Ctrl Pts',(-0.299293162852124,-2.49967896122964,
17.3412514821693));
#15341=CARTESIAN_POINT('Ctrl Pts',(-0.31204592046886,-2.49811902438594,
17.3404391051219));
#15342=CARTESIAN_POINT('Ctrl Pts',(-0.336376510593825,-2.49495364647654,
17.3388935122801));
#15343=CARTESIAN_POINT('Ctrl Pts',(-0.347956160916023,-2.49336507002573,
17.3381597907208));
#15344=CARTESIAN_POINT('Ctrl Pts',(-0.374515202248042,-2.4895328905997,
17.3364810306681));
#15345=CARTESIAN_POINT('Ctrl Pts',(-0.389486343124227,-2.48723461989581,
17.3355377292126));
#15346=CARTESIAN_POINT('Ctrl Pts',(-0.436284966240024,-2.47961749090798,
17.3325977646291));
#15347=CARTESIAN_POINT('Ctrl Pts',(-0.468032269140274,-2.473821621065,17.3306160580795));
#15348=CARTESIAN_POINT('Ctrl Pts',(-0.628555134452087,-2.44131518036286,
17.3206472409808));
#15349=CARTESIAN_POINT('Ctrl Pts',(-0.755213322066048,-2.4051527878217,
17.312963795227));
#15350=CARTESIAN_POINT('Ctrl Pts',(-1.01011534986747,-2.31023897717009,
17.2972746945933));
#15351=CARTESIAN_POINT('Ctrl Pts',(-1.13741126208741,-2.25029517202352,
17.2893089230232));
#15352=CARTESIAN_POINT('Ctrl Pts',(-1.31597236321481,-2.14717161568439,
17.2771259365905));
#15353=CARTESIAN_POINT('Ctrl Pts',(-1.37159344056241,-2.11207458757824,
17.2731708088443));
#15354=CARTESIAN_POINT('Ctrl Pts',(-1.4371224858811,-2.06704496328576,17.2682333979137));
#15355=CARTESIAN_POINT('Ctrl Pts',(-1.4484084966615,-2.05915242918485,17.267372675277));
#15356=CARTESIAN_POINT('Ctrl Pts',(-1.46588726439985,-2.04671438631972,
17.2660224823702));
#15357=CARTESIAN_POINT('Ctrl Pts',(-1.47212512858,-2.04223232106142,17.2655371706916));
#15358=CARTESIAN_POINT('Ctrl Pts',(-1.48309119450267,-2.03427657432648,
17.2646777043376));
#15359=CARTESIAN_POINT('Ctrl Pts',(-1.48782788829705,-2.03081482286425,
17.2643043643747));
#15360=CARTESIAN_POINT('Ctrl Pts',(-1.49902503710075,-2.02257133117975,
17.2634168335519));
#15361=CARTESIAN_POINT('Ctrl Pts',(-1.50547466017881,-2.01777523398066,
17.2629016683259));
#15362=CARTESIAN_POINT('Ctrl Pts',(-1.52459393713099,-2.0034149773373,17.2613630152951));
#15363=CARTESIAN_POINT('Ctrl Pts',(-1.53719594113133,-1.99376198496496,
17.2603337224881));
#15364=CARTESIAN_POINT('Ctrl Pts',(-1.66124153343151,-1.89686933218797,
17.2500579089718));
#15365=CARTESIAN_POINT('Ctrl Pts',(-1.76522068708018,-1.800506636014,17.2402943683696));
#15366=CARTESIAN_POINT('Ctrl Pts',(-1.9908605028757,-1.55296586749063,17.217154659469));
#15367=CARTESIAN_POINT('Ctrl Pts',(-2.10428986702762,-1.39542791838508,
17.2038855962678));
#15368=CARTESIAN_POINT('Ctrl Pts',(-2.21415981578012,-1.19846881134589,
17.1892427120159));
#15369=CARTESIAN_POINT('Ctrl Pts',(-2.22922187092713,-1.1702141624134,17.1871827037195));
#15370=CARTESIAN_POINT('Ctrl Pts',(-2.25051523571947,-1.12836631022428,
17.1841892486697));
#15371=CARTESIAN_POINT('Ctrl Pts',(-2.25717050774065,-1.11499357438125,
17.1832411284448));
#15372=CARTESIAN_POINT('Ctrl Pts',(-2.26882302673851,-1.09104768752096,
17.1815581356364));
#15373=CARTESIAN_POINT('Ctrl Pts',(-2.27386631628235,-1.08049755493998,
17.1808216890569));
#15374=CARTESIAN_POINT('Ctrl Pts',(-2.2842867905785,-1.05830270130007,17.1792827712986));
#15375=CARTESIAN_POINT('Ctrl Pts',(-2.28964887319293,-1.04665122957376,
17.1784808341678));
#15376=CARTESIAN_POINT('Ctrl Pts',(-2.30353301862119,-1.01586447963842,
17.1763771207906));
#15377=CARTESIAN_POINT('Ctrl Pts',(-2.31190582387938,-0.996662686845945,
17.1750804273303));
#15378=CARTESIAN_POINT('Ctrl Pts',(-2.35054783521849,-0.904934858698359,
17.1689557611542));
#15379=CARTESIAN_POINT('Ctrl Pts',(-2.3776514490624,-0.831118286420926,
17.1642342406773));
#15380=CARTESIAN_POINT('Ctrl Pts',(-2.44373228989777,-0.621269042164098,
17.1512420651925));
#15381=CARTESIAN_POINT('Ctrl Pts',(-2.47476609064376,-0.483050291452884,
17.1431862309463));
#15382=CARTESIAN_POINT('Ctrl Pts',(-2.50195272400195,-0.285342698903077,
17.1316932275178));
#15383=CARTESIAN_POINT('Ctrl Pts',(-2.50787587372179,-0.227477582243425,
17.1283304593088));
#15384=CARTESIAN_POINT('Ctrl Pts',(-2.51329123624318,-0.147210017682062,
17.1236095816729));
#15385=CARTESIAN_POINT('Ctrl Pts',(-2.51449667804207,-0.124940147803237,
17.1222937910304));
#15386=CARTESIAN_POINT('Ctrl Pts',(-2.51774068580823,-0.0454527179734783,
17.1175670775158));
#15387=CARTESIAN_POINT('Ctrl Pts',(-2.51812301768035,0.01181060981283,17.1141060973369));
#15388=CARTESIAN_POINT('Ctrl Pts',(-2.5161898701013,0.0822830847172104,
17.1097244262833));
#15389=CARTESIAN_POINT('Ctrl Pts',(-2.5157217375488,0.0955305703542631,
17.1088954189292));
#15390=CARTESIAN_POINT('Ctrl Pts',(-2.51482219019189,0.116330651720235,
17.1075845361629));
#15391=CARTESIAN_POINT('Ctrl Pts',(-2.51446130557067,0.12388627060511,17.1071064410165));
#15392=CARTESIAN_POINT('Ctrl Pts',(-2.51375936165838,0.137312420783076,
17.1062532872409));
#15393=CARTESIAN_POINT('Ctrl Pts',(-2.51343177838748,0.143183526404349,
17.1058789792501));
#15394=CARTESIAN_POINT('Ctrl Pts',(-2.51259883877228,0.157227128567068,
17.1049807090772));
#15395=CARTESIAN_POINT('Ctrl Pts',(-2.51207418207066,0.165398288499605,
17.104455696716));
#15396=CARTESIAN_POINT('Ctrl Pts',(-2.51036351088478,0.190151709419325,
17.102858381021));
#15397=CARTESIAN_POINT('Ctrl Pts',(-2.50905312027644,0.206724537112013,
17.1017796145281));
#15398=CARTESIAN_POINT('Ctrl Pts',(-2.49564153304598,0.357343549882187,
17.0918977360187));
#15399=CARTESIAN_POINT('Ctrl Pts',(-2.47297397648725,0.490217386015908,
17.0826310717887));
#15400=CARTESIAN_POINT('Ctrl Pts',(-2.39047438510124,0.81453871419814,17.059515922372));
#15401=CARTESIAN_POINT('Ctrl Pts',(-2.31819608817071,1.00191670106038,17.0457675949804));
#15402=CARTESIAN_POINT('Ctrl Pts',(-2.20975742059279,1.20655140952358,17.0307387114162));
#15403=CARTESIAN_POINT('Ctrl Pts',(-2.19452099841641,1.23404695822713,17.0287169450877));
#15404=CARTESIAN_POINT('Ctrl Pts',(-2.17126358267775,1.27422344232747,17.0257578820989));
#15405=CARTESIAN_POINT('Ctrl Pts',(-2.16363825053626,1.28712876709745,17.0248066183301));
#15406=CARTESIAN_POINT('Ctrl Pts',(-2.14987271574392,1.30995790351896,17.0231222368029));
#15407=CARTESIAN_POINT('Ctrl Pts',(-2.14377797723277,1.31990847963964,17.0223875054212));
#15408=CARTESIAN_POINT('Ctrl Pts',(-2.1307845751477,1.3407947309133,17.0208439532374));
#15409=CARTESIAN_POINT('Ctrl Pts',(-2.12387038762523,1.35172038625714,17.0200357265744));
#15410=CARTESIAN_POINT('Ctrl Pts',(-2.1052786611993,1.38060379103463,17.0178966212008));
#15411=CARTESIAN_POINT('Ctrl Pts',(-2.09345542343198,1.39846684013917,17.0165711451767));
#15412=CARTESIAN_POINT('Ctrl Pts',(-2.03379995725953,1.48614457009966,17.0100491507113));
#15413=CARTESIAN_POINT('Ctrl Pts',(-1.98269395186465,1.55367140362027,17.0049773569991));
#15414=CARTESIAN_POINT('Ctrl Pts',(-1.86426094576879,1.6947722449797,16.9941315085167));
#15415=CARTESIAN_POINT('Ctrl Pts',(-1.79577175247373,1.76718053498851,16.9884023009395));
#15416=CARTESIAN_POINT('Ctrl Pts',(-1.60595414008019,1.94539693318515,16.9734409095532));
#15417=CARTESIAN_POINT('Ctrl Pts',(-1.47847874253534,2.04395315689368,16.9642635590213));
#15418=CARTESIAN_POINT('Ctrl Pts',(-1.32516284582363,2.14060031858582,16.9531207272754));
#15419=CARTESIAN_POINT('Ctrl Pts',(-1.30769305100589,2.15131706505944,16.951849367027));
#15420=CARTESIAN_POINT('Ctrl Pts',(-1.28299466097652,2.16605616711589,16.9500467706899));
#15421=CARTESIAN_POINT('Ctrl Pts',(-1.27587359057164,2.1702583246172,16.9495264476917));
#15422=CARTESIAN_POINT('Ctrl Pts',(-1.26296498426474,2.17779022883212,16.9485819250208));
#15423=CARTESIAN_POINT('Ctrl Pts',(-1.25718459163581,2.18113221363248,16.9481584998522));
#15424=CARTESIAN_POINT('Ctrl Pts',(-1.24533274748168,2.18792169545012,16.9472892220381));
#15425=CARTESIAN_POINT('Ctrl Pts',(-1.23926015649566,2.1913669841099,16.9468432439203));
#15426=CARTESIAN_POINT('Ctrl Pts',(-1.22361179927868,2.20015924442058,16.945692673882));
#15427=CARTESIAN_POINT('Ctrl Pts',(-1.21401539841958,2.20546891569288,16.9449858036987));
#15428=CARTESIAN_POINT('Ctrl Pts',(-1.17344779959629,2.22756990430983,16.9419932027643));
#15429=CARTESIAN_POINT('Ctrl Pts',(-1.14216218370164,2.24377197341134,16.9396746249137));
#15430=CARTESIAN_POINT('Ctrl Pts',(-1.05570762704758,2.28626811364174,16.9332588189138));
#15431=CARTESIAN_POINT('Ctrl Pts',(-0.999906399621586,2.31121758519661,
16.9291087384412));
#15432=CARTESIAN_POINT('Ctrl Pts',(-0.769907649540935,2.4041642736662,16.9121072641027));
#15433=CARTESIAN_POINT('Ctrl Pts',(-0.589268904905663,2.45469747938334,
16.8990469173539));
#15434=CARTESIAN_POINT('Ctrl Pts',(-0.328019710017269,2.49724735320643,
16.8813303737569));
#15435=CARTESIAN_POINT('Ctrl Pts',(-0.250801782163873,2.50618072842428,
16.8762247917211));
#15436=CARTESIAN_POINT('Ctrl Pts',(-0.151648156964318,2.51302199753124,
16.8698343664724));
#15437=CARTESIAN_POINT('Ctrl Pts',(-0.129990276075862,2.514235331034,16.8684484209119));
#15438=CARTESIAN_POINT('Ctrl Pts',(-0.0953427365522925,2.51572747022526,
16.8662464797875));
#15439=CARTESIAN_POINT('Ctrl Pts',(-0.0823622982543662,2.51618588422144,
16.8654249534322));
#15440=CARTESIAN_POINT('Ctrl Pts',(-0.0577272197924998,2.51686504964141,
16.8638720936828));
#15441=CARTESIAN_POINT('Ctrl Pts',(-0.0460735021914871,2.51710535134083,
16.8631401736264));
#15442=CARTESIAN_POINT('Ctrl Pts',(-0.0195375784786025,2.51746817508612,
16.8614794388107));
#15443=CARTESIAN_POINT('Ctrl Pts',(-0.00465502397778445,2.51753968693572,
16.8605522284459));
#15444=CARTESIAN_POINT('Ctrl Pts',(0.0410955819904817,2.51735381988979,
16.8577141679389));
#15445=CARTESIAN_POINT('Ctrl Pts',(0.0719596710107643,2.51666069115791,
16.8558167976196));
#15446=CARTESIAN_POINT('Ctrl Pts',(0.222730710596222,2.51049868640108,16.8466211458042));
#15447=CARTESIAN_POINT('Ctrl Pts',(0.342160070320115,2.49702701188625,16.8395727410772));
#15448=CARTESIAN_POINT('Ctrl Pts',(0.551896097116948,2.45803149504487,16.8272310651655));
#15449=CARTESIAN_POINT('Ctrl Pts',(0.642589129244993,2.43589559007007,16.8219037203371));
#15450=CARTESIAN_POINT('Ctrl Pts',(0.850847305419339,2.37262177351255,16.8093448610315));
#15451=CARTESIAN_POINT('Ctrl Pts',(0.966992219218174,2.32770123747517,16.8020888789459));
#15452=CARTESIAN_POINT('Ctrl Pts',(1.09171545978951,2.26851309564244,16.7935331180829));
#15453=CARTESIAN_POINT('Ctrl Pts',(1.10405612927462,2.26253273001271,16.7926778683132));
#15454=CARTESIAN_POINT('Ctrl Pts',(1.12388270772251,2.25272381693973,16.7912887441196));
#15455=CARTESIAN_POINT('Ctrl Pts',(1.13139955807838,2.24895797455137,16.7907585580609));
#15456=CARTESIAN_POINT('Ctrl Pts',(1.14471441206514,2.24220376224245,16.7898128931002));
#15457=CARTESIAN_POINT('Ctrl Pts',(1.15051984913076,2.2392304195662,16.789398342989));
#15458=CARTESIAN_POINT('Ctrl Pts',(1.15634887610778,2.23621634201296,16.7889798335824));
#15459=CARTESIAN_POINT('Ctrl Pts',(1.15638397704102,2.23619819094917,16.7889773133415));
#15460=CARTESIAN_POINT('Ctrl Pts',(1.1564526386876,2.23616268323664,16.7889723832859));
#15461=CARTESIAN_POINT('Ctrl Pts',(1.15648619946039,2.236145326647,16.788969973474));
#15462=CARTESIAN_POINT('Ctrl Pts',(1.1565518499205,2.23611137239421,16.7889652593329));
#15463=CARTESIAN_POINT('Ctrl Pts',(1.15658393963845,2.23609477479726,16.7889629550081));
#15464=CARTESIAN_POINT('Ctrl Pts',(1.15665248055706,2.23605932186635,16.7889580330181));
#15465=CARTESIAN_POINT('Ctrl Pts',(1.15668893168188,2.23604046631738,16.7889554153385));
#15466=CARTESIAN_POINT('Ctrl Pts',(1.15676146848256,2.23600294201165,16.7889502060462));
#15467=CARTESIAN_POINT('Ctrl Pts',(1.15679755411129,2.23598427330176,16.7889476144387));
#15468=CARTESIAN_POINT('Ctrl Pts',(1.15686936439946,2.2359471204239,16.7889424569744));
#15469=CARTESIAN_POINT('Ctrl Pts',(1.15690508909205,2.23592863626075,16.788939891117));
#15470=CARTESIAN_POINT('Ctrl Pts',(1.15697618209334,2.23589185016955,16.7889347848285));
#15471=CARTESIAN_POINT('Ctrl Pts',(1.15701155040356,2.2358735482622,16.7889322443992));
#15472=CARTESIAN_POINT('Ctrl Pts',(1.15708193506811,2.23583712445553,16.788927188654));
#15473=CARTESIAN_POINT('Ctrl Pts',(1.15711695145003,2.23581900256294,16.7889246733378));
#15474=CARTESIAN_POINT('Ctrl Pts',(1.15718663671241,2.23578293654329,16.788919667504));
#15475=CARTESIAN_POINT('Ctrl Pts',(1.15722130559132,2.23576499243759,16.7889171769881));
#15476=CARTESIAN_POINT('Ctrl Pts',(1.15729030017731,2.23572927981218,16.7889122204486));
#15477=CARTESIAN_POINT('Ctrl Pts',(1.15732462589627,2.23571151130642,16.7889097544258));
#15478=CARTESIAN_POINT('Ctrl Pts',(1.15739293846639,2.235676147713,16.788904846568));
#15479=CARTESIAN_POINT('Ctrl Pts',(1.1574269253212,2.23565855264309,16.7889024047343));
#15480=CARTESIAN_POINT('Ctrl Pts',(1.1574945643791,2.23562353379743,16.7888975449567));
#15481=CARTESIAN_POINT('Ctrl Pts',(1.15752821659453,2.23560611003449,16.7888951270133));
#15482=CARTESIAN_POINT('Ctrl Pts',(1.15759519056256,2.23557143169134,16.7888903147196));
#15483=CARTESIAN_POINT('Ctrl Pts',(1.15762851231809,2.2355541771284,16.7888879203707));
#15484=CARTESIAN_POINT('Ctrl Pts',(1.15769482944929,2.23551983512718,16.788883154977));
#15485=CARTESIAN_POINT('Ctrl Pts',(1.15772782484072,2.23550274769911,16.7888807839326));
#15486=CARTESIAN_POINT('Ctrl Pts',(1.15779349337626,2.23546873788239,16.7888760648554));
#15487=CARTESIAN_POINT('Ctrl Pts',(1.15782616649475,2.23545181552499,16.7888737168259));
#15488=CARTESIAN_POINT('Ctrl Pts',(1.15789119438795,2.23541813388157,16.7888690435022));
#15489=CARTESIAN_POINT('Ctrl Pts',(1.15792354919917,2.23540137459422,16.7888667182068));
#15490=CARTESIAN_POINT('Ctrl Pts',(1.15798794447562,2.23536801707263,16.788862090068));
#15491=CARTESIAN_POINT('Ctrl Pts',(1.15801998493697,2.2353514188576,16.7888597872264));
#15492=CARTESIAN_POINT('Ctrl Pts',(1.15808375540778,2.23531838151474,16.7888552037195));
#15493=CARTESIAN_POINT('Ctrl Pts',(1.15811548541356,2.23530194240563,16.7888529230557));
#15494=CARTESIAN_POINT('Ctrl Pts',(1.15817863878579,2.2352692213496,16.7888483836346));
#15495=CARTESIAN_POINT('Ctrl Pts',(1.15821006216592,2.23525293941203,16.7888461248774));
#15496=CARTESIAN_POINT('Ctrl Pts',(1.15827260605423,2.23522053079621,16.7888416290025));
#15497=CARTESIAN_POINT('Ctrl Pts',(1.15830372658138,2.23520440412421,16.7888393918846));
#15498=CARTESIAN_POINT('Ctrl Pts',(1.1583656685171,2.23517230414258,16.7888349390222));
#15499=CARTESIAN_POINT('Ctrl Pts',(1.158396489928,2.23515633084749,16.7888327232787));
#15500=CARTESIAN_POINT('Ctrl Pts',(1.15845783728866,2.23512453577125,16.7888283129059));
#15501=CARTESIAN_POINT('Ctrl Pts',(1.1584883632538,2.23510871399753,16.7888261182766));
#15502=CARTESIAN_POINT('Ctrl Pts',(1.15854912333037,2.23507722014031,16.7888217498764));
#15503=CARTESIAN_POINT('Ctrl Pts',(1.15857935745914,2.23506154806289,16.7888195761055));
#15504=CARTESIAN_POINT('Ctrl Pts',(1.15863953749895,2.23503035175856,16.7888152491641));
#15505=CARTESIAN_POINT('Ctrl Pts',(1.15866948339032,2.23501482755658,16.7888130959963));
#15506=CARTESIAN_POINT('Ctrl Pts',(1.15872909039696,2.23498392526302,16.7888088100171));
#15507=CARTESIAN_POINT('Ctrl Pts',(1.1587587515387,2.23496854717214,16.7888066772051));
#15508=CARTESIAN_POINT('Ctrl Pts',(1.15881779260454,2.23493793529896,16.788802431685));
#15509=CARTESIAN_POINT('Ctrl Pts',(1.15884717250253,2.23492270154432,16.7888003189799));
#15510=CARTESIAN_POINT('Ctrl Pts',(1.15890565443687,2.23489237664567,16.788796113436));
#15511=CARTESIAN_POINT('Ctrl Pts',(1.1589347564993,2.23487728550195,16.7887940205962));
#15512=CARTESIAN_POINT('Ctrl Pts',(1.16596386831419,2.23123210032163,16.7882885168057));
#15513=CARTESIAN_POINT('Ctrl Pts',(1.17294667193779,2.22756919723958,16.7877830656492));
#15514=CARTESIAN_POINT('Ctrl Pts',(1.19364229379309,2.21658880102117,16.7862755062734));
#15515=CARTESIAN_POINT('Ctrl Pts',(1.20730438741661,2.20917720562903,16.7852678403533));
#15516=CARTESIAN_POINT('Ctrl Pts',(1.23874542671307,2.19174190270448,16.7829214176238));
#15517=CARTESIAN_POINT('Ctrl Pts',(1.25647266220078,2.18162764752998,16.7815778823021));
#15518=CARTESIAN_POINT('Ctrl Pts',(1.45450050518641,2.06542893160591,16.7663527645449));
#15519=CARTESIAN_POINT('Ctrl Pts',(1.62102341867364,1.93748633406573,16.7515932693172));
#15520=CARTESIAN_POINT('Ctrl Pts',(1.85413250927938,1.70706149253897,16.7292684387356));
#15521=CARTESIAN_POINT('Ctrl Pts',(1.93247656960569,1.6178404408104,16.7213655716422));
#15522=CARTESIAN_POINT('Ctrl Pts',(2.01867499737448,1.50443540966903,16.7121834708676));
#15523=CARTESIAN_POINT('Ctrl Pts',(2.03283199644166,1.48525041154071,16.7106571168647));
#15524=CARTESIAN_POINT('Ctrl Pts',(2.05463125985263,1.45481321337406,16.7082768056118));
#15525=CARTESIAN_POINT('Ctrl Pts',(2.0624582331433,1.44369565632973,16.7074158218379));
#15526=CARTESIAN_POINT('Ctrl Pts',(2.07672674084776,1.42307556476004,16.7058342215236));
#15527=CARTESIAN_POINT('Ctrl Pts',(2.08319404391952,1.41359138423154,16.7051126441305));
#15528=CARTESIAN_POINT('Ctrl Pts',(2.09738946126581,1.39246506121984,16.7035180989009));
#15529=CARTESIAN_POINT('Ctrl Pts',(2.1050860088038,1.38080208826186,16.7026463256163));
#15530=CARTESIAN_POINT('Ctrl Pts',(2.12698956236018,1.34700167723768,16.7001437507135));
#15531=CARTESIAN_POINT('Ctrl Pts',(2.14094751390689,1.32470447247281,16.69852211908));
#15532=CARTESIAN_POINT('Ctrl Pts',(2.23694643938591,1.16586855219531,16.6871649981279));
#15533=CARTESIAN_POINT('Ctrl Pts',(2.30621050315556,1.02204210687976,16.6779144161415));
#15534=CARTESIAN_POINT('Ctrl Pts',(2.36142200368728,0.872635302117406,16.6687517122259));
#15535=CARTESIAN_POINT('Origin',(0.,0.,10.));
#15536=CARTESIAN_POINT('',(2.36142199860763,0.87263531586336,15.670984110559));
#15537=CARTESIAN_POINT('',(2.36142200728636,0.872635292378008,15.9436790867324));
#15538=CARTESIAN_POINT('',(2.36142200728636,0.87263529237802,10.));
#15539=CARTESIAN_POINT('',(2.5174993049387,0.00187073064801871,16.8874166975661));
#15540=CARTESIAN_POINT('Ctrl Pts',(2.36142200728636,0.872635292378007,15.9436790867324));
#15541=CARTESIAN_POINT('Ctrl Pts',(2.33256006636991,0.950738049679249,15.9489328860113));
#15542=CARTESIAN_POINT('Ctrl Pts',(2.29984299449287,1.02734321032059,15.9541866852901));
#15543=CARTESIAN_POINT('Ctrl Pts',(2.263465206547,1.10205785181685,15.959440484569));
#15544=CARTESIAN_POINT('Ctrl Pts',(2.22701756461404,1.17691596315821,15.9647043723894));
#15545=CARTESIAN_POINT('Ctrl Pts',(2.18689538095588,1.24987589771121,15.9699682602098));
#15546=CARTESIAN_POINT('Ctrl Pts',(2.14333851663164,1.32057042717277,15.9752321480303));
#15547=CARTESIAN_POINT('Ctrl Pts',(2.09987283734388,1.39111695968029,15.9804850160537));
#15548=CARTESIAN_POINT('Ctrl Pts',(2.05298716645419,1.45940723729897,15.9857378840772));
#15549=CARTESIAN_POINT('Ctrl Pts',(2.00295963408966,1.5251094892523,15.9909907521006));
#15550=CARTESIAN_POINT('Ctrl Pts',(1.95290942195784,1.59084152703984,15.9962460014893));
#15551=CARTESIAN_POINT('Ctrl Pts',(1.89952761462273,1.65422856365248,16.0015012508779));
#15552=CARTESIAN_POINT('Ctrl Pts',(1.84306196642989,1.71491365319061,16.0067565002666));
#15553=CARTESIAN_POINT('Ctrl Pts',(1.78667637373961,1.77551270501385,16.0120042989016));
#15554=CARTESIAN_POINT('Ctrl Pts',(1.72721593632925,1.83341708376036,16.0172520975367));
#15555=CARTESIAN_POINT('Ctrl Pts',(1.66496986958113,1.88830124275418,16.0224998961717));
#15556=CARTESIAN_POINT('Ctrl Pts',(1.6022727760879,1.9435830850858,16.0277857196598));
#15557=CARTESIAN_POINT('Ctrl Pts',(1.536749801404,1.99580037773037,16.0330715431478));
#15558=CARTESIAN_POINT('Ctrl Pts',(1.46873581844402,2.0446567794179,16.0383573666359));
#15559=CARTESIAN_POINT('Ctrl Pts',(1.40133171264408,2.09307508878655,16.0435957924731));
#15560=CARTESIAN_POINT('Ctrl Pts',(1.3314814747371,2.13819226543406,16.0488342183103));
#15561=CARTESIAN_POINT('Ctrl Pts',(1.25954438553007,2.17976012232532,16.0540726441475));
#15562=CARTESIAN_POINT('Ctrl Pts',(1.18763095527944,2.22131430821425,16.0593093471503));
#15563=CARTESIAN_POINT('Ctrl Pts',(1.11363243602454,2.25932126202357,16.0645460501531));
#15564=CARTESIAN_POINT('Ctrl Pts',(1.0379353599718,2.29357721442296,16.069782753156));
#15565=CARTESIAN_POINT('Ctrl Pts',(0.962240345915608,2.32783223368651,16.0750193135105));
#15566=CARTESIAN_POINT('Ctrl Pts',(0.884847287860035,2.35833626539672,16.080255873865));
#15567=CARTESIAN_POINT('Ctrl Pts',(0.806164213719876,2.38493302013231,16.0854924342194));
#15568=CARTESIAN_POINT('Ctrl Pts',(0.726193308647712,2.4119650924227,16.0908147030249));
#15569=CARTESIAN_POINT('Ctrl Pts',(0.644890239921313,2.4349606605837,16.0961369718304));
#15570=CARTESIAN_POINT('Ctrl Pts',(0.562699290720848,2.45380841921741,16.1014592406358));
#15571=CARTESIAN_POINT('Ctrl Pts',(0.481715787896842,2.47237929021218,16.1067033213409));
#15572=CARTESIAN_POINT('Ctrl Pts',(0.399870790227692,2.48692339010019,16.111947402046));
#15573=CARTESIAN_POINT('Ctrl Pts',(0.317597611250558,2.49738623511221,16.1171914827511));
#15574=CARTESIAN_POINT('Ctrl Pts',(0.233484419523207,2.5080830782323,16.1225528456068));
#15575=CARTESIAN_POINT('Ctrl Pts',(0.148924173671973,2.51451387293495,16.1279142084624));
#15576=CARTESIAN_POINT('Ctrl Pts',(0.0643812902686016,2.51667663784272,
16.133275571318));
#15577=CARTESIAN_POINT('Ctrl Pts',(-0.020161593134758,2.51883940275049,
16.1386369341736));
#15578=CARTESIAN_POINT('Ctrl Pts',(-0.10468660780405,2.51673421729153,16.1439982970293));
#15579=CARTESIAN_POINT('Ctrl Pts',(-0.188735569826069,2.51041533111205,
16.1493596598849));
#15580=CARTESIAN_POINT('Ctrl Pts',(-0.271121035916884,2.50422150824325,
16.1546149107186));
#15581=CARTESIAN_POINT('Ctrl Pts',(-0.353353424571359,2.49395642717338,
16.1598701615524));
#15582=CARTESIAN_POINT('Ctrl Pts',(-0.434998441876353,2.47963356275986,
16.1651254123862));
#15583=CARTESIAN_POINT('Ctrl Pts',(-0.516527705220022,2.46533100489225,
16.1703732124762));
#15584=CARTESIAN_POINT('Ctrl Pts',(-0.597470800626601,2.4469821698992,16.1756210125662));
#15585=CARTESIAN_POINT('Ctrl Pts',(-0.677397198106076,2.4246524051909,16.1808688126562));
#15586=CARTESIAN_POINT('Ctrl Pts',(-0.757902703820998,2.40216084974706,
16.1861546357817));
#15587=CARTESIAN_POINT('Ctrl Pts',(-0.837376243884293,2.37563046891055,
16.1914404589073));
#15588=CARTESIAN_POINT('Ctrl Pts',(-0.91538692772202,2.34518080807337,16.1967262820328));
#15589=CARTESIAN_POINT('Ctrl Pts',(-0.992698121574452,2.315004176926,16.2019647093382));
#15590=CARTESIAN_POINT('Ctrl Pts',(-1.06857215004843,2.28097844032329,16.2072031366436));
#15591=CARTESIAN_POINT('Ctrl Pts',(-1.14260522462048,2.24326983456515,16.2124415639489));
#15592=CARTESIAN_POINT('Ctrl Pts',(-1.21661395093089,2.20557363054778,16.2176782684217));
#15593=CARTESIAN_POINT('Ctrl Pts',(-1.2887825149814,2.1641971722119,16.2229149728944));
#15594=CARTESIAN_POINT('Ctrl Pts',(-1.35872954841789,2.11935373740584,16.2281516773671));
#15595=CARTESIAN_POINT('Ctrl Pts',(-1.42867467648605,2.07451152414209,16.2333882391912));
#15596=CARTESIAN_POINT('Ctrl Pts',(-1.49639800636966,2.02620277208412,16.2386248010153));
#15597=CARTESIAN_POINT('Ctrl Pts',(-1.56154629212837,1.97468464002234,16.2438613628393));
#15598=CARTESIAN_POINT('Ctrl Pts',(-1.62776084044333,1.92232332606336,16.2491836299085));
#15599=CARTESIAN_POINT('Ctrl Pts',(-1.69131490038314,1.86664692509891,16.2545058969776));
#15600=CARTESIAN_POINT('Ctrl Pts',(-1.75187321961527,1.80796749760465,16.2598281640467));
#15601=CARTESIAN_POINT('Ctrl Pts',(-1.81154192795574,1.75015007979753,16.2650722462056));
#15602=CARTESIAN_POINT('Ctrl Pts',(-1.8683020524125,1.68941766349438,16.2703163283645));
#15603=CARTESIAN_POINT('Ctrl Pts',(-1.92187197401931,1.62610404509648,16.2755604105234));
#15604=CARTESIAN_POINT('Ctrl Pts',(-1.97663992019507,1.56137449648783,16.2809217700477));
#15605=CARTESIAN_POINT('Ctrl Pts',(-2.02807294138086,1.49394730907183,16.2862831295719));
#15606=CARTESIAN_POINT('Ctrl Pts',(-2.07591652376069,1.42421095220383,16.2916444890962));
#15607=CARTESIAN_POINT('Ctrl Pts',(-2.12376010614051,1.35447459533585,16.2970058486204));
#15608=CARTESIAN_POINT('Ctrl Pts',(-2.1680140406906,1.28242953692711,16.3023672081447));
#15609=CARTESIAN_POINT('Ctrl Pts',(-2.20847437293236,1.20848963342721,16.3077285676689));
#15610=CARTESIAN_POINT('Ctrl Pts',(-2.24813390682169,1.13601316212423,16.3129838141774));
#15611=CARTESIAN_POINT('Ctrl Pts',(-2.28429516385635,1.06144849006884,16.3182390606859));
#15612=CARTESIAN_POINT('Ctrl Pts',(-2.31673299462772,0.985167235348021,
16.3234943071943));
#15613=CARTESIAN_POINT('Ctrl Pts',(-2.34912483590618,0.908994130159408,
16.3287421029542));
#15614=CARTESIAN_POINT('Ctrl Pts',(-2.37780355744491,0.831109697474887,
16.3339898987141));
#15615=CARTESIAN_POINT('Ctrl Pts',(-2.40258956938183,0.751910640367356,
16.3392376944739));
#15616=CARTESIAN_POINT('Ctrl Pts',(-2.42755519455052,0.672137662830976,
16.3445235186814));
#15617=CARTESIAN_POINT('Ctrl Pts',(-2.44857122708091,0.591031343189288,
16.3498093428889));
#15618=CARTESIAN_POINT('Ctrl Pts',(-2.46550334123449,0.509018196493554,
16.3550951670963));
#15619=CARTESIAN_POINT('Ctrl Pts',(-2.48228361478307,0.427740511754887,
16.360333590091));
#15620=CARTESIAN_POINT('Ctrl Pts',(-2.49505282753447,0.345572659178892,
16.3655720130857));
#15621=CARTESIAN_POINT('Ctrl Pts',(-2.50373057391308,0.262943840492387,
16.3708104360804));
#15622=CARTESIAN_POINT('Ctrl Pts',(-2.51240546634888,0.180342196824877,
16.3760471362592));
#15623=CARTESIAN_POINT('Ctrl Pts',(-2.51699151669958,0.0972803466739266,
16.381283836438));
#15624=CARTESIAN_POINT('Ctrl Pts',(-2.51745998417278,0.0141942977555527,
16.3865205366168));
#15625=CARTESIAN_POINT('Ctrl Pts',(-2.51792843888685,-0.0688894882392182,
16.3917570941693));
#15626=CARTESIAN_POINT('Ctrl Pts',(-2.51427953212815,-0.151997010271273,
16.3969936517218));
#15627=CARTESIAN_POINT('Ctrl Pts',(-2.50653664139236,-0.23469195844231,
16.4022302092743));
#15628=CARTESIAN_POINT('Ctrl Pts',(-2.49866701109522,-0.318740499452894,
16.4075524814559));
#15629=CARTESIAN_POINT('Ctrl Pts',(-2.48656819550601,-0.402362347490421,
16.4128747536375));
#15630=CARTESIAN_POINT('Ctrl Pts',(-2.47031942034519,-0.485106391903289,
16.4181970258191));
#15631=CARTESIAN_POINT('Ctrl Pts',(-2.45430937027496,-0.566634770562661,
16.4234411038047));
#15632=CARTESIAN_POINT('Ctrl Pts',(-2.43427066495096,-0.647310528120108,
16.4286851817903));
#15633=CARTESIAN_POINT('Ctrl Pts',(-2.41032996240741,-0.726715709422255,
16.4339292597759));
#15634=CARTESIAN_POINT('Ctrl Pts',(-2.38585379185858,-0.807896901013318,
16.4392906290555));
#15635=CARTESIAN_POINT('Ctrl Pts',(-2.35729914260083,-0.887749511803182,
16.444651998335));
#15636=CARTESIAN_POINT('Ctrl Pts',(-2.32485329087844,-0.965848552254288,
16.4500133676146));
#15637=CARTESIAN_POINT('Ctrl Pts',(-2.29240743915605,-1.04394759270539,
16.4553747368941));
#15638=CARTESIAN_POINT('Ctrl Pts',(-2.25607066365104,-1.1202926327294,16.4607361061737));
#15639=CARTESIAN_POINT('Ctrl Pts',(-2.2160790626755,-1.19448726990759,16.4660974754532));
#15640=CARTESIAN_POINT('Ctrl Pts',(-2.17687902638735,-1.2672133523555,16.4713527256854));
#15641=CARTESIAN_POINT('Ctrl Pts',(-2.13402277703882,-1.33814202835465,
16.4766079759176));
#15642=CARTESIAN_POINT('Ctrl Pts',(-2.08769944242106,-1.40688211592685,
16.4818632261498));
#15643=CARTESIAN_POINT('Ctrl Pts',(-2.04144178397511,-1.47552474536399,
16.4871110256075));
#15644=CARTESIAN_POINT('Ctrl Pts',(-1.99172705969588,-1.54198457024853,
16.4923588250653));
#15645=CARTESIAN_POINT('Ctrl Pts',(-1.93879024342378,-1.60589496605624,
16.497606624523));
#15646=CARTESIAN_POINT('Ctrl Pts',(-1.88546986446111,-1.67026843548827,
16.5028924478028));
#15647=CARTESIAN_POINT('Ctrl Pts',(-1.8288807289112,-1.73205495816942,16.5081782710826));
#15648=CARTESIAN_POINT('Ctrl Pts',(-1.76930746003082,-1.79090964648674,
16.5134640943623));
#15649=CARTESIAN_POINT('Ctrl Pts',(-1.71026836998505,-1.84923659930446,
16.5187025209661));
#15650=CARTESIAN_POINT('Ctrl Pts',(-1.64829878254551,-1.90468375498875,
16.52394094757));
#15651=CARTESIAN_POINT('Ctrl Pts',(-1.58371493216762,-1.95694999006855,
16.5291793741738));
#15652=CARTESIAN_POINT('Ctrl Pts',(-1.51915232265853,-2.00919903539836,
16.5344160779207));
#15653=CARTESIAN_POINT('Ctrl Pts',(-1.45197751621885,-2.05826894782693,
16.5396527816677));
#15654=CARTESIAN_POINT('Ctrl Pts',(-1.3825405850962,-2.10389823436445,16.5448894854146));
#15655=CARTESIAN_POINT('Ctrl Pts',(-1.3131055457531,-2.14952627775153,16.5501260464898));
#15656=CARTESIAN_POINT('Ctrl Pts',(-1.24140889044425,-2.19171362908595,
16.5553626075649));
#15657=CARTESIAN_POINT('Ctrl Pts',(-1.16782932078672,-2.23024234725979,
16.5605991686401));
#15658=CARTESIAN_POINT('Ctrl Pts',(-1.09304547413255,-2.26940166505825,
16.5659214365232));
#15659=CARTESIAN_POINT('Ctrl Pts',(-1.01631695125543,-2.30478126775819,
16.5712437044063));
#15660=CARTESIAN_POINT('Ctrl Pts',(-0.938065273354438,-2.33620200173839,
16.5765659722894));
#15661=CARTESIAN_POINT('Ctrl Pts',(-0.860963147983039,-2.36716115092965,
16.5818100536509));
#15662=CARTESIAN_POINT('Ctrl Pts',(-0.782382784649652,-2.39427687982042,
16.5870541350123));
#15663=CARTESIAN_POINT('Ctrl Pts',(-0.702743720441128,-2.41742787139153,
16.5922982163738));
#15664=CARTESIAN_POINT('Ctrl Pts',(-0.621323590783215,-2.44109661680136,
16.5976595775177));
#15665=CARTESIAN_POINT('Ctrl Pts',(-0.538797333086823,-2.46062103062427,
16.6030209386616));
#15666=CARTESIAN_POINT('Ctrl Pts',(-0.455623385630417,-2.4759268124213,
16.6083822998056));
#15667=CARTESIAN_POINT('Ctrl Pts',(-0.372449438174011,-2.49123259421832,
16.6137436609495));
#15668=CARTESIAN_POINT('Ctrl Pts',(-0.288628313434993,-2.50231974358233,
16.6191050220934));
#15669=CARTESIAN_POINT('Ctrl Pts',(-0.204621052373853,-2.50917047546105,
16.6244663832373));
#15670=CARTESIAN_POINT('Ctrl Pts',(-0.122276319118097,-2.51588562938981,
16.6297216415056));
#15671=CARTESIAN_POINT('Ctrl Pts',(-0.0394486079889621,-2.51855536563663,
16.6349768997738));
#15672=CARTESIAN_POINT('Ctrl Pts',(0.0434309883450006,-2.51712534436634,
16.6402321580421));
#15673=CARTESIAN_POINT('Ctrl Pts',(0.126193081175941,-2.5156973505252,16.6454799656073));
#15674=CARTESIAN_POINT('Ctrl Pts',(0.209006455596838,-2.51018115234066,
16.6507277731726));
#15675=CARTESIAN_POINT('Ctrl Pts',(0.29143565672779,-2.50057423564821,16.6559755807379));
#15676=CARTESIAN_POINT('Ctrl Pts',(0.374461952664628,-2.49089772905342,
16.6612614019997));
#15677=CARTESIAN_POINT('Ctrl Pts',(0.457098013823339,-2.47707095133006,
16.6665472232615));
#15678=CARTESIAN_POINT('Ctrl Pts',(0.538899589046655,-2.45914486822663,
16.6718330445233));
#15679=CARTESIAN_POINT('Ctrl Pts',(0.619967827861354,-2.44137948923393,
16.6770714793483));
#15680=CARTESIAN_POINT('Ctrl Pts',(0.700216023835672,-2.41958811021566,
16.6823099141732));
#15681=CARTESIAN_POINT('Ctrl Pts',(0.779219421588435,-2.39387203981737,
16.6875483489982));
#15682=CARTESIAN_POINT('Ctrl Pts',(0.858196836457926,-2.36816442700034,
16.6927850609904));
#15683=CARTESIAN_POINT('Ctrl Pts',(0.935929827769396,-2.33853482903941,
16.6980217729826));
#15684=CARTESIAN_POINT('Ctrl Pts',(1.01200845890472,-2.30513451431913,16.7032584849748));
#15685=CARTESIAN_POINT('Ctrl Pts',(1.08808501750054,-2.27173510949261,16.7084950543081));
#15686=CARTESIAN_POINT('Ctrl Pts',(1.16250688344625,-2.23456537857441,16.7137316236414));
#15687=CARTESIAN_POINT('Ctrl Pts',(1.2348850638382,-2.19382431591715,16.7189681929747));
#15688=CARTESIAN_POINT('Ctrl Pts',(1.30844760783264,-2.15241658505302,16.7242904511453));
#15689=CARTESIAN_POINT('Ctrl Pts',(1.37989854415171,-2.10731981863762,16.7296127093159));
#15690=CARTESIAN_POINT('Ctrl Pts',(1.44885810514049,-2.0587900430031,16.7349349674864));
#15691=CARTESIAN_POINT('Ctrl Pts',(1.51680484930424,-2.01097302963929,16.7401790570529));
#15692=CARTESIAN_POINT('Ctrl Pts',(1.58233258353913,-1.95982351619309,16.7454231466194));
#15693=CARTESIAN_POINT('Ctrl Pts',(1.64511112944355,-1.9056273564842,16.7506672361858));
#15694=CARTESIAN_POINT('Ctrl Pts',(1.70929334453757,-1.85021942166199,16.7560285786584));
#15695=CARTESIAN_POINT('Ctrl Pts',(1.77060157946887,-1.79162731043557,16.7613899211311));
#15696=CARTESIAN_POINT('Ctrl Pts',(1.82872391766773,-1.73019509967807,16.7667512636037));
#15697=CARTESIAN_POINT('Ctrl Pts',(1.88684625586659,-1.66876288892055,16.7721126060763));
#15698=CARTESIAN_POINT('Ctrl Pts',(1.94178241797934,-1.60449100825937,16.7774739485489));
#15699=CARTESIAN_POINT('Ctrl Pts',(1.99326647407452,-1.53775648700648,16.7828352910216));
#15700=CARTESIAN_POINT('Ctrl Pts',(2.04375865853867,-1.47230764686464,16.788093343973));
#15701=CARTESIAN_POINT('Ctrl Pts',(2.0911200889309,-1.4042446607204,16.7933513969245));
#15702=CARTESIAN_POINT('Ctrl Pts',(2.13506909127537,-1.3338988812802,16.7986094498759));
#15703=CARTESIAN_POINT('Ctrl Pts',(2.17895674914168,-1.26365129121632,16.8038601635819));
#15704=CARTESIAN_POINT('Ctrl Pts',(2.21944119444765,-1.19112762062856,16.8091108772879));
#15705=CARTESIAN_POINT('Ctrl Pts',(2.25628160460562,-1.11669134980006,16.8143615909939));
#15706=CARTESIAN_POINT('Ctrl Pts',(2.29308163742164,-1.04233666163441,16.8196065498817));
#15707=CARTESIAN_POINT('Ctrl Pts',(2.32624536463931,-0.966073946613376,
16.8248515087695));
#15708=CARTESIAN_POINT('Ctrl Pts',(2.35557655574188,-0.888293498816241,
16.8300964676574));
#15709=CARTESIAN_POINT('Ctrl Pts',(2.3848851679442,-0.810572925743141,16.8353373890206));
#15710=CARTESIAN_POINT('Ctrl Pts',(2.41036694330135,-0.73133737020881,16.8405783103839));
#15711=CARTESIAN_POINT('Ctrl Pts',(2.43187326239833,-0.65099822244927,16.8458192317472));
#15712=CARTESIAN_POINT('Ctrl Pts',(2.45336962702427,-0.570696260677519,
16.8510577272839));
#15713=CARTESIAN_POINT('Ctrl Pts',(2.47089407458419,-0.489292166094003,
16.8562962228207));
#15714=CARTESIAN_POINT('Ctrl Pts',(2.48434787328852,-0.407212345695463,
16.8615347183574));
#15715=CARTESIAN_POINT('Ctrl Pts',(2.49780301782331,-0.325124314565895,
16.8667737379191));
#15716=CARTESIAN_POINT('Ctrl Pts',(2.50718661818065,-0.242360875602271,
16.8720127574809));
#15717=CARTESIAN_POINT('Ctrl Pts',(2.51245128260683,-0.159357467748757,
16.8772517770426));
#15718=CARTESIAN_POINT('Ctrl Pts',(2.51585617510238,-0.10567547443881,16.8806400838644));
#15719=CARTESIAN_POINT('Ctrl Pts',(2.51753925645563,-0.0518932709951306,
16.8840283906862));
#15720=CARTESIAN_POINT('Ctrl Pts',(2.51749930493939,0.00187072972653814,
16.887416697508));
#15721=CARTESIAN_POINT('Ctrl Pts',(2.5174993049387,0.00187073064803274,
16.8874166975661));
#15722=CARTESIAN_POINT('Ctrl Pts',(2.51742785555538,0.0980223455464406,
16.8934763502764));
#15723=CARTESIAN_POINT('Ctrl Pts',(2.51184391185846,0.193950007534804,16.8995360029868));
#15724=CARTESIAN_POINT('Ctrl Pts',(2.50084792088994,0.289077717198135,16.9055956556972));
#15725=CARTESIAN_POINT('Ctrl Pts',(2.4897455630997,0.385125619699227,16.9117139248616));
#15726=CARTESIAN_POINT('Ctrl Pts',(2.47312604616118,0.480357869841915,16.917832194026));
#15727=CARTESIAN_POINT('Ctrl Pts',(2.45114240622494,0.574201318707828,16.9239504631905));
#15728=CARTESIAN_POINT('Ctrl Pts',(2.43047752529607,0.662415267917,16.9297017083956));
#15729=CARTESIAN_POINT('Ctrl Pts',(2.4050733126551,0.749402139891612,16.9354529536007));
#15730=CARTESIAN_POINT('Ctrl Pts',(2.37509512959371,0.834703166029845,16.9412041988058));
#15731=CARTESIAN_POINT('Ctrl Pts',(2.37064009567936,0.847379683602514,16.9420588867762));
#15732=CARTESIAN_POINT('Ctrl Pts',(2.36608223827853,0.860024328645438,16.9429135747467));
#15733=CARTESIAN_POINT('Ctrl Pts',(2.36142200728636,0.872635292378013,16.9437682627171));
#15734=CARTESIAN_POINT('',(2.51750016131132,0.00131518048836379,16.6143270326092));
#15735=CARTESIAN_POINT('Ctrl Pts',(2.36142200368728,0.872635302117405,16.6687517122259));
#15736=CARTESIAN_POINT('Ctrl Pts',(2.36386197625392,0.866032538175512,16.6683467830721));
#15737=CARTESIAN_POINT('Ctrl Pts',(2.36627450067557,0.859418878191297,16.6679419651352));
#15738=CARTESIAN_POINT('Ctrl Pts',(2.40176087186149,0.760854533318875,16.6619195611102));
#15739=CARTESIAN_POINT('Ctrl Pts',(2.42947996278743,0.667068696889583,16.6563300599534));
#15740=CARTESIAN_POINT('Ctrl Pts',(2.46403571560758,0.518935114137275,16.6474234120279));
#15741=CARTESIAN_POINT('Ctrl Pts',(2.47467296806581,0.465573459107778,16.6441989244266));
#15742=CARTESIAN_POINT('Ctrl Pts',(2.48911195965705,0.378515460182014,16.6388530720024));
#15743=CARTESIAN_POINT('Ctrl Pts',(2.49397652107123,0.34501182288473,16.6367754829283));
#15744=CARTESIAN_POINT('Ctrl Pts',(2.49954909251244,0.300309820509292,16.633964475721));
#15745=CARTESIAN_POINT('Ctrl Pts',(2.5008601765897,0.289188555031691,16.6332619344937));
#15746=CARTESIAN_POINT('Ctrl Pts',(2.50287375753636,0.271069479635317,16.6321115906921));
#15747=CARTESIAN_POINT('Ctrl Pts',(2.50362121993825,0.264076680409275,16.6316662412482));
#15748=CARTESIAN_POINT('Ctrl Pts',(2.50496858734813,0.250951377569079,16.6308275702593));
#15749=CARTESIAN_POINT('Ctrl Pts',(2.50557529337874,0.244819655441212,16.6304346320055));
#15750=CARTESIAN_POINT('Ctrl Pts',(2.5067905206519,0.232059984209922,16.629614669477));
#15751=CARTESIAN_POINT('Ctrl Pts',(2.5073952811417,0.22543170232375,16.6291874416678));
#15752=CARTESIAN_POINT('Ctrl Pts',(2.50876413858236,0.209741392274904,16.6281732117087));
#15753=CARTESIAN_POINT('Ctrl Pts',(2.50950542443588,0.200677536296804,16.6275850269434));
#15754=CARTESIAN_POINT('Ctrl Pts',(2.51192971671358,0.168917963066522,16.6255164749279));
#15755=CARTESIAN_POINT('Ctrl Pts',(2.51335401207864,0.146204337379204,16.624023585749));
#15756=CARTESIAN_POINT('Ctrl Pts',(2.51646841711688,0.0827821850118265,
16.6198230050186));
#15757=CARTESIAN_POINT('Ctrl Pts',(2.51747843504179,0.0420488464344308,
16.6170884128516));
#15758=CARTESIAN_POINT('Ctrl Pts',(2.51749965834993,0.0013115669903107,
16.614327662638));
#15759=CARTESIAN_POINT('Ctrl Pts',(2.51749965649576,0.0013151211919122,
16.6143279035048));
#15760=CARTESIAN_POINT('Ctrl Pts',(2.51759289161941,-0.177162264168698,
16.6022325643764));
#15761=CARTESIAN_POINT('Ctrl Pts',(2.49870710678302,-0.355153439427492,
16.5897184849106));
#15762=CARTESIAN_POINT('Ctrl Pts',(2.43726528490359,-0.640649853452946,
16.5698726053172));
#15763=CARTESIAN_POINT('Ctrl Pts',(2.40589806630083,-0.749903381947059,
16.5623241462808));
#15764=CARTESIAN_POINT('Ctrl Pts',(2.35938061982181,-0.878444698619027,
16.5535212616552));
#15765=CARTESIAN_POINT('Ctrl Pts',(2.35120419892183,-0.900100478352394,
16.552040602573));
#15766=CARTESIAN_POINT('Ctrl Pts',(2.33785941558209,-0.934021738630407,
16.5497244548122));
#15767=CARTESIAN_POINT('Ctrl Pts',(2.3328906417668,-0.946363841163944,16.5488823916523));
#15768=CARTESIAN_POINT('Ctrl Pts',(2.32340323799045,-0.969401065830408,
16.5473116667831));
#15769=CARTESIAN_POINT('Ctrl Pts',(2.31890803128904,-0.980105393528043,
16.5465822450454));
#15770=CARTESIAN_POINT('Ctrl Pts',(2.30867634272983,-1.00400538456234,16.5449543920492));
#15771=CARTESIAN_POINT('Ctrl Pts',(2.30290042967158,-1.0171838045857,16.5440573176961));
#15772=CARTESIAN_POINT('Ctrl Pts',(2.28791197026316,-1.05059956672344,16.5417835160231));
#15773=CARTESIAN_POINT('Ctrl Pts',(2.27854360037989,-1.07076596078246,16.5404120938657));
#15774=CARTESIAN_POINT('Ctrl Pts',(2.19810978992022,-1.23807067337564,16.5290344982388));
#15775=CARTESIAN_POINT('Ctrl Pts',(2.11313902604193,-1.378099666811,16.5195468522991));
#15776=CARTESIAN_POINT('Ctrl Pts',(1.93712822666715,-1.61316467487242,16.5026564872387));
#15777=CARTESIAN_POINT('Ctrl Pts',(1.85110631844529,-1.71118874366793,16.4952363316092));
#15778=CARTESIAN_POINT('Ctrl Pts',(1.73000489045211,-1.82931884466891,16.4851849149801));
#15779=CARTESIAN_POINT('Ctrl Pts',(1.70148750335004,-1.85587292589741,16.4828423303225));
#15780=CARTESIAN_POINT('Ctrl Pts',(1.6592958469584,-1.89336983817612,16.4793911610366));
#15781=CARTESIAN_POINT('Ctrl Pts',(1.64610441488601,-1.90484967149928,16.4783141319773));
#15782=CARTESIAN_POINT('Ctrl Pts',(1.62516539795622,-1.92269190255638,16.4766056776944));
#15783=CARTESIAN_POINT('Ctrl Pts',(1.617497324431,-1.92914725222831,16.4759802597479));
#15784=CARTESIAN_POINT('Ctrl Pts',(1.60315590119635,-1.94107493017673,16.4748105475923));
#15785=CARTESIAN_POINT('Ctrl Pts',(1.59649253495555,-1.9465590946027,16.4742670686335));
#15786=CARTESIAN_POINT('Ctrl Pts',(1.58480568065266,-1.95607737918198,16.4733135929471));
#15787=CARTESIAN_POINT('Ctrl Pts',(1.57979459138374,-1.96012673239326,16.4729046728288));
#15788=CARTESIAN_POINT('Ctrl Pts',(1.56916424229675,-1.96864964341147,16.4720369042345));
#15789=CARTESIAN_POINT('Ctrl Pts',(1.5635413554041,-1.97311841121173,16.4715777422625));
#15790=CARTESIAN_POINT('Ctrl Pts',(1.54857089409316,-1.98491195428991,16.4703550169703));
#15791=CARTESIAN_POINT('Ctrl Pts',(1.53919061363268,-1.99219464964125,16.4695886228376));
#15792=CARTESIAN_POINT('Ctrl Pts',(1.49828695429828,-2.02349025176069,16.4662468719358));
#15793=CARTESIAN_POINT('Ctrl Pts',(1.4662523367576,-2.04682199414114,16.463630243415));
#15794=CARTESIAN_POINT('Ctrl Pts',(1.28087937831617,-2.17524942720514,16.4485512790733));
#15795=CARTESIAN_POINT('Ctrl Pts',(1.11682524071258,-2.26386031841253,16.4354948518298));
#15796=CARTESIAN_POINT('Ctrl Pts',(0.834698003934132,-2.37804964211992,
16.4146975686557));
#15797=CARTESIAN_POINT('Ctrl Pts',(0.721871972396797,-2.4146942946323,16.4067595857975));
#15798=CARTESIAN_POINT('Ctrl Pts',(0.577102821528507,-2.45065283711551,
16.397085751441));
#15799=CARTESIAN_POINT('Ctrl Pts',(0.547202113978372,-2.45750218245596,
16.3951137372499));
#15800=CARTESIAN_POINT('Ctrl Pts',(0.50265464564233,-2.46685324216732,16.3922130129569));
#15801=CARTESIAN_POINT('Ctrl Pts',(0.488099766178357,-2.46977433074594,
16.3912711175394));
#15802=CARTESIAN_POINT('Ctrl Pts',(0.46207588530407,-2.47475814754733,16.3895971989709));
#15803=CARTESIAN_POINT('Ctrl Pts',(0.450616899134009,-2.47687028933969,
16.3888636344728));
#15804=CARTESIAN_POINT('Ctrl Pts',(0.426333297382346,-2.48117218687824,
16.3873163189472));
#15805=CARTESIAN_POINT('Ctrl Pts',(0.413505505118304,-2.48334224559086,
16.3865032078872));
#15806=CARTESIAN_POINT('Ctrl Pts',(0.379149894493703,-2.48888054598132,
16.3843365400638));
#15807=CARTESIAN_POINT('Ctrl Pts',(0.357593902639592,-2.49206895198495,
16.3829886410434));
#15808=CARTESIAN_POINT('Ctrl Pts',(0.257918958424257,-2.50549218156433,
16.3768057569194));
#15809=CARTESIAN_POINT('Ctrl Pts',(0.179383957081291,-2.51233685060237,
16.372076860921));
#15810=CARTESIAN_POINT('Ctrl Pts',(-0.0661259408356384,-2.52216032100304,
16.35757867813));
#15811=CARTESIAN_POINT('Ctrl Pts',(-0.233148880538158,-2.51223152947583,
16.3481491135309));
#15812=CARTESIAN_POINT('Ctrl Pts',(-0.49975620372696,-2.4695501001532,16.3325004386518));
#15813=CARTESIAN_POINT('Ctrl Pts',(-0.600442451799385,-2.44701817055557,
16.3264382890751));
#15814=CARTESIAN_POINT('Ctrl Pts',(-0.716675633348967,-2.41340087224932,
16.318969233596));
#15815=CARTESIAN_POINT('Ctrl Pts',(-0.733845391944648,-2.40823558480896,
16.3178535163201));
#15816=CARTESIAN_POINT('Ctrl Pts',(-0.759014912144487,-2.40036952742121,
16.3161976698582));
#15817=CARTESIAN_POINT('Ctrl Pts',(-0.767059028962156,-2.39781107392871,
16.3156653967585));
#15818=CARTESIAN_POINT('Ctrl Pts',(-0.781298646312219,-2.39320313790047,
16.3147174713582));
#15819=CARTESIAN_POINT('Ctrl Pts',(-0.787499246513019,-2.39116995827077,
16.31430276528));
#15820=CARTESIAN_POINT('Ctrl Pts',(-0.800938615137099,-2.38670523818564,
16.313399650953));
#15821=CARTESIAN_POINT('Ctrl Pts',(-0.808174134120746,-2.38426490232591,
16.3129107568972));
#15822=CARTESIAN_POINT('Ctrl Pts',(-0.828238283458461,-2.37739600880764,
16.3115478337123));
#15823=CARTESIAN_POINT('Ctrl Pts',(-0.841042153799331,-2.37289665032012,
16.3106698685911));
#15824=CARTESIAN_POINT('Ctrl Pts',(-0.912313496079961,-2.34720216820449,
16.3057391968499));
#15825=CARTESIAN_POINT('Ctrl Pts',(-0.970011692361758,-2.32395135073942,
16.3015835485047));
#15826=CARTESIAN_POINT('Ctrl Pts',(-1.18887120298118,-2.22618642353206,
16.2853308152295));
#15827=CARTESIAN_POINT('Ctrl Pts',(-1.34284623923541,-2.13684099658062,
16.2728867280455));
#15828=CARTESIAN_POINT('Ctrl Pts',(-1.57768099278886,-1.96509257177471,
16.2531161751137));
#15829=CARTESIAN_POINT('Ctrl Pts',(-1.66459649026258,-1.89203354085314,
16.2455762824394));
#15830=CARTESIAN_POINT('Ctrl Pts',(-1.76296726235267,-1.79730024189398,
16.236781824801));
#15831=CARTESIAN_POINT('Ctrl Pts',(-1.77941358195077,-1.781019115675,16.2353015455611));
#15832=CARTESIAN_POINT('Ctrl Pts',(-1.80495763932047,-1.75502454158789,
16.2329858561261));
#15833=CARTESIAN_POINT('Ctrl Pts',(-1.81420652360025,-1.74546209414179,
16.2321438757622));
#15834=CARTESIAN_POINT('Ctrl Pts',(-1.83138425864606,-1.72741793794416,
16.2305732280437));
#15835=CARTESIAN_POINT('Ctrl Pts',(-1.8393310385493,-1.71895386006696,16.2298438013301));
#15836=CARTESIAN_POINT('Ctrl Pts',(-1.85699579174829,-1.69987645027589,
16.2282158385925));
#15837=CARTESIAN_POINT('Ctrl Pts',(-1.86668194087161,-1.68923410514482,
16.2273186603392));
#15838=CARTESIAN_POINT('Ctrl Pts',(-1.89110495250793,-1.66193349557615,
16.22504440843));
#15839=CARTESIAN_POINT('Ctrl Pts',(-1.90571347972684,-1.64516171444362,
16.2236726436586));
#15840=CARTESIAN_POINT('Ctrl Pts',(-2.02160224910991,-1.50849664043799,
16.2126904082288));
#15841=CARTESIAN_POINT('Ctrl Pts',(-2.11169609937389,-1.37956020168648,
16.2035542764276));
#15842=CARTESIAN_POINT('Ctrl Pts',(-2.24505023613386,-1.14470424688722,
16.1880088556805));
#15843=CARTESIAN_POINT('Ctrl Pts',(-2.29420258616721,-1.0427036265657,16.1815602012426));
#15844=CARTESIAN_POINT('Ctrl Pts',(-2.36605453057775,-0.863690071597645,
16.1702479232374));
#15845=CARTESIAN_POINT('Ctrl Pts',(-2.39223888327035,-0.788267117122985,
16.1654812347327));
#15846=CARTESIAN_POINT('Ctrl Pts',(-2.41875379370783,-0.698306789192273,
16.1596578469722));
#15847=CARTESIAN_POINT('Ctrl Pts',(-2.4225999686992,-0.684844257639382,
16.15878280108));
#15848=CARTESIAN_POINT('Ctrl Pts',(-2.42837278742728,-0.663980670796985,
16.157420178114));
#15849=CARTESIAN_POINT('Ctrl Pts',(-2.43037840550998,-0.656601498836276,
16.1569369817138));
#15850=CARTESIAN_POINT('Ctrl Pts',(-2.43403284599777,-0.642909730771618,
16.1560379115385));
#15851=CARTESIAN_POINT('Ctrl Pts',(-2.43569077904126,-0.636599750950935,
16.1556225619017));
#15852=CARTESIAN_POINT('Ctrl Pts',(-2.43943364212482,-0.622125991391422,
16.1546675670903));
#15853=CARTESIAN_POINT('Ctrl Pts',(-2.44150212120969,-0.613958166933839,
16.1541270108892));
#15854=CARTESIAN_POINT('Ctrl Pts',(-2.44684419526516,-0.592409898267039,
16.152696900001));
#15855=CARTESIAN_POINT('Ctrl Pts',(-2.4500489862197,-0.579012908933841,
16.1518036977012));
#15856=CARTESIAN_POINT('Ctrl Pts',(-2.47885905152827,-0.454054642828202,
16.1434388881598));
#15857=CARTESIAN_POINT('Ctrl Pts',(-2.49693503496261,-0.340906659924204,
16.1356215462103));
#15858=CARTESIAN_POINT('Ctrl Pts',(-2.52728333596821,-0.0056107239324921,
16.1124169950894));
#15859=CARTESIAN_POINT('Ctrl Pts',(-2.51792543437029,0.217445891382168,
16.0970339492602));
#15860=CARTESIAN_POINT('Ctrl Pts',(-2.47391616444877,0.467484091589759,
16.0805566478802));
#15861=CARTESIAN_POINT('Ctrl Pts',(-2.46786025408798,0.498466125902654,
16.0785261406324));
#15862=CARTESIAN_POINT('Ctrl Pts',(-2.45806615829862,0.544005919350389,
16.075556852166));
#15863=CARTESIAN_POINT('Ctrl Pts',(-2.45477796215965,0.558656290817961,
16.0746039641146));
#15864=CARTESIAN_POINT('Ctrl Pts',(-2.44870107279725,0.58464136612793,16.0729177681316));
#15865=CARTESIAN_POINT('Ctrl Pts',(-2.44596427222349,0.595987631851077,
16.0721828339529));
#15866=CARTESIAN_POINT('Ctrl Pts',(-2.44003290182603,0.619848772653278,
16.0706399172626));
#15867=CARTESIAN_POINT('Ctrl Pts',(-2.43682072120239,0.632358953098329,
16.0698325210998));
#15868=CARTESIAN_POINT('Ctrl Pts',(-2.42804166570517,0.66548935126612,16.0676980711492));
#15869=CARTESIAN_POINT('Ctrl Pts',(-2.42230834459651,0.686064671963054,
16.0663763776353));
#15870=CARTESIAN_POINT('Ctrl Pts',(-2.3954430660026,0.777938651026193,16.0604890705995));
#15871=CARTESIAN_POINT('Ctrl Pts',(-2.37141908583245,0.848356695051183,
16.0560171969866));
#15872=CARTESIAN_POINT('Ctrl Pts',(-2.27493468183705,1.09485429123281,16.0403612520508));
#15873=CARTESIAN_POINT('Ctrl Pts',(-2.18568686480429,1.26364718455792,16.0296822624048));
#15874=CARTESIAN_POINT('Ctrl Pts',(-2.02710574017071,1.49561652745872,16.0132887333093));
#15875=CARTESIAN_POINT('Ctrl Pts',(-1.97193758034223,1.56763674165819,16.0079048511246));
#15876=CARTESIAN_POINT('Ctrl Pts',(-1.90366402768768,1.64744540558377,16.0013874995212));
#15877=CARTESIAN_POINT('Ctrl Pts',(-1.8942216302322,1.65829354691348,16.0004890691247));
#15878=CARTESIAN_POINT('Ctrl Pts',(-1.87956350060414,1.67484537192479,15.9990977580429));
#15879=CARTESIAN_POINT('Ctrl Pts',(-1.874413406773,1.68060713713614,15.9986095550046));
#15880=CARTESIAN_POINT('Ctrl Pts',(-1.86487219101607,1.69118314201114,15.9977060506394));
#15881=CARTESIAN_POINT('Ctrl Pts',(-1.86048882638238,1.69600413692736,15.9972913185129));
#15882=CARTESIAN_POINT('Ctrl Pts',(-1.85046865409002,1.70693912124457,15.9963440708932));
#15883=CARTESIAN_POINT('Ctrl Pts',(-1.84482026449249,1.71304220334033,15.9958107020503));
#15884=CARTESIAN_POINT('Ctrl Pts',(-1.82998774095959,1.72891029914376,15.99441190415));
#15885=CARTESIAN_POINT('Ctrl Pts',(-1.82075580039909,1.73862999268947,15.9935430719766));
#15886=CARTESIAN_POINT('Ctrl Pts',(-1.75162844533053,1.81025517568678,15.9870537318084));
#15887=CARTESIAN_POINT('Ctrl Pts',(-1.68867429811614,1.86911797805562,15.9812357022869));
#15888=CARTESIAN_POINT('Ctrl Pts',(-1.50478902899741,2.02416860962639,15.9647659885821));
#15889=CARTESIAN_POINT('Ctrl Pts',(-1.37782621288012,2.11264005859239,15.9539931270428));
#15890=CARTESIAN_POINT('Ctrl Pts',(-1.14721582443178,2.24365314824624,15.9359872780276));
#15891=CARTESIAN_POINT('Ctrl Pts',(-1.04735623476565,2.29197172313424,15.9286265249638));
#15892=CARTESIAN_POINT('Ctrl Pts',(-0.923290051217735,2.34219373005328,
15.92000857197));
#15893=CARTESIAN_POINT('Ctrl Pts',(-0.901837712462627,2.35053712704448,
15.9185363874946));
#15894=CARTESIAN_POINT('Ctrl Pts',(-0.867835234898131,2.36322756249511,
15.9162304451631));
#15895=CARTESIAN_POINT('Ctrl Pts',(-0.855360380794269,2.36777134390335,
15.9153902091923));
#15896=CARTESIAN_POINT('Ctrl Pts',(-0.831907616156793,2.37610412618105,
15.9138211480979));
#15897=CARTESIAN_POINT('Ctrl Pts',(-0.82093834970085,2.37991624506652,15.9130915780007));
#15898=CARTESIAN_POINT('Ctrl Pts',(-0.796282577539754,2.38829404754364,
15.9114611588432));
#15899=CARTESIAN_POINT('Ctrl Pts',(-0.782582338762797,2.39281827508362,
15.9105616863973));
#15900=CARTESIAN_POINT('Ctrl Pts',(-0.747547802876016,2.40405463731448,
15.9082775535478));
#15901=CARTESIAN_POINT('Ctrl Pts',(-0.726161301554181,2.41060080271731,
15.9068982834207));
#15902=CARTESIAN_POINT('Ctrl Pts',(-0.554688243337949,2.46059760152126,
15.8959526373461));
#15903=CARTESIAN_POINT('Ctrl Pts',(-0.400933388541469,2.49027727997339,
15.886855644023));
#15904=CARTESIAN_POINT('Ctrl Pts',(-0.133708233663857,2.51645055530821,
15.8713997478473));
#15905=CARTESIAN_POINT('Ctrl Pts',(-0.0214131073894728,2.51990889726814,
15.8650007404159));
#15906=CARTESIAN_POINT('Ctrl Pts',(0.145430270638465,2.51389179599546,15.8552161590877));
#15907=CARTESIAN_POINT('Ctrl Pts',(0.200045295743299,2.5101360641009,15.8519677776078));
#15908=CARTESIAN_POINT('Ctrl Pts',(0.276411999706423,2.50237650075648,15.8473094807242));
#15909=CARTESIAN_POINT('Ctrl Pts',(0.298302127918328,2.49986149959144,15.8459607122724));
#15910=CARTESIAN_POINT('Ctrl Pts',(0.336661007584157,2.4949433904305,15.8435691075759));
#15911=CARTESIAN_POINT('Ctrl Pts',(0.353144478526909,2.49266365531695,15.8425322430868));
#15912=CARTESIAN_POINT('Ctrl Pts',(0.377706045048438,2.48901817770437,15.8409719481176));
#15913=CARTESIAN_POINT('Ctrl Pts',(0.385802413220178,2.48777608295063,15.8404551322775));
#15914=CARTESIAN_POINT('Ctrl Pts',(0.399700717814768,2.48557441426652,15.8395634631105));
#15915=CARTESIAN_POINT('Ctrl Pts',(0.405505564717805,2.48463399087122,15.8391896851294));
#15916=CARTESIAN_POINT('Ctrl Pts',(0.41876768858446,2.48243772508089,15.838332574971));
#15917=CARTESIAN_POINT('Ctrl Pts',(0.426222494394662,2.48116863949323,15.837848520655));
#15918=CARTESIAN_POINT('Ctrl Pts',(0.446719361255199,2.47758421035862,15.8365116035778));
#15919=CARTESIAN_POINT('Ctrl Pts',(0.459748826400814,2.47519952847301,15.8356550358795));
#15920=CARTESIAN_POINT('Ctrl Pts',(0.52884460967535,2.46198908661189,15.8310790700527));
#15921=CARTESIAN_POINT('Ctrl Pts',(0.584545101902249,2.44936171562828,15.8272729187443));
#15922=CARTESIAN_POINT('Ctrl Pts',(0.78168348264611,2.39756315553294,15.8134895325377));
#15923=CARTESIAN_POINT('Ctrl Pts',(0.920068473247469,2.34793766702451,15.8032493558316));
#15924=CARTESIAN_POINT('Ctrl Pts',(1.18281032727238,2.22690039498695,15.7833881009054));
#15925=CARTESIAN_POINT('Ctrl Pts',(1.30699644478953,2.1563621333607,15.7737943703504));
#15926=CARTESIAN_POINT('Ctrl Pts',(1.44712430400242,2.06019088908982,15.7628048887434));
#15927=CARTESIAN_POINT('Ctrl Pts',(1.46943576383536,2.0443370277864,15.7610489455182));
#15928=CARTESIAN_POINT('Ctrl Pts',(1.50291799094005,2.01971413011972,15.7584034285225));
#15929=CARTESIAN_POINT('Ctrl Pts',(1.51427986098309,2.01120962879152,15.7575038251017));
#15930=CARTESIAN_POINT('Ctrl Pts',(1.53479476913275,1.99558156035767,15.7558758549031));
#15931=CARTESIAN_POINT('Ctrl Pts',(1.54397158663948,1.98849000357109,15.7551462727766));
#15932=CARTESIAN_POINT('Ctrl Pts',(1.56368756266869,1.97303534111945,15.7535756869592));
#15933=CARTESIAN_POINT('Ctrl Pts',(1.57420938425578,1.96465062456972,15.7527355641207));
#15934=CARTESIAN_POINT('Ctrl Pts',(1.60269865975992,1.94157203415329,15.7504550687707));
#15935=CARTESIAN_POINT('Ctrl Pts',(1.62053120718329,1.92671316485822,15.7490213110135));
#15936=CARTESIAN_POINT('Ctrl Pts',(1.71743690111907,1.84366970388247,15.7411898989989));
#15937=CARTESIAN_POINT('Ctrl Pts',(1.79241960300952,1.77085944606404,15.734986805943));
#15938=CARTESIAN_POINT('Ctrl Pts',(1.97397931773628,1.57117422265329,15.7192423172525));
#15939=CARTESIAN_POINT('Ctrl Pts',(2.07294262786278,1.43808483452379,15.7099240427029));
#15940=CARTESIAN_POINT('Ctrl Pts',(2.20035052168185,1.22596375165347,15.6954290193888));
#15941=CARTESIAN_POINT('Ctrl Pts',(2.23910624318266,1.15365935879761,15.6905371491669));
#15942=CARTESIAN_POINT('Ctrl Pts',(2.28030223325077,1.06687693025528,15.6845731586594));
#15943=CARTESIAN_POINT('Ctrl Pts',(2.28623570035812,1.05410196872915,15.683692923656));
#15944=CARTESIAN_POINT('Ctrl Pts',(2.2952318659338,1.03429961038054,15.6823239315309));
#15945=CARTESIAN_POINT('Ctrl Pts',(2.29837030001894,1.02730665467101,15.6818396202343));
#15946=CARTESIAN_POINT('Ctrl Pts',(2.30412006610345,1.01433698099556,15.6809395779089));
#15947=CARTESIAN_POINT('Ctrl Pts',(2.30674015503032,1.00836434087861,15.6805243811195));
#15948=CARTESIAN_POINT('Ctrl Pts',(2.31268177619179,0.994675736080053,15.6795711799718));
#15949=CARTESIAN_POINT('Ctrl Pts',(2.31598790517059,0.986953310011539,15.6790322778378));
#15950=CARTESIAN_POINT('Ctrl Pts',(2.32458006008421,0.966602918775715,15.6776093934698));
#15951=CARTESIAN_POINT('Ctrl Pts',(2.32980175824751,0.953948324631367,15.6767218207374));
#15952=CARTESIAN_POINT('Ctrl Pts',(2.34408940327186,0.918505635343549,15.6742294616949));
#15953=CARTESIAN_POINT('Ctrl Pts',(2.35292426096839,0.895630883696691,15.672613486953));
#15954=CARTESIAN_POINT('Ctrl Pts',(2.36142199860763,0.87263531586336,15.670984110559));
#15955=CARTESIAN_POINT('Origin',(0.,0.,10.));
#15956=CARTESIAN_POINT('',(2.36142197356233,0.87263538363797,14.6670478768675));
#15957=CARTESIAN_POINT('',(2.36142200728636,0.87263529237801,14.9438284014526));
#15958=CARTESIAN_POINT('',(2.36142200728636,0.87263529237802,10.));
#15959=CARTESIAN_POINT('',(2.51749934288794,-0.0018189444229938,15.8874166974484));
#15960=CARTESIAN_POINT('Ctrl Pts',(2.36142200728636,0.872635292378009,14.9438284014526));
#15961=CARTESIAN_POINT('Ctrl Pts',(2.33277648153847,0.950152412648301,14.9490388977595));
#15962=CARTESIAN_POINT('Ctrl Pts',(2.30029580664879,1.02629583242825,14.9542493940664));
#15963=CARTESIAN_POINT('Ctrl Pts',(2.26414317539008,1.10066431364632,14.9594598903733));
#15964=CARTESIAN_POINT('Ctrl Pts',(2.22799445285202,1.17502475435369,14.9646698233361));
#15965=CARTESIAN_POINT('Ctrl Pts',(2.18817476734327,1.24761021831179,14.9698797562988));
#15966=CARTESIAN_POINT('Ctrl Pts',(2.1448943452171,1.31804191809505,14.9750896892615));
#15967=CARTESIAN_POINT('Ctrl Pts',(2.09942050746829,1.39204303756151,14.9805636572727));
#15968=CARTESIAN_POINT('Ctrl Pts',(2.0501261611078,1.46366582484097,14.9860376252838));
#15969=CARTESIAN_POINT('Ctrl Pts',(1.99730698814324,1.53250482710959,14.991511593295));
#15970=CARTESIAN_POINT('Ctrl Pts',(1.94696848714391,1.59811078021334,14.9967284743769));
#15971=CARTESIAN_POINT('Ctrl Pts',(1.89342914441608,1.66118820601892,15.0019453554588));
#15972=CARTESIAN_POINT('Ctrl Pts',(1.83698530511478,1.72142128451822,15.0071622365407));
#15973=CARTESIAN_POINT('Ctrl Pts',(1.78050276468467,1.78169566226574,15.0123826946151));
#15974=CARTESIAN_POINT('Ctrl Pts',(1.7211121013311,1.83912148975098,15.0176031526894));
#15975=CARTESIAN_POINT('Ctrl Pts',(1.65914462916598,1.89342159845864,15.0228236107638));
#15976=CARTESIAN_POINT('Ctrl Pts',(1.59708124854021,1.94780574867482,15.0280521486594));
#15977=CARTESIAN_POINT('Ctrl Pts',(1.5324334707376,1.99905424477454,15.033280686555));
#15978=CARTESIAN_POINT('Ctrl Pts',(1.46556295352631,2.04693221168929,15.0385092244506));
#15979=CARTESIAN_POINT('Ctrl Pts',(1.45589372738709,2.05385518624506,15.0392652514323));
#15980=CARTESIAN_POINT('Ctrl Pts',(1.44617807104084,2.06070776737762,15.0400212784139));
#15981=CARTESIAN_POINT('Ctrl Pts',(1.43641711978723,2.06748932475652,15.0407773053956));
#15982=CARTESIAN_POINT('Ctrl Pts',(1.36856738098678,2.11462887958713,15.046032554797));
#15983=CARTESIAN_POINT('Ctrl Pts',(1.2982693825395,2.15851196661367,15.0512878041983));
#15984=CARTESIAN_POINT('Ctrl Pts',(1.22586870228417,2.19887520672732,15.0565430535997));
#15985=CARTESIAN_POINT('Ctrl Pts',(1.15357066974716,2.23918122093527,15.0617908522512));
#15986=CARTESIAN_POINT('Ctrl Pts',(1.07917627644597,2.27597707769949,15.0670386509027));
#15987=CARTESIAN_POINT('Ctrl Pts',(1.00306088631776,2.30904203260561,15.0722864495542));
#15988=CARTESIAN_POINT('Ctrl Pts',(0.926393974459495,2.34234657166288,15.0775722730386));
#15989=CARTESIAN_POINT('Ctrl Pts',(0.847981409502392,2.37186564312825,15.082858096523));
#15990=CARTESIAN_POINT('Ctrl Pts',(0.76823300944464,2.39742034136687,15.0881439200074));
#15991=CARTESIAN_POINT('Ctrl Pts',(0.689199707900845,2.42274589235336,15.0933823458698));
#15992=CARTESIAN_POINT('Ctrl Pts',(0.608854879500604,2.44417773849274,15.0986207717323));
#15993=CARTESIAN_POINT('Ctrl Pts',(0.527616746581242,2.46159030277726,15.1038591975947));
#15994=CARTESIAN_POINT('Ctrl Pts',(0.446405331532488,2.47899714035902,15.109095900626));
#15995=CARTESIAN_POINT('Ctrl Pts',(0.36430164627102,2.492387224774,15.1143326036573));
#15996=CARTESIAN_POINT('Ctrl Pts',(0.281736172863987,2.50168562751197,15.1195693066886));
#15997=CARTESIAN_POINT('Ctrl Pts',(0.19917294849977,2.51098377696603,15.1248058670747));
#15998=CARTESIAN_POINT('Ctrl Pts',(0.116148419637579,2.51619041573157,15.1300424274607));
#15999=CARTESIAN_POINT('Ctrl Pts',(0.0330989093399816,2.51728240612779,
15.1352789878468));
#16000=CARTESIAN_POINT('Ctrl Pts',(-0.051309897791966,2.51839226946611,
15.1406012566246));
#16001=CARTESIAN_POINT('Ctrl Pts',(-0.13574401998502,2.51525155821139,15.1459235254023));
#16002=CARTESIAN_POINT('Ctrl Pts',(-0.219746481833127,2.50789109287504,
15.1512457941801));
#16003=CARTESIAN_POINT('Ctrl Pts',(-0.302514885877946,2.50063875817539,
15.1564898749241));
#16004=CARTESIAN_POINT('Ctrl Pts',(-0.384863772944501,2.48928995367179,
15.1617339556682));
#16005=CARTESIAN_POINT('Ctrl Pts',(-0.466364091257801,2.47392618814412,
15.1669780364122));
#16006=CARTESIAN_POINT('Ctrl Pts',(-0.549687135977597,2.45821881731883,
15.1723393992068));
#16007=CARTESIAN_POINT('Ctrl Pts',(-0.632122700302753,2.4383148521548,15.1777007620014));
#16008=CARTESIAN_POINT('Ctrl Pts',(-0.713228296029433,2.4143553275653,15.183062124796));
#16009=CARTESIAN_POINT('Ctrl Pts',(-0.794333891756125,2.3903958029758,15.1884234875906));
#16010=CARTESIAN_POINT('Ctrl Pts',(-0.874109061611535,2.36238095033946,
15.1937848503852));
#16011=CARTESIAN_POINT('Ctrl Pts',(-0.952134552185257,2.33050338865555,
15.1991462131798));
#16012=CARTESIAN_POINT('Ctrl Pts',(-1.0286157438934,2.29925675517194,15.2044014626206));
#16013=CARTESIAN_POINT('Ctrl Pts',(-1.10369839428042,2.26418355135292,15.2096567120615));
#16014=CARTESIAN_POINT('Ctrl Pts',(-1.17697343258409,2.22543024806243,15.2149119615023));
#16015=CARTESIAN_POINT('Ctrl Pts',(-1.25014458353137,2.18673188815134,15.2201597601934));
#16016=CARTESIAN_POINT('Ctrl Pts',(-1.32151280834504,2.14436400625807,15.2254075588846));
#16017=CARTESIAN_POINT('Ctrl Pts',(-1.3906885808284,2.09852127012177,15.2306553575757));
#16018=CARTESIAN_POINT('Ctrl Pts',(-1.4603655908628,2.05234636421029,15.2359411810502));
#16019=CARTESIAN_POINT('Ctrl Pts',(-1.52781780343736,2.0026462142322,15.2412270045247));
#16020=CARTESIAN_POINT('Ctrl Pts',(-1.59267202784433,1.94966716690881,15.2465128279992));
#16021=CARTESIAN_POINT('Ctrl Pts',(-1.65694470941202,1.89716317862567,15.2517512539014));
#16022=CARTESIAN_POINT('Ctrl Pts',(-1.71866544419385,1.84143915801312,15.2569896798036));
#16023=CARTESIAN_POINT('Ctrl Pts',(-1.77750119735707,1.78277753614807,15.2622281057058));
#16024=CARTESIAN_POINT('Ctrl Pts',(-1.83631760041949,1.72413520711493,15.2674648087768));
#16025=CARTESIAN_POINT('Ctrl Pts',(-1.89225057977768,1.66255752114573,15.2727015118479));
#16026=CARTESIAN_POINT('Ctrl Pts',(-1.94500290933897,1.59836476833761,15.2779382149189));
#16027=CARTESIAN_POINT('Ctrl Pts',(-1.99775380195184,1.5341737641096,15.2831747753446));
#16028=CARTESIAN_POINT('Ctrl Pts',(-2.04732392486907,1.46736819181756,15.2884113357704));
#16029=CARTESIAN_POINT('Ctrl Pts',(-2.09345631360712,1.39830143853838,15.2936478961961));
#16030=CARTESIAN_POINT('Ctrl Pts',(-2.14034376454627,1.32810424965462,15.2989701649267));
#16031=CARTESIAN_POINT('Ctrl Pts',(-2.18367964919649,1.25557159477232,15.3042924336574));
#16032=CARTESIAN_POINT('Ctrl Pts',(-2.22324101859935,1.1811035615971,15.3096147023881));
#16033=CARTESIAN_POINT('Ctrl Pts',(-2.26222120309141,1.10772951727694,15.3148587831711));
#16034=CARTESIAN_POINT('Ctrl Pts',(-2.29753689359051,1.03247703115664,15.3201028639542));
#16035=CARTESIAN_POINT('Ctrl Pts',(-2.32902286112003,0.955750366141851,
15.3253469447373));
#16036=CARTESIAN_POINT('Ctrl Pts',(-2.3612130006334,0.877307737726311,15.3307083074417));
#16037=CARTESIAN_POINT('Ctrl Pts',(-2.3893998792421,0.797324678732944,15.3360696701462));
#16038=CARTESIAN_POINT('Ctrl Pts',(-2.41346088255415,0.716249131504479,
15.3414310328506));
#16039=CARTESIAN_POINT('Ctrl Pts',(-2.43752188586621,0.635173584276002,
15.3467923955551));
#16040=CARTESIAN_POINT('Ctrl Pts',(-2.45745695899733,0.553006058343721,
15.3521537582595));
#16041=CARTESIAN_POINT('Ctrl Pts',(-2.47319940610295,0.470203091920946,
15.357515120964));
#16042=CARTESIAN_POINT('Ctrl Pts',(-2.4886302750115,0.389038981186634,15.3627703703231));
#16043=CARTESIAN_POINT('Ctrl Pts',(-2.50009000836156,0.306964573930027,
15.3680256196823));
#16044=CARTESIAN_POINT('Ctrl Pts',(-2.50747874556489,0.224402741828887,
15.3732808690415));
#16045=CARTESIAN_POINT('Ctrl Pts',(-2.51485700721747,0.141957963648953,
15.378528667651));
#16046=CARTESIAN_POINT('Ctrl Pts',(-2.51817569631215,0.0590275890165934,
15.3837764662605));
#16047=CARTESIAN_POINT('Ctrl Pts',(-2.51738602049689,-0.0239556633564388,
15.38902426487));
#16048=CARTESIAN_POINT('Ctrl Pts',(-2.51659062279048,-0.107540201887602,
15.3943100883649));
#16049=CARTESIAN_POINT('Ctrl Pts',(-2.51162698306217,-0.191177922134853,
15.3995959118598));
#16050=CARTESIAN_POINT('Ctrl Pts',(-2.5024985507745,-0.274421670739607,
15.4048817353547));
#16051=CARTESIAN_POINT('Ctrl Pts',(-2.49345197261146,-0.356918977462784,
15.4101201611759));
#16052=CARTESIAN_POINT('Ctrl Pts',(-2.4803150448715,-0.439028882564209,
15.4153585869972));
#16053=CARTESIAN_POINT('Ctrl Pts',(-2.46314334722548,-0.520318268965132,
15.4205970128184));
#16054=CARTESIAN_POINT('Ctrl Pts',(-2.445977297064,-0.601580920644586,15.4258337158088));
#16055=CARTESIAN_POINT('Ctrl Pts',(-2.42477920772006,-0.682023138468348,
15.4310704187993));
#16056=CARTESIAN_POINT('Ctrl Pts',(-2.39965591084302,-0.761221229049839,
15.4363071217897));
#16057=CARTESIAN_POINT('Ctrl Pts',(-2.37453329831013,-0.840417162320947,
15.4415436821354));
#16058=CARTESIAN_POINT('Ctrl Pts',(-2.34548583133283,-0.918368596220602,
15.4467802424811));
#16059=CARTESIAN_POINT('Ctrl Pts',(-2.31267002354775,-0.994667588787157,
15.4520168028267));
#16060=CARTESIAN_POINT('Ctrl Pts',(-2.27931710879627,-1.07221539170466,
15.4573390716535));
#16061=CARTESIAN_POINT('Ctrl Pts',(-2.2420715672161,-1.14805571627183,15.4626613404803));
#16062=CARTESIAN_POINT('Ctrl Pts',(-2.20114760439853,-1.22178372621778,
15.4679836093071));
#16063=CARTESIAN_POINT('Ctrl Pts',(-2.16082484529459,-1.29442861638924,
15.4732276900122));
#16064=CARTESIAN_POINT('Ctrl Pts',(-2.11693132432732,-1.36502247789413,
15.4784717707173));
#16065=CARTESIAN_POINT('Ctrl Pts',(-2.06971617492699,-1.43320661638355,
15.4837158514225));
#16066=CARTESIAN_POINT('Ctrl Pts',(-2.02144507385857,-1.50291567125448,
15.4890772143101));
#16067=CARTESIAN_POINT('Ctrl Pts',(-1.96970228962038,-1.57010551141682,
15.4944385771977));
#16068=CARTESIAN_POINT('Ctrl Pts',(-1.91479679524017,-1.6344294059206,15.4997999400853));
#16069=CARTESIAN_POINT('Ctrl Pts',(-1.85989130085996,-1.69875330042438,
15.5051613029729));
#16070=CARTESIAN_POINT('Ctrl Pts',(-1.80182349384693,-1.76021092581791,
15.5105226658605));
#16071=CARTESIAN_POINT('Ctrl Pts',(-1.74094000232509,-1.81849777517167,
15.5158840287482));
#16072=CARTESIAN_POINT('Ctrl Pts',(-1.68126153286005,-1.87563099589251,
15.5211392781332));
#16073=CARTESIAN_POINT('Ctrl Pts',(-1.61865742272164,-1.92992887109054,
15.5263945275182));
#16074=CARTESIAN_POINT('Ctrl Pts',(-1.55342800415825,-1.98107740532694,
15.5316497769033));
#16075=CARTESIAN_POINT('Ctrl Pts',(-1.4882910660995,-2.0321534225555,15.536897575538));
#16076=CARTESIAN_POINT('Ctrl Pts',(-1.42053657284844,-2.08008868537052,
15.5421453741726));
#16077=CARTESIAN_POINT('Ctrl Pts',(-1.35050092045069,-2.12460667274247,
15.5473931728073));
#16078=CARTESIAN_POINT('Ctrl Pts',(-1.27995779899129,-2.1694472315549,15.5526789962958));
#16079=CARTESIAN_POINT('Ctrl Pts',(-1.20710066325347,-2.21082045600598,
15.5579648197844));
#16080=CARTESIAN_POINT('Ctrl Pts',(-1.13230646008424,-2.24848578613508,
15.5632506432729));
#16081=CARTESIAN_POINT('Ctrl Pts',(-1.05818293179129,-2.2858133736377,15.5684890691175));
#16082=CARTESIAN_POINT('Ctrl Pts',(-0.98215735576056,-2.31949908603407,
15.573727494962));
#16083=CARTESIAN_POINT('Ctrl Pts',(-0.904623287695934,-2.34935373185014,
15.5789659208066));
#16084=CARTESIAN_POINT('Ctrl Pts',(-0.827114719301739,-2.37919855896783,
15.5842026238197));
#16085=CARTESIAN_POINT('Ctrl Pts',(-0.748099074453607,-2.40521465621004,
15.5894393268328));
#16086=CARTESIAN_POINT('Ctrl Pts',(-0.667989908555241,-2.42726095261065,
15.5946760298458));
#16087=CARTESIAN_POINT('Ctrl Pts',(-0.587882924796029,-2.44930664847965,
15.5999125902134));
#16088=CARTESIAN_POINT('Ctrl Pts',(-0.506682924365674,-2.46738263706995,
15.6051491505809));
#16089=CARTESIAN_POINT('Ctrl Pts',(-0.424817299930151,-2.4813980961708,
15.6103857109485));
#16090=CARTESIAN_POINT('Ctrl Pts',(-0.341611755062269,-2.4956429507004,
15.6157079797472));
#16091=CARTESIAN_POINT('Ctrl Pts',(-0.257719083109179,-2.50569306067364,
15.6210302485458));
#16092=CARTESIAN_POINT('Ctrl Pts',(-0.173595482170129,-2.51150768634502,
15.6263525173445));
#16093=CARTESIAN_POINT('Ctrl Pts',(-0.0907077192844954,-2.51723689085527,
15.6315965980694));
#16094=CARTESIAN_POINT('Ctrl Pts',(-0.00759623653741434,-2.51885428207375,
15.6368406787943));
#16095=CARTESIAN_POINT('Ctrl Pts',(0.0753024549304608,-2.51637353949716,
15.6420847595193));
#16096=CARTESIAN_POINT('Ctrl Pts',(0.160055147892539,-2.51383731594297,
15.6474461223548));
#16097=CARTESIAN_POINT('Ctrl Pts',(0.244584906330077,-2.50701748102916,
15.6528074851903));
#16098=CARTESIAN_POINT('Ctrl Pts',(0.328432674164168,-2.4959844207329,15.6581688480258));
#16099=CARTESIAN_POINT('Ctrl Pts',(0.412280441998259,-2.48495136043665,
15.6635302108613));
#16100=CARTESIAN_POINT('Ctrl Pts',(0.495445731495645,-2.46970523208183,
15.6688915736969));
#16101=CARTESIAN_POINT('Ctrl Pts',(0.577484402382204,-2.45037099538116,
15.6742529365324));
#16102=CARTESIAN_POINT('Ctrl Pts',(0.657899346862904,-2.43141942590716,
15.6795081861616));
#16103=CARTESIAN_POINT('Ctrl Pts',(0.73752889484594,-2.40847014295311,15.6847634357908));
#16104=CARTESIAN_POINT('Ctrl Pts',(0.815946152988599,-2.38160410761804,
15.69001868542));
#16105=CARTESIAN_POINT('Ctrl Pts',(0.894252233289506,-2.35477616221235,
15.6952664843002));
#16106=CARTESIAN_POINT('Ctrl Pts',(0.971349004820566,-2.32404264273536,
15.7005142831804));
#16107=CARTESIAN_POINT('Ctrl Pts',(1.04682137249731,-2.2895351633209,15.7057620820606));
#16108=CARTESIAN_POINT('Ctrl Pts',(1.12284059851767,-2.25477764930946,15.7110479054879));
#16109=CARTESIAN_POINT('Ctrl Pts',(1.19721131986629,-2.21619136251645,15.7163337289152));
#16110=CARTESIAN_POINT('Ctrl Pts',(1.26952652745185,-2.17396150980096,15.7216195523426));
#16111=CARTESIAN_POINT('Ctrl Pts',(1.34119329336554,-2.13211032703901,15.726857978434));
#16112=CARTESIAN_POINT('Ctrl Pts',(1.41084085516088,-2.08668089644513,15.7320964045255));
#16113=CARTESIAN_POINT('Ctrl Pts',(1.47809624844896,-2.03790032394156,15.737334830617));
#16114=CARTESIAN_POINT('Ctrl Pts',(1.54532952255311,-1.98913579455963,15.742571533877));
#16115=CARTESIAN_POINT('Ctrl Pts',(1.61017181744542,-1.93702258286824,15.747808237137));
#16116=CARTESIAN_POINT('Ctrl Pts',(1.67227964298106,-1.8818307696685,15.753044940397));
#16117=CARTESIAN_POINT('Ctrl Pts',(1.73438577672219,-1.82664045987361,15.7582815010111));
#16118=CARTESIAN_POINT('Ctrl Pts',(1.79375724497693,-1.76837202258052,15.7635180616252));
#16119=CARTESIAN_POINT('Ctrl Pts',(1.85008517215019,-1.70733450319204,15.7687546222393));
#16120=CARTESIAN_POINT('Ctrl Pts',(1.90733503039106,-1.64529796984657,15.7740768907457));
#16121=CARTESIAN_POINT('Ctrl Pts',(1.96144047700552,-1.58040124476285,15.7793991592521));
#16122=CARTESIAN_POINT('Ctrl Pts',(2.01211896210389,-1.51300480248476,15.7847214277586));
#16123=CARTESIAN_POINT('Ctrl Pts',(2.0620529477485,-1.44659845717513,15.7899655087267));
#16124=CARTESIAN_POINT('Ctrl Pts',(2.10865978046098,-1.37776577400283,15.7952095896948));
#16125=CARTESIAN_POINT('Ctrl Pts',(2.15171327529958,-1.30688034299225,15.8004536706629));
#16126=CARTESIAN_POINT('Ctrl Pts',(2.19572964050522,-1.23440959396672,15.8058150329385));
#16127=CARTESIAN_POINT('Ctrl Pts',(2.23603156928824,-1.15979362226863,15.8111763952141));
#16128=CARTESIAN_POINT('Ctrl Pts',(2.27242816711791,-1.08345580218537,15.8165377574897));
#16129=CARTESIAN_POINT('Ctrl Pts',(2.30882476494757,-1.00711798210211,15.8218991197653));
#16130=CARTESIAN_POINT('Ctrl Pts',(2.34131589823886,-0.929058808395344,
15.8272604820409));
#16131=CARTESIAN_POINT('Ctrl Pts',(2.36976456938881,-0.849718856839985,
15.8326218443165));
#16132=CARTESIAN_POINT('Ctrl Pts',(2.40208841605574,-0.759571502852221,
15.8387135120506));
#16133=CARTESIAN_POINT('Ctrl Pts',(2.42929323465991,-0.667497677878766,
15.8448051797847));
#16134=CARTESIAN_POINT('Ctrl Pts',(2.45117917360797,-0.574044343993166,
15.8508968475188));
#16135=CARTESIAN_POINT('Ctrl Pts',(2.47304705502787,-0.480668116061849,
15.8569834891737));
#16136=CARTESIAN_POINT('Ctrl Pts',(2.48960468448161,-0.385914782985989,
15.8630701308287));
#16137=CARTESIAN_POINT('Ctrl Pts',(2.50070035307118,-0.290351501028792,
15.8691567724836));
#16138=CARTESIAN_POINT('Ctrl Pts',(2.51179602166076,-0.194788219071594,
15.8752434141385));
#16139=CARTESIAN_POINT('Ctrl Pts',(2.51742955018304,-0.0984151276298001,
15.8813300557935));
#16140=CARTESIAN_POINT('Ctrl Pts',(2.51749934288794,-0.00181894442298069,
15.8874166974484));
#16141=CARTESIAN_POINT('Ctrl Pts',(2.51749934288862,-0.00181894347718374,
15.887416697508));
#16142=CARTESIAN_POINT('Ctrl Pts',(2.517559487875,0.0814244148722606,15.8926619616126));
#16143=CARTESIAN_POINT('Ctrl Pts',(2.51348653829097,0.164706578703061,15.8979072257173));
#16144=CARTESIAN_POINT('Ctrl Pts',(2.50529558016625,0.247588986022126,15.9031524898219));
#16145=CARTESIAN_POINT('Ctrl Pts',(2.49710604212937,0.330457023801282,15.9083968445414));
#16146=CARTESIAN_POINT('Ctrl Pts',(2.48479996515358,0.412924986783603,15.9136411992608));
#16147=CARTESIAN_POINT('Ctrl Pts',(2.46844432551966,0.494559260159785,15.9188855539803));
#16148=CARTESIAN_POINT('Ctrl Pts',(2.45208034576598,0.576235160744154,15.9241325829178));
#16149=CARTESIAN_POINT('Ctrl Pts',(2.4316627733015,0.657076073200728,15.9293796118553));
#16150=CARTESIAN_POINT('Ctrl Pts',(2.40730957902637,0.73665924329223,15.9346266407928));
#16151=CARTESIAN_POINT('Ctrl Pts',(2.39330444855097,0.782426244868507,15.9376441227726));
#16152=CARTESIAN_POINT('Ctrl Pts',(2.37799865629738,0.827777533216081,15.9406616047525));
#16153=CARTESIAN_POINT('Ctrl Pts',(2.36142200728636,0.872635292378007,15.9436790867324));
#16154=CARTESIAN_POINT('Ctrl Pts',(2.36142199860763,0.87263531586336,15.670984110559));
#16155=CARTESIAN_POINT('Ctrl Pts',(2.38881140575593,0.798517356856821,15.6657324005925));
#16156=CARTESIAN_POINT('Ctrl Pts',(2.41269859977669,0.723144194438671,15.6603427311849));
#16157=CARTESIAN_POINT('Ctrl Pts',(2.48897985726643,0.436189773331056,15.6399181512781));
#16158=CARTESIAN_POINT('Ctrl Pts',(2.51739377276997,0.219189285637256,15.6247664971261));
#16159=CARTESIAN_POINT('Ctrl Pts',(2.51751982902625,-0.0401892803670483,
15.6077912659681));
#16160=CARTESIAN_POINT('Ctrl Pts',(2.51651810043557,-0.0815980963299537,
15.6051113332934));
#16161=CARTESIAN_POINT('Ctrl Pts',(2.5136565021235,-0.14011433710098,15.601364814718));
#16162=CARTESIAN_POINT('Ctrl Pts',(2.51264244759951,-0.157254546783502,
15.600272320509));
#16163=CARTESIAN_POINT('Ctrl Pts',(2.51070321221152,-0.185183230864893,
15.5984998713506));
#16164=CARTESIAN_POINT('Ctrl Pts',(2.50988365856385,-0.195978251874473,
15.5978166571824));
#16165=CARTESIAN_POINT('Ctrl Pts',(2.50801290938118,-0.218678593221559,
15.5963837736142));
#16166=CARTESIAN_POINT('Ctrl Pts',(2.50694651663212,-0.230582417778358,
15.5956345955265));
#16167=CARTESIAN_POINT('Ctrl Pts',(2.50418055193433,-0.259166170399388,
15.5938407360676));
#16168=CARTESIAN_POINT('Ctrl Pts',(2.50239903003582,-0.275837735524215,
15.5927986313873));
#16169=CARTESIAN_POINT('Ctrl Pts',(2.49559433710554,-0.334009870738131,
15.5891759084683));
#16170=CARTESIAN_POINT('Ctrl Pts',(2.48970405154831,-0.375403424295379,
15.5866222670278));
#16171=CARTESIAN_POINT('Ctrl Pts',(2.4467489135997,-0.631380244526915,15.5709426874391));
#16172=CARTESIAN_POINT('Ctrl Pts',(2.38300758603946,-0.840534570131567,
15.5587213945927));
#16173=CARTESIAN_POINT('Ctrl Pts',(2.25010360397097,-1.13389598543474,15.5400367430987));
#16174=CARTESIAN_POINT('Ctrl Pts',(2.20120110001263,-1.22613000538683,15.5338902104286));
#16175=CARTESIAN_POINT('Ctrl Pts',(2.13957096552891,-1.32673661154938,15.5265782160125));
#16176=CARTESIAN_POINT('Ctrl Pts',(2.13231925254442,-1.33836039203338,15.5257237644765));
#16177=CARTESIAN_POINT('Ctrl Pts',(2.1204670366814,-1.35701747145425,15.5243356851403));
#16178=CARTESIAN_POINT('Ctrl Pts',(2.11592544650851,-1.36408810987468,15.5238057367336));
#16179=CARTESIAN_POINT('Ctrl Pts',(2.10779620020278,-1.37660596076598,15.5228603269342));
#16180=CARTESIAN_POINT('Ctrl Pts',(2.10422266555543,-1.38206214227595,15.5224457923324));
#16181=CARTESIAN_POINT('Ctrl Pts',(2.09640464151786,-1.39389832708489,15.5215411183615));
#16182=CARTESIAN_POINT('Ctrl Pts',(2.09215227908852,-1.40027276079334,15.5210504782031));
#16183=CARTESIAN_POINT('Ctrl Pts',(2.08000666891873,-1.41830060767409,15.5196533596124));
#16184=CARTESIAN_POINT('Ctrl Pts',(2.07204484475086,-1.42990716352752,15.5187425254391));
#16185=CARTESIAN_POINT('Ctrl Pts',(2.01720154697946,-1.50843651182806,15.512505498258));
#16186=CARTESIAN_POINT('Ctrl Pts',(1.96718763891124,-1.57310292610649,15.5070003396374));
#16187=CARTESIAN_POINT('Ctrl Pts',(1.84152149819552,-1.72020311889623,15.4937775149866));
#16188=CARTESIAN_POINT('Ctrl Pts',(1.76333971063287,-1.80025916687264,15.4860096425698));
#16189=CARTESIAN_POINT('Ctrl Pts',(1.56385461702373,-1.97902204085724,15.4675845595447));
#16190=CARTESIAN_POINT('Ctrl Pts',(1.43815965630078,-2.07216834872263,15.4570590777913));
#16191=CARTESIAN_POINT('Ctrl Pts',(1.2855460439328,-2.16464205996158,15.4455491516549));
#16192=CARTESIAN_POINT('Ctrl Pts',(1.26631427043085,-2.17594855169479,15.444119404117));
#16193=CARTESIAN_POINT('Ctrl Pts',(1.23441582180643,-2.19413570298014,15.4417811928913));
#16194=CARTESIAN_POINT('Ctrl Pts',(1.22183614917437,-2.20116567819165,15.4408674333296));
#16195=CARTESIAN_POINT('Ctrl Pts',(1.19901245798483,-2.21366442707653,15.4392243454714));
#16196=CARTESIAN_POINT('Ctrl Pts',(1.1887897274702,-2.21917103019417,15.4384936925878));
#16197=CARTESIAN_POINT('Ctrl Pts',(1.16678671473362,-2.23082755822618,15.4369321819197));
#16198=CARTESIAN_POINT('Ctrl Pts',(1.15499506001769,-2.23695535366888,15.4361021172352));
#16199=CARTESIAN_POINT('Ctrl Pts',(1.12259845212116,-2.25346651036378,15.4338396319747));
#16200=CARTESIAN_POINT('Ctrl Pts',(1.10189808677716,-2.26366058824857,15.4324137932811));
#16201=CARTESIAN_POINT('Ctrl Pts',(0.979934341541557,-2.32165316581012,
15.4241229314208));
#16202=CARTESIAN_POINT('Ctrl Pts',(0.875706732592535,-2.36294031080028,
15.4174851316121));
#16203=CARTESIAN_POINT('Ctrl Pts',(0.612895949574018,-2.44725641560329,
15.4014207549164));
#16204=CARTESIAN_POINT('Ctrl Pts',(0.452213364262973,-2.48197584425831,
15.392182657108));
#16205=CARTESIAN_POINT('Ctrl Pts',(0.213842815866966,-2.50955136071224,
15.378089232579));
#16206=CARTESIAN_POINT('Ctrl Pts',(0.1380329374517,-2.51486011073486,15.3735457787418));
#16207=CARTESIAN_POINT('Ctrl Pts',(0.0490628643820267,-2.51705568975932,
15.368023961927));
#16208=CARTESIAN_POINT('Ctrl Pts',(0.036016478002413,-2.51727616812457,
15.3672094718865));
#16209=CARTESIAN_POINT('Ctrl Pts',(0.0147608659385897,-2.51747010919017,
15.3658738352442));
#16210=CARTESIAN_POINT('Ctrl Pts',(0.0065522617272382,-2.5175048554485,
15.3653559325133));
#16211=CARTESIAN_POINT('Ctrl Pts',(-0.00816613720818674,-2.51749517241507,
15.3644233113043));
#16212=CARTESIAN_POINT('Ctrl Pts',(-0.0146757652788879,-2.51746564008284,
15.3640094184943));
#16213=CARTESIAN_POINT('Ctrl Pts',(-0.0289991101952524,-2.51734510179127,
15.3630955629884));
#16214=CARTESIAN_POINT('Ctrl Pts',(-0.0368124436567685,-2.51724296601848,
15.3625950156029));
#16215=CARTESIAN_POINT('Ctrl Pts',(-0.0594131698256786,-2.51684228399823,
15.361141475967));
#16216=CARTESIAN_POINT('Ctrl Pts',(-0.0741982781822732,-2.51644980040659,
15.3601835736814));
#16217=CARTESIAN_POINT('Ctrl Pts',(-0.195396873408821,-2.51216347321171,
15.3522784220622));
#16218=CARTESIAN_POINT('Ctrl Pts',(-0.30145770675546,-2.50165213318503,
15.3450302451222));
#16219=CARTESIAN_POINT('Ctrl Pts',(-0.418811623063205,-2.48245003380248,
15.3368466175873));
#16220=CARTESIAN_POINT('Ctrl Pts',(-0.431086785658288,-2.48034786394589,
15.3359885270153));
#16221=CARTESIAN_POINT('Ctrl Pts',(-0.636301071400487,-2.44363470479067,
15.321612183756));
#16222=CARTESIAN_POINT('Ctrl Pts',(-0.824599525550887,-2.38668996798914,
15.3080393549895));
#16223=CARTESIAN_POINT('Ctrl Pts',(-1.04713468432362,-2.28986624573079,
15.2920970503824));
#16224=CARTESIAN_POINT('Ctrl Pts',(-1.08934929702491,-2.27008745421015,
15.2890733021061));
#16225=CARTESIAN_POINT('Ctrl Pts',(-1.14707478540443,-2.24105995338555,
15.2849368436095));
#16226=CARTESIAN_POINT('Ctrl Pts',(-1.16306990017164,-2.23280064331093,
15.2837904565796));
#16227=CARTESIAN_POINT('Ctrl Pts',(-1.1886733129984,-2.21923015383286,15.281954716087));
#16228=CARTESIAN_POINT('Ctrl Pts',(-1.19833763043849,-2.21402656948294,
15.2812616259039));
#16229=CARTESIAN_POINT('Ctrl Pts',(-1.21834298804327,-2.20308566698797,
15.2798264310971));
#16230=CARTESIAN_POINT('Ctrl Pts',(-1.22867827250917,-2.19733834511559,
15.2790847020833));
#16231=CARTESIAN_POINT('Ctrl Pts',(-1.25295371490377,-2.18361424668106,
15.2773416766438));
#16232=CARTESIAN_POINT('Ctrl Pts',(-1.26685889988727,-2.17557641477953,
15.2763425846859));
#16233=CARTESIAN_POINT('Ctrl Pts',(-1.31291527988052,-2.14836241563089,
15.2730302719432));
#16234=CARTESIAN_POINT('Ctrl Pts',(-1.34471651039098,-2.12860173128764,
15.2707380947528));
#16235=CARTESIAN_POINT('Ctrl Pts',(-1.48882062067564,-2.03453919354006,
15.2603077924118));
#16236=CARTESIAN_POINT('Ctrl Pts',(-1.59549388633856,-1.95200957712699,
15.2524774388167));
#16237=CARTESIAN_POINT('Ctrl Pts',(-1.81300488204768,-1.753928719302,15.235538490969));
#16238=CARTESIAN_POINT('Ctrl Pts',(-1.92045942321415,-1.63556665368369,
15.2265001596354));
#16239=CARTESIAN_POINT('Ctrl Pts',(-2.03977441565233,-1.47604344114202,
15.2144986766687));
#16240=CARTESIAN_POINT('Ctrl Pts',(-2.0628068788277,-1.44367977347344,15.2120710098848));
#16241=CARTESIAN_POINT('Ctrl Pts',(-2.09172327607617,-1.40094298731833,
15.2088553258887));
#16242=CARTESIAN_POINT('Ctrl Pts',(-2.09831391981306,-1.39105219107801,
15.2081104297761));
#16243=CARTESIAN_POINT('Ctrl Pts',(-2.10877568167771,-1.37510835714715,
15.2069079558654));
#16244=CARTESIAN_POINT('Ctrl Pts',(-2.11269144420212,-1.36908463144331,
15.2064532623436));
#16245=CARTESIAN_POINT('Ctrl Pts',(-2.12017744243631,-1.35746012022529,
15.2055748876328));
#16246=CARTESIAN_POINT('Ctrl Pts',(-2.12375136059673,-1.35186187152455,
15.2051514522374));
#16247=CARTESIAN_POINT('Ctrl Pts',(-2.13227574337301,-1.33839189942268,
15.2041317199498));
#16248=CARTESIAN_POINT('Ctrl Pts',(-2.13720480023032,-1.3305068047939,15.2035340569879));
#16249=CARTESIAN_POINT('Ctrl Pts',(-2.15407972621147,-1.30317597643868,
15.2014604553677));
#16250=CARTESIAN_POINT('Ctrl Pts',(-2.1658043868312,-1.28359587260666,15.1999714007256));
#16251=CARTESIAN_POINT('Ctrl Pts',(-2.19398761626698,-1.23504441653125,
15.1962755836971));
#16252=CARTESIAN_POINT('Ctrl Pts',(-2.21014000107759,-1.20590104590893,
15.1940541475708));
#16253=CARTESIAN_POINT('Ctrl Pts',(-2.27530537861129,-1.08261533106032,
15.184669676121));
#16254=CARTESIAN_POINT('Ctrl Pts',(-2.31891642286823,-0.985745831882188,
15.1773317781199));
#16255=CARTESIAN_POINT('Ctrl Pts',(-2.42115219806167,-0.713982399962587,
15.1572729264982));
#16256=CARTESIAN_POINT('Ctrl Pts',(-2.46690840652586,-0.534915639120533,
15.1446676848096));
#16257=CARTESIAN_POINT('Ctrl Pts',(-2.49727129684068,-0.320163201604435,
15.1305791461148));
#16258=CARTESIAN_POINT('Ctrl Pts',(-2.50120688379339,-0.287806693320121,
15.1284813581798));
#16259=CARTESIAN_POINT('Ctrl Pts',(-2.5060391771045,-0.240416661009576,
15.1254438908344));
#16260=CARTESIAN_POINT('Ctrl Pts',(-2.50743099894337,-0.225438083781834,
15.124488917134));
#16261=CARTESIAN_POINT('Ctrl Pts',(-2.50966724307612,-0.198780434511985,
15.122798102588));
#16262=CARTESIAN_POINT('Ctrl Pts',(-2.51056458739767,-0.187106365737418,
15.1220606358));
#16263=CARTESIAN_POINT('Ctrl Pts',(-2.5122705510553,-0.162684008276177,
15.1205239076267));
#16264=CARTESIAN_POINT('Ctrl Pts',(-2.51306365425366,-0.149934944204064,
15.1197251490001));
#16265=CARTESIAN_POINT('Ctrl Pts',(-2.51488797229082,-0.116505214851965,
15.1176394154671));
#16266=CARTESIAN_POINT('Ctrl Pts',(-2.51576115537954,-0.0958166318843272,
15.1163573633316));
#16267=CARTESIAN_POINT('Ctrl Pts',(-2.5186384570955,0.000568677124928038,
15.1104222386679));
#16268=CARTESIAN_POINT('Ctrl Pts',(-2.5174821168074,0.0763244139333311,
15.1058674751591));
#16269=CARTESIAN_POINT('Ctrl Pts',(-2.50493933800149,0.283796631592991,
15.0935748077665));
#16270=CARTESIAN_POINT('Ctrl Pts',(-2.48659714810952,0.414847705627033,
15.0860204203589));
#16271=CARTESIAN_POINT('Ctrl Pts',(-2.42841472277007,0.677813731246231,
15.0705340399385));
#16272=CARTESIAN_POINT('Ctrl Pts',(-2.38787836655046,0.809108773280037,
15.0626207255028));
#16273=CARTESIAN_POINT('Ctrl Pts',(-2.32889676410057,0.956297121081916,
15.052882981077));
#16274=CARTESIAN_POINT('Ctrl Pts',(-2.3206829501584,0.97606090820723,15.0515564353465));
#16275=CARTESIAN_POINT('Ctrl Pts',(-2.30888747632026,1.00345194182823,15.0496881162314));
#16276=CARTESIAN_POINT('Ctrl Pts',(-2.30551773684484,1.0111701826154,15.0491583279628));
#16277=CARTESIAN_POINT('Ctrl Pts',(-2.29963581490471,1.0244602110262,15.0482400780457));
#16278=CARTESIAN_POINT('Ctrl Pts',(-2.2971419261892,1.0300400837845,15.0478527092524));
#16279=CARTESIAN_POINT('Ctrl Pts',(-2.29183545771371,1.0417977542909,15.0470324635551));
#16280=CARTESIAN_POINT('Ctrl Pts',(-2.28901818103231,1.04797332484206,15.0465992931731));
#16281=CARTESIAN_POINT('Ctrl Pts',(-2.281961819795,1.06327691346483,15.0455201599903));
#16282=CARTESIAN_POINT('Ctrl Pts',(-2.2776929397021,1.07239097627057,15.0448724251353));
#16283=CARTESIAN_POINT('Ctrl Pts',(-2.26136242005423,1.10671924959317,15.0424142477346));
#16284=CARTESIAN_POINT('Ctrl Pts',(-2.24893629088401,1.13175655434347,15.0405835595723));
#16285=CARTESIAN_POINT('Ctrl Pts',(-2.21592779748154,1.19557414097106,15.0358289372114));
#16286=CARTESIAN_POINT('Ctrl Pts',(-2.19474362889226,1.23403140130677,15.0328782670417));
#16287=CARTESIAN_POINT('Ctrl Pts',(-2.10996816826968,1.37883715093957,15.0214880860647));
#16288=CARTESIAN_POINT('Ctrl Pts',(-2.03956370666671,1.48099167872028,15.0128701946067));
#16289=CARTESIAN_POINT('Ctrl Pts',(-1.86060732884295,1.70355211466464,14.993207170834));
#16290=CARTESIAN_POINT('Ctrl Pts',(-1.74736961478691,1.81952351801807,14.982286003529));
#16291=CARTESIAN_POINT('Ctrl Pts',(-1.60677702348184,1.93818684678772,14.9704201840154));
#16292=CARTESIAN_POINT('Ctrl Pts',(-1.58959541222314,1.95230303320891,14.9689951585419));
#16293=CARTESIAN_POINT('Ctrl Pts',(-1.56099121460858,1.97517586556778,14.9666630443253));
#16294=CARTESIAN_POINT('Ctrl Pts',(-1.54967684211776,1.98406526379702,14.9657507069784));
#16295=CARTESIAN_POINT('Ctrl Pts',(-1.52909651461544,1.99995121980013,14.9641091512604));
#16296=CARTESIAN_POINT('Ctrl Pts',(-1.51985726059715,2.00698155130553,14.9633786192623));
#16297=CARTESIAN_POINT('Ctrl Pts',(-1.49992650584378,2.02193069327464,14.9618162618917));
#16298=CARTESIAN_POINT('Ctrl Pts',(-1.48922016222383,2.02982919738463,14.9609852380707));
#16299=CARTESIAN_POINT('Ctrl Pts',(-1.45971767887471,2.05123530286599,14.9587173122495));
#16300=CARTESIAN_POINT('Ctrl Pts',(-1.44079679234585,2.06456935650309,14.957287046414));
#16301=CARTESIAN_POINT('Ctrl Pts',(-1.32801153730688,2.1417463806301,14.948897744424));
#16302=CARTESIAN_POINT('Ctrl Pts',(-1.23009425552339,2.19944650556234,14.9421727064589));
#16303=CARTESIAN_POINT('Ctrl Pts',(-0.969073344892513,2.33035519740223,
14.9251860656122));
#16304=CARTESIAN_POINT('Ctrl Pts',(-0.801498018579548,2.39316763673473,
14.9151704027721));
#16305=CARTESIAN_POINT('Ctrl Pts',(-0.569392832980046,2.45302868214434,
14.9009671154989));
#16306=CARTESIAN_POINT('Ctrl Pts',(-0.509549310245642,2.46615411296971,
14.8972730613384));
#16307=CARTESIAN_POINT('Ctrl Pts',(-0.435999532412581,2.4794945389303,14.8926291769369));
#16308=CARTESIAN_POINT('Ctrl Pts',(-0.422687911373011,2.4817984752291,14.891784573943));
#16309=CARTESIAN_POINT('Ctrl Pts',(-0.401838141655966,2.48523448658922,
14.8904543485869));
#16310=CARTESIAN_POINT('Ctrl Pts',(-0.394312074285199,2.48643968956872,
14.8899726904463));
#16311=CARTESIAN_POINT('Ctrl Pts',(-0.380330784147522,2.48861354023739,
14.8890749464072));
#16312=CARTESIAN_POINT('Ctrl Pts',(-0.373877154234701,2.48959127733828,
14.8886593706427));
#16313=CARTESIAN_POINT('Ctrl Pts',(-0.359048939490664,2.49177882359664,
14.8877018327678));
#16314=CARTESIAN_POINT('Ctrl Pts',(-0.350672029781081,2.49297151392958,
14.8871589409402));
#16315=CARTESIAN_POINT('Ctrl Pts',(-0.324420325786182,2.49657425693135,
14.8854518519568));
#16316=CARTESIAN_POINT('Ctrl Pts',(-0.306525997128382,2.49883439573106,
14.8842798663823));
#16317=CARTESIAN_POINT('Ctrl Pts',(-0.141649521573048,2.51786150066191,
14.87341389261));
#16318=CARTESIAN_POINT('Ctrl Pts',(0.00650513065036972,2.52183274284893,
14.8631750668824));
#16319=CARTESIAN_POINT('Ctrl Pts',(0.336348971714478,2.5016000164923,14.8403463504556));
#16320=CARTESIAN_POINT('Ctrl Pts',(0.516838295960918,2.4706343014458,14.8278613649218));
#16321=CARTESIAN_POINT('Ctrl Pts',(0.723475030893875,2.41152107796648,14.8138987483381));
#16322=CARTESIAN_POINT('Ctrl Pts',(0.754363778964595,2.40203777595943,14.8118187778432));
#16323=CARTESIAN_POINT('Ctrl Pts',(0.799520622156711,2.38721690999601,14.8087874026054));
#16324=CARTESIAN_POINT('Ctrl Pts',(0.813935539385937,2.3823406043055,14.8078211419135));
#16325=CARTESIAN_POINT('Ctrl Pts',(0.839386144979637,2.37347315811431,14.8061173829471));
#16326=CARTESIAN_POINT('Ctrl Pts',(0.850439691476767,2.36953503273654,14.8053781727174));
#16327=CARTESIAN_POINT('Ctrl Pts',(0.87339104543088,2.36117670098505,14.8038446976425));
#16328=CARTESIAN_POINT('Ctrl Pts',(0.885283794193366,2.35674350421294,14.8030508859994));
#16329=CARTESIAN_POINT('Ctrl Pts',(0.915027327187574,2.34539924753365,14.8010672685988));
#16330=CARTESIAN_POINT('Ctrl Pts',(0.93283396080928,2.33837410881037,14.799881272571));
#16331=CARTESIAN_POINT('Ctrl Pts',(1.01005308277905,2.30688687962633,14.7947427787229));
#16332=CARTESIAN_POINT('Ctrl Pts',(1.06859977710096,2.2803573963202,14.7908596590706));
#16333=CARTESIAN_POINT('Ctrl Pts',(1.22815297925636,2.20056210977424,14.7802425810399));
#16334=CARTESIAN_POINT('Ctrl Pts',(1.32664980754301,2.14262368778261,14.773653449442));
#16335=CARTESIAN_POINT('Ctrl Pts',(1.56183499231316,1.98182592477016,14.7572750215297));
#16336=CARTESIAN_POINT('Ctrl Pts',(1.6926009103257,1.87137605714634,14.7475711753274));
#16337=CARTESIAN_POINT('Ctrl Pts',(1.82395545053425,1.73531894033377,14.7359355338547));
#16338=CARTESIAN_POINT('Ctrl Pts',(1.83659872920183,1.72193216282107,14.7347934592627));
#16339=CARTESIAN_POINT('Ctrl Pts',(1.85568782044743,1.70127110917447,14.733032725243));
#16340=CARTESIAN_POINT('Ctrl Pts',(1.86224052985465,1.694095887354,14.7324216023394));
#16341=CARTESIAN_POINT('Ctrl Pts',(1.87320854792724,1.68194537150281,14.7313869475562));
#16342=CARTESIAN_POINT('Ctrl Pts',(1.87764606076477,1.67699009119724,14.7309650497652));
#16343=CARTESIAN_POINT('Ctrl Pts',(1.88672632177683,1.66676912580199,14.7300948125163));
#16344=CARTESIAN_POINT('Ctrl Pts',(1.8913667453634,1.66150153886609,14.7296463210225));
#16345=CARTESIAN_POINT('Ctrl Pts',(1.90331460362784,1.64782398831414,14.7284819581567));
#16346=CARTESIAN_POINT('Ctrl Pts',(1.91058825832425,1.63938490692625,14.7277637061883));
#16347=CARTESIAN_POINT('Ctrl Pts',(1.94117681057694,1.60341521833078,14.7247040330188));
#16348=CARTESIAN_POINT('Ctrl Pts',(1.96395329172995,1.57543483711423,14.7223282075242));
#16349=CARTESIAN_POINT('Ctrl Pts',(2.04973601817565,1.46530082597472,14.7130235856465));
#16350=CARTESIAN_POINT('Ctrl Pts',(2.10824951106603,1.37978445616766,14.7059009304884));
#16351=CARTESIAN_POINT('Ctrl Pts',(2.21633923608816,1.19881426405434,14.6913445031883));
#16352=CARTESIAN_POINT('Ctrl Pts',(2.26540931700534,1.10328513542836,14.6839244519033));
#16353=CARTESIAN_POINT('Ctrl Pts',(2.32721433607724,0.961322021669879,14.6734116019023));
#16354=CARTESIAN_POINT('Ctrl Pts',(2.34494933737997,0.917211670335576,14.6702119075418));
#16355=CARTESIAN_POINT('Ctrl Pts',(2.36142197356233,0.872635383637971,14.6670478768675));
#16356=CARTESIAN_POINT('Origin',(0.,0.,10.));
#16357=CARTESIAN_POINT('',(2.36142191786124,0.872635534369624,13.6679749024944));
#16358=CARTESIAN_POINT('',(2.36142200728636,0.872635292378013,13.9438095899177));
#16359=CARTESIAN_POINT('',(2.36142200728636,0.87263529237802,10.));
#16360=CARTESIAN_POINT('',(2.5174999540924,-0.000480775158033205,14.8874166975507));
#16361=CARTESIAN_POINT('Ctrl Pts',(2.36142200728636,0.872635292378013,13.9438095899177));
#16362=CARTESIAN_POINT('Ctrl Pts',(2.33274328543006,0.950242244015014,13.9490591804899));
#16363=CARTESIAN_POINT('Ctrl Pts',(2.30018971864896,1.02655575865372,13.9543087710621));
#16364=CARTESIAN_POINT('Ctrl Pts',(2.26390046374053,1.1011634484832,13.9595583616344));
#16365=CARTESIAN_POINT('Ctrl Pts',(2.22616663310737,1.17874106585397,13.9650169240117));
#16366=CARTESIAN_POINT('Ctrl Pts',(2.18439357996264,1.25447371190632,13.9704754863891));
#16367=CARTESIAN_POINT('Ctrl Pts',(2.13879413279158,1.32791788433484,13.9759340487664));
#16368=CARTESIAN_POINT('Ctrl Pts',(2.09502845327483,1.39840852210115,13.9811730967472));
#16369=CARTESIAN_POINT('Ctrl Pts',(2.04773848948028,1.46679077534903,13.9864121447281));
#16370=CARTESIAN_POINT('Ctrl Pts',(1.99715956760326,1.53269694053676,13.9916511927089));
#16371=CARTESIAN_POINT('Ctrl Pts',(1.94660080083145,1.59857684289319,13.9968881529908));
#16372=CARTESIAN_POINT('Ctrl Pts',(1.89275595920445,1.66198225093666,14.0021251132727));
#16373=CARTESIAN_POINT('Ctrl Pts',(1.83590271087396,1.72257582886956,14.0073620735545));
#16374=CARTESIAN_POINT('Ctrl Pts',(1.77905496837645,1.78316353874514,14.012598526674));
#16375=CARTESIAN_POINT('Ctrl Pts',(1.71919971426181,1.84093962357419,14.0178349797935));
#16376=CARTESIAN_POINT('Ctrl Pts',(1.65665284537889,1.89560217342617,14.023071432913));
#16377=CARTESIAN_POINT('Ctrl Pts',(1.59409316714979,1.95027591794763,14.0283089584369));
#16378=CARTESIAN_POINT('Ctrl Pts',(1.52884112790565,2.00183455884925,14.0335464839608));
#16379=CARTESIAN_POINT('Ctrl Pts',(1.46124612495801,2.05001610049658,14.0387840094848));
#16380=CARTESIAN_POINT('Ctrl Pts',(1.39357582607775,2.09825131288812,14.0440273692324));
#16381=CARTESIAN_POINT('Ctrl Pts',(1.32355773220934,2.14310165189018,14.0492707289801));
#16382=CARTESIAN_POINT('Ctrl Pts',(1.25157017303084,2.18434849600048,14.0545140887277));
#16383=CARTESIAN_POINT('Ctrl Pts',(1.17953513628648,2.22562254341897,14.0597609066001));
#16384=CARTESIAN_POINT('Ctrl Pts',(1.10552845998846,2.26328815725627,14.0650077244724));
#16385=CARTESIAN_POINT('Ctrl Pts',(1.02995087051983,2.29717379715063,14.0702545423448));
#16386=CARTESIAN_POINT('Ctrl Pts',(0.954253109036032,2.33111331684798,14.0755097029108));
#16387=CARTESIAN_POINT('Ctrl Pts',(0.87697987943064,2.36126070341817,14.0807648634769));
#16388=CARTESIAN_POINT('Ctrl Pts',(0.798548999298957,2.38749361166028,14.0860200240429));
#16389=CARTESIAN_POINT('Ctrl Pts',(0.775944111138288,2.39505430657976,14.0875346355921));
#16390=CARTESIAN_POINT('Ctrl Pts',(0.7532431325843,2.4022901592352,14.0890492471413));
#16391=CARTESIAN_POINT('Ctrl Pts',(0.730456218411384,2.40919902934235,14.0905638586905));
#16392=CARTESIAN_POINT('Ctrl Pts',(0.651392436506789,2.43317074377522,14.0958191080976));
#16393=CARTESIAN_POINT('Ctrl Pts',(0.571001358182961,2.453290596041,14.1010743575047));
#16394=CARTESIAN_POINT('Ctrl Pts',(0.489692843030049,2.46941433734502,14.1063296069117));
#16395=CARTESIAN_POINT('Ctrl Pts',(0.408499604880611,2.48551521884673,14.111577405569));
#16396=CARTESIAN_POINT('Ctrl Pts',(0.326391962337084,2.49763115387252,14.1168252042263));
#16397=CARTESIAN_POINT('Ctrl Pts',(0.243794995117869,2.50566762567494,14.1220730028835));
#16398=CARTESIAN_POINT('Ctrl Pts',(0.160599541659662,2.51376232864425,14.1273588263665));
#16399=CARTESIAN_POINT('Ctrl Pts',(0.0769080959480587,2.51771806298627,
14.1326446498495));
#16400=CARTESIAN_POINT('Ctrl Pts',(-0.00683435580937276,2.51749072323627,
14.1379304733324));
#16401=CARTESIAN_POINT('Ctrl Pts',(-0.0898258947777812,2.51726542202612,
14.1431688992008));
#16402=CARTESIAN_POINT('Ctrl Pts',(-0.172867058799017,2.51293176621098,
14.1484073250692));
#16403=CARTESIAN_POINT('Ctrl Pts',(-0.255521276603785,2.50449897728124,
14.1536457509375));
#16404=CARTESIAN_POINT('Ctrl Pts',(-0.338148310811867,2.49606896175544,
14.1588824539748));
#16405=CARTESIAN_POINT('Ctrl Pts',(-0.420388192873449,2.48354253738479,
14.1641191570121));
#16406=CARTESIAN_POINT('Ctrl Pts',(-0.501808273384028,2.46698088901461,
14.1693558600494));
#16407=CARTESIAN_POINT('Ctrl Pts',(-0.583226136052318,2.45041969177546,
14.1745924204415));
#16408=CARTESIAN_POINT('Ctrl Pts',(-0.663823789613585,2.42982358206545,
14.1798289808336));
#16409=CARTESIAN_POINT('Ctrl Pts',(-0.743178965304525,2.40530481967024,
14.1850655412257));
#16410=CARTESIAN_POINT('Ctrl Pts',(-0.823832971322326,2.38038475122412,
14.1903878099965));
#16411=CARTESIAN_POINT('Ctrl Pts',(-0.903202986807447,2.35141259770563,
14.1957100787672));
#16412=CARTESIAN_POINT('Ctrl Pts',(-0.980863698073059,2.31855831408279,
14.201032347538));
#16413=CARTESIAN_POINT('Ctrl Pts',(-1.0573835166936,2.2861866839141,14.2062764282881));
#16414=CARTESIAN_POINT('Ctrl Pts',(-1.13224352479191,2.25004648791044,14.2115205090382));
#16415=CARTESIAN_POINT('Ctrl Pts',(-1.20506057604794,2.21034731615984,14.2167645897883));
#16416=CARTESIAN_POINT('Ctrl Pts',(-1.27950615517514,2.16976028632459,14.2221259525694));
#16417=CARTESIAN_POINT('Ctrl Pts',(-1.35181585815272,2.12545343681934,14.2274873153505));
#16418=CARTESIAN_POINT('Ctrl Pts',(-1.42161207295006,2.0776971300078,14.2328486781316));
#16419=CARTESIAN_POINT('Ctrl Pts',(-1.4914082877474,2.02994082319626,14.2382100409126));
#16420=CARTESIAN_POINT('Ctrl Pts',(-1.55869065048786,1.97873541994997,14.2435714036937));
#16421=CARTESIAN_POINT('Ctrl Pts',(-1.62311953090137,1.92439321304315,14.2489327664748));
#16422=CARTESIAN_POINT('Ctrl Pts',(-1.68627321952089,1.87112656007844,14.2541880158828));
#16423=CARTESIAN_POINT('Ctrl Pts',(-1.74691864447732,1.81464942874646,14.2594432652908));
#16424=CARTESIAN_POINT('Ctrl Pts',(-1.80471166230083,1.75522706962814,14.2646985146988));
#16425=CARTESIAN_POINT('Ctrl Pts',(-1.86242274275407,1.69588895791589,14.269946313357));
#16426=CARTESIAN_POINT('Ctrl Pts',(-1.91728912974502,1.63361424052214,14.2751941120152));
#16427=CARTESIAN_POINT('Ctrl Pts',(-1.96900010803878,1.56870801124469,14.2804419106734));
#16428=CARTESIAN_POINT('Ctrl Pts',(-2.02108577694166,1.50333148039134,14.2857277341562));
#16429=CARTESIAN_POINT('Ctrl Pts',(-2.06996975464811,1.43528544713269,14.2910135576389));
#16430=CARTESIAN_POINT('Ctrl Pts',(-2.11537277239941,1.36491914917743,14.2962993811216));
#16431=CARTESIAN_POINT('Ctrl Pts',(-2.16036866443207,1.29518382094713,14.3015378069909));
#16432=CARTESIAN_POINT('Ctrl Pts',(-2.20194551875351,1.22317006752683,14.3067762328602));
#16433=CARTESIAN_POINT('Ctrl Pts',(-2.23987337836964,1.14924910218411,14.3120146587295));
#16434=CARTESIAN_POINT('Ctrl Pts',(-2.27778876414393,1.07535244821671,14.3172513617677));
#16435=CARTESIAN_POINT('Ctrl Pts',(-2.31205732819042,0.999550238292341,
14.3224880648059));
#16436=CARTESIAN_POINT('Ctrl Pts',(-2.34249483524164,0.922238687578345,
14.3277247678441));
#16437=CARTESIAN_POINT('Ctrl Pts',(-2.37293151319036,0.844929242792407,
14.3329613282371));
#16438=CARTESIAN_POINT('Ctrl Pts',(-2.39953717355716,0.766110968683968,
14.3381978886301));
#16439=CARTESIAN_POINT('Ctrl Pts',(-2.42217607409677,0.686199181049617,
14.3434344490232));
#16440=CARTESIAN_POINT('Ctrl Pts',(-2.44518551240696,0.60497945288248,14.3487567177928));
#16441=CARTESIAN_POINT('Ctrl Pts',(-2.46409702237147,0.522630562025979,
14.3540789865624));
#16442=CARTESIAN_POINT('Ctrl Pts',(-2.4788215982056,0.439601790566655,14.3594012553321));
#16443=CARTESIAN_POINT('Ctrl Pts',(-2.49332985925757,0.357792772451314,
14.3646453360831));
#16444=CARTESIAN_POINT('Ctrl Pts',(-2.50377338992976,0.275324189044946,
14.3698894168341));
#16445=CARTESIAN_POINT('Ctrl Pts',(-2.51011938815899,0.192631532175615,
14.3751334975851));
#16446=CARTESIAN_POINT('Ctrl Pts',(-2.51660731241434,0.108089483019304,
14.3804948603641));
#16447=CARTESIAN_POINT('Ctrl Pts',(-2.5188121995278,0.0233137286734454,
14.385856223143));
#16448=CARTESIAN_POINT('Ctrl Pts',(-2.51675523590462,-0.0612317935935599,
14.391217585922));
#16449=CARTESIAN_POINT('Ctrl Pts',(-2.51469827228144,-0.145777315860577,
14.3965789487009));
#16450=CARTESIAN_POINT('Ctrl Pts',(-2.50837956250467,-0.230092104354747,
14.4019403114799));
#16451=CARTESIAN_POINT('Ctrl Pts',(-2.49787614311308,-0.313721251537898,
14.4073016742588));
#16452=CARTESIAN_POINT('Ctrl Pts',(-2.4875806099061,-0.395695190671064,
14.4125569236655));
#16453=CARTESIAN_POINT('Ctrl Pts',(-2.47322652414794,-0.477313167553763,
14.4178121730721));
#16454=CARTESIAN_POINT('Ctrl Pts',(-2.45484900653005,-0.55814210120581,
14.4230674224788));
#16455=CARTESIAN_POINT('Ctrl Pts',(-2.43649754405725,-0.638856437792109,
14.4283152211356));
#16456=CARTESIAN_POINT('Ctrl Pts',(-2.41413408159974,-0.718783506996741,
14.4335630197925));
#16457=CARTESIAN_POINT('Ctrl Pts',(-2.38784536008661,-0.797496574483465,
14.4388108184493));
#16458=CARTESIAN_POINT('Ctrl Pts',(-2.36136615411844,-0.876779986015132,
14.4440966419324));
#16459=CARTESIAN_POINT('Ctrl Pts',(-2.33090462435669,-0.954831258423609,
14.4493824654155));
#16460=CARTESIAN_POINT('Ctrl Pts',(-2.2966016603855,-1.03122600021263,14.4546682888985));
#16461=CARTESIAN_POINT('Ctrl Pts',(-2.26260628872966,-1.10693571561366,
14.4599067147665));
#16462=CARTESIAN_POINT('Ctrl Pts',(-2.22483829118455,-1.18101806071211,
14.4651451406344));
#16463=CARTESIAN_POINT('Ctrl Pts',(-2.18348383813068,-1.25307804171253,
14.4703835665024));
#16464=CARTESIAN_POINT('Ctrl Pts',(-2.14214298586814,-1.32511432338453,
14.4756202695393));
#16465=CARTESIAN_POINT('Ctrl Pts',(-2.09721825018888,-1.39512916204231,
14.4808569725762));
#16466=CARTESIAN_POINT('Ctrl Pts',(-2.04894166613948,-1.46275230259863,
14.486093675613));
#16467=CARTESIAN_POINT('Ctrl Pts',(-2.00066639712001,-1.53037360113451,
14.4913302360047));
#16468=CARTESIAN_POINT('Ctrl Pts',(-1.94903973020372,-1.59560295615947,
14.4965667963965));
#16469=CARTESIAN_POINT('Ctrl Pts',(-1.89433612399927,-1.65810038879177,
14.5018033567882));
#16470=CARTESIAN_POINT('Ctrl Pts',(-1.83873716720369,-1.72162073594717,
14.5071256255594));
#16471=CARTESIAN_POINT('Ctrl Pts',(-1.77995995396854,-1.78231854680815,
14.5124478943307));
#16472=CARTESIAN_POINT('Ctrl Pts',(-1.71833287930394,-1.83987455167547,
14.5177701631019));
#16473=CARTESIAN_POINT('Ctrl Pts',(-1.65761115144655,-1.89658501672892,
14.5230142438516));
#16474=CARTESIAN_POINT('Ctrl Pts',(-1.59412313651235,-1.9502451186521,14.5282583246014));
#16475=CARTESIAN_POINT('Ctrl Pts',(-1.5282162625524,-2.00059023912204,14.5335024053511));
#16476=CARTESIAN_POINT('Ctrl Pts',(-1.46083540440216,-2.05206131060698,
14.5388637681331));
#16477=CARTESIAN_POINT('Ctrl Pts',(-1.39092660988126,-2.1000670447314,14.5442251309151));
#16478=CARTESIAN_POINT('Ctrl Pts',(-1.31889056096353,-2.14437262111819,
14.5495864936971));
#16479=CARTESIAN_POINT('Ctrl Pts',(-1.24685451204578,-2.188678197505,14.5549478564791));
#16480=CARTESIAN_POINT('Ctrl Pts',(-1.17269168648866,-2.22928343072958,
14.5603092192611));
#16481=CARTESIAN_POINT('Ctrl Pts',(-1.09682559989037,-2.26600526332688,
14.5656705820431));
#16482=CARTESIAN_POINT('Ctrl Pts',(-1.02246107304345,-2.30200028862073,
14.5709258314492));
#16483=CARTESIAN_POINT('Ctrl Pts',(-0.946185439314126,-2.33439722714392,
14.5761810808553));
#16484=CARTESIAN_POINT('Ctrl Pts',(-0.868381085202565,-2.36298974624572,
14.5814363302613));
#16485=CARTESIAN_POINT('Ctrl Pts',(-0.790687039990303,-2.3915417276508,
14.5866841289176));
#16486=CARTESIAN_POINT('Ctrl Pts',(-0.711469008929585,-2.41629984546682,
14.5919319275739));
#16487=CARTESIAN_POINT('Ctrl Pts',(-0.631132159723589,-2.43710452114033,
14.5971797262301));
#16488=CARTESIAN_POINT('Ctrl Pts',(-0.550213200762819,-2.45805994463099,
14.6024655497133));
#16489=CARTESIAN_POINT('Ctrl Pts',(-0.468159568186418,-2.47500418557747,
14.6077513731966));
#16490=CARTESIAN_POINT('Ctrl Pts',(-0.385403945861432,-2.48782436046326,
14.6130371966798));
#16491=CARTESIAN_POINT('Ctrl Pts',(-0.303390387513959,-2.50052957772199,
14.6182756225471));
#16492=CARTESIAN_POINT('Ctrl Pts',(-0.220687842766615,-2.50918432118937,
14.6235140484144));
#16493=CARTESIAN_POINT('Ctrl Pts',(-0.137728990121894,-2.51372969415568,
14.6287524742818));
#16494=CARTESIAN_POINT('Ctrl Pts',(-0.0547974212632767,-2.51827357222446,
14.633989177318));
#16495=CARTESIAN_POINT('Ctrl Pts',(0.0283898277111877,-2.51871073872867,
14.6392258803543));
#16496=CARTESIAN_POINT('Ctrl Pts',(0.111395857847538,-2.51503423691496,
14.6444625833905));
#16497=CARTESIAN_POINT('Ctrl Pts',(0.19439962694111,-2.51135783524732,14.6496991437816));
#16498=CARTESIAN_POINT('Ctrl Pts',(0.277221726088093,-2.50356800950175,
14.6549357041727));
#16499=CARTESIAN_POINT('Ctrl Pts',(0.359427554207529,-2.49170987140887,
14.6601722645637));
#16500=CARTESIAN_POINT('Ctrl Pts',(0.442978870185704,-2.4796576475535,14.6654945333357));
#16501=CARTESIAN_POINT('Ctrl Pts',(0.525893071175531,-2.46340279242345,
14.6708168021077));
#16502=CARTESIAN_POINT('Ctrl Pts',(0.607723561040238,-2.44304693433355,
14.6761390708796));
#16503=CARTESIAN_POINT('Ctrl Pts',(0.688351901128603,-2.42299011869459,
14.6813831516287));
#16504=CARTESIAN_POINT('Ctrl Pts',(0.767927729473984,-2.39895218782986,
14.6866272323778));
#16505=CARTESIAN_POINT('Ctrl Pts',(0.846039928523892,-2.37108048984915,
14.6918713131269));
#16506=CARTESIAN_POINT('Ctrl Pts',(0.925899079622809,-2.34258545107803,
14.6972326759103));
#16507=CARTESIAN_POINT('Ctrl Pts',(1.00422787138072,-2.31008329044402,14.7025940386937));
#16508=CARTESIAN_POINT('Ctrl Pts',(1.08061118635039,-2.27378224857491,14.7079554014771));
#16509=CARTESIAN_POINT('Ctrl Pts',(1.15699450132007,-2.23748120670581,14.7133167642605));
#16510=CARTESIAN_POINT('Ctrl Pts',(1.23143192385297,-2.19738158338615,14.7186781270439));
#16511=CARTESIAN_POINT('Ctrl Pts',(1.30353932303076,-2.15373895431004,14.7240394898273));
#16512=CARTESIAN_POINT('Ctrl Pts',(1.37421955536285,-2.11096011055952,14.7292947392395));
#16513=CARTESIAN_POINT('Ctrl Pts',(1.44292224538896,-2.06461926113376,14.7345499886517));
#16514=CARTESIAN_POINT('Ctrl Pts',(1.50926613194603,-2.01492481074621,14.739805238064));
#16515=CARTESIAN_POINT('Ctrl Pts',(1.57551595794375,-1.9653008157999,14.7450530367264));
#16516=CARTESIAN_POINT('Ctrl Pts',(1.63941325689886,-1.91233293832158,14.7503008353889));
#16517=CARTESIAN_POINT('Ctrl Pts',(1.70060358136297,-1.85627414706326,14.7555486340513));
#16518=CARTESIAN_POINT('Ctrl Pts',(1.76223728240759,-1.79980916160033,14.760834457533));
#16519=CARTESIAN_POINT('Ctrl Pts',(1.82112420930131,-1.74020852606853,14.7661202810147));
#16520=CARTESIAN_POINT('Ctrl Pts',(1.87693410081557,-1.67777371275021,14.7714061044963));
#16521=CARTESIAN_POINT('Ctrl Pts',(1.93224354894996,-1.61589874802058,14.7766445303699));
#16522=CARTESIAN_POINT('Ctrl Pts',(1.98453061063023,-1.55124058003066,14.7818829562434));
#16523=CARTESIAN_POINT('Ctrl Pts',(2.03351031126417,-1.48413006976555,14.7871213821169));
#16524=CARTESIAN_POINT('Ctrl Pts',(2.08247390328959,-1.41704163103055,14.7923580851593));
#16525=CARTESIAN_POINT('Ctrl Pts',(2.12813202276749,-1.3475028242608,14.7975947882018));
#16526=CARTESIAN_POINT('Ctrl Pts',(2.17024096410897,-1.27587632931384,14.8028314912442));
#16527=CARTESIAN_POINT('Ctrl Pts',(2.21234875842374,-1.20425178543714,14.8080680516414));
#16528=CARTESIAN_POINT('Ctrl Pts',(2.25090733386203,-1.13054006474639,14.8133046120386));
#16529=CARTESIAN_POINT('Ctrl Pts',(2.28571791055815,-1.05513026842835,14.8185411724359));
#16530=CARTESIAN_POINT('Ctrl Pts',(2.32109824248877,-0.978486217172226,
14.8238634412005));
#16531=CARTESIAN_POINT('Ctrl Pts',(2.3526065614897,-0.900088443901519,14.8291857099651));
#16532=CARTESIAN_POINT('Ctrl Pts',(2.38008496264434,-0.8203668817025,14.8345079787297));
#16533=CARTESIAN_POINT('Ctrl Pts',(2.40715968604695,-0.74181648739041,14.8397520594849));
#16534=CARTESIAN_POINT('Ctrl Pts',(2.43032203904185,-0.661981407406311,
14.84499614024));
#16535=CARTESIAN_POINT('Ctrl Pts',(2.44947178249304,-0.581286707890679,
14.8502402209951));
#16536=CARTESIAN_POINT('Ctrl Pts',(2.46904980319419,-0.49878729991598,14.8556015837645));
#16537=CARTESIAN_POINT('Ctrl Pts',(2.48443347448112,-0.415389861801244,
14.8609629465339));
#16538=CARTESIAN_POINT('Ctrl Pts',(2.49557145564365,-0.331555967789178,
14.8663243093032));
#16539=CARTESIAN_POINT('Ctrl Pts',(2.50670943680618,-0.247722073777111,
14.8716856720726));
#16540=CARTESIAN_POINT('Ctrl Pts',(2.51360175300079,-0.163452235728656,
14.877047034842));
#16541=CARTESIAN_POINT('Ctrl Pts',(2.51625363846893,-0.0792078082760125,
14.8824083976114));
#16542=CARTESIAN_POINT('Ctrl Pts',(2.51707938858055,-0.0529755873869006,
14.8840778309102));
#16543=CARTESIAN_POINT('Ctrl Pts',(2.5174949411117,-0.0267303865065068,
14.8857472642091));
#16544=CARTESIAN_POINT('Ctrl Pts',(2.51749995409227,-0.000480775830062533,
14.887416697508));
#16545=CARTESIAN_POINT('Ctrl Pts',(2.5174999540924,-0.000480775158034882,
14.8874166975507));
#16546=CARTESIAN_POINT('Ctrl Pts',(2.51751564872697,0.0817015945668656,
14.8926433649588));
#16547=CARTESIAN_POINT('Ctrl Pts',(2.51350287472604,0.164042797258516,14.8978700323668));
#16548=CARTESIAN_POINT('Ctrl Pts',(2.5054410199567,0.246112871500738,14.9030966997749));
#16549=CARTESIAN_POINT('Ctrl Pts',(2.49738907413895,0.328082072133129,14.9083169430044));
#16550=CARTESIAN_POINT('Ctrl Pts',(2.4852979657381,0.409780345309913,14.9135371862339));
#16551=CARTESIAN_POINT('Ctrl Pts',(2.46919906474516,0.490777168032105,14.9187574294635));
#16552=CARTESIAN_POINT('Ctrl Pts',(2.4531173359169,0.571687594125189,14.9239721044324));
#16553=CARTESIAN_POINT('Ctrl Pts',(2.43303639711601,0.651897600727632,14.9291867794013));
#16554=CARTESIAN_POINT('Ctrl Pts',(2.40903928768665,0.730982872837808,14.9344014543702));
#16555=CARTESIAN_POINT('Ctrl Pts',(2.39457884786559,0.778638938308824,14.9375437700643));
#16556=CARTESIAN_POINT('Ctrl Pts',(2.37869738372328,0.825886720026406,14.9406860857585));
#16557=CARTESIAN_POINT('Ctrl Pts',(2.36142200728636,0.872635292378009,14.9438284014526));
#16558=CARTESIAN_POINT('',(2.51749903103506,-0.00220878644373725,14.6120681308043));
#16559=CARTESIAN_POINT('Ctrl Pts',(2.36142197356233,0.872635383637971,14.6670478768675));
#16560=CARTESIAN_POINT('Ctrl Pts',(2.3830264806342,0.814171838973078,14.662898126802));
#16561=CARTESIAN_POINT('Ctrl Pts',(2.40245955452755,0.754906799200612,14.6588100797912));
#16562=CARTESIAN_POINT('Ctrl Pts',(2.42615252031912,0.672413936199539,14.653279758481));
#16563=CARTESIAN_POINT('Ctrl Pts',(2.4323130090463,0.649776915793715,14.6517783272278));
#16564=CARTESIAN_POINT('Ctrl Pts',(2.44152137461929,0.613972427929959,14.6494282374261));
#16565=CARTESIAN_POINT('Ctrl Pts',(2.44478106226665,0.600861326874552,14.6485728408));
#16566=CARTESIAN_POINT('Ctrl Pts',(2.45064178630728,0.57645078367163,14.6469896307871));
#16567=CARTESIAN_POINT('Ctrl Pts',(2.45327059448336,0.565158445280051,14.6462609490147));
#16568=CARTESIAN_POINT('Ctrl Pts',(2.45826314377867,0.543020954942658,14.6448395336263));
#16569=CARTESIAN_POINT('Ctrl Pts',(2.46063335403456,0.532177550106636,14.6441466097339));
#16570=CARTESIAN_POINT('Ctrl Pts',(2.46579440974727,0.507794521789542,14.6425957117803));
#16571=CARTESIAN_POINT('Ctrl Pts',(2.46854561521828,0.494246805671042,14.641738999612));
#16572=CARTESIAN_POINT('Ctrl Pts',(2.47519637313375,0.460054910860904,14.6395889327426));
#16573=CARTESIAN_POINT('Ctrl Pts',(2.47894940738897,0.439383069791684,14.6383001296647));
#16574=CARTESIAN_POINT('Ctrl Pts',(2.50589531034888,0.279609775603074,14.6284185095174));
#16575=CARTESIAN_POINT('Ctrl Pts',(2.51762277134393,0.138826173536537,14.6201945782306));
#16576=CARTESIAN_POINT('Ctrl Pts',(2.51749903103506,-0.00220878644373725,
14.6120681308043));
#16577=CARTESIAN_POINT('Ctrl Pts',(2.51749903223328,-0.0022074203295025,
14.6120682095199));
#16578=CARTESIAN_POINT('Ctrl Pts',(2.51734625288752,-0.176447844755141,
14.6020284594246));
#16579=CARTESIAN_POINT('Ctrl Pts',(2.49910489813037,-0.350188088773951,
14.5921890872909));
#16580=CARTESIAN_POINT('Ctrl Pts',(2.45856792263053,-0.541964218877127,
14.58028939457));
#16581=CARTESIAN_POINT('Ctrl Pts',(2.45378307845243,-0.563231730425828,
14.578954613819));
#16582=CARTESIAN_POINT('Ctrl Pts',(2.44601366715268,-0.595784842741711,
14.5768845090396));
#16583=CARTESIAN_POINT('Ctrl Pts',(2.44322565862868,-0.607116799426908,
14.5761588308346));
#16584=CARTESIAN_POINT('Ctrl Pts',(2.43788093129379,-0.628207433113598,
14.5747980756725));
#16585=CARTESIAN_POINT('Ctrl Pts',(2.43534413365638,-0.637970968568624,
14.5741640632016));
#16586=CARTESIAN_POINT('Ctrl Pts',(2.4310011019985,-0.654282838740212,14.5730975889619));
#16587=CARTESIAN_POINT('Ctrl Pts',(2.42922688704112,-0.660839708525803,
14.572666935467));
#16588=CARTESIAN_POINT('Ctrl Pts',(2.42580703534214,-0.673278382807251,
14.5718460944824));
#16589=CARTESIAN_POINT('Ctrl Pts',(2.42416649032558,-0.679161526251899,
14.5714562138903));
#16590=CARTESIAN_POINT('Ctrl Pts',(2.42021743785845,-0.693126576022748,
14.5705269205205));
#16591=CARTESIAN_POINT('Ctrl Pts',(2.41788984890373,-0.701202945441875,
14.5699864382391));
#16592=CARTESIAN_POINT('Ctrl Pts',(2.40952032669336,-0.729706673432705,
14.5680685148678));
#16593=CARTESIAN_POINT('Ctrl Pts',(2.40325979961571,-0.750068196271464,
14.5666795054453));
#16594=CARTESIAN_POINT('Ctrl Pts',(2.35370687914706,-0.904239703959241,
14.5560304303478));
#16595=CARTESIAN_POINT('Ctrl Pts',(2.29953170732172,-1.03427864219943,14.5463032027858));
#16596=CARTESIAN_POINT('Ctrl Pts',(2.17424252029407,-1.27584085291948,14.5275040961828));
#16597=CARTESIAN_POINT('Ctrl Pts',(2.10463444026818,-1.38766737270961,14.518459516005));
#16598=CARTESIAN_POINT('Ctrl Pts',(1.98310654607306,-1.5525686782299,14.5047892093619));
#16599=CARTESIAN_POINT('Ctrl Pts',(1.93705179352577,-1.60966245078824,14.4999825989861));
#16600=CARTESIAN_POINT('Ctrl Pts',(1.87556965954321,-1.67941389037954,14.4940117351049));
#16601=CARTESIAN_POINT('Ctrl Pts',(1.86240059024153,-1.69400609215391,14.4927567045419));
#16602=CARTESIAN_POINT('Ctrl Pts',(1.840272037548,-1.71795600474581,14.4906864918425));
#16603=CARTESIAN_POINT('Ctrl Pts',(1.8314089940245,-1.72740126004728,14.4898673096871));
#16604=CARTESIAN_POINT('Ctrl Pts',(1.81442698629495,-1.74522118796995,14.4883163569763));
#16605=CARTESIAN_POINT('Ctrl Pts',(1.80632197230322,-1.75360862887468,14.487584020239));
#16606=CARTESIAN_POINT('Ctrl Pts',(1.78769787891087,-1.77261556828376,14.4859188900544));
#16607=CARTESIAN_POINT('Ctrl Pts',(1.77714186327992,-1.78319838272559,14.4849877334615));
#16608=CARTESIAN_POINT('Ctrl Pts',(1.74425669843902,-1.81558496429833,14.4821248942249));
#16609=CARTESIAN_POINT('Ctrl Pts',(1.72161538447477,-1.83706853219827,14.4802070430736));
#16610=CARTESIAN_POINT('Ctrl Pts',(1.54600115794843,-1.99760377336749,14.4657117114391));
#16611=CARTESIAN_POINT('Ctrl Pts',(1.37682758565216,-2.1177569598037,14.4539831362561));
#16612=CARTESIAN_POINT('Ctrl Pts',(1.08310027930611,-2.27614155980993,14.4347518683054));
#16613=CARTESIAN_POINT('Ctrl Pts',(0.966961136711867,-2.32785404201039,
14.4273690924806));
#16614=CARTESIAN_POINT('Ctrl Pts',(0.830949845217222,-2.3764753557936,14.4184476305572));
#16615=CARTESIAN_POINT('Ctrl Pts',(0.814403579517508,-2.38219636722863,
14.4173577332219));
#16616=CARTESIAN_POINT('Ctrl Pts',(0.789869955263508,-2.39039360807982,
14.4157331172956));
#16617=CARTESIAN_POINT('Ctrl Pts',(0.781927364103617,-2.39300349776436,
14.4152058371787));
#16618=CARTESIAN_POINT('Ctrl Pts',(0.767768653602804,-2.39757795361037,
14.414263297133));
#16619=CARTESIAN_POINT('Ctrl Pts',(0.761557715226591,-2.3995579997027,14.4138489416665));
#16620=CARTESIAN_POINT('Ctrl Pts',(0.747999255449551,-2.40382249048615,
14.4129423983532));
#16621=CARTESIAN_POINT('Ctrl Pts',(0.740649038230816,-2.40609734847353,
14.4124496920677));
#16622=CARTESIAN_POINT('Ctrl Pts',(0.720058648621119,-2.41236669095845,
14.4110661722716));
#16623=CARTESIAN_POINT('Ctrl Pts',(0.706796052690527,-2.4162857506115,14.4101712353938));
#16624=CARTESIAN_POINT('Ctrl Pts',(0.629272470710851,-2.43850089894496,
14.4049207295255));
#16625=CARTESIAN_POINT('Ctrl Pts',(0.564341138819439,-2.45434062533898,
14.4004463548239));
#16626=CARTESIAN_POINT('Ctrl Pts',(0.281632269446114,-2.51149508125784,
14.3808460556432));
#16627=CARTESIAN_POINT('Ctrl Pts',(0.0595073510815119,-2.52654052793513,
14.3652553615935));
#16628=CARTESIAN_POINT('Ctrl Pts',(-0.208041459279902,-2.50931864733981,
14.3473976783514));
#16629=CARTESIAN_POINT('Ctrl Pts',(-0.254279203346788,-2.50505565874671,
14.3443398744679));
#16630=CARTESIAN_POINT('Ctrl Pts',(-0.334326927527517,-2.49543606011436,
14.3390958261121));
#16631=CARTESIAN_POINT('Ctrl Pts',(-0.368193388823455,-2.49066445765854,
14.3368926872635));
#16632=CARTESIAN_POINT('Ctrl Pts',(-0.417252711845663,-2.48272966962158,
14.3337223255568));
#16633=CARTESIAN_POINT('Ctrl Pts',(-0.432528988805183,-2.48011393474472,
14.3327381093059));
#16634=CARTESIAN_POINT('Ctrl Pts',(-0.459329796269762,-2.47526970937939,
14.3310163700365));
#16635=CARTESIAN_POINT('Ctrl Pts',(-0.470864587517976,-2.47310140181741,
14.3302769770892));
#16636=CARTESIAN_POINT('Ctrl Pts',(-0.494832769384331,-2.46842209925745,
14.3287438063046));
#16637=CARTESIAN_POINT('Ctrl Pts',(-0.507263217263479,-2.4658976393093,
14.3279504767646));
#16638=CARTESIAN_POINT('Ctrl Pts',(-0.539531970799089,-2.45908995010045,
14.3258954323637));
#16639=CARTESIAN_POINT('Ctrl Pts',(-0.559338750579415,-2.4546605324642,
14.3246383720816));
#16640=CARTESIAN_POINT('Ctrl Pts',(-0.641625057460877,-2.43521099985357,
14.3194316741519));
#16641=CARTESIAN_POINT('Ctrl Pts',(-0.703574407161174,-2.41804040715723,
14.3155504950842));
#16642=CARTESIAN_POINT('Ctrl Pts',(-0.956481779059505,-2.33739710838233,
14.2997607199375));
#16643=CARTESIAN_POINT('Ctrl Pts',(-1.1401326653457,-2.25352569000999,14.2884897134711));
#16644=CARTESIAN_POINT('Ctrl Pts',(-1.36515191545438,-2.11614454985564,
14.2731171892448));
#16645=CARTESIAN_POINT('Ctrl Pts',(-1.41722859017158,-2.08162667313111,
14.2694305399331));
#16646=CARTESIAN_POINT('Ctrl Pts',(-1.48749692717594,-2.03119108300949,
14.2641971492547));
#16647=CARTESIAN_POINT('Ctrl Pts',(-1.50682696767897,-2.01689283964196,
14.2627290230078));
#16648=CARTESIAN_POINT('Ctrl Pts',(-1.54010956402366,-1.99152850417433,
14.2601454566726));
#16649=CARTESIAN_POINT('Ctrl Pts',(-1.55415525788796,-1.98058694456151,
14.2590374023261));
#16650=CARTESIAN_POINT('Ctrl Pts',(-1.57466838556011,-1.96425471319443,
14.2573908186262));
#16651=CARTESIAN_POINT('Ctrl Pts',(-1.58122706855388,-1.95897882980861,
14.2568600202831));
#16652=CARTESIAN_POINT('Ctrl Pts',(-1.5928216166371,-1.9495558738129,14.2559136923239));
#16653=CARTESIAN_POINT('Ctrl Pts',(-1.59786798261398,-1.94542198924811,
14.2554990966046));
#16654=CARTESIAN_POINT('Ctrl Pts',(-1.60879952922023,-1.93639585089276,
14.254594999978));
#16655=CARTESIAN_POINT('Ctrl Pts',(-1.61467839704372,-1.93149643722047,
14.2541050038002));
#16656=CARTESIAN_POINT('Ctrl Pts',(-1.63097763164425,-1.91778633542791,
14.2527361370296));
#16657=CARTESIAN_POINT('Ctrl Pts',(-1.64134865631302,-1.90891776461857,
14.2518532767759));
#16658=CARTESIAN_POINT('Ctrl Pts',(-1.69955808780646,-1.85831609948693,
14.2468330356465));
#16659=CARTESIAN_POINT('Ctrl Pts',(-1.74587270943177,-1.81487284860378,
14.2425883852418));
#16660=CARTESIAN_POINT('Ctrl Pts',(-1.93518223429473,-1.62334243535806,
14.2243171725942));
#16661=CARTESIAN_POINT('Ctrl Pts',(-2.06138052702461,-1.45975881848175,
14.2098472249371));
#16662=CARTESIAN_POINT('Ctrl Pts',(-2.21041326093247,-1.20805166917435,
14.1901938165273));
#16663=CARTESIAN_POINT('Ctrl Pts',(-2.25068743696326,-1.13124912266871,
14.1844848553704));
#16664=CARTESIAN_POINT('Ctrl Pts',(-2.29594132457244,-1.03292057246328,
14.1775261244116));
#16665=CARTESIAN_POINT('Ctrl Pts',(-2.30470694481398,-1.01321143929362,
14.1761480675076));
#16666=CARTESIAN_POINT('Ctrl Pts',(-2.31833302716469,-0.981481650712406,
14.1739556506734));
#16667=CARTESIAN_POINT('Ctrl Pts',(-2.32335565994743,-0.969532229028211,
14.1731358435942));
#16668=CARTESIAN_POINT('Ctrl Pts',(-2.3327213006881,-0.946759509891454,
14.1715843851601));
#16669=CARTESIAN_POINT('Ctrl Pts',(-2.33708181328242,-0.935943823970974,
14.17085216215));
#16670=CARTESIAN_POINT('Ctrl Pts',(-2.34685315966793,-0.911213139548342,
14.169188217121));
#16671=CARTESIAN_POINT('Ctrl Pts',(-2.35221571232524,-0.897279441734802,
14.1682581232099));
#16672=CARTESIAN_POINT('Ctrl Pts',(-2.36837167132169,-0.854160466355362,
14.1654019707286));
#16673=CARTESIAN_POINT('Ctrl Pts',(-2.37874843850869,-0.824821479105153,
14.1634896482738));
#16674=CARTESIAN_POINT('Ctrl Pts',(-2.45277431018102,-0.602493565493219,
14.1492127929861));
#16675=CARTESIAN_POINT('Ctrl Pts',(-2.49339098942343,-0.402629297198246,
14.1376649399018));
#16676=CARTESIAN_POINT('Ctrl Pts',(-2.51985688868026,-0.0706115310829718,
14.1184822633901));
#16677=CARTESIAN_POINT('Ctrl Pts',(-2.52014421841247,0.0594062770241095,
14.1109459826088));
#16678=CARTESIAN_POINT('Ctrl Pts',(-2.50905593034063,0.206806568299369,
14.1018223742667));
#16679=CARTESIAN_POINT('Ctrl Pts',(-2.50751227584696,0.224750443401174,
14.10070175336));
#16680=CARTESIAN_POINT('Ctrl Pts',(-2.50496111858431,0.251092725249343,
14.0990399816989));
#16681=CARTESIAN_POINT('Ctrl Pts',(-2.50410355922615,0.259505533805276,
14.0985067675563));
#16682=CARTESIAN_POINT('Ctrl Pts',(-2.50250904005756,0.274403636921412,
14.0975578195258));
#16683=CARTESIAN_POINT('Ctrl Pts',(-2.50178922407814,0.280890598715556,
14.0971430397181));
#16684=CARTESIAN_POINT('Ctrl Pts',(-2.50017372047505,0.294950445521417,
14.0962405378494));
#16685=CARTESIAN_POINT('Ctrl Pts',(-2.49926886428486,0.302521963207046,
14.0957523359419));
#16686=CARTESIAN_POINT('Ctrl Pts',(-2.49666373648765,0.323510986334988,
14.0943931419138));
#16687=CARTESIAN_POINT('Ctrl Pts',(-2.4948897453465,0.336918848998842,14.0935182473147));
#16688=CARTESIAN_POINT('Ctrl Pts',(-2.48444998949582,0.411213869045681,
14.0886358709595));
#16689=CARTESIAN_POINT('Ctrl Pts',(-2.47366400130315,0.471777145237108,
14.0845277090296));
#16690=CARTESIAN_POINT('Ctrl Pts',(-2.42302078937919,0.706071695280246,
14.0682805594306));
#16691=CARTESIAN_POINT('Ctrl Pts',(-2.3669790430704,0.875775041830177,14.055786168493));
#16692=CARTESIAN_POINT('Ctrl Pts',(-2.24668794350813,1.14152381647296,14.0359628702875));
#16693=CARTESIAN_POINT('Ctrl Pts',(-2.19295215680885,1.24163217314924,14.0284177440001));
#16694=CARTESIAN_POINT('Ctrl Pts',(-2.12033774262357,1.35739078723631,14.0196181388173));
#16695=CARTESIAN_POINT('Ctrl Pts',(-2.10776908820302,1.37682657633483,14.0181376283125));
#16696=CARTESIAN_POINT('Ctrl Pts',(-2.08755617416093,1.40715758233037,14.0158216603069));
#16697=CARTESIAN_POINT('Ctrl Pts',(-2.08009074729203,1.41816985437632,14.0149796300023));
#16698=CARTESIAN_POINT('Ctrl Pts',(-2.06594775968526,1.43868025901438,14.0134089364747));
#16699=CARTESIAN_POINT('Ctrl Pts',(-2.05929113966803,1.4481923362499,14.0126795134833));
#16700=CARTESIAN_POINT('Ctrl Pts',(-2.04423762951421,1.46938960130097,14.011051619493));
#16701=CARTESIAN_POINT('Ctrl Pts',(-2.0358058361225,1.48104959320312,14.0101545057334));
#16702=CARTESIAN_POINT('Ctrl Pts',(-2.01409004084545,1.51054362307848,14.0078805318625));
#16703=CARTESIAN_POINT('Ctrl Pts',(-2.00066869935664,1.52827534613825,14.0065089783501));
#16704=CARTESIAN_POINT('Ctrl Pts',(-1.88772051990814,1.67345947361546,13.9952350160761));
#16705=CARTESIAN_POINT('Ctrl Pts',(-1.77635704373441,1.79123434184884,13.9858393255165));
#16706=CARTESIAN_POINT('Ctrl Pts',(-1.56104769672598,1.97896254655044,13.9694063071358));
#16707=CARTESIAN_POINT('Ctrl Pts',(-1.46176418007724,2.05338858387265,13.9623434537998));
#16708=CARTESIAN_POINT('Ctrl Pts',(-1.32045192267171,2.14386075074272,13.9524218009888));
#16709=CARTESIAN_POINT('Ctrl Pts',(-1.28288173889696,2.16655168742379,13.9497946556163));
#16710=CARTESIAN_POINT('Ctrl Pts',(-1.22045084330304,2.20206422283044,13.9454144714827));
#16711=CARTESIAN_POINT('Ctrl Pts',(-1.19593454325564,2.21547455880243,13.9436908091261));
#16712=CARTESIAN_POINT('Ctrl Pts',(-1.16229325002607,2.23315514986017,13.9413137920888));
#16713=CARTESIAN_POINT('Ctrl Pts',(-1.15335736693984,2.23778334484619,13.9406812865326));
#16714=CARTESIAN_POINT('Ctrl Pts',(-1.13834831049038,2.24544326283981,13.9396166395329));
#16715=CARTESIAN_POINT('Ctrl Pts',(-1.13229007603068,2.24850428162906,13.9391862927821));
#16716=CARTESIAN_POINT('Ctrl Pts',(-1.12075323698775,2.25427500298419,13.9383654701466));
#16717=CARTESIAN_POINT('Ctrl Pts',(-1.11527700965938,2.25698932144274,13.9379752975234));
#16718=CARTESIAN_POINT('Ctrl Pts',(-1.10223101886484,2.26339655617169,13.9370445816514));
#16719=CARTESIAN_POINT('Ctrl Pts',(-1.09465255675428,2.26707145115132,13.9365029614504));
#16720=CARTESIAN_POINT('Ctrl Pts',(-1.06774768714296,2.27995161696867,13.9345770817294));
#16721=CARTESIAN_POINT('Ctrl Pts',(-1.04832307777891,2.28894804489453,13.9331811320847));
#16722=CARTESIAN_POINT('Ctrl Pts',(-0.903741556202521,2.3536840314239,13.9227627370341));
#16723=CARTESIAN_POINT('Ctrl Pts',(-0.774345782399214,2.39936638469497,
13.9132971001229));
#16724=CARTESIAN_POINT('Ctrl Pts',(-0.51401932129544,2.46801102296908,13.8946973100706));
#16725=CARTESIAN_POINT('Ctrl Pts',(-0.383678003792294,2.49160426722687,
13.885592891985));
#16726=CARTESIAN_POINT('Ctrl Pts',(-0.176694737400621,2.51243411061752,
13.8716927581285));
#16727=CARTESIAN_POINT('Ctrl Pts',(-0.101003386376267,2.51661408809667,
13.8667213425273));
#16728=CARTESIAN_POINT('Ctrl Pts',(-0.00452354997097181,2.51758111374386,
13.8605243958234));
#16729=CARTESIAN_POINT('Ctrl Pts',(0.0161870093766731,2.51753314762102,
13.8592022145615));
#16730=CARTESIAN_POINT('Ctrl Pts',(0.0496678897407512,2.51704241700615,
13.8570772958137));
#16731=CARTESIAN_POINT('Ctrl Pts',(0.0624392199115469,2.51675799032433,
13.856269689167));
#16732=CARTESIAN_POINT('Ctrl Pts',(0.086910777936425,2.51602659831334,13.8547276690753));
#16733=CARTESIAN_POINT('Ctrl Pts',(0.0986111028927149,2.51559519489167,
13.8539927932796));
#16734=CARTESIAN_POINT('Ctrl Pts',(0.125334640486415,2.51442313613797,13.8523196060479));
#16735=CARTESIAN_POINT('Ctrl Pts',(0.140355169244816,2.5136294320329,13.8513829638745));
#16736=CARTESIAN_POINT('Ctrl Pts',(0.18788779452626,2.5106903454381,13.8484303244437));
#16737=CARTESIAN_POINT('Ctrl Pts',(0.220366614327333,2.5080483524544,13.8464297136977));
#16738=CARTESIAN_POINT('Ctrl Pts',(0.436300996766045,2.48625589844649,13.833223247049));
#16739=CARTESIAN_POINT('Ctrl Pts',(0.61722731865483,2.44762461749861,13.8226674440063));
#16740=CARTESIAN_POINT('Ctrl Pts',(0.836793098595791,2.37482177662283,13.8093699713131));
#16741=CARTESIAN_POINT('Ctrl Pts',(0.880841212095109,2.35883865038029,13.806673117886));
#16742=CARTESIAN_POINT('Ctrl Pts',(1.01700119319479,2.30508623794732,13.7981792328358));
#16743=CARTESIAN_POINT('Ctrl Pts',(1.1073262797376,2.2630815336638,13.7923159518788));
#16744=CARTESIAN_POINT('Ctrl Pts',(1.21069705728322,2.20733783001997,13.7850662566939));
#16745=CARTESIAN_POINT('Ctrl Pts',(1.22638494623779,2.19866040615993,13.7839506642353));
#16746=CARTESIAN_POINT('Ctrl Pts',(1.24932050047618,2.18565225633742,13.7822949683913));
#16747=CARTESIAN_POINT('Ctrl Pts',(1.25664158595892,2.1814512183681,13.7817627190394));
#16748=CARTESIAN_POINT('Ctrl Pts',(1.26958483535283,2.17393725287522,13.7808148191869));
#16749=CARTESIAN_POINT('Ctrl Pts',(1.27521542841474,2.1706391785228,13.7804001147086));
#16750=CARTESIAN_POINT('Ctrl Pts',(1.28740736463745,2.16343403895374,13.7794969840274));
#16751=CARTESIAN_POINT('Ctrl Pts',(1.2939636709954,2.15951906171134,13.7790080718642));
#16752=CARTESIAN_POINT('Ctrl Pts',(1.31212344879682,2.14856289760869,13.7776450515702));
#16753=CARTESIAN_POINT('Ctrl Pts',(1.32368774293938,2.14145773008418,13.7767670065763));
#16754=CARTESIAN_POINT('Ctrl Pts',(1.38793472415581,2.10126479117447,13.7718348928233));
#16755=CARTESIAN_POINT('Ctrl Pts',(1.43943009917202,2.06632914607376,13.7676778134186));
#16756=CARTESIAN_POINT('Ctrl Pts',(1.63267084545332,1.92449976028815,13.7514248972784));
#16757=CARTESIAN_POINT('Ctrl Pts',(1.76426015988295,1.80463410216423,13.7389823071638));
#16758=CARTESIAN_POINT('Ctrl Pts',(1.9574622483997,1.58713804180118,13.7192133243873));
#16759=CARTESIAN_POINT('Ctrl Pts',(2.02696643708287,1.49735732030823,13.7116735878293));
#16760=CARTESIAN_POINT('Ctrl Pts',(2.103085049424,1.3839707358866,13.7028792834288));
#16761=CARTESIAN_POINT('Ctrl Pts',(2.1157176192637,1.36458079160921,13.7013990108488));
#16762=CARTESIAN_POINT('Ctrl Pts',(2.13518878351653,1.33377362379436,13.6990833292935));
#16763=CARTESIAN_POINT('Ctrl Pts',(2.14220702886513,1.32247203271281,13.6982413502282));
#16764=CARTESIAN_POINT('Ctrl Pts',(2.15518181285156,1.3012042071963,13.696670703484));
#16765=CARTESIAN_POINT('Ctrl Pts',(2.16115960237255,1.29125141456129,13.6959412764584));
#16766=CARTESIAN_POINT('Ctrl Pts',(2.17439198684188,1.26887068110694,13.6943133111727));
#16767=CARTESIAN_POINT('Ctrl Pts',(2.18160934280137,1.25642111045781,13.6934161307));
#16768=CARTESIAN_POINT('Ctrl Pts',(2.1997088306205,1.224574191558,13.6911418696493));
#16769=CARTESIAN_POINT('Ctrl Pts',(2.21044152737758,1.20509302236417,13.6897700980273));
#16770=CARTESIAN_POINT('Ctrl Pts',(2.27483086218884,1.08446320456598,13.6813894162444));
#16771=CARTESIAN_POINT('Ctrl Pts',(2.32176837437179,0.979941211286028,13.6746219436779));
#16772=CARTESIAN_POINT('Ctrl Pts',(2.36142191786124,0.872635534369624,13.6679749024944));
#16773=CARTESIAN_POINT('Origin',(0.,0.,10.));
#16774=CARTESIAN_POINT('',(2.36142200728627,0.872635292378268,12.6712695847815));
#16775=CARTESIAN_POINT('',(2.36142200728636,0.872635292378013,12.9436566100381));
#16776=CARTESIAN_POINT('',(2.36142200728636,0.87263529237802,10.));
#16777=CARTESIAN_POINT('',(2.51749904018606,0.00219833170478317,13.8874166975433));
#16778=CARTESIAN_POINT('Ctrl Pts',(2.36142200728636,0.872635292378012,12.9436566100381));
#16779=CARTESIAN_POINT('Ctrl Pts',(2.33220137935874,0.951708685876645,12.9489830833342));
#16780=CARTESIAN_POINT('Ctrl Pts',(2.29903614731653,1.0292286051767,12.9543095566304));
#16781=CARTESIAN_POINT('Ctrl Pts',(2.26213002722283,1.10479590419989,12.9596360299265));
#16782=CARTESIAN_POINT('Ctrl Pts',(2.22515491740963,1.1805044634463,12.9649724601592));
#16783=CARTESIAN_POINT('Ctrl Pts',(2.18442517141745,1.25425272759434,12.970308890392));
#16784=CARTESIAN_POINT('Ctrl Pts',(2.14018926508127,1.3256681936408,12.9756453206247));
#16785=CARTESIAN_POINT('Ctrl Pts',(2.12268150483724,1.35393312502382,12.9777573818169));
#16786=CARTESIAN_POINT('Ctrl Pts',(2.10462498722126,1.38183298711463,12.9798694430091));
#16787=CARTESIAN_POINT('Ctrl Pts',(2.08603685581894,1.40934612007307,12.9819815042013));
#16788=CARTESIAN_POINT('Ctrl Pts',(2.0397857022557,1.47780454173607,12.9872367536086));
#16789=CARTESIAN_POINT('Ctrl Pts',(1.99007561770278,1.54411020833861,12.9924920030159));
#16790=CARTESIAN_POINT('Ctrl Pts',(1.93713376492469,1.60789272863233,12.9977472524232));
#16791=CARTESIAN_POINT('Ctrl Pts',(1.8842669716669,1.67158481980191,13.0029950510807));
#16792=CARTESIAN_POINT('Ctrl Pts',(1.82817780344527,1.73276051803573,13.0082428497382));
#16793=CARTESIAN_POINT('Ctrl Pts',(1.7691365941095,1.79107843529608,13.0134906483957));
#16794=CARTESIAN_POINT('Ctrl Pts',(1.70966758031253,1.84981891614298,13.0187764718786));
#16795=CARTESIAN_POINT('Ctrl Pts',(1.64720383001802,1.90565963442675,13.0240622953615));
#16796=CARTESIAN_POINT('Ctrl Pts',(1.58206291381047,1.95828577759875,13.0293481188444));
#16797=CARTESIAN_POINT('Ctrl Pts',(1.51750611170216,2.01044002577748,13.034586544713));
#16798=CARTESIAN_POINT('Ctrl Pts',(1.45032032884751,2.05943682238185,13.0398249705816));
#16799=CARTESIAN_POINT('Ctrl Pts',(1.38085022903217,2.10500805104917,13.0450633964502));
#16800=CARTESIAN_POINT('Ctrl Pts',(1.31140297677652,2.15056429209778,13.0503000994877));
#16801=CARTESIAN_POINT('Ctrl Pts',(1.2396732851439,2.19269694983328,13.0555368025252));
#16802=CARTESIAN_POINT('Ctrl Pts',(1.16603553866809,2.23118071266382,13.0607735055627));
#16803=CARTESIAN_POINT('Ctrl Pts',(1.09239979804759,2.26966342721594,13.066010065955));
#16804=CARTESIAN_POINT('Ctrl Pts',(1.01685651534262,2.30449723168073,13.0712466263474));
#16805=CARTESIAN_POINT('Ctrl Pts',(0.939804222611933,2.33550300217336,13.0764831867397));
#16806=CARTESIAN_POINT('Ctrl Pts',(0.861490791548575,2.36701625355094,13.0818054555102));
#16807=CARTESIAN_POINT('Ctrl Pts',(0.781618959217072,2.39457483546,13.0871277242807));
#16808=CARTESIAN_POINT('Ctrl Pts',(0.700625999890145,2.4180424847959,13.0924499930512));
#16809=CARTESIAN_POINT('Ctrl Pts',(0.620822886361808,2.44116537720234,13.0976940738015));
#16810=CARTESIAN_POINT('Ctrl Pts',(0.539931837104895,2.46031668865462,13.1029381545518));
#16811=CARTESIAN_POINT('Ctrl Pts',(0.458382389107529,2.47541750728156,13.1081822353021));
#16812=CARTESIAN_POINT('Ctrl Pts',(0.375009116253195,2.49085605043086,13.1135435980827));
#16813=CARTESIAN_POINT('Ctrl Pts',(0.290948147124334,2.50206067115165,13.1189049608633));
#16814=CARTESIAN_POINT('Ctrl Pts',(0.206663042294907,2.50900311616973,13.1242663236438));
#16815=CARTESIAN_POINT('Ctrl Pts',(0.122377937465491,2.51594556118781,13.1296276864244));
#16816=CARTESIAN_POINT('Ctrl Pts',(0.0378692069044778,2.51862588116019,
13.1349890492049));
#16817=CARTESIAN_POINT('Ctrl Pts',(-0.0464026301349656,2.51707231638595,
13.1403504119855));
#16818=CARTESIAN_POINT('Ctrl Pts',(-0.129006538839045,2.51554950013696,
13.1456056613928));
#16819=CARTESIAN_POINT('Ctrl Pts',(-0.211687953583377,2.50995328840564,
13.1508609108001));
#16820=CARTESIAN_POINT('Ctrl Pts',(-0.294012513924601,2.50027256347298,
13.1561161602074));
#16821=CARTESIAN_POINT('Ctrl Pts',(-0.376220356740822,2.49060556360911,
13.1613639588649));
#16822=CARTESIAN_POINT('Ctrl Pts',(-0.458071895655358,2.47686560642358,
13.1666117575223));
#16823=CARTESIAN_POINT('Ctrl Pts',(-0.539133593329459,2.45909357661388,
13.1718595561798));
#16824=CARTESIAN_POINT('Ctrl Pts',(-0.620782652887027,2.44119277312683,
13.1771453796627));
#16825=CARTESIAN_POINT('Ctrl Pts',(-0.70162990293876,2.41920122751533,13.1824312031456));
#16826=CARTESIAN_POINT('Ctrl Pts',(-0.781238379347123,2.39321391535213,
13.1877170266285));
#16827=CARTESIAN_POINT('Ctrl Pts',(-0.860133012042394,2.36745962962336,
13.1929554524971));
#16828=CARTESIAN_POINT('Ctrl Pts',(-0.937810551387549,2.33778109568812,
13.1981938783657));
#16829=CARTESIAN_POINT('Ctrl Pts',(-1.01385845070989,2.30432143849857,13.2034323042343));
#16830=CARTESIAN_POINT('Ctrl Pts',(-1.08988133914377,2.27087278563343,13.2086690072718));
#16831=CARTESIAN_POINT('Ctrl Pts',(-1.16427522998869,2.23364566494832,13.2139057103093));
#16832=CARTESIAN_POINT('Ctrl Pts',(-1.23664729937582,2.19283143605396,13.2191424133468));
#16833=CARTESIAN_POINT('Ctrl Pts',(-1.30901739738391,2.15201831891883,13.2243789737391));
#16834=CARTESIAN_POINT('Ctrl Pts',(-1.37936538202707,2.10761851540647,13.2296155341314));
#16835=CARTESIAN_POINT('Ctrl Pts',(-1.44732402417111,2.05986878685443,13.2348520945238));
#16836=CARTESIAN_POINT('Ctrl Pts',(-1.5163949661006,2.01133752395814,13.2401743632943));
#16837=CARTESIAN_POINT('Ctrl Pts',(-1.58299723579261,1.95934596013539,13.2454966320647));
#16838=CARTESIAN_POINT('Ctrl Pts',(-1.64677846214582,1.90418668901257,13.2508189008352));
#16839=CARTESIAN_POINT('Ctrl Pts',(-1.70962269564365,1.84983774791796,13.2560629815856));
#16840=CARTESIAN_POINT('Ctrl Pts',(-1.76972792598289,1.79241392127716,13.2613070623359));
#16841=CARTESIAN_POINT('Ctrl Pts',(-1.82679410041109,1.73223253771058,13.2665511430862));
#16842=CARTESIAN_POINT('Ctrl Pts',(-1.88513653985392,1.6707052185675,13.2719125058668));
#16843=CARTESIAN_POINT('Ctrl Pts',(-1.94030201513782,1.60629589941926,13.2772738686474));
#16844=CARTESIAN_POINT('Ctrl Pts',(-1.99201444135622,1.53937802875976,13.2826352314279));
#16845=CARTESIAN_POINT('Ctrl Pts',(-2.04372686757461,1.47246015810027,13.2879965942085));
#16846=CARTESIAN_POINT('Ctrl Pts',(-2.09198600956482,1.40303419126785,13.2933579569891));
#16847=CARTESIAN_POINT('Ctrl Pts',(-2.13656482464556,1.33150178373418,13.2987193197697));
#16848=CARTESIAN_POINT('Ctrl Pts',(-2.18026132516609,1.26138516270311,13.303974569177));
#16849=CARTESIAN_POINT('Ctrl Pts',(-2.22058329126614,1.18898576367435,13.3092298185843));
#16850=CARTESIAN_POINT('Ctrl Pts',(-2.25728490926731,1.11466187177729,13.3144850679916));
#16851=CARTESIAN_POINT('Ctrl Pts',(-2.29393449271176,1.04044335427459,13.3197328666491));
#16852=CARTESIAN_POINT('Ctrl Pts',(-2.3269737207614,0.964306173763971,13.3249806653067));
#16853=CARTESIAN_POINT('Ctrl Pts',(-2.3562008471042,0.886636237757878,13.3302284639642));
#16854=CARTESIAN_POINT('Ctrl Pts',(-2.38563974917403,0.808403516106258,
13.3355142874471));
#16855=CARTESIAN_POINT('Ctrl Pts',(-2.4112108218721,0.728616135146873,13.34080011093));
#16856=CARTESIAN_POINT('Ctrl Pts',(-2.43275582416933,0.647692326626021,
13.3460859344129));
#16857=CARTESIAN_POINT('Ctrl Pts',(-2.45410763391817,0.567494156310112,
13.3513243602815));
#16858=CARTESIAN_POINT('Ctrl Pts',(-2.47150516617186,0.486180311444701,
13.3565627861501));
#16859=CARTESIAN_POINT('Ctrl Pts',(-2.48484386135612,0.404174757599766,
13.3618012120187));
#16860=CARTESIAN_POINT('Ctrl Pts',(-2.49817816966551,0.322196174016748,
13.3670379150562));
#16861=CARTESIAN_POINT('Ctrl Pts',(-2.50745621803746,0.239526788341009,
13.3722746180937));
#16862=CARTESIAN_POINT('Ctrl Pts',(-2.51262464386851,0.156600284241947,
13.3775113211312));
#16863=CARTESIAN_POINT('Ctrl Pts',(-2.51779292891423,0.0736760390193401,
13.3827478815236));
#16864=CARTESIAN_POINT('Ctrl Pts',(-2.51885178631918,-0.00950485011003217,
13.3879844419159));
#16865=CARTESIAN_POINT('Ctrl Pts',(-2.51579987119137,-0.092505449101692,
13.3932210023083));
#16866=CARTESIAN_POINT('Ctrl Pts',(-2.51269800443956,-0.176864544165065,
13.3985432710788));
#16867=CARTESIAN_POINT('Ctrl Pts',(-2.50534959151287,-0.261036902242081,
13.4038655398492));
#16868=CARTESIAN_POINT('Ctrl Pts',(-2.49380820869165,-0.344567654114772,
13.4091878086197));
#16869=CARTESIAN_POINT('Ctrl Pts',(-2.48243637722363,-0.426871278161132,
13.41443188937));
#16870=CARTESIAN_POINT('Ctrl Pts',(-2.46699410093623,-0.508551573724599,
13.4196759701204));
#16871=CARTESIAN_POINT('Ctrl Pts',(-2.44758418843864,-0.589184088808537,
13.4249200508707));
#16872=CARTESIAN_POINT('Ctrl Pts',(-2.42774018004294,-0.671619921865025,
13.4302814136513));
#16873=CARTESIAN_POINT('Ctrl Pts',(-2.40374906918141,-0.752960051296445,
13.4356427764318));
#16874=CARTESIAN_POINT('Ctrl Pts',(-2.37577378671128,-0.832769574597652,
13.4410041392123));
#16875=CARTESIAN_POINT('Ctrl Pts',(-2.34779850424114,-0.912579097898858,
13.4463655019928));
#16876=CARTESIAN_POINT('Ctrl Pts',(-2.315839304062,-0.990857569907541,13.4517268647733));
#16877=CARTESIAN_POINT('Ctrl Pts',(-2.28010947794251,-1.0671958670257,13.4570882275539));
#16878=CARTESIAN_POINT('Ctrl Pts',(-2.245086825079,-1.14202325832673,13.4623434769612));
#16879=CARTESIAN_POINT('Ctrl Pts',(-2.20631212510925,-1.21526297823414,
13.4675987263685));
#16880=CARTESIAN_POINT('Ctrl Pts',(-2.16395207119476,-1.2865137712329,13.4728539757758));
#16881=CARTESIAN_POINT('Ctrl Pts',(-2.12165207421362,-1.35766354679352,
13.4781017744333));
#16882=CARTESIAN_POINT('Ctrl Pts',(-2.07577705387296,-1.42682960317198,
13.4833495730908));
#16883=CARTESIAN_POINT('Ctrl Pts',(-2.02654086532252,-1.49363260917063,
13.4885973717483));
#16884=CARTESIAN_POINT('Ctrl Pts',(-1.97694791813944,-1.5609196605387,13.4938831952312));
#16885=CARTESIAN_POINT('Ctrl Pts',(-1.92394508898363,-1.62580884315633,
13.4991690187141));
#16886=CARTESIAN_POINT('Ctrl Pts',(-1.86779703284198,-1.68793971874196,
13.504454842197));
#16887=CARTESIAN_POINT('Ctrl Pts',(-1.81215245244416,-1.74951347105478,
13.5096932680656));
#16888=CARTESIAN_POINT('Ctrl Pts',(-1.75341914028644,-1.80837783666129,
13.5149316939342));
#16889=CARTESIAN_POINT('Ctrl Pts',(-1.69189578779466,-1.86421428308086,
13.5201701198028));
#16890=CARTESIAN_POINT('Ctrl Pts',(-1.63039266930961,-1.92003236582247,
13.5254068228403));
#16891=CARTESIAN_POINT('Ctrl Pts',(-1.56610167430368,-1.97282419729961,
13.5306435258778));
#16892=CARTESIAN_POINT('Ctrl Pts',(-1.49935751994023,-2.0223088976214,13.5358802289153));
#16893=CARTESIAN_POINT('Ctrl Pts',(-1.43261518365407,-2.07179225000477,
13.5411167893076));
#16894=CARTESIAN_POINT('Ctrl Pts',(-1.3634201921449,-2.11796837636223,13.5463533496999));
#16895=CARTESIAN_POINT('Ctrl Pts',(-1.2921383100898,-2.16059825918616,13.5515899100923));
#16896=CARTESIAN_POINT('Ctrl Pts',(-1.21968973577027,-2.20392587828038,
13.5569121788628));
#16897=CARTESIAN_POINT('Ctrl Pts',(-1.14508575630031,-2.24358985796068,
13.5622344476332));
#16898=CARTESIAN_POINT('Ctrl Pts',(-1.06873708216018,-2.27938748334191,
13.5675567164037));
#16899=CARTESIAN_POINT('Ctrl Pts',(-0.993510025873233,-2.31465921542922,
13.5728007971541));
#16900=CARTESIAN_POINT('Ctrl Pts',(-0.916589652672846,-2.34617731763926,
13.5780448779044));
#16901=CARTESIAN_POINT('Ctrl Pts',(-0.838387963927007,-2.3737969314881,
13.5832889586547));
#16902=CARTESIAN_POINT('Ctrl Pts',(-0.758437321787748,-2.40203424833212,
13.5886503214353));
#16903=CARTESIAN_POINT('Ctrl Pts',(-0.677147850984717,-2.42619645007277,
13.5940116842158));
#16904=CARTESIAN_POINT('Ctrl Pts',(-0.594973052343611,-2.44618341850829,
13.5993730469964));
#16905=CARTESIAN_POINT('Ctrl Pts',(-0.512798253702505,-2.46617038694382,
13.6047344097769));
#16906=CARTESIAN_POINT('Ctrl Pts',(-0.429738638858063,-2.48198209267391,
13.6100957725575));
#16907=CARTESIAN_POINT('Ctrl Pts',(-0.346253504564394,-2.49357469520704,
13.615457135338));
#16908=CARTESIAN_POINT('Ctrl Pts',(-0.264420727998077,-2.50493785418069,
13.6207123847453));
#16909=CARTESIAN_POINT('Ctrl Pts',(-0.18187687004404,-2.51228941481937,
13.6259676341526));
#16910=CARTESIAN_POINT('Ctrl Pts',(-0.0990492570846659,-2.51555073386942,
13.6312228835598));
#16911=CARTESIAN_POINT('Ctrl Pts',(-0.0163390748644514,-2.51880742910993,
13.6364706822173));
#16912=CARTESIAN_POINT('Ctrl Pts',(0.0666536060586472,-2.51798538333182,
13.6417184808747));
#16913=CARTESIAN_POINT('Ctrl Pts',(0.149494171832415,-2.51305744912211,
13.6469662795322));
#16914=CARTESIAN_POINT('Ctrl Pts',(0.232934988923193,-2.50809380778062,
13.6522521030151));
#16915=CARTESIAN_POINT('Ctrl Pts',(0.316221007768245,-2.49896446036265,
13.657537926498));
#16916=CARTESIAN_POINT('Ctrl Pts',(0.398905803696967,-2.4856951562444,13.6628237499809));
#16917=CARTESIAN_POINT('Ctrl Pts',(0.48084917076703,-2.47254483706041,13.6680621758495));
#16918=CARTESIAN_POINT('Ctrl Pts',(0.562201589998596,-2.45532858368356,
13.673300601718));
#16919=CARTESIAN_POINT('Ctrl Pts',(0.642533255791257,-2.4341235106712,13.6785390275865));
#16920=CARTESIAN_POINT('Ctrl Pts',(0.7228385018361,-2.41292541165441,13.683775730624));
#16921=CARTESIAN_POINT('Ctrl Pts',(0.802123215391075,-2.38774121609487,
13.6890124336615));
#16922=CARTESIAN_POINT('Ctrl Pts',(0.879969559288569,-2.35869875667188,
13.6942491366989));
#16923=CARTESIAN_POINT('Ctrl Pts',(0.957813782690483,-2.329657088351,13.6994856970912));
#16924=CARTESIAN_POINT('Ctrl Pts',(1.03421928238141,-2.29675752737838,13.7047222574835));
#16925=CARTESIAN_POINT('Ctrl Pts',(1.10878643117052,-2.26017674088823,13.7099588178758));
#16926=CARTESIAN_POINT('Ctrl Pts',(1.18457404318631,-2.22299722552834,13.7152810866463));
#16927=CARTESIAN_POINT('Ctrl Pts',(1.25846213642482,-2.18201509875874,13.7206033554169));
#16928=CARTESIAN_POINT('Ctrl Pts',(1.33005706324213,-2.13746449292607,13.7259256241874));
#16929=CARTESIAN_POINT('Ctrl Pts',(1.40060020822942,-2.09356836807152,13.7311697049377));
#16930=CARTESIAN_POINT('Ctrl Pts',(1.4689167664711,-2.04620823240741,13.736413785688));
#16931=CARTESIAN_POINT('Ctrl Pts',(1.53466091700049,-1.99565080107498,13.7416578664382));
#16932=CARTESIAN_POINT('Ctrl Pts',(1.60187541244369,-1.9439626704877,13.7470192292189));
#16933=CARTESIAN_POINT('Ctrl Pts',(1.66640066013281,-1.88893283796649,13.7523805919996));
#16934=CARTESIAN_POINT('Ctrl Pts',(1.7279057724601,-1.83088718699407,13.7577419547802));
#16935=CARTESIAN_POINT('Ctrl Pts',(1.7894108847874,-1.77284153602164,13.7631033175609));
#16936=CARTESIAN_POINT('Ctrl Pts',(1.8478955585318,-1.71178047974623,13.7684646803415));
#16937=CARTESIAN_POINT('Ctrl Pts',(1.90307295579245,-1.64806540371777,13.7738260431222));
#16938=CARTESIAN_POINT('Ctrl Pts',(1.9567066129225,-1.58613293297104,13.7790374069668));
#16939=CARTESIAN_POINT('Ctrl Pts',(2.00742189654929,-1.52145466982198,13.7842487708115));
#16940=CARTESIAN_POINT('Ctrl Pts',(2.0549218431537,-1.45433918620445,13.7894601346562));
#16941=CARTESIAN_POINT('Ctrl Pts',(2.10235895333399,-1.38731248788658,13.7946646045254));
#16942=CARTESIAN_POINT('Ctrl Pts',(2.14658889768453,-1.31785534577773,13.7998690743945));
#16943=CARTESIAN_POINT('Ctrl Pts',(2.18735350234999,-1.24631091857418,13.8050735442637));
#16944=CARTESIAN_POINT('Ctrl Pts',(2.22807698574385,-1.1748386617706,13.8102727641269));
#16945=CARTESIAN_POINT('Ctrl Pts',(2.26534183691485,-1.10128370481958,13.81547198399));
#16946=CARTESIAN_POINT('Ctrl Pts',(2.29893280601861,-1.02601861747796,13.8206712038532));
#16947=CARTESIAN_POINT('Ctrl Pts',(2.33250043822423,-0.950805819597609,
13.8258668116245));
#16948=CARTESIAN_POINT('Ctrl Pts',(2.36239906650766,-0.873885678457068,
13.8310624193959));
#16949=CARTESIAN_POINT('Ctrl Pts',(2.3884597893834,-0.795654500709079,13.8362580271672));
#16950=CARTESIAN_POINT('Ctrl Pts',(2.41451585326659,-0.717437308700311,
13.8414527060964));
#16951=CARTESIAN_POINT('Ctrl Pts',(2.43673521726414,-0.637909987838495,
13.8466473850256));
#16952=CARTESIAN_POINT('Ctrl Pts',(2.45499791486807,-0.557486760375013,
13.8518420639548));
#16953=CARTESIAN_POINT('Ctrl Pts',(2.47325894911898,-0.477070857799738,
13.8570362697565));
#16954=CARTESIAN_POINT('Ctrl Pts',(2.48756393628175,-0.395759670386109,
13.8622304755582));
#16955=CARTESIAN_POINT('Ctrl Pts',(2.49784379623378,-0.313978692933837,
13.8674246813599));
#16956=CARTESIAN_POINT('Ctrl Pts',(2.5081291916546,-0.232153678300999,13.8726216841222));
#16957=CARTESIAN_POINT('Ctrl Pts',(2.51438508505178,-0.149858835924081,
13.8778186868846));
#16958=CARTESIAN_POINT('Ctrl Pts',(2.51659425685167,-0.0675247834590446,
13.8830156896469));
#16959=CARTESIAN_POINT('Ctrl Pts',(2.51721785875597,-0.0442836430876919,
13.8844826922673));
#16960=CARTESIAN_POINT('Ctrl Pts',(2.51751933182793,-0.0210393816020136,
13.8859496948877));
#16961=CARTESIAN_POINT('Ctrl Pts',(2.51749904018654,0.00219833114617901,
13.887416697508));
#16962=CARTESIAN_POINT('Ctrl Pts',(2.51749904018606,0.0021983317047849,
13.8874166975433));
#16963=CARTESIAN_POINT('Ctrl Pts',(2.51741017424796,0.10396637397242,13.8938413395162));
#16964=CARTESIAN_POINT('Ctrl Pts',(2.51114671053784,0.205464160528413,13.9002659814891));
#16965=CARTESIAN_POINT('Ctrl Pts',(2.49882897256025,0.306039239140149,13.906690623462));
#16966=CARTESIAN_POINT('Ctrl Pts',(2.48631365676307,0.408227552647264,13.9132183173714));
#16967=CARTESIAN_POINT('Ctrl Pts',(2.46754833856782,0.509463401298269,13.9197460112809));
#16968=CARTESIAN_POINT('Ctrl Pts',(2.44270786672858,0.609084992281317,13.9262737051904));
#16969=CARTESIAN_POINT('Ctrl Pts',(2.43519696831622,0.639207111313228,13.9282474537624));
#16970=CARTESIAN_POINT('Ctrl Pts',(2.42713098016237,0.669181796373038,13.9302212023344));
#16971=CARTESIAN_POINT('Ctrl Pts',(2.41851558766797,0.698991131708456,13.9321949509065));
#16972=CARTESIAN_POINT('Ctrl Pts',(2.40161632718108,0.757462724627967,13.9360664972435));
#16973=CARTESIAN_POINT('Ctrl Pts',(2.38257241873794,0.815400560410186,13.9399380435806));
#16974=CARTESIAN_POINT('Ctrl Pts',(2.36142200728636,0.872635292378013,13.9438095899177));
#16975=CARTESIAN_POINT('Ctrl Pts',(2.36142191786124,0.872635534369624,13.6679749024944));
#16976=CARTESIAN_POINT('Ctrl Pts',(2.37809075863486,0.827528311023971,13.6651807393162));
#16977=CARTESIAN_POINT('Ctrl Pts',(2.39347242642984,0.781929253098341,13.6624065957962));
#16978=CARTESIAN_POINT('Ctrl Pts',(2.44479148206397,0.614034034977576,13.6523079455054));
#16979=CARTESIAN_POINT('Ctrl Pts',(2.4727309941405,0.489530988008946,13.6450467174458));
#16980=CARTESIAN_POINT('Ctrl Pts',(2.49706478605095,0.322747949202046,13.6350543391746));
#16981=CARTESIAN_POINT('Ctrl Pts',(2.50200522284528,0.281901199609186,13.6325856636504));
#16982=CARTESIAN_POINT('Ctrl Pts',(2.50849472206676,0.214409857885104,13.6284449640569));
#16983=CARTESIAN_POINT('Ctrl Pts',(2.51062499424916,0.187828018936672,13.6267984228798));
#16984=CARTESIAN_POINT('Ctrl Pts',(2.51296551022381,0.15135484437533,13.6245115902134));
#16985=CARTESIAN_POINT('Ctrl Pts',(2.51354036909397,0.141487631169278,13.6238901612926));
#16986=CARTESIAN_POINT('Ctrl Pts',(2.51441006086061,0.124875440192849,13.6228389055961));
#16987=CARTESIAN_POINT('Ctrl Pts',(2.51473589921992,0.118132067608455,13.6224107745233));
#16988=CARTESIAN_POINT('Ctrl Pts',(2.51530656429679,0.105246939291447,13.6215899081342));
#16989=CARTESIAN_POINT('Ctrl Pts',(2.51555602898852,0.0991054675449234,
13.6211974485973));
#16990=CARTESIAN_POINT('Ctrl Pts',(2.51609896969873,0.0844123345254984,
13.6202557206377));
#16991=CARTESIAN_POINT('Ctrl Pts',(2.51637133932898,0.075860036347716,13.6197053174528));
#16992=CARTESIAN_POINT('Ctrl Pts',(2.51719523687576,0.0450544589039541,
13.6177150116822));
#16993=CARTESIAN_POINT('Ctrl Pts',(2.51749518710519,0.022796223009124,13.6162623979861));
#16994=CARTESIAN_POINT('Ctrl Pts',(2.51750703494928,-0.0326589414498927,
13.6126118173863));
#16995=CARTESIAN_POINT('Ctrl Pts',(2.51685750509814,-0.0658510767202741,
13.6103987212928));
#16996=CARTESIAN_POINT('Ctrl Pts',(2.51140428215516,-0.204388794806129,
13.6010693947918));
#16997=CARTESIAN_POINT('Ctrl Pts',(2.5006404684397,-0.309388435010393,13.5937801096634));
#16998=CARTESIAN_POINT('Ctrl Pts',(2.45291424950533,-0.596085184335655,
13.573701268477));
#16999=CARTESIAN_POINT('Ctrl Pts',(2.40243068465968,-0.774890960910285,
13.5610264877404));
#17000=CARTESIAN_POINT('Ctrl Pts',(2.3205371506762,-0.976715181915555,13.5468788962842));
#17001=CARTESIAN_POINT('Ctrl Pts',(2.30771774987936,-1.00663010236431,13.5447843218245));
#17002=CARTESIAN_POINT('Ctrl Pts',(2.28813308902568,-1.0499901076307,13.5417505937046));
#17003=CARTESIAN_POINT('Ctrl Pts',(2.281822035993,-1.06363549736384,13.540796199055));
#17004=CARTESIAN_POINT('Ctrl Pts',(2.2703796854448,-1.08780484751768,13.5391060459477));
#17005=CARTESIAN_POINT('Ctrl Pts',(2.26529654221601,-1.09835098473381,13.5383686659501));
#17006=CARTESIAN_POINT('Ctrl Pts',(2.25451186580801,-1.12033288202263,13.5368317574778));
#17007=CARTESIAN_POINT('Ctrl Pts',(2.24879644807643,-1.13176148737903,13.5360327343738));
#17008=CARTESIAN_POINT('Ctrl Pts',(2.23358303614245,-1.16161208116453,13.5339455076524));
#17009=CARTESIAN_POINT('Ctrl Pts',(2.22394400716131,-1.17996139732444,13.5326622399996));
#17010=CARTESIAN_POINT('Ctrl Pts',(2.17792925906639,-1.26498989626293,13.526711697645));
#17011=CARTESIAN_POINT('Ctrl Pts',(2.13877259475649,-1.33012357331012,13.5221433803506));
#17012=CARTESIAN_POINT('Ctrl Pts',(2.02319963452841,-1.50403371917174,13.5097954818854));
#17013=CARTESIAN_POINT('Ctrl Pts',(1.94102663771021,-1.60868646600432,13.5022017477818));
#17014=CARTESIAN_POINT('Ctrl Pts',(1.75867271623855,-1.80649446145371,13.4867305559519));
#17015=CARTESIAN_POINT('Ctrl Pts',(1.65840654927995,-1.89895508917419,13.4788721412775));
#17016=CARTESIAN_POINT('Ctrl Pts',(1.5343066374832,-1.99603806000914,13.4691961797086));
#17017=CARTESIAN_POINT('Ctrl Pts',(1.51727370654132,-2.00901598406386,13.4678689624149));
#17018=CARTESIAN_POINT('Ctrl Pts',(1.49331298652176,-2.02679390492557,13.4659998451705));
#17019=CARTESIAN_POINT('Ctrl Pts',(1.48652297403821,-2.03177918378469,13.4654699436876));
#17020=CARTESIAN_POINT('Ctrl Pts',(1.47476311389155,-2.04032285895249,13.4645515513967));
#17021=CARTESIAN_POINT('Ctrl Pts',(1.46980503926398,-2.04389744251115,13.4641641542436));
#17022=CARTESIAN_POINT('Ctrl Pts',(1.45931393713159,-2.05140321531996,13.4633439146791));
#17023=CARTESIAN_POINT('Ctrl Pts',(1.45377796974234,-2.05533012682068,13.4629107792005));
#17024=CARTESIAN_POINT('Ctrl Pts',(1.43999604444607,-2.06502273163781,13.4618318470369));
#17025=CARTESIAN_POINT('Ctrl Pts',(1.43173133570106,-2.07076142141599,13.4611842796785));
#17026=CARTESIAN_POINT('Ctrl Pts',(1.40039401278373,-2.09224354771822,13.4587274821286));
#17027=CARTESIAN_POINT('Ctrl Pts',(1.37709527025043,-2.10765151708069,13.4568980347743));
#17028=CARTESIAN_POINT('Ctrl Pts',(1.31656470663896,-2.14624960109195,13.4521474046048));
#17029=CARTESIAN_POINT('Ctrl Pts',(1.27897528420057,-2.16885955426309,13.4491995381363));
#17030=CARTESIAN_POINT('Ctrl Pts',(1.13297376822004,-2.25156359832945,13.437809516732));
#17031=CARTESIAN_POINT('Ctrl Pts',(1.02076945468084,-2.30460339731891,13.4291886210193));
#17032=CARTESIAN_POINT('Ctrl Pts',(0.754220629113447,-2.40730299872092,
13.4095210718018));
#17033=CARTESIAN_POINT('Ctrl Pts',(0.598050074362739,-2.45077733867244,
13.39859835904));
#17034=CARTESIAN_POINT('Ctrl Pts',(0.416868001374833,-2.48284549033157,
13.3867311280604));
#17035=CARTESIAN_POINT('Ctrl Pts',(0.394922057865349,-2.48643063032723,
13.3853060979199));
#17036=CARTESIAN_POINT('Ctrl Pts',(0.358701370722863,-2.49185605508689,
13.3829739776756));
#17037=CARTESIAN_POINT('Ctrl Pts',(0.344453589169661,-2.4938654758297,13.3820616389215));
#17038=CARTESIAN_POINT('Ctrl Pts',(0.318679815629225,-2.49727535681125,
13.3804200816875));
#17039=CARTESIAN_POINT('Ctrl Pts',(0.307159965330567,-2.49871843063716,
13.3796895495698));
#17040=CARTESIAN_POINT('Ctrl Pts',(0.282418267232902,-2.50164409404214,
13.3781271930396));
#17041=CARTESIAN_POINT('Ctrl Pts',(0.26919377422902,-2.50310167065371,13.3772961701701));
#17042=CARTESIAN_POINT('Ctrl Pts',(0.232932535203316,-2.50680761137186,
13.3750282497524));
#17043=CARTESIAN_POINT('Ctrl Pts',(0.209875004720985,-2.50884326008693,
13.3735979883149));
#17044=CARTESIAN_POINT('Ctrl Pts',(0.073590212145572,-2.5189831937923,13.3652087853792));
#17045=CARTESIAN_POINT('Ctrl Pts',(-0.0400591223554762,-2.51974040778754,
13.3584838351933));
#17046=CARTESIAN_POINT('Ctrl Pts',(-0.331509641175326,-2.50195020746078,
13.3414980921401));
#17047=CARTESIAN_POINT('Ctrl Pts',(-0.507960568904698,-2.47216938436677,
13.3314831810998));
#17048=CARTESIAN_POINT('Ctrl Pts',(-0.738757301150904,-2.40744621896714,
13.3172800196309));
#17049=CARTESIAN_POINT('Ctrl Pts',(-0.797118086428009,-2.38875722866903,
13.3135851423482));
#17050=CARTESIAN_POINT('Ctrl Pts',(-0.867441885713224,-2.36337330082162,
13.3089403323355));
#17051=CARTESIAN_POINT('Ctrl Pts',(-0.8801124209655,-2.35868414413761,13.3080956764112));
#17052=CARTESIAN_POINT('Ctrl Pts',(-0.899871150864326,-2.35119039217152,
13.3067653854445));
#17053=CARTESIAN_POINT('Ctrl Pts',(-0.906985605970703,-2.34845512099487,
13.3062837152547));
#17054=CARTESIAN_POINT('Ctrl Pts',(-0.920169394286457,-2.34331755071924,
13.3053859608971));
#17055=CARTESIAN_POINT('Ctrl Pts',(-0.926241912820787,-2.34092391445327,
13.3049703869733));
#17056=CARTESIAN_POINT('Ctrl Pts',(-0.94016464059317,-2.33537326576604,
13.304012869329));
#17057=CARTESIAN_POINT('Ctrl Pts',(-0.948008269066632,-2.33220028272001,
13.3034699960396));
#17058=CARTESIAN_POINT('Ctrl Pts',(-0.972520217951942,-2.32214037900105,
13.3017630231271));
#17059=CARTESIAN_POINT('Ctrl Pts',(-0.989130198283595,-2.31511401900966,
13.3005911365514));
#17060=CARTESIAN_POINT('Ctrl Pts',(-1.14349679679879,-2.24784938389074,
13.2895671095692));
#17061=CARTESIAN_POINT('Ctrl Pts',(-1.27566014501487,-2.17556760450728,
13.2791528662349));
#17062=CARTESIAN_POINT('Ctrl Pts',(-1.55018979264058,-1.99176740576532,
13.2563319237504));
#17063=CARTESIAN_POINT('Ctrl Pts',(-1.68865442809921,-1.87581810887262,
13.2440271834098));
#17064=CARTESIAN_POINT('Ctrl Pts',(-1.83405660407491,-1.72479406241571,
13.2304071297146));
#17065=CARTESIAN_POINT('Ctrl Pts',(-1.85416158491882,-1.70316268234601,
13.2285044724803));
#17066=CARTESIAN_POINT('Ctrl Pts',(-1.88379652698458,-1.67013092713428,
13.2256692769152));
#17067=CARTESIAN_POINT('Ctrl Pts',(-1.8936132171945,-1.65899236524033,13.2247248418291));
#17068=CARTESIAN_POINT('Ctrl Pts',(-1.9104795445215,-1.63951012345845,13.2230927242107));
#17069=CARTESIAN_POINT('Ctrl Pts',(-1.91757439551896,-1.63120629556808,
13.2224031915989));
#17070=CARTESIAN_POINT('Ctrl Pts',(-1.93226378791115,-1.61378551506635,
13.2209691671538));
#17071=CARTESIAN_POINT('Ctrl Pts',(-1.93984837950974,-1.60466049585197,
13.2202250902542));
#17072=CARTESIAN_POINT('Ctrl Pts',(-1.95769337763586,-1.58287975384526,
13.2184654824269));
#17073=CARTESIAN_POINT('Ctrl Pts',(-1.96789608338595,-1.57017728315698,
13.2174522767995));
#17074=CARTESIAN_POINT('Ctrl Pts',(-2.00199461725012,-1.52686980477434,
13.2140405393533));
#17075=CARTESIAN_POINT('Ctrl Pts',(-2.02530621890243,-1.49581042094412,
13.2116648649744));
#17076=CARTESIAN_POINT('Ctrl Pts',(-2.12043525272134,-1.36276107700484,
13.2017621306102));
#17077=CARTESIAN_POINT('Ctrl Pts',(-2.1853427602699,-1.25604343837688,13.1944898670829));
#17078=CARTESIAN_POINT('Ctrl Pts',(-2.30840032196292,-1.01506700837394,
13.1788906795224));
#17079=CARTESIAN_POINT('Ctrl Pts',(-2.3633084477247,-0.879682099700715,
13.1706242151947));
#17080=CARTESIAN_POINT('Ctrl Pts',(-2.42334987876075,-0.684534769749036,
13.158502365031));
#17081=CARTESIAN_POINT('Ctrl Pts',(-2.43856617758191,-0.628176995431338,
13.1549765580319));
#17082=CARTESIAN_POINT('Ctrl Pts',(-2.45483434578437,-0.558365683251226,
13.1505219224476));
#17083=CARTESIAN_POINT('Ctrl Pts',(-2.45775605746228,-0.545361389739,13.1496884456733));
#17084=CARTESIAN_POINT('Ctrl Pts',(-2.46217731268002,-0.524925329418601,
13.1483720151933));
#17085=CARTESIAN_POINT('Ctrl Pts',(-2.46374682795991,-0.517508729087825,
13.147892894012));
#17086=CARTESIAN_POINT('Ctrl Pts',(-2.46659394342787,-0.503748392895903,
13.1470012404913));
#17087=CARTESIAN_POINT('Ctrl Pts',(-2.46788060677716,-0.497406707271335,
13.1465892221593));
#17088=CARTESIAN_POINT('Ctrl Pts',(-2.4707982469329,-0.482736264189013,
13.1456336173918));
#17089=CARTESIAN_POINT('Ctrl Pts',(-2.4724115631273,-0.474404189844925,
13.1450890621632));
#17090=CARTESIAN_POINT('Ctrl Pts',(-2.47734674171339,-0.448207059155325,
13.1433715385622));
#17091=CARTESIAN_POINT('Ctrl Pts',(-2.48051724127615,-0.430314556324609,
13.14219064942));
#17092=CARTESIAN_POINT('Ctrl Pts',(-2.50457703400831,-0.285421726013943,
13.1325731134126));
#17093=CARTESIAN_POINT('Ctrl Pts',(-2.51589036887427,-0.157036459991599,
13.1237217332443));
#17094=CARTESIAN_POINT('Ctrl Pts',(-2.51964136449002,0.175861940829714,
13.1007301925616));
#17095=CARTESIAN_POINT('Ctrl Pts',(-2.49708142069865,0.379651511722815,
13.0866816259376));
#17096=CARTESIAN_POINT('Ctrl Pts',(-2.4430074841959,0.608672204471248,13.0714164705259));
#17097=CARTESIAN_POINT('Ctrl Pts',(-2.43532632500538,0.638712181759205,
13.0694227651158));
#17098=CARTESIAN_POINT('Ctrl Pts',(-2.42313267639444,0.682976227054846,
13.0664965888944));
#17099=CARTESIAN_POINT('Ctrl Pts',(-2.41904575887019,0.697313506395124,
13.0655505943799));
#17100=CARTESIAN_POINT('Ctrl Pts',(-2.41153608953457,0.722797251760484,
13.0638721110112));
#17101=CARTESIAN_POINT('Ctrl Pts',(-2.40816283368252,0.73395773184295,13.0631380491776));
#17102=CARTESIAN_POINT('Ctrl Pts',(-2.40087234078289,0.757487010302141,
13.0615924408573));
#17103=CARTESIAN_POINT('Ctrl Pts',(-2.39693676518691,0.769849804332523,
13.0607815139856));
#17104=CARTESIAN_POINT('Ctrl Pts',(-2.38618713300383,0.802735836984656,
13.0586271611727));
#17105=CARTESIAN_POINT('Ctrl Pts',(-2.379203827701,0.823202920868137,13.0572892784912));
#17106=CARTESIAN_POINT('Ctrl Pts',(-2.3426622807203,0.925949789014163,13.0505840796357));
#17107=CARTESIAN_POINT('Ctrl Pts',(-2.30909433649126,1.00674490445486,13.0453504820223));
#17108=CARTESIAN_POINT('Ctrl Pts',(-2.18030220991975,1.27620599524215,13.0277903924667));
#17109=CARTESIAN_POINT('Ctrl Pts',(-2.06560711448605,1.45453570666296,13.0160466257753));
#17110=CARTESIAN_POINT('Ctrl Pts',(-1.89283715056426,1.66082056219731,13.0000662862577));
#17111=CARTESIAN_POINT('Ctrl Pts',(-1.8541508456278,1.70390168118828,12.9965681245321));
#17112=CARTESIAN_POINT('Ctrl Pts',(-1.80479716574065,1.75518952634118,12.9921445981148));
#17113=CARTESIAN_POINT('Ctrl Pts',(-1.79550103642579,1.76469801753502,12.9913130109086));
#17114=CARTESIAN_POINT('Ctrl Pts',(-1.7807927482699,1.77950577471563,12.9899989238631));
#17115=CARTESIAN_POINT('Ctrl Pts',(-1.77543110430399,1.78485517755347,12.9895202343738));
#17116=CARTESIAN_POINT('Ctrl Pts',(-1.76544316922027,1.79473077510757,12.9886289408832));
#17117=CARTESIAN_POINT('Ctrl Pts',(-1.76082348175553,1.79926340528292,12.9882168469099));
#17118=CARTESIAN_POINT('Ctrl Pts',(-1.75009798246767,1.80970591781176,12.9872604813368));
#17119=CARTESIAN_POINT('Ctrl Pts',(-1.74397970371148,1.81560272230545,12.9867152354569));
#17120=CARTESIAN_POINT('Ctrl Pts',(-1.72464383691172,1.83405074220905,12.9849933677446));
#17121=CARTESIAN_POINT('Ctrl Pts',(-1.7113200607685,1.84648912628948,12.9838087697132));
#17122=CARTESIAN_POINT('Ctrl Pts',(-1.59734150909223,1.95060032499522,12.9736998379727));
#17123=CARTESIAN_POINT('Ctrl Pts',(-1.48954756252013,2.0341047334634,12.9643130130075));
#17124=CARTESIAN_POINT('Ctrl Pts',(-1.21190425064778,2.21523592114061,12.9414120899283));
#17125=CARTESIAN_POINT('Ctrl Pts',(-1.03635926706881,2.30260042617566,12.9280032078562));
#17126=CARTESIAN_POINT('Ctrl Pts',(-0.822852325842711,2.37943475252667,
12.9132726593402));
#17127=CARTESIAN_POINT('Ctrl Pts',(-0.793057044007318,2.38953057374007,
12.9112485828575));
#17128=CARTESIAN_POINT('Ctrl Pts',(-0.748736707895591,2.40362769830424,
12.9082829694164));
#17129=CARTESIAN_POINT('Ctrl Pts',(-0.734353310004099,2.40806104613763,
12.9073274753791));
#17130=CARTESIAN_POINT('Ctrl Pts',(-0.708710408996641,2.41571374858801,
12.905636066239));
#17131=CARTESIAN_POINT('Ctrl Pts',(-0.697466682370646,2.41898400023712,
12.904898521237));
#17132=CARTESIAN_POINT('Ctrl Pts',(-0.673914463720985,2.42565632441566,
12.9033619539428));
#17133=CARTESIAN_POINT('Ctrl Pts',(-0.661602054593062,2.42904344125737,
12.9025634320681));
#17134=CARTESIAN_POINT('Ctrl Pts',(-0.629276203854807,2.43767218812735,
12.9004790352874));
#17135=CARTESIAN_POINT('Ctrl Pts',(-0.609222733539032,2.44276112994044,
12.8991980713526));
#17136=CARTESIAN_POINT('Ctrl Pts',(-0.515691001673122,2.46527308802374,
12.8932767042149));
#17137=CARTESIAN_POINT('Ctrl Pts',(-0.441511413653369,2.47963261209531,
12.888734033511));
#17138=CARTESIAN_POINT('Ctrl Pts',(-0.236721407293363,2.50979176322334,
12.8764904193053));
#17139=CARTESIAN_POINT('Ctrl Pts',(-0.105344108653229,2.51872918987127,
12.8689709390602));
#17140=CARTESIAN_POINT('Ctrl Pts',(0.164194273390748,2.51593117970867,12.8534726753599));
#17141=CARTESIAN_POINT('Ctrl Pts',(0.30188784765683,2.50314274929702,12.8455123787338));
#17142=CARTESIAN_POINT('Ctrl Pts',(0.458906817720091,2.47541296209981,12.8357205747889));
#17143=CARTESIAN_POINT('Ctrl Pts',(0.479945114370115,2.47142012159577,12.8343933497603));
#17144=CARTESIAN_POINT('Ctrl Pts',(0.509184385006529,2.46548341531214,12.8325242233235));
#17145=CARTESIAN_POINT('Ctrl Pts',(0.517431062808267,2.46376587759491,12.8319943205369));
#17146=CARTESIAN_POINT('Ctrl Pts',(0.531646451170755,2.46073071705992,12.8310759266064));
#17147=CARTESIAN_POINT('Ctrl Pts',(0.537619331044593,2.45943267114636,12.8306885291266));
#17148=CARTESIAN_POINT('Ctrl Pts',(0.550214638937756,2.45664734342314,12.8298682896324));
#17149=CARTESIAN_POINT('Ctrl Pts',(0.556835850641238,2.45515501565242,12.8294351545554));
#17150=CARTESIAN_POINT('Ctrl Pts',(0.573257368282003,2.45138399262925,12.828356224705));
#17151=CARTESIAN_POINT('Ctrl Pts',(0.583050124901039,2.44907330092699,12.8277086592742));
#17152=CARTESIAN_POINT('Ctrl Pts',(0.619974997666589,2.44012652219851,12.8252518775997));
#17153=CARTESIAN_POINT('Ctrl Pts',(0.647008773314897,2.43309801202393,12.8234224445204));
#17154=CARTESIAN_POINT('Ctrl Pts',(0.716177789675453,2.41388055000207,12.8186718602732));
#17155=CARTESIAN_POINT('Ctrl Pts',(0.758120588908801,2.4010378330102,12.8157240260535));
#17156=CARTESIAN_POINT('Ctrl Pts',(0.97681254444608,2.32777390142417,12.800068551787));
#17157=CARTESIAN_POINT('Ctrl Pts',(1.14677140277557,2.24891467940778,12.7869642211667));
#17158=CARTESIAN_POINT('Ctrl Pts',(1.393096444391,2.09937196476488,12.7674641387089));
#17159=CARTESIAN_POINT('Ctrl Pts',(1.47649307708827,2.04158102325674,12.7607469599041));
#17160=CARTESIAN_POINT('Ctrl Pts',(1.57429774356821,1.96466885436951,12.7527331957181));
#17161=CARTESIAN_POINT('Ctrl Pts',(1.59221273355169,1.95017839222046,12.7512590233193));
#17162=CARTESIAN_POINT('Ctrl Pts',(1.6202402878396,1.92686471400428,12.7489420238722));
#17163=CARTESIAN_POINT('Ctrl Pts',(1.63048522565309,1.91820336686881,12.7480927683579));
#17164=CARTESIAN_POINT('Ctrl Pts',(1.64944540036644,1.90191226617537,12.7465165044326));
#17165=CARTESIAN_POINT('Ctrl Pts',(1.65817811779051,1.89430349572399,12.7457886695384));
#17166=CARTESIAN_POINT('Ctrl Pts',(1.66706094061283,1.88645544435058,12.7450463484127));
#17167=CARTESIAN_POINT('Ctrl Pts',(1.66726371892795,1.88627622971385,12.7450294015419));
#17168=CARTESIAN_POINT('Ctrl Pts',(1.66764802512575,1.88593647109887,12.7449972817578));
#17169=CARTESIAN_POINT('Ctrl Pts',(1.66782955872015,1.88577593361091,12.7449821085776));
#17170=CARTESIAN_POINT('Ctrl Pts',(1.66817419178611,1.8854710719843,12.7449533013832));
#17171=CARTESIAN_POINT('Ctrl Pts',(1.668337295705,1.8853267528974,12.7449396671613));
#17172=CARTESIAN_POINT('Ctrl Pts',(1.66864741612383,1.88505227758218,12.7449137421899));
#17173=CARTESIAN_POINT('Ctrl Pts',(1.66879443612225,1.88492212532028,12.7449014512769));
#17174=CARTESIAN_POINT('Ctrl Pts',(1.66907436040821,1.88467425857843,12.74487804846));
#17175=CARTESIAN_POINT('Ctrl Pts',(1.66920726746409,1.88455654724535,12.744866936427));
#17176=CARTESIAN_POINT('Ctrl Pts',(1.66946063508355,1.88433210019086,12.7448457521065));
#17177=CARTESIAN_POINT('Ctrl Pts',(1.66958109786296,1.88422536697763,12.7448356797155));
#17178=CARTESIAN_POINT('Ctrl Pts',(1.66981099989146,1.88402162833352,12.7448164559359));
#17179=CARTESIAN_POINT('Ctrl Pts',(1.66992044092075,1.88392462492056,12.7448073044642));
#17180=CARTESIAN_POINT('Ctrl Pts',(1.67012952021494,1.88373927427328,12.7447898206331));
#17181=CARTESIAN_POINT('Ctrl Pts',(1.6702291599208,1.88365092867105,12.7447814882064));
#17182=CARTESIAN_POINT('Ctrl Pts',(1.67041969000504,1.88348196805897,12.7447655545256));
#17183=CARTESIAN_POINT('Ctrl Pts',(1.67051058155444,1.88340135437842,12.7447579532169));
#17184=CARTESIAN_POINT('Ctrl Pts',(1.67080491686272,1.88314026396033,12.7447333370999));
#17185=CARTESIAN_POINT('Ctrl Pts',(1.67100833726458,1.88295976078979,12.7447163233804));
#17186=CARTESIAN_POINT('Ctrl Pts',(1.68217384108825,1.87304892222698,12.7437824011769));
#17187=CARTESIAN_POINT('Ctrl Pts',(1.69305094316491,1.86322291067464,12.7428694618121));
#17188=CARTESIAN_POINT('Ctrl Pts',(1.72658826258211,1.83239022539699,12.7400441404101));
#17189=CARTESIAN_POINT('Ctrl Pts',(1.74894852584554,1.8110605037083,12.7381453846975));
#17190=CARTESIAN_POINT('Ctrl Pts',(1.80014866667017,1.7603872249161,12.7337565821545));
#17191=CARTESIAN_POINT('Ctrl Pts',(1.82867354011596,1.73073734368324,12.7312797525815));
#17192=CARTESIAN_POINT('Ctrl Pts',(1.92844346603761,1.6218107169829,12.7224745300691));
#17193=CARTESIAN_POINT('Ctrl Pts',(1.99536737966006,1.53872533332381,12.716300611589));
#17194=CARTESIAN_POINT('Ctrl Pts',(2.15310798789481,1.31522352293741,12.7005573373296));
#17195=CARTESIAN_POINT('Ctrl Pts',(2.23556694365276,1.16957872182038,12.6910969366956));
#17196=CARTESIAN_POINT('Ctrl Pts',(2.3153968018407,0.988780316548436,12.6790862762629));
#17197=CARTESIAN_POINT('Ctrl Pts',(2.3272824812662,0.96047119808167,12.6771976976479));
#17198=CARTESIAN_POINT('Ctrl Pts',(2.34263775694275,0.921938615522299,12.6746072249691));
#17199=CARTESIAN_POINT('Ctrl Pts',(2.34656416844794,0.911898604329127,12.6739304541055));
#17200=CARTESIAN_POINT('Ctrl Pts',(2.3526653155969,0.895997345504483,12.6728552887704));
#17201=CARTESIAN_POINT('Ctrl Pts',(2.35488296304312,0.890152547994118,12.6724593907968));
#17202=CARTESIAN_POINT('Ctrl Pts',(2.35853616202579,0.880415036445676,12.6717985584326));
#17203=CARTESIAN_POINT('Ctrl Pts',(2.35998390411294,0.876526916418576,12.6715343551603));
#17204=CARTESIAN_POINT('Ctrl Pts',(2.36142200728627,0.872635292378268,12.6712695847815));
#17205=CARTESIAN_POINT('Origin',(0.,0.,10.));
#17206=CARTESIAN_POINT('',(2.36142193605295,0.872635485141376,11.6676249231292));
#17207=CARTESIAN_POINT('',(2.36142200728635,0.872635292378037,11.9438279118171));
#17208=CARTESIAN_POINT('',(2.36142200728636,0.87263529237802,10.));
#17209=CARTESIAN_POINT('',(2.51749968849485,-0.00125236909203477,12.8874166974535));
#17210=CARTESIAN_POINT('Ctrl Pts',(2.36142200728635,0.872635292378036,11.9438279118171));
#17211=CARTESIAN_POINT('Ctrl Pts',(2.33294410961694,0.949698797447294,11.9490047738285));
#17212=CARTESIAN_POINT('Ctrl Pts',(2.30067936897463,1.02539487449982,11.95418163584));
#17213=CARTESIAN_POINT('Ctrl Pts',(2.26479238961036,1.09932783188773,11.9593584978515));
#17214=CARTESIAN_POINT('Ctrl Pts',(2.22890486521791,1.17326191212148,11.9645354384858));
#17215=CARTESIAN_POINT('Ctrl Pts',(2.18939520142238,1.24543239473698,11.9697123791201));
#17216=CARTESIAN_POINT('Ctrl Pts',(2.14647477656318,1.31546656497915,11.9748893197544));
#17217=CARTESIAN_POINT('Ctrl Pts',(2.10351230570705,1.38556934256892,11.9800713318583));
#17218=CARTESIAN_POINT('Ctrl Pts',(2.05713265121341,1.45353122561535,11.9852533439622));
#17219=CARTESIAN_POINT('Ctrl Pts',(2.00759113030992,1.51900760481998,11.9904353560661));
#17220=CARTESIAN_POINT('Ctrl Pts',(1.95802381995394,1.58451806856501,11.9956200657306));
#17221=CARTESIAN_POINT('Ctrl Pts',(1.90529167198153,1.64754009118975,12.0008047753951));
#17222=CARTESIAN_POINT('Ctrl Pts',(1.84968934232933,1.70776332870608,12.0059894850596));
#17223=CARTESIAN_POINT('Ctrl Pts',(1.79399353595335,1.76808781145754,12.0111829110797));
#17224=CARTESIAN_POINT('Ctrl Pts',(1.73541825291344,1.82560378477774,12.0163763370997));
#17225=CARTESIAN_POINT('Ctrl Pts',(1.67429355538389,1.8800391858682,12.0215697631197));
#17226=CARTESIAN_POINT('Ctrl Pts',(1.63428350827941,1.91567065808494,12.0249691945786));
#17227=CARTESIAN_POINT('Ctrl Pts',(1.59318183758348,1.94998307448256,12.0283686260374));
#17228=CARTESIAN_POINT('Ctrl Pts',(1.55108776789127,1.98291023152791,12.0317680574963));
#17229=CARTESIAN_POINT('Ctrl Pts',(1.4860136996306,2.03381298530929,12.0370233069036));
#17230=CARTESIAN_POINT('Ctrl Pts',(1.41831105347754,2.08160300135593,12.0422785563109));
#17231=CARTESIAN_POINT('Ctrl Pts',(1.34830995266707,2.12599777082172,12.0475338057182));
#17232=CARTESIAN_POINT('Ctrl Pts',(1.27840809751517,2.17032959858971,12.0527816043757));
#17233=CARTESIAN_POINT('Ctrl Pts',(1.20621464682175,2.21127549610313,12.0580294030332));
#17234=CARTESIAN_POINT('Ctrl Pts',(1.13209187433444,2.24859383572621,12.0632772016907));
#17235=CARTESIAN_POINT('Ctrl Pts',(1.05743201845915,2.28618257889205,12.0685630251736));
#17236=CARTESIAN_POINT('Ctrl Pts',(0.980815136875723,2.32009068081077,12.0738488486565));
#17237=CARTESIAN_POINT('Ctrl Pts',(0.902640269298452,2.35011633632057,12.0791346721394));
#17238=CARTESIAN_POINT('Ctrl Pts',(0.825166390362672,2.37987275384996,12.084373098008));
#17239=CARTESIAN_POINT('Ctrl Pts',(0.746162792910291,2.4058159048703,12.0896115238766));
#17240=CARTESIAN_POINT('Ctrl Pts',(0.66603992468444,2.42779675193916,12.0948499497452));
#17241=CARTESIAN_POINT('Ctrl Pts',(0.585943407536478,2.44977036987324,12.1000866527827));
#17242=CARTESIAN_POINT('Ctrl Pts',(0.504728795329191,2.46778414997608,12.1053233558202));
#17243=CARTESIAN_POINT('Ctrl Pts',(0.422821641415746,2.4817389285641,12.1105600588577));
#17244=CARTESIAN_POINT('Ctrl Pts',(0.34091671861231,2.49569332703091,12.1157966192501));
#17245=CARTESIAN_POINT('Ctrl Pts',(0.258319746649563,2.50558886733434,12.1210331796424));
#17246=CARTESIAN_POINT('Ctrl Pts',(0.175465040666664,2.51137776320167,12.1262697400347));
#17247=CARTESIAN_POINT('Ctrl Pts',(0.0912542264867864,2.51726140769003,
12.1315920088052));
#17248=CARTESIAN_POINT('Ctrl Pts',(0.00677765496035548,2.51890271813326,
12.1369142775757));
#17249=CARTESIAN_POINT('Ctrl Pts',(-0.0775066867448587,2.51630661158569,
12.1422365463461));
#17250=CARTESIAN_POINT('Ctrl Pts',(-0.160552829837487,2.5137486437417,12.1474806270965));
#17251=CARTESIAN_POINT('Ctrl Pts',(-0.243411892025351,2.50707703272407,
12.1527247078468));
#17252=CARTESIAN_POINT('Ctrl Pts',(-0.32565089727474,2.49634888248902,12.1579687885971));
#17253=CARTESIAN_POINT('Ctrl Pts',(-0.409729149087675,2.48538080092949,
12.1633301513777));
#17254=CARTESIAN_POINT('Ctrl Pts',(-0.49315877083768,2.47017263631205,12.1686915141582));
#17255=CARTESIAN_POINT('Ctrl Pts',(-0.575490003805714,2.45084016319296,
12.1740528769388));
#17256=CARTESIAN_POINT('Ctrl Pts',(-0.657821236773758,2.43150769007387,
12.1794142397194));
#17257=CARTESIAN_POINT('Ctrl Pts',(-0.739053611328862,2.40805111359026,
12.1847756024999));
#17258=CARTESIAN_POINT('Ctrl Pts',(-0.818757647879546,2.38063902430393,
12.1901369652805));
#17259=CARTESIAN_POINT('Ctrl Pts',(-0.896884163093578,2.35376948163886,
12.1953922146878));
#17260=CARTESIAN_POINT('Ctrl Pts',(-0.973830871246756,2.32300037319786,
12.2006474640951));
#17261=CARTESIAN_POINT('Ctrl Pts',(-1.04918106998781,2.28845479142133,12.2059027135024));
#17262=CARTESIAN_POINT('Ctrl Pts',(-1.12442443926459,2.25395818743193,12.2111505121599));
#17263=CARTESIAN_POINT('Ctrl Pts',(-1.19807537913551,2.21569593576888,12.2163983108174));
#17264=CARTESIAN_POINT('Ctrl Pts',(-1.26973397369639,2.17384035431334,12.2216461094749));
#17265=CARTESIAN_POINT('Ctrl Pts',(-1.34191179655186,2.1316814930864,12.2269319329578));
#17266=CARTESIAN_POINT('Ctrl Pts',(-1.41206783162651,2.08587716292094,12.2322177564407));
#17267=CARTESIAN_POINT('Ctrl Pts',(-1.47981554851215,2.03665220211544,12.2375035799236));
#17268=CARTESIAN_POINT('Ctrl Pts',(-1.54695577629684,1.98786863813568,12.2427420057922));
#17269=CARTESIAN_POINT('Ctrl Pts',(-1.61173032318671,1.93572581916218,12.2479804316608));
#17270=CARTESIAN_POINT('Ctrl Pts',(-1.67379070881036,1.88048688192715,12.2532188575294));
#17271=CARTESIAN_POINT('Ctrl Pts',(-1.73583068380593,1.82526611185936,12.2584555605669));
#17272=CARTESIAN_POINT('Ctrl Pts',(-1.79515792597853,1.76695155239302,12.2636922636044));
#17273=CARTESIAN_POINT('Ctrl Pts',(-1.85145756440794,1.7058461645754,12.2689289666419));
#17274=CARTESIAN_POINT('Ctrl Pts',(-1.90775566926345,1.6447424412379,12.2741655270342));
#17275=CARTESIAN_POINT('Ctrl Pts',(-1.96102602244995,1.58084838074151,12.2794020874266));
#17276=CARTESIAN_POINT('Ctrl Pts',(-2.01099207765506,1.51450226596351,12.2846386478189));
#17277=CARTESIAN_POINT('Ctrl Pts',(-2.06177594249721,1.44707024412675,12.2899609165894));
#17278=CARTESIAN_POINT('Ctrl Pts',(-2.10914606227333,1.37710556168465,12.2952831853599));
#17279=CARTESIAN_POINT('Ctrl Pts',(-2.15285720954222,1.30499505183816,12.3006054541303));
#17280=CARTESIAN_POINT('Ctrl Pts',(-2.19592620809399,1.23394389811207,12.3058495348807));
#17281=CARTESIAN_POINT('Ctrl Pts',(-2.23544285799706,1.16080998695817,12.311093615631));
#17282=CARTESIAN_POINT('Ctrl Pts',(-2.27121932313193,1.08598758567128,12.3163376963813));
#17283=CARTESIAN_POINT('Ctrl Pts',(-2.30779591638548,1.00949180757226,12.3216990591619));
#17284=CARTESIAN_POINT('Ctrl Pts',(-2.34046281303122,0.931231575526155,
12.3270604219424));
#17285=CARTESIAN_POINT('Ctrl Pts',(-2.3690722520371,0.851647177314573,12.332421784723));
#17286=CARTESIAN_POINT('Ctrl Pts',(-2.39768169104297,0.772062779102991,
12.3377831475035));
#17287=CARTESIAN_POINT('Ctrl Pts',(-2.42223358878511,0.691154720335989,
12.3431445102841));
#17288=CARTESIAN_POINT('Ctrl Pts',(-2.44263552689208,0.609375034576103,
12.3485058730646));
#17289=CARTESIAN_POINT('Ctrl Pts',(-2.46263366496502,0.529213951897958,
12.3537611224719));
#17290=CARTESIAN_POINT('Ctrl Pts',(-2.47871852955354,0.447919357606388,
12.3590163718793));
#17291=CARTESIAN_POINT('Ctrl Pts',(-2.49076649540138,0.365907796290177,
12.3642716212866));
#17292=CARTESIAN_POINT('Ctrl Pts',(-2.50279737997062,0.284012508737078,
12.3695194199441));
#17293=CARTESIAN_POINT('Ctrl Pts',(-2.51080266764662,0.201402725930073,
12.3747672186015));
#17294=CARTESIAN_POINT('Ctrl Pts',(-2.51470916250038,0.118507712983695,
12.380015017259));
#17295=CARTESIAN_POINT('Ctrl Pts',(-2.51864396327716,0.0350120542045962,
12.3853008407419));
#17296=CARTESIAN_POINT('Ctrl Pts',(-2.51842020731908,-0.0487725258359569,
12.3905866642249));
#17297=CARTESIAN_POINT('Ctrl Pts',(-2.5140160401722,-0.132399394851013,
12.3958724877078));
#17298=CARTESIAN_POINT('Ctrl Pts',(-2.50965136488812,-0.215276387503942,
12.4011109135763));
#17299=CARTESIAN_POINT('Ctrl Pts',(-2.50118097377524,-0.297998016898358,
12.4063493394449));
#17300=CARTESIAN_POINT('Ctrl Pts',(-2.48863585321229,-0.380128715182573,
12.4115877653135));
#17301=CARTESIAN_POINT('Ctrl Pts',(-2.47609485853071,-0.462232402046997,
12.416824468351));
#17302=CARTESIAN_POINT('Ctrl Pts',(-2.4594818655495,-0.543745088015308,
12.4220611713885));
#17303=CARTESIAN_POINT('Ctrl Pts',(-2.43887956369379,-0.624237714173704,
12.427297874426));
#17304=CARTESIAN_POINT('Ctrl Pts',(-2.41827782303446,-0.704728147753272,
12.4325344348183));
#17305=CARTESIAN_POINT('Ctrl Pts',(-2.39368710497056,-0.784198130013413,
12.4377709952107));
#17306=CARTESIAN_POINT('Ctrl Pts',(-2.36524059249831,-0.862231517400193,
12.443007555603));
#17307=CARTESIAN_POINT('Ctrl Pts',(-2.33632848729624,-0.941542100994626,
12.4483298243735));
#17308=CARTESIAN_POINT('Ctrl Pts',(-2.30343338708723,-1.01936817258425,
12.453652093144));
#17309=CARTESIAN_POINT('Ctrl Pts',(-2.26674625011272,-1.09529342534315,
12.4589743619144));
#17310=CARTESIAN_POINT('Ctrl Pts',(-2.23059807400783,-1.17010328061869,
12.4642184426648));
#17311=CARTESIAN_POINT('Ctrl Pts',(-2.19076881527345,-1.24306741378626,
12.4694625234151));
#17312=CARTESIAN_POINT('Ctrl Pts',(-2.14748691460629,-1.31381360991381,
12.4747066041654));
#17313=CARTESIAN_POINT('Ctrl Pts',(-2.10323702938211,-1.38614201995211,
12.480067966946));
#17314=CARTESIAN_POINT('Ctrl Pts',(-2.05537849337824,-1.45615166634425,
12.4854293297265));
#17315=CARTESIAN_POINT('Ctrl Pts',(-2.00420016786459,-1.52347889290648,
12.4907906925071));
#17316=CARTESIAN_POINT('Ctrl Pts',(-1.95302184235094,-1.59080611946871,
12.4961520552876));
#17317=CARTESIAN_POINT('Ctrl Pts',(-1.89852410590017,-1.65545058077777,
12.5015134180682));
#17318=CARTESIAN_POINT('Ctrl Pts',(-1.8410358034506,-1.71708864663797,12.5068747808488));
#17319=CARTESIAN_POINT('Ctrl Pts',(-1.78468532321994,-1.77750675717024,
12.5121300302561));
#17320=CARTESIAN_POINT('Ctrl Pts',(-1.7252534743354,-1.83525958626136,12.5173852796634));
#17321=CARTESIAN_POINT('Ctrl Pts',(-1.66302234322075,-1.89001664964851,
12.5226405290707));
#17322=CARTESIAN_POINT('Ctrl Pts',(-1.6008794417127,-1.94469607995917,12.5278883277282));
#17323=CARTESIAN_POINT('Ctrl Pts',(-1.53594548458524,-1.99638787870886,
12.5331361263857));
#17324=CARTESIAN_POINT('Ctrl Pts',(-1.46854068446692,-2.04479693565533,
12.5383839250432));
#17325=CARTESIAN_POINT('Ctrl Pts',(-1.40064747846204,-2.09355675795285,
12.5436697485261));
#17326=CARTESIAN_POINT('Ctrl Pts',(-1.33024779482607,-2.13898571857549,
12.548955572009));
#17327=CARTESIAN_POINT('Ctrl Pts',(-1.25770436658404,-2.18082231653004,
12.5542413954919));
#17328=CARTESIAN_POINT('Ctrl Pts',(-1.18581143025568,-2.22228376859854,
12.5594798213605));
#17329=CARTESIAN_POINT('Ctrl Pts',(-1.1118134480378,-2.26021679013605,12.5647182472291));
#17330=CARTESIAN_POINT('Ctrl Pts',(-1.03609264146632,-2.29441022668122,
12.5699566730977));
#17331=CARTESIAN_POINT('Ctrl Pts',(-0.960396738207965,-2.32859241757415,
12.5751933761352));
#17332=CARTESIAN_POINT('Ctrl Pts',(-0.882979556111035,-2.35903727634762,
12.5804300791727));
#17333=CARTESIAN_POINT('Ctrl Pts',(-0.80424600686889,-2.38558056045807,
12.5856667822102));
#17334=CARTESIAN_POINT('Ctrl Pts',(-0.725514602289312,-2.41212312154272,
12.5909033426025));
#17335=CARTESIAN_POINT('Ctrl Pts',(-0.645467339429018,-2.43476417284083,
12.5961399029949));
#17336=CARTESIAN_POINT('Ctrl Pts',(-0.564525787980757,-2.45338885721459,
12.6013764633872));
#17337=CARTESIAN_POINT('Ctrl Pts',(-0.482259441518213,-2.47231837746756,
12.6066987321577));
#17338=CARTESIAN_POINT('Ctrl Pts',(-0.399069744423423,-2.4870987473584,
12.6120210009282));
#17339=CARTESIAN_POINT('Ctrl Pts',(-0.315409859162885,-2.49766348228556,
12.6173432696986));
#17340=CARTESIAN_POINT('Ctrl Pts',(-0.232978998793114,-2.50807301353119,
12.622587350449));
#17341=CARTESIAN_POINT('Ctrl Pts',(-0.15009214470415,-2.51438997478315,
12.6278314311993));
#17342=CARTESIAN_POINT('Ctrl Pts',(-0.0671858828033769,-2.51660332733467,
12.6330755119496));
#17343=CARTESIAN_POINT('Ctrl Pts',(0.0175745486223677,-2.5188661807412,
12.6384368747302));
#17344=CARTESIAN_POINT('Ctrl Pts',(0.102354754540799,-2.51683967122696,
12.6437982375108));
#17345=CARTESIAN_POINT('Ctrl Pts',(0.186692431981194,-2.51056810021974,
12.6491596002913));
#17346=CARTESIAN_POINT('Ctrl Pts',(0.27103010942159,-2.50429652921252,12.6545209630719));
#17347=CARTESIAN_POINT('Ctrl Pts',(0.354924762531114,-2.49378002618991,
12.6598823258524));
#17348=CARTESIAN_POINT('Ctrl Pts',(0.437925892658355,-2.47911822278394,
12.665243688633));
#17349=CARTESIAN_POINT('Ctrl Pts',(0.519284244584921,-2.46474660929443,
12.6704989380403));
#17350=CARTESIAN_POINT('Ctrl Pts',(0.600084634974541,-2.44633925090901,
12.6757541874476));
#17351=CARTESIAN_POINT('Ctrl Pts',(0.679896273783434,-2.42395282687089,
12.6810094368549));
#17352=CARTESIAN_POINT('Ctrl Pts',(0.75959475781951,-2.40159814169649,12.6862572355124));
#17353=CARTESIAN_POINT('Ctrl Pts',(0.838306834140221,-2.37527571993383,
12.6915050341698));
#17354=CARTESIAN_POINT('Ctrl Pts',(0.915610626285604,-2.34509348023333,
12.6967528328273));
#17355=CARTESIAN_POINT('Ctrl Pts',(0.993474551048993,-2.31469254418597,
12.7020386563102));
#17356=CARTESIAN_POINT('Ctrl Pts',(1.06990923039545,-2.28037570120017,12.7073244797932));
#17357=CARTESIAN_POINT('Ctrl Pts',(1.14449782874756,-2.24230483431494,12.7126103032761));
#17358=CARTESIAN_POINT('Ctrl Pts',(1.21841759628679,-2.20457534626519,12.7178487291447));
#17359=CARTESIAN_POINT('Ctrl Pts',(1.29052383903844,-2.16315910245273,12.7230871550133));
#17360=CARTESIAN_POINT('Ctrl Pts',(1.36043134115744,-2.11826174397702,12.7283255808819));
#17361=CARTESIAN_POINT('Ctrl Pts',(1.43031585186234,-2.07337915149537,12.7335622839194));
#17362=CARTESIAN_POINT('Ctrl Pts',(1.49800267016891,-2.0250179672967,12.7387989869569));
#17363=CARTESIAN_POINT('Ctrl Pts',(1.56313357589519,-1.97342840607637,12.7440356899944));
#17364=CARTESIAN_POINT('Ctrl Pts',(1.6282627074881,-1.92184025012994,12.7492722503867));
#17365=CARTESIAN_POINT('Ctrl Pts',(1.69083570386656,-1.86702417931556,12.754508810779));
#17366=CARTESIAN_POINT('Ctrl Pts',(1.75052669947214,-1.8092712688912,12.7597453711714));
#17367=CARTESIAN_POINT('Ctrl Pts',(1.8111946757751,-1.75057309899965,12.7650676399418));
#17368=CARTESIAN_POINT('Ctrl Pts',(1.86888509645734,-1.6888414183296,12.7703899087123));
#17369=CARTESIAN_POINT('Ctrl Pts',(1.92329546973574,-1.62442013841678,12.7757121774828));
#17370=CARTESIAN_POINT('Ctrl Pts',(1.97690651484305,-1.56094525421398,12.7809562582331));
#17371=CARTESIAN_POINT('Ctrl Pts',(2.02733301030535,-1.49485967987571,12.7862003389835));
#17372=CARTESIAN_POINT('Ctrl Pts',(2.07432799706175,-1.42652361025178,12.7914444197338));
#17373=CARTESIAN_POINT('Ctrl Pts',(2.12237401024577,-1.35665922835262,12.7968057825144));
#17374=CARTESIAN_POINT('Ctrl Pts',(2.1668329051569,-1.28444290942349,12.8021671452949));
#17375=CARTESIAN_POINT('Ctrl Pts',(2.20749013991691,-1.21028654961112,12.8075285080755));
#17376=CARTESIAN_POINT('Ctrl Pts',(2.24814737467694,-1.13613018979875,12.812889870856));
#17377=CARTESIAN_POINT('Ctrl Pts',(2.2850027879228,-1.06003427551497,12.8182512336366));
#17378=CARTESIAN_POINT('Ctrl Pts',(2.31789467520479,-0.982430926150674,
12.8236125964172));
#17379=CARTESIAN_POINT('Ctrl Pts',(2.35361447071358,-0.898155562249387,
12.8294349069623));
#17380=CARTESIAN_POINT('Ctrl Pts',(2.38477328167352,-0.811838041542797,
12.8352572175074));
#17381=CARTESIAN_POINT('Ctrl Pts',(2.41115846466759,-0.723962090348533,
12.8410795280525));
#17382=CARTESIAN_POINT('Ctrl Pts',(2.437464413732,-0.636350028055026,12.84688435437));
#17383=CARTESIAN_POINT('Ctrl Pts',(2.45902521036186,-0.547189130624484,
12.8526891806875));
#17384=CARTESIAN_POINT('Ctrl Pts',(2.47567650290169,-0.456981512733812,
12.858494007005));
#17385=CARTESIAN_POINT('Ctrl Pts',(2.49224191268916,-0.367239160737021,
12.864268893637));
#17386=CARTESIAN_POINT('Ctrl Pts',(2.50394821153212,-0.276461124821933,
12.8700437802691));
#17387=CARTESIAN_POINT('Ctrl Pts',(2.51068155182407,-0.185160458333482,
12.8758186669011));
#17388=CARTESIAN_POINT('Ctrl Pts',(2.51518920085692,-0.124039032243293,
12.8796846770852));
#17389=CARTESIAN_POINT('Ctrl Pts',(2.51746912849982,-0.0626837621653072,
12.8835506872694));
#17390=CARTESIAN_POINT('Ctrl Pts',(2.51749968849485,-0.00125236909204737,
12.8874166974535));
#17391=CARTESIAN_POINT('Ctrl Pts',(2.51749968849528,-0.00125236822527237,
12.887416697508));
#17392=CARTESIAN_POINT('Ctrl Pts',(2.51754167409805,0.0831467244342282,
12.8927281146097));
#17393=CARTESIAN_POINT('Ctrl Pts',(2.51333509749615,0.167540690501748,12.8980395317113));
#17394=CARTESIAN_POINT('Ctrl Pts',(2.50490792228564,0.251480716697432,12.9033509488129));
#17395=CARTESIAN_POINT('Ctrl Pts',(2.49647888833066,0.335439257170471,12.9086635374302));
#17396=CARTESIAN_POINT('Ctrl Pts',(2.48382745746316,0.418943218731677,12.9139761260474));
#17397=CARTESIAN_POINT('Ctrl Pts',(2.46703330555087,0.501550515205346,12.9192887146647));
#17398=CARTESIAN_POINT('Ctrl Pts',(2.4502220639129,0.584241872847674,12.924606709371));
#17399=CARTESIAN_POINT('Ctrl Pts',(2.42925978258897,0.66603431133487,12.9299247040774));
#17400=CARTESIAN_POINT('Ctrl Pts',(2.40427682702775,0.746497949774397,12.9352426987838));
#17401=CARTESIAN_POINT('Ctrl Pts',(2.39110116072441,0.788933363271986,12.9380473358686));
#17402=CARTESIAN_POINT('Ctrl Pts',(2.37680803330578,0.830999455775601,12.9408519729533));
#17403=CARTESIAN_POINT('Ctrl Pts',(2.36142200728636,0.872635292378012,12.9436566100381));
#17404=CARTESIAN_POINT('',(2.51749934966675,0.00180953791660804,12.610970894458));
#17405=CARTESIAN_POINT('Ctrl Pts',(2.36142200728627,0.872635292378268,12.6712695847815));
#17406=CARTESIAN_POINT('Ctrl Pts',(2.3622945071155,0.870274236945268,12.6711089481077));
#17407=CARTESIAN_POINT('Ctrl Pts',(2.36316345899157,0.867911891698931,12.6709481031855));
#17408=CARTESIAN_POINT('Ctrl Pts',(2.36727334457552,0.856686765890141,12.6701832599527));
#17409=CARTESIAN_POINT('Ctrl Pts',(2.37046791552923,0.847807264339659,12.6695765880174));
#17410=CARTESIAN_POINT('Ctrl Pts',(2.3815053195227,0.816578034044917,12.66743765534));
#17411=CARTESIAN_POINT('Ctrl Pts',(2.38908231813799,0.794136546107376,12.6658911799632));
#17412=CARTESIAN_POINT('Ctrl Pts',(2.40707461124876,0.738257730667373,12.6620229098741));
#17413=CARTESIAN_POINT('Ctrl Pts',(2.41711073903533,0.704704258671639,12.6596847265558));
#17414=CARTESIAN_POINT('Ctrl Pts',(2.48670743765461,0.453014266688823,12.6420836116566));
#17415=CARTESIAN_POINT('Ctrl Pts',(2.51733680247564,0.227951496130733,12.6261205826785));
#17416=CARTESIAN_POINT('Ctrl Pts',(2.51749934966675,0.00180953791660804,
12.610970894458));
#17417=CARTESIAN_POINT('Ctrl Pts',(2.5174993518837,0.00180645098896169,
12.6109706876588));
#17418=CARTESIAN_POINT('Ctrl Pts',(2.51753502679323,-0.0479106806532836,
12.6076400421281));
#17419=CARTESIAN_POINT('Ctrl Pts',(2.51609793727693,-0.0976210787494668,
12.6043466370876));
#17420=CARTESIAN_POINT('Ctrl Pts',(2.51134124597573,-0.178800545830599,
12.5990304130993));
#17421=CARTESIAN_POINT('Ctrl Pts',(2.50889945893777,-0.210304875616481,
12.5969825419673));
#17422=CARTESIAN_POINT('Ctrl Pts',(2.50439206707403,-0.257025172510051,
12.5939674482425));
#17423=CARTESIAN_POINT('Ctrl Pts',(2.50277941099293,-0.272280740881106,
12.592986394353));
#17424=CARTESIAN_POINT('Ctrl Pts',(2.49970477899756,-0.299025714575572,
12.5912723517902));
#17425=CARTESIAN_POINT('Ctrl Pts',(2.49830278659595,-0.310521422626574,
12.5905375179727));
#17426=CARTESIAN_POINT('Ctrl Pts',(2.4954086528572,-0.332962334552027,12.5891066406945));
#17427=CARTESIAN_POINT('Ctrl Pts',(2.49392370133097,-0.3439081842779,12.5884103894646));
#17428=CARTESIAN_POINT('Ctrl Pts',(2.49082989607196,-0.365638567925284,
12.587031350738));
#17429=CARTESIAN_POINT('Ctrl Pts',(2.48922292550844,-0.376423121792505,
12.5863485205199));
#17430=CARTESIAN_POINT('Ctrl Pts',(2.48527387919882,-0.401793755381892,
12.5847456934798));
#17431=CARTESIAN_POINT('Ctrl Pts',(2.48287336620441,-0.416370434172154,
12.5838275452231));
#17432=CARTESIAN_POINT('Ctrl Pts',(2.47403688916322,-0.467231927160941,
12.5806328050258));
#17433=CARTESIAN_POINT('Ctrl Pts',(2.46693250069783,-0.503396912815185,
12.5783771391568));
#17434=CARTESIAN_POINT('Ctrl Pts',(2.44188583165782,-0.617581774736163,
12.571292907895));
#17435=CARTESIAN_POINT('Ctrl Pts',(2.4210151264175,-0.694910820068047,12.566553177363));
#17436=CARTESIAN_POINT('Ctrl Pts',(2.35621427086737,-0.896299674260321,
12.5542023333951));
#17437=CARTESIAN_POINT('Ctrl Pts',(2.30618943417384,-1.01813028628443,12.5467303653566));
#17438=CARTESIAN_POINT('Ctrl Pts',(2.19889978294303,-1.23043098565515,12.5329781504577));
#17439=CARTESIAN_POINT('Ctrl Pts',(2.14495939077477,-1.32221967013425,12.5267527110818));
#17440=CARTESIAN_POINT('Ctrl Pts',(2.07328091897847,-1.42820841116114,12.518892285439));
#17441=CARTESIAN_POINT('Ctrl Pts',(2.06094819817612,-1.44594795443168,12.5175525565895));
#17442=CARTESIAN_POINT('Ctrl Pts',(2.04309990110297,-1.47092889876943,12.5156280018374));
#17443=CARTESIAN_POINT('Ctrl Pts',(2.03777062349898,-1.47830305116941,12.5150551115847));
#17444=CARTESIAN_POINT('Ctrl Pts',(2.02850160420936,-1.49098328853693,12.5140614088374));
#17445=CARTESIAN_POINT('Ctrl Pts',(2.02458067313543,-1.49630311839935,12.5136418739513));
#17446=CARTESIAN_POINT('Ctrl Pts',(2.01630325866709,-1.50744162532234,12.5127577928314));
#17447=CARTESIAN_POINT('Ctrl Pts',(2.01194250467107,-1.513256898009,12.5122929680561));
#17448=CARTESIAN_POINT('Ctrl Pts',(2.00015559153102,-1.52883429693761,12.5110392410938));
#17449=CARTESIAN_POINT('Ctrl Pts',(1.9926832803624,-1.53856102496411,12.5102472571239));
#17450=CARTESIAN_POINT('Ctrl Pts',(1.95838778671657,-1.58253463224009,12.5066264560169));
#17451=CARTESIAN_POINT('Ctrl Pts',(1.93075240823426,-1.61613526630451,12.5037476749076));
#17452=CARTESIAN_POINT('Ctrl Pts',(1.78284352136868,-1.78676074313925,12.4886066925734));
#17453=CARTESIAN_POINT('Ctrl Pts',(1.64881631912947,-1.91113850022334,12.4758090773104));
#17454=CARTESIAN_POINT('Ctrl Pts',(1.43370485933303,-2.07114820920674,12.4574951990103));
#17455=CARTESIAN_POINT('Ctrl Pts',(1.36230101007205,-2.11879750899754,12.4517145093992));
#17456=CARTESIAN_POINT('Ctrl Pts',(1.25778789962102,-2.18106901929841,12.4436905551074));
#17457=CARTESIAN_POINT('Ctrl Pts',(1.22658834326324,-2.19876640738806,12.4413469831263));
#17458=CARTESIAN_POINT('Ctrl Pts',(1.17056568424307,-2.2289805252545,12.4372288802163));
#17459=CARTESIAN_POINT('Ctrl Pts',(1.14589398531373,-2.24176387660513,12.4354453957186));
#17460=CARTESIAN_POINT('Ctrl Pts',(1.10835981084241,-2.26043016692362,12.4327761325644));
#17461=CARTESIAN_POINT('Ctrl Pts',(1.09565175292343,-2.26661714001533,12.4318798744822));
#17462=CARTESIAN_POINT('Ctrl Pts',(1.0827761806386,-2.27275207823372,12.4309791978059));
#17463=CARTESIAN_POINT('Ctrl Pts',(1.08266030617716,-2.27280727909394,12.4309710927155));
#17464=CARTESIAN_POINT('Ctrl Pts',(1.08242158526773,-2.2729209797659,12.4309543961035));
#17465=CARTESIAN_POINT('Ctrl Pts',(1.0822987383012,-2.27297947847866,12.4309458046201));
#17466=CARTESIAN_POINT('Ctrl Pts',(1.0820456281083,-2.27309998229397,12.4309281043788));
#17467=CARTESIAN_POINT('Ctrl Pts',(1.08191536428114,-2.27316198616499,12.4309189956628));
#17468=CARTESIAN_POINT('Ctrl Pts',(1.08164694547373,-2.27328972169295,12.4309002280064));
#17469=CARTESIAN_POINT('Ctrl Pts',(1.08150878982745,-2.27335545195498,12.430890569114));
#17470=CARTESIAN_POINT('Ctrl Pts',(1.08122407962554,-2.2734908765978,12.4308706658953));
#17471=CARTESIAN_POINT('Ctrl Pts',(1.08107752432224,-2.27356056940229,12.4308604216237));
#17472=CARTESIAN_POINT('Ctrl Pts',(1.08077547179291,-2.2737041714376,12.4308393100165));
#17473=CARTESIAN_POINT('Ctrl Pts',(1.08061997372362,-2.27377807888799,12.4308284427426));
#17474=CARTESIAN_POINT('Ctrl Pts',(1.08029945483932,-2.27393037959636,12.430806044908));
#17475=CARTESIAN_POINT('Ctrl Pts',(1.08013443305777,-2.27400877084948,12.4307945144158));
#17476=CARTESIAN_POINT('Ctrl Pts',(1.07979424537833,-2.27417032678893,12.4307707471446));
#17477=CARTESIAN_POINT('Ctrl Pts',(1.07961907840034,-2.27425348920332,12.4307585104438));
#17478=CARTESIAN_POINT('Ctrl Pts',(1.07925793555186,-2.27442489454415,12.4307332847866));
#17479=CARTESIAN_POINT('Ctrl Pts',(1.07907195845855,-2.27451313490213,12.4307202959186));
#17480=CARTESIAN_POINT('Ctrl Pts',(1.07868848418916,-2.27469502392142,12.4306935167885));
#17481=CARTESIAN_POINT('Ctrl Pts',(1.0784909856272,-2.27478866967816,12.4306797266263));
#17482=CARTESIAN_POINT('Ctrl Pts',(1.0780837076643,-2.27498171930179,12.4306512923904));
#17483=CARTESIAN_POINT('Ctrl Pts',(1.07787392670094,-2.27508111987834,12.4306366484301));
#17484=CARTESIAN_POINT('Ctrl Pts',(1.07744127037446,-2.27528605228095,12.4306064504874));
#17485=CARTESIAN_POINT('Ctrl Pts',(1.07721839324281,-2.27539158038124,12.4305908966333));
#17486=CARTESIAN_POINT('Ctrl Pts',(1.07675867490992,-2.27560916562066,12.430558818982));
#17487=CARTESIAN_POINT('Ctrl Pts',(1.07652183169936,-2.27572121854266,12.4305422953296));
#17488=CARTESIAN_POINT('Ctrl Pts',(1.07613177902632,-2.2759056818959,12.4305150869449));
#17489=CARTESIAN_POINT('Ctrl Pts',(1.07597857978567,-2.27597811381367,12.4305044014736));
#17490=CARTESIAN_POINT('Ctrl Pts',(1.07562125605292,-2.27614701073974,12.4304794809875));
#17491=CARTESIAN_POINT('Ctrl Pts',(1.07541712587571,-2.27624346376778,12.4304652463851));
#17492=CARTESIAN_POINT('Ctrl Pts',(1.06471534816574,-2.28129837247681,12.4297190767861));
#17493=CARTESIAN_POINT('Ctrl Pts',(1.05418340088328,-2.28618424486074,12.4289896462315));
#17494=CARTESIAN_POINT('Ctrl Pts',(1.03052184163024,-2.29696279448139,12.4273616186799));
#17495=CARTESIAN_POINT('Ctrl Pts',(1.01737467487582,-2.30281613026747,12.426464379949));
#17496=CARTESIAN_POINT('Ctrl Pts',(0.983780310747627,-2.31742903458171,
12.4241898681064));
#17497=CARTESIAN_POINT('Ctrl Pts',(0.9632656275026,-2.32603104222524,12.4228179060099));
#17498=CARTESIAN_POINT('Ctrl Pts',(0.792808776154341,-2.39486330421806,
12.411551077741));
#17499=CARTESIAN_POINT('Ctrl Pts',(0.637494800194419,-2.44080433708856,
12.4021620679572));
#17500=CARTESIAN_POINT('Ctrl Pts',(0.357381015113579,-2.49507288997588,
12.3857481191458));
#17501=CARTESIAN_POINT('Ctrl Pts',(0.23436924749912,-2.50961700859083,12.3786973985936));
#17502=CARTESIAN_POINT('Ctrl Pts',(0.0667511149687532,-2.51700102679946,
12.3687782844453));
#17503=CARTESIAN_POINT('Ctrl Pts',(0.022666244979773,-2.51778388432851,
12.3661395576425));
#17504=CARTESIAN_POINT('Ctrl Pts',(-0.0494487216010663,-2.51717045189379,
12.3617419375182));
#17505=CARTESIAN_POINT('Ctrl Pts',(-0.077476295193672,-2.51646369580423,
12.3600127161011));
#17506=CARTESIAN_POINT('Ctrl Pts',(-0.115552088885675,-2.51486689357172,
12.3576292104596));
#17507=CARTESIAN_POINT('Ctrl Pts',(-0.125616505973406,-2.51438427114253,
12.3569959223817));
#17508=CARTESIAN_POINT('Ctrl Pts',(-0.142457978641892,-2.51347529974156,
12.3559303266728));
#17509=CARTESIAN_POINT('Ctrl Pts',(-0.14923682384159,-2.51308191800922,
12.3554998207836));
#17510=CARTESIAN_POINT('Ctrl Pts',(-0.162111950565015,-2.51228248704699,
12.3546789893125));
#17511=CARTESIAN_POINT('Ctrl Pts',(-0.168208496366009,-2.51188166104113,
12.3542889688832));
#17512=CARTESIAN_POINT('Ctrl Pts',(-0.182696756992745,-2.51087612837025,
12.353358993859));
#17513=CARTESIAN_POINT('Ctrl Pts',(-0.191086955732838,-2.51025154269353,
12.3528179661915));
#17514=CARTESIAN_POINT('Ctrl Pts',(-0.220758851074861,-2.50789307959591,
12.3508962330294));
#17515=CARTESIAN_POINT('Ctrl Pts',(-0.242020777320876,-2.50593057393651,
12.3495039009692));
#17516=CARTESIAN_POINT('Ctrl Pts',(-0.400500327497464,-2.48926705164925,
12.3390242943463));
#17517=CARTESIAN_POINT('Ctrl Pts',(-0.536314863442209,-2.4635767446743,
12.3294871342398));
#17518=CARTESIAN_POINT('Ctrl Pts',(-0.796167652203041,-2.39191049262016,
12.31086467475));
#17519=CARTESIAN_POINT('Ctrl Pts',(-0.920082980298449,-2.3470347978668,
12.3018081875349));
#17520=CARTESIAN_POINT('Ctrl Pts',(-1.08552342765433,-2.27199284000306,
12.2896710729925));
#17521=CARTESIAN_POINT('Ctrl Pts',(-1.13049101877052,-2.24995626269979,
12.2863652080218));
#17522=CARTESIAN_POINT('Ctrl Pts',(-1.20680989961236,-2.20968959398645,
12.2807434875941));
#17523=CARTESIAN_POINT('Ctrl Pts',(-1.2384784677822,-2.19209706516752,12.2784072668224));
#17524=CARTESIAN_POINT('Ctrl Pts',(-1.28344736547907,-2.16583020015199,
12.2750831676069));
#17525=CARTESIAN_POINT('Ctrl Pts',(-1.29706138900641,-2.15770465257502,
12.2740759007525));
#17526=CARTESIAN_POINT('Ctrl Pts',(-1.32066558176627,-2.14331232190712,
12.2723275885426));
#17527=CARTESIAN_POINT('Ctrl Pts',(-1.33069004234187,-2.13710301739542,
12.2715844916702));
#17528=CARTESIAN_POINT('Ctrl Pts',(-1.35128588144678,-2.12414453542423,
12.2700563279025));
#17529=CARTESIAN_POINT('Ctrl Pts',(-1.36185120870613,-2.11738632166915,
12.2692716189572));
#17530=CARTESIAN_POINT('Ctrl Pts',(-1.388829843696,-2.09984370663774,12.2672655363098));
#17531=CARTESIAN_POINT('Ctrl Pts',(-1.40516845638597,-2.08894556418483,
12.2660484007814));
#17532=CARTESIAN_POINT('Ctrl Pts',(-1.46979862521322,-2.04473467245724,
12.2612227813788));
#17533=CARTESIAN_POINT('Ctrl Pts',(-1.5170489259708,-2.00992816639374,12.2576705057414));
#17534=CARTESIAN_POINT('Ctrl Pts',(-1.72579779442693,-1.84459582756289,
12.2417770952425));
#17535=CARTESIAN_POINT('Ctrl Pts',(-1.87197322476266,-1.69606194493632,
12.2301558254995));
#17536=CARTESIAN_POINT('Ctrl Pts',(-2.03645719747082,-1.48141591856693,
12.2143912886018));
#17537=CARTESIAN_POINT('Ctrl Pts',(-2.07277844330027,-1.43015367259183,
12.210685005293));
#17538=CARTESIAN_POINT('Ctrl Pts',(-2.12034694811258,-1.35739358746677,
12.2054259727978));
#17539=CARTESIAN_POINT('Ctrl Pts',(-2.13325974157092,-1.33700834659444,
12.2039526674916));
#17540=CARTESIAN_POINT('Ctrl Pts',(-2.15521342002102,-1.30122255840699,
12.2013608065886));
#17541=CARTESIAN_POINT('Ctrl Pts',(-2.16438734261813,-1.28590529261611,
12.2002497016387));
#17542=CARTESIAN_POINT('Ctrl Pts',(-2.17765003278284,-1.26321716174244,
12.1985994297712));
#17543=CARTESIAN_POINT('Ctrl Pts',(-2.18186617108675,-1.25592088509911,
12.1980680435391));
#17544=CARTESIAN_POINT('Ctrl Pts',(-2.18928143734325,-1.24293829535928,
12.197121079376));
#17545=CARTESIAN_POINT('Ctrl Pts',(-2.19249519720356,-1.23726053310948,
12.1967064402557));
#17546=CARTESIAN_POINT('Ctrl Pts',(-2.19942742888982,-1.22490150561083,
12.1958027379516));
#17547=CARTESIAN_POINT('Ctrl Pts',(-2.20313748731257,-1.21821587648048,
12.1953131832861));
#17548=CARTESIAN_POINT('Ctrl Pts',(-2.21336956741047,-1.19957776227024,
12.1939466987359));
#17549=CARTESIAN_POINT('Ctrl Pts',(-2.21982504902044,-1.18758931534281,
12.1930658007409));
#17550=CARTESIAN_POINT('Ctrl Pts',(-2.25558281238821,-1.1198734739857,12.1880817056283));
#17551=CARTESIAN_POINT('Ctrl Pts',(-2.28288131199852,-1.06311895953314,
12.1838729962112));
#17552=CARTESIAN_POINT('Ctrl Pts',(-2.39800619574733,-0.798837093132328,
12.1643198150031));
#17553=CARTESIAN_POINT('Ctrl Pts',(-2.45986770478959,-0.581076485295152,
12.1484505317142));
#17554=CARTESIAN_POINT('Ctrl Pts',(-2.49856032727949,-0.311746033951842,
12.1303222117129));
#17555=CARTESIAN_POINT('Ctrl Pts',(-2.50391599256939,-0.26531953030825,
12.1272439758556));
#17556=CARTESIAN_POINT('Ctrl Pts',(-2.51096291740736,-0.18453306064284,
12.1219686601374));
#17557=CARTESIAN_POINT('Ctrl Pts',(-2.51324803412135,-0.150238917919318,
12.1197544124582));
#17558=CARTESIAN_POINT('Ctrl Pts',(-2.51554529255956,-0.100395507988638,
12.1165711760848));
#17559=CARTESIAN_POINT('Ctrl Pts',(-2.51611670303056,-0.0848771540916381,
12.1155849997241));
#17560=CARTESIAN_POINT('Ctrl Pts',(-2.51686795494256,-0.0576176892375606,
12.113861013185));
#17561=CARTESIAN_POINT('Ctrl Pts',(-2.51710930161321,-0.0458788841228253,
12.1131213177217));
#17562=CARTESIAN_POINT('Ctrl Pts',(-2.51741935106567,-0.0230168916542543,
12.1116858325763));
#17563=CARTESIAN_POINT('Ctrl Pts',(-2.51749647525531,-0.0118941091298984,
12.1109897988483));
#17564=CARTESIAN_POINT('Ctrl Pts',(-2.51750563405195,0.0180101399364491,
12.109124590416));
#17565=CARTESIAN_POINT('Ctrl Pts',(-2.51730121793708,0.036791174643719,
12.1079596596674));
#17566=CARTESIAN_POINT('Ctrl Pts',(-2.5157390714679,0.107546023137503,12.1035937154676));
#17567=CARTESIAN_POINT('Ctrl Pts',(-2.51298161306114,0.159477908940482,
12.1004358860706));
#17568=CARTESIAN_POINT('Ctrl Pts',(-2.49057414599155,0.425518691437462,
12.0844327093301));
#17569=CARTESIAN_POINT('Ctrl Pts',(-2.44516671392129,0.636540634410002,
12.0724081630507));
#17570=CARTESIAN_POINT('Ctrl Pts',(-2.35230662518016,0.899167255119664,
12.05617656775));
#17571=CARTESIAN_POINT('Ctrl Pts',(-2.32885134072189,0.958278965263406,
12.0524268683046));
#17572=CARTESIAN_POINT('Ctrl Pts',(-2.28857712867055,1.04953807732663,12.0463938697484));
#17573=CARTESIAN_POINT('Ctrl Pts',(-2.27325727258668,1.08231996759801,12.0441754055428));
#17574=CARTESIAN_POINT('Ctrl Pts',(-2.25233428925201,1.12468622344181,12.0412261952961));
#17575=CARTESIAN_POINT('Ctrl Pts',(-2.24736597711045,1.13458142328223,12.0405314138683));
#17576=CARTESIAN_POINT('Ctrl Pts',(-2.23914821849367,1.15068265638373,12.0393906069351));
#17577=CARTESIAN_POINT('Ctrl Pts',(-2.23593779605627,1.15690859163188,12.0389469584269));
#17578=CARTESIAN_POINT('Ctrl Pts',(-2.22962375471788,1.16902888690866,12.0380781890607));
#17579=CARTESIAN_POINT('Ctrl Pts',(-2.22652266056816,1.1749244504983,12.0376532235637));
#17580=CARTESIAN_POINT('Ctrl Pts',(-2.21954745574235,1.18805839315335,12.0367012914962));
#17581=CARTESIAN_POINT('Ctrl Pts',(-2.21566126416068,1.19529026260172,12.0361735846493));
#17582=CARTESIAN_POINT('Ctrl Pts',(-2.20211180975773,1.22021150702354,12.0343431311956));
#17583=CARTESIAN_POINT('Ctrl Pts',(-2.19227180478373,1.23780322277386,12.0330301104735));
#17584=CARTESIAN_POINT('Ctrl Pts',(-2.09862745198669,1.40059854144838,12.0206963188929));
#17585=CARTESIAN_POINT('Ctrl Pts',(-2.00073227821853,1.53719730463512,12.0090094862668));
#17586=CARTESIAN_POINT('Ctrl Pts',(-1.78975632717178,1.77696523595894,11.986986982023));
#17587=CARTESIAN_POINT('Ctrl Pts',(-1.67940565642236,1.88160644656731,11.9766721875944));
#17588=CARTESIAN_POINT('Ctrl Pts',(-1.53072294342952,1.99902788093899,11.9643152105487));
#17589=CARTESIAN_POINT('Ctrl Pts',(-1.50063967009827,2.02170869046113,11.9618837438889));
#17590=CARTESIAN_POINT('Ctrl Pts',(-1.45698744941406,2.05310813846939,11.9584502701666));
#17591=CARTESIAN_POINT('Ctrl Pts',(-1.44382744411486,2.06238400577086,11.9574270700946));
#17592=CARTESIAN_POINT('Ctrl Pts',(-1.42084297667296,2.07825683821559,11.9556602249378));
#17593=CARTESIAN_POINT('Ctrl Pts',(-1.41105943497202,2.08491187551337,11.9549144013992));
#17594=CARTESIAN_POINT('Ctrl Pts',(-1.39211855634074,2.09760159120119,11.9534823155637));
#17595=CARTESIAN_POINT('Ctrl Pts',(-1.38296801366096,2.10364588027217,11.9527957054004));
#17596=CARTESIAN_POINT('Ctrl Pts',(-1.35873721185581,2.11942482822684,11.9509911208822));
#17597=CARTESIAN_POINT('Ctrl Pts',(-1.34359166138221,2.12905845078916,11.9498768913881));
#17598=CARTESIAN_POINT('Ctrl Pts',(-1.28903641282525,2.16294535374278,11.9459107727317));
#17599=CARTESIAN_POINT('Ctrl Pts',(-1.24906136172821,2.18627390772019,11.943092297764));
#17600=CARTESIAN_POINT('Ctrl Pts',(-1.03619038619005,2.30275488909154,11.928490026143));
#17601=CARTESIAN_POINT('Ctrl Pts',(-0.853483432444309,2.37653967113284,
11.9173951817837));
#17602=CARTESIAN_POINT('Ctrl Pts',(-0.549542208086691,2.45965488016427,
11.8991886437835));
#17603=CARTESIAN_POINT('Ctrl Pts',(-0.432977306254001,2.48282542438193,
11.8922420461293));
#17604=CARTESIAN_POINT('Ctrl Pts',(-0.300339401330266,2.49956551554975,
11.883954204494));
#17605=CARTESIAN_POINT('Ctrl Pts',(-0.285432359299889,2.50131162899133,
11.8830172981414));
#17606=CARTESIAN_POINT('Ctrl Pts',(-0.262696777090993,2.50376884495363,
11.8815788692959));
#17607=CARTESIAN_POINT('Ctrl Pts',(-0.254878747263481,2.50457677979402,
11.8810825320049));
#17608=CARTESIAN_POINT('Ctrl Pts',(-0.240580866398312,2.50598672129961,
11.8801714830977));
#17609=CARTESIAN_POINT('Ctrl Pts',(-0.234102332032966,2.50660022660675,
11.8797574124748));
#17610=CARTESIAN_POINT('Ctrl Pts',(-0.219499358210026,2.50792599452817,
11.8788212279609));
#17611=CARTESIAN_POINT('Ctrl Pts',(-0.211373855558783,2.50862389588986,
11.8782983454335));
#17612=CARTESIAN_POINT('Ctrl Pts',(-0.190415326690593,2.51032148140501,
11.8769448352744));
#17613=CARTESIAN_POINT('Ctrl Pts',(-0.177577943914144,2.51126223125455,
11.8761111444935));
#17614=CARTESIAN_POINT('Ctrl Pts',(-0.0932844055489619,2.51678988008789,
11.8706088792076));
#17615=CARTESIAN_POINT('Ctrl Pts',(-0.0216737556048522,2.51842442015186,
11.865803100985));
#17616=CARTESIAN_POINT('Ctrl Pts',(0.210711685160005,2.51381718642206,11.8499739571947));
#17617=CARTESIAN_POINT('Ctrl Pts',(0.370847228036938,2.4952258230688,11.8387296494322));
#17618=CARTESIAN_POINT('Ctrl Pts',(0.605543147010275,2.44487096587333,11.8223839959206));
#17619=CARTESIAN_POINT('Ctrl Pts',(0.682144917858804,2.4246147732719,11.8170652946829));
#17620=CARTESIAN_POINT('Ctrl Pts',(0.790124429806865,2.39053713573412,11.8096113396093));
#17621=CARTESIAN_POINT('Ctrl Pts',(0.822368541463098,2.3796374880917,11.807390847196));
#17622=CARTESIAN_POINT('Ctrl Pts',(0.879654885388384,2.35896912522589,11.8034547681283));
#17623=CARTESIAN_POINT('Ctrl Pts',(0.90477991607114,2.34944705110204,11.8017315766919));
#17624=CARTESIAN_POINT('Ctrl Pts',(0.942841717193832,2.33432094043054,11.799125008086));
#17625=CARTESIAN_POINT('Ctrl Pts',(0.955891209509325,2.32900767824665,11.7982320454753));
#17626=CARTESIAN_POINT('Ctrl Pts',(0.978557491738719,2.31955622231094,11.7966820251234));
#17627=CARTESIAN_POINT('Ctrl Pts',(0.988194247505063,2.31546711650916,11.7960233413012));
#17628=CARTESIAN_POINT('Ctrl Pts',(1.00985878932688,2.30611444599358,11.7945431320623));
#17629=CARTESIAN_POINT('Ctrl Pts',(1.02187153075751,2.30081663706743,11.7937227850175));
#17630=CARTESIAN_POINT('Ctrl Pts',(1.05420796992306,2.28625254385818,11.791515287711));
#17631=CARTESIAN_POINT('Ctrl Pts',(1.07445098825068,2.27680922816071,11.7901341816849));
#17632=CARTESIAN_POINT('Ctrl Pts',(1.1719490907979,2.22973665045761,11.7834823499358));
#17633=CARTESIAN_POINT('Ctrl Pts',(1.2473732837918,2.18843605192168,11.7783394901813));
#17634=CARTESIAN_POINT('Ctrl Pts',(1.47325578203325,2.0492674530745,11.7627389764816));
#17635=CARTESIAN_POINT('Ctrl Pts',(1.6154678040361,1.93913398330687,11.7526594674976));
#17636=CARTESIAN_POINT('Ctrl Pts',(1.7879213438161,1.77333785295166,11.7386881385616));
#17637=CARTESIAN_POINT('Ctrl Pts',(1.82957964465381,1.73032576995872,11.735148398652));
#17638=CARTESIAN_POINT('Ctrl Pts',(1.88532101746347,1.66850761226299,11.7301071947024));
#17639=CARTESIAN_POINT('Ctrl Pts',(1.900736108857,1.65092554495815,11.7286782693222));
#17640=CARTESIAN_POINT('Ctrl Pts',(1.92720737005179,1.61987087061507,11.7261575781324));
#17641=CARTESIAN_POINT('Ctrl Pts',(1.93837289870792,1.60649318428139,11.7250727163868));
#17642=CARTESIAN_POINT('Ctrl Pts',(1.95467852464292,1.58653955128484,11.7234541977783));
#17643=CARTESIAN_POINT('Ctrl Pts',(1.95992650285732,1.58005189192766,11.7229278992065));
#17644=CARTESIAN_POINT('Ctrl Pts',(1.9688284828509,1.56893449215492,11.7220256883112));
#17645=CARTESIAN_POINT('Ctrl Pts',(1.97249861878599,1.56431781732018,11.7216509274027));
#17646=CARTESIAN_POINT('Ctrl Pts',(1.98077255356866,1.55383459544008,11.7207996534618));
#17647=CARTESIAN_POINT('Ctrl Pts',(1.98536643734936,1.54796058249875,11.7203224770519));
#17648=CARTESIAN_POINT('Ctrl Pts',(1.99776668440484,1.53195888810345,11.7190222725349));
#17649=CARTESIAN_POINT('Ctrl Pts',(2.00552196937138,1.52179215869184,11.7181958552676));
#17650=CARTESIAN_POINT('Ctrl Pts',(2.04383477821429,1.4707647702427,11.7140482184999));
#17651=CARTESIAN_POINT('Ctrl Pts',(2.07322046900851,1.42904362688158,11.7106578205151));
#17652=CARTESIAN_POINT('Ctrl Pts',(2.18455839123274,1.26030034281833,11.6970353900391));
#17653=CARTESIAN_POINT('Ctrl Pts',(2.25626729808039,1.12690223291128,11.6864831710867));
#17654=CARTESIAN_POINT('Ctrl Pts',(2.3318083941289,0.949835152145914,11.673258922542));
#17655=CARTESIAN_POINT('Ctrl Pts',(2.34709396730031,0.911408123072879,11.6704314740495));
#17656=CARTESIAN_POINT('Ctrl Pts',(2.36142193605295,0.872635485141376,11.6676249231292));
#17657=CARTESIAN_POINT('Origin',(0.,0.,10.));
#17658=CARTESIAN_POINT('',(2.3614219719961,0.872635387876314,10.6673175101421));
#17659=CARTESIAN_POINT('',(2.36142200728636,0.872635292378011,10.9438346412346));
#17660=CARTESIAN_POINT('',(2.36142200728636,0.87263529237802,10.));
#17661=CARTESIAN_POINT('',(2.51749968066629,-0.00126800833144993,11.8874166975493));
#17662=CARTESIAN_POINT('Ctrl Pts',(2.36142200728636,0.872635292378011,10.9438346412346));
#17663=CARTESIAN_POINT('Ctrl Pts',(2.33271572526319,0.95031682406596,10.9490804874489));
#17664=CARTESIAN_POINT('Ctrl Pts',(2.30013331963894,1.02668572932892,10.9543263336633));
#17665=CARTESIAN_POINT('Ctrl Pts',(2.26381902291199,1.10133086831425,10.9595721798777));
#17666=CARTESIAN_POINT('Ctrl Pts',(2.22754127086672,1.17590088859732,10.9648127469651));
#17667=CARTESIAN_POINT('Ctrl Pts',(2.1875392926656,1.24875017705897,10.9700533140526));
#17668=CARTESIAN_POINT('Ctrl Pts',(2.14400555146569,1.31948719026912,10.9752938811401));
#17669=CARTESIAN_POINT('Ctrl Pts',(2.10049529828321,1.39018603831924,10.9805316207533));
#17670=CARTESIAN_POINT('Ctrl Pts',(2.05345730675966,1.45877448166034,10.9857693603666));
#17671=CARTESIAN_POINT('Ctrl Pts',(2.00312957846779,1.52488627178143,10.9910070999799));
#17672=CARTESIAN_POINT('Ctrl Pts',(1.95281382251523,1.59098233473161,10.9962435936001));
#17673=CARTESIAN_POINT('Ctrl Pts',(1.89921016379548,1.65460254786909,11.0014800872204));
#17674=CARTESIAN_POINT('Ctrl Pts',(1.84259864664381,1.71541146008367,11.0067165808407));
#17675=CARTESIAN_POINT('Ctrl Pts',(1.78598352026102,1.77622424913162,11.0119534083103));
#17676=CARTESIAN_POINT('Ctrl Pts',(1.72636047011587,1.8342250446018,11.0171902357799));
#17677=CARTESIAN_POINT('Ctrl Pts',(1.66404741004881,1.88911420171197,11.0224270632495));
#17678=CARTESIAN_POINT('Ctrl Pts',(1.60167005533702,1.9440599934803,11.0276692940801));
#17679=CARTESIAN_POINT('Ctrl Pts',(1.53659749523301,1.99588743011063,11.0329115249107));
#17680=CARTESIAN_POINT('Ctrl Pts',(1.46918144404333,2.04433660009274,11.0381537557414));
#17681=CARTESIAN_POINT('Ctrl Pts',(1.40172945738266,2.09281159543413,11.0433987808922));
#17682=CARTESIAN_POINT('Ctrl Pts',(1.33193187978792,2.1379044875086,11.048643806043));
#17683=CARTESIAN_POINT('Ctrl Pts',(1.2601681220195,2.17939958572214,11.0538888311939));
#17684=CARTESIAN_POINT('Ctrl Pts',(1.18828032022182,2.22096640842917,11.059142922398));
#17685=CARTESIAN_POINT('Ctrl Pts',(1.11441996076285,2.258922804603,11.0643970136022));
#17686=CARTESIAN_POINT('Ctrl Pts',(1.03898945011338,2.29309990461669,11.0696511048063));
#17687=CARTESIAN_POINT('Ctrl Pts',(0.982025108734673,2.31891009701432,11.0736189401346));
#17688=CARTESIAN_POINT('Ctrl Pts',(0.924165769894775,2.34256589081392,11.0775867754629));
#17689=CARTESIAN_POINT('Ctrl Pts',(0.865590384616456,2.36401343821467,11.0815546107913));
#17690=CARTESIAN_POINT('Ctrl Pts',(0.788009478833835,2.39241991213302,11.0868098601986));
#17691=CARTESIAN_POINT('Ctrl Pts',(0.708885477546035,2.41705578739816,11.0920651096059));
#17692=CARTESIAN_POINT('Ctrl Pts',(0.628619422757704,2.43775385782317,11.0973203590132));
#17693=CARTESIAN_POINT('Ctrl Pts',(0.548467167000818,2.45842258308636,11.1025681576707));
#17694=CARTESIAN_POINT('Ctrl Pts',(0.467176516969301,2.47516447854801,11.1078159563282));
#17695=CARTESIAN_POINT('Ctrl Pts',(0.385166524084973,2.48786112930853,11.1130637549857));
#17696=CARTESIAN_POINT('Ctrl Pts',(0.302562298101252,2.5006497782496,11.1183495784686));
#17697=CARTESIAN_POINT('Ctrl Pts',(0.219228705756461,2.50933414962652,11.1236354019515));
#17698=CARTESIAN_POINT('Ctrl Pts',(0.135607525172923,2.51384503283645,11.1289212254344));
#17699=CARTESIAN_POINT('Ctrl Pts',(0.0527361699436561,2.51831546726799,
11.134159651303));
#17700=CARTESIAN_POINT('Ctrl Pts',(-0.0304171673727481,2.51868693520644,
11.1393980771716));
#17701=CARTESIAN_POINT('Ctrl Pts',(-0.113416093058638,2.51494394367654,
11.1446365030402));
#17702=CARTESIAN_POINT('Ctrl Pts',(-0.196387721779181,2.51120218315426,
11.1498732060777));
#17703=CARTESIAN_POINT('Ctrl Pts',(-0.279204579139248,2.50334867141901,
11.1551099091152));
#17704=CARTESIAN_POINT('Ctrl Pts',(-0.361431247096957,2.49142001750446,
11.1603466121527));
#17705=CARTESIAN_POINT('Ctrl Pts',(-0.443655675241373,2.47949168852048,
11.165583172545));
#17706=CARTESIAN_POINT('Ctrl Pts',(-0.525289489454989,2.46348850532878,
11.1708197329373));
#17707=CARTESIAN_POINT('Ctrl Pts',(-0.605904746066285,2.44349865739565,
11.1760562933297));
#17708=CARTESIAN_POINT('Ctrl Pts',(-0.687839457124779,2.42318162953576,
11.1813785621001));
#17709=CARTESIAN_POINT('Ctrl Pts',(-0.768721487248743,2.39874636322141,
11.1867008308706));
#17710=CARTESIAN_POINT('Ctrl Pts',(-0.848116588526167,2.37033847841753,
11.1920230996411));
#17711=CARTESIAN_POINT('Ctrl Pts',(-0.926345317708214,2.34234792621466,
11.1972671803914));
#17712=CARTESIAN_POINT('Ctrl Pts',(-1.00313010739058,2.31050093807348,11.2025112611417));
#17713=CARTESIAN_POINT('Ctrl Pts',(-1.07807656706871,2.27498509127804,11.2077553418921));
#17714=CARTESIAN_POINT('Ctrl Pts',(-1.15469917808144,2.23867494500185,11.2131167046726));
#17715=CARTESIAN_POINT('Ctrl Pts',(-1.22939978860919,2.19853009672522,11.2184780674532));
#17716=CARTESIAN_POINT('Ctrl Pts',(-1.30178609528692,2.15479911177763,11.2238394302337));
#17717=CARTESIAN_POINT('Ctrl Pts',(-1.37417240196464,2.11106812683003,11.2292007930143));
#17718=CARTESIAN_POINT('Ctrl Pts',(-1.44424402108168,2.06375134491811,11.2345621557948));
#17719=CARTESIAN_POINT('Ctrl Pts',(-1.51164419791891,2.0131413434973,11.2399235185753));
#17720=CARTESIAN_POINT('Ctrl Pts',(-1.57771037435095,1.96353302731782,11.2451787679827));
#17721=CARTESIAN_POINT('Ctrl Pts',(-1.6414539424788,1.91057746621052,11.25043401739));
#17722=CARTESIAN_POINT('Ctrl Pts',(-1.70251630309735,1.85452001544543,11.2556892667973));
#17723=CARTESIAN_POINT('Ctrl Pts',(-1.76349209116024,1.79854204141082,11.2609370654547));
#17724=CARTESIAN_POINT('Ctrl Pts',(-1.82179388522027,1.73947122242578,11.2661848641122));
#17725=CARTESIAN_POINT('Ctrl Pts',(-1.87709420657246,1.67759458441308,11.2714326627697));
#17726=CARTESIAN_POINT('Ctrl Pts',(-1.9327952264274,1.61526959681397,11.2767184862526));
#17727=CARTESIAN_POINT('Ctrl Pts',(-1.98545071457912,1.55009824201138,11.2820043097356));
#17728=CARTESIAN_POINT('Ctrl Pts',(-2.03476209091959,1.48241339826532,11.2872901332185));
#17729=CARTESIAN_POINT('Ctrl Pts',(-2.08363129555214,1.41533547984118,11.2925285590871));
#17730=CARTESIAN_POINT('Ctrl Pts',(-2.12921584430058,1.34578934831197,11.2977669849556));
#17731=CARTESIAN_POINT('Ctrl Pts',(-2.171265146536,1.27413261218682,11.3030054108242));
#17732=CARTESIAN_POINT('Ctrl Pts',(-2.21330061945572,1.20249944276962,11.3082421138617));
#17733=CARTESIAN_POINT('Ctrl Pts',(-2.2518029216706,1.12875744500906,11.3134788168993));
#17734=CARTESIAN_POINT('Ctrl Pts',(-2.28656569652305,1.05329177604502,11.3187155199368));
#17735=CARTESIAN_POINT('Ctrl Pts',(-2.32132752445488,0.977828162728087,
11.3239520803291));
#17736=CARTESIAN_POINT('Ctrl Pts',(-2.35234983543744,0.900641391085434,
11.3291886407214));
#17737=CARTESIAN_POINT('Ctrl Pts',(-2.37947360751471,0.82213843185982,11.3344252011138));
#17738=CARTESIAN_POINT('Ctrl Pts',(-2.40704132262709,0.742350590801221,
11.3397474698842));
#17739=CARTESIAN_POINT('Ctrl Pts',(-2.43058155731725,0.661203549034004,
11.3450697386547));
#17740=CARTESIAN_POINT('Ctrl Pts',(-2.44998002953474,0.579140833373839,
11.3503920074252));
#17741=CARTESIAN_POINT('Ctrl Pts',(-2.46909352401022,0.498283679015128,
11.3556360881755));
#17742=CARTESIAN_POINT('Ctrl Pts',(-2.4841861146577,0.416538047402362,11.3608801689259));
#17743=CARTESIAN_POINT('Ctrl Pts',(-2.49520041333004,0.334336876993229,
11.3661242496762));
#17744=CARTESIAN_POINT('Ctrl Pts',(-2.5064610429365,0.250297306183437,11.3714856124568));
#17745=CARTESIAN_POINT('Ctrl Pts',(-2.51345871792463,0.165782085062312,
11.3768469752373));
#17746=CARTESIAN_POINT('Ctrl Pts',(-2.51618834279567,0.081255606447549,
11.3822083380179));
#17747=CARTESIAN_POINT('Ctrl Pts',(-2.51891796766671,-0.00327087216720202,
11.3875697007985));
#17748=CARTESIAN_POINT('Ctrl Pts',(-2.51737961845211,-0.0878081014682281,
11.392931063579));
#17749=CARTESIAN_POINT('Ctrl Pts',(-2.51162447120054,-0.171897544097102,
11.3982924263596));
#17750=CARTESIAN_POINT('Ctrl Pts',(-2.50598323119857,-0.254322668384312,
11.4035476757669));
#17751=CARTESIAN_POINT('Ctrl Pts',(-2.4962698002576,-0.336622019470591,
11.4088029251742));
#17752=CARTESIAN_POINT('Ctrl Pts',(-2.4824947405883,-0.418361223049447,
11.4140581745815));
#17753=CARTESIAN_POINT('Ctrl Pts',(-2.46873921082429,-0.499984539006543,
11.419305973239));
#17754=CARTESIAN_POINT('Ctrl Pts',(-2.45093356636752,-0.581048833684736,
11.4245537718965));
#17755=CARTESIAN_POINT('Ctrl Pts',(-2.42914026605553,-0.661123148760993,
11.429801570554));
#17756=CARTESIAN_POINT('Ctrl Pts',(-2.40718905449474,-0.741777671282183,
11.4350873940369));
#17757=CARTESIAN_POINT('Ctrl Pts',(-2.38119218759287,-0.821427334373664,
11.4403732175198));
#17758=CARTESIAN_POINT('Ctrl Pts',(-2.35126631866039,-0.899640455255999,
11.4456590410027));
#17759=CARTESIAN_POINT('Ctrl Pts',(-2.32160879292897,-0.977152244482109,
11.4508974668713));
#17760=CARTESIAN_POINT('Ctrl Pts',(-2.28809261306326,-1.05325271217118,
11.4561358927399));
#17761=CARTESIAN_POINT('Ctrl Pts',(-2.25088130386272,-1.1275369643259,11.4613743186085));
#17762=CARTESIAN_POINT('Ctrl Pts',(-2.21368223284249,-1.20179678562636,
11.466611021646));
#17763=CARTESIAN_POINT('Ctrl Pts',(-2.17279065257139,-1.27424116548086,
11.4718477246835));
#17764=CARTESIAN_POINT('Ctrl Pts',(-2.1284172786826,-1.34448731411098,11.477084427721));
#17765=CARTESIAN_POINT('Ctrl Pts',(-2.08404511350235,-1.41473154927109,
11.4823209881133));
#17766=CARTESIAN_POINT('Ctrl Pts',(-2.03619159057178,-1.4827772827042,11.4875575485057));
#17767=CARTESIAN_POINT('Ctrl Pts',(-1.985111494058,-1.54826955216423,11.492794108898));
#17768=CARTESIAN_POINT('Ctrl Pts',(-1.93319535405385,-1.61483375353685,
11.4981163776685));
#17769=CARTESIAN_POINT('Ctrl Pts',(-1.87794635897837,-1.67875975435015,
11.503438646439));
#17770=CARTESIAN_POINT('Ctrl Pts',(-1.81967431466205,-1.73971021683474,
11.5087609152094));
#17771=CARTESIAN_POINT('Ctrl Pts',(-1.76225832928815,-1.79976527245543,
11.5140049959598));
#17772=CARTESIAN_POINT('Ctrl Pts',(-1.70190790868205,-1.85693135779365,
11.5192490767101));
#17773=CARTESIAN_POINT('Ctrl Pts',(-1.63895495321572,-1.9109246220952,11.5244931574604));
#17774=CARTESIAN_POINT('Ctrl Pts',(-1.57459407693794,-1.96612542685175,
11.529854520241));
#17775=CARTESIAN_POINT('Ctrl Pts',(-1.50751325655198,-2.01800946671689,
11.5352158830216));
#17776=CARTESIAN_POINT('Ctrl Pts',(-1.43809924691837,-2.06631962823103,
11.5405772458021));
#17777=CARTESIAN_POINT('Ctrl Pts',(-1.36868523728477,-2.11462978974516,
11.5459386085827));
#17778=CARTESIAN_POINT('Ctrl Pts',(-1.29693850490505,-2.15936586075083,
11.5512999713632));
#17779=CARTESIAN_POINT('Ctrl Pts',(-1.22327153025753,-2.20032111594226,
11.5566613341438));
#17780=CARTESIAN_POINT('Ctrl Pts',(-1.15106258997488,-2.24046577493673,
11.5619165835511));
#17781=CARTESIAN_POINT('Ctrl Pts',(-1.07674203656927,-2.2771262341722,11.5671718329584));
#17782=CARTESIAN_POINT('Ctrl Pts',(-1.00067997046994,-2.31007485738023,
11.5724270823657));
#17783=CARTESIAN_POINT('Ctrl Pts',(-0.924725743101172,-2.34297676692555,
11.5776748810232));
#17784=CARTESIAN_POINT('Ctrl Pts',(-0.847035327201545,-2.37217711150453,
11.5829226796807));
#17785=CARTESIAN_POINT('Ctrl Pts',(-0.768004213099251,-2.39749364517652,
11.5881704783382));
#17786=CARTESIAN_POINT('Ctrl Pts',(-0.68840045044239,-2.4229936189604,11.5934563018211));
#17787=CARTESIAN_POINT('Ctrl Pts',(-0.607436892756986,-2.44455303097054,
11.598742125304));
#17788=CARTESIAN_POINT('Ctrl Pts',(-0.525539144305069,-2.46203469874068,
11.6040279487869));
#17789=CARTESIAN_POINT('Ctrl Pts',(-0.444375767310484,-2.4793596096026,
11.6092663746555));
#17790=CARTESIAN_POINT('Ctrl Pts',(-0.362295345666159,-2.49267951493152,
11.6145048005241));
#17791=CARTESIAN_POINT('Ctrl Pts',(-0.279726532665681,-2.50191113289878,
11.6197432263927));
#17792=CARTESIAN_POINT('Ctrl Pts',(-0.197184875173657,-2.51113971474052,
11.6249799294302));
#17793=CARTESIAN_POINT('Ctrl Pts',(-0.114155603534914,-2.51628262838045,
11.6302166324677));
#17794=CARTESIAN_POINT('Ctrl Pts',(-0.0310745233178724,-2.51730820997362,
11.6354533355052));
#17795=CARTESIAN_POINT('Ctrl Pts',(0.0520042938120662,-2.51833376363045,
11.6406898958975));
#17796=CARTESIAN_POINT('Ctrl Pts',(0.135134455316132,-2.51524220356714,
11.6459264562899));
#17797=CARTESIAN_POINT('Ctrl Pts',(0.217879503963259,-2.50805398102846,
11.6511630166822));
#17798=CARTESIAN_POINT('Ctrl Pts',(0.30197886601233,-2.50074810666313,11.6564852854527));
#17799=CARTESIAN_POINT('Ctrl Pts',(0.385679903931784,-2.48921028676347,
11.6618075542231));
#17800=CARTESIAN_POINT('Ctrl Pts',(0.468530987135125,-2.47351671999487,
11.6671298229936));
#17801=CARTESIAN_POINT('Ctrl Pts',(0.550164927341342,-2.45805370319803,
11.672373903744));
#17802=CARTESIAN_POINT('Ctrl Pts',(0.630973279405442,-2.43855640038696,
11.6776179844943));
#17803=CARTESIAN_POINT('Ctrl Pts',(0.710537247829024,-2.41514866404691,
11.6828620652446));
#17804=CARTESIAN_POINT('Ctrl Pts',(0.791880636553999,-2.39121742187779,
11.6882234280252));
#17805=CARTESIAN_POINT('Ctrl Pts',(0.871922826291916,-2.36319889375187,
11.6935847908057));
#17806=CARTESIAN_POINT('Ctrl Pts',(0.950237582968915,-2.33127750083798,
11.6989461535863));
#17807=CARTESIAN_POINT('Ctrl Pts',(1.02855233964591,-2.2993561079241,11.7043075163668));
#17808=CARTESIAN_POINT('Ctrl Pts',(1.10513923131845,-2.26353212601067,11.7096688791474));
#17809=CARTESIAN_POINT('Ctrl Pts',(1.17960028275458,-2.22403898862527,11.7150302419279));
#17810=CARTESIAN_POINT('Ctrl Pts',(1.25258758326828,-2.18532750885186,11.7202854913353));
#17811=CARTESIAN_POINT('Ctrl Pts',(1.32380203496519,-2.14294784628386,11.7255407407426));
#17812=CARTESIAN_POINT('Ctrl Pts',(1.39285119654308,-2.09708650138436,11.7307959901499));
#17813=CARTESIAN_POINT('Ctrl Pts',(1.46180246209593,-2.0512901774535,11.7360437888074));
#17814=CARTESIAN_POINT('Ctrl Pts',(1.52859415406778,-2.00202222915312,11.7412915874649));
#17815=CARTESIAN_POINT('Ctrl Pts',(1.59285808064306,-1.94951516663249,11.7465393861223));
#17816=CARTESIAN_POINT('Ctrl Pts',(1.65758765476843,-1.89662764517746,11.7518252096052));
#17817=CARTESIAN_POINT('Ctrl Pts',(1.71975225860469,-1.84045409313397,11.7571110330882));
#17818=CARTESIAN_POINT('Ctrl Pts',(1.77900510365261,-1.78127681486566,11.7623968565711));
#17819=CARTESIAN_POINT('Ctrl Pts',(1.83772663252895,-1.72263017516685,11.7676352824396));
#17820=CARTESIAN_POINT('Ctrl Pts',(1.89358808005317,-1.66103379397625,11.7728737083082));
#17821=CARTESIAN_POINT('Ctrl Pts',(1.94628620911509,-1.59680187944793,11.7781121341768));
#17822=CARTESIAN_POINT('Ctrl Pts',(1.99896700663935,-1.53259108972735,11.7833488372143));
#17823=CARTESIAN_POINT('Ctrl Pts',(2.04848625947948,-1.465746844592,11.7885855402518));
#17824=CARTESIAN_POINT('Ctrl Pts',(2.09458013322459,-1.39661745496069,11.7938222432893));
#17825=CARTESIAN_POINT('Ctrl Pts',(2.14067275139564,-1.32748994837936,11.7990588036816));
#17826=CARTESIAN_POINT('Ctrl Pts',(2.18333992086565,-1.25607780554123,11.804295364074));
#17827=CARTESIAN_POINT('Ctrl Pts',(2.22236116616019,-1.18275825811665,11.8095319244663));
#17828=CARTESIAN_POINT('Ctrl Pts',(2.26202108405602,-1.10823866733811,11.8148541932368));
#17829=CARTESIAN_POINT('Ctrl Pts',(2.29791441049217,-1.0317490984141,11.8201764620073));
#17830=CARTESIAN_POINT('Ctrl Pts',(2.32985916934349,-0.953709862078643,
11.8254987307777));
#17831=CARTESIAN_POINT('Ctrl Pts',(2.36133463632767,-0.87681707919117,11.8307428115281));
#17832=CARTESIAN_POINT('Ctrl Pts',(2.38897668257414,-0.79842031994992,11.8359868922784));
#17833=CARTESIAN_POINT('Ctrl Pts',(2.41266118072916,-0.718938298466948,
11.8412309730287));
#17834=CARTESIAN_POINT('Ctrl Pts',(2.43687537439436,-0.637678689397213,
11.8465923358093));
#17835=CARTESIAN_POINT('Ctrl Pts',(2.45695274431194,-0.555285186779717,
11.8519536985898));
#17836=CARTESIAN_POINT('Ctrl Pts',(2.47281591772864,-0.472215720860557,
11.8573150613704));
#17837=CARTESIAN_POINT('Ctrl Pts',(2.48867909114535,-0.389146254941386,
11.8626764241509));
#17838=CARTESIAN_POINT('Ctrl Pts',(2.50032806421805,-0.305401338184903,
11.8680377869315));
#17839=CARTESIAN_POINT('Ctrl Pts',(2.5077419609525,-0.221441882393838,11.8733991497121));
#17840=CARTESIAN_POINT('Ctrl Pts',(2.51420329401791,-0.148269834375331,
11.878071665644));
#17841=CARTESIAN_POINT('Ctrl Pts',(2.51746263872295,-0.0748109262769095,
11.882744181576));
#17842=CARTESIAN_POINT('Ctrl Pts',(2.51749968066596,-0.00126800898217133,
11.887416697508));
#17843=CARTESIAN_POINT('Ctrl Pts',(2.51749968066629,-0.00126800833143484,
11.8874166975493));
#17844=CARTESIAN_POINT('Ctrl Pts',(2.51754083200788,0.080433733485191,11.8926075807009));
#17845=CARTESIAN_POINT('Ctrl Pts',(2.5136004923615,0.162294866749569,11.8977984638525));
#17846=CARTESIAN_POINT('Ctrl Pts',(2.50565840018274,0.243889793951418,11.9029893470041));
#17847=CARTESIAN_POINT('Ctrl Pts',(2.4977254437868,0.325390862568187,11.9081742590866));
#17848=CARTESIAN_POINT('Ctrl Pts',(2.48579990932845,0.406625865579958,11.9133591711691));
#17849=CARTESIAN_POINT('Ctrl Pts',(2.46991353201475,0.487168753483251,11.9185440832516));
#17850=CARTESIAN_POINT('Ctrl Pts',(2.45404174318634,0.567637678725842,11.9237242340212));
#17851=CARTESIAN_POINT('Ctrl Pts',(2.43421642376982,0.647415288567381,11.9289043847908));
#17852=CARTESIAN_POINT('Ctrl Pts',(2.41052097744956,0.726081859899853,11.9340845355604));
#17853=CARTESIAN_POINT('Ctrl Pts',(2.3956646756842,0.775403333180655,11.9373323276459));
#17854=CARTESIAN_POINT('Ctrl Pts',(2.37928809884128,0.824288196918462,11.9405801197315));
#17855=CARTESIAN_POINT('Ctrl Pts',(2.36142200728635,0.872635292378036,11.9438279118171));
#17856=CARTESIAN_POINT('Ctrl Pts',(2.36142193605295,0.872635485141379,11.6676249231292));
#17857=CARTESIAN_POINT('Ctrl Pts',(2.39733462200457,0.775452863264637,11.6605903752774));
#17858=CARTESIAN_POINT('Ctrl Pts',(2.42723136146153,0.676098638326863,11.653692497531));
#17859=CARTESIAN_POINT('Ctrl Pts',(2.45717869013096,0.548478592359361,11.6452161982623));
#17860=CARTESIAN_POINT('Ctrl Pts',(2.46299857004445,0.521722169439311,11.6434595024517));
#17861=CARTESIAN_POINT('Ctrl Pts',(2.47117118202385,0.480958117282357,11.6408130912722));
#17862=CARTESIAN_POINT('Ctrl Pts',(2.47384366205525,0.46701742000365,11.6399133359408));
#17863=CARTESIAN_POINT('Ctrl Pts',(2.47848523789497,0.441646550732813,11.6382852051423));
#17864=CARTESIAN_POINT('Ctrl Pts',(2.48049350670077,0.43022403548439,11.637555613152));
#17865=CARTESIAN_POINT('Ctrl Pts',(2.48466051193079,0.405523539298904,11.6359851326879));
#17866=CARTESIAN_POINT('Ctrl Pts',(2.48679190989915,0.392241263101315,11.6351451240798));
#17867=CARTESIAN_POINT('Ctrl Pts',(2.49230918754642,0.356004896870224,11.6328652520794));
#17868=CARTESIAN_POINT('Ctrl Pts',(2.49548442162297,0.33301971352108,11.6314319972977));
#17869=CARTESIAN_POINT('Ctrl Pts',(2.51117835423709,0.206536973781483,11.6236108013769));
#17870=CARTESIAN_POINT('Ctrl Pts',(2.51757761128408,0.102376427559413,11.6174167833035));
#17871=CARTESIAN_POINT('Ctrl Pts',(2.51741793553497,-0.110195921914664,
11.6050150424096));
#17872=CARTESIAN_POINT('Ctrl Pts',(2.51034757727641,-0.218384835402626,
11.5988290301993));
#17873=CARTESIAN_POINT('Ctrl Pts',(2.47987381666146,-0.451892398911848,
11.5852728567677));
#17874=CARTESIAN_POINT('Ctrl Pts',(2.45388512266596,-0.576559517709645,
11.5779033120999));
#17875=CARTESIAN_POINT('Ctrl Pts',(2.41264106487878,-0.719325857023597,
11.5687779373222));
#17876=CARTESIAN_POINT('Ctrl Pts',(2.40642315928923,-0.739860868354321,
11.5674481663356));
#17877=CARTESIAN_POINT('Ctrl Pts',(2.3973976420479,-0.768350097330235,11.5655760144903));
#17878=CARTESIAN_POINT('Ctrl Pts',(2.39481117317985,-0.776374114851892,
11.5650456829381));
#17879=CARTESIAN_POINT('Ctrl Pts',(2.39027949798047,-0.790194630478281,
11.5641267496927));
#17880=CARTESIAN_POINT('Ctrl Pts',(2.38835336851684,-0.795997372913695,
11.5637392446933));
#17881=CARTESIAN_POINT('Ctrl Pts',(2.38424507238018,-0.808225047074561,
11.5629190278164));
#17882=CARTESIAN_POINT('Ctrl Pts',(2.38205804528001,-0.814648241501571,
11.5624860244296));
#17883=CARTESIAN_POINT('Ctrl Pts',(2.37656669829816,-0.830564882332221,
11.5614078535492));
#17884=CARTESIAN_POINT('Ctrl Pts',(2.37323145959659,-0.840047454778009,
11.560760920611));
#17885=CARTESIAN_POINT('Ctrl Pts',(2.36043783596484,-0.875737263985224,
11.5583093432993));
#17886=CARTESIAN_POINT('Ctrl Pts',(2.35060177888145,-0.901805776198298,
11.5564845892203));
#17887=CARTESIAN_POINT('Ctrl Pts',(2.32422938779747,-0.968335856941044,
11.5517490492363));
#17888=CARTESIAN_POINT('Ctrl Pts',(2.30706862046077,-1.00853880933508,11.5488117769722));
#17889=CARTESIAN_POINT('Ctrl Pts',(2.23719436430341,-1.16110715123365,11.5374223580444));
#17890=CARTESIAN_POINT('Ctrl Pts',(2.17724603866038,-1.26996339033412,11.5287901057939));
#17891=CARTESIAN_POINT('Ctrl Pts',(2.02121642999805,-1.50952551202223,11.5091054489021));
#17892=CARTESIAN_POINT('Ctrl Pts',(1.92003972523376,-1.63629079817126,11.4981768932803));
#17893=CARTESIAN_POINT('Ctrl Pts',(1.79189727919847,-1.76844700605937,11.4863043246929));
#17894=CARTESIAN_POINT('Ctrl Pts',(1.77620740872702,-1.78420513546298,11.4848792754598));
#17895=CARTESIAN_POINT('Ctrl Pts',(1.75002419347935,-1.80981452017164,11.4825471305605));
#17896=CARTESIAN_POINT('Ctrl Pts',(1.73965175660351,-1.81978709054911,11.4816347860533));
#17897=CARTESIAN_POINT('Ctrl Pts',(1.72075658209769,-1.8376446386457,11.4799932226271));
#17898=CARTESIAN_POINT('Ctrl Pts',(1.7122637789379,-1.84556056291702,11.4792626900262));
#17899=CARTESIAN_POINT('Ctrl Pts',(1.6939217423108,-1.86242110709247,11.4777003369487));
#17900=CARTESIAN_POINT('Ctrl Pts',(1.68405571748575,-1.87134700160352,11.476869317981));
#17901=CARTESIAN_POINT('Ctrl Pts',(1.65683321967711,-1.89558582892479,11.4746014197013));
#17902=CARTESIAN_POINT('Ctrl Pts',(1.63933533477002,-1.91073851369584,11.4731711762786));
#17903=CARTESIAN_POINT('Ctrl Pts',(1.53480737469414,-1.99876380054203,11.4647823789306));
#17904=CARTESIAN_POINT('Ctrl Pts',(1.44313315820741,-2.06592877438447,11.4580577881623));
#17905=CARTESIAN_POINT('Ctrl Pts',(1.1965231600097,-2.22215329813713,11.4410757238237));
#17906=CARTESIAN_POINT('Ctrl Pts',(1.03610900383154,-2.30132636198947,11.4310638935683));
#17907=CARTESIAN_POINT('Ctrl Pts',(0.81113045191687,-2.38403736244201,11.4168612471783));
#17908=CARTESIAN_POINT('Ctrl Pts',(0.752824858510689,-2.40308555374831,
11.4131629968456));
#17909=CARTESIAN_POINT('Ctrl Pts',(0.680896920898376,-2.42370960772331,
11.408514393824));
#17910=CARTESIAN_POINT('Ctrl Pts',(0.667876892133936,-2.42732966809544,
11.407669521155));
#17911=CARTESIAN_POINT('Ctrl Pts',(0.647468050691093,-2.43282746694381,
11.4063389615243));
#17912=CARTESIAN_POINT('Ctrl Pts',(0.640098561790641,-2.4347768251201,11.4058572420002));
#17913=CARTESIAN_POINT('Ctrl Pts',(0.626402612903218,-2.43833316486429,
11.4049594453866));
#17914=CARTESIAN_POINT('Ctrl Pts',(0.620078646068015,-2.4399490416106,11.4045438789916));
#17915=CARTESIAN_POINT('Ctrl Pts',(0.605543715173644,-2.44360279735802,
11.4035864441435));
#17916=CARTESIAN_POINT('Ctrl Pts',(0.597328735560597,-2.44562388747316,
11.4030436467284));
#17917=CARTESIAN_POINT('Ctrl Pts',(0.571575479221172,-2.45182233543792,
11.4013371488221));
#17918=CARTESIAN_POINT('Ctrl Pts',(0.554002861577968,-2.45585261741511,
11.400165667376));
#17919=CARTESIAN_POINT('Ctrl Pts',(0.394372290485779,-2.49066349475816,
11.3894692705354));
#17920=CARTESIAN_POINT('Ctrl Pts',(0.249954017534687,-2.50927257987244,
11.3794176445737));
#17921=CARTESIAN_POINT('Ctrl Pts',(-0.0805325957285195,-2.52303614343129,
11.3565662917518));
#17922=CARTESIAN_POINT('Ctrl Pts',(-0.266136949880176,-2.51025724267252,
11.3438738372159));
#17923=CARTESIAN_POINT('Ctrl Pts',(-0.480685334711145,-2.47139757840306,
11.329711268035));
#17924=CARTESIAN_POINT('Ctrl Pts',(-0.512579264337335,-2.46498012993331,
11.3276175328131));
#17925=CARTESIAN_POINT('Ctrl Pts',(-0.559016808301207,-2.45469598871661,
11.3245847813435));
#17926=CARTESIAN_POINT('Ctrl Pts',(-0.573663345725554,-2.45131445774044,
11.3236305380125));
#17927=CARTESIAN_POINT('Ctrl Pts',(-0.599661484538509,-2.4450663382755,
11.3219405577085));
#17928=CARTESIAN_POINT('Ctrl Pts',(-0.611024919818703,-2.44225138948572,
11.3212032003458));
#17929=CARTESIAN_POINT('Ctrl Pts',(-0.634750652159168,-2.4361980950605,
11.3196662445311));
#17930=CARTESIAN_POINT('Ctrl Pts',(-0.647108784969866,-2.4329446723663,
11.3188671521334));
#17931=CARTESIAN_POINT('Ctrl Pts',(-0.679448917233236,-2.42416690688252,
11.3167795342191));
#17932=CARTESIAN_POINT('Ctrl Pts',(-0.699388645794815,-2.41848952559864,
11.3154959481257));
#17933=CARTESIAN_POINT('Ctrl Pts',(-0.792103332307921,-2.39084857161893,
11.3095413578145));
#17934=CARTESIAN_POINT('Ctrl Pts',(-0.863933568668204,-2.36584129036096,
11.3049694816425));
#17935=CARTESIAN_POINT('Ctrl Pts',(-1.05805885687285,-2.28823438307753,
11.2926070363392));
#17936=CARTESIAN_POINT('Ctrl Pts',(-1.17748619293803,-2.22913296196636,
11.2850029314329));
#17937=CARTESIAN_POINT('Ctrl Pts',(-1.40834098265433,-2.0911368230332,11.2695360682195));
#17938=CARTESIAN_POINT('Ctrl Pts',(-1.51914471610405,-2.01208043210366,
11.2616924757929));
#17939=CARTESIAN_POINT('Ctrl Pts',(-1.63938845857399,-1.91067280944356,
11.2520329516163));
#17940=CARTESIAN_POINT('Ctrl Pts',(-1.65558590818234,-1.89665503805232,
11.2507052973716));
#17941=CARTESIAN_POINT('Ctrl Pts',(-1.67790151135174,-1.87683876426748,
11.2488356608478));
#17942=CARTESIAN_POINT('Ctrl Pts',(-1.68417290717555,-1.87121320079613,
11.2483056857276));
#17943=CARTESIAN_POINT('Ctrl Pts',(-1.69494553626937,-1.8614519181657,11.2473872008259));
#17944=CARTESIAN_POINT('Ctrl Pts',(-1.69946020833582,-1.85733104559618,
11.2469997852196));
#17945=CARTESIAN_POINT('Ctrl Pts',(-1.70895589800082,-1.84860002514801,
11.2461795496073));
#17946=CARTESIAN_POINT('Ctrl Pts',(-1.71393333407742,-1.84398612717605,
11.2457464368011));
#17947=CARTESIAN_POINT('Ctrl Pts',(-1.72624217894296,-1.83248339593527,
11.2446676352453));
#17948=CARTESIAN_POINT('Ctrl Pts',(-1.73355100987166,-1.82557069015936,
11.2440201767197));
#17949=CARTESIAN_POINT('Ctrl Pts',(-1.76098721499923,-1.79930814723009,
11.2415642753773));
#17950=CARTESIAN_POINT('Ctrl Pts',(-1.78083282619967,-1.77966852873953,
11.2397356338672));
#17951=CARTESIAN_POINT('Ctrl Pts',(-1.83098620619575,-1.72835678738393,
11.2349875958374));
#17952=CARTESIAN_POINT('Ctrl Pts',(-1.86080008709392,-1.69621645878455,
11.232041549607));
#17953=CARTESIAN_POINT('Ctrl Pts',(-1.97166599481848,-1.57025740253802,
11.2206516318227));
#17954=CARTESIAN_POINT('Ctrl Pts',(-2.04658622852537,-1.47127795249396,
11.2120287854528));
#17955=CARTESIAN_POINT('Ctrl Pts',(-2.20173726091226,-1.23138706119628,
11.1923582977563));
#17956=CARTESIAN_POINT('Ctrl Pts',(-2.27628894104925,-1.08742203938476,
11.1814345814186));
#17957=CARTESIAN_POINT('Ctrl Pts',(-2.34479744928971,-0.916638196542017,
11.1695664337921));
#17958=CARTESIAN_POINT('Ctrl Pts',(-2.35280220109205,-0.89589202244469,
11.1681414005325));
#17959=CARTESIAN_POINT('Ctrl Pts',(-2.36553239402975,-0.861550791216074,
11.1658092762604));
#17960=CARTESIAN_POINT('Ctrl Pts',(-2.37041786212139,-0.848016772228323,
11.1648969365664));
#17961=CARTESIAN_POINT('Ctrl Pts',(-2.3790351887848,-0.82348807105769,11.1632553783208));
#17962=CARTESIAN_POINT('Ctrl Pts',(-2.38280749935209,-0.812508129783064,
11.1625248461243));
#17963=CARTESIAN_POINT('Ctrl Pts',(-2.39073944839949,-0.788890448991829,
11.1609624901581));
#17964=CARTESIAN_POINT('Ctrl Pts',(-2.39487514639262,-0.77624499652189,
11.160131467926));
#17965=CARTESIAN_POINT('Ctrl Pts',(-2.40593058696488,-0.741511951926544,
11.157863551125));
#17966=CARTESIAN_POINT('Ctrl Pts',(-2.41264638393,-0.719360441749694,11.1564332926306));
#17967=CARTESIAN_POINT('Ctrl Pts',(-2.45048890550599,-0.588043993508652,
11.1480441559588));
#17968=CARTESIAN_POINT('Ctrl Pts',(-2.47451096153681,-0.476960922333004,
11.1413192644936));
#17969=CARTESIAN_POINT('Ctrl Pts',(-2.51680047774478,-0.188057131813012,
11.1243341222338));
#17970=CARTESIAN_POINT('Ctrl Pts',(-2.52379800329334,-0.00925704089722142,
11.1143197143108));
#17971=CARTESIAN_POINT('Ctrl Pts',(-2.50772903572159,0.229904090897192,
11.1001166369944));
#17972=CARTESIAN_POINT('Ctrl Pts',(-2.50139100619104,0.290865149549083,
11.0964212088506));
#17973=CARTESIAN_POINT('Ctrl Pts',(-2.49094988651444,0.364907471250643,
11.0917757793895));
#17974=CARTESIAN_POINT('Ctrl Pts',(-2.48895565364245,0.37827045234536,11.0909310880515));
#17975=CARTESIAN_POINT('Ctrl Pts',(-2.48566829091056,0.399145960708781,
11.0896007531878));
#17976=CARTESIAN_POINT('Ctrl Pts',(-2.48444840247935,0.406669991729693,
11.0891190749371));
#17977=CARTESIAN_POINT('Ctrl Pts',(-2.48212046505666,0.420626740013686,
11.0882213136764));
#17978=CARTESIAN_POINT('Ctrl Pts',(-2.48102154900441,0.427060800681334,
11.0878057409841));
#17979=CARTESIAN_POINT('Ctrl Pts',(-2.47844071959789,0.441825121633087,
11.086848236874));
#17980=CARTESIAN_POINT('Ctrl Pts',(-2.47694182798876,0.450152212577691,
11.0863053759864));
#17981=CARTESIAN_POINT('Ctrl Pts',(-2.47211676075218,0.476203947033921,
11.0845984807209));
#17982=CARTESIAN_POINT('Ctrl Pts',(-2.4686421711388,0.493900055581935,11.0834266603707));
#17983=CARTESIAN_POINT('Ctrl Pts',(-2.43459210165735,0.657973106557688,
11.0724560828398));
#17984=CARTESIAN_POINT('Ctrl Pts',(-2.39122432622761,0.801376946139549,
11.0621010601758));
#17985=CARTESIAN_POINT('Ctrl Pts',(-2.26783491396871,1.10791068269773,11.0392753885434));
#17986=CARTESIAN_POINT('Ctrl Pts',(-2.18236567500239,1.26800756912656,11.0269078797221));
#17987=CARTESIAN_POINT('Ctrl Pts',(-2.06224972480371,1.4442913120166,11.0130495986418));
#17988=CARTESIAN_POINT('Ctrl Pts',(-2.04353289230858,1.47065454750975,11.0109683170281));
#17989=CARTESIAN_POINT('Ctrl Pts',(-2.01526406930795,1.50888987314861,11.007935401561));
#17990=CARTESIAN_POINT('Ctrl Pts',(-2.0061044420944,1.5210466469932,11.006968890362));
#17991=CARTESIAN_POINT('Ctrl Pts',(-1.98968887780072,1.5424273454487,11.0052648430355));
#17992=CARTESIAN_POINT('Ctrl Pts',(-1.98247771263297,1.55168491417507,11.0045255930391));
#17993=CARTESIAN_POINT('Ctrl Pts',(-1.9673339409232,1.57084832248744,11.0029921847298));
#17994=CARTESIAN_POINT('Ctrl Pts',(-1.95939061750972,1.58074530041335,11.0021984785472));
#17995=CARTESIAN_POINT('Ctrl Pts',(-1.93853216285496,1.6063350657589,11.0001413023145));
#17996=CARTESIAN_POINT('Ctrl Pts',(-1.92550107584605,1.62193246909921,10.998882505291));
#17997=CARTESIAN_POINT('Ctrl Pts',(-1.86582361245943,1.69162966811375,10.9932325047161));
#17998=CARTESIAN_POINT('Ctrl Pts',(-1.81707406750394,1.74388987759326,10.98892805379));
#17999=CARTESIAN_POINT('Ctrl Pts',(-1.59931214699988,1.95827182051405,10.9708135544456));
#18000=CARTESIAN_POINT('Ctrl Pts',(-1.41038339110225,2.09843488773873,10.9578827249366));
#18001=CARTESIAN_POINT('Ctrl Pts',(-1.15736137022779,2.23634607259549,10.9407222320724));
#18002=CARTESIAN_POINT('Ctrl Pts',(-1.10907399511331,2.26068198556832,10.9374478455764));
#18003=CARTESIAN_POINT('Ctrl Pts',(-1.04822098560862,2.28893183547811,10.933276444192));
#18004=CARTESIAN_POINT('Ctrl Pts',(-1.03635498831175,2.29432876968182,10.9324609656707));
#18005=CARTESIAN_POINT('Ctrl Pts',(-1.0175840439003,2.30269090978864,10.9311668635687));
#18006=CARTESIAN_POINT('Ctrl Pts',(-1.01070662764098,2.30571785389678,10.9306918635515));
#18007=CARTESIAN_POINT('Ctrl Pts',(-0.998416234301015,2.31106164802894,
10.9298413003156));
#18008=CARTESIAN_POINT('Ctrl Pts',(-0.993008552306173,2.31339035410235,
10.9294664598037));
#18009=CARTESIAN_POINT('Ctrl Pts',(-0.979995838311128,2.31893997709558,
10.9285630565051));
#18010=CARTESIAN_POINT('Ctrl Pts',(-0.972383134094452,2.32214243671705,
10.9280334079455));
#18011=CARTESIAN_POINT('Ctrl Pts',(-0.949066919331147,2.33181618311478,
10.9264080287004));
#18012=CARTESIAN_POINT('Ctrl Pts',(-0.93331392864005,2.33816590575514,10.925305507615));
#18013=CARTESIAN_POINT('Ctrl Pts',(-0.896431707738855,2.35260031146914,
10.9227160173604));
#18014=CARTESIAN_POINT('Ctrl Pts',(-0.875255593514787,2.36056044247229,
10.9212230562769));
#18015=CARTESIAN_POINT('Ctrl Pts',(-0.800407435936451,2.3875503964935,10.9159312862508));
#18016=CARTESIAN_POINT('Ctrl Pts',(-0.746202203458642,2.40504270691928,
10.9120727230693));
#18017=CARTESIAN_POINT('Ctrl Pts',(-0.530005995903139,2.46679796291472,
10.8966922480688));
#18018=CARTESIAN_POINT('Ctrl Pts',(-0.364333165218001,2.49665110955337,
10.8849616127632));
#18019=CARTESIAN_POINT('Ctrl Pts',(-0.0971860332738022,2.51761187361939,
10.866838087092));
#18020=CARTESIAN_POINT('Ctrl Pts',(0.0029367541128548,2.51948614030987,
10.8602112423803));
#18021=CARTESIAN_POINT('Ctrl Pts',(0.125871810457664,2.51445627167282,10.8522872724182));
#18022=CARTESIAN_POINT('Ctrl Pts',(0.148813271983063,2.51320288119465,10.8508173992024));
#18023=CARTESIAN_POINT('Ctrl Pts',(0.185103973421996,2.51072147680859,10.8485056218221));
#18024=CARTESIAN_POINT('Ctrl Pts',(0.198465641319012,2.50970062270158,10.8476573374664));
#18025=CARTESIAN_POINT('Ctrl Pts',(0.223378689272948,2.50759701636848,10.8460808623983));
#18026=CARTESIAN_POINT('Ctrl Pts',(0.234931911116423,2.50654101097681,10.8453518607697));
#18027=CARTESIAN_POINT('Ctrl Pts',(0.260668769256758,2.50400906183424,10.8437323230351));
#18028=CARTESIAN_POINT('Ctrl Pts',(0.274848067041515,2.50249238605967,10.8428430794495));
#18029=CARTESIAN_POINT('Ctrl Pts',(0.316533743979677,2.49767493737318,10.8402371409028));
#18030=CARTESIAN_POINT('Ctrl Pts',(0.343999959172452,2.49404046174496,10.8385308553767));
#18031=CARTESIAN_POINT('Ctrl Pts',(0.541732976115757,2.46454660348116,10.8263130586518));
#18032=CARTESIAN_POINT('Ctrl Pts',(0.70901385228238,2.42172946050181,10.8163732311916));
#18033=CARTESIAN_POINT('Ctrl Pts',(1.02260130307539,2.30614951468294,10.7971682262028));
#18034=CARTESIAN_POINT('Ctrl Pts',(1.16879242719175,2.23560930750595,10.787928182996));
#18035=CARTESIAN_POINT('Ctrl Pts',(1.32462344639371,2.1409333916849,10.7767165001997));
#18036=CARTESIAN_POINT('Ctrl Pts',(1.34194134790884,2.13012122190247,10.7754499427391));
#18037=CARTESIAN_POINT('Ctrl Pts',(1.36668613976552,2.11425067801649,10.7736074856101));
#18038=CARTESIAN_POINT('Ctrl Pts',(1.37422094001165,2.10936097820178,10.773042021912));
#18039=CARTESIAN_POINT('Ctrl Pts',(1.3871751458298,2.10085549422045,10.7720618764836));
#18040=CARTESIAN_POINT('Ctrl Pts',(1.39260706592421,2.09725874701013,10.7716484427858));
#18041=CARTESIAN_POINT('Ctrl Pts',(1.39826045702336,2.09348370533714,10.7712155386713));
#18042=CARTESIAN_POINT('Ctrl Pts',(1.39849592741285,2.09332641296019,10.7711975029857));
#18043=CARTESIAN_POINT('Ctrl Pts',(1.3989147409203,2.09304654660976,10.7711654158756));
#18044=CARTESIAN_POINT('Ctrl Pts',(1.39909809453178,2.09292398823192,10.771151365503));
#18045=CARTESIAN_POINT('Ctrl Pts',(1.39940806169558,2.0927167390894,10.7711276079094));
#18046=CARTESIAN_POINT('Ctrl Pts',(1.39953468372102,2.09263206089017,10.7711179015345));
#18047=CARTESIAN_POINT('Ctrl Pts',(1.39975277896695,2.09248618152838,10.7711011808126));
#18048=CARTESIAN_POINT('Ctrl Pts',(1.39984425588037,2.09242498584577,10.7710941668344));
#18049=CARTESIAN_POINT('Ctrl Pts',(1.40005856813296,2.09228159616287,10.771077732808));
#18050=CARTESIAN_POINT('Ctrl Pts',(1.40018140022948,2.09219939735575,10.7710683124367));
#18051=CARTESIAN_POINT('Ctrl Pts',(1.40042015178547,2.09203959521152,10.7710499993511));
#18052=CARTESIAN_POINT('Ctrl Pts',(1.4005360720393,2.09196199305253,10.7710411067161));
#18053=CARTESIAN_POINT('Ctrl Pts',(1.4007619906409,2.09181072592668,10.7710237735085));
#18054=CARTESIAN_POINT('Ctrl Pts',(1.40087198962762,2.09173706191837,10.7710153330003));
#18055=CARTESIAN_POINT('Ctrl Pts',(1.40108687499705,2.09159313315217,10.7709988422774));
#18056=CARTESIAN_POINT('Ctrl Pts',(1.40119176190284,2.09152286918262,10.7709907921157));
#18057=CARTESIAN_POINT('Ctrl Pts',(1.40139709362752,2.09138529462943,10.7709750308952));
#18058=CARTESIAN_POINT('Ctrl Pts',(1.40149753890377,2.09131798468491,10.7709673198786));
#18059=CARTESIAN_POINT('Ctrl Pts',(1.40169455003112,2.0911859438912,10.77095219398));
#18060=CARTESIAN_POINT('Ctrl Pts',(1.4017911162457,2.09112121359085,10.7709447791348));
#18061=CARTESIAN_POINT('Ctrl Pts',(1.40198084665936,2.09099401438221,10.7709302091109));
#18062=CARTESIAN_POINT('Ctrl Pts',(1.40207401116765,2.09093154593597,10.7709230539632));
#18063=CARTESIAN_POINT('Ctrl Pts',(1.40225734739891,2.09080859799612,10.7709089720652));
#18064=CARTESIAN_POINT('Ctrl Pts',(1.40234751939106,2.09074811889104,10.7709020453409));
#18065=CARTESIAN_POINT('Ctrl Pts',(1.40252522467712,2.09062891380924,10.7708883932264));
#18066=CARTESIAN_POINT('Ctrl Pts',(1.40261275819615,2.09057018816786,10.7708816678587));
#18067=CARTESIAN_POINT('Ctrl Pts',(1.40278549554194,2.09045428412731,10.7708683948329));
#18068=CARTESIAN_POINT('Ctrl Pts',(1.40287069955756,2.09039710601884,10.7708618471943));
#18069=CARTESIAN_POINT('Ctrl Pts',(1.40303904969481,2.09028411587032,10.77084890884));
#18070=CARTESIAN_POINT('Ctrl Pts',(1.40312219598932,2.09022830407359,10.7708425181405));
#18071=CARTESIAN_POINT('Ctrl Pts',(1.40328667162243,2.09011788587227,10.770829875232));
#18072=CARTESIAN_POINT('Ctrl Pts',(1.40336800109619,2.09006327968691,10.7708236230379));
#18073=CARTESIAN_POINT('Ctrl Pts',(1.40352905813526,2.08995512922967,10.7708112406832));
#18074=CARTESIAN_POINT('Ctrl Pts',(1.40360878582183,2.08990158514396,10.7708051105351));
#18075=CARTESIAN_POINT('Ctrl Pts',(1.40376683255596,2.08979542987289,10.7707929574762));
#18076=CARTESIAN_POINT('Ctrl Pts',(1.40384515171288,2.08974281884495,10.7707869345759));
#18077=CARTESIAN_POINT('Ctrl Pts',(1.4040005562267,2.08963841291741,10.7707749826228));
#18078=CARTESIAN_POINT('Ctrl Pts',(1.40407764167998,2.08958661815184,10.7707690535787));
#18079=CARTESIAN_POINT('Ctrl Pts',(1.4042307379417,2.08948373839258,10.7707572771445));
#18080=CARTESIAN_POINT('Ctrl Pts',(1.40430674883701,2.08943265351103,10.7707514297614));
#18081=CARTESIAN_POINT('Ctrl Pts',(1.40445784177767,2.08933109603385,10.7707398054744));
#18082=CARTESIAN_POINT('Ctrl Pts',(1.40453292388654,2.08928062354092,10.7707340285773));
#18083=CARTESIAN_POINT('Ctrl Pts',(1.40468229360237,2.08918020095291,10.7707225349601));
#18084=CARTESIAN_POINT('Ctrl Pts',(1.40475658125238,2.08913025095176,10.7707168182468));
#18085=CARTESIAN_POINT('Ctrl Pts',(1.40490448650718,2.08903079002271,10.7707054354491));
#18086=CARTESIAN_POINT('Ctrl Pts',(1.40497810417176,2.0889812791571,10.7706997693685));
#18087=CARTESIAN_POINT('Ctrl Pts',(1.40512478550771,2.08888261874761,10.7706884789288));
#18088=CARTESIAN_POINT('Ctrl Pts',(1.40519784922212,2.08883346925874,10.7706828545733));
#18089=CARTESIAN_POINT('Ctrl Pts',(1.40534353145249,2.08873545866046,10.7706716392288));
#18090=CARTESIAN_POINT('Ctrl Pts',(1.40541614999251,2.08868659760173,10.7706660482435));
#18091=CARTESIAN_POINT('Ctrl Pts',(1.40556104440565,2.08858909506851,10.7706548917615));
#18092=CARTESIAN_POINT('Ctrl Pts',(1.40563332029845,2.08854045363181,10.7706493262674));
#18093=CARTESIAN_POINT('Ctrl Pts',(1.40577762657922,2.08844332509855,10.7706382132981));
#18094=CARTESIAN_POINT('Ctrl Pts',(1.40584965698744,2.08839483802457,10.7706326658242));
#18095=CARTESIAN_POINT('Ctrl Pts',(1.40599356487939,2.08829795599818,10.7706215817738));
#18096=CARTESIAN_POINT('Ctrl Pts',(1.40606544237672,2.08824956105883,10.7706160451979));
#18097=CARTESIAN_POINT('Ctrl Pts',(1.41311305219985,2.08350389414276,10.7700731392783));
#18098=CARTESIAN_POINT('Ctrl Pts',(1.42006508721248,2.07877178123098,10.7695334630535));
#18099=CARTESIAN_POINT('Ctrl Pts',(1.44210436950111,2.06360792915573,10.7678097296066));
#18100=CARTESIAN_POINT('Ctrl Pts',(1.45710098439732,2.05304636405247,10.7666175248755));
#18101=CARTESIAN_POINT('Ctrl Pts',(1.59466926886422,1.95389560105135,10.7555112935215));
#18102=CARTESIAN_POINT('Ctrl Pts',(1.70912892953977,1.85460180676072,10.7450314383921));
#18103=CARTESIAN_POINT('Ctrl Pts',(1.93782765136039,1.61695171134747,10.7222502874169));
#18104=CARTESIAN_POINT('Ctrl Pts',(2.0476515188536,1.47541627528143,10.7100490039289));
#18105=CARTESIAN_POINT('Ctrl Pts',(2.15712861659806,1.29825940628082,10.6965184917753));
#18106=CARTESIAN_POINT('Ctrl Pts',(2.17223541240657,1.27282158573549,10.6946123108767));
#18107=CARTESIAN_POINT('Ctrl Pts',(2.19425209414119,1.23421424707339,10.6917727875705));
#18108=CARTESIAN_POINT('Ctrl Pts',(2.20149899958331,1.22124085691834,10.6908274979365));
#18109=CARTESIAN_POINT('Ctrl Pts',(2.21387391582671,1.19861916037615,10.6891943154352));
#18110=CARTESIAN_POINT('Ctrl Pts',(2.21905470931688,1.1890003406038,10.6885045666132));
#18111=CARTESIAN_POINT('Ctrl Pts',(2.22972998983283,1.16886746299885,10.6870704807308));
#18112=CARTESIAN_POINT('Ctrl Pts',(2.23521311664045,1.15834766134119,10.6863265561475));
#18113=CARTESIAN_POINT('Ctrl Pts',(2.24804292293344,1.13330234869151,10.684568005527));
#18114=CARTESIAN_POINT('Ctrl Pts',(2.2553235457549,1.11874345602014,10.683555697073));
#18115=CARTESIAN_POINT('Ctrl Pts',(2.27945219422264,1.06930098011352,10.6801503480015));
#18116=CARTESIAN_POINT('Ctrl Pts',(2.29563663540643,1.03409843624873,10.6777800458454));
#18117=CARTESIAN_POINT('Ctrl Pts',(2.32894184405087,0.957017070062897,10.6726957809908));
#18118=CARTESIAN_POINT('Ctrl Pts',(2.34575361275732,0.915035235837583,10.6699926192476));
#18119=CARTESIAN_POINT('Ctrl Pts',(2.3614219719961,0.872635387876314,10.6673175101421));
#18120=CARTESIAN_POINT('Origin',(0.,0.,10.));
#18121=CARTESIAN_POINT('',(2.36142200350084,0.872635302621937,9.67114329893353));
#18122=CARTESIAN_POINT('',(2.36142200728636,0.872635292378023,9.94365014611287));
#18123=CARTESIAN_POINT('',(2.36142200728636,0.87263529237802,10.));
#18124=CARTESIAN_POINT('',(2.51749898433573,0.00226138642591275,10.8874166974549));
#18125=CARTESIAN_POINT('Ctrl Pts',(2.36142200728636,0.872635292378024,9.94365014611287));
#18126=CARTESIAN_POINT('Ctrl Pts',(2.33166846731732,0.953150789162594,9.94908273018793));
#18127=CARTESIAN_POINT('Ctrl Pts',(2.29783002319381,1.0320428527644,9.95451531426299));
#18128=CARTESIAN_POINT('Ctrl Pts',(2.26012095724572,1.10890013464634,9.95994789833805));
#18129=CARTESIAN_POINT('Ctrl Pts',(2.22998573573739,1.17032067519298,9.96428935099269));
#18130=CARTESIAN_POINT('Ctrl Pts',(2.19737952459186,1.23044212633847,9.96863080364734));
#18131=CARTESIAN_POINT('Ctrl Pts',(2.1624315142936,1.28906795631179,9.97297225630198));
#18132=CARTESIAN_POINT('Ctrl Pts',(2.12012758401584,1.36003345627881,9.97822750570929));
#18133=CARTESIAN_POINT('Ctrl Pts',(2.07424846759199,1.42904534370428,9.98348275511659));
#18134=CARTESIAN_POINT('Ctrl Pts',(2.02500000847369,1.49572096852373,9.98873800452389));
#18135=CARTESIAN_POINT('Ctrl Pts',(1.97582137248252,1.56230206245406,9.99398580318139));
#18136=CARTESIAN_POINT('Ctrl Pts',(1.92328315409526,1.626553104896,9.99923360183888));
#18137=CARTESIAN_POINT('Ctrl Pts',(1.8676359396016,1.68811796006928,10.0044814004964));
#18138=CARTESIAN_POINT('Ctrl Pts',(1.81158551306532,1.75012890569351,10.0097672239793));
#18139=CARTESIAN_POINT('Ctrl Pts',(1.75238108825255,1.80941416526022,10.0150530474622));
#18140=CARTESIAN_POINT('Ctrl Pts',(1.69032191607646,1.86564146341992,10.0203388709451));
#18141=CARTESIAN_POINT('Ctrl Pts',(1.62881922421362,1.92136457527812,10.0255772968137));
#18142=CARTESIAN_POINT('Ctrl Pts',(1.56451312482682,1.97408403161953,10.0308157226823));
#18143=CARTESIAN_POINT('Ctrl Pts',(1.49773256054321,2.02351264564585,10.0360541485509));
#18144=CARTESIAN_POINT('Ctrl Pts',(1.43097395927577,2.07292500342366,10.0412908515884));
#18145=CARTESIAN_POINT('Ctrl Pts',(1.36174287997103,2.11904839410426,10.0465275546259));
#18146=CARTESIAN_POINT('Ctrl Pts',(1.29040036014567,2.16163668560097,10.0517642576634));
#18147=CARTESIAN_POINT('Ctrl Pts',(1.21905978365487,2.20422381701391,10.0570008180557));
#18148=CARTESIAN_POINT('Ctrl Pts',(1.1456082777219,2.24327580507479,10.0622373784481));
#18149=CARTESIAN_POINT('Ctrl Pts',(1.07043360185148,2.27859126523983,10.0674739388404));
#18150=CARTESIAN_POINT('Ctrl Pts',(0.994028519175117,2.31448474429274,10.0727962076109));
#18151=CARTESIAN_POINT('Ctrl Pts',(0.915843789831386,2.34651805717603,10.0781184763814));
#18152=CARTESIAN_POINT('Ctrl Pts',(0.836308278399151,2.37453041957374,10.0834407451518));
#18153=CARTESIAN_POINT('Ctrl Pts',(0.757941201790199,2.40213125988379,10.0886848259022));
#18154=CARTESIAN_POINT('Ctrl Pts',(0.678263233698535,2.42582843231022,10.0939289066525));
#18155=CARTESIAN_POINT('Ctrl Pts',(0.597698758546328,2.44551884965792,10.0991729874028));
#18156=CARTESIAN_POINT('Ctrl Pts',(0.515332487110007,2.4656496362967,10.1045343501834));
#18157=CARTESIAN_POINT('Ctrl Pts',(0.432040080192264,2.48159218961263,10.1098957129639));
#18158=CARTESIAN_POINT('Ctrl Pts',(0.348282757392841,2.49329207492882,10.1152570757445));
#18159=CARTESIAN_POINT('Ctrl Pts',(0.264525434593406,2.504991960245,10.1206184385251));
#18160=CARTESIAN_POINT('Ctrl Pts',(0.180303707930422,2.51244919928504,10.1259798013056));
#18161=CARTESIAN_POINT('Ctrl Pts',(0.0960789567655814,2.51566593252499,
10.1313411640862));
#18162=CARTESIAN_POINT('Ctrl Pts',(0.0135212020012339,2.51881899941202,
10.1365964134935));
#18163=CARTESIAN_POINT('Ctrl Pts',(-0.0693443933132752,2.51790958034371,
10.1418516629008));
#18164=CARTESIAN_POINT('Ctrl Pts',(-0.152084793467355,2.5129020007943,10.1471069123081));
#18165=CARTESIAN_POINT('Ctrl Pts',(-0.234707886530317,2.50790152085511,
10.1523547109656));
#18166=CARTESIAN_POINT('Ctrl Pts',(-0.317205680260735,2.49881444895049,
10.1576025096231));
#18167=CARTESIAN_POINT('Ctrl Pts',(-0.399143018617033,2.48565707624549,
10.1628503082806));
#18168=CARTESIAN_POINT('Ctrl Pts',(-0.481674063628092,2.47240436703224,
10.1681361317635));
#18169=CARTESIAN_POINT('Ctrl Pts',(-0.563636023487413,2.45502210436827,
10.1734219552464));
#18170=CARTESIAN_POINT('Ctrl Pts',(-0.64458726056848,2.43358038977816,10.1787077787293));
#18171=CARTESIAN_POINT('Ctrl Pts',(-0.724812613494356,2.41233094156275,
10.1839462045979));
#18172=CARTESIAN_POINT('Ctrl Pts',(-0.804044842948055,2.38709467180907,
10.1891846304665));
#18173=CARTESIAN_POINT('Ctrl Pts',(-0.881863965531894,2.35799113575441,
10.1944230563351));
#18174=CARTESIAN_POINT('Ctrl Pts',(-0.959657494701511,2.32889717136837,
10.1996597593726));
#18175=CARTESIAN_POINT('Ctrl Pts',(-1.03603840817081,2.29593862820907,10.2048964624101));
#18176=CARTESIAN_POINT('Ctrl Pts',(-1.11060368480479,2.25928433476135,10.2101331654476));
#18177=CARTESIAN_POINT('Ctrl Pts',(-1.18516693031777,2.22263103975832,10.21536972584));
#18178=CARTESIAN_POINT('Ctrl Pts',(-1.25791422369005,2.18228239910813,10.2206062862323));
#18179=CARTESIAN_POINT('Ctrl Pts',(-1.32846552885232,2.13845401836259,10.2258428466246));
#18180=CARTESIAN_POINT('Ctrl Pts',(-1.4001715687047,2.09390828516636,10.2311651153951));
#18181=CARTESIAN_POINT('Ctrl Pts',(-1.46960866236063,2.04576812457827,10.2364873841656));
#18182=CARTESIAN_POINT('Ctrl Pts',(-1.53640844918686,1.99430572562665,10.2418096529361));
#18183=CARTESIAN_POINT('Ctrl Pts',(-1.60222689829722,1.94359934694754,10.2470537336864));
#18184=CARTESIAN_POINT('Ctrl Pts',(-1.66548469781701,1.88966804453302,10.2522978144367));
#18185=CARTESIAN_POINT('Ctrl Pts',(-1.72586432224112,1.83281166277804,10.257541895187));
#18186=CARTESIAN_POINT('Ctrl Pts',(-1.78759431582885,1.77468370794838,10.2629032579676));
#18187=CARTESIAN_POINT('Ctrl Pts',(-1.84631548752542,1.71349862765125,10.2682646207481));
#18188=CARTESIAN_POINT('Ctrl Pts',(-1.90173106621274,1.64961365228388,10.2736259835287));
#18189=CARTESIAN_POINT('Ctrl Pts',(-1.95714664490007,1.5857286769165,10.2789873463093));
#18190=CARTESIAN_POINT('Ctrl Pts',(-2.00925637003065,1.51914424778319,10.2843487090898));
#18191=CARTESIAN_POINT('Ctrl Pts',(-2.05781083830561,1.4502485317186,10.2897100718704));
#18192=CARTESIAN_POINT('Ctrl Pts',(-2.10540430494241,1.38271641612896,10.2949653212777));
#18193=CARTESIAN_POINT('Ctrl Pts',(-2.14975779396929,1.31271425944068,10.300220570685));
#18194=CARTESIAN_POINT('Ctrl Pts',(-2.19060561490065,1.24058586561581,10.3054758200923));
#18195=CARTESIAN_POINT('Ctrl Pts',(-2.23139552290147,1.16855973346774,10.3107236187498));
#18196=CARTESIAN_POINT('Ctrl Pts',(-2.26868940967179,1.09441375005823,10.3159714174073));
#18197=CARTESIAN_POINT('Ctrl Pts',(-2.30226401872903,1.01852179066805,10.3212192160648));
#18198=CARTESIAN_POINT('Ctrl Pts',(-2.33608190477361,0.942079928605546,
10.3265050395477));
#18199=CARTESIAN_POINT('Ctrl Pts',(-2.36612611394324,0.863867068955288,
10.3317908630306));
#18200=CARTESIAN_POINT('Ctrl Pts',(-2.39221499656075,0.784291820835746,
10.3370766865135));
#18201=CARTESIAN_POINT('Ctrl Pts',(-2.41806994196864,0.705430118473343,
10.3423151123821));
#18202=CARTESIAN_POINT('Ctrl Pts',(-2.4400400646031,0.625230809207545,10.3475535382507));
#18203=CARTESIAN_POINT('Ctrl Pts',(-2.45799698585833,0.544111263907802,
10.3527919641193));
#18204=CARTESIAN_POINT('Ctrl Pts',(-2.47594800138103,0.463018397476416,
10.3580286671568));
#18205=CARTESIAN_POINT('Ctrl Pts',(-2.48988833722006,0.381006346250531,
10.3632653701943));
#18206=CARTESIAN_POINT('Ctrl Pts',(-2.49974017991993,0.298505080181056,
10.3685020732318));
#18207=CARTESIAN_POINT('Ctrl Pts',(-2.50959175426053,0.216006061404777,
10.3737386336242));
#18208=CARTESIAN_POINT('Ctrl Pts',(-2.51535500320341,0.133018312568195,
10.3789751940165));
#18209=CARTESIAN_POINT('Ctrl Pts',(-2.51700386379089,0.0499779917736052,
10.3842117544088));
#18210=CARTESIAN_POINT('Ctrl Pts',(-2.51867971178158,-0.0344214752318402,
10.3895340231793));
#18211=CARTESIAN_POINT('Ctrl Pts',(-2.51610525050777,-0.118874759276741,
10.3948562919498));
#18212=CARTESIAN_POINT('Ctrl Pts',(-2.50930823550473,-0.202924688562398,
10.4001785607203));
#18213=CARTESIAN_POINT('Ctrl Pts',(-2.5026110736224,-0.285739862925326,
10.4054226414706));
#18214=CARTESIAN_POINT('Ctrl Pts',(-2.49181472092364,-0.368162998928606,
10.4106667222209));
#18215=CARTESIAN_POINT('Ctrl Pts',(-2.47699780731677,-0.449764507879297,
10.4159108029712));
#18216=CARTESIAN_POINT('Ctrl Pts',(-2.46184951862394,-0.533191006012003,
10.4212721657518));
#18217=CARTESIAN_POINT('Ctrl Pts',(-2.44249877889863,-0.615758184287968,
10.4266335285323));
#18218=CARTESIAN_POINT('Ctrl Pts',(-2.41908365274357,-0.697022618735462,
10.4319948913129));
#18219=CARTESIAN_POINT('Ctrl Pts',(-2.3956685265885,-0.778287053182968,
10.4373562540934));
#18220=CARTESIAN_POINT('Ctrl Pts',(-2.36818924231083,-0.858248284987959,
10.442717616874));
#18221=CARTESIAN_POINT('Ctrl Pts',(-2.33683560324142,-0.936485778548348,
10.4480789796545));
#18222=CARTESIAN_POINT('Ctrl Pts',(-2.30610252288839,-1.01317477694144,
10.4533342290618));
#18223=CARTESIAN_POINT('Ctrl Pts',(-2.27153358025029,-1.08849092484316,
10.4585894784692));
#18224=CARTESIAN_POINT('Ctrl Pts',(-2.23327249983845,-1.1620241785201,10.4638447278765));
#18225=CARTESIAN_POINT('Ctrl Pts',(-2.19506566494669,-1.23545317874822,
10.469092526534));
#18226=CARTESIAN_POINT('Ctrl Pts',(-2.15317730095472,-1.3071038996678,10.4743403251915));
#18227=CARTESIAN_POINT('Ctrl Pts',(-2.10779945922323,-1.37658551848342,
10.479588123849));
#18228=CARTESIAN_POINT('Ctrl Pts',(-2.06209281590818,-1.44657059152742,
10.4848739473319));
#18229=CARTESIAN_POINT('Ctrl Pts',(-2.01284608921402,-1.51435455592319,
10.4901597708148));
#18230=CARTESIAN_POINT('Ctrl Pts',(-1.96030311786669,-1.57956257745052,
10.4954455942977));
#18231=CARTESIAN_POINT('Ctrl Pts',(-1.90823129571664,-1.64418588314981,
10.5006840201663));
#18232=CARTESIAN_POINT('Ctrl Pts',(-1.85292240139207,-1.70627889164405,
10.5059224460349));
#18233=CARTESIAN_POINT('Ctrl Pts',(-1.794656626426,-1.76550668172772,10.5111608719034));
#18234=CARTESIAN_POINT('Ctrl Pts',(-1.73641001410357,-1.82471499277701,
10.5163975749409));
#18235=CARTESIAN_POINT('Ctrl Pts',(-1.67520877585225,-1.88105962824554,
10.5216342779784));
#18236=CARTESIAN_POINT('Ctrl Pts',(-1.61137120149243,-1.93424122099619,
10.526870981016));
#18237=CARTESIAN_POINT('Ctrl Pts',(-1.54753536603621,-1.98742136510686,
10.5321075414083));
#18238=CARTESIAN_POINT('Ctrl Pts',(-1.48106369243104,-2.03743834325886,
10.5373441018006));
#18239=CARTESIAN_POINT('Ctrl Pts',(-1.41230783671028,-2.08403282708472,
10.542580662193));
#18240=CARTESIAN_POINT('Ctrl Pts',(-1.34242663296713,-2.13138993701242,
10.5479029309634));
#18241=CARTESIAN_POINT('Ctrl Pts',(-1.27018620039252,-2.17521122109056,
10.5532251997339));
#18242=CARTESIAN_POINT('Ctrl Pts',(-1.19598512270871,-2.21527105254852,
10.5585474685044));
#18243=CARTESIAN_POINT('Ctrl Pts',(-1.12287411311555,-2.25474237578864,
10.5637915492547));
#18244=CARTESIAN_POINT('Ctrl Pts',(-1.04786013143497,-2.29056188349954,
10.569035630005));
#18245=CARTESIAN_POINT('Ctrl Pts',(-0.971346323524718,-2.32256163960723,
10.5742797107554));
#18246=CARTESIAN_POINT('Ctrl Pts',(-0.893121311085303,-2.35527705905829,
10.5796410735359));
#18247=CARTESIAN_POINT('Ctrl Pts',(-0.813329058487404,-2.38399963696703,
10.5850024363165));
#18248=CARTESIAN_POINT('Ctrl Pts',(-0.732416675826054,-2.40860375798343,
10.590363799097));
#18249=CARTESIAN_POINT('Ctrl Pts',(-0.651504293164715,-2.43320787899983,
10.5957251618776));
#18250=CARTESIAN_POINT('Ctrl Pts',(-0.56947228959179,-2.45369348482417,
10.6010865246581));
#18251=CARTESIAN_POINT('Ctrl Pts',(-0.486776745845734,-2.46999081976104,
10.6064478874387));
#18252=CARTESIAN_POINT('Ctrl Pts',(-0.405717932061537,-2.48596559395061,
10.611703136846));
#18253=CARTESIAN_POINT('Ctrl Pts',(-0.323722213469202,-2.49797542585534,
10.6169583862533));
#18254=CARTESIAN_POINT('Ctrl Pts',(-0.241211782623407,-2.5059176215358,
10.6222136356606));
#18255=CARTESIAN_POINT('Ctrl Pts',(-0.158818332824435,-2.51384855698703,
10.6274614343181));
#18256=CARTESIAN_POINT('Ctrl Pts',(-0.0759120757247375,-2.51772326728586,
10.6327092329755));
#18257=CARTESIAN_POINT('Ctrl Pts',(0.00707460686686389,-2.51749005955092,
10.637957031633));
#18258=CARTESIAN_POINT('Ctrl Pts',(0.0906625995169013,-2.51725516202489,
10.6432428551159));
#18259=CARTESIAN_POINT('Ctrl Pts',(0.174331723135915,-2.51285247283202,
10.6485286785989));
#18260=CARTESIAN_POINT('Ctrl Pts',(0.25763481129679,-2.50428244293811,10.6538145020818));
#18261=CARTESIAN_POINT('Ctrl Pts',(0.340190926416144,-2.49578925991071,
10.6590529279504));
#18262=CARTESIAN_POINT('Ctrl Pts',(0.422387076759307,-2.48320322145356,
10.664291353819));
#18263=CARTESIAN_POINT('Ctrl Pts',(0.503789782285385,-2.46657700168976,
10.6695297796875));
#18264=CARTESIAN_POINT('Ctrl Pts',(0.585165715816503,-2.44995625001291,
10.6747664827251));
#18265=CARTESIAN_POINT('Ctrl Pts',(0.665748271062474,-2.42929804826106,
10.6800031857626));
#18266=CARTESIAN_POINT('Ctrl Pts',(0.745113047788698,-2.40470638457485,
10.6852398888001));
#18267=CARTESIAN_POINT('Ctrl Pts',(0.824475662657691,-2.38011539075338,
10.6904764491924));
#18268=CARTESIAN_POINT('Ctrl Pts',(0.902620124518652,-2.35159128558361,
10.6957130095847));
#18269=CARTESIAN_POINT('Ctrl Pts',(0.979137451061313,-2.31928784369883,
10.700949569977));
#18270=CARTESIAN_POINT('Ctrl Pts',(1.05690715998257,-2.2864556815462,10.7062718387475));
#18271=CARTESIAN_POINT('Ctrl Pts',(1.1329955312796,-2.24971953054739,10.711594107518));
#18272=CARTESIAN_POINT('Ctrl Pts',(1.20699630142809,-2.20929087680616,10.7169163762885));
#18273=CARTESIAN_POINT('Ctrl Pts',(1.27990994615004,-2.16945614955183,10.7221604570388));
#18274=CARTESIAN_POINT('Ctrl Pts',(1.35079655230279,-2.12603698732614,10.7274045377892));
#18275=CARTESIAN_POINT('Ctrl Pts',(1.41929576301148,-2.07928011270672,10.7326486185395));
#18276=CARTESIAN_POINT('Ctrl Pts',(1.4893269345886,-2.03147753695431,10.7380099813201));
#18277=CARTESIAN_POINT('Ctrl Pts',(1.55686222783487,-1.98018646343722,10.7433713441006));
#18278=CARTESIAN_POINT('Ctrl Pts',(1.62155284777459,-1.92571353318039,10.7487327068812));
#18279=CARTESIAN_POINT('Ctrl Pts',(1.6862434677143,-1.87124060292358,10.7540940696618));
#18280=CARTESIAN_POINT('Ctrl Pts',(1.74808908823758,-1.8135862112583,10.7594554324423));
#18281=CARTESIAN_POINT('Ctrl Pts',(1.80678288493526,-1.75309493659215,10.7648167952229));
#18282=CARTESIAN_POINT('Ctrl Pts',(1.86353796867841,-1.69460174731883,10.7700010669979));
#18283=CARTESIAN_POINT('Ctrl Pts',(1.91756794793396,-1.63322734809474,10.7751853387729));
#18284=CARTESIAN_POINT('Ctrl Pts',(1.96856067929309,-1.56925941193326,10.7803696105479));
#18285=CARTESIAN_POINT('Ctrl Pts',(2.0194881038542,-1.50537340001815,10.7855472427847));
#18286=CARTESIAN_POINT('Ctrl Pts',(2.06738570241999,-1.43890080617497,10.7907248750215));
#18287=CARTESIAN_POINT('Ctrl Pts',(2.11197797192582,-1.37016615638399,10.7959025072582));
#18288=CARTESIAN_POINT('Ctrl Pts',(2.15652744873156,-1.30149746738145,10.8010751708117));
#18289=CARTESIAN_POINT('Ctrl Pts',(2.19777763273926,-1.230571425196,10.8062478343652));
#18290=CARTESIAN_POINT('Ctrl Pts',(2.23549414426048,-1.15774443681543,10.8114204979187));
#18291=CARTESIAN_POINT('Ctrl Pts',(2.27318656404733,-1.08496396727738,10.8165898573905));
#18292=CARTESIAN_POINT('Ctrl Pts',(2.30734957417607,-1.01028538234413,10.8217592168623));
#18293=CARTESIAN_POINT('Ctrl Pts',(2.33779370789917,-0.934091445901874,
10.8269285763341));
#18294=CARTESIAN_POINT('Ctrl Pts',(2.36823897829908,-0.857894664646169,
10.8320981288115));
#18295=CARTESIAN_POINT('Ctrl Pts',(2.39496490115964,-0.780182852656203,
10.837267681289));
#18296=CARTESIAN_POINT('Ctrl Pts',(2.41782980818633,-0.701359585837148,
10.8424372337665));
#18297=CARTESIAN_POINT('Ctrl Pts',(2.44069380324846,-0.622539462876305,
10.8476065800568));
#18298=CARTESIAN_POINT('Ctrl Pts',(2.45969696387435,-0.542608431845676,
10.8527759263472));
#18299=CARTESIAN_POINT('Ctrl Pts',(2.47474785657928,-0.461984086691589,
10.8579452726376));
#18300=CARTESIAN_POINT('Ctrl Pts',(2.48981318905341,-0.381282390847459,
10.8631195783791));
#18301=CARTESIAN_POINT('Ctrl Pts',(2.50091860016248,-0.299886521460539,
10.8682938841207));
#18302=CARTESIAN_POINT('Ctrl Pts',(2.50802417071427,-0.218222384536952,
10.8734681898622));
#18303=CARTESIAN_POINT('Ctrl Pts',(2.51440905980166,-0.144841020876706,
10.8781176923931));
#18304=CARTESIAN_POINT('Ctrl Pts',(2.51756501124576,-0.0712433790694381,
10.882767194924));
#18305=CARTESIAN_POINT('Ctrl Pts',(2.51749898433573,0.00226138642592499,
10.8874166974549));
#18306=CARTESIAN_POINT('Ctrl Pts',(2.51749898433498,0.00226138726554988,
10.887416697508));
#18307=CARTESIAN_POINT('Ctrl Pts',(2.5173983212915,0.114324948237316,10.8945052149239));
#18308=CARTESIAN_POINT('Ctrl Pts',(2.50981145266277,0.226062019317946,10.9015937323398));
#18309=CARTESIAN_POINT('Ctrl Pts',(2.49489001405865,0.336645314463777,10.9086822497556));
#18310=CARTESIAN_POINT('Ctrl Pts',(2.48471334971823,0.412064924208791,10.9135167341728));
#18311=CARTESIAN_POINT('Ctrl Pts',(2.4711260222801,0.486948560768708,10.9183512185899));
#18312=CARTESIAN_POINT('Ctrl Pts',(2.4541882701679,0.561040270007676,10.923185703007));
#18313=CARTESIAN_POINT('Ctrl Pts',(2.4357768697415,0.64157823738605,10.9284408058016));
#18314=CARTESIAN_POINT('Ctrl Pts',(2.41336280308272,0.721357675404119,10.9336959085962));
#18315=CARTESIAN_POINT('Ctrl Pts',(2.38702415962054,0.799951193128594,10.9389510113908));
#18316=CARTESIAN_POINT('Ctrl Pts',(2.37886522088455,0.824297158291176,10.9405788880054));
#18317=CARTESIAN_POINT('Ctrl Pts',(2.37033006201922,0.848529372445582,10.94220676462));
#18318=CARTESIAN_POINT('Ctrl Pts',(2.36142200728636,0.872635292378011,10.9438346412346));
#18319=CARTESIAN_POINT('',(2.51749997867612,-0.000327667110924752,10.6149188233509));
#18320=CARTESIAN_POINT('Ctrl Pts',(2.3614219719961,0.872635387876314,10.6673175101421));
#18321=CARTESIAN_POINT('Ctrl Pts',(2.38753013195813,0.801984594384251,10.6628599804557));
#18322=CARTESIAN_POINT('Ctrl Pts',(2.41046358840151,0.730173114338968,10.6584813167228));
#18323=CARTESIAN_POINT('Ctrl Pts',(2.47566938108042,0.489138520415815,10.6440744556866));
#18324=CARTESIAN_POINT('Ctrl Pts',(2.50358581879094,0.316608122570416,10.6342474256015));
#18325=CARTESIAN_POINT('Ctrl Pts',(2.51540284035079,0.108321598130534,10.621654531346));
#18326=CARTESIAN_POINT('Ctrl Pts',(2.51664606178224,0.0740091890297152,
10.6195555519703));
#18327=CARTESIAN_POINT('Ctrl Pts',(2.5173298295721,0.0306372799154144,10.6168595333047));
#18328=CARTESIAN_POINT('Ctrl Pts',(2.51742367915042,0.0215899944366838,
10.6162947943949));
#18329=CARTESIAN_POINT('Ctrl Pts',(2.51749012946065,0.00825247343740583,
10.6154585264606));
#18330=CARTESIAN_POINT('Ctrl Pts',(2.51750053705118,0.00396238565652019,
10.6151889674799));
#18331=CARTESIAN_POINT('Ctrl Pts',(2.51749997867612,-0.000327667110924752,
10.6149188233509));
#18332=CARTESIAN_POINT('Ctrl Pts',(2.51749997858344,-0.000328378448568064,
10.6149187785581));
#18333=CARTESIAN_POINT('Ctrl Pts',(2.51749957459957,-0.00342550428806741,
10.6147237528536));
#18334=CARTESIAN_POINT('Ctrl Pts',(2.51749345531221,-0.0065226102894847,
10.6145284222777));
#18335=CARTESIAN_POINT('Ctrl Pts',(2.51745918050036,-0.0154923684534925,
10.6139618040555));
#18336=CARTESIAN_POINT('Ctrl Pts',(2.51741619102707,-0.0213648877897438,
10.6135897120455));
#18337=CARTESIAN_POINT('Ctrl Pts',(2.51728166745765,-0.033798035259292,
10.6127994435243));
#18338=CARTESIAN_POINT('Ctrl Pts',(2.51718503287258,-0.0403584823729039,
10.6123809765192));
#18339=CARTESIAN_POINT('Ctrl Pts',(2.51689072622532,-0.0561473645042193,
10.6113704201091));
#18340=CARTESIAN_POINT('Ctrl Pts',(2.51666794237783,-0.0653751923519982,
10.6107769720843));
#18341=CARTESIAN_POINT('Ctrl Pts',(2.51574187936881,-0.0966123993385475,
10.6087589821041));
#18342=CARTESIAN_POINT('Ctrl Pts',(2.51480059563153,-0.118613009291447,
10.6073223942329));
#18343=CARTESIAN_POINT('Ctrl Pts',(2.51235677467159,-0.162303085450508,
10.6044427754474));
#18344=CARTESIAN_POINT('Ctrl Pts',(2.51086160499253,-0.183991283202461,
10.603000168833));
#18345=CARTESIAN_POINT('Ctrl Pts',(2.49519664982502,-0.37510942135449,10.5901868837444));
#18346=CARTESIAN_POINT('Ctrl Pts',(2.46417812493984,-0.542712628507912,
10.5782847751557));
#18347=CARTESIAN_POINT('Ctrl Pts',(2.38190687746773,-0.824349383005594,
10.5581486165164));
#18348=CARTESIAN_POINT('Ctrl Pts',(2.33864240964159,-0.940101723006075,
10.5498223723753));
#18349=CARTESIAN_POINT('Ctrl Pts',(2.27083938297377,-1.08747416594008,10.5392326526807));
#18350=CARTESIAN_POINT('Ctrl Pts',(2.25380968384517,-1.12234297212867,10.5367268024903));
#18351=CARTESIAN_POINT('Ctrl Pts',(2.2284959682926,-1.17127163318593,10.5332082794644));
#18352=CARTESIAN_POINT('Ctrl Pts',(2.22087161105699,-1.18566471944585,10.5321729519042));
#18353=CARTESIAN_POINT('Ctrl Pts',(2.20745270224278,-1.21041297998127,10.5303919238626));
#18354=CARTESIAN_POINT('Ctrl Pts',(2.20172370535086,-1.22080291113549,10.5296439474443));
#18355=CARTESIAN_POINT('Ctrl Pts',(2.19057971398888,-1.24067968268403,10.5282123526258));
#18356=CARTESIAN_POINT('Ctrl Pts',(2.18517602014863,-1.25017251823079,10.527528354568));
#18357=CARTESIAN_POINT('Ctrl Pts',(2.17228005079754,-1.2724881836021,10.5259195527403));
#18358=CARTESIAN_POINT('Ctrl Pts',(2.16473570378715,-1.28528057016568,10.5249966324264));
#18359=CARTESIAN_POINT('Ctrl Pts',(2.14184472128715,-1.32332173346476,10.5222494223788));
#18360=CARTESIAN_POINT('Ctrl Pts',(2.12616602175079,-1.34836841364802,10.5204370824753));
#18361=CARTESIAN_POINT('Ctrl Pts',(2.01207723793185,-1.52368485441108,10.5077113295619));
#18362=CARTESIAN_POINT('Ctrl Pts',(1.898273111502,-1.663321474057,10.4974126751653));
#18363=CARTESIAN_POINT('Ctrl Pts',(1.69275831288387,-1.86664256412825,10.4807984124612));
#18364=CARTESIAN_POINT('Ctrl Pts',(1.61002111632048,-1.93845652730022,10.4745039220776));
#18365=CARTESIAN_POINT('Ctrl Pts',(1.48253288465022,-2.03530588075346,10.4649391348528));
#18366=CARTESIAN_POINT('Ctrl Pts',(1.44127115883748,-2.0647301136129,10.4618614093995));
#18367=CARTESIAN_POINT('Ctrl Pts',(1.39159715120258,-2.09793856647254,10.4581411117589));
#18368=CARTESIAN_POINT('Ctrl Pts',(1.38401397268012,-2.10294892416184,10.457572769733));
#18369=CARTESIAN_POINT('Ctrl Pts',(1.36955623184223,-2.11238937277149,10.456488090803));
#18370=CARTESIAN_POINT('Ctrl Pts',(1.36268686844723,-2.11682725523524,10.4559722541331));
#18371=CARTESIAN_POINT('Ctrl Pts',(1.35040395768513,-2.12467794131628,10.4550488382958));
#18372=CARTESIAN_POINT('Ctrl Pts',(1.34499886695179,-2.12810367458251,10.454642115582));
#18373=CARTESIAN_POINT('Ctrl Pts',(1.33310986540093,-2.13557550698314,10.4537466149593));
#18374=CARTESIAN_POINT('Ctrl Pts',(1.32662067451829,-2.13961263819215,10.4532572921579));
#18375=CARTESIAN_POINT('Ctrl Pts',(1.30875323543977,-2.15061600772809,10.4519087068624));
#18376=CARTESIAN_POINT('Ctrl Pts',(1.29733802407315,-2.15752132710056,10.4510457058427));
#18377=CARTESIAN_POINT('Ctrl Pts',(1.2340925713079,-2.19509653468859,10.4462588279196));
#18378=CARTESIAN_POINT('Ctrl Pts',(1.18123353221974,-2.22398726496045,10.4422383422976));
#18379=CARTESIAN_POINT('Ctrl Pts',(0.923549427309861,-2.35304891759812,
10.4227171027183));
#18380=CARTESIAN_POINT('Ctrl Pts',(0.70677037352199,-2.426990624531,10.4066489729991));
#18381=CARTESIAN_POINT('Ctrl Pts',(0.436908130361662,-2.47974193477186,
10.3883259121943));
#18382=CARTESIAN_POINT('Ctrl Pts',(0.3906037965418,-2.48745611209794,10.3852335239401));
#18383=CARTESIAN_POINT('Ctrl Pts',(0.309949773739372,-2.49858488164457,
10.3799365676373));
#18384=CARTESIAN_POINT('Ctrl Pts',(0.275696671197079,-2.50259601431372,
10.3777146410588));
#18385=CARTESIAN_POINT('Ctrl Pts',(0.225893044645415,-2.50739313981557,
10.3745225096445));
#18386=CARTESIAN_POINT('Ctrl Pts',(0.210401799524816,-2.5087405457031,10.3735349822504));
#18387=CARTESIAN_POINT('Ctrl Pts',(0.183189937584401,-2.51085356409409,
10.3718094453232));
#18388=CARTESIAN_POINT('Ctrl Pts',(0.171474722907431,-2.51168083173649,
10.3710695399124));
#18389=CARTESIAN_POINT('Ctrl Pts',(0.147117431978758,-2.51322960338131,
10.3695371897336));
#18390=CARTESIAN_POINT('Ctrl Pts',(0.134474816605329,-2.51393776994115,
10.3687451797638));
#18391=CARTESIAN_POINT('Ctrl Pts',(0.101656131209017,-2.5155277991798,10.3666976082304));
#18392=CARTESIAN_POINT('Ctrl Pts',(0.081473586061596,-2.5162623410592,10.365446636789));
#18393=CARTESIAN_POINT('Ctrl Pts',(-0.00205060046043071,-2.51829618693438,
10.3603012112854));
#18394=CARTESIAN_POINT('Ctrl Pts',(-0.0654241703440023,-2.51744723027823,
10.3564731484526));
#18395=CARTESIAN_POINT('Ctrl Pts',(-0.354587084316347,-2.50264496794959,
10.3392413479069));
#18396=CARTESIAN_POINT('Ctrl Pts',(-0.577860692956225,-2.46069716787177,
10.326692380744));
#18397=CARTESIAN_POINT('Ctrl Pts',(-0.83695234210536,-2.37476492721169,
10.3105936322072));
#18398=CARTESIAN_POINT('Ctrl Pts',(-0.880962771817687,-2.35879243945169,
10.3077980953124));
#18399=CARTESIAN_POINT('Ctrl Pts',(-0.951722428837876,-2.33085547876292,
10.303165253962));
#18400=CARTESIAN_POINT('Ctrl Pts',(-0.978754299980336,-2.31963417241312,
10.301361768732));
#18401=CARTESIAN_POINT('Ctrl Pts',(-1.01497268533276,-2.30385364134825,
10.2988917297993));
#18402=CARTESIAN_POINT('Ctrl Pts',(-1.02433708987833,-2.29970534428829,
10.2982481857628));
#18403=CARTESIAN_POINT('Ctrl Pts',(-1.03989884412982,-2.29269780477186,
10.2971701267101));
#18404=CARTESIAN_POINT('Ctrl Pts',(-1.04611045999065,-2.28987024376169,
10.2967375065194));
#18405=CARTESIAN_POINT('Ctrl Pts',(-1.05783496463517,-2.28447552399394,
10.295916425885));
#18406=CARTESIAN_POINT('Ctrl Pts',(-1.06335020373665,-2.2819135773415,10.2955282948099));
#18407=CARTESIAN_POINT('Ctrl Pts',(-1.07637049324967,-2.27580792146334,
10.2946076129807));
#18408=CARTESIAN_POINT('Ctrl Pts',(-1.0838673544966,-2.27224705685503,10.2940740377422));
#18409=CARTESIAN_POINT('Ctrl Pts',(-1.1099791569752,-2.25968582896782,10.2922038149076));
#18410=CARTESIAN_POINT('Ctrl Pts',(-1.12850013939999,-2.2504935336932,10.2908563148761));
#18411=CARTESIAN_POINT('Ctrl Pts',(-1.28754299472856,-2.16910085451562,
10.2791161168946));
#18412=CARTESIAN_POINT('Ctrl Pts',(-1.42108173315797,-2.0840547403687,10.2681331159879));
#18413=CARTESIAN_POINT('Ctrl Pts',(-1.64239481745146,-1.91189303956432,
10.2487801092099));
#18414=CARTESIAN_POINT('Ctrl Pts',(-1.73342657162677,-1.82976330741955,
10.2403986447282));
#18415=CARTESIAN_POINT('Ctrl Pts',(-1.84902955455047,-1.7090617178523,10.2292833192714));
#18416=CARTESIAN_POINT('Ctrl Pts',(-1.8790689352992,-1.67597809748634,10.2263441803925));
#18417=CARTESIAN_POINT('Ctrl Pts',(-1.92987233512501,-1.61694205003993,
10.221282307625));
#18418=CARTESIAN_POINT('Ctrl Pts',(-1.95103197319459,-1.59134635906815,
10.2191442233013));
#18419=CARTESIAN_POINT('Ctrl Pts',(-1.98120479631392,-1.5533410660387,10.2160494120328));
#18420=CARTESIAN_POINT('Ctrl Pts',(-1.99062016236569,-1.54125672698266,
10.2150768087034));
#18421=CARTESIAN_POINT('Ctrl Pts',(-2.00703784409035,-1.51978369797835,
10.2133683308657));
#18422=CARTESIAN_POINT('Ctrl Pts',(-2.01408596744621,-1.51043077281748,
10.212630677117));
#18423=CARTESIAN_POINT('Ctrl Pts',(-2.02867908161984,-1.49078179319963,
10.2110943309542));
#18424=CARTESIAN_POINT('Ctrl Pts',(-2.03621156347878,-1.48047683178363,
10.2102961357227));
#18425=CARTESIAN_POINT('Ctrl Pts',(-2.05573188399112,-1.45334085388171,
10.2082135834458));
#18426=CARTESIAN_POINT('Ctrl Pts',(-2.06759160317454,-1.43641853867961,
10.2069341211091));
#18427=CARTESIAN_POINT('Ctrl Pts',(-2.11728903364949,-1.36361559741499,
10.2015083685032));
#18428=CARTESIAN_POINT('Ctrl Pts',(-2.15308182660201,-1.30636908079411,
10.1974381523756));
#18429=CARTESIAN_POINT('Ctrl Pts',(-2.28446057396817,-1.0761433446066,10.1817007121886));
#18430=CARTESIAN_POINT('Ctrl Pts',(-2.36184108735325,-0.89361573269217,
10.1706262664755));
#18431=CARTESIAN_POINT('Ctrl Pts',(-2.43448126368547,-0.644187755481913,
10.1554761063338));
#18432=CARTESIAN_POINT('Ctrl Pts',(-2.44965576886291,-0.583834296811531,
10.1518033369345));
#18433=CARTESIAN_POINT('Ctrl Pts',(-2.46998643302507,-0.488103353977006,
10.1458814130446));
#18434=CARTESIAN_POINT('Ctrl Pts',(-2.47665197046114,-0.453070174549224,
10.1436942312045));
#18435=CARTESIAN_POINT('Ctrl Pts',(-2.48439939026788,-0.407046992703168,
10.1407809192934));
#18436=CARTESIAN_POINT('Ctrl Pts',(-2.48615658184325,-0.396172973255005,
10.1400896759648));
#18437=CARTESIAN_POINT('Ctrl Pts',(-2.48891246160676,-0.378377988306357,
10.1389532155672));
#18438=CARTESIAN_POINT('Ctrl Pts',(-2.48995379559916,-0.371463640900195,
10.1385103410759));
#18439=CARTESIAN_POINT('Ctrl Pts',(-2.49193211997425,-0.357945591364488,
10.1376418013031));
#18440=CARTESIAN_POINT('Ctrl Pts',(-2.49287169276949,-0.351342364016672,
10.1372162821138));
#18441=CARTESIAN_POINT('Ctrl Pts',(-2.49491356548371,-0.336571648608706,
10.1362617404116));
#18442=CARTESIAN_POINT('Ctrl Pts',(-2.49600201870287,-0.328402332515074,
10.1357319646937));
#18443=CARTESIAN_POINT('Ctrl Pts',(-2.49963744276939,-0.300054286493891,
10.1338875669656));
#18444=CARTESIAN_POINT('Ctrl Pts',(-2.50197989940242,-0.279850748376581,
10.1325624699713));
#18445=CARTESIAN_POINT('Ctrl Pts',(-2.52092357286169,-0.0971372093117507,
10.1204962948171));
#18446=CARTESIAN_POINT('Ctrl Pts',(-2.52191378982063,0.0665877779835312,
10.1091228666568));
#18447=CARTESIAN_POINT('Ctrl Pts',(-2.49129956622154,0.401395038494172,
10.0859288283872));
#18448=CARTESIAN_POINT('Ctrl Pts',(-2.45786506292514,0.571498928622087,
10.0741941900692));
#18449=CARTESIAN_POINT('Ctrl Pts',(-2.39948689554551,0.762215295139084,
10.0613076607371));
#18450=CARTESIAN_POINT('Ctrl Pts',(-2.39132445884022,0.787449641823742,
10.0596071326662));
#18451=CARTESIAN_POINT('Ctrl Pts',(-2.37824015787482,0.825818684746376,
10.0570275551696));
#18452=CARTESIAN_POINT('Ctrl Pts',(-2.37360495124534,0.839048447328103,
10.0561392224297));
#18453=CARTESIAN_POINT('Ctrl Pts',(-2.36531792395057,0.862082833196594,
10.0545942805152));
#18454=CARTESIAN_POINT('Ctrl Pts',(-2.36171507343008,0.871904587620782,
10.0539360796937));
#18455=CARTESIAN_POINT('Ctrl Pts',(-2.35343463355426,0.894050008575098,
10.052453135533));
#18456=CARTESIAN_POINT('Ctrl Pts',(-2.34872124634027,0.906360033174254,
10.0516295986676));
#18457=CARTESIAN_POINT('Ctrl Pts',(-2.33567290266129,0.939653167424983,
10.049404075569));
#18458=CARTESIAN_POINT('Ctrl Pts',(-2.32715188697292,0.960562402589358,
10.0480083076319));
#18459=CARTESIAN_POINT('Ctrl Pts',(-2.28341828692826,1.06387857650208,10.0411171406873));
#18460=CARTESIAN_POINT('Ctrl Pts',(-2.24410256816616,1.14448367673421,10.0357616948804));
#18461=CARTESIAN_POINT('Ctrl Pts',(-2.11500515130242,1.37680401994983,10.0201601264924));
#18462=CARTESIAN_POINT('Ctrl Pts',(-2.01352260459123,1.52136775236244,10.0102564927425));
#18463=CARTESIAN_POINT('Ctrl Pts',(-1.85885721426075,1.6988131419265,9.99650366605367));
#18464=CARTESIAN_POINT('Ctrl Pts',(-1.81836755050526,1.74208346018455,9.99299895726296));
#18465=CARTESIAN_POINT('Ctrl Pts',(-1.75993658156716,1.80026908820957,9.98800366674946));
#18466=CARTESIAN_POINT('Ctrl Pts',(-1.74325552388882,1.81642661851913,9.98658420739711));
#18467=CARTESIAN_POINT('Ctrl Pts',(-1.71373816425295,1.84423647881634,9.9840787237502));
#18468=CARTESIAN_POINT('Ctrl Pts',(-1.70100035531801,1.8559914973267,9.98299948974418));
#18469=CARTESIAN_POINT('Ctrl Pts',(-1.68196532890022,1.8731973249436,9.98138778796064));
#18470=CARTESIAN_POINT('Ctrl Pts',(-1.67576050226168,1.87875020164524,9.98086258934892));
#18471=CARTESIAN_POINT('Ctrl Pts',(-1.66511554724683,1.88818198920309,9.97996161212716));
#18472=CARTESIAN_POINT('Ctrl Pts',(-1.66068916591767,1.89207624142267,9.97958697611093));
#18473=CARTESIAN_POINT('Ctrl Pts',(-1.65062432977439,1.90086857857118,9.97873507813718));
#18474=CARTESIAN_POINT('Ctrl Pts',(-1.64497784619459,1.90575704462086,9.97825714630172));
#18475=CARTESIAN_POINT('Ctrl Pts',(-1.62956708164645,1.91897946139476,9.9769529222285));
#18476=CARTESIAN_POINT('Ctrl Pts',(-1.61976082684076,1.92726383617347,9.97612320684488));
#18477=CARTESIAN_POINT('Ctrl Pts',(-1.57035020650584,1.96836271573562,9.97194535575163));
#18478=CARTESIAN_POINT('Ctrl Pts',(-1.52981286797455,2.00003082825864,9.96852694758394));
#18479=CARTESIAN_POINT('Ctrl Pts',(-1.3666869264535,2.11960458498591,9.95489462403589));
#18480=CARTESIAN_POINT('Ctrl Pts',(-1.23727226613267,2.1976607084222,9.94436476990255));
#18481=CARTESIAN_POINT('Ctrl Pts',(-0.971402086897258,2.32705124523744,
9.92405367907568));
#18482=CARTESIAN_POINT('Ctrl Pts',(-0.835906816978862,2.37908838904751,
9.91429771706695));
#18483=CARTESIAN_POINT('Ctrl Pts',(-0.670357757058067,2.4267625166531,9.90315799669041));
#18484=CARTESIAN_POINT('Ctrl Pts',(-0.643925756265351,2.43390952003248,
9.90140135674121));
#18485=CARTESIAN_POINT('Ctrl Pts',(-0.603621092038556,2.44410500874085,
9.89875501193101));
#18486=CARTESIAN_POINT('Ctrl Pts',(-0.589831219859135,2.4474694813251,9.8978552678731));
#18487=CARTESIAN_POINT('Ctrl Pts',(-0.564723631774981,2.45337073630171,
9.89622714899279));
#18488=CARTESIAN_POINT('Ctrl Pts',(-0.553415516372069,2.45594625827215,
9.89549755773439));
#18489=CARTESIAN_POINT('Ctrl Pts',(-0.52895349010041,2.4613401653427,9.89392706945352));
#18490=CARTESIAN_POINT('Ctrl Pts',(-0.515793925170151,2.46413145796284,
9.89308705236989));
#18491=CARTESIAN_POINT('Ctrl Pts',(-0.47987712673323,2.4714494825323,9.89080713412552));
#18492=CARTESIAN_POINT('Ctrl Pts',(-0.457078328765627,2.47576736752077,
9.88937384203083));
#18493=CARTESIAN_POINT('Ctrl Pts',(-0.331523446930536,2.49775277893056,
9.88155187993226));
#18494=CARTESIAN_POINT('Ctrl Pts',(-0.227799753290429,2.50934009742363,
9.87535718135092));
#18495=CARTESIAN_POINT('Ctrl Pts',(0.0417160593748585,2.52259327000825,
9.8596143634522));
#18496=CARTESIAN_POINT('Ctrl Pts',(0.207468441432837,2.51439261681814,9.85029044450562));
#18497=CARTESIAN_POINT('Ctrl Pts',(0.452363150396881,2.47788338317032,9.83578656165403));
#18498=CARTESIAN_POINT('Ctrl Pts',(0.532868130982717,2.46182598414749,9.83089158469095));
#18499=CARTESIAN_POINT('Ctrl Pts',(0.626101070168777,2.43844256994088,9.82492410392657));
#18500=CARTESIAN_POINT('Ctrl Pts',(0.639736303658354,2.43490085168376,9.8240437431648));
#18501=CARTESIAN_POINT('Ctrl Pts',(0.660743542832745,2.4292556431424,9.82267459670275));
#18502=CARTESIAN_POINT('Ctrl Pts',(0.668137117730192,2.42723253878861,9.82219025841161));
#18503=CARTESIAN_POINT('Ctrl Pts',(0.681804255258157,2.42342562231827,9.82129019244053));
#18504=CARTESIAN_POINT('Ctrl Pts',(0.688080238292918,2.42165116641887,9.82087499924405));
#18505=CARTESIAN_POINT('Ctrl Pts',(0.702423293231371,2.41753558915091,9.81992184103611));
#18506=CARTESIAN_POINT('Ctrl Pts',(0.710485562041883,2.41517847559543,9.81938297856681));
#18507=CARTESIAN_POINT('Ctrl Pts',(0.731654057910166,2.4088744138878,9.81796026731902));
#18508=CARTESIAN_POINT('Ctrl Pts',(0.744739953539584,2.40486090750032,9.81707282940518));
#18509=CARTESIAN_POINT('Ctrl Pts',(0.856428648585164,2.36960645332421,9.80943414743815));
#18510=CARTESIAN_POINT('Ctrl Pts',(0.953042214726981,2.332425895425,9.80239952620401));
#18511=CARTESIAN_POINT('Ctrl Pts',(1.197221327585,2.22074845323684,9.78393008628809));
#18512=CARTESIAN_POINT('Ctrl Pts',(1.34025663832435,2.13747145108765,9.77244171894969));
#18513=CARTESIAN_POINT('Ctrl Pts',(1.54318947344083,1.99088768942309,9.75563412759824));
#18514=CARTESIAN_POINT('Ctrl Pts',(1.60969452066259,1.93751228449982,9.75002316110792));
#18515=CARTESIAN_POINT('Ctrl Pts',(1.68940639355854,1.86659394952443,9.74316482921825));
#18516=CARTESIAN_POINT('Ctrl Pts',(1.70525942239742,1.85212237282638,9.74179363094978));
#18517=CARTESIAN_POINT('Ctrl Pts',(1.73036941159569,1.82860475742239,9.73960949664));
#18518=CARTESIAN_POINT('Ctrl Pts',(1.73974478878245,1.81968726420496,9.73879118575063));
#18519=CARTESIAN_POINT('Ctrl Pts',(1.75744201355821,1.80259255514466,9.73724093439485));
#18520=CARTESIAN_POINT('Ctrl Pts',(1.7657765525782,1.79442902467809,9.73650843539827));
#18521=CARTESIAN_POINT('Ctrl Pts',(1.78467661374134,1.77565756192688,9.73484163468123));
#18522=CARTESIAN_POINT('Ctrl Pts',(1.79520492260039,1.76501266114465,9.73390898213249));
#18523=CARTESIAN_POINT('Ctrl Pts',(1.82747476225071,1.73179799026465,9.73103671347212));
#18524=CARTESIAN_POINT('Ctrl Pts',(1.84889081714552,1.70891520124081,9.72911106393133));
#18525=CARTESIAN_POINT('Ctrl Pts',(2.00449919592539,1.53629911474618,9.71495430327224));
#18526=CARTESIAN_POINT('Ctrl Pts',(2.12074928845023,1.37137273952955,9.7035194184664));
#18527=CARTESIAN_POINT('Ctrl Pts',(2.27205578341547,1.0906218481476,9.6851564163805));
#18528=CARTESIAN_POINT('Ctrl Pts',(2.32059591720706,0.983114007988647,9.67832658896893));
#18529=CARTESIAN_POINT('Ctrl Pts',(2.36142200350084,0.872635302621939,9.67114329893353));
#18530=CARTESIAN_POINT('Origin',(0.,0.,10.));
#18531=CARTESIAN_POINT('',(2.36142186693781,0.872635672172493,8.66836043115426));
#18532=CARTESIAN_POINT('',(2.36142200728636,0.872635292378026,8.94380698639026));
#18533=CARTESIAN_POINT('',(2.36142200728636,0.87263529237802,10.));
#18534=CARTESIAN_POINT('',(2.51749994136415,-0.000543352107728946,9.88741669745326));
#18535=CARTESIAN_POINT('Ctrl Pts',(2.36142200728635,0.872635292378026,8.94380698639026));
#18536=CARTESIAN_POINT('Ctrl Pts',(2.33302028921955,0.949492649252658,8.94896806576715));
#18537=CARTESIAN_POINT('Ctrl Pts',(2.30085777760834,1.02497408410551,8.95412914514404));
#18538=CARTESIAN_POINT('Ctrl Pts',(2.26510290562476,1.09868788877018,8.95929022452092));
#18539=CARTESIAN_POINT('Ctrl Pts',(2.22846148870633,1.17422943316732,8.96457927327726));
#18540=CARTESIAN_POINT('Ctrl Pts',(2.18804739574404,1.24791403963753,8.96986832203359));
#18541=CARTESIAN_POINT('Ctrl Pts',(2.14409230335549,1.31934621865974,8.97515737078992));
#18542=CARTESIAN_POINT('Ctrl Pts',(2.10114674343037,1.3891377890576,8.98032494405548));
#18543=CARTESIAN_POINT('Ctrl Pts',(2.05482143374227,1.45677892969738,8.98549251732103));
#18544=CARTESIAN_POINT('Ctrl Pts',(2.00537560108398,1.52193132189894,8.99066009058658));
#18545=CARTESIAN_POINT('Ctrl Pts',(1.95418626432411,1.58938104548163,8.99600987708831));
#18546=CARTESIAN_POINT('Ctrl Pts',(1.89965259770243,1.6541628068661,9.00135966359003));
#18547=CARTESIAN_POINT('Ctrl Pts',(1.84210502463234,1.71594152820668,9.00670945009175));
#18548=CARTESIAN_POINT('Ctrl Pts',(1.78455745156225,1.77772024954727,9.01205923659348));
#18549=CARTESIAN_POINT('Ctrl Pts',(1.72399642618433,1.8364955984303,9.0174090230952));
#18550=CARTESIAN_POINT('Ctrl Pts',(1.66078955074694,1.89197894230612,9.02275880959693));
#18551=CARTESIAN_POINT('Ctrl Pts',(1.59869961602288,1.9464818294633,9.02801405900423));
#18552=CARTESIAN_POINT('Ctrl Pts',(1.53380920573821,1.99802568053148,9.03326930841153));
#18553=CARTESIAN_POINT('Ctrl Pts',(1.46643193098255,2.04630976193606,9.03852455781883));
#18554=CARTESIAN_POINT('Ctrl Pts',(1.39915018189616,2.09452538748206,9.04377235647632));
#18555=CARTESIAN_POINT('Ctrl Pts',(1.32938894355375,2.13949015670334,9.04902015513382));
#18556=CARTESIAN_POINT('Ctrl Pts',(1.25749623897869,2.18094233278976,9.05426795379132));
#18557=CARTESIAN_POINT('Ctrl Pts',(1.18508260978013,2.22269486562794,9.05955377727422));
#18558=CARTESIAN_POINT('Ctrl Pts',(1.11050685153594,2.2608833743918,9.06483960075713));
#18559=CARTESIAN_POINT('Ctrl Pts',(1.0341559473649,2.2952838008686,9.07012542424004));
#18560=CARTESIAN_POINT('Ctrl Pts',(0.958489676481416,2.32937576109568,9.07536385010863));
#18561=CARTESIAN_POINT('Ctrl Pts',(0.881080395831208,2.3597471088514,9.08060227597723));
#18562=CARTESIAN_POINT('Ctrl Pts',(0.802329463704639,2.38622582369553,9.08584070184582));
#18563=CARTESIAN_POINT('Ctrl Pts',(0.723604431449088,2.41269583013101,9.09107740488332));
#18564=CARTESIAN_POINT('Ctrl Pts',(0.64353906107271,2.43527559930725,9.09631410792082));
#18565=CARTESIAN_POINT('Ctrl Pts',(0.562552613965812,2.45384205003505,9.10155081095832));
#18566=CARTESIAN_POINT('Ctrl Pts',(0.4815683728892,2.47240799502203,9.10678737135065));
#18567=CARTESIAN_POINT('Ctrl Pts',(0.39966355495031,2.4869607368158,9.11202393174299));
#18568=CARTESIAN_POINT('Ctrl Pts',(0.317269076047917,2.49742799363339,9.11726049213532));
#18569=CARTESIAN_POINT('Ctrl Pts',(0.233526021625283,2.50806657122995,9.1225827609058));
#18570=CARTESIAN_POINT('Ctrl Pts',(0.149277618914341,2.51448464551231,9.12790502967628));
#18571=CARTESIAN_POINT('Ctrl Pts',(0.0649813996984492,2.51666121432608,
9.13322729844677));
#18572=CARTESIAN_POINT('Ctrl Pts',(-0.018076446415588,2.51880580775237,
9.1384713791971));
#18573=CARTESIAN_POINT('Ctrl Pts',(-0.101180247008542,2.51683276258221,
9.14371545994744));
#18574=CARTESIAN_POINT('Ctrl Pts',(-0.183894488815157,2.51077459501713,
9.14895954069778));
#18575=CARTESIAN_POINT('Ctrl Pts',(-0.268458605684501,2.5045809386552,9.15432090347833));
#18576=CARTESIAN_POINT('Ctrl Pts',(-0.352615020686498,2.49411729347784,
9.15968226625889));
#18577=CARTESIAN_POINT('Ctrl Pts',(-0.435908145371969,2.47947380280542,
9.16504362903945));
#18578=CARTESIAN_POINT('Ctrl Pts',(-0.519201270057435,2.46483031213301,
9.17040499182));
#18579=CARTESIAN_POINT('Ctrl Pts',(-0.601630623941684,2.44600715420398,
9.17576635460055));
#18580=CARTESIAN_POINT('Ctrl Pts',(-0.682757877074033,2.42314835107002,
9.18112771738111));
#18581=CARTESIAN_POINT('Ctrl Pts',(-0.762279440227115,2.40074197482977,
9.18638296678842));
#18582=CARTESIAN_POINT('Ctrl Pts',(-0.840843710027793,2.3743755294766,9.19163821619573));
#18583=CARTESIAN_POINT('Ctrl Pts',(-0.918027687426472,2.34414833470888,
9.19689346560304));
#18584=CARTESIAN_POINT('Ctrl Pts',(-0.995102235479325,2.31396399523653,
9.20214126426054));
#18585=CARTESIAN_POINT('Ctrl Pts',(-1.07079995212278,2.27992994550431,9.20738906291804));
#18586=CARTESIAN_POINT('Ctrl Pts',(-1.14471181286138,2.24219560152445,9.21263686157554));
#18587=CARTESIAN_POINT('Ctrl Pts',(-1.2191592287505,2.20418783969166,9.21792268505845));
#18588=CARTESIAN_POINT('Ctrl Pts',(-1.29179434327592,2.16242606222498,9.22320850854136));
#18589=CARTESIAN_POINT('Ctrl Pts',(-1.36221852457427,2.11711287873526,9.22849433202426));
#18590=CARTESIAN_POINT('Ctrl Pts',(-1.43201121710003,2.07220601543409,9.23373275789286));
#18591=CARTESIAN_POINT('Ctrl Pts',(-1.49963207297705,2.02381143571954,9.23897118376145));
#18592=CARTESIAN_POINT('Ctrl Pts',(-1.56471828263945,1.97217213903195,9.24420960963005));
#18593=CARTESIAN_POINT('Ctrl Pts',(-1.62978308653067,1.92054982564965,9.24944631266755));
#18594=CARTESIAN_POINT('Ctrl Pts',(-1.69231453860351,1.86568520124345,9.25468301570506));
#18595=CARTESIAN_POINT('Ctrl Pts',(-1.75198113178758,1.80786292728743,9.25991971874256));
#18596=CARTESIAN_POINT('Ctrl Pts',(-1.81164609968345,1.75004222838129,9.26515627913489));
#18597=CARTESIAN_POINT('Ctrl Pts',(-1.8684460332117,1.68926436196184,9.27039283952722));
#18598=CARTESIAN_POINT('Ctrl Pts',(-1.92208569013667,1.62585142303097,9.27562939991955));
#18599=CARTESIAN_POINT('Ctrl Pts',(-1.97660328365647,1.56140058522333,9.28095166869003));
#18600=CARTESIAN_POINT('Ctrl Pts',(-2.02785588922117,1.49422800555234,9.2862739374605));
#18601=CARTESIAN_POINT('Ctrl Pts',(-2.07557678649202,1.42470602349237,9.29159620623098));
#18602=CARTESIAN_POINT('Ctrl Pts',(-2.12259662888613,1.35620537018672,9.29684028698132));
#18603=CARTESIAN_POINT('Ctrl Pts',(-2.16618764778015,1.28542431585706,9.30208436773166));
#18604=CARTESIAN_POINT('Ctrl Pts',(-2.20614000163594,1.21274586916706,9.30732844848199));
#18605=CARTESIAN_POINT('Ctrl Pts',(-2.24698587589978,1.13844199445904,9.31268981126254));
#18606=CARTESIAN_POINT('Ctrl Pts',(-2.28402814256931,1.06215529485584,9.31805117404309));
#18607=CARTESIAN_POINT('Ctrl Pts',(-2.31709436732389,0.984316993105329,
9.32341253682364));
#18608=CARTESIAN_POINT('Ctrl Pts',(-2.35016059207846,0.906478691354823,
9.32877389960418));
#18609=CARTESIAN_POINT('Ctrl Pts',(-2.37925066282246,0.827089287526063,
9.33413526238473));
#18610=CARTESIAN_POINT('Ctrl Pts',(-2.40424673471584,0.746594862430907,
9.33949662516528));
#18611=CARTESIAN_POINT('Ctrl Pts',(-2.42874807838152,0.66769360223127,9.34475187457258));
#18612=CARTESIAN_POINT('Ctrl Pts',(-2.44940654676642,0.58743924649994,9.35000712397989));
#18613=CARTESIAN_POINT('Ctrl Pts',(-2.4660751459744,0.506240678341169,9.35526237338719));
#18614=CARTESIAN_POINT('Ctrl Pts',(-2.48272011289535,0.425157231306012,
9.36051017204468));
#18615=CARTESIAN_POINT('Ctrl Pts',(-2.49538635454002,0.343132679074537,
9.36575797070217));
#18616=CARTESIAN_POINT('Ctrl Pts',(-2.50397650588169,0.26059145801906,9.37100576935966));
#18617=CARTESIAN_POINT('Ctrl Pts',(-2.51262890027544,0.177452154657975,
9.37629159284257));
#18618=CARTESIAN_POINT('Ctrl Pts',(-2.51714574501048,0.0937891160271414,
9.38157741632548));
#18619=CARTESIAN_POINT('Ctrl Pts',(-2.51747995172501,0.0100470225771085,
9.38686323980839));
#18620=CARTESIAN_POINT('Ctrl Pts',(-2.51781116163099,-0.072944161301374,
9.39210166567699));
#18621=CARTESIAN_POINT('Ctrl Pts',(-2.51403444206278,-0.156012517999937,
9.39734009154558));
#18622=CARTESIAN_POINT('Ctrl Pts',(-2.50615608684176,-0.238721424229121,
9.40257851741418));
#18623=CARTESIAN_POINT('Ctrl Pts',(-2.49828032268067,-0.321403128875424,
9.40781522045169));
#18624=CARTESIAN_POINT('Ctrl Pts',(-2.48630564569439,-0.403725158859143,
9.41305192348919));
#18625=CARTESIAN_POINT('Ctrl Pts',(-2.4702903381893,-0.485254464223237,
9.41828862652669));
#18626=CARTESIAN_POINT('Ctrl Pts',(-2.45427546693321,-0.566781548769688,
9.42352518691902));
#18627=CARTESIAN_POINT('Ctrl Pts',(-2.43422027394709,-0.647515499060678,
9.42876174731134));
#18628=CARTESIAN_POINT('Ctrl Pts',(-2.41023418493754,-0.727033303060081,
9.43399830770367));
#18629=CARTESIAN_POINT('Ctrl Pts',(-2.38585550830685,-0.807852599165939,
9.43932057647415));
#18630=CARTESIAN_POINT('Ctrl Pts',(-2.35741622780999,-0.887415105170079,
9.44464284524463));
#18631=CARTESIAN_POINT('Ctrl Pts',(-2.32508344262074,-0.965294377302017,
9.44996511401511));
#18632=CARTESIAN_POINT('Ctrl Pts',(-2.29322564968929,-1.04202954597707,
9.45520919476545));
#18633=CARTESIAN_POINT('Ctrl Pts',(-2.25758824566464,-1.11713021185032,
9.46045327551578));
#18634=CARTESIAN_POINT('Ctrl Pts',(-2.21837824670601,-1.19021183179364,
9.46569735626611));
#18635=CARTESIAN_POINT('Ctrl Pts',(-2.17829132984662,-1.26492789658387,
9.47105871904667));
#18636=CARTESIAN_POINT('Ctrl Pts',(-2.13447035466995,-1.33753307677758,
9.47642008182723));
#18637=CARTESIAN_POINT('Ctrl Pts',(-2.08718314535509,-1.40764795589865,
9.48178144460779));
#18638=CARTESIAN_POINT('Ctrl Pts',(-2.03989593604022,-1.47776283501973,
9.48714280738834));
#18639=CARTESIAN_POINT('Ctrl Pts',(-1.98914285101059,-1.54538704677986,
9.4925041701689));
#18640=CARTESIAN_POINT('Ctrl Pts',(-1.93523389860261,-1.61017887444201,
9.49786553294946));
#18641=CARTESIAN_POINT('Ctrl Pts',(-1.88239192506227,-1.67368832676902,
9.50312078235677));
#18642=CARTESIAN_POINT('Ctrl Pts',(-1.82632272598332,-1.73471109993205,
9.50837603176407));
#18643=CARTESIAN_POINT('Ctrl Pts',(-1.76728923830295,-1.79290127954067,
9.51363128117138));
#18644=CARTESIAN_POINT('Ctrl Pts',(-1.70833944669725,-1.85100895869389,
9.51887907982888));
#18645=CARTESIAN_POINT('Ctrl Pts',(-1.64643404012571,-1.90629169997373,
9.52412687848638));
#18646=CARTESIAN_POINT('Ctrl Pts',(-1.58187602200219,-1.95843674930147,
9.52937467714388));
#18647=CARTESIAN_POINT('Ctrl Pts',(-1.51685022538183,-2.01095963446589,
9.53466050062678));
#18648=CARTESIAN_POINT('Ctrl Pts',(-1.4491335171903,-2.06029880096679,9.53994632410969));
#18649=CARTESIAN_POINT('Ctrl Pts',(-1.37907325462678,-2.10617264448409,
9.5452321475926));
#18650=CARTESIAN_POINT('Ctrl Pts',(-1.30964121760168,-2.15163514041306,
9.55047057346119));
#18651=CARTESIAN_POINT('Ctrl Pts',(-1.23790787999561,-2.19369395365338,
9.55570899932979));
#18652=CARTESIAN_POINT('Ctrl Pts',(-1.16424290473617,-2.23211664318231,
9.56094742519839));
#18653=CARTESIAN_POINT('Ctrl Pts',(-1.09060215666123,-2.27052669612806,
9.56618412823589));
#18654=CARTESIAN_POINT('Ctrl Pts',(-1.0150314414322,-2.3053027871869,9.57142083127339));
#18655=CARTESIAN_POINT('Ctrl Pts',(-0.937925729904853,-2.33625802838266,
9.57665753431089));
#18656=CARTESIAN_POINT('Ctrl Pts',(-0.860822118698498,-2.36721242637315,
9.58189409470322));
#18657=CARTESIAN_POINT('Ctrl Pts',(-0.782184022913733,-2.39434601048332,
9.58713065509555));
#18658=CARTESIAN_POINT('Ctrl Pts',(-0.702425838779753,-2.41752025658826,
9.59236721548788));
#18659=CARTESIAN_POINT('Ctrl Pts',(-0.621362228164636,-2.44107380263432,
9.59768948425836));
#18660=CARTESIAN_POINT('Ctrl Pts',(-0.539142001277231,-2.46053708415148,
9.60301175302884));
#18661=CARTESIAN_POINT('Ctrl Pts',(-0.456213833268316,-2.47581808466103,
9.60833402179932));
#18662=CARTESIAN_POINT('Ctrl Pts',(-0.374503940688586,-2.49087459609889,
9.61357810254966));
#18663=CARTESIAN_POINT('Ctrl Pts',(-0.292107241289309,-2.50187089130879,
9.6188221833));
#18664=CARTESIAN_POINT('Ctrl Pts',(-0.209458997150726,-2.50877124874162,
9.62406626405033));
#18665=CARTESIAN_POINT('Ctrl Pts',(-0.124962353964239,-2.51582593025287,
9.62942762683089));
#18666=CARTESIAN_POINT('Ctrl Pts',(-0.0402032906123846,-2.51859923804143,
9.63478898961143));
#18667=CARTESIAN_POINT('Ctrl Pts',(0.0443541239994344,-2.51710924706979,
9.64015035239199));
#18668=CARTESIAN_POINT('Ctrl Pts',(0.128911538611253,-2.51561925609815,
9.64551171517254));
#18669=CARTESIAN_POINT('Ctrl Pts',(0.213266802099033,-2.50986606758288,
9.65087307795309));
#18670=CARTESIAN_POINT('Ctrl Pts',(0.296964500577313,-2.49992366591399,
9.65623444073364));
#18671=CARTESIAN_POINT('Ctrl Pts',(0.37900563420771,-2.49017804663468,9.66148969014094));
#18672=CARTESIAN_POINT('Ctrl Pts',(0.460718028521943,-2.47637157911841,
9.66674493954823));
#18673=CARTESIAN_POINT('Ctrl Pts',(0.541668376772104,-2.45853647920975,
9.67200018895553));
#18674=CARTESIAN_POINT('Ctrl Pts',(0.622503955817923,-2.44072666542116,
9.677247987613));
#18675=CARTESIAN_POINT('Ctrl Pts',(0.70257918795143,-2.41889966276629,9.68249578627047));
#18676=CARTESIAN_POINT('Ctrl Pts',(0.78146676678254,-2.39313934872469,9.68774358492795));
#18677=CARTESIAN_POINT('Ctrl Pts',(0.860925954131833,-2.36719237899971,
9.69302940841086));
#18678=CARTESIAN_POINT('Ctrl Pts',(0.939179733833506,-2.33725491281245,
9.69831523189377));
#18679=CARTESIAN_POINT('Ctrl Pts',(1.01580277918708,-2.30346499079014,9.70360105537668));
#18680=CARTESIAN_POINT('Ctrl Pts',(1.09173875098174,-2.2699780606663,9.70883948124527));
#18681=CARTESIAN_POINT('Ctrl Pts',(1.16607268668969,-2.23270767701616,9.71407790711385));
#18682=CARTESIAN_POINT('Ctrl Pts',(1.2384083530163,-2.19183735737382,9.71931633298244));
#18683=CARTESIAN_POINT('Ctrl Pts',(1.3107202293462,-2.15098047929938,9.72455303601994));
#18684=CARTESIAN_POINT('Ctrl Pts',(1.38103474011051,-2.10652624344335,9.72978973905744));
#18685=CARTESIAN_POINT('Ctrl Pts',(1.44898008261764,-2.05870419686204,9.73502644209495));
#18686=CARTESIAN_POINT('Ctrl Pts',(1.51692357432748,-2.01088345292947,9.74026300248727));
#18687=CARTESIAN_POINT('Ctrl Pts',(1.58249764935552,-1.95969534708922,9.74549956287959));
#18688=CARTESIAN_POINT('Ctrl Pts',(1.64536049606058,-1.90541205202531,9.75073612327192));
#18689=CARTESIAN_POINT('Ctrl Pts',(1.70925223811573,-1.85024028574499,9.75605839204241));
#18690=CARTESIAN_POINT('Ctrl Pts',(1.77034281937465,-1.79187140775071,9.7613806608129));
#18691=CARTESIAN_POINT('Ctrl Pts',(1.82831077523864,-1.73063166478205,9.76670292958339));
#18692=CARTESIAN_POINT('Ctrl Pts',(1.88542713944182,-1.67029157841926,9.77194701033372));
#18693=CARTESIAN_POINT('Ctrl Pts',(1.93951175864186,-1.60716481273136,9.77719109108406));
#18694=CARTESIAN_POINT('Ctrl Pts',(1.9902976907599,-1.54159701354011,9.78243517183439));
#18695=CARTESIAN_POINT('Ctrl Pts',(2.04221943247161,-1.47456281347266,9.78779653461496));
#18696=CARTESIAN_POINT('Ctrl Pts',(2.0906928660034,-1.40497749678828,9.79315789739553));
#18697=CARTESIAN_POINT('Ctrl Pts',(2.13548048945439,-1.33324016184618,9.7985192601761));
#18698=CARTESIAN_POINT('Ctrl Pts',(2.18026811290537,-1.26150282690409,9.80388062295667));
#18699=CARTESIAN_POINT('Ctrl Pts',(2.22136973765147,-1.18761395020763,9.80924198573724));
#18700=CARTESIAN_POINT('Ctrl Pts',(2.2585994704274,-1.11199581032712,9.81460334851781));
#18701=CARTESIAN_POINT('Ctrl Pts',(2.29771370768164,-1.0325500114058,9.82023609418019));
#18702=CARTESIAN_POINT('Ctrl Pts',(2.33268319210186,-0.950935265153575,
9.82586883984257));
#18703=CARTESIAN_POINT('Ctrl Pts',(2.36328009289161,-0.867590601921324,
9.83150158550495));
#18704=CARTESIAN_POINT('Ctrl Pts',(2.39377456178312,-0.784524958846109,
9.83711547393619));
#18705=CARTESIAN_POINT('Ctrl Pts',(2.41992549446168,-0.699741274925882,
9.84272936236742));
#18706=CARTESIAN_POINT('Ctrl Pts',(2.44155272692805,-0.613699056240259,
9.84834325079866));
#18707=CARTESIAN_POINT('Ctrl Pts',(2.46313411560376,-0.527839223417836,
9.85394523932886));
#18708=CARTESIAN_POINT('Ctrl Pts',(2.48021080455436,-0.440726511693493,
9.85954722785906));
#18709=CARTESIAN_POINT('Ctrl Pts',(2.49265158327791,-0.352837546729558,
9.86514921638926));
#18710=CARTESIAN_POINT('Ctrl Pts',(2.50505613088035,-0.265204539676687,
9.87073489031975));
#18711=CARTESIAN_POINT('Ctrl Pts',(2.51285161508252,-0.176800136802324,
9.87632056425024));
#18712=CARTESIAN_POINT('Ctrl Pts',(2.51595758515505,-0.0881117455323095,
9.88190623818073));
#18713=CARTESIAN_POINT('Ctrl Pts',(2.51697896722398,-0.058947030338859,
9.88374305793824));
#18714=CARTESIAN_POINT('Ctrl Pts',(2.51749363732466,-0.0297517030242967,
9.88557987769575));
#18715=CARTESIAN_POINT('Ctrl Pts',(2.51749994136415,-0.000543352107749378,
9.88741669745326));
#18716=CARTESIAN_POINT('Ctrl Pts',(2.51749994136434,-0.000543351237068014,
9.88741669750801));
#18717=CARTESIAN_POINT('Ctrl Pts',(2.51751848517122,0.0853753502565315,
9.89281984980827));
#18718=CARTESIAN_POINT('Ctrl Pts',(2.51313426321878,0.171241900920938,9.89822300210852));
#18719=CARTESIAN_POINT('Ctrl Pts',(2.50438935504415,0.256593469015731,9.90362615440877));
#18720=CARTESIAN_POINT('Ctrl Pts',(2.49563786110501,0.342009315124396,9.90903337580707));
#18721=CARTESIAN_POINT('Ctrl Pts',(2.48251919619281,0.42690899151922,9.91444059720537));
#18722=CARTESIAN_POINT('Ctrl Pts',(2.46512689921235,0.51083815517218,9.91984781860366));
#18723=CARTESIAN_POINT('Ctrl Pts',(2.4477056995384,0.594906793150723,9.92526402577668));
#18724=CARTESIAN_POINT('Ctrl Pts',(2.42599678269746,0.678001290366767,9.93068023294971));
#18725=CARTESIAN_POINT('Ctrl Pts',(2.40014405502514,0.759680699456999,9.93609644012273));
#18726=CARTESIAN_POINT('Ctrl Pts',(2.38812556449347,0.797652058503759,9.93861434211945));
#18727=CARTESIAN_POINT('Ctrl Pts',(2.37521222142059,0.835317852404866,9.94113224411616));
#18728=CARTESIAN_POINT('Ctrl Pts',(2.36142200728636,0.872635292378024,9.94365014611287));
#18729=CARTESIAN_POINT('Ctrl Pts',(2.36142200350084,0.872635302621937,9.67114329893353));
#18730=CARTESIAN_POINT('Ctrl Pts',(2.36647528649717,0.858960708411047,9.67025418119806));
#18731=CARTESIAN_POINT('Ctrl Pts',(2.37141038618732,0.84524060304922,9.66935958559407));
#18732=CARTESIAN_POINT('Ctrl Pts',(2.38200567353762,0.814960969193715,9.6673781273229));
#18733=CARTESIAN_POINT('Ctrl Pts',(2.38761217568937,0.798386165365412,9.66628884452266));
#18734=CARTESIAN_POINT('Ctrl Pts',(2.39564083768089,0.773809467664475,9.66466497258941));
#18735=CARTESIAN_POINT('Ctrl Pts',(2.3981967744251,0.765851383638769,9.66413781212311));
#18736=CARTESIAN_POINT('Ctrl Pts',(2.40267549959039,0.751664280709686,9.6631954002981));
#18737=CARTESIAN_POINT('Ctrl Pts',(2.40461378500539,0.745440333393591,9.66278105239958));
#18738=CARTESIAN_POINT('Ctrl Pts',(2.40878758851222,0.731852326300868,9.66187442319204));
#18739=CARTESIAN_POINT('Ctrl Pts',(2.41101348838801,0.724485630730547,9.66138162264118));
#18740=CARTESIAN_POINT('Ctrl Pts',(2.41714673468343,0.70384611189657,9.6599975922119));
#18741=CARTESIAN_POINT('Ctrl Pts',(2.42097841878177,0.69055134609642,9.65910223427123));
#18742=CARTESIAN_POINT('Ctrl Pts',(2.4427062790222,0.612758194322319,9.65384342587154));
#18743=CARTESIAN_POINT('Ctrl Pts',(2.45813246720599,0.547603584611023,9.64936074260902));
#18744=CARTESIAN_POINT('Ctrl Pts',(2.47571367516164,0.457459342572544,9.6431191754587));
#18745=CARTESIAN_POINT('Ctrl Pts',(2.48012050084405,0.43293129079698,9.64141681910491));
#18746=CARTESIAN_POINT('Ctrl Pts',(2.50623205226357,0.274080932159291,9.63038017599378));
#18747=CARTESIAN_POINT('Ctrl Pts',(2.51738163120652,0.138244323610536,9.62090456378432));
#18748=CARTESIAN_POINT('Ctrl Pts',(2.51760485864111,-0.120416906853857,
9.60326323783957));
#18749=CARTESIAN_POINT('Ctrl Pts',(2.50875650327208,-0.24286425338847,9.59508204491669));
#18750=CARTESIAN_POINT('Ctrl Pts',(2.48785268672985,-0.38584171060584,9.5857661484294));
#18751=CARTESIAN_POINT('Ctrl Pts',(2.48440587041795,-0.407446115295201,
9.5843645552423));
#18752=CARTESIAN_POINT('Ctrl Pts',(2.47824452681829,-0.443073589627441,
9.58206271849662));
#18753=CARTESIAN_POINT('Ctrl Pts',(2.47569155695518,-0.457123034891203,
9.58115745827956));
#18754=CARTESIAN_POINT('Ctrl Pts',(2.47084778377868,-0.482547502159364,
9.57952348346087));
#18755=CARTESIAN_POINT('Ctrl Pts',(2.4685976286522,-0.493929769828765,9.57879350981291));
#18756=CARTESIAN_POINT('Ctrl Pts',(2.46358221713985,-0.518409178853658,
9.57722672792726));
#18757=CARTESIAN_POINT('Ctrl Pts',(2.46079102065578,-0.531500687649627,
9.5763907644777));
#18758=CARTESIAN_POINT('Ctrl Pts',(2.45280735150639,-0.567534699657773,
9.57409477361229));
#18759=CARTESIAN_POINT('Ctrl Pts',(2.44739746577319,-0.59042801509282,9.57264166551865));
#18760=CARTESIAN_POINT('Ctrl Pts',(2.41190258342717,-0.731753281365565,
9.56370021676248));
#18761=CARTESIAN_POINT('Ctrl Pts',(2.37354752347173,-0.847947262627435,
9.55648609280943));
#18762=CARTESIAN_POINT('Ctrl Pts',(2.25344748185044,-1.13877712308217,9.53823408636118));
#18763=CARTESIAN_POINT('Ctrl Pts',(2.15985212332765,-1.30761718702181,9.52746597225172));
#18764=CARTESIAN_POINT('Ctrl Pts',(2.02411131459663,-1.49748476011527,9.51342044063668));
#18765=CARTESIAN_POINT('Ctrl Pts',(1.99945698954969,-1.53024786608671,9.51091667554503));
#18766=CARTESIAN_POINT('Ctrl Pts',(1.96655721170996,-1.57181532065612,9.50761382938489));
#18767=CARTESIAN_POINT('Ctrl Pts',(1.95903182517084,-1.58118467097132,9.50686081084206));
#18768=CARTESIAN_POINT('Ctrl Pts',(1.94688227215881,-1.5960913846239,9.50564833237535));
#18769=CARTESIAN_POINT('Ctrl Pts',(1.94230077535962,-1.60166350543643,9.50519184247834));
#18770=CARTESIAN_POINT('Ctrl Pts',(1.93346296805035,-1.61231856456575,9.50431247896849));
#18771=CARTESIAN_POINT('Ctrl Pts',(1.92921045667836,-1.61740446772248,9.5038898703138));
#18772=CARTESIAN_POINT('Ctrl Pts',(1.91899165868033,-1.62952827332452,9.50287566674407));
#18773=CARTESIAN_POINT('Ctrl Pts',(1.91300670647945,-1.63655024801305,9.5022827436402));
#18774=CARTESIAN_POINT('Ctrl Pts',(1.89237474955293,-1.66048932011846,9.50024289352669));
#18775=CARTESIAN_POINT('Ctrl Pts',(1.87754133671617,-1.67724339985583,9.49878340026861));
#18776=CARTESIAN_POINT('Ctrl Pts',(1.84065176452078,-1.71780691631435,9.49517552673694));
#18777=CARTESIAN_POINT('Ctrl Pts',(1.81835510221512,-1.74139140984504,9.49301330961599));
#18778=CARTESIAN_POINT('Ctrl Pts',(1.72456112953382,-1.83683705395011,9.48401518329662));
#18779=CARTESIAN_POINT('Ctrl Pts',(1.64921433424445,-1.90477591919613,9.4770169628648));
#18780=CARTESIAN_POINT('Ctrl Pts',(1.42058328305293,-2.08716902275808,9.45681124159363));
#18781=CARTESIAN_POINT('Ctrl Pts',(1.25807071934463,-2.18897577772168,9.44371043134116));
#18782=CARTESIAN_POINT('Ctrl Pts',(1.0565366857585,-2.28529482016103,9.42920589262093));
#18783=CARTESIAN_POINT('Ctrl Pts',(1.02723239650116,-2.29861609313234,9.42713464951643));
#18784=CARTESIAN_POINT('Ctrl Pts',(0.983936707440413,-2.31730422255812,
9.42412808951916));
#18785=CARTESIAN_POINT('Ctrl Pts',(0.970140987699629,-2.32311359685462,
9.42317791603781));
#18786=CARTESIAN_POINT('Ctrl Pts',(0.945473031784617,-2.33324320098661,
9.42149257642528));
#18787=CARTESIAN_POINT('Ctrl Pts',(0.934621051643274,-2.33761129918285,
9.42075582081989));
#18788=CARTESIAN_POINT('Ctrl Pts',(0.91182235817537,-2.34660400016268,9.41921755632303));
#18789=CARTESIAN_POINT('Ctrl Pts',(0.899869973409208,-2.35121338611812,
9.41841657206057));
#18790=CARTESIAN_POINT('Ctrl Pts',(0.868350149360071,-2.36309330922198,
9.41631827705893));
#18791=CARTESIAN_POINT('Ctrl Pts',(0.84872630732279,-2.37021215628358,9.41502600050449));
#18792=CARTESIAN_POINT('Ctrl Pts',(0.755643087744054,-2.40267519880789,
9.408959491603));
#18793=CARTESIAN_POINT('Ctrl Pts',(0.68112061180335,-2.4248548493827,9.40428917165514));
#18794=CARTESIAN_POINT('Ctrl Pts',(0.471279965914689,-2.47686822272979,
9.39151656271789));
#18795=CARTESIAN_POINT('Ctrl Pts',(0.334354027909021,-2.49903792946427,
9.38361897000609));
#18796=CARTESIAN_POINT('Ctrl Pts',(0.0682992559190702,-2.51984613277134,
9.36825909323298));
#18797=CARTESIAN_POINT('Ctrl Pts',(-0.0602596597745309,-2.52004962292166,
9.36082403409335));
#18798=CARTESIAN_POINT('Ctrl Pts',(-0.209695469693848,-2.5088436209334,
9.35162236078788));
#18799=CARTESIAN_POINT('Ctrl Pts',(-0.231113078438273,-2.50696134362511,
9.35028989132003));
#18800=CARTESIAN_POINT('Ctrl Pts',(-0.260898589216307,-2.50395874093345,
9.34841453336676));
#18801=CARTESIAN_POINT('Ctrl Pts',(-0.269289608415433,-2.50307022517838,
9.34788374802464));
#18802=CARTESIAN_POINT('Ctrl Pts',(-0.283754538422571,-2.50146497423133,
9.34696424379794));
#18803=CARTESIAN_POINT('Ctrl Pts',(-0.289830659632837,-2.50076825039936,
9.34657662481538));
#18804=CARTESIAN_POINT('Ctrl Pts',(-0.302640411658805,-2.49925209708182,
9.34575643084977));
#18805=CARTESIAN_POINT('Ctrl Pts',(-0.30937334052923,-2.4984275847554,9.3453235659978));
#18806=CARTESIAN_POINT('Ctrl Pts',(-0.326065202312927,-2.49631499905286,
9.34424619443894));
#18807=CARTESIAN_POINT('Ctrl Pts',(-0.336019840392307,-2.4949945389553,
9.34359992777618));
#18808=CARTESIAN_POINT('Ctrl Pts',(-0.373490671937523,-2.489795805394,9.34115382234958));
#18809=CARTESIAN_POINT('Ctrl Pts',(-0.40094879961149,-2.48552174476235,
9.33933398619751));
#18810=CARTESIAN_POINT('Ctrl Pts',(-0.471241468160891,-2.47338514778306,
9.3346142417374));
#18811=CARTESIAN_POINT('Ctrl Pts',(-0.513951969853503,-2.46486420674446,
9.33168805280143));
#18812=CARTESIAN_POINT('Ctrl Pts',(-0.678094326570187,-2.42766553885441,
9.32026622024919));
#18813=CARTESIAN_POINT('Ctrl Pts',(-0.797549924505594,-2.39108445777432,
9.31158751774704));
#18814=CARTESIAN_POINT('Ctrl Pts',(-1.06418579753438,-2.28721729995606,
9.29188638077167));
#18815=CARTESIAN_POINT('Ctrl Pts',(-1.20861318502091,-2.21430021351207,
9.28098607830016));
#18816=CARTESIAN_POINT('Ctrl Pts',(-1.36387873701221,-2.11616053669732,
9.26913929669441));
#18817=CARTESIAN_POINT('Ctrl Pts',(-1.38251586653006,-2.10403197621247,
9.26771431510549));
#18818=CARTESIAN_POINT('Ctrl Pts',(-1.41294464344692,-2.08365081064173,
9.26538225755767));
#18819=CARTESIAN_POINT('Ctrl Pts',(-1.42483025333498,-2.07554138222043,
9.2644699334336));
#18820=CARTESIAN_POINT('Ctrl Pts',(-1.4461794875036,-2.06070520020931,9.26282839194581));
#18821=CARTESIAN_POINT('Ctrl Pts',(-1.45566726714951,-2.05401408146994,
9.26209786105712));
#18822=CARTESIAN_POINT('Ctrl Pts',(-1.47592777422095,-2.03951476105089,
9.2605354957455));
#18823=CARTESIAN_POINT('Ctrl Pts',(-1.48668561076329,-2.0316862850355,9.25970446295303));
#18824=CARTESIAN_POINT('Ctrl Pts',(-1.51598794405718,-2.01000561064165,
9.25743648623442));
#18825=CARTESIAN_POINT('Ctrl Pts',(-1.53440454389709,-1.99598215220301,
9.25600617898162));
#18826=CARTESIAN_POINT('Ctrl Pts',(-1.64199400105456,-1.91168805488362,
9.24761594437005));
#18827=CARTESIAN_POINT('Ctrl Pts',(-1.72652968751229,-1.83570023815874,
9.24089007994945));
#18828=CARTESIAN_POINT('Ctrl Pts',(-1.93011070794262,-1.62615445052017,
9.2238949945278));
#18829=CARTESIAN_POINT('Ctrl Pts',(-2.04057104403988,-1.48518259249948,
9.21387226123886));
#18830=CARTESIAN_POINT('Ctrl Pts',(-2.16755882729801,-1.28188547036864,
9.19966778960911));
#18831=CARTESIAN_POINT('Ctrl Pts',(-2.19803665636954,-1.22889185391841,
9.19598147762745));
#18832=CARTESIAN_POINT('Ctrl Pts',(-2.23285443790405,-1.16290567150141,
9.19134629950591));
#18833=CARTESIAN_POINT('Ctrl Pts',(-2.23905890469332,-1.15091430795047,
9.19050219506075));
#18834=CARTESIAN_POINT('Ctrl Pts',(-2.2486137045485,-1.13207805610502,9.18917258768684));
#18835=CARTESIAN_POINT('Ctrl Pts',(-2.25203002396736,-1.12526667280146,
9.18869104303722));
#18836=CARTESIAN_POINT('Ctrl Pts',(-2.25831535986996,-1.11259183735401,
9.18779339612274));
#18837=CARTESIAN_POINT('Ctrl Pts',(-2.26119254661947,-1.10673263479187,
9.18737780295553));
#18838=CARTESIAN_POINT('Ctrl Pts',(-2.26774814163521,-1.09325031810593,
9.18642007424008));
#18839=CARTESIAN_POINT('Ctrl Pts',(-2.27141090503754,-1.08561981718363,
9.18587700757643));
#18840=CARTESIAN_POINT('Ctrl Pts',(-2.28276421040053,-1.06165890845496,
9.18416882368802));
#18841=CARTESIAN_POINT('Ctrl Pts',(-2.2903174427038,-1.045264581713,9.18299590420926));
#18842=CARTESIAN_POINT('Ctrl Pts',(-2.30769523368822,-1.006453164976,9.18021182397249));
#18843=CARTESIAN_POINT('Ctrl Pts',(-2.31737033072852,-0.983971504344939,
9.17859343360965));
#18844=CARTESIAN_POINT('Ctrl Pts',(-2.35122667259248,-0.902030675932925,
9.17268311619013));
#18845=CARTESIAN_POINT('Ctrl Pts',(-2.37345837403282,-0.841795996271935,
9.16831702166189));
#18846=CARTESIAN_POINT('Ctrl Pts',(-2.46056393453768,-0.57478775683513,
9.14904439575039));
#18847=CARTESIAN_POINT('Ctrl Pts',(-2.50090218333311,-0.360934568481369,
9.13392261081604));
#18848=CARTESIAN_POINT('Ctrl Pts',(-2.51621659285148,-0.0946480917806868,
9.11636057837711));
#18849=CARTESIAN_POINT('Ctrl Pts',(-2.51759985243393,-0.0446739804134837,
9.11311295916028));
#18850=CARTESIAN_POINT('Ctrl Pts',(-2.51745537497348,0.0238076706712868,
9.10872606252561));
#18851=CARTESIAN_POINT('Ctrl Pts',(-2.51721250838459,0.0423035177186008,
9.10754752802467));
#18852=CARTESIAN_POINT('Ctrl Pts',(-2.51649851536062,0.071860896210121,
9.10567385069298));
#18853=CARTESIAN_POINT('Ctrl Pts',(-2.51615823793766,0.0829246297629913,
9.10497467621193));
#18854=CARTESIAN_POINT('Ctrl Pts',(-2.51530563904789,0.105746364648813,
9.10353679445947));
#18855=CARTESIAN_POINT('Ctrl Pts',(-2.51478381303445,0.11750375613942,9.10279840022273));
#18856=CARTESIAN_POINT('Ctrl Pts',(-2.5133729325225,0.144946764559623,9.10108025546161));
#18857=CARTESIAN_POINT('Ctrl Pts',(-2.51241945238621,0.160628687832301,
9.10010252865361));
#18858=CARTESIAN_POINT('Ctrl Pts',(-2.50884053422694,0.211608596524839,
9.0969365402307));
#18859=CARTESIAN_POINT('Ctrl Pts',(-2.5056174318732,0.246861294623273,9.09476679857245));
#18860=CARTESIAN_POINT('Ctrl Pts',(-2.49621109839028,0.330295316195898,
9.08966948436537));
#18861=CARTESIAN_POINT('Ctrl Pts',(-2.48937477757095,0.378389317816642,
9.08676150987123));
#18862=CARTESIAN_POINT('Ctrl Pts',(-2.45705712119158,0.566503203603238,
9.07545818720507));
#18863=CARTESIAN_POINT('Ctrl Pts',(-2.42111584204072,0.704454558995143,
9.06734073357711));
#18864=CARTESIAN_POINT('Ctrl Pts',(-2.33044484490683,0.961093584693852,
9.05167764437746));
#18865=CARTESIAN_POINT('Ctrl Pts',(-2.27777380867821,1.08000569399528,9.04416119415918));
#18866=CARTESIAN_POINT('Ctrl Pts',(-2.20600614343839,1.21317873033923,9.03487128724458));
#18867=CARTESIAN_POINT('Ctrl Pts',(-2.19559681376915,1.23191732585953,9.03354273440847));
#18868=CARTESIAN_POINT('Ctrl Pts',(-2.18076376038303,1.25783412720895,9.03167203003952));
#18869=CARTESIAN_POINT('Ctrl Pts',(-2.17654100742291,1.26512707204384,9.03114190354894));
#18870=CARTESIAN_POINT('Ctrl Pts',(-2.16919200583589,1.2776735357655,9.03022322825833));
#18871=CARTESIAN_POINT('Ctrl Pts',(-2.16608305925666,1.28293717721042,9.029835774703));
#18872=CARTESIAN_POINT('Ctrl Pts',(-2.15948246982475,1.29402000265873,9.02901554712703));
#18873=CARTESIAN_POINT('Ctrl Pts',(-2.15598643163422,1.29983645431076,9.02858248085474));
#18874=CARTESIAN_POINT('Ctrl Pts',(-2.14725130437121,1.31423712621905,9.02750394744237));
#18875=CARTESIAN_POINT('Ctrl Pts',(-2.14198425381999,1.32280415644471,9.026856712368));
#18876=CARTESIAN_POINT('Ctrl Pts',(-2.12191414031491,1.35501467859251,9.02440265018545));
#18877=CARTESIAN_POINT('Ctrl Pts',(-2.10677038056677,1.37844216744733,9.02257566225857));
#18878=CARTESIAN_POINT('Ctrl Pts',(-2.06686679234994,1.43797934977472,9.01783294180737));
#18879=CARTESIAN_POINT('Ctrl Pts',(-2.04154913447083,1.47370269999305,9.01489062913552));
#18880=CARTESIAN_POINT('Ctrl Pts',(-1.94098394497538,1.60803314905606,9.00350092381855));
#18881=CARTESIAN_POINT('Ctrl Pts',(-1.85941964624749,1.70168938276722,8.99487407572329));
#18882=CARTESIAN_POINT('Ctrl Pts',(-1.65634442356775,1.90275946961818,8.97519755968456));
#18883=CARTESIAN_POINT('Ctrl Pts',(-1.53068343962811,2.00524204004788,8.96427178441155));
#18884=CARTESIAN_POINT('Ctrl Pts',(-1.3775310629047,2.10729894338544,8.95240175599791));
#18885=CARTESIAN_POINT('Ctrl Pts',(-1.35886453264704,2.11938384908532,8.95097671612602));
#18886=CARTESIAN_POINT('Ctrl Pts',(-1.32785922870589,2.13887894530634,8.9486445833152));
#18887=CARTESIAN_POINT('Ctrl Pts',(-1.31561298142216,2.14643326731657,8.94773224162875));
#18888=CARTESIAN_POINT('Ctrl Pts',(-1.29336968011474,2.15989256752792,8.94609068123867));
#18889=CARTESIAN_POINT('Ctrl Pts',(-1.28339534123931,2.16583412062632,8.94536014887469));
#18890=CARTESIAN_POINT('Ctrl Pts',(-1.26190338659983,2.17843592812391,8.94379779410433));
#18891=CARTESIAN_POINT('Ctrl Pts',(-1.25037331743632,2.1850743300599,8.94296677322355));
#18892=CARTESIAN_POINT('Ctrl Pts',(-1.21864165675435,2.20301032040406,8.94069886408962));
#18893=CARTESIAN_POINT('Ctrl Pts',(-1.19833572564897,2.21412138396209,8.93926861183428));
#18894=CARTESIAN_POINT('Ctrl Pts',(-1.07755813055978,2.27806048868268,8.93087961563217));
#18895=CARTESIAN_POINT('Ctrl Pts',(-0.97375375064002,2.32432772078794,8.92415484864632));
#18896=CARTESIAN_POINT('Ctrl Pts',(-0.699660671073356,2.42489545454157,
8.9071709802723));
#18897=CARTESIAN_POINT('Ctrl Pts',(-0.526105877073629,2.46836941257501,
8.89715763916029));
#18898=CARTESIAN_POINT('Ctrl Pts',(-0.288725520143927,2.50163963086478,
8.88295474023484));
#18899=CARTESIAN_POINT('Ctrl Pts',(-0.227738993692051,2.50792681547114,
8.8792581440627));
#18900=CARTESIAN_POINT('Ctrl Pts',(-0.153106759390012,2.51287627091878,
8.87461140114671));
#18901=CARTESIAN_POINT('Ctrl Pts',(-0.139617424933388,2.51366182860446,
8.87376663474007));
#18902=CARTESIAN_POINT('Ctrl Pts',(-0.118509703675461,2.51472062160851,
8.87243620682553));
#18903=CARTESIAN_POINT('Ctrl Pts',(-0.110895061522468,2.51506791882549,
8.87195451148787));
#18904=CARTESIAN_POINT('Ctrl Pts',(-0.0967571706041103,2.51564840685909,
8.8710567355929));
#18905=CARTESIAN_POINT('Ctrl Pts',(-0.0902344779359328,2.51589081492491,
8.87064116550925));
#18906=CARTESIAN_POINT('Ctrl Pts',(-0.0752550135229502,2.51638918190434,
8.86968369008033));
#18907=CARTESIAN_POINT('Ctrl Pts',(-0.0667978660740206,2.51662787714356,
8.86914085547557));
#18908=CARTESIAN_POINT('Ctrl Pts',(-0.0403127116606915,2.51724180138517,
8.86743412475642));
#18909=CARTESIAN_POINT('Ctrl Pts',(-0.0222822324136588,2.51746595996093,
8.86626244474766));
#18910=CARTESIAN_POINT('Ctrl Pts',(0.143554973629019,2.51774602412938,8.85540526024625));
#18911=CARTESIAN_POINT('Ctrl Pts',(0.291081968688955,2.50497823205498,8.84517579275143));
#18912=CARTESIAN_POINT('Ctrl Pts',(0.616535904009861,2.44766481881102,8.82234712184223));
#18913=CARTESIAN_POINT('Ctrl Pts',(0.792498801616777,2.39648652812175,8.80985292243285));
#18914=CARTESIAN_POINT('Ctrl Pts',(0.99125811164431,2.31435903973819,8.79588161340696));
#18915=CARTESIAN_POINT('Ctrl Pts',(1.02088323978874,2.30144475881326,8.79380125819369));
#18916=CARTESIAN_POINT('Ctrl Pts',(1.06408309181307,2.2816145618581,8.79076943099895));
#18917=CARTESIAN_POINT('Ctrl Pts',(1.07785588910503,2.27514055259541,8.78980309679165));
#18918=CARTESIAN_POINT('Ctrl Pts',(1.10214299834276,2.2634541629803,8.78809925320576));
#18919=CARTESIAN_POINT('Ctrl Pts',(1.11268105097236,2.25829245737752,8.78736003131039));
#18920=CARTESIAN_POINT('Ctrl Pts',(1.12409118435183,2.25260433488596,8.78655961864032));
#18921=CARTESIAN_POINT('Ctrl Pts',(1.12499932023364,2.25215092961444,8.78649591344023));
#18922=CARTESIAN_POINT('Ctrl Pts',(1.1263128507283,2.25149413012709,8.7864037697891));
#18923=CARTESIAN_POINT('Ctrl Pts',(1.12671846412425,2.25129117581764,8.78637531613239));
#18924=CARTESIAN_POINT('Ctrl Pts',(1.12742881301269,2.25093550280219,8.7863254853022));
#18925=CARTESIAN_POINT('Ctrl Pts',(1.12773357228416,2.25078283184539,8.78630410647829));
#18926=CARTESIAN_POINT('Ctrl Pts',(1.12826688649127,2.2505155294343,8.78626669451087));
#18927=CARTESIAN_POINT('Ctrl Pts',(1.12849545493568,2.25040092507252,8.78625066043071));
#18928=CARTESIAN_POINT('Ctrl Pts',(1.12889521767398,2.25020040756404,8.78622261704161));
#18929=CARTESIAN_POINT('Ctrl Pts',(1.12906641960202,2.25011450971181,8.78621060720375));
#18930=CARTESIAN_POINT('Ctrl Pts',(1.1294752501352,2.24990932706814,8.78618192766668));
#18931=CARTESIAN_POINT('Ctrl Pts',(1.12971286968457,2.24979002415011,8.78616525859452));
#18932=CARTESIAN_POINT('Ctrl Pts',(1.13017394099946,2.24955844014407,8.78613291428865));
#18933=CARTESIAN_POINT('Ctrl Pts',(1.1303973949333,2.24944616340684,8.78611723890492));
#18934=CARTESIAN_POINT('Ctrl Pts',(1.14249592626669,2.24336487336437,8.78526852112721));
#18935=CARTESIAN_POINT('Ctrl Pts',(1.15432374146975,2.2373018587586,8.78443874808158));
#18936=CARTESIAN_POINT('Ctrl Pts',(1.17870949822711,2.22455669715852,8.78272758794073));
#18937=CARTESIAN_POINT('Ctrl Pts',(1.19125995464662,2.21786120246362,8.78184669868728));
#18938=CARTESIAN_POINT('Ctrl Pts',(1.22305860582782,2.20054926384951,8.77961375049276));
#18939=CARTESIAN_POINT('Ctrl Pts',(1.24222597306976,2.18978631220626,8.77826678855427));
#18940=CARTESIAN_POINT('Ctrl Pts',(1.29744087969792,2.15782345617162,8.77438118290696));
#18941=CARTESIAN_POINT('Ctrl Pts',(1.33310509646883,2.13597424694994,8.77186467606242));
#18942=CARTESIAN_POINT('Ctrl Pts',(1.46011798923064,2.05374041427202,8.76285075555961));
#18943=CARTESIAN_POINT('Ctrl Pts',(1.54805083334395,1.98829961667938,8.75651649192456));
#18944=CARTESIAN_POINT('Ctrl Pts',(1.76742019693579,1.80164002657368,8.73994808503236));
#18945=CARTESIAN_POINT('Ctrl Pts',(1.89068018109402,1.67182264800081,8.72983492149918));
#18946=CARTESIAN_POINT('Ctrl Pts',(2.01094565721828,1.51468805641451,8.71764825393113));
#18947=CARTESIAN_POINT('Ctrl Pts',(2.02255368985017,1.4991527151326,8.71644364097489));
#18948=CARTESIAN_POINT('Ctrl Pts',(2.03868002113719,1.47704218623548,8.71472709788236));
#18949=CARTESIAN_POINT('Ctrl Pts',(2.04334864771464,1.47057680803253,8.71422491221487));
#18950=CARTESIAN_POINT('Ctrl Pts',(2.05182602342918,1.45871855028654,8.71330317408219));
#18951=CARTESIAN_POINT('Ctrl Pts',(2.05564446880157,1.45333260347049,8.71288427349661));
#18952=CARTESIAN_POINT('Ctrl Pts',(2.06353024875123,1.44211639502942,8.71201126415512));
#18953=CARTESIAN_POINT('Ctrl Pts',(2.06759411238707,1.43628387436127,8.71155694431904));
#18954=CARTESIAN_POINT('Ctrl Pts',(2.07819162105292,1.42093598299914,8.71036068927252));
#18955=CARTESIAN_POINT('Ctrl Pts',(2.08468453412916,1.4113928803266,8.70961613097328));
#18956=CARTESIAN_POINT('Ctrl Pts',(2.11381248734533,1.36794192493528,8.7062239307294));
#18957=CARTESIAN_POINT('Ctrl Pts',(2.13568612176331,1.33353391000531,8.70353193338342));
#18958=CARTESIAN_POINT('Ctrl Pts',(2.19605388452002,1.23327616511136,8.69570440061242));
#18959=CARTESIAN_POINT('Ctrl Pts',(2.23240280724681,1.16618994237024,8.69048738157978));
#18960=CARTESIAN_POINT('Ctrl Pts',(2.301214376549,1.0241453178954,8.67961586955767));
#18961=CARTESIAN_POINT('Ctrl Pts',(2.3331728339198,0.949079813084719,8.67396572716839));
#18962=CARTESIAN_POINT('Ctrl Pts',(2.36142186693781,0.872635672172493,8.66836043115426));
#18963=CARTESIAN_POINT('Origin',(0.,0.,10.));
#18964=CARTESIAN_POINT('',(2.36142200378576,0.872635301850924,7.66684133937673));
#18965=CARTESIAN_POINT('',(2.36142200728636,0.872635292378021,7.94384568391999));
#18966=CARTESIAN_POINT('',(2.36142200728636,0.87263529237802,10.));
#18967=CARTESIAN_POINT('',(2.51749930935125,-0.0018647830938552,8.88741669754404));
#18968=CARTESIAN_POINT('Ctrl Pts',(2.36142200728636,0.872635292378021,7.94384568391999));
#18969=CARTESIAN_POINT('Ctrl Pts',(2.33203545559993,0.952157689050145,7.94920817054382));
#18970=CARTESIAN_POINT('Ctrl Pts',(2.29859309494399,1.030287126504,7.95457065716764));
#18971=CARTESIAN_POINT('Ctrl Pts',(2.26125522707057,1.10658530988173,7.95993314379147));
#18972=CARTESIAN_POINT('Ctrl Pts',(2.22477931807968,1.18112212067366,7.96517183537179));
#18973=CARTESIAN_POINT('Ctrl Pts',(2.18458604395432,1.25391088226474,7.97041052695211));
#18974=CARTESIAN_POINT('Ctrl Pts',(2.1408736952347,1.32456259612451,7.97564921853243));
#18975=CARTESIAN_POINT('Ctrl Pts',(2.09717707316596,1.39518889119829,7.98088602535762));
#18976=CARTESIAN_POINT('Ctrl Pts',(2.04996413340203,1.46367927342139,7.98612283218281));
#18977=CARTESIAN_POINT('Ctrl Pts',(1.99947825686152,1.52967086340101,7.991359639008));
#18978=CARTESIAN_POINT('Ctrl Pts',(1.9489953151362,1.59565861719648,7.99659614141023));
#18979=CARTESIAN_POINT('Ctrl Pts',(1.89524009579892,1.65914750149198,8.00183264381245));
#18980=CARTESIAN_POINT('Ctrl Pts',(1.83849746441907,1.71980618772136,8.00706914621468));
#18981=CARTESIAN_POINT('Ctrl Pts',(1.77937255397181,1.78301156441867,8.01252549760445));
#18982=CARTESIAN_POINT('Ctrl Pts',(1.7170042125162,1.8431434499418,8.01798184899421));
#18983=CARTESIAN_POINT('Ctrl Pts',(1.65175734424917,1.89986944965146,8.02343820038398));
#18984=CARTESIAN_POINT('Ctrl Pts',(1.58905159374907,1.95438618706949,8.0286820476057));
#18985=CARTESIAN_POINT('Ctrl Pts',(1.52368778151637,2.0057571609586,8.03392589482741));
#18986=CARTESIAN_POINT('Ctrl Pts',(1.45602219672215,2.0537296834424,8.03916974204913));
#18987=CARTESIAN_POINT('Ctrl Pts',(1.38830887220202,2.10173605171473,8.04441728893338));
#18988=CARTESIAN_POINT('Ctrl Pts',(1.31829093226679,2.14633895037898,8.04966483581763));
#18989=CARTESIAN_POINT('Ctrl Pts',(1.24635127519451,2.18733050744989,8.05491238270188));
#18990=CARTESIAN_POINT('Ctrl Pts',(1.17430060942845,2.2283853177999,8.06016802697426));
#18991=CARTESIAN_POINT('Ctrl Pts',(1.10032272263448,2.26581746540645,8.06542367124664));
#18992=CARTESIAN_POINT('Ctrl Pts',(1.02482191817686,2.29946652204904,8.07067931551902));
#18993=CARTESIAN_POINT('Ctrl Pts',(1.01588625012767,2.30344895379247,8.07130133130998));
#18994=CARTESIAN_POINT('Ctrl Pts',(1.00692926837676,2.30737845228083,8.07192334710093));
#18995=CARTESIAN_POINT('Ctrl Pts',(0.997951656853134,2.31125479784988,8.07254536289189));
#18996=CARTESIAN_POINT('Ctrl Pts',(0.922102155402338,2.34400503192823,8.0778006122992));
#18997=CARTESIAN_POINT('Ctrl Pts',(0.844498702622624,2.37307800987226,8.08305586170651));
#18998=CARTESIAN_POINT('Ctrl Pts',(0.765532238206542,2.39828410374302,8.08831111111381));
#18999=CARTESIAN_POINT('Ctrl Pts',(0.686677730298033,2.4234544610988,8.09355890977131));
#19000=CARTESIAN_POINT('Ctrl Pts',(0.606464485047739,2.44476868481441,8.0988067084288));
#19001=CARTESIAN_POINT('Ctrl Pts',(0.52530418316165,2.46208484117686,8.10405450708629));
#19002=CARTESIAN_POINT('Ctrl Pts',(0.443555804919887,2.47952646802045,8.1093403305692));
#19003=CARTESIAN_POINT('Ctrl Pts',(0.360847022713483,2.49291165629838,8.11462615405211));
#19004=CARTESIAN_POINT('Ctrl Pts',(0.277614991356014,2.50214631198385,8.11991197753501));
#19005=CARTESIAN_POINT('Ctrl Pts',(0.195129295878602,2.51129816114922,8.12515040340361));
#19006=CARTESIAN_POINT('Ctrl Pts',(0.112130164601205,2.51637356285531,8.1303888292722));
#19007=CARTESIAN_POINT('Ctrl Pts',(0.0290524157150399,2.5173323592925,8.13562725514079));
#19008=CARTESIAN_POINT('Ctrl Pts',(-0.0539980102821334,2.51829084039749,
8.14086395817829));
#19009=CARTESIAN_POINT('Ctrl Pts',(-0.137126541510563,2.51513539979878,
8.14610066121579));
#19010=CARTESIAN_POINT('Ctrl Pts',(-0.219896386140231,2.50787795344241,
8.1513373642533));
#19011=CARTESIAN_POINT('Ctrl Pts',(-0.302663976160698,2.50062070477524,
8.15657392464563));
#19012=CARTESIAN_POINT('Ctrl Pts',(-0.385072439441506,2.48926171384237,
8.16181048503796));
#19013=CARTESIAN_POINT('Ctrl Pts',(-0.46668952830822,2.47386481727831,8.16704704543029));
#19014=CARTESIAN_POINT('Ctrl Pts',(-0.549642468915775,2.45821591502079,
8.17236931420076));
#19015=CARTESIAN_POINT('Ctrl Pts',(-0.631777410420044,2.438395813585,8.17769158297124));
#19016=CARTESIAN_POINT('Ctrl Pts',(-0.712652561784477,2.41452533144343,
8.18301385174172));
#19017=CARTESIAN_POINT('Ctrl Pts',(-0.792339598035419,2.39100552413982,
8.18825793249206));
#19018=CARTESIAN_POINT('Ctrl Pts',(-0.870803191428158,2.36355376477676,
8.19350201324239));
#19019=CARTESIAN_POINT('Ctrl Pts',(-0.947638970692298,2.33233501693587,
8.19874609399272));
#19020=CARTESIAN_POINT('Ctrl Pts',(-1.02619315526228,2.30041807272806,8.20410745677328));
#19021=CARTESIAN_POINT('Ctrl Pts',(-1.1030453720849,2.26456382854647,8.20946881955383));
#19022=CARTESIAN_POINT('Ctrl Pts',(-1.17778988319318,2.22499825641455,8.21483018233438));
#19023=CARTESIAN_POINT('Ctrl Pts',(-1.25253439430145,2.18543268428264,8.22019154511493));
#19024=CARTESIAN_POINT('Ctrl Pts',(-1.32517079737989,2.14215610165391,8.22555290789549));
#19025=CARTESIAN_POINT('Ctrl Pts',(-1.39532635611374,2.09544043340162,8.23091427067604));
#19026=CARTESIAN_POINT('Ctrl Pts',(-1.46409337926548,2.04964937281807,8.23616952008335));
#19027=CARTESIAN_POINT('Ctrl Pts',(-1.53073088988013,2.00038502354856,8.24142476949065));
#19028=CARTESIAN_POINT('Ctrl Pts',(-1.59486698177955,1.94787205956381,8.24668001889796));
#19029=CARTESIAN_POINT('Ctrl Pts',(-1.65891214327062,1.8954335470325,8.25192781755545));
#19030=CARTESIAN_POINT('Ctrl Pts',(-1.72046257628046,1.83975585812135,8.25717561621295));
#19031=CARTESIAN_POINT('Ctrl Pts',(-1.77917508770257,1.78110703139888,8.26242341487044));
#19032=CARTESIAN_POINT('Ctrl Pts',(-1.83831302188613,1.72203324336552,8.26770923835335));
#19033=CARTESIAN_POINT('Ctrl Pts',(-1.89457134013327,1.65994534158663,8.27299506183626));
#19034=CARTESIAN_POINT('Ctrl Pts',(-1.94763310747957,1.59515877850748,8.27828088531916));
#19035=CARTESIAN_POINT('Ctrl Pts',(-2.00021907362067,1.53095315206756,8.28351931118776));
#19036=CARTESIAN_POINT('Ctrl Pts',(-2.04966528800478,1.46409743145697,8.28875773705635));
#19037=CARTESIAN_POINT('Ctrl Pts',(-2.09570132912801,1.39493447483784,8.29399616292494));
#19038=CARTESIAN_POINT('Ctrl Pts',(-2.14172222976347,1.32579426476408,8.29923286596245));
#19039=CARTESIAN_POINT('Ctrl Pts',(-2.1843349291271,1.25434870953135,8.30446956899995));
#19040=CARTESIAN_POINT('Ctrl Pts',(-2.2233116102288,1.1809706744123,8.30970627203746));
#19041=CARTESIAN_POINT('Ctrl Pts',(-2.26228722962518,1.10759463807426,8.31494283242979));
#19042=CARTESIAN_POINT('Ctrl Pts',(-2.29762681213926,1.03228663449532,8.32017939282212));
#19043=CARTESIAN_POINT('Ctrl Pts',(-2.32914856552648,0.955443985645375,
8.32541595321445));
#19044=CARTESIAN_POINT('Ctrl Pts',(-2.36118624504783,0.877343629767864,
8.33073822198493));
#19045=CARTESIAN_POINT('Ctrl Pts',(-2.38927979398977,0.797658389323468,
8.33606049075541));
#19046=CARTESIAN_POINT('Ctrl Pts',(-2.41329002013544,0.716824615031257,
8.3413827595259));
#19047=CARTESIAN_POINT('Ctrl Pts',(-2.43694751850155,0.6371783479931,8.34662684027623));
#19048=CARTESIAN_POINT('Ctrl Pts',(-2.4566408204405,0.556417537949075,8.35187092102657));
#19049=CARTESIAN_POINT('Ctrl Pts',(-2.47228813556247,0.474971183080658,
8.3571150017769));
#19050=CARTESIAN_POINT('Ctrl Pts',(-2.4882853974096,0.391703308996976,8.36247636455746));
#19051=CARTESIAN_POINT('Ctrl Pts',(-2.50005344341738,0.307719363212413,
8.36783772733801));
#19052=CARTESIAN_POINT('Ctrl Pts',(-2.50756091250626,0.223482706424399,
8.37319909011857));
#19053=CARTESIAN_POINT('Ctrl Pts',(-2.51506838159514,0.139246049636391,
8.37856045289912));
#19054=CARTESIAN_POINT('Ctrl Pts',(-2.51831532100137,0.0547571921421189,
8.38392181567968));
#19055=CARTESIAN_POINT('Ctrl Pts',(-2.51732688234237,-0.0295231677914636,
8.38928317846023));
#19056=CARTESIAN_POINT('Ctrl Pts',(-2.5163580070975,-0.112135430702491,
8.39453842786754));
#19057=CARTESIAN_POINT('Ctrl Pts',(-2.51131634767356,-0.194852512373203,
8.39979367727485));
#19058=CARTESIAN_POINT('Ctrl Pts',(-2.50218787396462,-0.277240136676509,
8.40504892668215));
#19059=CARTESIAN_POINT('Ctrl Pts',(-2.49307234235767,-0.359510954044777,
8.41029672533965));
#19060=CARTESIAN_POINT('Ctrl Pts',(-2.47988155577698,-0.441452787045854,
8.41554452399715));
#19061=CARTESIAN_POINT('Ctrl Pts',(-2.46265349088341,-0.522631833932614,
8.42079232265464));
#19062=CARTESIAN_POINT('Ctrl Pts',(-2.44530059380733,-0.604399092998672,
8.42607814613755));
#19063=CARTESIAN_POINT('Ctrl Pts',(-2.42385166998306,-0.685391991366873,
8.43136396962046));
#19064=CARTESIAN_POINT('Ctrl Pts',(-2.39839876275192,-0.765172937857888,
8.43664979310337));
#19065=CARTESIAN_POINT('Ctrl Pts',(-2.37317408998301,-0.844238494108646,
8.44188821897196));
#19066=CARTESIAN_POINT('Ctrl Pts',(-2.34401709592337,-0.922113298716357,
8.44712664484055));
#19067=CARTESIAN_POINT('Ctrl Pts',(-2.31106813594437,-0.998383854548244,
8.45236507070915));
#19068=CARTESIAN_POINT('Ctrl Pts',(-2.27813001232996,-1.07462932626364,
8.45760177374665));
#19069=CARTESIAN_POINT('Ctrl Pts',(-2.24140258247872,-1.14927117381642,
8.46283847678415));
#19070=CARTESIAN_POINT('Ctrl Pts',(-2.2010745675889,-1.22191529899308,8.46807517982166));
#19071=CARTESIAN_POINT('Ctrl Pts',(-2.16074765121404,-1.29455744538009,
8.47331174021399));
#19072=CARTESIAN_POINT('Ctrl Pts',(-2.11682056966571,-1.36520157466179,
8.47854830060632));
#19073=CARTESIAN_POINT('Ctrl Pts',(-2.06952761647568,-1.43347887833915,
8.48378486099866));
#19074=CARTESIAN_POINT('Ctrl Pts',(-2.02146060512304,-1.50287369743199,
8.48910712976913));
#19075=CARTESIAN_POINT('Ctrl Pts',(-1.96991681677189,-1.56982310309958,
8.49442939853961));
#19076=CARTESIAN_POINT('Ctrl Pts',(-1.91518647561926,-1.6339727701541,8.49975166731009));
#19077=CARTESIAN_POINT('Ctrl Pts',(-1.86126016319972,-1.69718003169016,
8.50499574806043));
#19078=CARTESIAN_POINT('Ctrl Pts',(-1.80424066777231,-1.75766897052556,
8.51023982881076));
#19079=CARTESIAN_POINT('Ctrl Pts',(-1.74444329879661,-1.81513741278273,
8.51548390956109));
#19080=CARTESIAN_POINT('Ctrl Pts',(-1.68330858259666,-1.87389111663336,
8.52084527234165));
#19081=CARTESIAN_POINT('Ctrl Pts',(-1.61927062781268,-1.92948725322094,
8.5262066351222));
#19082=CARTESIAN_POINT('Ctrl Pts',(-1.55270102323419,-1.98164723965884,
8.53156799790275));
#19083=CARTESIAN_POINT('Ctrl Pts',(-1.48613141865571,-2.03380722609674,
8.53692936068331));
#19084=CARTESIAN_POINT('Ctrl Pts',(-1.41703061803393,-2.08253082417426,
8.54229072346386));
#19085=CARTESIAN_POINT('Ctrl Pts',(-1.34579874535832,-2.12758830298344,
8.54765208624441));
#19086=CARTESIAN_POINT('Ctrl Pts',(-1.27597671092752,-2.17175399340559,
8.55290733565172));
#19087=CARTESIAN_POINT('Ctrl Pts',(-1.20384932162568,-2.21256053261645,
8.55816258505902));
#19088=CARTESIAN_POINT('Ctrl Pts',(-1.12977320620478,-2.2497597099561,8.56341783446633));
#19089=CARTESIAN_POINT('Ctrl Pts',(-1.05580211388743,-2.28690614731295,
8.56866563312383));
#19090=CARTESIAN_POINT('Ctrl Pts',(-0.979888192187141,-2.32045517618541,
8.57391343178133));
#19091=CARTESIAN_POINT('Ctrl Pts',(-0.902415987114985,-2.35020246706519,
8.57916123043883));
#19092=CARTESIAN_POINT('Ctrl Pts',(-0.824382429128209,-2.38016530271256,
8.58444705392173));
#19093=CARTESIAN_POINT('Ctrl Pts',(-0.744768310763633,-2.40627082083289,
8.58973287740464));
#19094=CARTESIAN_POINT('Ctrl Pts',(-0.663990793267411,-2.4283579794701,
8.59501870088755));
#19095=CARTESIAN_POINT('Ctrl Pts',(-0.583937602194848,-2.45024708408039,
8.60025712675614));
#19096=CARTESIAN_POINT('Ctrl Pts',(-0.502742245948794,-2.46818948133829,
8.60549555262473));
#19097=CARTESIAN_POINT('Ctrl Pts',(-0.420827979435216,-2.48207777108705,
8.61073397849333));
#19098=CARTESIAN_POINT('Ctrl Pts',(-0.338940653160633,-2.49596149320846,
8.61597068153083));
#19099=CARTESIAN_POINT('Ctrl Pts',(-0.256335340766099,-2.50579367881355,
8.62120738456834));
#19100=CARTESIAN_POINT('Ctrl Pts',(-0.173445358343676,-2.51151805839995,
8.62644408760584));
#19101=CARTESIAN_POINT('Ctrl Pts',(-0.0905576338029299,-2.5172422820571,
8.63168064799818));
#19102=CARTESIAN_POINT('Ctrl Pts',(-0.00738571504710353,-2.51885889140939,
8.63691720839051));
#19103=CARTESIAN_POINT('Ctrl Pts',(0.0756334827210238,-2.51636361170072,
8.64215376878284));
#19104=CARTESIAN_POINT('Ctrl Pts',(0.160011480973147,-2.5138274909894,8.64747603755332));
#19105=CARTESIAN_POINT('Ctrl Pts',(0.244231221974307,-2.50704366739768,
8.6527983063238));
#19106=CARTESIAN_POINT('Ctrl Pts',(0.327837487473386,-2.49606266584137,
8.65812057509428));
#19107=CARTESIAN_POINT('Ctrl Pts',(0.41021551579522,-2.48524298322778,8.66336465584461));
#19108=CARTESIAN_POINT('Ctrl Pts',(0.49199752432431,-2.47034876753276,8.66860873659494));
#19109=CARTESIAN_POINT('Ctrl Pts',(0.572758381215893,-2.45147997885909,
8.67385281734527));
#19110=CARTESIAN_POINT('Ctrl Pts',(0.655325426400422,-2.432189196332,8.67921418012582));
#19111=CARTESIAN_POINT('Ctrl Pts',(0.736824601303901,-2.40874405725313,
8.68457554290638));
#19112=CARTESIAN_POINT('Ctrl Pts',(0.816819920653717,-2.3813045725449,8.68993690568693));
#19113=CARTESIAN_POINT('Ctrl Pts',(0.896815240003528,-2.35386508783667,
8.69529826846748));
#19114=CARTESIAN_POINT('Ctrl Pts',(0.975306256944832,-2.32243150840789,
8.70065963124803));
#19115=CARTESIAN_POINT('Ctrl Pts',(1.05188242683368,-2.28721437782261,8.70602099402858));
#19116=CARTESIAN_POINT('Ctrl Pts',(1.12694298287034,-2.25269427310095,8.71127624343589));
#19117=CARTESIAN_POINT('Ctrl Pts',(1.2004410628445,-2.2144115593781,8.7165314928432));
#19118=CARTESIAN_POINT('Ctrl Pts',(1.27197430248878,-2.17253023541864,8.72178674225051));
#19119=CARTESIAN_POINT('Ctrl Pts',(1.34340612424965,-2.13070828966226,8.72703454090801));
#19120=CARTESIAN_POINT('Ctrl Pts',(1.41287824401752,-2.08529809894302,8.7322823395655));
#19121=CARTESIAN_POINT('Ctrl Pts',(1.48000990510121,-2.03651096996857,8.737530138223));
#19122=CARTESIAN_POINT('Ctrl Pts',(1.54762799294374,-1.98737033618524,8.74281596170591));
#19123=CARTESIAN_POINT('Ctrl Pts',(1.61287113116809,-1.93480381800173,8.74810178518882));
#19124=CARTESIAN_POINT('Ctrl Pts',(1.67537711493224,-1.87907364750861,8.75338760867172));
#19125=CARTESIAN_POINT('Ctrl Pts',(1.73732261185449,-1.8238432056075,8.75862603454032));
#19126=CARTESIAN_POINT('Ctrl Pts',(1.79657949470934,-1.76550593339148,8.76386446040891));
#19127=CARTESIAN_POINT('Ctrl Pts',(1.85282723527963,-1.70435837962737,8.7691028862775));
#19128=CARTESIAN_POINT('Ctrl Pts',(1.90905647690416,-1.64323093627604,8.774339589315));
#19129=CARTESIAN_POINT('Ctrl Pts',(1.96227822961948,-1.57929538632552,8.77957629235251));
#19130=CARTESIAN_POINT('Ctrl Pts',(2.01220937537835,-1.51288455595246,8.78481299539001));
#19131=CARTESIAN_POINT('Ctrl Pts',(2.06213916103779,-1.4464755345772,8.79004955578234));
#19132=CARTESIAN_POINT('Ctrl Pts',(2.10877824149183,-1.37759173626641,8.79528611617467));
#19133=CARTESIAN_POINT('Ctrl Pts',(2.15188515194386,-1.30659731472383,8.80052267656701));
#19134=CARTESIAN_POINT('Ctrl Pts',(2.19569760632263,-1.23444090587049,8.80584494533749));
#19135=CARTESIAN_POINT('Ctrl Pts',(2.23586095688824,-1.16010457351426,8.81116721410797));
#19136=CARTESIAN_POINT('Ctrl Pts',(2.27216973926283,-1.08399765958155,8.81648948287845));
#19137=CARTESIAN_POINT('Ctrl Pts',(2.30794511907356,-1.00900881186765,8.82173356362878));
#19138=CARTESIAN_POINT('Ctrl Pts',(2.3399783080633,-0.932301515061035,8.82697764437911));
#19139=CARTESIAN_POINT('Ctrl Pts',(2.36812168829854,-0.854286789907267,
8.83222172512945));
#19140=CARTESIAN_POINT('Ctrl Pts',(2.39689448538076,-0.774527292735595,
8.83758308791));
#19141=CARTESIAN_POINT('Ctrl Pts',(2.42160123659593,-0.69340167100751,8.84294445069055));
#19142=CARTESIAN_POINT('Ctrl Pts',(2.44213878500907,-0.611362744002635,
8.8483058134711));
#19143=CARTESIAN_POINT('Ctrl Pts',(2.46267633342221,-0.529323816997754,
8.85366717625165));
#19144=CARTESIAN_POINT('Ctrl Pts',(2.47904464620288,-0.446372096142171,
8.85902853903221));
#19145=CARTESIAN_POINT('Ctrl Pts',(2.49119680399602,-0.362966573888061,
8.86438990181276));
#19146=CARTESIAN_POINT('Ctrl Pts',(2.50859444872508,-0.243559002877223,
8.87206550037784));
#19147=CARTESIAN_POINT('Ctrl Pts',(2.5174096762307,-0.12287148413771,8.87974109894292));
#19148=CARTESIAN_POINT('Ctrl Pts',(2.51749930935083,-0.00186478366189579,
8.88741669750801));
#19149=CARTESIAN_POINT('Ctrl Pts',(2.51749930935125,-0.00186478309385184,
8.88741669754404));
#19150=CARTESIAN_POINT('Ctrl Pts',(2.51755970653645,0.0796727815327686,
8.89258872199874));
#19151=CARTESIAN_POINT('Ctrl Pts',(2.51365459994446,0.161358301547571,8.89776074645344));
#19152=CARTESIAN_POINT('Ctrl Pts',(2.5057673658586,0.242767704190768,8.90293277090814));
#19153=CARTESIAN_POINT('Ctrl Pts',(2.49788815071092,0.324094338025553,8.90809953697391));
#19154=CARTESIAN_POINT('Ctrl Pts',(2.48603488288074,0.405144940630114,8.91326630303968));
#19155=CARTESIAN_POINT('Ctrl Pts',(2.47024295996914,0.485495590837766,8.91843306910546));
#19156=CARTESIAN_POINT('Ctrl Pts',(2.45446208214504,0.565790042698492,8.92359622146417));
#19157=CARTESIAN_POINT('Ctrl Pts',(2.43474810638477,0.645385047783456,8.92875937382288));
#19158=CARTESIAN_POINT('Ctrl Pts',(2.4111880499293,0.723863549212233,8.9339225261816));
#19159=CARTESIAN_POINT('Ctrl Pts',(2.39615340801751,0.773943911667475,8.93721734625115));
#19160=CARTESIAN_POINT('Ctrl Pts',(2.37955359253486,0.823569749410887,8.94051216632071));
#19161=CARTESIAN_POINT('Ctrl Pts',(2.36142200728635,0.872635292378026,8.94380698639026));
#19162=CARTESIAN_POINT('',(2.51749909420668,-0.00135787363871094,8.61075084542347));
#19163=CARTESIAN_POINT('Ctrl Pts',(2.36142186693781,0.872635672172493,8.66836043115426));
#19164=CARTESIAN_POINT('Ctrl Pts',(2.38766432837594,0.801621474313745,8.66315328780155));
#19165=CARTESIAN_POINT('Ctrl Pts',(2.4107055817133,0.729417533717104,8.65798469879897));
#19166=CARTESIAN_POINT('Ctrl Pts',(2.45152777444271,0.578228022230177,8.64746763910954));
#19167=CARTESIAN_POINT('Ctrl Pts',(2.46882533046289,0.499239322516955,8.64213924160784));
#19168=CARTESIAN_POINT('Ctrl Pts',(2.48627876218841,0.395974422567439,8.63538790124849));
#19169=CARTESIAN_POINT('Ctrl Pts',(2.48992714207542,0.372344891433137,8.63385720767189));
#19170=CARTESIAN_POINT('Ctrl Pts',(2.49512354268189,0.335186536182973,8.63147163611905));
#19171=CARTESIAN_POINT('Ctrl Pts',(2.49689929596445,0.321691505840321,8.63060968090192));
#19172=CARTESIAN_POINT('Ctrl Pts',(2.49985358529291,0.297739837343419,8.62908747963504));
#19173=CARTESIAN_POINT('Ctrl Pts',(2.50107616058215,0.287289058310349,8.62842587294413));
#19174=CARTESIAN_POINT('Ctrl Pts',(2.50343991969958,0.265923384065525,8.62707840247117));
#19175=CARTESIAN_POINT('Ctrl Pts',(2.50457532711521,0.255008067724658,8.62639273211866));
#19176=CARTESIAN_POINT('Ctrl Pts',(2.50692920549118,0.230844529274809,8.62488069701353));
#19177=CARTESIAN_POINT('Ctrl Pts',(2.5081141120614,0.217593312163377,8.62405538682484));
#19178=CARTESIAN_POINT('Ctrl Pts',(2.51142857636331,0.176891963405776,8.6215318582072));
#19179=CARTESIAN_POINT('Ctrl Pts',(2.51321297152733,0.14941522635885,8.61984422538577));
#19180=CARTESIAN_POINT('Ctrl Pts',(2.51653706826746,0.0808537709645683,
8.61566864809835));
#19181=CARTESIAN_POINT('Ctrl Pts',(2.51752185448915,0.0397499541746253,
8.6131971064922));
#19182=CARTESIAN_POINT('Ctrl Pts',(2.51749963220541,-0.00136082535489392,
8.61074973370103));
#19183=CARTESIAN_POINT('Ctrl Pts',(2.51749963382901,-0.00135781839193702,
8.6107499127091));
#19184=CARTESIAN_POINT('Ctrl Pts',(2.51737464808992,-0.233090982609691,
8.59695455967742));
#19185=CARTESIAN_POINT('Ctrl Pts',(2.4852569110145,-0.46368713501507,8.58412487491137));
#19186=CARTESIAN_POINT('Ctrl Pts',(2.41013441700624,-0.728675235698085,
8.56783566805232));
#19187=CARTESIAN_POINT('Ctrl Pts',(2.39712499375044,-0.770393956259634,
8.56521950708456));
#19188=CARTESIAN_POINT('Ctrl Pts',(2.37405534696998,-0.838118981753158,
8.56085586831821));
#19189=CARTESIAN_POINT('Ctrl Pts',(2.36463670135636,-0.864335201202673,
8.55913748803329));
#19190=CARTESIAN_POINT('Ctrl Pts',(2.35123051681317,-0.899790162408652,
8.55676663776672));
#19191=CARTESIAN_POINT('Ctrl Pts',(2.34761935723741,-0.909170294859618,
8.55613487769055));
#19192=CARTESIAN_POINT('Ctrl Pts',(2.34147656589317,-0.924845814336315,
8.55507113418019));
#19193=CARTESIAN_POINT('Ctrl Pts',(2.3389754317916,-0.931153164939045,8.55464093873036));
#19194=CARTESIAN_POINT('Ctrl Pts',(2.33417206311208,-0.943124813602679,
8.5538201231076));
#19195=CARTESIAN_POINT('Ctrl Pts',(2.33187463657746,-0.948790973615488,
8.55342980438863));
#19196=CARTESIAN_POINT('Ctrl Pts',(2.32636012689872,-0.96225043289266,8.55249837835992));
#19197=CARTESIAN_POINT('Ctrl Pts',(2.32312451342757,-0.970035992074675,
8.55195619037801));
#19198=CARTESIAN_POINT('Ctrl Pts',(2.31151513200617,-0.997579338570043,
8.55002633001605));
#19199=CARTESIAN_POINT('Ctrl Pts',(2.30292818396566,-1.01724552087722,8.54862690632044));
#19200=CARTESIAN_POINT('Ctrl Pts',(2.23938325271842,-1.15784934633412,8.53847862266113));
#19201=CARTESIAN_POINT('Ctrl Pts',(2.17518504586928,-1.27436882180376,8.52931295679336));
#19202=CARTESIAN_POINT('Ctrl Pts',(2.0276928550642,-1.49818382513107,8.51079520974065));
#19203=CARTESIAN_POINT('Ctrl Pts',(1.94429841729279,-1.60493096679138,8.5014754838603));
#19204=CARTESIAN_POINT('Ctrl Pts',(1.81831792885298,-1.74186934011822,8.4890361871044));
#19205=CARTESIAN_POINT('Ctrl Pts',(1.7827842255893,-1.77822098399486,8.48567866899807));
#19206=CARTESIAN_POINT('Ctrl Pts',(1.72804177147631,-1.83093183261729,8.48072608097172));
#19207=CARTESIAN_POINT('Ctrl Pts',(1.70964989923951,-1.84811715973801,8.47909709581625));
#19208=CARTESIAN_POINT('Ctrl Pts',(1.67555017835562,-1.87903510808308,8.47613927387552));
#19209=CARTESIAN_POINT('Ctrl Pts',(1.65992361592052,-1.89285365775568,8.47480693598427));
#19210=CARTESIAN_POINT('Ctrl Pts',(1.634617829585,-1.91467711804161,8.47268544841849));
#19211=CARTESIAN_POINT('Ctrl Pts',(1.62504758341077,-1.92280635428529,8.47189121301355));
#19212=CARTESIAN_POINT('Ctrl Pts',(1.60648814244898,-1.938333722254,8.4703662544326));
#19213=CARTESIAN_POINT('Ctrl Pts',(1.59750768697473,-1.94574175265601,8.46963514133291));
#19214=CARTESIAN_POINT('Ctrl Pts',(1.57703519686471,-1.96239234463157,8.46798352273246));
#19215=CARTESIAN_POINT('Ctrl Pts',(1.56551262079387,-1.97159680846695,8.46706455388978));
#19216=CARTESIAN_POINT('Ctrl Pts',(1.53017631787962,-1.99931904365559,8.46427783639052));
#19217=CARTESIAN_POINT('Ctrl Pts',(1.5061095338955,-2.01751094001382,8.46242285358293));
#19218=CARTESIAN_POINT('Ctrl Pts',(1.31079447398623,-2.15970479185445,8.4476911339114));
#19219=CARTESIAN_POINT('Ctrl Pts',(1.12487776398485,-2.26211520369748,8.43571270384987));
#19220=CARTESIAN_POINT('Ctrl Pts',(0.813875362275058,-2.38549275388142,
8.41642002826897));
#19221=CARTESIAN_POINT('Ctrl Pts',(0.696253449370582,-2.42243519113316,
8.40924954365842));
#19222=CARTESIAN_POINT('Ctrl Pts',(0.558894500901102,-2.45474383037895,
8.4005399526972));
#19223=CARTESIAN_POINT('Ctrl Pts',(0.541327222224817,-2.45867751677927,
8.39941981076524));
#19224=CARTESIAN_POINT('Ctrl Pts',(0.515449824455284,-2.46418124650907,
8.3977586177536));
#19225=CARTESIAN_POINT('Ctrl Pts',(0.50717112626941,-2.46589845309399,8.3972254954022));
#19226=CARTESIAN_POINT('Ctrl Pts',(0.492486662819062,-2.4688672983262,8.39627664719856));
#19227=CARTESIAN_POINT('Ctrl Pts',(0.486084471445781,-2.47013577259444,
8.39586187465994));
#19228=CARTESIAN_POINT('Ctrl Pts',(0.472190510290721,-2.4728324924096,8.39495931342163));
#19229=CARTESIAN_POINT('Ctrl Pts',(0.464697279245796,-2.47425157341053,
8.39447104429632));
#19230=CARTESIAN_POINT('Ctrl Pts',(0.443893438794687,-2.47809360376033,
8.39311148830178));
#19231=CARTESIAN_POINT('Ctrl Pts',(0.430569797360363,-2.48044329192573,
8.39223629570707));
#19232=CARTESIAN_POINT('Ctrl Pts',(0.356504087570587,-2.49289042031678,
8.38734871702509));
#19233=CARTESIAN_POINT('Ctrl Pts',(0.295431112545935,-2.50086323803604,
8.38323540522959));
#19234=CARTESIAN_POINT('Ctrl Pts',(0.056764030473468,-2.52315643000945,
8.36698759428564));
#19235=CARTESIAN_POINT('Ctrl Pts',(-0.121863623809035,-2.52085194192725,
8.35449859967775));
#19236=CARTESIAN_POINT('Ctrl Pts',(-0.411426366202344,-2.48624412087625,
8.33468096217839));
#19237=CARTESIAN_POINT('Ctrl Pts',(-0.523066232554378,-2.46517534363098,
8.32713640010854));
#19238=CARTESIAN_POINT('Ctrl Pts',(-0.655317832266786,-2.43082299089872,
8.31833734980553));
#19239=CARTESIAN_POINT('Ctrl Pts',(-0.677637339666892,-2.42469576827135,
8.31685686419236));
#19240=CARTESIAN_POINT('Ctrl Pts',(-0.712649121655435,-2.41456299752018,
8.31454092615491));
#19241=CARTESIAN_POINT('Ctrl Pts',(-0.725399115355684,-2.410763234761,8.31369890121087));
#19242=CARTESIAN_POINT('Ctrl Pts',(-0.749218013192332,-2.40345863337134,
8.31212821257802));
#19243=CARTESIAN_POINT('Ctrl Pts',(-0.760293902739406,-2.39997796288599,
8.31139878916497));
#19244=CARTESIAN_POINT('Ctrl Pts',(-0.785042307749389,-2.39201209542708,
8.30977088771807));
#19245=CARTESIAN_POINT('Ctrl Pts',(-0.798701316259831,-2.3874860231246,
8.30887376698085));
#19246=CARTESIAN_POINT('Ctrl Pts',(-0.833368841284254,-2.37566772108291,
8.30659976307365));
#19247=CARTESIAN_POINT('Ctrl Pts',(-0.854321184433942,-2.36821369576142,
8.3052281867491));
#19248=CARTESIAN_POINT('Ctrl Pts',(-1.02688164672101,-2.3042351847904,8.29394845952897));
#19249=CARTESIAN_POINT('Ctrl Pts',(-1.1728222245501,-2.23349125458446,8.28454767554206));
#19250=CARTESIAN_POINT('Ctrl Pts',(-1.41692888469482,-2.08459133975002,
8.26809879652324));
#19251=CARTESIAN_POINT('Ctrl Pts',(-1.51794929679112,-2.01222139487975,
8.26102541531852));
#19252=CARTESIAN_POINT('Ctrl Pts',(-1.64677294364045,-1.90469309904515,
8.25110154928247));
#19253=CARTESIAN_POINT('Ctrl Pts',(-1.67959341799864,-1.87581514430811,
8.24848445035755));
#19254=CARTESIAN_POINT('Ctrl Pts',(-1.73207627790999,-1.82715472862733,
8.24411939847138));
#19255=CARTESIAN_POINT('Ctrl Pts',(-1.75219200170792,-1.80787324646103,
8.24240056678593));
#19256=CARTESIAN_POINT('Ctrl Pts',(-1.77912312868682,-1.78118729876964,
8.24002918945711));
#19257=CARTESIAN_POINT('Ctrl Pts',(-1.78622107852673,-1.77406920691418,
8.23939736559858));
#19258=CARTESIAN_POINT('Ctrl Pts',(-1.79803841163796,-1.7620755267802,8.23833354479875));
#19259=CARTESIAN_POINT('Ctrl Pts',(-1.80278114649585,-1.75722293059777,
8.23790333641549));
#19260=CARTESIAN_POINT('Ctrl Pts',(-1.8117599738799,-1.7479615067211,8.23708252024665));
#19261=CARTESIAN_POINT('Ctrl Pts',(-1.81599972690298,-1.74355631451983,
8.2366922140699));
#19262=CARTESIAN_POINT('Ctrl Pts',(-1.82604727201779,-1.73304030058062,
8.23576084896937));
#19263=CARTESIAN_POINT('Ctrl Pts',(-1.83184045452337,-1.72691570941812,
8.23521870969261));
#19264=CARTESIAN_POINT('Ctrl Pts',(-1.85226731321811,-1.7051018590694,8.23328919107777));
#19265=CARTESIAN_POINT('Ctrl Pts',(-1.86673060489012,-1.68925525786975,
8.23189006568425));
#19266=CARTESIAN_POINT('Ctrl Pts',(-1.96694419050882,-1.57659826359056,
8.22197316778406));
#19267=CARTESIAN_POINT('Ctrl Pts',(-2.04531778775473,-1.47349935742758,
8.21305998009377));
#19268=CARTESIAN_POINT('Ctrl Pts',(-2.19277144766801,-1.24495675186071,
8.19427160147215));
#19269=CARTESIAN_POINT('Ctrl Pts',(-2.2598002872475,-1.11869322411117,8.18443217630014));
#19270=CARTESIAN_POINT('Ctrl Pts',(-2.34454518273031,-0.919942994800179,
8.17001376318646));
#19271=CARTESIAN_POINT('Ctrl Pts',(-2.37035589243968,-0.851235547118459,
8.16520466978328));
#19272=CARTESIAN_POINT('Ctrl Pts',(-2.39949401582388,-0.762007148649081,
8.15917738289421));
#19273=CARTESIAN_POINT('Ctrl Pts',(-2.40561907951748,-0.74244414700348,
8.15786891767906));
#19274=CARTESIAN_POINT('Ctrl Pts',(-2.41515908654987,-0.710615818501265,
8.15576057224085));
#19275=CARTESIAN_POINT('Ctrl Pts',(-2.41872103605421,-0.698395886482881,
8.1549559609172));
#19276=CARTESIAN_POINT('Ctrl Pts',(-2.42538505504475,-0.674871090933258,
8.15341610231489));
#19277=CARTESIAN_POINT('Ctrl Pts',(-2.42850113331093,-0.663570574678193,
8.15268042042152));
#19278=CARTESIAN_POINT('Ctrl Pts',(-2.43546012369153,-0.637627932097979,
8.15100048916356));
#19279=CARTESIAN_POINT('Ctrl Pts',(-2.4392501522418,-0.622971993294495,
8.15005795685465));
#19280=CARTESIAN_POINT('Ctrl Pts',(-2.45090892130213,-0.57614950877362,
8.14706680672387));
#19281=CARTESIAN_POINT('Ctrl Pts',(-2.45827551078707,-0.543860704749151,
8.14503416358954));
#19282=CARTESIAN_POINT('Ctrl Pts',(-2.49961667841714,-0.34460536143009,
8.13265669104477));
#19283=CARTESIAN_POINT('Ctrl Pts',(-2.51720653304508,-0.174688620952317,
8.12285330540817));
#19284=CARTESIAN_POINT('Ctrl Pts',(-2.51766562992915,0.0952434320171729,
8.10734351450212));
#19285=CARTESIAN_POINT('Ctrl Pts',(-2.51193289355596,0.194685999372743,
8.10163318409915));
#19286=CARTESIAN_POINT('Ctrl Pts',(-2.4950527900688,0.338476855747316,8.09308307747562));
#19287=CARTESIAN_POINT('Ctrl Pts',(-2.48856429327033,0.3832783608502,8.09037661033664));
#19288=CARTESIAN_POINT('Ctrl Pts',(-2.47601610355159,0.456033812292816,
8.08587718251499));
#19289=CARTESIAN_POINT('Ctrl Pts',(-2.47068131206139,0.48410358145907,8.08411565193481));
#19290=CARTESIAN_POINT('Ctrl Pts',(-2.46280586571477,0.522011993804842,
8.08169446565782));
#19291=CARTESIAN_POINT('Ctrl Pts',(-2.46068145006588,0.531936130489481,
8.08105667079656));
#19292=CARTESIAN_POINT('Ctrl Pts',(-2.45703238159988,0.548492880201491,
8.07998560484734));
#19293=CARTESIAN_POINT('Ctrl Pts',(-2.45554070858783,0.555132768166742,
8.07955417624436));
#19294=CARTESIAN_POINT('Ctrl Pts',(-2.45266165932137,0.567709615012644,
8.07873326517996));
#19295=CARTESIAN_POINT('Ctrl Pts',(-2.45127960323995,0.573647737657269,
8.07834409864006));
#19296=CARTESIAN_POINT('Ctrl Pts',(-2.44795081100352,0.587718475635898,
8.0774183008108));
#19297=CARTESIAN_POINT('Ctrl Pts',(-2.44598511085898,0.595846467177164,
8.07688061830548));
#19298=CARTESIAN_POINT('Ctrl Pts',(-2.43892972344113,0.624396526177035,
8.07498215129924));
#19299=CARTESIAN_POINT('Ctrl Pts',(-2.43362462574986,0.644763778933942,
8.07361009341827));
#19300=CARTESIAN_POINT('Ctrl Pts',(-2.38854986346771,0.809326728405822,
8.06239315346727));
#19301=CARTESIAN_POINT('Ctrl Pts',(-2.33625944751048,0.949770678525944,
8.0520197683175));
#19302=CARTESIAN_POINT('Ctrl Pts',(-2.21661803535369,1.20034354390598,8.03284351853884));
#19303=CARTESIAN_POINT('Ctrl Pts',(-2.15266556743567,1.31158583729764,8.02405411413298));
#19304=CARTESIAN_POINT('Ctrl Pts',(-2.05469925225694,1.4553760563597,8.01247067482682));
#19305=CARTESIAN_POINT('Ctrl Pts',(-2.02785168977947,1.49255701245392,8.00945181006693));
#19306=CARTESIAN_POINT('Ctrl Pts',(-1.97942987376889,1.55589555320451,8.00426743175082));
#19307=CARTESIAN_POINT('Ctrl Pts',(-1.95831586840964,1.5823883023995,8.00208553875647));
#19308=CARTESIAN_POINT('Ctrl Pts',(-1.92680814957182,1.6203255824475,7.99893982152219));
#19309=CARTESIAN_POINT('Ctrl Pts',(-1.91683430240607,1.63211240814546,7.99795937257309));
#19310=CARTESIAN_POINT('Ctrl Pts',(-1.89909460657724,1.65268976900617,7.99624194548377));
#19311=CARTESIAN_POINT('Ctrl Pts',(-1.89137466600175,1.66151908735217,7.99550312688755));
#19312=CARTESIAN_POINT('Ctrl Pts',(-1.87516099332643,1.67980326899045,7.99396897777136));
#19313=CARTESIAN_POINT('Ctrl Pts',(-1.86665678041011,1.6892484266645,7.99317411113845));
#19314=CARTESIAN_POINT('Ctrl Pts',(-1.84430919164595,1.7136938107486,7.99111036956656));
#19315=CARTESIAN_POINT('Ctrl Pts',(-1.83035409661777,1.72859098411185,7.98984622463906));
#19316=CARTESIAN_POINT('Ctrl Pts',(-1.77097689912881,1.79045121276967,7.98456682576103));
#19317=CARTESIAN_POINT('Ctrl Pts',(-1.72391462894867,1.83580885495681,7.98062253163847));
#19318=CARTESIAN_POINT('Ctrl Pts',(-1.52584839570059,2.01235889236698,7.96484999876149));
#19319=CARTESIAN_POINT('Ctrl Pts',(-1.36124366885512,2.1271612941855,7.95364432877833));
#19320=CARTESIAN_POINT('Ctrl Pts',(-1.12974841760269,2.25063690371914,7.9383454758762));
#19321=CARTESIAN_POINT('Ctrl Pts',(-1.07363646105424,2.27793803402906,7.93466314865816));
#19322=CARTESIAN_POINT('Ctrl Pts',(-0.98388970465471,2.31755120216156,7.92872740867969));
#19323=CARTESIAN_POINT('Ctrl Pts',(-0.950905355950302,2.3312788830228,7.92653632078502));
#19324=CARTESIAN_POINT('Ctrl Pts',(-0.907378010061243,2.34831703359879,
7.92361852470122));
#19325=CARTESIAN_POINT('Ctrl Pts',(-0.897087876634973,2.35226722005725,
7.92292683693532));
#19326=CARTESIAN_POINT('Ctrl Pts',(-0.880226635211065,2.35861320194372,
7.92178983062499));
#19327=CARTESIAN_POINT('Ctrl Pts',(-0.87367076998457,2.36104945914826,7.92134685897184));
#19328=CARTESIAN_POINT('Ctrl Pts',(-0.860844192792682,2.36575527021321,
7.92047829135203));
#19329=CARTESIAN_POINT('Ctrl Pts',(-0.854574482394941,2.36802727460356,
7.92005284264647));
#19330=CARTESIAN_POINT('Ctrl Pts',(-0.840540094581967,2.37305003259906,
7.91909863216753));
#19331=CARTESIAN_POINT('Ctrl Pts',(-0.832770801400698,2.3757876369001,7.91856911882831));
#19332=CARTESIAN_POINT('Ctrl Pts',(-0.80579443415389,2.38514450467108,7.91672649406695));
#19333=CARTESIAN_POINT('Ctrl Pts',(-0.786521347912426,2.39156916813997,
7.91540293331457));
#19334=CARTESIAN_POINT('Ctrl Pts',(-0.611055225459327,2.44771029748455,
7.90330190015009));
#19335=CARTESIAN_POINT('Ctrl Pts',(-0.450444886224806,2.48229034993314,
7.89188774136286));
#19336=CARTESIAN_POINT('Ctrl Pts',(-0.190566171215828,2.5121776452348,7.87384210604544));
#19337=CARTESIAN_POINT('Ctrl Pts',(-0.0929297295445561,2.5176812168465,
7.86714919964302));
#19338=CARTESIAN_POINT('Ctrl Pts',(0.0885422853935554,2.51733622264386,
7.85497386326368));
#19339=CARTESIAN_POINT('Ctrl Pts',(0.172245330360465,2.51299732701248,7.84946171354762));
#19340=CARTESIAN_POINT('Ctrl Pts',(0.276828897499114,2.50232452549987,7.84270486789271));
#19341=CARTESIAN_POINT('Ctrl Pts',(0.298045241888387,2.49988626723135,7.84134075284194));
#19342=CARTESIAN_POINT('Ctrl Pts',(0.33203919532441,2.49554062631197,7.83916517329379));
#19343=CARTESIAN_POINT('Ctrl Pts',(0.344837247835686,2.49380438836038,7.8383484082176));
#19344=CARTESIAN_POINT('Ctrl Pts',(0.369174734470975,2.49031172546414,7.8367993903288));
#19345=CARTESIAN_POINT('Ctrl Pts',(0.380716382724384,2.48857339008721,7.83606659262183));
#19346=CARTESIAN_POINT('Ctrl Pts',(0.407077902814832,2.48441528317325,7.83439677476896));
#19347=CARTESIAN_POINT('Ctrl Pts',(0.421889141030419,2.48194304654735,7.8334614260073));
#19348=CARTESIAN_POINT('Ctrl Pts',(0.467770520756483,2.47386211164416,7.83057211367006));
#19349=CARTESIAN_POINT('Ctrl Pts',(0.498758640351203,2.46780124039813,7.82863236254786));
#19350=CARTESIAN_POINT('Ctrl Pts',(0.723828231857169,2.41936770350154,7.81461117430008));
#19351=CARTESIAN_POINT('Ctrl Pts',(0.912401862226988,2.35473969720422,7.80330341300111));
#19352=CARTESIAN_POINT('Ctrl Pts',(1.17832828471452,2.22680211230946,7.78631724603764));
#19353=CARTESIAN_POINT('Ctrl Pts',(1.26274580993872,2.18004025600454,7.78073703524978));
#19354=CARTESIAN_POINT('Ctrl Pts',(1.37092066368093,2.11172359912494,7.77307222629464));
#19355=CARTESIAN_POINT('Ctrl Pts',(1.39725478287324,2.09439225466527,7.77116318943319));
#19356=CARTESIAN_POINT('Ctrl Pts',(1.44131402096562,2.06419462633159,7.76788293455805));
#19357=CARTESIAN_POINT('Ctrl Pts',(1.45920980659037,2.05158285910118,7.76652569597058));
#19358=CARTESIAN_POINT('Ctrl Pts',(1.48434531354932,2.03337377302988,7.76458029861017));
#19359=CARTESIAN_POINT('Ctrl Pts',(1.49172306209089,2.02796750728548,7.76400442900969));
#19360=CARTESIAN_POINT('Ctrl Pts',(1.50438656998002,2.01858145113807,7.76300726303883));
#19361=CARTESIAN_POINT('Ctrl Pts',(1.50968647758137,2.01462074977195,7.76258726930048));
#19362=CARTESIAN_POINT('Ctrl Pts',(1.52075911240334,2.00627777227604,7.76170410474754));
#19363=CARTESIAN_POINT('Ctrl Pts',(1.52652855707195,2.00189144030462,7.76124066839993));
#19364=CARTESIAN_POINT('Ctrl Pts',(1.54193500079129,1.99007306679771,7.75999455033995));
#19365=CARTESIAN_POINT('Ctrl Pts',(1.55153704097377,1.98259606431021,7.75920884922047));
#19366=CARTESIAN_POINT('Ctrl Pts',(1.59440894029345,1.94871001077266,7.75566130299178));
#19367=CARTESIAN_POINT('Ctrl Pts',(1.62705943610825,1.92153263700967,7.75285187299618));
#19368=CARTESIAN_POINT('Ctrl Pts',(1.68747338721567,1.86860173047059,7.74747002353398));
#19369=CARTESIAN_POINT('Ctrl Pts',(1.71537498394118,1.84302123966393,7.74490570707718));
#19370=CARTESIAN_POINT('Ctrl Pts',(1.78555450477,1.77570535738269,7.73827061628446));
#19371=CARTESIAN_POINT('Ctrl Pts',(1.826951155555,1.73308496705262,7.73417578307359));
#19372=CARTESIAN_POINT('Ctrl Pts',(1.96511040899497,1.58038550424474,7.71995367550269));
#19373=CARTESIAN_POINT('Ctrl Pts',(2.05375639382241,1.4633421695019,7.7098355341175));
#19374=CARTESIAN_POINT('Ctrl Pts',(2.1713043388427,1.27623673274407,7.69508160225339));
#19375=CARTESIAN_POINT('Ctrl Pts',(2.20807736402743,1.21150276350709,7.69020157538508));
#19376=CARTESIAN_POINT('Ctrl Pts',(2.25129880366988,1.12689128020244,7.6841000546184));
#19377=CARTESIAN_POINT('Ctrl Pts',(2.26044091766316,1.10843906449759,7.68278552761173));
#19378=CARTESIAN_POINT('Ctrl Pts',(2.27487489086101,1.07838444153065,7.68066985760226));
#19379=CARTESIAN_POINT('Ctrl Pts',(2.28030665785984,1.06685065901042,7.67986392266788));
#19380=CARTESIAN_POINT('Ctrl Pts',(2.29056158220675,1.04463924136709,7.67832311728845));
#19381=CARTESIAN_POINT('Ctrl Pts',(2.29539825934304,1.033968251417,7.67758779992275));
#19382=CARTESIAN_POINT('Ctrl Pts',(2.30629557412689,1.00947254200333,7.67591088872844));
#19383=CARTESIAN_POINT('Ctrl Pts',(2.31230675814033,0.99562621509304,7.67497099056746));
#19384=CARTESIAN_POINT('Ctrl Pts',(2.3310132988591,0.951453649614908,7.67199710374849));
#19385=CARTESIAN_POINT('Ctrl Pts',(2.34323965518116,0.920931657666336,7.66997882468211));
#19386=CARTESIAN_POINT('Ctrl Pts',(2.35707269506995,0.88433790948212,7.66759887766997));
#19387=CARTESIAN_POINT('Ctrl Pts',(2.35925833630511,0.878490361790436,7.66721976651879));
#19388=CARTESIAN_POINT('Ctrl Pts',(2.36142200378576,0.872635301850924,7.66684133937673));
#19389=CARTESIAN_POINT('Origin',(0.,0.,10.));
#19390=CARTESIAN_POINT('',(2.36142200703877,0.872635293048023,6.67067451578988));
#19391=CARTESIAN_POINT('',(2.36142200728636,0.872635292378025,6.9436622819569));
#19392=CARTESIAN_POINT('',(2.36142200728636,0.87263529237802,10.));
#19393=CARTESIAN_POINT('',(2.51749917428734,0.00203898566820233,7.8874166974512));
#19394=CARTESIAN_POINT('Ctrl Pts',(2.36142200728635,0.872635292378026,6.9436622819569));
#19395=CARTESIAN_POINT('Ctrl Pts',(2.33099320995247,0.954978090459999,6.94922798284441));
#19396=CARTESIAN_POINT('Ctrl Pts',(2.29629372475297,1.0356188703594,6.95479368373192));
#19397=CARTESIAN_POINT('Ctrl Pts',(2.25754798994522,1.11412895263263,6.96035938461943));
#19398=CARTESIAN_POINT('Ctrl Pts',(2.24918575763024,1.13107325760698,6.96156059254717));
#19399=CARTESIAN_POINT('Ctrl Pts',(2.24063521552867,1.14791841827325,6.96276180047491));
#19400=CARTESIAN_POINT('Ctrl Pts',(2.23189888544184,1.16466030032945,6.96396300840265));
#19401=CARTESIAN_POINT('Ctrl Pts',(2.19367769787667,1.23790554265705,6.96921825780996));
#19402=CARTESIAN_POINT('Ctrl Pts',(2.15177652201526,1.30940257330376,6.97447350721726));
#19403=CARTESIAN_POINT('Ctrl Pts',(2.1063792225828,1.37875770919747,6.97972875662457));
#19404=CARTESIAN_POINT('Ctrl Pts',(2.06104628620795,1.44801451526404,6.98497655528206));
#19405=CARTESIAN_POINT('Ctrl Pts',(2.01222732233057,1.51513507554269,6.99022435393955));
#19406=CARTESIAN_POINT('Ctrl Pts',(1.96015236693439,1.57974964738135,6.99547215259704));
#19407=CARTESIAN_POINT('Ctrl Pts',(1.9077000835924,1.64483240749739,7.00075797607995));
#19408=CARTESIAN_POINT('Ctrl Pts',(1.85194464393797,1.70737228971862,7.00604379956286));
#19409=CARTESIAN_POINT('Ctrl Pts',(1.79316602057124,1.76702062032923,7.01132962304577));
#19410=CARTESIAN_POINT('Ctrl Pts',(1.73491446106303,1.8261340884765,7.01656804891436));
#19411=CARTESIAN_POINT('Ctrl Pts',(1.67369404788882,1.88240731928882,7.02180647478295));
#19412=CARTESIAN_POINT('Ctrl Pts',(1.60981694875901,1.93553497552698,7.02704490065154));
#19413=CARTESIAN_POINT('Ctrl Pts',(1.54596085774405,1.98864515896316,7.03228160368904));
#19414=CARTESIAN_POINT('Ctrl Pts',(1.47945017054394,2.03861152762981,7.03751830672654));
#19415=CARTESIAN_POINT('Ctrl Pts',(1.41063142108491,2.08516791742247,7.04275500976405));
#19416=CARTESIAN_POINT('Ctrl Pts',(1.34181454621417,2.13172303904238,7.04799157015638));
#19417=CARTESIAN_POINT('Ctrl Pts',(1.27069011684549,2.17486810877582,7.05322813054871));
#19418=CARTESIAN_POINT('Ctrl Pts',(1.19763387775308,2.21438012654967,7.05846469094104));
#19419=CARTESIAN_POINT('Ctrl Pts',(1.12338190495437,2.25453884954737,7.06378695971153));
#19420=CARTESIAN_POINT('Ctrl Pts',(1.04713474113611,2.29094427560596,7.06910922848201));
#19421=CARTESIAN_POINT('Ctrl Pts',(0.96931146732795,2.32341161426609,7.07443149725249));
#19422=CARTESIAN_POINT('Ctrl Pts',(0.892631474320322,2.35540198397955,7.07967557800282));
#19423=CARTESIAN_POINT('Ctrl Pts',(0.814421833479111,2.38356910416803,7.08491965875315));
#19424=CARTESIAN_POINT('Ctrl Pts',(0.735100417157203,2.40778604254932,7.09016373950348));
#19425=CARTESIAN_POINT('Ctrl Pts',(0.654005005126743,2.43254458428005,7.09552510228404));
#19426=CARTESIAN_POINT('Ctrl Pts',(0.571747985256415,2.45317399867889,7.1008864650646));
#19427=CARTESIAN_POINT('Ctrl Pts',(0.488786758667984,2.46959384404619,7.10624782784515));
#19428=CARTESIAN_POINT('Ctrl Pts',(0.405825532079546,2.48601368941349,7.11160919062571));
#19429=CARTESIAN_POINT('Ctrl Pts',(0.322160611200065,2.49822395846984,7.11697055340626));
#19430=CARTESIAN_POINT('Ctrl Pts',(0.238252757484204,2.50620068501131,7.12233191618682));
#19431=CARTESIAN_POINT('Ctrl Pts',(0.15600562805885,2.51401953427504,7.12758716559413));
#19432=CARTESIAN_POINT('Ctrl Pts',(0.0732213097317949,2.51779982116763,
7.13284241500143));
#19433=CARTESIAN_POINT('Ctrl Pts',(-0.00966987373661683,2.51748142863893,
7.13809766440874));
#19434=CARTESIAN_POINT('Ctrl Pts',(-0.0924435363375321,2.51716348751851,
7.14334546306624));
#19435=CARTESIAN_POINT('Ctrl Pts',(-0.175323305567867,2.51275841106904,
7.14859326172374));
#19436=CARTESIAN_POINT('Ctrl Pts',(-0.257873800693118,2.50425784473486,
7.15384106038124));
#19437=CARTESIAN_POINT('Ctrl Pts',(-0.341022445322447,2.49569568446924,
7.15912688386415));
#19438=CARTESIAN_POINT('Ctrl Pts',(-0.423836552202102,2.48297838833264,
7.16441270734705));
#19439=CARTESIAN_POINT('Ctrl Pts',(-0.50587122499004,2.46615095923325,7.16969853082996));
#19440=CARTESIAN_POINT('Ctrl Pts',(-0.5871702985296,2.44947442052907,7.17493695669855));
#19441=CARTESIAN_POINT('Ctrl Pts',(-0.667703399917476,2.42876125862326,
7.18017538256715));
#19442=CARTESIAN_POINT('Ctrl Pts',(-0.747044454435779,2.40410707604648,
7.18541380843574));
#19443=CARTESIAN_POINT('Ctrl Pts',(-0.82635941500168,2.37946100182004,7.19065051147325));
#19444=CARTESIAN_POINT('Ctrl Pts',(-0.904482667029787,2.35087661793432,
7.19588721451076));
#19445=CARTESIAN_POINT('Ctrl Pts',(-0.98100228318559,2.31849968091105,7.20112391754826));
#19446=CARTESIAN_POINT('Ctrl Pts',(-1.05751981498533,2.28612362581935,7.2063604779406));
#19447=CARTESIAN_POINT('Ctrl Pts',(-1.13243337321921,2.24995540374432,7.21159703833294));
#19448=CARTESIAN_POINT('Ctrl Pts',(-1.20535133231742,2.21018877376585,7.21683359872527));
#19449=CARTESIAN_POINT('Ctrl Pts',(-1.27946276185111,2.16977127124811,7.22215586749575));
#19450=CARTESIAN_POINT('Ctrl Pts',(-1.35151223973342,2.12563672951816,7.22747813626623));
#19451=CARTESIAN_POINT('Ctrl Pts',(-1.4211165958319,2.07803606105648,7.23280040503671));
#19452=CARTESIAN_POINT('Ctrl Pts',(-1.48969841304116,2.03113468122247,7.23804448578704));
#19453=CARTESIAN_POINT('Ctrl Pts',(-1.55590613719537,1.98086867041449,7.24328856653737));
#19454=CARTESIAN_POINT('Ctrl Pts',(-1.61940578722062,1.92751942825912,7.24853264728771));
#19455=CARTESIAN_POINT('Ctrl Pts',(-1.68432558468972,1.87297704897861,7.25389401006826));
#19456=CARTESIAN_POINT('Ctrl Pts',(-1.74641434121004,1.81521221218204,7.25925537284881));
#19457=CARTESIAN_POINT('Ctrl Pts',(-1.80535555014973,1.75456478579264,7.26461673562936));
#19458=CARTESIAN_POINT('Ctrl Pts',(-1.86429675908941,1.69391735940324,7.26997809840991));
#19459=CARTESIAN_POINT('Ctrl Pts',(-1.92009013535083,1.63038776927758,7.27533946119046));
#19460=CARTESIAN_POINT('Ctrl Pts',(-1.97246471397379,1.564349450132,7.28070082397101));
#19461=CARTESIAN_POINT('Ctrl Pts',(-2.0238026824218,1.49961817717873,7.28595607337832));
#19462=CARTESIAN_POINT('Ctrl Pts',(-2.07204560924577,1.43223751273171,7.29121132278562));
#19463=CARTESIAN_POINT('Ctrl Pts',(-2.11690877828477,1.36253567821944,7.29646657219293));
#19464=CARTESIAN_POINT('Ctrl Pts',(-2.16170834154174,1.29293266507416,7.30171437085042));
#19465=CARTESIAN_POINT('Ctrl Pts',(-2.20313741713624,1.22101540329665,7.30696216950792));
#19466=CARTESIAN_POINT('Ctrl Pts',(-2.24095195361088,1.14714453823725,7.31220996816541));
#19467=CARTESIAN_POINT('Ctrl Pts',(-2.27904048900228,1.07273841507627,7.31749579164832));
#19468=CARTESIAN_POINT('Ctrl Pts',(-2.31346158888117,0.996350629387539,
7.32278161513123));
#19469=CARTESIAN_POINT('Ctrl Pts',(-2.34401077683183,0.918378858694077,
7.32806743861413));
#19470=CARTESIAN_POINT('Ctrl Pts',(-2.37428603232282,0.841106255486374,
7.33330586448272));
#19471=CARTESIAN_POINT('Ctrl Pts',(-2.4007583646804,0.762278398006722,7.33854429035132));
#19472=CARTESIAN_POINT('Ctrl Pts',(-2.42327598752445,0.682304725388445,
7.34378271621991));
#19473=CARTESIAN_POINT('Ctrl Pts',(-2.44578620469709,0.602357354780145,
7.34901941925741));
#19474=CARTESIAN_POINT('Ctrl Pts',(-2.46434417053717,0.521265361257688,
7.35425612229492));
#19475=CARTESIAN_POINT('Ctrl Pts',(-2.47884787001031,0.439453623657098,
7.35949282533242));
#19476=CARTESIAN_POINT('Ctrl Pts',(-2.49335117440993,0.357644114567342,
7.36472938572475));
#19477=CARTESIAN_POINT('Ctrl Pts',(-2.50380035248801,0.275115354896476,
7.36996594611708));
#19478=CARTESIAN_POINT('Ctrl Pts',(-2.51014470671314,0.192301329584641,
7.37520250650941));
#19479=CARTESIAN_POINT('Ctrl Pts',(-2.51659290091533,0.108131861908805,
7.38052477527989));
#19480=CARTESIAN_POINT('Ctrl Pts',(-2.51880063850722,0.0236681955690314,
7.38584704405037));
#19481=CARTESIAN_POINT('Ctrl Pts',(-2.51676976536495,-0.0606316595919791,
7.39116931282085));
#19482=CARTESIAN_POINT('Ctrl Pts',(-2.5147687272342,-0.143693088236424,
7.39641339357118));
#19483=CARTESIAN_POINT('Ctrl Pts',(-2.50865288393014,-0.226595024528087,
7.40165747432152));
#19484=CARTESIAN_POINT('Ctrl Pts',(-2.49847643477153,-0.308904119252801,
7.40690155507185));
#19485=CARTESIAN_POINT('Ctrl Pts',(-2.48807239288989,-0.393054028067616,
7.4122629178524));
#19486=CARTESIAN_POINT('Ctrl Pts',(-2.47342401384052,-0.476583753600546,
7.41762428063296));
#19487=CARTESIAN_POINT('Ctrl Pts',(-2.45464405368561,-0.559042770909252,
7.42298564341351));
#19488=CARTESIAN_POINT('Ctrl Pts',(-2.43586409353069,-0.641501788217963,
7.42834700619406));
#19489=CARTESIAN_POINT('Ctrl Pts',(-2.41295275425359,-0.722889626306476,
7.43370836897462));
#19490=CARTESIAN_POINT('Ctrl Pts',(-2.38607574271783,-0.802775684742356,
7.43906973175517));
#19491=CARTESIAN_POINT('Ctrl Pts',(-2.35973068741663,-0.881080619220939,
7.44432498116248));
#19492=CARTESIAN_POINT('Ctrl Pts',(-2.32947824272636,-0.958231921997537,
7.44958023056978));
#19493=CARTESIAN_POINT('Ctrl Pts',(-2.2954387040908,-1.03381207468376,7.45483547997709));
#19494=CARTESIAN_POINT('Ctrl Pts',(-2.26144742578818,-1.10928507188319,
7.46008327863458));
#19495=CARTESIAN_POINT('Ctrl Pts',(-2.22367990631756,-1.18319092631449,
7.46533107729208));
#19496=CARTESIAN_POINT('Ctrl Pts',(-2.18230577801954,-1.25512857557404,
7.47057887594957));
#19497=CARTESIAN_POINT('Ctrl Pts',(-2.14063185849326,-1.32758747512011,
7.47586469943248));
#19498=CARTESIAN_POINT('Ctrl Pts',(-2.09529899473707,-1.39804907730857,
7.48115052291539));
#19499=CARTESIAN_POINT('Ctrl Pts',(-2.04652942808554,-1.46612535275121,
7.48643634639829));
#19500=CARTESIAN_POINT('Ctrl Pts',(-1.99819717477185,-1.53359119293094,
7.49167477226689));
#19501=CARTESIAN_POINT('Ctrl Pts',(-1.94648987873685,-1.5987139311414,7.49691319813548));
#19502=CARTESIAN_POINT('Ctrl Pts',(-1.89166833403524,-1.66114333036266,
7.50215162400407));
#19503=CARTESIAN_POINT('Ctrl Pts',(-1.83686481922731,-1.7235521975935,7.50738832704157));
#19504=CARTESIAN_POINT('Ctrl Pts',(-1.77894939414191,-1.78326913862989,
7.51262503007908));
#19505=CARTESIAN_POINT('Ctrl Pts',(-1.71822290162412,-1.8399772581025,7.51786173311658));
#19506=CARTESIAN_POINT('Ctrl Pts',(-1.65749806326561,-1.8966838328743,7.52309829350892));
#19507=CARTESIAN_POINT('Ctrl Pts',(-1.59396264766415,-1.95038143486611,
7.52833485390125));
#19508=CARTESIAN_POINT('Ctrl Pts',(-1.52795307568929,-2.00079125560156,
7.53357141429358));
#19509=CARTESIAN_POINT('Ctrl Pts',(-1.46086310495409,-2.05202614921965,
7.53889368306406));
#19510=CARTESIAN_POINT('Ctrl Pts',(-1.39121763942827,-2.09986435746919,
7.54421595183454));
#19511=CARTESIAN_POINT('Ctrl Pts',(-1.31940185922458,-2.14405806448303,
7.54953822060503));
#19512=CARTESIAN_POINT('Ctrl Pts',(-1.24864110534737,-2.18760253362418,
7.55478230135536));
#19513=CARTESIAN_POINT('Ctrl Pts',(-1.17577382032524,-2.22760870007047,
7.56002638210569));
#19514=CARTESIAN_POINT('Ctrl Pts',(-1.10119300303954,-2.26388608813623,
7.56527046285603));
#19515=CARTESIAN_POINT('Ctrl Pts',(-1.02494421188322,-2.30097480728671,
7.57063182563658));
#19516=CARTESIAN_POINT('Ctrl Pts',(-0.946904789682583,-2.33416574940922,
7.57599318841714));
#19517=CARTESIAN_POINT('Ctrl Pts',(-0.867514023497643,-2.3633082044107,
7.58135455119769));
#19518=CARTESIAN_POINT('Ctrl Pts',(-0.788123257312707,-2.39245065941218,
7.58671591397825));
#19519=CARTESIAN_POINT('Ctrl Pts',(-0.707381652181406,-2.4175445402802,
7.5920772767588));
#19520=CARTESIAN_POINT('Ctrl Pts',(-0.625740611784981,-2.43849439957589,
7.59743863953936));
#19521=CARTESIAN_POINT('Ctrl Pts',(-0.54571543036819,-2.45902961425042,
7.60269388894667));
#19522=CARTESIAN_POINT('Ctrl Pts',(-0.464530522070502,-2.47565924426919,
7.60794913835397));
#19523=CARTESIAN_POINT('Ctrl Pts',(-0.382601593137168,-2.48825687398406,
7.61320438776128));
#19524=CARTESIAN_POINT('Ctrl Pts',(-0.300788820813074,-2.50083664312182,
7.61845218641877));
#19525=CARTESIAN_POINT('Ctrl Pts',(-0.21823457535389,-2.50939569697438,
7.62369998507627));
#19526=CARTESIAN_POINT('Ctrl Pts',(-0.135367621402295,-2.51385796278865,
7.62894778373376));
#19527=CARTESIAN_POINT('Ctrl Pts',(-0.0519002249295223,-2.51835256156567,
7.63423360721667));
#19528=CARTESIAN_POINT('Ctrl Pts',(0.031883971826203,-2.51869063448652,
7.63951943069957));
#19529=CARTESIAN_POINT('Ctrl Pts',(0.115538493166088,-2.51484733266195,
7.64480525418248));
#19530=CARTESIAN_POINT('Ctrl Pts',(0.19844289018743,-2.51103849345955,7.65004368005107));
#19531=CARTESIAN_POINT('Ctrl Pts',(0.281219458631735,-2.50312298893552,
7.65528210591966));
#19532=CARTESIAN_POINT('Ctrl Pts',(0.36343243265852,-2.4911288840387,7.66052053178826));
#19533=CARTESIAN_POINT('Ctrl Pts',(0.44561836820636,-2.47913872380338,7.66575723482576));
#19534=CARTESIAN_POINT('Ctrl Pts',(0.5272406212384,-2.46307269381636,7.67099393786327));
#19535=CARTESIAN_POINT('Ctrl Pts',(0.607869588007,-2.44301060455664,7.67623064090077));
#19536=CARTESIAN_POINT('Ctrl Pts',(0.688496358482866,-2.4229490617782,7.6814672012931));
#19537=CARTESIAN_POINT('Ctrl Pts',(0.76812944897189,-2.39889178856426,7.68670376168544));
#19538=CARTESIAN_POINT('Ctrl Pts',(0.846351832207465,-2.3709691744346,7.69194032207777));
#19539=CARTESIAN_POINT('Ctrl Pts',(0.925854505003288,-2.34258954237878,
7.69726259084825));
#19540=CARTESIAN_POINT('Ctrl Pts',(1.00389940744476,-2.31021705035651,7.70258485961873));
#19541=CARTESIAN_POINT('Ctrl Pts',(1.08006896158071,-2.27403986073903,7.70790712838921));
#19542=CARTESIAN_POINT('Ctrl Pts',(1.15511952926743,-2.23839414049158,7.71315120913954));
#19543=CARTESIAN_POINT('Ctrl Pts',(1.22834910012129,-2.19905504374563,7.71839528988987));
#19544=CARTESIAN_POINT('Ctrl Pts',(1.2993839357522,-2.15624851014653,7.72363937064021));
#19545=CARTESIAN_POINT('Ctrl Pts',(1.37200744061526,-2.1124846234085,7.72900073342076));
#19546=CARTESIAN_POINT('Ctrl Pts',(1.44233643204523,-2.06509661837745,7.73436209620131));
#19547=CARTESIAN_POINT('Ctrl Pts',(1.51000532505316,-2.01437091130484,7.73972345898186));
#19548=CARTESIAN_POINT('Ctrl Pts',(1.5776742180611,-1.96364520423223,7.74508482176241));
#19549=CARTESIAN_POINT('Ctrl Pts',(1.64268266469297,-1.90958217136595,7.75044618454297));
#19550=CARTESIAN_POINT('Ctrl Pts',(1.70470483693449,-1.85250848012422,7.75580754732352));
#19551=CARTESIAN_POINT('Ctrl Pts',(1.76459909663822,-1.7973929244779,7.76098496764176));
#19552=CARTESIAN_POINT('Ctrl Pts',(1.82194411214314,-1.73925298659712,7.76616238795999));
#19553=CARTESIAN_POINT('Ctrl Pts',(1.87641220836533,-1.67835737383239,7.77133980827823));
#19554=CARTESIAN_POINT('Ctrl Pts',(1.93078975802769,-1.61756299258898,7.77650862176731));
#19555=CARTESIAN_POINT('Ctrl Pts',(1.9822995759239,-1.55402238995363,7.78167743525639));
#19556=CARTESIAN_POINT('Ctrl Pts',(2.03064882854201,-1.48804287073356,7.78684624874548));
#19557=CARTESIAN_POINT('Ctrl Pts',(2.07895290625881,-1.42212499917313,7.7920102327775));
#19558=CARTESIAN_POINT('Ctrl Pts',(2.12410199614041,-1.35377311300361,7.79717421680953));
#19559=CARTESIAN_POINT('Ctrl Pts',(2.16584248281601,-1.28332871456591,7.80233820084155));
#19560=CARTESIAN_POINT('Ctrl Pts',(2.20755744793516,-1.2129273882348,7.8074990274377));
#19561=CARTESIAN_POINT('Ctrl Pts',(2.24586770342724,-1.14043649738504,7.81265985403386));
#19562=CARTESIAN_POINT('Ctrl Pts',(2.28056296879537,-1.06622642780942,7.81782068063001));
#19563=CARTESIAN_POINT('Ctrl Pts',(2.31524822027094,-0.992037777054395,
7.82298001768681));
#19564=CARTESIAN_POINT('Ctrl Pts',(2.34632035285082,-0.916131364616725,
7.82813935474361));
#19565=CARTESIAN_POINT('Ctrl Pts',(2.37361579836222,-0.838900644751972,
7.83329869180041));
#19566=CARTESIAN_POINT('Ctrl Pts',(2.40092462170801,-0.761632073159203,
7.83846055751191));
#19567=CARTESIAN_POINT('Ctrl Pts',(2.42445289854673,-0.683038346308388,
7.84362242322342));
#19568=CARTESIAN_POINT('Ctrl Pts',(2.44408620525132,-0.603530339999749,
7.84878428893492));
#19569=CARTESIAN_POINT('Ctrl Pts',(2.46372478256877,-0.524000989557537,
7.85394754036286));
#19570=CARTESIAN_POINT('Ctrl Pts',(2.47946621212717,-0.443557337995902,
7.8591107917908));
#19571=CARTESIAN_POINT('Ctrl Pts',(2.49124719851254,-0.362620526037097,
7.86427404321874));
#19572=CARTESIAN_POINT('Ctrl Pts',(2.50304227978826,-0.281586880464179,
7.86944347201251));
#19573=CARTESIAN_POINT('Ctrl Pts',(2.51086741194793,-0.200059370819776,
7.87461290080627));
#19574=CARTESIAN_POINT('Ctrl Pts',(2.51471124598385,-0.118463493627188,
7.87978232960004));
#19575=CARTESIAN_POINT('Ctrl Pts',(2.51660347587099,-0.0782957454756287,
7.88232711888376));
#19576=CARTESIAN_POINT('Ctrl Pts',(2.51753169311342,-0.0381114278833191,
7.88487190816748));
#19577=CARTESIAN_POINT('Ctrl Pts',(2.51749917428734,0.00203898566819532,
7.8874166974512));
#19578=CARTESIAN_POINT('Ctrl Pts',(2.51749917428662,0.00203898656449749,
7.88741669750801));
#19579=CARTESIAN_POINT('Ctrl Pts',(2.51739410665396,0.131764058348535,7.89563885372781));
#19580=CARTESIAN_POINT('Ctrl Pts',(2.50725905023964,0.261092140162662,7.9038610099476));
#19581=CARTESIAN_POINT('Ctrl Pts',(2.487294105771,0.388811369942864,7.91208316616739));
#19582=CARTESIAN_POINT('Ctrl Pts',(2.4855998057872,0.399650102266283,7.91278092914749));
#19583=CARTESIAN_POINT('Ctrl Pts',(2.48383473575149,0.410477266840176,7.91347869212759));
#19584=CARTESIAN_POINT('Ctrl Pts',(2.48199903094351,0.42129213189365,7.91417645510769));
#19585=CARTESIAN_POINT('Ctrl Pts',(2.46817693435167,0.502723584677579,7.91943032123432));
#19586=CARTESIAN_POINT('Ctrl Pts',(2.45031757063398,0.583624430079666,7.92468418736095));
#19587=CARTESIAN_POINT('Ctrl Pts',(2.42847467976397,0.663563847527349,7.92993805348757));
#19588=CARTESIAN_POINT('Ctrl Pts',(2.40920107270496,0.734100340594189,7.93457393029838));
#19589=CARTESIAN_POINT('Ctrl Pts',(2.38682672026174,0.803888074802876,7.93920980710918));
#19590=CARTESIAN_POINT('Ctrl Pts',(2.36142200728636,0.872635292378021,7.94384568391999));
#19591=CARTESIAN_POINT('Ctrl Pts',(2.36142200378576,0.872635301850921,7.66684133937673));
#19592=CARTESIAN_POINT('Ctrl Pts',(2.42086954617539,0.711765423710423,7.656443917513));
#19593=CARTESIAN_POINT('Ctrl Pts',(2.46373111482585,0.545222597560534,7.6466045117527));
#19594=CARTESIAN_POINT('Ctrl Pts',(2.49794968758694,0.318425823046622,7.63342394826705));
#19595=CARTESIAN_POINT('Ctrl Pts',(2.50460219122272,0.260988974035791,7.6300999936721));
#19596=CARTESIAN_POINT('Ctrl Pts',(2.51478615551483,0.135337905865415,7.62277330548585));
#19597=CARTESIAN_POINT('Ctrl Pts',(2.51753071680053,0.0671087438691356,
7.61875974364018));
#19598=CARTESIAN_POINT('Ctrl Pts',(2.5174828384576,-0.03838426666723,7.61238982392487));
#19599=CARTESIAN_POINT('Ctrl Pts',(2.51663955706866,-0.0756187800710945,
7.6101097592111));
#19600=CARTESIAN_POINT('Ctrl Pts',(2.51445058985874,-0.124415604668799,
7.6070641552816));
#19601=CARTESIAN_POINT('Ctrl Pts',(2.51385016514194,-0.13600862687656,7.60633632182352));
#19602=CARTESIAN_POINT('Ctrl Pts',(2.51275196666941,-0.154707939178105,
7.60515485894985));
#19603=CARTESIAN_POINT('Ctrl Pts',(2.51230416142923,-0.161817149623434,
7.60470393691037));
#19604=CARTESIAN_POINT('Ctrl Pts',(2.51137858811787,-0.175579999974779,
7.60382744031686));
#19605=CARTESIAN_POINT('Ctrl Pts',(2.51090453851276,-0.182233761054445,
7.60340207024887));
#19606=CARTESIAN_POINT('Ctrl Pts',(2.50969411076089,-0.198321093604625,
7.60236980833609));
#19607=CARTESIAN_POINT('Ctrl Pts',(2.50893098305654,-0.207752499849492,
7.60176146479519));
#19608=CARTESIAN_POINT('Ctrl Pts',(2.50605732921872,-0.240939165686356,
7.59961023555404));
#19609=CARTESIAN_POINT('Ctrl Pts',(2.50366250386092,-0.264667693276221,
7.59805292332056));
#19610=CARTESIAN_POINT('Ctrl Pts',(2.49688263338409,-0.323469647341974,
7.59415186332088));
#19611=CARTESIAN_POINT('Ctrl Pts',(2.49209541297209,-0.358490865017609,
7.591791389841));
#19612=CARTESIAN_POINT('Ctrl Pts',(2.46812431574152,-0.51000637690205,7.58144887362121));
#19613=CARTESIAN_POINT('Ctrl Pts',(2.44149695168975,-0.625167559692171,
7.57325977652352));
#19614=CARTESIAN_POINT('Ctrl Pts',(2.35764722451197,-0.898621273072675,
7.55351693658072));
#19615=CARTESIAN_POINT('Ctrl Pts',(2.29244872325207,-1.05390571419485,7.54207739813704));
#19616=CARTESIAN_POINT('Ctrl Pts',(2.19642386647353,-1.23070243644216,7.52900225495291));
#19617=CARTESIAN_POINT('Ctrl Pts',(2.18001894668773,-1.25953318799135,7.5268666764399));
#19618=CARTESIAN_POINT('Ctrl Pts',(2.15529873985325,-1.30104689539353,7.52378528451401));
#19619=CARTESIAN_POINT('Ctrl Pts',(2.14743161766961,-1.31399130354971,7.52282354351958));
#19620=CARTESIAN_POINT('Ctrl Pts',(2.13326912531708,-1.33682703688318,7.52112497942315));
#19621=CARTESIAN_POINT('Ctrl Pts',(2.12702064666858,-1.34674677045447,7.52038647885588));
#19622=CARTESIAN_POINT('Ctrl Pts',(2.11384651649111,-1.36734086711533,7.51885175949239));
#19623=CARTESIAN_POINT('Ctrl Pts',(2.1069087604897,-1.37800712139096,7.51805601344013));
#19624=CARTESIAN_POINT('Ctrl Pts',(2.08859499428624,-1.40570144194905,7.51598729921638));
#19625=CARTESIAN_POINT('Ctrl Pts',(2.07709141573814,-1.42264432767221,7.51471910438732));
#19626=CARTESIAN_POINT('Ctrl Pts',(2.02356866872017,-1.49944121594213,7.50895607026972));
#19627=CARTESIAN_POINT('Ctrl Pts',(1.97915849224262,-1.55759020817188,7.5045524668245));
#19628=CARTESIAN_POINT('Ctrl Pts',(1.84133275259981,-1.72262265491989,7.4918184183952));
#19629=CARTESIAN_POINT('Ctrl Pts',(1.74134649792106,-1.82363649798573,7.48372376864114));
#19630=CARTESIAN_POINT('Ctrl Pts',(1.53411076063925,-2.00033204983397,7.46805300434556));
#19631=CARTESIAN_POINT('Ctrl Pts',(1.4284257739737,-2.07711714193046,7.46050517015642));
#19632=CARTESIAN_POINT('Ctrl Pts',(1.29902481214428,-2.15657132556343,7.45118032750939));
#19633=CARTESIAN_POINT('Ctrl Pts',(1.28062391513368,-2.16754876822474,7.44985233013855));
#19634=CARTESIAN_POINT('Ctrl Pts',(1.25479533484955,-2.18251366828983,7.44798228585051));
#19635=CARTESIAN_POINT('Ctrl Pts',(1.24748377003217,-2.18670105029956,7.44745225291942));
#19636=CARTESIAN_POINT('Ctrl Pts',(1.234831706416,-2.1938628658829,7.44653369530755));
#19637=CARTESIAN_POINT('Ctrl Pts',(1.22950108523407,-2.19685472823494,7.4461462652104));
#19638=CARTESIAN_POINT('Ctrl Pts',(1.21822928731429,-2.20312725782635,7.44532603268121));
#19639=CARTESIAN_POINT('Ctrl Pts',(1.21228567728193,-2.20640335022703,7.44489293765851));
#19640=CARTESIAN_POINT('Ctrl Pts',(1.19750016516469,-2.21447528433339,7.44381423856481));
#19641=CARTESIAN_POINT('Ctrl Pts',(1.18864269717609,-2.21924220417729,7.44316686542151));
#19642=CARTESIAN_POINT('Ctrl Pts',(1.15510089447735,-2.23703535406014,7.44071166697805));
#19643=CARTESIAN_POINT('Ctrl Pts',(1.130230088021,-2.24970332421702,7.438883657464));
#19644=CARTESIAN_POINT('Ctrl Pts',(1.06578906603185,-2.28118818425783,7.43413765203379));
#19645=CARTESIAN_POINT('Ctrl Pts',(1.02592979365215,-2.29938980855323,7.43119303300765));
#19646=CARTESIAN_POINT('Ctrl Pts',(0.871522990269123,-2.36508524185316,
7.41980319646024));
#19647=CARTESIAN_POINT('Ctrl Pts',(0.754000131909261,-2.4051326827452,7.41117882048742));
#19648=CARTESIAN_POINT('Ctrl Pts',(0.477485186068167,-2.47708953127256,
7.39150602855232));
#19649=CARTESIAN_POINT('Ctrl Pts',(0.317378312306575,-2.50264912308864,
7.38058152522559));
#19650=CARTESIAN_POINT('Ctrl Pts',(0.133708044302341,-2.51404511139788,
7.36871265873431));
#19651=CARTESIAN_POINT('Ctrl Pts',(0.111497488915577,-2.51512803352212,
7.36728762298061));
#19652=CARTESIAN_POINT('Ctrl Pts',(0.0748956475640587,-2.51642681502144,
7.36495549548775));
#19653=CARTESIAN_POINT('Ctrl Pts',(0.0605120435658942,-2.51681377538387,
7.36404315504224));
#19654=CARTESIAN_POINT('Ctrl Pts',(0.0345180203202891,-2.51729011815153,
7.36240159598778));
#19655=CARTESIAN_POINT('Ctrl Pts',(0.0229088893203318,-2.51742253559902,
7.36167106372806));
#19656=CARTESIAN_POINT('Ctrl Pts',(-0.00200491774711399,-2.5175343554212,
7.36010870821292));
#19657=CARTESIAN_POINT('Ctrl Pts',(-0.0153093963244285,-2.51748860644803,
7.35927768649054));
#19658=CARTESIAN_POINT('Ctrl Pts',(-0.0517570586393679,-2.51707432731513,
7.35700977258154));
#19659=CARTESIAN_POINT('Ctrl Pts',(-0.0748968629791023,-2.51649209757656,
7.35557951644043));
#19660=CARTESIAN_POINT('Ctrl Pts',(-0.2114527605897,-2.51117087350629,7.34719043275331));
#19661=CARTESIAN_POINT('Ctrl Pts',(-0.324458229461923,-2.49908441014914,
7.34046558824129));
#19662=CARTESIAN_POINT('Ctrl Pts',(-0.61201477436361,-2.44848634141086,
7.32348092644027));
#19663=CARTESIAN_POINT('Ctrl Pts',(-0.783955939782015,-2.39896904096846,
7.31346692087066));
#19664=CARTESIAN_POINT('Ctrl Pts',(-1.00596542750272,-2.30859162573154,
7.29926391084281));
#19665=CARTESIAN_POINT('Ctrl Pts',(-1.0618571316909,-2.28342283877398,7.29556804216793));
#19666=CARTESIAN_POINT('Ctrl Pts',(-1.1288793337555,-2.25024893333476,7.29092211732648));
#19667=CARTESIAN_POINT('Ctrl Pts',(-1.14093994739004,-2.24415793334999,
7.29007739767234));
#19668=CARTESIAN_POINT('Ctrl Pts',(-1.15972674276995,-2.23447941008288,
7.28874702770951));
#19669=CARTESIAN_POINT('Ctrl Pts',(-1.16648685512989,-2.23095781339685,
7.2882653430135));
#19670=CARTESIAN_POINT('Ctrl Pts',(-1.17900602773341,-2.22436364919452,
7.28736757623295));
#19671=CARTESIAN_POINT('Ctrl Pts',(-1.18476923265915,-2.221299331308,7.2869520045249));
#19672=CARTESIAN_POINT('Ctrl Pts',(-1.19797544005754,-2.21421152583038,
7.28599451123468));
#19673=CARTESIAN_POINT('Ctrl Pts',(-1.20541010115261,-2.21017291613181,
7.2854516602621));
#19674=CARTESIAN_POINT('Ctrl Pts',(-1.22862677810239,-2.19740931307615,
7.28374482707147));
#19675=CARTESIAN_POINT('Ctrl Pts',(-1.24433509203443,-2.18855239459042,
7.28257305966513));
#19676=CARTESIAN_POINT('Ctrl Pts',(-1.38884285211712,-2.10501502151373,
7.27164523835278));
#19677=CARTESIAN_POINT('Ctrl Pts',(-1.51086285132787,-2.01922204570008,
7.26133757083595));
#19678=CARTESIAN_POINT('Ctrl Pts',(-1.76332579332913,-1.80595609454316,
7.2385080643547));
#19679=CARTESIAN_POINT('Ctrl Pts',(-1.88900737401213,-1.67405749725641,
7.22609022247482));
#19680=CARTESIAN_POINT('Ctrl Pts',(-2.01903637660224,-1.50410819492974,
7.21218873995391));
#19681=CARTESIAN_POINT('Ctrl Pts',(-2.0381669804889,-1.47808148284719,7.21010945771378));
#19682=CARTESIAN_POINT('Ctrl Pts',(-2.06556565544647,-1.4392624020203,7.20707889104254));
#19683=CARTESIAN_POINT('Ctrl Pts',(-2.07422638838818,-1.42675248207603,
7.20611276188839));
#19684=CARTESIAN_POINT('Ctrl Pts',(-2.08936444864689,-1.40445723544223,
7.20440915431779));
#19685=CARTESIAN_POINT('Ctrl Pts',(-2.09588770326426,-1.39470379231312,
7.20366996495082));
#19686=CARTESIAN_POINT('Ctrl Pts',(-2.10932501833041,-1.37430539610771,
7.2021364547265));
#19687=CARTESIAN_POINT('Ctrl Pts',(-2.11622725530086,-1.36365302333363,
7.20134258763454));
#19688=CARTESIAN_POINT('Ctrl Pts',(-2.13397743377333,-1.33579942278446,
7.19928450078525));
#19689=CARTESIAN_POINT('Ctrl Pts',(-2.14469817865072,-1.31851793534113,
7.19802496194301));
#19690=CARTESIAN_POINT('Ctrl Pts',(-2.19219451794774,-1.23984305548966,
7.19236614265402));
#19691=CARTESIAN_POINT('Ctrl Pts',(-2.22655347427037,-1.17702532900818,
7.1880539600011));
#19692=CARTESIAN_POINT('Ctrl Pts',(-2.36222514636639,-0.901714444178392,
7.16986113360819));
#19693=CARTESIAN_POINT('Ctrl Pts',(-2.43613021019673,-0.677087755563914,
7.15687005622727));
#19694=CARTESIAN_POINT('Ctrl Pts',(-2.48712479082669,-0.393460285449062,
7.13969386131856));
#19695=CARTESIAN_POINT('Ctrl Pts',(-2.49483742210367,-0.341154045320238,
7.13648987385414));
#19696=CARTESIAN_POINT('Ctrl Pts',(-2.50238203821092,-0.275786182520685,
7.13239797651873));
#19697=CARTESIAN_POINT('Ctrl Pts',(-2.50376725584618,-0.262913285256533,
7.13158793725552));
#19698=CARTESIAN_POINT('Ctrl Pts',(-2.50579735507217,-0.24257374926059,
7.13030058588439));
#19699=CARTESIAN_POINT('Ctrl Pts',(-2.50650831612172,-0.235113730497315,
7.12982683517828));
#19700=CARTESIAN_POINT('Ctrl Pts',(-2.50771868447863,-0.221783581787762,
7.12897729614917));
#19701=CARTESIAN_POINT('Ctrl Pts',(-2.50823080725063,-0.215914734671706,
7.12860221917862));
#19702=CARTESIAN_POINT('Ctrl Pts',(-2.50941388152144,-0.20178435057446,
7.12769664828832));
#19703=CARTESIAN_POINT('Ctrl Pts',(-2.51006463135081,-0.193521302954794,
7.12716505365914));
#19704=CARTESIAN_POINT('Ctrl Pts',(-2.51193561380513,-0.168164796620101,
7.1255278153761));
#19705=CARTESIAN_POINT('Ctrl Pts',(-2.51302209455952,-0.151062374675916,
7.12441524067728));
#19706=CARTESIAN_POINT('Ctrl Pts',(-2.51515149669146,-0.111098612961105,
7.12179814517295));
#19707=CARTESIAN_POINT('Ctrl Pts',(-2.51605743787149,-0.0882317652370027,
7.1202874643056));
#19708=CARTESIAN_POINT('Ctrl Pts',(-2.51815574540642,-0.00743339158061894,
7.11491008802558));
#19709=CARTESIAN_POINT('Ctrl Pts',(-2.51765970647078,0.0505210312757371,
7.11098171950916));
#19710=CARTESIAN_POINT('Ctrl Pts',(-2.50785362482535,0.278042039756813,
7.09539619441546));
#19711=CARTESIAN_POINT('Ctrl Pts',(-2.48339713259575,0.446523756409464,
7.08353462715593));
#19712=CARTESIAN_POINT('Ctrl Pts',(-2.41861731433399,0.705337811392432,
7.06551368229093));
#19713=CARTESIAN_POINT('Ctrl Pts',(-2.38965197754169,0.797984059906887,
7.05909644524408));
#19714=CARTESIAN_POINT('Ctrl Pts',(-2.34736056592555,0.91006833719209,7.05138258431398));
#19715=CARTESIAN_POINT('Ctrl Pts',(-2.33902269546803,0.931288833148569,
7.04992416233301));
#19716=CARTESIAN_POINT('Ctrl Pts',(-2.32534316838163,0.964761056583153,
7.04762629837541));
#19717=CARTESIAN_POINT('Ctrl Pts',(-2.32019040392467,0.977088147385552,
7.04678060405317));
#19718=CARTESIAN_POINT('Ctrl Pts',(-2.3103791762473,1.00004448547845,7.04520654015534));
#19719=CARTESIAN_POINT('Ctrl Pts',(-2.30574489831994,1.01068362116832,7.04447738077026));
#19720=CARTESIAN_POINT('Ctrl Pts',(-2.29523107927763,1.03437197312589,7.04285446389198));
#19721=CARTESIAN_POINT('Ctrl Pts',(-2.2893134593091,1.04740392612839,7.04196202520934));
#19722=CARTESIAN_POINT('Ctrl Pts',(-2.27150695398942,1.0857459700166,7.03933696433826));
#19723=CARTESIAN_POINT('Ctrl Pts',(-2.25930691941018,1.11090975905745,7.03761498939914));
#19724=CARTESIAN_POINT('Ctrl Pts',(-2.17751221303842,1.27269588043332,7.02653858240463));
#19725=CARTESIAN_POINT('Ctrl Pts',(-2.09597666478979,1.40292702264964,7.01762451166263));
#19726=CARTESIAN_POINT('Ctrl Pts',(-1.90128422003157,1.65866520065164,6.99912838210781));
#19727=CARTESIAN_POINT('Ctrl Pts',(-1.78635893107121,1.78184181425028,6.98960629277691));
#19728=CARTESIAN_POINT('Ctrl Pts',(-1.63787815670527,1.91207487812141,6.97758848348496));
#19729=CARTESIAN_POINT('Ctrl Pts',(-1.61537831608435,1.93112089686188,6.97577351135815));
#19730=CARTESIAN_POINT('Ctrl Pts',(-1.58433462449258,1.9564770835601,6.97326937013832));
#19731=CARTESIAN_POINT('Ctrl Pts',(-1.57607668008897,1.96313552001987,6.9726032447582));
#19732=CARTESIAN_POINT('Ctrl Pts',(-1.56291231315402,1.97361343980111,6.97154090058489));
#19733=CARTESIAN_POINT('Ctrl Pts',(-1.55803328739749,1.97746736552878,6.97114707517961));
#19734=CARTESIAN_POINT('Ctrl Pts',(-1.5478747479719,1.98543062703204,6.97032678232992));
#19735=CARTESIAN_POINT('Ctrl Pts',(-1.54259309688882,1.98953701739896,6.96990010620974));
#19736=CARTESIAN_POINT('Ctrl Pts',(-1.52971787966714,1.999465182298,6.9688596478821));
#19737=CARTESIAN_POINT('Ctrl Pts',(-1.52210740934946,2.00526477901384,6.96824435805372));
#19738=CARTESIAN_POINT('Ctrl Pts',(-1.49486506857249,2.0257805048549,6.96604142887106));
#19739=CARTESIAN_POINT('Ctrl Pts',(-1.47505205245633,2.04025232841725,6.96443845429551));
#19740=CARTESIAN_POINT('Ctrl Pts',(-1.42506245786211,2.07565698184861,6.96039837309672));
#19741=CARTESIAN_POINT('Ctrl Pts',(-1.3946339551262,2.09622297722418,6.95794307234788));
#19742=CARTESIAN_POINT('Ctrl Pts',(-1.25712482122973,2.1848431989041,6.94690011246475));
#19743=CARTESIAN_POINT('Ctrl Pts',(-1.14544277116187,2.24540895759377,6.9380810691353));
#19744=CARTESIAN_POINT('Ctrl Pts',(-0.886673841005095,2.36139230519445,
6.91853101820738));
#19745=CARTESIAN_POINT('Ctrl Pts',(-0.737979219513423,2.41200445029971,
6.90789386807265));
#19746=CARTESIAN_POINT('Ctrl Pts',(-0.553185453308542,2.45619574280637,
6.89554491724946));
#19747=CARTESIAN_POINT('Ctrl Pts',(-0.520698106691311,2.46328750391865,
6.89340401919077));
#19748=CARTESIAN_POINT('Ctrl Pts',(-0.47320454353213,2.47267336799684,6.89031645147102));
#19749=CARTESIAN_POINT('Ctrl Pts',(-0.458304082608395,2.47547844043885,
6.88935376412622));
#19750=CARTESIAN_POINT('Ctrl Pts',(-0.431836657858963,2.4802138696741,6.88765411354523));
#19751=CARTESIAN_POINT('Ctrl Pts',(-0.420279955113492,2.48219832109358,
6.8869154656276));
#19752=CARTESIAN_POINT('Ctrl Pts',(-0.39616143188712,2.48616654511661,6.88538101309589));
#19753=CARTESIAN_POINT('Ctrl Pts',(-0.383597572032591,2.48813602569373,
6.88458567710148));
#19754=CARTESIAN_POINT('Ctrl Pts',(-0.35079556229005,2.49302362545499,6.88251928125985));
#19755=CARTESIAN_POINT('Ctrl Pts',(-0.330535578046118,2.49579057483001,
6.88125297453443));
#19756=CARTESIAN_POINT('Ctrl Pts',(-0.238014243089519,2.50728000259833,
6.87551288149068));
#19757=CARTESIAN_POINT('Ctrl Pts',(-0.165425602166072,2.51311353095782,
6.87112941073162));
#19758=CARTESIAN_POINT('Ctrl Pts',(0.0478727385834268,2.52097134796037,
6.85848611970517));
#19759=CARTESIAN_POINT('Ctrl Pts',(0.188614261977942,2.51436187224441,6.85045753576906));
#19760=CARTESIAN_POINT('Ctrl Pts',(0.459028320221171,2.47881924209878,6.83476672284182));
#19761=CARTESIAN_POINT('Ctrl Pts',(0.588410568258542,2.45132948772839,6.82713045166811));
#19762=CARTESIAN_POINT('Ctrl Pts',(0.735569304664735,2.40773821142667,6.81770542617525));
#19763=CARTESIAN_POINT('Ctrl Pts',(0.756037481914017,2.40138975438664,6.81637721340887));
#19764=CARTESIAN_POINT('Ctrl Pts',(0.784436991520351,2.39218223822322,6.81450691315459));
#19765=CARTESIAN_POINT('Ctrl Pts',(0.792439420611852,2.38954326481827,6.8139768439395));
#19766=CARTESIAN_POINT('Ctrl Pts',(0.806224146581308,2.38492059506494,6.81305824069077));
#19767=CARTESIAN_POINT('Ctrl Pts',(0.812012804647827,2.38295590023679,6.81267080149711));
#19768=CARTESIAN_POINT('Ctrl Pts',(0.824212752112566,2.37876557222836,6.81185057089422));
#19769=CARTESIAN_POINT('Ctrl Pts',(0.830622266320938,2.3765350735141,6.81141748702581));
#19770=CARTESIAN_POINT('Ctrl Pts',(0.846508395869181,2.37093461524189,6.81033885220676));
#19771=CARTESIAN_POINT('Ctrl Pts',(0.855973908993297,2.36753375329956,6.80969153262531));
#19772=CARTESIAN_POINT('Ctrl Pts',(0.891622673758886,2.35448379227934,6.80723677503268));
#19773=CARTESIAN_POINT('Ctrl Pts',(0.917664189133221,2.34445669690555,6.80540916188624));
#19774=CARTESIAN_POINT('Ctrl Pts',(0.984140217100389,2.31758338921996,6.80066443109058));
#19775=CARTESIAN_POINT('Ctrl Pts',(1.02431054739924,2.3001113459173,6.79772070700575));
#19776=CARTESIAN_POINT('Ctrl Pts',(1.23269124837145,2.20293506466281,6.78211423221947));
#19777=CARTESIAN_POINT('Ctrl Pts',(1.39213918512665,2.10580309750223,6.76905649718064));
#19778=CARTESIAN_POINT('Ctrl Pts',(1.5793908308799,1.96109187594669,6.75303776944874));
#19779=CARTESIAN_POINT('Ctrl Pts',(1.61841443154039,1.929013213548,6.74965251004168));
#19780=CARTESIAN_POINT('Ctrl Pts',(1.70060695582346,1.85719705131927,6.74242575782365));
#19781=CARTESIAN_POINT('Ctrl Pts',(1.74340644117043,1.81708002357301,6.73860095886542));
#19782=CARTESIAN_POINT('Ctrl Pts',(1.79861698935554,1.76158131572853,6.73357923578153));
#19783=CARTESIAN_POINT('Ctrl Pts',(1.8123022330649,1.74749891502875,6.73232678688449));
#19784=CARTESIAN_POINT('Ctrl Pts',(1.83445584326564,1.72416219749561,6.73028610887836));
#19785=CARTESIAN_POINT('Ctrl Pts',(1.84302208823742,1.71500236608204,6.72949369709551));
#19786=CARTESIAN_POINT('Ctrl Pts',(1.85950936151041,1.69710642840791,6.72796185833734));
#19787=CARTESIAN_POINT('Ctrl Pts',(1.8674381438087,1.68837794392235,6.72722211447508));
#19788=CARTESIAN_POINT('Ctrl Pts',(1.88303595245279,1.67096263054701,6.72576053145248));
#19789=CARTESIAN_POINT('Ctrl Pts',(1.89070690629874,1.66227792876817,6.72503862251721));
#19790=CARTESIAN_POINT('Ctrl Pts',(1.91540776424453,1.63392054791466,6.72270355687474));
#19791=CARTESIAN_POINT('Ctrl Pts',(1.932193065581,1.61403633621696,6.72110038435432));
#19792=CARTESIAN_POINT('Ctrl Pts',(2.01823620896317,1.50884151779443,6.71278820706795));
#19793=CARTESIAN_POINT('Ctrl Pts',(2.08216626121359,1.41931950555954,6.70629179382278));
#19794=CARTESIAN_POINT('Ctrl Pts',(2.19361501752498,1.23943707110981,6.69399282060017));
#19795=CARTESIAN_POINT('Ctrl Pts',(2.24189448675934,1.14980892096917,6.68818467532153));
#19796=CARTESIAN_POINT('Ctrl Pts',(2.30948432068794,1.0037889419143,6.67891503959213));
#19797=CARTESIAN_POINT('Ctrl Pts',(2.33244594885261,0.949213082436155,6.67548944583528));
#19798=CARTESIAN_POINT('Ctrl Pts',(2.35614736665016,0.886810597765583,6.67156612518863));
#19799=CARTESIAN_POINT('Ctrl Pts',(2.35880073269644,0.879728674404211,6.6711207779961));
#19800=CARTESIAN_POINT('Ctrl Pts',(2.36142200703877,0.872635293048023,6.67067451578988));
#19801=CARTESIAN_POINT('Origin',(0.,0.,10.));
#19802=CARTESIAN_POINT('',(2.36142200559759,0.87263529694796,5.66918223051795));
#19803=CARTESIAN_POINT('',(2.36142200728636,0.872635292378019,5.94377298858649));
#19804=CARTESIAN_POINT('',(2.36142200728636,0.87263529237802,10.));
#19805=CARTESIAN_POINT('',(2.51749998978759,0.0002267586386634,6.8874166975502));
#19806=CARTESIAN_POINT('Ctrl Pts',(2.36142200728636,0.872635292378018,5.94377298858649));
#19807=CARTESIAN_POINT('Ctrl Pts',(2.33300945646759,0.949521963559691,5.94893586779302));
#19808=CARTESIAN_POINT('Ctrl Pts',(2.30084060580699,1.02501176309947,5.95409874699956));
#19809=CARTESIAN_POINT('Ctrl Pts',(2.26508957566429,1.09871536997394,5.95926162620609));
#19810=CARTESIAN_POINT('Ctrl Pts',(2.2293031348659,1.17249197874612,5.96442961913766));
#19811=CARTESIAN_POINT('Ctrl Pts',(2.18992764184852,1.24447843524094,5.96959761206923));
#19812=CARTESIAN_POINT('Ctrl Pts',(2.14718358488262,1.31430928734854,5.9747656050008));
#19813=CARTESIAN_POINT('Ctrl Pts',(2.10441596932025,1.38417862707248,5.979936446297));
#19814=CARTESIAN_POINT('Ctrl Pts',(2.0582763652583,1.45188960658155,5.9851072875932));
#19815=CARTESIAN_POINT('Ctrl Pts',(2.00902761483445,1.51710721204291,5.9902781288894));
#19816=CARTESIAN_POINT('Ctrl Pts',(1.95969848853396,1.58243125517357,5.99545740919976));
#19817=CARTESIAN_POINT('Ctrl Pts',(1.90725039554371,1.64525344003261,6.00063668951012));
#19818=CARTESIAN_POINT('Ctrl Pts',(1.85198488302567,1.70527365635091,6.00581596982048));
#19819=CARTESIAN_POINT('Ctrl Pts',(1.82376641798002,1.73591986406783,6.00846050044619));
#19820=CARTESIAN_POINT('Ctrl Pts',(1.79481399192534,1.7658361884047,6.0111050310719));
#19821=CARTESIAN_POINT('Ctrl Pts',(1.76517104191674,1.79498675281423,6.0137495616976));
#19822=CARTESIAN_POINT('Ctrl Pts',(1.70626414405401,1.85291517491172,6.01900481110491));
#19823=CARTESIAN_POINT('Ctrl Pts',(1.64439384420559,1.90804774175317,6.02426006051221));
#19824=CARTESIAN_POINT('Ctrl Pts',(1.57985623667156,1.96006645842685,6.02951530991952));
#19825=CARTESIAN_POINT('Ctrl Pts',(1.51541012880387,2.01201142437749,6.03476310857701));
#19826=CARTESIAN_POINT('Ctrl Pts',(1.44830458093836,2.06085102195825,6.0400109072345));
#19827=CARTESIAN_POINT('Ctrl Pts',(1.37887225049238,2.10630424365097,6.04525870589199));
#19828=CARTESIAN_POINT('Ctrl Pts',(1.30893682295451,2.1520868131202,6.0505445293749));
#19829=CARTESIAN_POINT('Ctrl Pts',(1.23664108935189,2.19443339293679,6.05583035285781));
#19830=CARTESIAN_POINT('Ctrl Pts',(1.16235873651848,2.23309838960113,6.06111617634071));
#19831=CARTESIAN_POINT('Ctrl Pts',(1.08874246841558,2.27141667990923,6.06635460220931));
#19832=CARTESIAN_POINT('Ctrl Pts',(1.01317548297763,2.30611893065896,6.07159302807789));
#19833=CARTESIAN_POINT('Ctrl Pts',(0.936048763302448,2.3370106894749,6.07683145394649));
#19834=CARTESIAN_POINT('Ctrl Pts',(0.858947409321755,2.36789228850549,6.08206815698399));
#19835=CARTESIAN_POINT('Ctrl Pts',(0.780287767893451,2.3949657131123,6.08730486002149));
#19836=CARTESIAN_POINT('Ctrl Pts',(0.700481465353148,2.41808435888757,6.092541563059));
#19837=CARTESIAN_POINT('Ctrl Pts',(0.620677336696681,2.44120237492247,6.09777812345133));
#19838=CARTESIAN_POINT('Ctrl Pts',(0.539727052516544,2.46036569891565,6.10301468384366));
#19839=CARTESIAN_POINT('Ctrl Pts',(0.458056749044402,2.47547778512651,6.10825124423598));
#19840=CARTESIAN_POINT('Ctrl Pts',(0.375049722851719,2.4908372154531,6.11357351300647));
#19841=CARTESIAN_POINT('Ctrl Pts',(0.291299376297725,2.5020114934577,6.11889578177695));
#19842=CARTESIAN_POINT('Ctrl Pts',(0.207261320091412,2.50895376505705,6.12421805054743));
#19843=CARTESIAN_POINT('Ctrl Pts',(0.124457844383674,2.51579404961007,6.12946213129776));
#19844=CARTESIAN_POINT('Ctrl Pts',(0.0413755260271846,2.51852589088098,
6.13470621204809));
#19845=CARTESIAN_POINT('Ctrl Pts',(-0.0415489796354925,2.51715711315191,
6.13995029279842));
#19846=CARTESIAN_POINT('Ctrl Pts',(-0.126328062838598,2.51575772318808,
6.14531165557898));
#19847=CARTESIAN_POINT('Ctrl Pts',(-0.210941678431173,2.51007211743798,
6.15067301835953));
#19848=CARTESIAN_POINT('Ctrl Pts',(-0.294929867698439,2.50016451921456,
6.15603438114009));
#19849=CARTESIAN_POINT('Ctrl Pts',(-0.378918056965711,2.49025692099114,
6.16139574392065));
#19850=CARTESIAN_POINT('Ctrl Pts',(-0.462280330108473,2.47612748106319,
6.16675710670121));
#19851=CARTESIAN_POINT('Ctrl Pts',(-0.544570910994263,2.45789519160172,
6.17211846948177));
#19852=CARTESIAN_POINT('Ctrl Pts',(-0.625232777039784,2.4400237599699,6.17737371888907));
#19853=CARTESIAN_POINT('Ctrl Pts',(-0.705162930103143,2.41814444185597,
6.18262896829638));
#19854=CARTESIAN_POINT('Ctrl Pts',(-0.783933429501754,2.39233246604848,
6.18788421770368));
#19855=CARTESIAN_POINT('Ctrl Pts',(-0.862592250226629,2.36655708575894,
6.19313201636117));
#19856=CARTESIAN_POINT('Ctrl Pts',(-0.940094248178497,2.33686026505975,
6.19837981501866));
#19857=CARTESIAN_POINT('Ctrl Pts',(-1.01602260056888,2.30336803944425,6.20362761367615));
#19858=CARTESIAN_POINT('Ctrl Pts',(-1.09250111933045,2.2696331337804,6.20891343715906));
#19859=CARTESIAN_POINT('Ctrl Pts',(-1.16738262880088,2.23204769166868,6.21419926064197));
#19860=CARTESIAN_POINT('Ctrl Pts',(-1.24025767266734,2.19079144497823,6.21948508412487));
#19861=CARTESIAN_POINT('Ctrl Pts',(-1.31247925104564,2.14990514020414,6.22472350999347));
#19862=CARTESIAN_POINT('Ctrl Pts',(-1.38272979443769,2.10541383039651,6.22996193586206));
#19863=CARTESIAN_POINT('Ctrl Pts',(-1.45063332633318,2.05753959926207,6.23520036173065));
#19864=CARTESIAN_POINT('Ctrl Pts',(-1.51851452588715,2.00968111316549,6.24043706476815));
#19865=CARTESIAN_POINT('Ctrl Pts',(-1.58404987014721,1.95844218107001,6.24567376780566));
#19866=CARTESIAN_POINT('Ctrl Pts',(-1.64689227786619,1.90408825297167,6.25091047084316));
#19867=CARTESIAN_POINT('Ctrl Pts',(-1.7097329737895,1.84973580544708,6.2561470312355));
#19868=CARTESIAN_POINT('Ctrl Pts',(-1.76988053070197,1.79226883325605,6.26138359162784));
#19869=CARTESIAN_POINT('Ctrl Pts',(-1.8270219562447,1.73199221170298,6.26662015202018));
#19870=CARTESIAN_POINT('Ctrl Pts',(-1.8850986328952,1.67072902433457,6.27194242079066));
#19871=CARTESIAN_POINT('Ctrl Pts',(-1.94006953799678,1.60656373286678,6.27726468956114));
#19872=CARTESIAN_POINT('Ctrl Pts',(-1.99164731274412,1.5398529902686,6.28258695833163));
#19873=CARTESIAN_POINT('Ctrl Pts',(-2.04246737226417,1.47412227726141,6.28783103908196));
#19874=CARTESIAN_POINT('Ctrl Pts',(-2.08999311757048,1.40592082483329,6.29307511983229));
#19875=CARTESIAN_POINT('Ctrl Pts',(-2.13399337392762,1.33561915605947,6.29831920058263));
#19876=CARTESIAN_POINT('Ctrl Pts',(-2.17897768061532,1.26374521507356,6.30368056336318));
#19877=CARTESIAN_POINT('Ctrl Pts',(-2.22027665347001,1.18967643016703,6.30904192614373));
#19878=CARTESIAN_POINT('Ctrl Pts',(-2.25769373727086,1.11383357764432,6.31440328892429));
#19879=CARTESIAN_POINT('Ctrl Pts',(-2.2951108210717,1.03799072512163,6.31976465170484));
#19880=CARTESIAN_POINT('Ctrl Pts',(-2.32864587561046,0.960374297908852,
6.3251260144854));
#19881=CARTESIAN_POINT('Ctrl Pts',(-2.35815600709098,0.881422995060092,
6.33048737726595));
#19882=CARTESIAN_POINT('Ctrl Pts',(-2.38708206699782,0.804034315262673,
6.33574262667326));
#19883=CARTESIAN_POINT('Ctrl Pts',(-2.41224796036822,0.725077290618015,
6.34099787608056));
#19884=CARTESIAN_POINT('Ctrl Pts',(-2.43348379555695,0.644951832900536,
6.34625312548787));
#19885=CARTESIAN_POINT('Ctrl Pts',(-2.45468952315561,0.564939974879646,
6.35150092414538));
#19886=CARTESIAN_POINT('Ctrl Pts',(-2.47197614282722,0.483763416523515,
6.35674872280288));
#19887=CARTESIAN_POINT('Ctrl Pts',(-2.48522243235339,0.40184040579251,6.36199652146039));
#19888=CARTESIAN_POINT('Ctrl Pts',(-2.49856470266681,0.319323792222941,
6.36728234494329));
#19889=CARTESIAN_POINT('Ctrl Pts',(-2.50780767851238,0.23605030714626,6.3725681684262));
#19890=CARTESIAN_POINT('Ctrl Pts',(-2.51287918846666,0.152461254655519,
6.3778539919091));
#19891=CARTESIAN_POINT('Ctrl Pts',(-2.51790522254124,0.0696217394286344,
6.3830924177777));
#19892=CARTESIAN_POINT('Ctrl Pts',(-2.5188342731305,-0.0135272374760142,
6.38833084364629));
#19893=CARTESIAN_POINT('Ctrl Pts',(-2.51564792133638,-0.0965493960413684,
6.39356926951489));
#19894=CARTESIAN_POINT('Ctrl Pts',(-2.51246261748033,-0.179544250000486,
6.39880597255239));
#19895=CARTESIAN_POINT('Ctrl Pts',(-2.50516461702319,-0.262411907738021,
6.4040426755899));
#19896=CARTESIAN_POINT('Ctrl Pts',(-2.4937876084469,-0.34471671551679,6.40927937862741));
#19897=CARTESIAN_POINT('Ctrl Pts',(-2.48241090977468,-0.427019281353452,
6.41451593901973));
#19898=CARTESIAN_POINT('Ctrl Pts',(-2.46695548810174,-0.50875857078144,
6.41975249941204));
#19899=CARTESIAN_POINT('Ctrl Pts',(-2.44750666130293,-0.589506058389383,
6.42498905980436));
#19900=CARTESIAN_POINT('Ctrl Pts',(-2.42773950963489,-0.671575164709831,
6.43031132857484));
#19901=CARTESIAN_POINT('Ctrl Pts',(-2.40384715326946,-0.752619228922703,
6.43563359734532));
#19902=CARTESIAN_POINT('Ctrl Pts',(-2.37597229701536,-0.832203036413311,
6.4409558661158));
#19903=CARTESIAN_POINT('Ctrl Pts',(-2.34850694278311,-0.910617699576286,
6.44619994686614));
#19904=CARTESIAN_POINT('Ctrl Pts',(-2.31717555686965,-0.987614315326444,
6.45144402761647));
#19905=CARTESIAN_POINT('Ctrl Pts',(-2.2821630677264,-1.06279724421248,6.45668810836681));
#19906=CARTESIAN_POINT('Ctrl Pts',(-2.24636753652009,-1.13966161298417,
6.46204947114736));
#19907=CARTESIAN_POINT('Ctrl Pts',(-2.20672450140766,-1.21462973836723,
6.46741083392791));
#19908=CARTESIAN_POINT('Ctrl Pts',(-2.16347989151026,-1.287307659043,6.47277219670846));
#19909=CARTESIAN_POINT('Ctrl Pts',(-2.12023528161285,-1.35998557971878,
6.47813355948902));
#19910=CARTESIAN_POINT('Ctrl Pts',(-2.07338943405647,-1.43037290970729,
6.48349492226957));
#19911=CARTESIAN_POINT('Ctrl Pts',(-2.02323252747283,-1.49811094040992,
6.48885628505012));
#19912=CARTESIAN_POINT('Ctrl Pts',(-1.9740683383692,-1.56450828382301,6.49411153445743));
#19913=CARTESIAN_POINT('Ctrl Pts',(-1.92154140516665,-1.62860551635464,
6.49936678386474));
#19914=CARTESIAN_POINT('Ctrl Pts',(-1.86589467300489,-1.69004240161363,
6.50462203327205));
#19915=CARTESIAN_POINT('Ctrl Pts',(-1.81032683526795,-1.75139218332606,
6.50986983192955));
#19916=CARTESIAN_POINT('Ctrl Pts',(-1.75164829144652,-1.81008877046015,
6.51511763058705));
#19917=CARTESIAN_POINT('Ctrl Pts',(-1.69014386507699,-1.8658027669994,6.52036542924455));
#19918=CARTESIAN_POINT('Ctrl Pts',(-1.62819378611535,-1.92192045947471,
6.52565125272745));
#19919=CARTESIAN_POINT('Ctrl Pts',(-1.56337698190049,-1.97501177524926,
6.53093707621036));
#19920=CARTESIAN_POINT('Ctrl Pts',(-1.49602432105693,-2.02477590878747,
6.53622289969326));
#19921=CARTESIAN_POINT('Ctrl Pts',(-1.42927560687406,-2.07409381077528,
6.54146132556186));
#19922=CARTESIAN_POINT('Ctrl Pts',(-1.36003670956918,-2.12014368151662,
6.54669975143045));
#19923=CARTESIAN_POINT('Ctrl Pts',(-1.28866354925699,-2.16267253804555,
6.55193817729905));
#19924=CARTESIAN_POINT('Ctrl Pts',(-1.21731386238938,-2.20518740754137,
6.55717488033656));
#19925=CARTESIAN_POINT('Ctrl Pts',(-1.14383170264659,-2.24418332667548,
6.56241158337407));
#19926=CARTESIAN_POINT('Ctrl Pts',(-1.06860083476897,-2.27945136072939,
6.56764828641158));
#19927=CARTESIAN_POINT('Ctrl Pts',(-0.993372016142759,-2.31471843409959,
6.5728848468039));
#19928=CARTESIAN_POINT('Ctrl Pts',(-0.916395002317771,-2.34625762936338,
6.57812140719623));
#19929=CARTESIAN_POINT('Ctrl Pts',(-0.838075688553231,-2.37390719916681,
6.58335796758855));
#19930=CARTESIAN_POINT('Ctrl Pts',(-0.758474498736846,-2.40200931789683,
6.58868023635903));
#19931=CARTESIAN_POINT('Ctrl Pts',(-0.677487132195189,-2.42609316097627,
6.59400250512951));
#19932=CARTESIAN_POINT('Ctrl Pts',(-0.59555633944533,-2.44604147482141,
6.59932477389999));
#19933=CARTESIAN_POINT('Ctrl Pts',(-0.514829169952893,-2.46569673334895,
6.60456885465032));
#19934=CARTESIAN_POINT('Ctrl Pts',(-0.433186580706483,-2.4813371362005,
6.60981293540065));
#19935=CARTESIAN_POINT('Ctrl Pts',(-0.351061115609648,-2.49290239341754,
6.61505701615098));
#19936=CARTESIAN_POINT('Ctrl Pts',(-0.267098943234972,-2.50472630356368,
6.62041837893153));
#19937=CARTESIAN_POINT('Ctrl Pts',(-0.182632545677713,-2.5122905444431,
6.62577974171208));
#19938=CARTESIAN_POINT('Ctrl Pts',(-0.0981262711465387,-2.51558690665039,
6.63114110449264));
#19939=CARTESIAN_POINT('Ctrl Pts',(-0.0136199966153704,-2.51888326885768,
6.63650246727319));
#19940=CARTESIAN_POINT('Ctrl Pts',(0.070925647583907,-2.51791182502412,
6.64186383005375));
#19941=CARTESIAN_POINT('Ctrl Pts',(0.155051791237123,-2.51272067529086,
6.6472251928343));
#19942=CARTESIAN_POINT('Ctrl Pts',(0.237512890153206,-2.50763227003354,
6.6524804422416));
#19943=CARTESIAN_POINT('Ctrl Pts',(0.319875525080888,-2.49847092200906,
6.6577356916489));
#19944=CARTESIAN_POINT('Ctrl Pts',(0.401705260653849,-2.48524428046078,
6.66299094105621));
#19945=CARTESIAN_POINT('Ctrl Pts',(0.483418980251289,-2.47203639128548,
6.6682387397137));
#19946=CARTESIAN_POINT('Ctrl Pts',(0.564600849488969,-2.4547747299151,6.6734865383712));
#19947=CARTESIAN_POINT('Ctrl Pts',(0.644819500910465,-2.43351886395926,
6.67873433702869));
#19948=CARTESIAN_POINT('Ctrl Pts',(0.725619405618183,-2.41210898092985,
6.6840201605116));
#19949=CARTESIAN_POINT('Ctrl Pts',(0.80544160193643,-2.38664679535527,6.68930598399451));
#19950=CARTESIAN_POINT('Ctrl Pts',(0.883853634563512,-2.35724606324178,
6.69459180747741));
#19951=CARTESIAN_POINT('Ctrl Pts',(0.961562551906455,-2.32810896546375,
6.69983023334601));
#19952=CARTESIAN_POINT('Ctrl Pts',(1.03788605394017,-2.29510383658063,6.7050686592146));
#19953=CARTESIAN_POINT('Ctrl Pts',(1.1124181592425,-2.25839148266803,6.71030708508319));
#19954=CARTESIAN_POINT('Ctrl Pts',(1.18692575217586,-2.22169120283763,6.7155437881207));
#19955=CARTESIAN_POINT('Ctrl Pts',(1.25964270487964,-2.18128632319353,6.72078049115821));
#19956=CARTESIAN_POINT('Ctrl Pts',(1.33018482321191,-2.13738498780559,6.72601719419572));
#19957=CARTESIAN_POINT('Ctrl Pts',(1.40072502001207,-2.09348484826812,6.73125375458805));
#19958=CARTESIAN_POINT('Ctrl Pts',(1.46909010902144,-2.04608868703051,6.73649031498038));
#19959=CARTESIAN_POINT('Ctrl Pts',(1.53492342749988,-1.99544890230545,6.74172687537271));
#19960=CARTESIAN_POINT('Ctrl Pts',(1.601834259944,-1.94398028080713,6.74704914414319));
#19961=CARTESIAN_POINT('Ctrl Pts',(1.66612929985463,-1.8891611885151,6.75237141291367));
#19962=CARTESIAN_POINT('Ctrl Pts',(1.72746913962016,-1.83129916225066,6.75769368168415));
#19963=CARTESIAN_POINT('Ctrl Pts',(1.78790785228484,-1.7742871714636,6.76293776243449));
#19964=CARTESIAN_POINT('Ctrl Pts',(1.84547733669641,-1.71432143920906,6.76818184318483));
#19965=CARTESIAN_POINT('Ctrl Pts',(1.8998915228993,-1.6517319550143,6.77342592393516));
#19966=CARTESIAN_POINT('Ctrl Pts',(1.95552266332814,-1.58774267891589,6.77878728671571));
#19967=CARTESIAN_POINT('Ctrl Pts',(2.00785535222641,-1.52101127904257,6.78414864949626));
#19968=CARTESIAN_POINT('Ctrl Pts',(2.05662988850108,-1.4519227774658,6.78951001227682));
#19969=CARTESIAN_POINT('Ctrl Pts',(2.10540442477576,-1.38283427588904,6.79487137505737));
#19970=CARTESIAN_POINT('Ctrl Pts',(2.15062059314599,-1.31138913767725,6.80023273783792));
#19971=CARTESIAN_POINT('Ctrl Pts',(2.19206890703465,-1.23799844782291,6.80559410061847));
#19972=CARTESIAN_POINT('Ctrl Pts',(2.23446890777386,-1.16292264829979,6.81107856462994));
#19973=CARTESIAN_POINT('Ctrl Pts',(2.27307163741378,-1.08555429773617,6.81656302864142));
#19974=CARTESIAN_POINT('Ctrl Pts',(2.30763425924484,-1.00629537192593,6.82204749265289));
#19975=CARTESIAN_POINT('Ctrl Pts',(2.3421071209173,-0.927242283907316,6.82751771334793));
#19976=CARTESIAN_POINT('Ctrl Pts',(2.37256061323794,-0.846308768248659,
6.83298793404297));
#19977=CARTESIAN_POINT('Ctrl Pts',(2.39879783154463,-0.76392094707293,6.83845815473802));
#19978=CARTESIAN_POINT('Ctrl Pts',(2.42499481295722,-0.681659474277432,
6.84391998640766));
#19979=CARTESIAN_POINT('Ctrl Pts',(2.44698825905869,-0.597948514162592,
6.8493818180773));
#19980=CARTESIAN_POINT('Ctrl Pts',(2.46462916087108,-0.513234205196725,
6.85484364974695));
#19981=CARTESIAN_POINT('Ctrl Pts',(2.48223686891343,-0.428679297792125,
6.86029520423312));
#19982=CARTESIAN_POINT('Ctrl Pts',(2.49550826265312,-0.343125195357741,
6.8657467587193));
#19983=CARTESIAN_POINT('Ctrl Pts',(2.50434439920537,-0.257031866056912,
6.87119831320548));
#19984=CARTESIAN_POINT('Ctrl Pts',(2.51310690653042,-0.171655930072285,
6.87660444130632));
#19985=CARTESIAN_POINT('Ctrl Pts',(2.51750773395471,-0.0857501128064433,
6.88201056940717));
#19986=CARTESIAN_POINT('Ctrl Pts',(2.51749998978765,0.000226757967686038,
6.88741669750801));
#19987=CARTESIAN_POINT('Ctrl Pts',(2.51749998978759,0.000226758638666253,
6.8874166975502));
#19988=CARTESIAN_POINT('Ctrl Pts',(2.51749207334366,0.0881160122807311,
6.89294307411638));
#19989=CARTESIAN_POINT('Ctrl Pts',(2.51287736989993,0.175904347014042,6.89846945068255));
#19990=CARTESIAN_POINT('Ctrl Pts',(2.50371314433435,0.263109750650595,6.90399582724873));
#19991=CARTESIAN_POINT('Ctrl Pts',(2.49453499561041,0.350447644985407,6.90953060000895));
#19992=CARTESIAN_POINT('Ctrl Pts',(2.48079359631616,0.43720046548662,6.91506537276916));
#19993=CARTESIAN_POINT('Ctrl Pts',(2.46259736788571,0.522896216932551,6.92060014552938));
#19994=CARTESIAN_POINT('Ctrl Pts',(2.44435527462668,0.60880797033544,6.92614886905993));
#19995=CARTESIAN_POINT('Ctrl Pts',(2.42163600591916,0.693656960244299,6.93169759259049));
#19996=CARTESIAN_POINT('Ctrl Pts',(2.39459808317596,0.776985373124874,6.93724631612104));
#19997=CARTESIAN_POINT('Ctrl Pts',(2.38417680414139,0.809102805014325,6.93938497139966));
#19998=CARTESIAN_POINT('Ctrl Pts',(2.37311446244257,0.840994558653117,6.94152362667828));
#19999=CARTESIAN_POINT('Ctrl Pts',(2.36142200728635,0.872635292378026,6.9436622819569));
#20000=CARTESIAN_POINT('',(2.51749891107627,0.00228349541106654,6.61240052779172));
#20001=CARTESIAN_POINT('Ctrl Pts',(2.36142200703877,0.872635293048023,6.67067451578988));
#20002=CARTESIAN_POINT('Ctrl Pts',(2.38467103606877,0.809721531444391,6.66671645507875));
#20003=CARTESIAN_POINT('Ctrl Pts',(2.40539555026188,0.745906400452688,6.66268671174773));
#20004=CARTESIAN_POINT('Ctrl Pts',(2.42706372989967,0.66883240968557,6.65771882192992));
#20005=CARTESIAN_POINT('Ctrl Pts',(2.43048394040097,0.656294857644221,6.65690755437749));
#20006=CARTESIAN_POINT('Ctrl Pts',(2.4359017972833,0.6358111417721,6.65557615329902));
#20007=CARTESIAN_POINT('Ctrl Pts',(2.43795803848093,0.627880539714219,6.65505922957548));
#20008=CARTESIAN_POINT('Ctrl Pts',(2.44157840260655,0.613631423224701,6.65412762765142));
#20009=CARTESIAN_POINT('Ctrl Pts',(2.44315677540427,0.607316711904609,6.65371376685591));
#20010=CARTESIAN_POINT('Ctrl Pts',(2.4465792908925,0.593394718934433,6.65279907558092));
#20011=CARTESIAN_POINT('Ctrl Pts',(2.44841242767532,0.58578502809641,6.65229765308281));
#20012=CARTESIAN_POINT('Ctrl Pts',(2.45214370450115,0.569972276258733,6.65125286516005));
#20013=CARTESIAN_POINT('Ctrl Pts',(2.45403623661321,0.561768001886577,6.65070920448268));
#20014=CARTESIAN_POINT('Ctrl Pts',(2.45885124073767,0.540405862953337,6.64928978862847));
#20015=CARTESIAN_POINT('Ctrl Pts',(2.46170922010563,0.527233931585121,6.64841079322574));
#20016=CARTESIAN_POINT('Ctrl Pts',(2.46993370875743,0.487803278738433,6.64576947173143));
#20017=CARTESIAN_POINT('Ctrl Pts',(2.47498664686636,0.46148189809904,6.6439930735918));
#20018=CARTESIAN_POINT('Ctrl Pts',(2.50469517508788,0.292168690199933,6.63250235207536));
#20019=CARTESIAN_POINT('Ctrl Pts',(2.51736734102002,0.147362881071231,6.6224012180816));
#20020=CARTESIAN_POINT('Ctrl Pts',(2.51749896391893,0.00228400243197625,
6.61240047030075));
#20021=CARTESIAN_POINT('Ctrl Pts',(2.51749896437308,0.00228350180114051,
6.61240043579068));
#20022=CARTESIAN_POINT('Ctrl Pts',(2.51764262912045,-0.156102995878949,
6.60148235182255));
#20023=CARTESIAN_POINT('Ctrl Pts',(2.50283907664945,-0.314178187571748,
6.59073840743485));
#20024=CARTESIAN_POINT('Ctrl Pts',(2.46917070021309,-0.491410592718018,
6.57903055701159));
#20025=CARTESIAN_POINT('Ctrl Pts',(2.4647909428422,-0.512926871148302,6.57761434418599));
#20026=CARTESIAN_POINT('Ctrl Pts',(2.4571129791369,-0.548273741161353,6.57529586558297));
#20027=CARTESIAN_POINT('Ctrl Pts',(2.45397817822452,-0.562138240850671,
6.57438851837946));
#20028=CARTESIAN_POINT('Ctrl Pts',(2.44763110369328,-0.589144486888082,
6.57262494229146));
#20029=CARTESIAN_POINT('Ctrl Pts',(2.44442999896002,-0.602288334602156,
6.57176839110694));
#20030=CARTESIAN_POINT('Ctrl Pts',(2.43857323921963,-0.625520269782588,
6.57025737715399));
#20031=CARTESIAN_POINT('Ctrl Pts',(2.43596055922672,-0.635618761611592,
6.56960155995007));
#20032=CARTESIAN_POINT('Ctrl Pts',(2.42979489923048,-0.65885368382676,6.56809478766277));
#20033=CARTESIAN_POINT('Ctrl Pts',(2.42619799965326,-0.671978204279829,
6.56724526228131));
#20034=CARTESIAN_POINT('Ctrl Pts',(2.41599242172552,-0.708066263611893,
6.56491332556017));
#20035=CARTESIAN_POINT('Ctrl Pts',(2.40916284800644,-0.730966242373608,
6.56343804479047));
#20036=CARTESIAN_POINT('Ctrl Pts',(2.36612829424863,-0.868103401182656,
6.55462425740325));
#20037=CARTESIAN_POINT('Ctrl Pts',(2.32212847682084,-0.979740342680465,
6.5475475943634));
#20038=CARTESIAN_POINT('Ctrl Pts',(2.2260048061575,-1.18035375868838,6.53463937488682));
#20039=CARTESIAN_POINT('Ctrl Pts',(2.17605756268362,-1.27008110973878,6.52878496287698));
#20040=CARTESIAN_POINT('Ctrl Pts',(2.0702389931808,-1.43551830349322,6.51745801455129));
#20041=CARTESIAN_POINT('Ctrl Pts',(2.01533173785899,-1.51163403156109,6.51200350096616));
#20042=CARTESIAN_POINT('Ctrl Pts',(1.93166392045488,-1.61493478907269,6.50398640288852));
#20043=CARTESIAN_POINT('Ctrl Pts',(1.90631064602362,-1.64478545996722,6.50159045911177));
#20044=CARTESIAN_POINT('Ctrl Pts',(1.87265745955274,-1.68258475532417,6.49843395943529));
#20045=CARTESIAN_POINT('Ctrl Pts',(1.86498363084858,-1.69108647461973,6.49771572571102));
#20046=CARTESIAN_POINT('Ctrl Pts',(1.85246658510197,-1.70476510224588,6.4965460787577));
#20047=CARTESIAN_POINT('Ctrl Pts',(1.84765894056843,-1.70997454341697,6.49609727528917));
#20048=CARTESIAN_POINT('Ctrl Pts',(1.83832436401742,-1.72000392664656,6.49522656451627));
#20049=CARTESIAN_POINT('Ctrl Pts',(1.83380035822558,-1.72482643106998,6.49480487203248));
#20050=CARTESIAN_POINT('Ctrl Pts',(1.82374968607531,-1.73545602069929,6.49386878388667));
#20051=CARTESIAN_POINT('Ctrl Pts',(1.81821417438852,-1.74125464224175,6.4933537272423));
#20052=CARTESIAN_POINT('Ctrl Pts',(1.79846577836947,-1.76174485810495,6.49151832115046));
#20053=CARTESIAN_POINT('Ctrl Pts',(1.78410219566875,-1.77628922011353,6.4901872096681));
#20054=CARTESIAN_POINT('Ctrl Pts',(1.64937474330208,-1.90942966451447,6.47775040913707));
#20055=CARTESIAN_POINT('Ctrl Pts',(1.51754305519328,-2.0157910269683,6.46596740877383));
#20056=CARTESIAN_POINT('Ctrl Pts',(1.27947782164855,-2.17118556082261,6.44636657095683));
#20057=CARTESIAN_POINT('Ctrl Pts',(1.17866325968881,-2.22752511464358,6.438492154302));
#20058=CARTESIAN_POINT('Ctrl Pts',(1.03531313466283,-2.29516760162362,6.42796476353293));
#20059=CARTESIAN_POINT('Ctrl Pts',(0.995826835890043,-2.31257364836771,
6.42512964081845));
#20060=CARTESIAN_POINT('Ctrl Pts',(0.926007551901459,-2.34123068113191,
6.42022828307746));
#20061=CARTESIAN_POINT('Ctrl Pts',(0.89586974705452,-2.3529276749184,6.41814798903026));
#20062=CARTESIAN_POINT('Ctrl Pts',(0.851281326778832,-2.36925221730586,
6.41512051641313));
#20063=CARTESIAN_POINT('Ctrl Pts',(0.83700179633168,-2.37433442796945,6.414158424086));
#20064=CARTESIAN_POINT('Ctrl Pts',(0.811629527554386,-2.38310729875188,
6.41246186480738));
#20065=CARTESIAN_POINT('Ctrl Pts',(0.800555456859901,-2.38685019540337,
6.41172570031532));
#20066=CARTESIAN_POINT('Ctrl Pts',(0.777261056146578,-2.39454305135542,
6.41018604902812));
#20067=CARTESIAN_POINT('Ctrl Pts',(0.765035734341543,-2.39847691444072,
6.40938310591206));
#20068=CARTESIAN_POINT('Ctrl Pts',(0.732720663011623,-2.40860303836279,
6.40727376137095));
#20069=CARTESIAN_POINT('Ctrl Pts',(0.712582265283442,-2.41463759662118,
6.40597249293455));
#20070=CARTESIAN_POINT('Ctrl Pts',(0.624223997608043,-2.43991281517091,
6.40031796042861));
#20071=CARTESIAN_POINT('Ctrl Pts',(0.555281092223001,-2.45652079187197,
6.39604924512552));
#20072=CARTESIAN_POINT('Ctrl Pts',(0.271994146491859,-2.51222454296997,
6.37894128547761));
#20073=CARTESIAN_POINT('Ctrl Pts',(0.0537343956660501,-2.52633247150004,
6.36683508631061));
#20074=CARTESIAN_POINT('Ctrl Pts',(-0.209791046977706,-2.50917040783561,
6.35125327565513));
#20075=CARTESIAN_POINT('Ctrl Pts',(-0.255882464528519,-2.50488963686466,
6.34848813789867));
#20076=CARTESIAN_POINT('Ctrl Pts',(-0.330648633776396,-2.49586068039505,
6.34390077324298));
#20077=CARTESIAN_POINT('Ctrl Pts',(-0.359406554799883,-2.49188198282343,
6.34211154031295));
#20078=CARTESIAN_POINT('Ctrl Pts',(-0.39817651573996,-2.48583305398359,
6.3396580874016));
#20079=CARTESIAN_POINT('Ctrl Pts',(-0.40825536533137,-2.48419766891451,
6.33901648352339));
#20080=CARTESIAN_POINT('Ctrl Pts',(-0.425047333157644,-2.48136807111227,
6.33794078620589));
#20081=CARTESIAN_POINT('Ctrl Pts',(-0.43176617225622,-2.48020779574439,
6.33750856988267));
#20082=CARTESIAN_POINT('Ctrl Pts',(-0.444473562776449,-2.47796015846696,
6.33668755472791));
#20083=CARTESIAN_POINT('Ctrl Pts',(-0.450463048201784,-2.47687834486623,
6.33629908076239));
#20084=CARTESIAN_POINT('Ctrl Pts',(-0.464631096237097,-2.47426623983085,
6.3353766983061));
#20085=CARTESIAN_POINT('Ctrl Pts',(-0.472806052021689,-2.47271711153767,
6.334841756449));
#20086=CARTESIAN_POINT('Ctrl Pts',(-0.501618220916195,-2.46710919515326,
6.33294711116231));
#20087=CARTESIAN_POINT('Ctrl Pts',(-0.522211451640957,-2.46283246529598,
6.3315761218241));
#20088=CARTESIAN_POINT('Ctrl Pts',(-0.690659741181082,-2.42564212631217,
6.32023669481753));
#20089=CARTESIAN_POINT('Ctrl Pts',(-0.835309564179003,-2.37970602818354,
6.30972613747561));
#20090=CARTESIAN_POINT('Ctrl Pts',(-1.04112724916594,-2.29325400895412,
6.2943107460072));
#20091=CARTESIAN_POINT('Ctrl Pts',(-1.10609724884355,-2.26263331728389,
6.28936833769292));
#20092=CARTESIAN_POINT('Ctrl Pts',(-1.238742405954,-2.19303616263861,6.27917404651769));
#20093=CARTESIAN_POINT('Ctrl Pts',(-1.30609616516309,-2.15360280351311,
6.27393809799044));
#20094=CARTESIAN_POINT('Ctrl Pts',(-1.39977026599398,-2.0927457440425,6.26658696488886));
#20095=CARTESIAN_POINT('Ctrl Pts',(-1.42765487181711,-2.07382335057029,
6.26438912432197));
#20096=CARTESIAN_POINT('Ctrl Pts',(-1.47690468943093,-2.03893829110284,
6.26048920128261));
#20097=CARTESIAN_POINT('Ctrl Pts',(-1.49841161713251,-2.02318549110424,
6.2587797136444));
#20098=CARTESIAN_POINT('Ctrl Pts',(-1.5308633246844,-1.99861477623512,6.2561894618137));
#20099=CARTESIAN_POINT('Ctrl Pts',(-1.54199068744078,-1.99004227982961,
6.25529929537964));
#20100=CARTESIAN_POINT('Ctrl Pts',(-1.56128157608125,-1.97492166610264,
6.25375234563691));
#20101=CARTESIAN_POINT('Ctrl Pts',(-1.5694770150833,-1.96841500997854,6.2530939570433));
#20102=CARTESIAN_POINT('Ctrl Pts',(-1.5878872597679,-1.9536103727868,6.25161211527055));
#20103=CARTESIAN_POINT('Ctrl Pts',(-1.59807809883172,-1.9452829714154,6.25078985732198));
#20104=CARTESIAN_POINT('Ctrl Pts',(-1.62549896937443,-1.92251520663694,
6.24857156387508));
#20105=CARTESIAN_POINT('Ctrl Pts',(-1.64260189478767,-1.90792313388635,
6.24718167660706));
#20106=CARTESIAN_POINT('Ctrl Pts',(-1.72578199286055,-1.83500689183502,
6.24038661615886));
#20107=CARTESIAN_POINT('Ctrl Pts',(-1.78896419196649,-1.77346646891228,
6.23511647398662));
#20108=CARTESIAN_POINT('Ctrl Pts',(-1.96922831725502,-1.57842657059376,
6.21951580690794));
#20109=CARTESIAN_POINT('Ctrl Pts',(-2.07554382487315,-1.43575955508333,
6.20954189931697));
#20110=CARTESIAN_POINT('Ctrl Pts',(-2.19629948248837,-1.23191507266479,
6.19570149942029));
#20111=CARTESIAN_POINT('Ctrl Pts',(-2.2247975460239,-1.17966992406611,6.19218250646721));
#20112=CARTESIAN_POINT('Ctrl Pts',(-2.26183683041802,-1.10564132577336,
6.1871684904197));
#20113=CARTESIAN_POINT('Ctrl Pts',(-2.27196736898275,-1.08467173988065,
6.18574516567033));
#20114=CARTESIAN_POINT('Ctrl Pts',(-2.28914374284474,-1.04782103196951,
6.18323347093917));
#20115=CARTESIAN_POINT('Ctrl Pts',(-2.29631892846367,-1.03200161361778,
6.18215193758628));
#20116=CARTESIAN_POINT('Ctrl Pts',(-2.30669339976604,-1.00848463871386,
6.18053745030711));
#20117=CARTESIAN_POINT('Ctrl Pts',(-2.31001925158052,-1.00084302449772,
6.18001180189886));
#20118=CARTESIAN_POINT('Ctrl Pts',(-2.31587817315683,-0.987196541443809,
6.17907100691467));
#20119=CARTESIAN_POINT('Ctrl Pts',(-2.31842594640675,-0.981198172534568,
6.17865675112962));
#20120=CARTESIAN_POINT('Ctrl Pts',(-2.32393861334242,-0.968078033439025,
6.17774902075387));
#20121=CARTESIAN_POINT('Ctrl Pts',(-2.32689403170536,-0.960952610090968,
6.17725501668204));
#20122=CARTESIAN_POINT('Ctrl Pts',(-2.33508972099295,-0.940933553534841,
6.17586446101935));
#20123=CARTESIAN_POINT('Ctrl Pts',(-2.34025579114612,-0.928010112279348,
6.17496372115736));
#20124=CARTESIAN_POINT('Ctrl Pts',(-2.37021276929685,-0.851228598166221,
6.16959693924877));
#20125=CARTESIAN_POINT('Ctrl Pts',(-2.39249394915815,-0.786428408410698,
6.16500603894688));
#20126=CARTESIAN_POINT('Ctrl Pts',(-2.47510092030687,-0.50999306334675,
6.14538475903113));
#20127=CARTESIAN_POINT('Ctrl Pts',(-2.51019960579048,-0.291785896529965,
6.12991464126099));
#20128=CARTESIAN_POINT('Ctrl Pts',(-2.51779611652691,-0.0255264967127382,
6.11217455402732));
#20129=CARTESIAN_POINT('Ctrl Pts',(-2.51783990854284,0.0207731010988608,
6.10912587337467));
#20130=CARTESIAN_POINT('Ctrl Pts',(-2.51569820002282,0.101158395823247,
6.103895795856));
#20131=CARTESIAN_POINT('Ctrl Pts',(-2.51409609117507,0.135246017962943,
6.10169762598872));
#20132=CARTESIAN_POINT('Ctrl Pts',(-2.51076017542635,0.184741330002574,
6.09853302560837));
#20133=CARTESIAN_POINT('Ctrl Pts',(-2.50957637538775,0.200181045749964,
6.09754968826761));
#20134=CARTESIAN_POINT('Ctrl Pts',(-2.50724518243701,0.227300559581401,
6.09582895586437));
#20135=CARTESIAN_POINT('Ctrl Pts',(-2.50615844354016,0.238984963220055,
6.09508969775372));
#20136=CARTESIAN_POINT('Ctrl Pts',(-2.50372654916484,0.263288141369486,
6.09355630303063));
#20137=CARTESIAN_POINT('Ctrl Pts',(-2.50236759773365,0.275905225729157,
6.09276261833018));
#20138=CARTESIAN_POINT('Ctrl Pts',(-2.49858436198463,0.308699546120931,
6.09070556367505));
#20139=CARTESIAN_POINT('Ctrl Pts',(-2.49601103316484,0.328858911285989,
6.08944686569461));
#20140=CARTESIAN_POINT('Ctrl Pts',(-2.48425174869456,0.412868665011913,
6.08422338922226));
#20141=CARTESIAN_POINT('Ctrl Pts',(-2.47285718629996,0.476388141691041,
6.08032764246175));
#20142=CARTESIAN_POINT('Ctrl Pts',(-2.41598692254536,0.735648212729541,
6.06454189794592));
#20143=CARTESIAN_POINT('Ctrl Pts',(-2.34960640922154,0.926023061614967,
6.05328600561617));
#20144=CARTESIAN_POINT('Ctrl Pts',(-2.23386081771046,1.16257094251553,6.03793050442848));
#20145=CARTESIAN_POINT('Ctrl Pts',(-2.20434065542979,1.21761512791022,6.03424483181116));
#20146=CARTESIAN_POINT('Ctrl Pts',(-2.15475215657273,1.3023545222563,6.02830425705274));
#20147=CARTESIAN_POINT('Ctrl Pts',(-2.13604310721858,1.33281795542462,6.02611180328649));
#20148=CARTESIAN_POINT('Ctrl Pts',(-2.11072452865471,1.37214057700311,6.02319243929303));
#20149=CARTESIAN_POINT('Ctrl Pts',(-2.10469538990937,1.38137073377817,6.02250059629575));
#20150=CARTESIAN_POINT('Ctrl Pts',(-2.09474246671518,1.39639148221189,6.02136339930581));
#20151=CARTESIAN_POINT('Ctrl Pts',(-2.09085475665357,1.4022059610428,6.02092039371176));
#20152=CARTESIAN_POINT('Ctrl Pts',(-2.08321336271889,1.41353203121619,6.02005181629774));
#20153=CARTESIAN_POINT('Ctrl Pts',(-2.07946193210531,1.41904502649759,6.01962639214683));
#20154=CARTESIAN_POINT('Ctrl Pts',(-2.0710282168807,1.43133371708985,6.01867229712303));
#20155=CARTESIAN_POINT('Ctrl Pts',(-2.06633449916899,1.43810146298348,6.01814287525579));
#20156=CARTESIAN_POINT('Ctrl Pts',(-2.04995275398882,1.46147608833569,6.01630086828549));
#20157=CARTESIAN_POINT('Ctrl Pts',(-2.03809740475567,1.47796399063211,6.01497784278345));
#20158=CARTESIAN_POINT('Ctrl Pts',(-1.92862734988289,1.62638819521802,6.00286387292814));
#20159=CARTESIAN_POINT('Ctrl Pts',(-1.81853600395081,1.74861676855274,5.99143463933209));
#20160=CARTESIAN_POINT('Ctrl Pts',(-1.60987589763608,1.93910631497473,5.97194476242831));
#20161=CARTESIAN_POINT('Ctrl Pts',(-1.51687216290424,2.01269417510598,5.96384920749629));
#20162=CARTESIAN_POINT('Ctrl Pts',(-1.38282625343039,2.10416686797863,5.9530645614086));
#20163=CARTESIAN_POINT('Ctrl Pts',(-1.34598830421661,2.12791976276554,5.95018339347335));
#20164=CARTESIAN_POINT('Ctrl Pts',(-1.28059835777471,2.1677048679725,5.94521088331135));
#20165=CARTESIAN_POINT('Ctrl Pts',(-1.25231975275721,2.18416390178316,5.94310491752272));
#20166=CARTESIAN_POINT('Ctrl Pts',(-1.21041859692883,2.20747026888751,5.94004750529565));
#20167=CARTESIAN_POINT('Ctrl Pts',(-1.19704283174079,2.2147520500952,5.93908072092514));
#20168=CARTESIAN_POINT('Ctrl Pts',(-1.17327642486921,2.22741229707972,5.93737885179961));
#20169=CARTESIAN_POINT('Ctrl Pts',(-1.16291292804173,2.23284048682187,5.93664203307494));
#20170=CARTESIAN_POINT('Ctrl Pts',(-1.14112599277617,2.24405920807533,5.93510391053287));
#20171=CARTESIAN_POINT('Ctrl Pts',(-1.12969542403539,2.2498352204772,5.934303129359));
#20172=CARTESIAN_POINT('Ctrl Pts',(-1.099533123351,2.26478878496928,5.93220598024121));
#20173=CARTESIAN_POINT('Ctrl Pts',(-1.08073029840269,2.27382131937554,5.93091463628026));
#20174=CARTESIAN_POINT('Ctrl Pts',(-0.998858166881356,2.31190616977218,
5.92535786513149));
#20175=CARTESIAN_POINT('Ctrl Pts',(-0.934711121816948,2.33857738123311,
5.92117334385899));
#20176=CARTESIAN_POINT('Ctrl Pts',(-0.705050342623193,2.42310374368821,
5.90666017056631));
#20177=CARTESIAN_POINT('Ctrl Pts',(-0.534693677424592,2.46629915494052,
5.89676193790825));
#20178=CARTESIAN_POINT('Ctrl Pts',(-0.251619936255753,2.50734128341228,
5.8801981352094));
#20179=CARTESIAN_POINT('Ctrl Pts',(-0.141094987856981,2.51598071206995,
5.8736904597384));
#20180=CARTESIAN_POINT('Ctrl Pts',(-0.0155015312881966,2.5174962230828,
5.86590237217017));
#20181=CARTESIAN_POINT('Ctrl Pts',(-0.000626224857081857,2.51754386530644,
5.8649736600194));
#20182=CARTESIAN_POINT('Ctrl Pts',(0.0220799689617035,2.51741535376739,
5.86354525662034));
#20183=CARTESIAN_POINT('Ctrl Pts',(0.0299113531311938,2.51733448223364,
5.86305064050257));
#20184=CARTESIAN_POINT('Ctrl Pts',(0.0442503720644473,2.51711948894187,
5.86214121999668));
#20185=CARTESIAN_POINT('Ctrl Pts',(0.0507579945147347,2.51699667068455,
5.86172704153836));
#20186=CARTESIAN_POINT('Ctrl Pts',(0.0654506991158243,2.5166623720372,5.8607886591277));
#20187=CARTESIAN_POINT('Ctrl Pts',(0.0736352119455181,2.51643619825982,
5.86026366945199));
#20188=CARTESIAN_POINT('Ctrl Pts',(0.0947900643359271,2.51574830563656,
5.85890109550621));
#20189=CARTESIAN_POINT('Ctrl Pts',(0.107758015593976,2.51522620989445,5.85806038132969));
#20190=CARTESIAN_POINT('Ctrl Pts',(0.194849099336523,2.51104514390699,5.85238016261128));
#20191=CARTESIAN_POINT('Ctrl Pts',(0.268776644480801,2.50421062328309,5.84739338082318));
#20192=CARTESIAN_POINT('Ctrl Pts',(0.402265388164401,2.48589099178223,5.83820729703165));
#20193=CARTESIAN_POINT('Ctrl Pts',(0.461926122795771,2.47549900149968,5.83403467532624));
#20194=CARTESIAN_POINT('Ctrl Pts',(0.62173698506213,2.4416837658413,5.82275368068259));
#20195=CARTESIAN_POINT('Ctrl Pts',(0.720928165416151,2.41425784866357,5.81564385606498));
#20196=CARTESIAN_POINT('Ctrl Pts',(0.926184677678503,2.34372220155681,5.80089070620759));
#20197=CARTESIAN_POINT('Ctrl Pts',(1.03156194926637,2.29929079358061,5.7932945120028));
#20198=CARTESIAN_POINT('Ctrl Pts',(1.15426592261674,2.23741226971139,5.78444470955402));
#20199=CARTESIAN_POINT('Ctrl Pts',(1.17481702349848,2.22669003337826,5.78296196079747));
#20200=CARTESIAN_POINT('Ctrl Pts',(1.20693309826492,2.20936550523106,5.78064329816586));
#20201=CARTESIAN_POINT('Ctrl Pts',(1.21859837794703,2.20295289185225,5.7798007859347));
#20202=CARTESIAN_POINT('Ctrl Pts',(1.24034085962375,2.19077510671482,5.77822965190946));
#20203=CARTESIAN_POINT('Ctrl Pts',(1.25043006066988,2.18503219355857,5.77750026638291));
#20204=CARTESIAN_POINT('Ctrl Pts',(1.27292575132958,2.1720204931856,5.77587304062748));
#20205=CARTESIAN_POINT('Ctrl Pts',(1.28531048293538,2.16471475424095,5.77497655249754));
#20206=CARTESIAN_POINT('Ctrl Pts',(1.31665850606506,2.14585871080158,5.77270527134266));
#20207=CARTESIAN_POINT('Ctrl Pts',(1.33553307244268,2.13416276062942,5.77133576283714));
#20208=CARTESIAN_POINT('Ctrl Pts',(1.49044716137565,2.03530745380056,5.76007220965784));
#20209=CARTESIAN_POINT('Ctrl Pts',(1.61796758928213,1.93548430355487,5.75068398696019));
#20210=CARTESIAN_POINT('Ctrl Pts',(1.82556859812181,1.73801924811472,5.73420126790117));
#20211=CARTESIAN_POINT('Ctrl Pts',(1.90954424125383,1.64531115857055,5.72708242144767));
#20212=CARTESIAN_POINT('Ctrl Pts',(2.01294746991208,1.51252489607689,5.71712629495188));
#20213=CARTESIAN_POINT('Ctrl Pts',(2.03871636746502,1.47760760512915,5.71452763058099));
#20214=CARTESIAN_POINT('Ctrl Pts',(2.07944486742211,1.41932501431833,5.71019036280101));
#20215=CARTESIAN_POINT('Ctrl Pts',(2.09494406099876,1.39634654999743,5.7084804154402));
#20216=CARTESIAN_POINT('Ctrl Pts',(2.11553174354946,1.36470961498031,5.70611941352598));
#20217=CARTESIAN_POINT('Ctrl Pts',(2.12095307622008,1.35626875348217,5.70548884757562));
#20218=CARTESIAN_POINT('Ctrl Pts',(2.12995417931019,1.3420683399604,5.7044265506527));
#20219=CARTESIAN_POINT('Ctrl Pts',(2.13356145796007,1.33632620958028,5.70399659693292));
#20220=CARTESIAN_POINT('Ctrl Pts',(2.14037890575465,1.32537610422837,5.7031757896568));
#20221=CARTESIAN_POINT('Ctrl Pts',(2.14359336835503,1.3201708779858,5.70278523464692));
#20222=CARTESIAN_POINT('Ctrl Pts',(2.15119994053834,1.30775241834254,5.70185266208054));
#20223=CARTESIAN_POINT('Ctrl Pts',(2.15557475603701,1.30052875329529,5.70130955784393));
#20224=CARTESIAN_POINT('Ctrl Pts',(2.1709795289709,1.27480123526098,5.69937337687495));
#20225=CARTESIAN_POINT('Ctrl Pts',(2.18180788290342,1.2561785677007,5.69796845186269));
#20226=CARTESIAN_POINT('Ctrl Pts',(2.25520805841346,1.12613200654281,5.688145840705));
#20227=CARTESIAN_POINT('Ctrl Pts',(2.30944999734189,1.01023324050885,5.6793424912854));
#20228=CARTESIAN_POINT('Ctrl Pts',(2.3569344417224,0.884707728550295,5.67007201361025));
#20229=CARTESIAN_POINT('Ctrl Pts',(2.35918987096009,0.878675634613511,5.6696271157682));
#20230=CARTESIAN_POINT('Ctrl Pts',(2.36142200559759,0.87263529694796,5.66918223051795));
#20231=CARTESIAN_POINT('Origin',(0.,0.,10.));
#20232=CARTESIAN_POINT('',(2.36142200727925,0.872635292397265,4.66658913197125));
#20233=CARTESIAN_POINT('',(2.36142200728636,0.872635292378022,4.94384492744144));
#20234=CARTESIAN_POINT('',(2.36142200728636,0.87263529237802,10.));
#20235=CARTESIAN_POINT('',(2.51749903524847,-0.00220397890970226,5.88741669756531));
#20236=CARTESIAN_POINT('Ctrl Pts',(2.36142200728636,0.872635292378022,4.94384492744144));
#20237=CARTESIAN_POINT('Ctrl Pts',(2.33267223382292,0.950434515437239,4.94908498406439));
#20238=CARTESIAN_POINT('Ctrl Pts',(2.30004677929906,1.02688413496855,4.95432504068734));
#20239=CARTESIAN_POINT('Ctrl Pts',(2.26369979786784,1.101575905298,4.95956509731029));
#20240=CARTESIAN_POINT('Ctrl Pts',(2.2273708295506,1.17623065931083,4.96480255702605));
#20241=CARTESIAN_POINT('Ctrl Pts',(2.1873241979168,1.2491288796774,4.97004001674182));
#20242=CARTESIAN_POINT('Ctrl Pts',(2.14376179350139,1.31988318525683,4.97527747645758));
#20243=CARTESIAN_POINT('Ctrl Pts',(2.10020783758702,1.39062376873271,4.98051392041941));
#20244=CARTESIAN_POINT('Ctrl Pts',(2.05313970549245,1.45922087074756,4.98575036438124));
#20245=CARTESIAN_POINT('Ctrl Pts',(2.00280406300176,1.52531378254562,4.99098680834306));
#20246=CARTESIAN_POINT('Ctrl Pts',(1.95246299932454,1.59141381259997,4.99622381627384));
#20247=CARTESIAN_POINT('Ctrl Pts',(1.89885400717399,1.65500875069382,5.00146082420462));
#20248=CARTESIAN_POINT('Ctrl Pts',(1.84226484542956,1.7157699406664,5.0066978321354));
#20249=CARTESIAN_POINT('Ctrl Pts',(1.78561580536273,1.77659542348254,5.01194038146738));
#20250=CARTESIAN_POINT('Ctrl Pts',(1.72598061546314,1.83458083389482,5.01718293079937));
#20251=CARTESIAN_POINT('Ctrl Pts',(1.66368442898251,1.88943387573134,5.02242548013135));
#20252=CARTESIAN_POINT('Ctrl Pts',(1.60135258097397,1.94431831825853,5.0276710305671));
#20253=CARTESIAN_POINT('Ctrl Pts',(1.53635706458887,1.99606653476143,5.03291658100284));
#20254=CARTESIAN_POINT('Ctrl Pts',(1.4690547859029,2.04442761818945,5.03816213143859));
#20255=CARTESIAN_POINT('Ctrl Pts',(1.40163917700721,2.09287013677589,5.04341651484912));
#20256=CARTESIAN_POINT('Ctrl Pts',(1.33190943726327,2.13791388323439,5.04867089825965));
#20257=CARTESIAN_POINT('Ctrl Pts',(1.2602496924962,2.17935241816536,5.05392528167019));
#20258=CARTESIAN_POINT('Ctrl Pts',(1.21655856142409,2.20461759971172,5.05712889277764));
#20259=CARTESIAN_POINT('Ctrl Pts',(1.17215044553941,2.22854349808343,5.06033250388509));
#20260=CARTESIAN_POINT('Ctrl Pts',(1.12711601958344,2.25109211903875,5.06353611499254));
#20261=CARTESIAN_POINT('Ctrl Pts',(1.05324090416664,2.28808119884167,5.06879136439984));
#20262=CARTESIAN_POINT('Ctrl Pts',(0.977406600329949,2.3214981450137,5.07404661380715));
#20263=CARTESIAN_POINT('Ctrl Pts',(0.899992693089727,2.35113151533152,5.07930186321445));
#20264=CARTESIAN_POINT('Ctrl Pts',(0.822688541183612,2.38072287226214,5.08454966187195));
#20265=CARTESIAN_POINT('Ctrl Pts',(0.743809661544648,2.40654114472748,5.08979746052945));
#20266=CARTESIAN_POINT('Ctrl Pts',(0.663759045355666,2.42842133488168,5.09504525918694));
#20267=CARTESIAN_POINT('Ctrl Pts',(0.583128393440619,2.4504600658765,5.10033108266985));
#20268=CARTESIAN_POINT('Ctrl Pts',(0.501309376583909,2.46850319198873,5.10561690615276));
#20269=CARTESIAN_POINT('Ctrl Pts',(0.418733125877458,2.48243203719516,5.11090272963567));
#20270=CARTESIAN_POINT('Ctrl Pts',(0.336897330711262,2.49623598340805,5.11614115550426));
#20271=CARTESIAN_POINT('Ctrl Pts',(0.254318290809087,2.50599905997798,5.12137958137285));
#20272=CARTESIAN_POINT('Ctrl Pts',(0.171427855908116,2.51165657290537,5.12661800724144));
#20273=CARTESIAN_POINT('Ctrl Pts',(0.088564682291696,2.51731222517091,5.13185471027894));
#20274=CARTESIAN_POINT('Ctrl Pts',(0.00539077706015141,2.51886496407217,
5.13709141331644));
#20275=CARTESIAN_POINT('Ctrl Pts',(-0.0776570934184586,2.51630197429518,
5.14232811635394));
#20276=CARTESIAN_POINT('Ctrl Pts',(-0.16070270171454,2.51373905433274,5.14756467674627));
#20277=CARTESIAN_POINT('Ctrl Pts',(-0.243621820914314,2.50706064386031,
5.15280123713859));
#20278=CARTESIAN_POINT('Ctrl Pts',(-0.325979284033456,2.49630602218178,
5.15803779753092));
#20279=CARTESIAN_POINT('Ctrl Pts',(-0.409684716824353,2.48537537633611,
5.1633600663014));
#20280=CARTESIAN_POINT('Ctrl Pts',(-0.492809452779872,2.47023393290528,
5.16868233507188));
#20281=CARTESIAN_POINT('Ctrl Pts',(-0.57490557300384,2.45097732183085,5.17400460384237));
#20282=CARTESIAN_POINT('Ctrl Pts',(-0.65579564118882,2.43200360445452,5.1792486845927));
#20283=CARTESIAN_POINT('Ctrl Pts',(-0.735686682421181,2.40903501479327,
5.18449276534303));
#20284=CARTESIAN_POINT('Ctrl Pts',(-0.814165640056451,2.38221337427013,
5.18973684609336));
#20285=CARTESIAN_POINT('Ctrl Pts',(-0.89439975210679,2.35479187714591,5.19509820887392));
#20286=CARTESIAN_POINT('Ctrl Pts',(-0.973157381352252,2.3233430951021,5.20045957165448));
#20287=CARTESIAN_POINT('Ctrl Pts',(-1.05002065499384,2.28806968296123,5.20582093443504));
#20288=CARTESIAN_POINT('Ctrl Pts',(-1.12688392863543,2.25279627082036,5.2111822972156));
#20289=CARTESIAN_POINT('Ctrl Pts',(-1.20185242704163,2.21369852276584,5.21654365999616));
#20290=CARTESIAN_POINT('Ctrl Pts',(-1.27453862635216,2.17102683998525,5.22190502277672));
#20291=CARTESIAN_POINT('Ctrl Pts',(-1.34578620303772,2.12919972534656,5.22716027218404));
#20292=CARTESIAN_POINT('Ctrl Pts',(-1.41510418478558,2.08378440484446,5.23241552159136));
#20293=CARTESIAN_POINT('Ctrl Pts',(-1.48210854983538,2.03498415141368,5.23767077099868));
#20294=CARTESIAN_POINT('Ctrl Pts',(-1.5490179179171,1.98625308565619,5.24291856965619));
#20295=CARTESIAN_POINT('Ctrl Pts',(-1.61361981483033,1.93414688869806,5.2481663683137));
#20296=CARTESIAN_POINT('Ctrl Pts',(-1.67555643247632,1.87891375309971,5.25341416697121));
#20297=CARTESIAN_POINT('Ctrl Pts',(-1.73794183431264,1.82328040581752,5.25869999045411));
#20298=CARTESIAN_POINT('Ctrl Pts',(-1.79762276074638,1.76447485387468,5.26398581393702));
#20299=CARTESIAN_POINT('Ctrl Pts',(-1.8542649372488,1.70279411335889,5.26927163741992));
#20300=CARTESIAN_POINT('Ctrl Pts',(-1.91039920726448,1.64166645978555,5.27451006328853));
#20301=CARTESIAN_POINT('Ctrl Pts',(-1.96354868775492,1.57771532047659,5.27974848915713));
#20302=CARTESIAN_POINT('Ctrl Pts',(-2.01342399262884,1.51126770491086,5.28498691502574));
#20303=CARTESIAN_POINT('Ctrl Pts',(-2.06328289434503,1.44484194286004,5.29022361806326));
#20304=CARTESIAN_POINT('Ctrl Pts',(-2.10986948229739,1.3759217039417,5.29546032110078));
#20305=CARTESIAN_POINT('Ctrl Pts',(-2.1529352089685,1.30486636709808,5.3006970241383));
#20306=CARTESIAN_POINT('Ctrl Pts',(-2.19599976255075,1.23381296576632,5.30593358453064));
#20307=CARTESIAN_POINT('Ctrl Pts',(-2.23554340725751,1.16062497728009,5.31117014492299));
#20308=CARTESIAN_POINT('Ctrl Pts',(-2.27136216292191,1.08568880202693,5.31640670531534));
#20309=CARTESIAN_POINT('Ctrl Pts',(-2.30776717506465,1.00952612358046,5.3217289740858));
#20310=CARTESIAN_POINT('Ctrl Pts',(-2.34032404138,0.931557953841109,5.32705124285626));
#20311=CARTESIAN_POINT('Ctrl Pts',(-2.36886910538294,0.852212069594317,
5.33237351162672));
#20312=CARTESIAN_POINT('Ctrl Pts',(-2.39699482152228,0.774031834408297,
5.33761759237707));
#20313=CARTESIAN_POINT('Ctrl Pts',(-2.42122574782482,0.694514560871142,
5.34286167312742));
#20314=CARTESIAN_POINT('Ctrl Pts',(-2.44145595367123,0.614083932604748,
5.34810575387777));
#20315=CARTESIAN_POINT('Ctrl Pts',(-2.46213860098934,0.531854501493749,
5.35346711665829));
#20316=CARTESIAN_POINT('Ctrl Pts',(-2.47863931941877,0.44867087120749,5.35882847943881));
#20317=CARTESIAN_POINT('Ctrl Pts',(-2.49090058276349,0.364993885960422,
5.36418984221933));
#20318=CARTESIAN_POINT('Ctrl Pts',(-2.50316184610821,0.28131690071336,5.36955120499985));
#20319=CARTESIAN_POINT('Ctrl Pts',(-2.51118367265795,0.197147072657779,
5.37491256778037));
#20320=CARTESIAN_POINT('Ctrl Pts',(-2.51496510902639,0.112945785135466,
5.38027393056089));
#20321=CARTESIAN_POINT('Ctrl Pts',(-2.51867170230267,0.0304110296152409,
5.38552917996819));
#20322=CARTESIAN_POINT('Ctrl Pts',(-2.51831796520711,-0.0524588008414003,
5.39078442937549));
#20323=CARTESIAN_POINT('Ctrl Pts',(-2.51386532026224,-0.135230919477881,
5.39603967878279));
#20324=CARTESIAN_POINT('Ctrl Pts',(-2.50941898815638,-0.217885686053684,
5.40128747744027));
#20325=CARTESIAN_POINT('Ctrl Pts',(-2.50088531575826,-0.300442559065994,
5.40653527609776));
#20326=CARTESIAN_POINT('Ctrl Pts',(-2.48827767589485,-0.38246628301505,
5.41178307475525));
#20327=CARTESIAN_POINT('Ctrl Pts',(-2.47557868281153,-0.46508433955709,
5.41706889823816));
#20328=CARTESIAN_POINT('Ctrl Pts',(-2.45874641307709,-0.547161014775412,
5.42235472172107));
#20329=CARTESIAN_POINT('Ctrl Pts',(-2.4378480052055,-0.628254210901584,
5.42764054520398));
#20330=CARTESIAN_POINT('Ctrl Pts',(-2.4171369919148,-0.708620249935456,
5.43287897107256));
#20331=CARTESIAN_POINT('Ctrl Pts',(-2.39243258725539,-0.788019921759011,
5.43811739694115));
#20332=CARTESIAN_POINT('Ctrl Pts',(-2.36385152754614,-0.866032450730203,
5.44335582280973));
#20333=CARTESIAN_POINT('Ctrl Pts',(-2.33527986767179,-0.944019322678919,
5.44859252584723));
#20334=CARTESIAN_POINT('Ctrl Pts',(-2.30283424350849,-1.02061952491235,
5.45382922888473));
#20335=CARTESIAN_POINT('Ctrl Pts',(-2.26668077725661,-1.09542891326429,
5.45906593192222));
#20336=CARTESIAN_POINT('Ctrl Pts',(-2.23052829580707,-1.17023626384591,
5.46430249231455));
#20337=CARTESIAN_POINT('Ctrl Pts',(-2.19066837478679,-1.24325248253438,
5.46953905270688));
#20338=CARTESIAN_POINT('Ctrl Pts',(-2.14731406653957,-1.31409609604523,
5.4747756130992));
#20339=CARTESIAN_POINT('Ctrl Pts',(-2.10325016513045,-1.38609922854609,
5.48009788186969));
#20340=CARTESIAN_POINT('Ctrl Pts',(-2.05557670255103,-1.45585756856753,
5.48542015064018));
#20341=CARTESIAN_POINT('Ctrl Pts',(-2.00456339163998,-1.52300093857385,
5.49074241941067));
#20342=CARTESIAN_POINT('Ctrl Pts',(-1.95429950356983,-1.58915792337601,
5.495986500161));
#20343=CARTESIAN_POINT('Ctrl Pts',(-1.90079359363922,-1.65277594112813,
5.50123058091132));
#20344=CARTESIAN_POINT('Ctrl Pts',(-1.84434337031048,-1.7135354628346,5.50647466166165));
#20345=CARTESIAN_POINT('Ctrl Pts',(-1.78663065749791,-1.77565384997461,
5.51183602444222));
#20346=CARTESIAN_POINT('Ctrl Pts',(-1.72584071206694,-1.83478398265607,
5.51719738722279));
#20347=CARTESIAN_POINT('Ctrl Pts',(-1.66232876636211,-1.89062670099759,
5.52255875000336));
#20348=CARTESIAN_POINT('Ctrl Pts',(-1.59881682065729,-1.9464694193391,5.52792011278393));
#20349=CARTESIAN_POINT('Ctrl Pts',(-1.53258331422587,-1.99902445983985,
5.5332814755645));
#20350=CARTESIAN_POINT('Ctrl Pts',(-1.46401473278279,-2.04803982192606,
5.53864283834507));
#20351=CARTESIAN_POINT('Ctrl Pts',(-1.39680327708826,-2.09608506025352,
5.54389808775238));
#20352=CARTESIAN_POINT('Ctrl Pts',(-1.32710010991282,-2.14090695686197,
5.54915333715968));
#20353=CARTESIAN_POINT('Ctrl Pts',(-1.25524724588119,-2.18223752183571,
5.55440858656699));
#20354=CARTESIAN_POINT('Ctrl Pts',(-1.18349625288774,-2.22350948945751,
5.55965638522449));
#20355=CARTESIAN_POINT('Ctrl Pts',(-1.10960201345748,-2.26129972927176,
5.56490418388198));
#20356=CARTESIAN_POINT('Ctrl Pts',(-1.03393689740224,-2.29538248276627,
5.57015198253948));
#20357=CARTESIAN_POINT('Ctrl Pts',(-0.957723522350152,-2.32971219519264,
5.57543780602239));
#20358=CARTESIAN_POINT('Ctrl Pts',(-0.879713884850836,-2.36028019114472,
5.58072362950529));
#20359=CARTESIAN_POINT('Ctrl Pts',(-0.800315366770485,-2.3869020850699,
5.5860094529882));
#20360=CARTESIAN_POINT('Ctrl Pts',(-0.721628809721245,-2.41328526230983,
5.59124787885679));
#20361=CARTESIAN_POINT('Ctrl Pts',(-0.641578625868135,-2.43579267354177,
5.59648630472538));
#20362=CARTESIAN_POINT('Ctrl Pts',(-0.560581315844548,-2.45429314433423,
5.60172473059397));
#20363=CARTESIAN_POINT('Ctrl Pts',(-0.479610644488222,-2.47278753062974,
5.60696143363148));
#20364=CARTESIAN_POINT('Ctrl Pts',(-0.397693915086651,-2.48727749107547,
5.61219813666898));
#20365=CARTESIAN_POINT('Ctrl Pts',(-0.315260566139868,-2.4976823307693,
5.61743483970649));
#20366=CARTESIAN_POINT('Ctrl Pts',(-0.232829462636283,-2.5080868870405,
5.62267140009882));
#20367=CARTESIAN_POINT('Ctrl Pts',(-0.149882225484674,-2.51440648704672,
5.62790796049115));
#20368=CARTESIAN_POINT('Ctrl Pts',(-0.0668548282142248,-2.51661214372506,
5.63314452088349));
#20369=CARTESIAN_POINT('Ctrl Pts',(0.0175315037440013,-2.51885390105774,
5.63846678965397));
#20370=CARTESIAN_POINT('Ctrl Pts',(0.102000152302478,-2.51684580555825,
5.64378905842444));
#20371=CARTESIAN_POINT('Ctrl Pts',(0.186093769824085,-2.51061254653773,
5.64911132719492));
#20372=CARTESIAN_POINT('Ctrl Pts',(0.268951990610853,-2.50447085865029,
5.65435540794526));
#20373=CARTESIAN_POINT('Ctrl Pts',(0.351445669286562,-2.49422744326407,
5.65959948869559));
#20374=CARTESIAN_POINT('Ctrl Pts',(0.433144699557753,-2.47995804788005,
5.66484356944592));
#20375=CARTESIAN_POINT('Ctrl Pts',(0.51667090004111,-2.46536952246346,5.67020493222648));
#20376=CARTESIAN_POINT('Ctrl Pts',(0.599365979841238,-2.44657287826214,
5.67556629500703));
#20377=CARTESIAN_POINT('Ctrl Pts',(0.680785599153083,-2.4237032033617,5.68092765778758));
#20378=CARTESIAN_POINT('Ctrl Pts',(0.762205218464927,-2.40083352846127,
5.68628902056813));
#20379=CARTESIAN_POINT('Ctrl Pts',(0.842348916953833,-2.37389104808713,
5.69165038334869));
#20380=CARTESIAN_POINT('Ctrl Pts',(0.920794895731843,-2.34306274136955,
5.69701174612924));
#20381=CARTESIAN_POINT('Ctrl Pts',(0.997688252953283,-2.31284459586492,
5.70226699553655));
#20382=CARTESIAN_POINT('Ctrl Pts',(1.07323451221374,-2.27878146856251,5.70752224494385));
#20383=CARTESIAN_POINT('Ctrl Pts',(1.14702267524311,-2.24101433116304,5.71277749435116));
#20384=CARTESIAN_POINT('Ctrl Pts',(1.22070622341987,-2.20330073898478,5.71802529300865));
#20385=CARTESIAN_POINT('Ctrl Pts',(1.29263621904077,-2.16189377609017,5.72327309166614));
#20386=CARTESIAN_POINT('Ctrl Pts',(1.36242056028213,-2.1169828688302,5.72852089032363));
#20387=CARTESIAN_POINT('Ctrl Pts',(1.43271054923708,-2.0717465433293,5.73380671380654));
#20388=CARTESIAN_POINT('Ctrl Pts',(1.50082321732777,-2.02295545433889,5.73909253728945));
#20389=CARTESIAN_POINT('Ctrl Pts',(1.56638210368218,-1.9708509216235,5.74437836077236));
#20390=CARTESIAN_POINT('Ctrl Pts',(1.63135312802791,-1.91921360665641,5.74961678664095));
#20391=CARTESIAN_POINT('Ctrl Pts',(1.69381561848899,-1.86432232519309,5.75485521250955));
#20392=CARTESIAN_POINT('Ctrl Pts',(1.75343278254427,-1.80645501662761,5.76009363837814));
#20393=CARTESIAN_POINT('Ctrl Pts',(1.81303033950647,-1.74860673965686,5.76533034141565));
#20394=CARTESIAN_POINT('Ctrl Pts',(1.86978409773885,-1.68778470059144,5.77056704445316));
#20395=CARTESIAN_POINT('Ctrl Pts',(1.92339256251835,-1.62430517466673,5.77580374749066));
#20396=CARTESIAN_POINT('Ctrl Pts',(1.97699956703006,-1.56082737789256,5.781040307883));
#20397=CARTESIAN_POINT('Ctrl Pts',(2.02746115151177,-1.49469259138107,5.78627686827533));
#20398=CARTESIAN_POINT('Ctrl Pts',(2.07451563537021,-1.42625072431342,5.79151342866767));
#20399=CARTESIAN_POINT('Ctrl Pts',(2.12234027429109,-1.35668864837122,5.79683569743815));
#20400=CARTESIAN_POINT('Ctrl Pts',(2.1666449868447,-1.28474368689114,5.80215796620862));
#20401=CARTESIAN_POINT('Ctrl Pts',(2.20720147859976,-1.21081290167681,5.8074802349791));
#20402=CARTESIAN_POINT('Ctrl Pts',(2.24716216583405,-1.1379682137591,5.81272431572944));
#20403=CARTESIAN_POINT('Ctrl Pts',(2.28348388016501,-1.0631961090121,5.81796839647978));
#20404=CARTESIAN_POINT('Ctrl Pts',(2.31599598596918,-0.986898598121723,
5.82321247723012));
#20405=CARTESIAN_POINT('Ctrl Pts',(2.34923521363833,-0.908894720109367,
5.82857384001067));
#20406=CARTESIAN_POINT('Ctrl Pts',(2.37849219878231,-0.829296862872776,
5.83393520279122));
#20407=CARTESIAN_POINT('Ctrl Pts',(2.40363833074468,-0.748551284131521,
5.83929656557177));
#20408=CARTESIAN_POINT('Ctrl Pts',(2.42878446270704,-0.667805705390267,
5.84465792835232));
#20409=CARTESIAN_POINT('Ctrl Pts',(2.44981967977522,-0.585912913893838,
5.85001929113287));
#20410=CARTESIAN_POINT('Ctrl Pts',(2.46667116953814,-0.503328512374697,
5.85538065391342));
#20411=CARTESIAN_POINT('Ctrl Pts',(2.49012320424341,-0.388396700541604,
5.8628420040828));
#20412=CARTESIAN_POINT('Ctrl Pts',(2.50554871649177,-0.271776010994806,
5.87030335425218));
#20413=CARTESIAN_POINT('Ctrl Pts',(2.51276111767348,-0.154394998326727,
5.87776470442156));
#20414=CARTESIAN_POINT('Ctrl Pts',(2.51587110200439,-0.103780355443389,
5.88098203545038));
#20415=CARTESIAN_POINT('Ctrl Pts',(2.51745454359309,-0.0530246346749052,
5.8841993664792));
#20416=CARTESIAN_POINT('Ctrl Pts',(2.51749903524768,-0.00220397981474928,
5.88741669750801));
#20417=CARTESIAN_POINT('Ctrl Pts',(2.51749903524847,-0.00220397890970059,
5.88741669756531));
#20418=CARTESIAN_POINT('Ctrl Pts',(2.51757053067679,0.0794618079230993,
5.89258675825598));
#20419=CARTESIAN_POINT('Ctrl Pts',(2.51366404213075,0.161254080397915,5.89775681894665));
#20420=CARTESIAN_POINT('Ctrl Pts',(2.5057692990165,0.242747749951151,5.90292687963733));
#20421=CARTESIAN_POINT('Ctrl Pts',(2.49788117536977,0.324173089896855,5.90809260541193));
#20422=CARTESIAN_POINT('Ctrl Pts',(2.48601147702744,0.405299852219512,5.91325833118653));
#20423=CARTESIAN_POINT('Ctrl Pts',(2.47020197026165,0.485704103457491,5.91842405696113));
#20424=CARTESIAN_POINT('Ctrl Pts',(2.45439918947274,0.566074147610928,5.92358758503579));
#20425=CARTESIAN_POINT('Ctrl Pts',(2.43466001342619,0.645721823650851,5.92875111311045));
#20426=CARTESIAN_POINT('Ctrl Pts',(2.41107772695427,0.724230933187066,5.93391464118511));
#20427=CARTESIAN_POINT('Ctrl Pts',(2.39606974731984,0.774194838020478,5.93720075698557));
#20428=CARTESIAN_POINT('Ctrl Pts',(2.37950628321881,0.823697772264239,5.94048687278603));
#20429=CARTESIAN_POINT('Ctrl Pts',(2.36142200728636,0.872635292378018,5.94377298858649));
#20430=CARTESIAN_POINT('Ctrl Pts',(2.36142200559759,0.872635296947961,5.66918223051795));
#20431=CARTESIAN_POINT('Ctrl Pts',(2.39783104698668,0.774109473113404,5.66192556901657));
#20432=CARTESIAN_POINT('Ctrl Pts',(2.42804248043668,0.673389919223703,5.65467850049511));
#20433=CARTESIAN_POINT('Ctrl Pts',(2.47501374093648,0.47171881947199,5.64067010978861));
#20434=CARTESIAN_POINT('Ctrl Pts',(2.49209560292995,0.371046896598681,5.63391380302999));
#20435=CARTESIAN_POINT('Ctrl Pts',(2.5054373914724,0.247180826666557,5.62589615657237));
#20436=CARTESIAN_POINT('Ctrl Pts',(2.50755126384116,0.224725603632017,5.62445411121646));
#20437=CARTESIAN_POINT('Ctrl Pts',(2.51042164432387,0.189111133098329,5.62218448477917));
#20438=CARTESIAN_POINT('Ctrl Pts',(2.51137702772495,0.175969566382344,5.62135076358077));
#20439=CARTESIAN_POINT('Ctrl Pts',(2.51298104593006,0.151220523591832,5.6197875217877));
#20440=CARTESIAN_POINT('Ctrl Pts',(2.51365253433375,0.139614927153138,5.61905731044915));
#20441=CARTESIAN_POINT('Ctrl Pts',(2.51498468159558,0.113449196171349,5.6174172010502));
#20442=CARTESIAN_POINT('Ctrl Pts',(2.51559933861532,0.0988870589969022,
5.61650875328282));
#20443=CARTESIAN_POINT('Ctrl Pts',(2.51703647558089,0.0560033358103809,
5.6138456553633));
#20444=CARTESIAN_POINT('Ctrl Pts',(2.51750737237581,0.0276716838714607,
5.61210188970108));
#20445=CARTESIAN_POINT('Ctrl Pts',(2.51747265449706,-0.104199967389831,
5.60405005134338));
#20446=CARTESIAN_POINT('Ctrl Pts',(2.51105833246633,-0.207643202004953,
5.59792487363476));
#20447=CARTESIAN_POINT('Ctrl Pts',(2.47687590215931,-0.482758338292225,
5.58179499959653));
#20448=CARTESIAN_POINT('Ctrl Pts',(2.43768600780875,-0.652418633881754,
5.5720364616246));
#20449=CARTESIAN_POINT('Ctrl Pts',(2.3599098385048,-0.879204334357425,5.55787415453548));
#20450=CARTESIAN_POINT('Ctrl Pts',(2.33601678259988,-0.940849987195239,
5.55389904250376));
#20451=CARTESIAN_POINT('Ctrl Pts',(2.30424270751658,-1.01413114795309,5.5489391888713));
#20452=CARTESIAN_POINT('Ctrl Pts',(2.29865284163117,-1.02673829875189,5.54807730597257));
#20453=CARTESIAN_POINT('Ctrl Pts',(2.28978699462535,-1.04629863674219,5.5467256699616));
#20454=CARTESIAN_POINT('Ctrl Pts',(2.2865821744531,-1.0532840422973,5.54624008944124));
#20455=CARTESIAN_POINT('Ctrl Pts',(2.28059952182967,-1.06616817726162,5.54533892952165));
#20456=CARTESIAN_POINT('Ctrl Pts',(2.27783071097401,-1.0720708978997,5.54492389581341));
#20457=CARTESIAN_POINT('Ctrl Pts',(2.27145410797361,-1.08552870991306,5.54397268782207));
#20458=CARTESIAN_POINT('Ctrl Pts',(2.26783155110192,-1.09307657358126,5.54343563055764));
#20459=CARTESIAN_POINT('Ctrl Pts',(2.25649076860869,-1.11640687884374,5.54176483477058));
#20460=CARTESIAN_POINT('Ctrl Pts',(2.24864512176733,-1.13212631077346,5.5406237595016));
#20461=CARTESIAN_POINT('Ctrl Pts',(2.22986181527336,-1.16879467666197,5.53792807393001));
#20462=CARTESIAN_POINT('Ctrl Pts',(2.21879255196787,-1.18967400472535,5.5363668114175));
#20463=CARTESIAN_POINT('Ctrl Pts',(2.17818180303355,-1.26373705706365,5.53074189303134));
#20464=CARTESIAN_POINT('Ctrl Pts',(2.14700993797586,-1.31599950790599,5.52661087654587));
#20465=CARTESIAN_POINT('Ctrl Pts',(2.01346722173593,-1.52250297695557,5.50975858512767));
#20466=CARTESIAN_POINT('Ctrl Pts',(1.89610733146566,-1.66639001829872,5.49682899394259));
#20467=CARTESIAN_POINT('Ctrl Pts',(1.70718628308946,-1.85193647878988,5.47908743713262));
#20468=CARTESIAN_POINT('Ctrl Pts',(1.64772250568898,-1.90503714795624,5.47384760369904));
#20469=CARTESIAN_POINT('Ctrl Pts',(1.56886942098742,-1.96899266999412,5.4673185314169));
#20470=CARTESIAN_POINT('Ctrl Pts',(1.55172562925484,-1.98253146639487,5.46592262179008));
#20471=CARTESIAN_POINT('Ctrl Pts',(1.52408399891509,-2.00378236723756,5.46370865119447));
#20472=CARTESIAN_POINT('Ctrl Pts',(1.51369907746407,-2.01163886526274,5.46288495309209));
#20473=CARTESIAN_POINT('Ctrl Pts',(1.49390886409483,-2.02637071292773,5.46133029742939));
#20474=CARTESIAN_POINT('Ctrl Pts',(1.48451592885888,-2.03326201575861,5.46059873439598));
#20475=CARTESIAN_POINT('Ctrl Pts',(1.46306251189895,-2.0487738012655,5.45894193223829));
#20476=CARTESIAN_POINT('Ctrl Pts',(1.45097297380197,-2.05735350550188,5.45801826834275));
#20477=CARTESIAN_POINT('Ctrl Pts',(1.41372720728206,-2.08329446596012,5.45520237251203));
#20478=CARTESIAN_POINT('Ctrl Pts',(1.38832944068451,-2.10030520075686,5.4533233096956));
#20479=CARTESIAN_POINT('Ctrl Pts',(1.26371508216894,-2.18052011764391,5.44428962807916));
#20480=CARTESIAN_POINT('Ctrl Pts',(1.16045619625476,-2.2371834521684,5.43737439906529));
#20481=CARTESIAN_POINT('Ctrl Pts',(0.887978982514378,-2.36274325372937,
5.42000525339764));
#20482=CARTESIAN_POINT('Ctrl Pts',(0.714570661034453,-2.42083425413133,
5.40976769672338));
#20483=CARTESIAN_POINT('Ctrl Pts',(0.493989579096829,-2.46894054252338,
5.39620999699039));
#20484=CARTESIAN_POINT('Ctrl Pts',(0.451319574014799,-2.4770957263316,5.39356156159059));
#20485=CARTESIAN_POINT('Ctrl Pts',(0.396365628675956,-2.48613170227601,
5.39009325859955));
#20486=CARTESIAN_POINT('Ctrl Pts',(0.384254192605346,-2.4880324061188,5.38932531531737));
#20487=CARTESIAN_POINT('Ctrl Pts',(0.36494204170022,-2.49091878066398,5.38809445220397));
#20488=CARTESIAN_POINT('Ctrl Pts',(0.357749927974798,-2.49196188805645,
5.38763466257352));
#20489=CARTESIAN_POINT('Ctrl Pts',(0.344008604780543,-2.49389414622446,
5.38675334150088));
#20490=CARTESIAN_POINT('Ctrl Pts',(0.337460301974299,-2.49478866304452,
5.38633210946532));
#20491=CARTESIAN_POINT('Ctrl Pts',(0.321886276455238,-2.49685368205619,
5.38532740676311));
#20492=CARTESIAN_POINT('Ctrl Pts',(0.312857636908472,-2.49800103632878,
5.38474267322363));
#20493=CARTESIAN_POINT('Ctrl Pts',(0.282358510436422,-2.50170890824558,
5.38276016628613));
#20494=CARTESIAN_POINT('Ctrl Pts',(0.260861986125186,-2.50404168101888,
5.38135073287078));
#20495=CARTESIAN_POINT('Ctrl Pts',(0.133269989665312,-2.51622705632052,
5.37292373061923));
#20496=CARTESIAN_POINT('Ctrl Pts',(0.0266748502186243,-2.51961177295505,
5.36563681993708));
#20497=CARTESIAN_POINT('Ctrl Pts',(-0.270519628149642,-2.51018626220693,
5.34513737730983));
#20498=CARTESIAN_POINT('Ctrl Pts',(-0.459963597470203,-2.48247262574406,
5.3319125261101));
#20499=CARTESIAN_POINT('Ctrl Pts',(-0.694773483722971,-2.42029002422557,
5.31589706063384));
#20500=CARTESIAN_POINT('Ctrl Pts',(-0.744653177009354,-2.40541187577891,
5.31251266403639));
#20501=CARTESIAN_POINT('Ctrl Pts',(-0.811868078652032,-2.38307143522336,
5.30797368071818));
#20502=CARTESIAN_POINT('Ctrl Pts',(-0.829630643553055,-2.37694599623925,
5.30677623025569));
#20503=CARTESIAN_POINT('Ctrl Pts',(-0.857798471472089,-2.36687806575736,
5.30488018697502));
#20504=CARTESIAN_POINT('Ctrl Pts',(-0.868248772877727,-2.36306455067636,
5.30417738532549));
#20505=CARTESIAN_POINT('Ctrl Pts',(-0.889675628291844,-2.35508415185207,
5.30273755970141));
#20506=CARTESIAN_POINT('Ctrl Pts',(-0.900649012105707,-2.35090949429513,
5.30200081375032));
#20507=CARTESIAN_POINT('Ctrl Pts',(-0.926063452541657,-2.34103689127228,
5.30029577581887));
#20508=CARTESIAN_POINT('Ctrl Pts',(-0.940481906354718,-2.33528179139785,
5.29932941236738));
#20509=CARTESIAN_POINT('Ctrl Pts',(-0.986621950089961,-2.3163684322425,
5.29623930884737));
#20510=CARTESIAN_POINT('Ctrl Pts',(-1.01812868814839,-2.30269401661894,
5.29413284744242));
#20511=CARTESIAN_POINT('Ctrl Pts',(-1.09177945566315,-2.26892110560911,
5.28920965306988));
#20512=CARTESIAN_POINT('Ctrl Pts',(-1.13366417879987,-2.24828629554803,
5.28641069389122));
#20513=CARTESIAN_POINT('Ctrl Pts',(-1.37379983546856,-2.12156348579047,
5.27030554327346));
#20514=CARTESIAN_POINT('Ctrl Pts',(-1.55767334296076,-1.99047711769316,
5.25783974244052));
#20515=CARTESIAN_POINT('Ctrl Pts',(-1.76803016161815,-1.79329575922209,
5.24078055354328));
#20516=CARTESIAN_POINT('Ctrl Pts',(-1.81270494747751,-1.74812461430787,
5.23695498945698));
#20517=CARTESIAN_POINT('Ctrl Pts',(-1.86484320538594,-1.69125761796496,
5.23216304485169));
#20518=CARTESIAN_POINT('Ctrl Pts',(-1.87398410878147,-1.68112344927229,
5.23130995820897));
#20519=CARTESIAN_POINT('Ctrl Pts',(-1.88812155839485,-1.66519122125636,
5.22996921899234));
#20520=CARTESIAN_POINT('Ctrl Pts',(-1.89317498215566,-1.65944367361167,
5.22948563235671));
#20521=CARTESIAN_POINT('Ctrl Pts',(-1.90248721580531,-1.64875443934342,
5.22858622295046));
#20522=CARTESIAN_POINT('Ctrl Pts',(-1.90675310206618,-1.64381915429765,
5.2281709278583));
#20523=CARTESIAN_POINT('Ctrl Pts',(-1.91647903501075,-1.63247823930534,
5.22721656550286));
#20524=CARTESIAN_POINT('Ctrl Pts',(-1.92192615375607,-1.62606179098011,
5.22667659187876));
#20525=CARTESIAN_POINT('Ctrl Pts',(-1.93879348003045,-1.60598972300047,
5.22498771447247));
#20526=CARTESIAN_POINT('Ctrl Pts',(-1.95010080566896,-1.59224054526798,
5.22383125059638));
#20527=CARTESIAN_POINT('Ctrl Pts',(-1.97633192303534,-1.55964618097085,
5.22109292579974));
#20528=CARTESIAN_POINT('Ctrl Pts',(-1.99113329443608,-1.54070509648409,
5.21950413730703));
#20529=CARTESIAN_POINT('Ctrl Pts',(-2.04339858759305,-1.47181084790265,
5.213742489502));
#20530=CARTESIAN_POINT('Ctrl Pts',(-2.07927053936707,-1.4206822273389,5.20949904134749));
#20531=CARTESIAN_POINT('Ctrl Pts',(-2.22238787113198,-1.19964805883782,
5.19144218569171));
#20532=CARTESIAN_POINT('Ctrl Pts',(-2.31101455648827,-1.01852606918758,
5.1774116300116));
#20533=CARTESIAN_POINT('Ctrl Pts',(-2.39839943693262,-0.767884266252309,
5.15977470738541));
#20534=CARTESIAN_POINT('Ctrl Pts',(-2.41728564940047,-0.706185116115677,
5.15555772546259));
#20535=CARTESIAN_POINT('Ctrl Pts',(-2.43897931291082,-0.624178737845461,
5.15011190534594));
#20536=CARTESIAN_POINT('Ctrl Pts',(-2.4439382176043,-0.604471019706533,
5.14881496257076));
#20537=CARTESIAN_POINT('Ctrl Pts',(-2.45160529217868,-0.572362441648023,
5.1467205395948));
#20538=CARTESIAN_POINT('Ctrl Pts',(-2.45445918741456,-0.559997660829141,
5.14591844311952));
#20539=CARTESIAN_POINT('Ctrl Pts',(-2.45977204724335,-0.536158023758772,
5.14438034527616));
#20540=CARTESIAN_POINT('Ctrl Pts',(-2.46224450211045,-0.524686544662356,
5.14364393290269));
#20541=CARTESIAN_POINT('Ctrl Pts',(-2.46779332284992,-0.498038299465238,
5.14194163364446));
#20542=CARTESIAN_POINT('Ctrl Pts',(-2.47081007162127,-0.482849499192106,
5.14097765538341));
#20543=CARTESIAN_POINT('Ctrl Pts',(-2.48002501804241,-0.43410430442964,
5.13790331653093));
#20544=CARTESIAN_POINT('Ctrl Pts',(-2.4856813568868,-0.400448498062643,
5.13580998245519));
#20545=CARTESIAN_POINT('Ctrl Pts',(-2.49739482298834,-0.320886960949656,
5.13092271934361));
#20546=CARTESIAN_POINT('Ctrl Pts',(-2.50287340265627,-0.274908056206649,
5.12814620071889));
#20547=CARTESIAN_POINT('Ctrl Pts',(-2.52708725807323,-0.00958669160281925,
5.11233812185545));
#20548=CARTESIAN_POINT('Ctrl Pts',(-2.51825552154817,0.211284599114498,
5.10010925068193));
#20549=CARTESIAN_POINT('Ctrl Pts',(-2.46917851291256,0.495629312918067,
5.08308886645551));
#20550=CARTESIAN_POINT('Ctrl Pts',(-2.4547925588343,0.562567934436855,5.07897784435588));
#20551=CARTESIAN_POINT('Ctrl Pts',(-2.43422362353306,0.642304621406732,
5.07386541939244));
#20552=CARTESIAN_POINT('Ctrl Pts',(-2.43063633277828,0.655749093308375,
5.07299592113837));
#20553=CARTESIAN_POINT('Ctrl Pts',(-2.42488760042545,0.676598753039767,
5.07163485508647));
#20554=CARTESIAN_POINT('Ctrl Pts',(-2.42280319906389,0.6840251473156,5.07114755319548));
#20555=CARTESIAN_POINT('Ctrl Pts',(-2.41889472268292,0.697708424927733,
5.07024485968005));
#20556=CARTESIAN_POINT('Ctrl Pts',(-2.41708044755187,0.703967920136713,
5.06983002920037));
#20557=CARTESIAN_POINT('Ctrl Pts',(-2.41289048720496,0.718216693059688,
5.06888144425261));
#20558=CARTESIAN_POINT('Ctrl Pts',(-2.41049942857921,0.726201226606091,
5.06834682639191));
#20559=CARTESIAN_POINT('Ctrl Pts',(-2.4030017259259,0.750793480825635,5.06669106566961));
#20560=CARTESIAN_POINT('Ctrl Pts',(-2.39776288664475,0.76735991920852,5.0655627692444));
#20561=CARTESIAN_POINT('Ctrl Pts',(-2.38509955493481,0.806008103160726,
5.0629023821986));
#20562=CARTESIAN_POINT('Ctrl Pts',(-2.37753927888408,0.828043383359886,
5.06136386287958));
#20563=CARTESIAN_POINT('Ctrl Pts',(-2.34957682770992,0.906001349191321,
5.05585083568419));
#20564=CARTESIAN_POINT('Ctrl Pts',(-2.32749925548017,0.96129913973336,5.05181156332078));
#20565=CARTESIAN_POINT('Ctrl Pts',(-2.23184105489407,1.17822777274019,5.03557425351062));
#20566=CARTESIAN_POINT('Ctrl Pts',(-2.14320051976757,1.33268035914081,5.02316971068235));
#20567=CARTESIAN_POINT('Ctrl Pts',(-1.98745293853806,1.54776421966146,5.00530566140899));
#20568=CARTESIAN_POINT('Ctrl Pts',(-1.9321612889552,1.61626081773016,4.99950345885724));
#20569=CARTESIAN_POINT('Ctrl Pts',(-1.85838124510524,1.69844936984479,4.99239617219218));
#20570=CARTESIAN_POINT('Ctrl Pts',(-1.84314792697643,1.71496847983924,4.9909595743883));
#20571=CARTESIAN_POINT('Ctrl Pts',(-1.81864656474489,1.74083429619041,4.98869651578299));
#20572=CARTESIAN_POINT('Ctrl Pts',(-1.80952316544436,1.75031577112604,4.98786397516013));
#20573=CARTESIAN_POINT('Ctrl Pts',(-1.79301112695942,1.7672087743431,4.98637506234196));
#20574=CARTESIAN_POINT('Ctrl Pts',(-1.78564987124667,1.77464652710094,4.98571753098342));
#20575=CARTESIAN_POINT('Ctrl Pts',(-1.76829735120659,1.79196208479789,4.98418193579814));
#20576=CARTESIAN_POINT('Ctrl Pts',(-1.75826928521604,1.8018026442891,4.98330551430559));
#20577=CARTESIAN_POINT('Ctrl Pts',(-1.72896599214416,1.83008040077963,4.98077563076421));
#20578=CARTESIAN_POINT('Ctrl Pts',(-1.70947911242897,1.84829622155621,4.97913165863776));
#20579=CARTESIAN_POINT('Ctrl Pts',(-1.66470943289628,1.88883186115741,4.97543720539586));
#20580=CARTESIAN_POINT('Ctrl Pts',(-1.63926004935121,1.91096047562378,4.97339446686066));
#20581=CARTESIAN_POINT('Ctrl Pts',(-1.5534247573338,1.98261852516899,4.96667961332971));
#20582=CARTESIAN_POINT('Ctrl Pts',(-1.49117773052985,2.02985098470629,4.96208958936225));
#20583=CARTESIAN_POINT('Ctrl Pts',(-1.29699391176685,2.16343446891779,4.94839785901126));
#20584=CARTESIAN_POINT('Ctrl Pts',(-1.1590633456091,2.24035934814638,4.93950759087748));
#20585=CARTESIAN_POINT('Ctrl Pts',(-0.980537396851379,2.31899952566037,
4.9280518150789));
#20586=CARTESIAN_POINT('Ctrl Pts',(-0.94588865729387,2.33334669678435,4.92582948336285));
#20587=CARTESIAN_POINT('Ctrl Pts',(-0.87103399495885,2.36240087034972,4.9210049780843));
#20588=CARTESIAN_POINT('Ctrl Pts',(-0.830748287170026,2.37686661068305,
4.91839436507727));
#20589=CARTESIAN_POINT('Ctrl Pts',(-0.778532670600854,2.3941265571579,4.91496913413278));
#20590=CARTESIAN_POINT('Ctrl Pts',(-0.766921661508516,2.39787118961044,
4.91420487082656));
#20591=CARTESIAN_POINT('Ctrl Pts',(-0.748364102276225,2.40370756214885,
4.91297854083794));
#20592=CARTESIAN_POINT('Ctrl Pts',(-0.741434764551357,2.40585397741949,
4.91251956454737));
#20593=CARTESIAN_POINT('Ctrl Pts',(-0.728170045990337,2.40990007676248,
4.91163874208495));
#20594=CARTESIAN_POINT('Ctrl Pts',(-0.721836350474372,2.41180477545543,
4.91121718691396));
#20595=CARTESIAN_POINT('Ctrl Pts',(-0.706740563891648,2.41627966227534,
4.91021021680694));
#20596=CARTESIAN_POINT('Ctrl Pts',(-0.697971904485111,2.41882716318682,
4.90962352338039));
#20597=CARTESIAN_POINT('Ctrl Pts',(-0.668221110241237,2.42729522366124,
4.90762740351304));
#20598=CARTESIAN_POINT('Ctrl Pts',(-0.647176655283755,2.43299072257802,
4.90620610507695));
#20599=CARTESIAN_POINT('Ctrl Pts',(-0.595697615316425,2.44620795496882,
4.9027110232013));
#20600=CARTESIAN_POINT('Ctrl Pts',(-0.565191888532306,2.45343574493739,
4.9006244390631));
#20601=CARTESIAN_POINT('Ctrl Pts',(-0.441218789015813,2.48037422811033,
4.89210297107627));
#20602=CARTESIAN_POINT('Ctrl Pts',(-0.346803498109627,2.4953267446186,4.88552086845927));
#20603=CARTESIAN_POINT('Ctrl Pts',(-0.0527297734357414,2.52488502687459,
4.86510603044115));
#20604=CARTESIAN_POINT('Ctrl Pts',(0.148028322265435,2.52109926485449,4.85136063564229));
#20605=CARTESIAN_POINT('Ctrl Pts',(0.377381707151431,2.4892523867735,4.83633409965327));
#20606=CARTESIAN_POINT('Ctrl Pts',(0.408435175550585,2.48434604097104,4.83431208699742));
#20607=CARTESIAN_POINT('Ctrl Pts',(0.454149540200648,2.47624294849541,4.83135274200616));
#20608=CARTESIAN_POINT('Ctrl Pts',(0.468885879539872,2.47349489440385,4.83040143843833));
#20609=CARTESIAN_POINT('Ctrl Pts',(0.495048174979353,2.46837389925695,4.82871701919486));
#20610=CARTESIAN_POINT('Ctrl Pts',(0.506483721125436,2.46605284811969,4.82798228952315));
#20611=CARTESIAN_POINT('Ctrl Pts',(0.530555048926457,2.46099263339741,4.82643877389073));
#20612=CARTESIAN_POINT('Ctrl Pts',(0.54318673069177,2.45823546209455,4.82563058182078));
#20613=CARTESIAN_POINT('Ctrl Pts',(0.576686211217743,2.45065256409399,4.82349164490495));
#20614=CARTESIAN_POINT('Ctrl Pts',(0.597514905203522,2.44565757167712,4.82216630136789));
#20615=CARTESIAN_POINT('Ctrl Pts',(0.700286369158245,2.41962028727449,4.8156461055526));
#20616=CARTESIAN_POINT('Ctrl Pts',(0.781200640062332,2.39472150350713,4.81057589382786));
#20617=CARTESIAN_POINT('Ctrl Pts',(1.04208450983859,2.29980768000398,4.79423109796298));
#20618=CARTESIAN_POINT('Ctrl Pts',(1.21525311579265,2.21318999624887,4.78342971419582));
#20619=CARTESIAN_POINT('Ctrl Pts',(1.44160217561186,2.06532729588902,4.76756265704338));
#20620=CARTESIAN_POINT('Ctrl Pts',(1.504391363471,2.02004897692823,4.7629382400568));
#20621=CARTESIAN_POINT('Ctrl Pts',(1.57525990343738,1.96380610075467,4.75732539260183));
#20622=CARTESIAN_POINT('Ctrl Pts',(1.58546614983903,1.95557542311832,4.75650702445257));
#20623=CARTESIAN_POINT('Ctrl Pts',(1.60197152502219,1.94205076653459,4.75516629177455));
#20624=CARTESIAN_POINT('Ctrl Pts',(1.60830995542125,1.93680485066354,4.75464721232406));
#20625=CARTESIAN_POINT('Ctrl Pts',(1.61961782581343,1.92735226133159,4.75371336168882));
#20626=CARTESIAN_POINT('Ctrl Pts',(1.62459680010945,1.92315726767796,4.75329942609349));
#20627=CARTESIAN_POINT('Ctrl Pts',(1.62960637340882,1.91890315584798,4.75288014057315));
#20628=CARTESIAN_POINT('Ctrl Pts',(1.62965322346661,1.91886336799233,4.75287621912359));
#20629=CARTESIAN_POINT('Ctrl Pts',(1.62974579673245,1.91878474343315,4.75286847005589));
#20630=CARTESIAN_POINT('Ctrl Pts',(1.62979152002562,1.91874590679733,4.75286464244233));
#20631=CARTESIAN_POINT('Ctrl Pts',(1.62988188058262,1.91866915042142,4.75285707766432));
#20632=CARTESIAN_POINT('Ctrl Pts',(1.62992651790169,1.91863123076616,4.75285334050626));
#20633=CARTESIAN_POINT('Ctrl Pts',(1.63001474534562,1.91855627575205,4.75284595342067));
#20634=CARTESIAN_POINT('Ctrl Pts',(1.63005833553188,1.9185192404651,4.75284230349837));
#20635=CARTESIAN_POINT('Ctrl Pts',(1.6301445057419,1.91844602309309,4.75283508781444));
#20636=CARTESIAN_POINT('Ctrl Pts',(1.6301870858217,1.91840984107733,4.75283152205789));
#20637=CARTESIAN_POINT('Ctrl Pts',(1.6302712711175,1.91833830060032,4.75282447177856));
#20638=CARTESIAN_POINT('Ctrl Pts',(1.63031287639333,1.91830294219848,4.75282098726));
#20639=CARTESIAN_POINT('Ctrl Pts',(1.6303951457655,1.91823302065012,4.75281409666296));
#20640=CARTESIAN_POINT('Ctrl Pts',(1.6304358099162,1.91819845756144,4.75281069058863));
#20641=CARTESIAN_POINT('Ctrl Pts',(1.6305162292395,1.91813009957854,4.75280395420877));
#20642=CARTESIAN_POINT('Ctrl Pts',(1.63055598444249,1.91809630475671,4.75280062390889));
#20643=CARTESIAN_POINT('Ctrl Pts',(1.6306346165123,1.91802945755159,4.75279403653548));
#20644=CARTESIAN_POINT('Ctrl Pts',(1.63067349345178,1.91799640519935,4.75279077946363));
#20645=CARTESIAN_POINT('Ctrl Pts',(1.63075039838825,1.91793101821943,4.75278433610682));
#20646=CARTESIAN_POINT('Ctrl Pts',(1.63078842642159,1.91789868364861,4.75278114982615));
#20647=CARTESIAN_POINT('Ctrl Pts',(1.63086366159562,1.91783470864212,4.75277484572332));
#20648=CARTESIAN_POINT('Ctrl Pts',(1.63090086877354,1.91780306825785,4.75277172790498));
#20649=CARTESIAN_POINT('Ctrl Pts',(1.63097448908139,1.91774045904306,4.75276555849799));
#20650=CARTESIAN_POINT('Ctrl Pts',(1.63101090224037,1.91770949026646,4.75276250691349));
#20651=CARTESIAN_POINT('Ctrl Pts',(1.63108296018502,1.91764820266488,4.75275646784209));
#20652=CARTESIAN_POINT('Ctrl Pts',(1.63111860500452,1.9176178838856,4.75275348035858));
#20653=CARTESIAN_POINT('Ctrl Pts',(1.63118915082847,1.91755787561133,4.75274756744943));
#20654=CARTESIAN_POINT('Ctrl Pts',(1.63122405188274,1.91752818614455,4.7527446420255));
#20655=CARTESIAN_POINT('Ctrl Pts',(1.63129313370655,1.91746941668853,4.75273885128076));
#20656=CARTESIAN_POINT('Ctrl Pts',(1.63132731452337,1.91744033672601,4.75273598596157));
#20657=CARTESIAN_POINT('Ctrl Pts',(1.6313949785099,1.91738276721824,4.75273031354528));
#20658=CARTESIAN_POINT('Ctrl Pts',(1.63142846168033,1.91735427773589,4.75272750645343));
#20659=CARTESIAN_POINT('Ctrl Pts',(1.63149475192016,1.91729787104473,4.75272194870129));
#20660=CARTESIAN_POINT('Ctrl Pts',(1.6315275590418,1.91726995385177,4.75271919804166));
#20661=CARTESIAN_POINT('Ctrl Pts',(1.63159251796458,1.91721467423563,4.75271375142668));
#20662=CARTESIAN_POINT('Ctrl Pts',(1.63162466978812,1.91718731185069,4.75271105547422));
#20663=CARTESIAN_POINT('Ctrl Pts',(1.63168833800625,1.91713312509258,4.75270571661992));
#20664=CARTESIAN_POINT('Ctrl Pts',(1.6317198544294,1.91710630074957,4.75270307372023));
#20665=CARTESIAN_POINT('Ctrl Pts',(1.63178227092494,1.91705317399953,4.75269783938514));
#20666=CARTESIAN_POINT('Ctrl Pts',(1.63181317103331,1.91702687161366,4.75269524795106));
#20667=CARTESIAN_POINT('Ctrl Pts',(1.63187437328153,1.9169747732849,4.75269011501845));
#20668=CARTESIAN_POINT('Ctrl Pts',(1.63190467542814,1.91694897738553,4.75268757352348));
#20669=CARTESIAN_POINT('Ctrl Pts',(1.63196469934903,1.91689787719699,4.75268253900554));
#20670=CARTESIAN_POINT('Ctrl Pts',(1.63199442114572,1.91687257293565,4.75268004598462));
#20671=CARTESIAN_POINT('Ctrl Pts',(1.63205330128584,1.91682244175839,4.75267510700729));
#20672=CARTESIAN_POINT('Ctrl Pts',(1.63208245965654,1.91679761486393,4.75267266105233));
#20673=CARTESIAN_POINT('Ctrl Pts',(1.63214022922484,1.91674842469169,4.75266781485241));
#20674=CARTESIAN_POINT('Ctrl Pts',(1.63216884044255,1.91672406143936,4.7526654146093));
#20675=CARTESIAN_POINT('Ctrl Pts',(1.63222553137195,1.91667578533717,4.75266065852934));
#20676=CARTESIAN_POINT('Ctrl Pts',(1.63225361109485,1.91665187251835,4.75265830269492));
#20677=CARTESIAN_POINT('Ctrl Pts',(1.63230925407908,1.91660448459212,4.75265363418023));
#20678=CARTESIAN_POINT('Ctrl Pts',(1.63233681736609,1.91658100950154,4.75265132150104));
#20679=CARTESIAN_POINT('Ctrl Pts',(1.63239144192669,1.91653448484187,4.75264673809416));
#20680=CARTESIAN_POINT('Ctrl Pts',(1.63241850324724,1.91651143526973,4.75264446736561));
#20681=CARTESIAN_POINT('Ctrl Pts',(1.63247213787864,1.91646574982922,4.75263996669418));
#20682=CARTESIAN_POINT('Ctrl Pts',(1.63249871119377,1.91644311399248,4.75263773675387));
#20683=CARTESIAN_POINT('Ctrl Pts',(1.63255138328412,1.91639824465391,4.75263331653733));
#20684=CARTESIAN_POINT('Ctrl Pts',(1.63257748205064,1.91637601119318,4.75263112626464));
#20685=CARTESIAN_POINT('Ctrl Pts',(1.63262921791013,1.91633193574613,4.75262678431195));
#20686=CARTESIAN_POINT('Ctrl Pts',(1.63265485504277,1.91631009375821,4.75262463263131));
#20687=CARTESIAN_POINT('Ctrl Pts',(1.63270568017682,1.91626679066704,4.75262036681807));
#20688=CARTESIAN_POINT('Ctrl Pts',(1.63273086817529,1.91624532959707,4.75261825268828));
#20689=CARTESIAN_POINT('Ctrl Pts',(1.63278080701975,1.91620277822712,4.75261406097898));
#20690=CARTESIAN_POINT('Ctrl Pts',(1.63280555789136,1.91618168793476,4.75261198339977));
#20691=CARTESIAN_POINT('Ctrl Pts',(1.6391588304552,1.9107678327417,4.75207867428604));
#20692=CARTESIAN_POINT('Ctrl Pts',(1.64546049089582,1.9053438404436,4.75154518615882));
#20693=CARTESIAN_POINT('Ctrl Pts',(1.66463752982013,1.88867160829619,4.74990815432789));
#20694=CARTESIAN_POINT('Ctrl Pts',(1.67742498848545,1.87732360559165,4.74879775780544));
#20695=CARTESIAN_POINT('Ctrl Pts',(1.70739940553356,1.85017259237463,4.7461521073417));
#20696=CARTESIAN_POINT('Ctrl Pts',(1.72448383043867,1.83425919316251,4.74461010133018));
#20697=CARTESIAN_POINT('Ctrl Pts',(1.78447788478779,1.7767983075371,4.73907998321365));
#20698=CARTESIAN_POINT('Ctrl Pts',(1.82612549743954,1.73396606487033,4.73502671276063));
#20699=CARTESIAN_POINT('Ctrl Pts',(1.98608829622687,1.55729300844135,4.71870252679664));
#20700=CARTESIAN_POINT('Ctrl Pts',(2.09155176009271,1.41249073707705,4.70622488586076));
#20701=CARTESIAN_POINT('Ctrl Pts',(2.22414725145006,1.18258318892851,4.68838087862704));
#20702=CARTESIAN_POINT('Ctrl Pts',(2.263583151661,1.10522767257613,4.6826600644618));
#20703=CARTESIAN_POINT('Ctrl Pts',(2.30807433911545,1.00553490477725,4.67563550199438));
#20704=CARTESIAN_POINT('Ctrl Pts',(2.31692654013989,0.98496652741267,4.67420400112456));
#20705=CARTESIAN_POINT('Ctrl Pts',(2.33053667777167,0.952143749777371,4.67194708862268));
#20706=CARTESIAN_POINT('Ctrl Pts',(2.33547492215656,0.939965863899505,4.67111565336464));
#20707=CARTESIAN_POINT('Ctrl Pts',(2.34417481929611,0.918019725400779,4.66962771806396));
#20708=CARTESIAN_POINT('Ctrl Pts',(2.34797130142708,0.90826569496149,4.66897006797735));
#20709=CARTESIAN_POINT('Ctrl Pts',(2.35499248616887,0.889888414752341,4.6677377694359));
#20710=CARTESIAN_POINT('Ctrl Pts',(2.35823090787457,0.881270666679349,4.66716267736481));
#20711=CARTESIAN_POINT('Ctrl Pts',(2.36142200727925,0.872635292397265,4.66658913197125));
#20712=CARTESIAN_POINT('Origin',(0.,0.,10.));
#20713=CARTESIAN_POINT('',(2.36142196837105,0.872635397685999,3.66998323165053));
#20714=CARTESIAN_POINT('',(2.36142200728636,0.872635292378021,3.9436931725108));
#20715=CARTESIAN_POINT('',(2.36142200728636,0.87263529237802,10.));
#20716=CARTESIAN_POINT('',(2.51749952702257,0.00154319187075679,4.88741669746642));
#20717=CARTESIAN_POINT('Ctrl Pts',(2.36142200728636,0.872635292378021,3.9436931725108));
#20718=CARTESIAN_POINT('Ctrl Pts',(2.34093516802426,0.928074344082446,3.94744670184164));
#20719=CARTESIAN_POINT('Ctrl Pts',(2.31851215292549,0.982746025527077,3.95120023117247));
#20720=CARTESIAN_POINT('Ctrl Pts',(2.29421643254441,1.03652168845771,3.95495376050331));
#20721=CARTESIAN_POINT('Ctrl Pts',(2.26020042817918,1.11181203409469,3.96020900990937));
#20722=CARTESIAN_POINT('Ctrl Pts',(2.22241142210613,1.18556516925875,3.96546425931544));
#20723=CARTESIAN_POINT('Ctrl Pts',(2.18101071131842,1.25737763902272,3.97071950872151));
#20724=CARTESIAN_POINT('Ctrl Pts',(2.13966869733361,1.32908829501817,3.97596730737775));
#20725=CARTESIAN_POINT('Ctrl Pts',(2.09472537813039,1.39886335432976,3.98121510603399));
#20726=CARTESIAN_POINT('Ctrl Pts',(2.04638950247262,1.46632065189366,3.98646290469024));
#20727=CARTESIAN_POINT('Ctrl Pts',(1.99770339171077,1.5342667357537,3.99174872817346));
#20728=CARTESIAN_POINT('Ctrl Pts',(1.94557554816624,1.5998608959182,3.99703455165667));
#20729=CARTESIAN_POINT('Ctrl Pts',(1.89026576924196,1.66273917727108,4.00232037513989));
#20730=CARTESIAN_POINT('Ctrl Pts',(1.83545194930389,1.72505363339665,4.00755880100723));
#20731=CARTESIAN_POINT('Ctrl Pts',(1.77751334019645,1.78470036898949,4.01279722687456));
#20732=CARTESIAN_POINT('Ctrl Pts',(1.71674433469282,1.84135687450861,4.0180356527419));
#20733=CARTESIAN_POINT('Ctrl Pts',(1.65599531510379,1.89799474664594,4.02327235577815));
#20734=CARTESIAN_POINT('Ctrl Pts',(1.59241808510542,1.95164402746345,4.02850905881439));
#20735=CARTESIAN_POINT('Ctrl Pts',(1.52634356492189,2.00201937348806,4.03374576185064));
#20736=CARTESIAN_POINT('Ctrl Pts',(1.46027084457531,2.05239334731339,4.03898232224171));
#20737=CARTESIAN_POINT('Ctrl Pts',(1.39170133686044,2.09949328472293,4.04421888263278));
#20738=CARTESIAN_POINT('Ctrl Pts',(1.32099756813324,2.14307528448864,4.04945544302385));
#20739=CARTESIAN_POINT('Ctrl Pts',(1.24913656926093,2.18737060413561,4.05477771179582));
#20740=CARTESIAN_POINT('Ctrl Pts',(1.17507122655244,2.22803151965106,4.06009998056779));
#20741=CARTESIAN_POINT('Ctrl Pts',(1.09920949497462,2.26484982640299,4.06542224933976));
#20742=CARTESIAN_POINT('Ctrl Pts',(1.02446222774625,2.30112724528657,4.07066633008885));
#20743=CARTESIAN_POINT('Ctrl Pts',(0.947971456517051,2.33367408067572,4.07591041083793));
#20744=CARTESIAN_POINT('Ctrl Pts',(0.870147202928374,2.36233996182512,4.08115449158702));
#20745=CARTESIAN_POINT('Ctrl Pts',(0.790582437090273,2.39164694539416,4.08651585437043));
#20746=CARTESIAN_POINT('Ctrl Pts',(0.70962431222964,2.41689713515886,4.09187721715384));
#20747=CARTESIAN_POINT('Ctrl Pts',(0.627724945719765,2.43798434008939,4.09723857993726));
#20748=CARTESIAN_POINT('Ctrl Pts',(0.545825579209892,2.45907154501993,4.10259994272067));
#20749=CARTESIAN_POINT('Ctrl Pts',(0.462985482245224,2.47599572885717,4.10796130550408));
#20750=CARTESIAN_POINT('Ctrl Pts',(0.379663322338168,2.48870689549234,4.11332266828749));
#20751=CARTESIAN_POINT('Ctrl Pts',(0.297990294582247,2.50116647967214,4.11857791769423));
#20752=CARTESIAN_POINT('Ctrl Pts',(0.21555245044207,2.50962436248483,4.12383316710096));
#20753=CARTESIAN_POINT('Ctrl Pts',(0.132776023197794,2.51399617693897,4.12908841650769));
#20754=CARTESIAN_POINT('Ctrl Pts',(0.0501169541230106,2.51836179315337,
4.1343362151646));
#20755=CARTESIAN_POINT('Ctrl Pts',(-0.0328792876339783,2.51865282369693,
4.13958401382151));
#20756=CARTESIAN_POINT('Ctrl Pts',(-0.115778491375535,2.51483629505676,
4.14483181247842));
#20757=CARTESIAN_POINT('Ctrl Pts',(-0.199278371327402,2.51099211237582,
4.15011763596147));
#20758=CARTESIAN_POINT('Ctrl Pts',(-0.282679332614184,2.50298052226196,
4.15540345944452));
#20759=CARTESIAN_POINT('Ctrl Pts',(-0.36553464539088,2.4908212848414,4.16068928292757));
#20760=CARTESIAN_POINT('Ctrl Pts',(-0.447647000285111,2.47877107846524,
4.16592770879555));
#20761=CARTESIAN_POINT('Ctrl Pts',(-0.529222988118453,2.46264737843161,
4.17116613466353));
#20762=CARTESIAN_POINT('Ctrl Pts',(-0.609831807771019,2.44252152830446,
4.1764045605315));
#20763=CARTESIAN_POINT('Ctrl Pts',(-0.690414116524153,2.4224022972345,4.18164126356838));
#20764=CARTESIAN_POINT('Ctrl Pts',(-0.77002944150669,2.39828364188206,4.18687796660525));
#20765=CARTESIAN_POINT('Ctrl Pts',(-0.848258268782068,2.37028777987882,
4.19211466964213));
#20766=CARTESIAN_POINT('Ctrl Pts',(-0.926484965143172,2.3422926804689,4.19735123003382));
#20767=CARTESIAN_POINT('Ctrl Pts',(-1.00332480479719,2.31042074083838,4.20258779042552));
#20768=CARTESIAN_POINT('Ctrl Pts',(-1.07837582723516,2.27484325289345,4.20782435081721));
#20769=CARTESIAN_POINT('Ctrl Pts',(-1.15465523262542,2.23868345736289,4.21314661958842));
#20770=CARTESIAN_POINT('Ctrl Pts',(-1.22908628631208,2.19869591822691,4.21846888835962));
#20771=CARTESIAN_POINT('Ctrl Pts',(-1.30127223613778,2.15510946762734,4.22379115713083));
#20772=CARTESIAN_POINT('Ctrl Pts',(-1.37239772155604,2.11216333387084,4.22903523788051));
#20773=CARTESIAN_POINT('Ctrl Pts',(-1.44134327579444,2.06572364040126,4.23427931863019));
#20774=CARTESIAN_POINT('Ctrl Pts',(-1.50775953210907,2.01605244062109,4.23952339937987));
#20775=CARTESIAN_POINT('Ctrl Pts',(-1.5756611647726,1.96527036182622,4.24488476216184));
#20776=CARTESIAN_POINT('Ctrl Pts',(-1.64091860658684,1.91111081651486,4.2502461249438));
#20777=CARTESIAN_POINT('Ctrl Pts',(-1.70319662932577,1.85389522137939,4.25560748772577));
#20778=CARTESIAN_POINT('Ctrl Pts',(-1.7654746520647,1.79667962624392,4.26096885050774));
#20779=CARTESIAN_POINT('Ctrl Pts',(-1.82477294699385,1.73640839032897,4.2663302132897));
#20780=CARTESIAN_POINT('Ctrl Pts',(-1.88079985551992,1.67343901994553,4.27169157607167));
#20781=CARTESIAN_POINT('Ctrl Pts',(-1.93571786607732,1.61171595439566,4.27694682547964));
#20782=CARTESIAN_POINT('Ctrl Pts',(-1.98769568587252,1.54717263420609,4.28220207488761));
#20783=CARTESIAN_POINT('Ctrl Pts',(-2.03643048514925,1.48012064682403,4.28745732429558));
#20784=CARTESIAN_POINT('Ctrl Pts',(-2.08509618955193,1.41316372392755,4.29270512295376));
#20785=CARTESIAN_POINT('Ctrl Pts',(-2.13052773711959,1.3437055686568,4.29795292161193));
#20786=CARTESIAN_POINT('Ctrl Pts',(-2.17246106323187,1.27209244111481,4.3032007202701));
#20787=CARTESIAN_POINT('Ctrl Pts',(-2.21469823243587,1.19996041473755,4.30848654375284));
#20788=CARTESIAN_POINT('Ctrl Pts',(-2.25338595601427,1.12564240909209,4.31377236723558));
#20789=CARTESIAN_POINT('Ctrl Pts',(-2.28829758584728,1.04952389615744,4.31905819071832));
#20790=CARTESIAN_POINT('Ctrl Pts',(-2.32289616551108,0.974087932661735,
4.32429661658761));
#20791=CARTESIAN_POINT('Ctrl Pts',(-2.35378590423559,0.896884049737827,
4.32953504245689));
#20792=CARTESIAN_POINT('Ctrl Pts',(-2.38079209410969,0.81831244315651,4.33477346832618));
#20793=CARTESIAN_POINT('Ctrl Pts',(-2.40778940209743,0.739766677468888,
4.34001017136439));
#20794=CARTESIAN_POINT('Ctrl Pts',(-2.4309055480264,0.659854517514087,4.34524687440259));
#20795=CARTESIAN_POINT('Ctrl Pts',(-2.45001464208563,0.578994389926193,
4.3504835774408));
#20796=CARTESIAN_POINT('Ctrl Pts',(-2.46912321562272,0.498136464927666,
4.35572013783384));
#20797=CARTESIAN_POINT('Ctrl Pts',(-2.48422484919077,0.416331072925899,
4.36095669822688));
#20798=CARTESIAN_POINT('Ctrl Pts',(-2.49524437309276,0.334008635440673,
4.36619325861992));
#20799=CARTESIAN_POINT('Ctrl Pts',(-2.50644425689397,0.250338801583255,
4.37151552738958));
#20800=CARTESIAN_POINT('Ctrl Pts',(-2.51342712092159,0.166135329894889,
4.37683779615924));
#20801=CARTESIAN_POINT('Ctrl Pts',(-2.51616889547945,0.0818556010405808,
4.3821600649289));
#20802=CARTESIAN_POINT('Ctrl Pts',(-2.51887039136492,-0.00118599699139293,
4.38740414567994));
#20803=CARTESIAN_POINT('Ctrl Pts',(-2.51745464937952,-0.0843011596064944,
4.39264822643099));
#20804=CARTESIAN_POINT('Ctrl Pts',(-2.51195126462655,-0.167054165291002,
4.39789230718203));
#20805=CARTESIAN_POINT('Ctrl Pts',(-2.50632479860254,-0.251657912942316,
4.403253669961));
#20806=CARTESIAN_POINT('Ctrl Pts',(-2.49642570589058,-0.335882600626038,
4.40861503273997));
#20807=CARTESIAN_POINT('Ctrl Pts',(-2.4823410728014,-0.419272045673439,
4.41397639551893));
#20808=CARTESIAN_POINT('Ctrl Pts',(-2.46825643971223,-0.502661490720837,
4.4193377582979));
#20809=CARTESIAN_POINT('Ctrl Pts',(-2.44998644125835,-0.585215211462834,
4.42469912107687));
#20810=CARTESIAN_POINT('Ctrl Pts',(-2.42767215699857,-0.666493922053232,
4.43006048385584));
#20811=CARTESIAN_POINT('Ctrl Pts',(-2.40579952237929,-0.746163945002343,
4.43531573326292));
#20812=CARTESIAN_POINT('Ctrl Pts',(-2.37996048847709,-0.824903250665136,
4.44057098267001));
#20813=CARTESIAN_POINT('Ctrl Pts',(-2.35025153630514,-0.902288183506419,
4.44582623207709));
#20814=CARTESIAN_POINT('Ctrl Pts',(-2.32058470467833,-0.979563402092642,
4.45107403073436));
#20815=CARTESIAN_POINT('Ctrl Pts',(-2.28705901689624,-1.05548763474825,
4.45632182939163));
#20816=CARTESIAN_POINT('Ctrl Pts',(-2.24982114286705,-1.12965086425338,
4.4615696280489));
#20817=CARTESIAN_POINT('Ctrl Pts',(-2.21231344833568,-1.20435147029651,
4.46685545153187));
#20818=CARTESIAN_POINT('Ctrl Pts',(-2.17103967004633,-1.27726498855752,
4.47214127501483));
#20819=CARTESIAN_POINT('Ctrl Pts',(-2.12619973999849,-1.34799143752116,
4.47742709849779));
#20820=CARTESIAN_POINT('Ctrl Pts',(-2.08176188651069,-1.41808368729509,
4.48266552436616));
#20821=CARTESIAN_POINT('Ctrl Pts',(-2.0338218316076,-1.48602753639573,4.48790395023452));
#20822=CARTESIAN_POINT('Ctrl Pts',(-1.98262013641925,-1.55145855396299,
4.49314237610289));
#20823=CARTESIAN_POINT('Ctrl Pts',(-1.93143528061632,-1.61686805235751,
4.49837907914017));
#20824=CARTESIAN_POINT('Ctrl Pts',(-1.87699119910284,-1.67976599745249,
4.50361578217744));
#20825=CARTESIAN_POINT('Ctrl Pts',(-1.81957032400716,-1.73981898081164,
4.50885248521472));
#20826=CARTESIAN_POINT('Ctrl Pts',(-1.76215101302744,-1.79987032835752,
4.51408904560682));
#20827=CARTESIAN_POINT('Ctrl Pts',(-1.7017553893145,-1.85707653546034,4.51932560599892));
#20828=CARTESIAN_POINT('Ctrl Pts',(-1.63870356085949,-1.91114020668982,
4.52456216639102));
#20829=CARTESIAN_POINT('Ctrl Pts',(-1.57461974392674,-1.96608875449054,
4.52988443516177));
#20830=CARTESIAN_POINT('Ctrl Pts',(-1.50779235269812,-2.01779063858759,
4.53520670393252));
#20831=CARTESIAN_POINT('Ctrl Pts',(-1.43859192976348,-2.0659766478882,4.54052897270327));
#20832=CARTESIAN_POINT('Ctrl Pts',(-1.37040811165095,-2.11345476947172,
4.54577305345338));
#20833=CARTESIAN_POINT('Ctrl Pts',(-1.29992095154826,-2.15751943604622,
4.55101713420348));
#20834=CARTESIAN_POINT('Ctrl Pts',(-1.22751204239967,-2.19795824249775,
4.55626121495359));
#20835=CARTESIAN_POINT('Ctrl Pts',(-1.15348373333534,-2.2393014487052,4.56162257773466));
#20836=CARTESIAN_POINT('Ctrl Pts',(-1.07744713857565,-2.27685442881522,
4.56698394051573));
#20837=CARTESIAN_POINT('Ctrl Pts',(-0.99983231490222,-2.31044186078708,
4.5723453032968));
#20838=CARTESIAN_POINT('Ctrl Pts',(-0.922217491228789,-2.34402929275895,
4.57770666607787));
#20839=CARTESIAN_POINT('Ctrl Pts',(-0.843024937947763,-2.37365106114631,
4.58306802885894));
#20840=CARTESIAN_POINT('Ctrl Pts',(-0.762699935624585,-2.3991863325299,
4.58842939164001));
#20841=CARTESIAN_POINT('Ctrl Pts',(-0.683964744949417,-2.42421620371794,
4.59368464104726));
#20842=CARTESIAN_POINT('Ctrl Pts',(-0.603850720472383,-2.44541235930782,
4.59893989045451));
#20843=CARTESIAN_POINT('Ctrl Pts',(-0.522765750426252,-2.46262506691158,
4.60419513986177));
#20844=CARTESIAN_POINT('Ctrl Pts',(-0.441795740447352,-2.47981337080623,
4.60944293851921));
#20845=CARTESIAN_POINT('Ctrl Pts',(-0.359857966786886,-2.49302934952906,
4.61469073717665));
#20846=CARTESIAN_POINT('Ctrl Pts',(-0.277376203386156,-2.50217279415213,
4.61993853583409));
#20847=CARTESIAN_POINT('Ctrl Pts',(-0.194296788500819,-2.5113824909142,
4.62522435931701));
#20848=CARTESIAN_POINT('Ctrl Pts',(-0.110665918879123,-2.5164602429421,
4.63051018279993));
#20849=CARTESIAN_POINT('Ctrl Pts',(-0.026927949219451,-2.51735598109422,
4.63579600628285));
#20850=CARTESIAN_POINT('Ctrl Pts',(0.0560591478451705,-2.51824368722415,
4.64103443215139));
#20851=CARTESIAN_POINT('Ctrl Pts',(0.139150962027135,-2.51502407372522,
4.64627285801992));
#20852=CARTESIAN_POINT('Ctrl Pts',(0.221910837649735,-2.50770050646675,
4.65151128388845));
#20853=CARTESIAN_POINT('Ctrl Pts',(0.304643494926548,-2.50037934780767,
4.65674798692589));
#20854=CARTESIAN_POINT('Ctrl Pts',(0.387043971197711,-2.48895695665212,
4.66198468996334));
#20855=CARTESIAN_POINT('Ctrl Pts',(0.468678835425855,-2.47348871014684,
4.66722139300078));
#20856=CARTESIAN_POINT('Ctrl Pts',(0.550311475961083,-2.45802088498886,
4.67245795339305));
#20857=CARTESIAN_POINT('Ctrl Pts',(0.631178092756059,-2.43850751051613,
4.67769451378532));
#20858=CARTESIAN_POINT('Ctrl Pts',(0.710854949522729,-2.4150551734358,4.68293107417759));
#20859=CARTESIAN_POINT('Ctrl Pts',(0.791835901662793,-2.3912189848141,4.68825334294814));
#20860=CARTESIAN_POINT('Ctrl Pts',(0.871587320643905,-2.36331385611791,
4.69357561171869));
#20861=CARTESIAN_POINT('Ctrl Pts',(0.949681651786961,-2.33150402321317,
4.69889788048924));
#20862=CARTESIAN_POINT('Ctrl Pts',(1.02662872009707,-2.30016150001554,4.70414196123951));
#20863=CARTESIAN_POINT('Ctrl Pts',(1.10196666682185,-2.26502849041801,4.70938604198977));
#20864=CARTESIAN_POINT('Ctrl Pts',(1.17530956931617,-2.22630942734245,4.71463012274004));
#20865=CARTESIAN_POINT('Ctrl Pts',(1.25029276015298,-2.18672442597381,4.71999148552073));
#20866=CARTESIAN_POINT('Ctrl Pts',(1.3231901528623,-2.14339129554255,4.72535284830142));
#20867=CARTESIAN_POINT('Ctrl Pts',(1.39362054358296,-2.09657531000046,4.73071421108212));
#20868=CARTESIAN_POINT('Ctrl Pts',(1.46405093430362,-2.04975932445837,4.73607557386281));
#20869=CARTESIAN_POINT('Ctrl Pts',(1.53201395435211,-1.99946083976464,4.7414369366435));
#20870=CARTESIAN_POINT('Ctrl Pts',(1.59716581588964,-1.94598756587846,4.74679829942419));
#20871=CARTESIAN_POINT('Ctrl Pts',(1.66018580041307,-1.89426402624049,4.75198422951874));
#20872=CARTESIAN_POINT('Ctrl Pts',(1.72082195295255,-1.83936794722174,4.7571701596133));
#20873=CARTESIAN_POINT('Ctrl Pts',(1.77873133380433,-1.7815501935513,4.76235608970785));
#20874=CARTESIAN_POINT('Ctrl Pts',(1.83691908277286,-1.72345451221237,4.76756694836446));
#20875=CARTESIAN_POINT('Ctrl Pts',(1.89235335502451,-1.66240923773946,4.77277780702107));
#20876=CARTESIAN_POINT('Ctrl Pts',(1.94471789917397,-1.5987115257708,4.77798866567767));
#20877=CARTESIAN_POINT('Ctrl Pts',(1.9966980531484,-1.53548139687862,4.78316127320647));
#20878=CARTESIAN_POINT('Ctrl Pts',(2.04565307367945,-1.4696379988575,4.78833388073526));
#20879=CARTESIAN_POINT('Ctrl Pts',(2.09131013993223,-1.40150923957591,4.79350648826406));
#20880=CARTESIAN_POINT('Ctrl Pts',(2.13693972349127,-1.33342148953955,4.79867598220716));
#20881=CARTESIAN_POINT('Ctrl Pts',(2.17927502808787,-1.26305150123698,4.80384547615025));
#20882=CARTESIAN_POINT('Ctrl Pts',(2.21808489358847,-1.19075843681018,4.80901497009335));
#20883=CARTESIAN_POINT('Ctrl Pts',(2.25688384820123,-1.11848569663618,4.8141830107006));
#20884=CARTESIAN_POINT('Ctrl Pts',(2.29215910763938,-1.04429137212952,4.81935105130785));
#20885=CARTESIAN_POINT('Ctrl Pts',(2.32372486071905,-0.968560282933497,
4.82451909191511));
#20886=CARTESIAN_POINT('Ctrl Pts',(2.35573909391718,-0.891753221060157,
4.82976055904438));
#20887=CARTESIAN_POINT('Ctrl Pts',(2.38393735988785,-0.813365831106525,
4.83500202617366));
#20888=CARTESIAN_POINT('Ctrl Pts',(2.40817655178341,-0.733820104276619,
4.84024349330293));
#20889=CARTESIAN_POINT('Ctrl Pts',(2.43209781731739,-0.655317716004383,
4.84541621224205));
#20890=CARTESIAN_POINT('Ctrl Pts',(2.45216318475617,-0.575687678729605,
4.85058893118116));
#20891=CARTESIAN_POINT('Ctrl Pts',(2.46828607655098,-0.495348457456518,
4.85576165012027));
#20892=CARTESIAN_POINT('Ctrl Pts',(2.48473039107651,-0.413407609613363,
4.86103749134463));
#20893=CARTESIAN_POINT('Ctrl Pts',(2.49707324762491,-0.330729506808876,
4.86631333256899));
#20894=CARTESIAN_POINT('Ctrl Pts',(2.50527825608034,-0.247764221813888,
4.87158917379334));
#20895=CARTESIAN_POINT('Ctrl Pts',(2.51348326453577,-0.1647989368189,4.8768650150177));
#20896=CARTESIAN_POINT('Ctrl Pts',(2.51755046013754,-0.0815469897731697,
4.88214085624206));
#20897=CARTESIAN_POINT('Ctrl Pts',(2.51749952702257,0.00154319187075648,
4.88741669746642));
#20898=CARTESIAN_POINT('Ctrl Pts',(2.51749952702217,0.00154319252581683,
4.88741669750801));
#20899=CARTESIAN_POINT('Ctrl Pts',(2.51744240569644,0.0947285262346869,
4.89333353407479));
#20900=CARTESIAN_POINT('Ctrl Pts',(2.51221164500483,0.187753544831829,4.89925037064158));
#20901=CARTESIAN_POINT('Ctrl Pts',(2.50185877901997,0.280194396519088,4.90516720720837));
#20902=CARTESIAN_POINT('Ctrl Pts',(2.49266337064657,0.362300296749366,4.91042253733531));
#20903=CARTESIAN_POINT('Ctrl Pts',(2.47940487600131,0.444104686115124,4.91567786746224));
#20904=CARTESIAN_POINT('Ctrl Pts',(2.46211260638418,0.525174031616275,4.92093319758918));
#20905=CARTESIAN_POINT('Ctrl Pts',(2.44484693031314,0.606118701674371,4.92618044561544));
#20906=CARTESIAN_POINT('Ctrl Pts',(2.42355990290171,0.686330126880152,4.9314276936417));
#20907=CARTESIAN_POINT('Ctrl Pts',(2.3983325070012,0.765380582364975,4.93667494166796));
#20908=CARTESIAN_POINT('Ctrl Pts',(2.3868420349923,0.801386163346109,4.93906493692579));
#20909=CARTESIAN_POINT('Ctrl Pts',(2.37453480876644,0.837150986090258,4.94145493218361));
#20910=CARTESIAN_POINT('Ctrl Pts',(2.36142200728636,0.872635292378022,4.94384492744144));
#20911=CARTESIAN_POINT('',(2.51749980506587,-0.00177349968566837,4.61406162840033));
#20912=CARTESIAN_POINT('Ctrl Pts',(2.36142200727925,0.872635292397265,4.66658913197125));
#20913=CARTESIAN_POINT('Ctrl Pts',(2.3631089532083,0.868070279640319,4.66628593237008));
#20914=CARTESIAN_POINT('Ctrl Pts',(2.36478267438196,0.86350034104399,4.6659831649262));
#20915=CARTESIAN_POINT('Ctrl Pts',(2.37558197045969,0.833746981502558,4.6640168308542));
#20916=CARTESIAN_POINT('Ctrl Pts',(2.38431862179719,0.808423479041231,4.6623660094523));
#20917=CARTESIAN_POINT('Ctrl Pts',(2.40319358021164,0.750743778121066,4.65865389320594));
#20918=CARTESIAN_POINT('Ctrl Pts',(2.41308584250394,0.718312241636577,4.65660045200013));
#20919=CARTESIAN_POINT('Ctrl Pts',(2.44376410437075,0.60993583797465,4.64983766640419));
#20920=CARTESIAN_POINT('Ctrl Pts',(2.46164346316683,0.533214366119594,4.64521179243));
#20921=CARTESIAN_POINT('Ctrl Pts',(2.50368455543998,0.304835965786213,4.63172626299532));
#20922=CARTESIAN_POINT('Ctrl Pts',(2.51760727523633,0.151684038986887,4.62306023742689));
#20923=CARTESIAN_POINT('Ctrl Pts',(2.51749937769237,-0.00177011822094938,
4.61406257126606));
#20924=CARTESIAN_POINT('Ctrl Pts',(2.51749937528208,-0.00177354288295418,
4.61406237046359));
#20925=CARTESIAN_POINT('Ctrl Pts',(2.51744798928901,-0.074714663546969,
4.6097855217469));
#20926=CARTESIAN_POINT('Ctrl Pts',(2.5142265643001,-0.147614065923254,4.60543620366339));
#20927=CARTESIAN_POINT('Ctrl Pts',(2.5067136734322,-0.233152702817736,4.60013979836202));
#20928=CARTESIAN_POINT('Ctrl Pts',(2.50548244364905,-0.24603116151992,4.59933719764383));
#20929=CARTESIAN_POINT('Ctrl Pts',(2.50330884937322,-0.267054823730848,
4.59801766304268));
#20930=CARTESIAN_POINT('Ctrl Pts',(2.50242583835527,-0.275206092752786,
4.59750376256807));
#20931=CARTESIAN_POINT('Ctrl Pts',(2.50078928885904,-0.289653925735625,
4.59658859503168));
#20932=CARTESIAN_POINT('Ctrl Pts',(2.50005174171018,-0.295952277669667,
4.59618818876115));
#20933=CARTESIAN_POINT('Ctrl Pts',(2.49858281402361,-0.308098861281167,
4.59541307615331));
#20934=CARTESIAN_POINT('Ctrl Pts',(2.49785469025906,-0.313947340020373,
4.59503855329779));
#20935=CARTESIAN_POINT('Ctrl Pts',(2.49615591669731,-0.327212212864726,
4.59418606597501));
#20936=CARTESIAN_POINT('Ctrl Pts',(2.49517276865825,-0.334626723071374,
4.59370742554324));
#20937=CARTESIAN_POINT('Ctrl Pts',(2.49240608059129,-0.354801618961238,
4.59239942839782));
#20938=CARTESIAN_POINT('Ctrl Pts',(2.49055762418982,-0.367552667451044,
4.59156661650582));
#20939=CARTESIAN_POINT('Ctrl Pts',(2.48075080098427,-0.431728584194256,
4.58734607722727));
#20940=CARTESIAN_POINT('Ctrl Pts',(2.47129775668273,-0.482908533398728,
4.58388640033651));
#20941=CARTESIAN_POINT('Ctrl Pts',(2.44745406651946,-0.592812672928028,
4.57630366372473));
#20942=CARTESIAN_POINT('Ctrl Pts',(2.43251963181112,-0.651387618516999,
4.57216618637696));
#20943=CARTESIAN_POINT('Ctrl Pts',(2.36635209388672,-0.876697742863623,
4.55599662172088));
#20944=CARTESIAN_POINT('Ctrl Pts',(2.29994927894316,-1.03849294306498,4.54387645177078));
#20945=CARTESIAN_POINT('Ctrl Pts',(2.19455542882569,-1.23452390324998,4.52903029996862));
#20946=CARTESIAN_POINT('Ctrl Pts',(2.17055167131663,-1.27625574720375,4.52585623893855));
#20947=CARTESIAN_POINT('Ctrl Pts',(2.12697109225534,-1.34723270256414,4.52043466639669));
#20948=CARTESIAN_POINT('Ctrl Pts',(2.10795123725415,-1.37680200726673,4.51816867482162));
#20949=CARTESIAN_POINT('Ctrl Pts',(2.07956736075055,-1.41896135419786,4.51492557004882));
#20950=CARTESIAN_POINT('Ctrl Pts',(2.0706959195927,-1.43187644693349,4.51393035071565));
#20951=CARTESIAN_POINT('Ctrl Pts',(2.05495444971835,-1.45434067759052,4.51219596546999));
#20952=CARTESIAN_POINT('Ctrl Pts',(2.04813706580728,-1.46392594217284,4.51145484323011));
#20953=CARTESIAN_POINT('Ctrl Pts',(2.03387025006481,-1.48369038244374,4.50992426356614));
#20954=CARTESIAN_POINT('Ctrl Pts',(2.02641097891935,-1.4938620748913,4.50913521028086));
#20955=CARTESIAN_POINT('Ctrl Pts',(2.00694517156414,-1.51999214853163,4.50710440826548));
#20956=CARTESIAN_POINT('Ctrl Pts',(1.99482448748306,-1.53586469228605,4.50586710620542));
#20957=CARTESIAN_POINT('Ctrl Pts',(1.94466273879563,-1.5999578856432,4.50085340107417));
#20958=CARTESIAN_POINT('Ctrl Pts',(1.90505029543186,-1.64692522077764,4.49713908020449));
#20959=CARTESIAN_POINT('Ctrl Pts',(1.74121030300414,-1.82735419379689,4.48261756620563));
#20960=CARTESIAN_POINT('Ctrl Pts',(1.6043719357939,-1.94859676368014,4.47232338479871));
#20961=CARTESIAN_POINT('Ctrl Pts',(1.39197377331506,-2.09911978196859,4.45726027364328));
#20962=CARTESIAN_POINT('Ctrl Pts',(1.32625146030379,-2.14124968082467,4.45269975540765));
#20963=CARTESIAN_POINT('Ctrl Pts',(1.23467467028978,-2.19411788625095,4.44633435250681));
#20964=CARTESIAN_POINT('Ctrl Pts',(1.21043869724606,-2.20758077371835,4.44464865928232));
#20965=CARTESIAN_POINT('Ctrl Pts',(1.16858530360595,-2.22993358740495,4.44172728066867));
#20966=CARTESIAN_POINT('Ctrl Pts',(1.15107620987603,-2.23902186667889,4.44050210802469));
#20967=CARTESIAN_POINT('Ctrl Pts',(1.12571314245084,-2.25181071511957,4.43872042207612));
#20968=CARTESIAN_POINT('Ctrl Pts',(1.11794350901209,-2.25567814220515,4.438173698644));
#20969=CARTESIAN_POINT('Ctrl Pts',(1.10434736264418,-2.26235828538219,4.43721509807269));
#20970=CARTESIAN_POINT('Ctrl Pts',(1.09852965225872,-2.26518889083171,4.43680431526626));
#20971=CARTESIAN_POINT('Ctrl Pts',(1.08612971779064,-2.27116307045286,4.43592738472692));
#20972=CARTESIAN_POINT('Ctrl Pts',(1.07954472926909,-2.27430047063708,4.43546088519819));
#20973=CARTESIAN_POINT('Ctrl Pts',(1.06174573697435,-2.28268603579702,4.4341979713399));
#20974=CARTESIAN_POINT('Ctrl Pts',(1.05050666751586,-2.28788008310356,4.43339839923334));
#20975=CARTESIAN_POINT('Ctrl Pts',(0.998485460932153,-2.31145714994828,
4.42968931897497));
#20976=CARTESIAN_POINT('Ctrl Pts',(0.957258736938432,-2.32883286562977,
4.42672691332104));
#20977=CARTESIAN_POINT('Ctrl Pts',(0.746502291969871,-2.41111821512607,
4.4115435181355));
#20978=CARTESIAN_POINT('Ctrl Pts',(0.570769684802599,-2.45865401231696,
4.39880315403903));
#20979=CARTESIAN_POINT('Ctrl Pts',(0.275834907844707,-2.5050788399438,4.37841181338006));
#20980=CARTESIAN_POINT('Ctrl Pts',(0.159076672967931,-2.51519504256211,
4.37057367471458));
#20981=CARTESIAN_POINT('Ctrl Pts',(0.0115384077442088,-2.51765818198488,
4.36100571210751));
#20982=CARTESIAN_POINT('Ctrl Pts',(-0.0189545506671911,-2.5176132972375,
4.35904562349324));
#20983=CARTESIAN_POINT('Ctrl Pts',(-0.0642470446742235,-2.51672364227029,
4.35615890513128));
#20984=CARTESIAN_POINT('Ctrl Pts',(-0.0790511865987438,-2.51630214789036,
4.35521927443884));
#20985=CARTESIAN_POINT('Ctrl Pts',(-0.105490832705892,-2.51531580686368,
4.35354787036417));
#20986=CARTESIAN_POINT('Ctrl Pts',(-0.117127656783522,-2.5148007959716,
4.3528145731037));
#20987=CARTESIAN_POINT('Ctrl Pts',(-0.141773591668861,-2.51353859718961,
4.35126627752719));
#20988=CARTESIAN_POINT('Ctrl Pts',(-0.154781355721146,-2.51277113421189,
4.35045193061832));
#20989=CARTESIAN_POINT('Ctrl Pts',(-0.189616500768391,-2.51044431749062,
4.34827829449673));
#20990=CARTESIAN_POINT('Ctrl Pts',(-0.211430795401036,-2.50870128829697,
4.34692472823319));
#20991=CARTESIAN_POINT('Ctrl Pts',(-0.313046573431349,-2.4992469893665,
4.34065150298943));
#20992=CARTESIAN_POINT('Ctrl Pts',(-0.392477531622812,-2.48801063872559,
4.33584201279791));
#20993=CARTESIAN_POINT('Ctrl Pts',(-0.634449916484938,-2.44190155405757,
4.3213171572279));
#20994=CARTESIAN_POINT('Ctrl Pts',(-0.794173080282035,-2.39472320081013,
4.31193143764029));
#20995=CARTESIAN_POINT('Ctrl Pts',(-1.03891968337528,-2.29522692923639,
4.29661534481884));
#20996=CARTESIAN_POINT('Ctrl Pts',(-1.12750998836885,-2.25302859825829,
4.29085029025559));
#20997=CARTESIAN_POINT('Ctrl Pts',(-1.231619824543,-2.19575751998811,4.28354315913374));
#20998=CARTESIAN_POINT('Ctrl Pts',(-1.2497101567384,-2.18551205400862,4.28225301975849));
#20999=CARTESIAN_POINT('Ctrl Pts',(-1.27541156447124,-2.17053262208112,
4.28038761485535));
#21000=CARTESIAN_POINT('Ctrl Pts',(-1.2831280082296,-2.16597992396813,4.2798233110935));
#21001=CARTESIAN_POINT('Ctrl Pts',(-1.29647556950908,-2.15800851336101,
4.27883951995507));
#21002=CARTESIAN_POINT('Ctrl Pts',(-1.3021178339861,-2.1546087328432,4.27842124599539));
#21003=CARTESIAN_POINT('Ctrl Pts',(-1.31401320986657,-2.1473773105845,4.27753421237516));
#21004=CARTESIAN_POINT('Ctrl Pts',(-1.32026283641549,-2.1435405452716,4.27706514263467));
#21005=CARTESIAN_POINT('Ctrl Pts',(-1.33716980493438,-2.13305904632379,
4.2757881079507));
#21006=CARTESIAN_POINT('Ctrl Pts',(-1.34779416642361,-2.12636188166849,
4.27497686695568));
#21007=CARTESIAN_POINT('Ctrl Pts',(-1.39766215347746,-2.09440324734153,
4.27112928987244));
#21008=CARTESIAN_POINT('Ctrl Pts',(-1.43624594734759,-2.06813476367657,
4.26803529049715));
#21009=CARTESIAN_POINT('Ctrl Pts',(-1.65439171066707,-1.91056845184088,
4.24995279725691));
#21010=CARTESIAN_POINT('Ctrl Pts',(-1.81665829245263,-1.75700089373511,
4.23424298515611));
#21011=CARTESIAN_POINT('Ctrl Pts',(-2.01256128725213,-1.51502489094334,
4.21330326755074));
#21012=CARTESIAN_POINT('Ctrl Pts',(-2.06478704277916,-1.44303878620737,
4.20744416857285));
#21013=CARTESIAN_POINT('Ctrl Pts',(-2.12491064956853,-1.35019739174296,
4.20033207579972));
#21014=CARTESIAN_POINT('Ctrl Pts',(-2.13648390135242,-1.3318088650073,4.19894382138404));
#21015=CARTESIAN_POINT('Ctrl Pts',(-2.15459736900602,-1.30218482590774,
4.19673909199813));
#21016=CARTESIAN_POINT('Ctrl Pts',(-2.16129091909579,-1.29104481590471,
4.19591706167645));
#21017=CARTESIAN_POINT('Ctrl Pts',(-2.17382289879586,-1.26981734099256,
4.19436378643572));
#21018=CARTESIAN_POINT('Ctrl Pts',(-2.17967810548655,-1.25974022664038,
4.19363195048458));
#21019=CARTESIAN_POINT('Ctrl Pts',(-2.19284359558402,-1.23671512100248,
4.19197213563917));
#21020=CARTESIAN_POINT('Ctrl Pts',(-2.20010961451792,-1.22374222133413,
4.19104575431238));
#21021=CARTESIAN_POINT('Ctrl Pts',(-2.22207121504036,-1.18370360610821,
4.18821288760459));
#21022=CARTESIAN_POINT('Ctrl Pts',(-2.23638576959146,-1.15643137619107,
4.18631980886489));
#21023=CARTESIAN_POINT('Ctrl Pts',(-2.34263351170426,-0.944651929046173,
4.17187998451683));
#21024=CARTESIAN_POINT('Ctrl Pts',(-2.41209127125278,-0.749748807333856,
4.16017838755981));
#21025=CARTESIAN_POINT('Ctrl Pts',(-2.48477485889716,-0.424187848460003,
4.14095889405291));
#21026=CARTESIAN_POINT('Ctrl Pts',(-2.50305361361178,-0.297918940740631,
4.13355452995335));
#21027=CARTESIAN_POINT('Ctrl Pts',(-2.51291935836652,-0.152862074446298,
4.12458054997968));
#21028=CARTESIAN_POINT('Ctrl Pts',(-2.51394843288695,-0.134884207099769,
4.12346010345837));
#21029=CARTESIAN_POINT('Ctrl Pts',(-2.51517717408223,-0.1084506160654,4.12179854246881));
#21030=CARTESIAN_POINT('Ctrl Pts',(-2.515527250423,-0.100002003188513,4.12126536174167));
#21031=CARTESIAN_POINT('Ctrl Pts',(-2.51607211081778,-0.0850293129558371,
4.12031645005344));
#21032=CARTESIAN_POINT('Ctrl Pts',(-2.51628409624932,-0.0785060283885452,
4.11990167289346));
#21033=CARTESIAN_POINT('Ctrl Pts',(-2.51668875814144,-0.0643591346285295,
4.11899914942007));
#21034=CARTESIAN_POINT('Ctrl Pts',(-2.51687216099032,-0.0567355720520758,
4.11851092304939));
#21035=CARTESIAN_POINT('Ctrl Pts',(-2.51728479638091,-0.0355874964734826,
4.11715159729157));
#21036=CARTESIAN_POINT('Ctrl Pts',(-2.51743966443228,-0.0220620218026809,
4.11627659424445));
#21037=CARTESIAN_POINT('Ctrl Pts',(-2.51769415614889,0.0529913523234178,
4.11139232549786));
#21038=CARTESIAN_POINT('Ctrl Pts',(-2.51564707031644,0.114500799560346,
4.10728229034464));
#21039=CARTESIAN_POINT('Ctrl Pts',(-2.49890169806237,0.353620788117591,
4.09103490019247));
#21040=CARTESIAN_POINT('Ctrl Pts',(-2.46761781469537,0.529551139057424,
4.07854247228994));
#21041=CARTESIAN_POINT('Ctrl Pts',(-2.38643388434348,0.809701166666007,
4.05872123340112));
#21042=CARTESIAN_POINT('Ctrl Pts',(-2.34751390807522,0.916442791962811,
4.0511763124758));
#21043=CARTESIAN_POINT('Ctrl Pts',(-2.29213875125551,1.04136536845466,4.04237690925929));
#21044=CARTESIAN_POINT('Ctrl Pts',(-2.28246824911139,1.06239382332507,4.04089640781739));
#21045=CARTESIAN_POINT('Ctrl Pts',(-2.26678421339043,1.09529565456573,4.0385804507244));
#21046=CARTESIAN_POINT('Ctrl Pts',(-2.26096436584289,1.10725940430399,4.037738422373));
#21047=CARTESIAN_POINT('Ctrl Pts',(-2.24988870012625,1.12957596935306,4.03616773063101));
#21048=CARTESIAN_POINT('Ctrl Pts',(-2.24465559573863,1.1399396024689,4.03543830748814));
#21049=CARTESIAN_POINT('Ctrl Pts',(-2.23277655353745,1.16306584057133,4.03381041078868));
#21050=CARTESIAN_POINT('Ctrl Pts',(-2.22609247742936,1.17580848059847,4.03291329449226));
#21051=CARTESIAN_POINT('Ctrl Pts',(-2.20880146406436,1.20809636548607,4.03063930969692));
#21052=CARTESIAN_POINT('Ctrl Pts',(-2.19804400544689,1.22755991072405,4.0292677478866));
#21053=CARTESIAN_POINT('Ctrl Pts',(-2.10692146373496,1.38738916238534,4.01799162421964));
#21054=CARTESIAN_POINT('Ctrl Pts',(-2.0134556447357,1.51985938665549,4.00859402375851));
#21055=CARTESIAN_POINT('Ctrl Pts',(-1.8270199675378,1.73642675999762,3.99215505830478));
#21056=CARTESIAN_POINT('Ctrl Pts',(-1.739299865033,1.82428406368276,3.9850882575277));
#21057=CARTESIAN_POINT('Ctrl Pts',(-1.61230661530876,1.9339580768998,3.97516577627883));
#21058=CARTESIAN_POINT('Ctrl Pts',(-1.57840182551127,1.9617272275819,3.9725423984803));
#21059=CARTESIAN_POINT('Ctrl Pts',(-1.52174235110174,2.00571325047913,3.9681678883919));
#21060=CARTESIAN_POINT('Ctrl Pts',(-1.49941092881506,2.02246190158252,3.9664460366982));
#21061=CARTESIAN_POINT('Ctrl Pts',(-1.46866008532416,2.04473592255081,3.96407113343376));
#21062=CARTESIAN_POINT('Ctrl Pts',(-1.46047829109749,2.05058786507156,3.96343888321199));
#21063=CARTESIAN_POINT('Ctrl Pts',(-1.44671806540844,2.06030559633666,3.96237454570308));
#21064=CARTESIAN_POINT('Ctrl Pts',(-1.44115857038415,2.06419821825453,3.9619442508103));
#21065=CARTESIAN_POINT('Ctrl Pts',(-1.43056191984243,2.07155405674072,3.96112343074273));
#21066=CARTESIAN_POINT('Ctrl Pts',(-1.42552776839172,2.07502149293185,3.960733208211));
#21067=CARTESIAN_POINT('Ctrl Pts',(-1.4135249184593,2.08322455445612,3.95980224961037));
#21068=CARTESIAN_POINT('Ctrl Pts',(-1.40654502839954,2.08794356189775,3.95926043531785));
#21069=CARTESIAN_POINT('Ctrl Pts',(-1.38173285553225,2.10453785443036,3.95733319561931));
#21070=CARTESIAN_POINT('Ctrl Pts',(-1.36377337835662,2.11622006549789,3.95593605920174));
#21071=CARTESIAN_POINT('Ctrl Pts',(-1.23519378924031,2.197541560704,3.94593014511059));
#21072=CARTESIAN_POINT('Ctrl Pts',(-1.11945610819381,2.25869524199001,3.93691735121521));
#21073=CARTESIAN_POINT('Ctrl Pts',(-0.869483556517382,2.36682791992753,
3.91810230171811));
#21074=CARTESIAN_POINT('Ctrl Pts',(-0.734930638955566,2.41200348908363,
3.90833609761946));
#21075=CARTESIAN_POINT('Ctrl Pts',(-0.526294355866242,2.46295759780508,
3.89400629362969));
#21076=CARTESIAN_POINT('Ctrl Pts',(-0.454581605793358,2.47719664283383,
3.88921622652109));
#21077=CARTESIAN_POINT('Ctrl Pts',(-0.362109163229426,2.49140569627182,
3.8832088763224));
#21078=CARTESIAN_POINT('Ctrl Pts',(-0.34183611138683,2.49426812971329,3.88190205532801));
#21079=CARTESIAN_POINT('Ctrl Pts',(-0.308911488984472,2.49850791603864,
3.87979569662749));
#21080=CARTESIAN_POINT('Ctrl Pts',(-0.296280761104125,2.50003716667972,
3.87899144427039));
#21081=CARTESIAN_POINT('Ctrl Pts',(-0.271989715869779,2.50279149953608,
3.87745184010376));
#21082=CARTESIAN_POINT('Ctrl Pts',(-0.260331400269903,2.50403100323958,
3.87671605703081));
#21083=CARTESIAN_POINT('Ctrl Pts',(-0.233589418796562,2.5066854083391,3.87503529557393));
#21084=CARTESIAN_POINT('Ctrl Pts',(-0.218500694778285,2.50804569637984,
3.87409204012157));
#21085=CARTESIAN_POINT('Ctrl Pts',(-0.170328953041776,2.51195047747566,
3.87109613906079));
#21086=CARTESIAN_POINT('Ctrl Pts',(-0.137206689401077,2.51397725426197,
3.86905954150488));
#21087=CARTESIAN_POINT('Ctrl Pts',(0.0630887435892422,2.52226290574743,
3.85686716284664));
#21088=CARTESIAN_POINT('Ctrl Pts',(0.2305083175267,2.51250165583614,3.84723060401108));
#21089=CARTESIAN_POINT('Ctrl Pts',(0.512861728766748,2.467558454867,3.83080257427056));
#21090=CARTESIAN_POINT('Ctrl Pts',(0.628513786338901,2.44066349071575,3.82400895071012));
#21091=CARTESIAN_POINT('Ctrl Pts',(0.775688520157098,2.39528055834854,3.81482386695236));
#21092=CARTESIAN_POINT('Ctrl Pts',(0.809320913102423,2.38412689409412,3.81268654724171));
#21093=CARTESIAN_POINT('Ctrl Pts',(0.865219012911848,2.36427010979438,3.80905237504293));
#21094=CARTESIAN_POINT('Ctrl Pts',(0.887617057871395,2.35595266394936,3.80757377048634));
#21095=CARTESIAN_POINT('Ctrl Pts',(0.91872139354652,2.34389567074444,3.80548448993186));
#21096=CARTESIAN_POINT('Ctrl Pts',(0.927530862207434,2.34042355294591,3.80488869226996));
#21097=CARTESIAN_POINT('Ctrl Pts',(0.942513635927006,2.3344204441844,3.80386809933771));
#21098=CARTESIAN_POINT('Ctrl Pts',(0.948696961229068,2.33191441501032,3.80344477605443));
#21099=CARTESIAN_POINT('Ctrl Pts',(0.96145908796655,2.32668291352529,3.80256651621827));
#21100=CARTESIAN_POINT('Ctrl Pts',(0.968036349294273,2.3239540833154,3.80211139472084));
#21101=CARTESIAN_POINT('Ctrl Pts',(0.985295243741117,2.31670758622374,3.8009107575322));
#21102=CARTESIAN_POINT('Ctrl Pts',(0.995957244739025,2.31214400757547,3.80016258477397));
#21103=CARTESIAN_POINT('Ctrl Pts',(1.04063556883363,2.29265430568783,3.79700135697263));
#21104=CARTESIAN_POINT('Ctrl Pts',(1.07434910270687,2.27705068431263,3.7945521714047));
#21105=CARTESIAN_POINT('Ctrl Pts',(1.27957306220259,2.17649493439499,3.7793003101533));
#21106=CARTESIAN_POINT('Ctrl Pts',(1.441275236585,2.07296008206912,3.76584384774829));
#21107=CARTESIAN_POINT('Ctrl Pts',(1.65548889862967,1.89851641530261,3.74698032153053));
#21108=CARTESIAN_POINT('Ctrl Pts',(1.7185463933416,1.84163207473074,3.74126397762998));
#21109=CARTESIAN_POINT('Ctrl Pts',(1.803819558469,1.75650494009893,3.73331900902989));
#21110=CARTESIAN_POINT('Ctrl Pts',(1.82848821148946,1.73081069762476,3.73099224160633));
#21111=CARTESIAN_POINT('Ctrl Pts',(1.87145654006031,1.68411159679977,3.72688710466982));
#21112=CARTESIAN_POINT('Ctrl Pts',(1.88996806643035,1.6633106328245,3.72510015771468));
#21113=CARTESIAN_POINT('Ctrl Pts',(1.9174515598588,1.63137669145542,3.72241783447421));
#21114=CARTESIAN_POINT('Ctrl Pts',(1.92667957399474,1.62046790362634,3.72151199976722));
#21115=CARTESIAN_POINT('Ctrl Pts',(1.94323225018751,1.60055905765305,3.71987741231498));
#21116=CARTESIAN_POINT('Ctrl Pts',(1.95058845549773,1.59158586314099,3.7191473960898));
#21117=CARTESIAN_POINT('Ctrl Pts',(1.96629256355762,1.5721573683499,3.7175809868224));
#21118=CARTESIAN_POINT('Ctrl Pts',(1.97461971784119,1.56168569732838,3.71674543498294));
#21119=CARTESIAN_POINT('Ctrl Pts',(1.99695978580558,1.53312794677522,3.7144898531122));
#21120=CARTESIAN_POINT('Ctrl Pts',(2.01081048229548,1.51491615101593,3.71307619427292));
#21121=CARTESIAN_POINT('Ctrl Pts',(2.08288641489722,1.41741556958778,3.7056331651904));
#21122=CARTESIAN_POINT('Ctrl Pts',(2.13667886061936,1.33494920078824,3.69977497513817));
#21123=CARTESIAN_POINT('Ctrl Pts',(2.254471578004,1.1289232096223,3.6858968307041));
#21124=CARTESIAN_POINT('Ctrl Pts',(2.31330030136958,1.0028565208644,3.67801546162231));
#21125=CARTESIAN_POINT('Ctrl Pts',(2.36142196837104,0.872635397686014,3.66998323165053));
#21126=CARTESIAN_POINT('Origin',(0.,0.,10.));
#21127=CARTESIAN_POINT('',(2.36142200370902,0.872635302058581,2.66999896006316));
#21128=CARTESIAN_POINT('',(2.36142200728636,0.872635292378021,2.94373350505074));
#21129=CARTESIAN_POINT('',(2.36142200728636,0.87263529237802,10.));
#21130=CARTESIAN_POINT('',(2.51749981257981,0.000971421949232871,3.88741669755218));
#21131=CARTESIAN_POINT('Ctrl Pts',(2.36142200728636,0.872635292378019,2.94373350505074));
#21132=CARTESIAN_POINT('Ctrl Pts',(2.33289170715608,0.949840602764351,2.94891972478529));
#21133=CARTESIAN_POINT('Ctrl Pts',(2.30058211384146,1.02561533123368,2.95410594451983));
#21134=CARTESIAN_POINT('Ctrl Pts',(2.2646748419411,1.09956996606812,2.95929216425438));
#21135=CARTESIAN_POINT('Ctrl Pts',(2.22875114002844,1.17355844016397,2.9644807570362));
#21136=CARTESIAN_POINT('Ctrl Pts',(2.18922670931926,1.24572474801263,2.96966934981803));
#21137=CARTESIAN_POINT('Ctrl Pts',(2.14632862703392,1.31570501054556,2.97485794259986));
#21138=CARTESIAN_POINT('Ctrl Pts',(2.10335434119307,1.38580958504156,2.9800557523256));
#21139=CARTESIAN_POINT('Ctrl Pts',(2.05699469910031,1.4537199663387,2.98525356205133));
#21140=CARTESIAN_POINT('Ctrl Pts',(2.00751934661653,1.5191024728307,2.99045137177706));
#21141=CARTESIAN_POINT('Ctrl Pts',(1.9621829145152,1.57901532675449,2.99521435245079));
#21142=CARTESIAN_POINT('Ctrl Pts',(1.91423093465632,1.63680574266011,2.99997733312453));
#21143=CARTESIAN_POINT('Ctrl Pts',(1.86389785875587,1.69224437423361,3.00474031379826));
#21144=CARTESIAN_POINT('Ctrl Pts',(1.80836270459021,1.7534127589605,3.00999556317994));
#21145=CARTESIAN_POINT('Ctrl Pts',(1.7497107152114,1.81195742573655,3.01525081256161));
#21146=CARTESIAN_POINT('Ctrl Pts',(1.68821951959702,1.86754413700229,3.02050606194329));
#21147=CARTESIAN_POINT('Ctrl Pts',(1.62681550452739,1.92305203894059,3.02575386057532));
#21148=CARTESIAN_POINT('Ctrl Pts',(1.56258061817866,1.975610008454,3.03100165920735));
#21149=CARTESIAN_POINT('Ctrl Pts',(1.49583108670036,2.02491866751749,3.03624945783939));
#21150=CARTESIAN_POINT('Ctrl Pts',(1.42859789691412,2.074584610626,3.04153528132868));
#21151=CARTESIAN_POINT('Ctrl Pts',(1.35881378520359,2.12095360559161,3.04682110481797));
#21152=CARTESIAN_POINT('Ctrl Pts',(1.28683794502615,2.16375931037648,3.05210692830727));
#21153=CARTESIAN_POINT('Ctrl Pts',(1.21550750766473,2.20618117910827,3.05734535415095));
#21154=CARTESIAN_POINT('Ctrl Pts',(1.14202489448295,2.2451031651063,3.06258377999464));
#21155=CARTESIAN_POINT('Ctrl Pts',(1.06676946087999,2.28030900698432,3.06782220583833));
#21156=CARTESIAN_POINT('Ctrl Pts',(0.991538777532885,2.31550327024865,3.0730589088512));
#21157=CARTESIAN_POINT('Ctrl Pts',(0.914536849353382,2.34698362133617,3.07829561186407));
#21158=CARTESIAN_POINT('Ctrl Pts',(0.836166348986227,2.37458040226543,3.08353231487695));
#21159=CARTESIAN_POINT('Ctrl Pts',(0.757797983387795,2.40217643147376,3.08876887524495));
#21160=CARTESIAN_POINT('Ctrl Pts',(0.678061555290332,2.42588894856972,3.09400543561296));
#21161=CARTESIAN_POINT('Ctrl Pts',(0.597377056140069,2.44559745313848,3.09924199598096));
#21162=CARTESIAN_POINT('Ctrl Pts',(0.515371968391089,2.46562853300615,3.10456426478108));
#21163=CARTESIAN_POINT('Ctrl Pts',(0.432387969400019,2.48152321851334,3.10988653358121));
#21164=CARTESIAN_POINT('Ctrl Pts',(0.348877289275957,2.49320895374364,3.11520880238133));
#21165=CARTESIAN_POINT('Ctrl Pts',(0.266593442934255,2.50472301686289,3.12045288310835));
#21166=CARTESIAN_POINT('Ctrl Pts',(0.183798759045822,2.5121509933318,3.12569696383536));
#21167=CARTESIAN_POINT('Ctrl Pts',(0.100929636214124,2.51547599045065,3.13094104456238));
#21168=CARTESIAN_POINT('Ctrl Pts',(0.0162071731961466,2.51887535001681,
3.13630240739905));
#21169=CARTESIAN_POINT('Ctrl Pts',(-0.0685925865370805,2.5179859975086,
3.14166377023573));
#21170=CARTESIAN_POINT('Ctrl Pts',(-0.153006787453389,2.51284603049872,
3.14702513307241));
#21171=CARTESIAN_POINT('Ctrl Pts',(-0.237420988369697,2.50770606348885,
3.15238649590908));
#21172=CARTESIAN_POINT('Ctrl Pts',(-0.321449132924398,2.49831560479349,
3.15774785874576));
#21173=CARTESIAN_POINT('Ctrl Pts',(-0.404639426819381,2.48476823552284,
3.16310922158244));
#21174=CARTESIAN_POINT('Ctrl Pts',(-0.486183197008939,2.47148899927115,
3.16836447094613));
#21175=CARTESIAN_POINT('Ctrl Pts',(-0.567223178648792,2.45416689838971,
3.17361972030981));
#21176=CARTESIAN_POINT('Ctrl Pts',(-0.647327860324917,2.43285282975505,
3.1788749696735));
#21177=CARTESIAN_POINT('Ctrl Pts',(-0.727318971746132,2.41156897963144,
3.18412276828653));
#21178=CARTESIAN_POINT('Ctrl Pts',(-0.806376974925999,2.38630452123467,
3.18937056689956));
#21179=CARTESIAN_POINT('Ctrl Pts',(-0.8840785840676,2.35716170577944,3.19461836551259));
#21180=CARTESIAN_POINT('Ctrl Pts',(-0.962343209180321,2.32780772519228,
3.19990418900651));
#21181=CARTESIAN_POINT('Ctrl Pts',(-1.03923123307102,2.29451902239971,3.20519001250043));
#21182=CARTESIAN_POINT('Ctrl Pts',(-1.11432368664947,2.25745187575991,3.21047583599435));
#21183=CARTESIAN_POINT('Ctrl Pts',(-1.18874279056827,2.22071710806612,3.21571426181672));
#21184=CARTESIAN_POINT('Ctrl Pts',(-1.26139797536918,2.1802715953004,3.22095268763908));
#21185=CARTESIAN_POINT('Ctrl Pts',(-1.3319013020307,2.13631579398948,3.22619111346145));
#21186=CARTESIAN_POINT('Ctrl Pts',(-1.40238144131381,2.09237444901484,3.23142781645218));
#21187=CARTESIAN_POINT('Ctrl Pts',(-1.47071073676316,2.04492535227277,3.23666451944291));
#21188=CARTESIAN_POINT('Ctrl Pts',(-1.53652764482227,1.99421389191253,3.24190122243364));
#21189=CARTESIAN_POINT('Ctrl Pts',(-1.60234276005534,1.94350381291203,3.24713778277869));
#21190=CARTESIAN_POINT('Ctrl Pts',(-1.66564525908662,1.88953182942044,3.25237434312373));
#21191=CARTESIAN_POINT('Ctrl Pts',(-1.7261054020982,1.83258462037839,3.25761090346878));
#21192=CARTESIAN_POINT('Ctrl Pts',(-1.78755511585904,1.77470533791553,3.2629331722936));
#21193=CARTESIAN_POINT('Ctrl Pts',(-1.84606822367696,1.71375288583823,3.26825544111842));
#21194=CARTESIAN_POINT('Ctrl Pts',(-1.90133764881034,1.65006708809562,3.27357770994324));
#21195=CARTESIAN_POINT('Ctrl Pts',(-1.95579512461805,1.58731688250739,3.27882179064555));
#21196=CARTESIAN_POINT('Ctrl Pts',(-2.00710334879779,1.52191351407604,3.28406587134786));
#21197=CARTESIAN_POINT('Ctrl Pts',(-2.05501055398101,1.45421383332255,3.28930995205017));
#21198=CARTESIAN_POINT('Ctrl Pts',(-2.10398918845009,1.38500007091213,3.29467131493624));
#21199=CARTESIAN_POINT('Ctrl Pts',(-2.14941256856701,1.31338647656395,3.30003267782232));
#21200=CARTESIAN_POINT('Ctrl Pts',(-2.19106064785408,1.23978203222392,3.30539404070839));
#21201=CARTESIAN_POINT('Ctrl Pts',(-2.23270872714114,1.16617758788389,3.31075540359447));
#21202=CARTESIAN_POINT('Ctrl Pts',(-2.27058133772659,1.09058277775616,3.31611676648054));
#21203=CARTESIAN_POINT('Ctrl Pts',(-2.30451099460484,1.01342751380915,3.32147812936661));
#21204=CARTESIAN_POINT('Ctrl Pts',(-2.33776910715393,0.937799326311952,
3.32673337880581));
#21205=CARTESIAN_POINT('Ctrl Pts',(-2.36736180743918,0.860392568794018,
3.331988628245));
#21206=CARTESIAN_POINT('Ctrl Pts',(-2.39309685031164,0.781596900600643,
3.3372438776842));
#21207=CARTESIAN_POINT('Ctrl Pts',(-2.41879540674197,0.702912946757253,
3.34249167637402));
#21208=CARTESIAN_POINT('Ctrl Pts',(-2.44064702728877,0.622844428524487,
3.34773947506385));
#21209=CARTESIAN_POINT('Ctrl Pts',(-2.45850702087654,0.541802065611387,
3.35298727375368));
#21210=CARTESIAN_POINT('Ctrl Pts',(-2.47649642537684,0.460172481539068,
3.35827309722856));
#21211=CARTESIAN_POINT('Ctrl Pts',(-2.490435922581,0.37755531436034,3.36355892070344));
#21212=CARTESIAN_POINT('Ctrl Pts',(-2.50022848920796,0.294387078101105,
3.36884474417831));
#21213=CARTESIAN_POINT('Ctrl Pts',(-2.5099332466421,0.211964605028515,3.37408317008008));
#21214=CARTESIAN_POINT('Ctrl Pts',(-2.51556509109816,0.129001372780505,
3.37932159598185));
#21215=CARTESIAN_POINT('Ctrl Pts',(-2.51708094996556,0.0459319204960778,
3.38456002188362));
#21216=CARTESIAN_POINT('Ctrl Pts',(-2.51859631029229,-0.037110211632046,
3.38979672495455));
#21217=CARTESIAN_POINT('Ctrl Pts',(-2.51599836509906,-0.12025803343577,
3.39503342802547));
#21218=CARTESIAN_POINT('Ctrl Pts',(-2.50929610112586,-0.203074682997528,
3.4002701310964));
#21219=CARTESIAN_POINT('Ctrl Pts',(-2.50259401971873,-0.28588907667826,
3.40550669152235));
#21220=CARTESIAN_POINT('Ctrl Pts',(-2.49178788006596,-0.368371856219138,
3.4107432519483));
#21221=CARTESIAN_POINT('Ctrl Pts',(-2.47693861889985,-0.450090355598209,
3.41597981237425));
#21222=CARTESIAN_POINT('Ctrl Pts',(-2.46184631556332,-0.533146365391441,
3.42130208110562));
#21223=CARTESIAN_POINT('Ctrl Pts',(-2.44257742174296,-0.615412364763316,
3.426624349837));
#21224=CARTESIAN_POINT('Ctrl Pts',(-2.41924979072903,-0.696445762466485,
3.43194661856838));
#21225=CARTESIAN_POINT('Ctrl Pts',(-2.39626485935617,-0.776288721402427,
3.43719069935248));
#21226=CARTESIAN_POINT('Ctrl Pts',(-2.36933986039222,-0.854934630968459,
3.44243478013658));
#21227=CARTESIAN_POINT('Ctrl Pts',(-2.33863704216953,-0.931978022805563,
3.44767886092068));
#21228=CARTESIAN_POINT('Ctrl Pts',(-2.30724756680958,-1.01074446151412,
3.4530402236257));
#21229=CARTESIAN_POINT('Ctrl Pts',(-2.27190946744169,-1.08783537264659,
3.45840158633072));
#21230=CARTESIAN_POINT('Ctrl Pts',(-2.23284599028985,-1.16284351210579,
3.46376294903574));
#21231=CARTESIAN_POINT('Ctrl Pts',(-2.19378251313801,-1.23785165156499,
3.46912431174075));
#21232=CARTESIAN_POINT('Ctrl Pts',(-2.15099397295079,-1.31077661491582,
3.47448567444577));
#21233=CARTESIAN_POINT('Ctrl Pts',(-2.10474978906033,-1.38124385082812,
3.47984703715079));
#21234=CARTESIAN_POINT('Ctrl Pts',(-2.05942088052246,-1.45031638326054,
3.48510228655188));
#21235=CARTESIAN_POINT('Ctrl Pts',(-2.01060448178666,-1.51728274144073,
3.49035753595296));
#21236=CARTESIAN_POINT('Ctrl Pts',(-1.95852276792631,-1.5817695209841,3.49561278535405));
#21237=CARTESIAN_POINT('Ctrl Pts',(-1.90651489410496,-1.64616487292335,
3.5008605840053));
#21238=CARTESIAN_POINT('Ctrl Pts',(-1.85125118814415,-1.7080872730199,3.50610838265656));
#21239=CARTESIAN_POINT('Ctrl Pts',(-1.79299738127787,-1.76719173853057,
3.51135618130781));
#21240=CARTESIAN_POINT('Ctrl Pts',(-1.73432147527304,-1.82672446693629,
3.51664200479228));
#21241=CARTESIAN_POINT('Ctrl Pts',(-1.67261221380116,-1.88339785551484,
3.52192782827674));
#21242=CARTESIAN_POINT('Ctrl Pts',(-1.60818291698439,-1.93689286113599,
3.5272136517612));
#21243=CARTESIAN_POINT('Ctrl Pts',(-1.54433135331982,-1.98990818065546,
3.53245207762355));
#21244=CARTESIAN_POINT('Ctrl Pts',(-1.47780870122699,-2.03980158942313,
3.53769050348591));
#21245=CARTESIAN_POINT('Ctrl Pts',(-1.40895599782697,-2.08630037295386,
3.54292892934826));
#21246=CARTESIAN_POINT('Ctrl Pts',(-1.34012593893504,-2.13278386380866,
3.54816563237953));
#21247=CARTESIAN_POINT('Ctrl Pts',(-1.26896773276627,-2.17587468869197,
3.55340233541081));
#21248=CARTESIAN_POINT('Ctrl Pts',(-1.19585270856544,-2.21534253545963,
3.55863903844209));
#21249=CARTESIAN_POINT('Ctrl Pts',(-1.12273967598102,-2.25480930714303,
3.56387559882821));
#21250=CARTESIAN_POINT('Ctrl Pts',(-1.04767033787355,-2.2906530786532,3.56911215921434));
#21251=CARTESIAN_POINT('Ctrl Pts',(-0.971040788257617,-2.32268939756051,
3.57434871960047));
#21252=CARTESIAN_POINT('Ctrl Pts',(-0.893157019273675,-2.35525006473628,
3.57967098837834));
#21253=CARTESIAN_POINT('Ctrl Pts',(-0.813661953682703,-2.38387731755965,
3.58499325715621));
#21254=CARTESIAN_POINT('Ctrl Pts',(-0.732990999032035,-2.40842904095969,
3.59031552593409));
#21255=CARTESIAN_POINT('Ctrl Pts',(-0.653505159898557,-2.43262008152783,
3.59555960667833));
#21256=CARTESIAN_POINT('Ctrl Pts',(-0.572878220599952,-2.45285448845586,
3.60080368742257));
#21257=CARTESIAN_POINT('Ctrl Pts',(-0.491538621220228,-2.46904759651346,
3.60604776816682));
#21258=CARTESIAN_POINT('Ctrl Pts',(-0.408379889858549,-2.48560285782704,
3.61140913096151));
#21259=CARTESIAN_POINT('Ctrl Pts',(-0.324476743563918,-2.49793380003589,
3.6167704937562));
#21260=CARTESIAN_POINT('Ctrl Pts',(-0.240292322326436,-2.5060059556655,
3.62213185655089));
#21261=CARTESIAN_POINT('Ctrl Pts',(-0.156107901088954,-2.51407811129511,
3.62749321934558));
#21262=CARTESIAN_POINT('Ctrl Pts',(-0.0716427155110961,-2.51789152415883,
3.63285458214027));
#21263=CARTESIAN_POINT('Ctrl Pts',(0.0126423778376351,-2.51746825606255,
3.63821594493496));
#21264=CARTESIAN_POINT('Ctrl Pts',(0.0952592801793968,-2.51705336539107,
3.64347119433707));
#21265=CARTESIAN_POINT('Ctrl Pts',(0.178008309290671,-2.51256648498689,
3.64872644373918));
#21266=CARTESIAN_POINT('Ctrl Pts',(0.260455292888836,-2.50399067298706,
3.65398169314129));
#21267=CARTESIAN_POINT('Ctrl Pts',(0.342785385391971,-2.49542701954066,
3.65922949179347));
#21268=CARTESIAN_POINT('Ctrl Pts',(0.424813827859746,-2.48278599672192,
3.66447729044565));
#21269=CARTESIAN_POINT('Ctrl Pts',(0.506106573643376,-2.46610267144638,
3.66972508909783));
#21270=CARTESIAN_POINT('Ctrl Pts',(0.587988355556145,-2.44929846107529,
3.67501091258205));
#21271=CARTESIAN_POINT('Ctrl Pts',(0.669123260401729,-2.42839312350843,
3.68029673606627));
#21272=CARTESIAN_POINT('Ctrl Pts',(0.749073089634344,-2.40347576571632,
3.68558255955049));
#21273=CARTESIAN_POINT('Ctrl Pts',(0.828306014163418,-2.37878184018383,
3.69082098541355));
#21274=CARTESIAN_POINT('Ctrl Pts',(0.906374582304272,-2.35014769710119,
3.69605941127661));
#21275=CARTESIAN_POINT('Ctrl Pts',(0.982864365057567,-2.31771091594702,
3.70129783713967));
#21276=CARTESIAN_POINT('Ctrl Pts',(1.05932899159329,-2.28528480271077,3.70653454017157));
#21277=CARTESIAN_POINT('Ctrl Pts',(1.13421543950595,-2.2490587152142,3.71177124320348));
#21278=CARTESIAN_POINT('Ctrl Pts',(1.20712835395856,-2.20921872775633,3.71700794623539));
#21279=CARTESIAN_POINT('Ctrl Pts',(1.28003928229874,-2.1693798255204,3.72224450662204));
#21280=CARTESIAN_POINT('Ctrl Pts',(1.35097637964091,-2.12592744120263,3.72748106700869));
#21281=CARTESIAN_POINT('Ctrl Pts',(1.41956927470519,-2.0790933899931,3.73271762739535));
#21282=CARTESIAN_POINT('Ctrl Pts',(1.48928485072602,-2.0314927914996,3.73803989617233));
#21283=CARTESIAN_POINT('Ctrl Pts',(1.5565783820882,-1.98039909625843,3.74336216494931));
#21284=CARTESIAN_POINT('Ctrl Pts',(1.62109360544763,-1.92610014598847,3.7486844337263));
#21285=CARTESIAN_POINT('Ctrl Pts',(1.68466105285133,-1.8725988871285,3.75392851447084));
#21286=CARTESIAN_POINT('Ctrl Pts',(1.74553098024876,-1.8159862868895,3.75917259521539));
#21287=CARTESIAN_POINT('Ctrl Pts',(1.80339910622492,-1.75657562139156,3.76441667595993));
#21288=CARTESIAN_POINT('Ctrl Pts',(1.8625614327859,-1.69583625694693,3.76977803875313));
#21289=CARTESIAN_POINT('Ctrl Pts',(1.91858573094579,-1.6321725458682,3.77513940154633));
#21290=CARTESIAN_POINT('Ctrl Pts',(1.971190932362,-1.5659542005352,3.78050076433954));
#21291=CARTESIAN_POINT('Ctrl Pts',(2.02379613377821,-1.49973585520219,3.78586212713274));
#21292=CARTESIAN_POINT('Ctrl Pts',(2.07298199720273,-1.43096332775857,3.79122348992594));
#21293=CARTESIAN_POINT('Ctrl Pts',(2.11851611382906,-1.36003519272356,3.79658485271914));
#21294=CARTESIAN_POINT('Ctrl Pts',(2.16415197869778,-1.28894856525233,3.80195819574346));
#21295=CARTESIAN_POINT('Ctrl Pts',(2.2062826727302,-1.21544362331868,3.80733153876778));
#21296=CARTESIAN_POINT('Ctrl Pts',(2.24465002146114,-1.1398914558652,3.81270488179211));
#21297=CARTESIAN_POINT('Ctrl Pts',(2.28295541767622,-1.06446128398889,3.81806954837331));
#21298=CARTESIAN_POINT('Ctrl Pts',(2.31750935406228,-0.986990841663087,
3.82343421495451));
#21299=CARTESIAN_POINT('Ctrl Pts',(2.34809743283373,-0.907879229809594,
3.82879888153571));
#21300=CARTESIAN_POINT('Ctrl Pts',(2.37863368176286,-0.828901668296364,
3.83415445798003));
#21301=CARTESIAN_POINT('Ctrl Pts',(2.40521729350954,-0.748288874715507,
3.83951003442434));
#21302=CARTESIAN_POINT('Ctrl Pts',(2.42768086926413,-0.666462187231165,
3.84486561086866));
#21303=CARTESIAN_POINT('Ctrl Pts',(2.45012200391775,-0.584717244566827,
3.85021583709479));
#21304=CARTESIAN_POINT('Ctrl Pts',(2.46845116965856,-0.501761234880452,
3.85556606332091));
#21305=CARTESIAN_POINT('Ctrl Pts',(2.4825500989695,-0.418032601726885,3.86091628954703));
#21306=CARTESIAN_POINT('Ctrl Pts',(2.49663704247012,-0.334375148128312,
3.86626196742801));
#21307=CARTESIAN_POINT('Ctrl Pts',(2.50650083257717,-0.249946804510473,
3.87160764530899));
#21308=CARTESIAN_POINT('Ctrl Pts',(2.51207407902142,-0.165197068704897,
3.87695332318996));
#21309=CARTESIAN_POINT('Ctrl Pts',(2.51571034773615,-0.109902041654824,
3.88044111462931));
#21310=CARTESIAN_POINT('Ctrl Pts',(2.51752120578827,-0.0544704354779488,
3.88392890606866));
#21311=CARTESIAN_POINT('Ctrl Pts',(2.51749981258008,0.000971421247064627,
3.88741669750801));
#21312=CARTESIAN_POINT('Ctrl Pts',(2.51749981257981,0.000971421949234606,
3.88741669755219));
#21313=CARTESIAN_POINT('Ctrl Pts',(2.51746490758839,0.0914298570691506,
3.89310734671633));
#21314=CARTESIAN_POINT('Ctrl Pts',(2.51255029559255,0.181738119631553,3.89879799588047));
#21315=CARTESIAN_POINT('Ctrl Pts',(2.50282942875531,0.271387362558304,3.90448864504461));
#21316=CARTESIAN_POINT('Ctrl Pts',(2.49308230922834,0.361278716996203,3.9101946626784));
#21317=CARTESIAN_POINT('Ctrl Pts',(2.47850306200983,0.450507179086973,3.91590068031219));
#21318=CARTESIAN_POINT('Ctrl Pts',(2.4592160192085,0.538574805266912,3.92160669794598));
#21319=CARTESIAN_POINT('Ctrl Pts',(2.43985725342605,0.626969929692968,3.92733393462299));
#21320=CARTESIAN_POINT('Ctrl Pts',(2.41575575171988,0.714195269642512,3.93306117130002));
#21321=CARTESIAN_POINT('Ctrl Pts',(2.38708587495822,0.799767013307601,3.93878840797704));
#21322=CARTESIAN_POINT('Ctrl Pts',(2.37890164914636,0.824194689753225,3.94042332948829));
#21323=CARTESIAN_POINT('Ctrl Pts',(2.37034544207401,0.84848775276759,3.94205825099955));
#21324=CARTESIAN_POINT('Ctrl Pts',(2.36142200728636,0.872635292378021,3.9436931725108));
#21325=CARTESIAN_POINT('Ctrl Pts',(2.36142196837104,0.872635397686016,3.66998323165053));
#21326=CARTESIAN_POINT('Ctrl Pts',(2.37171308987963,0.844786790496797,3.66826548869242));
#21327=CARTESIAN_POINT('Ctrl Pts',(2.38151450564319,0.816748213276368,3.66654020096058));
#21328=CARTESIAN_POINT('Ctrl Pts',(2.40889173926343,0.733740777454115,3.66142820138484));
#21329=CARTESIAN_POINT('Ctrl Pts',(2.42507293816446,0.678347504930899,3.65801142973578));
#21330=CARTESIAN_POINT('Ctrl Pts',(2.44497829488643,0.600340006610761,3.6531315422438));
#21331=CARTESIAN_POINT('Ctrl Pts',(2.45031934433564,0.578153977253145,3.65173604938153));
#21332=CARTESIAN_POINT('Ctrl Pts',(2.45913364056118,0.53922200803024,3.64926911247199));
#21333=CARTESIAN_POINT('Ctrl Pts',(2.46273927628498,0.52250727853566,3.64820417505802));
#21334=CARTESIAN_POINT('Ctrl Pts',(2.46783795430178,0.497645116948153,3.64660980248966));
#21335=CARTESIAN_POINT('Ctrl Pts',(2.46946158761549,0.489524558937571,3.64608741239728));
#21336=CARTESIAN_POINT('Ctrl Pts',(2.47217146575597,0.475614540417378,3.64518957261515));
#21337=CARTESIAN_POINT('Ctrl Pts',(2.47327750259242,0.469829055492997,3.64481524299538));
#21338=CARTESIAN_POINT('Ctrl Pts',(2.47574547546959,0.456669271492089,3.64396169082849));
#21339=CARTESIAN_POINT('Ctrl Pts',(2.47709474700074,0.449292881899078,3.64348178144294));
#21340=CARTESIAN_POINT('Ctrl Pts',(2.48068753908381,0.429143074010089,3.64216702075899));
#21341=CARTESIAN_POINT('Ctrl Pts',(2.48286530638019,0.416358376843797,3.64132865654332));
#21342=CARTESIAN_POINT('Ctrl Pts',(2.49346449598788,0.351092887361307,3.63702953903928));
#21343=CARTESIAN_POINT('Ctrl Pts',(2.50032050644018,0.298375384728944,3.63349369227555));
#21344=CARTESIAN_POINT('Ctrl Pts',(2.50839807836804,0.215932938583925,3.62790463997628));
#21345=CARTESIAN_POINT('Ctrl Pts',(2.51077038227164,0.186332871078375,3.62588602703367));
#21346=CARTESIAN_POINT('Ctrl Pts',(2.51582836012262,0.105229638886954,3.62033318810098));
#21347=CARTESIAN_POINT('Ctrl Pts',(2.51745592389102,0.053675300667166,3.61677955282314));
#21348=CARTESIAN_POINT('Ctrl Pts',(2.51767273534475,-0.205168317705718,
3.5989066387134));
#21349=CARTESIAN_POINT('Ctrl Pts',(2.49224625113157,-0.411717004261668,
3.58463819453919));
#21350=CARTESIAN_POINT('Ctrl Pts',(2.4343054571848,-0.6425756439213,3.56920234207048));
#21351=CARTESIAN_POINT('Ctrl Pts',(2.4262979681964,-0.67217915923025,3.56723083786128));
#21352=CARTESIAN_POINT('Ctrl Pts',(2.41361454144976,-0.715885055189095,
3.56433071215611));
#21353=CARTESIAN_POINT('Ctrl Pts',(2.40935169984168,-0.730103395954272,
3.56338891325753));
#21354=CARTESIAN_POINT('Ctrl Pts',(2.40151856909678,-0.755414171939983,
3.56171510177294));
#21355=CARTESIAN_POINT('Ctrl Pts',(2.39799657891024,-0.76652098717923,3.56098154858628));
#21356=CARTESIAN_POINT('Ctrl Pts',(2.39037887645708,-0.789977436969182,
3.55943419123705));
#21357=CARTESIAN_POINT('Ctrl Pts',(2.38626427071203,-0.802320611951452,
3.55862102752818));
#21358=CARTESIAN_POINT('Ctrl Pts',(2.375002138915,-0.835252074218305,3.55645406357455));
#21359=CARTESIAN_POINT('Ctrl Pts',(2.3676825553437,-0.85578066727183,3.55510592383193));
#21360=CARTESIAN_POINT('Ctrl Pts',(2.32882949577893,-0.960432259289628,
3.54824336988238));
#21361=CARTESIAN_POINT('Ctrl Pts',(2.29307425674893,-1.04292375489012,3.54287068636599));
#21362=CARTESIAN_POINT('Ctrl Pts',(2.14978889206595,-1.33029976436524,3.52401132456284));
#21363=CARTESIAN_POINT('Ctrl Pts',(2.01858682484259,-1.52202912021574,3.51124533961636));
#21364=CARTESIAN_POINT('Ctrl Pts',(1.83727275460247,-1.7215423723066,3.49498375102671));
#21365=CARTESIAN_POINT('Ctrl Pts',(1.81081543102841,-1.74935028689683,3.49263580341399));
#21366=CARTESIAN_POINT('Ctrl Pts',(1.77545113924399,-1.78485777812619,3.48951188901158));
#21367=CARTESIAN_POINT('Ctrl Pts',(1.76710986829707,-1.79311648723545,3.48877607258802));
#21368=CARTESIAN_POINT('Ctrl Pts',(1.75359392008409,-1.80631275399331,3.48758478064276));
#21369=CARTESIAN_POINT('Ctrl Pts',(1.74845530888824,-1.81128723055797,3.48713209471877));
#21370=CARTESIAN_POINT('Ctrl Pts',(1.73849316391186,-1.82084927474419,3.48625475489709));
#21371=CARTESIAN_POINT('Ctrl Pts',(1.73367254737565,-1.82543968859462,3.48583032499636));
#21372=CARTESIAN_POINT('Ctrl Pts',(1.72201250808263,-1.83645507190215,3.48480408717947));
#21373=CARTESIAN_POINT('Ctrl Pts',(1.71515529277909,-1.84286098881615,3.48420086870498));
#21374=CARTESIAN_POINT('Ctrl Pts',(1.6911094225939,-1.8650738544232,3.48208716537312));
#21375=CARTESIAN_POINT('Ctrl Pts',(1.67373736211122,-1.88067932200606,3.48056289556372));
#21376=CARTESIAN_POINT('Ctrl Pts',(1.63027458762246,-1.9186431471577,3.47676157242773));
#21377=CARTESIAN_POINT('Ctrl Pts',(1.60393890545098,-1.94071288771721,3.47446880780639));
#21378=CARTESIAN_POINT('Ctrl Pts',(1.48977456550939,-2.03247330753569,3.46460230041676));
#21379=CARTESIAN_POINT('Ctrl Pts',(1.39779778294782,-2.09679160269266,3.45683767390979));
#21380=CARTESIAN_POINT('Ctrl Pts',(1.151263233354,-2.24574071247285,3.4369449681719));
#21381=CARTESIAN_POINT('Ctrl Pts',(0.991534070169703,-2.32069790843866,
3.42493592058843));
#21382=CARTESIAN_POINT('Ctrl Pts',(0.794146002400204,-2.38918891138065,
3.41136014051053));
#21383=CARTESIAN_POINT('Ctrl Pts',(0.762812716553126,-2.39937668045928,
3.40923921039686));
#21384=CARTESIAN_POINT('Ctrl Pts',(0.716831965717704,-2.41333511848547,
3.4061748339182));
#21385=CARTESIAN_POINT('Ctrl Pts',(0.702337240403806,-2.4175931994747,3.40521570686261));
#21386=CARTESIAN_POINT('Ctrl Pts',(0.676533150631907,-2.4249219461005,3.40352014032761));
#21387=CARTESIAN_POINT('Ctrl Pts',(0.665239134635787,-2.42804457327948,
3.40278204330003));
#21388=CARTESIAN_POINT('Ctrl Pts',(0.641618365982783,-2.43439817942558,
3.40124656931451));
#21389=CARTESIAN_POINT('Ctrl Pts',(0.629288030963136,-2.43761465518074,
3.40044967658379));
#21390=CARTESIAN_POINT('Ctrl Pts',(0.596996005642966,-2.44577695727829,
3.39837448153957));
#21391=CARTESIAN_POINT('Ctrl Pts',(0.576996947687529,-2.45057212027743,
3.397101009265));
#21392=CARTESIAN_POINT('Ctrl Pts',(0.484673455937985,-2.47151557379813,
3.39127321743585));
#21393=CARTESIAN_POINT('Ctrl Pts',(0.411713150437736,-2.48471153322036,
3.38681276013958));
#21394=CARTESIAN_POINT('Ctrl Pts',(0.194177121897359,-2.51420890257995,
3.37381836547031));
#21395=CARTESIAN_POINT('Ctrl Pts',(0.048660402299325,-2.52122703488835,
3.36553363916592));
#21396=CARTESIAN_POINT('Ctrl Pts',(-0.142852604899192,-2.51386890608652,
3.35449845190083));
#21397=CARTESIAN_POINT('Ctrl Pts',(-0.188992894594998,-2.51082162631455,
3.35182787668881));
#21398=CARTESIAN_POINT('Ctrl Pts',(-0.263188565840582,-2.50386468497476,
3.34748090515114));
#21399=CARTESIAN_POINT('Ctrl Pts',(-0.291307966759062,-2.50074912227055,
3.34582116996553));
#21400=CARTESIAN_POINT('Ctrl Pts',(-0.382552431661657,-2.48907963642776,
3.34037919518763));
#21401=CARTESIAN_POINT('Ctrl Pts',(-0.445401720126896,-2.47860437691079,
3.33654292471539));
#21402=CARTESIAN_POINT('Ctrl Pts',(-0.521157792299076,-2.46300372564203,
3.33173895899301));
#21403=CARTESIAN_POINT('Ctrl Pts',(-0.534512312162776,-2.4601401110027,
3.33088522893934));
#21404=CARTESIAN_POINT('Ctrl Pts',(-0.555314694445819,-2.45550207676014,
3.32954369250539));
#21405=CARTESIAN_POINT('Ctrl Pts',(-0.562779112528652,-2.45380205511044,
3.32905995982354));
#21406=CARTESIAN_POINT('Ctrl Pts',(-0.57658933707655,-2.45059044729018,
3.32816042308855));
#21407=CARTESIAN_POINT('Ctrl Pts',(-0.582937135970413,-2.44908821731899,
3.32774514803687));
#21408=CARTESIAN_POINT('Ctrl Pts',(-0.597458810120976,-2.44559195448451,
3.32679102082923));
#21409=CARTESIAN_POINT('Ctrl Pts',(-0.60562854849773,-2.44358161190014,
3.3262512640499));
#21410=CARTESIAN_POINT('Ctrl Pts',(-0.631035500015342,-2.43719443774873,
3.32456373562764));
#21411=CARTESIAN_POINT('Ctrl Pts',(-0.64823608676926,-2.43267598814066,
3.32340842067298));
#21412=CARTESIAN_POINT('Ctrl Pts',(-0.688540729517259,-2.42163050087728,
3.32067328443048));
#21413=CARTESIAN_POINT('Ctrl Pts',(-0.711601855916282,-2.4149545189643,
3.319086556369));
#21414=CARTESIAN_POINT('Ctrl Pts',(-0.794170158447463,-2.38976644418621,
3.31333519381706));
#21415=CARTESIAN_POINT('Ctrl Pts',(-0.853077884324735,-2.36937692926746,
3.30910021546813));
#21416=CARTESIAN_POINT('Ctrl Pts',(-1.09672329928171,-2.2747805768987,3.2911784825484));
#21417=CARTESIAN_POINT('Ctrl Pts',(-1.2731140963201,-2.18096963974417,3.27727592078711));
#21418=CARTESIAN_POINT('Ctrl Pts',(-1.49093792685606,-2.02960248621425,
3.25963439224541));
#21419=CARTESIAN_POINT('Ctrl Pts',(-1.54375500766294,-1.98972459092971,
3.25530642923218));
#21420=CARTESIAN_POINT('Ctrl Pts',(-1.61080487683812,-1.93482147613294,
3.24974178241116));
#21421=CARTESIAN_POINT('Ctrl Pts',(-1.62650694528666,-1.92164036523148,
3.24843320757732));
#21422=CARTESIAN_POINT('Ctrl Pts',(-1.6516948543067,-1.89996641352216,3.2463247295588));
#21423=CARTESIAN_POINT('Ctrl Pts',(-1.66128009982131,-1.89159105090206,
3.24552009417809));
#21424=CARTESIAN_POINT('Ctrl Pts',(-1.67956975512852,-1.87536372195323,
3.24398021825313));
#21425=CARTESIAN_POINT('Ctrl Pts',(-1.68828362861271,-1.86752297141914,
3.24324454287149));
#21426=CARTESIAN_POINT('Ctrl Pts',(-1.70831560627555,-1.84924338367033,
3.24154841723865));
#21427=CARTESIAN_POINT('Ctrl Pts',(-1.71959341949941,-1.83876093902504,
3.24058983070305));
#21428=CARTESIAN_POINT('Ctrl Pts',(-1.75519832861889,-1.80505297681218,
3.23755092435718));
#21429=CARTESIAN_POINT('Ctrl Pts',(-1.7791571098717,-1.78144255130788,3.2354870714768));
#21430=CARTESIAN_POINT('Ctrl Pts',(-1.83434769453083,-1.72482998398978,
3.23068026805999));
#21431=CARTESIAN_POINT('Ctrl Pts',(-1.86517386625816,-1.69144811748293,
3.22795393026716));
#21432=CARTESIAN_POINT('Ctrl Pts',(-1.97805722934954,-1.5623648277117,3.21777166402914));
#21433=CARTESIAN_POINT('Ctrl Pts',(-2.05379396674959,-1.46137860112287,
3.21053271485628));
#21434=CARTESIAN_POINT('Ctrl Pts',(-2.20380360870498,-1.22651897647792,
3.19452017714683));
#21435=CARTESIAN_POINT('Ctrl Pts',(-2.27408017708267,-1.09070903769988,
3.18577779565248));
#21436=CARTESIAN_POINT('Ctrl Pts',(-2.33953929678176,-0.92994785828179,
3.17511175862017));
#21437=CARTESIAN_POINT('Ctrl Pts',(-2.34721388681938,-0.910403231290679,
3.17380971612176));
#21438=CARTESIAN_POINT('Ctrl Pts',(-2.35758517305081,-0.882987855629502,
3.17197291095029));
#21439=CARTESIAN_POINT('Ctrl Pts',(-2.36048891968801,-0.875195667738129,
3.17144967586976));
#21440=CARTESIAN_POINT('Ctrl Pts',(-2.36545060206652,-0.861676696728664,
3.17053964527978));
#21441=CARTESIAN_POINT('Ctrl Pts',(-2.36752649821355,-0.855956516928376,
3.17015389652312));
#21442=CARTESIAN_POINT('Ctrl Pts',(-2.37188486993873,-0.843809767980152,
3.16933317926256));
#21443=CARTESIAN_POINT('Ctrl Pts',(-2.3741619988306,-0.837381371283397,
3.16889789308085));
#21444=CARTESIAN_POINT('Ctrl Pts',(-2.37978555272848,-0.821298593474106,
3.16780667530516));
#21445=CARTESIAN_POINT('Ctrl Pts',(-2.38309934182735,-0.811633029811188,
3.16714888844337));
#21446=CARTESIAN_POINT('Ctrl Pts',(-2.39561913878663,-0.774377898401364,
3.16460663404196));
#21447=CARTESIAN_POINT('Ctrl Pts',(-2.40440521173164,-0.746650918215022,
3.16270014773739));
#21448=CARTESIAN_POINT('Ctrl Pts',(-2.42595743999321,-0.674307103136191,
3.15769953107164));
#21449=CARTESIAN_POINT('Ctrl Pts',(-2.43797347914089,-0.629479457219506,
3.15457534235658));
#21450=CARTESIAN_POINT('Ctrl Pts',(-2.49971753143807,-0.370737594176667,
3.13648773307066));
#21451=CARTESIAN_POINT('Ctrl Pts',(-2.52252971298457,-0.151331259863748,
3.12104593521538));
#21452=CARTESIAN_POINT('Ctrl Pts',(-2.51469800671796,0.137449642934256,
3.10179872673477));
#21453=CARTESIAN_POINT('Ctrl Pts',(-2.50996770517658,0.206548040190508,
3.09726400102883));
#21454=CARTESIAN_POINT('Ctrl Pts',(-2.50011539984802,0.296079994589264,
3.0914780765001));
#21455=CARTESIAN_POINT('Ctrl Pts',(-2.49757927136606,0.316762058377484,
3.09014768627992));
#21456=CARTESIAN_POINT('Ctrl Pts',(-2.49307084906653,0.350096950074888,
3.0880128489194));
#21457=CARTESIAN_POINT('Ctrl Pts',(-2.49125832461962,0.362770041155054,
3.08720344927099));
#21458=CARTESIAN_POINT('Ctrl Pts',(-2.48760437230363,0.386998229362491,
3.08566010392745));
#21459=CARTESIAN_POINT('Ctrl Pts',(-2.48577890713357,0.398555359898262,
3.08492567946336));
#21460=CARTESIAN_POINT('Ctrl Pts',(-2.48139045791008,0.42513512914044,3.08324048269309));
#21461=CARTESIAN_POINT('Ctrl Pts',(-2.47877148966601,0.440148157713901,
3.08229149444509));
#21462=CARTESIAN_POINT('Ctrl Pts',(-2.47009157229782,0.487368289417942,
3.07931497634118));
#21463=CARTESIAN_POINT('Ctrl Pts',(-2.46353783886127,0.519482139296874,
3.07730295206085));
#21464=CARTESIAN_POINT('Ctrl Pts',(-2.44673793709007,0.594313643730848,
3.07263681950008));
#21465=CARTESIAN_POINT('Ctrl Pts',(-2.435997030405,0.636909746295945,3.06999798211615));
#21466=CARTESIAN_POINT('Ctrl Pts',(-2.39207015336152,0.793688945211835,
3.06031716401303));
#21467=CARTESIAN_POINT('Ctrl Pts',(-2.35192235723,0.905762509449909,3.05346794087905));
#21468=CARTESIAN_POINT('Ctrl Pts',(-2.2381278782979,1.16417677531396,3.03724161255528));
#21469=CARTESIAN_POINT('Ctrl Pts',(-2.1578496306127,1.30697907522442,3.02792262634101));
#21470=CARTESIAN_POINT('Ctrl Pts',(-2.05267611894614,1.45764898203386,3.01662309222682));
#21471=CARTESIAN_POINT('Ctrl Pts',(-2.04083492552195,1.47418199365801,3.01536139924901));
#21472=CARTESIAN_POINT('Ctrl Pts',(-2.02391577071154,1.49721044572789,3.01357034872952));
#21473=CARTESIAN_POINT('Ctrl Pts',(-2.01900385365688,1.50382764976125,3.01305172188164));
#21474=CARTESIAN_POINT('Ctrl Pts',(-2.01005804303024,1.51575637809767,3.01210935373858));
#21475=CARTESIAN_POINT('Ctrl Pts',(-2.00603531737064,1.52107627623965,3.01168637542339));
#21476=CARTESIAN_POINT('Ctrl Pts',(-1.99775186904073,1.53194080040577,3.01081685069875));
#21477=CARTESIAN_POINT('Ctrl Pts',(-1.9934891235286,1.53748374226118,3.0103701713089));
#21478=CARTESIAN_POINT('Ctrl Pts',(-1.98245150853844,1.55171312430389,3.00921574652804));
#21479=CARTESIAN_POINT('Ctrl Pts',(-1.97564269978716,1.56037287724135,3.00850569441227));
#21480=CARTESIAN_POINT('Ctrl Pts',(-1.94654819574101,1.59688088240674,3.00548133484038));
#21481=CARTESIAN_POINT('Ctrl Pts',(-1.92372998622106,1.62429709914944,3.00313333120025));
#21482=CARTESIAN_POINT('Ctrl Pts',(-1.85951898013077,1.69819568486777,2.99661106303427));
#21483=CARTESIAN_POINT('Ctrl Pts',(-1.81697393802239,1.7436410594951,2.99238198517743));
#21484=CARTESIAN_POINT('Ctrl Pts',(-1.63229961464143,1.92679988488511,2.97454762553986));
#21485=CARTESIAN_POINT('Ctrl Pts',(-1.47584473239446,2.04911224221236,2.96072737486786));
#21486=CARTESIAN_POINT('Ctrl Pts',(-1.24922388776033,2.18672429166329,2.94308313956118));
#21487=CARTESIAN_POINT('Ctrl Pts',(-1.19039802918825,2.21929659168274,2.93868396082205));
#21488=CARTESIAN_POINT('Ctrl Pts',(-1.11190695324792,2.25873736342474,2.93304258489894));
#21489=CARTESIAN_POINT('Ctrl Pts',(-1.0933662242406,2.26777024644018,2.93172602637423));
#21490=CARTESIAN_POINT('Ctrl Pts',(-1.06318155788361,2.28201970226479,2.92960790181943));
#21491=CARTESIAN_POINT('Ctrl Pts',(-1.0516055990162,2.2873772361348,2.92880152340266));
#21492=CARTESIAN_POINT('Ctrl Pts',(-1.02932188052382,2.29748556560566,2.92726039813304));
#21493=CARTESIAN_POINT('Ctrl Pts',(-1.01862073081102,2.30225004552018,2.92652520025176));
#21494=CARTESIAN_POINT('Ctrl Pts',(-0.993831707052291,2.31308020454868,
2.92483317086968));
#21495=CARTESIAN_POINT('Ctrl Pts',(-0.979720784149016,2.31909221380158,
2.9238781732613));
#21496=CARTESIAN_POINT('Ctrl Pts',(-0.934793678844641,2.33775031374205,
2.9208626950068));
#21497=CARTESIAN_POINT('Ctrl Pts',(-0.903780261914417,2.34991428532921,
2.91881831672342));
#21498=CARTESIAN_POINT('Ctrl Pts',(-0.83045466926891,2.37700728712604,2.9140644857403));
#21499=CARTESIAN_POINT('Ctrl Pts',(-0.787966269845653,2.39142804494661,
2.91137113266122));
#21500=CARTESIAN_POINT('Ctrl Pts',(-0.627332967009044,2.44120128131698,
2.90138049976519));
#21501=CARTESIAN_POINT('Ctrl Pts',(-0.507024909679662,2.46899552152921,
2.89429073882447));
#21502=CARTESIAN_POINT('Ctrl Pts',(-0.373100388752179,2.48972915813977,
2.88650397502014));
#21503=CARTESIAN_POINT('Ctrl Pts',(-0.361026919649716,2.4915085277924,2.88580281368281));
#21504=CARTESIAN_POINT('Ctrl Pts',(-0.206630451209501,2.5131174066636,2.87684243796109));
#21505=CARTESIAN_POINT('Ctrl Pts',(-0.0628934766570935,2.52081119644265,
2.86857856377841));
#21506=CARTESIAN_POINT('Ctrl Pts',(0.101947062899903,2.51552484072547,2.85844853305551));
#21507=CARTESIAN_POINT('Ctrl Pts',(0.123190319662389,2.51457402046924,2.8571303815876));
#21508=CARTESIAN_POINT('Ctrl Pts',(0.152803218266471,2.51287245353318,2.85527204210989));
#21509=CARTESIAN_POINT('Ctrl Pts',(0.161185666735311,2.51234869541708,2.85474367295009));
#21510=CARTESIAN_POINT('Ctrl Pts',(0.175657399741574,2.51137173910912,2.85382720652775));
#21511=CARTESIAN_POINT('Ctrl Pts',(0.18174800831294,2.51093830940743,2.85344019210531));
#21512=CARTESIAN_POINT('Ctrl Pts',(0.194612585022782,2.50997576853738,2.85261986285461));
#21513=CARTESIAN_POINT('Ctrl Pts',(0.201386063150256,2.50944138547143,2.85218624937463));
#21514=CARTESIAN_POINT('Ctrl Pts',(0.21821934900887,2.50804475838059,2.85110457204126));
#21515=CARTESIAN_POINT('Ctrl Pts',(0.228276208659745,2.50714940892081,2.85045471865989));
#21516=CARTESIAN_POINT('Ctrl Pts',(0.26638712461251,2.503525240354,2.84797903568993));
#21517=CARTESIAN_POINT('Ctrl Pts',(0.294398890518322,2.50038594327313,2.84613259776715));
#21518=CARTESIAN_POINT('Ctrl Pts',(0.366401059950976,2.49108998215924,2.84132720683863));
#21519=CARTESIAN_POINT('Ctrl Pts',(0.410290872402409,2.4842383116301,2.83834084816532));
#21520=CARTESIAN_POINT('Ctrl Pts',(0.548304915399368,2.45893582690046,2.82881274187096));
#21521=CARTESIAN_POINT('Ctrl Pts',(0.641567526632519,2.43626632422023,2.82217353630221));
#21522=CARTESIAN_POINT('Ctrl Pts',(0.901082493008442,2.35724738529896,2.80343855349362));
#21523=CARTESIAN_POINT('Ctrl Pts',(1.06308842496709,2.28876121845641,2.79146798812186));
#21524=CARTESIAN_POINT('Ctrl Pts',(1.24504301358969,2.18831531239108,2.77796172802742));
#21525=CARTESIAN_POINT('Ctrl Pts',(1.27310407652904,2.1721100759696,2.77587520841093));
#21526=CARTESIAN_POINT('Ctrl Pts',(1.31389599146097,2.1474906109862,2.77283545736936));
#21527=CARTESIAN_POINT('Ctrl Pts',(1.32687481053861,2.13949570097053,2.77186727856046));
#21528=CARTESIAN_POINT('Ctrl Pts',(1.34934163025603,2.12537313255695,2.77018928761137));
#21529=CARTESIAN_POINT('Ctrl Pts',(1.35886238252501,2.11929866224996,2.76947755954944));
#21530=CARTESIAN_POINT('Ctrl Pts',(1.37746306078472,2.10725409985954,2.76808564045312));
#21531=CARTESIAN_POINT('Ctrl Pts',(1.38654583490639,2.10128888514113,2.76740529007627));
#21532=CARTESIAN_POINT('Ctrl Pts',(1.41048381300153,2.08534455405227,2.76561022065557));
#21533=CARTESIAN_POINT('Ctrl Pts',(1.4252718980391,2.07526541394443,2.76449925106208));
#21534=CARTESIAN_POINT('Ctrl Pts',(1.48067372532626,2.03663354087659,2.76032794016278));
#21535=CARTESIAN_POINT('Ctrl Pts',(1.52054891479112,2.00703820567017,2.75730705847066));
#21536=CARTESIAN_POINT('Ctrl Pts',(1.61993872037049,1.92860763391846,2.74970116868446));
#21537=CARTESIAN_POINT('Ctrl Pts',(1.67813746788893,1.87818657481302,2.74517492606913));
#21538=CARTESIAN_POINT('Ctrl Pts',(1.80775107238824,1.75505210947985,2.73478374756119));
#21539=CARTESIAN_POINT('Ctrl Pts',(1.87724313439426,1.68051492397956,2.72896981967822));
#21540=CARTESIAN_POINT('Ctrl Pts',(1.97971512538996,1.55629091919991,2.71969270406915));
#21541=CARTESIAN_POINT('Ctrl Pts',(2.01577470029517,1.50929297108582,2.71626548606949));
#21542=CARTESIAN_POINT('Ctrl Pts',(2.09345290729549,1.40029650535367,2.70839880870442));
#21543=CARTESIAN_POINT('Ctrl Pts',(2.13403574625664,1.33763395736447,2.70393206790445));
#21544=CARTESIAN_POINT('Ctrl Pts',(2.17834447459626,1.26205803152608,2.69849599581683));
#21545=CARTESIAN_POINT('Ctrl Pts',(2.18482995186509,1.25079702184486,2.69768476671425));
#21546=CARTESIAN_POINT('Ctrl Pts',(2.19526147742054,1.23235563727955,2.69635341592008));
#21547=CARTESIAN_POINT('Ctrl Pts',(2.19926025732571,1.22520516121395,2.69583650361944));
#21548=CARTESIAN_POINT('Ctrl Pts',(2.20637332013503,1.21233881061133,2.69490491367588));
#21549=CARTESIAN_POINT('Ctrl Pts',(2.20950042246204,1.20663022537022,2.69449105334225));
#21550=CARTESIAN_POINT('Ctrl Pts',(2.2163393576788,1.19402988783534,2.69357635275449));
#21551=CARTESIAN_POINT('Ctrl Pts',(2.22004115315811,1.18713301520003,2.69307492039927));
#21552=CARTESIAN_POINT('Ctrl Pts',(2.23067482018304,1.16709758389474,2.69161629212046));
#21553=CARTESIAN_POINT('Ctrl Pts',(2.23752250331571,1.15391505135971,2.69065413464249));
#21554=CARTESIAN_POINT('Ctrl Pts',(2.28848054339192,1.05365606101378,2.68332246710814));
#21555=CARTESIAN_POINT('Ctrl Pts',(2.32760090953802,0.964157929869422,2.67670089885606));
#21556=CARTESIAN_POINT('Ctrl Pts',(2.36142200370902,0.872635302058581,2.66999896006316));
#21557=CARTESIAN_POINT('Origin',(0.,0.,10.));
#21558=CARTESIAN_POINT('',(2.36142200724207,0.872635292497862,1.66658329180866));
#21559=CARTESIAN_POINT('',(2.36142200728636,0.872635292378021,1.94383454073647));
#21560=CARTESIAN_POINT('',(2.36142200728636,0.87263529237802,10.));
#21561=CARTESIAN_POINT('',(2.51749898697345,-0.00225844805835542,2.88741669746852));
#21562=CARTESIAN_POINT('Ctrl Pts',(2.36142200728636,0.872635292378021,1.94383454073647));
#21563=CARTESIAN_POINT('Ctrl Pts',(2.33265413141813,0.950483502015518,1.94907292625409));
#21564=CARTESIAN_POINT('Ctrl Pts',(2.30001172667712,1.02696408405365,1.95431131177171));
#21565=CARTESIAN_POINT('Ctrl Pts',(2.26365383506435,1.10167035223721,1.95954969728933));
#21566=CARTESIAN_POINT('Ctrl Pts',(2.2273076844016,1.1763524957391,1.96478639119009));
#21567=CARTESIAN_POINT('Ctrl Pts',(2.18724863159326,1.24926104878193,1.97002308509085));
#21568=CARTESIAN_POINT('Ctrl Pts',(2.14368314884031,1.32001091184054,1.97525977899161));
#21569=CARTESIAN_POINT('Ctrl Pts',(2.10011859343222,1.39075926890134,1.9804963614229));
#21570=CARTESIAN_POINT('Ctrl Pts',(2.05304799935803,1.45934863501175,1.9857329438542));
#21571=CARTESIAN_POINT('Ctrl Pts',(2.00272220913907,1.52542125428392,1.99096952628549));
#21572=CARTESIAN_POINT('Ctrl Pts',(1.95182111346055,1.5922491908284,1.9962659713528));
#21573=CARTESIAN_POINT('Ctrl Pts',(1.89759020054139,1.65650207795797,2.00156241642011));
#21574=CARTESIAN_POINT('Ctrl Pts',(1.8403309830746,1.71784403329746,2.00685886148742));
#21575=CARTESIAN_POINT('Ctrl Pts',(1.7836372765285,1.77858015525019,2.01210299711603));
#21576=CARTESIAN_POINT('Ctrl Pts',(1.72397519722586,1.83646231030203,2.01734713274463));
#21577=CARTESIAN_POINT('Ctrl Pts',(1.66167330739977,1.89120281024408,2.02259126837324));
#21578=CARTESIAN_POINT('Ctrl Pts',(1.59843924005638,1.94676235216823,2.0279138681599));
#21579=CARTESIAN_POINT('Ctrl Pts',(1.53248610333258,1.99908514507073,2.03323646794657));
#21580=CARTESIAN_POINT('Ctrl Pts',(1.4641892332896,2.04791507126609,2.03855906773323));
#21581=CARTESIAN_POINT('Ctrl Pts',(1.39589236324662,2.09674499746146,2.04388166751989));
#21582=CARTESIAN_POINT('Ctrl Pts',(1.32525220718384,2.14208184682114,2.04920426730656));
#21583=CARTESIAN_POINT('Ctrl Pts',(1.25266969650984,2.18371813232522,2.05452686709322));
#21584=CARTESIAN_POINT('Ctrl Pts',(1.18100561291598,2.22482757063473,2.05978211704952));
#21585=CARTESIAN_POINT('Ctrl Pts',(1.10718338004907,2.26248143958662,2.06503736700583));
#21586=CARTESIAN_POINT('Ctrl Pts',(1.03157001246663,2.29644716015405,2.07029261696213));
#21587=CARTESIAN_POINT('Ctrl Pts',(0.956063846954617,2.33036472527377,2.07554041620312));
#21588=CARTESIAN_POINT('Ctrl Pts',(0.878772008130202,2.36060434069963,2.08078821544411));
#21589=CARTESIAN_POINT('Ctrl Pts',(0.800087506862563,2.38697847316696,2.08603601468509));
#21590=CARTESIAN_POINT('Ctrl Pts',(0.720832879483858,2.41354370529602,2.09132183802644));
#21591=CARTESIAN_POINT('Ctrl Pts',(0.640165733872132,2.43618696587407,2.09660766136779));
#21592=CARTESIAN_POINT('Ctrl Pts',(0.558509796253283,2.45476537727929,2.10189348470913));
#21593=CARTESIAN_POINT('Ctrl Pts',(0.477586049366593,2.47317720017856,2.10713191124168));
#21594=CARTESIAN_POINT('Ctrl Pts',(0.395691630223132,2.48759667489879,2.11237033777423));
#21595=CARTESIAN_POINT('Ctrl Pts',(0.313254036815387,2.49793477865593,2.11760876430678));
#21596=CARTESIAN_POINT('Ctrl Pts',(0.230843555302572,2.50826948244018,2.1228454680371));
#21597=CARTESIAN_POINT('Ctrl Pts',(0.147890711783706,2.51452542371834,2.12808217176742));
#21598=CARTESIAN_POINT('Ctrl Pts',(0.0648308480982068,2.51666509713447,
2.13331887549774));
#21599=CARTESIAN_POINT('Ctrl Pts',(-0.0182267535231641,2.51880471227844,
2.13855543661092));
#21600=CARTESIAN_POINT('Ctrl Pts',(-0.101390908222088,2.51682827159825,
2.14379199772411));
#21601=CARTESIAN_POINT('Ctrl Pts',(-0.184224923671929,2.51075037140256,
2.1490285588373));
#21602=CARTESIAN_POINT('Ctrl Pts',(-0.268414684946125,2.50457299410477,
2.15435082684063));
#21603=CARTESIAN_POINT('Ctrl Pts',(-0.352262911315727,2.4941587115898,2.15967309484397));
#21604=CARTESIAN_POINT('Ctrl Pts',(-0.435316991251371,2.47957765902338,
2.16499536284731));
#21605=CARTESIAN_POINT('Ctrl Pts',(-0.517150970037226,2.46521080856497,
2.17023944438088));
#21606=CARTESIAN_POINT('Ctrl Pts',(-0.598213537433156,2.44679896233672,
2.17548352591445));
#21607=CARTESIAN_POINT('Ctrl Pts',(-0.678084274595561,2.42446034542663,
2.18072760744801));
#21608=CARTESIAN_POINT('Ctrl Pts',(-0.759741257148187,2.40162214315027,
2.18608896868624));
#21609=CARTESIAN_POINT('Ctrl Pts',(-0.840151972029443,2.37467957529194,
2.19145032992447));
#21610=CARTESIAN_POINT('Ctrl Pts',(-0.918887750789561,2.34381133017334,
2.19681169116269));
#21611=CARTESIAN_POINT('Ctrl Pts',(-0.997623529549678,2.31294308505473,
2.20217305240092));
#21612=CARTESIAN_POINT('Ctrl Pts',(-1.07468393658661,2.27814943264632,2.20753441363915));
#21613=CARTESIAN_POINT('Ctrl Pts',(-1.14966790242312,2.23965844809829,2.21289577487737));
#21614=CARTESIAN_POINT('Ctrl Pts',(-1.22316775138176,2.20192929468543,2.21815102160681));
#21615=CARTESIAN_POINT('Ctrl Pts',(-1.29494410802143,2.1605085163771,2.22340626833624));
#21616=CARTESIAN_POINT('Ctrl Pts',(-1.36460206538526,2.11557733329375,2.22866151506568));
#21617=CARTESIAN_POINT('Ctrl Pts',(-1.43416126292787,2.07070985284792,2.23390931099915));
#21618=CARTESIAN_POINT('Ctrl Pts',(-1.50160764236144,2.02234210140636,2.23915710693263));
#21619=CARTESIAN_POINT('Ctrl Pts',(-1.56656992694817,1.97070162987237,2.2444049028661));
#21620=CARTESIAN_POINT('Ctrl Pts',(-1.63200296161448,1.91868694495843,2.24969072702424));
#21621=CARTESIAN_POINT('Ctrl Pts',(-1.69491532586794,1.86335212458742,2.25497655118239));
#21622=CARTESIAN_POINT('Ctrl Pts',(-1.75495647585527,1.80497479701343,2.26026237534053));
#21623=CARTESIAN_POINT('Ctrl Pts',(-1.81445920139815,1.74712097340586,2.26550079839233));
#21624=CARTESIAN_POINT('Ctrl Pts',(-1.87114166523572,1.6862793195283,2.27073922144413));
#21625=CARTESIAN_POINT('Ctrl Pts',(-1.9246964437954,1.62275994812583,2.27597764449592));
#21626=CARTESIAN_POINT('Ctrl Pts',(-1.9782336087776,1.5592614675458,2.28121434468801));
#21627=CARTESIAN_POINT('Ctrl Pts',(-2.02864483426583,1.49308737099406,2.28645104488009));
#21628=CARTESIAN_POINT('Ctrl Pts',(-2.07566163847028,1.42458239936582,2.29168774507218));
#21629=CARTESIAN_POINT('Ctrl Pts',(-2.12267716173675,1.35607929410476,2.29692430259425));
#21630=CARTESIAN_POINT('Ctrl Pts',(-2.16629818733523,1.28524582104953,2.30216086011633));
#21631=CARTESIAN_POINT('Ctrl Pts',(-2.20629920064349,1.21245622075187,2.3073974176384));
#21632=CARTESIAN_POINT('Ctrl Pts',(-2.24695497031956,1.13847516427939,2.31271968972366));
#21633=CARTESIAN_POINT('Ctrl Pts',(-2.28387090180366,1.06247378967159,2.31804196180892));
#21634=CARTESIAN_POINT('Ctrl Pts',(-2.31685939799245,0.984869930464954,
2.32336423389419));
#21635=CARTESIAN_POINT('Ctrl Pts',(-2.3493632308149,0.908406218642723,2.32860831174196));
#21636=CARTESIAN_POINT('Ctrl Pts',(-2.37805416120823,0.830387257136895,
2.33385238958973));
#21637=CARTESIAN_POINT('Ctrl Pts',(-2.4028024577348,0.751230057374981,2.33909646743751));
#21638=CARTESIAN_POINT('Ctrl Pts',(-2.42810428556819,0.670302392798165,
2.34445783664152));
#21639=CARTESIAN_POINT('Ctrl Pts',(-2.44928485791634,0.588185454647371,
2.34981920584553));
#21640=CARTESIAN_POINT('Ctrl Pts',(-2.46626066743033,0.505336096361721,
2.35518057504954));
#21641=CARTESIAN_POINT('Ctrl Pts',(-2.48323647694432,0.422486738076075,
2.36054194425355));
#21642=CARTESIAN_POINT('Ctrl Pts',(-2.49600751290881,0.338905472027392,
2.36590331345755));
#21643=CARTESIAN_POINT('Ctrl Pts',(-2.50454672006448,0.255052890621214,
2.37126468266156));
#21644=CARTESIAN_POINT('Ctrl Pts',(-2.51291690935513,0.172860016495573,
2.37651993344498));
#21645=CARTESIAN_POINT('Ctrl Pts',(-2.51725222683093,0.0901028851533855,
2.38177518422839));
#21646=CARTESIAN_POINT('Ctrl Pts',(-2.51748967139839,0.0072114077971777,
2.38703043501181));
#21647=CARTESIAN_POINT('Ctrl Pts',(-2.51772677932425,-0.0755625485714478,
2.39227823506227));
#21648=CARTESIAN_POINT('Ctrl Pts',(-2.5138775530656,-0.158470015052679,
2.39752603511273));
#21649=CARTESIAN_POINT('Ctrl Pts',(-2.5059307189532,-0.241075676514023,
2.40277383516319));
#21650=CARTESIAN_POINT('Ctrl Pts',(-2.49792630582551,-0.324279859673127,
2.40805965829996));
#21651=CARTESIAN_POINT('Ctrl Pts',(-2.48576460762758,-0.407177374436601,
2.41334548143673));
#21652=CARTESIAN_POINT('Ctrl Pts',(-2.46948764310001,-0.489323032951007,
2.41863130457351));
#21653=CARTESIAN_POINT('Ctrl Pts',(-2.45335662754912,-0.570732124473509,
2.4238697318659));
#21654=CARTESIAN_POINT('Ctrl Pts',(-2.43318394130393,-0.651402327969849,
2.42910815915829));
#21655=CARTESIAN_POINT('Ctrl Pts',(-2.40906232782647,-0.730906937063328,
2.43434658645068));
#21656=CARTESIAN_POINT('Ctrl Pts',(-2.38494864750538,-0.810385398548718,
2.43958329092039));
#21657=CARTESIAN_POINT('Ctrl Pts',(-2.35688875315938,-0.888698585773644,
2.4448199953901));
#21658=CARTESIAN_POINT('Ctrl Pts',(-2.32502563597652,-0.965433603129697,
2.45005669985981));
#21659=CARTESIAN_POINT('Ctrl Pts',(-2.29316338668939,-1.04216653035772,
2.45529326169082));
#21660=CARTESIAN_POINT('Ctrl Pts',(-2.25749829843715,-1.11732094743798,
2.46052982352183));
#21661=CARTESIAN_POINT('Ctrl Pts',(-2.21822150001762,-1.19050393819575,
2.46576638535285));
#21662=CARTESIAN_POINT('Ctrl Pts',(-2.17830186984482,-1.26488469333735,
2.47108865244392));
#21663=CARTESIAN_POINT('Ctrl Pts',(-2.13465146028981,-1.3372284689841,2.47641091953499));
#21664=CARTESIAN_POINT('Ctrl Pts',(-2.08751860851424,-1.40715042163473,
2.48173318662607));
#21665=CARTESIAN_POINT('Ctrl Pts',(-2.04107814539084,-1.47604521032795,
2.4869772688164));
#21666=CARTESIAN_POINT('Ctrl Pts',(-1.99125720574241,-1.54258851974971,
2.49222135100673));
#21667=CARTESIAN_POINT('Ctrl Pts',(-1.93833494345258,-1.60644448923412,
2.49746543319706));
#21668=CARTESIAN_POINT('Ctrl Pts',(-1.88422914083846,-1.67172851775383,
2.50282679273851));
#21669=CARTESIAN_POINT('Ctrl Pts',(-1.82688197361883,-1.73420318074725,
2.50818815227995));
#21670=CARTESIAN_POINT('Ctrl Pts',(-1.7666311789406,-1.79354970034147,2.51354951182139));
#21671=CARTESIAN_POINT('Ctrl Pts',(-1.70638038426236,-1.85289621993568,
2.51891087136284));
#21672=CARTESIAN_POINT('Ctrl Pts',(-1.64322638605859,-1.90911430818517,
2.52427223090428));
#21673=CARTESIAN_POINT('Ctrl Pts',(-1.57754079279172,-1.96193050261167,
2.52963359044573));
#21674=CARTESIAN_POINT('Ctrl Pts',(-1.51315522620229,-2.01370137707772,
2.53488883980251));
#21675=CARTESIAN_POINT('Ctrl Pts',(-1.44609957370261,-2.06239504521322,
2.54014408915929));
#21676=CARTESIAN_POINT('Ctrl Pts',(-1.37670014015963,-2.10772459635609,
2.54539933851607));
#21677=CARTESIAN_POINT('Ctrl Pts',(-1.30739909920855,-2.1529898805187,2.55064713712609));
#21678=CARTESIAN_POINT('Ctrl Pts',(-1.23576126065028,-2.19490027118673,
2.5558949357361));
#21679=CARTESIAN_POINT('Ctrl Pts',(-1.16214562522365,-2.23320930406747,
2.56114273434611));
#21680=CARTESIAN_POINT('Ctrl Pts',(-1.08799658021141,-2.2717959193563,2.56642855784127));
#21681=CARTESIAN_POINT('Ctrl Pts',(-1.01184132497023,-2.30672846972519,
2.57171438133643));
#21682=CARTESIAN_POINT('Ctrl Pts',(-0.934076156963984,-2.33779981670617,
2.57700020483159));
#21683=CARTESIAN_POINT('Ctrl Pts',(-0.857008304613156,-2.36859254875914,
2.58223863066055));
#21684=CARTESIAN_POINT('Ctrl Pts',(-0.778359732224536,-2.39559287208768,
2.58747705648951));
#21685=CARTESIAN_POINT('Ctrl Pts',(-0.698538851910779,-2.41864625821371,
2.59271548231847));
#21686=CARTESIAN_POINT('Ctrl Pts',(-0.618744223309859,-2.44169206247807,
2.59795218531939));
#21687=CARTESIAN_POINT('Ctrl Pts',(-0.537778495463607,-2.4607933796665,
2.60318888832031));
#21688=CARTESIAN_POINT('Ctrl Pts',(-0.456065853583791,-2.47584534799629,
2.60842559132124));
#21689=CARTESIAN_POINT('Ctrl Pts',(-0.374355437466878,-2.49089690632695,
2.6136621516801));
#21690=CARTESIAN_POINT('Ctrl Pts',(-0.291898601740537,-2.50189925252725,
2.61889871203897));
#21691=CARTESIAN_POINT('Ctrl Pts',(-0.209128981627125,-2.50879878010246,
2.62413527239784));
#21692=CARTESIAN_POINT('Ctrl Pts',(-0.12500464463323,-2.51581123445517,
2.62945754121718));
#21693=CARTESIAN_POINT('Ctrl Pts',(-0.0405576809259553,-2.51858530024611,
2.63477981003652));
#21694=CARTESIAN_POINT('Ctrl Pts',(0.0437538975583074,-2.51711975210725,
2.64010207885586));
#21695=CARTESIAN_POINT('Ctrl Pts',(0.126826876137409,-2.51567573396247,
2.64534615958083));
#21696=CARTESIAN_POINT('Ctrl Pts',(0.209767958040033,-2.51011593374228,
2.6505902403058));
#21697=CARTESIAN_POINT('Ctrl Pts',(0.292143440366348,-2.50049164370748,
2.65583432103077));
#21698=CARTESIAN_POINT('Ctrl Pts',(0.376361223275997,-2.49065210958979,
2.66119568389729));
#21699=CARTESIAN_POINT('Ctrl Pts',(0.459987297506857,-2.47656417495975,
2.66655704676382));
#21700=CARTESIAN_POINT('Ctrl Pts',(0.542570392136683,-2.45833757233962,
2.67191840963034));
#21701=CARTESIAN_POINT('Ctrl Pts',(0.625153486766509,-2.44011096971949,
2.67727977249686));
#21702=CARTESIAN_POINT('Ctrl Pts',(0.706693129455465,-2.41774589792986,
2.68264113536339));
#21703=CARTESIAN_POINT('Ctrl Pts',(0.78675761828311,-2.39140517271195,2.68800249822991));
#21704=CARTESIAN_POINT('Ctrl Pts',(0.865237445155743,-2.36558579154721,
2.69325774728885));
#21705=CARTESIAN_POINT('Ctrl Pts',(0.942589867960649,-2.33585137359311,
2.69851299634779));
#21706=CARTESIAN_POINT('Ctrl Pts',(1.01839657108159,-2.30231941181263,2.70376824540673));
#21707=CARTESIAN_POINT('Ctrl Pts',(1.09409579741994,-2.2688349907801,2.70901604370951));
#21708=CARTESIAN_POINT('Ctrl Pts',(1.16825323853503,-2.23156390533443,2.71426384201229));
#21709=CARTESIAN_POINT('Ctrl Pts',(1.24046670358489,-2.19067309457555,2.71951164031506));
#21710=CARTESIAN_POINT('Ctrl Pts',(1.31320342357032,-2.14948599117189,2.72479746388586));
#21711=CARTESIAN_POINT('Ctrl Pts',(1.38396742657179,-2.10462663253549,2.73008328745665));
#21712=CARTESIAN_POINT('Ctrl Pts',(1.45236920159089,-2.05631465303106,2.73536911102744));
#21713=CARTESIAN_POINT('Ctrl Pts',(1.52015761673026,-2.00843588786837,2.74060753652839));
#21714=CARTESIAN_POINT('Ctrl Pts',(1.58562561464942,-1.95716644436069,2.74584596202934));
#21715=CARTESIAN_POINT('Ctrl Pts',(1.64842121744586,-1.90276476209602,2.75108438753029));
#21716=CARTESIAN_POINT('Ctrl Pts',(1.71119616776366,-1.84838097168254,2.75632109019611));
#21717=CARTESIAN_POINT('Ctrl Pts',(1.77130012004533,-1.79086729032705,2.76155779286192));
#21718=CARTESIAN_POINT('Ctrl Pts',(1.828414168735,-1.73052242908582,2.76679449552774));
#21719=CARTESIAN_POINT('Ctrl Pts',(1.88552666162767,-1.67017921164952,2.77203105554483));
#21720=CARTESIAN_POINT('Ctrl Pts',(1.93964909643247,-1.60700530349576,2.77726761556192));
#21721=CARTESIAN_POINT('Ctrl Pts',(1.99050041505611,-1.54133524830305,2.78250417557901));
#21722=CARTESIAN_POINT('Ctrl Pts',(2.04218404059567,-1.47459034111862,2.78782644478193));
#21723=CARTESIAN_POINT('Ctrl Pts',(2.09048819269342,-1.40526721925857,2.79314871398485));
#21724=CARTESIAN_POINT('Ctrl Pts',(2.13516247809648,-1.33374939255053,2.79847098318777));
#21725=CARTESIAN_POINT('Ctrl Pts',(2.17918045881088,-1.26328222584898,2.80371506355789));
#21726=CARTESIAN_POINT('Ctrl Pts',(2.21967434238095,-1.19068484919091,2.808959143928));
#21727=CARTESIAN_POINT('Ctrl Pts',(2.25645102213422,-1.11634897532512,2.81420322429812));
#21728=CARTESIAN_POINT('Ctrl Pts',(2.29405020806441,-1.0403505882626,2.81956458791744));
#21729=CARTESIAN_POINT('Ctrl Pts',(2.32776371056333,-0.962535472885557,
2.82492595153677));
#21730=CARTESIAN_POINT('Ctrl Pts',(2.35743787716961,-0.883341896032365,
2.8302873151561));
#21731=CARTESIAN_POINT('Ctrl Pts',(2.38711204377589,-0.804148319179173,
2.83564867877542));
#21732=CARTESIAN_POINT('Ctrl Pts',(2.4127467840924,-0.723576785293608,2.84101004239475));
#21733=CARTESIAN_POINT('Ctrl Pts',(2.43424362587157,-0.642078048140283,
2.84637140601408));
#21734=CARTESIAN_POINT('Ctrl Pts',(2.4616727216149,-0.538088974428746,2.85321228792315));
#21735=CARTESIAN_POINT('Ctrl Pts',(2.48245069282632,-0.432277824801234,
2.86005316983222));
#21736=CARTESIAN_POINT('Ctrl Pts',(2.49638302074693,-0.325389095893594,
2.8668940517413));
#21737=CARTESIAN_POINT('Ctrl Pts',(2.51031534866753,-0.21850036698595,2.87373493365037));
#21738=CARTESIAN_POINT('Ctrl Pts',(2.5174018532492,-0.110533708811776,2.88057581555944));
#21739=CARTESIAN_POINT('Ctrl Pts',(2.51749898697345,-0.00225844805835206,
2.88741669746852));
#21740=CARTESIAN_POINT('Ctrl Pts',(2.51749898697402,-0.00225844743326701,
2.88741669750801));
#21741=CARTESIAN_POINT('Ctrl Pts',(2.51757261561498,0.0798156475007308,
2.89260217743504));
#21742=CARTESIAN_POINT('Ctrl Pts',(2.51362838985468,0.161986453160739,2.89778765736208));
#21743=CARTESIAN_POINT('Ctrl Pts',(2.50566466175838,0.243825455634248,2.90297313728911));
#21744=CARTESIAN_POINT('Ctrl Pts',(2.49770584428074,0.325613994288886,2.90815541972948));
#21745=CARTESIAN_POINT('Ctrl Pts',(2.4857324912812,0.407070667135054,2.91333770216984));
#21746=CARTESIAN_POINT('Ctrl Pts',(2.46979497608291,0.487769439505618,2.9185199846102));
#21747=CARTESIAN_POINT('Ctrl Pts',(2.4538590637285,0.568460095960229,2.92370174586582));
#21748=CARTESIAN_POINT('Ctrl Pts',(2.4339598626489,0.648392538286256,2.92888350712144));
#21749=CARTESIAN_POINT('Ctrl Pts',(2.41019910481231,0.72714958926064,2.93406526837706));
#21750=CARTESIAN_POINT('Ctrl Pts',(2.39542133466959,0.776131764173706,2.93728801393495));
#21751=CARTESIAN_POINT('Ctrl Pts',(2.37915089320259,0.824659486525423,2.94051075949285));
#21752=CARTESIAN_POINT('Ctrl Pts',(2.36142200728636,0.872635292378019,2.94373350505074));
#21753=CARTESIAN_POINT('',(2.51749999784475,0.000104171493018674,2.61023257544742));
#21754=CARTESIAN_POINT('Ctrl Pts',(2.36142200370902,0.872635302058581,2.66999896006316));
#21755=CARTESIAN_POINT('Ctrl Pts',(2.36560483263882,0.861316227240872,2.66917009677071));
#21756=CARTESIAN_POINT('Ctrl Pts',(2.36970660561097,0.849966189911584,2.66833995597539));
#21757=CARTESIAN_POINT('Ctrl Pts',(2.44966690857208,0.623628147166383,2.65180981247241));
#21758=CARTESIAN_POINT('Ctrl Pts',(2.49607367105078,0.399296602080148,2.63599979237781));
#21759=CARTESIAN_POINT('Ctrl Pts',(2.51373507564165,0.141034278453407,2.61920134346827));
#21760=CARTESIAN_POINT('Ctrl Pts',(2.51527232959309,0.110272133569269,2.61722005897344));
#21761=CARTESIAN_POINT('Ctrl Pts',(2.51670862159752,0.0648055824669632,
2.61431949278353));
#21762=CARTESIAN_POINT('Ctrl Pts',(2.51704393563378,0.0501187643659415,
2.61338680522547));
#21763=CARTESIAN_POINT('Ctrl Pts',(2.51735379166243,0.0281036860631062,
2.61199492973371));
#21764=CARTESIAN_POINT('Ctrl Pts',(2.51742492146047,0.0207773004703606,
2.61153275554957));
#21765=CARTESIAN_POINT('Ctrl Pts',(2.51748783676618,0.00900187890311291,
2.61079154030412));
#21766=CARTESIAN_POINT('Ctrl Pts',(2.51749981375532,0.00455303872383315,
2.6105118753073));
#21767=CARTESIAN_POINT('Ctrl Pts',(2.51749999784475,0.000104171493018674,
2.61023257544742));
#21768=CARTESIAN_POINT('Ctrl Pts',(2.51749999784015,0.000104282475506742,
2.6102325824149));
#21769=CARTESIAN_POINT('Ctrl Pts',(2.51750022479702,-0.00537471984685295,
2.60988861067223));
#21770=CARTESIAN_POINT('Ctrl Pts',(2.51748256528205,-0.0108537515103197,
2.60954519348913));
#21771=CARTESIAN_POINT('Ctrl Pts',(2.51738144358299,-0.0264401591722797,
2.60856981810447));
#21772=CARTESIAN_POINT('Ctrl Pts',(2.51725499699461,-0.0365472206500459,
2.60793919480463));
#21773=CARTESIAN_POINT('Ctrl Pts',(2.51664876752044,-0.0692548427430348,
2.60590424622283));
#21774=CARTESIAN_POINT('Ctrl Pts',(2.51592544507136,-0.0918501948059999,
2.60450745476016));
#21775=CARTESIAN_POINT('Ctrl Pts',(2.51055257667226,-0.209929573437987,
2.59725081006728));
#21776=CARTESIAN_POINT('Ctrl Pts',(2.50077135808014,-0.30510696611966,2.59155198304949));
#21777=CARTESIAN_POINT('Ctrl Pts',(2.45882025594135,-0.566113290107611,
2.5760757995714));
#21778=CARTESIAN_POINT('Ctrl Pts',(2.41536020766425,-0.729598243129649,
2.56657451789204));
#21779=CARTESIAN_POINT('Ctrl Pts',(2.33486495002623,-0.943272842912999,
2.55323697219275));
#21780=CARTESIAN_POINT('Ctrl Pts',(2.31188277138799,-0.99827607715766,2.54971235222533));
#21781=CARTESIAN_POINT('Ctrl Pts',(2.27722642761517,-1.07358724792391,2.54469096161048));
#21782=CARTESIAN_POINT('Ctrl Pts',(2.2671870395028,-1.09462899172694,2.54326611708904));
#21783=CARTESIAN_POINT('Ctrl Pts',(2.24915360344967,-1.13111297926263,2.54075198124741));
#21784=CARTESIAN_POINT('Ctrl Pts',(2.24128895854769,-1.14661775202205,2.53966954485422));
#21785=CARTESIAN_POINT('Ctrl Pts',(2.22941641910484,-1.16943498521629,2.53805396455376));
#21786=CARTESIAN_POINT('Ctrl Pts',(2.22553157132549,-1.17681135903904,2.53752814049659));
#21787=CARTESIAN_POINT('Ctrl Pts',(2.21883643611925,-1.18937205870896,2.53662646318241));
#21788=CARTESIAN_POINT('Ctrl Pts',(2.21604446192654,-1.1945660158331,2.53625175754563));
#21789=CARTESIAN_POINT('Ctrl Pts',(2.20967806856464,-1.20631039347719,2.53540022030728));
#21790=CARTESIAN_POINT('Ctrl Pts',(2.20609283085704,-1.21285462867864,2.53492272254882));
#21791=CARTESIAN_POINT('Ctrl Pts',(2.19627463015713,-1.23058850053314,2.53362080340586));
#21792=CARTESIAN_POINT('Ctrl Pts',(2.18998537718652,-1.24174648784717,2.53279297834645));
#21793=CARTESIAN_POINT('Ctrl Pts',(2.15819618128822,-1.29715211045029,2.52864078190378));
#21794=CARTESIAN_POINT('Ctrl Pts',(2.1314408507088,-1.34066156928266,2.5252471349779));
#21795=CARTESIAN_POINT('Ctrl Pts',(2.09086086841776,-1.4023645892814,2.52027059419372));
#21796=CARTESIAN_POINT('Ctrl Pts',(2.0780807328474,-1.42123398151892,2.51872567664879));
#21797=CARTESIAN_POINT('Ctrl Pts',(1.9516489097758,-1.60255402837902,2.5036721197753));
#21798=CARTESIAN_POINT('Ctrl Pts',(1.81941891068677,-1.75124001647328,2.48976241523873));
#21799=CARTESIAN_POINT('Ctrl Pts',(1.60717857832517,-1.93961095658286,2.4707071243353));
#21800=CARTESIAN_POINT('Ctrl Pts',(1.54039068661423,-1.99306622145591,2.46507782694509));
#21801=CARTESIAN_POINT('Ctrl Pts',(1.45357079845143,-2.05557771053364,2.45820069727876));
#21802=CARTESIAN_POINT('Ctrl Pts',(1.43597592865269,-2.06790738893567,2.45682820446374));
#21803=CARTESIAN_POINT('Ctrl Pts',(1.40914459195788,-2.08620194459258,2.454766484838));
#21804=CARTESIAN_POINT('Ctrl Pts',(1.40002369501289,-2.09233379131881,2.45407099804921));
#21805=CARTESIAN_POINT('Ctrl Pts',(1.38213431595182,-2.10419120814286,2.45271720478694));
#21806=CARTESIAN_POINT('Ctrl Pts',(1.37336969813707,-2.10992217518418,2.45205870628358));
#21807=CARTESIAN_POINT('Ctrl Pts',(1.35352424940092,-2.12272256961129,2.4505782673358));
#21808=CARTESIAN_POINT('Ctrl Pts',(1.34242324566254,-2.12976027786114,2.44975751034793));
#21809=CARTESIAN_POINT('Ctrl Pts',(1.312082295444,-2.14866406178501,2.44753378448082));
#21810=CARTESIAN_POINT('Ctrl Pts',(1.29273654710529,-2.16035864414496,2.44613706835385));
#21811=CARTESIAN_POINT('Ctrl Pts',(1.19033445768652,-2.22039294032427,2.43884968431189));
#21812=CARTESIAN_POINT('Ctrl Pts',(1.10471341295377,-2.26421117102594,2.43312190391391));
#21813=CARTESIAN_POINT('Ctrl Pts',(0.881776871053521,-2.36263772187843,
2.41885789239743));
#21814=CARTESIAN_POINT('Ctrl Pts',(0.741788212895067,-2.41025672169114,
2.410499205523));
#21815=CARTESIAN_POINT('Ctrl Pts',(0.502840146069942,-2.46873321046211,
2.39623996392119));
#21816=CARTESIAN_POINT('Ctrl Pts',(0.405965795160245,-2.48649944424717,
2.39045479294018));
#21817=CARTESIAN_POINT('Ctrl Pts',(0.287642158107969,-2.50110015553808,
2.38312350322353));
#21818=CARTESIAN_POINT('Ctrl Pts',(0.266942202756421,-2.50339405497751,
2.3818311401278));
#21819=CARTESIAN_POINT('Ctrl Pts',(0.237294140502355,-2.50630766795479,
2.37996307821561));
#21820=CARTESIAN_POINT('Ctrl Pts',(0.228366863623841,-2.50713685413932,
2.37939838393723));
#21821=CARTESIAN_POINT('Ctrl Pts',(0.212872054347985,-2.50849260457689,
2.37841414210315));
#21822=CARTESIAN_POINT('Ctrl Pts',(0.206306578213213,-2.50904110243012,
2.37799581121172));
#21823=CARTESIAN_POINT('Ctrl Pts',(0.192431466204484,-2.51014543749658,
2.37710891200246));
#21824=CARTESIAN_POINT('Ctrl Pts',(0.185121657013629,-2.51069511398835,
2.3766400354175));
#21825=CARTESIAN_POINT('Ctrl Pts',(0.16529551279393,-2.51209892969087,2.37536408230954));
#21826=CARTESIAN_POINT('Ctrl Pts',(0.152775217827282,-2.5128914334879,2.37455373897499));
#21827=CARTESIAN_POINT('Ctrl Pts',(0.0938036517867975,-2.51618184731973,
2.37071706728717));
#21828=CARTESIAN_POINT('Ctrl Pts',(0.0472978336248556,-2.51748535224016,
2.3676334598008));
#21829=CARTESIAN_POINT('Ctrl Pts',(-0.0326801620692364,-2.51751032836194,
2.36225978815277));
#21830=CARTESIAN_POINT('Ctrl Pts',(-0.0661422488160582,-2.51685345064351,
2.35999019430042));
#21831=CARTESIAN_POINT('Ctrl Pts',(-0.158656355707367,-2.51319117636813,
2.35367213343477));
#21832=CARTESIAN_POINT('Ctrl Pts',(-0.217630409161568,-2.50877228192166,
2.34959621137581));
#21833=CARTESIAN_POINT('Ctrl Pts',(-0.421969968780054,-2.48620171532827,
2.33539773304633));
#21834=CARTESIAN_POINT('Ctrl Pts',(-0.565881758997117,-2.45744660560747,
2.32528446112953));
#21835=CARTESIAN_POINT('Ctrl Pts',(-0.777886672193769,-2.39546078138107,
2.31053636865557));
#21836=CARTESIAN_POINT('Ctrl Pts',(-0.848331731333832,-2.37142892868546,
2.30565756632621));
#21837=CARTESIAN_POINT('Ctrl Pts',(-0.936788748871013,-2.33680487856067,
2.29955731608922));
#21838=CARTESIAN_POINT('Ctrl Pts',(-0.955869977998377,-2.32906479660331,
2.29824288430192));
#21839=CARTESIAN_POINT('Ctrl Pts',(-0.986608206230737,-2.31615479066974,
2.29612732356208));
#21840=CARTESIAN_POINT('Ctrl Pts',(-0.998324342961222,-2.31112900611374,
2.29532140373033));
#21841=CARTESIAN_POINT('Ctrl Pts',(-1.02073366110338,-2.30131403881312,
2.29378059853873));
#21842=CARTESIAN_POINT('Ctrl Pts',(-1.03143254653928,-2.29653879164617,
2.29304526647651));
#21843=CARTESIAN_POINT('Ctrl Pts',(-1.05583912131422,-2.28544040980704,
2.29136828208717));
#21844=CARTESIAN_POINT('Ctrl Pts',(-1.06952413915976,-2.27906828512441,
2.290428325836));
#21845=CARTESIAN_POINT('Ctrl Pts',(-1.11283251538259,-2.258426697421,2.28745409324779));
#21846=CARTESIAN_POINT('Ctrl Pts',(-1.1422347663941,-2.24369945543102,2.28543553149689));
#21847=CARTESIAN_POINT('Ctrl Pts',(-1.32860154522244,-2.14573720157006,
2.27262697284913));
#21848=CARTESIAN_POINT('Ctrl Pts',(-1.47667366616995,-2.04665918456801,
2.26243304464846));
#21849=CARTESIAN_POINT('Ctrl Pts',(-1.65754905267989,-1.89570313683784,
2.24889460737264));
#21850=CARTESIAN_POINT('Ctrl Pts',(-1.70071134221037,-1.85707832599156,
2.24556495494219));
#21851=CARTESIAN_POINT('Ctrl Pts',(-1.80856586604532,-1.75364589905302,
2.23687992568517));
#21852=CARTESIAN_POINT('Ctrl Pts',(-1.87111819856363,-1.6867417203143,2.23147851143386));
#21853=CARTESIAN_POINT('Ctrl Pts',(-1.9427993712315,-1.60116878295874,2.22460785718118));
#21854=CARTESIAN_POINT('Ctrl Pts',(-1.95553036612376,-1.58559509227524,
2.22335882250004));
#21855=CARTESIAN_POINT('Ctrl Pts',(-1.97358638854975,-1.56295911362746,
2.2215425848302));
#21856=CARTESIAN_POINT('Ctrl Pts',(-1.97906331578201,-1.55601825519887,
2.22098556684161));
#21857=CARTESIAN_POINT('Ctrl Pts',(-1.98854662789488,-1.54386907976749,
2.22001010261365));
#21858=CARTESIAN_POINT('Ctrl Pts',(-1.99256935934669,-1.53867370616994,
2.21959280891932));
#21859=CARTESIAN_POINT('Ctrl Pts',(-2.00107505419219,-1.52759927160628,
2.2187028849454));
#21860=CARTESIAN_POINT('Ctrl Pts',(-2.00555239651119,-1.52171629702125,
2.21822990897928));
#21861=CARTESIAN_POINT('Ctrl Pts',(-2.01772912772273,-1.50556967330009,
2.21693133246535));
#21862=CARTESIAN_POINT('Ctrl Pts',(-2.02537594427001,-1.49526691327455,
2.21610227185164));
#21863=CARTESIAN_POINT('Ctrl Pts',(-2.06231407211538,-1.44469596449026,
2.21203235766072));
#21864=CARTESIAN_POINT('Ctrl Pts',(-2.09048301872307,-1.40362593035789,
2.20872574789864));
#21865=CARTESIAN_POINT('Ctrl Pts',(-2.13362218567366,-1.33654799236901,
2.20335591003126));
#21866=CARTESIAN_POINT('Ctrl Pts',(-2.14937906118414,-1.31105823982704,
2.20132213576879));
#21867=CARTESIAN_POINT('Ctrl Pts',(-2.24317752538977,-1.15308401081435,
2.18878360959522));
#21868=CARTESIAN_POINT('Ctrl Pts',(-2.30940209313332,-1.01395913328513,
2.17804683246056));
#21869=CARTESIAN_POINT('Ctrl Pts',(-2.40157803687309,-0.76355264308214,
2.15986799611763));
#21870=CARTESIAN_POINT('Ctrl Pts',(-2.43344731706674,-0.654927420935664,
2.1523203673732));
#21871=CARTESIAN_POINT('Ctrl Pts',(-2.46393348524573,-0.517314352749194,
2.14320230937293));
#21872=CARTESIAN_POINT('Ctrl Pts',(-2.4695073822765,-0.490016071083766,
2.14141429813739));
#21873=CARTESIAN_POINT('Ctrl Pts',(-2.47725339657793,-0.44858231429324,
2.13873072238977));
#21874=CARTESIAN_POINT('Ctrl Pts',(-2.47975997619498,-0.434512321720601,
2.13782468434218));
#21875=CARTESIAN_POINT('Ctrl Pts',(-2.48408431912514,-0.408981626612012,
2.1361898918949));
#21876=CARTESIAN_POINT('Ctrl Pts',(-2.4859429006225,-0.39752833552041,2.13545987234389));
#21877=CARTESIAN_POINT('Ctrl Pts',(-2.48977345262704,-0.372844894953186,
2.13389363311997));
#21878=CARTESIAN_POINT('Ctrl Pts',(-2.4917193051178,-0.35961100728991,2.13305825326488));
#21879=CARTESIAN_POINT('Ctrl Pts',(-2.49670570123404,-0.323712511507988,
2.13080356723848));
#21880=CARTESIAN_POINT('Ctrl Pts',(-2.49954311498457,-0.301020627110442,
2.12939062384565));
#21881=CARTESIAN_POINT('Ctrl Pts',(-2.51292293332564,-0.180725474898618,
2.12196052162249));
#21882=CARTESIAN_POINT('Ctrl Pts',(-2.51805950468641,-0.0826007767955057,
2.11611379869366));
#21883=CARTESIAN_POINT('Ctrl Pts',(-2.51640684271091,0.184398799697227,
2.10049861623488));
#21884=CARTESIAN_POINT('Ctrl Pts',(-2.49838437356912,0.35267353641864,2.09099564336493));
#21885=CARTESIAN_POINT('Ctrl Pts',(-2.45178286763654,0.574369063215822,
2.07774655092478));
#21886=CARTESIAN_POINT('Ctrl Pts',(-2.4379681123593,0.630436107401488,2.07432776116495));
#21887=CARTESIAN_POINT('Ctrl Pts',(-2.41601911304895,0.707940006103002,
2.06944522669334));
#21888=CARTESIAN_POINT('Ctrl Pts',(-2.40950038628094,0.729818621248891,
2.06804918640699));
#21889=CARTESIAN_POINT('Ctrl Pts',(-2.39757866579965,0.767929266536848,
2.06558137170981));
#21890=CARTESIAN_POINT('Ctrl Pts',(-2.39230597874035,0.784200793257984,
2.06451611056507));
#21891=CARTESIAN_POINT('Ctrl Pts',(-2.38423478344372,0.808269351151879,
2.06292135123098));
#21892=CARTESIAN_POINT('Ctrl Pts',(-2.3815628068336,0.816108717694153,2.06239890335881));
#21893=CARTESIAN_POINT('Ctrl Pts',(-2.37692440372529,0.829500648675597,
2.06150100576316));
#21894=CARTESIAN_POINT('Ctrl Pts',(-2.37497709962775,0.835059711927412,
2.06112667664012));
#21895=CARTESIAN_POINT('Ctrl Pts',(-2.37050665545302,0.847679577014091,
2.06027318516354));
#21896=CARTESIAN_POINT('Ctrl Pts',(-2.36797152035159,0.85473583296209,2.05979333641508));
#21897=CARTESIAN_POINT('Ctrl Pts',(-2.36096669852877,0.873962584112031,
2.05847887269019));
#21898=CARTESIAN_POINT('Ctrl Pts',(-2.35643452509574,0.886109847590886,
2.05764074715221));
#21899=CARTESIAN_POINT('Ctrl Pts',(-2.33286132897366,0.947831445650328,
2.05334493348961));
#21900=CARTESIAN_POINT('Ctrl Pts',(-2.31235025908706,0.996825866338199,
2.04981228270863));
#21901=CARTESIAN_POINT('Ctrl Pts',(-2.19271862139852,1.25898746302094,2.03037003294219));
#21902=CARTESIAN_POINT('Ctrl Pts',(-2.06565605735625,1.45813438501692,2.01376501548297));
#21903=CARTESIAN_POINT('Ctrl Pts',(-1.86627400937068,1.69113728768919,1.99332074143289));
#21904=CARTESIAN_POINT('Ctrl Pts',(-1.81746338161314,1.74348860633243,1.98863398682015));
#21905=CARTESIAN_POINT('Ctrl Pts',(-1.75199737476513,1.80796152945558,1.98273508253423));
#21906=CARTESIAN_POINT('Ctrl Pts',(-1.73733744101811,1.8220533331468,1.98143732819238));
#21907=CARTESIAN_POINT('Ctrl Pts',(-1.71325185510255,1.84465048787923,1.97934192634097));
#21908=CARTESIAN_POINT('Ctrl Pts',(-1.70393000710769,1.8532646551153,1.97853965446623));
#21909=CARTESIAN_POINT('Ctrl Pts',(-1.68586570463759,1.86970606088125,1.97700143879645));
#21910=CARTESIAN_POINT('Ctrl Pts',(-1.67713291177885,1.87754337682993,1.97626508231531));
#21911=CARTESIAN_POINT('Ctrl Pts',(-1.65695066385073,1.89540292992624,1.97457966403325));
#21912=CARTESIAN_POINT('Ctrl Pts',(-1.64546443038492,1.90538305690609,1.97363235812494));
#21913=CARTESIAN_POINT('Ctrl Pts',(-1.60931320740998,1.93622330846879,1.97068704487632));
#21914=CARTESIAN_POINT('Ctrl Pts',(-1.58433616989097,1.95671376179668,1.96870398387053));
#21915=CARTESIAN_POINT('Ctrl Pts',(-1.41643741785449,2.0891298042913,1.95569370805038));
#21916=CARTESIAN_POINT('Ctrl Pts',(-1.26216234749102,2.18579810029513,1.94529339369489));
#21917=CARTESIAN_POINT('Ctrl Pts',(-0.964779236302288,2.33006474161138,
1.92629611392895));
#21918=CARTESIAN_POINT('Ctrl Pts',(-0.825251536674082,2.38305441452863,
1.91772907586008));
#21919=CARTESIAN_POINT('Ctrl Pts',(-0.664509321501718,2.42828320333141,
1.90742293460748));
#21920=CARTESIAN_POINT('Ctrl Pts',(-0.647085178356231,2.43298431616534,
1.90630005073643));
#21921=CARTESIAN_POINT('Ctrl Pts',(-0.621417936861451,2.43961423802894,
1.90463553940599));
#21922=CARTESIAN_POINT('Ctrl Pts',(-0.613212808720353,2.44168956441407,
1.90410188560876));
#21923=CARTESIAN_POINT('Ctrl Pts',(-0.598660870817896,2.44529221685999,
1.90315243871837));
#21924=CARTESIAN_POINT('Ctrl Pts',(-0.592318377344968,2.446836284385,1.90273760318398));
#21925=CARTESIAN_POINT('Ctrl Pts',(-0.578557602613034,2.45012967789807,
1.90183530145457));
#21926=CARTESIAN_POINT('Ctrl Pts',(-0.571137478273156,2.45186996297007,
1.90134735785356));
#21927=CARTESIAN_POINT('Ctrl Pts',(-0.550547143093724,2.45660059652816,
1.89998968360787));
#21928=CARTESIAN_POINT('Ctrl Pts',(-0.537360821711074,2.45951864719021,
1.89911606500862));
#21929=CARTESIAN_POINT('Ctrl Pts',(-0.464323692886314,2.47506593446538,
1.89425671650388));
#21930=CARTESIAN_POINT('Ctrl Pts',(-0.404056113338046,2.48561566169853,
1.89017140535845));
#21931=CARTESIAN_POINT('Ctrl Pts',(-0.166614283085535,2.51831632051453,
1.87392865789657));
#21932=CARTESIAN_POINT('Ctrl Pts',(0.0123314257865917,2.52379279430711,
1.86141194082279));
#21933=CARTESIAN_POINT('Ctrl Pts',(0.303536657573069,2.50171035598399,1.84156580002127));
#21934=CARTESIAN_POINT('Ctrl Pts',(0.416016816254641,2.48548295025079,1.83401891064894));
#21935=CARTESIAN_POINT('Ctrl Pts',(0.549665061238158,2.45687002296113,1.82521749442003));
#21936=CARTESIAN_POINT('Ctrl Pts',(0.572230907692743,2.45171242929946,1.82373684788367));
#21937=CARTESIAN_POINT('Ctrl Pts',(0.607651323746474,2.44310113136202,1.82142067829603));
#21938=CARTESIAN_POINT('Ctrl Pts',(0.620554678088349,2.43985556372956,1.82057858165271));
#21939=CARTESIAN_POINT('Ctrl Pts',(0.644668820239365,2.4335864818603,1.81900776961239));
#21940=CARTESIAN_POINT('Ctrl Pts',(0.655885544201494,2.43058742131456,1.81827829434706));
#21941=CARTESIAN_POINT('Ctrl Pts',(0.680956591931032,2.4236978840098,1.81665028929571));
#21942=CARTESIAN_POINT('Ctrl Pts',(0.694799186698213,2.41976598389132,1.81575311681268));
#21943=CARTESIAN_POINT('Ctrl Pts',(0.72994662999056,2.40945610145229,1.81347900279893));
#21944=CARTESIAN_POINT('Ctrl Pts',(0.751202345189274,2.4029140376617,1.81210736814316));
#21945=CARTESIAN_POINT('Ctrl Pts',(0.926328524891839,2.34646290467242,1.80083003319136));
#21946=CARTESIAN_POINT('Ctrl Pts',(1.07515375563884,2.28211010879423,1.79143139705414));
#21947=CARTESIAN_POINT('Ctrl Pts',(1.32536533555651,2.1439670883371,1.77498943707993));
#21948=CARTESIAN_POINT('Ctrl Pts',(1.42935576611394,2.076084475189,1.76792071678127));
#21949=CARTESIAN_POINT('Ctrl Pts',(1.56271786500049,1.97424334219929,1.75799770766925));
#21950=CARTESIAN_POINT('Ctrl Pts',(1.59682012413603,1.94676371574629,1.75537601467513));
#21951=CARTESIAN_POINT('Ctrl Pts',(1.65144744876503,1.90034365583597,1.7510040334261));
#21952=CARTESIAN_POINT('Ctrl Pts',(1.67240562112858,1.88192560305948,1.74928298156938));
#21953=CARTESIAN_POINT('Ctrl Pts',(1.70049587031815,1.85640006495595,1.74690900168537));
#21954=CARTESIAN_POINT('Ctrl Pts',(1.70789863090861,1.84959175620835,1.74627685303655));
#21955=CARTESIAN_POINT('Ctrl Pts',(1.72022783664916,1.83811547453024,1.74521263327353));
#21956=CARTESIAN_POINT('Ctrl Pts',(1.72517665395886,1.83347152104003,1.74478235360709));
#21957=CARTESIAN_POINT('Ctrl Pts',(1.7345468485722,1.82460703749317,1.74396157623113));
#21958=CARTESIAN_POINT('Ctrl Pts',(1.73897174212099,1.82039031236408,1.74357138101861));
#21959=CARTESIAN_POINT('Ctrl Pts',(1.7494596066996,1.81032271359423,1.74264043584657));
#21960=CARTESIAN_POINT('Ctrl Pts',(1.75550860141213,1.80445747757804,1.74209860725028));
#21961=CARTESIAN_POINT('Ctrl Pts',(1.77683732280253,1.78356793540415,1.74017106712188));
#21962=CARTESIAN_POINT('Ctrl Pts',(1.7919540507707,1.76837950116006,1.73877363762351));
#21963=CARTESIAN_POINT('Ctrl Pts',(1.89755823187141,1.6595298514891,1.72879911891637));
#21964=CARTESIAN_POINT('Ctrl Pts',(1.98084395722714,1.55917202082583,1.71982091729261));
#21965=CARTESIAN_POINT('Ctrl Pts',(2.12265427685906,1.35848848506777,1.70284528725198));
#21966=CARTESIAN_POINT('Ctrl Pts',(2.18275402492497,1.25965886273768,1.69487041119613));
#21967=CARTESIAN_POINT('Ctrl Pts',(2.28013283157017,1.07148562326009,1.68057143425173));
#21968=CARTESIAN_POINT('Ctrl Pts',(2.31946612684565,0.983446993081237,1.67420304161951));
#21969=CARTESIAN_POINT('Ctrl Pts',(2.35627749479815,0.886463218134093,1.66752945036158));
#21970=CARTESIAN_POINT('Ctrl Pts',(2.35886495348818,0.879554887728603,1.66705586916765));
#21971=CARTESIAN_POINT('Ctrl Pts',(2.36142200724207,0.872635292497862,1.66658329180866));
#21972=CARTESIAN_POINT('Origin',(0.,0.,10.));
#21973=CARTESIAN_POINT('',(2.36142199806814,0.872635317323264,0.66916271832655));
#21974=CARTESIAN_POINT('',(2.36142200728636,0.872635292378021,0.943739684385603));
#21975=CARTESIAN_POINT('',(2.36142200728636,0.87263529237802,10.));
#21976=CARTESIAN_POINT('',(2.51749944581752,0.00167042164863851,0.612583302452829));
#21977=CARTESIAN_POINT('Ctrl Pts',(2.36142199806814,0.872635317323264,0.66916271832655));
#21978=CARTESIAN_POINT('Ctrl Pts',(2.37681768646397,0.830973334898781,0.666612244616638));
#21979=CARTESIAN_POINT('Ctrl Pts',(2.39111080605859,0.788903976832428,0.664061088185206));
#21980=CARTESIAN_POINT('Ctrl Pts',(2.42299547018568,0.686207656059237,0.657849231643885));
#21981=CARTESIAN_POINT('Ctrl Pts',(2.4394324974691,0.62526498961167,0.654176172148787));
#21982=CARTESIAN_POINT('Ctrl Pts',(2.46633440053622,0.508186762100082,0.647039638474432));
#21983=CARTESIAN_POINT('Ctrl Pts',(2.47721305089561,0.452187545013459,0.643591919008456));
#21984=CARTESIAN_POINT('Ctrl Pts',(2.48825441667045,0.382844904997875,0.639227439169845));
#21985=CARTESIAN_POINT('Ctrl Pts',(2.49022626481964,0.369801833019874,0.638402376229968));
#21986=CARTESIAN_POINT('Ctrl Pts',(2.49316143652721,0.34929770678135,0.637098032199428));
#21987=CARTESIAN_POINT('Ctrl Pts',(2.49419400660206,0.341846589068485,0.636622524686075));
#21988=CARTESIAN_POINT('Ctrl Pts',(2.49597303807743,0.328571631908365,0.63577248368067));
#21989=CARTESIAN_POINT('Ctrl Pts',(2.4967325409946,0.322749655427988,0.635398687562037));
#21990=CARTESIAN_POINT('Ctrl Pts',(2.49826595554394,0.310665857198052,0.634620831734606));
#21991=CARTESIAN_POINT('Ctrl Pts',(2.49903670379824,0.304403696526905,0.634216604903073));
#21992=CARTESIAN_POINT('Ctrl Pts',(2.50074151733824,0.290109463030347,0.633291448180771));
#21993=CARTESIAN_POINT('Ctrl Pts',(2.50166043510509,0.282075699662491,0.632769718083427));
#21994=CARTESIAN_POINT('Ctrl Pts',(2.50391801978371,0.261459208743697,0.631426548146041));
#21995=CARTESIAN_POINT('Ctrl Pts',(2.5052005339591,0.248870724191182,0.630602311351134));
#21996=CARTESIAN_POINT('Ctrl Pts',(2.51374345548572,0.158247419999016,0.624641789388791));
#21997=CARTESIAN_POINT('Ctrl Pts',(2.5174505050648,0.0799288784532003,0.619348271840614));
#21998=CARTESIAN_POINT('Ctrl Pts',(2.51749950767651,0.00157443594625835,
0.613985814047302));
#21999=CARTESIAN_POINT('',(-1.91346599666507,1.63598720337494,0.));
#22000=CARTESIAN_POINT('Ctrl Pts',(2.51749944581752,0.00167042164863862,
0.61258330245283));
#22001=CARTESIAN_POINT('Ctrl Pts',(2.51755363606023,-0.0799999195505381,
0.607399299002986));
#22002=CARTESIAN_POINT('Ctrl Pts',(2.5136294010915,-0.161821619082909,0.602215295553139));
#22003=CARTESIAN_POINT('Ctrl Pts',(2.50570901083512,-0.243369272957164,
0.597031292103296));
#22004=CARTESIAN_POINT('Ctrl Pts',(2.49779912369791,-0.324808787623776,
0.591854163088201));
#22005=CARTESIAN_POINT('Ctrl Pts',(2.48590365394244,-0.405974509605015,
0.586677034073107));
#22006=CARTESIAN_POINT('Ctrl Pts',(2.47005689828212,-0.486441331764581,
0.581499905058012));
#22007=CARTESIAN_POINT('Ctrl Pts',(2.45422172607578,-0.566849335340019,
0.576326560352901));
#22008=CARTESIAN_POINT('Ctrl Pts',(2.43444108857363,-0.646558988738404,
0.571153215647791));
#22009=CARTESIAN_POINT('Ctrl Pts',(2.41080092412554,-0.725151814612256,
0.56597987094268));
#22010=CARTESIAN_POINT('Ctrl Pts',(2.38717046687464,-0.803712368457708,
0.560808650532318));
#22011=CARTESIAN_POINT('Ctrl Pts',(2.35968376436198,-0.881156551101217,
0.555637430121958));
#22012=CARTESIAN_POINT('Ctrl Pts',(2.32847715353194,-0.957079095728153,
0.550466209711596));
#22013=CARTESIAN_POINT('Ctrl Pts',(2.29727336091083,-1.03299478393624,0.545295456304193));
#22014=CARTESIAN_POINT('Ctrl Pts',(2.26235050879355,-1.10738866876217,0.540124702896787));
#22015=CARTESIAN_POINT('Ctrl Pts',(2.22389323148074,-1.17987505481477,0.534953949489385));
#22016=CARTESIAN_POINT('Ctrl Pts',(2.18540220370415,-1.25242505559305,0.529778658180765));
#22017=CARTESIAN_POINT('Ctrl Pts',(2.1433707776255,-1.32306379366159,0.524603366872146));
#22018=CARTESIAN_POINT('Ctrl Pts',(2.09802942378302,-1.39143048225224,0.519428075563527));
#22019=CARTESIAN_POINT('Ctrl Pts',(2.05266856488632,-1.45982658099178,0.514250557935464));
#22020=CARTESIAN_POINT('Ctrl Pts',(2.00399522499661,-1.52594830190349,0.509073040307402));
#22021=CARTESIAN_POINT('Ctrl Pts',(1.95228156389339,-1.58946624540504,0.50389552267934));
#22022=CARTESIAN_POINT('Ctrl Pts',(1.90048050967036,-1.65309153058629,0.498709255343585));
#22023=CARTESIAN_POINT('Ctrl Pts',(1.84562918976615,-1.71410389642268,0.493522988007832));
#22024=CARTESIAN_POINT('Ctrl Pts',(1.78803790317884,-1.77220955498943,0.488336720672077));
#22025=CARTESIAN_POINT('Ctrl Pts',(1.73906674416392,-1.8216180960024,0.483926721565561));
#22026=CARTESIAN_POINT('Ctrl Pts',(1.68811520655394,-1.86892548692704,0.479516722459043));
#22027=CARTESIAN_POINT('Ctrl Pts',(1.63539196861162,-1.91397475401339,0.475106723352527));
#22028=CARTESIAN_POINT('Ctrl Pts',(1.57247470805091,-1.96773428370012,0.469844052210049));
#22029=CARTESIAN_POINT('Ctrl Pts',(1.50679114174476,-2.01848444144763,0.464581381067567));
#22030=CARTESIAN_POINT('Ctrl Pts',(1.43866062696852,-2.0659288105863,0.459318709925087));
#22031=CARTESIAN_POINT('Ctrl Pts',(1.37062496764678,-2.11330712478304,0.454063365794076));
#22032=CARTESIAN_POINT('Ctrl Pts',(1.30014950174808,-2.15738853258599,0.448808021663067));
#22033=CARTESIAN_POINT('Ctrl Pts',(1.22758734420499,-2.19791618637921,0.443552677532056));
#22034=CARTESIAN_POINT('Ctrl Pts',(1.15463018095667,-2.23866446005214,0.438268724950235));
#22035=CARTESIAN_POINT('Ctrl Pts',(1.07956389471693,-2.27581986235599,0.432984772368411));
#22036=CARTESIAN_POINT('Ctrl Pts',(1.00277781621867,-2.30916497922944,0.42770081978659));
#22037=CARTESIAN_POINT('Ctrl Pts',(0.926540176764554,-2.3422719310034,0.422454607456127));
#22038=CARTESIAN_POINT('Ctrl Pts',(0.848607660651047,-2.37162266619502,
0.417208395125666));
#22039=CARTESIAN_POINT('Ctrl Pts',(0.769385240476353,-2.39705081334067,
0.411962182795202));
#22040=CARTESIAN_POINT('Ctrl Pts',(0.690187749994883,-2.42247095876274,
0.406717621341645));
#22041=CARTESIAN_POINT('Ctrl Pts',(0.609701599172221,-2.44397082749234,
0.401473059888088));
#22042=CARTESIAN_POINT('Ctrl Pts',(0.528348914803874,-2.46143325609807,
0.396228498434532));
#22043=CARTESIAN_POINT('Ctrl Pts',(0.446997505831167,-2.47889541093896,
0.390984019201874));
#22044=CARTESIAN_POINT('Ctrl Pts',(0.364780040117444,-2.49232015610874,
0.385739539969215));
#22045=CARTESIAN_POINT('Ctrl Pts',(0.282129543584915,-2.50164129535722,
0.380495060736557));
#22046=CARTESIAN_POINT('Ctrl Pts',(0.198397557100848,-2.51108440263805,
0.37518195697254));
#22047=CARTESIAN_POINT('Ctrl Pts',(0.114221603733744,-2.516315660127,0.369868853208523));
#22048=CARTESIAN_POINT('Ctrl Pts',(0.0300561933397463,-2.51732057458758,
0.364555749444506));
#22049=CARTESIAN_POINT('Ctrl Pts',(-0.0531422727847476,-2.51831394396955,
0.359303685901333));
#22050=CARTESIAN_POINT('Ctrl Pts',(-0.136329974024215,-2.51517766013747,
0.35405162235816));
#22051=CARTESIAN_POINT('Ctrl Pts',(-0.219070760971157,-2.50795020917233,
0.348799558814987));
#22052=CARTESIAN_POINT('Ctrl Pts',(-0.303253985504742,-2.50059676053043,
0.343455934940547));
#22053=CARTESIAN_POINT('Ctrl Pts',(-0.386974071543444,-2.48900820957633,
0.338112311066108));
#22054=CARTESIAN_POINT('Ctrl Pts',(-0.469782010250341,-2.47327942474059,
0.332768687191669));
#22055=CARTESIAN_POINT('Ctrl Pts',(-0.552589948957238,-2.45755063990485,
0.327425063317229));
#22056=CARTESIAN_POINT('Ctrl Pts',(-0.634485275099095,-2.43768180027533,
0.322081439442788));
#22057=CARTESIAN_POINT('Ctrl Pts',(-0.715036549887057,-2.41382041219425,
0.316737815568349));
#22058=CARTESIAN_POINT('Ctrl Pts',(-0.793400342988758,-2.39060701323034,
0.311539305218113));
#22059=CARTESIAN_POINT('Ctrl Pts',(-0.870795262975601,-2.36352519602271,
0.306340794867879));
#22060=CARTESIAN_POINT('Ctrl Pts',(-0.946806110785062,-2.33267323870706,
0.301142284517644));
#22061=CARTESIAN_POINT('Ctrl Pts',(-1.0227074740887,-2.30186571993403,0.295951261997806));
#22062=CARTESIAN_POINT('Ctrl Pts',(-1.09722828924589,-2.26729901643482,
0.290760239477968));
#22063=CARTESIAN_POINT('Ctrl Pts',(-1.16996737546248,-2.22912148398275,
0.28556921695813));
#22064=CARTESIAN_POINT('Ctrl Pts',(-1.24423368667912,-2.19014237860704,
0.280269204075882));
#22065=CARTESIAN_POINT('Ctrl Pts',(-1.31664211485637,-2.14739921831778,
0.274969191193632));
#22066=CARTESIAN_POINT('Ctrl Pts',(-1.38678620559988,-2.10110215600239,
0.269669178311384));
#22067=CARTESIAN_POINT('Ctrl Pts',(-1.455367490382,-2.05583658934422,0.264487249385175));
#22068=CARTESIAN_POINT('Ctrl Pts',(-1.5217838796265,-2.00717412159218,0.259305320458967));
#22069=CARTESIAN_POINT('Ctrl Pts',(-1.58568124356746,-1.95535706299344,
0.254123391532758));
#22070=CARTESIAN_POINT('Ctrl Pts',(-1.64955996115625,-1.90355512550556,
0.24894297478273));
#22071=CARTESIAN_POINT('Ctrl Pts',(-1.71092074568316,-1.84860072127404,
0.243762558032702));
#22072=CARTESIAN_POINT('Ctrl Pts',(-1.76944123177445,-1.7907774784424,0.238582141282674));
#22073=CARTESIAN_POINT('Ctrl Pts',(-1.82796321126342,-1.73295276000619,
0.233401592332405));
#22074=CARTESIAN_POINT('Ctrl Pts',(-1.88364441326875,-1.67225939038837,
0.228221043382138));
#22075=CARTESIAN_POINT('Ctrl Pts',(-1.93619925700975,-1.60901792630004,
0.223040494431869));
#22076=CARTESIAN_POINT('Ctrl Pts',(-1.99087179530924,-1.54322815086992,
0.217651195544561));
#22077=CARTESIAN_POINT('Ctrl Pts',(-2.04216031683337,-1.4746809957138,0.212261896657254));
#22078=CARTESIAN_POINT('Ctrl Pts',(-2.08979094478388,-1.403773506339,0.206872597769946));
#22079=CARTESIAN_POINT('Ctrl Pts',(-2.13565388919363,-1.33549755904706,
0.201683308316679));
#22080=CARTESIAN_POINT('Ctrl Pts',(-2.17812547157535,-1.26503383316533,
0.196494018863409));
#22081=CARTESIAN_POINT('Ctrl Pts',(-2.21700767034701,-1.19276285975986,
0.191304729410142));
#22082=CARTESIAN_POINT('Ctrl Pts',(-2.25592163863668,-1.12043283583607,
0.186111199938822));
#22083=CARTESIAN_POINT('Ctrl Pts',(-2.2912401921896,-1.04629305424291,0.180917670467504));
#22084=CARTESIAN_POINT('Ctrl Pts',(-2.32281343696738,-0.970744037861583,
0.175724140996184));
#22085=CARTESIAN_POINT('Ctrl Pts',(-2.35444103009835,-0.895064975783177,
0.170521671684311));
#22086=CARTESIAN_POINT('Ctrl Pts',(-2.38231030568149,-0.81797228520106,
0.165319202372439));
#22087=CARTESIAN_POINT('Ctrl Pts',(-2.40632137520468,-0.739880861512898,
0.160116733060566));
#22088=CARTESIAN_POINT('Ctrl Pts',(-2.40901030051494,-0.731135644834104,
0.159534124635103));
#22089=CARTESIAN_POINT('Ctrl Pts',(-2.4116508929402,-0.722377911375065,
0.158951516209639));
#22090=CARTESIAN_POINT('Ctrl Pts',(-2.41424305246311,-0.71360824941532,
0.158368907784176));
#22091=CARTESIAN_POINT('Ctrl Pts',(-2.43827539171481,-0.63230326433367,
0.152967448804556));
#22092=CARTESIAN_POINT('Ctrl Pts',(-2.45823257024162,-0.549660683368054,
0.147565989824935));
#22093=CARTESIAN_POINT('Ctrl Pts',(-2.47397350173628,-0.466113036405061,
0.142164530845315));
#22094=CARTESIAN_POINT('Ctrl Pts',(-2.48968971854399,-0.38269656680855,
0.136771552645105));
#22095=CARTESIAN_POINT('Ctrl Pts',(-2.50120277584277,-0.298378277521893,
0.131378574444896));
#22096=CARTESIAN_POINT('Ctrl Pts',(-2.50842167175663,-0.213604697190072,
0.125985596244686));
#22097=CARTESIAN_POINT('Ctrl Pts',(-2.51562919183355,-0.128964706598124,
0.120601116524215));
#22098=CARTESIAN_POINT('Ctrl Pts',(-2.51855598739321,-0.0438712799426537,
0.115216636803746));
#22099=CARTESIAN_POINT('Ctrl Pts',(-2.51716249945789,0.0412213697360415,
0.109832157083275));
#22100=CARTESIAN_POINT('Ctrl Pts',(-2.51577030759958,0.126234875114859,
0.104452685443753));
#22101=CARTESIAN_POINT('Ctrl Pts',(-2.51006582998477,0.211247176543093,
0.0990732138042305));
#22102=CARTESIAN_POINT('Ctrl Pts',(-2.50006149470586,0.295801914613631,
0.0936937421647084));
#22103=CARTESIAN_POINT('Ctrl Pts',(-2.49006408324414,0.380298133898865,
0.0883179935589642));
#22104=CARTESIAN_POINT('Ctrl Pts',(-2.4757727839072,0.464336993480074,0.0829422449532235));
#22105=CARTESIAN_POINT('Ctrl Pts',(-2.45725194307627,0.547466106939874,
0.0775664963474796));
#22106=CARTESIAN_POINT('Ctrl Pts',(-2.43873951628433,0.630557454749165,
0.0721931899504231));
#22107=CARTESIAN_POINT('Ctrl Pts',(-2.41600146512598,0.712739459447074,
0.0668198835533652));
#22108=CARTESIAN_POINT('Ctrl Pts',(-2.38915325197096,0.793569775505975,
0.0614465771563086));
#22109=CARTESIAN_POINT('Ctrl Pts',(-2.36230312891944,0.874405841576472,
0.0560728885193252));
#22110=CARTESIAN_POINT('Ctrl Pts',(-2.33134238550205,0.953889615212508,
0.050699199882339));
#22111=CARTESIAN_POINT('Ctrl Pts',(-2.29643622565225,1.03159435414898,0.0453255112453554));
#22112=CARTESIAN_POINT('Ctrl Pts',(-2.26153094627027,1.10929713307259,0.0399519581535011));
#22113=CARTESIAN_POINT('Ctrl Pts',(-2.22268063027161,1.18522057628461,0.034578405061647));
#22114=CARTESIAN_POINT('Ctrl Pts',(-2.18009787371179,1.25895969396853,0.0292048519697925));
#22115=CARTESIAN_POINT('Ctrl Pts',(-2.13748475845543,1.3327513827793,0.0238274678890403));
#22116=CARTESIAN_POINT('Ctrl Pts',(-2.09113410476751,1.40435526322514,0.018450083808286));
#22117=CARTESIAN_POINT('Ctrl Pts',(-2.04130338933839,1.47339292881282,0.0130726997275339));
#22118=CARTESIAN_POINT('Ctrl Pts',(-2.00092303771321,1.52933764459313,0.00871513315168901));
#22119=CARTESIAN_POINT('Ctrl Pts',(-1.95825834189446,1.58359765574858,0.00435756657584321));
#22120=CARTESIAN_POINT('Ctrl Pts',(-1.91346599666507,1.63598720337494,-1.77635683940025E-15));
#22121=CARTESIAN_POINT('',(1.91360977481672,1.63581902413619,1.65132641005705E-6));
#22122=CARTESIAN_POINT('Origin',(0.,0.,0.));
#22123=CARTESIAN_POINT('',(2.51749949188307,0.00159949006993195,0.887416697568047));
#22124=CARTESIAN_POINT('Ctrl Pts',(1.91360977481672,1.63581902413619,1.65132641072319E-6));
#22125=CARTESIAN_POINT('Ctrl Pts',(1.86009423852759,1.69842243676096,0.00523991872577366));
#22126=CARTESIAN_POINT('Ctrl Pts',(1.80340192327242,1.7585155596962,0.0104781861251362));
#22127=CARTESIAN_POINT('Ctrl Pts',(1.74379813375851,1.81575723011099,0.0157164535244991));
#22128=CARTESIAN_POINT('Ctrl Pts',(1.68427848419545,1.87291809507072,0.0209473263007164));
#22129=CARTESIAN_POINT('Ctrl Pts',(1.62185585512159,1.92723518240283,0.0261781990769335));
#22130=CARTESIAN_POINT('Ctrl Pts',(1.55683525052212,1.97840093326195,0.031409071853151));
#22131=CARTESIAN_POINT('Ctrl Pts',(1.49188840291163,2.02950864356998,0.0366340109191525));
#22132=CARTESIAN_POINT('Ctrl Pts',(1.4243497999245,2.07747183574107,0.0418589499851537));
#22133=CARTESIAN_POINT('Ctrl Pts',(1.35455959449404,2.12202133706618,0.0470838890511551));
#22134=CARTESIAN_POINT('Ctrl Pts',(1.28481247118473,2.16654333758367,0.0523056027153035));
#22135=CARTESIAN_POINT('Ctrl Pts',(1.2128168951504,2.20765558081316,0.0575273163794534));
#22136=CARTESIAN_POINT('Ctrl Pts',(1.13894330276347,2.24513126633839,0.0627490300436016));
#22137=CARTESIAN_POINT('Ctrl Pts',(1.06509264495393,2.28259531727295,0.0679691225899423));
#22138=CARTESIAN_POINT('Ctrl Pts',(0.989365542862862,2.31642484251573,0.0731892151362824));
#22139=CARTESIAN_POINT('Ctrl Pts',(0.912157161652249,2.34643891087037,0.0784093076826231));
#22140=CARTESIAN_POINT('Ctrl Pts',(0.834949059074677,2.3764528709089,0.0836293813904616));
#22141=CARTESIAN_POINT('Ctrl Pts',(0.756260121759999,2.40265123454484,0.0888494550983027));
#22142=CARTESIAN_POINT('Ctrl Pts',(0.676504282709394,2.42490168985793,0.0940695288061413));
#22143=CARTESIAN_POINT('Ctrl Pts',(0.596671652308013,2.44717356858702,0.0992946285599214));
#22144=CARTESIAN_POINT('Ctrl Pts',(0.515770517139345,2.46548982200541,0.104519728313704));
#22145=CARTESIAN_POINT('Ctrl Pts',(0.434228159148547,2.47976856900044,0.109744828067484));
#22146=CARTESIAN_POINT('Ctrl Pts',(0.352646405999318,2.49405421441628,0.114972452198014));
#22147=CARTESIAN_POINT('Ctrl Pts',(0.270423274645153,2.50429841098978,0.120200076328541));
#22148=CARTESIAN_POINT('Ctrl Pts',(0.187991931561763,2.51047112782993,0.12542770045907));
#22149=CARTESIAN_POINT('Ctrl Pts',(0.105419192746191,2.51665443282484,0.130664291612505));
#22150=CARTESIAN_POINT('Ctrl Pts',(0.0226379940687081,2.51875229510584,
0.135900882765937));
#22151=CARTESIAN_POINT('Ctrl Pts',(-0.059917986517188,2.51678685726299,
0.141137473919372));
#22152=CARTESIAN_POINT('Ctrl Pts',(-0.128036847781654,2.5151651287487,0.145458307173946));
#22153=CARTESIAN_POINT('Ctrl Pts',(-0.196002288236653,2.51077797126332,
0.149779140428521));
#22154=CARTESIAN_POINT('Ctrl Pts',(-0.263574933994023,2.50366421553891,
0.154099973683095));
#22155=CARTESIAN_POINT('Ctrl Pts',(-0.345901347362564,2.49499724700738,
0.159364214865687));
#22156=CARTESIAN_POINT('Ctrl Pts',(-0.427945869163083,2.48224998394257,
0.16462845604828));
#22157=CARTESIAN_POINT('Ctrl Pts',(-0.509273485255483,2.46545062153265,
0.169892697230871));
#22158=CARTESIAN_POINT('Ctrl Pts',(-0.590488851465099,2.44867444591403,
0.175149672610233));
#22159=CARTESIAN_POINT('Ctrl Pts',(-0.670988831084925,2.42785737344303,
0.180406647989593));
#22160=CARTESIAN_POINT('Ctrl Pts',(-0.750343951568759,2.40307931711464,
0.185663623368955));
#22161=CARTESIAN_POINT('Ctrl Pts',(-0.830100257938074,2.37817599342596,
0.190947175789718));
#22162=CARTESIAN_POINT('Ctrl Pts',(-0.908699628614368,2.34927157097849,
0.196230728210483));
#22163=CARTESIAN_POINT('Ctrl Pts',(-0.985716841942823,2.3164992030023,0.201514280631246));
#22164=CARTESIAN_POINT('Ctrl Pts',(-1.06221560148537,2.2839474475037,0.206762265967234));
#22165=CARTESIAN_POINT('Ctrl Pts',(-1.13715301185763,2.24757984596568,0.212010251303225));
#22166=CARTESIAN_POINT('Ctrl Pts',(-1.21012965718489,2.20757615107647,0.217258236639212));
#22167=CARTESIAN_POINT('Ctrl Pts',(-1.28308404635457,2.16758465637175,0.222504621463309));
#22168=CARTESIAN_POINT('Ctrl Pts',(-1.35407845556301,2.1239594917239,0.227751006287403));
#22169=CARTESIAN_POINT('Ctrl Pts',(-1.42273741331739,2.07692669652709,0.2329973911115));
#22170=CARTESIAN_POINT('Ctrl Pts',(-1.49139593290246,2.02989420148526,0.238243742454098));
#22171=CARTESIAN_POINT('Ctrl Pts',(-1.55771865220263,1.9794543798231,0.243490093796699));
#22172=CARTESIAN_POINT('Ctrl Pts',(-1.62135961873937,1.92587622570126,0.248736445139297));
#22173=CARTESIAN_POINT('Ctrl Pts',(-1.68578524814015,1.87163747840884,0.254047481499962));
#22174=CARTESIAN_POINT('Ctrl Pts',(-1.74746216178544,1.81418277684423,0.259358517860623));
#22175=CARTESIAN_POINT('Ctrl Pts',(-1.8060678899512,1.75383152750976,0.264669554221287));
#22176=CARTESIAN_POINT('Ctrl Pts',(-1.86404468745398,1.69412794099672,0.26992359489699));
#22177=CARTESIAN_POINT('Ctrl Pts',(-1.91901564041973,1.63159006804883,0.275177635572696));
#22178=CARTESIAN_POINT('Ctrl Pts',(-1.97070862699392,1.56656112472247,0.2804316762484));
#22179=CARTESIAN_POINT('Ctrl Pts',(-2.0232427596572,1.50047403318335,0.285771210451545));
#22180=CARTESIAN_POINT('Ctrl Pts',(-2.07239100817816,1.43181448141849,0.291110744654691));
#22181=CARTESIAN_POINT('Ctrl Pts',(-2.11791413260419,1.36097243797053,0.296450278857836));
#22182=CARTESIAN_POINT('Ctrl Pts',(-2.16343725703023,1.29013039452256,0.301789813060982));
#22183=CARTESIAN_POINT('Ctrl Pts',(-2.20533506873481,1.21710631747659,0.307129347264126));
#22184=CARTESIAN_POINT('Ctrl Pts',(-2.24341839400878,1.14231351187976,0.312468881467272));
#22185=CARTESIAN_POINT('Ctrl Pts',(-2.28085037427587,1.06879989921385,0.317717092790461));
#22186=CARTESIAN_POINT('Ctrl Pts',(-2.31473604611418,0.993305135517561,
0.32296530411365));
#22187=CARTESIAN_POINT('Ctrl Pts',(-2.34486098057096,0.916205889413401,
0.32821351543684));
#22188=CARTESIAN_POINT('Ctrl Pts',(-2.37494258213299,0.839217545907933,
0.333454177525716));
#22189=CARTESIAN_POINT('Ctrl Pts',(-2.40127402338612,0.760629731212215,
0.338694839614592));
#22190=CARTESIAN_POINT('Ctrl Pts',(-2.42368708901712,0.680842966132206,
0.343935501703468));
#22191=CARTESIAN_POINT('Ctrl Pts',(-2.44630087689435,0.600341663426275,
0.349223097017967));
#22192=CARTESIAN_POINT('Ctrl Pts',(-2.46492552564214,0.518620248947559,
0.354510692332466));
#22193=CARTESIAN_POINT('Ctrl Pts',(-2.47943830443195,0.436110014234484,
0.359798287646965));
#22194=CARTESIAN_POINT('Ctrl Pts',(-2.49379602217835,0.354481355908151,
0.365029387919509));
#22195=CARTESIAN_POINT('Ctrl Pts',(-2.50412923353572,0.272081119207604,
0.370260488192053));
#22196=CARTESIAN_POINT('Ctrl Pts',(-2.51036984617185,0.189339603440867,
0.375491588464596));
#22197=CARTESIAN_POINT('Ctrl Pts',(-2.51660833788702,0.106626208024527,
0.380720910906854));
#22198=CARTESIAN_POINT('Ctrl Pts',(-2.51875695823721,0.0235722250301544,
0.38595023334911));
#22199=CARTESIAN_POINT('Ctrl Pts',(-2.516799449759,-0.0593866962608646,
0.391179555791368));
#22200=CARTESIAN_POINT('Ctrl Pts',(-2.51484201164508,-0.142342635523984,
0.396408690261251));
#22201=CARTESIAN_POINT('Ctrl Pts',(-2.50877875002578,-0.225203057176136,
0.401637824731133));
#22202=CARTESIAN_POINT('Ctrl Pts',(-2.49864551292181,-0.307533495339446,
0.406866959201016));
#22203=CARTESIAN_POINT('Ctrl Pts',(-2.48831506543297,-0.391466226751247,
0.412197861705219));
#22204=CARTESIAN_POINT('Ctrl Pts',(-2.47375459029873,-0.474847629671242,
0.417528764209423));
#22205=CARTESIAN_POINT('Ctrl Pts',(-2.45505711055919,-0.557226016884306,
0.422859666713626));
#22206=CARTESIAN_POINT('Ctrl Pts',(-2.43669032389862,-0.638147418295674,
0.428096284181162));
#22207=CARTESIAN_POINT('Ctrl Pts',(-2.41433187505233,-0.71810056085767,
0.433332901648697));
#22208=CARTESIAN_POINT('Ctrl Pts',(-2.38812046829166,-0.796672378664167,
0.438569519116234));
#22209=CARTESIAN_POINT('Ctrl Pts',(-2.3612011589213,-0.87736621896955,0.443947564138769));
#22210=CARTESIAN_POINT('Ctrl Pts',(-2.33021796121626,-0.956602555970598,
0.449325609161306));
#22211=CARTESIAN_POINT('Ctrl Pts',(-2.29537319685894,-1.03395751225162,
0.454703654183842));
#22212=CARTESIAN_POINT('Ctrl Pts',(-2.26052843250163,-1.11131246853263,
0.460081699206377));
#22213=CARTESIAN_POINT('Ctrl Pts',(-2.22182240094526,-1.18678561188465,
0.465459744228912));
#22214=CARTESIAN_POINT('Ctrl Pts',(-2.17950621167997,-1.25998369959632,
0.470837789251448));
#22215=CARTESIAN_POINT('Ctrl Pts',(-2.13814395334591,-1.33153168787354,
0.476094597376578));
#22216=CARTESIAN_POINT('Ctrl Pts',(-2.09317876908886,-1.40117236950367,
0.481351405501709));
#22217=CARTESIAN_POINT('Ctrl Pts',(-2.04481161312267,-1.46852024733698,
0.486608213626839));
#22218=CARTESIAN_POINT('Ctrl Pts',(-1.99651294033756,-1.53577276713608,
0.491857578623765));
#22219=CARTESIAN_POINT('Ctrl Pts',(-1.94482213045194,-1.60073856010646,
0.497106943620689));
#22220=CARTESIAN_POINT('Ctrl Pts',(-1.88998522071329,-1.66305806136928,
0.502356308617614));
#22221=CARTESIAN_POINT('Ctrl Pts',(-1.83477153213647,-1.72580575359677,
0.507641741468364));
#22222=CARTESIAN_POINT('Ctrl Pts',(-1.77636857449826,-1.7858702340872,0.512927174319118));
#22223=CARTESIAN_POINT('Ctrl Pts',(-1.71507102163768,-1.84291552729329,
0.518212607169868));
#22224=CARTESIAN_POINT('Ctrl Pts',(-1.65430038653143,-1.89947045544582,
0.523452606095797));
#22225=CARTESIAN_POINT('Ctrl Pts',(-1.5906850726739,-1.95305758349209,0.528692605021722));
#22226=CARTESIAN_POINT('Ctrl Pts',(-1.52455035578429,-2.00338525068894,
0.533932603947651));
#22227=CARTESIAN_POINT('Ctrl Pts',(-1.45843739621914,-2.05369636084229,
0.539170878992959));
#22228=CARTESIAN_POINT('Ctrl Pts',(-1.38980704643993,-2.1007498608487,0.54440915403827));
#22229=CARTESIAN_POINT('Ctrl Pts',(-1.31901721811137,-2.1442947158275,0.549647429083578));
#22230=CARTESIAN_POINT('Ctrl Pts',(-1.24822936107416,-2.18783835820842,
0.554885558258122));
#22231=CARTESIAN_POINT('Ctrl Pts',(-1.1752825383405,-2.22787330911488,0.560123687432665));
#22232=CARTESIAN_POINT('Ctrl Pts',(-1.10056197765173,-2.26419292096484,
0.56536181660721));
#22233=CARTESIAN_POINT('Ctrl Pts',(-1.0246677492648,-2.30108302044024,0.570682223309577));
#22234=CARTESIAN_POINT('Ctrl Pts',(-0.946944012562917,-2.33413982481418,
0.576002630011945));
#22235=CARTESIAN_POINT('Ctrl Pts',(-0.867816815767798,-2.36319703458485,
0.581323036714313));
#22236=CARTESIAN_POINT('Ctrl Pts',(-0.789801797256569,-2.39184582855153,
0.586568662038905));
#22237=CARTESIAN_POINT('Ctrl Pts',(-0.710422986118061,-2.41660666787764,
0.591814287363496));
#22238=CARTESIAN_POINT('Ctrl Pts',(-0.630103544308487,-2.43737066804577,
0.597059912688088));
#22239=CARTESIAN_POINT('Ctrl Pts',(-0.548066557454519,-2.45857868406843,
0.602417710079344));
#22240=CARTESIAN_POINT('Ctrl Pts',(-0.465048744752886,-2.47561684540565,
0.607775507470597));
#22241=CARTESIAN_POINT('Ctrl Pts',(-0.381509456210711,-2.48842455879655,
0.613133304861853));
#22242=CARTESIAN_POINT('Ctrl Pts',(-0.297970167668535,-2.50123227218746,
0.618491102253108));
#22243=CARTESIAN_POINT('Ctrl Pts',(-0.213909912770551,-2.50980955209961,
0.623848899644367));
#22244=CARTESIAN_POINT('Ctrl Pts',(-0.129788985686316,-2.51415215712862,
0.629206697035622));
#22245=CARTESIAN_POINT('Ctrl Pts',(-0.047261723163428,-2.51841249183587,
0.634462991363071));
#22246=CARTESIAN_POINT('Ctrl Pts',(0.0356272034635327,-2.51861290613602,
0.639719285690518));
#22247=CARTESIAN_POINT('Ctrl Pts',(0.118445090380389,-2.51471211286,0.644975580017967));
#22248=CARTESIAN_POINT('Ctrl Pts',(0.20114594817007,-2.51081683175591,0.650224446728505));
#22249=CARTESIAN_POINT('Ctrl Pts',(0.28377550876694,-2.50283187606817,0.655473313439045));
#22250=CARTESIAN_POINT('Ctrl Pts',(0.365898280032954,-2.49076789337524,
0.660722180149584));
#22251=CARTESIAN_POINT('Ctrl Pts',(0.448595137540521,-2.47861957638166,
0.666007739510843));
#22252=CARTESIAN_POINT('Ctrl Pts',(0.530777618532214,-2.46233494642037,
0.6712932988721));
#22253=CARTESIAN_POINT('Ctrl Pts',(0.61200339223134,-2.44197831642653,0.676578858233359));
#22254=CARTESIAN_POINT('Ctrl Pts',(0.69252200492473,-2.42179891361421,0.681818400901843));
#22255=CARTESIAN_POINT('Ctrl Pts',(0.772100048659439,-2.39761825181994,
0.687057943570328));
#22256=CARTESIAN_POINT('Ctrl Pts',(0.850315861233121,-2.36955041856791,
0.692297486238811));
#22257=CARTESIAN_POINT('Ctrl Pts',(0.928506192134854,-2.34149172944283,
0.697535321933946));
#22258=CARTESIAN_POINT('Ctrl Pts',(1.00533473952937,-2.30954853967114,0.70277315762908));
#22259=CARTESIAN_POINT('Ctrl Pts',(1.08039615906332,-2.27388442746794,0.708010993324216));
#22260=CARTESIAN_POINT('Ctrl Pts',(1.15545574030167,-2.23822118869854,0.713248700741863));
#22261=CARTESIAN_POINT('Ctrl Pts',(1.22874786360369,-2.19883740756184,0.71848640815951));
#22262=CARTESIAN_POINT('Ctrl Pts',(1.29988955463394,-2.15594373668553,0.723724115577157));
#22263=CARTESIAN_POINT('Ctrl Pts',(1.37216199747502,-2.11236829826457,0.729045073014044));
#22264=CARTESIAN_POINT('Ctrl Pts',(1.44221462172498,-2.06517065811216,0.734366030450932));
#22265=CARTESIAN_POINT('Ctrl Pts',(1.50967588999156,-2.01461781913548,0.739686987887819));
#22266=CARTESIAN_POINT('Ctrl Pts',(1.5761773301844,-1.96478423782033,0.74493223959817));
#22267=CARTESIAN_POINT('Ctrl Pts',(1.64016035927463,-1.91169066531786,0.750177491308521));
#22268=CARTESIAN_POINT('Ctrl Pts',(1.70130337941679,-1.85563279265727,0.755422743018872));
#22269=CARTESIAN_POINT('Ctrl Pts',(1.76377013300914,-1.79836127891361,0.760781553319027));
#22270=CARTESIAN_POINT('Ctrl Pts',(1.82327210965394,-1.73799597357039,0.766140363619182));
#22271=CARTESIAN_POINT('Ctrl Pts',(1.87950830977704,-1.67488947798924,0.771499173919336));
#22272=CARTESIAN_POINT('Ctrl Pts',(1.93574450990013,-1.61178298240809,0.776857984219491));
#22273=CARTESIAN_POINT('Ctrl Pts',(1.98871466811899,-1.54593573263283,0.782216794519645));
#22274=CARTESIAN_POINT('Ctrl Pts',(2.03816460106524,-1.47773181225977,0.7875756048198));
#22275=CARTESIAN_POINT('Ctrl Pts',(2.08698103976692,-1.4104016401092,0.79286576435987));
#22276=CARTESIAN_POINT('Ctrl Pts',(2.13254746814638,-1.34052609907627,0.79815592389994));
#22277=CARTESIAN_POINT('Ctrl Pts',(2.17459027483789,-1.26844920536081,0.80344608344001));
#22278=CARTESIAN_POINT('Ctrl Pts',(2.21657188440823,-1.19647722610625,0.808728542672704));
#22279=CARTESIAN_POINT('Ctrl Pts',(2.25503983332636,-1.12231064633767,0.814011001905399));
#22280=CARTESIAN_POINT('Ctrl Pts',(2.28976238804666,-1.04632425962838,0.819293461138093));
#22281=CARTESIAN_POINT('Ctrl Pts',(2.32444439986729,-0.970426596472905,
0.824569752442869));
#22282=CARTESIAN_POINT('Ctrl Pts',(2.35538951924606,-0.892713757994868,
0.829846043747642));
#22283=CARTESIAN_POINT('Ctrl Pts',(2.38241141190576,-0.813585960068888,
0.835122335052418));
#22284=CARTESIAN_POINT('Ctrl Pts',(2.4094079578325,-0.734532384596086,0.84039367715736));
#22285=CARTESIAN_POINT('Ctrl Pts',(2.43248844884065,-0.654066916378462,
0.845665019262304));
#22286=CARTESIAN_POINT('Ctrl Pts',(2.45151479060097,-0.57260936201279,0.850936361367246));
#22287=CARTESIAN_POINT('Ctrl Pts',(2.47053084747212,-0.491195840384925,
0.856204853992769));
#22288=CARTESIAN_POINT('Ctrl Pts',(2.4854970089497,-0.408791739321907,0.861473346618289));
#22289=CARTESIAN_POINT('Ctrl Pts',(2.49632544298429,-0.325830527589564,
0.866741839243812));
#22290=CARTESIAN_POINT('Ctrl Pts',(2.50715226328724,-0.242881679337623,
0.872009546720419));
#22291=CARTESIAN_POINT('Ctrl Pts',(2.51384252043204,-0.159376334278797,
0.877277254197028));
#22292=CARTESIAN_POINT('Ctrl Pts',(2.51635994169055,-0.0757554872939529,
0.882544961673636));
#22293=CARTESIAN_POINT('Ctrl Pts',(2.51713600423197,-0.0499771211156531,
0.884168873618426));
#22294=CARTESIAN_POINT('Ctrl Pts',(2.51751587579956,-0.0241878072630997,
0.885792785563215));
#22295=CARTESIAN_POINT('Ctrl Pts',(2.51749949188368,0.0015994891165021,
0.887416697508005));
#22296=CARTESIAN_POINT('Ctrl Pts',(2.51749949188307,0.00159949006993176,
0.88741669756805));
#22297=CARTESIAN_POINT('Ctrl Pts',(2.51743985264828,0.0954679961080183,
0.893327910048533));
#22298=CARTESIAN_POINT('Ctrl Pts',(2.51212612121857,0.18913758394578,0.899239122529015));
#22299=CARTESIAN_POINT('Ctrl Pts',(2.50164908824153,0.282060435545834,0.905150335009498));
#22300=CARTESIAN_POINT('Ctrl Pts',(2.49112317160026,0.375416845910796,0.911089127982165));
#22301=CARTESIAN_POINT('Ctrl Pts',(2.47538578820664,0.468019323633379,0.917027920954832));
#22302=CARTESIAN_POINT('Ctrl Pts',(2.45457854884019,0.559330311688543,0.922966713927499));
#22303=CARTESIAN_POINT('Ctrl Pts',(2.43365820860934,0.651137634288419,0.928937788098399));
#22304=CARTESIAN_POINT('Ctrl Pts',(2.407612866569,0.741639183707493,0.934908862269296));
#22305=CARTESIAN_POINT('Ctrl Pts',(2.37663455189708,0.83030985585442,0.940879936440195));
#22306=CARTESIAN_POINT('Ctrl Pts',(2.37168903348617,0.844465643419186,0.941833185755331));
#22307=CARTESIAN_POINT('Ctrl Pts',(2.36661788834054,0.858574816053316,0.942786435070469));
#22308=CARTESIAN_POINT('Ctrl Pts',(2.36142200728636,0.872635292378022,0.943739684385605));
#22309=CARTESIAN_POINT('Origin',(0.,0.,116.208423447177));
#22310=CARTESIAN_POINT('',(1.87238193903529,2.43733217358128,95.4372285454945));
#22311=CARTESIAN_POINT('',(1.87274665176455,2.43781213467006,95.3543119584347));
#22312=CARTESIAN_POINT('',(1.8723819390353,2.43733217358128,116.208423447177));
#22313=CARTESIAN_POINT('',(0.793799282532884,-2.96922295374569,95.));
#22314=CARTESIAN_POINT('Ctrl Pts',(1.87274665176427,2.43781213467027,95.3543119584347));
#22315=CARTESIAN_POINT('Ctrl Pts',(2.06600193866627,2.29241896294923,95.341787244146));
#22316=CARTESIAN_POINT('Ctrl Pts',(2.9817068419035,1.41812695324678,95.2764728939291));
#22317=CARTESIAN_POINT('Ctrl Pts',(3.44893401864242,-1.12662596907763,95.1583689077841));
#22318=CARTESIAN_POINT('Ctrl Pts',(1.77865212890006,-2.70592999965464,95.0527896359281));
#22319=CARTESIAN_POINT('Ctrl Pts',(0.7937992825328,-2.96922295374571,95.));
#22320=CARTESIAN_POINT('',(-0.793800297434324,-2.96922268241929,95.0000201645727));
#22321=CARTESIAN_POINT('Origin',(0.,0.,95.));
#22322=CARTESIAN_POINT('Ctrl Pts',(1.87238193903529,2.43733217358128,95.4372285454945));
#22323=CARTESIAN_POINT('Ctrl Pts',(1.95199907732151,2.3761695247718,95.43203022616));
#22324=CARTESIAN_POINT('Ctrl Pts',(2.02870034980563,2.31103702475557,95.4268319068256));
#22325=CARTESIAN_POINT('Ctrl Pts',(2.1020729328552,2.2422514655938,95.4216335874911));
#22326=CARTESIAN_POINT('Ctrl Pts',(2.17232729272017,2.17638918807797,95.416656188822));
#22327=CARTESIAN_POINT('Ctrl Pts',(2.2395297596846,2.10717834640106,95.411678790153));
#22328=CARTESIAN_POINT('Ctrl Pts',(2.30335166303348,2.03493817262366,95.4067013914839));
#22329=CARTESIAN_POINT('Ctrl Pts',(2.36715550913664,1.96271843788834,95.4017254010792));
#22330=CARTESIAN_POINT('Ctrl Pts',(2.42758040087319,1.88747140367397,95.3967494106744));
#22331=CARTESIAN_POINT('Ctrl Pts',(2.48433585976231,1.80955176380757,95.3917734202697));
#22332=CARTESIAN_POINT('Ctrl Pts',(2.5410908516842,1.73163276504104,95.386797470806));
#22333=CARTESIAN_POINT('Ctrl Pts',(2.59417621222107,1.65104156053901,95.3818215213422));
#22334=CARTESIAN_POINT('Ctrl Pts',(2.64334361325069,1.5681635094233,95.3768455718785));
#22335=CARTESIAN_POINT('Ctrl Pts',(2.69252411613971,1.48526337341901,95.371868296451));
#22336=CARTESIAN_POINT('Ctrl Pts',(2.7377843613136,1.400075558836,95.3668910210236));
#22337=CARTESIAN_POINT('Ctrl Pts',(2.77892151202516,1.31301084534888,95.3619137455961));
#22338=CARTESIAN_POINT('Ctrl Pts',(2.82010539412938,1.22584722721616,95.3569308160334));
#22339=CARTESIAN_POINT('Ctrl Pts',(2.85715664663417,1.13680285365857,95.3519478864708));
#22340=CARTESIAN_POINT('Ctrl Pts',(2.88992033600746,1.04630908508459,95.3469649569081));
#22341=CARTESIAN_POINT('Ctrl Pts',(2.92270594910692,0.955754762872091,95.3419786930328));
#22342=CARTESIAN_POINT('Ctrl Pts',(2.95119815856141,0.863749534894087,95.3369924291575));
#22343=CARTESIAN_POINT('Ctrl Pts',(2.9752923225259,0.770738506575633,95.3320061652822));
#22344=CARTESIAN_POINT('Ctrl Pts',(2.99942397267683,0.677582769822665,95.3270121436769));
#22345=CARTESIAN_POINT('Ctrl Pts',(3.01914383312545,0.58341853954865,95.3220181220717));
#22346=CARTESIAN_POINT('Ctrl Pts',(3.03439864879444,0.488699386325051,95.3170241004664));
#22347=CARTESIAN_POINT('Ctrl Pts',(3.03903679627405,0.45990051970302,95.3155056941333));
#22348=CARTESIAN_POINT('Ctrl Pts',(3.0432625449371,0.431050373549066,95.3139872878003));
#22349=CARTESIAN_POINT('Ctrl Pts',(3.04707535237419,0.40216171741438,95.3124688814672));
#22350=CARTESIAN_POINT('Ctrl Pts',(3.05965199261959,0.306871766014207,95.3074603803792));
#22351=CARTESIAN_POINT('Ctrl Pts',(3.06777615614939,0.21082657494261,95.3024518792911));
#22352=CARTESIAN_POINT('Ctrl Pts',(3.07136732883625,0.114476990514523,95.297443378203));
#22353=CARTESIAN_POINT('Ctrl Pts',(3.07495362336384,0.0182582849553239,
95.2924416805377));
#22354=CARTESIAN_POINT('Ctrl Pts',(3.0740191495951,-0.0782635588336074,
95.2874399828725));
#22355=CARTESIAN_POINT('Ctrl Pts',(3.06853490026756,-0.17463051233945,95.2824382852072));
#22356=CARTESIAN_POINT('Ctrl Pts',(3.06305646302346,-0.270895338326955,
95.277441888228));
#22357=CARTESIAN_POINT('Ctrl Pts',(3.05303786108569,-0.367005166113458,
95.2724454912488));
#22358=CARTESIAN_POINT('Ctrl Pts',(3.03850212533996,-0.46250090195001,95.2674490942696));
#22359=CARTESIAN_POINT('Ctrl Pts',(3.02397702351035,-0.557926775919026,
95.2624563525072));
#22360=CARTESIAN_POINT('Ctrl Pts',(3.00494142390259,-0.65273902012935,95.2574636107449));
#22361=CARTESIAN_POINT('Ctrl Pts',(2.9814701956168,-0.746483571586628,95.2524708689826));
#22362=CARTESIAN_POINT('Ctrl Pts',(2.95800776792021,-0.840192973316017,
95.2474799992599));
#22363=CARTESIAN_POINT('Ctrl Pts',(2.93011312251414,-0.932835054094185,
95.2424891295371));
#22364=CARTESIAN_POINT('Ctrl Pts',(2.89791205806607,-1.02396677373598,95.2374982598144));
#22365=CARTESIAN_POINT('Ctrl Pts',(2.86571436112259,-1.11508896305668,95.232507912024));
#22366=CARTESIAN_POINT('Ctrl Pts',(2.82921128645578,-1.20470069310555,95.2275175642337));
#22367=CARTESIAN_POINT('Ctrl Pts',(2.78857791297204,-1.29237590246975,95.2225272164433));
#22368=CARTESIAN_POINT('Ctrl Pts',(2.74793780284242,-1.38006564759083,95.2175360412984));
#22369=CARTESIAN_POINT('Ctrl Pts',(2.70316621786208,-1.46581783771117,95.2125448661535));
#22370=CARTESIAN_POINT('Ctrl Pts',(2.65448515558461,-1.54922910145044,95.2075536910085));
#22371=CARTESIAN_POINT('Ctrl Pts',(2.60575338765648,-1.63272724543024,95.2025573171113));
#22372=CARTESIAN_POINT('Ctrl Pts',(2.55310423340784,-1.71387921678865,95.1975609432141));
#22373=CARTESIAN_POINT('Ctrl Pts',(2.49680406636686,-1.79230904259671,95.1925645693169));
#22374=CARTESIAN_POINT('Ctrl Pts',(2.44047165355774,-1.87078378887499,95.1875653337601));
#22375=CARTESIAN_POINT('Ctrl Pts',(2.38048433483173,-1.94653294191964,95.1825660982033));
#22376=CARTESIAN_POINT('Ctrl Pts',(2.31714866444604,-2.01921378681306,95.1775668626465));
#22377=CARTESIAN_POINT('Ctrl Pts',(2.25371354258339,-2.09200875724311,95.1725597771474));
#22378=CARTESIAN_POINT('Ctrl Pts',(2.18691987252752,-2.16172548314829,95.1675526916483));
#22379=CARTESIAN_POINT('Ctrl Pts',(2.11711085813903,-2.22805831708908,95.1625456061491));
#22380=CARTESIAN_POINT('Ctrl Pts',(2.07786106046433,-2.26535364827477,95.1597303953271));
#22381=CARTESIAN_POINT('Ctrl Pts',(2.037658659917,-2.30157998686302,95.1569151845051));
#22382=CARTESIAN_POINT('Ctrl Pts',(1.99656891278477,-2.33668885958345,95.1540999736831));
#22383=CARTESIAN_POINT('Ctrl Pts',(1.92387856350215,-2.39879866553469,95.149119688521));
#22384=CARTESIAN_POINT('Ctrl Pts',(1.84815642390381,-2.45762505194757,95.1441394033589));
#22385=CARTESIAN_POINT('Ctrl Pts',(1.76973267449693,-2.51285664350714,95.1391591181968));
#22386=CARTESIAN_POINT('Ctrl Pts',(1.69141397285223,-2.56801425294854,95.1341855040727));
#22387=CARTESIAN_POINT('Ctrl Pts',(1.61040121108685,-2.61958638311514,95.1292118899486));
#22388=CARTESIAN_POINT('Ctrl Pts',(1.5270587811377,-2.66730083210542,95.1242382758245));
#22389=CARTESIAN_POINT('Ctrl Pts',(1.44032909978763,-2.71695451941985,95.119062521189));
#22390=CARTESIAN_POINT('Ctrl Pts',(1.35107671067972,-2.76242995177963,95.1138867665535));
#22391=CARTESIAN_POINT('Ctrl Pts',(1.25974732844742,-2.80346908641233,95.108711011918));
#22392=CARTESIAN_POINT('Ctrl Pts',(1.17213645803605,-2.84283729649127,95.103745990174));
#22393=CARTESIAN_POINT('Ctrl Pts',(1.08261487000877,-2.87812320383586,95.09878096843));
#22394=CARTESIAN_POINT('Ctrl Pts',(0.991601232680961,-2.9091457930715,95.093815946686));
#22395=CARTESIAN_POINT('Ctrl Pts',(0.900616750682097,-2.94015844452396,
95.0888525154381));
#22396=CARTESIAN_POINT('Ctrl Pts',(0.808141587604577,-2.9669103483976,95.0838890841903));
#22397=CARTESIAN_POINT('Ctrl Pts',(0.714612621221596,-2.98926931734008,
95.0789256529424));
#22398=CARTESIAN_POINT('Ctrl Pts',(0.621087571927549,-3.01162734986602,
95.0739624295682));
#22399=CARTESIAN_POINT('Ctrl Pts',(0.526509237787314,-3.02959271093489,
95.0689992061939));
#22400=CARTESIAN_POINT('Ctrl Pts',(0.431326729031135,-3.04308388034627,
95.0640359828197));
#22401=CARTESIAN_POINT('Ctrl Pts',(0.336121702034778,-3.05657824149315,
95.059071585248));
#22402=CARTESIAN_POINT('Ctrl Pts',(0.24031265481731,-3.06559624710674,95.0541071876763));
#22403=CARTESIAN_POINT('Ctrl Pts',(0.144354772265256,-3.07010813322988,
95.0491427901047));
#22404=CARTESIAN_POINT('Ctrl Pts',(0.048291499036758,-3.07462497476385,
95.0441729401282));
#22405=CARTESIAN_POINT('Ctrl Pts',(-0.0479204930664325,-3.07462580026007,
95.0392030901517));
#22406=CARTESIAN_POINT('Ctrl Pts',(-0.143825393015308,-3.07013297860597,
95.0342332401753));
#22407=CARTESIAN_POINT('Ctrl Pts',(-0.239792625173286,-3.06563723689775,
95.029260160106));
#22408=CARTESIAN_POINT('Ctrl Pts',(-0.335451927996392,-3.05664207694859,
95.0242870800367));
#22409=CARTESIAN_POINT('Ctrl Pts',(-0.430354103305085,-3.04322158177292,
95.0193139999675));
#22410=CARTESIAN_POINT('Ctrl Pts',(-0.525401275530676,-3.02978058200484,
95.0143333217449));
#22411=CARTESIAN_POINT('Ctrl Pts',(-0.619688578614677,-3.01190083860415,
95.0093526435223));
#22412=CARTESIAN_POINT('Ctrl Pts',(-0.712778776397496,-2.98970712042456,
95.0043719652997));
#22413=CARTESIAN_POINT('Ctrl Pts',(-0.739890879895944,-2.98324329932811,
95.0029213650574));
#22414=CARTESIAN_POINT('Ctrl Pts',(-0.766901553461834,-2.97641386787412,
95.001470764815));
#22415=CARTESIAN_POINT('Ctrl Pts',(-0.793800297434324,-2.96922268241929,
95.0000201645727));
#22416=CARTESIAN_POINT('Origin',(0.,0.,116.208423447177));
#22417=CARTESIAN_POINT('',(1.87462644597698,2.44029756596839,96.4374142054168));
#22418=CARTESIAN_POINT('',(1.87238193903531,2.43733217358126,96.3541439943328));
#22419=CARTESIAN_POINT('',(1.8723819390353,2.43733217358128,116.208423447177));
#22420=CARTESIAN_POINT('',(-3.073000247725,0.000543316047154233,95.7084234157772));
#22421=CARTESIAN_POINT('Ctrl Pts',(1.87238193903531,2.43733217358126,96.3541439943328));
#22422=CARTESIAN_POINT('Ctrl Pts',(1.94890039524938,2.37854996204234,96.3491622040271));
#22423=CARTESIAN_POINT('Ctrl Pts',(2.02266131396365,2.3161507538951,96.3441804137215));
#22424=CARTESIAN_POINT('Ctrl Pts',(2.09331377339724,2.25043100229831,96.3391986234159));
#22425=CARTESIAN_POINT('Ctrl Pts',(2.16397435585413,2.18470369479934,96.334216260346));
#22426=CARTESIAN_POINT('Ctrl Pts',(2.23152544809283,2.1156553848872,96.3292338972762));
#22427=CARTESIAN_POINT('Ctrl Pts',(2.29565207766036,2.04362026519941,96.3242515342064));
#22428=CARTESIAN_POINT('Ctrl Pts',(2.3598454088084,1.97151021788219,96.3192639887109));
#22429=CARTESIAN_POINT('Ctrl Pts',(2.42060687118491,1.89640748479273,96.3142764432154));
#22430=CARTESIAN_POINT('Ctrl Pts',(2.47766112968026,1.8186801743219,96.3092888977199));
#22431=CARTESIAN_POINT('Ctrl Pts',(2.53474566539261,1.74091161598093,96.3042987054632));
#22432=CARTESIAN_POINT('Ctrl Pts',(2.58811883594471,1.6605160719845,96.2993085132065));
#22433=CARTESIAN_POINT('Ctrl Pts',(2.63754929462482,1.57788971998175,96.2943183209498));
#22434=CARTESIAN_POINT('Ctrl Pts',(2.68706324692705,1.49512380274748,96.2893196996953));
#22435=CARTESIAN_POINT('Ctrl Pts',(2.73262097536261,1.41011993708907,96.2843210784408));
#22436=CARTESIAN_POINT('Ctrl Pts',(2.77403759886778,1.32329802012542,96.2793224571864));
#22437=CARTESIAN_POINT('Ctrl Pts',(2.80820522869565,1.25167221220823,96.2751987255487));
#22438=CARTESIAN_POINT('Ctrl Pts',(2.83955533933329,1.17880957773639,96.2710749939111));
#22439=CARTESIAN_POINT('Ctrl Pts',(2.86800958600607,1.10495396491316,96.2669512622734));
#22440=CARTESIAN_POINT('Ctrl Pts',(2.90250143644083,1.01542719653439,96.2619525309236));
#22441=CARTESIAN_POINT('Ctrl Pts',(2.93285800694782,0.924126318119108,96.2569537995738));
#22442=CARTESIAN_POINT('Ctrl Pts',(2.95889528436648,0.831469149249558,96.251955068224));
#22443=CARTESIAN_POINT('Ctrl Pts',(2.98489722985203,0.738937713836757,96.2469631200274));
#22444=CARTESIAN_POINT('Ctrl Pts',(3.00659141307212,0.645054064831401,96.2419711718308));
#22445=CARTESIAN_POINT('Ctrl Pts',(3.02384217706374,0.550255157368292,96.2369792236341));
#22446=CARTESIAN_POINT('Ctrl Pts',(3.04107473805111,0.455556281701891,96.2319925429407));
#22447=CARTESIAN_POINT('Ctrl Pts',(3.05387312238288,0.359944497192783,96.2270058622473));
#22448=CARTESIAN_POINT('Ctrl Pts',(3.06215199580362,0.263870052480181,96.2220191815539));
#22449=CARTESIAN_POINT('Ctrl Pts',(3.07042494913393,0.167864309071667,96.2170360667563));
#22450=CARTESIAN_POINT('Ctrl Pts',(3.07418477861356,0.0713969993844289,
96.2120529519588));
#22451=CARTESIAN_POINT('Ctrl Pts',(3.07339771727761,-0.0250743181916119,
96.2070698371612));
#22452=CARTESIAN_POINT('Ctrl Pts',(3.07261094230205,-0.121510536134186,
96.2020885353948));
#22453=CARTESIAN_POINT('Ctrl Pts',(3.06728056700538,-0.217950320417463,
96.1971072336284));
#22454=CARTESIAN_POINT('Ctrl Pts',(3.05742492024352,-0.31393487712244,96.192125931862));
#22455=CARTESIAN_POINT('Ctrl Pts',(3.04757016647388,-0.40991073693885,96.1871450814372));
#22456=CARTESIAN_POINT('Ctrl Pts',(3.03319100146494,-0.505431014383348,
96.1821642310125));
#22457=CARTESIAN_POINT('Ctrl Pts',(3.01435764138757,-0.600041881711913,
96.1771833805877));
#22458=CARTESIAN_POINT('Ctrl Pts',(2.99552084201603,-0.694670026605536,
96.1722016205743));
#22459=CARTESIAN_POINT('Ctrl Pts',(2.97222831790626,-0.788388000908782,
96.1672198605609));
#22460=CARTESIAN_POINT('Ctrl Pts',(2.94460120804333,-0.88075307299479,96.1622381005475));
#22461=CARTESIAN_POINT('Ctrl Pts',(2.91694425733271,-0.973217911290937,
96.1572509595897));
#22462=CARTESIAN_POINT('Ctrl Pts',(2.88494349992794,-1.0643265086119,96.152263818632));
#22463=CARTESIAN_POINT('Ctrl Pts',(2.84876962586883,-1.15365240377123,96.1472766776742));
#22464=CARTESIAN_POINT('Ctrl Pts',(2.81257434529212,-1.24303115907887,96.1422865854892));
#22465=CARTESIAN_POINT('Ctrl Pts',(2.77220121464559,-1.33062471308574,96.1372964933043));
#22466=CARTESIAN_POINT('Ctrl Pts',(2.7278677424662,-1.41602960054243,96.1323064011193));
#22467=CARTESIAN_POINT('Ctrl Pts',(2.68346248210394,-1.50157278219034,96.1273082285916));
#22468=CARTESIAN_POINT('Ctrl Pts',(2.63508429541024,-1.58491984109699,96.1223100560639));
#22469=CARTESIAN_POINT('Ctrl Pts',(2.58299496575557,-1.66569482705608,96.1173118835362));
#22470=CARTESIAN_POINT('Ctrl Pts',(2.55266952755875,-1.71272052043303,96.1144020405205));
#22471=CARTESIAN_POINT('Ctrl Pts',(2.52108704166495,-1.75887502791644,96.1114921975049));
#22472=CARTESIAN_POINT('Ctrl Pts',(2.4883053372942,-1.80408946518548,96.1085823544892));
#22473=CARTESIAN_POINT('Ctrl Pts',(2.43197076052523,-1.88178939678727,96.1035818586975));
#22474=CARTESIAN_POINT('Ctrl Pts',(2.3718945114762,-1.95698440230462,96.0985813629058));
#22475=CARTESIAN_POINT('Ctrl Pts',(2.30832713238641,-2.0292925121551,96.093580867114));
#22476=CARTESIAN_POINT('Ctrl Pts',(2.24484601165398,-2.10150250283078,96.0885871567925));
#22477=CARTESIAN_POINT('Ctrl Pts',(2.17788346331487,-2.17083305675957,96.0835934464709));
#22478=CARTESIAN_POINT('Ctrl Pts',(2.10773239764918,-2.2369323614942,96.0785997361493));
#22479=CARTESIAN_POINT('Ctrl Pts',(2.03765539409394,-2.3029618817721,96.0736112979462));
#22480=CARTESIAN_POINT('Ctrl Pts',(1.96439688289154,-2.36576663526249,96.068622859743));
#22481=CARTESIAN_POINT('Ctrl Pts',(1.88828831398959,-2.42502979223975,96.0636344215399));
#22482=CARTESIAN_POINT('Ctrl Pts',(1.81223436368252,-2.48425041957272,96.0586495632422));
#22483=CARTESIAN_POINT('Ctrl Pts',(1.73333476695209,-2.53993423425027,96.0536647049446));
#22484=CARTESIAN_POINT('Ctrl Pts',(1.65195517251102,-2.59180368817048,96.0486798466469));
#22485=CARTESIAN_POINT('Ctrl Pts',(1.57060532800669,-2.64365418017543,96.0436968106638));
#22486=CARTESIAN_POINT('Ctrl Pts',(1.48677765678592,-2.69169284641807,96.0387137746808));
#22487=CARTESIAN_POINT('Ctrl Pts',(1.4008672035044,-2.73568516612306,96.0337307386977));
#22488=CARTESIAN_POINT('Ctrl Pts',(1.31496472709016,-2.77967340109933,96.0287481653942));
#22489=CARTESIAN_POINT('Ctrl Pts',(1.22698024374369,-2.81961583669491,96.0237655920907));
#22490=CARTESIAN_POINT('Ctrl Pts',(1.13733288238007,-2.85532417855785,96.0187830187873));
#22491=CARTESIAN_POINT('Ctrl Pts',(1.04766939667527,-2.89103894306924,96.0137995492978));
#22492=CARTESIAN_POINT('Ctrl Pts',(0.956342846597565,-2.92251793905592,
96.0088160798083));
#22493=CARTESIAN_POINT('Ctrl Pts',(0.86379078274741,-2.94962162550396,96.0038326103188));
#22494=CARTESIAN_POINT('Ctrl Pts',(0.77113935568867,-2.97675441026853,95.9988437906135));
#22495=CARTESIAN_POINT('Ctrl Pts',(0.677260209959345,-2.99950238421146,
95.9938549709082));
#22496=CARTESIAN_POINT('Ctrl Pts',(0.582604231448032,-3.01777642636078,
95.9888661512028));
#22497=CARTESIAN_POINT('Ctrl Pts',(0.487892539284682,-3.03606122444588,
95.9838743951234));
#22498=CARTESIAN_POINT('Ctrl Pts',(0.392403537956677,-3.04986678451124,
95.978882639044));
#22499=CARTESIAN_POINT('Ctrl Pts',(0.296594328969761,-3.05915577472331,
95.9738908829645));
#22500=CARTESIAN_POINT('Ctrl Pts',(0.200630793355014,-3.06845972736488,
95.9688910863127));
#22501=CARTESIAN_POINT('Ctrl Pts',(0.104346458129836,-3.07323256149298,
95.9638912896608));
#22502=CARTESIAN_POINT('Ctrl Pts',(0.00819946362641492,-3.07348906274225,
95.9588914930089));
#22503=CARTESIAN_POINT('Ctrl Pts',(-0.0474273367138514,-3.07363746409223,
95.9559988109076));
#22504=CARTESIAN_POINT('Ctrl Pts',(-0.103008221685502,-3.07227507766361,
95.9531061288063));
#22505=CARTESIAN_POINT('Ctrl Pts',(-0.15845552235523,-3.06941266326884,
95.950213446705));
#22506=CARTESIAN_POINT('Ctrl Pts',(-0.254304418075243,-3.06446455478534,
95.9452130159946));
#22507=CARTESIAN_POINT('Ctrl Pts',(-0.350089038366274,-3.05501385990303,
95.9402125852842));
#22508=CARTESIAN_POINT('Ctrl Pts',(-0.445352560841227,-3.04106286461694,
95.9352121545737));
#22509=CARTESIAN_POINT('Ctrl Pts',(-0.540487134578819,-3.02713075340295,
95.930218492448));
#22510=CARTESIAN_POINT('Ctrl Pts',(-0.635101581926603,-3.00871051163352,
95.9252248303224));
#22511=CARTESIAN_POINT('Ctrl Pts',(-0.728741322152277,-2.98585638224409,
95.9202311681967));
#22512=CARTESIAN_POINT('Ctrl Pts',(-0.822282514218609,-2.96302630495454,
95.9152427614915));
#22513=CARTESIAN_POINT('Ctrl Pts',(-0.914850614413196,-2.93577171996645,
95.9102543547863));
#22514=CARTESIAN_POINT('Ctrl Pts',(-1.00599941533267,-2.90419824157207,
95.9052659480812));
#22515=CARTESIAN_POINT('Ctrl Pts',(-1.09708325569609,-2.87264726518203,
95.9002810965481));
#22516=CARTESIAN_POINT('Ctrl Pts',(-1.18674939422637,-2.83678365758152,
95.895296245015));
#22517=CARTESIAN_POINT('Ctrl Pts',(-1.27456596348003,-2.79676310307795,
95.8903113934819));
#22518=CARTESIAN_POINT('Ctrl Pts',(-1.3623506983059,-2.75675705644531,95.8853283490098));
#22519=CARTESIAN_POINT('Ctrl Pts',(-1.44828679720389,-2.71259723883619,
95.8803453045378));
#22520=CARTESIAN_POINT('Ctrl Pts',(-1.5319624912743,-2.66448741324268,95.8753622600657));
#22521=CARTESIAN_POINT('Ctrl Pts',(-1.61563067019821,-2.61638190852623,
95.8703796631346));
#22522=CARTESIAN_POINT('Ctrl Pts',(-1.69703846764458,-2.56432732002754,
95.8653970662036));
#22523=CARTESIAN_POINT('Ctrl Pts',(-1.77579978769978,-2.50857277430921,
95.8604144692726));
#22524=CARTESIAN_POINT('Ctrl Pts',(-1.85457551170371,-2.45280803214398,
95.8554309611193));
#22525=CARTESIAN_POINT('Ctrl Pts',(-1.93070343900024,-2.39334224243777,
95.8504474529659));
#22526=CARTESIAN_POINT('Ctrl Pts',(-2.00382834816003,-2.33046652005779,
95.8454639448126));
#22527=CARTESIAN_POINT('Ctrl Pts',(-2.07703209272744,-2.26752301184038,
95.8404750639771));
#22528=CARTESIAN_POINT('Ctrl Pts',(-2.14722602247896,-2.20116251823993,
95.8354861831416));
#22529=CARTESIAN_POINT('Ctrl Pts',(-2.2140899552858,-2.13171478390111,95.8304973023061));
#22530=CARTESIAN_POINT('Ctrl Pts',(-2.28099341415391,-2.06222599610808,
95.8255054723349));
#22531=CARTESIAN_POINT('Ctrl Pts',(-2.3445626674711,-1.98964666357807,95.8205136423637));
#22532=CARTESIAN_POINT('Ctrl Pts',(-2.40451759767676,-1.91433993127208,
95.8155218123926));
#22533=CARTESIAN_POINT('Ctrl Pts',(-2.46456933067151,-1.8389116092703,95.8105219226494));
#22534=CARTESIAN_POINT('Ctrl Pts',(-2.52099483136462,-1.76074744989398,
95.8055220329063));
#22535=CARTESIAN_POINT('Ctrl Pts',(-2.5735571384206,-1.68023983564382,95.8005221431632));
#22536=CARTESIAN_POINT('Ctrl Pts',(-2.60396546887915,-1.63366459426521,
95.7976296084158));
#22537=CARTESIAN_POINT('Ctrl Pts',(-2.63308169225606,-1.58630551453297,
95.7947370736683));
#22538=CARTESIAN_POINT('Ctrl Pts',(-2.66086712515347,-1.53824198105418,
95.7918445389209));
#22539=CARTESIAN_POINT('Ctrl Pts',(-2.71074598685348,-1.45196100252656,
95.7866520216345));
#22540=CARTESIAN_POINT('Ctrl Pts',(-2.75649795601848,-1.36312477777713,
95.7814595043481));
#22541=CARTESIAN_POINT('Ctrl Pts',(-2.79786374839681,-1.27214806347649,
95.7762669870617));
#22542=CARTESIAN_POINT('Ctrl Pts',(-2.83915701351187,-1.18133086001146,
95.7710835738936));
#22543=CARTESIAN_POINT('Ctrl Pts',(-2.87607924651253,-1.08838099000229,
95.7659001607256));
#22544=CARTESIAN_POINT('Ctrl Pts',(-2.9084162021105,-0.993739123362437,
95.7607167475575));
#22545=CARTESIAN_POINT('Ctrl Pts',(-2.94068575767816,-0.899294519098164,
95.7555441381957));
#22546=CARTESIAN_POINT('Ctrl Pts',(-2.96838895106745,-0.803165312865599,
95.7503715288339));
#22547=CARTESIAN_POINT('Ctrl Pts',(-2.99135941124075,-0.705812384973069,
95.7451989194722));
#22548=CARTESIAN_POINT('Ctrl Pts',(-3.01430118770704,-0.608581023772685,
95.7400327692588));
#22549=CARTESIAN_POINT('Ctrl Pts',(-3.03252190065904,-0.51012936038651,
95.7348666190454));
#22550=CARTESIAN_POINT('Ctrl Pts',(-3.04590469133192,-0.410934132583531,
95.7297004688321));
#22551=CARTESIAN_POINT('Ctrl Pts',(-3.05926884892359,-0.311877015939915,
95.7245415115353));
#22552=CARTESIAN_POINT('Ctrl Pts',(-3.06780845018851,-0.212078783790839,
95.7193825542385));
#22553=CARTESIAN_POINT('Ctrl Pts',(-3.07145769837096,-0.112026144795582,
95.7142235969417));
#22554=CARTESIAN_POINT('Ctrl Pts',(-3.07282529940395,-0.0745301769681272,
95.7122902136869));
#22555=CARTESIAN_POINT('Ctrl Pts',(-3.0735065820639,-0.0369985695992274,
95.7103568304322));
#22556=CARTESIAN_POINT('Ctrl Pts',(-3.07349995206979,0.000542795567035782,
95.7084234471775));
#22557=CARTESIAN_POINT('Ctrl Pts',(-3.06853913704955,0.000547962633554823,
95.7084231354506));
#22558=CARTESIAN_POINT('Ctrl Pts',(-3.06913019292027,0.484861479280904,
95.6834406340126));
#22559=CARTESIAN_POINT('Ctrl Pts',(-2.733190250717,1.9916708787895,95.6056684966466));
#22560=CARTESIAN_POINT('Ctrl Pts',(-0.606155923754067,3.45373062715694,
95.4876314376412));
#22561=CARTESIAN_POINT('Ctrl Pts',(1.25146230115526,2.90522756078225,95.394576880074));
#22562=CARTESIAN_POINT('Ctrl Pts',(1.87274665176427,2.43781213467027,95.3543119584347));
#22563=CARTESIAN_POINT('',(-3.07399806097456,0.000489289934194882,95.7915766089109));
#22564=CARTESIAN_POINT('Ctrl Pts',(-3.07349996089424,0.000490288814122033,
95.7915765528225));
#22565=CARTESIAN_POINT('Ctrl Pts',(-3.07349587727009,0.0260895240076914,
95.7902429034883));
#22566=CARTESIAN_POINT('Ctrl Pts',(-3.0731719752456,0.0516859350238667,
95.7889092541541));
#22567=CARTESIAN_POINT('Ctrl Pts',(-3.07252842825033,0.0772742362857353,
95.7875756048199));
#22568=CARTESIAN_POINT('Ctrl Pts',(-3.07011545939872,0.173217150113296,
95.7825751086228));
#22569=CARTESIAN_POINT('Ctrl Pts',(-3.06320007643443,0.269215187868969,
95.7775746124258));
#22570=CARTESIAN_POINT('Ctrl Pts',(-3.05177238829369,0.364811650099374,
95.7725741162287));
#22571=CARTESIAN_POINT('Ctrl Pts',(-3.04036020706927,0.46027839174918,95.7675804055052));
#22572=CARTESIAN_POINT('Ctrl Pts',(-3.02444794151189,0.555344208923741,
95.7625866947818));
#22573=CARTESIAN_POINT('Ctrl Pts',(-3.00407769839575,0.649553255708325,
95.7575929840583));
#22574=CARTESIAN_POINT('Ctrl Pts',(-2.98372896121357,0.743662841061493,
95.7526045454572));
#22575=CARTESIAN_POINT('Ctrl Pts',(-2.9589316950746,0.836917027616928,95.747616106856));
#22576=CARTESIAN_POINT('Ctrl Pts',(-2.92977958303345,0.92886696832234,95.7426276682549));
#22577=CARTESIAN_POINT('Ctrl Pts',(-2.90064839177123,1.02075092189175,95.7376428095666));
#22578=CARTESIAN_POINT('Ctrl Pts',(-2.8671686997368,1.11133207327179,95.7326579508783));
#22579=CARTESIAN_POINT('Ctrl Pts',(-2.82948462399554,1.20017457587338,95.72767309219));
#22580=CARTESIAN_POINT('Ctrl Pts',(-2.79181432445534,1.28898460024232,95.7226900558209));
#22581=CARTESIAN_POINT('Ctrl Pts',(-2.74994286626322,1.37605683518936,95.7177070194519));
#22582=CARTESIAN_POINT('Ctrl Pts',(-2.7040629642024,1.46097424194573,95.7127239830828));
#22583=CARTESIAN_POINT('Ctrl Pts',(-2.65818732218065,1.54588376395401,95.7077414093985));
#22584=CARTESIAN_POINT('Ctrl Pts',(-2.6083041850157,1.62863846962425,95.7027588357141));
#22585=CARTESIAN_POINT('Ctrl Pts',(-2.55465229994161,1.7088457731472,95.6977762620298));
#22586=CARTESIAN_POINT('Ctrl Pts',(-2.50099076488044,1.78906750299351,95.692792792165));
#22587=CARTESIAN_POINT('Ctrl Pts',(-2.4435593796705,1.86674055605838,95.6878093223002));
#22588=CARTESIAN_POINT('Ctrl Pts',(-2.38263968880861,1.94150208944364,95.6828258524354));
#22589=CARTESIAN_POINT('Ctrl Pts',(-2.32165459515316,2.01634388609131,95.6778370323653));
#22590=CARTESIAN_POINT('Ctrl Pts',(-2.25717399687822,2.0882675819913,95.6728482122952));
#22591=CARTESIAN_POINT('Ctrl Pts',(-2.18951898812381,2.15694433183736,95.6678593922252));
#22592=CARTESIAN_POINT('Ctrl Pts',(-2.12182415832039,2.22566150411882,95.6628676357864));
#22593=CARTESIAN_POINT('Ctrl Pts',(-2.05095151978951,2.29112762732478,95.6578758793477));
#22594=CARTESIAN_POINT('Ctrl Pts',(-1.97725662449484,2.35305301489177,95.6528841229089));
#22595=CARTESIAN_POINT('Ctrl Pts',(-1.90344302383817,2.41507814987707,95.6478843259098));
#22596=CARTESIAN_POINT('Ctrl Pts',(-1.82679843763728,2.4735508949663,95.6428845289107));
#22597=CARTESIAN_POINT('Ctrl Pts',(-1.74770879545561,2.52822392526594,95.6378847319115));
#22598=CARTESIAN_POINT('Ctrl Pts',(-1.70195075945917,2.55985550709481,95.6349920536195));
#22599=CARTESIAN_POINT('Ctrl Pts',(-1.65537479165772,2.59021604073263,95.6320993753275));
#22600=CARTESIAN_POINT('Ctrl Pts',(-1.60805923467315,2.6192647341921,95.6292066970355));
#22601=CARTESIAN_POINT('Ctrl Pts',(-1.52626713370109,2.66947979705859,95.6242062648306));
#22602=CARTESIAN_POINT('Ctrl Pts',(-1.44197754952503,2.71594785869701,95.6192058326257));
#22603=CARTESIAN_POINT('Ctrl Pts',(-1.35556824555185,2.75841203986125,95.6142054004208));
#22604=CARTESIAN_POINT('Ctrl Pts',(-1.26927590504828,2.80081874159058,95.6092117367914));
#22605=CARTESIAN_POINT('Ctrl Pts',(-1.18086993769247,2.8392321422873,95.604218073162));
#22606=CARTESIAN_POINT('Ctrl Pts',(-1.09075569008632,2.87343945030069,95.5992244095326));
#22607=CARTESIAN_POINT('Ctrl Pts',(-1.00073628019014,2.90761075798291,95.5942360013166));
#22608=CARTESIAN_POINT('Ctrl Pts',(-0.909012572083997,2.93758461792952,
95.5892475931007));
#22609=CARTESIAN_POINT('Ctrl Pts',(-0.816012110743412,2.96319531673497,
95.5842591848847));
#22610=CARTESIAN_POINT('Ctrl Pts',(-0.723077929512727,2.98878776315859,
95.5792743318364));
#22611=CARTESIAN_POINT('Ctrl Pts',(-0.62886922575727,3.01002311398092,95.5742894787882));
#22612=CARTESIAN_POINT('Ctrl Pts',(-0.533830088582683,3.0267850413473,95.56930462574));
#22613=CARTESIAN_POINT('Ctrl Pts',(-0.438825404042331,3.043540892348,95.5643215797507));
#22614=CARTESIAN_POINT('Ctrl Pts',(-0.342991315883686,3.05582646586484,
95.5593385337614));
#22615=CARTESIAN_POINT('Ctrl Pts',(-0.246782583713422,3.06357644043293,
95.5543554877721));
#22616=CARTESIAN_POINT('Ctrl Pts',(-0.150582492309382,3.07132571895487,
95.5493728893236));
#22617=CARTESIAN_POINT('Ctrl Pts',(-0.054008261156951,3.07454017339115,
95.5443902908752));
#22618=CARTESIAN_POINT('Ctrl Pts',(0.0424808114944798,3.07320640872929,
95.5394076924267));
#22619=CARTESIAN_POINT('Ctrl Pts',(0.138987530126228,3.07187240014773,95.5344241827576));
#22620=CARTESIAN_POINT('Ctrl Pts',(0.235408620609279,3.06598852661926,95.5294406730884));
#22621=CARTESIAN_POINT('Ctrl Pts',(0.331286444502977,3.05559348436414,95.5244571634193));
#22622=CARTESIAN_POINT('Ctrl Pts',(0.42726763329119,3.04518723532102,95.5194682810798));
#22623=CARTESIAN_POINT('Ctrl Pts',(0.522703949282092,3.03026015549755,95.5144793987402));
#22624=CARTESIAN_POINT('Ctrl Pts',(0.617144748484151,3.01090262370247,95.5094905164006));
#22625=CARTESIAN_POINT('Ctrl Pts',(0.711641375483698,2.99153364888305,95.5044986849298));
#22626=CARTESIAN_POINT('Ctrl Pts',(0.805140888896846,2.96772911533756,95.499506853459));
#22627=CARTESIAN_POINT('Ctrl Pts',(0.897206742691589,2.93962962137558,95.4945150219882));
#22628=CARTESIAN_POINT('Ctrl Pts',(0.989421244889705,2.91148475831376,95.4895151307672));
#22629=CARTESIAN_POINT('Ctrl Pts',(1.08019705249857,2.87903123556852,95.4845152395462));
#22630=CARTESIAN_POINT('Ctrl Pts',(1.16911662325572,2.84245819164102,95.4795153483253));
#22631=CARTESIAN_POINT('Ctrl Pts',(1.22055806427665,2.82130008138327,95.476622828634));
#22632=CARTESIAN_POINT('Ctrl Pts',(1.2713786822235,2.79876411974557,95.4737303089427));
#22633=CARTESIAN_POINT('Ctrl Pts',(1.32150163250936,2.77489381513511,95.4708377892515));
#22634=CARTESIAN_POINT('Ctrl Pts',(1.40804369735621,2.73367945249822,95.4658435775128));
#22635=CARTESIAN_POINT('Ctrl Pts',(1.49281002673697,2.68833922668901,95.4608493657742));
#22636=CARTESIAN_POINT('Ctrl Pts',(1.5753800256132,2.63904907587922,95.4558551540356));
#22637=CARTESIAN_POINT('Ctrl Pts',(1.65782752464194,2.58983205133852,95.4508683516488));
#22638=CARTESIAN_POINT('Ctrl Pts',(1.73808479715806,2.53667697695274,95.4458815492621));
#22639=CARTESIAN_POINT('Ctrl Pts',(1.81575327570771,2.47980690614344,95.4408947468753));
#22640=CARTESIAN_POINT('Ctrl Pts',(1.8347867338384,2.46587031137745,95.4396726797484));
#22641=CARTESIAN_POINT('Ctrl Pts',(1.85366483429822,2.45171083285497,95.4384506126214));
#22642=CARTESIAN_POINT('Ctrl Pts',(1.87238193903529,2.43733217358128,95.4372285454945));
#22643=CARTESIAN_POINT('Ctrl Pts',(1.87462644597698,2.44029756596839,96.4374142054168));
#22644=CARTESIAN_POINT('Ctrl Pts',(1.95834925157173,2.37696725901686,96.4319598822634));
#22645=CARTESIAN_POINT('Ctrl Pts',(2.81520938972617,1.65344307781877,96.3737159231819));
#22646=CARTESIAN_POINT('Ctrl Pts',(3.57003808721136,-0.655357920372746,
96.2626823281723));
#22647=CARTESIAN_POINT('Ctrl Pts',(1.39401266499885,-3.35130737712119,96.1043134203881));
#22648=CARTESIAN_POINT('Ctrl Pts',(-2.02307198855743,-2.99696810683408,
95.9472783470963));
#22649=CARTESIAN_POINT('Ctrl Pts',(-3.07630577576351,-0.988793015625566,
95.8430329097325));
#22650=CARTESIAN_POINT('Ctrl Pts',(-3.0784329222612,0.000480396352174041,
95.7915771082968));
#22651=CARTESIAN_POINT('Origin',(0.,0.,116.208423447177));
#22652=CARTESIAN_POINT('',(1.87238193903531,2.43733217358127,97.4373604997054));
#22653=CARTESIAN_POINT('',(1.87238193903531,2.43733217358127,97.3540855889292));
#22654=CARTESIAN_POINT('',(1.8723819390353,2.43733217358128,116.208423447177));
#22655=CARTESIAN_POINT('',(-3.07349878913888,-0.00272821586942156,96.7084234471429));
#22656=CARTESIAN_POINT('Ctrl Pts',(1.87238193903531,2.43733217358127,97.3540855889292));
#22657=CARTESIAN_POINT('Ctrl Pts',(1.94866488721299,2.37873088157338,97.3490953090774));
#22658=CARTESIAN_POINT('Ctrl Pts',(2.02229111276488,2.31647038074485,97.3441050292257));
#22659=CARTESIAN_POINT('Ctrl Pts',(2.09289233906605,2.25082293996632,97.339114749374));
#22660=CARTESIAN_POINT('Ctrl Pts',(2.16478061199566,2.18397875910626,97.3340334976909));
#22661=CARTESIAN_POINT('Ctrl Pts',(2.23353210894762,2.11362317016449,97.3289522460077));
#22662=CARTESIAN_POINT('Ctrl Pts',(2.29879203377926,2.04008760484274,97.3238709943246));
#22663=CARTESIAN_POINT('Ctrl Pts',(2.36278895497312,1.9679752052195,97.3188880823097));
#22664=CARTESIAN_POINT('Ctrl Pts',(2.42342794060438,1.89280516011432,97.3139051702948));
#22665=CARTESIAN_POINT('Ctrl Pts',(2.48041155381986,1.81492720891967,97.30892225828));
#22666=CARTESIAN_POINT('Ctrl Pts',(2.53738140951798,1.73706805974906,97.3039405492864));
#22667=CARTESIAN_POINT('Ctrl Pts',(2.5906973874908,1.65650265779948,97.2989588402928));
#22668=CARTESIAN_POINT('Ctrl Pts',(2.64010346854948,1.57361238090992,97.2939771312992));
#22669=CARTESIAN_POINT('Ctrl Pts',(2.68951110915327,1.49071948751804,97.2889952650537));
#22670=CARTESIAN_POINT('Ctrl Pts',(2.73500838355779,1.40550195090539,97.2840133988082));
#22671=CARTESIAN_POINT('Ctrl Pts',(2.77638415978595,1.31836764496465,97.2790315325627));
#22672=CARTESIAN_POINT('Ctrl Pts',(2.81920258234809,1.22819523319272,97.2738759639307));
#22673=CARTESIAN_POINT('Ctrl Pts',(2.85760659608389,1.13597038545078,97.2687203952986));
#22674=CARTESIAN_POINT('Ctrl Pts',(2.8914161828386,1.04216827221858,97.2635648266666));
#22675=CARTESIAN_POINT('Ctrl Pts',(2.92413458878274,0.951393556709182,97.2585756504132));
#22676=CARTESIAN_POINT('Ctrl Pts',(2.95255051386505,0.859142272147958,97.2535864741597));
#22677=CARTESIAN_POINT('Ctrl Pts',(2.97655192666899,0.765859567964746,97.2485972979063));
#22678=CARTESIAN_POINT('Ctrl Pts',(3.00175403432598,0.667910302537554,97.2433585330849));
#22679=CARTESIAN_POINT('Ctrl Pts',(3.0220883572468,0.56882428666938,97.2381197682636));
#22680=CARTESIAN_POINT('Ctrl Pts',(3.03748631368271,0.469125936386219,97.2328810034423));
#22681=CARTESIAN_POINT('Ctrl Pts',(3.05288427011861,0.369427586103058,97.227642238621));
#22682=CARTESIAN_POINT('Ctrl Pts',(3.06334587623904,0.269117458435972,97.2224034737997));
#22683=CARTESIAN_POINT('Ctrl Pts',(3.06886550244303,0.168721006146533,97.2171647089784));
#22684=CARTESIAN_POINT('Ctrl Pts',(3.07413303278099,0.0729099242519637,
97.212165212344));
#22685=CARTESIAN_POINT('Ctrl Pts',(3.07491863032797,-0.0233163652926922,
97.2071657157097));
#22686=CARTESIAN_POINT('Ctrl Pts',(3.07117585748342,-0.119503566520019,
97.2021662190754));
#22687=CARTESIAN_POINT('Ctrl Pts',(3.06743816170377,-0.215560289974863,
97.1971735042496));
#22688=CARTESIAN_POINT('Ctrl Pts',(3.05918432071533,-0.311577595611862,
97.1921807894238));
#22689=CARTESIAN_POINT('Ctrl Pts',(3.04641979592841,-0.407097871494691,
97.187188074598));
#22690=CARTESIAN_POINT('Ctrl Pts',(3.03366873739887,-0.502517375853227,
97.1822006269626));
#22691=CARTESIAN_POINT('Ctrl Pts',(3.01641651283108,-0.597440460058204,
97.1772131793273));
#22692=CARTESIAN_POINT('Ctrl Pts',(2.99472055478194,-0.691412357979333,
97.1722257316919));
#22693=CARTESIAN_POINT('Ctrl Pts',(2.97304012043542,-0.785317017947915,
97.1672418526316));
#22694=CARTESIAN_POINT('Ctrl Pts',(2.94692237185042,-0.878271418115299,
97.1622579735713));
#22695=CARTESIAN_POINT('Ctrl Pts',(2.91647605472128,-0.96982971301018,97.1572740945109));
#22696=CARTESIAN_POINT('Ctrl Pts',(2.88604082512443,-1.06135466543058,97.152292030413));
#22697=CARTESIAN_POINT('Ctrl Pts',(2.8512802973318,-1.15148410663098,97.147309966315));
#22698=CARTESIAN_POINT('Ctrl Pts',(2.81235316369519,-1.23978705133327,97.1423279022171));
#22699=CARTESIAN_POINT('Ctrl Pts',(2.77342957883461,-1.32808194593417,97.1373462923069));
#22700=CARTESIAN_POINT('Ctrl Pts',(2.73034032057302,-1.41455027350001,97.1323646823968));
#22701=CARTESIAN_POINT('Ctrl Pts',(2.68329192137924,-1.49878174350401,97.1273830724866));
#22702=CARTESIAN_POINT('Ctrl Pts',(2.63623496719825,-1.58302852963269,97.1224005567516));
#22703=CARTESIAN_POINT('Ctrl Pts',(2.5852176564402,-1.66503726720775,97.1174180410167));
#22704=CARTESIAN_POINT('Ctrl Pts',(2.53049155840198,-1.74442389425744,97.1124355252817));
#22705=CARTESIAN_POINT('Ctrl Pts',(2.47570647140233,-1.82389609171776,97.1074476389202));
#22706=CARTESIAN_POINT('Ctrl Pts',(2.417204865677,-1.90074017407882,97.1024597525588));
#22707=CARTESIAN_POINT('Ctrl Pts',(2.35528045009995,-1.97460280851035,97.0974718661974));
#22708=CARTESIAN_POINT('Ctrl Pts',(2.29331945369033,-2.04850907608139,97.0924810333239));
#22709=CARTESIAN_POINT('Ctrl Pts',(2.22793191877006,-2.11943006622527,97.0874902004505));
#22710=CARTESIAN_POINT('Ctrl Pts',(2.15944902676273,-2.18704873078162,97.082499367577));
#22711=CARTESIAN_POINT('Ctrl Pts',(2.09085546075036,-2.25477667268014,97.0775004691058));
#22712=CARTESIAN_POINT('Ctrl Pts',(2.01915687537714,-2.3191913393532,97.0725015706345));
#22713=CARTESIAN_POINT('Ctrl Pts',(1.9447181137197,-2.3800154848594,97.0675026721632));
#22714=CARTESIAN_POINT('Ctrl Pts',(1.90150001300119,-2.41532913043965,97.0646003818403));
#22715=CARTESIAN_POINT('Ctrl Pts',(1.85735882408159,-2.44943327562251,97.0616980915173));
#22716=CARTESIAN_POINT('Ctrl Pts',(1.81237015424912,-2.48228053893733,97.0587958011943));
#22717=CARTESIAN_POINT('Ctrl Pts',(1.73487214875217,-2.53886361646355,97.0537962821545));
#22718=CARTESIAN_POINT('Ctrl Pts',(1.65458565811884,-2.59191331061371,97.0487967631147));
#22719=CARTESIAN_POINT('Ctrl Pts',(1.57186646274079,-2.64114332691559,97.0437972440749));
#22720=CARTESIAN_POINT('Ctrl Pts',(1.48925947665256,-2.69030656228299,97.0388045069251));
#22721=CARTESIAN_POINT('Ctrl Pts',(1.40422671830548,-2.73566019496757,97.0338117697752));
#22722=CARTESIAN_POINT('Ctrl Pts',(1.31715500584991,-2.77695965771282,97.0288190326253));
#22723=CARTESIAN_POINT('Ctrl Pts',(1.23017515339638,-2.81821554983537,97.0238315627757));
#22724=CARTESIAN_POINT('Ctrl Pts',(1.14116101755377,-2.85542558755582,97.018844092926));
#22725=CARTESIAN_POINT('Ctrl Pts',(1.05052532509124,-2.88839034608239,97.0138566230763));
#22726=CARTESIAN_POINT('Ctrl Pts',(0.959954487793827,-2.92133151638671,
97.0088727220544));
#22727=CARTESIAN_POINT('Ctrl Pts',(0.867764811876671,-2.95003329678853,
97.0038888210325));
#22728=CARTESIAN_POINT('Ctrl Pts',(0.774389478947485,-2.97434416046554,
96.9989049200107));
#22729=CARTESIAN_POINT('Ctrl Pts',(0.681048153119648,-2.99864617017674,
96.9939228341151));
#22730=CARTESIAN_POINT('Ctrl Pts',(0.586522452611931,-3.01856033004005,
96.9889407482196));
#22731=CARTESIAN_POINT('Ctrl Pts',(0.491260287932881,-3.03398509876039,
96.9839586623241));
#22732=CARTESIAN_POINT('Ctrl Pts',(0.396006811374262,-3.04940846070766,
96.9789770308058));
#22733=CARTESIAN_POINT('Ctrl Pts',(0.300017437531326,-3.06034317557799,
96.9739953992876));
#22734=CARTESIAN_POINT('Ctrl Pts',(0.203748764977606,-3.06673909727745,
96.9690137677693));
#22735=CARTESIAN_POINT('Ctrl Pts',(0.107462591762245,-3.07313618169016,
96.9640312306413));
#22736=CARTESIAN_POINT('Ctrl Pts',(0.010897456992419,-3.07499280520594,
96.9590486935133));
#22737=CARTESIAN_POINT('Ctrl Pts',(-0.085487520602769,-3.07231087844658,
96.9540661563853));
#22738=CARTESIAN_POINT('Ctrl Pts',(-0.181976381768099,-3.06962606111098,
96.949078249087));
#22739=CARTESIAN_POINT('Ctrl Pts',(-0.278284258591738,-3.06239294001798,
96.9440903417887));
#22740=CARTESIAN_POINT('Ctrl Pts',(-0.373954864658887,-3.05066550267281,
96.9391024344904));
#22741=CARTESIAN_POINT('Ctrl Pts',(-0.469681981989062,-3.0389311380976,
96.9341115809064));
#22742=CARTESIAN_POINT('Ctrl Pts',(-0.564770646537324,-3.0226972451083,
96.9291207273223));
#22743=CARTESIAN_POINT('Ctrl Pts',(-0.658774604986502,-3.00206899817857,
96.9241298737383));
#22744=CARTESIAN_POINT('Ctrl Pts',(-0.75293047041527,-2.98140741675168,
96.9191309551163));
#22745=CARTESIAN_POINT('Ctrl Pts',(-0.845997706132988,-2.95633741612214,
96.9141320364943));
#22746=CARTESIAN_POINT('Ctrl Pts',(-0.937545117289906,-2.92701407633203,
96.9091331178723));
#22747=CARTESIAN_POINT('Ctrl Pts',(-0.990692099049544,-2.9099906893759,
96.9062310430516));
#22748=CARTESIAN_POINT('Ctrl Pts',(-1.04332721268546,-2.89153472117561,
96.9033289682308));
#22749=CARTESIAN_POINT('Ctrl Pts',(-1.0953695685853,-2.87168378450993,96.9004268934101));
#22750=CARTESIAN_POINT('Ctrl Pts',(-1.18502535444122,-2.83748565308476,
96.8954273542047));
#22751=CARTESIAN_POINT('Ctrl Pts',(-1.27323553386468,-2.79902477074773,
96.8904278149992));
#22752=CARTESIAN_POINT('Ctrl Pts',(-1.35956625780384,-2.75644369444421,
96.8854282757938));
#22753=CARTESIAN_POINT('Ctrl Pts',(-1.44577987898086,-2.71392037697119,
96.8804355181815));
#22754=CARTESIAN_POINT('Ctrl Pts',(-1.53011872108289,-2.66728816543942,
96.8754427605693));
#22755=CARTESIAN_POINT('Ctrl Pts',(-1.6121670374189,-2.6167383693178,96.870450002957));
#22756=CARTESIAN_POINT('Ctrl Pts',(-1.69412879811219,-2.56624189994666,
96.8654625123797));
#22757=CARTESIAN_POINT('Ctrl Pts',(-1.77380446487575,-2.51183629076463,
96.8604750218023));
#22758=CARTESIAN_POINT('Ctrl Pts',(-1.85080205055773,-2.45375916088994,
96.8554875312249));
#22759=CARTESIAN_POINT('Ctrl Pts',(-1.92774454489346,-2.39572358488013,
96.8505036091695));
#22760=CARTESIAN_POINT('Ctrl Pts',(-2.00201241792848,-2.33402197401046,
96.845519687114));
#22761=CARTESIAN_POINT('Ctrl Pts',(-2.073242722576,-2.26893518269819,96.8405357650585));
#22762=CARTESIAN_POINT('Ctrl Pts',(-2.14444708798958,-2.20387209339751,
96.8355536579486));
#22763=CARTESIAN_POINT('Ctrl Pts',(-2.21261575912116,-2.13542656878813,
96.8305715508386));
#22764=CARTESIAN_POINT('Ctrl Pts',(-2.27741969742316,-2.0639190322755,96.8255894437286));
#22765=CARTESIAN_POINT('Ctrl Pts',(-2.34221772748717,-1.9924180151744,96.8206077908421));
#22766=CARTESIAN_POINT('Ctrl Pts',(-2.40365133999704,-1.91785586658859,
96.8156261379557));
#22767=CARTESIAN_POINT('Ctrl Pts',(-2.46142987624377,-1.84058827941899,
96.8106444850693));
#22768=CARTESIAN_POINT('Ctrl Pts',(-2.51921891746298,-1.76330664388595,
96.8056619264464));
#22769=CARTESIAN_POINT('Ctrl Pts',(-2.57335129978882,-1.6833189444371,96.8006793678235));
#22770=CARTESIAN_POINT('Ctrl Pts',(-2.62357865729354,-1.60101133006417,
96.7956968092006));
#22771=CARTESIAN_POINT('Ctrl Pts',(-2.67386015012781,-1.51861500407966,
96.7907088803479));
#22772=CARTESIAN_POINT('Ctrl Pts',(-2.72022798650951,-1.4338941466383,96.7857209514952));
#22773=CARTESIAN_POINT('Ctrl Pts',(-2.76247902432589,-1.3472608842238,96.7807330226425));
#22774=CARTESIAN_POINT('Ctrl Pts',(-2.80475501967376,-1.26057644786218,
96.7757421474387));
#22775=CARTESIAN_POINT('Ctrl Pts',(-2.84290920085046,-1.17197776018121,
96.7707512722349));
#22776=CARTESIAN_POINT('Ctrl Pts',(-2.87678682353888,-1.08189640073026,
96.7657603970311));
#22777=CARTESIAN_POINT('Ctrl Pts',(-2.91071919022953,-0.991669475748106,
96.7607614569024));
#22778=CARTESIAN_POINT('Ctrl Pts',(-2.94036106451332,-0.89995551231489,
96.7557625167737));
#22779=CARTESIAN_POINT('Ctrl Pts',(-2.9656077610954,-0.807200630160035,
96.7507635766449));
#22780=CARTESIAN_POINT('Ctrl Pts',(-2.98026336204054,-0.753356812052726,
96.7478617129719));
#22781=CARTESIAN_POINT('Ctrl Pts',(-2.99343885263844,-0.699162428364548,
96.7449598492989));
#22782=CARTESIAN_POINT('Ctrl Pts',(-3.00512174427709,-0.644705787218516,
96.7420579856259));
#22783=CARTESIAN_POINT('Ctrl Pts',(-3.03303922606691,-0.51457599276761,
96.7351236812812));
#22784=CARTESIAN_POINT('Ctrl Pts',(-3.05251243821152,-0.382575811799598,
96.7281893769366));
#22785=CARTESIAN_POINT('Ctrl Pts',(-3.0633464197383,-0.2496216390391,96.7212550725919));
#22786=CARTESIAN_POINT('Ctrl Pts',(-3.07002902195233,-0.167613021333926,
96.7169778641204));
#22787=CARTESIAN_POINT('Ctrl Pts',(-3.07342554527863,-0.0852417967828543,
96.7127006556489));
#22788=CARTESIAN_POINT('Ctrl Pts',(-3.07349878913829,-0.00272821653494097,
96.7084234471774));
#22789=CARTESIAN_POINT('Ctrl Pts',(-3.07349878913888,-0.00272821586942156,
96.7084234471429));
#22790=CARTESIAN_POINT('Ctrl Pts',(-3.07358304670424,0.0921929844691349,
96.7035030720848));
#22791=CARTESIAN_POINT('Ctrl Pts',(-3.06926580554714,0.18724875112797,96.6985826970266));
#22792=CARTESIAN_POINT('Ctrl Pts',(-3.06053637932574,0.28199170346609,96.6936623219685));
#22793=CARTESIAN_POINT('Ctrl Pts',(-3.0518144921111,0.37665283281373,96.6887461963009));
#22794=CARTESIAN_POINT('Ctrl Pts',(-3.03868803264072,0.471001235998057,
96.6838300706332));
#22795=CARTESIAN_POINT('Ctrl Pts',(-3.0211983720668,0.564590689456483,96.6789139449656));
#22796=CARTESIAN_POINT('Ctrl Pts',(-3.0037165249272,0.658138332209337,96.674000015557));
#22797=CARTESIAN_POINT('Ctrl Pts',(-2.98187542952173,0.750927254409376,
96.6690860861484));
#22798=CARTESIAN_POINT('Ctrl Pts',(-2.95576803510189,0.842518588916523,
96.6641721567398));
#22799=CARTESIAN_POINT('Ctrl Pts',(-2.9296647045998,0.934095666173676,96.6592589922411));
#22800=CARTESIAN_POINT('Ctrl Pts',(-2.89929651865308,1.02447509116612,96.6543458277424));
#22801=CARTESIAN_POINT('Ctrl Pts',(-2.86480673424856,1.11323161354864,96.6494326632437));
#22802=CARTESIAN_POINT('Ctrl Pts',(-2.8303122788876,1.20200015623968,96.6445188333544));
#22803=CARTESIAN_POINT('Ctrl Pts',(-2.7916952822282,1.28914493889506,96.6396050034651));
#22804=CARTESIAN_POINT('Ctrl Pts',(-2.74914726062367,1.37426037904225,96.6346911735759));
#22805=CARTESIAN_POINT('Ctrl Pts',(-2.70655560981867,1.45946309748023,96.6297723049924));
#22806=CARTESIAN_POINT('Ctrl Pts',(-2.66002509260195,1.54263191558396,96.624853436409));
#22807=CARTESIAN_POINT('Ctrl Pts',(-2.60979313043381,1.62338598809417,96.6199345678255));
#22808=CARTESIAN_POINT('Ctrl Pts',(-2.55953193290358,1.70418706005351,96.6150128364253));
#22809=CARTESIAN_POINT('Ctrl Pts',(-2.5055652614669,1.78257021878091,96.610091105025));
#22810=CARTESIAN_POINT('Ctrl Pts',(-2.44817249361536,1.85818559124356,96.6051693736248));
#22811=CARTESIAN_POINT('Ctrl Pts',(-2.39069007411127,1.93391908038454,96.6002399541243));
#22812=CARTESIAN_POINT('Ctrl Pts',(-2.32977116879369,2.00687581022152,96.5953105346238));
#22813=CARTESIAN_POINT('Ctrl Pts',(-2.26573359723045,2.07674108072748,96.5903811151233));
#22814=CARTESIAN_POINT('Ctrl Pts',(-2.23675507915326,2.10835677062488,96.5881504360295));
#22815=CARTESIAN_POINT('Ctrl Pts',(-2.20713840149301,2.13933992704164,96.5859197569356));
#22816=CARTESIAN_POINT('Ctrl Pts',(-2.17691522278127,2.16966411290392,96.5836890778418));
#22817=CARTESIAN_POINT('Ctrl Pts',(-2.10917614296048,2.23762957961467,96.5786894664299));
#22818=CARTESIAN_POINT('Ctrl Pts',(-2.03813212500065,2.30253904379334,96.573689855018));
#22819=CARTESIAN_POINT('Ctrl Pts',(-1.96409002225505,2.36405427908882,96.5686902436061));
#22820=CARTESIAN_POINT('Ctrl Pts',(-1.89014836370427,2.42548606391423,96.5636974145778));
#22821=CARTESIAN_POINT('Ctrl Pts',(-1.81321703829942,2.48353249300041,96.5587045855495));
#22822=CARTESIAN_POINT('Ctrl Pts',(-1.73364005777044,2.53789172347713,96.5537117565212));
#22823=CARTESIAN_POINT('Ctrl Pts',(-1.6541470385018,2.59219359981109,96.5487241954009));
#22824=CARTESIAN_POINT('Ctrl Pts',(-1.57201427380566,2.64281576503736,96.5437366342807));
#22825=CARTESIAN_POINT('Ctrl Pts',(-1.4876183993823,2.68949693210817,96.5387490731605));
#22826=CARTESIAN_POINT('Ctrl Pts',(-1.40328293555489,2.73614468478352,96.5337650821382));
#22827=CARTESIAN_POINT('Ctrl Pts',(-1.316687965361,2.77885683541977,96.5287810911159));
#22828=CARTESIAN_POINT('Ctrl Pts',(-1.22823779052362,2.81741622411912,96.5237971000936));
#22829=CARTESIAN_POINT('Ctrl Pts',(-1.13981984296242,2.85596156350686,96.5188149250141));
#22830=CARTESIAN_POINT('Ctrl Pts',(-1.04954843576476,2.89035697205567,96.5138327499346));
#22831=CARTESIAN_POINT('Ctrl Pts',(-0.957850206143674,2.92043237082979,
96.5088505748551));
#22832=CARTESIAN_POINT('Ctrl Pts',(-0.86616035638254,2.95050502115795,96.5038688550726));
#22833=CARTESIAN_POINT('Ctrl Pts',(-0.773044360578548,2.97625830999605,
96.4988871352901));
#22834=CARTESIAN_POINT('Ctrl Pts',(-0.678945444151034,2.99757157276796,
96.4939054155076));
#22835=CARTESIAN_POINT('Ctrl Pts',(-0.584829441143728,3.01888870562444,
96.4889227911392));
#22836=CARTESIAN_POINT('Ctrl Pts',(-0.489730591155304,3.03576411432382,
96.4839401667708));
#22837=CARTESIAN_POINT('Ctrl Pts',(-0.394102718476329,3.04812816287137,
96.4789575424024));
#22838=CARTESIAN_POINT('Ctrl Pts',(-0.298371819986878,3.06050553197166,
96.4739695499452));
#22839=CARTESIAN_POINT('Ctrl Pts',(-0.202111196998124,3.06836178126515,
96.468981557488));
#22840=CARTESIAN_POINT('Ctrl Pts',(-0.105779988667777,3.07167915707312,
96.4639935650308));
#22841=CARTESIAN_POINT('Ctrl Pts',(-0.00939190008039556,3.07499849167713,
96.459002627336));
#22842=CARTESIAN_POINT('Ctrl Pts',(0.0870664181326297,3.07377362194052,
96.4540116896412));
#22843=CARTESIAN_POINT('Ctrl Pts',(0.18313776291556,3.06803891921114,96.4490207519465));
#22844=CARTESIAN_POINT('Ctrl Pts',(0.27936430523661,3.06229495241091,96.444021751689));
#22845=CARTESIAN_POINT('Ctrl Pts',(0.375202189722728,3.05202665207337,96.4390227514315));
#22846=CARTESIAN_POINT('Ctrl Pts',(0.470201313175157,3.03732003172013,96.434023751174));
#22847=CARTESIAN_POINT('Ctrl Pts',(0.525334508772668,3.02878497426857,96.4311225574685));
#22848=CARTESIAN_POINT('Ctrl Pts',(0.580185407945726,3.01875599274042,96.428221363763));
#22849=CARTESIAN_POINT('Ctrl Pts',(0.634668328288215,3.00725761501536,96.4253201700575));
#22850=CARTESIAN_POINT('Ctrl Pts',(0.728566358212649,2.98744085392906,96.4203201375397));
#22851=CARTESIAN_POINT('Ctrl Pts',(0.821700203521094,2.96318730838223,96.4153201050219));
#22852=CARTESIAN_POINT('Ctrl Pts',(0.91361899032501,2.93457025653119,96.4103200725041));
#22853=CARTESIAN_POINT('Ctrl Pts',(1.00539028441085,2.90599912354947,96.4053280630295));
#22854=CARTESIAN_POINT('Ctrl Pts',(1.09594998283726,2.87307854152665,96.4003360535548));
#22855=CARTESIAN_POINT('Ctrl Pts',(1.18485783210905,2.8359326803875,96.3953440440801));
#22856=CARTESIAN_POINT('Ctrl Pts',(1.27368277071042,2.79882145947726,96.3903566898845));
#22857=CARTESIAN_POINT('Ctrl Pts',(1.36085851744708,2.75749295450866,96.3853693356889));
#22858=CARTESIAN_POINT('Ctrl Pts',(1.44596091047329,2.7121208113547,96.3803819814933));
#22859=CARTESIAN_POINT('Ctrl Pts',(1.53100536935423,2.66677955565571,96.3753980224795));
#22860=CARTESIAN_POINT('Ctrl Pts',(1.61397889340451,2.61740033821018,96.3704140634658));
#22861=CARTESIAN_POINT('Ctrl Pts',(1.69447922616217,2.56420404845341,96.3654301044521));
#22862=CARTESIAN_POINT('Ctrl Pts',(1.75524321035264,2.5240499472337,96.3616680677457));
#22863=CARTESIAN_POINT('Ctrl Pts',(1.81459844688948,2.48172200613711,96.3579060310392));
#22864=CARTESIAN_POINT('Ctrl Pts',(1.87238193903531,2.43733217358126,96.3541439943328));
#22865=CARTESIAN_POINT('',(-3.07349915159075,0.00228367488303187,96.7915765528226));
#22866=CARTESIAN_POINT('Ctrl Pts',(-3.07056037769426,0.00230326753188174,
96.7915754276343));
#22867=CARTESIAN_POINT('Ctrl Pts',(-3.07296424660638,0.349288135212611,
96.7736466355977));
#22868=CARTESIAN_POINT('Ctrl Pts',(-2.85878184482725,1.71505316958018,96.7029282076332));
#22869=CARTESIAN_POINT('Ctrl Pts',(-0.943444564451998,3.44751893046241,
96.5848744668941));
#22870=CARTESIAN_POINT('Ctrl Pts',(1.14803854905623,2.98990927824168,96.4847495181914));
#22871=CARTESIAN_POINT('Ctrl Pts',(1.87462644597698,2.44029756596839,96.4374142054168));
#22872=CARTESIAN_POINT('Ctrl Pts',(1.8723819390353,2.43733217358127,97.4373604997054));
#22873=CARTESIAN_POINT('Ctrl Pts',(1.94890431270062,2.37854695261874,97.4323776874656));
#22874=CARTESIAN_POINT('Ctrl Pts',(2.02263347195522,2.3161715702656,97.4273948752259));
#22875=CARTESIAN_POINT('Ctrl Pts',(2.09322696924329,2.25051174296704,97.4224120629862));
#22876=CARTESIAN_POINT('Ctrl Pts',(2.16389828936707,2.18477953175001,97.4174237576544));
#22877=CARTESIAN_POINT('Ctrl Pts',(2.23142672611253,2.11575594801334,97.4124354523226));
#22878=CARTESIAN_POINT('Ctrl Pts',(2.29550652016526,2.04378376201563,97.4074471469909));
#22879=CARTESIAN_POINT('Ctrl Pts',(2.3596267818964,1.97176612413531,97.402455691444));
#22880=CARTESIAN_POINT('Ctrl Pts',(2.42029378929588,1.89679651771012,97.3974642358971));
#22881=CARTESIAN_POINT('Ctrl Pts',(2.47724324675447,1.81924933596508,97.3924727803502));
#22882=CARTESIAN_POINT('Ctrl Pts',(2.53428199789625,1.74158056441412,97.3874734984698));
#22883=CARTESIAN_POINT('Ctrl Pts',(2.5875913217096,1.66132651533092,97.3824742165893));
#22884=CARTESIAN_POINT('Ctrl Pts',(2.63695134636908,1.57888880130372,97.3774749347089));
#22885=CARTESIAN_POINT('Ctrl Pts',(2.65739016148488,1.54475329980844,97.3754048506931));
#22886=CARTESIAN_POINT('Ctrl Pts',(2.67715239088241,1.51024365654688,97.3733347666773));
#22887=CARTESIAN_POINT('Ctrl Pts',(2.69622482896227,1.47538941357438,97.3712646826615));
#22888=CARTESIAN_POINT('Ctrl Pts',(2.7422871163402,1.39121212331832,97.3662651747626));
#22889=CARTESIAN_POINT('Ctrl Pts',(2.78448445429822,1.30472778727541,97.3612656668637));
#22890=CARTESIAN_POINT('Ctrl Pts',(2.82257907131634,1.21632628688481,97.3562661589648));
#22891=CARTESIAN_POINT('Ctrl Pts',(2.86062201321497,1.12804470259924,97.3512734328684));
#22892=CARTESIAN_POINT('Ctrl Pts',(2.89457312263953,1.03785152220718,97.346280706772));
#22893=CARTESIAN_POINT('Ctrl Pts',(2.92424002577248,0.946161995469138,97.3412879806756));
#22894=CARTESIAN_POINT('Ctrl Pts',(2.95387563107546,0.854569198855065,97.3363005217785));
#22895=CARTESIAN_POINT('Ctrl Pts',(2.9792358806208,0.761483609495415,97.3313130628814));
#22896=CARTESIAN_POINT('Ctrl Pts',(3.00017652003359,0.667340316959154,97.3263256039843));
#22897=CARTESIAN_POINT('Ctrl Pts',(3.02110217596745,0.573264385978197,97.3213417137216));
#22898=CARTESIAN_POINT('Ctrl Pts',(3.03761441328648,0.478132683583798,97.3163578234589));
#22899=CARTESIAN_POINT('Ctrl Pts',(3.04961912253582,0.382394374257599,97.3113739331962));
#22900=CARTESIAN_POINT('Ctrl Pts',(3.06161945998259,0.286690930331169,97.3063918579365));
#22901=CARTESIAN_POINT('Ctrl Pts',(3.06911547633185,0.190381753504808,97.3014097826769));
#22902=CARTESIAN_POINT('Ctrl Pts',(3.07206453494666,0.0939241349331538,
97.2964277074172));
#22903=CARTESIAN_POINT('Ctrl Pts',(3.07501332468038,-0.00252468909283135,
97.2914460863994));
#22904=CARTESIAN_POINT('Ctrl Pts',(3.07341596769022,-0.0991214891924568,
97.2864644653817));
#22905=CARTESIAN_POINT('Ctrl Pts',(3.06728191506374,-0.195407020147495,
97.2814828443639));
#22906=CARTESIAN_POINT('Ctrl Pts',(3.06114674714497,-0.291710057719588,
97.2765003175887));
#22907=CARTESIAN_POINT('Ctrl Pts',(3.05047327335789,-0.387701275681762,
97.2715177908135));
#22908=CARTESIAN_POINT('Ctrl Pts',(3.03532288909604,-0.482925676403381,
97.2665352640384));
#22909=CARTESIAN_POINT('Ctrl Pts',(3.02015617486979,-0.57825271551669,97.2615473668064));
#22910=CARTESIAN_POINT('Ctrl Pts',(3.00050298564189,-0.672810853089337,
97.2565594695743));
#22911=CARTESIAN_POINT('Ctrl Pts',(2.97647598743741,-0.766154649015789,
97.2515715723423));
#22912=CARTESIAN_POINT('Ctrl Pts',(2.95243479609223,-0.859553584648742,
97.2465807286778));
#22913=CARTESIAN_POINT('Ctrl Pts',(2.92401478050595,-0.951736331027809,
97.2415898850134));
#22914=CARTESIAN_POINT('Ctrl Pts',(2.89137806169206,-1.04227403036142,97.2365990413489));
#22915=CARTESIAN_POINT('Ctrl Pts',(2.85868860087712,-1.13295804156727,97.2316001323184));
#22916=CARTESIAN_POINT('Ctrl Pts',(2.82176899815312,-1.22199129218172,97.226601223288));
#22917=CARTESIAN_POINT('Ctrl Pts',(2.78082890764678,-1.30896632362946,97.2216023142575));
#22918=CARTESIAN_POINT('Ctrl Pts',(2.75706062086986,-1.35946077697127,97.2187001344641));
#22919=CARTESIAN_POINT('Ctrl Pts',(2.73193807334052,-1.40926197064841,97.2157979546707));
#22920=CARTESIAN_POINT('Ctrl Pts',(2.70550904928966,-1.45829456359536,97.2128957748773));
#22921=CARTESIAN_POINT('Ctrl Pts',(2.65998045166647,-1.54276174597812,97.2078962646499));
#22922=CARTESIAN_POINT('Ctrl Pts',(2.61041244107992,-1.62524311105927,97.2028967544224));
#22923=CARTESIAN_POINT('Ctrl Pts',(2.55700259225754,-1.70532694612741,97.1978972441949));
#22924=CARTESIAN_POINT('Ctrl Pts',(2.50366519367961,-1.78530214779636,97.1929045157829));
#22925=CARTESIAN_POINT('Ctrl Pts',(2.44649655572826,-1.86288592099231,97.1879117873709));
#22926=CARTESIAN_POINT('Ctrl Pts',(2.38574024872595,-1.93769082043783,97.1829190589589));
#22927=CARTESIAN_POINT('Ctrl Pts',(2.32504803824859,-2.01241680241223,97.1779315977621));
#22928=CARTESIAN_POINT('Ctrl Pts',(2.26077595816414,-2.08436939965339,97.1729441365652));
#22929=CARTESIAN_POINT('Ctrl Pts',(2.19321041897331,-2.15319072729448,97.1679566753684));
#22930=CARTESIAN_POINT('Ctrl Pts',(2.12569322480403,-2.22196281136246,97.1629727828387));
#22931=CARTESIAN_POINT('Ctrl Pts',(2.05488756290188,-2.28760776751967,97.157988890309));
#22932=CARTESIAN_POINT('Ctrl Pts',(1.98111895117006,-2.34980210896894,97.1530049977793));
#22933=CARTESIAN_POINT('Ctrl Pts',(1.90737720434542,-2.41197380060588,97.1480229202737));
#22934=CARTESIAN_POINT('Ctrl Pts',(1.83067498688838,-2.47069709168082,97.1430408427681));
#22935=CARTESIAN_POINT('Ctrl Pts',(1.75137265774965,-2.52568724581785,97.1380587652625));
#22936=CARTESIAN_POINT('Ctrl Pts',(1.67207755939211,-2.5806723859562,97.1330771420224));
#22937=CARTESIAN_POINT('Ctrl Pts',(1.59018318153496,-2.63192481592623,97.1280955187823));
#22938=CARTESIAN_POINT('Ctrl Pts',(1.50607988143107,-2.67920242623595,97.1231138955423));
#22939=CARTESIAN_POINT('Ctrl Pts',(1.42196129013103,-2.72648863229888,97.118131366571));
#22940=CARTESIAN_POINT('Ctrl Pts',(1.33563336163968,-2.76979836839094,97.1131488375998));
#22941=CARTESIAN_POINT('Ctrl Pts',(1.24751117153615,-2.8089354081026,97.1081663086286));
#22942=CARTESIAN_POINT('Ctrl Pts',(1.15929399919801,-2.84811463155348,97.1031784092537));
#22943=CARTESIAN_POINT('Ctrl Pts',(1.06927910615813,-2.88311200125748,97.0981905098788));
#22944=CARTESIAN_POINT('Ctrl Pts',(0.97790146560417,-2.91377949981964,97.0932026105038));
#22945=CARTESIAN_POINT('Ctrl Pts',(0.88646984729801,-2.94446511400208,97.0882117647233));
#22946=CARTESIAN_POINT('Ctrl Pts',(0.793674300682157,-2.97081564438874,
97.0832209189427));
#22947=CARTESIAN_POINT('Ctrl Pts',(0.699962815698049,-2.99273358430717,
97.0782300731621));
#22948=CARTESIAN_POINT('Ctrl Pts',(0.606099891146746,-3.01468694403926,
97.0732311620785));
#22949=CARTESIAN_POINT('Ctrl Pts',(0.511318504016708,-3.03219333039695,
97.0682322509949));
#22950=CARTESIAN_POINT('Ctrl Pts',(0.41607457425234,-3.04520675794941,97.0632333399113));
#22951=CARTESIAN_POINT('Ctrl Pts',(0.360779952969739,-3.0527618068631,97.0603311823052));
#22952=CARTESIAN_POINT('Ctrl Pts',(0.305329505627397,-3.05880348903059,
97.0574290246992));
#22953=CARTESIAN_POINT('Ctrl Pts',(0.249812441843652,-3.06333086588767,
97.0545268670932));
#22954=CARTESIAN_POINT('Ctrl Pts',(0.154173822864202,-3.07113012688421,
97.0495273529513));
#22955=CARTESIAN_POINT('Ctrl Pts',(0.0580016288474361,-3.0744599702639,
97.0445278388095));
#22956=CARTESIAN_POINT('Ctrl Pts',(-0.0382512281636187,-3.07326196305228,
97.0395283246676));
#22957=CARTESIAN_POINT('Ctrl Pts',(-0.134373519396679,-3.07206558092223,
97.0345355923032));
#22958=CARTESIAN_POINT('Ctrl Pts',(-0.230575820989438,-3.06635356038032,
97.0295428599388));
#22959=CARTESIAN_POINT('Ctrl Pts',(-0.326400533937449,-3.05611926165282,
97.0245501275743));
#22960=CARTESIAN_POINT('Ctrl Pts',(-0.42212415468589,-3.04589575980367,
97.0195626623929));
#22961=CARTESIAN_POINT('Ctrl Pts',(-0.517470544516665,-3.03115951033572,
97.0145751972114));
#22962=CARTESIAN_POINT('Ctrl Pts',(-0.611983575133122,-3.01195590169698,
97.00958773203));
#22963=CARTESIAN_POINT('Ctrl Pts',(-0.70642897969296,-2.99276603364318,
97.0046038354845));
#22964=CARTESIAN_POINT('Ctrl Pts',(-0.800041781488772,-2.96911524804222,
96.999619938939));
#22965=CARTESIAN_POINT('Ctrl Pts',(-0.892373413025865,-2.94110046440521,
96.9946360423936));
#22966=CARTESIAN_POINT('Ctrl Pts',(-0.984671419767091,-2.91309588302897,
96.9896539608546));
#22967=CARTESIAN_POINT('Ctrl Pts',(-1.0756887636492,-2.88073058861448,96.9846718793155));
#22968=CARTESIAN_POINT('Ctrl Pts',(-1.16499041151238,-2.8441518227908,96.9796897977765));
#22969=CARTESIAN_POINT('Ctrl Pts',(-1.25428391709092,-2.80757639212084,
96.9747081704903));
#22970=CARTESIAN_POINT('Ctrl Pts',(-1.34186163153142,-2.76678842040393,
96.9697265432041));
#22971=CARTESIAN_POINT('Ctrl Pts',(-1.42730794418423,-2.72198351987454,
96.9647449159178));
#22972=CARTESIAN_POINT('Ctrl Pts',(-1.51276979233033,-2.67717047310444,
96.9597623828929));
#22973=CARTESIAN_POINT('Ctrl Pts',(-1.59609908033135,-2.62833925094222,
96.9547798498679));
#22974=CARTESIAN_POINT('Ctrl Pts',(-1.67690522600176,-2.57573118026862,
96.9497973168429));
#22975=CARTESIAN_POINT('Ctrl Pts',(-1.75779846804352,-2.5230664063329,96.9448094134276));
#22976=CARTESIAN_POINT('Ctrl Pts',(-1.83616276994022,-2.46661689670211,
96.9398215100122));
#22977=CARTESIAN_POINT('Ctrl Pts',(-1.91163715358443,-2.40666691568144,
96.9348336065969));
#22978=CARTESIAN_POINT('Ctrl Pts',(-1.98715612069678,-2.34668152161148,
96.9298427567775));
#22979=CARTESIAN_POINT('Ctrl Pts',(-2.05978144010712,-2.28319182767184,
96.924851906958));
#22980=CARTESIAN_POINT('Ctrl Pts',(-2.12918741472047,-2.21652051716107,
96.9198610571386));
#22981=CARTESIAN_POINT('Ctrl Pts',(-2.19870555004368,-2.14974146518342,
96.9148621420588));
#22982=CARTESIAN_POINT('Ctrl Pts',(-2.26499365065353,-2.07977084860068,
96.9098632269789));
#22983=CARTESIAN_POINT('Ctrl Pts',(-2.32776491757109,-2.00696605315716,
96.9048643118991));
#22984=CARTESIAN_POINT('Ctrl Pts',(-2.36420674368624,-1.96469926731411,
96.9019621943691));
#22985=CARTESIAN_POINT('Ctrl Pts',(-2.39946404159902,-1.92147784769679,
96.899060076839));
#22986=CARTESIAN_POINT('Ctrl Pts',(-2.43348745577258,-1.87737610845496,
96.896157959309));
#22987=CARTESIAN_POINT('Ctrl Pts',(-2.49213133510029,-1.80136089548879,
96.8911557737741));
#22988=CARTESIAN_POINT('Ctrl Pts',(-2.54731629060798,-1.72245755890727,
96.8861535882393));
#22989=CARTESIAN_POINT('Ctrl Pts',(-2.59874527060311,-1.64101348821939,
96.8811514027044));
#22990=CARTESIAN_POINT('Ctrl Pts',(-2.65010560182581,-1.55967813124652,
96.87615589422));
#22991=CARTESIAN_POINT('Ctrl Pts',(-2.69771968649096,-1.47580914427467,
96.8711603857356));
#22992=CARTESIAN_POINT('Ctrl Pts',(-2.74133111800883,-1.38978629703868,
96.8661648772513));
#22993=CARTESIAN_POINT('Ctrl Pts',(-2.78489616873654,-1.30385493516529,
96.8611746814939));
#22994=CARTESIAN_POINT('Ctrl Pts',(-2.82446682901955,-1.21577465312144,
96.8561844857365));
#22995=CARTESIAN_POINT('Ctrl Pts',(-2.8598309453293,-1.12595258076746,96.8511942899792));
#22996=CARTESIAN_POINT('Ctrl Pts',(-2.89516771522501,-1.03619996615305,
96.8462079530475));
#22997=CARTESIAN_POINT('Ctrl Pts',(-2.92630424711921,-0.944708644435166,
96.8412216161158));
#22998=CARTESIAN_POINT('Ctrl Pts',(-2.95307560184055,-0.851907706159584,
96.8362352791841));
#22999=CARTESIAN_POINT('Ctrl Pts',(-2.97983400188649,-0.759151674316428,
96.831251355144));
#23000=CARTESIAN_POINT('Ctrl Pts',(-3.00223130379482,-0.665087706013686,
96.8262674311039));
#23001=CARTESIAN_POINT('Ctrl Pts',(-3.0201520710862,-0.570161132938504,
96.8212835070637));
#23002=CARTESIAN_POINT('Ctrl Pts',(-3.03807483177263,-0.475224000819851,
96.8162990286428));
#23003=CARTESIAN_POINT('Ctrl Pts',(-3.05151996977012,-0.379424500303791,
96.8113145502219));
#23004=CARTESIAN_POINT('Ctrl Pts',(-3.06042308111738,-0.283218669165731,
96.806330071801));
#23005=CARTESIAN_POINT('Ctrl Pts',(-3.06920716450155,-0.188299038286348,
96.8014122321415));
#23006=CARTESIAN_POINT('Ctrl Pts',(-3.07356993770723,-0.0929842945523692,
96.7964943924821));
#23007=CARTESIAN_POINT('Ctrl Pts',(-3.07349915159074,0.00228367488303187,
96.7915765528226));
#23008=CARTESIAN_POINT('Origin',(0.,0.,116.208423447177));
#23009=CARTESIAN_POINT('',(1.8723819390353,2.43733217358127,98.4372333997809));
#23010=CARTESIAN_POINT('',(1.87238193903531,2.43733217358127,98.354260042891));
#23011=CARTESIAN_POINT('',(1.8723819390353,2.43733217358128,116.208423447177));
#23012=CARTESIAN_POINT('',(-3.07349950430575,0.00174557505997315,97.7084234472127));
#23013=CARTESIAN_POINT('Ctrl Pts',(1.87238193903531,2.43733217358127,98.354260042891));
#23014=CARTESIAN_POINT('Ctrl Pts',(1.94887360315701,2.37857054398451,98.3492617290814));
#23015=CARTESIAN_POINT('Ctrl Pts',(2.02251066494388,2.31627054257947,98.3442634152718));
#23016=CARTESIAN_POINT('Ctrl Pts',(2.09296620165726,2.25075425773681,98.3392651014622));
#23017=CARTESIAN_POINT('Ctrl Pts',(2.15648232986216,2.19169089747168,98.3347590887974));
#23018=CARTESIAN_POINT('Ctrl Pts',(2.21741311751157,2.13001428347652,98.3302530761326));
#23019=CARTESIAN_POINT('Ctrl Pts',(2.27554719676962,2.06598335067684,98.3257470634677));
#23020=CARTESIAN_POINT('Ctrl Pts',(2.3400480999962,1.99493977257722,98.3207475538764));
#23021=CARTESIAN_POINT('Ctrl Pts',(2.40133208819396,1.92074789682503,98.3157480442851));
#23022=CARTESIAN_POINT('Ctrl Pts',(2.4590766680417,1.84373105161598,98.3107485346938));
#23023=CARTESIAN_POINT('Ctrl Pts',(2.51674291773897,1.76681867926115,98.305755806905));
#23024=CARTESIAN_POINT('Ctrl Pts',(2.57087904005066,1.68708930160601,98.3007630791163));
#23025=CARTESIAN_POINT('Ctrl Pts',(2.62120073287719,1.60490154463259,98.2957703513275));
#23026=CARTESIAN_POINT('Ctrl Pts',(2.67146933758932,1.52280049366606,98.2907828907404));
#23027=CARTESIAN_POINT('Ctrl Pts',(2.7179312845413,1.4382465915319,98.2857954301533));
#23028=CARTESIAN_POINT('Ctrl Pts',(2.76034440402892,1.35162902497181,98.2808079695662));
#23029=CARTESIAN_POINT('Ctrl Pts',(2.80272717593779,1.26507343530597,98.2758240776237));
#23030=CARTESIAN_POINT('Ctrl Pts',(2.84106668705415,1.17645750973203,98.2708401856813));
#23031=CARTESIAN_POINT('Ctrl Pts',(2.87516621973593,1.08619586580386,98.2658562937389));
#23032=CARTESIAN_POINT('Ctrl Pts',(2.909253334212,0.995967092932087,98.2608742168065));
#23033=CARTESIAN_POINT('Ctrl Pts',(2.93910338322924,0.904094202725765,98.2558921398742));
#23034=CARTESIAN_POINT('Ctrl Pts',(2.96456778565997,0.811011771941172,98.2509100629418));
#23035=CARTESIAN_POINT('Ctrl Pts',(2.99002986632277,0.717937828133745,98.2459284402603));
#23036=CARTESIAN_POINT('Ctrl Pts',(3.01110697976169,0.623654986462369,98.2409468175788));
#23037=CARTESIAN_POINT('Ctrl Pts',(3.02770072523178,0.528611926114938,98.2359651948973));
#23038=CARTESIAN_POINT('Ctrl Pts',(3.04429748773597,0.43355158527145,98.2309826664694));
#23039=CARTESIAN_POINT('Ctrl Pts',(3.05640918791082,0.337731183667423,98.2260001380414));
#23040=CARTESIAN_POINT('Ctrl Pts',(3.06398891884574,0.241607440263167,98.2210176096135));
#23041=CARTESIAN_POINT('Ctrl Pts',(3.07157681961165,0.145380089653701,98.2160297107555));
#23042=CARTESIAN_POINT('Ctrl Pts',(3.07462296453397,0.0488491828327223,
98.2110418118975));
#23043=CARTESIAN_POINT('Ctrl Pts',(3.07313252958506,-0.0475258414563746,
98.2060539130394));
#23044=CARTESIAN_POINT('Ctrl Pts',(3.07164121421593,-0.143957795784586,
98.2010630677616));
#23045=CARTESIAN_POINT('Ctrl Pts',(3.0656080104583,-0.240233246332413,98.1960722224838));
#23046=CARTESIAN_POINT('Ctrl Pts',(3.05509005777202,-0.335897289215853,
98.191081377206));
#23047=CARTESIAN_POINT('Ctrl Pts',(3.04455510781254,-0.431715927572407,
98.1860824665981));
#23048=CARTESIAN_POINT('Ctrl Pts',(3.02952100576024,-0.526920752049771,
98.1810835559902));
#23049=CARTESIAN_POINT('Ctrl Pts',(3.01009611464282,-0.621066526720114,
98.1760846453823));
#23050=CARTESIAN_POINT('Ctrl Pts',(2.99881881660216,-0.675723716498384,
98.1731824821494));
#23051=CARTESIAN_POINT('Ctrl Pts',(2.98606255056658,-0.730024210174861,
98.1702803189164));
#23052=CARTESIAN_POINT('Ctrl Pts',(2.97185612004777,-0.783883570267034,
98.1673781556835));
#23053=CARTESIAN_POINT('Ctrl Pts',(2.94738293373129,-0.876666212090917,
98.162378646382));
#23054=CARTESIAN_POINT('Ctrl Pts',(2.91851752568576,-0.968464626203716,
98.1573791370805));
#23055=CARTESIAN_POINT('Ctrl Pts',(2.88535551907953,-1.05883227119186,98.152379627779));
#23056=CARTESIAN_POINT('Ctrl Pts',(2.85223849652507,-1.14907733304233,98.1473869002802));
#23057=CARTESIAN_POINT('Ctrl Pts',(2.81483660871829,-1.23789507447157,98.1423941727814));
#23058=CARTESIAN_POINT('Ctrl Pts',(2.77329587960945,-1.32485177062993,98.1374014452826));
#23059=CARTESIAN_POINT('Ctrl Pts',(2.73179897492065,-1.41171672967004,98.1324139849852));
#23060=CARTESIAN_POINT('Ctrl Pts',(2.68617209722699,-1.49672415249134,98.1274265246878));
#23061=CARTESIAN_POINT('Ctrl Pts',(2.63660984365751,-1.57945901571656,98.1224390643904));
#23062=CARTESIAN_POINT('Ctrl Pts',(2.587083053026,-1.66213468023488,98.1174551727361));
#23063=CARTESIAN_POINT('Ctrl Pts',(2.53362670923431,-1.74254064222001,98.1124712810818));
#23064=CARTESIAN_POINT('Ctrl Pts',(2.47648148702774,-1.8202861572865,98.1074873894275));
#23065=CARTESIAN_POINT('Ctrl Pts',(2.41935707568555,-1.89800335937587,98.1025053127822));
#23066=CARTESIAN_POINT('Ctrl Pts',(2.35854671482401,-1.97306168624915,98.097523236137));
#23067=CARTESIAN_POINT('Ctrl Pts',(2.29433402881454,-2.04509990323789,98.0925411594917));
#23068=CARTESIAN_POINT('Ctrl Pts',(2.23012719750764,-2.11713155201776,98.0875595370958));
#23069=CARTESIAN_POINT('Ctrl Pts',(2.16251895003478,-2.18614331082863,98.0825779147));
#23070=CARTESIAN_POINT('Ctrl Pts',(2.09183206056623,-2.25180835782871,98.0775962923042));
#23071=CARTESIAN_POINT('Ctrl Pts',(2.02113231895527,-2.31748534391032,98.0726137641602));
#23072=CARTESIAN_POINT('Ctrl Pts',(1.94735314530763,-2.37981411098498,98.0676312360162));
#23073=CARTESIAN_POINT('Ctrl Pts',(1.87085209339092,-2.43850665257547,98.0626487078722));
#23074=CARTESIAN_POINT('Ctrl Pts',(1.79426858456159,-2.49726245611664,98.0576608092937));
#23075=CARTESIAN_POINT('Ctrl Pts',(1.71495768928043,-2.55237394197662,98.0526729107152));
#23076=CARTESIAN_POINT('Ctrl Pts',(1.63330759925468,-2.60359530960879,98.0476850121367));
#23077=CARTESIAN_POINT('Ctrl Pts',(1.55160927737255,-2.65484693442313,98.0426941671364));
#23078=CARTESIAN_POINT('Ctrl Pts',(1.46756939161196,-2.70220365002367,98.0377033221361));
#23079=CARTESIAN_POINT('Ctrl Pts',(1.38160062147527,-2.74546571144845,98.0327124771357));
#23080=CARTESIAN_POINT('Ctrl Pts',(1.29549292355664,-2.78879768549646,98.0277135667993));
#23081=CARTESIAN_POINT('Ctrl Pts',(1.20745051774667,-2.82802161402931,98.0227146564629));
#23082=CARTESIAN_POINT('Ctrl Pts',(1.11790586289056,-2.86298598175313,98.0177157461265));
#23083=CARTESIAN_POINT('Ctrl Pts',(1.06591984151815,-2.88328488592205,98.0148135800507));
#23084=CARTESIAN_POINT('Ctrl Pts',(1.01342778663993,-2.9021490366,98.011911413975));
#23085=CARTESIAN_POINT('Ctrl Pts',(0.960516206142954,-2.91955662177269,
98.0090092478992));
#23086=CARTESIAN_POINT('Ctrl Pts',(0.869366374068857,-2.94954435697928,
98.0040097383784));
#23087=CARTESIAN_POINT('Ctrl Pts',(0.776650752559451,-2.97531206584531,
97.9990102288576));
#23088=CARTESIAN_POINT('Ctrl Pts',(0.682795959320957,-2.99669683617395,
97.9940107193368));
#23089=CARTESIAN_POINT('Ctrl Pts',(0.589068479545639,-3.01805259819012,
97.9890179916206));
#23090=CARTESIAN_POINT('Ctrl Pts',(0.4942053235143,-3.03503714113321,97.9840252639044));
#23091=CARTESIAN_POINT('Ctrl Pts',(0.39864979928181,-3.04753680659194,97.9790325361882));
#23092=CARTESIAN_POINT('Ctrl Pts',(0.303195083751813,-3.06002328521435,
97.9740450756756));
#23093=CARTESIAN_POINT('Ctrl Pts',(0.20704988501364,-3.06803423552479,97.9690576151631));
#23094=CARTESIAN_POINT('Ctrl Pts',(0.110668270214102,-3.07150692396547,
97.9640701546505));
#23095=CARTESIAN_POINT('Ctrl Pts',(0.0143556187644802,-3.07497712761453,
97.9590862627852));
#23096=CARTESIAN_POINT('Ctrl Pts',(-0.082192675041899,-3.07391550898284,
97.9541023709199));
#23097=CARTESIAN_POINT('Ctrl Pts',(-0.178517822059432,-3.06831120279661,
97.9491184790546));
#23098=CARTESIAN_POINT('Ctrl Pts',(-0.2748078898121,-3.06270893756175,97.9441364022009));
#23099=CARTESIAN_POINT('Ctrl Pts',(-0.370874534466474,-3.0525672972281,
97.9391543253472));
#23100=CARTESIAN_POINT('Ctrl Pts',(-0.466260335408199,-3.03792750894833,
97.9341722484936));
#23101=CARTESIAN_POINT('Ctrl Pts',(-0.561637439330315,-3.02328905548491,
97.9291906258922));
#23102=CARTESIAN_POINT('Ctrl Pts',(-0.656333389107419,-3.00415333626096,
97.9242090032908));
#23103=CARTESIAN_POINT('Ctrl Pts',(-0.749898314168346,-2.98061315309576,
97.9192273806894));
#23104=CARTESIAN_POINT('Ctrl Pts',(-0.843480250949397,-2.9570686899185,
97.914244852343));
#23105=CARTESIAN_POINT('Ctrl Pts',(-0.935930328930217,-2.92911827952979,
97.9092623239966));
#23106=CARTESIAN_POINT('Ctrl Pts',(-1.0268122997602,-2.8969050296931,97.9042797956501));
#23107=CARTESIAN_POINT('Ctrl Pts',(-1.11779222791188,-2.86465705873792,
97.8992918968751));
#23108=CARTESIAN_POINT('Ctrl Pts',(-1.20720026018258,-2.82813722231406,
97.8943039981001));
#23109=CARTESIAN_POINT('Ctrl Pts',(-1.2946188693551,-2.78753730613775,97.8893160993251));
#23110=CARTESIAN_POINT('Ctrl Pts',(-1.3820891178739,-2.74691340704579,97.8843252541313));
#23111=CARTESIAN_POINT('Ctrl Pts',(-1.4675672145334,-2.70220483253513,97.8793344089376));
#23112=CARTESIAN_POINT('Ctrl Pts',(-1.55066093076454,-2.65364898353201,
97.8743435637438));
#23113=CARTESIAN_POINT('Ctrl Pts',(-1.63388892849863,-2.60501466707458,
97.8693446532206));
#23114=CARTESIAN_POINT('Ctrl Pts',(-1.71472448388021,-2.55252090047919,
97.8643457426974));
#23115=CARTESIAN_POINT('Ctrl Pts',(-1.7928050541175,-2.49644793415179,97.8593468321742));
#23116=CARTESIAN_POINT('Ctrl Pts',(-1.83813545571699,-2.46389425178534,
97.8564446681545));
#23117=CARTESIAN_POINT('Ctrl Pts',(-1.88253790919386,-2.43013496034154,
97.8535425041349));
#23118=CARTESIAN_POINT('Ctrl Pts',(-1.92594701958118,-2.39523074624688,
97.8506403401152));
#23119=CARTESIAN_POINT('Ctrl Pts',(-1.99978831977924,-2.33585674553263,
97.8457035984338));
#23120=CARTESIAN_POINT('Ctrl Pts',(-2.07102703883305,-2.27294759451819,
97.8407668567525));
#23121=CARTESIAN_POINT('Ctrl Pts',(-2.1392990935973,-2.20676270544292,97.8358301150711));
#23122=CARTESIAN_POINT('Ctrl Pts',(-2.20747811774654,-2.14066800291552,
97.8309001004191));
#23123=CARTESIAN_POINT('Ctrl Pts',(-2.27269818618689,-2.07130673938253,
97.8259700857671));
#23124=CARTESIAN_POINT('Ctrl Pts',(-2.33462698575195,-1.9989795115005,97.8210400711151));
#23125=CARTESIAN_POINT('Ctrl Pts',(-2.39648614566971,-1.92673361641799,
97.8161156003212));
#23126=CARTESIAN_POINT('Ctrl Pts',(-2.45506110199223,-1.85152872758815,
97.8111911295274));
#23127=CARTESIAN_POINT('Ctrl Pts',(-2.51005617571016,-1.77370241156155,
97.8062666587335));
#23128=CARTESIAN_POINT('Ctrl Pts',(-2.56501759495709,-1.69592372168251,
97.8013452014907));
#23129=CARTESIAN_POINT('Ctrl Pts',(-2.61640322143425,-1.61552715686622,
97.7964237442478));
#23130=CARTESIAN_POINT('Ctrl Pts',(-2.66395808802082,-1.53288275979229,
97.791502287005));
#23131=CARTESIAN_POINT('Ctrl Pts',(-2.71149762595039,-1.45026500200278,
97.7865824161262));
#23132=CARTESIAN_POINT('Ctrl Pts',(-2.75520863196226,-1.36540124188588,
97.7816625452474));
#23133=CARTESIAN_POINT('Ctrl Pts',(-2.79488053362013,-1.27868880216856,
97.7767426743686));
#23134=CARTESIAN_POINT('Ctrl Pts',(-2.83455113660563,-1.19197920101063,
97.7718229645433));
#23135=CARTESIAN_POINT('Ctrl Pts',(-2.87018271202133,-1.10342145149765,
97.766903254718));
#23136=CARTESIAN_POINT('Ctrl Pts',(-2.90161208415863,-1.01343453812498,
97.7619835448928));
#23137=CARTESIAN_POINT('Ctrl Pts',(-2.93306694789383,-0.923374638559616,
97.7570598448107));
#23138=CARTESIAN_POINT('Ctrl Pts',(-2.9603126535254,-0.831883687086739,
97.7521361447287));
#23139=CARTESIAN_POINT('Ctrl Pts',(-2.98323552026053,-0.739397106199298,
97.7472124446467));
#23140=CARTESIAN_POINT('Ctrl Pts',(-3.00616832327337,-0.646870435546328,
97.7422866103093));
#23141=CARTESIAN_POINT('Ctrl Pts',(-3.024774468657,-0.55334771875868,97.7373607759719));
#23142=CARTESIAN_POINT('Ctrl Pts',(-3.03899158497072,-0.459273770726299,
97.7324349416345));
#23143=CARTESIAN_POINT('Ctrl Pts',(-3.05322924500887,-0.365063885896224,
97.7275019894695));
#23144=CARTESIAN_POINT('Ctrl Pts',(-3.06306516685465,-0.270301628072282,
97.7225690373045));
#23145=CARTESIAN_POINT('Ctrl Pts',(-3.06848896336662,-0.175435833561094,
97.7176360851395));
#23146=CARTESIAN_POINT('Ctrl Pts',(-3.0718654048822,-0.116379634404259,
97.7145652058306));
#23147=CARTESIAN_POINT('Ctrl Pts',(-3.0735330294058,-0.0572833264886464,
97.7114943265216));
#23148=CARTESIAN_POINT('Ctrl Pts',(-3.07349950430575,0.00174557505997277,
97.7084234472127));
#23149=CARTESIAN_POINT('Ctrl Pts',(-3.07349950430537,0.00174557573727362,
97.7084234471775));
#23150=CARTESIAN_POINT('Ctrl Pts',(-3.07344072655593,0.105237724430831,
97.7030394422287));
#23151=CARTESIAN_POINT('Ctrl Pts',(-3.06815507510877,0.208578390863187,
97.6976554372799));
#23152=CARTESIAN_POINT('Ctrl Pts',(-3.05768593427089,0.311382365207073,
97.692271432331));
#23153=CARTESIAN_POINT('Ctrl Pts',(-3.04796444388583,0.406844625540194,
97.6872719244293));
#23154=CARTESIAN_POINT('Ctrl Pts',(-3.03375103466145,0.502018859025492,
97.6822724165276));
#23155=CARTESIAN_POINT('Ctrl Pts',(-3.01507060365512,0.596449079951323,
97.6772729086259));
#23156=CARTESIAN_POINT('Ctrl Pts',(-2.99641551254137,0.690751206848963,
97.6722801825266));
#23157=CARTESIAN_POINT('Ctrl Pts',(-2.97330552693452,0.784310900067703,
97.6672874564274));
#23158=CARTESIAN_POINT('Ctrl Pts',(-2.94581732589708,0.87667698295587,97.6622947303281));
#23159=CARTESIAN_POINT('Ctrl Pts',(-2.91835812421426,0.968945621970214,
97.6573072714282));
#23160=CARTESIAN_POINT('Ctrl Pts',(-2.88653001374994,1.06002273543477,97.6523198125283));
#23161=CARTESIAN_POINT('Ctrl Pts',(-2.85046056698401,1.14946805352267,97.6473323536284));
#23162=CARTESIAN_POINT('Ctrl Pts',(-2.8144169286848,1.23884937155729,97.6423484633629));
#23163=CARTESIAN_POINT('Ctrl Pts',(-2.77413815075664,1.32660080937809,97.6373645730973));
#23164=CARTESIAN_POINT('Ctrl Pts',(-2.72980110282041,1.41229890215933,97.6323806828318));
#23165=CARTESIAN_POINT('Ctrl Pts',(-2.68548020128289,1.49796578592604,97.6273986075694));
#23166=CARTESIAN_POINT('Ctrl Pts',(-2.63710416769728,1.58158042092399,97.6224165323069));
#23167=CARTESIAN_POINT('Ctrl Pts',(-2.58489689381886,1.66274180146094,97.6174344570445));
#23168=CARTESIAN_POINT('Ctrl Pts',(-2.53269437995089,1.74389578208999,97.6124528360239));
#23169=CARTESIAN_POINT('Ctrl Pts',(-2.47666155792127,1.82259658388718,97.6074712150034));
#23170=CARTESIAN_POINT('Ctrl Pts',(-2.4170663519432,1.89847109546181,97.6024895939828));
#23171=CARTESIAN_POINT('Ctrl Pts',(-2.35746031037621,1.97435940252559,97.5975070672049));
#23172=CARTESIAN_POINT('Ctrl Pts',(-2.29429086967186,2.04742005362503,97.5925245404269));
#23173=CARTESIAN_POINT('Ctrl Pts',(-2.22786635543717,2.11731286122554,97.587542013649));
#23174=CARTESIAN_POINT('Ctrl Pts',(-2.16137024500247,2.18728100335412,97.5825541164142));
#23175=CARTESIAN_POINT('Ctrl Pts',(-2.09161235952636,2.25407416656305,97.5775662191795));
#23176=CARTESIAN_POINT('Ctrl Pts',(-2.0189378630642,2.31738908150655,97.5725783219447));
#23177=CARTESIAN_POINT('Ctrl Pts',(-1.94622043658912,2.38074139760518,97.5675874782776));
#23178=CARTESIAN_POINT('Ctrl Pts',(-1.87058331260046,2.44061110196734,97.5625966346104));
#23179=CARTESIAN_POINT('Ctrl Pts',(-1.79240301819493,2.49673660412261,97.5576057909433));
#23180=CARTESIAN_POINT('Ctrl Pts',(-1.71409638188708,2.55295280691754,97.5526068819102));
#23181=CARTESIAN_POINT('Ctrl Pts',(-1.63323873670845,2.60541248673435,97.5476079728771));
#23182=CARTESIAN_POINT('Ctrl Pts',(-1.55023366048267,2.65389861296668,97.542609063844));
#23183=CARTESIAN_POINT('Ctrl Pts',(-1.5020440152854,2.68204784583735,97.5397068840783));
#23184=CARTESIAN_POINT('Ctrl Pts',(-1.45313101222759,2.70885865259285,97.5368047043125));
#23185=CARTESIAN_POINT('Ctrl Pts',(-1.4035767066912,2.73429601148703,97.5339025245467));
#23186=CARTESIAN_POINT('Ctrl Pts',(-1.31821078268786,2.77811629355338,97.5289030143196));
#23187=CARTESIAN_POINT('Ctrl Pts',(-1.23064081993939,2.81801196854969,97.5239035040924));
#23188=CARTESIAN_POINT('Ctrl Pts',(-1.14126285133205,2.85375565775513,97.5189039938653));
#23189=CARTESIAN_POINT('Ctrl Pts',(-1.052006123578,2.88945086079059,97.5139112654536));
#23190=CARTESIAN_POINT('Ctrl Pts',(-0.960946668342703,2.92100510996173,
97.5089185370419));
#23191=CARTESIAN_POINT('Ctrl Pts',(-0.868504677489902,2.94823707920143,
97.5039258086301));
#23192=CARTESIAN_POINT('Ctrl Pts',(-0.776160210839561,2.97544031933158,
97.4989383474336));
#23193=CARTESIAN_POINT('Ctrl Pts',(-0.682436526901436,2.9983302209688,97.4939508862371));
#23194=CARTESIAN_POINT('Ctrl Pts',(-0.587772377970094,3.01677408529299,
97.4889634250405));
#23195=CARTESIAN_POINT('Ctrl Pts',(-0.493175963867824,3.03520475251975,
97.483979532511));
#23196=CARTESIAN_POINT('Ctrl Pts',(-0.397640852148199,3.04919562292873,
97.4789956399816));
#23197=CARTESIAN_POINT('Ctrl Pts',(-0.301618539097904,3.05866449727204,
97.4740117474521));
#23198=CARTESIAN_POINT('Ctrl Pts',(-0.205631195263303,3.06812992325947,
97.4690296699467));
#23199=CARTESIAN_POINT('Ctrl Pts',(-0.10915743902516,3.07307658218339,97.4640475924413));
#23200=CARTESIAN_POINT('Ctrl Pts',(-0.012655529398233,3.07347394450899,
97.459065514936));
#23201=CARTESIAN_POINT('Ctrl Pts',(0.0838375811911415,3.07387127060312,
97.4540838916961));
#23202=CARTESIAN_POINT('Ctrl Pts',(0.180358401106432,3.06972012318302,97.4491022684562));
#23203=CARTESIAN_POINT('Ctrl Pts',(0.276448095310002,3.06104209389539,97.4441206452164));
#23204=CARTESIAN_POINT('Ctrl Pts',(0.37255526000993,3.0523624868165,97.4391381162453));
#23205=CARTESIAN_POINT('Ctrl Pts',(0.468230706150381,3.03915440280407,97.4341555872743));
#23206=CARTESIAN_POINT('Ctrl Pts',(0.563021218355264,3.02149124732834,97.4291730583032));
#23207=CARTESIAN_POINT('Ctrl Pts',(0.657913900226234,3.00380905367405,97.4241851589285));
#23208=CARTESIAN_POINT('Ctrl Pts',(0.751919311691618,2.98166228258095,97.4191972595537));
#23209=CARTESIAN_POINT('Ctrl Pts',(0.844595147304252,2.95517533949343,97.4142093601789));
#23210=CARTESIAN_POINT('Ctrl Pts',(0.937325727527124,2.9286727502845,97.4092185143984));
#23211=CARTESIAN_POINT('Ctrl Pts',(1.02872475232966,2.89782502447123,97.404227668618));
#23212=CARTESIAN_POINT('Ctrl Pts',(1.11836780050234,2.86280556671241,97.3992368228375));
#23213=CARTESIAN_POINT('Ctrl Pts',(1.20815571357048,2.82772951683417,97.394237911754));
#23214=CARTESIAN_POINT('Ctrl Pts',(1.29618158314048,2.78846845221175,97.3892390006705));
#23215=CARTESIAN_POINT('Ctrl Pts',(1.38204363664166,2.74524272814232,97.384240089587));
#23216=CARTESIAN_POINT('Ctrl Pts',(1.43189153504418,2.72014769006757,97.3813379319789));
#23217=CARTESIAN_POINT('Ctrl Pts',(1.48101061626524,2.69371721716037,97.3784357743708));
#23218=CARTESIAN_POINT('Ctrl Pts',(1.52932683084278,2.66600106797885,97.3755336167627));
#23219=CARTESIAN_POINT('Ctrl Pts',(1.61255620384157,2.61825730869455,97.37053436837));
#23220=CARTESIAN_POINT('Ctrl Pts',(1.69369385600289,2.56652847870588,97.3655351199774));
#23221=CARTESIAN_POINT('Ctrl Pts',(1.77233350698893,2.51102293697296,97.3605358715848));
#23222=CARTESIAN_POINT('Ctrl Pts',(1.80615512289055,2.48715091962086,97.3583857773662));
#23223=CARTESIAN_POINT('Ctrl Pts',(1.83951493944344,2.46258091771763,97.3562356831477));
#23224=CARTESIAN_POINT('Ctrl Pts',(1.87238193903531,2.43733217358127,97.3540855889292));
#23225=CARTESIAN_POINT('',(-3.07349919776137,-0.00222066661297698,97.7915765528574));
#23226=CARTESIAN_POINT('Ctrl Pts',(-3.07349919776186,-0.00222066593792731,
97.7915765528225));
#23227=CARTESIAN_POINT('Ctrl Pts',(-3.07356904943382,0.0944571161890471,
97.7865867807264));
#23228=CARTESIAN_POINT('Ctrl Pts',(-3.06907304335083,0.191177787731082,
97.7815970086303));
#23229=CARTESIAN_POINT('Ctrl Pts',(-3.06002570027429,0.287480370914012,
97.7766072365341));
#23230=CARTESIAN_POINT('Ctrl Pts',(-3.05097913287416,0.383774697568821,
97.7716178922375));
#23231=CARTESIAN_POINT('Ctrl Pts',(-3.03738204494624,0.479650572509984,
97.7666285479408));
#23232=CARTESIAN_POINT('Ctrl Pts',(-3.01930089212336,0.574651522945046,
97.7616392036442));
#23233=CARTESIAN_POINT('Ctrl Pts',(-3.00121642371484,0.669669893938976,
97.7566489444391));
#23234=CARTESIAN_POINT('Ctrl Pts',(-2.97864633831454,0.76381259281622,97.7516586852341));
#23235=CARTESIAN_POINT('Ctrl Pts',(-2.95170812541139,0.856633756269486,
97.746668426029));
#23236=CARTESIAN_POINT('Ctrl Pts',(-2.9247387155029,0.949562415433147,97.7416723876305));
#23237=CARTESIAN_POINT('Ctrl Pts',(-2.89339119687211,1.04116606243066,97.7366763492321));
#23238=CARTESIAN_POINT('Ctrl Pts',(-2.85783282778683,1.13101449081077,97.7316803108336));
#23239=CARTESIAN_POINT('Ctrl Pts',(-2.82225376596991,1.22091520531829,97.7266813650554));
#23240=CARTESIAN_POINT('Ctrl Pts',(-2.78245915294648,1.3090582689151,97.7216824192772));
#23241=CARTESIAN_POINT('Ctrl Pts',(-2.73866333821666,1.39503597441355,97.7166834734989));
#23242=CARTESIAN_POINT('Ctrl Pts',(-2.69478773475782,1.48117031706761,97.7116754204685));
#23243=CARTESIAN_POINT('Ctrl Pts',(-2.64689658149737,1.56513103983351,97.7066673674381));
#23244=CARTESIAN_POINT('Ctrl Pts',(-2.5952490191003,1.64653720846476,97.7016593144077));
#23245=CARTESIAN_POINT('Ctrl Pts',(-2.54830188139988,1.72053463314501,97.6971070423484));
#23246=CARTESIAN_POINT('Ctrl Pts',(-2.49825164975594,1.79242150070637,97.6925547702891));
#23247=CARTESIAN_POINT('Ctrl Pts',(-2.44532132719365,1.86193605066658,97.6880024982298));
#23248=CARTESIAN_POINT('Ctrl Pts',(-2.38719087098629,1.93828004984554,97.6830029887091));
#23249=CARTESIAN_POINT('Ctrl Pts',(-2.32537964657829,2.01203324522605,97.6780034791883));
#23250=CARTESIAN_POINT('Ctrl Pts',(-2.2601469502219,2.08281972657325,97.6730039696676));
#23251=CARTESIAN_POINT('Ctrl Pts',(-2.19500274162626,2.15351018648371,97.6680112419515));
#23252=CARTESIAN_POINT('Ctrl Pts',(-2.12644658009942,2.2212416104132,97.6630185142354));
#23253=CARTESIAN_POINT('Ctrl Pts',(-2.05477941583094,2.28566922416115,97.6580257865192));
#23254=CARTESIAN_POINT('Ctrl Pts',(-1.98318785863915,2.35002886837825,97.6530383260068));
#23255=CARTESIAN_POINT('Ctrl Pts',(-1.90849214789139,2.41109133934675,97.6480508654943));
#23256=CARTESIAN_POINT('Ctrl Pts',(-1.83103094631659,2.46854773574079,97.6430634049818));
#23257=CARTESIAN_POINT('Ctrl Pts',(-1.75362517008367,2.52596302070938,97.6380795131166));
#23258=CARTESIAN_POINT('Ctrl Pts',(-1.67345818828568,2.57977709972297,97.6330956212513));
#23259=CARTESIAN_POINT('Ctrl Pts',(-1.59090193540887,2.62972114147343,97.6281117293861));
#23260=CARTESIAN_POINT('Ctrl Pts',(-1.50837574750221,2.6796469948242,97.6231296525325));
#23261=CARTESIAN_POINT('Ctrl Pts',(-1.42346239253632,2.72570538419995,97.6181475756789));
#23262=CARTESIAN_POINT('Ctrl Pts',(-1.3365621845007,2.76767118295558,97.6131654988253));
#23263=CARTESIAN_POINT('Ctrl Pts',(-1.24966989979133,2.80963315538302,97.608183876224));
#23264=CARTESIAN_POINT('Ctrl Pts',(-1.16079151754669,2.84750308835942,97.6032022536227));
#23265=CARTESIAN_POINT('Ctrl Pts',(-1.07035034378284,2.88110263468068,97.5982206310214));
#23266=CARTESIAN_POINT('Ctrl Pts',(-0.979892726250969,2.91470828997999,
97.5932381026751));
#23267=CARTESIAN_POINT('Ctrl Pts',(-0.887872164384384,2.94404186379848,
97.5882555743288));
#23268=CARTESIAN_POINT('Ctrl Pts',(-0.794729233475481,2.96897418234977,
97.5832730459824));
#23269=CARTESIAN_POINT('Ctrl Pts',(-0.701485908264306,2.99393337425259,
97.5782851472075));
#23270=CARTESIAN_POINT('Ctrl Pts',(-0.607118223597923,3.01448172643295,
97.5732972484326));
#23271=CARTESIAN_POINT('Ctrl Pts',(-0.512078899859159,3.03054078512714,
97.5683093496577));
#23272=CARTESIAN_POINT('Ctrl Pts',(-0.416983435115779,3.04660933012293,
97.563318504464));
#23273=CARTESIAN_POINT('Ctrl Pts',(-0.321215976901245,3.05818324865149,
97.5583276592703));
#23274=CARTESIAN_POINT('Ctrl Pts',(-0.225234235281423,3.06523600873688,
97.5533368140766));
#23275=CARTESIAN_POINT('Ctrl Pts',(-0.129097384790456,3.07230016625721,
97.5483379035535));
#23276=CARTESIAN_POINT('Ctrl Pts',(-0.0327459979506133,3.07482856475272,
97.5433389930304));
#23277=CARTESIAN_POINT('Ctrl Pts',(0.063362407555235,3.07284679984356,97.5383400825073));
#23278=CARTESIAN_POINT('Ctrl Pts',(0.119159036688698,3.07169626778464,97.5354379184868));
#23279=CARTESIAN_POINT('Ctrl Pts',(0.174873848989266,3.06902656260381,97.5325357544663));
#23280=CARTESIAN_POINT('Ctrl Pts',(0.230418577026407,3.06485065367974,97.5296335904458));
#23281=CARTESIAN_POINT('Ctrl Pts',(0.326094831378455,3.0576576159516,97.5246345888697));
#23282=CARTESIAN_POINT('Ctrl Pts',(0.421601973471025,3.04596752585046,97.5196355872936));
#23283=CARTESIAN_POINT('Ctrl Pts',(0.516483657699913,3.02979320768413,97.5146365857176));
#23284=CARTESIAN_POINT('Ctrl Pts',(0.611243167896439,3.0136397163158,97.5096440210865));
#23285=CARTESIAN_POINT('Ctrl Pts',(0.70537839149724,2.99301354198044,97.5046514564554));
#23286=CARTESIAN_POINT('Ctrl Pts',(0.798436325656736,2.96797939411172,97.4996588918244));
#23287=CARTESIAN_POINT('Ctrl Pts',(0.895202885872508,2.94194756352071,97.4944673591478));
#23288=CARTESIAN_POINT('Ctrl Pts',(0.990804017801527,2.911149102255,97.4892758264712));
#23289=CARTESIAN_POINT('Ctrl Pts',(1.08473981285586,2.87571587407474,97.4840842937946));
#23290=CARTESIAN_POINT('Ctrl Pts',(1.17491270328855,2.84170203940684,97.4791007248904));
#23291=CARTESIAN_POINT('Ctrl Pts',(1.2635506597892,2.80341779712293,97.4741171559862));
#23292=CARTESIAN_POINT('Ctrl Pts',(1.35022649850534,2.76103072288847,97.469133587082));
#23293=CARTESIAN_POINT('Ctrl Pts',(1.43686593133514,2.71866145221991,97.4641521113937));
#23294=CARTESIAN_POINT('Ctrl Pts',(1.52154449194907,2.67219297011668,97.4591706357054));
#23295=CARTESIAN_POINT('Ctrl Pts',(1.60385651248083,2.62184029593201,97.4541891600171));
#23296=CARTESIAN_POINT('Ctrl Pts',(1.68616392127089,2.57149044288482,97.4492079634288));
#23297=CARTESIAN_POINT('Ctrl Pts',(1.76610467867593,2.51725705834576,97.4442267668404));
#23298=CARTESIAN_POINT('Ctrl Pts',(1.84330001440335,2.45939978590318,97.439245570252));
#23299=CARTESIAN_POINT('Ctrl Pts',(1.85303787899999,2.4521013360724,97.4386172134031));
#23300=CARTESIAN_POINT('Ctrl Pts',(1.86273209567925,2.44474527574693,97.4379888565543));
#23301=CARTESIAN_POINT('Ctrl Pts',(1.8723819390353,2.43733217358127,97.4373604997054));
#23302=CARTESIAN_POINT('Ctrl Pts',(1.8723819390353,2.43733217358127,98.4372333997809));
#23303=CARTESIAN_POINT('Ctrl Pts',(1.94879667949973,2.3786296374754,98.4322491033839));
#23304=CARTESIAN_POINT('Ctrl Pts',(2.02250938947208,2.31628298897807,98.427264806987));
#23305=CARTESIAN_POINT('Ctrl Pts',(2.09315882163261,2.25057512592262,98.42228051059));
#23306=CARTESIAN_POINT('Ctrl Pts',(2.16377952620586,2.18489398110555,98.4172982409158));
#23307=CARTESIAN_POINT('Ctrl Pts',(2.23133910669081,2.11585463573883,98.4123159712416));
#23308=CARTESIAN_POINT('Ctrl Pts',(2.29551041638283,2.04377938591178,98.4073337015674));
#23309=CARTESIAN_POINT('Ctrl Pts',(2.35967315132447,1.97171376698176,98.402352097638));
#23310=CARTESIAN_POINT('Ctrl Pts',(2.42044822365573,1.89661337785966,98.3973704937086));
#23311=CARTESIAN_POINT('Ctrl Pts',(2.47754703950436,1.8188355937366,98.3923888897792));
#23312=CARTESIAN_POINT('Ctrl Pts',(2.53465381334927,1.74104696954082,98.387406591552));
#23313=CARTESIAN_POINT('Ctrl Pts',(2.58808305355812,1.66058056326875,98.3824242933247));
#23314=CARTESIAN_POINT('Ctrl Pts',(2.63758861081898,1.57782399844787,98.3774419950975));
#23315=CARTESIAN_POINT('Ctrl Pts',(2.68714635867861,1.49498018857999,98.3724544443463));
#23316=CARTESIAN_POINT('Ctrl Pts',(2.73277193785748,1.40984177645768,98.3674668935951));
#23317=CARTESIAN_POINT('Ctrl Pts',(2.77426454507443,1.32282216640899,98.3624793428438));
#23318=CARTESIAN_POINT('Ctrl Pts',(2.81578008312558,1.23575446508853,98.3574890357293));
#23319=CARTESIAN_POINT('Ctrl Pts',(2.8531579303546,1.14680390010304,98.3524987286148));
#23320=CARTESIAN_POINT('Ctrl Pts',(2.88624578645053,1.05640310023995,98.3475084215002));
#23321=CARTESIAN_POINT('Ctrl Pts',(2.91938864408817,0.965852028224121,98.3425098190587));
#23322=CARTESIAN_POINT('Ctrl Pts',(2.94822713534302,0.873846325235199,98.3375112166172));
#23323=CARTESIAN_POINT('Ctrl Pts',(2.97265908194401,0.780833037553993,98.3325126141758));
#23324=CARTESIAN_POINT('Ctrl Pts',(2.99063703656771,0.712390326351174,98.3288344525727));
#23325=CARTESIAN_POINT('Ctrl Pts',(3.00623009381549,0.643402335271145,98.3251562909697));
#23326=CARTESIAN_POINT('Ctrl Pts',(3.01941544185753,0.574049335399231,98.3214781293667));
#23327=CARTESIAN_POINT('Ctrl Pts',(3.03733751258853,0.479781867817168,98.316478619896));
#23328=CARTESIAN_POINT('Ctrl Pts',(3.05087222367182,0.38450871946811,98.3114791104254));
#23329=CARTESIAN_POINT('Ctrl Pts',(3.05991332529291,0.28867402324231,98.3064796009548));
#23330=CARTESIAN_POINT('Ctrl Pts',(3.06894216271708,0.192969326173176,98.301486873287));
#23331=CARTESIAN_POINT('Ctrl Pts',(3.07348946431034,0.0967050284110289,
98.2964941456192));
#23332=CARTESIAN_POINT('Ctrl Pts',(3.07349998169631,0.000335429283253844,
98.2915014179515));
#23333=CARTESIAN_POINT('Ctrl Pts',(3.07351048798669,-0.095932502347352,
98.2865139574855));
#23334=CARTESIAN_POINT('Ctrl Pts',(3.06899372468457,-0.192305077874619,
98.2815264970195));
#23335=CARTESIAN_POINT('Ctrl Pts',(3.05994633315224,-0.288323929336723,
98.2765390365535));
#23336=CARTESIAN_POINT('Ctrl Pts',(3.05090541523968,-0.384274077069903,
98.2715551447319));
#23337=CARTESIAN_POINT('Ctrl Pts',(3.03734035464377,-0.479870568110944,
98.2665712529103));
#23338=CARTESIAN_POINT('Ctrl Pts',(3.01929983554887,-0.574657074310022,
98.2615873610886));
#23339=CARTESIAN_POINT('Ctrl Pts',(3.00126588636379,-0.669409061613417,
98.2566052842769));
#23340=CARTESIAN_POINT('Ctrl Pts',(2.97875979900632,-0.763351219380252,
98.2516232074651));
#23341=CARTESIAN_POINT('Ctrl Pts',(2.95188173341891,-0.856035327488177,
98.2466411306533));
#23342=CARTESIAN_POINT('Ctrl Pts',(2.92500611849093,-0.948710984943907,
98.241659508092));
#23343=CARTESIAN_POINT('Ctrl Pts',(2.89375944030682,-1.04012839925424,98.2366778855306));
#23344=CARTESIAN_POINT('Ctrl Pts',(2.85829202006636,-1.12985352060564,98.2316962629693));
#23345=CARTESIAN_POINT('Ctrl Pts',(2.82281815122272,-1.21959495556821,98.226713734661));
#23346=CARTESIAN_POINT('Ctrl Pts',(2.78312217765326,-1.30764307829281,98.2217312063528));
#23347=CARTESIAN_POINT('Ctrl Pts',(2.73940253685439,-1.39358386582068,98.2167486780445));
#23348=CARTESIAN_POINT('Ctrl Pts',(2.69563577272231,-1.47961728485911,98.2117607793047));
#23349=CARTESIAN_POINT('Ctrl Pts',(2.64783688246335,-1.56353844217188,98.2067728805648));
#23350=CARTESIAN_POINT('Ctrl Pts',(2.59625014480326,-1.64495818658379,98.2017849818249));
#23351=CARTESIAN_POINT('Ctrl Pts',(2.54463293414702,-1.72642602675967,98.1967941366645));
#23352=CARTESIAN_POINT('Ctrl Pts',(2.48922367281748,-1.80538915269852,98.1918032915042));
#23353=CARTESIAN_POINT('Ctrl Pts',(2.43030859142751,-1.88148941013061,98.1868124463438));
#23354=CARTESIAN_POINT('Ctrl Pts',(2.37129830177163,-1.95771264750899,98.1818135358511));
#23355=CARTESIAN_POINT('Ctrl Pts',(2.30877116388989,-2.0310634445112,98.1768146253584));
#23356=CARTESIAN_POINT('Ctrl Pts',(2.24305204931632,-2.10121863547273,98.1718157148657));
#23357=CARTESIAN_POINT('Ctrl Pts',(2.20489820022924,-2.14194789036287,98.1689135504379));
#23358=CARTESIAN_POINT('Ctrl Pts',(2.16566916856287,-2.18160077883473,98.1660113860102));
#23359=CARTESIAN_POINT('Ctrl Pts',(2.12543360399782,-2.22012032218906,98.1631092215824));
#23360=CARTESIAN_POINT('Ctrl Pts',(2.05612047864035,-2.28647728688168,98.1581097120947));
#23361=CARTESIAN_POINT('Ctrl Pts',(1.98357509118963,-2.34970171259639,98.1531102026069));
#23362=CARTESIAN_POINT('Ctrl Pts',(1.90811212901156,-2.40946266896148,98.1481106931191));
#23363=CARTESIAN_POINT('Ctrl Pts',(1.83275153186626,-2.46914255996576,98.1431179654345));
#23364=CARTESIAN_POINT('Ctrl Pts',(1.75448156678403,-2.52536804874238,98.1381252377498));
#23365=CARTESIAN_POINT('Ctrl Pts',(1.67365321647241,-2.57784544939986,98.1331325100651));
#23366=CARTESIAN_POINT('Ctrl Pts',(1.59291013803702,-2.63026748771978,98.1281450495826));
#23367=CARTESIAN_POINT('Ctrl Pts',(1.50961440609933,-2.67894906074651,98.1231575891001));
#23368=CARTESIAN_POINT('Ctrl Pts',(1.42414866755533,-2.72363779212662,98.1181701286175));
#23369=CARTESIAN_POINT('Ctrl Pts',(1.33874408175006,-2.7682945476722,98.1131862367798));
#23370=CARTESIAN_POINT('Ctrl Pts',(1.25117296389306,-2.80896393827999,98.1082023449421));
#23371=CARTESIAN_POINT('Ctrl Pts',(1.16184458469751,-2.84543835129301,98.1032184531044));
#23372=CARTESIAN_POINT('Ctrl Pts',(1.0725487366886,-2.88189948122681,98.0982363762769));
#23373=CARTESIAN_POINT('Ctrl Pts',(0.981497304829406,-2.91416850318698,
98.0932542994494));
#23374=CARTESIAN_POINT('Ctrl Pts',(0.889120784939191,-2.94208539641342,
98.0882722226218));
#23375=CARTESIAN_POINT('Ctrl Pts',(0.796752687662835,-2.96999974426132,
98.0832906000451));
#23376=CARTESIAN_POINT('Ctrl Pts',(0.703060162809543,-2.99356262550506,
98.0783089774684));
#23377=CARTESIAN_POINT('Ctrl Pts',(0.608489130627945,-3.01266380930691,
98.0733273548917));
#23378=CARTESIAN_POINT('Ctrl Pts',(0.513900903769525,-3.03176846603991,
98.0683448265683));
#23379=CARTESIAN_POINT('Ctrl Pts',(0.418434282638778,-3.04640972738691,
98.063362298245));
#23380=CARTESIAN_POINT('Ctrl Pts',(0.322544586106083,-3.05652862574092,
98.0583797699217));
#23381=CARTESIAN_POINT('Ctrl Pts',(0.226551534616821,-3.06665843077559,
98.0533918711674));
#23382=CARTESIAN_POINT('Ctrl Pts',(0.13013493460024,-3.07225609530408,98.0484039724131));
#23383=CARTESIAN_POINT('Ctrl Pts',(0.0337542009956394,-3.07331464447023,
98.0434160736588));
#23384=CARTESIAN_POINT('Ctrl Pts',(-0.0626834660288813,-3.07437381893586,
98.0384252284843));
#23385=CARTESIAN_POINT('Ctrl Pts',(-0.159084785984224,-3.07088855494982,
98.0334343833099));
#23386=CARTESIAN_POINT('Ctrl Pts',(-0.254993503125497,-3.06290394288881,
98.0284435381354));
#23387=CARTESIAN_POINT('Ctrl Pts',(-0.351057211173044,-3.05490642749328,
98.0234446276293));
#23388=CARTESIAN_POINT('Ctrl Pts',(-0.446626291898313,-3.0423951022646,
98.0184457171231));
#23389=CARTESIAN_POINT('Ctrl Pts',(-0.54125279961846,-3.02546651888683,
98.013446806617));
#23390=CARTESIAN_POINT('Ctrl Pts',(-0.596189104167083,-3.01563847139332,
98.0105446423441));
#23391=CARTESIAN_POINT('Ctrl Pts',(-0.650807945735842,-3.00432253982776,
98.0076424780711));
#23392=CARTESIAN_POINT('Ctrl Pts',(-0.705024154619203,-2.99154528486591,
98.0047403137982));
#23393=CARTESIAN_POINT('Ctrl Pts',(-0.798421505988598,-2.96953412259938,
97.9997408042067));
#23394=CARTESIAN_POINT('Ctrl Pts',(-0.89095111788327,-2.94310624791073,
97.9947412946151));
#23395=CARTESIAN_POINT('Ctrl Pts',(-0.982164076418903,-2.912345442593,97.9897417850236));
#23396=CARTESIAN_POINT('Ctrl Pts',(-1.07325330516414,-2.88162636410943,
97.9847490572345));
#23397=CARTESIAN_POINT('Ctrl Pts',(-1.16302901778237,-2.84658617539717,
97.9797563294455));
#23398=CARTESIAN_POINT('Ctrl Pts',(-1.2510537797181,-2.80735938031686,97.9747636016565));
#23399=CARTESIAN_POINT('Ctrl Pts',(-1.33898567775394,-2.76817396851429,
97.9697761410692));
#23400=CARTESIAN_POINT('Ctrl Pts',(-1.42516989842704,-2.72481090833102,
97.9647886804818));
#23401=CARTESIAN_POINT('Ctrl Pts',(-1.50918641768823,-2.67745375434673,
97.9598012198945));
#23402=CARTESIAN_POINT('Ctrl Pts',(-1.59314282116564,-2.63013048551328,
97.9548173279518));
#23403=CARTESIAN_POINT('Ctrl Pts',(-1.67493422532557,-2.57881901911081,
97.9498334360091));
#23404=CARTESIAN_POINT('Ctrl Pts',(-1.75416365818427,-2.52374961323535,
97.9448495440664));
#23405=CARTESIAN_POINT('Ctrl Pts',(-1.83336423764461,-2.46870026227444,
97.9398674671338));
#23406=CARTESIAN_POINT('Ctrl Pts',(-1.9100043395087,-2.40989594127437,97.9348853902012));
#23407=CARTESIAN_POINT('Ctrl Pts',(-1.98371535546732,-2.34761062326851,
97.9299033132686));
#23408=CARTESIAN_POINT('Ctrl Pts',(-2.05741965067641,-2.28533098425129,
97.9249216905869));
#23409=CARTESIAN_POINT('Ctrl Pts',(-2.12819505578402,-2.21957126270958,
97.9199400679051));
#23410=CARTESIAN_POINT('Ctrl Pts',(-2.19570632802947,-2.15064547776972,
97.9149584452233));
#23411=CARTESIAN_POINT('Ctrl Pts',(-2.26322987500894,-2.0817071609126,97.9099759167951));
#23412=CARTESIAN_POINT('Ctrl Pts',(-2.32748780335053,-2.00960195103968,
97.904993388367));
#23413=CARTESIAN_POINT('Ctrl Pts',(-2.38818275240191,-1.93467966111448,
97.9000108599388));
#23414=CARTESIAN_POINT('Ctrl Pts',(-2.44894312164816,-1.85967661602127,
97.8950229610805));
#23415=CARTESIAN_POINT('Ctrl Pts',(-2.50613256789654,-1.78185077064053,
97.8900350622222));
#23416=CARTESIAN_POINT('Ctrl Pts',(-2.55949511150196,-1.70158368122098,
97.885047163364));
#23417=CARTESIAN_POINT('Ctrl Pts',(-2.6128891770883,-1.62126917693907,97.8800563180859));
#23418=CARTESIAN_POINT('Ctrl Pts',(-2.66245161337136,-1.53851093362595,
97.8750654728079));
#23419=CARTESIAN_POINT('Ctrl Pts',(-2.70797183264986,-1.45371620462007,
97.8700746275299));
#23420=CARTESIAN_POINT('Ctrl Pts',(-2.75356561373528,-1.36878444522237,
97.8650757169217));
#23421=CARTESIAN_POINT('Ctrl Pts',(-2.79510394516053,-1.28181002454817,
97.8600768063135));
#23422=CARTESIAN_POINT('Ctrl Pts',(-2.83242392899805,-1.19322124370934,
97.8550778957054));
#23423=CARTESIAN_POINT('Ctrl Pts',(-2.85409038662106,-1.14179021752574,
97.8521757324749));
#23424=CARTESIAN_POINT('Ctrl Pts',(-2.87433597636449,-1.08981539643607,
97.8492735692445));
#23425=CARTESIAN_POINT('Ctrl Pts',(-2.89313660636368,-1.03738268103842,
97.8463714060141));
#23426=CARTESIAN_POINT('Ctrl Pts',(-2.93067890649147,-0.932681682292151,
97.8405761809062));
#23427=CARTESIAN_POINT('Ctrl Pts',(-2.96256548532845,-0.825852277625856,
97.8347809557982));
#23428=CARTESIAN_POINT('Ctrl Pts',(-2.98858506992045,-0.717468835454609,
97.8289857306903));
#23429=CARTESIAN_POINT('Ctrl Pts',(-3.01448640612548,-0.609577951770032,
97.823216842514));
#23430=CARTESIAN_POINT('Ctrl Pts',(-3.03457384715709,-0.500147256877293,
97.8174479543377));
#23431=CARTESIAN_POINT('Ctrl Pts',(-3.04868590390206,-0.389764684584056,
97.8116790661614));
#23432=CARTESIAN_POINT('Ctrl Pts',(-3.062686713896,-0.280252269119051,97.8059556547061));
#23433=CARTESIAN_POINT('Ctrl Pts',(-3.07080588040819,-0.169803074558109,
97.8002322432507));
#23434=CARTESIAN_POINT('Ctrl Pts',(-3.07293345960593,-0.0590101926311166,
97.7945088317954));
#23435=CARTESIAN_POINT('Ctrl Pts',(-3.07329680092891,-0.0400893306770456,
97.7935314054827));
#23436=CARTESIAN_POINT('Ctrl Pts',(-3.07348551479518,-0.0211584870746742,
97.79255397917));
#23437=CARTESIAN_POINT('Ctrl Pts',(-3.07349919776137,-0.00222066661295415,
97.7915765528574));
#23438=CARTESIAN_POINT('Origin',(0.,0.,116.208423447177));
#23439=CARTESIAN_POINT('',(1.87238193903529,2.43733217358128,99.4373602300224));
#23440=CARTESIAN_POINT('',(1.87238193903531,2.43733217358127,99.3541713863777));
#23441=CARTESIAN_POINT('',(1.8723819390353,2.43733217358128,116.208423447177));
#23442=CARTESIAN_POINT('',(-3.07349970959527,0.00133608300057976,98.7084234471481));
#23443=CARTESIAN_POINT('Ctrl Pts',(1.87238193903531,2.43733217358127,99.3541713863777));
#23444=CARTESIAN_POINT('Ctrl Pts',(1.94890764724692,2.37854439098831,99.3491895972089));
#23445=CARTESIAN_POINT('Ctrl Pts',(2.02266023466669,2.31615050135599,99.3442078080402));
#23446=CARTESIAN_POINT('Ctrl Pts',(2.09329231361966,2.25045096363837,99.3392260188715));
#23447=CARTESIAN_POINT('Ctrl Pts',(2.16394410004746,2.18473309470346,99.3342428397042));
#23448=CARTESIAN_POINT('Ctrl Pts',(2.23147332718422,2.11570804446625,99.329259660537));
#23449=CARTESIAN_POINT('Ctrl Pts',(2.2955691098263,2.04371346132752,99.3242764813697));
#23450=CARTESIAN_POINT('Ctrl Pts',(2.35973727932181,1.97163757079034,99.3192876744272));
#23451=CARTESIAN_POINT('Ctrl Pts',(2.42046397465964,1.89658578347112,99.3142988674847));
#23452=CARTESIAN_POINT('Ctrl Pts',(2.47747849109117,1.81892896402818,99.3093100605422));
#23453=CARTESIAN_POINT('Ctrl Pts',(2.53453165653656,1.74121950256213,99.304317871786));
#23454=CARTESIAN_POINT('Ctrl Pts',(2.58786739174473,1.66090185891364,99.2993256830299));
#23455=CARTESIAN_POINT('Ctrl Pts',(2.63725936478344,1.57837425627196,99.2943334942738));
#23456=CARTESIAN_POINT('Ctrl Pts',(2.68672617834146,1.49572160479625,99.2893337411711));
#23457=CARTESIAN_POINT('Ctrl Pts',(2.73223709994962,1.41085269856006,99.2843339880684));
#23458=CARTESIAN_POINT('Ctrl Pts',(2.77361272540734,1.32418831721869,99.2793342349658));
#23459=CARTESIAN_POINT('Ctrl Pts',(2.78291918318436,1.3046952365268,99.2782096600348));
#23460=CARTESIAN_POINT('Ctrl Pts',(2.79201662624458,1.2851113883725,99.2770850851037));
#23461=CARTESIAN_POINT('Ctrl Pts',(2.80090335865005,1.26544167210617,99.2759605101727));
#23462=CARTESIAN_POINT('Ctrl Pts',(2.84041099999358,1.17799624670995,99.2709610006779));
#23463=CARTESIAN_POINT('Ctrl Pts',(2.87588898208135,1.08854528768625,99.2659614911831));
#23464=CARTESIAN_POINT('Ctrl Pts',(2.90712996357781,0.997495676616248,99.2609619816883));
#23465=CARTESIAN_POINT('Ctrl Pts',(2.93832856688126,0.906569573765421,99.2559692539964));
#23466=CARTESIAN_POINT('Ctrl Pts',(2.96530145105313,0.814049540389896,99.2509765263044));
#23467=CARTESIAN_POINT('Ctrl Pts',(2.9878884751466,0.720364289846532,99.2459837986125));
#23468=CARTESIAN_POINT('Ctrl Pts',(3.01045167049912,0.626777874880536,99.2409963381224));
#23469=CARTESIAN_POINT('Ctrl Pts',(3.02863810157716,0.532029110936636,99.2360088776323));
#23470=CARTESIAN_POINT('Ctrl Pts',(3.04233711995342,0.436562823146337,99.2310214171422));
#23471=CARTESIAN_POINT('Ctrl Pts',(3.05602633636178,0.341164843716829,99.2260375252967));
#23472=CARTESIAN_POINT('Ctrl Pts',(3.06523446091201,0.245050794331692,99.2210536334512));
#23473=CARTESIAN_POINT('Ctrl Pts',(3.06990191756383,0.148675709306916,99.2160697416057));
#23474=CARTESIAN_POINT('Ctrl Pts',(3.07456767444353,0.0523357217012599,
99.2110876647702));
#23475=CARTESIAN_POINT('Ctrl Pts',(3.07469602773365,-0.0442646746643785,
99.2061055879347));
#23476=CARTESIAN_POINT('Ctrl Pts',(3.07027934411709,-0.140666268479421,
99.2011235110992));
#23477=CARTESIAN_POINT('Ctrl Pts',(3.06586306320034,-0.237059072689754,
99.1961418885143));
#23478=CARTESIAN_POINT('Ctrl Pts',(3.05690258955944,-0.333252671893883,
99.1911602659294));
#23479=CARTESIAN_POINT('Ctrl Pts',(3.04344237491033,-0.428789879311707,
99.1861786433445));
#23480=CARTESIAN_POINT('Ctrl Pts',(3.02997971295706,-0.524344457077083,
99.1811961150129));
#23481=CARTESIAN_POINT('Ctrl Pts',(3.01201574645876,-0.619241971379589,
99.1762135866812));
#23482=CARTESIAN_POINT('Ctrl Pts',(2.98964639614413,-0.713033432611991,
99.1712310583496));
#23483=CARTESIAN_POINT('Ctrl Pts',(2.96725293496671,-0.806925987216338,
99.1662431595867));
#23484=CARTESIAN_POINT('Ctrl Pts',(2.94044471232729,-0.899709681014647,
99.1612552608239));
#23485=CARTESIAN_POINT('Ctrl Pts',(2.90936804124939,-0.990948964657948,
99.1562673620611));
#23486=CARTESIAN_POINT('Ctrl Pts',(2.87827301275542,-1.08224214459819,99.151276516878));
#23487=CARTESIAN_POINT('Ctrl Pts',(2.84290467611058,-1.17198868963417,99.1462856716949));
#23488=CARTESIAN_POINT('Ctrl Pts',(2.80345739047923,-1.25977335650798,99.1412948265118));
#23489=CARTESIAN_POINT('Ctrl Pts',(2.76394635703844,-1.34769988561961,99.1362959159969));
#23490=CARTESIAN_POINT('Ctrl Pts',(2.72034341092015,-1.43365781467906,99.131297005482));
#23491=CARTESIAN_POINT('Ctrl Pts',(2.6728886737526,-1.51725686280375,99.1262980949671));
#23492=CARTESIAN_POINT('Ctrl Pts',(2.64533838282884,-1.56579107106736,99.1233959307743));
#23493=CARTESIAN_POINT('Ctrl Pts',(2.61649066732709,-1.61353075371004,99.1204937665814));
#23494=CARTESIAN_POINT('Ctrl Pts',(2.58639891787788,-1.66040443494954,99.1175916023886));
#23495=CARTESIAN_POINT('Ctrl Pts',(2.53456036672751,-1.74115293801154,99.1125920928982));
#23496=CARTESIAN_POINT('Ctrl Pts',(2.47884563517596,-1.81961330989724,99.1075925834077));
#23497=CARTESIAN_POINT('Ctrl Pts',(2.41948312504004,-1.89539010698233,99.1025930739172));
#23498=CARTESIAN_POINT('Ctrl Pts',(2.36020113977226,-1.97106411332323,99.0976003462296));
#23499=CARTESIAN_POINT('Ctrl Pts',(2.29728147850438,-2.04406143702507,99.092607618542));
#23500=CARTESIAN_POINT('Ctrl Pts',(2.2309965537036,-2.11401433944112,99.0876148908544));
#23501=CARTESIAN_POINT('Ctrl Pts',(2.16478155782714,-2.18389344330894,99.0826274303687));
#23502=CARTESIAN_POINT('Ctrl Pts',(2.09520865645798,-2.2507341937906,99.0776399698829));
#23503=CARTESIAN_POINT('Ctrl Pts',(2.02259072277512,-2.31420159410195,99.0726525093971));
#23504=CARTESIAN_POINT('Ctrl Pts',(1.95002474892108,-2.37762358200499,99.0676686175559));
#23505=CARTESIAN_POINT('Ctrl Pts',(1.87441840365887,-2.43767673003947,99.0626847257147));
#23506=CARTESIAN_POINT('Ctrl Pts',(1.7961209299935,-2.49406332213905,99.0577008338735));
#23507=CARTESIAN_POINT('Ctrl Pts',(1.71785197032867,-2.55042937963845,99.0527187570422));
#23508=CARTESIAN_POINT('Ctrl Pts',(1.63689418534052,-2.60313127797436,99.047736680211));
#23509=CARTESIAN_POINT('Ctrl Pts',(1.55362860196168,-2.65191259606469,99.0427546033797));
#23510=CARTESIAN_POINT('Ctrl Pts',(1.47037061048527,-2.70068946642294,99.037772980799));
#23511=CARTESIAN_POINT('Ctrl Pts',(1.38480561781128,-2.74554624551174,99.0327913582184));
#23512=CARTESIAN_POINT('Ctrl Pts',(1.29734131048932,-2.78627130303168,99.0278097356377));
#23513=CARTESIAN_POINT('Ctrl Pts',(1.20986110061474,-2.82700376508485,99.0228272073103));
#23514=CARTESIAN_POINT('Ctrl Pts',(1.12048128821925,-2.86360282839112,99.0178446789829));
#23515=CARTESIAN_POINT('Ctrl Pts',(1.02963070651139,-2.89590449742543,99.0128621506554));
#23516=CARTESIAN_POINT('Ctrl Pts',(0.938682201265032,-2.9282409828987,99.0078742518967));
#23517=CARTESIAN_POINT('Ctrl Pts',(0.846260176139689,-2.95627067952686,
99.002886353138));
#23518=CARTESIAN_POINT('Ctrl Pts',(0.752809626922593,-2.9798791780226,98.9978984543793));
#23519=CARTESIAN_POINT('Ctrl Pts',(0.659303875182713,-3.00350162238262,
98.9929076092003));
#23520=CARTESIAN_POINT('Ctrl Pts',(0.564768819575584,-3.02269758105268,
98.9879167640213));
#23521=CARTESIAN_POINT('Ctrl Pts',(0.46965858209221,-3.03740400116072,98.9829259188423));
#23522=CARTESIAN_POINT('Ctrl Pts',(0.374394644062165,-3.05213418721519,
98.9779270083313));
#23523=CARTESIAN_POINT('Ctrl Pts',(0.278554104323566,-3.06236030112,98.9729280978205));
#23524=CARTESIAN_POINT('Ctrl Pts',(0.182595062064441,-3.06807126600894,
98.9679291873096));
#23525=CARTESIAN_POINT('Ctrl Pts',(0.126885142899932,-3.07138682007059,
98.9650270230745));
#23526=CARTESIAN_POINT('Ctrl Pts',(0.0711352808583605,-3.07318152364689,
98.9621248588395));
#23527=CARTESIAN_POINT('Ctrl Pts',(0.0154344978905465,-3.07346124528598,
98.9592226946044));
#23528=CARTESIAN_POINT('Ctrl Pts',(-0.0805203036166465,-3.0739431170466,
98.9542231851132));
#23529=CARTESIAN_POINT('Ctrl Pts',(-0.176666230816496,-3.06992790199966,
98.949223675622));
#23530=CARTESIAN_POINT('Ctrl Pts',(-0.272547234921952,-3.06139188192828,
98.9442241661308));
#23531=CARTESIAN_POINT('Ctrl Pts',(-0.368298177053213,-3.05286744091402,
98.9392314384426));
#23532=CARTESIAN_POINT('Ctrl Pts',(-0.463784476814253,-3.03983442129326,
98.9342387107543));
#23533=CARTESIAN_POINT('Ctrl Pts',(-0.558549362472165,-3.02232110466144,
98.929245983066));
#23534=CARTESIAN_POINT('Ctrl Pts',(-0.653214273563878,-3.00482626413731,
98.9242585225797));
#23535=CARTESIAN_POINT('Ctrl Pts',(-0.747158854163399,-2.98286060214701,
98.9192710620933));
#23536=CARTESIAN_POINT('Ctrl Pts',(-0.839931767261859,-2.95650416477711,
98.9142836016069));
#23537=CARTESIAN_POINT('Ctrl Pts',(-0.932638299171926,-2.93016658605436,
98.9092997097651));
#23538=CARTESIAN_POINT('Ctrl Pts',(-1.02417440914999,-2.89944459712448,
98.9043158179233));
#23539=CARTESIAN_POINT('Ctrl Pts',(-1.11410022935702,-2.86446904834851,
98.8993319260815));
#23540=CARTESIAN_POINT('Ctrl Pts',(-1.2039933008072,-2.82950623680129,98.8943498492497));
#23541=CARTESIAN_POINT('Ctrl Pts',(-1.29227683896434,-2.79029310213957,
98.8893677724179));
#23542=CARTESIAN_POINT('Ctrl Pts',(-1.37852830909465,-2.74700963795627,
98.8843856955861));
#23543=CARTESIAN_POINT('Ctrl Pts',(-1.46477191507737,-2.70373012022803,
98.879404073005));
#23544=CARTESIAN_POINT('Ctrl Pts',(-1.54898342914967,-2.65638120788158,
98.8744224504239));
#23545=CARTESIAN_POINT('Ctrl Pts',(-1.6307633718706,-2.60518964280247,98.8694408278427));
#23546=CARTESIAN_POINT('Ctrl Pts',(-1.71255818362577,-2.55398877019501,
98.8644582995149));
#23547=CARTESIAN_POINT('Ctrl Pts',(-1.7919201739585,-2.49894409024715,98.859475771187));
#23548=CARTESIAN_POINT('Ctrl Pts',(-1.86847830577755,-2.4403260173261,98.8544932428591));
#23549=CARTESIAN_POINT('Ctrl Pts',(-1.94511895597981,-2.38164476276138,
98.8495053441));
#23550=CARTESIAN_POINT('Ctrl Pts',(-2.01894936512326,-2.31938269317944,
98.8445174453409));
#23551=CARTESIAN_POINT('Ctrl Pts',(-2.08963128892913,-2.25385077729835,
98.8395295465818));
#23552=CARTESIAN_POINT('Ctrl Pts',(-2.16035496551738,-2.18828015081523,
98.8345387014024));
#23553=CARTESIAN_POINT('Ctrl Pts',(-2.22792614615563,-2.1194361451444,98.8295478562231));
#23554=CARTESIAN_POINT('Ctrl Pts',(-2.29204469515411,-2.04766534507372,
98.8245570110437));
#23555=CARTESIAN_POINT('Ctrl Pts',(-2.35626686134706,-1.97577856157759,
98.8195581005325));
#23556=CARTESIAN_POINT('Ctrl Pts',(-2.41702497826903,-1.90095587990278,
98.8145591900213));
#23557=CARTESIAN_POINT('Ctrl Pts',(-2.47406034191185,-1.82357551929692,
98.8095602795101));
#23558=CARTESIAN_POINT('Ctrl Pts',(-2.507172755474,-1.77865162755117,98.8066581152801));
#23559=CARTESIAN_POINT('Ctrl Pts',(-2.53903123834827,-1.73286620261018,
98.8037559510502));
#23560=CARTESIAN_POINT('Ctrl Pts',(-2.56959224488766,-1.68629711053931,
98.8008537868202));
#23561=CARTESIAN_POINT('Ctrl Pts',(-2.62325694576495,-1.60452243492808,
98.7957576269441));
#23562=CARTESIAN_POINT('Ctrl Pts',(-2.67310143600297,-1.52005111545229,
98.7906614670681));
#23563=CARTESIAN_POINT('Ctrl Pts',(-2.71885041936436,-1.43326712343592,
98.785565307192));
#23564=CARTESIAN_POINT('Ctrl Pts',(-2.76453038786018,-1.34661404985973,
98.7804768351543));
#23565=CARTESIAN_POINT('Ctrl Pts',(-2.80612694355087,-1.25765560699959,
98.7753883631166));
#23566=CARTESIAN_POINT('Ctrl Pts',(-2.84340806514103,-1.16680453594033,
98.7702998910789));
#23567=CARTESIAN_POINT('Ctrl Pts',(-2.88118664928777,-1.07474118895833,
98.7651435207538));
#23568=CARTESIAN_POINT('Ctrl Pts',(-2.91453352864961,-0.980734682921244,
98.7599871504287));
#23569=CARTESIAN_POINT('Ctrl Pts',(-2.94325508540529,-0.885241070124925,
98.7548307801035));
#23570=CARTESIAN_POINT('Ctrl Pts',(-2.9715268151876,-0.791243044882755,
98.7497551670464));
#23571=CARTESIAN_POINT('Ctrl Pts',(-2.99531692166486,-0.695804569698325,
98.7446795539893));
#23572=CARTESIAN_POINT('Ctrl Pts',(-3.014489253313,-0.59938033973466,98.7396039409322));
#23573=CARTESIAN_POINT('Ctrl Pts',(-3.03411915681741,-0.500654824006531,
98.7344071919731));
#23574=CARTESIAN_POINT('Ctrl Pts',(-3.04890789387831,-0.400896316070449,
98.729210443014));
#23575=CARTESIAN_POINT('Ctrl Pts',(-3.05876400967397,-0.300607689727384,
98.7240136940548));
#23576=CARTESIAN_POINT('Ctrl Pts',(-3.06862012546962,-0.20031906338432,
98.7188169450957));
#23577=CARTESIAN_POINT('Ctrl Pts',(-3.07354354443464,-0.0995007836641929,
98.7136201961365));
#23578=CARTESIAN_POINT('Ctrl Pts',(-3.07349970959552,0.00133608243214189,
98.7084234471774));
#23579=CARTESIAN_POINT('Ctrl Pts',(-3.07349970959527,0.00133608300055935,
98.7084234471481));
#23580=CARTESIAN_POINT('Ctrl Pts',(-3.07345335998039,0.107957848126409,
98.7029285664721));
#23581=CARTESIAN_POINT('Ctrl Pts',(-3.06785451553832,0.214401037669215,
98.6974336857961));
#23582=CARTESIAN_POINT('Ctrl Pts',(-3.05678458077965,0.320109788522285,
98.6919388051201));
#23583=CARTESIAN_POINT('Ctrl Pts',(-3.04577427243555,0.425249156272434,
98.6864735217308));
#23584=CARTESIAN_POINT('Ctrl Pts',(-3.02935184224795,0.529661712284398,
98.6810082383416));
#23585=CARTESIAN_POINT('Ctrl Pts',(-3.00764794743082,0.632815987720909,
98.6755429549523));
#23586=CARTESIAN_POINT('Ctrl Pts',(-2.98576774618479,0.736808212386391,
98.6700332756329));
#23587=CARTESIAN_POINT('Ctrl Pts',(-2.95852002197215,0.839521339036963,
98.6645235963136));
#23588=CARTESIAN_POINT('Ctrl Pts',(-2.92608819126525,0.940430830491022,
98.6590139169942));
#23589=CARTESIAN_POINT('Ctrl Pts',(-2.89365636055835,1.04134032194509,98.6535042376748));
#23590=CARTESIAN_POINT('Ctrl Pts',(-2.85604060187747,1.14044592852212,98.6479945583555));
#23591=CARTESIAN_POINT('Ctrl Pts',(-2.8134715159663,1.23724705651146,98.6424848790361));
#23592=CARTESIAN_POINT('Ctrl Pts',(-2.77484412300311,1.32508486486674,98.6374853695654));
#23593=CARTESIAN_POINT('Ctrl Pts',(-2.73203143908153,1.41126627409199,98.6324858600948));
#23594=CARTESIAN_POINT('Ctrl Pts',(-2.68519747882601,1.49536508910247,98.6274863506241));
#23595=CARTESIAN_POINT('Ctrl Pts',(-2.63842704854006,1.57934982460463,98.6224936229563));
#23596=CARTESIAN_POINT('Ctrl Pts',(-2.5876463947889,1.66125720022001,98.6175008952884));
#23597=CARTESIAN_POINT('Ctrl Pts',(-2.53306732127339,1.74068153201465,98.6125081676206));
#23598=CARTESIAN_POINT('Ctrl Pts',(-2.4785458273042,1.82002207314196,98.6075207071546));
#23599=CARTESIAN_POINT('Ctrl Pts',(-2.42023412700094,1.8968844180998,98.6025332466886));
#23600=CARTESIAN_POINT('Ctrl Pts',(-2.35838909114258,1.97088892248641,98.5975457862225));
#23601=CARTESIAN_POINT('Ctrl Pts',(-2.2965883068507,2.04484047492304,98.5925618944008));
#23602=CARTESIAN_POINT('Ctrl Pts',(-2.23125949359266,2.11593791599362,98.5875780025792));
#23603=CARTESIAN_POINT('Ctrl Pts',(-2.16270125530425,2.18383276152397,98.5825941107575));
#23604=CARTESIAN_POINT('Ctrl Pts',(-2.09416798422655,2.25170288143481,98.5776120339457));
#23605=CARTESIAN_POINT('Ctrl Pts',(-2.02240793643468,2.3163724145637,98.5726299571338));
#23606=CARTESIAN_POINT('Ctrl Pts',(-1.94775754441361,2.37752871658364,98.567647880322));
#23607=CARTESIAN_POINT('Ctrl Pts',(-1.87311395878615,2.43867944255968,98.5626662577606));
#23608=CARTESIAN_POINT('Ctrl Pts',(-1.79558089255998,2.49631729625335,98.5576846351993));
#23609=CARTESIAN_POINT('Ctrl Pts',(-1.71552808955889,2.5501697245349,98.5527030126379));
#23610=CARTESIAN_POINT('Ctrl Pts',(-1.63546073154467,2.60403194413882,98.5477204843296));
#23611=CARTESIAN_POINT('Ctrl Pts',(-1.5528730911389,2.65410712646822,98.5427379560213));
#23612=CARTESIAN_POINT('Ctrl Pts',(-1.46816322085729,2.70016647763095,98.537755427713));
#23613=CARTESIAN_POINT('Ctrl Pts',(-1.38336204581268,2.74627547399003,98.532767528973));
#23614=CARTESIAN_POINT('Ctrl Pts',(-1.29643446048882,2.78835978774973,98.5277796302331));
#23615=CARTESIAN_POINT('Ctrl Pts',(-1.20780220683728,2.82623708827816,98.5227917314932));
#23616=CARTESIAN_POINT('Ctrl Pts',(-1.11911759689321,2.8641367634495,98.5178008863328));
#23617=CARTESIAN_POINT('Ctrl Pts',(-1.02872672471051,2.89782432384418,98.5128100411724));
#23618=CARTESIAN_POINT('Ctrl Pts',(-0.937068346938756,2.92716674673061,
98.507819196012));
#23619=CARTESIAN_POINT('Ctrl Pts',(-0.845261846903743,2.95655658771665,
98.5028202855192));
#23620=CARTESIAN_POINT('Ctrl Pts',(-0.752184174851212,2.98158715618758,
98.4978213750265));
#23621=CARTESIAN_POINT('Ctrl Pts',(-0.658286112490856,3.00217615141112,
98.4928224645337));
#23622=CARTESIAN_POINT('Ctrl Pts',(-0.603772710666914,3.01412928592272,
98.4899203001064));
#23623=CARTESIAN_POINT('Ctrl Pts',(-0.548982947401211,3.02458635673339,
98.4870181356791));
#23624=CARTESIAN_POINT('Ctrl Pts',(-0.494005672129448,3.03353929361463,
98.4841159712518));
#23625=CARTESIAN_POINT('Ctrl Pts',(-0.399285209413585,3.04896432731927,
98.4791158260815));
#23626=CARTESIAN_POINT('Ctrl Pts',(-0.303675206864667,3.0599758189329,98.4741156809111));
#23627=CARTESIAN_POINT('Ctrl Pts',(-0.207622622940845,3.06647926724496,
98.4691155357407));
#23628=CARTESIAN_POINT('Ctrl Pts',(-0.111730386717616,3.07297185886851,
98.4641237376834));
#23629=CARTESIAN_POINT('Ctrl Pts',(-0.0153974733967171,3.07497135061767,
98.4591319396262));
#23630=CARTESIAN_POINT('Ctrl Pts',(0.0809207697427157,3.07243455243952,
98.4541401415689));
#23631=CARTESIAN_POINT('Ctrl Pts',(0.177147010391447,3.06990017739268,98.4491531116411));
#23632=CARTESIAN_POINT('Ctrl Pts',(0.273358172546258,3.06283813231317,98.4441660817132));
#23633=CARTESIAN_POINT('Ctrl Pts',(0.369096078452734,3.05125717285037,98.4391790517854));
#23634=CARTESIAN_POINT('Ctrl Pts',(0.46476867590044,3.03968411344143,98.4341954238042));
#23635=CARTESIAN_POINT('Ctrl Pts',(0.559968224302033,3.02359831840271,98.4292117958229));
#23636=CARTESIAN_POINT('Ctrl Pts',(0.654239913682788,3.00306050311084,98.4242281678417));
#23637=CARTESIAN_POINT('Ctrl Pts',(0.748473032011306,2.98253109082046,98.4192465789007));
#23638=CARTESIAN_POINT('Ctrl Pts',(0.841778617905281,2.95755337362891,98.4142649899598));
#23639=CARTESIAN_POINT('Ctrl Pts',(0.933711384315625,2.92823928339188,98.4092834010188));
#23640=CARTESIAN_POINT('Ctrl Pts',(1.02566263452351,2.89891929932907,98.4043008104907));
#23641=CARTESIAN_POINT('Ctrl Pts',(1.11624009255976,2.86526132485732,98.3993182199626));
#23642=CARTESIAN_POINT('Ctrl Pts',(1.2050135810746,2.82742719082663,98.3943356294344));
#23643=CARTESIAN_POINT('Ctrl Pts',(1.29379444950277,2.78958991157055,98.3893526246938));
#23644=CARTESIAN_POINT('Ctrl Pts',(1.38077064941425,2.7475759621702,98.3843696199532));
#23645=CARTESIAN_POINT('Ctrl Pts',(1.46553343141306,2.70159471635008,98.3793866152126));
#23646=CARTESIAN_POINT('Ctrl Pts',(1.55037166299099,2.65557254141505,98.3743991749686));
#23647=CARTESIAN_POINT('Ctrl Pts',(1.63299216003407,2.60557623509644,98.3694117347245));
#23648=CARTESIAN_POINT('Ctrl Pts',(1.71301247083479,2.55186020870354,98.3644242944805));
#23649=CARTESIAN_POINT('Ctrl Pts',(1.76737212438089,2.51536966579796,98.3610362106173));
#23650=CARTESIAN_POINT('Ctrl Pts',(1.82053241882744,2.47716347201369,98.3576481267542));
#23651=CARTESIAN_POINT('Ctrl Pts',(1.87238193903531,2.43733217358127,98.354260042891));
#23652=CARTESIAN_POINT('',(-3.07349994395351,-0.00058695637196295,98.7915765527878));
#23653=CARTESIAN_POINT('Ctrl Pts',(-3.07349994395351,-0.000586956371967045,
98.7915765527878));
#23654=CARTESIAN_POINT('Ctrl Pts',(-3.07351817682241,0.094886445460421,
98.7866030213858));
#23655=CARTESIAN_POINT('Ctrl Pts',(-3.0690835429351,0.190535387119877,98.7816294899839));
#23656=CARTESIAN_POINT('Ctrl Pts',(-3.06017303934281,0.285907711122693,
98.7766559585819));
#23657=CARTESIAN_POINT('Ctrl Pts',(-3.05127451808939,0.381151783843896,
98.7716891153024));
#23658=CARTESIAN_POINT('Ctrl Pts',(-3.03791212734771,0.47611953978147,98.7667222720228));
#23659=CARTESIAN_POINT('Ctrl Pts',(-3.02011486886673,0.570358158397045,
98.7617554287432));
#23660=CARTESIAN_POINT('Ctrl Pts',(-3.00167035590524,0.668024067131597,
98.7566079502512));
#23661=CARTESIAN_POINT('Ctrl Pts',(-2.97846221221157,0.764906306697993,
98.7514604717592));
#23662=CARTESIAN_POINT('Ctrl Pts',(-2.95058168534517,0.860505646759896,
98.7463129932672));
#23663=CARTESIAN_POINT('Ctrl Pts',(-2.92372606122301,0.952590705099405,
98.7413547387758));
#23664=CARTESIAN_POINT('Ctrl Pts',(-2.89253567597502,1.04348506014707,98.7363964842844));
#23665=CARTESIAN_POINT('Ctrl Pts',(-2.85714392584538,1.13275365239088,98.7314382297929));
#23666=CARTESIAN_POINT('Ctrl Pts',(-2.82176350666418,1.22199366458953,98.7264815627259));
#23667=CARTESIAN_POINT('Ctrl Pts',(-2.78218455822006,1.30960853552735,98.7215248956588));
#23668=CARTESIAN_POINT('Ctrl Pts',(-2.73858945230785,1.39518101395775,98.7165682285918));
#23669=CARTESIAN_POINT('Ctrl Pts',(-2.69499608012731,1.48075008926038,98.7116117586461));
#23670=CARTESIAN_POINT('Ctrl Pts',(-2.64738707020622,1.56427653816429,98.7066552887005));
#23671=CARTESIAN_POINT('Ctrl Pts',(-2.59599128452805,1.64536667665733,98.7016988187549));
#23672=CARTESIAN_POINT('Ctrl Pts',(-2.54458313179807,1.72647632737169,98.6967411561644));
#23673=CARTESIAN_POINT('Ctrl Pts',(-2.4893866319005,1.80514812878637,98.6917834935739));
#23674=CARTESIAN_POINT('Ctrl Pts',(-2.43067395941607,1.88101737180085,98.6868258309835));
#23675=CARTESIAN_POINT('Ctrl Pts',(-2.37189661767665,1.95697018122809,98.6818627077601));
#23676=CARTESIAN_POINT('Ctrl Pts',(-2.30959564770612,2.03011392141336,98.6768995845368));
#23677=CARTESIAN_POINT('Ctrl Pts',(-2.24408326980453,2.10011726534101,98.6719364613135));
#23678=CARTESIAN_POINT('Ctrl Pts',(-2.17852785422086,2.17016659724463,98.6669700776175));
#23679=CARTESIAN_POINT('Ctrl Pts',(-2.10975715023411,2.23707111855631,98.6620036939215));
#23680=CARTESIAN_POINT('Ctrl Pts',(-2.03811839317448,2.30053812517938,98.6570373102255));
#23681=CARTESIAN_POINT('Ctrl Pts',(-1.96637053317777,2.36410178949327,98.6520633629275));
#23682=CARTESIAN_POINT('Ctrl Pts',(-1.89174625052971,2.4242172172049,98.6470894156295));
#23683=CARTESIAN_POINT('Ctrl Pts',(-1.81462350537452,2.4806337463927,98.6421154683315));
#23684=CARTESIAN_POINT('Ctrl Pts',(-1.79446902637195,2.49537707212139,98.6408156271993));
#23685=CARTESIAN_POINT('Ctrl Pts',(-1.77414405639444,2.50986802799386,98.6395157860671));
#23686=CARTESIAN_POINT('Ctrl Pts',(-1.75365561779317,2.52410265721948,98.638215944935));
#23687=CARTESIAN_POINT('Ctrl Pts',(-1.67485203117638,2.57885255099956,98.6332164354438));
#23688=CARTESIAN_POINT('Ctrl Pts',(-1.59334360087784,2.63000464830929,98.6282169259526));
#23689=CARTESIAN_POINT('Ctrl Pts',(-1.50949272260857,2.67728107795797,98.6232174164614));
#23690=CARTESIAN_POINT('Ctrl Pts',(-1.42575558752384,2.72449337742968,98.6182246887732));
#23691=CARTESIAN_POINT('Ctrl Pts',(-1.33968269867362,2.76784024406897,98.6132319610849));
#23692=CARTESIAN_POINT('Ctrl Pts',(-1.25166650240203,2.80708625032518,98.6082392333967));
#23693=CARTESIAN_POINT('Ctrl Pts',(-1.16374316099921,2.84629085303392,98.6032517729103));
#23694=CARTESIAN_POINT('Ctrl Pts',(-1.07388098651105,2.88140301797678,98.5982643124239));
#23695=CARTESIAN_POINT('Ctrl Pts',(-0.982497268071358,2.91223305527431,
98.5932768519375));
#23696=CARTESIAN_POINT('Ctrl Pts',(-0.89117893681916,2.94304103295921,98.5882929600957));
#23697=CARTESIAN_POINT('Ctrl Pts',(-0.79834164063746,2.96957283409185,98.583309068254));
#23698=CARTESIAN_POINT('Ctrl Pts',(-0.704421994544591,2.9916871333082,98.5783251764122));
#23699=CARTESIAN_POINT('Ctrl Pts',(-0.610536551661147,3.01379337904437,
98.5733430995804));
#23700=CARTESIAN_POINT('Ctrl Pts',(-0.515569968870673,3.03148521876159,
98.5683610227486));
#23701=CARTESIAN_POINT('Ctrl Pts',(-0.41997241371209,3.04467164431911,98.5633789459169));
#23702=CARTESIAN_POINT('Ctrl Pts',(-0.324383574848405,3.05785686757838,
98.5583973233357));
#23703=CARTESIAN_POINT('Ctrl Pts',(-0.228164312867165,3.06653743360497,
98.5534157007546));
#23704=CARTESIAN_POINT('Ctrl Pts',(-0.13177227556886,3.07067391909193,98.5484340781734));
#23705=CARTESIAN_POINT('Ctrl Pts',(-0.0353627124998721,3.07481115666483,
98.5434515498455));
#23706=CARTESIAN_POINT('Ctrl Pts',(0.0612192497179335,3.07440265409146,
98.5384690215176));
#23707=CARTESIAN_POINT('Ctrl Pts',(0.157514664773568,3.06946108956951,98.5334864931898));
#23708=CARTESIAN_POINT('Ctrl Pts',(0.25391387209432,3.06451419876931,98.5284985944307));
#23709=CARTESIAN_POINT('Ctrl Pts',(0.350025476538818,3.05502451416117,98.5235106956716));
#23710=CARTESIAN_POINT('Ctrl Pts',(0.445394584749105,3.04105671007237,98.5185227969125));
#23711=CARTESIAN_POINT('Ctrl Pts',(0.540820028800482,3.02708065501,98.5135319517332));
#23712=CARTESIAN_POINT('Ctrl Pts',(0.63550167263886,3.00862129722929,98.5085411065538));
#23713=CARTESIAN_POINT('Ctrl Pts',(0.728995853848436,2.98579424861657,98.5035502613745));
#23714=CARTESIAN_POINT('Ctrl Pts',(0.822641124016088,2.96293031091679,98.4985513508633));
#23715=CARTESIAN_POINT('Ctrl Pts',(0.915094679021009,2.93568471252292,98.4935524403521));
#23716=CARTESIAN_POINT('Ctrl Pts',(1.00592908130586,2.90422260396533,98.4885535298409));
#23717=CARTESIAN_POINT('Ctrl Pts',(1.05866384272606,2.88595698271581,98.4856513656108));
#23718=CARTESIAN_POINT('Ctrl Pts',(1.11085324558548,2.86627109189438,98.4827492013808));
#23719=CARTESIAN_POINT('Ctrl Pts',(1.16241729726026,2.8452044350152,98.4798470371507));
#23720=CARTESIAN_POINT('Ctrl Pts',(1.25124149116091,2.80891502883593,98.4748477713846));
#23721=CARTESIAN_POINT('Ctrl Pts',(1.33852068826598,2.76839840732892,98.4698485056184));
#23722=CARTESIAN_POINT('Ctrl Pts',(1.42382456802978,2.72380723427243,98.4648492398523));
#23723=CARTESIAN_POINT('Ctrl Pts',(1.50900204416191,2.67928213659528,98.4598573820183));
#23724=CARTESIAN_POINT('Ctrl Pts',(1.5922096376006,2.63069469437216,98.4548655241842));
#23725=CARTESIAN_POINT('Ctrl Pts',(1.67303641751327,2.57824579814927,98.4498736663502));
#23726=CARTESIAN_POINT('Ctrl Pts',(1.74125898300543,2.53397583884341,98.4456602441604));
#23727=CARTESIAN_POINT('Ctrl Pts',(1.80778554719658,2.48695574098692,98.4414468219706));
#23728=CARTESIAN_POINT('Ctrl Pts',(1.8723819390353,2.43733217358127,98.4372333997809));
#23729=CARTESIAN_POINT('Ctrl Pts',(1.87238193903529,2.43733217358128,99.4373602300224));
#23730=CARTESIAN_POINT('Ctrl Pts',(1.90947719062037,2.4088352457334,99.4349269813002));
#23731=CARTESIAN_POINT('Ctrl Pts',(1.94589304168592,2.37951330214532,99.432493732578));
#23732=CARTESIAN_POINT('Ctrl Pts',(1.9815920072363,2.3494031937616,99.4300604838558));
#23733=CARTESIAN_POINT('Ctrl Pts',(2.05494140039069,2.28753702638926,99.4250609743626));
#23734=CARTESIAN_POINT('Ctrl Pts',(2.12551961643353,2.22212390310521,99.4200614648694));
#23735=CARTESIAN_POINT('Ctrl Pts',(2.19296414688146,2.15344154796281,99.4150619553762));
#23736=CARTESIAN_POINT('Ctrl Pts',(2.26031718925207,2.08485235999908,99.4100692276858));
#23737=CARTESIAN_POINT('Ctrl Pts',(2.32454468933311,2.01300306435795,99.4050764999955));
#23738=CARTESIAN_POINT('Ctrl Pts',(2.38531731363497,1.9382114340993,99.4000837723052));
#23739=CARTESIAN_POINT('Ctrl Pts',(2.44602582435009,1.86349870712528,99.3950963118167));
#23740=CARTESIAN_POINT('Ctrl Pts',(2.5032864295953,1.7858501551383,99.3901088513282));
#23741=CARTESIAN_POINT('Ctrl Pts',(2.55680750521989,1.70561942743721,99.3851213908398));
#23742=CARTESIAN_POINT('Ctrl Pts',(2.61029028526379,1.62544610669723,99.3801374989959));
#23743=CARTESIAN_POINT('Ctrl Pts',(2.66003861199281,1.54269464731914,99.3751536071519));
#23744=CARTESIAN_POINT('Ctrl Pts',(2.70580254100521,1.45774993023144,99.370169715308));
#23745=CARTESIAN_POINT('Ctrl Pts',(2.7515498039281,1.37283614790586,99.3651876384741));
#23746=CARTESIAN_POINT('Ctrl Pts',(2.79331534416602,1.28573108091295,99.3602055616402));
#23747=CARTESIAN_POINT('Ctrl Pts',(2.83089428315928,1.19684577434861,99.3552234848062));
#23748=CARTESIAN_POINT('Ctrl Pts',(2.86846979581905,1.10796857207647,99.3502418622229));
#23749=CARTESIAN_POINT('Ctrl Pts',(2.90185929540075,1.0173118573331,99.3452602396396));
#23750=CARTESIAN_POINT('Ctrl Pts',(2.93090577140742,0.925307305240087,99.3402786170563));
#23751=CARTESIAN_POINT('Ctrl Pts',(2.9599575285752,0.833286025098481,99.3352960887262));
#23752=CARTESIAN_POINT('Ctrl Pts',(2.98466456182656,0.739916839519692,99.3303135603962));
#23753=CARTESIAN_POINT('Ctrl Pts',(3.00491983427052,0.645646218611726,99.3253310320661));
#23754=CARTESIAN_POINT('Ctrl Pts',(3.02519693891298,0.551273987867915,99.3203431333048));
#23755=CARTESIAN_POINT('Ctrl Pts',(3.04101261093616,0.455998811935668,99.3153552345435));
#23756=CARTESIAN_POINT('Ctrl Pts',(3.05231107613794,0.360276760956968,99.3103673357823));
#23757=CARTESIAN_POINT('Ctrl Pts',(3.06361621549819,0.26449816564895,99.3053764906007));
#23758=CARTESIAN_POINT('Ctrl Pts',(3.07039880401429,0.168272607348081,99.3003856454192));
#23759=CARTESIAN_POINT('Ctrl Pts',(3.0726551735271,0.0720585497850684,99.2953948002376));
#23760=CARTESIAN_POINT('Ctrl Pts',(3.07491518939003,-0.0243109921245982,
99.2903958897243));
#23761=CARTESIAN_POINT('Ctrl Pts',(3.07263439122162,-0.12066855764159,99.2853969792109));
#23762=CARTESIAN_POINT('Ctrl Pts',(3.06586116397397,-0.216558475327454,
99.2803980686975));
#23763=CARTESIAN_POINT('Ctrl Pts',(3.06192890360598,-0.272228263040121,
99.2774959044889));
#23764=CARTESIAN_POINT('Ctrl Pts',(3.05648344205991,-0.327740558712226,
99.2745937402803));
#23765=CARTESIAN_POINT('Ctrl Pts',(3.04954213539397,-0.383007851690783,
99.2716915760716));
#23766=CARTESIAN_POINT('Ctrl Pts',(3.03758446309371,-0.4782158881838,99.2666920665789));
#23767=CARTESIAN_POINT('Ctrl Pts',(3.02114285983535,-0.573030628378096,
99.2616925570862));
#23768=CARTESIAN_POINT('Ctrl Pts',(3.00025291010258,-0.666996795660201,
99.2566930475935));
#23769=CARTESIAN_POINT('Ctrl Pts',(2.97939129745398,-0.760835498433068,
99.2517003199037));
#23770=CARTESIAN_POINT('Ctrl Pts',(2.95409342525884,-0.85382749116087,99.2467075922139));
#23771=CARTESIAN_POINT('Ctrl Pts',(2.92444653297567,-0.945523519414831,
99.241714864524));
#23772=CARTESIAN_POINT('Ctrl Pts',(2.89483091741653,-1.03712281067037,99.2367274040361));
#23773=CARTESIAN_POINT('Ctrl Pts',(2.8608755369712,-1.12742843992935,99.2317399435481));
#23774=CARTESIAN_POINT('Ctrl Pts',(2.8227182547191,-1.21600325019121,99.2267524830602));
#23775=CARTESIAN_POINT('Ctrl Pts',(2.78458827489435,-1.30451468310593,99.2217685912167));
#23776=CARTESIAN_POINT('Ctrl Pts',(2.7422625433336,-1.39129735699729,99.2167846993733));
#23777=CARTESIAN_POINT('Ctrl Pts',(2.69592781257063,-1.47593207140712,99.2118008075299));
#23778=CARTESIAN_POINT('Ctrl Pts',(2.64960995576901,-1.56053596395017,99.2068187306965));
#23779=CARTESIAN_POINT('Ctrl Pts',(2.59928621116296,-1.64299306658165,99.2018366538631));
#23780=CARTESIAN_POINT('Ctrl Pts',(2.54518981375611,-1.72290773460222,99.1968545770296));
#23781=CARTESIAN_POINT('Ctrl Pts',(2.49109834869436,-1.80281511624624,99.1918729544468));
#23782=CARTESIAN_POINT('Ctrl Pts',(2.43323516094607,-1.88018016075809,99.186891331864));
#23783=CARTESIAN_POINT('Ctrl Pts',(2.3718768516627,-1.95463614275052,99.1819097092812));
#23784=CARTESIAN_POINT('Ctrl Pts',(2.3105073863576,-2.02910566215235,99.1769271809516));
#23785=CARTESIAN_POINT('Ctrl Pts',(2.2456418166526,-2.10066472987187,99.171944652622));
#23786=CARTESIAN_POINT('Ctrl Pts',(2.17759636182742,-2.16898048284349,99.1669621242925));
#23787=CARTESIAN_POINT('Ctrl Pts',(2.10947756403026,-2.23736987012866,99.1619742255317));
#23788=CARTESIAN_POINT('Ctrl Pts',(2.03817234882155,-2.30250865206996,99.1569863267708));
#23789=CARTESIAN_POINT('Ctrl Pts',(1.96403289796642,-2.36410173759625,99.15199842801));
#23790=CARTESIAN_POINT('Ctrl Pts',(1.88984965192002,-2.42573120700361,99.147007582829));
#23791=CARTESIAN_POINT('Ctrl Pts',(1.81282918689692,-2.48381054535344,99.1420167376479));
#23792=CARTESIAN_POINT('Ctrl Pts',(1.73335406160244,-2.53808706452839,99.1370258924669));
#23793=CARTESIAN_POINT('Ctrl Pts',(1.65375050249836,-2.59245129592906,99.1320269819539));
#23794=CARTESIAN_POINT('Ctrl Pts',(1.57168473581269,-2.64300020698688,99.127028071441));
#23795=CARTESIAN_POINT('Ctrl Pts',(1.48756531849523,-2.68952629160047,99.1220291609281));
#23796=CARTESIAN_POINT('Ctrl Pts',(1.43872900466873,-2.71653744481296,99.1191269967146));
#23797=CARTESIAN_POINT('Ctrl Pts',(1.38920092920491,-2.74219358975948,99.1162248325011));
#23798=CARTESIAN_POINT('Ctrl Pts',(1.33906394489779,-2.76646163925596,99.1133226682876));
#23799=CARTESIAN_POINT('Ctrl Pts',(1.25269380505265,-2.80826780007209,99.108323158795));
#23800=CARTESIAN_POINT('Ctrl Pts',(1.16421227589896,-2.84609874340984,99.1033236493024));
#23801=CARTESIAN_POINT('Ctrl Pts',(1.07402061397536,-2.87973644119666,99.0983241398098));
#23802=CARTESIAN_POINT('Ctrl Pts',(0.98395129646859,-2.91332850965997,99.0933314121201));
#23803=CARTESIAN_POINT('Ctrl Pts',(0.892176864380095,-2.94273848523513,
99.0883386844303));
#23804=CARTESIAN_POINT('Ctrl Pts',(0.799121646518137,-2.9677949464318,99.0833459567406));
#23805=CARTESIAN_POINT('Ctrl Pts',(0.706164599565391,-2.99282497369351,
99.0783584962527));
#23806=CARTESIAN_POINT('Ctrl Pts',(0.611929874548104,-3.01351050335598,
99.0733710357649));
#23807=CARTESIAN_POINT('Ctrl Pts',(0.51685921515451,-3.02972916309525,99.0683835752771));
#23808=CARTESIAN_POINT('Ctrl Pts',(0.421856581040128,-3.04593621800435,
99.0633996834338));
#23809=CARTESIAN_POINT('Ctrl Pts',(0.326019633074976,-3.0576826831781,99.0584157915905));
#23810=CARTESIAN_POINT('Ctrl Pts',(0.229801671077851,-3.06489697085723,
99.0534318997472));
#23811=CARTESIAN_POINT('Ctrl Pts',(0.133618749279474,-3.07210863127146,
99.0484498229139));
#23812=CARTESIAN_POINT('Ctrl Pts',(0.037055526428251,-3.07479136078171,
99.0434677460806));
#23813=CARTESIAN_POINT('Ctrl Pts',(-0.0594291485925616,-3.07292538573548,
99.0384856692473));
#23814=CARTESIAN_POINT('Ctrl Pts',(-0.155905026433875,-3.07105958082318,
99.0335040466646));
#23815=CARTESIAN_POINT('Ctrl Pts',(-0.252301931807038,-3.06464590459951,
99.0285224240819));
#23816=CARTESIAN_POINT('Ctrl Pts',(-0.348161662357746,-3.05371670376679,
99.0235408014992));
#23817=CARTESIAN_POINT('Ctrl Pts',(-0.444038821896402,-3.0427855158128,
99.0185582731698));
#23818=CARTESIAN_POINT('Ctrl Pts',(-0.539378176515784,-3.02733722249843,
99.0135757448403));
#23819=CARTESIAN_POINT('Ctrl Pts',(-0.63372835716399,-3.00745583830025,
99.0085932165109));
#23820=CARTESIAN_POINT('Ctrl Pts',(-0.728180233401813,-2.98755302489997,
99.0036053177502));
#23821=CARTESIAN_POINT('Ctrl Pts',(-0.821640376889052,-2.96320767200392,
98.9986174189896));
#23822=CARTESIAN_POINT('Ctrl Pts',(-0.913669521600026,-2.93455452416533,
98.9936295202289));
#23823=CARTESIAN_POINT('Ctrl Pts',(-1.00575302918991,-2.90588445051903,
98.988638675048));
#23824=CARTESIAN_POINT('Ctrl Pts',(-1.09640344253843,-2.87290166508771,
98.9836478298671));
#23825=CARTESIAN_POINT('Ctrl Pts',(-1.18520052411789,-2.83578947872205,
98.9786569846862));
#23826=CARTESIAN_POINT('Ctrl Pts',(-1.27414110402368,-2.79861731812599,
98.9736580741734));
#23827=CARTESIAN_POINT('Ctrl Pts',(-1.361221975422,-2.75730261968959,98.9686591636606));
#23828=CARTESIAN_POINT('Ctrl Pts',(-1.4460466443268,-2.71207510080956,98.9636602531478));
#23829=CARTESIAN_POINT('Ctrl Pts',(-1.49529239857694,-2.68581784205611,
98.960758088933));
#23830=CARTESIAN_POINT('Ctrl Pts',(-1.54377821304985,-2.65824260261122,
98.9578559247182));
#23831=CARTESIAN_POINT('Ctrl Pts',(-1.59143122513768,-2.62940086439036,
98.9549537605033));
#23832=CARTESIAN_POINT('Ctrl Pts',(-1.67352226780585,-2.57971568691305,
98.9499542510085));
#23833=CARTESIAN_POINT('Ctrl Pts',(-1.75342847792337,-2.52609517900815,
98.9449547415137));
#23834=CARTESIAN_POINT('Ctrl Pts',(-1.83074851047602,-2.46875720584059,
98.9399552320189));
#23835=CARTESIAN_POINT('Ctrl Pts',(-1.90796365889549,-2.41149701126953,
98.934962504327));
#23836=CARTESIAN_POINT('Ctrl Pts',(-1.9825992523572,-2.35052963273801,98.929969776635));
#23837=CARTESIAN_POINT('Ctrl Pts',(-2.05428047735531,-2.28611766327913,
98.9249770489431));
#23838=CARTESIAN_POINT('Ctrl Pts',(-2.12588608046794,-2.22177364682438,
98.919989588453));
#23839=CARTESIAN_POINT('Ctrl Pts',(-2.19454318632489,-2.15399255536408,
98.9150021279629));
#23840=CARTESIAN_POINT('Ctrl Pts',(-2.25990864192412,-2.08307829429349,
98.9100146674729));
#23841=CARTESIAN_POINT('Ctrl Pts',(-2.32522732701191,-2.01221477403436,
98.9050307756274));
#23842=CARTESIAN_POINT('Ctrl Pts',(-2.38725874731746,-1.93822286270734,
98.9000468837819));
#23843=CARTESIAN_POINT('Ctrl Pts',(-2.44569605578645,-1.86144380863635,
98.8950629919364));
#23844=CARTESIAN_POINT('Ctrl Pts',(-2.50411208283503,-1.78469271559525,
98.8900809151008));
#23845=CARTESIAN_POINT('Ctrl Pts',(-2.55893633307966,-1.70515684546293,
98.8850988382653));
#23846=CARTESIAN_POINT('Ctrl Pts',(-2.60990239954228,-1.62321031134707,
98.8801167614298));
#23847=CARTESIAN_POINT('Ctrl Pts',(-2.66086381907369,-1.5412712488674,98.8751351388449));
#23848=CARTESIAN_POINT('Ctrl Pts',(-2.707967522548,-1.45692233224867,98.87015351626));
#23849=CARTESIAN_POINT('Ctrl Pts',(-2.75099117314239,-1.37056550930361,
98.8651718936751));
#23850=CARTESIAN_POINT('Ctrl Pts',(-2.79402264619452,-1.28419298516657,
98.8601893653434));
#23851=CARTESIAN_POINT('Ctrl Pts',(-2.8329723973875,-1.19581222258103,98.8552068370118));
#23852=CARTESIAN_POINT('Ctrl Pts',(-2.8676651488311,-1.10584756823872,98.8502243086801));
#23853=CARTESIAN_POINT('Ctrl Pts',(-2.90239529394758,-1.01578594525843,
98.8452364099173));
#23854=CARTESIAN_POINT('Ctrl Pts',(-2.93285912076048,-0.924137432494293,
98.8402485111544));
#23855=CARTESIAN_POINT('Ctrl Pts',(-2.95893049288799,-0.831343844782441,
98.8352606123916));
#23856=CARTESIAN_POINT('Ctrl Pts',(-2.98501726573278,-0.738495442624959,
98.8302697672085));
#23857=CARTESIAN_POINT('Ctrl Pts',(-3.00670631880345,-0.644501046197165,
98.8252789220254));
#23858=CARTESIAN_POINT('Ctrl Pts',(-3.02392261284924,-0.549812951374382,
98.8202880768423));
#23859=CARTESIAN_POINT('Ctrl Pts',(-3.04116672886086,-0.45497183819986,
98.8152891663274));
#23860=CARTESIAN_POINT('Ctrl Pts',(-3.05392359488709,-0.359435222980361,
98.8102902558125));
#23861=CARTESIAN_POINT('Ctrl Pts',(-3.0621700243383,-0.263660751808075,
98.8052913452975));
#23862=CARTESIAN_POINT('Ctrl Pts',(-3.0669575659837,-0.208057987967436,
98.8023891811047));
#23863=CARTESIAN_POINT('Ctrl Pts',(-3.07022584521813,-0.152375079105688,
98.7994870169119));
#23864=CARTESIAN_POINT('Ctrl Pts',(-3.07197837451438,-0.0967011712233662,
98.7965848527191));
#23865=CARTESIAN_POINT('Ctrl Pts',(-3.07298649485838,-0.064675458851045,
98.7949154194203));
#23866=CARTESIAN_POINT('Ctrl Pts',(-3.07349382383657,-0.0326338998043769,
98.7932459861214));
#23867=CARTESIAN_POINT('Ctrl Pts',(-3.07349994395338,-0.000586957040365301,
98.7915765528226));
#23868=CARTESIAN_POINT('Origin',(0.,0.,116.208423447177));
#23869=CARTESIAN_POINT('',(1.8723819390353,2.43733217358127,100.43738386173));
#23870=CARTESIAN_POINT('',(1.87238193903531,2.43733217358127,100.354075679943));
#23871=CARTESIAN_POINT('',(1.8723819390353,2.43733217358128,116.208423447177));
#23872=CARTESIAN_POINT('',(-3.0734987850259,-0.00273284546552975,99.7084234472081));
#23873=CARTESIAN_POINT('Ctrl Pts',(1.87238193903531,2.43733217358127,100.354075679943));
#23874=CARTESIAN_POINT('Ctrl Pts',(1.94872699621459,2.378683168843,100.349088366481));
#23875=CARTESIAN_POINT('Ctrl Pts',(2.02239556219247,2.31638085683682,100.34410105302));
#23876=CARTESIAN_POINT('Ctrl Pts',(2.09302229050685,2.25070209966611,100.339113739558));
#23877=CARTESIAN_POINT('Ctrl Pts',(2.1635994165791,2.18506946970099,100.334129928764));
#23878=CARTESIAN_POINT('Ctrl Pts',(2.23113863126896,2.11606540665456,100.32914611797));
#23879=CARTESIAN_POINT('Ctrl Pts',(2.29530794381499,2.04400677422062,100.324162307176));
#23880=CARTESIAN_POINT('Ctrl Pts',(2.35945446148497,1.97197373918721,100.319180266782));
#23881=CARTESIAN_POINT('Ctrl Pts',(2.4202331638817,1.89688861821699,100.314198226387));
#23882=CARTESIAN_POINT('Ctrl Pts',(2.47734988312798,1.81910412196932,100.309216185993));
#23883=CARTESIAN_POINT('Ctrl Pts',(2.534461905551,1.74132602209799,100.304234555282));
#23884=CARTESIAN_POINT('Ctrl Pts',(2.58791228391867,1.66084934224848,100.299252924571));
#23885=CARTESIAN_POINT('Ctrl Pts',(2.63744867501404,1.57805790028968,100.29427129386));
#23886=CARTESIAN_POINT('Ctrl Pts',(2.68699451579225,1.4952506648334,100.289288712841));
#23887=CARTESIAN_POINT('Ctrl Pts',(2.73262466108324,1.41012816697903,100.284306131822));
#23888=CARTESIAN_POINT('Ctrl Pts',(2.77413198545853,1.32310013878615,100.279323550803));
#23889=CARTESIAN_POINT('Ctrl Pts',(2.81568425155709,1.23597788169224,100.274335574935));
#23890=CARTESIAN_POINT('Ctrl Pts',(2.85310459601087,1.1469463723038,100.269347599066));
#23891=CARTESIAN_POINT('Ctrl Pts',(2.88623356395202,1.05643649327199,100.264359623197));
#23892=CARTESIAN_POINT('Ctrl Pts',(2.91938236737993,0.965872422769139,100.25936866085));
#23893=CARTESIAN_POINT('Ctrl Pts',(2.94823454715684,0.873828638819195,100.254377698504));
#23894=CARTESIAN_POINT('Ctrl Pts',(2.97268079764369,0.780750360435693,100.249386736157));
#23895=CARTESIAN_POINT('Ctrl Pts',(2.99716631982083,0.687522556409266,100.244387756077));
#23896=CARTESIAN_POINT('Ctrl Pts',(3.0172316893431,0.593257368747633,100.239388775997));
#23897=CARTESIAN_POINT('Ctrl Pts',(3.03281889489707,0.498409270334469,100.234389795916));
#23898=CARTESIAN_POINT('Ctrl Pts',(3.04135810155053,0.44644822380602,100.231651182904));
#23899=CARTESIAN_POINT('Ctrl Pts',(3.0485542237069,0.394312318422457,100.228912569891));
#23900=CARTESIAN_POINT('Ctrl Pts',(3.05440435245981,0.342076455890416,100.226173956878));
#23901=CARTESIAN_POINT('Ctrl Pts',(3.06508412871854,0.246716618853292,100.221174447385));
#23902=CARTESIAN_POINT('Ctrl Pts',(3.071312619333,0.150688668851936,100.216174937892));
#23903=CARTESIAN_POINT('Ctrl Pts',(3.07301775946222,0.0544435490191098,
100.211175428399));
#23904=CARTESIAN_POINT('Ctrl Pts',(3.07472058657968,-0.0416710149198213,
100.206182700709));
#23905=CARTESIAN_POINT('Ctrl Pts',(3.07191225019029,-0.138001728073925,
100.201189973019));
#23906=CARTESIAN_POINT('Ctrl Pts',(3.06457231374881,-0.234091400534577,
100.196197245329));
#23907=CARTESIAN_POINT('Ctrl Pts',(3.05724012075527,-0.330079700812884,
100.19120978484));
#23908=CARTESIAN_POINT('Ctrl Pts',(3.04538586475535,-0.425827030554686,
100.186222324352));
#23909=CARTESIAN_POINT('Ctrl Pts',(3.02904115811324,-0.520876100868515,
100.181234863864));
#23910=CARTESIAN_POINT('Ctrl Pts',(3.0127081464908,-0.61585716135073,100.17625097202));
#23911=CARTESIAN_POINT('Ctrl Pts',(2.99189114574195,-0.710140524255589,
100.171267080177));
#23912=CARTESIAN_POINT('Ctrl Pts',(2.9666735038666,-0.803274904037155,100.166283188333));
#23913=CARTESIAN_POINT('Ctrl Pts',(2.94146504563184,-0.896375366584292,
100.161301111499));
#23914=CARTESIAN_POINT('Ctrl Pts',(2.91185924507951,-0.988327254113311,
100.156319034665));
#23915=CARTESIAN_POINT('Ctrl Pts',(2.87799015759056,-1.07869129171041,100.151336957832));
#23916=CARTESIAN_POINT('Ctrl Pts',(2.84412415818208,-1.16904709018915,100.146355335249));
#23917=CARTESIAN_POINT('Ctrl Pts',(2.80599579890358,-1.25781491560126,100.141373712665));
#23918=CARTESIAN_POINT('Ctrl Pts',(2.76378806945563,-1.34457344802533,100.136392090082));
#23919=CARTESIAN_POINT('Ctrl Pts',(2.7215726658988,-1.43134775467922,100.131409561753));
#23920=CARTESIAN_POINT('Ctrl Pts',(2.67527661121658,-1.51611164810015,100.126427033423));
#23921=CARTESIAN_POINT('Ctrl Pts',(2.62512934372775,-1.59846744686887,100.121444505093));
#23922=CARTESIAN_POINT('Ctrl Pts',(2.57492802487519,-1.68091201305121,100.116456606332));
#23923=CARTESIAN_POINT('Ctrl Pts',(2.52086743472272,-1.76094292721634,100.111468707571));
#23924=CARTESIAN_POINT('Ctrl Pts',(2.46322082222888,-1.83819080373559,100.10648080881));
#23925=CARTESIAN_POINT('Ctrl Pts',(2.40554015708981,-1.91548431163577,100.101489963628));
#23926=CARTESIAN_POINT('Ctrl Pts',(2.34426953038545,-1.98999116957381,100.096499118447));
#23927=CARTESIAN_POINT('Ctrl Pts',(2.27972165651885,-2.06137609833794,100.091508273266));
#23928=CARTESIAN_POINT('Ctrl Pts',(2.21506947165803,-2.13287638694966,100.086509362752));
#23929=CARTESIAN_POINT('Ctrl Pts',(2.1471297736734,-2.20124436124788,100.081510452239));
#23930=CARTESIAN_POINT('Ctrl Pts',(2.07625113663158,-2.26618257597134,100.076511541726));
#23931=CARTESIAN_POINT('Ctrl Pts',(2.03510188157209,-2.30388306334367,100.073609377515));
#23932=CARTESIAN_POINT('Ctrl Pts',(1.99296267411118,-2.34042831230001,100.070707213305));
#23933=CARTESIAN_POINT('Ctrl Pts',(1.94990630988358,-2.37576674626871,100.067805049094));
#23934=CARTESIAN_POINT('Ctrl Pts',(1.87573383511689,-2.43664367233664,100.062805539601));
#23935=CARTESIAN_POINT('Ctrl Pts',(1.79857744293256,-2.49415064949343,100.057806030108));
#23936=CARTESIAN_POINT('Ctrl Pts',(1.71877614513625,-2.54798171361385,100.052806520615));
#23937=CARTESIAN_POINT('Ctrl Pts',(1.63908309729366,-2.60173975623762,100.047813792925));
#23938=CARTESIAN_POINT('Ctrl Pts',(1.55675263514356,-2.65183155249234,100.042821065235));
#23939=CARTESIAN_POINT('Ctrl Pts',(1.47215711934522,-2.6979910426021,100.037828337545));
#23940=CARTESIAN_POINT('Ctrl Pts',(1.38765084968367,-2.74410183561333,100.032840877057));
#23941=CARTESIAN_POINT('Ctrl Pts',(1.30088465998618,-2.78628836027702,100.027853416568));
#23942=CARTESIAN_POINT('Ctrl Pts',(1.21225933204805,-2.82432816114955,100.02286595608));
#23943=CARTESIAN_POINT('Ctrl Pts',(1.12369741760369,-2.86234074365537,100.017882064237));
#23944=CARTESIAN_POINT('Ctrl Pts',(1.03327941162508,-2.89621232814008,100.012898172393));
#23945=CARTESIAN_POINT('Ctrl Pts',(0.941429227895216,-2.92576712314303,
100.007914280549));
#23946=CARTESIAN_POINT('Ctrl Pts',(0.849612493727385,-2.95531115502162,
100.002932203716));
#23947=CARTESIAN_POINT('Ctrl Pts',(0.756365035534493,-2.98054138662742,
99.9979501268819));
#23948=CARTESIAN_POINT('Ctrl Pts',(0.662128300386727,-3.00133109866722,
99.9929680500482));
#23949=CARTESIAN_POINT('Ctrl Pts',(0.567900157458148,-3.02211891516424,
99.9879864274651));
#23950=CARTESIAN_POINT('Ctrl Pts',(0.472683345601994,-3.03846692267068,
99.9830048048821));
#23951=CARTESIAN_POINT('Ctrl Pts',(0.376930893746072,-3.05029922324676,
99.978023182299));
#23952=CARTESIAN_POINT('Ctrl Pts',(0.28116103240736,-3.06213367514355,99.9730406539692));
#23953=CARTESIAN_POINT('Ctrl Pts',(0.184855773303206,-3.06945073573493,
99.9680581256394));
#23954=CARTESIAN_POINT('Ctrl Pts',(0.0884736065908541,-3.0722263378431,
99.9630755973096));
#23955=CARTESIAN_POINT('Ctrl Pts',(-0.00801244589267319,-3.07500493164128,
99.9580876985486));
#23956=CARTESIAN_POINT('Ctrl Pts',(-0.104575131968766,-3.07323228183818,
99.9530997997875));
#23957=CARTESIAN_POINT('Ctrl Pts',(-0.200755842999826,-3.06693647497,99.9481119010265));
#23958=CARTESIAN_POINT('Ctrl Pts',(-0.296993369297024,-3.0606369490823,
99.9431210558452));
#23959=CARTESIAN_POINT('Ctrl Pts',(-0.392848035282793,-3.04980899520767,
99.9381302106639));
#23960=CARTESIAN_POINT('Ctrl Pts',(-0.487868353496007,-3.03453237248461,
99.9331393654826));
#23961=CARTESIAN_POINT('Ctrl Pts',(-0.583042226943077,-3.01923106235344,
99.9281404549695));
#23962=CARTESIAN_POINT('Ctrl Pts',(-0.677378630961432,-2.99946681815902,
99.9231415444563));
#23963=CARTESIAN_POINT('Ctrl Pts',(-0.770438289065952,-2.97537007660243,
99.9181426339432));
#23964=CARTESIAN_POINT('Ctrl Pts',(-0.824464943183301,-2.96138048811747,
99.915240469732));
#23965=CARTESIAN_POINT('Ctrl Pts',(-0.878061573359936,-2.94593156383606,
99.9123383055208));
#23966=CARTESIAN_POINT('Ctrl Pts',(-0.931145283868457,-2.92905628323007,
99.9094361413096));
#23967=CARTESIAN_POINT('Ctrl Pts',(-1.02259169947179,-2.89998552105208,
99.9044366318167));
#23968=CARTESIAN_POINT('Ctrl Pts',(-1.11283602642308,-2.86657709801935,
99.8994371223238));
#23969=CARTESIAN_POINT('Ctrl Pts',(-1.20143704886778,-2.82894879197342,
99.8944376128309));
#23970=CARTESIAN_POINT('Ctrl Pts',(-1.28991788458815,-2.79137152848571,
99.8894448851408));
#23971=CARTESIAN_POINT('Ctrl Pts',(-1.37675944547547,-2.74958592866531,
99.8844521574508));
#23972=CARTESIAN_POINT('Ctrl Pts',(-1.46153583030011,-2.70375946910019,
99.8794594297608));
#23973=CARTESIAN_POINT('Ctrl Pts',(-1.54622277817571,-2.65798135529477,
99.8744719692726));
#23974=CARTESIAN_POINT('Ctrl Pts',(-1.62884849702787,-2.6081710639704,99.8694845087845));
#23975=CARTESIAN_POINT('Ctrl Pts',(-1.70900818667259,-2.55454365159143,
99.8644970482963));
#23976=CARTESIAN_POINT('Ctrl Pts',(-1.78911052018557,-2.5009546108796,99.8595131564527));
#23977=CARTESIAN_POINT('Ctrl Pts',(-1.86674996843881,-2.44355412207145,
99.8545292646091));
#23978=CARTESIAN_POINT('Ctrl Pts',(-1.94154827839042,-2.38260205084256,
99.8495453727655));
#23979=CARTESIAN_POINT('Ctrl Pts',(-2.01631934865012,-2.32167217684838,
99.8445632959318));
#23980=CARTESIAN_POINT('Ctrl Pts',(-2.08825099645011,-2.25719356728725,
99.8395812190982));
#23981=CARTESIAN_POINT('Ctrl Pts',(-2.15699658407839,-2.18946751203897,
99.8345991422646));
#23982=CARTESIAN_POINT('Ctrl Pts',(-2.22573590369289,-2.12174763184662,
99.8296175196816));
#23983=CARTESIAN_POINT('Ctrl Pts',(-2.29128942811944,-2.0507812028496,99.8246358970986));
#23984=CARTESIAN_POINT('Ctrl Pts',(-2.35334684244476,-1.97690689946575,
99.8196542745156));
#23985=CARTESIAN_POINT('Ctrl Pts',(-2.41541553990144,-1.90301916443189,
99.8146717461858));
#23986=CARTESIAN_POINT('Ctrl Pts',(-2.47398658253122,-1.82622284113484,
99.8096892178561));
#23987=CARTESIAN_POINT('Ctrl Pts',(-2.52879015728921,-1.7468894041688,99.8047066895263));
#23988=CARTESIAN_POINT('Ctrl Pts',(-2.58365280222392,-1.66747045744974,
99.7997187907653));
#23989=CARTESIAN_POINT('Ctrl Pts',(-2.63473962241708,-1.5855092993811,99.7947308920043));
#23990=CARTESIAN_POINT('Ctrl Pts',(-2.68182448644991,-1.50140589910847,
99.7897429932433));
#23991=CARTESIAN_POINT('Ctrl Pts',(-2.72893716415821,-1.41725281780289,
99.7847521480621));
#23992=CARTESIAN_POINT('Ctrl Pts',(-2.77204298251292,-1.33095536708632,
99.7797613028808));
#23993=CARTESIAN_POINT('Ctrl Pts',(-2.8109630298111,-1.24293567614547,99.7747704576996));
#23994=CARTESIAN_POINT('Ctrl Pts',(-2.84994597288857,-1.15477374316127,
99.7697715471865));
#23995=CARTESIAN_POINT('Ctrl Pts',(-2.8847294797668,-1.06488442165541,99.7647726366734));
#23996=CARTESIAN_POINT('Ctrl Pts',(-2.91518379497631,-0.973707189820183,
99.7597737261603));
#23997=CARTESIAN_POINT('Ctrl Pts',(-2.93286433225755,-0.920773395854607,
99.7568715619486));
#23998=CARTESIAN_POINT('Ctrl Pts',(-2.94908666272494,-0.867405765000334,
99.7539693977369));
#23999=CARTESIAN_POINT('Ctrl Pts',(-2.96383331659686,-0.813691785278971,
99.7510672335252));
#24000=CARTESIAN_POINT('Ctrl Pts',(-2.99602294044364,-0.696442623702255,
99.7447322659369));
#24001=CARTESIAN_POINT('Ctrl Pts',(-3.02127028321447,-0.57721156375486,
99.7383972983485));
#24002=CARTESIAN_POINT('Ctrl Pts',(-3.03937583012655,-0.45672400116763,
99.7320623307601));
#24003=CARTESIAN_POINT('Ctrl Pts',(-3.05716351922146,-0.338351697170771,
99.7258385787555));
#24004=CARTESIAN_POINT('Ctrl Pts',(-3.06805797241941,-0.218766467410884,
99.7196148267509));
#24005=CARTESIAN_POINT('Ctrl Pts',(-3.0719155261535,-0.0986775059325435,
99.7133910747463));
#24006=CARTESIAN_POINT('Ctrl Pts',(-3.0729418572233,-0.0667269380851964,
99.7117351989002));
#24007=CARTESIAN_POINT('Ctrl Pts',(-3.07347032466039,-0.0347408385625631,
99.7100793230542));
#24008=CARTESIAN_POINT('Ctrl Pts',(-3.0734987850259,-0.0027328454655318,
99.7084234472081));
#24009=CARTESIAN_POINT('Ctrl Pts',(-3.07349878502643,-0.00273284487125647,
99.7084234471774));
#24010=CARTESIAN_POINT('Ctrl Pts',(-3.07358364945221,0.0927100806662572,
99.7034858794082));
#24011=CARTESIAN_POINT('Ctrl Pts',(-3.06921850417963,0.18825319576249,99.6985483116391));
#24012=CARTESIAN_POINT('Ctrl Pts',(-3.06040211108497,0.283445177180123,
99.6936107438699));
#24013=CARTESIAN_POINT('Ctrl Pts',(-3.05159013460821,0.378589471680395,
99.6886756496009));
#24014=CARTESIAN_POINT('Ctrl Pts',(-3.03833137923279,0.473382536297822,
99.683740555332));
#24015=CARTESIAN_POINT('Ctrl Pts',(-3.02067664917373,0.567375388201277,
99.678805461063));
#24016=CARTESIAN_POINT('Ctrl Pts',(-3.00302571337087,0.661348039684788,
99.673871427417));
#24017=CARTESIAN_POINT('Ctrl Pts',(-2.98098076247416,0.754520379674263,
99.668937393771));
#24018=CARTESIAN_POINT('Ctrl Pts',(-2.95464399798693,0.846452063119824,
99.664003360125));
#24019=CARTESIAN_POINT('Ctrl Pts',(-2.92830536019262,0.938390285571876,
99.6590689755262));
#24020=CARTESIAN_POINT('Ctrl Pts',(-2.89767442726149,1.02908724559419,99.6541345909275));
#24021=CARTESIAN_POINT('Ctrl Pts',(-2.86290337241046,1.11811740449775,99.6492002063287));
#24022=CARTESIAN_POINT('Ctrl Pts',(-2.82809727594385,1.2072372863222,99.6442608489499));
#24023=CARTESIAN_POINT('Ctrl Pts',(-2.78914288936945,1.29468659433648,99.639321491571));
#24024=CARTESIAN_POINT('Ctrl Pts',(-2.74624057952636,1.38005975572174,99.6343821341922));
#24025=CARTESIAN_POINT('Ctrl Pts',(-2.70331618395766,1.46547686644732,99.6294402340764));
#24026=CARTESIAN_POINT('Ctrl Pts',(-2.65644003945883,1.5488153123457,99.6244983339605));
#24027=CARTESIAN_POINT('Ctrl Pts',(-2.60585741201884,1.62969610609661,99.6195564338447));
#24028=CARTESIAN_POINT('Ctrl Pts',(-2.55518929445766,1.71071359715271,99.6146061813821));
#24029=CARTESIAN_POINT('Ctrl Pts',(-2.50080243814957,1.7892647716427,99.6096559289196));
#24030=CARTESIAN_POINT('Ctrl Pts',(-2.44298415873699,1.86500151478763,99.6047056764571));
#24031=CARTESIAN_POINT('Ctrl Pts',(-2.39623608114133,1.9262372897251,99.6007032262184));
#24032=CARTESIAN_POINT('Ctrl Pts',(-2.34724563429205,1.98563375214153,99.5967007759797));
#24033=CARTESIAN_POINT('Ctrl Pts',(-2.29618206789302,2.04302475782515,99.592698325741));
#24034=CARTESIAN_POINT('Ctrl Pts',(-2.23239794323971,2.11471256419374,99.5876988162483));
#24035=CARTESIAN_POINT('Ctrl Pts',(-2.16514138169983,2.18353636970958,99.5826993067556));
#24036=CARTESIAN_POINT('Ctrl Pts',(-2.0946995960865,2.24914113655747,99.5776997972629));
#24037=CARTESIAN_POINT('Ctrl Pts',(-2.02435336430823,2.31465691095556,99.5727070695731));
#24038=CARTESIAN_POINT('Ctrl Pts',(-1.95083081411207,2.37696202841577,99.5677143418832));
#24039=CARTESIAN_POINT('Ctrl Pts',(-1.8744583160611,2.43573567353877,99.5627216141934));
#24040=CARTESIAN_POINT('Ctrl Pts',(-1.79816638907032,2.49444731394778,99.5577341537054));
#24041=CARTESIAN_POINT('Ctrl Pts',(-1.71903083723589,2.54963462202604,99.5527466932175));
#24042=CARTESIAN_POINT('Ctrl Pts',(-1.63741289766001,2.60101542720851,99.5477592327295));
#24043=CARTESIAN_POINT('Ctrl Pts',(-1.55585335762769,2.65235946822385,99.5427753408861));
#24044=CARTESIAN_POINT('Ctrl Pts',(-1.47181533128459,2.69990218762713,99.5377914490427));
#24045=CARTESIAN_POINT('Ctrl Pts',(-1.38569017429653,2.74340390589101,99.5328075571993));
#24046=CARTESIAN_POINT('Ctrl Pts',(-1.29959638195762,2.78688978190649,99.5278254803658));
#24047=CARTESIAN_POINT('Ctrl Pts',(-1.21141736058979,2.8263373830523,99.5228434035324));
#24048=CARTESIAN_POINT('Ctrl Pts',(-1.12156942919324,2.86155277174808,99.517861326699));
#24049=CARTESIAN_POINT('Ctrl Pts',(-1.03172968985804,2.89676494961175,99.5128797041162));
#24050=CARTESIAN_POINT('Ctrl Pts',(-0.940221751787076,2.92774552221313,
99.5078980815334));
#24051=CARTESIAN_POINT('Ctrl Pts',(-0.847481291008796,2.95434894881936,
99.5029164589506));
#24052=CARTESIAN_POINT('Ctrl Pts',(-0.754723968380491,2.98095721239736,
99.497933930621));
#24053=CARTESIAN_POINT('Ctrl Pts',(-0.660734099943554,3.00318662843291,
99.4929514022914));
#24054=CARTESIAN_POINT('Ctrl Pts',(-0.565960830078548,3.02094200355068,
99.4879688739618));
#24055=CARTESIAN_POINT('Ctrl Pts',(-0.471085408596105,3.03871651634608,
99.482980975201));
#24056=CARTESIAN_POINT('Ctrl Pts',(-0.375425332107708,3.05200727986838,
99.4779930764402));
#24057=CARTESIAN_POINT('Ctrl Pts',(-0.279437986122745,3.06077059936083,
99.4730051776794));
#24058=CARTESIAN_POINT('Ctrl Pts',(-0.183393939094897,3.0695390954664,99.4680143324983));
#24059=CARTESIAN_POINT('Ctrl Pts',(-0.0870226759677632,3.07377480306248,
99.4630234873172));
#24060=CARTESIAN_POINT('Ctrl Pts',(0.00921740284671422,3.07348617850882,
99.4580326421362));
#24061=CARTESIAN_POINT('Ctrl Pts',(0.105613008058961,3.0731970875306,99.4530337316233));
#24062=CARTESIAN_POINT('Ctrl Pts',(0.201876567531194,3.06836908705604,99.4480348211103));
#24063=CARTESIAN_POINT('Ctrl Pts',(0.297553848616778,3.05906259451704,99.4430359105974));
#24064=CARTESIAN_POINT('Ctrl Pts',(0.353100188262375,3.05365962330366,99.4401337463839));
#24065=CARTESIAN_POINT('Ctrl Pts',(0.408449077096889,3.04674814463559,99.4372315821705));
#24066=CARTESIAN_POINT('Ctrl Pts',(0.463513494017044,3.03834782256148,99.434329417957));
#24067=CARTESIAN_POINT('Ctrl Pts',(0.558371274461476,3.02387684563053,99.4293299487685));
#24068=CARTESIAN_POINT('Ctrl Pts',(0.652717335024171,3.00493397786565,99.42433047958));
#24069=CARTESIAN_POINT('Ctrl Pts',(0.746097510232636,2.98156682890467,99.4193310103915));
#24070=CARTESIAN_POINT('Ctrl Pts',(0.839355661825531,2.95823021473328,99.4143380742096));
#24071=CARTESIAN_POINT('Ctrl Pts',(0.931650013755398,2.93048091252956,99.4093451380278));
#24072=CARTESIAN_POINT('Ctrl Pts',(1.02253371972923,2.89841802402909,99.404352201846));
#24073=CARTESIAN_POINT('Ctrl Pts',(1.11330987119278,2.86639307971492,99.3993651744549));
#24074=CARTESIAN_POINT('Ctrl Pts',(1.20267828575442,2.8300648489633,99.3943781470639));
#24075=CARTESIAN_POINT('Ctrl Pts',(1.29020571752677,2.78958266707786,99.3893911196728));
#24076=CARTESIAN_POINT('Ctrl Pts',(1.37767342091869,2.74912811007655,99.38440749541));
#24077=CARTESIAN_POINT('Ctrl Pts',(1.46330224105315,2.70452541902491,99.3794238711471));
#24078=CARTESIAN_POINT('Ctrl Pts',(1.54667812735834,2.65597233049429,99.3744402468842));
#24079=CARTESIAN_POINT('Ctrl Pts',(1.63002246332206,2.60743761498003,99.3694585084789));
#24080=CARTESIAN_POINT('Ctrl Pts',(1.71111518098379,2.55495569354762,99.3644767700737));
#24081=CARTESIAN_POINT('Ctrl Pts',(1.78956701695306,2.49877012584866,99.3594950316684));
#24082=CARTESIAN_POINT('Ctrl Pts',(1.81751239887433,2.47875622651269,99.3577204832382));
#24083=CARTESIAN_POINT('Ctrl Pts',(1.84512294216106,2.4582727962739,99.3559459348079));
#24084=CARTESIAN_POINT('Ctrl Pts',(1.87238193903531,2.43733217358127,99.3541713863777));
#24085=CARTESIAN_POINT('',(-3.07349882820719,0.0026838422157513,99.7915765527815));
#24086=CARTESIAN_POINT('Ctrl Pts',(-3.07349882820719,0.00268384221573294,
99.7915765527815));
#24087=CARTESIAN_POINT('Ctrl Pts',(-3.07339561550422,0.120881596078696,
99.7854645576999));
#24088=CARTESIAN_POINT('Ctrl Pts',(-3.06647036213536,0.238780932134677,
99.7793525626182));
#24089=CARTESIAN_POINT('Ctrl Pts',(-3.05284834088149,0.355695456222244,
99.7732405675365));
#24090=CARTESIAN_POINT('Ctrl Pts',(-3.03901199464307,0.474449479977432,
99.7670324080731));
#24091=CARTESIAN_POINT('Ctrl Pts',(-3.01826654307125,0.592187533253163,
99.7608242486097));
#24092=CARTESIAN_POINT('Ctrl Pts',(-2.99079197937576,0.708212952509057,
99.7546160891463));
#24093=CARTESIAN_POINT('Ctrl Pts',(-2.97925928798004,0.756915649635332,
99.7520101592389));
#24094=CARTESIAN_POINT('Ctrl Pts',(-2.96654152276501,0.80531684908909,99.7494042293315));
#24095=CARTESIAN_POINT('Ctrl Pts',(-2.95265448210355,0.853366134384175,
99.7467982994241));
#24096=CARTESIAN_POINT('Ctrl Pts',(-2.92601201892033,0.945549296057218,
99.7417987899312));
#24097=CARTESIAN_POINT('Ctrl Pts',(-2.89500162464424,1.03664549094737,99.7367992804382));
#24098=CARTESIAN_POINT('Ctrl Pts',(-2.85972936878449,1.1262105430653,99.7317997709453));
#24099=CARTESIAN_POINT('Ctrl Pts',(-2.82450495951587,1.2156541007587,99.7268070432552));
#24100=CARTESIAN_POINT('Ctrl Pts',(-2.78503033786379,1.30357023861343,99.7218143155651));
#24101=CARTESIAN_POINT('Ctrl Pts',(-2.7414616596724,1.38952877571724,99.7168215878751));
#24102=CARTESIAN_POINT('Ctrl Pts',(-2.69793894533826,1.47539662873118,99.7118341273869));
#24103=CARTESIAN_POINT('Ctrl Pts',(-2.65033095802679,1.55931059706762,99.7068466668987));
#24104=CARTESIAN_POINT('Ctrl Pts',(-2.59884197479933,1.64086033531837,99.7018592064105));
#24105=CARTESIAN_POINT('Ctrl Pts',(-2.54738983314294,1.72235172282517,99.6968753145668));
#24106=CARTESIAN_POINT('Ctrl Pts',(-2.49206244968104,1.80148187308355,99.6918914227232));
#24107=CARTESIAN_POINT('Ctrl Pts',(-2.43310959700793,1.87786579364658,99.6869075308795));
#24108=CARTESIAN_POINT('Ctrl Pts',(-2.37417821350366,1.95422189707758,99.6819254540459));
#24109=CARTESIAN_POINT('Ctrl Pts',(-2.31162425201878,2.02783341077531,99.6769433772122));
#24110=CARTESIAN_POINT('Ctrl Pts',(-2.24573973087618,2.09834585117997,99.6719613003785));
#24111=CARTESIAN_POINT('Ctrl Pts',(-2.17986121688395,2.16885186247465,99.6669796777955));
#24112=CARTESIAN_POINT('Ctrl Pts',(-2.11065304680986,2.23625904165095,99.6619980552124));
#24113=CARTESIAN_POINT('Ctrl Pts',(-2.03844557093221,2.30024822668052,99.6570164326294));
#24114=CARTESIAN_POINT('Ctrl Pts',(-1.96622496646332,2.36424904607125,99.6520339042996));
#24115=CARTESIAN_POINT('Ctrl Pts',(-1.89100430171671,2.42483034600694,99.6470513759698));
#24116=CARTESIAN_POINT('Ctrl Pts',(-1.81314778667537,2.48171258482408,99.64206884764));
#24117=CARTESIAN_POINT('Ctrl Pts',(-1.73520735378508,2.53865613431153,99.637080948879));
#24118=CARTESIAN_POINT('Ctrl Pts',(-1.65462575371984,2.59189240353175,99.632093050118));
#24119=CARTESIAN_POINT('Ctrl Pts',(-1.57179683613089,2.64118476368635,99.6271051513569));
#24120=CARTESIAN_POINT('Ctrl Pts',(-1.48891899036346,2.69050624151464,99.6221143061757));
#24121=CARTESIAN_POINT('Ctrl Pts',(-1.40379157095317,2.73587896504871,99.6171234609943));
#24122=CARTESIAN_POINT('Ctrl Pts',(-1.3168318284825,2.77711292271226,99.6121326158131));
#24123=CARTESIAN_POINT('Ctrl Pts',(-1.22973155687197,2.8184135154927,99.6071337052999));
#24124=CARTESIAN_POINT('Ctrl Pts',(-1.1407934543542,2.85556181817568,99.6021347947868));
#24125=CARTESIAN_POINT('Ctrl Pts',(-1.05045341429752,2.88841649946657,99.5971358842737));
#24126=CARTESIAN_POINT('Ctrl Pts',(-0.998005659851746,2.9074905917036,99.5942337200625));
#24127=CARTESIAN_POINT('Ctrl Pts',(-0.945085660605878,2.92511845906008,
99.5913315558513));
#24128=CARTESIAN_POINT('Ctrl Pts',(-0.891780412032025,2.94128032440228,
99.5884293916401));
#24129=CARTESIAN_POINT('Ctrl Pts',(-0.799949516312664,2.96912295923802,
99.5834297275138));
#24130=CARTESIAN_POINT('Ctrl Pts',(-0.706652142229662,2.99270974290835,
99.5784300633876));
#24131=CARTESIAN_POINT('Ctrl Pts',(-0.612318651122561,3.01188779994997,
99.5734303992613));
#24132=CARTESIAN_POINT('Ctrl Pts',(-0.518113881799054,3.03103968777342,
99.5684375573746));
#24133=CARTESIAN_POINT('Ctrl Pts',(-0.422876231971961,3.04579471883114,
99.563444715488));
#24134=CARTESIAN_POINT('Ctrl Pts',(-0.327051584553492,3.05604965781662,
99.5584518736014));
#24135=CARTESIAN_POINT('Ctrl Pts',(-0.230216586280553,3.06641272228594,
99.5534063884522));
#24136=CARTESIAN_POINT('Ctrl Pts',(-0.132782570099405,3.0721800947961,99.5483609033031));
#24137=CARTESIAN_POINT('Ctrl Pts',(-0.0352210732845736,3.07329818371024,
99.543315418154));
#24138=CARTESIAN_POINT('Ctrl Pts',(0.0611469184591723,3.07440259463837,
99.5383316562493));
#24139=CARTESIAN_POINT('Ctrl Pts',(0.1576388379333,3.07097083768206,99.5333478943445));
#24140=CARTESIAN_POINT('Ctrl Pts',(0.253795789654246,3.0630034193833,99.5283641324398));
#24141=CARTESIAN_POINT('Ctrl Pts',(0.349916924314426,3.05503896883154,99.5233822269137));
#24142=CARTESIAN_POINT('Ctrl Pts',(0.445702902217803,3.04254225069144,99.5184003213875));
#24143=CARTESIAN_POINT('Ctrl Pts',(0.540697505617908,3.02556580781489,99.5134184158613));
#24144=CARTESIAN_POINT('Ctrl Pts',(0.63568265805823,3.00859105391512,99.5084370059821));
#24145=CARTESIAN_POINT('Ctrl Pts',(0.729876160657855,2.98713753949268,99.5034555961029));
#24146=CARTESIAN_POINT('Ctrl Pts',(0.822830638672055,2.96130916826706,99.4984741862237));
#24147=CARTESIAN_POINT('Ctrl Pts',(0.917864240869227,2.93490309070206,99.4933813565403));
#24148=CARTESIAN_POINT('Ctrl Pts',(1.01160225962071,2.90392420678091,99.4882885268569));
#24149=CARTESIAN_POINT('Ctrl Pts',(1.10358298894315,2.86853740371558,99.4831956971734));
#24150=CARTESIAN_POINT('Ctrl Pts',(1.19365258115027,2.83388585284088,99.4782086841746));
#24151=CARTESIAN_POINT('Ctrl Pts',(1.28203681523046,2.7950080159714,99.4732216711759));
#24152=CARTESIAN_POINT('Ctrl Pts',(1.36832381372345,2.75210686398572,99.4682346581771));
#24153=CARTESIAN_POINT('Ctrl Pts',(1.45735712672751,2.70784026809427,99.4630889201513));
#24154=CARTESIAN_POINT('Ctrl Pts',(1.54415701328919,2.65929019006871,99.4579431821255));
#24155=CARTESIAN_POINT('Ctrl Pts',(1.62830142014859,2.60672912577085,99.4527974440998));
#24156=CARTESIAN_POINT('Ctrl Pts',(1.712445827008,2.554168061473,99.447651706074));
#24157=CARTESIAN_POINT('Ctrl Pts',(1.79393437018822,2.49759634793658,99.4425059680482));
#24158=CARTESIAN_POINT('Ctrl Pts',(1.87238193903529,2.43733217358128,99.4373602300224));
#24159=CARTESIAN_POINT('Ctrl Pts',(1.8723819390353,2.43733217358127,100.43738386173));
#24160=CARTESIAN_POINT('Ctrl Pts',(1.94893925283926,2.37852011126932,100.43239647173));
#24161=CARTESIAN_POINT('Ctrl Pts',(2.02268566713518,2.31612623548597,100.427409081731));
#24162=CARTESIAN_POINT('Ctrl Pts',(2.09328189820265,2.25046065165715,100.422421691731));
#24163=CARTESIAN_POINT('Ctrl Pts',(2.16391581914448,2.18476001032501,100.417431639067));
#24164=CARTESIAN_POINT('Ctrl Pts',(2.23139590007027,2.11578449591865,100.412441586403));
#24165=CARTESIAN_POINT('Ctrl Pts',(2.29542082359019,2.04388000935195,100.407451533738));
#24166=CARTESIAN_POINT('Ctrl Pts',(2.3595536676993,1.97185432038267,100.402453069827));
#24167=CARTESIAN_POINT('Ctrl Pts',(2.42021944330251,1.89689013799153,100.397454605916));
#24168=CARTESIAN_POINT('Ctrl Pts',(2.47715805099304,1.81936534000193,100.392456142005));
#24169=CARTESIAN_POINT('Ctrl Pts',(2.52341480577271,1.756384425726,100.388395404857));
#24170=CARTESIAN_POINT('Ctrl Pts',(2.56721243459908,1.69171419247052,100.384334667709));
#24171=CARTESIAN_POINT('Ctrl Pts',(2.60843375910548,1.62556930776848,100.380273930561));
#24172=CARTESIAN_POINT('Ctrl Pts',(2.65918474240463,1.54413286730871,100.375274421068));
#24173=CARTESIAN_POINT('Ctrl Pts',(2.70620748898614,1.46017440983936,100.370274911575));
#24174=CARTESIAN_POINT('Ctrl Pts',(2.7492425500123,1.37406974029772,100.365275402082));
#24175=CARTESIAN_POINT('Ctrl Pts',(2.79221923425145,1.28808187119356,100.360282674392));
#24176=CARTESIAN_POINT('Ctrl Pts',(2.8312187889334,1.19995396537158,100.355289946702));
#24177=CARTESIAN_POINT('Ctrl Pts',(2.8660256549653,1.11008972388754,100.350297219012));
#24178=CARTESIAN_POINT('Ctrl Pts',(2.90079580063089,1.02032028691314,100.345309758524));
#24179=CARTESIAN_POINT('Ctrl Pts',(2.93138189296096,0.92881856291917,100.340322298035));
#24180=CARTESIAN_POINT('Ctrl Pts',(2.95761529276879,0.836010783411429,100.335334837547));
#24181=CARTESIAN_POINT('Ctrl Pts',(2.98382992196587,0.743269410039213,100.330350945703));
#24182=CARTESIAN_POINT('Ctrl Pts',(3.00569793096851,0.649224260121703,100.32536705386));
#24183=CARTESIAN_POINT('Ctrl Pts',(3.02309994888467,0.554318454548931,100.320383162016));
#24184=CARTESIAN_POINT('Ctrl Pts',(3.0404956294169,0.459447211320003,100.315401085182));
#24185=CARTESIAN_POINT('Ctrl Pts',(3.05342847126171,0.363716366508996,100.310419008349));
#24186=CARTESIAN_POINT('Ctrl Pts',(3.061830034121,0.267580066810998,100.305436931515));
#24187=CARTESIAN_POINT('Ctrl Pts',(3.07023083095134,0.171452532528594,100.300455308932));
#24188=CARTESIAN_POINT('Ctrl Pts',(3.07410113217776,0.0749200541701876,
100.295473686349));
#24189=CARTESIAN_POINT('Ctrl Pts',(3.07342439124172,-0.0215583236932937,
100.290492063766));
#24190=CARTESIAN_POINT('Ctrl Pts',(3.07274752726225,-0.118054243026111,
100.285509535436));
#24191=CARTESIAN_POINT('Ctrl Pts',(3.06752198234294,-0.214495603382103,
100.280527007106));
#24192=CARTESIAN_POINT('Ctrl Pts',(3.057783311344,-0.310424662142246,100.275544478776));
#24193=CARTESIAN_POINT('Ctrl Pts',(3.04803414349302,-0.406457118289549,
100.270556580015));
#24194=CARTESIAN_POINT('Ctrl Pts',(3.03376218247675,-0.501975733011638,
100.265568681254));
#24195=CARTESIAN_POINT('Ctrl Pts',(3.01505471239693,-0.596529405187283,
100.260580782493));
#24196=CARTESIAN_POINT('Ctrl Pts',(2.99633619155775,-0.691138931514897,
100.255589937312));
#24197=CARTESIAN_POINT('Ctrl Pts',(2.97317704991245,-0.784781954398285,
100.25059909213));
#24198=CARTESIAN_POINT('Ctrl Pts',(2.94571488551018,-0.877021130465937,
100.245608246949));
#24199=CARTESIAN_POINT('Ctrl Pts',(2.91820834155675,-0.969409367371377,
100.240609336436));
#24200=CARTESIAN_POINT('Ctrl Pts',(2.88638503449228,-1.06038881339784,100.235610425923));
#24201=CARTESIAN_POINT('Ctrl Pts',(2.85043123004095,-1.14954080084493,100.23061151541));
#24202=CARTESIAN_POINT('Ctrl Pts',(2.82955791289528,-1.20129882024089,100.227709351199));
#24203=CARTESIAN_POINT('Ctrl Pts',(2.8072932968787,-1.2524413162764,100.224807186988));
#24204=CARTESIAN_POINT('Ctrl Pts',(2.78368082639769,-1.302890366357,100.221905022777));
#24205=CARTESIAN_POINT('Ctrl Pts',(2.74300402048885,-1.38979809674736,100.216905513284));
#24206=CARTESIAN_POINT('Ctrl Pts',(2.69818192186844,-1.47495172703947,100.211906003791));
#24207=CARTESIAN_POINT('Ctrl Pts',(2.64938849549389,-1.55792902596511,100.206906494298));
#24208=CARTESIAN_POINT('Ctrl Pts',(2.60066125709239,-1.64079376671167,100.201913766608));
#24209=CARTESIAN_POINT('Ctrl Pts',(2.5479736180061,-1.72148766820019,100.196921038918));
#24210=CARTESIAN_POINT('Ctrl Pts',(2.49154683808155,-1.79961012545658,100.191928311228));
#24211=CARTESIAN_POINT('Ctrl Pts',(2.43517958698741,-1.87765016548986,100.18694085074));
#24212=CARTESIAN_POINT('Ctrl Pts',(2.37508129253556,-1.9531238002365,100.181953390251));
#24213=CARTESIAN_POINT('Ctrl Pts',(2.31151765855626,-2.02565751403898,100.176965929763));
#24214=CARTESIAN_POINT('Ctrl Pts',(2.24799950584286,-2.09813932827378,100.17198203792));
#24215=CARTESIAN_POINT('Ctrl Pts',(2.18102123127155,-2.1676850741982,100.166998146076));
#24216=CARTESIAN_POINT('Ctrl Pts',(2.1108895295578,-2.23395336656861,100.162014254232));
#24217=CARTESIAN_POINT('Ctrl Pts',(2.04078336807288,-2.3001975256682,100.157032177399));
#24218=CARTESIAN_POINT('Ctrl Pts',(1.96752637992255,-2.36316630152999,100.152050100565));
#24219=CARTESIAN_POINT('Ctrl Pts',(1.89146223742386,-2.4225550260829,100.147068023731));
#24220=CARTESIAN_POINT('Ctrl Pts',(1.81540503022257,-2.48193833575235,100.142086401148));
#24221=CARTESIAN_POINT('Ctrl Pts',(1.73654152365057,-2.53774197309553,100.137104778565));
#24222=CARTESIAN_POINT('Ctrl Pts',(1.65524775195289,-2.58970213145352,100.132123155982));
#24223=CARTESIAN_POINT('Ctrl Pts',(1.57393919961505,-2.64167173708388,100.127140627652));
#24224=CARTESIAN_POINT('Ctrl Pts',(1.49019987448773,-2.68979623951408,100.122158099322));
#24225=CARTESIAN_POINT('Ctrl Pts',(1.40443308544748,-2.73385624320308,100.117175570992));
#24226=CARTESIAN_POINT('Ctrl Pts',(1.31857385244889,-2.77796373708253,100.112187672231));
#24227=CARTESIAN_POINT('Ctrl Pts',(1.23068318387448,-2.81799778518139,100.10719977347));
#24228=CARTESIAN_POINT('Ctrl Pts',(1.14118698183003,-2.85378599802117,100.102211874709));
#24229=CARTESIAN_POINT('Ctrl Pts',(1.05163791315072,-2.88959535144945,100.097221029528));
#24230=CARTESIAN_POINT('Ctrl Pts',(0.960481837174163,-2.92115373209521,
100.092230184347));
#24231=CARTESIAN_POINT('Ctrl Pts',(0.86816050961901,-2.9483384438592,100.087239339165));
#24232=CARTESIAN_POINT('Ctrl Pts',(0.775689988467065,-2.97556708680391,
100.082240428652));
#24233=CARTESIAN_POINT('Ctrl Pts',(0.682050881821392,-2.9984078437609,100.077241518139));
#24234=CARTESIAN_POINT('Ctrl Pts',(0.587695777583457,-3.01678900869958,
100.072242607626));
#24235=CARTESIAN_POINT('Ctrl Pts',(0.532917040111328,-3.0274603657686,100.069340443415));
#24236=CARTESIAN_POINT('Ctrl Pts',(0.477897104043139,-3.03662958942373,
100.066438279204));
#24237=CARTESIAN_POINT('Ctrl Pts',(0.422724983624898,-3.04429069541976,
100.063536114993));
#24238=CARTESIAN_POINT('Ctrl Pts',(0.327680899375573,-3.05748835391485,
100.0585366055));
#24239=CARTESIAN_POINT('Ctrl Pts',(0.231851229668309,-3.06625395032696,
100.053537096007));
#24240=CARTESIAN_POINT('Ctrl Pts',(0.135684854326108,-3.07050352064714,
100.048537586514));
#24241=CARTESIAN_POINT('Ctrl Pts',(0.0396489280611693,-3.07474732645219,
100.043544858824));
#24242=CARTESIAN_POINT('Ctrl Pts',(-0.0567223613169125,-3.07448726189378,
100.038552131134));
#24243=CARTESIAN_POINT('Ctrl Pts',(-0.152972524177658,-3.06969080802069,
100.033559403444));
#24244=CARTESIAN_POINT('Ctrl Pts',(-0.249121145542297,-3.06489941428556,
100.028571942955));
#24245=CARTESIAN_POINT('Ctrl Pts',(-0.345148458332253,-3.05558116680173,
100.023584482467));
#24246=CARTESIAN_POINT('Ctrl Pts',(-0.440596497630456,-3.04175557470941,
100.018597021979));
#24247=CARTESIAN_POINT('Ctrl Pts',(-0.535976241625584,-3.02793987515138,
100.013613130135));
#24248=CARTESIAN_POINT('Ctrl Pts',(-0.630777102920117,-3.00962330509827,
100.008629238292));
#24249=CARTESIAN_POINT('Ctrl Pts',(-0.724545749788833,-2.98687724998249,
100.003645346448));
#24250=CARTESIAN_POINT('Ctrl Pts',(-0.818280248438755,-2.96413947841662,
99.9986632696142));
#24251=CARTESIAN_POINT('Ctrl Pts',(-0.91098285339435,-2.93697553023507,
99.9936811927805));
#24252=CARTESIAN_POINT('Ctrl Pts',(-1.00221089849853,-2.90550779811908,
99.9886991159468));
#24253=CARTESIAN_POINT('Ctrl Pts',(-1.09343062570669,-2.87404293513531,
99.9837174933637));
#24254=CARTESIAN_POINT('Ctrl Pts',(-1.1831756454572,-2.83827521170346,99.9787358707807));
#24255=CARTESIAN_POINT('Ctrl Pts',(-1.27101994632812,-2.79837641249995,
99.9737542481976));
#24256=CARTESIAN_POINT('Ctrl Pts',(-1.35888021884078,-2.75847035899171,
99.9687717198678));
#24257=CARTESIAN_POINT('Ctrl Pts',(-1.4448386864932,-2.71443191958095,99.9637891915379));
#24258=CARTESIAN_POINT('Ctrl Pts',(-1.52849173985072,-2.66647993639707,
99.9588066632081));
#24259=CARTESIAN_POINT('Ctrl Pts',(-1.61223495887111,-2.6184762680424,99.953818764447));
#24260=CARTESIAN_POINT('Ctrl Pts',(-1.69366742126704,-2.56655085328486,
99.948830865686));
#24261=CARTESIAN_POINT('Ctrl Pts',(-1.77241264500758,-2.51096707780433,
99.9438429669249));
#24262=CARTESIAN_POINT('Ctrl Pts',(-1.85120438463253,-2.45535046822476,
99.9388521217436));
#24263=CARTESIAN_POINT('Ctrl Pts',(-1.92730537871458,-2.39607146455465,
99.9338612765623));
#24264=CARTESIAN_POINT('Ctrl Pts',(-2.00037219612163,-2.33343380599998,
99.928870431381));
#24265=CARTESIAN_POINT('Ctrl Pts',(-2.07355709135082,-2.27069492340725,
99.9238715208678));
#24266=CARTESIAN_POINT('Ctrl Pts',(-2.14369769986152,-2.20458684894214,
99.9188726103547));
#24267=CARTESIAN_POINT('Ctrl Pts',(-2.21048746299902,-2.13545016938447,
99.9138736998415));
#24268=CARTESIAN_POINT('Ctrl Pts',(-2.24926288410972,-2.09531222401513,
99.9109715356305));
#24269=CARTESIAN_POINT('Ctrl Pts',(-2.28690964825366,-2.05415412424212,
99.9080693714194));
#24270=CARTESIAN_POINT('Ctrl Pts',(-2.32337427194694,-2.01204727639662,
99.9051672072084));
#24271=CARTESIAN_POINT('Ctrl Pts',(-2.38566669364708,-1.94011625786977,
99.900209447644));
#24272=CARTESIAN_POINT('Ctrl Pts',(-2.44473485011727,-1.8651516831922,99.8952516880796));
#24273=CARTESIAN_POINT('Ctrl Pts',(-2.50026567549644,-1.78747693745524,
99.8902939285151));
#24274=CARTESIAN_POINT('Ctrl Pts',(-2.55572621153801,-1.70990051019973,
99.8853424443416));
#24275=CARTESIAN_POINT('Ctrl Pts',(-2.607658049446,-1.62962108272174,99.8803909601681));
#24276=CARTESIAN_POINT('Ctrl Pts',(-2.65578668753765,-1.54699687145701,
99.8754394759946));
#24277=CARTESIAN_POINT('Ctrl Pts',(-2.70386808833047,-1.46445375420853,
99.8704928516041));
#24278=CARTESIAN_POINT('Ctrl Pts',(-2.74815347955921,-1.379570807569,99.8655462272136));
#24279=CARTESIAN_POINT('Ctrl Pts',(-2.78841090588688,-1.29273619502632,
99.8605996028231));
#24280=CARTESIAN_POINT('Ctrl Pts',(-2.82864026125435,-1.20596213108732,
99.855656427647));
#24281=CARTESIAN_POINT('Ctrl Pts',(-2.86484704507828,-1.11723950925545,
99.850713252471));
#24282=CARTESIAN_POINT('Ctrl Pts',(-2.89684519413524,-1.02698109584137,
99.8457700772949));
#24283=CARTESIAN_POINT('Ctrl Pts',(-2.92883661597063,-0.936741658160721,
99.8408279413613));
#24284=CARTESIAN_POINT('Ctrl Pts',(-2.9566210024437,-0.844967487724284,
99.8358858054277));
#24285=CARTESIAN_POINT('Ctrl Pts',(-2.98006075985854,-0.75209049824561,
99.8309436694941));
#24286=CARTESIAN_POINT('Ctrl Pts',(-3.00349711253167,-0.659226999613062,
99.8260022514304));
#24287=CARTESIAN_POINT('Ctrl Pts',(-3.02258998671406,-0.565261435023065,
99.8210608333667));
#24288=CARTESIAN_POINT('Ctrl Pts',(-3.03725230660657,-0.470638583217584,
99.8161194153029));
#24289=CARTESIAN_POINT('Ctrl Pts',(-3.05192271450474,-0.375963535704594,
99.811175271462));
#24290=CARTESIAN_POINT('Ctrl Pts',(-3.06215762251637,-0.280630919460878,
99.8062311276211));
#24291=CARTESIAN_POINT('Ctrl Pts',(-3.0679215976678,-0.185092735036906,
99.8012869837802));
#24292=CARTESIAN_POINT('Ctrl Pts',(-3.07169513153947,-0.122546217140886,
99.798050173461));
#24293=CARTESIAN_POINT('Ctrl Pts',(-3.07355348791211,-0.0599117111426067,
99.7948133631418));
#24294=CARTESIAN_POINT('Ctrl Pts',(-3.07349882820788,0.00268384142361682,
99.7915765528225));
#24295=CARTESIAN_POINT('Origin',(0.,0.,116.208423447177));
#24296=CARTESIAN_POINT('',(1.87238193903531,2.43733217358127,101.437247300765));
#24297=CARTESIAN_POINT('',(1.8723819390353,2.43733217358127,101.354247327612));
#24298=CARTESIAN_POINT('',(1.8723819390353,2.43733217358128,116.208423447177));
#24299=CARTESIAN_POINT('',(-3.0734998880982,0.000829373466577904,100.708423447224));
#24300=CARTESIAN_POINT('Ctrl Pts',(1.8723819390353,2.43733217358127,101.354247327612));
#24301=CARTESIAN_POINT('Ctrl Pts',(1.94878097456855,2.37864170215407,101.349247767036));
#24302=CARTESIAN_POINT('Ctrl Pts',(2.02231682918563,2.31643333910141,101.34424820646));
#24303=CARTESIAN_POINT('Ctrl Pts',(2.09266737696025,2.25103209648514,101.339248645885));
#24304=CARTESIAN_POINT('Ctrl Pts',(2.11373844172856,2.23144342429015,101.337751201045));
#24305=CARTESIAN_POINT('Ctrl Pts',(2.13452402208501,2.21156855431721,101.336253756206));
#24306=CARTESIAN_POINT('Ctrl Pts',(2.15501616577209,2.19141679633541,101.334756311367));
#24307=CARTESIAN_POINT('Ctrl Pts',(2.22343315463915,2.12413625104229,101.329756801874));
#24308=CARTESIAN_POINT('Ctrl Pts',(2.28881650109087,2.05353044898987,101.324757292381));
#24309=CARTESIAN_POINT('Ctrl Pts',(2.35082593556615,1.97990395491033,101.319757782888));
#24310=CARTESIAN_POINT('Ctrl Pts',(2.41275125463732,1.90637733470247,101.314765055198));
#24311=CARTESIAN_POINT('Ctrl Pts',(2.47131147724654,1.82983849895284,101.309772327508));
#24312=CARTESIAN_POINT('Ctrl Pts',(2.52620246685421,1.75062941437065,101.304779599818));
#24313=CARTESIAN_POINT('Ctrl Pts',(2.58103554785143,1.67150389337614,101.29979213933));
#24314=CARTESIAN_POINT('Ctrl Pts',(2.63220684236026,1.58971408254266,101.294804678841));
#24315=CARTESIAN_POINT('Ctrl Pts',(2.67945254972848,1.50563484409519,101.289817218353));
#24316=CARTESIAN_POINT('Ctrl Pts',(2.72666445168872,1.42161576630816,101.28483332651));
#24317=CARTESIAN_POINT('Ctrl Pts',(2.76995613594748,1.33531089903656,101.279849434666));
#24318=CARTESIAN_POINT('Ctrl Pts',(2.80910774232447,1.24712306610563,101.274865542822));
#24319=CARTESIAN_POINT('Ctrl Pts',(2.84824509065609,1.1589673489993,101.269883465989));
#24320=CARTESIAN_POINT('Ctrl Pts',(2.88324517883544,1.06893042949496,101.264901389155));
#24321=CARTESIAN_POINT('Ctrl Pts',(2.91393507687157,0.977437782049311,101.259919312321));
#24322=CARTESIAN_POINT('Ctrl Pts',(2.94462217669606,0.885953476625236,101.254937689738));
#24323=CARTESIAN_POINT('Ctrl Pts',(2.97099972828884,0.793014123380588,101.249956067155));
#24324=CARTESIAN_POINT('Ctrl Pts',(2.99294410379898,0.699062115648467,101.244974444572));
#24325=CARTESIAN_POINT('Ctrl Pts',(3.01489246918324,0.605093025785963,101.239991916242));
#24326=CARTESIAN_POINT('Ctrl Pts',(3.03240595790338,0.510111343237367,101.235009387912));
#24327=CARTESIAN_POINT('Ctrl Pts',(3.0454118986007,0.414570401574087,101.230026859582));
#24328=CARTESIAN_POINT('Ctrl Pts',(3.05843185778529,0.318926480856358,101.225038960821));
#24329=CARTESIAN_POINT('Ctrl Pts',(3.06693451014776,0.222722533263559,101.22005106206));
#24330=CARTESIAN_POINT('Ctrl Pts',(3.07089902991346,0.126417554463543,101.215063163299));
#24331=CARTESIAN_POINT('Ctrl Pts',(3.07486589157541,0.0300556869906981,
101.210072318118));
#24332=CARTESIAN_POINT('Ctrl Pts',(3.07428928547725,-0.0664068917735554,
101.205081472937));
#24333=CARTESIAN_POINT('Ctrl Pts',(3.06920052266676,-0.162512773842821,
101.200090627755));
#24334=CARTESIAN_POINT('Ctrl Pts',(3.06410353628706,-0.258773965444505,
101.195091717242));
#24335=CARTESIAN_POINT('Ctrl Pts',(3.05447987696273,-0.354676872871681,
101.190092806729));
#24336=CARTESIAN_POINT('Ctrl Pts',(3.04041254424233,-0.44977084255639,101.185093896216));
#24337=CARTESIAN_POINT('Ctrl Pts',(3.0322456227786,-0.504978535267258,101.182191732005));
#24338=CARTESIAN_POINT('Ctrl Pts',(3.02258192059223,-0.559913777938571,
101.179289567794));
#24339=CARTESIAN_POINT('Ctrl Pts',(3.01144541790487,-0.614490638642901,
101.176387403583));
#24340=CARTESIAN_POINT('Ctrl Pts',(2.99226075196033,-0.708509278992459,
101.17138789409));
#24341=CARTESIAN_POINT('Ctrl Pts',(2.96863521495117,-0.801793764721477,
101.166388384597));
#24342=CARTESIAN_POINT('Ctrl Pts',(2.94063901313135,-0.893892859603363,
101.161388875104));
#24343=CARTESIAN_POINT('Ctrl Pts',(2.91268078798154,-0.985867022647843,
101.156396147414));
#24344=CARTESIAN_POINT('Ctrl Pts',(2.88036380765222,-1.07665857419504,101.151403419724));
#24345=CARTESIAN_POINT('Ctrl Pts',(2.84380932356711,-1.16582622255324,101.146410692034));
#24346=CARTESIAN_POINT('Ctrl Pts',(2.8072934035413,-1.25489980129004,101.141423231546));
#24347=CARTESIAN_POINT('Ctrl Pts',(2.76654903238328,-1.34235247853228,101.136435771057));
#24348=CARTESIAN_POINT('Ctrl Pts',(2.72174701495846,-1.42775888600447,101.131448310569));
#24349=CARTESIAN_POINT('Ctrl Pts',(2.67697705442436,-1.51310418319572,101.126464418726));
#24350=CARTESIAN_POINT('Ctrl Pts',(2.62815542265787,-1.5964057336758,101.121480526882));
#24351=CARTESIAN_POINT('Ctrl Pts',(2.57550030195752,-1.6772598023612,101.116496635038));
#24352=CARTESIAN_POINT('Ctrl Pts',(2.522864356948,-1.75808442599732,101.111514558204));
#24353=CARTESIAN_POINT('Ctrl Pts',(2.46639793613185,-1.83646297131814,101.106532481371));
#24354=CARTESIAN_POINT('Ctrl Pts',(2.40636377219734,-1.91201873574925,101.101550404537));
#24355=CARTESIAN_POINT('Ctrl Pts',(2.34633508199547,-1.98756761123537,101.096568781954));
#24356=CARTESIAN_POINT('Ctrl Pts',(2.282739568645,-2.0602938739694,101.091587159371));
#24357=CARTESIAN_POINT('Ctrl Pts',(2.21588099888434,-2.12985296412296,101.086605536788));
#24358=CARTESIAN_POINT('Ctrl Pts',(2.14901027305768,-2.19942470134469,101.081623008458));
#24359=CARTESIAN_POINT('Ctrl Pts',(2.0788756167751,-2.26582780590346,101.076640480128));
#24360=CARTESIAN_POINT('Ctrl Pts',(2.00581771670423,-2.32875450345361,101.071657951798));
#24361=CARTESIAN_POINT('Ctrl Pts',(1.93268107098425,-2.39174902670966,101.066670053037));
#24362=CARTESIAN_POINT('Ctrl Pts',(1.85661522429097,-2.45125937535987,101.061682154276));
#24363=CARTESIAN_POINT('Ctrl Pts',(1.777993840024,-2.50701817999725,101.056694255515));
#24364=CARTESIAN_POINT('Ctrl Pts',(1.69932601302621,-2.56280992212586,101.051703410334));
#24365=CARTESIAN_POINT('Ctrl Pts',(1.61810001205964,-2.61484547096914,101.046712565153));
#24366=CARTESIAN_POINT('Ctrl Pts',(1.5347165547633,-2.66290205350018,101.041721719971));
#24367=CARTESIAN_POINT('Ctrl Pts',(1.45119834769425,-2.71103629668218,101.036722809458));
#24368=CARTESIAN_POINT('Ctrl Pts',(1.36551611247566,-2.75517853314257,101.031723898945));
#24369=CARTESIAN_POINT('Ctrl Pts',(1.27809304307741,-2.7951530232238,101.026724988432));
#24370=CARTESIAN_POINT('Ctrl Pts',(1.22733876320914,-2.81836058698402,101.023822824221));
#24371=CARTESIAN_POINT('Ctrl Pts',(1.17599808773117,-2.84016432677214,101.02092066001));
#24372=CARTESIAN_POINT('Ctrl Pts',(1.1241561517504,-2.86053757124106,101.018018495799));
#24373=CARTESIAN_POINT('Ctrl Pts',(1.0348489202403,-2.89563421695802,101.013018986306));
#24374=CARTESIAN_POINT('Ctrl Pts',(0.943739652778536,-2.92660618265729,
101.008019476813));
#24375=CARTESIAN_POINT('Ctrl Pts',(0.851245066735334,-2.95326668053509,
101.00301996732));
#24376=CARTESIAN_POINT('Ctrl Pts',(0.758875949010772,-2.97989101361682,
100.99802723963));
#24377=CARTESIAN_POINT('Ctrl Pts',(0.665125665624834,-3.00221538180517,
100.99303451194));
#24378=CARTESIAN_POINT('Ctrl Pts',(0.570430384170966,-3.02010122790852,
100.98804178425));
#24379=CARTESIAN_POINT('Ctrl Pts',(0.475835003852092,-3.03796820489507,
100.983054323761));
#24380=CARTESIAN_POINT('Ctrl Pts',(0.380297036382195,-3.05140588734464,
100.978066863273));
#24381=CARTESIAN_POINT('Ctrl Pts',(0.284266272364707,-3.06032595263901,
100.973079402785));
#24382=CARTESIAN_POINT('Ctrl Pts',(0.188304220603611,-3.06923963541815,
100.968095510941));
#24383=CARTESIAN_POINT('Ctrl Pts',(0.0918505090894153,-3.07364208653821,
100.963111619098));
#24384=CARTESIAN_POINT('Ctrl Pts',(-0.00463742261154345,-3.07349650143148,
100.958127727254));
#24385=CARTESIAN_POINT('Ctrl Pts',(-0.101090215797521,-3.07335096934323,
100.95314565042));
#24386=CARTESIAN_POINT('Ctrl Pts',(-0.197576765896115,-3.06866069254261,
100.948163573586));
#24387=CARTESIAN_POINT('Ctrl Pts',(-0.293638052471836,-3.05944095287694,
100.943181496753));
#24388=CARTESIAN_POINT('Ctrl Pts',(-0.389690580471286,-3.05022205383911,
100.93819987417));
#24389=CARTESIAN_POINT('Ctrl Pts',(-0.485317485101434,-3.03647455514257,
100.933218251587));
#24390=CARTESIAN_POINT('Ctrl Pts',(-0.580064365961525,-3.01826565784751,
100.928236629004));
#24391=CARTESIAN_POINT('Ctrl Pts',(-0.674828473473925,-3.0000534498541,
100.923254100674));
#24392=CARTESIAN_POINT('Ctrl Pts',(-0.768711808385901,-2.97737831517518,
100.918271572344));
#24393=CARTESIAN_POINT('Ctrl Pts',(-0.861270724562729,-2.95035845093629,
100.913289044014));
#24394=CARTESIAN_POINT('Ctrl Pts',(-0.953929405610073,-2.92330946326588,
100.908301145253));
#24395=CARTESIAN_POINT('Ctrl Pts',(-1.04526039592031,-2.89190652011422,
100.903313246492));
#24396=CARTESIAN_POINT('Ctrl Pts',(-1.13483598647635,-2.85631747776718,
100.898325347731));
#24397=CARTESIAN_POINT('Ctrl Pts',(-1.22446449056317,-2.82070741248435,
100.89333450255));
#24398=CARTESIAN_POINT('Ctrl Pts',(-1.31233513051131,-2.78090650531461,
100.888343657368));
#24399=CARTESIAN_POINT('Ctrl Pts',(-1.39804287468036,-2.73712958599981,
100.883352812187));
#24400=CARTESIAN_POINT('Ctrl Pts',(-1.48388912472846,-2.69328192207785,
100.878353901674));
#24401=CARTESIAN_POINT('Ctrl Pts',(-1.56756511884022,-2.64544563374788,
100.873354991161));
#24402=CARTESIAN_POINT('Ctrl Pts',(-1.64869303932916,-2.59388001111608,
100.868356080647));
#24403=CARTESIAN_POINT('Ctrl Pts',(-1.69579261167301,-2.56394310703961,
100.865453916436));
#24404=CARTESIAN_POINT('Ctrl Pts',(-1.74203393130438,-2.53275002469661,
100.862551752225));
#24405=CARTESIAN_POINT('Ctrl Pts',(-1.78734827456124,-2.50035765350139,
100.859649588015));
#24406=CARTESIAN_POINT('Ctrl Pts',(-1.86486694926472,-2.44494443320328,
100.854684892352));
#24407=CARTESIAN_POINT('Ctrl Pts',(-1.93995177014106,-2.38581864905339,
100.84972019669));
#24408=CARTESIAN_POINT('Ctrl Pts',(-2.012222153803,-2.32322281620692,100.844755501028));
#24409=CARTESIAN_POINT('Ctrl Pts',(-2.0843942196799,-2.26071213973193,100.839797559417));
#24410=CARTESIAN_POINT('Ctrl Pts',(-2.1537591213382,-2.19474108272794,100.834839617806));
#24411=CARTESIAN_POINT('Ctrl Pts',(-2.21996586383073,-2.12559493164297,
100.829881676195));
#24412=CARTESIAN_POINT('Ctrl Pts',(-2.28754560356957,-2.05501482577546,
100.824820916654));
#24413=CARTESIAN_POINT('Ctrl Pts',(-2.35183433745526,-1.98112672110582,
100.819760157114));
#24414=CARTESIAN_POINT('Ctrl Pts',(-2.41249487126628,-1.90427696150374,
100.814699397573));
#24415=CARTESIAN_POINT('Ctrl Pts',(-2.47181879393756,-1.82912053096285,
100.809750148222));
#24416=CARTESIAN_POINT('Ctrl Pts',(-2.52767247112215,-1.75113198889134,
100.80480089887));
#24417=CARTESIAN_POINT('Ctrl Pts',(-2.57977928200124,-1.67067085512293,
100.799851649518));
#24418=CARTESIAN_POINT('Ctrl Pts',(-2.63186879451738,-1.59023643275504,
100.794904043213));
#24419=CARTESIAN_POINT('Ctrl Pts',(-2.68021366949828,-1.50733142313592,
100.789956436908));
#24420=CARTESIAN_POINT('Ctrl Pts',(-2.72458015982701,-1.42234496613058,
100.785008830603));
#24421=CARTESIAN_POINT('Ctrl Pts',(-2.76894446929391,-1.33736268668626,
100.7800614675));
#24422=CARTESIAN_POINT('Ctrl Pts',(-2.80933057728387,-1.25029955885745,
100.775114104398));
#24423=CARTESIAN_POINT('Ctrl Pts',(-2.84555087825066,-1.1615689601943,100.770166741295));
#24424=CARTESIAN_POINT('Ctrl Pts',(-2.88322011483119,-1.06928883485691,
100.765021466789));
#24425=CARTESIAN_POINT('Ctrl Pts',(-2.91638305279106,-0.975205509234439,
100.759876192283));
#24426=CARTESIAN_POINT('Ctrl Pts',(-2.94488468889632,-0.879804761923921,
100.754730917777));
#24427=CARTESIAN_POINT('Ctrl Pts',(-2.97232631723532,-0.787952075246951,
100.749777001793));
#24428=CARTESIAN_POINT('Ctrl Pts',(-2.99544715264274,-0.69487867798545,
100.744823085808));
#24429=CARTESIAN_POINT('Ctrl Pts',(-3.01416077415875,-0.601030013828543,
100.739869169823));
#24430=CARTESIAN_POINT('Ctrl Pts',(-3.03288686416883,-0.507118820272323,
100.734911953148));
#24431=CARTESIAN_POINT('Ctrl Pts',(-3.04719983161355,-0.412431771858417,
100.729954736472));
#24432=CARTESIAN_POINT('Ctrl Pts',(-3.05706504618843,-0.317420152751691,
100.724997519797));
#24433=CARTESIAN_POINT('Ctrl Pts',(-3.06694455849489,-0.222270832572669,
100.72003311859));
#24434=CARTESIAN_POINT('Ctrl Pts',(-3.07236343782549,-0.126796446613842,
100.715068717382));
#24435=CARTESIAN_POINT('Ctrl Pts',(-3.0733391029767,-0.0314484993980698,
100.710104316174));
#24436=CARTESIAN_POINT('Ctrl Pts',(-3.07344921798623,-0.0206873892944004,
100.709544026524));
#24437=CARTESIAN_POINT('Ctrl Pts',(-3.07350279090739,-0.00992788374707534,
100.708983736874));
#24438=CARTESIAN_POINT('Ctrl Pts',(-3.0734998880982,0.000829373466577527,
100.708423447224));
#24439=CARTESIAN_POINT('Ctrl Pts',(-3.07349988809796,0.000829374362847938,
100.708423447177));
#24440=CARTESIAN_POINT('Ctrl Pts',(-3.07348755274493,0.0465417906926426,
100.706042524862));
#24441=CARTESIAN_POINT('Ctrl Pts',(-3.07245544142314,0.0922390841767112,
100.703661602546));
#24442=CARTESIAN_POINT('Ctrl Pts',(-3.07040526815993,0.137890316033153,
100.701280680231));
#24443=CARTESIAN_POINT('Ctrl Pts',(-3.06610027230853,0.233749708641906,
100.696281170738));
#24444=CARTESIAN_POINT('Ctrl Pts',(-3.0572942542034,0.329575672356581,100.691281661245));
#24445=CARTESIAN_POINT('Ctrl Pts',(-3.04398627306699,0.424911543006023,
100.686282151752));
#24446=CARTESIAN_POINT('Ctrl Pts',(-3.0306963441225,0.520118091152141,100.681289424061));
#24447=CARTESIAN_POINT('Ctrl Pts',(-3.01291664934247,0.614835436466869,
100.676296696371));
#24448=CARTESIAN_POINT('Ctrl Pts',(-2.99069821909291,0.708608786506702,
100.671303968681));
#24449=CARTESIAN_POINT('Ctrl Pts',(-2.96850322872718,0.802283208026099,
100.666316508193));
#24450=CARTESIAN_POINT('Ctrl Pts',(-2.94187891259058,0.895015189177,100.661329047705));
#24451=CARTESIAN_POINT('Ctrl Pts',(-2.91092773001718,0.986357947510458,
100.656341587216));
#24452=CARTESIAN_POINT('Ctrl Pts',(-2.87999869373841,1.07763534796513,100.651357695373));
#24453=CARTESIAN_POINT('Ctrl Pts',(-2.84474908614237,1.16752508711852,100.646373803529));
#24454=CARTESIAN_POINT('Ctrl Pts',(-2.80533153550899,1.25559437155427,100.641389911685));
#24455=CARTESIAN_POINT('Ctrl Pts',(-2.76592833977128,1.34363158333789,100.636407834852));
#24456=CARTESIAN_POINT('Ctrl Pts',(-2.72236039596523,1.42984925738979,100.631425758018));
#24457=CARTESIAN_POINT('Ctrl Pts',(-2.67482854984605,1.51383436310861,100.626443681184));
#24458=CARTESIAN_POINT('Ctrl Pts',(-2.62730103753619,1.59781181132066,100.621462058601));
#24459=CARTESIAN_POINT('Ctrl Pts',(-2.57581055784407,1.67955671397915,100.616480436018));
#24460=CARTESIAN_POINT('Ctrl Pts',(-2.52060349661687,1.75868139890169,100.611498813435));
#24461=CARTESIAN_POINT('Ctrl Pts',(-2.46538639777322,1.83782047008608,100.606516285105));
#24462=CARTESIAN_POINT('Ctrl Pts',(-2.40645162657808,1.91433801742719,100.601533756775));
#24463=CARTESIAN_POINT('Ctrl Pts',(-2.34408776827968,1.98787695408986,100.596551228446));
#24464=CARTESIAN_POINT('Ctrl Pts',(-2.28165669093311,2.06149515488822,100.591563329684));
#24465=CARTESIAN_POINT('Ctrl Pts',(-2.21578943204242,2.13212800019319,100.586575430923));
#24466=CARTESIAN_POINT('Ctrl Pts',(-2.14681344500452,2.19945317803035,100.581587532162));
#24467=CARTESIAN_POINT('Ctrl Pts',(-2.07779671290436,2.26681812577413,100.576596686981));
#24468=CARTESIAN_POINT('Ctrl Pts',(-2.00566792421729,2.33087122420806,100.5716058418));
#24469=CARTESIAN_POINT('Ctrl Pts',(-1.93078820320179,2.39132999905425,100.566614996618));
#24470=CARTESIAN_POINT('Ctrl Pts',(-1.85578747466614,2.4518864768074,100.561616086105));
#24471=CARTESIAN_POINT('Ctrl Pts',(-1.77802729087215,2.50883677345381,100.556617175592));
#24472=CARTESIAN_POINT('Ctrl Pts',(-1.69789830452878,2.56194137276369,100.551618265079));
#24473=CARTESIAN_POINT('Ctrl Pts',(-1.65137867273835,2.59277174413127,100.548716100868));
#24474=CARTESIAN_POINT('Ctrl Pts',(-1.60406112681858,2.62230677207033,100.545813936657));
#24475=CARTESIAN_POINT('Ctrl Pts',(-1.55602560798124,2.65050684913407,100.542911772446));
#24476=CARTESIAN_POINT('Ctrl Pts',(-1.47327562728728,2.69908664777214,100.537912262953));
#24477=CARTESIAN_POINT('Ctrl Pts',(-1.38810309789947,2.7438728232548,100.53291275346));
#24478=CARTESIAN_POINT('Ctrl Pts',(-1.30089055399368,2.78461595494424,100.527913243967));
#24479=CARTESIAN_POINT('Ctrl Pts',(-1.21379631335,2.82530381883421,100.522920516277));
#24480=CARTESIAN_POINT('Ctrl Pts',(-1.12466795224931,2.86195935453384,100.517927788587));
#24481=CARTESIAN_POINT('Ctrl Pts',(-1.03391473064704,2.89437775346465,100.512935060897));
#24482=CARTESIAN_POINT('Ctrl Pts',(-0.94325725140587,2.92676195180178,100.507947600409));
#24483=CARTESIAN_POINT('Ctrl Pts',(-0.850978730544745,2.95491775272394,
100.50296013992));
#24484=CARTESIAN_POINT('Ctrl Pts',(-0.757509709879373,2.97868784692832,
100.497972679432));
#24485=CARTESIAN_POINT('Ctrl Pts',(-0.664107568483129,3.00244093307467,
100.492988787589));
#24486=CARTESIAN_POINT('Ctrl Pts',(-0.569517044882587,3.02181444297084,
100.488004895745));
#24487=CARTESIAN_POINT('Ctrl Pts',(-0.47418426156171,3.03670076498939,100.483021003901));
#24488=CARTESIAN_POINT('Ctrl Pts',(-0.378886196079398,3.05158166577816,
100.478038927068));
#24489=CARTESIAN_POINT('Ctrl Pts',(-0.282846841221909,3.0619785578591,100.473056850234));
#24490=CARTESIAN_POINT('Ctrl Pts',(-0.186521994656168,3.06783503394649,
100.4680747734));
#24491=CARTESIAN_POINT('Ctrl Pts',(-0.0902059306972084,3.0736909760582,
100.463093150817));
#24492=CARTESIAN_POINT('Ctrl Pts',(0.00639513505272708,3.07500729879151,
100.458111528234));
#24493=CARTESIAN_POINT('Ctrl Pts',(0.102821880998748,3.07177959996935,100.453129905651));
#24494=CARTESIAN_POINT('Ctrl Pts',(0.199266159026103,3.06855131429468,100.448147377321));
#24495=CARTESIAN_POINT('Ctrl Pts',(0.29553561559349,3.06077738098397,100.443164848991));
#24496=CARTESIAN_POINT('Ctrl Pts',(0.391173608329545,3.04850544663224,100.438182320662));
#24497=CARTESIAN_POINT('Ctrl Pts',(0.486914684726831,3.0362202849439,100.4331944219));
#24498=CARTESIAN_POINT('Ctrl Pts',(0.582022502373442,3.01942749922723,100.428206523139));
#24499=CARTESIAN_POINT('Ctrl Pts',(0.676048425958704,2.99822627160773,100.423218624378));
#24500=CARTESIAN_POINT('Ctrl Pts',(0.770129891947641,2.97701252013206,100.418227779197));
#24501=CARTESIAN_POINT('Ctrl Pts',(0.863127768352573,2.95138525807356,100.413236934016));
#24502=CARTESIAN_POINT('Ctrl Pts',(0.954608503262189,2.92149360011271,100.408246088834));
#24503=CARTESIAN_POINT('Ctrl Pts',(1.04623707334957,2.89155363647774,100.403247178321));
#24504=CARTESIAN_POINT('Ctrl Pts',(1.13634319626868,2.85733567212782,100.398248267808));
#24505=CARTESIAN_POINT('Ctrl Pts',(1.22451327617656,2.81903697855622,100.393249357295));
#24506=CARTESIAN_POINT('Ctrl Pts',(1.27570123997732,2.79680231411894,100.390347193084));
#24507=CARTESIAN_POINT('Ctrl Pts',(1.32623710529685,2.77319311371393,100.387445028873));
#24508=CARTESIAN_POINT('Ctrl Pts',(1.37604412559679,2.74825486707666,100.384542864662));
#24509=CARTESIAN_POINT('Ctrl Pts',(1.46319056629028,2.70462086892769,100.379465000542));
#24510=CARTESIAN_POINT('Ctrl Pts',(1.54841499802168,2.65675983856468,100.374387136422));
#24511=CARTESIAN_POINT('Ctrl Pts',(1.63128015375264,2.60486608292495,100.369309272302));
#24512=CARTESIAN_POINT('Ctrl Pts',(1.71414530948361,2.55297232728521,100.364231408183));
#24513=CARTESIAN_POINT('Ctrl Pts',(1.7946507457641,2.4970460213523,100.359153544063));
#24514=CARTESIAN_POINT('Ctrl Pts',(1.87238193903531,2.43733217358127,100.354075679943));
#24515=CARTESIAN_POINT('',(-3.0734996196979,-0.00152895940825499,100.791576552855));
#24516=CARTESIAN_POINT('Ctrl Pts',(-3.07349961969821,-0.00152895878437358,
100.791576552823));
#24517=CARTESIAN_POINT('Ctrl Pts',(-3.07354837615827,0.0964808522008683,
100.786524377151));
#24518=CARTESIAN_POINT('Ctrl Pts',(-3.06890468339488,0.19448503801226,100.781472201478));
#24519=CARTESIAN_POINT('Ctrl Pts',(-3.05959658800328,0.292011932425183,
100.776420025806));
#24520=CARTESIAN_POINT('Ctrl Pts',(-3.05028541410575,0.389571082322173,
100.771366179206));
#24521=CARTESIAN_POINT('Ctrl Pts',(-3.03630680849132,0.486652207185376,
100.766312332606));
#24522=CARTESIAN_POINT('Ctrl Pts',(-3.01774058051128,0.582789875285645,
100.761258486006));
#24523=CARTESIAN_POINT('Ctrl Pts',(-2.99916372480891,0.678982574727879,
100.756201746471));
#24524=CARTESIAN_POINT('Ctrl Pts',(-2.97599410203961,0.774230329524674,
100.751145006937));
#24525=CARTESIAN_POINT('Ctrl Pts',(-2.94836220263535,0.868079818951714,
100.746088267403));
#24526=CARTESIAN_POINT('Ctrl Pts',(-2.92068929198974,0.962068599710314,
100.74102402266));
#24527=CARTESIAN_POINT('Ctrl Pts',(-2.88854100335846,1.0546545678525,100.735959777917));
#24528=CARTESIAN_POINT('Ctrl Pts',(-2.85209712144358,1.14540135317419,100.730895533175));
#24529=CARTESIAN_POINT('Ctrl Pts',(-2.81562133876217,1.23622757273446,100.725826855499));
#24530=CARTESIAN_POINT('Ctrl Pts',(-2.77484264850276,1.32521102066264,100.720758177823));
#24531=CARTESIAN_POINT('Ctrl Pts',(-2.72998732910008,1.41193889136642,100.715689500148));
#24532=CARTESIAN_POINT('Ctrl Pts',(-2.68505404545288,1.49881750612927,100.710612012466));
#24533=CARTESIAN_POINT('Ctrl Pts',(-2.63603019868476,1.58343235411485,100.705534524784));
#24534=CARTESIAN_POINT('Ctrl Pts',(-2.58318596836571,1.66539860178833,100.700457037103));
#24535=CARTESIAN_POINT('Ctrl Pts',(-2.57123361704824,1.68393779485544,100.699308606778));
#24536=CARTESIAN_POINT('Ctrl Pts',(-2.5590859869867,1.70234162478948,100.698160176454));
#24537=CARTESIAN_POINT('Ctrl Pts',(-2.54674648514763,1.72060587886598,100.697011746129));
#24538=CARTESIAN_POINT('Ctrl Pts',(-2.49302841861834,1.80011641570814,100.692012236636));
#24539=CARTESIAN_POINT('Ctrl Pts',(-2.43548890078887,1.87724854367466,100.687012727143));
#24540=CARTESIAN_POINT('Ctrl Pts',(-2.37436554489057,1.9516122845577,100.68201321765));
#24541=CARTESIAN_POINT('Ctrl Pts',(-2.31332510243647,2.02587515149837,100.67702048996));
#24542=CARTESIAN_POINT('Ctrl Pts',(-2.24871076007897,2.09737675855472,100.67202776227));
#24543=CARTESIAN_POINT('Ctrl Pts',(-2.18080347983684,2.16575585704657,100.66703503458));
#24544=CARTESIAN_POINT('Ctrl Pts',(-2.11296784006364,2.23406281731314,100.662047574092));
#24545=CARTESIAN_POINT('Ctrl Pts',(-2.04184647611333,2.29925350781209,100.657060113603));
#24546=CARTESIAN_POINT('Ctrl Pts',(-1.96776003170119,2.36100036163473,100.652072653115));
#24547=CARTESIAN_POINT('Ctrl Pts',(-1.89372659787175,2.42270303414017,100.647088761271));
#24548=CARTESIAN_POINT('Ctrl Pts',(-1.81673263742507,2.48096648834149,100.642104869428));
#24549=CARTESIAN_POINT('Ctrl Pts',(-1.73713427956381,2.53550128076566,100.637120977584));
#24550=CARTESIAN_POINT('Ctrl Pts',(-1.65756490945309,2.59001621296908,100.63213890075));
#24551=CARTESIAN_POINT('Ctrl Pts',(-1.57539338816331,2.64080493352111,100.627156823917));
#24552=CARTESIAN_POINT('Ctrl Pts',(-1.49100665160184,2.68762002799486,100.622174747083));
#24553=CARTESIAN_POINT('Ctrl Pts',(-1.40662760916653,2.73443085401058,100.6171931245));
#24554=CARTESIAN_POINT('Ctrl Pts',(-1.32003413696557,2.77726856148609,100.612211501917));
#24555=CARTESIAN_POINT('Ctrl Pts',(-1.23163877272392,2.8159311396984,100.607229879334));
#24556=CARTESIAN_POINT('Ctrl Pts',(-1.14322733664759,2.85460074744863,100.602247351004));
#24557=CARTESIAN_POINT('Ctrl Pts',(-1.05301376007122,2.8890935424676,100.597264822674));
#24558=CARTESIAN_POINT('Ctrl Pts',(-0.961430604396251,2.91925563165172,
100.592282294344));
#24559=CARTESIAN_POINT('Ctrl Pts',(-0.869748735576916,2.9494502311227,100.587294395583));
#24560=CARTESIAN_POINT('Ctrl Pts',(-0.776694758177426,2.97530466826145,
100.582306496822));
#24561=CARTESIAN_POINT('Ctrl Pts',(-0.682716228799109,2.99671500161999,
100.577318598061));
#24562=CARTESIAN_POINT('Ctrl Pts',(-0.588682185013639,3.01813798235631,
100.57232775288));
#24563=CARTESIAN_POINT('Ctrl Pts',(-0.493722933696055,3.03511155492146,
100.567336907699));
#24564=CARTESIAN_POINT('Ctrl Pts',(-0.398293950692616,3.04758333419148,
100.562346062517));
#24565=CARTESIAN_POINT('Ctrl Pts',(-0.302710752042614,3.06007526817177,
100.557347152004));
#24566=CARTESIAN_POINT('Ctrl Pts',(-0.206656743117444,3.0680508459679,100.552348241491));
#24567=CARTESIAN_POINT('Ctrl Pts',(-0.110590156886658,3.0715097374418,100.547349330978));
#24568=CARTESIAN_POINT('Ctrl Pts',(-0.0548178025511639,3.07351782920876,
100.544447166767));
#24569=CARTESIAN_POINT('Ctrl Pts',(0.000958815562382781,3.07400455206058,
100.541545002556));
#24570=CARTESIAN_POINT('Ctrl Pts',(0.0566508376247306,3.07297786073971,
100.538642838345));
#24571=CARTESIAN_POINT('Ctrl Pts',(0.152574884939159,3.07120948560817,100.533644145053));
#24572=CARTESIAN_POINT('Ctrl Pts',(0.248584508306219,3.06494224889118,100.528645451761));
#24573=CARTESIAN_POINT('Ctrl Pts',(0.344223451978229,3.05416313662322,100.52364675847));
#24574=CARTESIAN_POINT('Ctrl Pts',(0.439740601233117,3.04339775135438,100.518654430921));
#24575=CARTESIAN_POINT('Ctrl Pts',(0.534887576440721,3.02813195419978,100.513662103372));
#24576=CARTESIAN_POINT('Ctrl Pts',(0.629208503991605,3.00840471155472,100.508669775823));
#24577=CARTESIAN_POINT('Ctrl Pts',(0.723435077350063,2.98869720310966,100.503682442363));
#24578=CARTESIAN_POINT('Ctrl Pts',(0.816836817974346,2.96453720784374,100.498695108902));
#24579=CARTESIAN_POINT('Ctrl Pts',(0.908964422445171,2.93601531479809,100.493707775442));
#24580=CARTESIAN_POINT('Ctrl Pts',(1.00102824561016,2.90751316788166,100.488723894786));
#24581=CARTESIAN_POINT('Ctrl Pts',(1.09181926773591,2.87465525458155,100.48374001413));
#24582=CARTESIAN_POINT('Ctrl Pts',(1.18090080967825,2.83758269090105,100.478756133474));
#24583=CARTESIAN_POINT('Ctrl Pts',(1.2699445459253,2.80052586060388,100.473774367949));
#24584=CARTESIAN_POINT('Ctrl Pts',(1.35727984015054,2.75925810589058,100.468792602424));
#24585=CARTESIAN_POINT('Ctrl Pts',(1.4424885671648,2.71396923040753,100.463810836898));
#24586=CARTESIAN_POINT('Ctrl Pts',(1.52770834936352,2.66867447903724,100.458828425027));
#24587=CARTESIAN_POINT('Ctrl Pts',(1.61080062163714,2.61935776367916,100.453846013155));
#24588=CARTESIAN_POINT('Ctrl Pts',(1.6913711379829,2.56625523352577,100.448863601284));
#24589=CARTESIAN_POINT('Ctrl Pts',(1.75325071004712,2.52547155743119,100.445037021432));
#24590=CARTESIAN_POINT('Ctrl Pts',(1.81364326519963,2.48245578586724,100.441210441581));
#24591=CARTESIAN_POINT('Ctrl Pts',(1.8723819390353,2.43733217358127,100.43738386173));
#24592=CARTESIAN_POINT('Ctrl Pts',(1.8723819390353,2.43733217358127,101.437247300765));
#24593=CARTESIAN_POINT('Ctrl Pts',(1.94884000716434,2.37859635274812,101.432264386686));
#24594=CARTESIAN_POINT('Ctrl Pts',(2.02257777502802,2.31622396885693,101.427281472606));
#24595=CARTESIAN_POINT('Ctrl Pts',(2.09323711758791,2.2505023038318,101.422298558526));
#24596=CARTESIAN_POINT('Ctrl Pts',(2.16387933174016,2.18479657028054,101.417316852346));
#24597=CARTESIAN_POINT('Ctrl Pts',(2.23144428227298,2.11574346786595,101.412335146166));
#24598=CARTESIAN_POINT('Ctrl Pts',(2.29560854168267,2.04366916925259,101.407353439986));
#24599=CARTESIAN_POINT('Ctrl Pts',(2.35977476377393,1.97159266600227,101.402371581424));
#24600=CARTESIAN_POINT('Ctrl Pts',(2.42053979676236,1.8964951113874,101.397389722861));
#24601=CARTESIAN_POINT('Ctrl Pts',(2.47761928898509,1.8187371742088,101.392407864299));
#24602=CARTESIAN_POINT('Ctrl Pts',(2.53674029629675,1.73819813306707,101.387247823712));
#24603=CARTESIAN_POINT('Ctrl Pts',(2.59190685923281,1.65480522729768,101.382087783126));
#24604=CARTESIAN_POINT('Ctrl Pts',(2.64285179868346,1.5689922307633,101.37692774254));
#24605=CARTESIAN_POINT('Ctrl Pts',(2.69210967599394,1.48602096608979,101.371938578772));
#24606=CARTESIAN_POINT('Ctrl Pts',(2.73742097378704,1.4007877967329,101.366949415003));
#24607=CARTESIAN_POINT('Ctrl Pts',(2.7785916612906,1.3137087309622,101.361960251234));
#24608=CARTESIAN_POINT('Ctrl Pts',(2.82187746759233,1.22215603164039,101.35671477224));
#24609=CARTESIAN_POINT('Ctrl Pts',(2.86058565957799,1.12856323312179,101.351469293245));
#24610=CARTESIAN_POINT('Ctrl Pts',(2.89454931285437,1.03343433533742,101.34622381425));
#24611=CARTESIAN_POINT('Ctrl Pts',(2.92851296613076,0.938305437553028,101.340978335255));
#24612=CARTESIAN_POINT('Ctrl Pts',(2.95773199094319,0.841640994127167,101.335732856261));
#24613=CARTESIAN_POINT('Ctrl Pts',(2.98210140691277,0.743957961775299,101.330487377266));
#24614=CARTESIAN_POINT('Ctrl Pts',(3.00532809919398,0.65085545425668,101.325487867773));
#24615=CARTESIAN_POINT('Ctrl Pts',(3.02423135712574,0.556500655140469,101.32048835828));
#24616=CARTESIAN_POINT('Ctrl Pts',(3.03867997357276,0.461330974689379,101.315488848787));
#24617=CARTESIAN_POINT('Ctrl Pts',(3.05310899056328,0.366290391305736,101.310496121097));
#24618=CARTESIAN_POINT('Ctrl Pts',(3.06309531019677,0.270437553736443,101.305503393407));
#24619=CARTESIAN_POINT('Ctrl Pts',(3.06855806990335,0.174222907882483,101.300510665717));
#24620=CARTESIAN_POINT('Ctrl Pts',(3.07401506653613,0.0781097660547342,
101.295523205229));
#24621=CARTESIAN_POINT('Ctrl Pts',(3.07495796541972,-0.0183639893377553,
101.29053574474));
#24622=CARTESIAN_POINT('Ctrl Pts',(3.07135748041999,-0.114740914534327,
101.285548284252));
#24623=CARTESIAN_POINT('Ctrl Pts',(3.06775957165143,-0.211048879788368,
101.280564392409));
#24624=CARTESIAN_POINT('Ctrl Pts',(3.05962475797039,-0.307259715181775,
101.275580500565));
#24625=CARTESIAN_POINT('Ctrl Pts',(3.04697582811149,-0.402915069095557,
101.270596608721));
#24626=CARTESIAN_POINT('Ctrl Pts',(3.03433150467958,-0.498535587698538,
101.265614531888));
#24627=CARTESIAN_POINT('Ctrl Pts',(3.01717638886501,-0.593600592025961,
101.260632455054));
#24628=CARTESIAN_POINT('Ctrl Pts',(2.99558512143411,-0.687656913178777,
101.25565037822));
#24629=CARTESIAN_POINT('Ctrl Pts',(2.97399582262933,-0.781704658562207,
101.250668755637));
#24630=CARTESIAN_POINT('Ctrl Pts',(2.94797127476999,-0.874743475828466,
101.245687133054));
#24631=CARTESIAN_POINT('Ctrl Pts',(2.91763700124182,-0.966331505739423,
101.240705510471));
#24632=CARTESIAN_POINT('Ctrl Pts',(2.88729721240838,-1.05793618796758,101.235722982141));
#24633=CARTESIAN_POINT('Ctrl Pts',(2.85264627975232,-1.14808914228928,101.230740453811));
#24634=CARTESIAN_POINT('Ctrl Pts',(2.81385889893677,-1.23636578198943,101.225757925482));
#24635=CARTESIAN_POINT('Ctrl Pts',(2.77502971104104,-1.3247375708973,101.220770026721));
#24636=CARTESIAN_POINT('Ctrl Pts',(2.7320553509119,-1.41122860512118,101.215782127959));
#24637=CARTESIAN_POINT('Ctrl Pts',(2.68515768917594,-1.49543653635295,101.210794229198));
#24638=CARTESIAN_POINT('Ctrl Pts',(2.6382323243475,-1.57969421036549,101.205803384017));
#24639=CARTESIAN_POINT('Ctrl Pts',(2.58737927459469,-1.66166572314443,101.200812538836));
#24640=CARTESIAN_POINT('Ctrl Pts',(2.53286404893341,-1.74097730014513,101.195821693655));
#24641=CARTESIAN_POINT('Ctrl Pts',(2.4782607252907,-1.82041704665726,101.190822783141));
#24642=CARTESIAN_POINT('Ctrl Pts',(2.41998367369567,-1.89718792478939,101.185823872628));
#24643=CARTESIAN_POINT('Ctrl Pts',(2.35833896172744,-1.9709489063896,101.180824962115));
#24644=CARTESIAN_POINT('Ctrl Pts',(2.32255054815166,-2.01377153352141,101.177922797904));
#24645=CARTESIAN_POINT('Ctrl Pts',(2.28562777722862,-2.05558034855792,101.175020633693));
#24646=CARTESIAN_POINT('Ctrl Pts',(2.24763596500687,-2.09631458011617,101.172118469482));
#24647=CARTESIAN_POINT('Ctrl Pts',(2.18218810883934,-2.16648675596708,101.167118959989));
#24648=CARTESIAN_POINT('Ctrl Pts',(2.11333593956034,-2.23371428055537,101.162119450496));
#24649=CARTESIAN_POINT('Ctrl Pts',(2.04137491759407,-2.29764894964783,101.157119941003));
#24650=CARTESIAN_POINT('Ctrl Pts',(1.96951151029715,-2.36149689176766,101.152127213313));
#24651=CARTESIAN_POINT('Ctrl Pts',(1.89454795694443,-2.42206056667833,101.147134485623));
#24652=CARTESIAN_POINT('Ctrl Pts',(1.81681806233013,-2.47902690150611,101.142141757933));
#24653=CARTESIAN_POINT('Ctrl Pts',(1.73917017079561,-2.53593313828639,101.137154297445));
#24654=CARTESIAN_POINT('Ctrl Pts',(1.65876209181881,-2.58924932131834,101.132166836956));
#24655=CARTESIAN_POINT('Ctrl Pts',(1.57596158081565,-2.63870182964901,101.127179376468));
#24656=CARTESIAN_POINT('Ctrl Pts',(1.49322031551337,-2.68811895355414,101.122195484625));
#24657=CARTESIAN_POINT('Ctrl Pts',(1.40809039702697,-2.73367767411584,101.117211592781));
#24658=CARTESIAN_POINT('Ctrl Pts',(1.3209686945205,-2.77514755609441,101.112227700937));
#24659=CARTESIAN_POINT('Ctrl Pts',(1.23387871958018,-2.81660233576914,101.107245624104));
#24660=CARTESIAN_POINT('Ctrl Pts',(1.14479879777426,-2.8539710469787,101.10226354727));
#24661=CARTESIAN_POINT('Ctrl Pts',(1.05414968196086,-2.88706956930757,101.097281470436));
#24662=CARTESIAN_POINT('Ctrl Pts',(0.963508831258191,-2.92016507381383,
101.092299847853));
#24663=CARTESIAN_POINT('Ctrl Pts',(0.87129948340515,-2.94899101314185,101.08731822527));
#24664=CARTESIAN_POINT('Ctrl Pts',(0.777960607925135,-2.97341210438727,
101.082336602687));
#24665=CARTESIAN_POINT('Ctrl Pts',(0.684604761793506,-2.99783763581723,
101.077354074357));
#24666=CARTESIAN_POINT('Ctrl Pts',(0.59011940484592,-3.01785661754358,101.072371546027));
#24667=CARTESIAN_POINT('Ctrl Pts',(0.494955790469876,-3.03338441604099,
101.067389017697));
#24668=CARTESIAN_POINT('Ctrl Pts',(0.399689603742445,-3.04892895121674,
101.062401118936));
#24669=CARTESIAN_POINT('Ctrl Pts',(0.303744134041005,-3.05997256807873,
101.057413220175));
#24670=CARTESIAN_POINT('Ctrl Pts',(0.207577665831377,-3.0664823108324,101.052425321414));
#24671=CARTESIAN_POINT('Ctrl Pts',(0.111354390769157,-3.07299589898045,
101.047434476233));
#24672=CARTESIAN_POINT('Ctrl Pts',(0.0149102959240317,-3.07497027126291,
101.042443631052));
#24673=CARTESIAN_POINT('Ctrl Pts',(-0.0812965427013993,-3.07242463245965,
101.03745278587));
#24674=CARTESIAN_POINT('Ctrl Pts',(-0.177658854007724,-3.06987487983979,
101.032453875357));
#24675=CARTESIAN_POINT('Ctrl Pts',(-0.273782706025204,-3.06279056299999,
101.027454964844));
#24676=CARTESIAN_POINT('Ctrl Pts',(-0.369215407999756,-3.05124273575466,
101.022456054331));
#24677=CARTESIAN_POINT('Ctrl Pts',(-0.42461975490707,-3.0445385367381,101.01955389012));
#24678=CARTESIAN_POINT('Ctrl Pts',(-0.479791326678711,-3.03633087595215,
101.016651725909));
#24679=CARTESIAN_POINT('Ctrl Pts',(-0.534643587322911,-3.02664145292013,
101.013749561698));
#24680=CARTESIAN_POINT('Ctrl Pts',(-0.629136654518057,-3.00994964676859,
101.008750052205));
#24681=CARTESIAN_POINT('Ctrl Pts',(-0.723013254539368,-2.98879910906617,
101.003750542712));
#24682=CARTESIAN_POINT('Ctrl Pts',(-0.815820452473183,-2.96324808939894,
100.998751033219));
#24683=CARTESIAN_POINT('Ctrl Pts',(-0.908501758032551,-2.93773172952757,
100.993758305529));
#24684=CARTESIAN_POINT('Ctrl Pts',(-1.00011612495393,-2.90782686665276,
100.988765577839));
#24685=CARTESIAN_POINT('Ctrl Pts',(-1.09021920958482,-2.87364304064584,
100.983772850148));
#24686=CARTESIAN_POINT('Ctrl Pts',(-1.18022723773209,-2.83949527771389,
100.97878538966));
#24687=CARTESIAN_POINT('Ctrl Pts',(-1.26872674485357,-2.80107768048225,
100.973797929172));
#24688=CARTESIAN_POINT('Ctrl Pts',(-1.3552879947946,-2.75854974600162,100.968810468684));
#24689=CARTESIAN_POINT('Ctrl Pts',(-1.44178730813832,-2.71605224125202,
100.96382657684));
#24690=CARTESIAN_POINT('Ctrl Pts',(-1.52635072847931,-2.66945043891615,
100.958842684996));
#24691=CARTESIAN_POINT('Ctrl Pts',(-1.60856889248042,-2.61895176896107,
100.953858793153));
#24692=CARTESIAN_POINT('Ctrl Pts',(-1.69075711466253,-2.56847148937086,
100.948876716319));
#24693=CARTESIAN_POINT('Ctrl Pts',(-1.77060140381673,-2.5140973913475,100.943894639485));
#24694=CARTESIAN_POINT('Ctrl Pts',(-1.84771824160846,-2.4560821544947,100.938912562652));
#24695=CARTESIAN_POINT('Ctrl Pts',(-1.92482804812148,-2.39807220729474,
100.933930940069));
#24696=CARTESIAN_POINT('Ctrl Pts',(-1.99921054702392,-2.33642204535948,
100.928949317485));
#24697=CARTESIAN_POINT('Ctrl Pts',(-2.07051326641702,-2.27142621795011,
100.923967694902));
#24698=CARTESIAN_POINT('Ctrl Pts',(-2.14182894990078,-2.20641857315415,
100.918985166573));
#24699=CARTESIAN_POINT('Ctrl Pts',(-2.21006341741581,-2.13806435053479,
100.914002638243));
#24700=CARTESIAN_POINT('Ctrl Pts',(-2.27489999340274,-2.06669597909712,
100.909020109913));
#24701=CARTESIAN_POINT('Ctrl Pts',(-2.33980645366294,-1.99525068307335,
100.904032211152));
#24702=CARTESIAN_POINT('Ctrl Pts',(-2.40130741504089,-1.92078507772949,
100.899044312391));
#24703=CARTESIAN_POINT('Ctrl Pts',(-2.45912572077757,-1.84366562570609,
100.89405641363));
#24704=CARTESIAN_POINT('Ctrl Pts',(-2.51697818058096,-1.76650061816396,
100.889065568448));
#24705=CARTESIAN_POINT('Ctrl Pts',(-2.571143406811,-1.68667900552759,100.884074723267));
#24706=CARTESIAN_POINT('Ctrl Pts',(-2.62138810809422,-1.60459547448638,
100.879083878086));
#24707=CARTESIAN_POINT('Ctrl Pts',(-2.67171400608364,-1.52237929438601,
100.874084967573));
#24708=CARTESIAN_POINT('Ctrl Pts',(-2.71810651705663,-1.43789428152925,
100.86908605706));
#24709=CARTESIAN_POINT('Ctrl Pts',(-2.76037877221685,-1.35155883478841,
100.864087146546));
#24710=CARTESIAN_POINT('Ctrl Pts',(-2.78492032496541,-1.30143598441692,
100.861184982335));
#24711=CARTESIAN_POINT('Ctrl Pts',(-2.80807405079476,-1.25068982192612,
100.858282818124));
#24712=CARTESIAN_POINT('Ctrl Pts',(-2.82981103644184,-1.19940474737762,
100.855380653913));
#24713=CARTESIAN_POINT('Ctrl Pts',(-2.87129753361498,-1.10152373780138,
100.849841678579));
#24714=CARTESIAN_POINT('Ctrl Pts',(-2.90774489594132,-1.00138651678959,
100.844302703245));
#24715=CARTESIAN_POINT('Ctrl Pts',(-2.93892843199391,-0.899500929192315,
100.838763727911));
#24716=CARTESIAN_POINT('Ctrl Pts',(-2.97002309322088,-0.797905721230475,
100.833240538968));
#24717=CARTESIAN_POINT('Ctrl Pts',(-2.9958837450267,-0.694572335139929,
100.827717350024));
#24718=CARTESIAN_POINT('Ctrl Pts',(-3.01633389163178,-0.590027206316343,
100.82219416108));
#24719=CARTESIAN_POINT('Ctrl Pts',(-3.03668036550995,-0.486012072646383,
100.816698972134));
#24720=CARTESIAN_POINT('Ctrl Pts',(-3.05167093851318,-0.38079770440686,
100.811203783188));
#24721=CARTESIAN_POINT('Ctrl Pts',(-3.0611795685935,-0.27492162305963,100.805708594242));
#24722=CARTESIAN_POINT('Ctrl Pts',(-3.06933072015189,-0.184160706063101,
100.80099791378));
#24723=CARTESIAN_POINT('Ctrl Pts',(-3.07345415884847,-0.0929139253420787,
100.796287233317));
#24724=CARTESIAN_POINT('Ctrl Pts',(-3.0734996196979,-0.00152895940824786,
100.791576552855));
#24725=CARTESIAN_POINT('Origin',(0.,0.,116.208423447177));
#24726=CARTESIAN_POINT('',(1.87238193903529,2.43733217358128,102.437311095123));
#24727=CARTESIAN_POINT('',(1.8723819390353,2.43733217358127,102.354198413529));
#24728=CARTESIAN_POINT('',(1.8723819390353,2.43733217358128,116.208423447177));
#24729=CARTESIAN_POINT('',(-3.0734992979985,0.00207730659809526,101.708423447141));
#24730=CARTESIAN_POINT('Ctrl Pts',(1.8723819390353,2.43733217358127,102.354198413529));
#24731=CARTESIAN_POINT('Ctrl Pts',(1.94890699904715,2.37854488894159,102.349215952023));
#24732=CARTESIAN_POINT('Ctrl Pts',(2.02264391055518,2.31616314582571,102.344233490517));
#24733=CARTESIAN_POINT('Ctrl Pts',(2.09324892654711,2.25049132002534,102.339251029012));
#24734=CARTESIAN_POINT('Ctrl Pts',(2.16392958878789,2.18474913339851,102.334263229294));
#24735=CARTESIAN_POINT('Ctrl Pts',(2.23147133415777,2.11571012581288,102.329275429577));
#24736=CARTESIAN_POINT('Ctrl Pts',(2.29556689235758,2.04371595206177,102.324287629859));
#24737=CARTESIAN_POINT('Ctrl Pts',(2.35969963902613,1.97168000703734,102.319296936203));
#24738=CARTESIAN_POINT('Ctrl Pts',(2.42038194099289,1.89668582278075,102.314306242547));
#24739=CARTESIAN_POINT('Ctrl Pts',(2.47734783506712,1.81910691112102,102.30931554889));
#24740=CARTESIAN_POINT('Ctrl Pts',(2.5344065073427,1.7414016496163,102.30431672708));
#24741=CARTESIAN_POINT('Ctrl Pts',(2.58773644184387,1.66110361976615,102.299317905269));
#24742=CARTESIAN_POINT('Ctrl Pts',(2.6371159008827,1.57861394118753,102.294319083458));
#24743=CARTESIAN_POINT('Ctrl Pts',(2.66790079696583,1.52718696664379,102.291202641663));
#24744=CARTESIAN_POINT('Ctrl Pts',(2.69715117320429,1.47490865119322,102.288086199867));
#24745=CARTESIAN_POINT('Ctrl Pts',(2.72482273064766,1.42188021174284,102.284969758072));
#24746=CARTESIAN_POINT('Ctrl Pts',(2.76921445146489,1.33681005679139,102.279970248579));
#24747=CARTESIAN_POINT('Ctrl Pts',(2.80969643364758,1.24950959633869,102.274970739086));
#24748=CARTESIAN_POINT('Ctrl Pts',(2.84603864801093,1.16037332959187,102.269971229593));
#24749=CARTESIAN_POINT('Ctrl Pts',(2.88233156439122,1.071357975625,102.264978501903));
#24750=CARTESIAN_POINT('Ctrl Pts',(2.91449570921459,0.980512167589046,102.259985774213));
#24751=CARTESIAN_POINT('Ctrl Pts',(2.94234694291599,0.888254871933135,102.254993046523));
#24752=CARTESIAN_POINT('Ctrl Pts',(2.97016879426802,0.796094905398126,102.250005586035));
#24753=CARTESIAN_POINT('Ctrl Pts',(2.99368665346061,0.702526829448201,102.245018125546));
#24754=CARTESIAN_POINT('Ctrl Pts',(3.01276488262564,0.607988496616256,102.240030665058));
#24755=CARTESIAN_POINT('Ctrl Pts',(3.03182946087167,0.513517808171705,102.235046773214));
#24756=CARTESIAN_POINT('Ctrl Pts',(3.04646063755337,0.418078672018671,102.230062881371));
#24757=CARTESIAN_POINT('Ctrl Pts',(3.05657318778474,0.32212202302148,102.225078989527));
#24758=CARTESIAN_POINT('Ctrl Pts',(3.06668205527578,0.226200319059179,102.220096912693));
#24759=CARTESIAN_POINT('Ctrl Pts',(3.07227551993007,0.1297619128116,102.21511483586));
#24760=CARTESIAN_POINT('Ctrl Pts',(3.07331998006636,0.0332648481871961,
102.210132759026));
#24761=CARTESIAN_POINT('Ctrl Pts',(3.07436434497195,-0.0632234181279897,
102.205151136443));
#24762=CARTESIAN_POINT('Ctrl Pts',(3.07086052542035,-0.159769893248088,
102.20016951386));
#24763=CARTESIAN_POINT('Ctrl Pts',(3.06282703587785,-0.255915607761009,
102.195187891277));
#24764=CARTESIAN_POINT('Ctrl Pts',(3.05479208570543,-0.352078803258626,
102.190205362947));
#24765=CARTESIAN_POINT('Ctrl Pts',(3.04222586650856,-0.447840656007861,
102.185222834617));
#24766=CARTESIAN_POINT('Ctrl Pts',(3.02519874309424,-0.542747468700733,
102.180240306287));
#24767=CARTESIAN_POINT('Ctrl Pts',(3.00815326695027,-0.637756576950667,
102.175252407526));
#24768=CARTESIAN_POINT('Ctrl Pts',(2.98663736511165,-0.731908372460368,
102.170264508765));
#24769=CARTESIAN_POINT('Ctrl Pts',(2.96077247436852,-0.824759725630283,
102.165276610004));
#24770=CARTESIAN_POINT('Ctrl Pts',(2.93489230487937,-0.91766592736909,102.160285764823));
#24771=CARTESIAN_POINT('Ctrl Pts',(2.90465816868865,-1.00926974052806,102.155294919642));
#24772=CARTESIAN_POINT('Ctrl Pts',(2.87024062061863,-1.09914559078896,102.15030407446));
#24773=CARTESIAN_POINT('Ctrl Pts',(2.8357674529218,-1.18916668269344,102.145305163947));
#24774=CARTESIAN_POINT('Ctrl Pts',(2.79709755011772,-1.27745383401738,102.140306253434));
#24775=CARTESIAN_POINT('Ctrl Pts',(2.75444856847819,-1.36360380375255,102.135307342921));
#24776=CARTESIAN_POINT('Ctrl Pts',(2.72968830365192,-1.41361897371482,102.13240517871));
#24777=CARTESIAN_POINT('Ctrl Pts',(2.7035877408453,-1.46291429447095,102.129503014499));
#24778=CARTESIAN_POINT('Ctrl Pts',(2.67619614131916,-1.51141538406504,102.126600850288));
#24779=CARTESIAN_POINT('Ctrl Pts',(2.6290090933427,-1.59496739567365,102.121601340795));
#24780=CARTESIAN_POINT('Ctrl Pts',(2.57782261901536,-1.67645424199027,102.116601831302));
#24781=CARTESIAN_POINT('Ctrl Pts',(2.52284238147984,-1.75546819060019,102.111602321809));
#24782=CARTESIAN_POINT('Ctrl Pts',(2.4679367242875,-1.83437495729044,102.106609594119));
#24783=CARTESIAN_POINT('Ctrl Pts',(2.40924778022428,-1.9108151358268,102.101616866429));
#24784=CARTESIAN_POINT('Ctrl Pts',(2.34702672004184,-1.98440616442543,102.096624138739));
#24785=CARTESIAN_POINT('Ctrl Pts',(2.28487130150936,-2.05791955634404,102.091636678251));
#24786=CARTESIAN_POINT('Ctrl Pts',(2.21919145641307,-2.1285894402129,102.086649217762));
#24787=CARTESIAN_POINT('Ctrl Pts',(2.15028060383059,-2.19606365453963,102.081661757274));
#24788=CARTESIAN_POINT('Ctrl Pts',(2.08141905857399,-2.26348958948873,102.076677865431));
#24789=CARTESIAN_POINT('Ctrl Pts',(2.0093314144485,-2.32772409427521,102.071693973587));
#24790=CARTESIAN_POINT('Ctrl Pts',(1.93434951131722,-2.3884501707314,102.066710081743));
#24791=CARTESIAN_POINT('Ctrl Pts',(1.85939491473803,-2.4491541322545,102.061728004909));
#24792=CARTESIAN_POINT('Ctrl Pts',(1.78154849414504,-2.50635192807946,102.056745928076));
#24793=CARTESIAN_POINT('Ctrl Pts',(1.70117615874711,-2.55976599065431,102.051763851242));
#24794=CARTESIAN_POINT('Ctrl Pts',(1.62081115145448,-2.61317518309725,102.046782228659));
#24795=CARTESIAN_POINT('Ctrl Pts',(1.53792105293775,-2.66280108538063,102.041800606076));
#24796=CARTESIAN_POINT('Ctrl Pts',(1.452900923429,-2.70840934068304,102.036818983493));
#24797=CARTESIAN_POINT('Ctrl Pts',(1.36786533576248,-2.75402588836998,102.031836455163));
#24798=CARTESIAN_POINT('Ctrl Pts',(1.28069933480315,-2.79562313087121,102.026853926833));
#24799=CARTESIAN_POINT('Ctrl Pts',(1.19182178858177,-2.83301307343644,102.021871398503));
#24800=CARTESIAN_POINT('Ctrl Pts',(1.10284844546438,-2.8704433168492,102.016883499742));
#24801=CARTESIAN_POINT('Ctrl Pts',(1.01216027941154,-2.90365703641808,102.011895600981));
#24802=CARTESIAN_POINT('Ctrl Pts',(0.920195100562621,-2.93251482978357,
102.00690770222));
#24803=CARTESIAN_POINT('Ctrl Pts',(0.828175596620137,-2.96138966984374,
102.001916857039));
#24804=CARTESIAN_POINT('Ctrl Pts',(0.734878002203351,-2.98590334872931,
101.996926011858));
#24805=CARTESIAN_POINT('Ctrl Pts',(0.640752144606385,-3.0059672219075,101.991935166676));
#24806=CARTESIAN_POINT('Ctrl Pts',(0.546474177246778,-3.02606351881139,
101.986936256163));
#24807=CARTESIAN_POINT('Ctrl Pts',(0.451365706888683,-3.04169558002853,
101.98193734565));
#24808=CARTESIAN_POINT('Ctrl Pts',(0.355883472275826,-3.05282642876415,
101.976938435137));
#24809=CARTESIAN_POINT('Ctrl Pts',(0.300450368732722,-3.0592885470104,101.974036270926));
#24810=CARTESIAN_POINT('Ctrl Pts',(0.244891341822553,-3.06423451062689,
101.971134106715));
#24811=CARTESIAN_POINT('Ctrl Pts',(0.189295602926459,-3.06766514220713,
101.968231942504));
#24812=CARTESIAN_POINT('Ctrl Pts',(0.0935217582459618,-3.07357503355216,
101.963232433011));
#24813=CARTESIAN_POINT('Ctrl Pts',(-0.00269733563999103,-3.07500585446188,
101.958232923518));
#24814=CARTESIAN_POINT('Ctrl Pts',(-0.0989077023084138,-3.07190812304406,
101.953233414025));
#24815=CARTESIAN_POINT('Ctrl Pts',(-0.194987560225561,-3.06881459367923,
101.948240686335));
#24816=CARTESIAN_POINT('Ctrl Pts',(-0.291058279471199,-3.06120473470361,
101.943247958645));
#24817=CARTESIAN_POINT('Ctrl Pts',(-0.386662219864625,-3.04908093984554,
101.938255230955));
#24818=CARTESIAN_POINT('Ctrl Pts',(-0.482165300510678,-3.03696993528546,
101.933267770466));
#24819=CARTESIAN_POINT('Ctrl Pts',(-0.577202148086172,-3.02035451651745,
101.928280309978));
#24820=CARTESIAN_POINT('Ctrl Pts',(-0.671317619773322,-2.99928906632587,
101.92329284949));
#24821=CARTESIAN_POINT('Ctrl Pts',(-0.765365749640313,-2.97823868895634,
101.918308957646));
#24822=CARTESIAN_POINT('Ctrl Pts',(-0.858493387073436,-2.95274470561038,
101.913325065802));
#24823=CARTESIAN_POINT('Ctrl Pts',(-0.950253965723744,-2.92291287085782,
101.908341173959));
#24824=CARTESIAN_POINT('Ctrl Pts',(-1.04198112744394,-2.89309190012063,
101.903359097125));
#24825=CARTESIAN_POINT('Ctrl Pts',(-1.13234180252452,-2.85893635232294,
101.898377020291));
#24826=CARTESIAN_POINT('Ctrl Pts',(-1.22090394960432,-2.82060202719926,
101.893394943458));
#24827=CARTESIAN_POINT('Ctrl Pts',(-1.30945802185682,-2.78227119728279,
101.888413320875));
#24828=CARTESIAN_POINT('Ctrl Pts',(-1.39621348936957,-2.73976252209492,
101.883431698292));
#24829=CARTESIAN_POINT('Ctrl Pts',(-1.48075868428877,-2.69327977917323,
101.878450075708));
#24830=CARTESIAN_POINT('Ctrl Pts',(-1.56531925101342,-2.64678858487022,
101.873467547379));
#24831=CARTESIAN_POINT('Ctrl Pts',(-1.64766836239948,-2.59632209935035,
101.868485019049));
#24832=CARTESIAN_POINT('Ctrl Pts',(-1.72742027654751,-2.54212931185109,
101.863502490719));
#24833=CARTESIAN_POINT('Ctrl Pts',(-1.80725815150581,-2.4878781125134,101.858514591958));
#24834=CARTESIAN_POINT('Ctrl Pts',(-1.88449287681768,-2.42989283993802,
101.853526693197));
#24835=CARTESIAN_POINT('Ctrl Pts',(-1.95876915644562,-2.36846482806001,
101.848538794436));
#24836=CARTESIAN_POINT('Ctrl Pts',(-2.03308931209126,-2.30700052981237,
101.843547949255));
#24837=CARTESIAN_POINT('Ctrl Pts',(-2.10444721774311,-2.24208973812568,
101.838557104073));
#24838=CARTESIAN_POINT('Ctrl Pts',(-2.17252360987847,-2.17406150200968,
101.833566258892));
#24839=CARTESIAN_POINT('Ctrl Pts',(-2.24071001518281,-2.10592333054606,
101.828567348379));
#24840=CARTESIAN_POINT('Ctrl Pts',(-2.30560402268783,-2.03465797948598,
101.823568437866));
#24841=CARTESIAN_POINT('Ctrl Pts',(-2.36692594442134,-1.96062842569038,
101.818569527352));
#24842=CARTESIAN_POINT('Ctrl Pts',(-2.40252695910958,-1.91764987646137,
101.815667363142));
#24843=CARTESIAN_POINT('Ctrl Pts',(-2.436924794165,-1.87374023092859,101.812765198931));
#24844=CARTESIAN_POINT('Ctrl Pts',(-2.47007156829697,-1.82897476677261,
101.80986303472));
#24845=CARTESIAN_POINT('Ctrl Pts',(-2.52743545420021,-1.75150354836611,
101.804840542455));
#24846=CARTESIAN_POINT('Ctrl Pts',(-2.58125253037607,-1.67119415335716,
101.79981805019));
#24847=CARTESIAN_POINT('Ctrl Pts',(-2.63123135768058,-1.58840290617916,
101.794795557926));
#24848=CARTESIAN_POINT('Ctrl Pts',(-2.68114177306052,-1.50572498516071,
101.78977994054));
#24849=CARTESIAN_POINT('Ctrl Pts',(-2.72722415798737,-1.4205723301425,101.784764323154));
#24850=CARTESIAN_POINT('Ctrl Pts',(-2.76922841947647,-1.33333274570298,
101.779748705768));
#24851=CARTESIAN_POINT('Ctrl Pts',(-2.81118629016578,-1.24618951134681,
101.774738627784));
#24852=CARTESIAN_POINT('Ctrl Pts',(-2.84907480323806,-1.15696431708763,
101.7697285498));
#24853=CARTESIAN_POINT('Ctrl Pts',(-2.88268867979694,-1.06607139787659,
101.764718471816));
#24854=CARTESIAN_POINT('Ctrl Pts',(-2.91627301188171,-0.975258367799869,
101.759712797375));
#24855=CARTESIAN_POINT('Ctrl Pts',(-2.94559003048157,-0.882780933297525,
101.754707122933));
#24856=CARTESIAN_POINT('Ctrl Pts',(-2.97048212200563,-0.789074275873267,
101.749701448491));
#24857=CARTESIAN_POINT('Ctrl Pts',(-2.99536106342461,-0.695417122219762,
101.744698418469));
#24858=CARTESIAN_POINT('Ctrl Pts',(-3.01581961525058,-0.600532455110712,
101.739695388448));
#24859=CARTESIAN_POINT('Ctrl Pts',(-3.03174994754577,-0.504870781048189,
101.734692358426));
#24860=CARTESIAN_POINT('Ctrl Pts',(-3.04767925349586,-0.409215270189851,
101.729689650735));
#24861=CARTESIAN_POINT('Ctrl Pts',(-3.0590808394957,-0.312783277793817,
101.724686943044));
#24862=CARTESIAN_POINT('Ctrl Pts',(-3.06589809758779,-0.21603496292859,
101.719684235353));
#24863=CARTESIAN_POINT('Ctrl Pts',(-3.07101317419916,-0.143443455335405,
101.715930639294));
#24864=CARTESIAN_POINT('Ctrl Pts',(-3.07354846896932,-0.0706741086632016,
101.712177043236));
#24865=CARTESIAN_POINT('Ctrl Pts',(-3.07349929799898,0.0020773059017772,
101.708423447177));
#24866=CARTESIAN_POINT('Ctrl Pts',(-3.0734992979985,0.00207730659811786,
101.708423447141));
#24867=CARTESIAN_POINT('Ctrl Pts',(-3.0734250223512,0.111972567151077,101.702753421076));
#24868=CARTESIAN_POINT('Ctrl Pts',(-3.06745263996542,0.221638779434296,
101.697083395011));
#24869=CARTESIAN_POINT('Ctrl Pts',(-3.0556797259961,0.330490033338945,101.691413368946));
#24870=CARTESIAN_POINT('Ctrl Pts',(-3.04384899836201,0.439875826943855,
101.685715498884));
#24871=CARTESIAN_POINT('Ctrl Pts',(-3.0261607520244,0.548438458319583,101.680017628821));
#24872=CARTESIAN_POINT('Ctrl Pts',(-3.00276350587291,0.655601691423871,
101.674319758759));
#24873=CARTESIAN_POINT('Ctrl Pts',(-2.97923000797706,0.763388979912571,
101.668588707666));
#24874=CARTESIAN_POINT('Ctrl Pts',(-2.9499209313853,0.869760348838303,101.662857656573));
#24875=CARTESIAN_POINT('Ctrl Pts',(-2.91503564058411,0.974150637285826,
101.65712660548));
#24876=CARTESIAN_POINT('Ctrl Pts',(-2.90360721621242,1.00834890507326,101.655249112632));
#24877=CARTESIAN_POINT('Ctrl Pts',(-2.8915807188752,1.04233473933062,101.653371619784));
#24878=CARTESIAN_POINT('Ctrl Pts',(-2.87896424539991,1.07608880846747,101.651494126936));
#24879=CARTESIAN_POINT('Ctrl Pts',(-2.84536828312015,1.1659713287875,101.646494617443));
#24880=CARTESIAN_POINT('Ctrl Pts',(-2.80750002023446,1.25443689238554,101.64149510795));
#24881=CARTESIAN_POINT('Ctrl Pts',(-2.76549909601532,1.3410507074449,101.636495598457));
#24882=CARTESIAN_POINT('Ctrl Pts',(-2.72355514578312,1.42754703141422,101.631502870766));
#24883=CARTESIAN_POINT('Ctrl Pts',(-2.67748986552272,1.51219620745576,101.626510143076));
#24884=CARTESIAN_POINT('Ctrl Pts',(-2.62749176748756,1.5945812183094,101.621517415386));
#24885=CARTESIAN_POINT('Ctrl Pts',(-2.57754641618561,1.67687931505313,101.616529954898));
#24886=CARTESIAN_POINT('Ctrl Pts',(-2.52367672164694,1.75691762180815,101.61154249441));
#24887=CARTESIAN_POINT('Ctrl Pts',(-2.46611766424434,1.83430256939853,101.606555033921));
#24888=CARTESIAN_POINT('Ctrl Pts',(-2.40859979169278,1.91163214625,101.601571142078));
#24889=CARTESIAN_POINT('Ctrl Pts',(-2.34739806535233,1.98631178694058,101.596587250234));
#24890=CARTESIAN_POINT('Ctrl Pts',(-2.28279089484515,2.05797667149365,101.59160335839));
#24891=CARTESIAN_POINT('Ctrl Pts',(-2.21820725266931,2.12961545747072,101.586621281557));
#24892=CARTESIAN_POINT('Ctrl Pts',(-2.15022092404982,2.19824134301865,101.581639204723));
#24893=CARTESIAN_POINT('Ctrl Pts',(-2.07915011426144,2.26352315039335,101.576657127889));
#24894=CARTESIAN_POINT('Ctrl Pts',(-2.00808578449351,2.32879900557126,101.571675505306));
#24895=CARTESIAN_POINT('Ctrl Pts',(-1.93393785610523,2.39073109196675,101.566693882723));
#24896=CARTESIAN_POINT('Ctrl Pts',(-1.85706006057578,2.44902637417695,101.56171226014));
#24897=CARTESIAN_POINT('Ctrl Pts',(-1.78016828730857,2.50733225549657,101.55672973181));
#24898=CARTESIAN_POINT('Ctrl Pts',(-1.70054601096407,2.56199975421964,101.55174720348));
#24899=CARTESIAN_POINT('Ctrl Pts',(-1.618577702117,2.61277792248205,101.546764675151));
#24900=CARTESIAN_POINT('Ctrl Pts',(-1.53652104351337,2.66361082212624,101.54177677639));
#24901=CARTESIAN_POINT('Ctrl Pts',(-1.45211367791652,2.71054579056809,101.536788877628));
#24902=CARTESIAN_POINT('Ctrl Pts',(-1.36576635612371,2.75337692851534,101.531800978867));
#24903=CARTESIAN_POINT('Ctrl Pts',(-1.27936802778278,2.79623336740364,101.526810133686));
#24904=CARTESIAN_POINT('Ctrl Pts',(-1.19102786326029,2.83498097260156,101.521819288505));
#24905=CARTESIAN_POINT('Ctrl Pts',(-1.10117639046943,2.86946211110597,101.516828443323));
#24906=CARTESIAN_POINT('Ctrl Pts',(-1.01117971542946,2.90399897200098,101.51182953281));
#24907=CARTESIAN_POINT('Ctrl Pts',(-0.91966727185571,2.93425546127084,101.506830622297));
#24908=CARTESIAN_POINT('Ctrl Pts',(-0.827084463136288,2.96012390633206,
101.501831711784));
#24909=CARTESIAN_POINT('Ctrl Pts',(-0.773334648389712,2.97514207384128,
101.498929547573));
#24910=CARTESIAN_POINT('Ctrl Pts',(-0.719224272794842,2.98868220974381,
101.496027383362));
#24911=CARTESIAN_POINT('Ctrl Pts',(-0.664841586868186,3.00073122994556,
101.493125219151));
#24912=CARTESIAN_POINT('Ctrl Pts',(-0.571149477978079,3.02148964033897,
101.488125284326));
#24913=CARTESIAN_POINT('Ctrl Pts',(-0.476319646934513,3.03789227190172,
101.4831253495));
#24914=CARTESIAN_POINT('Ctrl Pts',(-0.380792933756225,3.04981950147895,
101.478125414674));
#24915=CARTESIAN_POINT('Ctrl Pts',(-0.282177760885511,3.06213234850879,
101.472963827713));
#24916=CARTESIAN_POINT('Ctrl Pts',(-0.182820307436638,3.06967528480989,
101.467802240753));
#24917=CARTESIAN_POINT('Ctrl Pts',(-0.0832206554129855,3.07237311739844,
101.462640653792));
#24918=CARTESIAN_POINT('Ctrl Pts',(0.013007602662867,3.07497962982396,101.457653783737));
#24919=CARTESIAN_POINT('Ctrl Pts',(0.109461444457588,3.07306372397927,101.452666913682));
#24920=CARTESIAN_POINT('Ctrl Pts',(0.205682849278356,3.06660998751272,101.447680043627));
#24921=CARTESIAN_POINT('Ctrl Pts',(0.301840877117753,3.0601605018502,101.442696458213));
#24922=CARTESIAN_POINT('Ctrl Pts',(0.397766335590615,3.04917915399254,101.437712872799));
#24923=CARTESIAN_POINT('Ctrl Pts',(0.493001817994154,3.03370259871571,101.432729287385));
#24924=CARTESIAN_POINT('Ctrl Pts',(0.588200572705452,3.0182320119933,101.427747623897));
#24925=CARTESIAN_POINT('Ctrl Pts',(0.682709447625377,2.99826973462336,101.42276596041));
#24926=CARTESIAN_POINT('Ctrl Pts',(0.77607783639723,2.97390407408393,101.417784296922));
#24927=CARTESIAN_POINT('Ctrl Pts',(0.869435706496847,2.9495411585249,101.412803194658));
#24928=CARTESIAN_POINT('Ctrl Pts',(0.961652921895574,2.92077595894579,101.407822092393));
#24929=CARTESIAN_POINT('Ctrl Pts',(1.05229176659022,2.88774726871422,101.402840990129));
#24930=CARTESIAN_POINT('Ctrl Pts',(1.14298146039165,2.85470004912692,101.397857093427));
#24931=CARTESIAN_POINT('Ctrl Pts',(1.23209060240693,2.81738471281017,101.392873196724));
#24932=CARTESIAN_POINT('Ctrl Pts',(1.31919976902284,2.77598887234983,101.387889300022));
#24933=CARTESIAN_POINT('Ctrl Pts',(1.40633871728044,2.73457887911848,101.382903699382));
#24934=CARTESIAN_POINT('Ctrl Pts',(1.49147593915523,2.68908580625506,101.377918098742));
#24935=CARTESIAN_POINT('Ctrl Pts',(1.57421657404744,2.6397432503928,101.372932498101));
#24936=CARTESIAN_POINT('Ctrl Pts',(1.65704434652747,2.59034872984233,101.367941646919));
#24937=CARTESIAN_POINT('Ctrl Pts',(1.7374701273175,2.53709687465271,101.362950795736));
#24938=CARTESIAN_POINT('Ctrl Pts',(1.81512839634102,2.48026433163816,101.357959944553));
#24939=CARTESIAN_POINT('Ctrl Pts',(1.83438465776063,2.46617204862451,101.356722405573));
#24940=CARTESIAN_POINT('Ctrl Pts',(1.85347092013274,2.45185979957568,101.355484866592));
#24941=CARTESIAN_POINT('Ctrl Pts',(1.8723819390353,2.43733217358127,101.354247327612));
#24942=CARTESIAN_POINT('',(-3.07349961014009,-0.00154805320464923,101.791576552789));
#24943=CARTESIAN_POINT('Ctrl Pts',(-3.07349961014009,-0.00154805320462876,
101.791576552789));
#24944=CARTESIAN_POINT('Ctrl Pts',(-3.07354741658701,0.0933667052458107,
101.786637087407));
#24945=CARTESIAN_POINT('Ctrl Pts',(-3.06919431499038,0.188457621467398,
101.781697622025));
#24946=CARTESIAN_POINT('Ctrl Pts',(-3.06041767066042,0.283277127755595,
101.776758156643));
#24947=CARTESIAN_POINT('Ctrl Pts',(-3.05165206442623,0.377977382681551,
101.771824903463));
#24948=CARTESIAN_POINT('Ctrl Pts',(-3.03847400796433,0.472406461110176,
101.766891650284));
#24949=CARTESIAN_POINT('Ctrl Pts',(-3.02091288803395,0.566116218554452,
101.761958397104));
#24950=CARTESIAN_POINT('Ctrl Pts',(-3.00336870097853,0.659735618685973,
101.757029900692));
#24951=CARTESIAN_POINT('Ctrl Pts',(-2.98144993236622,0.752636635881347,
101.75210140428));
#24952=CARTESIAN_POINT('Ctrl Pts',(-2.95523770915002,0.844376890030603,
101.747172907867));
#24953=CARTESIAN_POINT('Ctrl Pts',(-2.92903900427722,0.936069831281267,
101.742246953212));
#24954=CARTESIAN_POINT('Ctrl Pts',(-2.89855136438474,1.02660276607848,101.737320998557));
#24955=CARTESIAN_POINT('Ctrl Pts',(-2.86390665014472,1.11554513546376,101.732395043902));
#24956=CARTESIAN_POINT('Ctrl Pts',(-2.82926981023108,1.20446728931945,101.727470208857));
#24957=CARTESIAN_POINT('Ctrl Pts',(-2.79047793620527,1.29179917656985,101.722545373812));
#24958=CARTESIAN_POINT('Ctrl Pts',(-2.7477118276345,1.37712815753562,101.717620538767));
#24959=CARTESIAN_POINT('Ctrl Pts',(-2.70494310387406,1.46246235645267,101.712695402564));
#24960=CARTESIAN_POINT('Ctrl Pts',(-2.65819986601987,1.54579300403043,101.707770266361));
#24961=CARTESIAN_POINT('Ctrl Pts',(-2.60770930769473,1.62673120599633,101.702845130157));
#24962=CARTESIAN_POINT('Ctrl Pts',(-2.55716897446221,1.7077491989497,101.697915138626));
#24963=CARTESIAN_POINT('Ctrl Pts',(-2.50287418324929,1.78636965428595,101.692985147095));
#24964=CARTESIAN_POINT('Ctrl Pts',(-2.44509579674928,1.86223220751844,101.688055155565));
#24965=CARTESIAN_POINT('Ctrl Pts',(-2.38728790612099,1.93813349943226,101.683122646568));
#24966=CARTESIAN_POINT('Ctrl Pts',(-2.32599316896728,2.01127374135177,101.678190137571));
#24967=CARTESIAN_POINT('Ctrl Pts',(-2.26152165329072,2.08132699537992,101.673257628575));
#24968=CARTESIAN_POINT('Ctrl Pts',(-2.19694352932644,2.15149608750158,101.66831696332));
#24969=CARTESIAN_POINT('Ctrl Pts',(-2.1291784570876,2.21856768184379,101.663376298065));
#24970=CARTESIAN_POINT('Ctrl Pts',(-2.05857205794463,2.28225400257062,101.65843563281));
#24971=CARTESIAN_POINT('Ctrl Pts',(-2.00516974882912,2.33042239278971,101.654698819485));
#24972=CARTESIAN_POINT('Ctrl Pts',(-1.95014280537916,2.37665504166767,101.650962006159));
#24973=CARTESIAN_POINT('Ctrl Pts',(-1.89365173966774,2.42084393112264,101.647225192834));
#24974=CARTESIAN_POINT('Ctrl Pts',(-1.8180719355148,2.47996456495532,101.642225683341));
#24975=CARTESIAN_POINT('Ctrl Pts',(-1.73958806921937,2.53564619575051,101.637226173848));
#24976=CARTESIAN_POINT('Ctrl Pts',(-1.65854623503812,2.58759089429548,101.632226664355));
#24977=CARTESIAN_POINT('Ctrl Pts',(-1.57761433359045,2.63946513018664,101.627233936665));
#24978=CARTESIAN_POINT('Ctrl Pts',(-1.49413172679109,2.6876122735277,101.622241208975));
#24979=CARTESIAN_POINT('Ctrl Pts',(-1.40847691271125,2.73177507060142,101.617248481285));
#24980=CARTESIAN_POINT('Ctrl Pts',(-1.32291246230095,2.77589127703755,101.612261020797));
#24981=CARTESIAN_POINT('Ctrl Pts',(-1.23518074830207,2.81603129319022,101.607273560308));
#24982=CARTESIAN_POINT('Ctrl Pts',(-1.1456876594634,2.85198212423452,101.60228609982));
#24983=CARTESIAN_POINT('Ctrl Pts',(-1.0562586050218,2.88790723161882,101.597302207976));
#24984=CARTESIAN_POINT('Ctrl Pts',(-0.965071087323808,2.91964894954352,
101.592318316133));
#24985=CARTESIAN_POINT('Ctrl Pts',(-0.872553026345084,2.94704147684013,
101.587334424289));
#24986=CARTESIAN_POINT('Ctrl Pts',(-0.780068658152789,2.97442402845671,
101.582352347455));
#24987=CARTESIAN_POINT('Ctrl Pts',(-0.686255129900967,2.99746041192585,
101.577370270622));
#24988=CARTESIAN_POINT('Ctrl Pts',(-0.591556739153066,3.01603429595265,
101.572388193788));
#24989=CARTESIAN_POINT('Ctrl Pts',(-0.496866982716663,3.03460648646914,
101.567406571205));
#24990=CARTESIAN_POINT('Ctrl Pts',(-0.401292954979292,3.04871690218318,
101.562424948622));
#24991=CARTESIAN_POINT('Ctrl Pts',(-0.305289340276359,3.05830029080102,
101.557443326039));
#24992=CARTESIAN_POINT('Ctrl Pts',(-0.209268270424516,3.06788542184779,
101.552460797709));
#24993=CARTESIAN_POINT('Ctrl Pts',(-0.112817895278018,3.07294184756764,
101.547478269379));
#24994=CARTESIAN_POINT('Ctrl Pts',(-0.0163971433261428,3.07345626025339,
101.542495741049));
#24995=CARTESIAN_POINT('Ctrl Pts',(0.080127535985788,3.0739712274002,101.537507842288));
#24996=CARTESIAN_POINT('Ctrl Pts',(0.176622088674992,3.06993440551272,101.532519943527));
#24997=CARTESIAN_POINT('Ctrl Pts',(0.272628690951967,3.06138462903142,101.527532044766));
#24998=CARTESIAN_POINT('Ctrl Pts',(0.368692005646722,3.05282980207979,101.522541199585));
#24999=CARTESIAN_POINT('Ctrl Pts',(0.464266361288784,3.03975677182418,101.517550354404));
#25000=CARTESIAN_POINT('Ctrl Pts',(0.55890226517057,3.02225586408352,101.512559509222));
#25001=CARTESIAN_POINT('Ctrl Pts',(0.653691103062858,3.004726674434,101.507560598709));
#25002=CARTESIAN_POINT('Ctrl Pts',(0.747538033838945,2.9827554192197,101.502561688196));
#25003=CARTESIAN_POINT('Ctrl Pts',(0.840006960936336,2.95648280150223,101.497562777683));
#25004=CARTESIAN_POINT('Ctrl Pts',(0.893690660642837,2.94122998778069,101.494660613472));
#25005=CARTESIAN_POINT('Ctrl Pts',(0.946910229263901,2.92452832489818,101.491758449261));
#25006=CARTESIAN_POINT('Ctrl Pts',(0.999583567331903,2.9064127273875,101.48885628505));
#25007=CARTESIAN_POINT('Ctrl Pts',(1.09030709198469,2.87521077745148,101.48385765432));
#25008=CARTESIAN_POINT('Ctrl Pts',(1.17972758713199,2.83970206790258,101.478859023589));
#25009=CARTESIAN_POINT('Ctrl Pts',(1.26740695051557,2.80001461992341,101.473860392859));
#25010=CARTESIAN_POINT('Ctrl Pts',(1.35498197212341,2.76037440151613,101.468867710689));
#25011=CARTESIAN_POINT('Ctrl Pts',(1.44081958027821,2.71656549895826,101.463875028519));
#25012=CARTESIAN_POINT('Ctrl Pts',(1.52449792699141,2.66876531763265,101.458882346349));
#25013=CARTESIAN_POINT('Ctrl Pts',(1.60808320110302,2.62101830283586,101.453895217372));
#25014=CARTESIAN_POINT('Ctrl Pts',(1.68951361054567,2.56928905370452,101.448908088394));
#25015=CARTESIAN_POINT('Ctrl Pts',(1.76838958458584,2.51380200634981,101.443920959416));
#25016=CARTESIAN_POINT('Ctrl Pts',(1.80357290875261,2.48905151929853,101.441696406532));
#25017=CARTESIAN_POINT('Ctrl Pts',(1.83824829490535,2.46355396619335,101.439471853649));
#25018=CARTESIAN_POINT('Ctrl Pts',(1.8723819390353,2.43733217358127,101.437247300765));
#25019=CARTESIAN_POINT('Ctrl Pts',(1.87238193903529,2.43733217358128,102.437311095123));
#25020=CARTESIAN_POINT('Ctrl Pts',(1.94849411630402,2.37886206942259,102.432312458847));
#25021=CARTESIAN_POINT('Ctrl Pts',(2.02199547848817,2.31672298377835,102.427313822571));
#25022=CARTESIAN_POINT('Ctrl Pts',(2.09251173940791,2.25117677458704,102.422315186295));
#25023=CARTESIAN_POINT('Ctrl Pts',(2.16293483738044,2.18571716213166,102.417323153995));
#25024=CARTESIAN_POINT('Ctrl Pts',(2.23038035341126,2.11685966892024,102.412331121694));
#25025=CARTESIAN_POINT('Ctrl Pts',(2.2945054394344,2.04490758676424,102.407339089394));
#25026=CARTESIAN_POINT('Ctrl Pts',(2.35856514009273,1.97302887079661,102.402352147237));
#25027=CARTESIAN_POINT('Ctrl Pts',(2.41931085091136,1.89806216492121,102.39736520508));
#25028=CARTESIAN_POINT('Ctrl Pts',(2.47643586927194,1.82034821816687,102.392378262922));
#25029=CARTESIAN_POINT('Ctrl Pts',(2.53352270357738,1.74268621771757,102.387394654185));
#25030=CARTESIAN_POINT('Ctrl Pts',(2.58699339693294,1.66228097941049,102.382411045448));
#25031=CARTESIAN_POINT('Ctrl Pts',(2.63658154685445,1.57950625094888,102.37742743671));
#25032=CARTESIAN_POINT('Ctrl Pts',(2.68615322426235,1.49675901913402,102.372445483461));
#25033=CARTESIAN_POINT('Ctrl Pts',(2.73184469549272,1.41164423737551,102.367463530211));
#25034=CARTESIAN_POINT('Ctrl Pts',(2.7734334696027,1.32456371673375,102.362481576961));
#25035=CARTESIAN_POINT('Ctrl Pts',(2.81501978212943,1.23748835027014,102.357499918586));
#25036=CARTESIAN_POINT('Ctrl Pts',(2.85250369151814,1.14844787255197,102.352518260211));
#25037=CARTESIAN_POINT('Ctrl Pts',(2.88570965194885,1.05786674711386,102.347536601837));
#25038=CARTESIAN_POINT('Ctrl Pts',(2.91892271199686,0.967266254932028,102.342553878356));
#25039=CARTESIAN_POINT('Ctrl Pts',(2.9478558553953,0.875124872908682,102.337571154875));
#25040=CARTESIAN_POINT('Ctrl Pts',(2.97238283161512,0.781883976252037,102.332588431394));
#25041=CARTESIAN_POINT('Ctrl Pts',(2.99693666972406,0.688540962375334,102.327600250846));
#25042=CARTESIAN_POINT('Ctrl Pts',(3.01707459646963,0.594096455340248,102.322612070298));
#25043=CARTESIAN_POINT('Ctrl Pts',(3.03272116605009,0.499003586151244,102.317623889749));
#25044=CARTESIAN_POINT('Ctrl Pts',(3.04837742712118,0.403851816405978,102.31263261952));
#25045=CARTESIAN_POINT('Ctrl Pts',(3.05953674162776,0.308051320573856,102.307641349291));
#25046=CARTESIAN_POINT('Ctrl Pts',(3.06617561067201,0.212059837121748,102.302650079062));
#25047=CARTESIAN_POINT('Ctrl Pts',(3.07282498283358,0.115916488976235,102.297650912323));
#25048=CARTESIAN_POINT('Ctrl Pts',(3.07493962318002,0.0195819881951491,
102.292651745584));
#25049=CARTESIAN_POINT('Ctrl Pts',(3.07254813663131,-0.0764865876048893,
102.287652578845));
#25050=CARTESIAN_POINT('Ctrl Pts',(3.07143961667606,-0.121017021365781,
102.28533532722));
#25051=CARTESIAN_POINT('Ctrl Pts',(3.06936365093371,-0.16549039982456,102.283018075596));
#25052=CARTESIAN_POINT('Ctrl Pts',(3.06632683703467,-0.209861808056952,
102.280700823971));
#25053=CARTESIAN_POINT('Ctrl Pts',(3.05977485978896,-0.305593870265763,
102.275701314478));
#25054=CARTESIAN_POINT('Ctrl Pts',(3.04872388231001,-0.401186951466522,
102.270701804985));
#25055=CARTESIAN_POINT('Ctrl Pts',(3.03318367410548,-0.496184491031267,
102.265702295492));
#25056=CARTESIAN_POINT('Ctrl Pts',(3.01766454609472,-0.591053167036798,
102.260709567802));
#25057=CARTESIAN_POINT('Ctrl Pts',(2.9976683603208,-0.685327477452969,102.255716840112));
#25058=CARTESIAN_POINT('Ctrl Pts',(2.97325679924304,-0.778553951730414,
102.250724112422));
#25059=CARTESIAN_POINT('Ctrl Pts',(2.94887099174687,-0.871682074427455,
102.245736651934));
#25060=CARTESIAN_POINT('Ctrl Pts',(2.92007917959053,-0.963764136147713,
102.240749191445));
#25061=CARTESIAN_POINT('Ctrl Pts',(2.88699427219932,-1.05435588028347,102.235761730957));
#25062=CARTESIAN_POINT('Ctrl Pts',(2.85393303783272,-1.14488280390867,102.230777839114));
#25063=CARTESIAN_POINT('Ctrl Pts',(2.81658496499745,-1.23392111867382,102.22579394727));
#25064=CARTESIAN_POINT('Ctrl Pts',(2.77511279018437,-1.32104172975539,102.220810055426));
#25065=CARTESIAN_POINT('Ctrl Pts',(2.7336557185102,-1.40813061366815,102.215827978592));
#25066=CARTESIAN_POINT('Ctrl Pts',(2.68807771744261,-1.49330278556179,102.210845901759));
#25067=CARTESIAN_POINT('Ctrl Pts',(2.63858926419319,-1.57615003882385,102.205863824925));
#25068=CARTESIAN_POINT('Ctrl Pts',(2.58910532315058,-1.65898973832508,102.200882202342));
#25069=CARTESIAN_POINT('Ctrl Pts',(2.53571186406559,-1.73950456389468,102.195900579759));
#25070=CARTESIAN_POINT('Ctrl Pts',(2.47866429699143,-1.81731272840422,102.190918957176));
#25071=CARTESIAN_POINT('Ctrl Pts',(2.42160635766439,-1.89513503980904,102.185936428846));
#25072=CARTESIAN_POINT('Ctrl Pts',(2.36089325046359,-1.97024935882309,102.180953900516));
#25073=CARTESIAN_POINT('Ctrl Pts',(2.29682185592593,-2.0423054649442,102.175971372186));
#25074=CARTESIAN_POINT('Ctrl Pts',(2.23268140186773,-2.11443923692817,102.170983473425));
#25075=CARTESIAN_POINT('Ctrl Pts',(2.16517572616756,-2.18350788667534,102.165995574664));
#25076=CARTESIAN_POINT('Ctrl Pts',(2.09463975125441,-2.24919687054399,102.161007675903));
#25077=CARTESIAN_POINT('Ctrl Pts',(2.02406210977271,-2.31492465779704,102.156016830722));
#25078=CARTESIAN_POINT('Ctrl Pts',(1.95045093962948,-2.3772685204187,102.151025985541));
#25079=CARTESIAN_POINT('Ctrl Pts',(1.87417389055081,-2.43595453118026,102.146035140359));
#25080=CARTESIAN_POINT('Ctrl Pts',(1.79777357583458,-2.49473538001722,102.141036229846));
#25081=CARTESIAN_POINT('Ctrl Pts',(1.71869913968857,-2.54984632285046,102.136037319333));
#25082=CARTESIAN_POINT('Ctrl Pts',(1.63734674468351,-2.60105707120669,102.13103840882));
#25083=CARTESIAN_POINT('Ctrl Pts',(1.59011685156191,-2.63078794970622,102.128136244609));
#25084=CARTESIAN_POINT('Ctrl Pts',(1.54211964313373,-2.65920512779243,102.125234080398));
#25085=CARTESIAN_POINT('Ctrl Pts',(1.49343596752582,-2.6862708837532,102.122331916187));
#25086=CARTESIAN_POINT('Ctrl Pts',(1.40956941806112,-2.73289660649784,102.117332406694));
#25087=CARTESIAN_POINT('Ctrl Pts',(1.32336995709366,-2.77567293412901,102.112332897201));
#25088=CARTESIAN_POINT('Ctrl Pts',(1.23522586317959,-2.81435948608777,102.107333387708));
#25089=CARTESIAN_POINT('Ctrl Pts',(1.14720133616926,-2.85299355998444,102.102340660018));
#25090=CARTESIAN_POINT('Ctrl Pts',(1.05723781734186,-2.88754870909612,102.097347932328));
#25091=CARTESIAN_POINT('Ctrl Pts',(0.965749257407004,-2.9178297794453,102.092355204638));
#25092=CARTESIAN_POINT('Ctrl Pts',(0.874357215596731,-2.94807890402856,
102.08736774415));
#25093=CARTESIAN_POINT('Ctrl Pts',(0.781443745548439,-2.97406277636264,
102.082380283661));
#25094=CARTESIAN_POINT('Ctrl Pts',(0.687442959990188,-2.99563422779884,
102.077392823173));
#25095=CARTESIAN_POINT('Ctrl Pts',(0.593509434191262,-3.0171902443573,102.07240893133));
#25096=CARTESIAN_POINT('Ctrl Pts',(0.498490566123605,-3.03434001846278,
102.067425039486));
#25097=CARTESIAN_POINT('Ctrl Pts',(0.402834879351311,-3.04698643088183,
102.062441147642));
#25098=CARTESIAN_POINT('Ctrl Pts',(0.307214028011036,-3.05962823779069,
102.057459070809));
#25099=CARTESIAN_POINT('Ctrl Pts',(0.210957253484139,-3.0677698840657,102.052476993975));
#25100=CARTESIAN_POINT('Ctrl Pts',(0.114521550974326,-3.07136566764077,
102.047494917141));
#25101=CARTESIAN_POINT('Ctrl Pts',(0.0180946411787591,-3.07496112336322,
102.042513294558));
#25102=CARTESIAN_POINT('Ctrl Pts',(-0.0785107255000115,-3.07401152427165,
102.037531671975));
#25103=CARTESIAN_POINT('Ctrl Pts',(-0.17483525056192,-3.06852324175017,
102.032550049392));
#25104=CARTESIAN_POINT('Ctrl Pts',(-0.271177289119651,-3.06303396136222,
102.027567521062));
#25105=CARTESIAN_POINT('Ctrl Pts',(-0.367237946406401,-3.05300438367627,
102.022584992732));
#25106=CARTESIAN_POINT('Ctrl Pts',(-0.462561823095072,-3.0384928516972,
102.017602464402));
#25107=CARTESIAN_POINT('Ctrl Pts',(-0.55798844487411,-3.02396567842534,
102.012614565641));
#25108=CARTESIAN_POINT('Ctrl Pts',(-0.652676265943998,-3.00494697261566,
102.00762666688));
#25109=CARTESIAN_POINT('Ctrl Pts',(-0.746179100485398,-2.98154641084099,
102.002638768119));
#25110=CARTESIAN_POINT('Ctrl Pts',(-0.839737168434552,-2.95813202603329,
101.997647922938));
#25111=CARTESIAN_POINT('Ctrl Pts',(-0.932108435924485,-2.93033075773942,
101.992657077757));
#25112=CARTESIAN_POINT('Ctrl Pts',(-1.02286296744176,-2.89830184760598,
101.987666232575));
#25113=CARTESIAN_POINT('Ctrl Pts',(-1.11376416057381,-2.86622117794494,
101.982667322062));
#25114=CARTESIAN_POINT('Ctrl Pts',(-1.20304299444944,-2.82989938980636,
101.977668411549));
#25115=CARTESIAN_POINT('Ctrl Pts',(-1.29029061354383,-2.78954340037948,
101.972669501036));
#25116=CARTESIAN_POINT('Ctrl Pts',(-1.3409430340988,-2.76611435360915,101.969767336825));
#25117=CARTESIAN_POINT('Ctrl Pts',(-1.39091129889851,-2.74132644243857,
101.966865172614));
#25118=CARTESIAN_POINT('Ctrl Pts',(-1.44011974937299,-2.71522694400779,
101.963963008403));
#25119=CARTESIAN_POINT('Ctrl Pts',(-1.52489031967731,-2.67026577686473,
101.95896349891));
#25120=CARTESIAN_POINT('Ctrl Pts',(-1.60770220436728,-2.62125197237255,
101.953963989417));
#25121=CARTESIAN_POINT('Ctrl Pts',(-1.68814237521852,-2.56838034001811,
101.948964479924));
#25122=CARTESIAN_POINT('Ctrl Pts',(-1.76847342948877,-2.51558042769725,
101.943971752234));
#25123=CARTESIAN_POINT('Ctrl Pts',(-1.84643880023916,-2.45893332703264,
101.938979024544));
#25124=CARTESIAN_POINT('Ctrl Pts',(-1.92164941770891,-2.39868000479827,
101.933986296854));
#25125=CARTESIAN_POINT('Ctrl Pts',(-1.99678068987299,-2.3384902483001,101.928998836366));
#25126=CARTESIAN_POINT('Ctrl Pts',(-2.06916264533529,-2.27470210628814,
101.924011375877));
#25127=CARTESIAN_POINT('Ctrl Pts',(-2.13843548681621,-2.20759958296905,
101.919023915389));
#25128=CARTESIAN_POINT('Ctrl Pts',(-2.20765876195982,-2.1405450730739,101.914040023545));
#25129=CARTESIAN_POINT('Ctrl Pts',(-2.27377703121969,-2.07018120087511,
101.909056131702));
#25130=CARTESIAN_POINT('Ctrl Pts',(-2.33646463237743,-1.99683130775972,
101.904072239858));
#25131=CARTESIAN_POINT('Ctrl Pts',(-2.39912940426343,-1.92350812685873,
101.899090163024));
#25132=CARTESIAN_POINT('Ctrl Pts',(-2.45836570549932,-1.84720141901281,
101.894108086191));
#25133=CARTESIAN_POINT('Ctrl Pts',(-2.5138863897926,-1.76826962571196,101.889126009357));
#25134=CARTESIAN_POINT('Ctrl Pts',(-2.56940201187861,-1.68934502917217,
101.884144386774));
#25135=CARTESIAN_POINT('Ctrl Pts',(-2.62120243817953,-1.60779618218701,
101.879162764191));
#25136=CARTESIAN_POINT('Ctrl Pts',(-2.66904294717785,-1.52401180970496,
101.874181141608));
#25137=CARTESIAN_POINT('Ctrl Pts',(-2.71689215442356,-1.44021220374788,
101.869198613278));
#25138=CARTESIAN_POINT('Ctrl Pts',(-2.76077979685105,-1.35417664627861,
101.864216084948));
#25139=CARTESIAN_POINT('Ctrl Pts',(-2.80050686924816,-1.2663188876795,101.859233556618));
#25140=CARTESIAN_POINT('Ctrl Pts',(-2.84027676157447,-1.17836643136481,
101.854245657857));
#25141=CARTESIAN_POINT('Ctrl Pts',(-2.87587694986003,-1.08858825348359,
101.849257759096));
#25142=CARTESIAN_POINT('Ctrl Pts',(-2.90715650340211,-0.997418324840106,
101.844269860335));
#25143=CARTESIAN_POINT('Ctrl Pts',(-2.93845453420578,-0.906194540868447,
101.839279015154));
#25144=CARTESIAN_POINT('Ctrl Pts',(-2.9654267256226,-0.813577790403893,
101.834288169973));
#25145=CARTESIAN_POINT('Ctrl Pts',(-2.98797256925578,-0.720015399401322,
101.829297324791));
#25146=CARTESIAN_POINT('Ctrl Pts',(-3.01055484754163,-0.626301809212099,
101.824298414278));
#25147=CARTESIAN_POINT('Ctrl Pts',(-3.02869641233825,-0.531639957875307,
101.819299503765));
#25148=CARTESIAN_POINT('Ctrl Pts',(-3.04234822215892,-0.43648544663761,
101.814300593252));
#25149=CARTESIAN_POINT('Ctrl Pts',(-3.05027390792034,-0.381242605962414,
101.811398429041));
#25150=CARTESIAN_POINT('Ctrl Pts',(-3.05668729903727,-0.32583379401264,
101.80849626483));
#25151=CARTESIAN_POINT('Ctrl Pts',(-3.06158685878352,-0.270348212725789,
101.805594100619));
#25152=CARTESIAN_POINT('Ctrl Pts',(-3.06947520324294,-0.181015823615497,
101.800921584687));
#25153=CARTESIAN_POINT('Ctrl Pts',(-3.07345438733466,-0.0913332202229314,
101.796249068755));
#25154=CARTESIAN_POINT('Ctrl Pts',(-3.07349961013976,-0.00154805386522649,
101.791576552823));
#25155=CARTESIAN_POINT('Origin',(0.,0.,116.208423447177));
#25156=CARTESIAN_POINT('',(1.87238193903529,2.43733217358128,103.43740200794));
#25157=CARTESIAN_POINT('',(1.87238193903529,2.43733217358128,103.354077375525));
#25158=CARTESIAN_POINT('',(1.8723819390353,2.43733217358128,116.208423447177));
#25159=CARTESIAN_POINT('',(-3.07349905914929,-0.00240487181663789,102.708423447209));
#25160=CARTESIAN_POINT('Ctrl Pts',(1.87238193903529,2.43733217358128,103.354077375525));
#25161=CARTESIAN_POINT('Ctrl Pts',(1.9487790670956,2.37864316749308,103.349092480919));
#25162=CARTESIAN_POINT('Ctrl Pts',(2.02248072686417,2.3163076435992,103.344107586313));
#25163=CARTESIAN_POINT('Ctrl Pts',(2.09312461075592,2.25060694343723,103.339122691707));
#25164=CARTESIAN_POINT('Ctrl Pts',(2.16373572233126,2.18493672240546,103.334140109638));
#25165=CARTESIAN_POINT('Ctrl Pts',(2.2312915552962,2.11590472503888,103.329157527568));
#25166=CARTESIAN_POINT('Ctrl Pts',(2.29546369119003,2.0438318650095,103.324174945498));
#25167=CARTESIAN_POINT('Ctrl Pts',(2.35962357603549,1.97177276434909,103.319193314649));
#25168=CARTESIAN_POINT('Ctrl Pts',(2.42040075586888,1.89667428258958,103.3142116838));
#25169=CARTESIAN_POINT('Ctrl Pts',(2.47750517899769,1.81889261311372,103.30923005295));
#25170=CARTESIAN_POINT('Ctrl Pts',(2.53461428964495,1.74110455879074,103.304248013175));
#25171=CARTESIAN_POINT('Ctrl Pts',(2.58804978543248,1.66063323350006,103.2992659734));
#25172=CARTESIAN_POINT('Ctrl Pts',(2.63756390184625,1.5778653027675,103.294283933625));
#25173=CARTESIAN_POINT('Ctrl Pts',(2.68712858603362,1.49501284280801,103.289296805792));
#25174=CARTESIAN_POINT('Ctrl Pts',(2.73276366546207,1.40985946992048,103.28430967796));
#25175=CARTESIAN_POINT('Ctrl Pts',(2.77426657811826,1.32281790263664,103.279322550127));
#25176=CARTESIAN_POINT('Ctrl Pts',(2.81579029511711,1.23573270365381,103.274332922376));
#25177=CARTESIAN_POINT('Ctrl Pts',(2.85317754883889,1.14675782977441,103.269343294624));
#25178=CARTESIAN_POINT('Ctrl Pts',(2.8862741907344,1.05632549240301,103.264353666873));
#25179=CARTESIAN_POINT('Ctrl Pts',(2.91942798705916,0.965736987869896,103.259355422558));
#25180=CARTESIAN_POINT('Ctrl Pts',(2.94827623441644,0.873686410270901,103.254357178242));
#25181=CARTESIAN_POINT('Ctrl Pts',(2.9727148166892,0.780620822574235,103.249358933927));
#25182=CARTESIAN_POINT('Ctrl Pts',(2.99581857748097,0.692638424410125,103.244633690877));
#25183=CARTESIAN_POINT('Ctrl Pts',(3.01498160827294,0.603749276804136,103.239908447827));
#25184=CARTESIAN_POINT('Ctrl Pts',(3.03015849914792,0.514336193594856,103.235183204777));
#25185=CARTESIAN_POINT('Ctrl Pts',(3.04621629960374,0.419733322681253,103.230183695284));
#25186=CARTESIAN_POINT('Ctrl Pts',(3.05786774372334,0.324211570568872,103.225184185791));
#25187=CARTESIAN_POINT('Ctrl Pts',(3.06501536928885,0.228217080918866,103.220184676298));
#25188=CARTESIAN_POINT('Ctrl Pts',(3.07215329914567,0.132352807184519,103.215191948608));
#25189=CARTESIAN_POINT('Ctrl Pts',(3.07479952016353,0.0360175043912559,
103.210199220918));
#25190=CARTESIAN_POINT('Ctrl Pts',(3.07290776230444,-0.0603335260788791,
103.205206493228));
#25191=CARTESIAN_POINT('Ctrl Pts',(3.07101800020222,-0.156582908640208,
103.20021903274));
#25192=CARTESIAN_POINT('Ctrl Pts',(3.0645997849622,-0.25284754934986,103.195231572251));
#25193=CARTESIAN_POINT('Ctrl Pts',(3.05365880648709,-0.348669103253849,
103.190244111763));
#25194=CARTESIAN_POINT('Ctrl Pts',(3.04272565653778,-0.444422094596621,
103.18526021992));
#25195=CARTESIAN_POINT('Ctrl Pts',(3.02727622630706,-0.539732194514151,
103.180276328076));
#25196=CARTESIAN_POINT('Ctrl Pts',(3.00736819811512,-0.634144124758574,
103.175292436232));
#25197=CARTESIAN_POINT('Ctrl Pts',(2.98746741993402,-0.728521672516159,
103.170310359399));
#25198=CARTESIAN_POINT('Ctrl Pts',(2.96311136040599,-0.822001271416911,
103.165328282565));
#25199=CARTESIAN_POINT('Ctrl Pts',(2.93440900753257,-0.91413676575866,103.160346205731));
#25200=CARTESIAN_POINT('Ctrl Pts',(2.90570927165249,-1.00626385946593,103.155364583148));
#25201=CARTESIAN_POINT('Ctrl Pts',(2.87266416104216,-1.0970466732265,103.150382960565));
#25202=CARTESIAN_POINT('Ctrl Pts',(2.83543253547438,-1.18605420903656,103.145401337982));
#25203=CARTESIAN_POINT('Ctrl Pts',(2.79819414054104,-1.27507792798496,103.140418809652));
#25204=CARTESIAN_POINT('Ctrl Pts',(2.75676788836646,-1.36232532300432,103.135436281322));
#25205=CARTESIAN_POINT('Ctrl Pts',(2.71136035032806,-1.44738636882793,103.130453752993));
#25206=CARTESIAN_POINT('Ctrl Pts',(2.66590386965575,-1.53253909792276,103.125465854232));
#25207=CARTESIAN_POINT('Ctrl Pts',(2.61645774311736,-1.61550038528,103.12047795547));
#25208=CARTESIAN_POINT('Ctrl Pts',(2.56327388343518,-1.69588597744634,103.115490056709));
#25209=CARTESIAN_POINT('Ctrl Pts',(2.51005860731703,-1.77631905448543,103.110499211528));
#25210=CARTESIAN_POINT('Ctrl Pts',(2.45310146076836,-1.85417305267103,103.105508366347));
#25211=CARTESIAN_POINT('Ctrl Pts',(2.39269568836607,-1.92909553751866,103.100517521166));
#25212=CARTESIAN_POINT('Ctrl Pts',(2.33219229871011,-2.00413909899388,103.095518610652));
#25213=CARTESIAN_POINT('Ctrl Pts',(2.26822944612697,-2.07624135943845,103.090519700139));
#25214=CARTESIAN_POINT('Ctrl Pts',(2.20113831793372,-2.14508562890247,103.085520789626));
#25215=CARTESIAN_POINT('Ctrl Pts',(2.16218793652437,-2.1850538128589,103.082618625415));
#25216=CARTESIAN_POINT('Ctrl Pts',(2.12218382895401,-2.223924616875,103.079716461204));
#25217=CARTESIAN_POINT('Ctrl Pts',(2.08119575623365,-2.26164242846544,103.076814296993));
#25218=CARTESIAN_POINT('Ctrl Pts',(2.01058629248019,-2.32661826835245,103.0718147875));
#25219=CARTESIAN_POINT('Ctrl Pts',(1.93680703068045,-2.38839837684193,103.066815278007));
#25220=CARTESIAN_POINT('Ctrl Pts',(1.86017912923882,-2.44665809976472,103.061815768514));
#25221=CARTESIAN_POINT('Ctrl Pts',(1.78365517305878,-2.50483879374341,103.056823040824));
#25222=CARTESIAN_POINT('Ctrl Pts',(1.7042906034489,-2.55950832950711,103.051830313134));
#25223=CARTESIAN_POINT('Ctrl Pts',(1.62244213190147,-2.61038000655671,103.046837585444));
#25224=CARTESIAN_POINT('Ctrl Pts',(1.54068000842812,-2.6611980152695,103.041850124956));
#25225=CARTESIAN_POINT('Ctrl Pts',(1.45643956315767,-2.7082258997491,103.036862664467));
#25226=CARTESIAN_POINT('Ctrl Pts',(1.37010835017788,-2.75121888601631,103.031875203979));
#25227=CARTESIAN_POINT('Ctrl Pts',(1.2838389091994,-2.79418110979668,103.026891312135));
#25228=CARTESIAN_POINT('Ctrl Pts',(1.19548206628228,-2.83311397959143,103.021907420292));
#25229=CARTESIAN_POINT('Ctrl Pts',(1.10545111053773,-2.86781800193299,103.016923528448));
#25230=CARTESIAN_POINT('Ctrl Pts',(1.01545294183751,-2.9025093859291,103.011941451614));
#25231=CARTESIAN_POINT('Ctrl Pts',(0.923782280826692,-2.93297482464625,
103.006959374781));
#25232=CARTESIAN_POINT('Ctrl Pts',(0.830872698153815,-2.95906282621079,
103.001977297947));
#25233=CARTESIAN_POINT('Ctrl Pts',(0.737971586694478,-2.98514844915059,
102.996995675364));
#25234=CARTESIAN_POINT('Ctrl Pts',(0.64383220082838,-3.00685730997497,102.992014052781));
#25235=CARTESIAN_POINT('Ctrl Pts',(0.548902549807335,-3.02408800149979,
102.987032430198));
#25236=CARTESIAN_POINT('Ctrl Pts',(0.453955638903061,-3.04132182586794,
102.982049901868));
#25237=CARTESIAN_POINT('Ctrl Pts',(0.358218609394035,-3.05407578555463,
102.977067373538));
#25238=CARTESIAN_POINT('Ctrl Pts',(0.262147855419645,-3.06229991214102,
102.972084845208));
#25239=CARTESIAN_POINT('Ctrl Pts',(0.165973551331058,-3.07053290312382,
102.967096946447));
#25240=CARTESIAN_POINT('Ctrl Pts',(0.0694652427456439,-3.07422627605857,
102.962109047686));
#25241=CARTESIAN_POINT('Ctrl Pts',(-0.026917607229562,-3.07338212600077,
102.957121148925));
#25242=CARTESIAN_POINT('Ctrl Pts',(-0.123357391876979,-3.07253747729195,
102.952130303744));
#25243=CARTESIAN_POINT('Ctrl Pts',(-0.219671132276306,-3.06714999302605,
102.947139458563));
#25244=CARTESIAN_POINT('Ctrl Pts',(-0.315403551633273,-3.05727376098659,
102.942148613381));
#25245=CARTESIAN_POINT('Ctrl Pts',(-0.411290676997528,-3.04738156870675,
102.937149702868));
#25246=CARTESIAN_POINT('Ctrl Pts',(-0.506594171739937,-3.03298620967511,
102.932150792355));
#25247=CARTESIAN_POINT('Ctrl Pts',(-0.600868083321939,-3.01419305892058,
102.927151881842));
#25248=CARTESIAN_POINT('Ctrl Pts',(-0.655599683637761,-3.00328251963658,
102.924249717631));
#25249=CARTESIAN_POINT('Ctrl Pts',(-0.709984512979015,-2.99089065275652,
102.92134755342));
#25250=CARTESIAN_POINT('Ctrl Pts',(-0.763937942530679,-2.97704569497379,
102.918445389209));
#25251=CARTESIAN_POINT('Ctrl Pts',(-0.856882608515816,-2.95319521897278,
102.913445879716));
#25252=CARTESIAN_POINT('Ctrl Pts',(-0.948872521153678,-2.92494601987692,
102.908446370223));
#25253=CARTESIAN_POINT('Ctrl Pts',(-1.03946050783718,-2.89239072440894,
102.90344686073));
#25254=CARTESIAN_POINT('Ctrl Pts',(-1.12992561249208,-2.8598795899925,102.89845413304));
#25255=CARTESIAN_POINT('Ctrl Pts',(-1.21899216114037,-2.82307411537473,
102.89346140535));
#25256=CARTESIAN_POINT('Ctrl Pts',(-1.30622545948642,-2.78211741286911,
102.88846867766));
#25257=CARTESIAN_POINT('Ctrl Pts',(-1.39336672890185,-2.74120391865212,
102.883481217171));
#25258=CARTESIAN_POINT('Ctrl Pts',(-1.47867819752179,-2.69614808817625,
102.878493756683));
#25259=CARTESIAN_POINT('Ctrl Pts',(-1.5617435463928,-2.64714173124531,102.873506296195));
#25260=CARTESIAN_POINT('Ctrl Pts',(-1.64474946006473,-2.59817043950848,
102.868522404351));
#25261=CARTESIAN_POINT('Ctrl Pts',(-1.72551207194326,-2.545254463062,102.863538512507));
#25262=CARTESIAN_POINT('Ctrl Pts',(-1.80363903254509,-2.48863185109405,
102.858554620664));
#25263=CARTESIAN_POINT('Ctrl Pts',(-1.88173754124283,-2.43202985967902,
102.85357254383));
#25264=CARTESIAN_POINT('Ctrl Pts',(-1.95720195069231,-2.37172417211283,
102.848590466996));
#25265=CARTESIAN_POINT('Ctrl Pts',(-2.02966913246221,-2.30799598412347,
102.843608390163));
#25266=CARTESIAN_POINT('Ctrl Pts',(-2.10212970689473,-2.24427360667661,
102.83862676758));
#25267=CARTESIAN_POINT('Ctrl Pts',(-2.1715932674645,-2.17712963924436,102.833645144997));
#25268=CARTESIAN_POINT('Ctrl Pts',(-2.23773083527129,-2.10688465723115,
102.828663522413));
#25269=CARTESIAN_POINT('Ctrl Pts',(-2.30388042805295,-2.03662690344283,
102.823680994084));
#25270=CARTESIAN_POINT('Ctrl Pts',(-2.3667025262089,-1.96326733494541,102.818698465754));
#25271=CARTESIAN_POINT('Ctrl Pts',(-2.42590673211331,-1.88716156623838,
102.813715937424));
#25272=CARTESIAN_POINT('Ctrl Pts',(-2.48517475142643,-1.81097376672883,
102.808728038663));
#25273=CARTESIAN_POINT('Ctrl Pts',(-2.54081682341287,-1.73203420469134,
102.803740139902));
#25274=CARTESIAN_POINT('Ctrl Pts',(-2.59258454998316,-1.65072941489168,
102.798752241141));
#25275=CARTESIAN_POINT('Ctrl Pts',(-2.64438285646005,-1.56937659723677,
102.79376139596));
#25276=CARTESIAN_POINT('Ctrl Pts',(-2.69230204253118,-1.48565615061415,
102.788770550778));
#25277=CARTESIAN_POINT('Ctrl Pts',(-2.73613960045076,-1.39997940586465,
102.783779705597));
#25278=CARTESIAN_POINT('Ctrl Pts',(-2.78004800097105,-1.31416420533189,
102.778780795084));
#25279=CARTESIAN_POINT('Ctrl Pts',(-2.8198614213579,-1.22638679349449,102.773781884571));
#25280=CARTESIAN_POINT('Ctrl Pts',(-2.85542544981684,-1.13707860350034,
102.768782974058));
#25281=CARTESIAN_POINT('Ctrl Pts',(-2.87607247886867,-1.08522989925403,
102.765880809847));
#25282=CARTESIAN_POINT('Ctrl Pts',(-2.89528818176262,-1.03286555270384,
102.762978645636));
#25283=CARTESIAN_POINT('Ctrl Pts',(-2.91305016692883,-0.98007192335866,
102.760076481425));
#25284=CARTESIAN_POINT('Ctrl Pts',(-2.94920738770469,-0.872602465754107,
102.75416868502));
#25285=CARTESIAN_POINT('Ctrl Pts',(-2.97944169451475,-0.763046477913077,
102.748260888615));
#25286=CARTESIAN_POINT('Ctrl Pts',(-3.0035458119629,-0.652008286327827,
102.742353092211));
#25287=CARTESIAN_POINT('Ctrl Pts',(-3.02740835185899,-0.542082947538994,
102.736504505233));
#25288=CARTESIAN_POINT('Ctrl Pts',(-3.04526290787279,-0.430705059004667,
102.730655918256));
#25289=CARTESIAN_POINT('Ctrl Pts',(-3.05695463632165,-0.318481712931148,
102.724807331279));
#25290=CARTESIAN_POINT('Ctrl Pts',(-3.0678721407958,-0.213689774919587,
102.719346036589));
#25291=CARTESIAN_POINT('Ctrl Pts',(-3.0734163099308,-0.108160880676264,
102.713884741899));
#25292=CARTESIAN_POINT('Ctrl Pts',(-3.07349905914929,-0.00240487181666147,
102.708423447209));
#25293=CARTESIAN_POINT('Ctrl Pts',(-3.07349905914978,-0.00240487119184143,
102.708423447177));
#25294=CARTESIAN_POINT('Ctrl Pts',(-3.07357440903969,0.0938945965503393,
102.703450493134));
#25295=CARTESIAN_POINT('Ctrl Pts',(-3.06911954638383,0.190252789663529,
102.698477539092));
#25296=CARTESIAN_POINT('Ctrl Pts',(-3.06014462176969,0.28621171159479,102.693504585049));
#25297=CARTESIAN_POINT('Ctrl Pts',(-3.05117154752427,0.382150849584176,
102.688532656285));
#25298=CARTESIAN_POINT('Ctrl Pts',(-3.03768030403397,0.477690441648064,
102.683560727521));
#25299=CARTESIAN_POINT('Ctrl Pts',(-3.01973301736177,0.572376409240639,
102.678588798757));
#25300=CARTESIAN_POINT('Ctrl Pts',(-3.00178449415828,0.667068900502399,
102.673616527437));
#25301=CARTESIAN_POINT('Ctrl Pts',(-2.97937940044342,0.760907217840844,
102.668644256118));
#25302=CARTESIAN_POINT('Ctrl Pts',(-2.95263100332805,0.85344736696881,102.663671984798));
#25303=CARTESIAN_POINT('Ctrl Pts',(-2.92485280817885,0.949550259060835,
102.658508283868));
#25304=CARTESIAN_POINT('Ctrl Pts',(-2.89239026140684,1.044252510288,102.653344582938));
#25305=CARTESIAN_POINT('Ctrl Pts',(-2.85542656316374,1.13707580766585,102.648180882009));
#25306=CARTESIAN_POINT('Ctrl Pts',(-2.81977708586454,1.22659883133477,102.643200773204));
#25307=CARTESIAN_POINT('Ctrl Pts',(-2.77994134730074,1.31437386440563,102.638220664399));
#25308=CARTESIAN_POINT('Ctrl Pts',(-2.7361315529654,1.39999513387268,102.633240555594));
#25309=CARTESIAN_POINT('Ctrl Pts',(-2.69228901873091,1.48568038975574,102.628256725059));
#25310=CARTESIAN_POINT('Ctrl Pts',(-2.6444667369319,1.56920829804548,102.623272894523));
#25311=CARTESIAN_POINT('Ctrl Pts',(-2.59292101568691,1.65020085335366,102.618289063988));
#25312=CARTESIAN_POINT('Ctrl Pts',(-2.54129576608687,1.73131836965841,102.613297544049));
#25313=CARTESIAN_POINT('Ctrl Pts',(-2.48593587132566,1.80989237281012,102.60830602411));
#25314=CARTESIAN_POINT('Ctrl Pts',(-2.42713849798024,1.88557708981155,102.603314504171));
#25315=CARTESIAN_POINT('Ctrl Pts',(-2.42082891055332,1.89369886994614,102.602778860661));
#25316=CARTESIAN_POINT('Ctrl Pts',(-2.41447977355874,1.90178741316457,102.602243217151));
#25317=CARTESIAN_POINT('Ctrl Pts',(-2.40809147900626,1.909842317768,102.60170757364));
#25318=CARTESIAN_POINT('Ctrl Pts',(-2.34846536825855,1.98502398479989,102.596708064147));
#25319=CARTESIAN_POINT('Ctrl Pts',(-2.28521034726891,2.05754269684241,102.591708554654));
#25320=CARTESIAN_POINT('Ctrl Pts',(-2.21859308199756,2.12702773524761,102.586709045161));
#25321=CARTESIAN_POINT('Ctrl Pts',(-2.15206618262348,2.19641851763949,102.581716317471));
#25322=CARTESIAN_POINT('Ctrl Pts',(-2.0821864045681,2.26278349084756,102.576723589781));
#25323=CARTESIAN_POINT('Ctrl Pts',(-2.00926144500736,2.32578388841417,102.571730862091));
#25324=CARTESIAN_POINT('Ctrl Pts',(-1.93641341944093,2.38871782214924,102.566743401603));
#25325=CARTESIAN_POINT('Ctrl Pts',(-1.86052692920946,2.4482939510788,102.561755941115));
#25326=CARTESIAN_POINT('Ctrl Pts',(-1.78194666857239,2.50421011905227,102.556768480626));
#25327=CARTESIAN_POINT('Ctrl Pts',(-1.7034226339486,2.56008627770052,102.551784588783));
#25328=CARTESIAN_POINT('Ctrl Pts',(-1.62220901723995,2.61230742764789,102.546800696939));
#25329=CARTESIAN_POINT('Ctrl Pts',(-1.53868298702377,2.66061213171774,102.541816805095));
#25330=CARTESIAN_POINT('Ctrl Pts',(-1.45518737491906,2.70889924441075,102.536834728262));
#25331=CARTESIAN_POINT('Ctrl Pts',(-1.36938140211987,2.75327252554234,102.531852651428));
#25332=CARTESIAN_POINT('Ctrl Pts',(-1.2816697484747,2.79351479427706,102.526870574594));
#25333=CARTESIAN_POINT('Ctrl Pts',(-1.19396609211161,2.83375339384399,102.521888952011));
#25334=CARTESIAN_POINT('Ctrl Pts',(-1.10435749940877,2.86986154698673,102.516907329428));
#25335=CARTESIAN_POINT('Ctrl Pts',(-1.01327071436459,2.90166929704456,102.511925706845));
#25336=CARTESIAN_POINT('Ctrl Pts',(-0.922167368138048,2.93348283031177,
102.506943178515));
#25337=CARTESIAN_POINT('Ctrl Pts',(-0.829585710238195,2.96099426297923,
102.501960650185));
#25338=CARTESIAN_POINT('Ctrl Pts',(-0.735968779922514,2.98408314310767,
102.496978121856));
#25339=CARTESIAN_POINT('Ctrl Pts',(-0.642250944353016,3.0071969096461,102.491990223095));
#25340=CARTESIAN_POINT('Ctrl Pts',(-0.547496035532473,3.02587850176356,
102.487002324334));
#25341=CARTESIAN_POINT('Ctrl Pts',(-0.452158234261135,3.04005841739758,
102.482014425572));
#25342=CARTESIAN_POINT('Ctrl Pts',(-0.356764115641836,3.05424670930241,
102.477023580391));
#25343=CARTESIAN_POINT('Ctrl Pts',(-0.260786855511279,3.06392798578358,
102.47203273521));
#25344=CARTESIAN_POINT('Ctrl Pts',(-0.164684598476815,3.06908475494316,
102.467041890028));
#25345=CARTESIAN_POINT('Ctrl Pts',(-0.0684270377681817,3.07424985757193,
102.462042979515));
#25346=CARTESIAN_POINT('Ctrl Pts',(0.0279554845327262,3.07487585014498,
102.457044069002));
#25347=CARTESIAN_POINT('Ctrl Pts',(0.12400604513015,3.07099735440641,102.452045158489));
#25348=CARTESIAN_POINT('Ctrl Pts',(0.179769095633911,3.0687456574626,102.449142994278));
#25349=CARTESIAN_POINT('Ctrl Pts',(0.235420357734847,3.06497669821165,102.446240830067));
#25350=CARTESIAN_POINT('Ctrl Pts',(0.290871837190732,3.05970518585195,102.443338665856));
#25351=CARTESIAN_POINT('Ctrl Pts',(0.38638965175104,3.05062475472607,102.43833954977));
#25352=CARTESIAN_POINT('Ctrl Pts',(0.481649606642594,3.03705127955959,102.433340433685));
#25353=CARTESIAN_POINT('Ctrl Pts',(0.576195666898044,3.01900659215046,102.428341317599));
#25354=CARTESIAN_POINT('Ctrl Pts',(0.670619518355395,3.00098522902955,102.423348663294));
#25355=CARTESIAN_POINT('Ctrl Pts',(0.764330881220847,2.97850421807133,102.41835600899));
#25356=CARTESIAN_POINT('Ctrl Pts',(0.856878093999578,2.95163720365895,102.413363354686));
#25357=CARTESIAN_POINT('Ctrl Pts',(0.949320810009901,2.92480052528911,102.408376337679));
#25358=CARTESIAN_POINT('Ctrl Pts',(1.04060157080027,2.89358781392061,102.403389320673));
#25359=CARTESIAN_POINT('Ctrl Pts',(1.13027937671876,2.8581236468292,102.398402303667));
#25360=CARTESIAN_POINT('Ctrl Pts',(1.21989649384948,2.82268347984894,102.393418661588));
#25361=CARTESIAN_POINT('Ctrl Pts',(1.30791240494778,2.78299773560621,102.388435019508));
#25362=CARTESIAN_POINT('Ctrl Pts',(1.39390252845336,2.73924040404841,102.383451377429));
#25363=CARTESIAN_POINT('Ctrl Pts',(1.47987428090962,2.69549242086766,102.378468800061));
#25364=CARTESIAN_POINT('Ctrl Pts',(1.56382071038342,2.64767476874144,102.373486222694));
#25365=CARTESIAN_POINT('Ctrl Pts',(1.64533919289062,2.59600870382556,102.368503645327));
#25366=CARTESIAN_POINT('Ctrl Pts',(1.72335375591205,2.54656340806587,102.363735234727));
#25367=CARTESIAN_POINT('Ctrl Pts',(1.79914446256703,2.49359390502932,102.358966824128));
#25368=CARTESIAN_POINT('Ctrl Pts',(1.8723819390353,2.43733217358127,102.354198413529));
#25369=CARTESIAN_POINT('',(-3.07349876002173,0.00276082323149203,102.791576552849));
#25370=CARTESIAN_POINT('Ctrl Pts',(-3.07349876002127,0.00276082373854232,
102.791576552823));
#25371=CARTESIAN_POINT('Ctrl Pts',(-3.0733818456602,0.132916233066199,102.784832988938));
#25372=CARTESIAN_POINT('Ctrl Pts',(-3.06499365801856,0.262711138894001,
102.778089425052));
#25373=CARTESIAN_POINT('Ctrl Pts',(-3.04849240550272,0.391275227419569,
102.771345861166));
#25374=CARTESIAN_POINT('Ctrl Pts',(-3.03581851156285,0.490019708839072,
102.766166423219));
#25375=CARTESIAN_POINT('Ctrl Pts',(-3.01835961128476,0.588038888602218,
102.760986985271));
#25376=CARTESIAN_POINT('Ctrl Pts',(-2.99620562000435,0.684948270057185,
102.755807547324));
#25377=CARTESIAN_POINT('Ctrl Pts',(-2.97482123605449,0.778491117264577,
102.750808037831));
#25378=CARTESIAN_POINT('Ctrl Pts',(-2.94901442045459,0.871195861184662,
102.745808528338));
#25379=CARTESIAN_POINT('Ctrl Pts',(-2.91886594287446,0.962613036233973,
102.740809018845));
#25380=CARTESIAN_POINT('Ctrl Pts',(-2.88875836151275,1.05390620446576,102.735816291154));
#25381=CARTESIAN_POINT('Ctrl Pts',(-2.85432095934281,1.14391486172565,102.730823563464));
#25382=CARTESIAN_POINT('Ctrl Pts',(-2.81568530393745,1.23220068137891,102.725830835774));
#25383=CARTESIAN_POINT('Ctrl Pts',(-2.77709040817466,1.32039336171788,102.720843375286));
#25384=CARTESIAN_POINT('Ctrl Pts',(-2.7343062389121,1.40686641762785,102.715855914798));
#25385=CARTESIAN_POINT('Ctrl Pts',(-2.68751353008668,1.49119860367459,102.710868454309));
#25386=CARTESIAN_POINT('Ctrl Pts',(-2.64075430253822,1.57547044807092,102.705884562466));
#25387=CARTESIAN_POINT('Ctrl Pts',(-2.58999244964522,1.65760408509986,102.700900670622));
#25388=CARTESIAN_POINT('Ctrl Pts',(-2.53545556238873,1.73720100769947,102.695916778778));
#25389=CARTESIAN_POINT('Ctrl Pts',(-2.48093853611586,1.81676894307126,102.690934701945));
#25390=CARTESIAN_POINT('Ctrl Pts',(-2.42264945486254,1.89380163777317,102.685952625111));
#25391=CARTESIAN_POINT('Ctrl Pts',(-2.3608598137594,1.96792865464578,102.680970548277));
#25392=CARTESIAN_POINT('Ctrl Pts',(-2.29907580644797,2.04204891284224,102.675988925694));
#25393=CARTESIAN_POINT('Ctrl Pts',(-2.23379215506017,2.11326368287658,102.671007303111));
#25394=CARTESIAN_POINT('Ctrl Pts',(-2.16532062365469,2.18123562385535,102.666025680528));
#25395=CARTESIAN_POINT('Ctrl Pts',(-2.09683664291834,2.24921992333066,102.661043152198));
#25396=CARTESIAN_POINT('Ctrl Pts',(-2.02516394260194,2.31395991357074,102.656060623868));
#25397=CARTESIAN_POINT('Ctrl Pts',(-1.9506503338181,2.37515589492044,102.651078095538));
#25398=CARTESIAN_POINT('Ctrl Pts',(-1.87605641034575,2.43641783651903,102.646090196777));
#25399=CARTESIAN_POINT('Ctrl Pts',(-1.79861580503093,2.4941278640542,102.641102298016));
#25400=CARTESIAN_POINT('Ctrl Pts',(-1.71870834904133,2.54802744509073,102.636114399255));
#25401=CARTESIAN_POINT('Ctrl Pts',(-1.63875369062066,2.60195886534962,102.631123554074));
#25402=CARTESIAN_POINT('Ctrl Pts',(-1.55632965489344,2.65207512928547,102.626132708893));
#25403=CARTESIAN_POINT('Ctrl Pts',(-1.47184207391802,2.69816292307279,102.621141863711));
#25404=CARTESIAN_POINT('Ctrl Pts',(-1.38721795887821,2.74432519589871,102.616142953198));
#25405=CARTESIAN_POINT('Ctrl Pts',(-1.30052403441139,2.78644580762637,102.611144042685));
#25406=CARTESIAN_POINT('Ctrl Pts',(-1.21218749966317,2.82435899199453,102.606145132172));
#25407=CARTESIAN_POINT('Ctrl Pts',(-1.16090289895004,2.84636984546106,102.603242967961));
#25408=CARTESIAN_POINT('Ctrl Pts',(-1.10906498743717,2.86696350849769,102.60034080375));
#25409=CARTESIAN_POINT('Ctrl Pts',(-1.05675950233097,2.88611531374496,102.597438639539));
#25410=CARTESIAN_POINT('Ctrl Pts',(-0.96665372253602,2.91910780665049,102.592439130046));
#25411=CARTESIAN_POINT('Ctrl Pts',(-0.874843137497201,2.94793449136314,
102.587439620553));
#25412=CARTESIAN_POINT('Ctrl Pts',(-0.781748730651191,2.97241840462026,
102.58244011106));
#25413=CARTESIAN_POINT('Ctrl Pts',(-0.688780605776904,2.99686910560452,
102.57744738337));
#25414=CARTESIAN_POINT('Ctrl Pts',(-0.594532541098022,3.01698863229479,
102.57245465568));
#25415=CARTESIAN_POINT('Ctrl Pts',(-0.499443833784544,3.0326486949356,102.56746192799));
#25416=CARTESIAN_POINT('Ctrl Pts',(-0.40445544266044,3.04829223660506,102.562474467502));
#25417=CARTESIAN_POINT('Ctrl Pts',(-0.308628602744227,3.05948559577763,
102.557487007013));
#25418=CARTESIAN_POINT('Ctrl Pts',(-0.212415052330399,3.066151022951,102.552499546525));
#25419=CARTESIAN_POINT('Ctrl Pts',(-0.116270344960902,3.07281168085543,
102.547515654681));
#25420=CARTESIAN_POINT('Ctrl Pts',(-0.019739913818218,3.07495081716137,
102.542531762838));
#25421=CARTESIAN_POINT('Ctrl Pts',(0.0767180641836116,3.07254236563598,
102.537547870994));
#25422=CARTESIAN_POINT('Ctrl Pts',(0.173140914578841,3.07013479120897,102.53256579416));
#25423=CARTESIAN_POINT('Ctrl Pts',(0.269490925881531,3.06318293042476,102.527583717327));
#25424=CARTESIAN_POINT('Ctrl Pts',(0.365309562312508,3.05171282621466,102.522601640493));
#25425=CARTESIAN_POINT('Ctrl Pts',(0.461119462291404,3.0402437678138,102.51762001791));
#25426=CARTESIAN_POINT('Ctrl Pts',(0.556397647895687,3.02425733739534,102.512638395327));
#25427=CARTESIAN_POINT('Ctrl Pts',(0.650691419758013,3.00383137447049,102.507656772744));
#25428=CARTESIAN_POINT('Ctrl Pts',(0.745002335889377,2.98340169774571,102.502674244414));
#25429=CARTESIAN_POINT('Ctrl Pts',(0.838328053816558,2.95853097840997,102.497691716084));
#25430=CARTESIAN_POINT('Ctrl Pts',(0.930227821477748,2.92934778579614,102.492709187754));
#25431=CARTESIAN_POINT('Ctrl Pts',(1.0222266435445,2.90013313800163,102.487721288993));
#25432=CARTESIAN_POINT('Ctrl Pts',(1.11279602787013,2.86659687028279,102.482733390232));
#25433=CARTESIAN_POINT('Ctrl Pts',(1.20151231977035,2.8289168237048,102.477745491471));
#25434=CARTESIAN_POINT('Ctrl Pts',(1.29028101760189,2.79121451900611,102.47275464629));
#25435=CARTESIAN_POINT('Ctrl Pts',(1.37719404807226,2.7493637518578,102.467763801109));
#25436=CARTESIAN_POINT('Ctrl Pts',(1.4618515292926,2.70358879201421,102.462772955927));
#25437=CARTESIAN_POINT('Ctrl Pts',(1.54664581914047,2.65773985867956,102.457774045414));
#25438=CARTESIAN_POINT('Ctrl Pts',(1.62917690581338,2.60795429647158,102.452775134901));
#25439=CARTESIAN_POINT('Ctrl Pts',(1.70907315660856,2.55450018503817,102.447776224388));
#25440=CARTESIAN_POINT('Ctrl Pts',(1.75545767160221,2.52346690114089,102.444874060177));
#25441=CARTESIAN_POINT('Ctrl Pts',(1.80095470912527,2.49119791287163,102.441971895966));
#25442=CARTESIAN_POINT('Ctrl Pts',(1.84549689863107,2.4577517057553,102.439069731755));
#25443=CARTESIAN_POINT('Ctrl Pts',(1.854494037828,2.45099585957051,102.438483519544));
#25444=CARTESIAN_POINT('Ctrl Pts',(1.86345592697286,2.44418922160882,102.437897307334));
#25445=CARTESIAN_POINT('Ctrl Pts',(1.87238193903529,2.43733217358128,102.437311095123));
#25446=CARTESIAN_POINT('Ctrl Pts',(1.87238193903529,2.43733217358128,103.43740200794));
#25447=CARTESIAN_POINT('Ctrl Pts',(1.94890807686061,2.37854406095496,103.432413164395));
#25448=CARTESIAN_POINT('Ctrl Pts',(2.02261042630876,2.31618872145143,103.42742432085));
#25449=CARTESIAN_POINT('Ctrl Pts',(2.09315372916472,2.25057986218748,103.422435477304));
#25450=CARTESIAN_POINT('Ctrl Pts',(2.16374507961965,2.18492631621293,103.417443235819));
#25451=CARTESIAN_POINT('Ctrl Pts',(2.23117279423004,2.11601515269204,103.412450994333));
#25452=CARTESIAN_POINT('Ctrl Pts',(2.29514009236418,2.04419524664905,103.407458752847));
#25453=CARTESIAN_POINT('Ctrl Pts',(2.35920408615418,1.97226677461809,103.402458964879));
#25454=CARTESIAN_POINT('Ctrl Pts',(2.41979695160821,1.89742112725603,103.397459176911));
#25455=CARTESIAN_POINT('Ctrl Pts',(2.47666379764105,1.82003809945128,103.392459388943));
#25456=CARTESIAN_POINT('Ctrl Pts',(2.48870571312885,1.80365175229081,103.391400652115));
#25457=CARTESIAN_POINT('Ctrl Pts',(2.50058071237939,1.78715172008231,103.390341915288));
#25458=CARTESIAN_POINT('Ctrl Pts',(2.51228663814601,1.7705417526263,103.38928317846));
#25459=CARTESIAN_POINT('Ctrl Pts',(2.56756372444965,1.69210706724807,103.384283668967));
#25460=CARTESIAN_POINT('Ctrl Pts',(2.61926123270116,1.61094347370205,103.379284159474));
#25461=CARTESIAN_POINT('Ctrl Pts',(2.6670988678853,1.52741149626582,103.374284649981));
#25462=CARTESIAN_POINT('Ctrl Pts',(2.71487161162101,1.44399282942666,103.369291922291));
#25463=CARTESIAN_POINT('Ctrl Pts',(2.75879467199935,1.35821254138241,103.364299194601));
#25464=CARTESIAN_POINT('Ctrl Pts',(2.79862999518409,1.27046149097715,103.359306466911));
#25465=CARTESIAN_POINT('Ctrl Pts',(2.83842329310691,1.18280301571834,103.354319006423));
#25466=CARTESIAN_POINT('Ctrl Pts',(2.87413724626096,1.09317830881245,103.349331545934));
#25467=CARTESIAN_POINT('Ctrl Pts',(2.90557937086777,1.00200337803205,103.344344085446));
#25468=CARTESIAN_POINT('Ctrl Pts',(2.93699899789952,0.910893685045682,103.339360193603));
#25469=CARTESIAN_POINT('Ctrl Pts',(2.96415273004939,0.818236387054327,103.334376301759));
#25470=CARTESIAN_POINT('Ctrl Pts',(2.98689631737574,0.724467141592515,103.329392409915));
#25471=CARTESIAN_POINT('Ctrl Pts',(3.00963162205088,0.630732044567546,103.324410333082));
#25472=CARTESIAN_POINT('Ctrl Pts',(3.02795986961644,0.535886230808812,103.319428256248));
#25473=CARTESIAN_POINT('Ctrl Pts',(3.04178703534541,0.440379247472645,103.314446179414));
#25474=CARTESIAN_POINT('Ctrl Pts',(3.05561294035544,0.344880972172903,103.309464556831));
#25475=CARTESIAN_POINT('Ctrl Pts',(3.0649385167558,0.248722081609561,103.304482934248));
#25476=CARTESIAN_POINT('Ctrl Pts',(3.06972127333403,0.152359948938327,103.299501311665));
#25477=CARTESIAN_POINT('Ctrl Pts',(3.07450489950169,0.0559802959333553,
103.294518783335));
#25478=CARTESIAN_POINT('Ctrl Pts',(3.07474404375544,-0.0406022341483371,
103.289536255005));
#25479=CARTESIAN_POINT('Ctrl Pts',(3.07044830650883,-0.136928620299167,
103.284553726675));
#25480=CARTESIAN_POINT('Ctrl Pts',(3.06614793909059,-0.23335883209767,103.279565827914));
#25481=CARTESIAN_POINT('Ctrl Pts',(3.05730295145221,-0.329531909532675,
103.274577929153));
#25482=CARTESIAN_POINT('Ctrl Pts',(3.04397496614524,-0.424992535794552,
103.269590030392));
#25483=CARTESIAN_POINT('Ctrl Pts',(3.03063910781443,-0.520509551958479,
103.264599185211));
#25484=CARTESIAN_POINT('Ctrl Pts',(3.01281505994994,-0.615312847756394,
103.25960834003));
#25485=CARTESIAN_POINT('Ctrl Pts',(2.99061545682705,-0.708957995502657,
103.254617494848));
#25486=CARTESIAN_POINT('Ctrl Pts',(2.96837997858488,-0.802754476172602,
103.249618584335));
#25487=CARTESIAN_POINT('Ctrl Pts',(2.94175494702062,-0.895388650028548,
103.244619673822));
#25488=CARTESIAN_POINT('Ctrl Pts',(2.91090264273685,-0.986431981693414,
103.239620763309));
#25489=CARTESIAN_POINT('Ctrl Pts',(2.89299104918402,-1.03928803865039,103.236718599098));
#25490=CARTESIAN_POINT('Ctrl Pts',(2.8736555610664,-1.09160827303963,103.233816434887));
#25491=CARTESIAN_POINT('Ctrl Pts',(2.85293514461264,-1.14331242914353,103.230914270676));
#25492=CARTESIAN_POINT('Ctrl Pts',(2.81724043155436,-1.23238230957604,103.225914761183));
#25493=CARTESIAN_POINT('Ctrl Pts',(2.77730782451965,-1.3199354258661,103.22091525169));
#25494=CARTESIAN_POINT('Ctrl Pts',(2.73328712143254,-1.40554038071164,103.215915742197));
#25495=CARTESIAN_POINT('Ctrl Pts',(2.68932613214967,-1.49102921297946,103.210923014507));
#25496=CARTESIAN_POINT('Ctrl Pts',(2.64128826710602,-1.57457474889841,103.205930286817));
#25497=CARTESIAN_POINT('Ctrl Pts',(2.58937176690187,-1.65576450703942,103.200937559127));
#25498=CARTESIAN_POINT('Ctrl Pts',(2.53751003729684,-1.73686861203202,103.195950098639));
#25499=CARTESIAN_POINT('Ctrl Pts',(2.48177804212799,-1.81562151199361,103.19096263815));
#25500=CARTESIAN_POINT('Ctrl Pts',(2.42241992741185,-1.89163525693458,103.185975177662));
#25501=CARTESIAN_POINT('Ctrl Pts',(2.3631042848142,-1.96759461226434,103.180991285819));
#25502=CARTESIAN_POINT('Ctrl Pts',(2.30016794995018,-2.04081836383862,103.176007393975));
#25503=CARTESIAN_POINT('Ctrl Pts',(2.23389781189284,-2.11094832149449,103.171023502131));
#25504=CARTESIAN_POINT('Ctrl Pts',(2.16765180777847,-2.18105273955668,103.166041425298));
#25505=CARTESIAN_POINT('Ctrl Pts',(2.0980747139139,-2.24806528357457,103.161059348464));
#25506=CARTESIAN_POINT('Ctrl Pts',(2.02549241507628,-2.31166232968149,103.15607727163));
#25507=CARTESIAN_POINT('Ctrl Pts',(1.95291673407208,-2.37525357720303,103.151095649047));
#25508=CARTESIAN_POINT('Ctrl Pts',(1.87733672314457,-2.43542965681751,103.146114026464));
#25509=CARTESIAN_POINT('Ctrl Pts',(1.79911288896127,-2.49190590969511,103.141132403881));
#25510=CARTESIAN_POINT('Ctrl Pts',(1.72087483230664,-2.54839243095058,103.136149875551));
#25511=CARTESIAN_POINT('Ctrl Pts',(1.63999235365309,-2.60117753257764,103.131167347221));
#25512=CARTESIAN_POINT('Ctrl Pts',(1.55685570324067,-2.650019352625,103.126184818892));
#25513=CARTESIAN_POINT('Ctrl Pts',(1.47362944377158,-2.69891381695617,103.12119692013));
#25514=CARTESIAN_POINT('Ctrl Pts',(1.38814454104967,-2.743856291702,103.116209021369));
#25515=CARTESIAN_POINT('Ctrl Pts',(1.30081646179655,-2.78465056743555,103.111221122608));
#25516=CARTESIAN_POINT('Ctrl Pts',(1.21343679664838,-2.82546894090769,103.106230277427));
#25517=CARTESIAN_POINT('Ctrl Pts',(1.12421219283913,-2.86213406945711,103.101239432246));
#25518=CARTESIAN_POINT('Ctrl Pts',(1.03357675678986,-2.89449846049774,103.096248587064));
#25519=CARTESIAN_POINT('Ctrl Pts',(0.942794851587153,-2.92691515321157,
103.091249676551));
#25520=CARTESIAN_POINT('Ctrl Pts',(0.850597981214573,-2.95501710270414,
103.086250766038));
#25521=CARTESIAN_POINT('Ctrl Pts',(0.757433951767733,-2.97870711193791,
103.081251855525));
#25522=CARTESIAN_POINT('Ctrl Pts',(0.703346703896485,-2.99246056817105,
103.078349691314));
#25523=CARTESIAN_POINT('Ctrl Pts',(0.648933658242725,-3.00472794319488,
103.075447527103));
#25524=CARTESIAN_POINT('Ctrl Pts',(0.594283347907237,-3.01549822623064,
103.072545362892));
#25525=CARTESIAN_POINT('Ctrl Pts',(0.500138177112909,-3.03405201173855,
103.067545853399));
#25526=CARTESIAN_POINT('Ctrl Pts',(0.404957928388729,-3.04822527986852,
103.062546343906));
#25527=CARTESIAN_POINT('Ctrl Pts',(0.309186012177099,-3.05790880502902,
103.057546834413));
#25528=CARTESIAN_POINT('Ctrl Pts',(0.213544009961789,-3.06757919454913,
103.052554106723));
#25529=CARTESIAN_POINT('Ctrl Pts',(0.117312368359615,-3.07277190140275,
103.047561379033));
#25530=CARTESIAN_POINT('Ctrl Pts',(0.020945006015351,-3.07342863211805,
103.042568651343));
#25531=CARTESIAN_POINT('Ctrl Pts',(-0.0753206911909299,-3.074084669999,
103.037581190855));
#25532=CARTESIAN_POINT('Ctrl Pts',(-0.171721387884164,-3.07021424173392,
103.032593730366));
#25533=CARTESIAN_POINT('Ctrl Pts',(-0.267798748926218,-3.06181091514051,
103.027606269878));
#25534=CARTESIAN_POINT('Ctrl Pts',(-0.363807364370635,-3.0534136013237,
103.022622378035));
#25535=CARTESIAN_POINT('Ctrl Pts',(-0.459492668046105,-3.04048987503179,
103.017638486191));
#25536=CARTESIAN_POINT('Ctrl Pts',(-0.55439801560365,-3.02308535941259,
103.012654594347));
#25537=CARTESIAN_POINT('Ctrl Pts',(-0.64926880098422,-3.0056871820869,103.007672517514));
#25538=CARTESIAN_POINT('Ctrl Pts',(-0.743359763284123,-2.98381153672753,
103.00269044068));
#25539=CARTESIAN_POINT('Ctrl Pts',(-0.836222020825068,-2.957555575452,102.997708363846));
#25540=CARTESIAN_POINT('Ctrl Pts',(-0.929075811467547,-2.93130200811525,
102.992726741263));
#25541=CARTESIAN_POINT('Ctrl Pts',(-1.02070069773359,-2.90066903851846,
102.98774511868));
#25542=CARTESIAN_POINT('Ctrl Pts',(-1.11066163157496,-2.86580407392886,
102.982763496097));
#25543=CARTESIAN_POINT('Ctrl Pts',(-1.20063892189915,-2.8309327702744,102.977780967767));
#25544=CARTESIAN_POINT('Ctrl Pts',(-1.28895124968016,-2.79182810215373,
102.972798439437));
#25545=CARTESIAN_POINT('Ctrl Pts',(-1.37518327062679,-2.74868572634054,
102.967815911107));
#25546=CARTESIAN_POINT('Ctrl Pts',(-1.46150823698312,-2.70549684940454,
102.962828012346));
#25547=CARTESIAN_POINT('Ctrl Pts',(-1.545748026809,-2.65826177303416,102.957840113585));
#25548=CARTESIAN_POINT('Ctrl Pts',(-1.62751185964566,-2.60722216098144,
102.952852214824));
#25549=CARTESIAN_POINT('Ctrl Pts',(-1.70932399150057,-2.55615239912937,
102.947861369643));
#25550=CARTESIAN_POINT('Ctrl Pts',(-1.78865689328987,-2.50127387628021,
102.942870524462));
#25551=CARTESIAN_POINT('Ctrl Pts',(-1.86515049945167,-2.44287041498217,
102.93787967928));
#25552=CARTESIAN_POINT('Ctrl Pts',(-1.94176772121277,-2.38437257221578,
102.932880768767));
#25553=CARTESIAN_POINT('Ctrl Pts',(-2.01553614964289,-2.3223386988988,102.927881858254));
#25554=CARTESIAN_POINT('Ctrl Pts',(-2.086130447889,-2.25709149225068,102.922882947741));
#25555=CARTESIAN_POINT('Ctrl Pts',(-2.12711462740793,-2.21921161672516,
102.91998078353));
#25556=CARTESIAN_POINT('Ctrl Pts',(-2.1670296745846,-2.1802493652989,102.917078619319));
#25557=CARTESIAN_POINT('Ctrl Pts',(-2.2058181516778,-2.14027300401812,102.914176455108));
#25558=CARTESIAN_POINT('Ctrl Pts',(-2.27409282468423,-2.06990744189837,
102.909068125847));
#25559=CARTESIAN_POINT('Ctrl Pts',(-2.33913739562393,-1.996126757291,102.903959796586));
#25560=CARTESIAN_POINT('Ctrl Pts',(-2.4005870002092,-1.9192666058749,102.898851467326));
#25561=CARTESIAN_POINT('Ctrl Pts',(-2.45984031151225,-1.84515354185449,
102.89392571677));
#25562=CARTESIAN_POINT('Ctrl Pts',(-2.51575090150008,-1.76817775298914,
102.888999966214));
#25563=CARTESIAN_POINT('Ctrl Pts',(-2.56802759118943,-1.68867893363121,
102.884074215659));
#25564=CARTESIAN_POINT('Ctrl Pts',(-2.62025593278434,-1.60925363875328,
102.879153020683));
#25565=CARTESIAN_POINT('Ctrl Pts',(-2.66885679969573,-1.52731032102897,
102.874231825708));
#25566=CARTESIAN_POINT('Ctrl Pts',(-2.71357986674681,-1.44322089673978,
102.869310630733));
#25567=CARTESIAN_POINT('Ctrl Pts',(-2.75827455989699,-1.35918482176559,
102.864392557938));
#25568=CARTESIAN_POINT('Ctrl Pts',(-2.7990961280248,-1.27300574208554,102.859474485143));
#25569=CARTESIAN_POINT('Ctrl Pts',(-2.83583876812314,-1.18508258413067,
102.854556412349));
#25570=CARTESIAN_POINT('Ctrl Pts',(-2.87256876478253,-1.09718968124397,
102.849640031903));
#25571=CARTESIAN_POINT('Ctrl Pts',(-2.90522244952974,-1.00755430938457,
102.844723651456));
#25572=CARTESIAN_POINT('Ctrl Pts',(-2.93364152684788,-0.91659677173425,
102.83980727101));
#25573=CARTESIAN_POINT('Ctrl Pts',(-2.96206829382904,-0.825614622700294,
102.834889560285));
#25574=CARTESIAN_POINT('Ctrl Pts',(-2.98625802504285,-0.733310023163684,
102.82997184956));
#25575=CARTESIAN_POINT('Ctrl Pts',(-3.0061020888235,-0.640119115142639,
102.825054138834));
#25576=CARTESIAN_POINT('Ctrl Pts',(-3.02594955728513,-0.546912218193335,
102.820135584369));
#25577=CARTESIAN_POINT('Ctrl Pts',(-3.04144979336049,-0.452819154589259,
102.815217029903));
#25578=CARTESIAN_POINT('Ctrl Pts',(-3.05254548904124,-0.358285203900466,
102.810298475437));
#25579=CARTESIAN_POINT('Ctrl Pts',(-3.06365068804381,-0.263670286088727,
102.805375708292));
#25580=CARTESIAN_POINT('Ctrl Pts',(-3.07034378241226,-0.168614177656698,
102.800452941148));
#25581=CARTESIAN_POINT('Ctrl Pts',(-3.07261946386603,-0.0735654828818875,
102.795530174003));
#25582=CARTESIAN_POINT('Ctrl Pts',(-3.07322868642112,-0.0481200021036727,
102.794212300285));
#25583=CARTESIAN_POINT('Ctrl Pts',(-3.07352160822751,-0.0226750436337593,
102.792894426567));
#25584=CARTESIAN_POINT('Ctrl Pts',(-3.07349876002173,0.00276082323151584,
102.791576552849));
#25585=CARTESIAN_POINT('Origin',(0.,0.,116.208423447177));
#25586=CARTESIAN_POINT('',(1.8723819390353,2.43733217358127,104.437267724146));
#25587=CARTESIAN_POINT('',(1.87238193903531,2.43733217358127,104.354220317975));
#25588=CARTESIAN_POINT('',(1.8723819390353,2.43733217358128,116.208423447177));
#25589=CARTESIAN_POINT('',(-3.07349999209142,-0.000220485887778205,103.708423447147));
#25590=CARTESIAN_POINT('Ctrl Pts',(1.87238193903531,2.43733217358127,104.354220317975));
#25591=CARTESIAN_POINT('Ctrl Pts',(1.92554476800143,2.39649197877191,104.350735398405));
#25592=CARTESIAN_POINT('Ctrl Pts',(1.97731444018826,2.35395489326419,104.347250478836));
#25593=CARTESIAN_POINT('Ctrl Pts',(2.02758160247093,2.30983010096444,104.343765559266));
#25594=CARTESIAN_POINT('Ctrl Pts',(2.09969550639227,2.24652811835879,104.338766049773));
#25595=CARTESIAN_POINT('Ctrl Pts',(2.1689687585394,2.17973457216113,104.33376654028));
#25596=CARTESIAN_POINT('Ctrl Pts',(2.23504440315198,2.10973428799435,104.328767030787));
#25597=CARTESIAN_POINT('Ctrl Pts',(2.3010304165722,2.03982895876856,104.323774303097));
#25598=CARTESIAN_POINT('Ctrl Pts',(2.36382714428195,1.96672585323331,104.318781575407));
#25599=CARTESIAN_POINT('Ctrl Pts',(2.42311158959213,1.89074918336206,104.313788847717));
#25600=CARTESIAN_POINT('Ctrl Pts',(2.48233349130688,1.81485266696239,104.308801387229));
#25601=CARTESIAN_POINT('Ctrl Pts',(2.53805020806858,1.7360889569736,104.30381392674));
#25602=CARTESIAN_POINT('Ctrl Pts',(2.58997715335333,1.65481739026026,104.298826466252));
#25603=CARTESIAN_POINT('Ctrl Pts',(2.64186694369491,1.57360397525267,104.293842574408));
#25604=CARTESIAN_POINT('Ctrl Pts',(2.68997211756546,1.48988663960697,104.288858682565));
#25605=CARTESIAN_POINT('Ctrl Pts',(2.73405037656118,1.40405512300111,104.283874790721));
#25606=CARTESIAN_POINT('Ctrl Pts',(2.77811258334667,1.3182548641078,104.278892713887));
#25607=CARTESIAN_POINT('Ctrl Pts',(2.81815058871434,1.23034234410879,104.273910637054));
#25608=CARTESIAN_POINT('Ctrl Pts',(2.85396766778545,1.14073257218127,104.26892856022));
#25609=CARTESIAN_POINT('Ctrl Pts',(2.88978148116412,1.05113097060046,104.263946937637));
#25610=CARTESIAN_POINT('Ctrl Pts',(2.92137497065069,0.959832832439655,104.258965315054));
#25611=CARTESIAN_POINT('Ctrl Pts',(2.94859967732581,0.867272847997753,104.253983692471));
#25612=CARTESIAN_POINT('Ctrl Pts',(2.97582933393228,0.774696034519856,104.249001164141));
#25613=CARTESIAN_POINT('Ctrl Pts',(2.9986885063732,0.68085734025023,104.244018635811));
#25614=CARTESIAN_POINT('Ctrl Pts',(3.01707899164171,0.58620526114514,104.239036107481));
#25615=CARTESIAN_POINT('Ctrl Pts',(3.03548929914299,0.491451161048425,104.23404820872));
#25616=CARTESIAN_POINT('Ctrl Pts',(3.0494212197408,0.395882357466433,104.229060309959));
#25617=CARTESIAN_POINT('Ctrl Pts',(3.05882799262756,0.299955932626856,104.224072411198));
#25618=CARTESIAN_POINT('Ctrl Pts',(3.06824032222418,0.203972842731484,104.219081566017));
#25619=CARTESIAN_POINT('Ctrl Pts',(3.07312215939221,0.107632149136793,104.214090720836));
#25620=CARTESIAN_POINT('Ctrl Pts',(3.0734788864626,0.0113922986534843,104.209099875654));
#25621=CARTESIAN_POINT('Ctrl Pts',(3.07383619001295,-0.0850030778585972,
104.204100965141));
#25622=CARTESIAN_POINT('Ctrl Pts',(3.06965380067041,-0.181296847600807,
104.199102054628));
#25623=CARTESIAN_POINT('Ctrl Pts',(3.0609890886171,-0.277034383005151,104.194103144115));
#25624=CARTESIAN_POINT('Ctrl Pts',(3.05595870906673,-0.332615703808248,
104.191200979904));
#25625=CARTESIAN_POINT('Ctrl Pts',(3.04941853195809,-0.388009693650793,
104.188298815693));
#25626=CARTESIAN_POINT('Ctrl Pts',(3.04138763737108,-0.443129201527433,
104.185396651482));
#25627=CARTESIAN_POINT('Ctrl Pts',(3.02755295028724,-0.538082651037559,
104.180397141989));
#25628=CARTESIAN_POINT('Ctrl Pts',(3.00924296930636,-0.632554371002716,
104.175397632496));
#25629=CARTESIAN_POINT('Ctrl Pts',(2.9865022588426,-0.726089875929984,104.170398123003));
#25630=CARTESIAN_POINT('Ctrl Pts',(2.9637923960082,-0.81949850053874,104.165405395313));
#25631=CARTESIAN_POINT('Ctrl Pts',(2.93666385149201,-0.911973011201854,
104.160412667623));
#25632=CARTESIAN_POINT('Ctrl Pts',(2.90521271574455,-1.00306596307329,104.155419939933));
#25633=CARTESIAN_POINT('Ctrl Pts',(2.87379476015253,-1.09406281417667,104.150432479445));
#25634=CARTESIAN_POINT('Ctrl Pts',(2.83806342127841,-1.18368059120868,104.145445018956));
#25635=CARTESIAN_POINT('Ctrl Pts',(2.79816516453479,-1.27148494367176,104.140457558468));
#25636=CARTESIAN_POINT('Ctrl Pts',(2.75829545592651,-1.3592264700682,104.135473666624));
#25637=CARTESIAN_POINT('Ctrl Pts',(2.71426493765869,-1.44515675286649,104.130489774781));
#25638=CARTESIAN_POINT('Ctrl Pts',(2.66626860062224,-1.52886035965876,104.125505882937));
#25639=CARTESIAN_POINT('Ctrl Pts',(2.61828974266299,-1.61253348367056,104.120523806103));
#25640=CARTESIAN_POINT('Ctrl Pts',(2.56634815364014,-1.69398116243539,104.11554172927));
#25641=CARTESIAN_POINT('Ctrl Pts',(2.51068483288244,-1.77281243224828,104.110559652436));
#25642=CARTESIAN_POINT('Ctrl Pts',(2.45502658733718,-1.85163651446555,104.105578029853));
#25643=CARTESIAN_POINT('Ctrl Pts',(2.39564753806593,-1.92784430355049,104.10059640727));
#25644=CARTESIAN_POINT('Ctrl Pts',(2.33283147124749,-2.00107460549507,104.095614784687));
#25645=CARTESIAN_POINT('Ctrl Pts',(2.27000398336133,-2.07431822199882,104.090632256357));
#25646=CARTESIAN_POINT('Ctrl Pts',(2.20373852267581,-2.14458294306888,104.085649728027));
#25647=CARTESIAN_POINT('Ctrl Pts',(2.13435781735861,-2.21154221245723,104.080667199697));
#25648=CARTESIAN_POINT('Ctrl Pts',(2.06490232986631,-2.27857365406961,104.075679300936));
#25649=CARTESIAN_POINT('Ctrl Pts',(1.99232521063532,-2.34229222588164,104.070691402175));
#25650=CARTESIAN_POINT('Ctrl Pts',(1.91698439771724,-2.40240984615629,104.065703503414));
#25651=CARTESIAN_POINT('Ctrl Pts',(1.84159907994687,-2.46256297873438,104.060712658233));
#25652=CARTESIAN_POINT('Ctrl Pts',(1.76344717327735,-2.51911066710761,104.055721813052));
#25653=CARTESIAN_POINT('Ctrl Pts',(1.68291614977514,-2.57180782385194,104.05073096787));
#25654=CARTESIAN_POINT('Ctrl Pts',(1.60225498610525,-2.62459014053234,104.045732057357));
#25655=CARTESIAN_POINT('Ctrl Pts',(1.5192074065279,-2.67350927787263,104.040733146844));
#25656=CARTESIAN_POINT('Ctrl Pts',(1.43418598442494,-2.71836583484988,104.035734236331));
#25657=CARTESIAN_POINT('Ctrl Pts',(1.38482600333623,-2.74440772816731,104.03283207212));
#25658=CARTESIAN_POINT('Ctrl Pts',(1.33480114237456,-2.76908122230678,104.029929907909));
#25659=CARTESIAN_POINT('Ctrl Pts',(1.28419489131014,-2.79235487199119,104.027027743698));
#25660=CARTESIAN_POINT('Ctrl Pts',(1.19701635343025,-2.83244799700915,104.022028234205));
#25661=CARTESIAN_POINT('Ctrl Pts',(1.10780530582788,-2.86852500162958,104.017028724712));
#25662=CARTESIAN_POINT('Ctrl Pts',(1.01696723059307,-2.9003758208032,104.012029215219));
#25663=CARTESIAN_POINT('Ctrl Pts',(0.926252376630513,-2.93218343454286,
104.007036487529));
#25664=CARTESIAN_POINT('Ctrl Pts',(0.833915292099658,-2.95977611238127,
104.002043759839));
#25665=CARTESIAN_POINT('Ctrl Pts',(0.740383606881194,-2.9829908422021,103.997051032149));
#25666=CARTESIAN_POINT('Ctrl Pts',(0.646950595232957,-3.00618108106815,
103.992063571661));
#25667=CARTESIAN_POINT('Ctrl Pts',(0.552325912015178,-3.02500244828318,
103.987076111172));
#25668=CARTESIAN_POINT('Ctrl Pts',(0.456953630396812,-3.03934131509891,
103.982088650684));
#25669=CARTESIAN_POINT('Ctrl Pts',(0.361649589875361,-3.05366992212025,
103.97710475884));
#25670=CARTESIAN_POINT('Ctrl Pts',(0.265599447196298,-3.06352233969462,
103.972120866997));
#25671=CARTESIAN_POINT('Ctrl Pts',(0.169257826953313,-3.06883594185402,
103.967136975153));
#25672=CARTESIAN_POINT('Ctrl Pts',(0.0729512919423281,-3.07414760893112,
103.962154898319));
#25673=CARTESIAN_POINT('Ctrl Pts',(-0.0236460718779519,-3.07492372062509,
103.957172821486));
#25674=CARTESIAN_POINT('Ctrl Pts',(-0.120075114707274,-3.07115356451416,
103.952190744652));
#25675=CARTESIAN_POINT('Ctrl Pts',(-0.216495365429501,-3.06738375215461,
103.947209122069));
#25676=CARTESIAN_POINT('Ctrl Pts',(-0.312746887053481,-3.059068513455,103.942227499486));
#25677=CARTESIAN_POINT('Ctrl Pts',(-0.408372205003796,-3.04624923343123,
103.937245876903));
#25678=CARTESIAN_POINT('Ctrl Pts',(-0.504014909321746,-3.03342762263648,
103.932263348573));
#25679=CARTESIAN_POINT('Ctrl Pts',(-0.599030748788974,-3.01610040251193,
103.927280820243));
#25680=CARTESIAN_POINT('Ctrl Pts',(-0.692970100689274,-2.99436048089583,
103.922298291913));
#25681=CARTESIAN_POINT('Ctrl Pts',(-0.787010705366312,-2.97259712684821,
103.917310393152));
#25682=CARTESIAN_POINT('Ctrl Pts',(-0.879972077686123,-2.94641167504668,
103.912322494391));
#25683=CARTESIAN_POINT('Ctrl Pts',(-0.971417696979223,-2.91594751461606,
103.90733459563));
#25684=CARTESIAN_POINT('Ctrl Pts',(-1.06291733445483,-2.88546535858772,
103.902343750449));
#25685=CARTESIAN_POINT('Ctrl Pts',(-1.15289902679166,-2.85069961940891,
103.897352905268));
#25686=CARTESIAN_POINT('Ctrl Pts',(-1.24094623677775,-2.8118418674291,103.892362060086));
#25687=CARTESIAN_POINT('Ctrl Pts',(-1.32913573327866,-2.7729213203408,103.887363149573));
#25688=CARTESIAN_POINT('Ctrl Pts',(-1.41538411261891,-2.72989575197777,
103.88236423906));
#25689=CARTESIAN_POINT('Ctrl Pts',(-1.49929949253701,-2.68300266151159,
103.877365328547));
#25690=CARTESIAN_POINT('Ctrl Pts',(-1.54801735049982,-2.65577843964668,
103.874463164336));
#25691=CARTESIAN_POINT('Ctrl Pts',(-1.59594940067385,-2.62725149460519,
103.871561000125));
#25692=CARTESIAN_POINT('Ctrl Pts',(-1.64302381086752,-2.59747473653207,
103.868658835914));
#25693=CARTESIAN_POINT('Ctrl Pts',(-1.72411810585929,-2.54617881602781,
103.863659326421));
#25694=CARTESIAN_POINT('Ctrl Pts',(-1.80295031313648,-2.49099145902901,
103.858659816928));
#25695=CARTESIAN_POINT('Ctrl Pts',(-1.87912346639947,-2.43213841054058,
103.853660307435));
#25696=CARTESIAN_POINT('Ctrl Pts',(-1.95519329126374,-2.37336519583872,
103.848667579745));
#25697=CARTESIAN_POINT('Ctrl Pts',(-2.02861088637677,-2.31093643822026,
103.843674852055));
#25698=CARTESIAN_POINT('Ctrl Pts',(-2.0990066946769,-2.24512207812884,103.838682124365));
#25699=CARTESIAN_POINT('Ctrl Pts',(-2.16932823717359,-2.17937715052848,
103.833694663876));
#25700=CARTESIAN_POINT('Ctrl Pts',(-2.23663401128075,-2.11025401901876,
103.828707203388));
#25701=CARTESIAN_POINT('Ctrl Pts',(-2.30058692975088,-2.03806330339845,
103.8237197429));
#25702=CARTESIAN_POINT('Ctrl Pts',(-2.36449408841299,-1.9659242419226,103.818735851056));
#25703=CARTESIAN_POINT('Ctrl Pts',(-2.42505287038437,-1.89072228738107,
103.813751959213));
#25704=CARTESIAN_POINT('Ctrl Pts',(-2.48196322441649,-1.81280467856968,
103.808768067369));
#25705=CARTESIAN_POINT('Ctrl Pts',(-2.53885285310721,-1.73491544542158,
103.803785990535));
#25706=CARTESIAN_POINT('Ctrl Pts',(-2.59209643513275,-1.65431287710342,
103.798803913701));
#25707=CARTESIAN_POINT('Ctrl Pts',(-2.64143500017088,-1.57137627253062,
103.793821836868));
#25708=CARTESIAN_POINT('Ctrl Pts',(-2.69076906666857,-1.48844722986545,
103.788840214285));
#25709=CARTESIAN_POINT('Ctrl Pts',(-2.73619859979841,-1.40318495139973,
103.783858591702));
#25710=CARTESIAN_POINT('Ctrl Pts',(-2.77750924024574,-1.31599569541451,
103.778876969119));
#25711=CARTESIAN_POINT('Ctrl Pts',(-2.81882739169535,-1.22879058688639,
103.773894440789));
#25712=CARTESIAN_POINT('Ctrl Pts',(-2.85602497525254,-1.13965820172586,
103.768911912459));
#25713=CARTESIAN_POINT('Ctrl Pts',(-2.88893512350555,-1.0490262638161,103.763929384129));
#25714=CARTESIAN_POINT('Ctrl Pts',(-2.92188074404815,-0.958296638034406,
103.758941485368));
#25715=CARTESIAN_POINT('Ctrl Pts',(-2.95052955336883,-0.866064646002697,
103.753953586607));
#25716=CARTESIAN_POINT('Ctrl Pts',(-2.97476416079934,-0.772774506323692,
103.748965687846));
#25717=CARTESIAN_POINT('Ctrl Pts',(-2.99901308394508,-0.679429258878735,
103.743974842665));
#25718=CARTESIAN_POINT('Ctrl Pts',(-3.0188425229909,-0.585025048572415,
103.738983997483));
#25719=CARTESIAN_POINT('Ctrl Pts',(-3.03418638133272,-0.490015564380421,
103.733993152302));
#25720=CARTESIAN_POINT('Ctrl Pts',(-3.04955503573711,-0.394852542462566,
103.728994241789));
#25721=CARTESIAN_POINT('Ctrl Pts',(-3.06042358569747,-0.299082729402581,
103.723995331276));
#25722=CARTESIAN_POINT('Ctrl Pts',(-3.06677788277764,-0.203164139812822,
103.718996420763));
#25723=CARTESIAN_POINT('Ctrl Pts',(-3.07046692932559,-0.147477706310342,
103.716094256552));
#25724=CARTESIAN_POINT('Ctrl Pts',(-3.072635427446,-0.0917411326516463,
103.713192092341));
#25725=CARTESIAN_POINT('Ctrl Pts',(-3.07328864861143,-0.0360434781358497,
103.71028992813));
#25726=CARTESIAN_POINT('Ctrl Pts',(-3.07342868489404,-0.0241031233202659,
103.709667767812));
#25727=CARTESIAN_POINT('Ctrl Pts',(-3.07349913543572,-0.0121619508103782,
103.709045607495));
#25728=CARTESIAN_POINT('Ctrl Pts',(-3.07349999209138,-0.00022048645764921,
103.708423447177));
#25729=CARTESIAN_POINT('Ctrl Pts',(-3.07349999209142,-0.000220485887798679,
103.708423447147));
#25730=CARTESIAN_POINT('Ctrl Pts',(-3.07350686177119,0.0955405667047918,
103.703434215918));
#25731=CARTESIAN_POINT('Ctrl Pts',(-3.06903399632083,0.19147336895022,103.698444984688));
#25732=CARTESIAN_POINT('Ctrl Pts',(-3.06005921735193,0.287123381666347,
103.693455753459));
#25733=CARTESIAN_POINT('Ctrl Pts',(-3.05109660653681,0.382643710512995,
103.688473286711));
#25734=CARTESIAN_POINT('Ctrl Pts',(-3.03764425268558,0.477881576496013,
103.683490819964));
#25735=CARTESIAN_POINT('Ctrl Pts',(-3.01973198023759,0.572381880854357,
103.678508353217));
#25736=CARTESIAN_POINT('Ctrl Pts',(-3.00183853139196,0.66678287697818,103.673531122431));
#25737=CARTESIAN_POINT('Ctrl Pts',(-2.97949456191652,0.760447421190341,
103.668553891645));
#25738=CARTESIAN_POINT('Ctrl Pts',(-2.95278164141698,0.852926039062489,
103.66357666086));
#25739=CARTESIAN_POINT('Ctrl Pts',(-2.92608756204122,0.945339430031195,
103.658602940608));
#25740=CARTESIAN_POINT('Ctrl Pts',(-2.89503077887684,1.0365681348272,103.653629220357));
#25741=CARTESIAN_POINT('Ctrl Pts',(-2.85974361903482,1.12617435745519,103.648655500106));
#25742=CARTESIAN_POINT('Ctrl Pts',(-2.8244689530173,1.21574885397023,103.643683540857));
#25743=CARTESIAN_POINT('Ctrl Pts',(-2.78496704750032,1.30370159967069,103.638711581608));
#25744=CARTESIAN_POINT('Ctrl Pts',(-2.74141929053079,1.38961236447639,103.63373962236));
#25745=CARTESIAN_POINT('Ctrl Pts',(-2.6978749304007,1.47551642801675,103.628768050937));
#25746=CARTESIAN_POINT('Ctrl Pts',(-2.65028554591197,1.5593784341012,103.623796479514));
#25747=CARTESIAN_POINT('Ctrl Pts',(-2.59887915058709,1.64080145375475,103.618824908091));
#25748=CARTESIAN_POINT('Ctrl Pts',(-2.54746257395873,1.72224059966009,103.613852352023));
#25749=CARTESIAN_POINT('Ctrl Pts',(-2.49222772076612,1.80123942705036,103.608879795955));
#25750=CARTESIAN_POINT('Ctrl Pts',(-2.43344610934209,1.87742970119466,103.603907239887));
#25751=CARTESIAN_POINT('Ctrl Pts',(-2.37460080953994,1.95370252555952,103.598929296181));
#25752=CARTESIAN_POINT('Ctrl Pts',(-2.31220135081348,2.02716037302272,103.593951352474));
#25753=CARTESIAN_POINT('Ctrl Pts',(-2.24655957870032,2.09746807111571,103.588973408768));
#25754=CARTESIAN_POINT('Ctrl Pts',(-2.1808777071248,2.16781871900732,103.58399242412));
#25755=CARTESIAN_POINT('Ctrl Pts',(-2.11194989471064,2.23501507910632,103.579011439471));
#25756=CARTESIAN_POINT('Ctrl Pts',(-2.04012333245904,2.29876032642732,103.574030454822));
#25757=CARTESIAN_POINT('Ctrl Pts',(-1.96818290487756,2.36260662791807,103.56904157391));
#25758=CARTESIAN_POINT('Ctrl Pts',(-1.893334896855,2.42299061889371,103.564052692998));
#25759=CARTESIAN_POINT('Ctrl Pts',(-1.81595775176263,2.47965717263762,103.559063812085));
#25760=CARTESIAN_POINT('Ctrl Pts',(-1.77902970834285,2.50670113962046,103.556682881505));
#25761=CARTESIAN_POINT('Ctrl Pts',(-1.74152601481376,2.53289905886596,103.554301950925));
#25762=CARTESIAN_POINT('Ctrl Pts',(-1.70348979365066,2.55822688065935,103.551921020345));
#25763=CARTESIAN_POINT('Ctrl Pts',(-1.62362083384975,2.6114105755376,103.546921510852));
#25764=CARTESIAN_POINT('Ctrl Pts',(-1.54111857553593,2.66094378308383,103.541922001359));
#25765=CARTESIAN_POINT('Ctrl Pts',(-1.45635082880781,2.70655583970307,103.536922491866));
#25766=CARTESIAN_POINT('Ctrl Pts',(-1.37169806898992,2.75210602385711,103.531929764176));
#25767=CARTESIAN_POINT('Ctrl Pts',(-1.2847863116298,2.79374542205784,103.526937036486));
#25768=CARTESIAN_POINT('Ctrl Pts',(-1.19601257379427,2.83124639926058,103.521944308796));
#25769=CARTESIAN_POINT('Ctrl Pts',(-1.10733249001449,2.86870781387764,103.516956848308));
#25770=CARTESIAN_POINT('Ctrl Pts',(-1.01679473296656,2.90203931679329,103.51196938782));
#25771=CARTESIAN_POINT('Ctrl Pts',(-0.924820254834743,2.93105949210305,
103.506981927331));
#25772=CARTESIAN_POINT('Ctrl Pts',(-0.832911586591893,2.96005890279904,
103.501998035488));
#25773=CARTESIAN_POINT('Ctrl Pts',(-0.739568658313955,2.98475298673084,
103.497014143644));
#25774=CARTESIAN_POINT('Ctrl Pts',(-0.645230789620226,3.00500906456637,
103.4920302518));
#25775=CARTESIAN_POINT('Ctrl Pts',(-0.55092727644181,3.02525776564004,103.487048174967));
#25776=CARTESIAN_POINT('Ctrl Pts',(-0.455629971504973,3.04107157979625,
103.482066098133));
#25777=CARTESIAN_POINT('Ctrl Pts',(-0.35979075107977,3.05236840264039,103.477084021299));
#25778=CARTESIAN_POINT('Ctrl Pts',(-0.26396026898355,3.06366419547454,103.472102398716));
#25779=CARTESIAN_POINT('Ctrl Pts',(-0.167588405601255,3.07044376461798,
103.467120776133));
#25780=CARTESIAN_POINT('Ctrl Pts',(-0.0711334977560217,3.07267672811459,
103.46213915355));
#25781=CARTESIAN_POINT('Ctrl Pts',(0.0253389472912264,3.07491009760332,
103.45715662522));
#25782=CARTESIAN_POINT('Ctrl Pts',(0.121894027946905,3.07259520958721,103.45217409689));
#25783=CARTESIAN_POINT('Ctrl Pts',(0.218073137580161,3.06575379909508,103.447191568561));
#25784=CARTESIAN_POINT('Ctrl Pts',(0.314355914118666,3.05890501457074,103.4422036698));
#25785=CARTESIAN_POINT('Ctrl Pts',(0.410261472025794,3.04751999844626,103.437215771038));
#25786=CARTESIAN_POINT('Ctrl Pts',(0.505336283203782,3.03167239174647,103.432227872277));
#25787=CARTESIAN_POINT('Ctrl Pts',(0.600467256377786,3.01581542364788,103.427237027096));
#25788=CARTESIAN_POINT('Ctrl Pts',(0.694766076784185,2.99549070848587,103.422246181915));
#25789=CARTESIAN_POINT('Ctrl Pts',(0.787791450553388,2.97082259322818,103.417255336733));
#25790=CARTESIAN_POINT('Ctrl Pts',(0.880967155675705,2.9461146136733,103.41225642622));
#25791=CARTESIAN_POINT('Ctrl Pts',(0.972864886699481,2.91704935082481,103.407257515707));
#25792=CARTESIAN_POINT('Ctrl Pts',(1.0630605493129,2.88380036037423,103.402258605194));
#25793=CARTESIAN_POINT('Ctrl Pts',(1.11542448408092,2.86449734827132,103.399356440983));
#25794=CARTESIAN_POINT('Ctrl Pts',(1.16721513135695,2.84378510836311,103.396454276772));
#25795=CARTESIAN_POINT('Ctrl Pts',(1.21835329387811,2.82170471546836,103.393552112561));
#25796=CARTESIAN_POINT('Ctrl Pts',(1.30644831913931,2.78366711939642,103.388552593281));
#25797=CARTESIAN_POINT('Ctrl Pts',(1.39291504089482,2.74143320287493,103.383553074001));
#25798=CARTESIAN_POINT('Ctrl Pts',(1.47732617133322,2.69516411995521,103.37855355472));
#25799=CARTESIAN_POINT('Ctrl Pts',(1.56161153330858,2.64896397570998,103.37356148448));
#25800=CARTESIAN_POINT('Ctrl Pts',(1.64384701257246,2.59874082935472,103.368569414239));
#25801=CARTESIAN_POINT('Ctrl Pts',(1.72362567342723,2.54470367388867,103.363577343999));
#25802=CARTESIAN_POINT('Ctrl Pts',(1.77423225055539,2.51042589275549,103.360410687841));
#25803=CARTESIAN_POINT('Ctrl Pts',(1.82385063493909,2.47461438658962,103.357244031683));
#25804=CARTESIAN_POINT('Ctrl Pts',(1.87238193903529,2.43733217358128,103.354077375525));
#25805=CARTESIAN_POINT('',(-3.07349992841428,-0.000663353166432896,103.791576552855));
#25806=CARTESIAN_POINT('Ctrl Pts',(-3.07349992841441,-0.000663352542477041,
103.791576552823));
#25807=CARTESIAN_POINT('Ctrl Pts',(-3.07352145853115,0.0990917671334288,
103.786438116722));
#25808=CARTESIAN_POINT('Ctrl Pts',(-3.06868209475957,0.198789365247624,
103.781299680621));
#25809=CARTESIAN_POINT('Ctrl Pts',(-3.05902469152581,0.297943260765191,
103.77616124452));
#25810=CARTESIAN_POINT('Ctrl Pts',(-3.04935854635228,0.397186910988275,
103.771018157076));
#25811=CARTESIAN_POINT('Ctrl Pts',(-3.03486571256589,0.495885482213515,
103.765875069631));
#25812=CARTESIAN_POINT('Ctrl Pts',(-3.0156405532298,0.593560699268277,103.760731982187));
#25813=CARTESIAN_POINT('Ctrl Pts',(-2.99637806306914,0.691425579062894,
103.755578908053));
#25814=CARTESIAN_POINT('Ctrl Pts',(-2.97236496789568,0.788262743622209,
103.75042583392));
#25815=CARTESIAN_POINT('Ctrl Pts',(-2.94374630484731,0.883606214723414,
103.745272759786));
#25816=CARTESIAN_POINT('Ctrl Pts',(-2.91509738297958,0.979050493499077,
103.740114237251));
#25817=CARTESIAN_POINT('Ctrl Pts',(-2.88183331879042,1.07299755565158,103.734955714717));
#25818=CARTESIAN_POINT('Ctrl Pts',(-2.84414762681942,1.16500065530346,103.729797192183));
#25819=CARTESIAN_POINT('Ctrl Pts',(-2.80638226408419,1.25719825734807,103.724627764092));
#25820=CARTESIAN_POINT('Ctrl Pts',(-2.7641767638206,1.34744332420583,103.719458336002));
#25821=CARTESIAN_POINT('Ctrl Pts',(-2.71777125569243,1.43531238820405,103.714288907911));
#25822=CARTESIAN_POINT('Ctrl Pts',(-2.69303114014139,1.48215792194269,103.711532936617));
#25823=CARTESIAN_POINT('Ctrl Pts',(-2.66709802246462,1.52832860739875,103.708776965323));
#25824=CARTESIAN_POINT('Ctrl Pts',(-2.64001321119417,1.57376379889748,103.706020994028));
#25825=CARTESIAN_POINT('Ctrl Pts',(-2.59087961849347,1.65618616363491,103.701021484535));
#25826=CARTESIAN_POINT('Ctrl Pts',(-2.53779613328403,1.73645013360103,103.696021975042));
#25827=CARTESIAN_POINT('Ctrl Pts',(-2.4809779245829,1.81415291189368,103.691022465549));
#25828=CARTESIAN_POINT('Ctrl Pts',(-2.42423678942116,1.89175028686088,103.686029737859));
#25829=CARTESIAN_POINT('Ctrl Pts',(-2.36377125624717,1.96679302367079,103.681037010169));
#25830=CARTESIAN_POINT('Ctrl Pts',(-2.29984139884962,2.03890455640704,103.676044282479));
#25831=CARTESIAN_POINT('Ctrl Pts',(-2.23597898584013,2.11094001329399,103.671056821991));
#25832=CARTESIAN_POINT('Ctrl Pts',(-2.16865980372973,2.1800500867846,103.666069361503));
#25833=CARTESIAN_POINT('Ctrl Pts',(-2.09818545004237,2.24588959373129,103.661081901014));
#25834=CARTESIAN_POINT('Ctrl Pts',(-2.02776152240241,2.31168199097176,103.656098009171));
#25835=CARTESIAN_POINT('Ctrl Pts',(-1.95418723102758,2.37420817500229,103.651114117327));
#25836=CARTESIAN_POINT('Ctrl Pts',(-1.87780175898322,2.43315901740094,103.646130225483));
#25837=CARTESIAN_POINT('Ctrl Pts',(-1.80144410463589,2.49208839136287,103.64114814865));
#25838=CARTESIAN_POINT('Ctrl Pts',(-1.72227765087632,2.54744474280995,103.636166071816));
#25839=CARTESIAN_POINT('Ctrl Pts',(-1.6406747159887,2.59895916210998,103.631183994982));
#25840=CARTESIAN_POINT('Ctrl Pts',(-1.5590792214087,2.65046888448181,103.626202372399));
#25841=CARTESIAN_POINT('Ctrl Pts',(-1.47504805866327,2.69813713699048,103.621220749816));
#25842=CARTESIAN_POINT('Ctrl Pts',(-1.38898167563165,2.74173889252049,103.616239127233));
#25843=CARTESIAN_POINT('Ctrl Pts',(-1.30289964421533,2.78534857561781,103.611256598903));
#25844=CARTESIAN_POINT('Ctrl Pts',(-1.21478204920664,2.82489009502186,103.606274070573));
#25845=CARTESIAN_POINT('Ctrl Pts',(-1.12505205241748,2.86018533129432,103.601291542243));
#25846=CARTESIAN_POINT('Ctrl Pts',(-1.03522533991596,2.89551861062976,103.596303643482));
#25847=CARTESIAN_POINT('Ctrl Pts',(-0.943783165187995,2.92659630859235,
103.591315744721));
#25848=CARTESIAN_POINT('Ctrl Pts',(-0.851166487319248,2.95328932901343,
103.58632784596));
#25849=CARTESIAN_POINT('Ctrl Pts',(-0.758495099507587,2.97999811736808,
103.581337000779));
#25850=CARTESIAN_POINT('Ctrl Pts',(-0.664648253947756,3.0023169693754,103.576346155598));
#25851=CARTESIAN_POINT('Ctrl Pts',(-0.570077733164632,3.02016781456757,
103.571355310416));
#25852=CARTESIAN_POINT('Ctrl Pts',(-0.475354384031829,3.03804750717635,
103.566356399903));
#25853=CARTESIAN_POINT('Ctrl Pts',(-0.379905458896058,3.05144471442974,
103.56135748939));
#25854=CARTESIAN_POINT('Ctrl Pts',(-0.284188438080711,3.06033318147898,
103.556358578877));
#25855=CARTESIAN_POINT('Ctrl Pts',(-0.228619027213755,3.06549346408315,
103.553456414666));
#25856=CARTESIAN_POINT('Ctrl Pts',(-0.172959285597081,3.06913505583286,
103.550554250455));
#25857=CARTESIAN_POINT('Ctrl Pts',(-0.11729838078186,3.07126087134681,103.547652086244));
#25858=CARTESIAN_POINT('Ctrl Pts',(-0.0214331825123264,3.07492217952003,
103.542653666825));
#25859=CARTESIAN_POINT('Ctrl Pts',(0.0747719474817214,3.07409716580575,
103.537655247406));
#25860=CARTESIAN_POINT('Ctrl Pts',(0.170862295476754,3.06874702867219,103.532656827988));
#25861=CARTESIAN_POINT('Ctrl Pts',(0.266831636419484,3.06340362899289,103.527664703103));
#25862=CARTESIAN_POINT('Ctrl Pts',(0.362686048388711,3.05354645028764,103.522672578219));
#25863=CARTESIAN_POINT('Ctrl Pts',(0.457968239139363,3.03918859927113,103.517680453334));
#25864=CARTESIAN_POINT('Ctrl Pts',(0.553156462986874,3.02484490790801,103.512693251663));
#25865=CARTESIAN_POINT('Ctrl Pts',(0.647773155437854,3.00600942913244,103.507706049991));
#25866=CARTESIAN_POINT('Ctrl Pts',(0.741364642876875,2.98274717605969,103.50271884832));
#25867=CARTESIAN_POINT('Ctrl Pts',(0.834889386692949,2.95950151217779,103.49773520321));
#25868=CARTESIAN_POINT('Ctrl Pts',(0.927389954212311,2.931835455185,103.492751558101));
#25869=CARTESIAN_POINT('Ctrl Pts',(1.01842244305371,2.89986516539727,103.487767912991));
#25870=CARTESIAN_POINT('Ctrl Pts',(1.10942726221678,2.8679045931032,103.482785782679));
#25871=CARTESIAN_POINT('Ctrl Pts',(1.19896447432909,2.83164252900669,103.477803652368));
#25872=CARTESIAN_POINT('Ctrl Pts',(1.28660578901007,2.79124484660264,103.472821522057));
#25873=CARTESIAN_POINT('Ctrl Pts',(1.37423185213238,2.75085419430334,103.467840258748));
#25874=CARTESIAN_POINT('Ctrl Pts',(1.45996227740941,2.70632954305835,103.462858995439));
#25875=CARTESIAN_POINT('Ctrl Pts',(1.54339036598283,2.65788420142627,103.45787773213));
#25876=CARTESIAN_POINT('Ctrl Pts',(1.62684889623697,2.60942118280259,103.452894651232));
#25877=CARTESIAN_POINT('Ctrl Pts',(1.70800303472105,2.55703484133616,103.447911570334));
#25878=CARTESIAN_POINT('Ctrl Pts',(1.78647284537127,2.50098321120936,103.442928489435));
#25879=CARTESIAN_POINT('Ctrl Pts',(1.81548180357218,2.48026187415033,103.441086328937));
#25880=CARTESIAN_POINT('Ctrl Pts',(1.84412420216451,2.45904003791276,103.439244168439));
#25881=CARTESIAN_POINT('Ctrl Pts',(1.87238193903529,2.43733217358128,103.43740200794));
#25882=CARTESIAN_POINT('Ctrl Pts',(1.8723819390353,2.43733217358127,104.437267724146));
#25883=CARTESIAN_POINT('Ctrl Pts',(1.94887274963103,2.37857119967135,104.432285699447));
#25884=CARTESIAN_POINT('Ctrl Pts',(2.02262578910975,2.31618218202684,104.427303674749));
#25885=CARTESIAN_POINT('Ctrl Pts',(2.09328617694461,2.25045667174745,104.42232165005));
#25886=CARTESIAN_POINT('Ctrl Pts',(2.16394103458939,2.18473630543311,104.417340015266));
#25887=CARTESIAN_POINT('Ctrl Pts',(2.23150340058652,2.11568026483155,104.412358380483));
#25888=CARTESIAN_POINT('Ctrl Pts',(2.29565367489618,2.04361847098123,104.407376745699));
#25889=CARTESIAN_POINT('Ctrl Pts',(2.35981644119198,1.97154264453417,104.402394140841));
#25890=CARTESIAN_POINT('Ctrl Pts',(2.42056550434251,1.89646023024797,104.397411535984));
#25891=CARTESIAN_POINT('Ctrl Pts',(2.47762084770206,1.8187350508065,104.392428931126));
#25892=CARTESIAN_POINT('Ctrl Pts',(2.53473809046188,1.74092554723849,104.387440920635));
#25893=CARTESIAN_POINT('Ctrl Pts',(2.5881533535492,1.66046790932871,104.382452910145));
#25894=CARTESIAN_POINT('Ctrl Pts',(2.63762950377971,1.57775563722359,104.377464899654));
#25895=CARTESIAN_POINT('Ctrl Pts',(2.68713545317714,1.49499354804921,104.372473884916));
#25896=CARTESIAN_POINT('Ctrl Pts',(2.73269735870101,1.40997450756545,104.367482870179));
#25897=CARTESIAN_POINT('Ctrl Pts',(2.77412467651314,1.32311546327631,104.362491855442));
#25898=CARTESIAN_POINT('Ctrl Pts',(2.81561837012091,1.23611725144075,104.357492843986));
#25899=CARTESIAN_POINT('Ctrl Pts',(2.85296407966245,1.14727355392855,104.352493832531));
#25900=CARTESIAN_POINT('Ctrl Pts',(2.88601992722648,1.05701997599461,104.347494821076));
#25901=CARTESIAN_POINT('Ctrl Pts',(2.90364922234982,1.00888607296121,104.344828755772));
#25902=CARTESIAN_POINT('Ctrl Pts',(2.92005921202746,0.96035140393487,104.342162690469));
#25903=CARTESIAN_POINT('Ctrl Pts',(2.93523429559057,0.911483340488959,104.339496625165));
#25904=CARTESIAN_POINT('Ctrl Pts',(2.96369120331487,0.819844044641818,104.334497115672));
#25905=CARTESIAN_POINT('Ctrl Pts',(2.98790245202407,0.726709858047175,104.329497606179));
#25906=CARTESIAN_POINT('Ctrl Pts',(3.0077122975794,0.632510067105379,104.324498096686));
#25907=CARTESIAN_POINT('Ctrl Pts',(3.02749527120502,0.538438057581826,104.319505368996));
#25908=CARTESIAN_POINT('Ctrl Pts',(3.04288861803811,0.443303742409854,104.314512641306));
#25909=CARTESIAN_POINT('Ctrl Pts',(3.05378612035519,0.347552271070138,104.309519913616));
#25910=CARTESIAN_POINT('Ctrl Pts',(3.06467212608201,0.251901815119079,104.304532453128));
#25911=CARTESIAN_POINT('Ctrl Pts',(3.07107166672151,0.155635931143929,104.299544992639));
#25912=CARTESIAN_POINT('Ctrl Pts',(3.07292962245941,0.0592096732929988,
104.294557532151));
#25913=CARTESIAN_POINT('Ctrl Pts',(3.07478624878655,-0.0371475893164126,
104.289573640307));
#25914=CARTESIAN_POINT('Ctrl Pts',(3.07210774185138,-0.133664560059064,
104.284589748464));
#25915=CARTESIAN_POINT('Ctrl Pts',(3.06489092193472,-0.229882332166164,
104.27960585662));
#25916=CARTESIAN_POINT('Ctrl Pts',(3.05767673020514,-0.326065064143557,
104.274623779786));
#25917=CARTESIAN_POINT('Ctrl Pts',(3.04592754210997,-0.421948376693134,
104.269641702953));
#25918=CARTESIAN_POINT('Ctrl Pts',(3.02969224012889,-0.517075603855755,
104.264659626119));
#25919=CARTESIAN_POINT('Ctrl Pts',(3.01345841843328,-0.61219415760705,104.259678003536));
#25920=CARTESIAN_POINT('Ctrl Pts',(2.99273937010984,-0.706556330357332,
104.254696380953));
#25921=CARTESIAN_POINT('Ctrl Pts',(2.96763541861875,-0.79971386893033,104.24971475837));
#25922=CARTESIAN_POINT('Ctrl Pts',(2.94252690278692,-0.892888345185374,
104.24473223004));
#25923=CARTESIAN_POINT('Ctrl Pts',(2.91303201469197,-0.98485732845272,104.23974970171));
#25924=CARTESIAN_POINT('Ctrl Pts',(2.87930114853018,-1.07518702841544,104.23476717338));
#25925=CARTESIAN_POINT('Ctrl Pts',(2.84553392546594,-1.16561409048185,104.229779274619));
#25926=CARTESIAN_POINT('Ctrl Pts',(2.80752176303124,-1.25439792987099,104.224791375858));
#25927=CARTESIAN_POINT('Ctrl Pts',(2.76546341299628,-1.34112429005627,104.219803477097));
#25928=CARTESIAN_POINT('Ctrl Pts',(2.72338021851669,-1.42790188069288,104.214812631916));
#25929=CARTESIAN_POINT('Ctrl Pts',(2.67724628711548,-1.51261918677559,104.209821786735));
#25930=CARTESIAN_POINT('Ctrl Pts',(2.62730555565989,-1.59488801086429,104.204830941553));
#25931=CARTESIAN_POINT('Ctrl Pts',(2.57728411872113,-1.67728978345024,104.19983203104));
#25932=CARTESIAN_POINT('Ctrl Pts',(2.52344384281173,-1.75723480932283,104.194833120527));
#25933=CARTESIAN_POINT('Ctrl Pts',(2.4660710110759,-1.83436529032009,104.189834210014));
#25934=CARTESIAN_POINT('Ctrl Pts',(2.4327626774887,-1.87914411181223,104.186932045803));
#25935=CARTESIAN_POINT('Ctrl Pts',(2.39826444550648,-1.92297492309074,104.184029881592));
#25936=CARTESIAN_POINT('Ctrl Pts',(2.36263808832369,-1.96579335475583,104.181127717381));
#25937=CARTESIAN_POINT('Ctrl Pts',(2.30126516178033,-2.0395559470916,104.176128207888));
#25938=CARTESIAN_POINT('Ctrl Pts',(2.23632677673238,-2.11057120900105,104.171128698395));
#25939=CARTESIAN_POINT('Ctrl Pts',(2.16809822016109,-2.17847477785131,104.166129188902));
#25940=CARTESIAN_POINT('Ctrl Pts',(2.09996221519368,-2.24628623594147,104.161136461212));
#25941=CARTESIAN_POINT('Ctrl Pts',(2.02854521728431,-2.31099408291181,104.156143733522));
#25942=CARTESIAN_POINT('Ctrl Pts',(1.95416278397776,-2.37226686182568,104.151151005832));
#25943=CARTESIAN_POINT('Ctrl Pts',(1.87985882226302,-2.43347499950262,104.146163545344));
#25944=CARTESIAN_POINT('Ctrl Pts',(1.80259598134922,-2.49125499562497,104.141176084855));
#25945=CARTESIAN_POINT('Ctrl Pts',(1.72272594707639,-2.54531286117635,104.136188624367));
#25946=CARTESIAN_POINT('Ctrl Pts',(1.64291306168037,-2.59933204706112,104.131204732523));
#25947=CARTESIAN_POINT('Ctrl Pts',(1.56049705395011,-2.64963415149563,104.12622084068));
#25948=CARTESIAN_POINT('Ctrl Pts',(1.47586112013985,-2.69596665484934,104.121236948836));
#25949=CARTESIAN_POINT('Ctrl Pts',(1.39125600864048,-2.74228228505286,104.116254872002));
#25950=CARTESIAN_POINT('Ctrl Pts',(1.30443296199666,-2.78463097591669,104.111272795169));
#25951=CARTESIAN_POINT('Ctrl Pts',(1.21580164223415,-2.82280509719335,104.106290718335));
#25952=CARTESIAN_POINT('Ctrl Pts',(1.12717840360608,-2.86097573786962,104.101309095752));
#25953=CARTESIAN_POINT('Ctrl Pts',(1.03674762288719,-2.89497239223644,104.096327473169));
#25954=CARTESIAN_POINT('Ctrl Pts',(0.944939912648046,-2.92463515869667,
104.091345850586));
#25955=CARTESIAN_POINT('Ctrl Pts',(0.853115510149806,-2.95430331837041,
104.086363322256));
#25956=CARTESIAN_POINT('Ctrl Pts',(0.759914098643544,-2.97963589029097,
104.081380793926));
#25957=CARTESIAN_POINT('Ctrl Pts',(0.665781420455429,-3.00052284613471,
104.076398265596));
#25958=CARTESIAN_POINT('Ctrl Pts',(0.571547281113173,-3.02143231503861,
104.071410366835));
#25959=CARTESIAN_POINT('Ctrl Pts',(0.476380300408673,-3.03788650639572,
104.066422468074));
#25960=CARTESIAN_POINT('Ctrl Pts',(0.380736164232095,-3.049826589045,104.061434569313));
#25961=CARTESIAN_POINT('Ctrl Pts',(0.285035529751468,-3.06177372486498,
104.056443724132));
#25962=CARTESIAN_POINT('Ctrl Pts',(0.188857616019592,-3.06920140866425,
104.051452878951));
#25963=CARTESIAN_POINT('Ctrl Pts',(0.0926608518625408,-3.07210289810288,
104.046462033769));
#25964=CARTESIAN_POINT('Ctrl Pts',(-0.00369136869463417,-3.07500907642171,
104.041463123256));
#25965=CARTESIAN_POINT('Ctrl Pts',(-0.100062061900924,-3.07337446249044,
104.036464212743));
#25966=CARTESIAN_POINT('Ctrl Pts',(-0.195995242113639,-3.067244384634,104.03146530223));
#25967=CARTESIAN_POINT('Ctrl Pts',(-0.251690146338518,-3.06368551065163,
104.028563138019));
#25968=CARTESIAN_POINT('Ctrl Pts',(-0.307237708948579,-3.05861241343464,
104.025660973808));
#25969=CARTESIAN_POINT('Ctrl Pts',(-0.362550304875721,-3.05204186184176,
104.022758809597));
#25970=CARTESIAN_POINT('Ctrl Pts',(-0.457836383924149,-3.04072288308156,
104.017759300104));
#25971=CARTESIAN_POINT('Ctrl Pts',(-0.552759242854784,-3.02491743689527,
104.012759790611));
#25972=CARTESIAN_POINT('Ctrl Pts',(-0.646863376675473,-3.00465805407471,
104.007760281118));
#25973=CARTESIAN_POINT('Ctrl Pts',(-0.740839858836012,-2.98442615297834,
104.002767553428));
#25974=CARTESIAN_POINT('Ctrl Pts',(-0.833999397662042,-2.95975241439547,
103.997774825738));
#25975=CARTESIAN_POINT('Ctrl Pts',(-0.925892163834386,-2.93072106331361,
103.992782098048));
#25976=CARTESIAN_POINT('Ctrl Pts',(-1.01768798545516,-2.90172033957523,
103.98779463756));
#25977=CARTESIAN_POINT('Ctrl Pts',(-1.10821927478628,-2.86837127377104,
103.982807177071));
#25978=CARTESIAN_POINT('Ctrl Pts',(-1.19704796020428,-2.83080879449156,
103.977819716583));
#25979=CARTESIAN_POINT('Ctrl Pts',(-1.28581308662117,-2.79327319204417,
103.972835824739));
#25980=CARTESIAN_POINT('Ctrl Pts',(-1.37287762781264,-2.75153033986734,
103.967851932896));
#25981=CARTESIAN_POINT('Ctrl Pts',(-1.45782114046193,-2.70576417531578,
103.962868041052));
#25982=CARTESIAN_POINT('Ctrl Pts',(-1.54273371878766,-2.66001467766788,
103.957885964218));
#25983=CARTESIAN_POINT('Ctrl Pts',(-1.62552641725117,-2.61024498681573,
103.952903887385));
#25984=CARTESIAN_POINT('Ctrl Pts',(-1.70580203607325,-2.55668567949374,
103.947921810551));
#25985=CARTESIAN_POINT('Ctrl Pts',(-1.78607033560831,-2.50313125554665,
103.942940187968));
#25986=CARTESIAN_POINT('Ctrl Pts',(-1.86382164674154,-2.44578814587672,
103.937958565385));
#25987=CARTESIAN_POINT('Ctrl Pts',(-1.93868739756062,-2.38493048631184,
103.932976942802));
#25988=CARTESIAN_POINT('Ctrl Pts',(-2.01356676029249,-2.32406176175202,
103.927994414472));
#25989=CARTESIAN_POINT('Ctrl Pts',(-2.08555918016921,-2.25967749513936,
103.923011886142));
#25990=CARTESIAN_POINT('Ctrl Pts',(-2.15432968117646,-2.1920916666057,103.918029357812));
#25991=CARTESIAN_POINT('Ctrl Pts',(-2.22317430664848,-2.12443299050959,
103.913041459051));
#25992=CARTESIAN_POINT('Ctrl Pts',(-2.28878976662176,-2.05356617146032,
103.90805356029));
#25993=CARTESIAN_POINT('Ctrl Pts',(-2.35087861507805,-1.97984140454954,
103.903065661529));
#25994=CARTESIAN_POINT('Ctrl Pts',(-2.41300414026913,-1.90607308740727,
103.898074816348));
#25995=CARTESIAN_POINT('Ctrl Pts',(-2.47159863940539,-1.82944380940346,
103.893083971167));
#25996=CARTESIAN_POINT('Ctrl Pts',(-2.52640686477412,-1.75033442622323,
103.888093125985));
#25997=CARTESIAN_POINT('Ctrl Pts',(-2.5813036616193,-1.67109720028177,103.883094215472));
#25998=CARTESIAN_POINT('Ctrl Pts',(-2.6324017344191,-1.58937223819583,103.878095304959));
#25999=CARTESIAN_POINT('Ctrl Pts',(-2.67949084212781,-1.5055666962819,103.873096394446));
#26000=CARTESIAN_POINT('Ctrl Pts',(-2.70682886363425,-1.45691260579936,
103.870194230235));
#26001=CARTESIAN_POINT('Ctrl Pts',(-2.73281654600128,-1.40755768312279,
103.867292066024));
#26002=CARTESIAN_POINT('Ctrl Pts',(-2.75742024721313,-1.3575845573146,103.864389901813));
#26003=CARTESIAN_POINT('Ctrl Pts',(-2.80284919410827,-1.26531281092261,
103.859031266432));
#26004=CARTESIAN_POINT('Ctrl Pts',(-2.84369889987435,-1.17064478182644,
103.853672631051));
#26005=CARTESIAN_POINT('Ctrl Pts',(-2.87972873844127,-1.07404126689594,
103.84831399567));
#26006=CARTESIAN_POINT('Ctrl Pts',(-2.91564169345326,-0.977751141164306,
103.842972744112));
#26007=CARTESIAN_POINT('Ctrl Pts',(-2.94676582982252,-0.879538363778252,
103.837631492554));
#26008=CARTESIAN_POINT('Ctrl Pts',(-2.97290811057071,-0.779884360724638,
103.832290240997));
#26009=CARTESIAN_POINT('Ctrl Pts',(-2.99899763374524,-0.680431468792797,
103.826959768586));
#26010=CARTESIAN_POINT('Ctrl Pts',(-3.02012523611837,-0.579543470887511,
103.821629296174));
#26011=CARTESIAN_POINT('Ctrl Pts',(-3.03614664061705,-0.477719401604962,
103.816298823763));
#26012=CARTESIAN_POINT('Ctrl Pts',(-3.05212172792721,-0.376189701309465,
103.810983761518));
#26013=CARTESIAN_POINT('Ctrl Pts',(-3.06301998403236,-0.273729658401492,
103.805668699272));
#26014=CARTESIAN_POINT('Ctrl Pts',(-3.06874773143845,-0.170849673079425,
103.800353637026));
#26015=CARTESIAN_POINT('Ctrl Pts',(-3.0719005901615,-0.114219022990934,
103.797427942303));
#26016=CARTESIAN_POINT('Ctrl Pts',(-3.0734876697023,-0.057461379173942,
103.794502247579));
#26017=CARTESIAN_POINT('Ctrl Pts',(-3.07349992841428,-0.0006633531664633,
103.791576552855));
#26018=CARTESIAN_POINT('Origin',(0.,0.,116.208423447177));
#26019=CARTESIAN_POINT('',(1.87238193903528,2.43733217358128,105.437268236956));
#26020=CARTESIAN_POINT('',(1.87238193903528,2.43733217358129,105.354223092666));
#26021=CARTESIAN_POINT('',(1.8723819390353,2.43733217358128,116.208423447177));
#26022=CARTESIAN_POINT('',(-3.07349891831708,0.00257858561311968,104.70842344715));
#26023=CARTESIAN_POINT('Ctrl Pts',(1.87238193903529,2.43733217358128,105.354223092666));
#26024=CARTESIAN_POINT('Ctrl Pts',(1.94945953133495,2.37812042834175,105.349202752108));
#26025=CARTESIAN_POINT('Ctrl Pts',(2.02369320136329,2.3152738620541,105.34418241155));
#26026=CARTESIAN_POINT('Ctrl Pts',(2.09473553780151,2.24910766231219,105.339162070992));
#26027=CARTESIAN_POINT('Ctrl Pts',(2.16534023155336,2.18334906675188,105.334172657279));
#26028=CARTESIAN_POINT('Ctrl Pts',(2.23279253492672,2.11431198189643,105.329183243567));
#26029=CARTESIAN_POINT('Ctrl Pts',(2.29678984415326,2.04234146552296,105.324193829854));
#26030=CARTESIAN_POINT('Ctrl Pts',(2.36138218367118,1.96970178605737,105.319158025873));
#26031=CARTESIAN_POINT('Ctrl Pts',(2.42245466520873,1.89407420271472,105.314122221893));
#26032=CARTESIAN_POINT('Ctrl Pts',(2.47973990076263,1.8158447826193,105.309086417912));
#26033=CARTESIAN_POINT('Ctrl Pts',(2.53702513631653,1.73761536252389,105.304050613932));
#26034=CARTESIAN_POINT('Ctrl Pts',(2.59052292778912,1.65678451783041,105.299014809952));
#26035=CARTESIAN_POINT('Ctrl Pts',(2.64001321119421,1.57376379889741,105.293979005971));
#26036=CARTESIAN_POINT('Ctrl Pts',(2.68914680389491,1.49134143415999,105.288979496478));
#26037=CARTESIAN_POINT('Ctrl Pts',(2.73450310331458,1.40647113676653,105.283979986985));
#26038=CARTESIAN_POINT('Ctrl Pts',(2.77583012931114,1.31953375978355,105.278980477492));
#26039=CARTESIAN_POINT('Ctrl Pts',(2.8171010954593,1.23271431280053,105.273987749802));
#26040=CARTESIAN_POINT('Ctrl Pts',(2.85435346402324,1.14383375201073,105.268995022112));
#26041=CARTESIAN_POINT('Ctrl Pts',(2.8873796867055,1.0532999548089,105.264002294422));
#26042=CARTESIAN_POINT('Ctrl Pts',(2.92037106755534,0.962861668480981,105.259014833934));
#26043=CARTESIAN_POINT('Ctrl Pts',(2.94914501607307,0.870774023139204,105.254027373445));
#26044=CARTESIAN_POINT('Ctrl Pts',(2.97354133946183,0.777466496070115,105.249039912957));
#26045=CARTESIAN_POINT('Ctrl Pts',(2.99792020671094,0.684225732717753,105.244056021114));
#26046=CARTESIAN_POINT('Ctrl Pts',(3.01792756496112,0.58976724629874,105.23907212927));
#26047=CARTESIAN_POINT('Ctrl Pts',(3.03345281349624,0.494536427669112,105.234088237426));
#26048=CARTESIAN_POINT('Ctrl Pts',(3.04897240812038,0.399340289744977,105.229106160593));
#26049=CARTESIAN_POINT('Ctrl Pts',(3.06001306562101,0.303372811251732,105.224124083759));
#26050=CARTESIAN_POINT('Ctrl Pts',(3.06651532359486,0.20708940136545,105.219142006925));
#26051=CARTESIAN_POINT('Ctrl Pts',(3.07301698871259,0.110814770307922,105.214160384342));
#26052=CARTESIAN_POINT('Ctrl Pts',(3.07498104761558,0.0142247031053793,
105.209178761759));
#26053=CARTESIAN_POINT('Ctrl Pts',(3.07240001820998,-0.0822215184931722,
105.204197139176));
#26054=CARTESIAN_POINT('Ctrl Pts',(3.06981851952776,-0.178685275714061,
105.199214610846));
#26055=CARTESIAN_POINT('Ctrl Pts',(3.06269030312906,-0.275004696589989,
105.194232082516));
#26056=CARTESIAN_POINT('Ctrl Pts',(3.05105995248765,-0.370722829518265,
105.189249554186));
#26057=CARTESIAN_POINT('Ctrl Pts',(3.03941706604231,-0.466544132487117,
105.184261655425));
#26058=CARTESIAN_POINT('Ctrl Pts',(3.02326241054735,-0.561762417156996,
105.179273756664));
#26059=CARTESIAN_POINT('Ctrl Pts',(3.00269215754031,-0.655928393230473,
105.174285857903));
#26060=CARTESIAN_POINT('Ctrl Pts',(2.98210975340248,-0.750149994438522,
105.169295012722));
#26061=CARTESIAN_POINT('Ctrl Pts',(2.95710667181709,-0.84331762555405,105.164304167541));
#26062=CARTESIAN_POINT('Ctrl Pts',(2.92782911689693,-0.934996744513346,
105.159313322359));
#26063=CARTESIAN_POINT('Ctrl Pts',(2.89850424870867,-1.02682401924407,105.154314411846));
#26064=CARTESIAN_POINT('Ctrl Pts',(2.86489126710132,-1.117157567493,105.149315501333));
#26065=CARTESIAN_POINT('Ctrl Pts',(2.82718466573472,-1.20558247989693,105.14431659082));
#26066=CARTESIAN_POINT('Ctrl Pts',(2.80529374596009,-1.25691838908413,105.141414426609));
#26067=CARTESIAN_POINT('Ctrl Pts',(2.78202394842517,-1.30761143150604,105.138512262398));
#26068=CARTESIAN_POINT('Ctrl Pts',(2.75742024721298,-1.35758455731491,105.135610098187));
#26069=CARTESIAN_POINT('Ctrl Pts',(2.71503586478997,-1.44367242096148,105.130610588694));
#26070=CARTESIAN_POINT('Ctrl Pts',(2.66854162211707,-1.52792470090094,105.125611079201));
#26071=CARTESIAN_POINT('Ctrl Pts',(2.61811978482655,-1.6099226820875,105.120611569708));
#26072=CARTESIAN_POINT('Ctrl Pts',(2.56776634443807,-1.69180943353335,105.115618842018));
#26073=CARTESIAN_POINT('Ctrl Pts',(2.51349612596166,-1.77144759295787,105.110626114328));
#26074=CARTESIAN_POINT('Ctrl Pts',(2.45553825381476,-1.84844100096605,105.105633386638));
#26075=CARTESIAN_POINT('Ctrl Pts',(2.39764152576222,-1.9253531828693,105.10064592615));
#26076=CARTESIAN_POINT('Ctrl Pts',(2.33606514047656,-1.99962581115889,105.095658465661));
#26077=CARTESIAN_POINT('Ctrl Pts',(2.2710821229741,-2.07089068777361,105.090671005173));
#26078=CARTESIAN_POINT('Ctrl Pts',(2.20614560233962,-2.14210457270332,105.085687113329));
#26079=CARTESIAN_POINT('Ctrl Pts',(2.13780759009278,-2.21031466083467,105.080703221486));
#26080=CARTESIAN_POINT('Ctrl Pts',(2.06638145991496,-2.27518568739339,105.075719329642));
#26081=CARTESIAN_POINT('Ctrl Pts',(1.99498134136481,-2.34003308953083,105.070737252808));
#26082=CARTESIAN_POINT('Ctrl Pts',(1.92049566398737,-2.40154355134022,105.065755175975));
#26083=CARTESIAN_POINT('Ctrl Pts',(1.84327404708782,-2.45941924797959,105.060773099141));
#26084=CARTESIAN_POINT('Ctrl Pts',(1.76605947102081,-2.51728966768868,105.055791476558));
#26085=CARTESIAN_POINT('Ctrl Pts',(1.68610980276192,-2.57152571801325,105.050809853975));
#26086=CARTESIAN_POINT('Ctrl Pts',(1.60380621066126,-2.62187106636547,105.045828231392));
#26087=CARTESIAN_POINT('Ctrl Pts',(1.52148765431711,-2.67222556838925,105.040845703062));
#26088=CARTESIAN_POINT('Ctrl Pts',(1.43681469862724,-2.71868773452121,105.035863174732));
#26089=CARTESIAN_POINT('Ctrl Pts',(1.35019490461258,-2.76104617302178,105.030880646402));
#26090=CARTESIAN_POINT('Ctrl Pts',(1.26348174722592,-2.80345026767631,105.025892747641));
#26091=CARTESIAN_POINT('Ctrl Pts',(1.17481795723416,-2.84174161100527,105.02090484888));
#26092=CARTESIAN_POINT('Ctrl Pts',(1.08463275661632,-2.87575625414862,105.015916950119));
#26093=CARTESIAN_POINT('Ctrl Pts',(0.994394282362713,-2.90979099020851,
105.010926104938));
#26094=CARTESIAN_POINT('Ctrl Pts',(0.902633025354364,-2.93954386046796,
105.005935259757));
#26095=CARTESIAN_POINT('Ctrl Pts',(0.809793077179332,-2.9649009127039,105.000944414575));
#26096=CARTESIAN_POINT('Ctrl Pts',(0.716803097303502,-2.99029894257662,
104.995945504062));
#26097=CARTESIAN_POINT('Ctrl Pts',(0.622731373631855,-3.01128687428064,
104.990946593549));
#26098=CARTESIAN_POINT('Ctrl Pts',(0.528031821313986,-3.02780194954687,
104.985947683036));
#26099=CARTESIAN_POINT('Ctrl Pts',(0.473053111291294,-3.03738993081861,
104.983045518825));
#26100=CARTESIAN_POINT('Ctrl Pts',(0.417862900802648,-3.04547131024891,
104.980143354614));
#26101=CARTESIAN_POINT('Ctrl Pts',(0.362550304875634,-3.05204186184177,
104.977241190403));
#26102=CARTESIAN_POINT('Ctrl Pts',(0.267264225827233,-3.06336084060196,
104.97224168091));
#26103=CARTESIAN_POINT('Ctrl Pts',(0.171280200402446,-3.07023311387662,
104.967242171417));
#26104=CARTESIAN_POINT('Ctrl Pts',(0.0750486783593991,-3.07258359461163,
104.962242661924));
#26105=CARTESIAN_POINT('Ctrl Pts',(-0.0210523062352704,-3.07493088693445,
104.957249934234));
#26106=CARTESIAN_POINT('Ctrl Pts',(-0.117399685134141,-3.07276856657818,
104.952257206544));
#26107=CARTESIAN_POINT('Ctrl Pts',(-0.213536415746227,-3.06607313173549,
104.947264478854));
#26108=CARTESIAN_POINT('Ctrl Pts',(-0.309571724530516,-3.0593847604078,
104.942277018366));
#26109=CARTESIAN_POINT('Ctrl Pts',(-0.405396391232003,-3.04817281189546,
104.937289557877));
#26110=CARTESIAN_POINT('Ctrl Pts',(-0.500552925261181,-3.03246583146661,
104.932302097389));
#26111=CARTESIAN_POINT('Ctrl Pts',(-0.595641372565858,-3.01677008974942,
104.927318205546));
#26112=CARTESIAN_POINT('Ctrl Pts',(-0.690062205708036,-2.99658578125377,
104.922334313702));
#26113=CARTESIAN_POINT('Ctrl Pts',(-0.783363590391523,-2.97199322597628,
104.917350421858));
#26114=CARTESIAN_POINT('Ctrl Pts',(-0.876630997021813,-2.94740962669825,
104.912368345025));
#26115=CARTESIAN_POINT('Ctrl Pts',(-0.968779341168995,-2.91842108210969,
104.907386268191));
#26116=CARTESIAN_POINT('Ctrl Pts',(-1.05936845887682,-2.88515869898641,
104.902404191357));
#26117=CARTESIAN_POINT('Ctrl Pts',(-1.14994931694398,-2.85189934862622,
104.897422568774));
#26118=CARTESIAN_POINT('Ctrl Pts',(-1.23897081922333,-2.81436708595139,
104.892440946191));
#26119=CARTESIAN_POINT('Ctrl Pts',(-1.32601042821453,-2.77274207135578,
104.887459323608));
#26120=CARTESIAN_POINT('Ctrl Pts',(-1.41306586254063,-2.73110948859891,
104.882476795278));
#26121=CARTESIAN_POINT('Ctrl Pts',(-1.49813829194838,-2.6853828654822,104.877494266948));
#26122=CARTESIAN_POINT('Ctrl Pts',(-1.58082850544345,-2.63578896848314,
104.872511738619));
#26123=CARTESIAN_POINT('Ctrl Pts',(-1.66360784680152,-2.58614161657243,
104.867523839858));
#26124=CARTESIAN_POINT('Ctrl Pts',(-1.7439994690437,-2.53261889520195,104.862535941096));
#26125=CARTESIAN_POINT('Ctrl Pts',(-1.82163216255449,-2.47549157024359,
104.857548042335));
#26126=CARTESIAN_POINT('Ctrl Pts',(-1.89931071476291,-2.41833049939025,
104.852557197154));
#26127=CARTESIAN_POINT('Ctrl Pts',(-1.97422675241966,-2.35756086159102,
104.847566351973));
#26128=CARTESIAN_POINT('Ctrl Pts',(-2.04604290692081,-2.29349311597813,
104.842575506792));
#26129=CARTESIAN_POINT('Ctrl Pts',(-2.11797511814123,-2.2293218352704,104.837576596278));
#26130=CARTESIAN_POINT('Ctrl Pts',(-2.18679713013914,-2.1618421113799,104.832577685765));
#26131=CARTESIAN_POINT('Ctrl Pts',(-2.25220916695079,-2.09140051599469,
104.827578775252));
#26132=CARTESIAN_POINT('Ctrl Pts',(-2.29018473616726,-2.05050498954941,
104.824676611041));
#26133=CARTESIAN_POINT('Ctrl Pts',(-2.32701173114118,-2.00861178642058,
104.82177444683));
#26134=CARTESIAN_POINT('Ctrl Pts',(-2.36263808832381,-1.96579335475569,
104.818872282619));
#26135=CARTESIAN_POINT('Ctrl Pts',(-2.42366151100837,-1.89245082240576,
104.813901244114));
#26136=CARTESIAN_POINT('Ctrl Pts',(-2.48138149360842,-1.81612585312949,
104.808930205609));
#26137=CARTESIAN_POINT('Ctrl Pts',(-2.53549054025688,-1.73714995618337,
104.803959167104));
#26138=CARTESIAN_POINT('Ctrl Pts',(-2.58953001315165,-1.658275606944,104.798994520392));
#26139=CARTESIAN_POINT('Ctrl Pts',(-2.63996752204625,-1.57675746166274,
104.79402987368));
#26140=CARTESIAN_POINT('Ctrl Pts',(-2.68653487203633,-1.49296102806896,
104.789065226968));
#26141=CARTESIAN_POINT('Ctrl Pts',(-2.73305541744705,-1.40924881779533,
104.784105570194));
#26142=CARTESIAN_POINT('Ctrl Pts',(-2.77571331674056,-1.32326325384198,
104.77914591342));
#26143=CARTESIAN_POINT('Ctrl Pts',(-2.81428353238982,-1.23539890291333,
104.774186256646));
#26144=CARTESIAN_POINT('Ctrl Pts',(-2.85282580546769,-1.14759820617634,
104.769230192944));
#26145=CARTESIAN_POINT('Ctrl Pts',(-2.88728610213059,-1.05792183275072,
104.764274129242));
#26146=CARTESIAN_POINT('Ctrl Pts',(-2.91748575996682,-0.966788027641428,
104.75931806554));
#26147=CARTESIAN_POINT('Ctrl Pts',(-2.94767654771691,-0.875680989878505,
104.754363457507));
#26148=CARTESIAN_POINT('Ctrl Pts',(-2.97360903798759,-0.783117790220548,
104.749408849474));
#26149=CARTESIAN_POINT('Ctrl Pts',(-2.99515341736076,-0.689534811646325,
104.744454241442));
#26150=CARTESIAN_POINT('Ctrl Pts',(-3.01669409614081,-0.595967907451499,
104.739500484442));
#26151=CARTESIAN_POINT('Ctrl Pts',(-3.03384806794806,-0.50138200653861,
104.734546727443));
#26152=CARTESIAN_POINT('Ctrl Pts',(-3.04653625570149,-0.406225421036614,
104.729592970444));
#26153=CARTESIAN_POINT('Ctrl Pts',(-3.05922958420412,-0.311030281869517,
104.724637206379));
#26154=CARTESIAN_POINT('Ctrl Pts',(-3.06745346148863,-0.215264437470324,
104.719681442315));
#26155=CARTESIAN_POINT('Ctrl Pts',(-3.07118057186357,-0.119382347973822,
104.71472567825));
#26156=CARTESIAN_POINT('Ctrl Pts',(-3.07276049041973,-0.0787380210932937,
104.712624934559));
#26157=CARTESIAN_POINT('Ctrl Pts',(-3.07353302379519,-0.0380728361124389,
104.710524190868));
#26158=CARTESIAN_POINT('Ctrl Pts',(-3.07349891831751,0.00257858509384388,
104.708423447177));
#26159=CARTESIAN_POINT('Ctrl Pts',(-3.07349891831708,0.00257858561313954,
104.70842344715));
#26160=CARTESIAN_POINT('Ctrl Pts',(-3.07340190154726,0.11821598603669,104.702447652648));
#26161=CARTESIAN_POINT('Ctrl Pts',(-3.06677494859755,0.233572640495253,
104.696471858145));
#26162=CARTESIAN_POINT('Ctrl Pts',(-3.05373569317267,0.347995066406445,
104.690496063642));
#26163=CARTESIAN_POINT('Ctrl Pts',(-3.04052691899684,0.463905057833428,
104.684442579947));
#26164=CARTESIAN_POINT('Ctrl Pts',(-3.02073810232729,0.578856352949399,
104.678389096252));
#26165=CARTESIAN_POINT('Ctrl Pts',(-2.99454061664833,0.692191263483916,
104.672335612557));
#26166=CARTESIAN_POINT('Ctrl Pts',(-2.97747193939876,0.766033350191337,
104.668391533316));
#26167=CARTESIAN_POINT('Ctrl Pts',(-2.95768375771646,0.839189719506165,
104.664447454075));
#26168=CARTESIAN_POINT('Ctrl Pts',(-2.93523429559051,0.911483340489175,
104.660503374835));
#26169=CARTESIAN_POINT('Ctrl Pts',(-2.90677738786623,1.00312263633624,104.655503865342));
#26170=CARTESIAN_POINT('Ctrl Pts',(-2.87397485611257,1.09358895707076,104.650504355849));
#26171=CARTESIAN_POINT('Ctrl Pts',(-2.83694151691682,1.18244030698961,104.645504846356));
#26172=CARTESIAN_POINT('Ctrl Pts',(-2.7999584132105,1.27117113061657,104.640512118666));
#26173=CARTESIAN_POINT('Ctrl Pts',(-2.75875607550427,1.35829093558367,104.635519390975));
#26174=CARTESIAN_POINT('Ctrl Pts',(-2.71349912070783,1.4433727072097,104.630526663285));
#26175=CARTESIAN_POINT('Ctrl Pts',(-2.66828991085796,1.52836471971121,104.625539202797));
#26176=CARTESIAN_POINT('Ctrl Pts',(-2.61903479241562,1.61132258760283,104.620551742309));
#26177=CARTESIAN_POINT('Ctrl Pts',(-2.56594610259187,1.69184007772413,104.615564281821));
#26178=CARTESIAN_POINT('Ctrl Pts',(-2.51289539896664,1.77229995569914,104.610580389977));
#26179=CARTESIAN_POINT('Ctrl Pts',(-2.45601681787269,1.85032256174038,104.605596498133));
#26180=CARTESIAN_POINT('Ctrl Pts',(-2.39556768273871,1.92552790876109,104.60061260629));
#26181=CARTESIAN_POINT('Ctrl Pts',(-2.33514056168258,2.00070586785708,104.595630529456));
#26182=CARTESIAN_POINT('Ctrl Pts',(-2.27114574488193,2.0730682646461,104.590648452622));
#26183=CARTESIAN_POINT('Ctrl Pts',(-2.20388219103734,2.14226644888736,104.585666375788));
#26184=CARTESIAN_POINT('Ctrl Pts',(-2.13662477007921,2.21145832384844,104.580684753205));
#26185=CARTESIAN_POINT('Ctrl Pts',(-2.06609951071634,2.27748624522545,104.575703130622));
#26186=CARTESIAN_POINT('Ctrl Pts',(-1.99264299891211,2.34003763407484,104.570721508039));
#26187=CARTESIAN_POINT('Ctrl Pts',(-1.91917313141978,2.40260039586882,104.565738979709));
#26188=CARTESIAN_POINT('Ctrl Pts',(-1.84277128726752,2.4616850852312,104.560756451379));
#26189=CARTESIAN_POINT('Ctrl Pts',(-1.763807123446,2.51701940423214,104.55577392305));
#26190=CARTESIAN_POINT('Ctrl Pts',(-1.68475784789349,2.5724133654739,104.550786024289));
#26191=CARTESIAN_POINT('Ctrl Pts',(-1.6031410990681,2.62404863385521,104.545798125528));
#26192=CARTESIAN_POINT('Ctrl Pts',(-1.51935532078173,2.67169640101795,104.540810226766));
#26193=CARTESIAN_POINT('Ctrl Pts',(-1.43552004908622,2.71937231437069,104.535819381585));
#26194=CARTESIAN_POINT('Ctrl Pts',(-1.34951358789181,2.76305583768599,104.530828536404));
#26195=CARTESIAN_POINT('Ctrl Pts',(-1.26175685718869,2.80256523266405,104.525837691223));
#26196=CARTESIAN_POINT('Ctrl Pts',(-1.17385830939251,2.84213847582219,104.520838780709));
#26197=CARTESIAN_POINT('Ctrl Pts',(-1.08420425227333,2.8775239603299,104.515839870196));
#26198=CARTESIAN_POINT('Ctrl Pts',(-0.993233284057695,2.90858898668065,
104.510840959683));
#26199=CARTESIAN_POINT('Ctrl Pts',(-0.940419238377377,2.92662407801726,
104.507938795472));
#26200=CARTESIAN_POINT('Ctrl Pts',(-0.887161587446126,2.94320390445115,
104.505036631261));
#26201=CARTESIAN_POINT('Ctrl Pts',(-0.833547700173576,2.95831040993594,
104.50213446705));
#26202=CARTESIAN_POINT('Ctrl Pts',(-0.741183834711446,2.98433529474063,
104.497134734362));
#26203=CARTESIAN_POINT('Ctrl Pts',(-0.647437746391747,3.00607609265561,
104.492135001674));
#26204=CARTESIAN_POINT('Ctrl Pts',(-0.55274274831966,3.02338844745098,104.487135268986));
#26205=CARTESIAN_POINT('Ctrl Pts',(-0.458177294599245,3.04067711865351,
104.482142376016));
#26206=CARTESIAN_POINT('Ctrl Pts',(-0.362665939390717,3.05354930928601,
104.477149483047));
#26207=CARTESIAN_POINT('Ctrl Pts',(-0.266656530519557,3.06191060364787,
104.472156590077));
#26208=CARTESIAN_POINT('Ctrl Pts',(-0.170760147999297,3.07026205473915,
104.467169574953));
#26209=CARTESIAN_POINT('Ctrl Pts',(-0.0743673130760004,3.07411313495795,
104.462182559829));
#26210=CARTESIAN_POINT('Ctrl Pts',(0.0220657436718747,3.0734207900898,104.457195544705));
#26211=CARTESIAN_POINT('Ctrl Pts',(0.1184357663145,3.07272889777745,104.452211789376));
#26212=CARTESIAN_POINT('Ctrl Pts',(0.214845520986163,3.067499483887,104.447228034047));
#26213=CARTESIAN_POINT('Ctrl Pts',(0.310836215005677,3.05774150271748,104.442244278719));
#26214=CARTESIAN_POINT('Ctrl Pts',(0.40679036992339,3.0479872359483,104.437262420469));
#26215=CARTESIAN_POINT('Ctrl Pts',(0.502325345044623,3.03370787233216,104.43228056222));
#26216=CARTESIAN_POINT('Ctrl Pts',(0.596985986216576,3.01496434178931,104.42729870397));
#26217=CARTESIAN_POINT('Ctrl Pts',(0.691636436486133,2.99622282912303,104.422317382054));
#26218=CARTESIAN_POINT('Ctrl Pts',(0.785412309697513,2.97301819146454,104.417336060137));
#26219=CARTESIAN_POINT('Ctrl Pts',(0.877868241469313,2.94546254442652,104.412354738221));
#26220=CARTESIAN_POINT('Ctrl Pts',(0.970389740926265,2.91788735553809,104.407369883662));
#26221=CARTESIAN_POINT('Ctrl Pts',(1.06158900682457,2.88595511628965,104.402385029103));
#26222=CARTESIAN_POINT('Ctrl Pts',(1.15103577723119,2.84982787015879,104.397400174544));
#26223=CARTESIAN_POINT('Ctrl Pts',(1.24051289750611,2.81368836581942,104.392413628592));
#26224=CARTESIAN_POINT('Ctrl Pts',(1.3282359367672,2.77335119885068,104.387427082639));
#26225=CARTESIAN_POINT('Ctrl Pts',(1.41379637619271,2.72902584389821,104.382440536687));
#26226=CARTESIAN_POINT('Ctrl Pts',(1.49947820590929,2.68463760161399,104.37744691599));
#26227=CARTESIAN_POINT('Ctrl Pts',(1.58299092297891,2.63625008317744,104.372453295293));
#26228=CARTESIAN_POINT('Ctrl Pts',(1.66395228944447,2.58411784337567,104.367459674596));
#26229=CARTESIAN_POINT('Ctrl Pts',(1.73550200378447,2.53804590772833,104.363046555722));
#26230=CARTESIAN_POINT('Ctrl Pts',(1.80505932822455,2.48905004853368,104.358633436849));
#26231=CARTESIAN_POINT('Ctrl Pts',(1.87238193903531,2.43733217358127,104.354220317975));
#26232=CARTESIAN_POINT('',(-3.07349915681862,-0.00227662804431954,104.791576552792));
#26233=CARTESIAN_POINT('Ctrl Pts',(-3.07349915681862,-0.00227662804430111,
104.791576552792));
#26234=CARTESIAN_POINT('Ctrl Pts',(-3.07356931928976,0.0924442889047205,
104.786655194444));
#26235=CARTESIAN_POINT('Ctrl Pts',(-3.06925653593697,0.187328717419588,
104.781733836096));
#26236=CARTESIAN_POINT('Ctrl Pts',(-3.06054199775665,0.281930718382627,
104.776812477748));
#26237=CARTESIAN_POINT('Ctrl Pts',(-3.05164555568275,0.378507404860657,
104.771788392872));
#26238=CARTESIAN_POINT('Ctrl Pts',(-3.03816145777448,0.474789267800039,
104.766764307997));
#26239=CARTESIAN_POINT('Ctrl Pts',(-3.02012579510685,0.570300299605607,
104.761740223121));
#26240=CARTESIAN_POINT('Ctrl Pts',(-3.00249201978596,0.663683066103453,
104.75682808956));
#26241=CARTESIAN_POINT('Ctrl Pts',(-2.98050749991343,0.756328525787592,
104.751915955999));
#26242=CARTESIAN_POINT('Ctrl Pts',(-2.95425829823731,0.847797238315873,
104.747003822437));
#26243=CARTESIAN_POINT('Ctrl Pts',(-2.9280187265775,0.93923239381623,104.742093490985));
#26244=CARTESIAN_POINT('Ctrl Pts',(-2.89751770441931,1.02949122436819,104.737183159533));
#26245=CARTESIAN_POINT('Ctrl Pts',(-2.86289185257744,1.11814690020842,104.732272828081));
#26246=CARTESIAN_POINT('Ctrl Pts',(-2.82826859954847,1.20679592207478,104.72736286517));
#26247=CARTESIAN_POINT('Ctrl Pts',(-2.78952129756073,1.29384160663761,104.722452902258));
#26248=CARTESIAN_POINT('Ctrl Pts',(-2.74683521027429,1.37887583835434,104.717542939347));
#26249=CARTESIAN_POINT('Ctrl Pts',(-2.70241837912313,1.4673578556188,104.712433897796));
#26250=CARTESIAN_POINT('Ctrl Pts',(-2.65373679550002,1.55366136045947,104.707324856245));
#26251=CARTESIAN_POINT('Ctrl Pts',(-2.60105180294079,1.63735511371799,104.702215814693));
#26252=CARTESIAN_POINT('Ctrl Pts',(-2.55035354038939,1.71789280899892,104.697299433057));
#26253=CARTESIAN_POINT('Ctrl Pts',(-2.4959486828039,1.79601368823005,104.69238305142));
#26254=CARTESIAN_POINT('Ctrl Pts',(-2.43811316796268,1.87136485758576,104.687466669784));
#26255=CARTESIAN_POINT('Ctrl Pts',(-2.38023908112461,1.94676628058018,104.682547009285));
#26256=CARTESIAN_POINT('Ctrl Pts',(-2.31893007893897,2.01939397562079,104.677627348787));
#26257=CARTESIAN_POINT('Ctrl Pts',(-2.25450042655716,2.0889303666359,104.672707688289));
#26258=CARTESIAN_POINT('Ctrl Pts',(-2.18997614221535,2.15856889020535,104.66778080197));
#26259=CARTESIAN_POINT('Ctrl Pts',(-2.12232239149969,2.22510674253026,104.662853915651));
#26260=CARTESIAN_POINT('Ctrl Pts',(-2.05188761562412,2.28826560146509,104.657927029332));
#26261=CARTESIAN_POINT('Ctrl Pts',(-2.04382186572228,2.29549815887612,104.657362833132));
#26262=CARTESIAN_POINT('Ctrl Pts',(-2.03571967892865,2.30268645256438,104.656798636933));
#26263=CARTESIAN_POINT('Ctrl Pts',(-2.02758160247084,2.30983010096452,104.656234440734));
#26264=CARTESIAN_POINT('Ctrl Pts',(-1.95546769854954,2.37313208357013,104.651234931241));
#26265=CARTESIAN_POINT('Ctrl Pts',(-1.880259817106,2.43316487332258,104.646235421748));
#26266=CARTESIAN_POINT('Ctrl Pts',(-1.80228664223904,2.48961143739474,104.641235912255));
#26267=CARTESIAN_POINT('Ctrl Pts',(-1.72441923748872,2.54598143206114,104.636243184565));
#26268=CARTESIAN_POINT('Ctrl Pts',(-1.6437943469127,2.59877461409763,104.631250456875));
#26269=CARTESIAN_POINT('Ctrl Pts',(-1.56077530780112,2.64771272772526,104.626257729185));
#26270=CARTESIAN_POINT('Ctrl Pts',(-1.477843851683,2.69659921287667,104.621270268696));
#26271=CARTESIAN_POINT('Ctrl Pts',(-1.39252364424015,2.74163849284233,104.616282808208));
#26272=CARTESIAN_POINT('Ctrl Pts',(-1.30520787358299,2.78259495017456,104.61129534772));
#26273=CARTESIAN_POINT('Ctrl Pts',(-1.21795457940088,2.82352210220415,104.606311455876));
#26274=CARTESIAN_POINT('Ctrl Pts',(-1.12870895682206,2.86037205323864,104.601327564033));
#26275=CARTESIAN_POINT('Ctrl Pts',(-1.03788885994979,2.89295505744423,104.596343672189));
#26276=CARTESIAN_POINT('Ctrl Pts',(-0.947101837507401,2.92552619572669,
104.591361595355));
#26277=CARTESIAN_POINT('Ctrl Pts',(-0.854741892778729,2.9538333265618,104.586379518521));
#26278=CARTESIAN_POINT('Ctrl Pts',(-0.761246030056902,2.97773516816432,
104.581397441688));
#26279=CARTESIAN_POINT('Ctrl Pts',(-0.66775869200392,3.00163483046951,104.576415819105));
#26280=CARTESIAN_POINT('Ctrl Pts',(-0.573136067203588,3.02112989357356,
104.571434196522));
#26281=CARTESIAN_POINT('Ctrl Pts',(-0.477828419957685,3.03612948522963,
104.566452573938));
#26282=CARTESIAN_POINT('Ctrl Pts',(-0.382503444102034,3.05113180407578,
104.561470045609));
#26283=CARTESIAN_POINT('Ctrl Pts',(-0.286493632072055,3.06163695999534,
104.556487517279));
#26284=CARTESIAN_POINT('Ctrl Pts',(-0.190256424370767,3.06760570200697,
104.551504988949));
#26285=CARTESIAN_POINT('Ctrl Pts',(-0.0939154871429441,3.07358087744281,
104.546517090188));
#26286=CARTESIAN_POINT('Ctrl Pts',(0.00265289622678519,3.07500985014687,
104.541529191427));
#26287=CARTESIAN_POINT('Ctrl Pts',(0.0989894381430324,3.07190549026758,
104.536541292666));
#26288=CARTESIAN_POINT('Ctrl Pts',(0.195382887376889,3.06879929660031,104.531550447484));
#26289=CARTESIAN_POINT('Ctrl Pts',(0.291543785086276,3.0611544729812,104.526559602303));
#26290=CARTESIAN_POINT('Ctrl Pts',(0.387018248209097,3.04903576980546,104.521568757122));
#26291=CARTESIAN_POINT('Ctrl Pts',(0.482647000475417,3.03689748249934,104.516569846609));
#26292=CARTESIAN_POINT('Ctrl Pts',(0.577586671046384,3.02027095479029,104.511570936095));
#26293=CARTESIAN_POINT('Ctrl Pts',(0.67139390137743,2.99927199153281,104.506572025582));
#26294=CARTESIAN_POINT('Ctrl Pts',(0.725854565532475,2.98708084718782,104.503669861371));
#26295=CARTESIAN_POINT('Ctrl Pts',(0.779933812901155,2.97341691542069,104.50076769716));
#26296=CARTESIAN_POINT('Ctrl Pts',(0.833547700173759,2.95831040993589,104.497865532949));
#26297=CARTESIAN_POINT('Ctrl Pts',(0.926836818625348,2.93202482142043,104.492815715549));
#26298=CARTESIAN_POINT('Ctrl Pts',(1.01904687568902,2.90127553014951,104.487765898149));
#26299=CARTESIAN_POINT('Ctrl Pts',(1.10971947703148,2.86616903414592,104.482716080748));
#26300=CARTESIAN_POINT('Ctrl Pts',(1.19935676078363,2.8314633910164,104.477723923156));
#26301=CARTESIAN_POINT('Ctrl Pts',(1.28749108347536,2.79249965768734,104.472731765564));
#26302=CARTESIAN_POINT('Ctrl Pts',(1.37369152560868,2.74943154896988,104.467739607972));
#26303=CARTESIAN_POINT('Ctrl Pts',(1.46138540044595,2.70561728025063,104.462660960667));
#26304=CARTESIAN_POINT('Ctrl Pts',(1.54707730635654,2.65755518789107,104.457582313363));
#26305=CARTESIAN_POINT('Ctrl Pts',(1.63033297575459,2.60545900719378,104.452503666059));
#26306=CARTESIAN_POINT('Ctrl Pts',(1.71358864515264,2.55336282649648,104.447425018755));
#26307=CARTESIAN_POINT('Ctrl Pts',(1.79440764694954,2.49723277219189,104.44234637145));
#26308=CARTESIAN_POINT('Ctrl Pts',(1.8723819390353,2.43733217358127,104.437267724146));
#26309=CARTESIAN_POINT('Ctrl Pts',(1.87238193903528,2.43733217358128,105.437268236956));
#26310=CARTESIAN_POINT('Ctrl Pts',(1.94857858758612,2.37879717777398,105.432273767433));
#26311=CARTESIAN_POINT('Ctrl Pts',(2.02214284670669,2.31659717020739,105.42727929791));
#26312=CARTESIAN_POINT('Ctrl Pts',(2.09270312766355,2.25099886038781,105.422284828387));
#26313=CARTESIAN_POINT('Ctrl Pts',(2.16318302679711,2.18547527974557,105.417296048531));
#26314=CARTESIAN_POINT('Ctrl Pts',(2.23066543068644,2.11656138927756,105.412307268676));
#26315=CARTESIAN_POINT('Ctrl Pts',(2.2948108199587,2.04456488050648,105.407318488821));
#26316=CARTESIAN_POINT('Ctrl Pts',(2.35890300902193,1.97262808342098,105.402333846506));
#26317=CARTESIAN_POINT('Ctrl Pts',(2.41966339522959,1.89761407787516,105.397349204191));
#26318=CARTESIAN_POINT('Ctrl Pts',(2.47678916287568,1.81986749316031,105.392364561876));
#26319=CARTESIAN_POINT('Ctrl Pts',(2.53388976982813,1.74215515145138,105.387382115016));
#26320=CARTESIAN_POINT('Ctrl Pts',(2.58735867913724,1.66171297490895,105.382399668156));
#26321=CARTESIAN_POINT('Ctrl Pts',(2.63693383328984,1.57891805007459,105.377417221296));
#26322=CARTESIAN_POINT('Ctrl Pts',(2.68650068635184,1.4961369888012,105.37243560872));
#26323=CARTESIAN_POINT('Ctrl Pts',(2.73217485472712,1.41100433882768,105.367453996144));
#26324=CARTESIAN_POINT('Ctrl Pts',(2.77373862360918,1.32392458165057,105.362472383567));
#26325=CARTESIAN_POINT('Ctrl Pts',(2.81530677959038,1.2368356331143,105.357490245177));
#26326=CARTESIAN_POINT('Ctrl Pts',(2.85276348569194,1.14779956557037,105.352508106786));
#26327=CARTESIAN_POINT('Ctrl Pts',(2.88593830961203,1.05724279288801,105.347525968396));
#26328=CARTESIAN_POINT('Ctrl Pts',(2.9191474671539,0.966592300281464,105.34253867384));
#26329=CARTESIAN_POINT('Ctrl Pts',(2.94806574065103,0.8744183723187,105.337551379285));
#26330=CARTESIAN_POINT('Ctrl Pts',(2.97257200930894,0.781164450978793,105.33256408473));
#26331=CARTESIAN_POINT('Ctrl Pts',(2.99709107801706,0.687861821494363,105.327574185224));
#26332=CARTESIAN_POINT('Ctrl Pts',(3.01719346026177,0.593478504598446,105.322584285718));
#26333=CARTESIAN_POINT('Ctrl Pts',(3.03280925406294,0.498467931235499,105.317594386212));
#26334=CARTESIAN_POINT('Ctrl Pts',(3.0484515967511,0.403295827500985,105.312596003226));
#26335=CARTESIAN_POINT('Ctrl Pts',(3.05959206077699,0.307494773333855,105.30759762024));
#26336=CARTESIAN_POINT('Ctrl Pts',(3.06621267375895,0.211523259430255,105.302599237253));
#26337=CARTESIAN_POINT('Ctrl Pts',(3.071903459219,0.129030400024395,105.298302848792));
#26338=CARTESIAN_POINT('Ctrl Pts',(3.07425568275345,0.0464118010204372,
105.294006460331));
#26339=CARTESIAN_POINT('Ctrl Pts',(3.07328864861143,-0.0360434781360978,
105.28971007187));
#26340=CARTESIAN_POINT('Ctrl Pts',(3.07216335549216,-0.131992891140951,
105.284710562377));
#26341=CARTESIAN_POINT('Ctrl Pts',(3.0665384052831,-0.22805808365021,105.279711052884));
#26342=CARTESIAN_POINT('Ctrl Pts',(3.05639772121958,-0.323782673600333,
105.274711543391));
#26343=CARTESIAN_POINT('Ctrl Pts',(3.0462707929296,-0.419377413752011,105.269718815701));
#26344=CARTESIAN_POINT('Ctrl Pts',(3.03164035078638,-0.514632036803301,
105.264726088011));
#26345=CARTESIAN_POINT('Ctrl Pts',(3.01254232265201,-0.609090308764181,
105.259733360321));
#26346=CARTESIAN_POINT('Ctrl Pts',(2.99346444245592,-0.70344892962915,105.254745899833));
#26347=CARTESIAN_POINT('Ctrl Pts',(2.9699284323356,-0.797012441563642,105.249758439344));
#26348=CARTESIAN_POINT('Ctrl Pts',(2.94202188636012,-0.889330911516094,
105.244770978856));
#26349=CARTESIAN_POINT('Ctrl Pts',(2.91413530817061,-0.981583325445304,
105.239787087013));
#26350=CARTESIAN_POINT('Ctrl Pts',(2.88188453754418,-1.07259204939377,105.234803195169));
#26351=CARTESIAN_POINT('Ctrl Pts',(2.84540777360706,-1.16191946876559,105.229819303325));
#26352=CARTESIAN_POINT('Ctrl Pts',(2.80894429360394,-1.25121435730368,105.224837226492));
#26353=CARTESIAN_POINT('Ctrl Pts',(2.76825804389783,-1.33882875184732,105.219855149658));
#26354=CARTESIAN_POINT('Ctrl Pts',(2.72353606965056,-1.42434319154913,105.214873072824));
#26355=CARTESIAN_POINT('Ctrl Pts',(2.67881817301702,-1.50984983430417,105.209891450241));
#26356=CARTESIAN_POINT('Ctrl Pts',(2.63006548701451,-1.59325651399534,105.204909827658));
#26357=CARTESIAN_POINT('Ctrl Pts',(2.5775114123991,-1.6741676047972,105.199928205075));
#26358=CARTESIAN_POINT('Ctrl Pts',(2.52494778252695,-1.75509340666099,105.194945676745));
#26359=CARTESIAN_POINT('Ctrl Pts',(2.46858163053288,-1.8335223504018,105.189963148415));
#26360=CARTESIAN_POINT('Ctrl Pts',(2.40868954716271,-1.90908798000226,105.184980620085));
#26361=CARTESIAN_POINT('Ctrl Pts',(2.34873290895347,-1.98473505821468,105.179992721324));
#26362=CARTESIAN_POINT('Ctrl Pts',(2.2852430252631,-2.05751231632888,105.175004822563));
#26363=CARTESIAN_POINT('Ctrl Pts',(2.21853648627002,-2.12708676576408,105.170016923802));
#26364=CARTESIAN_POINT('Ctrl Pts',(2.15179054280878,-2.1967023137815,105.165026078621));
#26365=CARTESIAN_POINT('Ctrl Pts',(2.08182447882346,-2.26311098389953,105.16003523344));
#26366=CARTESIAN_POINT('Ctrl Pts',(2.00898985730555,-2.32601848729614,105.155044388258));
#26367=CARTESIAN_POINT('Ctrl Pts',(1.93603753319994,-2.38902765080688,105.150045477745));
#26368=CARTESIAN_POINT('Ctrl Pts',(1.86020774028786,-2.44852407909202,105.145046567232));
#26369=CARTESIAN_POINT('Ctrl Pts',(1.7818829776655,-2.50425543902892,105.140047656719));
#26370=CARTESIAN_POINT('Ctrl Pts',(1.73641080481555,-2.53661080082469,105.137145492508));
#26371=CARTESIAN_POINT('Ctrl Pts',(1.6900982210611,-2.56769797845902,105.134243328297));
#26372=CARTESIAN_POINT('Ctrl Pts',(1.64302381086744,-2.59747473653212,105.131341164086));
#26373=CARTESIAN_POINT('Ctrl Pts',(1.56192951587574,-2.64877065703635,105.126341654593));
#26374=CARTESIAN_POINT('Ctrl Pts',(1.47828826060228,-2.69635533621959,105.1213421451));
#26375=CARTESIAN_POINT('Ctrl Pts',(1.39247410178145,-2.73996681108877,105.116342635607));
#26376=CARTESIAN_POINT('Ctrl Pts',(1.30677634932212,-2.78351912726922,105.111349907917));
#26377=CARTESIAN_POINT('Ctrl Pts',(1.21891193931509,-2.82310875348712,105.106357180227));
#26378=CARTESIAN_POINT('Ctrl Pts',(1.12928311829205,-2.85851742844793,105.101364452537));
#26379=CARTESIAN_POINT('Ctrl Pts',(1.03974885341599,-2.89388874814918,105.096376992049));
#26380=CARTESIAN_POINT('Ctrl Pts',(0.948454283980141,-2.92508772456526,
105.09138953156));
#26381=CARTESIAN_POINT('Ctrl Pts',(0.855824501084636,-2.95194286417323,
105.086402071072));
#26382=CARTESIAN_POINT('Ctrl Pts',(0.763260996964004,-2.97877878830107,
105.081418179229));
#26383=CARTESIAN_POINT('Ctrl Pts',(0.669364599019418,-3.00127693253031,
105.076434287385));
#26384=CARTESIAN_POINT('Ctrl Pts',(0.574577617727836,-3.01931495727196,
105.071450395541));
#26385=CARTESIAN_POINT('Ctrl Pts',(0.479825155507194,-3.03734641301177,
105.066468318707));
#26386=CARTESIAN_POINT('Ctrl Pts',(0.384183185127693,-3.05092089452402,
105.061486241874));
#26387=CARTESIAN_POINT('Ctrl Pts',(0.288105384142396,-3.05996691773427,
105.05650416504));
#26388=CARTESIAN_POINT('Ctrl Pts',(0.192036343239045,-3.06901211615561,
105.051522542457));
#26389=CARTESIAN_POINT('Ctrl Pts',(0.0955319877824317,-3.07352963621368,
105.046540919874));
#26390=CARTESIAN_POINT('Ctrl Pts',(-0.000948758931243446,-3.07349985356377,
105.041559297291));
#26391=CARTESIAN_POINT('Ctrl Pts',(-0.0974470475446472,-3.07347006549885,
105.036576768961));
#26392=CARTESIAN_POINT('Ctrl Pts',(-0.193921279932462,-3.06889133291107,
105.031594240631));
#26393=CARTESIAN_POINT('Ctrl Pts',(-0.289913485351131,-3.05979614043347,
105.026611712301));
#26394=CARTESIAN_POINT('Ctrl Pts',(-0.386009156219984,-3.05069114467882,
105.02162381354));
#26395=CARTESIAN_POINT('Ctrl Pts',(-0.481621325148319,-3.03706001184057,
105.016635914779));
#26396=CARTESIAN_POINT('Ctrl Pts',(-0.576298315866676,-3.01898699916532,
105.011648016018));
#26397=CARTESIAN_POINT('Ctrl Pts',(-0.671031233582986,-3.00090331051342,
105.006657170837));
#26398=CARTESIAN_POINT('Ctrl Pts',(-0.764827446503814,-2.97837261993017,
105.001666325656));
#26399=CARTESIAN_POINT('Ctrl Pts',(-0.857248698416135,-2.95152958973205,
104.996675480474));
#26400=CARTESIAN_POINT('Ctrl Pts',(-0.949819305405491,-2.92464318051925,
104.991676569961));
#26401=CARTESIAN_POINT('Ctrl Pts',(-1.04101009957125,-2.89343065849364,
104.986677659448));
#26402=CARTESIAN_POINT('Ctrl Pts',(-1.13040117360682,-2.85807547778366,
104.981678748935));
#26403=CARTESIAN_POINT('Ctrl Pts',(-1.18229799695739,-2.83754969724429,
104.978776584724));
#26404=CARTESIAN_POINT('Ctrl Pts',(-1.23358864024603,-2.81562852167547,
104.975874420513));
#26405=CARTESIAN_POINT('Ctrl Pts',(-1.28419489131042,-2.79235487199106,
104.972972256302));
#26406=CARTESIAN_POINT('Ctrl Pts',(-1.37137342919031,-2.7522617469731,104.967972746809));
#26407=CARTESIAN_POINT('Ctrl Pts',(-1.456825702983,-2.70801166018953,104.962973237316));
#26408=CARTESIAN_POINT('Ctrl Pts',(-1.54012832437796,-2.65977574138286,
104.957973727823));
#26409=CARTESIAN_POINT('Ctrl Pts',(-1.62331794629595,-2.61160525429376,
104.952981000133));
#26410=CARTESIAN_POINT('Ctrl Pts',(-1.70436333452886,-2.55945989883298,
104.947988272443));
#26411=CARTESIAN_POINT('Ctrl Pts',(-1.78286240943459,-2.50355824358554,
104.942995544753));
#26412=CARTESIAN_POINT('Ctrl Pts',(-1.861278669795,-2.44771556317528,104.938008084265));
#26413=CARTESIAN_POINT('Ctrl Pts',(-1.93715360136216,-2.38812471406588,
104.933020623776));
#26414=CARTESIAN_POINT('Ctrl Pts',(-2.01011191517901,-2.32504888947638,
104.928033163288));
#26415=CARTESIAN_POINT('Ctrl Pts',(-2.0830180256169,-2.2620181971138,104.923049271445));
#26416=CARTESIAN_POINT('Ctrl Pts',(-2.15301133586417,-2.19550777265747,
104.918065379601));
#26417=CARTESIAN_POINT('Ctrl Pts',(-2.21974841178776,-2.12582201474293,
104.913081487757));
#26418=CARTESIAN_POINT('Ctrl Pts',(-2.28646118372119,-2.05616163465552,
104.908099410924));
#26419=CARTESIAN_POINT('Ctrl Pts',(-2.34991977416294,-1.98332853541114,
104.90311733409));
#26420=CARTESIAN_POINT('Ctrl Pts',(-2.40981721737087,-1.90766433862535,
104.898135257256));
#26421=CARTESIAN_POINT('Ctrl Pts',(-2.46970919931195,-1.8320070406711,104.893153634673));
#26422=CARTESIAN_POINT('Ctrl Pts',(-2.52604040726019,-1.75351950267518,
104.88817201209));
#26423=CARTESIAN_POINT('Ctrl Pts',(-2.57854451896164,-1.67257598145282,
104.883190389507));
#26424=CARTESIAN_POINT('Ctrl Pts',(-2.63105817683576,-1.59161774327204,
104.878207861177));
#26425=CARTESIAN_POINT('Ctrl Pts',(-2.6797431176888,-1.50820300332114,104.873225332847));
#26426=CARTESIAN_POINT('Ctrl Pts',(-2.72437724649409,-1.42273359023582,
104.868242804517));
#26427=CARTESIAN_POINT('Ctrl Pts',(-2.76905948431207,-1.33717205371965,
104.863254905756));
#26428=CARTESIAN_POINT('Ctrl Pts',(-2.80968198987636,-1.24955181250041,
104.858267006995));
#26429=CARTESIAN_POINT('Ctrl Pts',(-2.8460695216654,-1.16029760313778,104.853279108234));
#26430=CARTESIAN_POINT('Ctrl Pts',(-2.88247854806892,-1.07099067008858,
104.848288263053));
#26431=CARTESIAN_POINT('Ctrl Pts',(-2.9146474731721,-0.980048260651874,
104.843297417872));
#26432=CARTESIAN_POINT('Ctrl Pts',(-2.94245064140778,-0.887911297866479,
104.83830657269));
#26433=CARTESIAN_POINT('Ctrl Pts',(-2.97029874026546,-0.795625439422457,
104.833307662177));
#26434=CARTESIAN_POINT('Ctrl Pts',(-2.99376688782516,-0.7021415984557,104.828308751664));
#26435=CARTESIAN_POINT('Ctrl Pts',(-3.01278034480596,-0.607911871862083,
104.823309841151));
#26436=CARTESIAN_POINT('Ctrl Pts',(-3.0238187849283,-0.553205923554098,
104.82040767694));
#26437=CARTESIAN_POINT('Ctrl Pts',(-3.03335674278417,-0.498248709403444,
104.817505512729));
#26438=CARTESIAN_POINT('Ctrl Pts',(-3.04138763737114,-0.443129201527042,
104.814603348518));
#26439=CARTESIAN_POINT('Ctrl Pts',(-3.06262762190927,-0.297349988219478,
104.806927749953));
#26440=CARTESIAN_POINT('Ctrl Pts',(-3.07338972786299,-0.150008145579605,
104.799252151388));
#26441=CARTESIAN_POINT('Ctrl Pts',(-3.07349915681818,-0.0022766286332329,
104.791576552823));
#26442=CARTESIAN_POINT('Origin',(0.,0.,116.208423447177));
#26443=CARTESIAN_POINT('',(1.87238193903529,2.43733217358128,106.437412799624));
#26444=CARTESIAN_POINT('',(1.87238193903529,2.43733217358128,106.354088497349));
#26445=CARTESIAN_POINT('',(1.8723819390353,2.43733217358128,116.208423447177));
#26446=CARTESIAN_POINT('',(-3.07349947605365,-0.00179463031419764,105.708423447212));
#26447=CARTESIAN_POINT('Ctrl Pts',(1.87238193903529,2.43733217358128,106.354088497349));
#26448=CARTESIAN_POINT('Ctrl Pts',(1.94882610271153,2.37860703428205,106.349105157254));
#26449=CARTESIAN_POINT('Ctrl Pts',(2.02255624584631,2.31624258933613,106.344121817158));
#26450=CARTESIAN_POINT('Ctrl Pts',(2.09321314072919,2.25052460494851,106.339138477063));
#26451=CARTESIAN_POINT('Ctrl Pts',(2.16384886215988,2.1848263139907,106.334156630304));
#26452=CARTESIAN_POINT('Ctrl Pts',(2.23141284411495,2.11577677922113,106.329174783545));
#26453=CARTESIAN_POINT('Ctrl Pts',(2.29558034985051,2.04370083607661,106.324192936786));
#26454=CARTESIAN_POINT('Ctrl Pts',(2.35974614434464,1.97162681507849,106.319211222884));
#26455=CARTESIAN_POINT('Ctrl Pts',(2.42051535126871,1.89652687448059,106.314229508983));
#26456=CARTESIAN_POINT('Ctrl Pts',(2.47760212909524,1.81876055045812,106.309247795082));
#26457=CARTESIAN_POINT('Ctrl Pts',(2.53470296884459,1.74097507061556,106.304264854058));
#26458=CARTESIAN_POINT('Ctrl Pts',(2.58811931807684,1.66052225656373,106.299281913034));
#26459=CARTESIAN_POINT('Ctrl Pts',(2.63760806823708,1.57779147176382,106.29429897201));
#26460=CARTESIAN_POINT('Ctrl Pts',(2.68715187132221,1.49496865449862,106.289310487797));
#26461=CARTESIAN_POINT('Ctrl Pts',(2.73275912984867,1.40986318619962,106.284322003584));
#26462=CARTESIAN_POINT('Ctrl Pts',(2.77423234473112,1.32288969587326,106.279333519372));
#26463=CARTESIAN_POINT('Ctrl Pts',(2.81573245764219,1.23585979768369,106.274341799809));
#26464=CARTESIAN_POINT('Ctrl Pts',(2.85309301960049,1.14695986977429,106.269350080245));
#26465=CARTESIAN_POINT('Ctrl Pts',(2.8861651946821,1.05662326257075,106.264358360682));
#26466=CARTESIAN_POINT('Ctrl Pts',(2.91928857655281,0.966146784083211,106.259358912267));
#26467=CARTESIAN_POINT('Ctrl Pts',(2.94811018886722,0.874229604593374,106.254359463852));
#26468=CARTESIAN_POINT('Ctrl Pts',(2.97253147258493,0.781318689455259,106.249360015438));
#26469=CARTESIAN_POINT('Ctrl Pts',(2.98094563523119,0.749306959006453,106.247637494517));
#26470=CARTESIAN_POINT('Ctrl Pts',(2.98883788747533,0.71717733402477,106.245914973597));
#26471=CARTESIAN_POINT('Ctrl Pts',(2.99620562000438,0.684948270057071,106.244192452677));
#26472=CARTESIAN_POINT('Ctrl Pts',(3.01759000395423,0.591405422849737,106.239192943184));
#26473=CARTESIAN_POINT('Ctrl Pts',(3.03462707651195,0.496695869818655,106.234193433691));
#26474=CARTESIAN_POINT('Ctrl Pts',(3.04719429030025,0.401259525944931,106.229193924198));
#26475=CARTESIAN_POINT('Ctrl Pts',(3.05974445674285,0.305952640865651,106.224201196508));
#26476=CARTESIAN_POINT('Ctrl Pts',(3.06783675807475,0.20992135581178,106.219208468818));
#26477=CARTESIAN_POINT('Ctrl Pts',(3.07139923898995,0.113617625093908,106.214215741128));
#26478=CARTESIAN_POINT('Ctrl Pts',(3.07495796157757,0.0174154923846215,
106.209228280639));
#26479=CARTESIAN_POINT('Ctrl Pts',(3.0739963476656,-0.0790580782787412,
106.204240820151));
#26480=CARTESIAN_POINT('Ctrl Pts',(3.06849414646785,-0.175345154174617,
106.199253359663));
#26481=CARTESIAN_POINT('Ctrl Pts',(3.06299588222366,-0.271563334417186,
106.194269467819));
#26482=CARTESIAN_POINT('Ctrl Pts',(3.05296351431736,-0.367594848176605,
106.189285575975));
#26483=CARTESIAN_POINT('Ctrl Pts',(3.03842887460575,-0.462981882973846,
106.184301684132));
#26484=CARTESIAN_POINT('Ctrl Pts',(3.02389952804996,-0.558334180175458,
106.179319607298));
#26485=CARTESIAN_POINT('Ctrl Pts',(3.00487123348384,-0.653042031234897,
106.174337530464));
#26486=CARTESIAN_POINT('Ctrl Pts',(2.98142756238955,-0.746653828908618,
106.169355453631));
#26487=CARTESIAN_POINT('Ctrl Pts',(2.95798602881796,-0.840257091343089,
106.164373831048));
#26488=CARTESIAN_POINT('Ctrl Pts',(2.93013002593912,-0.932764073312985,
106.159392208464));
#26489=CARTESIAN_POINT('Ctrl Pts',(2.89799377469533,-1.02373547942185,106.154410585881));
#26490=CARTESIAN_POINT('Ctrl Pts',(2.86585168051494,-1.11472342573497,106.149428057552));
#26491=CARTESIAN_POINT('Ctrl Pts',(2.82942793865795,-1.20417482782572,106.144445529222));
#26492=CARTESIAN_POINT('Ctrl Pts',(2.78890559181497,-1.29166863008404,106.139463000892));
#26493=CARTESIAN_POINT('Ctrl Pts',(2.74833956785412,-1.37925673776671,106.134475102131));
#26494=CARTESIAN_POINT('Ctrl Pts',(2.70366630417707,-1.46488263421209,106.12948720337));
#26495=CARTESIAN_POINT('Ctrl Pts',(2.65511557027466,-1.54814842908717,106.124499304609));
#26496=CARTESIAN_POINT('Ctrl Pts',(2.60653615678729,-1.63146341021025,106.119508459427));
#26497=CARTESIAN_POINT('Ctrl Pts',(2.55407495097874,-1.71241514559357,106.114517614246));
#26498=CARTESIAN_POINT('Ctrl Pts',(2.49800478819914,-1.79063517449372,106.109526769065));
#26499=CARTESIAN_POINT('Ctrl Pts',(2.44184401462058,-1.86898160893583,106.104527858552));
#26500=CARTESIAN_POINT('Ctrl Pts',(2.38206291060169,-1.94458717800361,106.099528948038));
#26501=CARTESIAN_POINT('Ctrl Pts',(2.31897421576095,-2.01711696156567,106.094530037525));
#26502=CARTESIAN_POINT('Ctrl Pts',(2.28234748443543,-2.0592248051711,106.091627873314));
#26503=CARTESIAN_POINT('Ctrl Pts',(2.24460662877106,-2.10029664273728,106.088725709103));
#26504=CARTESIAN_POINT('Ctrl Pts',(2.20581815167771,-2.14027300401821,106.085823544892));
#26505=CARTESIAN_POINT('Ctrl Pts',(2.13899789432946,-2.20913960948482,106.080824035399));
#26506=CARTESIAN_POINT('Ctrl Pts',(2.06883211266339,-2.27499493850143,106.075824525906));
#26507=CARTESIAN_POINT('Ctrl Pts',(1.99562308286094,-2.33749668687521,106.070825016413));
#26508=CARTESIAN_POINT('Ctrl Pts',(1.92251336064241,-2.39991365202433,106.065832288723));
#26509=CARTESIAN_POINT('Ctrl Pts',(1.84636892569537,-2.45898579500717,106.060839561033));
#26510=CARTESIAN_POINT('Ctrl Pts',(1.76752969763012,-2.51440669303826,106.055846833343));
#26511=CARTESIAN_POINT('Ctrl Pts',(1.68877364296334,-2.5697691234188,106.050859372855));
#26512=CARTESIAN_POINT('Ctrl Pts',(1.60732880397115,-2.62148771523487,106.045871912366));
#26513=CARTESIAN_POINT('Ctrl Pts',(1.52356826551536,-2.66929616009811,106.040884451878));
#26514=CARTESIAN_POINT('Ctrl Pts',(1.43986765968277,-2.71707039690151,106.035900560035));
#26515=CARTESIAN_POINT('Ctrl Pts',(1.35385502843941,-2.76093983167477,106.030916668191));
#26516=CARTESIAN_POINT('Ctrl Pts',(1.26593171226487,-2.80068190801493,106.025932776347));
#26517=CARTESIAN_POINT('Ctrl Pts',(1.17804041558438,-2.84040951127523,106.020950699513));
#26518=CARTESIAN_POINT('Ctrl Pts',(1.08824021608889,-2.87601256194491,106.01596862268));
#26519=CARTESIAN_POINT('Ctrl Pts',(0.996955419074167,-2.90731528086973,
106.010986545846));
#26520=CARTESIAN_POINT('Ctrl Pts',(0.90567894513013,-2.93861514570767,106.006004923263));
#26521=CARTESIAN_POINT('Ctrl Pts',(0.812918558076705,-2.96561531613726,
106.00102330068));
#26522=CARTESIAN_POINT('Ctrl Pts',(0.719115812304894,-2.98818920058504,
105.996041678097));
#26523=CARTESIAN_POINT('Ctrl Pts',(0.625296011541326,-3.01076718936272,
105.991059149767));
#26524=CARTESIAN_POINT('Ctrl Pts',(0.530433902455986,-3.02891719120094,
105.986076621437));
#26525=CARTESIAN_POINT('Ctrl Pts',(0.434982321124866,-3.04256349651225,
105.981094093108));
#26526=CARTESIAN_POINT('Ctrl Pts',(0.339427857056205,-3.05622451052956,
105.976106194346));
#26527=CARTESIAN_POINT('Ctrl Pts',(0.24328308756026,-3.0653720745883,105.971118295585));
#26528=CARTESIAN_POINT('Ctrl Pts',(0.147006858336642,-3.06998228555182,
105.966130396824));
#26529=CARTESIAN_POINT('Ctrl Pts',(0.0506737574230522,-3.07459521983023,
105.961139551643));
#26530=CARTESIAN_POINT('Ctrl Pts',(-0.0457905190849338,-3.07466546382483,
105.956148706462));
#26531=CARTESIAN_POINT('Ctrl Pts',(-0.14192836352605,-3.07022126069552,
105.951157861281));
#26532=CARTESIAN_POINT('Ctrl Pts',(-0.238221569151672,-3.06576987562172,
105.946158950767));
#26533=CARTESIAN_POINT('Ctrl Pts',(-0.334186852606287,-3.05678951687311,
105.941160040254));
#26534=CARTESIAN_POINT('Ctrl Pts',(-0.429373013894057,-3.04336016024057,
105.936161129741));
#26535=CARTESIAN_POINT('Ctrl Pts',(-0.484634229301692,-3.03556362175623,
105.93325896553));
#26536=CARTESIAN_POINT('Ctrl Pts',(-0.539633037571687,-3.02626850926642,
105.930356801319));
#26537=CARTESIAN_POINT('Ctrl Pts',(-0.594283347907387,-3.01549822623062,
105.927454637108));
#26538=CARTESIAN_POINT('Ctrl Pts',(-0.688428518701941,-2.99694444072266,
105.922455127615));
#26539=CARTESIAN_POINT('Ctrl Pts',(-0.781869329979001,-2.9739449610631,
105.917455618122));
#26540=CARTESIAN_POINT('Ctrl Pts',(-0.874154084883601,-2.94656696612877,
105.912456108629));
#26541=CARTESIAN_POINT('Ctrl Pts',(-0.966313656103778,-2.91922610927084,
105.907463380939));
#26542=CARTESIAN_POINT('Ctrl Pts',(-1.05731987037793,-2.8875186651387,105.902470653249));
#26543=CARTESIAN_POINT('Ctrl Pts',(-1.14673063287514,-2.85156292331518,
105.897477925559));
#26544=CARTESIAN_POINT('Ctrl Pts',(-1.23604706927213,-2.81564511389276,
105.892490465071));
#26545=CARTESIAN_POINT('Ctrl Pts',(-1.32377099481605,-2.77548807932703,
105.887503004583));
#26546=CARTESIAN_POINT('Ctrl Pts',(-1.40947590544984,-2.73125976830406,
105.882515544094));
#26547=CARTESIAN_POINT('Ctrl Pts',(-1.49511949221646,-2.6870631036716,105.877531652251));
#26548=CARTESIAN_POINT('Ctrl Pts',(-1.57874654700909,-2.63880115440058,
105.872547760407));
#26549=CARTESIAN_POINT('Ctrl Pts',(-1.65995188078329,-2.58668939060801,
105.867563868563));
#26550=CARTESIAN_POINT('Ctrl Pts',(-1.7411276415861,-2.53459660462918,105.86258179173));
#26551=CARTESIAN_POINT('Ctrl Pts',(-1.81988306461357,-2.47865702659944,
105.857599714896));
#26552=CARTESIAN_POINT('Ctrl Pts',(-1.89583969398661,-2.4191308572925,105.852617638062));
#26553=CARTESIAN_POINT('Ctrl Pts',(-1.97178939786516,-2.35961011540067,
105.847636015479));
#26554=CARTESIAN_POINT('Ctrl Pts',(-2.04494047005417,-2.29650370330816,
105.842654392896));
#26555=CARTESIAN_POINT('Ctrl Pts',(-2.11494632154101,-2.23011307045185,
105.837672770313));
#26556=CARTESIAN_POINT('Ctrl Pts',(-2.18496490132493,-2.16371036660889,
105.832690241983));
#26557=CARTESIAN_POINT('Ctrl Pts',(-2.25183680621799,-2.09402255818539,
105.827707713654));
#26558=CARTESIAN_POINT('Ctrl Pts',(-2.31525198429387,-2.02138826038525,
105.822725185324));
#26559=CARTESIAN_POINT('Ctrl Pts',(-2.37873551458575,-1.94867567351673,
105.817737286563));
#26560=CARTESIAN_POINT('Ctrl Pts',(-2.4387545905842,-1.87301058813429,105.812749387802));
#26561=CARTESIAN_POINT('Ctrl Pts',(-2.49503934326516,-1.79476486637079,
105.807761489041));
#26562=CARTESIAN_POINT('Ctrl Pts',(-2.55135734412205,-1.71647292378551,
105.802770643859));
#26563=CARTESIAN_POINT('Ctrl Pts',(-2.60393639017204,-1.63559767730731,
105.797779798678));
#26564=CARTESIAN_POINT('Ctrl Pts',(-2.65255102635424,-1.5525383417446,105.792788953497));
#26565=CARTESIAN_POINT('Ctrl Pts',(-2.70124422501623,-1.46934478019803,
105.787790042983));
#26566=CARTESIAN_POINT('Ctrl Pts',(-2.74596001776208,-1.3839604704515,105.78279113247));
#26567=CARTESIAN_POINT('Ctrl Pts',(-2.78651983112612,-1.29680741852476,
105.777792221957));
#26568=CARTESIAN_POINT('Ctrl Pts',(-2.81006720978768,-1.24620989982293,
105.774890057746));
#26569=CARTESIAN_POINT('Ctrl Pts',(-2.83221472815899,-1.19501658524713,
105.771987893535));
#26570=CARTESIAN_POINT('Ctrl Pts',(-2.85293514461266,-1.14331242914346,
105.769085729324));
#26571=CARTESIAN_POINT('Ctrl Pts',(-2.893051927116,-1.04320805191886,105.763466851407));
#26572=CARTESIAN_POINT('Ctrl Pts',(-2.92793512895817,-0.940893018626475,
105.75784797349));
#26573=CARTESIAN_POINT('Ctrl Pts',(-2.95736499242841,-0.836895782973556,
105.752229095573));
#26574=CARTESIAN_POINT('Ctrl Pts',(-2.98669778170527,-0.733241581455836,
105.746628751485));
#26575=CARTESIAN_POINT('Ctrl Pts',(-3.01061301739709,-0.627916464693566,
105.741028407397));
#26576=CARTESIAN_POINT('Ctrl Pts',(-3.02893966727519,-0.521465954791764,
105.735428063308));
#26577=CARTESIAN_POINT('Ctrl Pts',(-3.04715867314249,-0.415640696090364,
105.729860613584));
#26578=CARTESIAN_POINT('Ctrl Pts',(-3.05985444442008,-0.308703449488098,
105.72429316386));
#26579=CARTESIAN_POINT('Ctrl Pts',(-3.0669067781481,-0.201209006133457,
105.718725714136));
#26580=CARTESIAN_POINT('Ctrl Pts',(-3.07125676650912,-0.134904773307905,
105.715291625161));
#26581=CARTESIAN_POINT('Ctrl Pts',(-3.07346059135322,-0.0683889062706779,
105.711857536187));
#26582=CARTESIAN_POINT('Ctrl Pts',(-3.07349947605365,-0.00179463031418164,
105.708423447212));
#26583=CARTESIAN_POINT('Ctrl Pts',(-3.07349947605404,-0.00179462963607823,
105.708423447177));
#26584=CARTESIAN_POINT('Ctrl Pts',(-3.07355640778969,0.095707192560317,
105.70339553858));
#26585=CARTESIAN_POINT('Ctrl Pts',(-3.06896936787619,0.193220771531798,
105.698367629983));
#26586=CARTESIAN_POINT('Ctrl Pts',(-3.0597615284335,0.2902785543548,105.693339721386));
#26587=CARTESIAN_POINT('Ctrl Pts',(-3.05055210965956,0.387352984556402,
105.688310950401));
#26588=CARTESIAN_POINT('Ctrl Pts',(-3.03672035558937,0.483971037494733,
105.683282179415));
#26589=CARTESIAN_POINT('Ctrl Pts',(-3.01834127070958,0.579670788923594,
105.67825340843));
#26590=CARTESIAN_POINT('Ctrl Pts',(-2.99995437574094,0.675411207424039,
105.673222500497));
#26591=CARTESIAN_POINT('Ctrl Pts',(-2.97701638775837,0.770232128781307,
105.668191592563));
#26592=CARTESIAN_POINT('Ctrl Pts',(-2.94965312222315,0.863683222344401,
105.66316068463));
#26593=CARTESIAN_POINT('Ctrl Pts',(-2.92225260677349,0.957261531909367,
105.658122928066));
#26594=CARTESIAN_POINT('Ctrl Pts',(-2.89041490754594,1.04946588014872,105.653085171503));
#26595=CARTESIAN_POINT('Ctrl Pts',(-2.85431530228173,1.13986245010542,105.648047414939));
#26596=CARTESIAN_POINT('Ctrl Pts',(-2.81818801472202,1.23032833895201,105.643005795268));
#26597=CARTESIAN_POINT('Ctrl Pts',(-2.77779248930952,1.31898330026846,105.637964175596));
#26598=CARTESIAN_POINT('Ctrl Pts',(-2.73335070314102,1.40541672952846,105.632922555925));
#26599=CARTESIAN_POINT('Ctrl Pts',(-2.68883063971646,1.49200239775673,105.627872056229));
#26600=CARTESIAN_POINT('Ctrl Pts',(-2.64025029773579,1.57635835094933,105.622821556533));
#26601=CARTESIAN_POINT('Ctrl Pts',(-2.58787585624958,1.65810156583984,105.617771056836));
#26602=CARTESIAN_POINT('Ctrl Pts',(-2.56349136256802,1.69615957372393,105.615419645071));
#26603=CARTESIAN_POINT('Ctrl Pts',(-2.53828502684479,1.7336516852532,105.613068233305));
#26604=CARTESIAN_POINT('Ctrl Pts',(-2.51228663814599,1.77054175262633,105.61071682154));
#26605=CARTESIAN_POINT('Ctrl Pts',(-2.4570095518424,1.84897643800449,105.605717312047));
#26606=CARTESIAN_POINT('Ctrl Pts',(-2.39795870705164,1.92495774495692,105.600717802554));
#26607=CARTESIAN_POINT('Ctrl Pts',(-2.33537936862426,1.99810046158949,105.595718293061));
#26608=CARTESIAN_POINT('Ctrl Pts',(-2.272884918672,2.07114396059151,105.590725565371));
#26609=CARTESIAN_POINT('Ctrl Pts',(-2.20687177062592,2.14135619125706,105.585732837681));
#26610=CARTESIAN_POINT('Ctrl Pts',(-2.13762796257577,2.20838152129883,105.58074010999));
#26611=CARTESIAN_POINT('Ctrl Pts',(-2.06845720499776,2.27533614130686,105.575752649502));
#26612=CARTESIAN_POINT('Ctrl Pts',(-1.99606287656792,2.33911024066632,105.570765189014));
#26613=CARTESIAN_POINT('Ctrl Pts',(-1.9207720244847,2.39938264558969,105.565777728526));
#26614=CARTESIAN_POINT('Ctrl Pts',(-1.84553504476623,2.45961192419833,105.560793836682));
#26615=CARTESIAN_POINT('Ctrl Pts',(-1.76740600318806,2.51634421573316,105.555809944838));
#26616=CARTESIAN_POINT('Ctrl Pts',(-1.68674667299025,2.56929716287477,105.550826052995));
#26617=CARTESIAN_POINT('Ctrl Pts',(-1.60611671692275,2.62223082586454,105.545843976161));
#26618=CARTESIAN_POINT('Ctrl Pts',(-1.52295866966958,2.67138763844867,105.540861899327));
#26619=CARTESIAN_POINT('Ctrl Pts',(-1.43766427554716,2.7165278722692,105.535879822494));
#26620=CARTESIAN_POINT('Ctrl Pts',(-1.35237765830835,2.76166399034043,105.530898199911));
#26621=CARTESIAN_POINT('Ctrl Pts',(-1.2649554695348,2.80278405259261,105.525916577328));
#26622=CARTESIAN_POINT('Ctrl Pts',(-1.17581415413273,2.83969423088845,105.520934954745));
#26623=CARTESIAN_POINT('Ctrl Pts',(-1.08665663126879,2.87661112010509,105.515952426415));
#26624=CARTESIAN_POINT('Ctrl Pts',(-0.995779766595947,2.90931643732089,
105.510969898085));
#26625=CARTESIAN_POINT('Ctrl Pts',(-0.903619074985017,2.93766485789704,
105.505987369755));
#26626=CARTESIAN_POINT('Ctrl Pts',(-0.811359047731229,2.96604383389256,
105.500999470994));
#26627=CARTESIAN_POINT('Ctrl Pts',(-0.717812851215745,2.99005640866325,
105.496011572233));
#26628=CARTESIAN_POINT('Ctrl Pts',(-0.623430006574469,3.00960749548883,
105.491023673472));
#26629=CARTESIAN_POINT('Ctrl Pts',(-0.528991408691466,3.02917013140974,
105.486032828291));
#26630=CARTESIAN_POINT('Ctrl Pts',(-0.433715611962334,3.04426596308788,
105.481041983109));
#26631=CARTESIAN_POINT('Ctrl Pts',(-0.338059037536675,3.05485160640247,
105.476051137928));
#26632=CARTESIAN_POINT('Ctrl Pts',(-0.242247879670979,3.065454356384,105.471052227415));
#26633=CARTESIAN_POINT('Ctrl Pts',(-0.14605515319154,3.07153233665974,105.466053316902));
#26634=CARTESIAN_POINT('Ctrl Pts',(-0.0499390083025376,3.07309426237624,
105.461054406389));
#26635=CARTESIAN_POINT('Ctrl Pts',(0.00586211777445551,3.07400105294644,
105.458152242178));
#26636=CARTESIAN_POINT('Ctrl Pts',(0.0616374759675003,3.07338668686073,
105.455250077967));
#26637=CARTESIAN_POINT('Ctrl Pts',(0.117298380782215,3.07126087134679,105.452347913756));
#26638=CARTESIAN_POINT('Ctrl Pts',(0.213170815550757,3.06759928679534,105.447349117025));
#26639=CARTESIAN_POINT('Ctrl Pts',(0.309040004977434,3.05943784159464,105.442350320295));
#26640=CARTESIAN_POINT('Ctrl Pts',(0.404449496958352,3.04677253079552,105.437351523564));
#26641=CARTESIAN_POINT('Ctrl Pts',(0.499737015301177,3.03412341161428,105.432359117408));
#26642=CARTESIAN_POINT('Ctrl Pts',(0.594565572604177,3.01698192325251,105.427366711251));
#26643=CARTESIAN_POINT('Ctrl Pts',(0.6884801318473,2.99539602691389,105.422374305095));
#26644=CARTESIAN_POINT('Ctrl Pts',(0.782300280046847,2.9738318305866,105.417386917737));
#26645=CARTESIAN_POINT('Ctrl Pts',(0.875207830789812,2.94783220335917,105.41239953038));
#26646=CARTESIAN_POINT('Ctrl Pts',(0.966755342263142,2.91749659095014,105.407412143022));
#26647=CARTESIAN_POINT('Ctrl Pts',(1.05823691733825,2.88718282753501,105.402428347792));
#26648=CARTESIAN_POINT('Ctrl Pts',(1.14835998508706,2.85253942515601,105.397444552562));
#26649=CARTESIAN_POINT('Ctrl Pts',(1.23669075990271,2.81371608631206,105.392460757332));
#26650=CARTESIAN_POINT('Ctrl Pts',(1.32498387377679,2.77490930028902,105.387479087007));
#26651=CARTESIAN_POINT('Ctrl Pts',(1.41148581328142,2.73192629887186,105.382497416681));
#26652=CARTESIAN_POINT('Ctrl Pts',(1.49578230549484,2.6849650918715,105.377515746355));
#26653=CARTESIAN_POINT('Ctrl Pts',(1.58008336359877,2.63800134123351,105.372533806199));
#26654=CARTESIAN_POINT('Ctrl Pts',(1.66217834910624,2.58705916249099,105.367551866042));
#26655=CARTESIAN_POINT('Ctrl Pts',(1.7416778638474,2.53238237013765,105.362569925886));
#26656=CARTESIAN_POINT('Ctrl Pts',(1.78607617520012,2.50184687242328,105.359787648146));
#26657=CARTESIAN_POINT('Ctrl Pts',(1.82966546057547,2.47014738179717,105.357005370406));
#26658=CARTESIAN_POINT('Ctrl Pts',(1.87238193903529,2.43733217358128,105.354223092666));
#26659=CARTESIAN_POINT('',(-3.07349899192526,0.00248930400748836,105.791576552872));
#26660=CARTESIAN_POINT('Ctrl Pts',(-3.07349899192449,0.00248930494811218,
105.791576552823));
#26661=CARTESIAN_POINT('Ctrl Pts',(-3.0733769618853,0.153157547793597,105.783754517199));
#26662=CARTESIAN_POINT('Ctrl Pts',(-3.06217291351732,0.303387429693875,
105.775932481575));
#26663=CARTESIAN_POINT('Ctrl Pts',(-3.04009617916299,0.451904272427881,
105.768110445952));
#26664=CARTESIAN_POINT('Ctrl Pts',(-3.0369975376803,0.472749767163985,105.767012562376));
#26665=CARTESIAN_POINT('Ctrl Pts',(-3.03368476415738,0.493561567928361,
105.765914678799));
#26666=CARTESIAN_POINT('Ctrl Pts',(-3.03015849914789,0.514336193594988,
105.764816795223));
#26667=CARTESIAN_POINT('Ctrl Pts',(-3.01410069869206,0.608939064508622,
105.75981728573));
#26668=CARTESIAN_POINT('Ctrl Pts',(-2.99358013316199,0.702955380470386,
105.754817776237));
#26669=CARTESIAN_POINT('Ctrl Pts',(-2.96865201364476,0.79593182615278,105.749818266744));
#26670=CARTESIAN_POINT('Ctrl Pts',(-2.94375770896337,0.888782149876992,
105.744825539054));
#26671=CARTESIAN_POINT('Ctrl Pts',(-2.91446784550576,0.980594986390127,
105.739832811364));
#26672=CARTESIAN_POINT('Ctrl Pts',(-2.88088898110049,1.07092526750179,105.734840083674));
#26673=CARTESIAN_POINT('Ctrl Pts',(-2.84734554155075,1.16116025244383,105.729852623186));
#26674=CARTESIAN_POINT('Ctrl Pts',(-2.80952224819633,1.24991538197292,105.724865162698));
#26675=CARTESIAN_POINT('Ctrl Pts',(-2.76757571287371,1.33675986007644,105.719877702209));
#26676=CARTESIAN_POINT('Ctrl Pts',(-2.72565919127763,1.42354219892586,105.714893810366));
#26677=CARTESIAN_POINT('Ctrl Pts',(-2.67962548309349,1.50841620997487,105.709909918522));
#26678=CARTESIAN_POINT('Ctrl Pts',(-2.62967926860791,1.59097114815252,105.704926026678));
#26679=CARTESIAN_POINT('Ctrl Pts',(-2.57975124329663,1.67349602186633,105.699943949845));
#26680=CARTESIAN_POINT('Ctrl Pts',(-2.52591376967499,1.75370312554444,105.694961873011));
#26681=CARTESIAN_POINT('Ctrl Pts',(-2.46841694995455,1.83120725511261,105.689979796177));
#26682=CARTESIAN_POINT('Ctrl Pts',(-2.41092537261941,1.90870431808977,105.684998173594));
#26683=CARTESIAN_POINT('Ctrl Pts',(-2.34977537422278,1.98349854450907,105.680016551011));
#26684=CARTESIAN_POINT('Ctrl Pts',(-2.28525913387661,2.05523549527385,105.675034928428));
#26685=CARTESIAN_POINT('Ctrl Pts',(-2.22073116334122,2.12698548908021,105.670052400098));
#26686=CARTESIAN_POINT('Ctrl Pts',(-2.15283602889522,2.19567677692278,105.665069871768));
#26687=CARTESIAN_POINT('Ctrl Pts',(-2.08190402857787,2.26099046123402,105.660087343438));
#26688=CARTESIAN_POINT('Ctrl Pts',(-2.01089557401804,2.32637454407111,105.655099444677));
#26689=CARTESIAN_POINT('Ctrl Pts',(-1.93684404221188,2.38837345750345,105.650111545916));
#26690=CARTESIAN_POINT('Ctrl Pts',(-1.86011402906525,2.44670759366023,105.645123647155));
#26691=CARTESIAN_POINT('Ctrl Pts',(-1.78333869044674,2.50507618859188,105.640132801974));
#26692=CARTESIAN_POINT('Ctrl Pts',(-1.70388208143739,2.55977544691557,105.635141956793));
#26693=CARTESIAN_POINT('Ctrl Pts',(-1.62213731550006,2.61056943590134,105.630151111611));
#26694=CARTESIAN_POINT('Ctrl Pts',(-1.54026044795657,2.66144550925608,105.625152201098));
#26695=CARTESIAN_POINT('Ctrl Pts',(-1.45608842304143,2.70840349785718,105.620153290585));
#26696=CARTESIAN_POINT('Ctrl Pts',(-1.37003837715734,2.75125373150426,105.615154380072));
#26697=CARTESIAN_POINT('Ctrl Pts',(-1.32008121892035,2.77613083506423,105.612252215861));
#26698=CARTESIAN_POINT('Ctrl Pts',(-1.26949145639921,2.79962432257363,105.60935005165));
#26699=CARTESIAN_POINT('Ctrl Pts',(-1.21835329387792,2.82170471546844,105.606447887439));
#26700=CARTESIAN_POINT('Ctrl Pts',(-1.13025844107435,2.85974223707676,105.601448377946));
#26701=CARTESIAN_POINT('Ctrl Pts',(-1.04022582662802,2.89371707501104,105.596448868453));
#26702=CARTESIAN_POINT('Ctrl Pts',(-0.948665747700957,2.92342873166749,
105.59144935896));
#26703=CARTESIAN_POINT('Ctrl Pts',(-0.857229869439561,2.95310008465035,
105.58645663127));
#26704=CARTESIAN_POINT('Ctrl Pts',(-0.764271058609443,2.97851961531101,
105.58146390358));
#26705=CARTESIAN_POINT('Ctrl Pts',(-0.670220650551179,2.99953438546298,
105.57647117589));
#26706=CARTESIAN_POINT('Ctrl Pts',(-0.57626946330279,3.02052698556213,105.571483715401));
#26707=CARTESIAN_POINT('Ctrl Pts',(-0.48122939427299,3.03712396771852,105.566496254913));
#26708=CARTESIAN_POINT('Ctrl Pts',(-0.385547059392509,3.0492221491708,105.561508794425));
#26709=CARTESIAN_POINT('Ctrl Pts',(-0.289933187459186,3.06131167409146,
105.556524902581));
#26710=CARTESIAN_POINT('Ctrl Pts',(-0.193678397497479,3.06890874261549,
105.551541010737));
#26711=CARTESIAN_POINT('Ctrl Pts',(-0.0972386578056601,3.07196140819317,
105.546557118894));
#26712=CARTESIAN_POINT('Ctrl Pts',(-0.000834039078500506,3.07501296206565,
105.54157504206));
#26713=CARTESIAN_POINT('Ctrl Pts',(0.0957549572592695,3.07352338734202,
105.536592965226));
#26714=CARTESIAN_POINT('Ctrl Pts',(0.192069056462435,3.06749274286829,105.531610888393));
#26715=CARTESIAN_POINT('Ctrl Pts',(0.288374374038715,3.0614626482504,105.52662926581));
#26716=CARTESIAN_POINT('Ctrl Pts',(0.384404406220011,3.05089233468703,105.521647643226));
#26717=CARTESIAN_POINT('Ctrl Pts',(0.479702774852875,3.03583390484368,105.516666020643));
#26718=CARTESIAN_POINT('Ctrl Pts',(0.575018470408214,3.02077273711248,105.511683492314));
#26719=CARTESIAN_POINT('Ctrl Pts',(0.669601804645896,3.00122190103336,105.506700963984));
#26720=CARTESIAN_POINT('Ctrl Pts',(0.763005457463406,2.97728482377502,105.501718435654));
#26721=CARTESIAN_POINT('Ctrl Pts',(0.856509785653021,2.95332194587519,105.496730536893));
#26722=CARTESIAN_POINT('Ctrl Pts',(0.948831468019021,2.92496349749113,105.491742638132));
#26723=CARTESIAN_POINT('Ctrl Pts',(1.03953746682639,2.89236306591413,105.486754739371));
#26724=CARTESIAN_POINT('Ctrl Pts',(1.13029704691229,2.85974337681472,105.481763894189));
#26725=CARTESIAN_POINT('Ctrl Pts',(1.21943863760954,2.82287688275281,105.476773049008));
#26726=CARTESIAN_POINT('Ctrl Pts',(1.30655030912593,2.7819648703251,105.471782203827));
#26727=CARTESIAN_POINT('Ctrl Pts',(1.39380275530329,2.74098674305216,105.466783293313));
#26728=CARTESIAN_POINT('Ctrl Pts',(1.47901834423043,2.6959502481222,105.4617843828));
#26729=CARTESIAN_POINT('Ctrl Pts',(1.56181087144092,2.64710201009499,105.456785472287));
#26730=CARTESIAN_POINT('Ctrl Pts',(1.60987684677172,2.61874270904359,105.453883308076));
#26731=CARTESIAN_POINT('Ctrl Pts',(1.65712667802367,2.58909947248047,105.450981143865));
#26732=CARTESIAN_POINT('Ctrl Pts',(1.70348979365083,2.55822688065923,105.448078979654));
#26733=CARTESIAN_POINT('Ctrl Pts',(1.76105829279885,2.5198927706255,105.444475398755));
#26734=CARTESIAN_POINT('Ctrl Pts',(1.81740497180485,2.4795660067949,105.440871817856));
#26735=CARTESIAN_POINT('Ctrl Pts',(1.87238193903528,2.43733217358128,105.437268236956));
#26736=CARTESIAN_POINT('Ctrl Pts',(1.87238193903529,2.43733217358128,106.437412799624));
#26737=CARTESIAN_POINT('Ctrl Pts',(1.94886548644755,2.37857677931852,106.432422059601));
#26738=CARTESIAN_POINT('Ctrl Pts',(2.02251314091683,2.31626985199124,106.427431319579));
#26739=CARTESIAN_POINT('Ctrl Pts',(2.09299380989473,2.25072858464595,106.422440579557));
#26740=CARTESIAN_POINT('Ctrl Pts',(2.16358899334487,2.18508082819166,106.417441730758));
#26741=CARTESIAN_POINT('Ctrl Pts',(2.23100660916304,2.11618855151676,106.41244288196));
#26742=CARTESIAN_POINT('Ctrl Pts',(2.29495385707934,2.04440432495059,106.407444033162));
#26743=CARTESIAN_POINT('Ctrl Pts',(2.33397751316687,2.00059817126444,106.404393497561));
#26744=CARTESIAN_POINT('Ctrl Pts',(2.37170959517796,1.95571568837146,106.40134296196));
#26745=CARTESIAN_POINT('Ctrl Pts',(2.40809147900642,1.9098423177678,106.398292426359));
#26746=CARTESIAN_POINT('Ctrl Pts',(2.46771758975408,1.83466065073596,106.393292916866));
#26747=CARTESIAN_POINT('Ctrl Pts',(2.52392424819075,1.75655192635719,106.388293407373));
#26748=CARTESIAN_POINT('Ctrl Pts',(2.57641121104068,1.67586023332016,106.38329389788));
#26749=CARTESIAN_POINT('Ctrl Pts',(2.62882697565878,1.59527799805237,106.37830117019));
#26750=CARTESIAN_POINT('Ctrl Pts',(2.67753283546953,1.51212012247802,106.3733084425));
#26751=CARTESIAN_POINT('Ctrl Pts',(2.72226900449198,1.42676337112439,106.36831571481));
#26752=CARTESIAN_POINT('Ctrl Pts',(2.7669579779838,1.34149666899182,106.363328254322));
#26753=CARTESIAN_POINT('Ctrl Pts',(2.80768538333752,1.2540360893513,106.358340793833));
#26754=CARTESIAN_POINT('Ctrl Pts',(2.84423550879917,1.16478608357325,106.353353333345));
#26755=CARTESIAN_POINT('Ctrl Pts',(2.88075948179168,1.07559993826061,106.348369441502));
#26756=CARTESIAN_POINT('Ctrl Pts',(2.91311195088674,0.984627317191522,106.343385549658));
#26757=CARTESIAN_POINT('Ctrl Pts',(2.9411242491937,0.892295018928603,106.338401657814));
#26758=CARTESIAN_POINT('Ctrl Pts',(2.9691263461154,0.799996345801883,106.333419580981));
#26759=CARTESIAN_POINT('Ctrl Pts',(2.99279128538639,0.706339398938902,106.328437504147));
#26760=CARTESIAN_POINT('Ctrl Pts',(3.01199975905624,0.61176768584582,106.323455427313));
#26761=CARTESIAN_POINT('Ctrl Pts',(3.03120648135583,0.517204595514167,106.31847380473));
#26762=CARTESIAN_POINT('Ctrl Pts',(3.04595745871357,0.421727334993363,106.313492182147));
#26763=CARTESIAN_POINT('Ctrl Pts',(3.05618439138251,0.325790140842114,106.308510559564));
#26764=CARTESIAN_POINT('Ctrl Pts',(3.066413183488,0.229835503618627,106.303528031234));
#26765=CARTESIAN_POINT('Ctrl Pts',(3.07211625082295,0.13342120317577,106.298545502904));
#26766=CARTESIAN_POINT('Ctrl Pts',(3.07327720859963,0.0370060684490628,
106.293562974574));
#26767=CARTESIAN_POINT('Ctrl Pts',(3.0744394177177,-0.0595129875833855,
106.288575075813));
#26768=CARTESIAN_POINT('Ctrl Pts',(3.07104973812129,-0.156032440036609,
106.283587177052));
#26769=CARTESIAN_POINT('Ctrl Pts',(3.06314393340568,-0.252094215006907,
106.278599278291));
#26770=CARTESIAN_POINT('Ctrl Pts',(3.05523345862272,-0.348212734986186,
106.27360843311));
#26771=CARTESIAN_POINT('Ctrl Pts',(3.04280160336489,-0.443872604060372,
106.268617587929));
#26772=CARTESIAN_POINT('Ctrl Pts',(3.02593567731295,-0.538623733941043,
106.263626742747));
#26773=CARTESIAN_POINT('Ctrl Pts',(3.0090424954986,-0.633527984040376,106.258627832234));
#26774=CARTESIAN_POINT('Ctrl Pts',(2.98770103195925,-0.727520134807199,
106.253628921721));
#26775=CARTESIAN_POINT('Ctrl Pts',(2.96204906231461,-0.820163155988569,
106.248630011208));
#26776=CARTESIAN_POINT('Ctrl Pts',(2.94715657163131,-0.873947927642731,
106.245727846997));
#26777=CARTESIAN_POINT('Ctrl Pts',(2.93081215209482,-0.927278294014138,
106.242825682786));
#26778=CARTESIAN_POINT('Ctrl Pts',(2.91305016692873,-0.980071923358931,
106.239923518575));
#26779=CARTESIAN_POINT('Ctrl Pts',(2.88245189371046,-1.07101862102652,106.234924009082));
#26780=CARTESIAN_POINT('Ctrl Pts',(2.84753670122269,-1.16069074941787,106.229924499589));
#26781=CARTESIAN_POINT('Ctrl Pts',(2.80842974048269,-1.24864912716596,106.224924990096));
#26782=CARTESIAN_POINT('Ctrl Pts',(2.76937582808664,-1.33648818993311,106.219932262406));
#26783=CARTESIAN_POINT('Ctrl Pts',(2.72614162500837,-1.42261772455469,106.214939534716));
#26784=CARTESIAN_POINT('Ctrl Pts',(2.67890171754383,-1.50661469451904,106.209946807026));
#26785=CARTESIAN_POINT('Ctrl Pts',(2.63171164699089,-1.5905230497974,106.204959346538));
#26786=CARTESIAN_POINT('Ctrl Pts',(2.5805244869527,-1.67230293231822,106.199971886049));
#26787=CARTESIAN_POINT('Ctrl Pts',(2.52556204351732,-1.75155320054648,106.194984425561));
#26788=CARTESIAN_POINT('Ctrl Pts',(2.47063892699498,-1.83074676335533,106.190000533718));
#26789=CARTESIAN_POINT('Ctrl Pts',(2.41194614658162,-1.90741395039175,106.185016641874));
#26790=CARTESIAN_POINT('Ctrl Pts',(2.34974986666697,-1.98118091402541,106.18003275003));
#26791=CARTESIAN_POINT('Ctrl Pts',(2.28757623709703,-2.05492101355793,106.175050673196));
#26792=CARTESIAN_POINT('Ctrl Pts',(2.22190192574255,-2.12576265296943,106.170068596363));
#26793=CARTESIAN_POINT('Ctrl Pts',(2.15303398587826,-2.19336428931748,106.165086519529));
#26794=CARTESIAN_POINT('Ctrl Pts',(2.08417232518346,-2.26095976195375,106.160104896946));
#26795=CARTESIAN_POINT('Ctrl Pts',(2.01211792829748,-2.32531551149458,106.155123274363));
#26796=CARTESIAN_POINT('Ctrl Pts',(1.93721461943756,-2.38612693883569,106.15014165178));
#26797=CARTESIAN_POINT('Ctrl Pts',(1.86229769183634,-2.44694942276576,106.14515912345));
#26798=CARTESIAN_POINT('Ctrl Pts',(1.78453116435678,-2.50422602803077,106.14017659512));
#26799=CARTESIAN_POINT('Ctrl Pts',(1.70429097844695,-2.557693201067,106.13519406679));
#26800=CARTESIAN_POINT('Ctrl Pts',(1.62396430544236,-2.61121800383586,106.130206168029));
#26801=CARTESIAN_POINT('Ctrl Pts',(1.54115901700683,-2.66092493329992,106.125218269268));
#26802=CARTESIAN_POINT('Ctrl Pts',(1.45627881354207,-2.70659458863504,106.120230370507));
#26803=CARTESIAN_POINT('Ctrl Pts',(1.37134847017607,-2.75229122166243,106.115239525326));
#26804=CARTESIAN_POINT('Ctrl Pts',(1.28434116699327,-2.79394564242786,106.110248680145));
#26805=CARTESIAN_POINT('Ctrl Pts',(1.19568197046962,-2.83138603434676,106.105257834963));
#26806=CARTESIAN_POINT('Ctrl Pts',(1.10687949844549,-2.86888693088448,106.10025892445));
#26807=CARTESIAN_POINT('Ctrl Pts',(1.01642021437568,-2.90216004912354,106.095260013937));
#26808=CARTESIAN_POINT('Ctrl Pts',(0.924745708015972,-2.93108301238741,
106.090261103424));
#26809=CARTESIAN_POINT('Ctrl Pts',(0.871523216691855,-2.94787450898232,
106.087358939213));
#26810=CARTESIAN_POINT('Ctrl Pts',(0.817891372082622,-2.96320073719099,
106.084456775002));
#26811=CARTESIAN_POINT('Ctrl Pts',(0.763937942530578,-2.97704569497382,
106.081554610791));
#26812=CARTESIAN_POINT('Ctrl Pts',(0.67099327654534,-3.00089617097485,106.076555101298));
#26813=CARTESIAN_POINT('Ctrl Pts',(0.576767356000774,-3.02043170716477,
106.071555591805));
#26814=CARTESIAN_POINT('Ctrl Pts',(0.481696701506079,-3.03551816627049,
106.066556082312));
#26815=CARTESIAN_POINT('Ctrl Pts',(0.386755009750507,-3.05058416069024,
106.061563354622));
#26816=CARTESIAN_POINT('Ctrl Pts',(0.290971291227217,-3.06121300426841,
106.056570626932));
#26817=CARTESIAN_POINT('Ctrl Pts',(0.194795439479901,-3.06732081575401,
106.051577899242));
#26818=CARTESIAN_POINT('Ctrl Pts',(0.0987210508319767,-3.07342218365244,
106.046590438754));
#26819=CARTESIAN_POINT('Ctrl Pts',(0.00225578710244156,-3.075011973412,
106.041602978265));
#26820=CARTESIAN_POINT('Ctrl Pts',(-0.0941431146129687,-3.07205783213321,
106.036615517777));
#26821=CARTESIAN_POINT('Ctrl Pts',(-0.190473040660873,-3.06910580461155,
106.031631625934));
#26822=CARTESIAN_POINT('Ctrl Pts',(-0.286736261591445,-3.0616163228673,
106.02664773409));
#26823=CARTESIAN_POINT('Ctrl Pts',(-0.382474283279055,-3.04960910161125,
106.021663842246));
#26824=CARTESIAN_POINT('Ctrl Pts',(-0.478177439550352,-3.03760625308779,
106.016681765413));
#26825=CARTESIAN_POINT('Ctrl Pts',(-0.573355341495525,-3.02108898855307,
106.011699688579));
#26826=CARTESIAN_POINT('Ctrl Pts',(-0.667554329894647,-3.00012890833693,
106.006717611745));
#26827=CARTESIAN_POINT('Ctrl Pts',(-0.761744729516232,-2.9791707391972,
106.001735989162));
#26828=CARTESIAN_POINT('Ctrl Pts',(-0.854955964602517,-2.95377065527505,
105.996754366579));
#26829=CARTESIAN_POINT('Ctrl Pts',(-0.946745344142949,-2.92405121421354,
105.991772743996));
#26830=CARTESIAN_POINT('Ctrl Pts',(-1.03855141260981,-2.89432636963401,
105.986790215666));
#26831=CARTESIAN_POINT('Ctrl Pts',(-1.12893469451034,-2.86028074348624,
105.981807687336));
#26832=CARTESIAN_POINT('Ctrl Pts',(-1.21746944124027,-2.82208618040734,
105.976825159007));
#26833=CARTESIAN_POINT('Ctrl Pts',(-1.30609961537912,-2.78385044921848,
105.971837260246));
#26834=CARTESIAN_POINT('Ctrl Pts',(-1.3928768728847,-2.74145702744756,105.966849361484));
#26835=CARTESIAN_POINT('Ctrl Pts',(-1.47739738672443,-2.69512508275587,
105.961861462723));
#26836=CARTESIAN_POINT('Ctrl Pts',(-1.56196782799178,-2.64876576914852,
105.956870617542));
#26837=CARTESIAN_POINT('Ctrl Pts',(-1.64427849681322,-2.59846352889413,
105.951879772361));
#26838=CARTESIAN_POINT('Ctrl Pts',(-1.72395384665673,-2.54448135866574,
105.94688892718));
#26839=CARTESIAN_POINT('Ctrl Pts',(-1.80375795387767,-2.49041195188703,
105.941890016666));
#26840=CARTESIAN_POINT('Ctrl Pts',(-1.88091788718286,-2.43265100345196,
105.936891106153));
#26841=CARTESIAN_POINT('Ctrl Pts',(-1.95509057372824,-2.37150228726834,
105.93189219564));
#26842=CARTESIAN_POINT('Ctrl Pts',(-1.99815222001252,-2.33600182868072,
105.928990031429));
#26843=CARTESIAN_POINT('Ctrl Pts',(-2.04020768351381,-2.29936024005541,
105.926087867218));
#26844=CARTESIAN_POINT('Ctrl Pts',(-2.08119575623374,-2.26164242846535,
105.923185703007));
#26845=CARTESIAN_POINT('Ctrl Pts',(-2.15075950934304,-2.19762886649083,
105.918260235151));
#26846=CARTESIAN_POINT('Ctrl Pts',(-2.21750681602361,-2.13027396279245,
105.913334767295));
#26847=CARTESIAN_POINT('Ctrl Pts',(-2.28109244639444,-2.05985909736619,
105.90840929944));
#26848=CARTESIAN_POINT('Ctrl Pts',(-2.34457578858639,-1.98955750609177,
105.903491755027));
#26849=CARTESIAN_POINT('Ctrl Pts',(-2.40490726497281,-1.91620607231139,
105.898574210615));
#26850=CARTESIAN_POINT('Ctrl Pts',(-2.4617762523236,-1.84012497768374,105.893656666202));
#26851=CARTESIAN_POINT('Ctrl Pts',(-2.51859341366884,-1.76411321749329,
105.88874360326));
#26852=CARTESIAN_POINT('Ctrl Pts',(-2.57195407934606,-1.68537709464359,
105.883830540318));
#26853=CARTESIAN_POINT('Ctrl Pts',(-2.62158640063781,-1.60427148388011,
105.878917477376));
#26854=CARTESIAN_POINT('Ctrl Pts',(-2.67118799605383,-1.52321608315823,
105.874007455963));
#26855=CARTESIAN_POINT('Ctrl Pts',(-2.71706559402625,-1.43979449251477,
105.86909743455));
#26856=CARTESIAN_POINT('Ctrl Pts',(-2.75899012028278,-1.35439128990925,
105.864187413137));
#26857=CARTESIAN_POINT('Ctrl Pts',(-2.80090094098928,-1.26901600647109,
105.85927899686));
#26858=CARTESIAN_POINT('Ctrl Pts',(-2.83886105818303,-1.18166080472102,
105.854370580583));
#26859=CARTESIAN_POINT('Ctrl Pts',(-2.87268751225107,-1.09273450890725,
105.849462164305));
#26860=CARTESIAN_POINT('Ctrl Pts',(-2.90652877058643,-1.00376929418545,
105.844551599842));
#26861=CARTESIAN_POINT('Ctrl Pts',(-2.93623258264752,-0.913232033075345,
105.839641035379));
#26862=CARTESIAN_POINT('Ctrl Pts',(-2.96166455066047,-0.821550570178788,
105.834730470916));
#26863=CARTESIAN_POINT('Ctrl Pts',(-2.9871011391851,-0.729852450479684,
105.829819014295));
#26864=CARTESIAN_POINT('Ctrl Pts',(-3.00826423064648,-0.637010155946073,
105.824907557675));
#26865=CARTESIAN_POINT('Ctrl Pts',(-3.02507014949399,-0.543463743630075,
105.819996101054));
#26866=CARTESIAN_POINT('Ctrl Pts',(-3.0418970487393,-0.449800548592378,
105.815078513004));
#26867=CARTESIAN_POINT('Ctrl Pts',(-3.05435584318723,-0.355431929188649,
105.810160924953));
#26868=CARTESIAN_POINT('Ctrl Pts',(-3.06241458140855,-0.260804872608452,
105.805243336903));
#26869=CARTESIAN_POINT('Ctrl Pts',(-3.06988009998551,-0.173143500643975,
105.800687742226));
#26870=CARTESIAN_POINT('Ctrl Pts',(-3.07357006283488,-0.0852606728696437,
105.796132147549));
#26871=CARTESIAN_POINT('Ctrl Pts',(-3.07349899192525,0.00248930400749208,
105.791576552872));
#26872=CARTESIAN_POINT('Origin',(0.,0.,116.208423447177));
#26873=CARTESIAN_POINT('',(1.8723819390353,2.43733217358127,107.437292535812));
#26874=CARTESIAN_POINT('',(1.8723819390353,2.43733217358127,107.354176765664));
#26875=CARTESIAN_POINT('',(1.8723819390353,2.43733217358128,116.208423447177));
#26876=CARTESIAN_POINT('',(-3.07349975246569,-0.00123352880650566,106.708423447146));
#26877=CARTESIAN_POINT('Ctrl Pts',(1.8723819390353,2.43733217358127,107.354176765664));
#26878=CARTESIAN_POINT('Ctrl Pts',(1.87949704018099,2.43186628467864,107.353709446164));
#26879=CARTESIAN_POINT('Ctrl Pts',(1.88658706336632,2.42637011824953,107.353242126665));
#26880=CARTESIAN_POINT('Ctrl Pts',(1.89365173966783,2.42084393112257,107.352774807166));
#26881=CARTESIAN_POINT('Ctrl Pts',(1.96923154382078,2.36172329728988,107.347775297673));
#26882=CARTESIAN_POINT('Ctrl Pts',(2.04217278678712,2.29895597815628,107.34277578818));
#26883=CARTESIAN_POINT('Ctrl Pts',(2.11210297010482,2.23280614780468,107.337776278687));
#26884=CARTESIAN_POINT('Ctrl Pts',(2.18193829357291,2.1667460492779,107.332783550997));
#26885=CARTESIAN_POINT('Ctrl Pts',(2.24877035886731,2.09731285765864,107.327790823307));
#26886=CARTESIAN_POINT('Ctrl Pts',(2.31225834386002,2.02481199158088,107.322798095617));
#26887=CARTESIAN_POINT('Ctrl Pts',(2.3756793506289,1.95238761208931,107.317810635128));
#26888=CARTESIAN_POINT('Ctrl Pts',(2.43576300273951,1.87690232023088,107.31282317464));
#26889=CARTESIAN_POINT('Ctrl Pts',(2.49220483946106,1.79869877638443,107.307835714152));
#26890=CARTESIAN_POINT('Ctrl Pts',(2.54860629072909,1.72055118900166,107.302851822308));
#26891=CARTESIAN_POINT('Ctrl Pts',(2.60137085066683,1.63968957106517,107.297867930464));
#26892=CARTESIAN_POINT('Ctrl Pts',(2.65023455884298,1.55648932958578,107.292884038621));
#26893=CARTESIAN_POINT('Ctrl Pts',(2.69908047206682,1.4733193875737,107.287901961787));
#26894=CARTESIAN_POINT('Ctrl Pts',(2.7440281340211,1.3878128923161,107.282919884953));
#26895=CARTESIAN_POINT('Ctrl Pts',(2.78485765514179,1.30037305824067,107.27793780812));
#26896=CARTESIAN_POINT('Ctrl Pts',(2.82568345355081,1.2129411966636,107.272956185537));
#26897=CARTESIAN_POINT('Ctrl Pts',(2.86239167209386,1.12357674455337,107.267974562953));
#26898=CARTESIAN_POINT('Ctrl Pts',(2.89480949636708,1.03270529665679,107.26299294037));
#26899=CARTESIAN_POINT('Ctrl Pts',(2.92723321477193,0.941817326729887,107.258010412041));
#26900=CARTESIAN_POINT('Ctrl Pts',(2.95536484223045,0.849422230304534,107.253027883711));
#26901=CARTESIAN_POINT('Ctrl Pts',(2.97908095867815,0.755962228977924,107.248045355381));
#26902=CARTESIAN_POINT('Ctrl Pts',(3.00282263760414,0.66240149154387,107.24305745662));
#26903=CARTESIAN_POINT('Ctrl Pts',(3.02213919592931,0.567773983893576,107.238069557859));
#26904=CARTESIAN_POINT('Ctrl Pts',(3.03695808761004,0.472533410564768,107.233081659098));
#26905=CARTESIAN_POINT('Ctrl Pts',(3.05178573301348,0.377236577322067,107.228090813916));
#26906=CARTESIAN_POINT('Ctrl Pts',(3.06211037462238,0.281326393545326,107.223099968735));
#26907=CARTESIAN_POINT('Ctrl Pts',(3.06791144880873,0.18526087624835,107.218109123554));
#26908=CARTESIAN_POINT('Ctrl Pts',(3.07372189767746,0.0890401146494389,
107.21311021304));
#26909=CARTESIAN_POINT('Ctrl Pts',(3.07499417648102,-0.00733604307861015,
107.208111302527));
#26910=CARTESIAN_POINT('Ctrl Pts',(3.07175984225134,-0.103410451754141,
107.203112392014));
#26911=CARTESIAN_POINT('Ctrl Pts',(3.06988211929091,-0.159187347482755,
107.200210227803));
#26912=CARTESIAN_POINT('Ctrl Pts',(3.06648641852976,-0.214862631439177,
107.197308063592));
#26913=CARTESIAN_POINT('Ctrl Pts',(3.06158685878352,-0.270348212725877,
107.194405899381));
#26914=CARTESIAN_POINT('Ctrl Pts',(3.0531464695836,-0.365932290744841,107.189406389888));
#26915=CARTESIAN_POINT('Ctrl Pts',(3.04021070012985,-0.461288607501185,
107.184406880395));
#26916=CARTESIAN_POINT('Ctrl Pts',(3.0227983302358,-0.555960884166899,107.179407370902));
#26917=CARTESIAN_POINT('Ctrl Pts',(3.00540958011095,-0.650504738490473,
107.174414643212));
#26918=CARTESIAN_POINT('Ctrl Pts',(2.98355637692206,-0.744365968827277,
107.169421915522));
#26919=CARTESIAN_POINT('Ctrl Pts',(2.95730934232343,-0.837092410553675,
107.164429187832));
#26920=CARTESIAN_POINT('Ctrl Pts',(2.93108999768471,-0.92972102822135,107.159441727344));
#26921=CARTESIAN_POINT('Ctrl Pts',(2.90048615541362,-1.02121681706509,107.154454266855));
#26922=CARTESIAN_POINT('Ctrl Pts',(2.86561947227221,-1.1111378357946,107.149466806367));
#26923=CARTESIAN_POINT('Ctrl Pts',(2.83077773705761,-1.20099451393331,107.144482914524));
#26924=CARTESIAN_POINT('Ctrl Pts',(2.7916793827907,-1.2892782538538,107.13949902268));
#26925=CARTESIAN_POINT('Ctrl Pts',(2.74849558430707,-1.37556325664964,107.134515130836));
#26926=CARTESIAN_POINT('Ctrl Pts',(2.7053275122933,-1.4618168365845,107.129533054003));
#26927=CARTESIAN_POINT('Ctrl Pts',(2.65807714845424,-1.54607273349073,107.124550977169));
#26928=CARTESIAN_POINT('Ctrl Pts',(2.6069629867247,-1.62792697497383,107.119568900335));
#26929=CARTESIAN_POINT('Ctrl Pts',(2.5558534854291,-1.70977375323593,107.114587277752));
#26930=CARTESIAN_POINT('Ctrl Pts',(2.50088111931813,-1.78921893920546,107.109605655169));
#26931=CARTESIAN_POINT('Ctrl Pts',(2.44230878491009,-1.86588586176941,107.104624032586));
#26932=CARTESIAN_POINT('Ctrl Pts',(2.38372580101967,-1.94256672373068,107.099641504256));
#26933=CARTESIAN_POINT('Ctrl Pts',(2.32154181543371,-2.01646797029362,107.094658975926));
#26934=CARTESIAN_POINT('Ctrl Pts',(2.2560605639695,-2.0872453094214,107.089676447596));
#26935=CARTESIAN_POINT('Ctrl Pts',(2.19050873336672,-2.15809893608972,107.084688548835));
#26936=CARTESIAN_POINT('Ctrl Pts',(2.12165284031759,-2.22582161044657,107.079700650074));
#26937=CARTESIAN_POINT('Ctrl Pts',(2.04983395088141,-2.29010546128642,107.074712751313));
#26938=CARTESIAN_POINT('Ctrl Pts',(1.97797263704148,-2.35442728547931,107.069721906132));
#26939=CARTESIAN_POINT('Ctrl Pts',(1.90314518206019,-2.4153059644849,107.064731060951));
#26940=CARTESIAN_POINT('Ctrl Pts',(1.82572457117581,-2.47247488161253,107.059740215769));
#26941=CARTESIAN_POINT('Ctrl Pts',(1.74817884662911,-2.52973618515395,107.054741305256));
#26942=CARTESIAN_POINT('Ctrl Pts',(1.6680319632319,-2.58327551232093,107.049742394743));
#26943=CARTESIAN_POINT('Ctrl Pts',(1.58568455211106,-2.63287043950065,107.04474348423));
#26944=CARTESIAN_POINT('Ctrl Pts',(1.5378769930855,-2.66166323791702,107.041841320019));
#26945=CARTESIAN_POINT('Ctrl Pts',(1.48932819984732,-2.68912744557709,107.038939155808));
#26946=CARTESIAN_POINT('Ctrl Pts',(1.44011974937296,-2.7152269440078,107.036036991597));
#26947=CARTESIAN_POINT('Ctrl Pts',(1.35534917906867,-2.76018811115085,107.031037482104));
#26948=CARTESIAN_POINT('Ctrl Pts',(1.26832213635766,-2.80125458304302,107.026037972611));
#26949=CARTESIAN_POINT('Ctrl Pts',(1.17943156909956,-2.83819369032689,107.021038463118));
#26950=CARTESIAN_POINT('Ctrl Pts',(1.09066158133155,-2.87508268994626,107.016045735428));
#26951=CARTESIAN_POINT('Ctrl Pts',(1.00003349485742,-2.90785528508275,107.011053007738));
#26952=CARTESIAN_POINT('Ctrl Pts',(0.90796503194505,-2.93632453089999,107.006060280048));
#26953=CARTESIAN_POINT('Ctrl Pts',(0.815993698940238,-2.96476374238052,
107.00107281956));
#26954=CARTESIAN_POINT('Ctrl Pts',(0.722585427433058,-2.98890850065104,
106.996085359071));
#26955=CARTESIAN_POINT('Ctrl Pts',(0.628177150582328,-3.0086202348396,106.991097898583));
#26956=CARTESIAN_POINT('Ctrl Pts',(0.533836425060517,-3.02831786482157,
106.98611400674));
#26957=CARTESIAN_POINT('Ctrl Pts',(0.438497545093442,-3.04358868691319,
106.981130114896));
#26958=CARTESIAN_POINT('Ctrl Pts',(0.342610863925298,-3.05434445436666,
106.976146223052));
#26959=CARTESIAN_POINT('Ctrl Pts',(0.246759102311604,-3.06509630483601,
106.971164146219));
#26960=CARTESIAN_POINT('Ctrl Pts',(0.150360371653682,-3.07133631877303,
106.966182069385));
#26961=CARTESIAN_POINT('Ctrl Pts',(0.0538724802433375,-3.07302782380382,
106.961199992551));
#26962=CARTESIAN_POINT('Ctrl Pts',(-0.0426066136942767,-3.07471917460832,
106.956218369968));
#26963=CARTESIAN_POINT('Ctrl Pts',(-0.139174413323532,-3.07186283353432,
106.951236747385));
#26964=CARTESIAN_POINT('Ctrl Pts',(-0.235371835401016,-3.06447423697768,
106.946255124802));
#26965=CARTESIAN_POINT('Ctrl Pts',(-0.331586747864818,-3.05708429704401,
106.941272596472));
#26966=CARTESIAN_POINT('Ctrl Pts',(-0.427430711371173,-3.04516049872647,
106.936290068142));
#26967=CARTESIAN_POINT('Ctrl Pts',(-0.522449566975857,-3.02877016294844,
106.931307539812));
#26968=CARTESIAN_POINT('Ctrl Pts',(-0.617570838903127,-3.01236216080403,
106.926319641051));
#26969=CARTESIAN_POINT('Ctrl Pts',(-0.711864794142939,-2.99147808469634,
106.92133174229));
#26970=CARTESIAN_POINT('Ctrl Pts',(-0.804887498754871,-2.9662363972462,
106.916343843529));
#26971=CARTESIAN_POINT('Ctrl Pts',(-0.897965153155196,-2.94097979918483,
106.911352998348));
#26972=CARTESIAN_POINT('Ctrl Pts',(-0.989769644110338,-2.91136059904522,
106.906362153167));
#26973=CARTESIAN_POINT('Ctrl Pts',(-1.07987426320182,-2.87754649409429,
106.901371307985));
#26974=CARTESIAN_POINT('Ctrl Pts',(-1.1701244936332,-2.84367774469583,106.896372397472));
#26975=CARTESIAN_POINT('Ctrl Pts',(-1.25866896399276,-2.80560072747383,
106.891373486959));
#26976=CARTESIAN_POINT('Ctrl Pts',(-1.34510298282755,-2.76353038984348,
106.886374576446));
#26977=CARTESIAN_POINT('Ctrl Pts',(-1.39528306014903,-2.73910606220384,
106.883472412235));
#26978=CARTESIAN_POINT('Ctrl Pts',(-1.44475229191811,-2.71333663971388,
106.880570248024));
#26979=CARTESIAN_POINT('Ctrl Pts',(-1.49343596752607,-2.68627088375306,
106.877668083813));
#26980=CARTESIAN_POINT('Ctrl Pts',(-1.5773025169908,-2.6396451610084,106.87266857432));
#26981=CARTESIAN_POINT('Ctrl Pts',(-1.65913076605024,-2.58900625370816,
106.867669064827));
#26982=CARTESIAN_POINT('Ctrl Pts',(-1.73851161236678,-2.53455708629059,
106.862669555334));
#26983=CARTESIAN_POINT('Ctrl Pts',(-1.81778477906938,-2.48018177882287,
106.857676827644));
#26984=CARTESIAN_POINT('Ctrl Pts',(-1.89461678219015,-2.42200672964877,
106.852684099954));
#26985=CARTESIAN_POINT('Ctrl Pts',(-1.96862338430176,-2.36028053857593,
106.847691372264));
#26986=CARTESIAN_POINT('Ctrl Pts',(-2.04255191131358,-2.29861946707879,
106.842703911776));
#26987=CARTESIAN_POINT('Ctrl Pts',(-2.11366062751448,-2.23341498089758,
106.837716451288));
#26988=CARTESIAN_POINT('Ctrl Pts',(-2.18159541178576,-2.16495813106751,
106.832728990799));
#26989=CARTESIAN_POINT('Ctrl Pts',(-2.24948158713089,-2.0965502637137,106.827745098956));
#26990=CARTESIAN_POINT('Ctrl Pts',(-2.31419803691549,-2.02489496964545,
106.822761207112));
#26991=CARTESIAN_POINT('Ctrl Pts',(-2.37542554492148,-1.95032195561001,
106.817777315268));
#26992=CARTESIAN_POINT('Ctrl Pts',(-2.43663075538551,-1.87577609921931,
106.812795238435));
#26993=CARTESIAN_POINT('Ctrl Pts',(-2.49434927032418,-1.79831497297089,
106.807813161601));
#26994=CARTESIAN_POINT('Ctrl Pts',(-2.54830107479406,-1.71830261659681,
106.802831084767));
#26995=CARTESIAN_POINT('Ctrl Pts',(-2.60224796010231,-1.6382975555063,106.797849462184));
#26996=CARTESIAN_POINT('Ctrl Pts',(-2.65242857249977,-1.55574209082362,
106.792867839601));
#26997=CARTESIAN_POINT('Ctrl Pts',(-2.6986059113277,-1.47102970240142,106.787886217018));
#26998=CARTESIAN_POINT('Ctrl Pts',(-2.74479164600945,-1.38630191177441,
106.782903688688));
#26999=CARTESIAN_POINT('Ctrl Pts',(-2.78697245151776,-1.29941680399648,
106.777921160359));
#27000=CARTESIAN_POINT('Ctrl Pts',(-2.82495752857764,-1.21079197706811,
106.772938632029));
#27001=CARTESIAN_POINT('Ctrl Pts',(-2.86298354795241,-1.1220716256377,106.767950733268));
#27002=CARTESIAN_POINT('Ctrl Pts',(-2.89680463715693,-1.0316082156055,106.762962834507));
#27003=CARTESIAN_POINT('Ctrl Pts',(-2.92627846119675,-0.939838612494707,
106.757974935746));
#27004=CARTESIAN_POINT('Ctrl Pts',(-2.95576969582899,-0.848014799819735,
106.752984090564));
#27005=CARTESIAN_POINT('Ctrl Pts',(-2.98090843766949,-0.754883681308667,
106.747993245383));
#27006=CARTESIAN_POINT('Ctrl Pts',(-3.00160302782743,-0.660894479729704,
106.743002400202));
#27007=CARTESIAN_POINT('Ctrl Pts',(-3.02233106096569,-0.566753389227413,
106.738003489688));
#27008=CARTESIAN_POINT('Ctrl Pts',(-3.0386005277857,-0.471751879127948,
106.733004579175));
#27009=CARTESIAN_POINT('Ctrl Pts',(-3.05037138962777,-0.37634642995565,
106.728005668662));
#27010=CARTESIAN_POINT('Ctrl Pts',(-3.05720507346357,-0.320957904917864,
106.725103504451));
#27011=CARTESIAN_POINT('Ctrl Pts',(-3.06252348114542,-0.265433292654388,
106.72220134024));
#27012=CARTESIAN_POINT('Ctrl Pts',(-3.0663268370347,-0.209861808056603,
106.719299176029));
#27013=CARTESIAN_POINT('Ctrl Pts',(-3.07107780497571,-0.140444601398931,
106.715673933079));
#27014=CARTESIAN_POINT('Ctrl Pts',(-3.07347180662027,-0.0708642553406025,
106.712048690128));
#27015=CARTESIAN_POINT('Ctrl Pts',(-3.07349975246545,-0.0012335294098428,
106.708423447177));
#27016=CARTESIAN_POINT('Ctrl Pts',(-3.07349975246569,-0.00123352880650975,
106.708423447146));
#27017=CARTESIAN_POINT('Ctrl Pts',(-3.07353790671295,0.0938328116699644,
106.703473928438));
#27018=CARTESIAN_POINT('Ctrl Pts',(-3.06916108330069,0.18907672144084,106.69852440973));
#27019=CARTESIAN_POINT('Ctrl Pts',(-3.06034609058113,0.28404938983357,106.693574891022));
#27020=CARTESIAN_POINT('Ctrl Pts',(-3.05154252364177,0.378898956952153,
106.68863178776));
#27021=CARTESIAN_POINT('Ctrl Pts',(-3.03831225657513,0.473477538391671,
106.683688684499));
#27022=CARTESIAN_POINT('Ctrl Pts',(-3.02068411174001,0.567335656451707,
106.678745581237));
#27023=CARTESIAN_POINT('Ctrl Pts',(-3.00307397543663,0.661097891086995,
106.673807527743));
#27024=CARTESIAN_POINT('Ctrl Pts',(-2.98107497399975,0.75414068679251,106.668869474249));
#27025=CARTESIAN_POINT('Ctrl Pts',(-2.95476767376119,0.846020238585289,
106.663931420755));
#27026=CARTESIAN_POINT('Ctrl Pts',(-2.92847497441744,0.937848796028246,
106.658996107945));
#27027=CARTESIAN_POINT('Ctrl Pts',(-2.89787884709398,1.02851496137343,106.654060795135));
#27028=CARTESIAN_POINT('Ctrl Pts',(-2.86311061951497,1.11758660980731,106.649125482325));
#27029=CARTESIAN_POINT('Ctrl Pts',(-2.82835173619897,1.20663431946239,106.644191495923));
#27030=CARTESIAN_POINT('Ctrl Pts',(-2.7894231428698,1.29408794592081,106.639257509521));
#27031=CARTESIAN_POINT('Ctrl Pts',(-2.74650516220389,1.37953312536792,106.634323523119));
#27032=CARTESIAN_POINT('Ctrl Pts',(-2.70358643071273,1.46497979962902,106.6293894504));
#27033=CARTESIAN_POINT('Ctrl Pts',(-2.65667837574756,1.54841755690931,106.624455377681));
#27034=CARTESIAN_POINT('Ctrl Pts',(-2.60600780319389,1.62945560838354,106.619521304962));
#27035=CARTESIAN_POINT('Ctrl Pts',(-2.55528842710113,1.71057171194034,106.614582479974));
#27036=CARTESIAN_POINT('Ctrl Pts',(-2.50079953325928,1.78928311198955,106.609643654985));
#27037=CARTESIAN_POINT('Ctrl Pts',(-2.44281174149959,1.86522734421081,106.604704829997));
#27038=CARTESIAN_POINT('Ctrl Pts',(-2.38479683706134,1.94120708479504,106.599763695819));
#27039=CARTESIAN_POINT('Ctrl Pts',(-2.32328006610208,2.0144167378847,106.594822561642));
#27040=CARTESIAN_POINT('Ctrl Pts',(-2.25857142803395,2.0845280891532,106.589881427464));
#27041=CARTESIAN_POINT('Ctrl Pts',(-2.19375173689868,2.15475976563379,106.584931813304));
#27042=CARTESIAN_POINT('Ctrl Pts',(-2.12572955460516,2.2218822018932,106.579982199144));
#27043=CARTESIAN_POINT('Ctrl Pts',(-2.05485076363564,2.28560508163288,106.575032584985));
#27044=CARTESIAN_POINT('Ctrl Pts',(-1.98753540476063,2.34612429280382,106.570331812738));
#27045=CARTESIAN_POINT('Ctrl Pts',(-1.91764398370614,2.40357730667361,106.565631040491));
#27046=CARTESIAN_POINT('Ctrl Pts',(-1.84549689863096,2.45775170575539,106.560930268245));
#27047=CARTESIAN_POINT('Ctrl Pts',(-1.76876481764489,2.5153689244328,106.555930758752));
#27048=CARTESIAN_POINT('Ctrl Pts',(-1.68919712402311,2.56949048583303,106.550931249259));
#27049=CARTESIAN_POINT('Ctrl Pts',(-1.60714572551787,2.61982535046702,106.545931739766));
#27050=CARTESIAN_POINT('Ctrl Pts',(-1.52520562921355,2.67009193617684,106.540939012076));
#27051=CARTESIAN_POINT('Ctrl Pts',(-1.4407888949156,2.71658180626101,106.535946284386));
#27052=CARTESIAN_POINT('Ctrl Pts',(-1.35427902496947,2.75904522843098,106.530953556696));
#27053=CARTESIAN_POINT('Ctrl Pts',(-1.26786042075562,2.80146385276085,106.525966096207));
#27054=CARTESIAN_POINT('Ctrl Pts',(-1.17935346262849,2.83986428115655,106.520978635719));
#27055=CARTESIAN_POINT('Ctrl Pts',(-1.08916816463259,2.87404157227255,106.515991175231));
#27056=CARTESIAN_POINT('Ctrl Pts',(-0.999047396325561,2.90819440873783,
106.511007283387));
#27057=CARTESIAN_POINT('Ctrl Pts',(-0.907251084763536,2.93812995991572,
106.506023391544));
#27058=CARTESIAN_POINT('Ctrl Pts',(-0.81421033935335,2.96369090380392,106.5010394997));
#27059=CARTESIAN_POINT('Ctrl Pts',(-0.721203477078128,2.98924253902948,
106.496057422866));
#27060=CARTESIAN_POINT('Ctrl Pts',(-0.626953504244634,3.01042261616097,
106.491075346033));
#27061=CARTESIAN_POINT('Ctrl Pts',(-0.531906928153377,3.02712359671396,
106.486093269199));
#27062=CARTESIAN_POINT('Ctrl Pts',(-0.436869018120279,3.04382305452225,
106.481111646616));
#27063=CARTESIAN_POINT('Ctrl Pts',(-0.341035081605433,3.05604415192055,
106.476130024033));
#27064=CARTESIAN_POINT('Ctrl Pts',(-0.244861002391348,3.06373062450143,
106.47114840145));
#27065=CARTESIAN_POINT('Ctrl Pts',(-0.148669437035249,3.07141849461844,
106.46616587312));
#27066=CARTESIAN_POINT('Ctrl Pts',(-0.0521380437231236,3.07457006757433,
106.46118334479));
#27067=CARTESIAN_POINT('Ctrl Pts',(0.0442740757878782,3.07318109720419,
106.45620081646));
#27068=CARTESIAN_POINT('Ctrl Pts',(0.140790113354838,3.07179062972869,106.451212917699));
#27069=CARTESIAN_POINT('Ctrl Pts',(0.237186180818789,3.06584985476902,106.446225018938));
#27070=CARTESIAN_POINT('Ctrl Pts',(0.333005310159123,3.05540663634251,106.441237120177));
#27071=CARTESIAN_POINT('Ctrl Pts',(0.42888104117435,3.04495724896352,106.436246274996));
#27072=CARTESIAN_POINT('Ctrl Pts',(0.524178722015902,3.0300001903401,106.431255429815));
#27073=CARTESIAN_POINT('Ctrl Pts',(0.61845073052815,3.0106346413853,106.426264584633));
#27074=CARTESIAN_POINT('Ctrl Pts',(0.712875084986894,2.99123779721434,106.42126567412));
#27075=CARTESIAN_POINT('Ctrl Pts',(0.8062700323702,2.96741834560313,106.416266763607));
#27076=CARTESIAN_POINT('Ctrl Pts',(0.898202338471354,2.93932557046078,106.411267853094));
#27077=CARTESIAN_POINT('Ctrl Pts',(0.95157449784442,2.92301604733754,106.408365688883));
#27078=CARTESIAN_POINT('Ctrl Pts',(1.00445401722475,2.90526711899224,106.405463524672));
#27079=CARTESIAN_POINT('Ctrl Pts',(1.05675950233112,2.88611531374491,106.402561360461));
#27080=CARTESIAN_POINT('Ctrl Pts',(1.14685315663654,2.85312726062258,106.397562523749));
#27081=CARTESIAN_POINT('Ctrl Pts',(1.23555890822217,2.81585865486352,106.392563687038));
#27082=CARTESIAN_POINT('Ctrl Pts',(1.32244121367734,2.77444615849139,106.387564850326));
#27083=CARTESIAN_POINT('Ctrl Pts',(1.4092199524657,2.73308302722519,106.382571972399));
#27084=CARTESIAN_POINT('Ctrl Pts',(1.49417916876701,2.6875860016328,106.377579094471));
#27085=CARTESIAN_POINT('Ctrl Pts',(1.57690055060915,2.63814080433334,106.372586216543));
#27086=CARTESIAN_POINT('Ctrl Pts',(1.65952934396238,2.58875095011447,106.367598927049));
#27087=CARTESIAN_POINT('Ctrl Pts',(1.73992490908725,2.5354219361422,106.362611637556));
#27088=CARTESIAN_POINT('Ctrl Pts',(1.81769214758397,2.47838606891896,106.357624348063));
#27089=CARTESIAN_POINT('Ctrl Pts',(1.83607042340513,2.46490711660189,106.356445731158));
#27090=CARTESIAN_POINT('Ctrl Pts',(1.85430202037919,2.45122134039976,106.355267114254));
#27091=CARTESIAN_POINT('Ctrl Pts',(1.87238193903529,2.43733217358128,106.354088497349));
#27092=CARTESIAN_POINT('',(-3.07349998753216,0.000276838910911489,106.791576552796));
#27093=CARTESIAN_POINT('Ctrl Pts',(-3.07349998753216,0.000276838910921114,
106.791576552796));
#27094=CARTESIAN_POINT('Ctrl Pts',(-3.07349079945254,0.102284040620658,
106.786322773875));
#27095=CARTESIAN_POINT('Ctrl Pts',(-3.06839901409353,0.204179977417602,
106.781068994954));
#27096=CARTESIAN_POINT('Ctrl Pts',(-3.05828337165257,0.305458783919216,
106.775815216034));
#27097=CARTESIAN_POINT('Ctrl Pts',(-3.04813772460372,0.407037999504475,
106.770545853567));
#27098=CARTESIAN_POINT('Ctrl Pts',(-3.03293845951957,0.507996061930611,
106.765276491101));
#27099=CARTESIAN_POINT('Ctrl Pts',(-3.01279594210241,0.607834567338209,
106.760007128635));
#27100=CARTESIAN_POINT('Ctrl Pts',(-2.99262318887305,0.707822939728093,
106.75472985636));
#27101=CARTESIAN_POINT('Ctrl Pts',(-2.96749246796359,0.806688050718487,
106.749452584086));
#27102=CARTESIAN_POINT('Ctrl Pts',(-2.93756412737037,0.903946484913101,
106.744175311811));
#27103=CARTESIAN_POINT('Ctrl Pts',(-2.90755169174042,1.00147820360776,106.738883211036));
#27104=CARTESIAN_POINT('Ctrl Pts',(-2.87271479946202,1.09739387420478,106.733591110261));
#27105=CARTESIAN_POINT('Ctrl Pts',(-2.83326264746127,1.19122836622571,106.728299009486));
#27106=CARTESIAN_POINT('Ctrl Pts',(-2.80029014392485,1.26965141701237,106.723876086967));
#27107=CARTESIAN_POINT('Ctrl Pts',(-2.76409481162807,1.34662108790702,106.719453164447));
#27108=CARTESIAN_POINT('Ctrl Pts',(-2.72482273064761,1.42188021174292,106.715030241928));
#27109=CARTESIAN_POINT('Ctrl Pts',(-2.68043100983037,1.50695036669438,106.710030732435));
#27110=CARTESIAN_POINT('Ctrl Pts',(-2.63197360866318,1.59008905533461,106.705031222942));
#27111=CARTESIAN_POINT('Ctrl Pts',(-2.57964256266102,1.67088195241546,106.700031713449));
#27112=CARTESIAN_POINT('Ctrl Pts',(-2.52738250339044,1.75156525444448,106.695038985759));
#27113=CARTESIAN_POINT('Ctrl Pts',(-2.47125947900096,1.82990872375329,106.690046258069));
#27114=CARTESIAN_POINT('Ctrl Pts',(-2.41151184191223,1.90552168350745,106.685053530379));
#27115=CARTESIAN_POINT('Ctrl Pts',(-2.35182723707464,1.98105487349497,106.680066069891));
#27116=CARTESIAN_POINT('Ctrl Pts',(-2.288525891873,2.05386293783921,106.675078609403));
#27117=CARTESIAN_POINT('Ctrl Pts',(-2.2218893914809,2.12358418293804,106.670091148914));
#27118=CARTESIAN_POINT('Ctrl Pts',(-2.15530057106246,2.19325554085627,106.665107257071));
#27119=CARTESIAN_POINT('Ctrl Pts',(-2.08538164189137,2.25984415387907,106.660123365227));
#27120=CARTESIAN_POINT('Ctrl Pts',(-2.01245375433242,2.32302219891962,106.655139473383));
#27121=CARTESIAN_POINT('Ctrl Pts',(-1.93955242530391,2.38617723608091,106.65015739655));
#27122=CARTESIAN_POINT('Ctrl Pts',(-1.86364464653832,2.44592388593905,106.645175319716));
#27123=CARTESIAN_POINT('Ctrl Pts',(-1.78508692598574,2.50197260510078,106.640193242882));
#27124=CARTESIAN_POINT('Ctrl Pts',(-1.70653636808742,2.55801621391061,106.635211620299));
#27125=CARTESIAN_POINT('Ctrl Pts',(-1.62533670621702,2.61036230757285,106.630229997716));
#27126=CARTESIAN_POINT('Ctrl Pts',(-1.54187501558476,2.6587635634474,106.625248375133));
#27127=CARTESIAN_POINT('Ctrl Pts',(-1.45839815014669,2.70717361952301,106.620265846803));
#27128=CARTESIAN_POINT('Ctrl Pts',(-1.37265881889352,2.75163719318902,106.615283318473));
#27129=CARTESIAN_POINT('Ctrl Pts',(-1.28506942846085,2.79195250927291,106.610300790143));
#27130=CARTESIAN_POINT('Ctrl Pts',(-1.19738562957399,2.83231127932597,106.605312891382));
#27131=CARTESIAN_POINT('Ctrl Pts',(-1.10784818990129,2.86851268159844,106.600324992621));
#27132=CARTESIAN_POINT('Ctrl Pts',(-1.01689005841298,2.90040287875682,106.59533709386));
#27133=CARTESIAN_POINT('Ctrl Pts',(-0.925878196707886,2.93231191389239,
106.590346248679));
#27134=CARTESIAN_POINT('Ctrl Pts',(-0.833444392583745,2.95990454753966,
106.585355403498));
#27135=CARTESIAN_POINT('Ctrl Pts',(-0.740035287971699,2.98307727398347,
106.580364558316));
#27136=CARTESIAN_POINT('Ctrl Pts',(-0.646475231887759,3.00628744813838,
106.575365647803));
#27137=CARTESIAN_POINT('Ctrl Pts',(-0.551937158434959,3.02506336727993,
106.57036673729));
#27138=CARTESIAN_POINT('Ctrl Pts',(-0.45687632976544,3.03935293595529,106.565367826777));
#27139=CARTESIAN_POINT('Ctrl Pts',(-0.401687877380712,3.04764887857936,
106.562465662566));
#27140=CARTESIAN_POINT('Ctrl Pts',(-0.346323316646575,3.05443367349225,
106.559563498355));
#27141=CARTESIAN_POINT('Ctrl Pts',(-0.29087183719041,3.05970518585198,106.556661334144));
#27142=CARTESIAN_POINT('Ctrl Pts',(-0.195371922038768,3.06878391536491,
106.551663154859));
#27143=CARTESIAN_POINT('Ctrl Pts',(-0.0992788561140445,3.07340316998083,
106.546664975575));
#27144=CARTESIAN_POINT('Ctrl Pts',(-0.00304436420393871,3.07349849224733,
106.541666796291));
#27145=CARTESIAN_POINT('Ctrl Pts',(0.0930703047400408,3.07359369582668,
106.536674840312));
#27146=CARTESIAN_POINT('Ctrl Pts',(0.189325615191599,3.0691761555212,106.531682884333));
#27147=CARTESIAN_POINT('Ctrl Pts',(0.28526431249711,3.06023308295554,106.526690928355));
#27148=CARTESIAN_POINT('Ctrl Pts',(0.381109755113251,3.05129870326853,106.521703824676));
#27149=CARTESIAN_POINT('Ctrl Pts',(0.476638761596079,3.03784757214109,106.516716720997));
#27150=CARTESIAN_POINT('Ctrl Pts',(0.571394733447213,3.01991892417475,106.511729617318));
#27151=CARTESIAN_POINT('Ctrl Pts',(0.66608447301117,3.00200280792898,106.506745999512));
#27152=CARTESIAN_POINT('Ctrl Pts',(0.760001822005656,2.97961547692256,106.501762381706));
#27153=CARTESIAN_POINT('Ctrl Pts',(0.852697023548337,2.9528477840945,106.4967787639));
#27154=CARTESIAN_POINT('Ctrl Pts',(0.945373875724465,2.92608539003271,106.49179613262));
#27155=CARTESIAN_POINT('Ctrl Pts',(1.03682863681075,2.89494446814416,106.48681350134));
#27156=CARTESIAN_POINT('Ctrl Pts',(1.12662418519526,2.85956643485216,106.48183087006));
#27157=CARTESIAN_POINT('Ctrl Pts',(1.21640461430721,2.82419435831569,106.476849077727));
#27158=CARTESIAN_POINT('Ctrl Pts',(1.30452597941365,2.78458675430858,106.471867285395));
#27159=CARTESIAN_POINT('Ctrl Pts',(1.39057003262799,2.74093364282264,106.466885493063));
#27160=CARTESIAN_POINT('Ctrl Pts',(1.47666861947242,2.69725286454806,106.461900543334));
#27161=CARTESIAN_POINT('Ctrl Pts',(1.56068687181946,2.64952165515339,106.456915593604));
#27162=CARTESIAN_POINT('Ctrl Pts',(1.64223042811163,2.59797641848118,106.451930643875));
#27163=CARTESIAN_POINT('Ctrl Pts',(1.72139114950026,2.54793741718352,106.447091362458));
#27164=CARTESIAN_POINT('Ctrl Pts',(1.7982195086045,2.49430446352957,106.442252081041));
#27165=CARTESIAN_POINT('Ctrl Pts',(1.87238193903529,2.43733217358128,106.437412799624));
#27166=CARTESIAN_POINT('Ctrl Pts',(1.8723819390353,2.43733217358127,107.437292535812));
#27167=CARTESIAN_POINT('Ctrl Pts',(1.94889495900041,2.37855413822091,107.432310908554));
#27168=CARTESIAN_POINT('Ctrl Pts',(2.02265352062151,2.31615755441516,107.427329281296));
#27169=CARTESIAN_POINT('Ctrl Pts',(2.09330611117521,2.25043812954645,107.422347654038));
#27170=CARTESIAN_POINT('Ctrl Pts',(2.16396476603174,2.18471306380185,107.417365599194));
#27171=CARTESIAN_POINT('Ctrl Pts',(2.23151659924619,2.11566488992335,107.412383544349));
#27172=CARTESIAN_POINT('Ctrl Pts',(2.29564594777291,2.04362715104145,107.407401489504));
#27173=CARTESIAN_POINT('Ctrl Pts',(2.35984093096381,1.97151568347046,107.402414335661));
#27174=CARTESIAN_POINT('Ctrl Pts',(2.42060614030575,1.89640886787032,107.397427181817));
#27175=CARTESIAN_POINT('Ctrl Pts',(2.477665453007,1.81867428446537,107.392440027973));
#27176=CARTESIAN_POINT('Ctrl Pts',(2.53475355975952,1.7409004735711,107.387450357443));
#27177=CARTESIAN_POINT('Ctrl Pts',(2.58813180152419,1.66049661928838,107.382460686914));
#27178=CARTESIAN_POINT('Ctrl Pts',(2.6375679743032,1.57785849521752,107.377471016384));
#27179=CARTESIAN_POINT('Ctrl Pts',(2.68708930554924,1.49507801918921,107.372472750677));
#27180=CARTESIAN_POINT('Ctrl Pts',(2.73265479140424,1.41005597060174,107.367474484969));
#27181=CARTESIAN_POINT('Ctrl Pts',(2.7740786078095,1.32321204940618,107.362476219262));
#27182=CARTESIAN_POINT('Ctrl Pts',(2.81267233143673,1.24230134189105,107.357819437196));
#27183=CARTESIAN_POINT('Ctrl Pts',(2.84767136059942,1.15980968333125,107.353162655131));
#27184=CARTESIAN_POINT('Ctrl Pts',(2.87896424539992,1.07608880846743,107.348505873065));
#27185=CARTESIAN_POINT('Ctrl Pts',(2.91256020767963,0.986206288147527,107.343506363572));
#27186=CARTESIAN_POINT('Ctrl Pts',(2.94200188712549,0.894591066769858,107.338506854079));
#27187=CARTESIAN_POINT('Ctrl Pts',(2.96710950151711,0.801662931665718,107.333507344586));
#27188=CARTESIAN_POINT('Ctrl Pts',(2.99218305758924,0.708860852986766,107.328514616896));
#27189=CARTESIAN_POINT('Ctrl Pts',(3.01293411947688,0.614749820262306,107.323521889206));
#27190=CARTESIAN_POINT('Ctrl Pts',(3.02923145456839,0.51976826052911,107.318529161516));
#27191=CARTESIAN_POINT('Ctrl Pts',(3.04551159638223,0.424886903947011,107.313541701027));
#27192=CARTESIAN_POINT('Ctrl Pts',(3.05734727803285,0.329137276387487,107.308554240539));
#27193=CARTESIAN_POINT('Ctrl Pts',(3.0646577226006,0.232970584633594,107.303566780051));
#27194=CARTESIAN_POINT('Ctrl Pts',(3.07196293637436,0.136872702395668,107.298582888207));
#27195=CARTESIAN_POINT('Ctrl Pts',(3.0747493167053,0.0403587856510456,107.293598996363));
#27196=CARTESIAN_POINT('Ctrl Pts',(3.07298772560659,-0.0561131737763518,
107.28861510452));
#27197=CARTESIAN_POINT('Ctrl Pts',(3.07122677603572,-0.152550000505387,
107.283633027686));
#27198=CARTESIAN_POINT('Ctrl Pts',(3.06492115384708,-0.248944461835907,
107.278650950852));
#27199=CARTESIAN_POINT('Ctrl Pts',(3.05409382664008,-0.344837857664972,
107.273668874019));
#27200=CARTESIAN_POINT('Ctrl Pts',(3.04326748663586,-0.440722510225716,
107.268687251436));
#27201=CARTESIAN_POINT('Ctrl Pts',(3.0279203107254,-0.536105751946442,107.263705628852));
#27202=CARTESIAN_POINT('Ctrl Pts',(3.00812710105997,-0.630534371678943,
107.258724006269));
#27203=CARTESIAN_POINT('Ctrl Pts',(2.98833029264029,-0.724980160198237,
107.25374147794));
#27204=CARTESIAN_POINT('Ctrl Pts',(2.96408593513475,-0.818470552410832,
107.24875894961));
#27205=CARTESIAN_POINT('Ctrl Pts',(2.93551963948931,-0.910563944032784,
107.24377642128));
#27206=CARTESIAN_POINT('Ctrl Pts',(2.90692255358723,-1.00275659875831,107.238788522519));
#27207=CARTESIAN_POINT('Ctrl Pts',(2.87399435971913,-1.09354882683002,107.233800623758));
#27208=CARTESIAN_POINT('Ctrl Pts',(2.83691005410327,-1.18251579056172,107.228812724997));
#27209=CARTESIAN_POINT('Ctrl Pts',(2.79980384227905,-1.27153530830008,107.223821879815));
#27210=CARTESIAN_POINT('Ctrl Pts',(2.75853681795548,-1.35872701822674,107.218831034634));
#27211=CARTESIAN_POINT('Ctrl Pts',(2.71333056440642,-1.44368954358544,107.213840189453));
#27212=CARTESIAN_POINT('Ctrl Pts',(2.66805125641002,-1.5287893705307,107.208841278939));
#27213=CARTESIAN_POINT('Ctrl Pts',(2.61882023196572,-1.61165244254687,107.203842368426));
#27214=CARTESIAN_POINT('Ctrl Pts',(2.56590307268301,-1.69190533765807,107.198843457913));
#27215=CARTESIAN_POINT('Ctrl Pts',(2.53518152137457,-1.7384969058418,107.195941293702));
#27216=CARTESIAN_POINT('Ctrl Pts',(2.50321834242864,-1.78420930261705,107.193039129491));
#27217=CARTESIAN_POINT('Ctrl Pts',(2.47007156829692,-1.82897476677269,107.19013696528));
#27218=CARTESIAN_POINT('Ctrl Pts',(2.41297017778752,-1.90609147924455,107.185137455787));
#27219=CARTESIAN_POINT('Ctrl Pts',(2.35215360522443,-1.98066698312061,107.180137946294));
#27220=CARTESIAN_POINT('Ctrl Pts',(2.28787608227205,-2.05232192459358,107.175138436801));
#27221=CARTESIAN_POINT('Ctrl Pts',(2.22368575137137,-2.12387966659348,107.170145709111));
#27222=CARTESIAN_POINT('Ctrl Pts',(2.15604409120931,-2.19252439589207,107.165152981421));
#27223=CARTESIAN_POINT('Ctrl Pts',(2.08524740120169,-2.25790733330258,107.160160253731));
#27224=CARTESIAN_POINT('Ctrl Pts',(2.01452539991748,-2.32322129336222,107.155172793243));
#27225=CARTESIAN_POINT('Ctrl Pts',(1.94065530636213,-2.38528000601421,107.150185332754));
#27226=CARTESIAN_POINT('Ctrl Pts',(1.86397161018428,-2.44377005596415,107.145197872266));
#27227=CARTESIAN_POINT('Ctrl Pts',(1.78734278298354,-2.50221825491614,107.140213980423));
#27228=CARTESIAN_POINT('Ctrl Pts',(1.70790470332619,-2.55710260187487,107.135230088579));
#27229=CARTESIAN_POINT('Ctrl Pts',(1.6260256669984,-2.60814930175832,107.130246196735));
#27230=CARTESIAN_POINT('Ctrl Pts',(1.54417644898777,-2.65917741169793,107.125264119902));
#27231=CARTESIAN_POINT('Ctrl Pts',(1.45988841264542,-2.7063704193997,107.120282043068));
#27232=CARTESIAN_POINT('Ctrl Pts',(1.37355881682426,-2.74949784992175,107.115299966234));
#27233=CARTESIAN_POINT('Ctrl Pts',(1.28723709227335,-2.79262134821572,107.110318343651));
#27234=CARTESIAN_POINT('Ctrl Pts',(1.19887457110041,-2.8316798103144,107.105336721068));
#27235=CARTESIAN_POINT('Ctrl Pts',(1.10889212946815,-2.86648922816807,107.100355098485));
#27236=CARTESIAN_POINT('Ctrl Pts',(1.01889332744257,-2.90130497498723,107.095372570155));
#27237=CARTESIAN_POINT('Ctrl Pts',(0.927274429425749,-2.93186998493461,
107.090390041825));
#27238=CARTESIAN_POINT('Ctrl Pts',(0.834474238759778,-2.95804918736087,
107.085407513495));
#27239=CARTESIAN_POINT('Ctrl Pts',(0.741574023164935,-2.98425660710911,
107.080419614734));
#27240=CARTESIAN_POINT('Ctrl Pts',(0.64749039615016,-3.00606866243138,107.075431715973));
#27241=CARTESIAN_POINT('Ctrl Pts',(0.552674985253281,-3.02340083526404,
107.070443817212));
#27242=CARTESIAN_POINT('Ctrl Pts',(0.457803565591821,-3.04074324644908,
107.065452972031));
#27243=CARTESIAN_POINT('Ctrl Pts',(0.362199936161149,-3.05360044739323,
107.06046212685));
#27244=CARTESIAN_POINT('Ctrl Pts',(0.266321410047234,-3.0619397702356,107.055471281668));
#27245=CARTESIAN_POINT('Ctrl Pts',(0.170287941813845,-3.07029256963429,
107.050472371155));
#27246=CARTESIAN_POINT('Ctrl Pts',(0.0739791281699808,-3.07411289505045,
107.045473460642));
#27247=CARTESIAN_POINT('Ctrl Pts',(-0.0221472110899903,-3.07342020411153,
107.040474550129));
#27248=CARTESIAN_POINT('Ctrl Pts',(-0.07795425560488,-3.07301805591405,
107.037572385918));
#27249=CARTESIAN_POINT('Ctrl Pts',(-0.133699864030437,-3.07109577378738,
107.034670221707));
#27250=CARTESIAN_POINT('Ctrl Pts',(-0.189295602926625,-3.06766514220712,
107.031768057496));
#27251=CARTESIAN_POINT('Ctrl Pts',(-0.285069447607009,-3.06175525086209,
107.026768548003));
#27252=CARTESIAN_POINT('Ctrl Pts',(-0.380734482790873,-3.05134552848548,
107.02176903851));
#27253=CARTESIAN_POINT('Ctrl Pts',(-0.475834092604759,-3.03644268286345,
107.016769529017));
#27254=CARTESIAN_POINT('Ctrl Pts',(-0.570804700401915,-3.02156005285686,
107.011776801327));
#27255=CARTESIAN_POINT('Ctrl Pts',(-0.665210977222577,-3.00219648017965,
107.006784073637));
#27256=CARTESIAN_POINT('Ctrl Pts',(-0.7585990490962,-2.9784106051232,107.001791345947));
#27257=CARTESIAN_POINT('Ctrl Pts',(-0.851888598907823,-2.95464982356542,
106.996803885459));
#27258=CARTESIAN_POINT('Ctrl Pts',(-0.944161656058873,-2.92647612196491,
106.99181642497));
#27259=CARTESIAN_POINT('Ctrl Pts',(-1.03497321680699,-2.89399942821214,
106.986828964482));
#27260=CARTESIAN_POINT('Ctrl Pts',(-1.12571979976071,-2.86154597229288,
106.981845072639));
#27261=CARTESIAN_POINT('Ctrl Pts',(-1.21500655304231,-2.82479579230485,
106.976861180795));
#27262=CARTESIAN_POINT('Ctrl Pts',(-1.30240330023355,-2.78390874375235,
106.971877288951));
#27263=CARTESIAN_POINT('Ctrl Pts',(-1.38976821969396,-2.7430365852503,106.966895212118));
#27264=CARTESIAN_POINT('Ctrl Pts',(-1.47524410343219,-2.69803073734652,
106.961913135284));
#27265=CARTESIAN_POINT('Ctrl Pts',(-1.55842134264245,-2.64909893526016,
106.95693105845));
#27266=CARTESIAN_POINT('Ctrl Pts',(-1.64159099800491,-2.60017159462675,
106.951949435867));
#27267=CARTESIAN_POINT('Ctrl Pts',(-1.7224620472744,-2.54731923422894,106.946967813284));
#27268=CARTESIAN_POINT('Ctrl Pts',(-1.80065099923461,-2.49079469827511,
106.941986190701));
#27269=CARTESIAN_POINT('Ctrl Pts',(-1.87885416732379,-2.43425988516481,
106.937003662371));
#27270=CARTESIAN_POINT('Ctrl Pts',(-1.95437391391006,-2.37405182771042,
106.932021134041));
#27271=CARTESIAN_POINT('Ctrl Pts',(-2.02685803561019,-2.31046505134408,
106.927038605712));
#27272=CARTESIAN_POINT('Ctrl Pts',(-2.09942028451098,-2.24680973780409,
106.922050706951));
#27273=CARTESIAN_POINT('Ctrl Pts',(-2.16894004583562,-2.17976872487179,
106.91706280819));
#27274=CARTESIAN_POINT('Ctrl Pts',(-2.23510053716642,-2.10967481825005,
106.912074909429));
#27275=CARTESIAN_POINT('Ctrl Pts',(-2.30130011040751,-2.03953950619562,
106.907084064247));
#27276=CARTESIAN_POINT('Ctrl Pts',(-2.36413617665296,-1.9663480425184,106.902093219066));
#27277=CARTESIAN_POINT('Ctrl Pts',(-2.42333234952958,-1.89046623183897,
106.897102373885));
#27278=CARTESIAN_POINT('Ctrl Pts',(-2.4826241849165,-1.81446179423718,106.892103463372));
#27279=CARTESIAN_POINT('Ctrl Pts',(-2.53826412833264,-1.73575868649417,
106.887104552858));
#27280=CARTESIAN_POINT('Ctrl Pts',(-2.59001923998408,-1.6547515180571,106.882105642345));
#27281=CARTESIAN_POINT('Ctrl Pts',(-2.6200661536819,-1.60772204944488,106.879203478134));
#27282=CARTESIAN_POINT('Ctrl Pts',(-2.64880454179271,-1.55991647365968,
106.876301313923));
#27283=CARTESIAN_POINT('Ctrl Pts',(-2.67619614131924,-1.51141538406488,
106.873399149712));
#27284=CARTESIAN_POINT('Ctrl Pts',(-2.72544131435984,-1.42421914174836,
106.868181580047));
#27285=CARTESIAN_POINT('Ctrl Pts',(-2.77049117203041,-1.33449006635661,
106.862964010382));
#27286=CARTESIAN_POINT('Ctrl Pts',(-2.81108935767527,-1.24264993991263,
106.857746440717));
#27287=CARTESIAN_POINT('Ctrl Pts',(-2.85161438327567,-1.15097531415855,
106.852538273385));
#27288=CARTESIAN_POINT('Ctrl Pts',(-2.88770355110402,-1.05719755939782,
106.847330106052));
#27289=CARTESIAN_POINT('Ctrl Pts',(-2.91914588564462,-0.961763769500647,
106.842121938719));
#27290=CARTESIAN_POINT('Ctrl Pts',(-2.95051943878282,-0.86653874495124,
106.836925164467));
#27291=CARTESIAN_POINT('Ctrl Pts',(-2.97726629363181,-0.769665267032493,
106.831728390215));
#27292=CARTESIAN_POINT('Ctrl Pts',(-2.99922360632994,-0.67161001275536,
106.826531615963));
#27293=CARTESIAN_POINT('Ctrl Pts',(-3.02115180119315,-0.573684790634065,
106.821341733211));
#27294=CARTESIAN_POINT('Ctrl Pts',(-3.03830301001062,-0.47458128423278,
106.816151850459));
#27295=CARTESIAN_POINT('Ctrl Pts',(-3.05056405627992,-0.374781521066573,
106.810961967706));
#27296=CARTESIAN_POINT('Ctrl Pts',(-3.06280647431927,-0.275133383862565,
106.805779969952));
#27297=CARTESIAN_POINT('Ctrl Pts',(-3.07017348425895,-0.174791477730663,
106.800597972198));
#27298=CARTESIAN_POINT('Ctrl Pts',(-3.07260306387733,-0.0742473019824065,
106.795415974444));
#27299=CARTESIAN_POINT('Ctrl Pts',(-3.07320310147932,-0.0494157279708957,
106.794136167237));
#27300=CARTESIAN_POINT('Ctrl Pts',(-3.07350222572077,-0.0245718569904162,
106.79285636003));
#27301=CARTESIAN_POINT('Ctrl Pts',(-3.07349998753221,0.000276838377306025,
106.791576552823));
#27302=CARTESIAN_POINT('Origin',(0.,0.,116.208423447177));
#27303=CARTESIAN_POINT('',(1.87238193903529,2.43733217358128,108.437241832237));
#27304=CARTESIAN_POINT('',(1.8723819390353,2.43733217358127,108.354243299745));
#27305=CARTESIAN_POINT('',(1.8723819390353,2.43733217358128,116.208423447177));
#27306=CARTESIAN_POINT('',(-3.07349874901725,0.00277304695061168,107.708423447135));
#27307=CARTESIAN_POINT('Ctrl Pts',(1.8723819390353,2.43733217358127,108.354243299745));
#27308=CARTESIAN_POINT('Ctrl Pts',(1.9489202414689,2.37853471598626,108.349255013332));
#27309=CARTESIAN_POINT('Ctrl Pts',(2.02263916084149,2.31616481968597,108.344266726919));
#27310=CARTESIAN_POINT('Ctrl Pts',(2.09320201927132,2.25053494896624,108.339278440506));
#27311=CARTESIAN_POINT('Ctrl Pts',(2.16380931523457,2.18486374730219,108.334287012678));
#27312=CARTESIAN_POINT('Ctrl Pts',(2.23125628667876,2.11592879743876,108.329295584851));
#27313=CARTESIAN_POINT('Ctrl Pts',(2.29524455677507,2.04407795218148,108.324304157024));
#27314=CARTESIAN_POINT('Ctrl Pts',(2.35933328799668,1.97211430161227,108.319304892691));
#27315=CARTESIAN_POINT('Ctrl Pts',(2.41995220306546,1.89722595814191,108.314305628358));
#27316=CARTESIAN_POINT('Ctrl Pts',(2.47684458529493,1.81979206237834,108.309306364025));
#27317=CARTESIAN_POINT('Ctrl Pts',(2.50081160083218,1.78717153727201,108.307200327307));
#27318=CARTESIAN_POINT('Ctrl Pts',(2.52411782113852,1.75409958665616,108.305094290589));
#27319=CARTESIAN_POINT('Ctrl Pts',(2.54674648514769,1.7206058788659,108.302988253871));
#27320=CARTESIAN_POINT('Ctrl Pts',(2.60046455167701,1.6410953420237,108.297988744378));
#27321=CARTESIAN_POINT('Ctrl Pts',(2.6505498707295,1.55892708725271,108.292989234885));
#27322=CARTESIAN_POINT('Ctrl Pts',(2.69672931841694,1.47446710142698,108.287989725392));
#27323=CARTESIAN_POINT('Ctrl Pts',(2.74284612397695,1.39012168503551,108.282996997702));
#27324=CARTESIAN_POINT('Ctrl Pts',(2.7850673793875,1.30349109781853,108.278004270012));
#27325=CARTESIAN_POINT('Ctrl Pts',(2.82316279249373,1.21497082149284,108.273011542322));
#27326=CARTESIAN_POINT('Ctrl Pts',(2.8612180158994,1.12654393182736,108.268024081834));
#27327=CARTESIAN_POINT('Ctrl Pts',(2.89515587722372,1.03623171722334,108.263036621345));
#27328=CARTESIAN_POINT('Ctrl Pts',(2.92479214191414,0.944453903902824,108.258049160857));
#27329=CARTESIAN_POINT('Ctrl Pts',(2.95440720116434,0.852741759753303,108.253065269013));
#27330=CARTESIAN_POINT('Ctrl Pts',(2.97972664798471,0.759566518119873,108.24808137717));
#27331=CARTESIAN_POINT('Ctrl Pts',(3.00061486013517,0.665366599053461,108.243097485326));
#27332=CARTESIAN_POINT('Ctrl Pts',(3.02149546531612,0.57120098526449,108.238115408492));
#27333=CARTESIAN_POINT('Ctrl Pts',(3.03794794723341,0.476011863589975,108.233133331659));
#27334=CARTESIAN_POINT('Ctrl Pts',(3.04988717324782,0.380250549583362,108.228151254825));
#27335=CARTESIAN_POINT('Ctrl Pts',(3.06182531067985,0.284497966802541,108.223169632242));
#27336=CARTESIAN_POINT('Ctrl Pts',(3.06925095623096,0.188173731027255,108.218188009659));
#27337=CARTESIAN_POINT('Ctrl Pts',(3.07213065521582,0.0917359650475105,
108.213206387076));
#27338=CARTESIAN_POINT('Ctrl Pts',(3.0750108777807,-0.0047193350173881,
108.208223858746));
#27339=CARTESIAN_POINT('Ctrl Pts',(3.07334349921686,-0.101287767518089,
108.203241330416));
#27340=CARTESIAN_POINT('Ctrl Pts',(3.06714717884297,-0.197510590388534,
108.198258802086));
#27341=CARTESIAN_POINT('Ctrl Pts',(3.06094417974892,-0.293837127280852,
108.193270903325));
#27342=CARTESIAN_POINT('Ctrl Pts',(3.05020252157301,-0.389816872067273,
108.188283004564));
#27343=CARTESIAN_POINT('Ctrl Pts',(3.03499280251743,-0.484995813041077,
108.183295105803));
#27344=CARTESIAN_POINT('Ctrl Pts',(3.01977409887207,-0.580230977521588,
108.178304260622));
#27345=CARTESIAN_POINT('Ctrl Pts',(3.00008216854657,-0.674663966759862,
108.173313415441));
#27346=CARTESIAN_POINT('Ctrl Pts',(2.97603839658355,-0.767852662989717,
108.168322570259));
#27347=CARTESIAN_POINT('Ctrl Pts',(2.9519557692778,-0.861191954506244,108.163323659746));
#27348=CARTESIAN_POINT('Ctrl Pts',(2.92350738708946,-0.953282518749631,
108.158324749233));
#27349=CARTESIAN_POINT('Ctrl Pts',(2.89086395801154,-1.04369910715199,108.15332583872));
#27350=CARTESIAN_POINT('Ctrl Pts',(2.87191251022242,-1.0961913024507,108.150423674509));
#27351=CARTESIAN_POINT('Ctrl Pts',(2.85154802208845,-1.14811967283023,108.147521510298));
#27352=CARTESIAN_POINT('Ctrl Pts',(2.82981103644169,-1.19940474737797,108.144619346087));
#27353=CARTESIAN_POINT('Ctrl Pts',(2.79236509672558,-1.28775268306042,108.139619836594));
#27354=CARTESIAN_POINT('Ctrl Pts',(2.75071202868001,-1.37450049686041,108.134620327101));
#27355=CARTESIAN_POINT('Ctrl Pts',(2.70501011654409,-1.45921983244271,108.129620817608));
#27356=CARTESIAN_POINT('Ctrl Pts',(2.6593701987617,-1.54382424678441,108.124628089918));
#27357=CARTESIAN_POINT('Ctrl Pts',(2.60969255896058,-1.62640526853741,108.119635362228));
#27358=CARTESIAN_POINT('Ctrl Pts',(2.55618354123051,-1.70655440978078,108.114642634538));
#27359=CARTESIAN_POINT('Ctrl Pts',(2.50273097416546,-1.78661899570029,108.109655174049));
#27360=CARTESIAN_POINT('Ctrl Pts',(2.44545530687436,-1.86425643817653,108.104667713561));
#27361=CARTESIAN_POINT('Ctrl Pts',(2.38460829568444,-1.93908368209135,108.099680253073));
#27362=CARTESIAN_POINT('Ctrl Pts',(2.32380482195331,-2.01385738536408,108.094696361229));
#27363=CARTESIAN_POINT('Ctrl Pts',(2.25943536044716,-2.0858245477796,108.089712469385));
#27364=CARTESIAN_POINT('Ctrl Pts',(2.19179381478206,-2.15463271196812,108.084728577542));
#27365=CARTESIAN_POINT('Ctrl Pts',(2.12417690249259,-2.22341581792744,108.079746500708));
#27366=CARTESIAN_POINT('Ctrl Pts',(2.05329058106153,-2.2890418987214,108.074764423874));
#27367=CARTESIAN_POINT('Ctrl Pts',(1.97946705989498,-2.35119382629139,108.069782347041));
#27368=CARTESIAN_POINT('Ctrl Pts',(1.90565026973289,-2.41334008703737,108.064800724458));
#27369=CARTESIAN_POINT('Ctrl Pts',(1.82889714820048,-2.47201254177189,108.059819101874));
#27370=CARTESIAN_POINT('Ctrl Pts',(1.74957375070406,-2.52693370329483,108.054837479291));
#27371=CARTESIAN_POINT('Ctrl Pts',(1.67023593081595,-2.58186485045288,108.049854950962));
#27372=CARTESIAN_POINT('Ctrl Pts',(1.58832726777996,-2.63304309999932,108.044872422632));
#27373=CARTESIAN_POINT('Ctrl Pts',(1.50424270999716,-2.68023434039272,108.039889894302));
#27374=CARTESIAN_POINT('Ctrl Pts',(1.42006752145364,-2.72747644598811,108.034901995541));
#27375=CARTESIAN_POINT('Ctrl Pts',(1.33371213943096,-2.77072274785716,108.02991409678));
#27376=CARTESIAN_POINT('Ctrl Pts',(1.2455958227475,-2.80978527584475,108.024926198019));
#27377=CARTESIAN_POINT('Ctrl Pts',(1.15742745454628,-2.8488708786038,108.019935352837));
#27378=CARTESIAN_POINT('Ctrl Pts',(1.06749648950074,-2.8837676277708,108.014944507656));
#27379=CARTESIAN_POINT('Ctrl Pts',(0.976239860858216,-2.91433662847509,
108.009953662475));
#27380=CARTESIAN_POINT('Ctrl Pts',(0.884835759199264,-2.94495502945648,
108.004954751961));
#27381=CARTESIAN_POINT('Ctrl Pts',(0.792102138282386,-2.9712315974102,107.999955841448));
#27382=CARTESIAN_POINT('Ctrl Pts',(0.698488635558885,-2.99307799363717,
107.994956930935));
#27383=CARTESIAN_POINT('Ctrl Pts',(0.644140441777194,-3.00576112311136,
107.992054766724));
#27384=CARTESIAN_POINT('Ctrl Pts',(0.589495847966339,-3.01695202988825,
107.989152602513));
#27385=CARTESIAN_POINT('Ctrl Pts',(0.534643587322916,-3.02664145292013,
107.986250438302));
#27386=CARTESIAN_POINT('Ctrl Pts',(0.44015052012765,-3.04333325907169,107.981250928809));
#27387=CARTESIAN_POINT('Ctrl Pts',(0.344709045236271,-3.05562496958097,
107.976251419316));
#27388=CARTESIAN_POINT('Ctrl Pts',(0.248764642739155,-3.0634161327712,107.971251909823));
#27389=CARTESIAN_POINT('Ctrl Pts',(0.152950388214801,-3.07119672729804,
107.966259182133));
#27390=CARTESIAN_POINT('Ctrl Pts',(0.0566349957276155,-3.07448887249237,
107.961266454443));
#27391=CARTESIAN_POINT('Ctrl Pts',(-0.039726553843952,-3.07324324629856,
107.956273726753));
#27392=CARTESIAN_POINT('Ctrl Pts',(-0.135986444409814,-3.07199893420898,
107.951286266265));
#27393=CARTESIAN_POINT('Ctrl Pts',(-0.232291958666501,-3.06622637310776,
107.946298805777));
#27394=CARTESIAN_POINT('Ctrl Pts',(-0.328184723810764,-3.05592817930285,
107.941311345288));
#27395=CARTESIAN_POINT('Ctrl Pts',(-0.424008875439887,-3.04563735409636,
107.936327453445));
#27396=CARTESIAN_POINT('Ctrl Pts',(-0.519420429860693,-3.03082738030431,
107.931343561601));
#27397=CARTESIAN_POINT('Ctrl Pts',(-0.613963732267965,-3.01155288604726,
107.926359669757));
#27398=CARTESIAN_POINT('Ctrl Pts',(-0.70847260434631,-2.9922854110836,107.921377592924));
#27399=CARTESIAN_POINT('Ctrl Pts',(-0.802113422982623,-2.96855673367534,
107.91639551609));
#27400=CARTESIAN_POINT('Ctrl Pts',(-0.894439311678201,-2.94047284764281,
107.911413439256));
#27401=CARTESIAN_POINT('Ctrl Pts',(-0.98675678237983,-2.91239152221366,
107.906431816673));
#27402=CARTESIAN_POINT('Ctrl Pts',(-1.07775914159711,-2.87995590557865,
107.90145019409));
#27403=CARTESIAN_POINT('Ctrl Pts',(-1.16701433576996,-2.84332196384922,
107.896468571507));
#27404=CARTESIAN_POINT('Ctrl Pts',(-1.25628575811,-2.80668136142361,107.891486043177));
#27405=CARTESIAN_POINT('Ctrl Pts',(-1.34380897845139,-2.76584108463607,
107.886503514848));
#27406=CARTESIAN_POINT('Ctrl Pts',(-1.42917259556581,-2.72100495076428,
107.881520986518));
#27407=CARTESIAN_POINT('Ctrl Pts',(-1.51462822207821,-2.67612049014831,
107.876533087757));
#27408=CARTESIAN_POINT('Ctrl Pts',(-1.59791920899493,-2.62723177848541,
107.871545188996));
#27409=CARTESIAN_POINT('Ctrl Pts',(-1.6786596222819,-2.57458814619356,107.866557290235));
#27410=CARTESIAN_POINT('Ctrl Pts',(-1.7594477300391,-2.52191341658562,107.861566445053));
#27411=CARTESIAN_POINT('Ctrl Pts',(-1.83768190832291,-2.46547960646562,
107.856575599872));
#27412=CARTESIAN_POINT('Ctrl Pts',(-1.91300776419879,-2.40557759054144,
107.851584754691));
#27413=CARTESIAN_POINT('Ctrl Pts',(-1.98845534856018,-2.34557877144665,
107.846585844178));
#27414=CARTESIAN_POINT('Ctrl Pts',(-2.06098489570981,-2.28210084408562,
107.841586933664));
#27415=CARTESIAN_POINT('Ctrl Pts',(-2.13027750201616,-2.21547286474103,
107.836588023151));
#27416=CARTESIAN_POINT('Ctrl Pts',(-2.17050597211508,-2.17679136872447,
107.83368585894));
#27417=CARTESIAN_POINT('Ctrl Pts',(-2.20964415278631,-2.13704881167315,
107.830783694729));
#27418=CARTESIAN_POINT('Ctrl Pts',(-2.24763596500707,-2.09631458011596,
107.827881530518));
#27419=CARTESIAN_POINT('Ctrl Pts',(-2.31279465263703,-2.02645244628409,
107.822904110379));
#27420=CARTESIAN_POINT('Ctrl Pts',(-2.37482199766329,-1.95341089458772,
107.81792669024));
#27421=CARTESIAN_POINT('Ctrl Pts',(-2.43338709172439,-1.87750619488434,
107.812949270101));
#27422=CARTESIAN_POINT('Ctrl Pts',(-2.49142726776055,-1.80228182782095,
107.808016462501));
#27423=CARTESIAN_POINT('Ctrl Pts',(-2.54606669154666,-1.72424576440769,
107.803083654901));
#27424=CARTESIAN_POINT('Ctrl Pts',(-2.59701940177456,-1.64374343399647,
107.7981508473));
#27425=CARTESIAN_POINT('Ctrl Pts',(-2.64792390878895,-1.56331726187013,
107.793222706325));
#27426=CARTESIAN_POINT('Ctrl Pts',(-2.69514838800659,-1.48042983355373,
107.78829456535));
#27427=CARTESIAN_POINT('Ctrl Pts',(-2.73844827237939,-1.39545810023172,
107.783366424374));
#27428=CARTESIAN_POINT('Ctrl Pts',(-2.78171969930191,-1.31054221183658,
107.77844152226));
#27429=CARTESIAN_POINT('Ctrl Pts',(-2.82107145100596,-1.22354513949691,
107.773516620146));
#27430=CARTESIAN_POINT('Ctrl Pts',(-2.85630392453019,-1.13487009860753,
107.768591718033));
#27431=CARTESIAN_POINT('Ctrl Pts',(-2.89217396080832,-1.04459040446457,
107.763577695461));
#27432=CARTESIAN_POINT('Ctrl Pts',(-2.92377393693999,-0.952571834193836,
107.75856367289));
#27433=CARTESIAN_POINT('Ctrl Pts',(-2.95094401222761,-0.859262292142507,
107.753549650319));
#27434=CARTESIAN_POINT('Ctrl Pts',(-2.97762656940174,-0.767627021929973,
107.748625595361));
#27435=CARTESIAN_POINT('Ctrl Pts',(-3.00003679617018,-0.67474718207457,
107.743701540403));
#27436=CARTESIAN_POINT('Ctrl Pts',(-3.01807379931678,-0.581061779742557,
107.738777485445));
#27437=CARTESIAN_POINT('Ctrl Pts',(-3.03660513471701,-0.484808782578329,
107.733718479067));
#27438=CARTESIAN_POINT('Ctrl Pts',(-3.05051992970566,-0.387705913687277,
107.728659472689));
#27439=CARTESIAN_POINT('Ctrl Pts',(-3.05976537292283,-0.29023802759536,
107.723600466311));
#27440=CARTESIAN_POINT('Ctrl Pts',(-3.06901081613999,-0.192770141503442,
107.718541459933));
#27441=CARTESIAN_POINT('Ctrl Pts',(-3.07358690801022,-0.0949377524641238,
107.713482453555));
#27442=CARTESIAN_POINT('Ctrl Pts',(-3.07349874901799,0.00277304613428424,
107.708423447177));
#27443=CARTESIAN_POINT('Ctrl Pts',(-3.07349874901725,0.00277304695062745,
107.708423447135));
#27444=CARTESIAN_POINT('Ctrl Pts',(-3.07338535343165,0.128454723711174,
107.701916240015));
#27445=CARTESIAN_POINT('Ctrl Pts',(-3.06555916854414,0.253796631394034,
107.695409032895));
#27446=CARTESIAN_POINT('Ctrl Pts',(-3.050166873552,0.378000388208786,107.688901825776));
#27447=CARTESIAN_POINT('Ctrl Pts',(-3.03487898698839,0.501361650835883,
107.682438758095));
#27448=CARTESIAN_POINT('Ctrl Pts',(-3.01212748935548,0.623600593083645,
107.675975690415));
#27449=CARTESIAN_POINT('Ctrl Pts',(-2.98210140691276,0.743957961775346,
107.669512622734));
#27450=CARTESIAN_POINT('Ctrl Pts',(-2.95887471463155,0.837060469293967,
107.664513113241));
#27451=CARTESIAN_POINT('Ctrl Pts',(-2.93124299597944,0.929237740901595,
107.659513603748));
#27452=CARTESIAN_POINT('Ctrl Pts',(-2.89929587704686,1.02004199292926,107.654514094255));
#27453=CARTESIAN_POINT('Ctrl Pts',(-2.86739209417824,1.11072306956569,107.649521366565));
#27454=CARTESIAN_POINT('Ctrl Pts',(-2.83118468953308,1.20003441766224,107.644528638875));
#27455=CARTESIAN_POINT('Ctrl Pts',(-2.7908138573318,1.2875403930459,107.639535911185));
#27456=CARTESIAN_POINT('Ctrl Pts',(-2.75048561534092,1.37495405183118,107.634548450696));
#27457=CARTESIAN_POINT('Ctrl Pts',(-2.70600286035394,1.46056572770928,107.629560990208));
#27458=CARTESIAN_POINT('Ctrl Pts',(-2.65755460620401,1.54395782489155,107.62457352972));
#27459=CARTESIAN_POINT('Ctrl Pts',(-2.6091410179124,1.62729025307901,107.619589637876));
#27460=CARTESIAN_POINT('Ctrl Pts',(-2.5567677909679,1.70840588129053,107.614605746033));
#27461=CARTESIAN_POINT('Ctrl Pts',(-2.50067033827754,1.78691077260698,107.609621854189));
#27462=CARTESIAN_POINT('Ctrl Pts',(-2.44459331489007,1.86538707438638,107.604639777355));
#27463=CARTESIAN_POINT('Ctrl Pts',(-2.38479501546821,1.94125417155407,107.599657700522));
#27464=CARTESIAN_POINT('Ctrl Pts',(-2.32155419443271,2.01414705826359,107.594675623688));
#27465=CARTESIAN_POINT('Ctrl Pts',(-2.25831913950307,2.08703329882124,107.589694001105));
#27466=CARTESIAN_POINT('Ctrl Pts',(-2.1916424748109,2.15694553662771,107.584712378522));
#27467=CARTESIAN_POINT('Ctrl Pts',(-2.12184256256027,2.22355265053644,107.579730755939));
#27468=CARTESIAN_POINT('Ctrl Pts',(-2.05202995945583,2.29017187479201,107.574748227609));
#27469=CARTESIAN_POINT('Ctrl Pts',(-1.97909329861193,2.35348447868616,107.569765699279));
#27470=CARTESIAN_POINT('Ctrl Pts',(-1.90338623924964,2.41319768652199,107.564783170949));
#27471=CARTESIAN_POINT('Ctrl Pts',(-1.82759757883496,2.47297525639543,107.559795272188));
#27472=CARTESIAN_POINT('Ctrl Pts',(-1.74903290369471,2.52914541261508,107.554807373427));
#27473=CARTESIAN_POINT('Ctrl Pts',(-1.66807707425214,2.58145717073796,107.549819474666));
#27474=CARTESIAN_POINT('Ctrl Pts',(-1.58707342308996,2.63379983013437,107.544828629485));
#27475=CARTESIAN_POINT('Ctrl Pts',(-1.50367618445484,2.68227933265321,107.539837784304));
#27476=CARTESIAN_POINT('Ctrl Pts',(-1.41829532200881,2.7266904168915,107.534846939122));
#27477=CARTESIAN_POINT('Ctrl Pts',(-1.33277648193289,2.77117327056345,107.529848028609));
#27478=CARTESIAN_POINT('Ctrl Pts',(-1.24526801546849,2.81157439392441,107.524849118096));
#27479=CARTESIAN_POINT('Ctrl Pts',(-1.1562003106438,2.84773648564385,107.519850207583));
#27480=CARTESIAN_POINT('Ctrl Pts',(-1.10449122231035,2.86873072590998,107.516948043372));
#27481=CARTESIAN_POINT('Ctrl Pts',(-1.05225690540002,2.88829712987677,107.514045879161));
#27482=CARTESIAN_POINT('Ctrl Pts',(-0.999583567331795,2.90641272738753,
107.51114371495));
#27483=CARTESIAN_POINT('Ctrl Pts',(-0.90884356227205,2.93762034532239,107.506144176192));
#27484=CARTESIAN_POINT('Ctrl Pts',(-0.816481295459383,2.96462926578446,
107.501144637434));
#27485=CARTESIAN_POINT('Ctrl Pts',(-0.722921168961461,2.9872708671072,107.496145098676));
#27486=CARTESIAN_POINT('Ctrl Pts',(-0.6294881007632,3.00988172025255,107.491152349486));
#27487=CARTESIAN_POINT('Ctrl Pts',(-0.534860828948531,3.0281369394181,107.486159600297));
#27488=CARTESIAN_POINT('Ctrl Pts',(-0.439481103284817,3.04191693013724,
107.481166851107));
#27489=CARTESIAN_POINT('Ctrl Pts',(-0.344202148071791,3.05568236204039,
107.47617937685));
#27490=CARTESIAN_POINT('Ctrl Pts',(-0.248172751548078,3.06498190244422,
107.471191902593));
#27491=CARTESIAN_POINT('Ctrl Pts',(-0.151846102580116,3.06974673403707,
107.466204428336));
#27492=CARTESIAN_POINT('Ctrl Pts',(-0.0555890490807236,3.07450812306557,
107.461220557501));
#27493=CARTESIAN_POINT('Ctrl Pts',(0.0409643927297265,3.07474129518815,
107.456236686666));
#27494=CARTESIAN_POINT('Ctrl Pts',(0.137355626442126,3.07042923414377,107.451252815831));
#27495=CARTESIAN_POINT('Ctrl Pts',(0.233711544263408,3.06611875295548,107.44627077099));
#27496=CARTESIAN_POINT('Ctrl Pts',(0.32990493400896,3.05726636708296,107.44128872615));
#27497=CARTESIAN_POINT('Ctrl Pts',(0.425477872150161,3.04390716519255,107.436306681309));
#27498=CARTESIAN_POINT('Ctrl Pts',(0.521041885408221,3.03054921082386,107.431325101707));
#27499=CARTESIAN_POINT('Ctrl Pts',(0.615985127581939,3.01268533826579,107.426343522104));
#27500=CARTESIAN_POINT('Ctrl Pts',(0.709856535661639,2.99040230550648,107.421361942502));
#27501=CARTESIAN_POINT('Ctrl Pts',(0.803744804035921,2.96811527047955,107.416379468155));
#27502=CARTESIAN_POINT('Ctrl Pts',(0.896560428964477,2.94140760047606,107.411396993808));
#27503=CARTESIAN_POINT('Ctrl Pts',(0.987865296181821,2.91041653489661,107.406414519461));
#27504=CARTESIAN_POINT('Ctrl Pts',(1.07926604503664,2.8793929247858,107.401426812888));
#27505=CARTESIAN_POINT('Ctrl Pts',(1.16915245293809,2.84407708124595,107.396439106314));
#27506=CARTESIAN_POINT('Ctrl Pts',(1.2571045059371,2.80465515013034,107.39145139974));
#27507=CARTESIAN_POINT('Ctrl Pts',(1.3451084356226,2.76520996680979,107.386460751271));
#27508=CARTESIAN_POINT('Ctrl Pts',(1.43117534722427,2.72165407165248,107.381470102802));
#27509=CARTESIAN_POINT('Ctrl Pts',(1.51490990831687,2.67421955338064,107.376479454334));
#27510=CARTESIAN_POINT('Ctrl Pts',(1.59877453701659,2.62671135353448,107.371481053729));
#27511=CARTESIAN_POINT('Ctrl Pts',(1.68029921137597,2.57531273623145,107.366482653124));
#27512=CARTESIAN_POINT('Ctrl Pts',(1.75911776996604,2.52029897460395,107.36148425252));
#27513=CARTESIAN_POINT('Ctrl Pts',(1.79752776191253,2.49348957617218,107.359048423568));
#27514=CARTESIAN_POINT('Ctrl Pts',(1.83529560004653,2.46582225468724,107.356612594616));
#27515=CARTESIAN_POINT('Ctrl Pts',(1.8723819390353,2.43733217358127,107.354176765664));
#27516=CARTESIAN_POINT('',(-3.07349882217909,-0.00269073665490008,107.791576552773));
#27517=CARTESIAN_POINT('Ctrl Pts',(-3.07349882217909,-0.00269073665491237,
107.791576552773));
#27518=CARTESIAN_POINT('Ctrl Pts',(-3.07358187200602,0.0921730787232002,
107.786657377012));
#27519=CARTESIAN_POINT('Ctrl Pts',(-3.06926874327697,0.187176666217751,
107.781738201252));
#27520=CARTESIAN_POINT('Ctrl Pts',(-3.06054730741393,0.281873072643216,
107.776819025491));
#27521=CARTESIAN_POINT('Ctrl Pts',(-3.05183388741077,0.376482443729889,
107.771904370938));
#27522=CARTESIAN_POINT('Ctrl Pts',(-3.03872025258485,0.470784745941165,
107.766989716385));
#27523=CARTESIAN_POINT('Ctrl Pts',(-3.02124633039514,0.564333997800871,
107.762075061832));
#27524=CARTESIAN_POINT('Ctrl Pts',(-3.00378085462675,0.657838030482692,
107.75716278289));
#27525=CARTESIAN_POINT('Ctrl Pts',(-2.98195935853931,0.750589291234735,
107.752250503948));
#27526=CARTESIAN_POINT('Ctrl Pts',(-2.95587337232113,0.842148951672397,
107.747338225007));
#27527=CARTESIAN_POINT('Ctrl Pts',(-2.92979239116969,0.933691044738551,
107.742426888574));
#27528=CARTESIAN_POINT('Ctrl Pts',(-2.89944866934983,1.02404155637932,107.737515552141));
#27529=CARTESIAN_POINT('Ctrl Pts',(-2.86498409547437,1.11277508180176,107.732604215709));
#27530=CARTESIAN_POINT('Ctrl Pts',(-2.83051608758398,1.20151744854199,107.727692389916));
#27531=CARTESIAN_POINT('Ctrl Pts',(-2.7919265779177,1.28864208775896,107.722780564123));
#27532=CARTESIAN_POINT('Ctrl Pts',(-2.7494057890288,1.37374308269594,107.71786873833));
#27533=CARTESIAN_POINT('Ctrl Pts',(-2.70684237480604,1.45892938786388,107.712951988634));
#27534=CARTESIAN_POINT('Ctrl Pts',(-2.66034001805582,1.5420875940516,107.708035238939));
#27535=CARTESIAN_POINT('Ctrl Pts',(-2.61013494930664,1.62283634307593,107.703118489243));
#27536=CARTESIAN_POINT('Ctrl Pts',(-2.55990223283484,1.70362956010058,107.698199031914));
#27537=CARTESIAN_POINT('Ctrl Pts',(-2.5059630043373,1.78201030768138,107.693279574585));
#27538=CARTESIAN_POINT('Ctrl Pts',(-2.44859557061089,1.85762805254032,107.688360117256));
#27539=CARTESIAN_POINT('Ctrl Pts',(-2.39113686525471,1.93336610528762,107.683432833066));
#27540=CARTESIAN_POINT('Ctrl Pts',(-2.33023935839614,2.00633203475412,107.678505548877));
#27541=CARTESIAN_POINT('Ctrl Pts',(-2.26621999102241,2.07621029818523,107.673578264687));
#27542=CARTESIAN_POINT('Ctrl Pts',(-2.23012341355619,2.11561034621164,107.670800072669));
#27543=CARTESIAN_POINT('Ctrl Pts',(-2.1930350019475,2.1540294738056,107.668021880651));
#27544=CARTESIAN_POINT('Ctrl Pts',(-2.15501616577193,2.19141679633557,107.665243688633));
#27545=CARTESIAN_POINT('Ctrl Pts',(-2.08659917690485,2.25869734162871,107.66024417914));
#27546=CARTESIAN_POINT('Ctrl Pts',(-2.01490820660401,2.32288897701853,107.655244669647));
#27547=CARTESIAN_POINT('Ctrl Pts',(-1.94025347588031,2.38365658166909,107.650245160154));
#27548=CARTESIAN_POINT('Ctrl Pts',(-1.86570001382474,2.44434175544985,107.645252432464));
#27549=CARTESIAN_POINT('Ctrl Pts',(-1.78819111899622,2.50161185473757,107.640259704774));
#27550=CARTESIAN_POINT('Ctrl Pts',(-1.70807380396321,2.55516851307593,107.635266977084));
#27551=CARTESIAN_POINT('Ctrl Pts',(-1.62804101067826,2.60866867048961,107.630279516596));
#27552=CARTESIAN_POINT('Ctrl Pts',(-1.54540563062879,2.65846293222671,107.625292056108));
#27553=CARTESIAN_POINT('Ctrl Pts',(-1.46054689172002,2.70429381301052,107.620304595619));
#27554=CARTESIAN_POINT('Ctrl Pts',(-1.37574887122236,2.75009190072792,107.615320703776));
#27555=CARTESIAN_POINT('Ctrl Pts',(-1.28873103955456,2.79193203711114,107.610336811932));
#27556=CARTESIAN_POINT('Ctrl Pts',(-1.19989984636383,2.82960113950643,107.605352920088));
#27557=CARTESIAN_POINT('Ctrl Pts',(-1.1111010032936,2.86725652374756,107.600370843255));
#27558=CARTESIAN_POINT('Ctrl Pts',(-1.02049051452175,2.90074372086698,107.595388766421));
#27559=CARTESIAN_POINT('Ctrl Pts',(-0.928496691140395,2.92989695118128,
107.590406689587));
#27560=CARTESIAN_POINT('Ctrl Pts',(-0.836511255476247,2.95904752339264,
107.585425067004));
#27561=CARTESIAN_POINT('Ctrl Pts',(-0.743143154476894,2.98386478201134,
107.580443444421));
#27562=CARTESIAN_POINT('Ctrl Pts',(-0.648836790001705,3.00423252594407,
107.575461821838));
#27563=CARTESIAN_POINT('Ctrl Pts',(-0.55451327896797,3.02460397309149,107.570479293508));
#27564=CARTESIAN_POINT('Ctrl Pts',(-0.459251594733273,3.04052420624508,
107.565496765178));
#27565=CARTESIAN_POINT('Ctrl Pts',(-0.363506224416851,3.05192815688872,
107.560514236849));
#27566=CARTESIAN_POINT('Ctrl Pts',(-0.267657654701984,3.06334439931047,
107.555526338088));
#27567=CARTESIAN_POINT('Ctrl Pts',(-0.171324794697769,3.07023458893297,
107.550538439326));
#27568=CARTESIAN_POINT('Ctrl Pts',(-0.0749669244908475,3.07258559038351,
107.545550540565));
#27569=CARTESIAN_POINT('Ctrl Pts',(0.0214478656326629,3.07493798060288,
107.540559695384));
#27570=CARTESIAN_POINT('Ctrl Pts',(0.117887256732058,3.0727458535934,107.535568850203));
#27571=CARTESIAN_POINT('Ctrl Pts',(0.213894429392107,3.06604817690052,107.530578005021));
#27572=CARTESIAN_POINT('Ctrl Pts',(0.310056752067661,3.05933967659297,107.525579094508));
#27573=CARTESIAN_POINT('Ctrl Pts',(0.405785025922154,3.04811113899372,107.520580183995));
#27574=CARTESIAN_POINT('Ctrl Pts',(0.500630050715323,3.03245309977265,107.515581273482));
#27575=CARTESIAN_POINT('Ctrl Pts',(0.555693216143185,3.02336267878551,107.512679109271));
#27576=CARTESIAN_POINT('Ctrl Pts',(0.610458900941498,3.01278025014732,107.50977694506));
#27577=CARTESIAN_POINT('Ctrl Pts',(0.664841586868444,3.0007312299455,107.506874780849));
#27578=CARTESIAN_POINT('Ctrl Pts',(0.758533573162282,2.9799728467145,107.501874852566));
#27579=CARTESIAN_POINT('Ctrl Pts',(0.851416994428939,2.95478576871685,107.496874924283));
#27580=CARTESIAN_POINT('Ctrl Pts',(0.94304174075739,2.92524777158949,107.491874996));
#27581=CARTESIAN_POINT('Ctrl Pts',(1.03451892702328,2.89575734489346,107.486883120014));
#27582=CARTESIAN_POINT('Ctrl Pts',(1.12474105646772,2.86193007146443,107.481891244029));
#27583=CARTESIAN_POINT('Ctrl Pts',(1.21326915473125,2.82389451080909,107.476899368043));
#27584=CARTESIAN_POINT('Ctrl Pts',(1.3017145830081,2.78589446881228,107.47191215361));
#27585=CARTESIAN_POINT('Ctrl Pts',(1.38846872151956,2.74369411797663,107.466924939176));
#27586=CARTESIAN_POINT('Ctrl Pts',(1.4731091828196,2.69747133172765,107.461937724742));
#27587=CARTESIAN_POINT('Ctrl Pts',(1.55769020176563,2.65128100739089,107.456954012792));
#27588=CARTESIAN_POINT('Ctrl Pts',(1.6401601100366,2.60107407253766,107.451970300841));
#27589=CARTESIAN_POINT('Ctrl Pts',(1.72011892292524,2.54707540936552,107.44698658889));
#27590=CARTESIAN_POINT('Ctrl Pts',(1.77196280848986,2.5120636275118,107.443755237864));
#27591=CARTESIAN_POINT('Ctrl Pts',(1.82275148441596,2.47545876455751,107.440523886838));
#27592=CARTESIAN_POINT('Ctrl Pts',(1.8723819390353,2.43733217358127,107.437292535812));
#27593=CARTESIAN_POINT('Ctrl Pts',(1.87238193903529,2.43733217358128,108.437241832237));
#27594=CARTESIAN_POINT('Ctrl Pts',(1.94865272942512,2.37874022130256,108.432250974061));
#27595=CARTESIAN_POINT('Ctrl Pts',(2.02227039622087,2.31648811211804,108.427260115884));
#27596=CARTESIAN_POINT('Ctrl Pts',(2.09286615451889,2.25084728697202,108.422269257707));
#27597=CARTESIAN_POINT('Ctrl Pts',(2.16568347076244,2.18314082927003,108.417121343627));
#27598=CARTESIAN_POINT('Ctrl Pts',(2.23528511606183,2.11182907458801,108.411973429546));
#27599=CARTESIAN_POINT('Ctrl Pts',(2.30130181357665,2.03725604989378,108.406825515465));
#27600=CARTESIAN_POINT('Ctrl Pts',(2.36520480718796,1.96507068316075,108.401842425838));
#27601=CARTESIAN_POINT('Ctrl Pts',(2.4257486140982,1.88983006461674,108.396859336211));
#27602=CARTESIAN_POINT('Ctrl Pts',(2.48263561520456,1.8118837302978,108.391876246583));
#27603=CARTESIAN_POINT('Ctrl Pts',(2.53950742813583,1.73395820675374,108.386894487384));
#27604=CARTESIAN_POINT('Ctrl Pts',(2.59272411674773,1.65332875733658,108.381912728184));
#27605=CARTESIAN_POINT('Ctrl Pts',(2.64202944337277,1.57037660144036,108.376930968984));
#27606=CARTESIAN_POINT('Ctrl Pts',(2.69133506624758,1.48742394712827,108.371949179852));
#27607=CARTESIAN_POINT('Ctrl Pts',(2.73672905683115,1.40214893640555,108.36696739072));
#27608=CARTESIAN_POINT('Ctrl Pts',(2.77800003571611,1.31495933456563,108.361985601587));
#27609=CARTESIAN_POINT('Ctrl Pts',(2.81928252927881,1.22774540666913,108.357002422527));
#27610=CARTESIAN_POINT('Ctrl Pts',(2.85643953838532,1.13861622323021,108.352019243466));
#27611=CARTESIAN_POINT('Ctrl Pts',(2.88930736521566,1.04800057219,108.347036064405));
#27612=CARTESIAN_POINT('Ctrl Pts',(2.92221231123304,0.957282584621167,108.342047257606));
#27613=CARTESIAN_POINT('Ctrl Pts',(2.95081825925177,0.865075192659291,108.337058450806));
#27614=CARTESIAN_POINT('Ctrl Pts',(2.97501113763128,0.771823153947734,108.332069644006));
#27615=CARTESIAN_POINT('Ctrl Pts',(2.99922041557854,0.678507902703052,108.327077455456));
#27616=CARTESIAN_POINT('Ctrl Pts',(3.01901057937577,0.584147023968748,108.322085266906));
#27617=CARTESIAN_POINT('Ctrl Pts',(3.03431890787338,0.489194251113101,108.317093078356));
#27618=CARTESIAN_POINT('Ctrl Pts',(3.04965043232491,0.394097601011497,108.312093325389));
#27619=CARTESIAN_POINT('Ctrl Pts',(3.06048652234468,0.298407702000529,108.307093572422));
#27620=CARTESIAN_POINT('Ctrl Pts',(3.06681640165786,0.202581856350362,108.302093819456));
#27621=CARTESIAN_POINT('Ctrl Pts',(3.06824048373387,0.181023172138915,108.300968986227));
#27622=CARTESIAN_POINT('Ctrl Pts',(3.0694366926648,0.159457597829568,108.299844152998));
#27623=CARTESIAN_POINT('Ctrl Pts',(3.07040526815994,0.137890316033002,108.29871931977));
#27624=CARTESIAN_POINT('Ctrl Pts',(3.07471026401134,0.0420309234243816,
108.293719810277));
#27625=CARTESIAN_POINT('Ctrl Pts',(3.07452936043881,-0.0541986383047818,
108.288720300784));
#27626=CARTESIAN_POINT('Ctrl Pts',(3.06982068590681,-0.150343627662216,
108.283720791291));
#27627=CARTESIAN_POINT('Ctrl Pts',(3.06511839866191,-0.24635819695208,108.278728063601));
#27628=CARTESIAN_POINT('Ctrl Pts',(3.05590056835112,-0.342287987185902,
108.273735335911));
#27629=CARTESIAN_POINT('Ctrl Pts',(3.04217725314545,-0.437675462465506,
108.268742608221));
#27630=CARTESIAN_POINT('Ctrl Pts',(3.02846841569141,-0.532962306363106,
108.263755147732));
#27631=CARTESIAN_POINT('Ctrl Pts',(3.01026360454042,-0.627707540485188,
108.258767687244));
#27632=CARTESIAN_POINT('Ctrl Pts',(2.98762481780021,-0.721456996683966,
108.253780226756));
#27633=CARTESIAN_POINT('Ctrl Pts',(2.96500222964111,-0.815139372955408,
108.248796334912));
#27634=CARTESIAN_POINT('Ctrl Pts',(2.93795207564211,-0.907826962250595,
108.243812443068));
#27635=CARTESIAN_POINT('Ctrl Pts',(2.90658757484791,-0.999075032087041,
108.238828551225));
#27636=CARTESIAN_POINT('Ctrl Pts',(2.87523449622809,-1.09028987163643,108.233846474391));
#27637=CARTESIAN_POINT('Ctrl Pts',(2.83957033511733,-1.18006581863036,108.228864397557));
#27638=CARTESIAN_POINT('Ctrl Pts',(2.79975810543389,-1.2679735017173,108.223882320724));
#27639=CARTESIAN_POINT('Ctrl Pts',(2.75994950570858,-1.35587316964881,108.218900698141));
#27640=CARTESIAN_POINT('Ctrl Pts',(2.7159937706197,-1.44190451255567,108.213919075557));
#27641=CARTESIAN_POINT('Ctrl Pts',(2.66810154393361,-1.52565933329138,108.208937452974));
#27642=CARTESIAN_POINT('Ctrl Pts',(2.62020060959689,-1.60942938212918,108.203954924645));
#27643=CARTESIAN_POINT('Ctrl Pts',(2.56836198016065,-1.69092170572518,108.198972396315));
#27644=CARTESIAN_POINT('Ctrl Pts',(2.51284107052908,-1.76975478647814,108.193989867985));
#27645=CARTESIAN_POINT('Ctrl Pts',(2.45726031753948,-1.84867283767389,108.189001969224));
#27646=CARTESIAN_POINT('Ctrl Pts',(2.39798961388014,-1.92492556429635,108.184014070463));
#27647=CARTESIAN_POINT('Ctrl Pts',(2.33532620329136,-1.99816259954508,108.179026171702));
#27648=CARTESIAN_POINT('Ctrl Pts',(2.2726257765659,-2.07144289691571,108.17403532652));
#27649=CARTESIAN_POINT('Ctrl Pts',(2.20652895301756,-2.14170363626027,108.169044481339));
#27650=CARTESIAN_POINT('Ctrl Pts',(2.13737008268124,-2.2086311099093,108.164053636158));
#27651=CARTESIAN_POINT('Ctrl Pts',(2.06809944986392,-2.27566674004593,108.159054725645));
#27652=CARTESIAN_POINT('Ctrl Pts',(1.99575721875222,-2.33935805868163,108.154055815131));
#27653=CARTESIAN_POINT('Ctrl Pts',(1.92071099964292,-2.39943149638632,108.149056904618));
#27654=CARTESIAN_POINT('Ctrl Pts',(1.87714221586565,-2.4343076920052,108.146154740407));
#27655=CARTESIAN_POINT('Ctrl Pts',(1.83266261781819,-2.46796528230611,108.143252576196));
#27656=CARTESIAN_POINT('Ctrl Pts',(1.78734827456117,-2.50035765350143,108.140350411985));
#27657=CARTESIAN_POINT('Ctrl Pts',(1.70928601729026,-2.55615944675534,108.135350902492));
#27658=CARTESIAN_POINT('Ctrl Pts',(1.62847091007281,-2.60840004133588,108.130351392999));
#27659=CARTESIAN_POINT('Ctrl Pts',(1.54526158954139,-2.65679673100672,108.125351883506));
#27660=CARTESIAN_POINT('Ctrl Pts',(1.4621651419249,-2.70512777087534,108.120359155816));
#27661=CARTESIAN_POINT('Ctrl Pts',(1.37668131185539,-2.74962504996746,108.115366428126));
#27662=CARTESIAN_POINT('Ctrl Pts',(1.28919935310137,-2.79004789886536,108.110373700436));
#27663=CARTESIAN_POINT('Ctrl Pts',(1.20180968560867,-2.83042810267661,108.105386239948));
#27664=CARTESIAN_POINT('Ctrl Pts',(1.11242647631956,-2.86674223814872,108.100398779459));
#27665=CARTESIAN_POINT('Ctrl Pts',(1.02146443293911,-2.8987950362591,108.095411318971));
#27666=CARTESIAN_POINT('Ctrl Pts',(0.930567475027023,-2.93082489984317,
108.090427427128));
#27667=CARTESIAN_POINT('Ctrl Pts',(0.838094341622891,-2.95859934203647,
108.085443535284));
#27668=CARTESIAN_POINT('Ctrl Pts',(0.744479713187609,-2.98197119480589,
108.08045964344));
#27669=CARTESIAN_POINT('Ctrl Pts',(0.650899176881401,-3.0053345361254,108.075477566607));
#27670=CARTESIAN_POINT('Ctrl Pts',(0.556178396957965,-3.02429836741274,
108.070495489773));
#27671=CARTESIAN_POINT('Ctrl Pts',(0.460766279976702,-3.03876565158231,
108.065513412939));
#27672=CARTESIAN_POINT('Ctrl Pts',(0.365362862382369,-3.05323161666886,
108.060531790356));
#27673=CARTESIAN_POINT('Ctrl Pts',(0.269268667082403,-3.06320178413063,
108.055550167773));
#27674=CARTESIAN_POINT('Ctrl Pts',(0.172940772021517,-3.06863059676016,
108.05056854519));
#27675=CARTESIAN_POINT('Ctrl Pts',(0.0765953628520557,-3.07406039644347,
108.04558601686));
#27676=CARTESIAN_POINT('Ctrl Pts',(-0.019983392200641,-3.07494717679239,
108.04060348853));
#27677=CARTESIAN_POINT('Ctrl Pts',(-0.116336418072692,-3.07129746000449,
108.0356209602));
#27678=CARTESIAN_POINT('Ctrl Pts',(-0.212793298306262,-3.06764380935978,
108.030633061439));
#27679=CARTESIAN_POINT('Ctrl Pts',(-0.309023524252548,-3.05944391643599,
108.025645162678));
#27680=CARTESIAN_POINT('Ctrl Pts',(-0.404571376123934,-3.04675634923786,
108.020657263917));
#27681=CARTESIAN_POINT('Ctrl Pts',(-0.500175669422909,-3.03406128731963,
108.015666418736));
#27682=CARTESIAN_POINT('Ctrl Pts',(-0.595096354297082,-3.01687335086801,
108.010675573555));
#27683=CARTESIAN_POINT('Ctrl Pts',(-0.688888257775055,-2.99530219148246,
108.005684728373));
#27684=CARTESIAN_POINT('Ctrl Pts',(-0.782831731337599,-2.97369617255861,
108.00068581786));
#27685=CARTESIAN_POINT('Ctrl Pts',(-0.875642358700166,-2.94769290506496,
107.995686907347));
#27686=CARTESIAN_POINT('Ctrl Pts',(-0.966890525935409,-2.91745179237916,
107.990687996834));
#27687=CARTESIAN_POINT('Ctrl Pts',(-1.01986550209675,-2.89989503181987,
107.987785832623));
#27688=CARTESIAN_POINT('Ctrl Pts',(-1.07231421576993,-2.88091081570988,
107.984883668412));
#27689=CARTESIAN_POINT('Ctrl Pts',(-1.12415615175069,-2.86053757124095,
107.981981504201));
#27690=CARTESIAN_POINT('Ctrl Pts',(-1.21346338326081,-2.82544092552398,
107.976981994708));
#27691=CARTESIAN_POINT('Ctrl Pts',(-1.30128230224839,-2.78609631033271,
107.971982485215));
#27692=CARTESIAN_POINT('Ctrl Pts',(-1.387180516629,-2.74265062745602,107.966982975722));
#27693=CARTESIAN_POINT('Ctrl Pts',(-1.4729622106272,-2.6992638783723,107.961990248032));
#27694=CARTESIAN_POINT('Ctrl Pts',(-1.55682798976619,-2.6517873142658,107.956997520342));
#27695=CARTESIAN_POINT('Ctrl Pts',(-1.63836405257318,-2.60041640535434,
107.952004792652));
#27696=CARTESIAN_POINT('Ctrl Pts',(-1.71981409688917,-2.54909969145688,
107.947017332164));
#27697=CARTESIAN_POINT('Ctrl Pts',(-1.79893894139432,-2.49389703282588,
107.942029871675));
#27698=CARTESIAN_POINT('Ctrl Pts',(-1.87534900768155,-2.43504996856078,
107.937042411187));
#27699=CARTESIAN_POINT('Ctrl Pts',(-1.95170440078025,-2.37624501074571,
107.932058519344));
#27700=CARTESIAN_POINT('Ctrl Pts',(-2.0253485304533,-2.31380109826874,107.9270746275));
#27701=CARTESIAN_POINT('Ctrl Pts',(-2.09592129083439,-2.24800271188162,
107.922090735656));
#27702=CARTESIAN_POINT('Ctrl Pts',(-2.16646835036403,-2.18222828763719,
107.917108658823));
#27703=CARTESIAN_POINT('Ctrl Pts',(-2.23394594223746,-2.11310211573858,
107.912126581989));
#27704=CARTESIAN_POINT('Ctrl Pts',(-2.29802826461889,-2.04094790355185,
107.907144505155));
#27705=CARTESIAN_POINT('Ctrl Pts',(-2.36210474416887,-1.96880027016696,
107.902162882572));
#27706=CARTESIAN_POINT('Ctrl Pts',(-2.4227862783556,-1.89362547373688,107.897181259989));
#27707=CARTESIAN_POINT('Ctrl Pts',(-2.47978579734442,-1.81578210402265,
107.892199637406));
#27708=CARTESIAN_POINT('Ctrl Pts',(-2.53679567985015,-1.73792458101216,
107.887217109076));
#27709=CARTESIAN_POINT('Ctrl Pts',(-2.59012195831713,-1.65739787530658,
107.882234580746));
#27710=CARTESIAN_POINT('Ctrl Pts',(-2.63952015937921,-1.57459060654849,
107.877252052417));
#27711=CARTESIAN_POINT('Ctrl Pts',(-2.68897160442178,-1.49169408375873,
107.872264153656));
#27712=CARTESIAN_POINT('Ctrl Pts',(-2.73448629423355,-1.40651246813084,
107.867276254895));
#27713=CARTESIAN_POINT('Ctrl Pts',(-2.7758652378553,-1.31945990134849,107.862288356134));
#27714=CARTESIAN_POINT('Ctrl Pts',(-2.81726862458697,-1.23235591142012,
107.857297510952));
#27715=CARTESIAN_POINT('Ctrl Pts',(-2.85453123114773,-1.1433791744113,107.852306665771));
#27716=CARTESIAN_POINT('Ctrl Pts',(-2.88750265733404,-1.05296279796052,
107.84731582059));
#27717=CARTESIAN_POINT('Ctrl Pts',(-2.92052736617773,-0.962400306362025,
107.842316910077));
#27718=CARTESIAN_POINT('Ctrl Pts',(-2.94924691696304,-0.870393948568264,
107.837317999563));
#27719=CARTESIAN_POINT('Ctrl Pts',(-2.97356111204,-0.777390868844901,107.83231908905));
#27720=CARTESIAN_POINT('Ctrl Pts',(-2.98767694519709,-0.723397061839775,
107.829416924839));
#27721=CARTESIAN_POINT('Ctrl Pts',(-3.0003089152176,-0.669067499346808,
107.826514760628));
#27722=CARTESIAN_POINT('Ctrl Pts',(-3.01144541790491,-0.614490638642712,
107.823612596417));
#27723=CARTESIAN_POINT('Ctrl Pts',(-3.03868361335523,-0.481003920176118,
107.816514343202));
#27724=CARTESIAN_POINT('Ctrl Pts',(-3.057053505008,-0.345651342796672,107.809416089987));
#27725=CARTESIAN_POINT('Ctrl Pts',(-3.06635784075599,-0.209408315103014,
107.802317836772));
#27726=CARTESIAN_POINT('Ctrl Pts',(-3.07105103823203,-0.140686006383854,
107.798737408789));
#27727=CARTESIAN_POINT('Ctrl Pts',(-3.07343837424032,-0.0717374795268788,
107.795156980806));
#27728=CARTESIAN_POINT('Ctrl Pts',(-3.07349882217824,-0.00269073762031292,
107.791576552823));
#27729=CARTESIAN_POINT('Origin',(0.,0.,116.208423447177));
#27730=CARTESIAN_POINT('',(1.87238193903529,2.43733217358128,109.437414079767));
#27731=CARTESIAN_POINT('',(1.8723819390353,2.43733217358128,109.354106889186));
#27732=CARTESIAN_POINT('',(1.8723819390353,2.43733217358128,116.208423447177));
#27733=CARTESIAN_POINT('',(-3.07349984408606,-0.00097898058431413,108.708423447223));
#27734=CARTESIAN_POINT('Ctrl Pts',(1.8723819390353,2.43733217358128,109.354106889186));
#27735=CARTESIAN_POINT('Ctrl Pts',(1.9488625296069,2.37857905079185,109.349124610237));
#27736=CARTESIAN_POINT('Ctrl Pts',(2.02261135197631,2.31619480280882,109.344142331288));
#27737=CARTESIAN_POINT('Ctrl Pts',(2.09327238020598,2.25046950485155,109.339160052339));
#27738=CARTESIAN_POINT('Ctrl Pts',(2.16392383385049,2.18475311268688,109.33417844849));
#27739=CARTESIAN_POINT('Ctrl Pts',(2.23148800372025,2.11569686945201,109.32919684464));
#27740=CARTESIAN_POINT('Ctrl Pts',(2.29564394264312,2.04362940344035,109.324215240791));
#27741=CARTESIAN_POINT('Ctrl Pts',(2.35980870268412,1.97155202851547,109.319232951996));
#27742=CARTESIAN_POINT('Ctrl Pts',(2.42056400940447,1.89646293660758,109.314250663202));
#27743=CARTESIAN_POINT('Ctrl Pts',(2.47762832376815,1.81872486629007,109.309268374407));
#27744=CARTESIAN_POINT('Ctrl Pts',(2.53475273694755,1.74090492403534,109.304280838381));
#27745=CARTESIAN_POINT('Ctrl Pts',(2.58817813514947,1.66043078696199,109.299293302355));
#27746=CARTESIAN_POINT('Ctrl Pts',(2.6376656962614,1.57769513048809,109.294305766329));
#27747=CARTESIAN_POINT('Ctrl Pts',(2.68718052328823,1.49491388956193,109.289315482345));
#27748=CARTESIAN_POINT('Ctrl Pts',(2.73275298501038,1.40986903470771,109.284325198361));
#27749=CARTESIAN_POINT('Ctrl Pts',(2.77419073716893,1.3229769475717,109.279334914377));
#27750=CARTESIAN_POINT('Ctrl Pts',(2.81569745690376,1.23594024022016,109.274336324736));
#27751=CARTESIAN_POINT('Ctrl Pts',(2.85305555124296,1.14705056442657,109.269337735094));
#27752=CARTESIAN_POINT('Ctrl Pts',(2.88612121697342,1.0567433798874,109.264339145452));
#27753=CARTESIAN_POINT('Ctrl Pts',(2.91067927939797,0.989671708221202,109.260626663827));
#27754=CARTESIAN_POINT('Ctrl Pts',(2.93287061027351,0.921818508434118,109.256914182201));
#27755=CARTESIAN_POINT('Ctrl Pts',(2.95265448210382,0.853366134383247,109.253201700576));
#27756=CARTESIAN_POINT('Ctrl Pts',(2.97929694528728,0.761182972709294,109.248202191083));
#27757=CARTESIAN_POINT('Ctrl Pts',(3.00166506851,0.667589018095253,109.24320268159));
#27758=CARTESIAN_POINT('Ctrl Pts',(3.01961161181223,0.573016547587191,109.238203172097));
#27759=CARTESIAN_POINT('Ctrl Pts',(3.03753381074247,0.478572364034679,109.233210444407));
#27760=CARTESIAN_POINT('Ctrl Pts',(3.05104626893321,0.383152730186458,109.228217716717));
#27761=CARTESIAN_POINT('Ctrl Pts',(3.06005157631718,0.28720480545898,109.223224989027));
#27762=CARTESIAN_POINT('Ctrl Pts',(3.06904738332882,0.191358103373958,109.218237528538));
#27763=CARTESIAN_POINT('Ctrl Pts',(3.07354545124736,0.0949846530728144,
109.21325006805));
#27764=CARTESIAN_POINT('Ctrl Pts',(3.0734996534705,-0.00145949192962973,
109.208262607562));
#27765=CARTESIAN_POINT('Ctrl Pts',(3.07345388846303,-0.0978346288922086,
109.203278715718));
#27766=CARTESIAN_POINT('Ctrl Pts',(3.0688707212837,-0.194279922294424,109.198294823875));
#27767=CARTESIAN_POINT('Ctrl Pts',(3.05975603135353,-0.290336492015243,
109.193310932031));
#27768=CARTESIAN_POINT('Ctrl Pts',(3.05064466076767,-0.386358080312533,
109.188328855197));
#27769=CARTESIAN_POINT('Ctrl Pts',(3.03700508775893,-0.481990789647019,
109.183346778363));
#27770=CARTESIAN_POINT('Ctrl Pts',(3.01889519957126,-0.576779007944624,
109.17836470153));
#27771=CARTESIAN_POINT('Ctrl Pts',(3.00078696258817,-0.671558583740493,
109.173383078947));
#27772=CARTESIAN_POINT('Ctrl Pts',(2.97820930334661,-0.765493390456918,
109.168401456363));
#27773=CARTESIAN_POINT('Ctrl Pts',(2.95127137398542,-0.858137242574983,
109.16341983378));
#27774=CARTESIAN_POINT('Ctrl Pts',(2.92432854683401,-0.950797938977824,
109.158437305451));
#27775=CARTESIAN_POINT('Ctrl Pts',(2.89302399770608,-1.04216679314023,109.153454777121));
#27776=CARTESIAN_POINT('Ctrl Pts',(2.8575166542334,-1.1318130679484,109.148472248791));
#27777=CARTESIAN_POINT('Ctrl Pts',(2.82197103907754,-1.22155596822871,109.14348435003));
#27778=CARTESIAN_POINT('Ctrl Pts',(2.78221374777995,-1.3095721736594,109.138496451269));
#27779=CARTESIAN_POINT('Ctrl Pts',(2.73845167054005,-1.39545143165802,109.133508552508));
#27780=CARTESIAN_POINT('Ctrl Pts',(2.69466374244047,-1.48138141971308,109.128517707326));
#27781=CARTESIAN_POINT('Ctrl Pts',(2.64686653533936,-1.565171565732,109.123526862145));
#27782=CARTESIAN_POINT('Ctrl Pts',(2.59531160133992,-1.64643856306587,109.118536016963));
#27783=CARTESIAN_POINT('Ctrl Pts',(2.5436733532652,-1.72783688991971,109.11353710645));
#27784=CARTESIAN_POINT('Ctrl Pts',(2.48826550486169,-1.80670356733909,109.108538195937));
#27785=CARTESIAN_POINT('Ctrl Pts',(2.42938134619686,-1.88268651791815,109.103539285424));
#27786=CARTESIAN_POINT('Ctrl Pts',(2.39519559764185,-1.92679912989836,109.100637121213));
#27787=CARTESIAN_POINT('Ctrl Pts',(2.35983889563577,-1.96994042855624,109.097734957003));
#27788=CARTESIAN_POINT('Ctrl Pts',(2.32337427194717,-2.01204727639635,109.094832792792));
#27789=CARTESIAN_POINT('Ctrl Pts',(2.26055727778196,-2.08458403524721,109.089833283299));
#27790=CARTESIAN_POINT('Ctrl Pts',(2.19422975031862,-2.15430361913334,109.084833773806));
#27791=CARTESIAN_POINT('Ctrl Pts',(2.12467411518251,-2.22084717039994,109.079834264313));
#27792=CARTESIAN_POINT('Ctrl Pts',(2.05521283182369,-2.28730045576188,109.074841536623));
#27793=CARTESIAN_POINT('Ctrl Pts',(1.98253245805288,-2.35058597004816,109.069848808933));
#27794=CARTESIAN_POINT('Ctrl Pts',(1.90695503267566,-2.41037854980353,109.064856081243));
#27795=CARTESIAN_POINT('Ctrl Pts',(1.83145733957744,-2.4701080498942,109.059868620754));
#27796=CARTESIAN_POINT('Ctrl Pts',(1.75306901306894,-2.52635167002143,109.054881160266));
#27797=CARTESIAN_POINT('Ctrl Pts',(1.6721474736194,-2.57882242049899,109.049893699778));
#27798=CARTESIAN_POINT('Ctrl Pts',(1.59128383542269,-2.6312556269282,109.044909807934));
#27799=CARTESIAN_POINT('Ctrl Pts',(1.50789095485014,-2.67992109220403,109.039925916091));
#27800=CARTESIAN_POINT('Ctrl Pts',(1.42235693806705,-2.72457390994125,109.034942024247));
#27801=CARTESIAN_POINT('Ctrl Pts',(1.33685407065436,-2.7692104662282,109.029959947413));
#27802=CARTESIAN_POINT('Ctrl Pts',(1.24921200503772,-2.80983707549881,109.024977870579));
#27803=CARTESIAN_POINT('Ctrl Pts',(1.15984442191021,-2.84625423442175,109.019995793746));
#27804=CARTESIAN_POINT('Ctrl Pts',(1.07048498704748,-2.88266807293876,109.015014171163));
#27805=CARTESIAN_POINT('Ctrl Pts',(0.979400754045785,-2.9148730587022,109.01003254858));
#27806=CARTESIAN_POINT('Ctrl Pts',(0.887025407928533,-2.94271782128175,
109.005050925997));
#27807=CARTESIAN_POINT('Ctrl Pts',(0.794633266345759,-2.97056764652974,
109.000068397667));
#27808=CARTESIAN_POINT('Ctrl Pts',(0.700949965729004,-2.9940555475094,108.995085869337));
#27809=CARTESIAN_POINT('Ctrl Pts',(0.606423333443464,-3.01308031599812,
108.990103341007));
#27810=CARTESIAN_POINT('Ctrl Pts',(0.51179481537949,-3.03212559038343,108.985115442246));
#27811=CARTESIAN_POINT('Ctrl Pts',(0.416321581984284,-3.04669804160713,
108.980127543485));
#27812=CARTESIAN_POINT('Ctrl Pts',(0.320460391650988,-3.05674784491343,
108.975139644724));
#27813=CARTESIAN_POINT('Ctrl Pts',(0.224542574796665,-3.0668035847765,108.970148799543));
#27814=CARTESIAN_POINT('Ctrl Pts',(0.128236782722721,-3.07233133200704,
108.965157954361));
#27815=CARTESIAN_POINT('Ctrl Pts',(0.0320014880243871,-3.07333339466518,
108.96016710918));
#27816=CARTESIAN_POINT('Ctrl Pts',(-0.0643893253401735,-3.07433707668188,
108.955168198667));
#27817=CARTESIAN_POINT('Ctrl Pts',(-0.160708975473842,-3.07080048653805,
108.950169288154));
#27818=CARTESIAN_POINT('Ctrl Pts',(-0.256502460329738,-3.06277794458638,
108.945170377641));
#27819=CARTESIAN_POINT('Ctrl Pts',(-0.312116263111785,-3.05812038288913,
108.942268213429));
#27820=CARTESIAN_POINT('Ctrl Pts',(-0.36755286320686,-3.05195180141579,
108.939366049218));
#27821=CARTESIAN_POINT('Ctrl Pts',(-0.422724983626062,-3.0442906954196,
108.936463885007));
#27822=CARTESIAN_POINT('Ctrl Pts',(-0.517769067875486,-3.03109303692445,
108.931464375514));
#27823=CARTESIAN_POINT('Ctrl Pts',(-0.612361442832732,-3.01341695487468,
108.926464866021));
#27824=CARTESIAN_POINT('Ctrl Pts',(-0.706047334392842,-2.99130396509562,
108.921465356528));
#27825=CARTESIAN_POINT('Ctrl Pts',(-0.799606141635985,-2.96922097144676,
108.916472628838));
#27826=CARTESIAN_POINT('Ctrl Pts',(-0.89226048573956,-2.94271313168788,
108.911479901148));
#27827=CARTESIAN_POINT('Ctrl Pts',(-0.983562287575478,-2.91187353373379,
108.906487173458));
#27828=CARTESIAN_POINT('Ctrl Pts',(-1.07476776831182,-2.8810664707782,108.90149971297));
#27829=CARTESIAN_POINT('Ctrl Pts',(-1.16462312970035,-2.84593687403104,
108.896512252482));
#27830=CARTESIAN_POINT('Ctrl Pts',(-1.25269304887393,-2.80662829304184,
108.891524791993));
#27831=CARTESIAN_POINT('Ctrl Pts',(-1.34069995196168,-2.76734783826118,
108.88654090015));
#27832=CARTESIAN_POINT('Ctrl Pts',(-1.42692355279716,-2.72389452193577,
108.881557008306));
#27833=CARTESIAN_POINT('Ctrl Pts',(-1.51094712078631,-2.67646054485911,
108.876573116463));
#27834=CARTESIAN_POINT('Ctrl Pts',(-1.59494008947298,-2.62904384206214,
108.871591039629));
#27835=CARTESIAN_POINT('Ctrl Pts',(-1.67673423533987,-2.57764957440248,
108.866608962795));
#27836=CARTESIAN_POINT('Ctrl Pts',(-1.75593698743265,-2.52251611415387,
108.861626885961));
#27837=CARTESIAN_POINT('Ctrl Pts',(-1.83513251805927,-2.46738768080657,
108.856645263378));
#27838=CARTESIAN_POINT('Ctrl Pts',(-1.91173676450594,-2.40852098363493,
108.851663640795));
#27839=CARTESIAN_POINT('Ctrl Pts',(-1.98538663793553,-2.34619738042371,
108.846682018212));
#27840=CARTESIAN_POINT('Ctrl Pts',(-2.05904990220975,-2.28386244568333,
108.841699489883));
#27841=CARTESIAN_POINT('Ctrl Pts',(-2.12975739161074,-2.21806964022926,
108.836716961553));
#27842=CARTESIAN_POINT('Ctrl Pts',(-2.19718039315411,-2.14913949522575,
108.831734433223));
#27843=CARTESIAN_POINT('Ctrl Pts',(-2.26467606675646,-2.08013505368472,
108.826746534462));
#27844=CARTESIAN_POINT('Ctrl Pts',(-2.32887987737857,-2.00798683588808,
108.821758635701));
#27845=CARTESIAN_POINT('Ctrl Pts',(-2.38950134957952,-1.93305084008612,
108.81677073694));
#27846=CARTESIAN_POINT('Ctrl Pts',(-2.45015863171617,-1.85807057856289,
108.811779891758));
#27847=CARTESIAN_POINT('Ctrl Pts',(-2.50722910227927,-1.78029961376144,
108.806789046577));
#27848=CARTESIAN_POINT('Ctrl Pts',(-2.56046508113166,-1.70012376558457,
108.801798201396));
#27849=CARTESIAN_POINT('Ctrl Pts',(-2.61378709067025,-1.61981835121235,
108.796799290883));
#27850=CARTESIAN_POINT('Ctrl Pts',(-2.66326201001578,-1.53710066974384,
108.79180038037));
#27851=CARTESIAN_POINT('Ctrl Pts',(-2.70868767608633,-1.45238194818652,
108.786801469856));
#27852=CARTESIAN_POINT('Ctrl Pts',(-2.73505997100621,-1.40319770272766,
108.783899305645));
#27853=CARTESIAN_POINT('Ctrl Pts',(-2.76006835591568,-1.35333941643973,
108.780997141434));
#27854=CARTESIAN_POINT('Ctrl Pts',(-2.7836808263976,-1.30289036635719,108.778094977223));
#27855=CARTESIAN_POINT('Ctrl Pts',(-2.82776458090748,-1.20870354499948,
108.772676726104));
#27856=CARTESIAN_POINT('Ctrl Pts',(-2.8671157375435,-1.11216731993342,108.767258474984));
#27857=CARTESIAN_POINT('Ctrl Pts',(-2.90149899609407,-1.01375826786523,
108.761840223864));
#27858=CARTESIAN_POINT('Ctrl Pts',(-2.93575895679424,-0.915702109184439,
108.756441402512));
#27859=CARTESIAN_POINT('Ctrl Pts',(-2.96508642595566,-0.815786813333184,
108.75104258116));
#27860=CARTESIAN_POINT('Ctrl Pts',(-2.98929429006591,-0.714508150673832,
108.745643759808));
#27861=CARTESIAN_POINT('Ctrl Pts',(-3.0134461323165,-0.613463867181533,
108.740257432413));
#27862=CARTESIAN_POINT('Ctrl Pts',(-3.03250189335562,-0.511062811241492,
108.734871105017));
#27863=CARTESIAN_POINT('Ctrl Pts',(-3.04632357483707,-0.407817272061727,
108.729484777622));
#27864=CARTESIAN_POINT('Ctrl Pts',(-3.06009921045474,-0.30491568741747,
108.72411639436));
#27865=CARTESIAN_POINT('Ctrl Pts',(-3.06867547241194,-0.201175543042106,
108.718748011098));
#27866=CARTESIAN_POINT('Ctrl Pts',(-3.07196518096963,-0.0971193951289094,
108.713379627836));
#27867=CARTESIAN_POINT('Ctrl Pts',(-3.07297755216737,-0.0650972736407699,
108.711727567632));
#27868=CARTESIAN_POINT('Ctrl Pts',(-3.07348963021813,-0.0330453177270445,
108.710075507427));
#27869=CARTESIAN_POINT('Ctrl Pts',(-3.07349984408606,-0.000978980584313824,
108.708423447223));
#27870=CARTESIAN_POINT('Ctrl Pts',(-3.07349984408634,-0.000978979696610955,
108.708423447177));
#27871=CARTESIAN_POINT('Ctrl Pts',(-3.07353140800572,0.0981157223006356,
108.703318080358));
#27872=CARTESIAN_POINT('Ctrl Pts',(-3.0687661617826,0.19717128811251,108.69821271354));
#27873=CARTESIAN_POINT('Ctrl Pts',(-3.05924166423145,0.295707101420337,
108.693107346721));
#27874=CARTESIAN_POINT('Ctrl Pts',(-3.04971067839837,0.394310039333225,
108.687998502022));
#27875=CARTESIAN_POINT('Ctrl Pts',(-3.03541402516345,0.492392114361571,
108.682889657324));
#27876=CARTESIAN_POINT('Ctrl Pts',(-3.01644086918857,0.589480052833778,
108.677780812625));
#27877=CARTESIAN_POINT('Ctrl Pts',(-2.99743484423122,0.686736185872648,
108.672663117394));
#27878=CARTESIAN_POINT('Ctrl Pts',(-2.97373621135201,0.782994341219481,
108.667545422163));
#27879=CARTESIAN_POINT('Ctrl Pts',(-2.94548493282318,0.877793119426008,
108.662427726933));
#27880=CARTESIAN_POINT('Ctrl Pts',(-2.91720806099992,0.972677777393298,
108.657305395498));
#27881=CARTESIAN_POINT('Ctrl Pts',(-2.88437045851986,1.06610003899986,108.652183064064));
#27882=CARTESIAN_POINT('Ctrl Pts',(-2.84716073907503,1.15761737023496,108.647060732629));
#27883=CARTESIAN_POINT('Ctrl Pts',(-2.80987280649384,1.24932706673416,108.641927634287));
#27884=CARTESIAN_POINT('Ctrl Pts',(-2.76819456226925,1.33912346049446,108.636794535945));
#27885=CARTESIAN_POINT('Ctrl Pts',(-2.7223614801067,1.42658691345156,108.631661437603));
#27886=CARTESIAN_POINT('Ctrl Pts',(-2.68683811953932,1.4943762836895,108.627682981549));
#27887=CARTESIAN_POINT('Ctrl Pts',(-2.64881983239274,1.56076469042194,108.623704525494));
#27888=CARTESIAN_POINT('Ctrl Pts',(-2.60843375910547,1.62556930776849,108.619726069439));
#27889=CARTESIAN_POINT('Ctrl Pts',(-2.55768277580638,1.70700574822815,108.614726559946));
#27890=CARTESIAN_POINT('Ctrl Pts',(-2.50302527490195,1.78620624615312,108.609727050453));
#27891=CARTESIAN_POINT('Ctrl Pts',(-2.44468433443415,1.86277233041837,108.604727540961));
#27892=CARTESIAN_POINT('Ctrl Pts',(-2.38642253308163,1.9392345532765,108.59973481327));
#27893=CARTESIAN_POINT('Ctrl Pts',(-2.32448748627122,2.01306911853243,108.59474208558));
#27894=CARTESIAN_POINT('Ctrl Pts',(-2.25914665028472,2.08390466732702,108.58974935789));
#27895=CARTESIAN_POINT('Ctrl Pts',(-2.19387474723318,2.15466548640313,108.584761897402));
#27896=CARTESIAN_POINT('Ctrl Pts',(-2.1252044937598,2.22243325769432,108.579774436914));
#27897=CARTESIAN_POINT('Ctrl Pts',(-2.05344424231571,2.28686881864711,108.574786976426));
#27898=CARTESIAN_POINT('Ctrl Pts',(-1.98173533700892,2.35125827444988,108.569803084582));
#27899=CARTESIAN_POINT('Ctrl Pts',(-1.90694115470479,2.41231996730369,108.564819192738));
#27900=CARTESIAN_POINT('Ctrl Pts',(-1.82940691437592,2.46975152426992,108.559835300895));
#27901=CARTESIAN_POINT('Ctrl Pts',(-1.75190091009697,2.52716216608558,108.554853224061));
#27902=CARTESIAN_POINT('Ctrl Pts',(-1.67165718280875,2.58094503768329,108.549871147227));
#27903=CARTESIAN_POINT('Ctrl Pts',(-1.58905328635393,2.63083863114555,108.544889070393));
#27904=CARTESIAN_POINT('Ctrl Pts',(-1.50645692147157,2.68072767546145,108.53990744781));
#27905=CARTESIAN_POINT('Ctrl Pts',(-1.42150119110167,2.72672791988308,108.534925825227));
#27906=CARTESIAN_POINT('Ctrl Pts',(-1.3345909069889,2.76862228571948,108.529944202644));
#27907=CARTESIAN_POINT('Ctrl Pts',(-1.24766482105507,2.81052426868978,108.524961674314));
#27908=CARTESIAN_POINT('Ctrl Pts',(-1.15878387103893,2.84831869990831,108.519979145985));
#27909=CARTESIAN_POINT('Ctrl Pts',(-1.06837465226522,2.88183584758001,108.514996617655));
#27910=CARTESIAN_POINT('Ctrl Pts',(-0.977867985678008,2.9153891217972,108.510008718894));
#27911=CARTESIAN_POINT('Ctrl Pts',(-0.885830174024775,2.94465575562677,
108.505020820133));
#27912=CARTESIAN_POINT('Ctrl Pts',(-0.792704638749025,2.96951538229823,
108.500032921372));
#27913=CARTESIAN_POINT('Ctrl Pts',(-0.699524092941319,2.99438969389238,
108.49504207619));
#27914=CARTESIAN_POINT('Ctrl Pts',(-0.605254972895097,3.01485172170391,
108.490051231009));
#27915=CARTESIAN_POINT('Ctrl Pts',(-0.510350514170142,3.03083232836894,
108.485060385828));
#27916=CARTESIAN_POINT('Ctrl Pts',(-0.415292687443233,3.0468387600979,108.480061475314));
#27917=CARTESIAN_POINT('Ctrl Pts',(-0.319597907425214,3.05834925744096,
108.475062564801));
#27918=CARTESIAN_POINT('Ctrl Pts',(-0.223724083557654,3.06534660102839,
108.470063654288));
#27919=CARTESIAN_POINT('Ctrl Pts',(-0.1680636392132,3.06940897423512,108.467161490077));
#27920=CARTESIAN_POINT('Ctrl Pts',(-0.112342859687147,3.07195116941884,
108.464259325866));
#27921=CARTESIAN_POINT('Ctrl Pts',(-0.0566508376245821,3.07297786073971,
108.461357161655));
#27922=CARTESIAN_POINT('Ctrl Pts',(0.0392697134137614,3.07474617141685,
108.456358650558));
#27923=CARTESIAN_POINT('Ctrl Pts',(0.135441582109926,3.0720221593444,108.45136013946));
#27924=CARTESIAN_POINT('Ctrl Pts',(0.231409352307455,3.06477600513719,108.446361628363));
#27925=CARTESIAN_POINT('Ctrl Pts',(0.327255795233389,3.05753901188179,108.441369436634));
#27926=CARTESIAN_POINT('Ctrl Pts',(0.422898218666516,3.04579126670438,108.436377244905));
#27927=CARTESIAN_POINT('Ctrl Pts',(0.51787965982746,3.02955490261144,108.431385053176));
#27928=CARTESIAN_POINT('Ctrl Pts',(0.612766961614202,3.01333463093757,108.42639780938));
#27929=CARTESIAN_POINT('Ctrl Pts',(0.70699415276511,2.99263465446948,108.421410565584));
#27930=CARTESIAN_POINT('Ctrl Pts',(0.800108920153355,2.96752893261229,108.416423321788));
#27931=CARTESIAN_POINT('Ctrl Pts',(0.896853710889718,2.94144447924914,108.411241653284));
#27932=CARTESIAN_POINT('Ctrl Pts',(0.992397085932376,2.91060379138493,108.406059984781));
#27933=CARTESIAN_POINT('Ctrl Pts',(1.08624307984464,2.87514838251691,108.400878316277));
#27934=CARTESIAN_POINT('Ctrl Pts',(1.17647157100917,2.84105968131169,108.395896386721));
#27935=CARTESIAN_POINT('Ctrl Pts',(1.26513068520286,2.80270564861303,108.390914457165));
#27936=CARTESIAN_POINT('Ctrl Pts',(1.35179631350352,2.76026248331536,108.385932527609));
#27937=CARTESIAN_POINT('Ctrl Pts',(1.43844753217521,2.71782637491299,108.380951426383));
#27938=CARTESIAN_POINT('Ctrl Pts',(1.52310553228236,2.67130268361139,108.375970325157));
#27939=CARTESIAN_POINT('Ctrl Pts',(1.60536895169007,2.62091449287258,108.370989223932));
#27940=CARTESIAN_POINT('Ctrl Pts',(1.68765633080886,2.57051162627296,108.36600667193));
#27941=CARTESIAN_POINT('Ctrl Pts',(1.76754736597993,2.51624224784611,108.361024119929));
#27942=CARTESIAN_POINT('Ctrl Pts',(1.84466863322337,2.4583734223266,108.356041567928));
#27943=CARTESIAN_POINT('Ctrl Pts',(1.85394665788643,2.45141155033483,108.3554421452));
#27944=CARTESIAN_POINT('Ctrl Pts',(1.86318463274705,2.4443976324336,108.354842722473));
#27945=CARTESIAN_POINT('Ctrl Pts',(1.8723819390353,2.43733217358127,108.354243299745));
#27946=CARTESIAN_POINT('',(-3.07349942256353,0.00188401212038324,108.791576552858));
#27947=CARTESIAN_POINT('Ctrl Pts',(-3.07349942256311,0.00188401280239466,
108.791576552823));
#27948=CARTESIAN_POINT('Ctrl Pts',(-3.07342968576284,0.115649702238102,
108.785659716256));
#27949=CARTESIAN_POINT('Ctrl Pts',(-3.06704369053512,0.229219670324852,
108.779742879689));
#27950=CARTESIAN_POINT('Ctrl Pts',(-3.05440435245984,0.342076455890201,
108.773826043122));
#27951=CARTESIAN_POINT('Ctrl Pts',(-3.04372457620121,0.437436292926549,
108.768826533629));
#27952=CARTESIAN_POINT('Ctrl Pts',(-3.02855599778406,0.532463002358434,
108.763827024136));
#27953=CARTESIAN_POINT('Ctrl Pts',(-3.00892809284563,0.626700871296976,
108.758827514643));
#27954=CARTESIAN_POINT('Ctrl Pts',(-2.98932681303559,0.720810907164757,
108.753834786953));
#27955=CARTESIAN_POINT('Ctrl Pts',(-2.96527831752782,0.814133803142816,
108.748842059263));
#27956=CARTESIAN_POINT('Ctrl Pts',(-2.93686381305166,0.906219175248276,
108.743849331573));
#27957=CARTESIAN_POINT('Ctrl Pts',(-2.90847928516147,0.998207399607386,
108.738861871085));
#27958=CARTESIAN_POINT('Ctrl Pts',(-2.87573803355059,1.08896027824398,108.733874410597));
#27959=CARTESIAN_POINT('Ctrl Pts',(-2.83877204625355,1.17803884460972,108.728886950109));
#27960=CARTESIAN_POINT('Ctrl Pts',(-2.80183250898455,1.26705367317891,108.723903058265));
#27961=CARTESIAN_POINT('Ctrl Pts',(-2.76067441317311,1.35439616678808,108.718919166421));
#27962=CARTESIAN_POINT('Ctrl Pts',(-2.715478872724,1.43964465816727,108.713935274578));
#27963=CARTESIAN_POINT('Ctrl Pts',(-2.67029979137136,1.5248621041573,108.708953197744));
#27964=CARTESIAN_POINT('Ctrl Pts',(-2.62108639218397,1.60798667565565,108.70397112091));
#27965=CARTESIAN_POINT('Ctrl Pts',(-2.56806658325906,1.68861963566344,108.698989044076));
#27966=CARTESIAN_POINT('Ctrl Pts',(-2.51505160851921,1.76924524380298,108.694007421493));
#27967=CARTESIAN_POINT('Ctrl Pts',(-2.45823115537972,1.84737932544832,108.68902579891));
#27968=CARTESIAN_POINT('Ctrl Pts',(-2.39787688201833,1.92265147873504,108.684044176327));
#27969=CARTESIAN_POINT('Ctrl Pts',(-2.33751163518674,1.99793731782536,108.679061647997));
#27970=CARTESIAN_POINT('Ctrl Pts',(-2.27361156672695,2.07035985270018,108.674079119668));
#27971=CARTESIAN_POINT('Ctrl Pts',(-2.20648840350465,2.13958200945874,108.669096591338));
#27972=CARTESIAN_POINT('Ctrl Pts',(-2.1392928914048,2.20887877750054,108.664108692577));
#27973=CARTESIAN_POINT('Ctrl Pts',(-2.06886765506542,2.27496796508934,108.659120793816));
#27974=CARTESIAN_POINT('Ctrl Pts',(-1.99556088715803,2.33754978463455,108.654132895055));
#27975=CARTESIAN_POINT('Ctrl Pts',(-1.92221081593672,2.4001685721195,108.649142049873));
#27976=CARTESIAN_POINT('Ctrl Pts',(-1.84597617061308,2.45927559732614,108.644151204692));
#27977=CARTESIAN_POINT('Ctrl Pts',(-1.76723608672674,2.51461306442378,108.639160359511));
#27978=CARTESIAN_POINT('Ctrl Pts',(-1.68836875687637,2.57003995826571,108.634161448998));
#27979=CARTESIAN_POINT('Ctrl Pts',(-1.60698827418052,2.62168489517077,108.629162538484));
#27980=CARTESIAN_POINT('Ctrl Pts',(-1.52350037601449,2.66933490860246,108.624163627971));
#27981=CARTESIAN_POINT('Ctrl Pts',(-1.47503069657559,2.69699856916918,108.62126146376));
#27982=CARTESIAN_POINT('Ctrl Pts',(-1.42585114589775,2.7233166204389,108.618359299549));
#27983=CARTESIAN_POINT('Ctrl Pts',(-1.37604412559659,2.74825486707676,108.615457135338));
#27984=CARTESIAN_POINT('Ctrl Pts',(-1.29024240911845,2.79121556527847,108.610457625845));
#27985=CARTESIAN_POINT('Ctrl Pts',(-1.20227618216251,2.8302297190156,108.605458116352));
#27986=CARTESIAN_POINT('Ctrl Pts',(-1.11254374124092,2.86507393863154,108.600458606859));
#27987=CARTESIAN_POINT('Ctrl Pts',(-1.02293302180566,2.89987089228483,108.595465879169));
#27988=CARTESIAN_POINT('Ctrl Pts',(-0.931561255708334,2.93050899617858,
108.590473151479));
#27989=CARTESIAN_POINT('Ctrl Pts',(-0.838850434689728,2.95681115362832,
108.585480423789));
#27990=CARTESIAN_POINT('Ctrl Pts',(-0.746237421250267,2.98308556296498,
108.580492963301));
#27991=CARTESIAN_POINT('Ctrl Pts',(-0.652288581241642,3.00503300014899,
108.575505502812));
#27992=CARTESIAN_POINT('Ctrl Pts',(-0.557443977509493,3.02252517970296,
108.570518042324));
#27993=CARTESIAN_POINT('Ctrl Pts',(-0.462667237308462,3.04000484319355,
108.56553415048));
#27994=CARTESIAN_POINT('Ctrl Pts',(-0.366996437986369,3.05303550694457,
108.560550258637));
#27995=CARTESIAN_POINT('Ctrl Pts',(-0.270883878544352,3.06153951049872,
108.555566366793));
#27996=CARTESIAN_POINT('Ctrl Pts',(-0.174806320916051,3.07004041710541,
108.550584289959));
#27997=CARTESIAN_POINT('Ctrl Pts',(-0.0782877596223771,3.07401790025227,
108.545602213126));
#27998=CARTESIAN_POINT('Ctrl Pts',(0.0182132628988892,3.07344603451152,
108.540620136292));
#27999=CARTESIAN_POINT('Ctrl Pts',(0.114705486750156,3.07287422091175,108.535638513709));
#28000=CARTESIAN_POINT('Ctrl Pts',(0.211179736054938,3.06775388589978,108.530656891126));
#28001=CARTESIAN_POINT('Ctrl Pts',(0.307177415868004,3.05811122838602,108.525675268543));
#28002=CARTESIAN_POINT('Ctrl Pts',(0.403192549750659,3.04846681766723,108.520692740213));
#28003=CARTESIAN_POINT('Ctrl Pts',(0.498730505300663,3.03429849538734,108.515710211883));
#28004=CARTESIAN_POINT('Ctrl Pts',(0.593338827351907,3.01568421522491,108.510727683553));
#28005=CARTESIAN_POINT('Ctrl Pts',(0.688049123231148,2.99704987161179,108.505739784792));
#28006=CARTESIAN_POINT('Ctrl Pts',(0.781827353776249,2.97396008803848,108.500751886031));
#28007=CARTESIAN_POINT('Ctrl Pts',(0.874232485425454,2.94654370600995,108.49576398727));
#28008=CARTESIAN_POINT('Ctrl Pts',(0.966692202054234,2.91911112874824,108.490773142089));
#28009=CARTESIAN_POINT('Ctrl Pts',(1.05777679044951,2.88734700852904,108.485782296908));
#28010=CARTESIAN_POINT('Ctrl Pts',(1.14706359252094,2.85142900397554,108.480791451726));
#28011=CARTESIAN_POINT('Ctrl Pts',(1.2364946843193,2.81545295501964,108.475792541213));
#28012=CARTESIAN_POINT('Ctrl Pts',(1.32412178980594,2.77530980048739,108.4707936307));
#28013=CARTESIAN_POINT('Ctrl Pts',(1.40954536994573,2.73122391979577,108.465794720187));
#28014=CARTESIAN_POINT('Ctrl Pts',(1.45913882764104,2.70562944979741,108.462892555976));
#28015=CARTESIAN_POINT('Ctrl Pts',(1.50799008914338,2.67870692619813,108.459990391765));
#28016=CARTESIAN_POINT('Ctrl Pts',(1.55602560798143,2.65050684913396,108.457088227554));
#28017=CARTESIAN_POINT('Ctrl Pts',(1.63877545032361,2.60192713171767,108.45208872642));
#28018=CARTESIAN_POINT('Ctrl Pts',(1.71939343985904,2.54938315058608,108.447089225286));
#28019=CARTESIAN_POINT('Ctrl Pts',(1.7974753479185,2.49308736782835,108.442089724152));
#28020=CARTESIAN_POINT('Ctrl Pts',(1.82271337604429,2.47489116099998,108.44047376018));
#28021=CARTESIAN_POINT('Ctrl Pts',(1.84768661711419,2.45630335660053,108.438857796209));
#28022=CARTESIAN_POINT('Ctrl Pts',(1.87238193903529,2.43733217358128,108.437241832237));
#28023=CARTESIAN_POINT('Ctrl Pts',(1.87238193903529,2.43733217358128,109.437414079767));
#28024=CARTESIAN_POINT('Ctrl Pts',(1.94920407382002,2.37831667325343,109.432395345516));
#28025=CARTESIAN_POINT('Ctrl Pts',(2.02314962296453,2.31573001139801,109.427376611265));
#28026=CARTESIAN_POINT('Ctrl Pts',(2.09388683944776,2.24989780958769,109.422357877013));
#28027=CARTESIAN_POINT('Ctrl Pts',(2.16462405593099,2.18406560777736,109.417339142762));
#28028=CARTESIAN_POINT('Ctrl Pts',(2.2321526722981,2.11498822739159,109.41232040851));
#28029=CARTESIAN_POINT('Ctrl Pts',(2.29618206789388,2.04302475782419,109.407301674259));
#28030=CARTESIAN_POINT('Ctrl Pts',(2.35996619255337,1.97133695144861,109.402302164766));
#28031=CARTESIAN_POINT('Ctrl Pts',(2.42050194475992,1.89653331529101,109.397302655273));
#28032=CARTESIAN_POINT('Ctrl Pts',(2.47747009479805,1.81894040017295,109.392303145779));
#28033=CARTESIAN_POINT('Ctrl Pts',(2.53436096790243,1.7414527393515,109.387310418089));
#28034=CARTESIAN_POINT('Ctrl Pts',(2.58769359932268,1.6611836701117,109.382317690399));
#28035=CARTESIAN_POINT('Ctrl Pts',(2.63718730315004,1.57849465570975,109.377324962708));
#28036=CARTESIAN_POINT('Ctrl Pts',(2.68662879236747,1.49589287613361,109.37233750222));
#28037=CARTESIAN_POINT('Ctrl Pts',(2.73223918084695,1.41087660121226,109.367350041732));
#28038=CARTESIAN_POINT('Ctrl Pts',(2.77378021988544,1.32383743026562,109.362362581243));
#28039=CARTESIAN_POINT('Ctrl Pts',(2.81529153533949,1.2368605378803,109.357378689399));
#28040=CARTESIAN_POINT('Ctrl Pts',(2.85273910117318,1.14786402191088,109.352394797555));
#28041=CARTESIAN_POINT('Ctrl Pts',(2.88593037386635,1.05726445471115,109.347410905711));
#28042=CARTESIAN_POINT('Ctrl Pts',(2.91910955912007,0.966697881629828,109.342428828877));
#28043=CARTESIAN_POINT('Ctrl Pts',(2.94803538014164,0.874529829000709,109.337446752044));
#28044=CARTESIAN_POINT('Ctrl Pts',(2.97256362795683,0.781196343916247,109.33246467521));
#28045=CARTESIAN_POINT('Ctrl Pts',(2.99708963936092,0.687871368695325,109.327483052626));
#28046=CARTESIAN_POINT('Ctrl Pts',(3.01721876334168,0.593381596877724,109.322501430043));
#28047=CARTESIAN_POINT('Ctrl Pts',(3.03285711041393,0.498176673291401,109.31751980746));
#28048=CARTESIAN_POINT('Ctrl Pts',(3.04849830081322,0.402954439772503,109.31253727913));
#28049=CARTESIAN_POINT('Ctrl Pts',(3.05964702161439,0.307017229409604,109.3075547508));
#28050=CARTESIAN_POINT('Ctrl Pts',(3.06626095531663,0.210822209220869,109.30257222247));
#28051=CARTESIAN_POINT('Ctrl Pts',(3.07288201786465,0.114523504977408,109.297584323708));
#28052=CARTESIAN_POINT('Ctrl Pts',(3.07495850504839,0.0179668747989478,
109.292596424947));
#28053=CARTESIAN_POINT('Ctrl Pts',(3.07250020693919,-0.0783883177433252,
109.287608526186));
#28054=CARTESIAN_POINT('Ctrl Pts',(3.07004045667956,-0.174800428620378,
109.282617681004));
#28055=CARTESIAN_POINT('Ctrl Pts',(3.06304061911616,-0.271010427328123,
109.277626835823));
#28056=CARTESIAN_POINT('Ctrl Pts',(3.05156239964119,-0.366564006820237,
109.272635990641));
#28057=CARTESIAN_POINT('Ctrl Pts',(3.04006563107369,-0.462272003309829,
109.267637080128));
#28058=CARTESIAN_POINT('Ctrl Pts',(3.02407610232081,-0.557321029832261,
109.262638169614));
#28059=CARTESIAN_POINT('Ctrl Pts',(3.00370664265917,-0.651266961272567,
109.257639259101));
#28060=CARTESIAN_POINT('Ctrl Pts',(2.99188096251942,-0.705808149605373,
109.254737094892));
#28061=CARTESIAN_POINT('Ctrl Pts',(2.97857997045296,-0.759977805615262,
109.251834930684));
#28062=CARTESIAN_POINT('Ctrl Pts',(2.96383331659665,-0.813691785279715,
109.248932766475));
#28063=CARTESIAN_POINT('Ctrl Pts',(2.93842950390934,-0.906223955043927,
109.243933256982));
#28064=CARTESIAN_POINT('Ctrl Pts',(2.9086435757866,-0.997727833444311,109.238933747489));
#28065=CARTESIAN_POINT('Ctrl Pts',(2.87457563542129,-1.08775786195378,109.233934237996));
#28066=CARTESIAN_POINT('Ctrl Pts',(2.84055390800077,-1.17766576530123,109.228941510306));
#28067=CARTESIAN_POINT('Ctrl Pts',(2.80226186641799,-1.26610338513085,109.223948782616));
#28068=CARTESIAN_POINT('Ctrl Pts',(2.75984988338236,-1.35263848503375,109.218956054926));
#28069=CARTESIAN_POINT('Ctrl Pts',(2.71748264391977,-1.43908229258749,109.213968594438));
#28070=CARTESIAN_POINT('Ctrl Pts',(2.67100429561214,-1.52362717815871,109.20898113395));
#28071=CARTESIAN_POINT('Ctrl Pts',(2.62061359406956,-1.60586009371234,109.203993673462));
#28072=CARTESIAN_POINT('Ctrl Pts',(2.57025894825183,-1.68803416969268,109.199009781618));
#28073=CARTESIAN_POINT('Ctrl Pts',(2.51599774292866,-1.76789919105604,109.194025889775));
#28074=CARTESIAN_POINT('Ctrl Pts',(2.45807456515645,-1.84506685031489,109.189041997931));
#28075=CARTESIAN_POINT('Ctrl Pts',(2.40017248157099,-1.92220640702348,109.184059921097));
#28076=CARTESIAN_POINT('Ctrl Pts',(2.33861133850038,-1.99665020266829,109.179077844264));
#28077=CARTESIAN_POINT('Ctrl Pts',(2.27367837408059,-2.06803986935413,109.17409576743));
#28078=CARTESIAN_POINT('Ctrl Pts',(2.20875133005119,-2.13942302694709,109.169114144847));
#28079=CARTESIAN_POINT('Ctrl Pts',(2.14045337140159,-2.20775228461636,109.164132522264));
#28080=CARTESIAN_POINT('Ctrl Pts',(2.06911053846775,-2.27270407875766,109.159150899681));
#28081=CARTESIAN_POINT('Ctrl Pts',(1.99775473414986,-2.33766768227955,109.154168371351));
#28082=CARTESIAN_POINT('Ctrl Pts',(1.92335328068573,-2.39925230722043,109.149185843022));
#28083=CARTESIAN_POINT('Ctrl Pts',(1.84626660641381,-2.45717355269042,109.144203314692));
#28084=CARTESIAN_POINT('Ctrl Pts',(1.76909684406792,-2.51515722872669,109.139215415931));
#28085=CARTESIAN_POINT('Ctrl Pts',(1.68923643428642,-2.56946937818642,109.13422751717));
#28086=CARTESIAN_POINT('Ctrl Pts',(1.6070760179085,-2.61986811169253,109.129239618409));
#28087=CARTESIAN_POINT('Ctrl Pts',(1.5248670682449,-2.67029661642228,109.124248773228));
#28088=CARTESIAN_POINT('Ctrl Pts',(1.44035579108999,-2.71680689066201,109.119257928046));
#28089=CARTESIAN_POINT('Ctrl Pts',(1.35395685128638,-2.75920334423809,109.114267082865));
#28090=CARTESIAN_POINT('Ctrl Pts',(1.26741828861416,-2.80166831155383,109.109268172352));
#28091=CARTESIAN_POINT('Ctrl Pts',(1.17898637457032,-2.84000600906012,109.104269261839));
#28092=CARTESIAN_POINT('Ctrl Pts',(1.0890950679507,-2.87406927247161,109.099270351326));
#28093=CARTESIAN_POINT('Ctrl Pts',(1.03690782988644,-2.89384501835573,109.096368187114));
#28094=CARTESIAN_POINT('Ctrl Pts',(0.984228994385734,-2.91218100262128,
109.093466022903));
#28095=CARTESIAN_POINT('Ctrl Pts',(0.931145283869106,-2.92905628322986,
109.090563858691));
#28096=CARTESIAN_POINT('Ctrl Pts',(0.839698868264912,-2.95812704540814,
109.085564349198));
#28097=CARTESIAN_POINT('Ctrl Pts',(0.74672912593414,-2.9829622681281,109.080564839705));
#28098=CARTESIAN_POINT('Ctrl Pts',(0.652664289271526,-3.00340333214001,
109.075565330212));
#28099=CARTESIAN_POINT('Ctrl Pts',(0.558727050962504,-3.02381666797839,
109.070572602522));
#28100=CARTESIAN_POINT('Ctrl Pts',(0.463698095913494,-3.03984759908562,
109.065579874832));
#28101=CARTESIAN_POINT('Ctrl Pts',(0.368021851346044,-3.0513869251427,109.060587147142));
#28102=CARTESIAN_POINT('Ctrl Pts',(0.272446542804956,-3.06291407750166,
109.055599686653));
#28103=CARTESIAN_POINT('Ctrl Pts',(0.176225735744696,-3.0699589924401,109.050612226165));
#28104=CARTESIAN_POINT('Ctrl Pts',(0.0798141044726736,-3.07246349998291,
109.045624765677));
#28105=CARTESIAN_POINT('Ctrl Pts',(-0.0165285420234597,-3.07496621549203,
109.040640873833));
#28106=CARTESIAN_POINT('Ctrl Pts',(-0.113061303741829,-3.07293497063558,
109.03565698199));
#28107=CARTESIAN_POINT('Ctrl Pts',(-0.209325305552926,-3.06636350853175,
109.030673090146));
#28108=CARTESIAN_POINT('Ctrl Pts',(-0.305554250398746,-3.05979443959168,
109.025691013312));
#28109=CARTESIAN_POINT('Ctrl Pts',(-0.401514192310171,-3.04868846846501,
109.020708936479));
#28110=CARTESIAN_POINT('Ctrl Pts',(-0.496748147809946,-3.03309141432424,
109.015726859645));
#28111=CARTESIAN_POINT('Ctrl Pts',(-0.591973420167034,-3.01749578227547,
109.010745237062));
#28112=CARTESIAN_POINT('Ctrl Pts',(-0.686472404555486,-2.99740995246849,
109.005763614479));
#28113=CARTESIAN_POINT('Ctrl Pts',(-0.77979618515038,-2.97293124031231,
109.000781991896));
#28114=CARTESIAN_POINT('Ctrl Pts',(-0.873136933652916,-2.94844807749496,
108.995799463566));
#28115=CARTESIAN_POINT('Ctrl Pts',(-0.965301629421924,-2.91957055750715,
108.990816935236));
#28116=CARTESIAN_POINT('Ctrl Pts',(-1.05585548341354,-2.88644616235009,
108.985834406906));
#28117=CARTESIAN_POINT('Ctrl Pts',(-1.14650694111404,-2.85328606397688,
108.980846508145));
#28118=CARTESIAN_POINT('Ctrl Pts',(-1.23554367784378,-2.81587010291647,
108.975858609384));
#28119=CARTESIAN_POINT('Ctrl Pts',(-1.32255011364468,-2.77439424864211,
108.970870710623));
#28120=CARTESIAN_POINT('Ctrl Pts',(-1.40960794534142,-2.73289389401136,
108.965879865442));
#28121=CARTESIAN_POINT('Ctrl Pts',(-1.49463270132819,-2.68732907813605,
108.960889020261));
#28122=CARTESIAN_POINT('Ctrl Pts',(-1.57723455715542,-2.63794112931178,
108.955898175079));
#28123=CARTESIAN_POINT('Ctrl Pts',(-1.65996989966767,-2.58847336831499,
108.950899264566));
#28124=CARTESIAN_POINT('Ctrl Pts',(-1.7402741582147,-2.53517038030392,108.945900354053));
#28125=CARTESIAN_POINT('Ctrl Pts',(-1.8177876229855,-2.47831604274369,108.94090144354));
#28126=CARTESIAN_POINT('Ctrl Pts',(-1.86278878929052,-2.44530872579205,
108.937999279329));
#28127=CARTESIAN_POINT('Ctrl Pts',(-1.90684994564932,-2.41110518024289,
108.935097115118));
#28128=CARTESIAN_POINT('Ctrl Pts',(-1.94990630988446,-2.37576674626798,
108.932194950906));
#28129=CARTESIAN_POINT('Ctrl Pts',(-2.0231004133922,-2.31569281666177,108.927261387392));
#28130=CARTESIAN_POINT('Ctrl Pts',(-2.09366081744235,-2.25211385752092,
108.922327823877));
#28131=CARTESIAN_POINT('Ctrl Pts',(-2.16122630733891,-2.18529245147331,
108.917394260362));
#28132=CARTESIAN_POINT('Ctrl Pts',(-2.22869969055363,-2.11856213775694,
108.912467422383));
#28133=CARTESIAN_POINT('Ctrl Pts',(-2.29318595057505,-2.04859847115879,
108.907540584405));
#28134=CARTESIAN_POINT('Ctrl Pts',(-2.35435603555813,-1.97570491415875,
108.902613746427));
#28135=CARTESIAN_POINT('Ctrl Pts',(-2.41545719841484,-1.90289348846435,
108.897692459661));
#28136=CARTESIAN_POINT('Ctrl Pts',(-2.47324932477289,-1.82715907853984,
108.892771172895));
#28137=CARTESIAN_POINT('Ctrl Pts',(-2.52744035696434,-1.74884175727478,
108.887849886129));
#28138=CARTESIAN_POINT('Ctrl Pts',(-2.58159824008911,-1.67057234331099,
108.882931609752));
#28139=CARTESIAN_POINT('Ctrl Pts',(-2.63215914615633,-1.58972352521532,
108.878013333375));
#28140=CARTESIAN_POINT('Ctrl Pts',(-2.6788720486264,-1.50666744741107,108.873095056998));
#28141=CARTESIAN_POINT('Ctrl Pts',(-2.72556993900543,-1.42363806127736,
108.868178361204));
#28142=CARTESIAN_POINT('Ctrl Pts',(-2.76842206102694,-1.33840321788697,
108.863261665409));
#28143=CARTESIAN_POINT('Ctrl Pts',(-2.807222054207,-1.25136189344803,108.858344969615));
#28144=CARTESIAN_POINT('Ctrl Pts',(-2.8460208426018,-1.1643232717442,108.85342842649));
#28145=CARTESIAN_POINT('Ctrl Pts',(-2.88076757017542,-1.07547869384789,
108.848511883365));
#28146=CARTESIAN_POINT('Ctrl Pts',(-2.91130349058054,-0.985248311713113,
108.84359534024));
#28147=CARTESIAN_POINT('Ctrl Pts',(-2.94186355431931,-0.894946588607045,
108.838674909832));
#28148=CARTESIAN_POINT('Ctrl Pts',(-2.96820601882626,-0.803257302207185,
108.833754479425));
#28149=CARTESIAN_POINT('Ctrl Pts',(-2.99022180531312,-0.710616496452175,
108.828834049017));
#28150=CARTESIAN_POINT('Ctrl Pts',(-3.01224721691765,-0.617935188911903,
108.823911467439));
#28151=CARTESIAN_POINT('Ctrl Pts',(-3.02994210090026,-0.52430197769036,
108.818988885861));
#28152=CARTESIAN_POINT('Ctrl Pts',(-3.04324877593042,-0.430161757712154,
108.814066304282));
#28153=CARTESIAN_POINT('Ctrl Pts',(-3.05657391129479,-0.33589093712039,
108.809136893612));
#28154=CARTESIAN_POINT('Ctrl Pts',(-3.06549864354241,-0.241112153077702,
108.804207482942));
#28155=CARTESIAN_POINT('Ctrl Pts',(-3.07001730613623,-0.146273681925572,
108.799278072273));
#28156=CARTESIAN_POINT('Ctrl Pts',(-3.07237056700401,-0.0968830362889882,
108.796710899135));
#28157=CARTESIAN_POINT('Ctrl Pts',(-3.07352967967365,-0.0474761854540675,
108.794143725996));
#28158=CARTESIAN_POINT('Ctrl Pts',(-3.07349942256353,0.00188401212038081,
108.791576552858));
#28159=CARTESIAN_POINT('Origin',(0.,0.,116.208423447177));
#28160=CARTESIAN_POINT('',(1.8723819390353,2.43733217358127,110.437319612009));
#28161=CARTESIAN_POINT('',(1.8723819390353,2.43733217358127,110.35412809305));
#28162=CARTESIAN_POINT('',(1.8723819390353,2.43733217358128,116.208423447177));
#28163=CARTESIAN_POINT('',(-3.07349931288414,-0.0020551643988658,109.708423447143));
#28164=CARTESIAN_POINT('Ctrl Pts',(1.8723819390353,2.43733217358127,110.35412809305));
#28165=CARTESIAN_POINT('Ctrl Pts',(1.94855031136323,2.37881889983944,110.349132233708));
#28166=CARTESIAN_POINT('Ctrl Pts',(2.02209372129131,2.31663912935644,110.344136374365));
#28167=CARTESIAN_POINT('Ctrl Pts',(2.09263962734076,2.2510578935432,110.339140515023));
#28168=CARTESIAN_POINT('Ctrl Pts',(2.1631006932861,2.18555552720921,110.334150663814));
#28169=CARTESIAN_POINT('Ctrl Pts',(2.23057110136168,2.11666012335588,110.329160812605));
#28170=CARTESIAN_POINT('Ctrl Pts',(2.29471016091284,2.04467785418715,110.324170961396));
#28171=CARTESIAN_POINT('Ctrl Pts',(2.35938447039662,1.97209488234221,110.319139469141));
#28172=CARTESIAN_POINT('Ctrl Pts',(2.42067120798129,1.8963735556705,110.314107976887));
#28173=CARTESIAN_POINT('Ctrl Pts',(2.47825785808659,1.81786694750526,110.309076484632));
#28174=CARTESIAN_POINT('Ctrl Pts',(2.53528697316547,1.74012041452718,110.304093705632));
#28175=CARTESIAN_POINT('Ctrl Pts',(2.58868707596905,1.65964266323822,110.299110926632));
#28176=CARTESIAN_POINT('Ctrl Pts',(2.63819497902644,1.57680991328685,110.294128147632));
#28177=CARTESIAN_POINT('Ctrl Pts',(2.68769187402954,1.49399558115065,110.28914647655));
#28178=CARTESIAN_POINT('Ctrl Pts',(2.73329806407065,1.40882766764537,110.284164805469));
#28179=CARTESIAN_POINT('Ctrl Pts',(2.77479458668175,1.32170997261943,110.279183134387));
#28180=CARTESIAN_POINT('Ctrl Pts',(2.81629321096451,1.2345878653493,110.274201210999));
#28181=CARTESIAN_POINT('Ctrl Pts',(2.85368156621807,1.14551617705663,110.269219287611));
#28182=CARTESIAN_POINT('Ctrl Pts',(2.88678788139234,1.05492083961135,110.264237364222));
#28183=CARTESIAN_POINT('Ctrl Pts',(2.92046964321373,0.962750794050624,110.259168846144));
#28184=CARTESIAN_POINT('Ctrl Pts',(2.94971892598634,0.86900406897538,110.254100328066));
#28185=CARTESIAN_POINT('Ctrl Pts',(2.97440751960176,0.774146082685,110.249031809987));
#28186=CARTESIAN_POINT('Ctrl Pts',(2.99871037369669,0.680770176529102,110.244042483448));
#28187=CARTESIAN_POINT('Ctrl Pts',(3.0185940050598,0.586317934023058,110.239053156909));
#28188=CARTESIAN_POINT('Ctrl Pts',(3.033987916313,0.491242886632159,110.23406383037));
#28189=CARTESIAN_POINT('Ctrl Pts',(3.04974833019519,0.39390426540047,110.228955716522));
#28190=CARTESIAN_POINT('Ctrl Pts',(3.06080246555741,0.295913295032107,110.223847602674));
#28191=CARTESIAN_POINT('Ctrl Pts',(3.06713112097644,0.19775979555466,110.218739488825));
#28192=CARTESIAN_POINT('Ctrl Pts',(3.07345977639546,0.0996062960772201,
110.213631374977));
#28193=CARTESIAN_POINT('Ctrl Pts',(3.07506301017686,0.00129075512507518,
110.208523261129));
#28194=CARTESIAN_POINT('Ctrl Pts',(3.07197837451437,-0.0967011712238769,
110.203415147281));
#28195=CARTESIAN_POINT('Ctrl Pts',(3.06895932174052,-0.192609676936675,
110.198415637786));
#28196=CARTESIAN_POINT('Ctrl Pts',(3.06143920317429,-0.288545119294609,
110.193416128292));
#28197=CARTESIAN_POINT('Ctrl Pts',(3.04941095386831,-0.384050887810424,
110.188416618797));
#28198=CARTESIAN_POINT('Ctrl Pts',(3.03739902080607,-0.479427103358187,
110.183423891105));
#28199=CARTESIAN_POINT('Ctrl Pts',(3.02089116504168,-0.574374371642853,
110.178431163413));
#28200=CARTESIAN_POINT('Ctrl Pts',(2.99993231319909,-0.66843725675933,110.173438435721));
#28201=CARTESIAN_POINT('Ctrl Pts',(2.9789955724168,-0.762400907903461,110.168450975231));
#28202=CARTESIAN_POINT('Ctrl Pts',(2.95361726526135,-0.855481604453911,
110.163463514741));
#28203=CARTESIAN_POINT('Ctrl Pts',(2.92389385012061,-0.947231230073669,
110.158476054251));
#28204=CARTESIAN_POINT('Ctrl Pts',(2.89419170277803,-1.03891520669213,110.153492162406));
#28205=CARTESIAN_POINT('Ctrl Pts',(2.86015076294477,-1.1292695893327,110.14850827056));
#28206=CARTESIAN_POINT('Ctrl Pts',(2.8219178410477,-1.21785957662479,110.143524378715));
#28207=CARTESIAN_POINT('Ctrl Pts',(2.78369884263373,-1.30641730163792,110.138542301879));
#28208=CARTESIAN_POINT('Ctrl Pts',(2.74129106913517,-1.39321150535876,110.133560225044));
#28209=CARTESIAN_POINT('Ctrl Pts',(2.69488980915411,-1.4778265008171,110.128578148208));
#28210=CARTESIAN_POINT('Ctrl Pts',(2.64849277989884,-1.56243378133746,110.123596525624));
#28211=CARTESIAN_POINT('Ctrl Pts',(2.59810319931333,-1.64486186383458,110.118614903039));
#28212=CARTESIAN_POINT('Ctrl Pts',(2.54396223207421,-1.72471980674543,110.113633280454));
#28213=CARTESIAN_POINT('Ctrl Pts',(2.48981142105321,-1.80459226923751,110.108650752122));
#28214=CARTESIAN_POINT('Ctrl Pts',(2.43190811514426,-1.88189330078221,110.10366822379));
#28215=CARTESIAN_POINT('Ctrl Pts',(2.37053608480555,-1.95626197648341,110.098685695459));
#28216=CARTESIAN_POINT('Ctrl Pts',(2.30909790446301,-2.03071081065673,110.093697796696));
#28217=CARTESIAN_POINT('Ctrl Pts',(2.24418381543414,-2.10222063992062,110.088709897933));
#28218=CARTESIAN_POINT('Ctrl Pts',(2.17611691919086,-2.17046478985753,110.08372199917));
#28219=CARTESIAN_POINT('Ctrl Pts',(2.10800981489766,-2.23874925255054,110.078731153987));
#28220=CARTESIAN_POINT('Ctrl Pts',(2.03674651916761,-2.30376389908778,110.073740308804));
#28221=CARTESIAN_POINT('Ctrl Pts',(1.96268433556355,-2.36522143761075,110.068749463621));
#28222=CARTESIAN_POINT('Ctrl Pts',(1.88850246560064,-2.42677829306784,110.063750553106));
#28223=CARTESIAN_POINT('Ctrl Pts',(1.81151302658086,-2.48476629835775,110.058751642591));
#28224=CARTESIAN_POINT('Ctrl Pts',(1.73210342396602,-2.53894071980525,110.053752732076));
#28225=CARTESIAN_POINT('Ctrl Pts',(1.68600143742526,-2.57039218620459,110.050850567883));
#28226=CARTESIAN_POINT('Ctrl Pts',(1.63908423686524,-2.60055912638756,110.04794840369));
#28227=CARTESIAN_POINT('Ctrl Pts',(1.5914312251376,-2.62940086439041,110.045046239497));
#28228=CARTESIAN_POINT('Ctrl Pts',(1.50934018250595,-2.67908604184562,110.040046730004));
#28229=CARTESIAN_POINT('Ctrl Pts',(1.42477593332819,-2.72501042574185,110.035047220512));
#28230=CARTESIAN_POINT('Ctrl Pts',(1.33811763243627,-2.76691948776309,110.030047711019));
#28231=CARTESIAN_POINT('Ctrl Pts',(1.25157688297926,-2.80877170040781,110.02505498333));
#28232=CARTESIAN_POINT('Ctrl Pts',(1.16294811904434,-2.8466192267724,110.02006225564));
#28233=CARTESIAN_POINT('Ctrl Pts',(1.0726378171252,-2.88025178817285,110.01506952795));
#28234=CARTESIAN_POINT('Ctrl Pts',(0.982422790298312,-2.91384886806872,
110.010082067462));
#28235=CARTESIAN_POINT('Ctrl Pts',(0.89053016122757,-2.94323967035396,110.005094606974));
#28236=CARTESIAN_POINT('Ctrl Pts',(0.797388323358748,-2.96826112594076,
110.000107146487));
#28237=CARTESIAN_POINT('Ctrl Pts',(0.704313130652064,-2.99326467809123,
109.995123254643));
#28238=CARTESIAN_POINT('Ctrl Pts',(0.609990928771594,-3.01390498506074,
109.9901393628));
#28239=CARTESIAN_POINT('Ctrl Pts',(0.514866356918277,-3.0300684620176,109.985155470957));
#28240=CARTESIAN_POINT('Ctrl Pts',(0.419776427078054,-3.04622605263648,
109.980173394123));
#28241=CARTESIAN_POINT('Ctrl Pts',(0.323885140158247,-3.05790997911342,
109.97519131729));
#28242=CARTESIAN_POINT('Ctrl Pts',(0.227647496366421,-3.06505772660126,
109.970209240457));
#28243=CARTESIAN_POINT('Ctrl Pts',(0.13141862723048,-3.07220482237921,109.965227617874));
#28244=CARTESIAN_POINT('Ctrl Pts',(0.0348439017790225,-3.07481652914136,
109.960245995291));
#28245=CARTESIAN_POINT('Ctrl Pts',(-0.0616174587366106,-3.07288228521348,
109.955264372709));
#28246=CARTESIAN_POINT('Ctrl Pts',(-0.158096357627207,-3.07094768960598,
109.950281844379));
#28247=CARTESIAN_POINT('Ctrl Pts',(-0.25446141177816,-3.06446551064649,
109.94529931605));
#28248=CARTESIAN_POINT('Ctrl Pts',(-0.350255380902445,-3.05347726668284,
109.94031678772));
#28249=CARTESIAN_POINT('Ctrl Pts',(-0.44615260180752,-3.04247717901161,
109.93532888896));
#28250=CARTESIAN_POINT('Ctrl Pts',(-0.541477071980438,-3.02696138014293,
109.930340990199));
#28251=CARTESIAN_POINT('Ctrl Pts',(-0.635778866339523,-3.007023026702,109.925353091438));
#28252=CARTESIAN_POINT('Ctrl Pts',(-0.730136366062876,-2.98707289540202,
109.920362246258));
#28253=CARTESIAN_POINT('Ctrl Pts',(-0.823469562577525,-2.96269511856725,
109.915371401077));
#28254=CARTESIAN_POINT('Ctrl Pts',(-0.915342943206711,-2.93403298316868,
109.910380555896));
#28255=CARTESIAN_POINT('Ctrl Pts',(-1.00736479353926,-2.90532452903543,
109.905381645383));
#28256=CARTESIAN_POINT('Ctrl Pts',(-1.09792170524262,-2.87231804159566,
109.90038273487));
#28257=CARTESIAN_POINT('Ctrl Pts',(-1.18659747408996,-2.83520522793031,
109.895383824357));
#28258=CARTESIAN_POINT('Ctrl Pts',(-1.2380790204009,-2.81365903712443,109.892481660143));
#28259=CARTESIAN_POINT('Ctrl Pts',(-1.28892696056755,-2.79072968876361,
109.889579495928));
#28260=CARTESIAN_POINT('Ctrl Pts',(-1.33906394489701,-2.76646163925634,
109.886677331713));
#28261=CARTESIAN_POINT('Ctrl Pts',(-1.42543408474452,-2.72465547843908,
109.88167782222));
#28262=CARTESIAN_POINT('Ctrl Pts',(-1.5099962411333,-2.67872724112716,109.876678312727));
#28263=CARTESIAN_POINT('Ctrl Pts',(-1.59233048623538,-2.62885638112952,
109.871678803235));
#28264=CARTESIAN_POINT('Ctrl Pts',(-1.67455304545668,-2.57905317063686,
109.866686075545));
#28265=CARTESIAN_POINT('Ctrl Pts',(-1.75455332746351,-2.5253181920119,109.861693347855));
#28266=CARTESIAN_POINT('Ctrl Pts',(-1.83193364535642,-2.4678779080439,109.856700620165));
#28267=CARTESIAN_POINT('Ctrl Pts',(-1.90923232896429,-2.41049822212773,
109.851713159677));
#28268=CARTESIAN_POINT('Ctrl Pts',(-1.98391619252336,-2.34942126198035,
109.846725699189));
#28269=CARTESIAN_POINT('Ctrl Pts',(-2.05561521546054,-2.28491757749971,
109.841738238701));
#28270=CARTESIAN_POINT('Ctrl Pts',(-2.12726293607088,-2.22046004691305,
109.836754346858));
#28271=CARTESIAN_POINT('Ctrl Pts',(-2.19592973637622,-2.15258095900171,
109.831770455014));
#28272=CARTESIAN_POINT('Ctrl Pts',(-2.26127825778897,-2.08159143225824,
109.826786563171));
#28273=CARTESIAN_POINT('Ctrl Pts',(-2.32660298088865,-2.01062775814225,
109.821804486337));
#28274=CARTESIAN_POINT('Ctrl Pts',(-2.38861152913235,-1.93655621846444,
109.816822409504));
#28275=CARTESIAN_POINT('Ctrl Pts',(-2.44700373997525,-1.85972442758253,
109.811840332671));
#28276=CARTESIAN_POINT('Ctrl Pts',(-2.50539062679372,-1.78289964198995,
109.806858710088));
#28277=CARTESIAN_POINT('Ctrl Pts',(-2.56016156630613,-1.70331545515841,
109.801877087505));
#28278=CARTESIAN_POINT('Ctrl Pts',(-2.61105767573447,-1.62135130801073,
109.796895464922));
#28279=CARTESIAN_POINT('Ctrl Pts',(-2.66196303897232,-1.53937225833684,
109.791912936592));
#28280=CARTESIAN_POINT('Ctrl Pts',(-2.70899194143188,-1.45501276189719,
109.786930408263));
#28281=CARTESIAN_POINT('Ctrl Pts',(-2.75193026319493,-1.36867895304629,
109.781947879933));
#28282=CARTESIAN_POINT('Ctrl Pts',(-2.79491486614059,-1.28225208907334,
109.776959981172));
#28283=CARTESIAN_POINT('Ctrl Pts',(-2.83379989034128,-1.19384705798507,
109.771972082412));
#28284=CARTESIAN_POINT('Ctrl Pts',(-2.86841851244245,-1.10389197273894,
109.766984183651));
#28285=CARTESIAN_POINT('Ctrl Pts',(-2.90305758423886,-1.01388374978925,
109.76199333847));
#28286=CARTESIAN_POINT('Ctrl Pts',(-2.93342509763796,-0.922324065945445,
109.757002493289));
#28287=CARTESIAN_POINT('Ctrl Pts',(-2.95940412508885,-0.829656238695951,
109.752011648108));
#28288=CARTESIAN_POINT('Ctrl Pts',(-2.98542513530414,-0.736838657897498,
109.747012737595));
#28289=CARTESIAN_POINT('Ctrl Pts',(-3.00704340021671,-0.642909785376251,
109.742013827082));
#28290=CARTESIAN_POINT('Ctrl Pts',(-3.02419311920603,-0.548323105246242,
109.737014916569));
#28291=CARTESIAN_POINT('Ctrl Pts',(-3.03414954883091,-0.493409924175956,
109.734112752355));
#28292=CARTESIAN_POINT('Ctrl Pts',(-3.04260082871646,-0.438275144761581,
109.731210588142));
#28293=CARTESIAN_POINT('Ctrl Pts',(-3.04954213539411,-0.383007851689662,
109.728308423928));
#28294=CARTESIAN_POINT('Ctrl Pts',(-3.06539555968381,-0.256781495889267,
109.721680098345));
#28295=CARTESIAN_POINT('Ctrl Pts',(-3.07341405992647,-0.129550961238268,
109.715051772761));
#28296=CARTESIAN_POINT('Ctrl Pts',(-3.0734993128837,-0.00205516505886973,
109.708423447177));
#28297=CARTESIAN_POINT('Ctrl Pts',(-3.07349931288414,-0.0020551643988658,
109.708423447143));
#28298=CARTESIAN_POINT('Ctrl Pts',(-3.07356266900829,0.0926939486859775,
109.70349757516));
#28299=CARTESIAN_POINT('Ctrl Pts',(-3.06924046811866,0.187612347631797,
109.698571703178));
#28300=CARTESIAN_POINT('Ctrl Pts',(-3.0605122154393,0.282253838143699,109.693645831195));
#28301=CARTESIAN_POINT('Ctrl Pts',(-3.05137897652877,0.381286642926907,
109.688491401402));
#28302=CARTESIAN_POINT('Ctrl Pts',(-3.03742083355291,0.480015730082625,
109.683336971608));
#28303=CARTESIAN_POINT('Ctrl Pts',(-3.01867547972599,0.577927848525294,
109.678182541814));
#28304=CARTESIAN_POINT('Ctrl Pts',(-3.00079765234977,0.671308638651749,
109.673266656687));
#28305=CARTESIAN_POINT('Ctrl Pts',(-2.97856592490908,0.763945887153016,
109.66835077156));
#28306=CARTESIAN_POINT('Ctrl Pts',(-2.95206600206826,0.855399654800428,
109.663434886433));
#28307=CARTESIAN_POINT('Ctrl Pts',(-2.92557704384696,0.946815582497475,
109.658521035305));
#28308=CARTESIAN_POINT('Ctrl Pts',(-2.89482352222469,1.03704856765137,109.653607184177));
#28309=CARTESIAN_POINT('Ctrl Pts',(-2.85994172243619,1.12567117501904,109.648693333049));
#28310=CARTESIAN_POINT('Ctrl Pts',(-2.82506420199237,1.21428291004966,109.643780084758));
#28311=CARTESIAN_POINT('Ctrl Pts',(-2.78605957572621,1.30128423906308,109.638866836468));
#28312=CARTESIAN_POINT('Ctrl Pts',(-2.74311281379706,1.38626633111476,109.633953588177));
#28313=CARTESIAN_POINT('Ctrl Pts',(-2.70015881922103,1.47126273496634,109.629039512449));
#28314=CARTESIAN_POINT('Ctrl Pts',(-2.65326157639766,1.55423882374924,109.62412543672));
#28315=CARTESIAN_POINT('Ctrl Pts',(-2.6026520919461,1.63481018417692,109.619211360991));
#28316=CARTESIAN_POINT('Ctrl Pts',(-2.55198980139593,1.71546561302084,109.6142921579));
#28317=CARTESIAN_POINT('Ctrl Pts',(-2.49760778202127,1.79371092387224,109.609372954809));
#28318=CARTESIAN_POINT('Ctrl Pts',(-2.43978020987164,1.86919094196358,109.604453751718));
#28319=CARTESIAN_POINT('Ctrl Pts',(-2.38191726870418,1.94471712581991,109.5995315399));
#28320=CARTESIAN_POINT('Ctrl Pts',(-2.32060487432343,2.01747430775393,109.594609328082));
#28321=CARTESIAN_POINT('Ctrl Pts',(-2.25615582270311,2.08714234150018,109.589687116264));
#28322=CARTESIAN_POINT('Ctrl Pts',(-2.19160825703757,2.15691686680301,109.584757380564));
#28323=CARTESIAN_POINT('Ctrl Pts',(-2.1239147913646,2.22359250862423,109.579827644865));
#28324=CARTESIAN_POINT('Ctrl Pts',(-2.05342285426502,2.28688802340257,109.574897909166));
#28325=CARTESIAN_POINT('Ctrl Pts',(-2.02978894835492,2.30810917723027,109.573245111492));
#28326=CARTESIAN_POINT('Ctrl Pts',(-2.00584072734789,2.32895073584105,109.571592313818));
#28327=CARTESIAN_POINT('Ctrl Pts',(-1.9815920072361,2.34940319376177,109.569939516144));
#28328=CARTESIAN_POINT('Ctrl Pts',(-1.90824261408625,2.41126936113027,109.564940006651));
#28329=CARTESIAN_POINT('Ctrl Pts',(-1.83186437798168,2.46980589951436,109.559940497158));
#28330=CARTESIAN_POINT('Ctrl Pts',(-1.75279217700187,2.52470232586756,109.554940987665));
#28331=CARTESIAN_POINT('Ctrl Pts',(-1.67382723696063,2.57952428556696,109.549948259975));
#28332=CARTESIAN_POINT('Ctrl Pts',(-1.59217595231317,2.63071569856871,109.544955532285));
#28333=CARTESIAN_POINT('Ctrl Pts',(-1.5082070821448,2.67800553535056,109.539962804595));
#28334=CARTESIAN_POINT('Ctrl Pts',(-1.42432679701802,2.72524548254656,109.534975344107));
#28335=CARTESIAN_POINT('Ctrl Pts',(-1.33813416731467,2.76859182175116,109.529987883619));
#28336=CARTESIAN_POINT('Ctrl Pts',(-1.25002695547136,2.80781674270153,109.525000423131));
#28337=CARTESIAN_POINT('Ctrl Pts',(-1.16198278639743,2.84701359730415,109.520016531287));
#28338=CARTESIAN_POINT('Ctrl Pts',(-1.07202715840337,2.88209471804872,109.515032639443));
#28339=CARTESIAN_POINT('Ctrl Pts',(-0.980581589636902,2.91287864423926,
109.5100487476));
#28340=CARTESIAN_POINT('Ctrl Pts',(-0.889169323081802,2.94365135968629,
109.505066670766));
#28341=CARTESIAN_POINT('Ctrl Pts',(-0.796268609437589,2.97012985002376,
109.500084593933));
#28342=CARTESIAN_POINT('Ctrl Pts',(-0.702319156661911,2.99218148717382,
109.495102517099));
#28343=CARTESIAN_POINT('Ctrl Pts',(-0.608378269911635,3.01423111372265,
109.490120894516));
#28344=CARTESIAN_POINT('Ctrl Pts',(-0.513389261531923,3.03185458944141,
109.485139271933));
#28345=CARTESIAN_POINT('Ctrl Pts',(-0.417804101854027,3.04496994771278,
109.48015764935));
#28346=CARTESIAN_POINT('Ctrl Pts',(-0.322201563110231,3.05808769058732,
109.47517512102));
#28347=CARTESIAN_POINT('Ctrl Pts',(-0.226003092691896,3.06669562854235,
109.47019259269));
#28348=CARTESIAN_POINT('Ctrl Pts',(-0.129666816763162,3.0707635478217,109.465210064361));
#28349=CARTESIAN_POINT('Ctrl Pts',(-0.0332267045267823,3.07483585171851,
109.4602221656));
#28350=CARTESIAN_POINT('Ctrl Pts',(0.0633510704557592,3.07435834902676,
109.455234266839));
#28351=CARTESIAN_POINT('Ctrl Pts',(0.159607564124986,3.0693529734252,109.450246368078));
#28352=CARTESIAN_POINT('Ctrl Pts',(0.255920917826297,3.06434464107956,109.445255522897));
#28353=CARTESIAN_POINT('Ctrl Pts',(0.351912175715045,3.05480315350409,109.440264677715));
#28354=CARTESIAN_POINT('Ctrl Pts',(0.447128821294317,3.04080220783397,109.435273832534));
#28355=CARTESIAN_POINT('Ctrl Pts',(0.542499339377329,3.02677863628209,109.430274922021));
#28356=CARTESIAN_POINT('Ctrl Pts',(0.63709231508409,3.00828130083954,109.425276011508));
#28357=CARTESIAN_POINT('Ctrl Pts',(0.73046676216636,2.98543473540625,109.420277100995));
#28358=CARTESIAN_POINT('Ctrl Pts',(0.784676169975338,2.97217094834986,109.417374936783));
#28359=CARTESIAN_POINT('Ctrl Pts',(0.83847516344876,2.95744218974732,109.414472772572));
#28360=CARTESIAN_POINT('Ctrl Pts',(0.891780412031208,2.94128032440253,109.41157060836));
#28361=CARTESIAN_POINT('Ctrl Pts',(0.983586075158197,2.91344533995343,109.406572318003));
#28362=CARTESIAN_POINT('Ctrl Pts',(1.0742484876445,2.8812590886785,109.401574027646));
#28363=CARTESIAN_POINT('Ctrl Pts',(1.16332521637671,2.84483333271777,109.39657573729));
#28364=CARTESIAN_POINT('Ctrl Pts',(1.25229627227011,2.8084507890875,109.391583376467));
#28365=CARTESIAN_POINT('Ctrl Pts',(1.33968497736054,2.76783889229763,109.386591015645));
#28366=CARTESIAN_POINT('Ctrl Pts',(1.42506331255238,2.72315934260507,109.381598654823));
#28367=CARTESIAN_POINT('Ctrl Pts',(1.51035007260189,2.6785277153288,109.37661164871));
#28368=CARTESIAN_POINT('Ctrl Pts',(1.59363036303518,2.62983731152457,109.371624642597));
#28369=CARTESIAN_POINT('Ctrl Pts',(1.67449663930034,2.57729766518574,109.366637636483));
#28370=CARTESIAN_POINT('Ctrl Pts',(1.7422269802255,2.53329257031841,109.362460720718));
#28371=CARTESIAN_POINT('Ctrl Pts',(1.80826409501652,2.48658811596448,109.358283804952));
#28372=CARTESIAN_POINT('Ctrl Pts',(1.8723819390353,2.43733217358128,109.354106889186));
#28373=CARTESIAN_POINT('',(-3.07349977118745,0.0011859640259134,109.791576552796));
#28374=CARTESIAN_POINT('Ctrl Pts',(-3.07349977118745,0.0011859640259162,
109.791576552796));
#28375=CARTESIAN_POINT('Ctrl Pts',(-3.07345762578049,0.110408415828411,
109.785948464215));
#28376=CARTESIAN_POINT('Ctrl Pts',(-3.06758844717733,0.219451566251278,
109.780320375635));
#28377=CARTESIAN_POINT('Ctrl Pts',(-3.05597865567814,0.327714366544475,
109.774692287054));
#28378=CARTESIAN_POINT('Ctrl Pts',(-3.04477419212563,0.43219743155575,109.769260689649));
#28379=CARTESIAN_POINT('Ctrl Pts',(-3.02822341391354,0.535953470050506,
109.763829092245));
#28380=CARTESIAN_POINT('Ctrl Pts',(-3.00645543748823,0.638457478926707,
109.758397494841));
#28381=CARTESIAN_POINT('Ctrl Pts',(-2.98350625736496,0.746523700476025,
109.752671160672));
#28382=CARTESIAN_POINT('Ctrl Pts',(-2.95475800377033,0.85319780148342,109.746944826503));
#28383=CARTESIAN_POINT('Ctrl Pts',(-2.9204200294292,0.957887833573822,109.741218492334));
#28384=CARTESIAN_POINT('Ctrl Pts',(-2.88608205508808,1.06257786566422,109.735492158165));
#28385=CARTESIAN_POINT('Ctrl Pts',(-2.84615458915357,1.16528350101537,109.729765823996));
#28386=CARTESIAN_POINT('Ctrl Pts',(-2.80090335864964,1.26544167210708,109.724039489827));
#28387=CARTESIAN_POINT('Ctrl Pts',(-2.76139571732356,1.3528870974646,109.719039980335));
#28388=CARTESIAN_POINT('Ctrl Pts',(-2.71771963209727,1.43863417236837,109.714040470842));
#28389=CARTESIAN_POINT('Ctrl Pts',(-2.67004338980336,1.5222583705033,109.70904096135));
#28390=CARTESIAN_POINT('Ctrl Pts',(-2.62243182002944,1.60576913294437,109.70404823366));
#28391=CARTESIAN_POINT('Ctrl Pts',(-2.57083109292843,1.68716236368984,109.69905550597));
#28392=CARTESIAN_POINT('Ctrl Pts',(-2.51545707599578,1.76603452650925,109.69406277828));
#28393=CARTESIAN_POINT('Ctrl Pts',(-2.46014147725528,1.84482348118488,109.689075317793));
#28394=CARTESIAN_POINT('Ctrl Pts',(-2.40106075301206,1.92109629783268,109.684087857305));
#28395=CARTESIAN_POINT('Ctrl Pts',(-2.33847557403926,1.99447593107106,109.679100396817));
#28396=CARTESIAN_POINT('Ctrl Pts',(-2.2759351762249,2.06780305946666,109.674116504974));
#28397=CARTESIAN_POINT('Ctrl Pts',(-2.20989559254838,2.13824078676674,109.66913261313));
#28398=CARTESIAN_POINT('Ctrl Pts',(-2.14065891187789,2.2054436453915,109.664148721287));
#28399=CARTESIAN_POINT('Ctrl Pts',(-2.07144744549171,2.27262203039957,109.659166644454));
#28400=CARTESIAN_POINT('Ctrl Pts',(-1.99904151011945,2.33656758198775,109.65418456762));
#28401=CARTESIAN_POINT('Ctrl Pts',(-1.92378066131403,2.3969710505457,109.649202490787));
#28402=CARTESIAN_POINT('Ctrl Pts',(-1.84852667456408,2.45736901169896,109.644220868204));
#28403=CARTESIAN_POINT('Ctrl Pts',(-1.77041863436421,2.51422525730453,109.639239245622));
#28404=CARTESIAN_POINT('Ctrl Pts',(-1.68982900327128,2.56727096148871,109.634257623039));
#28405=CARTESIAN_POINT('Ctrl Pts',(-1.60922471956359,2.62032631031647,109.62927509471));
#28406=CARTESIAN_POINT('Ctrl Pts',(-1.52613831556261,2.66956950046214,109.62429256638));
#28407=CARTESIAN_POINT('Ctrl Pts',(-1.44097012159478,2.71477574739998,109.619310038051));
#28408=CARTESIAN_POINT('Ctrl Pts',(-1.35571012886561,2.7600307200097,109.61432213929));
#28409=CARTESIAN_POINT('Ctrl Pts',(-1.26836425487647,2.80123985644017,109.609334240529));
#28410=CARTESIAN_POINT('Ctrl Pts',(-1.17935605154246,2.83822507100656,109.604346341769));
#28411=CARTESIAN_POINT('Ctrl Pts',(-1.09029526984105,2.87523213324683,109.599355496588));
#28412=CARTESIAN_POINT('Ctrl Pts',(-0.99957061620157,2.90801015632687,109.594364651407));
#28413=CARTESIAN_POINT('Ctrl Pts',(-0.90762216115675,2.93643053086177,109.589373806226));
#28414=CARTESIAN_POINT('Ctrl Pts',(-0.815525115086421,2.96489683343968,
109.584374895713));
#28415=CARTESIAN_POINT('Ctrl Pts',(-0.722200743331968,2.98899131635566,
109.5793759852));
#28416=CARTESIAN_POINT('Ctrl Pts',(-0.628100631454975,3.00863621043919,
109.574377074688));
#28417=CARTESIAN_POINT('Ctrl Pts',(-0.573469932105146,3.02004123728803,
109.571474910473));
#28418=CARTESIAN_POINT('Ctrl Pts',(-0.518577910963521,3.02994750048335,
109.568572746258));
#28419=CARTESIAN_POINT('Ctrl Pts',(-0.463513494017647,3.03834782256139,
109.565670582043));
#28420=CARTESIAN_POINT('Ctrl Pts',(-0.368642163266014,3.05282086665209,
109.560670398687));
#28421=CARTESIAN_POINT('Ctrl Pts',(-0.272925651907291,3.06287158957453,
109.555670215331));
#28422=CARTESIAN_POINT('Ctrl Pts',(-0.176811855286777,3.06840998203142,
109.550670031975));
#28423=CARTESIAN_POINT('Ctrl Pts',(-0.0808588487974082,3.07393910923315,
109.545678213497));
#28424=CARTESIAN_POINT('Ctrl Pts',(0.0154896860225316,3.07497089992223,
109.540686395018));
#28425=CARTESIAN_POINT('Ctrl Pts',(0.111777985423372,3.07146673951952,109.53569457654));
#28426=CARTESIAN_POINT('Ctrl Pts',(0.207974068326147,3.06796593509467,109.530707538788));
#28427=CARTESIAN_POINT('Ctrl Pts',(0.304109594399434,3.05993782606783,109.525720501036));
#28428=CARTESIAN_POINT('Ctrl Pts',(0.399726494775764,3.04739577005913,109.520733463284));
#28429=CARTESIAN_POINT('Ctrl Pts',(0.495277928487216,3.03486230130409,109.51574984004));
#28430=CARTESIAN_POINT('Ctrl Pts',(0.590311008371727,3.01782108468474,109.510766216797));
#28431=CARTESIAN_POINT('Ctrl Pts',(0.68437155856275,2.99633740086633,109.505782593553));
#28432=CARTESIAN_POINT('Ctrl Pts',(0.778393387336073,2.97486256112435,109.500801021892));
#28433=CARTESIAN_POINT('Ctrl Pts',(0.871443055207516,2.94894898843552,109.495819450231));
#28434=CARTESIAN_POINT('Ctrl Pts',(0.96307642652806,2.91871308056581,109.49083787857));
#28435=CARTESIAN_POINT('Ctrl Pts',(1.05472610292954,2.88847179257183,109.485855420497));
#28436=CARTESIAN_POINT('Ctrl Pts',(1.14495855950261,2.853906761974,109.480872962423));
#28437=CARTESIAN_POINT('Ctrl Pts',(1.233345300022,2.81518411847496,109.47589050435));
#28438=CARTESIAN_POINT('Ctrl Pts',(1.32173929949388,2.77645829479497,109.470907637082));
#28439=CARTESIAN_POINT('Ctrl Pts',(1.40828688260833,2.73357436304779,109.465924769813));
#28440=CARTESIAN_POINT('Ctrl Pts',(1.49258145628562,2.68674577255688,109.460941902545));
#28441=CARTESIAN_POINT('Ctrl Pts',(1.5769463622301,2.63987811002617,109.455954877757));
#28442=CARTESIAN_POINT('Ctrl Pts',(1.6590541258067,2.58905943849805,109.450967852969));
#28443=CARTESIAN_POINT('Ctrl Pts',(1.73852496201855,2.53454792940248,109.445980828181));
#28444=CARTESIAN_POINT('Ctrl Pts',(1.78403016060481,2.50333450363685,109.443125245376));
#28445=CARTESIAN_POINT('Ctrl Pts',(1.8286713227525,2.47091108800218,109.440269662572));
#28446=CARTESIAN_POINT('Ctrl Pts',(1.87238193903529,2.43733217358128,109.437414079767));
#28447=CARTESIAN_POINT('Ctrl Pts',(1.8723819390353,2.43733217358127,110.437319612009));
#28448=CARTESIAN_POINT('Ctrl Pts',(1.94890666575668,2.37854514497852,110.432337890837));
#28449=CARTESIAN_POINT('Ctrl Pts',(2.02266101654233,2.31615004673507,110.427356169666));
#28450=CARTESIAN_POINT('Ctrl Pts',(2.09329697097887,2.25044663151355,110.422374448494));
#28451=CARTESIAN_POINT('Ctrl Pts',(2.16395057773146,2.18472679664483,110.417391482363));
#28452=CARTESIAN_POINT('Ctrl Pts',(2.23148391885292,2.11569730151574,110.412408516232));
#28453=CARTESIAN_POINT('Ctrl Pts',(2.29558537922392,2.0436951868352,110.4074255501));
#28454=CARTESIAN_POINT('Ctrl Pts',(2.35975826823993,1.97161283976277,110.40243703142));
#28455=CARTESIAN_POINT('Ctrl Pts',(2.42049135228201,1.8965515907143,110.397448512739));
#28456=CARTESIAN_POINT('Ctrl Pts',(2.47751310099432,1.81888182254964,110.392459994058));
#28457=CARTESIAN_POINT('Ctrl Pts',(2.53457201502878,1.74116143121013,110.387468223988));
#28458=CARTESIAN_POINT('Ctrl Pts',(2.58791453587653,1.6608295014096,110.382476453918));
#28459=CARTESIAN_POINT('Ctrl Pts',(2.6373134392608,1.57828390129734,110.377484683848));
#28460=CARTESIAN_POINT('Ctrl Pts',(2.68678864765634,1.49561079546099,110.37248520314));
#28461=CARTESIAN_POINT('Ctrl Pts',(2.73230787459593,1.41071758103269,110.367485722432));
#28462=CARTESIAN_POINT('Ctrl Pts',(2.77369074462531,1.32402488767389,110.362486241724));
#28463=CARTESIAN_POINT('Ctrl Pts',(2.78740678543857,1.29529124693134,110.360829201471));
#28464=CARTESIAN_POINT('Ctrl Pts',(2.80066883094348,1.2663600695108,110.359172161217));
#28465=CARTESIAN_POINT('Ctrl Pts',(2.8134715159664,1.23724705651124,110.357515120964));
#28466=CARTESIAN_POINT('Ctrl Pts',(2.85209890920228,1.14940924753587,110.352515611458));
#28467=CARTESIAN_POINT('Ctrl Pts',(2.88667670388421,1.05960647784786,110.347516101952));
#28468=CARTESIAN_POINT('Ctrl Pts',(2.91700165563847,0.968247690935769,110.342516592446));
#28469=CARTESIAN_POINT('Ctrl Pts',(2.94728547178935,0.877012831634629,110.337523864743));
#28470=CARTESIAN_POINT('Ctrl Pts',(2.9733277733235,0.78422656308776,110.33253113704));
#28471=CARTESIAN_POINT('Ctrl Pts',(2.99497273314224,0.690319185402311,110.327538409336));
#28472=CARTESIAN_POINT('Ctrl Pts',(3.01659485807464,0.596510877630301,110.322550948835));
#28473=CARTESIAN_POINT('Ctrl Pts',(3.03382876544318,0.501584237411476,110.317563488333));
#28474=CARTESIAN_POINT('Ctrl Pts',(3.04656827999061,0.405985178738126,110.312576027832));
#28475=CARTESIAN_POINT('Ctrl Pts',(3.05929867911811,0.310454523422114,110.307592135975));
#28476=CARTESIAN_POINT('Ctrl Pts',(3.06754102055111,0.214252839985739,110.302608244118));
#28477=CARTESIAN_POINT('Ctrl Pts',(3.07124030137914,0.117835738146636,110.29762435226));
#28478=CARTESIAN_POINT('Ctrl Pts',(3.0749382350208,0.0214537490259393,110.292642275413));
#28479=CARTESIAN_POINT('Ctrl Pts',(3.07409637849752,-0.0751430644344541,
110.287660198566));
#28480=CARTESIAN_POINT('Ctrl Pts',(3.06871171095375,-0.171495437418373,
110.282678121719));
#28481=CARTESIAN_POINT('Ctrl Pts',(3.06332753436751,-0.267839025287296,
110.277696499122));
#28482=CARTESIAN_POINT('Ctrl Pts',(3.0534013949426,-0.363937778722953,110.272714876525));
#28483=CARTESIAN_POINT('Ctrl Pts',(3.03898233389616,-0.459334980452197,
110.267733253928));
#28484=CARTESIAN_POINT('Ctrl Pts',(3.02456065121019,-0.554749527074792,
110.262750725585));
#28485=CARTESIAN_POINT('Ctrl Pts',(3.00564449019055,-0.649461834644932,
110.257768197241));
#28486=CARTESIAN_POINT('Ctrl Pts',(2.98233427614312,-0.743023899576512,
110.252785668898));
#28487=CARTESIAN_POINT('Ctrl Pts',(2.95899893712032,-0.83668681062525,110.247797770123));
#28488=CARTESIAN_POINT('Ctrl Pts',(2.93126019609635,-0.929196577256966,
110.242809871348));
#28489=CARTESIAN_POINT('Ctrl Pts',(2.89926873314341,-1.02011914157956,110.237821972573));
#28490=CARTESIAN_POINT('Ctrl Pts',(2.8672583723941,-1.11109541510914,110.232831127378));
#28491=CARTESIAN_POINT('Ctrl Pts',(2.8309904525927,-1.20048221288414,110.227840282183));
#28492=CARTESIAN_POINT('Ctrl Pts',(2.79066349358526,-1.28786626462942,110.222849436988));
#28493=CARTESIAN_POINT('Ctrl Pts',(2.7502713651945,-1.37539153120726,110.217850526461));
#28494=CARTESIAN_POINT('Ctrl Pts',(2.70580730207173,-1.46090720000393,110.212851615934));
#28495=CARTESIAN_POINT('Ctrl Pts',(2.65751533350989,-1.54402542147461,110.207852705408));
#28496=CARTESIAN_POINT('Ctrl Pts',(2.62947898127678,-1.59228047927282,110.204950541332));
#28497=CARTESIAN_POINT('Ctrl Pts',(2.60015324980404,-1.63972802094159,110.202048377256));
#28498=CARTESIAN_POINT('Ctrl Pts',(2.56959224488743,-1.68629711053965,110.19914621318));
#28499=CARTESIAN_POINT('Ctrl Pts',(2.51694531310072,-1.76652090194077,110.194146703689));
#28500=CARTESIAN_POINT('Ctrl Pts',(2.46044537719295,-1.84441774726801,110.189147194198));
#28501=CARTESIAN_POINT('Ctrl Pts',(2.40032479908744,-1.91959451678885,110.184147684707));
#28502=CARTESIAN_POINT('Ctrl Pts',(2.34028577416437,-1.99466930949921,110.179154957019));
#28503=CARTESIAN_POINT('Ctrl Pts',(2.27663613989706,-2.06703101968213,110.174162229331));
#28504=CARTESIAN_POINT('Ctrl Pts',(2.20965198838535,-2.13631466320499,110.169169501643));
#28505=CARTESIAN_POINT('Ctrl Pts',(2.14273850346508,-2.2055252142303,110.164182041156));
#28506=CARTESIAN_POINT('Ctrl Pts',(2.07249779802678,-2.27166384008945,110.15919458067));
#28507=CARTESIAN_POINT('Ctrl Pts',(1.99924609399943,-2.33439870322703,110.154207120184));
#28508=CARTESIAN_POINT('Ctrl Pts',(1.92604680327836,-2.39708867810378,110.149223228342));
#28509=CARTESIAN_POINT('Ctrl Pts',(1.84984112933959,-2.45637944714489,110.1442393365));
#28510=CARTESIAN_POINT('Ctrl Pts',(1.77098128767597,-2.51197681691164,110.139255444659));
#28511=CARTESIAN_POINT('Ctrl Pts',(1.69215016481352,-2.56755393949334,110.134273367827));
#28512=CARTESIAN_POINT('Ctrl Pts',(1.610667153118,-2.61944008258216,110.129291290995));
#28513=CARTESIAN_POINT('Ctrl Pts',(1.52691583566181,-2.66738266486179,110.124309214163));
#28514=CARTESIAN_POINT('Ctrl Pts',(1.44317215439605,-2.71532087588257,110.119327591582));
#28515=CARTESIAN_POINT('Ctrl Pts',(1.35716095961153,-2.75931602305225,110.114345969001));
#28516=CARTESIAN_POINT('Ctrl Pts',(1.26929204279809,-2.79916058133317,110.10936434642));
#28517=CARTESIAN_POINT('Ctrl Pts',(1.18140714986676,-2.8390123840571,110.104381818092));
#28518=CARTESIAN_POINT('Ctrl Pts',(1.09166426389277,-2.87471191790758,110.099399289764));
#28519=CARTESIAN_POINT('Ctrl Pts',(1.00049384353992,-2.9060995026046,110.094416761436));
#28520=CARTESIAN_POINT('Ctrl Pts',(0.9092251549101,-2.93752091849221,110.089428862677));
#28521=CARTESIAN_POINT('Ctrl Pts',(0.816526275827664,-2.96462096350184,
110.084440963918));
#28522=CARTESIAN_POINT('Ctrl Pts',(0.722843328701962,-2.98728970341865,
110.079453065158));
#28523=CARTESIAN_POINT('Ctrl Pts',(0.629105041773077,-3.00997183407138,
110.074462219979));
#28524=CARTESIAN_POINT('Ctrl Pts',(0.534381960170196,-3.0282173645088,110.0694713748));
#28525=CARTESIAN_POINT('Ctrl Pts',(0.439128816249519,-3.04196780599981,
110.06448052962));
#28526=CARTESIAN_POINT('Ctrl Pts',(0.343721740842073,-3.05574046855162,
110.059481619109));
#28527=CARTESIAN_POINT('Ctrl Pts',(0.247783329323794,-3.06500349504237,
110.054482708597));
#28528=CARTESIAN_POINT('Ctrl Pts',(0.151771769027837,-3.0697504100702,110.049483798086));
#28529=CARTESIAN_POINT('Ctrl Pts',(0.0960313601271893,-3.07250627596647,
110.046581633856));
#28530=CARTESIAN_POINT('Ctrl Pts',(0.0402662849811449,-3.07374096692459,
110.043679469626));
#28531=CARTESIAN_POINT('Ctrl Pts',(-0.0154344978905223,-3.07346124528598,
110.040777305396));
#28532=CARTESIAN_POINT('Ctrl Pts',(-0.111389299388775,-3.07297937352541,
110.035777795905));
#28533=CARTESIAN_POINT('Ctrl Pts',(-0.207490050581665,-3.06799872221208,
110.030778286414));
#28534=CARTESIAN_POINT('Ctrl Pts',(-0.303280487470693,-3.05850015463782,
110.025778776924));
#28535=CARTESIAN_POINT('Ctrl Pts',(-0.398940985239289,-3.04901447181025,
110.020786049236));
#28536=CARTESIAN_POINT('Ctrl Pts',(-0.49429157220971,-3.03502309570359,
110.015793321548));
#28537=CARTESIAN_POINT('Ctrl Pts',(-0.588875783732631,-3.01655889406013,
110.01080059386));
#28538=CARTESIAN_POINT('Ctrl Pts',(-0.683360211295895,-2.99811417168411,
110.005813133374));
#28539=CARTESIAN_POINT('Ctrl Pts',(-0.777079442135289,-2.97520608795508,
110.000825672888));
#28540=CARTESIAN_POINT('Ctrl Pts',(-0.869582965946565,-2.94791921791211,
109.995838212402));
#28541=CARTESIAN_POINT('Ctrl Pts',(-0.962020301323166,-2.92065187226283,
109.990854320561));
#28542=CARTESIAN_POINT('Ctrl Pts',(-1.0532432391063,-2.88901209264129,109.98587042872));
#28543=CARTESIAN_POINT('Ctrl Pts',(-1.14281324783431,-2.85313514060838,
109.980886536879));
#28544=CARTESIAN_POINT('Ctrl Pts',(-1.23235063738287,-2.8172712540731,109.975904460047));
#28545=CARTESIAN_POINT('Ctrl Pts',(-1.32023588682419,-2.77717342409716,
109.970922383216));
#28546=CARTESIAN_POINT('Ctrl Pts',(-1.40604829049614,-2.7330258789102,109.965940306385));
#28547=CARTESIAN_POINT('Ctrl Pts',(-1.49185287005355,-2.68888235896243,
109.960958683804));
#28548=CARTESIAN_POINT('Ctrl Pts',(-1.57558458934891,-2.6406900588997,109.955977061223));
#28549=CARTESIAN_POINT('Ctrl Pts',(-1.65684626636518,-2.58867972133127,
109.950995438643));
#28550=CARTESIAN_POINT('Ctrl Pts',(-1.73812271818616,-2.53665992736706,
109.946012910315));
#28551=CARTESIAN_POINT('Ctrl Pts',(-1.81692786612375,-2.48082095390266,
109.941030381988));
#28552=CARTESIAN_POINT('Ctrl Pts',(-1.89289340769943,-2.42143692816642,
109.936047853661));
#28553=CARTESIAN_POINT('Ctrl Pts',(-1.96894082893254,-2.36198889520291,
109.931059954902));
#28554=CARTESIAN_POINT('Ctrl Pts',(-2.04214218703748,-2.29898845240086,
109.926072056143));
#28555=CARTESIAN_POINT('Ctrl Pts',(-2.11216237800063,-2.23274994994037,
109.921084157385));
#28556=CARTESIAN_POINT('Ctrl Pts',(-2.1822239308512,-2.16647231948774,109.916093312206));
#28557=CARTESIAN_POINT('Ctrl Pts',(-2.24910027066741,-2.09695313694679,
109.911102467027));
#28558=CARTESIAN_POINT('Ctrl Pts',(-2.31249475781148,-2.02454198402859,
109.906111621849));
#28559=CARTESIAN_POINT('Ctrl Pts',(-2.37599169204783,-1.9520138128585,109.901112711338));
#28560=CARTESIAN_POINT('Ctrl Pts',(-2.43599526512317,-1.87658468266414,
109.896113800827));
#28561=CARTESIAN_POINT('Ctrl Pts',(-2.4922505847114,-1.7986353919029,109.891114890317));
#28562=CARTESIAN_POINT('Ctrl Pts',(-2.52491013646644,-1.75338120235213,
109.888212726082));
#28563=CARTESIAN_POINT('Ctrl Pts',(-2.55630716799028,-1.70727811687191,
109.885310561847));
#28564=CARTESIAN_POINT('Ctrl Pts',(-2.58639891787753,-1.66040443495009,
109.882408397611));
#28565=CARTESIAN_POINT('Ctrl Pts',(-2.63940236178393,-1.57784138761193,
109.877296541378));
#28566=CARTESIAN_POINT('Ctrl Pts',(-2.68853322212055,-1.49260657041294,
109.872184685144));
#28567=CARTESIAN_POINT('Ctrl Pts',(-2.73351906787153,-1.40508923402848,
109.867072828911));
#28568=CARTESIAN_POINT('Ctrl Pts',(-2.77843555048245,-1.31770683958322,
109.861968854587));
#28569=CARTESIAN_POINT('Ctrl Pts',(-2.81921954317603,-1.22804928973175,
109.856864880264));
#28570=CARTESIAN_POINT('Ctrl Pts',(-2.85564221881624,-1.13653410336614,
109.851760905941));
#28571=CARTESIAN_POINT('Ctrl Pts',(-2.89200450421949,-1.04517065279952,
109.846665394209));
#28572=CARTESIAN_POINT('Ctrl Pts',(-2.92401972075752,-0.951956080133295,
109.841569882477));
#28573=CARTESIAN_POINT('Ctrl Pts',(-2.95150578637871,-0.857330649733813,
109.836474370745));
#28574=CARTESIAN_POINT('Ctrl Pts',(-2.97896501450207,-0.762797611960408,
109.83138383429));
#28575=CARTESIAN_POINT('Ctrl Pts',(-3.00190377183239,-0.666856850360775,
109.826293297835));
#28576=CARTESIAN_POINT('Ctrl Pts',(-3.02018879123147,-0.569966591406704,
109.82120276138));
#28577=CARTESIAN_POINT('Ctrl Pts',(-3.03845833192543,-0.47315835236822,
109.816116534185));
#28578=CARTESIAN_POINT('Ctrl Pts',(-3.05208189904631,-0.375402620030141,
109.81103030699));
#28579=CARTESIAN_POINT('Ctrl Pts',(-3.06097682462202,-0.277169856093556,
109.805944079796));
#28580=CARTESIAN_POINT('Ctrl Pts',(-3.06935225879234,-0.184674192052551,
109.801154904138));
#28581=CARTESIAN_POINT('Ctrl Pts',(-3.07353563445906,-0.091755982939446,
109.796365728481));
#28582=CARTESIAN_POINT('Ctrl Pts',(-3.07349977118766,0.0011859635037227,
109.791576552823));
#28583=CARTESIAN_POINT('Origin',(0.,0.,116.208423447177));
#28584=CARTESIAN_POINT('',(1.87238193903529,2.43733217358128,111.437229631665));
#28585=CARTESIAN_POINT('',(1.87238193903529,2.43733217358128,111.354256900092));
#28586=CARTESIAN_POINT('',(1.8723819390353,2.43733217358128,116.208423447177));
#28587=CARTESIAN_POINT('',(-3.07349888025591,0.00262355973274775,110.708423447212));
#28588=CARTESIAN_POINT('Ctrl Pts',(1.87238193903529,2.43733217358128,111.354256900092));
#28589=CARTESIAN_POINT('Ctrl Pts',(1.948881640316,2.37856436976194,111.349266871793));
#28590=CARTESIAN_POINT('Ctrl Pts',(2.02254958126843,2.31623943328911,111.344276843494));
#28591=CARTESIAN_POINT('Ctrl Pts',(2.09305320063531,2.25067335464529,111.339286815196));
#28592=CARTESIAN_POINT('Ctrl Pts',(2.16367582243927,2.18499660759582,111.334288364272));
#28593=CARTESIAN_POINT('Ctrl Pts',(2.23112314536882,2.11606810346765,111.329289913349));
#28594=CARTESIAN_POINT('Ctrl Pts',(2.29510062670075,2.04423955624526,111.324291462425));
#28595=CARTESIAN_POINT('Ctrl Pts',(2.34755265303044,1.98535082271439,111.32019347554));
#28596=CARTESIAN_POINT('Ctrl Pts',(2.39767308367136,1.92451353072959,111.316095488655));
#28597=CARTESIAN_POINT('Ctrl Pts',(2.44532132719983,1.86193605065848,111.31199750177));
#28598=CARTESIAN_POINT('Ctrl Pts',(2.50345178104249,1.7855920545846,111.306997992453));
#28599=CARTESIAN_POINT('Ctrl Pts',(2.55810567098051,1.70638906934886,111.301998483135));
#28600=CARTESIAN_POINT('Ctrl Pts',(2.60898960431686,1.6246770431586,111.296998973818));
#28601=CARTESIAN_POINT('Ctrl Pts',(2.65980451388741,1.54307585886654,111.292006246307));
#28602=CARTESIAN_POINT('Ctrl Pts',(2.70685940038884,1.45897276728328,111.287013518795));
#28603=CARTESIAN_POINT('Ctrl Pts',(2.7499019655331,1.37274958749117,111.282020791284));
#28604=CARTESIAN_POINT('Ctrl Pts',(2.79289912183065,1.28661737103132,111.277033330977));
#28605=CARTESIAN_POINT('Ctrl Pts',(2.83189217650519,1.19836990332672,111.27204587067));
#28606=CARTESIAN_POINT('Ctrl Pts',(2.86667344342633,1.10841581491526,111.267058410363));
#28607=CARTESIAN_POINT('Ctrl Pts',(2.90142982351349,1.01852609082005,111.262074518705));
#28608=CARTESIAN_POINT('Ctrl Pts',(2.93198024896046,0.926932581812277,111.257090627046));
#28609=CARTESIAN_POINT('Ctrl Pts',(2.9581645104515,0.834065332636013,111.252106735387));
#28610=CARTESIAN_POINT('Ctrl Pts',(2.98433923627205,0.741231903450742,111.24712465874));
#28611=CARTESIAN_POINT('Ctrl Pts',(3.0061508383937,0.647126077804854,111.242142582093));
#28612=CARTESIAN_POINT('Ctrl Pts',(3.02348878664653,0.552193631820106,111.237160505446));
#28613=CARTESIAN_POINT('Ctrl Pts',(3.04082515407159,0.45726984152198,111.232178883052));
#28614=CARTESIAN_POINT('Ctrl Pts',(3.05368859991533,0.36152001258511,111.227197260657));
#28615=CARTESIAN_POINT('Ctrl Pts',(3.06201980405686,0.26539964122729,111.222215638263));
#28616=CARTESIAN_POINT('Ctrl Pts',(3.07035252295555,0.169261793521756,111.217233110123));
#28617=CARTESIAN_POINT('Ctrl Pts',(3.07415132573822,0.0727537069176042,
111.212250581984));
#28618=CARTESIAN_POINT('Ctrl Pts',(3.07340888777848,-0.0236655556506188,
111.207268053844));
#28619=CARTESIAN_POINT('Ctrl Pts',(3.07266564958019,-0.1201887439533,111.202280155275));
#28620=CARTESIAN_POINT('Ctrl Pts',(3.06737140203435,-0.216622477408389,
111.197292256705));
#28621=CARTESIAN_POINT('Ctrl Pts',(3.0575709438332,-0.312509477339433,111.192304358135));
#28622=CARTESIAN_POINT('Ctrl Pts',(3.04776469636858,-0.408453119020665,
111.187313513147));
#28623=CARTESIAN_POINT('Ctrl Pts',(3.03344700313358,-0.503848950208386,
111.182322668158));
#28624=CARTESIAN_POINT('Ctrl Pts',(3.0147140412321,-0.598248693770405,111.177331823169));
#28625=CARTESIAN_POINT('Ctrl Pts',(2.99595080638871,-0.692800989714087,
111.172332912848));
#28626=CARTESIAN_POINT('Ctrl Pts',(2.97275816104351,-0.786353558033525,
111.167334002527));
#28627=CARTESIAN_POINT('Ctrl Pts',(2.94528248064981,-0.878472173251547,
111.162335092206));
#28628=CARTESIAN_POINT('Ctrl Pts',(2.92933120680081,-0.931952532495746,
111.159432926132));
#28629=CARTESIAN_POINT('Ctrl Pts',(2.91193725478093,-0.984949914274633,
111.156530760059));
#28630=CARTESIAN_POINT('Ctrl Pts',(2.89313660636581,-1.03738268103249,111.153628593986));
#28631=CARTESIAN_POINT('Ctrl Pts',(2.86074906560292,-1.12770767053203,111.148629084399));
#28632=CARTESIAN_POINT('Ctrl Pts',(2.82407060568943,-1.21667312579871,111.143629574812));
#28633=CARTESIAN_POINT('Ctrl Pts',(2.7832350224323,-1.30384242142457,111.138630065224));
#28634=CARTESIAN_POINT('Ctrl Pts',(2.74245483237396,-1.39089347247704,111.133637337439));
#28635=CARTESIAN_POINT('Ctrl Pts',(2.69752891095457,-1.47615281212287,111.128644609653));
#28636=CARTESIAN_POINT('Ctrl Pts',(2.6486401609382,-1.55920093248602,111.123651881868));
#28637=CARTESIAN_POINT('Ctrl Pts',(2.59980298730962,-1.64216143919449,111.118664421283));
#28638=CARTESIAN_POINT('Ctrl Pts',(2.54701151753359,-1.72291498777456,111.113676960698));
#28639=CARTESIAN_POINT('Ctrl Pts',(2.49049543277262,-1.80106489315036,111.108689500114));
#28640=CARTESIAN_POINT('Ctrl Pts',(2.43401978657781,-1.87915888046086,111.103705608173));
#28641=CARTESIAN_POINT('Ctrl Pts',(2.37382507988143,-1.95465257338061,111.098721716231));
#28642=CARTESIAN_POINT('Ctrl Pts',(2.31018480474021,-2.0271774510258,111.09373782429));
#28643=CARTESIAN_POINT('Ctrl Pts',(2.24656770580208,-2.09967591691695,111.088755747358));
#28644=CARTESIAN_POINT('Ctrl Pts',(2.17950782077992,-2.16920738609092,111.083773670426));
#28645=CARTESIAN_POINT('Ctrl Pts',(2.10931888497435,-2.2354364431785,111.078791593494));
#28646=CARTESIAN_POINT('Ctrl Pts',(2.03913634877496,-2.30165946170919,111.073809970812));
#28647=CARTESIAN_POINT('Ctrl Pts',(1.96582564840985,-2.36458036568008,111.06882834813));
#28648=CARTESIAN_POINT('Ctrl Pts',(1.88973655370966,-2.4239014021972,111.063846725449));
#28649=CARTESIAN_POINT('Ctrl Pts',(1.81363362466495,-2.48323322432898,111.05886419702));
#28650=CARTESIAN_POINT('Ctrl Pts',(1.7347516442379,-2.53896360926549,111.05388166859));
#28651=CARTESIAN_POINT('Ctrl Pts',(1.65347168301933,-2.59083647562968,111.048899140161));
#28652=CARTESIAN_POINT('Ctrl Pts',(1.57210411398258,-2.64276525329817,111.043911241301));
#28653=CARTESIAN_POINT('Ctrl Pts',(1.48833377474077,-2.69082797511479,111.038923342441));
#28654=CARTESIAN_POINT('Ctrl Pts',(1.40256861788299,-2.73481325178334,111.03393544358));
#28655=CARTESIAN_POINT('Ctrl Pts',(1.31675279836798,-2.77882451115953,111.0289445983));
#28656=CARTESIAN_POINT('Ctrl Pts',(1.22894021432322,-2.81875334785365,111.023953753019));
#28657=CARTESIAN_POINT('Ctrl Pts',(1.13955924096691,-2.85443636929025,111.018962907738));
#28658=CARTESIAN_POINT('Ctrl Pts',(1.05003382571607,-2.89017705538439,111.013963997126));
#28659=CARTESIAN_POINT('Ctrl Pts',(0.958935374812929,-2.92165808235672,
111.008965086514));
#28660=CARTESIAN_POINT('Ctrl Pts',(0.866707807624285,-2.94876581406579,
111.003966175903));
#28661=CARTESIAN_POINT('Ctrl Pts',(0.813164250758867,-2.96450345540776,
111.001064012669));
#28662=CARTESIAN_POINT('Ctrl Pts',(0.759240344083131,-2.97876803448073,
110.998161849435));
#28663=CARTESIAN_POINT('Ctrl Pts',(0.705024154617008,-2.99154528486643,
110.995259686202));
#28664=CARTESIAN_POINT('Ctrl Pts',(0.611626805219617,-3.01355644666815,
110.990260176716));
#28665=CARTESIAN_POINT('Ctrl Pts',(0.517033625005757,-3.03122821826157,
110.98526066723));
#28666=CARTESIAN_POINT('Ctrl Pts',(0.421683697314452,-3.04443510514171,
110.980261157744));
#28667=CARTESIAN_POINT('Ctrl Pts',(0.326463111192108,-3.057624076964,110.975268430061));
#28668=CARTESIAN_POINT('Ctrl Pts',(0.23048824883096,-3.06636014142969,110.970275702377));
#28669=CARTESIAN_POINT('Ctrl Pts',(0.134210571877783,-3.070568314237,110.965282974694));
#28670=CARTESIAN_POINT('Ctrl Pts',(0.0380344654444882,-3.07477204752818,
110.960295514213));
#28671=CARTESIAN_POINT('Ctrl Pts',(-0.058443384298457,-3.07445736610732,
110.955308053731));
#28672=CARTESIAN_POINT('Ctrl Pts',(-0.154765190719179,-3.06960094894135,
110.95032059325));
#28673=CARTESIAN_POINT('Ctrl Pts',(-0.25101807664028,-3.06474800665516,
110.945336701412));
#28674=CARTESIAN_POINT('Ctrl Pts',(-0.347114704050907,-3.05535981094989,
110.940352809575));
#28675=CARTESIAN_POINT('Ctrl Pts',(-0.442597057314949,-3.04146512307081,
110.935368917738));
#28676=CARTESIAN_POINT('Ctrl Pts',(-0.538044638273774,-3.02757549529249,
110.930386840911));
#28677=CARTESIAN_POINT('Ctrl Pts',(-0.632877955617285,-3.00918269928038,
110.925404764083));
#28678=CARTESIAN_POINT('Ctrl Pts',(-0.726644851861425,-2.98636727635154,
110.920422687256));
#28679=CARTESIAN_POINT('Ctrl Pts',(-0.820403198727854,-2.9635539336629,
110.915441064679));
#28680=CARTESIAN_POINT('Ctrl Pts',(-0.913094891337656,-2.93631886973509,
110.910459442102));
#28681=CARTESIAN_POINT('Ctrl Pts',(-1.00427974414338,-2.90479335676452,
110.905477819525));
#28682=CARTESIAN_POINT('Ctrl Pts',(-1.09548117596486,-2.87326211189924,
110.900495291201));
#28683=CARTESIAN_POINT('Ctrl Pts',(-1.18517480902578,-2.83743901221733,
110.895512762877));
#28684=CARTESIAN_POINT('Ctrl Pts',(-1.27293836977718,-2.79750427287413,
110.890530234554));
#28685=CARTESIAN_POINT('Ctrl Pts',(-1.36079652671805,-2.75752648976496,
110.885542335798));
#28686=CARTESIAN_POINT('Ctrl Pts',(-1.44672005794881,-2.71342840153585,
110.880554437043));
#28687=CARTESIAN_POINT('Ctrl Pts',(-1.53030954134675,-2.6654371044283,110.875566538287));
#28688=CARTESIAN_POINT('Ctrl Pts',(-1.6139484022026,-2.61741745820125,110.870575693112));
#28689=CARTESIAN_POINT('Ctrl Pts',(-1.69525010010885,-2.56550026001342,
110.865584847936));
#28690=CARTESIAN_POINT('Ctrl Pts',(-1.77384435308946,-2.50995586833965,
110.86059400276));
#28691=CARTESIAN_POINT('Ctrl Pts',(-1.8525656163727,-2.45432171552269,110.855595092252));
#28692=CARTESIAN_POINT('Ctrl Pts',(-1.92857035231037,-2.39504893459013,
110.850596181744));
#28693=CARTESIAN_POINT('Ctrl Pts',(-2.0015215512034,-2.33244801229702,110.845597271236));
#28694=CARTESIAN_POINT('Ctrl Pts',(-2.04387405236461,-2.29610446106903,
110.842695106963));
#28695=CARTESIAN_POINT('Ctrl Pts',(-2.08519804158071,-2.25863986348709,
110.839792942691));
#28696=CARTESIAN_POINT('Ctrl Pts',(-2.12543360399879,-2.22012032218812,
110.836890778418));
#28697=CARTESIAN_POINT('Ctrl Pts',(-2.1937352854616,-2.15473166395198,110.831964223703));
#28698=CARTESIAN_POINT('Ctrl Pts',(-2.25915360617813,-2.08605668722672,
110.827037668989));
#28699=CARTESIAN_POINT('Ctrl Pts',(-2.32134887028838,-2.01438369542916,
110.822111114274));
#28700=CARTESIAN_POINT('Ctrl Pts',(-2.38344339011673,-1.94282679999672,
110.817192539624));
#28701=CARTESIAN_POINT('Ctrl Pts',(-2.44232493870375,-1.86828188317021,
110.812273964974));
#28702=CARTESIAN_POINT('Ctrl Pts',(-2.49768920318606,-1.79107534578749,
110.807355390324));
#28703=CARTESIAN_POINT('Ctrl Pts',(-2.55300266298286,-1.71393965652111,
110.802441329175));
#28704=CARTESIAN_POINT('Ctrl Pts',(-2.60480498295285,-1.63414756060737,
110.797527268025));
#28705=CARTESIAN_POINT('Ctrl Pts',(-2.65283131018544,-1.55205937054606,
110.792613206876));
#28706=CARTESIAN_POINT('Ctrl Pts',(-2.70082759207679,-1.47002253497767,
110.78770221997));
#28707=CARTESIAN_POINT('Ctrl Pts',(-2.74505234385498,-1.38569284746465,
110.782791233065));
#28708=CARTESIAN_POINT('Ctrl Pts',(-2.78528406969069,-1.29945946498045,
110.777880246159));
#28709=CARTESIAN_POINT('Ctrl Pts',(-2.82550237202281,-1.21325485466784,
110.772970897827));
#28710=CARTESIAN_POINT('Ctrl Pts',(-2.86173010459517,-1.12514822177586,
110.768061549496));
#28711=CARTESIAN_POINT('Ctrl Pts',(-2.89379235729422,-1.03555204739578,
110.763152201164));
#28712=CARTESIAN_POINT('Ctrl Pts',(-2.92586678026355,-0.945921863875121,
110.758240989329));
#28713=CARTESIAN_POINT('Ctrl Pts',(-2.95377240523807,-0.854801434026095,
110.753329777495));
#28714=CARTESIAN_POINT('Ctrl Pts',(-2.97738326655227,-0.76262122580908,
110.74841856566));
#28715=CARTESIAN_POINT('Ctrl Pts',(-3.00099833095211,-0.670424608139487,
110.743506479557));
#28716=CARTESIAN_POINT('Ctrl Pts',(-3.0203170106075,-0.577168279053442,
110.738594393453));
#28717=CARTESIAN_POINT('Ctrl Pts',(-3.03526427861237,-0.483293915728025,
110.733682307349));
#28718=CARTESIAN_POINT('Ctrl Pts',(-3.05022812720535,-0.389315420185806,
110.728764772406));
#28719=CARTESIAN_POINT('Ctrl Pts',(-3.06081082419188,-0.294717971407319,
110.723847237462));
#28720=CARTESIAN_POINT('Ctrl Pts',(-3.06698918420348,-0.199948978439139,
110.718929702518));
#28721=CARTESIAN_POINT('Ctrl Pts',(-3.07138918192552,-0.132458033852455,
110.715427617416));
#28722=CARTESIAN_POINT('Ctrl Pts',(-3.07355650191939,-0.0648801894581821,
110.711925532314));
#28723=CARTESIAN_POINT('Ctrl Pts',(-3.07349888025591,0.00262355973275451,
110.708423447212));
#28724=CARTESIAN_POINT('Ctrl Pts',(-3.07349888025533,0.00262356040959872,
110.708423447177));
#28725=CARTESIAN_POINT('Ctrl Pts',(-3.07337791850908,0.144330147494426,
110.701071729185));
#28726=CARTESIAN_POINT('Ctrl Pts',(-3.06345337427643,0.285630529407084,
110.693720011193));
#28727=CARTESIAN_POINT('Ctrl Pts',(-3.04391216934768,0.425442070436255,
110.6863682932));
#28728=CARTESIAN_POINT('Ctrl Pts',(-3.0369601185254,0.475181937671709,110.683752819011));
#28729=CARTESIAN_POINT('Ctrl Pts',(-3.02879130436724,0.524733671575758,
110.681137344822));
#28730=CARTESIAN_POINT('Ctrl Pts',(-3.01941544185788,0.574049335397397,
110.678521870633));
#28731=CARTESIAN_POINT('Ctrl Pts',(-3.00149337100039,0.668316803645044,
110.673522361128));
#28732=CARTESIAN_POINT('Ctrl Pts',(-2.97912098278221,0.761909739136843,
110.668522851622));
#28733=CARTESIAN_POINT('Ctrl Pts',(-2.95236242568487,0.854376004698248,
110.663523342116));
#28734=CARTESIAN_POINT('Ctrl Pts',(-2.9256401663993,0.946716840361099,110.658530614413));
#28735=CARTESIAN_POINT('Ctrl Pts',(-2.89454368406788,1.03793362547514,110.653537886709));
#28736=CARTESIAN_POINT('Ctrl Pts',(-2.85918830111607,1.12758348194758,110.648545159006));
#28737=CARTESIAN_POINT('Ctrl Pts',(-2.82387021720086,1.21713876008429,110.643557698505));
#28738=CARTESIAN_POINT('Ctrl Pts',(-2.78430232472978,1.30512998960044,110.638570238003));
#28739=CARTESIAN_POINT('Ctrl Pts',(-2.74064970866011,1.39112954983397,110.633582777502));
#28740=CARTESIAN_POINT('Ctrl Pts',(-2.69702832705611,1.47706757537488,110.628598885645));
#28741=CARTESIAN_POINT('Ctrl Pts',(-2.64932823018674,1.56101637433474,110.623614993787));
#28742=CARTESIAN_POINT('Ctrl Pts',(-2.59776216630118,1.64256932192654,110.61863110193));
#28743=CARTESIAN_POINT('Ctrl Pts',(-2.54621488149783,1.72409256995641,110.613649025083));
#28744=CARTESIAN_POINT('Ctrl Pts',(-2.49080466135627,1.80322132956271,110.608666948236));
#28745=CARTESIAN_POINT('Ctrl Pts',(-2.4317891630379,1.87957540857807,110.603684871389));
#28746=CARTESIAN_POINT('Ctrl Pts',(-2.37277904557233,1.95592252586183,110.598703248792));
#28747=CARTESIAN_POINT('Ctrl Pts',(-2.31016457207171,2.02949511833949,110.593721626195));
#28748=CARTESIAN_POINT('Ctrl Pts',(-2.24424486111886,2.09994458339777,110.588740003598));
#28749=CARTESIAN_POINT('Ctrl Pts',(-2.17831316480023,2.17040685741097,110.583757475255));
#28750=CARTESIAN_POINT('Ctrl Pts',(-2.10907533748121,2.23774455577521,110.578774946911));
#28751=CARTESIAN_POINT('Ctrl Pts',(-2.03686790767812,2.3016453629243,110.573792418568));
#28752=CARTESIAN_POINT('Ctrl Pts',(-1.96458264890743,2.36561504572598,110.568804519793));
#28753=CARTESIAN_POINT('Ctrl Pts',(-1.88932172683329,2.42614015030467,110.563816621018));
#28754=CARTESIAN_POINT('Ctrl Pts',(-1.81145518560296,2.48294832015331,110.558828722244));
#28755=CARTESIAN_POINT('Ctrl Pts',(-1.73354264753758,2.53979004736788,110.553837877048));
#28756=CARTESIAN_POINT('Ctrl Pts',(-1.65302179180727,2.59291022635424,110.548847031853));
#28757=CARTESIAN_POINT('Ctrl Pts',(-1.57029031244102,2.64208073015453,110.543856186658));
#28758=CARTESIAN_POINT('Ctrl Pts',(-1.48742513691665,2.69133069472962,110.538857276131));
#28759=CARTESIAN_POINT('Ctrl Pts',(-1.40234259164468,2.73661803301578,110.533858365605));
#28760=CARTESIAN_POINT('Ctrl Pts',(-1.31546347572111,2.77776134576816,110.528859455078));
#28761=CARTESIAN_POINT('Ctrl Pts',(-1.26502499560561,2.80164747927776,110.525957291002));
#28762=CARTESIAN_POINT('Ctrl Pts',(-1.21398134620056,2.82413777925323,110.523055126925));
#28763=CARTESIAN_POINT('Ctrl Pts',(-1.16241729725908,2.84520443501568,110.520152962849));
#28764=CARTESIAN_POINT('Ctrl Pts',(-1.07358877298922,2.88149561038098,110.515153453358));
#28765=CARTESIAN_POINT('Ctrl Pts',(-0.982903059359573,2.91368664349634,
110.510153943867));
#28766=CARTESIAN_POINT('Ctrl Pts',(-0.890774331281627,2.94158517482152,
110.505154434376));
#28767=CARTESIAN_POINT('Ctrl Pts',(-0.798770575238357,2.9694458619661,110.500161706688));
#28768=CARTESIAN_POINT('Ctrl Pts',(-0.705328111557418,2.99302549351996,
110.495168979));
#28769=CARTESIAN_POINT('Ctrl Pts',(-0.61088121043788,3.01217967537362,110.490176251312));
#28770=CARTESIAN_POINT('Ctrl Pts',(-0.516533948418184,3.03131365004827,
110.485188790825));
#28771=CARTESIAN_POINT('Ctrl Pts',(-0.421184783409245,3.04603136940846,
110.480201330339));
#28772=CARTESIAN_POINT('Ctrl Pts',(-0.32528228108335,3.0562384867044,110.475213869853));
#28773=CARTESIAN_POINT('Ctrl Pts',(-0.229448399239483,3.06643830056934,
110.470229978011));
#28774=CARTESIAN_POINT('Ctrl Pts',(-0.133062402405853,3.07213388204652,
110.465246086169));
#28775=CARTESIAN_POINT('Ctrl Pts',(-0.0365811954306498,3.07328229522458,
110.460262194327));
#28776=CARTESIAN_POINT('Ctrl Pts',(0.0598648754787269,3.07443029017901,
110.455280117496));
#28777=CARTESIAN_POINT('Ctrl Pts',(0.156405649155184,3.07103440183982,110.450298040664));
#28778=CARTESIAN_POINT('Ctrl Pts',(0.252581941500445,3.06310375482579,110.445315963832));
#28779=CARTESIAN_POINT('Ctrl Pts',(0.348749464783802,3.05517383090404,110.440334341251));
#28780=CARTESIAN_POINT('Ctrl Pts',(0.444552135345558,3.04271000661028,110.43535271867));
#28781=CARTESIAN_POINT('Ctrl Pts',(0.539534692425912,3.0257733830657,110.430371096089));
#28782=CARTESIAN_POINT('Ctrl Pts',(0.634534519008938,3.00883368014451,110.425388567761));
#28783=CARTESIAN_POINT('Ctrl Pts',(0.728713503840477,2.98741963998045,110.420406039433));
#28784=CARTESIAN_POINT('Ctrl Pts',(0.821626455559054,2.96164349939784,110.415423511105));
#28785=CARTESIAN_POINT('Ctrl Pts',(0.914639553746905,2.93583957593433,110.410435612346));
#28786=CARTESIAN_POINT('Ctrl Pts',(1.00638347084152,2.9056642830803,110.405447713587));
#28787=CARTESIAN_POINT('Ctrl Pts',(1.09642828519429,2.87127972608485,110.400459814827));
#28788=CARTESIAN_POINT('Ctrl Pts',(1.18652629025516,2.8368748576595,110.395468969648));
#28789=CARTESIAN_POINT('Ctrl Pts',(1.27492279201485,2.79825594977819,110.390478124468));
#28790=CARTESIAN_POINT('Ctrl Pts',(1.36120991420809,2.75563238104462,110.385487279289));
#28791=CARTESIAN_POINT('Ctrl Pts',(1.4476364785706,2.7129399315472,110.380488368778));
#28792=CARTESIAN_POINT('Ctrl Pts',(1.53194647301246,2.66623011136276,110.375489458266));
#28793=CARTESIAN_POINT('Ctrl Pts',(1.61375863652375,2.61575712042326,110.370490547755));
#28794=CARTESIAN_POINT('Ctrl Pts',(1.66125545287571,2.58645455368383,110.367588383525));
#28795=CARTESIAN_POINT('Ctrl Pts',(1.70791094010491,2.55588441173041,110.364686219295));
#28796=CARTESIAN_POINT('Ctrl Pts',(1.75365561779286,2.5241026572197,110.361784055065));
#28797=CARTESIAN_POINT('Ctrl Pts',(1.79388071499675,2.49615570843531,110.359232067727));
#28798=CARTESIAN_POINT('Ctrl Pts',(1.83347357344082,2.46722195299097,110.356680080389));
#28799=CARTESIAN_POINT('Ctrl Pts',(1.8723819390353,2.43733217358127,110.35412809305));
#28800=CARTESIAN_POINT('',(-3.07349876323956,-0.0027572386409777,110.791576552868));
#28801=CARTESIAN_POINT('Ctrl Pts',(-3.07349876324033,-0.00275723777476568,
110.791576552823));
#28802=CARTESIAN_POINT('Ctrl Pts',(-3.07358427951016,0.0925679285798107,
110.786643375934));
#28803=CARTESIAN_POINT('Ctrl Pts',(-3.06923075828948,0.187999943733393,
110.781710199046));
#28804=CARTESIAN_POINT('Ctrl Pts',(-3.06043513424029,0.283088394512365,
110.776777022157));
#28805=CARTESIAN_POINT('Ctrl Pts',(-3.05164431928817,0.378124854712078,
110.771846542533));
#28806=CARTESIAN_POINT('Ctrl Pts',(-3.03841626490044,0.472817677209372,
110.766916062909));
#28807=CARTESIAN_POINT('Ctrl Pts',(-3.02079995318321,0.566718530531958,
110.761985583285));
#28808=CARTESIAN_POINT('Ctrl Pts',(-3.00318821239493,0.660595019269262,
110.757056382979));
#28809=CARTESIAN_POINT('Ctrl Pts',(-2.98119055870853,0.753679505664892,
110.752127182674));
#28810=CARTESIAN_POINT('Ctrl Pts',(-2.9549074089867,0.845532053984643,110.747197982368));
#28811=CARTESIAN_POINT('Ctrl Pts',(-2.92862352816746,0.93738715729349,110.742268644951));
#28812=CARTESIAN_POINT('Ctrl Pts',(-2.8980540394572,1.02800982286176,110.737339307534));
#28813=CARTESIAN_POINT('Ctrl Pts',(-2.8633493971494,1.11697469973324,110.732409970117));
#28814=CARTESIAN_POINT('Ctrl Pts',(-2.82861089080364,1.20602638660381,110.727475822759));
#28815=CARTESIAN_POINT('Ctrl Pts',(-2.78972933545781,1.29341663443531,110.722541675401));
#28816=CARTESIAN_POINT('Ctrl Pts',(-2.74690347158547,1.37873984775652,110.717607528043));
#28817=CARTESIAN_POINT('Ctrl Pts',(-2.70405712231737,1.46410387472712,110.712671020477));
#28818=CARTESIAN_POINT('Ctrl Pts',(-2.65726292856968,1.54739850686877,110.707734512911));
#28819=CARTESIAN_POINT('Ctrl Pts',(-2.60676464434538,1.62824455748849,110.702798005345));
#28820=CARTESIAN_POINT('Ctrl Pts',(-2.55617956998138,1.70922955619597,110.697853013526));
#28821=CARTESIAN_POINT('Ctrl Pts',(-2.50187794378262,1.78775719671831,110.692908021708));
#28822=CARTESIAN_POINT('Ctrl Pts',(-2.44414575109866,1.86347895007869,110.687963029889));
#28823=CARTESIAN_POINT('Ctrl Pts',(-2.39079118008633,1.93345899897378,110.68339299877));
#28824=CARTESIAN_POINT('Ctrl Pts',(-2.33450720666026,2.001042708641,110.678822967651));
#28825=CARTESIAN_POINT('Ctrl Pts',(-2.2755471967709,2.06598335067544,110.674252936532));
#28826=CARTESIAN_POINT('Ctrl Pts',(-2.21104629490347,2.13702692727814,110.669253427046));
#28827=CARTESIAN_POINT('Ctrl Pts',(-2.1431018958045,2.20517177216898,110.66425391756));
#28828=CARTESIAN_POINT('Ctrl Pts',(-2.07200476361226,2.27006575005398,110.659254408074));
#28829=CARTESIAN_POINT('Ctrl Pts',(-2.00100407422677,2.33487169967151,110.654261680391));
#28830=CARTESIAN_POINT('Ctrl Pts',(-1.92685947277257,2.39643525303404,110.649268952708));
#28831=CARTESIAN_POINT('Ctrl Pts',(-1.84990053545108,2.45443888881712,110.644276225025));
#28832=CARTESIAN_POINT('Ctrl Pts',(-1.77302278786648,2.51238133222811,110.639288764543));
#28833=CARTESIAN_POINT('Ctrl Pts',(-1.69333695539624,2.56677106121078,110.634301304062));
#28834=CARTESIAN_POINT('Ctrl Pts',(-1.61120709089405,2.61732954750691,110.62931384358));
#28835=CARTESIAN_POINT('Ctrl Pts',(-1.52913599222579,2.6678518580267,110.624329951743));
#28836=CARTESIAN_POINT('Ctrl Pts',(-1.44462471072116,2.7145481460659,110.619346059906));
#28837=CARTESIAN_POINT('Ctrl Pts',(-1.35806698952089,2.75718267475582,110.614362168069));
#28838=CARTESIAN_POINT('Ctrl Pts',(-1.27154079049631,2.7998016770076,110.609380091241));
#28839=CARTESIAN_POINT('Ctrl Pts',(-1.18297002591487,2.83836166514092,110.604398014414));
#28840=CARTESIAN_POINT('Ctrl Pts',(-1.09277294158465,2.87267289264553,110.599415937587));
#28841=CARTESIAN_POINT('Ctrl Pts',(-1.00258408114756,2.9069809917578,110.59443431501));
#28842=CARTESIAN_POINT('Ctrl Pts',(-0.910769606120397,2.93704094454205,
110.589452692433));
#28843=CARTESIAN_POINT('Ctrl Pts',(-0.817766632290743,2.96271159330635,
110.584471069856));
#28844=CARTESIAN_POINT('Ctrl Pts',(-0.724746748878659,2.98838690944777,
110.579488541532));
#28845=CARTESIAN_POINT('Ctrl Pts',(-0.630538360653306,3.00967121987548,
110.574506013208));
#28846=CARTESIAN_POINT('Ctrl Pts',(-0.535591545412797,3.02647384698469,
110.569523484885));
#28847=CARTESIAN_POINT('Ctrl Pts',(-0.440542391492857,3.0432945848506,110.564535586129));
#28848=CARTESIAN_POINT('Ctrl Pts',(-0.344753654548596,3.05562391894161,
110.559547687374));
#28849=CARTESIAN_POINT('Ctrl Pts',(-0.248683135866333,3.06342275044364,
110.554559788619));
#28850=CARTESIAN_POINT('Ctrl Pts',(-0.152555867006806,3.07122618882275,
110.549568943443));
#28851=CARTESIAN_POINT('Ctrl Pts',(-0.0561469234809696,3.07449378093882,
110.544578098267));
#28852=CARTESIAN_POINT('Ctrl Pts',(0.0400854023518479,3.07323858665713,
110.539587253091));
#28853=CARTESIAN_POINT('Ctrl Pts',(0.136473242059387,3.07198136394969,110.534588342584));
#28854=CARTESIAN_POINT('Ctrl Pts',(0.232683456282823,3.06618678688432,110.529589432076));
#28855=CARTESIAN_POINT('Ctrl Pts',(0.328262442087564,3.05591983191881,110.524590521568));
#28856=CARTESIAN_POINT('Ctrl Pts',(0.383751716687541,3.04995925513941,110.521688357295));
#28857=CARTESIAN_POINT('Ctrl Pts',(0.439028399776211,3.04249223002058,110.518786193021));
#28858=CARTESIAN_POINT('Ctrl Pts',(0.494005672129351,3.03353929361464,110.515884028748));
#28859=CARTESIAN_POINT('Ctrl Pts',(0.588714582648808,3.01811614116157,110.5108844934));
#28860=CARTESIAN_POINT('Ctrl Pts',(0.682866871070267,2.99822634453998,110.505884958052));
#28861=CARTESIAN_POINT('Ctrl Pts',(0.776008855003659,2.97392207479549,110.500885422704));
#28862=CARTESIAN_POINT('Ctrl Pts',(0.869028892685815,2.94964962544455,110.495892433004));
#28863=CARTESIAN_POINT('Ctrl Pts',(0.961040833031793,2.92097429707105,110.490899443303));
#28864=CARTESIAN_POINT('Ctrl Pts',(1.05159883344927,2.88799967858172,110.485906453603));
#28865=CARTESIAN_POINT('Ctrl Pts',(1.14204898499438,2.85506433078527,110.480919410238));
#28866=CARTESIAN_POINT('Ctrl Pts',(1.23104823087104,2.81784002774614,110.475932366874));
#28867=CARTESIAN_POINT('Ctrl Pts',(1.31816484313995,2.77648045127457,110.47094532351));
#28868=CARTESIAN_POINT('Ctrl Pts',(1.40522191994573,2.73514913992345,110.465961688289));
#28869=CARTESIAN_POINT('Ctrl Pts',(1.4903985248001,2.68968835917862,110.460978053068));
#28870=CARTESIAN_POINT('Ctrl Pts',(1.57328261187453,2.64029999681348,110.455994417848));
#28871=CARTESIAN_POINT('Ctrl Pts',(1.65613361834081,2.59093134627868,110.45101277169));
#28872=CARTESIAN_POINT('Ctrl Pts',(1.73669354957927,2.53763845506773,110.446031125533));
#28873=CARTESIAN_POINT('Ctrl Pts',(1.8145756300531,2.48066876725157,110.441049479375));
#28874=CARTESIAN_POINT('Ctrl Pts',(1.83401296871451,2.46645061708428,110.439806190253));
#28875=CARTESIAN_POINT('Ctrl Pts',(1.85328364809906,2.45200366374706,110.438562901131));
#28876=CARTESIAN_POINT('Ctrl Pts',(1.8723819390353,2.43733217358127,110.437319612009));
#28877=CARTESIAN_POINT('Ctrl Pts',(1.87238193903529,2.43733217358128,111.437229631665));
#28878=CARTESIAN_POINT('Ctrl Pts',(1.94871667497837,2.3786910977156,111.432241834346));
#28879=CARTESIAN_POINT('Ctrl Pts',(2.02237837223609,2.31639560571599,111.427254037028));
#28880=CARTESIAN_POINT('Ctrl Pts',(2.09300115674764,2.25072175265026,111.42226623971));
#28881=CARTESIAN_POINT('Ctrl Pts',(2.16357129200264,2.18509685941473,111.417282160793));
#28882=CARTESIAN_POINT('Ctrl Pts',(2.23110669796282,2.11609891015331,111.412298081876));
#28883=CARTESIAN_POINT('Ctrl Pts',(2.29527476119916,2.04404403587647,111.407314002958));
#28884=CARTESIAN_POINT('Ctrl Pts',(2.35941815820086,1.97201685952826,111.402331839923));
#28885=CARTESIAN_POINT('Ctrl Pts',(2.42019649266593,1.89693542031554,111.397349676888));
#28886=CARTESIAN_POINT('Ctrl Pts',(2.47731487587539,1.8191517956912,111.392367513854));
#28887=CARTESIAN_POINT('Ctrl Pts',(2.53442689601226,1.74137683627798,111.387385905839));
#28888=CARTESIAN_POINT('Ctrl Pts',(2.58787951574812,1.66090064377156,111.382404297824));
#28889=CARTESIAN_POINT('Ctrl Pts',(2.63741958716114,1.57810651454797,111.37742268981));
#28890=CARTESIAN_POINT('Ctrl Pts',(2.68696766394427,1.49529900630356,111.372440276798));
#28891=CARTESIAN_POINT('Ctrl Pts',(2.73260171149074,1.41017319421669,111.367457863786));
#28892=CARTESIAN_POINT('Ctrl Pts',(2.77411373158308,1.32313841084076,111.362475450775));
#28893=CARTESIAN_POINT('Ctrl Pts',(2.81567003196019,1.23601078869223,111.357487723093));
#28894=CARTESIAN_POINT('Ctrl Pts',(2.85309533663416,1.14697052651153,111.352499995412));
#28895=CARTESIAN_POINT('Ctrl Pts',(2.88622925913025,1.05644825417076,111.347512267731));
#28896=CARTESIAN_POINT('Ctrl Pts',(2.91938215337648,0.965874150781834,111.342521684187));
#28897=CARTESIAN_POINT('Ctrl Pts',(2.94823864118371,0.873816766246551,111.337531100644));
#28898=CARTESIAN_POINT('Ctrl Pts',(2.9726884541713,0.780721207881932,111.3325405171));
#28899=CARTESIAN_POINT('Ctrl Pts',(2.99717831341183,0.687473168666888,111.327541759499));
#28900=CARTESIAN_POINT('Ctrl Pts',(3.01724699218182,0.593183989036835,111.322543001898));
#28901=CARTESIAN_POINT('Ctrl Pts',(3.03283549421489,0.498308253022458,111.317544244298));
#28902=CARTESIAN_POINT('Ctrl Pts',(3.04303880920497,0.436208186100302,111.314272352088));
#28903=CARTESIAN_POINT('Ctrl Pts',(3.05132377438297,0.373856959073547,111.311000459879));
#28904=CARTESIAN_POINT('Ctrl Pts',(3.05768593427511,0.31138236516561,111.307728567669));
#28905=CARTESIAN_POINT('Ctrl Pts',(3.06740742905065,0.21592006170639,111.302729057509));
#28906=CARTESIAN_POINT('Ctrl Pts',(3.07267115116372,0.119834385611258,111.297729547349));
#28907=CARTESIAN_POINT('Ctrl Pts',(3.07340956853436,0.0235769811771108,
111.292730037189));
#28908=CARTESIAN_POINT('Ctrl Pts',(3.0741469842478,-0.0725498508641107,
111.287737308824));
#28909=CARTESIAN_POINT('Ctrl Pts',(3.07037129182113,-0.168847513080869,
111.282744580459));
#28910=CARTESIAN_POINT('Ctrl Pts',(3.06206664760734,-0.264858633256908,
111.277751852094));
#28911=CARTESIAN_POINT('Ctrl Pts',(3.05377076457157,-0.360768464263453,
111.272764390924));
#28912=CARTESIAN_POINT('Ctrl Pts',(3.04095546559796,-0.45639191916809,111.267776929754));
#28913=CARTESIAN_POINT('Ctrl Pts',(3.0236569543179,-0.551272049540874,111.262789468585));
#28914=CARTESIAN_POINT('Ctrl Pts',(3.00637082050063,-0.646084291107248,
111.257805576052));
#28915=CARTESIAN_POINT('Ctrl Pts',(2.98460792991186,-0.740153834858849,
111.25282168352));
#28916=CARTESIAN_POINT('Ctrl Pts',(2.95845615891374,-0.833030255023996,
111.247837790988));
#28917=CARTESIAN_POINT('Ctrl Pts',(2.93231391171984,-0.925872851979168,
111.242855713461));
#28918=CARTESIAN_POINT('Ctrl Pts',(2.90178607865338,-1.01752276656253,111.237873635935));
#28919=CARTESIAN_POINT('Ctrl Pts',(2.86701112026954,-1.10754209231559,111.232891558408));
#28920=CARTESIAN_POINT('Ctrl Pts',(2.8322393325373,-1.19755321044073,111.227909935129));
#28921=CARTESIAN_POINT('Ctrl Pts',(2.79322134773867,-1.28593362591614,111.22292831185));
#28922=CARTESIAN_POINT('Ctrl Pts',(2.75014437794742,-1.37226387784718,111.217946688571));
#28923=CARTESIAN_POINT('Ctrl Pts',(2.70705957598402,-1.4586098261793,111.212964159542));
#28924=CARTESIAN_POINT('Ctrl Pts',(2.6599145193837,-1.54290447791132,111.207981630514));
#28925=CARTESIAN_POINT('Ctrl Pts',(2.60894262908064,-1.62475247596851,111.202999101486));
#28926=CARTESIAN_POINT('Ctrl Pts',(2.55791579860506,-1.70668869408397,111.198011202027));
#28927=CARTESIAN_POINT('Ctrl Pts',(2.50305413215539,-1.78617262050403,111.193023302568));
#28928=CARTESIAN_POINT('Ctrl Pts',(2.4446345749057,-1.86283763253152,111.188035403109));
#28929=CARTESIAN_POINT('Ctrl Pts',(2.38618050841788,-1.93954793163889,111.183044557229));
#28930=CARTESIAN_POINT('Ctrl Pts',(2.32416464838364,-2.0134356646547,111.178053711348));
#28931=CARTESIAN_POINT('Ctrl Pts',(2.25890306088313,-2.08416870994956,111.173062865468));
#28932=CARTESIAN_POINT('Ctrl Pts',(2.19353600909908,-2.15501606153439,111.168063954262));
#28933=CARTESIAN_POINT('Ctrl Pts',(2.12491306871472,-2.22269823768194,111.163065043056));
#28934=CARTESIAN_POINT('Ctrl Pts',(2.05338578367992,-2.28692130896128,111.15806613185));
#28935=CARTESIAN_POINT('Ctrl Pts',(2.01186005429569,-2.32420651944946,111.155163974528));
#28936=CARTESIAN_POINT('Ctrl Pts',(1.96935602978709,-2.36032661270555,111.152261817207));
#28937=CARTESIAN_POINT('Ctrl Pts',(1.92594701958487,-2.39523074624391,111.149359659885));
#28938=CARTESIAN_POINT('Ctrl Pts',(1.85116686987237,-2.45535965310967,111.144360150382));
#28939=CARTESIAN_POINT('Ctrl Pts',(1.77343679923049,-2.51208881208536,111.13936064088));
#28940=CARTESIAN_POINT('Ctrl Pts',(1.69309887531852,-2.56511567933985,111.134361131377));
#28941=CARTESIAN_POINT('Ctrl Pts',(1.61286992925858,-2.6180706160065,111.129368403676));
#28942=CARTESIAN_POINT('Ctrl Pts',(1.53004052376622,-2.66733300236767,111.124375675974));
#28943=CARTESIAN_POINT('Ctrl Pts',(1.44498567289287,-2.71264053186823,111.119382948272));
#28944=CARTESIAN_POINT('Ctrl Pts',(1.36002055271011,-2.75790026308486,111.114395487771));
#28945=CARTESIAN_POINT('Ctrl Pts',(1.27283503977061,-2.79921322638924,111.109408027269));
#28946=CARTESIAN_POINT('Ctrl Pts',(1.18383212988815,-2.83636100280703,111.104420566767));
#28947=CARTESIAN_POINT('Ctrl Pts',(1.09489290361739,-2.87348219914364,111.099436674907));
#28948=CARTESIAN_POINT('Ctrl Pts',(1.00413926944769,-2.90644396466975,111.094452783047));
#28949=CARTESIAN_POINT('Ctrl Pts',(0.911996885344304,-2.93507477436645,
111.089468891187));
#28950=CARTESIAN_POINT('Ctrl Pts',(0.819888057182536,-2.96369515744149,
111.084486814336));
#28951=CARTESIAN_POINT('Ctrl Pts',(0.726391902716913,-2.98798758834278,
111.079504737484));
#28952=CARTESIAN_POINT('Ctrl Pts',(0.631951119459168,-3.00782978783945,
111.074522660632));
#28953=CARTESIAN_POINT('Ctrl Pts',(0.537518946992066,-3.02767017819159,
111.069541038029));
#28954=CARTESIAN_POINT('Ctrl Pts',(0.442142746592162,-3.04306105378232,
111.064559415426));
#28955=CARTESIAN_POINT('Ctrl Pts',(0.346276286620338,-3.05393107049331,
111.059577792823));
#28956=CARTESIAN_POINT('Ctrl Pts',(0.250392396404009,-3.0648030635686,111.054595264472));
#28957=CARTESIAN_POINT('Ctrl Pts',(0.154018505754517,-3.07115251590384,
111.049612736121));
#28958=CARTESIAN_POINT('Ctrl Pts',(0.0576133234244592,-3.07295996637834,
111.044630207769));
#28959=CARTESIAN_POINT('Ctrl Pts',(-0.0388957695325551,-3.07476936501899,
111.039642308984));
#28960=CARTESIAN_POINT('Ctrl Pts',(-0.135435781891717,-3.07202697992187,
111.034654410199));
#28961=CARTESIAN_POINT('Ctrl Pts',(-0.23154841023164,-3.0647655022398,111.029666511414));
#28962=CARTESIAN_POINT('Ctrl Pts',(-0.327717813648208,-3.05749973510109,
111.024675666207));
#28963=CARTESIAN_POINT('Ctrl Pts',(-0.423458894885145,-3.04570961360995,
111.019684821));
#28964=CARTESIAN_POINT('Ctrl Pts',(-0.518320990312167,-3.02947942739373,
111.014693975793));
#28965=CARTESIAN_POINT('Ctrl Pts',(-0.613336385319549,-3.01322301278011,
111.009695065253));
#28966=CARTESIAN_POINT('Ctrl Pts',(-0.707469529745186,-2.99251230029474,
111.004696154712));
#28967=CARTESIAN_POINT('Ctrl Pts',(-0.80028247929883,-2.96748213193059,
110.999697244171));
#28968=CARTESIAN_POINT('Ctrl Pts',(-0.854165900677711,-2.95295063481046,
110.996795080148));
#28969=CARTESIAN_POINT('Ctrl Pts',(-0.90760466305668,-2.93696419463733,
110.993892916124));
#28970=CARTESIAN_POINT('Ctrl Pts',(-0.960516206135646,-2.91955662177509,
110.990990752101));
#28971=CARTESIAN_POINT('Ctrl Pts',(-1.05166603449257,-2.88956888779168,
110.985991242784));
#28972=CARTESIAN_POINT('Ctrl Pts',(-1.14157026989393,-2.85525578517736,
110.980991733467));
#28973=CARTESIAN_POINT('Ctrl Pts',(-1.22978890165704,-2.8167395171299,110.97599222415));
#28974=CARTESIAN_POINT('Ctrl Pts',(-1.31788786534854,-2.77827549618071,
110.970999496639));
#28975=CARTESIAN_POINT('Ctrl Pts',(-1.4043053708423,-2.73561981542936,110.966006769128));
#28976=CARTESIAN_POINT('Ctrl Pts',(-1.48861722045163,-2.6889442205027,110.961014041617));
#28977=CARTESIAN_POINT('Ctrl Pts',(-1.57284012313476,-2.64231786717987,
110.95602658131));
#28978=CARTESIAN_POINT('Ctrl Pts',(-1.65496140397517,-2.59168024183188,
110.951039121004));
#28979=CARTESIAN_POINT('Ctrl Pts',(-1.73457844313087,-2.53725045563612,
110.946051660697));
#28980=CARTESIAN_POINT('Ctrl Pts',(-1.81413851437789,-2.48285961526303,
110.941067769039));
#28981=CARTESIAN_POINT('Ctrl Pts',(-1.89119754470857,-2.42468225514321,
110.93608387738));
#28982=CARTESIAN_POINT('Ctrl Pts',(-1.96537991012113,-2.36298202678147,
110.931099985722));
#28983=CARTESIAN_POINT('Ctrl Pts',(-2.03953526012232,-2.30130426814069,
110.926117909075));
#28984=CARTESIAN_POINT('Ctrl Pts',(-2.11081568955522,-2.23610647073804,
110.921135832429));
#28985=CARTESIAN_POINT('Ctrl Pts',(-2.17887760419358,-2.16769339066752,
110.916153755782));
#28986=CARTESIAN_POINT('Ctrl Pts',(-2.24693331312855,-2.09928654831872,
110.911172133388));
#28987=CARTESIAN_POINT('Ctrl Pts',(-2.31177078124945,-2.0276653174803,110.906190510994));
#28988=CARTESIAN_POINT('Ctrl Pts',(-2.37308311076532,-1.95317147209363,
110.9012088886));
#28989=CARTESIAN_POINT('Ctrl Pts',(-2.43440658792414,-1.87866408243623,
110.896226360461));
#28990=CARTESIAN_POINT('Ctrl Pts',(-2.49220337466263,-1.80128337990646,
110.891243832322));
#28991=CARTESIAN_POINT('Ctrl Pts',(-2.54620740244167,-1.72140353019019,
110.886261304183));
#28992=CARTESIAN_POINT('Ctrl Pts',(-2.60026963859217,-1.64143758178544,
110.881273405613));
#28993=CARTESIAN_POINT('Ctrl Pts',(-2.65053070813879,-1.55896747270389,
110.876285507044));
#28994=CARTESIAN_POINT('Ctrl Pts',(-2.69676850814867,-1.47439542303197,
110.871297608475));
#28995=CARTESIAN_POINT('Ctrl Pts',(-2.74303362145348,-1.38977341550444,
110.866306763487));
#28996=CARTESIAN_POINT('Ctrl Pts',(-2.78527054091283,-1.30304738953272,
110.861315918498));
#28997=CARTESIAN_POINT('Ctrl Pts',(-2.82330460349125,-1.21464124987797,
110.85632507351));
#28998=CARTESIAN_POINT('Ctrl Pts',(-2.86140013008018,-1.12609224365762,
110.851326163189));
#28999=CARTESIAN_POINT('Ctrl Pts',(-2.89527908362788,-1.03585811296161,
110.846327252868));
#29000=CARTESIAN_POINT('Ctrl Pts',(-2.92481612909701,-0.944379616983535,
110.841328342548));
#29001=CARTESIAN_POINT('Ctrl Pts',(-2.94196414854108,-0.891270885123915,
110.838426176471));
#29002=CARTESIAN_POINT('Ctrl Pts',(-2.95764967560813,-0.83774298313627,
110.835524010394));
#29003=CARTESIAN_POINT('Ctrl Pts',(-2.97185612004942,-0.783883570260808,
110.832621844317));
#29004=CARTESIAN_POINT('Ctrl Pts',(-3.00334933232157,-0.664486635330965,
110.826188247741));
#29005=CARTESIAN_POINT('Ctrl Pts',(-3.02766111559864,-0.543122440475141,
110.819754651165));
#29006=CARTESIAN_POINT('Ctrl Pts',(-3.04459242176316,-0.420546353381311,
110.813321054589));
#29007=CARTESIAN_POINT('Ctrl Pts',(-3.06118864013233,-0.300396171908,110.807014785442));
#29008=CARTESIAN_POINT('Ctrl Pts',(-3.07069363673407,-0.179081372834902,
110.800708516296));
#29009=CARTESIAN_POINT('Ctrl Pts',(-3.07296516881628,-0.0573351658404085,
110.79440224715));
#29010=CARTESIAN_POINT('Ctrl Pts',(-3.07330444259114,-0.0391512733276938,
110.793460349056));
#29011=CARTESIAN_POINT('Ctrl Pts',(-3.07348243549809,-0.0209578007778193,
110.792518450962));
#29012=CARTESIAN_POINT('Ctrl Pts',(-3.07349876323956,-0.00275723864097975,
110.791576552868));
#29013=CARTESIAN_POINT('Origin',(0.,0.,116.208423447177));
#29014=CARTESIAN_POINT('',(1.87238193903529,2.43733217358128,112.437403601774));
#29015=CARTESIAN_POINT('',(1.86967294057238,2.43383856956498,112.354102866614));
#29016=CARTESIAN_POINT('',(1.8723819390353,2.43733217358128,116.208423447177));
#29017=CARTESIAN_POINT('',(-3.07300208187459,-5.30343035903902E-5,111.708423450995));
#29018=CARTESIAN_POINT('Ctrl Pts',(1.8696729405724,2.43383856956497,112.354102866614));
#29019=CARTESIAN_POINT('Ctrl Pts',(2.33883235148557,2.07028612302645,112.323472227234));
#29020=CARTESIAN_POINT('Ctrl Pts',(3.34734616429362,0.724855016743962,112.240051951927));
#29021=CARTESIAN_POINT('Ctrl Pts',(2.87385982532852,-2.21711305274817,112.103842040691));
#29022=CARTESIAN_POINT('Ctrl Pts',(-0.295019362129256,-3.61768143627294,
111.945473132907));
#29023=CARTESIAN_POINT('Ctrl Pts',(-2.70868458642244,-2.0401170948013,111.813666947708));
#29024=CARTESIAN_POINT('Ctrl Pts',(-3.06863383704806,-0.508468182011378,
111.734650398436));
#29025=CARTESIAN_POINT('Ctrl Pts',(-3.06855559257655,-5.3618658338984E-5,
111.708423485093));
#29026=CARTESIAN_POINT('Ctrl Pts',(-3.07349999954357,-5.29688675722701E-5,
111.708423447177));
#29027=CARTESIAN_POINT('Ctrl Pts',(-3.0735017428754,0.101103250511966,111.703213628981));
#29028=CARTESIAN_POINT('Ctrl Pts',(-3.06850524053228,0.202167062758812,
111.698003810785));
#29029=CARTESIAN_POINT('Ctrl Pts',(-3.05856358047855,0.302640172763362,
111.69279399259));
#29030=CARTESIAN_POINT('Ctrl Pts',(-3.04837689147292,0.405589611741622,
111.687455769652));
#29031=CARTESIAN_POINT('Ctrl Pts',(-3.03299816639765,0.507918428276897,
111.682117546715));
#29032=CARTESIAN_POINT('Ctrl Pts',(-3.01253985928769,0.609102492363057,
111.676779323777));
#29033=CARTESIAN_POINT('Ctrl Pts',(-2.99249659337028,0.708233817950399,
111.671549398286));
#29034=CARTESIAN_POINT('Ctrl Pts',(-2.96757807806514,0.806266060873926,
111.666319472794));
#29035=CARTESIAN_POINT('Ctrl Pts',(-2.93794030454541,0.902723111993713,
111.661089547303));
#29036=CARTESIAN_POINT('Ctrl Pts',(-2.90738195523853,1.00217620550186,111.655697175642));
#29037=CARTESIAN_POINT('Ctrl Pts',(-2.87180656578605,1.09995424282145,111.650304803981));
#29038=CARTESIAN_POINT('Ctrl Pts',(-2.83143769168113,1.19555963804716,111.644912432321));
#29039=CARTESIAN_POINT('Ctrl Pts',(-2.79106881757621,1.29116503327286,111.63952006066));
#29040=CARTESIAN_POINT('Ctrl Pts',(-2.74590671329826,1.38459743088285,111.634127688999));
#29041=CARTESIAN_POINT('Ctrl Pts',(-2.69622482898178,1.47538941353873,111.628735317339));
#29042=CARTESIAN_POINT('Ctrl Pts',(-2.65016252078614,1.55956674184112,111.62373580718));
#29043=CARTESIAN_POINT('Ctrl Pts',(-2.60007344932545,1.64173272528624,111.618736297021));
#29044=CARTESIAN_POINT('Ctrl Pts',(-2.54615779135673,1.72147690995652,111.613736786863));
#29045=CARTESIAN_POINT('Ctrl Pts',(-2.4923152695435,1.80111292228299,111.608744058499));
#29046=CARTESIAN_POINT('Ctrl Pts',(-2.43465672122309,1.87833330431815,111.603751330136));
#29047=CARTESIAN_POINT('Ctrl Pts',(-2.373428164222,1.95275216022869,111.598758601772));
#29048=CARTESIAN_POINT('Ctrl Pts',(-2.31226420171481,2.02709250623193,111.593771140604));
#29049=CARTESIAN_POINT('Ctrl Pts',(-2.24753799504432,2.09863686436192,111.588783679436));
#29050=CARTESIAN_POINT('Ctrl Pts',(-2.17953821425042,2.16702916976724,111.583796218267));
#29051=CARTESIAN_POINT('Ctrl Pts',(-2.11158708878564,2.2353725389835,111.578812325737));
#29052=CARTESIAN_POINT('Ctrl Pts',(-2.04036735421783,2.30056802863682,111.573828433206));
#29053=CARTESIAN_POINT('Ctrl Pts',(-1.96620656948055,2.36229421879061,111.568844540675));
#29054=CARTESIAN_POINT('Ctrl Pts',(-1.89207279219901,2.42399792984908,111.56386246315));
#29055=CARTESIAN_POINT('Ctrl Pts',(-1.81500042985993,2.48223457117628,111.558880385625));
#29056=CARTESIAN_POINT('Ctrl Pts',(-1.73535163647026,2.53672169301246,111.5538983081));
#29057=CARTESIAN_POINT('Ctrl Pts',(-1.655710105162,2.59120384691506,111.548916684823));
#29058=CARTESIAN_POINT('Ctrl Pts',(-1.57349297224867,2.64193691332774,111.543935061545));
#29059=CARTESIAN_POINT('Ctrl Pts',(-1.48909211962564,2.68868125839952,111.538953438267));
#29060=CARTESIAN_POINT('Ctrl Pts',(-1.40467592140137,2.73543410243851,111.533970909241));
#29061=CARTESIAN_POINT('Ctrl Pts',(-1.31807559896087,2.77819657220395,111.528988380214));
#29062=CARTESIAN_POINT('Ctrl Pts',(-1.22970746160734,2.81677507246625,111.524005851187));
#29063=CARTESIAN_POINT('Ctrl Pts',(-1.14124407644792,2.85539515465632,111.519017951729));
#29064=CARTESIAN_POINT('Ctrl Pts',(-1.05100947529692,2.88982208822087,111.514030052272));
#29065=CARTESIAN_POINT('Ctrl Pts',(-0.959439559524308,2.91991061192287,
111.509042152814));
#29066=CARTESIAN_POINT('Ctrl Pts',(-0.867815552139671,2.95001690933075,
111.504051306936));
#29067=CARTESIAN_POINT('Ctrl Pts',(-0.774855082346382,2.97577957682628,
111.499060461057));
#29068=CARTESIAN_POINT('Ctrl Pts',(-0.681006748292446,2.99710394527453,
111.494069615179));
#29069=CARTESIAN_POINT('Ctrl Pts',(-0.587006753089678,3.01846277441139,
111.489070703974));
#29070=CARTESIAN_POINT('Ctrl Pts',(-0.492116460493753,3.03536890586542,
111.48407179277));
#29071=CARTESIAN_POINT('Ctrl Pts',(-0.396792072387789,3.04777924090479,
111.479072881565));
#29072=CARTESIAN_POINT('Ctrl Pts',(-0.341450746844712,3.05498415881886,
111.476170724228));
#29073=CARTESIAN_POINT('Ctrl Pts',(-0.285963177142949,3.06067475437294,
111.473268566891));
#29074=CARTESIAN_POINT('Ctrl Pts',(-0.230418577022753,3.06485065368001,
111.470366409554));
#29075=CARTESIAN_POINT('Ctrl Pts',(-0.13475653099004,3.07204262321219,111.46536815035));
#29076=CARTESIAN_POINT('Ctrl Pts',(-0.0385894607515949,3.07476413519502,
111.460369891147));
#29077=CARTESIAN_POINT('Ctrl Pts',(0.057629702772162,3.07295965924683,111.455371631943));
#29078=CARTESIAN_POINT('Ctrl Pts',(0.153728586124074,3.07115743901018,111.450379620886));
#29079=CARTESIAN_POINT('Ctrl Pts',(0.249878998755944,3.06484047776547,111.44538760983));
#29080=CARTESIAN_POINT('Ctrl Pts',(0.345623507471124,3.05400501654522,111.440395598773));
#29081=CARTESIAN_POINT('Ctrl Pts',(0.441274476905546,3.04318014121926,111.435408464749));
#29082=CARTESIAN_POINT('Ctrl Pts',(0.536519896763965,3.02784558640366,111.430421330726));
#29083=CARTESIAN_POINT('Ctrl Pts',(0.630904023771938,3.00804959446954,111.425434196702));
#29084=CARTESIAN_POINT('Ctrl Pts',(0.725221712157909,2.98826753727707,111.420450573208));
#29085=CARTESIAN_POINT('Ctrl Pts',(0.818678884568398,2.96403037526767,111.415466949714));
#29086=CARTESIAN_POINT('Ctrl Pts',(0.910827663943631,2.93543782366362,111.410483326221));
#29087=CARTESIAN_POINT('Ctrl Pts',(1.00295458034917,2.90685205585087,111.405500885128));
#29088=CARTESIAN_POINT('Ctrl Pts',(1.09377329924995,2.87391307357728,111.400518444035));
#29089=CARTESIAN_POINT('Ctrl Pts',(1.18284962564052,2.83677087779787,111.395536002943));
#29090=CARTESIAN_POINT('Ctrl Pts',(1.27191077845996,2.79963500894921,111.390554410576));
#29091=CARTESIAN_POINT('Ctrl Pts',(1.35922972560432,2.75829752370882,111.38557281821));
#29092=CARTESIAN_POINT('Ctrl Pts',(1.44439210090478,2.71295663600506,111.380591225844));
#29093=CARTESIAN_POINT('Ctrl Pts',(1.52959967204653,2.66759168580237,111.375606989736));
#29094=CARTESIAN_POINT('Ctrl Pts',(1.61264799791362,2.6182192970358,111.370622753629));
#29095=CARTESIAN_POINT('Ctrl Pts',(1.69314762423507,2.56508350206131,111.365638517522));
#29096=CARTESIAN_POINT('Ctrl Pts',(1.75442187170347,2.52463790001969,111.361844645045));
#29097=CARTESIAN_POINT('Ctrl Pts',(1.81421992195117,2.48201279262311,111.358050772568));
#29098=CARTESIAN_POINT('Ctrl Pts',(1.87238193903529,2.43733217358128,111.354256900092));
#29099=CARTESIAN_POINT('',(-3.07349983534499,0.00100604885424971,111.791576552851));
#29100=CARTESIAN_POINT('Ctrl Pts',(-3.07349983534482,0.00100604938365495,
111.791576552823));
#29101=CARTESIAN_POINT('Ctrl Pts',(-3.07348152082622,0.0569572490138065,
111.788662798889));
#29102=CARTESIAN_POINT('Ctrl Pts',(-3.07193546894597,0.112881401490518,
111.785749044955));
#29103=CARTESIAN_POINT('Ctrl Pts',(-3.06886550242914,0.168721006399079,
111.782835291022));
#29104=CARTESIAN_POINT('Ctrl Pts',(-3.06359795374749,0.264532421803207,
111.777835776985));
#29105=CARTESIAN_POINT('Ctrl Pts',(-3.05382993681823,0.360265200941909,
111.772836262949));
#29106=CARTESIAN_POINT('Ctrl Pts',(-3.03956509812897,0.455462692474593,
111.767836748913));
#29107=CARTESIAN_POINT('Ctrl Pts',(-3.02531960945124,0.550531050226053,
111.762844016632));
#29108=CARTESIAN_POINT('Ctrl Pts',(-3.00658948658028,0.645065133062805,
111.757851284352));
#29109=CARTESIAN_POINT('Ctrl Pts',(-2.98343032572477,0.738610683341211,
111.752858552071));
#29110=CARTESIAN_POINT('Ctrl Pts',(-2.96029559699084,0.83205754626771,111.747871086952));
#29111=CARTESIAN_POINT('Ctrl Pts',(-2.93274122381603,0.924517525962698,
111.742883621833));
#29112=CARTESIAN_POINT('Ctrl Pts',(-2.90087414832287,1.01554489097826,111.737896156715));
#29113=CARTESIAN_POINT('Ctrl Pts',(-2.86902987418579,1.10650712459,111.7329122602));
#29114=CARTESIAN_POINT('Ctrl Pts',(-2.83287917678328,1.19603836816774,111.727928363685));
#29115=CARTESIAN_POINT('Ctrl Pts',(-2.79257902413718,1.28370738252493,111.72294446717));
#29116=CARTESIAN_POINT('Ctrl Pts',(-2.75229354760534,1.3713444704405,111.717962385641));
#29117=CARTESIAN_POINT('Ctrl Pts',(-2.70786180139085,1.45712027815022,111.712980304113));
#29118=CARTESIAN_POINT('Ctrl Pts',(-2.65948877004993,1.54062381260913,111.707998222584));
#29119=CARTESIAN_POINT('Ctrl Pts',(-2.6111201490396,1.62411973377235,111.703016595289));
#29120=CARTESIAN_POINT('Ctrl Pts',(-2.5588111775301,1.70534341383878,111.698034967993));
#29121=CARTESIAN_POINT('Ctrl Pts',(-2.50281212316432,1.78390967432258,111.693053340698));
#29122=CARTESIAN_POINT('Ctrl Pts',(-2.44680288705992,1.86249021971062,111.688070807643));
#29123=CARTESIAN_POINT('Ctrl Pts',(-2.3871024904373,1.93841202850577,111.683088274589));
#29124=CARTESIAN_POINT('Ctrl Pts',(-2.32400309100997,2.01132092988069,111.678105741535));
#29125=CARTESIAN_POINT('Ctrl Pts',(-2.26083567993026,2.08430841607417,111.673117838061));
#29126=CARTESIAN_POINT('Ctrl Pts',(-2.19426223971617,2.15427617912469,111.668129934586));
#29127=CARTESIAN_POINT('Ctrl Pts',(-2.12461344499306,2.22090521169966,111.663142031111));
#29128=CARTESIAN_POINT('Ctrl Pts',(-2.05492350779719,2.28757360293359,111.658151181216));
#29129=CARTESIAN_POINT('Ctrl Pts',(-1.98215492981803,2.35089904862615,111.65316033132));
#29130=CARTESIAN_POINT('Ctrl Pts',(-1.90667165472996,2.4106027153078,111.648169481424));
#29131=CARTESIAN_POINT('Ctrl Pts',(-1.83106639756289,2.47040286398995,111.643170566242));
#29132=CARTESIAN_POINT('Ctrl Pts',(-1.75273803992456,2.5265692911926,111.63817165106));
#29133=CARTESIAN_POINT('Ctrl Pts',(-1.67207962099826,2.57886641589717,111.633172735877));
#29134=CARTESIAN_POINT('Ctrl Pts',(-1.6252534188489,2.6092274837912,111.63027061833));
#29135=CARTESIAN_POINT('Ctrl Pts',(-1.57764237847426,2.63828530138454,111.627368500784));
#29136=CARTESIAN_POINT('Ctrl Pts',(-1.52932683085211,2.6660010679735,111.624466383237));
#29137=CARTESIAN_POINT('Ctrl Pts',(-1.44609310154743,2.71374732621273,111.619466873179));
#29138=CARTESIAN_POINT('Ctrl Pts',(-1.36047504679114,2.75767582035157,111.614467363121));
#29139=CARTESIAN_POINT('Ctrl Pts',(-1.272857686705,2.79754098439969,111.609467853063));
#29140=CARTESIAN_POINT('Ctrl Pts',(-1.18535917861251,2.83735207178744,111.604475124786));
#29141=CARTESIAN_POINT('Ctrl Pts',(-1.09586715131362,2.87311060331083,111.599482396509));
#29142=CARTESIAN_POINT('Ctrl Pts',(-1.00479290128081,2.90461589122137,111.594489668232));
#29143=CARTESIAN_POINT('Ctrl Pts',(-0.913814731890411,2.93608794198418,
111.589502207136));
#29144=CARTESIAN_POINT('Ctrl Pts',(-0.821258070667402,2.96331552636819,
111.584514746039));
#29145=CARTESIAN_POINT('Ctrl Pts',(-0.727555017792677,2.98614566725816,
111.579527284943));
#29146=CARTESIAN_POINT('Ctrl Pts',(-0.633919011088274,3.00895947278373,
111.574543392462));
#29147=CARTESIAN_POINT('Ctrl Pts',(-0.539138668639977,3.02738198619175,
111.569559499982));
#29148=CARTESIAN_POINT('Ctrl Pts',(-0.443661171355982,3.04131008202568,
111.564575607501));
#29149=CARTESIAN_POINT('Ctrl Pts',(-0.348218444266958,3.05523310564237,
111.559593530012));
#29150=CARTESIAN_POINT('Ctrl Pts',(-0.252079500703078,3.06466490040868,
111.554611452524));
#29151=CARTESIAN_POINT('Ctrl Pts',(-0.15570068197844,3.06955363980359,111.549629375035));
#29152=CARTESIAN_POINT('Ctrl Pts',(-0.0593306504513404,3.07444193347485,
111.54464775178));
#29153=CARTESIAN_POINT('Ctrl Pts',(0.0372787743465924,3.07478797323944,
111.539666128525));
#29154=CARTESIAN_POINT('Ctrl Pts',(0.133668249681294,3.07059197045572,111.53468450527));
#29155=CARTESIAN_POINT('Ctrl Pts',(0.230075250633477,3.06639520475116,111.529701976252));
#29156=CARTESIAN_POINT('Ctrl Pts',(0.326261784158633,3.05765477550851,111.524719447234));
#29157=CARTESIAN_POINT('Ctrl Pts',(0.421771709378268,3.04442291332333,111.519736918216));
#29158=CARTESIAN_POINT('Ctrl Pts',(0.517384580606425,3.03117678908745,111.514749018746));
#29159=CARTESIAN_POINT('Ctrl Pts',(0.612318952045057,3.01342962739635,111.509761119276));
#29160=CARTESIAN_POINT('Ctrl Pts',(0.706127207081683,2.99128511135582,111.504773219806));
#29161=CARTESIAN_POINT('Ctrl Pts',(0.799990876175341,2.96912751419067,111.499782373903));
#29162=CARTESIAN_POINT('Ctrl Pts',(0.892726682516278,2.94256751125802,111.494791528));
#29163=CARTESIAN_POINT('Ctrl Pts',(0.983902593640346,2.91175856420614,111.489800682096));
#29164=CARTESIAN_POINT('Ctrl Pts',(1.0752258475601,2.88089982904318,111.484801770848));
#29165=CARTESIAN_POINT('Ctrl Pts',(1.16498376420778,2.84577859889926,111.4798028596));
#29166=CARTESIAN_POINT('Ctrl Pts',(1.25276474985378,2.80659628937327,111.474803948352));
#29167=CARTESIAN_POINT('Ctrl Pts',(1.30372669833892,2.78384868834216,111.471901790719));
#29168=CARTESIAN_POINT('Ctrl Pts',(1.35402277901538,2.75973317641541,111.468999633086));
#29169=CARTESIAN_POINT('Ctrl Pts',(1.40357670663329,2.73429601151676,111.466097475453));
#29170=CARTESIAN_POINT('Ctrl Pts',(1.48892153014178,2.6904865608195,111.46109920099));
#29171=CARTESIAN_POINT('Ctrl Pts',(1.57236313612921,2.6426005861688,111.456100926526));
#29172=CARTESIAN_POINT('Ctrl Pts',(1.65348622624554,2.59082719408615,111.451102652063));
#29173=CARTESIAN_POINT('Ctrl Pts',(1.7285402802135,2.54292710845203,111.44647831193));
#29174=CARTESIAN_POINT('Ctrl Pts',(1.80160966012451,2.49170011663527,111.441853971797));
#29175=CARTESIAN_POINT('Ctrl Pts',(1.87238193903529,2.43733217358128,111.437229631665));
#29176=CARTESIAN_POINT('Ctrl Pts',(1.87238193903529,2.43733217358128,112.437403601774));
#29177=CARTESIAN_POINT('Ctrl Pts',(1.94879948025963,2.37862748590479,112.432404200454));
#29178=CARTESIAN_POINT('Ctrl Pts',(2.02235522355243,2.31640107103305,112.427404799134));
#29179=CARTESIAN_POINT('Ctrl Pts',(2.09272617106382,2.25097743723578,112.422405397814));
#29180=CARTESIAN_POINT('Ctrl Pts',(2.12132119668281,2.22439273785799,112.420373905928));
#29181=CARTESIAN_POINT('Ctrl Pts',(2.14939080333889,2.19728052007338,112.418342414043));
#29182=CARTESIAN_POINT('Ctrl Pts',(2.17691522061888,2.16966411507354,112.416310922158));
#29183=CARTESIAN_POINT('Ctrl Pts',(2.24465163213634,2.10170132571918,112.411311507677));
#29184=CARTESIAN_POINT('Ctrl Pts',(2.30932133936017,2.03044400536883,112.406312093196));
#29185=CARTESIAN_POINT('Ctrl Pts',(2.37058714894232,1.95620009694037,112.401312678715));
#29186=CARTESIAN_POINT('Ctrl Pts',(2.4317698329323,1.88205692281862,112.396320047451));
#29187=CARTESIAN_POINT('Ctrl Pts',(2.48955752105744,1.80493554979578,112.391327416187));
#29188=CARTESIAN_POINT('Ctrl Pts',(2.54364952514628,1.72518095955848,112.386334784923));
#29189=CARTESIAN_POINT('Ctrl Pts',(2.59768444864421,1.64551053035782,112.381347422133));
#29190=CARTESIAN_POINT('Ctrl Pts',(2.64803119571126,1.56321276920054,112.376360059344));
#29191=CARTESIAN_POINT('Ctrl Pts',(2.69442974111918,1.47866514808879,112.371372696554));
#29192=CARTESIAN_POINT('Ctrl Pts',(2.74079507273524,1.39417804928576,112.366388903903));
#29193=CARTESIAN_POINT('Ctrl Pts',(2.7832176105889,1.30744467592563,112.361405111252));
#29194=CARTESIAN_POINT('Ctrl Pts',(2.82148154763242,1.21887002029328,112.356421318601));
#29195=CARTESIAN_POINT('Ctrl Pts',(2.85973154280678,1.13032763777123,112.351439341847));
#29196=CARTESIAN_POINT('Ctrl Pts',(2.89382577385429,1.03994570853644,112.346457365094));
#29197=CARTESIAN_POINT('Ctrl Pts',(2.92359558836734,0.94815140440702,112.34147538834));
#29198=CARTESIAN_POINT('Ctrl Pts',(2.95336268392932,0.856365484079305,112.336493866603));
#29199=CARTESIAN_POINT('Ctrl Pts',(2.97880601296027,0.763167862951526,112.331512344865));
#29200=CARTESIAN_POINT('Ctrl Pts',(2.99980639222127,0.669002136908707,112.326530823128));
#29201=CARTESIAN_POINT('Ctrl Pts',(3.02081058708148,0.574819301714405,112.321548396289));
#29202=CARTESIAN_POINT('Ctrl Pts',(3.03737013346229,0.479668440734097,112.316565969449));
#29203=CARTESIAN_POINT('Ctrl Pts',(3.04941691172385,0.384003578749662,112.311583542609));
#29204=CARTESIAN_POINT('Ctrl Pts',(3.0614766740101,0.288235609120851,112.306595745707));
#29205=CARTESIAN_POINT('Ctrl Pts',(3.06901390298465,0.191952968761404,112.301607948805));
#29206=CARTESIAN_POINT('Ctrl Pts',(3.07201237877847,0.0956148243308455,
112.296620151903));
#29207=CARTESIAN_POINT('Ctrl Pts',(3.07501262563339,-0.00078022258996073,
112.29162940894));
#29208=CARTESIAN_POINT('Ctrl Pts',(3.07346878836156,-0.0972304001388508,
112.286638665976));
#29209=CARTESIAN_POINT('Ctrl Pts',(3.06741676537897,-0.193278652395989,
112.281647923013));
#29210=CARTESIAN_POINT('Ctrl Pts',(3.06135496143944,-0.289482132718584,
112.276649114277));
#29211=CARTESIAN_POINT('Ctrl Pts',(3.05077047165617,-0.385281954668675,
112.271650305541));
#29212=CARTESIAN_POINT('Ctrl Pts',(3.0357508125885,-0.480228335136801,112.266651496805));
#29213=CARTESIAN_POINT('Ctrl Pts',(3.02702783719739,-0.535370395057574,
112.263748335995));
#29214=CARTESIAN_POINT('Ctrl Pts',(3.01680985790913,-0.59022480529076,112.260845175184));
#29215=CARTESIAN_POINT('Ctrl Pts',(3.00512174396439,-0.644705788676058,
112.257942014374));
#29216=CARTESIAN_POINT('Ctrl Pts',(2.98499361965295,-0.738527598710917,
112.252942475358));
#29217=CARTESIAN_POINT('Ctrl Pts',(2.96043216917071,-0.831570661220707,
112.247942936343));
#29218=CARTESIAN_POINT('Ctrl Pts',(2.93151213234959,-0.923384463745818,
112.242943397327));
#29219=CARTESIAN_POINT('Ctrl Pts',(2.90263132364309,-1.01507372692849,112.237950639855));
#29220=CARTESIAN_POINT('Ctrl Pts',(2.86940380932578,-1.10553662889735,112.232957882383));
#29221=CARTESIAN_POINT('Ctrl Pts',(2.83195527184254,-1.19433311445478,112.227965124911));
#29222=CARTESIAN_POINT('Ctrl Pts',(2.79454623976421,-1.28303592636426,112.222977634424));
#29223=CARTESIAN_POINT('Ctrl Pts',(2.75292520621421,-1.37007541424261,112.217990143938));
#29224=CARTESIAN_POINT('Ctrl Pts',(2.70726724450543,-1.4550279436588,112.213002653451));
#29225=CARTESIAN_POINT('Ctrl Pts',(2.66164195014025,-1.53991969126688,112.208018731413));
#29226=CARTESIAN_POINT('Ctrl Pts',(2.61198567671238,-1.62272706323516,112.203034809374));
#29227=CARTESIAN_POINT('Ctrl Pts',(2.55852065513925,-1.70304853343227,112.198050887336));
#29228=CARTESIAN_POINT('Ctrl Pts',(2.50507510290357,-1.78334075449113,112.193068780197));
#29229=CARTESIAN_POINT('Ctrl Pts',(2.44782380124132,-1.86114850736622,112.188086673059));
#29230=CARTESIAN_POINT('Ctrl Pts',(2.38703325753857,-1.93609774479616,112.18310456592));
#29231=CARTESIAN_POINT('Ctrl Pts',(2.32624825561316,-2.01104014971631,112.178122912959));
#29232=CARTESIAN_POINT('Ctrl Pts',(2.26192492977835,-2.08312421648798,112.173141259999));
#29233=CARTESIAN_POINT('Ctrl Pts',(2.19437049641909,-2.15200845129508,112.168159607038));
#29234=CARTESIAN_POINT('Ctrl Pts',(2.12680378007173,-2.22090521087952,112.163177048296));
#29235=CARTESIAN_POINT('Ctrl Pts',(2.05600509681178,-2.28660066966237,112.158194489553));
#29236=CARTESIAN_POINT('Ctrl Pts',(1.9823182115159,-2.34879048837745,112.153211930811));
#29237=CARTESIAN_POINT('Ctrl Pts',(1.90855190506639,-2.4110473364849,112.14822400177));
#29238=CARTESIAN_POINT('Ctrl Pts',(1.83189151785293,-2.46979071762057,112.143236072729));
#29239=CARTESIAN_POINT('Ctrl Pts',(1.75271338391871,-2.52475702669232,112.138248143688));
#29240=CARTESIAN_POINT('Ctrl Pts',(1.67348847913685,-2.5797558045877,112.133257268257));
#29241=CARTESIAN_POINT('Ctrl Pts',(1.59174323809057,-2.63097283491827,112.128266392826));
#29242=CARTESIAN_POINT('Ctrl Pts',(1.50788059978875,-2.67818937843849,112.123275517395));
#29243=CARTESIAN_POINT('Ctrl Pts',(1.42388244400905,-2.72548222133374,112.11827657698));
#29244=CARTESIAN_POINT('Ctrl Pts',(1.33776045074766,-2.7687614721309,112.113277636565));
#29245=CARTESIAN_POINT('Ctrl Pts',(1.24993956183347,-2.80785564831306,112.108278696149));
#29246=CARTESIAN_POINT('Ctrl Pts',(1.19895991747353,-2.83054964769012,112.105376832963));
#29247=CARTESIAN_POINT('Ctrl Pts',(1.1474081292581,-2.85183429548936,112.102474969776));
#29248=CARTESIAN_POINT('Ctrl Pts',(1.09536956853821,-2.87168378452789,112.09957310659));
#29249=CARTESIAN_POINT('Ctrl Pts',(1.00571417110824,-2.90588176779091,112.094573589046));
#29250=CARTESIAN_POINT('Ctrl Pts',(0.914298255469063,-2.93593716116456,
112.089574071502));
#29251=CARTESIAN_POINT('Ctrl Pts',(0.82154039614416,-2.96166737286673,112.084574553959));
#29252=CARTESIAN_POINT('Ctrl Pts',(0.728908357998077,-2.98736268288411,
112.079581817999));
#29253=CARTESIAN_POINT('Ctrl Pts',(0.634938413216042,-3.00874435494215,
112.074589082039));
#29254=CARTESIAN_POINT('Ctrl Pts',(0.540068100907363,-3.02567822089235,
112.069596346079));
#29255=CARTESIAN_POINT('Ctrl Pts',(0.445297870295764,-3.04259422277105,
112.064608877114));
#29256=CARTESIAN_POINT('Ctrl Pts',(0.349629590187939,-3.05507166949399,
112.059621408149));
#29257=CARTESIAN_POINT('Ctrl Pts',(0.253513917243686,-3.06302676184257,
112.054633939184));
#29258=CARTESIAN_POINT('Ctrl Pts',(0.157467011910874,-3.07097616258349,
112.04965003859));
#29259=CARTESIAN_POINT('Ctrl Pts',(0.0609737862857786,-3.07440960505889,
112.044666137996));
#29260=CARTESIAN_POINT('Ctrl Pts',(-0.0355079720195087,-3.07329488235722,
112.039682237402));
#29261=CARTESIAN_POINT('Ctrl Pts',(-0.131954597342464,-3.072180565572,112.034700151651));
#29262=CARTESIAN_POINT('Ctrl Pts',(-0.228389325159465,-3.06652137931458,
112.0297180659));
#29263=CARTESIAN_POINT('Ctrl Pts',(-0.324353310408222,-3.05633721634692,
112.024735980149));
#29264=CARTESIAN_POINT('Ctrl Pts',(-0.420308548972106,-3.04615398161983,
112.019754348493));
#29265=CARTESIAN_POINT('Ctrl Pts',(-0.515792693782929,-3.0314466366791,
112.014772716837));
#29266=CARTESIAN_POINT('Ctrl Pts',(-0.610352041216524,-3.0122869444631,
112.009791085181));
#29267=CARTESIAN_POINT('Ctrl Pts',(-0.70492858393743,-2.99312376812393,
112.004808547633));
#29268=CARTESIAN_POINT('Ctrl Pts',(-0.79857956508617,-2.96950672376021,
111.999826010084));
#29269=CARTESIAN_POINT('Ctrl Pts',(-0.890862547100991,-2.94155845975781,
111.994843472536));
#29270=CARTESIAN_POINT('Ctrl Pts',(-0.983244999487806,-2.91358007076209,
111.989855564389));
#29271=CARTESIAN_POINT('Ctrl Pts',(-1.07425608813524,-2.88126126923715,
111.984867656242));
#29272=CARTESIAN_POINT('Ctrl Pts',(-1.16346981067153,-2.84477420011782,
111.979879748094));
#29273=CARTESIAN_POINT('Ctrl Pts',(-1.25273623481969,-2.80826557683282,
111.974888893419));
#29274=CARTESIAN_POINT('Ctrl Pts',(-1.34020278087729,-2.76758396806884,
111.969898038743));
#29275=CARTESIAN_POINT('Ctrl Pts',(-1.4254665945932,-2.72294826203123,111.964907184067));
#29276=CARTESIAN_POINT('Ctrl Pts',(-1.51086819786687,-2.67824042299924,
111.95990826398));
#29277=CARTESIAN_POINT('Ctrl Pts',(-1.59405958224704,-2.62956594886001,
111.954909343894));
#29278=CARTESIAN_POINT('Ctrl Pts',(-1.67466555268891,-2.57718791255841,
111.949910423808));
#29279=CARTESIAN_POINT('Ctrl Pts',(-1.72146057395033,-2.54678034710228,
111.947008348807));
#29280=CARTESIAN_POINT('Ctrl Pts',(-1.76738482178594,-2.51512536555158,
111.944106273806));
#29281=CARTESIAN_POINT('Ctrl Pts',(-1.81237015387301,-2.48228053921194,
111.941204198806));
#29282=CARTESIAN_POINT('Ctrl Pts',(-1.88923164428324,-2.42616219601858,
111.93624574236));
#29283=CARTESIAN_POINT('Ctrl Pts',(-1.96363015846744,-2.36636383511589,
111.931287285915));
#29284=CARTESIAN_POINT('Ctrl Pts',(-2.03518809297881,-2.30313084217924,
111.926328829469));
#29285=CARTESIAN_POINT('Ctrl Pts',(-2.10664864570303,-2.23998390178032,
111.92137712089));
#29286=CARTESIAN_POINT('Ctrl Pts',(-2.17527596659793,-2.17341190847224,
111.91642541231));
#29287=CARTESIAN_POINT('Ctrl Pts',(-2.24072242206252,-2.10370275401879,
111.911473703731));
#29288=CARTESIAN_POINT('Ctrl Pts',(-2.30675050290536,-2.03337409140347,
111.906477989111));
#29289=CARTESIAN_POINT('Ctrl Pts',(-2.36954051726184,-1.95985248829929,
111.901482274491));
#29290=CARTESIAN_POINT('Ctrl Pts',(-2.42877049203524,-1.88347448801912,
111.896486559871));
#29291=CARTESIAN_POINT('Ctrl Pts',(-2.48737632744141,-1.8079013254406,111.89154348789));
#29292=CARTESIAN_POINT('Ctrl Pts',(-2.54249651377506,-1.72953203929604,
111.886600415908));
#29293=CARTESIAN_POINT('Ctrl Pts',(-2.59385799705819,-1.64872767341888,
111.881657343927));
#29294=CARTESIAN_POINT('Ctrl Pts',(-2.6452024680113,-1.5679500721609,111.876715909226));
#29295=CARTESIAN_POINT('Ctrl Pts',(-2.69279046934162,-1.48473937024501,
111.871774474526));
#29296=CARTESIAN_POINT('Ctrl Pts',(-2.7363920694606,-1.39948586709303,111.866833039825));
#29297=CARTESIAN_POINT('Ctrl Pts',(-2.77999162848551,-1.31423635485925,
111.861891836445));
#29298=CARTESIAN_POINT('Ctrl Pts',(-2.81960495457762,-1.22694462992712,
111.856950633065));
#29299=CARTESIAN_POINT('Ctrl Pts',(-2.85504846778913,-1.13802482247749,
111.852009429685));
#29300=CARTESIAN_POINT('Ctrl Pts',(-2.89117248629991,-1.04739778019993,
111.846973356615));
#29301=CARTESIAN_POINT('Ctrl Pts',(-2.92296471426377,-0.95507992912274,
111.841937283546));
#29302=CARTESIAN_POINT('Ctrl Pts',(-2.95028314976414,-0.861528633428869,
111.836901210476));
#29303=CARTESIAN_POINT('Ctrl Pts',(-2.97712196335533,-0.769619790907143,
111.831953554292));
#29304=CARTESIAN_POINT('Ctrl Pts',(-2.99964275917986,-0.676520919820833,
111.827005898108));
#29305=CARTESIAN_POINT('Ctrl Pts',(-3.01776236287641,-0.582677072834153,
111.822058241924));
#29306=CARTESIAN_POINT('Ctrl Pts',(-3.03636767501656,-0.486317676963264,
111.816977960412));
#29307=CARTESIAN_POINT('Ctrl Pts',(-3.05033240432285,-0.389173298906863,
111.811897678899));
#29308=CARTESIAN_POINT('Ctrl Pts',(-3.05962341637771,-0.291730697653163,
111.806817397387));
#29309=CARTESIAN_POINT('Ctrl Pts',(-3.06891442843256,-0.194288096399463,
111.801737115875));
#29310=CARTESIAN_POINT('Ctrl Pts',(-3.07353176764381,-0.0965477774265246,
111.796656834363));
#29311=CARTESIAN_POINT('Ctrl Pts',(-3.07349983534499,0.0010060488542432,
111.791576552851));
#29312=CARTESIAN_POINT('Origin',(0.,0.,116.208423447177));
#29313=CARTESIAN_POINT('',(1.8723819390353,2.43733217358127,113.437353936953));
#29314=CARTESIAN_POINT('',(1.8746157427793,2.44019679077305,113.354075550313));
#29315=CARTESIAN_POINT('',(1.8723819390353,2.43733217358128,116.208423447177));
#29316=CARTESIAN_POINT('',(-3.07304940657614,-0.00348278968395837,113.791576743866));
#29317=CARTESIAN_POINT('Ctrl Pts',(-3.07349803031876,-0.00347960151198421,
113.791576552823));
#29318=CARTESIAN_POINT('Ctrl Pts',(-3.07360613510913,0.0920083039628076,
113.786645986316));
#29319=CARTESIAN_POINT('Ctrl Pts',(-3.06926002918478,0.187573875915372,
113.78171541981));
#29320=CARTESIAN_POINT('Ctrl Pts',(-3.0604649665282,0.282765695680308,113.776784853303));
#29321=CARTESIAN_POINT('Ctrl Pts',(-3.05167259930464,0.37792834189809,113.771855797873));
#29322=CARTESIAN_POINT('Ctrl Pts',(-3.0384340242833,0.472717016989944,113.766926742443));
#29323=CARTESIAN_POINT('Ctrl Pts',(-3.02080650617518,0.566683599771268,
113.761997687013));
#29324=CARTESIAN_POINT('Ctrl Pts',(-3.00317934056945,0.660648303476645,
113.757068730151));
#29325=CARTESIAN_POINT('Ctrl Pts',(-2.98116348973558,0.753790506665149,
113.752139773288));
#29326=CARTESIAN_POINT('Ctrl Pts',(-2.95486745376389,0.845671674284358,
113.747210816426));
#29327=CARTESIAN_POINT('Ctrl Pts',(-2.9285644100671,0.937577327646052,113.742280546028));
#29328=CARTESIAN_POINT('Ctrl Pts',(-2.89797904042123,1.02822084712495,113.73735027563));
#29329=CARTESIAN_POINT('Ctrl Pts',(-2.86326952617376,1.11717942627168,113.732420005232));
#29330=CARTESIAN_POINT('Ctrl Pts',(-2.82851938726505,1.20624212419447,113.727483964354));
#29331=CARTESIAN_POINT('Ctrl Pts',(-2.78963563639662,1.29361552880427,113.722547923476));
#29332=CARTESIAN_POINT('Ctrl Pts',(-2.74682422301602,1.37889772566801,113.717611882598));
#29333=CARTESIAN_POINT('Ctrl Pts',(-2.70398333184197,1.46423864357798,113.71267244301));
#29334=CARTESIAN_POINT('Ctrl Pts',(-2.65720961820313,1.54748509953168,113.707733003422));
#29335=CARTESIAN_POINT('Ctrl Pts',(-2.60675337106642,1.628262605489,113.702793563833));
#29336=CARTESIAN_POINT('Ctrl Pts',(-2.55621556095394,1.70917068900878,113.697846139597));
#29337=CARTESIAN_POINT('Ctrl Pts',(-2.50198359661781,1.78760149362166,113.69289871536));
#29338=CARTESIAN_POINT('Ctrl Pts',(-2.44434893228502,1.86321242676112,113.687951291123));
#29339=CARTESIAN_POINT('Ctrl Pts',(-2.42614046142172,1.88710012505789,113.686388255559));
#29340=CARTESIAN_POINT('Ctrl Pts',(-2.40759264321255,1.91070664089894,113.684825219995));
#29341=CARTESIAN_POINT('Ctrl Pts',(-2.38871541829762,1.93402194930337,113.683262184432));
#29342=CARTESIAN_POINT('Ctrl Pts',(-2.3282774956313,2.00866898098517,113.678257920142));
#29343=CARTESIAN_POINT('Ctrl Pts',(-2.26423183045799,2.08061038074523,113.673253655852));
#29344=CARTESIAN_POINT('Ctrl Pts',(-2.19684950773242,2.14947772502434,113.668249391562));
#29345=CARTESIAN_POINT('Ctrl Pts',(-2.12955880479925,2.21825143032619,113.663251931574));
#29346=CARTESIAN_POINT('Ctrl Pts',(-2.05894076516932,2.28395907721264,113.658254471586));
#29347=CARTESIAN_POINT('Ctrl Pts',(-1.98530715722022,2.34626463586062,113.653257011598));
#29348=CARTESIAN_POINT('Ctrl Pts',(-1.91175158892653,2.4085041607441,113.648264848105));
#29349=CARTESIAN_POINT('Ctrl Pts',(-1.8351871386764,2.46734848414005,113.643272684612));
#29350=CARTESIAN_POINT('Ctrl Pts',(-1.75596218297494,2.52249857521504,113.638280521119));
#29351=CARTESIAN_POINT('Ctrl Pts',(-1.67679488852393,2.57760852712951,113.633291991007));
#29352=CARTESIAN_POINT('Ctrl Pts',(-1.59497129682453,2.6290293427901,113.628303460894));
#29353=CARTESIAN_POINT('Ctrl Pts',(-1.51087183006416,2.67650304747044,113.623314930782));
#29354=CARTESIAN_POINT('Ctrl Pts',(-1.42680367119149,2.72395907901359,113.61832825776));
#29355=CARTESIAN_POINT('Ctrl Pts',(-1.34046170176576,2.7674707042323,113.613341584738));
#29356=CARTESIAN_POINT('Ctrl Pts',(-1.25225340771642,2.8068244784565,113.608354911716));
#29357=CARTESIAN_POINT('Ctrl Pts',(-1.16405400161499,2.84617428735863,113.603368741156));
#29358=CARTESIAN_POINT('Ctrl Pts',(-1.07398904484235,2.88136689997652,113.598382570596));
#29359=CARTESIAN_POINT('Ctrl Pts',(-0.982487622527084,2.91223630936452,
113.593396400036));
#29360=CARTESIAN_POINT('Ctrl Pts',(-0.890970576799521,2.94311098955048,
113.588409378112));
#29361=CARTESIAN_POINT('Ctrl Pts',(-0.798016993449633,2.96966086056145,
113.583422356188));
#29362=CARTESIAN_POINT('Ctrl Pts',(-0.704071778567027,2.99176957345071,
113.578435334264));
#29363=CARTESIAN_POINT('Ctrl Pts',(-0.610027500913148,3.01390159939931,
113.573443053656));
#29364=CARTESIAN_POINT('Ctrl Pts',(-0.514989931181838,3.03158301716507,
113.568450773048));
#29365=CARTESIAN_POINT('Ctrl Pts',(-0.419414628834668,3.04474853134368,
113.56345849244));
#29366=CARTESIAN_POINT('Ctrl Pts',(-0.323784005594781,3.05792166598468,
113.5584633222));
#29367=CARTESIAN_POINT('Ctrl Pts',(-0.227615465991627,3.06657365253343,
113.55346815196));
#29368=CARTESIAN_POINT('Ctrl Pts',(-0.131368064689393,3.0706912383989,113.54847298172));
#29369=CARTESIAN_POINT('Ctrl Pts',(-0.0349678284998302,3.07481536273464,
113.543469879461));
#29370=CARTESIAN_POINT('Ctrl Pts',(0.0615110817052908,3.07439071040301,
113.538466777202));
#29371=CARTESIAN_POINT('Ctrl Pts',(0.157611306929676,3.06945612868598,113.533463674942));
#29372=CARTESIAN_POINT('Ctrl Pts',(0.212485074158239,3.06663845486806,113.53060687551));
#29373=CARTESIAN_POINT('Ctrl Pts',(0.2672354795067,3.06235128439908,113.527750076079));
#29374=CARTESIAN_POINT('Ctrl Pts',(0.321778771217115,3.05660934245677,113.524893276647));
#29375=CARTESIAN_POINT('Ctrl Pts',(0.417380576494212,3.04654504310359,113.519885966409));
#29376=CARTESIAN_POINT('Ctrl Pts',(0.512671443783229,3.03197421992204,113.514878656172));
#29377=CARTESIAN_POINT('Ctrl Pts',(0.607194239830824,3.01292505799867,113.509871345934));
#29378=CARTESIAN_POINT('Ctrl Pts',(0.701597580057766,2.99389996998514,113.504870363824));
#29379=CARTESIAN_POINT('Ctrl Pts',(0.795234352760283,2.97040787511575,113.499869381714));
#29380=CARTESIAN_POINT('Ctrl Pts',(0.887652546274494,2.94252870964625,113.494868399605));
#29381=CARTESIAN_POINT('Ctrl Pts',(0.979969062029866,2.91468021661207,113.489872919536));
#29382=CARTESIAN_POINT('Ctrl Pts',(1.07106924864573,2.88245437851228,113.484877439466));
#29383=CARTESIAN_POINT('Ctrl Pts',(1.1605124657483,2.8459819161131,113.479881959397));
#29384=CARTESIAN_POINT('Ctrl Pts',(1.24989707729888,2.80953335143206,113.474889752498));
#29385=CARTESIAN_POINT('Ctrl Pts',(1.33762647348917,2.76884385735648,113.469897545599));
#29386=CARTESIAN_POINT('Ctrl Pts',(1.42327710334293,2.72409334221494,113.4649053387));
#29387=CARTESIAN_POINT('Ctrl Pts',(1.50890863332699,2.67935280632294,113.459914245051));
#29388=CARTESIAN_POINT('Ctrl Pts',(1.59246192734598,2.63055324429409,113.454923151401));
#29389=CARTESIAN_POINT('Ctrl Pts',(1.67353604504419,2.57792151857613,113.449932057751));
#29390=CARTESIAN_POINT('Ctrl Pts',(1.74164136207261,2.53370888367436,113.445739350819));
#29391=CARTESIAN_POINT('Ctrl Pts',(1.80799749284803,2.48679292230585,113.441546643886));
#29392=CARTESIAN_POINT('Ctrl Pts',(1.8723819390353,2.43733217358127,113.437353936953));
#29393=CARTESIAN_POINT('',(-0.793799282533091,-2.96922295374563,114.));
#29394=CARTESIAN_POINT('Ctrl Pts',(-0.793799282533038,-2.96922295374565,
114.));
#29395=CARTESIAN_POINT('Ctrl Pts',(-1.77865212890027,-2.7059299996545,113.947210364072));
#29396=CARTESIAN_POINT('Ctrl Pts',(-2.87774335179386,-1.66670642438129,
113.877736327106));
#29397=CARTESIAN_POINT('Ctrl Pts',(-3.07274765096662,-0.326293812111691,
113.808262290142));
#29398=CARTESIAN_POINT('Ctrl Pts',(-3.07036006322683,-0.00350190166640733,
113.791577889105));
#29399=CARTESIAN_POINT('',(0.794173972183063,-2.96912275797195,113.999999974814));
#29400=CARTESIAN_POINT('Origin',(0.,0.,114.));
#29401=CARTESIAN_POINT('',(-3.07349930869882,0.00206141404370558,113.708423447177));
#29402=CARTESIAN_POINT('Ctrl Pts',(0.794173972183063,-2.96912275797195,
113.999999974814));
#29403=CARTESIAN_POINT('Ctrl Pts',(0.701819794355633,-2.99382543624822,
113.995019289507));
#29404=CARTESIAN_POINT('Ctrl Pts',(0.608144005864226,-3.01425987787217,
113.990038604201));
#29405=CARTESIAN_POINT('Ctrl Pts',(0.513578555021576,-3.03028700254975,
113.985057918894));
#29406=CARTESIAN_POINT('Ctrl Pts',(0.419141384954323,-3.04629238596811,
113.980083990031));
#29407=CARTESIAN_POINT('Ctrl Pts',(0.32381738326219,-3.05790225921004,113.975110061168));
#29408=CARTESIAN_POINT('Ctrl Pts',(0.228052546930729,-3.06502761583618,
113.970136132306));
#29409=CARTESIAN_POINT('Ctrl Pts',(0.128387450814283,-3.07244317023184,
113.964959627889));
#29410=CARTESIAN_POINT('Ctrl Pts',(0.0282453099355113,-3.07500098941394,
113.959783123473));
#29411=CARTESIAN_POINT('Ctrl Pts',(-0.0718603908461009,-3.07265981426963,
113.954606619057));
#29412=CARTESIAN_POINT('Ctrl Pts',(-0.167878281058049,-3.07041424087852,
113.949641496903));
#29413=CARTESIAN_POINT('Ctrl Pts',(-0.263862157958898,-3.0636619461203,
113.944676374749));
#29414=CARTESIAN_POINT('Ctrl Pts',(-0.35935623066889,-3.05241958935521,
113.939711252594));
#29415=CARTESIAN_POINT('Ctrl Pts',(-0.454818200664135,-3.0411810119888,
113.93474779959));
#29416=CARTESIAN_POINT('Ctrl Pts',(-0.549790254354859,-3.02545542312751,
113.929784346585));
#29417=CARTESIAN_POINT('Ctrl Pts',(-0.643821149403549,-3.00531139444496,
113.924820893581));
#29418=CARTESIAN_POINT('Ctrl Pts',(-0.737846617600058,-2.98516852834483,
113.919857727034));
#29419=CARTESIAN_POINT('Ctrl Pts',(-0.830930602409861,-2.96060782271577,
113.914894560488));
#29420=CARTESIAN_POINT('Ctrl Pts',(-0.922632597200634,-2.93174885359964,
113.909931393942));
#29421=CARTESIAN_POINT('Ctrl Pts',(-1.01435483510214,-2.902883513899,113.904967131782));
#29422=CARTESIAN_POINT('Ctrl Pts',(-1.10469405510182,-2.86971815972228,
113.900002869622));
#29423=CARTESIAN_POINT('Ctrl Pts',(-1.1932265144058,-2.83242170859478,113.895038607463));
#29424=CARTESIAN_POINT('Ctrl Pts',(-1.28185417451937,-2.79508515181146,
113.890069007128));
#29425=CARTESIAN_POINT('Ctrl Pts',(-1.36867078859752,-2.7536088056063,113.885099406793));
#29426=CARTESIAN_POINT('Ctrl Pts',(-1.45327446783635,-2.70820892309567,
113.880129806458));
#29427=CARTESIAN_POINT('Ctrl Pts',(-1.53793198498444,-2.66278015017769,
113.875157043697));
#29428=CARTESIAN_POINT('Ctrl Pts',(-1.62037338541075,-2.6134230987979,113.870184280936));
#29429=CARTESIAN_POINT('Ctrl Pts',(-1.70022497884624,-2.56039787363357,
113.865211518175));
#29430=CARTESIAN_POINT('Ctrl Pts',(-1.78019708483401,-2.50729262244916,
113.860231250487));
#29431=CARTESIAN_POINT('Ctrl Pts',(-1.85757122926894,-2.4505084124833,113.8552509828));
#29432=CARTESIAN_POINT('Ctrl Pts',(-1.93200631417581,-2.39034596909836,
113.850270715113));
#29433=CARTESIAN_POINT('Ctrl Pts',(-1.95378108694139,-2.37274642534332,
113.848813818847));
#29434=CARTESIAN_POINT('Ctrl Pts',(-1.97530458760304,-2.35485802645277,
113.847356922582));
#29435=CARTESIAN_POINT('Ctrl Pts',(-1.99656889110003,-2.33668887811185,
113.845900026317));
#29436=CARTESIAN_POINT('Ctrl Pts',(-2.06860404074852,-2.27513890447132,
113.84096463116));
#29437=CARTESIAN_POINT('Ctrl Pts',(-2.13792989564559,-2.21013527188959,
113.836029236003));
#29438=CARTESIAN_POINT('Ctrl Pts',(-2.20419088223709,-2.1419488333438,113.831093840846));
#29439=CARTESIAN_POINT('Ctrl Pts',(-2.27281305813786,-2.07133259261707,
113.825982574443));
#29440=CARTESIAN_POINT('Ctrl Pts',(-2.33814741676195,-1.99730269472254,
113.820871308041));
#29441=CARTESIAN_POINT('Ctrl Pts',(-2.39983504643822,-1.92020675967117,
113.815760041638));
#29442=CARTESIAN_POINT('Ctrl Pts',(-2.45925381887982,-1.845946395883,113.810836766471));
#29443=CARTESIAN_POINT('Ctrl Pts',(-2.51528907345824,-1.76884194831064,
113.805913491304));
#29444=CARTESIAN_POINT('Ctrl Pts',(-2.56765762979606,-1.68924141144777,
113.800990216137));
#29445=CARTESIAN_POINT('Ctrl Pts',(-2.61999590973637,-1.60968689490063,
113.796069787317));
#29446=CARTESIAN_POINT('Ctrl Pts',(-2.66867145318846,-1.52763953052981,
113.791149358496));
#29447=CARTESIAN_POINT('Ctrl Pts',(-2.71344297688252,-1.44347825103358,
113.786228929675));
#29448=CARTESIAN_POINT('Ctrl Pts',(-2.7582015959496,-1.35934122958862,113.781309919084));
#29449=CARTESIAN_POINT('Ctrl Pts',(-2.79905821921307,-1.273091901828,113.776390908493));
#29450=CARTESIAN_POINT('Ctrl Pts',(-2.8358169452503,-1.18513480373806,113.771471897902));
#29451=CARTESIAN_POINT('Ctrl Pts',(-2.8725757322411,-1.09717755979707,113.766552879154));
#29452=CARTESIAN_POINT('Ctrl Pts',(-2.9052364368862,-1.00751295730005,113.761633860406));
#29453=CARTESIAN_POINT('Ctrl Pts',(-2.93365132713148,-0.916565404550987,
113.756714841659));
#29454=CARTESIAN_POINT('Ctrl Pts',(-2.96208830210682,-0.825547165195897,
113.751791999732));
#29455=CARTESIAN_POINT('Ctrl Pts',(-2.98627274234399,-0.733244416947654,
113.746869157806));
#29456=CARTESIAN_POINT('Ctrl Pts',(-3.00610700087766,-0.64009604691351,
113.741946315879));
#29457=CARTESIAN_POINT('Ctrl Pts',(-3.02595053053168,-0.54690413657019,
113.737021172871));
#29458=CARTESIAN_POINT('Ctrl Pts',(-3.04143975801272,-0.452866262744185,
113.732096029862));
#29459=CARTESIAN_POINT('Ctrl Pts',(-3.05252863509209,-0.358428768296877,
113.727170886853));
#29460=CARTESIAN_POINT('Ctrl Pts',(-3.06363167096095,-0.263870691702751,
113.722239455195));
#29461=CARTESIAN_POINT('Ctrl Pts',(-3.07032311601581,-0.168912425696858,
113.717308023536));
#29462=CARTESIAN_POINT('Ctrl Pts',(-3.07260897912071,-0.0740021042050705,
113.712376591878));
#29463=CARTESIAN_POINT('Ctrl Pts',(-3.07321977859683,-0.0486413664947478,
113.711058876978));
#29464=CARTESIAN_POINT('Ctrl Pts',(-3.07351630803801,-0.0232840314320732,
113.709741162077));
#29465=CARTESIAN_POINT('Ctrl Pts',(-3.07349930869882,0.00206141404370563,
113.708423447177));
#29466=CARTESIAN_POINT('Ctrl Pts',(-3.07651118397331,0.00206343412614721,
113.708423447177));
#29467=CARTESIAN_POINT('Ctrl Pts',(-3.0775723946044,0.136145886725428,113.701459337629));
#29468=CARTESIAN_POINT('Ctrl Pts',(-3.00879601357565,1.28554760232957,113.641705592153));
#29469=CARTESIAN_POINT('Ctrl Pts',(-1.56068784542394,3.27732114239516,113.529162210748));
#29470=CARTESIAN_POINT('Ctrl Pts',(0.867539436947584,3.14804109327096,113.418010354676));
#29471=CARTESIAN_POINT('Ctrl Pts',(1.79005390196206,2.5061803198351,113.359648134531));
#29472=CARTESIAN_POINT('Ctrl Pts',(1.8746157427793,2.44019679077305,113.354075550313));
#29473=CARTESIAN_POINT('Origin',(0.,0.,104.));
#29474=CARTESIAN_POINT('',(-2.36143112101026,0.872610629504498,95.3311773795575));
#29475=CARTESIAN_POINT('',(-2.3614311210294,0.872610629452704,95.0532830566435));
#29476=CARTESIAN_POINT('',(-2.36143112101026,0.872610629504505,104.));
#29477=CARTESIAN_POINT('',(-1.91346599666497,1.63598720337506,95.));
#29478=CARTESIAN_POINT('Ctrl Pts',(-2.36143112104854,0.872610629400893,
95.0532830566435));
#29479=CARTESIAN_POINT('Ctrl Pts',(-2.31579433560925,0.996111446111038,
95.0453131407852));
#29480=CARTESIAN_POINT('Ctrl Pts',(-2.26053801495448,1.11584628337841,95.0375896339826));
#29481=CARTESIAN_POINT('Ctrl Pts',(-2.13200539566163,1.34520787555974,95.0221295983418));
#29482=CARTESIAN_POINT('Ctrl Pts',(-2.05899555128104,1.45449729498176,95.0144128937844));
#29483=CARTESIAN_POINT('Ctrl Pts',(-1.96578302134751,1.57285764443762,95.0051301889263));
#29484=CARTESIAN_POINT('Ctrl Pts',(-1.95358099596075,1.58798781731369,95.0039247102501));
#29485=CARTESIAN_POINT('Ctrl Pts',(-1.93616947814021,1.60907319677807,95.0022158593805));
#29486=CARTESIAN_POINT('Ctrl Pts',(-1.93110497507636,1.61514778668851,95.0017201146326));
#29487=CARTESIAN_POINT('Ctrl Pts',(-1.92184895461832,1.62614410096873,95.0008162608354));
#29488=CARTESIAN_POINT('Ctrl Pts',(-1.91766692397879,1.6310737593378,95.0004086818932));
#29489=CARTESIAN_POINT('Ctrl Pts',(-1.91346599666497,1.63598720337506,95.));
#29490=CARTESIAN_POINT('',(-2.36143112101026,0.872610629504506,95.));
#29491=CARTESIAN_POINT('Origin',(0.,0.,95.));
#29492=CARTESIAN_POINT('',(-2.36143112101026,0.872610629504505,94.));
#29493=CARTESIAN_POINT('',(-2.36143112101026,0.872610629504505,104.));
#29494=CARTESIAN_POINT('Origin',(0.,0.,94.));
#29495=CARTESIAN_POINT('',(1.91365527685913,1.63576579355029,95.0000017045188));
#29496=CARTESIAN_POINT('Origin',(0.,0.,95.));
#29497=CARTESIAN_POINT('Ctrl Pts',(1.91365527685913,1.63576579355029,95.0000017045188));
#29498=CARTESIAN_POINT('Ctrl Pts',(1.86017230240225,1.69833463848829,95.0052371659376));
#29499=CARTESIAN_POINT('Ctrl Pts',(1.80351517637209,1.75839729036196,95.0104726273563));
#29500=CARTESIAN_POINT('Ctrl Pts',(1.74394864222121,1.81561267435948,95.0157080887751));
#29501=CARTESIAN_POINT('Ctrl Pts',(1.68446655011802,1.87274694932065,95.0209361283573));
#29502=CARTESIAN_POINT('Ctrl Pts',(1.62208357330082,1.92704165258672,95.0261641679395));
#29503=CARTESIAN_POINT('Ctrl Pts',(1.55710418779672,1.97818927262937,95.0313922075217));
#29504=CARTESIAN_POINT('Ctrl Pts',(1.49219891201617,2.0292785582333,95.0366142844656));
#29505=CARTESIAN_POINT('Ctrl Pts',(1.424703476094,2.07722760724393,95.0418363614096));
#29506=CARTESIAN_POINT('Ctrl Pts',(1.35495753679941,2.12176726420936,95.0470584383535));
#29507=CARTESIAN_POINT('Ctrl Pts',(1.2852548997391,2.16627926842998,95.052277273136));
#29508=CARTESIAN_POINT('Ctrl Pts',(1.21330492382474,2.20738583238343,95.0574961079185));
#29509=CARTESIAN_POINT('Ctrl Pts',(1.13947758010576,2.24486015030699,95.0627149427009));
#29510=CARTESIAN_POINT('Ctrl Pts',(1.06567335706128,2.28232273231452,95.0679321430892));
#29511=CARTESIAN_POINT('Ctrl Pts',(0.989993348399747,2.3161551167964,95.0731493434775));
#29512=CARTESIAN_POINT('Ctrl Pts',(0.912832280854548,2.34617635249993,95.0783665438658));
#29513=CARTESIAN_POINT('Ctrl Pts',(0.835671637012119,2.37619742335244,95.0835837156057));
#29514=CARTESIAN_POINT('Ctrl Pts',(0.75703038467285,2.40240721980204,95.0888008873455));
#29515=CARTESIAN_POINT('Ctrl Pts',(0.677322039911264,2.42467340156369,95.0940180590854));
#29516=CARTESIAN_POINT('Ctrl Pts',(0.597536860009014,2.44696104688996,95.0992402599364));
#29517=CARTESIAN_POINT('Ctrl Pts',(0.516682982388146,2.46529735964048,95.1044624607874));
#29518=CARTESIAN_POINT('Ctrl Pts',(0.435187289079247,2.47960042616222,95.1096846616385));
#29519=CARTESIAN_POINT('Ctrl Pts',(0.353652247998477,2.49391039849426,95.1149093838738));
#29520=CARTESIAN_POINT('Ctrl Pts',(0.271475236215456,2.50418318862084,95.1201341061092));
#29521=CARTESIAN_POINT('Ctrl Pts',(0.18908902819608,2.51038873272963,95.1253588283446));
#29522=CARTESIAN_POINT('Ctrl Pts',(0.106561009261774,2.51660495840646,95.1305925438649));
#29523=CARTESIAN_POINT('Ctrl Pts',(0.023823540639689,2.5187399408743,95.1358262593852));
#29524=CARTESIAN_POINT('Ctrl Pts',(-0.0586900854461119,2.51681579061129,
95.1410599749055));
#29525=CARTESIAN_POINT('Ctrl Pts',(-0.12721868487804,2.5152177597299,95.1454066411647));
#29526=CARTESIAN_POINT('Ctrl Pts',(-0.195592795310752,2.51082090606575,
95.1497533074239));
#29527=CARTESIAN_POINT('Ctrl Pts',(-0.263568565194451,2.50366488601037,
95.1540999736831));
#29528=CARTESIAN_POINT('Ctrl Pts',(-0.345886810085939,2.4949989891419,95.1593637601499));
#29529=CARTESIAN_POINT('Ctrl Pts',(-0.427923601593685,2.4822535690543,95.1646275466167));
#29530=CARTESIAN_POINT('Ctrl Pts',(-0.509243989845148,2.46545671404034,
95.1698913330835));
#29531=CARTESIAN_POINT('Ctrl Pts',(-0.59045192433296,2.4486830865294,95.175147840532));
#29532=CARTESIAN_POINT('Ctrl Pts',(-0.670944976960685,2.42786924586806,
95.1804043479804));
#29533=CARTESIAN_POINT('Ctrl Pts',(-0.750293725218741,2.40309499934925,
95.1856608554289));
#29534=CARTESIAN_POINT('Ctrl Pts',(-0.830052467389669,2.37819274463257,
95.1909445231805));
#29535=CARTESIAN_POINT('Ctrl Pts',(-0.908654577485922,2.34928908694531,
95.1962281909321));
#29536=CARTESIAN_POINT('Ctrl Pts',(-0.985674728067885,2.31651712284807,
95.2015118586837));
#29537=CARTESIAN_POINT('Ctrl Pts',(-1.06216749166448,2.28396956116006,95.2067593471032));
#29538=CARTESIAN_POINT('Ctrl Pts',(-1.13709946505231,2.24760668753531,95.2120068355227));
#29539=CARTESIAN_POINT('Ctrl Pts',(-1.21007126184921,2.207608160713,95.2172543239422));
#29540=CARTESIAN_POINT('Ctrl Pts',(-1.28302066508639,2.16762190862475,95.2225002020142));
#29541=CARTESIAN_POINT('Ctrl Pts',(-1.35401068378094,2.12400244024195,95.2277460800863));
#29542=CARTESIAN_POINT('Ctrl Pts',(-1.42266586687652,2.07697570549693,95.2329919581583));
#29543=CARTESIAN_POINT('Ctrl Pts',(-1.49132049147426,2.02994935330614,95.2382377935561));
#29544=CARTESIAN_POINT('Ctrl Pts',(-1.55763993968314,1.97951605058171,95.2434836289539));
#29545=CARTESIAN_POINT('Ctrl Pts',(-1.62127827210285,1.92594470699633,95.2487294643516));
#29546=CARTESIAN_POINT('Ctrl Pts',(-1.68571462823238,1.8717015795863,95.2540410824446));
#29547=CARTESIAN_POINT('Ctrl Pts',(-1.74740177712543,1.81424145821353,95.2593527005376));
#29548=CARTESIAN_POINT('Ctrl Pts',(-1.80601705811497,1.75388387181071,95.2646643186305));
#29549=CARTESIAN_POINT('Ctrl Pts',(-1.86399106750709,1.69418661843362,95.2699178257708));
#29550=CARTESIAN_POINT('Ctrl Pts',(-1.91895983457342,1.63165537912202,95.2751713329111));
#29551=CARTESIAN_POINT('Ctrl Pts',(-1.97065124961128,1.56663330183087,95.2804248400514));
#29552=CARTESIAN_POINT('Ctrl Pts',(-2.02320033095449,1.50053237528099,95.2857655136207));
#29553=CARTESIAN_POINT('Ctrl Pts',(-2.07236202720979,1.43185760662661,95.2911061871901));
#29554=CARTESIAN_POINT('Ctrl Pts',(-2.11789688966922,1.36099927065721,95.2964468607594));
#29555=CARTESIAN_POINT('Ctrl Pts',(-2.16343175212864,1.29014093468782,95.3017875343287));
#29556=CARTESIAN_POINT('Ctrl Pts',(-2.20533959179403,1.2170994902856,95.307128207898));
#29557=CARTESIAN_POINT('Ctrl Pts',(-2.24343108861944,1.14228858027024,95.3124688814673));
#29558=CARTESIAN_POINT('Ctrl Pts',(-2.28325410804496,1.06407699576786,95.3180523256746));
#29559=CARTESIAN_POINT('Ctrl Pts',(-2.31903886419149,0.983671855279027,
95.3236357698818));
#29560=CARTESIAN_POINT('Ctrl Pts',(-2.3505537867259,0.901500496787727,95.3292192140891));
#29561=CARTESIAN_POINT('Ctrl Pts',(-2.35423797822459,0.891894411922428,
95.3298719359119));
#29562=CARTESIAN_POINT('Ctrl Pts',(-2.35786386636583,0.882264220521029,
95.3305246577347));
#29563=CARTESIAN_POINT('Ctrl Pts',(-2.36143112101026,0.872610629504497,
95.3311773795575));
#29564=CARTESIAN_POINT('Origin',(0.,0.,104.));
#29565=CARTESIAN_POINT('',(-2.35791364508473,0.871329681353405,96.3311375631035));
#29566=CARTESIAN_POINT('',(-2.36143112101026,0.872610629504502,96.0561753867426));
#29567=CARTESIAN_POINT('',(-2.36143112101026,0.872610629504505,104.));
#29568=CARTESIAN_POINT('',(-2.51749766382103,-0.00342967281893025,95.1125851160815));
#29569=CARTESIAN_POINT('Ctrl Pts',(-2.36143112101026,0.872610629504502,
96.0561753867426));
#29570=CARTESIAN_POINT('Ctrl Pts',(-2.33265141387007,0.950493357260157,
96.0509366716251));
#29571=CARTESIAN_POINT('Ctrl Pts',(-2.29999690568281,1.02699878203394,96.0456979565076));
#29572=CARTESIAN_POINT('Ctrl Pts',(-2.26362920233033,1.10172096483518,96.0404592413902));
#29573=CARTESIAN_POINT('Ctrl Pts',(-2.22727000798159,1.17642566478007,96.0352217519824));
#29574=CARTESIAN_POINT('Ctrl Pts',(-2.18719954614185,1.24934753707113,96.0299842625746));
#29575=CARTESIAN_POINT('Ctrl Pts',(-2.14362668723944,1.32010260046516,96.0247467731668));
#29576=CARTESIAN_POINT('Ctrl Pts',(-2.10005089320364,1.39086243002679,96.0195089309538));
#29577=CARTESIAN_POINT('Ctrl Pts',(-2.05297247670035,1.45945476887936,96.0142710887409));
#29578=CARTESIAN_POINT('Ctrl Pts',(-2.00264446347711,1.5255233209966,96.0090332465279));
#29579=CARTESIAN_POINT('Ctrl Pts',(-1.95226457423269,1.59165997382732,96.0037900053652));
#29580=CARTESIAN_POINT('Ctrl Pts',(-1.89862867988026,1.65526727771402,95.9985467642025));
#29581=CARTESIAN_POINT('Ctrl Pts',(-1.84203073908618,1.71602127208891,95.9933035230399));
#29582=CARTESIAN_POINT('Ctrl Pts',(-1.78540246993703,1.77680782186576,95.9880574722541));
#29583=CARTESIAN_POINT('Ctrl Pts',(-1.72580932439884,1.83473769565866,95.9828114214684));
#29584=CARTESIAN_POINT('Ctrl Pts',(-1.66358109354304,1.88952485964227,95.9775653706826));
#29585=CARTESIAN_POINT('Ctrl Pts',(-1.60124600512162,1.94440610348145,95.9723103114419));
#29586=CARTESIAN_POINT('Ctrl Pts',(-1.5362671547045,1.99613357105326,95.9670552522011));
#29587=CARTESIAN_POINT('Ctrl Pts',(-1.46900605360172,2.04446263465036,95.9618001929604));
#29588=CARTESIAN_POINT('Ctrl Pts',(-1.41957195745204,2.07998247505607,95.9579379442086));
#29589=CARTESIAN_POINT('Ctrl Pts',(-1.36890572652446,2.11366750477514,95.9540756954568));
#29590=CARTESIAN_POINT('Ctrl Pts',(-1.31715930479627,2.1454364627713,95.950213446705));
#29591=CARTESIAN_POINT('Ctrl Pts',(-1.24673646073771,2.18867153681405,95.9449572273863));
#29592=CARTESIAN_POINT('Ctrl Pts',(-1.17405304514657,2.22851509199812,95.9397010080676));
#29593=CARTESIAN_POINT('Ctrl Pts',(-1.09946919902374,2.26472376470026,95.9344447887488));
#29594=CARTESIAN_POINT('Ctrl Pts',(-1.02499086952048,2.30088121160832,95.9291960056046));
#29595=CARTESIAN_POINT('Ctrl Pts',(-0.948617861385659,2.33341379073347,
95.9239472224604));
#29596=CARTESIAN_POINT('Ctrl Pts',(-0.870737623933377,2.36212240162674,
95.9186984393161));
#29597=CARTESIAN_POINT('Ctrl Pts',(-0.792311415316317,2.39103227119924,
95.913412860133));
#29598=CARTESIAN_POINT('Ctrl Pts',(-0.712357162115909,2.41606409095858,
95.9081272809498));
#29599=CARTESIAN_POINT('Ctrl Pts',(-0.631294033309228,2.43706259532006,
95.9028417017667));
#29600=CARTESIAN_POINT('Ctrl Pts',(-0.550938551744799,2.4578777915127,95.8976022634813));
#29601=CARTESIAN_POINT('Ctrl Pts',(-0.469493933549941,2.47472969831333,
95.8923628251958));
#29602=CARTESIAN_POINT('Ctrl Pts',(-0.387384999349596,2.48751665567869,
95.8871233869104));
#29603=CARTESIAN_POINT('Ctrl Pts',(-0.305302936472543,2.50029942832934,
95.8818856633061));
#29604=CARTESIAN_POINT('Ctrl Pts',(-0.222557444742411,2.50901982274132,
95.8766479397017));
#29605=CARTESIAN_POINT('Ctrl Pts',(-0.139582707846034,2.51362744209844,
95.8714102160974));
#29606=CARTESIAN_POINT('Ctrl Pts',(-0.056610124402918,2.51823494187347,
95.8661726284284));
#29607=CARTESIAN_POINT('Ctrl Pts',(0.026591231815042,2.51872985428838,95.8609350407593));
#29608=CARTESIAN_POINT('Ctrl Pts',(0.109584284531156,2.51511382139731,95.8556974530903));
#29609=CARTESIAN_POINT('Ctrl Pts',(0.193900268125644,2.51144014800006,95.8503763769095));
#29610=CARTESIAN_POINT('Ctrl Pts',(0.278000758163298,2.50352332510973,95.8450553007287));
#29611=CARTESIAN_POINT('Ctrl Pts',(0.361431683604489,2.49141995418011,95.8397342245479));
#29612=CARTESIAN_POINT('Ctrl Pts',(0.443671569616648,2.47948936800537,95.8344891107456));
#29613=CARTESIAN_POINT('Ctrl Pts',(0.525260437824858,2.4634911463882,95.8292439969433));
#29614=CARTESIAN_POINT('Ctrl Pts',(0.605774396105066,2.44353097607203,95.823998883141));
#29615=CARTESIAN_POINT('Ctrl Pts',(0.688037419897433,2.42313719590408,95.818639825771));
#29616=CARTESIAN_POINT('Ctrl Pts',(0.769177794999873,2.39860745724191,95.813280768401));
#29617=CARTESIAN_POINT('Ctrl Pts',(0.848762379063284,2.37010731273646,95.8079217110309));
#29618=CARTESIAN_POINT('Ctrl Pts',(0.928346963126706,2.341607168231,95.8025626536609));
#29619=CARTESIAN_POINT('Ctrl Pts',(1.00637531423859,2.30913687376708,95.7972035962909));
#29620=CARTESIAN_POINT('Ctrl Pts',(1.08244033181905,2.27291204802374,95.7918445389208));
#29621=CARTESIAN_POINT('Ctrl Pts',(1.15694499484728,2.23743031777356,95.7865954142088));
#29622=CARTESIAN_POINT('Ctrl Pts',(1.22984274428871,2.19821491727435,95.7813462894968));
#29623=CARTESIAN_POINT('Ctrl Pts',(1.30073401346762,2.15543435905815,95.7760971647847));
#29624=CARTESIAN_POINT('Ctrl Pts',(1.37152445649355,2.11271464612172,95.7708555057177));
#29625=CARTESIAN_POINT('Ctrl Pts',(1.44031369453238,2.06644008345905,95.7656138466507));
#29626=CARTESIAN_POINT('Ctrl Pts',(1.50672433125253,2.01682622940391,95.7603721875837));
#29627=CARTESIAN_POINT('Ctrl Pts',(1.57371394436528,1.9667798354476,95.7550848310651));
#29628=CARTESIAN_POINT('Ctrl Pts',(1.63828284277624,1.91333583623313,95.7497974745464));
#29629=CARTESIAN_POINT('Ctrl Pts',(1.70007126986955,1.85676167758927,95.7445101180278));
#29630=CARTESIAN_POINT('Ctrl Pts',(1.76121623418599,1.80077668049124,95.7392778238771));
#29631=CARTESIAN_POINT('Ctrl Pts',(1.81963802047758,1.74172673474641,95.7340455297265));
#29632=CARTESIAN_POINT('Ctrl Pts',(1.87502056171392,1.67991194505844,95.7288132355758));
#29633=CARTESIAN_POINT('Ctrl Pts',(1.9303850390111,1.61811731729469,95.7235826480251));
#29634=CARTESIAN_POINT('Ctrl Pts',(1.98271193141133,1.55355998075114,95.7183520604744));
#29635=CARTESIAN_POINT('Ctrl Pts',(2.03172305193611,1.48657582727267,95.7131214729237));
#29636=CARTESIAN_POINT('Ctrl Pts',(2.08073306299572,1.41959319011508,95.7078910037779));
#29637=CARTESIAN_POINT('Ctrl Pts',(2.12642717908222,1.35018421921784,95.702660534632));
#29638=CARTESIAN_POINT('Ctrl Pts',(2.16856928100672,1.27871557567507,95.6974300654862));
#29639=CARTESIAN_POINT('Ctrl Pts',(2.21150957016828,1.20589328918329,95.6921005292904));
#29640=CARTESIAN_POINT('Ctrl Pts',(2.25076163563882,1.130932923186,95.6867709930946));
#29641=CARTESIAN_POINT('Ctrl Pts',(2.28612453916548,1.05424894660863,95.6814414568988));
#29642=CARTESIAN_POINT('Ctrl Pts',(2.32088080922383,0.978880446477947,95.676203346313));
#29643=CARTESIAN_POINT('Ctrl Pts',(2.35188018984607,0.90184746780268,95.6709652357273));
#29644=CARTESIAN_POINT('Ctrl Pts',(2.378981170246,0.823562287635228,95.6657271251415));
#29645=CARTESIAN_POINT('Ctrl Pts',(2.40679167852567,0.743227531508555,95.6603518761407));
#29646=CARTESIAN_POINT('Ctrl Pts',(2.43049665313458,0.66157458996074,95.6549766271399));
#29647=CARTESIAN_POINT('Ctrl Pts',(2.44999868103596,0.579061924945903,95.6496013781391));
#29648=CARTESIAN_POINT('Ctrl Pts',(2.46950070893734,0.496549259931055,95.6442261291383));
#29649=CARTESIAN_POINT('Ctrl Pts',(2.48479976500474,0.413177394251107,95.6388508801375));
#29650=CARTESIAN_POINT('Ctrl Pts',(2.4958556042303,0.329410158969318,95.6334756311367));
#29651=CARTESIAN_POINT('Ctrl Pts',(2.50668406766696,0.247365691251163,95.6282109301873));
#29652=CARTESIAN_POINT('Ctrl Pts',(2.51348245591912,0.164637609670783,95.6229462292378));
#29653=CARTESIAN_POINT('Ctrl Pts',(2.51617541011446,0.0816551010979545,
95.6176815282883));
#29654=CARTESIAN_POINT('Ctrl Pts',(2.51886454077522,-0.00120958649902303,
95.6124243023141));
#29655=CARTESIAN_POINT('Ctrl Pts',(2.51745980182278,-0.0843275278565643,
95.60716707634));
#29656=CARTESIAN_POINT('Ctrl Pts',(2.51193738922762,-0.167262675454818,
95.6019098503658));
#29657=CARTESIAN_POINT('Ctrl Pts',(2.50638741549332,-0.250611734021007,
95.5966263867403));
#29658=CARTESIAN_POINT('Ctrl Pts',(2.49667848808217,-0.333775703050781,
95.5913429231147));
#29659=CARTESIAN_POINT('Ctrl Pts',(2.48283953433707,-0.41631009684233,95.5860594594891));
#29660=CARTESIAN_POINT('Ctrl Pts',(2.46909418980429,-0.498286212910473,
95.5808117341771));
#29661=CARTESIAN_POINT('Ctrl Pts',(2.45127459572428,-0.579640785447499,
95.5755640088651));
#29662=CARTESIAN_POINT('Ctrl Pts',(2.42946105419747,-0.659943358279883,
95.5703162835531));
#29663=CARTESIAN_POINT('Ctrl Pts',(2.40765495986179,-0.740218515636984,
95.5650703498261));
#29664=CARTESIAN_POINT('Ctrl Pts',(2.38185774685792,-0.819441943492977,
95.5598244160991));
#29665=CARTESIAN_POINT('Ctrl Pts',(2.35220035334611,-0.897195490246381,
95.5545784823721));
#29666=CARTESIAN_POINT('Ctrl Pts',(2.32254422495082,-0.974945720211436,
95.5493327724246));
#29667=CARTESIAN_POINT('Ctrl Pts',(2.28902840815539,-1.05122576465178,95.5440870624771));
#29668=CARTESIAN_POINT('Ctrl Pts',(2.25183256125782,-1.12563598292657,95.5388413525296));
#29669=CARTESIAN_POINT('Ctrl Pts',(2.21417220748495,-1.2009754462882,95.5335301334315));
#29670=CARTESIAN_POINT('Ctrl Pts',(2.17273947002901,-1.27439761774384,95.5282189143334));
#29671=CARTESIAN_POINT('Ctrl Pts',(2.12776869285796,-1.34551352267212,95.5229076952353));
#29672=CARTESIAN_POINT('Ctrl Pts',(2.08329138828702,-1.4158490597099,95.5176547571202));
#29673=CARTESIAN_POINT('Ctrl Pts',(2.03535362741242,-1.48392835009897,95.512401819005));
#29674=CARTESIAN_POINT('Ctrl Pts',(1.98422465432488,-1.54940594137537,95.5071488808899));
#29675=CARTESIAN_POINT('Ctrl Pts',(1.93224477263797,-1.6159732366321,95.5018085213003));
#29676=CARTESIAN_POINT('Ctrl Pts',(1.87696681445754,-1.67985107003741,95.4964681617107));
#29677=CARTESIAN_POINT('Ctrl Pts',(1.81871363381257,-1.74071449933189,95.4911278021212));
#29678=CARTESIAN_POINT('Ctrl Pts',(1.76046045316761,-1.80157792862636,95.4857874425316));
#29679=CARTESIAN_POINT('Ctrl Pts',(1.69923245075008,-1.85942666068594,95.480447082942));
#29680=CARTESIAN_POINT('Ctrl Pts',(1.63538709547285,-1.91397891784651,95.4751067233524));
#29681=CARTESIAN_POINT('Ctrl Pts',(1.57250694959504,-1.96770645798353,95.4698470989275));
#29682=CARTESIAN_POINT('Ctrl Pts',(1.50686280030885,-2.01842901296663,95.4645874745026));
#29683=CARTESIAN_POINT('Ctrl Pts',(1.4387734646105,-2.06585022872731,95.4593278500777));
#29684=CARTESIAN_POINT('Ctrl Pts',(1.37077917835537,-2.1132052467478,95.454075567836));
#29685=CARTESIAN_POINT('Ctrl Pts',(1.30034686084804,-2.15726781899979,95.4488232855942));
#29686=CARTESIAN_POINT('Ctrl Pts',(1.22782911905335,-2.1977811320522,95.4435710033524));
#29687=CARTESIAN_POINT('Ctrl Pts',(1.15486356538724,-2.23854462308984,95.4382862871948));
#29688=CARTESIAN_POINT('Ctrl Pts',(1.07978709863394,-2.27571455706946,95.4330015710371));
#29689=CARTESIAN_POINT('Ctrl Pts',(1.0029894234992,-2.30907307514265,95.4277168548794));
#29690=CARTESIAN_POINT('Ctrl Pts',(0.9267959794547,-2.34216913405014,95.4224737179727));
#29691=CARTESIAN_POINT('Ctrl Pts',(0.848908745038345,-2.37151335508,95.417230581066));
#29692=CARTESIAN_POINT('Ctrl Pts',(0.769732253879452,-2.39693940418561,
95.4119874441592));
#29693=CARTESIAN_POINT('Ctrl Pts',(0.690580662639252,-2.4223574571481,95.406745956147));
#29694=CARTESIAN_POINT('Ctrl Pts',(0.610141058004238,-2.44385964492363,
95.4015044681348));
#29695=CARTESIAN_POINT('Ctrl Pts',(0.528835141361276,-2.46132883688088,
95.3962629801226));
#29696=CARTESIAN_POINT('Ctrl Pts',(0.447530402502071,-2.47879777578237,
95.3910215680377));
#29697=CARTESIAN_POINT('Ctrl Pts',(0.365359826960715,-2.49223373940727,
95.3857801559528));
#29698=CARTESIAN_POINT('Ctrl Pts',(0.282756021243529,-2.50157056315638,
95.3805387438679));
#29699=CARTESIAN_POINT('Ctrl Pts',(0.198964996349559,-2.51104157995034,
95.3752219998429));
#29700=CARTESIAN_POINT('Ctrl Pts',(0.114728671082748,-2.51629461967136,
95.3699052558179));
#29701=CARTESIAN_POINT('Ctrl Pts',(0.0305028474469036,-2.51731520201536,
95.364588511793));
#29702=CARTESIAN_POINT('Ctrl Pts',(-0.0526504958620326,-2.51832278888554,
95.3593394679474));
#29703=CARTESIAN_POINT('Ctrl Pts',(-0.135793139660068,-2.51520516872692,
95.3540904241019));
#29704=CARTESIAN_POINT('Ctrl Pts',(-0.218489369668261,-2.50800092610469,
95.3488413802563));
#29705=CARTESIAN_POINT('Ctrl Pts',(-0.302785476655478,-2.50065730709346,
95.3434907861416));
#29706=CARTESIAN_POINT('Ctrl Pts',(-0.386617216445367,-2.48906734892347,
95.338140192027));
#29707=CARTESIAN_POINT('Ctrl Pts',(-0.469533550827451,-2.47332660492855,
95.3327895979123));
#29708=CARTESIAN_POINT('Ctrl Pts',(-0.552449885209547,-2.45758586093362,
95.3274390037977));
#29709=CARTESIAN_POINT('Ctrl Pts',(-0.634450344179456,-2.4376945126903,
95.322088409683));
#29710=CARTESIAN_POINT('Ctrl Pts',(-0.715101646661369,-2.4138011278774,
95.3167378155684));
#29711=CARTESIAN_POINT('Ctrl Pts',(-0.793553864869304,-2.39055923368122,
95.3115331137953));
#29712=CARTESIAN_POINT('Ctrl Pts',(-0.871032543613655,-2.3634408582058,
95.3063284120223));
#29713=CARTESIAN_POINT('Ctrl Pts',(-0.947121846064168,-2.33254506038104,
95.3011237102492));
#29714=CARTESIAN_POINT('Ctrl Pts',(-1.02310194916727,-2.30169360257323,
95.2959264779893));
#29715=CARTESIAN_POINT('Ctrl Pts',(-1.09769620193994,-2.2670756598159,95.2907292457293));
#29716=CARTESIAN_POINT('Ctrl Pts',(-1.17050286371611,-2.22884034781148,
95.2855320134693));
#29717=CARTESIAN_POINT('Ctrl Pts',(-1.24472763665675,-2.18986029732424,
95.2802335507324));
#29718=CARTESIAN_POINT('Ctrl Pts',(-1.31709396224004,-2.14712059290674,
95.2749350879955));
#29719=CARTESIAN_POINT('Ctrl Pts',(-1.38719665267716,-2.10083119188603,
95.2696366252586));
#29720=CARTESIAN_POINT('Ctrl Pts',(-1.45583983912076,-2.05550551372996,
95.2644484739445));
#29721=CARTESIAN_POINT('Ctrl Pts',(-1.52231232778246,-2.0067767973796,95.2592603226305));
#29722=CARTESIAN_POINT('Ctrl Pts',(-1.5862594930535,-1.95488799441238,95.2540721713164));
#29723=CARTESIAN_POINT('Ctrl Pts',(-1.65018796402017,-1.90301436060977,
95.2488855367056));
#29724=CARTESIAN_POINT('Ctrl Pts',(-1.71159221114548,-1.84798277033845,
95.2436989020949));
#29725=CARTESIAN_POINT('Ctrl Pts',(-1.77014939416049,-1.79007747663425,
95.2385122674842));
#29726=CARTESIAN_POINT('Ctrl Pts',(-1.8287079575656,-1.73217081790718,95.233325510607));
#29727=CARTESIAN_POINT('Ctrl Pts',(-1.8844189893606,-1.67139065339286,95.2281387537298));
#29728=CARTESIAN_POINT('Ctrl Pts',(-1.93699644193566,-1.60805815626444,
95.2229519968526));
#29729=CARTESIAN_POINT('Ctrl Pts',(-1.9915522781266,-1.54234258486113,95.2175700727636));
#29730=CARTESIAN_POINT('Ctrl Pts',(-2.04273367412091,-1.47387920327015,
95.2121881486745));
#29731=CARTESIAN_POINT('Ctrl Pts',(-2.09026826242715,-1.40306266470524,
95.2068062245855));
#29732=CARTESIAN_POINT('Ctrl Pts',(-2.13615558916376,-1.33470019940844,
95.2016108054613));
#29733=CARTESIAN_POINT('Ctrl Pts',(-2.1786445252822,-1.2641454407714,95.1964153863372));
#29734=CARTESIAN_POINT('Ctrl Pts',(-2.21753644921349,-1.19177948732542,
95.191219967213));
#29735=CARTESIAN_POINT('Ctrl Pts',(-2.2564599203922,-1.11935483411846,95.1860203338162));
#29736=CARTESIAN_POINT('Ctrl Pts',(-2.29178037823891,-1.04511648975722,
95.1808207004193));
#29737=CARTESIAN_POINT('Ctrl Pts',(-2.32334730809328,-0.969465592981872,
95.1756210670225));
#29738=CARTESIAN_POINT('Ctrl Pts',(-2.3549680583398,-0.893685714359086,
95.1704125684522));
#29739=CARTESIAN_POINT('Ctrl Pts',(-2.38282236627793,-0.816488923342303,
95.1652040698819));
#29740=CARTESIAN_POINT('Ctrl Pts',(-2.40680970688121,-0.738290786115048,
95.1599955713116));
#29741=CARTESIAN_POINT('Ctrl Pts',(-2.40930686491077,-0.730150112686395,
95.1594533501358));
#29742=CARTESIAN_POINT('Ctrl Pts',(-2.41176216078532,-0.721998594537591,
95.15891112896));
#29743=CARTESIAN_POINT('Ctrl Pts',(-2.41417551320215,-0.713836705034951,
95.1583689077841));
#29744=CARTESIAN_POINT('Ctrl Pts',(-2.44522521635681,-0.608827488614062,
95.1513928000114));
#29745=CARTESIAN_POINT('Ctrl Pts',(-2.46942455892676,-0.501773885157136,
95.1444166922386));
#29746=CARTESIAN_POINT('Ctrl Pts',(-2.48656498776096,-0.393447342907944,
95.1374405844659));
#29747=CARTESIAN_POINT('Ctrl Pts',(-2.50328860943498,-0.287754998372505,
95.1306341160702));
#29748=CARTESIAN_POINT('Ctrl Pts',(-2.51329252836617,-0.180850497788633,
95.1238276476745));
#29749=CARTESIAN_POINT('Ctrl Pts',(-2.51642765153617,-0.0734719305866939,
95.1170211792788));
#29750=CARTESIAN_POINT('Ctrl Pts',(-2.51710874897196,-0.050144213360273,
95.1155424915463));
#29751=CARTESIAN_POINT('Ctrl Pts',(-2.51746583350749,-0.0267942163812354,
95.1140638038139));
#29752=CARTESIAN_POINT('Ctrl Pts',(-2.51749766382103,-0.00342967281893025,
95.1125851160815));
#29753=CARTESIAN_POINT('Ctrl Pts',(-2.51749757130744,-0.00349692166510488,
95.1115697988903));
#29754=CARTESIAN_POINT('Ctrl Pts',(-2.51766860658887,0.119634491284325,
95.1030512768662));
#29755=CARTESIAN_POINT('Ctrl Pts',(-2.50880598011611,0.242625205407994,
95.0946581244734));
#29756=CARTESIAN_POINT('Ctrl Pts',(-2.48347800210713,0.415721636410033,
95.0830838099193));
#29757=CARTESIAN_POINT('Ctrl Pts',(-2.47440185369426,0.466715694875851,
95.0797022152716));
#29758=CARTESIAN_POINT('Ctrl Pts',(-2.46015542500379,0.534554887518458,
95.0752365418874));
#29759=CARTESIAN_POINT('Ctrl Pts',(-2.45637290771386,0.551675452432403,
95.0741123445084));
#29760=CARTESIAN_POINT('Ctrl Pts',(-2.44948335309491,0.581382464738478,
95.0721661139171));
#29761=CARTESIAN_POINT('Ctrl Pts',(-2.4464574163654,0.593986857357515,95.0713417440849));
#29762=CARTESIAN_POINT('Ctrl Pts',(-2.44017548710644,0.619291300554413,
95.0696893113859));
#29763=CARTESIAN_POINT('Ctrl Pts',(-2.43691736707658,0.631990410057167,
95.0688613392206));
#29764=CARTESIAN_POINT('Ctrl Pts',(-2.43050098128503,0.656211816588521,
95.0672843425808));
#29765=CARTESIAN_POINT('Ctrl Pts',(-2.42735961356931,0.667738183509839,
95.0665348553807));
#29766=CARTESIAN_POINT('Ctrl Pts',(-2.41897310744704,0.697668660180833,
95.0645908614003));
#29767=CARTESIAN_POINT('Ctrl Pts',(-2.41359990664641,0.716036292656748,
95.0634000524792));
#29768=CARTESIAN_POINT('Ctrl Pts',(-2.39410128500123,0.779975268331027,
95.0592603824716));
#29769=CARTESIAN_POINT('Ctrl Pts',(-2.37888995878851,0.825206231053676,
95.0563421777975));
#29770=CARTESIAN_POINT('Ctrl Pts',(-2.36207867090852,0.870856748450194,
95.053396239938));
#29771=CARTESIAN_POINT('Ctrl Pts',(-2.36175513843305,0.871733783864357,
95.0533396423838));
#29772=CARTESIAN_POINT('Ctrl Pts',(-2.36143112104854,0.872610629400897,
95.0532830566435));
#29773=CARTESIAN_POINT('',(-2.51439859764413,0.000444055452618797,95.387416697508));
#29774=CARTESIAN_POINT('Ctrl Pts',(-2.36143112101026,0.872610629504497,
95.3311773795575));
#29775=CARTESIAN_POINT('Ctrl Pts',(-2.39184210810317,0.790313383844522,
95.336741858942));
#29776=CARTESIAN_POINT('Ctrl Pts',(-2.4179880049747,0.706313645512247,95.3423063383265));
#29777=CARTESIAN_POINT('Ctrl Pts',(-2.43969002558945,0.62106266112154,95.347870817711));
#29778=CARTESIAN_POINT('Ctrl Pts',(-2.46134996455353,0.535976984017515,
95.3534245072026));
#29779=CARTESIAN_POINT('Ctrl Pts',(-2.47858308353986,0.449645249570044,
95.3589781966942));
#29780=CARTESIAN_POINT('Ctrl Pts',(-2.49125949193803,0.362536058659951,
95.3645318861859));
#29781=CARTESIAN_POINT('Ctrl Pts',(-2.50390335952531,0.275650480276184,
95.3700713191504));
#29782=CARTESIAN_POINT('Ctrl Pts',(-2.51201376412536,0.187991789932431,
95.375610752115));
#29783=CARTESIAN_POINT('Ctrl Pts',(-2.51551154229381,0.100039645074327,
95.3811501850796));
#29784=CARTESIAN_POINT('Ctrl Pts',(-2.51683050222496,0.066874204231872,
95.3832390225557));
#29785=CARTESIAN_POINT('Ctrl Pts',(-2.51749409347004,0.0336671575514469,
95.3853278600319));
#29786=CARTESIAN_POINT('Ctrl Pts',(-2.51749996074042,0.000444603168957273,
95.387416697508));
#29787=CARTESIAN_POINT('Ctrl Pts',(-2.51343655732594,0.000443885551454637,
95.387416697508));
#29788=CARTESIAN_POINT('Ctrl Pts',(-2.51289686506427,-0.441107800258806,
95.4152237280892));
#29789=CARTESIAN_POINT('Ctrl Pts',(-2.19219217530483,-1.7217534319749,95.4958203945983));
#29790=CARTESIAN_POINT('Ctrl Pts',(-0.1532262480843,-2.96902544840633,95.6292066970356));
#29791=CARTESIAN_POINT('Ctrl Pts',(2.40697591309465,-1.74517565678557,95.7875756048197));
#29792=CARTESIAN_POINT('Ctrl Pts',(2.77431937328859,1.06887020238785,95.945944512604));
#29793=CARTESIAN_POINT('Ctrl Pts',(0.613923595831106,2.90898477565689,96.1043134203881));
#29794=CARTESIAN_POINT('Ctrl Pts',(-1.59108002946992,2.25210786338312,96.232711103888));
#29795=CARTESIAN_POINT('Ctrl Pts',(-2.23357827729263,1.21153303328952,96.3083191514598));
#29796=CARTESIAN_POINT('Ctrl Pts',(-2.35791364508473,0.871329681353405,
96.3311375631035));
#29797=CARTESIAN_POINT('Origin',(0.,0.,104.));
#29798=CARTESIAN_POINT('',(-2.36143105416444,0.872610810400505,97.3312318328322));
#29799=CARTESIAN_POINT('',(-2.36143112101025,0.872610629504517,97.0562333997462));
#29800=CARTESIAN_POINT('',(-2.36143112101026,0.872610629504505,104.));
#29801=CARTESIAN_POINT('',(-2.51749996796861,0.000401594395392813,96.1125833025275));
#29802=CARTESIAN_POINT('Ctrl Pts',(-2.36143112101025,0.872610629504516,
97.0562333997462));
#29803=CARTESIAN_POINT('Ctrl Pts',(-2.33278461148586,0.950132902110356,
97.0509794704497));
#29804=CARTESIAN_POINT('Ctrl Pts',(-2.3002655010888,1.02638145292235,97.0457255411532));
#29805=CARTESIAN_POINT('Ctrl Pts',(-2.26400778685995,1.10094277373418,97.0404716118567));
#29806=CARTESIAN_POINT('Ctrl Pts',(-2.22779951602781,1.17540241783961,97.0352248471628));
#29807=CARTESIAN_POINT('Ctrl Pts',(-2.18786296857266,1.24817899050201,97.0299780824688));
#29808=CARTESIAN_POINT('Ctrl Pts',(-2.14438090452949,1.31887709294281,97.0247313177748));
#29809=CARTESIAN_POINT('Ctrl Pts',(-2.10094555076451,1.38949924848218,97.0194901893781));
#29810=CARTESIAN_POINT('Ctrl Pts',(-2.05397249102578,1.45804698034267,97.0142490609813));
#29811=CARTESIAN_POINT('Ctrl Pts',(-2.00369062619877,1.52414898368998,97.0090079325846));
#29812=CARTESIAN_POINT('Ctrl Pts',(-1.95343813060393,1.59021237738965,97.0037698654888));
#29813=CARTESIAN_POINT('Ctrl Pts',(-1.89988094561557,1.65383251233682,96.9985317983929));
#29814=CARTESIAN_POINT('Ctrl Pts',(-1.84329090933107,1.71466756940738,96.9932937312971));
#29815=CARTESIAN_POINT('Ctrl Pts',(-1.78671685664124,1.77548544389673,96.9880571436691));
#29816=CARTESIAN_POINT('Ctrl Pts',(-1.72711196820619,1.83351946532465,96.9828205560411));
#29817=CARTESIAN_POINT('Ctrl Pts',(-1.66478702169368,1.8884624492958,96.9775839684132));
#29818=CARTESIAN_POINT('Ctrl Pts',(-1.60246087887709,1.94340648787701,96.9723472802709));
#29819=CARTESIAN_POINT('Ctrl Pts',(-1.537414921354,1.99525906708839,96.9671105921285));
#29820=CARTESIAN_POINT('Ctrl Pts',(-1.46999424040511,2.04375223135678,96.9618739039862));
#29821=CARTESIAN_POINT('Ctrl Pts',(-1.40250584265483,2.09229410177774,96.9566319561556));
#29822=CARTESIAN_POINT('Ctrl Pts',(-1.33263833275752,2.13746954757229,96.9513900083249));
#29823=CARTESIAN_POINT('Ctrl Pts',(-1.26076671530658,2.17905335858833,96.9461480604942));
#29824=CARTESIAN_POINT('Ctrl Pts',(-1.18885965972192,2.22065767356277,96.9409035279875));
#29825=CARTESIAN_POINT('Ctrl Pts',(-1.11494693892174,2.25866661476735,96.9356589954808));
#29826=CARTESIAN_POINT('Ctrl Pts',(-1.03942695786404,2.29290162223884,96.9304144629741));
#29827=CARTESIAN_POINT('Ctrl Pts',(-0.963772929437472,2.32719739657774,
96.9251606214636));
#29828=CARTESIAN_POINT('Ctrl Pts',(-0.886506370644806,2.35770568296987,
96.9199067799532));
#29829=CARTESIAN_POINT('Ctrl Pts',(-0.808044271200453,2.38429668996543,
96.9146529384428));
#29830=CARTESIAN_POINT('Ctrl Pts',(-0.737225908558111,2.40829721492937,
96.9099109234319));
#29831=CARTESIAN_POINT('Ctrl Pts',(-0.665434042401576,2.42910711943873,
96.905168908421));
#29832=CARTESIAN_POINT('Ctrl Pts',(-0.592982192526457,2.44666678755946,
96.9004268934101));
#29833=CARTESIAN_POINT('Ctrl Pts',(-0.512688307529111,2.46612707704975,
96.8951716127155));
#29834=CARTESIAN_POINT('Ctrl Pts',(-0.431287177478855,2.48166652730587,
96.8899163320209));
#29835=CARTESIAN_POINT('Ctrl Pts',(-0.349196172064143,2.4931643113553,96.8846610513262));
#29836=CARTESIAN_POINT('Ctrl Pts',(-0.26722154874824,2.50464579476092,96.8794132211506));
#29837=CARTESIAN_POINT('Ctrl Pts',(-0.184559445904595,2.51209692985521,
96.874165390975));
#29838=CARTESIAN_POINT('Ctrl Pts',(-0.101639614812427,2.5154474032865,96.8689175607994));
#29839=CARTESIAN_POINT('Ctrl Pts',(-0.0181195837250174,2.51882212850546,
96.8636317451671));
#29840=CARTESIAN_POINT('Ctrl Pts',(0.0656614618329577,2.51803646644374,
96.8583459295349));
#29841=CARTESIAN_POINT('Ctrl Pts',(0.149256758489685,2.51307156086832,96.8530601139027));
#29842=CARTESIAN_POINT('Ctrl Pts',(0.232103088575756,2.50815113803837,96.8478216561885));
#29843=CARTESIAN_POINT('Ctrl Pts',(0.314766515769923,2.49912608718189,96.8425831984743));
#29844=CARTESIAN_POINT('Ctrl Pts',(0.396811685536492,2.48603031683479,96.8373447407601));
#29845=CARTESIAN_POINT('Ctrl Pts',(0.478829872982636,2.47293885331371,96.8321080058255));
#29846=CARTESIAN_POINT('Ctrl Pts',(0.560229751533338,2.45577940179306,96.8268712708909));
#29847=CARTESIAN_POINT('Ctrl Pts',(0.640582822350771,2.43463752901928,96.8216345359563));
#29848=CARTESIAN_POINT('Ctrl Pts',(0.720933704526701,2.41349623210378,96.8163979436589));
#29849=CARTESIAN_POINT('Ctrl Pts',(0.800237389695353,2.38837284801125,96.8111613513615));
#29850=CARTESIAN_POINT('Ctrl Pts',(0.878078632796223,2.359403349287,96.8059247590641));
#29851=CARTESIAN_POINT('Ctrl Pts',(0.957192885521912,2.32996008563771,96.8006025279442));
#29852=CARTESIAN_POINT('Ctrl Pts',(1.03479596623164,2.29654393433539,96.7952802968244));
#29853=CARTESIAN_POINT('Ctrl Pts',(1.11047287007365,2.25934863507835,96.7899580657046));
#29854=CARTESIAN_POINT('Ctrl Pts',(1.18503900163065,2.22269928188212,96.784713953357));
#29855=CARTESIAN_POINT('Ctrl Pts',(1.25773474598859,2.18238126500678,96.7794698410095));
#29856=CARTESIAN_POINT('Ctrl Pts',(1.32818942411985,2.13862551739574,96.774225728662));
#29857=CARTESIAN_POINT('Ctrl Pts',(1.40021839145288,2.09389206038616,96.768864438156));
#29858=CARTESIAN_POINT('Ctrl Pts',(1.4699045123945,2.04556568193834,96.76350314765));
#29859=CARTESIAN_POINT('Ctrl Pts',(1.5368860919091,1.99393765963141,96.758141857144));
#29860=CARTESIAN_POINT('Ctrl Pts',(1.60386767142369,1.94230963732448,96.752780566638));
#29861=CARTESIAN_POINT('Ctrl Pts',(1.66814436666828,1.88738035199303,96.747419276132));
#29862=CARTESIAN_POINT('Ctrl Pts',(1.7293947723073,1.82948079287982,96.7420579856259));
#29863=CARTESIAN_POINT('Ctrl Pts',(1.78943248688574,1.77272758172979,96.7368028428099));
#29864=CARTESIAN_POINT('Ctrl Pts',(1.84678445224079,1.71291103807284,96.7315476999939));
#29865=CARTESIAN_POINT('Ctrl Pts',(1.90112208808839,1.65031544141792,96.7262925571779));
#29866=CARTESIAN_POINT('Ctrl Pts',(1.95538268272115,1.58780859431448,96.7210448652305));
#29867=CARTESIAN_POINT('Ctrl Pts',(2.00663713686189,1.52253086616357,96.7157971732831));
#29868=CARTESIAN_POINT('Ctrl Pts',(2.05459249820959,1.45480442544724,96.7105494813357));
#29869=CARTESIAN_POINT('Ctrl Pts',(2.1028965633686,1.38658551699965,96.7052636311901));
#29870=CARTESIAN_POINT('Ctrl Pts',(2.14785300996875,1.3158824595113,96.6999777810446));
#29871=CARTESIAN_POINT('Ctrl Pts',(2.18920275961304,1.24305974406005,96.694691930899));
#29872=CARTESIAN_POINT('Ctrl Pts',(2.23018069123416,1.17089185235826,96.6894536112553));
#29873=CARTESIAN_POINT('Ctrl Pts',(2.26761629636635,1.09664267832251,96.6842152916115));
#29874=CARTESIAN_POINT('Ctrl Pts',(2.30130099255538,1.02069583699729,96.6789769719678));
#29875=CARTESIAN_POINT('Ctrl Pts',(2.33497461285341,0.944773967811713,96.67374037474));
#29876=CARTESIAN_POINT('Ctrl Pts',(2.36489958674497,0.86715596145425,96.6685037775122));
#29877=CARTESIAN_POINT('Ctrl Pts',(2.39091439469562,0.78824780826671,96.6632671802844));
#29878=CARTESIAN_POINT('Ctrl Pts',(2.41692849676088,0.709341796171769,96.6580307251464));
#29879=CARTESIAN_POINT('Ctrl Pts',(2.4390325003349,0.629146145411388,96.6527942700083));
#29880=CARTESIAN_POINT('Ctrl Pts',(2.45711438189941,0.548083172760395,96.6475578148703));
#29881=CARTESIAN_POINT('Ctrl Pts',(2.47549301954925,0.465689811435834,96.6422354201179));
#29882=CARTESIAN_POINT('Ctrl Pts',(2.48971620069626,0.382400879284435,96.6369130253655));
#29883=CARTESIAN_POINT('Ctrl Pts',(2.49972047828995,0.298670019281929,96.6315906306132));
#29884=CARTESIAN_POINT('Ctrl Pts',(2.50957735913563,0.216172797226468,96.6263466526851));
#29885=CARTESIAN_POINT('Ctrl Pts',(2.51533885485511,0.133247053970913,96.621102674757));
#29886=CARTESIAN_POINT('Ctrl Pts',(2.51699686113291,0.0503294252607898,
96.6158586968289));
#29887=CARTESIAN_POINT('Ctrl Pts',(2.51869205738044,-0.0344480903165743,
96.6104970936644));
#29888=CARTESIAN_POINT('Ctrl Pts',(2.51609746535214,-0.119216610928426,
96.6051354904999));
#29889=CARTESIAN_POINT('Ctrl Pts',(2.50926050336597,-0.203514068917991,
96.5997738873354));
#29890=CARTESIAN_POINT('Ctrl Pts',(2.5024235413798,-0.287811526907556,96.5944122841709));
#29891=CARTESIAN_POINT('Ctrl Pts',(2.49134434230851,-0.371637427127336,
96.5890506810063));
#29892=CARTESIAN_POINT('Ctrl Pts',(2.47612558791285,-0.45454188243027,96.5836890778418));
#29893=CARTESIAN_POINT('Ctrl Pts',(2.46120841128382,-0.535803487088283,
96.5784337212377));
#29894=CARTESIAN_POINT('Ctrl Pts',(2.44225918150389,-0.616480033833178,
96.5731783646336));
#29895=CARTESIAN_POINT('Ctrl Pts',(2.41933747240763,-0.696141109692764,
96.5679230080295));
#29896=CARTESIAN_POINT('Ctrl Pts',(2.39644826324253,-0.775689236754743,
96.5626751028212));
#29897=CARTESIAN_POINT('Ctrl Pts',(2.36959788897822,-0.85422431309093,96.5574271976129));
#29898=CARTESIAN_POINT('Ctrl Pts',(2.33889710181438,-0.931325183340554,
96.5521792924046));
#29899=CARTESIAN_POINT('Ctrl Pts',(2.30797464513566,-1.00898274656396,96.5468934956401));
#29900=CARTESIAN_POINT('Ctrl Pts',(2.27314602487704,-1.08518483970174,96.5416076988757));
#29901=CARTESIAN_POINT('Ctrl Pts',(2.23457590956298,-1.15951574133375,96.5363219021112));
#29902=CARTESIAN_POINT('Ctrl Pts',(2.19635069606593,-1.23318196092313,96.5310833720166));
#29903=CARTESIAN_POINT('Ctrl Pts',(2.15445085106199,-1.30500990341387,96.5258448419221));
#29904=CARTESIAN_POINT('Ctrl Pts',(2.10908459973996,-1.37461572853643,96.5206063118275));
#29905=CARTESIAN_POINT('Ctrl Pts',(2.06373327781223,-1.44419864736237,96.5153695056594));
#29906=CARTESIAN_POINT('Ctrl Pts',(2.01491806688972,-1.51156051491705,96.5101326994913));
#29907=CARTESIAN_POINT('Ctrl Pts',(1.96289158387131,-1.57634478461001,96.5048958933232));
#29908=CARTESIAN_POINT('Ctrl Pts',(1.91086653019555,-1.64112727446096,96.4996592310278));
#29909=CARTESIAN_POINT('Ctrl Pts',(1.85563066954816,-1.70333194814043,96.4944225687324));
#29910=CARTESIAN_POINT('Ctrl Pts',(1.79747726185939,-1.76263488649762,96.489185906437));
#29911=CARTESIAN_POINT('Ctrl Pts',(1.73837456763181,-1.82290587614074,96.4838637617387));
#29912=CARTESIAN_POINT('Ctrl Pts',(1.67625855285653,-1.88017918278022,96.4785416170404));
#29913=CARTESIAN_POINT('Ctrl Pts',(1.61147511189883,-1.93415465093427,96.4732194723421));
#29914=CARTESIAN_POINT('Ctrl Pts',(1.54764070768506,-1.98733941236153,96.4679752937228));
#29915=CARTESIAN_POINT('Ctrl Pts',(1.48121692313514,-2.03732208599083,96.4627311151035));
#29916=CARTESIAN_POINT('Ctrl Pts',(1.41256560716746,-2.08385811787838,96.4574869364842));
#29917=CARTESIAN_POINT('Ctrl Pts',(1.34238331533709,-2.13143193819811,96.4521258087464));
#29918=CARTESIAN_POINT('Ctrl Pts',(1.26987338288143,-2.17540327598279,96.4467646810087));
#29919=CARTESIAN_POINT('Ctrl Pts',(1.19544906565652,-2.2155603763881,96.4414035532709));
#29920=CARTESIAN_POINT('Ctrl Pts',(1.12102474843161,-2.2557174767934,96.4360424255331));
#29921=CARTESIAN_POINT('Ctrl Pts',(1.04468653373815,-2.29206018174533,96.4306812977953));
#29922=CARTESIAN_POINT('Ctrl Pts',(0.966867543843202,-2.32442969406747,
96.4253201700575));
#29923=CARTESIAN_POINT('Ctrl Pts',(0.890582723867995,-2.35616105454278,
96.4200647347853));
#29924=CARTESIAN_POINT('Ctrl Pts',(0.8125933817548,-2.38419164490845,96.4148092995131));
#29925=CARTESIAN_POINT('Ctrl Pts',(0.733293001241794,-2.40833710770104,
96.4095538642409));
#29926=CARTESIAN_POINT('Ctrl Pts',(0.654105018669554,-2.43244834745107,
96.4043058778624));
#29927=CARTESIAN_POINT('Ctrl Pts',(0.573610126382135,-2.45268526421946,
96.3990578914839));
#29928=CARTESIAN_POINT('Ctrl Pts',(0.492221904547019,-2.46891146999728,
96.3938099051053));
#29929=CARTESIAN_POINT('Ctrl Pts',(0.410247611457908,-2.48525451961997,
96.3885241283207));
#29930=CARTESIAN_POINT('Ctrl Pts',(0.327367506731554,-2.49752867233272,
96.383238351536));
#29931=CARTESIAN_POINT('Ctrl Pts',(0.244019939406591,-2.50564572898325,
96.3779525747513));
#29932=CARTESIAN_POINT('Ctrl Pts',(0.161416005165548,-2.51369036466143,
96.3727139580533));
#29933=CARTESIAN_POINT('Ctrl Pts',(0.0783533841716873,-2.51765174293905,
96.3674753413552));
#29934=CARTESIAN_POINT('Ctrl Pts',(-0.00473257817738232,-2.51749555167508,
96.3622367246571));
#29935=CARTESIAN_POINT('Ctrl Pts',(-0.0877912275859617,-2.51733941175603,
96.3569998300553));
#29936=CARTESIAN_POINT('Ctrl Pts',(-0.170872742092727,-2.51306839143966,
96.3517629354535));
#29937=CARTESIAN_POINT('Ctrl Pts',(-0.253540502778757,-2.50470027417468,
96.3465260408517));
#29938=CARTESIAN_POINT('Ctrl Pts',(-0.336206019147242,-2.49633238409272,
96.3412892884245));
#29939=CARTESIAN_POINT('Ctrl Pts',(-0.418457345096286,-2.48386766571071,
96.3360525359972));
#29940=CARTESIAN_POINT('Ctrl Pts',(-0.499863102816892,-2.46737575744804,
96.33081578357));
#29941=CARTESIAN_POINT('Ctrl Pts',(-0.582594716538996,-2.45061524538928,
96.3254937401286));
#29942=CARTESIAN_POINT('Ctrl Pts',(-0.664452486780437,-2.42969526837323,
96.3201716966873));
#29943=CARTESIAN_POINT('Ctrl Pts',(-0.744996360411872,-2.40474253777261,
96.3148496532459));
#29944=CARTESIAN_POINT('Ctrl Pts',(-0.82436323944698,-2.38015444358388,
96.3096053812859));
#29945=CARTESIAN_POINT('Ctrl Pts',(-0.902453950006558,-2.35165089785812,
96.304361109326));
#29946=CARTESIAN_POINT('Ctrl Pts',(-0.978866343377746,-2.31940227899394,
96.299116837366));
#29947=CARTESIAN_POINT('Ctrl Pts',(-1.05697850701551,-2.28643629948883,
96.2937559081839));
#29948=CARTESIAN_POINT('Ctrl Pts',(-1.1333363289692,-2.24955685305805,96.2883949790018));
#29949=CARTESIAN_POINT('Ctrl Pts',(-1.20753724918357,-2.20899525618191,
96.2830340498197));
#29950=CARTESIAN_POINT('Ctrl Pts',(-1.28173816939795,-2.16843365930577,
96.2776731206376));
#29951=CARTESIAN_POINT('Ctrl Pts',(-1.35378179009948,-2.1241902345683,96.2723121914555));
#29952=CARTESIAN_POINT('Ctrl Pts',(-1.42329914826855,-2.07654178492464,
96.2669512622735));
#29953=CARTESIAN_POINT('Ctrl Pts',(-1.49115044797179,-2.0300352817675,96.2617188135412));
#29954=CARTESIAN_POINT('Ctrl Pts',(-1.55685069166608,-1.98011000497322,
96.2564863648089));
#29955=CARTESIAN_POINT('Ctrl Pts',(-1.62003283028502,-1.92699244388729,
96.2512539160767));
#29956=CARTESIAN_POINT('Ctrl Pts',(-1.68312519141424,-1.87395035921604,
96.2460289022955));
#29957=CARTESIAN_POINT('Ctrl Pts',(-1.74370619932942,-1.81772529526381,
96.2408038885144));
#29958=CARTESIAN_POINT('Ctrl Pts',(-1.80143792018448,-1.75858683883436,
96.2355788747332));
#29959=CARTESIAN_POINT('Ctrl Pts',(-1.85910373811189,-1.69951589117404,
96.2303598255016));
#29960=CARTESIAN_POINT('Ctrl Pts',(-1.91392640870733,-1.63753849161027,
96.2251407762699));
#29961=CARTESIAN_POINT('Ctrl Pts',(-1.96560237125858,-1.57296330793272,
96.2199217270382));
#29962=CARTESIAN_POINT('Ctrl Pts',(-2.01724621436462,-1.50842826127385,
96.2147059217319));
#29963=CARTESIAN_POINT('Ctrl Pts',(-2.06574694108255,-1.4412989981258,96.2094901164256));
#29964=CARTESIAN_POINT('Ctrl Pts',(-2.11083986172856,-1.3719188489622,96.2042743111193));
#29965=CARTESIAN_POINT('Ctrl Pts',(-2.15591867107367,-1.30256041150293,
96.1990601380381));
#29966=CARTESIAN_POINT('Ctrl Pts',(-2.19759153829349,-1.230952877166,96.1938459649569));
#29967=CARTESIAN_POINT('Ctrl Pts',(-2.23563672808269,-1.15746907952124,
96.1886317918757));
#29968=CARTESIAN_POINT('Ctrl Pts',(-2.27368175334582,-1.08398559965646,
96.1834176413432));
#29969=CARTESIAN_POINT('Ctrl Pts',(-2.308098919539,-1.00862628711035,96.1782034908107));
#29970=CARTESIAN_POINT('Ctrl Pts',(-2.33871282661468,-0.931787832410345,
96.1729893402781));
#29971=CARTESIAN_POINT('Ctrl Pts',(-2.36935658379212,-0.85487445634579,
96.1677701056861));
#29972=CARTESIAN_POINT('Ctrl Pts',(-2.39618950242494,-0.776479491398637,
96.1625508710941));
#29973=CARTESIAN_POINT('Ctrl Pts',(-2.41908490056256,-0.697018288045754,
96.1573316365021));
#29974=CARTESIAN_POINT('Ctrl Pts',(-2.44199140476928,-0.61751853975865,
96.1521098701708));
#29975=CARTESIAN_POINT('Ctrl Pts',(-2.4609564779823,-0.536951977037695,
96.1468881038394));
#29976=CARTESIAN_POINT('Ctrl Pts',(-2.47590437245768,-0.455745310941257,
96.1416663375081));
#29977=CARTESIAN_POINT('Ctrl Pts',(-2.49087835027489,-0.374396943200185,
96.136435459451));
#29978=CARTESIAN_POINT('Ctrl Pts',(-2.50182108451074,-0.292406703397515,
96.1312045813938));
#29979=CARTESIAN_POINT('Ctrl Pts',(-2.508708654222,-0.21020736959398,96.1259737033366));
#29980=CARTESIAN_POINT('Ctrl Pts',(-2.51458576306344,-0.140067327212032,
96.1215102364002));
#29981=CARTESIAN_POINT('Ctrl Pts',(-2.51751116265911,-0.0697752639189464,
96.1170467694638));
#29982=CARTESIAN_POINT('Ctrl Pts',(-2.51749996796861,0.000401594395409275,
96.1125833025275));
#29983=CARTESIAN_POINT('Ctrl Pts',(-2.51749996796852,0.000401594953133782,
96.112583302492));
#29984=CARTESIAN_POINT('Ctrl Pts',(-2.5174966230771,0.0213698964335877,
96.1112496531577));
#29985=CARTESIAN_POINT('Ctrl Pts',(-2.51723131533456,0.0423358846343242,
96.1099160038235));
#29986=CARTESIAN_POINT('Ctrl Pts',(-2.51670418679687,0.0632952301448918,
96.1085823544893));
#29987=CARTESIAN_POINT('Ctrl Pts',(-2.51462701145563,0.145886538621763,
96.1033270451808));
#29988=CARTESIAN_POINT('Ctrl Pts',(-2.50847607316376,0.228527745844191,
96.0980717358723));
#29989=CARTESIAN_POINT('Ctrl Pts',(-2.49824322749019,0.310784533558853,
96.0928164265637));
#29990=CARTESIAN_POINT('Ctrl Pts',(-2.48802311238251,0.392938986547741,
96.0875676553252));
#29991=CARTESIAN_POINT('Ctrl Pts',(-2.47373122398474,0.474709515524631,
96.0823188840867));
#29992=CARTESIAN_POINT('Ctrl Pts',(-2.45541140221161,0.555662753735768,
96.0770701128482));
#29993=CARTESIAN_POINT('Ctrl Pts',(-2.43711230709236,0.636524403187498,
96.071827279957));
#29994=CARTESIAN_POINT('Ctrl Pts',(-2.41479443687441,0.716570152071475,
96.0665844470658));
#29995=CARTESIAN_POINT('Ctrl Pts',(-2.38855310451469,0.79537432502768,96.0613416141747));
#29996=CARTESIAN_POINT('Ctrl Pts',(-2.3799338018142,0.821258567925877,96.059619538364));
#29997=CARTESIAN_POINT('Ctrl Pts',(-2.37089161588231,0.847008939293941,
96.0578974625533));
#29998=CARTESIAN_POINT('Ctrl Pts',(-2.36143112101026,0.872610629504502,
96.0561753867426));
#29999=CARTESIAN_POINT('',(-2.51804717241927,-0.00223002504931176,96.387416372278));
#30000=CARTESIAN_POINT('Ctrl Pts',(-2.35791364508473,0.871329681353405,
96.3311375631035));
#30001=CARTESIAN_POINT('Ctrl Pts',(-2.46013294861404,0.591639756348386,
96.3498971661617));
#30002=CARTESIAN_POINT('Ctrl Pts',(-2.51533068634196,0.294269068221567,
96.3686567692199));
#30003=CARTESIAN_POINT('Ctrl Pts',(-2.51804717241927,-0.00223002504931176,
96.387416372278));
#30004=CARTESIAN_POINT('Ctrl Pts',(-2.51749899202554,-0.00225280944616036,
96.3871012985794));
#30005=CARTESIAN_POINT('Ctrl Pts',(-2.51736869845421,-0.147854975242588,
96.3954712422479));
#30006=CARTESIAN_POINT('Ctrl Pts',(-2.50460703660455,-0.293157170744765,
96.4038561557088));
#30007=CARTESIAN_POINT('Ctrl Pts',(-2.47713855551654,-0.449172301708327,
96.4136292598055));
#30008=CARTESIAN_POINT('Ctrl Pts',(-2.47481501998665,-0.461802751706162,
96.4144261123344));
#30009=CARTESIAN_POINT('Ctrl Pts',(-2.47085734709265,-0.482428025777387,
96.4157374330634));
#30010=CARTESIAN_POINT('Ctrl Pts',(-2.46928076369863,-0.490433823824153,
96.416248919652));
#30011=CARTESIAN_POINT('Ctrl Pts',(-2.46615177369721,-0.505925014025159,
96.4172437220335));
#30012=CARTESIAN_POINT('Ctrl Pts',(-2.46460413363991,-0.513411288839801,
96.4177267738757));
#30013=CARTESIAN_POINT('Ctrl Pts',(-2.46167272031015,-0.527272435975308,
96.4186256324734));
#30014=CARTESIAN_POINT('Ctrl Pts',(-2.46029824341979,-0.533649092358558,
96.419040915781));
#30015=CARTESIAN_POINT('Ctrl Pts',(-2.45709173712559,-0.54824942296337,
96.4199958092197));
#30016=CARTESIAN_POINT('Ctrl Pts',(-2.45524320293902,-0.556469265974654,
96.4205363306388));
#30017=CARTESIAN_POINT('Ctrl Pts',(-2.45026371327949,-0.578103569240206,
96.421966400759));
#30018=CARTESIAN_POINT('Ctrl Pts',(-2.44706390474626,-0.591501671672988,
96.4228595971909));
#30019=CARTESIAN_POINT('Ctrl Pts',(-2.41553413935428,-0.718885549531426,
96.4314195309139));
#30020=CARTESIAN_POINT('Ctrl Pts',(-2.37937258034627,-0.830771642697027,
96.4394499975993));
#30021=CARTESIAN_POINT('Ctrl Pts',(-2.29695512651911,-1.03561035858076,
96.4546748422432));
#30022=CARTESIAN_POINT('Ctrl Pts',(-2.25249859383891,-1.1290451952626,96.4618406556468));
#30023=CARTESIAN_POINT('Ctrl Pts',(-2.14168670374415,-1.32917466175404,
96.4774656388834));
#30024=CARTESIAN_POINT('Ctrl Pts',(-2.07283412553353,-1.43418762657598,
96.4858491771246));
#30025=CARTESIAN_POINT('Ctrl Pts',(-1.9813782849684,-1.55324077978427,96.4955397713327));
#30026=CARTESIAN_POINT('Ctrl Pts',(-1.96603707706141,-1.57261410104507,
96.4971235943012));
#30027=CARTESIAN_POINT('Ctrl Pts',(-1.94151940078541,-1.60265607756257,
96.499591283578));
#30028=CARTESIAN_POINT('Ctrl Pts',(-1.93253482708415,-1.61347861521284,
96.5004827052764));
#30029=CARTESIAN_POINT('Ctrl Pts',(-1.91670809061988,-1.63222114394683,
96.502030979773));
#30030=CARTESIAN_POINT('Ctrl Pts',(-1.90990643789813,-1.64017473800895,
96.5026894474174));
#30031=CARTESIAN_POINT('Ctrl Pts',(-1.89445073822101,-1.65802153426466,
96.5041703630596));
#30032=CARTESIAN_POINT('Ctrl Pts',(-1.88576836702892,-1.667889889638,96.5049916242427));
#30033=CARTESIAN_POINT('Ctrl Pts',(-1.86207567245965,-1.69439740997439,
96.5072045071578));
#30034=CARTESIAN_POINT('Ctrl Pts',(-1.84691960726537,-1.71090514263882,
96.508590032471));
#30035=CARTESIAN_POINT('Ctrl Pts',(-1.77181792987299,-1.79054351030284,
96.5153149543631));
#30036=CARTESIAN_POINT('Ctrl Pts',(-1.70884243550823,-1.8507416645472,96.5205228595494));
#30037=CARTESIAN_POINT('Ctrl Pts',(-1.49171958293045,-2.03773668503772,
96.5373633179015));
#30038=CARTESIAN_POINT('Ctrl Pts',(-1.32564751779107,-2.14947629899044,
96.5484980300191));
#30039=CARTESIAN_POINT('Ctrl Pts',(-1.08760705431638,-2.27146291121257,
96.5642849552167));
#30040=CARTESIAN_POINT('Ctrl Pts',(-1.02584674250349,-2.3000151272654,96.5683732811711));
#30041=CARTESIAN_POINT('Ctrl Pts',(-0.950853998876421,-2.33106329685779,
96.5734154553201));
#30042=CARTESIAN_POINT('Ctrl Pts',(-0.938656422552669,-2.3360016104919,
96.5742379770537));
#30043=CARTESIAN_POINT('Ctrl Pts',(-0.919218732074385,-2.3436943422727,
96.5755533950753));
#30044=CARTESIAN_POINT('Ctrl Pts',(-0.912003462970394,-2.34651143767192,
96.5760426940437));
#30045=CARTESIAN_POINT('Ctrl Pts',(-0.898696808362354,-2.35163618075541,
96.5769471450763));
#30046=CARTESIAN_POINT('Ctrl Pts',(-0.892609352845022,-2.35395352974292,
96.5773617178837));
#30047=CARTESIAN_POINT('Ctrl Pts',(-0.878752856314007,-2.35916688923337,
96.578307206302));
#30048=CARTESIAN_POINT('Ctrl Pts',(-0.870978499856468,-2.36204814554349,
96.5788389624841));
#30049=CARTESIAN_POINT('Ctrl Pts',(-0.850673276283677,-2.36945959514692,
96.5802308780278));
#30050=CARTESIAN_POINT('Ctrl Pts',(-0.83812060822937,-2.37392873187347,
96.5810943882574));
#30051=CARTESIAN_POINT('Ctrl Pts',(-0.746297215186853,-2.40580164232354,
96.587430035659));
#30052=CARTESIAN_POINT('Ctrl Pts',(-0.665743868903635,-2.42932567990088,
96.5930896452486));
#30053=CARTESIAN_POINT('Ctrl Pts',(-0.43442119867569,-2.48450947825652,
96.6093611230807));
#30054=CARTESIAN_POINT('Ctrl Pts',(-0.281693688112623,-2.50642412335036,
96.6201050150125));
#30055=CARTESIAN_POINT('Ctrl Pts',(-0.01462777033248,-2.52001211653579,
96.6382770469461));
#30056=CARTESIAN_POINT('Ctrl Pts',(0.0989383796333694,-2.51811288601598,
96.6458196306118));
#30057=CARTESIAN_POINT('Ctrl Pts',(0.235061587411381,-2.50660881794183,
96.6546166001066));
#30058=CARTESIAN_POINT('Ctrl Pts',(0.258092168782863,-2.50434227031001,
96.6560968632599));
#30059=CARTESIAN_POINT('Ctrl Pts',(0.294307558461799,-2.50027323518626,
96.6584124611988));
#30060=CARTESIAN_POINT('Ctrl Pts',(0.307514469074636,-2.49868326362219,
96.6592543664414));
#30061=CARTESIAN_POINT('Ctrl Pts',(0.332221808824444,-2.49550990096949,
96.6608248342909));
#30062=CARTESIAN_POINT('Ctrl Pts',(0.343725037358974,-2.4939515035475,96.6615541563901));
#30063=CARTESIAN_POINT('Ctrl Pts',(0.369460172429428,-2.49028360094326,
96.6631818328872));
#30064=CARTESIAN_POINT('Ctrl Pts',(0.383685676705576,-2.48813153736058,
96.6640788303803));
#30065=CARTESIAN_POINT('Ctrl Pts',(0.419846857765702,-2.48234349406893,
96.6663525193734));
#30066=CARTESIAN_POINT('Ctrl Pts',(0.441754523847646,-2.47853860077018,
96.6677239055907));
#30067=CARTESIAN_POINT('Ctrl Pts',(0.617903764149041,-2.44553544627036,
96.6787079687245));
#30068=CARTESIAN_POINT('Ctrl Pts',(0.769163806993482,-2.40225825460969,
96.6878460610998));
#30069=CARTESIAN_POINT('Ctrl Pts',(1.02082027151597,-2.30402544269776,96.70339569076));
#30070=CARTESIAN_POINT('Ctrl Pts',(1.1233190824176,-2.25582789362918,96.7098465679069));
#30071=CARTESIAN_POINT('Ctrl Pts',(1.29194759528697,-2.16218365981552,96.7211585768009));
#30072=CARTESIAN_POINT('Ctrl Pts',(1.35978451204018,-2.12017692513694,96.7259224771952));
#30073=CARTESIAN_POINT('Ctrl Pts',(1.4370440739107,-2.067100994749,96.7317426504604));
#30074=CARTESIAN_POINT('Ctrl Pts',(1.44851515365224,-2.05907892555464,96.7326174912785));
#30075=CARTESIAN_POINT('Ctrl Pts',(1.46614712528584,-2.04652811157846,96.733979819267));
#30076=CARTESIAN_POINT('Ctrl Pts',(1.47235549102788,-2.04206611274972,96.7344629280109));
#30077=CARTESIAN_POINT('Ctrl Pts',(1.48382314310826,-2.03374474421842,96.7353618487868));
#30078=CARTESIAN_POINT('Ctrl Pts',(1.48908784809098,-2.02989314547075,96.7357771369691));
#30079=CARTESIAN_POINT('Ctrl Pts',(1.50111750270568,-2.02102040285675,96.7367320025181));
#30080=CARTESIAN_POINT('Ctrl Pts',(1.50787223600282,-2.015985749133,96.7372724907548));
#30081=CARTESIAN_POINT('Ctrl Pts',(1.52560355928216,-2.00263070611328,96.7387024428408));
#30082=CARTESIAN_POINT('Ctrl Pts',(1.53653718614361,-1.99425410138389,96.7395955537004));
#30083=CARTESIAN_POINT('Ctrl Pts',(1.63758129532717,-1.91551672049043,96.7479514150837));
#30084=CARTESIAN_POINT('Ctrl Pts',(1.72286006376316,-1.83919116019482,96.7557591018763));
#30085=CARTESIAN_POINT('Ctrl Pts',(1.95750172031732,-1.59850081971393,96.778926717251));
#30086=CARTESIAN_POINT('Ctrl Pts',(2.09071643795581,-1.41984541168163,96.7942838728304));
#30087=CARTESIAN_POINT('Ctrl Pts',(2.21433353769386,-1.19814506270149,96.8107629793089));
#30088=CARTESIAN_POINT('Ctrl Pts',(2.22934366403865,-1.16997931080664,96.81281624481));
#30089=CARTESIAN_POINT('Ctrl Pts',(2.25065184014371,-1.1280956946248,96.8158120644517));
#30090=CARTESIAN_POINT('Ctrl Pts',(2.25736813462483,-1.1145953178947,96.8167690924862));
#30091=CARTESIAN_POINT('Ctrl Pts',(2.2690701561936,-1.09053346879776,96.8184598488054));
#30092=CARTESIAN_POINT('Ctrl Pts',(2.27410439477052,-1.07999621730903,96.8191952360079));
#30093=CARTESIAN_POINT('Ctrl Pts',(2.28453611738341,-1.05776502355943,96.8207363543664));
#30094=CARTESIAN_POINT('Ctrl Pts',(2.28991756455601,-1.0460638957742,96.8215415194635));
#30095=CARTESIAN_POINT('Ctrl Pts',(2.30391723192259,-1.01499797115693,96.8236637521622));
#30096=CARTESIAN_POINT('Ctrl Pts',(2.31238121449784,-0.995564490250916,
96.8249755693114));
#30097=CARTESIAN_POINT('Ctrl Pts',(2.3487777427595,-0.909028118383248,96.8307505985041));
#30098=CARTESIAN_POINT('Ctrl Pts',(2.37404354144121,-0.840837505874827,
96.835124562483));
#30099=CARTESIAN_POINT('Ctrl Pts',(2.45519220682739,-0.588831965276025,
96.8507971199932));
#30100=CARTESIAN_POINT('Ctrl Pts',(2.49294487011241,-0.399894162543879,
96.8615700915236));
#30101=CARTESIAN_POINT('Ctrl Pts',(2.51396283906021,-0.146992712775582,
96.876373814445));
#30102=CARTESIAN_POINT('Ctrl Pts',(2.51681064548625,-0.0853181810766132,
96.8800188223732));
#30103=CARTESIAN_POINT('Ctrl Pts',(2.51772190102843,0.0118611696635401,
96.8859005307417));
#30104=CARTESIAN_POINT('Ctrl Pts',(2.51730489349256,0.0473290425222484,
96.8880762732822));
#30105=CARTESIAN_POINT('Ctrl Pts',(2.51577740093312,0.0937612139800365,
96.8909763876195));
#30106=CARTESIAN_POINT('Ctrl Pts',(2.51534400302675,0.104745559996041,96.8916662618259));
#30107=CARTESIAN_POINT('Ctrl Pts',(2.51451751233488,0.122705933496783,96.8928009975015));
#30108=CARTESIAN_POINT('Ctrl Pts',(2.51416728639153,0.129683920177109,96.8932435293651));
#30109=CARTESIAN_POINT('Ctrl Pts',(2.51342584239047,0.143322362638641,96.8941118645075));
#30110=CARTESIAN_POINT('Ctrl Pts',(2.51303718676604,0.149982863058114,96.8945375250866));
#30111=CARTESIAN_POINT('Ctrl Pts',(2.51210863132155,0.164877429387833,96.8954928725087));
#30112=CARTESIAN_POINT('Ctrl Pts',(2.51155471380607,0.173110534955513,96.8960233169788));
#30113=CARTESIAN_POINT('Ctrl Pts',(2.50949076308395,0.201689339334537,96.8978724783795));
#30114=CARTESIAN_POINT('Ctrl Pts',(2.50777393767597,0.222018681227759,96.8992017402161));
#30115=CARTESIAN_POINT('Ctrl Pts',(2.49020576267543,0.403686569900397,96.9111914343765));
#30116=CARTESIAN_POINT('Ctrl Pts',(2.45905275197633,0.563150936138783,96.9224745232812));
#30117=CARTESIAN_POINT('Ctrl Pts',(2.38459567424872,0.81318520545695,96.9404746501786));
#30118=CARTESIAN_POINT('Ctrl Pts',(2.35084830705162,0.906135567231456,96.947245222874));
#30119=CARTESIAN_POINT('Ctrl Pts',(2.27835607887696,1.0742440202384,96.9595309643992));
#30120=CARTESIAN_POINT('Ctrl Pts',(2.24112323784498,1.14990257913459,96.965077506078));
#30121=CARTESIAN_POINT('Ctrl Pts',(2.18976502278141,1.24225318390907,96.9718695864845));
#30122=CARTESIAN_POINT('Ctrl Pts',(2.17913040673448,1.26081503183629,96.9732360717253));
#30123=CARTESIAN_POINT('Ctrl Pts',(2.16169416597186,1.2903687671375,96.9754144456115));
#30124=CARTESIAN_POINT('Ctrl Pts',(2.15504242208814,1.30144742172417,96.9762316600626));
#30125=CARTESIAN_POINT('Ctrl Pts',(2.1422225507075,1.32243144865635,96.9777809161396));
#30126=CARTESIAN_POINT('Ctrl Pts',(2.13607030080289,1.3323460776185,96.9785135074402));
#30127=CARTESIAN_POINT('Ctrl Pts',(2.12185325763241,1.35490587443932,96.9801820060662));
#30128=CARTESIAN_POINT('Ctrl Pts',(2.11374390273684,1.36752254259395,96.9811162505746));
#30129=CARTESIAN_POINT('Ctrl Pts',(2.08826416861913,1.40639614452347,96.9839989631298));
#30130=CARTESIAN_POINT('Ctrl Pts',(2.07051326833901,1.43240088442351,96.9859333128201));
#30131=CARTESIAN_POINT('Ctrl Pts',(1.93668811609335,1.62076434748675,97.0000068083844));
#30132=CARTESIAN_POINT('Ctrl Pts',(1.80216266846783,1.76914002491917,97.0113636465397));
#30133=CARTESIAN_POINT('Ctrl Pts',(1.55142643676616,1.98707519675985,97.0304880479226));
#30134=CARTESIAN_POINT('Ctrl Pts',(1.44463392168879,2.06601439443902,97.0381736802327));
#30135=CARTESIAN_POINT('Ctrl Pts',(1.3166970266823,2.14579738148926,97.0474774836565));
#30136=CARTESIAN_POINT('Ctrl Pts',(1.30115101569777,2.15525948613846,97.0486096512545));
#30137=CARTESIAN_POINT('Ctrl Pts',(1.2782032725643,2.16888790631447,97.0502853260724));
#30138=CARTESIAN_POINT('Ctrl Pts',(1.27088046722993,2.17318687397538,97.0508207053334));
#30139=CARTESIAN_POINT('Ctrl Pts',(1.25793946092228,2.18069631845741,97.0517682489921));
#30140=CARTESIAN_POINT('Ctrl Pts',(1.25233043839155,2.1839222954403,97.0521794156654));
#30141=CARTESIAN_POINT('Ctrl Pts',(1.24012711544488,2.1908784502098,97.0530750669781));
#30142=CARTESIAN_POINT('Ctrl Pts',(1.23352850387399,2.19460043574964,97.0535600315285));
#30143=CARTESIAN_POINT('Ctrl Pts',(1.21529119896742,2.20477905923512,97.0549019992571));
#30144=CARTESIAN_POINT('Ctrl Pts',(1.20361814052377,2.21117316189203,97.0557627523496));
#30145=CARTESIAN_POINT('Ctrl Pts',(1.14072903020723,2.24497613901738,97.0604075348055));
#30146=CARTESIAN_POINT('Ctrl Pts',(1.08863044425069,2.27069663241653,97.0642813579726));
#30147=CARTESIAN_POINT('Ctrl Pts',(0.825971085596482,2.38925142704281,97.0837788145354));
#30148=CARTESIAN_POINT('Ctrl Pts',(0.604250468243455,2.45472146883869,97.1000067331764));
#30149=CARTESIAN_POINT('Ctrl Pts',(0.330128578060306,2.49620490956519,97.1184837667602));
#30150=CARTESIAN_POINT('Ctrl Pts',(0.28337676540084,2.50194362445227,97.1215870442982));
#30151=CARTESIAN_POINT('Ctrl Pts',(0.202070612964586,2.50961528626762,97.1269005838679));
#30152=CARTESIAN_POINT('Ctrl Pts',(0.167587734951365,2.51215365027907,97.1291283529388));
#30153=CARTESIAN_POINT('Ctrl Pts',(0.117520123271069,2.51480367010516,97.1323271682915));
#30154=CARTESIAN_POINT('Ctrl Pts',(0.101970614308654,2.51548215857317,97.1333156406632));
#30155=CARTESIAN_POINT('Ctrl Pts',(0.0746774914852433,2.51641957276513,
97.1350421807336));
#30156=CARTESIAN_POINT('Ctrl Pts',(0.0629366247317871,2.51674058709904,
97.135782152265));
#30157=CARTESIAN_POINT('Ctrl Pts',(0.0385431276468122,2.51723673548667,
97.137314027442));
#30158=CARTESIAN_POINT('Ctrl Pts',(0.0258905370800573,2.51739866619819,
97.1381055008062));
#30159=CARTESIAN_POINT('Ctrl Pts',(-0.00692212389810397,2.51757119835855,
97.1401503682554));
#30160=CARTESIAN_POINT('Ctrl Pts',(-0.0270823072891021,2.51743505176332,
97.1413991943718));
#30161=CARTESIAN_POINT('Ctrl Pts',(-0.110287950182441,2.51587348052676,
97.1465245885052));
#30162=CARTESIAN_POINT('Ctrl Pts',(-0.173273414679198,2.51232165581684,
97.1503354272722));
#30163=CARTESIAN_POINT('Ctrl Pts',(-0.273033299736258,2.50292588396244,
97.1562998760702));
#30164=CARTESIAN_POINT('Ctrl Pts',(-0.309922823053082,2.49862625490241,
97.1584900008439));
#30165=CARTESIAN_POINT('Ctrl Pts',(-0.516659148436956,2.46988106653034,
97.1707136866586));
#30166=CARTESIAN_POINT('Ctrl Pts',(-0.683743833263817,2.42893812048489,
97.180367943746));
#30167=CARTESIAN_POINT('Ctrl Pts',(-0.900286280017697,2.35174212152534,
97.1938078005655));
#30168=CARTESIAN_POINT('Ctrl Pts',(-0.954510960348861,2.33026057545199,
97.1972595329997));
#30169=CARTESIAN_POINT('Ctrl Pts',(-1.02899490947952,2.29771708372573,97.2021852815925));
#30170=CARTESIAN_POINT('Ctrl Pts',(-1.04992477460914,2.2882290557155,97.2035902919113));
#30171=CARTESIAN_POINT('Ctrl Pts',(-1.08628043958002,2.27114434030453,97.2060725163512));
#30172=CARTESIAN_POINT('Ctrl Pts',(-1.10176402719163,2.26367351857929,97.2071431115649));
#30173=CARTESIAN_POINT('Ctrl Pts',(-1.12460623442567,2.25236230123277,97.2087443010268));
#30174=CARTESIAN_POINT('Ctrl Pts',(-1.13202469839731,2.24864296768326,97.2092677616357));
#30175=CARTESIAN_POINT('Ctrl Pts',(-1.14467824957472,2.242220477007,97.2101667505426));
#30176=CARTESIAN_POINT('Ctrl Pts',(-1.14992244278479,2.23953551818768,97.2105411499245));
#30177=CARTESIAN_POINT('Ctrl Pts',(-1.16180804725903,2.23339748836304,97.2113938921814));
#30178=CARTESIAN_POINT('Ctrl Pts',(-1.16844338071537,2.22993325960517,97.211872914691));
#30179=CARTESIAN_POINT('Ctrl Pts',(-1.18648273432046,2.22041250789946,97.2131831199835));
#30180=CARTESIAN_POINT('Ctrl Pts',(-1.19785558250237,2.21429785051938,97.2140177773428));
#30181=CARTESIAN_POINT('Ctrl Pts',(-1.25515630304325,2.18291927117981,97.2182650961704));
#30182=CARTESIAN_POINT('Ctrl Pts',(-1.30033095319087,2.15631454840361,97.2217507745425));
#30183=CARTESIAN_POINT('Ctrl Pts',(-1.5439540730968,2.00239747028653,97.2411852899693));
#30184=CARTESIAN_POINT('Ctrl Pts',(-1.72460488253679,1.84909555864324,97.2578426910313));
#30185=CARTESIAN_POINT('Ctrl Pts',(-1.92889053692023,1.61935656662453,97.2783386397707));
#30186=CARTESIAN_POINT('Ctrl Pts',(-1.97417430087555,1.56383243602918,97.2830302668108));
#30187=CARTESIAN_POINT('Ctrl Pts',(-2.02920284415557,1.49015291552007,97.2889341807666));
#30188=CARTESIAN_POINT('Ctrl Pts',(-2.04117542662496,1.47371055901491,97.2902322560841));
#30189=CARTESIAN_POINT('Ctrl Pts',(-2.06029392013924,1.44677444787349,97.2923279748971));
#30190=CARTESIAN_POINT('Ctrl Pts',(-2.06756183816379,1.43636882287495,97.293130246396));
#30191=CARTESIAN_POINT('Ctrl Pts',(-2.08139554654044,1.41624025365992,97.2946683272234));
#30192=CARTESIAN_POINT('Ctrl Pts',(-2.0879726579124,1.40652552928541,97.2954045501611));
#30193=CARTESIAN_POINT('Ctrl Pts',(-2.1029205020329,1.38411088902672,97.2970894735906));
#30194=CARTESIAN_POINT('Ctrl Pts',(-2.11124458202282,1.37138029803988,97.2980364205715));
#30195=CARTESIAN_POINT('Ctrl Pts',(-2.13687201109165,1.33140007140476,97.3009798983876));
#30196=CARTESIAN_POINT('Ctrl Pts',(-2.15376742209557,1.30389193499914,97.3029615083089));
#30197=CARTESIAN_POINT('Ctrl Pts',(-2.24575106326858,1.14746075079896,97.3140030727608));
#30198=CARTESIAN_POINT('Ctrl Pts',(-2.30975897673764,1.01244410929445,97.3226562753726));
#30199=CARTESIAN_POINT('Ctrl Pts',(-2.36143105416443,0.872610810400539,
97.3312318328322));
#30200=CARTESIAN_POINT('Origin',(0.,0.,104.));
#30201=CARTESIAN_POINT('',(-2.36143112099219,0.872610629553384,98.3289997116198));
#30202=CARTESIAN_POINT('',(-2.36143112101026,0.872610629504505,98.0563225720173));
#30203=CARTESIAN_POINT('',(-2.36143112101026,0.872610629504505,104.));
#30204=CARTESIAN_POINT('',(-2.51749930506837,0.00187055614564606,97.1125833024347));
#30205=CARTESIAN_POINT('Ctrl Pts',(-2.36143112101026,0.872610629504505,
98.0563225720173));
#30206=CARTESIAN_POINT('Ctrl Pts',(-2.33256999240762,0.950713697431207,
98.0510687730156));
#30207=CARTESIAN_POINT('Ctrl Pts',(-2.29985371519826,1.02731921157481,98.0458149740139));
#30208=CARTESIAN_POINT('Ctrl Pts',(-2.2634766993883,1.10203424689356,98.0405611750122));
#30209=CARTESIAN_POINT('Ctrl Pts',(-2.22702982976517,1.17689275550175,98.0352972872804));
#30210=CARTESIAN_POINT('Ctrl Pts',(-2.18690839552841,1.24985312765648,98.0300333995486));
#30211=CARTESIAN_POINT('Ctrl Pts',(-2.14335225325123,1.3205481318312,98.0247695118168));
#30212=CARTESIAN_POINT('Ctrl Pts',(-2.09988271562105,1.39110256993278,98.019516090511));
#30213=CARTESIAN_POINT('Ctrl Pts',(-2.05299243786544,1.45940031406957,98.0142626692052));
#30214=CARTESIAN_POINT('Ctrl Pts',(-2.0029596359888,1.52510948675812,98.0090092478994));
#30215=CARTESIAN_POINT('Ctrl Pts',(-1.95290942326789,1.59084152548915,98.0037539984629));
#30216=CARTESIAN_POINT('Ctrl Pts',(-1.89952761528302,1.65422856294524,97.9984987490264));
#30217=CARTESIAN_POINT('Ctrl Pts',(-1.84306196639629,1.71491365322673,97.9932434995899));
#30218=CARTESIAN_POINT('Ctrl Pts',(-1.78667637299258,1.77551270581432,97.9879957009051));
#30219=CARTESIAN_POINT('Ctrl Pts',(-1.72721593482255,1.83341708522346,97.9827479022204));
#30220=CARTESIAN_POINT('Ctrl Pts',(-1.66496986728393,1.88830124477969,97.9775001035356));
#30221=CARTESIAN_POINT('Ctrl Pts',(-1.60227277373286,1.94358308702674,97.9722142800598));
#30222=CARTESIAN_POINT('Ctrl Pts',(-1.53674979902648,1.99580037955735,97.9669284565839));
#30223=CARTESIAN_POINT('Ctrl Pts',(-1.46873581608155,2.04465678111493,97.9616426331081));
#30224=CARTESIAN_POINT('Ctrl Pts',(-1.4013317094487,2.09307509096382,97.9564042072171));
#30225=CARTESIAN_POINT('Ctrl Pts',(-1.33148147068404,2.13819226799277,97.9511657813261));
#30226=CARTESIAN_POINT('Ctrl Pts',(-1.25954438060733,2.17976012516986,97.9459273554351));
#30227=CARTESIAN_POINT('Ctrl Pts',(-1.18763094946768,2.22131431135586,97.940690652377));
#30228=CARTESIAN_POINT('Ctrl Pts',(-1.11363242931061,2.25932126536479,97.935453949319));
#30229=CARTESIAN_POINT('Ctrl Pts',(-1.03793535235416,2.29357721787025,97.9302172462609));
#30230=CARTESIAN_POINT('Ctrl Pts',(-0.962240337375317,2.32783223724844,
97.9249806858499));
#30231=CARTESIAN_POINT('Ctrl Pts',(-0.884847278394691,2.3583362689779,97.9197441254389));
#30232=CARTESIAN_POINT('Ctrl Pts',(-0.806164203337558,2.38493302364178,
97.9145075650279));
#30233=CARTESIAN_POINT('Ctrl Pts',(-0.726193299139214,2.41196509524889,
97.9091852962852));
#30234=CARTESIAN_POINT('Ctrl Pts',(-0.644890231355187,2.43496066281516,
97.9038630275425));
#30235=CARTESIAN_POINT('Ctrl Pts',(-0.562699283145033,2.45380842095467,
97.8985407587997));
#30236=CARTESIAN_POINT('Ctrl Pts',(-0.481715779428683,2.47237929189089,
97.8932966780355));
#30237=CARTESIAN_POINT('Ctrl Pts',(-0.399870780873901,2.486923391632,97.8880525972712));
#30238=CARTESIAN_POINT('Ctrl Pts',(-0.317597601026388,2.49738623641244,
97.8828085165069));
#30239=CARTESIAN_POINT('Ctrl Pts',(-0.233484411298407,2.50808307892834,
97.877447153775));
#30240=CARTESIAN_POINT('Ctrl Pts',(-0.14892416749316,2.5145138732317,97.872085791043));
#30241=CARTESIAN_POINT('Ctrl Pts',(-0.0643812861428095,2.51667663794827,
97.8667244283111));
#30242=CARTESIAN_POINT('Ctrl Pts',(0.0201615952075295,2.51883940266483,
97.8613630655791));
#30243=CARTESIAN_POINT('Ctrl Pts',(0.104686607816869,2.51673421722273,97.8560017028472));
#30244=CARTESIAN_POINT('Ctrl Pts',(0.188735567811208,2.51041533126353,97.8506403401152));
#30245=CARTESIAN_POINT('Ctrl Pts',(0.271121022824545,2.50422150929404,97.8453850899825));
#30246=CARTESIAN_POINT('Ctrl Pts',(0.353353400731598,2.49395643019617,97.8401298398498));
#30247=CARTESIAN_POINT('Ctrl Pts',(0.434998407716047,2.47963356875255,97.8348745897171));
#30248=CARTESIAN_POINT('Ctrl Pts',(0.516527660694896,2.46533101386097,97.8296267903309));
#30249=CARTESIAN_POINT('Ctrl Pts',(0.597470746163032,2.44698218284478,97.8243789909448));
#30250=CARTESIAN_POINT('Ctrl Pts',(0.677397134217739,2.42465242303997,97.8191311915586));
#30251=CARTESIAN_POINT('Ctrl Pts',(0.757902643912019,2.40216086877123,97.8138453682574));
#30252=CARTESIAN_POINT('Ctrl Pts',(0.837376188129912,2.37563048869662,97.8085595449563));
#30253=CARTESIAN_POINT('Ctrl Pts',(0.915386876163325,2.34518082819811,97.8032737216551));
#30254=CARTESIAN_POINT('Ctrl Pts',(0.992698061192939,2.31500420245316,97.7980352950553));
#30255=CARTESIAN_POINT('Ctrl Pts',(1.0685720813671,2.28097847213127,97.7927968684554));
#30256=CARTESIAN_POINT('Ctrl Pts',(1.14260514823941,2.24326987346971,97.7875584418555));
#30257=CARTESIAN_POINT('Ctrl Pts',(1.21661386686244,2.20557367654157,97.7823217380873));
#30258=CARTESIAN_POINT('Ctrl Pts',(1.28878242382462,2.16419722610919,97.7770850343192));
#30259=CARTESIAN_POINT('Ctrl Pts',(1.35872945084618,2.11935379995961,97.771848330551));
#30260=CARTESIAN_POINT('Ctrl Pts',(1.42867457252424,2.07451159533629,97.7666117694297));
#30261=CARTESIAN_POINT('Ctrl Pts',(1.49639789668942,2.0262028526693,97.7613752083083));
#30262=CARTESIAN_POINT('Ctrl Pts',(1.56154617747477,1.97468473068841,97.756138647187));
#30263=CARTESIAN_POINT('Ctrl Pts',(1.6277607400155,1.92232341172859,97.7508163792823));
#30264=CARTESIAN_POINT('Ctrl Pts',(1.69131481339937,1.86664700454359,97.7454941113776));
#30265=CARTESIAN_POINT('Ctrl Pts',(1.75187314508481,1.80796756982272,97.740171843473));
#30266=CARTESIAN_POINT('Ctrl Pts',(1.81154184846608,1.75015016159015,97.7349277620051));
#30267=CARTESIAN_POINT('Ctrl Pts',(1.86830196868316,1.68941775557057,97.7296836805371));
#30268=CARTESIAN_POINT('Ctrl Pts',(1.92187188685686,1.62610414811268,97.7244395990692));
#30269=CARTESIAN_POINT('Ctrl Pts',(1.97663985307147,1.56137458285676,97.7190782379462));
#30270=CARTESIAN_POINT('Ctrl Pts',(2.02807289226775,1.49394737715799,97.7137168768231));
#30271=CARTESIAN_POINT('Ctrl Pts',(2.07591649040969,1.42421100081594,97.7083555157001));
#30272=CARTESIAN_POINT('Ctrl Pts',(2.12376008855163,1.35447462447388,97.702994154577));
#30273=CARTESIAN_POINT('Ctrl Pts',(2.16801403661508,1.282429545401,97.697632793454));
#30274=CARTESIAN_POINT('Ctrl Pts',(2.20847437999406,1.20848962052218,97.692271432331));
#30275=CARTESIAN_POINT('Ctrl Pts',(2.24813392220464,1.1360131330067,97.6870161845993));
#30276=CARTESIAN_POINT('Ctrl Pts',(2.28429518581942,1.06144844418236,97.6817609368676));
#30277=CARTESIAN_POINT('Ctrl Pts',(2.31673302142714,0.985167172326145,97.6765056891359));
#30278=CARTESIAN_POINT('Ctrl Pts',(2.34912486754154,0.908994050011247,97.6712578921535));
#30279=CARTESIAN_POINT('Ctrl Pts',(2.37780359217612,0.83110959983421,97.6660100951711));
#30280=CARTESIAN_POINT('Ctrl Pts',(2.40258960547228,0.751910525047065,97.6607622981887));
#30281=CARTESIAN_POINT('Ctrl Pts',(2.42755522475012,0.672137552900731,97.655476474287));
#30282=CARTESIAN_POINT('Ctrl Pts',(2.44857125192748,0.59103123923539,97.6501906503852));
#30283=CARTESIAN_POINT('Ctrl Pts',(2.46550336138273,0.509018098902654,97.6449048264835));
#30284=CARTESIAN_POINT('Ctrl Pts',(2.4822836351284,0.427740396962234,97.6396664022767));
#30285=CARTESIAN_POINT('Ctrl Pts',(2.49505284639742,0.345572527047932,97.6344279780699));
#30286=CARTESIAN_POINT('Ctrl Pts',(2.50373058960798,0.262943691046724,97.6291895538631));
#30287=CARTESIAN_POINT('Ctrl Pts',(2.51240547886663,0.180342030166865,97.6239528524787));
#30288=CARTESIAN_POINT('Ctrl Pts',(2.51699152436522,0.0972801628280084,
97.6187161510943));
#30289=CARTESIAN_POINT('Ctrl Pts',(2.51745998530524,0.0141940969049517,
97.61347944971));
#30290=CARTESIAN_POINT('Ctrl Pts',(2.51792843348557,-0.068889705965877,
97.60824289096));
#30291=CARTESIAN_POINT('Ctrl Pts',(2.5142795185248,-0.151997244690935,97.60300633221));
#30292=CARTESIAN_POINT('Ctrl Pts',(2.50653661791235,-0.234692209211345,
97.59776977346));
#30293=CARTESIAN_POINT('Ctrl Pts',(2.49866698150394,-0.318740724897604,
97.5924475027172));
#30294=CARTESIAN_POINT('Ctrl Pts',(2.48656816229883,-0.402362547682886,
97.5871252319745));
#30295=CARTESIAN_POINT('Ctrl Pts',(2.47031938587987,-0.485106567411868,
97.5818029612317));
#30296=CARTESIAN_POINT('Ctrl Pts',(2.4543093266835,-0.566634961910552,97.5765588820805));
#30297=CARTESIAN_POINT('Ctrl Pts',(2.43427061054853,-0.647310735018868,
97.5713148029294));
#30298=CARTESIAN_POINT('Ctrl Pts',(2.41032989547979,-0.726715931404013,
97.5660707237782));
#30299=CARTESIAN_POINT('Ctrl Pts',(2.38585373007903,-0.807897078868578,
97.5607093572396));
#30300=CARTESIAN_POINT('Ctrl Pts',(2.3572990901666,-0.887749646995334,97.5553479907011));
#30301=CARTESIAN_POINT('Ctrl Pts',(2.32485325153221,-0.965848646962927,
97.5499866241625));
#30302=CARTESIAN_POINT('Ctrl Pts',(2.29240741289782,-1.04394764693051,97.5446252576239));
#30303=CARTESIAN_POINT('Ctrl Pts',(2.25607065422207,-1.12029264865219,97.5392638910854));
#30304=CARTESIAN_POINT('Ctrl Pts',(2.21607907323478,-1.19448725031742,97.5339025245468));
#30305=CARTESIAN_POINT('Ctrl Pts',(2.17687903689243,-1.26721333440516,97.5286472743675));
#30306=CARTESIAN_POINT('Ctrl Pts',(2.13402278743501,-1.33814201184334,97.5233920241881));
#30307=CARTESIAN_POINT('Ctrl Pts',(2.08769945270457,-1.40688210066694,97.5181367740087));
#30308=CARTESIAN_POINT('Ctrl Pts',(2.04144179405224,-1.47552473149299,97.5128889745931));
#30309=CARTESIAN_POINT('Ctrl Pts',(1.99172706954891,-1.54198455757053,97.5076411751774));
#30310=CARTESIAN_POINT('Ctrl Pts',(1.93879025308253,-1.60589495439526,97.5023933757618));
#30311=CARTESIAN_POINT('Ctrl Pts',(1.88546987337671,-1.67026842551265,97.4971075524702));
#30312=CARTESIAN_POINT('Ctrl Pts',(1.8288807370468,-1.73205494964748,97.4918217291785));
#30313=CARTESIAN_POINT('Ctrl Pts',(1.76930746740127,-1.7909096392052,97.4865359058869));
#30314=CARTESIAN_POINT('Ctrl Pts',(1.71026837691022,-1.84923659294294,97.4812974792991));
#30315=CARTESIAN_POINT('Ctrl Pts',(1.64829878907119,-1.90468374936841,97.4760590527113));
#30316=CARTESIAN_POINT('Ctrl Pts',(1.58371493837924,-1.95694998504163,97.4708206261234));
#30317=CARTESIAN_POINT('Ctrl Pts',(1.5191523284362,-2.00919903106177,97.4655839223828));
#30318=CARTESIAN_POINT('Ctrl Pts',(1.4519775216383,-2.05826894402127,97.4603472186421));
#30319=CARTESIAN_POINT('Ctrl Pts',(1.38254059026732,-2.10389823096634,97.4551105149015));
#30320=CARTESIAN_POINT('Ctrl Pts',(1.31310555054775,-2.14952627484517,97.4498739538229));
#30321=CARTESIAN_POINT('Ctrl Pts',(1.241408894964,-2.19171362653536,97.4446373927444));
#30322=CARTESIAN_POINT('Ctrl Pts',(1.16782932516116,-2.23024234496918,97.4394008316658));
#30323=CARTESIAN_POINT('Ctrl Pts',(1.09304547804947,-2.26940166319413,97.4340785637572));
#30324=CARTESIAN_POINT('Ctrl Pts',(1.01631695483261,-2.30478126619033,97.4287562958486));
#30325=CARTESIAN_POINT('Ctrl Pts',(0.938065276735081,-2.33620200038095,
97.42343402794));
#30326=CARTESIAN_POINT('Ctrl Pts',(0.860963151144127,-2.36716114978992,
97.4181899465517));
#30327=CARTESIAN_POINT('Ctrl Pts',(0.782382787729207,-2.39427687881259,
97.4129458651633));
#30328=CARTESIAN_POINT('Ctrl Pts',(0.702743723592735,-2.41742787047536,
97.407701783775));
#30329=CARTESIAN_POINT('Ctrl Pts',(0.621323594049227,-2.44109661596705,
97.4023404226063));
#30330=CARTESIAN_POINT('Ctrl Pts',(0.538797336628929,-2.46062102983402,
97.3969790614375));
#30331=CARTESIAN_POINT('Ctrl Pts',(0.455623389616077,-2.47592681168785,
97.3916177002688));
#30332=CARTESIAN_POINT('Ctrl Pts',(0.372449442603224,-2.49123259354168,
97.3862563391001));
#30333=CARTESIAN_POINT('Ctrl Pts',(0.288628318475212,-2.50231974297535,
97.3808949779313));
#30334=CARTESIAN_POINT('Ctrl Pts',(0.204621058188024,-2.50917047498691,
97.3755336167626));
#30335=CARTESIAN_POINT('Ctrl Pts',(0.122276388344548,-2.51588562393652,
97.3702783624686));
#30336=CARTESIAN_POINT('Ctrl Pts',(0.0394487396834575,-2.5185553615653,
97.3650231081747));
#30337=CARTESIAN_POINT('Ctrl Pts',(-0.0434307957414703,-2.51712534768955,
97.3597678538807));
#30338=CARTESIAN_POINT('Ctrl Pts',(-0.126192827362948,-2.51569736123914,
97.3545200503086));
#30339=CARTESIAN_POINT('Ctrl Pts',(-0.20900614212781,-2.51018117647843,
97.3492722467364));
#30340=CARTESIAN_POINT('Ctrl Pts',(-0.291435285714752,-2.50057427888882,
97.3440244431643));
#30341=CARTESIAN_POINT('Ctrl Pts',(-0.37446160251036,-2.49089778234903,
97.3387386209066));
#30342=CARTESIAN_POINT('Ctrl Pts',(-0.457097685928118,-2.4770710125533,
97.3334527986488));
#30343=CARTESIAN_POINT('Ctrl Pts',(-0.538899284068818,-2.45914493505977,
97.3281669763911));
#30344=CARTESIAN_POINT('Ctrl Pts',(-0.619967468262847,-2.44137957857343,
97.3229285455762));
#30345=CARTESIAN_POINT('Ctrl Pts',(-0.700215611826423,-2.41958822747458,
97.3176901147613));
#30346=CARTESIAN_POINT('Ctrl Pts',(-0.779218959865339,-2.3938721901109,
97.3124516839464));
#30347=CARTESIAN_POINT('Ctrl Pts',(-0.858196325055373,-2.36816461031174,
97.3072149759618));
#30348=CARTESIAN_POINT('Ctrl Pts',(-0.935929269381141,-2.33853505047875,
97.3019782679771));
#30349=CARTESIAN_POINT('Ctrl Pts',(-1.01200785669301,-2.30513477870419,
97.2967415599924));
#30350=CARTESIAN_POINT('Ctrl Pts',(-1.08808437157927,-2.27173541677274,
97.2915049946588));
#30351=CARTESIAN_POINT('Ctrl Pts',(-1.16250619697185,-2.23456573355622,
97.2862684293251));
#30352=CARTESIAN_POINT('Ctrl Pts',(-1.23488434042773,-2.19382472311859,
97.2810318639915));
#30353=CARTESIAN_POINT('Ctrl Pts',(-1.3084469686825,-2.15241697676801,97.2757096010737));
#30354=CARTESIAN_POINT('Ctrl Pts',(-1.37989798599608,-2.10732018730508,
97.270387338156));
#30355=CARTESIAN_POINT('Ctrl Pts',(-1.44885762334226,-2.05879038206492,
97.2650650752382));
#30356=CARTESIAN_POINT('Ctrl Pts',(-1.51680433109064,-2.01097341810402,
97.2598209896115));
#30357=CARTESIAN_POINT('Ctrl Pts',(-1.58233203236523,-1.95982395866017,
97.2545769039847));
#30358=CARTESIAN_POINT('Ctrl Pts',(-1.64511054929148,-1.90562785732417,
97.249332818358));
#30359=CARTESIAN_POINT('Ctrl Pts',(-1.70929289180417,-1.85021984660473,
97.2439714667947));
#30360=CARTESIAN_POINT('Ctrl Pts',(-1.7706012442335,-1.79162764845339,97.2386101152315));
#30361=CARTESIAN_POINT('Ctrl Pts',(-1.82872368836751,-1.73019534203613,
97.2332487636682));
#30362=CARTESIAN_POINT('Ctrl Pts',(-1.88684613250151,-1.66876303561888,
97.2278874121049));
#30363=CARTESIAN_POINT('Ctrl Pts',(-1.94178238898331,-1.60449105056951,
97.2225260605417));
#30364=CARTESIAN_POINT('Ctrl Pts',(-1.9932665267309,-1.53775641875237,97.2171647089784));
#30365=CARTESIAN_POINT('Ctrl Pts',(-2.04375879578633,-1.47230746432789,
97.2119066466416));
#30366=CARTESIAN_POINT('Ctrl Pts',(-2.09112029805458,-1.40424435744742,
97.2066485843049));
#30367=CARTESIAN_POINT('Ctrl Pts',(-2.13506935929913,-1.33389845227514,
97.2013905219681));
#30368=CARTESIAN_POINT('Ctrl Pts',(-2.1789570760028,-1.26365073662348,97.1961397988875));
#30369=CARTESIAN_POINT('Ctrl Pts',(-2.21944156720512,-1.19112693546319,
97.1908890758069));
#30370=CARTESIAN_POINT('Ctrl Pts',(-2.25628201011796,-1.11669053045957,
97.1856383527263));
#30371=CARTESIAN_POINT('Ctrl Pts',(-2.29308207556009,-1.04233570845343,
97.1803933844874));
#30372=CARTESIAN_POINT('Ctrl Pts',(-2.32624582231096,-0.966072856005633,
97.1751484162485));
#30373=CARTESIAN_POINT('Ctrl Pts',(-2.35557701969086,-0.888292268515459,
97.1699034480096));
#30374=CARTESIAN_POINT('Ctrl Pts',(-2.38488563777284,-0.810571556898563,
97.1646625173727));
#30375=CARTESIAN_POINT('Ctrl Pts',(-2.41036740587786,-0.73133586059678,
97.1594215867358));
#30376=CARTESIAN_POINT('Ctrl Pts',(-2.431873704451,-0.650996571112148,97.1541806560988));
#30377=CARTESIAN_POINT('Ctrl Pts',(-2.45337004841148,-0.570694468245425,
97.1489421513296));
#30378=CARTESIAN_POINT('Ctrl Pts',(-2.4708944621029,-0.489290231623965,
97.1437036465604));
#30379=CARTESIAN_POINT('Ctrl Pts',(-2.48434821360103,-0.407210269489083,
97.1384651417911));
#30380=CARTESIAN_POINT('Ctrl Pts',(-2.497803310619,-0.325122098475233,97.1332261131151));
#30381=CARTESIAN_POINT('Ctrl Pts',(-2.50718685030444,-0.242358519957874,
97.127987084439));
#30382=CARTESIAN_POINT('Ctrl Pts',(-2.51245144076967,-0.159354974112484,
97.1227480557629));
#30383=CARTESIAN_POINT('Ctrl Pts',(-2.51585622350457,-0.105673867918983,
97.1193598046726));
#30384=CARTESIAN_POINT('Ctrl Pts',(-2.51753925219785,-0.0518925558902497,
97.1159715535823));
#30385=CARTESIAN_POINT('Ctrl Pts',(-2.51749930506904,0.0018705552357781,
97.112583302492));
#30386=CARTESIAN_POINT('Ctrl Pts',(-2.51749930506837,0.00187055614564556,
97.1125833024347));
#30387=CARTESIAN_POINT('Ctrl Pts',(-2.51742786227618,0.0980222702224651,
97.1065236428793));
#30388=CARTESIAN_POINT('Ctrl Pts',(-2.51184391378265,0.193950035127749,
97.100463983324));
#30389=CARTESIAN_POINT('Ctrl Pts',(-2.5008479055551,0.28907784986171,97.0944043237686));
#30390=CARTESIAN_POINT('Ctrl Pts',(-2.48974553226095,0.385125841821851,
97.0882860487522));
#30391=CARTESIAN_POINT('Ctrl Pts',(-2.47312598902194,0.480358183904104,
97.0821677737357));
#30392=CARTESIAN_POINT('Ctrl Pts',(-2.45114231090937,0.574201725589434,
97.0760494987193));
#30393=CARTESIAN_POINT('Ctrl Pts',(-2.43047745948084,0.662415482929026,
97.070298266211));
#30394=CARTESIAN_POINT('Ctrl Pts',(-2.40507329585502,0.749402171584247,
97.0645470337027));
#30395=CARTESIAN_POINT('Ctrl Pts',(-2.37509517890798,0.834703025709186,
97.0587958011944));
#30396=CARTESIAN_POINT('Ctrl Pts',(-2.37064303349584,0.84737132662399,97.0579416673783));
#30397=CARTESIAN_POINT('Ctrl Pts',(-2.36608819785996,0.860007796311788,
97.0570875335623));
#30398=CARTESIAN_POINT('Ctrl Pts',(-2.36143112101025,0.872610629504516,
97.0562333997462));
#30399=CARTESIAN_POINT('Ctrl Pts',(-2.36143105416443,0.872610810400539,
97.3312318328322));
#30400=CARTESIAN_POINT('Ctrl Pts',(-2.37281360699947,0.841807715343776,
97.3331208944054));
#30401=CARTESIAN_POINT('Ctrl Pts',(-2.38359750920899,0.810770938666179,
97.3350072777569));
#30402=CARTESIAN_POINT('Ctrl Pts',(-2.43975997246009,0.638304921164849,
97.3454324317484));
#30403=CARTESIAN_POINT('Ctrl Pts',(-2.47315310182676,0.493318849580991,
97.3539746313534));
#30404=CARTESIAN_POINT('Ctrl Pts',(-2.4960546078397,0.328394506053,97.364251471772));
#30405=CARTESIAN_POINT('Ctrl Pts',(-2.49834319432965,0.310504101672879,
97.3653736840554));
#30406=CARTESIAN_POINT('Ctrl Pts',(-2.50142261429291,0.284187858038864,
97.3670373345829));
#30407=CARTESIAN_POINT('Ctrl Pts',(-2.50236355938732,0.275779705033789,
97.3675708097129));
#30408=CARTESIAN_POINT('Ctrl Pts',(-2.50395522976449,0.260877467930617,
97.3685199899254));
#30409=CARTESIAN_POINT('Ctrl Pts',(-2.5046231096316,0.254385383389946,97.3689347384058));
#30410=CARTESIAN_POINT('Ctrl Pts',(-2.5060161268914,0.240307085286784,97.3698368928681));
#30411=CARTESIAN_POINT('Ctrl Pts',(-2.5067320546669,0.23272027399879,97.3703247764144));
#30412=CARTESIAN_POINT('Ctrl Pts',(-2.50862130915018,0.211678508054357,
97.3716824300492));
#30413=CARTESIAN_POINT('Ctrl Pts',(-2.50972080149989,0.198217413372497,
97.3725560894118));
#30414=CARTESIAN_POINT('Ctrl Pts',(-2.51520391391042,0.123702507622724,
97.3774182431325));
#30415=CARTESIAN_POINT('Ctrl Pts',(-2.51746761848308,0.0625181454298513,
97.381506471314));
#30416=CARTESIAN_POINT('Ctrl Pts',(-2.51756609999443,-0.125612640580314,
97.3942560028986));
#30417=CARTESIAN_POINT('Ctrl Pts',(-2.50803295207504,-0.252362804816378,
97.4030866037753));
#30418=CARTESIAN_POINT('Ctrl Pts',(-2.46462296398122,-0.538313904815139,
97.4230024390044));
#30419=CARTESIAN_POINT('Ctrl Pts',(-2.42479939024921,-0.696069878556848,
97.43396711388));
#30420=CARTESIAN_POINT('Ctrl Pts',(-2.36255428111609,-0.869849386733493,
97.4458725758867));
#30421=CARTESIAN_POINT('Ctrl Pts',(-2.3547789886642,-0.890683250745074,
97.447297645885));
#30422=CARTESIAN_POINT('Ctrl Pts',(-2.34151978796341,-0.924823405229062,
97.4496297518918));
#30423=CARTESIAN_POINT('Ctrl Pts',(-2.33619613767803,-0.938190209165906,
97.4505420374371));
#30424=CARTESIAN_POINT('Ctrl Pts',(-2.32637072677582,-0.962257885902154,
97.4521834466888));
#30425=CARTESIAN_POINT('Ctrl Pts',(-2.32190901852356,-0.972974570252401,
97.4529138842239));
#30426=CARTESIAN_POINT('Ctrl Pts',(-2.31217600757012,-0.995904257287378,
97.4544759803793));
#30427=CARTESIAN_POINT('Ctrl Pts',(-2.30688169462198,-1.00810715574672,
97.4553068381418));
#30428=CARTESIAN_POINT('Ctrl Pts',(-2.29211353583333,-1.04142074762595,
97.4575741538986));
#30429=CARTESIAN_POINT('Ctrl Pts',(-2.28244482868597,-1.06244401903929,
97.4590039806668));
#30430=CARTESIAN_POINT('Ctrl Pts',(-2.22368670639655,-1.18569999899059,
97.4673861007413));
#30431=CARTESIAN_POINT('Ctrl Pts',(-2.16802172990752,-1.28466082291107,
97.4741048865652));
#30432=CARTESIAN_POINT('Ctrl Pts',(-2.00862344146145,-1.5279820934026,97.4910267562332));
#30433=CARTESIAN_POINT('Ctrl Pts',(-1.89596563923792,-1.66571423925124,
97.5009880948812));
#30434=CARTESIAN_POINT('Ctrl Pts',(-1.72548688834964,-1.83422429670881,
97.5151821352445));
#30435=CARTESIAN_POINT('Ctrl Pts',(-1.67959545783295,-1.87633725813853,
97.5189354148818));
#30436=CARTESIAN_POINT('Ctrl Pts',(-1.62185931615923,-1.92550328180932,
97.5236461257159));
#30437=CARTESIAN_POINT('Ctrl Pts',(-1.6114532467947,-1.93422050036199,97.524494741165));
#30438=CARTESIAN_POINT('Ctrl Pts',(-1.59508430424113,-1.9477090706605,97.5258299005359));
#30439=CARTESIAN_POINT('Ctrl Pts',(-1.58916917786768,-1.95253831768638,
97.5263124320269));
#30440=CARTESIAN_POINT('Ctrl Pts',(-1.57815940811866,-1.96144378031291,
97.5272108591022));
#30441=CARTESIAN_POINT('Ctrl Pts',(-1.57307080034118,-1.96552717471724,
97.5276262361295));
#30442=CARTESIAN_POINT('Ctrl Pts',(-1.56136463829118,-1.97484630301446,
97.5285820694113));
#30443=CARTESIAN_POINT('Ctrl Pts',(-1.55473661388178,-1.98006856214416,
97.5291234435864));
#30444=CARTESIAN_POINT('Ctrl Pts',(-1.53395297274917,-1.99627542486301,
97.5308212762787));
#30445=CARTESIAN_POINT('Ctrl Pts',(-1.51970661315254,-2.00714201324545,
97.5319854075817));
#30446=CARTESIAN_POINT('Ctrl Pts',(-1.38684868636179,-2.10625573571253,
97.5428356343875));
#30447=CARTESIAN_POINT('Ctrl Pts',(-1.26080637835686,-2.18403785035919,
97.5530668564912));
#30448=CARTESIAN_POINT('Ctrl Pts',(-0.965154630837059,-2.33232762971752,
97.5759159329082));
#30449=CARTESIAN_POINT('Ctrl Pts',(-0.793143586764814,-2.39629326884446,
97.5884284569396));
#30450=CARTESIAN_POINT('Ctrl Pts',(-0.584032937634819,-2.44903611769644,
97.6024378858756));
#30451=CARTESIAN_POINT('Ctrl Pts',(-0.552219357105514,-2.45640516265882,
97.6045396653788));
#30452=CARTESIAN_POINT('Ctrl Pts',(-0.505542694743742,-2.46626426174268,
97.607581697783));
#30453=CARTESIAN_POINT('Ctrl Pts',(-0.49078737478013,-2.46924291914619,
97.6085373118365));
#30454=CARTESIAN_POINT('Ctrl Pts',(-0.464508867927245,-2.47430290094711,
97.6102287752873));
#30455=CARTESIAN_POINT('Ctrl Pts',(-0.452996317369128,-2.47643648776811,
97.6109662560458));
#30456=CARTESIAN_POINT('Ctrl Pts',(-0.42890120789017,-2.48072831406022,
97.6125025311236));
#30457=CARTESIAN_POINT('Ctrl Pts',(-0.416316248486393,-2.4828713227058,
97.6133008263237));
#30458=CARTESIAN_POINT('Ctrl Pts',(-0.383306797932391,-2.48823424366376,
97.6153842761601));
#30459=CARTESIAN_POINT('Ctrl Pts',(-0.362857724829885,-2.49129846940272,
97.6166645270829));
#30460=CARTESIAN_POINT('Ctrl Pts',(-0.267674308370134,-2.50436453327672,
97.6225781716718));
#30461=CARTESIAN_POINT('Ctrl Pts',(-0.192548483506289,-2.51125823788772,
97.6271141508825));
#30462=CARTESIAN_POINT('Ctrl Pts',(0.0329049403354752,-2.52176727470881,
97.6404646416206));
#30463=CARTESIAN_POINT('Ctrl Pts',(0.183355378832519,-2.51530830826447,
97.6490107494887));
#30464=CARTESIAN_POINT('Ctrl Pts',(0.373159109006744,-2.49003104900377,
97.6600477066965));
#30465=CARTESIAN_POINT('Ctrl Pts',(0.41384196790483,-2.4835935711914,97.6624301333511));
#30466=CARTESIAN_POINT('Ctrl Pts',(0.541589500905969,-2.46015333929717,
97.6700105540017));
#30467=CARTESIAN_POINT('Ctrl Pts',(0.627915115593771,-2.43954765955099,
97.6752791662137));
#30468=CARTESIAN_POINT('Ctrl Pts',(0.725915818944569,-2.41060881689443,
97.6816141425477));
#30469=CARTESIAN_POINT('Ctrl Pts',(0.73883693893511,-2.4066799960731,97.6824566408256));
#30470=CARTESIAN_POINT('Ctrl Pts',(0.759689854632868,-2.40015566475958,
97.683829012624));
#30471=CARTESIAN_POINT('Ctrl Pts',(0.767641641638585,-2.39762428158098,
97.6843553392976));
#30472=CARTESIAN_POINT('Ctrl Pts',(0.781780759349992,-2.3930456677565,97.6852968055591));
#30473=CARTESIAN_POINT('Ctrl Pts',(0.787972913074359,-2.39101388752923,
97.685711048318));
#30474=CARTESIAN_POINT('Ctrl Pts',(0.801467635600247,-2.38652786011651,
97.6866180953795));
#30475=CARTESIAN_POINT('Ctrl Pts',(0.80876674422791,-2.38406416601737,97.6871114238652));
#30476=CARTESIAN_POINT('Ctrl Pts',(0.829554481414299,-2.37694115740719,
97.6885239521368));
#30477=CARTESIAN_POINT('Ctrl Pts',(0.843014704381204,-2.3722006848545,97.6894476566685));
#30478=CARTESIAN_POINT('Ctrl Pts',(0.938476132205947,-2.33766565653956,
97.6960598512106));
#30479=CARTESIAN_POINT('Ctrl Pts',(1.01891205295563,-2.30374329211678,97.701951990921));
#30480=CARTESIAN_POINT('Ctrl Pts',(1.25530101938894,-2.18924675681002,97.7199373960713));
#30481=CARTESIAN_POINT('Ctrl Pts',(1.4047781191554,-2.09647082363536,97.7321929472169));
#30482=CARTESIAN_POINT('Ctrl Pts',(1.61480439854475,-1.93348986294657,97.7500969924981));
#30483=CARTESIAN_POINT('Ctrl Pts',(1.6831840653497,-1.87426544511501,97.7560645103172));
#30484=CARTESIAN_POINT('Ctrl Pts',(1.76434277940056,-1.79594037453304,97.7633239603216));
#30485=CARTESIAN_POINT('Ctrl Pts',(1.78024138223736,-1.78018199797686,97.7647553930719));
#30486=CARTESIAN_POINT('Ctrl Pts',(1.80522386420587,-1.7547504113409,97.7670203718386));
#30487=CARTESIAN_POINT('Ctrl Pts',(1.81444480277616,-1.74521410566861,97.7678598736036));
#30488=CARTESIAN_POINT('Ctrl Pts',(1.83151923951415,-1.72727409646956,97.7694211815081));
#30489=CARTESIAN_POINT('Ctrl Pts',(1.83939131515179,-1.71888863101991,97.7701437749559));
#30490=CARTESIAN_POINT('Ctrl Pts',(1.85697936031183,-1.69989436070961,97.7717646610353));
#30491=CARTESIAN_POINT('Ctrl Pts',(1.86666247374198,-1.68925557713864,97.7726615524833));
#30492=CARTESIAN_POINT('Ctrl Pts',(1.89514449671421,-1.65741856707189,97.7753137545754));
#30493=CARTESIAN_POINT('Ctrl Pts',(1.91367771442445,-1.63598492486266,97.7770580744112));
#30494=CARTESIAN_POINT('Ctrl Pts',(1.95519658948156,-1.58629717841548,97.781012928919));
#30495=CARTESIAN_POINT('Ctrl Pts',(1.97793909233074,-1.55784773918961,97.7832139894324));
#30496=CARTESIAN_POINT('Ctrl Pts',(2.05340073033681,-1.45913217464225,97.7906550455423));
#30497=CARTESIAN_POINT('Ctrl Pts',(2.10305847857833,-1.38660305518453,97.7957907029949));
#30498=CARTESIAN_POINT('Ctrl Pts',(2.21176121903907,-1.20851578406784,97.8078604249669));
#30499=CARTESIAN_POINT('Ctrl Pts',(2.26719228766116,-1.10101592713616,97.8147271602574));
#30500=CARTESIAN_POINT('Ctrl Pts',(2.35277925420826,-0.900898334255344,
97.8273884471995));
#30501=CARTESIAN_POINT('Ctrl Pts',(2.38569165680028,-0.809727726736834,
97.8331180783741));
#30502=CARTESIAN_POINT('Ctrl Pts',(2.41713426828811,-0.703883902727919,
97.8399625019929));
#30503=CARTESIAN_POINT('Ctrl Pts',(2.42089544100432,-0.690837075177546,
97.84080946823));
#30504=CARTESIAN_POINT('Ctrl Pts',(2.42680329825976,-0.669702922670512,
97.8421876990666));
#30505=CARTESIAN_POINT('Ctrl Pts',(2.42901558002388,-0.661634007846177,
97.8427153674314));
#30506=CARTESIAN_POINT('Ctrl Pts',(2.43287986613074,-0.64725906828058,97.8436582710199));
#30507=CARTESIAN_POINT('Ctrl Pts',(2.43454765282329,-0.640957462791354,
97.8440725981799));
#30508=CARTESIAN_POINT('Ctrl Pts',(2.43812898014234,-0.627210032828775,
97.844978679935));
#30509=CARTESIAN_POINT('Ctrl Pts',(2.44003286808013,-0.619762009187752,
97.8454709496951));
#30510=CARTESIAN_POINT('Ctrl Pts',(2.44535500699364,-0.598537073706251,
97.8468774756022));
#30511=CARTESIAN_POINT('Ctrl Pts',(2.44869082809743,-0.584740066337355,
97.8477961784328));
#30512=CARTESIAN_POINT('Ctrl Pts',(2.47119225778582,-0.488103299000273,
97.8542581964196));
#30513=CARTESIAN_POINT('Ctrl Pts',(2.48626500098483,-0.404375197363053,
97.8599950908284));
#30514=CARTESIAN_POINT('Ctrl Pts',(2.51843418994899,-0.153390808775393,
97.8773090953986));
#30515=CARTESIAN_POINT('Ctrl Pts',(2.52305792026864,0.0150097981747123,
97.8890468033371));
#30516=CARTESIAN_POINT('Ctrl Pts',(2.50367702977971,0.281486739478573,97.9071101364023));
#30517=CARTESIAN_POINT('Ctrl Pts',(2.49065193401831,0.379856090177702,97.9136746690665));
#30518=CARTESIAN_POINT('Ctrl Pts',(2.46751176654368,0.499717209907458,97.9215361462574));
#30519=CARTESIAN_POINT('Ctrl Pts',(2.46285971084279,0.52216253155518,97.9230025477102));
#30520=CARTESIAN_POINT('Ctrl Pts',(2.45500600072512,0.557611869986909,97.9253100364121));
#30521=CARTESIAN_POINT('Ctrl Pts',(2.45200611315563,0.570658824034685,97.9261574654601));
#30522=CARTESIAN_POINT('Ctrl Pts',(2.44621270862469,0.594965715610145,97.9277330328811));
#30523=CARTESIAN_POINT('Ctrl Pts',(2.44344516872562,0.606231418903919,97.9284619759452));
#30524=CARTESIAN_POINT('Ctrl Pts',(2.43709915709077,0.631314225543083,97.9300822381141));
#30525=CARTESIAN_POINT('Ctrl Pts',(2.43348083657293,0.645120906622737,97.9309722576839));
#30526=CARTESIAN_POINT('Ctrl Pts',(2.42247660915201,0.685700083069867,97.9335832009061));
#30527=CARTESIAN_POINT('Ctrl Pts',(2.41476474117469,0.712382526551963,97.9352936517657));
#30528=CARTESIAN_POINT('Ctrl Pts',(2.35655958860768,0.901949523238102,97.9474117363831));
#30529=CARTESIAN_POINT('Ctrl Pts',(2.29007199876082,1.05946486753853,97.9572603741884));
#30530=CARTESIAN_POINT('Ctrl Pts',(2.1295535704852,1.35262596591857,97.9764676837467));
#30531=CARTESIAN_POINT('Ctrl Pts',(2.03714445278447,1.48816101619655,97.9857982361846));
#30532=CARTESIAN_POINT('Ctrl Pts',(1.91922667862163,1.62935212838372,97.9971107436977));
#30533=CARTESIAN_POINT('Ctrl Pts',(1.9060093580292,1.64479411141045,97.9983718362741));
#30534=CARTESIAN_POINT('Ctrl Pts',(1.88717425850953,1.66626751902552,98.0001621293693));
#30535=CARTESIAN_POINT('Ctrl Pts',(1.88171123466018,1.67243443872519,98.0006806102809));
#30536=CARTESIAN_POINT('Ctrl Pts',(1.87177189059984,1.68354409123085,98.0016227541463));
#30537=CARTESIAN_POINT('Ctrl Pts',(1.86730596417978,1.68849612148886,98.0020456548498));
#30538=CARTESIAN_POINT('Ctrl Pts',(1.85811715520747,1.69860406692417,98.0029150677586));
#30539=CARTESIAN_POINT('Ctrl Pts',(1.85339239879728,1.70375812598781,98.003361713218));
#30540=CARTESIAN_POINT('Ctrl Pts',(1.84116827032712,1.71698194887245,98.0045161294051));
#30541=CARTESIAN_POINT('Ctrl Pts',(1.83363738124604,1.72502218997871,98.0052262073246));
#30542=CARTESIAN_POINT('Ctrl Pts',(1.80149276094251,1.75889258294977,98.0082513718593));
#30543=CARTESIAN_POINT('Ctrl Pts',(1.77638541763499,1.78424601136328,98.010600178534));
#30544=CARTESIAN_POINT('Ctrl Pts',(1.70600382410769,1.85235918542044,98.0171255345371));
#30545=CARTESIAN_POINT('Ctrl Pts',(1.65966977088861,1.89398491661036,98.021356958145));
#30546=CARTESIAN_POINT('Ctrl Pts',(1.45949304357544,2.06083033133244,98.0392252916538));
#30547=CARTESIAN_POINT('Ctrl Pts',(1.29264373078522,2.16938535835508,98.0530775030175));
#30548=CARTESIAN_POINT('Ctrl Pts',(1.05487407908419,2.28681219353953,98.0707212031858));
#30549=CARTESIAN_POINT('Ctrl Pts',(0.993816664272778,2.31400067528736,98.0750932092784));
#30550=CARTESIAN_POINT('Ctrl Pts',(0.912634475287457,2.34634348291541,98.0807050057469));
#30551=CARTESIAN_POINT('Ctrl Pts',(0.893430985698294,2.35372269822172,98.0820182144541));
#30552=CARTESIAN_POINT('Ctrl Pts',(0.862188682874349,2.36529053315015,98.0841322197037));
#30553=CARTESIAN_POINT('Ctrl Pts',(0.850205041001811,2.36962444894422,98.0849377954015));
#30554=CARTESIAN_POINT('Ctrl Pts',(0.82714203928663,2.37776776459769,98.0864782088236));
#30555=CARTESIAN_POINT('Ctrl Pts',(0.816068012450916,2.38159117020877,98.0872134910557));
#30556=CARTESIAN_POINT('Ctrl Pts',(0.790415201640926,2.39024809314571,98.0889068928647));
#30557=CARTESIAN_POINT('Ctrl Pts',(0.775817973468088,2.39502580910364,98.0898631673919));
#30558=CARTESIAN_POINT('Ctrl Pts',(0.729311286397423,2.4097777775398,98.0928873979151));
#30559=CARTESIAN_POINT('Ctrl Pts',(0.697245641753475,2.41925041389897,98.0949391141746));
#30560=CARTESIAN_POINT('Ctrl Pts',(0.621526012239214,2.43998839888775,98.0997129787148));
#30561=CARTESIAN_POINT('Ctrl Pts',(0.577738804714182,2.45072564443698,98.1024188331686));
#30562=CARTESIAN_POINT('Ctrl Pts',(0.412167792175033,2.48664135144035,98.1124820576477));
#30563=CARTESIAN_POINT('Ctrl Pts',(0.288858932063695,2.50396302351564,98.1196283491873));
#30564=CARTESIAN_POINT('Ctrl Pts',(0.00999197980473201,2.52225415536473,
98.1356859488692));
#30565=CARTESIAN_POINT('Ctrl Pts',(-0.145374015523826,2.51807852617538,
98.1445612025003));
#30566=CARTESIAN_POINT('Ctrl Pts',(-0.320034961545601,2.49716201287453,
98.1553717404444));
#30567=CARTESIAN_POINT('Ctrl Pts',(-0.340693341883785,2.49442748484183,
98.1566640006003));
#30568=CARTESIAN_POINT('Ctrl Pts',(-0.369554961381498,2.49024189827448,
98.1584914767358));
#30569=CARTESIAN_POINT('Ctrl Pts',(-0.37778919061541,2.48900600727672,98.1590153791614));
#30570=CARTESIAN_POINT('Ctrl Pts',(-0.392032409704921,2.48679590962537,
98.1599262092788));
#30571=CARTESIAN_POINT('Ctrl Pts',(-0.398044337151493,2.48584070490485,
98.1603120853364));
#30572=CARTESIAN_POINT('Ctrl Pts',(-0.410779453852282,2.4837699040808,98.1611326209815));
#30573=CARTESIAN_POINT('Ctrl Pts',(-0.417501659141065,2.48264879867973,
98.1615675953625));
#30574=CARTESIAN_POINT('Ctrl Pts',(-0.434271712197452,2.47978191339147,
98.1626572341668));
#30575=CARTESIAN_POINT('Ctrl Pts',(-0.444313569685101,2.47800236104002,
98.1633137434831));
#30576=CARTESIAN_POINT('Ctrl Pts',(-0.482813842093714,2.47093805198034,
98.1658455797619));
#30577=CARTESIAN_POINT('Ctrl Pts',(-0.511189933465595,2.46522387326448,
98.1677427031991));
#30578=CARTESIAN_POINT('Ctrl Pts',(-0.584482348915421,2.44914499920631,
98.1727128230025));
#30579=CARTESIAN_POINT('Ctrl Pts',(-0.629222723096888,2.43803386323016,
98.1758154574126));
#30580=CARTESIAN_POINT('Ctrl Pts',(-0.880760921333106,2.3681803775212,98.1935628479852));
#30581=CARTESIAN_POINT('Ctrl Pts',(-1.07970973780586,2.28435230278158,98.2086755042068));
#30582=CARTESIAN_POINT('Ctrl Pts',(-1.32909493024918,2.1393249064049,98.2279415870915));
#30583=CARTESIAN_POINT('Ctrl Pts',(-1.39096536804762,2.09962413853786,98.2327625031926));
#30584=CARTESIAN_POINT('Ctrl Pts',(-1.46840891681978,2.04500232739952,98.2388531113517));
#30585=CARTESIAN_POINT('Ctrl Pts',(-1.4856462269452,2.03251435416267,98.2402126481037));
#30586=CARTESIAN_POINT('Ctrl Pts',(-1.51307201845986,2.01210975986223,98.2423826259386));
#30587=CARTESIAN_POINT('Ctrl Pts',(-1.52336133202795,2.00433103077238,98.2431983202902));
#30588=CARTESIAN_POINT('Ctrl Pts',(-1.54245930445251,1.98966092816235,98.2447154926867));
#30589=CARTESIAN_POINT('Ctrl Pts',(-1.55128266346323,1.9827893028434,98.2454177155535));
#30590=CARTESIAN_POINT('Ctrl Pts',(-1.56020685970427,1.97574311081126,98.2461293512056));
#30591=CARTESIAN_POINT('Ctrl Pts',(-1.56035365021658,1.97562718427395,98.246141056998));
#30592=CARTESIAN_POINT('Ctrl Pts',(-1.56063564896794,1.97540442716535,98.2461635456943));
#30593=CARTESIAN_POINT('Ctrl Pts',(-1.56077085916982,1.97529759906207,98.2461743286966));
#30594=CARTESIAN_POINT('Ctrl Pts',(-1.56103095389672,1.97509205768155,98.2461950718576));
#30595=CARTESIAN_POINT('Ctrl Pts',(-1.56115584001412,1.97499334645215,98.2462050320954));
#30596=CARTESIAN_POINT('Ctrl Pts',(-1.5613963655788,1.97480319558456,98.2462242156443));
#30597=CARTESIAN_POINT('Ctrl Pts',(-1.56151200635576,1.97471175763465,98.2462334390217));
#30598=CARTESIAN_POINT('Ctrl Pts',(-1.56173497338694,1.97453542425206,98.2462512230814));
#30599=CARTESIAN_POINT('Ctrl Pts',(-1.56184230074504,1.97445053023103,98.2462597838186));
#30600=CARTESIAN_POINT('Ctrl Pts',(-1.57332625660252,1.96536540422798,98.2471757991006));
#30601=CARTESIAN_POINT('Ctrl Pts',(-1.58462507082855,1.9562668735716,98.2480793652999));
#30602=CARTESIAN_POINT('Ctrl Pts',(-1.60839911360544,1.93678135824142,98.2499859344445));
#30603=CARTESIAN_POINT('Ctrl Pts',(-1.62085383291634,1.92637031992174,98.2509879338353));
#30604=CARTESIAN_POINT('Ctrl Pts',(-1.65367260613589,1.89839310099913,98.2536376247734));
#30605=CARTESIAN_POINT('Ctrl Pts',(-1.67385768124324,1.88061957821771,98.2552770552511));
#30606=CARTESIAN_POINT('Ctrl Pts',(-1.73513503392139,1.82489481040161,98.2602896863143));
#30607=CARTESIAN_POINT('Ctrl Pts',(-1.77525158559537,1.78589391181513,98.2636217760274));
#30608=CARTESIAN_POINT('Ctrl Pts',(-1.88291529018487,1.674008331585,98.2727640849382));
#30609=CARTESIAN_POINT('Ctrl Pts',(-1.94749849400705,1.59841324201354,98.2784799864133));
#30610=CARTESIAN_POINT('Ctrl Pts',(-2.10473141360437,1.39064773189292,98.2934522043514));
#30611=CARTESIAN_POINT('Ctrl Pts',(-2.18942968502766,1.2530678219741,98.3026522644494));
#30612=CARTESIAN_POINT('Ctrl Pts',(-2.26939443951164,1.08998799169555,98.3138197982368));
#30613=CARTESIAN_POINT('Ctrl Pts',(-2.27817843654644,1.07150729995071,98.315089157258));
#30614=CARTESIAN_POINT('Ctrl Pts',(-2.29019145720924,1.04541743011927,98.3168893207269));
#30615=CARTESIAN_POINT('Ctrl Pts',(-2.29361002473671,1.03789573840632,98.3174092495864));
#30616=CARTESIAN_POINT('Ctrl Pts',(-2.29972322432121,1.02426749049372,98.3183532289286));
#30617=CARTESIAN_POINT('Ctrl Pts',(-2.30243074466243,1.01816671774747,98.3187765072962));
#30618=CARTESIAN_POINT('Ctrl Pts',(-2.3079211188865,1.00566153320459,98.3196456999727));
#30619=CARTESIAN_POINT('Ctrl Pts',(-2.31070163110441,0.999256213157136,
98.3200917410988));
#30620=CARTESIAN_POINT('Ctrl Pts',(-2.3177835515073,0.98275434443663,98.3212428388734));
#30621=CARTESIAN_POINT('Ctrl Pts',(-2.32204559785041,0.972641210403324,
98.3219501782195));
#30622=CARTESIAN_POINT('Ctrl Pts',(-2.33854544639524,0.932763185612064,
98.324745857215));
#30623=CARTESIAN_POINT('Ctrl Pts',(-2.35027748300159,0.902794249797349,
98.3268610144102));
#30624=CARTESIAN_POINT('Ctrl Pts',(-2.36143112099219,0.872610629553384,
98.3289997116198));
#30625=CARTESIAN_POINT('Origin',(0.,0.,104.));
#30626=CARTESIAN_POINT('',(-2.36143108732087,0.87261072067364,99.3329358985331));
#30627=CARTESIAN_POINT('',(-2.36143112101025,0.872610629504521,99.0561732563161));
#30628=CARTESIAN_POINT('',(-2.36143112101026,0.872610629504505,104.));
#30629=CARTESIAN_POINT('',(-2.51749934288707,-0.00181894562271404,98.1125833025509));
#30630=CARTESIAN_POINT('Ctrl Pts',(-2.36143112101025,0.87261062950452,99.0561732563161));
#30631=CARTESIAN_POINT('Ctrl Pts',(-2.33278640704966,0.950128043012731,
99.050962759861));
#30632=CARTESIAN_POINT('Ctrl Pts',(-2.30030652899971,1.02627179950822,99.0457522634059));
#30633=CARTESIAN_POINT('Ctrl Pts',(-2.26415467450212,1.10064065885747,99.0405417669508));
#30634=CARTESIAN_POINT('Ctrl Pts',(-2.22800672982909,1.1750014752115,99.0353318340111));
#30635=CARTESIAN_POINT('Ctrl Pts',(-2.18818780234614,1.24758735633662,99.0301219010714));
#30636=CARTESIAN_POINT('Ctrl Pts',(-2.14490811357667,1.3180195121139,99.0249119681317));
#30637=CARTESIAN_POINT('Ctrl Pts',(-2.09943389879839,1.39202297817794,99.0194378620045));
#30638=CARTESIAN_POINT('Ctrl Pts',(-2.05013895512243,1.46364803471633,99.0139637558772));
#30639=CARTESIAN_POINT('Ctrl Pts',(-1.99731898245969,1.53248919484158,99.0084896497499));
#30640=CARTESIAN_POINT('Ctrl Pts',(-1.94698099158007,1.59809554629982,99.0032727688918));
#30641=CARTESIAN_POINT('Ctrl Pts',(-1.89344213718278,1.66117339722202,98.9980558880337));
#30642=CARTESIAN_POINT('Ctrl Pts',(-1.83699876145007,1.72140692470749,98.9928390071756));
#30643=CARTESIAN_POINT('Ctrl Pts',(-1.78051668615308,1.78168175041863,98.9876185494404));
#30644=CARTESIAN_POINT('Ctrl Pts',(-1.72112646326178,1.83910804989151,98.9823980917053));
#30645=CARTESIAN_POINT('Ctrl Pts',(-1.65915940431223,1.89340865136987,98.9771776339701));
#30646=CARTESIAN_POINT('Ctrl Pts',(-1.5970964362197,1.94779329627775,98.9719490963029));
#30647=CARTESIAN_POINT('Ctrl Pts',(-1.53244904350619,1.99904230777826,98.9667205586356));
#30648=CARTESIAN_POINT('Ctrl Pts',(-1.46557888184648,2.04692080723354,98.9614920209684));
#30649=CARTESIAN_POINT('Ctrl Pts',(-1.45590439728475,2.05384766059119,98.960735578847));
#30650=CARTESIAN_POINT('Ctrl Pts',(-1.44618343088935,2.06070404354763,98.9599791367257));
#30651=CARTESIAN_POINT('Ctrl Pts',(-1.43641711982849,2.06748932472785,98.9592226946043));
#30652=CARTESIAN_POINT('Ctrl Pts',(-1.36856738097082,2.11462887960022,98.9539674451989));
#30653=CARTESIAN_POINT('Ctrl Pts',(-1.29826938246395,2.15851196666169,98.9487121957935));
#30654=CARTESIAN_POINT('Ctrl Pts',(-1.22586870214749,2.19887520680352,98.943456946388));
#30655=CARTESIAN_POINT('Ctrl Pts',(-1.15357066954887,2.23918122103992,98.9382091477325));
#30656=CARTESIAN_POINT('Ctrl Pts',(-1.07917627618452,2.27597707782582,98.9329613490769));
#30657=CARTESIAN_POINT('Ctrl Pts',(-1.00306088599235,2.30904203274697,98.9277135504213));
#30658=CARTESIAN_POINT('Ctrl Pts',(-0.926393974143907,2.34234657178713,
98.922427726938));
#30659=CARTESIAN_POINT('Ctrl Pts',(-0.847981409199212,2.37186564323599,
98.9171419034546));
#30660=CARTESIAN_POINT('Ctrl Pts',(-0.768233009155977,2.39742034145937,
98.9118560799712));
#30661=CARTESIAN_POINT('Ctrl Pts',(-0.689199707548472,2.42274589245578,
98.9066176541046));
#30662=CARTESIAN_POINT('Ctrl Pts',(-0.608854879083993,2.44417773859863,
98.901379228238));
#30663=CARTESIAN_POINT('Ctrl Pts',(-0.527616746100529,2.46159030288029,
98.8961408023714));
#30664=CARTESIAN_POINT('Ctrl Pts',(-0.446405330987264,2.47899714045929,
98.8909040993359));
#30665=CARTESIAN_POINT('Ctrl Pts',(-0.364301645661412,2.49238722486515,
98.8856673963005));
#30666=CARTESIAN_POINT('Ctrl Pts',(-0.281736172190727,2.50168562758779,
98.880430693265));
#30667=CARTESIAN_POINT('Ctrl Pts',(-0.199172947762835,2.51098377702652,
98.8751941328747));
#30668=CARTESIAN_POINT('Ctrl Pts',(-0.116148418837698,2.51619041577051,
98.8699575724844));
#30669=CARTESIAN_POINT('Ctrl Pts',(-0.033098908478487,2.51728240613912,
98.8647210120941));
#30670=CARTESIAN_POINT('Ctrl Pts',(0.0513098985704013,2.51839226944745,
98.8593987433213));
#30671=CARTESIAN_POINT('Ctrl Pts',(0.135744020678939,2.51525155817116,98.8540764745485));
#30672=CARTESIAN_POINT('Ctrl Pts',(0.21974648244285,2.50789109282161,98.8487542057757));
#30673=CARTESIAN_POINT('Ctrl Pts',(0.302514886547704,2.50063875809643,98.8435101250274));
#30674=CARTESIAN_POINT('Ctrl Pts',(0.384863773673149,2.48928995356123,98.8382660442791));
#30675=CARTESIAN_POINT('Ctrl Pts',(0.466364092043617,2.47392618799598,98.8330219635309));
#30676=CARTESIAN_POINT('Ctrl Pts',(0.549687136607523,2.45821881717267,98.8276606007458));
#30677=CARTESIAN_POINT('Ctrl Pts',(0.632122700779561,2.43831485202597,98.8222992379607));
#30678=CARTESIAN_POINT('Ctrl Pts',(0.713228296358643,2.41435532746805,98.8169378751756));
#30679=CARTESIAN_POINT('Ctrl Pts',(0.794333891937714,2.39039580291013,98.8115765123905));
#30680=CARTESIAN_POINT('Ctrl Pts',(0.874109061651032,2.36238095031963,98.8062151496054));
#30681=CARTESIAN_POINT('Ctrl Pts',(0.952134552090648,2.3305033886942,98.8008537868203));
#30682=CARTESIAN_POINT('Ctrl Pts',(1.0286157435233,2.29925675532677,98.7955985373986));
#30683=CARTESIAN_POINT('Ctrl Pts',(1.10369839365188,2.26418355164877,98.790343287977));
#30684=CARTESIAN_POINT('Ctrl Pts',(1.17697343171605,2.22543024852152,98.7850880385553));
#30685=CARTESIAN_POINT('Ctrl Pts',(1.25014458242303,2.18673188877404,98.7798402398835));
#30686=CARTESIAN_POINT('Ctrl Pts',(1.32151280701535,2.14436400706664,98.7745924412116));
#30687=CARTESIAN_POINT('Ctrl Pts',(1.39068857929799,2.09852127113598,98.7693446425397));
#30688=CARTESIAN_POINT('Ctrl Pts',(1.46036558944912,2.05234636522027,98.7640588190604));
#30689=CARTESIAN_POINT('Ctrl Pts',(1.52781780214095,2.00264621522567,98.7587729955811));
#30690=CARTESIAN_POINT('Ctrl Pts',(1.59267202666219,1.94966716787449,98.7534871721018));
#30691=CARTESIAN_POINT('Ctrl Pts',(1.65694470804885,1.89716317980421,98.7482487462188));
#30692=CARTESIAN_POINT('Ctrl Pts',(1.7186654426701,1.84143915942296,98.7430103203358));
#30693=CARTESIAN_POINT('Ctrl Pts',(1.77750119569472,1.7827775378055,98.7377718944529));
#30694=CARTESIAN_POINT('Ctrl Pts',(1.83631759861892,1.72413520901953,98.732535191401));
#30695=CARTESIAN_POINT('Ctrl Pts',(1.89225057786082,1.66255752331376,98.7272984883492));
#30696=CARTESIAN_POINT('Ctrl Pts',(1.94500290732925,1.59836477078317,98.7220617852973));
#30697=CARTESIAN_POINT('Ctrl Pts',(1.99775379985013,1.53417376683165,98.7168252248907));
#30698=CARTESIAN_POINT('Ctrl Pts',(2.04732392269868,1.46736819483014,98.7115886644841));
#30699=CARTESIAN_POINT('Ctrl Pts',(2.09345631139287,1.39830144185341,98.7063521040775));
#30700=CARTESIAN_POINT('Ctrl Pts',(2.14034376265922,1.32810425272046,98.701029835324));
#30701=CARTESIAN_POINT('Ctrl Pts',(2.18367964760589,1.25557159756422,98.6957075665706));
#30702=CARTESIAN_POINT('Ctrl Pts',(2.22324101727091,1.18110356409767,98.6903852978171));
#30703=CARTESIAN_POINT('Ctrl Pts',(2.26222120171519,1.10772952006664,98.6851412170528));
#30704=CARTESIAN_POINT('Ctrl Pts',(2.29753689219085,1.03247703424813,98.6798971362884));
#30705=CARTESIAN_POINT('Ctrl Pts',(2.32902285972319,0.955750369545749,98.6746530555241));
#30706=CARTESIAN_POINT('Ctrl Pts',(2.36121299961584,0.877307740532357,98.6692916927761));
#30707=CARTESIAN_POINT('Ctrl Pts',(2.38939987853756,0.7973246809162,98.6639303300281));
#30708=CARTESIAN_POINT('Ctrl Pts',(2.41346088209449,0.716249133053366,98.6585689672801));
#30709=CARTESIAN_POINT('Ctrl Pts',(2.43752188565141,0.635173585190543,98.6532076045321));
#30710=CARTESIAN_POINT('Ctrl Pts',(2.45745695895928,0.553006058612372,98.6478462417841));
#30711=CARTESIAN_POINT('Ctrl Pts',(2.47319940617432,0.470203091545531,98.6424848790361));
#30712=CARTESIAN_POINT('Ctrl Pts',(2.48863027513713,0.389038980458705,98.6372296296523));
#30713=CARTESIAN_POINT('Ctrl Pts',(2.50009000850579,0.306964572849086,98.6319743802685));
#30714=CARTESIAN_POINT('Ctrl Pts',(2.50747874569295,0.224402740397944,98.6267191308847));
#30715=CARTESIAN_POINT('Ctrl Pts',(2.51485700732933,0.141957961869083,98.6214713322506));
#30716=CARTESIAN_POINT('Ctrl Pts',(2.5181756963732,0.0590275868908074,98.6162235336166));
#30717=CARTESIAN_POINT('Ctrl Pts',(2.51738602047343,-0.023955665821825,
98.6109757349825));
#30718=CARTESIAN_POINT('Ctrl Pts',(2.51659062268654,-0.107540204206683,
98.6056899114938));
#30719=CARTESIAN_POINT('Ctrl Pts',(2.51162698289234,-0.191177924300599,
98.600404088005));
#30720=CARTESIAN_POINT('Ctrl Pts',(2.50249855055409,-0.274421672749577,
98.5951182645162));
#30721=CARTESIAN_POINT('Ctrl Pts',(2.49345197228857,-0.356918979795724,
98.5898798386708));
#30722=CARTESIAN_POINT('Ctrl Pts',(2.48031504441379,-0.439028885213252,
98.5846414128253));
#30723=CARTESIAN_POINT('Ctrl Pts',(2.46314334660122,-0.520318271920331,
98.5794029869799));
#30724=CARTESIAN_POINT('Ctrl Pts',(2.44597729627376,-0.601580923903414,
98.5741662839654));
#30725=CARTESIAN_POINT('Ctrl Pts',(2.42477920673235,-0.682023142020918,
98.5689295809509));
#30726=CARTESIAN_POINT('Ctrl Pts',(2.39965590962701,-0.76122123288318,98.5636928779364));
#30727=CARTESIAN_POINT('Ctrl Pts',(2.37453329686682,-0.840417166431858,
98.5584563175669));
#30728=CARTESIAN_POINT('Ctrl Pts',(2.34548582963169,-0.91836860059621,98.5532197571974));
#30729=CARTESIAN_POINT('Ctrl Pts',(2.31267002155887,-0.994667593411446,
98.5479831968278));
#30730=CARTESIAN_POINT('Ctrl Pts',(2.2793171068472,-1.07221539580916,98.5426609280298));
#30731=CARTESIAN_POINT('Ctrl Pts',(2.24207156535357,-1.14805571987408,98.5373386592318));
#30732=CARTESIAN_POINT('Ctrl Pts',(2.20114760266341,-1.22178372934375,98.5320163904338));
#30733=CARTESIAN_POINT('Ctrl Pts',(2.16082484328938,-1.29442861975869,98.5267723097056));
#30734=CARTESIAN_POINT('Ctrl Pts',(2.11693132202151,-1.36502248149198,98.5215282289774));
#30735=CARTESIAN_POINT('Ctrl Pts',(2.06971617229043,-1.43320662019105,98.5162841482492));
#30736=CARTESIAN_POINT('Ctrl Pts',(2.02144507158909,-1.50291567425786,98.5109227854163));
#30737=CARTESIAN_POINT('Ctrl Pts',(1.96970228778801,-1.57010551367019,98.5055614225834));
#30738=CARTESIAN_POINT('Ctrl Pts',(1.91479679390173,-1.63442940748863,98.5002000597505));
#30739=CARTESIAN_POINT('Ctrl Pts',(1.85989130001545,-1.69875330130708,98.4948386969176));
#30740=CARTESIAN_POINT('Ctrl Pts',(1.80182349355314,-1.76021092607999,98.4894773340847));
#30741=CARTESIAN_POINT('Ctrl Pts',(1.74094000262391,-1.8184977748856,98.4841159712518));
#30742=CARTESIAN_POINT('Ctrl Pts',(1.6812615329398,-1.87563099583494,98.47886072185));
#30743=CARTESIAN_POINT('Ctrl Pts',(1.6186574225678,-1.92992887123232,98.4736054724482));
#30744=CARTESIAN_POINT('Ctrl Pts',(1.55342800376033,-1.98107740563896,98.4683502230463));
#30745=CARTESIAN_POINT('Ctrl Pts',(1.48829106545379,-2.03215342304069,98.4631024243945));
#30746=CARTESIAN_POINT('Ctrl Pts',(1.42053657194417,-2.08008868599946,98.4578546257428));
#30747=CARTESIAN_POINT('Ctrl Pts',(1.35050091928083,-2.12460667348609,98.452606827091));
#30748=CARTESIAN_POINT('Ctrl Pts',(1.27995779784039,-2.16944723223193,98.4473210036067));
#30749=CARTESIAN_POINT('Ctrl Pts',(1.2071006621332,-2.21082045661513,98.4420351801224));
#30750=CARTESIAN_POINT('Ctrl Pts',(1.13230645900514,-2.2484857866785,98.4367493566381));
#30751=CARTESIAN_POINT('Ctrl Pts',(1.05818293044283,-2.28581337427217,98.4315109307758));
#30752=CARTESIAN_POINT('Ctrl Pts',(0.982157354137152,-2.3194990867312,98.4262725049135));
#30753=CARTESIAN_POINT('Ctrl Pts',(0.904623285795088,-2.34935373258207,
98.4210340790513));
#30754=CARTESIAN_POINT('Ctrl Pts',(0.827114717120905,-2.37919855973556,
98.4157973760203));
#30755=CARTESIAN_POINT('Ctrl Pts',(0.748099071990192,-2.40521465698546,
98.4105606729893));
#30756=CARTESIAN_POINT('Ctrl Pts',(0.667989905809573,-2.42726095336627,
98.4053239699583));
#30757=CARTESIAN_POINT('Ctrl Pts',(0.587882921765202,-2.44930664921626,
98.4000874095727));
#30758=CARTESIAN_POINT('Ctrl Pts',(0.506682921049927,-2.46738263775978,
98.3948508491871));
#30759=CARTESIAN_POINT('Ctrl Pts',(0.42481729633244,-2.48139809678673,98.3896142888014));
#30760=CARTESIAN_POINT('Ctrl Pts',(0.341611751791082,-2.49564295113626,
98.3842920200236));
#30761=CARTESIAN_POINT('Ctrl Pts',(0.257719080177702,-2.50569306096329,
98.3789697512458));
#30762=CARTESIAN_POINT('Ctrl Pts',(0.173595479584124,-2.51150768652377,
98.373647482468));
#30763=CARTESIAN_POINT('Ctrl Pts',(0.0907077164253666,-2.51723689096714,
98.3684034017248));
#30764=CARTESIAN_POINT('Ctrl Pts',(0.00759623340742896,-2.51885428209207,
98.3631593209815));
#30765=CARTESIAN_POINT('Ctrl Pts',(-0.075302458326526,-2.51637353939553,
98.3579152402383));
#30766=CARTESIAN_POINT('Ctrl Pts',(-0.160055150626523,-2.51383731574667,
98.3525538774432));
#30767=CARTESIAN_POINT('Ctrl Pts',(-0.244584908401927,-2.50701748080513,
98.3471925146481));
#30768=CARTESIAN_POINT('Ctrl Pts',(-0.328432675586283,-2.49598442054578,
98.341831151853));
#30769=CARTESIAN_POINT('Ctrl Pts',(-0.412280442770639,-2.48495136028642,
98.3364697890579));
#30770=CARTESIAN_POINT('Ctrl Pts',(-0.495445731630717,-2.4697052320331,
98.3311084262627));
#30771=CARTESIAN_POINT('Ctrl Pts',(-0.57748440190406,-2.45037099549385,
98.3257470634676));
#30772=CARTESIAN_POINT('Ctrl Pts',(-0.657899344579412,-2.43141942646188,
98.3204918139567));
#30773=CARTESIAN_POINT('Ctrl Pts',(-0.737528890838629,-2.40847014411869,
98.3152365644458));
#30774=CARTESIAN_POINT('Ctrl Pts',(-0.81594614735313,-2.38160410954877,
98.3099813149348));
#30775=CARTESIAN_POINT('Ctrl Pts',(-0.894252226019699,-2.35477616491005,
98.3047335161734));
#30776=CARTESIAN_POINT('Ctrl Pts',(-0.97134899601205,-2.32404264635472,
98.2994857174119));
#30777=CARTESIAN_POINT('Ctrl Pts',(-1.04682136225834,-2.28953516800236,
98.2942379186504));
#30778=CARTESIAN_POINT('Ctrl Pts',(-1.12284058898346,-2.25477765407972,
98.2889520951935));
#30779=CARTESIAN_POINT('Ctrl Pts',(-1.19721131105349,-2.21619136730165,
98.2836662717365));
#30780=CARTESIAN_POINT('Ctrl Pts',(-1.2695265193546,-2.1739615145295,98.2783804482796));
#30781=CARTESIAN_POINT('Ctrl Pts',(-1.34119328395092,-2.13211033289482,
98.2731420223069));
#30782=CARTESIAN_POINT('Ctrl Pts',(-1.41084084453737,-2.0866809035605,98.2679035963341));
#30783=CARTESIAN_POINT('Ctrl Pts',(-1.47809623673638,-2.03790033243673,
98.2626651703614));
#30784=CARTESIAN_POINT('Ctrl Pts',(-1.54532950975434,-1.98913580443232,
98.25742846722));
#30785=CARTESIAN_POINT('Ctrl Pts',(-1.61017180367999,-1.93702259423835,
98.2521917640785));
#30786=CARTESIAN_POINT('Ctrl Pts',(-1.67227962837945,-1.88183078264415,
98.2469550609371));
#30787=CARTESIAN_POINT('Ctrl Pts',(-1.73438576128929,-1.82664047445043,
98.2417185004411));
#30788=CARTESIAN_POINT('Ctrl Pts',(-1.79375722884276,-1.76837203886615,
98.2364819399451));
#30789=CARTESIAN_POINT('Ctrl Pts',(-1.85008515545565,-1.70733452128241,
98.2312453794491));
#30790=CARTESIAN_POINT('Ctrl Pts',(-1.90733501593176,-1.64529798673193,
98.225923110802));
#30791=CARTESIAN_POINT('Ctrl Pts',(-1.96144046461852,-1.58040126026179,
98.2206008421549));
#30792=CARTESIAN_POINT('Ctrl Pts',(-2.01211895159742,-1.51300481645714,
98.2152785735077));
#30793=CARTESIAN_POINT('Ctrl Pts',(-2.06205293667055,-1.44659847286751,
98.2100344926556));
#30794=CARTESIAN_POINT('Ctrl Pts',(-2.10865976894878,-1.37776579151508,
98.2047904118035));
#30795=CARTESIAN_POINT('Ctrl Pts',(-2.15171326350379,-1.30688036241344,
98.1995463309513));
#30796=CARTESIAN_POINT('Ctrl Pts',(-2.1957296316017,-1.23440961010017,98.1941849684067));
#30797=CARTESIAN_POINT('Ctrl Pts',(-2.23603156289674,-1.15979363489705,
98.1888236058621));
#30798=CARTESIAN_POINT('Ctrl Pts',(-2.27242816283364,-1.08345581117115,
98.1834622433175));
#30799=CARTESIAN_POINT('Ctrl Pts',(-2.30882476277054,-1.00711798744524,
98.1781008807728));
#30800=CARTESIAN_POINT('Ctrl Pts',(-2.34131589776423,-0.929058809958435,
98.1727395182282));
#30801=CARTESIAN_POINT('Ctrl Pts',(-2.36976457020348,-0.849718854567983,
98.1673781556836));
#30802=CARTESIAN_POINT('Ctrl Pts',(-2.40208841952505,-0.759571492904689,
98.1612864874196));
#30803=CARTESIAN_POINT('Ctrl Pts',(-2.42929323988043,-0.667497660029118,
98.1551948191556));
#30804=CARTESIAN_POINT('Ctrl Pts',(-2.45117917966575,-0.574044318126351,
98.1491031508916));
#30805=CARTESIAN_POINT('Ctrl Pts',(-2.47304705906853,-0.48066809436979,
98.1430165095015));
#30806=CARTESIAN_POINT('Ctrl Pts',(-2.48960468697981,-0.385914765713439,
98.1369298681114));
#30807=CARTESIAN_POINT('Ctrl Pts',(-2.50070035454831,-0.290351488306736,
98.1308432267212));
#30808=CARTESIAN_POINT('Ctrl Pts',(-2.51179602211682,-0.194788210900033,
98.1247565853311));
#30809=CARTESIAN_POINT('Ctrl Pts',(-2.51742955013952,-0.0984151241393797,
98.118669943941));
#30810=CARTESIAN_POINT('Ctrl Pts',(-2.51749934288707,-0.00181894562268696,
98.1125833025509));
#30811=CARTESIAN_POINT('Ctrl Pts',(-2.51749934288774,-0.00181894468837515,
98.112583302492));
#30812=CARTESIAN_POINT('Ctrl Pts',(-2.51755948791397,0.0814244133741985,
98.107338038379));
#30813=CARTESIAN_POINT('Ctrl Pts',(-2.51348653839861,0.164706576949697,
98.102092774266));
#30814=CARTESIAN_POINT('Ctrl Pts',(-2.50529558036044,0.247588984057089,
98.096847510153));
#30815=CARTESIAN_POINT('Ctrl Pts',(-2.49710604242185,0.330457021505943,
98.0916031554326));
#30816=CARTESIAN_POINT('Ctrl Pts',(-2.48479996557399,0.412924984202785,
98.0863588007123));
#30817=CARTESIAN_POINT('Ctrl Pts',(-2.4684443260827,0.494559257349544,98.081114445992));
#30818=CARTESIAN_POINT('Ctrl Pts',(-2.45208034729026,0.576235153618919,
98.0758674173161));
#30819=CARTESIAN_POINT('Ctrl Pts',(-2.43166277620762,0.657076061900327,
98.0706203886402));
#30820=CARTESIAN_POINT('Ctrl Pts',(-2.40730958369761,0.736659228027211,
98.0653733599643));
#30821=CARTESIAN_POINT('Ctrl Pts',(-2.39330701863621,0.782417847190807,
98.0623564306486));
#30822=CARTESIAN_POINT('Ctrl Pts',(-2.37800426835301,0.827760905486719,
98.0593395013329));
#30823=CARTESIAN_POINT('Ctrl Pts',(-2.36143112101026,0.872610629504505,
98.0563225720173));
#30824=CARTESIAN_POINT('',(-2.51749969980483,0.00122942367908718,98.3894800759037));
#30825=CARTESIAN_POINT('Ctrl Pts',(-2.36143112099219,0.872610629553384,
98.3289997116198));
#30826=CARTESIAN_POINT('Ctrl Pts',(-2.36251252634525,0.86968416479508,98.3292070698479));
#30827=CARTESIAN_POINT('Ctrl Pts',(-2.36358849455286,0.866755681947571,
98.3294146496157));
#30828=CARTESIAN_POINT('Ctrl Pts',(-2.38569176180474,0.806249585917351,
98.3337050233089));
#30829=CARTESIAN_POINT('Ctrl Pts',(-2.4046133940344,0.747928505123625,98.3378683249366));
#30830=CARTESIAN_POINT('Ctrl Pts',(-2.48503075249899,0.465305249999661,
98.3580083728554));
#30831=CARTESIAN_POINT('Ctrl Pts',(-2.51738610202588,0.233844411718779,
98.3742563990415));
#30832=CARTESIAN_POINT('Ctrl Pts',(-2.51749969980483,0.00122942367908718,
98.3894800759037));
#30833=CARTESIAN_POINT('Ctrl Pts',(-2.51749970102175,0.00122692926385033,
98.3894802391527));
#30834=CARTESIAN_POINT('Ctrl Pts',(-2.51751699362345,-0.0342552463685801,
98.3918023979318));
#30835=CARTESIAN_POINT('Ctrl Pts',(-2.51678414767873,-0.0697355527763528,
98.3941023709484));
#30836=CARTESIAN_POINT('Ctrl Pts',(-2.51468428064402,-0.119947354296721,
98.3973271767744));
#30837=CARTESIAN_POINT('Ctrl Pts',(-2.51393727670791,-0.134698860759586,
98.3982709040074));
#30838=CARTESIAN_POINT('Ctrl Pts',(-2.51238467930962,-0.160807584097307,
98.3999348979899));
#30839=CARTESIAN_POINT('Ctrl Pts',(-2.51163178999321,-0.172167402147022,
98.4006567785607));
#30840=CARTESIAN_POINT('Ctrl Pts',(-2.50998576638091,-0.194687001615117,
98.4020837535092));
#30841=CARTESIAN_POINT('Ctrl Pts',(-2.50909519904191,-0.205846701982753,
98.4027889107625));
#30842=CARTESIAN_POINT('Ctrl Pts',(-2.50703690369869,-0.229636872795596,
98.4042880715654));
#30843=CARTESIAN_POINT('Ctrl Pts',(-2.50584809806961,-0.242265244382523,
98.4050813985938));
#30844=CARTESIAN_POINT('Ctrl Pts',(-2.5025086037242,-0.27508004554831,98.4071367631431));
#30845=CARTESIAN_POINT('Ctrl Pts',(-2.50020907757556,-0.295250654440163,
98.4083941422339));
#30846=CARTESIAN_POINT('Ctrl Pts',(-2.48960195094086,-0.37925114101235,
98.4136078207328));
#30847=CARTESIAN_POINT('Ctrl Pts',(-2.47909158077049,-0.44278128912095,
98.4174954056116));
#30848=CARTESIAN_POINT('Ctrl Pts',(-2.42391125053333,-0.711804189701246,
98.4338297233657));
#30849=CARTESIAN_POINT('Ctrl Pts',(-2.35603586036114,-0.911647589929297,
98.4455667959131));
#30850=CARTESIAN_POINT('Ctrl Pts',(-2.23948847655878,-1.15137727999021,
98.4611714800706));
#30851=CARTESIAN_POINT('Ctrl Pts',(-2.21317205832378,-1.20118563047322,
98.4645102083124));
#30852=CARTESIAN_POINT('Ctrl Pts',(-2.17405848863169,-1.26955907691938,
98.4692874520271));
#30853=CARTESIAN_POINT('Ctrl Pts',(-2.162647579165,-1.28890105826086,98.4706613819721));
#30854=CARTESIAN_POINT('Ctrl Pts',(-2.14220510259818,-1.32251606415087,
98.4730935572093));
#30855=CARTESIAN_POINT('Ctrl Pts',(-2.13328564759608,-1.33685592028066,
98.4741455453322));
#30856=CARTESIAN_POINT('Ctrl Pts',(-2.11980100133727,-1.35805664463297,
98.4757241647799));
#30857=CARTESIAN_POINT('Ctrl Pts',(-2.11534508855464,-1.36498691828661,
98.4762439509061));
#30858=CARTESIAN_POINT('Ctrl Pts',(-2.10764829526881,-1.3768295272819,98.4771388537794));
#30859=CARTESIAN_POINT('Ctrl Pts',(-2.10442409021737,-1.38175255789982,
98.4775128710844));
#30860=CARTESIAN_POINT('Ctrl Pts',(-2.09703725211919,-1.3929456746197,98.4783678683661));
#30861=CARTESIAN_POINT('Ctrl Pts',(-2.09286382753363,-1.39920830654091,
98.4788495506993));
#30862=CARTESIAN_POINT('Ctrl Pts',(-2.0813546906116,-1.41631220020541,98.4801739478363));
#30863=CARTESIAN_POINT('Ctrl Pts',(-2.07396252345917,-1.42711493246564,
98.4810202591172));
#30864=CARTESIAN_POINT('Ctrl Pts',(-2.0351665779363,-1.48287233928722,98.4854376591868));
#30865=CARTESIAN_POINT('Ctrl Pts',(-2.00238659106204,-1.52684653211508,
98.4890887172663));
#30866=CARTESIAN_POINT('Ctrl Pts',(-1.95146611126933,-1.59069372807524,
98.4946041354914));
#30867=CARTESIAN_POINT('Ctrl Pts',(-1.93439815217987,-1.61140629071393,
98.4964288023875));
#30868=CARTESIAN_POINT('Ctrl Pts',(-1.82945276958812,-1.73469068796356,
98.5074885870588));
#30869=CARTESIAN_POINT('Ctrl Pts',(-1.73376798993656,-1.83032752193577,
98.5169002565777));
#30870=CARTESIAN_POINT('Ctrl Pts',(-1.56194742099078,-1.97643930116815,
98.532338102714));
#30871=CARTESIAN_POINT('Ctrl Pts',(-1.48990865438214,-2.03129687856708,
98.5384488730024));
#30872=CARTESIAN_POINT('Ctrl Pts',(-1.38436608735715,-2.10302510487333,
98.5468759228934));
#30873=CARTESIAN_POINT('Ctrl Pts',(-1.35320715832976,-2.12320858021311,
98.5493039478005));
#30874=CARTESIAN_POINT('Ctrl Pts',(-1.30438961140577,-2.15331916827592,
98.5530173911187));
#30875=CARTESIAN_POINT('Ctrl Pts',(-1.28703947715253,-2.16373406914773,
98.5543200160027));
#30876=CARTESIAN_POINT('Ctrl Pts',(-1.25790319702832,-2.18074945458449,
98.5564794816089));
#30877=CARTESIAN_POINT('Ctrl Pts',(-1.24618636264018,-2.18746615926823,
98.5573404502793));
#30878=CARTESIAN_POINT('Ctrl Pts',(-1.22326125242602,-2.2003640534734,98.5590107797653));
#30879=CARTESIAN_POINT('Ctrl Pts',(-1.21205878877034,-2.20655468137506,
98.5598204589114));
#30880=CARTESIAN_POINT('Ctrl Pts',(-1.19109946262436,-2.21792929830086,
98.561323388808));
#30881=CARTESIAN_POINT('Ctrl Pts',(-1.18135479006627,-2.22313498653789,
98.562017393489));
#30882=CARTESIAN_POINT('Ctrl Pts',(-1.15884198390379,-2.23497169761749,
98.5636099864298));
#30883=CARTESIAN_POINT('Ctrl Pts',(-1.14605056677791,-2.24155779420834,
98.5645069851632));
#30884=CARTESIAN_POINT('Ctrl Pts',(-1.11334886549381,-2.25804227448824,
98.5667806794855));
#30885=CARTESIAN_POINT('Ctrl Pts',(-1.09336236924063,-2.2677873329584,98.5681520697682));
#30886=CARTESIAN_POINT('Ctrl Pts',(-0.927130462668619,-2.34613047095334,
98.5794152305849));
#30887=CARTESIAN_POINT('Ctrl Pts',(-0.774716962842792,-2.40077531994733,
98.5888014870537));
#30888=CARTESIAN_POINT('Ctrl Pts',(-0.498314926994687,-2.47078073313339,
98.6052044919033));
#30889=CARTESIAN_POINT('Ctrl Pts',(-0.376465446982886,-2.49225711870617,
98.6122472279382));
#30890=CARTESIAN_POINT('Ctrl Pts',(-0.209544896812296,-2.50915375730239,
98.6221647301031));
#30891=CARTESIAN_POINT('Ctrl Pts',(-0.165442618148325,-2.51244700340151,
98.6248111354426));
#30892=CARTESIAN_POINT('Ctrl Pts',(-0.0932156440727912,-2.51593054004382,
98.6292202654478));
#30893=CARTESIAN_POINT('Ctrl Pts',(-0.0651328580131158,-2.5168140966657,
98.6309531204751));
#30894=CARTESIAN_POINT('Ctrl Pts',(-0.026960124412928,-2.51737583188876,
98.6333408143243));
#30895=CARTESIAN_POINT('Ctrl Pts',(-0.0168771009210558,-2.51746362091817,
98.6339745602995));
#30896=CARTESIAN_POINT('Ctrl Pts',(-2.87216088621246E-6,-2.51750915987809,
98.635040669953));
#30897=CARTESIAN_POINT('Ctrl Pts',(0.00678825361368961,-2.51750000750709,
98.6354712274952));
#30898=CARTESIAN_POINT('Ctrl Pts',(0.0196863967509814,-2.5174304349512,
98.6362919498681));
#30899=CARTESIAN_POINT('Ctrl Pts',(0.0257933834337942,-2.51737526969945,
98.6366818083085));
#30900=CARTESIAN_POINT('Ctrl Pts',(0.0419340648825511,-2.51717072965315,
98.637715433853));
#30901=CARTESIAN_POINT('Ctrl Pts',(0.0519670494144753,-2.51698358471215,
98.6383612360471));
#30902=CARTESIAN_POINT('Ctrl Pts',(0.0876723555727046,-2.51610400377987,
98.6406706409705));
#30903=CARTESIAN_POINT('Ctrl Pts',(0.113333938011973,-2.51507874590665,
98.6423508974433));
#30904=CARTESIAN_POINT('Ctrl Pts',(0.310297827850211,-2.50418909695351,
98.6553826259731));
#30905=CARTESIAN_POINT('Ctrl Pts',(0.480193025962468,-2.47722750799108,
98.6673744499423));
#30906=CARTESIAN_POINT('Ctrl Pts',(0.796505995138727,-2.39324641363297,
98.6899025226779));
#30907=CARTESIAN_POINT('Ctrl Pts',(0.942987044736867,-2.33941031592157,
98.7004236803611));
#30908=CARTESIAN_POINT('Ctrl Pts',(1.1083308856421,-2.26056655500363,98.7122689446717));
#30909=CARTESIAN_POINT('Ctrl Pts',(1.13289370070507,-2.24835728070326,98.7140287624617));
#30910=CARTESIAN_POINT('Ctrl Pts',(1.16986600128615,-2.22921993154496,98.716678807802));
#30911=CARTESIAN_POINT('Ctrl Pts',(1.18242382800012,-2.22258450201499,98.7175791186557));
#30912=CARTESIAN_POINT('Ctrl Pts',(1.20513188855768,-2.21033885569095,98.7192077433897));
#30913=CARTESIAN_POINT('Ctrl Pts',(1.21530071682184,-2.20476413721329,98.7199372787107));
#30914=CARTESIAN_POINT('Ctrl Pts',(1.23717239769552,-2.19257642566458,98.7215070698305));
#30915=CARTESIAN_POINT('Ctrl Pts',(1.24886158098583,-2.18593954323024,98.7223464504472));
#30916=CARTESIAN_POINT('Ctrl Pts',(1.28054623452729,-2.16761252027556,98.7246232107151));
#30917=CARTESIAN_POINT('Ctrl Pts',(1.30043473743483,-2.15573937326398,98.7260540112355));
#30918=CARTESIAN_POINT('Ctrl Pts',(1.40829909415721,-2.0893098388904,98.7338280696146));
#30919=CARTESIAN_POINT('Ctrl Pts',(1.49301494487951,-2.02963838208085,98.7399803227214));
#30920=CARTESIAN_POINT('Ctrl Pts',(1.70345095965785,-1.86108686495952,98.7557145617346));
#30921=CARTESIAN_POINT('Ctrl Pts',(1.82247939099285,-1.74469330797658,98.7650668714782));
#30922=CARTESIAN_POINT('Ctrl Pts',(1.96492130134873,-1.57479712484879,98.7780521717106));
#30923=CARTESIAN_POINT('Ctrl Pts',(1.99924124099459,-1.53099163609463,98.7813520089986));
#30924=CARTESIAN_POINT('Ctrl Pts',(2.04522878744721,-1.46810818330624,98.7860780605237));
#30925=CARTESIAN_POINT('Ctrl Pts',(2.05813818263662,-1.44995502741673,98.7874411795667));
#30926=CARTESIAN_POINT('Ctrl Pts',(2.08034765104763,-1.41782986132642,98.7898559206268));
#30927=CARTESIAN_POINT('Ctrl Pts',(2.08975221065323,-1.40393145412892,98.7909014088085));
#30928=CARTESIAN_POINT('Ctrl Pts',(2.10355427283277,-1.38308828804054,98.7924721369203));
#30929=CARTESIAN_POINT('Ctrl Pts',(2.10805806111619,-1.37621400869465,98.7929906310838));
#30930=CARTESIAN_POINT('Ctrl Pts',(2.11572780997627,-1.36438143183146,98.793884104961));
#30931=CARTESIAN_POINT('Ctrl Pts',(2.11891016971707,-1.35943390757987,98.7942579955972));
#30932=CARTESIAN_POINT('Ctrl Pts',(2.12613225931577,-1.3481189588307,98.795113823292));
#30933=CARTESIAN_POINT('Ctrl Pts',(2.13016066271556,-1.34174463246024,98.7955964709219));
#30934=CARTESIAN_POINT('Ctrl Pts',(2.14113780895645,-1.32420095658078,98.7969260292657));
#30935=CARTESIAN_POINT('Ctrl Pts',(2.14802762637555,-1.31299527380286,98.7977765812414));
#30936=CARTESIAN_POINT('Ctrl Pts',(2.18366325818061,-1.25400583669762,98.8022589023628));
#30937=CARTESIAN_POINT('Ctrl Pts',(2.21090124289708,-1.20533419886879,98.8059733849085));
#30938=CARTESIAN_POINT('Ctrl Pts',(2.33440870036381,-0.966345106520117,
98.8241512694426));
#30939=CARTESIAN_POINT('Ctrl Pts',(2.40785316135883,-0.765209203929734,
98.8391750234135));
#30940=CARTESIAN_POINT('Ctrl Pts',(2.46790762697627,-0.500605938009424,
98.8574141232757));
#30941=CARTESIAN_POINT('Ctrl Pts',(2.47879254550975,-0.443579430810109,
98.8612661773974));
#30942=CARTESIAN_POINT('Ctrl Pts',(2.49390609296479,-0.346231944753901,
98.8677051805415));
#30943=CARTESIAN_POINT('Ctrl Pts',(2.4991500068134,-0.306094288218767,98.8703212997873));
#30944=CARTESIAN_POINT('Ctrl Pts',(2.50517238454175,-0.249382565083663,
98.8739652399694));
#30945=CARTESIAN_POINT('Ctrl Pts',(2.50675824026645,-0.232902310541583,
98.8750179675019));
#30946=CARTESIAN_POINT('Ctrl Pts',(2.50920534040131,-0.204540182300264,
98.8768193674926));
#30947=CARTESIAN_POINT('Ctrl Pts',(2.51014502032862,-0.192665802059044,
98.8775704576663));
#30948=CARTESIAN_POINT('Ctrl Pts',(2.51178056805739,-0.169948982264116,
98.8790015967649));
#30949=CARTESIAN_POINT('Ctrl Pts',(2.51249059156029,-0.159107862402842,
98.8796820696292));
#30950=CARTESIAN_POINT('Ctrl Pts',(2.51399123933149,-0.133671036346462,
98.881272975351));
#30951=CARTESIAN_POINT('Ctrl Pts',(2.5147249762436,-0.119072269529612,98.8821816282468));
#30952=CARTESIAN_POINT('Ctrl Pts',(2.51651852755542,-0.0758878556344527,
98.8848570935973));
#30953=CARTESIAN_POINT('Ctrl Pts',(2.51721836844828,-0.0472890303797434,
98.8866128267951));
#30954=CARTESIAN_POINT('Ctrl Pts',(2.51888958382193,0.177890982017307,98.9003251482861));
#30955=CARTESIAN_POINT('Ctrl Pts',(2.497321116647,0.373959927687693,98.9115238248948));
#30956=CARTESIAN_POINT('Ctrl Pts',(2.42226595916285,0.699529847463623,98.930750766372));
#30957=CARTESIAN_POINT('Ctrl Pts',(2.38045389933403,0.830748659818356,98.9387105772089));
#30958=CARTESIAN_POINT('Ctrl Pts',(2.32179454098603,0.973321748433057,98.948243862286));
#30959=CARTESIAN_POINT('Ctrl Pts',(2.31528735363616,0.988700941661192,98.9492843270587));
#30960=CARTESIAN_POINT('Ctrl Pts',(2.30535672658936,1.01153541133451,98.9508489540232));
#30961=CARTESIAN_POINT('Ctrl Pts',(2.30204891225037,1.01904088551106,98.9513664468257));
#30962=CARTESIAN_POINT('Ctrl Pts',(2.29630646334231,1.03189992925071,98.9522588160658));
#30963=CARTESIAN_POINT('Ctrl Pts',(2.2938896599225,1.03726132899413,98.9526326114611));
#30964=CARTESIAN_POINT('Ctrl Pts',(2.28832631590083,1.0494884269284,98.9534890970397));
#30965=CARTESIAN_POINT('Ctrl Pts',(2.28516771340179,1.05634833476745,98.9539725042462));
#30966=CARTESIAN_POINT('Ctrl Pts',(2.27640145300119,1.07516373420176,98.9553061277819));
#30967=CARTESIAN_POINT('Ctrl Pts',(2.27073061108246,1.08708928088393,98.9561600208168));
#30968=CARTESIAN_POINT('Ctrl Pts',(2.24029753181949,1.14981159478994,98.9606946003531));
#30969=CARTESIAN_POINT('Ctrl Pts',(2.21392576400893,1.19980472671081,98.9644602448049));
#30970=CARTESIAN_POINT('Ctrl Pts',(2.09744788662719,1.40367692515224,98.9803326742536));
#30971=CARTESIAN_POINT('Ctrl Pts',(1.99280345357862,1.54865568462149,98.9928370597096));
#30972=CARTESIAN_POINT('Ctrl Pts',(1.8211376922936,1.73996021357985,99.010336023566));
#30973=CARTESIAN_POINT('Ctrl Pts',(1.76583564903728,1.79605969141301,99.015622626624));
#30974=CARTESIAN_POINT('Ctrl Pts',(1.68308597709842,1.87247885525332,99.0230366522767));
#30975=CARTESIAN_POINT('Ctrl Pts',(1.65771833506833,1.89497376499894,99.0252483089887));
#30976=CARTESIAN_POINT('Ctrl Pts',(1.61150845941753,1.93431231005251,99.0291702459706));
#30977=CARTESIAN_POINT('Ctrl Pts',(1.59083746903626,1.95134821730251,99.0308880534518));
#30978=CARTESIAN_POINT('Ctrl Pts',(1.55889778375257,1.97682623079763,99.0334881386531));
#30979=CARTESIAN_POINT('Ctrl Pts',(1.54782414292937,1.98550867099786,99.0343799301567));
#30980=CARTESIAN_POINT('Ctrl Pts',(1.52838868740956,2.00048588854729,99.0359285845265));
#30981=CARTESIAN_POINT('Ctrl Pts',(1.52005942234716,2.00682214656534,99.0365870652251));
#30982=CARTESIAN_POINT('Ctrl Pts',(1.50118464189965,2.02099568069085,99.0380676724236));
#30983=CARTESIAN_POINT('Ctrl Pts',(1.49061674424518,2.02880275103887,99.0388886146387));
#30984=CARTESIAN_POINT('Ctrl Pts',(1.46187875495682,2.04968726858238,99.0410998056959));
#30985=CARTESIAN_POINT('Ctrl Pts',(1.44359429530408,2.06260586480312,99.042483973662));
#30986=CARTESIAN_POINT('Ctrl Pts',(1.35365026743666,2.12437239083864,99.0491872593423));
#30987=CARTESIAN_POINT('Ctrl Pts',(1.27966762159844,2.16974196526879,99.0543759556894));
#30988=CARTESIAN_POINT('Ctrl Pts',(1.04654538881708,2.29662247419423,99.0699767135842));
#30989=CARTESIAN_POINT('Ctrl Pts',(0.880967243998219,2.3650847480179,99.0800184088173));
#30990=CARTESIAN_POINT('Ctrl Pts',(0.624982175647708,2.44028085453877,99.0956015921277));
#30991=CARTESIAN_POINT('Ctrl Pts',(0.539186741567531,2.46065998944262,99.100842112574));
#30992=CARTESIAN_POINT('Ctrl Pts',(0.438442990266717,2.47906806768612,99.1071980010465));
#30993=CARTESIAN_POINT('Ctrl Pts',(0.424354630710516,2.48151845956877,99.1080913909655));
#30994=CARTESIAN_POINT('Ctrl Pts',(0.402639616267851,2.48510503466635,99.1094764810659));
#30995=CARTESIAN_POINT('Ctrl Pts',(0.395027076194549,2.48632646674423,99.1099635680923));
#30996=CARTESIAN_POINT('Ctrl Pts',(0.380970151714646,2.48851571424831,99.1108660033671));
#30997=CARTESIAN_POINT('Ctrl Pts',(0.374527501603449,2.48949349546782,99.1112807919467));
#30998=CARTESIAN_POINT('Ctrl Pts',(0.359833889308503,2.49166517109962,99.1122294573842));
#30999=CARTESIAN_POINT('Ctrl Pts',(0.351580783123815,2.49284309593926,99.1127641989881));
#31000=CARTESIAN_POINT('Ctrl Pts',(0.329970364214883,2.49581799344352,99.114169085439));
#31001=CARTESIAN_POINT('Ctrl Pts',(0.316604403689426,2.4975487043405,99.1150426808899));
#31002=CARTESIAN_POINT('Ctrl Pts',(0.215821389323318,2.50977674799173,99.121661819589));
#31003=CARTESIAN_POINT('Ctrl Pts',(0.1279298592638,2.51578792258693,99.1276135051862));
#31004=CARTESIAN_POINT('Ctrl Pts',(-0.00828600142811408,2.51794786567276,
99.1369474368046));
#31005=CARTESIAN_POINT('Ctrl Pts',(-0.0564975498331805,2.51732754540024,
99.1402726909946));
#31006=CARTESIAN_POINT('Ctrl Pts',(-0.227141696781966,2.51022718001341,
99.1520691875792));
#31007=CARTESIAN_POINT('Ctrl Pts',(-0.349095860765041,2.49619110546966,
99.1605386739852));
#31008=CARTESIAN_POINT('Ctrl Pts',(-0.56195856385726,2.45578017283049,99.1751458661343));
#31009=CARTESIAN_POINT('Ctrl Pts',(-0.653321333576555,2.43306978720321,
99.1813588140841));
#31010=CARTESIAN_POINT('Ctrl Pts',(-0.764296576239692,2.39877972270679,
99.1888300983966));
#31011=CARTESIAN_POINT('Ctrl Pts',(-0.785298568465696,2.39198654334872,
99.1902408465567));
#31012=CARTESIAN_POINT('Ctrl Pts',(-0.818590861470113,2.3807322570265,99.1924726533573));
#31013=CARTESIAN_POINT('Ctrl Pts',(-0.830940059036212,2.37645023236023,
99.1932995094898));
#31014=CARTESIAN_POINT('Ctrl Pts',(-0.854222109443938,2.36817362158646,
99.1948566996009));
#31015=CARTESIAN_POINT('Ctrl Pts',(-0.865161655149543,2.36419902546531,
99.195587666996));
#31016=CARTESIAN_POINT('Ctrl Pts',(-0.889889440708315,2.35502021590934,
99.1972385291194));
#31017=CARTESIAN_POINT('Ctrl Pts',(-0.903660415365992,2.34977047864266,
99.1981568915802));
#31018=CARTESIAN_POINT('Ctrl Pts',(-0.945434112719405,2.33342405666579,
99.2009402451735));
#31019=CARTESIAN_POINT('Ctrl Pts',(-0.973285116314992,2.32194523850266,
99.2027925150356));
#31020=CARTESIAN_POINT('Ctrl Pts',(-1.19530910431112,2.22574082244616,99.2175478919344));
#31021=CARTESIAN_POINT('Ctrl Pts',(-1.37828220071341,2.11731727543549,99.2295483855258));
#31022=CARTESIAN_POINT('Ctrl Pts',(-1.64278533664376,1.91160762569995,99.2488711704504));
#31023=CARTESIAN_POINT('Ctrl Pts',(-1.73434933352431,1.82893741228284,99.2560474614189));
#31024=CARTESIAN_POINT('Ctrl Pts',(-1.83173235238424,1.72710074748358,99.2647478964081));
#31025=CARTESIAN_POINT('Ctrl Pts',(-1.84384609874572,1.71416216439873,99.2658510502251));
#31026=CARTESIAN_POINT('Ctrl Pts',(-1.8614987313224,1.69490392265879,99.2674916646551));
#31027=CARTESIAN_POINT('Ctrl Pts',(-1.86714450740241,1.68868239093063,99.268021473472));
#31028=CARTESIAN_POINT('Ctrl Pts',(-1.87711721794238,1.67758151214792,99.26896668032));
#31029=CARTESIAN_POINT('Ctrl Pts',(-1.88145647247008,1.67271346038088,99.2693811523807));
#31030=CARTESIAN_POINT('Ctrl Pts',(-1.89085309742834,1.6620889041754,99.2702857399228));
#31031=CARTESIAN_POINT('Ctrl Pts',(-1.89590304035709,1.65632624180449,99.2707763564439));
#31032=CARTESIAN_POINT('Ctrl Pts',(-1.90990248676862,1.6402030896841,99.2721487480768));
#31033=CARTESIAN_POINT('Ctrl Pts',(-1.91879374491143,1.6297926951168,99.2730345454454));
#31034=CARTESIAN_POINT('Ctrl Pts',(-1.96895578313804,1.57008066906743,99.2781108995259));
#31035=CARTESIAN_POINT('Ctrl Pts',(-2.00840742653807,1.51928874754185,99.282411487989));
#31036=CARTESIAN_POINT('Ctrl Pts',(-2.06229364670572,1.44414183428322,99.2886878372842));
#31037=CARTESIAN_POINT('Ctrl Pts',(-2.07833276406017,1.4209621988587,99.2906126766852));
#31038=CARTESIAN_POINT('Ctrl Pts',(-2.17748209749237,1.27240131684512,99.3028590059017));
#31039=CARTESIAN_POINT('Ctrl Pts',(-2.2496092496616,1.14004211783502,99.3133447890744));
#31040=CARTESIAN_POINT('Ctrl Pts',(-2.32799801044045,0.959371796268697,
99.3267118840795));
#31041=CARTESIAN_POINT('Ctrl Pts',(-2.34531855308029,0.916213942992361,
99.3298409628682));
#31042=CARTESIAN_POINT('Ctrl Pts',(-2.36143108732087,0.87261072067364,99.3329358985331));
#31043=CARTESIAN_POINT('Origin',(0.,0.,104.));
#31044=CARTESIAN_POINT('',(-2.36143107613328,0.872610750949147,100.332008666168));
#31045=CARTESIAN_POINT('',(-2.36143112101026,0.8726106295045,100.056192078358));
#31046=CARTESIAN_POINT('',(-2.36143112101026,0.872610629504505,104.));
#31047=CARTESIAN_POINT('',(-2.51749995409241,-0.000480775099579418,99.1125833024489));
#31048=CARTESIAN_POINT('Ctrl Pts',(-2.36143112101026,0.8726106295045,100.056192078358));
#31049=CARTESIAN_POINT('Ctrl Pts',(-2.33275321512777,0.950217865935678,
100.050942487041));
#31050=CARTESIAN_POINT('Ctrl Pts',(-2.30020045113898,1.0265317094225,100.045692895725));
#31051=CARTESIAN_POINT('Ctrl Pts',(-2.26391198059064,1.10113977048245,100.040443304408));
#31052=CARTESIAN_POINT('Ctrl Pts',(-2.22617849102928,1.17871874944353,100.034984672612));
#31053=CARTESIAN_POINT('Ctrl Pts',(-2.18440565730927,1.25445275645764,100.029526040816));
#31054=CARTESIAN_POINT('Ctrl Pts',(-2.13880631067855,1.32789826997462,100.02406740902));
#31055=CARTESIAN_POINT('Ctrl Pts',(-2.09504128200363,1.39838930203143,100.018828360773));
#31056=CARTESIAN_POINT('Ctrl Pts',(-2.04775194893672,1.46677198470564,100.013589312525));
#31057=CARTESIAN_POINT('Ctrl Pts',(-1.99717363357701,1.53267861188991,100.008350264277));
#31058=CARTESIAN_POINT('Ctrl Pts',(-1.94661547449549,1.59855897421539,100.003113303875));
#31059=CARTESIAN_POINT('Ctrl Pts',(-1.89277121654677,1.66196487490729,99.9978763434726));
#31060=CARTESIAN_POINT('Ctrl Pts',(-1.83591852413709,1.7225589751095,99.9926393830704));
#31061=CARTESIAN_POINT('Ctrl Pts',(-1.77907133909669,1.78314720550904,99.987402929977));
#31062=CARTESIAN_POINT('Ctrl Pts',(-1.71921661485095,1.84092384063048,99.9821664768837));
#31063=CARTESIAN_POINT('Ctrl Pts',(-1.65667024491431,1.89558696704096,99.9769300237903));
#31064=CARTESIAN_POINT('Ctrl Pts',(-1.59411106748309,1.95026128671008,99.971692498439));
#31065=CARTESIAN_POINT('Ctrl Pts',(-1.52885949824838,2.00182052920588,99.9664549730876));
#31066=CARTESIAN_POINT('Ctrl Pts',(-1.46126493165182,2.05000269500423,99.9612174477363));
#31067=CARTESIAN_POINT('Ctrl Pts',(-1.39359507066367,2.09823853149006,99.9559740882432));
#31068=CARTESIAN_POINT('Ctrl Pts',(-1.32357738102401,2.14308951729394,99.95073072875));
#31069=CARTESIAN_POINT('Ctrl Pts',(-1.25159019006132,2.1843370266839,99.9454873692569));
#31070=CARTESIAN_POINT('Ctrl Pts',(-1.17955552358119,2.22561173878625,99.9402405517708));
#31071=CARTESIAN_POINT('Ctrl Pts',(-1.10554918158347,2.26327803598502,99.9349937342846));
#31072=CARTESIAN_POINT('Ctrl Pts',(-1.02997188865551,2.29716437343508,99.9297469167985));
#31073=CARTESIAN_POINT('Ctrl Pts',(-0.954274422211247,2.33110459268176,
99.9244917564824));
#31074=CARTESIAN_POINT('Ctrl Pts',(-0.877001449681806,2.36125269283684,
99.9192365961662));
#31075=CARTESIAN_POINT('Ctrl Pts',(-0.798570787510214,2.38748632401011,
99.9139814358501));
#31076=CARTESIAN_POINT('Ctrl Pts',(-0.775958698366631,2.39504965689837,
99.9124663376698));
#31077=CARTESIAN_POINT('Ctrl Pts',(-0.753250453814723,2.40228793947742,
99.9109512394895));
#31078=CARTESIAN_POINT('Ctrl Pts',(-0.73045621841153,2.40919902934231,99.9094361413093));
#31079=CARTESIAN_POINT('Ctrl Pts',(-0.651392436504516,2.43317074377591,
99.904180891902));
#31080=CARTESIAN_POINT('Ctrl Pts',(-0.571001358178255,2.45329059604218,
99.8989256424948));
#31081=CARTESIAN_POINT('Ctrl Pts',(-0.489692843022924,2.46941433734643,
99.8936703930876));
#31082=CARTESIAN_POINT('Ctrl Pts',(-0.408499604871022,2.48551521884839,
99.8884225944301));
#31083=CARTESIAN_POINT('Ctrl Pts',(-0.326391962325043,2.49763115387418,
99.8831747957727));
#31084=CARTESIAN_POINT('Ctrl Pts',(-0.243794995103415,2.50566762567634,
99.8779269971153));
#31085=CARTESIAN_POINT('Ctrl Pts',(-0.16059954164588,2.51376232864511,99.8726411736324));
#31086=CARTESIAN_POINT('Ctrl Pts',(-0.0769080959350252,2.51771806298665,
99.8673553501494));
#31087=CARTESIAN_POINT('Ctrl Pts',(0.00683435582160804,2.51749072323624,
99.8620695266665));
#31088=CARTESIAN_POINT('Ctrl Pts',(0.0898258947923132,2.51726542202568,
99.856831100798));
#31089=CARTESIAN_POINT('Ctrl Pts',(0.172867058815803,2.5129317662099,99.8515926749295));
#31090=CARTESIAN_POINT('Ctrl Pts',(0.255521276622755,2.5044989772793,99.846354249061));
#31091=CARTESIAN_POINT('Ctrl Pts',(0.338148310833058,2.49606896175264,99.8411175460235));
#31092=CARTESIAN_POINT('Ctrl Pts',(0.420388192896793,2.48354253738092,99.8358808429861));
#31093=CARTESIAN_POINT('Ctrl Pts',(0.501808273409439,2.46698088900945,99.8306441399487));
#31094=CARTESIAN_POINT('Ctrl Pts',(0.583226136079772,2.450419691769,99.8254075795564));
#31095=CARTESIAN_POINT('Ctrl Pts',(0.663823789642993,2.4298235820575,99.8201710191642));
#31096=CARTESIAN_POINT('Ctrl Pts',(0.743178965335783,2.40530481966058,99.8149344587719));
#31097=CARTESIAN_POINT('Ctrl Pts',(0.823832971350214,2.38038475121435,99.8096121900014));
#31098=CARTESIAN_POINT('Ctrl Pts',(0.903202986832025,2.35141259769608,99.8042899212308));
#31099=CARTESIAN_POINT('Ctrl Pts',(0.980863698094443,2.31855831407375,99.7989676524603));
#31100=CARTESIAN_POINT('Ctrl Pts',(1.05738351671678,2.28618668390347,99.79372357171));
#31101=CARTESIAN_POINT('Ctrl Pts',(1.13224352481678,2.25004648789801,99.7884794909598));
#31102=CARTESIAN_POINT('Ctrl Pts',(1.2050605760744,2.21034731614541,99.7832354102096));
#31103=CARTESIAN_POINT('Ctrl Pts',(1.27950615519606,2.16976028631203,99.7778740474289));
#31104=CARTESIAN_POINT('Ctrl Pts',(1.35181585816839,2.12545343680915,99.7725126846481));
#31105=CARTESIAN_POINT('Ctrl Pts',(1.42161207296085,2.07769713000041,99.7671513218674));
#31106=CARTESIAN_POINT('Ctrl Pts',(1.49140828775331,2.02994082319168,99.7617899590867));
#31107=CARTESIAN_POINT('Ctrl Pts',(1.55869065048926,1.97873541994863,99.756428596306));
#31108=CARTESIAN_POINT('Ctrl Pts',(1.62311953089869,1.92439321304541,99.7510672335253));
#31109=CARTESIAN_POINT('Ctrl Pts',(1.68627321951298,1.87112656008526,99.7458119841178));
#31110=CARTESIAN_POINT('Ctrl Pts',(1.74691864446473,1.81464942875828,99.7405567347102));
#31111=CARTESIAN_POINT('Ctrl Pts',(1.80471166228413,1.75522706964531,99.7353014853027));
#31112=CARTESIAN_POINT('Ctrl Pts',(1.86242274273326,1.69588895793843,99.7300536866449));
#31113=CARTESIAN_POINT('Ctrl Pts',(1.91728912972066,1.63361424055039,99.7248058879872));
#31114=CARTESIAN_POINT('Ctrl Pts',(1.96900010801149,1.56870801127895,99.7195580893294));
#31115=CARTESIAN_POINT('Ctrl Pts',(2.02108577691702,1.5033314804246,99.7142722658466));
#31116=CARTESIAN_POINT('Ctrl Pts',(2.06996975462605,1.43528544716466,99.7089864423638));
#31117=CARTESIAN_POINT('Ctrl Pts',(2.11537277237975,1.36491914920789,99.7037006188809));
#31118=CARTESIAN_POINT('Ctrl Pts',(2.16036866440994,1.29518382098363,99.6984621930121));
#31119=CARTESIAN_POINT('Ctrl Pts',(2.20194551872949,1.22317006756963,99.6932237671432));
#31120=CARTESIAN_POINT('Ctrl Pts',(2.23987337834433,1.14924910223343,99.6879853412744));
#31121=CARTESIAN_POINT('Ctrl Pts',(2.27778876411735,1.07535244827252,99.6827486382366));
#31122=CARTESIAN_POINT('Ctrl Pts',(2.31205732816317,0.999550238354843,99.6775119351988));
#31123=CARTESIAN_POINT('Ctrl Pts',(2.34249483521434,0.922238687647695,99.6722752321611));
#31124=CARTESIAN_POINT('Ctrl Pts',(2.37293151316303,0.844929242868551,99.6670386717685));
#31125=CARTESIAN_POINT('Ctrl Pts',(2.39953717353041,0.766110968767055,99.6618021113759));
#31126=CARTESIAN_POINT('Ctrl Pts',(2.42217607407124,0.686199181139743,99.6565655509833));
#31127=CARTESIAN_POINT('Ctrl Pts',(2.44518551238695,0.604979452964636,99.6512432822131));
#31128=CARTESIAN_POINT('Ctrl Pts',(2.46409702235611,0.52263056209984,99.645921013443));
#31129=CARTESIAN_POINT('Ctrl Pts',(2.478821598194,0.43960179063209,99.6405987446728));
#31130=CARTESIAN_POINT('Ctrl Pts',(2.49332985924698,0.357792772523543,99.6353546639222));
#31131=CARTESIAN_POINT('Ctrl Pts',(2.50377338992084,0.275324189124085,99.6301105831716));
#31132=CARTESIAN_POINT('Ctrl Pts',(2.51011938815238,0.192631532261719,99.624866502421));
#31133=CARTESIAN_POINT('Ctrl Pts',(2.51660731241188,0.108089483089288,99.619505139641));
#31134=CARTESIAN_POINT('Ctrl Pts',(2.51881219952784,0.0233137287272409,
99.6141437768611));
#31135=CARTESIAN_POINT('Ctrl Pts',(2.51675523590554,-0.0612317935557103,
99.6087824140811));
#31136=CARTESIAN_POINT('Ctrl Pts',(2.51469827228324,-0.145777315838661,
99.6034210513011));
#31137=CARTESIAN_POINT('Ctrl Pts',(2.50837956250575,-0.230092104348521,
99.5980596885211));
#31138=CARTESIAN_POINT('Ctrl Pts',(2.49787614311196,-0.313721251546827,
99.5926983257411));
#31139=CARTESIAN_POINT('Ctrl Pts',(2.48758060990405,-0.395695190685063,
99.5874430763341));
#31140=CARTESIAN_POINT('Ctrl Pts',(2.47322652414446,-0.477313167572697,
99.5821878269271));
#31141=CARTESIAN_POINT('Ctrl Pts',(2.45484900652466,-0.558142101229502,
99.57693257752));
#31142=CARTESIAN_POINT('Ctrl Pts',(2.43649754404998,-0.638856437820514,
99.5716847788628));
#31143=CARTESIAN_POINT('Ctrl Pts',(2.41413408159011,-0.71878350702968,99.5664369802056));
#31144=CARTESIAN_POINT('Ctrl Pts',(2.38784536007417,-0.797496574520719,
99.5611891815484));
#31145=CARTESIAN_POINT('Ctrl Pts',(2.36136615410554,-0.876779986049647,
99.5559033580654));
#31146=CARTESIAN_POINT('Ctrl Pts',(2.33090462434359,-0.954831258455381,
99.5506175345824));
#31147=CARTESIAN_POINT('Ctrl Pts',(2.29660166037244,-1.03122600024173,99.5453317110994));
#31148=CARTESIAN_POINT('Ctrl Pts',(2.26260628871365,-1.10693571564675,99.5400932852311));
#31149=CARTESIAN_POINT('Ctrl Pts',(2.22483829116516,-1.18101806074897,99.5348548593628));
#31150=CARTESIAN_POINT('Ctrl Pts',(2.18348383810752,-1.2530780417529,99.5296164334945));
#31151=CARTESIAN_POINT('Ctrl Pts',(2.14214298584121,-1.32511432342837,99.5243797304572));
#31152=CARTESIAN_POINT('Ctrl Pts',(2.09721825015777,-1.39512916208937,99.51914302742));
#31153=CARTESIAN_POINT('Ctrl Pts',(2.0489416661038,-1.4627523026486,99.5139063243828));
#31154=CARTESIAN_POINT('Ctrl Pts',(2.00066639707982,-1.53037360118732,99.5086697639907));
#31155=CARTESIAN_POINT('Ctrl Pts',(1.94903973015863,-1.59560295621481,99.5034332035986));
#31156=CARTESIAN_POINT('Ctrl Pts',(1.89433612394891,-1.6581003888493,99.4981966432066));
#31157=CARTESIAN_POINT('Ctrl Pts',(1.83873716715634,-1.72162073599736,99.4928743744358));
#31158=CARTESIAN_POINT('Ctrl Pts',(1.77995995392479,-1.7823185468515,99.4875521056649));
#31159=CARTESIAN_POINT('Ctrl Pts',(1.71833287926423,-1.83987455171256,99.4822298368941));
#31160=CARTESIAN_POINT('Ctrl Pts',(1.65761115140187,-1.89658501676819,99.4769857561441));
#31161=CARTESIAN_POINT('Ctrl Pts',(1.59412313646232,-1.95024511869322,99.471741675394));
#31162=CARTESIAN_POINT('Ctrl Pts',(1.52821626249666,-2.00059023916462,99.4664975946439));
#31163=CARTESIAN_POINT('Ctrl Pts',(1.46083540435537,-2.05206131063975,99.4611362318628));
#31164=CARTESIAN_POINT('Ctrl Pts',(1.39092660984415,-2.10006704475547,99.4557748690816));
#31165=CARTESIAN_POINT('Ctrl Pts',(1.31889056093659,-2.14437262113476,99.4504135063004));
#31166=CARTESIAN_POINT('Ctrl Pts',(1.24685451202902,-2.18867819751406,99.4450521435193));
#31167=CARTESIAN_POINT('Ctrl Pts',(1.17269168648258,-2.22928343073232,99.4396907807381));
#31168=CARTESIAN_POINT('Ctrl Pts',(1.0968255998952,-2.26600526332455,99.4343294179569));
#31169=CARTESIAN_POINT('Ctrl Pts',(1.02246107303578,-2.30200028862464,99.42907416855));
#31170=CARTESIAN_POINT('Ctrl Pts',(0.946185439293675,-2.33439722715269,
99.4238189191431));
#31171=CARTESIAN_POINT('Ctrl Pts',(0.868381085169217,-2.36298974625798,
99.4185636697362));
#31172=CARTESIAN_POINT('Ctrl Pts',(0.790687039943935,-2.3915417276666,99.4133158710791));
#31173=CARTESIAN_POINT('Ctrl Pts',(0.711469008870073,-2.41629984548479,
99.408068072422));
#31174=CARTESIAN_POINT('Ctrl Pts',(0.631132159650954,-2.43710452115914,
99.4028202737649));
#31175=CARTESIAN_POINT('Ctrl Pts',(0.550213200693043,-2.45805994464649,
99.3975344502819));
#31176=CARTESIAN_POINT('Ctrl Pts',(0.468159568119976,-2.4750041855899,99.3922486267989));
#31177=CARTESIAN_POINT('Ctrl Pts',(0.385403945798672,-2.48782436047298,
99.3869628033159));
#31178=CARTESIAN_POINT('Ctrl Pts',(0.303390387438331,-2.50052957773159,
99.3817243774477));
#31179=CARTESIAN_POINT('Ctrl Pts',(0.220687842678183,-2.50918432119756,
99.3764859515795));
#31180=CARTESIAN_POINT('Ctrl Pts',(0.137728990020848,-2.51372969416122,
99.3712475257113));
#31181=CARTESIAN_POINT('Ctrl Pts',(0.0547974211495223,-2.51827357222735,
99.3660108226742));
#31182=CARTESIAN_POINT('Ctrl Pts',(-0.0283898278374614,-2.51871073872765,
99.3607741196371));
#31183=CARTESIAN_POINT('Ctrl Pts',(-0.111395857986024,-2.51503423690883,
99.3555374166));
#31184=CARTESIAN_POINT('Ctrl Pts',(-0.194399627091786,-2.51135783523607,
99.3503008562081));
#31185=CARTESIAN_POINT('Ctrl Pts',(-0.277221726250651,-2.50356800948417,
99.3450642958162));
#31186=CARTESIAN_POINT('Ctrl Pts',(-0.359427554381548,-2.49170987138377,
99.3398277354243));
#31187=CARTESIAN_POINT('Ctrl Pts',(-0.442978870342003,-2.47965764752499,
99.3345054666533));
#31188=CARTESIAN_POINT('Ctrl Pts',(-0.525893071314123,-2.46340279239329,
99.3291831978823));
#31189=CARTESIAN_POINT('Ctrl Pts',(-0.607723561161488,-2.44304693430339,
99.3238609291114));
#31190=CARTESIAN_POINT('Ctrl Pts',(-0.688351901260997,-2.42299011865741,
99.3186168483614));
#31191=CARTESIAN_POINT('Ctrl Pts',(-0.76792772961714,-2.39895218778448,
99.3133727676115));
#31192=CARTESIAN_POINT('Ctrl Pts',(-0.846039928677307,-2.37108048979441,
99.3081286868616));
#31193=CARTESIAN_POINT('Ctrl Pts',(-0.925899079745084,-2.34258545102857,
99.3027673240801));
#31194=CARTESIAN_POINT('Ctrl Pts',(-1.00422787147293,-2.31008329040283,
99.2974059612987));
#31195=CARTESIAN_POINT('Ctrl Pts',(-1.08061118641412,-2.27378224854463,
99.2920445985172));
#31196=CARTESIAN_POINT('Ctrl Pts',(-1.15699450135531,-2.23748120668643,
99.2866832357357));
#31197=CARTESIAN_POINT('Ctrl Pts',(-1.23143192386132,-2.19738158338034,
99.2813218729542));
#31198=CARTESIAN_POINT('Ctrl Pts',(-1.30353932301423,-2.15373895432005,
99.2759605101728));
#31199=CARTESIAN_POINT('Ctrl Pts',(-1.374219555307,-2.11096011059407,99.2707052607635));
#31200=CARTESIAN_POINT('Ctrl Pts',(-1.44292224529696,-2.06461926119626,
99.2654500113543));
#31201=CARTESIAN_POINT('Ctrl Pts',(-1.50926613182133,-2.01492481083962,
99.260194761945));
#31202=CARTESIAN_POINT('Ctrl Pts',(-1.57551595778619,-1.96530081592432,
99.2549469632856));
#31203=CARTESIAN_POINT('Ctrl Pts',(-1.63941325671187,-1.91233293847999,
99.2496991646262));
#31204=CARTESIAN_POINT('Ctrl Pts',(-1.70060358115018,-1.85627414725821,
99.2444513659668));
#31205=CARTESIAN_POINT('Ctrl Pts',(-1.76223728221295,-1.79980916179165,
99.2391655424843));
#31206=CARTESIAN_POINT('Ctrl Pts',(-1.82112420912457,-1.7402085262543,99.2338797190019));
#31207=CARTESIAN_POINT('Ctrl Pts',(-1.87693410065596,-1.67777371292877,
99.2285938955195));
#31208=CARTESIAN_POINT('Ctrl Pts',(-1.93224354876778,-1.61589874823624,
99.223355469649));
#31209=CARTESIAN_POINT('Ctrl Pts',(-1.98453061042904,-1.55124058028577,
99.2181170437784));
#31210=CARTESIAN_POINT('Ctrl Pts',(-2.03351031104773,-1.48413007006211,
99.2128786179079));
#31211=CARTESIAN_POINT('Ctrl Pts',(-2.08247390305797,-1.41704163136847,
99.2076419148685));
#31212=CARTESIAN_POINT('Ctrl Pts',(-2.12813202252442,-1.34750282464206,
99.2024052118291));
#31213=CARTESIAN_POINT('Ctrl Pts',(-2.17024096385839,-1.27587632974007,
99.1971685087896));
#31214=CARTESIAN_POINT('Ctrl Pts',(-2.21234875816577,-1.20425178590814,
99.1919319483954));
#31215=CARTESIAN_POINT('Ctrl Pts',(-2.25090733360058,-1.13054006526377,
99.1866953880011));
#31216=CARTESIAN_POINT('Ctrl Pts',(-2.28571791029733,-1.05513026899337,
99.1814588276069));
#31217=CARTESIAN_POINT('Ctrl Pts',(-2.32109824227236,-0.978486217690824,
99.1761365588387));
#31218=CARTESIAN_POINT('Ctrl Pts',(-2.35260656131234,-0.900088444370652,
99.1708142900705));
#31219=CARTESIAN_POINT('Ctrl Pts',(-2.38008496250032,-0.820366882120347,
99.1654920213023));
#31220=CARTESIAN_POINT('Ctrl Pts',(-2.40715968590261,-0.741816487853945,
99.1602479405501));
#31221=CARTESIAN_POINT('Ctrl Pts',(-2.43032203890123,-0.661981407916923,
99.1550038597979));
#31222=CARTESIAN_POINT('Ctrl Pts',(-2.44947178236045,-0.581286708449395,
99.1497597790457));
#31223=CARTESIAN_POINT('Ctrl Pts',(-2.46904980310552,-0.498787300373405,
99.1443984162695));
#31224=CARTESIAN_POINT('Ctrl Pts',(-2.48443347442554,-0.415389862155177,
99.1390370534934));
#31225=CARTESIAN_POINT('Ctrl Pts',(-2.49557145561039,-0.331555968039523,
99.1336756907172));
#31226=CARTESIAN_POINT('Ctrl Pts',(-2.50670943679524,-0.247722073923868,
99.128314327941));
#31227=CARTESIAN_POINT('Ctrl Pts',(-2.5136017530014,-0.163452235771735,
99.1229529651648));
#31228=CARTESIAN_POINT('Ctrl Pts',(-2.51625363847077,-0.079207808217358,
99.1175916023886));
#31229=CARTESIAN_POINT('Ctrl Pts',(-2.51707938858173,-0.0529755873299053,
99.1159221690898));
#31230=CARTESIAN_POINT('Ctrl Pts',(-2.51749494111227,-0.0267303864513461,
99.1142527357909));
#31231=CARTESIAN_POINT('Ctrl Pts',(-2.51749995409228,-0.00048077577683593,
99.112583302492));
#31232=CARTESIAN_POINT('Ctrl Pts',(-2.51749995409241,-0.000480775099579418,
99.1125833024489));
#31233=CARTESIAN_POINT('Ctrl Pts',(-2.51751564872535,0.0817015960768791,
99.1073566349482));
#31234=CARTESIAN_POINT('Ctrl Pts',(-2.51350287458033,0.16404280022504,99.1021299674474));
#31235=CARTESIAN_POINT('Ctrl Pts',(-2.50544101952395,0.246112875906163,
99.0969032999467));
#31236=CARTESIAN_POINT('Ctrl Pts',(-2.49738907342895,0.328082077879528,
99.0916830566307));
#31237=CARTESIAN_POINT('Ctrl Pts',(-2.48529796461774,0.409780352380315,
99.0864628133147));
#31238=CARTESIAN_POINT('Ctrl Pts',(-2.46919906308424,0.490777176388562,
99.0812425699987));
#31239=CARTESIAN_POINT('Ctrl Pts',(-2.45311733396175,0.571687602529829,
99.0760278950232));
#31240=CARTESIAN_POINT('Ctrl Pts',(-2.43303639485911,0.651897609163979,
99.0708132200476));
#31241=CARTESIAN_POINT('Ctrl Pts',(-2.40903928512245,0.730982881288401,
99.065598545072));
#31242=CARTESIAN_POINT('Ctrl Pts',(-2.39458138892031,0.77863056336517,99.0624567821534));
#31243=CARTESIAN_POINT('Ctrl Pts',(-2.37870296850341,0.825870105370799,
99.0593150192347));
#31244=CARTESIAN_POINT('Ctrl Pts',(-2.36143112101025,0.87261062950452,99.0561732563161));
#31245=CARTESIAN_POINT('Ctrl Pts',(-2.36143108732087,0.87261072067364,99.3329358985331));
#31246=CARTESIAN_POINT('Ctrl Pts',(-2.38350361458074,0.812878756795239,
99.3371756444856));
#31247=CARTESIAN_POINT('Ctrl Pts',(-2.40330917650767,0.752310976484073,
99.3413508841152));
#31248=CARTESIAN_POINT('Ctrl Pts',(-2.42710975634389,0.668934068856912,
99.3469335538277));
#31249=CARTESIAN_POINT('Ctrl Pts',(-2.43311614183059,0.646746051710752,
99.3484037148847));
#31250=CARTESIAN_POINT('Ctrl Pts',(-2.44210925342362,0.611624633902569,
99.3507071482415));
#31251=CARTESIAN_POINT('Ctrl Pts',(-2.44529890896816,0.598744983451393,
99.3515468762135));
#31252=CARTESIAN_POINT('Ctrl Pts',(-2.45108873153855,0.574547742247975,
99.3531153651944));
#31253=CARTESIAN_POINT('Ctrl Pts',(-2.45371269678936,0.563236262040109,
99.353844867736));
#31254=CARTESIAN_POINT('Ctrl Pts',(-2.45942266551899,0.537824079487287,
99.3554756174414));
#31255=CARTESIAN_POINT('Ctrl Pts',(-2.4624658658942,0.52371410250307,99.3563754841404));
#31256=CARTESIAN_POINT('Ctrl Pts',(-2.4699195078865,0.487652697582533,99.3586615322447));
#31257=CARTESIAN_POINT('Ctrl Pts',(-2.47415882993385,0.465666900772979,
99.3600423065247));
#31258=CARTESIAN_POINT('Ctrl Pts',(-2.50444437449513,0.296491547298753,
99.3705741160288));
#31259=CARTESIAN_POINT('Ctrl Pts',(-2.51763009975741,0.147294862717954,
99.3792994844789));
#31260=CARTESIAN_POINT('Ctrl Pts',(-2.51736624855715,-0.153667235191149,
99.3966409705038));
#31261=CARTESIAN_POINT('Ctrl Pts',(-2.50356545338128,-0.304793761042445,
99.4052239540686));
#31262=CARTESIAN_POINT('Ctrl Pts',(-2.4671480155389,-0.503536313841017,
99.4172876465437));
#31263=CARTESIAN_POINT('Ctrl Pts',(-2.45652651072161,-0.553032434548504,
99.4203597266038));
#31264=CARTESIAN_POINT('Ctrl Pts',(-2.4413360492093,-0.614695809172208,
99.4243102694106));
#31265=CARTESIAN_POINT('Ctrl Pts',(-2.43815446225405,-0.627196496088505,
99.4251175746218));
#31266=CARTESIAN_POINT('Ctrl Pts',(-2.43299484213032,-0.646836316304257,
99.4263968732795));
#31267=CARTESIAN_POINT('Ctrl Pts',(-2.43108107133862,-0.653992311233613,
99.4268652974623));
#31268=CARTESIAN_POINT('Ctrl Pts',(-2.42741138985683,-0.667475324425731,
99.4277524005593));
#31269=CARTESIAN_POINT('Ctrl Pts',(-2.42566228055569,-0.673804022803481,
99.4281706932355));
#31270=CARTESIAN_POINT('Ctrl Pts',(-2.4215080367134,-0.688609261340399,
99.4291536319278));
#31271=CARTESIAN_POINT('Ctrl Pts',(-2.41908313957884,-0.697080085015698,
99.4297193901709));
#31272=CARTESIAN_POINT('Ctrl Pts',(-2.41102350834638,-0.724685998092114,
99.4315737818691));
#31273=CARTESIAN_POINT('Ctrl Pts',(-2.40520596708076,-0.743766328134072,
99.4328721769997));
#31274=CARTESIAN_POINT('Ctrl Pts',(-2.37190210432902,-0.848517271839642,
99.4400851232568));
#31275=CARTESIAN_POINT('Ctrl Pts',(-2.34006731138586,-0.932728779619282,
99.4461958166118));
#31276=CARTESIAN_POINT('Ctrl Pts',(-2.30124781520773,-1.02083532040833,
99.4528094388848));
#31277=CARTESIAN_POINT('Ctrl Pts',(-2.29867571243539,-1.02661396197294,
99.4532442590251));
#31278=CARTESIAN_POINT('Ctrl Pts',(-2.27569957632008,-1.0777142786758,99.4570984021582));
#31279=CARTESIAN_POINT('Ctrl Pts',(-2.25397947675746,-1.12243176106848,
99.4605340104382));
#31280=CARTESIAN_POINT('Ctrl Pts',(-2.1468152438127,-1.32738921994537,99.4765107392243));
#31281=CARTESIAN_POINT('Ctrl Pts',(-2.04550368744715,-1.47875439981819,
99.4889251030126));
#31282=CARTESIAN_POINT('Ctrl Pts',(-1.90801155467121,-1.64266287107209,
99.5028235107663));
#31283=CARTESIAN_POINT('Ctrl Pts',(-1.88677973864446,-1.66700683165984,
99.5049028408222));
#31284=CARTESIAN_POINT('Ctrl Pts',(-1.85486588270896,-1.70220746786093,
99.5079333864175));
#31285=CARTESIAN_POINT('Ctrl Pts',(-1.84454512048291,-1.71338583557381,
99.5088994479938));
#31286=CARTESIAN_POINT('Ctrl Pts',(-1.82608709798173,-1.73301754220954,
99.5106028960883));
#31287=CARTESIAN_POINT('Ctrl Pts',(-1.81799096578936,-1.74150875589474,
99.5113419935818));
#31288=CARTESIAN_POINT('Ctrl Pts',(-1.80101437973741,-1.75906637213317,
99.5128752722766));
#31289=CARTESIAN_POINT('Ctrl Pts',(-1.79212411715161,-1.76812286216456,
99.5136690001466));
#31290=CARTESIAN_POINT('Ctrl Pts',(-1.76881427923021,-1.79151210525207,
99.5157266333546));
#31291=CARTESIAN_POINT('Ctrl Pts',(-1.75428871311169,-1.80573827734058,
99.5169858606241));
#31292=CARTESIAN_POINT('Ctrl Pts',(-1.6878884445282,-1.86921238954983,99.5226421387201));
#31293=CARTESIAN_POINT('Ctrl Pts',(-1.63409894406825,-1.91641446185513,
99.526952186908));
#31294=CARTESIAN_POINT('Ctrl Pts',(-1.39527342814532,-2.1086141768126,99.5451237231192));
#31295=CARTESIAN_POINT('Ctrl Pts',(-1.19247242616962,-2.22958136458589,
99.5580984578959));
#31296=CARTESIAN_POINT('Ctrl Pts',(-0.926826816288691,-2.34128764152677,
99.5752705816891));
#31297=CARTESIAN_POINT('Ctrl Pts',(-0.877155130666692,-2.36034610883845,
99.578493960378));
#31298=CARTESIAN_POINT('Ctrl Pts',(-0.814670057285158,-2.3820762356174,
99.5826076995543));
#31299=CARTESIAN_POINT('Ctrl Pts',(-0.802386401142647,-2.38624192844866,
99.5834191881031));
#31300=CARTESIAN_POINT('Ctrl Pts',(-0.782951577521749,-2.39266573248303,
99.584708299063));
#31301=CARTESIAN_POINT('Ctrl Pts',(-0.775821375847051,-2.39498719609388,
99.5851823433075));
#31302=CARTESIAN_POINT('Ctrl Pts',(-0.76307277731967,-2.39907500355149,
99.5860320564837));
#31303=CARTESIAN_POINT('Ctrl Pts',(-0.757458421221817,-2.40085353025583,
99.5864070109938));
#31304=CARTESIAN_POINT('Ctrl Pts',(-0.743936881683051,-2.40508476048013,
99.5873118180892));
#31305=CARTESIAN_POINT('Ctrl Pts',(-0.736023846607228,-2.40751815810598,
99.5878427666852));
#31306=CARTESIAN_POINT('Ctrl Pts',(-0.711739695433816,-2.41485505052959,
99.5894762824282));
#31307=CARTESIAN_POINT('Ctrl Pts',(-0.695330919672426,-2.41963079490134,
99.5905857371124));
#31308=CARTESIAN_POINT('Ctrl Pts',(-0.656916164928314,-2.43038832742408,
99.5931943085517));
#31309=CARTESIAN_POINT('Ctrl Pts',(-0.634875258379955,-2.43623882220654,
99.5946995337551));
#31310=CARTESIAN_POINT('Ctrl Pts',(-0.556854527964823,-2.45581786387308,
99.6000506865114));
#31311=CARTESIAN_POINT('Ctrl Pts',(-0.500488343834589,-2.46792198666117,
99.6039576994706));
#31312=CARTESIAN_POINT('Ctrl Pts',(-0.278042158974925,-2.50775636219712,
99.6194213700015));
#31313=CARTESIAN_POINT('Ctrl Pts',(-0.109748558572827,-2.52073636635111,
99.6311818878833));
#31314=CARTESIAN_POINT('Ctrl Pts',(0.15725323059623,-2.51452163981783,99.6492346988049));
#31315=CARTESIAN_POINT('Ctrl Pts',(0.255713856971508,-2.5064242014543,99.655769548375));
#31316=CARTESIAN_POINT('Ctrl Pts',(0.37612500224252,-2.48934940422941,99.6636012876936));
#31317=CARTESIAN_POINT('Ctrl Pts',(0.39874982503602,-2.48582563894636,99.6650660771872));
#31318=CARTESIAN_POINT('Ctrl Pts',(0.434516683811463,-2.4797541334284,99.6673716073837));
#31319=CARTESIAN_POINT('Ctrl Pts',(0.447691451196276,-2.47740947090541,
99.6682186718712));
#31320=CARTESIAN_POINT('Ctrl Pts',(0.472251899395199,-2.47283622032223,
99.6697938993378));
#31321=CARTESIAN_POINT('Ctrl Pts',(0.483642026420423,-2.47063377021909,
99.6705228640406));
#31322=CARTESIAN_POINT('Ctrl Pts',(0.509017696476248,-2.46554479723182,
99.6721435992095));
#31323=CARTESIAN_POINT('Ctrl Pts',(0.522994793607886,-2.46261783913498,
99.6730340664564));
#31324=CARTESIAN_POINT('Ctrl Pts',(0.564114795353025,-2.45364097696741,
99.6756476877903));
#31325=CARTESIAN_POINT('Ctrl Pts',(0.591183774112016,-2.44725997501708,
99.6773603358368));
#31326=CARTESIAN_POINT('Ctrl Pts',(0.652613089805557,-2.43170040762843,
99.6812326616919));
#31327=CARTESIAN_POINT('Ctrl Pts',(0.686896127418619,-2.42223958458449,
99.6833834357499));
#31328=CARTESIAN_POINT('Ctrl Pts',(0.802091440564606,-2.38780745940144,
99.6905898518851));
#31329=CARTESIAN_POINT('Ctrl Pts',(0.881943642260125,-2.35948133346607,
99.6955486757934));
#31330=CARTESIAN_POINT('Ctrl Pts',(1.13990184797048,-2.25304499243265,99.7117117745281));
#31331=CARTESIAN_POINT('Ctrl Pts',(1.310369432877,-2.15835649099085,99.7225908748216));
#31332=CARTESIAN_POINT('Ctrl Pts',(1.49666661801921,-2.02460387426945,99.736468233969));
#31333=CARTESIAN_POINT('Ctrl Pts',(1.52467384326875,-2.00359706627596,99.7386149116104));
#31334=CARTESIAN_POINT('Ctrl Pts',(1.56116154476958,-1.97502139580867,99.741506091522));
#31335=CARTESIAN_POINT('Ctrl Pts',(1.57004320118683,-1.96796829695185,99.7422174640866));
#31336=CARTESIAN_POINT('Ctrl Pts',(1.58437854132509,-1.95642551189073,99.7433786294224));
#31337=CARTESIAN_POINT('Ctrl Pts',(1.58986163259488,-1.95197236969748,99.7438258811177));
#31338=CARTESIAN_POINT('Ctrl Pts',(1.60051022876152,-1.94324938484815,99.7447007422064));
#31339=CARTESIAN_POINT('Ctrl Pts',(1.60567752318345,-1.93898191112802,99.7451281882358));
#31340=CARTESIAN_POINT('Ctrl Pts',(1.6182307175091,-1.92853011218795,99.7461736144245));
#31341=CARTESIAN_POINT('Ctrl Pts',(1.62559823757108,-1.9223239611282,99.7467931366474));
#31342=CARTESIAN_POINT('Ctrl Pts',(1.65193150097515,-1.89988206665984,99.7490283888691));
#31343=CARTESIAN_POINT('Ctrl Pts',(1.67069041255477,-1.88340728073437,99.7506600381524));
#31344=CARTESIAN_POINT('Ctrl Pts',(1.71708108420924,-1.8414268103847,99.7547882251664));
#31345=CARTESIAN_POINT('Ctrl Pts',(1.74439164039583,-1.81557639863167,99.7573039218401));
#31346=CARTESIAN_POINT('Ctrl Pts',(1.94085087424065,-1.62109522841749,99.77597832516));
#31347=CARTESIAN_POINT('Ctrl Pts',(2.08582754727152,-1.42975713546375,99.7928462800587));
#31348=CARTESIAN_POINT('Ctrl Pts',(2.23329401056134,-1.16381007579665,99.8130598913627));
#31349=CARTESIAN_POINT('Ctrl Pts',(2.26268275595813,-1.10558764396749,99.8173233836058));
#31350=CARTESIAN_POINT('Ctrl Pts',(2.29825613872131,-1.02773580990944,99.8228189056339));
#31351=CARTESIAN_POINT('Ctrl Pts',(2.30650655545125,-1.0090836059402,99.8241206163115));
#31352=CARTESIAN_POINT('Ctrl Pts',(2.31952722985832,-0.978652686080276,
99.8262207283625));
#31353=CARTESIAN_POINT('Ctrl Pts',(2.32443644003715,-0.96693479400513,99.8270237938747));
#31354=CARTESIAN_POINT('Ctrl Pts',(2.33370639022585,-0.944329533064323,
99.8285624282832));
#31355=CARTESIAN_POINT('Ctrl Pts',(2.3380801552854,-0.933447897704011,99.829298418254));
#31356=CARTESIAN_POINT('Ctrl Pts',(2.3480374689279,-0.908165641413657,99.8309978196828));
#31357=CARTESIAN_POINT('Ctrl Pts',(2.35356489082611,-0.893743312777121,
99.8319593424349));
#31358=CARTESIAN_POINT('Ctrl Pts',(2.37080160048548,-0.847499654454535,
99.8350179471396));
#31359=CARTESIAN_POINT('Ctrl Pts',(2.3820012059711,-0.81549145619755,99.8370982505718));
#31360=CARTESIAN_POINT('Ctrl Pts',(2.4068356229774,-0.739632620068523,99.8419500028941));
#31361=CARTESIAN_POINT('Ctrl Pts',(2.41992431723751,-0.695615400200794,
99.8447043948388));
#31362=CARTESIAN_POINT('Ctrl Pts',(2.46502712732749,-0.52720241740103,99.8550526473507));
#31363=CARTESIAN_POINT('Ctrl Pts',(2.48871107969751,-0.400775635599492,
99.8624211203637));
#31364=CARTESIAN_POINT('Ctrl Pts',(2.51882209365799,-0.124833290852954,
99.8783715774892));
#31365=CARTESIAN_POINT('Ctrl Pts',(2.52179178959734,0.0245492073282939,
99.8869276120713));
#31366=CARTESIAN_POINT('Ctrl Pts',(2.51007837505082,0.194310620125791,99.8973821092228));
#31367=CARTESIAN_POINT('Ctrl Pts',(2.50836451956261,0.215307770712928,99.8986882551669));
#31368=CARTESIAN_POINT('Ctrl Pts',(2.50560231962577,0.244608342566125,99.9005322689086));
#31369=CARTESIAN_POINT('Ctrl Pts',(2.50477571856571,0.252932442346295,99.9010585534075));
#31370=CARTESIAN_POINT('Ctrl Pts',(2.50327494596153,0.267316233350858,99.9019723680417));
#31371=CARTESIAN_POINT('Ctrl Pts',(2.5026202114308,0.273377941928626,99.9023588298144));
#31372=CARTESIAN_POINT('Ctrl Pts',(2.50118831913558,0.286198405402891,99.9031791768506));
#31373=CARTESIAN_POINT('Ctrl Pts',(2.50040577515912,0.292956466604461,99.9036133680493));
#31374=CARTESIAN_POINT('Ctrl Pts',(2.49838846916877,0.309780831070077,99.9046985478704));
#31375=CARTESIAN_POINT('Ctrl Pts',(2.49712026275552,0.319842916402753,99.9053513506574));
#31376=CARTESIAN_POINT('Ctrl Pts',(2.49205349760046,0.358174862206502,99.9078520028741));
#31377=CARTESIAN_POINT('Ctrl Pts',(2.48783553122931,0.38638591304184,99.9097209856019));
#31378=CARTESIAN_POINT('Ctrl Pts',(2.47570363209417,0.45906119966978,99.9145994787303));
#31379=CARTESIAN_POINT('Ctrl Pts',(2.46707106238824,0.503394046827024,99.9176373758836));
#31380=CARTESIAN_POINT('Ctrl Pts',(2.43570506126359,0.644176966686166,99.9274366972328));
#31381=CARTESIAN_POINT('Ctrl Pts',(2.40846892117756,0.739526469686777,99.9343008425818));
#31382=CARTESIAN_POINT('Ctrl Pts',(2.3191026329755,0.994389894783269,99.9529475504126));
#31383=CARTESIAN_POINT('Ctrl Pts',(2.24621594600339,1.14960031661482,99.9646037198963));
#31384=CARTESIAN_POINT('Ctrl Pts',(2.14109869930211,1.32461238864522,99.9778706347512));
#31385=CARTESIAN_POINT('Ctrl Pts',(2.123499187026,1.35264666236637,99.9800015895634));
#31386=CARTESIAN_POINT('Ctrl Pts',(2.09705392522325,1.39298244581963,99.9830775331366));
#31387=CARTESIAN_POINT('Ctrl Pts',(2.08864248956696,1.40556317066546,99.9840383718916));
#31388=CARTESIAN_POINT('Ctrl Pts',(2.07351628226033,1.4277513213686,99.9857358185416));
#31389=CARTESIAN_POINT('Ctrl Pts',(2.06684696104278,1.43738904114406,99.986474097569));
#31390=CARTESIAN_POINT('Ctrl Pts',(2.05279516786746,1.457395017114,99.9880088222405));
#31391=CARTESIAN_POINT('Ctrl Pts',(2.04540086811087,1.46775458961472,99.9888047919328));
#31392=CARTESIAN_POINT('Ctrl Pts',(2.02589224956218,1.49465283695458,99.9908751037702));
#31393=CARTESIAN_POINT('Ctrl Pts',(2.01365376730967,1.51110061005555,99.992144657532));
#31394=CARTESIAN_POINT('Ctrl Pts',(1.95668383846331,1.58574333173377,99.9979254903962));
#31395=CARTESIAN_POINT('Ctrl Pts',(1.90961931177131,1.64211727161478,100.002344811465));
#31396=CARTESIAN_POINT('Ctrl Pts',(1.76389951369148,1.80190746587991,100.015150560017));
#31397=CARTESIAN_POINT('Ctrl Pts',(1.65883485042892,1.89907385266144,100.02329753858));
#31398=CARTESIAN_POINT('Ctrl Pts',(1.44419225937166,2.06610414381818,100.038950030559));
#31399=CARTESIAN_POINT('Ctrl Pts',(1.33635521910781,2.13743403016492,100.046425109566));
#31400=CARTESIAN_POINT('Ctrl Pts',(1.20478495203594,2.21060173083181,100.055669691945));
#31401=CARTESIAN_POINT('Ctrl Pts',(1.18589784753166,2.22079107926653,100.056999742303));
#31402=CARTESIAN_POINT('Ctrl Pts',(1.15941309549036,2.23464507287224,100.058872184406));
#31403=CARTESIAN_POINT('Ctrl Pts',(1.15192320709902,2.23851518821925,100.059402521055));
#31404=CARTESIAN_POINT('Ctrl Pts',(1.13896873938926,2.2451266861324,100.060321425775));
#31405=CARTESIAN_POINT('Ctrl Pts',(1.133513296191,2.24788594718178,100.060708896916));
#31406=CARTESIAN_POINT('Ctrl Pts',(1.12198301678767,2.25366510016705,100.061528993487));
#31407=CARTESIAN_POINT('Ctrl Pts',(1.11590595980867,2.25668034048018,100.061961910039));
#31408=CARTESIAN_POINT('Ctrl Pts',(1.10079728291441,2.26410083023689,100.063039775806));
#31409=CARTESIAN_POINT('Ctrl Pts',(1.0917514027577,2.26847660204163,100.063686488898));
#31410=CARTESIAN_POINT('Ctrl Pts',(1.05754263982345,2.28477243421418,100.066136646998));
#31411=CARTESIAN_POINT('Ctrl Pts',(1.03220980906839,2.29632843239281,100.067960174099));
#31412=CARTESIAN_POINT('Ctrl Pts',(0.966666143371022,2.32492361230966,100.072691880931));
#31413=CARTESIAN_POINT('Ctrl Pts',(0.926195056687779,2.3413405399953,100.075626498917));
#31414=CARTESIAN_POINT('Ctrl Pts',(0.768639052117084,2.40052827063299,100.087049427278));
#31415=CARTESIAN_POINT('Ctrl Pts',(0.648867022426873,2.43563389143778,100.095719729962));
#31416=CARTESIAN_POINT('Ctrl Pts',(0.369239986869788,2.49549468436993,100.1154075499));
#31417=CARTESIAN_POINT('Ctrl Pts',(0.208585270639053,2.5140288243754,100.126302880078));
#31418=CARTESIAN_POINT('Ctrl Pts',(0.0250081221962085,2.5174739586208,100.138145005431));
#31419=CARTESIAN_POINT('Ctrl Pts',(0.0027743267229852,2.51759665025779,
100.139569857757));
#31420=CARTESIAN_POINT('Ctrl Pts',(-0.0338447596654966,2.51731359810553,
100.141901682248));
#31421=CARTESIAN_POINT('Ctrl Pts',(-0.0482297650618556,2.51707908551078,
100.142813901784));
#31422=CARTESIAN_POINT('Ctrl Pts',(-0.0742166170519933,2.5164325719562,
100.144455239401));
#31423=CARTESIAN_POINT('Ctrl Pts',(-0.0858190349131048,2.51606361127331,
100.145185670808));
#31424=CARTESIAN_POINT('Ctrl Pts',(-0.110710887058315,2.5150996596882,100.146747804681));
#31425=CARTESIAN_POINT('Ctrl Pts',(-0.123999038446791,2.51447955806498,
100.147578705901));
#31426=CARTESIAN_POINT('Ctrl Pts',(-0.160389147140787,2.5124922111058,100.149846270356));
#31427=CARTESIAN_POINT('Ctrl Pts',(-0.183478505368552,2.51091168349873,
100.151276299863));
#31428=CARTESIAN_POINT('Ctrl Pts',(-0.319638003657398,2.49970295503817,
100.159662995256));
#31429=CARTESIAN_POINT('Ctrl Pts',(-0.431981189574384,2.48275656701698,
100.166385835976));
#31430=CARTESIAN_POINT('Ctrl Pts',(-0.716732383987043,2.41988122040865,
100.183349575387));
#31431=CARTESIAN_POINT('Ctrl Pts',(-0.88607518290481,2.3631320803081,100.193346019235));
#31432=CARTESIAN_POINT('Ctrl Pts',(-1.1040166779255,2.26334904939646,100.20754577466));
#31433=CARTESIAN_POINT('Ctrl Pts',(-1.15906728588436,2.23565727376039,100.211260555814));
#31434=CARTESIAN_POINT('Ctrl Pts',(-1.22490312215346,2.19945489149915,100.215928039093));
#31435=CARTESIAN_POINT('Ctrl Pts',(-1.2367112009774,2.19283717245522,100.216774272211));
#31436=CARTESIAN_POINT('Ctrl Pts',(-1.25508846518467,2.1823421757574,100.218106478637));
#31437=CARTESIAN_POINT('Ctrl Pts',(-1.26169456921249,2.17852960455198,100.218588468017));
#31438=CARTESIAN_POINT('Ctrl Pts',(-1.2738114515064,2.17146300755805,100.219478436802));
#31439=CARTESIAN_POINT('Ctrl Pts',(-1.27932725244667,2.16821792844192,100.219885847926));
#31440=CARTESIAN_POINT('Ctrl Pts',(-1.29187069108932,2.16077379347895,100.220817525588));
#31441=CARTESIAN_POINT('Ctrl Pts',(-1.29889023902018,2.1565614787385,100.221342627287));
#31442=CARTESIAN_POINT('Ctrl Pts',(-1.31367741888495,2.14758955090531,100.22245646249));
#31443=CARTESIAN_POINT('Ctrl Pts',(-1.32143999531492,2.14282187149945,100.223045683224));
#31444=CARTESIAN_POINT('Ctrl Pts',(-1.34207234909262,2.12999498642356,100.22462350113));
#31445=CARTESIAN_POINT('Ctrl Pts',(-1.35489516581668,2.12186142268706,100.225616344208));
#31446=CARTESIAN_POINT('Ctrl Pts',(-1.39433617550252,2.09634055297995,100.228706409022));
#31447=CARTESIAN_POINT('Ctrl Pts',(-1.42069827649272,2.07856520277309,100.230823409188));
#31448=CARTESIAN_POINT('Ctrl Pts',(-1.52679116202141,2.00406804702355,100.239534748647));
#31449=CARTESIAN_POINT('Ctrl Pts',(-1.60351631104104,1.94322239379069,100.246282271396));
#31450=CARTESIAN_POINT('Ctrl Pts',(-1.82304009585914,1.74725961386189,100.266610225599));
#31451=CARTESIAN_POINT('Ctrl Pts',(-1.95379324117827,1.59972212968044,100.280094468558));
#31452=CARTESIAN_POINT('Ctrl Pts',(-2.08242009810825,1.4149740410807,100.29470727203));
#31453=CARTESIAN_POINT('Ctrl Pts',(-2.0983685382003,1.39121335166108,100.296549850248));
#31454=CARTESIAN_POINT('Ctrl Pts',(-2.12184816567641,1.35490971203528,100.299311062109));
#31455=CARTESIAN_POINT('Ctrl Pts',(-2.12968041605005,1.3425651962399,100.300240747771));
#31456=CARTESIAN_POINT('Ctrl Pts',(-2.14314531557536,1.32092863069683,100.301854462248));
#31457=CARTESIAN_POINT('Ctrl Pts',(-2.14882609944345,1.31166714200441,100.302540240768));
#31458=CARTESIAN_POINT('Ctrl Pts',(-2.16060852563175,1.29217603793948,100.303973240295));
#31459=CARTESIAN_POINT('Ctrl Pts',(-2.166697897209,1.28193929033195,100.30472000344));
#31460=CARTESIAN_POINT('Ctrl Pts',(-2.1810757595999,1.25737376156694,100.30649834743));
#31461=CARTESIAN_POINT('Ctrl Pts',(-2.18929609688322,1.2430055776523,100.307527464739));
#31462=CARTESIAN_POINT('Ctrl Pts',(-2.21711572337141,1.19324791288143,100.311054625445));
#31463=CARTESIAN_POINT('Ctrl Pts',(-2.2360040118263,1.15746665181497,100.313527601605));
#31464=CARTESIAN_POINT('Ctrl Pts',(-2.27985520585807,1.06931316215215,100.319481384804));
#31465=CARTESIAN_POINT('Ctrl Pts',(-2.30388655375325,1.01650273290238,100.322932025619));
#31466=CARTESIAN_POINT('Ctrl Pts',(-2.33844529612365,0.933019893775969,
100.328243924807));
#31467=CARTESIAN_POINT('Ctrl Pts',(-2.35023265669797,0.902915552522292,
100.330131448148));
#31468=CARTESIAN_POINT('Ctrl Pts',(-2.36143107613335,0.872610750948945,
100.332008666168));
#31469=CARTESIAN_POINT('Origin',(0.,0.,104.));
#31470=CARTESIAN_POINT('',(-2.36143112101024,0.872610629504535,101.328714168996));
#31471=CARTESIAN_POINT('',(-2.36143112101025,0.872610629504514,101.056345051278));
#31472=CARTESIAN_POINT('',(-2.36143112101026,0.872610629504505,104.));
#31473=CARTESIAN_POINT('',(-2.51749904018607,0.00219833169228679,100.112583302458));
#31474=CARTESIAN_POINT('Ctrl Pts',(-2.36143112101025,0.872610629504513,
101.056345051278));
#31475=CARTESIAN_POINT('Ctrl Pts',(-2.33221131544371,0.951684337618625,
101.051018578518));
#31476=CARTESIAN_POINT('Ctrl Pts',(-2.29904688773595,1.02920461468538,101.045692105757));
#31477=CARTESIAN_POINT('Ctrl Pts',(-2.26214154918255,1.10477231204533,101.040365632997));
#31478=CARTESIAN_POINT('Ctrl Pts',(-2.22516722098647,1.18048127320729,101.035029203102));
#31479=CARTESIAN_POINT('Ctrl Pts',(-2.18443823344539,1.25422997984213,101.029692773206));
#31480=CARTESIAN_POINT('Ctrl Pts',(-2.14020305802366,1.32564592573815,101.024356343311));
#31481=CARTESIAN_POINT('Ctrl Pts',(-2.12269098834624,1.35391847148228,101.022243727473));
#31482=CARTESIAN_POINT('Ctrl Pts',(-2.10462986862105,1.3818257619343,101.020131111636));
#31483=CARTESIAN_POINT('Ctrl Pts',(-2.08603685581883,1.40934612007324,101.018018495799));
#31484=CARTESIAN_POINT('Ctrl Pts',(-2.03978570225557,1.47780454173625,101.012763246392));
#31485=CARTESIAN_POINT('Ctrl Pts',(-1.99007561770263,1.5441102083388,101.007507996984));
#31486=CARTESIAN_POINT('Ctrl Pts',(-1.93713376492452,1.60789272863253,101.002252747577));
#31487=CARTESIAN_POINT('Ctrl Pts',(-1.88426697166669,1.67158481980214,100.99700494892));
#31488=CARTESIAN_POINT('Ctrl Pts',(-1.82817780344503,1.73276051803598,100.991757150262));
#31489=CARTESIAN_POINT('Ctrl Pts',(-1.76913659410922,1.79107843529635,100.986509351605));
#31490=CARTESIAN_POINT('Ctrl Pts',(-1.70966758031225,1.84981891614324,100.981223528122));
#31491=CARTESIAN_POINT('Ctrl Pts',(-1.64720383001774,1.90565963442698,100.975937704639));
#31492=CARTESIAN_POINT('Ctrl Pts',(-1.58206291381019,1.95828577759897,100.970651881156));
#31493=CARTESIAN_POINT('Ctrl Pts',(-1.51750611170184,2.01044002577772,100.965413455287));
#31494=CARTESIAN_POINT('Ctrl Pts',(-1.45032032884715,2.0594368223821,100.960175029419));
#31495=CARTESIAN_POINT('Ctrl Pts',(-1.38085022903176,2.10500805104943,100.95493660355));
#31496=CARTESIAN_POINT('Ctrl Pts',(-1.31140297677613,2.15056429209802,100.949699900513));
#31497=CARTESIAN_POINT('Ctrl Pts',(-1.23967328514353,2.19269694983349,100.944463197475));
#31498=CARTESIAN_POINT('Ctrl Pts',(-1.16603553866773,2.23118071266401,100.939226494438));
#31499=CARTESIAN_POINT('Ctrl Pts',(-1.09239979804728,2.26966342721609,100.933989934045));
#31500=CARTESIAN_POINT('Ctrl Pts',(-1.01685651534236,2.30449723168084,100.928753373653));
#31501=CARTESIAN_POINT('Ctrl Pts',(-0.939804222611727,2.33550300217344,
100.923516813261));
#31502=CARTESIAN_POINT('Ctrl Pts',(-0.861490791548369,2.36701625355101,
100.91819454449));
#31503=CARTESIAN_POINT('Ctrl Pts',(-0.781618959216873,2.39457483546007,
100.91287227572));
#31504=CARTESIAN_POINT('Ctrl Pts',(-0.700625999889945,2.41804248479596,
100.907550006949));
#31505=CARTESIAN_POINT('Ctrl Pts',(-0.62082288636162,2.44116537720239,100.902305926199));
#31506=CARTESIAN_POINT('Ctrl Pts',(-0.539931837104716,2.46031668865465,
100.897061845448));
#31507=CARTESIAN_POINT('Ctrl Pts',(-0.458382389107362,2.4754175072816,100.891817764698));
#31508=CARTESIAN_POINT('Ctrl Pts',(-0.37500911625304,2.49085605043088,100.886456401918));
#31509=CARTESIAN_POINT('Ctrl Pts',(-0.290948147124191,2.50206067115167,
100.881095039137));
#31510=CARTESIAN_POINT('Ctrl Pts',(-0.206663042294775,2.50900311616974,
100.875733676356));
#31511=CARTESIAN_POINT('Ctrl Pts',(-0.122377937465359,2.51594556118781,
100.870372313576));
#31512=CARTESIAN_POINT('Ctrl Pts',(-0.0378692069043505,2.51862588116019,
100.865010950795));
#31513=CARTESIAN_POINT('Ctrl Pts',(0.046402630135093,2.51707231638595,100.859649588015));
#31514=CARTESIAN_POINT('Ctrl Pts',(0.129006538839197,2.51554950013695,100.854394338607));
#31515=CARTESIAN_POINT('Ctrl Pts',(0.211687953583553,2.50995328840563,100.8491390892));
#31516=CARTESIAN_POINT('Ctrl Pts',(0.294012513924796,2.50027256347296,100.843883839793));
#31517=CARTESIAN_POINT('Ctrl Pts',(0.376220356741427,2.49060556360904,100.838636041135));
#31518=CARTESIAN_POINT('Ctrl Pts',(0.458071895656362,2.47686560642341,100.833388242478));
#31519=CARTESIAN_POINT('Ctrl Pts',(0.539133593330857,2.45909357661358,100.82814044382));
#31520=CARTESIAN_POINT('Ctrl Pts',(0.620782652888353,2.44119277312649,100.822854620337));
#31521=CARTESIAN_POINT('Ctrl Pts',(0.701629902940013,2.41920122751496,100.817568796854));
#31522=CARTESIAN_POINT('Ctrl Pts',(0.781238379348301,2.39321391535175,100.812282973371));
#31523=CARTESIAN_POINT('Ctrl Pts',(0.860133012043689,2.3674596296229,100.807044547503));
#31524=CARTESIAN_POINT('Ctrl Pts',(0.937810551388953,2.33778109568757,100.801806121634));
#31525=CARTESIAN_POINT('Ctrl Pts',(1.0138584507114,2.30432143849791,100.796567695766));
#31526=CARTESIAN_POINT('Ctrl Pts',(1.08988133914533,2.27087278563268,100.791330992728));
#31527=CARTESIAN_POINT('Ctrl Pts',(1.16427522999031,2.23364566494747,100.78609428969));
#31528=CARTESIAN_POINT('Ctrl Pts',(1.23664729937749,2.19283143605302,100.780857586653));
#31529=CARTESIAN_POINT('Ctrl Pts',(1.30901739738581,2.15201831891769,100.775621026261));
#31530=CARTESIAN_POINT('Ctrl Pts',(1.37936538202917,2.10761851540511,100.770384465868));
#31531=CARTESIAN_POINT('Ctrl Pts',(1.4473240241734,2.05986878685282,100.765147905476));
#31532=CARTESIAN_POINT('Ctrl Pts',(1.51639496610264,2.0113375239566,100.759825636705));
#31533=CARTESIAN_POINT('Ctrl Pts',(1.58299723579442,1.95934596013392,100.754503367935));
#31534=CARTESIAN_POINT('Ctrl Pts',(1.6467784621474,1.9041866890112,100.749181099164));
#31535=CARTESIAN_POINT('Ctrl Pts',(1.70962269564533,1.84983774791642,100.743937018414));
#31536=CARTESIAN_POINT('Ctrl Pts',(1.76972792598464,1.79241392127543,100.738692937664));
#31537=CARTESIAN_POINT('Ctrl Pts',(1.82679410041291,1.73223253770866,100.733448856913));
#31538=CARTESIAN_POINT('Ctrl Pts',(1.88513653985536,1.67070521856585,100.728087494133));
#31539=CARTESIAN_POINT('Ctrl Pts',(1.94030201513892,1.6062958994179,100.722726131352));
#31540=CARTESIAN_POINT('Ctrl Pts',(1.99201444135701,1.53937802875874,100.717364768572));
#31541=CARTESIAN_POINT('Ctrl Pts',(2.0437268675751,1.47246015809956,100.712003405791));
#31542=CARTESIAN_POINT('Ctrl Pts',(2.09198600956505,1.40303419126748,100.70664204301));
#31543=CARTESIAN_POINT('Ctrl Pts',(2.13656482464557,1.33150178373416,100.70128068023));
#31544=CARTESIAN_POINT('Ctrl Pts',(2.18026132516602,1.26138516270322,100.696025430823));
#31545=CARTESIAN_POINT('Ctrl Pts',(2.220583291266,1.18898576367459,100.690770181415));
#31546=CARTESIAN_POINT('Ctrl Pts',(2.25728490926713,1.11466187177766,100.685514932008));
#31547=CARTESIAN_POINT('Ctrl Pts',(2.2939344927115,1.04044335427516,100.68026713335));
#31548=CARTESIAN_POINT('Ctrl Pts',(2.32697372076107,0.964306173764744,100.675019334693));
#31549=CARTESIAN_POINT('Ctrl Pts',(2.35620084710383,0.88663623775886,100.669771536035));
#31550=CARTESIAN_POINT('Ctrl Pts',(2.38563974917372,0.808403516107192,100.664485712553));
#31551=CARTESIAN_POINT('Ctrl Pts',(2.41121082187184,0.728616135147747,100.65919988907));
#31552=CARTESIAN_POINT('Ctrl Pts',(2.43275582416911,0.647692326626838,100.653914065587));
#31553=CARTESIAN_POINT('Ctrl Pts',(2.45410763391796,0.567494156311032,100.648675639718));
#31554=CARTESIAN_POINT('Ctrl Pts',(2.47150516617165,0.486180311445731,100.64343721385));
#31555=CARTESIAN_POINT('Ctrl Pts',(2.48484386135593,0.404174757600901,100.638198787981));
#31556=CARTESIAN_POINT('Ctrl Pts',(2.49817816966534,0.322196174018033,100.632962084944));
#31557=CARTESIAN_POINT('Ctrl Pts',(2.50745621803731,0.239526788342451,100.627725381906));
#31558=CARTESIAN_POINT('Ctrl Pts',(2.51262464386841,0.15660028424354,100.622488678869));
#31559=CARTESIAN_POINT('Ctrl Pts',(2.51779292891417,0.0736760390211448,
100.617252118476));
#31560=CARTESIAN_POINT('Ctrl Pts',(2.51885178631918,-0.0095048501080237,
100.612015558084));
#31561=CARTESIAN_POINT('Ctrl Pts',(2.51579987119145,-0.0925054490994754,
100.606778997692));
#31562=CARTESIAN_POINT('Ctrl Pts',(2.51269800443971,-0.176864544163071,
100.601456728921));
#31563=CARTESIAN_POINT('Ctrl Pts',(2.50534959151306,-0.261036902240307,
100.596134460151));
#31564=CARTESIAN_POINT('Ctrl Pts',(2.49380820869186,-0.344567654113217,
100.59081219138));
#31565=CARTESIAN_POINT('Ctrl Pts',(2.48243637722391,-0.426871278159488,
100.58556811063));
#31566=CARTESIAN_POINT('Ctrl Pts',(2.46699410093658,-0.508551573722867,
100.58032402988));
#31567=CARTESIAN_POINT('Ctrl Pts',(2.44758418843908,-0.589184088806719,
100.575079949129));
#31568=CARTESIAN_POINT('Ctrl Pts',(2.42774018004335,-0.671619921863586,
100.569718586349));
#31569=CARTESIAN_POINT('Ctrl Pts',(2.40374906918176,-0.752960051295377,
100.564357223568));
#31570=CARTESIAN_POINT('Ctrl Pts',(2.37577378671153,-0.832769574596934,
100.558995860788));
#31571=CARTESIAN_POINT('Ctrl Pts',(2.3477985042413,-0.912579097898504,100.553634498007));
#31572=CARTESIAN_POINT('Ctrl Pts',(2.31583930406201,-0.990857569907529,
100.548273135227));
#31573=CARTESIAN_POINT('Ctrl Pts',(2.28010947794237,-1.06719586702601,100.542911772446));
#31574=CARTESIAN_POINT('Ctrl Pts',(2.24508682507885,-1.14202325832703,100.537656523039));
#31575=CARTESIAN_POINT('Ctrl Pts',(2.20631212510909,-1.21526297823443,100.532401273631));
#31576=CARTESIAN_POINT('Ctrl Pts',(2.16395207119459,-1.28651377123318,100.527146024224));
#31577=CARTESIAN_POINT('Ctrl Pts',(2.12165207421342,-1.35766354679385,100.521898225567));
#31578=CARTESIAN_POINT('Ctrl Pts',(2.07577705387272,-1.42682960317234,100.516650426909));
#31579=CARTESIAN_POINT('Ctrl Pts',(2.02654086532222,-1.49363260917103,100.511402628252));
#31580=CARTESIAN_POINT('Ctrl Pts',(1.97694791813915,-1.56091966053906,100.506116804769));
#31581=CARTESIAN_POINT('Ctrl Pts',(1.92394508898334,-1.62580884315666,100.500830981286));
#31582=CARTESIAN_POINT('Ctrl Pts',(1.8677970328417,-1.68793971874227,100.495545157803));
#31583=CARTESIAN_POINT('Ctrl Pts',(1.81215245244386,-1.74951347105509,100.490306731934));
#31584=CARTESIAN_POINT('Ctrl Pts',(1.75341914028613,-1.80837783666159,100.485068306066));
#31585=CARTESIAN_POINT('Ctrl Pts',(1.69189578779433,-1.86421428308116,100.479829880197));
#31586=CARTESIAN_POINT('Ctrl Pts',(1.63039266930932,-1.92003236582271,100.47459317716));
#31587=CARTESIAN_POINT('Ctrl Pts',(1.56610167430342,-1.97282419729981,100.469356474122));
#31588=CARTESIAN_POINT('Ctrl Pts',(1.49935751994002,-2.02230889762156,100.464119771085));
#31589=CARTESIAN_POINT('Ctrl Pts',(1.43261518365403,-2.0717922500048,100.458883210692));
#31590=CARTESIAN_POINT('Ctrl Pts',(1.36342019214502,-2.11796837636214,100.4536466503));
#31591=CARTESIAN_POINT('Ctrl Pts',(1.29213831009011,-2.16059825918598,100.448410089908));
#31592=CARTESIAN_POINT('Ctrl Pts',(1.21968973577056,-2.20392587828022,100.443087821137));
#31593=CARTESIAN_POINT('Ctrl Pts',(1.14508575630058,-2.24358985796055,100.437765552367));
#31594=CARTESIAN_POINT('Ctrl Pts',(1.06873708216042,-2.27938748334179,100.432443283596));
#31595=CARTESIAN_POINT('Ctrl Pts',(0.993510025873493,-2.31465921542911,
100.427199202846));
#31596=CARTESIAN_POINT('Ctrl Pts',(0.916589652673124,-2.34617731763915,
100.421955122096));
#31597=CARTESIAN_POINT('Ctrl Pts',(0.838387963927298,-2.373796931488,100.416711041345));
#31598=CARTESIAN_POINT('Ctrl Pts',(0.758437321787985,-2.40203424833205,
100.411349678565));
#31599=CARTESIAN_POINT('Ctrl Pts',(0.677147850984888,-2.42619645007273,
100.405988315784));
#31600=CARTESIAN_POINT('Ctrl Pts',(0.594973052343718,-2.44618341850827,
100.400626953004));
#31601=CARTESIAN_POINT('Ctrl Pts',(0.512798253702537,-2.46617038694381,
100.395265590223));
#31602=CARTESIAN_POINT('Ctrl Pts',(0.429738638858018,-2.48198209267392,
100.389904227443));
#31603=CARTESIAN_POINT('Ctrl Pts',(0.346253504564266,-2.49357469520706,
100.384542864662));
#31604=CARTESIAN_POINT('Ctrl Pts',(0.264420727997514,-2.50493785418077,
100.379287615255));
#31605=CARTESIAN_POINT('Ctrl Pts',(0.181876870043046,-2.51228941481946,
100.374032365847));
#31606=CARTESIAN_POINT('Ctrl Pts',(0.0990492570832516,-2.51555073386948,
100.36877711644));
#31607=CARTESIAN_POINT('Ctrl Pts',(0.0163390748624143,-2.51880742910996,
100.363529317783));
#31608=CARTESIAN_POINT('Ctrl Pts',(-0.0666536060613034,-2.51798538333177,
100.358281519125));
#31609=CARTESIAN_POINT('Ctrl Pts',(-0.149494171835672,-2.51305744912192,
100.353033720468));
#31610=CARTESIAN_POINT('Ctrl Pts',(-0.232934988926288,-2.50809380778033,
100.347747896985));
#31611=CARTESIAN_POINT('Ctrl Pts',(-0.316221007771172,-2.49896446036227,
100.342462073502));
#31612=CARTESIAN_POINT('Ctrl Pts',(-0.398905803699714,-2.48569515624396,
100.337176250019));
#31613=CARTESIAN_POINT('Ctrl Pts',(-0.48084917077028,-2.47254483705979,
100.33193782415));
#31614=CARTESIAN_POINT('Ctrl Pts',(-0.562201590002327,-2.45532858368273,
100.326699398282));
#31615=CARTESIAN_POINT('Ctrl Pts',(-0.642533255795456,-2.43412351067009,
100.321460972413));
#31616=CARTESIAN_POINT('Ctrl Pts',(-0.72283850184065,-2.41292541165306,
100.316224269376));
#31617=CARTESIAN_POINT('Ctrl Pts',(-0.802123215395963,-2.38774121609325,
100.310987566338));
#31618=CARTESIAN_POINT('Ctrl Pts',(-0.879969559293769,-2.35869875666994,
100.305750863301));
#31619=CARTESIAN_POINT('Ctrl Pts',(-0.957813782695915,-2.32965708834878,
100.300514302908));
#31620=CARTESIAN_POINT('Ctrl Pts',(-1.03421928238705,-2.29675752737585,
100.295277742516));
#31621=CARTESIAN_POINT('Ctrl Pts',(-1.10878643117635,-2.26017674088537,
100.290041182124));
#31622=CARTESIAN_POINT('Ctrl Pts',(-1.1845740431915,-2.22299722552555,100.284718913353));
#31623=CARTESIAN_POINT('Ctrl Pts',(-1.25846213642939,-2.18201509875608,
100.279396644583));
#31624=CARTESIAN_POINT('Ctrl Pts',(-1.33005706324611,-2.1374644929236,100.274074375812));
#31625=CARTESIAN_POINT('Ctrl Pts',(-1.40060020823375,-2.09356836806864,
100.268830295062));
#31626=CARTESIAN_POINT('Ctrl Pts',(-1.46891676647575,-2.04620823240409,
100.263586214312));
#31627=CARTESIAN_POINT('Ctrl Pts',(-1.53466091700543,-1.99565080107118,
100.258342133561));
#31628=CARTESIAN_POINT('Ctrl Pts',(-1.6018754124476,-1.94396267048442,100.252980770781));
#31629=CARTESIAN_POINT('Ctrl Pts',(-1.66640066013577,-1.88893283796383,
100.247619408));
#31630=CARTESIAN_POINT('Ctrl Pts',(-1.72790577246219,-1.8308871869921,100.24225804522));
#31631=CARTESIAN_POINT('Ctrl Pts',(-1.78941088478861,-1.77284153602037,
100.236896682439));
#31632=CARTESIAN_POINT('Ctrl Pts',(-1.84789555853221,-1.71178047974573,
100.231535319659));
#31633=CARTESIAN_POINT('Ctrl Pts',(-1.90307295579216,-1.64806540371809,
100.226173956878));
#31634=CARTESIAN_POINT('Ctrl Pts',(-1.95670661292151,-1.5861329329722,100.220962593033));
#31635=CARTESIAN_POINT('Ctrl Pts',(-2.00742189654769,-1.52145466982403,
100.215751229189));
#31636=CARTESIAN_POINT('Ctrl Pts',(-2.05492184315158,-1.45433918620744,
100.210539865344));
#31637=CARTESIAN_POINT('Ctrl Pts',(-2.10235895333139,-1.38731248789047,
100.205335395475));
#31638=CARTESIAN_POINT('Ctrl Pts',(-2.14658889768153,-1.31785534578256,
100.200130925606));
#31639=CARTESIAN_POINT('Ctrl Pts',(-2.18735350234669,-1.24631091857997,
100.194926455737));
#31640=CARTESIAN_POINT('Ctrl Pts',(-2.22807698574017,-1.17483866177749,
100.189727235874));
#31641=CARTESIAN_POINT('Ctrl Pts',(-2.2653418369109,-1.10128370482761,100.184528016011));
#31642=CARTESIAN_POINT('Ctrl Pts',(-2.29893280601451,-1.02601861748716,
100.179328796148));
#31643=CARTESIAN_POINT('Ctrl Pts',(-2.33250043822008,-0.950805819607697,
100.174133188376));
#31644=CARTESIAN_POINT('Ctrl Pts',(-2.36239906650357,-0.873885678468057,
100.168937580605));
#31645=CARTESIAN_POINT('Ctrl Pts',(-2.38845978937943,-0.79565450072098,
100.163741972834));
#31646=CARTESIAN_POINT('Ctrl Pts',(-2.41451585326278,-0.717437308713033,
100.158547293905));
#31647=CARTESIAN_POINT('Ctrl Pts',(-2.43673521726057,-0.637909987852045,
100.153352614975));
#31648=CARTESIAN_POINT('Ctrl Pts',(-2.45499791486481,-0.557486760389387,
100.148157936046));
#31649=CARTESIAN_POINT('Ctrl Pts',(-2.47325894911605,-0.477070857814841,
100.142963730245));
#31650=CARTESIAN_POINT('Ctrl Pts',(-2.48756393627921,-0.395759670401945,
100.137769524443));
#31651=CARTESIAN_POINT('Ctrl Pts',(-2.49784379623169,-0.313978692950392,
100.132575318641));
#31652=CARTESIAN_POINT('Ctrl Pts',(-2.50812919165291,-0.232153678318772,
100.127378315879));
#31653=CARTESIAN_POINT('Ctrl Pts',(-2.51438508505061,-0.149858835943071,
100.122181313117));
#31654=CARTESIAN_POINT('Ctrl Pts',(-2.51659425685113,-0.0675247834792372,
100.116984310354));
#31655=CARTESIAN_POINT('Ctrl Pts',(-2.51721785875581,-0.044283643100605,
100.115517307734));
#31656=CARTESIAN_POINT('Ctrl Pts',(-2.51751933182795,-0.021039381607636,
100.114050305113));
#31657=CARTESIAN_POINT('Ctrl Pts',(-2.51749904018654,0.00219833114783364,
100.112583302492));
#31658=CARTESIAN_POINT('Ctrl Pts',(-2.51749904018607,0.00219833169228797,
100.112583302458));
#31659=CARTESIAN_POINT('Ctrl Pts',(-2.51741017424848,0.103966373959212,
100.106158660485));
#31660=CARTESIAN_POINT('Ctrl Pts',(-2.51114671053894,0.205464160514488,
100.099734018512));
#31661=CARTESIAN_POINT('Ctrl Pts',(-2.49882897256204,0.30603923912551,100.093309376539));
#31662=CARTESIAN_POINT('Ctrl Pts',(-2.48631365676557,0.408227552631852,
100.08678168263));
#31663=CARTESIAN_POINT('Ctrl Pts',(-2.46754833857112,0.509463401282088,
100.080253988721));
#31664=CARTESIAN_POINT('Ctrl Pts',(-2.4427078667328,0.609084992264386,100.073726294811));
#31665=CARTESIAN_POINT('Ctrl Pts',(-2.43519696831913,0.639207111302466,
100.071752546239));
#31666=CARTESIAN_POINT('Ctrl Pts',(-2.42713098016373,0.669181796368386,
100.069778797666));
#31667=CARTESIAN_POINT('Ctrl Pts',(-2.41851558766757,0.698991131709841,
100.067805049094));
#31668=CARTESIAN_POINT('Ctrl Pts',(-2.40161875451569,0.757454326028318,
100.063934058849));
#31669=CARTESIAN_POINT('Ctrl Pts',(-2.38257788982076,0.815383916593283,
100.060063068603));
#31670=CARTESIAN_POINT('Ctrl Pts',(-2.36143112101026,0.8726106295045,100.056192078358));
#31671=CARTESIAN_POINT('',(-2.51749994369438,0.000532446056795771,100.385185287451));
#31672=CARTESIAN_POINT('Ctrl Pts',(-2.36143107613335,0.872610750948947,
100.332008666168));
#31673=CARTESIAN_POINT('Ctrl Pts',(-2.43054338807988,0.685581240945225,
100.343594129468));
#31674=CARTESIAN_POINT('Ctrl Pts',(-2.47722505275429,0.490913466893775,
100.354730759386));
#31675=CARTESIAN_POINT('Ctrl Pts',(-2.50506290388481,0.253091072209852,
100.369154925959));
#31676=CARTESIAN_POINT('Ctrl Pts',(-2.50875596153332,0.213397201095081,
100.371591126473));
#31677=CARTESIAN_POINT('Ctrl Pts',(-2.51232472874635,0.161777557736847,
100.374815693234));
#31678=CARTESIAN_POINT('Ctrl Pts',(-2.51306050061653,0.149914736060504,
100.375560598103));
#31679=CARTESIAN_POINT('Ctrl Pts',(-2.51410616662273,0.130874153104245,
100.376763043139));
#31680=CARTESIAN_POINT('Ctrl Pts',(-2.51446939378066,0.123699335771165,
100.377217698691));
#31681=CARTESIAN_POINT('Ctrl Pts',(-2.51509055639182,0.110293410338815,
100.378070273606));
#31682=CARTESIAN_POINT('Ctrl Pts',(-2.51535605427957,0.104062769533399,
100.378467771644));
#31683=CARTESIAN_POINT('Ctrl Pts',(-2.51585327150832,0.0912775083612031,
100.379285929411));
#31684=CARTESIAN_POINT('Ctrl Pts',(-2.516082532118,0.0847228219647258,100.379706719003));
#31685=CARTESIAN_POINT('Ctrl Pts',(-2.5166489074665,0.0664906381077124,
100.380880754559));
#31686=CARTESIAN_POINT('Ctrl Pts',(-2.51693035026904,0.0548117507589939,
100.381636892936));
#31687=CARTESIAN_POINT('Ctrl Pts',(-2.51737379221875,0.028932779951975,
100.383320851271));
#31688=CARTESIAN_POINT('Ctrl Pts',(-2.51749694040091,0.0147325533313436,
100.384250501894));
#31689=CARTESIAN_POINT('Ctrl Pts',(-2.51749994369438,0.000532446056795771,
100.385185287451));
#31690=CARTESIAN_POINT('Ctrl Pts',(-2.51749994318663,0.000534841376573433,
100.385185129769));
#31691=CARTESIAN_POINT('Ctrl Pts',(-2.51752973780924,-0.139708535471339,
100.394417271433));
#31692=CARTESIAN_POINT('Ctrl Pts',(-2.50584061409508,-0.279702207492776,
100.404120224013));
#31693=CARTESIAN_POINT('Ctrl Pts',(-2.46143942510912,-0.543416172880637,
100.422594579596));
#31694=CARTESIAN_POINT('Ctrl Pts',(-2.43084320016804,-0.667077391207286,
100.43134273588));
#31695=CARTESIAN_POINT('Ctrl Pts',(-2.36715576456412,-0.860347345119606,
100.444943440311));
#31696=CARTESIAN_POINT('Ctrl Pts',(-2.34000254505476,-0.931672720395224,
100.44994937167));
#31697=CARTESIAN_POINT('Ctrl Pts',(-2.30139294388001,-1.02069945985187,
100.456182180973));
#31698=CARTESIAN_POINT('Ctrl Pts',(-2.29290112967272,-1.03963518656407,
100.457507093384));
#31699=CARTESIAN_POINT('Ctrl Pts',(-2.27880177953355,-1.07006171928804,
100.459635240386));
#31700=CARTESIAN_POINT('Ctrl Pts',(-2.27333929020811,-1.08161828519615,
100.460443372284));
#31701=CARTESIAN_POINT('Ctrl Pts',(-2.26270711370638,-1.10367555908132,
100.461985646782));
#31702=CARTESIAN_POINT('Ctrl Pts',(-2.25755176746683,-1.11418277080741,
100.462720257459));
#31703=CARTESIAN_POINT('Ctrl Pts',(-2.24561386540841,-1.1380905855448,100.464391815965));
#31704=CARTESIAN_POINT('Ctrl Pts',(-2.23878424739747,-1.15146729107778,
100.465327104939));
#31705=CARTESIAN_POINT('Ctrl Pts',(-2.21681343613066,-1.1935654838543,100.468271364172));
#31706=CARTESIAN_POINT('Ctrl Pts',(-2.20123576423728,-1.22205631315929,
100.47026507277));
#31707=CARTESIAN_POINT('Ctrl Pts',(-2.09244022226173,-1.41220422413403,
100.483597045362));
#31708=CARTESIAN_POINT('Ctrl Pts',(-1.98204949032737,-1.56336674323794,
100.494267458906));
#31709=CARTESIAN_POINT('Ctrl Pts',(-1.78535499606566,-1.77798546479413,
100.511004895734));
#31710=CARTESIAN_POINT('Ctrl Pts',(-1.71003240461132,-1.85054337514874,
100.517028044717));
#31711=CARTESIAN_POINT('Ctrl Pts',(-1.60526470560482,-1.93959325553429,
100.525250826708));
#31712=CARTESIAN_POINT('Ctrl Pts',(-1.57968561426048,-1.96048206515904,
100.527247591794));
#31713=CARTESIAN_POINT('Ctrl Pts',(-1.54143627863174,-1.99048324446703,
100.530230060865));
#31714=CARTESIAN_POINT('Ctrl Pts',(-1.52907945201058,-1.99999133768001,
100.531193077928));
#31715=CARTESIAN_POINT('Ctrl Pts',(-1.5092341647605,-2.01497009201315,100.532740332215));
#31716=CARTESIAN_POINT('Ctrl Pts',(-1.50180220830475,-2.02051536912354,
100.533319910044));
#31717=CARTESIAN_POINT('Ctrl Pts',(-1.48778105545493,-2.03085701184175,
100.534413957143));
#31718=CARTESIAN_POINT('Ctrl Pts',(-1.48119884839694,-2.03566270257414,
100.53492780706));
#31719=CARTESIAN_POINT('Ctrl Pts',(-1.47456163479772,-2.04045932003837,
100.535446331092));
#31720=CARTESIAN_POINT('Ctrl Pts',(-1.47452973746517,-2.04048237063682,
100.53544882304));
#31721=CARTESIAN_POINT('Ctrl Pts',(-1.47446555227998,-2.04052875175198,
100.535453837463));
#31722=CARTESIAN_POINT('Ctrl Pts',(-1.47443326437138,-2.04055208228116,
100.535456359942));
#31723=CARTESIAN_POINT('Ctrl Pts',(-1.47436828569953,-2.04059903208592,
100.535461436392));
#31724=CARTESIAN_POINT('Ctrl Pts',(-1.47433559497287,-2.04062265130585,
100.53546399036));
#31725=CARTESIAN_POINT('Ctrl Pts',(-1.47426979792777,-2.04067018760653,
100.535469130782));
#31726=CARTESIAN_POINT('Ctrl Pts',(-1.47423669158589,-2.04069410467369,
100.535471717239));
#31727=CARTESIAN_POINT('Ctrl Pts',(-1.47417005008962,-2.04074224612766,
100.535476923672));
#31728=CARTESIAN_POINT('Ctrl Pts',(-1.47413651492153,-2.0407664704925,100.535479543651));
#31729=CARTESIAN_POINT('Ctrl Pts',(-1.47406900203198,-2.0408152363713,100.535484818203));
#31730=CARTESIAN_POINT('Ctrl Pts',(-1.47403502428251,-2.04083977787215,
100.535487472778));
#31731=CARTESIAN_POINT('Ctrl Pts',(-1.47396661192414,-2.04088918825523,
100.535492817643));
#31732=CARTESIAN_POINT('Ctrl Pts',(-1.47393217732338,-2.04091405709672,
100.535495507931));
#31733=CARTESIAN_POINT('Ctrl Pts',(-1.47386283644238,-2.04096413275879,
100.535500925381));
#31734=CARTESIAN_POINT('Ctrl Pts',(-1.47382793010014,-2.04098933958769,
100.535503652546));
#31735=CARTESIAN_POINT('Ctrl Pts',(-1.4737576302921,-2.04104010226688,100.535509144957));
#31736=CARTESIAN_POINT('Ctrl Pts',(-1.47372223678655,-2.04106565810771,
100.535511910206));
#31737=CARTESIAN_POINT('Ctrl Pts',(-1.47365094652265,-2.04111713034141,
100.535517480044));
#31738=CARTESIAN_POINT('Ctrl Pts',(-1.47361504978321,-2.04114304668063,
100.535520284632));
#31739=CARTESIAN_POINT('Ctrl Pts',(-1.47354273632298,-2.04119525186765,
100.535525934456));
#31740=CARTESIAN_POINT('Ctrl Pts',(-1.47350631956427,-2.04122154070092,
100.535528779696));
#31741=CARTESIAN_POINT('Ctrl Pts',(-1.47343294860229,-2.04127450335575,
100.53553451219));
#31742=CARTESIAN_POINT('Ctrl Pts',(-1.47339599441321,-2.04130117712311,
100.535537399443));
#31743=CARTESIAN_POINT('Ctrl Pts',(-1.47332153040682,-2.04135492263829,
100.535543217385));
#31744=CARTESIAN_POINT('Ctrl Pts',(-1.47328402057315,-2.04138199435178,
100.535546148076));
#31745=CARTESIAN_POINT('Ctrl Pts',(-1.46810454667195,-2.04511992320656,
100.535950828614));
#31746=CARTESIAN_POINT('Ctrl Pts',(-1.46294876346809,-2.04881121000888,
100.536353901632));
#31747=CARTESIAN_POINT('Ctrl Pts',(-1.45151404511931,-2.056932734988,100.537248441393));
#31748=CARTESIAN_POINT('Ctrl Pts',(-1.44522884787628,-2.06135365063044,
100.537740499733));
#31749=CARTESIAN_POINT('Ctrl Pts',(-1.42760949516564,-2.07362665364172,
100.539120687512));
#31750=CARTESIAN_POINT('Ctrl Pts',(-1.41623112356966,-2.08141436378788,
100.540012910354));
#31751=CARTESIAN_POINT('Ctrl Pts',(-1.35022360077575,-2.12580014252044,
100.545191419694));
#31752=CARTESIAN_POINT('Ctrl Pts',(-1.29424569805979,-2.16033712830925,
100.549592743342));
#31753=CARTESIAN_POINT('Ctrl Pts',(-1.08585130542124,-2.27790356877152,
100.565844555821));
#31754=CARTESIAN_POINT('Ctrl Pts',(-0.926305199992865,-2.34731358354033,
100.577998967716));
#31755=CARTESIAN_POINT('Ctrl Pts',(-0.652745184636279,-2.43404989738921,
100.59750089615));
#31756=CARTESIAN_POINT('Ctrl Pts',(-0.542404047051818,-2.46099152771537,
100.605043522307));
#31757=CARTESIAN_POINT('Ctrl Pts',(-0.407808109120123,-2.48435791799471,
100.613840533917));
#31758=CARTESIAN_POINT('Ctrl Pts',(-0.384954846368719,-2.48800151591862,
100.615320800282));
#31759=CARTESIAN_POINT('Ctrl Pts',(-0.34889035509464,-2.49324260955437,
100.617636402209));
#31760=CARTESIAN_POINT('Ctrl Pts',(-0.335711599323228,-2.49505128666623,
100.618478308275));
#31761=CARTESIAN_POINT('Ctrl Pts',(-0.311006546606393,-2.4982425671217,
100.620048777101));
#31762=CARTESIAN_POINT('Ctrl Pts',(-0.299483875279866,-2.49965005789153,
100.62077809936));
#31763=CARTESIAN_POINT('Ctrl Pts',(-0.273659274240288,-2.50262339029238,
100.622405775569));
#31764=CARTESIAN_POINT('Ctrl Pts',(-0.25935275315271,-2.50414644041181,
100.623302772622));
#31765=CARTESIAN_POINT('Ctrl Pts',(-0.222905182427715,-2.50771088550437,
100.625576459702));
#31766=CARTESIAN_POINT('Ctrl Pts',(-0.200748425042117,-2.50958178264796,
100.626947844484));
#31767=CARTESIAN_POINT('Ctrl Pts',(-0.0175577544293523,-2.52260852386498,
100.638203970951));
#31768=CARTESIAN_POINT('Ctrl Pts',(0.144189140867329,-2.51854738858078,
100.647583991415));
#31769=CARTESIAN_POINT('Ctrl Pts',(0.428316965986693,-2.4839326107074,100.664050429519));
#31770=CARTESIAN_POINT('Ctrl Pts',(0.550881788152934,-2.45965491945854,
100.671161290666));
#31771=CARTESIAN_POINT('Ctrl Pts',(0.713091661984844,-2.41478812658416,
100.681116238134));
#31772=CARTESIAN_POINT('Ctrl Pts',(0.754739344349178,-2.40209690002524,
100.683723091115));
#31773=CARTESIAN_POINT('Ctrl Pts',(0.822390400142762,-2.37954871150869,
100.688072658506));
#31774=CARTESIAN_POINT('Ctrl Pts',(0.848597674510532,-2.3703290657677,100.689786509709));
#31775=CARTESIAN_POINT('Ctrl Pts',(0.884060450968069,-2.35718988910627,
100.692152019308));
#31776=CARTESIAN_POINT('Ctrl Pts',(0.893454018587902,-2.35364546245515,
100.69278308648));
#31777=CARTESIAN_POINT('Ctrl Pts',(0.909157060713876,-2.34761276359627,
100.693845949014));
#31778=CARTESIAN_POINT('Ctrl Pts',(0.915478255372784,-2.34515496523902,
100.694275962354));
#31779=CARTESIAN_POINT('Ctrl Pts',(0.927479896712491,-2.34043258537347,
100.695096657117));
#31780=CARTESIAN_POINT('Ctrl Pts',(0.933162161070506,-2.33817279616173,
100.695487038634));
#31781=CARTESIAN_POINT('Ctrl Pts',(0.946664424333978,-2.33274599999782,
100.69641890245));
#31782=CARTESIAN_POINT('Ctrl Pts',(0.9544767879934,-2.32956036392274,100.696961468087));
#31783=CARTESIAN_POINT('Ctrl Pts',(0.98213832168642,-2.31811835900239,100.698894235719));
#31784=CARTESIAN_POINT('Ctrl Pts',(1.0018969496591,-2.30964734086693,100.70029623475));
#31785=CARTESIAN_POINT('Ctrl Pts',(1.13895276789552,-2.24879852893442,100.710159480568));
#31786=CARTESIAN_POINT('Ctrl Pts',(1.25218880544355,-2.18776716672089,100.719010663151));
#31787=CARTESIAN_POINT('Ctrl Pts',(1.46171080475726,-2.05322751427586,100.736210891805));
#31788=CARTESIAN_POINT('Ctrl Pts',(1.55835624891013,-1.98087644707488,100.744535329385));
#31789=CARTESIAN_POINT('Ctrl Pts',(1.71994735376084,-1.84073233757755,100.758951118939));
#31790=CARTESIAN_POINT('Ctrl Pts',(1.78699754995469,-1.77571331625135,100.765113382837));
#31791=CARTESIAN_POINT('Ctrl Pts',(1.86522348224368,-1.69092656821955,100.77253337927));
#31792=CARTESIAN_POINT('Ctrl Pts',(1.87994511134387,-1.6745440354028,100.773941005402));
#31793=CARTESIAN_POINT('Ctrl Pts',(1.90305106604264,-1.6481424225682,100.776169044908));
#31794=CARTESIAN_POINT('Ctrl Pts',(1.91157540483741,-1.63824793212065,100.776995221986));
#31795=CARTESIAN_POINT('Ctrl Pts',(1.9275515513349,-1.61940939010025,100.778551836963));
#31796=CARTESIAN_POINT('Ctrl Pts',(1.93501903943477,-1.6104791461357,100.779282902469));
#31797=CARTESIAN_POINT('Ctrl Pts',(1.95181042099421,-1.5901132114171,100.780934927466));
#31798=CARTESIAN_POINT('Ctrl Pts',(1.96109631449772,-1.57864663700044,100.781854346018));
#31799=CARTESIAN_POINT('Ctrl Pts',(1.98908614633528,-1.54345560040798,100.784644243067));
#31800=CARTESIAN_POINT('Ctrl Pts',(2.00746475018736,-1.51947500284881,100.786501910579));
#31801=CARTESIAN_POINT('Ctrl Pts',(2.15079634878779,-1.32531298603206,100.801217378728));
#31802=CARTESIAN_POINT('Ctrl Pts',(2.25432000658865,-1.14036354187834,100.813180005293));
#31803=CARTESIAN_POINT('Ctrl Pts',(2.37987546058945,-0.830206190917561,
100.83247331388));
#31804=CARTESIAN_POINT('Ctrl Pts',(2.41771590813143,-0.712524801985291,
100.839662104704));
#31805=CARTESIAN_POINT('Ctrl Pts',(2.45099165677794,-0.575124328726661,
100.848388804461));
#31806=CARTESIAN_POINT('Ctrl Pts',(2.45502768435253,-0.557644260879512,
100.849505138059));
#31807=CARTESIAN_POINT('Ctrl Pts',(2.46068773667247,-0.531877230564108,
100.851161686432));
#31808=CARTESIAN_POINT('Ctrl Pts',(2.46245753159908,-0.523622407856458,
100.85169403476));
#31809=CARTESIAN_POINT('Ctrl Pts',(2.46552146717394,-0.508972219075985,
100.852641990214));
#31810=CARTESIAN_POINT('Ctrl Pts',(2.46683231035741,-0.502580517009345,
100.85305665015));
#31811=CARTESIAN_POINT('Ctrl Pts',(2.46962277753576,-0.488700166624528,
100.853959536102));
#31812=CARTESIAN_POINT('Ctrl Pts',(2.47109317259254,-0.481209980026606,
100.854448246804));
#31813=CARTESIAN_POINT('Ctrl Pts',(2.47508136688199,-0.460393745800301,
100.855810356001));
#31814=CARTESIAN_POINT('Ctrl Pts',(2.47752553816796,-0.447054093272045,
100.856687683765));
#31815=CARTESIAN_POINT('Ctrl Pts',(2.4905503793018,-0.372578359732025,100.861608164114));
#31816=CARTESIAN_POINT('Ctrl Pts',(2.4989750429939,-0.311091946583115,100.865753776924));
#31817=CARTESIAN_POINT('Ctrl Pts',(2.52271833705488,-0.0725650432881702,
100.882005482591));
#31818=CARTESIAN_POINT('Ctrl Pts',(2.52155245773363,0.105600344880335,100.894460344976));
#31819=CARTESIAN_POINT('Ctrl Pts',(2.48892511090094,0.39486921629796,100.914242202577));
#31820=CARTESIAN_POINT('Ctrl Pts',(2.46861013541699,0.506596656144003,100.921783224797));
#31821=CARTESIAN_POINT('Ctrl Pts',(2.43515773256779,0.639021506479516,100.93057865893));
#31822=CARTESIAN_POINT('Ctrl Pts',(2.42918131339852,0.661377254858567,100.932058854489));
#31823=CARTESIAN_POINT('Ctrl Pts',(2.41928518229816,0.696449847755285,100.934374371168));
#31824=CARTESIAN_POINT('Ctrl Pts',(2.41557155146907,0.709223007592049,100.935216261984));
#31825=CARTESIAN_POINT('Ctrl Pts',(2.40842785420372,0.733086807857943,100.936786716888));
#31826=CARTESIAN_POINT('Ctrl Pts',(2.40502199129611,0.744184268444779,100.937516040346));
#31827=CARTESIAN_POINT('Ctrl Pts',(2.39722324296314,0.768982421632546,100.939143737769));
#31828=CARTESIAN_POINT('Ctrl Pts',(2.39278939897798,0.782669883859632,100.940040754674));
#31829=CARTESIAN_POINT('Ctrl Pts',(2.38120510360909,0.817412324265511,100.942314527208));
#31830=CARTESIAN_POINT('Ctrl Pts',(2.37389250883944,0.838412224459458,100.943685976889));
#31831=CARTESIAN_POINT('Ctrl Pts',(2.31108835374086,1.01135691993694,100.954963047209));
#31832=CARTESIAN_POINT('Ctrl Pts',(2.24134704658691,1.15773272525539,100.964361590552));
#31833=CARTESIAN_POINT('Ctrl Pts',(2.0941690288881,1.40272664227861,100.980802937861));
#31834=CARTESIAN_POINT('Ctrl Pts',(2.02254178811072,1.50416328124464,100.987871150068));
#31835=CARTESIAN_POINT('Ctrl Pts',(1.9159036005538,1.63371903738617,100.997793984006));
#31836=CARTESIAN_POINT('Ctrl Pts',(1.88719331809692,1.66680096401974,101.00041607461));
#31837=CARTESIAN_POINT('Ctrl Pts',(1.83880437782748,1.71970441338077,101.004788600888));
#31838=CARTESIAN_POINT('Ctrl Pts',(1.81963215780414,1.7399780085652,101.006509787682));
#31839=CARTESIAN_POINT('Ctrl Pts',(1.79309732213232,1.76711895047295,101.008883862739));
#31840=CARTESIAN_POINT('Ctrl Pts',(1.78602386268772,1.77426777731719,101.009515966861));
#31841=CARTESIAN_POINT('Ctrl Pts',(1.77410636777221,1.786168774638,101.010580085872));
#31842=CARTESIAN_POINT('Ctrl Pts',(1.76928551771567,1.79094417853476,101.011010309415));
#31843=CARTESIAN_POINT('Ctrl Pts',(1.76008578125356,1.79998379171951,101.011831012765));
#31844=CARTESIAN_POINT('Ctrl Pts',(1.75571056606676,1.8042516493297,101.012221190147));
#31845=CARTESIAN_POINT('Ctrl Pts',(1.745267702285,1.81436431733466,101.01315206251));
#31846=CARTESIAN_POINT('Ctrl Pts',(1.73918621542923,1.8201946412156,101.013693835635));
#31847=CARTESIAN_POINT('Ctrl Pts',(1.71753583431571,1.84074330911238,101.015621044044));
#31848=CARTESIAN_POINT('Ctrl Pts',(1.70180893731338,1.85529284519244,101.017018190788));
#31849=CARTESIAN_POINT('Ctrl Pts',(1.58893400648367,1.95707489480401,101.027014245241));
#31850=CARTESIAN_POINT('Ctrl Pts',(1.4853230278282,2.03682657618432,101.036016252602));
#31851=CARTESIAN_POINT('Ctrl Pts',(1.21961451622876,2.21025457964653,101.05793576285));
#31852=CARTESIAN_POINT('Ctrl Pts',(1.05232100302387,2.29463030545178,101.070765283594));
#31853=CARTESIAN_POINT('Ctrl Pts',(0.841749979897506,2.3729084213946,101.085419390914));
#31854=CARTESIAN_POINT('Ctrl Pts',(0.805996154787807,2.38528988948957,101.087861499123));
#31855=CARTESIAN_POINT('Ctrl Pts',(0.754622327257322,2.40179337757583,101.091307075695));
#31856=CARTESIAN_POINT('Ctrl Pts',(0.739222139259993,2.40657784705255,101.092331943959));
#31857=CARTESIAN_POINT('Ctrl Pts',(0.712441143248606,2.41461672758033,101.094100657476));
#31858=CARTESIAN_POINT('Ctrl Pts',(0.701081534144246,2.41793941485759,101.094846695066));
#31859=CARTESIAN_POINT('Ctrl Pts',(0.677731263547966,2.42459098138732,101.096371803482));
#31860=CARTESIAN_POINT('Ctrl Pts',(0.665738491730634,2.42791131677277,101.097150580848));
#31861=CARTESIAN_POINT('Ctrl Pts',(0.635191156459858,2.43612533393225,101.099123051274));
#31862=CARTESIAN_POINT('Ctrl Pts',(0.616604146978061,2.44089610706203,101.100312783088));
#31863=CARTESIAN_POINT('Ctrl Pts',(0.54442695384488,2.45854492113576,101.104894294869));
#31864=CARTESIAN_POINT('Ctrl Pts',(0.490471830884562,2.46987487344048,101.108237006871));
#31865=CARTESIAN_POINT('Ctrl Pts',(0.251030773908175,2.51199779071189,101.122780074389));
#31866=CARTESIAN_POINT('Ctrl Pts',(0.0628150882582449,2.52372867381365,
101.133397622241));
#31867=CARTESIAN_POINT('Ctrl Pts',(-0.240441823326435,2.5086576842004,101.15095578306));
#31868=CARTESIAN_POINT('Ctrl Pts',(-0.355378645883619,2.49496989932756,
101.15773259091));
#31869=CARTESIAN_POINT('Ctrl Pts',(-0.483649517092121,2.47065035617073,
101.165826760622));
#31870=CARTESIAN_POINT('Ctrl Pts',(-0.498321681213659,2.46773286938623,
101.166760628198));
#31871=CARTESIAN_POINT('Ctrl Pts',(-0.520650675099819,2.46308561115013,
101.168195298953));
#31872=CARTESIAN_POINT('Ctrl Pts',(-0.528327149139011,2.46145044087237,
101.168690957622));
#31873=CARTESIAN_POINT('Ctrl Pts',(-0.542353770502052,2.45839398424644,
101.169601300505));
#31874=CARTESIAN_POINT('Ctrl Pts',(-0.548706183004426,2.4569839470671,101.170015349237));
#31875=CARTESIAN_POINT('Ctrl Pts',(-0.563017731495372,2.45374896042638,
101.170952166158));
#31876=CARTESIAN_POINT('Ctrl Pts',(-0.570973438404357,2.45190991982809,
101.171475708719));
#31877=CARTESIAN_POINT('Ctrl Pts',(-0.591481206634859,2.44706412415595,
101.172832178246));
#31878=CARTESIAN_POINT('Ctrl Pts',(-0.604019169467984,2.44399952372491,
101.173668190619));
#31879=CARTESIAN_POINT('Ctrl Pts',(-0.686812521720767,2.42308670865737,
101.179230644361));
#31880=CARTESIAN_POINT('Ctrl Pts',(-0.756286362660291,2.40230921071231,
101.184097665248));
#31881=CARTESIAN_POINT('Ctrl Pts',(-0.969798124340045,2.32827471894551,
101.199493395555));
#31882=CARTESIAN_POINT('Ctrl Pts',(-1.10993300101494,2.26482286205766,101.210215688445));
#31883=CARTESIAN_POINT('Ctrl Pts',(-1.31581021125568,2.14787830702839,101.226371104731));
#31884=CARTESIAN_POINT('Ctrl Pts',(-1.38612282166367,2.10318888260151,101.231974675893));
#31885=CARTESIAN_POINT('Ctrl Pts',(-1.48280787509193,2.03477862282894,101.239780825843));
#31886=CARTESIAN_POINT('Ctrl Pts',(-1.51109087144459,2.01386390196833,101.242077806613));
#31887=CARTESIAN_POINT('Ctrl Pts',(-1.56074624829605,1.97550942366426,101.246135609531));
#31888=CARTESIAN_POINT('Ctrl Pts',(-1.58228735581412,1.95829853618454,101.247904731141));
#31889=CARTESIAN_POINT('Ctrl Pts',(-1.61451317864024,1.93167181019443,101.250565825627));
#31890=CARTESIAN_POINT('Ctrl Pts',(-1.62540735345955,1.92251391026502,101.251468009934));
#31891=CARTESIAN_POINT('Ctrl Pts',(-1.64503775469752,1.90572598983213,101.253098620193));
#31892=CARTESIAN_POINT('Ctrl Pts',(-1.65379995978832,1.89812709346959,101.253828282061));
#31893=CARTESIAN_POINT('Ctrl Pts',(-1.67258595652183,1.88160636930958,101.255396798162));
#31894=CARTESIAN_POINT('Ctrl Pts',(-1.68259159484296,1.87266437115923,101.256234789241));
#31895=CARTESIAN_POINT('Ctrl Pts',(-1.70959656273743,1.84813896429857,101.258503972631));
#31896=CARTESIAN_POINT('Ctrl Pts',(-1.72645429793493,1.83240106147024,101.259928660132));
#31897=CARTESIAN_POINT('Ctrl Pts',(-1.8164306964207,1.74605750913695,101.267582286731));
#31898=CARTESIAN_POINT('Ctrl Pts',(-1.88544308284351,1.67130044129759,101.273627577863));
#31899=CARTESIAN_POINT('Ctrl Pts',(-2.05555084997692,1.46304051714021,101.289331741976));
#31900=CARTESIAN_POINT('Ctrl Pts',(-2.14817370866746,1.32330005985822,101.298747639354));
#31901=CARTESIAN_POINT('Ctrl Pts',(-2.26509091513141,1.10185672581284,101.313408050624));
#31902=CARTESIAN_POINT('Ctrl Pts',(-2.30025380543939,1.02642806158329,101.318367374668));
#31903=CARTESIAN_POINT('Ctrl Pts',(-2.33694414465476,0.936321486141466,
101.324407073096));
#31904=CARTESIAN_POINT('Ctrl Pts',(-2.34216188340931,0.923192044570125,
101.325289923329));
#31905=CARTESIAN_POINT('Ctrl Pts',(-2.35004248008801,0.902865147073397,
101.326662084427));
#31906=CARTESIAN_POINT('Ctrl Pts',(-2.35278349490963,0.895698026344049,
101.327146916219));
#31907=CARTESIAN_POINT('Ctrl Pts',(-2.35748940257802,0.88322251231285,101.327992793097));
#31908=CARTESIAN_POINT('Ctrl Pts',(-2.35946921738775,0.877919870664267,
101.328352947803));
#31909=CARTESIAN_POINT('Ctrl Pts',(-2.3614311210104,0.872610629504102,101.328714168996));
#31910=CARTESIAN_POINT('Origin',(0.,0.,104.));
#31911=CARTESIAN_POINT('',(-2.36143111379333,0.872610649034711,102.332358906943));
#31912=CARTESIAN_POINT('',(-2.36143112101026,0.872610629504504,102.056173744947));
#31913=CARTESIAN_POINT('',(-2.36143112101026,0.872610629504505,104.));
#31914=CARTESIAN_POINT('',(-2.51749968849485,-0.00125236908425632,101.112583302546));
#31915=CARTESIAN_POINT('Ctrl Pts',(-2.36143112101026,0.872610629504504,
102.056173744947));
#31916=CARTESIAN_POINT('Ctrl Pts',(-2.33295402998363,0.949674427162242,
102.050996882856));
#31917=CARTESIAN_POINT('Ctrl Pts',(-2.30069008088684,1.02537084001563,102.045820020765));
#31918=CARTESIAN_POINT('Ctrl Pts',(-2.26480387283096,1.0993041742893,102.040643158674));
#31919=CARTESIAN_POINT('Ctrl Pts',(-2.22891712097872,1.17323862890085,102.035466218136));
#31920=CARTESIAN_POINT('Ctrl Pts',(-2.18940820972554,1.245409527097,102.030289277598));
#31921=CARTESIAN_POINT('Ctrl Pts',(-2.14648851258624,1.31544415135547,102.02511233706));
#31922=CARTESIAN_POINT('Ctrl Pts',(-2.10352677109179,1.38554738189058,102.019930325165));
#31923=CARTESIAN_POINT('Ctrl Pts',(-2.05714782123045,1.45350975648183,102.014748313269));
#31924=CARTESIAN_POINT('Ctrl Pts',(-2.00760697580321,1.51898666245174,102.009566301374));
#31925=CARTESIAN_POINT('Ctrl Pts',(-1.95804034278516,1.58449765124048,102.004381592076));
#31926=CARTESIAN_POINT('Ctrl Pts',(-1.90530884315185,1.64752023431275,101.999196882778));
#31927=CARTESIAN_POINT('Ctrl Pts',(-1.84970712889199,1.70774406376545,101.99401217348));
#31928=CARTESIAN_POINT('Ctrl Pts',(-1.79401193718764,1.76806914134962,101.988818747664));
#31929=CARTESIAN_POINT('Ctrl Pts',(-1.73543723557534,1.82558574091428,101.983625321847));
#31930=CARTESIAN_POINT('Ctrl Pts',(-1.67431308288007,1.88002179521851,101.978431896031));
#31931=CARTESIAN_POINT('Ctrl Pts',(-1.63429688170024,1.91565949332018,101.975031911522));
#31932=CARTESIAN_POINT('Ctrl Pts',(-1.59318868582522,1.9499777175966,101.971631927013));
#31933=CARTESIAN_POINT('Ctrl Pts',(-1.55108776789116,1.98291023152799,101.968231942504));
#31934=CARTESIAN_POINT('Ctrl Pts',(-1.48601369963049,2.03381298530937,101.962976693097));
#31935=CARTESIAN_POINT('Ctrl Pts',(-1.41831105347741,2.08160300135602,101.957721443689));
#31936=CARTESIAN_POINT('Ctrl Pts',(-1.34830995266693,2.12599777082181,101.952466194282));
#31937=CARTESIAN_POINT('Ctrl Pts',(-1.27840809751515,2.17032959858972,101.947218395625));
#31938=CARTESIAN_POINT('Ctrl Pts',(-1.20621464682185,2.21127549610306,101.941970596967));
#31939=CARTESIAN_POINT('Ctrl Pts',(-1.13209187433468,2.24859383572609,101.93672279831));
#31940=CARTESIAN_POINT('Ctrl Pts',(-1.05743201845937,2.28618257889195,101.931436974827));
#31941=CARTESIAN_POINT('Ctrl Pts',(-0.98081513687593,2.32009068081068,101.926151151344));
#31942=CARTESIAN_POINT('Ctrl Pts',(-0.90264026929864,2.3501163363205,101.920865327861));
#31943=CARTESIAN_POINT('Ctrl Pts',(-0.825166390362852,2.37987275384989,
101.915626901992));
#31944=CARTESIAN_POINT('Ctrl Pts',(-0.746162792910464,2.40581590487025,
101.910388476124));
#31945=CARTESIAN_POINT('Ctrl Pts',(-0.666039924684604,2.42779675193912,
101.905150050255));
#31946=CARTESIAN_POINT('Ctrl Pts',(-0.585943407536667,2.4497703698732,101.899913347218));
#31947=CARTESIAN_POINT('Ctrl Pts',(-0.504728795329403,2.46778414997604,
101.89467664418));
#31948=CARTESIAN_POINT('Ctrl Pts',(-0.422821641415984,2.48173892856406,
101.889439941143));
#31949=CARTESIAN_POINT('Ctrl Pts',(-0.340916718612409,2.4956933270309,101.88420338075));
#31950=CARTESIAN_POINT('Ctrl Pts',(-0.258319746649519,2.50558886733435,
101.878966820358));
#31951=CARTESIAN_POINT('Ctrl Pts',(-0.175465040666476,2.51137776320169,
101.873730259966));
#31952=CARTESIAN_POINT('Ctrl Pts',(-0.0912542264866104,2.51726140769004,
101.868407991195));
#31953=CARTESIAN_POINT('Ctrl Pts',(-0.00677765496019131,2.51890271813326,
101.863085722425));
#31954=CARTESIAN_POINT('Ctrl Pts',(0.0775066867450106,2.51630661158568,
101.857763453654));
#31955=CARTESIAN_POINT('Ctrl Pts',(0.160552829837627,2.51374864374169,101.852519372904));
#31956=CARTESIAN_POINT('Ctrl Pts',(0.243411892025474,2.50707703272406,101.847275292154));
#31957=CARTESIAN_POINT('Ctrl Pts',(0.325650897274851,2.496348882489,101.842031211403));
#31958=CARTESIAN_POINT('Ctrl Pts',(0.409729149087786,2.48538080092947,101.836669848623));
#31959=CARTESIAN_POINT('Ctrl Pts',(0.493158770837792,2.47017263631202,101.831308485842));
#31960=CARTESIAN_POINT('Ctrl Pts',(0.575490003805824,2.45084016319294,101.825947123061));
#31961=CARTESIAN_POINT('Ctrl Pts',(0.657821236773869,2.43150769007384,101.820585760281));
#31962=CARTESIAN_POINT('Ctrl Pts',(0.739053611328975,2.40805111359022,101.8152243975));
#31963=CARTESIAN_POINT('Ctrl Pts',(0.818757647879658,2.38063902430389,101.80986303472));
#31964=CARTESIAN_POINT('Ctrl Pts',(0.896884163093645,2.35376948163883,101.804607785312));
#31965=CARTESIAN_POINT('Ctrl Pts',(0.973830871246779,2.32300037319785,101.799352535905));
#31966=CARTESIAN_POINT('Ctrl Pts',(1.04918106998779,2.28845479142134,101.794097286498));
#31967=CARTESIAN_POINT('Ctrl Pts',(1.12442443926455,2.25395818743195,101.78884948784));
#31968=CARTESIAN_POINT('Ctrl Pts',(1.19807537913545,2.21569593576891,101.783601689183));
#31969=CARTESIAN_POINT('Ctrl Pts',(1.26973397369632,2.17384035431339,101.778353890525));
#31970=CARTESIAN_POINT('Ctrl Pts',(1.3419117965518,2.13168149308644,101.773068067042));
#31971=CARTESIAN_POINT('Ctrl Pts',(1.41206783162646,2.08587716292098,101.767782243559));
#31972=CARTESIAN_POINT('Ctrl Pts',(1.4798155485121,2.03665220211548,101.762496420076));
#31973=CARTESIAN_POINT('Ctrl Pts',(1.54695577629672,1.98786863813576,101.757257994208));
#31974=CARTESIAN_POINT('Ctrl Pts',(1.61173032318653,1.93572581916233,101.752019568339));
#31975=CARTESIAN_POINT('Ctrl Pts',(1.67379070881012,1.88048688192737,101.746781142471));
#31976=CARTESIAN_POINT('Ctrl Pts',(1.73583068380572,1.82526611185956,101.741544439433));
#31977=CARTESIAN_POINT('Ctrl Pts',(1.79515792597834,1.76695155239321,101.736307736395));
#31978=CARTESIAN_POINT('Ctrl Pts',(1.85145756440779,1.70584616457556,101.731071033358));
#31979=CARTESIAN_POINT('Ctrl Pts',(1.90775566926326,1.64474244123812,101.725834472966));
#31980=CARTESIAN_POINT('Ctrl Pts',(1.96102602244972,1.58084838074178,101.720597912573));
#31981=CARTESIAN_POINT('Ctrl Pts',(2.0109920776548,1.51450226596385,101.715361352181));
#31982=CARTESIAN_POINT('Ctrl Pts',(2.06177594249699,1.44707024412706,101.71003908341));
#31983=CARTESIAN_POINT('Ctrl Pts',(2.10914606227315,1.37710556168493,101.70471681464));
#31984=CARTESIAN_POINT('Ctrl Pts',(2.15285720954208,1.3049950518384,101.699394545869));
#31985=CARTESIAN_POINT('Ctrl Pts',(2.19592620809382,1.23394389811238,101.694150465119));
#31986=CARTESIAN_POINT('Ctrl Pts',(2.23544285799687,1.16080998695854,101.688906384369));
#31987=CARTESIAN_POINT('Ctrl Pts',(2.27121932313172,1.08598758567172,101.683662303618));
#31988=CARTESIAN_POINT('Ctrl Pts',(2.30779591638533,1.00949180757261,101.678300940838));
#31989=CARTESIAN_POINT('Ctrl Pts',(2.34046281303112,0.931231575526403,101.672939578057));
#31990=CARTESIAN_POINT('Ctrl Pts',(2.36907225203704,0.85164717731472,101.667578215277));
#31991=CARTESIAN_POINT('Ctrl Pts',(2.39768169104296,0.772062779103038,101.662216852496));
#31992=CARTESIAN_POINT('Ctrl Pts',(2.42223358878513,0.691154720335934,101.656855489715));
#31993=CARTESIAN_POINT('Ctrl Pts',(2.44263552689213,0.609375034575942,101.651494126935));
#31994=CARTESIAN_POINT('Ctrl Pts',(2.46263366496506,0.529213951897807,101.646238877528));
#31995=CARTESIAN_POINT('Ctrl Pts',(2.47871852955357,0.447919357606244,101.64098362812));
#31996=CARTESIAN_POINT('Ctrl Pts',(2.4907664954014,0.365907796290044,101.635728378713));
#31997=CARTESIAN_POINT('Ctrl Pts',(2.50279737997062,0.284012508737074,101.630480580055));
#31998=CARTESIAN_POINT('Ctrl Pts',(2.5108026676466,0.201402725930201,101.625232781398));
#31999=CARTESIAN_POINT('Ctrl Pts',(2.51470916250037,0.118507712983954,101.61998498274));
#32000=CARTESIAN_POINT('Ctrl Pts',(2.51864396327716,0.0350120542048318,
101.614699159258));
#32001=CARTESIAN_POINT('Ctrl Pts',(2.51842020731909,-0.0487725258357472,
101.609413335775));
#32002=CARTESIAN_POINT('Ctrl Pts',(2.51401604017221,-0.132399394850828,
101.604127512292));
#32003=CARTESIAN_POINT('Ctrl Pts',(2.50965136488813,-0.215276387503841,
101.598889086423));
#32004=CARTESIAN_POINT('Ctrl Pts',(2.50118097377524,-0.297998016898339,
101.593650660555));
#32005=CARTESIAN_POINT('Ctrl Pts',(2.48863585321228,-0.380128715182637,
101.588412234686));
#32006=CARTESIAN_POINT('Ctrl Pts',(2.47609485853068,-0.462232402047155,
101.583175531649));
#32007=CARTESIAN_POINT('Ctrl Pts',(2.45948186554945,-0.543745088015556,
101.577938828611));
#32008=CARTESIAN_POINT('Ctrl Pts',(2.4388795636937,-0.624237714174042,101.572702125574));
#32009=CARTESIAN_POINT('Ctrl Pts',(2.41827782303442,-0.704728147753364,
101.567465565181));
#32010=CARTESIAN_POINT('Ctrl Pts',(2.3936871049706,-0.78419813001327,101.562229004789));
#32011=CARTESIAN_POINT('Ctrl Pts',(2.36524059249845,-0.862231517399819,
101.556992444397));
#32012=CARTESIAN_POINT('Ctrl Pts',(2.33632848729637,-0.941542100994302,
101.551670175626));
#32013=CARTESIAN_POINT('Ctrl Pts',(2.30343338708735,-1.01936817258397,101.546347906856));
#32014=CARTESIAN_POINT('Ctrl Pts',(2.26674625011283,-1.09529342534292,101.541025638085));
#32015=CARTESIAN_POINT('Ctrl Pts',(2.23059807400799,-1.17010328061838,101.535781557335));
#32016=CARTESIAN_POINT('Ctrl Pts',(2.19076881527365,-1.24306741378589,101.530537476585));
#32017=CARTESIAN_POINT('Ctrl Pts',(2.14748691460656,-1.31381360991337,101.525293395834));
#32018=CARTESIAN_POINT('Ctrl Pts',(2.10323702938233,-1.38614201995179,101.519932033054));
#32019=CARTESIAN_POINT('Ctrl Pts',(2.0553784933784,-1.45615166634403,101.514570670273));
#32020=CARTESIAN_POINT('Ctrl Pts',(2.00420016786468,-1.52347889290636,101.509209307493));
#32021=CARTESIAN_POINT('Ctrl Pts',(1.95302184235097,-1.59080611946867,101.503847944712));
#32022=CARTESIAN_POINT('Ctrl Pts',(1.89852410590013,-1.65545058077782,101.498486581932));
#32023=CARTESIAN_POINT('Ctrl Pts',(1.84103580345049,-1.71708864663809,101.493125219151));
#32024=CARTESIAN_POINT('Ctrl Pts',(1.78468532321976,-1.77750675717042,101.487869969744));
#32025=CARTESIAN_POINT('Ctrl Pts',(1.72525347433516,-1.83525958626159,101.482614720336));
#32026=CARTESIAN_POINT('Ctrl Pts',(1.66302234322044,-1.89001664964878,101.477359470929));
#32027=CARTESIAN_POINT('Ctrl Pts',(1.6008794417125,-1.94469607995933,101.472111672272));
#32028=CARTESIAN_POINT('Ctrl Pts',(1.53594548458515,-1.99638787870892,101.466863873614));
#32029=CARTESIAN_POINT('Ctrl Pts',(1.46854068446697,-2.0447969356553,101.461616074957));
#32030=CARTESIAN_POINT('Ctrl Pts',(1.40064747846208,-2.09355675795282,101.456330251474));
#32031=CARTESIAN_POINT('Ctrl Pts',(1.33024779482609,-2.13898571857547,101.451044427991));
#32032=CARTESIAN_POINT('Ctrl Pts',(1.25770436658405,-2.18082231653003,101.445758604508));
#32033=CARTESIAN_POINT('Ctrl Pts',(1.18581143025572,-2.22228376859851,101.440520178639));
#32034=CARTESIAN_POINT('Ctrl Pts',(1.11181344803786,-2.26021679013602,101.435281752771));
#32035=CARTESIAN_POINT('Ctrl Pts',(1.03609264146641,-2.29441022668118,101.430043326902));
#32036=CARTESIAN_POINT('Ctrl Pts',(0.960396738207992,-2.32859241757414,
101.424806623865));
#32037=CARTESIAN_POINT('Ctrl Pts',(0.882979556110991,-2.35903727634764,
101.419569920827));
#32038=CARTESIAN_POINT('Ctrl Pts',(0.80424600686878,-2.38558056045811,101.41433321779));
#32039=CARTESIAN_POINT('Ctrl Pts',(0.725514602289,-2.41212312154282,101.409096657397));
#32040=CARTESIAN_POINT('Ctrl Pts',(0.645467339428495,-2.43476417284098,
101.403860097005));
#32041=CARTESIAN_POINT('Ctrl Pts',(0.564525787980021,-2.45338885721476,
101.398623536613));
#32042=CARTESIAN_POINT('Ctrl Pts',(0.482259441517519,-2.4723183774677,101.393301267842));
#32043=CARTESIAN_POINT('Ctrl Pts',(0.399069744422781,-2.4870987473585,101.387978999072));
#32044=CARTESIAN_POINT('Ctrl Pts',(0.31540985916229,-2.49766348228564,101.382656730301));
#32045=CARTESIAN_POINT('Ctrl Pts',(0.232978998792484,-2.50807301353125,
101.377412649551));
#32046=CARTESIAN_POINT('Ctrl Pts',(0.150092144703488,-2.51438997478319,
101.372168568801));
#32047=CARTESIAN_POINT('Ctrl Pts',(0.0671858828026818,-2.51660332733469,
101.36692448805));
#32048=CARTESIAN_POINT('Ctrl Pts',(-0.0175745486229646,-2.51886618074119,
101.36156312527));
#32049=CARTESIAN_POINT('Ctrl Pts',(-0.102354754541292,-2.51683967122694,
101.356201762489));
#32050=CARTESIAN_POINT('Ctrl Pts',(-0.186692431981587,-2.51056810021971,
101.350840399709));
#32051=CARTESIAN_POINT('Ctrl Pts',(-0.271030109421882,-2.50429652921248,
101.345479036928));
#32052=CARTESIAN_POINT('Ctrl Pts',(-0.354924762531309,-2.49378002618988,
101.340117674148));
#32053=CARTESIAN_POINT('Ctrl Pts',(-0.437925892658451,-2.47911822278392,
101.334756311367));
#32054=CARTESIAN_POINT('Ctrl Pts',(-0.519284244585212,-2.46474660929437,
101.32950106196));
#32055=CARTESIAN_POINT('Ctrl Pts',(-0.600084634975024,-2.4463392509089,
101.324245812552));
#32056=CARTESIAN_POINT('Ctrl Pts',(-0.679896273784101,-2.42395282687071,
101.318990563145));
#32057=CARTESIAN_POINT('Ctrl Pts',(-0.759594757820063,-2.40159814169631,
101.313742764488));
#32058=CARTESIAN_POINT('Ctrl Pts',(-0.838306834140659,-2.37527571993368,
101.30849496583));
#32059=CARTESIAN_POINT('Ctrl Pts',(-0.915610626285933,-2.3450934802332,
101.303247167173));
#32060=CARTESIAN_POINT('Ctrl Pts',(-0.993474551049313,-2.31469254418583,
101.29796134369));
#32061=CARTESIAN_POINT('Ctrl Pts',(-1.06990923039576,-2.28037570120002,
101.292675520207));
#32062=CARTESIAN_POINT('Ctrl Pts',(-1.14449782874786,-2.24230483431478,
101.287389696724));
#32063=CARTESIAN_POINT('Ctrl Pts',(-1.21841759628706,-2.20457534626504,
101.282151270855));
#32064=CARTESIAN_POINT('Ctrl Pts',(-1.29052383903869,-2.16315910245258,
101.276912844987));
#32065=CARTESIAN_POINT('Ctrl Pts',(-1.36043134115765,-2.11826174397688,
101.271674419118));
#32066=CARTESIAN_POINT('Ctrl Pts',(-1.43031585186252,-2.07337915149524,
101.266437716081));
#32067=CARTESIAN_POINT('Ctrl Pts',(-1.49800267016906,-2.02501796729658,
101.261201013043));
#32068=CARTESIAN_POINT('Ctrl Pts',(-1.56313357589532,-1.97342840607627,
101.255964310006));
#32069=CARTESIAN_POINT('Ctrl Pts',(-1.62826270748839,-1.92184025012971,
101.250727749613));
#32070=CARTESIAN_POINT('Ctrl Pts',(-1.69083570386698,-1.86702417931519,
101.245491189221));
#32071=CARTESIAN_POINT('Ctrl Pts',(-1.75052669947269,-1.80927126889067,
101.240254628829));
#32072=CARTESIAN_POINT('Ctrl Pts',(-1.8111946757756,-1.75057309899913,101.234932360058));
#32073=CARTESIAN_POINT('Ctrl Pts',(-1.86888509645779,-1.6888414183291,101.229610091288));
#32074=CARTESIAN_POINT('Ctrl Pts',(-1.92329546973613,-1.62442013841631,
101.224287822517));
#32075=CARTESIAN_POINT('Ctrl Pts',(-1.9769065148435,-1.56094525421343,101.219043741767));
#32076=CARTESIAN_POINT('Ctrl Pts',(-2.02733301030583,-1.49485967987507,
101.213799661017));
#32077=CARTESIAN_POINT('Ctrl Pts',(-2.07432799706226,-1.42652361025105,
101.208555580266));
#32078=CARTESIAN_POINT('Ctrl Pts',(-2.12237401024619,-1.35665922835195,
101.203194217486));
#32079=CARTESIAN_POINT('Ctrl Pts',(-2.16683290515724,-1.28444290942289,
101.197832854705));
#32080=CARTESIAN_POINT('Ctrl Pts',(-2.20749013991719,-1.21028654961061,
101.192471491925));
#32081=CARTESIAN_POINT('Ctrl Pts',(-2.24814737467715,-1.13613018979832,
101.187110129144));
#32082=CARTESIAN_POINT('Ctrl Pts',(-2.28500278792296,-1.06003427551463,
101.181748766363));
#32083=CARTESIAN_POINT('Ctrl Pts',(-2.3178946752049,-0.982430926150415,
101.176387403583));
#32084=CARTESIAN_POINT('Ctrl Pts',(-2.35361447071378,-0.898155562248903,
101.170565093038));
#32085=CARTESIAN_POINT('Ctrl Pts',(-2.38477328167377,-0.811838041542081,
101.164742782493));
#32086=CARTESIAN_POINT('Ctrl Pts',(-2.41115846466788,-0.723962090347565,
101.158920471948));
#32087=CARTESIAN_POINT('Ctrl Pts',(-2.4374644137324,-0.636350028053568,
101.15311564563));
#32088=CARTESIAN_POINT('Ctrl Pts',(-2.45902521036231,-0.547189130622515,
101.147310819312));
#32089=CARTESIAN_POINT('Ctrl Pts',(-2.47567650290214,-0.456981512731327,
101.141505992995));
#32090=CARTESIAN_POINT('Ctrl Pts',(-2.49224191268966,-0.367239160733822,
101.135731106363));
#32091=CARTESIAN_POINT('Ctrl Pts',(-2.50394821153258,-0.276461124818012,
101.129956219731));
#32092=CARTESIAN_POINT('Ctrl Pts',(-2.51068155182442,-0.18516045832883,
101.124181333099));
#32093=CARTESIAN_POINT('Ctrl Pts',(-2.51518920085722,-0.12403903223759,
101.120315322914));
#32094=CARTESIAN_POINT('Ctrl Pts',(-2.51746912850001,-0.0626837621585557,
101.11644931273));
#32095=CARTESIAN_POINT('Ctrl Pts',(-2.51749968849485,-0.00125236908424377,
101.112583302546));
#32096=CARTESIAN_POINT('Ctrl Pts',(-2.51749968849528,-0.00125236822532715,
101.112583302492));
#32097=CARTESIAN_POINT('Ctrl Pts',(-2.51754167409677,0.083146721867559,
101.107271885552));
#32098=CARTESIAN_POINT('Ctrl Pts',(-2.51333509775226,0.167540685368797,
101.101960468612));
#32099=CARTESIAN_POINT('Ctrl Pts',(-2.50490792305447,0.251480709039413,
101.096649051672));
#32100=CARTESIAN_POINT('Ctrl Pts',(-2.49647888961856,0.335439246924613,
101.09133646322));
#32101=CARTESIAN_POINT('Ctrl Pts',(-2.48382745953182,0.418943205939949,
101.086023874768));
#32102=CARTESIAN_POINT('Ctrl Pts',(-2.46703330865219,0.501550499950555,
101.080711286317));
#32103=CARTESIAN_POINT('Ctrl Pts',(-2.45022206899961,0.584241850446145,
101.075393292077));
#32104=CARTESIAN_POINT('Ctrl Pts',(-2.42925979038389,0.666034281971585,
101.070075297837));
#32105=CARTESIAN_POINT('Ctrl Pts',(-2.4042768382142,0.746497913745721,101.064757303598));
#32106=CARTESIAN_POINT('Ctrl Pts',(-2.39110377033219,0.788924960645322,
101.061953219491));
#32107=CARTESIAN_POINT('Ctrl Pts',(-2.37681368205517,0.830982832244095,
101.059149135384));
#32108=CARTESIAN_POINT('Ctrl Pts',(-2.36143112101025,0.872610629504513,
101.056345051278));
#32109=CARTESIAN_POINT('Ctrl Pts',(-2.3614311210104,0.872610629504102,101.328714168996));
#32110=CARTESIAN_POINT('Ctrl Pts',(-2.36172918736716,0.87180401181328,101.32876904829));
#32111=CARTESIAN_POINT('Ctrl Pts',(-2.36202684029789,0.870997241779622,
101.32882395201));
#32112=CARTESIAN_POINT('Ctrl Pts',(-2.36522277224922,0.862321177659682,
101.329414540597));
#32113=CARTESIAN_POINT('Ctrl Pts',(-2.36808207781547,0.854437735427849,
101.329952500584));
#32114=CARTESIAN_POINT('Ctrl Pts',(-2.37548955523205,0.833691644041302,
101.33137140068));
#32115=CARTESIAN_POINT('Ctrl Pts',(-2.37997257734536,0.820806247606163,
101.332255900535));
#32116=CARTESIAN_POINT('Ctrl Pts',(-2.41665618100022,0.712540185518066,
101.339710875365));
#32117=CARTESIAN_POINT('Ctrl Pts',(-2.44321033835195,0.61535305269985,101.346550076335));
#32118=CARTESIAN_POINT('Ctrl Pts',(-2.49940153361352,0.347484055687169,
101.365365167741));
#32119=CARTESIAN_POINT('Ctrl Pts',(-2.51737555155781,0.174885346556131,
101.377416472145));
#32120=CARTESIAN_POINT('Ctrl Pts',(-2.51755617191668,-0.0776304462386804,
101.394332960011));
#32121=CARTESIAN_POINT('Ctrl Pts',(-2.51385374182857,-0.157026032853185,
101.399556554048));
#32122=CARTESIAN_POINT('Ctrl Pts',(-2.50435559508939,-0.257847910187009,
101.406068721468));
#32123=CARTESIAN_POINT('Ctrl Pts',(-2.50202630676959,-0.279547671549114,
101.407463286211));
#32124=CARTESIAN_POINT('Ctrl Pts',(-2.49785775514308,-0.314137389021349,
101.40967556161));
#32125=CARTESIAN_POINT('Ctrl Pts',(-2.49620020432483,-0.327047724918777,
101.410498895477));
#32126=CARTESIAN_POINT('Ctrl Pts',(-2.49286963686515,-0.351486718145176,
101.412053127542));
#32127=CARTESIAN_POINT('Ctrl Pts',(-2.4912165884664,-0.363017707715161,
101.412784628888));
#32128=CARTESIAN_POINT('Ctrl Pts',(-2.48727744870282,-0.389200500062406,
101.414441645585));
#32129=CARTESIAN_POINT('Ctrl Pts',(-2.48494180482339,-0.403844496752386,
101.415365582878));
#32130=CARTESIAN_POINT('Ctrl Pts',(-2.47739135894408,-0.44863607148298,
101.418183580184));
#32131=CARTESIAN_POINT('Ctrl Pts',(-2.47175616434693,-0.478710620372423,
101.420064440261));
#32132=CARTESIAN_POINT('Ctrl Pts',(-2.4417557181073,-0.624124042715217,
101.429114724524));
#32133=CARTESIAN_POINT('Ctrl Pts',(-2.40985715131089,-0.737763463489458,
101.436043690325));
#32134=CARTESIAN_POINT('Ctrl Pts',(-2.30850872053919,-1.02077256024703,
101.453445916921));
#32135=CARTESIAN_POINT('Ctrl Pts',(-2.22837341446319,-1.1855497579761,101.463702586228));
#32136=CARTESIAN_POINT('Ctrl Pts',(-2.10829047188926,-1.3765019799792,101.477254844456));
#32137=CARTESIAN_POINT('Ctrl Pts',(-2.08453131581174,-1.41222346464157,
101.479871221915));
#32138=CARTESIAN_POINT('Ctrl Pts',(-2.05285448779753,-1.45730701588315,
101.483302949146));
#32139=CARTESIAN_POINT('Ctrl Pts',(-2.04576364091668,-1.46724449157694,
101.484067706087));
#32140=CARTESIAN_POINT('Ctrl Pts',(-2.03434391142491,-1.48300496984466,
101.4852946045));
#32141=CARTESIAN_POINT('Ctrl Pts',(-2.03006154129942,-1.48886165439053,
101.485753650007));
#32142=CARTESIAN_POINT('Ctrl Pts',(-2.02182807915965,-1.50002039695321,
101.486634429349));
#32143=CARTESIAN_POINT('Ctrl Pts',(-2.01788134988087,-1.50532548861657,
101.48705587088));
#32144=CARTESIAN_POINT('Ctrl Pts',(-2.00843843572285,-1.51791454468206,
101.48806231573));
#32145=CARTESIAN_POINT('Ctrl Pts',(-2.00292349153935,-1.52518424983481,
101.488648594527));
#32146=CARTESIAN_POINT('Ctrl Pts',(-1.98411891016749,-1.54969424217938,
101.49064211295));
#32147=CARTESIAN_POINT('Ctrl Pts',(-1.97064564706049,-1.56679154717359,
101.492061184998));
#32148=CARTESIAN_POINT('Ctrl Pts',(-1.93727145438188,-1.60803121257369,
101.495549793263));
#32149=CARTESIAN_POINT('Ctrl Pts',(-1.91713922736513,-1.63198102623633,
101.497632072998));
#32150=CARTESIAN_POINT('Ctrl Pts',(-1.83396174471256,-1.72726768161193,
101.506127287737));
#32151=CARTESIAN_POINT('Ctrl Pts',(-1.76734236855021,-1.79537410662982,
101.512686630651));
#32152=CARTESIAN_POINT('Ctrl Pts',(-1.54888968240569,-1.9947357411201,101.533114330001));
#32153=CARTESIAN_POINT('Ctrl Pts',(-1.38509360214154,-2.11177056368132,
101.546896691837));
#32154=CARTESIAN_POINT('Ctrl Pts',(-1.18159057604464,-2.22320374128811,
101.561952462386));
#32155=CARTESIAN_POINT('Ctrl Pts',(-1.15378344491456,-2.23776117406832,
101.563971101042));
#32156=CARTESIAN_POINT('Ctrl Pts',(-1.11231236310428,-2.25849326398709,
101.566926417194));
#32157=CARTESIAN_POINT('Ctrl Pts',(-1.0988546673236,-2.26507153363681,101.567877012767));
#32158=CARTESIAN_POINT('Ctrl Pts',(-1.07481286846283,-2.27655872698203,
101.569560553352));
#32159=CARTESIAN_POINT('Ctrl Pts',(-1.06425194631923,-2.28151487870729,
101.570295107451));
#32160=CARTESIAN_POINT('Ctrl Pts',(-1.04191223017021,-2.29180984882758,
101.571838628463));
#32161=CARTESIAN_POINT('Ctrl Pts',(-1.03012595204267,-2.29713169222341,
101.57264699892));
#32162=CARTESIAN_POINT('Ctrl Pts',(-0.998694193774606,-2.31103346814054,
101.574787272472));
#32163=CARTESIAN_POINT('Ctrl Pts',(-0.978978975170113,-2.31945381363046,
101.576113760895));
#32164=CARTESIAN_POINT('Ctrl Pts',(-0.880682351119668,-2.35995954239794,
101.582652075516));
#32165=CARTESIAN_POINT('Ctrl Pts',(-0.800616476209311,-2.38831026217681,
101.587738382793));
#32166=CARTESIAN_POINT('Ctrl Pts',(-0.53273968207224,-2.46817311667891,
101.604193756111));
#32167=CARTESIAN_POINT('Ctrl Pts',(-0.340408869308689,-2.50196042748617,
101.615080348334));
#32168=CARTESIAN_POINT('Ctrl Pts',(-0.0706608672599164,-2.51764290021729,
101.630953348771));
#32169=CARTESIAN_POINT('Ctrl Pts',(0.00494464605481614,-2.518628991865,
101.635474852003));
#32170=CARTESIAN_POINT('Ctrl Pts',(0.0934973024873506,-2.51579695911163,
101.640972057355));
#32171=CARTESIAN_POINT('Ctrl Pts',(0.106518970630747,-2.51527926427425,
101.641785548451));
#32172=CARTESIAN_POINT('Ctrl Pts',(0.127729731795672,-2.51427099957564,
101.643119835508));
#32173=CARTESIAN_POINT('Ctrl Pts',(0.135921663376561,-2.51384145097431,
101.643637397917));
#32174=CARTESIAN_POINT('Ctrl Pts',(0.150609338600618,-2.5129992919997,101.644569609295));
#32175=CARTESIAN_POINT('Ctrl Pts',(0.157105756180925,-2.51260151914006,
101.644983435099));
#32176=CARTESIAN_POINT('Ctrl Pts',(0.171400691760376,-2.51167058975998,
101.645897384837));
#32177=CARTESIAN_POINT('Ctrl Pts',(0.179198195729925,-2.51112631130291,
101.646398095255));
#32178=CARTESIAN_POINT('Ctrl Pts',(0.201757361004582,-2.5094460375886,101.647852766465));
#32179=CARTESIAN_POINT('Ctrl Pts',(0.21651140642045,-2.50821614584709,101.648811649398));
#32180=CARTESIAN_POINT('Ctrl Pts',(0.338067315599042,-2.49700281527279,
101.656768964609));
#32181=CARTESIAN_POINT('Ctrl Pts',(0.444130892964582,-2.48033367283814,
101.664072657662));
#32182=CARTESIAN_POINT('Ctrl Pts',(0.711067452958561,-2.42070969192047,
101.682898692485));
#32183=CARTESIAN_POINT('Ctrl Pts',(0.869368700839968,-2.36847221888829,
101.694460466903));
#32184=CARTESIAN_POINT('Ctrl Pts',(1.09454319307913,-2.26852173666696,101.710969828079));
#32185=CARTESIAN_POINT('Ctrl Pts',(1.16613199664307,-2.23256671433604,101.716235893064));
#32186=CARTESIAN_POINT('Ctrl Pts',(1.25494705283373,-2.18251976536889,101.722791932291));
#32187=CARTESIAN_POINT('Ctrl Pts',(1.27386171536046,-2.17153425280453,101.724189682161));
#32188=CARTESIAN_POINT('Ctrl Pts',(1.30380961784052,-2.15361473400303,101.726405802222));
#32189=CARTESIAN_POINT('Ctrl Pts',(1.31493600915743,-2.14683936154327,101.727229829755));
#32190=CARTESIAN_POINT('Ctrl Pts',(1.33590956352097,-2.13384337083717,101.728784639368));
#32191=CARTESIAN_POINT('Ctrl Pts',(1.34576708713398,-2.12764020635169,101.729516030584));
#32192=CARTESIAN_POINT('Ctrl Pts',(1.36806117869079,-2.11339400127814,101.731171810828));
#32193=CARTESIAN_POINT('Ctrl Pts',(1.38047060334552,-2.1053091272699,101.732094630978));
#32194=CARTESIAN_POINT('Ctrl Pts',(1.4182143928178,-2.08024142402063,101.734905665642));
#32195=CARTESIAN_POINT('Ctrl Pts',(1.44331267452209,-2.06290695201871,101.73678077715));
#32196=CARTESIAN_POINT('Ctrl Pts',(1.56324554824217,-1.97681307029793,101.745780547244));
#32197=CARTESIAN_POINT('Ctrl Pts',(1.65352296875486,-1.90194450478809,101.752667972112));
#32198=CARTESIAN_POINT('Ctrl Pts',(1.87087562321093,-1.69447290384077,101.770066608593));
#32199=CARTESIAN_POINT('Ctrl Pts',(1.9892475516853,-1.55380028613859,101.780355127044));
#32200=CARTESIAN_POINT('Ctrl Pts',(2.11530275363044,-1.36570904831162,101.793955891469));
#32201=CARTESIAN_POINT('Ctrl Pts',(2.1383907588902,-1.3292672435408,101.796586418493));
#32202=CARTESIAN_POINT('Ctrl Pts',(2.16680766557815,-1.28175675262042,101.800034256593));
#32203=CARTESIAN_POINT('Ctrl Pts',(2.17300890448883,-1.27121521363664,101.800800389005));
#32204=CARTESIAN_POINT('Ctrl Pts',(2.18276851790485,-1.2543446732966,101.802028981774));
#32205=CARTESIAN_POINT('Ctrl Pts',(2.18637683743974,-1.24804458403013,101.8024883313));
#32206=CARTESIAN_POINT('Ctrl Pts',(2.19321837662858,-1.23597860081223,101.803369296461));
#32207=CARTESIAN_POINT('Ctrl Pts',(2.19645619243537,-1.23021548514261,101.803790616648));
#32208=CARTESIAN_POINT('Ctrl Pts',(2.20410387926704,-1.21647663338506,101.804796211397));
#32209=CARTESIAN_POINT('Ctrl Pts',(2.20849318307504,-1.20848962112337,101.805381755583));
#32210=CARTESIAN_POINT('Ctrl Pts',(2.22318708358302,-1.18140440554198,101.807370167952));
#32211=CARTESIAN_POINT('Ctrl Pts',(2.23328775291323,-1.16219745139941,101.808784788955));
#32212=CARTESIAN_POINT('Ctrl Pts',(2.29188988975984,-1.0471769328964,101.817272767998));
#32213=CARTESIAN_POINT('Ctrl Pts',(2.33446419818119,-0.948478350966228,
101.824619422664));
#32214=CARTESIAN_POINT('Ctrl Pts',(2.43567639175228,-0.665328501455818,
101.845352659632));
#32215=CARTESIAN_POINT('Ctrl Pts',(2.47957350143165,-0.476360166230241,
101.858745741571));
#32216=CARTESIAN_POINT('Ctrl Pts',(2.50698160996559,-0.23513613647249,101.874724462154));
#32217=CARTESIAN_POINT('Ctrl Pts',(2.51111250586123,-0.185904105703202,
101.877933024791));
#32218=CARTESIAN_POINT('Ctrl Pts',(2.5147912768141,-0.118195043006874,101.882276357249));
#32219=CARTESIAN_POINT('Ctrl Pts',(2.51558845086623,-0.0997998467113807,
101.883449381315));
#32220=CARTESIAN_POINT('Ctrl Pts',(2.51654109464776,-0.0703513128390186,
101.885316482728));
#32221=CARTESIAN_POINT('Ctrl Pts',(2.51682568664899,-0.0593030994945107,
101.886014540997));
#32222=CARTESIAN_POINT('Ctrl Pts',(2.51726322565758,-0.0364797112806158,
101.887451719616));
#32223=CARTESIAN_POINT('Ctrl Pts',(2.51740632533036,-0.0247046013295393,
101.88819051691));
#32224=CARTESIAN_POINT('Ctrl Pts',(2.51754775425828,0.00283420997172765,
101.889912318829));
#32225=CARTESIAN_POINT('Ctrl Pts',(2.51748065830297,0.0185978641871937,
101.890893272061));
#32226=CARTESIAN_POINT('Ctrl Pts',(2.51677818651749,0.0700618057000397,
101.894081507818));
#32227=CARTESIAN_POINT('Ctrl Pts',(2.51553138671735,0.105750335333389,101.896269895965));
#32228=CARTESIAN_POINT('Ctrl Pts',(2.5107664008115,0.19045169630388,101.901418908085));
#32229=CARTESIAN_POINT('Ctrl Pts',(2.50657174313088,0.239412390919124,101.90435937046));
#32230=CARTESIAN_POINT('Ctrl Pts',(2.48429458526032,0.432715221182628,101.915877200006));
#32231=CARTESIAN_POINT('Ctrl Pts',(2.45515175006029,0.575494889199207,101.924163957067));
#32232=CARTESIAN_POINT('Ctrl Pts',(2.40050256925057,0.759999869101461,101.935243793087));
#32233=CARTESIAN_POINT('Ctrl Pts',(2.38590588137352,0.80465229124762,101.937957072073));
#32234=CARTESIAN_POINT('Ctrl Pts',(2.33998842558295,0.932855257071136,101.945903207168));
#32235=CARTESIAN_POINT('Ctrl Pts',(2.30546799976501,1.01517414679257,101.951200755784));
#32236=CARTESIAN_POINT('Ctrl Pts',(2.26077090167604,1.10765705734199,101.957568574702));
#32237=CARTESIAN_POINT('Ctrl Pts',(2.25478682874172,1.11978817860489,101.958412392653));
#32238=CARTESIAN_POINT('Ctrl Pts',(2.24495060009248,1.13932997879792,101.959786495274));
#32239=CARTESIAN_POINT('Ctrl Pts',(2.24115872768089,1.14677092309987,101.960313218542));
#32240=CARTESIAN_POINT('Ctrl Pts',(2.23434183455633,1.15998504131652,101.961255109214));
#32241=CARTESIAN_POINT('Ctrl Pts',(2.2313313294498,1.1657655108954,101.961669376467));
#32242=CARTESIAN_POINT('Ctrl Pts',(2.22471559754283,1.17834885922855,101.962576136081));
#32243=CARTESIAN_POINT('Ctrl Pts',(2.22110165356873,1.18514681147389,101.963069149946));
#32244=CARTESIAN_POINT('Ctrl Pts',(2.21071077874187,1.2044779413438,101.964479893279));
#32245=CARTESIAN_POINT('Ctrl Pts',(2.20385867773175,1.21697007552952,101.965402110189));
#32246=CARTESIAN_POINT('Ctrl Pts',(2.15462284931333,1.30495281456214,101.971968880341));
#32247=CARTESIAN_POINT('Ctrl Pts',(2.10847983104193,1.37826379468537,101.97781401008));
#32248=CARTESIAN_POINT('Ctrl Pts',(1.95902734123117,1.59059108685737,101.995589684895));
#32249=CARTESIAN_POINT('Ctrl Pts',(1.84505144901853,1.72149991230264,102.007682034587));
#32250=CARTESIAN_POINT('Ctrl Pts',(1.65049431142722,1.90324624530085,102.025634751009));
#32251=CARTESIAN_POINT('Ctrl Pts',(1.5789650858613,1.96299530129438,102.031788447827));
#32252=CARTESIAN_POINT('Ctrl Pts',(1.4862001328979,2.03212299867471,102.039235810936));
#32253=CARTESIAN_POINT('Ctrl Pts',(1.46793845223857,2.04535362987872,102.040678027916));
#32254=CARTESIAN_POINT('Ctrl Pts',(1.43862464046938,2.06599669703487,102.042956121989));
#32255=CARTESIAN_POINT('Ctrl Pts',(1.42768760277896,2.07356970662602,102.043798072823));
#32256=CARTESIAN_POINT('Ctrl Pts',(1.40709532834494,2.08758801767768,102.045368582532));
#32257=CARTESIAN_POINT('Ctrl Pts',(1.39745458616321,2.0940538869551,102.046097901273));
#32258=CARTESIAN_POINT('Ctrl Pts',(1.37576658061112,2.10838315308245,102.047725515224));
#32259=CARTESIAN_POINT('Ctrl Pts',(1.36369588030189,2.11621047255517,102.048622454014));
#32260=CARTESIAN_POINT('Ctrl Pts',(1.32765221650936,2.13914674143955,102.051274941111));
#32261=CARTESIAN_POINT('Ctrl Pts',(1.30349004682474,2.15395519601591,102.053019494989));
#32262=CARTESIAN_POINT('Ctrl Pts',(1.24771043709163,2.18685883634807,102.056974960525));
#32263=CARTESIAN_POINT('Ctrl Pts',(1.21593967212873,2.20468224660051,102.059176393726));
#32264=CARTESIAN_POINT('Ctrl Pts',(1.10625261587917,2.26312407522971,102.066619203297));
#32265=CARTESIAN_POINT('Ctrl Pts',(1.0265995718532,2.30035225228205,102.071756184157));
#32266=CARTESIAN_POINT('Ctrl Pts',(0.832735420481711,2.37888013945891,102.083856062264));
#32267=CARTESIAN_POINT('Ctrl Pts',(0.717171235759592,2.41623327313614,102.090750583046));
#32268=CARTESIAN_POINT('Ctrl Pts',(0.505797278098832,2.46804718008178,102.103413272922));
#32269=CARTESIAN_POINT('Ctrl Pts',(0.410997770687885,2.48559133947329,102.1091137378));
#32270=CARTESIAN_POINT('Ctrl Pts',(0.301976193924167,2.4993600686096,102.115925550792));
#32271=CARTESIAN_POINT('Ctrl Pts',(0.288500707560359,2.50095135844207,102.116771963719));
#32272=CARTESIAN_POINT('Ctrl Pts',(0.266699318406875,2.50334729546376,102.118149469117));
#32273=CARTESIAN_POINT('Ctrl Pts',(0.258380915102101,2.50421954031975,102.118676971487));
#32274=CARTESIAN_POINT('Ctrl Pts',(0.24357211845672,2.50569778005592,102.119619696994));
#32275=CARTESIAN_POINT('Ctrl Pts',(0.237083520288757,2.50632004036768,102.120034013459));
#32276=CARTESIAN_POINT('Ctrl Pts',(0.222935205337559,2.50762143751097,102.120940213473));
#32277=CARTESIAN_POINT('Ctrl Pts',(0.215274884125142,2.50829067297999,102.121432613296));
#32278=CARTESIAN_POINT('Ctrl Pts',(0.193456111303942,2.51009616088944,102.1228398761));
#32279=CARTESIAN_POINT('Ctrl Pts',(0.17929120698126,2.51114767485487,102.123759192873));
#32280=CARTESIAN_POINT('Ctrl Pts',(0.0800077748094564,2.51767355857795,
102.130239263557));
#32281=CARTESIAN_POINT('Ctrl Pts',(-0.00532378543316241,2.51893826357532,
102.135994793692));
#32282=CARTESIAN_POINT('Ctrl Pts',(-0.259645833197371,2.50978533121428,
102.153409511484));
#32283=CARTESIAN_POINT('Ctrl Pts',(-0.427719297121613,2.48666482807939,
102.165230256701));
#32284=CARTESIAN_POINT('Ctrl Pts',(-0.687266663619545,2.42384763050094,
102.183273992997));
#32285=CARTESIAN_POINT('Ctrl Pts',(-0.780918006447934,2.39531708987386,
102.189747966364));
#32286=CARTESIAN_POINT('Ctrl Pts',(-0.894110023229313,2.35348579646905,
102.197518661793));
#32287=CARTESIAN_POINT('Ctrl Pts',(-0.915429978700684,2.34527527981217,
102.198980112063));
#32288=CARTESIAN_POINT('Ctrl Pts',(-0.949045752935968,2.33180126902361,
102.201281584918));
#32289=CARTESIAN_POINT('Ctrl Pts',(-0.961416063958937,2.32672820986001,
102.202127894035));
#32290=CARTESIAN_POINT('Ctrl Pts',(-0.9844443545709,2.31706930496512,102.203702418765));
#32291=CARTESIAN_POINT('Ctrl Pts',(-0.995112130544635,2.3125078823973,102.204431429945));
#32292=CARTESIAN_POINT('Ctrl Pts',(-1.00588014631224,2.3078152876672,102.205166988493));
#32293=CARTESIAN_POINT('Ctrl Pts',(-1.00601214941439,2.30775774854429,102.205176005522));
#32294=CARTESIAN_POINT('Ctrl Pts',(-1.00626873776199,2.30764587748561,102.205193532784));
#32295=CARTESIAN_POINT('Ctrl Pts',(-1.00639332353623,2.30759154678967,102.205202043057));
#32296=CARTESIAN_POINT('Ctrl Pts',(-1.006635523316,2.3074859023761,102.205218587293));
#32297=CARTESIAN_POINT('Ctrl Pts',(-1.00675313779619,2.30743458975627,102.205226621292));
#32298=CARTESIAN_POINT('Ctrl Pts',(-1.00698181168126,2.30733480354001,102.205242241457));
#32299=CARTESIAN_POINT('Ctrl Pts',(-1.0070928715131,2.30728633091591,102.205249827656));
#32300=CARTESIAN_POINT('Ctrl Pts',(-1.00730882554319,2.30719205812677,102.205264578833));
#32301=CARTESIAN_POINT('Ctrl Pts',(-1.00741372011044,2.30714625883009,102.20527174384));
#32302=CARTESIAN_POINT('Ctrl Pts',(-1.00761770774491,2.30705717673657,102.205285677517));
#32303=CARTESIAN_POINT('Ctrl Pts',(-1.00771680115004,2.30701389470735,102.205292446213));
#32304=CARTESIAN_POINT('Ctrl Pts',(-1.00790952710494,2.30692970105548,102.205305610545));
#32305=CARTESIAN_POINT('Ctrl Pts',(-1.00800315995954,2.30688879011373,102.205312006204));
#32306=CARTESIAN_POINT('Ctrl Pts',(-1.00818528366029,2.30680920171942,102.20532444625));
#32307=CARTESIAN_POINT('Ctrl Pts',(-1.00827377476478,2.30677052487849,102.205330490657));
#32308=CARTESIAN_POINT('Ctrl Pts',(-1.0084459135437,2.30669527631879,102.2053422486));
#32309=CARTESIAN_POINT('Ctrl Pts',(-1.00852956144568,2.30665870514574,102.205347962153));
#32310=CARTESIAN_POINT('Ctrl Pts',(-1.00869229353554,2.30658754752828,102.205359077502));
#32311=CARTESIAN_POINT('Ctrl Pts',(-1.00877137795136,2.30655296155901,102.205364479314));
#32312=CARTESIAN_POINT('Ctrl Pts',(-1.00892524528203,2.30648566136781,102.205374989096));
#32313=CARTESIAN_POINT('Ctrl Pts',(-1.00900002838378,2.30645294757648,102.205380097081));
#32314=CARTESIAN_POINT('Ctrl Pts',(-1.02195129036639,2.30078668084318,102.20626471746));
#32315=CARTESIAN_POINT('Ctrl Pts',(-1.03478056851933,2.29504531072591,102.207140578595));
#32316=CARTESIAN_POINT('Ctrl Pts',(-1.07383726669698,2.27717254103202,102.209806223099));
#32317=CARTESIAN_POINT('Ctrl Pts',(-1.09990504095687,2.26469650567027,102.211584259757));
#32318=CARTESIAN_POINT('Ctrl Pts',(-1.1594819676016,2.23491158575601,102.215649616219));
#32319=CARTESIAN_POINT('Ctrl Pts',(-1.19282887405432,2.21729287995418,102.217926350863));
#32320=CARTESIAN_POINT('Ctrl Pts',(-1.3067695500755,2.15377796747743,102.225728165427));
#32321=CARTESIAN_POINT('Ctrl Pts',(-1.3852178436821,2.10418146640345,102.231136726129));
#32322=CARTESIAN_POINT('Ctrl Pts',(-1.55484898303669,1.98333015279238,102.243164782171));
#32323=CARTESIAN_POINT('Ctrl Pts',(-1.64421455413009,1.90989820394562,102.249739042851));
#32324=CARTESIAN_POINT('Ctrl Pts',(-1.79710703433492,1.76555590827235,102.261980744939));
#32325=CARTESIAN_POINT('Ctrl Pts',(-1.86226116432162,1.69669107390033,102.267590972833));
#32326=CARTESIAN_POINT('Ctrl Pts',(-1.93211057729572,1.61398214365726,102.27430205417));
#32327=CARTESIAN_POINT('Ctrl Pts',(-1.94076440164278,1.60356576468318,102.275146814554));
#32328=CARTESIAN_POINT('Ctrl Pts',(-1.95462129051345,1.58661012369885,102.276522153058));
#32329=CARTESIAN_POINT('Ctrl Pts',(-1.95987669833531,1.58011372899273,102.277049159366));
#32330=CARTESIAN_POINT('Ctrl Pts',(-1.96917371556974,1.56850362192962,102.277991353126));
#32331=CARTESIAN_POINT('Ctrl Pts',(-1.97322793209571,1.56340022404815,102.278405638058));
#32332=CARTESIAN_POINT('Ctrl Pts',(-1.98202574031839,1.55223691364614,102.279312193489));
#32333=CARTESIAN_POINT('Ctrl Pts',(-1.98676130965998,1.54617106623109,102.279804983587));
#32334=CARTESIAN_POINT('Ctrl Pts',(-2.00017537856742,1.52882544968786,102.281214458159));
#32335=CARTESIAN_POINT('Ctrl Pts',(-2.00878597807941,1.51749387896731,102.282135617796));
#32336=CARTESIAN_POINT('Ctrl Pts',(-2.06881130035086,1.43709426650933,102.288670502877));
#32337=CARTESIAN_POINT('Ctrl Pts',(-2.11674395867628,1.36550796291995,102.294482661709));
#32338=CARTESIAN_POINT('Ctrl Pts',(-2.22849033970987,1.17855304495393,102.309391289842));
#32339=CARTESIAN_POINT('Ctrl Pts',(-2.28709287016483,1.06036032991809,102.318564208382));
#32340=CARTESIAN_POINT('Ctrl Pts',(-2.3449014233359,0.916401356570871,102.329174466241));
#32341=CARTESIAN_POINT('Ctrl Pts',(-2.35331951990706,0.89456198575824,102.330769975562));
#32342=CARTESIAN_POINT('Ctrl Pts',(-2.36143111379333,0.872610649034711,
102.332358906943));
#32343=CARTESIAN_POINT('Origin',(0.,0.,104.));
#32344=CARTESIAN_POINT('',(-2.36143100149827,0.872610952923958,103.332666057199));
#32345=CARTESIAN_POINT('',(-2.36143112101026,0.872610629504504,103.05616702425));
#32346=CARTESIAN_POINT('',(-2.36143112101026,0.872610629504505,104.));
#32347=CARTESIAN_POINT('',(-2.51749968066629,-0.00126800832535854,102.11258330245));
#32348=CARTESIAN_POINT('Ctrl Pts',(-2.36143112101026,0.872610629504504,
103.05616702425));
#32349=CARTESIAN_POINT('Ctrl Pts',(-2.33272565502948,0.950292448196763,
103.050921177399));
#32350=CARTESIAN_POINT('Ctrl Pts',(-2.30014405188381,1.02666168444337,103.045675330547));
#32351=CARTESIAN_POINT('Ctrl Pts',(-2.26383053884827,1.10130719664312,103.040429483695));
#32352=CARTESIAN_POINT('Ctrl Pts',(-2.22755357146253,1.17587758615385,103.035188916225));
#32353=CARTESIAN_POINT('Ctrl Pts',(-2.1875523595261,1.24872728615334,103.029948348755));
#32354=CARTESIAN_POINT('Ctrl Pts',(-2.14401936121982,1.319464750842,103.024707781285));
#32355=CARTESIAN_POINT('Ctrl Pts',(-2.1005098519192,1.39016404786996,103.019470041456));
#32356=CARTESIAN_POINT('Ctrl Pts',(-2.05347258115096,1.45875298021808,103.014232301627));
#32357=CARTESIAN_POINT('Ctrl Pts',(-2.00314554584338,1.5248652964009,103.008994561799));
#32358=CARTESIAN_POINT('Ctrl Pts',(-1.95283048431597,1.59096188317835,103.00375806813));
#32359=CARTESIAN_POINT('Ctrl Pts',(-1.89922749246793,1.65458265733426,102.998521574462));
#32360=CARTESIAN_POINT('Ctrl Pts',(-1.84261661039682,1.71539216422652,102.993285080793));
#32361=CARTESIAN_POINT('Ctrl Pts',(-1.78600212094128,1.77620554604988,102.988048253442));
#32362=CARTESIAN_POINT('Ctrl Pts',(-1.72637967611523,1.83420696813375,102.982811426092));
#32363=CARTESIAN_POINT('Ctrl Pts',(-1.66406718599625,1.88909678166327,102.977574598741));
#32364=CARTESIAN_POINT('Ctrl Pts',(-1.60169040302655,1.94404322946596,102.972332368131));
#32365=CARTESIAN_POINT('Ctrl Pts',(-1.53661837932049,1.99587135211307,102.96709013752));
#32366=CARTESIAN_POINT('Ctrl Pts',(-1.46920282596402,2.04432123360771,102.96184790691));
#32367=CARTESIAN_POINT('Ctrl Pts',(-1.40175133933086,2.09279693945459,102.95660288213));
#32368=CARTESIAN_POINT('Ctrl Pts',(-1.33195422328854,2.13789056774503,102.951357857349));
#32369=CARTESIAN_POINT('Ctrl Pts',(-1.2601908859708,2.17938642303657,102.946112832569));
#32370=CARTESIAN_POINT('Ctrl Pts',(-1.18830350299189,2.22095400549406,102.940858741563));
#32371=CARTESIAN_POINT('Ctrl Pts',(-1.11444352097549,2.25891118210886,102.935604650558));
#32372=CARTESIAN_POINT('Ctrl Pts',(-1.03901334447018,2.29308907808068,102.930350559552));
#32373=CARTESIAN_POINT('Ctrl Pts',(-0.982041288511566,2.31890348144108,
102.926382169438));
#32374=CARTESIAN_POINT('Ctrl Pts',(-0.924173959955293,2.34256289199948,
102.922413779323));
#32375=CARTESIAN_POINT('Ctrl Pts',(-0.865590384616286,2.36401343821473,
102.918445389209));
#32376=CARTESIAN_POINT('Ctrl Pts',(-0.788009478833714,2.39241991213306,
102.913190139802));
#32377=CARTESIAN_POINT('Ctrl Pts',(-0.708885477545965,2.41705578739818,
102.907934890394));
#32378=CARTESIAN_POINT('Ctrl Pts',(-0.628619422757687,2.43775385782318,
102.902679640987));
#32379=CARTESIAN_POINT('Ctrl Pts',(-0.548467167000853,2.45842258308635,
102.89743184233));
#32380=CARTESIAN_POINT('Ctrl Pts',(-0.46717651696939,2.47516447854799,102.892184043672));
#32381=CARTESIAN_POINT('Ctrl Pts',(-0.385166524085117,2.4878611293085,102.886936245015));
#32382=CARTESIAN_POINT('Ctrl Pts',(-0.302562298101391,2.50064977824959,
102.881650421532));
#32383=CARTESIAN_POINT('Ctrl Pts',(-0.219228705756596,2.50933414962651,
102.876364598049));
#32384=CARTESIAN_POINT('Ctrl Pts',(-0.135607525173053,2.51384503283644,
102.871078774566));
#32385=CARTESIAN_POINT('Ctrl Pts',(-0.0527361699438051,2.51831546726799,
102.865840348697));
#32386=CARTESIAN_POINT('Ctrl Pts',(0.0304171673725803,2.51868693520644,
102.860601922829));
#32387=CARTESIAN_POINT('Ctrl Pts',(0.113416093058451,2.51494394367655,102.85536349696));
#32388=CARTESIAN_POINT('Ctrl Pts',(0.19638772177894,2.51120218315428,102.850126793923));
#32389=CARTESIAN_POINT('Ctrl Pts',(0.279204579138952,2.50334867141904,102.844890090885));
#32390=CARTESIAN_POINT('Ctrl Pts',(0.361431247096607,2.49142001750451,102.839653387848));
#32391=CARTESIAN_POINT('Ctrl Pts',(0.443655675240946,2.47949168852056,102.834416827455));
#32392=CARTESIAN_POINT('Ctrl Pts',(0.525289489454487,2.46348850532888,102.829180267063));
#32393=CARTESIAN_POINT('Ctrl Pts',(0.605904746065709,2.44349865739579,102.823943706671));
#32394=CARTESIAN_POINT('Ctrl Pts',(0.687839457124257,2.42318162953591,102.8186214379));
#32395=CARTESIAN_POINT('Ctrl Pts',(0.768721487248275,2.39874636322157,102.81329916913));
#32396=CARTESIAN_POINT('Ctrl Pts',(0.84811658852575,2.37033847841768,102.807976900359));
#32397=CARTESIAN_POINT('Ctrl Pts',(0.926345317707781,2.34234792621483,102.802732819609));
#32398=CARTESIAN_POINT('Ctrl Pts',(1.00313010739013,2.31050093807368,102.797488738859));
#32399=CARTESIAN_POINT('Ctrl Pts',(1.07807656706824,2.27498509127826,102.792244658108));
#32400=CARTESIAN_POINT('Ctrl Pts',(1.15469917808106,2.23867494500205,102.786883295328));
#32401=CARTESIAN_POINT('Ctrl Pts',(1.22939978860889,2.19853009672539,102.781521932547));
#32402=CARTESIAN_POINT('Ctrl Pts',(1.30178609528669,2.15479911177776,102.776160569766));
#32403=CARTESIAN_POINT('Ctrl Pts',(1.3741724019645,2.11106812683013,102.770799206986));
#32404=CARTESIAN_POINT('Ctrl Pts',(1.44424402108161,2.06375134491817,102.765437844205));
#32405=CARTESIAN_POINT('Ctrl Pts',(1.51164419791891,2.0131413434973,102.760076481425));
#32406=CARTESIAN_POINT('Ctrl Pts',(1.57771037435099,1.9635330273178,102.754821232017));
#32407=CARTESIAN_POINT('Ctrl Pts',(1.64145394247886,1.91057746621046,102.74956598261));
#32408=CARTESIAN_POINT('Ctrl Pts',(1.70251630309744,1.85452001544535,102.744310733203));
#32409=CARTESIAN_POINT('Ctrl Pts',(1.76349209116036,1.7985420414107,102.739062934545));
#32410=CARTESIAN_POINT('Ctrl Pts',(1.82179388522043,1.73947122242562,102.733815135888));
#32411=CARTESIAN_POINT('Ctrl Pts',(1.87709420657265,1.67759458441288,102.72856733723));
#32412=CARTESIAN_POINT('Ctrl Pts',(1.93279522642758,1.61526959681376,102.723281513747));
#32413=CARTESIAN_POINT('Ctrl Pts',(1.9854507145793,1.55009824201116,102.717995690264));
#32414=CARTESIAN_POINT('Ctrl Pts',(2.03476209091976,1.48241339826509,102.712709866781));
#32415=CARTESIAN_POINT('Ctrl Pts',(2.08363129555232,1.41533547984091,102.707471440913));
#32416=CARTESIAN_POINT('Ctrl Pts',(2.12921584430077,1.34578934831167,102.702233015044));
#32417=CARTESIAN_POINT('Ctrl Pts',(2.1712651465362,1.27413261218647,102.696994589176));
#32418=CARTESIAN_POINT('Ctrl Pts',(2.21330061945593,1.20249944276924,102.691757886138));
#32419=CARTESIAN_POINT('Ctrl Pts',(2.25180292167082,1.12875744500863,102.6865211831));
#32420=CARTESIAN_POINT('Ctrl Pts',(2.28656569652326,1.05329177604455,102.681284480063));
#32421=CARTESIAN_POINT('Ctrl Pts',(2.32132752445511,0.977828162727556,102.676047919671));
#32422=CARTESIAN_POINT('Ctrl Pts',(2.35234983543767,0.900641391084837,102.670811359278));
#32423=CARTESIAN_POINT('Ctrl Pts',(2.37947360751494,0.822138431859156,102.665574798886));
#32424=CARTESIAN_POINT('Ctrl Pts',(2.40704132262729,0.742350590800591,102.660252530115));
#32425=CARTESIAN_POINT('Ctrl Pts',(2.43058155731741,0.66120354903341,102.654930261345));
#32426=CARTESIAN_POINT('Ctrl Pts',(2.44998002953487,0.579140833373282,102.649607992574));
#32427=CARTESIAN_POINT('Ctrl Pts',(2.46909352401034,0.498283679014527,102.644363911824));
#32428=CARTESIAN_POINT('Ctrl Pts',(2.48418611465781,0.416538047401716,102.639119831074));
#32429=CARTESIAN_POINT('Ctrl Pts',(2.49520041333014,0.334336876992537,102.633875750323));
#32430=CARTESIAN_POINT('Ctrl Pts',(2.50646104293656,0.250297306182818,102.628514387543));
#32431=CARTESIAN_POINT('Ctrl Pts',(2.51345871792467,0.165782085061767,102.623153024762));
#32432=CARTESIAN_POINT('Ctrl Pts',(2.51618834279569,0.0812556064470767,
102.617791661982));
#32433=CARTESIAN_POINT('Ctrl Pts',(2.51891796766671,-0.00327087216761331,
102.612430299201));
#32434=CARTESIAN_POINT('Ctrl Pts',(2.51737961845209,-0.087808101468579,
102.60706893642));
#32435=CARTESIAN_POINT('Ctrl Pts',(2.51162447120052,-0.171897544097395,
102.60170757364));
#32436=CARTESIAN_POINT('Ctrl Pts',(2.50598323119854,-0.254322668384581,
102.596452324233));
#32437=CARTESIAN_POINT('Ctrl Pts',(2.49626980025757,-0.336622019470838,
102.591197074825));
#32438=CARTESIAN_POINT('Ctrl Pts',(2.48249474058826,-0.41836122304967,102.585941825418));
#32439=CARTESIAN_POINT('Ctrl Pts',(2.46873921082425,-0.499984539006743,
102.58069402676));
#32440=CARTESIAN_POINT('Ctrl Pts',(2.45093356636748,-0.581048833684912,
102.575446228103));
#32441=CARTESIAN_POINT('Ctrl Pts',(2.42914026605549,-0.661123148761145,
102.570198429445));
#32442=CARTESIAN_POINT('Ctrl Pts',(2.40718905449469,-0.741777671282336,
102.564912605963));
#32443=CARTESIAN_POINT('Ctrl Pts',(2.38119218759281,-0.821427334373817,
102.55962678248));
#32444=CARTESIAN_POINT('Ctrl Pts',(2.35126631866033,-0.899640455256151,
102.554340958997));
#32445=CARTESIAN_POINT('Ctrl Pts',(2.32160879292891,-0.977152244482249,
102.549102533128));
#32446=CARTESIAN_POINT('Ctrl Pts',(2.2880926130632,-1.0532527121713,102.54386410726));
#32447=CARTESIAN_POINT('Ctrl Pts',(2.25088130386266,-1.12753696432602,102.538625681391));
#32448=CARTESIAN_POINT('Ctrl Pts',(2.21368223284243,-1.20179678562646,102.533388978354));
#32449=CARTESIAN_POINT('Ctrl Pts',(2.17279065257134,-1.27424116548096,102.528152275316));
#32450=CARTESIAN_POINT('Ctrl Pts',(2.12841727868255,-1.34448731411106,102.522915572279));
#32451=CARTESIAN_POINT('Ctrl Pts',(2.08404511350229,-1.41473154927118,102.517679011886));
#32452=CARTESIAN_POINT('Ctrl Pts',(2.0361915905717,-1.4827772827043,102.512442451494));
#32453=CARTESIAN_POINT('Ctrl Pts',(1.98511149405792,-1.54826955216433,102.507205891102));
#32454=CARTESIAN_POINT('Ctrl Pts',(1.93319535405377,-1.61483375353694,102.501883622331));
#32455=CARTESIAN_POINT('Ctrl Pts',(1.8779463589783,-1.67875975435023,102.496561353561));
#32456=CARTESIAN_POINT('Ctrl Pts',(1.81967431466198,-1.73971021683482,102.49123908479));
#32457=CARTESIAN_POINT('Ctrl Pts',(1.76225832928811,-1.79976527245548,102.48599500404));
#32458=CARTESIAN_POINT('Ctrl Pts',(1.70190790868203,-1.85693135779367,102.48075092329));
#32459=CARTESIAN_POINT('Ctrl Pts',(1.63895495321572,-1.91092462209519,102.475506842539));
#32460=CARTESIAN_POINT('Ctrl Pts',(1.57459407693793,-1.96612542685176,102.470145479759));
#32461=CARTESIAN_POINT('Ctrl Pts',(1.50751325655197,-2.0180094667169,102.464784116978));
#32462=CARTESIAN_POINT('Ctrl Pts',(1.43809924691835,-2.06631962823104,102.459422754198));
#32463=CARTESIAN_POINT('Ctrl Pts',(1.36868523728473,-2.11462978974519,102.454061391417));
#32464=CARTESIAN_POINT('Ctrl Pts',(1.29693850490501,-2.15936586075086,102.448700028637));
#32465=CARTESIAN_POINT('Ctrl Pts',(1.22327153025748,-2.20032111594229,102.443338665856));
#32466=CARTESIAN_POINT('Ctrl Pts',(1.15106258997487,-2.24046577493673,102.438083416449));
#32467=CARTESIAN_POINT('Ctrl Pts',(1.0767420365693,-2.27712623417218,102.432828167041));
#32468=CARTESIAN_POINT('Ctrl Pts',(1.00067997047002,-2.31007485738019,102.427572917634));
#32469=CARTESIAN_POINT('Ctrl Pts',(0.92472574310124,-2.34297676692552,102.422325118977));
#32470=CARTESIAN_POINT('Ctrl Pts',(0.847035327201603,-2.37217711150451,
102.417077320319));
#32471=CARTESIAN_POINT('Ctrl Pts',(0.768004213099297,-2.39749364517651,
102.411829521662));
#32472=CARTESIAN_POINT('Ctrl Pts',(0.688400450442436,-2.42299361896039,
102.406543698179));
#32473=CARTESIAN_POINT('Ctrl Pts',(0.607436892757032,-2.44455303097053,
102.401257874696));
#32474=CARTESIAN_POINT('Ctrl Pts',(0.525539144305114,-2.46203469874067,
102.395972051213));
#32475=CARTESIAN_POINT('Ctrl Pts',(0.444375767310515,-2.4793596096026,102.390733625344));
#32476=CARTESIAN_POINT('Ctrl Pts',(0.362295345666176,-2.49267951493152,
102.385495199476));
#32477=CARTESIAN_POINT('Ctrl Pts',(0.279726532665683,-2.50191113289878,
102.380256773607));
#32478=CARTESIAN_POINT('Ctrl Pts',(0.19718487517368,-2.51113971474052,102.37502007057));
#32479=CARTESIAN_POINT('Ctrl Pts',(0.11415560353496,-2.51628262838044,102.369783367532));
#32480=CARTESIAN_POINT('Ctrl Pts',(0.0310745233179384,-2.51730820997361,
102.364546664495));
#32481=CARTESIAN_POINT('Ctrl Pts',(-0.0520042938120273,-2.51833376363045,
102.359310104102));
#32482=CARTESIAN_POINT('Ctrl Pts',(-0.13513445531612,-2.51524220356714,
102.35407354371));
#32483=CARTESIAN_POINT('Ctrl Pts',(-0.217879503963275,-2.50805398102846,
102.348836983318));
#32484=CARTESIAN_POINT('Ctrl Pts',(-0.301978866012361,-2.50074810666312,
102.343514714547));
#32485=CARTESIAN_POINT('Ctrl Pts',(-0.385679903931832,-2.48921028676346,
102.338192445777));
#32486=CARTESIAN_POINT('Ctrl Pts',(-0.468530987135187,-2.47351671999486,
102.332870177006));
#32487=CARTESIAN_POINT('Ctrl Pts',(-0.550164927341432,-2.45805370319801,
102.327626096256));
#32488=CARTESIAN_POINT('Ctrl Pts',(-0.630973279405555,-2.43855640038693,
102.322382015506));
#32489=CARTESIAN_POINT('Ctrl Pts',(-0.710537247829162,-2.41514866404687,
102.317137934755));
#32490=CARTESIAN_POINT('Ctrl Pts',(-0.791880636554139,-2.39121742187774,
102.311776571975));
#32491=CARTESIAN_POINT('Ctrl Pts',(-0.871922826292059,-2.36319889375182,
102.306415209194));
#32492=CARTESIAN_POINT('Ctrl Pts',(-0.950237582969059,-2.33127750083792,
102.301053846414));
#32493=CARTESIAN_POINT('Ctrl Pts',(-1.02855233964605,-2.29935610792404,
102.295692483633));
#32494=CARTESIAN_POINT('Ctrl Pts',(-1.10513923131857,-2.26353212601061,
102.290331120853));
#32495=CARTESIAN_POINT('Ctrl Pts',(-1.17960028275469,-2.22403898862521,
102.284969758072));
#32496=CARTESIAN_POINT('Ctrl Pts',(-1.25258758326841,-2.18532750885178,
102.279714508665));
#32497=CARTESIAN_POINT('Ctrl Pts',(-1.32380203496534,-2.14294784628376,
102.274459259257));
#32498=CARTESIAN_POINT('Ctrl Pts',(-1.39285119654326,-2.09708650138425,
102.26920400985));
#32499=CARTESIAN_POINT('Ctrl Pts',(-1.46180246209607,-2.0512901774534,102.263956211193));
#32500=CARTESIAN_POINT('Ctrl Pts',(-1.52859415406789,-2.00202222915303,
102.258708412535));
#32501=CARTESIAN_POINT('Ctrl Pts',(-1.59285808064314,-1.94951516663242,
102.253460613878));
#32502=CARTESIAN_POINT('Ctrl Pts',(-1.65758765476851,-1.89662764517739,
102.248174790395));
#32503=CARTESIAN_POINT('Ctrl Pts',(-1.71975225860477,-1.8404540931339,102.242888966912));
#32504=CARTESIAN_POINT('Ctrl Pts',(-1.77900510365269,-1.78127681486558,
102.237603143429));
#32505=CARTESIAN_POINT('Ctrl Pts',(-1.83772663252902,-1.72263017516676,
102.23236471756));
#32506=CARTESIAN_POINT('Ctrl Pts',(-1.89358808005325,-1.66103379397616,
102.227126291692));
#32507=CARTESIAN_POINT('Ctrl Pts',(-1.94628620911516,-1.59680187944784,
102.221887865823));
#32508=CARTESIAN_POINT('Ctrl Pts',(-1.99896700663946,-1.5325910897272,102.216651162786));
#32509=CARTESIAN_POINT('Ctrl Pts',(-2.04848625947963,-1.46574684459179,
102.211414459748));
#32510=CARTESIAN_POINT('Ctrl Pts',(-2.09458013322477,-1.39661745496041,
102.206177756711));
#32511=CARTESIAN_POINT('Ctrl Pts',(-2.14067275139581,-1.32748994837909,
102.200941196318));
#32512=CARTESIAN_POINT('Ctrl Pts',(-2.18333992086581,-1.25607780554095,
102.195704635926));
#32513=CARTESIAN_POINT('Ctrl Pts',(-2.22236116616033,-1.18275825811638,
102.190468075534));
#32514=CARTESIAN_POINT('Ctrl Pts',(-2.26202108405615,-1.10823866733784,
102.185145806763));
#32515=CARTESIAN_POINT('Ctrl Pts',(-2.29791441049229,-1.03174909841384,
102.179823537993));
#32516=CARTESIAN_POINT('Ctrl Pts',(-2.32985916934359,-0.953709862078392,
102.174501269222));
#32517=CARTESIAN_POINT('Ctrl Pts',(-2.36133463632777,-0.876817079190902,
102.169257188472));
#32518=CARTESIAN_POINT('Ctrl Pts',(-2.38897668257423,-0.79842031994964,
102.164013107722));
#32519=CARTESIAN_POINT('Ctrl Pts',(-2.41266118072925,-0.718938298466652,
102.158769026971));
#32520=CARTESIAN_POINT('Ctrl Pts',(-2.43687537439444,-0.637678689396935,
102.153407664191));
#32521=CARTESIAN_POINT('Ctrl Pts',(-2.456952744312,-0.555285186779454,102.14804630141));
#32522=CARTESIAN_POINT('Ctrl Pts',(-2.47281591772869,-0.472215720860313,
102.14268493863));
#32523=CARTESIAN_POINT('Ctrl Pts',(-2.48867909114538,-0.38914625494116,
102.137323575849));
#32524=CARTESIAN_POINT('Ctrl Pts',(-2.50032806421808,-0.305401338184696,
102.131962213068));
#32525=CARTESIAN_POINT('Ctrl Pts',(-2.50774196095251,-0.221441882393651,
102.126600850288));
#32526=CARTESIAN_POINT('Ctrl Pts',(-2.51420329401792,-0.148269834375223,
102.121928334356));
#32527=CARTESIAN_POINT('Ctrl Pts',(-2.51746263872295,-0.0748109262768815,
102.117255818424));
#32528=CARTESIAN_POINT('Ctrl Pts',(-2.51749968066596,-0.00126800898220263,
102.112583302492));
#32529=CARTESIAN_POINT('Ctrl Pts',(-2.51749968066629,-0.00126800832534177,
102.11258330245));
#32530=CARTESIAN_POINT('Ctrl Pts',(-2.51754083200824,0.0804337345976501,
102.107392419228));
#32531=CARTESIAN_POINT('Ctrl Pts',(-2.51360049225428,0.162294868972713,
102.102201536007));
#32532=CARTESIAN_POINT('Ctrl Pts',(-2.50565839985951,0.243889797272241,
102.097010652785));
#32533=CARTESIAN_POINT('Ctrl Pts',(-2.49772544325755,0.325390866885326,
102.091825740638));
#32534=CARTESIAN_POINT('Ctrl Pts',(-2.48579990849483,0.406625870881061,
102.086640828492));
#32535=CARTESIAN_POINT('Ctrl Pts',(-2.46991353078061,0.487168759740263,
102.081455916346));
#32536=CARTESIAN_POINT('Ctrl Pts',(-2.45404174187781,0.567637684286298,
102.076275765619));
#32537=CARTESIAN_POINT('Ctrl Pts',(-2.43421642245339,0.647415293431656,
102.071095614892));
#32538=CARTESIAN_POINT('Ctrl Pts',(-2.41052097619079,0.726081864078853,
102.065915464165));
#32539=CARTESIAN_POINT('Ctrl Pts',(-2.39566720092542,0.775394949316457,
102.062668224425));
#32540=CARTESIAN_POINT('Ctrl Pts',(-2.37929366785987,0.824271573567107,
102.059420984686));
#32541=CARTESIAN_POINT('Ctrl Pts',(-2.36143112101026,0.872610629504504,
102.056173744947));
#32542=CARTESIAN_POINT('',(-2.51749892479438,-0.00189520973707386,102.388647960208));
#32543=CARTESIAN_POINT('Ctrl Pts',(-2.36143111379333,0.872610649034711,
102.332358906943));
#32544=CARTESIAN_POINT('Ctrl Pts',(-2.38167255387254,0.81783390932394,102.336323881003));
#32545=CARTESIAN_POINT('Ctrl Pts',(-2.400005456087,0.762359938864054,102.340247356964));
#32546=CARTESIAN_POINT('Ctrl Pts',(-2.43298340665052,0.649533881196489,
102.348032574994));
#32547=CARTESIAN_POINT('Ctrl Pts',(-2.44756857832329,0.592209019412611,
102.351890070134));
#32548=CARTESIAN_POINT('Ctrl Pts',(-2.46430302505784,0.515174439931453,
102.356947278273));
#32549=CARTESIAN_POINT('Ctrl Pts',(-2.46825782248767,0.495880490231162,
102.358203518278));
#32550=CARTESIAN_POINT('Ctrl Pts',(-2.474361959814,0.464216225329726,102.36024870174));
#32551=CARTESIAN_POINT('Ctrl Pts',(-2.47664583673482,0.451873013884803,
102.361041864692));
#32552=CARTESIAN_POINT('Ctrl Pts',(-2.48089469194113,0.427909627950764,
102.362574010339));
#32553=CARTESIAN_POINT('Ctrl Pts',(-2.4828705790581,0.416291745552828,102.363313318437));
#32554=CARTESIAN_POINT('Ctrl Pts',(-2.48662534698678,0.393236070607597,
102.364773717817));
#32555=CARTESIAN_POINT('Ctrl Pts',(-2.48840706519073,0.381799041999803,
102.36549488103));
#32556=CARTESIAN_POINT('Ctrl Pts',(-2.49236442873955,0.355191048042248,
102.367165254244));
#32557=CARTESIAN_POINT('Ctrl Pts',(-2.49448055866104,0.340011594931609,
102.368112601438));
#32558=CARTESIAN_POINT('Ctrl Pts',(-2.50142524011857,0.28663602605955,102.3714251183));
#32559=CARTESIAN_POINT('Ctrl Pts',(-2.5055162804201,0.248348235283293,102.373767724152));
#32560=CARTESIAN_POINT('Ctrl Pts',(-2.51462593031466,0.139511104565593,
102.380346387944));
#32561=CARTESIAN_POINT('Ctrl Pts',(-2.51755260110758,0.0688228082331917,
102.384522807845));
#32562=CARTESIAN_POINT('Ctrl Pts',(-2.51749928456623,-0.00189794850746936,
102.388648747491));
#32563=CARTESIAN_POINT('Ctrl Pts',(-2.51749928665677,-0.001895173516098,
102.388648585595));
#32564=CARTESIAN_POINT('Ctrl Pts',(-2.51738362772184,-0.155533499352556,
102.397612045468));
#32565=CARTESIAN_POINT('Ctrl Pts',(-2.50320419797107,-0.308839288588633,
102.40629201102));
#32566=CARTESIAN_POINT('Ctrl Pts',(-2.46354884846836,-0.522261120674775,
102.418941987187));
#32567=CARTESIAN_POINT('Ctrl Pts',(-2.4496094044207,-0.58415948973351,102.422683426095));
#32568=CARTESIAN_POINT('Ctrl Pts',(-2.42408646069048,-0.680379425043883,
102.428704454135));
#32569=CARTESIAN_POINT('Ctrl Pts',(-2.4140741531442,-0.715092305514733,
102.430919516845));
#32570=CARTESIAN_POINT('Ctrl Pts',(-2.40002439675338,-0.760139190160104,
102.43386476658));
#32571=CARTESIAN_POINT('Ctrl Pts',(-2.39666017356873,-0.770680670101884,
102.434559106641));
#32572=CARTESIAN_POINT('Ctrl Pts',(-2.39105361636841,-0.787856517963723,
102.435699331359));
#32573=CARTESIAN_POINT('Ctrl Pts',(-2.38885285789073,-0.794504442866894,
102.436142843075));
#32574=CARTESIAN_POINT('Ctrl Pts',(-2.38450457701741,-0.807458076994481,
102.437011466609));
#32575=CARTESIAN_POINT('Ctrl Pts',(-2.38235971969409,-0.813764576692406,
102.437436423997));
#32576=CARTESIAN_POINT('Ctrl Pts',(-2.37751496396946,-0.827826237226315,
102.438388463557));
#32577=CARTESIAN_POINT('Ctrl Pts',(-2.37480210062592,-0.835576843466313,
102.438916286986));
#32578=CARTESIAN_POINT('Ctrl Pts',(-2.36529464143894,-0.862319177183936,
102.440747760597));
#32579=CARTESIAN_POINT('Ctrl Pts',(-2.35830995182773,-0.881241859515909,
102.442061700365));
#32580=CARTESIAN_POINT('Ctrl Pts',(-2.2912579183836,-1.05638888913749,102.454378340713));
#32581=CARTESIAN_POINT('Ctrl Pts',(-2.21598289091404,-1.2063299337195,102.466044872105));
#32582=CARTESIAN_POINT('Ctrl Pts',(-2.06414888723597,-1.44589649694668,
102.485603242282));
#32583=CARTESIAN_POINT('Ctrl Pts',(-1.99516590995544,-1.5396900257187,102.493544571162));
#32584=CARTESIAN_POINT('Ctrl Pts',(-1.89189916779521,-1.66144604537815,
102.504149853271));
#32585=CARTESIAN_POINT('Ctrl Pts',(-1.86300912178895,-1.69377767128789,
102.506998936773));
#32586=CARTESIAN_POINT('Ctrl Pts',(-1.81125385555683,-1.7487710627214,102.511903753183));
#32587=CARTESIAN_POINT('Ctrl Pts',(-1.78876303182323,-1.77176966091257,
102.51397404432));
#32588=CARTESIAN_POINT('Ctrl Pts',(-1.75539796790109,-1.80460486755361,
102.516959343884));
#32589=CARTESIAN_POINT('Ctrl Pts',(-1.74486954165176,-1.81478677841368,
102.517889357872));
#32590=CARTESIAN_POINT('Ctrl Pts',(-1.72622127333777,-1.83250896993319,
102.519515950083));
#32591=CARTESIAN_POINT('Ctrl Pts',(-1.718139469951,-1.84008852437888,102.520214204376));
#32592=CARTESIAN_POINT('Ctrl Pts',(-1.70087545799637,-1.85606674582451,
102.521691837917));
#32593=CARTESIAN_POINT('Ctrl Pts',(-1.69168046265567,-1.86445120872301,
102.522470605455));
#32594=CARTESIAN_POINT('Ctrl Pts',(-1.66814980582276,-1.88559026410293,
102.524443019386));
#32595=CARTESIAN_POINT('Ctrl Pts',(-1.65372963604511,-1.8982499153901,102.525632704994));
#32596=CARTESIAN_POINT('Ctrl Pts',(-1.59733936071315,-1.9466253254089,102.530213812539));
#32597=CARTESIAN_POINT('Ctrl Pts',(-1.55434395182887,-1.98112562449927,
102.533556177902));
#32598=CARTESIAN_POINT('Ctrl Pts',(-1.34101933116887,-2.14107742255326,
102.549505816003));
#32599=CARTESIAN_POINT('Ctrl Pts',(-1.15648519806792,-2.24612681314428,
102.561340359612));
#32600=CARTESIAN_POINT('Ctrl Pts',(-0.902554173308147,-2.35099964323332,
102.577352426539));
#32601=CARTESIAN_POINT('Ctrl Pts',(-0.843234281619375,-2.37292188018799,
102.581082163725));
#32602=CARTESIAN_POINT('Ctrl Pts',(-0.760125206045787,-2.40012566221989,
102.586371767267));
#32603=CARTESIAN_POINT('Ctrl Pts',(-0.736987121664504,-2.40733118141019,
102.587851193457));
#32604=CARTESIAN_POINT('Ctrl Pts',(-0.696571593415484,-2.41927988015266,
102.590452825256));
#32605=CARTESIAN_POINT('Ctrl Pts',(-0.679340515732245,-2.42417481726747,
102.591567502736));
#32606=CARTESIAN_POINT('Ctrl Pts',(-0.65391888261364,-2.43110417997221,
102.593222049707));
#32607=CARTESIAN_POINT('Ctrl Pts',(-0.645767556050396,-2.43328208344487,
102.593754079877));
#32608=CARTESIAN_POINT('Ctrl Pts',(-0.631293804746132,-2.43707138819131,
102.594701690055));
#32609=CARTESIAN_POINT('Ctrl Pts',(-0.624975860400547,-2.43869924172159,
102.595116325528));
#32610=CARTESIAN_POINT('Ctrl Pts',(-0.61124888880824,-2.44217922500546,
102.596019420535));
#32611=CARTESIAN_POINT('Ctrl Pts',(-0.603837855717199,-2.444022179,102.59650836678));
#32612=CARTESIAN_POINT('Ctrl Pts',(-0.583227450922472,-2.44904804890784,
102.597871745425));
#32613=CARTESIAN_POINT('Ctrl Pts',(-0.570010768033392,-2.45215788854564,
102.598750118524));
#32614=CARTESIAN_POINT('Ctrl Pts',(-0.495995283226894,-2.46894277684054,
102.603689511775));
#32615=CARTESIAN_POINT('Ctrl Pts',(-0.434735010062842,-2.48046242671523,
102.607853896467));
#32616=CARTESIAN_POINT('Ctrl Pts',(-0.231744205592185,-2.51088347797545,
102.62177198319));
#32617=CARTESIAN_POINT('Ctrl Pts',(-0.088826954223493,-2.51999019966902,
102.631743944321));
#32618=CARTESIAN_POINT('Ctrl Pts',(0.186648054686333,-2.51407012709301,
102.650653081945));
#32619=CARTESIAN_POINT('Ctrl Pts',(0.318789920484328,-2.50075355891401,
102.659584459724));
#32620=CARTESIAN_POINT('Ctrl Pts',(0.481158364700997,-2.47130374948898,
102.670301829104));
#32621=CARTESIAN_POINT('Ctrl Pts',(0.512918502786566,-2.46490777987964,
102.672386686747));
#32622=CARTESIAN_POINT('Ctrl Pts',(0.559356598471792,-2.45461942400073,
102.675419405697));
#32623=CARTESIAN_POINT('Ctrl Pts',(0.574135898987559,-2.45120466441293,
102.676382256309));
#32624=CARTESIAN_POINT('Ctrl Pts',(0.600248772738025,-2.44492214645146,
102.678079588396));
#32625=CARTESIAN_POINT('Ctrl Pts',(0.611594811928431,-2.44210865541391,
102.678815773851));
#32626=CARTESIAN_POINT('Ctrl Pts',(0.635355540528583,-2.43604069931775,
102.680354913031));
#32627=CARTESIAN_POINT('Ctrl Pts',(0.647765796243572,-2.43277011543186,
102.681157327286));
#32628=CARTESIAN_POINT('Ctrl Pts',(0.680403551654847,-2.42390134343649,
102.683264020846));
#32629=CARTESIAN_POINT('Ctrl Pts',(0.700587262337777,-2.4181447940243,102.684563189834));
#32630=CARTESIAN_POINT('Ctrl Pts',(0.788341933381007,-2.39192548969818,
102.690198597133));
#32631=CARTESIAN_POINT('Ctrl Pts',(0.855110519443737,-2.36887692477376,
102.694450997935));
#32632=CARTESIAN_POINT('Ctrl Pts',(1.10160037687089,-2.27200557293898,102.710147068473));
#32633=CARTESIAN_POINT('Ctrl Pts',(1.27353554913689,-2.18028383510349,102.72103888105));
#32634=CARTESIAN_POINT('Ctrl Pts',(1.5082181965256,-2.01777279508252,102.737688709874));
#32635=CARTESIAN_POINT('Ctrl Pts',(1.58033430860803,-1.96180245939454,102.743104498823));
#32636=CARTESIAN_POINT('Ctrl Pts',(1.6601241095028,-1.8926176305945,102.749657701103));
#32637=CARTESIAN_POINT('Ctrl Pts',(1.67092089174682,-1.88309237838327,102.750557112652));
#32638=CARTESIAN_POINT('Ctrl Pts',(1.68738818347471,-1.86831130524999,102.751949586056));
#32639=CARTESIAN_POINT('Ctrl Pts',(1.69311737844635,-1.86312091772818,102.752437957361));
#32640=CARTESIAN_POINT('Ctrl Pts',(1.70363036797095,-1.85350809594487,102.753341548518));
#32641=CARTESIAN_POINT('Ctrl Pts',(1.70842099312952,-1.84909339936437,102.753756197223));
#32642=CARTESIAN_POINT('Ctrl Pts',(1.71928318439554,-1.83900533761206,102.754702958101));
#32643=CARTESIAN_POINT('Ctrl Pts',(1.72534380085671,-1.8333205022769,102.755235920716));
#32644=CARTESIAN_POINT('Ctrl Pts',(1.74109414425502,-1.81839946924077,102.756633080516));
#32645=CARTESIAN_POINT('Ctrl Pts',(1.75073839842545,-1.80911594179759,102.757500668789));
#32646=CARTESIAN_POINT('Ctrl Pts',(1.82154010904192,-1.73986611105077,102.763956873288));
#32647=CARTESIAN_POINT('Ctrl Pts',(1.87966989575546,-1.67689608128999,102.769740836745));
#32648=CARTESIAN_POINT('Ctrl Pts',(1.96320419216849,-1.57659484543098,102.778677205794));
#32649=CARTESIAN_POINT('Ctrl Pts',(1.99100792627152,-1.54133360746604,102.781771417119));
#32650=CARTESIAN_POINT('Ctrl Pts',(2.10750504768939,-1.38517435215583,102.795223097379));
#32651=CARTESIAN_POINT('Ctrl Pts',(2.18625148611282,-1.25721863938396,102.805587850679));
#32652=CARTESIAN_POINT('Ctrl Pts',(2.28673886885793,-1.05560544542765,102.82063621328));
#32653=CARTESIAN_POINT('Ctrl Pts',(2.31729350216908,-0.986727046111983,
102.82557694532));
#32654=CARTESIAN_POINT('Ctrl Pts',(2.35224131080748,-0.897326164255197,
102.831741764531));
#32655=CARTESIAN_POINT('Ctrl Pts',(2.35952910329158,-0.877983987129867,
102.833061280816));
#32656=CARTESIAN_POINT('Ctrl Pts',(2.37093102798794,-0.846554919300016,
102.835182907652));
#32657=CARTESIAN_POINT('Ctrl Pts',(2.37519275210273,-0.834522960119893,
102.835989860898));
#32658=CARTESIAN_POINT('Ctrl Pts',(2.38318807275546,-0.811392602715328,
102.837531271266));
#32659=CARTESIAN_POINT('Ctrl Pts',(2.38693609781429,-0.800299580314415,
102.838266185632));
#32660=CARTESIAN_POINT('Ctrl Pts',(2.39532634855802,-0.774883613867455,
102.839940333077));
#32661=CARTESIAN_POINT('Ctrl Pts',(2.39991777942336,-0.760544277904604,
102.840877888933));
#32662=CARTESIAN_POINT('Ctrl Pts',(2.41406377516442,-0.714961352578325,
102.843836904041));
#32663=CARTESIAN_POINT('Ctrl Pts',(2.4231391695579,-0.683571767506233,102.845842878585));
#32664=CARTESIAN_POINT('Ctrl Pts',(2.47888434173951,-0.475677175089883,
102.858939292507));
#32665=CARTESIAN_POINT('Ctrl Pts',(2.50684786037321,-0.294718525591058,
102.869394955126));
#32666=CARTESIAN_POINT('Ctrl Pts',(2.52160117602881,0.0356550025147606,
102.88840324135));
#32667=CARTESIAN_POINT('Ctrl Pts',(2.5151369975468,0.183895567378174,102.896924479903));
#32668=CARTESIAN_POINT('Ctrl Pts',(2.49332445685361,0.348515283333323,102.907174362191));
#32669=CARTESIAN_POINT('Ctrl Pts',(2.49077096611955,0.366319125114966,102.908293509865));
#32670=CARTESIAN_POINT('Ctrl Pts',(2.48673761854896,0.392445779545791,102.9099534585));
#32671=CARTESIAN_POINT('Ctrl Pts',(2.48540619074844,0.400791386509681,102.910486346817));
#32672=CARTESIAN_POINT('Ctrl Pts',(2.48297226810997,0.415568948198591,102.911434888883));
#32673=CARTESIAN_POINT('Ctrl Pts',(2.48188675281953,0.422003530456306,102.911849590931));
#32674=CARTESIAN_POINT('Ctrl Pts',(2.4794782033649,0.435949839461696,102.912752124723));
#32675=CARTESIAN_POINT('Ctrl Pts',(2.47814606783039,0.443459678349607,102.91324043773));
#32676=CARTESIAN_POINT('Ctrl Pts',(2.4743553013391,0.464279322736735,102.914600404419));
#32677=CARTESIAN_POINT('Ctrl Pts',(2.47182346836101,0.477575301788284,102.915475968119));
#32678=CARTESIAN_POINT('Ctrl Pts',(2.45715687160118,0.55135455191865,102.920371306461));
#32679=CARTESIAN_POINT('Ctrl Pts',(2.4429102956263,0.611391593122609,102.924492378826));
#32680=CARTESIAN_POINT('Ctrl Pts',(2.41832586866082,0.700315277299747,102.930746284369));
#32681=CARTESIAN_POINT('Ctrl Pts',(2.40964051525969,0.729639626790019,102.93283360638));
#32682=CARTESIAN_POINT('Ctrl Pts',(2.38845956461168,0.79664464058407,102.937651241461));
#32683=CARTESIAN_POINT('Ctrl Pts',(2.37560253685304,0.834202769407093,102.940387134229));
#32684=CARTESIAN_POINT('Ctrl Pts',(2.32808391915122,0.96299235943133,102.949864906768));
#32685=CARTESIAN_POINT('Ctrl Pts',(2.28900872840419,1.05250626518966,102.956618001894));
#32686=CARTESIAN_POINT('Ctrl Pts',(2.20789218951705,1.21230330659508,102.96883600389));
#32687=CARTESIAN_POINT('Ctrl Pts',(2.16743014891732,1.28324428050476,102.974324647245));
#32688=CARTESIAN_POINT('Ctrl Pts',(2.10494478236901,1.38138294537662,102.981988990236));
#32689=CARTESIAN_POINT('Ctrl Pts',(2.0856956596084,1.41027840716407,102.984255345133));
#32690=CARTESIAN_POINT('Ctrl Pts',(2.05025860344977,1.46116069627317,102.988264450922));
#32691=CARTESIAN_POINT('Ctrl Pts',(2.03429941089601,1.4832993372348,102.990015219669));
#32692=CARTESIAN_POINT('Ctrl Pts',(2.00950821673279,1.5165368083286,102.992654513098));
#32693=CARTESIAN_POINT('Ctrl Pts',(2.00093760430525,1.52782717647838,102.993552997161));
#32694=CARTESIAN_POINT('Ctrl Pts',(1.9858678342209,1.5473347835457,102.995109033521));
#32695=CARTESIAN_POINT('Ctrl Pts',(1.97941196298716,1.55558486541144,102.995768253427));
#32696=CARTESIAN_POINT('Ctrl Pts',(1.96478871033027,1.57403376246048,102.997245131064));
#32697=CARTESIAN_POINT('Ctrl Pts',(1.95659300885593,1.58420982497115,102.998061643811));
#32698=CARTESIAN_POINT('Ctrl Pts',(1.93435331534736,1.61138752724046,103.00024782837));
#32699=CARTESIAN_POINT('Ctrl Pts',(1.9201643499337,1.62826945817043,103.0016116579));
#32700=CARTESIAN_POINT('Ctrl Pts',(1.85188088878139,1.70737855336194,103.008034207367));
#32701=CARTESIAN_POINT('Ctrl Pts',(1.79496974808412,1.76711346006148,103.012975902951));
#32702=CARTESIAN_POINT('Ctrl Pts',(1.60296239432799,1.94978046202481,103.028585409076));
#32703=CARTESIAN_POINT('Ctrl Pts',(1.45741348575376,2.06084339030448,103.038839083895));
#32704=CARTESIAN_POINT('Ctrl Pts',(1.24940878521563,2.18642063792493,103.05302422054));
#32705=CARTESIAN_POINT('Ctrl Pts',(1.1965749310008,2.21577638896681,103.056595815593));
#32706=CARTESIAN_POINT('Ctrl Pts',(1.12177728622576,2.25388008633242,103.061678696079));
#32707=CARTESIAN_POINT('Ctrl Pts',(1.10066669833238,2.26426422060688,103.063116142953));
#32708=CARTESIAN_POINT('Ctrl Pts',(1.06359804418931,2.28185712923467,103.065650488227));
#32709=CARTESIAN_POINT('Ctrl Pts',(1.04770424088273,2.28919823123452,103.06674037892));
#32710=CARTESIAN_POINT('Ctrl Pts',(1.02411018956133,2.29979878590641,103.068364944057));
#32711=CARTESIAN_POINT('Ctrl Pts',(1.01646780542663,2.30318677745033,103.068892179867));
#32712=CARTESIAN_POINT('Ctrl Pts',(1.0028367834599,2.3091485711002,103.069834619553));
#32713=CARTESIAN_POINT('Ctrl Pts',(0.996854843031237,2.31173725973907,103.070248918987));
#32714=CARTESIAN_POINT('Ctrl Pts',(0.983790943167309,2.31733053511908,103.0711553096));
#32715=CARTESIAN_POINT('Ctrl Pts',(0.976705348806667,2.32032585787243,103.071647918837));
#32716=CARTESIAN_POINT('Ctrl Pts',(0.956847061234565,2.32861355819018,103.073031089374));
#32717=CARTESIAN_POINT('Ctrl Pts',(0.944044559690628,2.33383316690007,103.073925771448));
#32718=CARTESIAN_POINT('Ctrl Pts',(0.869170460330283,2.36364263600486,103.07917273897));
#32719=CARTESIAN_POINT('Ctrl Pts',(0.806188476133523,2.38585881677424,103.083643654219));
#32720=CARTESIAN_POINT('Ctrl Pts',(0.53058432282325,2.47091640141351,103.103243642836));
#32721=CARTESIAN_POINT('Ctrl Pts',(0.311012600706783,2.50803561483774,103.118838266533));
#32722=CARTESIAN_POINT('Ctrl Pts',(0.0430231587831401,2.51756045804307,
103.136699712326));
#32723=CARTESIAN_POINT('Ctrl Pts',(-0.00341280010986838,2.51792582277355,
103.139757752228));
#32724=CARTESIAN_POINT('Ctrl Pts',(-0.0840253450051838,2.51632975651196,
103.145002104969));
#32725=CARTESIAN_POINT('Ctrl Pts',(-0.118199842720637,2.5149561998046,103.147205316341));
#32726=CARTESIAN_POINT('Ctrl Pts',(-0.167805709718507,2.51194897418758,
103.150375681418));
#32727=CARTESIAN_POINT('Ctrl Pts',(-0.183265536838815,2.51086840866851,
103.151359830341));
#32728=CARTESIAN_POINT('Ctrl Pts',(-0.210413127081642,2.50871885181465,
103.153081410469));
#32729=CARTESIAN_POINT('Ctrl Pts',(-0.222105103615359,2.50771076720999,
103.153820711617));
#32730=CARTESIAN_POINT('Ctrl Pts',(-0.244871979625545,2.50558732584508,
103.155256259153));
#32731=CARTESIAN_POINT('Ctrl Pts',(-0.255947355615494,2.50448020382286,
103.15595274391));
#32732=CARTESIAN_POINT('Ctrl Pts',(-0.285734991922991,2.50130289713291,
103.157821161271));
#32733=CARTESIAN_POINT('Ctrl Pts',(-0.304432209953688,2.49909618228299,
103.158988822031));
#32734=CARTESIAN_POINT('Ctrl Pts',(-0.374995315988209,2.48996438536853,
103.163377928873));
#32735=CARTESIAN_POINT('Ctrl Pts',(-0.426667793213562,2.48163238620764,
103.166555579521));
#32736=CARTESIAN_POINT('Ctrl Pts',(-0.688858428111269,2.43092259228202,
103.182559213639));
#32737=CARTESIAN_POINT('Ctrl Pts',(-0.893575907568189,2.36335167336494,
103.194568682619));
#32738=CARTESIAN_POINT('Ctrl Pts',(-1.14447771162261,2.24321308626393,103.210779304644));
#32739=CARTESIAN_POINT('Ctrl Pts',(-1.20065933392525,2.21365089432038,103.214522779327));
#32740=CARTESIAN_POINT('Ctrl Pts',(-1.27671698230111,2.16988253611406,103.219830309439));
#32741=CARTESIAN_POINT('Ctrl Pts',(-1.29759653687485,2.15746138122721,103.221313339242));
#32742=CARTESIAN_POINT('Ctrl Pts',(-1.33358240917717,2.13534220311773,103.223920738389));
#32743=CARTESIAN_POINT('Ctrl Pts',(-1.3487711160743,2.12578098599448,103.225037534022));
#32744=CARTESIAN_POINT('Ctrl Pts',(-1.37095325482857,2.11148400967517,103.226694640719));
#32745=CARTESIAN_POINT('Ctrl Pts',(-1.37802753581731,2.10687390598048,103.227227077759));
#32746=CARTESIAN_POINT('Ctrl Pts',(-1.39052710240531,2.09863841668815,103.228175129535));
#32747=CARTESIAN_POINT('Ctrl Pts',(-1.39596166328973,2.09502741265236,103.228589796338));
#32748=CARTESIAN_POINT('Ctrl Pts',(-1.40772264917479,2.08714672313838,103.229492624206));
#32749=CARTESIAN_POINT('Ctrl Pts',(-1.41404361611555,2.08286945077209,103.229981269393));
#32750=CARTESIAN_POINT('Ctrl Pts',(-1.4315385735023,2.07091462077226,103.231343025565));
#32751=CARTESIAN_POINT('Ctrl Pts',(-1.44266995044122,2.06317557391335,103.232220062645));
#32752=CARTESIAN_POINT('Ctrl Pts',(-1.50433122448289,2.0195628276572,103.237135299966));
#32753=CARTESIAN_POINT('Ctrl Pts',(-1.55358165593755,1.9819256114295,103.241275710444));
#32754=CARTESIAN_POINT('Ctrl Pts',(-1.73853897458603,1.82944863505302,103.257526741096));
#32755=CARTESIAN_POINT('Ctrl Pts',(-1.86333045345889,1.70217638075084,103.269987037853));
#32756=CARTESIAN_POINT('Ctrl Pts',(-2.04409315011653,1.47389109263844,103.289774592164));
#32757=CARTESIAN_POINT('Ctrl Pts',(-2.10842329333798,1.38030041793534,103.297316178222));
#32758=CARTESIAN_POINT('Ctrl Pts',(-2.17801818550521,1.26276619749444,103.306112166897));
#32759=CARTESIAN_POINT('Ctrl Pts',(-2.18953308782272,1.2426932854245,103.307592387349));
#32760=CARTESIAN_POINT('Ctrl Pts',(-2.20722906075781,1.21083568632134,103.309907934));
#32761=CARTESIAN_POINT('Ctrl Pts',(-2.21359603568314,1.19915628162888,103.310749830178));
#32762=CARTESIAN_POINT('Ctrl Pts',(-2.22534539612983,1.17719109089835,103.312320289976));
#32763=CARTESIAN_POINT('Ctrl Pts',(-2.23074976104873,1.16691752382361,103.313049613013));
#32764=CARTESIAN_POINT('Ctrl Pts',(-2.24269275756942,1.14382797361972,103.314677302977));
#32765=CARTESIAN_POINT('Ctrl Pts',(-2.24919300793412,1.13099251311799,103.315574312901));
#32766=CARTESIAN_POINT('Ctrl Pts',(-2.2654581616758,1.09818029223132,103.31784805539));
#32767=CARTESIAN_POINT('Ctrl Pts',(-2.27506922062494,1.0781283440497,103.319219482253));
#32768=CARTESIAN_POINT('Ctrl Pts',(-2.31255454723068,0.997187001461094,
103.324686558703));
#32769=CARTESIAN_POINT('Ctrl Pts',(-2.33824458908796,0.93535725801648,103.328707268518));
#32770=CARTESIAN_POINT('Ctrl Pts',(-2.36143100149827,0.872610952923958,
103.332666057199));
#32771=CARTESIAN_POINT('Origin',(0.,0.,104.));
#32772=CARTESIAN_POINT('',(-2.36143112095504,0.87261062965393,104.32884037888));
#32773=CARTESIAN_POINT('',(-2.36143112101026,0.872610629504495,104.05635151795));
#32774=CARTESIAN_POINT('',(-2.36143112101026,0.872610629504505,104.));
#32775=CARTESIAN_POINT('',(-2.51749898433586,0.00226138628059867,103.112583302554));
#32776=CARTESIAN_POINT('Ctrl Pts',(-2.36143112101026,0.872610629504494,
104.05635151795));
#32777=CARTESIAN_POINT('Ctrl Pts',(-2.33167841640509,0.953126452041245,
104.050918934233));
#32778=CARTESIAN_POINT('Ctrl Pts',(-2.29784078860177,1.03201888497832,104.045486350517));
#32779=CARTESIAN_POINT('Ctrl Pts',(-2.26013251530705,1.10887657710488,104.0400537668));
#32780=CARTESIAN_POINT('Ctrl Pts',(-2.22999407261371,1.17030530208506,104.035711759099));
#32781=CARTESIAN_POINT('Ctrl Pts',(-2.19738399262468,1.23043463114403,104.031369751399));
#32782=CARTESIAN_POINT('Ctrl Pts',(-2.16243151429358,1.28906795631184,104.027027743698));
#32783=CARTESIAN_POINT('Ctrl Pts',(-2.12012758401577,1.36003345627892,104.021772494291));
#32784=CARTESIAN_POINT('Ctrl Pts',(-2.07424846759187,1.42904534370445,104.016517244883));
#32785=CARTESIAN_POINT('Ctrl Pts',(-2.02500000847352,1.49572096852395,104.011261995476));
#32786=CARTESIAN_POINT('Ctrl Pts',(-1.97582137248236,1.56230206245426,104.006014196819));
#32787=CARTESIAN_POINT('Ctrl Pts',(-1.92328315409511,1.62655310489617,104.000766398161));
#32788=CARTESIAN_POINT('Ctrl Pts',(-1.86763593960146,1.68811796006943,103.995518599504));
#32789=CARTESIAN_POINT('Ctrl Pts',(-1.81158551306518,1.75012890569366,103.990232776021));
#32790=CARTESIAN_POINT('Ctrl Pts',(-1.75238108825241,1.80941416526036,103.984946952538));
#32791=CARTESIAN_POINT('Ctrl Pts',(-1.69032191607632,1.86564146342004,103.979661129055));
#32792=CARTESIAN_POINT('Ctrl Pts',(-1.62881922421346,1.92136457527826,103.974422703186));
#32793=CARTESIAN_POINT('Ctrl Pts',(-1.56451312482664,1.97408403161967,103.969184277318));
#32794=CARTESIAN_POINT('Ctrl Pts',(-1.49773256054301,2.023512645646,103.963945851449));
#32795=CARTESIAN_POINT('Ctrl Pts',(-1.43097395927558,2.07292500342379,103.958709148412));
#32796=CARTESIAN_POINT('Ctrl Pts',(-1.36174287997084,2.11904839410438,103.953472445374));
#32797=CARTESIAN_POINT('Ctrl Pts',(-1.29040036014548,2.16163668560108,103.948235742337));
#32798=CARTESIAN_POINT('Ctrl Pts',(-1.21905978365467,2.20422381701402,103.942999181944));
#32799=CARTESIAN_POINT('Ctrl Pts',(-1.1456082777217,2.2432758050749,103.937762621552));
#32800=CARTESIAN_POINT('Ctrl Pts',(-1.07043360185127,2.27859126523993,103.93252606116));
#32801=CARTESIAN_POINT('Ctrl Pts',(-0.994028519174909,2.31448474429283,
103.927203792389));
#32802=CARTESIAN_POINT('Ctrl Pts',(-0.915843789831181,2.34651805717611,
103.921881523619));
#32803=CARTESIAN_POINT('Ctrl Pts',(-0.836308278398951,2.37453041957381,
103.916559254848));
#32804=CARTESIAN_POINT('Ctrl Pts',(-0.757941201789924,2.40213125988388,
103.911315174098));
#32805=CARTESIAN_POINT('Ctrl Pts',(-0.678263233698182,2.42582843231033,
103.906071093348));
#32806=CARTESIAN_POINT('Ctrl Pts',(-0.597698758545896,2.44551884965802,
103.900827012597));
#32807=CARTESIAN_POINT('Ctrl Pts',(-0.515332487109612,2.46564963629678,
103.895465649817));
#32808=CARTESIAN_POINT('Ctrl Pts',(-0.43204008019191,2.48159218961269,103.890104287036));
#32809=CARTESIAN_POINT('Ctrl Pts',(-0.348282757392524,2.49329207492886,
103.884742924256));
#32810=CARTESIAN_POINT('Ctrl Pts',(-0.264525434593138,2.50499196024503,
103.879381561475));
#32811=CARTESIAN_POINT('Ctrl Pts',(-0.180303707930204,2.51244919928506,
103.874020198695));
#32812=CARTESIAN_POINT('Ctrl Pts',(-0.0960789567654115,2.515665932525,103.868658835914));
#32813=CARTESIAN_POINT('Ctrl Pts',(-0.0135212020010645,2.51881899941202,
103.863403586507));
#32814=CARTESIAN_POINT('Ctrl Pts',(0.0693443933134434,2.5179095803437,103.858148337099));
#32815=CARTESIAN_POINT('Ctrl Pts',(0.152084793467522,2.51290200079429,103.852893087692));
#32816=CARTESIAN_POINT('Ctrl Pts',(0.234707886530424,2.5079015208551,103.847645289035));
#32817=CARTESIAN_POINT('Ctrl Pts',(0.317205680260782,2.49881444895048,103.842397490377));
#32818=CARTESIAN_POINT('Ctrl Pts',(0.39914301861702,2.48565707624549,103.83714969172));
#32819=CARTESIAN_POINT('Ctrl Pts',(0.48167406362809,2.47240436703224,103.831863868237));
#32820=CARTESIAN_POINT('Ctrl Pts',(0.563636023487427,2.45502210436827,103.826578044754));
#32821=CARTESIAN_POINT('Ctrl Pts',(0.644587260568504,2.43358038977815,103.821292221271));
#32822=CARTESIAN_POINT('Ctrl Pts',(0.724812613494425,2.41233094156273,103.816053795402));
#32823=CARTESIAN_POINT('Ctrl Pts',(0.804044842948165,2.38709467180903,103.810815369534));
#32824=CARTESIAN_POINT('Ctrl Pts',(0.881863965532047,2.35799113575435,103.805576943665));
#32825=CARTESIAN_POINT('Ctrl Pts',(0.959657494701617,2.32889717136832,103.800340240628));
#32826=CARTESIAN_POINT('Ctrl Pts',(1.03603840817087,2.29593862820904,103.79510353759));
#32827=CARTESIAN_POINT('Ctrl Pts',(1.11060368480481,2.25928433476134,103.789866834553));
#32828=CARTESIAN_POINT('Ctrl Pts',(1.1851669303178,2.22263103975831,103.78463027416));
#32829=CARTESIAN_POINT('Ctrl Pts',(1.25791422369009,2.18228239910811,103.779393713768));
#32830=CARTESIAN_POINT('Ctrl Pts',(1.32846552885237,2.13845401836256,103.774157153376));
#32831=CARTESIAN_POINT('Ctrl Pts',(1.40017156870476,2.09390828516632,103.768834884605));
#32832=CARTESIAN_POINT('Ctrl Pts',(1.46960866236069,2.04576812457823,103.763512615835));
#32833=CARTESIAN_POINT('Ctrl Pts',(1.53640844918693,1.9943057256266,103.758190347064));
#32834=CARTESIAN_POINT('Ctrl Pts',(1.60222689829729,1.94359934694748,103.752946266314));
#32835=CARTESIAN_POINT('Ctrl Pts',(1.66548469781709,1.88966804453295,103.747702185564));
#32836=CARTESIAN_POINT('Ctrl Pts',(1.72586432224121,1.83281166277796,103.742458104813));
#32837=CARTESIAN_POINT('Ctrl Pts',(1.78759431582893,1.7746837079483,103.737096742033));
#32838=CARTESIAN_POINT('Ctrl Pts',(1.8463154875255,1.71349862765116,103.731735379252));
#32839=CARTESIAN_POINT('Ctrl Pts',(1.90173106621282,1.64961365228379,103.726374016472));
#32840=CARTESIAN_POINT('Ctrl Pts',(1.95714664490014,1.58572867691641,103.721012653691));
#32841=CARTESIAN_POINT('Ctrl Pts',(2.00925637003074,1.51914424778308,103.715651290911));
#32842=CARTESIAN_POINT('Ctrl Pts',(2.0578108383057,1.45024853171848,103.71028992813));
#32843=CARTESIAN_POINT('Ctrl Pts',(2.10540430494247,1.38271641612886,103.705034678723));
#32844=CARTESIAN_POINT('Ctrl Pts',(2.14975779396932,1.31271425944062,103.699779429315));
#32845=CARTESIAN_POINT('Ctrl Pts',(2.19060561490067,1.24058586561578,103.694524179908));
#32846=CARTESIAN_POINT('Ctrl Pts',(2.23139552290158,1.16855973346755,103.689276381251));
#32847=CARTESIAN_POINT('Ctrl Pts',(2.26868940967196,1.09441375005787,103.684028582593));
#32848=CARTESIAN_POINT('Ctrl Pts',(2.30226401872926,1.01852179066753,103.678780783936));
#32849=CARTESIAN_POINT('Ctrl Pts',(2.33608190477382,0.942079928605025,103.673494960453));
#32850=CARTESIAN_POINT('Ctrl Pts',(2.36612611394342,0.863867068954772,103.66820913697));
#32851=CARTESIAN_POINT('Ctrl Pts',(2.39221499656092,0.784291820835234,103.662923313487));
#32852=CARTESIAN_POINT('Ctrl Pts',(2.41806994196878,0.705430118472858,103.657684887618));
#32853=CARTESIAN_POINT('Ctrl Pts',(2.44004006460321,0.625230809207092,103.65244646175));
#32854=CARTESIAN_POINT('Ctrl Pts',(2.45799698585843,0.544111263907379,103.647208035881));
#32855=CARTESIAN_POINT('Ctrl Pts',(2.4759480013811,0.463018397476046,103.641971332844));
#32856=CARTESIAN_POINT('Ctrl Pts',(2.48988833722011,0.381006346250213,103.636734629806));
#32857=CARTESIAN_POINT('Ctrl Pts',(2.49974017991996,0.298505080180794,103.631497926769));
#32858=CARTESIAN_POINT('Ctrl Pts',(2.50959175426053,0.216006061404678,103.626261366376));
#32859=CARTESIAN_POINT('Ctrl Pts',(2.5153550032034,0.133018312568258,103.621024805984));
#32860=CARTESIAN_POINT('Ctrl Pts',(2.51700386379089,0.0499779917738332,
103.615788245592));
#32861=CARTESIAN_POINT('Ctrl Pts',(2.51867971178159,-0.0344214752316504,
103.610465976821));
#32862=CARTESIAN_POINT('Ctrl Pts',(2.51610525050778,-0.118874759276591,
103.605143708051));
#32863=CARTESIAN_POINT('Ctrl Pts',(2.50930823550474,-0.202924688562287,
103.59982143928));
#32864=CARTESIAN_POINT('Ctrl Pts',(2.5026110736224,-0.285739862925301,103.59457735853));
#32865=CARTESIAN_POINT('Ctrl Pts',(2.49181472092363,-0.36816299892866,103.589333277779));
#32866=CARTESIAN_POINT('Ctrl Pts',(2.47699780731675,-0.449764507879434,
103.584089197029));
#32867=CARTESIAN_POINT('Ctrl Pts',(2.46184951862391,-0.533191006012152,
103.578727834249));
#32868=CARTESIAN_POINT('Ctrl Pts',(2.44249877889859,-0.615758184288129,
103.573366471468));
#32869=CARTESIAN_POINT('Ctrl Pts',(2.41908365274352,-0.697022618735634,
103.568005108687));
#32870=CARTESIAN_POINT('Ctrl Pts',(2.39566852658844,-0.778287053183139,
103.562643745907));
#32871=CARTESIAN_POINT('Ctrl Pts',(2.36818924231077,-0.858248284988129,
103.557282383126));
#32872=CARTESIAN_POINT('Ctrl Pts',(2.33683560324135,-0.936485778548516,
103.551921020346));
#32873=CARTESIAN_POINT('Ctrl Pts',(2.3061025228883,-1.01317477694163,103.546665770938));
#32874=CARTESIAN_POINT('Ctrl Pts',(2.27153358025019,-1.08849092484336,103.541410521531));
#32875=CARTESIAN_POINT('Ctrl Pts',(2.23327249983834,-1.16202417852032,103.536155272124));
#32876=CARTESIAN_POINT('Ctrl Pts',(2.19506566494663,-1.23545317874833,103.530907473466));
#32877=CARTESIAN_POINT('Ctrl Pts',(2.15317730095472,-1.30710389966781,103.525659674809));
#32878=CARTESIAN_POINT('Ctrl Pts',(2.10779945922329,-1.37658551848332,103.520411876151));
#32879=CARTESIAN_POINT('Ctrl Pts',(2.06209281590823,-1.44657059152734,103.515126052668));
#32880=CARTESIAN_POINT('Ctrl Pts',(2.01284608921407,-1.51435455592313,103.509840229185));
#32881=CARTESIAN_POINT('Ctrl Pts',(1.96030311786674,-1.57956257745046,103.504554405702));
#32882=CARTESIAN_POINT('Ctrl Pts',(1.90823129571663,-1.64418588314982,103.499315979834));
#32883=CARTESIAN_POINT('Ctrl Pts',(1.85292240139199,-1.70627889164413,103.494077553965));
#32884=CARTESIAN_POINT('Ctrl Pts',(1.79465662642586,-1.76550668172787,103.488839128097));
#32885=CARTESIAN_POINT('Ctrl Pts',(1.73641001410332,-1.82471499277725,103.483602425059));
#32886=CARTESIAN_POINT('Ctrl Pts',(1.67520877585189,-1.88105962824586,103.478365722021));
#32887=CARTESIAN_POINT('Ctrl Pts',(1.61137120149195,-1.9342412209966,103.473129018984));
#32888=CARTESIAN_POINT('Ctrl Pts',(1.54753536603575,-1.98742136510721,103.467892458592));
#32889=CARTESIAN_POINT('Ctrl Pts',(1.48106369243062,-2.03743834325917,103.462655898199));
#32890=CARTESIAN_POINT('Ctrl Pts',(1.41230783670988,-2.08403282708499,103.457419337807));
#32891=CARTESIAN_POINT('Ctrl Pts',(1.34242663296675,-2.13138993701266,103.452097069036));
#32892=CARTESIAN_POINT('Ctrl Pts',(1.27018620039215,-2.17521122109078,103.446774800266));
#32893=CARTESIAN_POINT('Ctrl Pts',(1.19598512270835,-2.21527105254871,103.441452531495));
#32894=CARTESIAN_POINT('Ctrl Pts',(1.12287411311507,-2.25474237578889,103.436208450745));
#32895=CARTESIAN_POINT('Ctrl Pts',(1.04786013143435,-2.29056188349983,103.430964369995));
#32896=CARTESIAN_POINT('Ctrl Pts',(0.971346323523955,-2.32256163960755,
103.425720289244));
#32897=CARTESIAN_POINT('Ctrl Pts',(0.893121311084641,-2.35527705905854,
103.420358926464));
#32898=CARTESIAN_POINT('Ctrl Pts',(0.813329058486849,-2.38399963696721,
103.414997563683));
#32899=CARTESIAN_POINT('Ctrl Pts',(0.732416675825609,-2.40860375798357,
103.409636200903));
#32900=CARTESIAN_POINT('Ctrl Pts',(0.651504293164368,-2.43320787899992,
103.404274838122));
#32901=CARTESIAN_POINT('Ctrl Pts',(0.569472289591547,-2.45369348482422,
103.398913475341));
#32902=CARTESIAN_POINT('Ctrl Pts',(0.486776745845593,-2.46999081976107,
103.393552112561));
#32903=CARTESIAN_POINT('Ctrl Pts',(0.405717932061407,-2.48596559395063,
103.388296863154));
#32904=CARTESIAN_POINT('Ctrl Pts',(0.323722213469075,-2.49797542585536,
103.383041613746));
#32905=CARTESIAN_POINT('Ctrl Pts',(0.241211782623291,-2.50591762153581,
103.377786364339));
#32906=CARTESIAN_POINT('Ctrl Pts',(0.158818332824318,-2.51384855698704,
103.372538565681));
#32907=CARTESIAN_POINT('Ctrl Pts',(0.0759120757246245,-2.51772326728586,
103.367290767024));
#32908=CARTESIAN_POINT('Ctrl Pts',(-0.00707460686697792,-2.51749005955092,
103.362042968367));
#32909=CARTESIAN_POINT('Ctrl Pts',(-0.0906625995170283,-2.51725516202488,
103.356757144884));
#32910=CARTESIAN_POINT('Ctrl Pts',(-0.174331723136054,-2.51285247283201,
103.351471321401));
#32911=CARTESIAN_POINT('Ctrl Pts',(-0.257634811296941,-2.50428244293809,
103.346185497918));
#32912=CARTESIAN_POINT('Ctrl Pts',(-0.340190926416332,-2.49578925991069,
103.340947072049));
#32913=CARTESIAN_POINT('Ctrl Pts',(-0.422387076759521,-2.48320322145352,
103.335708646181));
#32914=CARTESIAN_POINT('Ctrl Pts',(-0.503789782285635,-2.46657700168971,
103.330470220312));
#32915=CARTESIAN_POINT('Ctrl Pts',(-0.585165715816659,-2.44995625001287,
103.325233517275));
#32916=CARTESIAN_POINT('Ctrl Pts',(-0.665748271062551,-2.42929804826103,
103.319996814237));
#32917=CARTESIAN_POINT('Ctrl Pts',(-0.745113047788685,-2.40470638457485,
103.3147601112));
#32918=CARTESIAN_POINT('Ctrl Pts',(-0.824475662658091,-2.38011539075326,
103.309523550807));
#32919=CARTESIAN_POINT('Ctrl Pts',(-0.902620124519449,-2.35159128558332,
103.304286990415));
#32920=CARTESIAN_POINT('Ctrl Pts',(-0.979137451062491,-2.31928784369833,
103.299050430023));
#32921=CARTESIAN_POINT('Ctrl Pts',(-1.05690715998365,-2.28645568154569,
103.293728161252));
#32922=CARTESIAN_POINT('Ctrl Pts',(-1.13299553128059,-2.24971953054689,
103.288405892482));
#32923=CARTESIAN_POINT('Ctrl Pts',(-1.20699630142899,-2.20929087680566,
103.283083623711));
#32924=CARTESIAN_POINT('Ctrl Pts',(-1.27990994615088,-2.16945614955134,
103.277839542961));
#32925=CARTESIAN_POINT('Ctrl Pts',(-1.35079655230355,-2.12603698732565,
103.272595462211));
#32926=CARTESIAN_POINT('Ctrl Pts',(-1.41929576301218,-2.07928011270624,
103.26735138146));
#32927=CARTESIAN_POINT('Ctrl Pts',(-1.48932693458919,-2.03147753695387,
103.26199001868));
#32928=CARTESIAN_POINT('Ctrl Pts',(-1.55686222783535,-1.98018646343684,
103.256628655899));
#32929=CARTESIAN_POINT('Ctrl Pts',(-1.62155284777497,-1.92571353318007,
103.251267293119));
#32930=CARTESIAN_POINT('Ctrl Pts',(-1.68624346771459,-1.87124060292331,
103.245905930338));
#32931=CARTESIAN_POINT('Ctrl Pts',(-1.74808908823779,-1.81358621125809,
103.240544567558));
#32932=CARTESIAN_POINT('Ctrl Pts',(-1.80678288493539,-1.75309493659201,
103.235183204777));
#32933=CARTESIAN_POINT('Ctrl Pts',(-1.86353796867853,-1.69460174731868,
103.229998933002));
#32934=CARTESIAN_POINT('Ctrl Pts',(-1.91756794793409,-1.63322734809459,
103.224814661227));
#32935=CARTESIAN_POINT('Ctrl Pts',(-1.96856067929322,-1.5692594119331,103.219630389452));
#32936=CARTESIAN_POINT('Ctrl Pts',(-2.01948810385429,-1.50537340001803,
103.214452757215));
#32937=CARTESIAN_POINT('Ctrl Pts',(-2.06738570242004,-1.4389008061749,103.209275124979));
#32938=CARTESIAN_POINT('Ctrl Pts',(-2.11197797192584,-1.37016615638397,
103.204097492742));
#32939=CARTESIAN_POINT('Ctrl Pts',(-2.1565274487315,-1.30149746738154,103.198924829188));
#32940=CARTESIAN_POINT('Ctrl Pts',(-2.19777763273914,-1.23057142519621,
103.193752165635));
#32941=CARTESIAN_POINT('Ctrl Pts',(-2.23549414426031,-1.15774443681577,
103.188579502081));
#32942=CARTESIAN_POINT('Ctrl Pts',(-2.2731865640472,-1.08496396727765,103.18341014261));
#32943=CARTESIAN_POINT('Ctrl Pts',(-2.30734957417599,-1.01028538234433,
103.178240783138));
#32944=CARTESIAN_POINT('Ctrl Pts',(-2.33779370789912,-0.93409144590199,
103.173071423666));
#32945=CARTESIAN_POINT('Ctrl Pts',(-2.36823897829903,-0.857894664646306,
103.167901871188));
#32946=CARTESIAN_POINT('Ctrl Pts',(-2.39496490115959,-0.780182852656354,
103.162732318711));
#32947=CARTESIAN_POINT('Ctrl Pts',(-2.41782980818628,-0.701359585837319,
103.157562766234));
#32948=CARTESIAN_POINT('Ctrl Pts',(-2.44069380324843,-0.622539462876451,
103.152393419943));
#32949=CARTESIAN_POINT('Ctrl Pts',(-2.45969696387433,-0.542608431845804,
103.147224073653));
#32950=CARTESIAN_POINT('Ctrl Pts',(-2.47474785657926,-0.46198408669169,
103.142054727362));
#32951=CARTESIAN_POINT('Ctrl Pts',(-2.48981318905338,-0.381282390847674,
103.136880421621));
#32952=CARTESIAN_POINT('Ctrl Pts',(-2.50091860016243,-0.29988652146086,
103.131706115879));
#32953=CARTESIAN_POINT('Ctrl Pts',(-2.50802417071423,-0.218222384537388,
103.126531810138));
#32954=CARTESIAN_POINT('Ctrl Pts',(-2.51440905979744,-0.144841020925352,
103.12188230761));
#32955=CARTESIAN_POINT('Ctrl Pts',(-2.5175650112416,-0.0712433791665783,
103.117232805082));
#32956=CARTESIAN_POINT('Ctrl Pts',(-2.51749898433586,0.00226138628061706,
103.112583302554));
#32957=CARTESIAN_POINT('Ctrl Pts',(-2.51749898433498,0.00226138726559125,
103.112583302492));
#32958=CARTESIAN_POINT('Ctrl Pts',(-2.5173983212915,0.114324948237909,103.105494785076));
#32959=CARTESIAN_POINT('Ctrl Pts',(-2.50981145266269,0.226062019319086,
103.09840626766));
#32960=CARTESIAN_POINT('Ctrl Pts',(-2.49489001405843,0.33664531446545,103.091317750244));
#32961=CARTESIAN_POINT('Ctrl Pts',(-2.48471334971802,0.41206492420996,103.086483265827));
#32962=CARTESIAN_POINT('Ctrl Pts',(-2.47112602227995,0.486948560769381,
103.08164878141));
#32963=CARTESIAN_POINT('Ctrl Pts',(-2.45418827016786,0.561040270007863,
103.076814296993));
#32964=CARTESIAN_POINT('Ctrl Pts',(-2.43577686875584,0.641578241697638,
103.071559193917));
#32965=CARTESIAN_POINT('Ctrl Pts',(-2.41336280068244,0.721357683945833,
103.066304090841));
#32966=CARTESIAN_POINT('Ctrl Pts',(-2.38702415539055,0.79995120575071,103.061048987765));
#32967=CARTESIAN_POINT('Ctrl Pts',(-2.37886800041174,0.824288863859839,
103.059421666594));
#32968=CARTESIAN_POINT('Ctrl Pts',(-2.37033588202498,0.848512848576402,
103.057794345422));
#32969=CARTESIAN_POINT('Ctrl Pts',(-2.36143112101026,0.872610629504504,
103.05616702425));
#32970=CARTESIAN_POINT('Ctrl Pts',(-2.36143100149827,0.872610952923958,
103.332666057199));
#32971=CARTESIAN_POINT('Ctrl Pts',(-2.39387776714414,0.784804585105903,
103.338205934878));
#32972=CARTESIAN_POINT('Ctrl Pts',(-2.42142173855965,0.695203230517513,
103.343622852339));
#32973=CARTESIAN_POINT('Ctrl Pts',(-2.47308432792982,0.486240117551232,
103.356007258809));
#32974=CARTESIAN_POINT('Ctrl Pts',(-2.49366949579794,0.366312548876271,
103.362934183258));
#32975=CARTESIAN_POINT('Ctrl Pts',(-2.51219498632938,0.177149514409093,
103.374151232098));
#32976=CARTESIAN_POINT('Ctrl Pts',(-2.51608648166396,0.108685954016836,
103.378271619745));
#32977=CARTESIAN_POINT('Ctrl Pts',(-2.51739500684821,0.0266607260762851,
103.38336960666));
#32978=CARTESIAN_POINT('Ctrl Pts',(-2.51750175646071,0.0131644323603149,
103.384213655136));
#32979=CARTESIAN_POINT('Ctrl Pts',(-2.51749898494065,-0.00786943934477994,
103.385538157595));
#32980=CARTESIAN_POINT('Ctrl Pts',(-2.51746413837851,-0.0154070020419334,
103.386014610995));
#32981=CARTESIAN_POINT('Ctrl Pts',(-2.51734182315744,-0.0288272163592207,
103.386866318177));
#32982=CARTESIAN_POINT('Ctrl Pts',(-2.51726758336298,-0.0347098592457373,
103.387240835722));
#32983=CARTESIAN_POINT('Ctrl Pts',(-2.51704014568502,-0.0488135624563618,
103.388141547836));
#32984=CARTESIAN_POINT('Ctrl Pts',(-2.51686729162727,-0.0570341183803992,
103.388668810118));
#32985=CARTESIAN_POINT('Ctrl Pts',(-2.51621865873184,-0.0820501507030038,
103.390279931391));
#32986=CARTESIAN_POINT('Ctrl Pts',(-2.51561501371179,-0.0988414524631855,
103.391370414343));
#32987=CARTESIAN_POINT('Ctrl Pts',(-2.51381866011755,-0.137912167079226,
103.393926978865));
#32988=CARTESIAN_POINT('Ctrl Pts',(-2.51249776720093,-0.160184015435006,
103.395398855545));
#32989=CARTESIAN_POINT('Ctrl Pts',(-2.50683959371106,-0.238058532460376,
103.400589689845));
#32990=CARTESIAN_POINT('Ctrl Pts',(-2.50095106569157,-0.293529571549378,
103.404366174094));
#32991=CARTESIAN_POINT('Ctrl Pts',(-2.47018418420475,-0.513479547637946,
103.419549570944));
#32992=CARTESIAN_POINT('Ctrl Pts',(-2.43087166419543,-0.675529644001177,
103.431171483305));
#32993=CARTESIAN_POINT('Ctrl Pts',(-2.37335574321666,-0.839670302552693,
103.442949384595));
#32994=CARTESIAN_POINT('Ctrl Pts',(-2.37081691040832,-0.846812186781872,
103.443461942661));
#32995=CARTESIAN_POINT('Ctrl Pts',(-2.3356075428061,-0.944458614156251,
103.450470848504));
#32996=CARTESIAN_POINT('Ctrl Pts',(-2.29780380514396,-1.03303738765478,
103.456836237442));
#32997=CARTESIAN_POINT('Ctrl Pts',(-2.24490261732576,-1.13962099139342,
103.464497698606));
#32998=CARTESIAN_POINT('Ctrl Pts',(-2.23451276328894,-1.15986056553296,
103.465952919309));
#32999=CARTESIAN_POINT('Ctrl Pts',(-2.21759348130645,-1.19174811536402,
103.468246821602));
#33000=CARTESIAN_POINT('Ctrl Pts',(-2.2112434812625,-1.20348938364089,103.46909172047));
#33001=CARTESIAN_POINT('Ctrl Pts',(-2.19919929437049,-1.22534213934016,
103.470664938552));
#33002=CARTESIAN_POINT('Ctrl Pts',(-2.19352802346135,-1.23546578760557,
103.471394041815));
#33003=CARTESIAN_POINT('Ctrl Pts',(-2.18069997767442,-1.25799802660365,
103.473017634773));
#33004=CARTESIAN_POINT('Ctrl Pts',(-2.17350684911057,-1.27038553905599,
103.473910799068));
#33005=CARTESIAN_POINT('Ctrl Pts',(-2.15192767687599,-1.30682786656698,
103.476540582205));
#33006=CARTESIAN_POINT('Ctrl Pts',(-2.137244929362,-1.33070507902403,103.478266493266));
#33007=CARTESIAN_POINT('Ctrl Pts',(-2.03592203954007,-1.48947254348868,
103.489773361189));
#33008=CARTESIAN_POINT('Ctrl Pts',(-1.93696376566969,-1.61607151098729,
103.499068104887));
#33009=CARTESIAN_POINT('Ctrl Pts',(-1.70652830626777,-1.85903878799125,
103.518323913763));
#33010=CARTESIAN_POINT('Ctrl Pts',(-1.57360687543323,-1.97281731350898,
103.528226249721));
#33011=CARTESIAN_POINT('Ctrl Pts',(-1.41370660726907,-2.08317846930345,
103.540185219019));
#33012=CARTESIAN_POINT('Ctrl Pts',(-1.39726650007648,-2.09424095507144,
103.54141556868));
#33013=CARTESIAN_POINT('Ctrl Pts',(-1.37396967275914,-2.10952087815147,
103.543162743387));
#33014=CARTESIAN_POINT('Ctrl Pts',(-1.3672202161803,-2.11390157607166,103.543669355663));
#33015=CARTESIAN_POINT('Ctrl Pts',(-1.35488060431832,-2.12182671548781,
103.54459656563));
#33016=CARTESIAN_POINT('Ctrl Pts',(-1.34929718746911,-2.12538165075333,
103.545016481409));
#33017=CARTESIAN_POINT('Ctrl Pts',(-1.33771808202371,-2.13268999591267,
103.545888218649));
#33018=CARTESIAN_POINT('Ctrl Pts',(-1.33172053129223,-2.1364401955636,103.546340228764));
#33019=CARTESIAN_POINT('Ctrl Pts',(-1.31602757920993,-2.14616106367415,
103.547524031721));
#33020=CARTESIAN_POINT('Ctrl Pts',(-1.3063074618291,-2.15209123969874,103.548258352521));
#33021=CARTESIAN_POINT('Ctrl Pts',(-1.26295253481293,-2.17813984870985,
103.55153729419));
#33022=CARTESIAN_POINT('Ctrl Pts',(-1.22889272951616,-2.19753602221635,
103.554122828524));
#33023=CARTESIAN_POINT('Ctrl Pts',(-1.13123724558799,-2.25016807087677,
103.561534060052));
#33024=CARTESIAN_POINT('Ctrl Pts',(-1.06665563573238,-2.28149040835823,
103.566432224306));
#33025=CARTESIAN_POINT('Ctrl Pts',(-0.960599112610984,-2.3274401971895,
103.574383870678));
#33026=CARTESIAN_POINT('Ctrl Pts',(-0.919920804693266,-2.34381615501612,
103.577413000992));
#33027=CARTESIAN_POINT('Ctrl Pts',(-0.703194079703188,-2.42455268033462,
103.593390992463));
#33028=CARTESIAN_POINT('Ctrl Pts',(-0.520762904952517,-2.47017565024896,
103.606226448787));
#33029=CARTESIAN_POINT('Ctrl Pts',(-0.302801517057759,-2.49943362395204,
103.62050961445));
#33030=CARTESIAN_POINT('Ctrl Pts',(-0.270589889383164,-2.50312574016055,
103.622596096085));
#33031=CARTESIAN_POINT('Ctrl Pts',(-0.223372238297469,-2.50761567791858,
103.625620326093));
#33032=CARTESIAN_POINT('Ctrl Pts',(-0.208417147586175,-2.50890291830514,
103.626573182138));
#33033=CARTESIAN_POINT('Ctrl Pts',(-0.181783521121086,-2.51095558385689,
103.628261495969));
#33034=CARTESIAN_POINT('Ctrl Pts',(-0.170109588218879,-2.51177346273865,
103.628998564153));
#33035=CARTESIAN_POINT('Ctrl Pts',(-0.145669004281273,-2.51331460171821,
103.630535701862));
#33036=CARTESIAN_POINT('Ctrl Pts',(-0.13290166478888,-2.5140220570073,103.63133525981));
#33037=CARTESIAN_POINT('Ctrl Pts',(-0.0993813966819019,-2.51562339110421,
103.633425838072));
#33038=CARTESIAN_POINT('Ctrl Pts',(-0.0786215600205884,-2.51635776433888,
103.634711891664));
#33039=CARTESIAN_POINT('Ctrl Pts',(0.018637267882308,-2.51859345419065,
103.640699272084));
#33040=CARTESIAN_POINT('Ctrl Pts',(0.0951740369102882,-2.51686390333626,
103.645300077656));
#33041=CARTESIAN_POINT('Ctrl Pts',(0.305818486820041,-2.50247911687551,
103.657781794824));
#33042=CARTESIAN_POINT('Ctrl Pts',(0.439167412864043,-2.48255130475694,
103.665470898837));
#33043=CARTESIAN_POINT('Ctrl Pts',(0.700407224694442,-2.42179326969231,
103.680898401929));
#33044=CARTESIAN_POINT('Ctrl Pts',(0.827895161868327,-2.38122525506859,
103.688615973074));
#33045=CARTESIAN_POINT('Ctrl Pts',(0.97148404881323,-2.3226038801022,103.698138909585));
#33046=CARTESIAN_POINT('Ctrl Pts',(0.991316228323331,-2.31420874279741,
103.699473548711));
#33047=CARTESIAN_POINT('Ctrl Pts',(1.01877019545961,-2.30216959236784,103.701351459402));
#33048=CARTESIAN_POINT('Ctrl Pts',(1.02648565514014,-2.29873981524347,103.701882584412));
#33049=CARTESIAN_POINT('Ctrl Pts',(1.03976048072132,-2.29275855872406,103.702802481271));
#33050=CARTESIAN_POINT('Ctrl Pts',(1.04532812808651,-2.29022548422419,103.703190150617));
#33051=CARTESIAN_POINT('Ctrl Pts',(1.05704787279382,-2.28484179304104,103.70401020839));
#33052=CARTESIAN_POINT('Ctrl Pts',(1.06319774976688,-2.28198658323001,103.704442885096));
#33053=CARTESIAN_POINT('Ctrl Pts',(1.07841713219861,-2.27484578869245,103.705519366091));
#33054=CARTESIAN_POINT('Ctrl Pts',(1.08747263111089,-2.27053080619043,103.706164924753));
#33055=CARTESIAN_POINT('Ctrl Pts',(1.12145091404538,-2.254090121947,103.708605612451));
#33056=CARTESIAN_POINT('Ctrl Pts',(1.14619766165188,-2.24160772683778,103.710420629532));
#33057=CARTESIAN_POINT('Ctrl Pts',(1.20914684358895,-2.2085409324695,103.715125021244));
#33058=CARTESIAN_POINT('Ctrl Pts',(1.24703141732688,-2.18737316481083,103.71804047918));
#33059=CARTESIAN_POINT('Ctrl Pts',(1.39178567227098,-2.10150972186441,103.729461005882));
#33060=CARTESIAN_POINT('Ctrl Pts',(1.49432852909416,-2.02987476963691,103.738150507394));
#33061=CARTESIAN_POINT('Ctrl Pts',(1.71627785401383,-1.84885825314889,103.757869425521));
#33062=CARTESIAN_POINT('Ctrl Pts',(1.83133409454045,-1.7349694099233,103.768776753568));
#33063=CARTESIAN_POINT('Ctrl Pts',(1.94892500024888,-1.59373520128016,103.78062981604));
#33064=CARTESIAN_POINT('Ctrl Pts',(1.96292405764026,-1.5764611457634,103.782054682875));
#33065=CARTESIAN_POINT('Ctrl Pts',(1.98560188846137,-1.5477074534434,103.784386526103));
#33066=CARTESIAN_POINT('Ctrl Pts',(1.99441411087351,-1.53633511619186,103.785298750011));
#33067=CARTESIAN_POINT('Ctrl Pts',(2.0101596528762,-1.51565139973249,103.786940092334));
#33068=CARTESIAN_POINT('Ctrl Pts',(2.01712691793259,-1.50636648920261,103.787670524108));
#33069=CARTESIAN_POINT('Ctrl Pts',(2.03193994857154,-1.48633887212167,103.789232655357));
#33070=CARTESIAN_POINT('Ctrl Pts',(2.03976531693737,-1.47558146504539,103.790063553612));
#33071=CARTESIAN_POINT('Ctrl Pts',(2.06096964222586,-1.44594118579236,103.792331101244));
#33072=CARTESIAN_POINT('Ctrl Pts',(2.07417428590734,-1.42693477969431,103.793761117063));
#33073=CARTESIAN_POINT('Ctrl Pts',(2.15056737226987,-1.31367507366855,103.802147504405));
#33074=CARTESIAN_POINT('Ctrl Pts',(2.20759088404041,-1.21541322704999,103.80887007214));
#33075=CARTESIAN_POINT('Ctrl Pts',(2.33656453993592,-0.953929202174542,
103.825831001799));
#33076=CARTESIAN_POINT('Ctrl Pts',(2.39816219060529,-0.786336391452298,
103.835825090898));
#33077=CARTESIAN_POINT('Ctrl Pts',(2.45659294105046,-0.553858763133373,
103.8500250316));
#33078=CARTESIAN_POINT('Ctrl Pts',(2.46941998587658,-0.493530153092568,
103.853742986836));
#33079=CARTESIAN_POINT('Ctrl Pts',(2.48234532074541,-0.41946526816815,103.858413674917));
#33080=CARTESIAN_POINT('Ctrl Pts',(2.48456431889281,-0.406115167208964,
103.859259736029));
#33081=CARTESIAN_POINT('Ctrl Pts',(2.48786535012506,-0.385214768027129,
103.860591729263));
#33082=CARTESIAN_POINT('Ctrl Pts',(2.48902092522443,-0.377676115230287,
103.861073679511));
#33083=CARTESIAN_POINT('Ctrl Pts',(2.49110165857439,-0.363677553379477,
103.861971605708));
#33084=CARTESIAN_POINT('Ctrl Pts',(2.49203597222829,-0.357219184753035,
103.86238706839));
#33085=CARTESIAN_POINT('Ctrl Pts',(2.49412272673484,-0.342387947188415,
103.863343863585));
#33086=CARTESIAN_POINT('Ctrl Pts',(2.49525811751567,-0.334012880657101,
103.863886121089));
#33087=CARTESIAN_POINT('Ctrl Pts',(2.49867811721182,-0.307794603119102,
103.865589472183));
#33088=CARTESIAN_POINT('Ctrl Pts',(2.50081360349901,-0.289932971700124,
103.866758307899));
#33089=CARTESIAN_POINT('Ctrl Pts',(2.50539061636632,-0.247826272509079,
103.869531071063));
#33090=CARTESIAN_POINT('Ctrl Pts',(2.50767186666554,-0.22356591512065,103.871142153422));
#33091=CARTESIAN_POINT('Ctrl Pts',(2.51464730060758,-0.135720698402123,
103.877015825201));
#33092=CARTESIAN_POINT('Ctrl Pts',(2.5172775419411,-0.0719992546959435,
103.881351696753));
#33093=CARTESIAN_POINT('Ctrl Pts',(2.51819290377348,0.207284718027779,103.900513238944));
#33094=CARTESIAN_POINT('Ctrl Pts',(2.49121506644567,0.422064839390602,103.915558581474));
#33095=CARTESIAN_POINT('Ctrl Pts',(2.42432877236368,0.680494037955959,103.933150916291));
#33096=CARTESIAN_POINT('Ctrl Pts',(2.40994657293799,0.729794679059438,103.936489037007));
#33097=CARTESIAN_POINT('Ctrl Pts',(2.38828658793369,0.796393480172014,103.940976328755));
#33098=CARTESIAN_POINT('Ctrl Pts',(2.38230964334191,0.814098394141081,103.942167130181));
#33099=CARTESIAN_POINT('Ctrl Pts',(2.37246759445412,0.842215561312557,103.944055243054));
#33100=CARTESIAN_POINT('Ctrl Pts',(2.36872985157804,0.85267135234073,103.944756701115));
#33101=CARTESIAN_POINT('Ctrl Pts',(2.36089530244754,0.87413822529171,103.946195633144));
#33102=CARTESIAN_POINT('Ctrl Pts',(2.35679034440409,0.885146059170485,103.946932817321));
#33103=CARTESIAN_POINT('Ctrl Pts',(2.347061143097,0.910688258471362,103.948641988885));
#33104=CARTESIAN_POINT('Ctrl Pts',(2.34137865830064,0.925200037389391,103.949612016571));
#33105=CARTESIAN_POINT('Ctrl Pts',(2.32261512723451,0.971837608401551,103.952726895427));
#33106=CARTESIAN_POINT('Ctrl Pts',(2.30900446000084,1.00374695449878,103.954854065937));
#33107=CARTESIAN_POINT('Ctrl Pts',(2.275286842434,1.07847714596994,103.959834170742));
#33108=CARTESIAN_POINT('Ctrl Pts',(2.25462371775412,1.12103320564527,103.962668745218));
#33109=CARTESIAN_POINT('Ctrl Pts',(2.12517940517811,1.36954893250977,103.979280379542));
#33110=CARTESIAN_POINT('Ctrl Pts',(1.98945662788042,1.56015938306679,103.992149818749));
#33111=CARTESIAN_POINT('Ctrl Pts',(1.79149926896549,1.76957470315813,104.009295266606));
#33112=CARTESIAN_POINT('Ctrl Pts',(1.75220083533936,1.80849536997681,104.012642042198));
#33113=CARTESIAN_POINT('Ctrl Pts',(1.70203370257971,1.85500935870737,104.0168950149));
#33114=CARTESIAN_POINT('Ctrl Pts',(1.6923417025111,1.86385567850046,104.01771581325));
#33115=CARTESIAN_POINT('Ctrl Pts',(1.67697763586337,1.87766051496428,104.019016477323));
#33116=CARTESIAN_POINT('Ctrl Pts',(1.67135155468716,1.88267017232798,104.019492657996));
#33117=CARTESIAN_POINT('Ctrl Pts',(1.66129129872783,1.89154753882451,104.020344137058));
#33118=CARTESIAN_POINT('Ctrl Pts',(1.65686594389805,1.89542504794065,104.020718701669));
#33119=CARTESIAN_POINT('Ctrl Pts',(1.64621903116203,1.90468812753593,104.021619866632));
#33120=CARTESIAN_POINT('Ctrl Pts',(1.63998467141384,1.91005869928306,104.022147537837));
#33121=CARTESIAN_POINT('Ctrl Pts',(1.62091631724366,1.92632290297196,104.023761134662));
#33122=CARTESIAN_POINT('Ctrl Pts',(1.60799958550767,1.93711820263747,104.02485371313));
#33123=CARTESIAN_POINT('Ctrl Pts',(1.5776721507108,1.9619523525148,104.02741601137));
#33124=CARTESIAN_POINT('Ctrl Pts',(1.56018088840414,1.97589017175661,104.028891560371));
#33125=CARTESIAN_POINT('Ctrl Pts',(1.49826972460489,2.0238891435732,104.034099951038));
#33126=CARTESIAN_POINT('Ctrl Pts',(1.4529036240984,2.0566987418208,104.037890704739));
#33127=CARTESIAN_POINT('Ctrl Pts',(1.26818883053807,2.18112530640414,104.053118223817));
#33128=CARTESIAN_POINT('Ctrl Pts',(1.12096607590401,2.26032119749295,104.064769256644));
#33129=CARTESIAN_POINT('Ctrl Pts',(0.928852586041864,2.34024478674086,104.078855894059));
#33130=CARTESIAN_POINT('Ctrl Pts',(0.890325110723717,2.3551718104359,104.081630622758));
#33131=CARTESIAN_POINT('Ctrl Pts',(0.788900541379837,2.39162275689454,104.088799878732));
#33132=CARTESIAN_POINT('Ctrl Pts',(0.725485101710259,2.41161692201443,104.093148762845));
#33133=CARTESIAN_POINT('Ctrl Pts',(0.641536230320368,2.4344730632923,104.098735719866));
#33134=CARTESIAN_POINT('Ctrl Pts',(0.621659241682069,2.43962449133796,104.100046408423));
#33135=CARTESIAN_POINT('Ctrl Pts',(0.589355628408675,2.44757601700117,104.102157368533));
#33136=CARTESIAN_POINT('Ctrl Pts',(0.576967198032266,2.45052591861508,104.102962393943));
#33137=CARTESIAN_POINT('Ctrl Pts',(0.55313736990064,2.45600948835446,104.104502413175));
#33138=CARTESIAN_POINT('Ctrl Pts',(0.541699650689299,2.4585575146338,104.105237846392));
#33139=CARTESIAN_POINT('Ctrl Pts',(0.515212124770009,2.46426442892456,104.10693254275));
#33140=CARTESIAN_POINT('Ctrl Pts',(0.500150234825214,2.46736549142861,104.107889951416));
#33141=CARTESIAN_POINT('Ctrl Pts',(0.452155487794997,2.4767894858813,104.110921587775));
#33142=CARTESIAN_POINT('Ctrl Pts',(0.4191234489377,2.48259268487586,104.112979460435));
#33143=CARTESIAN_POINT('Ctrl Pts',(0.341264757513149,2.49467283942801,104.117770072956));
#33144=CARTESIAN_POINT('Ctrl Pts',(0.296364760548544,2.50040446389215,104.120486356639));
#33145=CARTESIAN_POINT('Ctrl Pts',(0.126747036677982,2.51742314238566,104.130610212274));
#33146=CARTESIAN_POINT('Ctrl Pts',(0.00139654736664436,2.52061201911248,
104.137803709537));
#33147=CARTESIAN_POINT('Ctrl Pts',(-0.277374990281951,2.5069005376098,104.153840800988));
#33148=CARTESIAN_POINT('Ctrl Pts',(-0.430038592648369,2.4852648650098,104.162650889239));
#33149=CARTESIAN_POINT('Ctrl Pts',(-0.600042952386263,2.44503366335934,
104.173386903523));
#33150=CARTESIAN_POINT('Ctrl Pts',(-0.620275712715725,2.43997933083985,
104.174680132825));
#33151=CARTESIAN_POINT('Ctrl Pts',(-0.648497803208608,2.43255549282413,
104.176508763767));
#33152=CARTESIAN_POINT('Ctrl Pts',(-0.656542324134751,2.43039663397824,
104.177032833131));
#33153=CARTESIAN_POINT('Ctrl Pts',(-0.670447958610272,2.42659078737335,
104.177943872225));
#33154=CARTESIAN_POINT('Ctrl Pts',(-0.6763141433339,2.42496236923534,104.178329789151));
#33155=CARTESIAN_POINT('Ctrl Pts',(-0.688733643045075,2.42146621979154,
104.179150310578));
#33156=CARTESIAN_POINT('Ctrl Pts',(-0.69528536085527,2.41959313697012,104.179585229249));
#33157=CARTESIAN_POINT('Ctrl Pts',(-0.711619539386714,2.41485150832662,
104.180674551665));
#33158=CARTESIAN_POINT('Ctrl Pts',(-0.721392245235629,2.41195012306551,
104.181330798121));
#33159=CARTESIAN_POINT('Ctrl Pts',(-0.758815515955138,2.40059187240579,
104.183860411409));
#33160=CARTESIAN_POINT('Ctrl Pts',(-0.786336071535937,2.39171857432284,
104.185755527085));
#33161=CARTESIAN_POINT('Ctrl Pts',(-0.857252244842686,2.36749725907046,
104.190719090296));
#33162=CARTESIAN_POINT('Ctrl Pts',(-0.900389641879886,2.35142992405045,
104.193817085444));
#33163=CARTESIAN_POINT('Ctrl Pts',(-1.14147464116673,2.25402674091749,104.211493028684));
#33164=CARTESIAN_POINT('Ctrl Pts',(-1.32889471629403,2.1488740421352,104.226536632923));
#33165=CARTESIAN_POINT('Ctrl Pts',(-1.56048454409993,1.97692434033028,104.245809189719));
#33166=CARTESIAN_POINT('Ctrl Pts',(-1.61822985796482,1.92994192730616,104.250692770374));
#33167=CARTESIAN_POINT('Ctrl Pts',(-1.6897690692209,1.86626444817063,104.256848527777));
#33168=CARTESIAN_POINT('Ctrl Pts',(-1.70554305239767,1.85185999474962,104.258212990566));
#33169=CARTESIAN_POINT('Ctrl Pts',(-1.73055744801084,1.82842663642423,104.260388918363));
#33170=CARTESIAN_POINT('Ctrl Pts',(-1.73991474752255,1.81952458820983,104.261205688064));
#33171=CARTESIAN_POINT('Ctrl Pts',(-1.75759580607391,1.80244262307174,104.262754584547));
#33172=CARTESIAN_POINT('Ctrl Pts',(-1.76593197332259,1.79427609356988,104.263487257118));
#33173=CARTESIAN_POINT('Ctrl Pts',(-1.77430838224018,1.78595521598048,104.264226006925));
#33174=CARTESIAN_POINT('Ctrl Pts',(-1.77440558691462,1.78585863995499,104.264234580152));
#33175=CARTESIAN_POINT('Ctrl Pts',(-1.77459141069251,1.78567398780044,104.264250970046));
#33176=CARTESIAN_POINT('Ctrl Pts',(-1.77468003113393,1.78558591300034,104.264258786772));
#33177=CARTESIAN_POINT('Ctrl Pts',(-1.77484958072505,1.78541738224506,104.264273742372));
#33178=CARTESIAN_POINT('Ctrl Pts',(-1.77493051095504,1.78533692739034,104.264280881293));
#33179=CARTESIAN_POINT('Ctrl Pts',(-1.7853627920837,1.77496451387658,104.265201152514));
#33180=CARTESIAN_POINT('Ctrl Pts',(-1.79562460687889,1.7645825597548,104.266110347399));
#33181=CARTESIAN_POINT('Ctrl Pts',(-1.82707988470309,1.73220046922871,104.268910249619));
#33182=CARTESIAN_POINT('Ctrl Pts',(-1.8479641503524,1.70990291917768,104.270787696295));
#33183=CARTESIAN_POINT('Ctrl Pts',(-1.89568954674353,1.65705182649992,104.275127247451));
#33184=CARTESIAN_POINT('Ctrl Pts',(-1.92220679614154,1.62621674548608,104.277576437106));
#33185=CARTESIAN_POINT('Ctrl Pts',(-2.01421626505934,1.51382847889194,104.28623859431));
#33186=CARTESIAN_POINT('Ctrl Pts',(-2.07536241552043,1.42885164841835,104.292302871935));
#33187=CARTESIAN_POINT('Ctrl Pts',(-2.21685757591394,1.20387962267085,104.307603582226));
#33188=CARTESIAN_POINT('Ctrl Pts',(-2.28935763884659,1.05953511150167,104.316735614932));
#33189=CARTESIAN_POINT('Ctrl Pts',(-2.35227831645096,0.897086230223406,
104.327251000269));
#33190=CARTESIAN_POINT('Ctrl Pts',(-2.35690249744092,0.884865846514591,
104.328043545471));
#33191=CARTESIAN_POINT('Ctrl Pts',(-2.36143112095504,0.87261062965393,104.32884037888));
#33192=CARTESIAN_POINT('Origin',(0.,0.,104.));
#33193=CARTESIAN_POINT('',(-2.36143106504625,0.872610780952508,105.331623435588));
#33194=CARTESIAN_POINT('',(-2.36143112101025,0.872610629504508,105.056194669753));
#33195=CARTESIAN_POINT('',(-2.36143112101026,0.872610629504505,104.));
#33196=CARTESIAN_POINT('',(-2.51749994136415,-0.000543352100661543,104.112583302546));
#33197=CARTESIAN_POINT('Ctrl Pts',(-2.36143112101026,0.872610629504506,
105.056194669753));
#33198=CARTESIAN_POINT('Ctrl Pts',(-2.33303020666493,0.949468280251065,
105.051033590384));
#33199=CARTESIAN_POINT('Ctrl Pts',(-2.30086848333539,1.02495005197359,105.045872511015));
#33200=CARTESIAN_POINT('Ctrl Pts',(-2.265114379073,1.09866423429397,105.040711431645));
#33201=CARTESIAN_POINT('Ctrl Pts',(-2.22847279274693,1.17420813703378,105.035422244875));
#33202=CARTESIAN_POINT('Ctrl Pts',(-2.18805831165858,1.24789504763111,105.030133058105));
#33203=CARTESIAN_POINT('Ctrl Pts',(-2.14410262607408,1.31932944288462,105.024843871335));
#33204=CARTESIAN_POINT('Ctrl Pts',(-2.10115760903028,1.38912135446288,105.01967629829));
#33205=CARTESIAN_POINT('Ctrl Pts',(-2.05483282336813,1.45676286489124,105.014508725245));
#33206=CARTESIAN_POINT('Ctrl Pts',(-2.00538749260778,1.52191565288366,105.0093411522));
#33207=CARTESIAN_POINT('Ctrl Pts',(-1.95419669134617,1.58936840060466,105.003991158567));
#33208=CARTESIAN_POINT('Ctrl Pts',(-1.89966127698031,1.65415300688264,104.998641164935));
#33209=CARTESIAN_POINT('Ctrl Pts',(-1.84211170893855,1.71593435241314,104.993291171302));
#33210=CARTESIAN_POINT('Ctrl Pts',(-1.78456214089678,1.77771569794364,104.987941177669));
#33211=CARTESIAN_POINT('Ctrl Pts',(-1.72399887340572,1.83649345024587,104.982591184036));
#33212=CARTESIAN_POINT('Ctrl Pts',(-1.66078955074686,1.89197894230619,104.977241190403));
#33213=CARTESIAN_POINT('Ctrl Pts',(-1.59869961602271,1.94648182946345,104.971985940996));
#33214=CARTESIAN_POINT('Ctrl Pts',(-1.53380920573794,1.9980256805317,104.966730691588));
#33215=CARTESIAN_POINT('Ctrl Pts',(-1.46643193098218,2.04630976193632,104.961475442181));
#33216=CARTESIAN_POINT('Ctrl Pts',(-1.39915018189582,2.09452538748228,104.956227643524));
#33217=CARTESIAN_POINT('Ctrl Pts',(-1.32938894355345,2.13949015670352,104.950979844866));
#33218=CARTESIAN_POINT('Ctrl Pts',(-1.25749623897844,2.18094233278991,104.945732046209));
#33219=CARTESIAN_POINT('Ctrl Pts',(-1.18508260977988,2.22269486562808,104.940446222726));
#33220=CARTESIAN_POINT('Ctrl Pts',(-1.11050685153569,2.26088337439192,104.935160399243));
#33221=CARTESIAN_POINT('Ctrl Pts',(-1.03415594736465,2.29528380086871,104.92987457576));
#33222=CARTESIAN_POINT('Ctrl Pts',(-0.958489676481174,2.32937576109578,
104.924636149891));
#33223=CARTESIAN_POINT('Ctrl Pts',(-0.881080395830975,2.35974710885148,
104.919397724023));
#33224=CARTESIAN_POINT('Ctrl Pts',(-0.802329463704414,2.38622582369561,
104.914159298154));
#33225=CARTESIAN_POINT('Ctrl Pts',(-0.72360443144881,2.4126958301311,104.908922595117));
#33226=CARTESIAN_POINT('Ctrl Pts',(-0.643539061072373,2.43527559930734,
104.903685892079));
#33227=CARTESIAN_POINT('Ctrl Pts',(-0.56255261396542,2.45384205003514,104.898449189042));
#33228=CARTESIAN_POINT('Ctrl Pts',(-0.481568372888753,2.47240799502212,
104.893212628649));
#33229=CARTESIAN_POINT('Ctrl Pts',(-0.399663554949806,2.48696073681588,
104.887976068257));
#33230=CARTESIAN_POINT('Ctrl Pts',(-0.317269076047356,2.49742799363346,
104.882739507865));
#33231=CARTESIAN_POINT('Ctrl Pts',(-0.233526021624755,2.50806657123,104.877417239094));
#33232=CARTESIAN_POINT('Ctrl Pts',(-0.14927761891385,2.51448464551234,104.872094970324));
#33233=CARTESIAN_POINT('Ctrl Pts',(-0.0649813996979932,2.51666121432609,
104.866772701553));
#33234=CARTESIAN_POINT('Ctrl Pts',(0.0180764464160268,2.51880580775236,
104.861528620803));
#33235=CARTESIAN_POINT('Ctrl Pts',(0.101180247008966,2.51683276258219,104.856284540053));
#33236=CARTESIAN_POINT('Ctrl Pts',(0.183894488815563,2.5107745950171,104.851040459302));
#33237=CARTESIAN_POINT('Ctrl Pts',(0.26845860568486,2.50458093865516,104.845679096522));
#33238=CARTESIAN_POINT('Ctrl Pts',(0.352615020686807,2.49411729347779,104.840317733741));
#33239=CARTESIAN_POINT('Ctrl Pts',(0.435908145372231,2.47947380280537,104.834956370961));
#33240=CARTESIAN_POINT('Ctrl Pts',(0.51920127005765,2.46483031213296,104.82959500818));
#33241=CARTESIAN_POINT('Ctrl Pts',(0.60163062394185,2.44600715420394,104.8242336454));
#33242=CARTESIAN_POINT('Ctrl Pts',(0.682757877074153,2.42314835106999,104.818872282619));
#33243=CARTESIAN_POINT('Ctrl Pts',(0.762279440227179,2.40074197482975,104.813617033212));
#33244=CARTESIAN_POINT('Ctrl Pts',(0.840843710027796,2.3743755294766,104.808361783804));
#33245=CARTESIAN_POINT('Ctrl Pts',(0.918027687426422,2.3441483347089,104.803106534397));
#33246=CARTESIAN_POINT('Ctrl Pts',(0.99510223547909,2.31396399523662,104.79785873574));
#33247=CARTESIAN_POINT('Ctrl Pts',(1.07079995212236,2.2799299455045,104.792610937082));
#33248=CARTESIAN_POINT('Ctrl Pts',(1.1447118128608,2.24219560152475,104.787363138425));
#33249=CARTESIAN_POINT('Ctrl Pts',(1.21915922874995,2.20418783969196,104.782077314942));
#33250=CARTESIAN_POINT('Ctrl Pts',(1.29179434327542,2.16242606222529,104.776791491459));
#33251=CARTESIAN_POINT('Ctrl Pts',(1.3622185245738,2.11711287873556,104.771505667976));
#33252=CARTESIAN_POINT('Ctrl Pts',(1.43201121709949,2.07220601543446,104.766267242107));
#33253=CARTESIAN_POINT('Ctrl Pts',(1.49963207297644,2.02381143571998,104.761028816239));
#33254=CARTESIAN_POINT('Ctrl Pts',(1.56471828263879,1.97217213903247,104.75579039037));
#33255=CARTESIAN_POINT('Ctrl Pts',(1.62978308653003,1.9205498256502,104.750553687333));
#33256=CARTESIAN_POINT('Ctrl Pts',(1.69231453860289,1.86568520124402,104.745316984295));
#33257=CARTESIAN_POINT('Ctrl Pts',(1.75198113178698,1.80786292728802,104.740080281258));
#33258=CARTESIAN_POINT('Ctrl Pts',(1.8116460996829,1.75004222838186,104.734843720865));
#33259=CARTESIAN_POINT('Ctrl Pts',(1.8684460332112,1.6892643619624,104.729607160473));
#33260=CARTESIAN_POINT('Ctrl Pts',(1.92208569013621,1.62585142303151,104.724370600081));
#33261=CARTESIAN_POINT('Ctrl Pts',(1.97660328365608,1.56140058522383,104.71904833131));
#33262=CARTESIAN_POINT('Ctrl Pts',(2.02785588922083,1.4942280055528,104.71372606254));
#33263=CARTESIAN_POINT('Ctrl Pts',(2.07557678649174,1.42470602349278,104.708403793769));
#33264=CARTESIAN_POINT('Ctrl Pts',(2.12259662888583,1.35620537018719,104.703159713019));
#33265=CARTESIAN_POINT('Ctrl Pts',(2.16618764777983,1.28542431585759,104.697915632269));
#33266=CARTESIAN_POINT('Ctrl Pts',(2.20614000163562,1.21274586916765,104.692671551518));
#33267=CARTESIAN_POINT('Ctrl Pts',(2.24698587589954,1.13844199445953,104.687310188738));
#33268=CARTESIAN_POINT('Ctrl Pts',(2.28402814256915,1.06215529485621,104.681948825957));
#33269=CARTESIAN_POINT('Ctrl Pts',(2.31709436732378,0.98431699310558,104.676587463177));
#33270=CARTESIAN_POINT('Ctrl Pts',(2.35016059207842,0.906478691354946,104.671226100396));
#33271=CARTESIAN_POINT('Ctrl Pts',(2.37925066282247,0.827089287526055,104.665864737616));
#33272=CARTESIAN_POINT('Ctrl Pts',(2.40424673471588,0.746594862430761,104.660503374835));
#33273=CARTESIAN_POINT('Ctrl Pts',(2.42874807838157,0.667693602231119,104.655248125428));
#33274=CARTESIAN_POINT('Ctrl Pts',(2.44940654676645,0.587439246499782,104.64999287602));
#33275=CARTESIAN_POINT('Ctrl Pts',(2.46607514597444,0.506240678341004,104.644737626613));
#33276=CARTESIAN_POINT('Ctrl Pts',(2.48272011289541,0.425157231305679,104.639489827956));
#33277=CARTESIAN_POINT('Ctrl Pts',(2.4953863545401,0.343132679074028,104.634242029298));
#33278=CARTESIAN_POINT('Ctrl Pts',(2.50397650588177,0.260591458018378,104.628994230641));
#33279=CARTESIAN_POINT('Ctrl Pts',(2.51262890027548,0.177452154657314,104.623708407158));
#33280=CARTESIAN_POINT('Ctrl Pts',(2.5171457450105,0.0937891160265086,104.618422583675));
#33281=CARTESIAN_POINT('Ctrl Pts',(2.51747995172501,0.0100470225765003,
104.613136760192));
#33282=CARTESIAN_POINT('Ctrl Pts',(2.51781116163097,-0.072944161301868,
104.607898334323));
#33283=CARTESIAN_POINT('Ctrl Pts',(2.51403444206276,-0.156012518000315,
104.602659908455));
#33284=CARTESIAN_POINT('Ctrl Pts',(2.50615608684174,-0.238721424229384,
104.597421482586));
#33285=CARTESIAN_POINT('Ctrl Pts',(2.49828032268064,-0.321403128875668,
104.592184779549));
#33286=CARTESIAN_POINT('Ctrl Pts',(2.48630564569435,-0.403725158859374,
104.586948076511));
#33287=CARTESIAN_POINT('Ctrl Pts',(2.47029033818926,-0.485254464223448,
104.581711373474));
#33288=CARTESIAN_POINT('Ctrl Pts',(2.45427546693312,-0.56678154877009,104.576474813081));
#33289=CARTESIAN_POINT('Ctrl Pts',(2.43422027394694,-0.647515499061263,
104.571238252689));
#33290=CARTESIAN_POINT('Ctrl Pts',(2.41023418493731,-0.727033303060847,
104.566001692297));
#33291=CARTESIAN_POINT('Ctrl Pts',(2.38585550830661,-0.807852599166646,
104.560679423526));
#33292=CARTESIAN_POINT('Ctrl Pts',(2.35741622780974,-0.887415105170729,
104.555357154756));
#33293=CARTESIAN_POINT('Ctrl Pts',(2.32508344262049,-0.96529437730261,104.550034885985));
#33294=CARTESIAN_POINT('Ctrl Pts',(2.29322564968901,-1.04202954597769,104.544790805235));
#33295=CARTESIAN_POINT('Ctrl Pts',(2.25758824566432,-1.11713021185096,104.539546724484));
#33296=CARTESIAN_POINT('Ctrl Pts',(2.21837824670566,-1.19021183179429,104.534302643734));
#33297=CARTESIAN_POINT('Ctrl Pts',(2.17829132984629,-1.26492789658442,104.528941280954));
#33298=CARTESIAN_POINT('Ctrl Pts',(2.13447035466966,-1.33753307677803,104.523579918173));
#33299=CARTESIAN_POINT('Ctrl Pts',(2.08718314535484,-1.40764795589902,104.518218555392));
#33300=CARTESIAN_POINT('Ctrl Pts',(2.03989593604002,-1.47776283502,104.512857192612));
#33301=CARTESIAN_POINT('Ctrl Pts',(1.98914285101044,-1.54538704678005,104.507495829831));
#33302=CARTESIAN_POINT('Ctrl Pts',(1.93523389860253,-1.61017887444211,104.502134467051));
#33303=CARTESIAN_POINT('Ctrl Pts',(1.88239192506217,-1.67368832676914,104.496879217643));
#33304=CARTESIAN_POINT('Ctrl Pts',(1.8263227259832,-1.73471109993217,104.491623968236));
#33305=CARTESIAN_POINT('Ctrl Pts',(1.76728923830282,-1.7929012795408,104.486368718829));
#33306=CARTESIAN_POINT('Ctrl Pts',(1.70833944669724,-1.85100895869389,104.481120920171));
#33307=CARTESIAN_POINT('Ctrl Pts',(1.64643404012584,-1.90629169997362,104.475873121514));
#33308=CARTESIAN_POINT('Ctrl Pts',(1.58187602200247,-1.95843674930125,104.470625322856));
#33309=CARTESIAN_POINT('Ctrl Pts',(1.5168502253821,-2.01095963446569,104.465339499373));
#33310=CARTESIAN_POINT('Ctrl Pts',(1.44913351719056,-2.06029880096661,104.46005367589));
#33311=CARTESIAN_POINT('Ctrl Pts',(1.37907325462703,-2.10617264448393,104.454767852407));
#33312=CARTESIAN_POINT('Ctrl Pts',(1.30964121760201,-2.15163514041286,104.449529426539));
#33313=CARTESIAN_POINT('Ctrl Pts',(1.23790787999602,-2.19369395365314,104.44429100067));
#33314=CARTESIAN_POINT('Ctrl Pts',(1.16424290473668,-2.23211664318205,104.439052574802));
#33315=CARTESIAN_POINT('Ctrl Pts',(1.09060215666171,-2.27052669612783,104.433815871764));
#33316=CARTESIAN_POINT('Ctrl Pts',(1.01503144143266,-2.3053027871867,104.428579168726));
#33317=CARTESIAN_POINT('Ctrl Pts',(0.937925729905276,-2.33625802838249,
104.423342465689));
#33318=CARTESIAN_POINT('Ctrl Pts',(0.860822118699087,-2.36721242637293,
104.418105905297));
#33319=CARTESIAN_POINT('Ctrl Pts',(0.78218402291449,-2.39434601048306,104.412869344904));
#33320=CARTESIAN_POINT('Ctrl Pts',(0.702425838780685,-2.41752025658799,
104.407632784512));
#33321=CARTESIAN_POINT('Ctrl Pts',(0.621362228165491,-2.44107380263411,
104.402310515741));
#33322=CARTESIAN_POINT('Ctrl Pts',(0.539142001278009,-2.46053708415131,
104.396988246971));
#33323=CARTESIAN_POINT('Ctrl Pts',(0.456213833269011,-2.47581808466091,
104.3916659782));
#33324=CARTESIAN_POINT('Ctrl Pts',(0.374503940689362,-2.49087459609877,
104.38642189745));
#33325=CARTESIAN_POINT('Ctrl Pts',(0.292107241290161,-2.50187089130869,
104.3811778167));
#33326=CARTESIAN_POINT('Ctrl Pts',(0.209458997151658,-2.50877124874155,
104.375933735949));
#33327=CARTESIAN_POINT('Ctrl Pts',(0.124962353964994,-2.51582593025284,
104.370572373169));
#33328=CARTESIAN_POINT('Ctrl Pts',(0.0402032906129579,-2.51859923804143,
104.365211010388));
#33329=CARTESIAN_POINT('Ctrl Pts',(-0.0443541239990409,-2.5171092470698,
104.359849647608));
#33330=CARTESIAN_POINT('Ctrl Pts',(-0.12891153861104,-2.51561925609817,
104.354488284827));
#33331=CARTESIAN_POINT('Ctrl Pts',(-0.213266802098999,-2.50986606758289,
104.349126922046));
#33332=CARTESIAN_POINT('Ctrl Pts',(-0.296964500577455,-2.49992366591398,
104.343765559266));
#33333=CARTESIAN_POINT('Ctrl Pts',(-0.379005634207852,-2.49017804663466,
104.338510309859));
#33334=CARTESIAN_POINT('Ctrl Pts',(-0.460718028522092,-2.47637157911839,
104.333255060451));
#33335=CARTESIAN_POINT('Ctrl Pts',(-0.541668376772253,-2.45853647920972,
104.327999811044));
#33336=CARTESIAN_POINT('Ctrl Pts',(-0.622503955818408,-2.44072666542105,
104.322752012386));
#33337=CARTESIAN_POINT('Ctrl Pts',(-0.702579187952239,-2.41889966276607,
104.317504213729));
#33338=CARTESIAN_POINT('Ctrl Pts',(-0.781466766783666,-2.39313934872432,
104.312256415071));
#33339=CARTESIAN_POINT('Ctrl Pts',(-0.860925954132904,-2.36719237899932,
104.306970591589));
#33340=CARTESIAN_POINT('Ctrl Pts',(-0.939179733834524,-2.33725491281204,
104.301684768106));
#33341=CARTESIAN_POINT('Ctrl Pts',(-1.01580277918804,-2.30346499078971,
104.296398944623));
#33342=CARTESIAN_POINT('Ctrl Pts',(-1.09173875098279,-2.2699780606658,104.291160518754));
#33343=CARTESIAN_POINT('Ctrl Pts',(-1.1660726866908,-2.23270767701558,104.285922092886));
#33344=CARTESIAN_POINT('Ctrl Pts',(-1.23840835301748,-2.19183735737316,
104.280683667017));
#33345=CARTESIAN_POINT('Ctrl Pts',(-1.31072022934732,-2.15098047929869,
104.27544696398));
#33346=CARTESIAN_POINT('Ctrl Pts',(-1.38103474011157,-2.10652624344265,
104.270210260942));
#33347=CARTESIAN_POINT('Ctrl Pts',(-1.44898008261864,-2.05870419686133,
104.264973557905));
#33348=CARTESIAN_POINT('Ctrl Pts',(-1.51692357432857,-2.01088345292865,
104.259736997512));
#33349=CARTESIAN_POINT('Ctrl Pts',(-1.58249764935668,-1.95969534708828,
104.25450043712));
#33350=CARTESIAN_POINT('Ctrl Pts',(-1.6453604960618,-1.90541205202425,104.249263876728));
#33351=CARTESIAN_POINT('Ctrl Pts',(-1.70925223811683,-1.85024028574396,
104.243941607957));
#33352=CARTESIAN_POINT('Ctrl Pts',(-1.77034281937563,-1.79187140774975,
104.238619339187));
#33353=CARTESIAN_POINT('Ctrl Pts',(-1.8283107752395,-1.73063166478114,104.233297070416));
#33354=CARTESIAN_POINT('Ctrl Pts',(-1.88542713944256,-1.67029157841842,
104.228052989666));
#33355=CARTESIAN_POINT('Ctrl Pts',(-1.93951175864249,-1.6071648127306,104.222808908916));
#33356=CARTESIAN_POINT('Ctrl Pts',(-1.99029769076042,-1.54159701353945,
104.217564828165));
#33357=CARTESIAN_POINT('Ctrl Pts',(-2.04221943247203,-1.47456281347207,
104.212203465385));
#33358=CARTESIAN_POINT('Ctrl Pts',(-2.09069286600373,-1.40497749678778,
104.206842102604));
#33359=CARTESIAN_POINT('Ctrl Pts',(-2.13548048945464,-1.33324016184578,
104.201480739824));
#33360=CARTESIAN_POINT('Ctrl Pts',(-2.18026811290555,-1.26150282690377,
104.196119377043));
#33361=CARTESIAN_POINT('Ctrl Pts',(-2.2213697376516,-1.1876139502074,104.190758014263));
#33362=CARTESIAN_POINT('Ctrl Pts',(-2.25859947042747,-1.11199581032698,
104.185396651482));
#33363=CARTESIAN_POINT('Ctrl Pts',(-2.29771370768151,-1.03255001140606,
104.17976390582));
#33364=CARTESIAN_POINT('Ctrl Pts',(-2.33268319210157,-0.950935265154256,
104.174131160157));
#33365=CARTESIAN_POINT('Ctrl Pts',(-2.3632800928912,-0.867590601922441,
104.168498414495));
#33366=CARTESIAN_POINT('Ctrl Pts',(-2.39377456178273,-0.784524958847305,
104.162884526064));
#33367=CARTESIAN_POINT('Ctrl Pts',(-2.41992549446131,-0.699741274927147,
104.157270637633));
#33368=CARTESIAN_POINT('Ctrl Pts',(-2.44155272692772,-0.613699056241603,
104.151656749201));
#33369=CARTESIAN_POINT('Ctrl Pts',(-2.46313411560349,-0.527839223419127,
104.146054760671));
#33370=CARTESIAN_POINT('Ctrl Pts',(-2.48021080455414,-0.44072651169474,
104.140452772141));
#33371=CARTESIAN_POINT('Ctrl Pts',(-2.49265158327774,-0.352837546730744,
104.134850783611));
#33372=CARTESIAN_POINT('Ctrl Pts',(-2.50505613088024,-0.265204539677777,
104.12926510968));
#33373=CARTESIAN_POINT('Ctrl Pts',(-2.51285161508245,-0.176800136803316,
104.12367943575));
#33374=CARTESIAN_POINT('Ctrl Pts',(-2.51595758515502,-0.0881117455332033,
104.118093761819));
#33375=CARTESIAN_POINT('Ctrl Pts',(-2.51697896722405,-0.0589470303370983,
104.116256942062));
#33376=CARTESIAN_POINT('Ctrl Pts',(-2.51749363732475,-0.0297517030198697,
104.114420122304));
#33377=CARTESIAN_POINT('Ctrl Pts',(-2.51749994136415,-0.000543352100661293,
104.112583302546));
#33378=CARTESIAN_POINT('Ctrl Pts',(-2.51749994136434,-0.000543351236957333,
104.112583302492));
#33379=CARTESIAN_POINT('Ctrl Pts',(-2.51751848517037,0.0853753463440664,
104.107180150438));
#33380=CARTESIAN_POINT('Ctrl Pts',(-2.51313426361846,0.171241893100704,
104.101776998384));
#33381=CARTESIAN_POINT('Ctrl Pts',(-2.50438935623882,0.256593457355597,
104.096373846329));
#33382=CARTESIAN_POINT('Ctrl Pts',(-2.49563786309435,0.342009299630279,
104.090966625177));
#33383=CARTESIAN_POINT('Ctrl Pts',(-2.48251919937096,0.426908972259079,
104.085559404024));
#33384=CARTESIAN_POINT('Ctrl Pts',(-2.46512690395723,0.510838132275033,
104.080152182872));
#33385=CARTESIAN_POINT('Ctrl Pts',(-2.44770570697484,0.594906761195075,
104.074735976293));
#33386=CARTESIAN_POINT('Ctrl Pts',(-2.42599679375752,0.678001249607856,
104.069319769715));
#33387=CARTESIAN_POINT('Ctrl Pts',(-2.40014407058638,0.759680650292643,
104.063903563137));
#33388=CARTESIAN_POINT('Ctrl Pts',(-2.38812822328385,0.797643660993429,
104.061386214742));
#33389=CARTESIAN_POINT('Ctrl Pts',(-2.37521791696454,0.835301240958594,
104.058868866346));
#33390=CARTESIAN_POINT('Ctrl Pts',(-2.36143112101026,0.872610629504494,
104.05635151795));
#33391=CARTESIAN_POINT('',(-2.51749878614078,0.00217395721947723,104.388357324048));
#33392=CARTESIAN_POINT('Ctrl Pts',(-2.36143112095504,0.87261062965393,104.32884037888));
#33393=CARTESIAN_POINT('Ctrl Pts',(-2.36994372294453,0.849574097006755,
104.330338212745));
#33394=CARTESIAN_POINT('Ctrl Pts',(-2.37811868251946,0.82641448493804,104.331851197041));
#33395=CARTESIAN_POINT('Ctrl Pts',(-2.38967067758178,0.792096000718289,
104.334108788615));
#33396=CARTESIAN_POINT('Ctrl Pts',(-2.39331116459058,0.781027322701226,
104.334839298037));
#33397=CARTESIAN_POINT('Ctrl Pts',(-2.39905590931377,0.763143410196021,
104.336024015738));
#33398=CARTESIAN_POINT('Ctrl Pts',(-2.40120831839551,0.756343658132843,
104.33647548894));
#33399=CARTESIAN_POINT('Ctrl Pts',(-2.40531609083367,0.743172371081131,
104.337352148091));
#33400=CARTESIAN_POINT('Ctrl Pts',(-2.40727508292726,0.736802104376359,
104.337777122774));
#33401=CARTESIAN_POINT('Ctrl Pts',(-2.41194565227788,0.721396843246568,
104.338807098303));
#33402=CARTESIAN_POINT('Ctrl Pts',(-2.4146317722416,0.712354288755783,104.339413535808));
#33403=CARTESIAN_POINT('Ctrl Pts',(-2.4238789211069,0.680571376831846,104.341551062752));
#33404=CARTESIAN_POINT('Ctrl Pts',(-2.43016979895327,0.657754571033595,
104.343096343929));
#33405=CARTESIAN_POINT('Ctrl Pts',(-2.48997770515915,0.428252319084638,
104.358724032165));
#33406=CARTESIAN_POINT('Ctrl Pts',(-2.51731451133507,0.215658486073652,
104.373797644526));
#33407=CARTESIAN_POINT('Ctrl Pts',(-2.51749905933581,0.00217629118206962,
104.388357642272));
#33408=CARTESIAN_POINT('Ctrl Pts',(-2.51749906132417,0.00217398986072041,
104.388357799227));
#33409=CARTESIAN_POINT('Ctrl Pts',(-2.51759705576998,-0.111304425924101,
104.396097297547));
#33410=CARTESIAN_POINT('Ctrl Pts',(-2.51002239620448,-0.224674609144805,
104.403685278352));
#33411=CARTESIAN_POINT('Ctrl Pts',(-2.49202450093169,-0.35784890421739,
104.412393645945));
#33412=CARTESIAN_POINT('Ctrl Pts',(-2.48897173933918,-0.378499240382162,
104.41373838398));
#33413=CARTESIAN_POINT('Ctrl Pts',(-2.48347979364576,-0.412703174110995,
104.415956789967));
#33414=CARTESIAN_POINT('Ctrl Pts',(-2.4811856609536,-0.426278692344601,
104.416834930007));
#33415=CARTESIAN_POINT('Ctrl Pts',(-2.47684388210193,-0.450747680262971,
104.418413657293));
#33416=CARTESIAN_POINT('Ctrl Pts',(-2.47483545520061,-0.461647661793919,
104.419115458553));
#33417=CARTESIAN_POINT('Ctrl Pts',(-2.47079094447573,-0.482812447619622,
104.42047544179));
#33418=CARTESIAN_POINT('Ctrl Pts',(-2.46876271547497,-0.493078503782115,
104.421133856617));
#33419=CARTESIAN_POINT('Ctrl Pts',(-2.46404228637102,-0.516211841699916,
104.422614827664));
#33420=CARTESIAN_POINT('Ctrl Pts',(-2.46131318076387,-0.529071347882821,
104.423436195842));
#33421=CARTESIAN_POINT('Ctrl Pts',(-2.4536577064387,-0.563802001677604,
104.425649793425));
#33422=CARTESIAN_POINT('Ctrl Pts',(-2.44853964364161,-0.585630003466548,
104.427035918781));
#33423=CARTESIAN_POINT('Ctrl Pts',(-2.42208859806725,-0.692025641742305,
104.433771175174));
#33424=CARTESIAN_POINT('Ctrl Pts',(-2.39666137425239,-0.775518712718171,
104.438988286628));
#33425=CARTESIAN_POINT('Ctrl Pts',(-2.33319474884591,-0.950698787142168,
104.449937633954));
#33426=CARTESIAN_POINT('Ctrl Pts',(-2.29396787372504,-1.0417958409853,104.455632884603));
#33427=CARTESIAN_POINT('Ctrl Pts',(-2.21290939211794,-1.20310827165754,
104.466006020939));
#33428=CARTESIAN_POINT('Ctrl Pts',(-2.17283888657701,-1.27405172977227,
104.470679265308));
#33429=CARTESIAN_POINT('Ctrl Pts',(-2.08366744399577,-1.41544588724591,
104.480453786612));
#33430=CARTESIAN_POINT('Ctrl Pts',(-2.03426223784131,-1.48557430605187,
104.485558513338));
#33431=CARTESIAN_POINT('Ctrl Pts',(-1.97261100150029,-1.56422961146285,
104.49176165647));
#33432=CARTESIAN_POINT('Ctrl Pts',(-1.96374468859346,-1.57534606256729,
104.492650095827));
#33433=CARTESIAN_POINT('Ctrl Pts',(-1.94993732297004,-1.5923598420077,104.494029114021));
#33434=CARTESIAN_POINT('Ctrl Pts',(-1.94506244473924,-1.5983108309357,104.494515142902));
#33435=CARTESIAN_POINT('Ctrl Pts',(-1.93600676094677,-1.60926273793144,
104.495416634101));
#33436=CARTESIAN_POINT('Ctrl Pts',(-1.93183373327006,-1.61426985413066,
104.495831546242));
#33437=CARTESIAN_POINT('Ctrl Pts',(-1.92226434411328,-1.6256616885958,104.496781817996));
#33438=CARTESIAN_POINT('Ctrl Pts',(-1.9168556175426,-1.63203574444419,104.497318054359));
#33439=CARTESIAN_POINT('Ctrl Pts',(-1.90259415430328,-1.64867384778636,
104.498729443671));
#33440=CARTESIAN_POINT('Ctrl Pts',(-1.89369022706055,-1.65889338937834,
104.499608097677));
#33441=CARTESIAN_POINT('Ctrl Pts',(-1.82139122917186,-1.74053446506236,
104.506719063702));
#33442=CARTESIAN_POINT('Ctrl Pts',(-1.75406773897452,-1.80836075757747,
104.513193656654));
#33443=CARTESIAN_POINT('Ctrl Pts',(-1.59779231913719,-1.94884927253105,
104.527621178152));
#33444=CARTESIAN_POINT('Ctrl Pts',(-1.50738300055502,-2.01959182732876,
104.53558998574));
#33445=CARTESIAN_POINT('Ctrl Pts',(-1.33565847272146,-2.13598501867354,
104.549802292006));
#33446=CARTESIAN_POINT('Ctrl Pts',(-1.25602695061295,-2.18376161411814,
104.556075890789));
#33447=CARTESIAN_POINT('Ctrl Pts',(-1.14056181732992,-2.2446264702294,104.564700606796));
#33448=CARTESIAN_POINT('Ctrl Pts',(-1.1067990198121,-2.26146532669062,104.567169314603));
#33449=CARTESIAN_POINT('Ctrl Pts',(-1.04652949196028,-2.28985089286147,
104.571483857217));
#33450=CARTESIAN_POINT('Ctrl Pts',(-1.02017910749754,-2.30171149173258,
104.573339907378));
#33451=CARTESIAN_POINT('Ctrl Pts',(-0.980712421350819,-2.31866492494391,
104.576076160567));
#33452=CARTESIAN_POINT('Ctrl Pts',(-0.967748930751122,-2.32410539942738,
104.576968033364));
#33453=CARTESIAN_POINT('Ctrl Pts',(-0.954667741871376,-2.32946684002677,
104.577861214339));
#33454=CARTESIAN_POINT('Ctrl Pts',(-0.954595152639167,-2.32949658740079,
104.577866170508));
#33455=CARTESIAN_POINT('Ctrl Pts',(-0.954445826567376,-2.32955777370407,
104.577876365601));
#33456=CARTESIAN_POINT('Ctrl Pts',(-0.954369089564325,-2.32958921223488,
104.577881604512));
#33457=CARTESIAN_POINT('Ctrl Pts',(-0.954211215777274,-2.32965388274147,
104.577892382229));
#33458=CARTESIAN_POINT('Ctrl Pts',(-0.954130078808578,-2.32968711427099,
104.577897921021));
#33459=CARTESIAN_POINT('Ctrl Pts',(-0.953963136003445,-2.32975547938909,
104.577909316785));
#33460=CARTESIAN_POINT('Ctrl Pts',(-0.953877329947913,-2.32979061248183,
104.577915173741));
#33461=CARTESIAN_POINT('Ctrl Pts',(-0.953700761651266,-2.32986289657649,
104.577927225353));
#33462=CARTESIAN_POINT('Ctrl Pts',(-0.953609999195669,-2.32990004700889,
104.577933419987));
#33463=CARTESIAN_POINT('Ctrl Pts',(-0.953423211188627,-2.32997648939459,
104.577946167795));
#33464=CARTESIAN_POINT('Ctrl Pts',(-0.953327185384246,-2.33001578071311,
104.577952720947));
#33465=CARTESIAN_POINT('Ctrl Pts',(-0.953129542660793,-2.33009663682879,
104.577966208055));
#33466=CARTESIAN_POINT('Ctrl Pts',(-0.953027925444611,-2.33013820091779,
104.577973141988));
#33467=CARTESIAN_POINT('Ctrl Pts',(-0.952818749103518,-2.33022374351904,
104.577987414462));
#33468=CARTESIAN_POINT('Ctrl Pts',(-0.95271118963862,-2.33026772123729,
104.577994752977));
#33469=CARTESIAN_POINT('Ctrl Pts',(-0.952489753423229,-2.33035824172119,
104.578009860074));
#33470=CARTESIAN_POINT('Ctrl Pts',(-0.952375876312009,-2.33040478358441,
104.578017628626));
#33471=CARTESIAN_POINT('Ctrl Pts',(-0.952141402930466,-2.33050059339113,
104.578033623044));
#33472=CARTESIAN_POINT('Ctrl Pts',(-0.95202080624327,-2.33054986032282,
104.578041848876));
#33473=CARTESIAN_POINT('Ctrl Pts',(-0.951772463216978,-2.33065129251508,
104.578058787026));
#33474=CARTESIAN_POINT('Ctrl Pts',(-0.951644716414116,-2.33070345663309,
104.578067499306));
#33475=CARTESIAN_POINT('Ctrl Pts',(-0.951381611756175,-2.3308108675279,
104.578085441605));
#33476=CARTESIAN_POINT('Ctrl Pts',(-0.951246253372611,-2.33086611301862,
104.578094671581));
#33477=CARTESIAN_POINT('Ctrl Pts',(-0.950967430754681,-2.33097988400824,
104.578113682769));
#33478=CARTESIAN_POINT('Ctrl Pts',(-0.950823965931995,-2.33103840805264,
104.578123463932));
#33479=CARTESIAN_POINT('Ctrl Pts',(-0.950528399567668,-2.33115894751862,
104.578143613415));
#33480=CARTESIAN_POINT('Ctrl Pts',(-0.950376297342477,-2.33122096130556,
104.578153981681));
#33481=CARTESIAN_POINT('Ctrl Pts',(-0.950062886302104,-2.33134870673876,
104.578175343907));
#33482=CARTESIAN_POINT('Ctrl Pts',(-0.949901576727771,-2.33141443653232,
104.578186337805));
#33483=CARTESIAN_POINT('Ctrl Pts',(-0.949569138981177,-2.33154985673396,
104.578208992657));
#33484=CARTESIAN_POINT('Ctrl Pts',(-0.949398009956761,-2.33161954504412,
104.578220653541));
#33485=CARTESIAN_POINT('Ctrl Pts',(-0.94904527580149,-2.33176314254297,
104.578244686773));
#33486=CARTESIAN_POINT('Ctrl Pts',(-0.948863669699855,-2.33183704935974,
104.578257059043));
#33487=CARTESIAN_POINT('Ctrl Pts',(-0.948489274743593,-2.33198936297135,
104.578282562742));
#33488=CARTESIAN_POINT('Ctrl Pts',(-0.948296484791196,-2.33206776707879,
104.578295694082));
#33489=CARTESIAN_POINT('Ctrl Pts',(-0.94789896247512,-2.33222937460635,
104.57832276716));
#33490=CARTESIAN_POINT('Ctrl Pts',(-0.947694228862453,-2.33231257498196,
104.578336708796));
#33491=CARTESIAN_POINT('Ctrl Pts',(-0.947272002425946,-2.33248409609232,
104.578365457515));
#33492=CARTESIAN_POINT('Ctrl Pts',(-0.947054508193853,-2.33257241336971,
104.578380264481));
#33493=CARTESIAN_POINT('Ctrl Pts',(-0.946605882228841,-2.33275451257663,
104.578410803006));
#33494=CARTESIAN_POINT('Ctrl Pts',(-0.946374748899497,-2.33284829058008,
104.578426534432));
#33495=CARTESIAN_POINT('Ctrl Pts',(-0.945897900405061,-2.33304168036229,
104.578458985413));
#33496=CARTESIAN_POINT('Ctrl Pts',(-0.945652183424224,-2.33314128768137,
104.578475704817));
#33497=CARTESIAN_POINT('Ctrl Pts',(-0.945231257997559,-2.3333118425611,
104.578504341919));
#33498=CARTESIAN_POINT('Ctrl Pts',(-0.945056057322434,-2.33338280919564,
104.578516260256));
#33499=CARTESIAN_POINT('Ctrl Pts',(-0.944646797051759,-2.33354853015362,
104.578544098091));
#33500=CARTESIAN_POINT('Ctrl Pts',(-0.944412731158613,-2.33364326900832,
104.57856001707));
#33501=CARTESIAN_POINT('Ctrl Pts',(-0.943865901467322,-2.33386450417965,
104.578597202294));
#33502=CARTESIAN_POINT('Ctrl Pts',(-0.943553126433803,-2.33399097286593,
104.578618467611));
#33503=CARTESIAN_POINT('Ctrl Pts',(-0.942822351462466,-2.33428628638717,
104.578668143423));
#33504=CARTESIAN_POINT('Ctrl Pts',(-0.942404331476356,-2.33445508186545,
104.578696552262));
#33505=CARTESIAN_POINT('Ctrl Pts',(-0.931175254538073,-2.3389858488409,
104.579459501581));
#33506=CARTESIAN_POINT('Ctrl Pts',(-0.920333931203409,-2.3432728433032,
104.580191520365));
#33507=CARTESIAN_POINT('Ctrl Pts',(-0.895558632189609,-2.35287129652931,
104.581854153513));
#33508=CARTESIAN_POINT('Ctrl Pts',(-0.88160637719201,-2.35813460440708,
104.582783148238));
#33509=CARTESIAN_POINT('Ctrl Pts',(-0.838480638018669,-2.37396697850917,
104.585632796169));
#33510=CARTESIAN_POINT('Ctrl Pts',(-0.809157214191989,-2.3841211645656,
104.587539804161));
#33511=CARTESIAN_POINT('Ctrl Pts',(-0.585919781147914,-2.45683093528707,
104.601845315785));
#33512=CARTESIAN_POINT('Ctrl Pts',(-0.385245473996142,-2.49618004428777,
104.613421818613));
#33513=CARTESIAN_POINT('Ctrl Pts',(-0.0528506681205948,-2.52027423854299,
104.632617043671));
#33514=CARTESIAN_POINT('Ctrl Pts',(0.0768201698871136,-2.51965581059027,
104.640134829666));
#33515=CARTESIAN_POINT('Ctrl Pts',(0.223761401582444,-2.50760046651374,
104.649235348058));
#33516=CARTESIAN_POINT('Ctrl Pts',(0.241656982558344,-2.50593917017126,
104.650353671097));
#33517=CARTESIAN_POINT('Ctrl Pts',(0.26793630722683,-2.50321548521441,104.652012623391));
#33518=CARTESIAN_POINT('Ctrl Pts',(0.276335387717901,-2.5023022157141,104.652545353551));
#33519=CARTESIAN_POINT('Ctrl Pts',(0.291213183389695,-2.50060866866025,
104.653493723728));
#33520=CARTESIAN_POINT('Ctrl Pts',(0.297693673143479,-2.49984545673397,
104.653908413365));
#33521=CARTESIAN_POINT('Ctrl Pts',(0.311744289574365,-2.4981352942714,104.654811049956));
#33522=CARTESIAN_POINT('Ctrl Pts',(0.319312982675524,-2.49717914175093,
104.655299479174));
#33523=CARTESIAN_POINT('Ctrl Pts',(0.340305308334726,-2.49443018666976,
104.656660071816));
#33524=CARTESIAN_POINT('Ctrl Pts',(0.353718767410586,-2.49256347430356,
104.657536150878));
#33525=CARTESIAN_POINT('Ctrl Pts',(0.428274013284006,-2.4815739297311,104.6624405244));
#33526=CARTESIAN_POINT('Ctrl Pts',(0.489073902976107,-2.47031033844066,
104.666570544537));
#33527=CARTESIAN_POINT('Ctrl Pts',(0.72300867334983,-2.41799809231037,104.682820772379));
#33528=CARTESIAN_POINT('Ctrl Pts',(0.892022280454537,-2.36088061983492,
104.695292560618));
#33529=CARTESIAN_POINT('Ctrl Pts',(1.1566397939054,-2.23894173065663,104.715092162913));
#33530=CARTESIAN_POINT('Ctrl Pts',(1.25635434969884,-2.18454931396937,104.722634943283));
#33531=CARTESIAN_POINT('Ctrl Pts',(1.37159134604528,-2.111179505125,104.731432106561));
#33532=CARTESIAN_POINT('Ctrl Pts',(1.39093930183575,-2.09848269957238,104.732912379732));
#33533=CARTESIAN_POINT('Ctrl Pts',(1.42112940635216,-2.07806987394011,104.735227989854));
#33534=CARTESIAN_POINT('Ctrl Pts',(1.43208976878401,-2.07053183886651,104.736069897385));
#33535=CARTESIAN_POINT('Ctrl Pts',(1.4525019688657,-2.05625363868356,104.73764036755));
#33536=CARTESIAN_POINT('Ctrl Pts',(1.46196788666106,-2.0495343133963,104.738369689694));
#33537=CARTESIAN_POINT('Ctrl Pts',(1.48306088740548,-2.03434108137355,104.739997363864));
#33538=CARTESIAN_POINT('Ctrl Pts',(1.49466254736297,-2.02583244968708,104.740894359008));
#33539=CARTESIAN_POINT('Ctrl Pts',(1.52400650935799,-2.00392234392493,104.743168037876));
#33540=CARTESIAN_POINT('Ctrl Pts',(1.54164560485165,-1.99038425396033,104.744539416419));
#33541=CARTESIAN_POINT('Ctrl Pts',(1.68579856627099,-1.87668001410425,104.755792241897));
#33542=CARTESIAN_POINT('Ctrl Pts',(1.80259850823902,-1.76479254080282,104.765169338915));
#33543=CARTESIAN_POINT('Ctrl Pts',(1.98924918055955,-1.54798015692163,104.781627760049));
#33544=CARTESIAN_POINT('Ctrl Pts',(2.06346452103391,-1.44757227243226,104.788733640141));
#33545=CARTESIAN_POINT('Ctrl Pts',(2.15318648358678,-1.30518085087529,104.798687823221));
#33546=CARTESIAN_POINT('Ctrl Pts',(2.17547683047469,-1.26767867569951,104.801299750945));
#33547=CARTESIAN_POINT('Ctrl Pts',(2.2103693348331,-1.20534131971021,104.805656966285));
#33548=CARTESIAN_POINT('Ctrl Pts',(2.22355418953852,-1.18084161150694,104.807373262537));
#33549=CARTESIAN_POINT('Ctrl Pts',(2.24094307285037,-1.14720587126872,104.809741627424));
#33550=CARTESIAN_POINT('Ctrl Pts',(2.24550290235323,-1.13825474931395,104.810373040634));
#33551=CARTESIAN_POINT('Ctrl Pts',(2.25305177911631,-1.12321411363711,104.811436322397));
#33552=CARTESIAN_POINT('Ctrl Pts',(2.25607006405686,-1.11713926110719,104.811866405819));
#33553=CARTESIAN_POINT('Ctrl Pts',(2.2617621010825,-1.10556584199093,104.81268710315));
#33554=CARTESIAN_POINT('Ctrl Pts',(2.26444043949696,-1.10006960094475,104.81307741631));
#33555=CARTESIAN_POINT('Ctrl Pts',(2.27076518559023,-1.08696956552533,104.814008948343));
#33556=CARTESIAN_POINT('Ctrl Pts',(2.27439343345416,-1.07935715567501,104.814551248814));
#33557=CARTESIAN_POINT('Ctrl Pts',(2.28712477982981,-1.05229634620056,104.8164821568));
#33558=CARTESIAN_POINT('Ctrl Pts',(2.29601692548621,-1.03275048511012,104.817882532695));
#33559=CARTESIAN_POINT('Ctrl Pts',(2.35652724839298,-0.89509734690931,104.82777244643));
#33560=CARTESIAN_POINT('Ctrl Pts',(2.39925346854901,-0.773302294330039,
104.836654676793));
#33561=CARTESIAN_POINT('Ctrl Pts',(2.46931439236541,-0.510625801779804,
104.855434305709));
#33562=CARTESIAN_POINT('Ctrl Pts',(2.49433017729159,-0.369563542430787,
104.865296078724));
#33563=CARTESIAN_POINT('Ctrl Pts',(2.51385894751855,-0.153989521823215,
104.879741376855));
#33564=CARTESIAN_POINT('Ctrl Pts',(2.51728161193147,-0.0805894472093046,
104.88455613113));
#33565=CARTESIAN_POINT('Ctrl Pts',(2.51754801788225,0.0133656453069901,
104.890589233768));
#33566=CARTESIAN_POINT('Ctrl Pts',(2.51735566210889,0.0338699555761138,
104.89189807357));
#33567=CARTESIAN_POINT('Ctrl Pts',(2.51663792898245,0.0670953968228259,
104.894006799795));
#33568=CARTESIAN_POINT('Ctrl Pts',(2.51626653245155,0.0798185767291909,
104.894811421546));
#33569=CARTESIAN_POINT('Ctrl Pts',(2.51536785665976,0.104250410665722,104.896351153088));
#33570=CARTESIAN_POINT('Ctrl Pts',(2.51485527703259,0.115959240586989,104.897086698517));
#33571=CARTESIAN_POINT('Ctrl Pts',(2.51349362407948,0.142776078541068,104.898766112685));
#33572=CARTESIAN_POINT('Ctrl Pts',(2.51259006313106,0.157880959224034,104.899708266891));
#33573=CARTESIAN_POINT('Ctrl Pts',(2.50927696888736,0.205985627054936,104.90269736361));
#33574=CARTESIAN_POINT('Ctrl Pts',(2.50635299467243,0.238947289144724,104.904728361448));
#33575=CARTESIAN_POINT('Ctrl Pts',(2.48427372609774,0.442224775271648,104.917165384629));
#33576=CARTESIAN_POINT('Ctrl Pts',(2.44841789532362,0.61027616968858,104.927022652062));
#33577=CARTESIAN_POINT('Ctrl Pts',(2.36539923989853,0.867444251348764,104.942549959779));
#33578=CARTESIAN_POINT('Ctrl Pts',(2.32952862069943,0.959618406818162,104.948221790185));
#33579=CARTESIAN_POINT('Ctrl Pts',(2.26953520044176,1.0904358375706,104.956722348909));
#33580=CARTESIAN_POINT('Ctrl Pts',(2.24963730313713,1.13091639256554,104.959419483739));
#33581=CARTESIAN_POINT('Ctrl Pts',(2.21541065616835,1.19606603827347,104.963904857656));
#33582=CARTESIAN_POINT('Ctrl Pts',(2.20173040474449,1.22106568607888,104.965661910853));
#33583=CARTESIAN_POINT('Ctrl Pts',(2.18261239492136,1.25463626855605,104.968077826023));
#33584=CARTESIAN_POINT('Ctrl Pts',(2.1775422749966,1.26341547608539,104.968714947705));
#33585=CARTESIAN_POINT('Ctrl Pts',(2.16898186732908,1.27803371762194,104.969785154701));
#33586=CARTESIAN_POINT('Ctrl Pts',(2.16552062631111,1.28388976909503,104.970216403368));
#33587=CARTESIAN_POINT('Ctrl Pts',(2.15891186501839,1.29496833567877,104.971037185294));
#33588=CARTESIAN_POINT('Ctrl Pts',(2.15576902399851,1.30019357966128,104.971426404097));
#33589=CARTESIAN_POINT('Ctrl Pts',(2.14826837977797,1.31256208828681,104.972352594519));
#33590=CARTESIAN_POINT('Ctrl Pts',(2.14389391624238,1.31969509294647,104.972890619782));
#33591=CARTESIAN_POINT('Ctrl Pts',(2.1283732376717,1.34472229610727,104.97479171101));
#33592=CARTESIAN_POINT('Ctrl Pts',(2.11703823794499,1.36249760481806,104.976166090807));
#33593=CARTESIAN_POINT('Ctrl Pts',(2.0238963654023,1.50459206985361,104.987335888974));
#33594=CARTESIAN_POINT('Ctrl Pts',(1.93144244473804,1.62156599097165,104.997654366076));
#33595=CARTESIAN_POINT('Ctrl Pts',(1.70246116578491,1.86372352780306,105.020671661358));
#33596=CARTESIAN_POINT('Ctrl Pts',(1.56133922687283,1.98345234380917,105.033250747543));
#33597=CARTESIAN_POINT('Ctrl Pts',(1.38547032736212,2.10215169548993,105.046973723862));
#33598=CARTESIAN_POINT('Ctrl Pts',(1.36231316589544,2.11723232456532,105.04874692172));
#33599=CARTESIAN_POINT('Ctrl Pts',(1.3268490498326,2.13950478974092,105.051412855372));
#33600=CARTESIAN_POINT('Ctrl Pts',(1.31472218944968,2.1469780447203,105.052315858959));
#33601=CARTESIAN_POINT('Ctrl Pts',(1.29260678411515,2.1603491572363,105.053947339268));
#33602=CARTESIAN_POINT('Ctrl Pts',(1.28263973558793,2.1662816288428,105.054677058231));
#33603=CARTESIAN_POINT('Ctrl Pts',(1.26106254025512,2.17892343044826,105.056245025315));
#33604=CARTESIAN_POINT('Ctrl Pts',(1.24943903019509,2.18560933541595,105.057082415493));
#33605=CARTESIAN_POINT('Ctrl Pts',(1.2177196178447,2.20351876873095,105.059348323905));
#33606=CARTESIAN_POINT('Ctrl Pts',(1.19752201611124,2.21456025131756,105.060770369337));
#33607=CARTESIAN_POINT('Ctrl Pts',(1.08802984425337,2.27248058597765,105.068373070932));
#33608=CARTESIAN_POINT('Ctrl Pts',(0.996125567614707,2.31424160906338,105.07437313917));
#33609=CARTESIAN_POINT('Ctrl Pts',(0.745434497035487,2.4104439287012,105.090059656377));
#33610=CARTESIAN_POINT('Ctrl Pts',(0.583314222531473,2.45472067248762,105.099497837987));
#33611=CARTESIAN_POINT('Ctrl Pts',(0.362245593961423,2.49194328174458,105.112619621451));
#33612=CARTESIAN_POINT('Ctrl Pts',(0.306191907154722,2.49944971927846,105.115970895383));
#33613=CARTESIAN_POINT('Ctrl Pts',(0.227532768844672,2.5072977543434,105.120764643803));
#33614=CARTESIAN_POINT('Ctrl Pts',(0.205100498085318,2.50923233337952,105.12214204862));
#33615=CARTESIAN_POINT('Ctrl Pts',(0.165768996766808,2.51209339676708,105.124579824829));
#33616=CARTESIAN_POINT('Ctrl Pts',(0.148880456153644,2.51315084470318,105.125633899139));
#33617=CARTESIAN_POINT('Ctrl Pts',(0.12374846507899,2.51447023507061,105.127215050591));
#33618=CARTESIAN_POINT('Ctrl Pts',(0.115511919892945,2.51486207126377,105.127735250478));
#33619=CARTESIAN_POINT('Ctrl Pts',(0.10139330866418,2.51546422937995,105.128630611878));
#33620=CARTESIAN_POINT('Ctrl Pts',(0.0955122084070213,2.51569439904605,
105.129004670631));
#33621=CARTESIAN_POINT('Ctrl Pts',(0.0821137823100427,2.51617172421599,
105.129859406256));
#33622=CARTESIAN_POINT('Ctrl Pts',(0.0745962689008002,2.51640581229185,
105.130340782879));
#33623=CARTESIAN_POINT('Ctrl Pts',(0.0540130574060407,2.51695443979007,
105.131663546601));
#33624=CARTESIAN_POINT('Ctrl Pts',(0.0409459926615565,2.51720091981361,
105.132508516053));
#33625=CARTESIAN_POINT('Ctrl Pts',(-0.0266678848650488,2.51794969876221,
105.136905709292));
#33626=CARTESIAN_POINT('Ctrl Pts',(-0.0812146599716767,2.51678069612995,
105.140537058365));
#33627=CARTESIAN_POINT('Ctrl Pts',(-0.349818292313885,2.50228376583181,
105.158700921316));
#33628=CARTESIAN_POINT('Ctrl Pts',(-0.561613107896594,2.46341283872791,
105.173813682377));
#33629=CARTESIAN_POINT('Ctrl Pts',(-0.821319004749718,2.38046668827618,
105.192141388752));
#33630=CARTESIAN_POINT('Ctrl Pts',(-0.876076989834283,2.36086350903953,
105.196000664315));
#33631=CARTESIAN_POINT('Ctrl Pts',(-0.967768752494942,2.32440792596896,
105.202450348893));
#33632=CARTESIAN_POINT('Ctrl Pts',(-1.0050615898854,2.30852768580505,105.205070055219));
#33633=CARTESIAN_POINT('Ctrl Pts',(-1.05703555986599,2.28489747057786,105.208718066688));
#33634=CARTESIAN_POINT('Ctrl Pts',(-1.07204677304168,2.27789296580849,105.209771353353));
#33635=CARTESIAN_POINT('Ctrl Pts',(-1.09773316138717,2.2655970670739,105.211573412267));
#33636=CARTESIAN_POINT('Ctrl Pts',(-1.10844176623854,2.26037718593465,105.212324606801));
#33637=CARTESIAN_POINT('Ctrl Pts',(-1.12884317540422,2.25025272505381,105.213755745863));
#33638=CARTESIAN_POINT('Ctrl Pts',(-1.13854204952455,2.24536105084339,105.214436115717));
#33639=CARTESIAN_POINT('Ctrl Pts',(-1.16121066431388,2.23374337916769,105.216026484743));
#33640=CARTESIAN_POINT('Ctrl Pts',(-1.17415420572936,2.22696690728908,105.216934707069));
#33641=CARTESIAN_POINT('Ctrl Pts',(-1.21223835509208,2.2066039556023,105.219608012372));
#33642=CARTESIAN_POINT('Ctrl Pts',(-1.23720795864221,2.19270139642965,105.221362041804));
#33643=CARTESIAN_POINT('Ctrl Pts',(-1.43230114220424,2.07968365901404,105.235091694373));
#33644=CARTESIAN_POINT('Ctrl Pts',(-1.59050117252569,1.96134789102037,105.246306601521));
#33645=CARTESIAN_POINT('Ctrl Pts',(-1.83285101434336,1.73127218128131,105.265537561742));
#33646=CARTESIAN_POINT('Ctrl Pts',(-1.92448718562338,1.62879864978661,105.273484019249));
#33647=CARTESIAN_POINT('Ctrl Pts',(-2.01737907981476,1.50607654231052,105.283001658974));
#33648=CARTESIAN_POINT('Ctrl Pts',(-2.02732080192222,1.49266715463548,105.284041732361));
#33649=CARTESIAN_POINT('Ctrl Pts',(-2.04194656879639,1.47252426623806,105.285605883881));
#33650=CARTESIAN_POINT('Ctrl Pts',(-2.04673247305317,1.46586482451579,105.286123298558));
#33651=CARTESIAN_POINT('Ctrl Pts',(-2.05489438791523,1.45438986883172,105.287015581725));
#33652=CARTESIAN_POINT('Ctrl Pts',(-2.0582861883408,1.44958573457389,105.287389369799));
#33653=CARTESIAN_POINT('Ctrl Pts',(-2.06599586401125,1.43858416158218,105.288245907235));
#33654=CARTESIAN_POINT('Ctrl Pts',(-2.07030261921346,1.43237926590076,105.288729374126));
#33655=CARTESIAN_POINT('Ctrl Pts',(-2.0820643543736,1.41526985426939,105.290063317241));
#33656=CARTESIAN_POINT('Ctrl Pts',(-2.08946141076274,1.40432607724334,105.290917472962));
#33657=CARTESIAN_POINT('Ctrl Pts',(-2.12808095540209,1.34620871086016,105.295456201663));
#33658=CARTESIAN_POINT('Ctrl Pts',(-2.15779058112502,1.29805438528717,105.299225912155));
#33659=CARTESIAN_POINT('Ctrl Pts',(-2.25471729885706,1.12841730702219,105.31243368686));
#33660=CARTESIAN_POINT('Ctrl Pts',(-2.31341953218434,1.00253803793281,105.322096532151));
#33661=CARTESIAN_POINT('Ctrl Pts',(-2.36143106504627,0.872610780952442,
105.331623435588));
#33662=CARTESIAN_POINT('Origin',(0.,0.,104.));
#33663=CARTESIAN_POINT('',(-2.36143111532954,0.872610644877486,106.333142274553));
#33664=CARTESIAN_POINT('',(-2.36143112101026,0.872610629504504,106.056155979185));
#33665=CARTESIAN_POINT('',(-2.36143112101026,0.872610629504505,104.));
#33666=CARTESIAN_POINT('',(-2.51749930935125,-0.00186478308576427,105.112583302455));
#33667=CARTESIAN_POINT('Ctrl Pts',(-2.36143112101026,0.872610629504504,
106.056155979185));
#33668=CARTESIAN_POINT('Ctrl Pts',(-2.3320450272244,0.952134341506782,106.050793423265));
#33669=CARTESIAN_POINT('Ctrl Pts',(-2.29860300576651,1.03026510446364,106.045430867345));
#33670=CARTESIAN_POINT('Ctrl Pts',(-2.26126535934404,1.10656460481558,106.040068311425));
#33671=CARTESIAN_POINT('Ctrl Pts',(-2.22479013631369,1.18110174250636,106.034829619597));
#33672=CARTESIAN_POINT('Ctrl Pts',(-2.18459753161513,1.25389086788927,106.029590927769));
#33673=CARTESIAN_POINT('Ctrl Pts',(-2.14088583146978,1.3245429802811,106.024352235941));
#33674=CARTESIAN_POINT('Ctrl Pts',(-2.09718985896252,1.39516967177075,106.019115429014));
#33675=CARTESIAN_POINT('Ctrl Pts',(-2.04997754811381,1.46366048524139,106.013878622088));
#33676=CARTESIAN_POINT('Ctrl Pts',(-1.99949227582444,1.52965253862385,106.008641815161));
#33677=CARTESIAN_POINT('Ctrl Pts',(-1.94900993972484,1.5956407539525,106.003405312804));
#33678=CARTESIAN_POINT('Ctrl Pts',(-1.89525530153011,1.65913013206876,105.998168810447));
#33679=CARTESIAN_POINT('Ctrl Pts',(-1.83851322315744,1.71978934124946,105.99293230809));
#33680=CARTESIAN_POINT('Ctrl Pts',(-1.7793875752057,1.78299666727467,105.987475835508));
#33681=CARTESIAN_POINT('Ctrl Pts',(-1.71701832140262,1.84313039699446,105.982019362926));
#33682=CARTESIAN_POINT('Ctrl Pts',(-1.65177038710584,1.8998581100388,105.976562890344));
#33683=CARTESIAN_POINT('Ctrl Pts',(-1.58906500733386,1.95437528101715,105.97131904333));
#33684=CARTESIAN_POINT('Ctrl Pts',(-1.52370154234258,2.005746707741,105.966075196316));
#33685=CARTESIAN_POINT('Ctrl Pts',(-1.45603627926231,2.0537196993436,105.960831349301));
#33686=CARTESIAN_POINT('Ctrl Pts',(-1.38832327795329,2.10172653616519,105.955583802723));
#33687=CARTESIAN_POINT('Ctrl Pts',(-1.31830563575006,2.14632991980948,105.950336256144));
#33688=CARTESIAN_POINT('Ctrl Pts',(-1.24636624928542,2.18732197507413,105.945088709566));
#33689=CARTESIAN_POINT('Ctrl Pts',(-1.17431585319227,2.22837728515718,105.939833065501));
#33690=CARTESIAN_POINT('Ctrl Pts',(-1.10033820878909,2.2658099456108,105.934577421437));
#33691=CARTESIAN_POINT('Ctrl Pts',(-1.02483761825963,2.29945952480141,105.929321777372));
#33692=CARTESIAN_POINT('Ctrl Pts',(-1.01589674182243,2.30344435098088,105.928699397284));
#33693=CARTESIAN_POINT('Ctrl Pts',(-1.00693452631,2.30737618201483,105.928077017196));
#33694=CARTESIAN_POINT('Ctrl Pts',(-0.997951656852982,2.31125479784994,
105.927454637108));
#33695=CARTESIAN_POINT('Ctrl Pts',(-0.922102155402193,2.34400503192829,
105.922199387701));
#33696=CARTESIAN_POINT('Ctrl Pts',(-0.844498702622488,2.37307800987231,
105.916944138294));
#33697=CARTESIAN_POINT('Ctrl Pts',(-0.765532238206415,2.39828410374307,
105.911688888886));
#33698=CARTESIAN_POINT('Ctrl Pts',(-0.68667773029783,2.42345446109886,105.906441090229));
#33699=CARTESIAN_POINT('Ctrl Pts',(-0.606464485047457,2.44476868481448,
105.901193291571));
#33700=CARTESIAN_POINT('Ctrl Pts',(-0.525304183161289,2.46208484117693,
105.895945492914));
#33701=CARTESIAN_POINT('Ctrl Pts',(-0.443555804919529,2.47952646802052,
105.890659669431));
#33702=CARTESIAN_POINT('Ctrl Pts',(-0.360847022713129,2.49291165629843,
105.885373845948));
#33703=CARTESIAN_POINT('Ctrl Pts',(-0.277614991355664,2.50214631198389,
105.880088022465));
#33704=CARTESIAN_POINT('Ctrl Pts',(-0.195129295878244,2.51129816114925,
105.874849596596));
#33705=CARTESIAN_POINT('Ctrl Pts',(-0.112130164600841,2.51637356285532,
105.869611170728));
#33706=CARTESIAN_POINT('Ctrl Pts',(-0.0290524157146699,2.5173323592925,
105.864372744859));
#33707=CARTESIAN_POINT('Ctrl Pts',(0.0539980102825035,2.51829084039748,
105.859136041822));
#33708=CARTESIAN_POINT('Ctrl Pts',(0.137126541510933,2.51513539979876,105.853899338784));
#33709=CARTESIAN_POINT('Ctrl Pts',(0.2198963861406,2.50787795344237,105.848662635747));
#33710=CARTESIAN_POINT('Ctrl Pts',(0.302663976161101,2.50062070477519,105.843426075354));
#33711=CARTESIAN_POINT('Ctrl Pts',(0.385072439441943,2.4892617138423,105.838189514962));
#33712=CARTESIAN_POINT('Ctrl Pts',(0.466689528308689,2.47386481727822,105.83295295457));
#33713=CARTESIAN_POINT('Ctrl Pts',(0.549642468916212,2.45821591502069,105.827630685799));
#33714=CARTESIAN_POINT('Ctrl Pts',(0.631777410420446,2.43839581358489,105.822308417029));
#33715=CARTESIAN_POINT('Ctrl Pts',(0.712652561784847,2.41452533144332,105.816986148258));
#33716=CARTESIAN_POINT('Ctrl Pts',(0.792339598035796,2.39100552413969,105.811742067508));
#33717=CARTESIAN_POINT('Ctrl Pts',(0.870803191428542,2.36355376477662,105.806497986758));
#33718=CARTESIAN_POINT('Ctrl Pts',(0.947638970692687,2.33233501693571,105.801253906007));
#33719=CARTESIAN_POINT('Ctrl Pts',(1.02619315526263,2.3004180727279,105.795892543227));
#33720=CARTESIAN_POINT('Ctrl Pts',(1.1030453720852,2.26456382854632,105.790531180446));
#33721=CARTESIAN_POINT('Ctrl Pts',(1.17778988319344,2.22499825641442,105.785169817666));
#33722=CARTESIAN_POINT('Ctrl Pts',(1.25253439430167,2.18543268428251,105.779808454885));
#33723=CARTESIAN_POINT('Ctrl Pts',(1.32517079738007,2.14215610165379,105.774447092105));
#33724=CARTESIAN_POINT('Ctrl Pts',(1.39532635611388,2.09544043340152,105.769085729324));
#33725=CARTESIAN_POINT('Ctrl Pts',(1.46409337926563,2.04964937281796,105.763830479917));
#33726=CARTESIAN_POINT('Ctrl Pts',(1.53073088988028,2.00038502354845,105.758575230509));
#33727=CARTESIAN_POINT('Ctrl Pts',(1.59486698177971,1.94787205956368,105.753319981102));
#33728=CARTESIAN_POINT('Ctrl Pts',(1.65891214327077,1.89543354703236,105.748072182445));
#33729=CARTESIAN_POINT('Ctrl Pts',(1.72046257628061,1.8397558581212,105.742824383787));
#33730=CARTESIAN_POINT('Ctrl Pts',(1.77917508770272,1.78110703139874,105.73757658513));
#33731=CARTESIAN_POINT('Ctrl Pts',(1.83831302188627,1.72203324336537,105.732290761647));
#33732=CARTESIAN_POINT('Ctrl Pts',(1.89457134013341,1.65994534158647,105.727004938164));
#33733=CARTESIAN_POINT('Ctrl Pts',(1.9476331074797,1.59515877850733,105.721719114681));
#33734=CARTESIAN_POINT('Ctrl Pts',(2.00021907362082,1.53095315206737,105.716480688812));
#33735=CARTESIAN_POINT('Ctrl Pts',(2.04966528800493,1.46409743145675,105.711242262944));
#33736=CARTESIAN_POINT('Ctrl Pts',(2.09570132912817,1.39493447483759,105.706003837075));
#33737=CARTESIAN_POINT('Ctrl Pts',(2.14172222976363,1.32579426476382,105.700767134038));
#33738=CARTESIAN_POINT('Ctrl Pts',(2.18433492912726,1.25434870953106,105.695530431));
#33739=CARTESIAN_POINT('Ctrl Pts',(2.22331161022896,1.18097067441199,105.690293727963));
#33740=CARTESIAN_POINT('Ctrl Pts',(2.26228722962535,1.10759463807392,105.68505716757));
#33741=CARTESIAN_POINT('Ctrl Pts',(2.29762681213943,1.03228663449493,105.679820607178));
#33742=CARTESIAN_POINT('Ctrl Pts',(2.32914856552666,0.955443985644953,105.674584046786));
#33743=CARTESIAN_POINT('Ctrl Pts',(2.36118624504798,0.877343629767458,105.669261778015));
#33744=CARTESIAN_POINT('Ctrl Pts',(2.3892797939899,0.79765838932308,105.663939509245));
#33745=CARTESIAN_POINT('Ctrl Pts',(2.41329002013555,0.716824615030886,105.658617240474));
#33746=CARTESIAN_POINT('Ctrl Pts',(2.43694751850165,0.637178347992719,105.653373159724));
#33747=CARTESIAN_POINT('Ctrl Pts',(2.45664082044059,0.556417537948684,105.648129078974));
#33748=CARTESIAN_POINT('Ctrl Pts',(2.47228813556255,0.474971183080256,105.642884998223));
#33749=CARTESIAN_POINT('Ctrl Pts',(2.48828539740965,0.391703308996611,105.637523635443));
#33750=CARTESIAN_POINT('Ctrl Pts',(2.50005344341742,0.307719363212086,105.632162272662));
#33751=CARTESIAN_POINT('Ctrl Pts',(2.50756091250629,0.22348270642411,105.626800909882));
#33752=CARTESIAN_POINT('Ctrl Pts',(2.51506838159515,0.139246049636133,105.621439547101));
#33753=CARTESIAN_POINT('Ctrl Pts',(2.51831532100137,0.0547571921418939,
105.616078184321));
#33754=CARTESIAN_POINT('Ctrl Pts',(2.51732688234237,-0.0295231677916568,
105.61071682154));
#33755=CARTESIAN_POINT('Ctrl Pts',(2.51635800709749,-0.112135430702664,
105.605461572133));
#33756=CARTESIAN_POINT('Ctrl Pts',(2.51131634767354,-0.194852512373357,
105.600206322725));
#33757=CARTESIAN_POINT('Ctrl Pts',(2.50218787396461,-0.277240136676642,
105.594951073318));
#33758=CARTESIAN_POINT('Ctrl Pts',(2.49307234235765,-0.359510954044879,
105.589703274661));
#33759=CARTESIAN_POINT('Ctrl Pts',(2.47988155577697,-0.441452787045925,
105.584455476003));
#33760=CARTESIAN_POINT('Ctrl Pts',(2.4626534908834,-0.522631833932654,105.579207677346));
#33761=CARTESIAN_POINT('Ctrl Pts',(2.44530059380732,-0.604399092998717,
105.573921853863));
#33762=CARTESIAN_POINT('Ctrl Pts',(2.42385166998305,-0.685391991366922,
105.56863603038));
#33763=CARTESIAN_POINT('Ctrl Pts',(2.3983987627519,-0.76517293785794,105.563350206897));
#33764=CARTESIAN_POINT('Ctrl Pts',(2.373174089983,-0.84423849410868,105.558111781028));
#33765=CARTESIAN_POINT('Ctrl Pts',(2.34401709592337,-0.922113298716373,
105.55287335516));
#33766=CARTESIAN_POINT('Ctrl Pts',(2.31106813594437,-0.998383854548242,
105.547634929291));
#33767=CARTESIAN_POINT('Ctrl Pts',(2.27813001232997,-1.07462932626362,105.542398226254));
#33768=CARTESIAN_POINT('Ctrl Pts',(2.24140258247874,-1.14927117381638,105.537161523216));
#33769=CARTESIAN_POINT('Ctrl Pts',(2.20107456758893,-1.22191529899303,105.531924820179));
#33770=CARTESIAN_POINT('Ctrl Pts',(2.16074765121408,-1.29455744538003,105.526688259786));
#33771=CARTESIAN_POINT('Ctrl Pts',(2.11682056966576,-1.36520157466171,105.521451699394));
#33772=CARTESIAN_POINT('Ctrl Pts',(2.06952761647574,-1.43347887833907,105.516215139002));
#33773=CARTESIAN_POINT('Ctrl Pts',(2.02146060512309,-1.50287369743192,105.510892870231));
#33774=CARTESIAN_POINT('Ctrl Pts',(1.96991681677193,-1.56982310309953,105.505570601461));
#33775=CARTESIAN_POINT('Ctrl Pts',(1.9151864756193,-1.63397277015406,105.50024833269));
#33776=CARTESIAN_POINT('Ctrl Pts',(1.86126016319977,-1.69718003169011,105.49500425194));
#33777=CARTESIAN_POINT('Ctrl Pts',(1.80424066777238,-1.7576689705255,105.48976017119));
#33778=CARTESIAN_POINT('Ctrl Pts',(1.74444329879669,-1.81513741278266,105.484516090439));
#33779=CARTESIAN_POINT('Ctrl Pts',(1.68330858259673,-1.87389111663331,105.479154727659));
#33780=CARTESIAN_POINT('Ctrl Pts',(1.61927062781272,-1.9294872532209,105.473793364878));
#33781=CARTESIAN_POINT('Ctrl Pts',(1.55270102323422,-1.98164723965882,105.468432002097));
#33782=CARTESIAN_POINT('Ctrl Pts',(1.48613141865572,-2.03380722609673,105.463070639317));
#33783=CARTESIAN_POINT('Ctrl Pts',(1.41703061803392,-2.08253082417426,105.457709276536));
#33784=CARTESIAN_POINT('Ctrl Pts',(1.3457987453583,-2.12758830298346,105.452347913756));
#33785=CARTESIAN_POINT('Ctrl Pts',(1.27597671092749,-2.1717539934056,105.447092664348));
#33786=CARTESIAN_POINT('Ctrl Pts',(1.20384932162565,-2.21256053261647,105.441837414941));
#33787=CARTESIAN_POINT('Ctrl Pts',(1.12977320620474,-2.24975970995612,105.436582165534));
#33788=CARTESIAN_POINT('Ctrl Pts',(1.05580211388747,-2.28690614731293,105.431334366876));
#33789=CARTESIAN_POINT('Ctrl Pts',(0.979888192187262,-2.32045517618535,
105.426086568219));
#33790=CARTESIAN_POINT('Ctrl Pts',(0.90241598711519,-2.35020246706511,105.420838769561));
#33791=CARTESIAN_POINT('Ctrl Pts',(0.824382429128403,-2.38016530271249,
105.415552946078));
#33792=CARTESIAN_POINT('Ctrl Pts',(0.744768310763816,-2.40627082083284,
105.410267122595));
#33793=CARTESIAN_POINT('Ctrl Pts',(0.663990793267582,-2.42835797947005,
105.404981299112));
#33794=CARTESIAN_POINT('Ctrl Pts',(0.583937602195017,-2.45024708408035,
105.399742873244));
#33795=CARTESIAN_POINT('Ctrl Pts',(0.502742245948962,-2.46818948133825,
105.394504447375));
#33796=CARTESIAN_POINT('Ctrl Pts',(0.420827979435382,-2.48207777108703,
105.389266021507));
#33797=CARTESIAN_POINT('Ctrl Pts',(0.338940653160792,-2.49596149320844,
105.384029318469));
#33798=CARTESIAN_POINT('Ctrl Pts',(0.256335340766251,-2.50579367881354,
105.378792615431));
#33799=CARTESIAN_POINT('Ctrl Pts',(0.173445358343819,-2.51151805839994,
105.373555912394));
#33800=CARTESIAN_POINT('Ctrl Pts',(0.090557633803088,-2.51724228205709,
105.368319352002));
#33801=CARTESIAN_POINT('Ctrl Pts',(0.00738571504727582,-2.51885889140939,
105.363082791609));
#33802=CARTESIAN_POINT('Ctrl Pts',(-0.0756334827208372,-2.51636361170072,
105.357846231217));
#33803=CARTESIAN_POINT('Ctrl Pts',(-0.160011480972994,-2.51382749098941,
105.352523962446));
#33804=CARTESIAN_POINT('Ctrl Pts',(-0.244231221974189,-2.50704366739769,
105.347201693676));
#33805=CARTESIAN_POINT('Ctrl Pts',(-0.327837487473301,-2.49606266584138,
105.341879424905));
#33806=CARTESIAN_POINT('Ctrl Pts',(-0.410215515795193,-2.48524298322779,
105.336635344155));
#33807=CARTESIAN_POINT('Ctrl Pts',(-0.491997524324338,-2.47034876753276,
105.331391263405));
#33808=CARTESIAN_POINT('Ctrl Pts',(-0.572758381215976,-2.45147997885907,
105.326147182654));
#33809=CARTESIAN_POINT('Ctrl Pts',(-0.65532542640052,-2.43218919633198,
105.320785819874));
#33810=CARTESIAN_POINT('Ctrl Pts',(-0.736824601304015,-2.4087440572531,
105.315424457093));
#33811=CARTESIAN_POINT('Ctrl Pts',(-0.816819920653845,-2.38130457254486,
105.310063094313));
#33812=CARTESIAN_POINT('Ctrl Pts',(-0.896815240003676,-2.35386508783662,
105.304701731532));
#33813=CARTESIAN_POINT('Ctrl Pts',(-0.975306256944999,-2.32243150840783,
105.299340368751));
#33814=CARTESIAN_POINT('Ctrl Pts',(-1.05188242683387,-2.28721437782253,
105.293979005971));
#33815=CARTESIAN_POINT('Ctrl Pts',(-1.1269429828705,-2.25269427310087,105.288723756564));
#33816=CARTESIAN_POINT('Ctrl Pts',(-1.20044106284464,-2.21441155937803,
105.283468507156));
#33817=CARTESIAN_POINT('Ctrl Pts',(-1.2719743024889,-2.17253023541857,105.278213257749));
#33818=CARTESIAN_POINT('Ctrl Pts',(-1.34340612424973,-2.13070828966221,
105.272965459091));
#33819=CARTESIAN_POINT('Ctrl Pts',(-1.41287824401757,-2.08529809894299,
105.267717660434));
#33820=CARTESIAN_POINT('Ctrl Pts',(-1.48000990510123,-2.03651096996855,
105.262469861776));
#33821=CARTESIAN_POINT('Ctrl Pts',(-1.54762799294376,-1.98737033618523,
105.257184038294));
#33822=CARTESIAN_POINT('Ctrl Pts',(-1.61287113116811,-1.93480381800172,
105.251898214811));
#33823=CARTESIAN_POINT('Ctrl Pts',(-1.67537711493227,-1.87907364750859,
105.246612391328));
#33824=CARTESIAN_POINT('Ctrl Pts',(-1.73732261185454,-1.82384320560745,
105.241373965459));
#33825=CARTESIAN_POINT('Ctrl Pts',(-1.79657949470942,-1.76550593339141,
105.236135539591));
#33826=CARTESIAN_POINT('Ctrl Pts',(-1.85282723527973,-1.70435837962726,
105.230897113722));
#33827=CARTESIAN_POINT('Ctrl Pts',(-1.90905647690427,-1.64323093627591,
105.225660410685));
#33828=CARTESIAN_POINT('Ctrl Pts',(-1.9622782296196,-1.57929538632537,105.220423707647));
#33829=CARTESIAN_POINT('Ctrl Pts',(-2.01220937537848,-1.51288455595229,
105.21518700461));
#33830=CARTESIAN_POINT('Ctrl Pts',(-2.06213916103795,-1.44647553457697,
105.209950444217));
#33831=CARTESIAN_POINT('Ctrl Pts',(-2.10877824149203,-1.37759173626612,
105.204713883825));
#33832=CARTESIAN_POINT('Ctrl Pts',(-2.15188515194408,-1.30659731472347,
105.199477323433));
#33833=CARTESIAN_POINT('Ctrl Pts',(-2.19569760632283,-1.23444090587015,
105.194155054662));
#33834=CARTESIAN_POINT('Ctrl Pts',(-2.2358609568884,-1.16010457351394,105.188832785892));
#33835=CARTESIAN_POINT('Ctrl Pts',(-2.27216973926298,-1.08399765958124,
105.183510517121));
#33836=CARTESIAN_POINT('Ctrl Pts',(-2.30794511907369,-1.00900881186736,
105.178266436371));
#33837=CARTESIAN_POINT('Ctrl Pts',(-2.33997830806341,-0.932301515060755,
105.173022355621));
#33838=CARTESIAN_POINT('Ctrl Pts',(-2.36812168829864,-0.854286789907003,
105.16777827487));
#33839=CARTESIAN_POINT('Ctrl Pts',(-2.39689448538084,-0.774527292735347,
105.16241691209));
#33840=CARTESIAN_POINT('Ctrl Pts',(-2.42160123659599,-0.693401671007281,
105.157055549309));
#33841=CARTESIAN_POINT('Ctrl Pts',(-2.44213878500912,-0.611362744002423,
105.151694186529));
#33842=CARTESIAN_POINT('Ctrl Pts',(-2.46267633342225,-0.529323816997564,
105.146332823748));
#33843=CARTESIAN_POINT('Ctrl Pts',(-2.47904464620291,-0.446372096142003,
105.140971460968));
#33844=CARTESIAN_POINT('Ctrl Pts',(-2.49119680399604,-0.362966573887916,
105.135610098187));
#33845=CARTESIAN_POINT('Ctrl Pts',(-2.50859444872508,-0.24355900287716,
105.127934499622));
#33846=CARTESIAN_POINT('Ctrl Pts',(-2.51740967623069,-0.12287148413773,
105.120258901057));
#33847=CARTESIAN_POINT('Ctrl Pts',(-2.51749930935083,-0.00186478366199865,
105.112583302492));
#33848=CARTESIAN_POINT('Ctrl Pts',(-2.51749930935125,-0.00186478308577434,
105.112583302455));
#33849=CARTESIAN_POINT('Ctrl Pts',(-2.5175597065367,0.0796727822241211,
105.107411277957));
#33850=CARTESIAN_POINT('Ctrl Pts',(-2.51365459987842,0.161358302924671,
105.102239253459));
#33851=CARTESIAN_POINT('Ctrl Pts',(-2.50576736565954,0.242767706245406,
105.097067228961));
#33852=CARTESIAN_POINT('Ctrl Pts',(-2.49788815038873,0.324094340656303,
105.091900462859));
#33853=CARTESIAN_POINT('Ctrl Pts',(-2.48603488237869,0.40514494382945,105.086733696756));
#33854=CARTESIAN_POINT('Ctrl Pts',(-2.47024295923186,0.485495594589114,
105.081566930653));
#33855=CARTESIAN_POINT('Ctrl Pts',(-2.45446208158943,0.565790044881075,
105.076403778394));
#33856=CARTESIAN_POINT('Ctrl Pts',(-2.43474810616352,0.645385048417688,
105.071240626135));
#33857=CARTESIAN_POINT('Ctrl Pts',(-2.41118805019035,0.72386354834269,105.066077473876));
#33858=CARTESIAN_POINT('Ctrl Pts',(-2.39615592726708,0.7739355201177,105.062783205835));
#33859=CARTESIAN_POINT('Ctrl Pts',(-2.37955915543172,0.823553119547407,
105.059488937794));
#33860=CARTESIAN_POINT('Ctrl Pts',(-2.36143112101026,0.872610629504506,
105.056194669753));
#33861=CARTESIAN_POINT('Ctrl Pts',(-2.36143106504627,0.872610780952441,
105.331623435588));
#33862=CARTESIAN_POINT('Ctrl Pts',(-2.39352196172693,0.785767434547548,
105.337991215488));
#33863=CARTESIAN_POINT('Ctrl Pts',(-2.42083637768937,0.697115782413577,
105.344302156859));
#33864=CARTESIAN_POINT('Ctrl Pts',(-2.4545969372037,0.561238145578153,105.353634028697));
#33865=CARTESIAN_POINT('Ctrl Pts',(-2.46468897516356,0.515114648938842,
105.356744922903));
#33866=CARTESIAN_POINT('Ctrl Pts',(-2.47992709244794,0.434703781335813,
105.362070098137));
#33867=CARTESIAN_POINT('Ctrl Pts',(-2.48567292855367,0.400544689760486,
105.36430198973));
#33868=CARTESIAN_POINT('Ctrl Pts',(-2.49297832660727,0.350867338513951,
105.367505577799));
#33869=CARTESIAN_POINT('Ctrl Pts',(-2.49510134151263,0.335437236340905,
105.368494773181));
#33870=CARTESIAN_POINT('Ctrl Pts',(-2.49857412633694,0.308336777931283,
105.370222144256));
#33871=CARTESIAN_POINT('Ctrl Pts',(-2.49998564241973,0.296674954585462,
105.370962229453));
#33872=CARTESIAN_POINT('Ctrl Pts',(-2.50274744007373,0.272436210589003,
105.372493933803));
#33873=CARTESIAN_POINT('Ctrl Pts',(-2.50408466476423,0.259858112501073,
105.373285125583));
#33874=CARTESIAN_POINT('Ctrl Pts',(-2.50730502910332,0.227229582499644,
105.375328395664));
#33875=CARTESIAN_POINT('Ctrl Pts',(-2.50904250889579,0.207165434328679,
105.376575919717));
#33876=CARTESIAN_POINT('Ctrl Pts',(-2.51521141134491,0.124382165587546,
105.381688661802));
#33877=CARTESIAN_POINT('Ctrl Pts',(-2.51753349719247,0.0615258153455552,
105.385488569262));
#33878=CARTESIAN_POINT('Ctrl Pts',(-2.51743889339061,-0.114151683195328,
105.395946872353));
#33879=CARTESIAN_POINT('Ctrl Pts',(-2.50979754438263,-0.22682169639588,
105.402462588056));
#33880=CARTESIAN_POINT('Ctrl Pts',(-2.47136408136718,-0.50997548796669,
105.418892328511));
#33881=CARTESIAN_POINT('Ctrl Pts',(-2.43050971079906,-0.678469643761034,
105.42871156683));
#33882=CARTESIAN_POINT('Ctrl Pts',(-2.36596485482824,-0.860479801024286,
105.440596079517));
#33883=CARTESIAN_POINT('Ctrl Pts',(-2.35897690821076,-0.879456121124482,
105.44185163018));
#33884=CARTESIAN_POINT('Ctrl Pts',(-2.34891331819353,-0.905801399600665,
105.443620530715));
#33885=CARTESIAN_POINT('Ctrl Pts',(-2.34602985661011,-0.913243592765757,
105.444123115966));
#33886=CARTESIAN_POINT('Ctrl Pts',(-2.34069627491772,-0.92681756567609,
105.445045308973));
#33887=CARTESIAN_POINT('Ctrl Pts',(-2.33825729966128,-0.932953723978231,
105.445464261891));
#33888=CARTESIAN_POINT('Ctrl Pts',(-2.33314425558839,-0.945671507567461,
105.446337019053));
#33889=CARTESIAN_POINT('Ctrl Pts',(-2.33046644529192,-0.952251469932218,
105.446791031924));
#33890=CARTESIAN_POINT('Ctrl Pts',(-2.32337172682301,-0.969475567765736,
105.447985786039));
#33891=CARTESIAN_POINT('Ctrl Pts',(-2.31890957668818,-0.980100719606244,
105.448729139318));
#33892=CARTESIAN_POINT('Ctrl Pts',(-2.29840204664799,-1.02800863051862,
105.452108377022));
#33893=CARTESIAN_POINT('Ctrl Pts',(-2.28153031238456,-1.06492849979142,
105.45478821802));
#33894=CARTESIAN_POINT('Ctrl Pts',(-2.23063600162743,-1.16953261093582,
105.462567809591));
#33895=CARTESIAN_POINT('Ctrl Pts',(-2.19444225908793,-1.2361088958505,105.467747986373));
#33896=CARTESIAN_POINT('Ctrl Pts',(-2.06528675333901,-1.45008331740098,
105.484960912937));
#33897=CARTESIAN_POINT('Ctrl Pts',(-1.96001973139913,-1.58949264202145,
105.497063780135));
#33898=CARTESIAN_POINT('Ctrl Pts',(-1.79300813828961,-1.7685925837549,105.513392617223));
#33899=CARTESIAN_POINT('Ctrl Pts',(-1.742666851341,-1.81821664089991,105.518023378132));
#33900=CARTESIAN_POINT('Ctrl Pts',(-1.67474239029629,-1.87975660669075,
105.52391209139));
#33901=CARTESIAN_POINT('Ctrl Pts',(-1.65900856701762,-1.89365720034632,
105.525252732417));
#33902=CARTESIAN_POINT('Ctrl Pts',(-1.63337802386371,-1.91573672964483,
105.527399883355));
#33903=CARTESIAN_POINT('Ctrl Pts',(-1.62358967771431,-1.92403938485612,
105.528211451082));
#33904=CARTESIAN_POINT('Ctrl Pts',(-1.60476639536951,-1.93975970146391,
105.529756300674));
#33905=CARTESIAN_POINT('Ctrl Pts',(-1.59574248203678,-1.94718998085793,
105.530490081863));
#33906=CARTESIAN_POINT('Ctrl Pts',(-1.57489279768188,-1.96411530074756,
105.532170095239));
#33907=CARTESIAN_POINT('Ctrl Pts',(-1.56303225094643,-1.97356693253041,
105.53311458007));
#33908=CARTESIAN_POINT('Ctrl Pts',(-1.5255834322984,-2.00286041539864,105.536062537394));
#33909=CARTESIAN_POINT('Ctrl Pts',(-1.49969671931488,-2.02231662922032,
105.538050932682));
#33910=CARTESIAN_POINT('Ctrl Pts',(-1.36602901649228,-2.11880145803573,
105.548084030797));
#33911=CARTESIAN_POINT('Ctrl Pts',(-1.25265952444321,-2.18773965820178,
105.555820311298));
#33912=CARTESIAN_POINT('Ctrl Pts',(-1.00701172452887,-2.31172858399199,
105.571688766981));
#33913=CARTESIAN_POINT('Ctrl Pts',(-0.874418169902418,-2.36506863001192,
105.579778102985));
#33914=CARTESIAN_POINT('Ctrl Pts',(-0.678075839251542,-2.42527358735326,
105.591935241963));
#33915=CARTESIAN_POINT('Ctrl Pts',(-0.61746012150452,-2.4414095161025,105.595714113065));
#33916=CARTESIAN_POINT('Ctrl Pts',(-0.543046757652888,-2.45827000997418,
105.600453557576));
#33917=CARTESIAN_POINT('Ctrl Pts',(-0.529758707412121,-2.46116779511449,
105.601303740268));
#33918=CARTESIAN_POINT('Ctrl Pts',(-0.508968740001284,-2.4655253945856,
105.602640841554));
#33919=CARTESIAN_POINT('Ctrl Pts',(-0.501482321399643,-2.46705900361328,
105.603123728906));
#33920=CARTESIAN_POINT('Ctrl Pts',(-0.48759206646943,-2.46983861581964,
105.60402246342));
#33921=CARTESIAN_POINT('Ctrl Pts',(-0.48119025622526,-2.47109383583127,
105.604437788788));
#33922=CARTESIAN_POINT('Ctrl Pts',(-0.466504900406724,-2.47391400282253,
105.605393036766));
#33923=CARTESIAN_POINT('Ctrl Pts',(-0.458218349779135,-2.47546223047425,
105.605933872992));
#33924=CARTESIAN_POINT('Ctrl Pts',(-0.432337658382364,-2.48016327985293,
105.607628350653));
#33925=CARTESIAN_POINT('Ctrl Pts',(-0.41471805298476,-2.48317027996274,
105.608789622871));
#33926=CARTESIAN_POINT('Ctrl Pts',(-0.37320472754113,-2.48980089371614,
105.611541353253));
#33927=CARTESIAN_POINT('Ctrl Pts',(-0.349288192518539,-2.493268522841,105.61313882741));
#33928=CARTESIAN_POINT('Ctrl Pts',(-0.262901163276538,-2.50452636639286,
105.618944134036));
#33929=CARTESIAN_POINT('Ctrl Pts',(-0.200196549302332,-2.51031664788374,
105.623223602155));
#33930=CARTESIAN_POINT('Ctrl Pts',(0.0731473964442369,-2.52525149692107,
105.641999497277));
#33931=CARTESIAN_POINT('Ctrl Pts',(0.284293349342089,-2.51026864132188,
105.656720343178));
#33932=CARTESIAN_POINT('Ctrl Pts',(0.54598044546324,-2.45821917704242,105.674356487106));
#33933=CARTESIAN_POINT('Ctrl Pts',(0.600475436914682,-2.44547873122814,
105.678001354921));
#33934=CARTESIAN_POINT('Ctrl Pts',(0.673136360955237,-2.42591549906605,
105.682826434895));
#33935=CARTESIAN_POINT('Ctrl Pts',(0.691710543507755,-2.42068484667083,
105.68405681457));
#33936=CARTESIAN_POINT('Ctrl Pts',(0.722183342883347,-2.4117240480384,105.686070783091));
#33937=CARTESIAN_POINT('Ctrl Pts',(0.734117383096413,-2.40811821585418,
105.686858345729));
#33938=CARTESIAN_POINT('Ctrl Pts',(0.757316978604474,-2.40092004126222,
105.688387258258));
#33939=CARTESIAN_POINT('Ctrl Pts',(0.768584961307669,-2.39733669214709,
105.689128876702));
#33940=CARTESIAN_POINT('Ctrl Pts',(0.795095098629307,-2.38870003900381,
105.690871603665));
#33941=CARTESIAN_POINT('Ctrl Pts',(0.810315091568749,-2.38357998886868,
105.691870508782));
#33942=CARTESIAN_POINT('Ctrl Pts',(0.86084055752127,-2.36604318706098,105.695182005602));
#33943=CARTESIAN_POINT('Ctrl Pts',(0.895919053097665,-2.35298450937276,
105.697473566341));
#33944=CARTESIAN_POINT('Ctrl Pts',(1.06267081978998,-2.28663770236431,105.708351249084));
#33945=CARTESIAN_POINT('Ctrl Pts',(1.18997206271003,-2.2230505754236,105.716589461816));
#33946=CARTESIAN_POINT('Ctrl Pts',(1.4611171104913,-2.05761224115616,105.734861481182));
#33947=CARTESIAN_POINT('Ctrl Pts',(1.60099470020489,-1.95075122194353,105.744808463872));
#33948=CARTESIAN_POINT('Ctrl Pts',(1.74433326219988,-1.81537215380788,105.756912877276));
#33949=CARTESIAN_POINT('Ctrl Pts',(1.75987354532094,-1.80031097834116,105.75825391033));
#33950=CARTESIAN_POINT('Ctrl Pts',(1.78121673688669,-1.77908537772112,105.760139445103));
#33951=CARTESIAN_POINT('Ctrl Pts',(1.78718612260268,-1.77308871840858,105.760671672328));
#33952=CARTESIAN_POINT('Ctrl Pts',(1.79742175495483,-1.762702117921,105.761592957279));
#33953=CARTESIAN_POINT('Ctrl Pts',(1.80170247390046,-1.75832645300342,105.7619809047));
#33954=CARTESIAN_POINT('Ctrl Pts',(1.81068758573955,-1.74907479079575,105.762800913492));
#33955=CARTESIAN_POINT('Ctrl Pts',(1.81538830113156,-1.74419536450768,105.763233259183));
#33956=CARTESIAN_POINT('Ctrl Pts',(1.82698263233916,-1.73206259852588,105.764307824333));
#33957=CARTESIAN_POINT('Ctrl Pts',(1.83385275588654,-1.72478707259447,105.764951785019));
#33958=CARTESIAN_POINT('Ctrl Pts',(1.85946764254119,-1.69733462036419,105.767379416451));
#33959=CARTESIAN_POINT('Ctrl Pts',(1.87792351697907,-1.67689231744877,105.769182709327));
#33960=CARTESIAN_POINT('Ctrl Pts',(2.01978754316611,-1.51447985755666,105.783447587917));
#33961=CARTESIAN_POINT('Ctrl Pts',(2.12726146304627,-1.35939157789997,105.796653099726));
#33962=CARTESIAN_POINT('Ctrl Pts',(2.28378925633807,-1.06877275823182,105.819290044746));
#33963=CARTESIAN_POINT('Ctrl Pts',(2.34043375793168,-0.938269778745885,
105.828824043614));
#33964=CARTESIAN_POINT('Ctrl Pts',(2.39287916441563,-0.782579484474979,
105.83942010666));
#33965=CARTESIAN_POINT('Ctrl Pts',(2.39970261433892,-0.761399211744634,
105.840846142309));
#33966=CARTESIAN_POINT('Ctrl Pts',(2.41047568794179,-0.72637478974724,105.843179494826));
#33967=CARTESIAN_POINT('Ctrl Pts',(2.41458886372809,-0.712582634159106,
105.844092070889));
#33968=CARTESIAN_POINT('Ctrl Pts',(2.42180562879597,-0.68760344755235,105.845733792333));
#33969=CARTESIAN_POINT('Ctrl Pts',(2.4249505146959,-0.676428867885624,105.846464253785));
#33970=CARTESIAN_POINT('Ctrl Pts',(2.43153201033684,-0.652407216277687,
105.848026174135));
#33971=CARTESIAN_POINT('Ctrl Pts',(2.4349443561787,-0.639553818089912,105.848856833913));
#33972=CARTESIAN_POINT('Ctrl Pts',(2.44401077611605,-0.604278301621236,
105.85112302857));
#33973=CARTESIAN_POINT('Ctrl Pts',(2.44945811710471,-0.58180402789837,105.852551943408));
#33974=CARTESIAN_POINT('Ctrl Pts',(2.47971691079009,-0.448997376902675,
105.860913634063));
#33975=CARTESIAN_POINT('Ctrl Pts',(2.49738270605797,-0.33716284815677,105.867614316008));
#33976=CARTESIAN_POINT('Ctrl Pts',(2.52302803343273,-0.050736749581071,
105.884345417257));
#33977=CARTESIAN_POINT('Ctrl Pts',(2.52048013210104,0.124167879640361,105.894146345345));
#33978=CARTESIAN_POINT('Ctrl Pts',(2.49215911842413,0.362233327032045,105.908315257117));
#33979=CARTESIAN_POINT('Ctrl Pts',(2.48192636097651,0.426743534254404,105.912244249825));
#33980=CARTESIAN_POINT('Ctrl Pts',(2.46651932795349,0.504259472625395,105.917152249462));
#33981=CARTESIAN_POINT('Ctrl Pts',(2.46372922549626,0.517719513436078,105.918011390141));
#33982=CARTESIAN_POINT('Ctrl Pts',(2.45920981896702,0.538657795058667,105.91935959002));
#33983=CARTESIAN_POINT('Ctrl Pts',(2.45755625753106,0.546152351681175,105.919844509758));
#33984=CARTESIAN_POINT('Ctrl Pts',(2.45443459094082,0.559999643923158,105.920745019647));
#33985=CARTESIAN_POINT('Ctrl Pts',(2.45297605102233,0.566354352231889,105.921160069608));
#33986=CARTESIAN_POINT('Ctrl Pts',(2.4495855564149,0.580867579425493,105.922112062175));
#33987=CARTESIAN_POINT('Ctrl Pts',(2.44763752804677,0.58902212989969,105.922649894333));
#33988=CARTESIAN_POINT('Ctrl Pts',(2.44146596947612,0.614297260154735,105.924325709525));
#33989=CARTESIAN_POINT('Ctrl Pts',(2.43710336671447,0.631382881225102,105.925471091796));
#33990=CARTESIAN_POINT('Ctrl Pts',(2.40674080226692,0.74528858406175,105.933184858485));
#33991=CARTESIAN_POINT('Ctrl Pts',(2.37515929513042,0.840517973094675,105.940007705263));
#33992=CARTESIAN_POINT('Ctrl Pts',(2.32177709389228,0.974201565986207,105.949910775536));
#33993=CARTESIAN_POINT('Ctrl Pts',(2.30450959601247,1.01437321334719,105.952931225032));
#33994=CARTESIAN_POINT('Ctrl Pts',(2.2076733664515,1.22440342367536,105.968909392239));
#33995=CARTESIAN_POINT('Ctrl Pts',(2.11033867889845,1.38545309421955,105.981754034073));
#33996=CARTESIAN_POINT('Ctrl Pts',(1.97624426696516,1.55990875298976,105.996044919658));
#33997=CARTESIAN_POINT('Ctrl Pts',(1.95599730945183,1.5852228252493,105.99813091688));
#33998=CARTESIAN_POINT('Ctrl Pts',(1.92566725984355,1.62167725173096,106.001154582924));
#33999=CARTESIAN_POINT('Ctrl Pts',(1.91596500831242,1.63312877852177,106.002107351422));
#34000=CARTESIAN_POINT('Ctrl Pts',(1.89851668046733,1.65335344140096,106.003795565375));
#34001=CARTESIAN_POINT('Ctrl Pts',(1.89081081908427,1.66216053439715,106.004532620561));
#34002=CARTESIAN_POINT('Ctrl Pts',(1.87455659397339,1.68047830663406,106.006069786151));
#34003=CARTESIAN_POINT('Ctrl Pts',(1.86599659409139,1.68997824942282,106.00686938458));
#34004=CARTESIAN_POINT('Ctrl Pts',(1.8433407587136,1.71473982930815,106.008960191329));
#34005=CARTESIAN_POINT('Ctrl Pts',(1.82912756565793,1.72989312487497,106.010246430901));
#34006=CARTESIAN_POINT('Ctrl Pts',(1.76167297888014,1.80004837774472,106.016236194987));
#34007=CARTESIAN_POINT('Ctrl Pts',(1.70612562779904,1.85278246456659,106.020839096882));
#34008=CARTESIAN_POINT('Ctrl Pts',(1.54642075545973,1.99111536460875,106.033329483093));
#34009=CARTESIAN_POINT('Ctrl Pts',(1.43766720439114,2.07100769537146,106.041024783751));
#34010=CARTESIAN_POINT('Ctrl Pts',(1.20941287214989,2.21200449930339,106.056457087221));
#34011=CARTESIAN_POINT('Ctrl Pts',(1.09039575888854,2.27303138479676,106.064173169772));
#34012=CARTESIAN_POINT('Ctrl Pts',(0.947312211208525,2.33256640444476,106.073689800145));
#34013=CARTESIAN_POINT('Ctrl Pts',(0.927402113636948,2.340553717791,106.075019374245));
#34014=CARTESIAN_POINT('Ctrl Pts',(0.899530277256461,2.35132358175623,106.076891250466));
#34015=CARTESIAN_POINT('Ctrl Pts',(0.891652326545413,2.35432228669465,106.077421506985));
#34016=CARTESIAN_POINT('Ctrl Pts',(0.878035388899877,2.35942736228369,106.078340310896));
#34017=CARTESIAN_POINT('Ctrl Pts',(0.872303456056896,2.36155251914801,106.078727761924));
#34018=CARTESIAN_POINT('Ctrl Pts',(0.860194062657157,2.36599206534157,106.079547862615));
#34019=CARTESIAN_POINT('Ctrl Pts',(0.853814919065881,2.36830157692148,106.079980803691));
#34020=CARTESIAN_POINT('Ctrl Pts',(0.837962599137786,2.37396839620913,106.081058810891));
#34021=CARTESIAN_POINT('Ctrl Pts',(0.828478578015414,2.37729478639092,106.081705641863));
#34022=CARTESIAN_POINT('Ctrl Pts',(0.792633749318139,2.38962632581186,106.084156768804));
#34023=CARTESIAN_POINT('Ctrl Pts',(0.766145082158192,2.3982501534697,106.085981166771));
#34024=CARTESIAN_POINT('Ctrl Pts',(0.697750561326767,2.41926845721426,106.090715671808));
#34025=CARTESIAN_POINT('Ctrl Pts',(0.655656143056743,2.43101425473521,106.093652253629));
#34026=CARTESIAN_POINT('Ctrl Pts',(0.492902173102709,2.47189374712834,106.105041670535));
#34027=CARTESIAN_POINT('Ctrl Pts',(0.370456339809665,2.4931851583422,106.113674704845));
#34028=CARTESIAN_POINT('Ctrl Pts',(0.0859199573453927,2.52123068446959,
106.13336083853));
#34029=CARTESIAN_POINT('Ctrl Pts',(-0.0762816828006424,2.52154407170327,
106.144290082977));
#34030=CARTESIAN_POINT('Ctrl Pts',(-0.259550307404212,2.50418334522028,
106.156163154833));
#34031=CARTESIAN_POINT('Ctrl Pts',(-0.28165675068904,2.50179337978175,106.15758808061));
#34032=CARTESIAN_POINT('Ctrl Pts',(-0.318010893627006,2.49737508202679,
106.159919999951));
#34033=CARTESIAN_POINT('Ctrl Pts',(-0.33227765635651,2.49551694081023,106.16083224162));
#34034=CARTESIAN_POINT('Ctrl Pts',(-0.358025473566206,2.49193875452469,
106.16247360306));
#34035=CARTESIAN_POINT('Ctrl Pts',(-0.369511958688839,2.4902614151307,106.163204036326));
#34036=CARTESIAN_POINT('Ctrl Pts',(-0.394135342293437,2.48649160949141,
106.164766156918));
#34037=CARTESIAN_POINT('Ctrl Pts',(-0.407268129954352,2.48437434240983,
106.16559704313));
#34038=CARTESIAN_POINT('Ctrl Pts',(-0.443199399477272,2.47828893167073,
106.167864522431));
#34039=CARTESIAN_POINT('Ctrl Pts',(-0.465961272990795,2.47411032160621,
106.169294482643));
#34040=CARTESIAN_POINT('Ctrl Pts',(-0.599957824267533,2.44759645053261,
106.177679618943));
#34041=CARTESIAN_POINT('Ctrl Pts',(-0.709644186108853,2.41807516523421,
106.184401078037));
#34042=CARTESIAN_POINT('Ctrl Pts',(-0.974362659558696,2.3272537335617,106.200681700565));
#34043=CARTESIAN_POINT('Ctrl Pts',(-1.12599858094617,2.25778976432643,106.210048264149));
#34044=CARTESIAN_POINT('Ctrl Pts',(-1.33207323811583,2.1374307820088,106.224093335637));
#34045=CARTESIAN_POINT('Ctrl Pts',(-1.39287605639833,2.09831449564818,106.228424762657));
#34046=CARTESIAN_POINT('Ctrl Pts',(-1.46244223111181,2.04920357798446,106.233709590173));
#34047=CARTESIAN_POINT('Ctrl Pts',(-1.47292073709227,2.04168486046258,106.234514799906));
#34048=CARTESIAN_POINT('Ctrl Pts',(-1.4899358914265,2.02927669776175,106.23583819953));
#34049=CARTESIAN_POINT('Ctrl Pts',(-1.4965074894668,2.02443528081114,106.236353242984));
#34050=CARTESIAN_POINT('Ctrl Pts',(-1.50810604285753,2.01580307900998,106.237269464396));
#34051=CARTESIAN_POINT('Ctrl Pts',(-1.51314246973389,2.01202528674545,106.23766975048));
#34052=CARTESIAN_POINT('Ctrl Pts',(-1.5182151886982,2.00819045282177,106.238075406396));
#34053=CARTESIAN_POINT('Ctrl Pts',(-1.51826562863857,2.00815231864845,106.238079440231));
#34054=CARTESIAN_POINT('Ctrl Pts',(-1.51836532222937,2.008076941271,106.238087413521));
#34055=CARTESIAN_POINT('Ctrl Pts',(-1.51841457594033,2.00803969815961,106.238091352968));
#34056=CARTESIAN_POINT('Ctrl Pts',(-1.5185119423902,2.00796606905025,106.23809914107));
#34057=CARTESIAN_POINT('Ctrl Pts',(-1.51856005518335,2.0079296831414,106.238102989719));
#34058=CARTESIAN_POINT('Ctrl Pts',(-1.51865518282569,2.00785773628304,106.238110599635));
#34059=CARTESIAN_POINT('Ctrl Pts',(-1.5187021977253,2.00782217541776,106.238114360896));
#34060=CARTESIAN_POINT('Ctrl Pts',(-1.51879517046939,2.00775184808275,106.238121799278));
#34061=CARTESIAN_POINT('Ctrl Pts',(-1.51884112836308,2.00771708169094,106.238125476392));
#34062=CARTESIAN_POINT('Ctrl Pts',(-1.51893202591893,2.00764831427555,106.238132749558));
#34063=CARTESIAN_POINT('Ctrl Pts',(-1.51897696565627,2.00761431330356,106.238136345607));
#34064=CARTESIAN_POINT('Ctrl Pts',(-1.51906586390531,2.00754704905175,106.238143459576));
#34065=CARTESIAN_POINT('Ctrl Pts',(-1.51910982246958,2.00751378583442,106.238146977491));
#34066=CARTESIAN_POINT('Ctrl Pts',(-1.51919679355273,2.00744797077504,106.238153937985));
#34067=CARTESIAN_POINT('Ctrl Pts',(-1.51923980612523,2.00741541898887,106.238157380559));
#34068=CARTESIAN_POINT('Ctrl Pts',(-1.51932491883692,2.00735100164097,106.238164193035));
#34069=CARTESIAN_POINT('Ctrl Pts',(-1.51936701897824,2.00731913616869,106.238167562929));
#34070=CARTESIAN_POINT('Ctrl Pts',(-1.51945033873661,2.00725606756734,106.238174232578));
#34071=CARTESIAN_POINT('Ctrl Pts',(-1.51949155840269,2.0072248644872,106.238177532329));
#34072=CARTESIAN_POINT('Ctrl Pts',(-1.51957314759574,2.00716309792448,106.238184064103));
#34073=CARTESIAN_POINT('Ctrl Pts',(-1.51961351722166,2.00713253444835,106.238187296126));
#34074=CARTESIAN_POINT('Ctrl Pts',(-1.51969343548718,2.00707202526417,106.238193694758));
#34075=CARTESIAN_POINT('Ctrl Pts',(-1.51973298416023,2.00704207960777,106.238196861363));
#34076=CARTESIAN_POINT('Ctrl Pts',(-1.51981128834638,2.0069827852222,106.238203131366));
#34077=CARTESIAN_POINT('Ctrl Pts',(-1.5198500438576,2.00695343656732,106.238206234758));
#34078=CARTESIAN_POINT('Ctrl Pts',(-1.51992678814661,2.00689531638929,106.238212380436));
#34079=CARTESIAN_POINT('Ctrl Pts',(-1.51996477697941,2.00686654489353,106.238215422719));
#34080=CARTESIAN_POINT('Ctrl Pts',(-1.52004001333529,2.00680955998396,106.238221448197));
#34081=CARTESIAN_POINT('Ctrl Pts',(-1.52007726086863,2.00678134662785,106.238224431387));
#34082=CARTESIAN_POINT('Ctrl Pts',(-1.52015103876086,2.00672545991089,106.238230340595));
#34083=CARTESIAN_POINT('Ctrl Pts',(-1.52018756919179,2.00669778655757,106.238233266613));
#34084=CARTESIAN_POINT('Ctrl Pts',(-1.52025993610152,2.00664296243901,106.238239063324));
#34085=CARTESIAN_POINT('Ctrl Pts',(-1.52029577260332,2.00661581171531,106.238241934012));
#34086=CARTESIAN_POINT('Ctrl Pts',(-1.5203667740048,2.00656201609837,106.238247621838));
#34087=CARTESIAN_POINT('Ctrl Pts',(-1.52040193884303,2.00653537130769,106.238250438965));
#34088=CARTESIAN_POINT('Ctrl Pts',(-1.520471617968,2.00648257177307,106.238256021341));
#34089=CARTESIAN_POINT('Ctrl Pts',(-1.52050613232808,2.0064564170268,106.238258786592));
#34090=CARTESIAN_POINT('Ctrl Pts',(-1.52057453095547,2.00640458223589,106.238264266839));
#34091=CARTESIAN_POINT('Ctrl Pts',(-1.52060841522901,2.00637890223714,106.238266981833));
#34092=CARTESIAN_POINT('Ctrl Pts',(-1.52067557317113,2.00632800232261,106.238272363117));
#34093=CARTESIAN_POINT('Ctrl Pts',(-1.52070884686618,2.00630278243493,106.238275029406));
#34094=CARTESIAN_POINT('Ctrl Pts',(-1.52077480241013,2.00625278866754,106.23828031477));
#34095=CARTESIAN_POINT('Ctrl Pts',(-1.52080748427373,2.00622801482255,106.238282933843));
#34096=CARTESIAN_POINT('Ctrl Pts',(-1.52087227396967,2.00617889977284,106.238288126193));
#34097=CARTESIAN_POINT('Ctrl Pts',(-1.52090438189069,2.00615455854456,106.238290699474));
#34098=CARTESIAN_POINT('Ctrl Pts',(-1.52096804114101,2.00610629563725,106.238295801626));
#34099=CARTESIAN_POINT('Ctrl Pts',(-1.5209995924226,2.00608237403602,106.23829833049));
#34100=CARTESIAN_POINT('Ctrl Pts',(-1.52106215488206,2.00603493800586,106.238303345121));
#34101=CARTESIAN_POINT('Ctrl Pts',(-1.52109316607101,2.00601142360822,106.238305830885));
#34102=CARTESIAN_POINT('Ctrl Pts',(-1.52115466419343,2.00596479008643,106.238310760576));
#34103=CARTESIAN_POINT('Ctrl Pts',(-1.52118515117764,2.0059416709617,106.238313204504));
#34104=CARTESIAN_POINT('Ctrl Pts',(-1.52124561616672,2.00589581651419,106.238318051737));
#34105=CARTESIAN_POINT('Ctrl Pts',(-1.52127559421915,2.00587308119152,106.238320455043));
#34106=CARTESIAN_POINT('Ctrl Pts',(-1.52133505606685,2.00582798329055,106.238325222206));
#34107=CARTESIAN_POINT('Ctrl Pts',(-1.52136453987596,2.00580562073632,106.238327586059));
#34108=CARTESIAN_POINT('Ctrl Pts',(-1.52142302745861,2.00576125768844,106.238332275448));
#34109=CARTESIAN_POINT('Ctrl Pts',(-1.52145203119468,2.00573925725624,106.238334600978));
#34110=CARTESIAN_POINT('Ctrl Pts',(-1.52150957216221,2.00569560828701,106.238339214794));
#34111=CARTESIAN_POINT('Ctrl Pts',(-1.52153810941493,2.00567395976542,106.23834150308));
#34112=CARTESIAN_POINT('Ctrl Pts',(-1.52159473045282,2.0056310048214,106.238346043448));
#34113=CARTESIAN_POINT('Ctrl Pts',(-1.52162281428758,2.00560969839154,106.238348295531));
#34114=CARTESIAN_POINT('Ctrl Pts',(-1.52167854116102,2.00556741810743,106.238352764501));
#34115=CARTESIAN_POINT('Ctrl Pts',(-1.52170618420044,2.0055464442815,106.238354981386));
#34116=CARTESIAN_POINT('Ctrl Pts',(-1.52176104161755,2.00550482008449,106.238359380926));
#34117=CARTESIAN_POINT('Ctrl Pts',(-1.52178825599615,2.00548416974038,106.238361563578));
#34118=CARTESIAN_POINT('Ctrl Pts',(-1.5218422678636,2.00544318365678,106.238365895591));
#34119=CARTESIAN_POINT('Ctrl Pts',(-1.52186906532566,2.0054228479641,106.238368044947));
#34120=CARTESIAN_POINT('Ctrl Pts',(-1.52849164415888,2.00039698644006,106.238899242306));
#34121=CARTESIAN_POINT('Ctrl Pts',(-1.53506258031548,1.99535903523944,106.239430527626));
#34122=CARTESIAN_POINT('Ctrl Pts',(-1.54896739544983,1.98458884964416,106.240563591107));
#34123=CARTESIAN_POINT('Ctrl Pts',(-1.55629455755438,1.97884818472817,106.241165919939));
#34124=CARTESIAN_POINT('Ctrl Pts',(-1.57587883034914,1.96332830474971,106.24278964481));
#34125=CARTESIAN_POINT('Ctrl Pts',(-1.58807648536065,1.9534751520086,106.243815600405));
#34126=CARTESIAN_POINT('Ctrl Pts',(-1.62588329083977,1.92234705799058,106.247039602589));
#34127=CARTESIAN_POINT('Ctrl Pts',(-1.65116209677604,1.90067835341579,106.249259302077));
#34128=CARTESIAN_POINT('Ctrl Pts',(-1.75509558929767,1.80794940734993,106.258632655889));
#34129=CARTESIAN_POINT('Ctrl Pts',(-1.82964894287989,1.7324618421866,106.265960816481));
#34130=CARTESIAN_POINT('Ctrl Pts',(-2.02028319468862,1.51336651497345,106.28602408217));
#34131=CARTESIAN_POINT('Ctrl Pts',(-2.12571178610571,1.36132099860141,106.298643650481));
#34132=CARTESIAN_POINT('Ctrl Pts',(-2.2291063244802,1.17044976988128,106.31274427953));
#34133=CARTESIAN_POINT('Ctrl Pts',(-2.24406707185061,1.14150374904687,106.314841325137));
#34134=CARTESIAN_POINT('Ctrl Pts',(-2.26510692023375,1.09878253947643,106.317877850261));
#34135=CARTESIAN_POINT('Ctrl Pts',(-2.27163060166272,1.08523124482096,106.318832612282));
#34136=CARTESIAN_POINT('Ctrl Pts',(-2.28301563303063,1.06102917464459,106.320523102128));
#34137=CARTESIAN_POINT('Ctrl Pts',(-2.28792481215159,1.05040151919514,106.321260454836));
#34138=CARTESIAN_POINT('Ctrl Pts',(-2.29803470469356,1.0281079094436,106.322796993301));
#34139=CARTESIAN_POINT('Ctrl Pts',(-2.30322113915874,1.01643581752206,106.323595676108));
#34140=CARTESIAN_POINT('Ctrl Pts',(-2.31658205675916,0.985739589933278,
106.325681314138));
#34141=CARTESIAN_POINT('Ctrl Pts',(-2.32461116787492,0.966652948400143,
106.326963346341));
#34142=CARTESIAN_POINT('Ctrl Pts',(-2.34247802360866,0.922669737893518,
106.329885333479));
#34143=CARTESIAN_POINT('Ctrl Pts',(-2.35215484568137,0.897713790146171,
106.331519808921));
#34144=CARTESIAN_POINT('Ctrl Pts',(-2.36143111532954,0.872610644877486,
106.333142274553));
#34145=CARTESIAN_POINT('Origin',(0.,0.,104.));
#34146=CARTESIAN_POINT('',(-2.36143111856514,0.872610636121403,107.329309102664));
#34147=CARTESIAN_POINT('',(-2.36143112101026,0.872610629504506,107.056339385048));
#34148=CARTESIAN_POINT('',(-2.36143112101026,0.872610629504505,104.));
#34149=CARTESIAN_POINT('',(-2.51749917428736,0.00203898565078566,106.11258330255));
#34150=CARTESIAN_POINT('Ctrl Pts',(-2.36143112101026,0.872610629504506,
107.056339385048));
#34151=CARTESIAN_POINT('Ctrl Pts',(-2.33100317881425,0.954953758525005,
107.050773684733));
#34152=CARTESIAN_POINT('Ctrl Pts',(-2.29630452944505,1.03559491387476,107.045207984417));
#34153=CARTESIAN_POINT('Ctrl Pts',(-2.25755960665741,1.11410541349948,107.039642284101));
#34154=CARTESIAN_POINT('Ctrl Pts',(-2.24919367653911,1.13105765668792,107.038440519933));
#34155=CARTESIAN_POINT('Ctrl Pts',(-2.2406392610389,1.14791066565236,107.037238755765));
#34156=CARTESIAN_POINT('Ctrl Pts',(-2.23189888544177,1.16466030032959,107.036036991597));
#34157=CARTESIAN_POINT('Ctrl Pts',(-2.19367769787657,1.23790554265723,107.03078174219));
#34158=CARTESIAN_POINT('Ctrl Pts',(-2.15177652201512,1.30940257330399,107.025526492782));
#34159=CARTESIAN_POINT('Ctrl Pts',(-2.10637922258263,1.37875770919774,107.020271243375));
#34160=CARTESIAN_POINT('Ctrl Pts',(-2.06104628620771,1.44801451526437,107.015023444718));
#34161=CARTESIAN_POINT('Ctrl Pts',(-2.01222732233027,1.51513507554309,107.00977564606));
#34162=CARTESIAN_POINT('Ctrl Pts',(-1.96015236693402,1.57974964738181,107.004527847403));
#34163=CARTESIAN_POINT('Ctrl Pts',(-1.90770008359203,1.64483240749782,106.99924202392));
#34164=CARTESIAN_POINT('Ctrl Pts',(-1.8519446439376,1.70737228971902,106.993956200437));
#34165=CARTESIAN_POINT('Ctrl Pts',(-1.79316602057087,1.76702062032961,106.988670376954));
#34166=CARTESIAN_POINT('Ctrl Pts',(-1.73491446106262,1.8261340884769,106.983431951085));
#34167=CARTESIAN_POINT('Ctrl Pts',(-1.67369404788836,1.88240731928923,106.978193525217));
#34168=CARTESIAN_POINT('Ctrl Pts',(-1.60981694875851,1.9355349755274,106.972955099348));
#34169=CARTESIAN_POINT('Ctrl Pts',(-1.54596085774349,1.9886451589636,106.967718396311));
#34170=CARTESIAN_POINT('Ctrl Pts',(-1.47945017054332,2.03861152763026,106.962481693273));
#34171=CARTESIAN_POINT('Ctrl Pts',(-1.41063142108424,2.08516791742293,106.957244990236));
#34172=CARTESIAN_POINT('Ctrl Pts',(-1.34181454621347,2.13172303904282,106.952008429843));
#34173=CARTESIAN_POINT('Ctrl Pts',(-1.27069011684476,2.17486810877624,106.946771869451));
#34174=CARTESIAN_POINT('Ctrl Pts',(-1.19763387775233,2.21438012655007,106.941535309059));
#34175=CARTESIAN_POINT('Ctrl Pts',(-1.12338190495366,2.25453884954772,106.936213040288));
#34176=CARTESIAN_POINT('Ctrl Pts',(-1.04713474113545,2.29094427560626,106.930890771518));
#34177=CARTESIAN_POINT('Ctrl Pts',(-0.969311467327336,2.32341161426634,
106.925568502747));
#34178=CARTESIAN_POINT('Ctrl Pts',(-0.892631474319646,2.3554019839798,106.920324421997));
#34179=CARTESIAN_POINT('Ctrl Pts',(-0.814421833478372,2.38356910416829,
106.915080341247));
#34180=CARTESIAN_POINT('Ctrl Pts',(-0.7351004171564,2.40778604254956,106.909836260496));
#34181=CARTESIAN_POINT('Ctrl Pts',(-0.654005005126036,2.43254458428023,
106.904474897716));
#34182=CARTESIAN_POINT('Ctrl Pts',(-0.571747985255809,2.45317399867903,
106.899113534935));
#34183=CARTESIAN_POINT('Ctrl Pts',(-0.48878675866748,2.46959384404629,106.893752172155));
#34184=CARTESIAN_POINT('Ctrl Pts',(-0.405825532079157,2.48601368941355,
106.888390809374));
#34185=CARTESIAN_POINT('Ctrl Pts',(-0.322160611199794,2.49822395846987,
106.883029446594));
#34186=CARTESIAN_POINT('Ctrl Pts',(-0.23825275748405,2.50620068501133,106.877668083813));
#34187=CARTESIAN_POINT('Ctrl Pts',(-0.156005628058678,2.51401953427505,
106.872412834406));
#34188=CARTESIAN_POINT('Ctrl Pts',(-0.0732213097316059,2.51779982116764,
106.867157584998));
#34189=CARTESIAN_POINT('Ctrl Pts',(0.00966987373682366,2.51748142863893,
106.861902335591));
#34190=CARTESIAN_POINT('Ctrl Pts',(0.0924435363376794,2.5171634875185,106.856654536934));
#34191=CARTESIAN_POINT('Ctrl Pts',(0.175323305567954,2.51275841106903,106.851406738276));
#34192=CARTESIAN_POINT('Ctrl Pts',(0.257873800693145,2.50425784473486,106.846158939619));
#34193=CARTESIAN_POINT('Ctrl Pts',(0.341022445322474,2.49569568446924,106.840873116136));
#34194=CARTESIAN_POINT('Ctrl Pts',(0.423836552202129,2.48297838833264,106.835587292653));
#34195=CARTESIAN_POINT('Ctrl Pts',(0.505871224990067,2.46615095923324,106.83030146917));
#34196=CARTESIAN_POINT('Ctrl Pts',(0.587170298529627,2.44947442052906,106.825063043301));
#34197=CARTESIAN_POINT('Ctrl Pts',(0.667703399917501,2.42876125862325,106.819824617433));
#34198=CARTESIAN_POINT('Ctrl Pts',(0.747044454435803,2.40410707604647,106.814586191564));
#34199=CARTESIAN_POINT('Ctrl Pts',(0.826359415001698,2.37946100182003,106.809349488527));
#34200=CARTESIAN_POINT('Ctrl Pts',(0.904482667029798,2.35087661793432,106.804112785489));
#34201=CARTESIAN_POINT('Ctrl Pts',(0.981002283185595,2.31849968091105,106.798876082452));
#34202=CARTESIAN_POINT('Ctrl Pts',(1.0575198149853,2.28612362581937,106.793639522059));
#34203=CARTESIAN_POINT('Ctrl Pts',(1.13243337321914,2.24995540374435,106.788402961667));
#34204=CARTESIAN_POINT('Ctrl Pts',(1.20535133231732,2.21018877376591,106.783166401275));
#34205=CARTESIAN_POINT('Ctrl Pts',(1.27946276185102,2.16977127124816,106.777844132504));
#34206=CARTESIAN_POINT('Ctrl Pts',(1.35151223973336,2.1256367295182,106.772521863734));
#34207=CARTESIAN_POINT('Ctrl Pts',(1.42111659583186,2.07803606105651,106.767199594963));
#34208=CARTESIAN_POINT('Ctrl Pts',(1.48969841304111,2.0311346812225,106.761955514213));
#34209=CARTESIAN_POINT('Ctrl Pts',(1.55590613719532,1.98086867041453,106.756711433463));
#34210=CARTESIAN_POINT('Ctrl Pts',(1.61940578722056,1.92751942825917,106.751467352712));
#34211=CARTESIAN_POINT('Ctrl Pts',(1.6843255846897,1.87297704897863,106.746105989932));
#34212=CARTESIAN_POINT('Ctrl Pts',(1.74641434121004,1.81521221218204,106.740744627151));
#34213=CARTESIAN_POINT('Ctrl Pts',(1.80535555014975,1.75456478579261,106.735383264371));
#34214=CARTESIAN_POINT('Ctrl Pts',(1.86429675908946,1.69391735940319,106.73002190159));
#34215=CARTESIAN_POINT('Ctrl Pts',(1.9200901353509,1.6303877692775,106.72466053881));
#34216=CARTESIAN_POINT('Ctrl Pts',(1.97246471397388,1.56434945013189,106.719299176029));
#34217=CARTESIAN_POINT('Ctrl Pts',(2.02380268242187,1.49961817717862,106.714043926622));
#34218=CARTESIAN_POINT('Ctrl Pts',(2.07204560924584,1.43223751273161,106.708788677214));
#34219=CARTESIAN_POINT('Ctrl Pts',(2.11690877828482,1.36253567821935,106.703533427807));
#34220=CARTESIAN_POINT('Ctrl Pts',(2.16170834154179,1.29293266507408,106.69828562915));
#34221=CARTESIAN_POINT('Ctrl Pts',(2.20313741713628,1.22101540329658,106.693037830492));
#34222=CARTESIAN_POINT('Ctrl Pts',(2.24095195361092,1.14714453823719,106.687790031835));
#34223=CARTESIAN_POINT('Ctrl Pts',(2.27904048900231,1.07273841507621,106.682504208352));
#34224=CARTESIAN_POINT('Ctrl Pts',(2.3134615888812,0.996350629387463,106.677218384869));
#34225=CARTESIAN_POINT('Ctrl Pts',(2.34401077683186,0.918378858693995,106.671932561386));
#34226=CARTESIAN_POINT('Ctrl Pts',(2.37428603232284,0.841106255486301,106.666694135517));
#34227=CARTESIAN_POINT('Ctrl Pts',(2.40075836468042,0.76227839800666,106.661455709649));
#34228=CARTESIAN_POINT('Ctrl Pts',(2.42327598752447,0.682304725388393,106.65621728378));
#34229=CARTESIAN_POINT('Ctrl Pts',(2.4457862046971,0.602357354780098,106.650980580743));
#34230=CARTESIAN_POINT('Ctrl Pts',(2.46434417053718,0.521265361257645,106.645743877705));
#34231=CARTESIAN_POINT('Ctrl Pts',(2.47884787001032,0.43945362365706,106.640507174668));
#34232=CARTESIAN_POINT('Ctrl Pts',(2.49335117440993,0.357644114567297,106.635270614275));
#34233=CARTESIAN_POINT('Ctrl Pts',(2.50380035248801,0.275115354896424,106.630034053883));
#34234=CARTESIAN_POINT('Ctrl Pts',(2.51014470671314,0.192301329584582,106.624797493491));
#34235=CARTESIAN_POINT('Ctrl Pts',(2.51659290091533,0.108131861908733,106.61947522472));
#34236=CARTESIAN_POINT('Ctrl Pts',(2.51880063850722,0.0236681955689467,
106.61415295595));
#34237=CARTESIAN_POINT('Ctrl Pts',(2.51676976536494,-0.0606316595920765,
106.608830687179));
#34238=CARTESIAN_POINT('Ctrl Pts',(2.5147687272342,-0.14369308823651,106.603586606429));
#34239=CARTESIAN_POINT('Ctrl Pts',(2.50865288393013,-0.226595024528162,
106.598342525679));
#34240=CARTESIAN_POINT('Ctrl Pts',(2.49847643477152,-0.308904119252864,
106.593098444928));
#34241=CARTESIAN_POINT('Ctrl Pts',(2.48807239288988,-0.393054028067697,
106.587737082148));
#34242=CARTESIAN_POINT('Ctrl Pts',(2.4734240138405,-0.476583753600645,106.582375719367));
#34243=CARTESIAN_POINT('Ctrl Pts',(2.45464405368558,-0.559042770909367,
106.577014356587));
#34244=CARTESIAN_POINT('Ctrl Pts',(2.43586409353066,-0.64150178821809,106.571652993806));
#34245=CARTESIAN_POINT('Ctrl Pts',(2.41295275425355,-0.722889626306614,
106.566291631026));
#34246=CARTESIAN_POINT('Ctrl Pts',(2.38607574271778,-0.802775684742503,
106.560930268245));
#34247=CARTESIAN_POINT('Ctrl Pts',(2.35973068741657,-0.88108061922109,106.555675018838));
#34248=CARTESIAN_POINT('Ctrl Pts',(2.3294782427263,-0.958231921997691,106.55041976943));
#34249=CARTESIAN_POINT('Ctrl Pts',(2.29543870409073,-1.03381207468392,106.545164520023));
#34250=CARTESIAN_POINT('Ctrl Pts',(2.26144742578811,-1.10928507188334,106.539916721366));
#34251=CARTESIAN_POINT('Ctrl Pts',(2.22367990631748,-1.18319092631463,106.534668922708));
#34252=CARTESIAN_POINT('Ctrl Pts',(2.18230577801946,-1.25512857557418,106.529421124051));
#34253=CARTESIAN_POINT('Ctrl Pts',(2.14063185849318,-1.32758747512024,106.524135300568));
#34254=CARTESIAN_POINT('Ctrl Pts',(2.09529899473699,-1.39804907730869,106.518849477085));
#34255=CARTESIAN_POINT('Ctrl Pts',(2.04652942808546,-1.46612535275133,106.513563653602));
#34256=CARTESIAN_POINT('Ctrl Pts',(1.99819717477175,-1.53359119293106,106.508325227733));
#34257=CARTESIAN_POINT('Ctrl Pts',(1.94648987873675,-1.59871393114153,106.503086801865));
#34258=CARTESIAN_POINT('Ctrl Pts',(1.89166833403513,-1.66114333036279,106.497848375996));
#34259=CARTESIAN_POINT('Ctrl Pts',(1.83686481922718,-1.72355219759363,106.492611672959));
#34260=CARTESIAN_POINT('Ctrl Pts',(1.77894939414177,-1.78326913863002,106.487374969921));
#34261=CARTESIAN_POINT('Ctrl Pts',(1.71822290162397,-1.83997725810264,106.482138266884));
#34262=CARTESIAN_POINT('Ctrl Pts',(1.65749806326547,-1.89668383287443,106.476901706491));
#34263=CARTESIAN_POINT('Ctrl Pts',(1.593962647664,-1.95038143486623,106.471665146099));
#34264=CARTESIAN_POINT('Ctrl Pts',(1.52795307568914,-2.00079125560167,106.466428585707));
#34265=CARTESIAN_POINT('Ctrl Pts',(1.46086310495394,-2.05202614921975,106.461106316936));
#34266=CARTESIAN_POINT('Ctrl Pts',(1.39121763942812,-2.09986435746929,106.455784048166));
#34267=CARTESIAN_POINT('Ctrl Pts',(1.31940185922442,-2.14405806448313,106.450461779395));
#34268=CARTESIAN_POINT('Ctrl Pts',(1.24864110534721,-2.18760253362428,106.445217698645));
#34269=CARTESIAN_POINT('Ctrl Pts',(1.17577382032506,-2.22760870007057,106.439973617895));
#34270=CARTESIAN_POINT('Ctrl Pts',(1.10119300303935,-2.26388608813632,106.434729537144));
#34271=CARTESIAN_POINT('Ctrl Pts',(1.02494421188303,-2.30097480728679,106.429368174364));
#34272=CARTESIAN_POINT('Ctrl Pts',(0.946904789682408,-2.3341657494093,106.424006811583));
#34273=CARTESIAN_POINT('Ctrl Pts',(0.867514023497477,-2.36330820441076,
106.418645448802));
#34274=CARTESIAN_POINT('Ctrl Pts',(0.788123257312551,-2.39245065941223,
106.413284086022));
#34275=CARTESIAN_POINT('Ctrl Pts',(0.707381652181258,-2.41754454028025,
106.407922723241));
#34276=CARTESIAN_POINT('Ctrl Pts',(0.625740611784842,-2.43849439957592,
106.402561360461));
#34277=CARTESIAN_POINT('Ctrl Pts',(0.545715430368026,-2.45902961425046,
106.397306111053));
#34278=CARTESIAN_POINT('Ctrl Pts',(0.464530522070312,-2.47565924426923,
106.392050861646));
#34279=CARTESIAN_POINT('Ctrl Pts',(0.382601593136953,-2.48825687398409,
106.386795612239));
#34280=CARTESIAN_POINT('Ctrl Pts',(0.30078882081284,-2.50083664312184,106.381547813581));
#34281=CARTESIAN_POINT('Ctrl Pts',(0.218234575353637,-2.5093956969744,106.376300014924));
#34282=CARTESIAN_POINT('Ctrl Pts',(0.135367621402023,-2.51385796278866,
106.371052216266));
#34283=CARTESIAN_POINT('Ctrl Pts',(0.0519002249292542,-2.51835256156568,
106.365766392783));
#34284=CARTESIAN_POINT('Ctrl Pts',(-0.0318839718264673,-2.51869063448652,
106.3604805693));
#34285=CARTESIAN_POINT('Ctrl Pts',(-0.115538493166347,-2.51484733266193,
106.355194745817));
#34286=CARTESIAN_POINT('Ctrl Pts',(-0.198442890187689,-2.51103849345953,
106.349956319949));
#34287=CARTESIAN_POINT('Ctrl Pts',(-0.281219458631995,-2.50312298893549,
106.34471789408));
#34288=CARTESIAN_POINT('Ctrl Pts',(-0.36343243265878,-2.49112888403866,
106.339479468212));
#34289=CARTESIAN_POINT('Ctrl Pts',(-0.445618368206609,-2.47913872380333,
106.334242765174));
#34290=CARTESIAN_POINT('Ctrl Pts',(-0.527240621238637,-2.46307269381631,
106.329006062136));
#34291=CARTESIAN_POINT('Ctrl Pts',(-0.607869588007225,-2.44301060455658,
106.323769359099));
#34292=CARTESIAN_POINT('Ctrl Pts',(-0.688496358483101,-2.42294906177813,
106.318532798707));
#34293=CARTESIAN_POINT('Ctrl Pts',(-0.768129448972136,-2.39889178856418,
106.313296238314));
#34294=CARTESIAN_POINT('Ctrl Pts',(-0.846351832207721,-2.3709691744345,
106.308059677922));
#34295=CARTESIAN_POINT('Ctrl Pts',(-0.925854505003531,-2.34258954237868,
106.302737409151));
#34296=CARTESIAN_POINT('Ctrl Pts',(-1.00389940744499,-2.31021705035641,
106.297415140381));
#34297=CARTESIAN_POINT('Ctrl Pts',(-1.08006896158092,-2.27403986073892,
106.29209287161));
#34298=CARTESIAN_POINT('Ctrl Pts',(-1.15511952926764,-2.23839414049147,
106.28684879086));
#34299=CARTESIAN_POINT('Ctrl Pts',(-1.2283491001215,-2.19905504374551,106.28160471011));
#34300=CARTESIAN_POINT('Ctrl Pts',(-1.2993839357524,-2.15624851014641,106.276360629359));
#34301=CARTESIAN_POINT('Ctrl Pts',(-1.37200744061546,-2.11248462340838,
106.270999266579));
#34302=CARTESIAN_POINT('Ctrl Pts',(-1.44233643204541,-2.06509661837732,
106.265637903798));
#34303=CARTESIAN_POINT('Ctrl Pts',(-1.51000532505333,-2.01437091130471,
106.260276541018));
#34304=CARTESIAN_POINT('Ctrl Pts',(-1.57767421806126,-1.9636452042321,106.254915178237));
#34305=CARTESIAN_POINT('Ctrl Pts',(-1.64268266469312,-1.90958217136583,
106.249553815457));
#34306=CARTESIAN_POINT('Ctrl Pts',(-1.70470483693462,-1.8525084801241,106.244192452676));
#34307=CARTESIAN_POINT('Ctrl Pts',(-1.76459909663839,-1.79739292447774,
106.239015032358));
#34308=CARTESIAN_POINT('Ctrl Pts',(-1.82194411214334,-1.73925298659691,
106.23383761204));
#34309=CARTESIAN_POINT('Ctrl Pts',(-1.87641220836556,-1.67835737383214,
106.228660191721));
#34310=CARTESIAN_POINT('Ctrl Pts',(-1.9307897580279,-1.61756299258873,106.223491378232));
#34311=CARTESIAN_POINT('Ctrl Pts',(-1.98229957592409,-1.55402238995337,
106.218322564743));
#34312=CARTESIAN_POINT('Ctrl Pts',(-2.0306488285422,-1.4880428707333,106.213153751254));
#34313=CARTESIAN_POINT('Ctrl Pts',(-2.07895290625897,-1.42212499917289,
106.207989767222));
#34314=CARTESIAN_POINT('Ctrl Pts',(-2.12410199614056,-1.35377311300338,
106.20282578319));
#34315=CARTESIAN_POINT('Ctrl Pts',(-2.16584248281613,-1.2833287145657,106.197661799158));
#34316=CARTESIAN_POINT('Ctrl Pts',(-2.2075574479352,-1.2129273882347,106.192500972562));
#34317=CARTESIAN_POINT('Ctrl Pts',(-2.24586770342721,-1.14043649738507,
106.187340145966));
#34318=CARTESIAN_POINT('Ctrl Pts',(-2.2805629687953,-1.06622642780958,106.18217931937));
#34319=CARTESIAN_POINT('Ctrl Pts',(-2.31524822027081,-0.992037777054693,
106.177019982313));
#34320=CARTESIAN_POINT('Ctrl Pts',(-2.34632035285064,-0.916131364617167,
106.171860645256));
#34321=CARTESIAN_POINT('Ctrl Pts',(-2.37361579836201,-0.83890064475256,
106.166701308199));
#34322=CARTESIAN_POINT('Ctrl Pts',(-2.40092462170781,-0.761632073159825,
106.161539442488));
#34323=CARTESIAN_POINT('Ctrl Pts',(-2.42445289854654,-0.68303834630904,
106.156377576776));
#34324=CARTESIAN_POINT('Ctrl Pts',(-2.44408620525115,-0.603530340000433,
106.151215711065));
#34325=CARTESIAN_POINT('Ctrl Pts',(-2.46372478256864,-0.524000989558178,
106.146052459637));
#34326=CARTESIAN_POINT('Ctrl Pts',(-2.47946621212706,-0.443557337996501,
106.140889208209));
#34327=CARTESIAN_POINT('Ctrl Pts',(-2.49124719851246,-0.36262052603765,
106.135725956781));
#34328=CARTESIAN_POINT('Ctrl Pts',(-2.50304227978819,-0.281586880464768,
106.130556527987));
#34329=CARTESIAN_POINT('Ctrl Pts',(-2.51086741194788,-0.200059370820398,
106.125387099194));
#34330=CARTESIAN_POINT('Ctrl Pts',(-2.51471124598382,-0.118463493627845,
106.1202176704));
#34331=CARTESIAN_POINT('Ctrl Pts',(-2.5166034758707,-0.0782957454818718,
106.117672881117));
#34332=CARTESIAN_POINT('Ctrl Pts',(-2.51753169311315,-0.0381114278951565,
106.115128091833));
#34333=CARTESIAN_POINT('Ctrl Pts',(-2.51749917428736,0.00203898565078367,
106.11258330255));
#34334=CARTESIAN_POINT('Ctrl Pts',(-2.51749917428662,0.00203898656446618,
106.112583302492));
#34335=CARTESIAN_POINT('Ctrl Pts',(-2.51739410665396,0.131764058349367,
106.104361146272));
#34336=CARTESIAN_POINT('Ctrl Pts',(-2.50725905023951,0.261092140164354,
106.096138990052));
#34337=CARTESIAN_POINT('Ctrl Pts',(-2.4872941057706,0.388811369945391,106.087916833832));
#34338=CARTESIAN_POINT('Ctrl Pts',(-2.48559980578692,0.399650102268016,
106.087219070852));
#34339=CARTESIAN_POINT('Ctrl Pts',(-2.48383473575133,0.410477266841117,
106.086521307872));
#34340=CARTESIAN_POINT('Ctrl Pts',(-2.48199903094348,0.421292131893801,
106.085823544892));
#34341=CARTESIAN_POINT('Ctrl Pts',(-2.46817693389102,0.502723587391459,
106.08056967859));
#34342=CARTESIAN_POINT('Ctrl Pts',(-2.45031756944332,0.58362443547189,106.075315812289));
#34343=CARTESIAN_POINT('Ctrl Pts',(-2.42847467758016,0.663563855519524,
106.070061945987));
#34344=CARTESIAN_POINT('Ctrl Pts',(-2.40920337579527,0.734091910957334,
106.065426623719));
#34345=CARTESIAN_POINT('Ctrl Pts',(-2.38683207102609,0.803871386774122,
106.060791301452));
#34346=CARTESIAN_POINT('Ctrl Pts',(-2.36143112101026,0.872610629504504,
106.056155979185));
#34347=CARTESIAN_POINT('',(-2.51749974387929,-0.00113559134422,106.385343084406));
#34348=CARTESIAN_POINT('Ctrl Pts',(-2.36143111532954,0.872610644877486,
106.333142274553));
#34349=CARTESIAN_POINT('Ctrl Pts',(-2.37840222838592,0.826683959627441,
106.336110606514));
#34350=CARTESIAN_POINT('Ctrl Pts',(-2.39403264494922,0.780264573325589,
106.339038531095));
#34351=CARTESIAN_POINT('Ctrl Pts',(-2.48082626973949,0.495260363424947,
106.356658330302));
#34352=CARTESIAN_POINT('Ctrl Pts',(-2.51761199924472,0.247724049190195,
106.370316362223));
#34353=CARTESIAN_POINT('Ctrl Pts',(-2.51749974387929,-0.00113559134422,
106.385343084406));
#34354=CARTESIAN_POINT('Ctrl Pts',(-2.51749974245381,-0.00113874712773204,
106.38534327496));
#34355=CARTESIAN_POINT('Ctrl Pts',(-2.5174886769077,-0.0256020443719995,
106.386820426755));
#34356=CARTESIAN_POINT('Ctrl Pts',(-2.51712103637506,-0.0500631483503205,
106.38831115182));
#34357=CARTESIAN_POINT('Ctrl Pts',(-2.51590148255077,-0.0912483122380716,
106.390849931066));
#34358=CARTESIAN_POINT('Ctrl Pts',(-2.51523906686123,-0.107976511726821,
106.391889134037));
#34359=CARTESIAN_POINT('Ctrl Pts',(-2.5140400509716,-0.132153782305922,
106.393404299523));
#34360=CARTESIAN_POINT('Ctrl Pts',(-2.51363704738602,-0.139609422307697,
106.393873354727));
#34361=CARTESIAN_POINT('Ctrl Pts',(-2.51284220378002,-0.153192723263485,
106.394731410201));
#34362=CARTESIAN_POINT('Ctrl Pts',(-2.51246109876711,-0.15932098678088,
106.395119828112));
#34363=CARTESIAN_POINT('Ctrl Pts',(-2.51164734611005,-0.17167651256996,
106.395905663239));
#34364=CARTESIAN_POINT('Ctrl Pts',(-2.51121395728993,-0.177903552065781,
106.396303126556));
#34365=CARTESIAN_POINT('Ctrl Pts',(-2.51014024441833,-0.192544560959587,
106.397240925798));
#34366=CARTESIAN_POINT('Ctrl Pts',(-2.50948077436851,-0.200956942598961,
106.397782301401));
#34367=CARTESIAN_POINT('Ctrl Pts',(-2.5076297546577,-0.223137268022371,
106.399216124558));
#34368=CARTESIAN_POINT('Ctrl Pts',(-2.50636712718199,-0.23689877699717,
106.400112249799));
#34369=CARTESIAN_POINT('Ctrl Pts',(-2.49983804137136,-0.302150641058131,
106.404390150203));
#34370=CARTESIAN_POINT('Ctrl Pts',(-2.49309808721478,-0.353477521822113,
106.407840193943));
#34371=CARTESIAN_POINT('Ctrl Pts',(-2.45039581229338,-0.615754713508913,
106.425791061583));
#34372=CARTESIAN_POINT('Ctrl Pts',(-2.38922456477507,-0.821714523814122,
106.440867787194));
#34373=CARTESIAN_POINT('Ctrl Pts',(-2.2673384725194,-1.09756545525668,106.461138692496));
#34374=CARTESIAN_POINT('Ctrl Pts',(-2.22779112997989,-1.17576500379407,
106.466909277117));
#34375=CARTESIAN_POINT('Ctrl Pts',(-2.17348812189932,-1.27052099109105,
106.473930898796));
#34376=CARTESIAN_POINT('Ctrl Pts',(-2.16249039112194,-1.28915071300985,
106.475313064241));
#34377=CARTESIAN_POINT('Ctrl Pts',(-2.14451449585696,-1.31872368623372,
106.47751037029));
#34378=CARTESIAN_POINT('Ctrl Pts',(-2.13768967215345,-1.32975842143583,
106.478331002013));
#34379=CARTESIAN_POINT('Ctrl Pts',(-2.12457174787982,-1.35060616654113,
106.479883008618));
#34380=CARTESIAN_POINT('Ctrl Pts',(-2.1182952230244,-1.36042915451066,106.480614963194));
#34381=CARTESIAN_POINT('Ctrl Pts',(-2.10384015801193,-1.38270925803018,
106.482276915269));
#34382=CARTESIAN_POINT('Ctrl Pts',(-2.09561873828371,-1.39513813707365,
106.483205298159));
#34383=CARTESIAN_POINT('Ctrl Pts',(-2.06996941460449,-1.43317561839316,
106.486051105667));
#34384=CARTESIAN_POINT('Ctrl Pts',(-2.05217846194298,-1.45853673915997,
106.487954939507));
#34385=CARTESIAN_POINT('Ctrl Pts',(-1.91340326130433,-1.64879353647585,
106.502304452549));
#34386=CARTESIAN_POINT('Ctrl Pts',(-1.77320115967382,-1.79872133068051,
106.513920857825));
#34387=CARTESIAN_POINT('Ctrl Pts',(-1.54528393003118,-1.98959975225619,
106.531045769329));
#34388=CARTESIAN_POINT('Ctrl Pts',(-1.4709417104943,-2.0451742212175,106.536423246696));
#34389=CARTESIAN_POINT('Ctrl Pts',(-1.36805384530418,-2.11357138570874,
106.543831345724));
#34390=CARTESIAN_POINT('Ctrl Pts',(-1.34208865201766,-2.13015332933239,
106.545698345049));
#34391=CARTESIAN_POINT('Ctrl Pts',(-1.30316267420755,-2.1540180966544,106.548503645364));
#34392=CARTESIAN_POINT('Ctrl Pts',(-1.29043027905398,-2.16166986104699,
106.549422228113));
#34393=CARTESIAN_POINT('Ctrl Pts',(-1.26989609879762,-2.17376418612735,
106.550906490124));
#34394=CARTESIAN_POINT('Ctrl Pts',(-1.26213676920833,-2.17827858845475,
106.551467991951));
#34395=CARTESIAN_POINT('Ctrl Pts',(-1.24734474990491,-2.18677906326363,
106.552539945485));
#34396=CARTESIAN_POINT('Ctrl Pts',(-1.24031666126126,-2.19077296225725,
106.553049911725));
#34397=CARTESIAN_POINT('Ctrl Pts',(-1.22769644399515,-2.19786454508185,
106.553967036993));
#34398=CARTESIAN_POINT('Ctrl Pts',(-1.22211160398293,-2.2009748619724,106.554373387341));
#34399=CARTESIAN_POINT('Ctrl Pts',(-1.20977891756267,-2.20778178638898,
106.555271844535));
#34400=CARTESIAN_POINT('Ctrl Pts',(-1.20302605189916,-2.21146868853847,
106.555764525401));
#34401=CARTESIAN_POINT('Ctrl Pts',(-1.18408705283165,-2.22169651118994,
106.557148083931));
#34402=CARTESIAN_POINT('Ctrl Pts',(-1.17186397637098,-2.22816793285224,
106.558043085935));
#34403=CARTESIAN_POINT('Ctrl Pts',(-1.10031765231315,-2.26529609607387,
106.56329115958));
#34404=CARTESIAN_POINT('Ctrl Pts',(-1.03985169351275,-2.29368091646447,
106.567762891552));
#34405=CARTESIAN_POINT('Ctrl Pts',(-0.774096630116817,-2.40576687398546,
106.587362643806));
#34406=CARTESIAN_POINT('Ctrl Pts',(-0.559332233676539,-2.46457119808922,
106.602955951201));
#34407=CARTESIAN_POINT('Ctrl Pts',(-0.293643990155972,-2.5007468333505,
106.620816114834));
#34408=CARTESIAN_POINT('Ctrl Pts',(-0.247476936706913,-2.50573684319135,
106.623874056116));
#34409=CARTESIAN_POINT('Ctrl Pts',(-0.167108753650601,-2.51218038975102,
106.62911825787));
#34410=CARTESIAN_POINT('Ctrl Pts',(-0.132968270019118,-2.51421862076372,
106.631321415561));
#34411=CARTESIAN_POINT('Ctrl Pts',(-0.0833105800665508,-2.51616886314197,
106.634491718405));
#34412=CARTESIAN_POINT('Ctrl Pts',(-0.0678201651223361,-2.51663403046701,
106.63547585784));
#34413=CARTESIAN_POINT('Ctrl Pts',(-0.0405936575150107,-2.51720005481548,
106.637197427096));
#34414=CARTESIAN_POINT('Ctrl Pts',(-0.0288594408697667,-2.51736193289732,
106.637936726786));
#34415=CARTESIAN_POINT('Ctrl Pts',(-0.00599425838749794,-2.51751746840598,
106.639372275662));
#34416=CARTESIAN_POINT('Ctrl Pts',(0.00513636111921546,-2.51751936616252,
106.640068763188));
#34417=CARTESIAN_POINT('Ctrl Pts',(0.0350926329951424,-2.5173258003219,
106.641937198091));
#34418=CARTESIAN_POINT('Ctrl Pts',(0.0539169212550774,-2.51699298239075,
106.643104873476));
#34419=CARTESIAN_POINT('Ctrl Pts',(0.125040839673735,-2.51493719775465,
106.647494107486));
#34420=CARTESIAN_POINT('Ctrl Pts',(0.177288196806846,-2.51179493474101,
106.650671867291));
#34421=CARTESIAN_POINT('Ctrl Pts',(0.419181729845457,-2.48966074300661,
106.665228510676));
#34422=CARTESIAN_POINT('Ctrl Pts',(0.606371057255961,-2.45080421165191,
106.675992382609));
#34423=CARTESIAN_POINT('Ctrl Pts',(0.898128086010245,-2.35473242022073,
106.693750428235));
#34424=CARTESIAN_POINT('Ctrl Pts',(1.00618565585988,-2.31062377853236,106.700580180374));
#34425=CARTESIAN_POINT('Ctrl Pts',(1.12422216626366,-2.25258851585288,106.708734677337));
#34426=CARTESIAN_POINT('Ctrl Pts',(1.13760108703273,-2.24586158130117,106.709669493805));
#34427=CARTESIAN_POINT('Ctrl Pts',(1.15790223958993,-2.23542620265445,106.711105325391));
#34428=CARTESIAN_POINT('Ctrl Pts',(1.16486871567246,-2.23180392849727,106.711601183228));
#34429=CARTESIAN_POINT('Ctrl Pts',(1.17757722062226,-2.22512032973606,106.71251171493));
#34430=CARTESIAN_POINT('Ctrl Pts',(1.18332444369557,-2.22206927222134,106.712925751572));
#34431=CARTESIAN_POINT('Ctrl Pts',(1.19625390988776,-2.21514095472807,106.713862315884));
#34432=CARTESIAN_POINT('Ctrl Pts',(1.20342911054679,-2.2112510571332,106.714385615959));
#34433=CARTESIAN_POINT('Ctrl Pts',(1.22189132611882,-2.20112564752323,106.715741042883));
#34434=CARTESIAN_POINT('Ctrl Pts',(1.23314941870801,-2.19483826824055,106.716576247476));
#34435=CARTESIAN_POINT('Ctrl Pts',(1.30711216556026,-2.15278314078093,106.722118352285));
#34436=CARTESIAN_POINT('Ctrl Pts',(1.36829633275082,-2.11442204870785,106.726964688546));
#34437=CARTESIAN_POINT('Ctrl Pts',(1.55428769103191,-1.98635408150379,106.742347306281));
#34438=CARTESIAN_POINT('Ctrl Pts',(1.67259169940009,-1.88781673830012,106.753079315354));
#34439=CARTESIAN_POINT('Ctrl Pts',(1.84009812473606,-1.72011532924929,106.769253029855));
#34440=CARTESIAN_POINT('Ctrl Pts',(1.89605714629313,-1.65823019504619,106.774865064157));
#34441=CARTESIAN_POINT('Ctrl Pts',(1.97113171652223,-1.56642438114409,106.782681640062));
#34442=CARTESIAN_POINT('Ctrl Pts',(1.99284411990497,-1.53870663191259,106.78498086224));
#34443=CARTESIAN_POINT('Ctrl Pts',(2.0305234632661,-1.48846966088346,106.789042226085));
#34444=CARTESIAN_POINT('Ctrl Pts',(2.04671456062163,-1.46612655403242,106.790812688018));
#34445=CARTESIAN_POINT('Ctrl Pts',(2.07069829632754,-1.43185804823379,106.793475373802));
#34446=CARTESIAN_POINT('Ctrl Pts',(2.07876202172337,-1.42012583079747,106.794377827601));
#34447=CARTESIAN_POINT('Ctrl Pts',(2.09321413239448,-1.39871203760131,106.796008723936));
#34448=CARTESIAN_POINT('Ctrl Pts',(2.09963590355781,-1.38905357993688,106.796738404468));
#34449=CARTESIAN_POINT('Ctrl Pts',(2.11334116573075,-1.36812840804141,106.798306739406));
#34450=CARTESIAN_POINT('Ctrl Pts',(2.12060183297364,-1.35684711766214,106.799144532376));
#34451=CARTESIAN_POINT('Ctrl Pts',(2.1400893987707,-1.32602969115209,106.80141263594));
#34452=CARTESIAN_POINT('Ctrl Pts',(2.15213895821762,-1.30638253785931,106.802836452287));
#34453=CARTESIAN_POINT('Ctrl Pts',(2.21572749191487,-1.19943142137683,106.81047321577));
#34454=CARTESIAN_POINT('Ctrl Pts',(2.26223011997917,-1.10923505101745,106.816503531559));
#34455=CARTESIAN_POINT('Ctrl Pts',(2.37075433132497,-0.863335526133497,
106.832202296985));
#34456=CARTESIAN_POINT('Ctrl Pts',(2.42289426067117,-0.703849578767558,
106.841625986407));
#34457=CARTESIAN_POINT('Ctrl Pts',(2.47091192097962,-0.485359139711029,
106.854721856653));
#34458=CARTESIAN_POINT('Ctrl Pts',(2.48115219321345,-0.429956056647078,
106.858061058317));
#34459=CARTESIAN_POINT('Ctrl Pts',(2.49286405119169,-0.352050398636419,
106.862838924928));
#34460=CARTESIAN_POINT('Ctrl Pts',(2.49590542355734,-0.32979797667032,106.864212986107));
#34461=CARTESIAN_POINT('Ctrl Pts',(2.5007115231282,-0.290746217752555,106.866645372895));
#34462=CARTESIAN_POINT('Ctrl Pts',(2.50260568054328,-0.273963970336145,
106.86769743983));
#34463=CARTESIAN_POINT('Ctrl Pts',(2.50517245796069,-0.248968060895189,
106.869276154933));
#34464=CARTESIAN_POINT('Ctrl Pts',(2.50597387153135,-0.240767709911513,
106.869795956693));
#34465=CARTESIAN_POINT('Ctrl Pts',(2.50727865814311,-0.226703803424934,
106.87069087688));
#34466=CARTESIAN_POINT('Ctrl Pts',(2.50780174795306,-0.220842197136975,
106.87106489574));
#34467=CARTESIAN_POINT('Ctrl Pts',(2.50894693872986,-0.20748046942414,106.871919883087));
#34468=CARTESIAN_POINT('Ctrl Pts',(2.50955595289047,-0.199979504802744,
106.872401553832));
#34469=CARTESIAN_POINT('Ctrl Pts',(2.51113205142319,-0.179425183925563,
106.873725889042));
#34470=CARTESIAN_POINT('Ctrl Pts',(2.51203096385962,-0.166367050592956,
106.874572149448));
#34471=CARTESIAN_POINT('Ctrl Pts',(2.5161666262377,-0.0985782977269599,
106.878988780419));
#34472=CARTESIAN_POINT('Ctrl Pts',(2.51771641335306,-0.0437635962055014,
106.882639088061));
#34473=CARTESIAN_POINT('Ctrl Pts',(2.51645126434022,0.244386296747995,106.902099691672));
#34474=CARTESIAN_POINT('Ctrl Pts',(2.48299555575205,0.476456519781788,106.918572983341));
#34475=CARTESIAN_POINT('Ctrl Pts',(2.40487006445882,0.746087354917213,106.937285614347));
#34476=CARTESIAN_POINT('Ctrl Pts',(2.39041801702914,0.791169097729831,106.940405141234));
#34477=CARTESIAN_POINT('Ctrl Pts',(2.36318048929641,0.868555503862495,106.945743498774));
#34478=CARTESIAN_POINT('Ctrl Pts',(2.35098215947258,0.901051480322453,106.947980057709));
#34479=CARTESIAN_POINT('Ctrl Pts',(2.33233670789758,0.94776299795592,106.951189047578));
#34480=CARTESIAN_POINT('Ctrl Pts',(2.32642369775259,0.962186060828268,106.952179060037));
#34481=CARTESIAN_POINT('Ctrl Pts',(2.31581967285404,0.987382155442238,106.953907370227));
#34482=CARTESIAN_POINT('Ctrl Pts',(2.31118653816699,0.998178877466677,106.954647583877));
#34483=CARTESIAN_POINT('Ctrl Pts',(2.3020283553739,1.01911479569419,106.956082349339));
#34484=CARTESIAN_POINT('Ctrl Pts',(2.29751148651414,1.02925725228618,106.956777156834));
#34485=CARTESIAN_POINT('Ctrl Pts',(2.28521533274418,1.05638349278913,106.958634928802));
#34486=CARTESIAN_POINT('Ctrl Pts',(2.27731376972384,1.07331133616501,106.959793710683));
#34487=CARTESIAN_POINT('Ctrl Pts',(2.24700895384686,1.13639295301249,106.964111538885));
#34488=CARTESIAN_POINT('Ctrl Pts',(2.22338418791763,1.18194817248927,106.967228639571));
#34489=CARTESIAN_POINT('Ctrl Pts',(2.09333387098665,1.41500286422539,106.983233410034));
#34490=CARTESIAN_POINT('Ctrl Pts',(1.96454871445951,1.58897034589151,106.995291075475));
#34491=CARTESIAN_POINT('Ctrl Pts',(1.77097214112476,1.79040036688358,107.011567665163));
#34492=CARTESIAN_POINT('Ctrl Pts',(1.72503973352877,1.8346968791506,107.01532959863));
#34493=CARTESIAN_POINT('Ctrl Pts',(1.65043719390017,1.90136225680395,107.021380176019));
#34494=CARTESIAN_POINT('Ctrl Pts',(1.6228788549393,1.92493773219777,107.023603522261));
#34495=CARTESIAN_POINT('Ctrl Pts',(1.58624914291547,1.95492779508859,107.026558273332));
#34496=CARTESIAN_POINT('Ctrl Pts',(1.57762957652766,1.96189039858094,107.027253543476));
#34497=CARTESIAN_POINT('Ctrl Pts',(1.56348542193121,1.97316209955616,107.028394910984));
#34498=CARTESIAN_POINT('Ctrl Pts',(1.55798820457407,1.97750552142392,107.028838626335));
#34499=CARTESIAN_POINT('Ctrl Pts',(1.54723073535155,1.9859324376366,107.029707312746));
#34500=CARTESIAN_POINT('Ctrl Pts',(1.5419723026253,1.99001809277611,107.030132126949));
#34501=CARTESIAN_POINT('Ctrl Pts',(1.5301998914087,1.99909025320383,107.031083489174));
#34502=CARTESIAN_POINT('Ctrl Pts',(1.52367762884071,2.00406587392741,107.031610775091));
#34503=CARTESIAN_POINT('Ctrl Pts',(1.50107238146822,2.02113653917867,107.033438637201));
#34504=CARTESIAN_POINT('Ctrl Pts',(1.48486924715709,2.03307020620374,107.034749451249));
#34505=CARTESIAN_POINT('Ctrl Pts',(1.33188109177482,2.1429421376612,107.04711864875));
#34506=CARTESIAN_POINT('Ctrl Pts',(1.18575540582497,2.22712462742915,107.058847785858));
#34507=CARTESIAN_POINT('Ctrl Pts',(0.894088247691019,2.35825995116277,107.080897556558));
#34508=CARTESIAN_POINT('Ctrl Pts',(0.750485771436709,2.4078139260615,107.091199139716));
#34509=CARTESIAN_POINT('Ctrl Pts',(0.566954225203103,2.45311412334179,107.103526365418));
#34510=CARTESIAN_POINT('Ctrl Pts',(0.530434314292028,2.4612691195923,107.105940994534));
#34511=CARTESIAN_POINT('Ctrl Pts',(0.478000741989728,2.47175632357832,107.109355088195));
#34512=CARTESIAN_POINT('Ctrl Pts',(0.462226900996958,2.47475460277658,107.110375421833));
#34513=CARTESIAN_POINT('Ctrl Pts',(0.434789115058307,2.4796984632526,107.11213884487));
#34514=CARTESIAN_POINT('Ctrl Pts',(0.423138294957362,2.48171312489638,107.112884090315));
#34515=CARTESIAN_POINT('Ctrl Pts',(0.399174030091159,2.48568336160188,107.114409849717));
#34516=CARTESIAN_POINT('Ctrl Pts',(0.38685936972341,2.48762969861274,107.115190054142));
#34517=CARTESIAN_POINT('Ctrl Pts',(0.355446806058426,2.4923555628087,107.11717071872));
#34518=CARTESIAN_POINT('Ctrl Pts',(0.336330252339824,2.49500714968275,107.118367150429));
#34519=CARTESIAN_POINT('Ctrl Pts',(0.261661547090632,2.50449037300758,107.123007537263));
#34520=CARTESIAN_POINT('Ctrl Pts',(0.205915947458594,2.50968884843986,107.126400750155));
#34521=CARTESIAN_POINT('Ctrl Pts',(-0.0368404706516668,2.52418261208097,
107.140940069409));
#34522=CARTESIAN_POINT('Ctrl Pts',(-0.224377970224939,2.51446063642063,
107.151513092457));
#34523=CARTESIAN_POINT('Ctrl Pts',(-0.513036974492457,2.4669197658741,107.168431695489));
#34524=CARTESIAN_POINT('Ctrl Pts',(-0.615776510393933,2.44329991054807,
107.174599657339));
#34525=CARTESIAN_POINT('Ctrl Pts',(-0.737337379113756,2.40719801554209,
107.182390887225));
#34526=CARTESIAN_POINT('Ctrl Pts',(-0.757871962789267,2.4008120945672,107.183724497829));
#34527=CARTESIAN_POINT('Ctrl Pts',(-0.786957265933539,2.39135672184425,
107.185641718282));
#34528=CARTESIAN_POINT('Ctrl Pts',(-0.795577700844144,2.38850263249566,
107.186213514532));
#34529=CARTESIAN_POINT('Ctrl Pts',(-0.810441489727181,2.38349207475983,
107.187205902519));
#34530=CARTESIAN_POINT('Ctrl Pts',(-0.816692227877049,2.38135752939939,
107.187625225523));
#34531=CARTESIAN_POINT('Ctrl Pts',(-0.829809872755465,2.37682030264468,
107.188509503655));
#34532=CARTESIAN_POINT('Ctrl Pts',(-0.836674792114363,2.37441244627528,
107.18897474171));
#34533=CARTESIAN_POINT('Ctrl Pts',(-0.85511522574752,2.36785460206178,107.190230912942));
#34534=CARTESIAN_POINT('Ctrl Pts',(-0.866670756161856,2.36364956194156,
107.19102494862));
#34535=CARTESIAN_POINT('Ctrl Pts',(-0.919285349757061,2.34406549830082,
107.194670294172));
#34536=CARTESIAN_POINT('Ctrl Pts',(-0.959966617936126,2.32770104847975,
107.197572379141));
#34537=CARTESIAN_POINT('Ctrl Pts',(-1.167547076091,2.23783273385408,107.212743041166));
#34538=CARTESIAN_POINT('Ctrl Pts',(-1.32652653616748,2.1474146382059,107.225543998172));
#34539=CARTESIAN_POINT('Ctrl Pts',(-1.5693600164499,1.9719675435252,107.246005999776));
#34540=CARTESIAN_POINT('Ctrl Pts',(-1.65947508724273,1.89675931944158,107.253856652104));
#34541=CARTESIAN_POINT('Ctrl Pts',(-1.76603399516982,1.79439713634079,107.263437784845));
#34542=CARTESIAN_POINT('Ctrl Pts',(-1.78765196214386,1.77286145842605,107.265399266362));
#34543=CARTESIAN_POINT('Ctrl Pts',(-1.81917607289125,1.74029424969281,107.268287543781));
#34544=CARTESIAN_POINT('Ctrl Pts',(-1.82938429156376,1.72956028768908,107.269227362632));
#34545=CARTESIAN_POINT('Ctrl Pts',(-1.84744883653704,1.71022650405974,107.270898888472));
#34546=CARTESIAN_POINT('Ctrl Pts',(-1.8553412677625,1.70166115496169,107.271632121366));
#34547=CARTESIAN_POINT('Ctrl Pts',(-1.87193369860679,1.68340135913011,107.273180061547));
#34548=CARTESIAN_POINT('Ctrl Pts',(-1.88061849757676,1.67369351573479,107.273994119252));
#34549=CARTESIAN_POINT('Ctrl Pts',(-1.90367977858585,1.64750953545306,107.276166455543));
#34550=CARTESIAN_POINT('Ctrl Pts',(-1.91791780425728,1.63091253946289,107.277519022239));
#34551=CARTESIAN_POINT('Ctrl Pts',(-1.98321983997168,1.55275318554288,107.28377972546));
#34552=CARTESIAN_POINT('Ctrl Pts',(-2.03155053152866,1.48896195220122,107.288578251208));
#34553=CARTESIAN_POINT('Ctrl Pts',(-2.17073612603328,1.28582671935263,107.303099701702));
#34554=CARTESIAN_POINT('Ctrl Pts',(-2.25088842806099,1.13971363888592,107.312491585597));
#34555=CARTESIAN_POINT('Ctrl Pts',(-2.33210770891705,0.949082516362216,
107.324503685888));
#34556=CARTESIAN_POINT('Ctrl Pts',(-2.34723801617531,0.911019557884368,
107.32689269747));
#34557=CARTESIAN_POINT('Ctrl Pts',(-2.36143111856514,0.872610636121403,
107.329309102664));
#34558=CARTESIAN_POINT('Origin',(0.,0.,104.));
#34559=CARTESIAN_POINT('',(-2.36143103931299,0.872610850591009,108.330801621721));
#34560=CARTESIAN_POINT('',(-2.36143112101026,0.872610629504501,108.056228667503));
#34561=CARTESIAN_POINT('',(-2.36143112101026,0.872610629504505,104.));
#34562=CARTESIAN_POINT('',(-2.51749998978759,0.000226758633992978,107.11258330245));
#34563=CARTESIAN_POINT('Ctrl Pts',(-2.36143112101026,0.8726106295045,108.056228667503));
#34564=CARTESIAN_POINT('Ctrl Pts',(-2.3330193732305,0.949497597346625,108.051065788408));
#34565=CARTESIAN_POINT('Ctrl Pts',(-2.30085130969319,1.0249877363886,108.045902909314));
#34566=CARTESIAN_POINT('Ctrl Pts',(-2.26510104568141,1.09869172330229,108.04074003022));
#34567=CARTESIAN_POINT('Ctrl Pts',(-2.22931537254852,1.17246871089086,108.035572037513));
#34568=CARTESIAN_POINT('Ctrl Pts',(-2.1899406263118,1.24445558689348,108.030404044806));
#34569=CARTESIAN_POINT('Ctrl Pts',(-2.1471972905072,1.31428689624395,108.025236052099));
#34570=CARTESIAN_POINT('Ctrl Pts',(-2.10443039782417,1.38415669130532,108.020065211187));
#34571=CARTESIAN_POINT('Ctrl Pts',(-2.05829149119642,1.4518681640573,108.014894370275));
#34572=CARTESIAN_POINT('Ctrl Pts',(-2.00904340845741,1.51708629712809,108.009723529363));
#34573=CARTESIAN_POINT('Ctrl Pts',(-1.95971494943521,1.5824108707107,108.00454424928));
#34574=CARTESIAN_POINT('Ctrl Pts',(-1.90726749368202,1.64523362034305,107.999364969198));
#34575=CARTESIAN_POINT('Ctrl Pts',(-1.85200258460678,1.7052544316347,107.994185689115));
#34576=CARTESIAN_POINT('Ctrl Pts',(-1.82377852594175,1.7359073527625,107.991540605511));
#34577=CARTESIAN_POINT('Ctrl Pts',(-1.79482019034814,1.76583009294109,107.988895521906));
#34578=CARTESIAN_POINT('Ctrl Pts',(-1.76517104191664,1.79498675281433,107.986250438302));
#34579=CARTESIAN_POINT('Ctrl Pts',(-1.70626414405387,1.85291517491186,107.980995188895));
#34580=CARTESIAN_POINT('Ctrl Pts',(-1.64439384420539,1.90804774175334,107.975739939487));
#34581=CARTESIAN_POINT('Ctrl Pts',(-1.57985623667132,1.96006645842705,107.97048469008));
#34582=CARTESIAN_POINT('Ctrl Pts',(-1.51541012880355,2.01201142437774,107.965236891423));
#34583=CARTESIAN_POINT('Ctrl Pts',(-1.44830458093796,2.06085102195854,107.959989092765));
#34584=CARTESIAN_POINT('Ctrl Pts',(-1.37887225049189,2.10630424365129,107.954741294108));
#34585=CARTESIAN_POINT('Ctrl Pts',(-1.30893682295402,2.1520868131205,107.949455470625));
#34586=CARTESIAN_POINT('Ctrl Pts',(-1.23664108935141,2.19443339293706,107.944169647142));
#34587=CARTESIAN_POINT('Ctrl Pts',(-1.162358736518,2.23309838960138,107.938883823659));
#34588=CARTESIAN_POINT('Ctrl Pts',(-1.08874246841506,2.27141667990948,107.93364539779));
#34589=CARTESIAN_POINT('Ctrl Pts',(-1.01317548297708,2.30611893065921,107.928406971922));
#34590=CARTESIAN_POINT('Ctrl Pts',(-0.93604876330185,2.33701068947514,107.923168546053));
#34591=CARTESIAN_POINT('Ctrl Pts',(-0.858947409321192,2.3678922885057,107.917931843016));
#34592=CARTESIAN_POINT('Ctrl Pts',(-0.780287767892922,2.39496571311247,
107.912695139978));
#34593=CARTESIAN_POINT('Ctrl Pts',(-0.700481465352659,2.41808435888771,
107.907458436941));
#34594=CARTESIAN_POINT('Ctrl Pts',(-0.620677336696214,2.44120237492259,
107.902221876548));
#34595=CARTESIAN_POINT('Ctrl Pts',(-0.539727052516102,2.46036569891574,
107.896985316156));
#34596=CARTESIAN_POINT('Ctrl Pts',(-0.458056749043987,2.47547778512659,
107.891748755764));
#34597=CARTESIAN_POINT('Ctrl Pts',(-0.375049722851323,2.49083721545316,
107.886426486993));
#34598=CARTESIAN_POINT('Ctrl Pts',(-0.291299376297351,2.50201149345775,
107.881104218223));
#34599=CARTESIAN_POINT('Ctrl Pts',(-0.20726132009106,2.50895376505708,107.875781949452));
#34600=CARTESIAN_POINT('Ctrl Pts',(-0.124457844383297,2.51579404961009,
107.870537868702));
#34601=CARTESIAN_POINT('Ctrl Pts',(-0.0413755260267815,2.51852589088099,
107.865293787952));
#34602=CARTESIAN_POINT('Ctrl Pts',(0.0415489796359196,2.5171571131519,107.860049707201));
#34603=CARTESIAN_POINT('Ctrl Pts',(0.126328062838983,2.51575772318806,107.854688344421));
#34604=CARTESIAN_POINT('Ctrl Pts',(0.210941678431518,2.51007211743795,107.84932698164));
#34605=CARTESIAN_POINT('Ctrl Pts',(0.294929867698741,2.50016451921453,107.84396561886));
#34606=CARTESIAN_POINT('Ctrl Pts',(0.378918056965965,2.4902569209911,107.838604256079));
#34607=CARTESIAN_POINT('Ctrl Pts',(0.462280330108677,2.47612748106315,107.833242893299));
#34608=CARTESIAN_POINT('Ctrl Pts',(0.544570910994421,2.45789519160169,107.827881530518));
#34609=CARTESIAN_POINT('Ctrl Pts',(0.625232777039974,2.44002375996985,107.822626281111));
#34610=CARTESIAN_POINT('Ctrl Pts',(0.705162930103362,2.41814444185591,107.817371031703));
#34611=CARTESIAN_POINT('Ctrl Pts',(0.783933429502005,2.3923324660484,107.812115782296));
#34612=CARTESIAN_POINT('Ctrl Pts',(0.8625922502269,2.36655708575884,107.806867983639));
#34613=CARTESIAN_POINT('Ctrl Pts',(0.940094248178786,2.33686026505963,107.801620184981));
#34614=CARTESIAN_POINT('Ctrl Pts',(1.01602260056919,2.30336803944411,107.796372386324));
#34615=CARTESIAN_POINT('Ctrl Pts',(1.09250111933074,2.26963313378026,107.791086562841));
#34616=CARTESIAN_POINT('Ctrl Pts',(1.16738262880117,2.23204769166853,107.785800739358));
#34617=CARTESIAN_POINT('Ctrl Pts',(1.24025767266762,2.19079144497807,107.780514915875));
#34618=CARTESIAN_POINT('Ctrl Pts',(1.31247925104597,2.14990514020395,107.775276490006));
#34619=CARTESIAN_POINT('Ctrl Pts',(1.38272979443805,2.10541383039628,107.770038064138));
#34620=CARTESIAN_POINT('Ctrl Pts',(1.45063332633357,2.0575395992618,107.764799638269));
#34621=CARTESIAN_POINT('Ctrl Pts',(1.51851452588748,2.00968111316523,107.759562935232));
#34622=CARTESIAN_POINT('Ctrl Pts',(1.58404987014748,1.95844218106979,107.754326232194));
#34623=CARTESIAN_POINT('Ctrl Pts',(1.6468922778664,1.90408825297149,107.749089529157));
#34624=CARTESIAN_POINT('Ctrl Pts',(1.70973297378955,1.84973580544703,107.743852968764));
#34625=CARTESIAN_POINT('Ctrl Pts',(1.76988053070187,1.79226883325615,107.738616408372));
#34626=CARTESIAN_POINT('Ctrl Pts',(1.82702195624446,1.73199221170323,107.73337984798));
#34627=CARTESIAN_POINT('Ctrl Pts',(1.885098632895,1.6707290243348,107.728057579209));
#34628=CARTESIAN_POINT('Ctrl Pts',(1.94006953799661,1.60656373286699,107.722735310439));
#34629=CARTESIAN_POINT('Ctrl Pts',(1.99164731274398,1.53985299026877,107.717413041668));
#34630=CARTESIAN_POINT('Ctrl Pts',(2.04246737226403,1.4741222772616,107.712168960918));
#34631=CARTESIAN_POINT('Ctrl Pts',(2.08999311757033,1.4059208248335,107.706924880168));
#34632=CARTESIAN_POINT('Ctrl Pts',(2.13399337392747,1.33561915605971,107.701680799417));
#34633=CARTESIAN_POINT('Ctrl Pts',(2.17897768061521,1.26374521507374,107.696319436637));
#34634=CARTESIAN_POINT('Ctrl Pts',(2.22027665346995,1.18967643016715,107.690958073856));
#34635=CARTESIAN_POINT('Ctrl Pts',(2.25769373727083,1.11383357764438,107.685596711076));
#34636=CARTESIAN_POINT('Ctrl Pts',(2.29511082107171,1.03799072512162,107.680235348295));
#34637=CARTESIAN_POINT('Ctrl Pts',(2.32864587561049,0.960374297908778,107.674873985515));
#34638=CARTESIAN_POINT('Ctrl Pts',(2.35815600709104,0.881422995059944,107.669512622734));
#34639=CARTESIAN_POINT('Ctrl Pts',(2.38708206699787,0.804034315262545,107.664257373327));
#34640=CARTESIAN_POINT('Ctrl Pts',(2.41224796036825,0.725077290617908,107.659002123919));
#34641=CARTESIAN_POINT('Ctrl Pts',(2.43348379555697,0.644951832900452,107.653746874512));
#34642=CARTESIAN_POINT('Ctrl Pts',(2.45468952315555,0.56493997487986,107.648499075855));
#34643=CARTESIAN_POINT('Ctrl Pts',(2.47197614282711,0.483763416524039,107.643251277197));
#34644=CARTESIAN_POINT('Ctrl Pts',(2.48522243235326,0.401840405793344,107.63800347854));
#34645=CARTESIAN_POINT('Ctrl Pts',(2.49856470266671,0.31932379222374,107.632717655057));
#34646=CARTESIAN_POINT('Ctrl Pts',(2.50780767851231,0.236050307147021,107.627431831574));
#34647=CARTESIAN_POINT('Ctrl Pts',(2.51287918846662,0.15246125465624,107.622146008091));
#34648=CARTESIAN_POINT('Ctrl Pts',(2.51790522254122,0.0696217394294053,
107.616907582222));
#34649=CARTESIAN_POINT('Ctrl Pts',(2.51883427313051,-0.0135272374751904,
107.611669156354));
#34650=CARTESIAN_POINT('Ctrl Pts',(2.51564792133641,-0.096549396040497,
107.606430730485));
#34651=CARTESIAN_POINT('Ctrl Pts',(2.51246261748039,-0.179544249999562,
107.601194027448));
#34652=CARTESIAN_POINT('Ctrl Pts',(2.50516461702329,-0.262411907737051,
107.59595732441));
#34653=CARTESIAN_POINT('Ctrl Pts',(2.49378760844704,-0.344716715515772,
107.590720621373));
#34654=CARTESIAN_POINT('Ctrl Pts',(2.48241090977482,-0.427019281352698,
107.58548406098));
#34655=CARTESIAN_POINT('Ctrl Pts',(2.46695548810185,-0.508758570780944,
107.580247500588));
#34656=CARTESIAN_POINT('Ctrl Pts',(2.44750666130299,-0.589506058389143,
107.575010940196));
#34657=CARTESIAN_POINT('Ctrl Pts',(2.42773950963495,-0.671575164709622,
107.569688671425));
#34658=CARTESIAN_POINT('Ctrl Pts',(2.40384715326952,-0.752619228922522,
107.564366402655));
#34659=CARTESIAN_POINT('Ctrl Pts',(2.37597229701542,-0.832203036413159,
107.559044133884));
#34660=CARTESIAN_POINT('Ctrl Pts',(2.34850694278321,-0.910617699576022,
107.553800053134));
#34661=CARTESIAN_POINT('Ctrl Pts',(2.3171755568698,-0.987614315326077,107.548555972384));
#34662=CARTESIAN_POINT('Ctrl Pts',(2.28216306772662,-1.06279724421201,107.543311891633));
#34663=CARTESIAN_POINT('Ctrl Pts',(2.24636753652028,-1.13966161298381,107.537950528853));
#34664=CARTESIAN_POINT('Ctrl Pts',(2.2067245014078,-1.21462973836698,107.532589166072));
#34665=CARTESIAN_POINT('Ctrl Pts',(2.16347989151034,-1.28730765904285,107.527227803292));
#34666=CARTESIAN_POINT('Ctrl Pts',(2.12023528161289,-1.35998557971873,107.521866440511));
#34667=CARTESIAN_POINT('Ctrl Pts',(2.07338943405645,-1.43037290970733,107.516505077731));
#34668=CARTESIAN_POINT('Ctrl Pts',(2.02323252747275,-1.49811094041004,107.51114371495));
#34669=CARTESIAN_POINT('Ctrl Pts',(1.97406833836912,-1.56450828382311,107.505888465543));
#34670=CARTESIAN_POINT('Ctrl Pts',(1.92154140516658,-1.62860551635473,107.500633216135));
#34671=CARTESIAN_POINT('Ctrl Pts',(1.86589467300482,-1.69004240161371,107.495377966728));
#34672=CARTESIAN_POINT('Ctrl Pts',(1.81032683526791,-1.75139218332611,107.490130168071));
#34673=CARTESIAN_POINT('Ctrl Pts',(1.7516482914465,-1.81008877046016,107.484882369413));
#34674=CARTESIAN_POINT('Ctrl Pts',(1.69014386507701,-1.86580276699938,107.479634570756));
#34675=CARTESIAN_POINT('Ctrl Pts',(1.62819378611536,-1.9219204594747,107.474348747273));
#34676=CARTESIAN_POINT('Ctrl Pts',(1.56337698190051,-1.97501177524924,107.46906292379));
#34677=CARTESIAN_POINT('Ctrl Pts',(1.49602432105695,-2.02477590878746,107.463777100307));
#34678=CARTESIAN_POINT('Ctrl Pts',(1.42927560687408,-2.07409381077527,107.458538674438));
#34679=CARTESIAN_POINT('Ctrl Pts',(1.3600367095692,-2.12014368151661,107.45330024857));
#34680=CARTESIAN_POINT('Ctrl Pts',(1.28866354925701,-2.16267253804554,107.448061822701));
#34681=CARTESIAN_POINT('Ctrl Pts',(1.2173138623895,-2.20518740754129,107.442825119664));
#34682=CARTESIAN_POINT('Ctrl Pts',(1.14383170264682,-2.24418332667537,107.437588416626));
#34683=CARTESIAN_POINT('Ctrl Pts',(1.06860083476931,-2.27945136072923,107.432351713589));
#34684=CARTESIAN_POINT('Ctrl Pts',(0.993372016143048,-2.31471843409947,
107.427115153196));
#34685=CARTESIAN_POINT('Ctrl Pts',(0.916395002318008,-2.34625762936329,
107.421878592804));
#34686=CARTESIAN_POINT('Ctrl Pts',(0.838075688553412,-2.37390719916675,
107.416642032412));
#34687=CARTESIAN_POINT('Ctrl Pts',(0.758474498737001,-2.40200931789678,
107.411319763641));
#34688=CARTESIAN_POINT('Ctrl Pts',(0.677487132195316,-2.42609316097623,
107.405997494871));
#34689=CARTESIAN_POINT('Ctrl Pts',(0.595556339445428,-2.44604147482138,
107.4006752261));
#34690=CARTESIAN_POINT('Ctrl Pts',(0.514829169952915,-2.46569673334894,
107.39543114535));
#34691=CARTESIAN_POINT('Ctrl Pts',(0.433186580706433,-2.48133713620051,
107.3901870646));
#34692=CARTESIAN_POINT('Ctrl Pts',(0.351061115609519,-2.49290239341756,
107.384942983849));
#34693=CARTESIAN_POINT('Ctrl Pts',(0.267098943234842,-2.50472630356369,
107.379581621069));
#34694=CARTESIAN_POINT('Ctrl Pts',(0.182632545677586,-2.51229054444311,
107.374220258288));
#34695=CARTESIAN_POINT('Ctrl Pts',(0.0981262711464113,-2.51558690665039,
107.368858895508));
#34696=CARTESIAN_POINT('Ctrl Pts',(0.0136199966152368,-2.51888326885768,
107.363497532727));
#34697=CARTESIAN_POINT('Ctrl Pts',(-0.0709256475840465,-2.51791182502412,
107.358136169947));
#34698=CARTESIAN_POINT('Ctrl Pts',(-0.155051791237268,-2.51272067529085,
107.352774807166));
#34699=CARTESIAN_POINT('Ctrl Pts',(-0.237512890153433,-2.50763227003352,
107.347519557759));
#34700=CARTESIAN_POINT('Ctrl Pts',(-0.319875525081196,-2.49847092200903,
107.342264308351));
#34701=CARTESIAN_POINT('Ctrl Pts',(-0.401705260654237,-2.48524428046072,
107.337009058944));
#34702=CARTESIAN_POINT('Ctrl Pts',(-0.483418980251928,-2.47203639128536,
107.331761260287));
#34703=CARTESIAN_POINT('Ctrl Pts',(-0.564600849489855,-2.4547747299149,
107.326513461629));
#34704=CARTESIAN_POINT('Ctrl Pts',(-0.644819500911588,-2.43351886395896,
107.321265662972));
#34705=CARTESIAN_POINT('Ctrl Pts',(-0.725619405619257,-2.41210898092952,
107.315979839489));
#34706=CARTESIAN_POINT('Ctrl Pts',(-0.805441601937452,-2.38664679535493,
107.310694016006));
#34707=CARTESIAN_POINT('Ctrl Pts',(-0.883853634564483,-2.35724606324142,
107.305408192523));
#34708=CARTESIAN_POINT('Ctrl Pts',(-0.961562551907393,-2.32810896546336,
107.300169766654));
#34709=CARTESIAN_POINT('Ctrl Pts',(-1.03788605394107,-2.29510383658022,
107.294931340786));
#34710=CARTESIAN_POINT('Ctrl Pts',(-1.11241815924337,-2.25839148266761,
107.289692914917));
#34711=CARTESIAN_POINT('Ctrl Pts',(-1.18692575217654,-2.22169120283726,
107.28445621188));
#34712=CARTESIAN_POINT('Ctrl Pts',(-1.25964270488015,-2.18128632319323,
107.279219508842));
#34713=CARTESIAN_POINT('Ctrl Pts',(-1.33018482321224,-2.13738498780538,
107.273982805805));
#34714=CARTESIAN_POINT('Ctrl Pts',(-1.40072502001217,-2.09348484826804,
107.268746245412));
#34715=CARTESIAN_POINT('Ctrl Pts',(-1.46909010902132,-2.04608868703059,
107.26350968502));
#34716=CARTESIAN_POINT('Ctrl Pts',(-1.53492342749955,-1.9954489023057,107.258273124628));
#34717=CARTESIAN_POINT('Ctrl Pts',(-1.60183425994372,-1.94398028080736,
107.252950855857));
#34718=CARTESIAN_POINT('Ctrl Pts',(-1.6661292998544,-1.88916118851532,107.247628587087));
#34719=CARTESIAN_POINT('Ctrl Pts',(-1.72746913961996,-1.83129916225085,
107.242306318316));
#34720=CARTESIAN_POINT('Ctrl Pts',(-1.78790785228463,-1.7742871714638,107.237062237566));
#34721=CARTESIAN_POINT('Ctrl Pts',(-1.8454773366962,-1.71432143920929,107.231818156815));
#34722=CARTESIAN_POINT('Ctrl Pts',(-1.89989152289909,-1.65173195501455,
107.226574076065));
#34723=CARTESIAN_POINT('Ctrl Pts',(-1.95552266332799,-1.58774267891609,
107.221212713285));
#34724=CARTESIAN_POINT('Ctrl Pts',(-2.0078553522263,-1.52101127904271,107.215851350504));
#34725=CARTESIAN_POINT('Ctrl Pts',(-2.05662988850103,-1.45192277746588,
107.210489987723));
#34726=CARTESIAN_POINT('Ctrl Pts',(-2.10540442477575,-1.38283427588906,
107.205128624943));
#34727=CARTESIAN_POINT('Ctrl Pts',(-2.15062059314602,-1.31138913767721,
107.199767262162));
#34728=CARTESIAN_POINT('Ctrl Pts',(-2.19206890703471,-1.2379984478228,107.194405899382));
#34729=CARTESIAN_POINT('Ctrl Pts',(-2.23446890777379,-1.16292264829992,
107.18892143537));
#34730=CARTESIAN_POINT('Ctrl Pts',(-2.27307163741358,-1.08555429773656,
107.183436971359));
#34731=CARTESIAN_POINT('Ctrl Pts',(-2.30763425924455,-1.00629537192658,
107.177952507347));
#34732=CARTESIAN_POINT('Ctrl Pts',(-2.34210712091703,-0.927242283907992,
107.172482286652));
#34733=CARTESIAN_POINT('Ctrl Pts',(-2.37256061323769,-0.846308768249363,
107.167012065957));
#34734=CARTESIAN_POINT('Ctrl Pts',(-2.39879783154439,-0.763920947073663,
107.161541845262));
#34735=CARTESIAN_POINT('Ctrl Pts',(-2.42499481295695,-0.681659474278365,
107.156080013592));
#34736=CARTESIAN_POINT('Ctrl Pts',(-2.4469882590584,-0.597948514163733,
107.150618181923));
#34737=CARTESIAN_POINT('Ctrl Pts',(-2.4646291608708,-0.513234205198073,
107.145156350253));
#34738=CARTESIAN_POINT('Ctrl Pts',(-2.48223686891322,-0.428679297793389,
107.139704795767));
#34739=CARTESIAN_POINT('Ctrl Pts',(-2.49550826265296,-0.343125195358922,
107.134253241281));
#34740=CARTESIAN_POINT('Ctrl Pts',(-2.50434439920526,-0.257031866058002,
107.128801686795));
#34741=CARTESIAN_POINT('Ctrl Pts',(-2.51310690653038,-0.171655930072997,
107.123395558694));
#34742=CARTESIAN_POINT('Ctrl Pts',(-2.51750773395471,-0.0857501128067695,
107.117989430593));
#34743=CARTESIAN_POINT('Ctrl Pts',(-2.51749998978765,0.000226757967744173,
107.112583302492));
#34744=CARTESIAN_POINT('Ctrl Pts',(-2.51749998978759,0.000226758633996389,
107.11258330245));
#34745=CARTESIAN_POINT('Ctrl Pts',(-2.51749207334436,0.0881160063818547,
107.107056926255));
#34746=CARTESIAN_POINT('Ctrl Pts',(-2.51287737051979,0.175904335234615,
107.101530550059));
#34747=CARTESIAN_POINT('Ctrl Pts',(-2.5037131461786,0.263109733100915,107.096004173863));
#34748=CARTESIAN_POINT('Ctrl Pts',(-2.49453499866111,0.350447621845197,
107.090469401462));
#34749=CARTESIAN_POINT('Ctrl Pts',(-2.48079360116063,0.437200436864105,
107.084934629061));
#34750=CARTESIAN_POINT('Ctrl Pts',(-2.46259737508519,0.522896183026359,
107.07939985666));
#34751=CARTESIAN_POINT('Ctrl Pts',(-2.44435528551196,0.608807924892799,
107.073851133893));
#34752=CARTESIAN_POINT('Ctrl Pts',(-2.42163602170516,0.693656903619571,
107.068302411125));
#34753=CARTESIAN_POINT('Ctrl Pts',(-2.39459810500259,0.776985305857198,
107.062753688358));
#34754=CARTESIAN_POINT('Ctrl Pts',(-2.38417952725892,0.809094415686877,
107.060615587255));
#34755=CARTESIAN_POINT('Ctrl Pts',(-2.37312021907302,0.840977964248501,
107.058477486152));
#34756=CARTESIAN_POINT('Ctrl Pts',(-2.36143112101026,0.872610629504506,
107.056339385048));
#34757=CARTESIAN_POINT('Ctrl Pts',(-2.36143111856514,0.872610636121403,
107.329309102664));
#34758=CARTESIAN_POINT('Ctrl Pts',(-2.37273689814697,0.84201529540582,107.331233935146));
#34759=CARTESIAN_POINT('Ctrl Pts',(-2.38344800047675,0.811200434712442,
107.33317617158));
#34760=CARTESIAN_POINT('Ctrl Pts',(-2.40590495362348,0.742303791526028,
107.337544213279));
#34761=CARTESIAN_POINT('Ctrl Pts',(-2.41735015134349,0.704138768383658,
107.339980917275));
#34762=CARTESIAN_POINT('Ctrl Pts',(-2.43091236365006,0.654677368318164,
107.343179686073));
#34763=CARTESIAN_POINT('Ctrl Pts',(-2.43386499499604,0.64361366578133,107.343897802894));
#34764=CARTESIAN_POINT('Ctrl Pts',(-2.43852283196717,0.625669949665931,
107.345067266237));
#34765=CARTESIAN_POINT('Ctrl Pts',(-2.44027467697771,0.618802057110833,
107.345516003933));
#34766=CARTESIAN_POINT('Ctrl Pts',(-2.44360454133335,0.605513673250652,
107.346386590374));
#34767=CARTESIAN_POINT('Ctrl Pts',(-2.44518630160325,0.599094240915663,
107.346808224389));
#34768=CARTESIAN_POINT('Ctrl Pts',(-2.44862974977171,0.584878489911253,
107.347744182174));
#34769=CARTESIAN_POINT('Ctrl Pts',(-2.45047952588004,0.577079360666258,
107.348259166738));
#34770=CARTESIAN_POINT('Ctrl Pts',(-2.45691366547512,0.549362560083878,
107.35009430998));
#34771=CARTESIAN_POINT('Ctrl Pts',(-2.46129254261949,0.529398657675405,
107.351425227625));
#34772=CARTESIAN_POINT('Ctrl Pts',(-2.49990059893568,0.342535127648288,
107.363953619616));
#34773=CARTESIAN_POINT('Ctrl Pts',(-2.51734456373288,0.172630788688992,
107.375839042506));
#34774=CARTESIAN_POINT('Ctrl Pts',(-2.5176397475312,-0.153039840341469,
107.39828852783));
#34775=CARTESIAN_POINT('Ctrl Pts',(-2.50340621560271,-0.308062823131997,
107.408829194306));
#34776=CARTESIAN_POINT('Ctrl Pts',(-2.46882862719299,-0.493777574152181,
107.421109713271));
#34777=CARTESIAN_POINT('Ctrl Pts',(-2.46203120364396,-0.526624735993077,
107.423269681965));
#34778=CARTESIAN_POINT('Ctrl Pts',(-2.45119930196303,-0.574159955287971,
107.426379296072));
#34779=CARTESIAN_POINT('Ctrl Pts',(-2.44768500646156,-0.588961626850756,
107.42734528467));
#34780=CARTESIAN_POINT('Ctrl Pts',(-2.44122323026002,-0.615120335428029,
107.429048648769));
#34781=CARTESIAN_POINT('Ctrl Pts',(-2.43833014717352,-0.626490213755297,
107.42978773469));
#34782=CARTESIAN_POINT('Ctrl Pts',(-2.43214223862213,-0.650116483086283,
107.431321032895));
#34783=CARTESIAN_POINT('Ctrl Pts',(-2.42883399453497,-0.662369041288485,
107.432114791536));
#34784=CARTESIAN_POINT('Ctrl Pts',(-2.41998475919982,-0.694185449099741,
107.434172598875));
#34785=CARTESIAN_POINT('Ctrl Pts',(-2.41429908822412,-0.713708359657247,
107.435431967996));
#34786=CARTESIAN_POINT('Ctrl Pts',(-2.3875395192746,-0.801611517651557,
107.441089933652));
#34787=CARTESIAN_POINT('Ctrl Pts',(-2.36379169565279,-0.86914681868696,
107.445401461449));
#34788=CARTESIAN_POINT('Ctrl Pts',(-2.24976858893047,-1.15398984590854,
107.463588057807));
#34789=CARTESIAN_POINT('Ctrl Pts',(-2.13217136208571,-1.35903578456481,
107.476574377692));
#34790=CARTESIAN_POINT('Ctrl Pts',(-1.95534159602503,-1.58658455450562,
107.493749563226));
#34791=CARTESIAN_POINT('Ctrl Pts',(-1.92153396896601,-1.62736524213994,
107.496959424955));
#34792=CARTESIAN_POINT('Ctrl Pts',(-1.87789067353578,-1.67675301318114,
107.50105789196));
#34793=CARTESIAN_POINT('Ctrl Pts',(-1.86923835645084,-1.6863931923179,107.501868323682));
#34794=CARTESIAN_POINT('Ctrl Pts',(-1.85546325871562,-1.70150478009377,
107.503156122928));
#34795=CARTESIAN_POINT('Ctrl Pts',(-1.85038964103753,-1.70702097058127,
107.503629924334));
#34796=CARTESIAN_POINT('Ctrl Pts',(-1.84128479801558,-1.71683174382802,
107.504479439222));
#34797=CARTESIAN_POINT('Ctrl Pts',(-1.83726303814441,-1.7211349366474,107.504854440493));
#34798=CARTESIAN_POINT('Ctrl Pts',(-1.82754816163319,-1.73145678619184,
107.505759672488));
#34799=CARTESIAN_POINT('Ctrl Pts',(-1.82184044073542,-1.73746144975727,
107.506291002147));
#34800=CARTESIAN_POINT('Ctrl Pts',(-1.80424748488139,-1.75578767062189,
107.507926842971));
#34801=CARTESIAN_POINT('Ctrl Pts',(-1.79226639939556,-1.76801596338372,
107.509038269328));
#34802=CARTESIAN_POINT('Ctrl Pts',(-1.76400093125974,-1.79628208595371,
107.511652258178));
#34803=CARTESIAN_POINT('Ctrl Pts',(-1.74762118959818,-1.81222203874087,
107.513160962257));
#34804=CARTESIAN_POINT('Ctrl Pts',(-1.68903451856967,-1.86770271170236,
107.518528955032));
#34805=CARTESIAN_POINT('Ctrl Pts',(-1.64568636780856,-1.90600801817147,
107.522449708055));
#34806=CARTESIAN_POINT('Ctrl Pts',(-1.47041986490487,-2.05044624877503,
107.537992097549));
#34807=CARTESIAN_POINT('Ctrl Pts',(-1.32923894108942,-2.14466679944575,
107.549817972916));
#34808=CARTESIAN_POINT('Ctrl Pts',(-1.09345534932311,-2.26973247681531,
107.56785046946));
#34809=CARTESIAN_POINT('Ctrl Pts',(-1.00464834151209,-2.31041465803188,
107.574309502234));
#34810=CARTESIAN_POINT('Ctrl Pts',(-0.892417811418203,-2.35412786357626,
107.582065204711));
#34811=CARTESIAN_POINT('Ctrl Pts',(-0.871030385627863,-2.36212482134271,
107.583525828777));
#34812=CARTESIAN_POINT('Ctrl Pts',(-0.836953763574405,-2.37434060741084,
107.585826297673));
#34813=CARTESIAN_POINT('Ctrl Pts',(-0.824335072346266,-2.37875106349208,
107.586672419832));
#34814=CARTESIAN_POINT('Ctrl Pts',(-0.800699199987404,-2.38680155187183,
107.588246770937));
#34815=CARTESIAN_POINT('Ctrl Pts',(-0.789690876675213,-2.39046631087393,
107.588975793924));
#34816=CARTESIAN_POINT('Ctrl Pts',(-0.765059694475698,-2.39847751141546,
107.590597762841));
#34817=CARTESIAN_POINT('Ctrl Pts',(-0.751424278540976,-2.40278427575851,
107.591489395961));
#34818=CARTESIAN_POINT('Ctrl Pts',(-0.711074736937883,-2.41515166064484,
107.594109997489));
#34819=CARTESIAN_POINT('Ctrl Pts',(-0.68426192011347,-2.42288475684472,
107.595828372961));
#34820=CARTESIAN_POINT('Ctrl Pts',(-0.515246274224209,-2.46860098913525,
107.606526678152));
#34821=CARTESIAN_POINT('Ctrl Pts',(-0.370063688639742,-2.49449995921898,
107.615104390183));
#34822=CARTESIAN_POINT('Ctrl Pts',(-0.0679157977862989,-2.521422548848,
107.632575484822));
#34823=CARTESIAN_POINT('Ctrl Pts',(0.0885398498160474,-2.52078086286033,
107.641422385245));
#34824=CARTESIAN_POINT('Ctrl Pts',(0.287894343465228,-2.5013747994269,107.653443049762));
#34825=CARTESIAN_POINT('Ctrl Pts',(0.331753499104943,-2.49593632124955,
107.656136061144));
#34826=CARTESIAN_POINT('Ctrl Pts',(0.387635271294029,-2.4875082234345,107.659655108473));
#34827=CARTESIAN_POINT('Ctrl Pts',(0.399812874536767,-2.48557999591668,
107.660427339813));
#34828=CARTESIAN_POINT('Ctrl Pts',(0.419159555203438,-2.48237075144017,
107.661663445374));
#34829=CARTESIAN_POINT('Ctrl Pts',(0.426338266092768,-2.4811479117533,107.662124142499));
#34830=CARTESIAN_POINT('Ctrl Pts',(0.440015683495928,-2.47875695580567,
107.663005948195));
#34831=CARTESIAN_POINT('Ctrl Pts',(0.446515207308212,-2.47759440047486,
107.66342674747));
#34832=CARTESIAN_POINT('Ctrl Pts',(0.461926892671691,-2.47477513481603,
107.664428651862));
#34833=CARTESIAN_POINT('Ctrl Pts',(0.470834768384566,-2.47309584062801,
107.665011001159));
#34834=CARTESIAN_POINT('Ctrl Pts',(0.50075171350041,-2.46728847023686,107.666977318281));
#34835=CARTESIAN_POINT('Ctrl Pts',(0.521716494107387,-2.46294062085169,
107.668372697634));
#34836=CARTESIAN_POINT('Ctrl Pts',(0.644520579454797,-2.43583426928961,
107.67663911985));
#34837=CARTESIAN_POINT('Ctrl Pts',(0.744912145804099,-2.40703073883812,
107.683769243345));
#34838=CARTESIAN_POINT('Ctrl Pts',(1.01690754978523,-2.31034328907831,107.703663216678));
#34839=CARTESIAN_POINT('Ctrl Pts',(1.18331889751004,-2.229699782988,107.716452910183));
#34840=CARTESIAN_POINT('Ctrl Pts',(1.38948780979697,-2.10014844737259,107.732579459345));
#34841=CARTESIAN_POINT('Ctrl Pts',(1.43841432564662,-2.06694582650521,107.736435458679));
#34842=CARTESIAN_POINT('Ctrl Pts',(1.50202424560496,-2.02042499510938,107.741491039627));
#34843=CARTESIAN_POINT('Ctrl Pts',(1.5177818467596,-2.00861452172274,107.742747102242));
#34844=CARTESIAN_POINT('Ctrl Pts',(1.54335440051805,-1.9889748594715,107.744792071503));
#34845=CARTESIAN_POINT('Ctrl Pts',(1.55325199953916,-1.98125516589704,107.74558519594));
#34846=CARTESIAN_POINT('Ctrl Pts',(1.57232955797509,-1.9661446765782,107.74711731818));
#34847=CARTESIAN_POINT('Ctrl Pts',(1.58151615113009,-1.95876282367395,107.747856641001));
#34848=CARTESIAN_POINT('Ctrl Pts',(1.60291250815966,-1.94132120007636,107.749582441287));
#34849=CARTESIAN_POINT('Ctrl Pts',(1.61508004419543,-1.93121023699515,107.750566838334));
#34850=CARTESIAN_POINT('Ctrl Pts',(1.65464479149441,-1.89769730325464,107.753778452495));
#34851=CARTESIAN_POINT('Ctrl Pts',(1.68163577053573,-1.87382116955119,107.755986379395));
#34852=CARTESIAN_POINT('Ctrl Pts',(1.74462897033323,-1.8156397926821,107.761189604843));
#34853=CARTESIAN_POINT('Ctrl Pts',(1.78014612075191,-1.78083079818497,107.764164142176));
#34854=CARTESIAN_POINT('Ctrl Pts',(1.91777692789404,-1.63770895711041,107.775911732827));
#34855=CARTESIAN_POINT('Ctrl Pts',(2.01122624469881,-1.52148947275829,107.784380158775));
#34856=CARTESIAN_POINT('Ctrl Pts',(2.12439767532785,-1.35194876269409,107.796125722356));
#34857=CARTESIAN_POINT('Ctrl Pts',(2.153423502941,-1.30521943538464,107.799308739364));
#34858=CARTESIAN_POINT('Ctrl Pts',(2.19219183319685,-1.23798734341174,107.80386313478));
#34859=CARTESIAN_POINT('Ctrl Pts',(2.20322414981745,-1.21824504784661,107.805197583276));
#34860=CARTESIAN_POINT('Ctrl Pts',(2.24106598413371,-1.14833150984222,107.80992221766));
#34861=CARTESIAN_POINT('Ctrl Pts',(2.2664377331786,-1.09740645814627,107.813361653027));
#34862=CARTESIAN_POINT('Ctrl Pts',(2.29555642396273,-1.03363533027569,107.817719004292));
#34863=CARTESIAN_POINT('Ctrl Pts',(2.30095668485284,-1.021557442505,107.818546441299));
#34864=CARTESIAN_POINT('Ctrl Pts',(2.30929185406096,-1.00251409226718,107.819855341307));
#34865=CARTESIAN_POINT('Ctrl Pts',(2.31229110630431,-0.99557682204169,107.820333042218));
#34866=CARTESIAN_POINT('Ctrl Pts',(2.31756825163488,-0.983218301060807,
107.821185800388));
#34867=CARTESIAN_POINT('Ctrl Pts',(2.31985844539506,-0.977802443984049,
107.821560110185));
#34868=CARTESIAN_POINT('Ctrl Pts',(2.32529465394902,-0.964820277694676,
107.822458784537));
#34869=CARTESIAN_POINT('Ctrl Pts',(2.32842269464495,-0.957246648724728,
107.822984202635));
#34870=CARTESIAN_POINT('Ctrl Pts',(2.3377979674255,-0.934229334897529,107.824584186073));
#34871=CARTESIAN_POINT('Ctrl Pts',(2.34392878405485,-0.918739139793101,
107.825665246166));
#34872=CARTESIAN_POINT('Ctrl Pts',(2.39868530283107,-0.776274468189472,
107.835639745301));
#34873=CARTESIAN_POINT('Ctrl Pts',(2.43709837862244,-0.64562907928827,107.845005744956));
#34874=CARTESIAN_POINT('Ctrl Pts',(2.50516842552434,-0.318283069590887,
107.86810138086));
#34875=CARTESIAN_POINT('Ctrl Pts',(2.52246433399614,-0.119895850838917,
107.881728559255));
#34876=CARTESIAN_POINT('Ctrl Pts',(2.51529125392845,0.110063913837987,107.896660858092));
#34877=CARTESIAN_POINT('Ctrl Pts',(2.51371212515731,0.141617997356326,107.89869301647));
#34878=CARTESIAN_POINT('Ctrl Pts',(2.51050664270669,0.188117467548634,107.901664158685));
#34879=CARTESIAN_POINT('Ctrl Pts',(2.50933976865435,0.203090438096633,107.902617276328));
#34880=CARTESIAN_POINT('Ctrl Pts',(2.50702813035546,0.229678911893988,107.904303644521));
#34881=CARTESIAN_POINT('Ctrl Pts',(2.50593645270978,0.241298469426901,107.90503852366));
#34882=CARTESIAN_POINT('Ctrl Pts',(2.50346696871456,0.265755668878032,107.906581089356));
#34883=CARTESIAN_POINT('Ctrl Pts',(2.50207112271808,0.278591180274351,107.907388191469));
#34884=CARTESIAN_POINT('Ctrl Pts',(2.49810622332229,0.312613158775157,107.90952131565));
#34885=CARTESIAN_POINT('Ctrl Pts',(2.49536637464797,0.333778953187105,107.910841988435));
#34886=CARTESIAN_POINT('Ctrl Pts',(2.48057161178308,0.43767589124299,107.917296716172));
#34887=CARTESIAN_POINT('Ctrl Pts',(2.46466929813009,0.519810615605896,107.922309250048));
#34888=CARTESIAN_POINT('Ctrl Pts',(2.42145986710482,0.695572546135234,107.932970764743));
#34889=CARTESIAN_POINT('Ctrl Pts',(2.39274418269861,0.7887114204011,107.938578592326));
#34890=CARTESIAN_POINT('Ctrl Pts',(2.3012189893111,1.03404301987399,107.953626784182));
#34891=CARTESIAN_POINT('Ctrl Pts',(2.22878086077839,1.18210609476309,107.962998935097));
#34892=CARTESIAN_POINT('Ctrl Pts',(2.13178222107162,1.33929934022117,107.974358420027));
#34893=CARTESIAN_POINT('Ctrl Pts',(2.12091621140433,1.35644112473726,107.975617653109));
#34894=CARTESIAN_POINT('Ctrl Pts',(2.1053526965474,1.38034925396387,107.977405725032));
#34895=CARTESIAN_POINT('Ctrl Pts',(2.10082709740946,1.38722728567323,107.977923879195));
#34896=CARTESIAN_POINT('Ctrl Pts',(2.09257601745881,1.39963434870028,107.978865609198));
#34897=CARTESIAN_POINT('Ctrl Pts',(2.0888621151652,1.40517107902617,107.979288425012));
#34898=CARTESIAN_POINT('Ctrl Pts',(2.0812070926189,1.41648586492994,107.98015788932));
#34899=CARTESIAN_POINT('Ctrl Pts',(2.07726382989551,1.4222623337698,107.980604672529));
#34900=CARTESIAN_POINT('Ctrl Pts',(2.06704224577365,1.43710270214981,107.981759844823));
#34901=CARTESIAN_POINT('Ctrl Pts',(2.06072843375132,1.44614180979949,107.982470546693));
#34902=CARTESIAN_POINT('Ctrl Pts',(2.03368248268498,1.48432510538756,107.98550197938));
#34903=CARTESIAN_POINT('Ctrl Pts',(2.01239096355288,1.5130656831663,107.987856599212));
#34904=CARTESIAN_POINT('Ctrl Pts',(1.95223488177878,1.59075155172447,107.994403082894));
#34905=CARTESIAN_POINT('Ctrl Pts',(1.91214975774352,1.63871713307986,107.99865021433));
#34906=CARTESIAN_POINT('Ctrl Pts',(1.73528554908213,1.83501760207041,108.016769321747));
#34907=CARTESIAN_POINT('Ctrl Pts',(1.58269507948169,1.96814698947047,108.030859084748));
#34908=CARTESIAN_POINT('Ctrl Pts',(1.36313489513516,2.11748256622686,108.048494486417));
#34909=CARTESIAN_POINT('Ctrl Pts',(1.30908380261991,2.15131818668927,108.052660770032));
#34910=CARTESIAN_POINT('Ctrl Pts',(1.23625364841554,2.19314675845504,108.058052147831));
#34911=CARTESIAN_POINT('Ctrl Pts',(1.21858367241051,2.20301376748668,108.059343649117));
#34912=CARTESIAN_POINT('Ctrl Pts',(1.18966024886055,2.21871027277269,108.061431425591));
#34913=CARTESIAN_POINT('Ctrl Pts',(1.17847866304134,2.22466960075153,108.06223226367));
#34914=CARTESIAN_POINT('Ctrl Pts',(1.15685145289476,2.23598720260113,108.063769362043));
#34915=CARTESIAN_POINT('Ctrl Pts',(1.14641242940057,2.24135731276086,108.064506022363));
#34916=CARTESIAN_POINT('Ctrl Pts',(1.12208247172748,2.25365883907981,108.066210957893));
#34917=CARTESIAN_POINT('Ctrl Pts',(1.10816413229903,2.26053522626595,108.067177304173));
#34918=CARTESIAN_POINT('Ctrl Pts',(1.06324954787257,2.28221085152783,108.070267736891));
#34919=CARTESIAN_POINT('Ctrl Pts',(1.0320129367722,2.29650504981211,108.072374537644));
#34920=CARTESIAN_POINT('Ctrl Pts',(0.957645544975907,2.32871240160955,108.077298755507));
#34921=CARTESIAN_POINT('Ctrl Pts',(0.914289070389287,2.34607380723462,108.080098387069));
#34922=CARTESIAN_POINT('Ctrl Pts',(0.659359741120222,2.44001469863309,108.096213240708));
#34923=CARTESIAN_POINT('Ctrl Pts',(0.438793948486696,2.48915137675487,108.10868681219));
#34924=CARTESIAN_POINT('Ctrl Pts',(0.151521070688895,2.51373468206869,108.125747685716));
#34925=CARTESIAN_POINT('Ctrl Pts',(0.0882162564628579,2.51675130863097,
108.129564269507));
#34926=CARTESIAN_POINT('Ctrl Pts',(0.0112339803149129,2.51751187393382,
108.134346057575));
#34927=CARTESIAN_POINT('Ctrl Pts',(-0.00240360133929631,2.51753578745429,
108.135198528975));
#34928=CARTESIAN_POINT('Ctrl Pts',(-0.0236905794401699,2.51740015390106,
108.136538466333));
#34929=CARTESIAN_POINT('Ctrl Pts',(-0.0313404288354343,2.51731653795564,
108.137021873519));
#34930=CARTESIAN_POINT('Ctrl Pts',(-0.0455117849561255,2.51709703344466,
108.137921059261));
#34931=CARTESIAN_POINT('Ctrl Pts',(-0.0520332607158115,2.51697066626515,
108.138336311306));
#34932=CARTESIAN_POINT('Ctrl Pts',(-0.0669700053182231,2.51662316076199,
108.139290713749));
#34933=CARTESIAN_POINT('Ctrl Pts',(-0.0753846782449455,2.51638515738663,
108.139830771532));
#34934=CARTESIAN_POINT('Ctrl Pts',(-0.101599905143106,2.51551206990412,
108.141520401152));
#34935=CARTESIAN_POINT('Ctrl Pts',(-0.119394575348378,2.51473028524736,
108.142677543281));
#34936=CARTESIAN_POINT('Ctrl Pts',(-0.161199968462996,2.5124489154723,108.145417803337));
#34937=CARTESIAN_POINT('Ctrl Pts',(-0.185200156337948,2.51079385758992,
108.1470078621));
#34938=CARTESIAN_POINT('Ctrl Pts',(-0.271473199747342,2.50360080182631,
108.152776066349));
#34939=CARTESIAN_POINT('Ctrl Pts',(-0.333555510673574,2.49608781873919,
108.1570249602));
#34940=CARTESIAN_POINT('Ctrl Pts',(-0.594944163996494,2.45452994704682,
108.175174886114));
#34941=CARTESIAN_POINT('Ctrl Pts',(-0.790083902045263,2.3988464338153,108.18929401947));
#34942=CARTESIAN_POINT('Ctrl Pts',(-1.03487448804734,2.29583460928733,108.206928798769));
#34943=CARTESIAN_POINT('Ctrl Pts',(-1.09233663048296,2.26905786766917,108.211070080065));
#34944=CARTESIAN_POINT('Ctrl Pts',(-1.16670129227178,2.23092406339511,108.216434544981));
#34945=CARTESIAN_POINT('Ctrl Pts',(-1.18456009379324,2.22149308012234,108.217723307061));
#34946=CARTESIAN_POINT('Ctrl Pts',(-1.21342769651984,2.20580139071252,108.219807774026));
#34947=CARTESIAN_POINT('Ctrl Pts',(-1.22450586771664,2.19967087069475,108.220608014776));
#34948=CARTESIAN_POINT('Ctrl Pts',(-1.24556470046214,2.18780878363184,108.222129994019));
#34949=CARTESIAN_POINT('Ctrl Pts',(-1.25555319814988,2.18209185655596,108.222852227994));
#34950=CARTESIAN_POINT('Ctrl Pts',(-1.27838095320674,2.16881772664195,108.224503796395));
#34951=CARTESIAN_POINT('Ctrl Pts',(-1.29119311329453,2.16121460112651,108.225431456564));
#34952=CARTESIAN_POINT('Ctrl Pts',(-1.31813272050178,2.14490274187768,108.227383968589));
#34953=CARTESIAN_POINT('Ctrl Pts',(-1.33224310921159,2.13616711870962,108.228407807582));
#34954=CARTESIAN_POINT('Ctrl Pts',(-1.36974994519367,2.11243075313723,108.231133290806));
#34955=CARTESIAN_POINT('Ctrl Pts',(-1.39298647640837,2.09718081348469,108.232826020154));
#34956=CARTESIAN_POINT('Ctrl Pts',(-1.46447572565446,2.0485504970995,108.238053027727));
#34957=CARTESIAN_POINT('Ctrl Pts',(-1.51181881173821,2.01386515197023,108.241541868679));
#34958=CARTESIAN_POINT('Ctrl Pts',(-1.73135137361525,1.84091839519729,108.25796442526));
#34959=CARTESIAN_POINT('Ctrl Pts',(-1.88604367990163,1.68207600870287,108.270198713614));
#34960=CARTESIAN_POINT('Ctrl Pts',(-2.04690585806332,1.46639557031896,108.28629234842));
#34961=CARTESIAN_POINT('Ctrl Pts',(-2.07466267311769,1.42685446636724,108.289228390637));
#34962=CARTESIAN_POINT('Ctrl Pts',(-2.1082589665769,1.37594030815489,108.29302426831));
#34963=CARTESIAN_POINT('Ctrl Pts',(-2.11517446530262,1.36528552593771,108.293819457996));
#34964=CARTESIAN_POINT('Ctrl Pts',(-2.12597137066416,1.34837169016418,108.295083839822));
#34965=CARTESIAN_POINT('Ctrl Pts',(-2.12990655673148,1.34214698897622,108.295549600311));
#34966=CARTESIAN_POINT('Ctrl Pts',(-2.13730464089937,1.33033017905094,108.296434791846));
#34967=CARTESIAN_POINT('Ctrl Pts',(-2.14077299234516,1.32474167466878,108.296853862742));
#34968=CARTESIAN_POINT('Ctrl Pts',(-2.14887966770191,1.31156453353929,108.297842948205));
#34969=CARTESIAN_POINT('Ctrl Pts',(-2.15349971822447,1.30396484224259,108.298414118023));
#34970=CARTESIAN_POINT('Ctrl Pts',(-2.16859273918081,1.27883878576177,108.300304510656));
#34971=CARTESIAN_POINT('Ctrl Pts',(-2.17889246462463,1.26121000363504,108.301634011481));
#34972=CARTESIAN_POINT('Ctrl Pts',(-2.23561321498277,1.16135917054091,108.309173865764));
#34973=CARTESIAN_POINT('Ctrl Pts',(-2.27759005986772,1.07670868388783,108.31559905276));
#34974=CARTESIAN_POINT('Ctrl Pts',(-2.33127140486613,0.951185466908145,
108.324987841862));
#34975=CARTESIAN_POINT('Ctrl Pts',(-2.34684876526915,0.912072925269062,
108.327895159897));
#34976=CARTESIAN_POINT('Ctrl Pts',(-2.36143103931297,0.872610850591077,
108.330801621721));
#34977=CARTESIAN_POINT('Origin',(0.,0.,104.));
#34978=CARTESIAN_POINT('',(-2.36143112100138,0.872610629528524,109.333394523839));
#34979=CARTESIAN_POINT('',(-2.36143112101026,0.8726106295045,109.056156733688));
#34980=CARTESIAN_POINT('',(-2.36143112101026,0.872610629504505,104.));
#34981=CARTESIAN_POINT('',(-2.5174990352485,-0.00220397887332777,108.112583302432));
#34982=CARTESIAN_POINT('Ctrl Pts',(-2.36143112101026,0.8726106295045,109.056156733688));
#34983=CARTESIAN_POINT('Ctrl Pts',(-2.33268216378951,0.950410142806583,
109.050916676707));
#34984=CARTESIAN_POINT('Ctrl Pts',(-2.30005751129571,1.02686009642425,109.045676619726));
#34985=CARTESIAN_POINT('Ctrl Pts',(-2.26371131250978,1.10155224279888,109.040436562745));
#34986=CARTESIAN_POINT('Ctrl Pts',(-2.22738312760807,1.17620737029062,109.035199102838));
#34987=CARTESIAN_POINT('Ctrl Pts',(-2.18733726025505,1.24910600616275,109.029961642932));
#34988=CARTESIAN_POINT('Ctrl Pts',(-2.14377559608639,1.31986076675703,109.024724183025));
#34989=CARTESIAN_POINT('Ctrl Pts',(-2.10022238166327,1.39060180290497,109.01948773904));
#34990=CARTESIAN_POINT('Ctrl Pts',(-2.05315496725343,1.45919939721905,109.014251295054));
#34991=CARTESIAN_POINT('Ctrl Pts',(-2.00282001409352,1.52529283783359,109.009014851069));
#34992=CARTESIAN_POINT('Ctrl Pts',(-1.95247964142512,1.59139339465545,109.003777843281));
#34993=CARTESIAN_POINT('Ctrl Pts',(-1.89887131212628,1.65498889619735,108.998540835493));
#34994=CARTESIAN_POINT('Ctrl Pts',(-1.84228278095399,1.71575068264606,108.993303827705));
#34995=CARTESIAN_POINT('Ctrl Pts',(-1.78563437319289,1.77657676142447,108.988061278615));
#34996=CARTESIAN_POINT('Ctrl Pts',(-1.72599978335873,1.83456280099905,108.982818729525));
#34997=CARTESIAN_POINT('Ctrl Pts',(-1.66370416107772,1.88941650104276,108.977576180435));
#34998=CARTESIAN_POINT('Ctrl Pts',(-1.6013728793718,1.94430160058657,108.972330630391));
#34999=CARTESIAN_POINT('Ctrl Pts',(-1.53637789353067,1.99605050335782,108.967085080347));
#35000=CARTESIAN_POINT('Ctrl Pts',(-1.4690761065609,2.04441229773543,108.961839530303));
#35001=CARTESIAN_POINT('Ctrl Pts',(-1.4016609880652,2.09285553000942,108.956585147118));
#35002=CARTESIAN_POINT('Ctrl Pts',(-1.33193169961201,2.13790001469722,108.951330763933));
#35003=CARTESIAN_POINT('Ctrl Pts',(-1.26027236462642,2.17933930744135,108.946076380748));
#35004=CARTESIAN_POINT('Ctrl Pts',(-1.21657392417061,2.20460932239298,108.942872215501));
#35005=CARTESIAN_POINT('Ctrl Pts',(-1.17215823529164,2.22853959777458,108.939668050255));
#35006=CARTESIAN_POINT('Ctrl Pts',(-1.12711601958332,2.25109211903881,108.936463885008));
#35007=CARTESIAN_POINT('Ctrl Pts',(-1.05324090416649,2.28808119884174,108.931208635601));
#35008=CARTESIAN_POINT('Ctrl Pts',(-0.977406600329775,2.32149814501377,
108.925953386194));
#35009=CARTESIAN_POINT('Ctrl Pts',(-0.899992693089532,2.3511315153316,108.920698136786));
#35010=CARTESIAN_POINT('Ctrl Pts',(-0.822688541183468,2.38072287226219,
108.915450338129));
#35011=CARTESIAN_POINT('Ctrl Pts',(-0.743809661544561,2.40654114472751,
108.910202539471));
#35012=CARTESIAN_POINT('Ctrl Pts',(-0.663759045355638,2.42842133488169,
108.904954740814));
#35013=CARTESIAN_POINT('Ctrl Pts',(-0.583128393440582,2.45046006587651,
108.899668917331));
#35014=CARTESIAN_POINT('Ctrl Pts',(-0.501309376583863,2.46850319198874,
108.894383093848));
#35015=CARTESIAN_POINT('Ctrl Pts',(-0.418733125877407,2.48243203719516,
108.889097270365));
#35016=CARTESIAN_POINT('Ctrl Pts',(-0.336897330711175,2.49623598340806,
108.883858844496));
#35017=CARTESIAN_POINT('Ctrl Pts',(-0.254318290808967,2.505999059978,108.878620418628));
#35018=CARTESIAN_POINT('Ctrl Pts',(-0.171427855907963,2.51165657290538,
108.873381992759));
#35019=CARTESIAN_POINT('Ctrl Pts',(-0.0885646822915049,2.51731222517092,
108.868145289722));
#35020=CARTESIAN_POINT('Ctrl Pts',(-0.00539077705992319,2.51886496407218,
108.862908586684));
#35021=CARTESIAN_POINT('Ctrl Pts',(0.0776570934187217,2.51630197429517,
108.857671883646));
#35022=CARTESIAN_POINT('Ctrl Pts',(0.160702701714922,2.51373905433272,108.852435323254));
#35023=CARTESIAN_POINT('Ctrl Pts',(0.243621820914811,2.50706064386026,108.847198762862));
#35024=CARTESIAN_POINT('Ctrl Pts',(0.325979284034066,2.4963060221817,108.841962202469));
#35025=CARTESIAN_POINT('Ctrl Pts',(0.40968471682491,2.48537537633602,108.836639933699));
#35026=CARTESIAN_POINT('Ctrl Pts',(0.492809452780374,2.47023393290518,108.831317664928));
#35027=CARTESIAN_POINT('Ctrl Pts',(0.574905573004285,2.45097732183075,108.825995396157));
#35028=CARTESIAN_POINT('Ctrl Pts',(0.655795641189291,2.4320036044544,108.820751315407));
#35029=CARTESIAN_POINT('Ctrl Pts',(0.735686682421675,2.40903501479311,108.815507234657));
#35030=CARTESIAN_POINT('Ctrl Pts',(0.814165640056965,2.38221337426995,108.810263153906));
#35031=CARTESIAN_POINT('Ctrl Pts',(0.894399752107213,2.35479187714574,108.804901791126));
#35032=CARTESIAN_POINT('Ctrl Pts',(0.973157381352583,2.32334309510195,108.799540428345));
#35033=CARTESIAN_POINT('Ctrl Pts',(1.05002065499409,2.28806968296112,108.794179065564));
#35034=CARTESIAN_POINT('Ctrl Pts',(1.12688392863559,2.25279627082028,108.788817702784));
#35035=CARTESIAN_POINT('Ctrl Pts',(1.2018524270417,2.2136985227658,108.783456340003));
#35036=CARTESIAN_POINT('Ctrl Pts',(1.27453862635215,2.17102683998526,108.778094977223));
#35037=CARTESIAN_POINT('Ctrl Pts',(1.34578620303758,2.12919972534665,108.772839727815));
#35038=CARTESIAN_POINT('Ctrl Pts',(1.41510418478533,2.08378440484462,108.767584478408));
#35039=CARTESIAN_POINT('Ctrl Pts',(1.48210854983503,2.03498415141394,108.762329229001));
#35040=CARTESIAN_POINT('Ctrl Pts',(1.54901791791665,1.98625308565653,108.757081430343));
#35041=CARTESIAN_POINT('Ctrl Pts',(1.6136198148298,1.9341468886985,108.751833631686));
#35042=CARTESIAN_POINT('Ctrl Pts',(1.67555643247572,1.87891375310024,108.746585833028));
#35043=CARTESIAN_POINT('Ctrl Pts',(1.73794183431208,1.82328040581805,108.741300009545));
#35044=CARTESIAN_POINT('Ctrl Pts',(1.79762276074586,1.76447485387521,108.736014186062));
#35045=CARTESIAN_POINT('Ctrl Pts',(1.85426493724833,1.70279411335941,108.730728362579));
#35046=CARTESIAN_POINT('Ctrl Pts',(1.91039920726393,1.64166645978618,108.725489936711));
#35047=CARTESIAN_POINT('Ctrl Pts',(1.96354868775432,1.57771532047734,108.720251510842));
#35048=CARTESIAN_POINT('Ctrl Pts',(2.01342399262818,1.51126770491174,108.715013084974));
#35049=CARTESIAN_POINT('Ctrl Pts',(2.06328289434433,1.44484194286104,108.709776381936));
#35050=CARTESIAN_POINT('Ctrl Pts',(2.10986948229665,1.37592170394282,108.704539678899));
#35051=CARTESIAN_POINT('Ctrl Pts',(2.15293520896774,1.30486636709934,108.699302975861));
#35052=CARTESIAN_POINT('Ctrl Pts',(2.19599976254997,1.2338129657677,108.694066415469));
#35053=CARTESIAN_POINT('Ctrl Pts',(2.23554340725672,1.1606249772816,108.688829855077));
#35054=CARTESIAN_POINT('Ctrl Pts',(2.27136216292113,1.08568880202857,108.683593294684));
#35055=CARTESIAN_POINT('Ctrl Pts',(2.307767175064,1.00952612358196,108.678271025914));
#35056=CARTESIAN_POINT('Ctrl Pts',(2.34032404137947,0.93155795384246,108.672948757144));
#35057=CARTESIAN_POINT('Ctrl Pts',(2.36886910538251,0.852212069595514,108.667626488373));
#35058=CARTESIAN_POINT('Ctrl Pts',(2.39699482152184,0.774031834409633,108.662382407623));
#35059=CARTESIAN_POINT('Ctrl Pts',(2.4212257478244,0.694514560872618,108.657138326873));
#35060=CARTESIAN_POINT('Ctrl Pts',(2.44145595367082,0.614083932606366,108.651894246122));
#35061=CARTESIAN_POINT('Ctrl Pts',(2.46213860098907,0.531854501495064,108.646532883342));
#35062=CARTESIAN_POINT('Ctrl Pts',(2.4786393194186,0.448670871208492,108.641171520561));
#35063=CARTESIAN_POINT('Ctrl Pts',(2.49090058276339,0.364993885961109,108.635810157781));
#35064=CARTESIAN_POINT('Ctrl Pts',(2.50316184610818,0.281316900713732,108.630448795));
#35065=CARTESIAN_POINT('Ctrl Pts',(2.51118367265796,0.197147072657835,108.62508743222));
#35066=CARTESIAN_POINT('Ctrl Pts',(2.5149651090264,0.112945785135207,108.619726069439));
#35067=CARTESIAN_POINT('Ctrl Pts',(2.51867170230268,0.0304110296148989,
108.614470820032));
#35068=CARTESIAN_POINT('Ctrl Pts',(2.5183179652071,-0.0524588008418233,
108.609215570625));
#35069=CARTESIAN_POINT('Ctrl Pts',(2.51386532026221,-0.135230919478382,
108.603960321217));
#35070=CARTESIAN_POINT('Ctrl Pts',(2.50941898815634,-0.217885686054263,
108.59871252256));
#35071=CARTESIAN_POINT('Ctrl Pts',(2.50088531575818,-0.300442559066649,
108.593464723902));
#35072=CARTESIAN_POINT('Ctrl Pts',(2.48827767589473,-0.382466283015776,
108.588216925245));
#35073=CARTESIAN_POINT('Ctrl Pts',(2.4755786828114,-0.465084339557793,108.582931101762));
#35074=CARTESIAN_POINT('Ctrl Pts',(2.45874641307694,-0.547161014776089,
108.577645278279));
#35075=CARTESIAN_POINT('Ctrl Pts',(2.43784800520533,-0.628254210902234,
108.572359454796));
#35076=CARTESIAN_POINT('Ctrl Pts',(2.4171369919146,-0.70862024993616,108.567121028928));
#35077=CARTESIAN_POINT('Ctrl Pts',(2.39243258725514,-0.788019921759766,
108.561882603059));
#35078=CARTESIAN_POINT('Ctrl Pts',(2.36385152754585,-0.866032450731004,
108.55664417719));
#35079=CARTESIAN_POINT('Ctrl Pts',(2.33527986767144,-0.944019322679784,
108.551407474153));
#35080=CARTESIAN_POINT('Ctrl Pts',(2.30283424350808,-1.02061952491328,108.546170771115));
#35081=CARTESIAN_POINT('Ctrl Pts',(2.26668077725614,-1.09542891326526,108.540934068078));
#35082=CARTESIAN_POINT('Ctrl Pts',(2.23052829580655,-1.1702362638469,108.535697507686));
#35083=CARTESIAN_POINT('Ctrl Pts',(2.19066837478622,-1.24325248253537,108.530460947293));
#35084=CARTESIAN_POINT('Ctrl Pts',(2.14731406653896,-1.31409609604623,108.525224386901));
#35085=CARTESIAN_POINT('Ctrl Pts',(2.10325016512985,-1.38609922854699,108.51990211813));
#35086=CARTESIAN_POINT('Ctrl Pts',(2.05557670255045,-1.45585756856834,108.51457984936));
#35087=CARTESIAN_POINT('Ctrl Pts',(2.00456339163943,-1.52300093857457,108.509257580589));
#35088=CARTESIAN_POINT('Ctrl Pts',(1.95429950356922,-1.58915792337676,108.504013499839));
#35089=CARTESIAN_POINT('Ctrl Pts',(1.90079359363855,-1.65277594112891,108.498769419089));
#35090=CARTESIAN_POINT('Ctrl Pts',(1.84434337030973,-1.7135354628354,108.493525338338));
#35091=CARTESIAN_POINT('Ctrl Pts',(1.78663065749725,-1.77565384997527,108.488163975558));
#35092=CARTESIAN_POINT('Ctrl Pts',(1.72584071206637,-1.8347839826566,108.482802612777));
#35093=CARTESIAN_POINT('Ctrl Pts',(1.66232876636165,-1.89062670099799,108.477441249997));
#35094=CARTESIAN_POINT('Ctrl Pts',(1.59881682065693,-1.94646941933939,108.472079887216));
#35095=CARTESIAN_POINT('Ctrl Pts',(1.53258331422562,-1.99902445984004,108.466718524435));
#35096=CARTESIAN_POINT('Ctrl Pts',(1.46401473278267,-2.04803982192615,108.461357161655));
#35097=CARTESIAN_POINT('Ctrl Pts',(1.39680327708815,-2.0960850602536,108.456101912248));
#35098=CARTESIAN_POINT('Ctrl Pts',(1.32710010991272,-2.14090695686203,108.45084666284));
#35099=CARTESIAN_POINT('Ctrl Pts',(1.2552472458811,-2.18223752183577,108.445591413433));
#35100=CARTESIAN_POINT('Ctrl Pts',(1.18349625288767,-2.22350948945755,108.440343614775));
#35101=CARTESIAN_POINT('Ctrl Pts',(1.10960201345743,-2.26129972927178,108.435095816118));
#35102=CARTESIAN_POINT('Ctrl Pts',(1.03393689740221,-2.29538248276628,108.42984801746));
#35103=CARTESIAN_POINT('Ctrl Pts',(0.957723522350116,-2.32971219519266,
108.424562193978));
#35104=CARTESIAN_POINT('Ctrl Pts',(0.879713884850795,-2.36028019114474,
108.419276370495));
#35105=CARTESIAN_POINT('Ctrl Pts',(0.800315366770437,-2.38690208506991,
108.413990547012));
#35106=CARTESIAN_POINT('Ctrl Pts',(0.721628809721186,-2.41328526230985,
108.408752121143));
#35107=CARTESIAN_POINT('Ctrl Pts',(0.641578625868065,-2.43579267354179,
108.403513695275));
#35108=CARTESIAN_POINT('Ctrl Pts',(0.560581315844466,-2.45429314433425,
108.398275269406));
#35109=CARTESIAN_POINT('Ctrl Pts',(0.47961064448814,-2.47278753062976,108.393038566369));
#35110=CARTESIAN_POINT('Ctrl Pts',(0.397693915086567,-2.48727749107548,
108.387801863331));
#35111=CARTESIAN_POINT('Ctrl Pts',(0.315260566139785,-2.49768233076931,
108.382565160294));
#35112=CARTESIAN_POINT('Ctrl Pts',(0.232829462636183,-2.50808688704051,
108.377328599901));
#35113=CARTESIAN_POINT('Ctrl Pts',(0.149882225484559,-2.51440648704673,
108.372092039509));
#35114=CARTESIAN_POINT('Ctrl Pts',(0.0668548282140929,-2.51661214372506,
108.366855479117));
#35115=CARTESIAN_POINT('Ctrl Pts',(-0.0175315037441317,-2.51885390105774,
108.361533210346));
#35116=CARTESIAN_POINT('Ctrl Pts',(-0.102000152302608,-2.51684580555824,
108.356210941576));
#35117=CARTESIAN_POINT('Ctrl Pts',(-0.186093769824212,-2.51061254653772,
108.350888672805));
#35118=CARTESIAN_POINT('Ctrl Pts',(-0.268951990610984,-2.50447085865027,
108.345644592055));
#35119=CARTESIAN_POINT('Ctrl Pts',(-0.351445669286695,-2.49422744326405,
108.340400511305));
#35120=CARTESIAN_POINT('Ctrl Pts',(-0.433144699557888,-2.47995804788003,
108.335156430554));
#35121=CARTESIAN_POINT('Ctrl Pts',(-0.516670900041242,-2.46536952246344,
108.329795067774));
#35122=CARTESIAN_POINT('Ctrl Pts',(-0.599365979841367,-2.44657287826211,
108.324433704993));
#35123=CARTESIAN_POINT('Ctrl Pts',(-0.680785599153208,-2.42370320336167,
108.319072342213));
#35124=CARTESIAN_POINT('Ctrl Pts',(-0.762205218465049,-2.40083352846123,
108.313710979432));
#35125=CARTESIAN_POINT('Ctrl Pts',(-0.842348916953951,-2.37389104808709,
108.308349616652));
#35126=CARTESIAN_POINT('Ctrl Pts',(-0.920794895731956,-2.3430627413695,
108.302988253871));
#35127=CARTESIAN_POINT('Ctrl Pts',(-0.997688252953404,-2.31284459586487,
108.297733004464));
#35128=CARTESIAN_POINT('Ctrl Pts',(-1.07323451221387,-2.27878146856245,
108.292477755056));
#35129=CARTESIAN_POINT('Ctrl Pts',(-1.14702267524325,-2.24101433116297,
108.287222505649));
#35130=CARTESIAN_POINT('Ctrl Pts',(-1.22070622342013,-2.20330073898465,
108.281974706992));
#35131=CARTESIAN_POINT('Ctrl Pts',(-1.29263621904113,-2.16189377608995,
108.276726908334));
#35132=CARTESIAN_POINT('Ctrl Pts',(-1.3624205602826,-2.1169828688299,108.271479109677));
#35133=CARTESIAN_POINT('Ctrl Pts',(-1.43271054923752,-2.07174654332899,
108.266193286194));
#35134=CARTESIAN_POINT('Ctrl Pts',(-1.50082321732818,-2.02295545433858,
108.260907462711));
#35135=CARTESIAN_POINT('Ctrl Pts',(-1.56638210368257,-1.97085092162319,
108.255621639228));
#35136=CARTESIAN_POINT('Ctrl Pts',(-1.63135312802827,-1.9192136066561,108.250383213359));
#35137=CARTESIAN_POINT('Ctrl Pts',(-1.69381561848933,-1.86432232519278,
108.245144787491));
#35138=CARTESIAN_POINT('Ctrl Pts',(-1.75343278254459,-1.8064550166273,108.239906361622));
#35139=CARTESIAN_POINT('Ctrl Pts',(-1.81303033950678,-1.74860673965654,
108.234669658585));
#35140=CARTESIAN_POINT('Ctrl Pts',(-1.86978409773914,-1.68778470059112,
108.229432955547));
#35141=CARTESIAN_POINT('Ctrl Pts',(-1.92339256251863,-1.6243051746664,108.22419625251));
#35142=CARTESIAN_POINT('Ctrl Pts',(-1.97699956703033,-1.56082737789222,
108.218959692117));
#35143=CARTESIAN_POINT('Ctrl Pts',(-2.02746115151203,-1.49469259138072,
108.213723131725));
#35144=CARTESIAN_POINT('Ctrl Pts',(-2.07451563537045,-1.42625072431307,
108.208486571333));
#35145=CARTESIAN_POINT('Ctrl Pts',(-2.1223402742913,-1.35668864837088,108.203164302562));
#35146=CARTESIAN_POINT('Ctrl Pts',(-2.16664498684489,-1.28474368689081,
108.197842033792));
#35147=CARTESIAN_POINT('Ctrl Pts',(-2.20720147859993,-1.2108129016765,108.192519765021));
#35148=CARTESIAN_POINT('Ctrl Pts',(-2.2471621658342,-1.13796821375881,108.187275684271));
#35149=CARTESIAN_POINT('Ctrl Pts',(-2.28348388016513,-1.06319610901183,
108.18203160352));
#35150=CARTESIAN_POINT('Ctrl Pts',(-2.31599598596929,-0.986898598121488,
108.17678752277));
#35151=CARTESIAN_POINT('Ctrl Pts',(-2.34923521363841,-0.908894720109143,
108.171426159989));
#35152=CARTESIAN_POINT('Ctrl Pts',(-2.37849219878238,-0.829296862872565,
108.166064797209));
#35153=CARTESIAN_POINT('Ctrl Pts',(-2.40363833074474,-0.748551284131325,
108.160703434428));
#35154=CARTESIAN_POINT('Ctrl Pts',(-2.42878446270709,-0.667805705390085,
108.155342071648));
#35155=CARTESIAN_POINT('Ctrl Pts',(-2.44981967977525,-0.585912913893669,
108.149980708867));
#35156=CARTESIAN_POINT('Ctrl Pts',(-2.46667116953818,-0.503328512374544,
108.144619346087));
#35157=CARTESIAN_POINT('Ctrl Pts',(-2.4901232042434,-0.388396700541625,
108.137157995917));
#35158=CARTESIAN_POINT('Ctrl Pts',(-2.50554871649174,-0.271776010995007,
108.129696645748));
#35159=CARTESIAN_POINT('Ctrl Pts',(-2.51276111767346,-0.154394998327111,
108.122235295578));
#35160=CARTESIAN_POINT('Ctrl Pts',(-2.51587110200439,-0.103780355443597,
108.11901796455));
#35161=CARTESIAN_POINT('Ctrl Pts',(-2.5174545435931,-0.0530246346749353,
108.115800633521));
#35162=CARTESIAN_POINT('Ctrl Pts',(-2.51749903524768,-0.00220397981460282,
108.112583302492));
#35163=CARTESIAN_POINT('Ctrl Pts',(-2.5174990352485,-0.00220397887333112,
108.112583302432));
#35164=CARTESIAN_POINT('Ctrl Pts',(-2.51757053067579,0.0794618081286696,
108.107413241731));
#35165=CARTESIAN_POINT('Ctrl Pts',(-2.51366404211222,0.161254080773151,
108.10224318103));
#35166=CARTESIAN_POINT('Ctrl Pts',(-2.50576929896393,0.242747750493866,
108.097073120328));
#35167=CARTESIAN_POINT('Ctrl Pts',(-2.49788117529288,0.3241730905068,108.091907394549));
#35168=CARTESIAN_POINT('Ctrl Pts',(-2.48601147691956,0.405299852895239,
108.08674166877));
#35169=CARTESIAN_POINT('Ctrl Pts',(-2.47020197011635,0.48570410419649,108.081575942991));
#35170=CARTESIAN_POINT('Ctrl Pts',(-2.45439918980559,0.56607414579113,108.076412415081));
#35171=CARTESIAN_POINT('Ctrl Pts',(-2.43466001448788,0.645721819316943,
108.07124888717));
#35172=CARTESIAN_POINT('Ctrl Pts',(-2.41107772898596,0.724230926423269,
108.06608535926));
#35173=CARTESIAN_POINT('Ctrl Pts',(-2.39607226998297,0.77418644019011,108.062799795341));
#35174=CARTESIAN_POINT('Ctrl Pts',(-2.3795118491617,0.823681138270154,108.059514231422));
#35175=CARTESIAN_POINT('Ctrl Pts',(-2.36143112101026,0.8726106295045,108.056228667503));
#35176=CARTESIAN_POINT('',(-2.51749991139346,-0.000667932580992832,108.389610494019));
#35177=CARTESIAN_POINT('Ctrl Pts',(-2.36143103931297,0.872610850591077,
108.330801621721));
#35178=CARTESIAN_POINT('Ctrl Pts',(-2.41699789040957,0.722237649469957,
108.341876912921));
#35179=CARTESIAN_POINT('Ctrl Pts',(-2.45811556380063,0.566786644106253,
108.35290722707));
#35180=CARTESIAN_POINT('Ctrl Pts',(-2.49286589157802,0.355398459208296,
108.367046773783));
#35181=CARTESIAN_POINT('Ctrl Pts',(-2.49987821345447,0.302155671775727,
108.370540950515));
#35182=CARTESIAN_POINT('Ctrl Pts',(-2.50705947385862,0.229825560448704,
108.375200002371));
#35183=CARTESIAN_POINT('Ctrl Pts',(-2.50872207453657,0.210904193218192,
108.376410764129));
#35184=CARTESIAN_POINT('Ctrl Pts',(-2.51111609185144,0.179599636397731,
108.378401073442));
#35185=CARTESIAN_POINT('Ctrl Pts',(-2.5119703885151,0.167226888682806,108.379184411809));
#35186=CARTESIAN_POINT('Ctrl Pts',(-2.51341356707306,0.143808315729925,
108.380660998116));
#35187=CARTESIAN_POINT('Ctrl Pts',(-2.51402114612365,0.132763978260241,
108.381354809862));
#35188=CARTESIAN_POINT('Ctrl Pts',(-2.51511445898997,0.110176975016777,
108.382768670918));
#35189=CARTESIAN_POINT('Ctrl Pts',(-2.51559356833387,0.0986342416272372,
108.383488499357));
#35190=CARTESIAN_POINT('Ctrl Pts',(-2.5164777214697,0.0730909819278779,
108.385075666263));
#35191=CARTESIAN_POINT('Ctrl Pts',(-2.51684541818914,0.0590894867524746,
108.385941840848));
#35192=CARTESIAN_POINT('Ctrl Pts',(-2.5173693966288,0.0298360417485043,
108.387743962294));
#35193=CARTESIAN_POINT('Ctrl Pts',(-2.5175039580511,0.0145842957774581,
108.388679221811));
#35194=CARTESIAN_POINT('Ctrl Pts',(-2.51749991139346,-0.000667932580992832,
108.389610494019));
#35195=CARTESIAN_POINT('Ctrl Pts',(-2.51749991190576,-0.000665998854557162,
108.389610375949));
#35196=CARTESIAN_POINT('Ctrl Pts',(-2.51746333858691,-0.138914475365931,
108.398051569454));
#35197=CARTESIAN_POINT('Ctrl Pts',(-2.50603947464677,-0.276938265112995,
108.406130853442));
#35198=CARTESIAN_POINT('Ctrl Pts',(-2.46726158300713,-0.509911691712988,
108.419750920604));
#35199=CARTESIAN_POINT('Ctrl Pts',(-2.44556977785967,-0.605456467028899,
108.425337009676));
#35200=CARTESIAN_POINT('Ctrl Pts',(-2.39826491729595,-0.769004275891744,
108.435212037579));
#35201=CARTESIAN_POINT('Ctrl Pts',(-2.37517335532977,-0.837611053587795,
108.439455650568));
#35202=CARTESIAN_POINT('Ctrl Pts',(-2.33499235898631,-0.941897032090542,
108.446194928368));
#35203=CARTESIAN_POINT('Ctrl Pts',(-2.31996281270867,-0.978330971549724,
108.448605911819));
#35204=CARTESIAN_POINT('Ctrl Pts',(-2.29948862147339,-1.02483582835349,
108.451775331619));
#35205=CARTESIAN_POINT('Ctrl Pts',(-2.29482104528161,-1.03524526269562,
108.452490803074));
#35206=CARTESIAN_POINT('Ctrl Pts',(-2.28714303859006,-1.05206134544333,
108.453657011255));
#35207=CARTESIAN_POINT('Ctrl Pts',(-2.28417599065181,-1.05848778657624,
108.454105165809));
#35208=CARTESIAN_POINT('Ctrl Pts',(-2.27838309933927,-1.07089704557172,
108.454975499619));
#35209=CARTESIAN_POINT('Ctrl Pts',(-2.2755607178232,-1.07688135150353,108.455397470688));
#35210=CARTESIAN_POINT('Ctrl Pts',(-2.26925827442145,-1.09010903689316,
108.456335098059));
#35211=CARTESIAN_POINT('Ctrl Pts',(-2.26576705434302,-1.09734701877104,
108.456851423583));
#35212=CARTESIAN_POINT('Ctrl Pts',(-2.2532166134995,-1.12305129815746,108.458696394838));
#35213=CARTESIAN_POINT('Ctrl Pts',(-2.24396608378319,-1.14142256697539,
108.460035947309));
#35214=CARTESIAN_POINT('Ctrl Pts',(-2.15687780182908,-1.30922613306967,
108.472451063908));
#35215=CARTESIAN_POINT('Ctrl Pts',(-2.06445305756935,-1.45059306180974,
108.48419898562));
#35216=CARTESIAN_POINT('Ctrl Pts',(-1.86535522708747,-1.69714152118424,
108.506048822544));
#35217=CARTESIAN_POINT('Ctrl Pts',(-1.76205530324812,-1.80416536657462,
108.516140092782));
#35218=CARTESIAN_POINT('Ctrl Pts',(-1.62955327403261,-1.91913751840924,
108.527597786545));
#35219=CARTESIAN_POINT('Ctrl Pts',(-1.60891302327847,-1.93647402825981,
108.529345254292));
#35220=CARTESIAN_POINT('Ctrl Pts',(-1.57538320841784,-1.96373070313886,
108.532125507894));
#35221=CARTESIAN_POINT('Ctrl Pts',(-1.56266947363193,-1.97386287878403,
108.533166627106));
#35222=CARTESIAN_POINT('Ctrl Pts',(-1.53867115513765,-1.99261106568585,
108.535107762159));
#35223=CARTESIAN_POINT('Ctrl Pts',(-1.52741016601901,-2.00125610078862,
108.536008898644));
#35224=CARTESIAN_POINT('Ctrl Pts',(-1.51592641023422,-2.00991875559233,
108.536918196063));
#35225=CARTESIAN_POINT('Ctrl Pts',(-1.5157763459574,-2.01003192869255,108.536930076669));
#35226=CARTESIAN_POINT('Ctrl Pts',(-1.51546785880682,-2.01026452445519,
108.536954496221));
#35227=CARTESIAN_POINT('Ctrl Pts',(-1.51530943447976,-2.01038394520456,
108.536967035091));
#35228=CARTESIAN_POINT('Ctrl Pts',(-1.51498324303016,-2.01062976886877,
108.536992848482));
#35229=CARTESIAN_POINT('Ctrl Pts',(-1.51481547419925,-2.01075616951684,
108.537006122914));
#35230=CARTESIAN_POINT('Ctrl Pts',(-1.51446944965376,-2.01101680397236,
108.537033497261));
#35231=CARTESIAN_POINT('Ctrl Pts',(-1.5142911918994,-2.01115103508656,108.537047597072));
#35232=CARTESIAN_POINT('Ctrl Pts',(-1.51392285031801,-2.011428325813,108.537076727281));
#35233=CARTESIAN_POINT('Ctrl Pts',(-1.5137327640548,-2.01157138218482,108.537091757552));
#35234=CARTESIAN_POINT('Ctrl Pts',(-1.51333918605269,-2.01186749633094,
108.537122872578));
#35235=CARTESIAN_POINT('Ctrl Pts',(-1.51313569135498,-2.01202055018911,
108.53713895718));
#35236=CARTESIAN_POINT('Ctrl Pts',(-1.51271341830748,-2.01233805285787,
108.537172328122));
#35237=CARTESIAN_POINT('Ctrl Pts',(-1.5124946363424,-2.01250249687868,108.537189614276));
#35238=CARTESIAN_POINT('Ctrl Pts',(-1.51203953482206,-2.01284445064483,
108.537225564941));
#35239=CARTESIAN_POINT('Ctrl Pts',(-1.51180321080559,-2.01302195446414,
108.537244229221));
#35240=CARTESIAN_POINT('Ctrl Pts',(-1.51131029278324,-2.01339205120609,
108.537283150117));
#35241=CARTESIAN_POINT('Ctrl Pts',(-1.51105369319284,-2.01358463671654,
108.537303406445));
#35242=CARTESIAN_POINT('Ctrl Pts',(-1.51051687384625,-2.01398737496365,
108.537345773628));
#35243=CARTESIAN_POINT('Ctrl Pts',(-1.51023664701592,-2.01419751829296,
108.537367884117));
#35244=CARTESIAN_POINT('Ctrl Pts',(-1.50964841276359,-2.01463844596748,
108.537414284993));
#35245=CARTESIAN_POINT('Ctrl Pts',(-1.50934039623226,-2.01486921819546,
108.537438574908));
#35246=CARTESIAN_POINT('Ctrl Pts',(-1.50017571663267,-2.02173230108417,
108.538161087501));
#35247=CARTESIAN_POINT('Ctrl Pts',(-1.49127536609841,-2.02830630497187,
108.538857036846));
#35248=CARTESIAN_POINT('Ctrl Pts',(-1.47144444523328,-2.04275278370774,
108.540395212104));
#35249=CARTESIAN_POINT('Ctrl Pts',(-1.46049339993789,-2.05059667674585,
108.54123632755));
#35250=CARTESIAN_POINT('Ctrl Pts',(-1.43043967229383,-2.07176033625264,
108.543522555112));
#35251=CARTESIAN_POINT('Ctrl Pts',(-1.41121399978581,-2.0849037506754,108.544960994706));
#35252=CARTESIAN_POINT('Ctrl Pts',(-1.30596207449112,-2.15473498859743,
108.552711416484));
#35253=CARTESIAN_POINT('Ctrl Pts',(-1.21669521133149,-2.20637172091286,
108.558834577188));
#35254=CARTESIAN_POINT('Ctrl Pts',(-0.998250752172163,-2.3154298165149,
108.573084285152));
#35255=CARTESIAN_POINT('Ctrl Pts',(-0.866921960984713,-2.36773428392264,
108.581082679637));
#35256=CARTESIAN_POINT('Ctrl Pts',(-0.662212604872423,-2.42993537835929,
108.593489635586));
#35257=CARTESIAN_POINT('Ctrl Pts',(-0.591640190933045,-2.44807514075426,
108.597759977346));
#35258=CARTESIAN_POINT('Ctrl Pts',(-0.481663310697931,-2.47130999478101,
108.604537157694));
#35259=CARTESIAN_POINT('Ctrl Pts',(-0.442755389331779,-2.47857618449848,
108.606958169524));
#35260=CARTESIAN_POINT('Ctrl Pts',(-0.392417861308584,-2.48675390836866,
108.610139034492));
#35261=CARTESIAN_POINT('Ctrl Pts',(-0.381128703346094,-2.48850912767786,
108.61085554078));
#35262=CARTESIAN_POINT('Ctrl Pts',(-0.362822979665856,-2.49122778796279,
108.612023022286));
#35263=CARTESIAN_POINT('Ctrl Pts',(-0.355813461566265,-2.4922385888413,
108.612471404918));
#35264=CARTESIAN_POINT('Ctrl Pts',(-0.34224904229243,-2.49413624254058,
108.613341836605));
#35265=CARTESIAN_POINT('Ctrl Pts',(-0.335694785065585,-2.49502685571191,
108.61376367491));
#35266=CARTESIAN_POINT('Ctrl Pts',(-0.321178115962958,-2.49694119209988,
108.614700645817));
#35267=CARTESIAN_POINT('Ctrl Pts',(-0.313214164012915,-2.49795267814626,
108.615216444332));
#35268=CARTESIAN_POINT('Ctrl Pts',(-0.284879494293792,-2.50141377874519,
108.617057548712));
#35269=CARTESIAN_POINT('Ctrl Pts',(-0.264484455369829,-2.50365235765994,
108.618393703052));
#35270=CARTESIAN_POINT('Ctrl Pts',(-0.0755845507974478,-2.52205238877293,
108.630856500826));
#35271=CARTESIAN_POINT('Ctrl Pts',(0.0941080406935608,-2.5214275092692,
108.642661974447));
#35272=CARTESIAN_POINT('Ctrl Pts',(0.426934503078466,-2.48654159468299,
108.665733434406));
#35273=CARTESIAN_POINT('Ctrl Pts',(0.589355177573529,-2.45312868676567,
108.676944953262));
#35274=CARTESIAN_POINT('Ctrl Pts',(0.773808198014051,-2.39578692895605,
108.689438858101));
#35275=CARTESIAN_POINT('Ctrl Pts',(0.80013297455786,-2.38712409804105,108.691217200007));
#35276=CARTESIAN_POINT('Ctrl Pts',(0.839780322442438,-2.37334755370228,
108.693889238942));
#35277=CARTESIAN_POINT('Ctrl Pts',(0.853210612960806,-2.3685525673245,108.694793275094));
#35278=CARTESIAN_POINT('Ctrl Pts',(0.877490380605397,-2.35965070152689,
108.696425853453));
#35279=CARTESIAN_POINT('Ctrl Pts',(0.888353513293747,-2.35558248506623,
108.697155645875));
#35280=CARTESIAN_POINT('Ctrl Pts',(0.911701088606557,-2.3466543930261,108.698722928328));
#35281=CARTESIAN_POINT('Ctrl Pts',(0.924175683487847,-2.34176963690626,
108.699559566943));
#35282=CARTESIAN_POINT('Ctrl Pts',(0.957925098484118,-2.32824247746864,
108.701821380599));
#35283=CARTESIAN_POINT('Ctrl Pts',(0.979121947515239,-2.31940806967414,
108.70324012276));
#35284=CARTESIAN_POINT('Ctrl Pts',(1.09184924120375,-2.27060484844487,108.710780038984));
#35285=CARTESIAN_POINT('Ctrl Pts',(1.18106650315315,-2.22550362656058,108.716724356643));
#35286=CARTESIAN_POINT('Ctrl Pts',(1.41254605896588,-2.09063347878695,108.732381286424));
#35287=CARTESIAN_POINT('Ctrl Pts',(1.54887690997742,-1.99173584295994,108.741839705979));
#35288=CARTESIAN_POINT('Ctrl Pts',(1.73728240666024,-1.82394101861242,108.756602160552));
#35289=CARTESIAN_POINT('Ctrl Pts',(1.79736592419613,-1.76476164604931,108.761624645243));
#35290=CARTESIAN_POINT('Ctrl Pts',(1.86394491425296,-1.69225185866636,108.767735328594));
#35291=CARTESIAN_POINT('Ctrl Pts',(1.87343912186556,-1.68173506582467,108.76862064406));
#35292=CARTESIAN_POINT('Ctrl Pts',(1.88794318951693,-1.66539358008089,108.769995829921));
#35293=CARTESIAN_POINT('Ctrl Pts',(1.89301617777139,-1.65962496076666,108.77048119004));
#35294=CARTESIAN_POINT('Ctrl Pts',(1.90234542403943,-1.6489180210646,108.771382088526));
#35295=CARTESIAN_POINT('Ctrl Pts',(1.90660898007681,-1.6439862975236,108.771797082733));
#35296=CARTESIAN_POINT('Ctrl Pts',(1.91630551108093,-1.63268171053714,108.772748387447));
#35297=CARTESIAN_POINT('Ctrl Pts',(1.92172585364824,-1.62629828701506,108.773285582395));
#35298=CARTESIAN_POINT('Ctrl Pts',(1.93586748090133,-1.60947457499884,108.774701147161));
#35299=CARTESIAN_POINT('Ctrl Pts',(1.94453603364752,-1.598990589669,108.775583050609));
#35300=CARTESIAN_POINT('Ctrl Pts',(2.01516647525875,-1.51214443660754,108.782882983432));
#35301=CARTESIAN_POINT('Ctrl Pts',(2.07268396817956,-1.43228965011507,108.789557663786));
#35302=CARTESIAN_POINT('Ctrl Pts',(2.18935272312382,-1.24851455922901,108.804513568481));
#35303=CARTESIAN_POINT('Ctrl Pts',(2.24608159076478,-1.1433165920949,108.812810456099));
#35304=CARTESIAN_POINT('Ctrl Pts',(2.34450257311796,-0.924958688047079,
108.829185953278));
#35305=CARTESIAN_POINT('Ctrl Pts',(2.38597350632561,-0.812021187139037,
108.837241374193));
#35306=CARTESIAN_POINT('Ctrl Pts',(2.42776742182877,-0.666862274751989,
108.8470393948));
#35307=CARTESIAN_POINT('Ctrl Pts',(2.43576532750426,-0.637030105837842,
108.849025189864));
#35308=CARTESIAN_POINT('Ctrl Pts',(2.44680155591433,-0.592612789132666,
108.851942010241));
#35309=CARTESIAN_POINT('Ctrl Pts',(2.45026241064343,-0.578136581056765,
108.85288643593));
#35310=CARTESIAN_POINT('Ctrl Pts',(2.45620405288014,-0.552271430060218,
108.854563084024));
#35311=CARTESIAN_POINT('Ctrl Pts',(2.45873448767691,-0.54089445211354,108.855296867868));
#35312=CARTESIAN_POINT('Ctrl Pts',(2.46391683492136,-0.516806225463399,
108.856842850126));
#35313=CARTESIAN_POINT('Ctrl Pts',(2.46654960292947,-0.504091172727498,
108.857654422037));
#35314=CARTESIAN_POINT('Ctrl Pts',(2.47331500824227,-0.470094744218063,
108.85981274229));
#35315=CARTESIAN_POINT('Ctrl Pts',(2.47727139383357,-0.448779105049962,
108.861153909465));
#35316=CARTESIAN_POINT('Ctrl Pts',(2.49412221726988,-0.350967529750927,
108.867256245764));
#35317=CARTESIAN_POINT('Ctrl Pts',(2.50375278175546,-0.27394811607055,108.871914795089));
#35318=CARTESIAN_POINT('Ctrl Pts',(2.52442382519882,-0.0100610028700596,
108.887543249065));
#35319=CARTESIAN_POINT('Ctrl Pts',(2.51819422098116,0.177516684600116,108.898046085373));
#35320=CARTESIAN_POINT('Ctrl Pts',(2.48243448512861,0.423156610254938,108.912531765076));
#35321=CARTESIAN_POINT('Ctrl Pts',(2.47142941830604,0.483299230818696,108.916142924413));
#35322=CARTESIAN_POINT('Ctrl Pts',(2.45064801600347,0.577383837320642,108.921975621837));
#35323=CARTESIAN_POINT('Ctrl Pts',(2.44232730426858,0.611624758267027,108.924137432778));
#35324=CARTESIAN_POINT('Ctrl Pts',(2.4304784776155,0.656278064802941,108.927021548435));
#35325=CARTESIAN_POINT('Ctrl Pts',(2.42759649009636,0.666859654983338,108.927709828053));
#35326=CARTESIAN_POINT('Ctrl Pts',(2.42276697668829,0.684145572261141,108.928842608653));
#35327=CARTESIAN_POINT('Ctrl Pts',(2.42086050256178,0.690861354888463,108.929284795501));
#35328=CARTESIAN_POINT('Ctrl Pts',(2.41707635562121,0.703983457042877,108.930153039899));
#35329=CARTESIAN_POINT('Ctrl Pts',(2.41520109472548,0.710390375221268,108.930578958957));
#35330=CARTESIAN_POINT('Ctrl Pts',(2.41094676380002,0.724713934070805,108.931535517147));
#35331=CARTESIAN_POINT('Ctrl Pts',(2.40855414147304,0.73262645813286,108.932066919892));
#35332=CARTESIAN_POINT('Ctrl Pts',(2.40009642940454,0.760107285400779,108.933922583181));
#35333=CARTESIAN_POINT('Ctrl Pts',(2.39383166342938,0.779612634500628,108.935257483357));
#35334=CARTESIAN_POINT('Ctrl Pts',(2.3362658198685,0.951605141823017,108.947173152212));
#35335=CARTESIAN_POINT('Ctrl Pts',(2.27069886475129,1.09891258036199,108.958366828552));
#35336=CARTESIAN_POINT('Ctrl Pts',(2.13220371766402,1.34389279173709,108.97778587728));
#35337=CARTESIAN_POINT('Ctrl Pts',(2.06540573043216,1.44445325698215,108.986033146747));
#35338=CARTESIAN_POINT('Ctrl Pts',(1.9645685702433,1.57487685459164,108.996993444172));
#35339=CARTESIAN_POINT('Ctrl Pts',(1.936565054912,1.60918704634741,108.999905506404));
#35340=CARTESIAN_POINT('Ctrl Pts',(1.88615183195814,1.66773047365585,109.004925615677));
#35341=CARTESIAN_POINT('Ctrl Pts',(1.86414436128791,1.69229419268715,109.00704867235));
#35342=CARTESIAN_POINT('Ctrl Pts',(1.83124496865168,1.72759412376548,109.010125913908));
#35343=CARTESIAN_POINT('Ctrl Pts',(1.82072851487356,1.7386740015226,109.011095722724));
#35344=CARTESIAN_POINT('Ctrl Pts',(1.80197762972351,1.75807276537668,109.012800940214));
#35345=CARTESIAN_POINT('Ctrl Pts',(1.79378489550945,1.76643114286886,109.013538106927));
#35346=CARTESIAN_POINT('Ctrl Pts',(1.77652361843944,1.78379748022837,109.015075034738));
#35347=CARTESIAN_POINT('Ctrl Pts',(1.76744414296857,1.79279414000099,109.015874287265));
#35348=CARTESIAN_POINT('Ctrl Pts',(1.74344715693463,1.81621275203769,109.017963141571));
#35349=CARTESIAN_POINT('Ctrl Pts',(1.72841899227392,1.83052030217492,109.019247791894));
#35350=CARTESIAN_POINT('Ctrl Pts',(1.66307518755323,1.89120854487413,109.024736454857));
#35351=CARTESIAN_POINT('Ctrl Pts',(1.61105444541873,1.93571527797469,109.028862064715));
#35352=CARTESIAN_POINT('Ctrl Pts',(1.40282363979073,2.09965141435771,109.044587988333));
#35353=CARTESIAN_POINT('Ctrl Pts',(1.23466418538949,2.20273746325408,109.055607880864));
#35354=CARTESIAN_POINT('Ctrl Pts',(0.999823223430909,2.31128120473676,109.070695919608));
#35355=CARTESIAN_POINT('Ctrl Pts',(0.942477087573467,2.33525228024153,109.074364333308));
#35356=CARTESIAN_POINT('Ctrl Pts',(0.850948628480963,2.36959112447785,109.080279902329));
#35357=CARTESIAN_POINT('Ctrl Pts',(0.81733017887474,2.38139596608829,109.082465243418));
#35358=CARTESIAN_POINT('Ctrl Pts',(0.773010520174252,2.39590947755397,109.085376383704));
#35359=CARTESIAN_POINT('Ctrl Pts',(0.762524312630417,2.39926741968057,109.086067358711));
#35360=CARTESIAN_POINT('Ctrl Pts',(0.74534501647702,2.40464465729226,109.087203449577));
#35361=CARTESIAN_POINT('Ctrl Pts',(0.738664819041111,2.40670509279752,109.087646225212));
#35362=CARTESIAN_POINT('Ctrl Pts',(0.725595049539507,2.41067678333594,109.088514631593));
#35363=CARTESIAN_POINT('Ctrl Pts',(0.719206329340282,2.41259051268546,109.088940116727));
#35364=CARTESIAN_POINT('Ctrl Pts',(0.704905608604688,2.41681241749096,109.089894642457));
#35365=CARTESIAN_POINT('Ctrl Pts',(0.696989733440576,2.41910716698275,109.09042443662));
#35366=CARTESIAN_POINT('Ctrl Pts',(0.669495559641228,2.42693136122433,109.092269198296));
#35367=CARTESIAN_POINT('Ctrl Pts',(0.649862194865251,2.43226215740726,109.093594646919));
#35368=CARTESIAN_POINT('Ctrl Pts',(0.472145256735906,2.47821008405001,109.105652198853));
#35369=CARTESIAN_POINT('Ctrl Pts',(0.3105379007965,2.50359828578337,109.117015584906));
#35370=CARTESIAN_POINT('Ctrl Pts',(-0.0250773544836534,2.52331264180319,
109.140209223901));
#35371=CARTESIAN_POINT('Ctrl Pts',(-0.198394193695286,2.51563024589888,
109.151952980096));
#35372=CARTESIAN_POINT('Ctrl Pts',(-0.395812286315085,2.48633108232782,
109.164847881198));
#35373=CARTESIAN_POINT('Ctrl Pts',(-0.421983631928079,2.48202327127825,
109.166548530343));
#35374=CARTESIAN_POINT('Ctrl Pts',(-0.461876063855393,2.4748077154357,109.169128178034));
#35375=CARTESIAN_POINT('Ctrl Pts',(-0.475648411716759,2.47219767172996,
109.170016462));
#35376=CARTESIAN_POINT('Ctrl Pts',(-0.49965905895639,2.46743925746936,109.171561271319));
#35377=CARTESIAN_POINT('Ctrl Pts',(-0.509906994914169,2.46534186805006,
109.17221938842));
#35378=CARTESIAN_POINT('Ctrl Pts',(-0.533035750388499,2.46045784546207,
109.173702080205));
#35379=CARTESIAN_POINT('Ctrl Pts',(-0.545908425246748,2.45763380555895,
109.174525449243));
#35380=CARTESIAN_POINT('Ctrl Pts',(-0.580765552836482,2.44969937457842,
109.17675035579));
#35381=CARTESIAN_POINT('Ctrl Pts',(-0.602704743495286,2.44439413686139,
109.178145679838));
#35382=CARTESIAN_POINT('Ctrl Pts',(-0.711301645720829,2.41658269598789,
109.185031397582));
#35383=CARTESIAN_POINT('Ctrl Pts',(-0.796791996511805,2.38975877237735,
109.19038211359));
#35384=CARTESIAN_POINT('Ctrl Pts',(-1.0457741304706,2.29678467592964,109.205984010064));
#35385=CARTESIAN_POINT('Ctrl Pts',(-1.20393176061232,2.21797401137319,109.215891885325));
#35386=CARTESIAN_POINT('Ctrl Pts',(-1.40253973374737,2.09145886075199,109.229649947858));
#35387=CARTESIAN_POINT('Ctrl Pts',(-1.45137675709278,2.05786843024439,109.233155447749));
#35388=CARTESIAN_POINT('Ctrl Pts',(-1.51763988347758,2.00875953646937,109.238151730462));
#35389=CARTESIAN_POINT('Ctrl Pts',(-1.53610687086798,1.99467322974401,109.23957135806));
#35390=CARTESIAN_POINT('Ctrl Pts',(-1.56801122628479,1.96963131584228,109.242077084624));
#35391=CARTESIAN_POINT('Ctrl Pts',(-1.58153547696412,1.95878845788043,109.243156390919));
#35392=CARTESIAN_POINT('Ctrl Pts',(-1.60138840778976,1.94253204495766,109.244768137679));
#35393=CARTESIAN_POINT('Ctrl Pts',(-1.60780425245238,1.93722509260327,109.245293307571));
#35394=CARTESIAN_POINT('Ctrl Pts',(-1.61919371185878,1.92770859572735,109.246233538929));
#35395=CARTESIAN_POINT('Ctrl Pts',(-1.62417745930115,1.92351144672044,109.246647713261));
#35396=CARTESIAN_POINT('Ctrl Pts',(-1.63502895684537,1.91430042754033,109.247555611739));
#35397=CARTESIAN_POINT('Ctrl Pts',(-1.64088987842461,1.90927897901221,109.248049867951));
#35398=CARTESIAN_POINT('Ctrl Pts',(-1.65727001709763,1.89511387568682,109.249441969225));
#35399=CARTESIAN_POINT('Ctrl Pts',(-1.66773633683908,1.88590986033912,109.250344017501));
#35400=CARTESIAN_POINT('Ctrl Pts',(-1.72949579221855,1.83068284061257,109.255739106464));
#35401=CARTESIAN_POINT('Ctrl Pts',(-1.77895368377705,1.78266019255683,109.260358508032));
#35402=CARTESIAN_POINT('Ctrl Pts',(-1.94400044518552,1.60868797362264,109.276670219196));
#35403=CARTESIAN_POINT('Ctrl Pts',(-2.0486967105319,1.47304489841446,109.288634065611));
#35404=CARTESIAN_POINT('Ctrl Pts',(-2.19828907335813,1.23208470389072,109.307902200272));
#35405=CARTESIAN_POINT('Ctrl Pts',(-2.25124153304283,1.13244217619082,109.315393695307));
#35406=CARTESIAN_POINT('Ctrl Pts',(-2.30679254905932,1.00848809634885,109.324140394719));
#35407=CARTESIAN_POINT('Ctrl Pts',(-2.31595136907461,0.987273730573168,
109.325618389642));
#35408=CARTESIAN_POINT('Ctrl Pts',(-2.32991797368891,0.95365886216644,109.327931256745));
#35409=CARTESIAN_POINT('Ctrl Pts',(-2.33492160985876,0.941341636358608,
109.328772673544));
#35410=CARTESIAN_POINT('Ctrl Pts',(-2.34411129147988,0.91819565842027,109.330342696065));
#35411=CARTESIAN_POINT('Ctrl Pts',(-2.34832043804173,0.907376515852697,
109.331072057258));
#35412=CARTESIAN_POINT('Ctrl Pts',(-2.35548722762594,0.888571148750481,
109.332332140506));
#35413=CARTESIAN_POINT('Ctrl Pts',(-2.35847942165005,0.880598424396253,
109.332863994183));
#35414=CARTESIAN_POINT('Ctrl Pts',(-2.36143112100139,0.87261062952849,109.333394523839));
#35415=CARTESIAN_POINT('Origin',(0.,0.,104.));
#35416=CARTESIAN_POINT('',(-2.36143112015948,0.872610631806858,110.330000354267));
#35417=CARTESIAN_POINT('',(-2.36143112101026,0.872610629504504,110.0563084973));
#35418=CARTESIAN_POINT('',(-2.36143112101026,0.872610629504505,104.));
#35419=CARTESIAN_POINT('',(-2.51749952702257,0.00154319186397671,109.112583302534));
#35420=CARTESIAN_POINT('Ctrl Pts',(-2.36143112101026,0.872610629504504,
110.0563084973));
#35421=CARTESIAN_POINT('Ctrl Pts',(-2.34094181790185,0.928058129651828,
110.052554411366));
#35422=CARTESIAN_POINT('Ctrl Pts',(-2.31851575568189,0.982738051259023,
110.048800325432));
#35423=CARTESIAN_POINT('Ctrl Pts',(-2.29421643253635,1.03652168847553,110.045046239498));
#35424=CARTESIAN_POINT('Ctrl Pts',(-2.26020042816479,1.11181203412497,110.039790990091));
#35425=CARTESIAN_POINT('Ctrl Pts',(-2.22241142208431,1.18556516930059,110.034535740684));
#35426=CARTESIAN_POINT('Ctrl Pts',(-2.18101071128821,1.2573776390751,110.029280491277));
#35427=CARTESIAN_POINT('Ctrl Pts',(-2.13966869729493,1.32908829508128,110.02403269262));
#35428=CARTESIAN_POINT('Ctrl Pts',(-2.09472537808228,1.39886335440258,110.018784893963));
#35429=CARTESIAN_POINT('Ctrl Pts',(-2.04638950241424,1.46632065197514,110.013537095306));
#35430=CARTESIAN_POINT('Ctrl Pts',(-1.99770339165185,1.53426673583022,110.008251271823));
#35431=CARTESIAN_POINT('Ctrl Pts',(-1.94557554810732,1.59986089598963,110.00296544834));
#35432=CARTESIAN_POINT('Ctrl Pts',(-1.89026576918357,1.66273917733746,109.997679624857));
#35433=CARTESIAN_POINT('Ctrl Pts',(-1.83545194923493,1.72505363347063,109.992441198989));
#35434=CARTESIAN_POINT('Ctrl Pts',(-1.77751334011617,1.78470036907002,109.98720277312));
#35435=CARTESIAN_POINT('Ctrl Pts',(-1.71674433460059,1.8413568745946,109.981964347252));
#35436=CARTESIAN_POINT('Ctrl Pts',(-1.65599531499959,1.8979947467374,109.976727644215));
#35437=CARTESIAN_POINT('Ctrl Pts',(-1.59241808498862,1.95164402755928,109.971490941178));
#35438=CARTESIAN_POINT('Ctrl Pts',(-1.52634356479197,2.00201937358712,109.966254238141));
#35439=CARTESIAN_POINT('Ctrl Pts',(-1.46027084443221,2.05239334741571,109.961017677749));
#35440=CARTESIAN_POINT('Ctrl Pts',(-1.39170133670365,2.09949328482736,109.955781117357));
#35441=CARTESIAN_POINT('Ctrl Pts',(-1.32099756796234,2.14307528459398,109.950544556965));
#35442=CARTESIAN_POINT('Ctrl Pts',(-1.24913656910106,2.18737060422625,109.945222288194));
#35443=CARTESIAN_POINT('Ctrl Pts',(-1.17507122640473,2.22803151972832,109.939900019423));
#35444=CARTESIAN_POINT('Ctrl Pts',(-1.09920949483988,2.26484982646838,109.934577750652));
#35445=CARTESIAN_POINT('Ctrl Pts',(-1.02446222759804,2.30112724535301,109.929333669902));
#35446=CARTESIAN_POINT('Ctrl Pts',(-0.94797145635493,2.33367408074203,109.924089589152));
#35447=CARTESIAN_POINT('Ctrl Pts',(-0.870147202752004,2.36233996189009,
109.918845508402));
#35448=CARTESIAN_POINT('Ctrl Pts',(-0.790582436940955,2.39164694544241,
109.91348414562));
#35449=CARTESIAN_POINT('Ctrl Pts',(-0.70962431210848,2.41689713519337,109.908122782839));
#35450=CARTESIAN_POINT('Ctrl Pts',(-0.627724945627277,2.43798434011321,
109.902761420057));
#35451=CARTESIAN_POINT('Ctrl Pts',(-0.545825579146075,2.45907154503304,
109.897400057275));
#35452=CARTESIAN_POINT('Ctrl Pts',(-0.46298548221059,2.47599572886265,109.892038694494));
#35453=CARTESIAN_POINT('Ctrl Pts',(-0.379663322332631,2.48870689549319,
109.886677331712));
#35454=CARTESIAN_POINT('Ctrl Pts',(-0.297990294570631,2.50116647967373,
109.881422082305));
#35455=CARTESIAN_POINT('Ctrl Pts',(-0.215552450424524,2.50962436248652,
109.876166832898));
#35456=CARTESIAN_POINT('Ctrl Pts',(-0.132776023174533,2.5139961769402,109.870911583491));
#35457=CARTESIAN_POINT('Ctrl Pts',(-0.0501169540939206,2.51836179315414,
109.865663784834));
#35458=CARTESIAN_POINT('Ctrl Pts',(0.0328792876686863,2.51865282369666,
109.860415986177));
#35459=CARTESIAN_POINT('Ctrl Pts',(0.115778491415589,2.51483629505492,109.855168187519));
#35460=CARTESIAN_POINT('Ctrl Pts',(0.199278371366194,2.5109921123727,109.849882364036));
#35461=CARTESIAN_POINT('Ctrl Pts',(0.282679332651454,2.5029805222577,109.844596540553));
#35462=CARTESIAN_POINT('Ctrl Pts',(0.365534645426433,2.49082128483618,109.83931071707));
#35463=CARTESIAN_POINT('Ctrl Pts',(0.447647000325784,2.47877107845807,109.834072291202));
#35464=CARTESIAN_POINT('Ctrl Pts',(0.529222988163966,2.462647378422,109.828833865334));
#35465=CARTESIAN_POINT('Ctrl Pts',(0.609831807821048,2.44252152829196,109.823595439465));
#35466=CARTESIAN_POINT('Ctrl Pts',(0.69041411657882,2.4224022972191,109.818358736428));
#35467=CARTESIAN_POINT('Ctrl Pts',(0.77002944156567,2.3982836418633,109.813122033391));
#35468=CARTESIAN_POINT('Ctrl Pts',(0.848258268845002,2.37028777985629,109.807885330354));
#35469=CARTESIAN_POINT('Ctrl Pts',(0.926484965210141,2.34229268044259,109.802648769961));
#35470=CARTESIAN_POINT('Ctrl Pts',(1.00332480486783,2.31042074080787,109.797412209569));
#35471=CARTESIAN_POINT('Ctrl Pts',(1.07837582730909,2.27484325285841,109.792175649177));
#35472=CARTESIAN_POINT('Ctrl Pts',(1.15465523269139,2.23868345732858,109.786853380407));
#35473=CARTESIAN_POINT('Ctrl Pts',(1.22908628637025,2.19869591819411,109.781531111636));
#35474=CARTESIAN_POINT('Ctrl Pts',(1.30127223618843,2.15510946759676,109.776208842865));
#35475=CARTESIAN_POINT('Ctrl Pts',(1.37239772160992,2.11216333383603,109.770964762115));
#35476=CARTESIAN_POINT('Ctrl Pts',(1.44134327585117,2.06572364036187,109.765720681365));
#35477=CARTESIAN_POINT('Ctrl Pts',(1.50775953216826,2.01605244057682,109.760476600615));
#35478=CARTESIAN_POINT('Ctrl Pts',(1.57566116481919,1.96527036178826,109.755115237834));
#35479=CARTESIAN_POINT('Ctrl Pts',(1.6409186066216,1.9111108164844,109.749753875053));
#35480=CARTESIAN_POINT('Ctrl Pts',(1.70319662934966,1.85389522135744,109.744392512272));
#35481=CARTESIAN_POINT('Ctrl Pts',(1.76547465207773,1.79667962623047,109.73903114949));
#35482=CARTESIAN_POINT('Ctrl Pts',(1.82477294699697,1.73640839032503,109.733669786709));
#35483=CARTESIAN_POINT('Ctrl Pts',(1.88079985551424,1.67343901995191,109.728308423928));
#35484=CARTESIAN_POINT('Ctrl Pts',(1.93571786606685,1.61171595440785,109.723053174521));
#35485=CARTESIAN_POINT('Ctrl Pts',(1.98769568585796,1.54717263422441,109.717797925113));
#35486=CARTESIAN_POINT('Ctrl Pts',(2.03643048513133,1.48012064684868,109.712542675705));
#35487=CARTESIAN_POINT('Ctrl Pts',(2.08509618953059,1.41316372395862,109.707294877048));
#35488=CARTESIAN_POINT('Ctrl Pts',(2.13052773709554,1.34370556869451,109.70204707839));
#35489=CARTESIAN_POINT('Ctrl Pts',(2.17246106320583,1.27209244115928,109.696799279732));
#35490=CARTESIAN_POINT('Ctrl Pts',(2.21469823241219,1.19996041478137,109.691513456249));
#35491=CARTESIAN_POINT('Ctrl Pts',(2.25338595599294,1.12564240913494,109.686227632767));
#35492=CARTESIAN_POINT('Ctrl Pts',(2.28829758582821,1.04952389619903,109.680941809284));
#35493=CARTESIAN_POINT('Ctrl Pts',(2.32289616549057,0.974087932710064,109.675703383415));
#35494=CARTESIAN_POINT('Ctrl Pts',(2.35378590421434,0.896884049792989,109.670464957546));
#35495=CARTESIAN_POINT('Ctrl Pts',(2.38079209408838,0.818312443218525,109.665226531677));
#35496=CARTESIAN_POINT('Ctrl Pts',(2.40778940207603,0.739766677537807,109.659989828639));
#35497=CARTESIAN_POINT('Ctrl Pts',(2.4309055480056,0.659854517589931,109.654753125602));
#35498=CARTESIAN_POINT('Ctrl Pts',(2.45001464206608,0.578994390008915,109.649516422564));
#35499=CARTESIAN_POINT('Ctrl Pts',(2.46912321560441,0.498136465017324,109.644279862171));
#35500=CARTESIAN_POINT('Ctrl Pts',(2.48422484917438,0.416331073022448,109.639043301779));
#35501=CARTESIAN_POINT('Ctrl Pts',(2.49524437307892,0.334008635544001,109.633806741386));
#35502=CARTESIAN_POINT('Ctrl Pts',(2.50644425688482,0.250338801677915,109.628484472616));
#35503=CARTESIAN_POINT('Ctrl Pts',(2.51342712091624,0.166135329980568,109.623162203846));
#35504=CARTESIAN_POINT('Ctrl Pts',(2.51616889547696,0.0818556011171571,
109.617839935076));
#35505=CARTESIAN_POINT('Ctrl Pts',(2.51887039136475,-0.00118599690829541,
109.612595854325));
#35506=CARTESIAN_POINT('Ctrl Pts',(2.5174546493823,-0.084301159516965,109.607351773574));
#35507=CARTESIAN_POINT('Ctrl Pts',(2.51195126463292,-0.16705416519519,109.602107692824));
#35508=CARTESIAN_POINT('Ctrl Pts',(2.50632479861102,-0.25165791286358,109.596746330044));
#35509=CARTESIAN_POINT('Ctrl Pts',(2.49642570589944,-0.335882600564322,
109.591384967264));
#35510=CARTESIAN_POINT('Ctrl Pts',(2.48234107280901,-0.419272045628374,
109.586023604484));
#35511=CARTESIAN_POINT('Ctrl Pts',(2.46825643971858,-0.502661490692423,
109.580662241704));
#35512=CARTESIAN_POINT('Ctrl Pts',(2.44998644126181,-0.585215211450702,
109.575300878924));
#35513=CARTESIAN_POINT('Ctrl Pts',(2.42767215699761,-0.666493922056721,
109.569939516144));
#35514=CARTESIAN_POINT('Ctrl Pts',(2.40579952237753,-0.746163945008328,
109.564684266737));
#35515=CARTESIAN_POINT('Ctrl Pts',(2.37996048847428,-0.824903250673477,
109.55942901733));
#35516=CARTESIAN_POINT('Ctrl Pts',(2.3502515363011,-0.902288183516956,109.554173767922));
#35517=CARTESIAN_POINT('Ctrl Pts',(2.32058470467304,-0.979563402105383,
109.548925969265));
#35518=CARTESIAN_POINT('Ctrl Pts',(2.2870590168895,-1.05548763476304,109.543678170607));
#35519=CARTESIAN_POINT('Ctrl Pts',(2.24982114285869,-1.12965086427003,109.53843037195));
#35520=CARTESIAN_POINT('Ctrl Pts',(2.21231344832706,-1.20435147031229,109.533144548467));
#35521=CARTESIAN_POINT('Ctrl Pts',(2.17103967003756,-1.27726498857237,109.527858724984));
#35522=CARTESIAN_POINT('Ctrl Pts',(2.12619973998966,-1.34799143753508,109.522572901501));
#35523=CARTESIAN_POINT('Ctrl Pts',(2.08176188650013,-1.41808368731073,109.517334475633));
#35524=CARTESIAN_POINT('Ctrl Pts',(2.03382183159514,-1.48602753641291,109.512096049764));
#35525=CARTESIAN_POINT('Ctrl Pts',(1.98262013640475,-1.55145855398152,109.506857623896));
#35526=CARTESIAN_POINT('Ctrl Pts',(1.93143528059979,-1.61686805237737,109.501620920858));
#35527=CARTESIAN_POINT('Ctrl Pts',(1.87699119908413,-1.67976599747351,109.496384217821));
#35528=CARTESIAN_POINT('Ctrl Pts',(1.81957032398615,-1.73981898083362,109.491147514783));
#35529=CARTESIAN_POINT('Ctrl Pts',(1.76215101300411,-1.79987032838048,109.485910954391));
#35530=CARTESIAN_POINT('Ctrl Pts',(1.70175538928872,-1.85707653548407,109.480674393999));
#35531=CARTESIAN_POINT('Ctrl Pts',(1.63870356083115,-1.91114020671413,109.475437833607));
#35532=CARTESIAN_POINT('Ctrl Pts',(1.57461974390001,-1.96608875451181,109.470115564836));
#35533=CARTESIAN_POINT('Ctrl Pts',(1.50779235267326,-2.01779063860604,109.464793296066));
#35534=CARTESIAN_POINT('Ctrl Pts',(1.43859192974068,-2.06597664790408,109.459471027295));
#35535=CARTESIAN_POINT('Ctrl Pts',(1.37040811162573,-2.11345476948817,109.454226946545));
#35536=CARTESIAN_POINT('Ctrl Pts',(1.2999209515205,-2.15751943606303,109.448982865794));
#35537=CARTESIAN_POINT('Ctrl Pts',(1.22751204236929,-2.19795824251472,109.443738785044));
#35538=CARTESIAN_POINT('Ctrl Pts',(1.15348373330948,-2.2393014487183,109.438377422264));
#35539=CARTESIAN_POINT('Ctrl Pts',(1.0774471385546,-2.27685442882497,109.433016059483));
#35540=CARTESIAN_POINT('Ctrl Pts',(0.999832314886172,-2.31044186079403,
109.427654696702));
#35541=CARTESIAN_POINT('Ctrl Pts',(0.922217491217744,-2.34402929276309,
109.422293333921));
#35542=CARTESIAN_POINT('Ctrl Pts',(0.843024937941911,-2.3736510611482,109.416931971141));
#35543=CARTESIAN_POINT('Ctrl Pts',(0.762699935624001,-2.39918633253008,
109.41157060836));
#35544=CARTESIAN_POINT('Ctrl Pts',(0.683964744948231,-2.4242162037183,109.406315358953));
#35545=CARTESIAN_POINT('Ctrl Pts',(0.603850720470603,-2.44541235930828,
109.401060109545));
#35546=CARTESIAN_POINT('Ctrl Pts',(0.522765750423893,-2.46262506691208,
109.395804860138));
#35547=CARTESIAN_POINT('Ctrl Pts',(0.441795740444478,-2.47981337080675,
109.390557061481));
#35548=CARTESIAN_POINT('Ctrl Pts',(0.359857966783513,-2.49302934952956,
109.385309262823));
#35549=CARTESIAN_POINT('Ctrl Pts',(0.277376203382308,-2.50217279415256,
109.380061464166));
#35550=CARTESIAN_POINT('Ctrl Pts',(0.194296788497055,-2.51138249091449,
109.374775640683));
#35551=CARTESIAN_POINT('Ctrl Pts',(0.110665918875473,-2.51646024294225,
109.3694898172));
#35552=CARTESIAN_POINT('Ctrl Pts',(0.0269279492159412,-2.51735598109426,
109.364203993717));
#35553=CARTESIAN_POINT('Ctrl Pts',(-0.0560591478492334,-2.51824368722407,
109.358965567848));
#35554=CARTESIAN_POINT('Ctrl Pts',(-0.139150962031731,-2.51502407372498,
109.35372714198));
#35555=CARTESIAN_POINT('Ctrl Pts',(-0.221910837654832,-2.5077005064663,
109.348488716111));
#35556=CARTESIAN_POINT('Ctrl Pts',(-0.304643494932171,-2.50037934780701,
109.343252013074));
#35557=CARTESIAN_POINT('Ctrl Pts',(-0.38704397120383,-2.48895695665119,
109.338015310036));
#35558=CARTESIAN_POINT('Ctrl Pts',(-0.468678835432439,-2.47348871014559,
109.332778606999));
#35559=CARTESIAN_POINT('Ctrl Pts',(-0.550311475968167,-2.45802088498729,
109.327542046607));
#35560=CARTESIAN_POINT('Ctrl Pts',(-0.631178092763609,-2.43850751051419,
109.322305486214));
#35561=CARTESIAN_POINT('Ctrl Pts',(-0.710854949530708,-2.41505517343345,
109.317068925822));
#35562=CARTESIAN_POINT('Ctrl Pts',(-0.791835901669957,-2.3912189848117,
109.311746657051));
#35563=CARTESIAN_POINT('Ctrl Pts',(-0.871587320650252,-2.36331385611554,
109.306424388281));
#35564=CARTESIAN_POINT('Ctrl Pts',(-0.949681651792507,-2.33150402321091,
109.30110211951));
#35565=CARTESIAN_POINT('Ctrl Pts',(-1.02662872010301,-2.30016150001291,
109.29585803876));
#35566=CARTESIAN_POINT('Ctrl Pts',(-1.10196666682814,-2.26502849041496,
109.29061395801));
#35567=CARTESIAN_POINT('Ctrl Pts',(-1.17530956932278,-2.22630942733895,
109.28536987726));
#35568=CARTESIAN_POINT('Ctrl Pts',(-1.2502927601582,-2.18672442597076,109.280008514479));
#35569=CARTESIAN_POINT('Ctrl Pts',(-1.3231901528662,-2.14339129554009,109.274647151698));
#35570=CARTESIAN_POINT('Ctrl Pts',(-1.39362054358561,-2.0965753099987,109.269285788918));
#35571=CARTESIAN_POINT('Ctrl Pts',(-1.46405093430502,-2.04975932445731,
109.263924426137));
#35572=CARTESIAN_POINT('Ctrl Pts',(-1.53201395435234,-1.99946083976441,
109.258563063356));
#35573=CARTESIAN_POINT('Ctrl Pts',(-1.5971658158888,-1.94598756587915,109.253201700576));
#35574=CARTESIAN_POINT('Ctrl Pts',(-1.66018580041137,-1.89426402624193,
109.248015770481));
#35575=CARTESIAN_POINT('Ctrl Pts',(-1.7208219529501,-1.83936794722398,109.242829840387));
#35576=CARTESIAN_POINT('Ctrl Pts',(-1.77873133380123,-1.78155019355439,
109.237643910292));
#35577=CARTESIAN_POINT('Ctrl Pts',(-1.8369190827697,-1.72345451221573,109.232433051636));
#35578=CARTESIAN_POINT('Ctrl Pts',(-1.89235335502134,-1.66240923774307,
109.227222192979));
#35579=CARTESIAN_POINT('Ctrl Pts',(-1.94471789917081,-1.59871152577464,
109.222011334322));
#35580=CARTESIAN_POINT('Ctrl Pts',(-1.99669805314474,-1.53548139688332,
109.216838726794));
#35581=CARTESIAN_POINT('Ctrl Pts',(-2.04565307367539,-1.4696379988631,109.211666119265));
#35582=CARTESIAN_POINT('Ctrl Pts',(-2.09131013992786,-1.40150923958243,
109.206493511736));
#35583=CARTESIAN_POINT('Ctrl Pts',(-2.1369397234866,-1.33342148954696,109.201324017793));
#35584=CARTESIAN_POINT('Ctrl Pts',(-2.179275028083,-1.26305150124533,109.19615452385));
#35585=CARTESIAN_POINT('Ctrl Pts',(-2.21808489358349,-1.19075843681946,
109.190985029907));
#35586=CARTESIAN_POINT('Ctrl Pts',(-2.25688384819613,-1.1184856966464,109.1858169893));
#35587=CARTESIAN_POINT('Ctrl Pts',(-2.29215910763426,-1.04429137214069,
109.180648948693));
#35588=CARTESIAN_POINT('Ctrl Pts',(-2.323724860714,-0.968560282945616,109.175480908086));
#35589=CARTESIAN_POINT('Ctrl Pts',(-2.35573909391273,-0.891753221071957,
109.170239440956));
#35590=CARTESIAN_POINT('Ctrl Pts',(-2.38393735988397,-0.813365831117959,
109.164997973827));
#35591=CARTESIAN_POINT('Ctrl Pts',(-2.40817655178005,-0.733820104287649,
109.159756506698));
#35592=CARTESIAN_POINT('Ctrl Pts',(-2.43209781731412,-0.655317716016403,
109.154583787759));
#35593=CARTESIAN_POINT('Ctrl Pts',(-2.45216318475308,-0.575687678742618,
109.14941106882));
#35594=CARTESIAN_POINT('Ctrl Pts',(-2.46828607654817,-0.495348457470522,
109.14423834988));
#35595=CARTESIAN_POINT('Ctrl Pts',(-2.48473039107442,-0.413407609626218,
109.138962508656));
#35596=CARTESIAN_POINT('Ctrl Pts',(-2.49707324762341,-0.33072950682054,
109.133686667432));
#35597=CARTESIAN_POINT('Ctrl Pts',(-2.50527825607931,-0.247764221824343,
109.128410826207));
#35598=CARTESIAN_POINT('Ctrl Pts',(-2.51348326453521,-0.16479893682814,
109.123134984983));
#35599=CARTESIAN_POINT('Ctrl Pts',(-2.51755046013732,-0.0815469897811725,
109.117859143758));
#35600=CARTESIAN_POINT('Ctrl Pts',(-2.51749952702257,0.00154319186397808,
109.112583302534));
#35601=CARTESIAN_POINT('Ctrl Pts',(-2.51749952702217,0.00154319252614217,
109.112583302492));
#35602=CARTESIAN_POINT('Ctrl Pts',(-2.51744240569643,0.0947285262351732,
109.106666465925));
#35603=CARTESIAN_POINT('Ctrl Pts',(-2.51221164500478,0.18775354483245,109.100749629358));
#35604=CARTESIAN_POINT('Ctrl Pts',(-2.50185877901989,0.280194396519821,
109.094832792791));
#35605=CARTESIAN_POINT('Ctrl Pts',(-2.49266337038751,0.362300299062281,
109.089577462516));
#35606=CARTESIAN_POINT('Ctrl Pts',(-2.47940487525419,0.44410469072322,109.084322132241));
#35607=CARTESIAN_POINT('Ctrl Pts',(-2.46211260492313,0.525174038465942,
109.079066801966));
#35608=CARTESIAN_POINT('Ctrl Pts',(-2.44484692813231,0.606118710794753,
109.07381955379));
#35609=CARTESIAN_POINT('Ctrl Pts',(-2.42355989977268,0.686330138217152,
109.068572305614));
#35610=CARTESIAN_POINT('Ctrl Pts',(-2.39833250270469,0.76538059582816,109.063325057437));
#35611=CARTESIAN_POINT('Ctrl Pts',(-2.38684469401716,0.801377830550768,
109.060935616187));
#35612=CARTESIAN_POINT('Ctrl Pts',(-2.37454050980643,0.837134418656268,
109.058546174938));
#35613=CARTESIAN_POINT('Ctrl Pts',(-2.36143112101026,0.8726106295045,109.056156733688));
#35614=CARTESIAN_POINT('Ctrl Pts',(-2.36143112100139,0.87261062952849,109.333394523839));
#35615=CARTESIAN_POINT('Ctrl Pts',(-2.36346984958465,0.867093487104515,
109.333760958848));
#35616=CARTESIAN_POINT('Ctrl Pts',(-2.36548925970523,0.861569155118568,
109.334126762288));
#35617=CARTESIAN_POINT('Ctrl Pts',(-2.37506141720324,0.835096045723733,
109.335874488354));
#35618=CARTESIAN_POINT('Ctrl Pts',(-2.38235550549763,0.814054319465642,
109.337247961307));
#35619=CARTESIAN_POINT('Ctrl Pts',(-2.438745542544,0.644129267194206,109.348220758002));
#35620=CARTESIAN_POINT('Ctrl Pts',(-2.47411894835068,0.491046575985721,
109.357347000226));
#35621=CARTESIAN_POINT('Ctrl Pts',(-2.51007103693908,0.223800113368748,
109.372868433239));
#35622=CARTESIAN_POINT('Ctrl Pts',(-2.51757913315039,0.111069461290839,
109.37930321569));
#35623=CARTESIAN_POINT('Ctrl Pts',(-2.51748053141364,-0.0284342513975516,
109.387482928585));
#35624=CARTESIAN_POINT('Ctrl Pts',(-2.5170383666155,-0.0550864820178238,
109.38905572446));
#35625=CARTESIAN_POINT('Ctrl Pts',(-2.51439311537659,-0.136528308785591,
109.393905511809));
#35626=CARTESIAN_POINT('Ctrl Pts',(-2.51082333543405,-0.191253570963997,
109.397224888042));
#35627=CARTESIAN_POINT('Ctrl Pts',(-2.50419226738626,-0.258841019621582,
109.401446971244));
#35628=CARTESIAN_POINT('Ctrl Pts',(-2.50281263159588,-0.271857498427805,
109.40226575223));
#35629=CARTESIAN_POINT('Ctrl Pts',(-2.5004800230266,-0.29233977185561,109.403563913153));
#35630=CARTESIAN_POINT('Ctrl Pts',(-2.49959494432716,-0.299813272812452,
109.404039631313));
#35631=CARTESIAN_POINT('Ctrl Pts',(-2.49795805589807,-0.31312367426411,
109.404890724882));
#35632=CARTESIAN_POINT('Ctrl Pts',(-2.49721927243702,-0.318962046818765,
109.40526537069));
#35633=CARTESIAN_POINT('Ctrl Pts',(-2.49539701410415,-0.332968286145085,
109.406167309786));
#35634=CARTESIAN_POINT('Ctrl Pts',(-2.4942939136824,-0.341133412569161,
109.406695679288));
#35635=CARTESIAN_POINT('Ctrl Pts',(-2.49080758458314,-0.366017816506546,
109.408313508455));
#35636=CARTESIAN_POINT('Ctrl Pts',(-2.48829623603564,-0.382718265534257,
109.409409670501));
#35637=CARTESIAN_POINT('Ctrl Pts',(-2.48205424858673,-0.421565325297277,
109.411981780215));
#35638=CARTESIAN_POINT('Ctrl Pts',(-2.47819493482364,-0.443689539333963,
109.413463615741));
#35639=CARTESIAN_POINT('Ctrl Pts',(-2.46361967436347,-0.521111197328586,
109.418702116494));
#35640=CARTESIAN_POINT('Ctrl Pts',(-2.45134493936348,-0.57609546026345,
109.422517357224));
#35641=CARTESIAN_POINT('Ctrl Pts',(-2.39532394427507,-0.792607583981021,
109.437811005721));
#35642=CARTESIAN_POINT('Ctrl Pts',(-2.33736025802409,-0.950030092836987,
109.449502067731));
#35643=CARTESIAN_POINT('Ctrl Pts',(-2.21986824165573,-1.19175400172207,
109.467689887044));
#35644=CARTESIAN_POINT('Ctrl Pts',(-2.17005539982266,-1.28021744699912,
109.474411240295));
#35645=CARTESIAN_POINT('Ctrl Pts',(-2.10253295841837,-1.38480780114625,
109.482429521941));
#35646=CARTESIAN_POINT('Ctrl Pts',(-2.08976618527293,-1.40399958544812,
109.483904251773));
#35647=CARTESIAN_POINT('Ctrl Pts',(-2.06915392804172,-1.43408098113171,
109.4862218571));
#35648=CARTESIAN_POINT('Ctrl Pts',(-2.06148210285805,-1.44508746769828,
109.487071167814));
#35649=CARTESIAN_POINT('Ctrl Pts',(-2.04701457617386,-1.46549380489623,
109.488648496492));
#35650=CARTESIAN_POINT('Ctrl Pts',(-2.04024122290779,-1.47490898934411,
109.489377334437));
#35651=CARTESIAN_POINT('Ctrl Pts',(-2.02501023821994,-1.49577485600221,
109.490995187945));
#35652=CARTESIAN_POINT('Ctrl Pts',(-2.01652002237354,-1.50720134596288,
109.49188292278));
#35653=CARTESIAN_POINT('Ctrl Pts',(-1.99129290285451,-1.54055829234207,
109.494480221376));
#35654=CARTESIAN_POINT('Ctrl Pts',(-1.97429158922705,-1.56228681409909,
109.496179480908));
#35655=CARTESIAN_POINT('Ctrl Pts',(-1.93479290357716,-1.61109329947915,
109.50001702054));
#35656=CARTESIAN_POINT('Ctrl Pts',(-1.9120776619221,-1.6379879079882,109.502146631196));
#35657=CARTESIAN_POINT('Ctrl Pts',(-1.83369471278203,-1.72693903970804,
109.509255455459));
#35658=CARTESIAN_POINT('Ctrl Pts',(-1.77550937380536,-1.78670724155929,
109.514140886404));
#35659=CARTESIAN_POINT('Ctrl Pts',(-1.64411754920209,-1.90890338974462,
109.524539441658));
#35660=CARTESIAN_POINT('Ctrl Pts',(-1.57008586047114,-1.9702449534474,109.530025511459));
#35661=CARTESIAN_POINT('Ctrl Pts',(-1.47237922826388,-2.04219106653644,
109.537021166083));
#35662=CARTESIAN_POINT('Ctrl Pts',(-1.45180447133898,-2.05686866191258,
109.538481671739));
#35663=CARTESIAN_POINT('Ctrl Pts',(-1.34625820570126,-2.12979042484566,
109.545927628196));
#35664=CARTESIAN_POINT('Ctrl Pts',(-1.25799940137787,-2.18308287036585,
109.552002056204));
#35665=CARTESIAN_POINT('Ctrl Pts',(-1.1546145115725,-2.23715415990781,109.559232998796));
#35666=CARTESIAN_POINT('Ctrl Pts',(-1.1424407580423,-2.24339530639306,109.560086225954));
#35667=CARTESIAN_POINT('Ctrl Pts',(-1.12271371071132,-2.25330661156631,
109.561472663653));
#35668=CARTESIAN_POINT('Ctrl Pts',(-1.11519167762764,-2.25703882981834,
109.562002208242));
#35669=CARTESIAN_POINT('Ctrl Pts',(-1.10179520818773,-2.26360245946967,
109.562947130089));
#35670=CARTESIAN_POINT('Ctrl Pts',(-1.09592825977956,-2.26644876916602,
109.563361583586));
#35671=CARTESIAN_POINT('Ctrl Pts',(-1.08314060552501,-2.27259134851176,
109.564266352561));
#35672=CARTESIAN_POINT('Ctrl Pts',(-1.07621598820648,-2.27587876471487,
109.564757170805));
#35673=CARTESIAN_POINT('Ctrl Pts',(-1.05652005003723,-2.28511929253639,
109.566155484484));
#35674=CARTESIAN_POINT('Ctrl Pts',(-1.04371384608329,-2.29099676629381,
109.567067347726));
#35675=CARTESIAN_POINT('Ctrl Pts',(-0.95590180266367,-2.33040951181688,
109.573334927669));
#35676=CARTESIAN_POINT('Ctrl Pts',(-0.879349628913439,-2.36035975501343,
109.578871567652));
#35677=CARTESIAN_POINT('Ctrl Pts',(-0.644383220125851,-2.43927021755126,
109.595814669249));
#35678=CARTESIAN_POINT('Ctrl Pts',(-0.482447046194343,-2.47639249119478,
109.607394073785));
#35679=CARTESIAN_POINT('Ctrl Pts',(-0.214874691263757,-2.51046816798263,
109.625666546562));
#35680=CARTESIAN_POINT('Ctrl Pts',(-0.110986203589693,-2.5172025135603,
109.63256452816));
#35681=CARTESIAN_POINT('Ctrl Pts',(0.0162200407558962,-2.51755452374944,
109.640758791927));
#35682=CARTESIAN_POINT('Ctrl Pts',(0.0394069677846057,-2.51729835724784,
109.642242511613));
#35683=CARTESIAN_POINT('Ctrl Pts',(0.0760307746945406,-2.51638756939638,
109.644571033584));
#35684=CARTESIAN_POINT('Ctrl Pts',(0.0894711651940837,-2.5159455479244,
109.645422372565));
#35685=CARTESIAN_POINT('Ctrl Pts',(0.114493880676477,-2.51492184137784,
109.647001612961));
#35686=CARTESIAN_POINT('Ctrl Pts',(0.126076916518214,-2.51436778043953,
109.647730350782));
#35687=CARTESIAN_POINT('Ctrl Pts',(0.151830052040208,-2.51295749969201,
109.649345671937));
#35688=CARTESIAN_POINT('Ctrl Pts',(0.165997640259432,-2.5120614157388,109.650230994418));
#35689=CARTESIAN_POINT('Ctrl Pts',(0.207478766265878,-2.50908531662416,
109.652813924134));
#35690=CARTESIAN_POINT('Ctrl Pts',(0.234767371536839,-2.50667926461903,
109.654501403183));
#35691=CARTESIAN_POINT('Ctrl Pts',(0.409372627539705,-2.48840776669711,
109.665233473326));
#35692=CARTESIAN_POINT('Ctrl Pts',(0.555091765975768,-2.46000814296342,
109.673868613575));
#35693=CARTESIAN_POINT('Ctrl Pts',(0.847737503890756,-2.37562646291455,
109.691409784299));
#35694=CARTESIAN_POINT('Ctrl Pts',(0.993615204999481,-2.3184002987068,109.700270387116));
#35695=CARTESIAN_POINT('Ctrl Pts',(1.17239575523607,-2.22827700514637,109.712289230991));
#35696=CARTESIAN_POINT('Ctrl Pts',(1.21103827733235,-2.2075135297388,109.714962857984));
#35697=CARTESIAN_POINT('Ctrl Pts',(1.25979404845179,-2.17965053703283,109.718459806681));
#35698=CARTESIAN_POINT('Ctrl Pts',(1.27042695876615,-2.17347022896262,109.719230145277));
#35699=CARTESIAN_POINT('Ctrl Pts',(1.28727700254527,-2.16351036517836,109.720463919338));
#35700=CARTESIAN_POINT('Ctrl Pts',(1.29352392836076,-2.15978124473093,109.720924198332));
#35701=CARTESIAN_POINT('Ctrl Pts',(1.30541129630678,-2.15261497394746,109.721805740327));
#35702=CARTESIAN_POINT('Ctrl Pts',(1.31105446944537,-2.14918264758338,109.722226698313));
#35703=CARTESIAN_POINT('Ctrl Pts',(1.3244229870632,-2.14097931926834,109.723229734364));
#35704=CARTESIAN_POINT('Ctrl Pts',(1.33213610497564,-2.1361886822006,109.723813064418));
#35705=CARTESIAN_POINT('Ctrl Pts',(1.35802489082578,-2.11991435625366,109.725786145086));
#35706=CARTESIAN_POINT('Ctrl Pts',(1.3760787582864,-2.10823994370133,109.727187411152));
#35707=CARTESIAN_POINT('Ctrl Pts',(1.48164213695745,-2.03804449734193,109.735521148586));
#35708=CARTESIAN_POINT('Ctrl Pts',(1.56555319278055,-1.97431700619429,109.742716984641));
#35709=CARTESIAN_POINT('Ctrl Pts',(1.78678930491417,-1.78330363322121,109.762863477234));
#35710=CARTESIAN_POINT('Ctrl Pts',(1.91431841023979,-1.64565848939293,109.775834612889));
#35711=CARTESIAN_POINT('Ctrl Pts',(2.05876710896484,-1.44997777030523,109.791913260181));
#35712=CARTESIAN_POINT('Ctrl Pts',(2.09058847857081,-1.40370872004539,109.795570851985));
#35713=CARTESIAN_POINT('Ctrl Pts',(2.13124773119218,-1.34013529890697,109.800409868807));
#35714=CARTESIAN_POINT('Ctrl Pts',(2.14146971785509,-1.32373977525013,109.801641831734));
#35715=CARTESIAN_POINT('Ctrl Pts',(2.15797823903794,-1.29656920952478,109.803657710542));
#35716=CARTESIAN_POINT('Ctrl Pts',(2.16437508709541,-1.28586246803049,109.804445615109));
#35717=CARTESIAN_POINT('Ctrl Pts',(2.17667959459117,-1.26491578073643,109.805974714704));
#35718=CARTESIAN_POINT('Ctrl Pts',(2.18259520292458,-1.25468090671586,109.806716181823));
#35719=CARTESIAN_POINT('Ctrl Pts',(2.19636825885272,-1.23045929348502,109.808457816894));
#35720=CARTESIAN_POINT('Ctrl Pts',(2.20416459824456,-1.21643826147093,109.809455789388));
#35721=CARTESIAN_POINT('Ctrl Pts',(2.22965681919375,-1.16954286512847,109.81276079625));
#35722=CARTESIAN_POINT('Ctrl Pts',(2.24675593487772,-1.1363485534053,109.815046915215));
#35723=CARTESIAN_POINT('Ctrl Pts',(2.34240742133841,-0.940054646262984,
109.828282878177));
#35724=CARTESIAN_POINT('Ctrl Pts',(2.40392278574608,-0.76924523925228,109.838626697978));
#35725=CARTESIAN_POINT('Ctrl Pts',(2.47888245101036,-0.46013491701283,109.856916111287));
#35726=CARTESIAN_POINT('Ctrl Pts',(2.5002453912599,-0.324570399740312,109.864820011941));
#35727=CARTESIAN_POINT('Ctrl Pts',(2.51207333564027,-0.166592293806112,
109.8745484853));
#35728=CARTESIAN_POINT('Ctrl Pts',(2.51340027666628,-0.145204734981214,
109.875876613134));
#35729=CARTESIAN_POINT('Ctrl Pts',(2.51486834015722,-0.115388348748911,
109.877746770805));
#35730=CARTESIAN_POINT('Ctrl Pts',(2.51524042787282,-0.106971139050084,
109.87827678384));
#35731=CARTESIAN_POINT('Ctrl Pts',(2.51580952623664,-0.0924447807835918,
109.879195281467));
#35732=CARTESIAN_POINT('Ctrl Pts',(2.51602655575973,-0.0863364268397177,
109.879582671416));
#35733=CARTESIAN_POINT('Ctrl Pts',(2.51643757768587,-0.0734452965639899,
109.880402784831));
#35734=CARTESIAN_POINT('Ctrl Pts',(2.51662639417135,-0.0666624536343644,
109.880835800592));
#35735=CARTESIAN_POINT('Ctrl Pts',(2.51702696808261,-0.0498258560599105,
109.881914238328));
#35736=CARTESIAN_POINT('Ctrl Pts',(2.51720590979569,-0.0397715167232285,
109.882561428108));
#35737=CARTESIAN_POINT('Ctrl Pts',(2.51765389437049,-0.00182224345531749,
109.885015506109));
#35738=CARTESIAN_POINT('Ctrl Pts',(2.51751949958342,0.0260742971917743,
109.886842557029));
#35739=CARTESIAN_POINT('Ctrl Pts',(2.515983127897,0.0977352401847407,109.891585589694));
#35740=CARTESIAN_POINT('Ctrl Pts',(2.51390289075263,0.141474738151433,109.894528157572));
#35741=CARTESIAN_POINT('Ctrl Pts',(2.5015626962541,0.308824500872177,109.905917914244));
#35742=CARTESIAN_POINT('Ctrl Pts',(2.48331440821473,0.431667625630043,109.914544530062));
#35743=CARTESIAN_POINT('Ctrl Pts',(2.42057821092703,0.710473413325409,109.934220995561));
#35744=CARTESIAN_POINT('Ctrl Pts',(2.36993616672713,0.864517724247111,109.945146938457));
#35745=CARTESIAN_POINT('Ctrl Pts',(2.29590555748541,1.03301415870238,109.95701699396));
#35746=CARTESIAN_POINT('Ctrl Pts',(2.28669267099375,1.0532508063944,109.958441908611));
#35747=CARTESIAN_POINT('Ctrl Pts',(2.27107873114421,1.08637683344634,109.960773813584));
#35748=CARTESIAN_POINT('Ctrl Pts',(2.26483326338453,1.09933776900559,109.9616860519));
#35749=CARTESIAN_POINT('Ctrl Pts',(2.2533484462779,1.12265835212401,109.963327409729));
#35750=CARTESIAN_POINT('Ctrl Pts',(2.24814793446607,1.13303656956481,109.964057842713));
#35751=CARTESIAN_POINT('Ctrl Pts',(2.23683435812628,1.15522952153017,109.965619965314));
#35752=CARTESIAN_POINT('Ctrl Pts',(2.2306990387499,1.16703256270518,109.966450853798));
#35753=CARTESIAN_POINT('Ctrl Pts',(2.21363500498472,1.19923384260389,109.96871834599));
#35754=CARTESIAN_POINT('Ctrl Pts',(2.20251797246947,1.21953121335917,109.970148316695));
#35755=CARTESIAN_POINT('Ctrl Pts',(2.13525389273553,1.33842049743581,109.978533689033));
#35756=CARTESIAN_POINT('Ctrl Pts',(2.0727704661541,1.43328497146815,109.985255357299));
#35757=CARTESIAN_POINT('Ctrl Pts',(1.89641154450373,1.66525865298754,110.002207016496));
#35758=CARTESIAN_POINT('Ctrl Pts',(1.77402711162415,1.79507187028435,110.012193334975));
#35759=CARTESIAN_POINT('Ctrl Pts',(1.59207714147863,1.95113219459781,110.026391986564));
#35760=CARTESIAN_POINT('Ctrl Pts',(1.54370027120321,1.98962674905459,110.030118445536));
#35761=CARTESIAN_POINT('Ctrl Pts',(1.48306078753487,2.03433535628456,110.034798695307));
#35762=CARTESIAN_POINT('Ctrl Pts',(1.47209647748619,2.04228342387063,110.035645298137));
#35763=CARTESIAN_POINT('Ctrl Pts',(1.45485631443609,2.05456991914629,110.036977962798));
#35764=CARTESIAN_POINT('Ctrl Pts',(1.44862377075494,2.05896906617798,110.037460036284));
#35765=CARTESIAN_POINT('Ctrl Pts',(1.43702309065858,2.06707848660173,110.038358068399));
#35766=CARTESIAN_POINT('Ctrl Pts',(1.43166042965011,2.0707962825175,110.038773512639));
#35767=CARTESIAN_POINT('Ctrl Pts',(1.4193212636266,2.07927987157974,110.039730102644));
#35768=CARTESIAN_POINT('Ctrl Pts',(1.41233519957301,2.08403140880092,110.040272171893));
#35769=CARTESIAN_POINT('Ctrl Pts',(1.39041282617187,2.09878095040168,110.041974346044));
#35770=CARTESIAN_POINT('Ctrl Pts',(1.37539365486613,2.10865396772303,110.043142178256));
#35771=CARTESIAN_POINT('Ctrl Pts',(1.33978923477499,2.1315167157797,110.045912148842));
#35772=CARTESIAN_POINT('Ctrl Pts',(1.31911901981497,2.14437021581,110.047521423599));
#35773=CARTESIAN_POINT('Ctrl Pts',(1.24373340008868,2.18974536147545,110.053385993537));
#35774=CARTESIAN_POINT('Ctrl Pts',(1.18797839541248,2.22048729241579,110.057714350784));
#35775=CARTESIAN_POINT('Ctrl Pts',(0.938813812376638,2.34579873148568,110.076848734929));
#35776=CARTESIAN_POINT('Ctrl Pts',(0.73485300110441,2.41747031016112,110.091875517807));
#35777=CARTESIAN_POINT('Ctrl Pts',(0.473733481223952,2.47306492985238,110.109473561756));
#35778=CARTESIAN_POINT('Ctrl Pts',(0.422897961496968,2.48226338438602,110.112832051939));
#35779=CARTESIAN_POINT('Ctrl Pts',(0.353272504175593,2.49266046113153,110.117343059449));
#35780=CARTESIAN_POINT('Ctrl Pts',(0.334702023936276,2.4952218784915,110.118537734943));
#35781=CARTESIAN_POINT('Ctrl Pts',(0.305077306451513,2.49897131401624,110.120430429919));
#35782=CARTESIAN_POINT('Ctrl Pts',(0.294041102889617,2.50029390820895,110.121132632443));
#35783=CARTESIAN_POINT('Ctrl Pts',(0.271328371682351,2.50286337001245,110.122571975704));
#35784=CARTESIAN_POINT('Ctrl Pts',(0.259651139208311,2.50410172070423,110.123308833754));
#35785=CARTESIAN_POINT('Ctrl Pts',(0.232494453781475,2.50678963564373,110.125015376843));
#35786=CARTESIAN_POINT('Ctrl Pts',(0.217009280925179,2.50817761282148,110.125983121273));
#35787=CARTESIAN_POINT('Ctrl Pts',(0.167147064172982,2.51218165558898,110.129082822464));
#35788=CARTESIAN_POINT('Ctrl Pts',(0.132727917554875,2.51423512964181,110.131197344345));
#35789=CARTESIAN_POINT('Ctrl Pts',(0.0513909479018113,2.5174127185878,110.136142727679));
#35790=CARTESIAN_POINT('Ctrl Pts',(0.00446189482594016,2.51793333820691,
110.138955587364));
#35791=CARTESIAN_POINT('Ctrl Pts',(-0.270322207029544,2.5132985785105,110.15525326836));
#35792=CARTESIAN_POINT('Ctrl Pts',(-0.496585165582177,2.47853447527572,
110.167872582218));
#35793=CARTESIAN_POINT('Ctrl Pts',(-0.77294120111929,2.39666673196435,110.184961338577));
#35794=CARTESIAN_POINT('Ctrl Pts',(-0.830174527957854,2.37744790123484,
110.188603487654));
#35795=CARTESIAN_POINT('Ctrl Pts',(-0.899256002207809,2.35145191526845,
110.19318940675));
#35796=CARTESIAN_POINT('Ctrl Pts',(-0.911816598428019,2.34660988226944,
110.194031062936));
#35797=CARTESIAN_POINT('Ctrl Pts',(-0.931416421807931,2.33887315164513,
110.195357595893));
#35798=CARTESIAN_POINT('Ctrl Pts',(-0.938482591291469,2.33604678731531,
110.195838543262));
#35799=CARTESIAN_POINT('Ctrl Pts',(-0.951528148091245,2.33076001336847,
110.196731668242));
#35800=CARTESIAN_POINT('Ctrl Pts',(-0.957510980919255,2.32830856517606,
110.197143314625));
#35801=CARTESIAN_POINT('Ctrl Pts',(-0.971124928183119,2.32266894361101,
110.198084663355));
#35802=CARTESIAN_POINT('Ctrl Pts',(-0.978749804297957,2.31946620232442,
110.198615217839));
#35803=CARTESIAN_POINT('Ctrl Pts',(-1.00207311581661,2.30953403266787,110.200248008988));
#35804=CARTESIAN_POINT('Ctrl Pts',(-1.01771859107161,2.30268252466107,110.201357113242));
#35805=CARTESIAN_POINT('Ctrl Pts',(-1.05436616772552,2.28618728436905,110.203985658807));
#35806=CARTESIAN_POINT('Ctrl Pts',(-1.07530732243676,2.27641261571774,110.205511582211));
#35807=CARTESIAN_POINT('Ctrl Pts',(-1.14905385211283,2.24074545575631,110.210963253567));
#35808=CARTESIAN_POINT('Ctrl Pts',(-1.20108085237109,2.21329366978944,110.214952362949));
#35809=CARTESIAN_POINT('Ctrl Pts',(-1.4063694961024,2.09560346987792,110.231153431149));
#35810=CARTESIAN_POINT('Ctrl Pts',(-1.55085631513265,1.99105094290367,110.243579060927));
#35811=CARTESIAN_POINT('Ctrl Pts',(-1.74906870344958,1.81285123428931,110.261515451035));
#35812=CARTESIAN_POINT('Ctrl Pts',(-1.81184466034434,1.75011226518961,110.267366783505));
#35813=CARTESIAN_POINT('Ctrl Pts',(-1.88624639705353,1.66744945425621,110.274523852778));
#35814=CARTESIAN_POINT('Ctrl Pts',(-1.90108360634812,1.65051335298086,110.275963399404));
#35815=CARTESIAN_POINT('Ctrl Pts',(-1.92423450504423,1.62336107290992,110.278229941457));
#35816=CARTESIAN_POINT('Ctrl Pts',(-1.93269838498003,1.6132751057523,110.279063049797));
#35817=CARTESIAN_POINT('Ctrl Pts',(-1.94774475117345,1.5950567637726,110.280552362701));
#35818=CARTESIAN_POINT('Ctrl Pts',(-1.95435635505879,1.58694893999044,110.281209731729));
#35819=CARTESIAN_POINT('Ctrl Pts',(-1.96971792895204,1.5678694014886,110.282744165839));
#35820=CARTESIAN_POINT('Ctrl Pts',(-1.97842713849519,1.55686519970285,110.283619595965));
#35821=CARTESIAN_POINT('Ctrl Pts',(-2.00337651649327,1.52479385868837,110.286143999506));
#35822=CARTESIAN_POINT('Ctrl Pts',(-2.01937569930384,1.50354103564462,110.287783546316));
#35823=CARTESIAN_POINT('Ctrl Pts',(-2.09140652708025,1.40463311715435,110.295268923289));
#35824=CARTESIAN_POINT('Ctrl Pts',(-2.14331893088709,1.32407035491419,110.300958584952));
#35825=CARTESIAN_POINT('Ctrl Pts',(-2.2573087540372,1.12282171676607,110.314467186735));
#35826=CARTESIAN_POINT('Ctrl Pts',(-2.31446337576209,0.999713246903394,
110.322160480437));
#35827=CARTESIAN_POINT('Ctrl Pts',(-2.36143112015948,0.872610631806857,
110.330000354267));
#35828=CARTESIAN_POINT('Origin',(0.,0.,104.));
#35829=CARTESIAN_POINT('',(-2.36143104183299,0.872610843771477,111.329984892853));
#35830=CARTESIAN_POINT('',(-2.36143112101025,0.872610629504508,111.056268151607));
#35831=CARTESIAN_POINT('',(-2.36143112101026,0.872610629504505,104.));
#35832=CARTESIAN_POINT('',(-2.51749981257983,0.000971421916385074,110.112583302448));
#35833=CARTESIAN_POINT('Ctrl Pts',(-2.36143112101026,0.872610629504506,
111.056268151607));
#35834=CARTESIAN_POINT('Ctrl Pts',(-2.33290162629547,0.94981624035577,111.051081932139));
#35835=CARTESIAN_POINT('Ctrl Pts',(-2.30059282193492,1.02559131211717,111.04589571267));
#35836=CARTESIAN_POINT('Ctrl Pts',(-2.26468631750998,1.09954633066692,111.040709493202));
#35837=CARTESIAN_POINT('Ctrl Pts',(-2.22876338451224,1.17353518641205,111.035520900843));
#35838=CARTESIAN_POINT('Ctrl Pts',(-2.18923970143173,1.24570191647689,111.030332308485));
#35839=CARTESIAN_POINT('Ctrl Pts',(-2.14634234083047,1.31568263876908,111.025143716127));
#35840=CARTESIAN_POINT('Ctrl Pts',(-2.10336877650249,1.38578767621173,111.019945906649));
#35841=CARTESIAN_POINT('Ctrl Pts',(-2.05700982965078,1.4536985579788,111.014748097172));
#35842=CARTESIAN_POINT('Ctrl Pts',(-2.0075351419556,1.51908159880018,111.009550287694));
#35843=CARTESIAN_POINT('Ctrl Pts',(-1.96219405170571,1.57900190335994,111.004786753863));
#35844=CARTESIAN_POINT('Ctrl Pts',(-1.91423677985947,1.6367993045682,111.000023220032));
#35845=CARTESIAN_POINT('Ctrl Pts',(-1.86389785842549,1.69224437459749,110.995259686201));
#35846=CARTESIAN_POINT('Ctrl Pts',(-1.80836270405406,1.75341275952704,110.990004436801));
#35847=CARTESIAN_POINT('Ctrl Pts',(-1.74971071445244,1.81195742648223,110.984749187401));
#35848=CARTESIAN_POINT('Ctrl Pts',(-1.68821951860107,1.8675441379026,110.979493938002));
#35849=CARTESIAN_POINT('Ctrl Pts',(-1.62681550329481,1.92305203999531,110.974246139351));
#35850=CARTESIAN_POINT('Ctrl Pts',(-1.56258061669531,1.97561000963871,110.968998340701));
#35851=CARTESIAN_POINT('Ctrl Pts',(-1.49583108495485,2.02491866880692,110.963750542051));
#35852=CARTESIAN_POINT('Ctrl Pts',(-1.42859789519625,2.07458461180543,110.958464718566));
#35853=CARTESIAN_POINT('Ctrl Pts',(-1.35881378352396,2.12095360666406,110.953178895081));
#35854=CARTESIAN_POINT('Ctrl Pts',(-1.28683794339329,2.16375931134757,110.947893071597));
#35855=CARTESIAN_POINT('Ctrl Pts',(-1.21550750577025,2.20618118016209,110.942654645735));
#35856=CARTESIAN_POINT('Ctrl Pts',(-1.14202489231661,2.24510316621814,110.937416219873));
#35857=CARTESIAN_POINT('Ctrl Pts',(-1.06676945843396,2.28030900812861,110.932177794011));
#35858=CARTESIAN_POINT('Ctrl Pts',(-0.991538774808701,2.31550327142471,
110.926941090981));
#35859=CARTESIAN_POINT('Ctrl Pts',(-0.914536846343273,2.3469836225186,110.92170438795));
#35860=CARTESIAN_POINT('Ctrl Pts',(-0.836166345684795,2.37458040342797,
110.916467684919));
#35861=CARTESIAN_POINT('Ctrl Pts',(-0.757797979796856,2.40217643261578,
110.911231124533));
#35862=CARTESIAN_POINT('Ctrl Pts',(-0.678061551404548,2.42588894966515,
110.905994564147));
#35863=CARTESIAN_POINT('Ctrl Pts',(-0.597377051956488,2.44559745416039,
110.900758003761));
#35864=CARTESIAN_POINT('Ctrl Pts',(-0.515371964515496,2.46562853380418,
110.895435734983));
#35865=CARTESIAN_POINT('Ctrl Pts',(-0.432387965843948,2.48152321912133,
110.890113466204));
#35866=CARTESIAN_POINT('Ctrl Pts',(-0.348877286043428,2.49320895419597,
110.884791197426));
#35867=CARTESIAN_POINT('Ctrl Pts',(-0.266593439415926,2.50472301724645,
110.879547116681));
#35868=CARTESIAN_POINT('Ctrl Pts',(-0.183798755238067,2.51215099361981,
110.874303035937));
#35869=CARTESIAN_POINT('Ctrl Pts',(-0.100929632115851,2.51547599061509,
110.869058955193));
#35870=CARTESIAN_POINT('Ctrl Pts',(-0.0162071697278075,2.51887535001771,
110.863697592397));
#35871=CARTESIAN_POINT('Ctrl Pts',(0.0685925893749563,2.51798599741062,
110.858336229601));
#35872=CARTESIAN_POINT('Ctrl Pts',(0.153006789672422,2.51284603036361,110.852974866805));
#35873=CARTESIAN_POINT('Ctrl Pts',(0.237420989969885,2.5077060633166,110.847613504009));
#35874=CARTESIAN_POINT('Ctrl Pts',(0.321449133917394,2.49831560464582,110.842252141214));
#35875=CARTESIAN_POINT('Ctrl Pts',(0.40463942722808,2.48476823545628,110.836890778418));
#35876=CARTESIAN_POINT('Ctrl Pts',(0.486183197812372,2.47148899912655,110.831635529032));
#35877=CARTESIAN_POINT('Ctrl Pts',(0.567223179826133,2.4541668981303,110.826380279646));
#35878=CARTESIAN_POINT('Ctrl Pts',(0.647327861852357,2.43285282934863,110.82112503026));
#35879=CARTESIAN_POINT('Ctrl Pts',(0.727318973630284,2.41156897907633,110.815877231624));
#35880=CARTESIAN_POINT('Ctrl Pts',(0.806376977142961,2.38630452049806,110.810629432989));
#35881=CARTESIAN_POINT('Ctrl Pts',(0.884078586591063,2.35716170483299,110.805381634353));
#35882=CARTESIAN_POINT('Ctrl Pts',(0.962343211590781,2.32780772419264,110.800095810864));
#35883=CARTESIAN_POINT('Ctrl Pts',(1.03923123535665,2.29451902136058,110.794809987376));
#35884=CARTESIAN_POINT('Ctrl Pts',(1.11432368880329,2.25745187469674,110.789524163888));
#35885=CARTESIAN_POINT('Ctrl Pts',(1.18874279300605,2.22071710677448,110.784285738042));
#35886=CARTESIAN_POINT('Ctrl Pts',(1.26139797806441,2.18027159375407,110.779047312196));
#35887=CARTESIAN_POINT('Ctrl Pts',(1.33190130495525,2.13631579216616,110.77380888635));
#35888=CARTESIAN_POINT('Ctrl Pts',(1.40238144447153,2.09237444691215,110.768572183335));
#35889=CARTESIAN_POINT('Ctrl Pts',(1.47071074012569,2.04492534986803,110.76333548032));
#35890=CARTESIAN_POINT('Ctrl Pts',(1.53652764835991,1.9942138891868,110.758098777306));
#35891=CARTESIAN_POINT('Ctrl Pts',(1.60234276377146,1.94350380986272,110.752862216936));
#35892=CARTESIAN_POINT('Ctrl Pts',(1.66564526295127,1.88953182602826,110.747625656567));
#35893=CARTESIAN_POINT('Ctrl Pts',(1.72610540608032,1.83258461662764,110.742389096198));
#35894=CARTESIAN_POINT('Ctrl Pts',(1.7875551193565,1.7747053343693,110.737066827401));
#35895=CARTESIAN_POINT('Ctrl Pts',(1.84606822671548,1.71375288254076,110.731744558604));
#35896=CARTESIAN_POINT('Ctrl Pts',(1.90133765142355,1.65006708508447,110.726422289807));
#35897=CARTESIAN_POINT('Ctrl Pts',(1.95579512735124,1.58731687915724,110.72117820908));
#35898=CARTESIAN_POINT('Ctrl Pts',(2.00710335162121,1.52191351037076,110.715934128353));
#35899=CARTESIAN_POINT('Ctrl Pts',(2.05501055686366,1.45421382924896,110.710690047626));
#35900=CARTESIAN_POINT('Ctrl Pts',(2.10398919067139,1.38500006748214,110.705328684794));
#35901=CARTESIAN_POINT('Ctrl Pts',(2.1494125701995,1.31338647383459,110.699967321962));
#35902=CARTESIAN_POINT('Ctrl Pts',(2.19106064897833,1.23978203023703,110.694605959129));
#35903=CARTESIAN_POINT('Ctrl Pts',(2.23270872775716,1.16617758663948,110.689244596297));
#35904=CARTESIAN_POINT('Ctrl Pts',(2.27058133791497,1.09058277729602,110.683883233465));
#35905=CARTESIAN_POINT('Ctrl Pts',(2.30451099445111,1.01342751415874,110.678521870633));
#35906=CARTESIAN_POINT('Ctrl Pts',(2.33776910688383,0.93779932695729,110.673266621212));
#35907=CARTESIAN_POINT('Ctrl Pts',(2.36736180708549,0.860392569738316,110.668011371791));
#35908=CARTESIAN_POINT('Ctrl Pts',(2.39309684990577,0.781596901843338,110.66275612237));
#35909=CARTESIAN_POINT('Ctrl Pts',(2.41879540628265,0.70291294830205,110.657508323699));
#35910=CARTESIAN_POINT('Ctrl Pts',(2.44064702680772,0.622844430370973,110.652260525027));
#35911=CARTESIAN_POINT('Ctrl Pts',(2.45850702040397,0.541802067755736,110.647012726356));
#35912=CARTESIAN_POINT('Ctrl Pts',(2.47649642499183,0.460172483624873,110.641726902876));
#35913=CARTESIAN_POINT('Ctrl Pts',(2.49043592227857,0.377555316375038,110.636441079397));
#35914=CARTESIAN_POINT('Ctrl Pts',(2.50022848898027,0.294387080034804,110.631155255918));
#35915=CARTESIAN_POINT('Ctrl Pts',(2.50993324644491,0.211964607252194,110.625916830035));
#35916=CARTESIAN_POINT('Ctrl Pts',(2.51556509096039,0.129001375289329,110.620678404152));
#35917=CARTESIAN_POINT('Ctrl Pts',(2.51708094991472,0.0459319232824279,
110.615439978269));
#35918=CARTESIAN_POINT('Ctrl Pts',(2.51859631032829,-0.0371102085658783,
110.610203275217));
#35919=CARTESIAN_POINT('Ctrl Pts',(2.51599836524963,-0.120258030097391,
110.604966572166));
#35920=CARTESIAN_POINT('Ctrl Pts',(2.50929610141724,-0.203074679397106,
110.599729869114));
#35921=CARTESIAN_POINT('Ctrl Pts',(2.50259402015106,-0.285889072814097,
110.594493308707));
#35922=CARTESIAN_POINT('Ctrl Pts',(2.49178788066565,-0.368371852101413,
110.5892567483));
#35923=CARTESIAN_POINT('Ctrl Pts',(2.47693861969188,-0.450090351239497,
110.584020187894));
#35924=CARTESIAN_POINT('Ctrl Pts',(2.46184631643197,-0.533146361441927,
110.57869791914));
#35925=CARTESIAN_POINT('Ctrl Pts',(2.44257742264818,-0.615412361223516,
110.573375650386));
#35926=CARTESIAN_POINT('Ctrl Pts',(2.41924979163227,-0.696445759328899,
110.568053381633));
#35927=CARTESIAN_POINT('Ctrl Pts',(2.39626486043877,-0.776288718031306,
110.562809300868));
#35928=CARTESIAN_POINT('Ctrl Pts',(2.36933986167899,-0.854934627375409,
110.557565220103));
#35929=CARTESIAN_POINT('Ctrl Pts',(2.33863704368428,-0.931978019004564,
110.552321139338));
#35930=CARTESIAN_POINT('Ctrl Pts',(2.30724756818869,-1.01074445842575,110.54695977659));
#35931=CARTESIAN_POINT('Ctrl Pts',(2.27190946861718,-1.08783537024603,110.541598413842));
#35932=CARTESIAN_POINT('Ctrl Pts',(2.2328459912008,-1.16284351035662,110.536237051094));
#35933=CARTESIAN_POINT('Ctrl Pts',(2.19378251378443,-1.2378516504672,110.530875688346));
#35934=CARTESIAN_POINT('Ctrl Pts',(2.15099397327178,-1.31077661443296,110.525514325597));
#35935=CARTESIAN_POINT('Ctrl Pts',(2.10474978900411,-1.38124385091379,110.520152962849));
#35936=CARTESIAN_POINT('Ctrl Pts',(2.05942088042597,-1.45031638340145,110.514897713444));
#35937=CARTESIAN_POINT('Ctrl Pts',(2.01060448164522,-1.51728274163174,110.509642464039));
#35938=CARTESIAN_POINT('Ctrl Pts',(1.95852276773595,-1.5817695212198,110.504387214633));
#35939=CARTESIAN_POINT('Ctrl Pts',(1.90651489386549,-1.646164873204,110.499139415978));
#35940=CARTESIAN_POINT('Ctrl Pts',(1.85125118785159,-1.70808727334008,110.493891617323));
#35941=CARTESIAN_POINT('Ctrl Pts',(1.79299738092891,-1.76719173888463,110.488643818667));
#35942=CARTESIAN_POINT('Ctrl Pts',(1.73432147492567,-1.82672446726521,110.483357995184));
#35943=CARTESIAN_POINT('Ctrl Pts',(1.67261221345808,-1.8833978558186,110.4780721717));
#35944=CARTESIAN_POINT('Ctrl Pts',(1.60818291664799,-1.9368928614153,110.472786348217));
#35945=CARTESIAN_POINT('Ctrl Pts',(1.5443313529261,-1.98990818096363,110.46754792235));
#35946=CARTESIAN_POINT('Ctrl Pts',(1.47780870077296,-2.03980158975459,110.462309496484));
#35947=CARTESIAN_POINT('Ctrl Pts',(1.4089559973102,-2.08630037330285,110.457071070617));
#35948=CARTESIAN_POINT('Ctrl Pts',(1.34012593835553,-2.1327838641752,110.451834367582));
#35949=CARTESIAN_POINT('Ctrl Pts',(1.26896773212161,-2.17587468907029,110.446597664546));
#35950=CARTESIAN_POINT('Ctrl Pts',(1.19585270785378,-2.21534253584379,110.441360961511));
#35951=CARTESIAN_POINT('Ctrl Pts',(1.12273967520259,-2.2548093075329,110.43612440112));
#35952=CARTESIAN_POINT('Ctrl Pts',(1.04767033702651,-2.29065307904286,110.43088784073));
#35953=CARTESIAN_POINT('Ctrl Pts',(0.971040787340695,-2.32268939794385,
110.42565128034));
#35954=CARTESIAN_POINT('Ctrl Pts',(0.893157018421006,-2.35525006505663,
110.420329011567));
#35955=CARTESIAN_POINT('Ctrl Pts',(0.813661952898577,-2.38387731782439,
110.415006742794));
#35956=CARTESIAN_POINT('Ctrl Pts',(0.732990998319023,-2.40842904117669,
110.409684474021));
#35957=CARTESIAN_POINT('Ctrl Pts',(0.653505159118581,-2.4326200817395,110.404440393273));
#35958=CARTESIAN_POINT('Ctrl Pts',(0.572878219751572,-2.45285448865618,
110.399196312524));
#35959=CARTESIAN_POINT('Ctrl Pts',(0.49153862030256,-2.46904759669615,110.393952231776));
#35960=CARTESIAN_POINT('Ctrl Pts',(0.408379889083523,-2.4856028579492,110.388590868991));
#35961=CARTESIAN_POINT('Ctrl Pts',(0.324476742934424,-2.49793380011266,
110.383229506206));
#35962=CARTESIAN_POINT('Ctrl Pts',(0.240292321842426,-2.50600595571191,
110.37786814342));
#35963=CARTESIAN_POINT('Ctrl Pts',(0.156107900750426,-2.51407811131116,
110.372506780635));
#35964=CARTESIAN_POINT('Ctrl Pts',(0.0716427153179948,-2.51789152415955,
110.36714541785));
#35965=CARTESIAN_POINT('Ctrl Pts',(-0.0126423778882081,-2.51746825606229,
110.361784055065));
#35966=CARTESIAN_POINT('Ctrl Pts',(-0.095259280281888,-2.5170533653889,
110.35652880566));
#35967=CARTESIAN_POINT('Ctrl Pts',(-0.178008309443103,-2.51256648497769,
110.351273556255));
#35968=CARTESIAN_POINT('Ctrl Pts',(-0.260455293088755,-2.50399067296627,
110.34601830685));
#35969=CARTESIAN_POINT('Ctrl Pts',(-0.342785385640271,-2.49542701950819,
110.340770508195));
#35970=CARTESIAN_POINT('Ctrl Pts',(-0.424813828153972,-2.48278599667312,
110.33552270954));
#35971=CARTESIAN_POINT('Ctrl Pts',(-0.506106573980688,-2.46610267137715,
110.330274910885));
#35972=CARTESIAN_POINT('Ctrl Pts',(-0.587988355880546,-2.44929846099704,
110.324989087401));
#35973=CARTESIAN_POINT('Ctrl Pts',(-0.669123260711364,-2.42839312342264,
110.319703263918));
#35974=CARTESIAN_POINT('Ctrl Pts',(-0.749073089927936,-2.40347576562482,
110.314417440434));
#35975=CARTESIAN_POINT('Ctrl Pts',(-0.828306014497535,-2.37878184006907,
110.309179014568));
#35976=CARTESIAN_POINT('Ctrl Pts',(-0.906374582676004,-2.35014769695937,
110.303940588702));
#35977=CARTESIAN_POINT('Ctrl Pts',(-0.982864365463725,-2.31771091577478,
110.298702162836));
#35978=CARTESIAN_POINT('Ctrl Pts',(-1.05932899203433,-2.28528480250793,
110.293465459801));
#35979=CARTESIAN_POINT('Ctrl Pts',(-1.13421543997866,-2.24905871497737,
110.288228756766));
#35980=CARTESIAN_POINT('Ctrl Pts',(-1.20712835445952,-2.20921872748261,
110.282992053731));
#35981=CARTESIAN_POINT('Ctrl Pts',(-1.28003928282855,-2.16937982520944,
110.277755493342));
#35982=CARTESIAN_POINT('Ctrl Pts',(-1.35097638019609,-2.12592744085146,
110.272518932952));
#35983=CARTESIAN_POINT('Ctrl Pts',(-1.41956927528209,-2.0790933895992,110.267282372562));
#35984=CARTESIAN_POINT('Ctrl Pts',(-1.48928485123735,-2.03149279112211,
110.261960103789));
#35985=CARTESIAN_POINT('Ctrl Pts',(-1.55657838253628,-1.98039909590352,
110.256637835015));
#35986=CARTESIAN_POINT('Ctrl Pts',(-1.62109360583593,-1.92610014566166,
110.251315566242));
#35987=CARTESIAN_POINT('Ctrl Pts',(-1.6846610532615,-1.87259888676139,110.246071485494));
#35988=CARTESIAN_POINT('Ctrl Pts',(-1.74553098067731,-1.81598628647952,
110.240827404746));
#35989=CARTESIAN_POINT('Ctrl Pts',(-1.80339910666816,-1.75657562093651,
110.235583323999));
#35990=CARTESIAN_POINT('Ctrl Pts',(-1.86256143313221,-1.69583625656073,
110.230221961212));
#35991=CARTESIAN_POINT('Ctrl Pts',(-1.91858573120319,-1.63217254555964,
110.224860598426));
#35992=CARTESIAN_POINT('Ctrl Pts',(-1.97119093253988,-1.56595420031129,
110.21949923564));
#35993=CARTESIAN_POINT('Ctrl Pts',(-2.02379613387657,-1.49973585506294,
110.214137872853));
#35994=CARTESIAN_POINT('Ctrl Pts',(-2.07298199723095,-1.43096332771099,
110.208776510067));
#35995=CARTESIAN_POINT('Ctrl Pts',(-2.11851611379751,-1.36003519277271,
110.203415147281));
#35996=CARTESIAN_POINT('Ctrl Pts',(-2.16415197863569,-1.28894856535267,
110.19804180426));
#35997=CARTESIAN_POINT('Ctrl Pts',(-2.20628267264359,-1.21544362347196,
110.192668461239));
#35998=CARTESIAN_POINT('Ctrl Pts',(-2.24465002135591,-1.13989145607242,
110.187295118218));
#35999=CARTESIAN_POINT('Ctrl Pts',(-2.28295541755198,-1.0644612842508,110.18193045164));
#36000=CARTESIAN_POINT('Ctrl Pts',(-2.317509353925,-0.986990841980724,110.176565785063));
#36001=CARTESIAN_POINT('Ctrl Pts',(-2.34809743268924,-0.907879230183296,
110.171201118485));
#36002=CARTESIAN_POINT('Ctrl Pts',(-2.37863368161104,-0.828901668726391,
110.165845542044));
#36003=CARTESIAN_POINT('Ctrl Pts',(-2.40521729335624,-0.74828887520221,
110.160489965604));
#36004=CARTESIAN_POINT('Ctrl Pts',(-2.42768086911504,-0.666462187774268,
110.155134389163));
#36005=CARTESIAN_POINT('Ctrl Pts',(-2.45012200377272,-0.584717245166741,
110.14978416294));
#36006=CARTESIAN_POINT('Ctrl Pts',(-2.46845116952332,-0.501761235536918,
110.144433936718));
#36007=CARTESIAN_POINT('Ctrl Pts',(-2.48255009884958,-0.418032602439035,
110.139083710495));
#36008=CARTESIAN_POINT('Ctrl Pts',(-2.49663704236547,-0.334375148896358,
110.133738032618));
#36009=CARTESIAN_POINT('Ctrl Pts',(-2.50650083249334,-0.249946805333563,
110.12839235474));
#36010=CARTESIAN_POINT('Ctrl Pts',(-2.51207407896376,-0.165197069581622,
110.123046676863));
#36011=CARTESIAN_POINT('Ctrl Pts',(-2.5157103477164,-0.10990204224983,110.119558885406));
#36012=CARTESIAN_POINT('Ctrl Pts',(-2.51752120578779,-0.0544704357890657,
110.116071093949));
#36013=CARTESIAN_POINT('Ctrl Pts',(-2.5174998125801,0.000971421219968912,
110.112583302492));
#36014=CARTESIAN_POINT('Ctrl Pts',(-2.51749981257983,0.000971421916383455,
110.112583302448));
#36015=CARTESIAN_POINT('Ctrl Pts',(-2.5174649075931,0.0914298479257806,
110.106892653857));
#36016=CARTESIAN_POINT('Ctrl Pts',(-2.51255029658571,0.181738101408035,
110.101202005267));
#36017=CARTESIAN_POINT('Ctrl Pts',(-2.50282943169604,0.27138733543788,110.095511356676));
#36018=CARTESIAN_POINT('Ctrl Pts',(-2.49308231405315,0.361278681588806,
110.089805339577));
#36019=CARTESIAN_POINT('Ctrl Pts',(-2.47850306961473,0.450507135567614,
110.084099322478));
#36020=CARTESIAN_POINT('Ctrl Pts',(-2.45921603044753,0.538574753947772,
110.07839330538));
#36021=CARTESIAN_POINT('Ctrl Pts',(-2.43985726985429,0.626969863505942,
110.072666069695));
#36022=CARTESIAN_POINT('Ctrl Pts',(-2.41575577495363,0.71419518908884,110.066938834011));
#36023=CARTESIAN_POINT('Ctrl Pts',(-2.38708590651013,0.799766919133763,
110.061211598327));
#36024=CARTESIAN_POINT('Ctrl Pts',(-2.37890445742615,0.824186311004028,
110.059577231318));
#36025=CARTESIAN_POINT('Ctrl Pts',(-2.37035127937335,0.848471180762149,
110.057942864309));
#36026=CARTESIAN_POINT('Ctrl Pts',(-2.36143112101026,0.872610629504504,
110.0563084973));
#36027=CARTESIAN_POINT('',(-2.51749930920945,0.00210565722249706,110.386763667368));
#36028=CARTESIAN_POINT('Ctrl Pts',(-2.36143112015948,0.872610631806858,
110.330000354267));
#36029=CARTESIAN_POINT('Ctrl Pts',(-2.36296399590596,0.868462412246907,
110.330256222472));
#36030=CARTESIAN_POINT('Ctrl Pts',(-2.36448602047482,0.86430993896747,110.330512261035));
#36031=CARTESIAN_POINT('Ctrl Pts',(-2.40316528250013,0.757916079188607,
110.337070542764));
#36032=CARTESIAN_POINT('Ctrl Pts',(-2.4336632123791,0.653389373353525,110.343466229615));
#36033=CARTESIAN_POINT('Ctrl Pts',(-2.46029282490902,0.533811334540226,
110.351057984404));
#36034=CARTESIAN_POINT('Ctrl Pts',(-2.46317169506485,0.520365742903747,
110.351915497782));
#36035=CARTESIAN_POINT('Ctrl Pts',(-2.46763513881816,0.498652115547464,
110.353307551631));
#36036=CARTESIAN_POINT('Ctrl Pts',(-2.46928867943535,0.490398331419059,
110.353838378079));
#36037=CARTESIAN_POINT('Ctrl Pts',(-2.47214998174644,0.475734448201513,
110.354784684309));
#36038=CARTESIAN_POINT('Ctrl Pts',(-2.47337426686735,0.469327744784659,
110.355199229615));
#36039=CARTESIAN_POINT('Ctrl Pts',(-2.47598044322707,0.455396119768616,
110.356103126194));
#36040=CARTESIAN_POINT('Ctrl Pts',(-2.47735291470224,0.447869750556951,
110.356592971902));
#36041=CARTESIAN_POINT('Ctrl Pts',(-2.48011967607558,0.432295449558692,
110.357609601127));
#36042=CARTESIAN_POINT('Ctrl Pts',(-2.48150914672819,0.42424676048847,110.358136636322));
#36043=CARTESIAN_POINT('Ctrl Pts',(-2.48498571496911,0.403506720311722,
110.359498706434));
#36044=CARTESIAN_POINT('Ctrl Pts',(-2.48701473576366,0.390806045783101,
110.360336647044));
#36045=CARTESIAN_POINT('Ctrl Pts',(-2.50785197421962,0.253635865350339,
110.369424037005));
#36046=CARTESIAN_POINT('Ctrl Pts',(-2.51739394917129,0.127954017128451,
110.378073632483));
#36047=CARTESIAN_POINT('Ctrl Pts',(-2.51749912091712,0.0021038492205399,
110.386763463131));
#36048=CARTESIAN_POINT('Ctrl Pts',(-2.51749911942459,0.0021056344473654,
110.386763339863));
#36049=CARTESIAN_POINT('Ctrl Pts',(-2.51764329833865,-0.170274851464046,
110.398666042829));
#36050=CARTESIAN_POINT('Ctrl Pts',(-2.50008177033433,-0.342246676778853,
110.410566416665));
#36051=CARTESIAN_POINT('Ctrl Pts',(-2.45545670408571,-0.557478736267895,
110.42508713168));
#36052=CARTESIAN_POINT('Ctrl Pts',(-2.44453208447062,-0.603583914935035,
110.428178433417));
#36053=CARTESIAN_POINT('Ctrl Pts',(-2.42634831314994,-0.671695416985644,
110.432718035789));
#36054=CARTESIAN_POINT('Ctrl Pts',(-2.42007670117976,-0.693952223558913,
110.434197108021));
#36055=CARTESIAN_POINT('Ctrl Pts',(-2.40971649144246,-0.728868654455705,
110.436511272229));
#36056=CARTESIAN_POINT('Ctrl Pts',(-2.40583279957737,-0.741587241047874,
110.437352921095));
#36057=CARTESIAN_POINT('Ctrl Pts',(-2.39837042256289,-0.7653498034775,110.438923155181));
#36058=CARTESIAN_POINT('Ctrl Pts',(-2.39481578578661,-0.776400904761422,
110.439652497783));
#36059=CARTESIAN_POINT('Ctrl Pts',(-2.3866831242604,-0.801097406431204,
110.441280532335));
#36060=CARTESIAN_POINT('Ctrl Pts',(-2.38206424300593,-0.814729001574641,
110.442177864633));
#36061=CARTESIAN_POINT('Ctrl Pts',(-2.3700071018441,-0.849333708582673,
110.444452994953));
#36062=CARTESIAN_POINT('Ctrl Pts',(-2.36240711075495,-0.87024944861862,
110.445825475878));
#36063=CARTESIAN_POINT('Ctrl Pts',(-2.29794020685439,-1.04059591718973,
110.456988449925));
#36064=CARTESIAN_POINT('Ctrl Pts',(-2.22723159648514,-1.18440607317206,
110.466284810636));
#36065=CARTESIAN_POINT('Ctrl Pts',(-2.07236844857468,-1.43575982673904,
110.483272012167));
#36066=CARTESIAN_POINT('Ctrl Pts',(-1.99221931021569,-1.54504835624853,
110.490972141341));
#36067=CARTESIAN_POINT('Ctrl Pts',(-1.87882400547249,-1.67608769707031,
110.501278484627));
#36068=CARTESIAN_POINT('Ctrl Pts',(-1.85331782356258,-1.70424832738821,
110.503564715586));
#36069=CARTESIAN_POINT('Ctrl Pts',(-1.81009660686039,-1.74984960487127,
110.507408245809));
#36070=CARTESIAN_POINT('Ctrl Pts',(-1.79274241516079,-1.76762492956887,
110.508943793693));
#36071=CARTESIAN_POINT('Ctrl Pts',(-1.76842553870494,-1.79180543838547,
110.51108992227));
#36072=CARTESIAN_POINT('Ctrl Pts',(-1.76168490739144,-1.79843317789301,
110.51168426053));
#36073=CARTESIAN_POINT('Ctrl Pts',(-1.75003919197618,-1.80975555658372,
110.512710464341));
#36074=CARTESIAN_POINT('Ctrl Pts',(-1.74515207398136,-1.81446867838519,
110.513140922979));
#36075=CARTESIAN_POINT('Ctrl Pts',(-1.73583180624045,-1.82338462940491,
110.513961639012));
#36076=CARTESIAN_POINT('Ctrl Pts',(-1.73140231587304,-1.82759119744597,
110.514351591185));
#36077=CARTESIAN_POINT('Ctrl Pts',(-1.71965051990675,-1.83867049539541,
110.51538580572));
#36078=CARTESIAN_POINT('Ctrl Pts',(-1.71230241387873,-1.84551552054584,
110.516032107405));
#36079=CARTESIAN_POINT('Ctrl Pts',(-1.68598309736712,-1.86974041359636,
110.518345084864));
#36080=CARTESIAN_POINT('Ctrl Pts',(-1.66678734393684,-1.88687255747639,
110.520028479651));
#36081=CARTESIAN_POINT('Ctrl Pts',(-1.46354085495847,-2.06274771198428,
110.537785324103));
#36082=CARTESIAN_POINT('Ctrl Pts',(-1.25768649220713,-2.19433807223394,
110.555052539306));
#36083=CARTESIAN_POINT('Ctrl Pts',(-0.950715499486211,-2.33296668823648,
110.577757280399));
#36084=CARTESIAN_POINT('Ctrl Pts',(-0.863186945362496,-2.36674997844094,
110.583948379089));
#36085=CARTESIAN_POINT('Ctrl Pts',(-0.752984734023684,-2.40235436498814,
110.591397561033));
#36086=CARTESIAN_POINT('Ctrl Pts',(-0.731912822413238,-2.40885785707047,
110.592806967996));
#36087=CARTESIAN_POINT('Ctrl Pts',(-0.698223518727957,-2.41877259755477,
110.595037156421));
#36088=CARTESIAN_POINT('Ctrl Pts',(-0.685660703036756,-2.4223637983495,
110.59586372085));
#36089=CARTESIAN_POINT('Ctrl Pts',(-0.661854342247283,-2.42896903266096,
110.597420663598));
#36090=CARTESIAN_POINT('Ctrl Pts',(-0.65061678576954,-2.43200319435752,
110.598151672839));
#36091=CARTESIAN_POINT('Ctrl Pts',(-0.625097279860039,-2.43870396798316,
110.59980303306));
#36092=CARTESIAN_POINT('Ctrl Pts',(-0.610803268316554,-2.44232328629008,
110.600721848056));
#36093=CARTESIAN_POINT('Ctrl Pts',(-0.567178033251368,-2.45296246985002,
110.603508004502));
#36094=CARTESIAN_POINT('Ctrl Pts',(-0.537751086756829,-2.45958120165861,
110.60536258629));
#36095=CARTESIAN_POINT('Ctrl Pts',(-0.301082449323961,-2.50836213760925,
110.620097502664));
#36096=CARTESIAN_POINT('Ctrl Pts',(-0.0894038025816362,-2.52478641643537,
110.632078951845));
#36097=CARTESIAN_POINT('Ctrl Pts',(0.244908168020617,-2.50858624571339,
110.651378927812));
#36098=CARTESIAN_POINT('Ctrl Pts',(0.367347059302306,-2.49359848791987,
110.658553452984));
#36099=CARTESIAN_POINT('Ctrl Pts',(0.505768845967032,-2.46623713093697,
110.667263469902));
#36100=CARTESIAN_POINT('Ctrl Pts',(0.523319645846156,-2.46257268267309,
110.668379150227));
#36101=CARTESIAN_POINT('Ctrl Pts',(0.54907262591235,-2.45690796388606,110.670034909156));
#36102=CARTESIAN_POINT('Ctrl Pts',(0.557306715375849,-2.45505330118695,
110.670567132018));
#36103=CARTESIAN_POINT('Ctrl Pts',(0.571889187600747,-2.45169157515576,
110.671514951305));
#36104=CARTESIAN_POINT('Ctrl Pts',(0.57824124413233,-2.45020119271443,110.671929601588));
#36105=CARTESIAN_POINT('Ctrl Pts',(0.592013518152153,-2.44691326617059,
110.672832569946));
#36106=CARTESIAN_POINT('Ctrl Pts',(0.599431258679526,-2.44510668484646,
110.673321373505));
#36107=CARTESIAN_POINT('Ctrl Pts',(0.620008583542812,-2.43999584019113,
110.674683982924));
#36108=CARTESIAN_POINT('Ctrl Pts',(0.633149619978672,-2.4366189450218,110.675561722554));
#36109=CARTESIAN_POINT('Ctrl Pts',(0.706331848654608,-2.41718110067154,
110.680489642497));
#36110=CARTESIAN_POINT('Ctrl Pts',(0.765784781830726,-2.39900843149059,
110.684642638261));
#36111=CARTESIAN_POINT('Ctrl Pts',(0.992271495586989,-2.32050276135613,
110.700895299131));
#36112=CARTESIAN_POINT('Ctrl Pts',(1.153422131308,-2.24476232836648,110.713342448533));
#36113=CARTESIAN_POINT('Ctrl Pts',(1.40224111491262,-2.0938928176765,110.733116221043));
#36114=CARTESIAN_POINT('Ctrl Pts',(1.49514037930865,-2.02860266874869,110.740656443378));
#36115=CARTESIAN_POINT('Ctrl Pts',(1.60132042408556,-1.94270804358123,110.749451090932));
#36116=CARTESIAN_POINT('Ctrl Pts',(1.61910876371784,-1.9279078071364,110.750931251268));
#36117=CARTESIAN_POINT('Ctrl Pts',(1.64679788193825,-1.9042163523838,110.753246725604));
#36118=CARTESIAN_POINT('Ctrl Pts',(1.65683619805588,-1.89548859255138,110.754088608896));
#36119=CARTESIAN_POINT('Ctrl Pts',(1.67550441776598,-1.8789959933731,110.755659057023));
#36120=CARTESIAN_POINT('Ctrl Pts',(1.68415066144695,-1.8712502648957,110.756388381168));
#36121=CARTESIAN_POINT('Ctrl Pts',(1.70339261395467,-1.85377098068766,110.758016089393));
#36122=CARTESIAN_POINT('Ctrl Pts',(1.71395913390444,-1.8440057882232,110.758913116331));
#36123=CARTESIAN_POINT('Ctrl Pts',(1.74064159773811,-1.81891932352864,110.761186931874));
#36124=CARTESIAN_POINT('Ctrl Pts',(1.75663953666859,-1.80347394320802,110.76255841418));
#36125=CARTESIAN_POINT('Ctrl Pts',(1.87205792432113,-1.68904891988188,110.772519591715));
#36126=CARTESIAN_POINT('Ctrl Pts',(1.96326066391103,-1.58211946020137,110.780738609599));
#36127=CARTESIAN_POINT('Ctrl Pts',(2.15574901970139,-1.31398633388733,110.799790462211));
#36128=CARTESIAN_POINT('Ctrl Pts',(2.24861184733092,-1.14784146530307,110.810451683602));
#36129=CARTESIAN_POINT('Ctrl Pts',(2.33259982649779,-0.947389891033239,
110.823710363112));
#36130=CARTESIAN_POINT('Ctrl Pts',(2.3428557902465,-0.921735405158754,110.825414972068));
#36131=CARTESIAN_POINT('Ctrl Pts',(2.35625249026904,-0.886555599091831,
110.827769685938));
#36132=CARTESIAN_POINT('Ctrl Pts',(2.35976198099206,-0.877171598542212,
110.828399441413));
#36133=CARTESIAN_POINT('Ctrl Pts',(2.36555159457127,-0.861404575828846,
110.829460715437));
#36134=CARTESIAN_POINT('Ctrl Pts',(2.3678621656094,-0.855032720284201,110.82989046374));
#36135=CARTESIAN_POINT('Ctrl Pts',(2.37220971985199,-0.842890703919863,
110.830711151496));
#36136=CARTESIAN_POINT('Ctrl Pts',(2.37425144596497,-0.837122310732061,
110.831101794246));
#36137=CARTESIAN_POINT('Ctrl Pts',(2.37960687987857,-0.821814654359174,
110.83214033244));
#36138=CARTESIAN_POINT('Ctrl Pts',(2.38288421396437,-0.812262915249904,
110.832790298342));
#36139=CARTESIAN_POINT('Ctrl Pts',(2.39441755864728,-0.777978579479148,
110.835129504385));
#36140=CARTESIAN_POINT('Ctrl Pts',(2.40234637176346,-0.753138698998407,
110.836835946197));
#36141=CARTESIAN_POINT('Ctrl Pts',(2.48090624281213,-0.493147885579695,
110.854785551936));
#36142=CARTESIAN_POINT('Ctrl Pts',(2.51716358381374,-0.248987751820035,
110.872236167635));
#36143=CARTESIAN_POINT('Ctrl Pts',(2.5176216474378,0.0877017228365608,110.894904945598));
#36144=CARTESIAN_POINT('Ctrl Pts',(2.51279781121409,0.178776008820882,110.900917916456));
#36145=CARTESIAN_POINT('Ctrl Pts',(2.50070308824772,0.291151166824925,110.908186495869));
#36146=CARTESIAN_POINT('Ctrl Pts',(2.49807828607229,0.312873558370864,110.90958470036));
#36147=CARTESIAN_POINT('Ctrl Pts',(2.49343921493223,0.347472104184843,110.911801369078));
#36148=CARTESIAN_POINT('Ctrl Pts',(2.49160762867454,0.36037122088898,110.91262549553));
#36149=CARTESIAN_POINT('Ctrl Pts',(2.487949229522,0.384773333181392,110.914180387578));
#36150=CARTESIAN_POINT('Ctrl Pts',(2.48614257036175,0.396278959529849,110.914911763166));
#36151=CARTESIAN_POINT('Ctrl Pts',(2.48185764350168,0.422383893568352,110.916567367625));
#36152=CARTESIAN_POINT('Ctrl Pts',(2.47933026533961,0.436974789095167,110.917490028922));
#36153=CARTESIAN_POINT('Ctrl Pts',(2.47120631175511,0.481533992124443,110.920300074781));
#36154=CARTESIAN_POINT('Ctrl Pts',(2.46519388526105,0.511424336201167,110.922174370069));
#36155=CARTESIAN_POINT('Ctrl Pts',(2.41374593185286,0.745149747006543,110.936763458479));
#36156=CARTESIAN_POINT('Ctrl Pts',(2.34365232581276,0.94271933301619,110.948606305652));
#36157=CARTESIAN_POINT('Ctrl Pts',(2.19375913317683,1.24133829274307,110.967865195147));
#36158=CARTESIAN_POINT('Ctrl Pts',(2.12928795658594,1.348934648664,110.97515283595));
#36159=CARTESIAN_POINT('Ctrl Pts',(2.04673092243822,1.46595417215013,110.983992650407));
#36160=CARTESIAN_POINT('Ctrl Pts',(2.03621622391404,1.48052441740371,110.985110700126));
#36161=CARTESIAN_POINT('Ctrl Pts',(2.02053020003841,1.50177738913931,110.986769322118));
#36162=CARTESIAN_POINT('Ctrl Pts',(2.01547948648121,1.50854898843145,110.987301999782));
#36163=CARTESIAN_POINT('Ctrl Pts',(2.00646719936282,1.5205059055601,110.988250312824));
#36164=CARTESIAN_POINT('Ctrl Pts',(2.00251942084914,1.52570141204202,110.988664998259));
#36165=CARTESIAN_POINT('Ctrl Pts',(1.99391193254135,1.53693840630447,110.989567668675));
#36166=CARTESIAN_POINT('Ctrl Pts',(1.9892450181865,1.54297398340292,110.990056136251));
#36167=CARTESIAN_POINT('Ctrl Pts',(1.97621645630644,1.5596660691145,110.991416935954));
#36168=CARTESIAN_POINT('Ctrl Pts',(1.96779627073543,1.57027626454492,110.992293185582));
#36169=CARTESIAN_POINT('Ctrl Pts',(1.92044609161951,1.62896284405293,110.997200557076));
#36170=CARTESIAN_POINT('Ctrl Pts',(1.8798429750062,1.67565574524605,111.001333546881));
#36171=CARTESIAN_POINT('Ctrl Pts',(1.71599060106809,1.85062621329894,111.017584161762));
#36172=CARTESIAN_POINT('Ctrl Pts',(1.5809995624089,1.96720264391738,111.030052847615));
#36173=CARTESIAN_POINT('Ctrl Pts',(1.34163221489586,2.13323642262933,111.049849200214));
#36174=CARTESIAN_POINT('Ctrl Pts',(1.24414846610622,2.19152355668126,111.057391660969));
#36175=CARTESIAN_POINT('Ctrl Pts',(1.12243469940877,2.25354877002397,111.066188509777));
#36176=CARTESIAN_POINT('Ctrl Pts',(1.10167293224502,2.26377086341799,111.06766876876));
#36177=CARTESIAN_POINT('Ctrl Pts',(1.06875889310635,2.27941606945674,111.069984361724));
#36178=CARTESIAN_POINT('Ctrl Pts',(1.05669993667899,2.28503138800181,111.070826266126));
#36179=CARTESIAN_POINT('Ctrl Pts',(1.03403527199155,2.29536752013784,111.072396733316));
#36180=CARTESIAN_POINT('Ctrl Pts',(1.02344036850641,2.30011104418824,111.073126055589));
#36181=CARTESIAN_POINT('Ctrl Pts',(0.999641626306764,2.31056916188519,111.074753733701));
#36182=CARTESIAN_POINT('Ctrl Pts',(0.986420778775437,2.31624422151011,111.075650732627));
#36183=CARTESIAN_POINT('Ctrl Pts',(0.952645918878369,2.33040047278099,111.077924427997));
#36184=CARTESIAN_POINT('Ctrl Pts',(0.93202660782502,2.33872338272945,111.079295819125));
#36185=CARTESIAN_POINT('Ctrl Pts',(0.760783654652436,2.4052204919798,111.090554863484));
#36186=CARTESIAN_POINT('Ctrl Pts',(0.604987457403047,2.44905634527811,111.099937467251));
#36187=CARTESIAN_POINT('Ctrl Pts',(0.323164559339578,2.49979211058615,111.116410999687));
#36188=CARTESIAN_POINT('Ctrl Pts',(0.198813172750137,2.51274066839984,111.123526272158));
#36189=CARTESIAN_POINT('Ctrl Pts',(0.0305860775248409,2.51768924404162,
111.133481900247));
#36190=CARTESIAN_POINT('Ctrl Pts',(-0.0128741655536576,2.51784202757347,
111.136084261461));
#36191=CARTESIAN_POINT('Ctrl Pts',(-0.0840523629938136,2.51624944081131,
111.140427058072));
#36192=CARTESIAN_POINT('Ctrl Pts',(-0.111777184821294,2.51517032467341,
111.142138743466));
#36193=CARTESIAN_POINT('Ctrl Pts',(-0.149496912776967,2.51307732224715,
111.144501723648));
#36194=CARTESIAN_POINT('Ctrl Pts',(-0.159513051122024,2.51246144906779,
111.145132484003));
#36195=CARTESIAN_POINT('Ctrl Pts',(-0.176290874480291,2.511329082898,111.146194974938));
#36196=CARTESIAN_POINT('Ctrl Pts',(-0.183054766898247,2.51084511381333,
111.146624926254));
#36197=CARTESIAN_POINT('Ctrl Pts',(-0.195915258578477,2.50987267968945,
111.147445619513));
#36198=CARTESIAN_POINT('Ctrl Pts',(-0.202012179560194,2.50938931498974,
111.147836062298));
#36199=CARTESIAN_POINT('Ctrl Pts',(-0.216518914339997,2.5081860085542,111.148768222285));
#36200=CARTESIAN_POINT('Ctrl Pts',(-0.224926924535857,2.50744598497346,
111.149311024371));
#36201=CARTESIAN_POINT('Ctrl Pts',(-0.254757061301248,2.50466926907201,
111.15124539124));
#36202=CARTESIAN_POINT('Ctrl Pts',(-0.276155932536117,2.50240027495241,
111.152648777436));
#36203=CARTESIAN_POINT('Ctrl Pts',(-0.424750308401898,2.48471521378279,
111.162491659274));
#36204=CARTESIAN_POINT('Ctrl Pts',(-0.550624975280106,2.45988382505115,
111.171318960531));
#36205=CARTESIAN_POINT('Ctrl Pts',(-0.81232890958307,2.38715851098287,111.190081669048));
#36206=CARTESIAN_POINT('Ctrl Pts',(-0.947083159303446,2.33697358364249,
111.199981762439));
#36207=CARTESIAN_POINT('Ctrl Pts',(-1.14334995170638,2.24409714444885,111.214473325633));
#36208=CARTESIAN_POINT('Ctrl Pts',(-1.20845710557636,2.20971815671582,111.219297945602));
#36209=CARTESIAN_POINT('Ctrl Pts',(-1.28967573089423,2.16216643855821,111.225341380822));
#36210=CARTESIAN_POINT('Ctrl Pts',(-1.30725439326156,2.15158387958411,111.22665106952));
#36211=CARTESIAN_POINT('Ctrl Pts',(-1.33552819121489,2.13408827863243,111.228760821941));
#36212=CARTESIAN_POINT('Ctrl Pts',(-1.34630341301713,2.12730709120473,111.22956562949));
#36213=CARTESIAN_POINT('Ctrl Pts',(-1.36689747730258,2.11412744844487,111.231105494151));
#36214=CARTESIAN_POINT('Ctrl Pts',(-1.37672396433045,2.10774161490821,111.231840988625));
#36215=CARTESIAN_POINT('Ctrl Pts',(-1.39913027009237,2.0929571210878,111.233519978948));
#36216=CARTESIAN_POINT('Ctrl Pts',(-1.4116797841383,2.08451318685592,111.234461763272));
#36217=CARTESIAN_POINT('Ctrl Pts',(-1.45140864262269,2.05725830032516,111.237448430081));
#36218=CARTESIAN_POINT('Ctrl Pts',(-1.47829465102032,2.03802449499353,111.239477405331));
#36219=CARTESIAN_POINT('Ctrl Pts',(-1.64314642487512,1.91511298206485,111.251985100253));
#36220=CARTESIAN_POINT('Ctrl Pts',(-1.7705287216286,1.7980057007078,111.261906290343));
#36221=CARTESIAN_POINT('Ctrl Pts',(-1.94989840103383,1.59540149108219,111.277454413042));
#36222=CARTESIAN_POINT('Ctrl Pts',(-2.01051478956918,1.51830102061003,111.283080421963));
#36223=CARTESIAN_POINT('Ctrl Pts',(-2.09212920244327,1.40100620191224,111.29152201836));
#36224=CARTESIAN_POINT('Ctrl Pts',(-2.11678601996941,1.36346597643312,111.294208050461));
#36225=CARTESIAN_POINT('Ctrl Pts',(-2.1553800283297,1.3011342341153,111.298676752008));
#36226=CARTESIAN_POINT('Ctrl Pts',(-2.16992510023507,1.2767295187199,111.300428526105));
#36227=CARTESIAN_POINT('Ctrl Pts',(-2.18908971810314,1.24330004359021,111.302838287168));
#36228=CARTESIAN_POINT('Ctrl Pts',(-2.19407291621182,1.23448484091084,111.303474675938));
#36229=CARTESIAN_POINT('Ctrl Pts',(-2.20231328604422,1.21970024216596,111.304543992961));
#36230=CARTESIAN_POINT('Ctrl Pts',(-2.20559975925482,1.21374716914736,111.304975091204));
#36231=CARTESIAN_POINT('Ctrl Pts',(-2.21178839982244,1.20242901282071,111.305795857677));
#36232=CARTESIAN_POINT('Ctrl Pts',(-2.21469526273643,1.19706655945658,111.306185213192));
#36233=CARTESIAN_POINT('Ctrl Pts',(-2.22154739615755,1.18431565533583,111.307112075069));
#36234=CARTESIAN_POINT('Ctrl Pts',(-2.22547530924003,1.17691802946674,111.307650638592));
#36235=CARTESIAN_POINT('Ctrl Pts',(-2.23918245250679,1.15078873182618,111.309555463624));
#36236=CARTESIAN_POINT('Ctrl Pts',(-2.24876238074172,1.13195426011333,111.310933095378));
#36237=CARTESIAN_POINT('Ctrl Pts',(-2.29670992164692,1.03467635481964,111.318063501898));
#36238=CARTESIAN_POINT('Ctrl Pts',(-2.33119449209657,0.954436009772043,
111.323993087481));
#36239=CARTESIAN_POINT('Ctrl Pts',(-2.36143104183299,0.872610843771477,
111.329984892853));
#36240=CARTESIAN_POINT('Origin',(0.,0.,104.));
#36241=CARTESIAN_POINT('',(-2.36143112095426,0.872610629656035,112.333400434891));
#36242=CARTESIAN_POINT('',(-2.36143112101026,0.872610629504506,112.056167113269));
#36243=CARTESIAN_POINT('',(-2.36143112101026,0.872610629504505,104.));
#36244=CARTESIAN_POINT('',(-2.51749898697117,-0.00225845060319292,111.11258330253));
#36245=CARTESIAN_POINT('Ctrl Pts',(-2.36143112101026,0.872610629504506,
112.056167113269));
#36246=CARTESIAN_POINT('Ctrl Pts',(-2.33266408168154,0.950459076031816,
112.050928731472));
#36247=CARTESIAN_POINT('Ctrl Pts',(-2.30002250408097,1.02693994154336,112.045690349676));
#36248=CARTESIAN_POINT('Ctrl Pts',(-2.26366542465182,1.10164653824895,112.040451967879));
#36249=CARTESIAN_POINT('Ctrl Pts',(-2.22732008720791,1.1763290075007,112.035215277885));
#36250=CARTESIAN_POINT('Ctrl Pts',(-2.18726183293021,1.249237931436,112.029978587892));
#36251=CARTESIAN_POINT('Ctrl Pts',(-2.14369712875725,1.31998820834049,112.024741897898));
#36252=CARTESIAN_POINT('Ctrl Pts',(-2.10013335341261,1.39073697680224,112.019505319554));
#36253=CARTESIAN_POINT('Ctrl Pts',(-2.05306351968801,1.45932679740954,112.014268741209));
#36254=CARTESIAN_POINT('Ctrl Pts',(-2.00273846521359,1.52539991148351,112.009032162865));
#36255=CARTESIAN_POINT('Ctrl Pts',(-1.95183672119319,1.59223017673308,112.003735577035));
#36256=CARTESIAN_POINT('Ctrl Pts',(-1.89760495238244,1.6564852927305,111.998438991206));
#36257=CARTESIAN_POINT('Ctrl Pts',(-1.84034469218861,1.71782934656886,111.993142405376));
#36258=CARTESIAN_POINT('Ctrl Pts',(-1.78365150597444,1.77856588279169,111.987898274005));
#36259=CARTESIAN_POINT('Ctrl Pts',(-1.72398992664513,1.83644848078674,111.982654142635));
#36260=CARTESIAN_POINT('Ctrl Pts',(-1.66168851342568,1.89118944961872,111.977410011265));
#36261=CARTESIAN_POINT('Ctrl Pts',(-1.59845234474376,1.94675173881877,111.972087198205));
#36262=CARTESIAN_POINT('Ctrl Pts',(-1.53249686008921,1.99907704075062,111.966764385146));
#36263=CARTESIAN_POINT('Ctrl Pts',(-1.46419743944608,2.04790920412003,111.961441572086));
#36264=CARTESIAN_POINT('Ctrl Pts',(-1.39589801880295,2.09674136748945,111.956118759026));
#36265=CARTESIAN_POINT('Ctrl Pts',(-1.32525510956176,2.14208018212246,111.950795945967));
#36266=CARTESIAN_POINT('Ctrl Pts',(-1.25266969144954,2.18371813522801,111.945473132907));
#36267=CARTESIAN_POINT('Ctrl Pts',(-1.18100560812644,2.22482757316149,111.940217882906));
#36268=CARTESIAN_POINT('Ctrl Pts',(-1.10718337541876,2.26248144184893,111.934962632905));
#36269=CARTESIAN_POINT('Ctrl Pts',(-1.03157000785796,2.29644716222428,111.929707382903));
#36270=CARTESIAN_POINT('Ctrl Pts',(-0.956063842513632,2.33036472708657,
111.924459583628));
#36271=CARTESIAN_POINT('Ctrl Pts',(-0.87877200372657,2.3606043423413,111.919211784352));
#36272=CARTESIAN_POINT('Ctrl Pts',(-0.800087502345774,2.38697847468093,
111.913963985076));
#36273=CARTESIAN_POINT('Ctrl Pts',(-0.720832875525854,2.41354370645587,
111.908678161745));
#36274=CARTESIAN_POINT('Ctrl Pts',(-0.640165730344157,2.43618696679044,
111.903392338414));
#36275=CARTESIAN_POINT('Ctrl Pts',(-0.558509793004058,2.45476537801855,
111.898106515082));
#36276=CARTESIAN_POINT('Ctrl Pts',(-0.477586046098783,2.4731772008094,111.892868088541));
#36277=CARTESIAN_POINT('Ctrl Pts',(-0.395691626781038,2.48759667545717,
111.887629661999));
#36278=CARTESIAN_POINT('Ctrl Pts',(-0.313254033035,2.49793477913001,111.882391235457));
#36279=CARTESIAN_POINT('Ctrl Pts',(-0.230843551335432,2.508269482811,111.877154531727));
#36280=CARTESIAN_POINT('Ctrl Pts',(-0.147890707467881,2.51452542398895,
111.871917827997));
#36281=CARTESIAN_POINT('Ctrl Pts',(-0.0648308432706447,2.51666509725883,
111.866681124267));
#36282=CARTESIAN_POINT('Ctrl Pts',(0.0182267587089307,2.5188047122526,111.861444563164));
#36283=CARTESIAN_POINT('Ctrl Pts',(0.101390913928715,2.51682827139128,111.856208002061));
#36284=CARTESIAN_POINT('Ctrl Pts',(0.184224930055796,2.51075037093414,111.850971440958));
#36285=CARTESIAN_POINT('Ctrl Pts',(0.268414691909898,2.5045729933786,111.845649172972));
#36286=CARTESIAN_POINT('Ctrl Pts',(0.352262919021846,2.49415871053369,111.840326904985));
#36287=CARTESIAN_POINT('Ctrl Pts',(0.435316999847022,2.47957765751432,111.835004636999));
#36288=CARTESIAN_POINT('Ctrl Pts',(0.517150979240378,2.46521080665683,111.8297605555));
#36289=CARTESIAN_POINT('Ctrl Pts',(0.59821354739173,2.44679895993656,111.824516474));
#36290=CARTESIAN_POINT('Ctrl Pts',(0.678084285437258,2.42446034239437,111.819272392501));
#36291=CARTESIAN_POINT('Ctrl Pts',(0.759741269292391,2.40162213936001,111.813911031271));
#36292=CARTESIAN_POINT('Ctrl Pts',(0.840151985597406,2.37467957055689,111.808549670041));
#36293=CARTESIAN_POINT('Ctrl Pts',(0.918887765864556,2.34381132426321,111.803188308812));
#36294=CARTESIAN_POINT('Ctrl Pts',(0.997623546131707,2.31294307796952,111.797826947582));
#36295=CARTESIAN_POINT('Ctrl Pts',(1.07468395475887,2.27814942415562,111.792465586352));
#36296=CARTESIAN_POINT('Ctrl Pts',(1.14966792222199,2.23965843793507,111.787104225123));
#36297=CARTESIAN_POINT('Ctrl Pts',(1.22316778867983,2.20192927471852,111.781848977265));
#36298=CARTESIAN_POINT('Ctrl Pts',(1.29494416129683,2.1605084851675,111.776593729406));
#36299=CARTESIAN_POINT('Ctrl Pts',(1.36460213303968,2.1155772896549,111.771338481548));
#36300=CARTESIAN_POINT('Ctrl Pts',(1.43416134522127,2.0707097966166,111.766090684466));
#36301=CARTESIAN_POINT('Ctrl Pts',(1.50160773768334,2.02234203137133,111.760842887384));
#36302=CARTESIAN_POINT('Ctrl Pts',(1.56657003363604,1.97070154506297,111.755595090303));
#36303=CARTESIAN_POINT('Ctrl Pts',(1.63200306190929,1.91868685945026,111.750309266429));
#36304=CARTESIAN_POINT('Ctrl Pts',(1.6949154194594,1.8633520392084,111.745023442556));
#36305=CARTESIAN_POINT('Ctrl Pts',(1.75495656268644,1.80497471258846,111.739737618682));
#36306=CARTESIAN_POINT('Ctrl Pts',(1.81445929822488,1.74712087369383,111.734499194443));
#36307=CARTESIAN_POINT('Ctrl Pts',(1.87114177041857,1.68627920366057,111.729260770203));
#36308=CARTESIAN_POINT('Ctrl Pts',(1.92469655566788,1.62275981543795,111.724022345963));
#36309=CARTESIAN_POINT('Ctrl Pts',(1.97823372746608,1.5592613178908,111.718785644571));
#36310=CARTESIAN_POINT('Ctrl Pts',(2.0286449580902,1.49308720369504,111.713548943179));
#36311=CARTESIAN_POINT('Ctrl Pts',(2.07566176573437,1.42458221393799,111.708312241787));
#36312=CARTESIAN_POINT('Ctrl Pts',(2.12267729253595,1.35607909040949,111.703075683055));
#36313=CARTESIAN_POINT('Ctrl Pts',(2.16629831995995,1.2852455985925,111.697839124322));
#36314=CARTESIAN_POINT('Ctrl Pts',(2.20629933337562,1.21245597921999,111.69260256559));
#36315=CARTESIAN_POINT('Ctrl Pts',(2.24695508308651,1.1384749398896,111.687280294902));
#36316=CARTESIAN_POINT('Ctrl Pts',(2.28387099652829,1.06247358409721,111.681958024214));
#36317=CARTESIAN_POINT('Ctrl Pts',(2.31685947685962,0.984869744933706,111.676635753527));
#36318=CARTESIAN_POINT('Ctrl Pts',(2.34936331018264,0.908406014926671,111.671391674454));
#36319=CARTESIAN_POINT('Ctrl Pts',(2.37805423941063,0.830387034882338,111.666147595382));
#36320=CARTESIAN_POINT('Ctrl Pts',(2.40280253307926,0.751229816386359,111.66090351631));
#36321=CARTESIAN_POINT('Ctrl Pts',(2.42810433929985,0.670302192439338,111.655542149815));
#36322=CARTESIAN_POINT('Ctrl Pts',(2.44928489436196,0.588185296471621,111.650180783319));
#36323=CARTESIAN_POINT('Ctrl Pts',(2.46626069105269,0.505335981074263,111.644819416824));
#36324=CARTESIAN_POINT('Ctrl Pts',(2.48323648774343,0.422486665676905,111.639458050329));
#36325=CARTESIAN_POINT('Ctrl Pts',(2.49600751534742,0.338905443219578,111.634096683833));
#36326=CARTESIAN_POINT('Ctrl Pts',(2.50454671857413,0.255052905256035,111.628735317338));
#36327=CARTESIAN_POINT('Ctrl Pts',(2.51291690716762,0.172860042741429,111.623480067229));
#36328=CARTESIAN_POINT('Ctrl Pts',(2.51725222512239,0.0901029227652949,
111.618224817121));
#36329=CARTESIAN_POINT('Ctrl Pts',(2.51748967125913,0.00721145641435616,
111.612969567012));
#36330=CARTESIAN_POINT('Ctrl Pts',(2.51772678075161,-0.0755624888167714,
111.607721767645));
#36331=CARTESIAN_POINT('Ctrl Pts',(2.5138775571612,-0.158469944519678,111.602473968278));
#36332=CARTESIAN_POINT('Ctrl Pts',(2.50593072673114,-0.24107559566393,111.59722616891));
#36333=CARTESIAN_POINT('Ctrl Pts',(2.4979263160133,-0.324279781935754,111.591940345604));
#36334=CARTESIAN_POINT('Ctrl Pts',(2.48576461990296,-0.407177300180112,
111.586654522297));
#36335=CARTESIAN_POINT('Ctrl Pts',(2.46948765707609,-0.489322962417326,
111.581368698991));
#36336=CARTESIAN_POINT('Ctrl Pts',(2.45335664588034,-0.570732044156025,
111.576130272397));
#36337=CARTESIAN_POINT('Ctrl Pts',(2.43318396494953,-0.651402238350493,
111.570891845803));
#36338=CARTESIAN_POINT('Ctrl Pts',(2.40906235766797,-0.730906838706032,
111.56565341921));
#36339=CARTESIAN_POINT('Ctrl Pts',(2.38494868356147,-0.810385291388008,
111.560416715443));
#36340=CARTESIAN_POINT('Ctrl Pts',(2.35688879631775,-0.888698470374929,
111.555180011676));
#36341=CARTESIAN_POINT('Ctrl Pts',(2.32502568704904,-0.965433480133231,
111.54994330791));
#36342=CARTESIAN_POINT('Ctrl Pts',(2.29316344569622,-1.04216639971462,111.544706746785));
#36343=CARTESIAN_POINT('Ctrl Pts',(2.25749836619498,-1.11732080979032,111.53947018566));
#36344=CARTESIAN_POINT('Ctrl Pts',(2.21822157726942,-1.19050379425535,111.534233624536));
#36345=CARTESIAN_POINT('Ctrl Pts',(2.17830194518036,-1.26488456455099,111.528911356621));
#36346=CARTESIAN_POINT('Ctrl Pts',(2.13465153231263,-1.33722835490508,111.523589088705));
#36347=CARTESIAN_POINT('Ctrl Pts',(2.08751867597528,-1.40715032155574,111.51826682079));
#36348=CARTESIAN_POINT('Ctrl Pts',(2.04107822181224,-1.47604510408256,111.513022739307));
#36349=CARTESIAN_POINT('Ctrl Pts',(1.99125729187287,-1.54258840801495,111.507778657824));
#36350=CARTESIAN_POINT('Ctrl Pts',(1.93833503998196,-1.60644437276183,111.502534576342));
#36351=CARTESIAN_POINT('Ctrl Pts',(1.88422922465678,-1.67172842460315,111.49717321521));
#36352=CARTESIAN_POINT('Ctrl Pts',(1.82688204264785,-1.73420310927673,111.491811854079));
#36353=CARTESIAN_POINT('Ctrl Pts',(1.76663123148277,-1.79354964858787,111.486450492948));
#36354=CARTESIAN_POINT('Ctrl Pts',(1.70638042031768,-1.85289618789902,111.481089131817));
#36355=CARTESIAN_POINT('Ctrl Pts',(1.64322640393058,-1.90911429390156,111.475727770685));
#36356=CARTESIAN_POINT('Ctrl Pts',(1.57754079121682,-1.961930503878,111.470366409554));
#36357=CARTESIAN_POINT('Ctrl Pts',(1.51315522391518,-2.01370137883163,111.465111160137));
#36358=CARTESIAN_POINT('Ctrl Pts',(1.44609957065455,-2.06239504738502,111.459855910719));
#36359=CARTESIAN_POINT('Ctrl Pts',(1.37670013630848,-2.10772459887155,111.454600661302));
#36360=CARTESIAN_POINT('Ctrl Pts',(1.30739909456602,-2.1529898833704,111.449352862632));
#36361=CARTESIAN_POINT('Ctrl Pts',(1.23576125517507,-2.19490027430168,111.444105063962));
#36362=CARTESIAN_POINT('Ctrl Pts',(1.16214561888101,-2.23320930736814,111.438857265293));
#36363=CARTESIAN_POINT('Ctrl Pts',(1.08799657404998,-2.27179592229504,111.433571441813));
#36364=CARTESIAN_POINT('Ctrl Pts',(1.01184131901189,-2.30672847232742,111.428285618332));
#36365=CARTESIAN_POINT('Ctrl Pts',(0.934076151220512,-2.33779981900099,
111.422999794852));
#36366=CARTESIAN_POINT('Ctrl Pts',(0.857008298023256,-2.3685925511726,111.417761368966));
#36367=CARTESIAN_POINT('Ctrl Pts',(0.778359724756236,-2.39559287454398,
111.41252294308));
#36368=CARTESIAN_POINT('Ctrl Pts',(0.698538843538567,-2.41864626063172,
111.407284517194));
#36369=CARTESIAN_POINT('Ctrl Pts',(0.618744214050853,-2.44169206485295,
111.402047814137));
#36370=CARTESIAN_POINT('Ctrl Pts',(0.537778485292789,-2.46079338191883,
111.39681111108));
#36371=CARTESIAN_POINT('Ctrl Pts',(0.456065842483091,-2.47584535004111,
111.391574408024));
#36372=CARTESIAN_POINT('Ctrl Pts',(0.37435542545508,-2.49089690816081,111.38633784761));
#36373=CARTESIAN_POINT('Ctrl Pts',(0.2918985887999,-2.50189925406705,111.381101287196));
#36374=CARTESIAN_POINT('Ctrl Pts',(0.209128967747527,-2.50879878125944,
111.375864726783));
#36375=CARTESIAN_POINT('Ctrl Pts',(0.125004631758573,-2.51581123505973,
111.370542458032));
#36376=CARTESIAN_POINT('Ctrl Pts',(0.040557669060788,-2.51858530040419,
111.36522018928));
#36377=CARTESIAN_POINT('Ctrl Pts',(-0.0437539084321868,-2.51711975191823,
111.359897920529));
#36378=CARTESIAN_POINT('Ctrl Pts',(-0.126826887911599,-2.51567573339883,
111.354653839753));
#36379=CARTESIAN_POINT('Ctrl Pts',(-0.209767970726271,-2.51011593271426,
111.349409758977));
#36380=CARTESIAN_POINT('Ctrl Pts',(-0.292143453966913,-2.50049164211846,
111.344165678201));
#36381=CARTESIAN_POINT('Ctrl Pts',(-0.376361234977798,-2.49065210775829,
111.338804315462));
#36382=CARTESIAN_POINT('Ctrl Pts',(-0.459987307352202,-2.47656417307093,
111.333442952724));
#36383=CARTESIAN_POINT('Ctrl Pts',(-0.542570400201254,-2.45833757055972,
111.328081589985));
#36384=CARTESIAN_POINT('Ctrl Pts',(-0.625153493050303,-2.44011096804851,
111.322720227247));
#36385=CARTESIAN_POINT('Ctrl Pts',(-0.706693134034247,-2.41774589653397,
111.317358864508));
#36386=CARTESIAN_POINT('Ctrl Pts',(-0.786757621261283,-2.39140517173215,
111.31199750177));
#36387=CARTESIAN_POINT('Ctrl Pts',(-0.865237450878734,-2.36558578955607,
111.306742252548));
#36388=CARTESIAN_POINT('Ctrl Pts',(-0.94258987623988,-2.33585137034942,
111.301487003325));
#36389=CARTESIAN_POINT('Ctrl Pts',(-1.01839658171196,-2.30231940711045,
111.296231754103));
#36390=CARTESIAN_POINT('Ctrl Pts',(-1.09409581044478,-2.26883498460085,
111.290983955634));
#36391=CARTESIAN_POINT('Ctrl Pts',(-1.16825325374797,-2.23156389746811,
111.285736157165));
#36392=CARTESIAN_POINT('Ctrl Pts',(-1.2404667207669,-2.19067308484626,111.280488358696));
#36393=CARTESIAN_POINT('Ctrl Pts',(-1.31320343986261,-2.14948598119299,
111.275202535166));
#36394=CARTESIAN_POINT('Ctrl Pts',(-1.38396744190819,-2.10462662241895,
111.269916711637));
#36395=CARTESIAN_POINT('Ctrl Pts',(-1.45236921594197,-2.05631464289493,
111.264630888107));
#36396=CARTESIAN_POINT('Ctrl Pts',(-1.52015763286562,-2.0084358757629,111.259392462434));
#36397=CARTESIAN_POINT('Ctrl Pts',(-1.58562563235106,-1.95716643012531,
111.25415403676));
#36398=CARTESIAN_POINT('Ctrl Pts',(-1.64842123648773,-1.90276474559948,
111.248915611087));
#36399=CARTESIAN_POINT('Ctrl Pts',(-1.71119618816908,-1.84838095290501,
111.243678908246));
#36400=CARTESIAN_POINT('Ctrl Pts',(-1.77130014158641,-1.79086726913501,
111.238442205406));
#36401=CARTESIAN_POINT('Ctrl Pts',(-1.82841419117776,-1.73052240537353,
111.233205502566));
#36402=CARTESIAN_POINT('Ctrl Pts',(-1.88552668499061,-1.67017918539746,
111.227968942373));
#36403=CARTESIAN_POINT('Ctrl Pts',(-1.93964912047973,-1.60700527459635,
111.22273238218));
#36404=CARTESIAN_POINT('Ctrl Pts',(-1.99050043954715,-1.54133521667501,
111.217495821986));
#36405=CARTESIAN_POINT('Ctrl Pts',(-2.04218406182935,-1.47459031150634,
111.212173552986));
#36406=CARTESIAN_POINT('Ctrl Pts',(-2.09048821090684,-1.40526719194838,
111.206851283986));
#36407=CARTESIAN_POINT('Ctrl Pts',(-2.13516249357516,-1.33374936777114,
111.201529014986));
#36408=CARTESIAN_POINT('Ctrl Pts',(-2.17918047477147,-1.26328219847807,
111.196284934438));
#36409=CARTESIAN_POINT('Ctrl Pts',(-2.21967435859153,-1.19068481914261,
111.191040853889));
#36410=CARTESIAN_POINT('Ctrl Pts',(-2.25645103835623,-1.11634894253593,
111.18579677334));
#36411=CARTESIAN_POINT('Ctrl Pts',(-2.29405022025787,-1.04035056083767,
111.180435410114));
#36412=CARTESIAN_POINT('Ctrl Pts',(-2.32776371931494,-0.962535451149197,
111.175074046889));
#36413=CARTESIAN_POINT('Ctrl Pts',(-2.35743788310572,-0.883341880190247,
111.169712683663));
#36414=CARTESIAN_POINT('Ctrl Pts',(-2.38711204689649,-0.804148309231296,
111.164351320437));
#36415=CARTESIAN_POINT('Ctrl Pts',(-2.4127467850239,-0.723576781445333,
111.158989957212));
#36416=CARTESIAN_POINT('Ctrl Pts',(-2.43424362525605,-0.642078050473828,
111.153628593986));
#36417=CARTESIAN_POINT('Ctrl Pts',(-2.46167272104034,-0.538088977011254,
111.146787712076));
#36418=CARTESIAN_POINT('Ctrl Pts',(-2.48245069235363,-0.432277827512794,
111.139946830167));
#36419=CARTESIAN_POINT('Ctrl Pts',(-2.49638302038995,-0.325389098632332,
111.133105948258));
#36420=CARTESIAN_POINT('Ctrl Pts',(-2.51031534842627,-0.218500369751869,
111.126265066348));
#36421=CARTESIAN_POINT('Ctrl Pts',(-2.51740185313733,-0.110533711503309,
111.119424184439));
#36422=CARTESIAN_POINT('Ctrl Pts',(-2.51749898697117,-0.00225845060319963,
111.11258330253));
#36423=CARTESIAN_POINT('Ctrl Pts',(-2.51749898697171,-0.00225845000779732,
111.112583302492));
#36424=CARTESIAN_POINT('Ctrl Pts',(-2.51757261569501,0.0798156431506282,
111.107397822684));
#36425=CARTESIAN_POINT('Ctrl Pts',(-2.51362839019092,0.161986447060072,
111.102212342876));
#36426=CARTESIAN_POINT('Ctrl Pts',(-2.50566466251812,0.243825447826831,
111.097026863068));
#36427=CARTESIAN_POINT('Ctrl Pts',(-2.49770584547388,0.325613984671257,
111.091844580753));
#36428=CARTESIAN_POINT('Ctrl Pts',(-2.48573249308511,0.40707065575182,111.086662298438));
#36429=CARTESIAN_POINT('Ctrl Pts',(-2.46979497866708,0.487769426420808,
111.081480016123));
#36430=CARTESIAN_POINT('Ctrl Pts',(-2.45385906771586,0.568460078019457,
111.076298255196));
#36431=CARTESIAN_POINT('Ctrl Pts',(-2.43395986851913,0.648392515612904,
111.071116494268));
#36432=CARTESIAN_POINT('Ctrl Pts',(-2.41019911302312,0.727149562045231,
111.06593473334));
#36433=CARTESIAN_POINT('Ctrl Pts',(-2.39542387295519,0.776123352810164,
111.062712539429));
#36434=CARTESIAN_POINT('Ctrl Pts',(-2.37915647272574,0.82464284667384,111.059490345518));
#36435=CARTESIAN_POINT('Ctrl Pts',(-2.36143112101026,0.872610629504506,
111.056268151607));
#36436=CARTESIAN_POINT('Ctrl Pts',(-2.36143104183299,0.872610843771477,
111.329984892853));
#36437=CARTESIAN_POINT('Ctrl Pts',(-2.38229711288321,0.816143761966584,
111.334119803671));
#36438=CARTESIAN_POINT('Ctrl Pts',(-2.40114012091893,0.75892196203164,111.338284776278));
#36439=CARTESIAN_POINT('Ctrl Pts',(-2.45397655537651,0.57669045218432,111.351389496961));
#36440=CARTESIAN_POINT('Ctrl Pts',(-2.48038965065677,0.449718197749219,
111.36027728338));
#36441=CARTESIAN_POINT('Ctrl Pts',(-2.50280298128401,0.275519363787184,
111.371972880807));
#36442=CARTESIAN_POINT('Ctrl Pts',(-2.50743097882214,0.229617084015653,
111.375010368583));
#36443=CARTESIAN_POINT('Ctrl Pts',(-2.51327703119018,0.14967507360673,111.380223240681));
#36444=CARTESIAN_POINT('Ctrl Pts',(-2.51507054653771,0.115690941624686,
111.382415250734));
#36445=CARTESIAN_POINT('Ctrl Pts',(-2.51667641816118,0.066221318604821,
111.385572625589));
#36446=CARTESIAN_POINT('Ctrl Pts',(-2.51703576466368,0.0507585812687205,
111.386554790778));
#36447=CARTESIAN_POINT('Ctrl Pts',(-2.51741704981101,0.0235638166596553,
111.388274098202));
#36448=CARTESIAN_POINT('Ctrl Pts',(-2.51749952096065,0.0118332422881704,
111.389013094862));
#36449=CARTESIAN_POINT('Ctrl Pts',(-2.51750051406999,-0.0125924704623981,
111.390546540677));
#36450=CARTESIAN_POINT('Ctrl Pts',(-2.51740500723337,-0.025287301469883,
111.391340533799));
#36451=CARTESIAN_POINT('Ctrl Pts',(-2.51690645117222,-0.0583293546827333,
111.393399671163));
#36452=CARTESIAN_POINT('Ctrl Pts',(-2.51635269694493,-0.0786736282879076,
111.394660124281));
#36453=CARTESIAN_POINT('Ctrl Pts',(-2.51273062852249,-0.170700247685259,
111.400331018358));
#36454=CARTESIAN_POINT('Ctrl Pts',(-2.50684544331757,-0.242241844617296,
111.404653883072));
#36455=CARTESIAN_POINT('Ctrl Pts',(-2.46839587202294,-0.548660119344687,
111.422957309732));
#36456=CARTESIAN_POINT('Ctrl Pts',(-2.40581011773477,-0.778501324702915,
111.436033522515));
#36457=CARTESIAN_POINT('Ctrl Pts',(-2.29176568242305,-1.04318555947838,
111.45323335973));
#36458=CARTESIAN_POINT('Ctrl Pts',(-2.27008475429137,-1.08955975546668,
111.456338779605));
#36459=CARTESIAN_POINT('Ctrl Pts',(-2.24122796721196,-1.14667681291608,
111.460319083837));
#36460=CARTESIAN_POINT('Ctrl Pts',(-2.23536135591467,-1.15807171912494,
111.461121080619));
#36461=CARTESIAN_POINT('Ctrl Pts',(-2.2259413211573,-1.17603026546513,111.462398408591));
#36462=CARTESIAN_POINT('Ctrl Pts',(-2.22244518318594,-1.18262392789843,
111.462870269199));
#36463=CARTESIAN_POINT('Ctrl Pts',(-2.21613482111481,-1.19439836938347,
111.463718217072));
#36464=CARTESIAN_POINT('Ctrl Pts',(-2.2133316523582,-1.19958492996755,111.464093609856));
#36465=CARTESIAN_POINT('Ctrl Pts',(-2.20652289883753,-1.21207770885202,
111.465002317962));
#36466=CARTESIAN_POINT('Ctrl Pts',(-2.20249926041712,-1.21937388791465,
111.465536756066));
#36467=CARTESIAN_POINT('Ctrl Pts',(-2.18997874533529,-1.24181353999731,
111.467191638406));
#36468=CARTESIAN_POINT('Ctrl Pts',(-2.18136155740626,-1.256888813542,111.468319226414));
#36469=CARTESIAN_POINT('Ctrl Pts',(-2.16082899745834,-1.29196213747666,
111.470977710746));
#36470=CARTESIAN_POINT('Ctrl Pts',(-2.14879096499259,-1.31188620997376,
111.47251502445));
#36471=CARTESIAN_POINT('Ctrl Pts',(-2.10502673364014,-1.38210141427275,
111.47802234941));
#36472=CARTESIAN_POINT('Ctrl Pts',(-2.07179858577641,-1.43142991344348,
111.482056997129));
#36473=CARTESIAN_POINT('Ctrl Pts',(-1.93269916909471,-1.62292669528796,
111.498266504626));
#36474=CARTESIAN_POINT('Ctrl Pts',(-1.8136762573168,-1.75493751377668,111.510647824571));
#36475=CARTESIAN_POINT('Ctrl Pts',(-1.61602745460668,-1.93237347880955,
111.528518899809));
#36476=CARTESIAN_POINT('Ctrl Pts',(-1.54721634787599,-1.9878975381383,111.534347594578));
#36477=CARTESIAN_POINT('Ctrl Pts',(-1.45739679203625,-2.05287767866344,
111.541481669317));
#36478=CARTESIAN_POINT('Ctrl Pts',(-1.43899671046783,-2.06581719759917,
111.542919799444));
#36479=CARTESIAN_POINT('Ctrl Pts',(-1.40955861375282,-2.08593480081386,
111.54518463337));
#36480=CARTESIAN_POINT('Ctrl Pts',(-1.39863381125282,-2.09327565111773,
111.546017434415));
#36481=CARTESIAN_POINT('Ctrl Pts',(-1.37892240917232,-2.10629739046327,
111.547506473789));
#36482=CARTESIAN_POINT('Ctrl Pts',(-1.37015708031947,-2.11200977463559,
111.548163874056));
#36483=CARTESIAN_POINT('Ctrl Pts',(-1.34954652799984,-2.12525940237391,
111.549698730898));
#36484=CARTESIAN_POINT('Ctrl Pts',(-1.33767328192528,-2.13275257872918,
111.550574549437));
#36485=CARTESIAN_POINT('Ctrl Pts',(-1.30309911291886,-2.15416993933617,
111.553101240828));
#36486=CARTESIAN_POINT('Ctrl Pts',(-1.28023872677981,-2.16783401367335,
111.554742660105));
#36487=CARTESIAN_POINT('Ctrl Pts',(-1.22800821524524,-2.19793872198445,
111.558430601004));
#36488=CARTESIAN_POINT('Ctrl Pts',(-1.19851631910115,-2.21415843773837,
111.560469419978));
#36489=CARTESIAN_POINT('Ctrl Pts',(-1.09974253052201,-2.26592923685664,
111.567166984433));
#36490=CARTESIAN_POINT('Ctrl Pts',(-1.02913506058263,-2.29885869710453,
111.571744130763));
#36491=CARTESIAN_POINT('Ctrl Pts',(-0.863938634819748,-2.36676234934217,
111.582120812596));
#36492=CARTESIAN_POINT('Ctrl Pts',(-0.768552083639069,-2.39943368171147,
111.587873512919));
#36493=CARTESIAN_POINT('Ctrl Pts',(-0.615375170747078,-2.44182442556879,
111.597030208845));
#36494=CARTESIAN_POINT('Ctrl Pts',(-0.558766982987014,-2.45539653080876,
111.600398314467));
#36495=CARTESIAN_POINT('Ctrl Pts',(-0.428001626262012,-2.48199181126257,
111.608238753064));
#36496=CARTESIAN_POINT('Ctrl Pts',(-0.353633507436423,-2.49367396204227,
111.612741249147));
#36497=CARTESIAN_POINT('Ctrl Pts',(-0.265923136866028,-2.5034497453985,
111.618217208517));
#36498=CARTESIAN_POINT('Ctrl Pts',(-0.252973651521361,-2.50479141995599,
111.619029893264));
#36499=CARTESIAN_POINT('Ctrl Pts',(-0.231852694931628,-2.50681427445869,
111.620363120844));
#36500=CARTESIAN_POINT('Ctrl Pts',(-0.223687093462902,-2.50755609279657,
111.620880438663));
#36501=CARTESIAN_POINT('Ctrl Pts',(-0.209033393997464,-2.50881518903251,
111.621812397235));
#36502=CARTESIAN_POINT('Ctrl Pts',(-0.202546740222107,-2.50934721166434,
111.622226216904));
#36503=CARTESIAN_POINT('Ctrl Pts',(-0.188261769184757,-2.51046308643859,
111.623140382446));
#36504=CARTESIAN_POINT('Ctrl Pts',(-0.180462867634823,-2.51103575274764,
111.62364131666));
#36505=CARTESIAN_POINT('Ctrl Pts',(-0.157874957975957,-2.51258859033894,
111.625097261471));
#36506=CARTESIAN_POINT('Ctrl Pts',(-0.143080092410167,-2.51347448541747,
111.626057206997));
#36507=CARTESIAN_POINT('Ctrl Pts',(-0.0203654575983437,-2.51973551769987,
111.634067000898));
#36508=CARTESIAN_POINT('Ctrl Pts',(0.0877787246391703,-2.51828740509499,
111.641426483692));
#36509=CARTESIAN_POINT('Ctrl Pts',(0.362032782808291,-2.49692731611548,
111.660363496811));
#36510=CARTESIAN_POINT('Ctrl Pts',(0.526898845618981,-2.46740794424107,
111.671977547523));
#36511=CARTESIAN_POINT('Ctrl Pts',(0.763389533845402,-2.40025926108424,
111.688440367221));
#36512=CARTESIAN_POINT('Ctrl Pts',(0.838101609340371,-2.37520440864219,
111.693617737743));
#36513=CARTESIAN_POINT('Ctrl Pts',(0.931767489828273,-2.33882176946208,
111.700078724876));
#36514=CARTESIAN_POINT('Ctrl Pts',(0.951909859335047,-2.33069637499014,
111.701466469118));
#36515=CARTESIAN_POINT('Ctrl Pts',(0.98393080097929,-2.31729481284869,111.703670514166));
#36516=CARTESIAN_POINT('Ctrl Pts',(0.995877677547504,-2.31218570456943,
111.704492365309));
#36517=CARTESIAN_POINT('Ctrl Pts',(1.01846326482464,-2.30231940049616,111.706045377038));
#36518=CARTESIAN_POINT('Ctrl Pts',(1.02910950381845,-2.29758039689254,111.706777127885));
#36519=CARTESIAN_POINT('Ctrl Pts',(1.05326379797822,-2.2866269248687,111.708436849598));
#36520=CARTESIAN_POINT('Ctrl Pts',(1.06675055270763,-2.28036632910666,111.709363222423));
#36521=CARTESIAN_POINT('Ctrl Pts',(1.10800435606921,-2.26077008872686,111.712196416476));
#36522=CARTESIAN_POINT('Ctrl Pts',(1.13558339739316,-2.24704372926393,111.714089825076));
#36523=CARTESIAN_POINT('Ctrl Pts',(1.26890715327651,-2.17760543952424,111.72325101599));
#36524=CARTESIAN_POINT('Ctrl Pts',(1.37084998143279,-2.11491510187378,111.730271171286));
#36525=CARTESIAN_POINT('Ctrl Pts',(1.55269538046208,-1.98439456118379,111.74322271115));
#36526=CARTESIAN_POINT('Ctrl Pts',(1.63356601333388,-1.91837079876647,111.749168590198));
#36527=CARTESIAN_POINT('Ctrl Pts',(1.79366086666738,-1.77018341521113,111.761787913692));
#36528=CARTESIAN_POINT('Ctrl Pts',(1.87186117358412,-1.68727526079769,111.768464567702));
#36529=CARTESIAN_POINT('Ctrl Pts',(1.9529239624428,-1.58873659216649,111.776371431333));
#36530=CARTESIAN_POINT('Ctrl Pts',(1.96158670312308,-1.57802837394737,111.777230362504));
#36531=CARTESIAN_POINT('Ctrl Pts',(1.97540567417953,-1.56065680043112,111.778624274475));
#36532=CARTESIAN_POINT('Ctrl Pts',(1.98061721478924,-1.55403753814311,111.779155525308));
#36533=CARTESIAN_POINT('Ctrl Pts',(1.98980498109427,-1.54224671890582,111.780102289748));
#36534=CARTESIAN_POINT('Ctrl Pts',(1.9937944597679,-1.53708570208269,111.780516865322));
#36535=CARTESIAN_POINT('Ctrl Pts',(2.00241630724092,-1.52584194402355,111.781420471881));
#36536=CARTESIAN_POINT('Ctrl Pts',(2.00704096790004,-1.51975368238673,111.781909994538));
#36537=CARTESIAN_POINT('Ctrl Pts',(2.02005422863553,-1.50245902320068,111.783301008822));
#36538=CARTESIAN_POINT('Ctrl Pts',(2.02837704111314,-1.49120379591061,111.784206798787));
#36539=CARTESIAN_POINT('Ctrl Pts',(2.083492475056,-1.41535414432738,111.7903112832));
#36540=CARTESIAN_POINT('Ctrl Pts',(2.12728196775874,-1.34864267619319,111.795680620909));
#36541=CARTESIAN_POINT('Ctrl Pts',(2.2253461372201,-1.18255627346517,111.808853489364));
#36542=CARTESIAN_POINT('Ctrl Pts',(2.27623252583276,-1.08137411602237,111.816716347026));
#36543=CARTESIAN_POINT('Ctrl Pts',(2.38104602525567,-0.832496058697998,
111.835294276462));
#36544=CARTESIAN_POINT('Ctrl Pts',(2.42830522530029,-0.682480177323201,
111.845877998643));
#36545=CARTESIAN_POINT('Ctrl Pts',(2.46596634230732,-0.507258807512532,
111.857437486713));
#36546=CARTESIAN_POINT('Ctrl Pts',(2.47035415572538,-0.485439899886147,
111.858863748363));
#36547=CARTESIAN_POINT('Ctrl Pts',(2.47710245681933,-0.449418316911209,
111.861197387093));
#36548=CARTESIAN_POINT('Ctrl Pts',(2.47963139714493,-0.435248840845943,
111.862110025733));
#36549=CARTESIAN_POINT('Ctrl Pts',(2.483980249321,-0.409613384289519,111.863751806883));
#36550=CARTESIAN_POINT('Ctrl Pts',(2.4858426170471,-0.398155113187746,111.864482266014));
#36551=CARTESIAN_POINT('Ctrl Pts',(2.48966812999361,-0.373544736174674,
111.866044124285));
#36552=CARTESIAN_POINT('Ctrl Pts',(2.49160646643803,-0.360389087803307,
111.866874724751));
#36553=CARTESIAN_POINT('Ctrl Pts',(2.49662916817981,-0.324320133712944,
111.869140611059));
#36554=CARTESIAN_POINT('Ctrl Pts',(2.49950232713127,-0.301378373349695,
111.870569279755));
#36555=CARTESIAN_POINT('Ctrl Pts',(2.51455567263471,-0.166089569936953,
111.878925695353));
#36556=CARTESIAN_POINT('Ctrl Pts',(2.51947720137194,-0.0530581234540805,
111.885621709153));
#36557=CARTESIAN_POINT('Ctrl Pts',(2.51265170387703,0.233566240413223,111.902302873451));
#36558=CARTESIAN_POINT('Ctrl Pts',(2.49056046207414,0.406292574422091,111.912061708187));
#36559=CARTESIAN_POINT('Ctrl Pts',(2.43576554085955,0.639703725203097,111.926224330721));
#36560=CARTESIAN_POINT('Ctrl Pts',(2.41813351061093,0.703422597384991,111.93019941436));
#36561=CARTESIAN_POINT('Ctrl Pts',(2.39381942274178,0.77950303052444,111.935159157788));
#36562=CARTESIAN_POINT('Ctrl Pts',(2.3895139011996,0.792603115905413,111.93602095817));
#36563=CARTESIAN_POINT('Ctrl Pts',(2.38264182050799,0.812947266442638,111.937372449032));
#36564=CARTESIAN_POINT('Ctrl Pts',(2.38014926590214,0.820216295350178,111.937857967591));
#36565=CARTESIAN_POINT('Ctrl Pts',(2.37548077362315,0.833630518924669,111.938759000705));
#36566=CARTESIAN_POINT('Ctrl Pts',(2.37331420922904,0.839778785760929,111.939173969626));
#36567=CARTESIAN_POINT('Ctrl Pts',(2.36831113619256,0.853802482704644,111.940125007452));
#36568=CARTESIAN_POINT('Ctrl Pts',(2.36545922406888,0.861672195075561,111.940661958888));
#36569=CARTESIAN_POINT('Ctrl Pts',(2.35650168939696,0.886010457680317,111.942332343444));
#36570=CARTESIAN_POINT('Ctrl Pts',(2.35026307801699,0.902429036898991,111.943473109261));
#36571=CARTESIAN_POINT('Ctrl Pts',(2.33523147200849,0.940775391603699,111.946167993238));
#36572=CARTESIAN_POINT('Ctrl Pts',(2.32630069286313,0.962647062292938,111.947728759237));
#36573=CARTESIAN_POINT('Ctrl Pts',(2.29328563902398,1.04035820034957,111.953351435431));
#36574=CARTESIAN_POINT('Ctrl Pts',(2.26748879668205,1.0954441231953,111.957480658369));
#36575=CARTESIAN_POINT('Ctrl Pts',(2.15528270723519,1.31406298953152,111.974319816998));
#36576=CARTESIAN_POINT('Ctrl Pts',(2.05295671387077,1.46880457820489,111.987238051842));
#36577=CARTESIAN_POINT('Ctrl Pts',(1.88349774221641,1.67230969081851,112.004982769701));
#36578=CARTESIAN_POINT('Ctrl Pts',(1.82950223408957,1.73121555619502,112.010235200587));
#36579=CARTESIAN_POINT('Ctrl Pts',(1.75727395606073,1.80285112891874,112.016777166042));
#36580=CARTESIAN_POINT('Ctrl Pts',(1.74155549111149,1.81803973286882,112.018173902209));
#36581=CARTESIAN_POINT('Ctrl Pts',(1.716158463428,1.84194896288625,112.020388798612));
#36582=CARTESIAN_POINT('Ctrl Pts',(1.70660685462993,1.85080223350775,112.021212605329));
#36583=CARTESIAN_POINT('Ctrl Pts',(1.68838347405453,1.86743223496468,112.022767230626));
#36584=CARTESIAN_POINT('Ctrl Pts',(1.67972562537669,1.87522365024132,112.023498656438));
#36585=CARTESIAN_POINT('Ctrl Pts',(1.65993229419706,1.89278909120363,112.025154828225));
#36586=CARTESIAN_POINT('Ctrl Pts',(1.64876390939381,1.9025255191411,112.026078002413));
#36587=CARTESIAN_POINT('Ctrl Pts',(1.61432154261329,1.93202076745023,112.028891243156));
#36588=CARTESIAN_POINT('Ctrl Pts',(1.59077303389617,1.95145575576374,112.03076817607));
#36589=CARTESIAN_POINT('Ctrl Pts',(1.47501005172878,2.04350857684085,112.039783952679));
#36590=CARTESIAN_POINT('Ctrl Pts',(1.37814270631383,2.1100495741371,112.046684545069));
#36591=CARTESIAN_POINT('Ctrl Pts',(1.12002051686159,2.26197468025798,112.064026113519));
#36592=CARTESIAN_POINT('Ctrl Pts',(0.953520813800322,2.33704107421866,112.074250439112));
#36593=CARTESIAN_POINT('Ctrl Pts',(0.738654526577406,2.40709862065585,112.087816802761));
#36594=CARTESIAN_POINT('Ctrl Pts',(0.696562033847317,2.41961465635794,112.09049317055));
#36595=CARTESIAN_POINT('Ctrl Pts',(0.642286257365155,2.43421978905894,112.093993249389));
#36596=CARTESIAN_POINT('Ctrl Pts',(0.630382717951387,2.43732952888696,112.094763862593));
#36597=CARTESIAN_POINT('Ctrl Pts',(0.611403679682745,2.44213937711137,112.095997978751));
#36598=CARTESIAN_POINT('Ctrl Pts',(0.604342601114428,2.44389631818982,112.096458322325));
#36599=CARTESIAN_POINT('Ctrl Pts',(0.590857455825236,2.44718968331548,112.097339931052));
#36600=CARTESIAN_POINT('Ctrl Pts',(0.584434853091539,2.4487314629538,112.09776089071));
#36601=CARTESIAN_POINT('Ctrl Pts',(0.569170414552988,2.45233229962099,112.09876383604));
#36602=CARTESIAN_POINT('Ctrl Pts',(0.560323419139634,2.45436882486701,112.099347072797));
#36603=CARTESIAN_POINT('Ctrl Pts',(0.530498549867877,2.46106467225022,112.10131937713));
#36604=CARTESIAN_POINT('Ctrl Pts',(0.509472734492231,2.46550309117595,112.102719946813));
#36605=CARTESIAN_POINT('Ctrl Pts',(0.385231283500474,2.49007264101417,112.111045412677));
#36606=CARTESIAN_POINT('Ctrl Pts',(0.280901792470644,2.50398776696118,112.118233119482));
#36607=CARTESIAN_POINT('Ctrl Pts',(-0.0102396569414233,2.52439385968174,
112.138349353213));
#36608=CARTESIAN_POINT('Ctrl Pts',(-0.197403401790635,2.51668828409672,
112.151299005578));
#36609=CARTESIAN_POINT('Ctrl Pts',(-0.437825881043689,2.47977900007459,
112.167382242781));
#36610=CARTESIAN_POINT('Ctrl Pts',(-0.493343578136614,2.46933358089448,
112.171062260673));
#36611=CARTESIAN_POINT('Ctrl Pts',(-0.567364900802064,2.45281027721735,
112.175925861383));
#36612=CARTESIAN_POINT('Ctrl Pts',(-0.5862141870893,2.44837377615213,112.177160635127));
#36613=CARTESIAN_POINT('Ctrl Pts',(-0.617126518722295,2.44072056916095,
112.179179929749));
#36614=CARTESIAN_POINT('Ctrl Pts',(-0.629219884878387,2.43763089544132,
112.179968465449));
#36615=CARTESIAN_POINT('Ctrl Pts',(-0.65271740419986,2.43144111352305,112.181497964349));
#36616=CARTESIAN_POINT('Ctrl Pts',(-0.664123672032448,2.42835039772998,
112.182239205783));
#36617=CARTESIAN_POINT('Ctrl Pts',(-0.690937107355352,2.42088180079674,
112.183979039497));
#36618=CARTESIAN_POINT('Ctrl Pts',(-0.706325209677865,2.41643694238857,
112.184975449882));
#36619=CARTESIAN_POINT('Ctrl Pts',(-0.757289062893238,2.40118758611259,
112.188269447425));
#36620=CARTESIAN_POINT('Ctrl Pts',(-0.792668834338255,2.38974159395874,
112.190546315903));
#36621=CARTESIAN_POINT('Ctrl Pts',(-0.997083239671975,2.31857029305641,
112.203668196522));
#36622=CARTESIAN_POINT('Ctrl Pts',(-1.15960518299079,2.24171068333428,112.213920002746));
#36623=CARTESIAN_POINT('Ctrl Pts',(-1.43129821580121,2.07570281156209,112.232225164233));
#36624=CARTESIAN_POINT('Ctrl Pts',(-1.54377004544984,1.99346959907223,112.240241665327));
#36625=CARTESIAN_POINT('Ctrl Pts',(-1.66500051199955,1.88839500978216,112.250094379419));
#36626=CARTESIAN_POINT('Ctrl Pts',(-1.68096076346272,1.87420203289338,112.251418221307));
#36627=CARTESIAN_POINT('Ctrl Pts',(-1.70295360638334,1.85413755061158,112.253283284331));
#36628=CARTESIAN_POINT('Ctrl Pts',(-1.70914074916309,1.84843580816176,112.253812574051));
#36629=CARTESIAN_POINT('Ctrl Pts',(-1.71977086123151,1.83854066008376,112.254730164414));
#36630=CARTESIAN_POINT('Ctrl Pts',(-1.72422740800457,1.83436185566017,112.255117375558));
#36631=CARTESIAN_POINT('Ctrl Pts',(-1.73360359792454,1.82550565501097,112.255937490958));
#36632=CARTESIAN_POINT('Ctrl Pts',(-1.73851958622172,1.82082453194555,112.25637068992));
#36633=CARTESIAN_POINT('Ctrl Pts',(-1.7502330242428,1.80958003280287,112.257410454314));
#36634=CARTESIAN_POINT('Ctrl Pts',(-1.75701253213182,1.80299819451964,112.258018406027));
#36635=CARTESIAN_POINT('Ctrl Pts',(-1.78150075794305,1.77895469591384,112.260236326502));
#36636=CARTESIAN_POINT('Ctrl Pts',(-1.79898688021145,1.76126967146124,112.261862135518));
#36637=CARTESIAN_POINT('Ctrl Pts',(-1.84253758800642,1.71589837260386,112.266012638196));
#36638=CARTESIAN_POINT('Ctrl Pts',(-1.86824166146068,1.68787581911322,112.268557339162));
#36639=CARTESIAN_POINT('Ctrl Pts',(-1.9814001918855,1.5587580191167,112.280159426443));
#36640=CARTESIAN_POINT('Ctrl Pts',(-2.06135163454704,1.45137899828533,112.289465148528));
#36641=CARTESIAN_POINT('Ctrl Pts',(-2.21825237761731,1.20135364584752,112.309788295908));
#36642=CARTESIAN_POINT('Ctrl Pts',(-2.29075388481616,1.05657832094613,112.320697349063));
#36643=CARTESIAN_POINT('Ctrl Pts',(-2.35314765889223,0.894786252596313,
112.331881384402));
#36644=CARTESIAN_POINT('Ctrl Pts',(-2.35732850676449,0.883712993638031,
112.332642198402));
#36645=CARTESIAN_POINT('Ctrl Pts',(-2.36143112095427,0.872610629656001,
112.333400434891));
#36646=CARTESIAN_POINT('Origin',(0.,0.,104.));
#36647=CARTESIAN_POINT('',(-2.36143112101026,0.872610629504504,113.330979739671));
#36648=CARTESIAN_POINT('',(-2.36143112101026,0.872610629504504,113.056261826378));
#36649=CARTESIAN_POINT('',(-2.36143112101026,0.872610629504505,104.));
#36650=CARTESIAN_POINT('',(-2.51749943375649,0.00168850103947855,113.387416697547));
#36651=CARTESIAN_POINT('Ctrl Pts',(-2.36143112101026,0.872610629504504,
113.330979739671));
#36652=CARTESIAN_POINT('Ctrl Pts',(-2.390175081664,0.794824637753064,113.33622078171));
#36653=CARTESIAN_POINT('Ctrl Pts',(-2.41504172891221,0.715697691567379,
113.341461823748));
#36654=CARTESIAN_POINT('Ctrl Pts',(-2.43592936053144,0.635652735777082,
113.346702865786));
#36655=CARTESIAN_POINT('Ctrl Pts',(-2.45685043664356,0.555479615003627,
113.351952299585));
#36656=CARTESIAN_POINT('Ctrl Pts',(-2.47377969301068,0.474386003757832,
113.357201733383));
#36657=CARTESIAN_POINT('Ctrl Pts',(-2.48666679435607,0.392803390829163,
113.362451167182));
#36658=CARTESIAN_POINT('Ctrl Pts',(-2.48999996417262,0.371702547770623,
113.363808901076));
#36659=CARTESIAN_POINT('Ctrl Pts',(-2.49306299843523,0.350569005603976,
113.365166634969));
#36660=CARTESIAN_POINT('Ctrl Pts',(-2.49585559325281,0.329410242142917,
113.366524368863));
#36661=CARTESIAN_POINT('Ctrl Pts',(-2.51017941349532,0.220882387524782,
113.373488478412));
#36662=CARTESIAN_POINT('Ctrl Pts',(-2.51742584483449,0.111407119474494,
113.38045258796));
#36663=CARTESIAN_POINT('Ctrl Pts',(-2.51749943375607,0.00168850166091125,
113.387416697508));
#36664=CARTESIAN_POINT('',(1.91346599666509,1.63598720337492,114.));
#36665=CARTESIAN_POINT('Ctrl Pts',(-2.51749943375649,0.00168850103947504,
113.387416697547));
#36666=CARTESIAN_POINT('Ctrl Pts',(-2.51755421150463,-0.0799833171623861,
113.392600607993));
#36667=CARTESIAN_POINT('Ctrl Pts',(-2.51363042105735,-0.161806285473799,
113.397784518439));
#36668=CARTESIAN_POINT('Ctrl Pts',(-2.50571039821078,-0.243354988233973,
113.402968428884));
#36669=CARTESIAN_POINT('Ctrl Pts',(-2.49780084907216,-0.32479584821237,
113.40814548395));
#36670=CARTESIAN_POINT('Ctrl Pts',(-2.48590561137912,-0.405962694191178,
113.413322539016));
#36671=CARTESIAN_POINT('Ctrl Pts',(-2.47005904803184,-0.486430415615699,
113.418499594082));
#36672=CARTESIAN_POINT('Ctrl Pts',(-2.45422403262535,-0.566839497418313,
113.423672876448));
#36673=CARTESIAN_POINT('Ctrl Pts',(-2.43444349473638,-0.646550001534911,
113.428846158814));
#36674=CARTESIAN_POINT('Ctrl Pts',(-2.41080343797533,-0.72514345714924,
113.43401944118));
#36675=CARTESIAN_POINT('Ctrl Pts',(-2.38717303572815,-0.803704815479894,
113.439190610796));
#36676=CARTESIAN_POINT('Ctrl Pts',(-2.35968637923368,-0.881149576872663,
113.444361780413));
#36677=CARTESIAN_POINT('Ctrl Pts',(-2.32847986839699,-0.957072490707963,
113.449532950029));
#36678=CARTESIAN_POINT('Ctrl Pts',(-2.29727610643059,-1.03298871676443,
113.454703664135));
#36679=CARTESIAN_POINT('Ctrl Pts',(-2.2623533225281,-1.10738292322524,113.459874378242));
#36680=CARTESIAN_POINT('Ctrl Pts',(-2.22389621033664,-1.17986944008663,
113.465045092348));
#36681=CARTESIAN_POINT('Ctrl Pts',(-2.18540521498254,-1.25241982218125,
113.470220362183));
#36682=CARTESIAN_POINT('Ctrl Pts',(-2.14337389406924,-1.32305873727335,
113.475395632017));
#36683=CARTESIAN_POINT('Ctrl Pts',(-2.09803277362101,-1.39142543127979,
113.480570901852));
#36684=CARTESIAN_POINT('Ctrl Pts',(-2.05267206221442,-1.45982166511767,
113.485748407813));
#36685=CARTESIAN_POINT('Ctrl Pts',(-2.00399898569736,-1.52594334083173,
113.490925913774));
#36686=CARTESIAN_POINT('Ctrl Pts',(-1.95228575326899,-1.58946109973882,
113.496103419735));
#36687=CARTESIAN_POINT('Ctrl Pts',(-1.90048496764483,-1.65308639751981,
113.501289691484));
#36688=CARTESIAN_POINT('Ctrl Pts',(-1.84563406334905,-1.71409861995426,
113.506475963233));
#36689=CARTESIAN_POINT('Ctrl Pts',(-1.78804338289506,-1.77220402631446,
113.511662234981));
#36690=CARTESIAN_POINT('Ctrl Pts',(-1.73906891532323,-1.82161621101349,
113.516072582203));
#36691=CARTESIAN_POINT('Ctrl Pts',(-1.68811389733081,-1.86892683868316,
113.520482929426));
#36692=CARTESIAN_POINT('Ctrl Pts',(-1.63538707771097,-1.91397893302303,
113.524893276648));
#36693=CARTESIAN_POINT('Ctrl Pts',(-1.57250705357179,-1.9677063681317,113.530152891049));
#36694=CARTESIAN_POINT('Ctrl Pts',(-1.50686303370176,-2.01842883236994,
113.53541250545));
#36695=CARTESIAN_POINT('Ctrl Pts',(-1.4387738333564,-2.06584997191203,113.540672119851));
#36696=CARTESIAN_POINT('Ctrl Pts',(-1.37077968294609,-2.11320491334619,
113.545924392031));
#36697=CARTESIAN_POINT('Ctrl Pts',(-1.30034750725321,-2.15726742356124,
113.55117666421));
#36698=CARTESIAN_POINT('Ctrl Pts',(-1.22782991160256,-2.19778068928045,
113.556428936389));
#36699=CARTESIAN_POINT('Ctrl Pts',(-1.15486433052847,-2.23854423015475,
113.561713655058));
#36700=CARTESIAN_POINT('Ctrl Pts',(-1.0797878306465,-2.27571421165269,113.566998373726));
#36701=CARTESIAN_POINT('Ctrl Pts',(-1.00299011791318,-2.30907277351072,
113.572283092395));
#36702=CARTESIAN_POINT('Ctrl Pts',(-0.926796819238338,-2.34216879651128,
113.577526219222));
#36703=CARTESIAN_POINT('Ctrl Pts',(-0.848909733928286,-2.37151299596481,
113.58276934605));
#36704=CARTESIAN_POINT('Ctrl Pts',(-0.76973339418745,-2.39693903799673,
113.588012472877));
#36705=CARTESIAN_POINT('Ctrl Pts',(-0.690581954112356,-2.42235708395368,
113.593253950827));
#36706=CARTESIAN_POINT('Ctrl Pts',(-0.610142502947859,-2.44385927919593,
113.598495428776));
#36707=CARTESIAN_POINT('Ctrl Pts',(-0.528836740693188,-2.46132849325177,
113.603736906726));
#36708=CARTESIAN_POINT('Ctrl Pts',(-0.447532155743138,-2.47879745435398,
113.608978308779));
#36709=CARTESIAN_POINT('Ctrl Pts',(-0.365361735020498,-2.49223345476331,
113.614219710832));
#36710=CARTESIAN_POINT('Ctrl Pts',(-0.282758083655926,-2.50157033003816,
113.619461112886));
#36711=CARTESIAN_POINT('Ctrl Pts',(-0.198966866834742,-2.51104143848994,
113.624777868848));
#36712=CARTESIAN_POINT('Ctrl Pts',(-0.114730345459241,-2.51629454991259,
113.63009462481));
#36713=CARTESIAN_POINT('Ctrl Pts',(-0.0305043257572554,-2.51731518410192,
113.635411380772));
#36714=CARTESIAN_POINT('Ctrl Pts',(0.0526488683712037,-2.51832281800389,
113.640660414767));
#36715=CARTESIAN_POINT('Ctrl Pts',(0.135791363028913,-2.51520525956991,
113.645909448762));
#36716=CARTESIAN_POINT('Ctrl Pts',(0.218487445379377,-2.5080010937421,113.651158482757));
#36717=CARTESIAN_POINT('Ctrl Pts',(0.302783919745552,-2.50065750789411,
113.656509099702));
#36718=CARTESIAN_POINT('Ctrl Pts',(0.386616022731536,-2.48906754631549,
113.661859716648));
#36719=CARTESIAN_POINT('Ctrl Pts',(0.469532709508704,-2.47332676464341,
113.667210333594));
#36720=CARTESIAN_POINT('Ctrl Pts',(0.552449396285871,-2.45758598297132,
113.67256095054));
#36721=CARTESIAN_POINT('Ctrl Pts',(0.634450196834202,-2.43769456279067,
113.677911567486));
#36722=CARTESIAN_POINT('Ctrl Pts',(0.715101824085999,-2.41380107531438,
113.683262184432));
#36723=CARTESIAN_POINT('Ctrl Pts',(0.793554342076212,-2.39055908603338,
113.688466907344));
#36724=CARTESIAN_POINT('Ctrl Pts',(0.871033305088665,-2.36344058807609,
113.693671630255));
#36725=CARTESIAN_POINT('Ctrl Pts',(0.947122874109041,-2.33254464294672,
113.698876353167));
#36726=CARTESIAN_POINT('Ctrl Pts',(1.02310324455864,-2.30169303757501,113.704073606614));
#36727=CARTESIAN_POINT('Ctrl Pts',(1.09769774699205,-2.26707492238892,113.709270860061));
#36728=CARTESIAN_POINT('Ctrl Pts',(1.17050463881239,-2.22883941559698,113.714468113509));
#36729=CARTESIAN_POINT('Ctrl Pts',(1.2447292695713,-2.18985936436068,113.719766570955));
#36730=CARTESIAN_POINT('Ctrl Pts',(1.31709545147365,-2.14711967416191,113.725065028401));
#36731=CARTESIAN_POINT('Ctrl Pts',(1.38719800100625,-2.10083030157227,113.730363485847));
#36732=CARTESIAN_POINT('Ctrl Pts',(1.45584139845677,-2.055504420822,113.735551658357));
#36733=CARTESIAN_POINT('Ctrl Pts',(1.52231407870445,-2.00677548085572,113.740739830867));
#36734=CARTESIAN_POINT('Ctrl Pts',(1.58626141440623,-1.95488643536292,113.745928003376));
#36735=CARTESIAN_POINT('Ctrl Pts',(1.65019005547335,-1.9030125593332,113.751114659154));
#36736=CARTESIAN_POINT('Ctrl Pts',(1.71159445158167,-1.84798070796214,113.756301314931));
#36737=CARTESIAN_POINT('Ctrl Pts',(1.77015176078904,-1.79007513634916,113.761487970709));
#36738=CARTESIAN_POINT('Ctrl Pts',(1.82871044984529,-1.73216820024489,113.766674748705));
#36739=CARTESIAN_POINT('Ctrl Pts',(1.88442158455526,-1.67138774159439,113.771861526701));
#36740=CARTESIAN_POINT('Ctrl Pts',(1.9369991156543,-1.60805493561459,113.777048304698));
#36741=CARTESIAN_POINT('Ctrl Pts',(1.99155455645801,-1.54233961815218,113.782430203657));
#36742=CARTESIAN_POINT('Ctrl Pts',(2.04273558987152,-1.47387652273846,113.787812102617));
#36743=CARTESIAN_POINT('Ctrl Pts',(2.09026985344726,-1.40306029441701,113.793194001577));
#36744=CARTESIAN_POINT('Ctrl Pts',(2.13615726482396,-1.33469753549987,113.798389441518));
#36745=CARTESIAN_POINT('Ctrl Pts',(2.17864626181776,-1.26414246756954,113.80358488146));
#36746=CARTESIAN_POINT('Ctrl Pts',(2.21753822073832,-1.19177619105465,113.808780321401));
#36747=CARTESIAN_POINT('Ctrl Pts',(2.25646172605579,-1.11935121615208,113.813979975514));
#36748=CARTESIAN_POINT('Ctrl Pts',(2.29178219227516,-1.045112536375,113.819179629628));
#36749=CARTESIAN_POINT('Ctrl Pts',(2.32334910253939,-0.969461292537977,
113.824379283741));
#36750=CARTESIAN_POINT('Ctrl Pts',(2.35496983129941,-0.893681070726442,
113.829587802756));
#36751=CARTESIAN_POINT('Ctrl Pts',(2.38282409013507,-0.816483924998248,
113.834796321772));
#36752=CARTESIAN_POINT('Ctrl Pts',(2.40681135176588,-0.738285423810404,
113.840004840787));
#36753=CARTESIAN_POINT('Ctrl Pts',(2.40930785914718,-0.730146806804966,
113.840546924597));
#36754=CARTESIAN_POINT('Ctrl Pts',(2.41176252558664,-0.721997350558678,
113.841089008406));
#36755=CARTESIAN_POINT('Ctrl Pts',(2.4141752698409,-0.713837528075284,113.841631092216));
#36756=CARTESIAN_POINT('Ctrl Pts',(2.43819602524483,-0.632600115669368,
113.847027960358));
#36757=CARTESIAN_POINT('Ctrl Pts',(2.45814875987533,-0.550025254596369,
113.852424828499));
#36758=CARTESIAN_POINT('Ctrl Pts',(2.47389213394086,-0.466544702708686,
113.857821696641));
#36759=CARTESIAN_POINT('Ctrl Pts',(2.48961070129014,-0.38319569049949,113.863210060978));
#36760=CARTESIAN_POINT('Ctrl Pts',(2.50113302019914,-0.298944246618516,
113.868598425315));
#36761=CARTESIAN_POINT('Ctrl Pts',(2.50836781699562,-0.214236188961182,
113.873986789652));
#36762=CARTESIAN_POINT('Ctrl Pts',(2.51559120170127,-0.129661748885135,
113.879366654441));
#36763=CARTESIAN_POINT('Ctrl Pts',(2.51854049285268,-0.0446325564713008,
113.884746519229));
#36764=CARTESIAN_POINT('Ctrl Pts',(2.51717585105964,0.0403978321467932,
113.890126384018));
#36765=CARTESIAN_POINT('Ctrl Pts',(2.515812477245,0.125349213441812,113.895501250021));
#36766=CARTESIAN_POINT('Ctrl Pts',(2.51014314800948,0.210301359333818,113.900876116024));
#36767=CARTESIAN_POINT('Ctrl Pts',(2.50018000938136,0.29479852558964,113.906250982027));
#36768=CARTESIAN_POINT('Ctrl Pts',(2.49022373185465,0.379237502990729,113.911622146636));
#36769=CARTESIAN_POINT('Ctrl Pts',(2.47597957677018,0.463221696707422,113.916993311245));
#36770=CARTESIAN_POINT('Ctrl Pts',(2.45751161106588,0.546299305762291,113.922364475854));
#36771=CARTESIAN_POINT('Ctrl Pts',(2.43905192557554,0.629339666514449,113.927733232272));
#36772=CARTESIAN_POINT('Ctrl Pts',(2.41637229132917,0.711473830977599,113.933101988689));
#36773=CARTESIAN_POINT('Ctrl Pts',(2.3895878950694,0.792260021544572,113.938470745107));
#36774=CARTESIAN_POINT('Ctrl Pts',(2.36280113558813,0.873053339980342,113.943839975217));
#36775=CARTESIAN_POINT('Ctrl Pts',(2.3319090164842,0.952498034205536,113.949209205327));
#36776=CARTESIAN_POINT('Ctrl Pts',(2.2970764722723,1.03016791375632,113.954578435437));
#36777=CARTESIAN_POINT('Ctrl Pts',(2.26224447137888,1.10783658181131,113.959947581798));
#36778=CARTESIAN_POINT('Ctrl Pts',(2.22347234975331,1.18373009898536,113.965316728159));
#36779=CARTESIAN_POINT('Ctrl Pts',(2.18097243197872,1.2574440349172,113.97068587452));
#36780=CARTESIAN_POINT('Ctrl Pts',(2.13844113945146,1.33121238875449,113.97605898455));
#36781=CARTESIAN_POINT('Ctrl Pts',(2.09217677159438,1.40279757420296,113.98143209458));
#36782=CARTESIAN_POINT('Ctrl Pts',(2.0424365335209,1.47182174754252,113.986805204611));
#36783=CARTESIAN_POINT('Ctrl Pts',(2.00172068117099,1.52832284522758,113.991203469741));
#36784=CARTESIAN_POINT('Ctrl Pts',(1.95867669090703,1.58310835081476,113.99560173487));
#36785=CARTESIAN_POINT('Ctrl Pts',(1.91346599666509,1.63598720337492,114.));
#36786=CARTESIAN_POINT('',(-1.91365515010967,1.63576594183237,113.999998295674));
#36787=CARTESIAN_POINT('Origin',(0.,0.,114.));
#36788=CARTESIAN_POINT('',(-2.51749949088407,0.00160106165700581,113.112583302433));
#36789=CARTESIAN_POINT('Ctrl Pts',(-1.91365515010967,1.63576594183237,113.999998295674));
#36790=CARTESIAN_POINT('Ctrl Pts',(-1.86017206798978,1.69833490290746,113.994762825085));
#36791=CARTESIAN_POINT('Ctrl Pts',(-1.80351482559582,1.75839765718748,113.989527354496));
#36792=CARTESIAN_POINT('Ctrl Pts',(-1.74394816828049,1.81561312959318,113.984291883907));
#36793=CARTESIAN_POINT('Ctrl Pts',(-1.68446595189907,1.87274749407471,113.979063835054));
#36794=CARTESIAN_POINT('Ctrl Pts',(-1.62208284389702,1.92704227278225,113.973835786202));
#36795=CARTESIAN_POINT('Ctrl Pts',(-1.55710332208692,1.9781899540605,113.968607737349));
#36796=CARTESIAN_POINT('Ctrl Pts',(-1.49219790864146,2.02927930202221,113.963385651023));
#36797=CARTESIAN_POINT('Ctrl Pts',(-1.42470232982389,2.07722839907304,113.958163564698));
#36798=CARTESIAN_POINT('Ctrl Pts',(-1.35495624407953,2.12176808973787,113.952941478372));
#36799=CARTESIAN_POINT('Ctrl Pts',(-1.28525345971406,2.16628012824128,113.947722634143));
#36800=CARTESIAN_POINT('Ctrl Pts',(-1.21330333288295,2.20738671206429,113.942503789914));
#36801=CARTESIAN_POINT('Ctrl Pts',(-1.13947583620391,2.24486103550028,113.937284945685));
#36802=CARTESIAN_POINT('Ctrl Pts',(-1.06567145944788,2.28232362342428,113.932067735796));
#36803=CARTESIAN_POINT('Ctrl Pts',(-0.989991294991094,2.31615599939776,
113.926850525907));
#36804=CARTESIAN_POINT('Ctrl Pts',(-0.912830071039806,2.34617721227649,
113.921633316019));
#36805=CARTESIAN_POINT('Ctrl Pts',(-0.835669270168312,2.37619826054704,
113.916416134737));
#36806=CARTESIAN_POINT('Ctrl Pts',(-0.757027860163825,2.40240802003829,
113.911198953454));
#36807=CARTESIAN_POINT('Ctrl Pts',(-0.677319358495791,2.42467415060392,
113.905981772172));
#36808=CARTESIAN_POINT('Ctrl Pts',(-0.59753402159868,2.44696174466726,113.900759561773));
#36809=CARTESIAN_POINT('Ctrl Pts',(-0.516679987743237,2.46529799189702,
113.895537351375));
#36810=CARTESIAN_POINT('Ctrl Pts',(-0.435184140292947,2.47960097879427,
113.890315140976));
#36811=CARTESIAN_POINT('Ctrl Pts',(-0.353648944782196,2.49391087150096,
113.885090409175));
#36812=CARTESIAN_POINT('Ctrl Pts',(-0.271471780659217,2.50418356786419,
113.879865677374));
#36813=CARTESIAN_POINT('Ctrl Pts',(-0.189085423689017,2.5103890042279,113.874640945573));
#36814=CARTESIAN_POINT('Ctrl Pts',(-0.106557256956499,2.51660512186808,
113.869407220559));
#36815=CARTESIAN_POINT('Ctrl Pts',(-0.0238196439423053,2.51873998240891,
113.864173495546));
#36816=CARTESIAN_POINT('Ctrl Pts',(0.0586941218575013,2.51681569648224,
113.858939770533));
#36817=CARTESIAN_POINT('Ctrl Pts',(0.12722137524081,2.5152175870274,113.854593189128));
#36818=CARTESIAN_POINT('Ctrl Pts',(0.195594143011457,2.51082076482695,113.850246607722));
#36819=CARTESIAN_POINT('Ctrl Pts',(0.263568588429768,2.50366488356432,113.845900026317));
#36820=CARTESIAN_POINT('Ctrl Pts',(0.345886857750583,2.49499898335168,113.840636238483));
#36821=CARTESIAN_POINT('Ctrl Pts',(0.427923672364484,2.4822535576129,113.83537245065));
#36822=CARTESIAN_POINT('Ctrl Pts',(0.509244082206853,2.46545669496288,113.830108662817));
#36823=CARTESIAN_POINT('Ctrl Pts',(0.590452038900465,2.44868305969327,113.824852153962));
#36824=CARTESIAN_POINT('Ctrl Pts',(0.670945112211881,2.42786920923019,113.819595645108));
#36825=CARTESIAN_POINT('Ctrl Pts',(0.750293879482346,2.4030949511851,113.814339136253));
#36826=CARTESIAN_POINT('Ctrl Pts',(0.830052614195825,2.37819269317767,113.809055468848));
#36827=CARTESIAN_POINT('Ctrl Pts',(0.908654715917763,2.34928903312637,113.803771801443));
#36828=CARTESIAN_POINT('Ctrl Pts',(0.985674857527892,2.31651706776302,113.798488134038));
#36829=CARTESIAN_POINT('Ctrl Pts',(1.0621676390054,2.2839694934179,113.793240644125));
#36830=CARTESIAN_POINT('Ctrl Pts',(1.13709962859141,2.24760660554363,113.787993154212));
#36831=CARTESIAN_POINT('Ctrl Pts',(1.21007143981663,2.20760806316251,113.782745664299));
#36832=CARTESIAN_POINT('Ctrl Pts',(1.28302085789761,2.16762179529004,113.777499784703));
#36833=CARTESIAN_POINT('Ctrl Pts',(1.35401088964504,2.12400230977291,113.772253905108));
#36834=CARTESIAN_POINT('Ctrl Pts',(1.42266608394282,2.07697555681303,113.767008025512));
#36835=CARTESIAN_POINT('Ctrl Pts',(1.49132072010692,2.02994918615801,113.761762188563));
#36836=CARTESIAN_POINT('Ctrl Pts',(1.55764017800716,1.9795158638528,113.756516351614));
#36837=CARTESIAN_POINT('Ctrl Pts',(1.62127851820578,1.92594449982456,113.751270514665));
#36838=CARTESIAN_POINT('Ctrl Pts',(1.68571484194417,1.87170138561295,113.745958898321));
#36839=CARTESIAN_POINT('Ctrl Pts',(1.74740195992598,1.81424128057953,113.740647281976));
#36840=CARTESIAN_POINT('Ctrl Pts',(1.80601721206052,1.75388371328921,113.735335665632));
#36841=CARTESIAN_POINT('Ctrl Pts',(1.86399122970701,1.69418644092815,113.730082156887));
#36842=CARTESIAN_POINT('Ctrl Pts',(1.91896000322127,1.63165518174354,113.724828648142));
#36843=CARTESIAN_POINT('Ctrl Pts',(1.97065142286629,1.56663308389523,113.719575139397));
#36844=CARTESIAN_POINT('Ctrl Pts',(2.0232004591392,1.50053219903201,113.714234469253));
#36845=CARTESIAN_POINT('Ctrl Pts',(2.0723621148443,1.43185747623515,113.708893799109));
#36846=CARTESIAN_POINT('Ctrl Pts',(2.11789694190401,1.36099918937288,113.703553128965));
#36847=CARTESIAN_POINT('Ctrl Pts',(2.16343176896373,1.29014090251061,113.698212458821));
#36848=CARTESIAN_POINT('Ctrl Pts',(2.20533957838103,1.21709951046272,113.692871788677));
#36849=CARTESIAN_POINT('Ctrl Pts',(2.24343105055273,1.14228865503246,113.687531118533));
#36850=CARTESIAN_POINT('Ctrl Pts',(2.28087180004238,1.06875580535301,113.682281683907));
#36851=CARTESIAN_POINT('Ctrl Pts',(2.31476407192179,0.993241483549429,113.677032249281));
#36852=CARTESIAN_POINT('Ctrl Pts',(2.34489351657419,0.916122615116727,113.671782814655));
#36853=CARTESIAN_POINT('Ctrl Pts',(2.3749797309288,0.83911439829699,113.666540912018));
#36854=CARTESIAN_POINT('Ctrl Pts',(2.4013136743019,0.760506634589067,113.66129900938));
#36855=CARTESIAN_POINT('Ctrl Pts',(2.42372722344526,0.680700078103652,113.656057106742));
#36856=CARTESIAN_POINT('Ctrl Pts',(2.44633483038983,0.600202551849299,113.650769819409));
#36857=CARTESIAN_POINT('Ctrl Pts',(2.46495359977937,0.518485794368826,113.645482532076));
#36858=CARTESIAN_POINT('Ctrl Pts',(2.47946100625358,0.435980926725019,113.640195244743));
#36859=CARTESIAN_POINT('Ctrl Pts',(2.49381774094527,0.354332942459809,113.634962870396));
#36860=CARTESIAN_POINT('Ctrl Pts',(2.50414803386643,0.271913608038802,113.629730496049));
#36861=CARTESIAN_POINT('Ctrl Pts',(2.51038388229762,0.1891534126056,113.624498121702));
#36862=CARTESIAN_POINT('Ctrl Pts',(2.51661762373109,0.106421180575309,113.619267515294));
#36863=CARTESIAN_POINT('Ctrl Pts',(2.51875963333115,0.0233487771706928,
113.614036908886));
#36864=CARTESIAN_POINT('Ctrl Pts',(2.51679374497759,-0.0596279736504867,
113.608806302478));
#36865=CARTESIAN_POINT('Ctrl Pts',(2.51482792416235,-0.142601873795793,
113.603575875768));
#36866=CARTESIAN_POINT('Ctrl Pts',(2.50875449790617,-0.22547966543505,113.598345449058));
#36867=CARTESIAN_POINT('Ctrl Pts',(2.49860940534716,-0.307826719942721,
113.593115022348));
#36868=CARTESIAN_POINT('Ctrl Pts',(2.48827233935064,-0.391732010319809,
113.587785621381));
#36869=CARTESIAN_POINT('Ctrl Pts',(2.47370796649111,-0.475085773950252,
113.582456220415));
#36870=CARTESIAN_POINT('Ctrl Pts',(2.45500924246962,-0.557436874801747,
113.577126819448));
#36871=CARTESIAN_POINT('Ctrl Pts',(2.4366314972481,-0.638374352055361,113.571888901982));
#36872=CARTESIAN_POINT('Ctrl Pts',(2.41426041510205,-0.718342884315836,
113.566650984516));
#36873=CARTESIAN_POINT('Ctrl Pts',(2.38803476196017,-0.796929247593444,
113.56141306705));
#36874=CARTESIAN_POINT('Ctrl Pts',(2.36112203769729,-0.877574450756549,
113.556037924333));
#36875=CARTESIAN_POINT('Ctrl Pts',(2.33015013274271,-0.956763560776925,
113.550662781616));
#36876=CARTESIAN_POINT('Ctrl Pts',(2.29532093802874,-1.0340735183955,113.545287638899));
#36877=CARTESIAN_POINT('Ctrl Pts',(2.26049174331478,-1.11138347601407,113.539912496182));
#36878=CARTESIAN_POINT('Ctrl Pts',(2.22180555688258,-1.18681385088719,113.534537353466));
#36879=CARTESIAN_POINT('Ctrl Pts',(2.17951291006165,-1.25997211273686,113.529162210749));
#36880=CARTESIAN_POINT('Ctrl Pts',(2.13815552656625,-1.33151254632535,113.523905934412));
#36881=CARTESIAN_POINT('Ctrl Pts',(2.09319585109432,-1.40114634549873,113.518649658076));
#36882=CARTESIAN_POINT('Ctrl Pts',(2.04483473617717,-1.46848804956774,113.51339338174));
#36883=CARTESIAN_POINT('Ctrl Pts',(1.99654215127683,-1.53573432721573,113.508144553799));
#36884=CARTESIAN_POINT('Ctrl Pts',(1.94485796776963,-1.60069458982375,113.502895725858));
#36885=CARTESIAN_POINT('Ctrl Pts',(1.89002812601534,-1.66300930029599,113.497646897917));
#36886=CARTESIAN_POINT('Ctrl Pts',(1.83481450963244,-1.72576017480049,113.492361331461));
#36887=CARTESIAN_POINT('Ctrl Pts',(1.77641125714273,-1.78582790185507,113.487075765005));
#36888=CARTESIAN_POINT('Ctrl Pts',(1.71511306460385,-1.84287639998596,113.481790198548));
#36889=CARTESIAN_POINT('Ctrl Pts',(1.65434966255228,-1.8994271837006,113.476550745534));
#36890=CARTESIAN_POINT('Ctrl Pts',(1.59074198040323,-1.95301089524435,113.47131129252));
#36891=CARTESIAN_POINT('Ctrl Pts',(1.5246152113669,-2.00333589476869,113.466071839506));
#36892=CARTESIAN_POINT('Ctrl Pts',(1.45851022582843,-2.05364431621829,113.460834112474));
#36893=CARTESIAN_POINT('Ctrl Pts',(1.38988816825624,-2.10069587858728,113.455596385441));
#36894=CARTESIAN_POINT('Ctrl Pts',(1.31910687156902,-2.14423956482931,113.450358658409));
#36895=CARTESIAN_POINT('Ctrl Pts',(1.2483275644794,-2.18778202709809,113.445121078605));
#36896=CARTESIAN_POINT('Ctrl Pts',(1.17538953231913,-2.2278165685016,113.4398834988));
#36897=CARTESIAN_POINT('Ctrl Pts',(1.10067792697136,-2.26413655751547,113.434645918996));
#36898=CARTESIAN_POINT('Ctrl Pts',(1.02477563959907,-2.30103537973536,113.42932486766));
#36899=CARTESIAN_POINT('Ctrl Pts',(0.947043186099315,-2.33409998341538,
113.424003816324));
#36900=CARTESIAN_POINT('Ctrl Pts',(0.867906828277549,-2.36316397810842,
113.418682764988));
#36901=CARTESIAN_POINT('Ctrl Pts',(0.789900366584946,-2.39181300178175,
113.413437686763));
#36902=CARTESIAN_POINT('Ctrl Pts',(0.710530296499695,-2.41657483980014,
113.408192608538));
#36903=CARTESIAN_POINT('Ctrl Pts',(0.630219709544866,-2.43734063431872,
113.402947530313));
#36904=CARTESIAN_POINT('Ctrl Pts',(0.548164216731687,-2.4585576066693,113.397588492422));
#36905=CARTESIAN_POINT('Ctrl Pts',(0.46512735781871,-2.47560275032423,113.39222945453));
#36906=CARTESIAN_POINT('Ctrl Pts',(0.381568868438044,-2.4884154493651,113.386870416639));
#36907=CARTESIAN_POINT('Ctrl Pts',(0.298010379057378,-2.50122814840597,
113.381511378747));
#36908=CARTESIAN_POINT('Ctrl Pts',(0.213930769663557,-2.50980841740042,
113.376152340855));
#36909=CARTESIAN_POINT('Ctrl Pts',(0.129790714023531,-2.51415206790545,
113.370793302964));
#36910=CARTESIAN_POINT('Ctrl Pts',(0.0472656661578695,-2.51841234516714,
113.365537127945));
#36911=CARTESIAN_POINT('Ctrl Pts',(-0.0356211275015085,-2.51861292477043,
113.360280952927));
#36912=CARTESIAN_POINT('Ctrl Pts',(-0.118436984617641,-2.51471249463526,
113.355024777908));
#36913=CARTESIAN_POINT('Ctrl Pts',(-0.201135760636818,-2.51081757874162,
113.349776033818));
#36914=CARTESIAN_POINT('Ctrl Pts',(-0.283763342413377,-2.50283319092071,
113.344527289729));
#36915=CARTESIAN_POINT('Ctrl Pts',(-0.365884255560971,-2.49076995355504,
113.339278545639));
#36916=CARTESIAN_POINT('Ctrl Pts',(-0.448581647023647,-2.47862203380478,
113.333992956037));
#36917=CARTESIAN_POINT('Ctrl Pts',(-0.530764754398789,-2.46233774014118,
113.328707366434));
#36918=CARTESIAN_POINT('Ctrl Pts',(-0.611991222275894,-2.44198136640255,
113.323421776832));
#36919=CARTESIAN_POINT('Ctrl Pts',(-0.692508066750636,-2.4218028332074,
113.318182364026));
#36920=CARTESIAN_POINT('Ctrl Pts',(-0.77208446623163,-2.39762320674597,
113.31294295122));
#36921=CARTESIAN_POINT('Ctrl Pts',(-0.850298770475567,-2.36955655153612,
113.307703538414));
#36922=CARTESIAN_POINT('Ctrl Pts',(-0.928487556411774,-2.34149905339224,
113.302465835026));
#36923=CARTESIAN_POINT('Ctrl Pts',(-1.00531469593654,-2.30955720088386,
113.297228131638));
#36924=CARTESIAN_POINT('Ctrl Pts',(-1.08037485415755,-2.27389454999656,
113.29199042825));
#36925=CARTESIAN_POINT('Ctrl Pts',(-1.15543314141069,-2.23823278804522,
113.286752855419));
#36926=CARTESIAN_POINT('Ctrl Pts',(-1.22872411878293,-2.19885061099978,
113.281515282587));
#36927=CARTESIAN_POINT('Ctrl Pts',(-1.29986481932664,-2.15595865022429,
113.276277709755));
#36928=CARTESIAN_POINT('Ctrl Pts',(-1.37214017913248,-2.11238258372319,
113.270956600207));
#36929=CARTESIAN_POINT('Ctrl Pts',(-1.442195639441,-2.06518403122962,113.26563549066));
#36930=CARTESIAN_POINT('Ctrl Pts',(-1.50965960883331,-2.0146300194967,113.260314381112));
#36931=CARTESIAN_POINT('Ctrl Pts',(-1.57616004961209,-1.964798026306,113.255069268297));
#36932=CARTESIAN_POINT('Ctrl Pts',(-1.6401422257576,-1.91170614836506,113.249824155483));
#36933=CARTESIAN_POINT('Ctrl Pts',(-1.70128454596898,-1.85565005958751,
113.244579042668));
#36934=CARTESIAN_POINT('Ctrl Pts',(-1.76375570793684,-1.79837567109193,
113.239219934754));
#36935=CARTESIAN_POINT('Ctrl Pts',(-1.82326176568727,-1.73800707625495,
113.233860826839));
#36936=CARTESIAN_POINT('Ctrl Pts',(-1.87950165344929,-1.67489694748107,
113.228501718924));
#36937=CARTESIAN_POINT('Ctrl Pts',(-1.9357415412113,-1.61178681870719,113.223142611009));
#36938=CARTESIAN_POINT('Ctrl Pts',(-1.98871499347162,-1.54593559223706,
113.217783503095));
#36939=CARTESIAN_POINT('Ctrl Pts',(-2.03816777581588,-1.47772743346862,
113.21242439518));
#36940=CARTESIAN_POINT('Ctrl Pts',(-2.08698649321268,-1.41039381401942,
113.207133999728));
#36941=CARTESIAN_POINT('Ctrl Pts',(-2.13255478527078,-1.3405147003582,113.201843604277));
#36942=CARTESIAN_POINT('Ctrl Pts',(-2.17459904927782,-1.26843416261152,
113.196553208825));
#36943=CARTESIAN_POINT('Ctrl Pts',(-2.21658214617846,-1.19645848953606,
113.19127050998));
#36944=CARTESIAN_POINT('Ctrl Pts',(-2.25505117194463,-1.12228814139204,
113.185987811136));
#36945=CARTESIAN_POINT('Ctrl Pts',(-2.28977440510418,-1.04629796125663,
113.180705112291));
#36946=CARTESIAN_POINT('Ctrl Pts',(-2.32445711796564,-0.970396457908242,
113.175428578095));
#36947=CARTESIAN_POINT('Ctrl Pts',(-2.3554025359366,-0.892679751782247,
113.170152043899));
#36948=CARTESIAN_POINT('Ctrl Pts',(-2.38242433929953,-0.813548103994591,
113.164875509703));
#36949=CARTESIAN_POINT('Ctrl Pts',(-2.40942081620889,-0.734490623129741,
113.159603920991));
#36950=CARTESIAN_POINT('Ctrl Pts',(-2.43250084524009,-0.654021265133354,
113.154332332279));
#36951=CARTESIAN_POINT('Ctrl Pts',(-2.45152634821391,-0.572559878102677,
113.149060743568));
#36952=CARTESIAN_POINT('Ctrl Pts',(-2.47054157481037,-0.491142491378067,
113.143792002236));
#36953=CARTESIAN_POINT('Ctrl Pts',(-2.48550652623066,-0.408734581394225,
113.138523260904));
#36954=CARTESIAN_POINT('Ctrl Pts',(-2.49633338758601,-0.325769654853503,
113.133254519572));
#36955=CARTESIAN_POINT('Ctrl Pts',(-2.5071586393188,-0.242817062655348,
113.12798656154));
#36956=CARTESIAN_POINT('Ctrl Pts',(-2.51384696245808,-0.15930806729188,
113.122718603509));
#36957=CARTESIAN_POINT('Ctrl Pts',(-2.51636210187741,-0.0756836986086212,
113.117450645477));
#36958=CARTESIAN_POINT('Ctrl Pts',(-2.51713672499427,-0.0499287171486604,
113.115828197815));
#36959=CARTESIAN_POINT('Ctrl Pts',(-2.51751587600766,-0.0241628209646658,
113.114205750154));
#36960=CARTESIAN_POINT('Ctrl Pts',(-2.51749949088467,0.00160106071358734,
113.112583302492));
#36961=CARTESIAN_POINT('Ctrl Pts',(-2.51749949088407,0.00160106165700588,
113.112583302433));
#36962=CARTESIAN_POINT('Ctrl Pts',(-2.51743978923143,0.0954755726528559,
113.106671674567));
#36963=CARTESIAN_POINT('Ctrl Pts',(-2.51212532380063,0.18915115378945,113.100760046701));
#36964=CARTESIAN_POINT('Ctrl Pts',(-2.50164689230095,0.282079911090854,
113.094848418835));
#36965=CARTESIAN_POINT('Ctrl Pts',(-2.49111954918855,0.375442444705727,
113.088909196452));
#36966=CARTESIAN_POINT('Ctrl Pts',(-2.47538004733398,0.468050954361973,
113.08296997407));
#36967=CARTESIAN_POINT('Ctrl Pts',(-2.45457000539992,0.559367802604915,
113.077030751687));
#36968=CARTESIAN_POINT('Ctrl Pts',(-2.43364683981328,0.65118105039612,113.071059243616));
#36969=CARTESIAN_POINT('Ctrl Pts',(-2.40759797707336,0.74168835061026,113.065087735545));
#36970=CARTESIAN_POINT('Ctrl Pts',(-2.37661545553252,0.830364514248985,
113.059116227474));
#36971=CARTESIAN_POINT('Ctrl Pts',(-2.37167887209854,0.844493683168649,
113.058164760442));
#36972=CARTESIAN_POINT('Ctrl Pts',(-2.36661713203812,0.858576411468391,
113.05721329341));
#36973=CARTESIAN_POINT('Ctrl Pts',(-2.36143112101026,0.872610629504505,
113.056261826378));
#36974=CARTESIAN_POINT('Origin',(0.,0.,104.));
#36975=CARTESIAN_POINT('',(-2.51749986513132,0.000824053271277057,112.112583302525));
#36976=CARTESIAN_POINT('Ctrl Pts',(-2.36143112101026,0.872610629504505,
113.056261826378));
#36977=CARTESIAN_POINT('Ctrl Pts',(-2.35742253990996,0.883458524133866,
113.055526380051));
#36978=CARTESIAN_POINT('Ctrl Pts',(-2.35333971150685,0.894277435752685,
113.054790933724));
#36979=CARTESIAN_POINT('Ctrl Pts',(-2.34918305681532,0.90506641500601,113.054055487397));
#36980=CARTESIAN_POINT('Ctrl Pts',(-2.31947994965906,0.982163559380531,
113.048800049387));
#36981=CARTESIAN_POINT('Ctrl Pts',(-2.28592265483531,1.05793922995017,113.043544611376));
#36982=CARTESIAN_POINT('Ctrl Pts',(-2.24864941558701,1.13198147324953,113.038289173366));
#36983=CARTESIAN_POINT('Ctrl Pts',(-2.21142901042525,1.20591876311934,113.033041184837));
#36984=CARTESIAN_POINT('Ctrl Pts',(-2.17050332894378,1.27812709757133,113.027793196307));
#36985=CARTESIAN_POINT('Ctrl Pts',(-2.12605919360101,1.34821309714177,113.022545207777));
#36986=CARTESIAN_POINT('Ctrl Pts',(-2.08129504247615,1.41880374430617,113.017259431604));
#36987=CARTESIAN_POINT('Ctrl Pts',(-2.03296172678269,1.48724092295824,113.01197365543));
#36988=CARTESIAN_POINT('Ctrl Pts',(-1.98129803209388,1.55314659901147,113.006687879257));
#36989=CARTESIAN_POINT('Ctrl Pts',(-1.93009527182849,1.61846427618127,113.001449261851));
#36990=CARTESIAN_POINT('Ctrl Pts',(-1.87562161171082,1.68129507221643,112.996210644446));
#36991=CARTESIAN_POINT('Ctrl Pts',(-1.81815275188423,1.74130032470444,112.99097202704));
#36992=CARTESIAN_POINT('Ctrl Pts',(-1.76070278980934,1.801285845387,112.985735132273));
#36993=CARTESIAN_POINT('Ctrl Pts',(-1.70025990302305,1.85844733489328,112.980498237507));
#36994=CARTESIAN_POINT('Ctrl Pts',(-1.63713836248182,1.91248117169565,112.97526134274));
#36995=CARTESIAN_POINT('Ctrl Pts',(-1.57401854213981,1.96651353595848,112.97002459069));
#36996=CARTESIAN_POINT('Ctrl Pts',(-1.5082205643552,2.01741811773257,112.96478783864));
#36997=CARTESIAN_POINT('Ctrl Pts',(-1.44009259967277,2.06493088367812,112.95955108659));
#36998=CARTESIAN_POINT('Ctrl Pts',(-1.37085504500771,2.11321748294433,112.954229044342));
#36999=CARTESIAN_POINT('Ctrl Pts',(-1.29921132121754,2.15800049824826,112.948907002094));
#37000=CARTESIAN_POINT('Ctrl Pts',(-1.2255568803691,2.19904901786658,112.943584959845));
#37001=CARTESIAN_POINT('Ctrl Pts',(-1.15297876560743,2.23949768780877,112.938340689594));
#37002=CARTESIAN_POINT('Ctrl Pts',(-1.07844875856923,2.27632013507848,112.933096419342));
#37003=CARTESIAN_POINT('Ctrl Pts',(-1.00236773890926,2.30934301609656,112.92785214909));
#37004=CARTESIAN_POINT('Ctrl Pts',(-0.924594308532173,2.34310048608301,
112.922491220844));
#37005=CARTESIAN_POINT('Ctrl Pts',(-0.845200512098593,2.37288713906597,
112.917130292597));
#37006=CARTESIAN_POINT('Ctrl Pts',(-0.76463160291642,2.39857140019251,112.911769364351));
#37007=CARTESIAN_POINT('Ctrl Pts',(-0.684062693734246,2.42425566131905,
112.906408436104));
#37008=CARTESIAN_POINT('Ctrl Pts',(-0.602319179784995,2.4458374654769,112.901047507858));
#37009=CARTESIAN_POINT('Ctrl Pts',(-0.519856031971376,2.46324094558835,
112.895686579612));
#37010=CARTESIAN_POINT('Ctrl Pts',(-0.439017021013886,2.48030165884911,
112.890431236483));
#37011=CARTESIAN_POINT('Ctrl Pts',(-0.35718804757108,2.49341016839008,112.885175893354));
#37012=CARTESIAN_POINT('Ctrl Pts',(-0.274789908521613,2.50245814274179,
112.879920550225));
#37013=CARTESIAN_POINT('Ctrl Pts',(-0.192508554083284,2.51149329320963,
112.874672655604));
#37014=CARTESIAN_POINT('Ctrl Pts',(-0.109660091183823,2.51647928983228,
112.869424760983));
#37015=CARTESIAN_POINT('Ctrl Pts',(-0.02667618636761,2.51735866158974,112.864176866363));
#37016=CARTESIAN_POINT('Ctrl Pts',(0.0569071050046635,2.51824438498382,
112.85889106659));
#37017=CARTESIAN_POINT('Ctrl Pts',(0.140627339457404,2.51496381246618,112.853605266818));
#37018=CARTESIAN_POINT('Ctrl Pts',(0.224037401075276,2.50751141431489,112.848319467046));
#37019=CARTESIAN_POINT('Ctrl Pts',(0.306701490974546,2.50012566613541,112.843080940433));
#37020=CARTESIAN_POINT('Ctrl Pts',(0.389060465882272,2.48864245688889,112.83784241382));
#37021=CARTESIAN_POINT('Ctrl Pts',(0.470680165815713,2.47310865744061,112.832603887207));
#37022=CARTESIAN_POINT('Ctrl Pts',(0.552273047443024,2.45757996203203,112.82736708185));
#37023=CARTESIAN_POINT('Ctrl Pts',(0.633126683617536,2.43800340591899,112.822130276494));
#37024=CARTESIAN_POINT('Ctrl Pts',(0.712815306971328,2.41447729087423,112.816893471137));
#37025=CARTESIAN_POINT('Ctrl Pts',(0.792501781614026,2.39095181018382,112.811656806985));
#37026=CARTESIAN_POINT('Ctrl Pts',(0.871022863666545,2.3634771139357,112.806420142832));
#37027=CARTESIAN_POINT('Ctrl Pts',(0.947967536103355,2.33220149225879,112.80118347868));
#37028=CARTESIAN_POINT('Ctrl Pts',(1.02616829911449,2.30041530874115,112.795861328109));
#37029=CARTESIAN_POINT('Ctrl Pts',(1.10274026042232,2.26470315876107,112.790539177538));
#37030=CARTESIAN_POINT('Ctrl Pts',(1.17727439967341,2.22527104818124,112.785217026967));
#37031=CARTESIAN_POINT('Ctrl Pts',(1.25071669726387,2.18641657385681,112.779972839941));
#37032=CARTESIAN_POINT('Ctrl Pts',(1.32218011034016,2.14395069601214,112.774728652915));
#37033=CARTESIAN_POINT('Ctrl Pts',(1.39130099717206,2.09811529360711,112.769484465889));
#37034=CARTESIAN_POINT('Ctrl Pts',(1.46196327907883,2.0512577621936,112.764123333546));
#37035=CARTESIAN_POINT('Ctrl Pts',(1.53017688912916,2.00087892113285,112.758762201202));
#37036=CARTESIAN_POINT('Ctrl Pts',(1.59558900860551,1.94728065918021,112.753401068859));
#37037=CARTESIAN_POINT('Ctrl Pts',(1.66100112808185,1.89368239722757,112.748039936515));
#37038=CARTESIAN_POINT('Ctrl Pts',(1.72361142572262,1.83686510516709,112.742678804172));
#37039=CARTESIAN_POINT('Ctrl Pts',(1.78310853031011,1.77716915884092,112.737317671828));
#37040=CARTESIAN_POINT('Ctrl Pts',(1.84142945236355,1.71865332589856,112.732062522293));
#37041=CARTESIAN_POINT('Ctrl Pts',(1.89697461828024,1.6571554909892,112.726807372758));
#37042=CARTESIAN_POINT('Ctrl Pts',(1.94942405491907,1.59296958668484,112.721552223222));
#37043=CARTESIAN_POINT('Ctrl Pts',(2.0017991132017,1.52887470417901,112.716304525996));
#37044=CARTESIAN_POINT('Ctrl Pts',(2.05108687255724,1.46209967823052,112.711056828769));
#37045=CARTESIAN_POINT('Ctrl Pts',(2.09700409958307,1.39297525330919,112.705809131542));
#37046=CARTESIAN_POINT('Ctrl Pts',(2.1432551506256,1.32334828512306,112.700523282896));
#37047=CARTESIAN_POINT('Ctrl Pts',(2.18608611890685,1.25133794816154,112.695237434251));
#37048=CARTESIAN_POINT('Ctrl Pts',(2.22524889018405,1.1773162815211,112.689951585605));
#37049=CARTESIAN_POINT('Ctrl Pts',(2.26405953268012,1.10396017450275,112.684713264225));
#37050=CARTESIAN_POINT('Ctrl Pts',(2.29926745803909,1.02862917736508,112.679474942845));
#37051=CARTESIAN_POINT('Ctrl Pts',(2.33067559396206,0.951712942913775,112.674236621465));
#37052=CARTESIAN_POINT('Ctrl Pts',(2.36207339457172,0.874822018891059,112.669000023833));
#37053=CARTESIAN_POINT('Ctrl Pts',(2.38967371475449,0.796347320430814,112.6637634262));
#37054=CARTESIAN_POINT('Ctrl Pts',(2.41332719013228,0.716699465165306,112.658526828567));
#37055=CARTESIAN_POINT('Ctrl Pts',(2.4369800176874,0.637053791299605,112.653290374355));
#37056=CARTESIAN_POINT('Ctrl Pts',(2.45668608498179,0.556235467152466,112.648053920143));
#37057=CARTESIAN_POINT('Ctrl Pts',(2.47234598758015,0.474669956597551,112.64281746593));
#37058=CARTESIAN_POINT('Ctrl Pts',(2.48826289130412,0.391765840780482,112.637495074107));
#37059=CARTESIAN_POINT('Ctrl Pts',(2.49999951690567,0.30809027249351,112.632172682283));
#37060=CARTESIAN_POINT('Ctrl Pts',(2.50750594724184,0.224098582206117,112.626850290459));
#37061=CARTESIAN_POINT('Ctrl Pts',(2.5149017807015,0.141344393391824,112.621606316722));
#37062=CARTESIAN_POINT('Ctrl Pts',(2.51819128388743,0.0582838059104078,
112.616362342986));
#37063=CARTESIAN_POINT('Ctrl Pts',(2.51737935166998,-0.0246464964168013,
112.61111836925));
#37064=CARTESIAN_POINT('Ctrl Pts',(2.51654920706964,-0.109437001340971,
112.605756768382));
#37065=CARTESIAN_POINT('Ctrl Pts',(2.51143143353047,-0.194090794260034,
112.600395167514));
#37066=CARTESIAN_POINT('Ctrl Pts',(2.50208718104879,-0.278147422118786,
112.595033566647));
#37067=CARTESIAN_POINT('Ctrl Pts',(2.4927429285671,-0.362204049977539,112.589671965779));
#37068=CARTESIAN_POINT('Ctrl Pts',(2.47917234468489,-0.44566302179835,112.584310364911));
#37069=CARTESIAN_POINT('Ctrl Pts',(2.4614914561348,-0.528077703918061,112.578948764044));
#37070=CARTESIAN_POINT('Ctrl Pts',(2.4441611792165,-0.608858104700658,112.573693483603));
#37071=CARTESIAN_POINT('Ctrl Pts',(2.4228181518075,-0.688933658633213,112.568438203163));
#37072=CARTESIAN_POINT('Ctrl Pts',(2.39753473630544,-0.767875926311536,
112.563182922723));
#37073=CARTESIAN_POINT('Ctrl Pts',(2.37228716535847,-0.846706276734757,
112.557935092747));
#37074=CARTESIAN_POINT('Ctrl Pts',(2.34311044196548,-0.92440609646199,112.552687262772));
#37075=CARTESIAN_POINT('Ctrl Pts',(2.31012780853102,-1.00055772359804,112.547439432796));
#37076=CARTESIAN_POINT('Ctrl Pts',(2.27690643472855,-1.07726056407256,112.542153617107));
#37077=CARTESIAN_POINT('Ctrl Pts',(2.23982392090673,-1.15239224138215,112.536867801418));
#37078=CARTESIAN_POINT('Ctrl Pts',(2.19905724983395,-1.22554210941638,112.531581985729));
#37079=CARTESIAN_POINT('Ctrl Pts',(2.15865582601481,-1.29803659432266,112.52634352808));
#37080=CARTESIAN_POINT('Ctrl Pts',(2.1146362256131,-1.36858422924356,112.521105070432));
#37081=CARTESIAN_POINT('Ctrl Pts',(2.06721801032139,-1.43680755419885,112.515866612784));
#37082=CARTESIAN_POINT('Ctrl Pts',(2.01981538907437,-1.50500844310142,112.510629877864));
#37083=CARTESIAN_POINT('Ctrl Pts',(1.9690166358365,-1.57088616154709,112.505393142945));
#37084=CARTESIAN_POINT('Ctrl Pts',(1.91508487122922,-1.63409185359604,112.500156408026));
#37085=CARTESIAN_POINT('Ctrl Pts',(1.86115457508603,-1.69729582466869,112.494919815693));
#37086=CARTESIAN_POINT('Ctrl Pts',(1.80409173746947,-1.75782756366648,112.489683223361));
#37087=CARTESIAN_POINT('Ctrl Pts',(1.74419913189159,-1.81537203853883,112.484446631028));
#37088=CARTESIAN_POINT('Ctrl Pts',(1.68332704644748,-1.87385759209704,112.479124399797));
#37089=CARTESIAN_POINT('Ctrl Pts',(1.61953214840592,-1.92925694349847,112.473802168567));
#37090=CARTESIAN_POINT('Ctrl Pts',(1.55316914556331,-1.9812803575643,112.468479937336));
#37091=CARTESIAN_POINT('Ctrl Pts',(1.48778020658823,-2.03254018159147,112.46323582483));
#37092=CARTESIAN_POINT('Ctrl Pts',(1.41989846878913,-2.08052229379791,112.457991712323));
#37093=CARTESIAN_POINT('Ctrl Pts',(1.34989290014419,-2.12499303719807,112.452747599817));
#37094=CARTESIAN_POINT('Ctrl Pts',(1.27832307852287,-2.17045746573032,112.447386309224));
#37095=CARTESIAN_POINT('Ctrl Pts',(1.20453381450385,-2.21225146025582,112.442025018631));
#37096=CARTESIAN_POINT('Ctrl Pts',(1.1289445359492,-2.25017565642117,112.436663728038));
#37097=CARTESIAN_POINT('Ctrl Pts',(1.05335525739454,-2.28809985258653,112.431302437445));
#37098=CARTESIAN_POINT('Ctrl Pts',(0.975966456223256,-2.32215410689282,
112.425941146852));
#37099=CARTESIAN_POINT('Ctrl Pts',(0.897215841482083,-2.35219259071055,
112.420579856259));
#37100=CARTESIAN_POINT('Ctrl Pts',(0.820022714062956,-2.38163698954401,
112.415324598389));
#37101=CARTESIAN_POINT('Ctrl Pts',(0.741236063657785,-2.40733180564496,
112.410069340519));
#37102=CARTESIAN_POINT('Ctrl Pts',(0.66125465588879,-2.429104470801,112.404814082649));
#37103=CARTESIAN_POINT('Ctrl Pts',(0.581386639723933,-2.45084626831545,
112.399566275287));
#37104=CARTESIAN_POINT('Ctrl Pts',(0.50032767215338,-2.46867683953436,112.394318467926));
#37105=CARTESIAN_POINT('Ctrl Pts',(0.418495180676302,-2.48247216172724,
112.389070660564));
#37106=CARTESIAN_POINT('Ctrl Pts',(0.336069912429048,-2.49636741423369,
112.383784839227));
#37107=CARTESIAN_POINT('Ctrl Pts',(0.252860309293708,-2.50616854129163,
112.37849901789));
#37108=CARTESIAN_POINT('Ctrl Pts',(0.169307180293646,-2.5118004157777,112.373213196553));
#37109=CARTESIAN_POINT('Ctrl Pts',(0.0865030868762668,-2.51738180173703,
112.367974761451));
#37110=CARTESIAN_POINT('Ctrl Pts',(0.00336207105493,-2.518868357077,112.36273632635));
#37111=CARTESIAN_POINT('Ctrl Pts',(-0.0796797191176613,-2.51623873914248,
112.357497891249));
#37112=CARTESIAN_POINT('Ctrl Pts',(-0.162694201103312,-2.51360998595447,
112.3522611788));
#37113=CARTESIAN_POINT('Ctrl Pts',(-0.245609061421601,-2.50686776240543,
112.347024466351));
#37114=CARTESIAN_POINT('Ctrl Pts',(-0.327988429067703,-2.49604283625055,
112.341787753903));
#37115=CARTESIAN_POINT('Ctrl Pts',(-0.410365555359416,-2.48521820461718,
112.336551183933));
#37116=CARTESIAN_POINT('Ctrl Pts',(-0.492206760595113,-2.47031115237332,
112.331314613964));
#37117=CARTESIAN_POINT('Ctrl Pts',(-0.57308295589743,-2.45140412328524,
112.326078043994));
#37118=CARTESIAN_POINT('Ctrl Pts',(-0.655282559208771,-2.43218771127393,
112.320755786034));
#37119=CARTESIAN_POINT('Ctrl Pts',(-0.736484804272134,-2.4088393344905,
112.315433528074));
#37120=CARTESIAN_POINT('Ctrl Pts',(-0.816253533495705,-2.38149877578297,
112.310111270114));
#37121=CARTESIAN_POINT('Ctrl Pts',(-0.894850709663508,-2.35455976434104,
112.304867179472));
#37122=CARTESIAN_POINT('Ctrl Pts',(-0.972055786362678,-2.32374528861014,
112.299623088829));
#37123=CARTESIAN_POINT('Ctrl Pts',(-1.04747189214599,-2.2892376209481,112.294378998187));
#37124=CARTESIAN_POINT('Ctrl Pts',(-1.12457420295903,-2.25395840717967,
112.289017656568));
#37125=CARTESIAN_POINT('Ctrl Pts',(-1.19980612546018,-2.21481909560088,
112.283656314949));
#37126=CARTESIAN_POINT('Ctrl Pts',(-1.27277206411672,-2.17206296474206,
112.278294973331));
#37127=CARTESIAN_POINT('Ctrl Pts',(-1.34573800277327,-2.12930683388324,
112.272933631712));
#37128=CARTESIAN_POINT('Ctrl Pts',(-1.41643756936656,-2.0829342182641,112.267572290094));
#37129=CARTESIAN_POINT('Ctrl Pts',(-1.48451012278353,-2.03323288025578,
112.262210948475));
#37130=CARTESIAN_POINT('Ctrl Pts',(-1.55068772048485,-1.98491509302979,
112.256998852102));
#37131=CARTESIAN_POINT('Ctrl Pts',(-1.61463601602439,-1.93326638368646,
112.251786755729));
#37132=CARTESIAN_POINT('Ctrl Pts',(-1.67599642208737,-1.87852129164147,
112.246574659355));
#37133=CARTESIAN_POINT('Ctrl Pts',(-1.73726957135127,-1.82385404917089,
112.241369974779));
#37134=CARTESIAN_POINT('Ctrl Pts',(-1.79596179018046,-1.76609947623745,
112.236165290202));
#37135=CARTESIAN_POINT('Ctrl Pts',(-1.85174473417749,-1.70553442927604,
112.230960605626));
#37136=CARTESIAN_POINT('Ctrl Pts',(-1.90746426549754,-1.64503823116848,
112.225761837606));
#37137=CARTESIAN_POINT('Ctrl Pts',(-1.9602807762888,-1.58173825061738,112.220563069587));
#37138=CARTESIAN_POINT('Ctrl Pts',(-2.00990135412894,-1.51594947035535,
112.215364301568));
#37139=CARTESIAN_POINT('Ctrl Pts',(-2.05949157030876,-1.45020094469505,
112.210168714552));
#37140=CARTESIAN_POINT('Ctrl Pts',(-2.10588945199941,-1.38196701550506,
112.204973127536));
#37141=CARTESIAN_POINT('Ctrl Pts',(-2.14884192972162,-1.31159620732536,
112.19977754052));
#37142=CARTESIAN_POINT('Ctrl Pts',(-2.19178162429527,-1.24124634230291,
112.19458349977));
#37143=CARTESIAN_POINT('Ctrl Pts',(-2.23127770634118,-1.16876126189922,
112.18938945902));
#37144=CARTESIAN_POINT('Ctrl Pts',(-2.26712091182993,-1.09451771166274,
112.18419541827));
#37145=CARTESIAN_POINT('Ctrl Pts',(-2.30296471405867,-1.02027292537342,
112.179001291047));
#37146=CARTESIAN_POINT('Ctrl Pts',(-2.33515531662749,-0.944270035186615,
112.173807163823));
#37147=CARTESIAN_POINT('Ctrl Pts',(-2.3635304945719,-0.866908213843155,
112.1686130366));
#37148=CARTESIAN_POINT('Ctrl Pts',(-2.39193263046187,-0.789472894607527,
112.163413974676));
#37149=CARTESIAN_POINT('Ctrl Pts',(-2.41651194329919,-0.710676508807594,
112.158214912753));
#37150=CARTESIAN_POINT('Ctrl Pts',(-2.43715550178047,-0.630935266205005,
112.153015850829));
#37151=CARTESIAN_POINT('Ctrl Pts',(-2.45780970186655,-0.551152917569743,
112.147814108826));
#37152=CARTESIAN_POINT('Ctrl Pts',(-2.47452401436576,-0.470425202882062,
112.142612366824));
#37153=CARTESIAN_POINT('Ctrl Pts',(-2.48723676413951,-0.389178017252802,
112.137410624821));
#37154=CARTESIAN_POINT('Ctrl Pts',(-2.49997002052968,-0.307799773835037,
112.13220049202));
#37155=CARTESIAN_POINT('Ctrl Pts',(-2.50868877897406,-0.225900853751341,
112.126990359219));
#37156=CARTESIAN_POINT('Ctrl Pts',(-2.51338333819124,-0.143911241057328,
112.121780226417));
#37157=CARTESIAN_POINT('Ctrl Pts',(-2.51614561607506,-0.0956685662137815,
112.11871458512));
#37158=CARTESIAN_POINT('Ctrl Pts',(-2.51751564850944,-0.0473944948304982,
112.115648943822));
#37159=CARTESIAN_POINT('Ctrl Pts',(-2.51749986513132,0.000824053271280102,
112.112583302525));
#37160=CARTESIAN_POINT('Ctrl Pts',(-2.51749986513115,0.000824053789601987,
112.112583302492));
#37161=CARTESIAN_POINT('Ctrl Pts',(-2.51748486373191,0.0466536113198584,
112.109669548558));
#37162=CARTESIAN_POINT('Ctrl Pts',(-2.51621849457345,0.0924610145605964,
112.106755794625));
#37163=CARTESIAN_POINT('Ctrl Pts',(-2.51370388884508,0.138199164994239,
112.103842040691));
#37164=CARTESIAN_POINT('Ctrl Pts',(-2.50916909978691,0.220682419441518,
112.098587435841));
#37165=CARTESIAN_POINT('Ctrl Pts',(-2.50056179900052,0.303094538210816,
112.093332830991));
#37166=CARTESIAN_POINT('Ctrl Pts',(-2.48788671813419,0.385001204844178,
112.088078226141));
#37167=CARTESIAN_POINT('Ctrl Pts',(-2.47505746494527,0.467904136603143,
112.082759707329));
#37168=CARTESIAN_POINT('Ctrl Pts',(-2.45806075103824,0.550288760222616,
112.077441188517));
#37169=CARTESIAN_POINT('Ctrl Pts',(-2.43695593026938,0.631705662413221,
112.072122669705));
#37170=CARTESIAN_POINT('Ctrl Pts',(-2.41585110950051,0.713122564603827,
112.066804150893));
#37171=CARTESIAN_POINT('Ctrl Pts',(-2.39063823988411,0.79357125371448,112.061485632081));
#37172=CARTESIAN_POINT('Ctrl Pts',(-2.36143112101026,0.872610629504506,
112.056167113269));
#37173=CARTESIAN_POINT('',(-2.51749910744234,-0.00211991202945377,112.387416697508));
#37174=CARTESIAN_POINT('Ctrl Pts',(-2.36143112095427,0.872610629656001,
112.333400434891));
#37175=CARTESIAN_POINT('Ctrl Pts',(-2.3650344949,0.862859293737455,112.334066402852));
#37176=CARTESIAN_POINT('Ctrl Pts',(-2.36857751691473,0.853085505298505,
112.334730382634));
#37177=CARTESIAN_POINT('Ctrl Pts',(-2.37687869028287,0.829735429620577,
112.336308382216));
#37178=CARTESIAN_POINT('Ctrl Pts',(-2.38158121680321,0.816139763304604,
112.337220539836));
#37179=CARTESIAN_POINT('Ctrl Pts',(-2.38986696712902,0.791502905673892,
112.338861746031));
#37180=CARTESIAN_POINT('Ctrl Pts',(-2.39349082628695,0.780475907393607,
112.339592108014));
#37181=CARTESIAN_POINT('Ctrl Pts',(-2.4011034084151,0.756759920999845,112.341154070631));
#37182=CARTESIAN_POINT('Ctrl Pts',(-2.40506810801852,0.744063547359317,
112.341984870282));
#37183=CARTESIAN_POINT('Ctrl Pts',(-2.4156536523985,0.709196055633934,112.344252095484));
#37184=CARTESIAN_POINT('Ctrl Pts',(-2.42206985904975,0.686963802837211,
112.345681889193));
#37185=CARTESIAN_POINT('Ctrl Pts',(-2.44042072433761,0.619921791530085,
112.3499487849));
#37186=CARTESIAN_POINT('Ctrl Pts',(-2.45142517742808,0.574866362517649,
112.352756647249));
#37187=CARTESIAN_POINT('Ctrl Pts',(-2.49877388886716,0.354796558801355,
112.366229596784));
#37188=CARTESIAN_POINT('Ctrl Pts',(-2.51765262075168,0.176565366880527,
112.376362442797));
#37189=CARTESIAN_POINT('Ctrl Pts',(-2.51749907092304,-0.00216284572706931,
112.386672407636));
#37190=CARTESIAN_POINT('Ctrl Pts',(-2.51749910744234,-0.00211991202945377,
112.387416697508));
#37191=CARTESIAN_POINT('Ctrl Pts',(-2.517394492057,-0.126355793312804,112.395287272283));
#37192=CARTESIAN_POINT('Ctrl Pts',(-2.50809026557141,-0.250215159424013,
112.403157847058));
#37193=CARTESIAN_POINT('Ctrl Pts',(-2.48977141696794,-0.372618492897856,
112.411028421832));
#37194=CARTESIAN_POINT('Ctrl Pts',(-2.48567305793243,-0.400003009172713,
112.412789255275));
#37195=CARTESIAN_POINT('Ctrl Pts',(-2.48112366278329,-0.427314773939724,
112.414550088717));
#37196=CARTESIAN_POINT('Ctrl Pts',(-2.47612558836571,-0.454541879963322,
112.416310922159));
#37197=CARTESIAN_POINT('Ctrl Pts',(-2.46120841196053,-0.535803483857776,
112.421566278699));
#37198=CARTESIAN_POINT('Ctrl Pts',(-2.44225918248003,-0.616480029859821,
112.426821635238));
#37199=CARTESIAN_POINT('Ctrl Pts',(-2.41933747375667,-0.696141105004374,
112.432076991778));
#37200=CARTESIAN_POINT('Ctrl Pts',(-2.39644826496086,-0.775689231363018,
112.437324896923));
#37201=CARTESIAN_POINT('Ctrl Pts',(-2.36959789113806,-0.854224307023324,
112.442572802068));
#37202=CARTESIAN_POINT('Ctrl Pts',(-2.33889710448583,-0.931325176631549,
112.447820707212));
#37203=CARTESIAN_POINT('Ctrl Pts',(-2.30797464785383,-1.00898274038578,
112.453106503993));
#37204=CARTESIAN_POINT('Ctrl Pts',(-2.27314602759454,-1.0851848340452,112.458392300773));
#37205=CARTESIAN_POINT('Ctrl Pts',(-2.23457591223811,-1.15951573617836,
112.463678097553));
#37206=CARTESIAN_POINT('Ctrl Pts',(-2.19635069926193,-1.23318195517964,
112.468916627587));
#37207=CARTESIAN_POINT('Ctrl Pts',(-2.15445085484626,-1.30500989711631,
112.47415515762));
#37208=CARTESIAN_POINT('Ctrl Pts',(-2.10908460417848,-1.37461572172637,
112.479393687653));
#37209=CARTESIAN_POINT('Ctrl Pts',(-2.06373328289616,-1.44419864005322,
112.484630493761));
#37210=CARTESIAN_POINT('Ctrl Pts',(-2.01491807268369,-1.51156050714949,
112.489867299869));
#37211=CARTESIAN_POINT('Ctrl Pts',(-1.96289159043833,-1.57634477643264,
112.495104105976));
#37212=CARTESIAN_POINT('Ctrl Pts',(-1.91086653752487,-1.64112726588717,
112.500340768213));
#37213=CARTESIAN_POINT('Ctrl Pts',(-1.85563067770148,-1.70333193921773,
112.505577430449));
#37214=CARTESIAN_POINT('Ctrl Pts',(-1.79747727089641,-1.76263487728196,
112.510814092685));
#37215=CARTESIAN_POINT('Ctrl Pts',(-1.73837457608633,-1.82290586813724,
112.516136237456));
#37216=CARTESIAN_POINT('Ctrl Pts',(-1.67625856063912,-1.88017917589626,
112.521458382228));
#37217=CARTESIAN_POINT('Ctrl Pts',(-1.61147511894358,-1.93415464506481,
112.526780526999));
#37218=CARTESIAN_POINT('Ctrl Pts',(-1.54764071556149,-1.98733940619305,
112.532024705562));
#37219=CARTESIAN_POINT('Ctrl Pts',(-1.48121693190589,-2.03732207957786,
112.537268884126));
#37220=CARTESIAN_POINT('Ctrl Pts',(-1.41256561689279,-2.08385811128596,
112.542513062689));
#37221=CARTESIAN_POINT('Ctrl Pts',(-1.34238332348644,-2.13143193315203,
112.547874190564));
#37222=CARTESIAN_POINT('Ctrl Pts',(-1.26987338934837,-2.17540327228873,
112.55323531844));
#37223=CARTESIAN_POINT('Ctrl Pts',(-1.19544907037609,-2.21556037384156,
112.558596446315));
#37224=CARTESIAN_POINT('Ctrl Pts',(-1.12102475140381,-2.25571747539439,
112.563957574191));
#37225=CARTESIAN_POINT('Ctrl Pts',(-1.04468653489811,-2.29206018128933,
112.569318702066));
#37226=CARTESIAN_POINT('Ctrl Pts',(-0.96686754316836,-2.32442969434818,
112.574679829942));
#37227=CARTESIAN_POINT('Ctrl Pts',(-0.89058272767988,-2.35616105293121,
112.579935264916));
#37228=CARTESIAN_POINT('Ctrl Pts',(-0.812593390130238,-2.38419164189191,
112.58519069989));
#37229=CARTESIAN_POINT('Ctrl Pts',(-0.733293014203989,-2.4083371037543,
112.590446134864));
#37230=CARTESIAN_POINT('Ctrl Pts',(-0.654105036246838,-2.43244834256484,
112.595694120943));
#37231=CARTESIAN_POINT('Ctrl Pts',(-0.573610148598829,-2.45268525887052,
112.600942107022));
#37232=CARTESIAN_POINT('Ctrl Pts',(-0.492221931378017,-2.46891146464803,
112.6061900931));
#37233=CARTESIAN_POINT('Ctrl Pts',(-0.4102476370936,-2.48525451543531,112.61147586996));
#37234=CARTESIAN_POINT('Ctrl Pts',(-0.327367531017245,-2.49752866920101,
112.616761646819));
#37235=CARTESIAN_POINT('Ctrl Pts',(-0.244019962235263,-2.50564572676001,
112.622047423679));
#37236=CARTESIAN_POINT('Ctrl Pts',(-0.161416032483974,-2.51369036276067,
112.627286040075));
#37237=CARTESIAN_POINT('Ctrl Pts',(-0.0783534159409274,-2.51765174180607,
112.632524656471));
#37238=CARTESIAN_POINT('Ctrl Pts',(0.00473254203868963,-2.51749555174301,
112.637763272866));
#37239=CARTESIAN_POINT('Ctrl Pts',(0.0877911870741211,-2.5173394130245,
112.643000167166));
#37240=CARTESIAN_POINT('Ctrl Pts',(0.170872697288985,-2.51306839434201,
112.648237061465));
#37241=CARTESIAN_POINT('Ctrl Pts',(0.253540453805012,-2.50470027913209,
112.653473955765));
#37242=CARTESIAN_POINT('Ctrl Pts',(0.336205966006391,-2.49633239110485,
112.65871070789));
#37243=CARTESIAN_POINT('Ctrl Pts',(0.418457287910135,-2.48386767519843,
112.663947460015));
#37244=CARTESIAN_POINT('Ctrl Pts',(0.49986304174694,-2.46737576982013,112.66918421214));
#37245=CARTESIAN_POINT('Ctrl Pts',(0.582594661855428,-2.4506152585993,112.674506255939));
#37246=CARTESIAN_POINT('Ctrl Pts',(0.664452438431347,-2.42969528180324,
112.679828299738));
#37247=CARTESIAN_POINT('Ctrl Pts',(0.744996318223181,-2.40474255084279,
112.685150343537));
#37248=CARTESIAN_POINT('Ctrl Pts',(0.824363193475616,-2.38015445935199,
112.690394615198));
#37249=CARTESIAN_POINT('Ctrl Pts',(0.902453900400525,-2.35165091673453,
112.695638886859));
#37250=CARTESIAN_POINT('Ctrl Pts',(0.978866290327585,-2.3194023013829,112.70088315852));
#37251=CARTESIAN_POINT('Ctrl Pts',(1.05697846488503,-2.28643631937415,112.706244088388));
#37252=CARTESIAN_POINT('Ctrl Pts',(1.13333629730785,-2.24955686941383,112.711605018256));
#37253=CARTESIAN_POINT('Ctrl Pts',(1.2075372273684,-2.20899526810707,112.716965948124));
#37254=CARTESIAN_POINT('Ctrl Pts',(1.28173815742895,-2.16843366680032,112.722326877992));
#37255=CARTESIAN_POINT('Ctrl Pts',(1.35378178735331,-2.12419023673152,112.72768780786));
#37256=CARTESIAN_POINT('Ctrl Pts',(1.42329915397842,-2.076541781011,112.733048737727));
#37257=CARTESIAN_POINT('Ctrl Pts',(1.49143551226082,-2.02983989329299,112.738303169187));
#37258=CARTESIAN_POINT('Ctrl Pts',(1.55739689094368,-1.97969447023556,112.743557600647));
#37259=CARTESIAN_POINT('Ctrl Pts',(1.6208144873514,-1.92633502994464,112.748812032107));
#37260=CARTESIAN_POINT('Ctrl Pts',(1.68414214036774,-1.87305126784548,112.754059011354));
#37261=CARTESIAN_POINT('Ctrl Pts',(1.74493282690168,-1.81656283733393,112.759305990602));
#37262=CARTESIAN_POINT('Ctrl Pts',(1.80284702815229,-1.75714223757853,112.76455296985));
#37263=CARTESIAN_POINT('Ctrl Pts',(1.86119223666162,-1.69727941969252,112.769838998002));
#37264=CARTESIAN_POINT('Ctrl Pts',(1.91661756868385,-1.63444086821441,112.775125026155));
#37265=CARTESIAN_POINT('Ctrl Pts',(1.96881021294934,-1.5689463328573,112.780411054307));
#37266=CARTESIAN_POINT('Ctrl Pts',(2.02052477966809,-1.50405171856625,112.785648663159));
#37267=CARTESIAN_POINT('Ctrl Pts',(2.06906534526677,-1.43654994610255,112.79088627201));
#37268=CARTESIAN_POINT('Ctrl Pts',(2.11416615756703,-1.36678736758804,112.796123880861));
#37269=CARTESIAN_POINT('Ctrl Pts',(2.15925215781729,-1.29704770056335,112.801359769572));
#37270=CARTESIAN_POINT('Ctrl Pts',(2.2009003979641,-1.22504908943391,112.806595658283));
#37271=CARTESIAN_POINT('Ctrl Pts',(2.23888812772545,-1.151167321257,112.811831546994));
#37272=CARTESIAN_POINT('Ctrl Pts',(2.27687484992131,-1.07728751267919,112.817067296831));
#37273=CARTESIAN_POINT('Ctrl Pts',(2.31120104462378,-1.00152505733288,112.822303046668));
#37274=CARTESIAN_POINT('Ctrl Pts',(2.3416903101504,-0.924279579644446,112.827538796505));
#37275=CARTESIAN_POINT('Ctrl Pts',(2.37268904082374,-0.845743356575832,
112.832862033922));
#37276=CARTESIAN_POINT('Ctrl Pts',(2.39972124217637,-0.765674547015846,
112.838185271339));
#37277=CARTESIAN_POINT('Ctrl Pts',(2.4226535098227,-0.684511666331364,112.843508508756));
#37278=CARTESIAN_POINT('Ctrl Pts',(2.44524135761816,-0.60456777138757,112.848751796442));
#37279=CARTESIAN_POINT('Ctrl Pts',(2.4638515439096,-0.523562915881689,112.853995084128));
#37280=CARTESIAN_POINT('Ctrl Pts',(2.4784081037197,-0.441927054406641,112.859238371814));
#37281=CARTESIAN_POINT('Ctrl Pts',(2.49329760150187,-0.35842401562299,112.864601584097));
#37282=CARTESIAN_POINT('Ctrl Pts',(2.50394569344754,-0.274261259748748,
112.869964796379));
#37283=CARTESIAN_POINT('Ctrl Pts',(2.51032728221455,-0.189903096787059,
112.875328008662));
#37284=CARTESIAN_POINT('Ctrl Pts',(2.51670887098156,-0.10554493382537,112.880691220945));
#37285=CARTESIAN_POINT('Ctrl Pts',(2.51882401098646,-0.0209918748079631,
112.886054433228));
#37286=CARTESIAN_POINT('Ctrl Pts',(2.51670418718245,0.0632952148137509,
112.891417645511));
#37287=CARTESIAN_POINT('Ctrl Pts',(2.51462662621131,0.145901876479592,112.896673931669));
#37288=CARTESIAN_POINT('Ctrl Pts',(2.50847378596393,0.228558455639894,112.901930217827));
#37289=CARTESIAN_POINT('Ctrl Pts',(2.49823752228716,0.310830391429945,112.907186503985));
#37290=CARTESIAN_POINT('Ctrl Pts',(2.48801577640484,0.392985643331266,112.912435335306));
#37291=CARTESIAN_POINT('Ctrl Pts',(2.47372216709517,0.474756881565425,112.917684166627));
#37292=CARTESIAN_POINT('Ctrl Pts',(2.45540054576482,0.555710724980039,112.922932997947));
#37293=CARTESIAN_POINT('Ctrl Pts',(2.4369507021753,0.637231116764084,112.928218562754));
#37294=CARTESIAN_POINT('Ctrl Pts',(2.41441624917947,0.717922152827627,112.93350412756));
#37295=CARTESIAN_POINT('Ctrl Pts',(2.38789507312428,0.797347709439735,112.938789692366));
#37296=CARTESIAN_POINT('Ctrl Pts',(2.36160532964296,0.87608017231575,112.944029133581));
#37297=CARTESIAN_POINT('Ctrl Pts',(2.33139831929238,0.953568710295907,112.949268574797));
#37298=CARTESIAN_POINT('Ctrl Pts',(2.29741997646057,1.0294016231578,112.954508016012));
#37299=CARTESIAN_POINT('Ctrl Pts',(2.26345286275538,1.10520947483927,112.959745725703));
#37300=CARTESIAN_POINT('Ctrl Pts',(2.22571708035768,1.17936236751307,112.964983435394));
#37301=CARTESIAN_POINT('Ctrl Pts',(2.1844066653329,1.25146864541194,112.970221145084));
#37302=CARTESIAN_POINT('Ctrl Pts',(2.14309745424578,1.32357282186827,112.975458702129));
#37303=CARTESIAN_POINT('Ctrl Pts',(2.09821404782988,1.39363010244888,112.980696259173));
#37304=CARTESIAN_POINT('Ctrl Pts',(2.04999571311091,1.46127472647237,112.985933816217));
#37305=CARTESIAN_POINT('Ctrl Pts',(2.00100861500654,1.52999783465486,112.99125487764));
#37306=CARTESIAN_POINT('Ctrl Pts',(1.9485795864765,1.5962302700184,112.996575939064));
#37307=CARTESIAN_POINT('Ctrl Pts',(1.89300325696989,1.65962192052931,113.001897000487));
#37308=CARTESIAN_POINT('Ctrl Pts',(1.83822091095501,1.72210793505335,113.007142043307));
#37309=CARTESIAN_POINT('Ctrl Pts',(1.78038098060945,1.78183351701213,113.012387086127));
#37310=CARTESIAN_POINT('Ctrl Pts',(1.71980284219268,1.83850059395856,113.017632128947));
#37311=CARTESIAN_POINT('Ctrl Pts',(1.65790772726718,1.89639962043509,113.022991199672));
#37312=CARTESIAN_POINT('Ctrl Pts',(1.593154337339,1.95110526570919,113.028350270397));
#37313=CARTESIAN_POINT('Ctrl Pts',(1.52591732836573,2.00234426535329,113.033709341121));
#37314=CARTESIAN_POINT('Ctrl Pts',(1.45868031939246,2.05358326499738,113.039068411846));
#37315=CARTESIAN_POINT('Ctrl Pts',(1.38896014656823,2.10135538743775,113.04442748257));
#37316=CARTESIAN_POINT('Ctrl Pts',(1.31715929980568,2.14543646583519,113.049786553295));
#37317=CARTESIAN_POINT('Ctrl Pts',(1.24673647755657,2.1886715262628,113.055042771043));
#37318=CARTESIAN_POINT('Ctrl Pts',(1.17405308457764,2.22851507030959,113.060298988791));
#37319=CARTESIAN_POINT('Ctrl Pts',(1.0994692615796,2.26472373433088,113.065555206539));
#37320=CARTESIAN_POINT('Ctrl Pts',(1.02499095534393,2.30088117248518,113.070803988102));
#37321=CARTESIAN_POINT('Ctrl Pts',(0.948617970996891,2.33341374532276,113.076052769665));
#37322=CARTESIAN_POINT('Ctrl Pts',(0.870737757582827,2.36212235236019,113.081301551228));
#37323=CARTESIAN_POINT('Ctrl Pts',(0.792311543702488,2.39103222891322,113.086587130805));
#37324=CARTESIAN_POINT('Ctrl Pts',(0.71235728434331,2.41606405520106,113.091872710382));
#37325=CARTESIAN_POINT('Ctrl Pts',(0.631294148703212,2.43706256542853,113.097158289959));
#37326=CARTESIAN_POINT('Ctrl Pts',(0.550938690802791,2.45787775955137,113.102397726651));
#37327=CARTESIAN_POINT('Ctrl Pts',(0.469494096436055,2.47472966663647,113.107637163342));
#37328=CARTESIAN_POINT('Ctrl Pts',(0.387385185996597,2.48751662661185,113.112876600033));
#37329=CARTESIAN_POINT('Ctrl Pts',(0.305303146901558,2.50029940186715,113.118114322042));
#37330=CARTESIAN_POINT('Ctrl Pts',(0.222557678887009,2.50901980121052,113.123352044051));
#37331=CARTESIAN_POINT('Ctrl Pts',(0.139582965417676,2.51362742779538,113.12858976606));
#37332=CARTESIAN_POINT('Ctrl Pts',(0.0566104053883257,2.51823493479865,
113.133827352135));
#37333=CARTESIAN_POINT('Ctrl Pts',(-0.0265909277041498,2.51872985673671,
113.139064938209));
#37334=CARTESIAN_POINT('Ctrl Pts',(-0.109583957800032,2.51511383563307,
113.144302524284));
#37335=CARTESIAN_POINT('Ctrl Pts',(-0.193899973960553,2.51144017179094,
113.14962360235));
#37336=CARTESIAN_POINT('Ctrl Pts',(-0.278000496800515,2.50352335519607,
113.154944680416));
#37337=CARTESIAN_POINT('Ctrl Pts',(-0.361431454613059,2.49141998740001,
113.160265758482));
#37338=CARTESIAN_POINT('Ctrl Pts',(-0.443671318679541,2.47948941212686,
113.165510870709));
#37339=CARTESIAN_POINT('Ctrl Pts',(-0.525260165375897,2.4634912036727,113.170755982935));
#37340=CARTESIAN_POINT('Ctrl Pts',(-0.605774102804838,2.44353104878391,
113.176001095161));
#37341=CARTESIAN_POINT('Ctrl Pts',(-0.68803718552538,2.42313726448811,113.181360156147));
#37342=CARTESIAN_POINT('Ctrl Pts',(-0.769177618051617,2.39860751598606,
113.186719217133));
#37343=CARTESIAN_POINT('Ctrl Pts',(-0.848762257034507,2.37010735643635,
113.19207827812));
#37344=CARTESIAN_POINT('Ctrl Pts',(-0.928346896017398,2.34160719688663,
113.197437339106));
#37345=CARTESIAN_POINT('Ctrl Pts',(-1.00637529954214,2.30913688217573,113.202796400093));
#37346=CARTESIAN_POINT('Ctrl Pts',(-1.08244036615458,2.27291203167196,113.208155461079));
#37347=CARTESIAN_POINT('Ctrl Pts',(-1.15692394512336,2.23744034100905,113.213403100501));
#37348=CARTESIAN_POINT('Ctrl Pts',(-1.22980151935485,2.1982370958742,113.218650739923));
#37349=CARTESIAN_POINT('Ctrl Pts',(-1.30067385925454,2.15547065900974,113.223898379344));
#37350=CARTESIAN_POINT('Ctrl Pts',(-1.37145410650413,2.11275979353621,113.2291391999));
#37351=CARTESIAN_POINT('Ctrl Pts',(-1.44023389914469,2.06649516329565,113.234380020455));
#37352=CARTESIAN_POINT('Ctrl Pts',(-1.50663601379298,2.01689220632685,113.23962084101));
#37353=CARTESIAN_POINT('Ctrl Pts',(-1.57297200614256,1.96733864329009,113.24485644283));
#37354=CARTESIAN_POINT('Ctrl Pts',(-1.63693465311243,1.91445362927206,113.250092044649));
#37355=CARTESIAN_POINT('Ctrl Pts',(-1.69817449725118,1.85849660394786,113.255327646469));
#37356=CARTESIAN_POINT('Ctrl Pts',(-1.75937195072917,1.80257831247921,113.260559624167));
#37357=CARTESIAN_POINT('Ctrl Pts',(-1.81785000481565,1.74359254496606,113.265791601865));
#37358=CARTESIAN_POINT('Ctrl Pts',(-1.87329228644203,1.68183895173016,113.271023579563));
#37359=CARTESIAN_POINT('Ctrl Pts',(-1.92872820551493,1.62009244533354,113.27625495684));
#37360=CARTESIAN_POINT('Ctrl Pts',(-1.98112872478702,1.55557907868882,113.281486334116));
#37361=CARTESIAN_POINT('Ctrl Pts',(-2.03021511929681,1.48863454863127,113.286717711393));
#37362=CARTESIAN_POINT('Ctrl Pts',(-2.07929599431949,1.42169754610706,113.291948500431));
#37363=CARTESIAN_POINT('Ctrl Pts',(-2.12506321658873,1.35233030042306,113.297179289469));
#37364=CARTESIAN_POINT('Ctrl Pts',(-2.16728017390901,1.28089925356405,113.302410078507));
#37365=CARTESIAN_POINT('Ctrl Pts',(-2.20952850283878,1.20941512597516,113.307644754567));
#37366=CARTESIAN_POINT('Ctrl Pts',(-2.24822106488964,1.13586453494511,113.312879430628));
#37367=CARTESIAN_POINT('Ctrl Pts',(-2.2831665462605,1.06063979372684,113.318114106689));
#37368=CARTESIAN_POINT('Ctrl Pts',(-2.31179587196648,0.999011407652224,
113.322402651016));
#37369=CARTESIAN_POINT('Ctrl Pts',(-2.33791103692983,0.936259932685513,
113.326691195344));
#37370=CARTESIAN_POINT('Ctrl Pts',(-2.36143112101026,0.872610629504504,
113.330979739671));
#37371=CARTESIAN_POINT('Origin',(0.,0.,116.208423447177));
#37372=CARTESIAN_POINT('',(-3.07507881988988,-0.00258943352280184,112.708423447177));
#37373=CARTESIAN_POINT('Ctrl Pts',(1.8746157427793,2.44019679077305,113.354075550313));
#37374=CARTESIAN_POINT('Ctrl Pts',(2.59111649989829,1.8811118882516,113.306858498602));
#37375=CARTESIAN_POINT('Ctrl Pts',(3.57307016162635,-0.0172528294224368,
113.206851810963));
#37376=CARTESIAN_POINT('Ctrl Pts',(2.0520963509033,-2.99395850450348,113.054055487396));
#37377=CARTESIAN_POINT('Ctrl Pts',(-1.39401273850626,-3.35130756079173,
112.895686579612));
#37378=CARTESIAN_POINT('Ctrl Pts',(-2.97703420005838,-1.39005018037111,
112.780475899539));
#37379=CARTESIAN_POINT('Ctrl Pts',(-3.07674611060127,-0.188293282082768,
112.718054855394));
#37380=CARTESIAN_POINT('Ctrl Pts',(-3.07507881988988,-0.00258943352280184,
112.708423447177));
#37381=CARTESIAN_POINT('Ctrl Pts',(-3.07507881988988,-0.00258943352280184,
112.708423447177));
#37382=CARTESIAN_POINT('Ctrl Pts',(-3.06760770968837,0.829547342602012,
112.665265219466));
#37383=CARTESIAN_POINT('Ctrl Pts',(-2.28977932831436,2.69183713313171,112.569317355827));
#37384=CARTESIAN_POINT('Ctrl Pts',(0.207333768054169,3.35545528762516,112.451210495639));
#37385=CARTESIAN_POINT('Ctrl Pts',(1.53027089159208,2.69684180982145,112.376261863162));
#37386=CARTESIAN_POINT('Ctrl Pts',(1.8696729405724,2.43383856956497,112.354102866614));
#37387=CARTESIAN_POINT('',(-3.07349937844406,0.00195466210857263,112.791576552787));
#37388=CARTESIAN_POINT('Ctrl Pts',(-3.07349937844406,0.00195466210857065,
112.791576552787));
#37389=CARTESIAN_POINT('Ctrl Pts',(-3.07343002419229,0.11100688591123,112.78595145356));
#37390=CARTESIAN_POINT('Ctrl Pts',(-3.06755261508276,0.219839360792043,
112.780326354332));
#37391=CARTESIAN_POINT('Ctrl Pts',(-3.05596138339884,0.327875392756234,
112.774701255105));
#37392=CARTESIAN_POINT('Ctrl Pts',(-3.04431879347594,0.436390108996588,
112.76905123228));
#37393=CARTESIAN_POINT('Ctrl Pts',(-3.02691175843935,0.544101106734187,
112.763401209456));
#37394=CARTESIAN_POINT('Ctrl Pts',(-3.00388543327814,0.650441814261192,
112.757751186631));
#37395=CARTESIAN_POINT('Ctrl Pts',(-2.9807318632009,0.757370167202966,112.752069941426));
#37396=CARTESIAN_POINT('Ctrl Pts',(-2.95189683807177,0.862912846042479,
112.746388696222));
#37397=CARTESIAN_POINT('Ctrl Pts',(-2.91757627648976,0.966514832200808,
112.740707451017));
#37398=CARTESIAN_POINT('Ctrl Pts',(-2.90215410924504,1.01306905753307,112.738154546587));
#37399=CARTESIAN_POINT('Ctrl Pts',(-2.88562493226943,1.05923171481558,112.735601642157));
#37400=CARTESIAN_POINT('Ctrl Pts',(-2.86800958296797,1.10495397279882,112.733048737727));
#37401=CARTESIAN_POINT('Ctrl Pts',(-2.83351112480162,1.19449789141844,112.728049048809));
#37402=CARTESIAN_POINT('Ctrl Pts',(-2.79475452621709,1.28258180731632,112.723049359891));
#37403=CARTESIAN_POINT('Ctrl Pts',(-2.75188381854915,1.36877233286159,112.718049670973));
#37404=CARTESIAN_POINT('Ctrl Pts',(-2.70907125272974,1.4548459656203,112.713056762703));
#37405=CARTESIAN_POINT('Ctrl Pts',(-2.66215586076226,1.53903092181659,112.708063854433));
#37406=CARTESIAN_POINT('Ctrl Pts',(-2.61133036493258,1.62091208126199,112.703070946162));
#37407=CARTESIAN_POINT('Ctrl Pts',(-2.56055847765614,1.70270687597206,112.698083304198));
#37408=CARTESIAN_POINT('Ctrl Pts',(-2.50588491546618,1.78220233358484,112.693095662233));
#37409=CARTESIAN_POINT('Ctrl Pts',(-2.44754862974388,1.85900724986183,112.688108020268));
#37410=CARTESIAN_POINT('Ctrl Pts',(-2.38925407682615,1.93575722118439,112.683123946379));
#37411=CARTESIAN_POINT('Ctrl Pts',(-2.32730227404646,2.00982012899545,112.67813987249));
#37412=CARTESIAN_POINT('Ctrl Pts',(-2.26197530990461,2.08083395478398,112.673155798601));
#37413=CARTESIAN_POINT('Ctrl Pts',(-2.19667213165785,2.15182192406086,112.66817353944));
#37414=CARTESIAN_POINT('Ctrl Pts',(-2.12799653063372,2.21976269443926,112.663191280279));
#37415=CARTESIAN_POINT('Ctrl Pts',(-2.0562700499957,2.28432828890479,112.658209021118));
#37416=CARTESIAN_POINT('Ctrl Pts',(-1.98455010812994,2.34888799740304,112.653227216152));
#37417=CARTESIAN_POINT('Ctrl Pts',(-1.90978016596492,2.41007284821533,112.648245411187));
#37418=CARTESIAN_POINT('Ctrl Pts',(-1.83231690711452,2.46759336234767,112.643263606221));
#37419=CARTESIAN_POINT('Ctrl Pts',(-1.75483956727324,2.52512433235092,112.638280895681));
#37420=CARTESIAN_POINT('Ctrl Pts',(-1.67466829084932,2.57898938117476,112.633298185141));
#37421=CARTESIAN_POINT('Ctrl Pts',(-1.59219007572955,2.62894142436615,112.628315474601));
#37422=CARTESIAN_POINT('Ctrl Pts',(-1.50962298743371,2.67894729264,112.623327395015));
#37423=CARTESIAN_POINT('Ctrl Pts',(-1.42474437381568,2.72503150986534,112.61833931543));
#37424=CARTESIAN_POINT('Ctrl Pts',(-1.33796705881446,2.76699230203616,112.613351235844));
#37425=CARTESIAN_POINT('Ctrl Pts',(-1.2511384940778,2.80897787579302,112.608360210353));
#37426=CARTESIAN_POINT('Ctrl Pts',(-1.16240939868322,2.84683500333169,112.603369184862));
#37427=CARTESIAN_POINT('Ctrl Pts',(-1.07221188821519,2.88041037297987,112.598378159371));
#37428=CARTESIAN_POINT('Ctrl Pts',(-0.981868668646718,2.91403998178479,
112.593379071153));
#37429=CARTESIAN_POINT('Ctrl Pts',(-0.890052715180372,2.94337388759342,
112.588379982936));
#37430=CARTESIAN_POINT('Ctrl Pts',(-0.797210516660054,2.96830888590231,
112.583380894719));
#37431=CARTESIAN_POINT('Ctrl Pts',(-0.743345628491891,2.9827755930332,112.580480539793));
#37432=CARTESIAN_POINT('Ctrl Pts',(-0.689135496025451,2.99576256182403,
112.577580184868));
#37433=CARTESIAN_POINT('Ctrl Pts',(-0.634668327413694,3.00725761519992,
112.574679829942));
#37434=CARTESIAN_POINT('Ctrl Pts',(-0.54076977135301,3.0270744872964,112.569679769419));
#37435=CARTESIAN_POINT('Ctrl Pts',(-0.445777316233022,3.04252410781941,
112.564679708896));
#37436=CARTESIAN_POINT('Ctrl Pts',(-0.350133011604329,3.05349130082024,
112.559679648374));
#37437=CARTESIAN_POINT('Ctrl Pts',(-0.252675795866729,3.06466637390449,
112.554584813099));
#37438=CARTESIAN_POINT('Ctrl Pts',(-0.15454219264561,3.07118717701671,112.549489977824));
#37439=CARTESIAN_POINT('Ctrl Pts',(-0.0562137622642027,3.07298588720028,
112.544395142549));
#37440=CARTESIAN_POINT('Ctrl Pts',(0.040033845638921,3.07474653314783,112.539408123983));
#37441=CARTESIAN_POINT('Ctrl Pts',(0.136467652143309,3.07198294492465,112.534421105417));
#37442=CARTESIAN_POINT('Ctrl Pts',(0.232629515719199,3.06468363104844,112.529434086851));
#37443=CARTESIAN_POINT('Ctrl Pts',(0.328727479536893,3.05738916758147,112.524450382169));
#37444=CARTESIAN_POINT('Ctrl Pts',(0.424553423212515,3.04556500077522,112.519466677487));
#37445=CARTESIAN_POINT('Ctrl Pts',(0.519650264770887,3.02925169841061,112.514482972805));
#37446=CARTESIAN_POINT('Ctrl Pts',(0.614709873716475,3.01294478308115,112.509501219359));
#37447=CARTESIAN_POINT('Ctrl Pts',(0.709040516019149,2.99215230062805,112.504519465913));
#37448=CARTESIAN_POINT('Ctrl Pts',(0.802192351484012,2.96696641053123,112.499537712467));
#37449=CARTESIAN_POINT('Ctrl Pts',(0.899010779616596,2.94078916691465,112.494359869909));
#37450=CARTESIAN_POINT('Ctrl Pts',(0.994555193225898,2.90986560914487,112.489182027351));
#37451=CARTESIAN_POINT('Ctrl Pts',(1.08833567477371,2.87435692095029,112.484004184794));
#37452=CARTESIAN_POINT('Ctrl Pts',(1.17860282536295,2.84017850715262,112.479020321561));
#37453=CARTESIAN_POINT('Ctrl Pts',(1.26723543317313,2.80175257466065,112.474036458329));
#37454=CARTESIAN_POINT('Ctrl Pts',(1.35381659437577,2.75927216468271,112.469052595097));
#37455=CARTESIAN_POINT('Ctrl Pts',(1.44042783864438,2.71677699466969,112.464067000196));
#37456=CARTESIAN_POINT('Ctrl Pts',(1.52498583030879,2.67022474944789,112.459081405295));
#37457=CARTESIAN_POINT('Ctrl Pts',(1.60709882997935,2.61985411820563,112.454095810394));
#37458=CARTESIAN_POINT('Ctrl Pts',(1.68929350361451,2.5694333856497,112.449105256555));
#37459=CARTESIAN_POINT('Ctrl Pts',(1.76903796889166,2.51518693317379,112.444114702716));
#37460=CARTESIAN_POINT('Ctrl Pts',(1.84597045576914,2.45739604590458,112.439124148876));
#37461=CARTESIAN_POINT('Ctrl Pts',(1.85481155648619,2.4507547026228,112.438550633176));
#37462=CARTESIAN_POINT('Ctrl Pts',(1.86361555744202,2.44406659195225,112.437977117475));
#37463=CARTESIAN_POINT('Ctrl Pts',(1.87238193903529,2.43733217358128,112.437403601774));
#37464=CARTESIAN_POINT('Ctrl Pts',(1.8723819390353,2.43733217358127,113.437353936953));
#37465=CARTESIAN_POINT('Ctrl Pts',(1.94902778074786,2.37845210328134,113.432362769506));
#37466=CARTESIAN_POINT('Ctrl Pts',(2.0228783853614,2.31596491432207,113.427371602059));
#37467=CARTESIAN_POINT('Ctrl Pts',(2.09358857238406,2.25017535751836,113.422380434612));
#37468=CARTESIAN_POINT('Ctrl Pts',(2.16437424616697,2.18431556698014,113.417383938837));
#37469=CARTESIAN_POINT('Ctrl Pts',(2.23201248708662,2.11514666725556,113.412387443062));
#37470=CARTESIAN_POINT('Ctrl Pts',(2.29619450083181,2.0430107841981,113.407390947287));
#37471=CARTESIAN_POINT('Ctrl Pts',(2.3604125894477,1.97083435562795,113.402391643125));
#37472=CARTESIAN_POINT('Ctrl Pts',(2.42117030685143,1.89568796237903,113.397392338963));
#37473=CARTESIAN_POINT('Ctrl Pts',(2.47820008932934,1.81794569975235,113.392393034801));
#37474=CARTESIAN_POINT('Ctrl Pts',(2.53532458293881,1.74007432813483,113.387385428139));
#37475=CARTESIAN_POINT('Ctrl Pts',(2.58870853348055,1.6595988406701,113.382377821478));
#37476=CARTESIAN_POINT('Ctrl Pts',(2.63812849265039,1.57692114776427,113.377370214816));
#37477=CARTESIAN_POINT('Ctrl Pts',(2.6738076304336,1.51723132109631,113.373754932832));
#37478=CARTESIAN_POINT('Ctrl Pts',(2.70742158929765,1.45639421551074,113.370139650847));
#37479=CARTESIAN_POINT('Ctrl Pts',(2.73890182080391,1.39456769860665,113.366524368863));
#37480=CARTESIAN_POINT('Ctrl Pts',(2.78238710748423,1.3091635041843,113.361530391183));
#37481=CARTESIAN_POINT('Ctrl Pts',(2.82195198542918,1.22157018123046,113.356536413502));
#37482=CARTESIAN_POINT('Ctrl Pts',(2.85737001572186,1.13218321982516,113.351542435822));
#37483=CARTESIAN_POINT('Ctrl Pts',(2.89273942558394,1.04291896520276,113.346555313671));
#37484=CARTESIAN_POINT('Ctrl Pts',(2.92397314004963,0.951866370848382,113.34156819152));
#37485=CARTESIAN_POINT('Ctrl Pts',(2.95089079206454,0.85944504379785,113.336581069369));
#37486=CARTESIAN_POINT('Ctrl Pts',(2.97777966031034,0.76712254535755,113.331599280081));
#37487=CARTESIAN_POINT('Ctrl Pts',(3.00036151800224,0.673434643831087,113.326617490794));
#37488=CARTESIAN_POINT('Ctrl Pts',(3.01850464563966,0.578819448750456,113.321635701507));
#37489=CARTESIAN_POINT('Ctrl Pts',(3.03663450464151,0.484273448715349,113.316657555558));
#37490=CARTESIAN_POINT('Ctrl Pts',(3.0503320039826,0.388801934157765,113.311679409608));
#37491=CARTESIAN_POINT('Ctrl Pts',(3.05951594227669,0.292855679396463,113.306701263659));
#37492=CARTESIAN_POINT('Ctrl Pts',(3.06869645062395,0.196945257906474,113.30172497691));
#37493=CARTESIAN_POINT('Ctrl Pts',(3.07336670507928,0.100560886087044,113.29674869016));
#37494=CARTESIAN_POINT('Ctrl Pts',(3.07349718469151,0.00416001121787148,
113.291772403411));
#37495=CARTESIAN_POINT('Ctrl Pts',(3.07362765141657,-0.0922313423484138,
113.286796608158));
#37496=CARTESIAN_POINT('Ctrl Pts',(3.06921923426622,-0.188638755635504,
113.281820812906));
#37497=CARTESIAN_POINT('Ctrl Pts',(3.06029453420285,-0.284604311155291,
113.276845017653));
#37498=CARTESIAN_POINT('Ctrl Pts',(3.05136826397639,-0.380586750331861,
113.271868346986));
#37499=CARTESIAN_POINT('Ctrl Pts',(3.03792417377253,-0.476126739170055,
113.266891676319));
#37500=CARTESIAN_POINT('Ctrl Pts',(3.0200366652607,-0.570772100300162,113.261915005653));
#37501=CARTESIAN_POINT('Ctrl Pts',(3.00212989325235,-0.665519387340322,
113.256932975487));
#37502=CARTESIAN_POINT('Ctrl Pts',(2.97977023157995,-0.759369690085068,
113.251950945322));
#37503=CARTESIAN_POINT('Ctrl Pts',(2.95308305439377,-0.851881872005937,
113.246968915156));
#37504=CARTESIAN_POINT('Ctrl Pts',(2.92638017443914,-0.944448488210441,
113.241983953558));
#37505=CARTESIAN_POINT('Ctrl Pts',(2.89534485085943,-1.03567499950709,113.236998991959));
#37506=CARTESIAN_POINT('Ctrl Pts',(2.86015140590259,-1.12513829608338,113.232014030361));
#37507=CARTESIAN_POINT('Ctrl Pts',(2.82490077734008,-1.21474695591924,113.227020969014));
#37508=CARTESIAN_POINT('Ctrl Pts',(2.78547871686333,-1.30258627922447,113.222027907666));
#37509=CARTESIAN_POINT('Ctrl Pts',(2.74210643107271,-1.38825594566337,113.217034846319));
#37510=CARTESIAN_POINT('Ctrl Pts',(2.71639613649571,-1.43903935078733,113.214075051239));
#37511=CARTESIAN_POINT('Ctrl Pts',(2.68929863301414,-1.489060862037,113.211115256159));
#37512=CARTESIAN_POINT('Ctrl Pts',(2.66086710191638,-1.53824202124994,113.208155461079));
#37513=CARTESIAN_POINT('Ctrl Pts',(2.61283286910437,-1.62133213846793,113.203154974631));
#37514=CARTESIAN_POINT('Ctrl Pts',(2.56081879647391,-1.70231576269226,113.198154488184));
#37515=CARTESIAN_POINT('Ctrl Pts',(2.50503479940379,-1.78078715847123,113.193154001736));
#37516=CARTESIAN_POINT('Ctrl Pts',(2.44932643402042,-1.85915216309257,113.188160294925));
#37517=CARTESIAN_POINT('Ctrl Pts',(2.38985855462289,-1.9350113541123,113.183166588113));
#37518=CARTESIAN_POINT('Ctrl Pts',(2.32688632254462,-2.0079846343921,113.178172881302));
#37519=CARTESIAN_POINT('Ctrl Pts',(2.26398050177324,-2.08088095613397,113.173184440917));
#37520=CARTESIAN_POINT('Ctrl Pts',(2.19757796042873,-2.15089708710934,113.168196000532));
#37521=CARTESIAN_POINT('Ctrl Pts',(2.12797579427881,-2.21768376216345,113.163207560147));
#37522=CARTESIAN_POINT('Ctrl Pts',(2.05842346278849,-2.28442261842972,113.158222691449));
#37523=CARTESIAN_POINT('Ctrl Pts',(1.98567637646282,-2.34793631260673,113.153237822752));
#37524=CARTESIAN_POINT('Ctrl Pts',(1.91006969057551,-2.40791113356469,113.148252954055));
#37525=CARTESIAN_POINT('Ctrl Pts',(1.83449056775726,-2.46786409018469,113.143269902635));
#37526=CARTESIAN_POINT('Ctrl Pts',(1.75605426011781,-2.5242804645642,113.138286851214));
#37527=CARTESIAN_POINT('Ctrl Pts',(1.6751295900509,-2.57688632006457,113.133303799794));
#37528=CARTESIAN_POINT('Ctrl Pts',(1.5942123538351,-2.62948734311894,113.128321206124));
#37529=CARTESIAN_POINT('Ctrl Pts',(1.51080757763404,-2.67827830426429,113.123338612453));
#37530=CARTESIAN_POINT('Ctrl Pts',(1.42531279674618,-2.72302876985014,113.118356018783));
#37531=CARTESIAN_POINT('Ctrl Pts',(1.33980255567569,-2.76778732774717,113.113372524101));
#37532=CARTESIAN_POINT('Ctrl Pts',(1.25220194807059,-2.80850373556424,113.108389029419));
#37533=CARTESIAN_POINT('Ctrl Pts',(1.16293184976043,-2.84499415866057,113.103405534736));
#37534=CARTESIAN_POINT('Ctrl Pts',(1.07356578717905,-2.88152380851845,113.098416682858));
#37535=CARTESIAN_POINT('Ctrl Pts',(0.982527057780247,-2.9138182378906,113.09342783098));
#37536=CARTESIAN_POINT('Ctrl Pts',(0.890254990788898,-2.94174239208253,
113.088438979101));
#37537=CARTESIAN_POINT('Ctrl Pts',(0.797928540084588,-2.96968300433415,
113.083447186871));
#37538=CARTESIAN_POINT('Ctrl Pts',(0.704367729648516,-2.99324810541254,
113.078455394642));
#37539=CARTESIAN_POINT('Ctrl Pts',(0.610023400508049,-3.01235351524893,
113.073463602412));
#37540=CARTESIAN_POINT('Ctrl Pts',(0.515526997266067,-3.03148972119211,
113.068463763887));
#37541=CARTESIAN_POINT('Ctrl Pts',(0.420244986836002,-3.04615181509973,
113.063463925362));
#37542=CARTESIAN_POINT('Ctrl Pts',(0.32463460720452,-3.05630735067748,113.058464086837));
#37543=CARTESIAN_POINT('Ctrl Pts',(0.269322002464767,-3.0621825404581,113.055571575657));
#37544=CARTESIAN_POINT('Ctrl Pts',(0.213899540344203,-3.0665504184687,113.052679064476));
#37545=CARTESIAN_POINT('Ctrl Pts',(0.158455515214029,-3.0694126636375,113.049786553295));
#37546=CARTESIAN_POINT('Ctrl Pts',(0.0626073974904463,-3.07436073173408,
113.044786163234));
#37547=CARTESIAN_POINT('Ctrl Pts',(-0.0336403558292232,-3.07482359911457,
113.039785773174));
#37548=CARTESIAN_POINT('Ctrl Pts',(-0.129833121082185,-3.07075652090329,
113.034785383113));
#37549=CARTESIAN_POINT('Ctrl Pts',(-0.225895770170549,-3.0666949440685,
113.029791756883));
#37550=CARTESIAN_POINT('Ctrl Pts',(-0.321903144356099,-3.05811561812003,
113.024798130653));
#37551=CARTESIAN_POINT('Ctrl Pts',(-0.417397502528618,-3.04502571005285,
113.019804504424));
#37552=CARTESIAN_POINT('Ctrl Pts',(-0.51279145266298,-3.0319495654374,113.014816128768));
#37553=CARTESIAN_POINT('Ctrl Pts',(-0.607673026698114,-3.01437232623717,
113.009827753112));
#37554=CARTESIAN_POINT('Ctrl Pts',(-0.701587525637013,-2.99235311984908,
113.004839377457));
#37555=CARTESIAN_POINT('Ctrl Pts',(-0.795435235314147,-2.97034957288053,
112.999854549389));
#37556=CARTESIAN_POINT('Ctrl Pts',(-0.888316811141023,-2.94391043854237,
112.994869721321));
#37557=CARTESIAN_POINT('Ctrl Pts',(-0.979786664578253,-2.91314612436703,
112.989884893253));
#37558=CARTESIAN_POINT('Ctrl Pts',(-1.07122344596474,-2.88239293340792,
112.984901867511));
#37559=CARTESIAN_POINT('Ctrl Pts',(-1.16124910366457,-2.84731780952579,
112.979918841769));
#37560=CARTESIAN_POINT('Ctrl Pts',(-1.24943309351804,-2.80808105203926,
112.974935816027));
#37561=CARTESIAN_POINT('Ctrl Pts',(-1.33760924880958,-2.76884778047809,
112.969953232994));
#37562=CARTESIAN_POINT('Ctrl Pts',(-1.42394366075278,-2.72545378896544,
112.96497064996));
#37563=CARTESIAN_POINT('Ctrl Pts',(-1.50802665397815,-2.67810714141378,
112.959988066927));
#37564=CARTESIAN_POINT('Ctrl Pts',(-1.59212510768468,-2.63075178815452,
112.955004567738));
#37565=CARTESIAN_POINT('Ctrl Pts',(-1.67397093819443,-2.57944255075047,
112.950021068549));
#37566=CARTESIAN_POINT('Ctrl Pts',(-1.7531808602772,-2.52443243545112,112.94503756936));
#37567=CARTESIAN_POINT('Ctrl Pts',(-1.8324763021253,-2.469362927944,112.940048689687));
#37568=CARTESIAN_POINT('Ctrl Pts',(-1.90912979301477,-2.41058481622441,
112.935059810014));
#37569=CARTESIAN_POINT('Ctrl Pts',(-1.98278892570486,-2.34839313704119,
112.930070930341));
#37570=CARTESIAN_POINT('Ctrl Pts',(-2.05649166654478,-2.28616463874315,
112.92507909712));
#37571=CARTESIAN_POINT('Ctrl Pts',(-2.12719619794431,-2.22051884737279,
112.920087263899));
#37572=CARTESIAN_POINT('Ctrl Pts',(-2.1945865282105,-2.15178814482211,112.915095430678));
#37573=CARTESIAN_POINT('Ctrl Pts',(-2.26208576240159,-2.08294637228203,
112.910095530569));
#37574=CARTESIAN_POINT('Ctrl Pts',(-2.32625980919352,-2.01101006127668,
112.905095630461));
#37575=CARTESIAN_POINT('Ctrl Pts',(-2.38683259562793,-1.93634511656575,
112.900095730352));
#37576=CARTESIAN_POINT('Ctrl Pts',(-2.42187701440332,-1.89314767189933,
112.897203035405));
#37577=CARTESIAN_POINT('Ctrl Pts',(-2.45571680882079,-1.84903746242192,
112.894310340458));
#37578=CARTESIAN_POINT('Ctrl Pts',(-2.48830532630393,-1.8040894803439,112.891417645511));
#37579=CARTESIAN_POINT('Ctrl Pts',(-2.54500547120761,-1.72588533686696,
112.88638470031));
#37580=CARTESIAN_POINT('Ctrl Pts',(-2.59811448861188,-1.64486892120071,
112.881351755109));
#37581=CARTESIAN_POINT('Ctrl Pts',(-2.64734378267396,-1.561401020346,112.876318809909));
#37582=CARTESIAN_POINT('Ctrl Pts',(-2.69650461378654,-1.47804919791147,
112.871292864002));
#37583=CARTESIAN_POINT('Ctrl Pts',(-2.7417962276114,-1.39225303355378,112.866266918094));
#37584=CARTESIAN_POINT('Ctrl Pts',(-2.7829717140169,-1.30440434259544,112.861240972187));
#37585=CARTESIAN_POINT('Ctrl Pts',(-2.8241006655227,-1.21665493473923,112.856220706405));
#37586=CARTESIAN_POINT('Ctrl Pts',(-2.86112255541327,-1.12685799962256,
112.851200440622));
#37587=CARTESIAN_POINT('Ctrl Pts',(-2.89383555741939,-1.0354313191203,112.846180174839));
#37588=CARTESIAN_POINT('Ctrl Pts',(-2.92651788308417,-0.944090373215514,
112.841164616768));
#37589=CARTESIAN_POINT('Ctrl Pts',(-2.95489921487249,-0.851123126818456,
112.836149058698));
#37590=CARTESIAN_POINT('Ctrl Pts',(-2.97882560649874,-0.756967803851286,
112.831133500627));
#37591=CARTESIAN_POINT('Ctrl Pts',(-3.00273870135661,-0.662864806430717,
112.826120729884));
#37592=CARTESIAN_POINT('Ctrl Pts',(-3.02220167352493,-0.56757546246408,
112.821107959142));
#37593=CARTESIAN_POINT('Ctrl Pts',(-3.03711049196263,-0.471552870429743,
112.8160951884));
#37594=CARTESIAN_POINT('Ctrl Pts',(-3.05201703766413,-0.375544916310658,
112.811083181816));
#37595=CARTESIAN_POINT('Ctrl Pts',(-3.0623707379808,-0.278804361265467,
112.806071175233));
#37596=CARTESIAN_POINT('Ctrl Pts',(-3.06811886878855,-0.181793445931633,
112.80105916865));
#37597=CARTESIAN_POINT('Ctrl Pts',(-3.071743984815,-0.120612544577855,112.797898296707));
#37598=CARTESIAN_POINT('Ctrl Pts',(-3.07353835017132,-0.0593242779513427,
112.794737424765));
#37599=CARTESIAN_POINT('Ctrl Pts',(-3.07349937844451,0.00195466141179594,
112.791576552823));
#37600=CARTESIAN_POINT('Origin',(0.,0.,10.));
#37601=CARTESIAN_POINT('',(2.51749986510683,0.000824128084735556,1.88741669747532));
#37602=CARTESIAN_POINT('Ctrl Pts',(2.36142200728636,0.872635292378022,0.943739684385605));
#37603=CARTESIAN_POINT('Ctrl Pts',(2.35741605103208,0.88347573550666,0.944474627125061));
#37604=CARTESIAN_POINT('Ctrl Pts',(2.3533359497583,0.894287232847126,0.945209569864519));
#37605=CARTESIAN_POINT('Ctrl Pts',(2.34918212370971,0.905068836963642,0.945944512603976));
#37606=CARTESIAN_POINT('Ctrl Pts',(2.31947828172392,0.982167651715261,0.951200058393829));
#37607=CARTESIAN_POINT('Ctrl Pts',(2.28592010378836,1.05794487781423,0.95645560418368));
#37608=CARTESIAN_POINT('Ctrl Pts',(2.24864585244449,1.13198855130438,0.961711149973533));
#37609=CARTESIAN_POINT('Ctrl Pts',(2.21142442782955,1.2059272868031,0.96695924736985));
#37610=CARTESIAN_POINT('Ctrl Pts',(2.17049759653951,1.27813694111076,0.972207344766169));
#37611=CARTESIAN_POINT('Ctrl Pts',(2.12605219964104,1.34822412617543,0.977455442162485));
#37612=CARTESIAN_POINT('Ctrl Pts',(2.08128793583427,1.41881414135464,0.982741191255221));
#37613=CARTESIAN_POINT('Ctrl Pts',(2.03295457895778,1.48725066327916,0.988026940347957));
#37614=CARTESIAN_POINT('Ctrl Pts',(1.98129091356592,1.5531556798406,0.993312689440693));
#37615=CARTESIAN_POINT('Ctrl Pts',(1.93008683787469,1.61847441847148,0.998551417559892));
#37616=CARTESIAN_POINT('Ctrl Pts',(1.8756117595696,1.68130614258371,1.00379014567909));
#37617=CARTESIAN_POINT('Ctrl Pts',(1.81814139472729,1.74131218303298,1.00902887379829));
#37618=CARTESIAN_POINT('Ctrl Pts',(1.76068992282892,1.80129849695431,1.01426587972559));
#37619=CARTESIAN_POINT('Ctrl Pts',(1.70024543888877,1.85846063917763,1.0195028856529));
#37620=CARTESIAN_POINT('Ctrl Pts',(1.63712222913025,1.91249498218625,1.0247398915802));
#37621=CARTESIAN_POINT('Ctrl Pts',(1.57400073599957,1.96652785573764,1.02997675508778));
#37622=CARTESIAN_POINT('Ctrl Pts',(1.50820101304804,2.01743279995885,1.03521361859535));
#37623=CARTESIAN_POINT('Ctrl Pts',(1.44007124555414,2.0649457759777,1.04045048210293));
#37624=CARTESIAN_POINT('Ctrl Pts',(1.37083503303633,2.11323037500102,1.0457723936267));
#37625=CARTESIAN_POINT('Ctrl Pts',(1.29919281266649,2.15801155432841,1.05109430515047));
#37626=CARTESIAN_POINT('Ctrl Pts',(1.22553999658496,2.19905842732078,1.05641621667424));
#37627=CARTESIAN_POINT('Ctrl Pts',(1.15296016317774,2.23950732475839,1.06166059798038));
#37628=CARTESIAN_POINT('Ctrl Pts',(1.07842837649574,2.27632985131858,1.06690497928653));
#37629=CARTESIAN_POINT('Ctrl Pts',(1.00234552948139,2.30935265594683,1.07214936059267));
#37630=CARTESIAN_POINT('Ctrl Pts',(0.92457552834666,2.34310774864106,1.07751003722525));
#37631=CARTESIAN_POINT('Ctrl Pts',(0.845185332141628,2.37289240318282,1.08287071385783));
#37632=CARTESIAN_POINT('Ctrl Pts',(0.764620117506867,2.39857506155296,1.08823139049041));
#37633=CARTESIAN_POINT('Ctrl Pts',(0.684054902872107,2.4242577199231,1.09359206712299));
#37634=CARTESIAN_POINT('Ctrl Pts',(0.602315177591028,2.44583831702018,1.09895274375557));
#37635=CARTESIAN_POINT('Ctrl Pts',(0.519855834697462,2.46324098722212,1.10431342038815));
#37636=CARTESIAN_POINT('Ctrl Pts',(0.439016490774304,2.48030176399125,1.10956878099078));
#37637=CARTESIAN_POINT('Ctrl Pts',(0.357187192540811,2.4934103011927,1.11482414159342));
#37638=CARTESIAN_POINT('Ctrl Pts',(0.274788740783649,2.50245827096848,1.12007950219605));
#37639=CARTESIAN_POINT('Ctrl Pts',(0.192507064452293,2.51149341792416,1.12532741487995));
#37640=CARTESIAN_POINT('Ctrl Pts',(0.109658291574247,2.51647937795004,1.13057532756386));
#37641=CARTESIAN_POINT('Ctrl Pts',(0.0266740919933808,2.51735868378273,
1.13582324024776));
#37642=CARTESIAN_POINT('Ctrl Pts',(-0.0569091383392196,2.51824433698319,
1.14110903557795));
#37643=CARTESIAN_POINT('Ctrl Pts',(-0.14062929514562,2.51496370024881,1.14639483090814));
#37644=CARTESIAN_POINT('Ctrl Pts',(-0.224039265615039,2.50751124772406,
1.15168062623833));
#37645=CARTESIAN_POINT('Ctrl Pts',(-0.306703640454684,2.50012541212775,
1.15691917223039));
#37646=CARTESIAN_POINT('Ctrl Pts',(-0.389062884281737,2.48864208789595,
1.16215771822245));
#37647=CARTESIAN_POINT('Ctrl Pts',(-0.470682834843838,2.47310814947171,
1.16739626421452));
#37648=CARTESIAN_POINT('Ctrl Pts',(-0.552275974182039,2.45757931376927,
1.1726330894039));
#37649=CARTESIAN_POINT('Ctrl Pts',(-0.633129849663377,2.43800259268168,
1.17786991459328));
#37650=CARTESIAN_POINT('Ctrl Pts',(-0.712818692105644,2.41447629149362,
1.18310673978267));
#37651=CARTESIAN_POINT('Ctrl Pts',(-0.792505392365057,2.39095062273587,
1.18834342419654));
#37652=CARTESIAN_POINT('Ctrl Pts',(-0.87102667963085,2.36347571660908,1.19358010861042));
#37653=CARTESIAN_POINT('Ctrl Pts',(-0.94797153545844,2.33219986664106,1.1988167930243));
#37654=CARTESIAN_POINT('Ctrl Pts',(-1.02617184959384,2.3004137093204,1.2041389209533));
#37655=CARTESIAN_POINT('Ctrl Pts',(-1.10274336598909,2.2647016303736,1.2094610488823));
#37656=CARTESIAN_POINT('Ctrl Pts',(-1.17727707310553,2.22526963380622,1.2147831768113));
#37657=CARTESIAN_POINT('Ctrl Pts',(-1.25071955316008,2.18641495002018,1.22002738496082));
#37658=CARTESIAN_POINT('Ctrl Pts',(-1.32218312830499,2.1439488445509,1.22527159311034));
#37659=CARTESIAN_POINT('Ctrl Pts',(-1.39130415572782,2.09811319910402,1.23051580125985));
#37660=CARTESIAN_POINT('Ctrl Pts',(-1.46196570987878,2.05125599712731,1.2358768890786));
#37661=CARTESIAN_POINT('Ctrl Pts',(-1.53017863021198,2.00087755633266,1.24123797689734));
#37662=CARTESIAN_POINT('Ctrl Pts',(-1.59559010990904,1.94727975677879,1.24659906471609));
#37663=CARTESIAN_POINT('Ctrl Pts',(-1.66100158960609,1.89368195722492,1.25196015253483));
#37664=CARTESIAN_POINT('Ctrl Pts',(-1.72361129743041,1.8368651896704,1.25732124035358));
#37665=CARTESIAN_POINT('Ctrl Pts',(-1.78310787212359,1.77716981922688,1.26268232817233));
#37666=CARTESIAN_POINT('Ctrl Pts',(-1.84142826271774,1.71865456286325,1.26793743297813));
#37667=CARTESIAN_POINT('Ctrl Pts',(-1.89697297047442,1.65715734036253,1.27319253778393));
#37668=CARTESIAN_POINT('Ctrl Pts',(-1.94942202226096,1.59297207418209,1.27844764258973));
#37669=CARTESIAN_POINT('Ctrl Pts',(-2.00179668862533,1.52887783821019,1.28369529438778));
#37670=CARTESIAN_POINT('Ctrl Pts',(-2.05108413004565,1.46210348521478,1.28894294618583));
#37671=CARTESIAN_POINT('Ctrl Pts',(-2.09700111239218,1.39297975025697,1.29419059798388));
#37672=CARTESIAN_POINT('Ctrl Pts',(-2.1432524159786,1.32335272584946,1.29947645789941));
#37673=CARTESIAN_POINT('Ctrl Pts',(-2.18608363723758,1.25134229844012,1.30476231781493));
#37674=CARTESIAN_POINT('Ctrl Pts',(-2.2252466527171,1.17732051055408,1.31004817773046));
#37675=CARTESIAN_POINT('Ctrl Pts',(-2.26405710768549,1.10396509524056,1.31528645230428));
#37676=CARTESIAN_POINT('Ctrl Pts',(-2.29926491670469,1.0286348033467,1.32052472687811));
#37677=CARTESIAN_POINT('Ctrl Pts',(-2.33067300630846,0.951719279864126,
1.32576300145193));
#37678=CARTESIAN_POINT('Ctrl Pts',(-2.36207075803671,0.874829072888122,
1.33099955186389));
#37679=CARTESIAN_POINT('Ctrl Pts',(-2.3896710999261,0.796355097461274,1.33623610227585));
#37680=CARTESIAN_POINT('Ctrl Pts',(-2.41332466618592,0.716707963942493,
1.3414726526878));
#37681=CARTESIAN_POINT('Ctrl Pts',(-2.43697758302428,0.637063017178899,
1.34670905932743));
#37682=CARTESIAN_POINT('Ctrl Pts',(-2.4566838092984,0.556245419012755,1.35194546596706));
#37683=CARTESIAN_POINT('Ctrl Pts',(-2.47234393902441,0.474680626494553,
1.35718187260669));
#37684=CARTESIAN_POINT('Ctrl Pts',(-2.48826138305951,0.391775628716241,
1.36250431955251));
#37685=CARTESIAN_POINT('Ctrl Pts',(-2.49999845664743,0.308099140257614,
1.36782676649832));
#37686=CARTESIAN_POINT('Ctrl Pts',(-2.50750523858282,0.224106511462149,
1.37314921344414));
#37687=CARTESIAN_POINT('Ctrl Pts',(-2.51490127421607,0.14135301191348,1.37839313921769));
#37688=CARTESIAN_POINT('Ctrl Pts',(-2.51819104635629,0.0582931078956557,
1.38363706499124));
#37689=CARTESIAN_POINT('Ctrl Pts',(-2.51737944929493,-0.0246365230413177,
1.38888099076478));
#37690=CARTESIAN_POINT('Ctrl Pts',(-2.51654962327054,-0.109428803866461,
1.39424269829674));
#37691=CARTESIAN_POINT('Ctrl Pts',(-2.51143198821274,-0.194084377305427,
1.39960440582869));
#37692=CARTESIAN_POINT('Ctrl Pts',(-2.50208769964345,-0.278142757038487,
1.40496611336064));
#37693=CARTESIAN_POINT('Ctrl Pts',(-2.49274341107416,-0.362201136771545,
1.41032782089259));
#37694=CARTESIAN_POINT('Ctrl Pts',(-2.47917261656255,-0.445661831741165,
1.41568952842455));
#37695=CARTESIAN_POINT('Ctrl Pts',(-2.46149135464734,-0.528078176974207,
1.4210512359565));
#37696=CARTESIAN_POINT('Ctrl Pts',(-2.44416098751678,-0.608858922562213,
1.42630653732701));
#37697=CARTESIAN_POINT('Ctrl Pts',(-2.42281783783166,-0.688934803476395,
1.43156183869753));
#37698=CARTESIAN_POINT('Ctrl Pts',(-2.39753427145321,-0.767877377715569,
1.43681714006804));
#37699=CARTESIAN_POINT('Ctrl Pts',(-2.37228654861054,-0.846708038115462,
1.44206499120073));
#37700=CARTESIAN_POINT('Ctrl Pts',(-2.34310964442233,-0.924408147350833,
1.44731284233341));
#37701=CARTESIAN_POINT('Ctrl Pts',(-2.31012680467993,-1.0005600413265,1.4525606934661));
#37702=CARTESIAN_POINT('Ctrl Pts',(-2.27690539007593,-1.07726276499748,
1.45784650389421));
#37703=CARTESIAN_POINT('Ctrl Pts',(-2.23982284843275,-1.15239431832373,
1.46313231432231));
#37704=CARTESIAN_POINT('Ctrl Pts',(-2.19905616306047,-1.22554405947145,
1.46841812475042));
#37705=CARTESIAN_POINT('Ctrl Pts',(-2.15865451862396,-1.29803878906462,
1.47365660395286));
#37706=CARTESIAN_POINT('Ctrl Pts',(-2.11463467386477,-1.36858664591832,
1.47889508315531));
#37707=CARTESIAN_POINT('Ctrl Pts',(-2.06721619339767,-1.43681016830841,
1.48413356235775));
#37708=CARTESIAN_POINT('Ctrl Pts',(-2.01981330608276,-1.5050112559904,1.48937031893217));
#37709=CARTESIAN_POINT('Ctrl Pts',(-1.96901426583195,-1.57088914864235,
1.49460707550659));
#37710=CARTESIAN_POINT('Ctrl Pts',(-1.91508219607761,-1.63409498875266,
1.499843832081));
#37711=CARTESIAN_POINT('Ctrl Pts',(-1.86115159404794,-1.69729910875893,
1.50508044614064));
#37712=CARTESIAN_POINT('Ctrl Pts',(-1.80408843232335,-1.757830970477,1.51031706020028));
#37713=CARTESIAN_POINT('Ctrl Pts',(-1.74419548713124,-1.81537554039681,
1.51555367425992));
#37714=CARTESIAN_POINT('Ctrl Pts',(-1.68332360005784,-1.87386066832983,
1.52087588004998));
#37715=CARTESIAN_POINT('Ctrl Pts',(-1.61952893661369,-1.92925962070465,
1.52619808584005));
#37716=CARTESIAN_POINT('Ctrl Pts',(-1.55316619771348,-1.98128266844493,
1.53152029163011));
#37717=CARTESIAN_POINT('Ctrl Pts',(-1.48777693586776,-2.03254258850062,
1.53676442582003));
#37718=CARTESIAN_POINT('Ctrl Pts',(-1.41989485917923,-2.080524769985,1.54200856000995));
#37719=CARTESIAN_POINT('Ctrl Pts',(-1.34988893798851,-2.12499555413565,
1.54725269419986));
#37720=CARTESIAN_POINT('Ctrl Pts',(-1.27831970603312,-2.17045942079122,
1.55261393579));
#37721=CARTESIAN_POINT('Ctrl Pts',(-1.20453107637456,-2.21225292119087,
1.55797517738014));
#37722=CARTESIAN_POINT('Ctrl Pts',(-1.12894246264074,-2.25017669662777,
1.56333641897027));
#37723=CARTESIAN_POINT('Ctrl Pts',(-1.05335384890691,-2.28810047206467,
1.56869766056041));
#37724=CARTESIAN_POINT('Ctrl Pts',(-0.975965742979037,-2.32215437904821,
1.57405890215054));
#37725=CARTESIAN_POINT('Ctrl Pts',(-0.897215838955941,-2.35219259167411,
1.57942014374068));
#37726=CARTESIAN_POINT('Ctrl Pts',(-0.820022679874984,-2.38163700248964,
1.58467540316064));
#37727=CARTESIAN_POINT('Ctrl Pts',(-0.741235998405527,-2.40733182677623,
1.58993066258061));
#37728=CARTESIAN_POINT('Ctrl Pts',(-0.661254560651124,-2.42910449672674,
1.59518592200058));
#37729=CARTESIAN_POINT('Ctrl Pts',(-0.581386513209035,-2.45084629939211,
1.600433730998));
#37730=CARTESIAN_POINT('Ctrl Pts',(-0.500327515397368,-2.46867687225071,
1.60568153999542));
#37731=CARTESIAN_POINT('Ctrl Pts',(-0.418494995123038,-2.4824721930078,
1.61092934899284));
#37732=CARTESIAN_POINT('Ctrl Pts',(-0.336069729768283,-2.49636743869064,
1.61621516993167));
#37733=CARTESIAN_POINT('Ctrl Pts',(-0.252860131598111,-2.50616855897815,
1.62150099087051));
#37734=CARTESIAN_POINT('Ctrl Pts',(-0.169307009444033,-2.51180042729376,
1.62678681180934));
#37735=CARTESIAN_POINT('Ctrl Pts',(-0.0865028875865664,-2.51738180951226,
1.63202524874446));
#37736=CARTESIAN_POINT('Ctrl Pts',(-0.00336184488425226,-2.5188683582142,
1.63726368567957));
#37737=CARTESIAN_POINT('Ctrl Pts',(0.0796799703382311,-2.51623873118727,
1.64250212261468));
#37738=CARTESIAN_POINT('Ctrl Pts',(0.162694478496319,-2.51360996887402,
1.64773883696781));
#37739=CARTESIAN_POINT('Ctrl Pts',(0.245609363154774,-2.50686773363573,
1.65297555132094));
#37740=CARTESIAN_POINT('Ctrl Pts',(0.327988753101664,-2.49604279367138,
1.65821226567407));
#37741=CARTESIAN_POINT('Ctrl Pts',(0.410365902771813,-2.48521814808722,
1.66344883761671));
#37742=CARTESIAN_POINT('Ctrl Pts',(0.492207129333078,-2.47031107966633,
1.66868540955935));
#37743=CARTESIAN_POINT('Ctrl Pts',(0.573083343760946,-2.45140403261147,
1.67392198150199));
#37744=CARTESIAN_POINT('Ctrl Pts',(0.65528290272542,-2.43218761725098,1.67924423733723));
#37745=CARTESIAN_POINT('Ctrl Pts',(0.736485102719983,-2.40883924168981,
1.68456649317246));
#37746=CARTESIAN_POINT('Ctrl Pts',(0.816253787080165,-2.38149868886743,
1.6898887490077));
#37747=CARTESIAN_POINT('Ctrl Pts',(0.894850982246054,-2.35455966156167,
1.69513284177368));
#37748=CARTESIAN_POINT('Ctrl Pts',(0.972056075902965,-2.32374516825423,
1.70037693453966));
#37749=CARTESIAN_POINT('Ctrl Pts',(1.04747219653616,-2.2892374816702,1.70562102730564));
#37750=CARTESIAN_POINT('Ctrl Pts',(1.12457443020833,-2.25395829080027,1.71098236467551));
#37751=CARTESIAN_POINT('Ctrl Pts',(1.19980627785168,-2.21481900996775,1.71634370204538));
#37752=CARTESIAN_POINT('Ctrl Pts',(1.27277214531568,-2.17206291716159,1.72170503941524));
#37753=CARTESIAN_POINT('Ctrl Pts',(1.34573801277968,-2.12930682435543,1.72706637678511));
#37754=CARTESIAN_POINT('Ctrl Pts',(1.4164375118487,-2.08293425409358,1.73242771415498));
#37755=CARTESIAN_POINT('Ctrl Pts',(1.48451000265987,-2.03323296796083,1.73778905152485));
#37756=CARTESIAN_POINT('Ctrl Pts',(1.55068750294995,-1.98491525785101,1.74300114088902));
#37757=CARTESIAN_POINT('Ctrl Pts',(1.61463571171944,-1.93326663287857,1.74821323025319));
#37758=CARTESIAN_POINT('Ctrl Pts',(1.67599604186995,-1.87852163086728,1.75342531961736));
#37759=CARTESIAN_POINT('Ctrl Pts',(1.73726911392309,-1.82385447955698,1.7586299970755));
#37760=CARTESIAN_POINT('Ctrl Pts',(1.79596126648459,-1.76610000357143,1.76383467453364));
#37761=CARTESIAN_POINT('Ctrl Pts',(1.8517441552362,-1.705535057848,1.76903935199177));
#37762=CARTESIAN_POINT('Ctrl Pts',(1.90746362981707,-1.64503896255333,1.77423811275552));
#37763=CARTESIAN_POINT('Ctrl Pts',(1.96028009502652,-1.58173908925178,1.77943687351927));
#37764=CARTESIAN_POINT('Ctrl Pts',(2.00990063841765,-1.51595041927113,1.78463563428302));
#37765=CARTESIAN_POINT('Ctrl Pts',(2.05949081933144,-1.45020200493593,1.78983121395996));
#37766=CARTESIAN_POINT('Ctrl Pts',(2.10588867698112,-1.3819681901832,1.79502679363691));
#37767=CARTESIAN_POINT('Ctrl Pts',(2.14884114177652,-1.3115974982473,1.80022237331385));
#37768=CARTESIAN_POINT('Ctrl Pts',(2.19178082278171,-1.2412477504916,1.80541640664878));
#37769=CARTESIAN_POINT('Ctrl Pts',(2.2312769024684,-1.16876278922474,1.81061043998372));
#37770=CARTESIAN_POINT('Ctrl Pts',(2.26712011663423,-1.09451935878376,1.81580447331866));
#37771=CARTESIAN_POINT('Ctrl Pts',(2.30296392706817,-1.02027469326965,1.82099859305869));
#37772=CARTESIAN_POINT('Ctrl Pts',(2.3351545489735,-0.944271924563801,1.82619271279873));
#37773=CARTESIAN_POINT('Ctrl Pts',(2.36352975717215,-0.866910224280322,
1.83138683253876));
#37774=CARTESIAN_POINT('Ctrl Pts',(2.3919319230396,-0.789475027052617,1.83658588691606));
#37775=CARTESIAN_POINT('Ctrl Pts',(2.41651127687384,-0.710678762869131,
1.84178494129336));
#37776=CARTESIAN_POINT('Ctrl Pts',(2.43715488713422,-0.630937640435078,
1.84698399567066));
#37777=CARTESIAN_POINT('Ctrl Pts',(2.45780913885177,-0.551155412703653,
1.85218573007891));
#37778=CARTESIAN_POINT('Ctrl Pts',(2.47452351384133,-0.470427817487587,
1.85738746448715));
#37779=CARTESIAN_POINT('Ctrl Pts',(2.48723633671725,-0.389180748898689,
1.8625891988954));
#37780=CARTESIAN_POINT('Ctrl Pts',(2.49996966634842,-0.307802622576515,
1.86779932409894));
#37781=CARTESIAN_POINT('Ctrl Pts',(2.50868850866609,-0.225903817148933,
1.87300944930248));
#37782=CARTESIAN_POINT('Ctrl Pts',(2.51338316214037,-0.143914315720466,
1.87821957450602));
#37783=CARTESIAN_POINT('Ctrl Pts',(2.51614555930706,-0.0956705917298165,
1.88128528216246));
#37784=CARTESIAN_POINT('Ctrl Pts',(2.51751565026114,-0.0473954685790145,
1.88435098981889));
#37785=CARTESIAN_POINT('Ctrl Pts',(2.51749986510683,0.000824128084736925,
1.88741669747533));
#37786=CARTESIAN_POINT('Ctrl Pts',(2.51749986510666,0.000824128598839498,
1.88741669750801));
#37787=CARTESIAN_POINT('Ctrl Pts',(2.51748486234407,0.0466536907109408,
1.89033045144168));
#37788=CARTESIAN_POINT('Ctrl Pts',(2.5162184915714,0.092461097738171,1.89324420537535));
#37789=CARTESIAN_POINT('Ctrl Pts',(2.51370388411283,0.13819925106905,1.89615795930902));
#37790=CARTESIAN_POINT('Ctrl Pts',(2.50916908870937,0.220682569402365,1.90141256789624));
#37791=CARTESIAN_POINT('Ctrl Pts',(2.50056177537896,0.303094749686193,1.90666717648346));
#37792=CARTESIAN_POINT('Ctrl Pts',(2.4878866763403,0.385001474917191,1.91192178507068));
#37793=CARTESIAN_POINT('Ctrl Pts',(2.47505675342768,0.467908674895217,1.91724057768164));
#37794=CARTESIAN_POINT('Ctrl Pts',(2.45805894040082,0.550297511071083,1.92255937029261));
#37795=CARTESIAN_POINT('Ctrl Pts',(2.43695260213126,0.631718501364096,1.92787816290357));
#37796=CARTESIAN_POINT('Ctrl Pts',(2.41584626386169,0.713139491657106,1.93319695551454));
#37797=CARTESIAN_POINT('Ctrl Pts',(2.39063145838279,0.793592144292747,1.93851574812551));
#37798=CARTESIAN_POINT('Ctrl Pts',(2.36142200728636,0.872635292378021,1.94383454073647));
#37799=CARTESIAN_POINT('Ctrl Pts',(2.36142200724207,0.872635292497862,1.66658329180866));
#37800=CARTESIAN_POINT('Ctrl Pts',(2.36656543969622,0.858716746348728,1.66563271745266));
#37801=CARTESIAN_POINT('Ctrl Pts',(2.37158585374055,0.844752622564022,1.66468620664304));
#37802=CARTESIAN_POINT('Ctrl Pts',(2.38080595803352,0.818376983810189,1.66291166730899));
#37803=CARTESIAN_POINT('Ctrl Pts',(2.38503272622791,0.805975683755325,1.6620827793949));
#37804=CARTESIAN_POINT('Ctrl Pts',(2.39282966260543,0.782500991670894,1.66052385439014));
#37805=CARTESIAN_POINT('Ctrl Pts',(2.39642023989896,0.771434791357363,1.65979316648514));
#37806=CARTESIAN_POINT('Ctrl Pts',(2.40436963235919,0.746343492191642,1.6581457159186));
#37807=CARTESIAN_POINT('Ctrl Pts',(2.4086827141935,0.732304263350909,1.65723046023622));
#37808=CARTESIAN_POINT('Ctrl Pts',(2.42139113165543,0.689610577587668,1.65446630588026));
#37809=CARTESIAN_POINT('Ctrl Pts',(2.42939997034476,0.660843143891866,1.65262986890035));
#37810=CARTESIAN_POINT('Ctrl Pts',(2.49059591268727,0.424858194389506,1.63776019526306));
#37811=CARTESIAN_POINT('Ctrl Pts',(2.51768324236378,0.211782042153157,1.62565128598905));
#37812=CARTESIAN_POINT('Ctrl Pts',(2.51739093025033,-0.127785717720968,
1.60606337558893));
#37813=CARTESIAN_POINT('Ctrl Pts',(2.50788069886021,-0.253203986703153,
1.59873916266813));
#37814=CARTESIAN_POINT('Ctrl Pts',(2.48700526467906,-0.3908940581761,1.59010798259596));
#37815=CARTESIAN_POINT('Ctrl Pts',(2.48484474075353,-0.404400725109235,
1.58925487696615));
#37816=CARTESIAN_POINT('Ctrl Pts',(2.48118054135853,-0.426168831867675,
1.58786859686673));
#37817=CARTESIAN_POINT('Ctrl Pts',(2.47974537598193,-0.434441730935338,
1.58733908762811));
#37818=CARTESIAN_POINT('Ctrl Pts',(2.47712211251085,-0.449126725621398,
1.58639419630881));
#37819=CARTESIAN_POINT('Ctrl Pts',(2.4759504515319,-0.45554158541987,1.58597973779078));
#37820=CARTESIAN_POINT('Ctrl Pts',(2.47334715535131,-0.46948787875069,1.58507491750255));
#37821=CARTESIAN_POINT('Ctrl Pts',(2.47190606094343,-0.477017233788878,
1.58458405255122));
#37822=CARTESIAN_POINT('Ctrl Pts',(2.46771816485463,-0.498369261827021,
1.58318553733568));
#37823=CARTESIAN_POINT('Ctrl Pts',(2.46488970136792,-0.512175361361853,
1.58227351696751));
#37824=CARTESIAN_POINT('Ctrl Pts',(2.44477084175596,-0.60634955073007,1.57600275167017));
#37825=CARTESIAN_POINT('Ctrl Pts',(2.4236703567482,-0.685845053535465,1.57046285555256));
#37826=CARTESIAN_POINT('Ctrl Pts',(2.3483866980391,-0.922163718528844,1.5535083985936));
#37827=CARTESIAN_POINT('Ctrl Pts',(2.28255663280725,-1.07482428696749,1.5419208038596));
#37828=CARTESIAN_POINT('Ctrl Pts',(2.15183824649078,-1.31079994526167,1.5236467305738));
#37829=CARTESIAN_POINT('Ctrl Pts',(2.09590038454559,-1.39850304947431,1.51675438044685));
#37830=CARTESIAN_POINT('Ctrl Pts',(2.02104047874389,-1.50124587682293,1.50856553305453));
#37831=CARTESIAN_POINT('Ctrl Pts',(2.00712864537521,-1.51979553198557,1.50708190695098));
#37832=CARTESIAN_POINT('Ctrl Pts',(1.98474553343597,-1.54879704001827,1.50475341472479));
#37833=CARTESIAN_POINT('Ctrl Pts',(1.97644361486455,-1.55937736046654,1.50390201356791));
#37834=CARTESIAN_POINT('Ctrl Pts',(1.96082482738877,-1.57895749080838,1.50232258882636));
#37835=CARTESIAN_POINT('Ctrl Pts',(1.95352981079476,-1.58797419596896,1.50159372919805));
#37836=CARTESIAN_POINT('Ctrl Pts',(1.93716559474296,-1.60791707663917,1.49997805037261));
#37837=CARTESIAN_POINT('Ctrl Pts',(1.92806569741186,-1.61881763838051,1.49909249317092));
#37838=CARTESIAN_POINT('Ctrl Pts',(1.90113476112544,-1.65052835088087,1.49650859240089));
#37839=CARTESIAN_POINT('Ctrl Pts',(1.88305523784894,-1.67112545256159,1.49482038667756));
#37840=CARTESIAN_POINT('Ctrl Pts',(1.76354870964592,-1.80287063360472,1.48394694410274));
#37841=CARTESIAN_POINT('Ctrl Pts',(1.65266250970589,-1.90503574388943,1.47518536761765));
#37842=CARTESIAN_POINT('Ctrl Pts',(1.40600277148995,-2.09445070982781,1.45727959958589));
#37843=CARTESIAN_POINT('Ctrl Pts',(1.26965976969582,-2.179798451262,1.44818533483113));
#37844=CARTESIAN_POINT('Ctrl Pts',(1.09175449762358,-2.26877861709355,1.43618752125606));
#37845=CARTESIAN_POINT('Ctrl Pts',(1.05698270855391,-2.28518521912782,1.43383570487106));
#37846=CARTESIAN_POINT('Ctrl Pts',(1.01111560348713,-2.30555621739638,1.43070726752831));
#37847=CARTESIAN_POINT('Ctrl Pts',(1.00034708024753,-2.31024889171167,1.42997092878311));
#37848=CARTESIAN_POINT('Ctrl Pts',(0.982967518019296,-2.31767821291206,
1.42877894484695));
#37849=CARTESIAN_POINT('Ctrl Pts',(0.976376817056206,-2.32046239964535,
1.42832609374267));
#37850=CARTESIAN_POINT('Ctrl Pts',(0.963628097224575,-2.32578406140048,
1.42744836388935));
#37851=CARTESIAN_POINT('Ctrl Pts',(0.95747176652422,-2.32832523979474,1.42702370890395));
#37852=CARTESIAN_POINT('Ctrl Pts',(0.942613873060686,-2.33438931317987,
1.42599701260429));
#37853=CARTESIAN_POINT('Ctrl Pts',(0.93390259285422,-2.33788800406963,1.42539356082793));
#37854=CARTESIAN_POINT('Ctrl Pts',(0.903454709871901,-2.34991938714786,
1.42327967486417));
#37855=CARTESIAN_POINT('Ctrl Pts',(0.881619858616303,-2.35819801369008,
1.4217554696473));
#37856=CARTESIAN_POINT('Ctrl Pts',(0.827386175562193,-2.37790211697935,
1.41795467061492));
#37857=CARTESIAN_POINT('Ctrl Pts',(0.794863207675124,-2.38897019878293,
1.41566238926392));
#37858=CARTESIAN_POINT('Ctrl Pts',(0.65531274963024,-2.43329643217257,1.40579971212265));
#37859=CARTESIAN_POINT('Ctrl Pts',(0.546358666576271,-2.46005207385707,
1.39803880137519));
#37860=CARTESIAN_POINT('Ctrl Pts',(0.262868816349941,-2.50990121328572,
1.37816170852405));
#37861=CARTESIAN_POINT('Ctrl Pts',(0.0870067161732809,-2.52213284563033,
1.36616427820632));
#37862=CARTESIAN_POINT('Ctrl Pts',(-0.121636934455914,-2.5147754627749,
1.35259908983483));
#37863=CARTESIAN_POINT('Ctrl Pts',(-0.15452987533737,-2.51296873385376,
1.35047852459925));
#37864=CARTESIAN_POINT('Ctrl Pts',(-0.202446906603256,-2.50939231696444,
1.34741431040695));
#37865=CARTESIAN_POINT('Ctrl Pts',(-0.217504439501805,-2.50813205103853,
1.34645499664912));
#37866=CARTESIAN_POINT('Ctrl Pts',(-0.24422201692004,-2.5056534607268,1.3447589458145));
#37867=CARTESIAN_POINT('Ctrl Pts',(-0.2558864989076,-2.50448912275189,1.34402055233592));
#37868=CARTESIAN_POINT('Ctrl Pts',(-0.280220601410862,-2.50188833337961,
1.34248430342288));
#37869=CARTESIAN_POINT('Ctrl Pts',(-0.292888322795294,-2.50043701341345,
1.34168693361905));
#37870=CARTESIAN_POINT('Ctrl Pts',(-0.325975323416193,-2.49639139380267,
1.3396101343631));
#37871=CARTESIAN_POINT('Ctrl Pts',(-0.34637503332979,-2.49364277267559,
1.33833554342853));
#37872=CARTESIAN_POINT('Ctrl Pts',(-0.440190940368616,-2.47982868701533,
1.33249805008895));
#37873=CARTESIAN_POINT('Ctrl Pts',(-0.513132614592708,-2.46576861029378,
1.32802935804034));
#37874=CARTESIAN_POINT('Ctrl Pts',(-0.727243864530593,-2.414582092351,1.31499916526967));
#37875=CARTESIAN_POINT('Ctrl Pts',(-0.865919528759469,-2.36839103674545,
1.30668866142716));
#37876=CARTESIAN_POINT('Ctrl Pts',(-1.04957041471071,-2.28891828583806,
1.29516554157286));
#37877=CARTESIAN_POINT('Ctrl Pts',(-1.09861214049467,-2.26578816326281,
1.29203207360484));
#37878=CARTESIAN_POINT('Ctrl Pts',(-1.17895241075164,-2.22467447114124,
1.28674773770486));
#37879=CARTESIAN_POINT('Ctrl Pts',(-1.21067995163597,-2.20756860751117,
1.28462002908492));
#37880=CARTESIAN_POINT('Ctrl Pts',(-1.28484763643677,-2.16550136465571,
1.27952356771145));
#37881=CARTESIAN_POINT('Ctrl Pts',(-1.32694241878387,-2.13996558501632,
1.27653312981781));
#37882=CARTESIAN_POINT('Ctrl Pts',(-1.37898932053784,-2.10626639598085,
1.27267529347276));
#37883=CARTESIAN_POINT('Ctrl Pts',(-1.38966687462304,-2.09923691815071,
1.27187509398411));
#37884=CARTESIAN_POINT('Ctrl Pts',(-1.406426091292,-2.08801973545374,1.27060446596708));
#37885=CARTESIAN_POINT('Ctrl Pts',(-1.41254382697707,-2.08388596124216,
1.27013752462182));
#37886=CARTESIAN_POINT('Ctrl Pts',(-1.42406967394163,-2.07602383463924,
1.26925172190527));
#37887=CARTESIAN_POINT('Ctrl Pts',(-1.42948146327859,-2.07230117032128,
1.26883323387935));
#37888=CARTESIAN_POINT('Ctrl Pts',(-1.44215159956868,-2.06351238505439,
1.26784747427176));
#37889=CARTESIAN_POINT('Ctrl Pts',(-1.4493978514199,-2.05842912486194,1.26727906805272));
#37890=CARTESIAN_POINT('Ctrl Pts',(-1.47309527551402,-2.04161816728942,
1.26540534249235));
#37891=CARTESIAN_POINT('Ctrl Pts',(-1.48943161417041,-2.02973097663667,
1.26408996742194));
#37892=CARTESIAN_POINT('Ctrl Pts',(-1.57971103058448,-1.96236211027759,
1.25669561353447));
#37893=CARTESIAN_POINT('Ctrl Pts',(-1.65069118883201,-1.90304157608034,
1.25040991818945));
#37894=CARTESIAN_POINT('Ctrl Pts',(-1.76600654219503,-1.79535462737379,
1.23956359173785));
#37895=CARTESIAN_POINT('Ctrl Pts',(-1.81201595312015,-1.74890691488186,
1.23504028551456));
#37896=CARTESIAN_POINT('Ctrl Pts',(-1.97026482301445,-1.57619433766027,
1.21886823707869));
#37897=CARTESIAN_POINT('Ctrl Pts',(-2.0715606228624,-1.44048142063773,1.20736201829065));
#37898=CARTESIAN_POINT('Ctrl Pts',(-2.1755690361032,-1.26720336113626,1.19422814539507));
#37899=CARTESIAN_POINT('Ctrl Pts',(-2.19206581820173,-1.23844766104923,
1.19209385732476));
#37900=CARTESIAN_POINT('Ctrl Pts',(-2.21526099540895,-1.1960995056953,1.18901456229561));
#37901=CARTESIAN_POINT('Ctrl Pts',(-2.22241172162173,-1.18276010298937,
1.18805362881769));
#37902=CARTESIAN_POINT('Ctrl Pts',(-2.23488197523751,-1.15898489114969,
1.18635660193945));
#37903=CARTESIAN_POINT('Ctrl Pts',(-2.24024972895498,-1.14857502174127,
1.18561883144596));
#37904=CARTESIAN_POINT('Ctrl Pts',(-2.25129047338053,-1.12679145533303,
1.18408575018006));
#37905=CARTESIAN_POINT('Ctrl Pts',(-2.25695038380481,-1.11541147288014,
1.18329091072057));
#37906=CARTESIAN_POINT('Ctrl Pts',(-2.27149189740842,-1.08560997626709,
1.18122484708161));
#37907=CARTESIAN_POINT('Ctrl Pts',(-2.28023575827393,-1.06712201058154,
1.17995838622634));
#37908=CARTESIAN_POINT('Ctrl Pts',(-2.31914163026448,-0.982197374822059,
1.17420746917555));
#37909=CARTESIAN_POINT('Ctrl Pts',(-2.34663354137771,-0.914572072470814,
1.16981388960174));
#37910=CARTESIAN_POINT('Ctrl Pts',(-2.41863151487462,-0.712740190435884,
1.15712255284373));
#37911=CARTESIAN_POINT('Ctrl Pts',(-2.45482131764587,-0.575874891250182,
1.14905874520011));
#37912=CARTESIAN_POINT('Ctrl Pts',(-2.50210461114167,-0.307421040012571,
1.13337671137171));
#37913=CARTESIAN_POINT('Ctrl Pts',(-2.51472556831109,-0.176584357740824,
1.12578562450538));
#37914=CARTESIAN_POINT('Ctrl Pts',(-2.51747699164142,-0.0239675245480319,
1.11641198267612));
#37915=CARTESIAN_POINT('Ctrl Pts',(-2.51758977161679,-0.00255291875063406,
1.11508469686271));
#37916=CARTESIAN_POINT('Ctrl Pts',(-2.51736627858063,0.0272793813710361,
1.11321572584653));
#37917=CARTESIAN_POINT('Ctrl Pts',(-2.51726096245127,0.0356985622833955,
1.11268605584854));
#37918=CARTESIAN_POINT('Ctrl Pts',(-2.51700638023353,0.0502238825068801,
1.11176817023207));
#37919=CARTESIAN_POINT('Ctrl Pts',(-2.5168771215311,0.0563303622931436,
1.11138104914158));
#37920=CARTESIAN_POINT('Ctrl Pts',(-2.51655739789115,0.0692180181425276,
1.11056130419081));
#37921=CARTESIAN_POINT('Ctrl Pts',(-2.51636174345143,0.0759989717104931,
1.11012838721149));
#37922=CARTESIAN_POINT('Ctrl Pts',(-2.51580817111654,0.0928252914642239,
1.10905030570795));
#37923=CARTESIAN_POINT('Ctrl Pts',(-2.51541749435442,0.102869381056326,
1.10840337456075));
#37924=CARTESIAN_POINT('Ctrl Pts',(-2.51371669962756,0.140752802940339,
1.10595120031646));
#37925=CARTESIAN_POINT('Ctrl Pts',(-2.51200451551857,0.16857093217028,1.10412582232164));
#37926=CARTESIAN_POINT('Ctrl Pts',(-2.50642071789218,0.239944187505855,
1.09938838297947));
#37927=CARTESIAN_POINT('Ctrl Pts',(-2.50187559255897,0.283436266433752,
1.09644979197519));
#37928=CARTESIAN_POINT('Ctrl Pts',(-2.48000642087177,0.450487332390012,
1.08501403096829));
#37929=CARTESIAN_POINT('Ctrl Pts',(-2.45463985197404,0.572811289169149,
1.07633449028049));
#37930=CARTESIAN_POINT('Ctrl Pts',(-2.37586517245021,0.848032835916339,
1.05662272753545));
#37931=CARTESIAN_POINT('Ctrl Pts',(-2.31657169888543,0.998702906564747,
1.04571316478046));
#37932=CARTESIAN_POINT('Ctrl Pts',(-2.23313614944323,1.16249913871672,1.03385680195097));
#37933=CARTESIAN_POINT('Ctrl Pts',(-2.22277443712753,1.18219083188889,1.03243078460233));
#37934=CARTESIAN_POINT('Ctrl Pts',(-2.2052806196052,1.21439321907345,1.03009714934354));
#37935=CARTESIAN_POINT('Ctrl Pts',(-2.19829999591787,1.22698436978636,1.02918427653099));
#37936=CARTESIAN_POINT('Ctrl Pts',(-2.18549288326325,1.24962474966612,1.02754182461858));
#37937=CARTESIAN_POINT('Ctrl Pts',(-2.17970416578576,1.25969477045726,1.02681093050002));
#37938=CARTESIAN_POINT('Ctrl Pts',(-2.16713323835683,1.28121696579934,1.02524786792946));
#37939=CARTESIAN_POINT('Ctrl Pts',(-2.16032946261532,1.29265618398572,1.02441650086985));
#37940=CARTESIAN_POINT('Ctrl Pts',(-2.14144275436363,1.32384485015468,1.02214779819336));
#37941=CARTESIAN_POINT('Ctrl Pts',(-2.12917741681121,1.34348272789404,1.02071709777966));
#37942=CARTESIAN_POINT('Ctrl Pts',(-2.05517542143316,1.45840688211109,1.01232588492245));
#37943=CARTESIAN_POINT('Ctrl Pts',(-1.98731729199051,1.5496035716431,1.00559927193119));
#37944=CARTESIAN_POINT('Ctrl Pts',(-1.84647924280528,1.71434140723486,0.992990036373422));
#37945=CARTESIAN_POINT('Ctrl Pts',(-1.77467308201424,1.78857147535461,0.987096789431059));
#37946=CARTESIAN_POINT('Ctrl Pts',(-1.65419597377087,1.89869618159393,0.977693553605859));
#37947=CARTESIAN_POINT('Ctrl Pts',(-1.60844356219811,1.93760685230893,0.974219198148781));
#37948=CARTESIAN_POINT('Ctrl Pts',(-1.50268902896809,2.02121824115617,0.966295336365825));
#37949=CARTESIAN_POINT('Ctrl Pts',(-1.44200096120561,2.06495242296029,0.961819855323459));
#37950=CARTESIAN_POINT('Ctrl Pts',(-1.36857846245463,2.11304722288093,0.956373645305415));
#37951=CARTESIAN_POINT('Ctrl Pts',(-1.35763854417802,2.12009271986527,0.955561358746048));
#37952=CARTESIAN_POINT('Ctrl Pts',(-1.33971318339815,2.1314413295364,0.954228254723307));
#37953=CARTESIAN_POINT('Ctrl Pts',(-1.33276030356428,2.13579575891417,0.953710649395945));
#37954=CARTESIAN_POINT('Ctrl Pts',(-1.32023670507718,2.14355403738605,0.952777165954427));
#37955=CARTESIAN_POINT('Ctrl Pts',(-1.31467388413465,2.14697029434183,0.952362100371873));
#37956=CARTESIAN_POINT('Ctrl Pts',(-1.30237757332989,2.15445603456975,0.951443662991297));
#37957=CARTESIAN_POINT('Ctrl Pts',(-1.29563833649191,2.15851556525145,0.950939687533825));
#37958=CARTESIAN_POINT('Ctrl Pts',(-1.27604270308395,2.17019460299725,0.949472774181139));
#37959=CARTESIAN_POINT('Ctrl Pts',(-1.26313760098367,2.17773115202909,0.948504838792789));
#37960=CARTESIAN_POINT('Ctrl Pts',(-1.15265456121644,2.24094057200843,0.940207266830241));
#37961=CARTESIAN_POINT('Ctrl Pts',(-1.05152801730223,2.290133260865,0.932545733957284));
#37962=CARTESIAN_POINT('Ctrl Pts',(-0.780969670107453,2.40003935503442,
0.912437887868524));
#37963=CARTESIAN_POINT('Ctrl Pts',(-0.607682965337253,2.4496611024057,0.899971032799213));
#37964=CARTESIAN_POINT('Ctrl Pts',(-0.368361763167782,2.4912051683072,0.883847074843666));
#37965=CARTESIAN_POINT('Ctrl Pts',(-0.305758577773296,2.49966126030663,
0.879721041319345));
#37966=CARTESIAN_POINT('Ctrl Pts',(-0.222793506888974,2.5077035962604,0.874370822732703));
#37967=CARTESIAN_POINT('Ctrl Pts',(-0.202664970584672,2.50941053274065,
0.873081794874619));
#37968=CARTESIAN_POINT('Ctrl Pts',(-0.169865486393625,2.51179475432956,
0.870995499692251));
#37969=CARTESIAN_POINT('Ctrl Pts',(-0.157206437510141,2.5126188164712,0.870193717441192));
#37970=CARTESIAN_POINT('Ctrl Pts',(-0.132780564651753,2.51402353787054,
0.868653089468399));
#37971=CARTESIAN_POINT('Ctrl Pts',(-0.121014859847978,2.51461735430326,
0.867913855711089));
#37972=CARTESIAN_POINT('Ctrl Pts',(-0.0936402624622615,2.51580637700057,
0.866200390827621));
#37973=CARTESIAN_POINT('Ctrl Pts',(-0.078029028714933,2.51633895038967,
0.865228121713024));
#37974=CARTESIAN_POINT('Ctrl Pts',(-0.0276854629661903,2.51758744598396,
0.862107690332712));
#37975=CARTESIAN_POINT('Ctrl Pts',(0.00705795139312717,2.51772981026285,
0.859977222248272));
#37976=CARTESIAN_POINT('Ctrl Pts',(0.0891350918806768,2.5163670107066,0.854990676225652));
#37977=CARTESIAN_POINT('Ctrl Pts',(0.136445916993481,2.51424559199206,0.852152956507963));
#37978=CARTESIAN_POINT('Ctrl Pts',(0.415894458664718,2.49380320122993,0.835541552342684));
#37979=CARTESIAN_POINT('Ctrl Pts',(0.644609876897895,2.44468485578048,0.822674399909907));
#37980=CARTESIAN_POINT('Ctrl Pts',(0.915564057244588,2.34577152690151,0.805516637889768));
#37981=CARTESIAN_POINT('Ctrl Pts',(0.967175439674964,2.3249671528889,0.802150154356566));
#37982=CARTESIAN_POINT('Ctrl Pts',(1.03007820508638,2.29715434293162,0.797874728427992));
#37983=CARTESIAN_POINT('Ctrl Pts',(1.04206326138337,2.29174242133527,0.797052206144096));
#37984=CARTESIAN_POINT('Ctrl Pts',(1.06085439440756,2.28307929958075,0.795749254049853));
#37985=CARTESIAN_POINT('Ctrl Pts',(1.06768939223993,2.2798908948638,0.795272526338978));
#37986=CARTESIAN_POINT('Ctrl Pts',(1.0803382042062,2.27392109603348,0.794384909369086));
#37987=CARTESIAN_POINT('Ctrl Pts',(1.0861557561688,2.27114804826618,0.793974528119976));
#37988=CARTESIAN_POINT('Ctrl Pts',(1.09944351722231,2.26475145105282,0.793032277277408));
#37989=CARTESIAN_POINT('Ctrl Pts',(1.10690642264452,2.26111329866756,0.792499529111765));
#37990=CARTESIAN_POINT('Ctrl Pts',(1.1301119031017,2.24965825636622,0.790832221380776));
#37991=CARTESIAN_POINT('Ctrl Pts',(1.14579031064432,2.2417135648613,0.789690227407963));
#37992=CARTESIAN_POINT('Ctrl Pts',(1.18262143696868,2.22256288323565,0.786972932151512));
#37993=CARTESIAN_POINT('Ctrl Pts',(1.20369977129088,2.21121821730328,0.785390543523805));
#37994=CARTESIAN_POINT('Ctrl Pts',(1.27895341386057,2.16932079241609,0.779650522444104));
#37995=CARTESIAN_POINT('Ctrl Pts',(1.33215134737835,2.13706488542584,0.775421939469041));
#37996=CARTESIAN_POINT('Ctrl Pts',(1.54739685076904,1.99539187579499,0.757741237801217));
#37997=CARTESIAN_POINT('Ctrl Pts',(1.69764724291739,1.86923442008128,0.744071612891362));
#37998=CARTESIAN_POINT('Ctrl Pts',(1.88022188371325,1.67557675566218,0.726320675551551));
#37999=CARTESIAN_POINT('Ctrl Pts',(1.92647841543517,1.62218196228031,0.721692405615313));
#38000=CARTESIAN_POINT('Ctrl Pts',(1.98344694453827,1.55054238344843,0.715812239542089));
#38001=CARTESIAN_POINT('Ctrl Pts',(1.99625717361339,1.5340146038628,0.71447706447666));
#38002=CARTESIAN_POINT('Ctrl Pts',(2.01654999056128,1.50714802297689,0.712340315980959));
#38003=CARTESIAN_POINT('Ctrl Pts',(2.02416226702043,1.49690886635203,0.711533676958355));
#38004=CARTESIAN_POINT('Ctrl Pts',(2.03854723543726,1.47724947481052,0.709999345304622));
#38005=CARTESIAN_POINT('Ctrl Pts',(2.04533326912431,1.46783945560564,0.709271147858374));
#38006=CARTESIAN_POINT('Ctrl Pts',(2.06075770921005,1.44613610924909,0.707605620887821));
#38007=CARTESIAN_POINT('Ctrl Pts',(2.06935165275714,1.43381161080969,0.706670008377926));
#38008=CARTESIAN_POINT('Ctrl Pts',(2.09588090904142,1.39503083157344,0.703756918313447));
#38009=CARTESIAN_POINT('Ctrl Pts',(2.1134234986342,1.36830883320872,0.701794195195356));
#38010=CARTESIAN_POINT('Ctrl Pts',(2.19955504256816,1.2314976679287,0.691954816867849));
#38011=CARTESIAN_POINT('Ctrl Pts',(2.26007538360321,1.11655441533893,0.684374831861546));
#38012=CARTESIAN_POINT('Ctrl Pts',(2.32923370738789,0.956287682709663,0.674308477894333));
#38013=CARTESIAN_POINT('Ctrl Pts',(2.34588901247795,0.914668837099738,0.671735936903445));
#38014=CARTESIAN_POINT('Ctrl Pts',(2.36142199806814,0.872635317323264,0.66916271832655));
#38015=CARTESIAN_POINT('Origin',(0.,0.,-2.20842344717744));
#38016=CARTESIAN_POINT('',(3.07504124793238,-0.00259082838863623,1.29157655282254));
#38017=CARTESIAN_POINT('Ctrl Pts',(-1.87460960294492,2.44013607231272,0.645925936011554));
#38018=CARTESIAN_POINT('Ctrl Pts',(-2.59108721142439,1.88105535536774,0.693142492280968));
#38019=CARTESIAN_POINT('Ctrl Pts',(-3.57302986143905,-0.0172401031001995,
0.793148684478441));
#38020=CARTESIAN_POINT('Ctrl Pts',(-2.05206621173493,-2.99393512365163,
0.945944512603972));
#38021=CARTESIAN_POINT('Ctrl Pts',(1.39399303947859,-3.35125838105565,1.10431342038815));
#38022=CARTESIAN_POINT('Ctrl Pts',(2.97699768626307,-1.39003409856734,1.219524100461));
#38023=CARTESIAN_POINT('Ctrl Pts',(3.076708517471,-0.188292403425034,1.2819451446058));
#38024=CARTESIAN_POINT('Ctrl Pts',(3.07504124793238,-0.00259082838863623,
1.29157655282254));
#38025=CARTESIAN_POINT('Ctrl Pts',(3.07504124793238,-0.00259082838863623,
1.29157655282254));
#38026=CARTESIAN_POINT('Ctrl Pts',(3.06757023260577,0.829535760103501,1.33473478053386));
#38027=CARTESIAN_POINT('Ctrl Pts',(2.28975044149764,2.69180612852788,1.43068264417324));
#38028=CARTESIAN_POINT('Ctrl Pts',(-0.207342744971815,3.35541631029136,
1.54879005713849));
#38029=CARTESIAN_POINT('Ctrl Pts',(-1.53027139183725,2.69679833931267,1.62373924239242));
#38030=CARTESIAN_POINT('Ctrl Pts',(-1.86967516139566,2.43378849843609,1.64589879171829));
#38031=CARTESIAN_POINT('',(3.07349937966369,0.00195274342530456,1.20842344721377));
#38032=CARTESIAN_POINT('Ctrl Pts',(3.07349937966369,0.00195274342531009,
1.20842344721377));
#38033=CARTESIAN_POINT('Ctrl Pts',(3.07343009793609,0.110997968751781,1.21404815002136));
#38034=CARTESIAN_POINT('Ctrl Pts',(3.06755350611745,0.219823458127608,1.21967285282894));
#38035=CARTESIAN_POINT('Ctrl Pts',(3.05596382899217,0.327852597811126,1.22529755563653));
#38036=CARTESIAN_POINT('Ctrl Pts',(3.0443228227567,0.436360183922003,1.230947169491));
#38037=CARTESIAN_POINT('Ctrl Pts',(3.02691813728145,0.544064148491547,1.23659678334547));
#38038=CARTESIAN_POINT('Ctrl Pts',(3.0038949192498,0.650398004382886,1.24224639719993));
#38039=CARTESIAN_POINT('Ctrl Pts',(2.98074448250616,0.757319426103119,1.24792722895786));
#38040=CARTESIAN_POINT('Ctrl Pts',(2.95191336117846,0.862855358188295,1.25360806071578));
#38041=CARTESIAN_POINT('Ctrl Pts',(2.91759746433215,0.96645087103411,1.2592888924737));
#38042=CARTESIAN_POINT('Ctrl Pts',(2.90216890839473,1.01302780218549,1.26184301574027));
#38043=CARTESIAN_POINT('Ctrl Pts',(2.88563227776604,1.05921278948065,1.26439713900684));
#38044=CARTESIAN_POINT('Ctrl Pts',(2.86800844378224,1.10495692965552,1.2669512622734));
#38045=CARTESIAN_POINT('Ctrl Pts',(2.83350913215343,1.19450278832257,1.27195105372586));
#38046=CARTESIAN_POINT('Ctrl Pts',(2.79475151626034,1.28258851739022,1.27695084517831));
#38047=CARTESIAN_POINT('Ctrl Pts',(2.75187964773997,1.36878071814098,1.28195063663076));
#38048=CARTESIAN_POINT('Ctrl Pts',(2.70906591298316,1.45485604325297,1.28694364842317));
#38049=CARTESIAN_POINT('Ctrl Pts',(2.66214920708533,1.53904255338566,1.29193666021558));
#38050=CARTESIAN_POINT('Ctrl Pts',(2.61132227195232,1.62092511918526,1.29692967200798));
#38051=CARTESIAN_POINT('Ctrl Pts',(2.56054893723817,1.70272133431641,1.30191741833391));
#38052=CARTESIAN_POINT('Ctrl Pts',(2.50587380102546,1.78221806423109,1.30690516465983));
#38053=CARTESIAN_POINT('Ctrl Pts',(2.44753583352583,1.8590240971023,1.31189291098575));
#38054=CARTESIAN_POINT('Ctrl Pts',(2.38923958960003,1.93577519795718,1.31687709005332));
#38055=CARTESIAN_POINT('Ctrl Pts',(2.32728598690376,2.009839078879,1.32186126912088));
#38056=CARTESIAN_POINT('Ctrl Pts',(2.26195713196696,2.08085371497946,1.32684544818845));
#38057=CARTESIAN_POINT('Ctrl Pts',(2.1966520569979,2.15184250146479,1.33182781299465));
#38058=CARTESIAN_POINT('Ctrl Pts',(2.12797446775194,2.21978392577767,1.33681017780085));
#38059=CARTESIAN_POINT('Ctrl Pts',(2.05624592462546,2.28435000546352,1.34179254260705));
#38060=CARTESIAN_POINT('Ctrl Pts',(1.98452391546502,2.34891020363341,1.34677445355484));
#38061=CARTESIAN_POINT('Ctrl Pts',(1.90975183131845,2.41009537498492,1.35175636450264));
#38062=CARTESIAN_POINT('Ctrl Pts',(1.83228637233234,2.4676160357246,1.35673827545043));
#38063=CARTESIAN_POINT('Ctrl Pts',(1.75480682901544,2.52514715454488,1.36172109218104));
#38064=CARTESIAN_POINT('Ctrl Pts',(1.67463329072286,2.57901217792974,1.36670390891165));
#38065=CARTESIAN_POINT('Ctrl Pts',(1.59215277132944,2.62896401701278,1.37168672564226));
#38066=CARTESIAN_POINT('Ctrl Pts',(1.50958338360504,2.67896967652034,1.37667491109036));
#38067=CARTESIAN_POINT('Ctrl Pts',(1.42470242845596,2.72505350663459,1.38166309653845));
#38068=CARTESIAN_POINT('Ctrl Pts',(1.33792274537938,2.76701372916661,1.38665128198655));
#38069=CARTESIAN_POINT('Ctrl Pts',(1.25109181275541,2.80899873218107,1.39164241331134));
#38070=CARTESIAN_POINT('Ctrl Pts',(1.16236032294793,2.84685510639286,1.39663354463613));
#38071=CARTESIAN_POINT('Ctrl Pts',(1.07216040699722,2.88042953596639,1.40162467596093));
#38072=CARTESIAN_POINT('Ctrl Pts',(0.981814800859125,2.91405819469174,1.40662386892137));
#38073=CARTESIAN_POINT('Ctrl Pts',(0.889996450440418,2.94339096524173,1.41162306188182));
#38074=CARTESIAN_POINT('Ctrl Pts',(0.797151859972865,2.96832463894059,1.41662225484226));
#38075=CARTESIAN_POINT('Ctrl Pts',(0.743306210453191,2.98278503828606,1.41952155991403));
#38076=CARTESIAN_POINT('Ctrl Pts',(0.689115582699021,2.99576676899764,1.42242086498581));
#38077=CARTESIAN_POINT('Ctrl Pts',(0.634668086571051,3.00725766602868,1.42532017005758));
#38078=CARTESIAN_POINT('Ctrl Pts',(0.54076914544621,3.02707461153619,1.43032024711525));
#38079=CARTESIAN_POINT('Ctrl Pts',(0.445776314329343,3.04252426601338,1.43532032417293));
#38080=CARTESIAN_POINT('Ctrl Pts',(0.350131646875332,3.05349145730856,1.44032040123061));
#38081=CARTESIAN_POINT('Ctrl Pts',(0.252673050139253,3.06466664461609,1.44541530622202));
#38082=CARTESIAN_POINT('Ctrl Pts',(0.154538065542236,3.07118742824564,1.45051021121343));
#38083=CARTESIAN_POINT('Ctrl Pts',(0.0562082719914919,3.07298598762828,
1.45560511620484));
#38084=CARTESIAN_POINT('Ctrl Pts',(-0.0400396967687125,3.0747464681604,
1.46059215257238));
#38085=CARTESIAN_POINT('Ctrl Pts',(-0.136473842897125,3.07198268032219,
1.46557918893991));
#38086=CARTESIAN_POINT('Ctrl Pts',(-0.232636021868556,3.06468313718224,
1.47056622530744));
#38087=CARTESIAN_POINT('Ctrl Pts',(-0.328734310230141,3.05738844389353,
1.47554994826425));
#38088=CARTESIAN_POINT('Ctrl Pts',(-0.42456055420376,3.04556401678089,1.48053367122106));
#38089=CARTESIAN_POINT('Ctrl Pts',(-0.519657669423997,3.02925042817672,
1.48551739417788));
#38090=CARTESIAN_POINT('Ctrl Pts',(-0.614717560680323,3.0129432252177,1.49049916635076));
#38091=CARTESIAN_POINT('Ctrl Pts',(-0.709048458548368,2.99215042840172,
1.49548093852365));
#38092=CARTESIAN_POINT('Ctrl Pts',(-0.802200520997021,2.96696420169036,
1.50046271069654));
#38093=CARTESIAN_POINT('Ctrl Pts',(-0.899020846212493,2.94078615906797,
1.5056406615572));
#38094=CARTESIAN_POINT('Ctrl Pts',(-0.994567082253931,2.9098616152258,1.51081861241787));
#38095=CARTESIAN_POINT('Ctrl Pts',(-1.08834928517019,2.87435176752421,1.51599656327853));
#38096=CARTESIAN_POINT('Ctrl Pts',(-1.17861656379949,2.84017281654109,1.52098044634519));
#38097=CARTESIAN_POINT('Ctrl Pts',(-1.26724926143468,2.80174633023389,1.52596432941184));
#38098=CARTESIAN_POINT('Ctrl Pts',(-1.35383047369533,2.75926535485333,1.5309482124785));
#38099=CARTESIAN_POINT('Ctrl Pts',(-1.44044177501539,2.71676961630928,1.53593382756473));
#38100=CARTESIAN_POINT('Ctrl Pts',(-1.52499978465994,2.67021679040478,1.54091944265095));
#38101=CARTESIAN_POINT('Ctrl Pts',(-1.60711276316665,2.61984557111042,1.54590505773717));
#38102=CARTESIAN_POINT('Ctrl Pts',(-1.68930742471596,2.56942424433577,1.55089563233427));
#38103=CARTESIAN_POINT('Ctrl Pts',(-1.76905183814869,2.5151771894122,1.55588620693136));
#38104=CARTESIAN_POINT('Ctrl Pts',(-1.84598423370511,2.45738569600137,1.56087678152846));
#38105=CARTESIAN_POINT('Ctrl Pts',(-1.85482935887853,2.45074125201285,1.56145056136047));
#38106=CARTESIAN_POINT('Ctrl Pts',(-1.86363734989752,2.44404999788814,1.56202434119248));
#38107=CARTESIAN_POINT('Ctrl Pts',(-1.87240768645123,2.4373123939533,1.56259812102449));
#38108=CARTESIAN_POINT('Ctrl Pts',(-1.87240768645124,2.43731239395329,0.562647869306095));
#38109=CARTESIAN_POINT('Ctrl Pts',(-1.94905896554419,2.37842685900668,0.567639530215172));
#38110=CARTESIAN_POINT('Ctrl Pts',(-2.02291441462503,2.31593375215335,0.57263119112425));
#38111=CARTESIAN_POINT('Ctrl Pts',(-2.09362883246835,2.25013789840917,0.577622852033327));
#38112=CARTESIAN_POINT('Ctrl Pts',(-2.16441886594012,2.18427168850591,0.582619850574929));
#38113=CARTESIAN_POINT('Ctrl Pts',(-2.23206084063887,2.11509597791773,0.587616849116532));
#38114=CARTESIAN_POINT('Ctrl Pts',(-2.29624594476156,2.04295296352268,0.592613847658134));
#38115=CARTESIAN_POINT('Ctrl Pts',(-2.36046719375466,1.97076932288044,0.597613660183871));
#38116=CARTESIAN_POINT('Ctrl Pts',(-2.42122742015232,1.89561539037743,0.602613472709608));
#38117=CARTESIAN_POINT('Ctrl Pts',(-2.47825904536878,1.81786532890855,0.607613285235344));
#38118=CARTESIAN_POINT('Ctrl Pts',(-2.5353854370201,1.73998607427524,0.612621405685083));
#38119=CARTESIAN_POINT('Ctrl Pts',(-2.58877061037479,1.6595024385294,0.617629526134822));
#38120=CARTESIAN_POINT('Ctrl Pts',(-2.63819110377384,1.57681639703821,0.622637646584561));
#38121=CARTESIAN_POINT('Ctrl Pts',(-2.67384110789506,1.51716993223815,0.626250308101941));
#38122=CARTESIAN_POINT('Ctrl Pts',(-2.70742899249457,1.45637798245718,0.629862969619322));
#38123=CARTESIAN_POINT('Ctrl Pts',(-2.73888636901132,1.39459804518865,0.633475631136703));
#38124=CARTESIAN_POINT('Ctrl Pts',(-2.78236147074177,1.30921619345601,0.638468445044824));
#38125=CARTESIAN_POINT('Ctrl Pts',(-2.82191856036241,1.22164556821355,0.643461258952946));
#38126=CARTESIAN_POINT('Ctrl Pts',(-2.85733111600709,1.13228138883303,0.648454072861068));
#38127=CARTESIAN_POINT('Ctrl Pts',(-2.89269493641044,1.04304019365317,0.653440015590695));
#38128=CARTESIAN_POINT('Ctrl Pts',(-2.92392539698329,0.952010755250424,
0.658425958320322));
#38129=CARTESIAN_POINT('Ctrl Pts',(-2.95084203474825,0.859612433578535,
0.66341190104995));
#38130=CARTESIAN_POINT('Ctrl Pts',(-2.97772980731311,0.767313199172595,
0.668392496892055));
#38131=CARTESIAN_POINT('Ctrl Pts',(-3.00031283028168,0.673648419926478,
0.673373092734159));
#38132=CARTESIAN_POINT('Ctrl Pts',(-3.018459279418,0.579055980450372,0.678353688576264));
#38133=CARTESIAN_POINT('Ctrl Pts',(-3.03659239523886,0.484533043874101,
0.683330624867396));
#38134=CARTESIAN_POINT('Ctrl Pts',(-3.0502953346203,0.389084233159763,0.688307561158528));
#38135=CARTESIAN_POINT('Ctrl Pts',(-3.05948678636867,0.29316011672043,0.693284497449659));
#38136=CARTESIAN_POINT('Ctrl Pts',(-3.0686747867071,0.197272019993435,0.698259564890494));
#38137=CARTESIAN_POINT('Ctrl Pts',(-3.07335462310795,0.100909409968239,
0.703234632331328));
#38138=CARTESIAN_POINT('Ctrl Pts',(-3.07349666230747,0.00452954576419626,
0.708209699772163));
#38139=CARTESIAN_POINT('Ctrl Pts',(-3.07363868723893,-0.0918406369259107,
0.71318426745939));
#38140=CARTESIAN_POINT('Ctrl Pts',(-3.06924382066654,-0.188227630029704,
0.718158835146618));
#38141=CARTESIAN_POINT('Ctrl Pts',(-3.06033455102816,-0.2841736894634,0.723133402833845));
#38142=CARTESIAN_POINT('Ctrl Pts',(-3.05142372585751,-0.380136500796889,
0.72810883906596));
#38143=CARTESIAN_POINT('Ctrl Pts',(-3.03799697319906,-0.475657787148692,
0.733084275298076));
#38144=CARTESIAN_POINT('Ctrl Pts',(-3.02012858349012,-0.570285533032338,
0.738059711530191));
#38145=CARTESIAN_POINT('Ctrl Pts',(-3.00224095756202,-0.665015150438181,
0.743040504069357));
#38146=CARTESIAN_POINT('Ctrl Pts',(-2.97990223035542,-0.758848873551352,
0.748021296608524));
#38147=CARTESIAN_POINT('Ctrl Pts',(-2.9532376668212,-0.851345719005196,
0.753002089147691));
#38148=CARTESIAN_POINT('Ctrl Pts',(-2.92655742970267,-0.943896934638524,
0.757985809425452));
#38149=CARTESIAN_POINT('Ctrl Pts',(-2.89554643530498,-1.03510929134487,
0.762969529703214));
#38150=CARTESIAN_POINT('Ctrl Pts',(-2.86037889876275,-1.12455982744931,
0.767953249980975));
#38151=CARTESIAN_POINT('Ctrl Pts',(-2.82515416180484,-1.21415585591263,
0.772945076338932));
#38152=CARTESIAN_POINT('Ctrl Pts',(-2.78575956342682,-1.30198394035763,
0.777936902696889));
#38153=CARTESIAN_POINT('Ctrl Pts',(-2.74241620542279,-1.38764390469402,
0.782928729054846));
#38154=CARTESIAN_POINT('Ctrl Pts',(-2.71661127878151,-1.43864247050864,
0.785900665676857));
#38155=CARTESIAN_POINT('Ctrl Pts',(-2.68940756252767,-1.48887304044717,
0.788872602298868));
#38156=CARTESIAN_POINT('Ctrl Pts',(-2.66085892417018,-1.53825616711389,
0.791844538920878));
#38157=CARTESIAN_POINT('Ctrl Pts',(-2.61281902951214,-1.62135505867035,
0.79684553127869));
#38158=CARTESIAN_POINT('Ctrl Pts',(-2.56079859453099,-1.70234671456233,
0.8018465236365));
#38159=CARTESIAN_POINT('Ctrl Pts',(-2.50500764161483,-1.78082536073903,
0.806847515994311));
#38160=CARTESIAN_POINT('Ctrl Pts',(-2.44929226877616,-1.85919769179027,
0.81184173350118));
#38161=CARTESIAN_POINT('Ctrl Pts',(-2.38981678184086,-1.93506342472989,
0.81683595100805));
#38162=CARTESIAN_POINT('Ctrl Pts',(-2.32683644438054,-2.00804243259511,
0.821830168514919));
#38163=CARTESIAN_POINT('Ctrl Pts',(-2.26392246891729,-2.08094454292532,
0.826819123645293));
#38164=CARTESIAN_POINT('Ctrl Pts',(-2.19751126966771,-2.15096564470491,
0.831808078775667));
#38165=CARTESIAN_POINT('Ctrl Pts',(-2.12790003961761,-2.21775644997267,
0.836797033906041));
#38166=CARTESIAN_POINT('Ctrl Pts',(-2.05833859131106,-2.28449949049418,
0.841782421237301));
#38167=CARTESIAN_POINT('Ctrl Pts',(-1.9855819772832,-2.34801652415295,0.84676780856856));
#38168=CARTESIAN_POINT('Ctrl Pts',(-1.9099654452319,-2.40799382225539,0.851753195899819));
#38169=CARTESIAN_POINT('Ctrl Pts',(-1.83437644348645,-2.46794928395095,
0.856736768161883));
#38170=CARTESIAN_POINT('Ctrl Pts',(-1.75592993590305,-2.52436729840681,
0.861720340423947));
#38171=CARTESIAN_POINT('Ctrl Pts',(-1.6749948327486,-2.57697391532501,0.866703912686011));
#38172=CARTESIAN_POINT('Ctrl Pts',(-1.59406713818946,-2.6295757167661,0.871687028764434));
#38173=CARTESIAN_POINT('Ctrl Pts',(-1.51065166887184,-2.67836657542674,
0.876670144842856));
#38174=CARTESIAN_POINT('Ctrl Pts',(-1.42514604412366,-2.72311604653909,
0.881653260921278));
#38175=CARTESIAN_POINT('Ctrl Pts',(-1.33962494296209,-2.76787361725092,
0.886637278937609));
#38176=CARTESIAN_POINT('Ctrl Pts',(-1.25201332369129,-2.80858814429552,
0.891621296953941));
#38177=CARTESIAN_POINT('Ctrl Pts',(-1.16273214328596,-2.84507578334385,
0.896605314970273));
#38178=CARTESIAN_POINT('Ctrl Pts',(-1.07335502862711,-2.88160262902452,
0.901594688404685));
#38179=CARTESIAN_POINT('Ctrl Pts',(-0.982305178048635,-2.91389335302891,
0.906584061839098));
#38180=CARTESIAN_POINT('Ctrl Pts',(-0.890021999705784,-2.94181289174545,
0.911573435273511));
#38181=CARTESIAN_POINT('Ctrl Pts',(-0.797684441172705,-2.96974888275431,
0.916565748822053));
#38182=CARTESIAN_POINT('Ctrl Pts',(-0.704112532915942,-2.99330845238699,
0.921558062370594));
#38183=CARTESIAN_POINT('Ctrl Pts',(-0.609757194458012,-3.01240741165711,
0.926550375919135));
#38184=CARTESIAN_POINT('Ctrl Pts',(-0.515249884375504,-3.03153713230137,
0.931550730242187));
#38185=CARTESIAN_POINT('Ctrl Pts',(-0.419957057788829,-3.04619183021403,
0.936551084565239));
#38186=CARTESIAN_POINT('Ctrl Pts',(-0.324336030925877,-3.05633905007989,
0.94155143888829));
#38187=CARTESIAN_POINT('Ctrl Pts',(-0.269121938175487,-3.06219832138468,
0.94443877482721));
#38188=CARTESIAN_POINT('Ctrl Pts',(-0.213798459573521,-3.0665556748148,
0.94732611076613));
#38189=CARTESIAN_POINT('Ctrl Pts',(-0.158453405166694,-3.06941277256596,
0.950213446705049));
#38190=CARTESIAN_POINT('Ctrl Pts',(-0.0626027152455783,-3.07436090738228,
0.955213950268477));
#38191=CARTESIAN_POINT('Ctrl Pts',(0.0336475200514081,-3.07482359536837,
0.960214453831906));
#38192=CARTESIAN_POINT('Ctrl Pts',(0.129842654367104,-3.07075611781641,
0.965214957395334));
#38193=CARTESIAN_POINT('Ctrl Pts',(0.225907730009681,-3.06669413961468,
0.970208700129714));
#38194=CARTESIAN_POINT('Ctrl Pts',(0.321917418088531,-3.05811418728265,
0.975202442864094));
#38195=CARTESIAN_POINT('Ctrl Pts',(0.417413958539367,-3.04502345429662,
0.980196185598474));
#38196=CARTESIAN_POINT('Ctrl Pts',(0.512810145125333,-3.03194647788902,
0.985184680588997));
#38197=CARTESIAN_POINT('Ctrl Pts',(0.607693823691037,-3.01436820348801,
0.990173175579519));
#38198=CARTESIAN_POINT('Ctrl Pts',(0.701610279724667,-2.99234778483128,
0.995161670570041));
#38199=CARTESIAN_POINT('Ctrl Pts',(0.795460017432848,-2.97034300949758,
1.00014662172973));
#38200=CARTESIAN_POINT('Ctrl Pts',(0.888343472603172,-2.94390246317094,
1.00513157288943));
#38201=CARTESIAN_POINT('Ctrl Pts',(0.979815043976995,-2.91313657928981,
1.01011652404912));
#38202=CARTESIAN_POINT('Ctrl Pts',(1.07125358537939,-2.88238180483045,1.01509967516546));
#38203=CARTESIAN_POINT('Ctrl Pts',(1.16128084051803,-2.8473049358334,1.02008282628179));
#38204=CARTESIAN_POINT('Ctrl Pts',(1.24946625528609,-2.80806629674254,1.02506597739813));
#38205=CARTESIAN_POINT('Ctrl Pts',(1.33764387342051,-2.76883112681145,1.03004868794497));
#38206=CARTESIAN_POINT('Ctrl Pts',(1.42397957415623,-2.72543509689045,1.03503139849181));
#38207=CARTESIAN_POINT('Ctrl Pts',(1.50806367453896,-2.67808629501293,1.04001410903866));
#38208=CARTESIAN_POINT('Ctrl Pts',(1.59216326892317,-2.63072876827062,1.04499773773916));
#38209=CARTESIAN_POINT('Ctrl Pts',(1.67401005665726,-2.57941723830154,1.04998136643966));
#38210=CARTESIAN_POINT('Ctrl Pts',(1.75322074687176,-2.52440473433609,1.05496499514017));
#38211=CARTESIAN_POINT('Ctrl Pts',(1.83251699190992,-2.46933281181154,1.05995400661758));
#38212=CARTESIAN_POINT('Ctrl Pts',(1.90917109423952,-2.41055218556782,1.064943018095));
#38213=CARTESIAN_POINT('Ctrl Pts',(1.98283064243665,-2.34835791424865,1.06993202957242));
#38214=CARTESIAN_POINT('Ctrl Pts',(2.0565338198878,-2.28612680466847,1.074923996089));
#38215=CARTESIAN_POINT('Ctrl Pts',(2.12723859006732,-2.22047832237597,1.07991596260557));
#38216=CARTESIAN_POINT('Ctrl Pts',(2.19462895830496,-2.15174486995305,1.08490792912214));
#38217=CARTESIAN_POINT('Ctrl Pts',(2.26212824199178,-2.08290033140552,1.089907963591));
#38218=CARTESIAN_POINT('Ctrl Pts',(2.32630213572037,-2.01096119419358,1.09490799805986));
#38219=CARTESIAN_POINT('Ctrl Pts',(2.38687456445779,-1.93629338261133,1.09990803252872));
#38220=CARTESIAN_POINT('Ctrl Pts',(2.42190263956881,-1.89311417109553,1.10279947318222));
#38221=CARTESIAN_POINT('Ctrl Pts',(2.45572713142748,-1.84902302175565,1.10569091383573));
#38222=CARTESIAN_POINT('Ctrl Pts',(2.48830145039687,-1.80409482620865,1.10858235448924));
#38223=CARTESIAN_POINT('Ctrl Pts',(2.54499894872664,-1.72589468657169,1.11361507525852));
#38224=CARTESIAN_POINT('Ctrl Pts',(2.59810577807862,-1.64488241326908,1.11864779602781));
#38225=CARTESIAN_POINT('Ctrl Pts',(2.6473333336295,-1.56141873648747,1.1236805167971));
#38226=CARTESIAN_POINT('Ctrl Pts',(2.69649239275006,-1.47807119311645,1.12870623491506));
#38227=CARTESIAN_POINT('Ctrl Pts',(2.74178268845003,-1.39227939287324,1.13373195303301));
#38228=CARTESIAN_POINT('Ctrl Pts',(2.78295729814532,-1.30443509869204,1.13875767115097));
#38229=CARTESIAN_POINT('Ctrl Pts',(2.82408534728155,-1.21669013950095,1.14377770614899));
#38230=CARTESIAN_POINT('Ctrl Pts',(2.8611067804729,-1.12689768830382,1.14879774114701));
#38231=CARTESIAN_POINT('Ctrl Pts',(2.89381975642089,-1.03547547887341,1.15381777614503));
#38232=CARTESIAN_POINT('Ctrl Pts',(2.92650203182348,-0.944139067558604,
1.15883309992959));
#38233=CARTESIAN_POINT('Ctrl Pts',(2.95488374949979,-0.851176345363529,
1.16384842371416));
#38234=CARTESIAN_POINT('Ctrl Pts',(2.97881094644113,-0.757025491884187,
1.16886374749872));
#38235=CARTESIAN_POINT('Ctrl Pts',(3.00272483622375,-0.662927000591433,
1.17387628200088));
#38236=CARTESIAN_POINT('Ctrl Pts',(3.02218902592584,-0.567642109118777,
1.17888881650303));
#38237=CARTESIAN_POINT('Ctrl Pts',(3.03709946663982,-0.471623875282121,
1.18390135100518));
#38238=CARTESIAN_POINT('Ctrl Pts',(3.05200762896964,-0.375620313474767,
1.18891311956892));
#38239=CARTESIAN_POINT('Ctrl Pts',(3.06236335379107,-0.278884057045305,
1.19392488813267));
#38240=CARTESIAN_POINT('Ctrl Pts',(3.06811389854472,-0.181877309075922,
1.19893665669641));
#38241=CARTESIAN_POINT('Ctrl Pts',(3.0717423058648,-0.120669195843547,1.20209892019009));
#38242=CARTESIAN_POINT('Ctrl Pts',(3.0735383305219,-0.0593535603866601,
1.20526118368377));
#38243=CARTESIAN_POINT('Ctrl Pts',(3.07349937966414,0.00195274272110892,
1.20842344717745));
#38244=CARTESIAN_POINT('Origin',(3.42660592399111E-16,1.36827403442078E-16,
19.));
#38245=CARTESIAN_POINT('Ctrl Pts',(1.91346599666504,1.63598720337497,19.));
#38246=CARTESIAN_POINT('Ctrl Pts',(1.97549316674761,1.57769689441576,19.));
#38247=CARTESIAN_POINT('Ctrl Pts',(2.0341596855751,1.51616828548999,19.));
#38248=CARTESIAN_POINT('Ctrl Pts',(2.08945330857753,1.45177509691646,19.));
#38249=CARTESIAN_POINT('Ctrl Pts',(2.14629304460953,1.38558135445508,19.));
#38250=CARTESIAN_POINT('Ctrl Pts',(2.19956910898861,1.31636012908618,19.));
#38251=CARTESIAN_POINT('Ctrl Pts',(2.24923921204997,1.24447092433007,19.));
#38252=CARTESIAN_POINT('Ctrl Pts',(2.26226627213726,1.22561642368954,19.));
#38253=CARTESIAN_POINT('Ctrl Pts',(2.27504511769678,1.20657818234704,19.));
#38254=CARTESIAN_POINT('Ctrl Pts',(2.28757460208665,1.18736224336636,19.));
#38255=CARTESIAN_POINT('Ctrl Pts',(2.29767202536097,1.17187625340348,19.));
#38256=CARTESIAN_POINT('Ctrl Pts',(2.30760787575165,1.15627404914224,19.));
#38257=CARTESIAN_POINT('Ctrl Pts',(2.3173728786525,1.14057310445739,19.));
#38258=CARTESIAN_POINT('Ctrl Pts',(2.36626838236995,1.06195504289599,19.));
#38259=CARTESIAN_POINT('Ctrl Pts',(2.41093732554403,0.980784092604621,19.));
#38260=CARTESIAN_POINT('Ctrl Pts',(2.45134078885768,0.897488002841355,19.));
#38261=CARTESIAN_POINT('Ctrl Pts',(2.49174425217133,0.814191913078089,19.));
#38262=CARTESIAN_POINT('Ctrl Pts',(2.52788268151298,0.728769767807054,19.));
#38263=CARTESIAN_POINT('Ctrl Pts',(2.55967588129444,0.641608270327732,19.));
#38264=CARTESIAN_POINT('Ctrl Pts',(2.56709861757521,0.621258736022559,19.));
#38265=CARTESIAN_POINT('Ctrl Pts',(2.57428579191308,0.600809491436937,19.));
#38266=CARTESIAN_POINT('Ctrl Pts',(2.58122657684236,0.580294271376261,19.));
#38267=CARTESIAN_POINT('Ctrl Pts',(2.61095617640783,0.492421028851814,19.));
#38268=CARTESIAN_POINT('Ctrl Pts',(2.63620257234987,0.403252571641342,19.));
#38269=CARTESIAN_POINT('Ctrl Pts',(2.65693219715155,0.313192377058794,19.));
#38270=CARTESIAN_POINT('Ctrl Pts',(2.67785890801516,0.222275938851151,19.));
#38271=CARTESIAN_POINT('Ctrl Pts',(2.69418301617952,0.130449883986704,19.));
#38272=CARTESIAN_POINT('Ctrl Pts',(2.70582812757014,0.0380961537513598,
19.));
#38273=CARTESIAN_POINT('Ctrl Pts',(2.7173871594921,-0.053574907185146,19.));
#38274=CARTESIAN_POINT('Ctrl Pts',(2.72433645988727,-0.145766797275223,
19.));
#38275=CARTESIAN_POINT('Ctrl Pts',(2.72655438838951,-0.238125122553047,
19.));
#38276=CARTESIAN_POINT('Ctrl Pts',(2.72766307746563,-0.284292826435247,
19.));
#38277=CARTESIAN_POINT('Ctrl Pts',(2.72758874267574,-0.330502332613507,
19.));
#38278=CARTESIAN_POINT('Ctrl Pts',(2.7263113205947,-0.376710079492555,19.));
#38279=CARTESIAN_POINT('Ctrl Pts',(2.72590026760623,-0.391578956997802,
19.));
#38280=CARTESIAN_POINT('Ctrl Pts',(2.72536453099617,-0.406449511013278,
19.));
#38281=CARTESIAN_POINT('Ctrl Pts',(2.72470363155247,-0.421314426811493,
19.));
#38282=CARTESIAN_POINT('Ctrl Pts',(2.72044884926157,-0.517012768060392,
19.));
#38283=CARTESIAN_POINT('Ctrl Pts',(2.71102631571702,-0.612146448503198,
19.));
#38284=CARTESIAN_POINT('Ctrl Pts',(2.69637150956148,-0.706317860645507,
19.));
#38285=CARTESIAN_POINT('Ctrl Pts',(2.69188202618866,-0.735167166772145,
19.));
#38286=CARTESIAN_POINT('Ctrl Pts',(2.68690115838408,-0.763926315013593,
19.));
#38287=CARTESIAN_POINT('Ctrl Pts',(2.68142612955932,-0.792584206033749,
19.));
#38288=CARTESIAN_POINT('Ctrl Pts',(2.66426531149033,-0.882408911944773,
19.));
#38289=CARTESIAN_POINT('Ctrl Pts',(2.64225376298974,-0.971238746161415,
19.));
#38290=CARTESIAN_POINT('Ctrl Pts',(2.6156937144733,-1.05884271791686,19.));
#38291=CARTESIAN_POINT('Ctrl Pts',(2.58843258219245,-1.1487590996914,19.));
#38292=CARTESIAN_POINT('Ctrl Pts',(2.55637947329957,-1.23738475688051,19.));
#38293=CARTESIAN_POINT('Ctrl Pts',(2.51980654956128,-1.32446593606375,19.));
#38294=CARTESIAN_POINT('Ctrl Pts',(2.50496207587815,-1.35981105317639,19.0000000000001));
#38295=CARTESIAN_POINT('Ctrl Pts',(2.48937238980909,-1.39490162057123,19.));
#38296=CARTESIAN_POINT('Ctrl Pts',(2.47305333806873,-1.42972006310193,19.));
#38297=CARTESIAN_POINT('Ctrl Pts',(2.46410614090769,-1.4488098653232,19.));
#38298=CARTESIAN_POINT('Ctrl Pts',(2.45493674697894,-1.4678235108951,19.));
#38299=CARTESIAN_POINT('Ctrl Pts',(2.4455633016621,-1.48672715429945,19.));
#38300=CARTESIAN_POINT('Ctrl Pts',(2.40280960551886,-1.57294951958685,19.));
#38301=CARTESIAN_POINT('Ctrl Pts',(2.35577316937404,-1.65697997837645,19.0000000000001));
#38302=CARTESIAN_POINT('Ctrl Pts',(2.30479723925007,-1.73857029447992,19.0000000000001));
#38303=CARTESIAN_POINT('Ctrl Pts',(2.25290166294845,-1.82163256454589,19.0000000000001));
#38304=CARTESIAN_POINT('Ctrl Pts',(2.19692283851795,-1.90216661241328,19.));
#38305=CARTESIAN_POINT('Ctrl Pts',(2.13716847969409,-1.97990352796869,19.));
#38306=CARTESIAN_POINT('Ctrl Pts',(2.0767383010823,-2.05851964542366,19.));
#38307=CARTESIAN_POINT('Ctrl Pts',(2.0124462676305,-2.13427584401283,19.));
#38308=CARTESIAN_POINT('Ctrl Pts',(1.94456136809724,-2.20687471793412,19.));
#38309=CARTESIAN_POINT('Ctrl Pts',(1.90683095180258,-2.24722516043911,19.));
#38310=CARTESIAN_POINT('Ctrl Pts',(1.86798981428088,-2.28659984954058,19.));
#38311=CARTESIAN_POINT('Ctrl Pts',(1.82807845289491,-2.32494369604583,19.));
#38312=CARTESIAN_POINT('Ctrl Pts',(1.81563649922765,-2.33689699317917,19.));
#38313=CARTESIAN_POINT('Ctrl Pts',(1.8030905122664,-2.3487500864603,19.));
#38314=CARTESIAN_POINT('Ctrl Pts',(1.79044164710463,-2.36050123580217,19.));
#38315=CARTESIAN_POINT('Ctrl Pts',(1.77881491495006,-2.37130279500602,19.));
#38316=CARTESIAN_POINT('Ctrl Pts',(1.76710642618068,-2.38201336392629,19.));
#38317=CARTESIAN_POINT('Ctrl Pts',(1.75532326360259,-2.3926265773167,19.));
#38318=CARTESIAN_POINT('Ctrl Pts',(1.67947459249907,-2.46094424046239,19.));
#38319=CARTESIAN_POINT('Ctrl Pts',(1.60046191187938,-2.52529830027693,19.));
#38320=CARTESIAN_POINT('Ctrl Pts',(1.51861373809775,-2.58540650642712,19.));
#38321=CARTESIAN_POINT('Ctrl Pts',(1.43669065585186,-2.64556972435346,19.));
#38322=CARTESIAN_POINT('Ctrl Pts',(1.3519263069689,-2.70148015019673,19.));
#38323=CARTESIAN_POINT('Ctrl Pts',(1.26460510700938,-2.75282858062769,19.));
#38324=CARTESIAN_POINT('Ctrl Pts',(1.17908172869413,-2.80311981853642,19.));
#38325=CARTESIAN_POINT('Ctrl Pts',(1.09110502956105,-2.84903564783563,19.));
#38326=CARTESIAN_POINT('Ctrl Pts',(1.00090853688297,-2.89024952005485,19.));
#38327=CARTESIAN_POINT('Ctrl Pts',(0.958564568973025,-2.90959793184868,
19.));
#38328=CARTESIAN_POINT('Ctrl Pts',(0.915730940586028,-2.92790946721792,
19.));
#38329=CARTESIAN_POINT('Ctrl Pts',(0.872429800746574,-2.9451468693802,19.));
#38330=CARTESIAN_POINT('Ctrl Pts',(0.847090664778629,-2.95523392202463,
19.));
#38331=CARTESIAN_POINT('Ctrl Pts',(0.821591411205071,-2.96495310066958,
19.));
#38332=CARTESIAN_POINT('Ctrl Pts',(0.795939046661962,-2.9743059911117,19.));
#38333=CARTESIAN_POINT('Ctrl Pts',(-0.793799282532847,-2.9692229537457,
19.));
#38334=CARTESIAN_POINT('Ctrl Pts',(-0.888615130963527,-2.93453889285012,
19.));
#38335=CARTESIAN_POINT('Ctrl Pts',(-0.981388558303585,-2.89487155596002,
19.));
#38336=CARTESIAN_POINT('Ctrl Pts',(-1.07187896565258,-2.85054012617705,
19.));
#38337=CARTESIAN_POINT('Ctrl Pts',(-1.15599932688489,-2.80932939460297,
19.));
#38338=CARTESIAN_POINT('Ctrl Pts',(-1.23814690070078,-2.76408714469173,
19.));
#38339=CARTESIAN_POINT('Ctrl Pts',(-1.31810348196186,-2.71503958519401,
19.));
#38340=CARTESIAN_POINT('Ctrl Pts',(-1.35017372493085,-2.69536681873353,
19.));
#38341=CARTESIAN_POINT('Ctrl Pts',(-1.38189112492164,-2.67508161858673,
19.));
#38342=CARTESIAN_POINT('Ctrl Pts',(-1.41324046584797,-2.65419744845672,
19.));
#38343=CARTESIAN_POINT('Ctrl Pts',(-1.43613725714475,-2.63894416176093,
19.));
#38344=CARTESIAN_POINT('Ctrl Pts',(-1.45883823398285,-2.62337064619425,
19.));
#38345=CARTESIAN_POINT('Ctrl Pts',(-1.48131237055426,-2.60750044237383,
19.));
#38346=CARTESIAN_POINT('Ctrl Pts',(-1.56372381597803,-2.54930526180017,
19.));
#38347=CARTESIAN_POINT('Ctrl Pts',(-1.64317247712071,-2.48706837685107,
19.));
#38348=CARTESIAN_POINT('Ctrl Pts',(-1.71939078398944,-2.42108429282079,
19.));
#38349=CARTESIAN_POINT('Ctrl Pts',(-1.79517577692462,-2.35547533944059,
19.));
#38350=CARTESIAN_POINT('Ctrl Pts',(-1.86776755723005,-2.28616087364922,
19.));
#38351=CARTESIAN_POINT('Ctrl Pts',(-1.93685978978932,-2.21340329421133,
19.));
#38352=CARTESIAN_POINT('Ctrl Pts',(-1.94744191636753,-2.20225978521449,
19.));
#38353=CARTESIAN_POINT('Ctrl Pts',(-1.957941859472,-2.19103546959794,19.));
#38354=CARTESIAN_POINT('Ctrl Pts',(-1.96835841626289,-2.17973125176718,
19.));
#38355=CARTESIAN_POINT('Ctrl Pts',(-1.97910256215294,-2.16807152888707,
19.));
#38356=CARTESIAN_POINT('Ctrl Pts',(-1.98975557035597,-2.15632935540799,
19.));
#38357=CARTESIAN_POINT('Ctrl Pts',(-2.00030982273794,-2.14451320385199,
19.));
#38358=CARTESIAN_POINT('Ctrl Pts',(-2.06583921208678,-2.07114891731656,
19.));
#38359=CARTESIAN_POINT('Ctrl Pts',(-2.12764079549692,-1.99485340794642,
19.));
#38360=CARTESIAN_POINT('Ctrl Pts',(-2.18547080821429,-1.91590255754304,
19.));
#38361=CARTESIAN_POINT('Ctrl Pts',(-2.2427282128697,-1.83773344470661,19.));
#38362=CARTESIAN_POINT('Ctrl Pts',(-2.29609272962286,-1.75696053678876,
19.));
#38363=CARTESIAN_POINT('Ctrl Pts',(-2.34528221055344,-1.67382965172358,
19.));
#38364=CARTESIAN_POINT('Ctrl Pts',(-2.39315017704695,-1.59293214385006,
19.));
#38365=CARTESIAN_POINT('Ctrl Pts',(-2.43706464605655,-1.50980096441262,
19.));
#38366=CARTESIAN_POINT('Ctrl Pts',(-2.47671778170977,-1.42465253741248,
19.));
#38367=CARTESIAN_POINT('Ctrl Pts',(-2.4975495968377,-1.37991972472364,19.));
#38368=CARTESIAN_POINT('Ctrl Pts',(-2.51720448567013,-1.33463005646684,
19.));
#38369=CARTESIAN_POINT('Ctrl Pts',(-2.53563199193951,-1.28881469101987,
19.));
#38370=CARTESIAN_POINT('Ctrl Pts',(-2.54352364960637,-1.26919406657378,
19.));
#38371=CARTESIAN_POINT('Ctrl Pts',(-2.55119015084139,-1.24947702985283,
19.));
#38372=CARTESIAN_POINT('Ctrl Pts',(-2.558627292172,-1.22966604205277,19.));
#38373=CARTESIAN_POINT('Ctrl Pts',(-2.56380159783432,-1.21588277482774,
19.));
#38374=CARTESIAN_POINT('Ctrl Pts',(-2.56886136486992,-1.2020633573541,19.));
#38375=CARTESIAN_POINT('Ctrl Pts',(-2.57380496377742,-1.1882106589647,19.));
#38376=CARTESIAN_POINT('Ctrl Pts',(-2.60500114582706,-1.10079432343262,
19.));
#38377=CARTESIAN_POINT('Ctrl Pts',(-2.63158503259151,-1.01202802807364,
19.));
#38378=CARTESIAN_POINT('Ctrl Pts',(-2.65330350896804,-0.922133451262639,
19.));
#38379=CARTESIAN_POINT('Ctrl Pts',(-2.657652648649,-0.904132001053431,19.));
#38380=CARTESIAN_POINT('Ctrl Pts',(-2.66180651953586,-0.886085276269219,
19.));
#38381=CARTESIAN_POINT('Ctrl Pts',(-2.66576283715123,-0.867995020296969,
19.));
#38382=CARTESIAN_POINT('Ctrl Pts',(-2.68634765000717,-0.773870996417419,
19.));
#38383=CARTESIAN_POINT('Ctrl Pts',(-2.70158902014984,-0.678568135390762,
19.));
#38384=CARTESIAN_POINT('Ctrl Pts',(-2.71160493858769,-0.582507485590656,
19.));
#38385=CARTESIAN_POINT('Ctrl Pts',(-2.72162085702555,-0.486446835790551,
19.));
#38386=CARTESIAN_POINT('Ctrl Pts',(-2.72641091914393,-0.389627299878367,
19.));
#38387=CARTESIAN_POINT('Ctrl Pts',(-2.72603908754498,-0.292484286395949,
19.));
#38388=CARTESIAN_POINT('Ctrl Pts',(-2.72590978680933,-0.258703770857363,
19.));
#38389=CARTESIAN_POINT('Ctrl Pts',(-2.72515584320796,-0.224884343071014,
19.));
#38390=CARTESIAN_POINT('Ctrl Pts',(-2.72377855213201,-0.191045091866269,
19.));
#38391=CARTESIAN_POINT('Ctrl Pts',(-2.7231767189462,-0.176258395928407,
19.));
#38392=CARTESIAN_POINT('Ctrl Pts',(-2.72245573154192,-0.161467085930695,
19.));
#38393=CARTESIAN_POINT('Ctrl Pts',(-2.72161681874514,-0.146689284135826,
19.));
#38394=CARTESIAN_POINT('Ctrl Pts',(-2.71634351414503,-0.0537978054471125,
19.));
#38395=CARTESIAN_POINT('Ctrl Pts',(-2.70640974169451,0.0387150029297866,
19.));
#38396=CARTESIAN_POINT('Ctrl Pts',(-2.69194108921809,0.13047643871239,19.));
#38397=CARTESIAN_POINT('Ctrl Pts',(-2.67748555890325,0.222154652620047,
19.));
#38398=CARTESIAN_POINT('Ctrl Pts',(-2.65850296606126,0.313083812823312,
19.));
#38399=CARTESIAN_POINT('Ctrl Pts',(-2.63506963364658,0.402875196637659,
19.));
#38400=CARTESIAN_POINT('Ctrl Pts',(-2.61213985997088,0.490737053946578,
19.));
#38401=CARTESIAN_POINT('Ctrl Pts',(-2.58494807707803,0.577510266859945,
19.));
#38402=CARTESIAN_POINT('Ctrl Pts',(-2.55352582338791,0.662801815998425,
19.));
#38403=CARTESIAN_POINT('Ctrl Pts',(-2.53742957959053,0.706492939567349,
19.));
#38404=CARTESIAN_POINT('Ctrl Pts',(-2.52022262780236,0.749794726035084,
19.));
#38405=CARTESIAN_POINT('Ctrl Pts',(-2.50190563126205,0.792650359973834,
19.));
#38406=CARTESIAN_POINT('Ctrl Pts',(-2.49657257443339,0.80512792586302,19.));
#38407=CARTESIAN_POINT('Ctrl Pts',(-2.49114540403142,0.81756765143535,19.));
#38408=CARTESIAN_POINT('Ctrl Pts',(-2.48562410083644,0.829968083953126,
19.));
#38409=CARTESIAN_POINT('Ctrl Pts',(-2.47996475337123,0.84267855353951,19.));
#38410=CARTESIAN_POINT('Ctrl Pts',(-2.47421005306852,0.855339737996612,
19.));
#38411=CARTESIAN_POINT('Ctrl Pts',(-2.46836165037947,0.867947484860423,
19.));
#38412=CARTESIAN_POINT('Ctrl Pts',(-2.43086233923552,0.948786963194456,
19.));
#38413=CARTESIAN_POINT('Ctrl Pts',(-2.38949695437655,1.02747039787255,19.));
#38414=CARTESIAN_POINT('Ctrl Pts',(-2.34433717506969,1.10364922240285,18.9999999999999));
#38415=CARTESIAN_POINT('Ctrl Pts',(-2.29994053932711,1.17854072045439,19.));
#38416=CARTESIAN_POINT('Ctrl Pts',(-2.25187620865753,1.25101221296806,19.));
#38417=CARTESIAN_POINT('Ctrl Pts',(-2.20017617040085,1.32069832886965,19.));
#38418=CARTESIAN_POINT('Ctrl Pts',(-2.15008171884632,1.3882202858114,19.));
#38419=CARTESIAN_POINT('Ctrl Pts',(-2.09657342616567,1.45312762148621,18.9999999999999));
#38420=CARTESIAN_POINT('Ctrl Pts',(-2.03965286195605,1.51504773829594,19.));
#38421=CARTESIAN_POINT('Ctrl Pts',(-2.01565725834268,1.54115096828483,19.));
#38422=CARTESIAN_POINT('Ctrl Pts',(-1.99105493705542,1.5667227863261,19.));
#38423=CARTESIAN_POINT('Ctrl Pts',(-1.96584476256622,1.59173275781375,19.));
#38424=CARTESIAN_POINT('Ctrl Pts',(-1.94982433031677,1.60762596608768,19.));
#38425=CARTESIAN_POINT('Ctrl Pts',(-1.93355840885751,1.62329224800863,19.));
#38426=CARTESIAN_POINT('Ctrl Pts',(-1.91705291980301,1.6387286579029,19.));
#38427=CARTESIAN_POINT('Ctrl Pts',(-1.90925347387187,1.63408080983891,0.00248200680218311));
#38428=CARTESIAN_POINT('Ctrl Pts',(-2.45156644640155,1.00049596865414,0.0552988434666635));
#38429=CARTESIAN_POINT('Ctrl Pts',(-2.84651267184705,-0.837496618391379,
0.160905316059202));
#38430=CARTESIAN_POINT('Ctrl Pts',(-0.842979713689217,-2.8475711288532,
0.3193014245798));
#38431=CARTESIAN_POINT('Ctrl Pts',(1.92769349397626,-2.25538582349437,0.477670332363976));
#38432=CARTESIAN_POINT('Ctrl Pts',(2.94229596891705,0.387912730907106,0.636039240148151));
#38433=CARTESIAN_POINT('Ctrl Pts',(1.2760586532515,2.67973607720936,0.794408147932327));
#38434=CARTESIAN_POINT('Ctrl Pts',(-1.55272782208431,2.52904086654082,0.952777055716503));
#38435=CARTESIAN_POINT('Ctrl Pts',(-2.96686221862994,0.0746779472267705,
1.11114596350068));
#38436=CARTESIAN_POINT('Ctrl Pts',(-1.67788023304716,-2.44800315617183,
1.26951487128486));
#38437=CARTESIAN_POINT('Ctrl Pts',(1.13980404363706,-2.74016996198817,1.42788377906903));
#38438=CARTESIAN_POINT('Ctrl Pts',(2.91902120615094,-0.535853057404118,
1.5862526868532));
#38439=CARTESIAN_POINT('Ctrl Pts',(2.03872475226955,2.15671799727073,1.74462159463738));
#38440=CARTESIAN_POINT('Ctrl Pts',(-0.699046144647114,2.88428901959944,
1.90299050242156));
#38441=CARTESIAN_POINT('Ctrl Pts',(-2.79991896953276,0.984004316378271,
2.06135941020573));
#38442=CARTESIAN_POINT('Ctrl Pts',(-2.34979400265249,-1.81280940468846,
2.21972831798991));
#38443=CARTESIAN_POINT('Ctrl Pts',(0.241220755203426,-2.95797512221762,
2.37809722577408));
#38444=CARTESIAN_POINT('Ctrl Pts',(2.61246013485936,-1.40814051945854,2.53646613355826));
#38445=CARTESIAN_POINT('Ctrl Pts',(2.60349519023718,1.42464734080985,2.69483504134244));
#38446=CARTESIAN_POINT('Ctrl Pts',(0.222493933180336,2.95944302392479,2.85320394912661));
#38447=CARTESIAN_POINT('Ctrl Pts',(-2.36122086593176,1.79789963417574,3.01157285691079));
#38448=CARTESIAN_POINT('Ctrl Pts',(-2.79363469858403,-1.00170461775365,
3.16994176469496));
#38449=CARTESIAN_POINT('Ctrl Pts',(-0.680776683187599,-2.88865885771179,
3.32831067247914));
#38450=CARTESIAN_POINT('Ctrl Pts',(2.05233484485897,-2.14376506356077,3.48667958026332));
#38451=CARTESIAN_POINT('Ctrl Pts',(2.91557050223709,0.554306404036049,3.64504848804749));
#38452=CARTESIAN_POINT('Ctrl Pts',(1.12243897822204,2.74735102858266,3.80341739583167));
#38453=CARTESIAN_POINT('Ctrl Pts',(-1.6933431948019,2.4372927131013,3.96178630361584));
#38454=CARTESIAN_POINT('Ctrl Pts',(-2.96632566963744,-0.0933753863158161,
4.12015521140002));
#38455=CARTESIAN_POINT('Ctrl Pts',(-1.53669808804495,-2.5389694615051,4.27852411918419));
#38456=CARTESIAN_POINT('Ctrl Pts',(1.29301032391677,-2.67131638784702,4.43689302696837));
#38457=CARTESIAN_POINT('Ctrl Pts',(2.94466106661435,-0.369835292927075,
4.59526193475254));
#38458=CARTESIAN_POINT('Ctrl Pts',(1.91344030499105,2.26860158254042,4.75363084253672));
#38459=CARTESIAN_POINT('Ctrl Pts',(-0.861109944606757,2.84012263900151,
4.91199975032089));
#38460=CARTESIAN_POINT('Ctrl Pts',(-2.85110561212216,0.824016826100779,
5.07036865810507));
#38461=CARTESIAN_POINT('Ctrl Pts',(-2.24346785780728,-1.9428481443896,5.22873756588924));
#38462=CARTESIAN_POINT('Ctrl Pts',(0.408186457476231,-2.93959023626285,
5.38710647367343));
#38463=CARTESIAN_POINT('Ctrl Pts',(2.68794336574243,-1.2580808414982,5.54547538145759));
#38464=CARTESIAN_POINT('Ctrl Pts',(2.51872346544836,1.56966208012581,5.70384428924178));
#38465=CARTESIAN_POINT('Ctrl Pts',(0.054702479433918,2.9672907811558,5.86221319702594));
#38466=CARTESIAN_POINT('Ctrl Pts',(-2.45915776480731,1.66143011558536,6.02058210481013));
#38467=CARTESIAN_POINT('Ctrl Pts',(-2.73248704721367,-1.15815434118082,
6.1789510125943));
#38468=CARTESIAN_POINT('Ctrl Pts',(-0.516255911939875,-2.92254799354502,
6.33731992037847));
#38469=CARTESIAN_POINT('Ctrl Pts',(2.17033437291138,-2.02421729341143,6.49568882816265));
#38470=CARTESIAN_POINT('Ctrl Pts',(2.87953978655513,0.718371462986052,6.65405773594683));
#38471=CARTESIAN_POINT('Ctrl Pts',(0.965205490814753,2.80645422226833,6.812426643731));
#38472=CARTESIAN_POINT('Ctrl Pts',(-1.82852451416062,2.3375853016094,6.97079555151518));
#38473=CARTESIAN_POINT('Ctrl Pts',(-2.95629154307943,-0.261050289223455,
7.12916445929935));
#38474=CARTESIAN_POINT('Ctrl Pts',(-1.39059057686979,-2.62184377656405,
7.28753336708353));
#38475=CARTESIAN_POINT('Ctrl Pts',(1.44207312239444,-2.5938835846765,7.4459022748677));
#38476=CARTESIAN_POINT('Ctrl Pts',(2.96086850210907,-0.202644157095674,
7.60427118265188));
#38477=CARTESIAN_POINT('Ctrl Pts',(1.78202583361296,2.37322372934426,7.76264009043606));
#38478=CARTESIAN_POINT('Ctrl Pts',(-1.02041500826522,2.78685488536697,7.92100899822022));
#38479=CARTESIAN_POINT('Ctrl Pts',(-2.89315892192767,0.661391256108661,
8.07937790600442));
#38480=CARTESIAN_POINT('Ctrl Pts',(-2.12995477448807,-2.06666388167551,
8.23774681378858));
#38481=CARTESIAN_POINT('Ctrl Pts',(0.573844518103784,-2.91178800914985,
8.39611572157276));
#38482=CARTESIAN_POINT('Ctrl Pts',(2.75481586183833,-1.1039911723155,8.55448462935694));
#38483=CARTESIAN_POINT('Ctrl Pts',(2.42588307460051,1.70964857486957,8.7128535371411));
#38484=CARTESIAN_POINT('Ctrl Pts',(-0.113264208110999,2.96563284314625,
8.8712224449253));
#38485=CARTESIAN_POINT('Ctrl Pts',(-2.54921682443218,1.51963828696783,9.02959135270946));
#38486=CARTESIAN_POINT('Ctrl Pts',(-2.66258595086561,-1.3108939680385,9.18796026049363));
#38487=CARTESIAN_POINT('Ctrl Pts',(-0.350081330264974,-2.94707482147749,
9.34632916827782));
#38488=CARTESIAN_POINT('Ctrl Pts',(2.28138129735905,-1.89818500606422,9.50469807606198));
#38489=CARTESIAN_POINT('Ctrl Pts',(2.83428454760838,0.880135242093526,9.66306698384617));
#38490=CARTESIAN_POINT('Ctrl Pts',(0.804879995387632,2.85656701903027,9.82143589163034));
#38491=CARTESIAN_POINT('Ctrl Pts',(-1.95784820773308,2.23038950335204,9.97980479941452));
#38492=CARTESIAN_POINT('Ctrl Pts',(-2.93678702134196,-0.427888925381411,
10.1381737071986));
#38493=CARTESIAN_POINT('Ctrl Pts',(-1.24002834868274,-2.69631909010226,
10.2965426149829));
#38494=CARTESIAN_POINT('Ctrl Pts',(1.58651628099675,-2.50814134994797,10.4549115227671));
#38495=CARTESIAN_POINT('Ctrl Pts',(2.96759088028684,-0.0348038564676998,
10.6132804305513));
#38496=CARTESIAN_POINT('Ctrl Pts',(1.6449026935962,2.47024332197998,10.7716493383355));
#38497=CARTESIAN_POINT('Ctrl Pts',(-1.17645120171631,2.72465952206268,10.9300182461196));
#38498=CARTESIAN_POINT('Ctrl Pts',(-2.92594408011687,0.496646938192196,
11.0883871539037));
#38499=CARTESIAN_POINT('Ctrl Pts',(-2.00961844214704,-2.18385912049501,
11.2467560616879));
#38500=CARTESIAN_POINT('Ctrl Pts',(0.73766428427855,-2.87465795267654,11.4051249694722));
#38501=CARTESIAN_POINT('Ctrl Pts',(2.81286338434295,-0.946364899079276,
11.5634938772563));
#38502=CARTESIAN_POINT('Ctrl Pts',(2.32527143690989,1.84415825944458,11.7218627850405));
#38503=CARTESIAN_POINT('Ctrl Pts',(-0.280868057014231,2.95447458539345,
11.8802316928247));
#38504=CARTESIAN_POINT('Ctrl Pts',(-2.6311095410845,1.37297834068884,12.0386006006089));
#38505=CARTESIAN_POINT('Ctrl Pts',(-2.5841553368005,-1.4594341836726,12.196969508393));
#38506=CARTESIAN_POINT('Ctrl Pts',(-0.182785273090703,-2.96216077975654,
12.3553384161772));
#38507=CARTESIAN_POINT('Ctrl Pts',(2.38511988226226,-1.7660719374997,12.5137073239614));
#38508=CARTESIAN_POINT('Ctrl Pts',(2.7799497594151,1.03907953319971,12.6720762317456));
#38509=CARTESIAN_POINT('Ctrl Pts',(0.641976089983368,2.89752888528765,12.8304451395297));
#38510=CARTESIAN_POINT('Ctrl Pts',(-2.08089999073317,2.11604871629969,12.9888140473139));
#38511=CARTESIAN_POINT('Ctrl Pts',(-2.9078745866236,-0.593356831641015,
13.1471829550981));
#38512=CARTESIAN_POINT('Ctrl Pts',(-1.08549372525115,-2.76215682277935,
13.3055518628823));
#38513=CARTESIAN_POINT('Ctrl Pts',(1.72587708020246,-2.41436435635144,13.4639207706664));
#38514=CARTESIAN_POINT('Ctrl Pts',(2.96480666620496,0.133147937316626,13.6222896784505));
#38515=CARTESIAN_POINT('Ctrl Pts',(1.50251015498524,2.55934956099197,13.7806585862348));
#38516=CARTESIAN_POINT('Ctrl Pts',(-1.32871866749039,2.6537357901384,13.939027494019));
#38517=CARTESIAN_POINT('Ctrl Pts',(-2.94935606037441,0.330311626052199,
14.0973964018031));
#38518=CARTESIAN_POINT('Ctrl Pts',(-1.88284435477652,-2.29405842925977,
14.2557653095873));
#38519=CARTESIAN_POINT('Ctrl Pts',(0.899120964085925,-2.828319011924,14.4141342173715));
#38520=CARTESIAN_POINT('Ctrl Pts',(2.86189997966902,-0.785706973011972,
14.5725031251557));
#38521=CARTESIAN_POINT('Ctrl Pts',(2.21721085889867,1.97276023589046,14.7308720329398));
#38522=CARTESIAN_POINT('Ctrl Pts',(-0.447572153204858,2.93385175314142,
14.889240940724));
#38523=CARTESIAN_POINT('Ctrl Pts',(-2.70457357369761,1.22192009751584,15.0476098485082));
#38524=CARTESIAN_POINT('Ctrl Pts',(-2.49744645542791,-1.60329914345083,
15.2059787562924));
#38525=CARTESIAN_POINT('Ctrl Pts',(-0.0149036681797597,-2.96775754154435,
15.3643476640765));
#38526=CARTESIAN_POINT('Ctrl Pts',(2.48121780335728,-1.6283013070035,15.5227165718607));
#38527=CARTESIAN_POINT('Ctrl Pts',(2.71670948321466,1.19469516065056,15.6810854796449));
#38528=CARTESIAN_POINT('Ctrl Pts',(0.47701563009963,2.92920860503424,15.8394543874291));
#38529=CARTESIAN_POINT('Ctrl Pts',(-2.19728566554779,1.99492921994414,15.9978232952133));
#38530=CARTESIAN_POINT('Ctrl Pts',(-2.86964686816259,-0.756923921148106,
16.1561922029974));
#38531=CARTESIAN_POINT('Ctrl Pts',(-0.927481736461798,-2.81914609426518,
16.3145611107816));
#38532=CARTESIAN_POINT('Ctrl Pts',(1.85970904856091,-2.31285296049272,16.4729300185658));
#38533=CARTESIAN_POINT('Ctrl Pts',(2.95252484228036,0.300673089886709,16.6312989263498));
#38534=CARTESIAN_POINT('Ctrl Pts',(1.35530424736705,2.64025719880453,16.7896678341341));
#38535=CARTESIAN_POINT('Ctrl Pts',(-1.47672939037767,2.57431050652288,16.9480367419183));
#38536=CARTESIAN_POINT('Ctrl Pts',(-2.9633203037766,0.162918905759724,17.1064056497025));
#38537=CARTESIAN_POINT('Ctrl Pts',(-1.75003778792055,-2.39691019261269,
17.2647745574867));
#38538=CARTESIAN_POINT('Ctrl Pts',(1.05769572839716,-2.77291694918154,17.4231434652708));
#38539=CARTESIAN_POINT('Ctrl Pts',(2.90177163005296,-0.622537181450101,
17.581512373055));
#38540=CARTESIAN_POINT('Ctrl Pts',(2.10204164733985,2.09505231770878,17.7398812808392));
#38541=CARTESIAN_POINT('Ctrl Pts',(-0.612831269401328,2.90381172146501,
17.8982501886234));
#38542=CARTESIAN_POINT('Ctrl Pts',(-2.7693949632942,1.06698316123474,18.0566190964075));
#38543=CARTESIAN_POINT('Ctrl Pts',(-2.40269624306919,-1.74209614650769,
18.2149880041917));
#38544=CARTESIAN_POINT('Ctrl Pts',(0.152947696564397,-2.96371698990033,
18.3733569119759));
#38545=CARTESIAN_POINT('Ctrl Pts',(2.56951616178647,-1.48556313374885,18.53172581976));
#38546=CARTESIAN_POINT('Ctrl Pts',(2.64448170946715,1.34695892431768,18.6900947275442));
#38547=CARTESIAN_POINT('Ctrl Pts',(0.311071818696124,2.95059345609503,18.8484636353284));
#38548=CARTESIAN_POINT('Ctrl Pts',(-2.30768370382183,1.86919021361793,19.0068325431126));
#38549=CARTESIAN_POINT('Ctrl Pts',(-2.8201996789474,-0.922146939298692,
19.1652256218881));
#38550=CARTESIAN_POINT('Ctrl Pts',(-1.45369664976329,-2.21310559305866,
19.2708290647355));
#38551=CARTESIAN_POINT('Ctrl Pts',(-0.647946980571831,-2.42809259672558,
19.3236428716548));
#38552=CARTESIAN_POINT('Ctrl Pts',(-2.05218096726007,1.75640876541957,-0.106134133512484));
#38553=CARTESIAN_POINT('Ctrl Pts',(-2.63509170999486,1.07539350473389,-0.0533172968480037));
#38554=CARTESIAN_POINT('Ctrl Pts',(-3.0596037708826,-0.900191956661482,
0.0522891757445352));
#38555=CARTESIAN_POINT('Ctrl Pts',(-0.906085518708576,-3.06074146441173,
0.210685284265133));
#38556=CARTESIAN_POINT('Ctrl Pts',(2.0720014147868,-2.42422492568104,0.369054192049308));
#38557=CARTESIAN_POINT('Ctrl Pts',(3.1625574446187,0.416952036080915,0.527423099833484));
#38558=CARTESIAN_POINT('Ctrl Pts',(1.37158492423724,2.88034221238152,0.685792007617659));
#38559=CARTESIAN_POINT('Ctrl Pts',(-1.66896565983697,2.7183658968093,0.844160915401836));
#38560=CARTESIAN_POINT('Ctrl Pts',(-3.18896273379987,0.0802683687996882,
1.00252982318601));
#38561=CARTESIAN_POINT('Ctrl Pts',(-1.80348703130465,-2.63126167040592,
1.16089873097018));
#38562=CARTESIAN_POINT('Ctrl Pts',(1.22513023900094,-2.94530020241159,1.31926763875436));
#38563=CARTESIAN_POINT('Ctrl Pts',(3.13754032362361,-0.575967235729459,
1.47763654653853));
#38564=CARTESIAN_POINT('Ctrl Pts',(2.19134451833939,2.31817078576297,1.63600545432271));
#38565=CARTESIAN_POINT('Ctrl Pts',(-0.75137702401143,3.1002080714278,1.79437436210689));
#38566=CARTESIAN_POINT('Ctrl Pts',(-3.0095220450185,1.05766728064561,1.95274326989106));
#38567=CARTESIAN_POINT('Ctrl Pts',(-2.52570053961777,-1.94851705574079,
2.11111217767524));
#38568=CARTESIAN_POINT('Ctrl Pts',(0.259278639275,-3.17941034572717,2.26948108545941));
#38569=CARTESIAN_POINT('Ctrl Pts',(2.80802996556119,-1.51355449279358,2.42784999324359));
#38570=CARTESIAN_POINT('Ctrl Pts',(2.79839390152992,1.53129702152048,2.58621890102776));
#38571=CARTESIAN_POINT('Ctrl Pts',(0.239149919721012,3.18098813515455,2.74458780881194));
#38572=CARTESIAN_POINT('Ctrl Pts',(-2.53798282254046,1.93249113372931,2.90295671659612));
#38573=CARTESIAN_POINT('Ctrl Pts',(-3.00276733098466,-1.07669263379773,
3.06132562438029));
#38574=CARTESIAN_POINT('Ctrl Pts',(-0.731739903219251,-3.10490503740267,
3.21969453216447));
#38575=CARTESIAN_POINT('Ctrl Pts',(2.20597346800839,-2.30424819015504,3.37806343994865));
#38576=CARTESIAN_POINT('Ctrl Pts',(3.13383129860806,0.595802007413021,3.53643234773282));
#38577=CARTESIAN_POINT('Ctrl Pts',(1.20646521770984,2.95301884657881,3.694801255517));
#38578=CARTESIAN_POINT('Ctrl Pts',(-1.82010755668003,2.61974943920086,3.85317016330117));
#38579=CARTESIAN_POINT('Ctrl Pts',(-3.18838601853105,-0.100365505801211,
4.01153907108535));
#38580=CARTESIAN_POINT('Ctrl Pts',(-1.65173593337267,-2.72903775044013,
4.16990797886952));
#38581=CARTESIAN_POINT('Ctrl Pts',(1.38980560387911,-2.8712922216411,4.3282768866537));
#38582=CARTESIAN_POINT('Ctrl Pts',(3.16509959449378,-0.39752131372418,4.48664579443787));
#38583=CARTESIAN_POINT('Ctrl Pts',(2.05668122626364,2.43843002183688,4.64501470222205));
#38584=CARTESIAN_POINT('Ctrl Pts',(-0.925572986103647,3.05273537757325,
4.80338361000622));
#38585=CARTESIAN_POINT('Ctrl Pts',(-3.06454054053909,0.885703061624783,
4.9617525177904));
#38586=CARTESIAN_POINT('Ctrl Pts',(-2.41141477622409,-2.0882905485081,5.12012142557457));
#38587=CARTESIAN_POINT('Ctrl Pts',(0.438743462085874,-3.15964915971496,
5.27849033335875));
#38588=CARTESIAN_POINT('Ctrl Pts',(2.88916390187998,-1.35226128616718,5.43685924114294));
#38589=CARTESIAN_POINT('Ctrl Pts',(2.70727613086501,1.68716762333896,5.5952281489271));
#38590=CARTESIAN_POINT('Ctrl Pts',(0.0587975293445813,3.18942337869112,
5.75359705671128));
#38591=CARTESIAN_POINT('Ctrl Pts',(-2.64325131759118,1.78580545134354,5.91196596449545));
#38592=CARTESIAN_POINT('Ctrl Pts',(-2.93704214150503,-1.24485424729959,
6.07033487227964));
#38593=CARTESIAN_POINT('Ctrl Pts',(-0.554903039966712,-3.14133112775976,
6.22870378006381));
#38594=CARTESIAN_POINT('Ctrl Pts',(2.33280648883499,-2.17575102519698,6.38707268784798));
#38595=CARTESIAN_POINT('Ctrl Pts',(3.0951033088617,0.77214904355946,6.54544159563215));
#38596=CARTESIAN_POINT('Ctrl Pts',(1.0374611673368,3.01654652943803,6.70381050341633));
#38597=CARTESIAN_POINT('Ctrl Pts',(-1.96540860471453,2.51257789023753,6.86217941120051));
#38598=CARTESIAN_POINT('Ctrl Pts',(-3.17760073316836,-0.280592620295555,
7.02054831898468));
#38599=CARTESIAN_POINT('Ctrl Pts',(-1.49469075434814,-2.81811607050928,
7.17891722676886));
#38600=CARTESIAN_POINT('Ctrl Pts',(1.55002730421837,-2.78806276725866,7.33728613455304));
#38601=CARTESIAN_POINT('Ctrl Pts',(3.18252032521683,-0.217814181306611,
7.49565504233721));
#38602=CARTESIAN_POINT('Ctrl Pts',(1.91542901398523,2.55088422520114,7.65402395012139));
#38603=CARTESIAN_POINT('Ctrl Pts',(-1.09680369177055,2.99547997818629,7.81239285790555));
#38604=CARTESIAN_POINT('Ctrl Pts',(-3.10974197826028,0.710903275166445,
7.97076176568975));
#38605=CARTESIAN_POINT('Ctrl Pts',(-2.2894040572124,-2.22137518236246,8.1291306734739));
#38606=CARTESIAN_POINT('Ctrl Pts',(0.616802752664856,-3.12976564654632,
8.28749958125809));
#38607=CARTESIAN_POINT('Ctrl Pts',(2.96104250029515,-1.18663640153263,8.44586848904227));
#38608=CARTESIAN_POINT('Ctrl Pts',(2.60748567051059,1.83763356414668,8.60423739682644));
#38609=CARTESIAN_POINT('Ctrl Pts',(-0.121743212903944,3.18764132676628,
8.76260630461062));
#38610=CARTESIAN_POINT('Ctrl Pts',(-2.74005223513341,1.63339902863226,8.9209752123948));
#38611=CARTESIAN_POINT('Ctrl Pts',(-2.86190822058818,-1.40902802489031,
9.07934412017897));
#38612=CARTESIAN_POINT('Ctrl Pts',(-0.376288561364208,-3.16769404402997,
9.23771302796314));
#38613=CARTESIAN_POINT('Ctrl Pts',(2.45216643131664,-2.04028390944011,9.39608193574732));
#38614=CARTESIAN_POINT('Ctrl Pts',(3.04646024427847,0.946022525116211,9.55445084353148));
#38615=CARTESIAN_POINT('Ctrl Pts',(0.865133639963048,3.07041079059476,9.71281975131568));
#38616=CARTESIAN_POINT('Ctrl Pts',(-2.10441352270846,2.39735737082276,9.87118865909984));
#38617=CARTESIAN_POINT('Ctrl Pts',(-3.15663609498233,-0.459920864770426,
10.029557566884));
#38618=CARTESIAN_POINT('Ctrl Pts',(-1.3328573763802,-2.89816663637986,10.1879264746682));
#38619=CARTESIAN_POINT('Ctrl Pts',(1.70528353655795,-2.69590183388433,10.3462953824524));
#38620=CARTESIAN_POINT('Ctrl Pts',(3.18974594336544,-0.0374092873511558,
10.5046642902366));
#38621=CARTESIAN_POINT('Ctrl Pts',(1.76804077980663,2.65516674409297,10.6630331980207));
#38622=CARTESIAN_POINT('Ctrl Pts',(-1.26452081827374,2.92862864463024,10.8214021058049));
#38623=CARTESIAN_POINT('Ctrl Pts',(-3.14498144675684,0.533826130450403,
10.9797710135891));
#38624=CARTESIAN_POINT('Ctrl Pts',(-2.1600592979755,-2.34734370453628,11.1381399213733));
#38625=CARTESIAN_POINT('Ctrl Pts',(0.792886133318907,-3.08985601890883,
11.2965088291574));
#38626=CARTESIAN_POINT('Ctrl Pts',(3.02343548399835,-1.01721016122337,11.4548777369416));
#38627=CARTESIAN_POINT('Ctrl Pts',(2.4993422046067,1.98221269854377,11.6132466447258));
#38628=CARTESIAN_POINT('Ctrl Pts',(-0.301893954262147,3.17564775728929,
11.77161555251));
#38629=CARTESIAN_POINT('Ctrl Pts',(-2.82807547393906,1.47576005898683,11.9299844602941));
#38630=CARTESIAN_POINT('Ctrl Pts',(-2.77760625878081,-1.56868802162129,
12.0883533680783));
#38631=CARTESIAN_POINT('Ctrl Pts',(-0.196468653149268,-3.18390934329579,
12.2467222758625));
#38632=CARTESIAN_POINT('Ctrl Pts',(2.56367092897621,-1.89828080270509,12.4050911836467));
#38633=CARTESIAN_POINT('Ctrl Pts',(2.9880579316907,1.11686545065049,12.5634600914308));
#38634=CARTESIAN_POINT('Ctrl Pts',(0.690034681790139,3.11443907885885,12.721828999215));
#38635=CARTESIAN_POINT('Ctrl Pts',(-2.23667701234773,2.27445698583902,12.8801979069992));
#38636=CARTESIAN_POINT('Ctrl Pts',(-3.12555926361439,-0.637775765947956,
13.0385668147834));
#38637=CARTESIAN_POINT('Ctrl Pts',(-1.1667542280403,-2.96893300856485,13.1969357225676));
#38638=CARTESIAN_POINT('Ctrl Pts',(1.85507694200457,-2.59510465631764,13.3553046303517));
#38639=CARTESIAN_POINT('Ctrl Pts',(3.18675330188238,0.143115446183788,13.5136735381359));
#38640=CARTESIAN_POINT('Ctrl Pts',(1.61498867770692,2.75094351248282,13.6720424459201));
#38641=CARTESIAN_POINT('Ctrl Pts',(-1.42818708860966,2.85239553322103,13.8304113537043));
#38642=CARTESIAN_POINT('Ctrl Pts',(-3.17014605740068,0.355038889034663,
13.9887802614884));
#38643=CARTESIAN_POINT('Ctrl Pts',(-2.02379485074318,-2.46579257847948,
14.1471491692726));
#38644=CARTESIAN_POINT('Ctrl Pts',(0.96642952599676,-3.04004812616082,14.3055180770568));
#38645=CARTESIAN_POINT('Ctrl Pts',(3.07614297884099,-0.844525317316191,
14.463886984841));
#38646=CARTESIAN_POINT('Ctrl Pts',(2.38319216767315,2.12044187137279,14.6222558926251));
#38647=CARTESIAN_POINT('Ctrl Pts',(-0.481077587052887,3.15348109140769,
14.7806248004093));
#38648=CARTESIAN_POINT('Ctrl Pts',(-2.90703905398222,1.31339353414885,14.9389937081935));
#38649=CARTESIAN_POINT('Ctrl Pts',(-2.68440631520056,-1.72332277093709,
15.0973626159776));
#38650=CARTESIAN_POINT('Ctrl Pts',(-0.0160193628553846,-3.18992508095263,
15.2557315237618));
#38651=CARTESIAN_POINT('Ctrl Pts',(2.66696277962007,-1.7501966066458,15.414100431546));
#38652=CARTESIAN_POINT('Ctrl Pts',(2.9200834626331,1.28413052741122,15.5724693393302));
#38653=CARTESIAN_POINT('Ctrl Pts',(0.512725214631047,3.14849035534036,15.7308382471144));
#38654=CARTESIAN_POINT('Ctrl Pts',(-2.36177536622523,2.14427043461023,15.8892071548985));
#38655=CARTESIAN_POINT('Ctrl Pts',(-3.08446980256532,-0.81358755445598,
16.0475760626827));
#38656=CARTESIAN_POINT('Ctrl Pts',(-0.99691339735436,-3.03018852014659,
16.2059449704669));
#38657=CARTESIAN_POINT('Ctrl Pts',(1.99892762607284,-2.48599407598237,16.364313878251));
#38658=CARTESIAN_POINT('Ctrl Pts',(3.17355205561192,0.323181599969261,16.5226827860353));
#38659=CARTESIAN_POINT('Ctrl Pts',(1.45676287583387,2.83790792904517,16.6810516938194));
#38660=CARTESIAN_POINT('Ctrl Pts',(-1.58727795455092,2.76702444049522,16.8394206016036));
#38661=CARTESIAN_POINT('Ctrl Pts',(-3.18515566975668,0.175115081461092,
16.9977895093878));
#38662=CARTESIAN_POINT('Ctrl Pts',(-1.88104633015191,-2.57634386676597,
17.1561584171719));
#38663=CARTESIAN_POINT('Ctrl Pts',(1.13687526180957,-2.98049864241602,17.3145273249561));
#38664=CARTESIAN_POINT('Ctrl Pts',(3.11899943722691,-0.669140568639529,
17.4728962327403));
#38665=CARTESIAN_POINT('Ctrl Pts',(2.25940134198667,2.25188878829013,17.6312651405244));
#38666=CARTESIAN_POINT('Ctrl Pts',(-0.658708068058032,3.12119225071374,
17.7896340483087));
#38667=CARTESIAN_POINT('Ctrl Pts',(-2.97671299922937,1.14685795565552,17.9480029560928));
#38668=CARTESIAN_POINT('Ctrl Pts',(-2.58256306331841,-1.87251017422536,
18.106371863877));
#38669=CARTESIAN_POINT('Ctrl Pts',(0.164397423480497,-3.18558205196536,
18.2647407716612));
#38670=CARTESIAN_POINT('Ctrl Pts',(2.76187118915734,-1.59677299555207,18.4231096794454));
#38671=CARTESIAN_POINT('Ctrl Pts',(2.84244868829818,1.44779281849893,18.5814785872295));
#38672=CARTESIAN_POINT('Ctrl Pts',(0.334358781856534,3.1714760850694,18.7398474950137));
#38673=CARTESIAN_POINT('Ctrl Pts',(-2.48043784664977,2.00911855501116,18.8982164027979));
#38674=CARTESIAN_POINT('Ctrl Pts',(-3.03132097660764,-0.991179235100812,
19.0566094815733));
#38675=CARTESIAN_POINT('Ctrl Pts',(-1.56252097358454,-2.37877957995877,
19.1622129244208));
#38676=CARTESIAN_POINT('Ctrl Pts',(-0.696452555682176,-2.60986059836271,
19.2150267313402));
#38677=CARTESIAN_POINT('Ctrl Pts',(-2.19510846064826,1.87873672100023,-0.214750273827152));
#38678=CARTESIAN_POINT('Ctrl Pts',(-2.81861697358817,1.15029104081366,-0.161933437162671));
#38679=CARTESIAN_POINT('Ctrl Pts',(-3.27269486991817,-0.962887294931585,
-0.0563269645701317));
#38680=CARTESIAN_POINT('Ctrl Pts',(-0.969191323727936,-3.27391179997027,
0.102069143950466));
#38681=CARTESIAN_POINT('Ctrl Pts',(2.21630933559734,-2.59306402786772,0.260438051734641));
#38682=CARTESIAN_POINT('Ctrl Pts',(3.38281892032033,0.445991341254727,0.418806959518817));
#38683=CARTESIAN_POINT('Ctrl Pts',(1.46711119522298,3.08094834755367,0.577175867302993));
#38684=CARTESIAN_POINT('Ctrl Pts',(-1.78520349758962,2.90769092707777,0.735544775087169));
#38685=CARTESIAN_POINT('Ctrl Pts',(-3.41106324896979,0.0858587903725989,
0.893913682871344));
#38686=CARTESIAN_POINT('Ctrl Pts',(-1.92909382956213,-2.81452018464,1.05228259065552));
#38687=CARTESIAN_POINT('Ctrl Pts',(1.31045643436484,-3.15043044283502,1.2106514984397));
#38688=CARTESIAN_POINT('Ctrl Pts',(3.35605944109629,-0.616081414054793,
1.36902040622387));
#38689=CARTESIAN_POINT('Ctrl Pts',(2.34396428440923,2.4796235742552,1.52738931400805));
#38690=CARTESIAN_POINT('Ctrl Pts',(-0.803707903375748,3.31612712325617,
1.68575822179222));
#38691=CARTESIAN_POINT('Ctrl Pts',(-3.21912512050423,1.13133024491295,1.8441271295764));
#38692=CARTESIAN_POINT('Ctrl Pts',(-2.70160707658305,-2.08422470679312,
2.00249603736058));
#38693=CARTESIAN_POINT('Ctrl Pts',(0.277336523346577,-3.40084556923671,
2.16086494514475));
#38694=CARTESIAN_POINT('Ctrl Pts',(3.00359979626304,-1.61896846612861,2.31923385292893));
#38695=CARTESIAN_POINT('Ctrl Pts',(2.99329261282266,1.63794670223112,2.4776027607131));
#38696=CARTESIAN_POINT('Ctrl Pts',(0.255805906261685,3.4025332463843,2.63597166849728));
#38697=CARTESIAN_POINT('Ctrl Pts',(-2.71474477914914,2.06708263328288,2.79434057628146));
#38698=CARTESIAN_POINT('Ctrl Pts',(-3.2118999633853,-1.1516806498418,2.95270948406563));
#38699=CARTESIAN_POINT('Ctrl Pts',(-0.782703123250905,-3.32115121709356,
3.11107839184981));
#38700=CARTESIAN_POINT('Ctrl Pts',(2.35961209115783,-2.46473131674929,3.26944729963398));
#38701=CARTESIAN_POINT('Ctrl Pts',(3.352092094979,0.637297610789994,3.42781620741816));
#38702=CARTESIAN_POINT('Ctrl Pts',(1.29049145719765,3.15868666457495,3.58618511520233));
#38703=CARTESIAN_POINT('Ctrl Pts',(-1.94687191855818,2.80220616530042,3.74455402298651));
#38704=CARTESIAN_POINT('Ctrl Pts',(-3.41044636742465,-0.107355625286608,
3.90292293077069));
#38705=CARTESIAN_POINT('Ctrl Pts',(-1.76677377870039,-2.91910603937516,
4.06129183855486));
#38706=CARTESIAN_POINT('Ctrl Pts',(1.48660088384143,-3.07126805543518,4.21966074633904));
#38707=CARTESIAN_POINT('Ctrl Pts',(3.3855381223732,-0.425207334521279,4.3780296541232));
#38708=CARTESIAN_POINT('Ctrl Pts',(2.19992214753625,2.60825846113332,4.5363985619074));
#38709=CARTESIAN_POINT('Ctrl Pts',(-0.99003602760054,3.26534811614501,4.69476746969156));
#38710=CARTESIAN_POINT('Ctrl Pts',(-3.27797546895602,0.947389297148782,
4.85313637747574));
#38711=CARTESIAN_POINT('Ctrl Pts',(-2.5793616946409,-2.23373295262659,5.01150528525992));
#38712=CARTESIAN_POINT('Ctrl Pts',(0.46930046669552,-3.37970808316707,5.16987419304408));
#38713=CARTESIAN_POINT('Ctrl Pts',(3.09038443801754,-1.44644173083616,5.32824310082827));
#38714=CARTESIAN_POINT('Ctrl Pts',(2.89582879628167,1.80467316655209,5.48661200861244));
#38715=CARTESIAN_POINT('Ctrl Pts',(0.0628925792552412,3.41155597622644,
5.64498091639662));
#38716=CARTESIAN_POINT('Ctrl Pts',(-2.82734487037505,1.91018078710171,5.8033498241808));
#38717=CARTESIAN_POINT('Ctrl Pts',(-3.14159723579638,-1.33155415341836,
5.96171873196497));
#38718=CARTESIAN_POINT('Ctrl Pts',(-0.593550167993543,-3.36011426197451,
6.12008763974915));
#38719=CARTESIAN_POINT('Ctrl Pts',(2.4952786047586,-2.32728475698253,6.27845654753331));
#38720=CARTESIAN_POINT('Ctrl Pts',(3.31066683116828,0.825926624132867,6.43682545531751));
#38721=CARTESIAN_POINT('Ctrl Pts',(1.10971684385883,3.22663883660774,6.59519436310167));
#38722=CARTESIAN_POINT('Ctrl Pts',(-2.10229269526844,2.68757047886569,6.75356327088585));
#38723=CARTESIAN_POINT('Ctrl Pts',(-3.39890992325729,-0.300134951367665,
6.91193217867001));
#38724=CARTESIAN_POINT('Ctrl Pts',(-1.59879093182649,-3.0143883644545,7.07030108645421));
#38725=CARTESIAN_POINT('Ctrl Pts',(1.65798148604228,-2.98224194984082,7.22866999423837));
#38726=CARTESIAN_POINT('Ctrl Pts',(3.40417214832457,-0.232984205517543,
7.38703890202256));
#38727=CARTESIAN_POINT('Ctrl Pts',(2.04883219435749,2.72854472105802,7.54540780980672));
#38728=CARTESIAN_POINT('Ctrl Pts',(-1.17319237527587,3.20410507100562,7.7037767175909));
#38729=CARTESIAN_POINT('Ctrl Pts',(-3.32632503459287,0.760415294224224,
7.86214562537508));
#38730=CARTESIAN_POINT('Ctrl Pts',(-2.44885333993672,-2.3760864830494,8.02051453315925));
#38731=CARTESIAN_POINT('Ctrl Pts',(0.659760987225929,-3.34774328394278,
8.17888344094343));
#38732=CARTESIAN_POINT('Ctrl Pts',(3.16726913875196,-1.26928163074977,8.3372523487276));
#38733=CARTESIAN_POINT('Ctrl Pts',(2.78908826642068,1.9656185534238,8.49562125651178));
#38734=CARTESIAN_POINT('Ctrl Pts',(-0.130222217696887,3.40964981038632,
8.65399016429595));
#38735=CARTESIAN_POINT('Ctrl Pts',(-2.93088764583465,1.74715977029668,8.81235907208013));
#38736=CARTESIAN_POINT('Ctrl Pts',(-3.06123049031075,-1.50716208174212,
8.97072797986429));
#38737=CARTESIAN_POINT('Ctrl Pts',(-0.402495792463442,-3.38831326658245,
9.12909688764848));
#38738=CARTESIAN_POINT('Ctrl Pts',(2.62295156527424,-2.182382812816,9.28746579543266));
#38739=CARTESIAN_POINT('Ctrl Pts',(3.25863594094856,1.0119098081389,9.44583470321683));
#38740=CARTESIAN_POINT('Ctrl Pts',(0.925387284538464,3.28425456215925,9.604203611001));
#38741=CARTESIAN_POINT('Ctrl Pts',(-2.25097883768382,2.56432523829347,9.76257251878518));
#38742=CARTESIAN_POINT('Ctrl Pts',(-3.37648516862269,-0.49195280415944,
9.92094142656936));
#38743=CARTESIAN_POINT('Ctrl Pts',(-1.42568640407767,-3.10001418265748,
10.0793103343535));
#38744=CARTESIAN_POINT('Ctrl Pts',(1.82405079211913,-2.88366231782067,10.2376792421377));
#38745=CARTESIAN_POINT('Ctrl Pts',(3.41190100644405,-0.0400147182346128,
10.3960481499219));
#38746=CARTESIAN_POINT('Ctrl Pts',(1.89117886601706,2.84009016620598,10.554417057706));
#38747=CARTESIAN_POINT('Ctrl Pts',(-1.35259043483117,3.13259776719778,10.7127859654902));
#38748=CARTESIAN_POINT('Ctrl Pts',(-3.36401881339682,0.571005322708608,
10.8711548732744));
#38749=CARTESIAN_POINT('Ctrl Pts',(-2.31050015380398,-2.51082828857755,
11.0295237810586));
#38750=CARTESIAN_POINT('Ctrl Pts',(0.848107982359261,-3.30505408514111,
11.1878926888427));
#38751=CARTESIAN_POINT('Ctrl Pts',(3.23400758365375,-1.08805542336746,11.3462615966269));
#38752=CARTESIAN_POINT('Ctrl Pts',(2.67341297230351,2.12026713764294,11.5046305044111));
#38753=CARTESIAN_POINT('Ctrl Pts',(-0.32291985151006,3.39682092918513,11.6629994121952));
#38754=CARTESIAN_POINT('Ctrl Pts',(-3.02504140679361,1.5785417772848,11.8213683199794));
#38755=CARTESIAN_POINT('Ctrl Pts',(-2.97105718076111,-1.67794185956998,
11.9797372277636));
#38756=CARTESIAN_POINT('Ctrl Pts',(-0.210152033207837,-3.40565790683504,
12.1381061355478));
#38757=CARTESIAN_POINT('Ctrl Pts',(2.74222197569018,-2.03048966791049,12.296475043332));
#38758=CARTESIAN_POINT('Ctrl Pts',(3.19616610396629,1.19465136810128,12.4548439511161));
#38759=CARTESIAN_POINT('Ctrl Pts',(0.738093273596913,3.33134927243006,12.6132128589003));
#38760=CARTESIAN_POINT('Ctrl Pts',(-2.39245403396228,2.43286525537836,12.7715817666845));
#38761=CARTESIAN_POINT('Ctrl Pts',(-3.34324394060518,-0.682194700254892,
12.9299506744687));
#38762=CARTESIAN_POINT('Ctrl Pts',(-1.24801473082944,-3.17570919435036,
13.0883195822528));
#38763=CARTESIAN_POINT('Ctrl Pts',(1.9842768038067,-2.77584495628384,13.246688490037));
#38764=CARTESIAN_POINT('Ctrl Pts',(3.40869993755978,0.153082955050945,13.4050573978212));
#38765=CARTESIAN_POINT('Ctrl Pts',(1.7274672004286,2.94253746397368,13.5634263056053));
#38766=CARTESIAN_POINT('Ctrl Pts',(-1.52765550972892,3.05105527630366,13.7217952133896));
#38767=CARTESIAN_POINT('Ctrl Pts',(-3.39093605442697,0.379766152017132,
13.8801641211737));
#38768=CARTESIAN_POINT('Ctrl Pts',(-2.16474534670984,-2.63752672769918,
14.0385330289579));
#38769=CARTESIAN_POINT('Ctrl Pts',(1.03373808790759,-3.25177724039764,14.1969019367421));
#38770=CARTESIAN_POINT('Ctrl Pts',(3.29038597801295,-0.903343661620412,
14.3552708445262));
#38771=CARTESIAN_POINT('Ctrl Pts',(2.54917347644763,2.26812350685512,14.5136397523104));
#38772=CARTESIAN_POINT('Ctrl Pts',(-0.514583020900911,3.37311042967397,
14.6720086600946));
#38773=CARTESIAN_POINT('Ctrl Pts',(-3.10950453426685,1.40486697078187,14.8303775678788));
#38774=CARTESIAN_POINT('Ctrl Pts',(-2.87136617497321,-1.84334639842336,
14.9887464756629));
#38775=CARTESIAN_POINT('Ctrl Pts',(-0.0171350575310117,-3.41209262036092,
15.1471153834471));
#38776=CARTESIAN_POINT('Ctrl Pts',(2.85270775588288,-1.8720919062881,15.3054842912313));
#38777=CARTESIAN_POINT('Ctrl Pts',(3.12345744205154,1.37356589417187,15.4638531990155));
#38778=CARTESIAN_POINT('Ctrl Pts',(0.548434799162462,3.36777210564648,15.6222221067996));
#38779=CARTESIAN_POINT('Ctrl Pts',(-2.52626506690267,2.29361164927632,15.7805910145838));
#38780=CARTESIAN_POINT('Ctrl Pts',(-3.29929273696804,-0.870251187763856,
15.938959922368));
#38781=CARTESIAN_POINT('Ctrl Pts',(-1.06634505824692,-3.24123094602799,
16.0973288301521));
#38782=CARTESIAN_POINT('Ctrl Pts',(2.13814620358477,-2.65913519147203,16.2556977379364));
#38783=CARTESIAN_POINT('Ctrl Pts',(3.39457926894347,0.345690110051812,16.4140666457205));
#38784=CARTESIAN_POINT('Ctrl Pts',(1.55822150430069,3.03555865928581,16.5724355535047));
#38785=CARTESIAN_POINT('Ctrl Pts',(-1.69782651872419,2.95973837446756,16.7308044612889));
#38786=CARTESIAN_POINT('Ctrl Pts',(-3.40699103573678,0.187311257162456,
16.8891733690731));
#38787=CARTESIAN_POINT('Ctrl Pts',(-2.01205487238326,-2.75577754091925,
17.0475422768572));
#38788=CARTESIAN_POINT('Ctrl Pts',(1.21605479522199,-3.18808033565051,17.2059111846414));
#38789=CARTESIAN_POINT('Ctrl Pts',(3.33622724440086,-0.715743955828957,
17.3642800924256));
#38790=CARTESIAN_POINT('Ctrl Pts',(2.4167610366335,2.40872525887147,17.5226490002097));
#38791=CARTESIAN_POINT('Ctrl Pts',(-0.704584866714741,3.33857277996247,
17.6810179079939));
#38792=CARTESIAN_POINT('Ctrl Pts',(-3.18403103516454,1.22673275007632,17.8393868157781));
#38793=CARTESIAN_POINT('Ctrl Pts',(-2.76242988356763,-2.00292420194302,
17.9977557235623));
#38794=CARTESIAN_POINT('Ctrl Pts',(0.175847150396599,-3.40744711403038,
18.1561246313465));
#38795=CARTESIAN_POINT('Ctrl Pts',(2.95422621652823,-1.70798285735531,18.3144935391306));
#38796=CARTESIAN_POINT('Ctrl Pts',(3.04041566712921,1.54862671268017,18.4728624469148));
#38797=CARTESIAN_POINT('Ctrl Pts',(0.357645745016943,3.39235871404377,18.631231354699));
#38798=CARTESIAN_POINT('Ctrl Pts',(-2.65319198947773,2.14904689640439,18.7896002624832));
#38799=CARTESIAN_POINT('Ctrl Pts',(-3.24244227426787,-1.06021153090294,
18.9479933412587));
#38800=CARTESIAN_POINT('Ctrl Pts',(-1.67134529740578,-2.5444535668589,19.0535967841062));
#38801=CARTESIAN_POINT('Ctrl Pts',(-0.74495813079252,-2.79162859999982,
19.1064105910255));
#38802=CARTESIAN_POINT('Ctrl Pts',(-2.33803595403645,2.00106467658089,-0.323366414141818));
#38803=CARTESIAN_POINT('Ctrl Pts',(-3.00214223718147,1.22518857689341,-0.270549577477338));
#38804=CARTESIAN_POINT('Ctrl Pts',(-3.48578596895374,-1.02558263320169,
-0.164943104884798));
#38805=CARTESIAN_POINT('Ctrl Pts',(-1.0322971287473,-3.48708213552881,-0.00654699636420169));
#38806=CARTESIAN_POINT('Ctrl Pts',(2.36061725640788,-2.76190313005438,0.151821911419974));
#38807=CARTESIAN_POINT('Ctrl Pts',(3.60308039602196,0.475030646428534,0.31019081920415));
#38808=CARTESIAN_POINT('Ctrl Pts',(1.56263746620872,3.28155448272582,0.468559726988325));
#38809=CARTESIAN_POINT('Ctrl Pts',(-1.90144133534228,3.09701595734625,0.626928634772501));
#38810=CARTESIAN_POINT('Ctrl Pts',(-3.63316376413971,0.0914492119455178,
0.785297542556676));
#38811=CARTESIAN_POINT('Ctrl Pts',(-2.05470062781962,-2.99777869887408,
0.943666450340852));
#38812=CARTESIAN_POINT('Ctrl Pts',(1.39578262972872,-3.35556068325843,1.10203535812503));
#38813=CARTESIAN_POINT('Ctrl Pts',(3.57457855856896,-0.656195592380133,
1.2604042659092));
#38814=CARTESIAN_POINT('Ctrl Pts',(2.49658405047906,2.64107636274744,1.41877317369338));
#38815=CARTESIAN_POINT('Ctrl Pts',(-0.856038782740064,3.53204617508454,
1.57714208147756));
#38816=CARTESIAN_POINT('Ctrl Pts',(-3.42872819598997,1.20499320918028,1.73551098926173));
#38817=CARTESIAN_POINT('Ctrl Pts',(-2.87751361354832,-2.21993235784546,
1.89387989704591));
#38818=CARTESIAN_POINT('Ctrl Pts',(0.29539440741815,-3.62228079274625,2.05224880483008));
#38819=CARTESIAN_POINT('Ctrl Pts',(3.19916962696489,-1.72438243946365,2.21061771261426));
#38820=CARTESIAN_POINT('Ctrl Pts',(3.18819132411539,1.74459638294176,2.36898662039843));
#38821=CARTESIAN_POINT('Ctrl Pts',(0.272461892802362,3.62407835761407,2.52735552818261));
#38822=CARTESIAN_POINT('Ctrl Pts',(-2.89150673575782,2.20167413283645,2.68572443596679));
#38823=CARTESIAN_POINT('Ctrl Pts',(-3.42103259578594,-1.22666866588587,
2.84409334375096));
#38824=CARTESIAN_POINT('Ctrl Pts',(-0.833666343282555,-3.53739739678445,
3.00246225153514));
#38825=CARTESIAN_POINT('Ctrl Pts',(2.51325071430724,-2.62521444334356,3.16083115931931));
#38826=CARTESIAN_POINT('Ctrl Pts',(3.57035289134998,0.678793214166964,3.31920006710349));
#38827=CARTESIAN_POINT('Ctrl Pts',(1.37451769668545,3.3643544825711,3.47756897488767));
#38828=CARTESIAN_POINT('Ctrl Pts',(-2.07363628043631,2.98466289139998,3.63593788267183));
#38829=CARTESIAN_POINT('Ctrl Pts',(-3.63250671631828,-0.114345744772007,
3.79430679045602));
#38830=CARTESIAN_POINT('Ctrl Pts',(-1.88181162402811,-3.10917432831019,
3.95267569824018));
#38831=CARTESIAN_POINT('Ctrl Pts',(1.58339616380376,-3.27124388922926,4.11104460602437));
#38832=CARTESIAN_POINT('Ctrl Pts',(3.60597665025262,-0.452893355318378,
4.26941351380853));
#38833=CARTESIAN_POINT('Ctrl Pts',(2.34316306880883,2.77808690042977,4.42778242159272));
#38834=CARTESIAN_POINT('Ctrl Pts',(-1.05449906909743,3.47796085471677,4.58615132937689));
#38835=CARTESIAN_POINT('Ctrl Pts',(-3.49141039737296,1.00907553267278,4.74452023716107));
#38836=CARTESIAN_POINT('Ctrl Pts',(-2.7473086130577,-2.37917535674507,4.90288914494524));
#38837=CARTESIAN_POINT('Ctrl Pts',(0.499857471305165,-3.59976700661918,
5.06125805272942));
#38838=CARTESIAN_POINT('Ctrl Pts',(3.2916049741551,-1.54062217550514,5.2196269605136));
#38839=CARTESIAN_POINT('Ctrl Pts',(3.08438146169832,1.92217870976522,5.37799586829777));
#38840=CARTESIAN_POINT('Ctrl Pts',(0.0669876291659018,3.63368857376175,
5.53636477608195));
#38841=CARTESIAN_POINT('Ctrl Pts',(-3.01143842315892,2.03455612285989,5.69473368386612));
#38842=CARTESIAN_POINT('Ctrl Pts',(-3.34615233008773,-1.41825405953713,
5.85310259165031));
#38843=CARTESIAN_POINT('Ctrl Pts',(-0.632197296020375,-3.57889739618926,
6.01147149943446));
#38844=CARTESIAN_POINT('Ctrl Pts',(2.6577507206822,-2.47881848876807,6.16984040721865));
#38845=CARTESIAN_POINT('Ctrl Pts',(3.52623035347487,0.879704204706274,6.32820931500282));
#38846=CARTESIAN_POINT('Ctrl Pts',(1.18197252038088,3.43673114377745,6.48657822278701));
#38847=CARTESIAN_POINT('Ctrl Pts',(-2.23917678582234,2.86256306749383,6.64494713057117));
#38848=CARTESIAN_POINT('Ctrl Pts',(-3.62021911334622,-0.319677282439768,
6.80331603835535));
#38849=CARTESIAN_POINT('Ctrl Pts',(-1.70289110930486,-3.21066065839974,
6.96168494613953));
#38850=CARTESIAN_POINT('Ctrl Pts',(1.76593566786621,-3.17642113242298,7.12005385392371));
#38851=CARTESIAN_POINT('Ctrl Pts',(3.62582397143231,-0.248154229728482,
7.27842276170788));
#38852=CARTESIAN_POINT('Ctrl Pts',(2.18223537472976,2.90620521691491,7.43679166949206));
#38853=CARTESIAN_POINT('Ctrl Pts',(-1.2495810587812,3.41273016382494,7.59516057727622));
#38854=CARTESIAN_POINT('Ctrl Pts',(-3.54290809092547,0.809927313282007,
7.75352948506041));
#38855=CARTESIAN_POINT('Ctrl Pts',(-2.60830262266105,-2.53079778373636,
7.91189839284458));
#38856=CARTESIAN_POINT('Ctrl Pts',(0.702719221787002,-3.56572092133924,
8.07026730062876));
#38857=CARTESIAN_POINT('Ctrl Pts',(3.37349577720877,-1.35192685996691,8.22863620841293));
#38858=CARTESIAN_POINT('Ctrl Pts',(2.97069086233078,2.09360354270093,8.38700511619711));
#38859=CARTESIAN_POINT('Ctrl Pts',(-0.138701222489833,3.63165829400636,
8.54537402398129));
#38860=CARTESIAN_POINT('Ctrl Pts',(-3.12172305653588,1.86092051196111,8.70374293176545));
#38861=CARTESIAN_POINT('Ctrl Pts',(-3.26055276003331,-1.60529613859391,
8.86211183954965));
#38862=CARTESIAN_POINT('Ctrl Pts',(-0.428703023562676,-3.60893248913491,
9.0204807473338));
#38863=CARTESIAN_POINT('Ctrl Pts',(2.79373669923185,-2.3244817161919,9.178849655118));
#38864=CARTESIAN_POINT('Ctrl Pts',(3.47081163761864,1.07779709116158,9.33721856290215));
#38865=CARTESIAN_POINT('Ctrl Pts',(0.985640929113881,3.49809833372375,9.49558747068635));
#38866=CARTESIAN_POINT('Ctrl Pts',(-2.3975441526592,2.73129310576418,9.6539563784705));
#38867=CARTESIAN_POINT('Ctrl Pts',(-3.59633424226306,-0.523984743548459,
9.8123252862547));
#38868=CARTESIAN_POINT('Ctrl Pts',(-1.51851543177513,-3.30186172893509,
9.97069419403885));
#38869=CARTESIAN_POINT('Ctrl Pts',(1.94281804768031,-3.07142280175702,10.1290631018231));
#38870=CARTESIAN_POINT('Ctrl Pts',(3.63405606952266,-0.0426201491180682,
10.2874320096072));
#38871=CARTESIAN_POINT('Ctrl Pts',(2.01431695222748,3.02501358831897,10.4458009173914));
#38872=CARTESIAN_POINT('Ctrl Pts',(-1.4406600513886,3.33656688976533,10.6041698251756));
#38873=CARTESIAN_POINT('Ctrl Pts',(-3.5830561800368,0.608184514966817,10.7625387329598));
#38874=CARTESIAN_POINT('Ctrl Pts',(-2.46094100963244,-2.67431287261882,
10.9209076407439));
#38875=CARTESIAN_POINT('Ctrl Pts',(0.903329831399618,-3.52025215137339,
11.0792765485281));
#38876=CARTESIAN_POINT('Ctrl Pts',(3.44457968330915,-1.15890068551155,11.2376454563123));
#38877=CARTESIAN_POINT('Ctrl Pts',(2.84748374000033,2.25832157674212,11.3960143640965));
#38878=CARTESIAN_POINT('Ctrl Pts',(-0.343945748757976,3.61799410108097,
11.5543832718806));
#38879=CARTESIAN_POINT('Ctrl Pts',(-3.22200733964816,1.68132349558278,11.7127521796648));
#38880=CARTESIAN_POINT('Ctrl Pts',(-3.16450810274141,-1.78719569751867,
11.871121087449));
#38881=CARTESIAN_POINT('Ctrl Pts',(-0.223835413266404,-3.62740647037429,
12.0294899952332));
#38882=CARTESIAN_POINT('Ctrl Pts',(2.92077302240413,-2.16269853311588,12.1878589030173));
#38883=CARTESIAN_POINT('Ctrl Pts',(3.40427427624188,1.27243728555206,12.3462278108015));
#38884=CARTESIAN_POINT('Ctrl Pts',(0.786151865403689,3.54825946600126,12.5045967185857));
#38885=CARTESIAN_POINT('Ctrl Pts',(-2.54823105557683,2.59127352491771,12.6629656263699));
#38886=CARTESIAN_POINT('Ctrl Pts',(-3.56092861759596,-0.726613634561833,
12.8213345341541));
#38887=CARTESIAN_POINT('Ctrl Pts',(-1.32927523361859,-3.38248538013586,
12.9797034419382));
#38888=CARTESIAN_POINT('Ctrl Pts',(2.11347666560882,-2.95658525625003,13.1380723497224));
#38889=CARTESIAN_POINT('Ctrl Pts',(3.6306465732372,0.163050463918102,13.2964412575066));
#38890=CARTESIAN_POINT('Ctrl Pts',(1.83994572315028,3.13413141546453,13.4548101652907));
#38891=CARTESIAN_POINT('Ctrl Pts',(-1.62712393084818,3.24971501938629,13.6131790730749));
#38892=CARTESIAN_POINT('Ctrl Pts',(-3.61172605145325,0.4044934149996,13.7715479808591));
#38893=CARTESIAN_POINT('Ctrl Pts',(-2.30569584267649,-2.80926087691889,
13.9299168886433));
#38894=CARTESIAN_POINT('Ctrl Pts',(1.10104664981842,-3.46350635463446,14.0882857964275));
#38895=CARTESIAN_POINT('Ctrl Pts',(3.50462897718492,-0.962162005924634,
14.2466547042116));
#38896=CARTESIAN_POINT('Ctrl Pts',(2.7151547852221,2.41580514233745,14.4050236119958));
#38897=CARTESIAN_POINT('Ctrl Pts',(-0.548088454748935,3.59273976794022,
14.56339251978));
#38898=CARTESIAN_POINT('Ctrl Pts',(-3.31197001455146,1.4963404074149,14.7217614275642));
#38899=CARTESIAN_POINT('Ctrl Pts',(-3.05832603474587,-1.96337002590963,
14.8801303353483));
#38900=CARTESIAN_POINT('Ctrl Pts',(-0.0182507522066404,-3.6342601597692,
15.0384992431325));
#38901=CARTESIAN_POINT('Ctrl Pts',(3.03845273214569,-1.99398720593042,15.1968681509167));
#38902=CARTESIAN_POINT('Ctrl Pts',(3.32683142146999,1.46300126093254,15.3552370587008));
#38903=CARTESIAN_POINT('Ctrl Pts',(0.584144383693881,3.5870538559526,15.513605966485));
#38904=CARTESIAN_POINT('Ctrl Pts',(-2.69075476758011,2.44295286394241,15.6719748742692));
#38905=CARTESIAN_POINT('Ctrl Pts',(-3.51411567137077,-0.926914821071728,
15.8303437820534));
#38906=CARTESIAN_POINT('Ctrl Pts',(-1.13577671913948,-3.45227337190941,
15.9887126898375));
#38907=CARTESIAN_POINT('Ctrl Pts',(2.2773647810967,-2.83227630696169,16.1470815976217));
#38908=CARTESIAN_POINT('Ctrl Pts',(3.61560648227504,0.36819862013436,16.3054505054059));
#38909=CARTESIAN_POINT('Ctrl Pts',(1.6596801327675,3.23320938952646,16.4638194131901));
#38910=CARTESIAN_POINT('Ctrl Pts',(-1.80837508289745,3.1524523084399,16.6221883209743));
#38911=CARTESIAN_POINT('Ctrl Pts',(-3.62882640171686,0.199507432863826,
16.7805572287584));
#38912=CARTESIAN_POINT('Ctrl Pts',(-2.14306341461461,-2.93521121507253,
16.9389261365426));
#38913=CARTESIAN_POINT('Ctrl Pts',(1.2952343286344,-3.39566202888499,17.0972950443268));
#38914=CARTESIAN_POINT('Ctrl Pts',(3.55345505157481,-0.762347343018389,
17.255663952111));
#38915=CARTESIAN_POINT('Ctrl Pts',(2.57412073128032,2.56556172945283,17.4140328598952));
#38916=CARTESIAN_POINT('Ctrl Pts',(-0.750461665371445,3.55595330921119,
17.5724017676793));
#38917=CARTESIAN_POINT('Ctrl Pts',(-3.39134907109971,1.3066075444971,17.7307706754635));
#38918=CARTESIAN_POINT('Ctrl Pts',(-2.94229670381685,-2.13333822966068,
17.8891395832477));
#38919=CARTESIAN_POINT('Ctrl Pts',(0.187296877312696,-3.62931217609541,
18.0475084910319));
#38920=CARTESIAN_POINT('Ctrl Pts',(3.14658124389912,-1.81919271915853,18.205877398816));
#38921=CARTESIAN_POINT('Ctrl Pts',(3.23838264596023,1.64946060686142,18.3642463066002));
#38922=CARTESIAN_POINT('Ctrl Pts',(0.38093270817736,3.61324134301813,18.5226152143844));
#38923=CARTESIAN_POINT('Ctrl Pts',(-2.82594613230569,2.28897523779762,18.6809841221686));
#38924=CARTESIAN_POINT('Ctrl Pts',(-3.45356357192809,-1.12924382670507,
18.839377200944));
#38925=CARTESIAN_POINT('Ctrl Pts',(-1.78016962122703,-2.71012755375903,
18.9449806437914));
#38926=CARTESIAN_POINT('Ctrl Pts',(-0.793463705902866,-2.97339660163694,
18.9977944507108));
#38927=CARTESIAN_POINT('Ctrl Pts',(-1.91346599666507,1.63598720337494,-1.49186218934005E-15));
#38928=CARTESIAN_POINT('Ctrl Pts',(-1.97562728140449,1.57757085957046,-2.50614906192051E-15));
#38929=CARTESIAN_POINT('Ctrl Pts',(-2.03436145510481,1.51595110656798,-4.44124286950301E-15));
#38930=CARTESIAN_POINT('Ctrl Pts',(-2.08967050234655,1.45152218121991,-3.68455266297474E-15));
#38931=CARTESIAN_POINT('Ctrl Pts',(-2.14612535197374,1.38575852276691,-2.91218658627838E-15));
#38932=CARTESIAN_POINT('Ctrl Pts',(-2.1990121164881,1.31706760569438,-1.5430458858727E-15));
#38933=CARTESIAN_POINT('Ctrl Pts',(-2.24830698708946,1.24581947769238,-1.76247905159244E-15));
#38934=CARTESIAN_POINT('Ctrl Pts',(-2.29883933734524,1.1727827638245,-1.98742078391902E-15));
#38935=CARTESIAN_POINT('Ctrl Pts',(-2.34559771595042,1.09705825975981,-6.50009313603642E-16));
#38936=CARTESIAN_POINT('Ctrl Pts',(-2.38852219321958,1.0190015549115,1.2490009027033E-16));
#38937=CARTESIAN_POINT('Ctrl Pts',(-2.41751206249941,0.966284461683361,
6.48250023716466E-16));
#38938=CARTESIAN_POINT('Ctrl Pts',(-2.44475247983232,0.912502700494791,
2.25064873853325E-15));
#38939=CARTESIAN_POINT('Ctrl Pts',(-2.47021462141466,0.857757311203253,
1.31838984174237E-15));
#38940=CARTESIAN_POINT('Ctrl Pts',(-2.47883400081736,0.83922504127118,1.06850379779826E-15));
#38941=CARTESIAN_POINT('Ctrl Pts',(-2.48725198934881,0.820576366164846,
-8.41426332219623E-16));
#38942=CARTESIAN_POINT('Ctrl Pts',(-2.49545335573811,0.801847661549147,
-6.52256026967279E-16));
#38943=CARTESIAN_POINT('Ctrl Pts',(-2.53213167303446,0.718088768477345,
-9.03468916911122E-16));
#38944=CARTESIAN_POINT('Ctrl Pts',(-2.56452720083354,0.632638163527894,
-2.74682372953375E-16));
#38945=CARTESIAN_POINT('Ctrl Pts',(-2.59261423848372,0.545897077960933,
1.01307850997046E-15));
#38946=CARTESIAN_POINT('Ctrl Pts',(-2.62108392241438,0.457974267422819,
2.31838331896207E-15));
#38947=CARTESIAN_POINT('Ctrl Pts',(-2.64512739967565,0.368724800334353,
-2.85563347547353E-15));
#38948=CARTESIAN_POINT('Ctrl Pts',(-2.66467879117549,0.278529425245449,
-1.1518563880486E-15));
#38949=CARTESIAN_POINT('Ctrl Pts',(-2.68425447613445,0.188221978457852,
5.5403771693064E-16));
#38950=CARTESIAN_POINT('Ctrl Pts',(-2.69932732669291,0.0969653795285389,
-3.58400398648576E-16));
#38951=CARTESIAN_POINT('Ctrl Pts',(-2.70978561266556,0.00511753876573948,
1.80411241501588E-16));
#38952=CARTESIAN_POINT('Ctrl Pts',(-2.71365156263523,-0.0288344069106642,
3.79585260011577E-16));
#38953=CARTESIAN_POINT('Ctrl Pts',(-2.71688647879056,-0.0628673128703889,
-1.31650542657094E-15));
#38954=CARTESIAN_POINT('Ctrl Pts',(-2.71948296230813,-0.0969635581463529,
-1.37390099297363E-15));
#38955=CARTESIAN_POINT('Ctrl Pts',(-2.72117333325281,-0.119161004017789,
-1.37858239915481E-15));
#38956=CARTESIAN_POINT('Ctrl Pts',(-2.72259309670265,-0.141385298884962,
1.35912043257924E-15));
#38957=CARTESIAN_POINT('Ctrl Pts',(-2.72373998089586,-0.163631606082652,
4.02455846426619E-16));
#38958=CARTESIAN_POINT('Ctrl Pts',(-2.72438165410587,-0.17607825015966,
-5.8898284204301E-16));
#38959=CARTESIAN_POINT('Ctrl Pts',(-2.72493780860265,-0.18853085131645,
1.50166758541897E-16));
#38960=CARTESIAN_POINT('Ctrl Pts',(-2.72540781340729,-0.200978281065814,
-1.38777878078145E-16));
#38961=CARTESIAN_POINT('Ctrl Pts',(-2.72916559147235,-0.300497856221906,
-8.51642209848428E-16));
#38962=CARTESIAN_POINT('Ctrl Pts',(-2.72743044903818,-0.399859077131394,
-9.16883136981344E-17));
#38963=CARTESIAN_POINT('Ctrl Pts',(-2.72013295703714,-0.498607340903291,
-1.80411241501588E-15));
#38964=CARTESIAN_POINT('Ctrl Pts',(-2.71283546503611,-0.597355604675174,
-4.27462052636193E-15));
#38965=CARTESIAN_POINT('Ctrl Pts',(-2.69997611686452,-0.695492103877208,
-1.71117497003209E-15));
#38966=CARTESIAN_POINT('Ctrl Pts',(-2.68142706905932,-0.792583196929577,
-2.19269047363468E-15));
#38967=CARTESIAN_POINT('Ctrl Pts',(-2.664117508035,-0.88318645687896,-2.61840637124098E-15));
#38968=CARTESIAN_POINT('Ctrl Pts',(-2.64185312691352,-0.972880370486868,
-5.09040680058174E-15));
#38969=CARTESIAN_POINT('Ctrl Pts',(-2.61490988468309,-1.06142534465363,
-4.91273688396632E-15));
#38970=CARTESIAN_POINT('Ctrl Pts',(-2.60515225760836,-1.09349234052115,
-4.84839285387875E-15));
#38971=CARTESIAN_POINT('Ctrl Pts',(-2.59478046819329,-1.12540860314951,
-4.2189522678695E-15));
#38972=CARTESIAN_POINT('Ctrl Pts',(-2.58380597441444,-1.15716250955434,
-3.83026943495679E-15));
#38973=CARTESIAN_POINT('Ctrl Pts',(-2.57707836097892,-1.17662837391802,
-3.42200387609689E-15));
#38974=CARTESIAN_POINT('Ctrl Pts',(-2.57012423657022,-1.19603322188682,
-6.35130850184293E-15));
#38975=CARTESIAN_POINT('Ctrl Pts',(-2.56294608765656,-1.21537433488221,
-5.82867087928207E-15));
#38976=CARTESIAN_POINT('Ctrl Pts',(-2.55803440850288,-1.22860857432904,
-5.55861431346926E-15));
#38977=CARTESIAN_POINT('Ctrl Pts',(-2.55301817112519,-1.24181188707138,
-4.25409719012689E-15));
#38978=CARTESIAN_POINT('Ctrl Pts',(-2.54790299736969,-1.25497158263782,
-4.30211422042248E-15));
#38979=CARTESIAN_POINT('Ctrl Pts',(-2.51363258640273,-1.3431383188659,-3.82292319133049E-15));
#38980=CARTESIAN_POINT('Ctrl Pts',(-2.47487338179404,-1.42948978193878,
-3.5983761671373E-15));
#38981=CARTESIAN_POINT('Ctrl Pts',(-2.43197011073125,-1.5137843727111,-4.69069227904129E-15));
#38982=CARTESIAN_POINT('Ctrl Pts',(-2.38822425227513,-1.59973444470317,
-5.80446064301425E-15));
#38983=CARTESIAN_POINT('Ctrl Pts',(-2.34016967457277,-1.68354677501953,
-4.78147958264788E-15));
#38984=CARTESIAN_POINT('Ctrl Pts',(-2.2881164923778,-1.76496219714289,-5.80091530366644E-15));
#38985=CARTESIAN_POINT('Ctrl Pts',(-2.23518331119972,-1.84775400944371,
-6.8375853677168E-15));
#38986=CARTESIAN_POINT('Ctrl Pts',(-2.17811482141291,-1.92806801277158,
-4.24679705205495E-15));
#38987=CARTESIAN_POINT('Ctrl Pts',(-2.11718543714367,-2.00561675751096,
-6.30051566474776E-15));
#38988=CARTESIAN_POINT('Ctrl Pts',(-2.07494196997557,-2.05938273416762,
-7.72439670061111E-15));
#38989=CARTESIAN_POINT('Ctrl Pts',(-2.03084151659921,-2.11181917678613,
-7.36061663108968E-15));
#38990=CARTESIAN_POINT('Ctrl Pts',(-1.98496281732071,-2.16282291589316,
-6.93889390390723E-15));
#38991=CARTESIAN_POINT('Ctrl Pts',(-1.97399768439553,-2.1750129471666,-6.87133739263459E-15));
#38992=CARTESIAN_POINT('Ctrl Pts',(-1.96293062927649,-2.18712132010553,
-7.50498138722435E-15));
#38993=CARTESIAN_POINT('Ctrl Pts',(-1.95177323750925,-2.19913549001593,
-7.18869408444789E-15));
#38994=CARTESIAN_POINT('Ctrl Pts',(-1.88308475485779,-2.27309857374356,
-6.58819740314064E-15));
#38995=CARTESIAN_POINT('Ctrl Pts',(-1.81088310049948,-2.34359790276572,
-8.33506234338686E-15));
#38996=CARTESIAN_POINT('Ctrl Pts',(-1.73548098567592,-2.41034417373154,
-7.27196081129478E-15));
#38997=CARTESIAN_POINT('Ctrl Pts',(-1.67159483308639,-2.4668964662194,-6.3827680954257E-15));
#38998=CARTESIAN_POINT('Ctrl Pts',(-1.60541009649036,-2.52075457683924,
-8.56307881259928E-15));
#38999=CARTESIAN_POINT('Ctrl Pts',(-1.53709204750604,-2.57172803359375,
-7.04991620636974E-15));
#39000=CARTESIAN_POINT('Ctrl Pts',(-1.51139262450419,-2.59090288484428,
-5.70535958527313E-15));
#39001=CARTESIAN_POINT('Ctrl Pts',(-1.48539160198016,-2.60966903460802,
-8.28152629487784E-15));
#39002=CARTESIAN_POINT('Ctrl Pts',(-1.45909549992335,-2.62801676553979,
-8.38218383591993E-15));
#39003=CARTESIAN_POINT('Ctrl Pts',(-1.43771162959308,-2.64293705670128,
-8.46403808948036E-15));
#39004=CARTESIAN_POINT('Ctrl Pts',(-1.41613408952649,-2.65757933351224,
-8.74660806298987E-15));
#39005=CARTESIAN_POINT('Ctrl Pts',(-1.39438874927187,-2.67192417048441,
-8.32667268468867E-15));
#39006=CARTESIAN_POINT('Ctrl Pts',(-1.30923746902616,-2.72809626155285,
-6.6822727965235E-15));
#39007=CARTESIAN_POINT('Ctrl Pts',(-1.22144049509827,-2.77976395162219,
-5.87210663195867E-15));
#39008=CARTESIAN_POINT('Ctrl Pts',(-1.13128845941444,-2.8266186852154,-4.77395900588817E-15));
#39009=CARTESIAN_POINT('Ctrl Pts',(-1.04699210296153,-2.87043004559701,
-3.74713977742599E-15));
#39010=CARTESIAN_POINT('Ctrl Pts',(-0.960635894698547,-2.91003369441993,
-3.99091700432708E-15));
#39011=CARTESIAN_POINT('Ctrl Pts',(-0.872429377952129,-2.94514712713841,
-4.77395900588817E-15));
#39012=CARTESIAN_POINT('Ctrl Pts',(-0.847142239363335,-2.95521348359633,
-4.82011908673854E-15));
#39013=CARTESIAN_POINT('Ctrl Pts',(-0.821702883756235,-2.96491059049498,
-4.33795729134559E-15));
#39014=CARTESIAN_POINT('Ctrl Pts',(-0.796118629904262,-2.97424061993174,
1.66533453693773E-16));
#39015=CARTESIAN_POINT('Ctrl Pts',(0.794818364480303,-2.97303485125766,
0.00227809062281707));
#39016=CARTESIAN_POINT('Ctrl Pts',(1.78093556794474,-2.7094038808666,0.0550677265508756));
#39017=CARTESIAN_POINT('Ctrl Pts',(3.4534673386373,-1.12871913187498,0.160646998406993));
#39018=CARTESIAN_POINT('Ctrl Pts',(2.82594663323224,2.28897348571344,0.319015906191168));
#39019=CARTESIAN_POINT('Ctrl Pts',(-0.380932805352938,3.61324274555714,
0.477384813975344));
#39020=CARTESIAN_POINT('Ctrl Pts',(-3.23838288724328,1.6494600182536,0.635753721759519));
#39021=CARTESIAN_POINT('Ctrl Pts',(-3.14658141599552,-1.81919242326023,
0.794122629543696));
#39022=CARTESIAN_POINT('Ctrl Pts',(-0.187296929226849,-3.62931267164117,
0.952491537327871));
#39023=CARTESIAN_POINT('Ctrl Pts',(2.94229693385074,-2.13333823050325,1.11086044511205));
#39024=CARTESIAN_POINT('Ctrl Pts',(3.3913492823706,1.30660755011612,1.26922935289622));
#39025=CARTESIAN_POINT('Ctrl Pts',(0.750461729472986,3.55595359950969,1.4275982606804));
#39026=CARTESIAN_POINT('Ctrl Pts',(-2.57412091487803,2.56556187728594,1.58596716846457));
#39027=CARTESIAN_POINT('Ctrl Pts',(-3.5534552890492,-0.762347379687072,
1.74433607624876));
#39028=CARTESIAN_POINT('Ctrl Pts',(-1.29523441987398,-3.39566226908073,
1.90270498403292));
#39029=CARTESIAN_POINT('Ctrl Pts',(2.14306356247744,-2.93521141044675,2.06107389181711));
#39030=CARTESIAN_POINT('Ctrl Pts',(3.62882664822082,0.1995074437915,2.21944279960128));
#39031=CARTESIAN_POINT('Ctrl Pts',(1.80837520679842,3.15245252492811,2.37781170738546));
#39032=CARTESIAN_POINT('Ctrl Pts',(-1.65968024628328,3.23320960921406,2.53618061516963));
#39033=CARTESIAN_POINT('Ctrl Pts',(-3.61560672868174,0.368198645699416,
2.69454952295381));
#39034=CARTESIAN_POINT('Ctrl Pts',(-2.27736493651933,-2.83227650037644,
2.85291843073798));
#39035=CARTESIAN_POINT('Ctrl Pts',(1.13577679665878,-3.45227360722268,3.01128733852215));
#39036=CARTESIAN_POINT('Ctrl Pts',(3.51411591100643,-0.926914884363649,
3.16965624630634));
#39037=CARTESIAN_POINT('Ctrl Pts',(2.69075495111143,2.44295303059633,3.32802515409051));
#39038=CARTESIAN_POINT('Ctrl Pts',(-0.584144423543271,3.58705410057259,
3.48639406187469));
#39039=CARTESIAN_POINT('Ctrl Pts',(-3.3268316483593,1.46300136072356,3.64476296965886));
#39040=CARTESIAN_POINT('Ctrl Pts',(-3.03845293937564,-1.99398734192987,
3.80313187744304));
#39041=CARTESIAN_POINT('Ctrl Pts',(0.0182507534530098,-3.63426040762749,
3.96150078522721));
#39042=CARTESIAN_POINT('Ctrl Pts',(3.05832624332729,-1.9633701598163,4.11986969301138));
#39043=CARTESIAN_POINT('Ctrl Pts',(3.31197024043316,1.49634050946856,4.27823860079557));
#39044=CARTESIAN_POINT('Ctrl Pts',(0.548088492129132,3.59274001296977,4.43660750857973));
#39045=CARTESIAN_POINT('Ctrl Pts',(-2.71515497039948,2.41580530709925,4.59497641636392));
#39046=CARTESIAN_POINT('Ctrl Pts',(-3.50462921620585,-0.962162071545632,
4.75334532414809));
#39047=CARTESIAN_POINT('Ctrl Pts',(-1.1010467249114,-3.46350659085057,4.91171423193227));
#39048=CARTESIAN_POINT('Ctrl Pts',(2.3056959999283,-2.80926106851468,5.07008313971643));
#39049=CARTESIAN_POINT('Ctrl Pts',(3.61172629777829,0.404493442586659,5.22845204750063));
#39050=CARTESIAN_POINT('Ctrl Pts',(1.62712404182042,3.2497152410216,5.38682095528478));
#39051=CARTESIAN_POINT('Ctrl Pts',(-1.83994584863726,3.13413162921692,5.54518986306898));
#39052=CARTESIAN_POINT('Ctrl Pts',(-3.63064682085263,0.163050475038392,
5.70355877085314));
#39053=CARTESIAN_POINT('Ctrl Pts',(-2.11347680975103,-2.95658545789347,
5.86192767863733));
#39054=CARTESIAN_POINT('Ctrl Pts',(1.32927532427707,-3.38248561082633,6.02029658642149));
#39055=CARTESIAN_POINT('Ctrl Pts',(3.56092886045652,-0.726613684117993,
6.17866549420568));
#39056=CARTESIAN_POINT('Ctrl Pts',(2.54823122936997,2.59127370164634,6.33703440198984));
#39057=CARTESIAN_POINT('Ctrl Pts',(-0.786151919020366,3.54825970799776,
6.49540330977403));
#39058=CARTESIAN_POINT('Ctrl Pts',(-3.40427450841839,1.27243737233417,6.6537722175582));
#39059=CARTESIAN_POINT('Ctrl Pts',(-2.92077322160515,-2.16269868061508,
6.81214112534238));
#39060=CARTESIAN_POINT('Ctrl Pts',(0.223835428532286,-3.62740671776872,
6.97051003312655));
#39061=CARTESIAN_POINT('Ctrl Pts',(3.1645083185655,-1.78719581940807,7.12887894091072));
#39062=CARTESIAN_POINT('Ctrl Pts',(3.2220075593938,1.6813236102515,7.28724784869491));
#39063=CARTESIAN_POINT('Ctrl Pts',(0.343945772215585,3.61799434783347,7.44561675647908));
#39064=CARTESIAN_POINT('Ctrl Pts',(-2.8474839342029,2.25832173076298,7.60398566426325));
#39065=CARTESIAN_POINT('Ctrl Pts',(-3.44457991823455,-1.15890076455028,
7.76235457204742));
#39066=CARTESIAN_POINT('Ctrl Pts',(-0.903329893008045,-3.52025239145974,
7.9207234798316));
#39067=CARTESIAN_POINT('Ctrl Pts',(2.46094117747219,-2.6743130550109,8.07909238761578));
#39068=CARTESIAN_POINT('Ctrl Pts',(3.5830564244065,0.608184556445852,8.23746129539996));
#39069=CARTESIAN_POINT('Ctrl Pts',(1.44066014964377,3.33656711732408,8.39583020318411));
#39070=CARTESIAN_POINT('Ctrl Pts',(-2.01431708960681,3.02501379462936,8.5541991109683));
#39071=CARTESIAN_POINT('Ctrl Pts',(-3.63405631737063,-0.0426201520247982,
8.71256801875249));
#39072=CARTESIAN_POINT('Ctrl Pts',(-1.94281818018336,-3.07142301123257,
8.87093692653665));
#39073=CARTESIAN_POINT('Ctrl Pts',(1.5185155353401,-3.3018619541269,9.02930583432084));
#39074=CARTESIAN_POINT('Ctrl Pts',(3.59633448753833,-0.523984779285016,
9.18767474210499));
#39075=CARTESIAN_POINT('Ctrl Pts',(2.39754431617524,2.73129329204238,9.34604364988919));
#39076=CARTESIAN_POINT('Ctrl Pts',(-0.985640996336014,3.49809857229919,
9.50441255767334));
#39077=CARTESIAN_POINT('Ctrl Pts',(-3.47081187433309,1.07779716466894,9.66278146545754));
#39078=CARTESIAN_POINT('Ctrl Pts',(-2.79373688976881,-2.32448187472495,
9.82115037324171));
#39079=CARTESIAN_POINT('Ctrl Pts',(0.42870305280083,-3.60893273526941,9.97951928102589));
#39080=CARTESIAN_POINT('Ctrl Pts',(3.26055298240778,-1.60529624807749,10.13788818881));
#39081=CARTESIAN_POINT('Ctrl Pts',(3.121723269442,1.86092063887863,10.2962570965942));
#39082=CARTESIAN_POINT('Ctrl Pts',(0.138701231949454,3.63165854169077,10.4546260043784));
#39083=CARTESIAN_POINT('Ctrl Pts',(-2.97069106493622,2.09360368548778,10.6129949121626));
#39084=CARTESIAN_POINT('Ctrl Pts',(-3.37349600728616,-1.35192695217027,
10.7713638199467));
#39085=CARTESIAN_POINT('Ctrl Pts',(-0.702719269713518,-3.56572116452664,
10.9297327277309));
#39086=CARTESIAN_POINT('Ctrl Pts',(2.60830280055109,-2.5307979563405,11.0881016355151));
#39087=CARTESIAN_POINT('Ctrl Pts',(3.54290833255702,0.809927368520206,11.2464705432993));
#39088=CARTESIAN_POINT('Ctrl Pts',(1.24958114400447,3.41273039657815,11.4048394510835));
#39089=CARTESIAN_POINT('Ctrl Pts',(-2.1822355235614,2.90620541512237,11.5632083588676));
#39090=CARTESIAN_POINT('Ctrl Pts',(-3.62582421871883,-0.248154246652957,
11.7215772666518));
#39091=CARTESIAN_POINT('Ctrl Pts',(-1.76593578830562,-3.17642134905957,
11.879946174436));
#39092=CARTESIAN_POINT('Ctrl Pts',(1.70289122544452,-3.21066087737151,12.0383150822201));
#39093=CARTESIAN_POINT('Ctrl Pts',(3.62021936025047,-0.319677304242251,
12.1966839900043));
#39094=CARTESIAN_POINT('Ctrl Pts',(2.23917693853751,2.86256326272481,12.3550528977885));
#39095=CARTESIAN_POINT('Ctrl Pts',(-1.18197260099312,3.43673137816756,12.5134218055727));
#39096=CARTESIAN_POINT('Ctrl Pts',(-3.52623059396893,0.879704264703417,
12.6717907133568));
#39097=CARTESIAN_POINT('Ctrl Pts',(-2.65775090194473,-2.47881865782711,
12.8301596211411));
#39098=CARTESIAN_POINT('Ctrl Pts',(0.632197339137122,-3.57889764027531,
12.9885285289252));
#39099=CARTESIAN_POINT('Ctrl Pts',(3.34615255830021,-1.41825415626418,13.1468974367094));
#39100=CARTESIAN_POINT('Ctrl Pts',(3.01143862854347,2.03455626161957,13.3052663444935));
#39101=CARTESIAN_POINT('Ctrl Pts',(-0.0669876337345568,3.63368882158465,
13.4636352522777));
#39102=CARTESIAN_POINT('Ctrl Pts',(-3.08438167205765,1.92217884086064,13.6220041600619));
#39103=CARTESIAN_POINT('Ctrl Pts',(-3.29160519864739,-1.54062228057782,
13.7803730678461));
#39104=CARTESIAN_POINT('Ctrl Pts',(-0.499857505396188,-3.59976725212857,
13.9387419756303));
#39105=CARTESIAN_POINT('Ctrl Pts',(2.74730880042816,-2.37917551900835,14.0971108834144));
#39106=CARTESIAN_POINT('Ctrl Pts',(3.49141063549228,1.00907560149324,14.2554797911986));
#39107=CARTESIAN_POINT('Ctrl Pts',(1.05449914101583,3.47796109191871,14.4138486989828));
#39108=CARTESIAN_POINT('Ctrl Pts',(-2.34316322861594,2.77808708989957,14.572217606767));
#39109=CARTESIAN_POINT('Ctrl Pts',(-3.60597689618556,-0.452893386206675,
14.7305865145511));
#39110=CARTESIAN_POINT('Ctrl Pts',(-1.58339627179364,-3.27124411233226,
14.8889554223353));
#39111=CARTESIAN_POINT('Ctrl Pts',(1.88181175237025,-3.10917454036161,15.0473243301195));
#39112=CARTESIAN_POINT('Ctrl Pts',(3.63250696406091,-0.114345752568428,
15.2056932379037));
#39113=CARTESIAN_POINT('Ctrl Pts',(2.07363642186069,2.98466309495445,15.3640621456878));
#39114=CARTESIAN_POINT('Ctrl Pts',(-1.3745177904283,3.36435471203218,15.522431053472));
#39115=CARTESIAN_POINT('Ctrl Pts',(-3.57035313485565,0.678793260448534,
15.6807999612562));
#39116=CARTESIAN_POINT('Ctrl Pts',(-2.51325088571015,-2.62521462236299,
15.8391688690404));
#39117=CARTESIAN_POINT('Ctrl Pts',(0.833666400131346,-3.53739763808404,
15.9975377768245));
#39118=CARTESIAN_POINT('Ctrl Pts',(3.42103282912131,-1.22666874946649,16.1559066846087));
#39119=CARTESIAN_POINT('Ctrl Pts',(2.89150693293287,2.20167428284837,16.3142755923929));
#39120=CARTESIAN_POINT('Ctrl Pts',(-0.272461911328257,3.62407860504538,
16.4726445001771));
#39121=CARTESIAN_POINT('Ctrl Pts',(-3.18819154166072,1.74459650144857,16.6310134079612));
#39122=CARTESIAN_POINT('Ctrl Pts',(-3.19916984495366,-1.72438255620852,
16.7893823157454));
#39123=CARTESIAN_POINT('Ctrl Pts',(-0.29539442793911,-3.62228104133726,
16.9477512235296));
#39124=CARTESIAN_POINT('Ctrl Pts',(2.87751381050283,-2.21993250648107,17.1061201313138));
#39125=CARTESIAN_POINT('Ctrl Pts',(3.42872842851207,1.20499328643291,17.2644890390979));
#39126=CARTESIAN_POINT('Ctrl Pts',(0.856038843606223,3.53204642471219,17.4228579468821));
#39127=CARTESIAN_POINT('Ctrl Pts',(-2.49658422541149,2.64107652748156,17.5812268546663));
#39128=CARTESIAN_POINT('Ctrl Pts',(-3.57457879361101,-0.656195610212313,
17.7395957624505));
#39129=CARTESIAN_POINT('Ctrl Pts',(-1.39578274133968,-3.35556095880372,
17.8979646702347));
#39130=CARTESIAN_POINT('Ctrl Pts',(2.05470079874548,-2.99777882317738,18.0563335780188));
#39131=CARTESIAN_POINT('Ctrl Pts',(3.63316395418835,0.0914490823390936,
18.214702485803));
#39132=CARTESIAN_POINT('Ctrl Pts',(1.90144157325746,3.09701639513276,18.3730713935872));
#39133=CARTESIAN_POINT('Ctrl Pts',(-1.56263777564272,3.28155433635805,18.5314403013714));
#39134=CARTESIAN_POINT('Ctrl Pts',(-3.60308026145187,0.47503126817419,18.6898092091555));
#39135=CARTESIAN_POINT('Ctrl Pts',(-2.36061813094683,-2.76190423084517,
18.8481781169397));
#39136=CARTESIAN_POINT('Ctrl Pts',(1.03229853401496,-3.48708097537846,19.0065470247239));
#39137=CARTESIAN_POINT('Ctrl Pts',(3.48536252450907,-1.02600760740019,19.164915932508));
#39138=CARTESIAN_POINT('Ctrl Pts',(3.00239128577455,1.22402918834916,19.2704952043642));
#39139=CARTESIAN_POINT('Ctrl Pts',(2.33906170208295,1.99986569877995,19.3232848402922));
#39140=CARTESIAN_POINT('Ctrl Pts',(0.746306651681278,-2.79157576665282,
-0.106166650550309));
#39141=CARTESIAN_POINT('Ctrl Pts',(1.67223622398558,-2.54403550389017,-0.0533770146222503));
#39142=CARTESIAN_POINT('Ctrl Pts',(3.24268507292766,-1.05982779669291,0.0522022572338669));
#39143=CARTESIAN_POINT('Ctrl Pts',(2.6534650731888,2.14926606411138,0.210571165018042));
#39144=CARTESIAN_POINT('Ctrl Pts',(-0.357682584076165,3.39270859312819,
0.368940072802219));
#39145=CARTESIAN_POINT('Ctrl Pts',(-3.04072829396782,1.54878528015627,0.527308980586394));
#39146=CARTESIAN_POINT('Ctrl Pts',(-2.95452992250576,-1.70815807339205,
0.68567788837057));
#39147=CARTESIAN_POINT('Ctrl Pts',(-0.175865267296476,-3.40779769180092,
0.844046796154745));
#39148=CARTESIAN_POINT('Ctrl Pts',(2.76271393702636,-2.00313000159674,1.00241570393892));
#39149=CARTESIAN_POINT('Ctrl Pts',(3.18435839018718,1.22685880116299,1.16078461172309));
#39150=CARTESIAN_POINT('Ctrl Pts',(0.704657322436346,3.33891608823015,1.31915351950727));
#39151=CARTESIAN_POINT('Ctrl Pts',(-2.41700952929224,2.40897289227878,1.47752242729144));
#39152=CARTESIAN_POINT('Ctrl Pts',(-3.33657026206665,-0.715817532379567,
1.63589133507562));
#39153=CARTESIAN_POINT('Ctrl Pts',(-1.21617982955205,-3.18840813389497,
1.7942602428598));
#39154=CARTESIAN_POINT('Ctrl Pts',(2.01226174825295,-2.75606087831087,1.95262915064397));
#39155=CARTESIAN_POINT('Ctrl Pts',(3.40734133280407,0.187330513505284,2.11099805842815));
#39156=CARTESIAN_POINT('Ctrl Pts',(1.69800108538207,2.96004268849728,2.26936696621232));
#39157=CARTESIAN_POINT('Ctrl Pts',(-1.55838171690348,3.03587076679338,2.4277358739965));
#39158=CARTESIAN_POINT('Ctrl Pts',(-3.39492829062034,0.345725653439304,
2.58610478178067));
#39159=CARTESIAN_POINT('Ctrl Pts',(-2.13836604233647,-2.65940859709953,
2.74447368956486));
#39160=CARTESIAN_POINT('Ctrl Pts',(1.06645469713818,-3.24156420087077,2.90284259734902));
#39161=CARTESIAN_POINT('Ctrl Pts',(3.29963196167206,-0.87034066480747,3.0612115051332));
#39162=CARTESIAN_POINT('Ctrl Pts',(2.52652481095076,2.29384747252421,3.21958041291738));
#39163=CARTESIAN_POINT('Ctrl Pts',(-0.548491187817377,3.36811837123105,
3.37794932070155));
#39164=CARTESIAN_POINT('Ctrl Pts',(-3.12377858785101,1.37370712067109,3.53631822848573));
#39165=CARTESIAN_POINT('Ctrl Pts',(-2.8530010639088,-1.87228438993549,3.6946871362699));
#39166=CARTESIAN_POINT('Ctrl Pts',(0.0171368193147903,-3.41244344288364,
3.85305604405408));
#39167=CARTESIAN_POINT('Ctrl Pts',(2.8716614014058,-1.84353592652772,4.01142495183826));
#39168=CARTESIAN_POINT('Ctrl Pts',(3.10982424547006,1.40501141556627,4.16979385962243));
#39169=CARTESIAN_POINT('Ctrl Pts',(0.514635928994152,3.37345724415162,4.32816276740661));
#39170=CARTESIAN_POINT('Ctrl Pts',(-2.5494355758621,2.26835670944009,4.48653167519078));
#39171=CARTESIAN_POINT('Ctrl Pts',(-3.29072428697737,-0.903436541076219,
4.64490058297496));
#39172=CARTESIAN_POINT('Ctrl Pts',(-1.03384437418045,-3.25211157971146,
4.80326949075913));
#39173=CARTESIAN_POINT('Ctrl Pts',(2.16496792021978,-2.63779791136634,4.96163839854332));
#39174=CARTESIAN_POINT('Ctrl Pts',(3.39128470168976,0.379805198589325,5.12000730632749));
#39175=CARTESIAN_POINT('Ctrl Pts',(1.52781257931188,3.05136897790507,5.27837621411166));
#39176=CARTESIAN_POINT('Ctrl Pts',(-1.72764481413208,2.94284000805473,5.43674512189584));
#39177=CARTESIAN_POINT('Ctrl Pts',(-3.40905041125902,0.153098694643912,
5.59511402968001));
#39178=CARTESIAN_POINT('Ctrl Pts',(-1.98448082200849,-2.77613036147294,
5.75348293746419));
#39179=CARTESIAN_POINT('Ctrl Pts',(1.24814304847173,-3.17603571254481,5.91185184524837));
#39180=CARTESIAN_POINT('Ctrl Pts',(3.34358768428832,-0.682264841747166,
6.07022075303254));
#39181=CARTESIAN_POINT('Ctrl Pts',(2.39270001988976,2.43311539628292,6.22858966081672));
#39182=CARTESIAN_POINT('Ctrl Pts',(-0.738169162435656,3.33169179313424,
6.38695856860088));
#39183=CARTESIAN_POINT('Ctrl Pts',(-3.1964947254872,1.19477419906089,6.54532747638508));
#39184=CARTESIAN_POINT('Ctrl Pts',(-2.74250392385152,-2.03069843759927,
6.70369638416923));
#39185=CARTESIAN_POINT('Ctrl Pts',(0.210173640495589,-3.40600806776054,
6.86206529195343));
#39186=CARTESIAN_POINT('Ctrl Pts',(2.97136265716555,-1.67811438120623,7.02043419973758));
#39187=CARTESIAN_POINT('Ctrl Pts',(3.02535243371638,1.578704078862,7.17880310752178));
#39188=CARTESIAN_POINT('Ctrl Pts',(0.322953053292851,3.39717018151548,7.33717201530594));
#39189=CARTESIAN_POINT('Ctrl Pts',(-2.67368784570132,2.12048513801866,7.49554092309013));
#39190=CARTESIAN_POINT('Ctrl Pts',(-3.23434009593761,-1.08816729440808,
7.65390983087429));
#39191=CARTESIAN_POINT('Ctrl Pts',(-0.848195182625461,-3.30539390224222,
7.81227873865848));
#39192=CARTESIAN_POINT('Ctrl Pts',(2.31073771344569,-2.51108644543929,7.97064764644264));
#39193=CARTESIAN_POINT('Ctrl Pts',(3.3643646930986,0.571064031996978,8.12901655422683));
#39194=CARTESIAN_POINT('Ctrl Pts',(1.35272950467657,3.13291985278694,8.287385462011));
#39195=CARTESIAN_POINT('Ctrl Pts',(-1.89137331212997,2.8403821769212,8.44575436979517));
#39196=CARTESIAN_POINT('Ctrl Pts',(-3.41225180926891,-0.0400188324442784,
8.60412327757936));
#39197=CARTESIAN_POINT('Ctrl Pts',(-1.82423833629739,-2.88395880851166,
8.76249218536352));
#39198=CARTESIAN_POINT('Ctrl Pts',(1.42583298946127,-3.10033291808686,8.9208610931477));
#39199=CARTESIAN_POINT('Ctrl Pts',(3.37683233008282,-0.492003385472662,
9.07923000093188));
#39200=CARTESIAN_POINT('Ctrl Pts',(2.25121027749802,2.564588895573,9.23759890871605));
#39201=CARTESIAN_POINT('Ctrl Pts',(-0.925482430462337,3.2845922407073,9.39596781650024));
#39202=CARTESIAN_POINT('Ctrl Pts',(-3.25897098545631,1.0120138500846,9.55433672428439));
#39203=CARTESIAN_POINT('Ctrl Pts',(-2.6232212503609,-2.18260719976455,9.71270563206859));
#39204=CARTESIAN_POINT('Ctrl Pts',(0.402537176038361,-3.38866164417696,
9.87107453985274));
#39205=CARTESIAN_POINT('Ctrl Pts',(3.06154523810132,-1.50731704424391,10.0294434476369));
#39206=CARTESIAN_POINT('Ctrl Pts',(2.93118899211157,1.74733940873922,10.1878123554211));
#39207=CARTESIAN_POINT('Ctrl Pts',(0.130235606808038,3.410000381749,10.3461812632053));
#39208=CARTESIAN_POINT('Ctrl Pts',(-2.78937503325262,1.96582065323264,10.5045501709895));
#39209=CARTESIAN_POINT('Ctrl Pts',(-3.16759478916177,-1.26941213499964,
10.6629190787736));
#39210=CARTESIAN_POINT('Ctrl Pts',(-0.659828822141922,-3.34808749023676,
10.8212879865578));
#39211=CARTESIAN_POINT('Ctrl Pts',(2.44910512469472,-2.37633078610767,10.979656894342));
#39212=CARTESIAN_POINT('Ctrl Pts',(3.32666703871794,0.760493478155309,11.1380258021261));
#39213=CARTESIAN_POINT('Ctrl Pts',(1.1733129998774,3.20443450879057,11.2963947099104));
#39214=CARTESIAN_POINT('Ctrl Pts',(-2.04904284997734,2.72882526295945,11.4547636176945));
#39215=CARTESIAN_POINT('Ctrl Pts',(-3.40452215648823,-0.233008160350131,
11.6131325254787));
#39216=CARTESIAN_POINT('Ctrl Pts',(-1.6581519554046,-2.98254857623426,11.7715014332628));
#39217=CARTESIAN_POINT('Ctrl Pts',(1.59895531536931,-3.01469829605903,11.9298703410471));
#39218=CARTESIAN_POINT('Ctrl Pts',(3.3992593903726,-0.300165810466054,12.0882392488312));
#39219=CARTESIAN_POINT('Ctrl Pts',(2.10250884755856,2.68784680790165,12.2466081566154));
#39220=CARTESIAN_POINT('Ctrl Pts',(-1.10983094207061,3.2269705912561,12.4049770643995));
#39221=CARTESIAN_POINT('Ctrl Pts',(-3.3110072253574,0.826011543769279,12.5633459721838));
#39222=CARTESIAN_POINT('Ctrl Pts',(-2.49553516284214,-2.32752404237368,
12.7217148799679));
#39223=CARTESIAN_POINT('Ctrl Pts',(0.593611195284521,-3.36045974022041,
12.8800837877521));
#39224=CARTESIAN_POINT('Ctrl Pts',(3.14192024668758,-1.3316910603678,13.0384526955363));
#39225=CARTESIAN_POINT('Ctrl Pts',(2.82763557065198,1.91037718694295,13.1968216033204));
#39226=CARTESIAN_POINT('Ctrl Pts',(-0.0628990457073522,3.41190674357617,
13.3551905111046));
#39227=CARTESIAN_POINT('Ctrl Pts',(-2.89612653789845,1.80485871837307,13.5135594188888));
#39228=CARTESIAN_POINT('Ctrl Pts',(-3.09070218334153,-1.44659045022871,
13.671928326673));
#39229=CARTESIAN_POINT('Ctrl Pts',(-0.469348718954053,-3.38005557599891,
13.8302972344571));
#39230=CARTESIAN_POINT('Ctrl Pts',(2.57962689792991,-2.23396261926356,13.9886661422413));
#39231=CARTESIAN_POINT('Ctrl Pts',(3.27831250190397,0.947486705262652,14.1470350500255));
#39232=CARTESIAN_POINT('Ctrl Pts',(0.990137820540776,3.26568385078115,14.3054039578097));
#39233=CARTESIAN_POINT('Ctrl Pts',(-2.20014833783372,2.60852663551323,14.4637728655938));
#39234=CARTESIAN_POINT('Ctrl Pts',(-3.38588621463462,-0.425251053238435,
14.6221417733781));
#39235=CARTESIAN_POINT('Ctrl Pts',(-1.48675373229403,-3.07158383526162,
14.7805106811622));
#39236=CARTESIAN_POINT('Ctrl Pts',(1.7669554338043,-2.91940617429889,14.9388795889464));
#39237=CARTESIAN_POINT('Ctrl Pts',(3.41079702068761,-0.107366663311963,
15.0972484967305));
#39238=CARTESIAN_POINT('Ctrl Pts',(1.94707209088592,2.8024942808771,15.2556174045147));
#39239=CARTESIAN_POINT('Ctrl Pts',(-1.29062414218578,3.15901143256371,15.4139863122989));
#39240=CARTESIAN_POINT('Ctrl Pts',(-3.35243674840872,0.637363136067446,
15.5723552200831));
#39241=CARTESIAN_POINT('Ctrl Pts',(-2.35985470035756,-2.46498473401718,
15.7307241278673));
#39242=CARTESIAN_POINT('Ctrl Pts',(0.782783598750917,-3.32149268930132,
15.8890930356514));
#39243=CARTESIAN_POINT('Ctrl Pts',(3.21223020263583,-1.15179906258833,16.0474619434356));
#39244=CARTESIAN_POINT('Ctrl Pts',(2.71502390214816,2.06729516522899,16.2058308512198));
#39245=CARTESIAN_POINT('Ctrl Pts',(-0.255832207509483,3.40288308628807,
16.364199759004));
#39246=CARTESIAN_POINT('Ctrl Pts',(-2.99360037551616,1.63811511122076,16.5225686667881));
#39247=CARTESIAN_POINT('Ctrl Pts',(-3.0039086184278,-1.61913492346524,16.6809375745723));
#39248=CARTESIAN_POINT('Ctrl Pts',(-0.277365038721381,-3.40119523682191,
16.8393064823565));
#39249=CARTESIAN_POINT('Ctrl Pts',(2.70188484948655,-2.0844389987813,16.9976753901407));
#39250=CARTESIAN_POINT('Ctrl Pts',(3.21945610137027,1.13144656072985,17.1560442979248));
#39251=CARTESIAN_POINT('Ctrl Pts',(0.803790540872318,3.31646808706206,17.314413205709));
#39252=CARTESIAN_POINT('Ctrl Pts',(-2.34420528912341,2.47987850827725,17.4727821134932));
#39253=CARTESIAN_POINT('Ctrl Pts',(-3.35640449422057,-0.616144732671989,
17.6311510212774));
#39254=CARTESIAN_POINT('Ctrl Pts',(-1.31059118751595,-3.15075440577503,
17.7895199290615));
#39255=CARTESIAN_POINT('Ctrl Pts',(1.92929220290631,-2.81480949105824,17.9478888368457));
#39256=CARTESIAN_POINT('Ctrl Pts',(3.41141391144418,0.0858674905988609,
18.1062577446299));
#39257=CARTESIAN_POINT('Ctrl Pts',(1.78538714921769,2.90799010106519,18.264626652414));
#39258=CARTESIAN_POINT('Ctrl Pts',(-1.46726223027463,3.08126477510226,18.4229955601983));
#39259=CARTESIAN_POINT('Ctrl Pts',(-3.38316637590686,0.44603775030638,18.5813644679824));
#39260=CARTESIAN_POINT('Ctrl Pts',(-2.21653788077352,-2.59333149673027,
18.7397333757666));
#39261=CARTESIAN_POINT('Ctrl Pts',(0.969292226859822,-3.27424710245315,
18.8981022835507));
#39262=CARTESIAN_POINT('Ctrl Pts',(3.27263353717619,-0.963385266744592,
19.056471191335));
#39263=CARTESIAN_POINT('Ctrl Pts',(2.81914043215213,1.14932060699719,19.1620504631911));
#39264=CARTESIAN_POINT('Ctrl Pts',(2.19629714783811,1.87780396146808,19.2148400991191));
#39265=CARTESIAN_POINT('Ctrl Pts',(0.697794938882252,-2.61011668204799,
-0.214611391723435));
#39266=CARTESIAN_POINT('Ctrl Pts',(1.56353688002641,-2.37866712691375,-0.161821755795376));
#39267=CARTESIAN_POINT('Ctrl Pts',(3.03190280721802,-0.990936461510826,
-0.056242483939259));
#39268=CARTESIAN_POINT('Ctrl Pts',(2.48098351314537,2.00955864250931,0.102126423844917));
#39269=CARTESIAN_POINT('Ctrl Pts',(-0.334432362799391,3.17217444069923,
0.260495331629093));
#39270=CARTESIAN_POINT('Ctrl Pts',(-2.84307370069235,1.44811054205896,0.418864239413268));
#39271=CARTESIAN_POINT('Ctrl Pts',(-2.76247842901601,-1.59712372352387,
0.577233147197444));
#39272=CARTESIAN_POINT('Ctrl Pts',(-0.164433605366102,-3.18628271196066,
0.73560205498162));
#39273=CARTESIAN_POINT('Ctrl Pts',(2.58313094020199,-1.87292177269022,0.893970962765795));
#39274=CARTESIAN_POINT('Ctrl Pts',(2.97736749800375,1.14711005220988,1.05233987054997));
#39275=CARTESIAN_POINT('Ctrl Pts',(0.658852915399703,3.12187857695061,1.21070877833415));
#39276=CARTESIAN_POINT('Ctrl Pts',(-2.25989814370645,2.25238390727161,1.36907768611832));
#39277=CARTESIAN_POINT('Ctrl Pts',(-3.1196852350841,-0.66928768507206,1.5274465939025));
#39278=CARTESIAN_POINT('Ctrl Pts',(-1.13712523923012,-2.98115399870921,
1.68581550168667));
#39279=CARTESIAN_POINT('Ctrl Pts',(1.88145993402846,-2.576910346175,1.84418440947086));
#39280=CARTESIAN_POINT('Ctrl Pts',(3.18585601738733,0.175153583219069,2.00255331725503));
#39281=CARTESIAN_POINT('Ctrl Pts',(1.58762696396573,2.76763285206644,2.16092222503921));
#39282=CARTESIAN_POINT('Ctrl Pts',(-1.45708318752367,2.8385319243727,2.31929113282338));
#39283=CARTESIAN_POINT('Ctrl Pts',(-3.17424985255893,0.323252661179191,
2.47766004060756));
#39284=CARTESIAN_POINT('Ctrl Pts',(-1.99936714815359,-2.48654069382262,
2.63602894839173));
#39285=CARTESIAN_POINT('Ctrl Pts',(0.997132597617568,-3.03085479451885,
2.7943978561759));
#39286=CARTESIAN_POINT('Ctrl Pts',(3.08514801233767,-0.813766445251292,
2.95276676396009));
#39287=CARTESIAN_POINT('Ctrl Pts',(2.36229467079009,2.14474191445211,3.11113567174426));
#39288=CARTESIAN_POINT('Ctrl Pts',(-0.512837952091488,3.14918264188951,
3.26950457952844));
#39289=CARTESIAN_POINT('Ctrl Pts',(-2.92072552734273,1.28441288061864,3.4278734873126));
#39290=CARTESIAN_POINT('Ctrl Pts',(-2.66754918844198,-1.75058143794112,
3.58624239509679));
#39291=CARTESIAN_POINT('Ctrl Pts',(0.0160228851765723,-3.19062647813978,
3.74461130288096));
#39292=CARTESIAN_POINT('Ctrl Pts',(2.6849965594843,-1.72370169323913,3.90298021066514));
#39293=CARTESIAN_POINT('Ctrl Pts',(2.90767825050696,1.31368232166397,4.06134911844931));
#39294=CARTESIAN_POINT('Ctrl Pts',(0.48118336585917,3.15417447533345,4.21971802623349));
#39295=CARTESIAN_POINT('Ctrl Pts',(-2.38371618132472,2.12090811178094,4.37808693401766));
#39296=CARTESIAN_POINT('Ctrl Pts',(-3.0768193577489,-0.844711010606807,
4.53645584180184));
#39297=CARTESIAN_POINT('Ctrl Pts',(-0.966642023449493,-3.04071656857237,
4.69482474958602));
#39298=CARTESIAN_POINT('Ctrl Pts',(2.02423984051125,-2.46633475421801,4.85319365737019));
#39299=CARTESIAN_POINT('Ctrl Pts',(3.17084310560123,0.355116954591987,5.01156256515437));
#39300=CARTESIAN_POINT('Ctrl Pts',(1.42850111680335,2.85302271478855,5.16993147293854));
#39301=CARTESIAN_POINT('Ctrl Pts',(-1.61534377962691,2.75154838689254,5.32830038072272));
#39302=CARTESIAN_POINT('Ctrl Pts',(-3.18745400166542,0.143146914249436,
5.48666928850689));
#39303=CARTESIAN_POINT('Ctrl Pts',(-1.85548483426596,-2.59567526505241,
5.64503819629107));
#39304=CARTESIAN_POINT('Ctrl Pts',(1.1670107726664,-2.96958581426328,5.80340710407524));
#39305=CARTESIAN_POINT('Ctrl Pts',(3.12624650812014,-0.637915999376343,
5.96177601185942));
#39306=CARTESIAN_POINT('Ctrl Pts',(2.23716881040954,2.27495709091949,6.1201449196436));
#39307=CARTESIAN_POINT('Ctrl Pts',(-0.690186405850939,3.1151238782707,6.27851382742777));
#39308=CARTESIAN_POINT('Ctrl Pts',(-2.98871494255602,1.1171110257876,6.43688273521195));
#39309=CARTESIAN_POINT('Ctrl Pts',(-2.56423462609788,-1.89869819458346,
6.59525164299611));
#39310=CARTESIAN_POINT('Ctrl Pts',(0.19651185245889,-3.18460941775236,6.75362055078031));
#39311=CARTESIAN_POINT('Ctrl Pts',(2.77821699576559,-1.56903294300439,6.91198945856447));
#39312=CARTESIAN_POINT('Ctrl Pts',(2.82869730803894,1.47608454747249,7.07035836634865));
#39313=CARTESIAN_POINT('Ctrl Pts',(0.30196033437012,3.17634601519748,7.22872727413282));
#39314=CARTESIAN_POINT('Ctrl Pts',(-2.49989175719976,1.98264854527436,7.387096181917));
#39315=CARTESIAN_POINT('Ctrl Pts',(-3.02410027364065,-1.01743382426589,
7.54546508970118));
#39316=CARTESIAN_POINT('Ctrl Pts',(-0.793060472242878,-3.09053541302469,
7.70383399748535));
#39317=CARTESIAN_POINT('Ctrl Pts',(2.16053424941917,-2.34785983586768,7.86220290526953));
#39318=CARTESIAN_POINT('Ctrl Pts',(3.1456729617907,0.533943507548107,8.0205718130537));
#39319=CARTESIAN_POINT('Ctrl Pts',(1.26479885970938,2.92927258824979,8.17894072083787));
#39320=CARTESIAN_POINT('Ctrl Pts',(-1.76842953465313,2.65575055921304,8.33730962862206));
#39321=CARTESIAN_POINT('Ctrl Pts',(-3.19044730116719,-0.0374175128637604,
8.49567853640622));
#39322=CARTESIAN_POINT('Ctrl Pts',(-1.70565849241141,-2.69649460579077,
8.65404744419042));
#39323=CARTESIAN_POINT('Ctrl Pts',(1.33315044358244,-2.89880388204682,8.81241635197457));
#39324=CARTESIAN_POINT('Ctrl Pts',(3.1573301726273,-0.460021991660309,8.97078525975877));
#39325=CARTESIAN_POINT('Ctrl Pts',(2.10487623882079,2.39788449910363,9.12915416754292));
#39326=CARTESIAN_POINT('Ctrl Pts',(-0.865323864588658,3.07108590911539,
9.28752307532712));
#39327=CARTESIAN_POINT('Ctrl Pts',(-3.04713009657952,0.946230535500251,
9.44589198311128));
#39328=CARTESIAN_POINT('Ctrl Pts',(-2.45270561095299,-2.04073252480415,
9.60426089089545));
#39329=CARTESIAN_POINT('Ctrl Pts',(0.37637129927589,-3.16839055308451,9.76262979867964));
#39330=CARTESIAN_POINT('Ctrl Pts',(2.86253749379487,-1.40933784041033,9.9209987064638));
#39331=CARTESIAN_POINT('Ctrl Pts',(2.74065471478115,1.63375817859982,10.079367614248));
#39332=CARTESIAN_POINT('Ctrl Pts',(0.121769981666623,3.18834222180723,10.2377365220322));
#39333=CARTESIAN_POINT('Ctrl Pts',(-2.60805900156902,1.8380376209775,10.3961054298164));
#39334=CARTESIAN_POINT('Ctrl Pts',(-2.96169357103739,-1.18689731782901,
10.5544743376005));
#39335=CARTESIAN_POINT('Ctrl Pts',(-0.616938374570327,-3.13045381594687,
10.7128432453847));
#39336=CARTESIAN_POINT('Ctrl Pts',(2.28990744883834,-2.22186361587486,10.8712121531689));
#39337=CARTESIAN_POINT('Ctrl Pts',(3.11042574487886,0.711059587790419,11.029581060953));
#39338=CARTESIAN_POINT('Ctrl Pts',(1.09704485575034,2.99613862100298,11.1879499687372));
#39339=CARTESIAN_POINT('Ctrl Pts',(-1.91585017639328,2.55144511079655,11.3463188765214));
#39340=CARTESIAN_POINT('Ctrl Pts',(-3.18322009425763,-0.217862074047309,
11.5046877843056));
#39341=CARTESIAN_POINT('Ctrl Pts',(-1.55036812250359,-2.78867580340896,
11.6630566920897));
#39342=CARTESIAN_POINT('Ctrl Pts',(1.49501940529411,-2.81873571474656,11.821425599874));
#39343=CARTESIAN_POINT('Ctrl Pts',(3.17829942049473,-0.280654316689852,
11.9797945076581));
#39344=CARTESIAN_POINT('Ctrl Pts',(1.96584075657961,2.51313035307848,12.1381634154423));
#39345=CARTESIAN_POINT('Ctrl Pts',(-1.03768928314808,3.01720980434465,12.2965323232264));
#39346=CARTESIAN_POINT('Ctrl Pts',(-3.09578385674587,0.772318822835137,
12.4549012310106));
#39347=CARTESIAN_POINT('Ctrl Pts',(-2.33331942373952,-2.17622942692025,
12.6132701387948));
#39348=CARTESIAN_POINT('Ctrl Pts',(0.555025051431915,-3.14202184016551,
12.771639046579));
#39349=CARTESIAN_POINT('Ctrl Pts',(2.93768793507494,-1.24512796447142,12.9300079543632));
#39350=CARTESIAN_POINT('Ctrl Pts',(2.64383251276049,1.78619811226633,13.0883768621473));
#39351=CARTESIAN_POINT('Ctrl Pts',(-0.0588104576801453,3.19012466556769,
13.2467457699315));
#39352=CARTESIAN_POINT('Ctrl Pts',(-2.70787140373924,1.6875385958855,13.4051146777157));
#39353=CARTESIAN_POINT('Ctrl Pts',(-2.88979916803567,-1.35255861987959,
13.5634835854999));
#39354=CARTESIAN_POINT('Ctrl Pts',(-0.438839932511918,-3.16034389986926,
13.721852493284));
#39355=CARTESIAN_POINT('Ctrl Pts',(2.41194499543166,-2.08874971951875,13.8802214010682));
#39356=CARTESIAN_POINT('Ctrl Pts',(3.06521436831565,0.885897809032061,14.0385903088524));
#39357=CARTESIAN_POINT('Ctrl Pts',(0.925776500065717,3.05340660964359,14.1969592166366));
#39358=CARTESIAN_POINT('Ctrl Pts',(-2.0571334470515,2.43896618112689,14.3553281244207));
#39359=CARTESIAN_POINT('Ctrl Pts',(-3.16579553308368,-0.397608720270194,
14.5136970322049));
#39360=CARTESIAN_POINT('Ctrl Pts',(-1.39011119279443,-2.871923558191,14.6720659399891));
#39361=CARTESIAN_POINT('Ctrl Pts',(1.65209911523836,-2.72963780823618,14.8304348477733));
#39362=CARTESIAN_POINT('Ctrl Pts',(3.18908707731431,-0.100387574055494,
14.9888037555574));
#39363=CARTESIAN_POINT('Ctrl Pts',(1.82050775991116,2.62032546679975,15.1471726633416));
#39364=CARTESIAN_POINT('Ctrl Pts',(-1.20673049394325,2.95366815309523,15.3055415711258));
#39365=CARTESIAN_POINT('Ctrl Pts',(-3.13452036196177,0.595933011686356,
15.46391047891));
#39366=CARTESIAN_POINT('Ctrl Pts',(-2.20645851500496,-2.30475484567138,
15.6222793866941));
#39367=CARTESIAN_POINT('Ctrl Pts',(0.731900797370488,-3.1055877405186,15.7806482944783));
#39368=CARTESIAN_POINT('Ctrl Pts',(3.00342757615037,-1.07692937571016,15.9390172022625));
#39369=CARTESIAN_POINT('Ctrl Pts',(2.53854087136345,1.93291604760962,16.0973861100467));
#39370=CARTESIAN_POINT('Ctrl Pts',(-0.239202503690712,3.18168756753077,
16.2557550178309));
#39371=CARTESIAN_POINT('Ctrl Pts',(-2.79900920937161,1.53163372099295,16.414123925615));
#39372=CARTESIAN_POINT('Ctrl Pts',(-2.80864739190195,-1.51388729072196,
16.5724928333992));
#39373=CARTESIAN_POINT('Ctrl Pts',(-0.259335649503649,-3.18010943230655,
16.7308617411834));
#39374=CARTESIAN_POINT('Ctrl Pts',(2.52625588847025,-1.94894549108153,16.8892306489676));
#39375=CARTESIAN_POINT('Ctrl Pts',(3.01018377422847,1.05789983502679,17.0475995567517));
#39376=CARTESIAN_POINT('Ctrl Pts',(0.751542238138412,3.10088974941192,17.2059684645359));
#39377=CARTESIAN_POINT('Ctrl Pts',(-2.19182635283533,2.31868048907294,17.3643373723201));
#39378=CARTESIAN_POINT('Ctrl Pts',(-3.13823019483013,-0.576093855131663,
17.5227062801042));
#39379=CARTESIAN_POINT('Ctrl Pts',(-1.22539963369223,-2.94594785274635,
17.6810751878884));
#39380=CARTESIAN_POINT('Ctrl Pts',(1.80388360706713,-2.63184015893912,17.8394440956726));
#39381=CARTESIAN_POINT('Ctrl Pts',(3.18966386870002,0.0802858988586278,
17.9978130034568));
#39382=CARTESIAN_POINT('Ctrl Pts',(1.66933272517792,2.71896380699763,18.1561819112409));
#39383=CARTESIAN_POINT('Ctrl Pts',(-1.37188668490652,2.88097521384648,18.3145508190252));
#39384=CARTESIAN_POINT('Ctrl Pts',(-3.16325249036186,0.417044232438571,
18.4729197268093));
#39385=CARTESIAN_POINT('Ctrl Pts',(-2.0724576306002,-2.42475876261538,18.6312886345935));
#39386=CARTESIAN_POINT('Ctrl Pts',(0.906285919704686,-3.06141322952783,
18.7896575423776));
#39387=CARTESIAN_POINT('Ctrl Pts',(3.05990454984331,-0.900762926088991,
18.9480264501619));
#39388=CARTESIAN_POINT('Ctrl Pts',(2.63588957852971,1.07461202564522,19.053605722018));
#39389=CARTESIAN_POINT('Ctrl Pts',(2.05353259359326,1.75574222415622,19.106395357946));
#39390=CARTESIAN_POINT('Ctrl Pts',(0.649283226083226,-2.42865759744316,
-0.323056132896561));
#39391=CARTESIAN_POINT('Ctrl Pts',(1.45483753606724,-2.21329874993732,-0.270266496968503));
#39392=CARTESIAN_POINT('Ctrl Pts',(2.82112054150838,-0.922045126328744,
-0.164687225112385));
#39393=CARTESIAN_POINT('Ctrl Pts',(2.30850195310193,1.86985122090724,-0.00631831732820976));
#39394=CARTESIAN_POINT('Ctrl Pts',(-0.311182141522623,2.95164028827028,
0.152050590455966));
#39395=CARTESIAN_POINT('Ctrl Pts',(-2.64541910741689,1.34743580396164,0.310419498240141));
#39396=CARTESIAN_POINT('Ctrl Pts',(-2.57042693552626,-1.48608937365568,
0.468788406024318));
#39397=CARTESIAN_POINT('Ctrl Pts',(-0.153001943435726,-2.96476773212039,
0.627157313808493));
#39398=CARTESIAN_POINT('Ctrl Pts',(2.40354794337761,-1.7427135437837,0.785526221592669));
#39399=CARTESIAN_POINT('Ctrl Pts',(2.77037660582034,1.06736130325675,0.943895129376844));
#39400=CARTESIAN_POINT('Ctrl Pts',(0.613048508363059,2.90484106567108,1.10226403716102));
#39401=CARTESIAN_POINT('Ctrl Pts',(-2.10278675812066,2.09579492226445,1.2606329449452));
#39402=CARTESIAN_POINT('Ctrl Pts',(-2.90280020810156,-0.622757837764556,
1.41900185272937));
#39403=CARTESIAN_POINT('Ctrl Pts',(-1.05807064890818,-2.77389986352343,
1.57737076051355));
#39404=CARTESIAN_POINT('Ctrl Pts',(1.75065811980397,-2.39775981403912,1.73573966829772));
#39405=CARTESIAN_POINT('Ctrl Pts',(2.9643707019706,0.162976652932851,1.8941085760819));
#39406=CARTESIAN_POINT('Ctrl Pts',(1.4772528425494,2.57522301563561,2.05247748386607));
#39407=CARTESIAN_POINT('Ctrl Pts',(-1.35578465814388,2.64119308195202,2.21084639165025));
#39408=CARTESIAN_POINT('Ctrl Pts',(-2.95357141449753,0.30077966891908,2.36921529943442));
#39409=CARTESIAN_POINT('Ctrl Pts',(-1.86036825397072,-2.3136727905457,2.5275842072186));
#39410=CARTESIAN_POINT('Ctrl Pts',(0.927810498096964,-2.82014538816694,
2.68595311500277));
#39411=CARTESIAN_POINT('Ctrl Pts',(2.87066406300329,-0.757192225695111,
2.84432202278695));
#39412=CARTESIAN_POINT('Ctrl Pts',(2.19806453062942,1.99563635637999,3.00269093057112));
#39413=CARTESIAN_POINT('Ctrl Pts',(-0.477184716365594,2.93024691254798,
3.16105983835531));
#39414=CARTESIAN_POINT('Ctrl Pts',(-2.71767246683444,1.19511864056618,3.31942874613947));
#39415=CARTESIAN_POINT('Ctrl Pts',(-2.48209731297516,-1.62887848594674,
3.47779765392366));
#39416=CARTESIAN_POINT('Ctrl Pts',(0.0149089510383518,-2.96880951339593,
3.63616656170783));
#39417=CARTESIAN_POINT('Ctrl Pts',(2.49833171756281,-1.60386745995054,3.79453546949201));
#39418=CARTESIAN_POINT('Ctrl Pts',(2.70553225554386,1.22235322776168,3.95290437727618));
#39419=CARTESIAN_POINT('Ctrl Pts',(0.447730802724189,2.93489170651531,4.11127328506035));
#39420=CARTESIAN_POINT('Ctrl Pts',(-2.21799678678734,1.97345951412179,4.26964219284454));
#39421=CARTESIAN_POINT('Ctrl Pts',(-2.86291442852043,-0.785985480137393,
4.42801110062871));
#39422=CARTESIAN_POINT('Ctrl Pts',(-0.899439672718537,-2.82932155743327,
4.58638000841288));
#39423=CARTESIAN_POINT('Ctrl Pts',(1.88351176080272,-2.29487159706967,4.74474891619707));
#39424=CARTESIAN_POINT('Ctrl Pts',(2.95040150951271,0.330428710594652,4.90311782398123));
#39425=CARTESIAN_POINT('Ctrl Pts',(1.32918965429481,2.65467645167202,5.06148673176541));
#39426=CARTESIAN_POINT('Ctrl Pts',(-1.50304274512173,2.56025676573035,5.21985563954959));
#39427=CARTESIAN_POINT('Ctrl Pts',(-2.96585759207181,0.133195133854954,
5.37822454733376));
#39428=CARTESIAN_POINT('Ctrl Pts',(-1.72648884652342,-2.41522016863187,
5.53659345511794));
#39429=CARTESIAN_POINT('Ctrl Pts',(1.08587849686107,-2.76313591598177,5.69496236290211));
#39430=CARTESIAN_POINT('Ctrl Pts',(2.90890533195194,-0.593567157005514,
5.85333127068629));
#39431=CARTESIAN_POINT('Ctrl Pts',(2.08163760092934,2.11679878555605,6.01170017847047));
#39432=CARTESIAN_POINT('Ctrl Pts',(-0.642203649266225,2.89855596340717,
6.17006908625463));
#39433=CARTESIAN_POINT('Ctrl Pts',(-2.78093515962483,1.03944785251432,6.32843799403883));
#39434=CARTESIAN_POINT('Ctrl Pts',(-2.38596532834426,-1.76669795156764,
6.48680690182298));
#39435=CARTESIAN_POINT('Ctrl Pts',(0.182850064422192,-2.96321076774417,
6.64517580960718));
#39436=CARTESIAN_POINT('Ctrl Pts',(2.58507133436564,-1.45995150480255,6.80354471739134));
#39437=CARTESIAN_POINT('Ctrl Pts',(2.63204218236152,1.37346501608299,6.96191362517552));
#39438=CARTESIAN_POINT('Ctrl Pts',(0.280967615447384,2.95552184887948,7.12028253295969));
#39439=CARTESIAN_POINT('Ctrl Pts',(-2.32609566869819,1.84481195253004,7.27865144074388));
#39440=CARTESIAN_POINT('Ctrl Pts',(-2.81386045134371,-0.946700354123697,
7.43702034852803));
#39441=CARTESIAN_POINT('Ctrl Pts',(-0.737925761860293,-2.87567692380717,
7.59538925631224));
#39442=CARTESIAN_POINT('Ctrl Pts',(2.01033078539266,-2.18463322629606,7.75375816409638));
#39443=CARTESIAN_POINT('Ctrl Pts',(2.9269812304828,0.496822983099234,7.91212707188058));
#39444=CARTESIAN_POINT('Ctrl Pts',(1.17686821474219,2.72562532371265,8.07049597966474));
#39445=CARTESIAN_POINT('Ctrl Pts',(-1.64548575717628,2.47111894150488,8.22886488744892));
#39446=CARTESIAN_POINT('Ctrl Pts',(-2.96864279306547,-0.0348161932832441,
8.3872337952331));
#39447=CARTESIAN_POINT('Ctrl Pts',(-1.58707864852543,-2.50903040306986,
8.54560270301728));
#39448=CARTESIAN_POINT('Ctrl Pts',(1.24046789770362,-2.69727484600679,8.70397161080145));
#39449=CARTESIAN_POINT('Ctrl Pts',(2.93782801517178,-0.428040597847953,
8.86234051858563));
#39450=CARTESIAN_POINT('Ctrl Pts',(1.95854220014356,2.23118010263425,9.02070942636979));
#39451=CARTESIAN_POINT('Ctrl Pts',(-0.805165298714976,2.8575795775235,9.17907833415399));
#39452=CARTESIAN_POINT('Ctrl Pts',(-2.83528920770275,0.880447220915903,
9.33744724193814));
#39453=CARTESIAN_POINT('Ctrl Pts',(-2.28218997154508,-1.89885784984376,
9.49581614972234));
#39454=CARTESIAN_POINT('Ctrl Pts',(0.35020542251342,-2.94811946199206,9.6541850575065));
#39455=CARTESIAN_POINT('Ctrl Pts',(2.66352974948841,-1.31135863657675,9.81255396529068));
#39456=CARTESIAN_POINT('Ctrl Pts',(2.55012043745071,1.52017694846043,9.97092287307486));
#39457=CARTESIAN_POINT('Ctrl Pts',(0.11330435652521,2.96668406186547,10.1292917808591));
#39458=CARTESIAN_POINT('Ctrl Pts',(-2.42674296988542,1.71025458872235,10.2876606886432));
#39459=CARTESIAN_POINT('Ctrl Pts',(-2.755792352913,-1.10438250065839,10.4460295964274));
#39460=CARTESIAN_POINT('Ctrl Pts',(-0.574047926998734,-2.91282014165699,
10.6043985042116));
#39461=CARTESIAN_POINT('Ctrl Pts',(2.13070977298197,-2.06739644564203,10.7627674119958));
#39462=CARTESIAN_POINT('Ctrl Pts',(2.89418445103978,0.661625697425526,10.9211363197799));
#39463=CARTESIAN_POINT('Ctrl Pts',(1.02077671162327,2.78784273321539,11.0795052275641));
#39464=CARTESIAN_POINT('Ctrl Pts',(-1.78265750280922,2.37406495863365,11.2378741353483));
#39465=CARTESIAN_POINT('Ctrl Pts',(-2.96191803202705,-0.202715987744488,
11.3962430431325));
#39466=CARTESIAN_POINT('Ctrl Pts',(-1.44258428960257,-2.59480303058365,
11.5546119509167));
#39467=CARTESIAN_POINT('Ctrl Pts',(1.39108349521891,-2.6227731334341,11.7129808587008));
#39468=CARTESIAN_POINT('Ctrl Pts',(2.95733945061687,-0.261142822913652,
11.871349766485));
#39469=CARTESIAN_POINT('Ctrl Pts',(1.82917266560066,2.33841389825531,12.0297186742692));
#39470=CARTESIAN_POINT('Ctrl Pts',(-0.965547624225554,2.80744901743319,
12.1880875820533));
#39471=CARTESIAN_POINT('Ctrl Pts',(-2.88056048813434,0.718626101900998,
12.3464564898375));
#39472=CARTESIAN_POINT('Ctrl Pts',(-2.17110368463692,-2.02493481146681,
12.5048253976217));
#39473=CARTESIAN_POINT('Ctrl Pts',(0.51643890757931,-2.92358394011061,12.6631943054059));
#39474=CARTESIAN_POINT('Ctrl Pts',(2.73345562346231,-1.15856486857504,12.8215632131901));
#39475=CARTESIAN_POINT('Ctrl Pts',(2.460029454869,1.66201903758971,12.9799321209742));
#39476=CARTESIAN_POINT('Ctrl Pts',(-0.0547218696529407,2.96834258755921,
13.1383010287584));
#39477=CARTESIAN_POINT('Ctrl Pts',(-2.51961626958004,1.57021847339793,13.2966699365426));
#39478=CARTESIAN_POINT('Ctrl Pts',(-2.68889615272982,-1.25852678953048,
13.4550388443267));
#39479=CARTESIAN_POINT('Ctrl Pts',(-0.408331146069782,-2.94063222373961,
13.6134077521109));
#39480=CARTESIAN_POINT('Ctrl Pts',(2.24426309293342,-1.94353681977395,13.7717766598951));
#39481=CARTESIAN_POINT('Ctrl Pts',(2.85211623472735,0.824308912801474,13.9301455676793));
#39482=CARTESIAN_POINT('Ctrl Pts',(0.861415179590656,2.84112936850602,14.0885144754634));
#39483=CARTESIAN_POINT('Ctrl Pts',(-1.91411855626928,2.26940572674055,14.2468833832476));
#39484=CARTESIAN_POINT('Ctrl Pts',(-2.94570485153274,-0.369966387301956,
14.4052522910318));
#39485=CARTESIAN_POINT('Ctrl Pts',(-1.29346865329481,-2.67226328112036,
14.563621198816));
#39486=CARTESIAN_POINT('Ctrl Pts',(1.53724279667241,-2.53986944217347,14.7219901066002));
#39487=CARTESIAN_POINT('Ctrl Pts',(2.96737713394102,-0.0934084847990243,
14.8803590143843));
#39488=CARTESIAN_POINT('Ctrl Pts',(1.69394342893639,2.43815665272238,15.0387279221685));
#39489=CARTESIAN_POINT('Ctrl Pts',(-1.12283684570072,2.74832487362677,15.1970968299527));
#39490=CARTESIAN_POINT('Ctrl Pts',(-2.91660397551482,0.554502887305266,
15.3554657377369));
#39491=CARTESIAN_POINT('Ctrl Pts',(-2.05306232965237,-2.14452495732557,
15.513834645521));
#39492=CARTESIAN_POINT('Ctrl Pts',(0.681017995990055,-2.88968279173588,
15.6722035533052));
#39493=CARTESIAN_POINT('Ctrl Pts',(2.7946249496649,-1.00205968883199,15.8305724610894));
#39494=CARTESIAN_POINT('Ctrl Pts',(2.36205784057873,1.79853692999024,15.9889413688736));
#39495=CARTESIAN_POINT('Ctrl Pts',(-0.222572799871934,2.96049204877346,
16.1473102766577));
#39496=CARTESIAN_POINT('Ctrl Pts',(-2.60441804322706,1.42515233076513,16.3056791844419));
#39497=CARTESIAN_POINT('Ctrl Pts',(-2.6133861653761,-1.40863965797868,16.4640480922261));
#39498=CARTESIAN_POINT('Ctrl Pts',(-0.241306260285921,-2.95902362779119,
16.6224170000102));
#39499=CARTESIAN_POINT('Ctrl Pts',(2.35062692745395,-1.81345198338176,16.7807859077945));
#39500=CARTESIAN_POINT('Ctrl Pts',(2.80091144708667,0.984353109323726,16.9391548155786));
#39501=CARTESIAN_POINT('Ctrl Pts',(0.699293935404505,2.88531141176178,17.0975237233628));
#39502=CARTESIAN_POINT('Ctrl Pts',(-2.03944741654725,2.15748246986864,17.255892631147));
#39503=CARTESIAN_POINT('Ctrl Pts',(-2.92005589543968,-0.536042977591341,
17.4142615389312));
#39504=CARTESIAN_POINT('Ctrl Pts',(-1.14020807986851,-2.74114129971766,
17.5726304467153));
#39505=CARTESIAN_POINT('Ctrl Pts',(1.67847501122794,-2.44887082681998,17.7309993544995));
#39506=CARTESIAN_POINT('Ctrl Pts',(2.96791382595584,0.0747043071183943,
17.8893682622837));
#39507=CARTESIAN_POINT('Ctrl Pts',(1.55327830113815,2.52993751293006,18.0477371700679));
#39508=CARTESIAN_POINT('Ctrl Pts',(-1.27651113953843,2.68068565259069,18.206106077852));
#39509=CARTESIAN_POINT('Ctrl Pts',(-2.94333860481685,0.388050714570759,
18.3644749856362));
#39510=CARTESIAN_POINT('Ctrl Pts',(-1.92837738042689,-2.25618602850048,
18.5228438934204));
#39511=CARTESIAN_POINT('Ctrl Pts',(0.843279612549552,-2.84857935660253,
18.6812128012046));
#39512=CARTESIAN_POINT('Ctrl Pts',(2.84717556251043,-0.838140585433388,
18.8395817089887));
#39513=CARTESIAN_POINT('Ctrl Pts',(2.45263872490728,0.999903444293248,18.9451609808448));
#39514=CARTESIAN_POINT('Ctrl Pts',(1.91076803934841,1.63368048684437,18.9979506167729));
#39515=CARTESIAN_POINT('Ctrl Pts',(0.793799282532864,-2.9692229537457,-2.78423117894278E-16));
#39516=CARTESIAN_POINT('Ctrl Pts',(0.887766721915256,-2.9348492446698,-2.60122598584039E-15));
#39517=CARTESIAN_POINT('Ctrl Pts',(0.979628067005363,-2.89561800221144,
-3.49555003596041E-15));
#39518=CARTESIAN_POINT('Ctrl Pts',(1.06916866443155,-2.85186613382074,-3.23005511226881E-15));
#39519=CARTESIAN_POINT('Ctrl Pts',(1.16002904452701,-2.80746938523814,-2.96064692901515E-15));
#39520=CARTESIAN_POINT('Ctrl Pts',(1.24850040694621,-2.75841707910134,-1.70928927322073E-15));
#39521=CARTESIAN_POINT('Ctrl Pts',(1.33432908742408,-2.70501521020721,-1.35308431126191E-15));
#39522=CARTESIAN_POINT('Ctrl Pts',(1.42022858512866,-2.65156927944197,-9.96585444661768E-16));
#39523=CARTESIAN_POINT('Ctrl Pts',(1.50348162410068,-2.59376582386862,-1.74304591459404E-15));
#39524=CARTESIAN_POINT('Ctrl Pts',(1.58379549048954,-2.53187705873125,-9.22872889219661E-16));
#39525=CARTESIAN_POINT('Ctrl Pts',(1.64739785919492,-2.48286594476085,-2.73359305730904E-16));
#39526=CARTESIAN_POINT('Ctrl Pts',(1.70915630400023,-2.43129195631135,-1.21478549956335E-15));
#39527=CARTESIAN_POINT('Ctrl Pts',(1.76890471985533,-2.37727978170559,-1.85268467234323E-15));
#39528=CARTESIAN_POINT('Ctrl Pts',(1.78260832618103,-2.36489181179879,-1.69449446100029E-15));
#39529=CARTESIAN_POINT('Ctrl Pts',(1.79620839750475,-2.3523732880026,-1.18822258932526E-16));
#39530=CARTESIAN_POINT('Ctrl Pts',(1.80968464748918,-2.33974304084967,-5.13478148889135E-16));
#39531=CARTESIAN_POINT('Ctrl Pts',(1.88211680870653,-2.27185797645468,-2.7899651133437E-15));
#39532=CARTESIAN_POINT('Ctrl Pts',(1.95108361340707,-2.20065250268282,-1.95723578809634E-15));
#39533=CARTESIAN_POINT('Ctrl Pts',(2.01634525032625,-2.12641641087435,-2.42861286636753E-15));
#39534=CARTESIAN_POINT('Ctrl Pts',(2.08117756282225,-2.05266868204296,-2.89688898515044E-15));
#39535=CARTESIAN_POINT('Ctrl Pts',(2.14235377267705,-1.97592928079205,8.44765968358672E-17));
#39536=CARTESIAN_POINT('Ctrl Pts',(2.19959532795681,-1.8964556490341,-9.71445146547012E-17));
#39537=CARTESIAN_POINT('Ctrl Pts',(2.25534354159704,-1.81905535862701,-2.74027418612624E-16));
#39538=CARTESIAN_POINT('Ctrl Pts',(2.30735997993029,-1.73906090637942,-2.45691015070983E-16));
#39539=CARTESIAN_POINT('Ctrl Pts',(2.35534084620635,-1.6566960329301,-3.33066907387547E-16));
#39540=CARTESIAN_POINT('Ctrl Pts',(2.39218550638746,-1.59344778402104,-4.00163133660391E-16));
#39541=CARTESIAN_POINT('Ctrl Pts',(2.4266496194399,-1.52880139924722,-3.4098607149105E-15));
#39542=CARTESIAN_POINT('Ctrl Pts',(2.45857474179235,-1.46285623457986,-1.30451205393456E-15));
#39543=CARTESIAN_POINT('Ctrl Pts',(2.46497201772008,-1.4496418947938,-7.93110398226214E-16));
#39544=CARTESIAN_POINT('Ctrl Pts',(2.47126331594316,-1.43638355863672,-2.07413338548309E-15));
#39545=CARTESIAN_POINT('Ctrl Pts',(2.47744641392549,-1.42308498824342,-1.88737914186277E-15));
#39546=CARTESIAN_POINT('Ctrl Pts',(2.51763430459499,-1.3366491118342,-8.64305086289203E-16));
#39547=CARTESIAN_POINT('Ctrl Pts',(2.55327433966832,-1.24847578889075,-1.3994068644472E-15));
#39548=CARTESIAN_POINT('Ctrl Pts',(2.58410580530037,-1.15880673981673,-1.33226762955019E-15));
#39549=CARTESIAN_POINT('Ctrl Pts',(2.61493727093243,-1.0691376907427,-1.26512839465317E-15));
#39550=CARTESIAN_POINT('Ctrl Pts',(2.64096062227041,-0.977972194521965,
-2.18326778438127E-15));
#39551=CARTESIAN_POINT('Ctrl Pts',(2.66185969210236,-0.885542657827795,
-4.16333634234434E-16));
#39552=CARTESIAN_POINT('Ctrl Pts',(2.66318121106867,-0.879698025182872,
-4.41723660151723E-16));
#39553=CARTESIAN_POINT('Ctrl Pts',(2.66448222104045,-0.873848337361808,
-3.11073001984487E-15));
#39554=CARTESIAN_POINT('Ctrl Pts',(2.66576263396923,-0.867993652908594,
-3.05311331771918E-15));
#39555=CARTESIAN_POINT('Ctrl Pts',(2.68612379311485,-0.774892310974501,
-2.15199967091541E-15));
#39556=CARTESIAN_POINT('Ctrl Pts',(2.70128071441176,-0.680526434244495,
-1.93615779328757E-15));
#39557=CARTESIAN_POINT('Ctrl Pts',(2.71131135145323,-0.585305736937107,
4.9960036108132E-16));
#39558=CARTESIAN_POINT('Ctrl Pts',(2.71436145645041,-0.556351132808682,
1.24026300173247E-15));
#39559=CARTESIAN_POINT('Ctrl Pts',(2.71693721397202,-0.527317589420452,
1.97945944668223E-16));
#39560=CARTESIAN_POINT('Ctrl Pts',(2.71903992025458,-0.498216958905591,
-8.60422844084496E-16));
#39561=CARTESIAN_POINT('Ctrl Pts',(2.72066941215208,-0.475665429940494,
-1.37880795766708E-15));
#39562=CARTESIAN_POINT('Ctrl Pts',(2.72201480614158,-0.453073615260271,
8.79161143954925E-16));
#39563=CARTESIAN_POINT('Ctrl Pts',(2.72307654238584,-0.430447121184021,
-8.32667268468867E-16));
#39564=CARTESIAN_POINT('Ctrl Pts',(2.72389118828461,-0.413086330589785,
-1.4285468048314E-15));
#39565=CARTESIAN_POINT('Ctrl Pts',(2.72453854393588,-0.395709062278408,
-1.32916983722708E-15));
#39566=CARTESIAN_POINT('Ctrl Pts',(2.72501883608608,-0.378334978099651,
-1.4432899320127E-15));
#39567=CARTESIAN_POINT('Ctrl Pts',(2.72759253700532,-0.285233942817064,
-2.05481563096606E-15));
#39568=CARTESIAN_POINT('Ctrl Pts',(2.72538042696458,-0.192083586758562,
-2.13427839413234E-15));
#39569=CARTESIAN_POINT('Ctrl Pts',(2.71851698412385,-0.0992587649797202,
-9.71445146547012E-16));
#39570=CARTESIAN_POINT('Ctrl Pts',(2.71162359278202,-0.00602890387282495,
1.96462101593499E-16));
#39571=CARTESIAN_POINT('Ctrl Pts',(2.70003782829147,0.0868735649517466,
3.96254244904816E-17));
#39572=CARTESIAN_POINT('Ctrl Pts',(2.68384500310791,0.179056180964395,0.));
#39573=CARTESIAN_POINT('Ctrl Pts',(2.66789631164747,0.269848990998196,-3.90280054297808E-17));
#39574=CARTESIAN_POINT('Ctrl Pts',(2.64747795906825,0.359944334746189,-1.65158417179709E-16));
#39575=CARTESIAN_POINT('Ctrl Pts',(2.62262856771139,0.448941443309629,-9.15933995315754E-16));
#39576=CARTESIAN_POINT('Ctrl Pts',(2.61402331282022,0.479760822052851,-1.17592487892117E-15));
#39577=CARTESIAN_POINT('Ctrl Pts',(2.60488633276693,0.510448211838593,-1.13142427929418E-15));
#39578=CARTESIAN_POINT('Ctrl Pts',(2.59521816034902,0.540985954218381,-1.11022302462516E-16));
#39579=CARTESIAN_POINT('Ctrl Pts',(2.58935888158599,0.55949298301996,5.41220718109879E-16));
#39580=CARTESIAN_POINT('Ctrl Pts',(2.58330449519924,0.577945037913408,-2.99423739596185E-16));
#39581=CARTESIAN_POINT('Ctrl Pts',(2.57705502797514,0.596338078066865,-5.82867087928207E-16));
#39582=CARTESIAN_POINT('Ctrl Pts',(2.57172583534412,0.612022623730196,-7.85788564701402E-16));
#39583=CARTESIAN_POINT('Ctrl Pts',(2.56625440043226,0.62766507688344,1.26864793468056E-15));
#39584=CARTESIAN_POINT('Ctrl Pts',(2.56064652768341,0.643247423606782,6.38378239159465E-16));
#39585=CARTESIAN_POINT('Ctrl Pts',(2.53007794912311,0.728186974002932,-1.52047584428395E-15));
#39586=CARTESIAN_POINT('Ctrl Pts',(2.49542222163634,0.81145269313479,-1.76096677592892E-15));
#39587=CARTESIAN_POINT('Ctrl Pts',(2.45674013243295,0.892671608124275,-2.27595720048157E-15));
#39588=CARTESIAN_POINT('Ctrl Pts',(2.42447605561005,0.960414932403238,-2.70550200953925E-15));
#39589=CARTESIAN_POINT('Ctrl Pts',(2.38941000579241,1.02673410646938,3.17065263267535E-16));
#39590=CARTESIAN_POINT('Ctrl Pts',(2.35155730975954,1.0913933075816,-2.16493489801906E-15));
#39591=CARTESIAN_POINT('Ctrl Pts',(2.33605432532997,1.11787518848119,-3.35396722920609E-15));
#39592=CARTESIAN_POINT('Ctrl Pts',(2.320083711266,1.1440783883098,2.22663090102326E-15));
#39593=CARTESIAN_POINT('Ctrl Pts',(2.30364573463797,1.16998563950688,1.0547118733939E-15));
#39594=CARTESIAN_POINT('Ctrl Pts',(2.28749640854811,1.19543795989525,-9.12481855642604E-17));
#39595=CARTESIAN_POINT('Ctrl Pts',(2.270909458915,1.22058319968122,-2.3008581611839E-16));
#39596=CARTESIAN_POINT('Ctrl Pts',(2.25389204750165,1.24539904737372,-1.66533453693773E-16));
#39597=CARTESIAN_POINT('Ctrl Pts',(2.20547130452195,1.31600918623414,1.42961996517205E-17));
#39598=CARTESIAN_POINT('Ctrl Pts',(2.1535546231662,1.38397612037656,2.23917548796031E-15));
#39599=CARTESIAN_POINT('Ctrl Pts',(2.09817041824585,1.44894279750897,9.99200722162641E-16));
#39600=CARTESIAN_POINT('Ctrl Pts',(2.05606612958433,1.49833189195019,5.65446788514969E-17));
#39601=CARTESIAN_POINT('Ctrl Pts',(2.01195712795118,1.54598639386782,-9.49244954967883E-16));
#39602=CARTESIAN_POINT('Ctrl Pts',(1.96584492925679,1.59173238567462,-1.0547118733939E-15));
#39603=CARTESIAN_POINT('Ctrl Pts',(1.94982090639806,1.60762915137139,-9.57905766773421E-16));
#39604=CARTESIAN_POINT('Ctrl Pts',(1.93355490152675,1.62329530307694,-1.35256693880661E-15));
#39605=CARTESIAN_POINT('Ctrl Pts',(1.91705309021378,1.63872826997869,-1.11022302462516E-16));
#39606=CARTESIAN_POINT('Origin',(0.,0.,20.));
#39607=CARTESIAN_POINT('Origin',(-3.42660592399111E-16,1.36827403442078E-16,
95.));
#39608=CARTESIAN_POINT('Ctrl Pts',(-1.91346599666497,1.63598720337506,95.));
#39609=CARTESIAN_POINT('Ctrl Pts',(-1.97637476724345,1.57686840642878,95.));
#39610=CARTESIAN_POINT('Ctrl Pts',(-2.03582478755404,1.5144166806707,95.));
#39611=CARTESIAN_POINT('Ctrl Pts',(-2.09180351026492,1.44902198639524,95.));
#39612=CARTESIAN_POINT('Ctrl Pts',(-2.1477822329758,1.38362729211977,95.));
#39613=CARTESIAN_POINT('Ctrl Pts',(-2.20029000314911,1.31528896999456,95.));
#39614=CARTESIAN_POINT('Ctrl Pts',(-2.24928637120995,1.24435238874975,95.));
#39615=CARTESIAN_POINT('Ctrl Pts',(-2.26224868442742,1.22558564702861,95.));
#39616=CARTESIAN_POINT('Ctrl Pts',(-2.27496506671204,1.20663684103107,95.));
#39617=CARTESIAN_POINT('Ctrl Pts',(-2.28743439477761,1.18751193473744,95.));
#39618=CARTESIAN_POINT('Ctrl Pts',(-2.29756668986916,1.17197146670692,95.));
#39619=CARTESIAN_POINT('Ctrl Pts',(-2.30753626837218,1.15631386661634,95.));
#39620=CARTESIAN_POINT('Ctrl Pts',(-2.317333768862,1.14055678391561,95.));
#39621=CARTESIAN_POINT('Ctrl Pts',(-2.36475924951746,1.06428353222387,95.));
#39622=CARTESIAN_POINT('Ctrl Pts',(-2.40820610202563,0.985606532640625,
95.));
#39623=CARTESIAN_POINT('Ctrl Pts',(-2.44763974844671,0.904917347557528,
95.));
#39624=CARTESIAN_POINT('Ctrl Pts',(-2.47963771154829,0.83944306857721,95.));
#39625=CARTESIAN_POINT('Ctrl Pts',(-2.50899276273707,0.772642817262913,
95.));
#39626=CARTESIAN_POINT('Ctrl Pts',(-2.53566897579507,0.70470769674724,95.));
#39627=CARTESIAN_POINT('Ctrl Pts',(-2.5438361703979,0.683908666974472,95.));
#39628=CARTESIAN_POINT('Ctrl Pts',(-2.55175214712428,0.663003164647788,
95.));
#39629=CARTESIAN_POINT('Ctrl Pts',(-2.55941554913515,0.641996437555638,
95.));
#39630=CARTESIAN_POINT('Ctrl Pts',(-2.56690183605693,0.621475213942943,
95.));
#39631=CARTESIAN_POINT('Ctrl Pts',(-2.5741486191131,0.600852476167031,95.));
#39632=CARTESIAN_POINT('Ctrl Pts',(-2.5811448836277,0.580162579357833,95.));
#39633=CARTESIAN_POINT('Ctrl Pts',(-2.61086044692886,0.492285407612116,
95.));
#39634=CARTESIAN_POINT('Ctrl Pts',(-2.63609351198065,0.403113198746262,
95.));
#39635=CARTESIAN_POINT('Ctrl Pts',(-2.65681095036009,0.313049768475568,
95.));
#39636=CARTESIAN_POINT('Ctrl Pts',(-2.67772663470034,0.222124517793465,
95.));
#39637=CARTESIAN_POINT('Ctrl Pts',(-2.69404032074682,0.130290065147494,
95.));
#39638=CARTESIAN_POINT('Ctrl Pts',(-2.70567605344102,0.0379287688478774,
95.));
#39639=CARTESIAN_POINT('Ctrl Pts',(-2.71722674145791,-0.0537574658251947,
95.));
#39640=CARTESIAN_POINT('Ctrl Pts',(-2.72416795527845,-0.145963797732815,
95.));
#39641=CARTESIAN_POINT('Ctrl Pts',(-2.72637845709328,-0.238335333551318,
95.));
#39642=CARTESIAN_POINT('Ctrl Pts',(-2.72748334696664,-0.284506014718901,
95.));
#39643=CARTESIAN_POINT('Ctrl Pts',(-2.72740556351808,-0.330718183947068,
95.));
#39644=CARTESIAN_POINT('Ctrl Pts',(-2.72612509839621,-0.376928226489462,
95.));
#39645=CARTESIAN_POINT('Ctrl Pts',(-2.72571336712059,-0.391786983231473,
95.));
#39646=CARTESIAN_POINT('Ctrl Pts',(-2.72517717633184,-0.406647371787764,
95.));
#39647=CARTESIAN_POINT('Ctrl Pts',(-2.72451604953527,-0.421502101712759,
95.));
#39648=CARTESIAN_POINT('Ctrl Pts',(-2.72025658293429,-0.517207231666559,
95.));
#39649=CARTESIAN_POINT('Ctrl Pts',(-2.71083095742351,-0.612346052400123,
95.));
#39650=CARTESIAN_POINT('Ctrl Pts',(-2.69617509433104,-0.706520494550697,
95.));
#39651=CARTESIAN_POINT('Ctrl Pts',(-2.69168471229759,-0.735374422864327,
95.));
#39652=CARTESIAN_POINT('Ctrl Pts',(-2.68670301102806,-0.764137972115757,
95.));
#39653=CARTESIAN_POINT('Ctrl Pts',(-2.6812272256085,-0.792800025397099,
95.));
#39654=CARTESIAN_POINT('Ctrl Pts',(-2.66406428539495,-0.882636472440427,
95.));
#39655=CARTESIAN_POINT('Ctrl Pts',(-2.6420515107896,-0.97147573332325,95.));
#39656=CARTESIAN_POINT('Ctrl Pts',(-2.61549087324854,-1.05908709780632,
95.));
#39657=CARTESIAN_POINT('Ctrl Pts',(-2.58823061274624,-1.14900619764259,
95.));
#39658=CARTESIAN_POINT('Ctrl Pts',(-2.55617956561799,-1.23763257002399,
95.));
#39659=CARTESIAN_POINT('Ctrl Pts',(-2.51960956826968,-1.3247127800465,95.));
#39660=CARTESIAN_POINT('Ctrl Pts',(-2.50475369780857,-1.36008747005534,
95.));
#39661=CARTESIAN_POINT('Ctrl Pts',(-2.48915149373411,-1.39520690037994,
95.));
#39662=CARTESIAN_POINT('Ctrl Pts',(-2.47281882090415,-1.43005347129214,
95.));
#39663=CARTESIAN_POINT('Ctrl Pts',(-2.46389555630005,-1.44909170073766,
95.));
#39664=CARTESIAN_POINT('Ctrl Pts',(-2.4547513259397,-1.46805407731575,94.9999999999999));
#39665=CARTESIAN_POINT('Ctrl Pts',(-2.44540417178415,-1.48690693831173,
94.9999999999999));
#39666=CARTESIAN_POINT('Ctrl Pts',(-2.40260336851074,-1.57323456073041,
94.9999999999999));
#39667=CARTESIAN_POINT('Ctrl Pts',(-2.35550976886648,-1.65736332426466,
94.9999999999999));
#39668=CARTESIAN_POINT('Ctrl Pts',(-2.30446753854991,-1.73904441047229,
94.9999999999999));
#39669=CARTESIAN_POINT('Ctrl Pts',(-2.25252507412462,-1.82216610966616,
94.9999999999999));
#39670=CARTESIAN_POINT('Ctrl Pts',(-2.19649313273819,-1.90275379234213,
94.9999999999999));
#39671=CARTESIAN_POINT('Ctrl Pts',(-2.13667978629767,-1.98053818479137,
94.9999999999999));
#39672=CARTESIAN_POINT('Ctrl Pts',(-2.07625803606746,-2.05911377723128,
94.9999999999999));
#39673=CARTESIAN_POINT('Ctrl Pts',(-2.01197711887089,-2.13482959939233,
94.9999999999999));
#39674=CARTESIAN_POINT('Ctrl Pts',(-1.94410535934088,-2.20738878038354,
94.9999999999999));
#39675=CARTESIAN_POINT('Ctrl Pts',(-1.89472368162325,-2.26018090064055,
94.9999999999999));
#39676=CARTESIAN_POINT('Ctrl Pts',(-1.84344008591747,-2.31130166154995,
94.9999999999999));
#39677=CARTESIAN_POINT('Ctrl Pts',(-1.79034391139651,-2.36062647407542,
94.9999999999999));
#39678=CARTESIAN_POINT('Ctrl Pts',(-1.77873832587776,-2.37140772781214,
94.9999999999999));
#39679=CARTESIAN_POINT('Ctrl Pts',(-1.76705130310331,-2.3820982531773,94.9999999999999));
#39680=CARTESIAN_POINT('Ctrl Pts',(-1.75528982662668,-2.39269177675974,
94.9999999999999));
#39681=CARTESIAN_POINT('Ctrl Pts',(-1.67945270486208,-2.46099802550614,
94.9999999999999));
#39682=CARTESIAN_POINT('Ctrl Pts',(-1.60045108818537,-2.52534093466199,
94.9999999999999));
#39683=CARTESIAN_POINT('Ctrl Pts',(-1.51861308701732,-2.58543865751991,
94.9999999999999));
#39684=CARTESIAN_POINT('Ctrl Pts',(-1.4367014765316,-2.6455904353683,95.));
#39685=CARTESIAN_POINT('Ctrl Pts',(-1.35194779658761,-2.70149022283026,
94.9999999999999));
#39686=CARTESIAN_POINT('Ctrl Pts',(-1.26463604590252,-2.75282922856233,
95.));
#39687=CARTESIAN_POINT('Ctrl Pts',(-1.17912004925445,-2.80311233716627,
95.));
#39688=CARTESIAN_POINT('Ctrl Pts',(-1.09114945513696,-2.84902100918829,
94.9999999999999));
#39689=CARTESIAN_POINT('Ctrl Pts',(-1.00095740892384,-2.89022906672385,
95.));
#39690=CARTESIAN_POINT('Ctrl Pts',(-0.958622435866522,-2.9095715927975,
95.));
#39691=CARTESIAN_POINT('Ctrl Pts',(-0.915797596451656,-2.92787787654872,
95.));
#39692=CARTESIAN_POINT('Ctrl Pts',(-0.872504988190697,-2.94511071874119,
95.));
#39693=CARTESIAN_POINT('Ctrl Pts',(-0.847139851648223,-2.95520743993184,
95.));
#39694=CARTESIAN_POINT('Ctrl Pts',(-0.821614117149488,-2.96493562401012,
94.9999999999999));
#39695=CARTESIAN_POINT('Ctrl Pts',(-0.795934819193142,-2.97429685620567,
94.9999999999999));
#39696=CARTESIAN_POINT('Ctrl Pts',(0.7937992825328,-2.96922295374571,95.));
#39697=CARTESIAN_POINT('Ctrl Pts',(0.889394081720711,-2.93425394918359,
95.));
#39698=CARTESIAN_POINT('Ctrl Pts',(0.982912280288356,-2.89421630604824,
95.));
#39699=CARTESIAN_POINT('Ctrl Pts',(1.07410729213453,-2.84943761375707,95.));
#39700=CARTESIAN_POINT('Ctrl Pts',(1.16513952621937,-2.80473884881213,95.));
#39701=CARTESIAN_POINT('Ctrl Pts',(1.25385743011116,-2.75531514973328,95.));
#39702=CARTESIAN_POINT('Ctrl Pts',(1.33998246484742,-2.70145265972436,95.));
#39703=CARTESIAN_POINT('Ctrl Pts',(1.36671560562667,-2.68473378660531,95.));
#39704=CARTESIAN_POINT('Ctrl Pts',(1.39319836634562,-2.66758719835479,95.));
#39705=CARTESIAN_POINT('Ctrl Pts',(1.41942255413576,-2.65002023451661,95.));
#39706=CARTESIAN_POINT('Ctrl Pts',(1.43652086410149,-2.63856648062858,95.));
#39707=CARTESIAN_POINT('Ctrl Pts',(1.45350887484186,-2.62693412288624,95.));
#39708=CARTESIAN_POINT('Ctrl Pts',(1.4703707131843,-2.61513499781576,95.));
#39709=CARTESIAN_POINT('Ctrl Pts',(1.55302591511012,-2.55729675708287,95.));
#39710=CARTESIAN_POINT('Ctrl Pts',(1.63273013133474,-2.49540305169935,95.));
#39711=CARTESIAN_POINT('Ctrl Pts',(1.70921781353368,-2.42975035881223,95.));
#39712=CARTESIAN_POINT('Ctrl Pts',(1.78531329212295,-2.36443431128283,95.));
#39713=CARTESIAN_POINT('Ctrl Pts',(1.85822565958198,-2.29539692708298,95.));
#39714=CARTESIAN_POINT('Ctrl Pts',(1.9276504475844,-2.22290249111416,95.));
#39715=CARTESIAN_POINT('Ctrl Pts',(1.94134566301126,-2.20860173562885,95.));
#39716=CARTESIAN_POINT('Ctrl Pts',(1.95490501326262,-2.1941663864582,95.));
#39717=CARTESIAN_POINT('Ctrl Pts',(1.96832593513303,-2.17959838567023,95.));
#39718=CARTESIAN_POINT('Ctrl Pts',(1.98260623147684,-2.16409756013845,95.));
#39719=CARTESIAN_POINT('Ctrl Pts',(1.99672372437399,-2.14845301269264,95.));
#39720=CARTESIAN_POINT('Ctrl Pts',(2.01066679948485,-2.13267784635066,95.));
#39721=CARTESIAN_POINT('Ctrl Pts',(2.07578057768892,-2.05900825236527,95.));
#39722=CARTESIAN_POINT('Ctrl Pts',(2.13715676450789,-1.98242441972866,95.));
#39723=CARTESIAN_POINT('Ctrl Pts',(2.194549598969,-1.9032011297646,95.));
#39724=CARTESIAN_POINT('Ctrl Pts',(2.25134918206036,-1.82479674560523,95.));
#39725=CARTESIAN_POINT('Ctrl Pts',(2.30424775307981,-1.7438064127902,94.9999999999999));
#39726=CARTESIAN_POINT('Ctrl Pts',(2.35296126981416,-1.66047518094658,94.9999999999999));
#39727=CARTESIAN_POINT('Ctrl Pts',(2.40036568860705,-1.5793833428355,94.9999999999999));
#39728=CARTESIAN_POINT('Ctrl Pts',(2.4438071815732,-1.49607404530473,95.));
#39729=CARTESIAN_POINT('Ctrl Pts',(2.48297596815033,-1.41076355819206,94.9999999999999));
#39730=CARTESIAN_POINT('Ctrl Pts',(2.50148013223893,-1.37046107782537,94.9999999999999));
#39731=CARTESIAN_POINT('Ctrl Pts',(2.51902998170372,-1.32971189089598,94.9999999999999));
#39732=CARTESIAN_POINT('Ctrl Pts',(2.53558876169176,-1.28853867411852,94.9999999999999));
#39733=CARTESIAN_POINT('Ctrl Pts',(2.54347893045625,-1.26891985985895,94.9999999999999));
#39734=CARTESIAN_POINT('Ctrl Pts',(2.55114403973676,-1.24920477206754,95.));
#39735=CARTESIAN_POINT('Ctrl Pts',(2.55857988947091,-1.22939587775288,95.));
#39736=CARTESIAN_POINT('Ctrl Pts',(2.56375525722037,-1.21560884379528,95.));
#39737=CARTESIAN_POINT('Ctrl Pts',(2.56881605398952,-1.20178568693359,95.));
#39738=CARTESIAN_POINT('Ctrl Pts',(2.57376064275323,-1.18792929888989,95.));
#39739=CARTESIAN_POINT('Ctrl Pts',(2.6049580470237,-1.10050375954049,95.));
#39740=CARTESIAN_POINT('Ctrl Pts',(2.63154314967493,-1.01173042098719,94.9999999999999));
#39741=CARTESIAN_POINT('Ctrl Pts',(2.65326289575206,-0.921831545713812,
94.9999999999999));
#39742=CARTESIAN_POINT('Ctrl Pts',(2.65761145312367,-0.903832697321139,
94.9999999999999));
#39743=CARTESIAN_POINT('Ctrl Pts',(2.66176481894967,-0.885788701871771,
95.));
#39744=CARTESIAN_POINT('Ctrl Pts',(2.66572071053984,-0.867701306572206,
95.));
#39745=CARTESIAN_POINT('Ctrl Pts',(2.68630633473123,-0.773578322220572,
95.));
#39746=CARTESIAN_POINT('Ctrl Pts',(2.70154908258618,-0.678279708787185,
95.));
#39747=CARTESIAN_POINT('Ctrl Pts',(2.71156683220905,-0.582225910335545,
95.));
#39748=CARTESIAN_POINT('Ctrl Pts',(2.72158458183192,-0.486172111883905,
95.));
#39749=CARTESIAN_POINT('Ctrl Pts',(2.72637692884362,-0.389362032339101,
95.));
#39750=CARTESIAN_POINT('Ctrl Pts',(2.72600772437218,-0.292230486803331,
95.));
#39751=CARTESIAN_POINT('Ctrl Pts',(2.72587933530249,-0.258453461515866,
95.));
#39752=CARTESIAN_POINT('Ctrl Pts',(2.725126326345,-0.224637766094994,95.));
#39753=CARTESIAN_POINT('Ctrl Pts',(2.72374998821602,-0.190802465141519,
95.));
#39754=CARTESIAN_POINT('Ctrl Pts',(2.72314858458174,-0.17601781845347,95.));
#39755=CARTESIAN_POINT('Ctrl Pts',(2.72242803550975,-0.161228600798757,
95.));
#39756=CARTESIAN_POINT('Ctrl Pts',(2.72158956888809,-0.146452928724579,
95.));
#39757=CARTESIAN_POINT('Ctrl Pts',(2.71631906770851,-0.0535748163660937,
95.));
#39758=CARTESIAN_POINT('Ctrl Pts',(2.7063884100378,0.0389231339706655,95.));
#39759=CARTESIAN_POINT('Ctrl Pts',(2.69192307739847,0.130668782477267,95.));
#39760=CARTESIAN_POINT('Ctrl Pts',(2.67747069981536,0.222332264187943,95.));
#39761=CARTESIAN_POINT('Ctrl Pts',(2.6584913618998,0.313245746507116,95.0000000000001));
#39762=CARTESIAN_POINT('Ctrl Pts',(2.63506128485434,0.403021048770596,95.0000000000001));
#39763=CARTESIAN_POINT('Ctrl Pts',(2.61213349833566,0.490871761380415,95.0000000000001));
#39764=CARTESIAN_POINT('Ctrl Pts',(2.58494325798982,0.577633328616342,95.0000000000001));
#39765=CARTESIAN_POINT('Ctrl Pts',(2.55352200789815,0.662913185460221,95.0000000000001));
#39766=CARTESIAN_POINT('Ctrl Pts',(2.53742751811359,0.706594954352263,95.0000000000001));
#39767=CARTESIAN_POINT('Ctrl Pts',(2.52022234983568,0.749887433972256,95.0000000000001));
#39768=CARTESIAN_POINT('Ctrl Pts',(2.50190715230985,0.792733884454138,95.0000000000001));
#39769=CARTESIAN_POINT('Ctrl Pts',(2.49657565883769,0.80520634459154,95.0000000000001));
#39770=CARTESIAN_POINT('Ctrl Pts',(2.49115008979521,0.817640989633295,95.0000000000001));
#39771=CARTESIAN_POINT('Ctrl Pts',(2.48563042562688,0.830036369593218,95.0000000000001));
#39772=CARTESIAN_POINT('Ctrl Pts',(2.47997189811484,0.84274359169704,95.0000000000001));
#39773=CARTESIAN_POINT('Ctrl Pts',(2.47421802933406,0.855401541926264,95.0000000000001));
#39774=CARTESIAN_POINT('Ctrl Pts',(2.4683704650422,0.868006079871034,95.0000000000001));
#39775=CARTESIAN_POINT('Ctrl Pts',(2.43080699529853,0.948974865520953,95.0000000000001));
#39776=CARTESIAN_POINT('Ctrl Pts',(2.38936345000638,1.02778052674691,95.0000000000001));
#39777=CARTESIAN_POINT('Ctrl Pts',(2.34411176247456,1.10407309709342,95.0000000000001));
#39778=CARTESIAN_POINT('Ctrl Pts',(2.30016849871569,1.17815971627689,95.0000000000001));
#39779=CARTESIAN_POINT('Ctrl Pts',(2.25263361346913,1.24987705073289,95.0000000000001));
#39780=CARTESIAN_POINT('Ctrl Pts',(2.20153811786332,1.31887168138104,95.0000000000001));
#39781=CARTESIAN_POINT('Ctrl Pts',(2.15104877950881,1.38704781334994,95.0000000000001));
#39782=CARTESIAN_POINT('Ctrl Pts',(2.09708244939439,1.45256603784657,95.0000000000001));
#39783=CARTESIAN_POINT('Ctrl Pts',(2.03964076081768,1.51504411883957,95.0000000000001));
#39784=CARTESIAN_POINT('Ctrl Pts',(2.01565998812739,1.5411274860863,95.0000000000001));
#39785=CARTESIAN_POINT('Ctrl Pts',(1.99107318468021,1.56668043915507,95.0000000000001));
#39786=CARTESIAN_POINT('Ctrl Pts',(1.96587920978157,1.59167263744915,95.0000000000001));
#39787=CARTESIAN_POINT('Ctrl Pts',(1.94985907681406,1.60756446640559,95.0000000000001));
#39788=CARTESIAN_POINT('Ctrl Pts',(1.93359342372445,1.62322952717531,95.0000000000001));
#39789=CARTESIAN_POINT('Ctrl Pts',(1.91708817308061,1.63866486770395,95.0000000000001));
#39790=CARTESIAN_POINT('Ctrl Pts',(1.90919204567957,1.63405297314213,113.997481789454));
#39791=CARTESIAN_POINT('Ctrl Pts',(2.45150048983647,1.00048419650343,113.944664556026));
#39792=CARTESIAN_POINT('Ctrl Pts',(2.84607223516907,-0.837858370588297,
113.839057686671));
#39793=CARTESIAN_POINT('Ctrl Pts',(0.84317678352709,-2.84731406332924,113.680661181388));
#39794=CARTESIAN_POINT('Ctrl Pts',(-1.92777411460126,-2.25549477905844,
113.522292273603));
#39795=CARTESIAN_POINT('Ctrl Pts',(-2.94220166301464,0.387995676951446,
113.363923365819));
#39796=CARTESIAN_POINT('Ctrl Pts',(-1.27606983691641,2.67964581640148,113.205554458035));
#39797=CARTESIAN_POINT('Ctrl Pts',(1.55272161995431,2.5290395279534,113.047185550251));
#39798=CARTESIAN_POINT('Ctrl Pts',(2.96681482889055,0.0746577552526638,
112.888816642467));
#39799=CARTESIAN_POINT('Ctrl Pts',(1.6778616323001,-2.44795918144571,112.730447734683));
#39800=CARTESIAN_POINT('Ctrl Pts',(-1.13979077436967,-2.74013955134929,
112.572078826898));
#39801=CARTESIAN_POINT('Ctrl Pts',(-2.91898098009258,-0.535842258547723,
112.413709919114));
#39802=CARTESIAN_POINT('Ctrl Pts',(-2.0386979343972,2.15668702450009,112.25534101133));
#39803=CARTESIAN_POINT('Ctrl Pts',(0.699037044459727,2.88425144150759,112.096972103546));
#39804=CARTESIAN_POINT('Ctrl Pts',(2.79988124597661,0.983990481949177,111.938603195762));
#39805=CARTESIAN_POINT('Ctrl Pts',(2.34976254180504,-1.81278472818317,111.780234287978));
#39806=CARTESIAN_POINT('Ctrl Pts',(-0.241217557004296,-2.95793561405378,
111.621865380193));
#39807=CARTESIAN_POINT('Ctrl Pts',(-2.6124250528005,-1.40812151641157,111.463496472409));
#39808=CARTESIAN_POINT('Ctrl Pts',(-2.60346025937764,1.42462816365992,111.305127564625));
#39809=CARTESIAN_POINT('Ctrl Pts',(-0.2224909416266,2.9594033363853,111.146758656841));
#39810=CARTESIAN_POINT('Ctrl Pts',(2.36118917324051,1.7978754877943,110.988389749057));
#39811=CARTESIAN_POINT('Ctrl Pts',(2.79359720679656,-1.00169116479646,110.830020841272));
#39812=CARTESIAN_POINT('Ctrl Pts',(0.680767545745605,-2.88862009406214,
110.671651933488));
#39813=CARTESIAN_POINT('Ctrl Pts',(-2.05230730015675,-2.14373628951773,
110.513283025704));
#39814=CARTESIAN_POINT('Ctrl Pts',(-2.91553137268672,0.554298963281664,
110.35491411792));
#39815=CARTESIAN_POINT('Ctrl Pts',(-1.12242391390563,2.74731415726134,110.196545210136));
#39816=CARTESIAN_POINT('Ctrl Pts',(1.69332046845399,2.43726000187965,110.038176302352));
#39817=CARTESIAN_POINT('Ctrl Pts',(2.9662858587266,-0.0933741329074965,
109.879807394567));
#39818=CARTESIAN_POINT('Ctrl Pts',(1.53667746406551,-2.53893538621435,109.721438486783));
#39819=CARTESIAN_POINT('Ctrl Pts',(-1.29299297046839,-2.67128053615198,
109.563069578999));
#39820=CARTESIAN_POINT('Ctrl Pts',(-2.94462154643842,-0.369830329415952,
109.404700671215));
#39821=CARTESIAN_POINT('Ctrl Pts',(-1.9134146247821,2.26857113574608,109.246331763431));
#39822=CARTESIAN_POINT('Ctrl Pts',(0.86109838768306,2.84008452181803,109.087962855647));
#39823=CARTESIAN_POINT('Ctrl Pts',(2.85106734754679,0.824005767008581,108.929593947862));
#39824=CARTESIAN_POINT('Ctrl Pts',(2.24343774831338,-1.94282206950403,108.771225040078));
#39825=CARTESIAN_POINT('Ctrl Pts',(-0.408180979221735,-2.93955078413682,
108.612856132294));
#39826=CARTESIAN_POINT('Ctrl Pts',(-2.68790729096064,-1.25806395684563,
108.45448722451));
#39827=CARTESIAN_POINT('Ctrl Pts',(-2.51868966176006,1.56964101375337,108.296118316726));
#39828=CARTESIAN_POINT('Ctrl Pts',(-0.0547017452741313,2.96725095726307,
108.137749408941));
#39829=CARTESIAN_POINT('Ctrl Pts',(2.45912476054798,1.66140781759745,107.979380501157));
#39830=CARTESIAN_POINT('Ctrl Pts',(2.73245037461282,-1.15813879763718,107.821011593373));
#39831=CARTESIAN_POINT('Ctrl Pts',(0.51624898328965,-2.92250877014367,107.662642685589));
#39832=CARTESIAN_POINT('Ctrl Pts',(-2.1703052449394,-2.02419012647102,107.504273777805));
#39833=CARTESIAN_POINT('Ctrl Pts',(-2.87950114036526,0.718361821750989,
107.345904870021));
#39834=CARTESIAN_POINT('Ctrl Pts',(-0.965192536829941,2.80641655695694,
107.187535962237));
#39835=CARTESIAN_POINT('Ctrl Pts',(1.82849997360527,2.33755392896929,107.029167054452));
#39836=CARTESIAN_POINT('Ctrl Pts',(2.95625186680727,-0.261046785677825,
106.870798146668));
#39837=CARTESIAN_POINT('Ctrl Pts',(1.39057191380851,-2.62180858890217,106.712429238884));
#39838=CARTESIAN_POINT('Ctrl Pts',(-1.44205376838795,-2.59384877226725,
106.5540603311));
#39839=CARTESIAN_POINT('Ctrl Pts',(-2.96082876440973,-0.202641437416436,
106.395691423316));
#39840=CARTESIAN_POINT('Ctrl Pts',(-1.78200191711455,2.37319187840222,106.237322515531));
#39841=CARTESIAN_POINT('Ctrl Pts',(1.02040131331566,2.78681748309749,106.078953607747));
#39842=CARTESIAN_POINT('Ctrl Pts',(2.89312009295593,0.661382379602711,105.920584699963));
#39843=CARTESIAN_POINT('Ctrl Pts',(2.12992618844909,-2.0666361450611,105.762215792179));
#39844=CARTESIAN_POINT('Ctrl Pts',(-0.573836816559167,-2.91174893015787,
105.603846884395));
#39845=CARTESIAN_POINT('Ctrl Pts',(-2.75477888956335,-1.10397635569352,
105.44547797661));
#39846=CARTESIAN_POINT('Ctrl Pts',(-2.42585051691946,1.7096256297435,105.287109068826));
#39847=CARTESIAN_POINT('Ctrl Pts',(0.113262687996535,2.96559304150486,105.128740161042));
#39848=CARTESIAN_POINT('Ctrl Pts',(2.54918261149376,1.51961789196234,104.970371253258));
#39849=CARTESIAN_POINT('Ctrl Pts',(2.66255021640461,-1.31087637458229,104.812002345474));
#39850=CARTESIAN_POINT('Ctrl Pts',(0.350076631837247,-2.94703526890258,
104.65363343769));
#39851=CARTESIAN_POINT('Ctrl Pts',(-2.28135067903068,-1.89815953059813,
104.495264529906));
#39852=CARTESIAN_POINT('Ctrl Pts',(-2.83424650878728,0.880123429833188,
104.336895622121));
#39853=CARTESIAN_POINT('Ctrl Pts',(-0.804869193124953,2.85652868115701,
104.178526714337));
#39854=CARTESIAN_POINT('Ctrl Pts',(1.95782193152955,2.23035956938251,104.020157806553));
#39855=CARTESIAN_POINT('Ctrl Pts',(2.93674760683921,-0.427883182701047,
103.861788898769));
#39856=CARTESIAN_POINT('Ctrl Pts',(1.24001170631118,-2.69628290291013,103.703419990985));
#39857=CARTESIAN_POINT('Ctrl Pts',(-1.58649498842436,-2.50810768828187,
103.5450510832));
#39858=CARTESIAN_POINT('Ctrl Pts',(-2.96755105236673,-0.0348033893664811,
103.386682175416));
#39859=CARTESIAN_POINT('Ctrl Pts',(-1.64488061742202,2.47021016894182,103.228313267632));
#39860=CARTESIAN_POINT('Ctrl Pts',(1.17643541261118,2.72462295451473,103.069944359848));
#39861=CARTESIAN_POINT('Ctrl Pts',(2.92590481113682,0.496640272713199,102.911575452064));
#39862=CARTESIAN_POINT('Ctrl Pts',(2.00959147113718,-2.18382981100793,102.75320654428));
#39863=CARTESIAN_POINT('Ctrl Pts',(-0.737654384115308,-2.87461937200557,
102.594837636495));
#39864=CARTESIAN_POINT('Ctrl Pts',(-2.81282563301446,-0.946352197953286,
102.436468728711));
#39865=CARTESIAN_POINT('Ctrl Pts',(-2.32524022953366,1.84413350906936,102.278099820927));
#39866=CARTESIAN_POINT('Ctrl Pts',(0.280864287495135,2.95443493350659,102.119730913143));
#39867=CARTESIAN_POINT('Ctrl Pts',(2.63107422906718,1.37295991400069,101.961362005359));
#39868=CARTESIAN_POINT('Ctrl Pts',(2.58412065495367,-1.45941459666404,101.802993097575));
#39869=CARTESIAN_POINT('Ctrl Pts',(0.182782819936727,-2.96212102471358,
101.64462418979));
#39870=CARTESIAN_POINT('Ctrl Pts',(-2.38508787166244,-1.76604823511788,
101.486255282006));
#39871=CARTESIAN_POINT('Ctrl Pts',(-2.77991244981906,1.03906558775433,101.327886374222));
#39872=CARTESIAN_POINT('Ctrl Pts',(-0.641967474047549,2.89748999766681,
101.169517466438));
#39873=CARTESIAN_POINT('Ctrl Pts',(2.08087206305652,2.1160203168933,101.011148558654));
#39874=CARTESIAN_POINT('Ctrl Pts',(2.90783556015353,-0.593348868222388,
100.852779650869));
#39875=CARTESIAN_POINT('Ctrl Pts',(1.08547915688257,-2.76211975198173,100.694410743085));
#39876=CARTESIAN_POINT('Ctrl Pts',(-1.72585391727417,-2.41433195326245,
100.536041835301));
#39877=CARTESIAN_POINT('Ctrl Pts',(-2.96476687565186,0.133146150343083,
100.377672927517));
#39878=CARTESIAN_POINT('Ctrl Pts',(-1.50248998985534,2.55931521206319,100.219304019733));
#39879=CARTESIAN_POINT('Ctrl Pts',(1.32870083480892,2.65370017445376,100.060935111949));
#39880=CARTESIAN_POINT('Ctrl Pts',(2.94931647718439,0.330307192955261,99.9025662041639));
#39881=CARTESIAN_POINT('Ctrl Pts',(1.88281908519425,-2.29402764079667,99.7441972963799));
#39882=CARTESIAN_POINT('Ctrl Pts',(-0.899108897014456,-2.82828105315757,
99.5858283885955));
#39883=CARTESIAN_POINT('Ctrl Pts',(-2.86186157023077,-0.785696428085674,
99.4274594808116));
#39884=CARTESIAN_POINT('Ctrl Pts',(-2.21718110178343,1.97273375958331,99.2690905730271));
#39885=CARTESIAN_POINT('Ctrl Pts',(0.447566146327358,2.93381237797627,99.1107216652432));
#39886=CARTESIAN_POINT('Ctrl Pts',(2.70453727577697,1.22190369828033,98.9523527574589));
#39887=CARTESIAN_POINT('Ctrl Pts',(2.49741293719626,-1.60327762583477,98.7939838496747));
#39888=CARTESIAN_POINT('Ctrl Pts',(0.0149034683458423,-2.96771771101614,
98.6356149418906));
#39889=CARTESIAN_POINT('Ctrl Pts',(-2.48118450337799,-1.62827945432984,
98.4772460341062));
#39890=CARTESIAN_POINT('Ctrl Pts',(-2.71667302172388,1.19467912798932,98.3188771263223));
#39891=CARTESIAN_POINT('Ctrl Pts',(-0.477009229269139,2.92916928982671,
98.1605082185381));
#39892=CARTESIAN_POINT('Ctrl Pts',(2.19725617802395,1.99490245057136,98.0021393107537));
#39893=CARTESIAN_POINT('Ctrl Pts',(2.86960835079419,-0.756913770851785,
97.8437704029698));
#39894=CARTESIAN_POINT('Ctrl Pts',(0.927469295965859,-2.81910824312945,
97.6854014951854));
#39895=CARTESIAN_POINT('Ctrl Pts',(-1.85968410254603,-2.31282194845431,
97.5270325874014));
#39896=CARTESIAN_POINT('Ctrl Pts',(-2.9524851929573,0.30066910752466,97.3686636796171));
#39897=CARTESIAN_POINT('Ctrl Pts',(-1.35528610028854,2.64022166642226,97.210294771833));
#39898=CARTESIAN_POINT('Ctrl Pts',(1.47670964695599,2.57427613617538,97.0519258640487));
#39899=CARTESIAN_POINT('Ctrl Pts',(2.96328039903411,0.162916390533464,96.8935569562647));
#39900=CARTESIAN_POINT('Ctrl Pts',(1.7500145362593,-2.39687742344476,96.7351880484805));
#39901=CARTESIAN_POINT('Ctrl Pts',(-1.05768194208838,-2.77288082627902,
96.5768191406962));
#39902=CARTESIAN_POINT('Ctrl Pts',(-2.90173198512928,-0.62252684748547,
96.4184502329122));
#39903=CARTESIAN_POINT('Ctrl Pts',(-2.10201461388728,2.09502063264114,96.2600813251278));
#39904=CARTESIAN_POINT('Ctrl Pts',(0.612824978782371,2.90377914373446,96.1017124173438));
#39905=CARTESIAN_POINT('Ctrl Pts',(2.76935472527221,1.06695745781245,95.9433435095596));
#39906=CARTESIAN_POINT('Ctrl Pts',(2.40266862666488,-1.74205266274717,95.7849746017753));
#39907=CARTESIAN_POINT('Ctrl Pts',(-0.152952049520368,-2.96371237362396,
95.6266056939912));
#39908=CARTESIAN_POINT('Ctrl Pts',(-2.56947425079852,-1.48548241474925,
95.4682367862071));
#39909=CARTESIAN_POINT('Ctrl Pts',(-2.64445097587162,1.34683714954358,95.3098678784228));
#39910=CARTESIAN_POINT('Ctrl Pts',(-0.311076541356304,2.95072891345583,
95.1514989706387));
#39911=CARTESIAN_POINT('Ctrl Pts',(2.30770049687633,1.86886673688316,94.9931300628545));
#39912=CARTESIAN_POINT('Ctrl Pts',(2.81996216194598,-0.921166536179545,
94.8347611550703));
#39913=CARTESIAN_POINT('Ctrl Pts',(1.45428462117612,-2.21245757983627,94.7291818832142));
#39914=CARTESIAN_POINT('Ctrl Pts',(0.649036464259029,-2.42773457963693,
94.6763922472862));
#39915=CARTESIAN_POINT('Ctrl Pts',(2.0520964948903,1.75636305747151,114.106081112791));
#39916=CARTESIAN_POINT('Ctrl Pts',(2.63499713074943,1.07537118514814,114.053263879364));
#39917=CARTESIAN_POINT('Ctrl Pts',(3.0591028656398,-0.900572694815907,113.947657010009));
#39918=CARTESIAN_POINT('Ctrl Pts',(0.906289194931637,-3.06043764556437,
113.789260504724));
#39919=CARTESIAN_POINT('Ctrl Pts',(-2.07206944553626,-2.42432024626506,
113.63089159694));
#39920=CARTESIAN_POINT('Ctrl Pts',(-3.162427652889,0.417037442883985,113.472522689156));
#39921=CARTESIAN_POINT('Ctrl Pts',(-1.37158461638119,2.8802193052442,113.314153781372));
#39922=CARTESIAN_POINT('Ctrl Pts',(1.66894399181015,2.71834002372711,113.155784873588));
#39923=CARTESIAN_POINT('Ctrl Pts',(3.18888313259644,0.0802459439410872,
112.997415965804));
#39924=CARTESIAN_POINT('Ctrl Pts',(1.80345082745639,-2.63119075278318,112.839047058019));
#39925=CARTESIAN_POINT('Ctrl Pts',(-1.22510496431476,-2.94524104139177,
112.680678150235));
#39926=CARTESIAN_POINT('Ctrl Pts',(-3.13746888452353,-0.575950451432188,
112.522309242451));
#39927=CARTESIAN_POINT('Ctrl Pts',(-2.19129599601253,2.31811665755014,112.363940334667));
#39928=CARTESIAN_POINT('Ctrl Pts',(0.751360488841596,3.10013981406113,112.205571426883));
#39929=CARTESIAN_POINT('Ctrl Pts',(3.00945444643971,1.05764290375229,112.047202519098));
#39930=CARTESIAN_POINT('Ctrl Pts',(2.52564402139353,-1.94847301774256,111.888833611314));
#39931=CARTESIAN_POINT('Ctrl Pts',(-0.259272871136612,-3.17933930190371,
111.73046470353));
#39932=CARTESIAN_POINT('Ctrl Pts',(-2.80796701732922,-1.51352046262023,
111.572095795746));
#39933=CARTESIAN_POINT('Ctrl Pts',(-2.79833120242936,1.53126264473197,111.413726887962));
#39934=CARTESIAN_POINT('Ctrl Pts',(-0.239144554624559,3.18091688434692,
111.255357980177));
#39935=CARTESIAN_POINT('Ctrl Pts',(2.5379259447182,1.93244780958568,111.096989072394));
#39936=CARTESIAN_POINT('Ctrl Pts',(3.00270004223804,-1.0766684959185,110.938620164609));
#39937=CARTESIAN_POINT('Ctrl Pts',(0.731723504516477,-3.10483546351917,
110.780251256825));
#39938=CARTESIAN_POINT('Ctrl Pts',(-2.20592403295415,-2.30419655039083,
110.621882349041));
#39939=CARTESIAN_POINT('Ctrl Pts',(-3.13376107142933,0.595788654287395,
110.463513441257));
#39940=CARTESIAN_POINT('Ctrl Pts',(-1.20643818138628,2.95295267190985,110.305144533473));
#39941=CARTESIAN_POINT('Ctrl Pts',(1.82006676903139,2.61969073164313,110.146775625688));
#39942=CARTESIAN_POINT('Ctrl Pts',(3.18831456862103,-0.100363256429076,
109.988406717904));
#39943=CARTESIAN_POINT('Ctrl Pts',(1.65169891888132,-2.72897659436294,109.83003781012));
#39944=CARTESIAN_POINT('Ctrl Pts',(-1.38977445910716,-2.87122787752605,
109.671668902336));
#39945=CARTESIAN_POINT('Ctrl Pts',(-3.1650286663927,-0.397512405530931,
109.513299994552));
#39946=CARTESIAN_POINT('Ctrl Pts',(-2.05663513718945,2.43837537800804,109.354931086767));
#39947=CARTESIAN_POINT('Ctrl Pts',(0.92555224453134,3.05266696747654,109.196562178983));
#39948=CARTESIAN_POINT('Ctrl Pts',(3.06447186590621,0.885683213521782,109.038193271199));
#39949=CARTESIAN_POINT('Ctrl Pts',(2.41136073777209,-2.08824375109192,108.879824363415));
#39950=CARTESIAN_POINT('Ctrl Pts',(-0.438733630090977,-3.15957835374916,
108.721455455631));
#39951=CARTESIAN_POINT('Ctrl Pts',(-2.88909915733862,-1.35223098275157,
108.563086547847));
#39952=CARTESIAN_POINT('Ctrl Pts',(-2.70721546232639,1.6871298148599,108.404717640063));
#39953=CARTESIAN_POINT('Ctrl Pts',(-0.0587962117249828,3.1893519055031,
108.246348732278));
#39954=CARTESIAN_POINT('Ctrl Pts',(2.64319208381275,1.78576543244581,108.087979824494));
#39955=CARTESIAN_POINT('Ctrl Pts',(2.93697632403909,-1.24482635081468,107.92961091671));
#39956=CARTESIAN_POINT('Ctrl Pts',(0.554890604901032,-3.14126073229229,
107.771242008926));
#39957=CARTESIAN_POINT('Ctrl Pts',(-2.33275421195092,-2.17570226783771,
107.612873101142));
#39958=CARTESIAN_POINT('Ctrl Pts',(-3.09503394933374,0.772131740132777,
107.454504193357));
#39959=CARTESIAN_POINT('Ctrl Pts',(-1.03743791841433,3.0164789303234,107.296135285573));
#39960=CARTESIAN_POINT('Ctrl Pts',(1.96536456101083,2.51252158477725,107.137766377789));
#39961=CARTESIAN_POINT('Ctrl Pts',(3.17752952491941,-0.280586332372429,
106.979397470005));
#39962=CARTESIAN_POINT('Ctrl Pts',(1.49465725916726,-2.81805291810986,106.821028562221));
#39963=CARTESIAN_POINT('Ctrl Pts',(-1.54999256897645,-2.7880002883369,106.662659654437));
#39964=CARTESIAN_POINT('Ctrl Pts',(-3.18244900672259,-0.217809300213058,
106.504290746652));
#39965=CARTESIAN_POINT('Ctrl Pts',(-1.91538609029609,2.5508270613174,106.345921838868));
#39966=CARTESIAN_POINT('Ctrl Pts',(1.09677911301541,2.99541285116125,106.187552931084));
#39967=CARTESIAN_POINT('Ctrl Pts',(3.10967229068793,0.710887344223057,106.0291840233));
#39968=CARTESIAN_POINT('Ctrl Pts',(2.28935275295246,-2.22132540259141,105.870815115516));
#39969=CARTESIAN_POINT('Ctrl Pts',(-0.616788930461382,-3.12969551025482,
105.712446207732));
#39970=CARTESIAN_POINT('Ctrl Pts',(-2.96097614499467,-1.18660980967688,
105.554077299947));
#39971=CARTESIAN_POINT('Ctrl Pts',(-2.6074272382202,1.83759238380993,105.395708392163));
#39972=CARTESIAN_POINT('Ctrl Pts',(0.121740484706877,3.18756989351327,105.237339484379));
#39973=CARTESIAN_POINT('Ctrl Pts',(2.73999083210073,1.6333624250768,105.078970576595));
#39974=CARTESIAN_POINT('Ctrl Pts',(2.86184408683125,-1.40899644936311,104.920601668811));
#39975=CARTESIAN_POINT('Ctrl Pts',(0.376280128948743,-3.16762305778437,
104.762232761026));
#39976=CARTESIAN_POINT('Ctrl Pts',(-2.45211147964326,-2.04023818782284,
104.603863853242));
#39977=CARTESIAN_POINT('Ctrl Pts',(-3.04639197481427,0.946001325282417,
104.445494945458));
#39978=CARTESIAN_POINT('Ctrl Pts',(-0.86511425280373,3.07034198441227,104.287126037674));
#39979=CARTESIAN_POINT('Ctrl Pts',(2.10436636398257,2.39730364738964,104.12875712989));
#39980=CARTESIAN_POINT('Ctrl Pts',(3.15656535653917,-0.459910558202012,
103.970388222106));
#39981=CARTESIAN_POINT('Ctrl Pts',(1.33282750779448,-2.8981016900922,103.812019314321));
#39982=CARTESIAN_POINT('Ctrl Pts',(-1.70524532211103,-2.69584142023735,
103.653650406537));
#39983=CARTESIAN_POINT('Ctrl Pts',(-3.18967446294917,-0.037408449029986,
103.495281498753));
#39984=CARTESIAN_POINT('Ctrl Pts',(-1.76800115900506,2.65510724329652,103.336912590969));
#39985=CARTESIAN_POINT('Ctrl Pts',(1.26449248107197,2.92856301570605,103.178543683185));
#39986=CARTESIAN_POINT('Ctrl Pts',(3.14491096948782,0.533814167706403,103.020174775401));
#39987=CARTESIAN_POINT('Ctrl Pts',(2.16001089225898,-2.34729110188136,102.861805867616));
#39988=CARTESIAN_POINT('Ctrl Pts',(-0.792868365185695,-3.08978677696968,
102.703436959832));
#39989=CARTESIAN_POINT('Ctrl Pts',(-3.02336773050613,-1.01718736611457,
102.545068052048));
#39990=CARTESIAN_POINT('Ctrl Pts',(-2.49928619575068,1.98216827826976,102.386699144264));
#39991=CARTESIAN_POINT('Ctrl Pts',(0.301887188988093,3.17557659280544,102.22833023648));
#39992=CARTESIAN_POINT('Ctrl Pts',(2.82801209835501,1.47572698803218,102.069961328695));
#39993=CARTESIAN_POINT('Ctrl Pts',(2.77754401418352,-1.56865286820322,101.911592420911));
#39994=CARTESIAN_POINT('Ctrl Pts',(0.196464250396984,-3.18383799367443,
101.753223513127));
#39995=CARTESIAN_POINT('Ctrl Pts',(-2.56361347854963,-1.89823826329772,
101.594854605343));
#39996=CARTESIAN_POINT('Ctrl Pts',(-2.98799097098955,1.11684042232264,101.436485697559));
#39997=CARTESIAN_POINT('Ctrl Pts',(-0.690019218500169,3.11436928602715,
101.278116789774));
#39998=CARTESIAN_POINT('Ctrl Pts',(2.23662688967128,2.2744060165345,101.119747881991));
#39999=CARTESIAN_POINT('Ctrl Pts',(3.1254892215856,-0.637761473751003,100.961378974206));
#40000=CARTESIAN_POINT('Ctrl Pts',(1.16672808173278,-2.96886647644263,100.803010066422));
#40001=CARTESIAN_POINT('Ctrl Pts',(-1.85503537077141,-2.59504650147861,
100.644641158638));
#40002=CARTESIAN_POINT('Ctrl Pts',(-3.18668188852971,0.143112239046609,
100.486272250854));
#40003=CARTESIAN_POINT('Ctrl Pts',(-1.61495248671667,2.75088186538348,100.327903343069));
#40004=CARTESIAN_POINT('Ctrl Pts',(1.42815508373788,2.8523316126367,100.169534435285));
#40005=CARTESIAN_POINT('Ctrl Pts',(3.17007501620824,0.355030932814977,100.011165527501));
#40006=CARTESIAN_POINT('Ctrl Pts',(2.02374949863382,-2.46573732145668,99.8527966197172));
#40007=CARTESIAN_POINT('Ctrl Pts',(-0.966407868848687,-3.0399800003794,
99.694427711933));
#40008=CARTESIAN_POINT('Ctrl Pts',(-3.07607404421248,-0.844506391995024,
99.5360588041488));
#40009=CARTESIAN_POINT('Ctrl Pts',(-2.38313876165731,2.120394353493,99.3776898963646));
#40010=CARTESIAN_POINT('Ctrl Pts',(0.48106680634269,3.15341042360563,99.2193209885805));
#40011=CARTESIAN_POINT('Ctrl Pts',(2.90697390892733,1.31336410185077,99.0609520807963));
#40012=CARTESIAN_POINT('Ctrl Pts',(2.68434615905282,-1.72328415245439,98.9025831730122));
#40013=CARTESIAN_POINT('Ctrl Pts',(0.0160190040721257,-3.18985359612286,
98.7442142652279));
#40014=CARTESIAN_POINT('Ctrl Pts',(-2.66690301485401,-1.75015738646807,
98.5858453574439));
#40015=CARTESIAN_POINT('Ctrl Pts',(-2.92001802451376,1.28410175215917,98.4274764496595));
#40016=CARTESIAN_POINT('Ctrl Pts',(-0.512713726012357,3.14841979684353,
98.2691075418755));
#40017=CARTESIAN_POINT('Ctrl Pts',(2.36172244248695,2.14422238754322,98.1107386340912));
#40018=CARTESIAN_POINT('Ctrl Pts',(3.08440067708151,-0.813569331390272,
97.9523697263072));
#40019=CARTESIAN_POINT('Ctrl Pts',(0.996891064823428,-3.03012059867614,
97.7940008185227));
#40020=CARTESIAN_POINT('Ctrl Pts',(-1.99888284527162,-2.48593839706633,
97.6356319107388));
#40021=CARTESIAN_POINT('Ctrl Pts',(-3.17348091272117,0.323174414574692,
97.4772630029545));
#40022=CARTESIAN_POINT('Ctrl Pts',(-1.45673027617593,2.83784422822171,97.3188940951704));
#40023=CARTESIAN_POINT('Ctrl Pts',(1.58724246591466,2.76696262582893,97.1605251873862));
#40024=CARTESIAN_POINT('Ctrl Pts',(3.18508414802795,0.175110803929055,97.0021562796021));
#40025=CARTESIAN_POINT('Ctrl Pts',(1.88100443011564,-2.57628548707993,96.8437873718179));
#40026=CARTESIAN_POINT('Ctrl Pts',(-1.13685022466966,-2.9804330251807,96.6854184640336));
#40027=CARTESIAN_POINT('Ctrl Pts',(-3.11892878941644,-0.669123446533811,
96.5270495562496));
#40028=CARTESIAN_POINT('Ctrl Pts',(-2.25935197620778,2.25183449024662,96.3686806484653));
#40029=CARTESIAN_POINT('Ctrl Pts',(0.65869538571899,3.12112917937077,96.2103117406811));
#40030=CARTESIAN_POINT('Ctrl Pts',(2.97664299288246,1.14682001966684,96.0519428328971));
#40031=CARTESIAN_POINT('Ctrl Pts',(2.58251016618233,-1.87244660443017,95.8935739251127));
#40032=CARTESIAN_POINT('Ctrl Pts',(-0.164400624555983,-3.18554845623818,
95.7352050173288));
#40033=CARTESIAN_POINT('Ctrl Pts',(-2.76180131574857,-1.59667188192327,
95.5768361095443));
#40034=CARTESIAN_POINT('Ctrl Pts',(-2.84239010463917,1.44764891516331,95.4184672017605));
#40035=CARTESIAN_POINT('Ctrl Pts',(-0.334360852594403,3.17159317438854,
95.2600982939759));
#40036=CARTESIAN_POINT('Ctrl Pts',(2.48043360101624,2.00875280664075,95.1017293861921));
#40037=CARTESIAN_POINT('Ctrl Pts',(3.03103843395327,-0.990116538764143,
94.9433604784076));
#40038=CARTESIAN_POINT('Ctrl Pts',(1.56313891022217,-2.37806168056784,94.8377812065516));
#40039=CARTESIAN_POINT('Ctrl Pts',(0.697617327903685,-2.60945232443793,
94.7849915706236));
#40040=CARTESIAN_POINT('Ctrl Pts',(2.19500094410104,1.87867314180088,114.214680436129));
#40041=CARTESIAN_POINT('Ctrl Pts',(2.81849377166239,1.15025817379284,114.161863202702));
#40042=CARTESIAN_POINT('Ctrl Pts',(3.27213349611052,-0.963287019043518,
114.056256333345));
#40043=CARTESIAN_POINT('Ctrl Pts',(0.969401606336187,-3.27356122779951,
113.897859828062));
#40044=CARTESIAN_POINT('Ctrl Pts',(-2.21636477647126,-2.5931457134717,113.739490920278));
#40045=CARTESIAN_POINT('Ctrl Pts',(-3.38265364276335,0.446079208816524,
113.581122012494));
#40046=CARTESIAN_POINT('Ctrl Pts',(-1.46709939584595,3.08079279408692,113.42275310471));
#40047=CARTESIAN_POINT('Ctrl Pts',(1.78516636366599,2.90764051950081,113.264384196926));
#40048=CARTESIAN_POINT('Ctrl Pts',(3.41095143630235,0.0858341326295093,
113.106015289141));
#40049=CARTESIAN_POINT('Ctrl Pts',(1.92904002261267,-2.81442232412067,112.947646381357));
#40050=CARTESIAN_POINT('Ctrl Pts',(-1.31041915425987,-3.15034253143425,
112.789277473573));
#40051=CARTESIAN_POINT('Ctrl Pts',(-3.35595678895446,-0.616058644316651,
112.630908565789));
#40052=CARTESIAN_POINT('Ctrl Pts',(-2.34389405762786,2.47954629060019,112.472539658005));
#40053=CARTESIAN_POINT('Ctrl Pts',(0.803683933223465,3.31602818661467,112.31417075022));
#40054=CARTESIAN_POINT('Ctrl Pts',(3.21902764690281,1.13129532555542,112.155801842436));
#40055=CARTESIAN_POINT('Ctrl Pts',(2.701525500982,-2.08416130730195,111.997432934652));
#40056=CARTESIAN_POINT('Ctrl Pts',(-0.277328185268923,-3.40074298975362,
111.839064026868));
#40057=CARTESIAN_POINT('Ctrl Pts',(-3.00350898185795,-1.6189194088289,111.680695119084));
#40058=CARTESIAN_POINT('Ctrl Pts',(-2.99320214548107,1.63789712580403,111.5223262113));
#40059=CARTESIAN_POINT('Ctrl Pts',(-0.255798167622519,3.40243043230853,
111.363957303515));
#40060=CARTESIAN_POINT('Ctrl Pts',(2.71466271619589,2.06702013137707,111.205588395731));
#40061=CARTESIAN_POINT('Ctrl Pts',(3.21180287767952,-1.15164582704055,111.047219487947));
#40062=CARTESIAN_POINT('Ctrl Pts',(0.782679463287348,-3.3210508329762,110.888850580163));
#40063=CARTESIAN_POINT('Ctrl Pts',(-2.35954076575154,-2.46465681126394,
110.730481672379));
#40064=CARTESIAN_POINT('Ctrl Pts',(-3.35199077017193,0.637278345293128,
110.572112764595));
#40065=CARTESIAN_POINT('Ctrl Pts',(-1.29045244886692,3.15859118655836,110.41374385681));
#40066=CARTESIAN_POINT('Ctrl Pts',(1.94681306960879,2.80212146140662,110.255374949026));
#40067=CARTESIAN_POINT('Ctrl Pts',(3.41034327851545,-0.107352379950659,
110.097006041242));
#40068=CARTESIAN_POINT('Ctrl Pts',(1.76672037369713,-2.91901780251153,109.938637133458));
#40069=CARTESIAN_POINT('Ctrl Pts',(-1.48655594774592,-3.07117521890013,
109.780268225674));
#40070=CARTESIAN_POINT('Ctrl Pts',(-3.38543578634698,-0.42519448164591,
109.62189931789));
#40071=CARTESIAN_POINT('Ctrl Pts',(-2.1998556495968,2.60817962027,109.463530410105));
#40072=CARTESIAN_POINT('Ctrl Pts',(0.990006101379621,3.26524941313507,109.305161502321));
#40073=CARTESIAN_POINT('Ctrl Pts',(3.27787638426565,0.947360660034989,109.146792594537));
#40074=CARTESIAN_POINT('Ctrl Pts',(2.57928372723081,-2.2336654326798,108.988423686753));
#40075=CARTESIAN_POINT('Ctrl Pts',(-0.469286280960221,-3.37960592336147,
108.830054778969));
#40076=CARTESIAN_POINT('Ctrl Pts',(-3.0902910237166,-1.4463980086575,108.671685871184));
#40077=CARTESIAN_POINT('Ctrl Pts',(-2.89574126289272,1.80461861596644,108.5133169634));
#40078=CARTESIAN_POINT('Ctrl Pts',(-0.0628906781758312,3.41145285374311,
108.354948055616));
#40079=CARTESIAN_POINT('Ctrl Pts',(2.8272594070775,1.91012304729417,108.196579147832));
#40080=CARTESIAN_POINT('Ctrl Pts',(3.14150227346538,-1.3315139039922,108.038210240048));
#40081=CARTESIAN_POINT('Ctrl Pts',(0.593532226512415,-3.3600126944409,107.879841332264));
#40082=CARTESIAN_POINT('Ctrl Pts',(-2.49520317896243,-2.3272144092044,107.721472424479));
#40083=CARTESIAN_POINT('Ctrl Pts',(-3.31056675830222,0.825901658514566,
107.563103516695));
#40084=CARTESIAN_POINT('Ctrl Pts',(-1.10968329999871,3.22654130368988,107.404734608911));
#40085=CARTESIAN_POINT('Ctrl Pts',(2.10222914841638,2.68748924058522,107.246365701127));
#40086=CARTESIAN_POINT('Ctrl Pts',(3.39880718303156,-0.300125879067034,
107.087996793343));
#40087=CARTESIAN_POINT('Ctrl Pts',(1.59874260452601,-3.01429724731755,106.929627885559));
#40088=CARTESIAN_POINT('Ctrl Pts',(-1.65793136956495,-2.98215180440655,
106.771258977774));
#40089=CARTESIAN_POINT('Ctrl Pts',(-3.40406924903544,-0.232977163009677,
106.61289006999));
#40090=CARTESIAN_POINT('Ctrl Pts',(-2.04877026347763,2.72846224423256,106.454521162206));
#40091=CARTESIAN_POINT('Ctrl Pts',(1.17315691271518,3.20400821922499,106.296152254422));
#40092=CARTESIAN_POINT('Ctrl Pts',(3.32622448841996,0.760392308843405,106.137783346638));
#40093=CARTESIAN_POINT('Ctrl Pts',(2.44877931745582,-2.37601466012173,105.979414438853));
#40094=CARTESIAN_POINT('Ctrl Pts',(-0.659741044363595,-3.34764209035177,
105.821045531069));
#40095=CARTESIAN_POINT('Ctrl Pts',(-3.16717340042598,-1.26924326366024,
105.662676623285));
#40096=CARTESIAN_POINT('Ctrl Pts',(-2.78900395952094,1.96555913787636,105.504307715501));
#40097=CARTESIAN_POINT('Ctrl Pts',(0.130218281417219,3.40954674552168,105.345938807717));
#40098=CARTESIAN_POINT('Ctrl Pts',(2.93079905270771,1.74710695819127,105.187569899933));
#40099=CARTESIAN_POINT('Ctrl Pts',(3.0611379572579,-1.50711652414395,105.029200992148));
#40100=CARTESIAN_POINT('Ctrl Pts',(0.402483626060236,-3.38821084666616,
104.870832084364));
#40101=CARTESIAN_POINT('Ctrl Pts',(-2.62287228025585,-2.18231684504754,
104.71246317658));
#40102=CARTESIAN_POINT('Ctrl Pts',(-3.25853744084126,1.01187922073165,104.554094268796));
#40103=CARTESIAN_POINT('Ctrl Pts',(-0.925359312482507,3.28415528766754,
104.395725361012));
#40104=CARTESIAN_POINT('Ctrl Pts',(2.25091079643559,2.56424772539676,104.237356453228));
#40105=CARTESIAN_POINT('Ctrl Pts',(3.37638310623911,-0.491937933702975,
104.078987545443));
#40106=CARTESIAN_POINT('Ctrl Pts',(1.42564330927776,-3.09992047727427,103.920618637659));
#40107=CARTESIAN_POINT('Ctrl Pts',(-1.8239956557977,-2.88357515219282,103.762249729875));
#40108=CARTESIAN_POINT('Ctrl Pts',(-3.41179787353161,-0.0400135086934916,
103.603880822091));
#40109=CARTESIAN_POINT('Ctrl Pts',(-1.89112170058811,2.84000431765121,103.445511914307));
#40110=CARTESIAN_POINT('Ctrl Pts',(1.35254954953276,3.13250307689736,103.287143006522));
#40111=CARTESIAN_POINT('Ctrl Pts',(3.36391712783881,0.570988062699605,103.128774098738));
#40112=CARTESIAN_POINT('Ctrl Pts',(2.31043031338077,-2.51075239275481,102.970405190954));
#40113=CARTESIAN_POINT('Ctrl Pts',(-0.848082346256082,-3.30495418193377,
102.81203628317));
#40114=CARTESIAN_POINT('Ctrl Pts',(-3.2339098279978,-1.08802253427584,102.653667375386));
#40115=CARTESIAN_POINT('Ctrl Pts',(-2.67333216196771,2.12020304747017,102.495298467602));
#40116=CARTESIAN_POINT('Ctrl Pts',(0.322910090481049,3.39671825210427,102.336929559818));
#40117=CARTESIAN_POINT('Ctrl Pts',(3.02494996764285,1.57849406206368,102.178560652033));
#40118=CARTESIAN_POINT('Ctrl Pts',(2.97096737341337,-1.6778911397424,102.020191744249));
#40119=CARTESIAN_POINT('Ctrl Pts',(0.210145680857242,-3.40555496263529,
101.861822836465));
#40120=CARTESIAN_POINT('Ctrl Pts',(-2.74213908543681,-2.03042829147757,
101.703453928681));
#40121=CARTESIAN_POINT('Ctrl Pts',(-3.19606949216004,1.19461525689096,101.545085020896));
#40122=CARTESIAN_POINT('Ctrl Pts',(-0.738070962952793,3.33124857438748,
101.386716113112));
#40123=CARTESIAN_POINT('Ctrl Pts',(2.39238171628604,2.4327917161757,101.228347205328));
#40124=CARTESIAN_POINT('Ctrl Pts',(3.34314288301767,-0.682174079279619,
101.069978297544));
#40125=CARTESIAN_POINT('Ctrl Pts',(1.247977006583,-3.17561320090353,100.91160938976));
#40126=CARTESIAN_POINT('Ctrl Pts',(-1.98421682426866,-2.77576104969477,
100.753240481976));
#40127=CARTESIAN_POINT('Ctrl Pts',(-3.40859690140757,0.153078327750135,
100.594871574191));
#40128=CARTESIAN_POINT('Ctrl Pts',(-1.72741498357801,2.94244851870377,100.436502666407));
#40129=CARTESIAN_POINT('Ctrl Pts',(1.52760933266685,3.05096305081963,100.278133758623));
#40130=CARTESIAN_POINT('Ctrl Pts',(3.39083355523211,0.379754672674693,100.119764850839));
#40131=CARTESIAN_POINT('Ctrl Pts',(2.16467991207339,-2.63744700211668,99.9613959430545));
#40132=CARTESIAN_POINT('Ctrl Pts',(-1.03370684068292,-3.25167894760123,
99.8030270352703));
#40133=CARTESIAN_POINT('Ctrl Pts',(-3.29028651819418,-0.90331635590437,
99.6446581274863));
#40134=CARTESIAN_POINT('Ctrl Pts',(-2.5490964215312,2.26805494740268,99.4862892197019));
#40135=CARTESIAN_POINT('Ctrl Pts',(0.514567466358019,3.37300846923499,99.3279203119179));
#40136=CARTESIAN_POINT('Ctrl Pts',(3.10941054207769,1.4048245054212,99.1695514041337));
#40137=CARTESIAN_POINT('Ctrl Pts',(2.87127938090939,-1.84329067907401,99.0111824963495));
#40138=CARTESIAN_POINT('Ctrl Pts',(0.0171345397984093,-3.41198948122956,
98.8528135885653));
#40139=CARTESIAN_POINT('Ctrl Pts',(-2.85262152633003,-1.8720353186063,98.6944446807813));
#40140=CARTESIAN_POINT('Ctrl Pts',(-3.12336302730363,1.37352437632903,98.5360757729969));
#40141=CARTESIAN_POINT('Ctrl Pts',(-0.548418222755575,3.36767030386034,
98.3777068652128));
#40142=CARTESIAN_POINT('Ctrl Pts',(2.52618870694997,2.29354232451508,98.2193379574286));
#40143=CARTESIAN_POINT('Ctrl Pts',(3.29919300336885,-0.870224891928761,
98.0609690496445));
#40144=CARTESIAN_POINT('Ctrl Pts',(1.06631283368099,-3.24113295422285,97.9026001418602));
#40145=CARTESIAN_POINT('Ctrl Pts',(-2.13808158799722,-2.65905484567836,
97.7442312340761));
#40146=CARTESIAN_POINT('Ctrl Pts',(-3.39447663248505,0.345679721624724,
97.5858623262918));
#40147=CARTESIAN_POINT('Ctrl Pts',(-1.5581744520633,3.03546679002117,97.4274934185078));
#40148=CARTESIAN_POINT('Ctrl Pts',(1.69777528487333,2.9596491154825,97.2691245107234));
#40149=CARTESIAN_POINT('Ctrl Pts',(3.4068878970218,0.18730521732464,97.1107556029395));
#40150=CARTESIAN_POINT('Ctrl Pts',(2.01199432397197,-2.75569355071509,96.9523866951552));
#40151=CARTESIAN_POINT('Ctrl Pts',(-1.21601850725094,-3.1879852240824,96.7940177873711));
#40152=CARTESIAN_POINT('Ctrl Pts',(-3.33612559370361,-0.715720045582149,
96.6356488795868));
#40153=CARTESIAN_POINT('Ctrl Pts',(-2.41668933852826,2.4086483478521,96.4772799718027));
#40154=CARTESIAN_POINT('Ctrl Pts',(0.70456579265561,3.33847921500707,96.3189110640184));
#40155=CARTESIAN_POINT('Ctrl Pts',(3.18393126049271,1.22668258152122,96.1605421562345));
#40156=CARTESIAN_POINT('Ctrl Pts',(2.76235170569977,-2.00284054611316,96.00217324845));
#40157=CARTESIAN_POINT('Ctrl Pts',(-0.175849199591597,-3.40738453885239,
95.843804340666));
#40158=CARTESIAN_POINT('Ctrl Pts',(-2.95412838069862,-1.7078613490973,95.6854354328817));
#40159=CARTESIAN_POINT('Ctrl Pts',(-3.04032923340671,1.54846068078304,95.5270665250977));
#40160=CARTESIAN_POINT('Ctrl Pts',(-0.357645163832503,3.39245743532123,
95.3686976173134));
#40161=CARTESIAN_POINT('Ctrl Pts',(2.65316670515616,2.14863887639834,95.2103287095293));
#40162=CARTESIAN_POINT('Ctrl Pts',(3.24211470596056,-1.05906654134874,95.0519598017451));
#40163=CARTESIAN_POINT('Ctrl Pts',(1.67199319926822,-2.54366578129941,94.9463805298889));
#40164=CARTESIAN_POINT('Ctrl Pts',(0.746198191548342,-2.79117006923892,
94.8935908939609));
#40165=CARTESIAN_POINT('Ctrl Pts',(2.33790539331178,2.00098322613026,114.323279759466));
#40166=CARTESIAN_POINT('Ctrl Pts',(3.00199041257534,1.22514516243756,114.270462526038));
#40167=CARTESIAN_POINT('Ctrl Pts',(3.48516412658124,-1.02600134327114,114.164855656683));
#40168=CARTESIAN_POINT('Ctrl Pts',(1.03251401774073,-3.48668481003465,114.006459151399));
#40169=CARTESIAN_POINT('Ctrl Pts',(-2.36066010740627,-2.76197118067833,
113.848090243615));
#40170=CARTESIAN_POINT('Ctrl Pts',(-3.60287963263771,0.475120974749064,
113.689721335831));
#40171=CARTESIAN_POINT('Ctrl Pts',(-1.56261417531073,3.28136628292964,113.531352428046));
#40172=CARTESIAN_POINT('Ctrl Pts',(1.90138873552182,3.09694101527453,113.372983520263));
#40173=CARTESIAN_POINT('Ctrl Pts',(3.63301974000825,0.0914223213179323,
113.214614612478));
#40174=CARTESIAN_POINT('Ctrl Pts',(2.05462921776896,-2.99765389545814,113.056245704694));
#40175=CARTESIAN_POINT('Ctrl Pts',(-1.39573334420497,-3.35544402147674,
112.89787679691));
#40176=CARTESIAN_POINT('Ctrl Pts',(-3.57444469338541,-0.656166837201114,
112.739507889126));
#40177=CARTESIAN_POINT('Ctrl Pts',(-2.49649211924318,2.64097592365024,112.581138981341));
#40178=CARTESIAN_POINT('Ctrl Pts',(0.856007377605333,3.53191655916822,112.422770073557));
#40179=CARTESIAN_POINT('Ctrl Pts',(3.42860084736592,1.20494774735854,112.264401165773));
#40180=CARTESIAN_POINT('Ctrl Pts',(2.87740698057048,-2.21984959686134,112.106032257989));
#40181=CARTESIAN_POINT('Ctrl Pts',(-0.295383499401239,-3.62214667760355,
111.947663350205));
#40182=CARTESIAN_POINT('Ctrl Pts',(-3.19905094638667,-1.72431835503756,
111.789294442421));
#40183=CARTESIAN_POINT('Ctrl Pts',(-3.18807308853279,1.74453160687608,111.630925534636));
#40184=CARTESIAN_POINT('Ctrl Pts',(-0.272451780620475,3.62394398027014,
111.472556626852));
#40185=CARTESIAN_POINT('Ctrl Pts',(2.89139948767358,2.20159245316845,111.314187719068));
#40186=CARTESIAN_POINT('Ctrl Pts',(3.42090571312101,-1.2266231581626,111.155818811284));
#40187=CARTESIAN_POINT('Ctrl Pts',(0.833635422058219,-3.53726620243323,
110.9974499035));
#40188=CARTESIAN_POINT('Ctrl Pts',(-2.51315749854894,-2.62511707213705,
110.839080995716));
#40189=CARTESIAN_POINT('Ctrl Pts',(-3.57022046891454,0.678768036298866,
110.680712087931));
#40190=CARTESIAN_POINT('Ctrl Pts',(-1.37446671634757,3.36422970120687,110.522343180147));
#40191=CARTESIAN_POINT('Ctrl Pts',(2.07355937018619,2.98455219117012,110.363974272363));
#40192=CARTESIAN_POINT('Ctrl Pts',(3.63237198840987,-0.114341503472241,
110.205605364579));
#40193=CARTESIAN_POINT('Ctrl Pts',(1.88174182851294,-3.10905901066011,110.047236456795));
#40194=CARTESIAN_POINT('Ctrl Pts',(-1.58333743638467,-3.27112256027421,
109.888867549011));
#40195=CARTESIAN_POINT('Ctrl Pts',(-3.60584290630127,-0.452876557760886,
109.730498641226));
#40196=CARTESIAN_POINT('Ctrl Pts',(-2.34307616200414,2.77798386253196,109.572129733442));
#40197=CARTESIAN_POINT('Ctrl Pts',(1.0544599582279,3.47783185879359,109.413760825658));
#40198=CARTESIAN_POINT('Ctrl Pts',(3.49128090262507,1.00903810654819,109.255391917874));
#40199=CARTESIAN_POINT('Ctrl Pts',(2.74720671668951,-2.3790871142677,109.09702301009));
#40200=CARTESIAN_POINT('Ctrl Pts',(-0.49983893182946,-3.59963349297381,
108.938654102305));
#40201=CARTESIAN_POINT('Ctrl Pts',(-3.29148289009458,-1.54056503456343,
108.780285194521));
#40202=CARTESIAN_POINT('Ctrl Pts',(-3.08426706345904,1.92210741707296,108.621916286737));
#40203=CARTESIAN_POINT('Ctrl Pts',(-0.066985144626685,3.63355380198312,
108.463547378953));
#40204=CARTESIAN_POINT('Ctrl Pts',(3.01132673034226,2.03448066214254,108.305178471169));
#40205=CARTESIAN_POINT('Ctrl Pts',(3.34602822289167,-1.4182014571697,108.146809563385));
#40206=CARTESIAN_POINT('Ctrl Pts',(0.632173848123799,-3.57876465658952,
107.9884406556));
#40207=CARTESIAN_POINT('Ctrl Pts',(-2.65765214597394,-2.47872655057109,
107.830071747816));
#40208=CARTESIAN_POINT('Ctrl Pts',(-3.52609956727071,0.879671576896354,
107.671702840032));
#40209=CARTESIAN_POINT('Ctrl Pts',(-1.18192868158311,3.43660367705634,107.513333932248));
#40210=CARTESIAN_POINT('Ctrl Pts',(2.23909373582195,2.86245689639317,107.354965024464));
#40211=CARTESIAN_POINT('Ctrl Pts',(3.62008484114372,-0.319665425761639,
107.196596116679));
#40212=CARTESIAN_POINT('Ctrl Pts',(1.70282794988475,-3.21054157652525,107.038227208895));
#40213=CARTESIAN_POINT('Ctrl Pts',(-1.76587017015344,-3.17630332047621,
106.879858301111));
#40214=CARTESIAN_POINT('Ctrl Pts',(-3.62568949134831,-0.248145025806301,
106.721489393327));
#40215=CARTESIAN_POINT('Ctrl Pts',(-2.18215443665916,2.90609742714773,106.563120485543));
#40216=CARTESIAN_POINT('Ctrl Pts',(1.24953471241494,3.41260358728873,106.404751577759));
#40217=CARTESIAN_POINT('Ctrl Pts',(3.54277668615197,0.809897273463753,106.246382669975));
#40218=CARTESIAN_POINT('Ctrl Pts',(2.60820588195919,-2.53070391765205,106.08801376219));
#40219=CARTESIAN_POINT('Ctrl Pts',(-0.702693158265811,-3.56558867044873,
105.929644854406));
#40220=CARTESIAN_POINT('Ctrl Pts',(-3.3733706558573,-1.3518767176436,105.771275946622));
#40221=CARTESIAN_POINT('Ctrl Pts',(-2.9705806808217,2.09352589194279,105.612907038838));
#40222=CARTESIAN_POINT('Ctrl Pts',(0.13869607812756,3.6315235975301,105.454538131054));
#40223=CARTESIAN_POINT('Ctrl Pts',(3.12160727331468,1.86085149130572,105.296169223269));
#40224=CARTESIAN_POINT('Ctrl Pts',(3.26043182768453,-1.60523659892479,105.137800315485));
#40225=CARTESIAN_POINT('Ctrl Pts',(0.428687123171732,-3.60879863554794,
104.979431407701));
#40226=CARTESIAN_POINT('Ctrl Pts',(-2.79363308086844,-2.32439550227224,
104.821062499917));
#40227=CARTESIAN_POINT('Ctrl Pts',(-3.47068290686825,1.07775711618088,104.662693592133));
#40228=CARTESIAN_POINT('Ctrl Pts',(-0.985604372161288,3.4979685909228,104.504324684348));
#40229=CARTESIAN_POINT('Ctrl Pts',(2.39745522888862,2.73119180340389,104.345955776564));
#40230=CARTESIAN_POINT('Ctrl Pts',(3.59620085593905,-0.523965309203938,
104.18758686878));
#40231=CARTESIAN_POINT('Ctrl Pts',(1.51845911076105,-3.30173926445634,104.029217960996));
#40232=CARTESIAN_POINT('Ctrl Pts',(-1.94274598948437,-3.07130888414831,
103.870849053212));
#40233=CARTESIAN_POINT('Ctrl Pts',(-3.63392128411406,-0.042618568356995,
103.712480145428));
#40234=CARTESIAN_POINT('Ctrl Pts',(-2.01424224217116,3.0249013920059,103.554111237643));
#40235=CARTESIAN_POINT('Ctrl Pts',(1.44060661799356,3.33644313808868,103.395742329859));
#40236=CARTESIAN_POINT('Ctrl Pts',(3.58292328618981,0.608161957692807,103.237373422075));
#40237=CARTESIAN_POINT('Ctrl Pts',(2.46084973450257,-2.67421368362825,103.079004514291));
#40238=CARTESIAN_POINT('Ctrl Pts',(-0.903296327326473,-3.52012158689788,
102.920635606507));
#40239=CARTESIAN_POINT('Ctrl Pts',(-3.44445192548946,-1.15885770243712,
102.762266698723));
#40240=CARTESIAN_POINT('Ctrl Pts',(-2.84737812818474,2.25823781667056,102.603897790938));
#40241=CARTESIAN_POINT('Ctrl Pts',(0.343932991974009,3.61785991140311,102.445528883154));
#40242=CARTESIAN_POINT('Ctrl Pts',(3.22188783693069,1.68126113609517,102.28715997537));
#40243=CARTESIAN_POINT('Ctrl Pts',(3.16439073264322,-1.78712941128159,102.128791067586));
#40244=CARTESIAN_POINT('Ctrl Pts',(0.223827111317502,-3.62727193159614,
101.970422159802));
#40245=CARTESIAN_POINT('Ctrl Pts',(-2.92066469232399,-2.16261831965741,
101.812053252017));
#40246=CARTESIAN_POINT('Ctrl Pts',(-3.40414801333053,1.27239009145927,101.653684344234));
#40247=CARTESIAN_POINT('Ctrl Pts',(-0.786122707405416,3.54812786274783,
101.495315436449));
#40248=CARTESIAN_POINT('Ctrl Pts',(2.54813654290081,2.5911774158169,101.336946528665));
#40249=CARTESIAN_POINT('Ctrl Pts',(3.56079654444974,-0.726586684808233,
101.178577620881));
#40250=CARTESIAN_POINT('Ctrl Pts',(1.32922593143321,-3.38235992536443,101.020208713097));
#40251=CARTESIAN_POINT('Ctrl Pts',(-2.11339827776591,-2.95647559791092,
100.861839805313));
#40252=CARTESIAN_POINT('Ctrl Pts',(-3.63051191428542,0.16304441645366,100.703470897528));
#40253=CARTESIAN_POINT('Ctrl Pts',(-1.83987748043935,3.13401517202406,100.545101989744));
#40254=CARTESIAN_POINT('Ctrl Pts',(1.62706358159582,3.24959448900257,100.38673308196));
#40255=CARTESIAN_POINT('Ctrl Pts',(3.61159209425597,0.404478412534406,100.228364174176));
#40256=CARTESIAN_POINT('Ctrl Pts',(2.30561032551295,-2.80915668277669,100.069995266392));
#40257=CARTESIAN_POINT('Ctrl Pts',(-1.10100581251714,-3.46337789482306,
99.9116263586078));
#40258=CARTESIAN_POINT('Ctrl Pts',(-3.50449899217589,-0.962126319813717,
99.7532574508236));
#40259=CARTESIAN_POINT('Ctrl Pts',(-2.71505408140509,2.41571554131236,99.5948885430393));
#40260=CARTESIAN_POINT('Ctrl Pts',(0.54806812637335,3.59260651486435,99.4365196352553));
#40261=CARTESIAN_POINT('Ctrl Pts',(3.31184717522804,1.49628490899163,99.278150727471));
#40262=CARTESIAN_POINT('Ctrl Pts',(3.05821260276595,-1.96329720569364,99.1197818196869));
#40263=CARTESIAN_POINT('Ctrl Pts',(0.0182500755246922,-3.63412536633627,
98.9614129119027));
#40264=CARTESIAN_POINT('Ctrl Pts',(-3.03834003780604,-1.99391325074452,
98.8030440041185));
#40265=CARTESIAN_POINT('Ctrl Pts',(-3.32670803009352,1.46294700049888,98.6446750963343));
#40266=CARTESIAN_POINT('Ctrl Pts',(-0.584122719498795,3.58692081087714,
98.4863061885502));
#40267=CARTESIAN_POINT('Ctrl Pts',(2.69065497141298,2.44286226148695,98.3279372807659));
#40268=CARTESIAN_POINT('Ctrl Pts',(3.51398532965618,-0.926880452467247,
98.1695683729819));
#40269=CARTESIAN_POINT('Ctrl Pts',(1.13573460253856,-3.45214530976955,98.0111994651975));
#40270=CARTESIAN_POINT('Ctrl Pts',(-2.27728033072282,-2.83217129429038,
97.8528305574135));
#40271=CARTESIAN_POINT('Ctrl Pts',(-3.61547235224893,0.368185028674753,
97.6944616496293));
#40272=CARTESIAN_POINT('Ctrl Pts',(-1.65961862795068,3.23308935182062,97.536092741845));
#40273=CARTESIAN_POINT('Ctrl Pts',(1.808308103832,3.15233560513605,97.377723834061));
#40274=CARTESIAN_POINT('Ctrl Pts',(3.62869164601564,0.199499630720231,97.2193549262767));
#40275=CARTESIAN_POINT('Ctrl Pts',(2.14298421782831,-2.93510161435026,97.0609860184926));
#40276=CARTESIAN_POINT('Ctrl Pts',(-1.29518678983222,-3.39553742298411,
96.9026171107084));
#40277=CARTESIAN_POINT('Ctrl Pts',(-3.55332239799077,-0.762316644630488,
96.7442482029242));
#40278=CARTESIAN_POINT('Ctrl Pts',(-2.57402670084876,2.5654622054576,96.5858792951401));
#40279=CARTESIAN_POINT('Ctrl Pts',(0.750436199592229,3.55582925064338,96.4275103873558));
#40280=CARTESIAN_POINT('Ctrl Pts',(3.39121952810296,1.30654514337561,96.2691414795717));
#40281=CARTESIAN_POINT('Ctrl Pts',(2.94219324521721,-2.13323448779617,96.1107725717875));
#40282=CARTESIAN_POINT('Ctrl Pts',(-0.187297774627212,-3.62922062146662,
95.9524036640034));
#40283=CARTESIAN_POINT('Ctrl Pts',(-3.14645544564867,-1.81905081627131,
95.7940347562191));
#40284=CARTESIAN_POINT('Ctrl Pts',(-3.23826836217426,1.64927244640277,95.6356658484351));
#40285=CARTESIAN_POINT('Ctrl Pts',(-0.380929475070602,3.61332169625394,
95.4772969406507));
#40286=CARTESIAN_POINT('Ctrl Pts',(2.82589980929608,2.28852494615592,95.3189280328667));
#40287=CARTESIAN_POINT('Ctrl Pts',(3.45319097796785,-1.12801654393334,95.1605591250824));
#40288=CARTESIAN_POINT('Ctrl Pts',(1.78084748831427,-2.70926988203097,95.0549798532264));
#40289=CARTESIAN_POINT('Ctrl Pts',(0.794779055193,-2.97288781403991,95.0021902172983));
#40290=CARTESIAN_POINT('Ctrl Pts',(1.9134659966651,1.63598720337492,114.));
#40291=CARTESIAN_POINT('Ctrl Pts',(1.97550038889691,1.57769010736882,114.));
#40292=CARTESIAN_POINT('Ctrl Pts',(2.0341197291836,1.51620065598168,114.));
#40293=CARTESIAN_POINT('Ctrl Pts',(2.08932641459958,1.45191113897336,114.));
#40294=CARTESIAN_POINT('Ctrl Pts',(2.14568689999563,1.38627799405325,114.));
#40295=CARTESIAN_POINT('Ctrl Pts',(2.19849101332626,1.31772603672195,114.));
#40296=CARTESIAN_POINT('Ctrl Pts',(2.24771556153909,1.24662378886774,114.));
#40297=CARTESIAN_POINT('Ctrl Pts',(2.29816664594502,1.17374987456722,114.));
#40298=CARTESIAN_POINT('Ctrl Pts',(2.34485807578261,1.09819642150282,114.));
#40299=CARTESIAN_POINT('Ctrl Pts',(2.38773087568948,1.02031743916418,114.));
#40300=CARTESIAN_POINT('Ctrl Pts',(2.40643444456904,0.986342170145018,114.));
#40301=CARTESIAN_POINT('Ctrl Pts',(2.42441077356168,0.951923818009723,114.));
#40302=CARTESIAN_POINT('Ctrl Pts',(2.4416526189394,0.917089771608395,114.));
#40303=CARTESIAN_POINT('Ctrl Pts',(2.45250309293484,0.895168341137736,114.));
#40304=CARTESIAN_POINT('Ctrl Pts',(2.46306223222539,0.873083189209911,114.));
#40305=CARTESIAN_POINT('Ctrl Pts',(2.47332929073886,0.850837952133165,114.));
#40306=CARTESIAN_POINT('Ctrl Pts',(2.48084188372401,0.834560708578284,114.));
#40307=CARTESIAN_POINT('Ctrl Pts',(2.48819808553823,0.81819734264052,114.));
#40308=CARTESIAN_POINT('Ctrl Pts',(2.49538774583109,0.801772443778709,114.));
#40309=CARTESIAN_POINT('Ctrl Pts',(2.53205184816493,0.718012690443779,114.));
#40310=CARTESIAN_POINT('Ctrl Pts',(2.56443370917822,0.632561132627693,114.));
#40311=CARTESIAN_POINT('Ctrl Pts',(2.59250806912875,0.545819305993932,114.));
#40312=CARTESIAN_POINT('Ctrl Pts',(2.62096652553687,0.457890730013266,114.));
#40313=CARTESIAN_POINT('Ctrl Pts',(2.64499928611092,0.368635563742515,114.));
#40314=CARTESIAN_POINT('Ctrl Pts',(2.66454092159011,0.27843493656148,114.));
#40315=CARTESIAN_POINT('Ctrl Pts',(2.68410865469452,0.188113847499725,114.));
#40316=CARTESIAN_POINT('Ctrl Pts',(2.69917368039218,0.0968438779961723,
114.));
#40317=CARTESIAN_POINT('Ctrl Pts',(2.7096246951451,0.00498341951435599,
114.));
#40318=CARTESIAN_POINT('Ctrl Pts',(2.71348879003703,-0.0289805099970009,
114.));
#40319=CARTESIAN_POINT('Ctrl Pts',(2.71672165473184,-0.0630253317880274,
114.));
#40320=CARTESIAN_POINT('Ctrl Pts',(2.71931590711735,-0.0971333890683507,
114.));
#40321=CARTESIAN_POINT('Ctrl Pts',(2.72100442149991,-0.119333212647831,
114.));
#40322=CARTESIAN_POINT('Ctrl Pts',(2.72242238171113,-0.141559828395214,
114.));
#40323=CARTESIAN_POINT('Ctrl Pts',(2.7235675220808,-0.163808393204148,114.));
#40324=CARTESIAN_POINT('Ctrl Pts',(2.72420819736649,-0.176255867760832,
114.));
#40325=CARTESIAN_POINT('Ctrl Pts',(2.72476337873092,-0.188709282612654,
114.));
#40326=CARTESIAN_POINT('Ctrl Pts',(2.7252324368028,-0.201157503848221,114.));
#40327=CARTESIAN_POINT('Ctrl Pts',(2.72898278021086,-0.300686980583852,
114.));
#40328=CARTESIAN_POINT('Ctrl Pts',(2.72724148462551,-0.400056709441885,
114.));
#40329=CARTESIAN_POINT('Ctrl Pts',(2.71993962742201,-0.498811550184699,
114.));
#40330=CARTESIAN_POINT('Ctrl Pts',(2.71263777021851,-0.597566390927493,
114.));
#40331=CARTESIAN_POINT('Ctrl Pts',(2.69977584370241,-0.695707537343122,
114.));
#40332=CARTESIAN_POINT('Ctrl Pts',(2.68122651196178,-0.792800808383239,
114.));
#40333=CARTESIAN_POINT('Ctrl Pts',(2.66387227429393,-0.883638566052308,
114.));
#40334=CARTESIAN_POINT('Ctrl Pts',(2.6415397886767,-0.973560147194905,114.));
#40335=CARTESIAN_POINT('Ctrl Pts',(2.61450671787376,-1.06232446094815,114.));
#40336=CARTESIAN_POINT('Ctrl Pts',(2.59875842933366,-1.11403468045077,114.));
#40337=CARTESIAN_POINT('Ctrl Pts',(2.58141387131424,-1.16535211779573,114.));
#40338=CARTESIAN_POINT('Ctrl Pts',(2.56251994638479,-1.21622780801466,114.));
#40339=CARTESIAN_POINT('Ctrl Pts',(2.55761297680077,-1.22944080983416,114.));
#40340=CARTESIAN_POINT('Ctrl Pts',(2.55260194342609,-1.24262256219186,114.));
#40341=CARTESIAN_POINT('Ctrl Pts',(2.54749229902281,-1.25576083529272,114.));
#40342=CARTESIAN_POINT('Ctrl Pts',(2.5132016869521,-1.34393124219844,114.));
#40343=CARTESIAN_POINT('Ctrl Pts',(2.47442287157765,-1.43028360326182,114.));
#40344=CARTESIAN_POINT('Ctrl Pts',(2.43150025930897,-1.51457657732671,114.));
#40345=CARTESIAN_POINT('Ctrl Pts',(2.38773715221989,-1.60052014543408,114.));
#40346=CARTESIAN_POINT('Ctrl Pts',(2.33966609261984,-1.68432359939539,114.));
#40347=CARTESIAN_POINT('Ctrl Pts',(2.28759680182187,-1.76572803828939,114.));
#40348=CARTESIAN_POINT('Ctrl Pts',(2.23465317175456,-1.84849940760502,114.));
#40349=CARTESIAN_POINT('Ctrl Pts',(2.17757554498291,-1.92879134450094,114.));
#40350=CARTESIAN_POINT('Ctrl Pts',(2.11663783812543,-2.00631672329851,114.));
#40351=CARTESIAN_POINT('Ctrl Pts',(2.07420548151236,-2.06029946550106,114.));
#40352=CARTESIAN_POINT('Ctrl Pts',(2.02990040888812,-2.11294049801343,114.));
#40353=CARTESIAN_POINT('Ctrl Pts',(1.98380220585711,-2.16413538567044,114.));
#40354=CARTESIAN_POINT('Ctrl Pts',(1.97305120009932,-2.17607503832023,114.));
#40355=CARTESIAN_POINT('Ctrl Pts',(1.9622027172611,-2.18793578502567,114.));
#40356=CARTESIAN_POINT('Ctrl Pts',(1.95126749026891,-2.19970603226562,114.));
#40357=CARTESIAN_POINT('Ctrl Pts',(1.88257352086365,-2.27364551284258,114.));
#40358=CARTESIAN_POINT('Ctrl Pts',(1.81036676090401,-2.34412026577735,114.));
#40359=CARTESIAN_POINT('Ctrl Pts',(1.73495944557455,-2.4108413165029,114.));
#40360=CARTESIAN_POINT('Ctrl Pts',(1.67111364979667,-2.46733263382534,114.));
#40361=CARTESIAN_POINT('Ctrl Pts',(1.6049724199379,-2.52113307849603,114.));
#40362=CARTESIAN_POINT('Ctrl Pts',(1.53670040710693,-2.57205276284475,114.));
#40363=CARTESIAN_POINT('Ctrl Pts',(1.51106812286496,-2.59117022794673,114.));
#40364=CARTESIAN_POINT('Ctrl Pts',(1.48513572033671,-2.60988115577991,114.));
#40365=CARTESIAN_POINT('Ctrl Pts',(1.45890980106933,-2.62817581421199,114.));
#40366=CARTESIAN_POINT('Ctrl Pts',(1.43763441829496,-2.64301708085742,114.));
#40367=CARTESIAN_POINT('Ctrl Pts',(1.4161671835519,-2.65758318957349,114.));
#40368=CARTESIAN_POINT('Ctrl Pts',(1.3945338103328,-2.67185485201352,114.));
#40369=CARTESIAN_POINT('Ctrl Pts',(1.30939543171884,-2.72802113676084,114.));
#40370=CARTESIAN_POINT('Ctrl Pts',(1.22161013194401,-2.77968415206107,114.));
#40371=CARTESIAN_POINT('Ctrl Pts',(1.13146814684533,-2.82653576956066,114.));
#40372=CARTESIAN_POINT('Ctrl Pts',(1.04714058572959,-2.87036531950615,114.));
#40373=CARTESIAN_POINT('Ctrl Pts',(0.960749769307409,-2.9099844694343,114.));
#40374=CARTESIAN_POINT('Ctrl Pts',(0.872505205252779,-2.94511065658153,
114.));
#40375=CARTESIAN_POINT('Ctrl Pts',(0.847218614713906,-2.95517610957684,
114.));
#40376=CARTESIAN_POINT('Ctrl Pts',(0.82177966221848,-2.96487242144315,114.));
#40377=CARTESIAN_POINT('Ctrl Pts',(0.796195672661137,-2.97420175871636,
114.));
#40378=CARTESIAN_POINT('Ctrl Pts',(-0.794822165015276,-2.97304906723816,
113.997713413532));
#40379=CARTESIAN_POINT('Ctrl Pts',(-1.78094408373656,-2.70941683625881,
113.944923777604));
#40380=CARTESIAN_POINT('Ctrl Pts',(-3.45337864756995,-1.12808000940134,
113.839344505748));
#40381=CARTESIAN_POINT('Ctrl Pts',(-2.82605277153101,2.28865011881991,113.680975597964));
#40382=CARTESIAN_POINT('Ctrl Pts',(0.380950093949879,3.61351685606822,113.522606690179));
#40383=CARTESIAN_POINT('Ctrl Pts',(3.23844382823359,1.64936220470124,113.364237782395));
#40384=CARTESIAN_POINT('Ctrl Pts',(3.14662599275776,-1.81914961314222,113.205868874611));
#40385=CARTESIAN_POINT('Ctrl Pts',(0.187307898924319,-3.62941717620368,
113.047499966827));
#40386=CARTESIAN_POINT('Ctrl Pts',(-2.94235267289263,-2.1333501625449,112.889131059043));
#40387=CARTESIAN_POINT('Ctrl Pts',(-3.3914033194749,1.30661598684926,112.730762151259));
#40388=CARTESIAN_POINT('Ctrl Pts',(-0.750476860684186,3.55602193007364,
112.572393243474));
#40389=CARTESIAN_POINT('Ctrl Pts',(2.5741661903379,2.56560124653058,112.41402433569));
#40390=CARTESIAN_POINT('Ctrl Pts',(3.55351496501208,-0.762357962940957,
112.255655427906));
#40391=CARTESIAN_POINT('Ctrl Pts',(1.29525697823035,-3.3957214333461,112.097286520122));
#40392=CARTESIAN_POINT('Ctrl Pts',(-2.1431003513736,-2.93526067758035,111.938917612338));
#40393=CARTESIAN_POINT('Ctrl Pts',(-3.62888829547523,0.19951044313998,111.780548704554));
#40394=CARTESIAN_POINT('Ctrl Pts',(-1.80840610088971,3.15250643855389,111.622179796769));
#40395=CARTESIAN_POINT('Ctrl Pts',(1.65970856721919,3.23326456230892,111.463810888985));
#40396=CARTESIAN_POINT('Ctrl Pts',(3.61566828494496,0.368204981509806,111.305441981201));
#40397=CARTESIAN_POINT('Ctrl Pts',(2.27740374291247,-2.83232477754531,111.147073073417));
#40398=CARTESIAN_POINT('Ctrl Pts',(-1.13579615117146,-3.4523323912807,110.988704165633));
#40399=CARTESIAN_POINT('Ctrl Pts',(-3.51417576242243,-0.926930682705363,
110.830335257848));
#40400=CARTESIAN_POINT('Ctrl Pts',(-2.69080078557179,2.44299464705653,110.671966350064));
#40401=CARTESIAN_POINT('Ctrl Pts',(0.584154374749769,3.58711519621666,110.51359744228));
#40402=CARTESIAN_POINT('Ctrl Pts',(3.32688831376596,1.4630262817106,110.355228534496));
#40403=CARTESIAN_POINT('Ctrl Pts',(3.03850469400245,-1.9940213065136,110.196859626712));
#40404=CARTESIAN_POINT('Ctrl Pts',(-0.0182510645473885,-3.63432230981833,
110.038490718928));
#40405=CARTESIAN_POINT('Ctrl Pts',(-3.05837833591408,-1.96340360229389,
109.880121811143));
#40406=CARTESIAN_POINT('Ctrl Pts',(-3.31202665354681,1.49636599688186,109.721752903359));
#40407=CARTESIAN_POINT('Ctrl Pts',(-0.548097827727379,3.59280120832229,
109.563383995575));
#40408=CARTESIAN_POINT('Ctrl Pts',(2.71520121782699,2.41584645573589,109.405015087791));
#40409=CARTESIAN_POINT('Ctrl Pts',(3.50468891083895,-0.962178460146911,
109.246646180007));
#40410=CARTESIAN_POINT('Ctrl Pts',(1.1010654791205,-3.46356558501832,109.088277272223));
#40411=CARTESIAN_POINT('Ctrl Pts',(-2.30573527302542,-2.80930891888302,
108.929908364438));
#40412=CARTESIAN_POINT('Ctrl Pts',(-3.61178781659568,0.404500332358161,
108.771539456654));
#40413=CARTESIAN_POINT('Ctrl Pts',(-1.62715175675016,3.24977059367342,108.61317054887));
#40414=CARTESIAN_POINT('Ctrl Pts',(1.83997718857821,3.13418501312623,108.454801641086));
#40415=CARTESIAN_POINT('Ctrl Pts',(3.63070866194348,0.163053252289208,108.296432733302));
#40416=CARTESIAN_POINT('Ctrl Pts',(2.11351280876615,-2.95663581764418,108.138063825517));
#40417=CARTESIAN_POINT('Ctrl Pts',(-1.32929796592752,-3.38254322496773,
107.979694917733));
#40418=CARTESIAN_POINT('Ctrl Pts',(-3.56098951403573,-0.726626060585297,
107.821326009949));
#40419=CARTESIAN_POINT('Ctrl Pts',(-2.54827463359117,2.59131783901361,107.662957102165));
#40420=CARTESIAN_POINT('Ctrl Pts',(0.78616530960755,3.54832014578222,107.504588194381));
#40421=CARTESIAN_POINT('Ctrl Pts',(3.40433249369181,1.27245904585901,107.346219286597));
#40422=CARTESIAN_POINT('Ctrl Pts',(2.92082297136322,-2.16273551803063,107.187850378812));
#40423=CARTESIAN_POINT('Ctrl Pts',(-0.223839241138819,-3.62746850367038,
107.029481471028));
#40424=CARTESIAN_POINT('Ctrl Pts',(-3.16456221988273,-1.78722626085373,
106.871112563244));
#40425=CARTESIAN_POINT('Ctrl Pts',(-3.22206244009988,1.68135224836795,106.71274365546));
#40426=CARTESIAN_POINT('Ctrl Pts',(-0.343951630670548,3.61805597341353,
106.554374747676));
#40427=CARTESIAN_POINT('Ctrl Pts',(2.84753243561908,2.25836019693307,106.396005839891));
#40428=CARTESIAN_POINT('Ctrl Pts',(3.44463859003301,-1.15892050419763,106.237636932107));
#40429=CARTESIAN_POINT('Ctrl Pts',(0.903345279496379,-3.52031235219348,
106.079268024323));
#40430=CARTESIAN_POINT('Ctrl Pts',(-2.46098309487547,-2.67435860679368,
105.920899116539));
#40431=CARTESIAN_POINT('Ctrl Pts',(-3.58311745488613,0.60819491570108,105.762530208755));
#40432=CARTESIAN_POINT('Ctrl Pts',(-1.4406846885203,3.33662394933224,105.604161300971));
#40433=CARTESIAN_POINT('Ctrl Pts',(2.01435139962717,3.02506531992523,105.445792393186));
#40434=CARTESIAN_POINT('Ctrl Pts',(3.63411821653544,-0.0426208779773826,
105.287423485402));
#40435=CARTESIAN_POINT('Ctrl Pts',(1.94285127235686,-3.0714753270205,105.129054577618));
#40436=CARTESIAN_POINT('Ctrl Pts',(-1.51854140033388,-3.30191819499912,
104.970685669834));
#40437=CARTESIAN_POINT('Ctrl Pts',(-3.59639574418431,-0.523993704358454,
104.81231676205));
#40438=CARTESIAN_POINT('Ctrl Pts',(-2.39758515373452,2.73133981437429,104.653947854266));
#40439=CARTESIAN_POINT('Ctrl Pts',(0.985657784836226,3.49815815568509,104.495578946481));
#40440=CARTESIAN_POINT('Ctrl Pts',(3.47087099294263,1.07781552287194,104.337210038697));
#40441=CARTESIAN_POINT('Ctrl Pts',(2.79378447570712,-2.32452146780626,104.178841130913));
#40442=CARTESIAN_POINT('Ctrl Pts',(-0.428710354933595,-3.60899420650229,
104.020472223129));
#40443=CARTESIAN_POINT('Ctrl Pts',(-3.26060851966125,-1.60532359121354,
103.862103315345));
#40444=CARTESIAN_POINT('Ctrl Pts',(-3.12177644199792,1.86095233608523,103.703734407561));
#40445=CARTESIAN_POINT('Ctrl Pts',(-0.138703594458174,3.63172040001413,
103.545365499776));
#40446=CARTESIAN_POINT('Ctrl Pts',(2.97074166494909,2.09363934600253,103.386996591992));
#40447=CARTESIAN_POINT('Ctrl Pts',(3.37355346830678,-1.35194997964774,103.228627684208));
#40448=CARTESIAN_POINT('Ctrl Pts',(0.702731239185455,-3.56578189973352,
103.070258776424));
#40449=CARTESIAN_POINT('Ctrl Pts',(-2.6083472279764,-2.5308410636194,102.91188986864));
#40450=CARTESIAN_POINT('Ctrl Pts',(-3.54296867919103,0.809941164076495,
102.753520960855));
#40451=CARTESIAN_POINT('Ctrl Pts',(-1.24960242821741,3.41278852588135,102.595152053071));
#40452=CARTESIAN_POINT('Ctrl Pts',(2.18227269374953,2.90625491674587,102.436783145287));
#40453=CARTESIAN_POINT('Ctrl Pts',(3.62588597766565,-0.248158473483804,
102.278414237503));
#40454=CARTESIAN_POINT('Ctrl Pts',(1.76596586762753,-3.17647545329235,102.120045329719));
#40455=CARTESIAN_POINT('Ctrl Pts',(-1.70292023092382,-3.21071556480869,
101.961676421935));
#40456=CARTESIAN_POINT('Ctrl Pts',(-3.62028102372934,-0.319682749330519,
101.80330751415));
#40457=CARTESIAN_POINT('Ctrl Pts',(-2.23921507861287,2.86261202098834,101.644938606366));
#40458=CARTESIAN_POINT('Ctrl Pts',(1.18199273362486,3.43678991628124,101.486569698582));
#40459=CARTESIAN_POINT('Ctrl Pts',(3.52629065652986,0.879719248774588,101.328200790798));
#40460=CARTESIAN_POINT('Ctrl Pts',(2.65779617162307,-2.47886087973892,101.169831883014));
#40461=CARTESIAN_POINT('Ctrl Pts',(-0.632208107403957,-3.578958599918,101.01146297523));
#40462=CARTESIAN_POINT('Ctrl Pts',(-3.34620955357793,-1.41827831349775,
100.853094067445));
#40463=CARTESIAN_POINT('Ctrl Pts',(-3.01148992261249,2.03459091637546,100.694725159661));
#40464=CARTESIAN_POINT('Ctrl Pts',(0.0669887747403652,3.63375071448961,
100.536356251877));
#40465=CARTESIAN_POINT('Ctrl Pts',(3.08443420857142,1.92221158148316,100.377987344093));
#40466=CARTESIAN_POINT('Ctrl Pts',(3.29166126481559,-1.54064852211846,100.219618436309));
#40467=CARTESIAN_POINT('Ctrl Pts',(0.499866019507705,-3.59982856724333,
100.061249528525));
#40468=CARTESIAN_POINT('Ctrl Pts',(-2.74735559555312,-2.37921604369379,
99.9028806207401));
#40469=CARTESIAN_POINT('Ctrl Pts',(-3.49147010496271,1.00909278916312,99.7445117129559));
#40470=CARTESIAN_POINT('Ctrl Pts',(-1.05451710238043,3.4780203322898,99.5861428051718));
#40471=CARTESIAN_POINT('Ctrl Pts',(2.34320313989566,2.77813440929543,99.4277738973876));
#40472=CARTESIAN_POINT('Ctrl Pts',(3.60603831707632,-0.452901100416202,
99.2694049896035));
#40473=CARTESIAN_POINT('Ctrl Pts',(1.5834232418962,-3.27129983161196,99.1110360818192));
#40474=CARTESIAN_POINT('Ctrl Pts',(-1.88184380539861,-3.1092274993174,98.9526671740351));
#40475=CARTESIAN_POINT('Ctrl Pts',(-3.63256883687055,-0.11434769996046,
98.794298266251));
#40476=CARTESIAN_POINT('Ctrl Pts',(-2.07367174220406,2.98471393245394,98.6359293584666));
#40477=CARTESIAN_POINT('Ctrl Pts',(1.37454120256743,3.3644120182804,98.4775604506826));
#40478=CARTESIAN_POINT('Ctrl Pts',(3.57041394920919,0.6788048206525,98.3191915428984));
#40479=CARTESIAN_POINT('Ctrl Pts',(2.51329369362716,-2.62525933462612,98.1608226351142));
#40480=CARTESIAN_POINT('Ctrl Pts',(-0.833680599109368,-3.5374578968306,
98.00245372733));
#40481=CARTESIAN_POINT('Ctrl Pts',(-3.42109110162642,-1.2266896323482,97.8440848195459));
#40482=CARTESIAN_POINT('Ctrl Pts',(-2.89155618075458,2.2017117637061,97.6857159117615));
#40483=CARTESIAN_POINT('Ctrl Pts',(0.272466545560592,3.624140371906,97.5273470039775));
#40484=CARTESIAN_POINT('Ctrl Pts',(3.1882458591633,1.74462614811699,97.3689780961933));
#40485=CARTESIAN_POINT('Ctrl Pts',(3.19922431200574,-1.72441180100781,97.2106091884092));
#40486=CARTESIAN_POINT('Ctrl Pts',(0.295399506973262,-3.6223429713569,97.0522402806248));
#40487=CARTESIAN_POINT('Ctrl Pts',(-2.87756291517,-2.21996989781333,96.8938713728408));
#40488=CARTESIAN_POINT('Ctrl Pts',(-3.4287866532623,1.20501304881627,96.7355024650567));
#40489=CARTESIAN_POINT('Ctrl Pts',(-0.856053766316002,3.53210796008794,
96.5771335572723));
#40490=CARTESIAN_POINT('Ctrl Pts',(2.49662740969472,2.64111905210372,96.4187646494883));
#40491=CARTESIAN_POINT('Ctrl Pts',(3.57463840557985,-0.656202408584182,
96.2603957417041));
#40492=CARTESIAN_POINT('Ctrl Pts',(1.39580897694624,-3.35562584110079,96.1020268339198));
#40493=CARTESIAN_POINT('Ctrl Pts',(-2.0547405519129,-2.99781638476409,95.9436579261358));
#40494=CARTESIAN_POINT('Ctrl Pts',(-3.63321664764495,0.0914273426514201,
95.7852890183515));
#40495=CARTESIAN_POINT('Ctrl Pts',(-1.90149172882987,3.09710873123844,95.6269201105673));
#40496=CARTESIAN_POINT('Ctrl Pts',(1.56269876086743,3.28154430658457,95.4685512027832));
#40497=CARTESIAN_POINT('Ctrl Pts',(3.60307507738476,0.475146396019093,95.310182294999));
#40498=CARTESIAN_POINT('Ctrl Pts',(2.36078764608376,-2.76212033287254,95.1518133872148));
#40499=CARTESIAN_POINT('Ctrl Pts',(-1.03256917122443,-3.4868746092295,94.9934444794307));
#40500=CARTESIAN_POINT('Ctrl Pts',(-3.48492740853102,-1.02648407117314,
94.8350755716465));
#40501=CARTESIAN_POINT('Ctrl Pts',(-3.00240564212693,1.22403504121547,94.7294962997903));
#40502=CARTESIAN_POINT('Ctrl Pts',(-2.33907288663243,1.99987526141664,94.6767066638623));
#40503=CARTESIAN_POINT('Ctrl Pts',(-0.746309486510706,-2.79158637039142,
114.106160313476));
#40504=CARTESIAN_POINT('Ctrl Pts',(-1.67224257593793,-2.54404516735251,
114.053370677548));
#40505=CARTESIAN_POINT('Ctrl Pts',(-3.24259860713048,-1.0592266416515,113.947791405692));
#40506=CARTESIAN_POINT('Ctrl Pts',(-2.6535621244696,2.1489603211384,113.789422497907));
#40507=CARTESIAN_POINT('Ctrl Pts',(0.357698465790113,3.39296263749542,113.631053590123));
#40508=CARTESIAN_POINT('Ctrl Pts',(3.04078252585762,1.54869191404229,113.472684682339));
#40509=CARTESIAN_POINT('Ctrl Pts',(2.95456887371925,-1.70811619684037,113.314315774555));
#40510=CARTESIAN_POINT('Ctrl Pts',(0.175875394545547,-3.40789246743471,
113.155946866771));
#40511=CARTESIAN_POINT('Ctrl Pts',(-2.76276355780503,-2.00313923596458,
112.997577958987));
#40512=CARTESIAN_POINT('Ctrl Pts',(-3.1844059983649,1.22686551675796,112.839209051202));
#40513=CARTESIAN_POINT('Ctrl Pts',(-0.704670837311911,3.33897696549902,
112.680840143418));
#40514=CARTESIAN_POINT('Ctrl Pts',(2.4170496650246,2.40900749018828,112.522471235634));
#40515=CARTESIAN_POINT('Ctrl Pts',(3.33662301528205,-0.715826765914207,
112.36410232785));
#40516=CARTESIAN_POINT('Ctrl Pts',(1.2161998153435,-3.18846055231137,112.205733420066));
#40517=CARTESIAN_POINT('Ctrl Pts',(-2.01229431333713,-2.75610442874092,
112.047364512282));
#40518=CARTESIAN_POINT('Ctrl Pts',(-3.4073958674124,0.18733314561058,111.888995604497));
#40519=CARTESIAN_POINT('Ctrl Pts',(-1.69802842442358,2.96009040127061,111.730626696713));
#40520=CARTESIAN_POINT('Ctrl Pts',(1.55840677711217,3.03591938103998,111.572257788929));
#40521=CARTESIAN_POINT('Ctrl Pts',(3.39498275199517,0.345731262635315,111.413888881145));
#40522=CARTESIAN_POINT('Ctrl Pts',(2.13840037779758,-2.65945131301259,111.255519973361));
#40523=CARTESIAN_POINT('Ctrl Pts',(-1.06647182183869,-3.24161621002536,
111.097151065577));
#40524=CARTESIAN_POINT('Ctrl Pts',(-3.29968491594777,-0.870354643201932,
110.938782157792));
#40525=CARTESIAN_POINT('Ctrl Pts',(-2.52656536389381,2.29388429367482,110.780413250008));
#40526=CARTESIAN_POINT('Ctrl Pts',(0.548499992390253,3.36817242645937,110.622044342224));
#40527=CARTESIAN_POINT('Ctrl Pts',(3.12382872346976,1.37372917001392,110.46367543444));
#40528=CARTESIAN_POINT('Ctrl Pts',(2.85304685469831,-1.87231444071136,110.305306526655));
#40529=CARTESIAN_POINT('Ctrl Pts',(-0.0171370945730645,-3.41249821185194,
110.146937618871));
#40530=CARTESIAN_POINT('Ctrl Pts',(-2.87170749118155,-1.84356551532891,
109.988568711087));
#40531=CARTESIAN_POINT('Ctrl Pts',(-3.10987415791403,1.40503396598599,109.830199803303));
#40532=CARTESIAN_POINT('Ctrl Pts',(-0.514644188817999,3.37351138775366,
109.671830895519));
#40533=CARTESIAN_POINT('Ctrl Pts',(2.5494764940416,2.26839311638259,109.513461987735));
#40534=CARTESIAN_POINT('Ctrl Pts',(3.29077710279722,-0.903451041164788,
109.35509307995));
#40535=CARTESIAN_POINT('Ctrl Pts',(1.03386096727849,-3.25216377578184,109.196724172166));
#40536=CARTESIAN_POINT('Ctrl Pts',(-2.16500266774537,-2.63784024777573,
109.038355264382));
#40537=CARTESIAN_POINT('Ctrl Pts',(-3.39133913148654,0.379811294429396,
108.879986356598));
#40538=CARTESIAN_POINT('Ctrl Pts',(-1.52783710055678,3.05141795208415,108.721617448814));
#40539=CARTESIAN_POINT('Ctrl Pts',(1.72767254266597,2.94288724035625,108.56324854103));
#40540=CARTESIAN_POINT('Ctrl Pts',(3.40910512619251,0.153101151862722,108.404879633246));
#40541=CARTESIAN_POINT('Ctrl Pts',(1.98451267273572,-2.7761749180998,108.246510725461));
#40542=CARTESIAN_POINT('Ctrl Pts',(-1.24816308104848,-3.17608668761447,
108.088141817677));
#40543=CARTESIAN_POINT('Ctrl Pts',(-3.34364134855115,-0.682275792032408,
107.929772909893));
#40544=CARTESIAN_POINT('Ctrl Pts',(-2.39273842249622,2.43315444755258,107.771404002109));
#40545=CARTESIAN_POINT('Ctrl Pts',(0.738181009980343,3.33174526646904,107.613035094325));
#40546=CARTESIAN_POINT('Ctrl Pts',(3.1965460289221,1.19479337507238,107.45466618654));
#40547=CARTESIAN_POINT('Ctrl Pts',(2.74254794077725,-2.03073103011525,107.296297278756));
#40548=CARTESIAN_POINT('Ctrl Pts',(-0.210177013762628,-3.40606273386447,
107.137928370972));
#40549=CARTESIAN_POINT('Ctrl Pts',(-2.97141034725229,-1.67814131478147,
106.979559463188));
#40550=CARTESIAN_POINT('Ctrl Pts',(-3.02540099033367,1.57872941691175,106.821190555404));
#40551=CARTESIAN_POINT('Ctrl Pts',(-0.322958236658289,3.3972247057722,106.66282164762));
#40552=CARTESIAN_POINT('Ctrl Pts',(2.67373075813582,2.1205191716023,106.504452739835));
#40553=CARTESIAN_POINT('Ctrl Pts',(3.23439200678694,-1.08818475938934,106.346083832051));
#40554=CARTESIAN_POINT('Ctrl Pts',(0.848208796076863,-3.30544695349847,
106.187714924267));
#40555=CARTESIAN_POINT('Ctrl Pts',(-2.31077480056528,-2.51112674813657,
106.029346016483));
#40556=CARTESIAN_POINT('Ctrl Pts',(-3.36441869083031,0.571073197520321,
105.870977108699));
#40557=CARTESIAN_POINT('Ctrl Pts',(-1.35275121585564,3.13297013585121,105.712608200914));
#40558=CARTESIAN_POINT('Ctrl Pts',(1.89140366849103,2.84042776478352,105.55423929313));
#40559=CARTESIAN_POINT('Ctrl Pts',(3.41230657558429,-0.0400194747429137,
105.395870385346));
#40560=CARTESIAN_POINT('Ctrl Pts',(1.82426761514817,-2.88400509577499,105.237501477562));
#40561=CARTESIAN_POINT('Ctrl Pts',(-1.42585587394465,-3.10038267813378,
105.079132569778));
#40562=CARTESIAN_POINT('Ctrl Pts',(-3.37688652791896,-0.49201128207979,
104.920763661994));
#40563=CARTESIAN_POINT('Ctrl Pts',(-2.25124640920767,2.56463005697977,104.762394754209));
#40564=CARTESIAN_POINT('Ctrl Pts',(0.925497284367084,3.28464495809877,104.604025846425));
#40565=CARTESIAN_POINT('Ctrl Pts',(3.25902329162918,1.01203009280996,104.445656938641));
#40566=CARTESIAN_POINT('Ctrl Pts',(2.62326335281111,-2.18264223040164,104.287288030857));
#40567=CARTESIAN_POINT('Ctrl Pts',(-0.402543636721763,-3.38871603187245,
104.128919123073));
#40568=CARTESIAN_POINT('Ctrl Pts',(-3.06159437560986,-1.50734123653821,
103.970550215289));
#40569=CARTESIAN_POINT('Ctrl Pts',(-2.93123603741461,1.74736745336986,103.812181307504));
#40570=CARTESIAN_POINT('Ctrl Pts',(-0.130237697076901,3.41005511192923,
103.65381239972));
#40571=CARTESIAN_POINT('Ctrl Pts',(2.78941980245543,1.96585220446606,103.495443491936));
#40572=CARTESIAN_POINT('Ctrl Pts',(3.16764562875528,-1.26943250894327,103.337074584152));
#40573=CARTESIAN_POINT('Ctrl Pts',(0.659839412331244,-3.348141226721,103.178705676368));
#40574=CARTESIAN_POINT('Ctrl Pts',(-2.44914443259804,-2.37636892598951,
103.020336768584));
#40575=CARTESIAN_POINT('Ctrl Pts',(-3.32672043140588,0.760505684003158,
102.861967860799));
#40576=CARTESIAN_POINT('Ctrl Pts',(-1.17333183143872,3.2044859396582,102.703598953015));
#40577=CARTESIAN_POINT('Ctrl Pts',(2.04907573691939,2.72886906034401,102.545230045231));
#40578=CARTESIAN_POINT('Ctrl Pts',(3.40457679874342,-0.233011900109024,
102.386861137447));
#40579=CARTESIAN_POINT('Ctrl Pts',(1.65817856858484,-2.98259644585391,102.228492229663));
#40580=CARTESIAN_POINT('Ctrl Pts',(-1.59898097844946,-3.01474668167847,
102.070123321878));
#40581=CARTESIAN_POINT('Ctrl Pts',(-3.39931394816092,-0.300170628098432,
101.911754414094));
#40582=CARTESIAN_POINT('Ctrl Pts',(-2.10254259262445,2.68788994758611,101.75338550631));
#40583=CARTESIAN_POINT('Ctrl Pts',(1.10984875475132,3.22702238382561,101.595016598526));
#40584=CARTESIAN_POINT('Ctrl Pts',(3.31106036670697,0.826024801175402,101.436647690742));
#40585=CARTESIAN_POINT('Ctrl Pts',(2.4955752159428,-2.32756139891226,101.278278782958));
#40586=CARTESIAN_POINT('Ctrl Pts',(-0.593620722687675,-3.36051367527798,
101.119909875173));
#40587=CARTESIAN_POINT('Ctrl Pts',(-3.14197067420732,-1.3317124338819,100.961540967389));
#40588=CARTESIAN_POINT('Ctrl Pts',(-2.8276809539325,1.91040784831451,100.803172059605));
#40589=CARTESIAN_POINT('Ctrl Pts',(0.0629000552312259,3.41196150435303,
100.644803151821));
#40590=CARTESIAN_POINT('Ctrl Pts',(2.89617302045262,1.80488768618331,100.486434244037));
#40591=CARTESIAN_POINT('Ctrl Pts',(3.09075178881617,-1.44661366786822,100.328065336253));
#40592=CARTESIAN_POINT('Ctrl Pts',(0.469356251955776,-3.38010982556621,
100.169696428468));
#40593=CARTESIAN_POINT('Ctrl Pts',(-2.57966830069486,-2.23399847415303,
100.011327520684));
#40594=CARTESIAN_POINT('Ctrl Pts',(-3.27836511850688,0.947501912339738,
99.8529586129002));
#40595=CARTESIAN_POINT('Ctrl Pts',(-0.990153712156691,3.26573626468394,
99.6945897051162));
#40596=CARTESIAN_POINT('Ctrl Pts',(2.20018365000201,2.60856850213676,99.5362207973317));
#40597=CARTESIAN_POINT('Ctrl Pts',(3.38594055778935,-0.425257878515824,
99.3778518895479));
#40598=CARTESIAN_POINT('Ctrl Pts',(1.48677759454023,-3.07163313381674,99.2194829817636));
#40599=CARTESIAN_POINT('Ctrl Pts',(-1.76698379325318,-2.91945303062344,
99.0611140739795));
#40600=CARTESIAN_POINT('Ctrl Pts',(-3.41085176368671,-0.107368386284913,
98.9027451661953));
#40601=CARTESIAN_POINT('Ctrl Pts',(-1.94710334114339,2.80253926017304,98.7443762584111));
#40602=CARTESIAN_POINT('Ctrl Pts',(1.29064485645816,3.15906213527026,98.5860073506268));
#40603=CARTESIAN_POINT('Ctrl Pts',(3.35249055493281,0.637373364056125,98.4276384428428));
#40604=CARTESIAN_POINT('Ctrl Pts',(2.3598925753479,-2.46502429376086,98.2692695350585));
#40605=CARTESIAN_POINT('Ctrl Pts',(-0.782796161482605,-3.32154600455329,
98.1109006272744));
#40606=CARTESIAN_POINT('Ctrl Pts',(-3.21228176030053,-1.15181753846559,
97.9525317194901));
#40607=CARTESIAN_POINT('Ctrl Pts',(-2.71506747479084,2.06732832593376,97.7941628117061));
#40608=CARTESIAN_POINT('Ctrl Pts',(0.255836307364129,3.4029377375855,97.6357939039218));
#40609=CARTESIAN_POINT('Ctrl Pts',(2.99364843452285,1.63814133785425,97.4774249961376));
#40610=CARTESIAN_POINT('Ctrl Pts',(3.00395680772149,-1.61916079141855,97.3190560883535));
#40611=CARTESIAN_POINT('Ctrl Pts',(0.27736953505882,-3.4012500429792,97.1606871805693));
#40612=CARTESIAN_POINT('Ctrl Pts',(-2.70192830062999,-2.08447205856978,
97.0023182727851));
#40613=CARTESIAN_POINT('Ctrl Pts',(-3.21950760709066,1.13146400450909,96.8439493650011));
#40614=CARTESIAN_POINT('Ctrl Pts',(-0.803803762509031,3.31652260596299,
96.6855804572166));
#40615=CARTESIAN_POINT('Ctrl Pts',(2.34424353289394,2.47991599926166,96.5272115494327));
#40616=CARTESIAN_POINT('Ctrl Pts',(3.35645716784768,-0.616150510332253,
96.3688426416484));
#40617=CARTESIAN_POINT('Ctrl Pts',(1.31061453329219,-3.1508122302375,96.2104737338642));
#40618=CARTESIAN_POINT('Ctrl Pts',(-1.92932763290688,-2.81484199264079,
96.0521048260802));
#40619=CARTESIAN_POINT('Ctrl Pts',(-3.41146003475373,0.0858469933911683,
95.8937359182958));
#40620=CARTESIAN_POINT('Ctrl Pts',(-1.78543248818445,2.90807394234403,95.7353670105118));
#40621=CARTESIAN_POINT('Ctrl Pts',(1.4673180506629,3.08125232813832,95.5769981027275));
#40622=CARTESIAN_POINT('Ctrl Pts',(3.38315818207064,0.446145412695689,95.4186291949435));
#40623=CARTESIAN_POINT('Ctrl Pts',(2.2166948701987,-2.59353185912633,95.2602602871591));
#40624=CARTESIAN_POINT('Ctrl Pts',(-0.969545392519947,-3.2740501129473,
95.101891379375));
#40625=CARTESIAN_POINT('Ctrl Pts',(-3.27222176137714,-0.963831701968104,
94.9435224715908));
#40626=CARTESIAN_POINT('Ctrl Pts',(-2.81915114059448,1.14932497266615,94.8379431997347));
#40627=CARTESIAN_POINT('Ctrl Pts',(-2.19630549042403,1.87781109426488,94.7851535638067));
#40628=CARTESIAN_POINT('Ctrl Pts',(-0.697796808006135,-2.61012367354467,
114.214607213421));
#40629=CARTESIAN_POINT('Ctrl Pts',(-1.56354106813931,-2.37867349844622,
114.161817577493));
#40630=CARTESIAN_POINT('Ctrl Pts',(-3.03181856669101,-0.990373273901665,
114.056238305636));
#40631=CARTESIAN_POINT('Ctrl Pts',(-2.4810714774082,2.00927052345691,113.897869397852));
#40632=CARTESIAN_POINT('Ctrl Pts',(0.334446837630344,3.17240841892262,113.739500490068));
#40633=CARTESIAN_POINT('Ctrl Pts',(2.84312122348166,1.44802162338334,113.581131582284));
#40634=CARTESIAN_POINT('Ctrl Pts',(2.76251175468075,-1.59708278053852,113.4227626745));
#40635=CARTESIAN_POINT('Ctrl Pts',(0.164442890166777,-3.18636775866573,
113.264393766716));
#40636=CARTESIAN_POINT('Ctrl Pts',(-2.58317444271743,-1.87292830938426,
113.106024858931));
#40637=CARTESIAN_POINT('Ctrl Pts',(-2.97740867725489,1.14711504666666,112.947655951147));
#40638=CARTESIAN_POINT('Ctrl Pts',(-0.658864813939638,3.12193200092439,
112.789287043363));
#40639=CARTESIAN_POINT('Ctrl Pts',(2.2599331397113,2.25241373384597,112.630918135579));
#40640=CARTESIAN_POINT('Ctrl Pts',(3.11973106555201,-0.669295568887458,
112.472549227795));
#40641=CARTESIAN_POINT('Ctrl Pts',(1.13714265245665,-2.98119967127663,112.314180320011));
#40642=CARTESIAN_POINT('Ctrl Pts',(-1.88148827530065,-2.5769481799015,112.155811412226));
#40643=CARTESIAN_POINT('Ctrl Pts',(-3.18590343934957,0.175155848081176,
111.997442504442));
#40644=CARTESIAN_POINT('Ctrl Pts',(-1.58765074795745,2.76767436398734,111.839073596658));
#40645=CARTESIAN_POINT('Ctrl Pts',(1.45710498700515,2.83857419977103,111.680704688874));
#40646=CARTESIAN_POINT('Ctrl Pts',(3.17429721904537,0.323257543760826,111.52233578109));
#40647=CARTESIAN_POINT('Ctrl Pts',(1.99939701268271,-2.48657784847987,111.363966873305));
#40648=CARTESIAN_POINT('Ctrl Pts',(-0.997147492505912,-3.03090002877003,
111.205597965521));
#40649=CARTESIAN_POINT('Ctrl Pts',(-3.0851940694731,-0.813778603698501,
111.047229057737));
#40650=CARTESIAN_POINT('Ctrl Pts',(-2.36232994221583,2.14477394029311,110.888860149953));
#40651=CARTESIAN_POINT('Ctrl Pts',(0.512845610030737,3.14922965670211,110.730491242169));
#40652=CARTESIAN_POINT('Ctrl Pts',(2.92076913317356,1.28443205831725,110.572122334385));
#40653=CARTESIAN_POINT('Ctrl Pts',(2.66758901539418,-1.75060757490912,110.4137534266));
#40654=CARTESIAN_POINT('Ctrl Pts',(-0.0160231245987433,-3.19067411388555,
110.255384518816));
#40655=CARTESIAN_POINT('Ctrl Pts',(-2.68503664644901,-1.72372742836392,
110.097015611032));
#40656=CARTESIAN_POINT('Ctrl Pts',(-2.90772166228126,1.31370193509011,109.938646703248));
#40657=CARTESIAN_POINT('Ctrl Pts',(-0.48119054990862,3.15422156718503,109.780277795464));
#40658=CARTESIAN_POINT('Ctrl Pts',(2.38375177025621,2.12093977702929,109.62190888768));
#40659=CARTESIAN_POINT('Ctrl Pts',(3.07686529475549,-0.844723622182665,
109.463539979895));
#40660=CARTESIAN_POINT('Ctrl Pts',(0.966656455436494,-3.04076196654535,
109.305171072111));
#40661=CARTESIAN_POINT('Ctrl Pts',(-2.02427006246532,-2.46637157666842,
109.146802164327));
#40662=CARTESIAN_POINT('Ctrl Pts',(-3.17089044637737,0.355122256500635,
108.988433256543));
#40663=CARTESIAN_POINT('Ctrl Pts',(-1.4285224443634,2.85306531049488,108.830064348759));
#40664=CARTESIAN_POINT('Ctrl Pts',(1.61536789675373,2.75158946758626,108.671695440975));
#40665=CARTESIAN_POINT('Ctrl Pts',(3.18750159044155,0.143149051436234,108.51332653319));
#40666=CARTESIAN_POINT('Ctrl Pts',(1.8555125367053,-2.59571401855541,108.354957625406));
#40667=CARTESIAN_POINT('Ctrl Pts',(-1.16702819616944,-2.96963015026121,
108.196588717622));
#40668=CARTESIAN_POINT('Ctrl Pts',(-3.12629318306656,-0.63792552347952,
108.038219809838));
#40669=CARTESIAN_POINT('Ctrl Pts',(-2.23720221140127,2.27499105609152,107.879850902054));
#40670=CARTESIAN_POINT('Ctrl Pts',(0.690196710353136,3.11517038715585,107.72148199427));
#40671=CARTESIAN_POINT('Ctrl Pts',(2.98875956415239,1.11712770428576,107.563113086485));
#40672=CARTESIAN_POINT('Ctrl Pts',(2.56427291019128,-1.89872654219987,107.404744178701));
#40673=CARTESIAN_POINT('Ctrl Pts',(-0.196514786386437,-3.18465696405854,
107.246375270917));
#40674=CARTESIAN_POINT('Ctrl Pts',(-2.77825847462185,-1.56905636870923,
107.088006363133));
#40675=CARTESIAN_POINT('Ctrl Pts',(-2.82873954056747,1.47610658545555,106.929637455349));
#40676=CARTESIAN_POINT('Ctrl Pts',(-0.30196484264603,3.17639343813087,106.771268547564));
#40677=CARTESIAN_POINT('Ctrl Pts',(2.49992908065257,1.98267814627153,106.61289963978));
#40678=CARTESIAN_POINT('Ctrl Pts',(3.02414542354086,-1.01744901458105,106.454530731996));
#40679=CARTESIAN_POINT('Ctrl Pts',(0.793072312657348,-3.09058155480347,
106.296161824212));
#40680=CARTESIAN_POINT('Ctrl Pts',(-2.16056650625509,-2.34789488947946,
106.137792916428));
#40681=CARTESIAN_POINT('Ctrl Pts',(-3.1457199267745,0.533951479339558,105.979424008644));
#40682=CARTESIAN_POINT('Ctrl Pts',(-1.26481774319096,2.92931632237019,105.821055100859));
#40683=CARTESIAN_POINT('Ctrl Pts',(1.76845593735489,2.65579020964182,105.662686193075));
#40684=CARTESIAN_POINT('Ctrl Pts',(3.19049493463312,-0.0374180715084452,
105.504317285291));
#40685=CARTESIAN_POINT('Ctrl Pts',(1.70568395793947,-2.69653486452949,105.345948377507));
#40686=CARTESIAN_POINT('Ctrl Pts',(-1.3331703475554,-2.89884716126845,105.187579469723));
#40687=CARTESIAN_POINT('Ctrl Pts',(-3.15737731165363,-0.460028859801123,
105.029210561938));
#40688=CARTESIAN_POINT('Ctrl Pts',(-2.10490766468081,2.39792029958526,104.870841654154));
#40689=CARTESIAN_POINT('Ctrl Pts',(0.865336783897941,3.07113176051245,104.71247274637));
#40690=CARTESIAN_POINT('Ctrl Pts',(3.04717559031573,0.946244662747985,104.554103838586));
#40691=CARTESIAN_POINT('Ctrl Pts',(2.45274222991511,-2.04076299299701,104.395734930802));
#40692=CARTESIAN_POINT('Ctrl Pts',(-0.376376918509931,-3.16843785724261,
104.237366023018));
#40693=CARTESIAN_POINT('Ctrl Pts',(-2.86258023155845,-1.40935888186287,
104.078997115233));
#40694=CARTESIAN_POINT('Ctrl Pts',(-2.74069563283132,1.6337825706545,103.920628207449));
#40695=CARTESIAN_POINT('Ctrl Pts',(-0.121771799695632,3.18838982384432,
103.762259299665));
#40696=CARTESIAN_POINT('Ctrl Pts',(2.60809793996178,1.83806506292957,103.603890391881));
#40697=CARTESIAN_POINT('Ctrl Pts',(2.96173778920377,-1.1869150382388,103.445521484097));
#40698=CARTESIAN_POINT('Ctrl Pts',(0.616947585477037,-3.13050055370848,
103.287152576312));
#40699=CARTESIAN_POINT('Ctrl Pts',(-2.28994163721969,-2.22189678835962,
103.128783668528));
#40700=CARTESIAN_POINT('Ctrl Pts',(-3.11047218362072,0.711070203929821,
102.970414760744));
#40701=CARTESIAN_POINT('Ctrl Pts',(-1.09706123466004,2.99618335343504,102.81204585296));
#40702=CARTESIAN_POINT('Ctrl Pts',(1.91587878008926,2.55148320394214,102.653676945176));
#40703=CARTESIAN_POINT('Ctrl Pts',(3.18326761982119,-0.217865326734245,
102.495308037392));
#40704=CARTESIAN_POINT('Ctrl Pts',(1.55039126954215,-2.78871743841547,102.336939129607));
#40705=CARTESIAN_POINT('Ctrl Pts',(-1.49504172597511,-2.81877779854825,
102.178570221823));
#40706=CARTESIAN_POINT('Ctrl Pts',(-3.17834687259251,-0.280658506866343,
102.020201314039));
#40707=CARTESIAN_POINT('Ctrl Pts',(-1.96587010663603,2.51316787418387,101.861832406255));
#40708=CARTESIAN_POINT('Ctrl Pts',(1.03770477587778,3.01725485136997,101.703463498471));
#40709=CARTESIAN_POINT('Ctrl Pts',(3.09583007688406,0.772330353576217,101.545094590687));
#40710=CARTESIAN_POINT('Ctrl Pts',(2.33335426026256,-2.1762619180856,101.386725682902));
#40711=CARTESIAN_POINT('Ctrl Pts',(-0.555033337971393,-3.14206875063794,
101.228356775118));
#40712=CARTESIAN_POINT('Ctrl Pts',(-2.9377317948367,-1.24514655426605,101.069987867334));
#40713=CARTESIAN_POINT('Ctrl Pts',(-2.6438719852525,1.78622478025355,100.91161895955));
#40714=CARTESIAN_POINT('Ctrl Pts',(0.058811335722083,3.19017229421644,100.753250051766));
#40715=CARTESIAN_POINT('Ctrl Pts',(2.70791183233384,1.68756379088345,100.594881143982));
#40716=CARTESIAN_POINT('Ctrl Pts',(2.88984231281674,-1.35257881361797,100.436512236197));
#40717=CARTESIAN_POINT('Ctrl Pts',(0.438846484403849,-3.16039108388907,
100.278143328413));
#40718=CARTESIAN_POINT('Ctrl Pts',(-2.41198100583659,-2.08878090461229,
100.119774420629));
#40719=CARTESIAN_POINT('Ctrl Pts',(-3.06526013205104,0.885911035516352,
99.9614055128444));
#40720=CARTESIAN_POINT('Ctrl Pts',(-0.925790321932956,3.05345219707809,
99.8030366050604));
#40721=CARTESIAN_POINT('Ctrl Pts',(2.05716416010835,2.43900259497809,99.6446676972761));
#40722=CARTESIAN_POINT('Ctrl Pts',(3.16584279850237,-0.397614656615443,
99.4862987894921));
#40723=CARTESIAN_POINT('Ctrl Pts',(1.39013194718426,-2.87196643602151,99.3279298817077));
#40724=CARTESIAN_POINT('Ctrl Pts',(-1.65212378110773,-2.72967856192949,
99.1695609739237));
#40725=CARTESIAN_POINT('Ctrl Pts',(-3.18913469050289,-0.100389072609364,
99.0111920661394));
#40726=CARTESIAN_POINT('Ctrl Pts',(-1.82053494008273,2.62036458789214,98.8528231583554));
#40727=CARTESIAN_POINT('Ctrl Pts',(1.2067485103489,2.95371225226013,98.694454250571));
#40728=CARTESIAN_POINT('Ctrl Pts',(3.13456716065645,0.59594190745975,98.536085342787));
#40729=CARTESIAN_POINT('Ctrl Pts',(2.20649145706861,-2.30478925289559,98.3777164350027));
#40730=CARTESIAN_POINT('Ctrl Pts',(-0.731911723855837,-3.10563411227598,
98.2193475272186));
#40731=CARTESIAN_POINT('Ctrl Pts',(-3.00347241897466,-1.07694544458298,
98.0609786194345));
#40732=CARTESIAN_POINT('Ctrl Pts',(-2.53857876882709,1.93294488816143,97.9026097116503));
#40733=CARTESIAN_POINT('Ctrl Pts',(0.239206069167667,3.18173510326499,97.7442408038659));
#40734=CARTESIAN_POINT('Ctrl Pts',(2.79905100988241,1.53165652759152,97.5858718960819));
#40735=CARTESIAN_POINT('Ctrl Pts',(2.80868930343724,-1.51390978182928,97.4275029882977));
#40736=CARTESIAN_POINT('Ctrl Pts',(0.259339563144376,-3.18015711460151,
97.2691340805136));
#40737=CARTESIAN_POINT('Ctrl Pts',(-2.52629368608997,-1.94897421932625,
97.1107651727293));
#40738=CARTESIAN_POINT('Ctrl Pts',(-3.01022856091902,1.05791496020191,96.9523962649453));
#40739=CARTESIAN_POINT('Ctrl Pts',(-0.751553758702059,3.10093725183804,
96.7940273571609));
#40740=CARTESIAN_POINT('Ctrl Pts',(2.19185965609315,2.31871294641959,96.6356584493769));
#40741=CARTESIAN_POINT('Ctrl Pts',(3.13827593011553,-0.576098612080323,
96.4772895415926));
#40742=CARTESIAN_POINT('Ctrl Pts',(1.22542008963813,-2.94599861937422,96.3189206338085));
#40743=CARTESIAN_POINT('Ctrl Pts',(-1.80391471390086,-2.6318676005175,96.1605517260244));
#40744=CARTESIAN_POINT('Ctrl Pts',(-3.18970342186251,0.0802666441309152,
96.0021828182401));
#40745=CARTESIAN_POINT('Ctrl Pts',(-1.66937324753903,2.7190391534496,95.843813910456));
#40746=CARTESIAN_POINT('Ctrl Pts',(1.37193734045838,2.88096034969207,95.6854450026717));
#40747=CARTESIAN_POINT('Ctrl Pts',(3.16324128675654,0.417144429372286,95.5270760948876));
#40748=CARTESIAN_POINT('Ctrl Pts',(2.07260209431364,-2.42494338538013,95.3687071871034));
#40749=CARTESIAN_POINT('Ctrl Pts',(-0.906521613815463,-3.06122561666511,
95.2103382793192));
#40750=CARTESIAN_POINT('Ctrl Pts',(-3.05951611422325,-0.901179332763063,
95.0519693715352));
#40751=CARTESIAN_POINT('Ctrl Pts',(-2.63589663906204,1.07461490411683,94.946390099679));
#40752=CARTESIAN_POINT('Ctrl Pts',(-2.05353809421562,1.75574692711312,94.8936004637509));
#40753=CARTESIAN_POINT('Ctrl Pts',(-0.649284129501564,-2.42866097669793,
114.323054113364));
#40754=CARTESIAN_POINT('Ctrl Pts',(-1.45483956034068,-2.21330182953991,
114.270264477436));
#40755=CARTESIAN_POINT('Ctrl Pts',(-2.82103852625153,-0.921519906151827,
114.16468520558));
#40756=CARTESIAN_POINT('Ctrl Pts',(-2.30858083034679,1.8695807257754,114.006316297796));
#40757=CARTESIAN_POINT('Ctrl Pts',(0.311195209470579,2.95185420034983,113.847947390012));
#40758=CARTESIAN_POINT('Ctrl Pts',(2.64545992110568,1.3473513327244,113.689578482228));
#40759=CARTESIAN_POINT('Ctrl Pts',(2.57045463564224,-1.48604936423666,113.531209574444));
#40760=CARTESIAN_POINT('Ctrl Pts',(0.153010385788004,-2.96484304989676,
113.372840666659));
#40761=CARTESIAN_POINT('Ctrl Pts',(-2.40358532762983,-1.74271738280394,
113.214471758875));
#40762=CARTESIAN_POINT('Ctrl Pts',(-2.77041135614488,1.06736457657537,113.056102851091));
#40763=CARTESIAN_POINT('Ctrl Pts',(-0.613058790567363,2.90488703634978,
112.897733943307));
#40764=CARTESIAN_POINT('Ctrl Pts',(2.10281661439799,2.09581997750367,112.739365035523));
#40765=CARTESIAN_POINT('Ctrl Pts',(2.90283911582197,-0.622764371860707,
112.580996127739));
#40766=CARTESIAN_POINT('Ctrl Pts',(1.0580854895698,-2.7739387902419,112.422627219954));
#40767=CARTESIAN_POINT('Ctrl Pts',(-1.75068223726419,-2.39779193106209,
112.26425831217));
#40768=CARTESIAN_POINT('Ctrl Pts',(-2.96441101128674,0.162978550551776,
112.105889404386));
#40769=CARTESIAN_POINT('Ctrl Pts',(-1.47727307149132,2.57525832670406,111.947520496602));
#40770=CARTESIAN_POINT('Ctrl Pts',(1.35580319689812,2.64122901850209,111.789151588818));
#40771=CARTESIAN_POINT('Ctrl Pts',(2.95361168609557,0.300783824886337,111.630782681033));
#40772=CARTESIAN_POINT('Ctrl Pts',(1.86039364756782,-2.31370438394716,111.472413773249));
#40773=CARTESIAN_POINT('Ctrl Pts',(-0.927823163173134,-2.82018384751469,
111.314044865465));
#40774=CARTESIAN_POINT('Ctrl Pts',(-2.87070322299844,-0.757202564195071,
111.155675957681));
#40775=CARTESIAN_POINT('Ctrl Pts',(-2.19809452053784,1.99566358691141,110.997307049897));
#40776=CARTESIAN_POINT('Ctrl Pts',(0.477191227671217,2.93028688694483,110.838938142113));
#40777=CARTESIAN_POINT('Ctrl Pts',(2.71770954287736,1.19513494662057,110.680569234328));
#40778=CARTESIAN_POINT('Ctrl Pts',(2.48213117609004,-1.62890070910689,110.522200326544));
#40779=CARTESIAN_POINT('Ctrl Pts',(-0.014909154624417,-2.96885001591916,
110.36383141876));
#40780=CARTESIAN_POINT('Ctrl Pts',(-2.49836580171648,-1.60388934139893,
110.205462510976));
#40781=CARTESIAN_POINT('Ctrl Pts',(-2.70556916664848,1.22236990419424,110.047093603192));
#40782=CARTESIAN_POINT('Ctrl Pts',(-0.447736910999243,2.93493174661639,
109.888724695407));
#40783=CARTESIAN_POINT('Ctrl Pts',(2.21802704647083,1.97348643767599,109.730355787623));
#40784=CARTESIAN_POINT('Ctrl Pts',(2.86295348671375,-0.785996203200543,
109.571986879839));
#40785=CARTESIAN_POINT('Ctrl Pts',(0.899451943594493,-2.82936015730887,
109.413617972055));
#40786=CARTESIAN_POINT('Ctrl Pts',(-1.88353745718526,-2.29490290556113,
109.255249064271));
#40787=CARTESIAN_POINT('Ctrl Pts',(-2.95044176126821,0.330433218571872,
109.096880156487));
#40788=CARTESIAN_POINT('Ctrl Pts',(-1.32920778817003,2.6547126689056,108.938511248703));
#40789=CARTESIAN_POINT('Ctrl Pts',(1.5030632508415,2.56029169481628,108.780142340918));
#40790=CARTESIAN_POINT('Ctrl Pts',(2.96589805469058,0.133196951009745,108.621773433134));
#40791=CARTESIAN_POINT('Ctrl Pts',(1.72651240067488,-2.41525311901104,108.46340452535));
#40792=CARTESIAN_POINT('Ctrl Pts',(-1.08589331129042,-2.76317361290795,
108.305035617566));
#40793=CARTESIAN_POINT('Ctrl Pts',(-2.90894501758196,-0.593575254926628,
108.146666709782));
#40794=CARTESIAN_POINT('Ctrl Pts',(-2.08166600030632,2.11682766463048,107.988297801997));
#40795=CARTESIAN_POINT('Ctrl Pts',(0.642212410725931,2.89859550784268,107.829928894213));
#40796=CARTESIAN_POINT('Ctrl Pts',(2.78097309938266,1.03946203349913,107.671559986429));
#40797=CARTESIAN_POINT('Ctrl Pts',(2.38599787960529,-1.76672205428449,107.513191078645));
#40798=CARTESIAN_POINT('Ctrl Pts',(-0.182852559010247,-2.96325119425262,
107.354822170861));
#40799=CARTESIAN_POINT('Ctrl Pts',(-2.58510660199141,-1.45997142263697,
107.196453263076));
#40800=CARTESIAN_POINT('Ctrl Pts',(-2.63207809080127,1.37348375399935,107.038084355292));
#40801=CARTESIAN_POINT('Ctrl Pts',(-0.28097144863377,2.95556217048953,106.879715447508));
#40802=CARTESIAN_POINT('Ctrl Pts',(2.32612740316932,1.84483712094075,106.721346539724));
#40803=CARTESIAN_POINT('Ctrl Pts',(2.81389884029478,-0.946713269772759,
106.56297763194));
#40804=CARTESIAN_POINT('Ctrl Pts',(0.73793582923783,-2.87571615610847,106.404608724156));
#40805=CARTESIAN_POINT('Ctrl Pts',(-2.0103582119449,-2.18466303082235,106.246239816371));
#40806=CARTESIAN_POINT('Ctrl Pts',(-2.92702116271869,0.496829761158795,
106.087870908587));
#40807=CARTESIAN_POINT('Ctrl Pts',(-1.1768842705263,2.72566250888916,105.929502000803));
#40808=CARTESIAN_POINT('Ctrl Pts',(1.64550820621875,2.47115265450012,105.771133093019));
#40809=CARTESIAN_POINT('Ctrl Pts',(2.96868329368197,-0.0348166682739743,
105.612764185235));
#40810=CARTESIAN_POINT('Ctrl Pts',(1.58710030073077,-2.50906463328398,105.454395277451));
#40811=CARTESIAN_POINT('Ctrl Pts',(-1.24048482116616,-2.6973116444031,105.296026369666));
#40812=CARTESIAN_POINT('Ctrl Pts',(-2.9378680953883,-0.42804643752246,105.137657461882));
#40813=CARTESIAN_POINT('Ctrl Pts',(-1.95856892015396,2.23121054219076,104.979288554098));
#40814=CARTESIAN_POINT('Ctrl Pts',(0.805176283428797,2.85761856292613,104.820919646314));
#40815=CARTESIAN_POINT('Ctrl Pts',(2.83532788900229,0.880459232686007,104.66255073853));
#40816=CARTESIAN_POINT('Ctrl Pts',(2.2822211070191,-1.8988837555924,104.504181830746));
#40817=CARTESIAN_POINT('Ctrl Pts',(-0.350210200298097,-2.94815968261277,
104.345812922961));
#40818=CARTESIAN_POINT('Ctrl Pts',(-2.66356608750706,-1.31137652718754,
104.187444015177));
#40819=CARTESIAN_POINT('Ctrl Pts',(-2.55015522824801,1.52019768793913,104.029075107393));
#40820=CARTESIAN_POINT('Ctrl Pts',(-0.113305902314361,2.96672453575942,
103.870706199609));
#40821=CARTESIAN_POINT('Ctrl Pts',(2.42677607746812,1.71027792139309,103.712337291825));
#40822=CARTESIAN_POINT('Ctrl Pts',(2.75582994965227,-1.10439756753432,103.553968384041));
#40823=CARTESIAN_POINT('Ctrl Pts',(0.574055758622828,-2.91285988069597,
103.395599476256));
#40824=CARTESIAN_POINT('Ctrl Pts',(-2.13073884184133,-2.06742465072972,
103.237230568472));
#40825=CARTESIAN_POINT('Ctrl Pts',(-2.89422393583557,0.661634723856482,
103.078861660688));
#40826=CARTESIAN_POINT('Ctrl Pts',(-1.02079063788135,2.78788076721189,102.920492752904));
#40827=CARTESIAN_POINT('Ctrl Pts',(1.78268182325912,2.37409734754027,102.76212384512));
#40828=CARTESIAN_POINT('Ctrl Pts',(2.96195844089894,-0.202718753359468,
102.603754937335));
#40829=CARTESIAN_POINT('Ctrl Pts',(1.44260397049946,-2.59483843097703,102.445386029551));
#40830=CARTESIAN_POINT('Ctrl Pts',(-1.39110247350075,-2.62280891541804,
102.287017121767));
#40831=CARTESIAN_POINT('Ctrl Pts',(-2.9573797970241,-0.261146385634254,
102.128648213983));
#40832=CARTESIAN_POINT('Ctrl Pts',(-1.82919762064763,2.33844580078163,101.970279306199));
#40833=CARTESIAN_POINT('Ctrl Pts',(0.965560797004244,2.80748731891433,101.811910398415));
#40834=CARTESIAN_POINT('Ctrl Pts',(2.88059978706116,0.718635905977031,101.65354149063));
#40835=CARTESIAN_POINT('Ctrl Pts',(2.1711333045823,-2.02496243725894,101.495172582846));
#40836=CARTESIAN_POINT('Ctrl Pts',(-0.516445953255115,-2.92362382599791,
101.336803675062));
#40837=CARTESIAN_POINT('Ctrl Pts',(-2.73349291546608,-1.15858067465021,
101.178434767278));
#40838=CARTESIAN_POINT('Ctrl Pts',(-2.46006301657252,1.66204171219262,101.020065859494));
#40839=CARTESIAN_POINT('Ctrl Pts',(0.0547226162129466,2.96838308407986,
100.861696951709));
#40840=CARTESIAN_POINT('Ctrl Pts',(2.51965064421505,1.57023989558361,100.703328043925));
#40841=CARTESIAN_POINT('Ctrl Pts',(2.68893283681732,-1.25854395936773,100.544959136141));
#40842=CARTESIAN_POINT('Ctrl Pts',(0.408336716851919,-2.94067234221196,
100.386590228357));
#40843=CARTESIAN_POINT('Ctrl Pts',(-2.24429371097833,-1.94356333507155,
100.228221320573));
#40844=CARTESIAN_POINT('Ctrl Pts',(-2.85215514559521,0.82432015869297,100.069852412789));
#40845=CARTESIAN_POINT('Ctrl Pts',(-0.861426931709219,2.84116812947223,
99.9114835050046));
#40846=CARTESIAN_POINT('Ctrl Pts',(1.91414467021469,2.26943668781942,99.7531145972204));
#40847=CARTESIAN_POINT('Ctrl Pts',(2.94574503921539,-0.369971434715065,
99.5947456894364));
#40848=CARTESIAN_POINT('Ctrl Pts',(1.29348629982829,-2.6722997382263,99.4363767816521));
#40849=CARTESIAN_POINT('Ctrl Pts',(-1.53726376896229,-2.53990409323553,
99.2780078738679));
#40850=CARTESIAN_POINT('Ctrl Pts',(-2.96741761731905,-0.0934097589338181,
99.1196389660839));
#40851=CARTESIAN_POINT('Ctrl Pts',(-1.69396653902206,2.43818991561124,98.9612700582995));
#40852=CARTESIAN_POINT('Ctrl Pts',(1.12285216423963,2.74836236925,98.8029011505155));
#40853=CARTESIAN_POINT('Ctrl Pts',(2.91664376638008,0.554510450863373,98.6445322427313));
#40854=CARTESIAN_POINT('Ctrl Pts',(2.05309033878933,-2.14455421203033,98.4861633349471));
#40855=CARTESIAN_POINT('Ctrl Pts',(-0.681027286229073,-2.88972221999867,
98.3277944271628));
#40856=CARTESIAN_POINT('Ctrl Pts',(-2.79466307764877,-1.00207335070038,
98.1694255193788));
#40857=CARTESIAN_POINT('Ctrl Pts',(-2.36209006286334,1.79856145038909,98.0110566115945));
#40858=CARTESIAN_POINT('Ctrl Pts',(0.222575830971204,2.96053246894448,97.8526877038105));
#40859=CARTESIAN_POINT('Ctrl Pts',(2.60445358524196,1.42517171732879,97.694318796026));
#40860=CARTESIAN_POINT('Ctrl Pts',(2.61342179915298,-1.40865877224002,97.5359498882422));
#40861=CARTESIAN_POINT('Ctrl Pts',(0.241309591229933,-2.95906418622381,
97.3775809804578));
#40862=CARTESIAN_POINT('Ctrl Pts',(-2.35065907154996,-1.81347638008271,
97.2192120726736));
#40863=CARTESIAN_POINT('Ctrl Pts',(-2.80094951474737,0.984365915894731,
97.0608431648896));
#40864=CARTESIAN_POINT('Ctrl Pts',(-0.699303754895083,2.88535189771308,
96.9024742571053));
#40865=CARTESIAN_POINT('Ctrl Pts',(2.03947577929237,2.15750989357752,96.7441053493211));
#40866=CARTESIAN_POINT('Ctrl Pts',(2.92009469238337,-0.536046713828397,
96.5857364415371));
#40867=CARTESIAN_POINT('Ctrl Pts',(1.14022564598408,-2.74118500851093,96.4273675337527));
#40868=CARTESIAN_POINT('Ctrl Pts',(-1.67850179489484,-2.4488932083942,96.2689986259687));
#40869=CARTESIAN_POINT('Ctrl Pts',(-2.96794680897129,0.0746862948706615,
96.1106297181844));
#40870=CARTESIAN_POINT('Ctrl Pts',(-1.55331400689361,2.53000436455518,95.9522608104003));
#40871=CARTESIAN_POINT('Ctrl Pts',(1.27655663025386,2.68066837124582,95.7938919026161));
#40872=CARTESIAN_POINT('Ctrl Pts',(2.94332439144243,0.388143446048883,95.6355229948319));
#40873=CARTESIAN_POINT('Ctrl Pts',(1.92850931842858,-2.25635491163392,95.4771540870476));
#40874=CARTESIAN_POINT('Ctrl Pts',(-0.84349783511098,-2.84840112038291,
95.3187851792635));
#40875=CARTESIAN_POINT('Ctrl Pts',(-2.84681046706935,-0.838526963558023,
95.1604162714794));
#40876=CARTESIAN_POINT('Ctrl Pts',(-2.4526421375296,0.999904835567503,95.0548369996233));
#40877=CARTESIAN_POINT('Ctrl Pts',(-1.91077069800722,1.63368275996136,95.0020473636952));
#40878=CARTESIAN_POINT('Ctrl Pts',(-0.793799282533084,-2.96922295374563,
114.));
#40879=CARTESIAN_POINT('Ctrl Pts',(-0.887756405416284,-2.93485301849123,
114.));
#40880=CARTESIAN_POINT('Ctrl Pts',(-0.979607394515572,-2.89562354334601,
114.));
#40881=CARTESIAN_POINT('Ctrl Pts',(-1.06913777784631,-2.8518719612289,114.));
#40882=CARTESIAN_POINT('Ctrl Pts',(-1.15999321053621,-2.80747285584995,
114.));
#40883=CARTESIAN_POINT('Ctrl Pts',(-1.24845948656086,-2.7584161121202,114.));
#40884=CARTESIAN_POINT('Ctrl Pts',(-1.33428309468856,-2.70500832173497,
114.));
#40885=CARTESIAN_POINT('Ctrl Pts',(-1.4201843897322,-2.65155218700005,114.));
#40886=CARTESIAN_POINT('Ctrl Pts',(-1.50343881675033,-2.59373634276815,
114.));
#40887=CARTESIAN_POINT('Ctrl Pts',(-1.58375375152654,-2.53183366530801,
114.));
#40888=CARTESIAN_POINT('Ctrl Pts',(-1.64735338850338,-2.48281429144772,
114.));
#40889=CARTESIAN_POINT('Ctrl Pts',(-1.70910910828567,-2.43123137544921,
114.));
#40890=CARTESIAN_POINT('Ctrl Pts',(-1.76885487784217,-2.37720991548722,
114.));
#40891=CARTESIAN_POINT('Ctrl Pts',(-1.78256802692274,-2.36481063869311,
114.));
#40892=CARTESIAN_POINT('Ctrl Pts',(-1.79617749974221,-2.3522805878216,114.));
#40893=CARTESIAN_POINT('Ctrl Pts',(-1.80966297662315,-2.33963863235335,
114.));
#40894=CARTESIAN_POINT('Ctrl Pts',(-1.88210098192872,-2.2717316502446,114.));
#40895=CARTESIAN_POINT('Ctrl Pts',(-1.95107281091722,-2.20050300321149,
114.));
#40896=CARTESIAN_POINT('Ctrl Pts',(-2.01633867799913,-2.12624319266344,
114.));
#40897=CARTESIAN_POINT('Ctrl Pts',(-2.08124950129726,-2.05238735260256,
114.));
#40898=CARTESIAN_POINT('Ctrl Pts',(-2.14249506046558,-1.97553244140376,
114.));
#40899=CARTESIAN_POINT('Ctrl Pts',(-2.19979582352635,-1.89593746805701,
114.));
#40900=CARTESIAN_POINT('Ctrl Pts',(-2.25579080895265,-1.81815631586134,
114.));
#40901=CARTESIAN_POINT('Ctrl Pts',(-2.30801903030654,-1.73775782070226,
114.));
#40902=CARTESIAN_POINT('Ctrl Pts',(-2.35617234908628,-1.6549694155717,114.));
#40903=CARTESIAN_POINT('Ctrl Pts',(-2.37613161281103,-1.620654114919,114.));
#40904=CARTESIAN_POINT('Ctrl Pts',(-2.39539019249454,-1.58592810520914,
114.));
#40905=CARTESIAN_POINT('Ctrl Pts',(-2.41392350328627,-1.55080728403562,
114.));
#40906=CARTESIAN_POINT('Ctrl Pts',(-2.42930717614674,-1.52165506025888,
114.));
#40907=CARTESIAN_POINT('Ctrl Pts',(-2.44419111793619,-1.49223081023459,
114.));
#40908=CARTESIAN_POINT('Ctrl Pts',(-2.45856039815702,-1.46254361992092,
114.));
#40909=CARTESIAN_POINT('Ctrl Pts',(-2.46495040099425,-1.44934175960374,
114.));
#40910=CARTESIAN_POINT('Ctrl Pts',(-2.47123463557079,-1.4360960866698,114.));
#40911=CARTESIAN_POINT('Ctrl Pts',(-2.47741091898805,-1.42281028747023,
114.));
#40912=CARTESIAN_POINT('Ctrl Pts',(-2.51759768923482,-1.33636455240484,
114.));
#40913=CARTESIAN_POINT('Ctrl Pts',(-2.55323686315738,-1.24818320074038,
114.));
#40914=CARTESIAN_POINT('Ctrl Pts',(-2.58406781887899,-1.15850854008231,
114.));
#40915=CARTESIAN_POINT('Ctrl Pts',(-2.6148987746006,-1.06883387942424,114.));
#40916=CARTESIAN_POINT('Ctrl Pts',(-2.64092196711114,-0.977665187699464,
114.));
#40917=CARTESIAN_POINT('Ctrl Pts',(-2.66182132438789,-0.885235488973918,
114.));
#40918=CARTESIAN_POINT('Ctrl Pts',(-2.66314166753101,-0.879396126675976,
114.));
#40919=CARTESIAN_POINT('Ctrl Pts',(-2.66444154050489,-0.873551730452811,
114.));
#40920=CARTESIAN_POINT('Ctrl Pts',(-2.66572085552459,-0.867702358851152,
114.));
#40921=CARTESIAN_POINT('Ctrl Pts',(-2.68608266907363,-0.774602682775677,
114.));
#40922=CARTESIAN_POINT('Ctrl Pts',(-2.7012408677073,-0.680241604070945,
114.));
#40923=CARTESIAN_POINT('Ctrl Pts',(-2.71127329807981,-0.58502826549681,
114.));
#40924=CARTESIAN_POINT('Ctrl Pts',(-2.71432415693148,-0.556073919839703,
114.));
#40925=CARTESIAN_POINT('Ctrl Pts',(-2.71690065119253,-0.527040860992301,
114.));
#40926=CARTESIAN_POINT('Ctrl Pts',(-2.71900407437446,-0.497940927530195,
114.));
#40927=CARTESIAN_POINT('Ctrl Pts',(-2.72063483457608,-0.475380078259617,
114.));
#40928=CARTESIAN_POINT('Ctrl Pts',(-2.72198123645291,-0.452779035766268,
114.));
#40929=CARTESIAN_POINT('Ctrl Pts',(-2.72304371940055,-0.430143407437012,
114.));
#40930=CARTESIAN_POINT('Ctrl Pts',(-2.72369452838722,-0.41627827165448,
114.));
#40931=CARTESIAN_POINT('Ctrl Pts',(-2.72423869350137,-0.402401224478398,
114.));
#40932=CARTESIAN_POINT('Ctrl Pts',(-2.72467613491267,-0.388526209993681,
114.));
#40933=CARTESIAN_POINT('Ctrl Pts',(-2.72760970254779,-0.29547764993958,
114.));
#40934=CARTESIAN_POINT('Ctrl Pts',(-2.72575570446157,-0.202367859072132,
114.));
#40935=CARTESIAN_POINT('Ctrl Pts',(-2.71925034893427,-0.109570485685123,
114.));
#40936=CARTESIAN_POINT('Ctrl Pts',(-2.71271344795737,-0.0163231238456995,
114.));
#40937=CARTESIAN_POINT('Ctrl Pts',(-2.70147961390672,0.0766097727305058,
114.));
#40938=CARTESIAN_POINT('Ctrl Pts',(-2.68563588787195,0.168836959232147,
114.));
#40939=CARTESIAN_POINT('Ctrl Pts',(-2.67002467875455,0.259710652177,114.));
#40940=CARTESIAN_POINT('Ctrl Pts',(-2.6499374210433,0.349900044984494,114.));
#40941=CARTESIAN_POINT('Ctrl Pts',(-2.62541421207747,0.439005547405842,
114.));
#40942=CARTESIAN_POINT('Ctrl Pts',(-2.61599341629587,0.473236171240522,
114.));
#40943=CARTESIAN_POINT('Ctrl Pts',(-2.60591755234073,0.507306502518509,
114.));
#40944=CARTESIAN_POINT('Ctrl Pts',(-2.59518738165598,0.541192473955113,
114.));
#40945=CARTESIAN_POINT('Ctrl Pts',(-2.5893302318919,0.559689403355105,114.));
#40946=CARTESIAN_POINT('Ctrl Pts',(-2.58327811024553,0.578131385467199,
114.));
#40947=CARTESIAN_POINT('Ctrl Pts',(-2.57703104241714,0.596514388648216,
114.));
#40948=CARTESIAN_POINT('Ctrl Pts',(-2.57101572615014,0.614215425536017,
114.));
#40949=CARTESIAN_POINT('Ctrl Pts',(-2.56481956583144,0.63186163539755,114.));
#40950=CARTESIAN_POINT('Ctrl Pts',(-2.55844967245198,0.649430828571657,
114.));
#40951=CARTESIAN_POINT('Ctrl Pts',(-2.52769580588534,0.73425495204952,114.));
#40952=CARTESIAN_POINT('Ctrl Pts',(-2.49285847495252,0.817397602756055,
114.));
#40953=CARTESIAN_POINT('Ctrl Pts',(-2.45399738165239,0.898485836372846,
114.));
#40954=CARTESIAN_POINT('Ctrl Pts',(-2.4224968286348,0.964215438533597,114.));
#40955=CARTESIAN_POINT('Ctrl Pts',(-2.38835153732701,1.02859487584379,114.));
#40956=CARTESIAN_POINT('Ctrl Pts',(-2.35157529000334,1.09140786163922,114.));
#40957=CARTESIAN_POINT('Ctrl Pts',(-2.33607146419489,1.1178880400465,114.));
#40958=CARTESIAN_POINT('Ctrl Pts',(-2.32009987385018,1.14408960317399,114.));
#40959=CARTESIAN_POINT('Ctrl Pts',(-2.30366078197046,1.16999529935414,114.));
#40960=CARTESIAN_POINT('Ctrl Pts',(-2.28749242428528,1.19547435653008,114.));
#40961=CARTESIAN_POINT('Ctrl Pts',(-2.27088535181155,1.22064570837715,114.));
#40962=CARTESIAN_POINT('Ctrl Pts',(-2.25384672324409,1.24548702198906,114.));
#40963=CARTESIAN_POINT('Ctrl Pts',(-2.2054204117729,1.31608972252691,114.));
#40964=CARTESIAN_POINT('Ctrl Pts',(-2.15349724301452,1.38404994787183,114.));
#40965=CARTESIAN_POINT('Ctrl Pts',(-2.09810553423573,1.4490110003995,114.));
#40966=CARTESIAN_POINT('Ctrl Pts',(-2.05603144768597,1.49835370902269,114.));
#40967=CARTESIAN_POINT('Ctrl Pts',(-2.01195547754715,1.54596540514302,114.));
#40968=CARTESIAN_POINT('Ctrl Pts',(-1.96587909147006,1.59167278088311,114.));
#40969=CARTESIAN_POINT('Ctrl Pts',(-1.94985536550434,1.60756817819673,114.));
#40970=CARTESIAN_POINT('Ctrl Pts',(-1.93358962678968,1.62323311874396,114.));
#40971=CARTESIAN_POINT('Ctrl Pts',(-1.91708805188416,1.63866502517338,114.));
#40972=CARTESIAN_POINT('Origin',(0.,0.,94.));
#40973=CARTESIAN_POINT('Origin',(0.,0.,0.));
#40974=CARTESIAN_POINT('',(-8.,-9.79717439317883E-16,114.));
#40975=CARTESIAN_POINT('Origin',(0.,0.,114.));
#40976=CARTESIAN_POINT('',(-8.,-9.79717439317883E-16,0.));
#40977=CARTESIAN_POINT('',(-8.,-9.79717439317883E-16,0.));
#40978=CARTESIAN_POINT('Origin',(0.,0.,0.));
#40979=CARTESIAN_POINT('Origin',(0.,0.,114.));
#40980=CARTESIAN_POINT('Origin',(0.,0.,0.));
#40981=CARTESIAN_POINT('',(0.,0.,0.));
#40982=CARTESIAN_POINT('Origin',(0.,0.,-1.84858989190501));
#40983=CARTESIAN_POINT('',(-2.36545134966535,0.172736721244679,0.83705293121947));
#40984=CARTESIAN_POINT('',(-2.36545134966535,0.172736721244682,0.639882202840047));
#40985=CARTESIAN_POINT('',(-2.36545134966535,0.172736721244682,-1.84858989190501));
#40986=CARTESIAN_POINT('',(-1.37697654870914,-1.93109648821727,7.5238082697382E-5));
#40987=CARTESIAN_POINT('Ctrl Pts',(-1.37697654870914,-1.93109648821727,
7.5238082697604E-5));
#40988=CARTESIAN_POINT('Ctrl Pts',(-1.31325509998115,-1.97653333773959,
0.00535249991746657));
#40989=CARTESIAN_POINT('Ctrl Pts',(-1.24716040592176,-2.01889953805901,
0.0106297617522353));
#40990=CARTESIAN_POINT('Ctrl Pts',(-1.17902429120828,-2.05793580639456,
0.0159070235870042));
#40991=CARTESIAN_POINT('Ctrl Pts',(-1.11077485413276,-2.09703699892121,
0.0211930624378784));
#40992=CARTESIAN_POINT('Ctrl Pts',(-1.04047756431894,-2.13279685390308,
0.0264791012887525));
#40993=CARTESIAN_POINT('Ctrl Pts',(-0.968497728889413,-2.16499658467076,
0.0317651401396266));
#40994=CARTESIAN_POINT('Ctrl Pts',(-0.896801545952434,-2.19706942526375,
0.0370303481829998));
#40995=CARTESIAN_POINT('Ctrl Pts',(-0.823436481138263,-2.22560992756757,
0.0422955562263733));
#40996=CARTESIAN_POINT('Ctrl Pts',(-0.748789098656628,-2.25044727737243,
0.0475607642697464));
#40997=CARTESIAN_POINT('Ctrl Pts',(-0.674178268397067,-2.27527246519257,
0.0528233941242097));
#40998=CARTESIAN_POINT('Ctrl Pts',(-0.598286820096588,-2.29639794759183,
0.0580860239786726));
#40999=CARTESIAN_POINT('Ctrl Pts',(-0.521519812123941,-2.31370161171708,
0.0633486538331358));
#41000=CARTESIAN_POINT('Ctrl Pts',(-0.444765325767524,-2.33100245340797,
0.0686104252897907));
#41001=CARTESIAN_POINT('Ctrl Pts',(-0.367136030644985,-2.34448261023254,
0.0738721967464463));
#41002=CARTESIAN_POINT('Ctrl Pts',(-0.289049019812454,-2.35407067154864,
0.0791339682031011));
#41003=CARTESIAN_POINT('Ctrl Pts',(-0.210347700874272,-2.36373416184737,
0.0844371338535079));
#41004=CARTESIAN_POINT('Ctrl Pts',(-0.131181919288033,-2.36944396338326,
0.0897402995039141));
#41005=CARTESIAN_POINT('Ctrl Pts',(-0.0519839748310875,-2.37118023964033,
0.0950434651543208));
#41006=CARTESIAN_POINT('Ctrl Pts',(0.0266910588187834,-2.37290505199357,
0.100311616226391));
#41007=CARTESIAN_POINT('Ctrl Pts',(0.105397349674217,-2.3707087231638,0.105579767298461));
#41008=CARTESIAN_POINT('Ctrl Pts',(0.183713167325577,-2.36462418465413,
0.110847918370531));
#41009=CARTESIAN_POINT('Ctrl Pts',(0.262809769913051,-2.35847898514194,
0.116168591310106));
#41010=CARTESIAN_POINT('Ctrl Pts',(0.341507573963179,-2.3483676763795,0.121489264249681));
#41011=CARTESIAN_POINT('Ctrl Pts',(0.41938164989237,-2.33437723905832,0.126809937189256));
#41012=CARTESIAN_POINT('Ctrl Pts',(0.49725572582156,-2.32038680173715,0.132130610128831));
#41013=CARTESIAN_POINT('Ctrl Pts',(0.57430560516479,-2.30251741176943,0.137451283068406));
#41014=CARTESIAN_POINT('Ctrl Pts',(0.650123141366246,-2.28090726763718,
0.142771956007981));
#41015=CARTESIAN_POINT('Ctrl Pts',(0.726320721013956,-2.25918880036411,
0.148119299385315));
#41016=CARTESIAN_POINT('Ctrl Pts',(0.801563345012648,-2.23360957253032,
0.15346664276265));
#41017=CARTESIAN_POINT('Ctrl Pts',(0.875433222024128,-2.20427192884101,
0.158813986139985));
#41018=CARTESIAN_POINT('Ctrl Pts',(0.949201129375983,-2.17497478270851,
0.164153948067584));
#41019=CARTESIAN_POINT('Ctrl Pts',(1.02159962420124,-2.14192969644625,0.169493909995184));
#41020=CARTESIAN_POINT('Ctrl Pts',(1.0922254709914,-2.105288954756,0.174833871922784));
#41021=CARTESIAN_POINT('Ctrl Pts',(1.1627745208271,-2.06868805538268,0.180168027296104));
#41022=CARTESIAN_POINT('Ctrl Pts',(1.2315543421985,-2.02849948476341,0.185502182669422));
#41023=CARTESIAN_POINT('Ctrl Pts',(1.29818246975213,-1.98492325739013,0.190836338042741));
#41024=CARTESIAN_POINT('Ctrl Pts',(1.36477125603836,-1.94137276005125,0.196167343808821));
#41025=CARTESIAN_POINT('Ctrl Pts',(1.42921048209172,-1.89443883140355,0.201498349574901));
#41026=CARTESIAN_POINT('Ctrl Pts',(1.49114410933806,-1.84436637024383,0.206829355340981));
#41027=CARTESIAN_POINT('Ctrl Pts',(1.55306012909141,-1.79430814449302,0.212158845522541));
#41028=CARTESIAN_POINT('Ctrl Pts',(1.61247160311578,-1.74111345109366,0.217488335704101));
#41029=CARTESIAN_POINT('Ctrl Pts',(1.66905438187736,-1.68506840598119,0.22281782588566));
#41030=CARTESIAN_POINT('Ctrl Pts',(1.7256383972715,-1.62902213598849,0.228147432544728));
#41031=CARTESIAN_POINT('Ctrl Pts',(1.77939326494072,-1.57012571929049,0.233477039203796));
#41032=CARTESIAN_POINT('Ctrl Pts',(1.83003166647521,-1.50870214495704,0.238806645862863));
#41033=CARTESIAN_POINT('Ctrl Pts',(1.88072081430783,-1.4472170161724,0.244141593484524));
#41034=CARTESIAN_POINT('Ctrl Pts',(1.9282869615661,-1.38320003164342,0.249476541106185));
#41035=CARTESIAN_POINT('Ctrl Pts',(1.97248347534309,-1.31700683445396,0.254811488727847));
#41036=CARTESIAN_POINT('Ctrl Pts',(2.01670221749346,-1.25078034579019,0.260149119529642));
#41037=CARTESIAN_POINT('Ctrl Pts',(2.05754771094884,-1.18237586412966,0.265486750331438));
#41038=CARTESIAN_POINT('Ctrl Pts',(2.09481835040345,-1.11217540941749,0.270824381133234));
#41039=CARTESIAN_POINT('Ctrl Pts',(2.13215413564378,-1.04185225051118,0.276171341642205));
#41040=CARTESIAN_POINT('Ctrl Pts',(2.16590238523173,-0.969727269235076,
0.281518302151176));
#41041=CARTESIAN_POINT('Ctrl Pts',(2.19590899540261,-0.896204076318512,
0.286865262660148));
#41042=CARTESIAN_POINT('Ctrl Pts',(2.22067994092979,-0.835509482815629,
0.291279265666469));
#41043=CARTESIAN_POINT('Ctrl Pts',(2.24290190653961,-0.773862515759138,
0.295693268672789));
#41044=CARTESIAN_POINT('Ctrl Pts',(2.26251409998074,-0.711497020294777,
0.30010727167911));
#41045=CARTESIAN_POINT('Ctrl Pts',(2.28620292971343,-0.636168087420177,
0.305438779649915));
#41046=CARTESIAN_POINT('Ctrl Pts',(2.30617025515604,-0.55951282801373,0.310770287620719));
#41047=CARTESIAN_POINT('Ctrl Pts',(2.3222700872644,-0.481933298597426,0.316101795591524));
#41048=CARTESIAN_POINT('Ctrl Pts',(2.33834675774283,-0.404465377074862,
0.321425633518702));
#41049=CARTESIAN_POINT('Ctrl Pts',(2.35056688962335,-0.32607628139956,0.326749471445881));
#41050=CARTESIAN_POINT('Ctrl Pts',(2.3588340904911,-0.247183729312878,0.33207330937306));
#41051=CARTESIAN_POINT('Ctrl Pts',(2.36709172107772,-0.168382504861136,
0.33739098431636));
#41052=CARTESIAN_POINT('Ctrl Pts',(2.3714054657222,-0.0890794461318766,
0.34270865925966));
#41053=CARTESIAN_POINT('Ctrl Pts',(2.37173015832874,-0.00970147277017596,
0.34802633420296));
#41054=CARTESIAN_POINT('Ctrl Pts',(2.3720546458506,0.0696263633028662,0.353340650358017));
#41055=CARTESIAN_POINT('Ctrl Pts',(2.36839508053346,0.14902855246632,0.358654966513075));
#41056=CARTESIAN_POINT('Ctrl Pts',(2.36075829608094,0.228075272629455,0.363969282668133));
#41057=CARTESIAN_POINT('Ctrl Pts',(2.35312395550452,0.307096696754529,0.369281898168901));
#41058=CARTESIAN_POINT('Ctrl Pts',(2.34151496834921,0.385762411435533,0.374594513669668));
#41059=CARTESIAN_POINT('Ctrl Pts',(2.32599014549971,0.463646315134985,0.379907129170436));
#41060=CARTESIAN_POINT('Ctrl Pts',(2.310465453176,0.54152956402124,0.385219700005098));
#41061=CARTESIAN_POINT('Ctrl Pts',(2.29102508376493,0.618630555491412,0.390532270839759));
#41062=CARTESIAN_POINT('Ctrl Pts',(2.26777893925327,0.694533473044543,0.395844841674421));
#41063=CARTESIAN_POINT('Ctrl Pts',(2.2445100106022,0.770510784983969,0.401162619495317));
#41064=CARTESIAN_POINT('Ctrl Pts',(2.21742799400823,0.845287228269891,0.406480397316214));
#41065=CARTESIAN_POINT('Ctrl Pts',(2.18669248809532,0.918462859895552,0.41179817513711));
#41066=CARTESIAN_POINT('Ctrl Pts',(2.15594205066763,0.991674040733512,0.417118536370114));
#41067=CARTESIAN_POINT('Ctrl Pts',(2.12153479162253,1.0632824376745,0.422438897603118));
#41068=CARTESIAN_POINT('Ctrl Pts',(2.0836771562134,1.13291110470965,0.427759258836121));
#41069=CARTESIAN_POINT('Ctrl Pts',(2.04575292380814,1.20266225853034,0.4330889793456));
#41070=CARTESIAN_POINT('Ctrl Pts',(2.00436643334651,1.2704263236269,0.438418699855078));
#41071=CARTESIAN_POINT('Ctrl Pts',(1.95976834177835,1.33585407476391,0.443748420364556));
#41072=CARTESIAN_POINT('Ctrl Pts',(1.92157161006786,1.39189069356813,0.448313142693117));
#41073=CARTESIAN_POINT('Ctrl Pts',(1.88101988697258,1.44621391972536,0.452877865021678));
#41074=CARTESIAN_POINT('Ctrl Pts',(1.838293254832,1.49862469342366,0.457442587350239));
#41075=CARTESIAN_POINT('Ctrl Pts',(1.78830766153796,1.5599396973699,0.462782824630466));
#41076=CARTESIAN_POINT('Ctrl Pts',(1.73515966602798,1.61886321765742,0.468123061910692));
#41077=CARTESIAN_POINT('Ctrl Pts',(1.67910660018427,1.67505196567677,0.473463299190919));
#41078=CARTESIAN_POINT('Ctrl Pts',(1.62313286426383,1.73116119174667,0.478795978622039));
#41079=CARTESIAN_POINT('Ctrl Pts',(1.56426255103442,1.7845430045804,0.48412865805316));
#41080=CARTESIAN_POINT('Ctrl Pts',(1.50279323671745,1.83488706741759,0.48946133748428));
#41081=CARTESIAN_POINT('Ctrl Pts',(1.4413935039843,1.88517414215156,0.494787980468028));
#41082=CARTESIAN_POINT('Ctrl Pts',(1.37740097674126,1.93243000641459,0.500114623451776));
#41083=CARTESIAN_POINT('Ctrl Pts',(1.31114898180007,1.97638215181797,0.505441266435525));
#41084=CARTESIAN_POINT('Ctrl Pts',(1.24493785724153,2.02030718345668,0.510764623451248));
#41085=CARTESIAN_POINT('Ctrl Pts',(1.17647042019243,2.0609322844446,0.516087980466972));
#41086=CARTESIAN_POINT('Ctrl Pts',(1.10611091149314,2.09802686207203,0.521411337482695));
#41087=CARTESIAN_POINT('Ctrl Pts',(1.03577308794568,2.13511000696546,0.526733053813212));
#41088=CARTESIAN_POINT('Ctrl Pts',(0.96354476380698,2.16866457193147,0.53205477014373));
#41089=CARTESIAN_POINT('Ctrl Pts',(0.88981556110165,2.19850547639103,0.537376486474247));
#41090=CARTESIAN_POINT('Ctrl Pts',(0.816086323548374,2.22834639495484,0.542698205320061));
#41091=CARTESIAN_POINT('Ctrl Pts',(0.740856639558851,2.25447347577933,0.548019924165875));
#41092=CARTESIAN_POINT('Ctrl Pts',(0.664535558446455,2.27674999814654,0.55334164301169));
#41093=CARTESIAN_POINT('Ctrl Pts',(0.588139649237234,2.29904836126533,0.558668579473493));
#41094=CARTESIAN_POINT('Ctrl Pts',(0.51065065500065,2.31748849433755,0.563995515935295));
#41095=CARTESIAN_POINT('Ctrl Pts',(0.432491633224321,2.33198392998129,0.569322452397098));
#41096=CARTESIAN_POINT('Ctrl Pts',(0.354294414425984,2.34648644967573,0.574651992181008));
#41097=CARTESIAN_POINT('Ctrl Pts',(0.275426979207465,2.35704036931227,0.579981531964919));
#41098=CARTESIAN_POINT('Ctrl Pts',(0.196318902637212,2.36361099823286,0.585311071748829));
#41099=CARTESIAN_POINT('Ctrl Pts',(0.117072958990159,2.37019307823962,0.590649899687661));
#41100=CARTESIAN_POINT('Ctrl Pts',(0.0375860038524554,2.37277798287157,
0.595988727626492));
#41101=CARTESIAN_POINT('Ctrl Pts',(-0.0417112580064065,2.3713831899243,
0.601327555565324));
#41102=CARTESIAN_POINT('Ctrl Pts',(-0.108303634743619,2.37021186855407,
0.605811004717334));
#41103=CARTESIAN_POINT('Ctrl Pts',(-0.174762115708698,2.36623487599976,
0.610294453869343));
#41104=CARTESIAN_POINT('Ctrl Pts',(-0.240835850885874,2.3594906559315,0.614777903021352));
#41105=CARTESIAN_POINT('Ctrl Pts',(-0.319526047864752,2.35145865949272,
0.620117445215696));
#41106=CARTESIAN_POINT('Ctrl Pts',(-0.397957859843874,2.33947115381473,
0.62545698741004));
#41107=CARTESIAN_POINT('Ctrl Pts',(-0.475703142599591,2.32355429947761,
0.630796529604384));
#41108=CARTESIAN_POINT('Ctrl Pts',(-0.553338566404695,2.3076599366519,0.636128526691405));
#41109=CARTESIAN_POINT('Ctrl Pts',(-0.630288933620861,2.28784734575792,
0.641460523778426));
#41110=CARTESIAN_POINT('Ctrl Pts',(-0.706131494106662,2.26419442087704,
0.646792520865447));
#41111=CARTESIAN_POINT('Ctrl Pts',(-0.781888514598013,2.24056817324769,
0.652118504191879));
#41112=CARTESIAN_POINT('Ctrl Pts',(-0.856539767648141,2.21311033818684,
0.657444487518312));
#41113=CARTESIAN_POINT('Ctrl Pts',(-0.929674440966726,2.18194947153072,
0.662770470844744));
#41114=CARTESIAN_POINT('Ctrl Pts',(-1.00276418804744,2.150807746828,0.668093182448162));
#41115=CARTESIAN_POINT('Ctrl Pts',(-1.07433877602337,2.11596768884218,0.673415894051581));
#41116=CARTESIAN_POINT('Ctrl Pts',(-1.14400540778191,2.07760672155866,0.678738605654999));
#41117=CARTESIAN_POINT('Ctrl Pts',(-1.21365076471705,2.03925746896242,0.684059691806655));
#41118=CARTESIAN_POINT('Ctrl Pts',(-1.28138891363587,1.9973896677277,0.689380777958311));
#41119=CARTESIAN_POINT('Ctrl Pts',(-1.34685112030407,1.95222696483674,0.694701864109966));
#41120=CARTESIAN_POINT('Ctrl Pts',(-1.41231355765948,1.90706410279353,0.700022969012999));
#41121=CARTESIAN_POINT('Ctrl Pts',(-1.47549965318234,1.85860658265147,0.70534407391603));
#41122=CARTESIAN_POINT('Ctrl Pts',(-1.53607038904226,1.80712086546738,0.710665178819062));
#41123=CARTESIAN_POINT('Ctrl Pts',(-1.59670085789442,1.75558437465636,0.715991531231694));
#41124=CARTESIAN_POINT('Ctrl Pts',(-1.65471045884588,1.70101402542165,0.721317883644325));
#41125=CARTESIAN_POINT('Ctrl Pts',(-1.70979445051785,1.64371560784656,0.726644236056956));
#41126=CARTESIAN_POINT('Ctrl Pts',(-1.76490552656311,1.58638901708205,0.731973207395934));
#41127=CARTESIAN_POINT('Ctrl Pts',(-1.81708782084753,1.52633203883876,0.737302178734913));
#41128=CARTESIAN_POINT('Ctrl Pts',(-1.8660762626614,1.46388436853177,0.74263115007389));
#41129=CARTESIAN_POINT('Ctrl Pts',(-1.91515038989168,1.40132747134522,0.747969442287575));
#41130=CARTESIAN_POINT('Ctrl Pts',(-1.96101923363549,1.33637191017052,0.753307734501259));
#41131=CARTESIAN_POINT('Ctrl Pts',(-2.00346068159012,1.26938700159662,0.758646026714944));
#41132=CARTESIAN_POINT('Ctrl Pts',(-2.03915044306756,1.21305821158582,0.763135090707457));
#41133=CARTESIAN_POINT('Ctrl Pts',(-2.07241726709839,1.1552950002603,0.76762415469997));
#41134=CARTESIAN_POINT('Ctrl Pts',(-2.10315499186712,1.09632893908919,0.772113218692483));
#41135=CARTESIAN_POINT('Ctrl Pts',(-2.14175463753469,1.02228087324364,0.777750470011304));
#41136=CARTESIAN_POINT('Ctrl Pts',(-2.17649347082348,0.946089393183921,
0.783387721330125));
#41137=CARTESIAN_POINT('Ctrl Pts',(-2.20714291909767,0.868169451879649,
0.789024972648946));
#41138=CARTESIAN_POINT('Ctrl Pts',(-2.23773470878619,0.790396095713576,
0.79465161901543));
#41139=CARTESIAN_POINT('Ctrl Pts',(-2.26425227792704,0.710901105848379,
0.800278265381915));
#41140=CARTESIAN_POINT('Ctrl Pts',(-2.28651336647709,0.630122755835394,
0.805904911748399));
#41141=CARTESIAN_POINT('Ctrl Pts',(-2.30871711961896,0.549552457628127,
0.811517066188068));
#41142=CARTESIAN_POINT('Ctrl Pts',(-2.32668612814396,0.467705755804625,
0.817129220627735));
#41143=CARTESIAN_POINT('Ctrl Pts',(-2.34028712478705,0.385037967031752,
0.822741375067404));
#41144=CARTESIAN_POINT('Ctrl Pts',(-2.35184842620135,0.314767585504852,
0.827511893784759));
#41145=CARTESIAN_POINT('Ctrl Pts',(-2.36025434182662,0.243904386798142,
0.832282412502115));
#41146=CARTESIAN_POINT('Ctrl Pts',(-2.36545134966535,0.172736721244678,
0.837052931219471));
#41147=CARTESIAN_POINT('',(1.37702479013102,-1.93106208855765,0.));
#41148=CARTESIAN_POINT('Origin',(0.,0.,0.));
#41149=CARTESIAN_POINT('Ctrl Pts',(1.37702479013101,-1.93106208855765,-2.44249065417534E-15));
#41150=CARTESIAN_POINT('Ctrl Pts',(1.44329081618841,-1.88380832019609,0.00546153625436459));
#41151=CARTESIAN_POINT('Ctrl Pts',(1.50716795013277,-1.83310728246389,0.0109230725087317));
#41152=CARTESIAN_POINT('Ctrl Pts',(1.56829444550799,-1.77922752752109,0.0163846087630988));
#41153=CARTESIAN_POINT('Ctrl Pts',(1.62938466103035,-1.7253797513392,0.0218429034815246));
#41154=CARTESIAN_POINT('Ctrl Pts',(1.68772716014062,-1.66835729997501,0.027301198199951));
#41155=CARTESIAN_POINT('Ctrl Pts',(1.74299340962789,-1.60846884846855,0.0327594929183768));
#41156=CARTESIAN_POINT('Ctrl Pts',(1.79825459974566,-1.5485858794728,0.0382172879551702));
#41157=CARTESIAN_POINT('Ctrl Pts',(1.85043979750689,-1.48583774573482,0.0436750829919633));
#41158=CARTESIAN_POINT('Ctrl Pts',(1.8992580012273,-1.42056928985322,0.0491328780287568));
#41159=CARTESIAN_POINT('Ctrl Pts',(1.94807564400118,-1.35530158394011,0.0545906103526478));
#41160=CARTESIAN_POINT('Ctrl Pts',(1.99352610807435,-1.28751396261289,0.0600483426765391));
#41161=CARTESIAN_POINT('Ctrl Pts',(2.03536010969931,-1.21758255832811,0.0655060750004302));
#41162=CARTESIAN_POINT('Ctrl Pts',(2.07720378652246,-1.14763498059184,0.0709650695665131));
#41163=CARTESIAN_POINT('Ctrl Pts',(2.11542911331289,-1.07554300813758,0.0764240641325964));
#41164=CARTESIAN_POINT('Ctrl Pts',(2.14983194318074,-1.00170887915588,0.0818830586986794));
#41165=CARTESIAN_POINT('Ctrl Pts',(2.18425108443838,-0.927839743249973,
0.087344641534058));
#41166=CARTESIAN_POINT('Ctrl Pts',(2.21484393973068,-0.85222720308178,0.0928062243694362));
#41167=CARTESIAN_POINT('Ctrl Pts',(2.2414542624766,-0.775294042106259,0.0982678072048149));
#41168=CARTESIAN_POINT('Ctrl Pts',(2.26810339717719,-0.698248671805628,
0.103737355922737));
#41169=CARTESIAN_POINT('Ctrl Pts',(2.29075825754318,-0.619879247457034,
0.109206904640659));
#41170=CARTESIAN_POINT('Ctrl Pts',(2.30931234658886,-0.540624221055853,
0.11467645335858));
#41171=CARTESIAN_POINT('Ctrl Pts',(2.32788094035391,-0.461307236780397,
0.120150277913975));
#41172=CARTESIAN_POINT('Ctrl Pts',(2.34234229640014,-0.381103699970898,
0.125624102469369));
#41173=CARTESIAN_POINT('Ctrl Pts',(2.35264140166807,-0.300460476031863,
0.131097927024764));
#41174=CARTESIAN_POINT('Ctrl Pts',(2.36295968183619,-0.219667110334866,
0.136581942760538));
#41175=CARTESIAN_POINT('Ctrl Pts',(2.36910019563012,-0.138432857311421,
0.142065958496312));
#41176=CARTESIAN_POINT('Ctrl Pts',(2.37105995620251,-0.0572079242145295,
0.147549974232085));
#41177=CARTESIAN_POINT('Ctrl Pts',(2.37220213875243,-0.00986862036883413,
0.150746153992562));
#41178=CARTESIAN_POINT('Ctrl Pts',(2.37192519994692,0.0374675362085513,
0.15394233375304));
#41179=CARTESIAN_POINT('Ctrl Pts',(2.37023667769141,0.084712184639374,0.157138513513516));
#41180=CARTESIAN_POINT('Ctrl Pts',(2.36744413080288,0.162847308736816,0.162424485798573));
#41181=CARTESIAN_POINT('Ctrl Pts',(2.36077748227605,0.241017935962905,0.167710458083629));
#41182=CARTESIAN_POINT('Ctrl Pts',(2.35022604973245,0.318803352647091,0.172996430368686));
#41183=CARTESIAN_POINT('Ctrl Pts',(2.33969127462521,0.396465970306297,0.1782740577445));
#41184=CARTESIAN_POINT('Ctrl Pts',(2.32528395068704,0.473744115683103,0.183551685120315));
#41185=CARTESIAN_POINT('Ctrl Pts',(2.30704538116865,0.55021784024912,0.188829312496129));
#41186=CARTESIAN_POINT('Ctrl Pts',(2.28883093718442,0.626590407240669,0.194099958755391));
#41187=CARTESIAN_POINT('Ctrl Pts',(2.26679542482695,0.702160205168564,0.199370605014654));
#41188=CARTESIAN_POINT('Ctrl Pts',(2.24103162067994,0.776514866317857,0.204641251273917));
#41189=CARTESIAN_POINT('Ctrl Pts',(2.2152865989447,0.850815321191758,0.209908055109609));
#41190=CARTESIAN_POINT('Ctrl Pts',(2.18581883281674,0.923901946362171,0.2151748589453));
#41191=CARTESIAN_POINT('Ctrl Pts',(2.15277128772683,0.995376233008883,0.220441662780992));
#41192=CARTESIAN_POINT('Ctrl Pts',(2.1197370814658,1.0668216708175,0.225706340800837));
#41193=CARTESIAN_POINT('Ctrl Pts',(2.08312616405238,1.13665562810727,0.230971018820683));
#41194=CARTESIAN_POINT('Ctrl Pts',(2.0431295094889,1.20449984223977,0.236235696840528));
#41195=CARTESIAN_POINT('Ctrl Pts',(2.00313598427935,1.27233874821438,0.241499962949903));
#41196=CARTESIAN_POINT('Ctrl Pts',(1.95975749191866,1.33818780901973,0.246764229059279));
#41197=CARTESIAN_POINT('Ctrl Pts',(1.91323000399408,1.40169505040034,0.252028495168653));
#41198=CARTESIAN_POINT('Ctrl Pts',(1.86665894877539,1.46526175853462,0.257297690618512));
#41199=CARTESIAN_POINT('Ctrl Pts',(1.81693329080277,1.52648188012333,0.26256688606837));
#41200=CARTESIAN_POINT('Ctrl Pts',(1.76433079845327,1.58503466716954,0.267836081518229));
#41201=CARTESIAN_POINT('Ctrl Pts',(1.71170476509385,1.64361365814029,0.273107635072747));
#41202=CARTESIAN_POINT('Ctrl Pts',(1.65619967103344,1.69952259795037,0.278379188627265));
#41203=CARTESIAN_POINT('Ctrl Pts',(1.5981299772164,1.75247785675663,0.283650742181783));
#41204=CARTESIAN_POINT('Ctrl Pts',(1.53995581739583,1.805528380819,0.288931779136265));
#41205=CARTESIAN_POINT('Ctrl Pts',(1.47920821056172,1.85561430383625,0.294212816090746));
#41206=CARTESIAN_POINT('Ctrl Pts',(1.41623422365411,1.9024927558997,0.299493853045228));
#41207=CARTESIAN_POINT('Ctrl Pts',(1.35747332670612,1.94623494257153,0.304421577705825));
#41208=CARTESIAN_POINT('Ctrl Pts',(1.2967745557132,1.98718474081386,0.309349302366423));
#41209=CARTESIAN_POINT('Ctrl Pts',(1.23443937156907,2.02518085622499,0.314277027027021));
#41210=CARTESIAN_POINT('Ctrl Pts',(1.16679049745889,2.06641590611558,0.319624809820821));
#41211=CARTESIAN_POINT('Ctrl Pts',(1.09695195078784,2.10433161823903,0.324972592614622));
#41212=CARTESIAN_POINT('Ctrl Pts',(1.02528200200408,2.13868999129526,0.330320375408422));
#41213=CARTESIAN_POINT('Ctrl Pts',(0.953712963733243,2.17299998813374,0.335660628581874));
#41214=CARTESIAN_POINT('Ctrl Pts',(0.880318061697311,2.20376239492551,0.341000881755326));
#41215=CARTESIAN_POINT('Ctrl Pts',(0.805482457184367,2.23078373529758,0.346341134928778));
#41216=CARTESIAN_POINT('Ctrl Pts',(0.730731435113846,2.25777453498009,0.351675352316731));
#41217=CARTESIAN_POINT('Ctrl Pts',(0.654543382842364,2.28103251516069,0.357009569704682));
#41218=CARTESIAN_POINT('Ctrl Pts',(0.577324500590568,2.30041180737664,0.362343787092635));
#41219=CARTESIAN_POINT('Ctrl Pts',(0.50015322956025,2.31977915080822,0.36767471553625));
#41220=CARTESIAN_POINT('Ctrl Pts',(0.421952840784171,2.33527244119564,0.373005643979866));
#41221=CARTESIAN_POINT('Ctrl Pts',(0.343144670295126,2.34679564464997,0.378336572423482));
#41222=CARTESIAN_POINT('Ctrl Pts',(0.264360971746756,2.35831526985664,0.383665845478274));
#41223=CARTESIAN_POINT('Ctrl Pts',(0.184970326640474,2.36586718957559,0.388995118533067));
#41224=CARTESIAN_POINT('Ctrl Pts',(0.105402811188834,2.36940674218115,0.394324391587859));
#41225=CARTESIAN_POINT('Ctrl Pts',(0.0258356529750808,2.37294627889502,
0.399653640715572));
#41226=CARTESIAN_POINT('Ctrl Pts',(-0.0539079089206988,2.37247346521709,
0.404982889843285));
#41227=CARTESIAN_POINT('Ctrl Pts',(-0.133395599791717,2.3679957087073,0.410312138970998));
#41228=CARTESIAN_POINT('Ctrl Pts',(-0.212959413064762,2.36351366401683,
0.41564649172218));
#41229=CARTESIAN_POINT('Ctrl Pts',(-0.292266400132336,2.3550190420733,0.420980844473363));
#41230=CARTESIAN_POINT('Ctrl Pts',(-0.370887824258233,2.34257129759523,
0.426315197224544));
#41231=CARTESIAN_POINT('Ctrl Pts',(-0.449547011114101,2.33011757432933,
0.4316521121237));
#41232=CARTESIAN_POINT('Ctrl Pts',(-0.527519522867585,2.31370704118153,
0.436989027022855));
#41233=CARTESIAN_POINT('Ctrl Pts',(-0.604387690555749,2.29345014814028,
0.44232594192201));
#41234=CARTESIAN_POINT('Ctrl Pts',(-0.68138671233925,2.27315877141752,0.447671941949536));
#41235=CARTESIAN_POINT('Ctrl Pts',(-0.757277189581784,2.24900809422682,
0.453017941977062));
#41236=CARTESIAN_POINT('Ctrl Pts',(-0.83165774481026,2.22115813439681,0.458363942004587));
#41237=CARTESIAN_POINT('Ctrl Pts',(-0.892188056615047,2.19849405576654,
0.462714474849906));
#41238=CARTESIAN_POINT('Ctrl Pts',(-0.95171866636475,2.17338107488758,0.467065007695225));
#41239=CARTESIAN_POINT('Ctrl Pts',(-1.01004516747242,2.14592796294881,0.471415540540543));
#41240=CARTESIAN_POINT('Ctrl Pts',(-1.08174595762753,2.11217984192586,0.476763652233876));
#41241=CARTESIAN_POINT('Ctrl Pts',(-1.15187962006272,2.07477490174953,0.482111763927208));
#41242=CARTESIAN_POINT('Ctrl Pts',(-1.22005032815419,2.03388182037965,0.48745987562054));
#41243=CARTESIAN_POINT('Ctrl Pts',(-1.28812716923514,1.99304504635067,0.492800623282156));
#41244=CARTESIAN_POINT('Ctrl Pts',(-1.35424602863012,1.9487299090355,0.498141370943772));
#41245=CARTESIAN_POINT('Ctrl Pts',(-1.41803353126763,1.90115201041386,0.503482118605387));
#41246=CARTESIAN_POINT('Ctrl Pts',(-1.4817519108599,1.85362566937172,0.50881707878941));
#41247=CARTESIAN_POINT('Ctrl Pts',(-1.54314358348597,1.80284387121132,0.514152038973432));
#41248=CARTESIAN_POINT('Ctrl Pts',(-1.60186339745384,1.74906595598841,0.519486999157454));
#41249=CARTESIAN_POINT('Ctrl Pts',(-1.66054868190695,1.69531966425324,0.524818822179181));
#41250=CARTESIAN_POINT('Ctrl Pts',(-1.71656488456289,1.63858106693363,0.530150645200908));
#41251=CARTESIAN_POINT('Ctrl Pts',(-1.7696001976057,1.57914951892905,0.535482468222635));
#41252=CARTESIAN_POINT('Ctrl Pts',(-1.82262054620086,1.51973474013423,0.540812786816804));
#41253=CARTESIAN_POINT('Ctrl Pts',(-1.87266136618552,1.45762886700911,0.546143105410973));
#41254=CARTESIAN_POINT('Ctrl Pts',(-1.91944898854585,1.39316676778853,0.551473424005142));
#41255=CARTESIAN_POINT('Ctrl Pts',(-1.96623772002074,1.32870314047463,0.556803868956105));
#41256=CARTESIAN_POINT('Ctrl Pts',(-2.00977282860423,1.26188355369521,0.562134313907067));
#41257=CARTESIAN_POINT('Ctrl Pts',(-2.04982295656368,1.19307330422088,0.567464758858029));
#41258=CARTESIAN_POINT('Ctrl Pts',(-2.08991314485198,1.1241942269709,0.572800535611623));
#41259=CARTESIAN_POINT('Ctrl Pts',(-2.12651115585645,1.05332091333084,0.578136312365216));
#41260=CARTESIAN_POINT('Ctrl Pts',(-2.15943106457146,0.980844299501093,
0.583472089118809));
#41261=CARTESIAN_POINT('Ctrl Pts',(-2.19236757196774,0.908331141942655,
0.588810556246135));
#41262=CARTESIAN_POINT('Ctrl Pts',(-2.22162211137489,0.834213507035436,
0.594149023373461));
#41263=CARTESIAN_POINT('Ctrl Pts',(-2.24705745683915,0.758901079300586,
0.599487490500786));
#41264=CARTESIAN_POINT('Ctrl Pts',(-2.27253702841281,0.683457700890284,
0.604835239972304));
#41265=CARTESIAN_POINT('Ctrl Pts',(-2.29418401214726,0.606815827876289,
0.610182989443822));
#41266=CARTESIAN_POINT('Ctrl Pts',(-2.31191155015882,0.529398759672008,
0.615530738915341));
#41267=CARTESIAN_POINT('Ctrl Pts',(-2.32630210923964,0.466554449698934,
0.619871843961577));
#41268=CARTESIAN_POINT('Ctrl Pts',(-2.3381108747471,0.40319963826319,0.624212949007814));
#41269=CARTESIAN_POINT('Ctrl Pts',(-2.34731653972495,0.339563138213948,
0.62855405405405));
#41270=CARTESIAN_POINT('Ctrl Pts',(-2.35532395883693,0.284209817411997,
0.632330103649382));
#41271=CARTESIAN_POINT('Ctrl Pts',(-2.36137449625126,0.228565026548074,
0.636106153244714));
#41272=CARTESIAN_POINT('Ctrl Pts',(-2.36545134966535,0.172736721244682,
0.639882202840047));
#41273=CARTESIAN_POINT('Origin',(0.,0.,-1.84858989190501));
#41274=CARTESIAN_POINT('',(-2.36545132977957,0.17273699355969,1.83684621836633));
#41275=CARTESIAN_POINT('',(-2.3654513498954,0.172736718094382,1.63785909343774));
#41276=CARTESIAN_POINT('',(-2.36545134966535,0.172736721244682,-1.84858989190501));
#41277=CARTESIAN_POINT('',(-2.37174999149347,0.00019724836186693,0.848751148665265));
#41278=CARTESIAN_POINT('Ctrl Pts',(-2.36545132977956,0.172736993559942,
1.83684621836632));
#41279=CARTESIAN_POINT('Ctrl Pts',(-2.35464804740561,0.320676575758163,
1.8277274167204));
#41280=CARTESIAN_POINT('Ctrl Pts',(-2.32998181411189,0.467398739448049,
1.81858518484146));
#41281=CARTESIAN_POINT('Ctrl Pts',(-2.28259556239425,0.645140233773284,
1.80672465140104));
#41282=CARTESIAN_POINT('Ctrl Pts',(-2.27272401047721,0.679097774815498,
1.80442343594766));
#41283=CARTESIAN_POINT('Ctrl Pts',(-2.25564957646514,0.73328256320601,1.80068757430668));
#41284=CARTESIAN_POINT('Ctrl Pts',(-2.2489245512852,0.753655519605635,1.79926820645086));
#41285=CARTESIAN_POINT('Ctrl Pts',(-2.2354785472076,0.792605774192321,1.79652475289482));
#41286=CARTESIAN_POINT('Ctrl Pts',(-2.22879999767541,0.811195894221982,
1.79520213923863));
#41287=CARTESIAN_POINT('Ctrl Pts',(-2.21267165189738,0.85438670407692,1.79209722876589));
#41288=CARTESIAN_POINT('Ctrl Pts',(-2.2030426526902,0.87891720555185,1.79030920336862));
#41289=CARTESIAN_POINT('Ctrl Pts',(-2.16907136675365,0.961393474542494,
1.78421130849708));
#41290=CARTESIAN_POINT('Ctrl Pts',(-2.14283715579601,1.01852624007698,1.77984046139933));
#41291=CARTESIAN_POINT('Ctrl Pts',(-2.06996539938773,1.16191488806456,1.76848579076181));
#41292=CARTESIAN_POINT('Ctrl Pts',(-2.02019466103313,1.24644026871397,1.76141583426954));
#41293=CARTESIAN_POINT('Ctrl Pts',(-1.88198291394013,1.45103935633154,1.74346126613437));
#41294=CARTESIAN_POINT('Ctrl Pts',(-1.78718026286442,1.56632298732763,1.73252966648431));
#41295=CARTESIAN_POINT('Ctrl Pts',(-1.66566776307086,1.6885786939201,1.7204796952185));
#41296=CARTESIAN_POINT('Ctrl Pts',(-1.64890356547969,1.70495285413968,1.71885569819598));
#41297=CARTESIAN_POINT('Ctrl Pts',(-1.62256842834581,1.72992343132611,1.71636698809508));
#41298=CARTESIAN_POINT('Ctrl Pts',(-1.61316609545785,1.7386944959781,1.71549042383356));
#41299=CARTESIAN_POINT('Ctrl Pts',(-1.59548765626292,1.75491915122687,1.71386523393306));
#41300=CARTESIAN_POINT('Ctrl Pts',(-1.58723005301484,1.76239123153072,1.71311535360085));
#41301=CARTESIAN_POINT('Ctrl Pts',(-1.5673305219545,1.78014446125934,1.71132968584785));
#41302=CARTESIAN_POINT('Ctrl Pts',(-1.55563975286473,1.79036986653117,1.71029784306977));
#41303=CARTESIAN_POINT('Ctrl Pts',(-1.51381833989229,1.82623027357081,1.70666364432644));
#41304=CARTESIAN_POINT('Ctrl Pts',(-1.4831461024168,1.85122689995472,1.7041016511453));
#41305=CARTESIAN_POINT('Ctrl Pts',(-1.40135799279215,1.91454248028618,1.69749204081709));
#41306=CARTESIAN_POINT('Ctrl Pts',(-1.34929319965399,1.9515855140747,1.69350107331283));
#41307=CARTESIAN_POINT('Ctrl Pts',(-1.1280557030759,2.09589987375625,1.67714158346809));
#41308=CARTESIAN_POINT('Ctrl Pts',(-0.947149752408485,2.18362302817075,
1.66507327098708));
#41309=CARTESIAN_POINT('Ctrl Pts',(-0.722521704518835,2.25931695648376,
1.64981128904514));
#41310=CARTESIAN_POINT('Ctrl Pts',(-0.687401910936438,2.27024868784409,
1.64742046279927));
#41311=CARTESIAN_POINT('Ctrl Pts',(-0.631137911039719,2.2863367601363,1.64357502739875));
#41312=CARTESIAN_POINT('Ctrl Pts',(-0.610151609211697,2.29202657175618,
1.64213740362893));
#41313=CARTESIAN_POINT('Ctrl Pts',(-0.570036573505999,2.30231259684495,
1.63938167749373));
#41314=CARTESIAN_POINT('Ctrl Pts',(-0.550923001188113,2.30696094378568,
1.63806535251114));
#41315=CARTESIAN_POINT('Ctrl Pts',(-0.506681300738281,2.31713919530339,
1.6350098310146));
#41316=CARTESIAN_POINT('Ctrl Pts',(-0.481516985704815,2.32249893317183,
1.63326546406677));
#41317=CARTESIAN_POINT('Ctrl Pts',(-0.398656387857117,2.33874286640403,
1.62749834876422));
#41318=CARTESIAN_POINT('Ctrl Pts',(-0.340646599130598,2.34789352304172,
1.62342336536928));
#41319=CARTESIAN_POINT('Ctrl Pts',(-0.195052606014149,2.36535090716893,
1.61309893372714));
#41320=CARTESIAN_POINT('Ctrl Pts',(-0.107237002091558,2.37095512134007,
1.60678289174567));
#41321=CARTESIAN_POINT('Ctrl Pts',(0.119026523861113,2.37279830575996,1.59036990779681));
#41322=CARTESIAN_POINT('Ctrl Pts',(0.257208585780112,2.36181813063321,1.58020166716128));
#41323=CARTESIAN_POINT('Ctrl Pts',(0.434056895759979,2.3320531299917,1.56745246526195));
#41324=CARTESIAN_POINT('Ctrl Pts',(0.474285525021769,2.32420543229086,1.56457202356149));
#41325=CARTESIAN_POINT('Ctrl Pts',(0.530052594517722,2.31181809885717,1.56062403552056));
#41326=CARTESIAN_POINT('Ctrl Pts',(0.545776387002374,2.30815659049947,1.55951593499902));
#41327=CARTESIAN_POINT('Ctrl Pts',(0.572369449341775,2.301677064512,1.55765180784972));
#41328=CARTESIAN_POINT('Ctrl Pts',(0.58325812904105,2.29894194623905,1.55689140381995));
#41329=CARTESIAN_POINT('Ctrl Pts',(0.606285120919396,2.29298367127748,1.55528984356908));
#41330=CARTESIAN_POINT('Ctrl Pts',(0.618417838186489,2.28974128661817,1.55444974049966));
#41331=CARTESIAN_POINT('Ctrl Pts',(0.652357883281247,2.28038159105728,1.55210867908778));
#41332=CARTESIAN_POINT('Ctrl Pts',(0.67410480187661,2.27404789200983,1.55061916582575));
#41333=CARTESIAN_POINT('Ctrl Pts',(0.799742383327257,2.23549567465549,1.54205718662485));
#41334=CARTESIAN_POINT('Ctrl Pts',(0.901420676276634,2.19646876201649,1.53529754222402));
#41335=CARTESIAN_POINT('Ctrl Pts',(1.16622545863182,2.07332913834315,1.51729376176956));
#41336=CARTESIAN_POINT('Ctrl Pts',(1.32285040011715,1.97707761353991,1.50616207489864));
#41337=CARTESIAN_POINT('Ctrl Pts',(1.49464348893898,1.84187176215918,1.49206666883163));
#41338=CARTESIAN_POINT('Ctrl Pts',(1.52196143823089,1.81936360306158,1.48976336520943));
#41339=CARTESIAN_POINT('Ctrl Pts',(1.56501858401806,1.78223890114579,1.48602487214174));
#41340=CARTESIAN_POINT('Ctrl Pts',(1.58108128568205,1.76800469099866,1.48460499728036));
#41341=CARTESIAN_POINT('Ctrl Pts',(1.61155250686322,1.74025479667892,1.48186105875631));
#41342=CARTESIAN_POINT('Ctrl Pts',(1.62598972051335,1.726773183908,1.48053847378397));
#41343=CARTESIAN_POINT('Ctrl Pts',(1.65928205316862,1.6948967343755,1.47743438854282));
#41344=CARTESIAN_POINT('Ctrl Pts',(1.67800214005842,1.67636529277775,1.47564717165789));
#41345=CARTESIAN_POINT('Ctrl Pts',(1.74027007152932,1.61263666922781,1.4695561952939));
#41346=CARTESIAN_POINT('Ctrl Pts',(1.78232823487315,1.56602739057756,1.46519165738248));
#41347=CARTESIAN_POINT('Ctrl Pts',(1.88505892168161,1.44267508313141,1.45385986364717));
#41348=CARTESIAN_POINT('Ctrl Pts',(1.94292055342253,1.36375038880253,1.44680695292137));
#41349=CARTESIAN_POINT('Ctrl Pts',(2.07643395921466,1.15582142048797,1.42883895203757));
#41350=CARTESIAN_POINT('Ctrl Pts',(2.14508106227687,1.02280715781205,1.41787522279012));
#41351=CARTESIAN_POINT('Ctrl Pts',(2.20948528617555,0.862507949569433,1.405799169735));
#41352=CARTESIAN_POINT('Ctrl Pts',(2.21788446555892,0.840674604372123,1.40417807212877));
#41353=CARTESIAN_POINT('Ctrl Pts',(2.23039516910707,0.806660124877918,1.40169280594942));
#41354=CARTESIAN_POINT('Ctrl Pts',(2.23473276105734,0.794564454924873,1.40081683620472));
#41355=CARTESIAN_POINT('Ctrl Pts',(2.242646454656,0.771919039650832,1.3991921427615));
#41356=CARTESIAN_POINT('Ctrl Pts',(2.2462467040576,0.761378929568453,1.39844217282981));
#41357=CARTESIAN_POINT('Ctrl Pts',(2.25469406728847,0.736066844893238,1.39665543138161));
#41358=CARTESIAN_POINT('Ctrl Pts',(2.25947041125486,0.721271952624277,1.39562261907189));
#41359=CARTESIAN_POINT('Ctrl Pts',(2.27591681237142,0.668561452349381,1.39198025899634));
#41360=CARTESIAN_POINT('Ctrl Pts',(2.28678137634935,0.630399167458296,1.38941132134774));
#41361=CARTESIAN_POINT('Ctrl Pts',(2.31269378923288,0.529867653087519,1.38277780427696));
#41362=CARTESIAN_POINT('Ctrl Pts',(2.32617823563843,0.467127544589651,1.37877039518622));
#41363=CARTESIAN_POINT('Ctrl Pts',(2.37109181040211,0.207251502796512,1.36243890650623));
#41364=CARTESIAN_POINT('Ctrl Pts',(2.38012086018376,0.00710148455932806,
1.35040995572103));
#41365=CARTESIAN_POINT('Ctrl Pts',(2.36099495772909,-0.228613223734846,
1.33518557292967));
#41366=CARTESIAN_POINT('Ctrl Pts',(2.35715029368854,-0.265336494569707,
1.33278578873205));
#41367=CARTESIAN_POINT('Ctrl Pts',(2.34967853496698,-0.323547236235964,
1.32892950709386));
#41368=CARTESIAN_POINT('Ctrl Pts',(2.34660972503881,-0.345101113126554,
1.32749017331415));
#41369=CARTESIAN_POINT('Ctrl Pts',(2.3402056851717,-0.386033626716818,1.32473342967413));
#41370=CARTESIAN_POINT('Ctrl Pts',(2.33692531641986,-0.405419086950399,
1.32341782769056));
#41371=CARTESIAN_POINT('Ctrl Pts',(2.32880791734409,-0.450011629192578,
1.32036734362408));
#41372=CARTESIAN_POINT('Ctrl Pts',(2.32380202601752,-0.475185056562063,
1.31862734446474));
#41373=CARTESIAN_POINT('Ctrl Pts',(2.30608680057119,-0.55728204188785,1.31289157957098));
#41374=CARTESIAN_POINT('Ctrl Pts',(2.29168712816545,-0.613814892254642,
1.30884435797765));
#41375=CARTESIAN_POINT('Ctrl Pts',(2.25064268309215,-0.753246518820026,
1.29861331140109));
#41376=CARTESIAN_POINT('Ctrl Pts',(2.2214907019716,-0.835313984454225,1.29236450136531));
#41377=CARTESIAN_POINT('Ctrl Pts',(2.13543055612175,-1.04096422827599,1.27619811812788));
#41378=CARTESIAN_POINT('Ctrl Pts',(2.07228291301253,-1.16160032931202,1.26621050543948));
#41379=CARTESIAN_POINT('Ctrl Pts',(1.97551187223355,-1.31319488213282,1.25339818423819));
#41380=CARTESIAN_POINT('Ctrl Pts',(1.95084819330827,-1.34956283179926,1.25030446045176));
#41381=CARTESIAN_POINT('Ctrl Pts',(1.91551449459827,-1.39866955941618,1.24612014442449));
#41382=CARTESIAN_POINT('Ctrl Pts',(1.90570137134627,-1.41201084877623,1.24498263784939));
#41383=CARTESIAN_POINT('Ctrl Pts',(1.88902868851754,-1.43418748435966,1.24309206880024));
#41384=CARTESIAN_POINT('Ctrl Pts',(1.88224503683565,-1.44307891971692,1.24233415629681));
#41385=CARTESIAN_POINT('Ctrl Pts',(1.8678449097303,-1.46167906951128,1.24074932216542));
#41386=CARTESIAN_POINT('Ctrl Pts',(1.86021517904386,-1.47137684279918,1.23992330908665));
#41387=CARTESIAN_POINT('Ctrl Pts',(1.8390138662032,-1.49789625328526,1.23766392946694));
#41388=CARTESIAN_POINT('Ctrl Pts',(1.82528713287918,-1.51459306337046,1.23624076231451));
#41389=CARTESIAN_POINT('Ctrl Pts',(1.79359239987193,-1.55208879144417,1.23303720058768));
#41390=CARTESIAN_POINT('Ctrl Pts',(1.77548706839401,-1.57276797893649,1.23126494883763));
#41391=CARTESIAN_POINT('Ctrl Pts',(1.71375476790853,-1.64085113825727,1.22539329143886));
#41392=CARTESIAN_POINT('Ctrl Pts',(1.66855475869492,-1.68679397789092,1.22136928279714));
#41393=CARTESIAN_POINT('Ctrl Pts',(1.47635145197169,-1.86685945081195,1.20506183220831));
#41394=CARTESIAN_POINT('Ctrl Pts',(1.31464165814232,-1.98405928836357,1.19306871053852));
#41395=CARTESIAN_POINT('Ctrl Pts',(1.10770064399898,-2.09751547300224,1.17787772412464));
#41396=CARTESIAN_POINT('Ctrl Pts',(1.07478804155704,-2.11456905898879,1.17546880631996));
#41397=CARTESIAN_POINT('Ctrl Pts',(1.02190320813182,-2.1404175349209,1.171601232347));
#41398=CARTESIAN_POINT('Ctrl Pts',(1.0021851697813,-2.14972049904551,1.1701599156739));
#41399=CARTESIAN_POINT('Ctrl Pts',(0.964450889725479,-2.16689153553028,
1.16740150302429));
#41400=CARTESIAN_POINT('Ctrl Pts',(0.946459517789672,-2.17481005777178,
1.16608624425905));
#41401=CARTESIAN_POINT('Ctrl Pts',(0.904802392982881,-2.1925297601584,1.16303968855379));
#41402=CARTESIAN_POINT('Ctrl Pts',(0.881072497691933,-2.20217285554434,
1.16130332308496));
#41403=CARTESIAN_POINT('Ctrl Pts',(0.803130633843565,-2.23238459540515,
1.15559493610862));
#41404=CARTESIAN_POINT('Ctrl Pts',(0.748323476888627,-2.2513486618235,1.15157215961699));
#41405=CARTESIAN_POINT('Ctrl Pts',(0.610396831172572,-2.29348035447054,
1.14142296165023));
#41406=CARTESIAN_POINT('Ctrl Pts',(0.526607457732485,-2.31415614238286,
1.13523297528626));
#41407=CARTESIAN_POINT('Ctrl Pts',(0.310403281285454,-2.35515540625786,
1.11927933476394));
#41408=CARTESIAN_POINT('Ctrl Pts',(0.177046256836943,-2.36891601756291,
1.10944685395313));
#41409=CARTESIAN_POINT('Ctrl Pts',(-0.00323629014956441,-2.3722032443458,
1.09658012018351));
#41410=CARTESIAN_POINT('Ctrl Pts',(-0.0497297408774496,-2.37168427538983,
1.09330174506795));
#41411=CARTESIAN_POINT('Ctrl Pts',(-0.113076200900375,-2.36911328318783,
1.08891403328352));
#41412=CARTESIAN_POINT('Ctrl Pts',(-0.12996405346272,-2.3682468961745,1.08775198206795));
#41413=CARTESIAN_POINT('Ctrl Pts',(-0.158068013671682,-2.36650355561102,
1.08583251261782));
#41414=CARTESIAN_POINT('Ctrl Pts',(-0.169289546561466,-2.36572729742231,
1.08506992399689));
#41415=CARTESIAN_POINT('Ctrl Pts',(-0.192694447740749,-2.36394085050548,
1.08348788754328));
#41416=CARTESIAN_POINT('Ctrl Pts',(-0.204876206756606,-2.36291625987324,
1.08266920595484));
#41417=CARTESIAN_POINT('Ctrl Pts',(-0.238006403714775,-2.35987158577458,
1.08045424470994));
#41418=CARTESIAN_POINT('Ctrl Pts',(-0.25893728863444,-2.35766674993709,
1.07906749155779));
#41419=CARTESIAN_POINT('Ctrl Pts',(-0.306183623860976,-2.35205306061748,
1.07596017688574));
#41420=CARTESIAN_POINT('Ctrl Pts',(-0.332477092089665,-2.34848059715367,
1.07424704437971));
#41421=CARTESIAN_POINT('Ctrl Pts',(-0.418852426913508,-2.33526507357372,
1.0686564357062));
#41422=CARTESIAN_POINT('Ctrl Pts',(-0.478626152164646,-2.3237509001182,
1.0648467014174));
#41423=CARTESIAN_POINT('Ctrl Pts',(-0.740448165038656,-2.26278310196466,
1.04817166483396));
#41424=CARTESIAN_POINT('Ctrl Pts',(-0.93590276929647,-2.18918563957954,
1.03566627579771));
#41425=CARTESIAN_POINT('Ctrl Pts',(-1.15019441625413,-2.07448364215316,
1.01998979754206));
#41426=CARTESIAN_POINT('Ctrl Pts',(-1.18076124768336,-2.05723898711783,
1.01770543780304));
#41427=CARTESIAN_POINT('Ctrl Pts',(-1.22933840958818,-2.02839427546507,
1.01398974945035));
#41428=CARTESIAN_POINT('Ctrl Pts',(-1.2475944629091,-2.01721696125745,1.01257337151276));
#41429=CARTESIAN_POINT('Ctrl Pts',(-1.28242628158196,-1.99523738906493,
1.00983083738293));
#41430=CARTESIAN_POINT('Ctrl Pts',(-1.29902313477684,-1.98447178405137,
1.00850609029389));
#41431=CARTESIAN_POINT('Ctrl Pts',(-1.33753656318517,-1.95879975139335,
1.0053885364006));
#41432=CARTESIAN_POINT('Ctrl Pts',(-1.35934140348433,-1.94373130232705,
1.00358987253713));
#41433=CARTESIAN_POINT('Ctrl Pts',(-1.43279842120747,-1.89112751344668,
0.997411981686479));
#41434=CARTESIAN_POINT('Ctrl Pts',(-1.48318167605389,-1.85187618865771,
0.992969601369592));
#41435=CARTESIAN_POINT('Ctrl Pts',(-1.60868449666613,-1.74569301666673,
0.981357150716677));
#41436=CARTESIAN_POINT('Ctrl Pts',(-1.68123734883176,-1.6759318505116,0.974095627242334));
#41437=CARTESIAN_POINT('Ctrl Pts',(-1.8466793688405,-1.49527011490924,0.956274130076739));
#41438=CARTESIAN_POINT('Ctrl Pts',(-1.93429347589134,-1.38006236221279,
0.945684068816811));
#41439=CARTESIAN_POINT('Ctrl Pts',(-2.02349685345405,-1.23742646019694,
0.933918328788326));
#41440=CARTESIAN_POINT('Ctrl Pts',(-2.03580479229626,-1.21707136719064,
0.932269296470122));
#41441=CARTESIAN_POINT('Ctrl Pts',(-2.05433054010817,-1.18536551513263,
0.929750542546412));
#41442=CARTESIAN_POINT('Ctrl Pts',(-2.06076480599553,-1.17414386091902,
0.928868543619198));
#41443=CARTESIAN_POINT('Ctrl Pts',(-2.07255539196082,-1.15318501920323,
0.927239516810714));
#41444=CARTESIAN_POINT('Ctrl Pts',(-2.07793533401818,-1.14346241518685,
0.92649114925813));
#41445=CARTESIAN_POINT('Ctrl Pts',(-2.09059823752764,-1.12019354729023,
0.924716966866783));
#41446=CARTESIAN_POINT('Ctrl Pts',(-2.09781808350303,-1.10661370564523,
0.923694962010024));
#41447=CARTESIAN_POINT('Ctrl Pts',(-2.12268368389257,-1.05872582188888,
0.920134403586227));
#41448=CARTESIAN_POINT('Ctrl Pts',(-2.13962496476518,-1.02405653596338,
0.917634149250662));
#41449=CARTESIAN_POINT('Ctrl Pts',(-2.18135678665411,-0.933092897859914,
0.911233316040393));
#41450=CARTESIAN_POINT('Ctrl Pts',(-2.20481773771799,-0.876218850789425,
0.907385114852131));
#41451=CARTESIAN_POINT('Ctrl Pts',(-2.28521664448587,-0.657559434172317,
0.892941572194925));
#41452=CARTESIAN_POINT('Ctrl Pts',(-2.32676218537592,-0.490689728306029,
0.882590252418731));
#41453=CARTESIAN_POINT('Ctrl Pts',(-2.35754816176512,-0.265172945859477,
0.868172710527603));
#41454=CARTESIAN_POINT('Ctrl Pts',(-2.3631638913273,-0.209298115508005,
0.864570841929052));
#41455=CARTESIAN_POINT('Ctrl Pts',(-2.36842780337635,-0.128018092227238,
0.859258561225237));
#41456=CARTESIAN_POINT('Ctrl Pts',(-2.36965921881742,-0.102732656837708,
0.857595897147773));
#41457=CARTESIAN_POINT('Ctrl Pts',(-2.37096058569031,-0.0628934828436836,
0.854958239102695));
#41458=CARTESIAN_POINT('Ctrl Pts',(-2.37130174057408,-0.0483500622696361,
0.853991585794441));
#41459=CARTESIAN_POINT('Ctrl Pts',(-2.37167126373329,-0.0224268086792617,
0.85226145946354));
#41460=CARTESIAN_POINT('Ctrl Pts',(-2.37175156271517,-0.0110481096338858,
0.85149960721778));
#41461=CARTESIAN_POINT('Ctrl Pts',(-2.37174997696831,0.000330531137167949,
0.850735237974249));
#41462=CARTESIAN_POINT('Ctrl Pts',(-2.36545134966535,0.172736721244678,
0.837052931219471));
#41463=CARTESIAN_POINT('Ctrl Pts',(-2.36964080846894,0.115366401199833,
0.840898584768258));
#41464=CARTESIAN_POINT('Ctrl Pts',(-2.37174546446208,0.057798410806183,
0.844744238317046));
#41465=CARTESIAN_POINT('Ctrl Pts',(-2.37174999267401,0.000186415808278105,
0.848589891865832));
#41466=CARTESIAN_POINT('',(-2.37174928376065,0.00184322565632311,0.651410108094984));
#41467=CARTESIAN_POINT('Ctrl Pts',(-2.36545134966535,0.172736721244682,
0.639882202840047));
#41468=CARTESIAN_POINT('Ctrl Pts',(-2.36960009283458,0.115923959844792,
0.643724837925026));
#41469=CARTESIAN_POINT('Ctrl Pts',(-2.37170492520006,0.0589210901913182,
0.647567473010006));
#41470=CARTESIAN_POINT('Ctrl Pts',(-2.37174928376066,0.00184322565632311,
0.651410108094985));
#41471=CARTESIAN_POINT('Ctrl Pts',(-2.37174922947978,0.00191179551492997,
0.652512471420324));
#41472=CARTESIAN_POINT('Ctrl Pts',(-2.37191126216802,-0.199103899144939,
0.665016268510595));
#41473=CARTESIAN_POINT('Ctrl Pts',(-2.34651945566196,-0.399324539138869,
0.677075520136256));
#41474=CARTESIAN_POINT('Ctrl Pts',(-2.28520666596991,-0.636354103094203,
0.692736184251922));
#41475=CARTESIAN_POINT('Ctrl Pts',(-2.27306750346192,-0.678439235429362,
0.695568368220726));
#41476=CARTESIAN_POINT('Ctrl Pts',(-2.25264373364539,-0.74252623970411,
0.699974677491279));
#41477=CARTESIAN_POINT('Ctrl Pts',(-2.24518521081825,-0.764782525883648,
0.701522499479531));
#41478=CARTESIAN_POINT('Ctrl Pts',(-2.23076691243074,-0.805776925393405,
0.704408099382541));
#41479=CARTESIAN_POINT('Ctrl Pts',(-2.22389816069032,-0.82454496585285,
0.705742810651493));
#41480=CARTESIAN_POINT('Ctrl Pts',(-2.2080731687877,-0.866148093963545,
0.708733065856802));
#41481=CARTESIAN_POINT('Ctrl Pts',(-2.19899832240328,-0.888935284605259,
0.710392393200129));
#41482=CARTESIAN_POINT('Ctrl Pts',(-2.17479194600454,-0.947078050459369,
0.714683448015121));
#41483=CARTESIAN_POINT('Ctrl Pts',(-2.15915144930666,-0.982212588466088,
0.717331639947056));
#41484=CARTESIAN_POINT('Ctrl Pts',(-2.05821227939559,-1.19488660051909,
0.733709689733471));
#41485=CARTESIAN_POINT('Ctrl Pts',(-1.95193344448354,-1.36158818032688,
0.748149173304034));
#41486=CARTESIAN_POINT('Ctrl Pts',(-1.78822553465202,-1.55916991681346,
0.766771877128838));
#41487=CARTESIAN_POINT('Ctrl Pts',(-1.748416248211,-1.6036841440578,0.771076524526458));
#41488=CARTESIAN_POINT('Ctrl Pts',(-1.68059420543115,-1.67399049534243,
0.77800378582117));
#41489=CARTESIAN_POINT('Ctrl Pts',(-1.65356602181679,-1.70069422726658,
0.780667661284586));
#41490=CARTESIAN_POINT('Ctrl Pts',(-1.61462030824582,-1.73736571491181,
0.784358915898909));
#41491=CARTESIAN_POINT('Ctrl Pts',(-1.6032300434013,-1.74788209763561,0.785421461407439));
#41492=CARTESIAN_POINT('Ctrl Pts',(-1.58329869885147,-1.76592549543948,
0.787250264384511));
#41493=CARTESIAN_POINT('Ctrl Pts',(-1.57480537351169,-1.77350378600904,
0.788020108656043));
#41494=CARTESIAN_POINT('Ctrl Pts',(-1.55608156126111,-1.78996979313978,
0.789696545966776));
#41495=CARTESIAN_POINT('Ctrl Pts',(-1.54582906513156,-1.7988313452953,0.790601330730788));
#41496=CARTESIAN_POINT('Ctrl Pts',(-1.51601355261087,-1.8241586434434,0.793196716777426));
#41497=CARTESIAN_POINT('Ctrl Pts',(-1.49625886437082,-1.84039707250557,
0.794872456336476));
#41498=CARTESIAN_POINT('Ctrl Pts',(-1.39186518699151,-1.92341676842146,
0.803525211988779));
#41499=CARTESIAN_POINT('Ctrl Pts',(-1.30299922090806,-1.9846961458972,0.810212632602846));
#41500=CARTESIAN_POINT('Ctrl Pts',(-1.12436746591585,-2.09068684003399,
0.823013037413721));
#41501=CARTESIAN_POINT('Ctrl Pts',(-1.03534010255263,-2.13617509073719,
0.829119809993047));
#41502=CARTESIAN_POINT('Ctrl Pts',(-0.861063347311503,-2.21176028439724,
0.840949468662011));
#41503=CARTESIAN_POINT('Ctrl Pts',(-0.776448029666017,-2.24286413884088,
0.846641027254705));
#41504=CARTESIAN_POINT('Ctrl Pts',(-0.661428498930152,-2.27785414852269,
0.854441562293542));
#41505=CARTESIAN_POINT('Ctrl Pts',(-0.632418529197615,-2.28607826940603,
0.856413863146435));
#41506=CARTESIAN_POINT('Ctrl Pts',(-0.583041475695171,-2.29906454762876,
0.859783238447097));
#41507=CARTESIAN_POINT('Ctrl Pts',(-0.562753399642459,-2.30411452005984,
0.861171133227325));
#41508=CARTESIAN_POINT('Ctrl Pts',(-0.521668025104564,-2.31376622521375,
0.863990061846888));
#41509=CARTESIAN_POINT('Ctrl Pts',(-0.500870237089178,-2.31835731263685,
0.865421285266575));
#41510=CARTESIAN_POINT('Ctrl Pts',(-0.448469685563391,-2.32918667050399,
0.869039248180442));
#41511=CARTESIAN_POINT('Ctrl Pts',(-0.416797228329559,-2.33506220536889,
0.871236951790047));
#41512=CARTESIAN_POINT('Ctrl Pts',(-0.278256467903017,-2.35785443334156,
0.880902088855557));
#41513=CARTESIAN_POINT('Ctrl Pts',(-0.170434327431137,-2.36809010273844,
0.888566613256902));
#41514=CARTESIAN_POINT('Ctrl Pts',(0.0576981276387517,-2.3740849016633,
0.905017240485764));
#41515=CARTESIAN_POINT('Ctrl Pts',(0.17776088966951,-2.3681233153469,0.913812339441916));
#41516=CARTESIAN_POINT('Ctrl Pts',(0.371124861478,-2.34372957930793,0.927891197594405));
#41517=CARTESIAN_POINT('Ctrl Pts',(0.44491778864012,-2.33084797457111,0.933240060042184));
#41518=CARTESIAN_POINT('Ctrl Pts',(0.536947687548176,-2.3102516917753,0.93979052373252));
#41519=CARTESIAN_POINT('Ctrl Pts',(0.555859317464115,-2.3057745287176,0.941130029945019));
#41520=CARTESIAN_POINT('Ctrl Pts',(0.58649552343711,-2.29812282387941,0.943286998527937));
#41521=CARTESIAN_POINT('Ctrl Pts',(0.598254092126595,-2.29508988280001,
0.944111740096526));
#41522=CARTESIAN_POINT('Ctrl Pts',(0.62033426106946,-2.28921341697813,0.94565387573166));
#41523=CARTESIAN_POINT('Ctrl Pts',(0.630660827984366,-2.28639007921324,
0.946372388625348));
#41524=CARTESIAN_POINT('Ctrl Pts',(0.65854503996355,-2.27856309581989,0.94830605285849));
#41525=CARTESIAN_POINT('Ctrl Pts',(0.676065026682413,-2.27342637455781,
0.949514005244516));
#41526=CARTESIAN_POINT('Ctrl Pts',(0.746357213305388,-2.2519327784342,0.954338708032254));
#41527=CARTESIAN_POINT('Ctrl Pts',(0.798613683144038,-2.2339354325253,0.957875997934973));
#41528=CARTESIAN_POINT('Ctrl Pts',(1.01206442875967,-2.15197297034043,0.97229938017342));
#41529=CARTESIAN_POINT('Ctrl Pts',(1.1666328977421,-2.07225392823316,0.982719219503754));
#41530=CARTESIAN_POINT('Ctrl Pts',(1.38109739063671,-1.92997847127507,0.998788098801221));
#41531=CARTESIAN_POINT('Ctrl Pts',(1.44853940187333,-1.87988785728605,1.00410655736001));
#41532=CARTESIAN_POINT('Ctrl Pts',(1.53588868338096,-1.80751589902515,1.01147241576628));
#41533=CARTESIAN_POINT('Ctrl Pts',(1.55824392718966,-1.78827948404009,1.01340273218654));
#41534=CARTESIAN_POINT('Ctrl Pts',(1.59570725418244,-1.75480682083839,1.01671968588537));
#41535=CARTESIAN_POINT('Ctrl Pts',(1.61099807016648,-1.74077965065701,1.01809775766645));
#41536=CARTESIAN_POINT('Ctrl Pts',(1.6416716930361,-1.71189063033207,1.02091327919703));
#41537=CARTESIAN_POINT('Ctrl Pts',(1.65704140523732,-1.69701773961953,1.0223511194052));
#41538=CARTESIAN_POINT('Ctrl Pts',(1.69549797911102,-1.6587836815328,1.02601956610504));
#41539=CARTESIAN_POINT('Ctrl Pts',(1.71830396213562,-1.63514770270913,1.02826187424703));
#41540=CARTESIAN_POINT('Ctrl Pts',(1.82774739959666,-1.51690257081733,1.03936266243522));
#41541=CARTESIAN_POINT('Ctrl Pts',(1.90708930317009,-1.41585851877461,1.04850864411624));
#41542=CARTESIAN_POINT('Ctrl Pts',(2.03072211240654,-1.22903990540586,1.06474758053518));
#41543=CARTESIAN_POINT('Ctrl Pts',(2.07869221514349,-1.14604097547829,1.07175479705561));
#41544=CARTESIAN_POINT('Ctrl Pts',(2.15681060526284,-0.989747209267179,
1.08439979836071));
#41545=CARTESIAN_POINT('Ctrl Pts',(2.1885640305246,-0.917399274419508,1.09005304862441));
#41546=CARTESIAN_POINT('Ctrl Pts',(2.22363848928257,-0.825236812181466,
1.0969066102231));
#41547=CARTESIAN_POINT('Ctrl Pts',(2.23039729851647,-0.806791100429943,
1.09826131052796));
#41548=CARTESIAN_POINT('Ctrl Pts',(2.24096444596045,-0.776803727452273,
1.10043394241082));
#41549=CARTESIAN_POINT('Ctrl Pts',(2.24491447757594,-0.765313454563482,
1.10125943754474));
#41550=CARTESIAN_POINT('Ctrl Pts',(2.25215366614211,-0.743716923281928,
1.1027972645983));
#41551=CARTESIAN_POINT('Ctrl Pts',(2.25546350178369,-0.733618020407526,
1.10351078088389));
#41552=CARTESIAN_POINT('Ctrl Pts',(2.2641731667591,-0.706427074629628,1.10541775036709));
#41553=CARTESIAN_POINT('Ctrl Pts',(2.26944743503956,-0.689295094743829,
1.10660431245804));
#41554=CARTESIAN_POINT('Ctrl Pts',(2.28935989085404,-0.62190760940321,1.11121919188182));
#41555=CARTESIAN_POINT('Ctrl Pts',(2.30252806493034,-0.571229522221275,
1.11457632443595));
#41556=CARTESIAN_POINT('Ctrl Pts',(2.34541138388366,-0.380454245494688,
1.12693425727061));
#41557=CARTESIAN_POINT('Ctrl Pts',(2.36410029454129,-0.238190831549242,
1.13560901022335));
#41558=CARTESIAN_POINT('Ctrl Pts',(2.373424692229,-0.00583977620744467,
1.1499829964217));
#41559=CARTESIAN_POINT('Ctrl Pts',(2.37196049852422,0.0835479996810568,
1.15555847964464));
#41560=CARTESIAN_POINT('Ctrl Pts',(2.36222366855902,0.216962633049453,1.16411334252959));
#41561=CARTESIAN_POINT('Ctrl Pts',(2.3577433969088,0.261187912047189,1.16698718051451));
#41562=CARTESIAN_POINT('Ctrl Pts',(2.3489751644962,0.328747199732648,1.1714499398246));
#41563=CARTESIAN_POINT('Ctrl Pts',(2.34557517404521,0.352187566022606,1.17301179425879));
#41564=CARTESIAN_POINT('Ctrl Pts',(2.33864087326628,0.395425346752585,1.1759196530551));
#41565=CARTESIAN_POINT('Ctrl Pts',(2.33520469769557,0.415236459204942,1.17726250468013));
#41566=CARTESIAN_POINT('Ctrl Pts',(2.32700354786808,0.459192960234471,1.18026652517117));
#41567=CARTESIAN_POINT('Ctrl Pts',(2.32211384883979,0.483312406198441,1.18193143678596));
#41568=CARTESIAN_POINT('Ctrl Pts',(2.30627951227469,0.555620938536484,1.18697472469319));
#41569=CARTESIAN_POINT('Ctrl Pts',(2.2942039232873,0.603545826024765,1.19038756115135));
#41570=CARTESIAN_POINT('Ctrl Pts',(2.2331810183158,0.817308387369813,1.20593640691556));
#41571=CARTESIAN_POINT('Ctrl Pts',(2.16768914440289,0.977853807280558,1.21856242851948));
#41572=CARTESIAN_POINT('Ctrl Pts',(2.05328810121645,1.18900628121615,1.23601762489984));
#41573=CARTESIAN_POINT('Ctrl Pts',(2.01871999839616,1.24679530499095,1.24088534818926));
#41574=CARTESIAN_POINT('Ctrl Pts',(1.95913936471236,1.33740909480629,1.24859136379094));
#41575=CARTESIAN_POINT('Ctrl Pts',(1.93564794366562,1.37118840546614,1.25148125758077));
#41576=CARTESIAN_POINT('Ctrl Pts',(1.90179867757114,1.41725675172584,1.25542925324394));
#41577=CARTESIAN_POINT('Ctrl Pts',(1.8921782219736,1.4300757048678,1.25652855837444));
#41578=CARTESIAN_POINT('Ctrl Pts',(1.87544434064011,1.45190853368045,1.25840077599928));
#41579=CARTESIAN_POINT('Ctrl Pts',(1.86839422807745,1.46096984749999,1.25917773579917));
#41580=CARTESIAN_POINT('Ctrl Pts',(1.85302702110034,1.48042769280371,1.26084567646308));
#41581=CARTESIAN_POINT('Ctrl Pts',(1.84468782628783,1.49080586893371,1.26173514709399));
#41582=CARTESIAN_POINT('Ctrl Pts',(1.8207812217944,1.52005000922234,1.26424288320383));
#41583=CARTESIAN_POINT('Ctrl Pts',(1.80500828083771,1.53874673205063,1.26584776889485));
#41584=CARTESIAN_POINT('Ctrl Pts',(1.69849461256428,1.66111239361092,1.27638791884378));
#41585=CARTESIAN_POINT('Ctrl Pts',(1.59914726608953,1.75696203934371,1.28483147287725));
#41586=CARTESIAN_POINT('Ctrl Pts',(1.41161768434159,1.90872578278869,1.29966783380997));
#41587=CARTESIAN_POINT('Ctrl Pts',(1.32703916719225,1.96846740887906,1.30602945227724));
#41588=CARTESIAN_POINT('Ctrl Pts',(1.20064955030336,2.0458846445821,1.31537187367624));
#41589=CARTESIAN_POINT('Ctrl Pts',(1.16181063614574,2.06818737521527,1.31822124648786));
#41590=CARTESIAN_POINT('Ctrl Pts',(1.09011313618483,2.10670163465591,1.3234638559335));
#41591=CARTESIAN_POINT('Ctrl Pts',(1.05746558234757,2.12327688757886,1.32584473413999));
#41592=CARTESIAN_POINT('Ctrl Pts',(1.00447214297391,2.1486564116057,1.32970704263957));
#41593=CARTESIAN_POINT('Ctrl Pts',(0.984363007648859,2.15794301960502,1.33117210058001));
#41594=CARTESIAN_POINT('Ctrl Pts',(0.945500914593175,2.17523371279521,1.33400393593717));
#41595=CARTESIAN_POINT('Ctrl Pts',(0.926768955101656,2.1832803175405,1.33536913987012));
#41596=CARTESIAN_POINT('Ctrl Pts',(0.883217490626617,2.2013270657985,1.33854489002083));
#41597=CARTESIAN_POINT('Ctrl Pts',(0.85832824731487,2.21115049390966,1.34036105690564));
#41598=CARTESIAN_POINT('Ctrl Pts',(0.788824073810611,2.23723248076674,1.34543836227829));
#41599=CARTESIAN_POINT('Ctrl Pts',(0.743881087860137,2.25257474556141,1.34872799989816));
#41600=CARTESIAN_POINT('Ctrl Pts',(0.53685201675325,2.31637723436353,1.36391618862283));
#41601=CARTESIAN_POINT('Ctrl Pts',(0.370344477178653,2.34875372249066,1.37627457767995));
#41602=CARTESIAN_POINT('Ctrl Pts',(0.135771072431408,2.36878896842941,1.39337989428021));
#41603=CARTESIAN_POINT('Ctrl Pts',(0.0694911106989449,2.3716591070089,1.39817299464699));
#41604=CARTESIAN_POINT('Ctrl Pts',(-0.0375725223054501,2.37180241770526,
1.40577785610045));
#41605=CARTESIAN_POINT('Ctrl Pts',(-0.0783172833811533,2.37080687981982,
1.40863961680838));
#41606=CARTESIAN_POINT('Ctrl Pts',(-0.134985165715778,2.3679595933879,1.41255750300973));
#41607=CARTESIAN_POINT('Ctrl Pts',(-0.150943559825744,2.36699592466261,
1.41365392878035));
#41608=CARTESIAN_POINT('Ctrl Pts',(-0.178348807825658,2.36506272386894,
1.41552359723415));
#41609=CARTESIAN_POINT('Ctrl Pts',(-0.189800316596872,2.36417128118926,
1.41630083785366));
#41610=CARTESIAN_POINT('Ctrl Pts',(-0.214550942478451,2.36206356212865,
1.41797170730982));
#41611=CARTESIAN_POINT('Ctrl Pts',(-0.22784686885415,2.36081812169737,1.41886379366944));
#41612=CARTESIAN_POINT('Ctrl Pts',(-0.265654009311369,2.35695431044917,
1.4213865987279));
#41613=CARTESIAN_POINT('Ctrl Pts',(-0.290136656495056,2.35406595240916,
1.42300368563891));
#41614=CARTESIAN_POINT('Ctrl Pts',(-0.483790682796548,2.32815220962286,
1.43569428799089));
#41615=CARTESIAN_POINT('Ctrl Pts',(-0.650092674923883,2.28729990221417,
1.44601133815751));
#41616=CARTESIAN_POINT('Ctrl Pts',(-0.88801217705426,2.2007773020901,1.46162602566395));
#41617=CARTESIAN_POINT('Ctrl Pts',(-0.963918203657382,2.16860478602989,
1.46674179712511));
#41618=CARTESIAN_POINT('Ctrl Pts',(-1.08883338780146,2.10780385165979,1.47554677031167));
#41619=CARTESIAN_POINT('Ctrl Pts',(-1.13876963467015,2.0812491872958,1.4791765932924));
#41620=CARTESIAN_POINT('Ctrl Pts',(-1.21007887980382,2.03999392478637,1.48455343370311));
#41621=CARTESIAN_POINT('Ctrl Pts',(-1.23223732888119,2.02668625820122,1.48625242413198));
#41622=CARTESIAN_POINT('Ctrl Pts',(-1.27132719058742,2.00233207000811,1.48930294541399));
#41623=CARTESIAN_POINT('Ctrl Pts',(-1.2883434173872,1.99142605707816,1.4906493466567));
#41624=CARTESIAN_POINT('Ctrl Pts',(-1.32428496462124,1.96773699653786,1.49353403372071));
#41625=CARTESIAN_POINT('Ctrl Pts',(-1.34316908379902,1.95489547176612,1.49507436708538));
#41626=CARTESIAN_POINT('Ctrl Pts',(-1.39378969747723,1.91939285218127,1.49927242251767));
#41627=CARTESIAN_POINT('Ctrl Pts',(-1.4251563456092,1.8962193248837,1.50194893353141));
#41628=CARTESIAN_POINT('Ctrl Pts',(-1.62892492623571,1.73776367777958,1.51985267697584));
#41629=CARTESIAN_POINT('Ctrl Pts',(-1.78241538033212,1.57993040584799,1.53598997546018));
#41630=CARTESIAN_POINT('Ctrl Pts',(-1.95464163831369,1.34527349619535,1.55700646335));
#41631=CARTESIAN_POINT('Ctrl Pts',(-1.99459158501783,1.28529804733741,1.56214776874525));
#41632=CARTESIAN_POINT('Ctrl Pts',(-2.04165535094396,1.20714949575484,1.56848337287424));
#41633=CARTESIAN_POINT('Ctrl Pts',(-2.05135808238401,1.19058664231235,1.56980626267898));
#41634=CARTESIAN_POINT('Ctrl Pts',(-2.06682629918302,1.1634313315272,1.57194084467282));
#41635=CARTESIAN_POINT('Ctrl Pts',(-2.07271377772006,1.1529098089861,1.57275964132894));
#41636=CARTESIAN_POINT('Ctrl Pts',(-2.08367601906124,1.13296375274879,1.57429568885592));
#41637=CARTESIAN_POINT('Ctrl Pts',(-2.08876766516299,1.1235489618026,1.57501400923182));
#41638=CARTESIAN_POINT('Ctrl Pts',(-2.1024018330279,1.09792544068666,1.5769517524714));
#41639=CARTESIAN_POINT('Ctrl Pts',(-2.11082075532756,1.08165129770391,1.57816388657386));
#41640=CARTESIAN_POINT('Ctrl Pts',(-2.14423006842767,1.01519366988212,1.58304547596345));
#41641=CARTESIAN_POINT('Ctrl Pts',(-2.16762798873382,0.964225451219779,
1.58663283713487));
#41642=CARTESIAN_POINT('Ctrl Pts',(-2.27429536440735,0.708309455603149,
1.60411171063068));
#41643=CARTESIAN_POINT('Ctrl Pts',(-2.3304158127949,0.493248120243888,1.61725279128887));
#41644=CARTESIAN_POINT('Ctrl Pts',(-2.35981811703602,0.239990689206501,
1.63350195156645));
#41645=CARTESIAN_POINT('Ctrl Pts',(-2.36299379611575,0.206390384608692,
1.63567032553817));
#41646=CARTESIAN_POINT('Ctrl Pts',(-2.3654513498954,0.172736718094382,1.63785909343774));
#41647=CARTESIAN_POINT('Origin',(0.,0.,-1.84858989190501));
#41648=CARTESIAN_POINT('',(-2.36545134753269,0.172736750449338,2.83572259012909));
#41649=CARTESIAN_POINT('',(-2.36545139057093,0.172736161084027,2.64008830168392));
#41650=CARTESIAN_POINT('',(-2.36545134966535,0.172736721244682,-1.84858989190501));
#41651=CARTESIAN_POINT('Ctrl Pts',(-2.36545134753269,0.172736750449338,
2.83572259012909));
#41652=CARTESIAN_POINT('Ctrl Pts',(-2.36334042788976,0.201643614222682,
2.83363353379938));
#41653=CARTESIAN_POINT('Ctrl Pts',(-2.36069940514974,0.230514817336211,
2.8315546832682));
#41654=CARTESIAN_POINT('Ctrl Pts',(-2.35369907162262,0.294152347824024,
2.826998243979));
#41655=CARTESIAN_POINT('Ctrl Pts',(-2.34909811675042,0.328881796846493,
2.82452864919489));
#41656=CARTESIAN_POINT('Ctrl Pts',(-2.34145312675036,0.378174407967134,
2.82105880332428));
#41657=CARTESIAN_POINT('Ctrl Pts',(-2.33903910560916,0.392829118240582,
2.82003169899207));
#41658=CARTESIAN_POINT('Ctrl Pts',(-2.33459966990723,0.418286023279023,
2.8182563934489));
#41659=CARTESIAN_POINT('Ctrl Pts',(-2.33263656645484,0.429098446100914,
2.81750516261938));
#41660=CARTESIAN_POINT('Ctrl Pts',(-2.3285451644487,0.450774912959025,2.81600526353117));
#41661=CARTESIAN_POINT('Ctrl Pts',(-2.32641584106716,0.461638340572145,
2.81525673515386));
#41662=CARTESIAN_POINT('Ctrl Pts',(-2.32157869365001,0.485432740955418,
2.81362434620353));
#41663=CARTESIAN_POINT('Ctrl Pts',(-2.31883880354422,0.498356499140129,
2.81274222866067));
#41664=CARTESIAN_POINT('Ctrl Pts',(-2.31058207310167,0.535759431525327,
2.8102005708944));
#41665=CARTESIAN_POINT('Ctrl Pts',(-2.30478439591019,0.560175591159726,
2.80855548904454));
#41666=CARTESIAN_POINT('Ctrl Pts',(-2.27402972870867,0.681121920390583,
2.80045594428058));
#41667=CARTESIAN_POINT('Ctrl Pts',(-2.24338838325232,0.776112753777745,
2.79424969793554));
#41668=CARTESIAN_POINT('Ctrl Pts',(-2.15926203390543,0.989778768504046,
2.78008121501327));
#41669=CARTESIAN_POINT('Ctrl Pts',(-2.10182014360091,1.10653762206543,2.77217228203211));
#41670=CARTESIAN_POINT('Ctrl Pts',(-1.99817070695529,1.27972073209173,2.75951087324629));
#41671=CARTESIAN_POINT('Ctrl Pts',(-1.95844837833089,1.33972005915607,2.75493492323077));
#41672=CARTESIAN_POINT('Ctrl Pts',(-1.89923602888978,1.42088558859733,2.74840672041238));
#41673=CARTESIAN_POINT('Ctrl Pts',(-1.88199328350514,1.44364625774669,2.74653689660864));
#41674=CARTESIAN_POINT('Ctrl Pts',(-1.85191329759649,1.48189730595256,2.74332334559211));
#41675=CARTESIAN_POINT('Ctrl Pts',(-1.83928195160299,1.49754610891323,2.74198765767879));
#41676=CARTESIAN_POINT('Ctrl Pts',(-1.8132380342129,1.52898496990926,2.73926001118541));
#41677=CARTESIAN_POINT('Ctrl Pts',(-1.79981454262205,1.54476366247098,2.73786769031826));
#41678=CARTESIAN_POINT('Ctrl Pts',(-1.76531542316314,1.58425563754174,2.73432191565675));
#41679=CARTESIAN_POINT('Ctrl Pts',(-1.7439680673205,1.60772500217544,2.73215754368813));
#41680=CARTESIAN_POINT('Ctrl Pts',(-1.64678726836699,1.71035249010092,2.72242913161553));
#41681=CARTESIAN_POINT('Ctrl Pts',(-1.56600038750526,1.78461504463547,2.71465986523717));
#41682=CARTESIAN_POINT('Ctrl Pts',(-1.3913907473097,1.92411094899125,2.69853542409325));
#41683=CARTESIAN_POINT('Ctrl Pts',(-1.29739773871484,1.98870034069226,2.69018951502757));
#41684=CARTESIAN_POINT('Ctrl Pts',(-1.15142809630391,2.07423929167262,2.6779356901154));
#41685=CARTESIAN_POINT('Ctrl Pts',(-1.10275750478588,2.10051943275307,2.67395909258983));
#41686=CARTESIAN_POINT('Ctrl Pts',(-1.02102520403788,2.14102683591385,2.66750313941681));
#41687=CARTESIAN_POINT('Ctrl Pts',(-0.988479873407547,2.15624586852976,
2.66498829682542));
#41688=CARTESIAN_POINT('Ctrl Pts',(-0.941886196949669,2.17675743939155,
2.66147834913373));
#41689=CARTESIAN_POINT('Ctrl Pts',(-0.928115652818932,2.18266440891562,
2.66045199643191));
#41690=CARTESIAN_POINT('Ctrl Pts',(-0.904072297315916,2.19270927355332,
2.65868016148559));
#41691=CARTESIAN_POINT('Ctrl Pts',(-0.893825096838485,2.19690632288673,
2.65793137308261));
#41692=CARTESIAN_POINT('Ctrl Pts',(-0.871309683423988,2.20594456327904,
2.65630020261092));
#41693=CARTESIAN_POINT('Ctrl Pts',(-0.859030017648339,2.21075539796449,
2.6554195407495));
#41694=CARTESIAN_POINT('Ctrl Pts',(-0.822652904847154,2.22465807837024,
2.65283525139086));
#41695=CARTESIAN_POINT('Ctrl Pts',(-0.798445958004287,2.23346044260092,
2.65114717788715));
#41696=CARTESIAN_POINT('Ctrl Pts',(-0.673520313924219,2.27659629465779,
2.64257353688474));
#41697=CARTESIAN_POINT('Ctrl Pts',(-0.5707068745239,2.3045213888288,2.63597077709296));
#41698=CARTESIAN_POINT('Ctrl Pts',(-0.346511365080279,2.34948254797305,
2.6218811497574));
#41699=CARTESIAN_POINT('Ctrl Pts',(-0.22499302241912,2.36421556408556,2.61442480574035));
#41700=CARTESIAN_POINT('Ctrl Pts',(-0.0526794870834247,2.3716972935954,
2.60360652990194));
#41701=CARTESIAN_POINT('Ctrl Pts',(-0.0024222066320971,2.37228093742978,
2.60042362342617));
#41702=CARTESIAN_POINT('Ctrl Pts',(0.0874870177756139,2.37046803678667,
2.59464938941809));
#41703=CARTESIAN_POINT('Ctrl Pts',(0.127132278463775,2.3686725794343,2.59207542061028));
#41704=CARTESIAN_POINT('Ctrl Pts',(0.188987207371859,2.36431396840485,2.58800604883393));
#41705=CARTESIAN_POINT('Ctrl Pts',(0.211238368949565,2.3624298934581,2.58653135328852));
#41706=CARTESIAN_POINT('Ctrl Pts',(0.252927148626647,2.35830630682148,2.58374649913439));
#41707=CARTESIAN_POINT('Ctrl Pts',(0.272370212695668,2.3561398956583,2.58243869983621));
#41708=CARTESIAN_POINT('Ctrl Pts',(0.316306578329727,2.35069326383021,2.5794620185146));
#41709=CARTESIAN_POINT('Ctrl Pts',(0.340779551043279,2.34727030633404,2.57778886685938));
#41710=CARTESIAN_POINT('Ctrl Pts',(0.404921617976307,2.33727473200564,2.573362141352));
#41711=CARTESIAN_POINT('Ctrl Pts',(0.444483395951404,2.33007486339111,2.57058976938614));
#41712=CARTESIAN_POINT('Ctrl Pts',(0.658658014303677,2.28544431167203,2.55534515743));
#41713=CARTESIAN_POINT('Ctrl Pts',(0.828779053912086,2.22939283654233,2.54231476710808));
#41714=CARTESIAN_POINT('Ctrl Pts',(1.05384041460813,2.12588976412907,2.52429933854261));
#41715=CARTESIAN_POINT('Ctrl Pts',(1.11542002318246,2.0942364099189,2.51929022682933));
#41716=CARTESIAN_POINT('Ctrl Pts',(1.20046390046497,2.04570492371843,2.51232930970138));
#41717=CARTESIAN_POINT('Ctrl Pts',(1.22513839085955,2.03102394978628,2.51030446664061));
#41718=CARTESIAN_POINT('Ctrl Pts',(1.26852998466481,2.00412795069126,2.50674183794915));
#41719=CARTESIAN_POINT('Ctrl Pts',(1.28735225424754,1.99208971350519,2.50519583318597));
#41720=CARTESIAN_POINT('Ctrl Pts',(1.31643067667237,1.97290760243381,2.50280973965758));
#41721=CARTESIAN_POINT('Ctrl Pts',(1.32680471069011,1.96594593298879,2.50195894692974));
#41722=CARTESIAN_POINT('Ctrl Pts',(1.34641537558599,1.95255992594008,2.50035226455621));
#41723=CARTESIAN_POINT('Ctrl Pts',(1.35566195670665,1.94615140520819,2.49959548313258));
#41724=CARTESIAN_POINT('Ctrl Pts',(1.37818477762112,1.93030311879665,2.49775328466571));
#41725=CARTESIAN_POINT('Ctrl Pts',(1.391410305204,1.92079171448511,2.49667249579058));
#41726=CARTESIAN_POINT('Ctrl Pts',(1.43829320496628,1.8863365600018,2.49284057348281));
#41727=CARTESIAN_POINT('Ctrl Pts',(1.47138835234922,1.86063692353074,2.49013431894508));
#41728=CARTESIAN_POINT('Ctrl Pts',(1.62302667067938,1.73630605430581,2.47763797038065));
#41729=CARTESIAN_POINT('Ctrl Pts',(1.73245697380583,1.6271370904306,2.46831424669657));
#41730=CARTESIAN_POINT('Ctrl Pts',(1.87984941930382,1.44823427371662,2.45399900593351));
#41731=CARTESIAN_POINT('Ctrl Pts',(1.92620814829436,1.38597882338579,2.44917031781089));
#41732=CARTESIAN_POINT('Ctrl Pts',(1.99955555997284,1.27667476233576,2.44081425599431));
#41733=CARTESIAN_POINT('Ctrl Pts',(2.02813449121015,1.23076833470534,2.43733900084326));
#41734=CARTESIAN_POINT('Ctrl Pts',(2.06758748648854,1.162283955079,2.43217718438621));
#41735=CARTESIAN_POINT('Ctrl Pts',(2.07971330954708,1.14044486048034,2.43053445725686));
#41736=CARTESIAN_POINT('Ctrl Pts',(2.10072825431499,1.10114601009879,2.4275819916053));
#41737=CARTESIAN_POINT('Ctrl Pts',(2.10975035138646,1.08375972906174,2.42627701377475));
#41738=CARTESIAN_POINT('Ctrl Pts',(2.12851804620491,1.04647027257227,2.42347969146593));
#41739=CARTESIAN_POINT('Ctrl Pts',(2.13820205243666,1.02653837271674,2.4219853904321));
#41740=CARTESIAN_POINT('Ctrl Pts',(2.16365155921366,0.972234460786808,2.41791522740838));
#41741=CARTESIAN_POINT('Ctrl Pts',(2.17887606577426,0.937617580699433,2.41532163738879));
#41742=CARTESIAN_POINT('Ctrl Pts',(2.24598467258466,0.774557150989222,2.40310293836556));
#41743=CARTESIAN_POINT('Ctrl Pts',(2.28737253639754,0.642107684911512,2.39315065803889));
#41744=CARTESIAN_POINT('Ctrl Pts',(2.33942868543062,0.404131130618277,2.37543102833928));
#41745=CARTESIAN_POINT('Ctrl Pts',(2.35504065377719,0.300055587120037,2.36774052726046));
#41746=CARTESIAN_POINT('Ctrl Pts',(2.36808922825888,0.142117955501362,2.35639138080684));
#41747=CARTESIAN_POINT('Ctrl Pts',(2.37068708483292,0.0888131858678933,
2.35261686586998));
#41748=CARTESIAN_POINT('Ctrl Pts',(2.37174265137471,0.0182234767299164,
2.34772798243264));
#41749=CARTESIAN_POINT('Ctrl Pts',(2.37181246691622,0.000981914649346083,
2.34654253800131));
#41750=CARTESIAN_POINT('Ctrl Pts',(2.37161597671251,-0.0276791809721018,
2.34458798610151));
#41751=CARTESIAN_POINT('Ctrl Pts',(2.37145520730219,-0.0390985767487486,
2.3438134797004));
#41752=CARTESIAN_POINT('Ctrl Pts',(2.37095334572605,-0.0626554661950777,
2.3422250672482));
#41753=CARTESIAN_POINT('Ctrl Pts',(2.37060152970334,-0.0747922357072169,
2.3414117267864));
#41754=CARTESIAN_POINT('Ctrl Pts',(2.36939857456663,-0.10759241905691,2.33922594058344));
#41755=CARTESIAN_POINT('Ctrl Pts',(2.36837033650107,-0.12824879409271,2.33786261733806));
#41756=CARTESIAN_POINT('Ctrl Pts',(2.35971143109423,-0.265909244036946,
2.32884946034921));
#41757=CARTESIAN_POINT('Ctrl Pts',(2.34368246171409,-0.382237021521754,
2.32157786325115));
#41758=CARTESIAN_POINT('Ctrl Pts',(2.29381421198584,-0.614973497550293,
2.30691633521917));
#41759=CARTESIAN_POINT('Ctrl Pts',(2.25954070074646,-0.7309244331178,2.2995471268618));
#41760=CARTESIAN_POINT('Ctrl Pts',(2.19043844425199,-0.912458706760118,
2.28736064012625));
#41761=CARTESIAN_POINT('Ctrl Pts',(2.16111028196973,-0.979899115424568,
2.28268198580112));
#41762=CARTESIAN_POINT('Ctrl Pts',(2.11644772781317,-1.07080302756555,2.27609421212494));
#41763=CARTESIAN_POINT('Ctrl Pts',(2.10375827394799,-1.09552322156963,2.274273136907));
#41764=CARTESIAN_POINT('Ctrl Pts',(2.08120412750174,-1.13762318995999,2.27111715546875));
#41765=CARTESIAN_POINT('Ctrl Pts',(2.07154851745287,-1.15511204732381,2.26978956171781));
#41766=CARTESIAN_POINT('Ctrl Pts',(2.05132523403797,-1.19067251115208,2.26705486739343));
#41767=CARTESIAN_POINT('Ctrl Pts',(2.04073693973913,-1.20873030064777,2.26564712666204));
#41768=CARTESIAN_POINT('Ctrl Pts',(2.01294570671396,-1.25472056961508,2.26201132249815));
#41769=CARTESIAN_POINT('Ctrl Pts',(1.99540024645773,-1.28243978385698,2.25977119321619));
#41770=CARTESIAN_POINT('Ctrl Pts',(1.90351103905125,-1.42115816879178,2.24830453649796));
#41771=CARTESIAN_POINT('Ctrl Pts',(1.82046949371683,-1.52608176236397,2.23876270080917));
#41772=CARTESIAN_POINT('Ctrl Pts',(1.65154206630797,-1.70599817253438,2.22085092420353));
#41773=CARTESIAN_POINT('Ctrl Pts',(1.56821830625224,-1.78289454833961,2.21255115864241));
#41774=CARTESIAN_POINT('Ctrl Pts',(1.4333989783112,-1.89052331311069,2.20015928783483));
#41775=CARTESIAN_POINT('Ctrl Pts',(1.38570464114618,-1.92575566781719,2.19595305570193));
#41776=CARTESIAN_POINT('Ctrl Pts',(1.32201074710681,-1.96921391409807,2.19060796559253));
#41777=CARTESIAN_POINT('Ctrl Pts',(1.30717174272897,-1.97909523193783,2.18938116819368));
#41778=CARTESIAN_POINT('Ctrl Pts',(1.28254933383123,-1.99509356500489,2.1873775190909));
#41779=CARTESIAN_POINT('Ctrl Pts',(1.27283041275375,-2.00130804386985,2.18659471417639));
#41780=CARTESIAN_POINT('Ctrl Pts',(1.25418813482182,-2.01303755740389,2.18510908094778));
#41781=CARTESIAN_POINT('Ctrl Pts',(1.245272926418,-2.01856469657572,2.1844054312002));
#41782=CARTESIAN_POINT('Ctrl Pts',(1.22067686485566,-2.03358848130557,2.18248195195641));
#41783=CARTESIAN_POINT('Ctrl Pts',(1.20492174909996,-2.04296298264404,2.18126957625663));
#41784=CARTESIAN_POINT('Ctrl Pts',(1.13736696082669,-2.08210556972155,2.17614756533318));
#41785=CARTESIAN_POINT('Ctrl Pts',(1.08455713275543,-2.11009579781193,2.17233256785448));
#41786=CARTESIAN_POINT('Ctrl Pts',(0.833311477659495,-2.23133257502607,
2.15478757739932));
#41787=CARTESIAN_POINT('Ctrl Pts',(0.623629037850769,-2.29877101113557,
2.14175345959954));
#41788=CARTESIAN_POINT('Ctrl Pts',(0.360532544108672,-2.34467541369039,
2.12472189895163));
#41789=CARTESIAN_POINT('Ctrl Pts',(0.313171501010043,-2.3514696761712,2.12163557715339));
#41790=CARTESIAN_POINT('Ctrl Pts',(0.241897493407644,-2.35950302456354,
2.11694266858223));
#41791=CARTESIAN_POINT('Ctrl Pts',(0.218116849781469,-2.36182003811804,
2.11536893238843));
#41792=CARTESIAN_POINT('Ctrl Pts',(0.176745371104177,-2.3652208340448,2.11261538452592));
#41793=CARTESIAN_POINT('Ctrl Pts',(0.15916966564872,-2.36646857352011,2.1114407009258));
#41794=CARTESIAN_POINT('Ctrl Pts',(0.119403087795279,-2.36884668815227,
2.10877099791222));
#41795=CARTESIAN_POINT('Ctrl Pts',(0.0972072219740444,-2.36986126770937,
2.1072725383911));
#41796=CARTESIAN_POINT('Ctrl Pts',(0.0369280851861319,-2.37176840716111,
2.10317892860491));
#41797=CARTESIAN_POINT('Ctrl Pts',(-0.00116633259554981,-2.37205552537581,
2.10056570214269));
#41798=CARTESIAN_POINT('Ctrl Pts',(-0.167155880341428,-2.36930824017253,
2.08905891438497));
#41799=CARTESIAN_POINT('Ctrl Pts',(-0.294663533878714,-2.356846954488,2.07989277137061));
#41800=CARTESIAN_POINT('Ctrl Pts',(-0.531500669652834,-2.31417797928882,
2.0624116941614));
#41801=CARTESIAN_POINT('Ctrl Pts',(-0.640907713365617,-2.28629635454371,
2.05415008350441));
#41802=CARTESIAN_POINT('Ctrl Pts',(-0.800443066188376,-2.23328289640376,
2.04209786324687));
#41803=CARTESIAN_POINT('Ctrl Pts',(-0.85234569383876,-2.21399400131151,
2.0381776781263));
#41804=CARTESIAN_POINT('Ctrl Pts',(-0.919661519618189,-2.18625825645097,
2.03313404613041));
#41805=CARTESIAN_POINT('Ctrl Pts',(-0.935720043385641,-2.17943353175747,
2.0319340116131));
#41806=CARTESIAN_POINT('Ctrl Pts',(-0.962199258403491,-2.16783347620682,
2.02996218076256));
#41807=CARTESIAN_POINT('Ctrl Pts',(-0.972663065306776,-2.16315879565978,
2.02918479080003));
#41808=CARTESIAN_POINT('Ctrl Pts',(-0.994083743563671,-2.15340229153987,
2.02759769567279));
#41809=CARTESIAN_POINT('Ctrl Pts',(-1.00503638094071,-2.14831231604814,
2.02678847534491));
#41810=CARTESIAN_POINT('Ctrl Pts',(-1.03436461743194,-2.13440933359863,
2.02462648597835));
#41811=CARTESIAN_POINT('Ctrl Pts',(-1.05266675366861,-2.12544257468181,
2.02328250217499));
#41812=CARTESIAN_POINT('Ctrl Pts',(-1.15920044921697,-2.07153481334418,
2.01547683169071));
#41813=CARTESIAN_POINT('Ctrl Pts',(-1.24467354114231,-2.02133482243089,
2.00928286398295));
#41814=CARTESIAN_POINT('Ctrl Pts',(-1.44016653204764,-1.88940074161149,
1.99469894881576));
#41815=CARTESIAN_POINT('Ctrl Pts',(-1.54672960284108,-1.80320319075302,
1.98638927235827));
#41816=CARTESIAN_POINT('Ctrl Pts',(-1.69973664815756,-1.65584185129473,
1.97307606276733));
#41817=CARTESIAN_POINT('Ctrl Pts',(-1.75166096847359,-1.60081201310641,
1.96826751018936));
#41818=CARTESIAN_POINT('Ctrl Pts',(-1.81911346214293,-1.52210730741402,
1.96152778895392));
#41819=CARTESIAN_POINT('Ctrl Pts',(-1.83698219572638,-1.50049350182988,
1.95969040205577));
#41820=CARTESIAN_POINT('Ctrl Pts',(-1.86694413498688,-1.46291438462146,
1.95651520823513));
#41821=CARTESIAN_POINT('Ctrl Pts',(-1.87922629867624,-1.44710309839294,
1.95518495500906));
#41822=CARTESIAN_POINT('Ctrl Pts',(-1.90389153966823,-1.41450700277021,
1.95245292311002));
#41823=CARTESIAN_POINT('Ctrl Pts',(-1.9162562811197,-1.3977105829214,1.95105059983466));
#41824=CARTESIAN_POINT('Ctrl Pts',(-1.94727411379477,-1.3543902483671,1.9474463936452));
#41825=CARTESIAN_POINT('Ctrl Pts',(-1.9656071975433,-1.32764362202015,1.94523285225192));
#41826=CARTESIAN_POINT('Ctrl Pts',(-2.05459898517378,-1.1919259309087,1.93405339279219));
#41827=CARTESIAN_POINT('Ctrl Pts',(-2.11676108894222,-1.0776722766733,1.92479034279789));
#41828=CARTESIAN_POINT('Ctrl Pts',(-2.2178710010374,-0.84894362716249,1.90665506299714));
#41829=CARTESIAN_POINT('Ctrl Pts',(-2.25805354808094,-0.735426308349322,
1.89783375800942));
#41830=CARTESIAN_POINT('Ctrl Pts',(-2.30438429372222,-0.564162802279199,
1.88510243910304));
#41831=CARTESIAN_POINT('Ctrl Pts',(-2.31731482045602,-0.508448398162815,
1.88104941324044));
#41832=CARTESIAN_POINT('Ctrl Pts',(-2.33158167486305,-0.435012298465262,
1.87586539028095));
#41833=CARTESIAN_POINT('Ctrl Pts',(-2.33475059823288,-0.417670319863833,
1.87465262086695));
#41834=CARTESIAN_POINT('Ctrl Pts',(-2.33966615602071,-0.388963351298039,
1.87266566716924));
#41835=CARTESIAN_POINT('Ctrl Pts',(-2.34152399418825,-0.377618345455078,
1.87188571857914));
#41836=CARTESIAN_POINT('Ctrl Pts',(-2.34515606463268,-0.354380666805676,
1.87029957447984));
#41837=CARTESIAN_POINT('Ctrl Pts',(-2.34692248183306,-0.34248723251976,
1.86949379534961));
#41838=CARTESIAN_POINT('Ctrl Pts',(-2.35140408449674,-0.31064783758922,
1.86735156450242));
#41839=CARTESIAN_POINT('Ctrl Pts',(-2.35395598882936,-0.290679403076856,
1.86602362271669));
#41840=CARTESIAN_POINT('Ctrl Pts',(-2.36650432268375,-0.181446938995612,
1.85883256437167));
#41841=CARTESIAN_POINT('Ctrl Pts',(-2.37167906593707,-0.0916932481035841,
1.85318862828644));
#41842=CARTESIAN_POINT('Ctrl Pts',(-2.37179484178429,0.0564523055511605,
1.84400223820082));
#41843=CARTESIAN_POINT('Ctrl Pts',(-2.36969033606028,0.114688263886919,
1.8404242658626));
#41844=CARTESIAN_POINT('Ctrl Pts',(-2.36545132977956,0.172736993559942,
1.83684621836632));
#41845=CARTESIAN_POINT('Ctrl Pts',(-2.3654513498954,0.172736718094382,1.63785909343774));
#41846=CARTESIAN_POINT('Ctrl Pts',(-2.36654719596649,0.157730235415224,
1.63883508538677));
#41847=CARTESIAN_POINT('Ctrl Pts',(-2.36750025325823,0.142713141653489,
1.63981511942869));
#41848=CARTESIAN_POINT('Ctrl Pts',(-2.36962990794866,0.103212916705495,
1.64240262684809));
#41849=CARTESIAN_POINT('Ctrl Pts',(-2.3705699460905,0.0787201675594078,
1.64401682505237));
#41850=CARTESIAN_POINT('Ctrl Pts',(-2.37154534091713,0.036062942540206,
1.64684724059731));
#41851=CARTESIAN_POINT('Ctrl Pts',(-2.3717519367411,0.0179041825275535,
1.64805813099086));
#41852=CARTESIAN_POINT('Ctrl Pts',(-2.37174751163658,-0.0232946734318096,
1.65081992710143));
#41853=CARTESIAN_POINT('Ctrl Pts',(-2.37140931205067,-0.0463326228033727,
1.65237459638538));
#41854=CARTESIAN_POINT('Ctrl Pts',(-2.3695342497042,-0.110421327414875,
1.65672980933126));
#41855=CARTESIAN_POINT('Ctrl Pts',(-2.36726651100573,-0.15144088271088,
1.65955211068397));
#41856=CARTESIAN_POINT('Ctrl Pts',(-2.35969524824681,-0.244475938589024,
1.6660359407548));
#41857=CARTESIAN_POINT('Ctrl Pts',(-2.35373478989167,-0.296415304166481,
1.669714930991));
#41858=CARTESIAN_POINT('Ctrl Pts',(-2.3253747220977,-0.487544759041735,
1.68346486913336));
#41859=CARTESIAN_POINT('Ctrl Pts',(-2.29229751164423,-0.624846928967425,
1.69378209767941));
#41860=CARTESIAN_POINT('Ctrl Pts',(-2.21779108325948,-0.845622755576177,
1.7106983813133));
#41861=CARTESIAN_POINT('Ctrl Pts',(-2.18329272077936,-0.931080769404213,
1.71732614367497));
#41862=CARTESIAN_POINT('Ctrl Pts',(-2.1351133200973,-1.03291439904969,1.72516634258405));
#41863=CARTESIAN_POINT('Ctrl Pts',(-2.1260758353813,-1.05139082065905,1.72658629267499));
#41864=CARTESIAN_POINT('Ctrl Pts',(-2.1112288379414,-1.08076979912125,1.72883736596415));
#41865=CARTESIAN_POINT('Ctrl Pts',(-2.10557273999476,-1.09174814792008,
1.72967701414564));
#41866=CARTESIAN_POINT('Ctrl Pts',(-2.09428981179005,-1.11323416090081,
1.73131656358107));
#41867=CARTESIAN_POINT('Ctrl Pts',(-2.08866907864324,-1.12374445614983,
1.7321167523793));
#41868=CARTESIAN_POINT('Ctrl Pts',(-2.07411171327606,-1.15047891219663,
1.73414858721058));
#41869=CARTESIAN_POINT('Ctrl Pts',(-2.06506359447816,-1.16664198834318,
1.73537361767912));
#41870=CARTESIAN_POINT('Ctrl Pts',(-2.02421612041418,-1.23764517585572,
1.74074754181101));
#41871=CARTESIAN_POINT('Ctrl Pts',(-1.99041237346468,-1.29130806603578,
1.74478920201906));
#41872=CARTESIAN_POINT('Ctrl Pts',(-1.86979535448828,-1.46677184212455,
1.75815821860776));
#41873=CARTESIAN_POINT('Ctrl Pts',(-1.77363062110573,-1.58170559429831,
1.76719613909452));
#41874=CARTESIAN_POINT('Ctrl Pts',(-1.59987921910734,-1.75344397644576,
1.78237190486569));
#41875=CARTESIAN_POINT('Ctrl Pts',(-1.52855209563023,-1.81595840926948,
1.7883407466005));
#41876=CARTESIAN_POINT('Ctrl Pts',(-1.42878216562506,-1.89334958496809,
1.79651915603755));
#41877=CARTESIAN_POINT('Ctrl Pts',(-1.40350078251773,-1.91216540397392,
1.79857757024046));
#41878=CARTESIAN_POINT('Ctrl Pts',(-1.36237723014878,-1.94151689379679,
1.80190843934111));
#41879=CARTESIAN_POINT('Ctrl Pts',(-1.34676963614764,-1.95237575240946,
1.80316868883825));
#41880=CARTESIAN_POINT('Ctrl Pts',(-1.31397202734376,-1.97461401260761,
1.80580991903696));
#41881=CARTESIAN_POINT('Ctrl Pts',(-1.29676089158136,-1.98595924737829,
1.80719201414072));
#41882=CARTESIAN_POINT('Ctrl Pts',(-1.25521473956508,-2.01257529514511,
1.81052012431879));
#41883=CARTESIAN_POINT('Ctrl Pts',(-1.23074635485711,-2.02763079675443,
1.81247366545656));
#41884=CARTESIAN_POINT('Ctrl Pts',(-1.139576297964,-2.08146984577536,1.81973211141));
#41885=CARTESIAN_POINT('Ctrl Pts',(-1.07127323573097,-2.11743295375691,
1.82513233190086));
#41886=CARTESIAN_POINT('Ctrl Pts',(-0.872973816873279,-2.209789276814,1.84070018983906));
#41887=CARTESIAN_POINT('Ctrl Pts',(-0.739512781128365,-2.25795633813337,
1.85106693815446));
#41888=CARTESIAN_POINT('Ctrl Pts',(-0.514336564277445,-2.31710549841442,
1.86796609553948));
#41889=CARTESIAN_POINT('Ctrl Pts',(-0.424832284520196,-2.33517468839432,
1.87453078407858));
#41890=CARTESIAN_POINT('Ctrl Pts',(-0.314168352659941,-2.35093984180814,
1.88230973266009));
#41891=CARTESIAN_POINT('Ctrl Pts',(-0.293797495290138,-2.35357239005546,
1.88372769062193));
#41892=CARTESIAN_POINT('Ctrl Pts',(-0.261131577271575,-2.35736309430761,
1.88597649192701));
#41893=CARTESIAN_POINT('Ctrl Pts',(-0.248857699329382,-2.3586903827263,
1.88681582713224));
#41894=CARTESIAN_POINT('Ctrl Pts',(-0.224709241457831,-2.36111117882403,
1.88845541479804));
#41895=CARTESIAN_POINT('Ctrl Pts',(-0.212835808804666,-2.3622110766265,
1.88925594681536));
#41896=CARTESIAN_POINT('Ctrl Pts',(-0.182472497352711,-2.36479299293019,
1.89128986106421));
#41897=CARTESIAN_POINT('Ctrl Pts',(-0.163972134449447,-2.3661477770163,
1.89251660057047));
#41898=CARTESIAN_POINT('Ctrl Pts',(-0.0818734459237205,-2.37119230452873,
1.89791251117477));
#41899=CARTESIAN_POINT('Ctrl Pts',(-0.01815225922352,-2.37253623255923,
1.90197335576717));
#41900=CARTESIAN_POINT('Ctrl Pts',(0.196845610564631,-2.36840628692787,
1.91547268789195));
#41901=CARTESIAN_POINT('Ctrl Pts',(0.347519075781397,-2.35102762939105,
1.92461558103027));
#41902=CARTESIAN_POINT('Ctrl Pts',(0.586445551710573,-2.29998380133406,
1.93980225343132));
#41903=CARTESIAN_POINT('Ctrl Pts',(0.676146672386169,-2.27522896257397,
1.94566306210147));
#41904=CARTESIAN_POINT('Ctrl Pts',(0.793817755561029,-2.23518077025074,
1.95371571285254));
#41905=CARTESIAN_POINT('Ctrl Pts',(0.823274064726649,-2.22449980276319,
1.95576260561974));
#41906=CARTESIAN_POINT('Ctrl Pts',(0.870221161956724,-2.20641642823471,
1.9590797366206));
#41907=CARTESIAN_POINT('Ctrl Pts',(0.887850252337718,-2.19938178141263,
1.96033796217619));
#41908=CARTESIAN_POINT('Ctrl Pts',(0.924466365445204,-2.18425865459622,
1.96297881103345));
#41909=CARTESIAN_POINT('Ctrl Pts',(0.943435973877932,-2.17613245203599,
1.96436259105091));
#41910=CARTESIAN_POINT('Ctrl Pts',(0.988684108260003,-2.15604622099577,
1.96770224662581));
#41911=CARTESIAN_POINT('Ctrl Pts',(1.01485446048899,-2.14385211058749,1.96966578677096));
#41912=CARTESIAN_POINT('Ctrl Pts',(1.1112273581862,-2.09678699705268,1.9770196338284));
#41913=CARTESIAN_POINT('Ctrl Pts',(1.17990417459937,-2.05892345458027,1.98250864731601));
#41914=CARTESIAN_POINT('Ctrl Pts',(1.37123128507644,-1.9407197557494,1.998523852608));
#41915=CARTESIAN_POINT('Ctrl Pts',(1.488475949544,-1.85232328560055,2.00926540172555));
#41916=CARTESIAN_POINT('Ctrl Pts',(1.6598440323203,-1.69628558433629,2.02606679136148));
#41917=CARTESIAN_POINT('Ctrl Pts',(1.7197498710968,-1.63552139311466,2.03218829732791));
#41918=CARTESIAN_POINT('Ctrl Pts',(1.7897013536335,-1.55646352464351,2.03953177587582));
#41919=CARTESIAN_POINT('Ctrl Pts',(1.8029499684322,-1.54109737446693,2.04093196651037));
#41920=CARTESIAN_POINT('Ctrl Pts',(1.82390564601439,-1.51615213820122,2.0431593841685));
#41921=CARTESIAN_POINT('Ctrl Pts',(1.83173793933251,-1.50668020832993,2.04399483810991));
#41922=CARTESIAN_POINT('Ctrl Pts',(1.84704906109139,-1.48786793152956,2.04563319536527));
#41923=CARTESIAN_POINT('Ctrl Pts',(1.85453147343717,-1.47853110924855,2.04643630854342));
#41924=CARTESIAN_POINT('Ctrl Pts',(1.8735575028594,-1.45441806712347,2.04848597520045));
#41925=CARTESIAN_POINT('Ctrl Pts',(1.88499742426595,-1.43956048655148,2.04972567741397));
#41926=CARTESIAN_POINT('Ctrl Pts',(1.93598244172652,-1.37169370037781,2.05529215505019));
#41927=CARTESIAN_POINT('Ctrl Pts',(1.97347943298454,-1.31717583229765,2.05950193928785));
#41928=CARTESIAN_POINT('Ctrl Pts',(2.09722486672678,-1.12008581911671,2.07409085967496));
#41929=CARTESIAN_POINT('Ctrl Pts',(2.17069203216557,-0.970074474317937,
2.08412099742966));
#41930=CARTESIAN_POINT('Ctrl Pts',(2.25486304642878,-0.739593060952089,
2.09946653763378));
#41931=CARTESIAN_POINT('Ctrl Pts',(2.27818293213832,-0.664293585535105,
2.10446458509643));
#41932=CARTESIAN_POINT('Ctrl Pts',(2.30505131001156,-0.559296898056516,
2.11150076645997));
#41933=CARTESIAN_POINT('Ctrl Pts',(2.31185289062396,-0.530481525902981,
2.1134382791473));
#41934=CARTESIAN_POINT('Ctrl Pts',(2.32246050689161,-0.481453946559815,
2.11674974631156));
#41935=CARTESIAN_POINT('Ctrl Pts',(2.32654637016368,-0.461305378419504,
2.11811485356412));
#41936=CARTESIAN_POINT('Ctrl Pts',(2.3343314156325,-0.420176935455452,2.120911190234));
#41937=CARTESIAN_POINT('Ctrl Pts',(2.33801088154881,-0.399195294041209,
2.12234289466152));
#41938=CARTESIAN_POINT('Ctrl Pts',(2.34657899441084,-0.34614620754104,2.12597703930065));
#41939=CARTESIAN_POINT('Ctrl Pts',(2.35109318640605,-0.314023607666797,
2.12819075162327));
#41940=CARTESIAN_POINT('Ctrl Pts',(2.3696820198827,-0.158691327416637,2.13896390528826));
#41941=CARTESIAN_POINT('Ctrl Pts',(2.37473564361942,-0.0346151462326547,
2.14779094708367));
#41942=CARTESIAN_POINT('Ctrl Pts',(2.3636818580042,0.25885386791482,2.16905448838635));
#41943=CARTESIAN_POINT('Ctrl Pts',(2.3391122421271,0.427265330510222,2.18157852282985));
#41944=CARTESIAN_POINT('Ctrl Pts',(2.29058335972866,0.61566433998418,2.19519917302738));
#41945=CARTESIAN_POINT('Ctrl Pts',(2.28401151629569,0.639614116995389,2.19692233546188));
#41946=CARTESIAN_POINT('Ctrl Pts',(2.27331852205391,0.67631374221941,2.19954552916359));
#41947=CARTESIAN_POINT('Ctrl Pts',(2.26946369569198,0.68913854618233,2.20045892647933));
#41948=CARTESIAN_POINT('Ctrl Pts',(2.26210544288602,0.712887516914196,2.20214337313136));
#41949=CARTESIAN_POINT('Ctrl Pts',(2.2586312311089,0.723819462909523,2.2029158750223));
#41950=CARTESIAN_POINT('Ctrl Pts',(2.25015115622019,0.749847145849368,2.20474882985971));
#41951=CARTESIAN_POINT('Ctrl Pts',(2.2450725648758,0.764918414125853,2.20580521498074));
#41952=CARTESIAN_POINT('Ctrl Pts',(2.22661991997986,0.817911116336573,2.2095057478403));
#41953=CARTESIAN_POINT('Ctrl Pts',(2.21243281491838,0.855544467836024,2.21210854298126));
#41954=CARTESIAN_POINT('Ctrl Pts',(2.17283760329181,0.952993192564637,2.21882657644898));
#41955=CARTESIAN_POINT('Ctrl Pts',(2.14591595133694,1.01215861297101,2.22288389865251));
#41956=CARTESIAN_POINT('Ctrl Pts',(2.02818561000403,1.24501229011298,2.23903908820727));
#41957=CARTESIAN_POINT('Ctrl Pts',(1.91845402014795,1.40823387897523,2.25086585964863));
#41958=CARTESIAN_POINT('Ctrl Pts',(1.76509493988458,1.5846348038616,2.26590461970806));
#41959=CARTESIAN_POINT('Ctrl Pts',(1.73961070548738,1.6125699836099,2.26836108307984));
#41960=CARTESIAN_POINT('Ctrl Pts',(1.69799245970479,1.65605579837115,2.27231532172865));
#41961=CARTESIAN_POINT('Ctrl Pts',(1.68228643563223,1.67200822153385,2.2737952303158));
#41962=CARTESIAN_POINT('Ctrl Pts',(1.65190819199447,1.70200167173956,2.2766360539972));
#41963=CARTESIAN_POINT('Ctrl Pts',(1.63727677971212,1.71608131184288,2.277995127723));
#41964=CARTESIAN_POINT('Ctrl Pts',(1.60300849844241,1.74822008626292,2.28115838970975));
#41965=CARTESIAN_POINT('Ctrl Pts',(1.58324442948389,1.76613892259814,2.28296818540969));
#41966=CARTESIAN_POINT('Ctrl Pts',(1.51667532359892,1.82447750443183,2.28901880161535));
#41967=CARTESIAN_POINT('Ctrl Pts',(1.4685953396413,1.86339710252776,2.29331770780599));
#41968=CARTESIAN_POINT('Ctrl Pts',(1.34311505976353,1.95709529108439,2.30436599142154));
#41969=CARTESIAN_POINT('Ctrl Pts',(1.26385294231681,2.00919209831419,2.31119377511628));
#41970=CARTESIAN_POINT('Ctrl Pts',(1.0487023163016,2.13282644491195,2.3292224757838));
#41971=CARTESIAN_POINT('Ctrl Pts',(0.90860329398233,2.19617198053371,2.34049057208151));
#41972=CARTESIAN_POINT('Ctrl Pts',(0.741191978470014,2.25308250126753,2.35284402226576));
#41973=CARTESIAN_POINT('Ctrl Pts',(0.718911870851121,2.26029027537264,2.3544658167008));
#41974=CARTESIAN_POINT('Ctrl Pts',(0.684147020658825,2.27097086396686,2.35695819240205));
#41975=CARTESIAN_POINT('Ctrl Pts',(0.671735050921496,2.27467313072325,2.35784054553979));
#41976=CARTESIAN_POINT('Ctrl Pts',(0.648153882010265,2.28149711350644,2.35950194032967));
#41977=CARTESIAN_POINT('Ctrl Pts',(0.636991275923464,2.28463884528914,2.3602819849293));
#41978=CARTESIAN_POINT('Ctrl Pts',(0.609623388168784,2.29212540119212,2.36217961556006));
#41979=CARTESIAN_POINT('Ctrl Pts',(0.593393861678064,2.29638047683091,2.3632923202811));
#41980=CARTESIAN_POINT('Ctrl Pts',(0.531831379473651,2.31182473180188,2.36747023293445));
#41981=CARTESIAN_POINT('Ctrl Pts',(0.4862136975798,2.32184734565715,2.37047864595902));
#41982=CARTESIAN_POINT('Ctrl Pts',(0.359291850114696,2.34582788666199,2.37868266362779));
#41983=CARTESIAN_POINT('Ctrl Pts',(0.277508407270747,2.35690260772842,2.38378385170301));
#41984=CARTESIAN_POINT('Ctrl Pts',(0.0249800131020579,2.37776877591972,
2.39938974117179));
#41985=CARTESIAN_POINT('Ctrl Pts',(-0.146354628853781,2.37339046599887,
2.40981451058443));
#41986=CARTESIAN_POINT('Ctrl Pts',(-0.352627515240425,2.34568502630476,
2.42321251274684));
#41987=CARTESIAN_POINT('Ctrl Pts',(-0.389406246152691,2.33986045383947,
2.42563265525156));
#41988=CARTESIAN_POINT('Ctrl Pts',(-0.447938143061073,2.32917268604736,
2.42954249705843));
#41989=CARTESIAN_POINT('Ctrl Pts',(-0.469787103924929,2.32486429778378,
2.43101504862357));
#41990=CARTESIAN_POINT('Ctrl Pts',(-0.511466963434117,2.31603393790522,
2.43385082297768));
#41991=CARTESIAN_POINT('Ctrl Pts',(-0.531306783926268,2.31156326199547,
2.43521233002938));
#41992=CARTESIAN_POINT('Ctrl Pts',(-0.577272120095192,2.30058249139106,
2.43839503564563));
#41993=CARTESIAN_POINT('Ctrl Pts',(-0.60334871334723,2.293881672843,2.44022206801229));
#41994=CARTESIAN_POINT('Ctrl Pts',(-0.690524329046958,2.2698911633327,2.44640493076675));
#41995=CARTESIAN_POINT('Ctrl Pts',(-0.751037438165423,2.25059353249019,
2.45082244216168));
#41996=CARTESIAN_POINT('Ctrl Pts',(-0.903681953558604,2.19507325329013,
2.46229351040683));
#41997=CARTESIAN_POINT('Ctrl Pts',(-0.994449394707747,2.15547091956026,
2.46943387768338));
#41998=CARTESIAN_POINT('Ctrl Pts',(-1.21201834639803,2.04387073742402,2.48721410283684));
#41999=CARTESIAN_POINT('Ctrl Pts',(-1.33517973024596,1.96562892411218,2.49789013064329));
#42000=CARTESIAN_POINT('Ctrl Pts',(-1.4693002142571,1.8619682891847,2.50974418884147));
#42001=CARTESIAN_POINT('Ctrl Pts',(-1.48798538419434,1.84707028342696,2.51140072467));
#42002=CARTESIAN_POINT('Ctrl Pts',(-1.516631205429,1.82351359779278,2.51394430278957));
#42003=CARTESIAN_POINT('Ctrl Pts',(-1.52674959428197,1.81505034403511,2.51484354412293));
#42004=CARTESIAN_POINT('Ctrl Pts',(-1.54557133490461,1.79903863562786,2.51651692269486));
#42005=CARTESIAN_POINT('Ctrl Pts',(-1.55429070116523,1.79151086676417,2.51729229850691));
#42006=CARTESIAN_POINT('Ctrl Pts',(-1.57519395151704,1.77319678400936,2.51915222073237));
#42007=CARTESIAN_POINT('Ctrl Pts',(-1.58732225850853,1.76234812208739,2.5202323463702));
#42008=CARTESIAN_POINT('Ctrl Pts',(-1.63096360932807,1.72249527428285,2.52412671424529));
#42009=CARTESIAN_POINT('Ctrl Pts',(-1.66180306751072,1.69276204616273,2.52689364616598));
#42010=CARTESIAN_POINT('Ctrl Pts',(-1.7420574487651,1.6110778225241,2.53419033041726));
#42011=CARTESIAN_POINT('Ctrl Pts',(-1.78995209193275,1.55769339364596,2.53864905113636));
#42012=CARTESIAN_POINT('Ctrl Pts',(-1.95712380270183,1.35344887476906,2.55494915465022));
#42013=CARTESIAN_POINT('Ctrl Pts',(-2.06033953236469,1.19044207352411,2.56659783522856));
#42014=CARTESIAN_POINT('Ctrl Pts',(-2.15749649940084,0.985692756810211,
2.58122954597995));
#42015=CARTESIAN_POINT('Ctrl Pts',(-2.17156489320032,0.954299260830908,
2.58347062928558));
#42016=CARTESIAN_POINT('Ctrl Pts',(-2.19338411794321,0.902626618631597,
2.58716195755577));
#42017=CARTESIAN_POINT('Ctrl Pts',(-2.20154833519359,0.88252681430177,2.58859842555104));
#42018=CARTESIAN_POINT('Ctrl Pts',(-2.21691021404479,0.843166549286795,
2.59141401724238));
#42019=CARTESIAN_POINT('Ctrl Pts',(-2.22413542343369,0.823918867562813,
2.59279208825022));
#42020=CARTESIAN_POINT('Ctrl Pts',(-2.24074498307047,0.777860384310956,
2.59609378211293));
#42021=CARTESIAN_POINT('Ctrl Pts',(-2.24989950488411,0.750970675547836,
2.59802462346734));
#42022=CARTESIAN_POINT('Ctrl Pts',(-2.28130217590741,0.652997565999373,
2.60507455568915));
#42023=CARTESIAN_POINT('Ctrl Pts',(-2.3006799337004,0.581046721417356,2.61028182104385));
#42024=CARTESIAN_POINT('Ctrl Pts',(-2.34091354263455,0.397680607579599,
2.62362330555379));
#42025=CARTESIAN_POINT('Ctrl Pts',(-2.35721448697413,0.285532433415052,
2.63185297112801));
#42026=CARTESIAN_POINT('Ctrl Pts',(-2.36545139057093,0.172736161084002,
2.64008830168392));
#42027=CARTESIAN_POINT('Origin',(0.,0.,-1.84858989190501));
#42028=CARTESIAN_POINT('',(-2.36545134965682,0.17273672136148,3.83914957969666));
#42029=CARTESIAN_POINT('',(-2.3654513605298,0.172736572467239,3.64082947459234));
#42030=CARTESIAN_POINT('',(-2.36545134966535,0.172736721244682,-1.84858989190501));
#42031=CARTESIAN_POINT('',(-2.37174919235095,0.0019573151533352,2.84812596863768));
#42032=CARTESIAN_POINT('Ctrl Pts',(-2.36545134965682,0.17273672136148,3.83914957969666));
#42033=CARTESIAN_POINT('Ctrl Pts',(-2.36496531051115,0.179392526473733,
3.83870004047593));
#42034=CARTESIAN_POINT('Ctrl Pts',(-2.36445118140828,0.186046256021305,
3.8382496373551));
#42035=CARTESIAN_POINT('Ctrl Pts',(-2.36132563377815,0.22438874170804,3.83564829188122));
#42036=CARTESIAN_POINT('Ctrl Pts',(-2.35810538440664,0.256023212159722,
3.83347885285856));
#42037=CARTESIAN_POINT('Ctrl Pts',(-2.33944156017782,0.408811963707815,
3.82288325940782));
#42038=CARTESIAN_POINT('Ctrl Pts',(-2.31529341069665,0.528698882910509,
3.81419633380283));
#42039=CARTESIAN_POINT('Ctrl Pts',(-2.23452559481581,0.813936547990445,
3.79273931456493));
#42040=CARTESIAN_POINT('Ctrl Pts',(-2.16866932197986,0.975948323225499,
3.7798550951437));
#42041=CARTESIAN_POINT('Ctrl Pts',(-2.07424916464073,1.15033102575288,3.76598350972286));
#42042=CARTESIAN_POINT('Ctrl Pts',(-2.06253304411047,1.17120818580878,3.76432359254829));
#42043=CARTESIAN_POINT('Ctrl Pts',(-2.04398617676241,1.20311541334203,3.76179191220107));
#42044=CARTESIAN_POINT('Ctrl Pts',(-2.03737802793863,1.21427220148476,3.7609076811755));
#42045=CARTESIAN_POINT('Ctrl Pts',(-2.0249371331119,1.23488912870589,3.75927634952197));
#42046=CARTESIAN_POINT('Ctrl Pts',(-2.01912915659518,1.2443628925082,3.75852788236576));
#42047=CARTESIAN_POINT('Ctrl Pts',(-2.00514565369015,1.26681658368055,3.75675617775592));
#42048=CARTESIAN_POINT('Ctrl Pts',(-1.99691046536362,1.27975856047989,3.75573670656421));
#42049=CARTESIAN_POINT('Ctrl Pts',(-1.96770379435595,1.32468972345186,3.75220003223985));
#42050=CARTESIAN_POINT('Ctrl Pts',(-1.94608344699825,1.356252441299,3.74972037846208));
#42051=CARTESIAN_POINT('Ctrl Pts',(-1.88820597716092,1.43650971228254,3.74338942979372));
#42052=CARTESIAN_POINT('Ctrl Pts',(-1.85082530978085,1.48436132875604,3.73958900239957));
#42053=CARTESIAN_POINT('Ctrl Pts',(-1.67952830912838,1.68709471662873,3.72312580439512));
#42054=CARTESIAN_POINT('Ctrl Pts',(-1.52773254041533,1.82568740013169,3.71081558557811));
#42055=CARTESIAN_POINT('Ctrl Pts',(-1.32966995051729,1.9643189861908,3.69525387651646));
#42056=CARTESIAN_POINT('Ctrl Pts',(-1.29881865935231,1.98485291908901,3.6928454878576));
#42057=CARTESIAN_POINT('Ctrl Pts',(-1.24907422896689,2.01630525567888,3.68897856807118));
#42058=CARTESIAN_POINT('Ctrl Pts',(-1.23048895088978,2.02770071836518,3.68753736526352));
#42059=CARTESIAN_POINT('Ctrl Pts',(-1.19485187791865,2.04888102403419,3.68477904020907));
#42060=CARTESIAN_POINT('Ctrl Pts',(-1.17783027272596,2.05871325594797,3.68346375335926));
#42061=CARTESIAN_POINT('Ctrl Pts',(-1.13834901662877,2.08086900352375,3.68041693778062));
#42062=CARTESIAN_POINT('Ctrl Pts',(-1.11580832925897,2.09304227815921,3.67868033741289));
#42063=CARTESIAN_POINT('Ctrl Pts',(-1.04160111852939,2.13157907780519,3.67297024844625));
#42064=CARTESIAN_POINT('Ctrl Pts',(-0.989167450738712,2.15641114694513,
3.66894595952278));
#42065=CARTESIAN_POINT('Ctrl Pts',(-0.856591164501748,2.21334492664889,
3.65879194246473));
#42066=CARTESIAN_POINT('Ctrl Pts',(-0.77550996172097,2.2430394827655,3.65259856302511));
#42067=CARTESIAN_POINT('Ctrl Pts',(-0.564920384808152,2.30737903955457,
3.63663425020827));
#42068=CARTESIAN_POINT('Ctrl Pts',(-0.4337579726088,2.33559165911594,3.62679442473676));
#42069=CARTESIAN_POINT('Ctrl Pts',(-0.254911908563656,2.35846746221174,
3.61392909283571));
#42070=CARTESIAN_POINT('Ctrl Pts',(-0.208743858329438,2.36300137378563,
3.61065837530656));
#42071=CARTESIAN_POINT('Ctrl Pts',(-0.145615466565604,2.3673359689762,3.60627916146979));
#42072=CARTESIAN_POINT('Ctrl Pts',(-0.128749123430831,2.36831314607568,
3.60511818905557));
#42073=CARTESIAN_POINT('Ctrl Pts',(-0.100642888636665,2.36964036773299,
3.60320013220399));
#42074=CARTESIAN_POINT('Ctrl Pts',(-0.0894085569419681,2.37009084086739,
3.6024378888533));
#42075=CARTESIAN_POINT('Ctrl Pts',(-0.0659584618580572,2.37086415689739,
3.60085654991306));
#42076=CARTESIAN_POINT('Ctrl Pts',(-0.0537427255754355,2.37117251691621,
3.60003822126383));
#42077=CARTESIAN_POINT('Ctrl Pts',(-0.020483171645991,2.37175491753093,
3.59782362974894));
#42078=CARTESIAN_POINT('Ctrl Pts',(0.000563325769140379,2.37184331386325,
3.59643690395749));
#42079=CARTESIAN_POINT('Ctrl Pts',(0.147784986859749,2.3705019178284,3.5868218610713));
#42080=CARTESIAN_POINT('Ctrl Pts',(0.273684902223934,2.35928473486872,3.57903067362696));
#42081=CARTESIAN_POINT('Ctrl Pts',(0.560624806980556,2.31042755041321,3.56112250808857));
#42082=CARTESIAN_POINT('Ctrl Pts',(0.719797439871965,2.26589074819803,3.55104890807293));
#42083=CARTESIAN_POINT('Ctrl Pts',(0.907880707879646,2.19142721041078,3.53803290704875));
#42084=CARTESIAN_POINT('Ctrl Pts',(0.942368469223541,2.17681924439915,3.53559965615468));
#42085=CARTESIAN_POINT('Ctrl Pts',(0.996434283501278,2.15239297760444,3.53170232929647));
#42086=CARTESIAN_POINT('Ctrl Pts',(1.01624788086959,2.14310919073928,3.53025607253192));
#42087=CARTESIAN_POINT('Ctrl Pts',(1.05359641205499,2.12497490762278,3.52749400360351));
#42088=CARTESIAN_POINT('Ctrl Pts',(1.07115546643094,2.11617808445448,3.52618010814896));
#42089=CARTESIAN_POINT('Ctrl Pts',(1.11122699224198,2.09547634180801,3.52314518941859));
#42090=CARTESIAN_POINT('Ctrl Pts',(1.13366067471577,2.08342504444885,3.52141922947268));
#42091=CARTESIAN_POINT('Ctrl Pts',(1.20570456972575,2.04321520289551,3.51578635106114));
#42092=CARTESIAN_POINT('Ctrl Pts',(1.25449088008122,2.01362945393628,3.51183054090305));
#42093=CARTESIAN_POINT('Ctrl Pts',(1.37245771762206,1.93613842592178,3.50190403980025));
#42094=CARTESIAN_POINT('Ctrl Pts',(1.44024321020899,1.88625805735089,3.49587350235481));
#42095=CARTESIAN_POINT('Ctrl Pts',(1.63538614460526,1.72599982981445,3.4775797798561));
#42096=CARTESIAN_POINT('Ctrl Pts',(1.75378885886107,1.60555052427525,3.46514962819775));
#42097=CARTESIAN_POINT('Ctrl Pts',(1.87395401107852,1.45400075834754,3.45160353440071));
#42098=CARTESIAN_POINT('Ctrl Pts',(1.88916202079736,1.43418576904441,3.44986984885094));
#42099=CARTESIAN_POINT('Ctrl Pts',(1.91191689168535,1.4035475521836,3.44725021458056));
#42100=CARTESIAN_POINT('Ctrl Pts',(1.91969070881282,1.39289609618989,3.4463504913652));
#42101=CARTESIAN_POINT('Ctrl Pts',(1.93382894443396,1.37318108940664,3.44470610932978));
#42102=CARTESIAN_POINT('Ctrl Pts',(1.94021906016955,1.36413734513345,3.4439598610505));
#42103=CARTESIAN_POINT('Ctrl Pts',(1.95510792123208,1.34274929100654,3.44221348877139));
#42104=CARTESIAN_POINT('Ctrl Pts',(1.9635533524251,1.33036870942975,3.44121680314907));
#42105=CARTESIAN_POINT('Ctrl Pts',(1.99185125563075,1.28802881955324,3.43785320810683));
#42106=CARTESIAN_POINT('Ctrl Pts',(2.01114091158604,1.25769718944114,3.43551912013507));
#42107=CARTESIAN_POINT('Ctrl Pts',(2.05835904054724,1.17958373922833,3.42966600445682));
#42108=CARTESIAN_POINT('Ctrl Pts',(2.08531912489945,1.13124030541228,3.42618870170665));
#42109=CARTESIAN_POINT('Ctrl Pts',(2.1625908721236,0.98051226067201,3.41565066818045));
#42110=CARTESIAN_POINT('Ctrl Pts',(2.2072304852554,0.875407497879184,3.40870977820598));
#42111=CARTESIAN_POINT('Ctrl Pts',(2.2795442896056,0.663964378204742,3.3948901449483));
#42112=CARTESIAN_POINT('Ctrl Pts',(2.30774194590003,0.558116455860594,3.38803656110826));
#42113=CARTESIAN_POINT('Ctrl Pts',(2.3345586010097,0.419571231901951,3.37890212065695));
#42114=CARTESIAN_POINT('Ctrl Pts',(2.33996001118584,0.388318006552668,3.37683170790399));
#42115=CARTESIAN_POINT('Ctrl Pts',(2.3478505654471,0.336489008829084,3.37337709063717));
#42116=CARTESIAN_POINT('Ctrl Pts',(2.35069969057951,0.315971597548835,3.37200409873295));
#42117=CARTESIAN_POINT('Ctrl Pts',(2.35578469666723,0.275465063603467,3.36928152986511));
#42118=CARTESIAN_POINT('Ctrl Pts',(2.35803576681631,0.255479585395643,3.36793254437998));
#42119=CARTESIAN_POINT('Ctrl Pts',(2.36286783440648,0.207049156803198,3.36464868742119));
#42120=CARTESIAN_POINT('Ctrl Pts',(2.36518964585235,0.178582121186022,3.36270604930908));
#42121=CARTESIAN_POINT('Ctrl Pts',(2.37206739816128,0.070110004797668,3.35525328110018));
#42122=CARTESIAN_POINT('Ctrl Pts',(2.37308144147758,-0.010058136187945,
3.34963854699891));
#42123=CARTESIAN_POINT('Ctrl Pts',(2.36414040774578,-0.245204303170176,
3.33286688036197));
#42124=CARTESIAN_POINT('Ctrl Pts',(2.3430347746088,-0.399332341407755,3.32146107362126));
#42125=CARTESIAN_POINT('Ctrl Pts',(2.28930142624893,-0.624609359746595,
3.30470821324799));
#42126=CARTESIAN_POINT('Ctrl Pts',(2.26798731288799,-0.698049895537723,
3.29924000878697));
#42127=CARTESIAN_POINT('Ctrl Pts',(2.2367968940019,-0.788873728356599,3.29256432594585));
#42128=CARTESIAN_POINT('Ctrl Pts',(2.2302021058487,-0.807329383066043,3.29121250946687));
#42129=CARTESIAN_POINT('Ctrl Pts',(2.21923293017176,-0.836866236036345,
3.28905893062079));
#42130=CARTESIAN_POINT('Ctrl Pts',(2.2150026567167,-0.847999493803162,3.28824947213989));
#42131=CARTESIAN_POINT('Ctrl Pts',(2.20649393707898,-0.869894632662896,
3.28666272770784));
#42132=CARTESIAN_POINT('Ctrl Pts',(2.20222021493609,-0.880657879806769,
3.2858852331419));
#42133=CARTESIAN_POINT('Ctrl Pts',(2.1910852558284,-0.908112953807342,3.28390740777524));
#42134=CARTESIAN_POINT('Ctrl Pts',(2.18411186395595,-0.924758968044414,
3.28271340791755));
#42135=CARTESIAN_POINT('Ctrl Pts',(2.15245710759393,-0.997965175055557,
3.27747838998661));
#42136=CARTESIAN_POINT('Ctrl Pts',(2.12576182562203,-1.05363376785842,3.27353975523884));
#42137=CARTESIAN_POINT('Ctrl Pts',(2.03071779237441,-1.23347460936641,3.26075588976711));
#42138=CARTESIAN_POINT('Ctrl Pts',(1.95341758325166,-1.35256716708233,3.25217763128086));
#42139=CARTESIAN_POINT('Ctrl Pts',(1.80115701151872,-1.54662449257737,3.2369050784427));
#42140=CARTESIAN_POINT('Ctrl Pts',(1.73096602550294,-1.62479748812019,3.23031969847355));
#42141=CARTESIAN_POINT('Ctrl Pts',(1.63329502933882,-1.72003968782065,3.22148685959775));
#42142=CARTESIAN_POINT('Ctrl Pts',(1.61032090532284,-1.74156699944358,3.21943119209404));
#42143=CARTESIAN_POINT('Ctrl Pts',(1.57156621659445,-1.77645851108627,3.21599444910875));
#42144=CARTESIAN_POINT('Ctrl Pts',(1.55602680485632,-1.79008540372232,3.21462434212483));
#42145=CARTESIAN_POINT('Ctrl Pts',(1.52499378691393,-1.81658960741378,3.2119023566361));
#42146=CARTESIAN_POINT('Ctrl Pts',(1.50951024938476,-1.82947604972054,3.21055100710892));
#42147=CARTESIAN_POINT('Ctrl Pts',(1.47154048211866,-1.86026685858309,3.20725222448123));
#42148=CARTESIAN_POINT('Ctrl Pts',(1.44888976531283,-1.87796232655483,3.20529685156905));
#42149=CARTESIAN_POINT('Ctrl Pts',(1.36056030280287,-1.94441882480595,3.19771562625172));
#42150=CARTESIAN_POINT('Ctrl Pts',(1.2927035622622,-1.99017682536731,3.1919803503454));
#42151=CARTESIAN_POINT('Ctrl Pts',(1.08287713841389,-2.11640559949154,3.17451367873617));
#42152=CARTESIAN_POINT('Ctrl Pts',(0.93483353083411,-2.18583504112227,3.1625033573219));
#42153=CARTESIAN_POINT('Ctrl Pts',(0.717052637924405,-2.26176916254781,
3.14587048381918));
#42154=CARTESIAN_POINT('Ctrl Pts',(0.652318788811348,-2.28128167770181,
3.1410534887113));
#42155=CARTESIAN_POINT('Ctrl Pts',(0.568401635671625,-2.30271135217159,
3.13503795696152));
#42156=CARTESIAN_POINT('Ctrl Pts',(0.54991205703135,-2.30719673562864,3.13372659957361));
#42157=CARTESIAN_POINT('Ctrl Pts',(0.519882866350561,-2.31409999581352,
3.13162162914518));
#42158=CARTESIAN_POINT('Ctrl Pts',(0.508376094621702,-2.31665507720023,
3.13082090036402));
#42159=CARTESIAN_POINT('Ctrl Pts',(0.48542357474766,-2.32157243741844,3.1292359920404));
#42160=CARTESIAN_POINT('Ctrl Pts',(0.473978491943804,-2.32393610742068,
3.12845176478038));
#42161=CARTESIAN_POINT('Ctrl Pts',(0.444318251115926,-2.32983338648486,
3.12643401410098));
#42162=CARTESIAN_POINT('Ctrl Pts',(0.426077850714125,-2.33323810060432,
3.12520733621009));
#42163=CARTESIAN_POINT('Ctrl Pts',(0.340885267093001,-2.34810755786689,
3.11953617647634));
#42164=CARTESIAN_POINT('Ctrl Pts',(0.273494443330123,-2.35690780685675,
3.11521637599224));
#42165=CARTESIAN_POINT('Ctrl Pts',(0.0249017643008804,-2.3785615611046,
3.09958980409025));
#42166=CARTESIAN_POINT('Ctrl Pts',(-0.157220504902397,-2.3734913192797,
3.08869288087847));
#42167=CARTESIAN_POINT('Ctrl Pts',(-0.403007374462072,-2.33821124249097,
3.07306724511153));
#42168=CARTESIAN_POINT('Ctrl Pts',(-0.468595086142282,-2.32595447480647,
3.06881173397738));
#42169=CARTESIAN_POINT('Ctrl Pts',(-0.560431777004879,-2.30475031478132,
3.06267939008483));
#42170=CARTESIAN_POINT('Ctrl Pts',(-0.587177282125869,-2.2980819236241,
3.06087245299169));
#42171=CARTESIAN_POINT('Ctrl Pts',(-0.633060205886138,-2.28578879978997,
3.05773305331591));
#42172=CARTESIAN_POINT('Ctrl Pts',(-0.652254428287186,-2.28038588442379,
3.05640769519611));
#42173=CARTESIAN_POINT('Ctrl Pts',(-0.691521671280252,-2.26879636918036,
3.05367034680632));
#42174=CARTESIAN_POINT('Ctrl Pts',(-0.71158514005088,-2.26258386075118,
3.05225763095738));
#42175=CARTESIAN_POINT('Ctrl Pts',(-0.763096051207286,-2.24588097771203,
3.04859293120847));
#42176=CARTESIAN_POINT('Ctrl Pts',(-0.794409911375765,-2.23499656669142,
3.04632850539249));
#42177=CARTESIAN_POINT('Ctrl Pts',(-0.970132617614989,-2.16975756937009,
3.03340637419198));
#42178=CARTESIAN_POINT('Ctrl Pts',(-1.10917176046243,-2.10207713982111,
3.02231642798197));
#42179=CARTESIAN_POINT('Ctrl Pts',(-1.35924902342421,-1.94859172727142,
3.00096001913634));
#42180=CARTESIAN_POINT('Ctrl Pts',(-1.47123503541127,-1.8654867715933,2.99076869723717));
#42181=CARTESIAN_POINT('Ctrl Pts',(-1.59328992644848,-1.75704435564816,
2.9793458450475));
#42182=CARTESIAN_POINT('Ctrl Pts',(-1.61104370724045,-1.740780267361,2.97767617604026));
#42183=CARTESIAN_POINT('Ctrl Pts',(-1.6379953051163,-1.71532455507567,2.97513284738791));
#42184=CARTESIAN_POINT('Ctrl Pts',(-1.64736982214983,-1.70632342697059,
2.97424655021329));
#42185=CARTESIAN_POINT('Ctrl Pts',(-1.66381872974742,-1.69026775611832,
2.97268921888215));
#42186=CARTESIAN_POINT('Ctrl Pts',(-1.67092294119698,-1.68324519385593,
2.97201594268709));
#42187=CARTESIAN_POINT('Ctrl Pts',(-1.68827298766562,-1.66587645958595,
2.97036966318114));
#42188=CARTESIAN_POINT('Ctrl Pts',(-1.69846824762546,-1.65548050359335,
2.96940046329458));
#42189=CARTESIAN_POINT('Ctrl Pts',(-1.73166768976955,-1.62099795260456,
2.96623568627904));
#42190=CARTESIAN_POINT('Ctrl Pts',(-1.75426136064373,-1.59651955526325,
2.9640679078593));
#42191=CARTESIAN_POINT('Ctrl Pts',(-1.80917120256205,-1.53445547004214,
2.95873955027437));
#42192=CARTESIAN_POINT('Ctrl Pts',(-1.84083978651161,-1.4963166395412,2.95561176719031));
#42193=CARTESIAN_POINT('Ctrl Pts',(-1.98447785519668,-1.31186245852775,
2.94101067545729));
#42194=CARTESIAN_POINT('Ctrl Pts',(-2.08034327435035,-1.1538241375076,2.92995190101031));
#42195=CARTESIAN_POINT('Ctrl Pts',(-2.18200528241339,-0.931493502422634,
2.91451037783979));
#42196=CARTESIAN_POINT('Ctrl Pts',(-2.20495854843782,-0.875776281825256,
2.9106549035364));
#42197=CARTESIAN_POINT('Ctrl Pts',(-2.23407838063787,-0.796662486810262,
2.90516356765353));
#42198=CARTESIAN_POINT('Ctrl Pts',(-2.24204738332637,-0.773951414327082,
2.90358539003129));
#42199=CARTESIAN_POINT('Ctrl Pts',(-2.25597669366231,-0.732232131626875,
2.90068087047535));
#42200=CARTESIAN_POINT('Ctrl Pts',(-2.26204585114382,-0.713262408976186,
2.89935815168019));
#42201=CARTESIAN_POINT('Ctrl Pts',(-2.27392309393666,-0.674461820250767,
2.89664740905895));
#42202=CARTESIAN_POINT('Ctrl Pts',(-2.27971234738101,-0.65462703234631,
2.89525891395057));
#42203=CARTESIAN_POINT('Ctrl Pts',(-2.29365916324721,-0.604412984476821,
2.89173562107873));
#42204=CARTESIAN_POINT('Ctrl Pts',(-2.30147267868288,-0.573943168353824,
2.88959018617532));
#42205=CARTESIAN_POINT('Ctrl Pts',(-2.31947076974247,-0.497466755750736,
2.88418411341739));
#42206=CARTESIAN_POINT('Ctrl Pts',(-2.32889427525843,-0.451296760904466,
2.8809012195654));
#42207=CARTESIAN_POINT('Ctrl Pts',(-2.36021728362533,-0.270502473907583,
2.86797109305728));
#42208=CARTESIAN_POINT('Ctrl Pts',(-2.37186171063907,-0.134385142783268,
2.85805660689887));
#42209=CARTESIAN_POINT('Ctrl Pts',(-2.37174919235095,0.0019573151533352,
2.84812596863768));
#42210=CARTESIAN_POINT('Ctrl Pts',(-2.3717491913197,0.00195856436296467,
2.84812587765026));
#42211=CARTESIAN_POINT('Ctrl Pts',(-2.37170212969245,0.058948458838013,
2.84397496217231));
#42212=CARTESIAN_POINT('Ctrl Pts',(-2.36960100172951,0.115911523124276,
2.83982926533819));
#42213=CARTESIAN_POINT('Ctrl Pts',(-2.36545134753269,0.172736750449338,
2.83572259012909));
#42214=CARTESIAN_POINT('',(-2.37174994626123,-0.00144183595024523,2.65273840708708));
#42215=CARTESIAN_POINT('Ctrl Pts',(-2.36545139057093,0.172736161084002,
2.64008830168392));
#42216=CARTESIAN_POINT('Ctrl Pts',(-2.36968143502358,0.114809873560342,
2.64431753830474));
#42217=CARTESIAN_POINT('Ctrl Pts',(-2.37178483994934,0.0567125215558486,
2.64854624104343));
#42218=CARTESIAN_POINT('Ctrl Pts',(-2.37174956359742,-0.00143877568085956,
2.65273885301577));
#42219=CARTESIAN_POINT('Ctrl Pts',(-2.3717495617682,-0.00144178789911513,
2.65273907019167));
#42220=CARTESIAN_POINT('Ctrl Pts',(-2.37170869729105,-0.0686640928088483,
2.65758568513456));
#42221=CARTESIAN_POINT('Ctrl Pts',(-2.36880991714627,-0.135861689288376,
2.66237712047973));
#42222=CARTESIAN_POINT('Ctrl Pts',(-2.36181720656935,-0.217321062812207,
2.66805674192593));
#42223=CARTESIAN_POINT('Ctrl Pts',(-2.36044222872002,-0.23177892708601,
2.66905980331548));
#42224=CARTESIAN_POINT('Ctrl Pts',(-2.35778607167011,-0.257226117679556,
2.67081546264293));
#42225=CARTESIAN_POINT('Ctrl Pts',(-2.35656065453419,-0.268220671806938,
2.67157076376477));
#42226=CARTESIAN_POINT('Ctrl Pts',(-2.35391963901662,-0.290499069624113,
2.67309413547133));
#42227=CARTESIAN_POINT('Ctrl Pts',(-2.35249977548238,-0.301781704034808,
2.67386184141381));
#42228=CARTESIAN_POINT('Ctrl Pts',(-2.34909542746515,-0.327347920252172,
2.67559294360465));
#42229=CARTESIAN_POINT('Ctrl Pts',(-2.34706176639614,-0.341624177694819,
2.67655370196905));
#42230=CARTESIAN_POINT('Ctrl Pts',(-2.34024572931977,-0.386534953235174,
2.67956001105642));
#42231=CARTESIAN_POINT('Ctrl Pts',(-2.33499260563589,-0.417096019625067,
2.68158213554441));
#42232=CARTESIAN_POINT('Ctrl Pts',(-2.30237959156813,-0.586821949158959,
2.69272418458075));
#42233=CARTESIAN_POINT('Ctrl Pts',(-2.26317650691132,-0.723431075731699,
2.70137278566001));
#42234=CARTESIAN_POINT('Ctrl Pts',(-2.1677453946956,-0.970113232282793,
2.7176478621772));
#42235=CARTESIAN_POINT('Ctrl Pts',(-2.11469384064466,-1.08088193735488,
2.72522965488955));
#42236=CARTESIAN_POINT('Ctrl Pts',(-2.03172695762217,-1.22439569879042,
2.73584337196682));
#42237=CARTESIAN_POINT('Ctrl Pts',(-2.00912096630732,-1.26114703289005,
2.73863549283612));
#42238=CARTESIAN_POINT('Ctrl Pts',(-1.97270169640577,-1.31688869970518,
2.74299960806788));
#42239=CARTESIAN_POINT('Ctrl Pts',(-1.95958699942411,-1.33632576792876,
2.74454649935343));
#42240=CARTESIAN_POINT('Ctrl Pts',(-1.93467517493862,-1.37209172002778,
2.74744198051341));
#42241=CARTESIAN_POINT('Ctrl Pts',(-1.92295394121791,-1.38847103630833,
2.74878766269736));
#42242=CARTESIAN_POINT('Ctrl Pts',(-1.89624604308154,-1.42480586311497,
2.75181840953896));
#42243=CARTESIAN_POINT('Ctrl Pts',(-1.88115034328365,-1.4446778563513,2.75350751363571));
#42244=CARTESIAN_POINT('Ctrl Pts',(-1.84125803292543,-1.49550656698913,
2.75791233091133));
#42245=CARTESIAN_POINT('Ctrl Pts',(-1.81599428612828,-1.52608501441929,
2.76064573332724));
#42246=CARTESIAN_POINT('Ctrl Pts',(-1.66256155153225,-1.70258794352608,
2.77693210955796));
#42247=CARTESIAN_POINT('Ctrl Pts',(-1.51763938085684,-1.83293857533994,
2.79116073647266));
#42248=CARTESIAN_POINT('Ctrl Pts',(-1.3099706068955,-1.97804924258223,2.80953258374712));
#42249=CARTESIAN_POINT('Ctrl Pts',(-1.26019499741816,-2.01012715015836,
2.81379770168163));
#42250=CARTESIAN_POINT('Ctrl Pts',(-1.17674325712806,-2.0595880396713,2.82067308876567));
#42251=CARTESIAN_POINT('Ctrl Pts',(-1.14375932565918,-2.07808627448954,
2.82332341174638));
#42252=CARTESIAN_POINT('Ctrl Pts',(-1.09660846847167,-2.10306671068279,
2.82700464563663));
#42253=CARTESIAN_POINT('Ctrl Pts',(-1.08280012498202,-2.11020938397262,
2.82807000103581));
#42254=CARTESIAN_POINT('Ctrl Pts',(-1.05880850911127,-2.12232206794716,
2.82989791188266));
#42255=CARTESIAN_POINT('Ctrl Pts',(-1.04865833133323,-2.12735566911528,
2.8306641316177));
#42256=CARTESIAN_POINT('Ctrl Pts',(-1.02627730086469,-2.13825558377023,
2.83233783131822));
#42257=CARTESIAN_POINT('Ctrl Pts',(-1.01403169139831,-2.14408996790642,
2.83324345225128));
#42258=CARTESIAN_POINT('Ctrl Pts',(-0.978483987704463,-2.16065388523661,
2.83584512121146));
#42259=CARTESIAN_POINT('Ctrl Pts',(-0.955056255819943,-2.17111119037089,
2.83752617952256));
#42260=CARTESIAN_POINT('Ctrl Pts',(-0.834770283286746,-2.22247857202935,
2.84601019745816));
#42261=CARTESIAN_POINT('Ctrl Pts',(-0.735428734554925,-2.25729964674856,
2.85253882433277));
#42262=CARTESIAN_POINT('Ctrl Pts',(-0.516518127194684,-2.31803700057488,
2.86654457838164));
#42263=CARTESIAN_POINT('Ctrl Pts',(-0.396603811041486,-2.34153597365893,
2.87399001547749));
#42264=CARTESIAN_POINT('Ctrl Pts',(-0.201714657456177,-2.3643213392082,
2.88629683201334));
#42265=CARTESIAN_POINT('Ctrl Pts',(-0.12765566015911,-2.36947392041282,
2.89101798779091));
#42266=CARTESIAN_POINT('Ctrl Pts',(-0.0251190536508085,-2.37178665750307,
2.89768729834219));
#42267=CARTESIAN_POINT('Ctrl Pts',(0.00325183424697385,-2.37191741649685,
2.89954641851911));
#42268=CARTESIAN_POINT('Ctrl Pts',(0.0521687217423089,-2.37126525783505,
2.90277913286163));
#42269=CARTESIAN_POINT('Ctrl Pts',(0.0727151572509987,-2.37072414260413,
2.9041452422231));
#42270=CARTESIAN_POINT('Ctrl Pts',(0.114940132748127,-2.36906267456761,
2.9069709925939));
#42271=CARTESIAN_POINT('Ctrl Pts',(0.136615452463394,-2.36791160208015,
2.90843144486063));
#42272=CARTESIAN_POINT('Ctrl Pts',(0.192649239668986,-2.36416400876877,
2.91223396326531));
#42273=CARTESIAN_POINT('Ctrl Pts',(0.226971345674578,-2.3611160468859,2.91458951885383));
#42274=CARTESIAN_POINT('Ctrl Pts',(0.451946523280566,-2.33618668167587,
2.93021159344092));
#42275=CARTESIAN_POINT('Ctrl Pts',(0.639379483619011,-2.29198418673891,
2.94417220709906));
#42276=CARTESIAN_POINT('Ctrl Pts',(0.886826411991718,-2.20088608415034,
2.96335244675838));
#42277=CARTESIAN_POINT('Ctrl Pts',(0.953094164954423,-2.1730101839167,2.96855805817798));
#42278=CARTESIAN_POINT('Ctrl Pts',(1.04470191421914,-2.12947650195746,2.97577389887777));
#42279=CARTESIAN_POINT('Ctrl Pts',(1.07116835719663,-2.11628702534304,2.97786085362024));
#42280=CARTESIAN_POINT('Ctrl Pts',(1.11774477167394,-2.09197807253441,2.98152932473105));
#42281=CARTESIAN_POINT('Ctrl Pts',(1.13795261407804,-2.08105491854414,2.98311949058891));
#42282=CARTESIAN_POINT('Ctrl Pts',(1.1692214333354,-2.06356115771325,2.98557419632987));
#42283=CARTESIAN_POINT('Ctrl Pts',(1.18039248042138,-2.05719153774944,2.98644997306991));
#42284=CARTESIAN_POINT('Ctrl Pts',(1.20145531498705,-2.04495365431395,2.98809819320477));
#42285=CARTESIAN_POINT('Ctrl Pts',(1.21135698728067,-2.03910386610605,2.98887164389015));
#42286=CARTESIAN_POINT('Ctrl Pts',(1.23569536293664,-2.02448519981646,2.99077019600599));
#42287=CARTESIAN_POINT('Ctrl Pts',(1.25008200183002,-2.01563349420413,2.99189021737386));
#42288=CARTESIAN_POINT('Ctrl Pts',(1.30176854107398,-1.98306589071793,2.99591060864418));
#42289=CARTESIAN_POINT('Ctrl Pts',(1.33850046938457,-1.95846080140712,2.99876117696602));
#42290=CARTESIAN_POINT('Ctrl Pts',(1.525461798208,-1.82550467312162,3.01335305733504));
#42291=CARTESIAN_POINT('Ctrl Pts',(1.66331491984682,-1.70085137525861,3.02444387549821));
#42292=CARTESIAN_POINT('Ctrl Pts',(1.84182812308832,-1.49674610267465,3.04135778370217));
#42293=CARTESIAN_POINT('Ctrl Pts',(1.89482945900008,-1.42905520387532,3.04679530488164));
#42294=CARTESIAN_POINT('Ctrl Pts',(1.96104640828997,-1.33430751236478,3.05429899253281));
#42295=CARTESIAN_POINT('Ctrl Pts',(1.97759500212729,-1.30965546416525,3.05624184506948));
#42296=CARTESIAN_POINT('Ctrl Pts',(2.00493187577039,-1.26723243831559,3.05957330477027));
#42297=CARTESIAN_POINT('Ctrl Pts',(2.01595747690404,-1.24961805565776,3.06095314156852));
#42298=CARTESIAN_POINT('Ctrl Pts',(2.03782668444745,-1.21363721386525,3.06376615313881));
#42299=CARTESIAN_POINT('Ctrl Pts',(2.04865681946319,-1.19526485288394,3.06519964438768));
#42300=CARTESIAN_POINT('Ctrl Pts',(2.07539313195629,-1.14847798923203,3.06884426975619));
#42301=CARTESIAN_POINT('Ctrl Pts',(2.09096418385581,-1.11987809472681,3.07106680985079));
#42302=CARTESIAN_POINT('Ctrl Pts',(2.16091639211851,-0.984846422819331,
3.08154083021186));
#42303=CARTESIAN_POINT('Ctrl Pts',(2.20778402647267,-0.874736764386953,
3.09003859613071));
#42304=CARTESIAN_POINT('Ctrl Pts',(2.29898296873842,-0.605760685433158,
3.11058309603114));
#42305=CARTESIAN_POINT('Ctrl Pts',(2.33545821977983,-0.444866603385176,
3.12272155662123));
#42306=CARTESIAN_POINT('Ctrl Pts',(2.35867617574538,-0.250621661283876,
3.13650514429128));
#42307=CARTESIAN_POINT('Ctrl Pts',(2.36175877074828,-0.219682150610599,
3.13867354568708));
#42308=CARTESIAN_POINT('Ctrl Pts',(2.36538067359745,-0.17430056120115,3.14180641172339));
#42309=CARTESIAN_POINT('Ctrl Pts',(2.36639769489325,-0.159901195871341,
3.14279343932768));
#42310=CARTESIAN_POINT('Ctrl Pts',(2.36798079961768,-0.134142861683774,
3.144545510243));
#42311=CARTESIAN_POINT('Ctrl Pts',(2.36859673361779,-0.122788035389571,
3.14531306499731));
#42312=CARTESIAN_POINT('Ctrl Pts',(2.36981314247163,-0.0969254128201573,
3.14705052339805));
#42313=CARTESIAN_POINT('Ctrl Pts',(2.37036210334426,-0.0824159646999778,
3.14801769161402));
#42314=CARTESIAN_POINT('Ctrl Pts',(2.37168150301097,-0.0363494837505168,
3.15106691468105));
#42315=CARTESIAN_POINT('Ctrl Pts',(2.37195527154187,-0.00478033147960674,
3.15312458579082));
#42316=CARTESIAN_POINT('Ctrl Pts',(2.36993836421144,0.173790001941277,3.16463012809853));
#42317=CARTESIAN_POINT('Ctrl Pts',(2.35461347417735,0.320336493127514,3.17357490168829));
#42318=CARTESIAN_POINT('Ctrl Pts',(2.3080747450888,0.553345658031935,3.18820349770689));
#42319=CARTESIAN_POINT('Ctrl Pts',(2.2852645916663,0.64106525268589,3.19380458947351));
#42320=CARTESIAN_POINT('Ctrl Pts',(2.24475830558875,0.766801052793803,3.20215724048862));
#42321=CARTESIAN_POINT('Ctrl Pts',(2.23098440894213,0.80599750929483,3.20480803646782));
#42322=CARTESIAN_POINT('Ctrl Pts',(2.20386793164277,0.87713208433436,3.20972197587692));
#42323=CARTESIAN_POINT('Ctrl Pts',(2.19084188433596,0.909178858723863,3.21197515521205));
#42324=CARTESIAN_POINT('Ctrl Pts',(2.16849826684493,0.960877540818893,3.21568121938285));
#42325=CARTESIAN_POINT('Ctrl Pts',(2.15960277024621,0.980706992374399,3.21712010860713));
#42326=CARTESIAN_POINT('Ctrl Pts',(2.14177249127744,1.01903412338137,3.2199367738348));
#42327=CARTESIAN_POINT('Ctrl Pts',(2.13286739554234,1.037543530314,3.22131344970243));
#42328=CARTESIAN_POINT('Ctrl Pts',(2.11112929013862,1.08126378144751,3.22460568461241));
#42329=CARTESIAN_POINT('Ctrl Pts',(2.09808367154296,1.10636478359268,3.2265283514266));
#42330=CARTESIAN_POINT('Ctrl Pts',(2.0519911694297,1.19130283357977,3.23314936028095));
#42331=CARTESIAN_POINT('Ctrl Pts',(2.01681078386904,1.24993716329735,3.23791962013976));
#42332=CARTESIAN_POINT('Ctrl Pts',(1.88089501049086,1.45575565166071,3.25540155615017));
#42333=CARTESIAN_POINT('Ctrl Pts',(1.76617746856635,1.59298341511564,3.2685397477923));
#42334=CARTESIAN_POINT('Ctrl Pts',(1.58817033892526,1.76281122453687,3.28627500219807));
#42335=CARTESIAN_POINT('Ctrl Pts',(1.5371629890109,1.80746232737251,3.29110251065013));
#42336=CARTESIAN_POINT('Ctrl Pts',(1.46958442724663,1.86168635502307,3.29711676999495));
#42337=CARTESIAN_POINT('Ctrl Pts',(1.45471855140829,1.87332550954975,3.29841736731983));
#42338=CARTESIAN_POINT('Ctrl Pts',(1.43018551950645,1.89206533487532,3.30052532236282));
#42339=CARTESIAN_POINT('Ctrl Pts',(1.42060093914961,1.89927218764784,3.30133946905811));
#42340=CARTESIAN_POINT('Ctrl Pts',(1.40231491803986,1.91280596438696,3.30287439882048));
#42341=CARTESIAN_POINT('Ctrl Pts',(1.39362440054565,1.9191469011636,3.3035961662468));
#42342=CARTESIAN_POINT('Ctrl Pts',(1.36977934916997,1.93629777980115,3.30555649570193));
#42343=CARTESIAN_POINT('Ctrl Pts',(1.35453986316615,1.94698905208411,3.30678746743322));
#42344=CARTESIAN_POINT('Ctrl Pts',(1.29027885036009,1.99095164023283,3.31189455206704));
#42345=CARTESIAN_POINT('Ctrl Pts',(1.24014164315954,2.02256220131441,3.3156785327761));
#42346=CARTESIAN_POINT('Ctrl Pts',(0.997432216105636,2.16316286972624,3.33332581258172));
#42347=CARTESIAN_POINT('Ctrl Pts',(0.791423528607317,2.24673135908165,3.34648101948516));
#42348=CARTESIAN_POINT('Ctrl Pts',(0.53181706790111,2.31182183270309,3.36357114111945));
#42349=CARTESIAN_POINT('Ctrl Pts',(0.486506539856596,2.3217796027777,3.36656673318472));
#42350=CARTESIAN_POINT('Ctrl Pts',(0.417288587778491,2.33487633254923,3.37117844049166));
#42351=CARTESIAN_POINT('Ctrl Pts',(0.393575761727071,2.33899023181909,3.37276453461936));
#42352=CARTESIAN_POINT('Ctrl Pts',(0.349933726448231,2.34587918726324,3.37569706552008));
#42353=CARTESIAN_POINT('Ctrl Pts',(0.330023752625998,2.34876287757548,3.37704000932117));
#42354=CARTESIAN_POINT('Ctrl Pts',(0.286046573754407,2.35456218235334,3.38001864168513));
#42355=CARTESIAN_POINT('Ctrl Pts',(0.261966754130693,2.35736273377595,3.38165771728396));
#42356=CARTESIAN_POINT('Ctrl Pts',(0.192236835076011,2.36439097124383,3.38642941922871));
#42357=CARTESIAN_POINT('Ctrl Pts',(0.146503854923845,2.36766462933651,3.3895904387194));
#42358=CARTESIAN_POINT('Ctrl Pts',(-0.0754299931378458,2.37709670728848,
3.40509044877301));
#42359=CARTESIAN_POINT('Ctrl Pts',(-0.251831275948877,2.36491896207247,
3.41795608159483));
#42360=CARTESIAN_POINT('Ctrl Pts',(-0.492245535190987,2.32110616074103,
3.43571979797412));
#42361=CARTESIAN_POINT('Ctrl Pts',(-0.558716006568461,2.30600887242064,
3.44064841396094));
#42362=CARTESIAN_POINT('Ctrl Pts',(-0.652074495569949,2.28052998600842,
3.44752621947062));
#42363=CARTESIAN_POINT('Ctrl Pts',(-0.679563995253629,2.27249006373039,
3.44954564714763));
#42364=CARTESIAN_POINT('Ctrl Pts',(-0.728304607186525,2.25727117947073,
3.45310841482403));
#42365=CARTESIAN_POINT('Ctrl Pts',(-0.749612012442071,2.25028502605011,
3.45465974966162));
#42366=CARTESIAN_POINT('Ctrl Pts',(-0.782870253818592,2.23885565369224,
3.45706813988182));
#42367=CARTESIAN_POINT('Ctrl Pts',(-0.794889216424853,2.234616661659,3.45793578829303));
#42368=CARTESIAN_POINT('Ctrl Pts',(-0.8177333154705,2.22635209533754,3.45957896815401));
#42369=CARTESIAN_POINT('Ctrl Pts',(-0.828564054573966,2.2223440419134,3.4603553781085));
#42370=CARTESIAN_POINT('Ctrl Pts',(-0.852838866431851,2.21315870650631,
3.46209037358421));
#42371=CARTESIAN_POINT('Ctrl Pts',(-0.866266127783814,2.20793763796001,
3.46304650259064));
#42372=CARTESIAN_POINT('Ctrl Pts',(-0.914165292375105,2.18880825164705,
3.46644736992822));
#42373=CARTESIAN_POINT('Ctrl Pts',(-0.948358536649344,2.17421162209463,
3.46885658300752));
#42374=CARTESIAN_POINT('Ctrl Pts',(-1.11062211103469,2.10038656899485,3.48026465218472));
#42375=CARTESIAN_POINT('Ctrl Pts',(-1.23358925492092,2.03060829229769,3.48884781043404));
#42376=CARTESIAN_POINT('Ctrl Pts',(-1.42234393182489,1.89998807652394,3.50298517135967));
#42377=CARTESIAN_POINT('Ctrl Pts',(-1.49218149884534,1.84564618450459,3.50845926883154));
#42378=CARTESIAN_POINT('Ctrl Pts',(-1.60343430999369,1.74862825668671,3.51779831633965));
#42379=CARTESIAN_POINT('Ctrl Pts',(-1.64657454617898,1.70806726050829,3.52159300242642));
#42380=CARTESIAN_POINT('Ctrl Pts',(-1.70660287183484,1.647238555026,3.52716698980351));
#42381=CARTESIAN_POINT('Ctrl Pts',(-1.7247431566068,1.62823498745683,3.5288928961914));
#42382=CARTESIAN_POINT('Ctrl Pts',(-1.7563047318699,1.59405208917849,3.53197315804465));
#42383=CARTESIAN_POINT('Ctrl Pts',(-1.76985439745985,1.57899453563827,3.53332199436456));
#42384=CARTESIAN_POINT('Ctrl Pts',(-1.79810614875913,1.5467782106517,3.53619229919335));
#42385=CARTESIAN_POINT('Ctrl Pts',(-1.81275914635655,1.52957927959192,3.53771556894155));
#42386=CARTESIAN_POINT('Ctrl Pts',(-1.85192700685686,1.48225265582605,3.54188439343084));
#42387=CARTESIAN_POINT('Ctrl Pts',(-1.87595019515784,1.45172901697744,3.54454873509709));
#42388=CARTESIAN_POINT('Ctrl Pts',(-2.01046652038272,1.27189691712276,3.5601162516265));
#42389=CARTESIAN_POINT('Ctrl Pts',(-2.10384784974602,1.11062998564555,3.57364648591392));
#42390=CARTESIAN_POINT('Ctrl Pts',(-2.2053649595544,0.875512551861624,3.59227050289971));
#42391=CARTESIAN_POINT('Ctrl Pts',(-2.23038737330346,0.809648116073871,
3.59736950337685));
#42392=CARTESIAN_POINT('Ctrl Pts',(-2.26570522777612,0.702546289675075,
3.60538969190063));
#42393=CARTESIAN_POINT('Ctrl Pts',(-2.27788901986706,0.661977028589482,
3.6083670451995));
#42394=CARTESIAN_POINT('Ctrl Pts',(-2.29322443061286,0.605460481594743,
3.6124125733104));
#42395=CARTESIAN_POINT('Ctrl Pts',(-2.29730800040423,0.589776797882458,
3.6135244791844));
#42396=CARTESIAN_POINT('Ctrl Pts',(-2.30401647472113,0.562884203400059,
3.61541130790141));
#42397=CARTESIAN_POINT('Ctrl Pts',(-2.3067210592276,0.551696039161641,3.61619044235533));
#42398=CARTESIAN_POINT('Ctrl Pts',(-2.31235796835592,0.527611203434994,
3.61785478453473));
#42399=CARTESIAN_POINT('Ctrl Pts',(-2.31526402920089,0.514709093841059,
3.61873858398443));
#42400=CARTESIAN_POINT('Ctrl Pts',(-2.32315097230029,0.478274171339033,
3.62121423802244));
#42401=CARTESIAN_POINT('Ctrl Pts',(-2.32788215867647,0.454688227809483,
3.62279323670354));
#42402=CARTESIAN_POINT('Ctrl Pts',(-2.34804842952469,0.345571689858489,
3.63000670355621));
#42403=CARTESIAN_POINT('Ctrl Pts',(-2.35912700921337,0.25934211993323,3.63545031325973));
#42404=CARTESIAN_POINT('Ctrl Pts',(-2.3654513605298,0.172736572467239,3.64082947459234));
#42405=CARTESIAN_POINT('Origin',(0.,0.,-1.84858989190501));
#42406=CARTESIAN_POINT('',(-2.36545132791903,0.1727370190379,4.83597583405742));
#42407=CARTESIAN_POINT('',(-2.36545134967025,0.172736721177577,4.63766477577655));
#42408=CARTESIAN_POINT('',(-2.36545134966535,0.172736721244682,-1.84858989190501));
#42409=CARTESIAN_POINT('Ctrl Pts',(-2.36545132791902,0.172737019038084,
4.83597583405741));
#42410=CARTESIAN_POINT('Ctrl Pts',(-2.35533920084846,0.311211936229127,
4.8273804069956));
#42411=CARTESIAN_POINT('Ctrl Pts',(-2.33307831419588,0.448655167420158,
4.81894726446124));
#42412=CARTESIAN_POINT('Ctrl Pts',(-2.27985950504,0.658333687173865,4.80540068318638));
#42413=CARTESIAN_POINT('Ctrl Pts',(-2.25721668224938,0.732211515671099,
4.80049355440317));
#42414=CARTESIAN_POINT('Ctrl Pts',(-2.22143223906243,0.831404766665299,
4.79363876603281));
#42415=CARTESIAN_POINT('Ctrl Pts',(-2.2113788978478,0.857786884880636,4.7917893762288));
#42416=CARTESIAN_POINT('Ctrl Pts',(-2.19338316387111,0.902590994150976,
4.78860002368318));
#42417=CARTESIAN_POINT('Ctrl Pts',(-2.18567344329208,0.921103557966245,
4.78726779366037));
#42418=CARTESIAN_POINT('Ctrl Pts',(-2.17046577729332,0.956353839490573,
4.78470222692556));
#42419=CARTESIAN_POINT('Ctrl Pts',(-2.16300659469204,0.973106775224658,
4.78347026205697));
#42420=CARTESIAN_POINT('Ctrl Pts',(-2.14284622428484,1.01700857704299,4.78020743663232));
#42421=CARTESIAN_POINT('Ctrl Pts',(-2.12982371695856,1.0440053550073,4.7781658990363));
#42422=CARTESIAN_POINT('Ctrl Pts',(-2.07650950324224,1.14937900582047,4.77005409527662));
#42423=CARTESIAN_POINT('Ctrl Pts',(-2.0323785694822,1.22572344466343,4.76385604898489));
#42424=CARTESIAN_POINT('Ctrl Pts',(-1.87704633839646,1.46290141534091,4.7435641143981));
#42425=CARTESIAN_POINT('Ctrl Pts',(-1.75020241730722,1.61250399735342,4.72905819340805));
#42426=CARTESIAN_POINT('Ctrl Pts',(-1.58044458899366,1.7687969978942,4.71273499996434));
#42427=CARTESIAN_POINT('Ctrl Pts',(-1.55390201327748,1.79215980434077,4.71026089624965));
#42428=CARTESIAN_POINT('Ctrl Pts',(-1.51544854352607,1.82450968491369,4.70679695876194));
#42429=CARTESIAN_POINT('Ctrl Pts',(-1.50396125123935,1.83399031123718,4.70577692342823));
#42430=CARTESIAN_POINT('Ctrl Pts',(-1.48378540523275,1.85032466360741,4.70401200215828));
#42431=CARTESIAN_POINT('Ctrl Pts',(-1.47513706944861,1.85722673188737,4.70326389326465));
#42432=CARTESIAN_POINT('Ctrl Pts',(-1.45602765726471,1.87225987622076,4.70162943429373));
#42433=CARTESIAN_POINT('Ctrl Pts',(-1.44554636281364,1.88036414457384,4.70074486556295));
#42434=CARTESIAN_POINT('Ctrl Pts',(-1.41487396139246,1.90367238089014,4.69818888484657));
#42435=CARTESIAN_POINT('Ctrl Pts',(-1.39450639890883,1.91864245907507,4.69653217935403));
#42436=CARTESIAN_POINT('Ctrl Pts',(-1.28574126179139,1.99593717064376,4.68787413960963));
#42437=CARTESIAN_POINT('Ctrl Pts',(-1.19338763413892,2.05249283079977,4.68116688604259));
#42438=CARTESIAN_POINT('Ctrl Pts',(-0.987908459136713,2.15974857313577,
4.66688780324374));
#42439=CARTESIAN_POINT('Ctrl Pts',(-0.874031061820946,2.20829012649557,
4.65934588701707));
#42440=CARTESIAN_POINT('Ctrl Pts',(-0.688842117005726,2.27064978358214,
4.64707531866328));
#42441=CARTESIAN_POINT('Ctrl Pts',(-0.619792511658483,2.29046058541658,
4.6425014300596));
#42442=CARTESIAN_POINT('Ctrl Pts',(-0.523134082372167,2.31350146799972,
4.63603644830036));
#42443=CARTESIAN_POINT('Ctrl Pts',(-0.496204472435919,2.3194265088973,4.63422891156447));
#42444=CARTESIAN_POINT('Ctrl Pts',(-0.449631193469407,2.32882535060369,
4.63108880958931));
#42445=CARTESIAN_POINT('Ctrl Pts',(-0.430035363246038,2.33252336958963,
4.62976335760313));
#42446=CARTESIAN_POINT('Ctrl Pts',(-0.392195173266823,2.33917132610175,
4.62719465345623));
#42447=CARTESIAN_POINT('Ctrl Pts',(-0.373958330635711,2.34215598988121,
4.625952586358));
#42448=CARTESIAN_POINT('Ctrl Pts',(-0.325256456820483,2.34954330502224,
4.62262381879196));
#42449=CARTESIAN_POINT('Ctrl Pts',(-0.294738318932124,2.35356637394792,
4.62052560741231));
#42450=CARTESIAN_POINT('Ctrl Pts',(-0.169110742250879,2.36764563601103,
4.61183388790019));
#42451=CARTESIAN_POINT('Ctrl Pts',(-0.0735242936022879,2.37253755618989,
4.60508789161921));
#42452=CARTESIAN_POINT('Ctrl Pts',(0.172700275231606,2.37024453528281,4.58740801448852));
#42453=CARTESIAN_POINT('Ctrl Pts',(0.322828557722016,2.35449844494837,4.57631970401873));
#42454=CARTESIAN_POINT('Ctrl Pts',(0.532515091441941,2.31206318918483,4.56092360538795));
#42455=CARTESIAN_POINT('Ctrl Pts',(0.594062722750231,2.29701968435132,4.55642056150683));
#42456=CARTESIAN_POINT('Ctrl Pts',(0.672417848373035,2.27450720298909,4.55076583973866));
#42457=CARTESIAN_POINT('Ctrl Pts',(0.689838685459744,2.26928434029901,4.54951371376772));
#42458=CARTESIAN_POINT('Ctrl Pts',(0.718279162576799,2.26039993652056,4.54747981774688));
#42459=CARTESIAN_POINT('Ctrl Pts',(0.72933475775657,2.25685703077833,4.54669175116885));
#42460=CARTESIAN_POINT('Ctrl Pts',(0.751644990510565,2.24952636449015,4.54510724255995));
#42461=CARTESIAN_POINT('Ctrl Pts',(0.762898028898242,2.24573499526698,4.54431101832711));
#42462=CARTESIAN_POINT('Ctrl Pts',(0.792490735548514,2.23551652214644,4.54222385876069));
#42463=CARTESIAN_POINT('Ctrl Pts',(0.810781126820546,2.2289481174238,4.54094068189317));
#42464=CARTESIAN_POINT('Ctrl Pts',(0.898018622680762,2.19640360596706,4.53484400803493));
#42465=CARTESIAN_POINT('Ctrl Pts',(0.965817447190775,2.1674466648487,4.53017623245889));
#42466=CARTESIAN_POINT('Ctrl Pts',(1.17405132807904,2.06679394261757,4.51574101130685));
#42467=CARTESIAN_POINT('Ctrl Pts',(1.30875037884268,1.98424003605602,4.50623148452605));
#42468=CARTESIAN_POINT('Ctrl Pts',(1.49850413438474,1.84015992845678,4.49133614751729));
#42469=CARTESIAN_POINT('Ctrl Pts',(1.56020438685097,1.78814527301783,4.48621940281624));
#42470=CARTESIAN_POINT('Ctrl Pts',(1.64004348709731,1.71355607329565,4.47912052725525));
#42471=CARTESIAN_POINT('Ctrl Pts',(1.6605992909546,1.69364309622624,4.47724658632478));
#42472=CARTESIAN_POINT('Ctrl Pts',(1.69498587280874,1.65910392819048,4.47402814862422));
#42473=CARTESIAN_POINT('Ctrl Pts',(1.70900025333188,1.64466441750671,4.47269175326272));
#42474=CARTESIAN_POINT('Ctrl Pts',(1.73705485203183,1.61501298909412,4.46996456822377));
#42475=CARTESIAN_POINT('Ctrl Pts',(1.75108300152111,1.59979210824652,4.46857343866579));
#42476=CARTESIAN_POINT('Ctrl Pts',(1.78604606314704,1.56084547885679,4.46503465736285));
#42477=CARTESIAN_POINT('Ctrl Pts',(1.80670818861305,1.53688142195913,4.46287617509905));
#42478=CARTESIAN_POINT('Ctrl Pts',(1.89565350540297,1.42944904939384,4.45327699969444));
#42479=CARTESIAN_POINT('Ctrl Pts',(1.95866883423737,1.34180385285562,4.44563829551699));
#42480=CARTESIAN_POINT('Ctrl Pts',(2.07621621608734,1.15229906065967,4.42955787068833));
#42481=CARTESIAN_POINT('Ctrl Pts',(2.12972211315881,1.05011868691001,4.42111709254652));
#42482=CARTESIAN_POINT('Ctrl Pts',(2.19777178096194,0.893364491764287,4.40873801253511));
#42483=CARTESIAN_POINT('Ctrl Pts',(2.21814788009371,0.841499620128731,4.40473098883347));
#42484=CARTESIAN_POINT('Ctrl Pts',(2.24868922244876,0.754916048377608,4.39823211089958));
#42485=CARTESIAN_POINT('Ctrl Pts',(2.25992058240464,0.720597496013535,4.39570423142441));
#42486=CARTESIAN_POINT('Ctrl Pts',(2.2747068023682,0.671663885094339,4.39217958096344));
#42487=CARTESIAN_POINT('Ctrl Pts',(2.27891256197112,0.657252596288559,4.39115122434867));
#42488=CARTESIAN_POINT('Ctrl Pts',(2.28595658141371,0.632234989374813,4.38938386532933));
#42489=CARTESIAN_POINT('Ctrl Pts',(2.28885846343327,0.621647429222014,4.38864145456694));
#42490=CARTESIAN_POINT('Ctrl Pts',(2.29506794827501,0.598358924379397,4.38702078795241));
#42491=CARTESIAN_POINT('Ctrl Pts',(2.29834378645797,0.585650193141942,4.38614426885179));
#42492=CARTESIAN_POINT('Ctrl Pts',(2.30747533593123,0.548966905690562,4.38363517920957));
#42493=CARTESIAN_POINT('Ctrl Pts',(2.31306276024204,0.524926538515636,4.3820165102701));
#42494=CARTESIAN_POINT('Ctrl Pts',(2.35419977880891,0.334498297046135,4.36936506194432));
#42495=CARTESIAN_POINT('Ctrl Pts',(2.37213092636178,0.164789843839533,4.35908533922349));
#42496=CARTESIAN_POINT('Ctrl Pts',(2.37155429665257,-0.0887445981140952,
4.34345590425478));
#42497=CARTESIAN_POINT('Ctrl Pts',(2.36697110684533,-0.172022624026459,
4.33828342413938));
#42498=CARTESIAN_POINT('Ctrl Pts',(2.35192072355321,-0.311259544608725,
4.32940923804492));
#42499=CARTESIAN_POINT('Ctrl Pts',(2.34380731883432,-0.367396344244507,
4.32576943930545));
#42500=CARTESIAN_POINT('Ctrl Pts',(2.32915663570164,-0.448188751199906,
4.32041049142159));
#42501=CARTESIAN_POINT('Ctrl Pts',(2.32422119253587,-0.473116854293194,
4.318740296194));
#42502=CARTESIAN_POINT('Ctrl Pts',(2.31476429381294,-0.517155470210715,
4.31575752318676));
#42503=CARTESIAN_POINT('Ctrl Pts',(2.31040417986393,-0.536298427363922,
4.31445009146337));
#42504=CARTESIAN_POINT('Ctrl Pts',(2.30067656473446,-0.576684862531626,
4.31166765705939));
#42505=CARTESIAN_POINT('Ctrl Pts',(2.29525135705422,-0.597912401069293,
4.31019094430137));
#42506=CARTESIAN_POINT('Ctrl Pts',(2.27972045298151,-0.655351828128441,
4.30615490243695));
#42507=CARTESIAN_POINT('Ctrl Pts',(2.26904695497142,-0.691402201519372,
4.30357793279273));
#42508=CARTESIAN_POINT('Ctrl Pts',(2.20757027202545,-0.882255310364198,
4.28969246087521));
#42509=CARTESIAN_POINT('Ctrl Pts',(2.14178112470122,-1.03174520612798,4.27791140636574));
#42510=CARTESIAN_POINT('Ctrl Pts',(1.99778278893594,-1.28471841436772,4.25670762396453));
#42511=CARTESIAN_POINT('Ctrl Pts',(1.92541768269389,-1.39083082973557,4.24736377186084));
#42512=CARTESIAN_POINT('Ctrl Pts',(1.83171394136996,-1.50680361095169,4.23697994213884));
#42513=CARTESIAN_POINT('Ctrl Pts',(1.81839177303455,-1.52285406975997,4.23553899634747));
#42514=CARTESIAN_POINT('Ctrl Pts',(1.79695756363907,-1.54799544836842,4.23327848894684));
#42515=CARTESIAN_POINT('Ctrl Pts',(1.78898458279312,-1.55720280392728,4.2324498967008));
#42516=CARTESIAN_POINT('Ctrl Pts',(1.77350168266863,-1.57480688581067,4.23086490331018));
#42517=CARTESIAN_POINT('Ctrl Pts',(1.76600233757626,-1.58321214486592,4.23010785608293));
#42518=CARTESIAN_POINT('Ctrl Pts',(1.74702887345391,-1.60417502458731,4.22821818908068));
#42519=CARTESIAN_POINT('Ctrl Pts',(1.73547873112509,-1.61666354223325,4.22709096759598));
#42520=CARTESIAN_POINT('Ctrl Pts',(1.69132911642183,-1.6633815342127,4.22286363577812));
#42521=CARTESIAN_POINT('Ctrl Pts',(1.65784118379842,-1.6967603208233,4.21982150740373));
#42522=CARTESIAN_POINT('Ctrl Pts',(1.52626679361792,-1.82028839641133,4.20837166987277));
#42523=CARTESIAN_POINT('Ctrl Pts',(1.42164366637919,-1.90312231413506,4.20027205452098));
#42524=CARTESIAN_POINT('Ctrl Pts',(1.23891701230126,-2.02427333805394,4.18676585288513));
#42525=CARTESIAN_POINT('Ctrl Pts',(1.16469226662965,-2.06787049484582,4.18143464743203));
#42526=CARTESIAN_POINT('Ctrl Pts',(1.03683565587186,-2.13389797640278,4.17232357454245));
#42527=CARTESIAN_POINT('Ctrl Pts',(0.984452202697774,-2.15856475342659,
4.16861043597579));
#42528=CARTESIAN_POINT('Ctrl Pts',(0.907678919324832,-2.19134030582006,
4.16316385752261));
#42529=CARTESIAN_POINT('Ctrl Pts',(0.883975480973467,-2.20100900114747,
4.16148174551434));
#42530=CARTESIAN_POINT('Ctrl Pts',(0.841804104769304,-2.21741972206334,
4.15848567289322));
#42531=CARTESIAN_POINT('Ctrl Pts',(0.823399875402378,-2.22431944219372,
4.15717702602271));
#42532=CARTESIAN_POINT('Ctrl Pts',(0.784397135021651,-2.2383911322332,4.15440029709406));
#42533=CARTESIAN_POINT('Ctrl Pts',(0.763781285710771,-2.24550925624015,
4.15293060548619));
#42534=CARTESIAN_POINT('Ctrl Pts',(0.707835563669785,-2.26396632606916,
4.14893552860718));
#42535=CARTESIAN_POINT('Ctrl Pts',(0.672334227341257,-2.27476177515535,
4.14639311095681));
#42536=CARTESIAN_POINT('Ctrl Pts',(0.445171119375501,-2.33805667972721,
4.13007036386436));
#42537=CARTESIAN_POINT('Ctrl Pts',(0.247829089144496,-2.36711624780666,
4.11554939457764));
#42538=CARTESIAN_POINT('Ctrl Pts',(-0.0152522898383138,-2.37257761960759,
4.09643317317025));
#42539=CARTESIAN_POINT('Ctrl Pts',(-0.0797612949147726,-2.37128578429372,
4.09177428400151));
#42540=CARTESIAN_POINT('Ctrl Pts',(-0.183878533504297,-2.36494644698234,
4.08436904923799));
#42541=CARTESIAN_POINT('Ctrl Pts',(-0.223551933365702,-2.36152661972962,
4.08157448848722));
#42542=CARTESIAN_POINT('Ctrl Pts',(-0.278594222621748,-2.3553822754953,
4.07775127244517));
#42543=CARTESIAN_POINT('Ctrl Pts',(-0.29404860883251,-2.35350288984531,
4.07668376842345));
#42544=CARTESIAN_POINT('Ctrl Pts',(-0.320529943956432,-2.35001760561564,
4.07486605537547));
#42545=CARTESIAN_POINT('Ctrl Pts',(-0.33156588213832,-2.3484859543524,4.07411200027414));
#42546=CARTESIAN_POINT('Ctrl Pts',(-0.355295073656612,-2.34502202524333,
4.07249843400206));
#42547=CARTESIAN_POINT('Ctrl Pts',(-0.367983973486608,-2.34306438286093,
4.07164028153028));
#42548=CARTESIAN_POINT('Ctrl Pts',(-0.403695745629255,-2.33725750377567,
4.06923671243015));
#42549=CARTESIAN_POINT('Ctrl Pts',(-0.426679263027888,-2.33317118925555,
4.06770346356701));
#42550=CARTESIAN_POINT('Ctrl Pts',(-0.596691244203305,-2.30034779928361,
4.05643827957072));
#42551=CARTESIAN_POINT('Ctrl Pts',(-0.740780913110152,-2.25807344158744,
4.04730166392353));
#42552=CARTESIAN_POINT('Ctrl Pts',(-0.970491859088624,-2.16629950108058,
4.03209070553291));
#42553=CARTESIAN_POINT('Ctrl Pts',(-1.0587290796595,-2.12457031573233,4.02607907387049));
#42554=CARTESIAN_POINT('Ctrl Pts',(-1.19902827893452,-2.04730439715628,
4.01596856749238));
#42555=CARTESIAN_POINT('Ctrl Pts',(-1.25269025191291,-2.0149169286898,4.01195928824721));
#42556=CARTESIAN_POINT('Ctrl Pts',(-1.32698508103623,-1.96596073772651,
4.00616029355871));
#42557=CARTESIAN_POINT('Ctrl Pts',(-1.34872277788352,-1.95111194110456,
4.00443207728883));
#42558=CARTESIAN_POINT('Ctrl Pts',(-1.38632837230736,-1.92449519335386,
4.0013838282368));
#42559=CARTESIAN_POINT('Ctrl Pts',(-1.40230503574717,-1.91288490308539,
4.00006976231903));
#42560=CARTESIAN_POINT('Ctrl Pts',(-1.43534069669859,-1.88824149545334,
3.99731147140708));
#42561=CARTESIAN_POINT('Ctrl Pts',(-1.45237139751333,-1.87517362741355,
3.99586599532996));
#42562=CARTESIAN_POINT('Ctrl Pts',(-1.49702739805236,-1.83993521839389,
3.99201155288803));
#42563=CARTESIAN_POINT('Ctrl Pts',(-1.52433652561458,-1.81737463531964,
3.98958757527384));
#42564=CARTESIAN_POINT('Ctrl Pts',(-1.70746246487127,-1.65905891767343,
3.97285967033546));
#42565=CARTESIAN_POINT('Ctrl Pts',(-1.84543803044489,-1.50407164627297,
3.9577383814089));
#42566=CARTESIAN_POINT('Ctrl Pts',(-1.99608799350086,-1.28242091397494,
3.93828569461351));
#42567=CARTESIAN_POINT('Ctrl Pts',(-2.02863031900023,-1.23029694342907,
3.93385475699824));
#42568=CARTESIAN_POINT('Ctrl Pts',(-2.07824548590066,-1.14349468073653,
3.92676366373243));
#42569=CARTESIAN_POINT('Ctrl Pts',(-2.09655944375571,-1.10955994799909,
3.92405969200348));
#42570=CARTESIAN_POINT('Ctrl Pts',(-2.12101311390812,-1.06147920455946,
3.92033743725976));
#42571=CARTESIAN_POINT('Ctrl Pts',(-2.12785385098453,-1.04769878837094,
3.91928284683628));
#42572=CARTESIAN_POINT('Ctrl Pts',(-2.1394064881051,-1.02384644609176,3.91747967296125));
#42573=CARTESIAN_POINT('Ctrl Pts',(-2.14418242035695,-1.01380640878957,
3.91672741261281));
#42574=CARTESIAN_POINT('Ctrl Pts',(-2.1543642493024,-0.992008163241909,
3.91510897200189));
#42575=CARTESIAN_POINT('Ctrl Pts',(-2.15974475185589,-0.980238818137827,
3.91424425763458));
#42576=CARTESIAN_POINT('Ctrl Pts',(-2.17475319854271,-0.946685681550879,
3.9118032097439));
#42577=CARTESIAN_POINT('Ctrl Pts',(-2.18415003046844,-0.924799438856245,
3.91023964763168));
#42578=CARTESIAN_POINT('Ctrl Pts',(-2.24794313921791,-0.76981933469923,
3.89934320563914));
#42579=CARTESIAN_POINT('Ctrl Pts',(-2.29047421117901,-0.632145921168367,
3.89055388067386));
#42580=CARTESIAN_POINT('Ctrl Pts',(-2.34118487377328,-0.392728065915054,
3.87550826850697));
#42581=CARTESIAN_POINT('Ctrl Pts',(-2.35577248521001,-0.292773319784415,
3.86929636123911));
#42582=CARTESIAN_POINT('Ctrl Pts',(-2.36913414046138,-0.128431366297866,
3.85889647990566));
#42583=CARTESIAN_POINT('Ctrl Pts',(-2.37173602461579,-0.0644852799020278,
3.85480552060976));
#42584=CARTESIAN_POINT('Ctrl Pts',(-2.37175513931822,0.0233609360900335,
3.84908163765761));
#42585=CARTESIAN_POINT('Ctrl Pts',(-2.37139977101542,0.0472359383233294,
3.84751557724493));
#42586=CARTESIAN_POINT('Ctrl Pts',(-2.37008832420336,0.0909629385895274,
3.84462609560508));
#42587=CARTESIAN_POINT('Ctrl Pts',(-2.36924305174823,0.1108162556765,3.84330615667556));
#42588=CARTESIAN_POINT('Ctrl Pts',(-2.36737410016197,0.144691093524926,
3.84103935124155));
#42589=CARTESIAN_POINT('Ctrl Pts',(-2.36647502731241,0.158718511030017,
3.84009638256154));
#42590=CARTESIAN_POINT('Ctrl Pts',(-2.36545134965682,0.17273672136148,3.83914957969666));
#42591=CARTESIAN_POINT('Ctrl Pts',(-2.3654513605298,0.172736572467239,3.64082947459234));
#42592=CARTESIAN_POINT('Ctrl Pts',(-2.36959701486398,0.115966060322647,
3.64435555060821));
#42593=CARTESIAN_POINT('Ctrl Pts',(-2.37169985081302,0.0590339790747697,
3.64785365633938));
#42594=CARTESIAN_POINT('Ctrl Pts',(-2.37186929854398,-0.13697030543108,
3.65990871287198));
#42595=CARTESIAN_POINT('Ctrl Pts',(-2.3597667239314,-0.275718044079579,
3.66848094369881));
#42596=CARTESIAN_POINT('Ctrl Pts',(-2.32885929991368,-0.450674302687589,
3.67990230286747));
#42597=CARTESIAN_POINT('Ctrl Pts',(-2.3212034515273,-0.488576745812499,
3.68241265533684));
#42598=CARTESIAN_POINT('Ctrl Pts',(-2.30761936118775,-0.548269861809052,
3.68643274490679));
#42599=CARTESIAN_POINT('Ctrl Pts',(-2.30230033262587,-0.570193018636082,
3.68792352524549));
#42600=CARTESIAN_POINT('Ctrl Pts',(-2.29161130574658,-0.611658651311513,
3.69077218950729));
#42601=CARTESIAN_POINT('Ctrl Pts',(-2.28630193730051,-0.631214774057751,
3.6921280498678));
#42602=CARTESIAN_POINT('Ctrl Pts',(-2.27351712965478,-0.676026298859747,
3.6952645906173));
#42603=CARTESIAN_POINT('Ctrl Pts',(-2.2658703920914,-0.701229610653536,
3.69705056751702));
#42604=CARTESIAN_POINT('Ctrl Pts',(-2.23954823443694,-0.783055797232476,
3.70292326638485));
#42605=CARTESIAN_POINT('Ctrl Pts',(-2.21915856600873,-0.839098852087853,
3.70706342124196));
#42606=CARTESIAN_POINT('Ctrl Pts',(-2.16296380620328,-0.977129175176385,
3.71756249663213));
#42607=CARTESIAN_POINT('Ctrl Pts',(-2.12459301006574,-1.05796779322785,
3.72398967843638));
#42608=CARTESIAN_POINT('Ctrl Pts',(-2.01284523644896,-1.26266944110875,
3.7409111983272));
#42609=CARTESIAN_POINT('Ctrl Pts',(-1.93259673664931,-1.38237224467905,
3.75147964219424));
#42610=CARTESIAN_POINT('Ctrl Pts',(-1.82048765813362,-1.52058821520228,
3.76406400339948));
#42611=CARTESIAN_POINT('Ctrl Pts',(-1.79840778894284,-1.54663943383508,
3.76645336699156));
#42612=CARTESIAN_POINT('Ctrl Pts',(-1.76653256182472,-1.58264178957273,
3.76977012327999));
#42613=CARTESIAN_POINT('Ctrl Pts',(-1.75720123467197,-1.59299597301356,
3.77072577889181));
#42614=CARTESIAN_POINT('Ctrl Pts',(-1.7399655167019,-1.61178524077673,3.77246226563935));
#42615=CARTESIAN_POINT('Ctrl Pts',(-1.73208974569331,-1.62024590657604,
3.77324503365964));
#42616=CARTESIAN_POINT('Ctrl Pts',(-1.71518447059434,-1.63814249514453,
3.77490217599846));
#42617=CARTESIAN_POINT('Ctrl Pts',(-1.70613844806886,-1.64756190120004,
3.77577532647589));
#42618=CARTESIAN_POINT('Ctrl Pts',(-1.68029427497409,-1.6740316797195,3.77823340594831));
#42619=CARTESIAN_POINT('Ctrl Pts',(-1.66331468424705,-1.69090368781637,
3.77980547565187));
#42620=CARTESIAN_POINT('Ctrl Pts',(-1.62359797152988,-1.7291914337846,3.78339370949207));
#42621=CARTESIAN_POINT('Ctrl Pts',(-1.60068713051918,-1.75042117250121,
3.7853988669567));
#42622=CARTESIAN_POINT('Ctrl Pts',(-1.51847301399674,-1.82363818622084,
3.79239830905289));
#42623=CARTESIAN_POINT('Ctrl Pts',(-1.45700059481048,-1.87311701832676,
3.7972848712947));
#42624=CARTESIAN_POINT('Ctrl Pts',(-1.24941469120838,-2.02378735028783,
3.81309428183043));
#42625=CARTESIAN_POINT('Ctrl Pts',(-1.09440358357304,-2.11164076288625,
3.82390642296878));
#42626=CARTESIAN_POINT('Ctrl Pts',(-0.897525844218545,-2.19567155091186,
3.837697356745));
#42627=CARTESIAN_POINT('Ctrl Pts',(-0.863683849776956,-2.20920261249745,
3.8400676319614));
#42628=CARTESIAN_POINT('Ctrl Pts',(-0.808832466806698,-2.22968089771886,
3.84391655636787));
#42629=CARTESIAN_POINT('Ctrl Pts',(-0.788013490900771,-2.23712349882225,
3.84537902567851));
#42630=CARTESIAN_POINT('Ctrl Pts',(-0.747802481056421,-2.25086764529329,
3.84820835485844));
#42631=CARTESIAN_POINT('Ctrl Pts',(-0.728427195358609,-2.25721232600311,
3.84957367594173));
#42632=CARTESIAN_POINT('Ctrl Pts',(-0.68293297459544,-2.2714632364996,3.85278542883885));
#42633=CARTESIAN_POINT('Ctrl Pts',(-0.656755062654135,-2.27916988498903,
3.85463803161126));
#42634=CARTESIAN_POINT('Ctrl Pts',(-0.566795950278192,-2.30397492198413,
3.86102255758896));
#42635=CARTESIAN_POINT('Ctrl Pts',(-0.502441468264347,-2.3188594720347,
3.86562186567931));
#42636=CARTESIAN_POINT('Ctrl Pts',(-0.333719670755148,-2.35052991440881,
3.87776417190233));
#42637=CARTESIAN_POINT('Ctrl Pts',(-0.228706999775877,-2.36305928100741,
3.88540842552406));
#42638=CARTESIAN_POINT('Ctrl Pts',(0.00999595579355788,-2.37547725565066,
3.90280516817964));
#42639=CARTESIAN_POINT('Ctrl Pts',(0.143567155264895,-2.371157091238,3.912558114431));
#42640=CARTESIAN_POINT('Ctrl Pts',(0.30097034944349,-2.35270976067056,3.9236566697985));
#42641=CARTESIAN_POINT('Ctrl Pts',(0.325819405575156,-2.3493974131832,3.92539645250121));
#42642=CARTESIAN_POINT('Ctrl Pts',(0.363905308127659,-2.34370468220607,
3.9280394695584));
#42643=CARTESIAN_POINT('Ctrl Pts',(0.377181448267994,-2.34160476751479,
3.92895636749114));
#42644=CARTESIAN_POINT('Ctrl Pts',(0.400606678112143,-2.33769514795478,
3.93056555234368));
#42645=CARTESIAN_POINT('Ctrl Pts',(0.410762458876981,-2.33593204598352,
3.93126024206808));
#42646=CARTESIAN_POINT('Ctrl Pts',(0.435726916999368,-2.3314302236727,3.93296097130487));
#42647=CARTESIAN_POINT('Ctrl Pts',(0.450521506849136,-2.32861659253567,
3.93396294336805));
#42648=CARTESIAN_POINT('Ctrl Pts',(0.499353312476416,-2.31884694883676,
3.93725348306805));
#42649=CARTESIAN_POINT('Ctrl Pts',(0.533266098946622,-2.31128372617966,
3.93951191798685));
#42650=CARTESIAN_POINT('Ctrl Pts',(0.617749244398843,-2.29048363245666,
3.94509843053944));
#42651=CARTESIAN_POINT('Ctrl Pts',(0.66807228948704,-2.27631488643149,3.94839018079369));
#42652=CARTESIAN_POINT('Ctrl Pts',(0.810617366573668,-2.2310453514565,3.9577146334586));
#42653=CARTESIAN_POINT('Ctrl Pts',(0.901448439913645,-2.19591795516649,
3.96365956172259));
#42654=CARTESIAN_POINT('Ctrl Pts',(1.10660342129562,-2.10169661411891,3.97757063293859));
#42655=CARTESIAN_POINT('Ctrl Pts',(1.21877781753522,-2.03869441880731,3.98555890524226));
#42656=CARTESIAN_POINT('Ctrl Pts',(1.35253402169478,-1.94857095101678,3.99598943318772));
#42657=CARTESIAN_POINT('Ctrl Pts',(1.37938967441525,-1.92965307488603,3.99813236598012));
#42658=CARTESIAN_POINT('Ctrl Pts',(1.42306457500007,-1.89750955641875,4.00170440222749));
#42659=CARTESIAN_POINT('Ctrl Pts',(1.44011367101772,-1.88460284054043,4.00312145660147));
#42660=CARTESIAN_POINT('Ctrl Pts',(1.47335116914279,-1.85872659814813,4.00593052163419));
#42661=CARTESIAN_POINT('Ctrl Pts',(1.48954857365625,-1.8457717179745,4.00732188311774));
#42662=CARTESIAN_POINT('Ctrl Pts',(1.52834292922249,-1.81390030474475,4.0107104244733));
#42663=CARTESIAN_POINT('Ctrl Pts',(1.55076077025568,-1.79477222105789,4.01271584787354));
#42664=CARTESIAN_POINT('Ctrl Pts',(1.63552406159507,-1.71967385926942,4.02048669602019));
#42665=CARTESIAN_POINT('Ctrl Pts',(1.6952377698661,-1.66083812169591,4.02636636913664));
#42666=CARTESIAN_POINT('Ctrl Pts',(1.86782285883982,-1.47176747154114,4.04464388194149));
#42667=CARTESIAN_POINT('Ctrl Pts',(1.96972502139181,-1.33230558346584,4.05735306779864));
#42668=CARTESIAN_POINT('Ctrl Pts',(2.08386102263331,-1.13398657558563,4.07377303001559));
#42669=CARTESIAN_POINT('Ctrl Pts',(2.11033358798511,-1.08392597799857,4.07778723693651));
#42670=CARTESIAN_POINT('Ctrl Pts',(2.14299417604124,-1.01642101449627,4.082988333703));
#42671=CARTESIAN_POINT('Ctrl Pts',(2.15080496593952,-0.999786860782929,
4.08425336371895));
#42672=CARTESIAN_POINT('Ctrl Pts',(2.16286266366618,-0.973312871353701,
4.08623871421392));
#42673=CARTESIAN_POINT('Ctrl Pts',(2.16723739152076,-0.963532535748515,
4.0869661853375));
#42674=CARTESIAN_POINT('Ctrl Pts',(2.17638962172718,-0.942693681843332,
4.08850302284787));
#42675=CARTESIAN_POINT('Ctrl Pts',(2.18114946461862,-0.931627709978138,
4.0893112886481));
#42676=CARTESIAN_POINT('Ctrl Pts',(2.19325346078083,-0.902886289245861,
4.09139156433872));
#42677=CARTESIAN_POINT('Ctrl Pts',(2.20046851059907,-0.885156926746334,
4.09265631658826));
#42678=CARTESIAN_POINT('Ctrl Pts',(2.23352089112106,-0.801035404537531,
4.09857921752201));
#42679=CARTESIAN_POINT('Ctrl Pts',(2.25657526875353,-0.73358251957858,4.1031011108126));
#42680=CARTESIAN_POINT('Ctrl Pts',(2.33550922792691,-0.463436511503453,
4.120696639232));
#42681=CARTESIAN_POINT('Ctrl Pts',(2.36737862340621,-0.254751785075263,
4.13325968599711));
#42682=CARTESIAN_POINT('Ctrl Pts',(2.37209574148656,-0.00391372846938446,
4.14929610723635));
#42683=CARTESIAN_POINT('Ctrl Pts',(2.37181378855006,0.0367774094967678,
4.15192306620879));
#42684=CARTESIAN_POINT('Ctrl Pts',(2.36966135224321,0.102665293149738,4.15622981959101));
#42685=CARTESIAN_POINT('Ctrl Pts',(2.36843468145974,0.127875593091838,4.1578902756474));
#42686=CARTESIAN_POINT('Ctrl Pts',(2.36550499903268,0.173177798722209,4.1608991172681));
#42687=CARTESIAN_POINT('Ctrl Pts',(2.3639476408708,0.193276899115214,4.16224292907959));
#42688=CARTESIAN_POINT('Ctrl Pts',(2.36004416271809,0.236494154304883,4.1651526980586));
#42689=CARTESIAN_POINT('Ctrl Pts',(2.35761414460571,0.259602417121173,4.16672109542269));
#42690=CARTESIAN_POINT('Ctrl Pts',(2.34983258483826,0.324428294961655,4.17115792094549));
#42691=CARTESIAN_POINT('Ctrl Pts',(2.34371054418482,0.366042893678182,4.17404945855088));
#42692=CARTESIAN_POINT('Ctrl Pts',(2.32721355582752,0.460638622281026,4.18072529803128));
#42693=CARTESIAN_POINT('Ctrl Pts',(2.31612986698481,0.513471128124007,4.18452864575801));
#42694=CARTESIAN_POINT('Ctrl Pts',(2.26701627807338,0.713375339508083,4.19919668728086));
#42695=CARTESIAN_POINT('Ctrl Pts',(2.21669430461229,0.857045569807947,4.21034719239739));
#42696=CARTESIAN_POINT('Ctrl Pts',(2.11995620683581,1.06638891943087,4.22703740811421));
#42697=CARTESIAN_POINT('Ctrl Pts',(2.08337882964004,1.13619306230513,4.23267755211699));
#42698=CARTESIAN_POINT('Ctrl Pts',(2.03321412302157,1.22132729939304,4.239549184619));
#42699=CARTESIAN_POINT('Ctrl Pts',(2.02281669094517,1.23847193850463,4.24093254207919));
#42700=CARTESIAN_POINT('Ctrl Pts',(2.00572370398829,1.2658674068242,4.24313977039542));
#42701=CARTESIAN_POINT('Ctrl Pts',(1.99916426064522,1.27620145118244,4.24397161782834));
#42702=CARTESIAN_POINT('Ctrl Pts',(1.98601190431793,1.29657200142261,4.24560914605082));
#42703=CARTESIAN_POINT('Ctrl Pts',(1.97942222955367,1.30661007518579,4.24641496883988));
#42704=CARTESIAN_POINT('Ctrl Pts',(1.9622337228158,1.33236489217494,4.24848078794539));
#42705=CARTESIAN_POINT('Ctrl Pts',(1.95152193438601,1.34800578023285,4.24973371934177));
#42706=CARTESIAN_POINT('Ctrl Pts',(1.90109730646082,1.41977254243833,4.25548340941102));
#42707=CARTESIAN_POINT('Ctrl Pts',(1.8591399272787,1.47428815574891,4.2598534761862));
#42708=CARTESIAN_POINT('Ctrl Pts',(1.69490179762089,1.66950009505479,4.27582346863329));
#42709=CARTESIAN_POINT('Ctrl Pts',(1.55854950481684,1.79745652873527,4.28700229857499));
#42710=CARTESIAN_POINT('Ctrl Pts',(1.35921490686768,1.94460899715166,4.30264156805711));
#42711=CARTESIAN_POINT('Ctrl Pts',(1.30841409108551,1.97914651727392,4.30656933940486));
#42712=CARTESIAN_POINT('Ctrl Pts',(1.23541347204958,2.02473700818823,4.31217363062635));
#42713=CARTESIAN_POINT('Ctrl Pts',(1.21429166743376,2.03747443490682,4.31379056115342));
#42714=CARTESIAN_POINT('Ctrl Pts',(1.17525730393103,2.06019139944019,4.31677281205536));
#42715=CARTESIAN_POINT('Ctrl Pts',(1.15740646060623,2.07027258447125,4.31813440469737));
#42716=CARTESIAN_POINT('Ctrl Pts',(1.12066957834967,2.09039594355557,4.32093327441707));
#42717=CARTESIAN_POINT('Ctrl Pts',(1.10177393638872,2.10041654132479,4.32237114336336));
#42718=CARTESIAN_POINT('Ctrl Pts',(1.05349951526259,2.12518643361744,4.32604156483767));
#42719=CARTESIAN_POINT('Ctrl Pts',(1.02394566111259,2.13958260078573,4.32828585614312));
#42720=CARTESIAN_POINT('Ctrl Pts',(0.871218946592627,2.2100892463976,4.33987558761203));
#42721=CARTESIAN_POINT('Ctrl Pts',(0.743723233567563,2.25618754713974,4.34954459695592));
#42722=CARTESIAN_POINT('Ctrl Pts',(0.471507779731947,2.32902026419796,4.36999584339015));
#42723=CARTESIAN_POINT('Ctrl Pts',(0.326795493038871,2.35369143786506,4.38076137547229));
#42724=CARTESIAN_POINT('Ctrl Pts',(0.148683895114844,2.36730308969311,4.39335994106292));
#42725=CARTESIAN_POINT('Ctrl Pts',(0.116592428726733,2.36910051809704,4.39560334664939));
#42726=CARTESIAN_POINT('Ctrl Pts',(0.0698627596221165,2.37076590461429,
4.39882252750585));
#42727=CARTESIAN_POINT('Ctrl Pts',(0.0552479967207604,2.37115150625911,
4.39982257121407));
#42728=CARTESIAN_POINT('Ctrl Pts',(0.029259149947314,2.37159678321582,4.40158782058091));
#42729=CARTESIAN_POINT('Ctrl Pts',(0.017887022491942,2.3717098197621,4.40235571844826));
#42730=CARTESIAN_POINT('Ctrl Pts',(-0.0078245996975554,2.37178043420015,
4.4040816972023));
#42731=CARTESIAN_POINT('Ctrl Pts',(-0.0221634587373503,2.37168978977999,
4.40503722022514));
#42732=CARTESIAN_POINT('Ctrl Pts',(-0.0670490634442839,2.37099892187294,
4.40800881262807));
#42733=CARTESIAN_POINT('Ctrl Pts',(-0.0975868348555995,2.36993849707445,
4.41000221612063));
#42734=CARTESIAN_POINT('Ctrl Pts',(-0.171574392440073,2.36593661873287,
4.41478147822842));
#42735=CARTESIAN_POINT('Ctrl Pts',(-0.214981016099167,2.36238807950973,
4.41754316594666));
#42736=CARTESIAN_POINT('Ctrl Pts',(-0.410936050032594,2.34092224864457,
4.42991536637424));
#42737=CARTESIAN_POINT('Ctrl Pts',(-0.561623213991225,2.30940873238947,
4.43918979904656));
#42738=CARTESIAN_POINT('Ctrl Pts',(-0.7955124154501,2.23623026714634,4.45443597512809));
#42739=CARTESIAN_POINT('Ctrl Pts',(-0.88115282773577,2.2038903954872,4.4602079157636));
#42740=CARTESIAN_POINT('Ctrl Pts',(-0.992830350896185,2.15416659808128,
4.46813276762702));
#42741=CARTESIAN_POINT('Ctrl Pts',(-1.02070698939691,2.1410985358678,4.47014510947494));
#42742=CARTESIAN_POINT('Ctrl Pts',(-1.06526228311548,2.11914394261611,4.47342134614995));
#42743=CARTESIAN_POINT('Ctrl Pts',(-1.08210344060334,2.11059396643435,4.47467380449814));
#42744=CARTESIAN_POINT('Ctrl Pts',(-1.11720042389382,2.09224532585545,4.47731467890076));
#42745=CARTESIAN_POINT('Ctrl Pts',(-1.1354334832107,2.08240679262041,4.4787043850232));
#42746=CARTESIAN_POINT('Ctrl Pts',(-1.17917009098673,2.05806140440532,4.48208236233983));
#42747=CARTESIAN_POINT('Ctrl Pts',(-1.20453733373699,2.04331801938028,4.48407875137095));
#42748=CARTESIAN_POINT('Ctrl Pts',(-1.30023322007292,1.98529847663583,4.49175671920609));
#42749=CARTESIAN_POINT('Ctrl Pts',(-1.3685512687438,1.93883501837791,4.49754897289493));
#42750=CARTESIAN_POINT('Ctrl Pts',(-1.56631458050422,1.78866776506741,4.51526812946975));
#42751=CARTESIAN_POINT('Ctrl Pts',(-1.68745208630786,1.67486488031832,4.52748100502024));
#42752=CARTESIAN_POINT('Ctrl Pts',(-1.83706803298036,1.50146089929052,4.54396672173134));
#42753=CARTESIAN_POINT('Ctrl Pts',(-1.87648278969722,1.45190135212583,4.54846951132244));
#42754=CARTESIAN_POINT('Ctrl Pts',(-1.92509118871346,1.38549012627206,4.55418333457826));
#42755=CARTESIAN_POINT('Ctrl Pts',(-1.93612759149335,1.37002517515135,4.55549233038461));
#42756=CARTESIAN_POINT('Ctrl Pts',(-1.95316152532907,1.34553906940437,4.55752928321059));
#42757=CARTESIAN_POINT('Ctrl Pts',(-1.95928485152688,1.33660697792828,4.55826501792636));
#42758=CARTESIAN_POINT('Ctrl Pts',(-1.97201511605928,1.31776187120408,4.55980148729828));
#42759=CARTESIAN_POINT('Ctrl Pts',(-1.97860894145919,1.30784044660455,4.56060128907068));
#42760=CARTESIAN_POINT('Ctrl Pts',(-1.99524735136364,1.28239153280117,4.56263081248285));
#42761=CARTESIAN_POINT('Ctrl Pts',(-2.00518585492076,1.26679508018082,4.56385394851374));
#42762=CARTESIAN_POINT('Ctrl Pts',(-2.04820232339298,1.19751460011362,4.56920416851125));
#42763=CARTESIAN_POINT('Ctrl Pts',(-2.07931696096085,1.14263571858385,4.57322518079343));
#42764=CARTESIAN_POINT('Ctrl Pts',(-2.17164580349763,0.963496528046234,
4.58588154134459));
#42765=CARTESIAN_POINT('Ctrl Pts',(-2.22418404544549,0.835092703635923,
4.5942739590145));
#42766=CARTESIAN_POINT('Ctrl Pts',(-2.29653487403135,0.601907278282683,
4.60939282451259));
#42767=CARTESIAN_POINT('Ctrl Pts',(-2.3210662687693,0.499011514499828,4.61602278866778));
#42768=CARTESIAN_POINT('Ctrl Pts',(-2.34394193075249,0.363514674476526,
4.62492060515917));
#42769=CARTESIAN_POINT('Ctrl Pts',(-2.34859916807399,0.332097107268569,
4.62699459821716));
#42770=CARTESIAN_POINT('Ctrl Pts',(-2.35503908188814,0.281695028335984,
4.63034390390299));
#42771=CARTESIAN_POINT('Ctrl Pts',(-2.35722621796972,0.26276546315654,4.63160674528801));
#42772=CARTESIAN_POINT('Ctrl Pts',(-2.36116115002608,0.224690098143811,
4.63415777395436));
#42773=CARTESIAN_POINT('Ctrl Pts',(-2.36290471661995,0.205545323697977,
4.63544598974069));
#42774=CARTESIAN_POINT('Ctrl Pts',(-2.36477379335609,0.181834475928732,
4.63704878560607));
#42775=CARTESIAN_POINT('Ctrl Pts',(-2.36511913544288,0.177286052594564,
4.63735658114384));
#42776=CARTESIAN_POINT('Ctrl Pts',(-2.36545134967025,0.172736721177577,
4.63766477577655));
#42777=CARTESIAN_POINT('Origin',(0.,0.,-1.84858989190501));
#42778=CARTESIAN_POINT('',(-2.36545133284689,0.172736951556046,5.836583843094));
#42779=CARTESIAN_POINT('',(-2.36545134983051,0.172736718982988,5.64123248379855));
#42780=CARTESIAN_POINT('',(-2.36545134966535,0.172736721244682,-1.84858989190501));
#42781=CARTESIAN_POINT('',(-2.37174965175948,-0.00128525436374919,4.84688602397483));
#42782=CARTESIAN_POINT('Ctrl Pts',(-2.36545133284689,0.172736951556046,
5.836583843094));
#42783=CARTESIAN_POINT('Ctrl Pts',(-2.35983651434252,0.249626000454991,
5.83096966813975));
#42784=CARTESIAN_POINT('Ctrl Pts',(-2.35047365701173,0.326229766732311,
5.8253661914758));
#42785=CARTESIAN_POINT('Ctrl Pts',(-2.32956379880885,0.447724696538534,
5.81657106413305));
#42786=CARTESIAN_POINT('Ctrl Pts',(-2.32041718088337,0.49293978679623,5.81331910439767));
#42787=CARTESIAN_POINT('Ctrl Pts',(-2.30613380496632,0.554282574352545,
5.80896045886768));
#42788=CARTESIAN_POINT('Ctrl Pts',(-2.30213536430365,0.570661986976835,
5.8078019002244));
#42789=CARTESIAN_POINT('Ctrl Pts',(-2.29518143793053,0.59788501570341,5.80588667218263));
#42790=CARTESIAN_POINT('Ctrl Pts',(-2.29232297990814,0.608752578186658,
5.8051248758443));
#42791=CARTESIAN_POINT('Ctrl Pts',(-2.28619197080939,0.631406316164129,
5.80354319707501));
#42792=CARTESIAN_POINT('Ctrl Pts',(-2.28290531676541,0.643188148672387,
5.80272409584545));
#42793=CARTESIAN_POINT('Ctrl Pts',(-2.27370053826859,0.67522529260106,5.80050503703187));
#42794=CARTESIAN_POINT('Ctrl Pts',(-2.26760285882853,0.695428416428523,
5.79911468149373));
#42795=CARTESIAN_POINT('Ctrl Pts',(-2.25320214180448,0.740936764783969,
5.79599767779488));
#42796=CARTESIAN_POINT('Ctrl Pts',(-2.24474082441348,0.76618922871637,5.79427853762823));
#42797=CARTESIAN_POINT('Ctrl Pts',(-2.21543190440487,0.849003506085373,
5.78865906853966));
#42798=CARTESIAN_POINT('Ctrl Pts',(-2.19278025961378,0.905903495369401,
5.78482732084784));
#42799=CARTESIAN_POINT('Ctrl Pts',(-2.0839284368528,1.15124463554459,5.76818287956512));
#42800=CARTESIAN_POINT('Ctrl Pts',(-1.97546316278137,1.32878292144953,5.75572348062973));
#42801=CARTESIAN_POINT('Ctrl Pts',(-1.8231379551919,1.51743603271154,5.74008857939321));
#42802=CARTESIAN_POINT('Ctrl Pts',(-1.80035284539538,1.54440070674248,5.73779121446811));
#42803=CARTESIAN_POINT('Ctrl Pts',(-1.7627743021259,1.58691038309416,5.73406004428108));
#42804=CARTESIAN_POINT('Ctrl Pts',(-1.74835642117146,1.60278120126657,5.7326414452077));
#42805=CARTESIAN_POINT('Ctrl Pts',(-1.72024337623466,1.63289655267585,5.72989843924121));
#42806=CARTESIAN_POINT('Ctrl Pts',(-1.70658144095262,1.64716974556969,5.72857549078604));
#42807=CARTESIAN_POINT('Ctrl Pts',(-1.6742643236744,1.68009911305064,5.72546818068498));
#42808=CARTESIAN_POINT('Ctrl Pts',(-1.65547332016843,1.69861768672768,5.72367806386286));
#42809=CARTESIAN_POINT('Ctrl Pts',(-1.59073712136371,1.76032071365969,5.71756396410465));
#42810=CARTESIAN_POINT('Ctrl Pts',(-1.54338364568856,1.80198204375279,5.71317855851379));
#42811=CARTESIAN_POINT('Ctrl Pts',(-1.41792535371578,1.90378375833569,5.70177148837119));
#42812=CARTESIAN_POINT('Ctrl Pts',(-1.3376331501234,1.96103015710688,5.69466261665056));
#42813=CARTESIAN_POINT('Ctrl Pts',(-1.12843124466399,2.09134749485002,5.6767380436381));
#42814=CARTESIAN_POINT('Ctrl Pts',(-0.995787731911431,2.15766176086079,
5.66587905030475));
#42815=CARTESIAN_POINT('Ctrl Pts',(-0.835893066226128,2.21969233797341,
5.65388825973334));
#42816=CARTESIAN_POINT('Ctrl Pts',(-0.813838179902742,2.22787315887062,
5.65225792753819));
#42817=CARTESIAN_POINT('Ctrl Pts',(-0.779525726150336,2.24002310777201,
5.64976162452941));
#42818=CARTESIAN_POINT('Ctrl Pts',(-0.76735204258696,2.24422252525514,5.64888369492357));
#42819=CARTESIAN_POINT('Ctrl Pts',(-0.744591327685893,2.25186716929118,
5.64725741071244));
#42820=CARTESIAN_POINT('Ctrl Pts',(-0.734013808511635,2.25533716502136,
5.64650778162859));
#42821=CARTESIAN_POINT('Ctrl Pts',(-0.708653554826448,2.26345937517038,
5.64472460991575));
#42822=CARTESIAN_POINT('Ctrl Pts',(-0.693849037172218,2.26804139047526,
5.64369497980043));
#42823=CARTESIAN_POINT('Ctrl Pts',(-0.641325327004928,2.28373509900227,
5.64007849088617));
#42824=CARTESIAN_POINT('Ctrl Pts',(-0.603373807978468,2.29405419213439,
5.63753147455735));
#42825=CARTESIAN_POINT('Ctrl Pts',(-0.503721144162228,2.31850550335701,
5.63097302123838));
#42826=CARTESIAN_POINT('Ctrl Pts',(-0.441678563563814,2.33112071992003,
5.62701714561831));
#42827=CARTESIAN_POINT('Ctrl Pts',(-0.180051174976883,2.37349555920616,
5.61059795370754));
#42828=CARTESIAN_POINT('Ctrl Pts',(0.0223849324246697,2.38020899460828,
5.59844591271183));
#42829=CARTESIAN_POINT('Ctrl Pts',(0.259531218346824,2.35778951913976,5.58310421238673));
#42830=CARTESIAN_POINT('Ctrl Pts',(0.295750228301503,2.35352064921956,5.58073309322422));
#42831=CARTESIAN_POINT('Ctrl Pts',(0.353321685541067,2.34538522878325,5.57691175297781));
#42832=CARTESIAN_POINT('Ctrl Pts',(0.374745204281869,2.3420576563193,5.57547813515316));
#42833=CARTESIAN_POINT('Ctrl Pts',(0.415529824577874,2.33514894557895,5.57272522501834));
#42834=CARTESIAN_POINT('Ctrl Pts',(0.434897919747119,2.33161947862673,5.57140764420607));
#42835=CARTESIAN_POINT('Ctrl Pts',(0.479597990855436,2.32289742070321,5.5683419345559));
#42836=CARTESIAN_POINT('Ctrl Pts',(0.504893055628163,2.31753092151006,5.56658852023571));
#42837=CARTESIAN_POINT('Ctrl Pts',(0.588134927158108,2.29844320973825,5.56075440018524));
#42838=CARTESIAN_POINT('Ctrl Pts',(0.64564882979788,2.28295431792562,5.55661974714181));
#42839=CARTESIAN_POINT('Ctrl Pts',(0.78837678704089,2.23869188423944,5.54609264564333));
#42840=CARTESIAN_POINT('Ctrl Pts',(0.872647787070976,2.20720695701663,5.53962999957555));
#42841=CARTESIAN_POINT('Ctrl Pts',(1.08641916555434,2.11317966515402,5.52268023440513));
#42842=CARTESIAN_POINT('Ctrl Pts',(1.21239308135347,2.04351192242557,5.51211949869314));
#42843=CARTESIAN_POINT('Ctrl Pts',(1.36013008809604,1.9433112025839,5.49949005398249));
#42844=CARTESIAN_POINT('Ctrl Pts',(1.38853582243527,1.9231174832937,5.49705073319995));
#42845=CARTESIAN_POINT('Ctrl Pts',(1.42746342260215,1.89413132947216,5.49370311310393));
#42846=CARTESIAN_POINT('Ctrl Pts',(1.43836835859807,1.88586367563031,5.49276480453541));
#42847=CARTESIAN_POINT('Ctrl Pts',(1.45810390234321,1.87063025350073,5.49106660516452));
#42848=CARTESIAN_POINT('Ctrl Pts',(1.46695766140168,1.86369519410678,5.49030475680871));
#42849=CARTESIAN_POINT('Ctrl Pts',(1.48554969912342,1.84891764761507,5.48870537956168));
#42850=CARTESIAN_POINT('Ctrl Pts',(1.49527578168365,1.84106076226913,5.48786884253952));
#42851=CARTESIAN_POINT('Ctrl Pts',(1.52224234652545,1.81892206299536,5.48554841901247));
#42852=CARTESIAN_POINT('Ctrl Pts',(1.53934391466039,1.8044721202348,5.48407565823806));
#42853=CARTESIAN_POINT('Ctrl Pts',(1.57796207581588,1.77089311184019,5.4807403232036));
#42854=CARTESIAN_POINT('Ctrl Pts',(1.59934040855064,1.7516098689334,5.47888690682706));
#42855=CARTESIAN_POINT('Ctrl Pts',(1.67112545772865,1.68444947713912,5.47261764241429));
#42856=CARTESIAN_POINT('Ctrl Pts',(1.71977848410962,1.63474570818768,5.46828849406543));
#42857=CARTESIAN_POINT('Ctrl Pts',(1.88620036279507,1.44906283626675,5.45288118057935));
#42858=CARTESIAN_POINT('Ctrl Pts',(1.99059346289233,1.30194805649066,5.44199618722029));
#42859=CARTESIAN_POINT('Ctrl Pts',(2.09629805536048,1.11007785770259,5.42797764919269));
#42860=CARTESIAN_POINT('Ctrl Pts',(2.11437904391868,1.0752392174298,5.42544131297186));
#42861=CARTESIAN_POINT('Ctrl Pts',(2.14230512564725,1.0180001713845,5.42127821304472));
#42862=CARTESIAN_POINT('Ctrl Pts',(2.15268301391176,0.995867144617789,5.41966942702183));
#42863=CARTESIAN_POINT('Ctrl Pts',(2.1707385919924,0.95575830222694,5.4167536347155));
#42864=CARTESIAN_POINT('Ctrl Pts',(2.17853977120631,0.937840281716509,5.41545091406078));
#42865=CARTESIAN_POINT('Ctrl Pts',(2.19484969511452,0.899077151868505,5.41263132802331));
#42866=CARTESIAN_POINT('Ctrl Pts',(2.20328476776369,0.878203326015486,5.41111216799049));
#42867=CARTESIAN_POINT('Ctrl Pts',(2.2260950966414,0.819357702511538,5.40682565126848));
#42868=CARTESIAN_POINT('Ctrl Pts',(2.23979375712705,0.781133794847414,5.40403673838727));
#42869=CARTESIAN_POINT('Ctrl Pts',(2.26873040703623,0.693358738045418,5.39761866404703));
#42870=CARTESIAN_POINT('Ctrl Pts',(2.28333809055135,0.643622964301902,5.39397203732664));
#42871=CARTESIAN_POINT('Ctrl Pts',(2.3313110147999,0.457996298894227,5.38033256503023));
#42872=CARTESIAN_POINT('Ctrl Pts',(2.3542613151249,0.319717561064668,5.37009440142709));
#42873=CARTESIAN_POINT('Ctrl Pts',(2.37211308487593,0.0854853880717415,
5.35302706169835));
#42874=CARTESIAN_POINT('Ctrl Pts',(2.37363418225915,-0.00962548594368886,
5.3461787562647));
#42875=CARTESIAN_POINT('Ctrl Pts',(2.36854805337011,-0.12486126208412,5.33815179423761));
#42876=CARTESIAN_POINT('Ctrl Pts',(2.36739246938358,-0.145131593875779,
5.33675015968628));
#42877=CARTESIAN_POINT('Ctrl Pts',(2.36513570838378,-0.1774164502631,5.33453677978305));
#42878=CARTESIAN_POINT('Ctrl Pts',(2.3642029413978,-0.189441240740074,5.33371660195758));
#42879=CARTESIAN_POINT('Ctrl Pts',(2.36220410897676,-0.212888216794355,
5.33212624756636));
#42880=CARTESIAN_POINT('Ctrl Pts',(2.36114683879175,-0.22431062942299,5.33135567438545));
#42881=CARTESIAN_POINT('Ctrl Pts',(2.35826720248799,-0.253140654950356,
5.32942035755941));
#42882=CARTESIAN_POINT('Ctrl Pts',(2.3563348967022,-0.270537036741587,5.32826140518265));
#42883=CARTESIAN_POINT('Ctrl Pts',(2.34742496258216,-0.343392374366385,
5.32343889512857));
#42884=CARTESIAN_POINT('Ctrl Pts',(2.33868005416297,-0.398621292932018,
5.31985880299081));
#42885=CARTESIAN_POINT('Ctrl Pts',(2.30601380863896,-0.56631199619505,5.30908161051705));
#42886=CARTESIAN_POINT('Ctrl Pts',(2.27586364903919,-0.677389577911156,
5.30206656579179));
#42887=CARTESIAN_POINT('Ctrl Pts',(2.19275543315795,-0.914047990051146,
5.28663093986359));
#42888=CARTESIAN_POINT('Ctrl Pts',(2.13680738856947,-1.03812726825105,5.27820758601029));
#42889=CARTESIAN_POINT('Ctrl Pts',(2.05453625263995,-1.18539319646175,5.26730207458688));
#42890=CARTESIAN_POINT('Ctrl Pts',(2.03792904927482,-1.21372207111858,5.26516062861634));
#42891=CARTESIAN_POINT('Ctrl Pts',(2.00977723386111,-1.25953641855663,5.26161969661488));
#42892=CARTESIAN_POINT('Ctrl Pts',(1.99857925015029,-1.27723038403366,5.26023262482767));
#42893=CARTESIAN_POINT('Ctrl Pts',(1.97624494093414,-1.31150788601183,5.25750574510989));
#42894=CARTESIAN_POINT('Ctrl Pts',(1.96513046900119,-1.32810361047556,5.2561668175452));
#42895=CARTESIAN_POINT('Ctrl Pts',(1.93806811730361,-1.36742857516302,5.2529479908486));
#42896=CARTESIAN_POINT('Ctrl Pts',(1.921928421539,-1.39002157048769,5.25106107268301));
#42897=CARTESIAN_POINT('Ctrl Pts',(1.86172555493616,-1.47124246918038,5.24413596563973));
#42898=CARTESIAN_POINT('Ctrl Pts',(1.81534987304086,-1.52809664970729,5.23901170306047));
#42899=CARTESIAN_POINT('Ctrl Pts',(1.68620132630663,-1.672236098016,5.22526610473913));
#42900=CARTESIAN_POINT('Ctrl Pts',(1.59929886448346,-1.75553043511646,5.21651511940835));
#42901=CARTESIAN_POINT('Ctrl Pts',(1.41536576130241,-1.90679047771282,5.19917109576228));
#42902=CARTESIAN_POINT('Ctrl Pts',(1.31879384896392,-1.97481604771594,5.19060384247161));
#42903=CARTESIAN_POINT('Ctrl Pts',(1.19977622159638,-2.04601176707779,5.18094702497339));
#42904=CARTESIAN_POINT('Ctrl Pts',(1.18186066160913,-2.05641255129386,5.17951621115076));
#42905=CARTESIAN_POINT('Ctrl Pts',(1.15322497579121,-2.07253897569914,5.17726784418582));
#42906=CARTESIAN_POINT('Ctrl Pts',(1.1425936073757,-2.07841899413828,5.17644141602583));
#42907=CARTESIAN_POINT('Ctrl Pts',(1.1218852334152,-2.08966550203978,5.17484837771745));
#42908=CARTESIAN_POINT('Ctrl Pts',(1.11181393878483,-2.09504132641319,5.17408126538524));
#42909=CARTESIAN_POINT('Ctrl Pts',(1.08645623726605,-2.10834232782184,5.17216798820957));
#42910=CARTESIAN_POINT('Ctrl Pts',(1.07112123076078,-2.11617434961667,5.17102733755447));
#42911=CARTESIAN_POINT('Ctrl Pts',(1.00811921344539,-2.1474909143601,5.16640219539893));
#42912=CARTESIAN_POINT('Ctrl Pts',(0.959751291244879,-2.16953911145561,
5.16299285209468));
#42913=CARTESIAN_POINT('Ctrl Pts',(0.814335582076024,-2.23000963224693,
5.15303909169019));
#42914=CARTESIAN_POINT('Ctrl Pts',(0.715446723791671,-2.26367489001098,
5.14664629577101));
#42915=CARTESIAN_POINT('Ctrl Pts',(0.479863094888836,-2.32688784537193,
5.13165021929414));
#42916=CARTESIAN_POINT('Ctrl Pts',(0.342154011499422,-2.35108501746986,
5.12304683303129));
#42917=CARTESIAN_POINT('Ctrl Pts',(0.165457461621328,-2.36627368878776,
5.11164422385195));
#42918=CARTESIAN_POINT('Ctrl Pts',(0.127720289175776,-2.36861027186162,
5.10918964455716));
#42919=CARTESIAN_POINT('Ctrl Pts',(0.06780306886953,-2.37088417607716,5.10525320287712));
#42920=CARTESIAN_POINT('Ctrl Pts',(0.0456511166297272,-2.37141412527839,
5.10378941463638));
#42921=CARTESIAN_POINT('Ctrl Pts',(0.00390879856295782,-2.3718276631876,
5.10101361448089));
#42922=CARTESIAN_POINT('Ctrl Pts',(-0.0156791323647055,-2.3717790513836,
5.09970379477545));
#42923=CARTESIAN_POINT('Ctrl Pts',(-0.060242389168304,-2.37111640128047,
5.09670636877949));
#42924=CARTESIAN_POINT('Ctrl Pts',(-0.0852127699032866,-2.37035036152854,
5.09501425371175));
#42925=CARTESIAN_POINT('Ctrl Pts',(-0.164186061918645,-2.36667816136069,
5.08962078494959));
#42926=CARTESIAN_POINT('Ctrl Pts',(-0.218100797522671,-2.36231958651618,
5.08587621475144));
#42927=CARTESIAN_POINT('Ctrl Pts',(-0.348916604859631,-2.34722791523376,
5.07663381456617));
#42928=CARTESIAN_POINT('Ctrl Pts',(-0.425527737333055,-2.33455477371267,
5.07108675024579));
#42929=CARTESIAN_POINT('Ctrl Pts',(-0.652284268152342,-2.28551142151962,
5.05432164901246));
#42930=CARTESIAN_POINT('Ctrl Pts',(-0.799644697274543,-2.23821494534555,
5.04293997512563));
#42931=CARTESIAN_POINT('Ctrl Pts',(-0.979647580033029,-2.16037692293081,
5.02899055876038));
#42932=CARTESIAN_POINT('Ctrl Pts',(-1.01749132139787,-2.14281350661744,
5.02605715399275));
#42933=CARTESIAN_POINT('Ctrl Pts',(-1.06941906810972,-2.1170274799708,5.02204941448369));
#42934=CARTESIAN_POINT('Ctrl Pts',(-1.08390930638961,-2.10964526547953,
5.02093300712275));
#42935=CARTESIAN_POINT('Ctrl Pts',(-1.10828966663745,-2.09690689591035,
5.01905930388239));
#42936=CARTESIAN_POINT('Ctrl Pts',(-1.11821952898874,-2.09162846170564,
5.01829752110859));
#42937=CARTESIAN_POINT('Ctrl Pts',(-1.13911175640631,-2.08033142575201,
5.01669805684348));
#42938=CARTESIAN_POINT('Ctrl Pts',(-1.15006460891892,-2.07429647044581,
5.01586136985217));
#42939=CARTESIAN_POINT('Ctrl Pts',(-1.18050063976755,-2.05721121212241,
5.01354006903425));
#42940=CARTESIAN_POINT('Ctrl Pts',(-1.1998763281987,-2.04597082491982,5.01206659454421));
#42941=CARTESIAN_POINT('Ctrl Pts',(-1.24379966177214,-2.01965101396301,
5.00872935385576));
#42942=CARTESIAN_POINT('Ctrl Pts',(-1.26823795712945,-2.00439528293902,
5.00687476071485));
#42943=CARTESIAN_POINT('Ctrl Pts',(-1.35074439431465,-1.9507768863627,5.00059961628949));
#42944=CARTESIAN_POINT('Ctrl Pts',(-1.40740208496645,-1.91030402855942,
4.99626593753506));
#42945=CARTESIAN_POINT('Ctrl Pts',(-1.60402844081316,-1.75634241355609,
4.98083531419186));
#42946=CARTESIAN_POINT('Ctrl Pts',(-1.73273267552638,-1.62950283785317,
4.96993151329039));
#42947=CARTESIAN_POINT('Ctrl Pts',(-1.87033877347285,-1.45895620246359,
4.95590499940489));
#42948=CARTESIAN_POINT('Ctrl Pts',(-1.89408454084166,-1.42799293199246,
4.953383137315));
#42949=CARTESIAN_POINT('Ctrl Pts',(-1.93140966728029,-1.37675312149897,
4.94923887472202));
#42950=CARTESIAN_POINT('Ctrl Pts',(-1.94545933719025,-1.35682731255793,
4.94763417324986));
#42951=CARTESIAN_POINT('Ctrl Pts',(-1.9702102512868,-1.32054964227576,4.94472272706631));
#42952=CARTESIAN_POINT('Ctrl Pts',(-1.981021435069,-1.30427521156576,4.94342021079128));
#42953=CARTESIAN_POINT('Ctrl Pts',(-2.00388005504848,-1.26892542211526,
4.94059761244707));
#42954=CARTESIAN_POINT('Ctrl Pts',(-2.01585876493428,-1.249808138038,4.93907519211629));
#42955=CARTESIAN_POINT('Ctrl Pts',(-2.04874849083197,-1.1956149578706,4.93476919471659));
#42956=CARTESIAN_POINT('Ctrl Pts',(-2.06902812589879,-1.16016713041531,
4.93196374242355));
#42957=CARTESIAN_POINT('Ctrl Pts',(-2.11313935191103,-1.07822457384409,
4.92549991870341));
#42958=CARTESIAN_POINT('Ctrl Pts',(-2.13636944626691,-1.03143157021321,
4.92182370936814));
#42959=CARTESIAN_POINT('Ctrl Pts',(-2.21583607572108,-0.857135867678792,
4.90819181365658));
#42960=CARTESIAN_POINT('Ctrl Pts',(-2.26234976598788,-0.725519872764137,
4.89799515111079));
#42961=CARTESIAN_POINT('Ctrl Pts',(-2.32060810414617,-0.498932803671791,
4.88099784086205));
#42962=CARTESIAN_POINT('Ctrl Pts',(-2.33867064841662,-0.405929940600503,
4.87417747595414));
#42963=CARTESIAN_POINT('Ctrl Pts',(-2.35380885558994,-0.291885700629591,
4.86617071983084));
#42964=CARTESIAN_POINT('Ctrl Pts',(-2.35623013046204,-0.271648728433522,
4.86476356480965));
#42965=CARTESIAN_POINT('Ctrl Pts',(-2.35967040226515,-0.2393731642305,4.86254356312469));
#42966=CARTESIAN_POINT('Ctrl Pts',(-2.36085874751695,-0.227354149563595,
4.8617222009013));
#42967=CARTESIAN_POINT('Ctrl Pts',(-2.36289841662166,-0.204980625550495,
4.86020378989359));
#42968=CARTESIAN_POINT('Ctrl Pts',(-2.36377359581518,-0.194628818536194,
4.85950549340648));
#42969=CARTESIAN_POINT('Ctrl Pts',(-2.36547442213167,-0.172803726398664,
4.85804159350378));
#42970=CARTESIAN_POINT('Ctrl Pts',(-2.36628468549959,-0.161329382698505,
4.85727680634689));
#42971=CARTESIAN_POINT('Ctrl Pts',(-2.36830893667634,-0.129354424462884,
4.85515797272806));
#42972=CARTESIAN_POINT('Ctrl Pts',(-2.36934022612258,-0.108842750727502,
4.85381289252438));
#42973=CARTESIAN_POINT('Ctrl Pts',(-2.37118557821475,-0.0593216529717983,
4.85059401951231));
#42974=CARTESIAN_POINT('Ctrl Pts',(-2.37173392573361,-0.0303053436508547,
4.84873154878914));
#42975=CARTESIAN_POINT('Ctrl Pts',(-2.37174965175948,-0.00128525436374919,
4.84688602397483));
#42976=CARTESIAN_POINT('Ctrl Pts',(-2.3717496500648,-0.00128837785816269,
4.84688622261268));
#42977=CARTESIAN_POINT('Ctrl Pts',(-2.371781216878,0.056822352373548,4.84319068379912));
#42978=CARTESIAN_POINT('Ctrl Pts',(-2.36967708807495,0.114869689684006,
4.83956777994056));
#42979=CARTESIAN_POINT('Ctrl Pts',(-2.36545132791902,0.172737019038084,
4.83597583405741));
#42980=CARTESIAN_POINT('',(-2.37174912486677,-0.00129108034661244,4.64962605624969));
#42981=CARTESIAN_POINT('Ctrl Pts',(-2.36545134967025,0.172736721177577,
4.63766477577655));
#42982=CARTESIAN_POINT('Ctrl Pts',(-2.36658296888664,0.157240362415775,
4.6387145771999));
#42983=CARTESIAN_POINT('Ctrl Pts',(-2.36756226778942,0.141733467563053,
4.63976901278111));
#42984=CARTESIAN_POINT('Ctrl Pts',(-2.37065240762875,0.0837493591564288,
4.64372701539268));
#42985=CARTESIAN_POINT('Ctrl Pts',(-2.37177284112994,0.041230125981495,
4.64666004539431));
#42986=CARTESIAN_POINT('Ctrl Pts',(-2.37174964720368,-0.00129363410709259,
4.64962532548984));
#42987=CARTESIAN_POINT('Ctrl Pts',(-2.37174964856074,-0.00129114368864713,
4.64962515182724));
#42988=CARTESIAN_POINT('Ctrl Pts',(-2.37165110338696,-0.182312422208469,
4.66224817878405));
#42989=CARTESIAN_POINT('Ctrl Pts',(-2.35082803275891,-0.362713863320744,
4.675471399105));
#42990=CARTESIAN_POINT('Ctrl Pts',(-2.29472645522795,-0.60313390397009,
4.69340839884554));
#42991=CARTESIAN_POINT('Ctrl Pts',(-2.27708403754593,-0.666655278982695,
4.69817091492568));
#42992=CARTESIAN_POINT('Ctrl Pts',(-2.248187994304,-0.756066384117575,4.70484479801763));
#42993=CARTESIAN_POINT('Ctrl Pts',(-2.23908413951427,-0.782616120552576,
4.70682257672485));
#42994=CARTESIAN_POINT('Ctrl Pts',(-2.22197921086113,-0.829755382450694,
4.71031992200118));
#42995=CARTESIAN_POINT('Ctrl Pts',(-2.214157796454,-0.850406341721413,4.71184709082956));
#42996=CARTESIAN_POINT('Ctrl Pts',(-2.20139536674833,-0.882732736820557,
4.71422661614696));
#42997=CARTESIAN_POINT('Ctrl Pts',(-2.19664742706446,-0.894482389346666,
4.71508917241692));
#42998=CARTESIAN_POINT('Ctrl Pts',(-2.18738020811822,-0.916896956367165,
4.71672942425424));
#42999=CARTESIAN_POINT('Ctrl Pts',(-2.18287664792323,-0.927567652135011,
4.71750791612136));
#43000=CARTESIAN_POINT('Ctrl Pts',(-2.17254069258638,-0.95156534707847,
4.71925416987481));
#43001=CARTESIAN_POINT('Ctrl Pts',(-2.16666339030451,-0.964872763365423,
4.72021936711099));
#43002=CARTESIAN_POINT('Ctrl Pts',(-2.14458497625673,-1.01364362465095,
4.72374812597013));
#43003=CARTESIAN_POINT('Ctrl Pts',(-2.12763169684756,-1.0487620689161,4.72627219296531));
#43004=CARTESIAN_POINT('Ctrl Pts',(-2.03829367049038,-1.22273160849175,
4.73876847555801));
#43005=CARTESIAN_POINT('Ctrl Pts',(-1.95314563859356,-1.35460126906985,
4.74823774858585));
#43006=CARTESIAN_POINT('Ctrl Pts',(-1.79764613744162,-1.54994499577224,
4.76365949818677));
#43007=CARTESIAN_POINT('Ctrl Pts',(-1.73544703424529,-1.61928457174219,
4.769461707163));
#43008=CARTESIAN_POINT('Ctrl Pts',(-1.63765290788172,-1.71618199961081,
4.77826530960326));
#43009=CARTESIAN_POINT('Ctrl Pts',(-1.60508956957666,-1.74667535022641,
4.78114933774708));
#43010=CARTESIAN_POINT('Ctrl Pts',(-1.55391613248898,-1.79195585995192,
4.78562539877054));
#43011=CARTESIAN_POINT('Ctrl Pts',(-1.53591040487013,-1.80741260168723,
4.78719015760944));
#43012=CARTESIAN_POINT('Ctrl Pts',(-1.50221084466508,-1.83547423480581,
4.79010217698707));
#43013=CARTESIAN_POINT('Ctrl Pts',(-1.48658250753474,-1.84815461877676,
4.79144626087941));
#43014=CARTESIAN_POINT('Ctrl Pts',(-1.45148886169345,-1.87589546122685,
4.79445152143152));
#43015=CARTESIAN_POINT('Ctrl Pts',(-1.43194692010397,-1.89085473730379,
4.79611642288232));
#43016=CARTESIAN_POINT('Ctrl Pts',(-1.37383487442656,-1.93392173579044,
4.80104440013107));
#43017=CARTESIAN_POINT('Ctrl Pts',(-1.33464701784071,-1.96117116287171,
4.80433880445198));
#43018=CARTESIAN_POINT('Ctrl Pts',(-1.14880685008554,-2.08224540972875,
4.81983898563114));
#43019=CARTESIAN_POINT('Ctrl Pts',(-0.992945463331488,-2.16091317060829,
4.83254805105607));
#43020=CARTESIAN_POINT('Ctrl Pts',(-0.766607802552961,-2.2454569982077,
4.85010899360453));
#43021=CARTESIAN_POINT('Ctrl Pts',(-0.702318041090329,-2.26638810199638,
4.85499661336951));
#43022=CARTESIAN_POINT('Ctrl Pts',(-0.597488569635666,-2.29562775342633,
4.86273019202159));
#43023=CARTESIAN_POINT('Ctrl Pts',(-0.557473020839824,-2.30567206577461,
4.86562807191041));
#43024=CARTESIAN_POINT('Ctrl Pts',(-0.501547974343546,-2.3181685323608,
4.86958560992966));
#43025=CARTESIAN_POINT('Ctrl Pts',(-0.485847064565066,-2.32150993536767,
4.87068665295815));
#43026=CARTESIAN_POINT('Ctrl Pts',(-0.458851539734028,-2.32696912997076,
4.87256120100941));
#43027=CARTESIAN_POINT('Ctrl Pts',(-0.44757351532359,-2.32916466523366,
4.8733387713707));
#43028=CARTESIAN_POINT('Ctrl Pts',(-0.42319904605979,-2.33372614390257,
4.87500695287501));
#43029=CARTESIAN_POINT('Ctrl Pts',(-0.410098048240426,-2.33606394580354,
4.87589606556439));
#43030=CARTESIAN_POINT('Ctrl Pts',(-0.372883612360168,-2.34238193530011,
4.87840215368309));
#43031=CARTESIAN_POINT('Ctrl Pts',(-0.348726629173498,-2.34609999108689,
4.88000577168433));
#43032=CARTESIAN_POINT('Ctrl Pts',(-0.187920195213922,-2.368311271314,4.89055288782546));
#43033=CARTESIAN_POINT('Ctrl Pts',(-0.0499225087589769,-2.37523247260828,
4.89900353008266));
#43034=CARTESIAN_POINT('Ctrl Pts',(0.191198713584041,-2.36628922170586,
4.91384228154988));
#43035=CARTESIAN_POINT('Ctrl Pts',(0.294124070915623,-2.35571028587255,
4.92019896519204));
#43036=CARTESIAN_POINT('Ctrl Pts',(0.440152342953531,-2.33097982454859,
4.92953465697416));
#43037=CARTESIAN_POINT('Ctrl Pts',(0.484056076565638,-2.3222597603063,4.93238241454375));
#43038=CARTESIAN_POINT('Ctrl Pts',(0.563359202703935,-2.30416218942303,
4.9376221174143));
#43039=CARTESIAN_POINT('Ctrl Pts',(0.59883856704674,-2.29519696962475,4.94000171672073));
#43040=CARTESIAN_POINT('Ctrl Pts',(0.655427892318291,-2.27949610006659,
4.94386202939001));
#43041=CARTESIAN_POINT('Ctrl Pts',(0.676676344311584,-2.27327896724064,
4.94532638364013));
#43042=CARTESIAN_POINT('Ctrl Pts',(0.717309449702917,-2.26076988060579,
4.94815687727492));
#43043=CARTESIAN_POINT('Ctrl Pts',(0.736706215216213,-2.25452372099153,
4.94952144438719));
#43044=CARTESIAN_POINT('Ctrl Pts',(0.781368425072409,-2.2395036691234,4.95269568387034));
#43045=CARTESIAN_POINT('Ctrl Pts',(0.806570330594091,-2.23055094138072,
4.95451097405464));
#43046=CARTESIAN_POINT('Ctrl Pts',(0.887170580026883,-2.2003739553889,4.96039718478683));
#43047=CARTESIAN_POINT('Ctrl Pts',(0.941922140556682,-2.17749829641362,
4.96452032493413));
#43048=CARTESIAN_POINT('Ctrl Pts',(1.16134654918115,-2.07599623855053,4.98156450553382));
#43049=CARTESIAN_POINT('Ctrl Pts',(1.31753445314707,-1.98054897154749,4.99498604056335));
#43050=CARTESIAN_POINT('Ctrl Pts',(1.50118294470875,-1.83690574075698,5.01183579483194));
#43051=CARTESIAN_POINT('Ctrl Pts',(1.54014085461459,-1.80436683146923,5.01547568107742));
#43052=CARTESIAN_POINT('Ctrl Pts',(1.60343686299302,-1.74795503832035,5.02146584641049));
#43053=CARTESIAN_POINT('Ctrl Pts',(1.62835801764578,-1.72476289289692,5.02384537098807));
#43054=CARTESIAN_POINT('Ctrl Pts',(1.66348981771552,-1.69062798247203,5.02722026216105));
#43055=CARTESIAN_POINT('Ctrl Pts',(1.67410860957276,-1.68011360953002,5.02824312855876));
#43056=CARTESIAN_POINT('Ctrl Pts',(1.69187424080273,-1.66218699243977,5.02995808389872));
#43057=CARTESIAN_POINT('Ctrl Pts',(1.69907319907929,-1.65482758101297,5.03065400987143));
#43058=CARTESIAN_POINT('Ctrl Pts',(1.71561581946345,-1.63769448541001,5.03225537496554));
#43059=CARTESIAN_POINT('Ctrl Pts',(1.72492414200704,-1.62788746340444,5.03315820950765));
#43060=CARTESIAN_POINT('Ctrl Pts',(1.75150759098343,-1.59939573685941,5.03574363077265));
#43061=CARTESIAN_POINT('Ctrl Pts',(1.76856711081288,-1.5805113295587,5.0374115114201));
#43062=CARTESIAN_POINT('Ctrl Pts',(1.85194715336425,-1.48517102486712,5.04562938953061));
#43063=CARTESIAN_POINT('Ctrl Pts',(1.91363662188265,-1.40479193998499,5.05192546535555));
#43064=CARTESIAN_POINT('Ctrl Pts',(2.01778352495627,-1.24944354097062,5.06346468403217));
#43065=CARTESIAN_POINT('Ctrl Pts',(2.06165808021096,-1.17563830349169,5.06871334819673));
#43066=CARTESIAN_POINT('Ctrl Pts',(2.13482061768018,-1.03582027923389,5.0784820183481));
#43067=CARTESIAN_POINT('Ctrl Pts',(2.16527966060376,-0.970538851958767,
5.08297784731948));
#43068=CARTESIAN_POINT('Ctrl Pts',(2.21240472916112,-0.856230396023313,
5.09084107249904));
#43069=CARTESIAN_POINT('Ctrl Pts',(2.23052259857101,-0.807857362597834,
5.09416561744907));
#43070=CARTESIAN_POINT('Ctrl Pts',(2.25505218039733,-0.735230363445715,
5.0991755035198));
#43071=CARTESIAN_POINT('Ctrl Pts',(2.26268222692542,-0.711402197407416,
5.10082199721662));
#43072=CARTESIAN_POINT('Ctrl Pts',(2.27577265455452,-0.668178639355362,
5.10381604699735));
#43073=CARTESIAN_POINT('Ctrl Pts',(2.28136561259387,-0.64882568471274,5.10515923091088));
#43074=CARTESIAN_POINT('Ctrl Pts',(2.29292035873469,-0.606845725485791,
5.10807962909838));
#43075=CARTESIAN_POINT('Ctrl Pts',(2.29879513492063,-0.584197198847938,
5.10965943980867));
#43076=CARTESIAN_POINT('Ctrl Pts',(2.31420011263372,-0.520973066361815,
5.11408294913696));
#43077=CARTESIAN_POINT('Ctrl Pts',(2.32299689316245,-0.480229280151128,
5.11694899654504));
#43078=CARTESIAN_POINT('Ctrl Pts',(2.36431719483691,-0.260992070817214,
5.13246099549679));
#43079=CARTESIAN_POINT('Ctrl Pts',(2.37734679262253,-0.0794641915102049,
5.14568820799574));
#43080=CARTESIAN_POINT('Ctrl Pts',(2.36659072666646,0.171057333192036,5.16392008314734));
#43081=CARTESIAN_POINT('Ctrl Pts',(2.3605737986665,0.240217961819762,5.16894215865201));
#43082=CARTESIAN_POINT('Ctrl Pts',(2.34606670065391,0.350612346769363,5.1768583145386));
#43083=CARTESIAN_POINT('Ctrl Pts',(2.33949779738781,0.392056794425747,5.1798070040956));
#43084=CARTESIAN_POINT('Ctrl Pts',(2.32888177577863,0.449186570935638,5.18382083543816));
#43085=CARTESIAN_POINT('Ctrl Pts',(2.32576893887404,0.465035245760649,5.18492885552106));
#43086=CARTESIAN_POINT('Ctrl Pts',(2.32016232005791,0.492115004611031,5.18681128264761));
#43087=CARTESIAN_POINT('Ctrl Pts',(2.31774833507715,0.503361745429486,5.18758984898347));
#43088=CARTESIAN_POINT('Ctrl Pts',(2.31237683771739,0.527529227465505,5.18925552445166));
#43089=CARTESIAN_POINT('Ctrl Pts',(2.3093927205057,0.540443344324526,5.19014119344737));
#43090=CARTESIAN_POINT('Ctrl Pts',(2.30065716648568,0.576853323694828,5.19262753914778));
#43091=CARTESIAN_POINT('Ctrl Pts',(2.29465415994562,0.600287888253987,5.19421518475187));
#43092=CARTESIAN_POINT('Ctrl Pts',(2.25124025447184,0.759587698018044,5.20494643553421));
#43093=CARTESIAN_POINT('Ctrl Pts',(2.20213883935107,0.891992437052478,5.2135727046943));
#43094=CARTESIAN_POINT('Ctrl Pts',(2.07668361361566,1.15558442530973,5.23152603669983));
#43095=CARTESIAN_POINT('Ctrl Pts',(1.99894431816741,1.28538123317038,5.24082935445429));
#43096=CARTESIAN_POINT('Ctrl Pts',(1.88933054733923,1.4341454558541,5.25276667180737));
#43097=CARTESIAN_POINT('Ctrl Pts',(1.8686779708433,1.46095364898792,5.25497230353333));
#43098=CARTESIAN_POINT('Ctrl Pts',(1.83392627778115,1.50412041442188,5.2586204864492));
#43099=CARTESIAN_POINT('Ctrl Pts',(1.82016436689223,1.52074502804192,5.26004989434407));
#43100=CARTESIAN_POINT('Ctrl Pts',(1.79296456102121,1.55270466626286,5.26284724608678));
#43101=CARTESIAN_POINT('Ctrl Pts',(1.77955197594444,1.56805880592934,5.26421409831973));
#43102=CARTESIAN_POINT('Ctrl Pts',(1.74685277984816,1.60453149123839,5.26751785476558));
#43103=CARTESIAN_POINT('Ctrl Pts',(1.72737926010606,1.62547737945573,5.26946232587143));
#43104=CARTESIAN_POINT('Ctrl Pts',(1.65864419332484,1.69677914344971,5.27625053930209));
#43105=CARTESIAN_POINT('Ctrl Pts',(1.60752552256837,1.74528508462493,5.28117120312147));
#43106=CARTESIAN_POINT('Ctrl Pts',(1.39025754495403,1.933795816761,5.30158376068989));
#43107=CARTESIAN_POINT('Ctrl Pts',(1.20743280282681,2.05291818166336,5.31775448736565));
#43108=CARTESIAN_POINT('Ctrl Pts',(0.979494169096872,2.16032398550873,5.33556845606557));
#43109=CARTESIAN_POINT('Ctrl Pts',(0.947696643084033,2.17446083439009,5.3380021090852));
#43110=CARTESIAN_POINT('Ctrl Pts',(0.9016981795616,2.19371043807433,5.3414385918448));
#43111=CARTESIAN_POINT('Ctrl Pts',(0.887743097695399,2.19939476109261,5.34247025485715));
#43112=CARTESIAN_POINT('Ctrl Pts',(0.864150742059678,2.20874349456479,5.34419497424904));
#43113=CARTESIAN_POINT('Ctrl Pts',(0.854542378580899,2.21247862536741,5.34489198165544));
#43114=CARTESIAN_POINT('Ctrl Pts',(0.832356030646821,2.22093718812977,5.34648881934817));
#43115=CARTESIAN_POINT('Ctrl Pts',(0.819761846707342,2.22561656431074,5.3473861326129));
#43116=CARTESIAN_POINT('Ctrl Pts',(0.783583980828815,2.23870970515927,5.34993949957969));
#43117=CARTESIAN_POINT('Ctrl Pts',(0.759905173631907,2.24685763782029,5.35158139935531));
#43118=CARTESIAN_POINT('Ctrl Pts',(0.609758667198756,2.29587808563206,5.36183503662984));
#43119=CARTESIAN_POINT('Ctrl Pts',(0.480157420582651,2.32643913705813,5.36999430703003));
#43120=CARTESIAN_POINT('Ctrl Pts',(0.243819935023265,2.3615641471679,5.38468873245931));
#43121=CARTESIAN_POINT('Ctrl Pts',(0.138051933709894,2.37009985653739,5.39120050065762));
#43122=CARTESIAN_POINT('Ctrl Pts',(-0.0340796963843198,2.37242778751211,
5.40204530382957));
#43123=CARTESIAN_POINT('Ctrl Pts',(-0.100235773192517,2.37055408272223,
5.40627102428342));
#43124=CARTESIAN_POINT('Ctrl Pts',(-0.193461720510762,2.36400427995252,
5.41235713792293));
#43125=CARTESIAN_POINT('Ctrl Pts',(-0.220664413446217,2.36162037392588,
5.41414873359078));
#43126=CARTESIAN_POINT('Ctrl Pts',(-0.268097355340189,2.35663693022035,
5.41730325899755));
#43127=CARTESIAN_POINT('Ctrl Pts',(-0.288346836832517,2.35424507461221,
5.41865971031016));
#43128=CARTESIAN_POINT('Ctrl Pts',(-0.330475866091216,2.34871714557575,
5.42150337084423));
#43129=CARTESIAN_POINT('Ctrl Pts',(-0.352347367323676,2.34553571806251,
5.42299185353294));
#43130=CARTESIAN_POINT('Ctrl Pts',(-0.41012085590314,2.3363057065339,5.42695743813941));
#43131=CARTESIAN_POINT('Ctrl Pts',(-0.445932304636449,2.32973552186478,
5.42945030421442));
#43132=CARTESIAN_POINT('Ctrl Pts',(-0.655821475485251,2.28621150450753,
5.44427414732502));
#43133=CARTESIAN_POINT('Ctrl Pts',(-0.825419083931088,2.23058899133352,
5.45718409978112));
#43134=CARTESIAN_POINT('Ctrl Pts',(-1.05873146646179,2.12378900845944,5.47586369815742));
#43135=CARTESIAN_POINT('Ctrl Pts',(-1.12862122409183,2.08748831090851,5.48157964825219));
#43136=CARTESIAN_POINT('Ctrl Pts',(-1.22351292835331,2.03204017152364,5.4894119693805));
#43137=CARTESIAN_POINT('Ctrl Pts',(-1.25013437683699,2.01577165594001,5.49161731552381));
#43138=CARTESIAN_POINT('Ctrl Pts',(-1.29658348095563,1.98611208212418,5.49547003381992));
#43139=CARTESIAN_POINT('Ctrl Pts',(-1.31654379186555,1.97293752473937,5.49712725662053));
#43140=CARTESIAN_POINT('Ctrl Pts',(-1.34708781085225,1.95210730270141,5.49966173970242));
#43141=CARTESIAN_POINT('Ctrl Pts',(-1.35781269977561,1.94466274288617,5.50055138332652));
#43142=CARTESIAN_POINT('Ctrl Pts',(-1.37791785696558,1.93045955279906,5.50221777364405));
#43143=CARTESIAN_POINT('Ctrl Pts',(-1.38731059142363,1.92372062260659,5.50299561104756));
#43144=CARTESIAN_POINT('Ctrl Pts',(-1.40792455599873,1.90870137966437,5.50470191185869));
#43145=CARTESIAN_POINT('Ctrl Pts',(-1.41912258964514,1.90039038371628,5.50562833468664));
#43146=CARTESIAN_POINT('Ctrl Pts',(-1.45751559345723,1.87136711004092,5.50880543138979));
#43147=CARTESIAN_POINT('Ctrl Pts',(-1.48433698533777,1.85016500788029,5.51102638857135));
#43148=CARTESIAN_POINT('Ctrl Pts',(-1.62152198039556,1.73681698897707,5.5224485253824));
#43149=CARTESIAN_POINT('Ctrl Pts',(-1.72380705779316,1.63534832659884,5.5311948392174));
#43150=CARTESIAN_POINT('Ctrl Pts',(-1.87377211965941,1.45676660934416,5.54555460638491));
#43151=CARTESIAN_POINT('Ctrl Pts',(-1.92734549629563,1.38510964880787,5.55108670487353));
#43152=CARTESIAN_POINT('Ctrl Pts',(-2.00968597081519,1.26091800275511,5.56051148598884));
#43153=CARTESIAN_POINT('Ctrl Pts',(-2.04074085321657,1.21001148773585,5.56433205257));
#43154=CARTESIAN_POINT('Ctrl Pts',(-2.0827018671235,1.13500862488954,5.56993692251447));
#43155=CARTESIAN_POINT('Ctrl Pts',(-2.09517610034106,1.11181323303174,5.57166696263946));
#43156=CARTESIAN_POINT('Ctrl Pts',(-2.1165602725007,1.07041173891797,5.57475183190208));
#43157=CARTESIAN_POINT('Ctrl Pts',(-2.12562806533239,1.05228986660156,5.57610108195207));
#43158=CARTESIAN_POINT('Ctrl Pts',(-2.14429785436192,1.01375228318112,5.57896937725715));
#43159=CARTESIAN_POINT('Ctrl Pts',(-2.15384293249525,0.993311402531853,
5.5804901876685));
#43160=CARTESIAN_POINT('Ctrl Pts',(-2.17895320975329,0.937473238005745,
5.58464457123343));
#43161=CARTESIAN_POINT('Ctrl Pts',(-2.19394611875703,0.901827751408585,
5.5872967094198));
#43162=CARTESIAN_POINT('Ctrl Pts',(-2.25868233697933,0.736736555146988,
5.59958715013205));
#43163=CARTESIAN_POINT('Ctrl Pts',(-2.29787792279577,0.603467666674163,
5.60955064411162));
#43164=CARTESIAN_POINT('Ctrl Pts',(-2.34477954047919,0.370222179973078,
5.62685247337639));
#43165=CARTESIAN_POINT('Ctrl Pts',(-2.35822058487779,0.27175459322788,5.6341098994282));
#43166=CARTESIAN_POINT('Ctrl Pts',(-2.36545134983051,0.172736718982988,
5.64123248379855));
#43167=CARTESIAN_POINT('Origin',(0.,0.,-1.84858989190501));
#43168=CARTESIAN_POINT('',(-2.36545134966528,0.172736721245734,6.83902895557492));
#43169=CARTESIAN_POINT('',(-2.36545136499511,0.172736511319393,6.6396530072276));
#43170=CARTESIAN_POINT('',(-2.36545134966535,0.172736721244682,-1.84858989190501));
#43171=CARTESIAN_POINT('Ctrl Pts',(-2.36545134966532,0.172736721245143,
6.83902895557496));
#43172=CARTESIAN_POINT('Ctrl Pts',(-2.36542532467499,0.173093106662592,
6.83900560678643));
#43173=CARTESIAN_POINT('Ctrl Pts',(-2.36539921913017,0.173449486382915,
6.83898225563025));
#43174=CARTESIAN_POINT('Ctrl Pts',(-2.3639291327463,0.193456307102682,6.8376711896765));
#43175=CARTESIAN_POINT('Ctrl Pts',(-2.36224045459217,0.213087504274731,
6.83637638238029));
#43176=CARTESIAN_POINT('Ctrl Pts',(-2.35849122463444,0.251117278926783,
6.8338505940092));
#43177=CARTESIAN_POINT('Ctrl Pts',(-2.35645945002291,0.269517295416842,
6.83262057564433));
#43178=CARTESIAN_POINT('Ctrl Pts',(-2.35170092552846,0.308429833699506,
6.83000150861523));
#43179=CARTESIAN_POINT('Ctrl Pts',(-2.34892070930324,0.328934128388039,
6.82861090973337));
#43180=CARTESIAN_POINT('Ctrl Pts',(-2.3412170627432,0.380656599659059,6.82507524540553));
#43181=CARTESIAN_POINT('Ctrl Pts',(-2.33593740339763,0.411816785893085,
6.82291938843814));
#43182=CARTESIAN_POINT('Ctrl Pts',(-2.30897578139668,0.553670738115659,
6.81298205457405));
#43183=CARTESIAN_POINT('Ctrl Pts',(-2.28003987291106,0.662821430618337,
6.80498159700965));
#43184=CARTESIAN_POINT('Ctrl Pts',(-2.19825955134394,0.901253604394254,
6.78678097333404));
#43185=CARTESIAN_POINT('Ctrl Pts',(-2.14154523272019,1.02877910230439,6.7765348047321));
#43186=CARTESIAN_POINT('Ctrl Pts',(-2.04634395039736,1.2003819879763,6.76245446212597));
#43187=CARTESIAN_POINT('Ctrl Pts',(-2.0169333247234,1.24916834045662,6.75841815581534));
#43188=CARTESIAN_POINT('Ctrl Pts',(-1.9761659607068,1.31159296812389,6.75325176968593));
#43189=CARTESIAN_POINT('Ctrl Pts',(-1.96637520310589,1.32622646045377,6.75204057795236));
#43190=CARTESIAN_POINT('Ctrl Pts',(-1.94992614204335,1.35022892431204,6.75005550178593));
#43191=CARTESIAN_POINT('Ctrl Pts',(-1.94336120026763,1.35966075649119,6.74927587419132));
#43192=CARTESIAN_POINT('Ctrl Pts',(-1.92978363109161,1.37886834775541,6.74768961917059));
#43193=CARTESIAN_POINT('Ctrl Pts',(-1.92276473136573,1.3886391132304,6.74688341655464));
#43194=CARTESIAN_POINT('Ctrl Pts',(-1.90378576072101,1.4146392640734,6.74473877917064));
#43195=CARTESIAN_POINT('Ctrl Pts',(-1.89169231926433,1.43077066814459,6.74340888745887));
#43196=CARTESIAN_POINT('Ctrl Pts',(-1.82412853727094,1.51853930910172,6.73616513714645));
#43197=CARTESIAN_POINT('Ctrl Pts',(-1.76478817211058,1.58711464082255,6.7304743645058));
#43198=CARTESIAN_POINT('Ctrl Pts',(-1.60174843662205,1.75504226204715,6.71596463527191));
#43199=CARTESIAN_POINT('Ctrl Pts',(-1.49270676434456,1.84867466489829,6.70727132185702));
#43200=CARTESIAN_POINT('Ctrl Pts',(-1.31286736355104,1.97675510243706,6.6934462843553));
#43201=CARTESIAN_POINT('Ctrl Pts',(-1.24770883019535,2.01851489099284,6.68853168445244));
#43202=CARTESIAN_POINT('Ctrl Pts',(-1.15613376662309,2.07107474300824,6.68166818213167));
#43203=CARTESIAN_POINT('Ctrl Pts',(-1.1313880620436,2.08469585822529,6.67981789415524));
#43204=CARTESIAN_POINT('Ctrl Pts',(-1.08866580632776,2.10722734119433,6.6766274799188));
#43205=CARTESIAN_POINT('Ctrl Pts',(-1.07080829587183,2.11635768662975,6.67529509979448));
#43206=CARTESIAN_POINT('Ctrl Pts',(-1.03640761869444,2.1333995177124,6.67272957969641));
#43207=CARTESIAN_POINT('Ctrl Pts',(-1.01988422210213,2.14134779887459,6.67149781545816));
#43208=CARTESIAN_POINT('Ctrl Pts',(-0.976126976102489,2.16177509015727,
6.66823631177346));
#43209=CARTESIAN_POINT('Ctrl Pts',(-0.948746719658261,2.17393075693665,
6.66619591181752));
#43210=CARTESIAN_POINT('Ctrl Pts',(-0.840110769079175,2.21971729761167,
6.65809819071309));
#43211=CARTESIAN_POINT('Ctrl Pts',(-0.757249583070241,2.24933342793609,
6.65191368241777));
#43212=CARTESIAN_POINT('Ctrl Pts',(-0.485410935009481,2.32976865411779,
6.63162530989638));
#43213=CARTESIAN_POINT('Ctrl Pts',(-0.291750328215603,2.36184706564075,
6.61710725986489));
#43214=CARTESIAN_POINT('Ctrl Pts',(-0.0609873882252387,2.37122998970069,
6.60076898323319));
#43215=CARTESIAN_POINT('Ctrl Pts',(-0.0255879450803394,2.37187619749758,
6.59829162742651));
#43216=CARTESIAN_POINT('Ctrl Pts',(0.0247153748751761,2.37166802974491,
6.59482401331062));
#43217=CARTESIAN_POINT('Ctrl Pts',(0.0396155094544078,2.37146594600062,
6.5938034705129));
#43218=CARTESIAN_POINT('Ctrl Pts',(0.06557563217951,2.37086911080748,6.59203799528834));
#43219=CARTESIAN_POINT('Ctrl Pts',(0.076636230171716,2.37053736737872,6.59128983321678));
#43220=CARTESIAN_POINT('Ctrl Pts',(0.100929210243043,2.36963852652243,6.58965564475329));
#43221=CARTESIAN_POINT('Ctrl Pts',(0.114159670552405,2.36903799924672,6.58877139473487));
#43222=CARTESIAN_POINT('Ctrl Pts',(0.152599071684038,2.36697046562635,6.58621727861332));
#43223=CARTESIAN_POINT('Ctrl Pts',(0.177791298605128,2.36521162639432,6.58456208658935));
#43224=CARTESIAN_POINT('Ctrl Pts',(0.317055483434422,2.35325085106747,6.57549211726679));
#43225=CARTESIAN_POINT('Ctrl Pts',(0.430312859504358,2.33519815961538,6.56840918207765));
#43226=CARTESIAN_POINT('Ctrl Pts',(0.655496726036591,2.28235689072448,6.55417236284696));
#43227=CARTESIAN_POINT('Ctrl Pts',(0.767031136827342,2.24732968264644,6.54703643569882));
#43228=CARTESIAN_POINT('Ctrl Pts',(0.921178344166718,2.18610178183194,6.53662333564196));
#43229=CARTESIAN_POINT('Ctrl Pts',(0.96624966207171,2.16655756696394,6.53350948154794));
#43230=CARTESIAN_POINT('Ctrl Pts',(1.04597382433044,2.12900419839743,6.52784744369699));
#43231=CARTESIAN_POINT('Ctrl Pts',(1.08085055314369,2.11151176322449,6.52531558436485));
#43232=CARTESIAN_POINT('Ctrl Pts',(1.13486771600584,2.08273042119615,6.52129767930024));
#43233=CARTESIAN_POINT('Ctrl Pts',(1.15430885891841,2.07201876045021,6.51983145696891));
#43234=CARTESIAN_POINT('Ctrl Pts',(1.19061274640348,2.05134658162497,6.51705366765181));
#43235=CARTESIAN_POINT('Ctrl Pts',(1.20750812261734,2.04144693903642,6.51574433042117));
#43236=CARTESIAN_POINT('Ctrl Pts',(1.24562112562161,2.01847641479658,6.51275169187655));
#43237=CARTESIAN_POINT('Ctrl Pts',(1.26675891460345,2.00527823437122,6.51106393679386));
#43238=CARTESIAN_POINT('Ctrl Pts',(1.33278573402331,1.96259130330786,6.50570066036345));
#43239=CARTESIAN_POINT('Ctrl Pts',(1.37688056729968,1.93191137482338,6.50198261237318));
#43240=CARTESIAN_POINT('Ctrl Pts',(1.57952985708404,1.78045020609046,6.48423034828215));
#43241=CARTESIAN_POINT('Ctrl Pts',(1.72347801509004,1.64149924780821,6.46953611437609));
#43242=CARTESIAN_POINT('Ctrl Pts',(1.89215701684174,1.43172312985216,6.45011264262666));
#43243=CARTESIAN_POINT('Ctrl Pts',(1.93355444575195,1.37530299678486,6.44512450608028));
#43244=CARTESIAN_POINT('Ctrl Pts',(1.98278763930992,1.30157637529536,6.43897014364482));
#43245=CARTESIAN_POINT('Ctrl Pts',(1.99299051498817,1.2858991968201,6.43768145326722));
#43246=CARTESIAN_POINT('Ctrl Pts',(2.00928231419232,1.26020631356106,6.43560372108651));
#43247=CARTESIAN_POINT('Ctrl Pts',(2.0154841308751,1.25026361392333,6.43480788113702));
#43248=CARTESIAN_POINT('Ctrl Pts',(2.02775841297569,1.23025689250392,6.43322348315045));
#43249=CARTESIAN_POINT('Ctrl Pts',(2.03383026413275,1.22019288409894,6.43243497279787));
#43250=CARTESIAN_POINT('Ctrl Pts',(2.04945443853848,1.19385535786401,6.4303923388121));
#43251=CARTESIAN_POINT('Ctrl Pts',(2.05888802490903,1.17751189652115,6.42914538505867));
#43252=CARTESIAN_POINT('Ctrl Pts',(2.10013455670182,1.10404175409316,6.4236231282517));
#43253=CARTESIAN_POINT('Ctrl Pts',(2.12977480253932,1.0457218620721,6.41946172680066));
#43254=CARTESIAN_POINT('Ctrl Pts',(2.22561266703555,0.836119767353759,6.40501562865975));
#43255=CARTESIAN_POINT('Ctrl Pts',(2.27839686035632,0.679234708973688,6.39507692935581));
#43256=CARTESIAN_POINT('Ctrl Pts',(2.33241831302828,0.437925538951538,6.37962819857534));
#43257=CARTESIAN_POINT('Ctrl Pts',(2.34619134424461,0.356844627523759,6.37441735047596));
#43258=CARTESIAN_POINT('Ctrl Pts',(2.35906792130351,0.246627599565111,6.36720915662877));
#43259=CARTESIAN_POINT('Ctrl Pts',(2.3618872360025,0.217979814007121,6.36532462449572));
#43260=CARTESIAN_POINT('Ctrl Pts',(2.36579270835301,0.169201134070067,6.36209360071417));
#43261=CARTESIAN_POINT('Ctrl Pts',(2.36714490439128,0.14909434144515,6.36075537079677));
#43262=CARTESIAN_POINT('Ctrl Pts',(2.36936399731871,0.108346778454531,6.35802928724783));
#43263=CARTESIAN_POINT('Ctrl Pts',(2.37021775364071,0.0877070733611477,
6.35664115069178));
#43264=CARTESIAN_POINT('Ctrl Pts',(2.37169040373146,0.0356433515391833,
6.35311996733857));
#43265=CARTESIAN_POINT('Ctrl Pts',(2.37195444720267,0.00421410901337383,
6.35097630965169));
#43266=CARTESIAN_POINT('Ctrl Pts',(2.3703997750263,-0.131290118411623,6.341651980117));
#43267=CARTESIAN_POINT('Ctrl Pts',(2.36235569961672,-0.235165147250278,
6.33428800792809));
#43268=CARTESIAN_POINT('Ctrl Pts',(2.32719970021587,-0.47921597985295,6.31652958673824));
#43269=CARTESIAN_POINT('Ctrl Pts',(2.29421094254769,-0.618142938735001,
6.30604590380047));
#43270=CARTESIAN_POINT('Ctrl Pts',(2.22930560262247,-0.811924538389362,
6.29134842433696));
#43271=CARTESIAN_POINT('Ctrl Pts',(2.20736911906492,-0.869797592671791,
6.28695273727277));
#43272=CARTESIAN_POINT('Ctrl Pts',(2.17613591017555,-0.943375172592391,
6.28140964945651));
#43273=CARTESIAN_POINT('Ctrl Pts',(2.1688892407961,-0.95991860375963,6.2801664102373));
#43274=CARTESIAN_POINT('Ctrl Pts',(2.15668571918784,-0.986934108320738,
6.27814313877535));
#43275=CARTESIAN_POINT('Ctrl Pts',(2.15183997357075,-0.997455248131422,
6.27735693083482));
#43276=CARTESIAN_POINT('Ctrl Pts',(2.14185741769152,-1.01871812390797,6.27577220072896));
#43277=CARTESIAN_POINT('Ctrl Pts',(2.13671644670183,-1.02945745680394,6.27497393971008));
#43278=CARTESIAN_POINT('Ctrl Pts',(2.12290721246118,-1.05775538073396,6.27287504344825));
#43279=CARTESIAN_POINT('Ctrl Pts',(2.11410180617813,-1.07524652597635,6.27158232457971));
#43280=CARTESIAN_POINT('Ctrl Pts',(2.07003500371878,-1.16014662388675,6.26532057805561));
#43281=CARTESIAN_POINT('Ctrl Pts',(2.03175772002092,-1.22594779437349,6.26050716376725));
#43282=CARTESIAN_POINT('Ctrl Pts',(1.90582494383209,-1.42028324048335,6.24607016420576));
#43283=CARTESIAN_POINT('Ctrl Pts',(1.80864460958961,-1.54213482558072,6.23668192429487));
#43284=CARTESIAN_POINT('Ctrl Pts',(1.64432334523634,-1.71109031693999,6.22194410999281));
#43285=CARTESIAN_POINT('Ctrl Pts',(1.58553583781208,-1.7657019891943,6.21685544961642));
#43286=CARTESIAN_POINT('Ctrl Pts',(1.50221137590773,-1.83558577721047,6.20978922977191));
#43287=CARTESIAN_POINT('Ctrl Pts',(1.47999396530646,-1.85354576777793,6.20791850088244));
#43288=CARTESIAN_POINT('Ctrl Pts',(1.44159107126498,-1.88345899155765,6.20470387574747));
#43289=CARTESIAN_POINT('Ctrl Pts',(1.42556766372122,-1.89561583248758,6.2033680324422));
#43290=CARTESIAN_POINT('Ctrl Pts',(1.39273351113588,-1.91987510553488,6.20064048857699));
#43291=CARTESIAN_POINT('Ctrl Pts',(1.37591499233533,-1.93196401146227,6.19924843066712));
#43292=CARTESIAN_POINT('Ctrl Pts',(1.33295577146983,-1.96199699389624,6.19570419980298));
#43293=CARTESIAN_POINT('Ctrl Pts',(1.3066102739149,-1.97963954275863,6.19354112804837));
#43294=CARTESIAN_POINT('Ctrl Pts',(1.18798153421953,-2.05568084013864,6.18384253785017));
#43295=CARTESIAN_POINT('Ctrl Pts',(1.09209513517765,-2.10818553320995,6.17610347514817));
#43296=CARTESIAN_POINT('Ctrl Pts',(0.889233005668803,-2.2017049855788,6.1599888998064));
#43297=CARTESIAN_POINT('Ctrl Pts',(0.782204118916242,-2.24196245435948,
6.15162074190443));
#43298=CARTESIAN_POINT('Ctrl Pts',(0.619587887031015,-2.29006031654228,
6.13933794723494));
#43299=CARTESIAN_POINT('Ctrl Pts',(0.565941583773536,-2.30390456202802,
6.13535459203533));
#43300=CARTESIAN_POINT('Ctrl Pts',(0.476743005521254,-2.3236194590524,6.12888910013483));
#43301=CARTESIAN_POINT('Ctrl Pts',(0.441454813231906,-2.33058131352853,
6.12637135719678));
#43302=CARTESIAN_POINT('Ctrl Pts',(0.391251564421225,-2.33930437553239,
6.12285813748782));
#43303=CARTESIAN_POINT('Ctrl Pts',(0.376458848129943,-2.34173045262465,
6.12183133806096));
#43304=CARTESIAN_POINT('Ctrl Pts',(0.35069936955868,-2.34570472207914,6.1200590123873));
#43305=CARTESIAN_POINT('Ctrl Pts',(0.339743269926519,-2.34731659980889,
6.11931017410947));
#43306=CARTESIAN_POINT('Ctrl Pts',(0.315719261384868,-2.35067930993816,
6.11767922811137));
#43307=CARTESIAN_POINT('Ctrl Pts',(0.302647540104854,-2.35239800135795,
6.11679883634816));
#43308=CARTESIAN_POINT('Ctrl Pts',(0.264020877357473,-2.35714939016802,
6.11421620555426));
#43309=CARTESIAN_POINT('Ctrl Pts',(0.238429275463149,-2.35987539513475,
6.11252949050779));
#43310=CARTESIAN_POINT('Ctrl Pts',(0.107097806058428,-2.37170637756908,
6.1039750688423));
#43311=CARTESIAN_POINT('Ctrl Pts',(0.000866616818803647,-2.37412408417339,
6.09738870717227));
#43312=CARTESIAN_POINT('Ctrl Pts',(-0.227511513130802,-2.36398631128562,
6.08330183214533));
#43313=CARTESIAN_POINT('Ctrl Pts',(-0.349235020293758,-2.34909054807512,
6.0758325011141));
#43314=CARTESIAN_POINT('Ctrl Pts',(-0.541849729439626,-2.31021223325413,
6.06350784294496));
#43315=CARTESIAN_POINT('Ctrl Pts',(-0.613705324291566,-2.29217056406882,
6.05879578316037));
#43316=CARTESIAN_POINT('Ctrl Pts',(-0.711261791736611,-2.26275948565538,
6.05216890181641));
#43317=CARTESIAN_POINT('Ctrl Pts',(-0.737784179258192,-2.25425114532952,
6.05034358157497));
#43318=CARTESIAN_POINT('Ctrl Pts',(-0.783072163553667,-2.23883799811418,
6.04718260831492));
#43319=CARTESIAN_POINT('Ctrl Pts',(-0.801911945278698,-2.23215922067777,
6.04585433041541));
#43320=CARTESIAN_POINT('Ctrl Pts',(-0.84028527334229,-2.21800722577292,
6.0431203689425));
#43321=CARTESIAN_POINT('Ctrl Pts',(-0.859808837423326,-2.21051218266549,
6.04171407037881));
#43322=CARTESIAN_POINT('Ctrl Pts',(-0.909602896822906,-2.19063691761851,
6.03808666325165));
#43323=CARTESIAN_POINT('Ctrl Pts',(-0.93972021886839,-2.17788733947459,
6.03585359748941));
#43324=CARTESIAN_POINT('Ctrl Pts',(-1.09486508333506,-2.10839259934208,
6.02413972769836));
#43325=CARTESIAN_POINT('Ctrl Pts',(-1.21503704678675,-2.04150017996007,
6.01432371358579));
#43326=CARTESIAN_POINT('Ctrl Pts',(-1.423215504033,-1.90070146021737,5.99607237790804));
#43327=CARTESIAN_POINT('Ctrl Pts',(-1.51296612243999,-1.8300663650977,5.9877132809889));
#43328=CARTESIAN_POINT('Ctrl Pts',(-1.63844391685033,-1.71575039899171,
5.9755420935242));
#43329=CARTESIAN_POINT('Ctrl Pts',(-1.67827141089234,-1.67681364774516,
5.97159808391528));
#43330=CARTESIAN_POINT('Ctrl Pts',(-1.72875584480334,-1.62385555182175,
5.96652922454154));
#43331=CARTESIAN_POINT('Ctrl Pts',(-1.74067747001173,-1.61106971113231,
5.96532686819106));
#43332=CARTESIAN_POINT('Ctrl Pts',(-1.76018344541345,-1.58968040151759,
5.96335228483598));
#43333=CARTESIAN_POINT('Ctrl Pts',(-1.76784855976269,-1.58115180502976,
5.96257443309881));
#43334=CARTESIAN_POINT('Ctrl Pts',(-1.7834527168597,-1.56353448334302,5.96098753857058));
#43335=CARTESIAN_POINT('Ctrl Pts',(-1.79138476577734,-1.55444019204796,
5.96017896790289));
#43336=CARTESIAN_POINT('Ctrl Pts',(-1.81249444659139,-1.52986121594332,
5.9580206872017));
#43337=CARTESIAN_POINT('Ctrl Pts',(-1.82554326987668,-1.51426658675174,
5.95667971067277));
#43338=CARTESIAN_POINT('Ctrl Pts',(-1.89923366372438,-1.42386203317637,
5.94905412357267));
#43339=CARTESIAN_POINT('Ctrl Pts',(-1.95548155277556,-1.34557337778903,
5.94302230431289));
#43340=CARTESIAN_POINT('Ctrl Pts',(-2.08084801854272,-1.14654397330121,
5.92846612325855));
#43341=CARTESIAN_POINT('Ctrl Pts',(-2.14440897219707,-1.02274206232494,
5.92003520173132));
#43342=CARTESIAN_POINT('Ctrl Pts',(-2.22548945135277,-0.823528089592046,
5.9065595876468));
#43343=CARTESIAN_POINT('Ctrl Pts',(-2.25078946237846,-0.751629507688478,
5.90171672577152));
#43344=CARTESIAN_POINT('Ctrl Pts',(-2.28062770994385,-0.651709605948943,
5.89493693985247));
#43345=CARTESIAN_POINT('Ctrl Pts',(-2.28819089818765,-0.624636268233069,
5.89309534782173));
#43346=CARTESIAN_POINT('Ctrl Pts',(-2.30031694357159,-0.578049574094697,
5.88991520475524));
#43347=CARTESIAN_POINT('Ctrl Pts',(-2.30511703895668,-0.558600704225646,
5.88858427017787));
#43348=CARTESIAN_POINT('Ctrl Pts',(-2.31440630517847,-0.51880217886128,
5.88585291106844));
#43349=CARTESIAN_POINT('Ctrl Pts',(-2.31887478124092,-0.498449544221166,
5.88445196627546));
#43350=CARTESIAN_POINT('Ctrl Pts',(-2.32959051049132,-0.446375715583181,
5.88085574884813));
#43351=CARTESIAN_POINT('Ctrl Pts',(-2.33545821234231,-0.414581703621275,
5.87864891951459));
#43352=CARTESIAN_POINT('Ctrl Pts',(-2.3614719843078,-0.255467243426252,
5.86754402908281));
#43353=CARTESIAN_POINT('Ctrl Pts',(-2.37186176843005,-0.126791202973871,
5.85835348480349));
#43354=CARTESIAN_POINT('Ctrl Pts',(-2.37169928118365,0.0590433526103015,
5.84488022648407));
#43355=CARTESIAN_POINT('Ctrl Pts',(-2.36959688997047,0.11596789586163,5.84072892506888));
#43356=CARTESIAN_POINT('Ctrl Pts',(-2.36545133284689,0.172736951556046,
5.836583843094));
#43357=CARTESIAN_POINT('Ctrl Pts',(-2.36545134983051,0.172736718982988,
5.64123248379855));
#43358=CARTESIAN_POINT('Ctrl Pts',(-2.36578023953226,0.168232913460231,
5.64155645293107));
#43359=CARTESIAN_POINT('Ctrl Pts',(-2.36609628100516,0.163727968708386,
5.64188013254837));
#43360=CARTESIAN_POINT('Ctrl Pts',(-2.36997300544558,0.106111042944931,
5.64601495739026));
#43361=CARTESIAN_POINT('Ctrl Pts',(-2.37175781277497,0.0528904143435972,
5.64978090317875));
#43362=CARTESIAN_POINT('Ctrl Pts',(-2.37174739206271,-0.0178879215464695,
5.6546827610044));
#43363=CARTESIAN_POINT('Ctrl Pts',(-2.37155026538341,-0.0354267308714001,
5.65588871844607));
#43364=CARTESIAN_POINT('Ctrl Pts',(-2.37089929323082,-0.0645711640244984,
5.65787646073038));
#43365=CARTESIAN_POINT('Ctrl Pts',(-2.37055474079148,-0.0761783255766588,
5.65866381833403));
#43366=CARTESIAN_POINT('Ctrl Pts',(-2.36965812363536,-0.100386816681599,
5.66029646047557));
#43367=CARTESIAN_POINT('Ctrl Pts',(-2.36909077150643,-0.112987035396042,
5.66114093693192));
#43368=CARTESIAN_POINT('Ctrl Pts',(-2.36726870980262,-0.147350209519865,
5.66343099269311));
#43369=CARTESIAN_POINT('Ctrl Pts',(-2.36581441562608,-0.169101923713969,
5.66486636017696));
#43370=CARTESIAN_POINT('Ctrl Pts',(-2.36184033382696,-0.218333699791606,
5.66808907103359));
#43371=CARTESIAN_POINT('Ctrl Pts',(-2.35914044609461,-0.245796370245136,
5.66986835907773));
#43372=CARTESIAN_POINT('Ctrl Pts',(-2.34857920697284,-0.336869771363608,
5.67572596145446));
#43373=CARTESIAN_POINT('Ctrl Pts',(-2.33861869041828,-0.400211415621115,
5.67973041794787));
#43374=CARTESIAN_POINT('Ctrl Pts',(-2.28741722256558,-0.65740483951979,
5.69597340927771));
#43375=CARTESIAN_POINT('Ctrl Pts',(-2.22453614031546,-0.846105073321273,
5.70792513214723));
#43376=CARTESIAN_POINT('Ctrl Pts',(-2.12278265817708,-1.05848374713708,
5.72308321076931));
#43377=CARTESIAN_POINT('Ctrl Pts',(-2.10584559360362,-1.0917912580745,5.72551151576248));
#43378=CARTESIAN_POINT('Ctrl Pts',(-2.07755706944244,-1.14431279608638,
5.72943133345789));
#43379=CARTESIAN_POINT('Ctrl Pts',(-2.0667085910341,-1.16379151755075,5.73090553787557));
#43380=CARTESIAN_POINT('Ctrl Pts',(-2.04544631841972,-1.20073340531113,
5.73374242287402));
#43381=CARTESIAN_POINT('Ctrl Pts',(-2.03507937768889,-1.21822134087508,
5.73510335925646));
#43382=CARTESIAN_POINT('Ctrl Pts',(-2.01049313543848,-1.25850594175691,
5.73828157647416));
#43383=CARTESIAN_POINT('Ctrl Pts',(-1.99610896212891,-1.2811981749897,5.74010463891316));
#43384=CARTESIAN_POINT('Ctrl Pts',(-1.94665401431654,-1.35636246888808,
5.74625678965326));
#43385=CARTESIAN_POINT('Ctrl Pts',(-1.90987758691654,-1.40767445204668,
5.75064671376742));
#43386=CARTESIAN_POINT('Ctrl Pts',(-1.81090534128857,-1.53473642310342,
5.7620184417255));
#43387=CARTESIAN_POINT('Ctrl Pts',(-1.74598405672104,-1.60820726509411,
5.76908503403594));
#43388=CARTESIAN_POINT('Ctrl Pts',(-1.57254212223241,-1.78157311921658,
5.78691360739987));
#43389=CARTESIAN_POINT('Ctrl Pts',(-1.45889240237088,-1.87577461744847,
5.79771824808407));
#43390=CARTESIAN_POINT('Ctrl Pts',(-1.31757944812477,-1.9722445697237,5.8096820714659));
#43391=CARTESIAN_POINT('Ctrl Pts',(-1.29772579011068,-1.9853644812301,5.81133147976303));
#43392=CARTESIAN_POINT('Ctrl Pts',(-1.26658234576733,-2.00527819683184,
5.81386652601018));
#43393=CARTESIAN_POINT('Ctrl Pts',(-1.25542832057329,-2.0122801091089,5.81476424061711));
#43394=CARTESIAN_POINT('Ctrl Pts',(-1.23440383249583,-2.02523531532749,
5.81643648125875));
#43395=CARTESIAN_POINT('Ctrl Pts',(-1.22454786762937,-2.03120984382484,
5.81721222245939));
#43396=CARTESIAN_POINT('Ctrl Pts',(-1.2006359027733,-2.04546758464899,5.81907530223929));
#43397=CARTESIAN_POINT('Ctrl Pts',(-1.18653733726933,-2.05367801626033,
5.82015817910857));
#43398=CARTESIAN_POINT('Ctrl Pts',(-1.13485255696043,-2.08306718206789,
5.8240756579843));
#43399=CARTESIAN_POINT('Ctrl Pts',(-1.09677287852343,-2.10336610922076,
5.82686221126415));
#43400=CARTESIAN_POINT('Ctrl Pts',(-0.993262452344374,-2.15496770666979,
5.83423000112154));
#43401=CARTESIAN_POINT('Ctrl Pts',(-0.92691311317928,-2.18432816279766,
5.83873849797822));
#43402=CARTESIAN_POINT('Ctrl Pts',(-0.681791379413475,-2.27961332944921,
5.8549758357128));
#43403=CARTESIAN_POINT('Ctrl Pts',(-0.496615512133596,-2.32698157941617,
5.86652307955466));
#43404=CARTESIAN_POINT('Ctrl Pts',(-0.273401907431081,-2.35619419560885,
5.88105293264485));
#43405=CARTESIAN_POINT('Ctrl Pts',(-0.238937509337316,-2.35993821141071,
5.88331080145762));
#43406=CARTESIAN_POINT('Ctrl Pts',(-0.182737798023221,-2.36479976554458,
5.88702257907744));
#43407=CARTESIAN_POINT('Ctrl Pts',(-0.16104667010228,-2.36637591102542,
5.88846240713598));
#43408=CARTESIAN_POINT('Ctrl Pts',(-0.118840285173875,-2.36885977646934,
5.89127949944095));
#43409=CARTESIAN_POINT('Ctrl Pts',(-0.0983288208485738,-2.36979979159629,
5.89265564526774));
#43410=CARTESIAN_POINT('Ctrl Pts',(-0.049580496321132,-2.37139990353691,
5.89594427208569));
#43411=CARTESIAN_POINT('Ctrl Pts',(-0.0213395146880917,-2.37182213418319,
5.89786381868385));
#43412=CARTESIAN_POINT('Ctrl Pts',(0.0800890165780273,-2.37152699831633,
5.9048126218662));
#43413=CARTESIAN_POINT('Ctrl Pts',(0.153220490005098,-2.36792654937597,
5.90992669463199));
#43414=CARTESIAN_POINT('Ctrl Pts',(0.344371412835014,-2.34962374146219,
5.92356411964682));
#43415=CARTESIAN_POINT('Ctrl Pts',(0.461652738406823,-2.3294196266039,5.93221180444539));
#43416=CARTESIAN_POINT('Ctrl Pts',(0.691479882900604,-2.27178433819866,
5.94946333371919));
#43417=CARTESIAN_POINT('Ctrl Pts',(0.803749709636661,-2.23453358046326,
5.9580418122213));
#43418=CARTESIAN_POINT('Ctrl Pts',(0.932245340392641,-2.18095419918627,
5.96773783947919));
#43419=CARTESIAN_POINT('Ctrl Pts',(0.951597052417868,-2.17258042857045,
5.969194410356));
#43420=CARTESIAN_POINT('Ctrl Pts',(0.982204145092333,-2.15884884725206,
5.97148945065426));
#43421=CARTESIAN_POINT('Ctrl Pts',(0.993532919795582,-2.15365867366831,
5.97233700354946));
#43422=CARTESIAN_POINT('Ctrl Pts',(1.01554654926933,-2.14336265761326,5.97397943526246));
#43423=CARTESIAN_POINT('Ctrl Pts',(1.02623492847852,-2.13826568871588,5.97477474167052));
#43424=CARTESIAN_POINT('Ctrl Pts',(1.05319463069071,-2.12516069872611,5.9767763780805));
#43425=CARTESIAN_POINT('Ctrl Pts',(1.06941353060286,-2.11704550607595,5.97797648681104));
#43426=CARTESIAN_POINT('Ctrl Pts',(1.13809299574232,-2.08169073307758,5.98304770001403));
#43427=CARTESIAN_POINT('Ctrl Pts',(1.1896225859989,-2.05267905187098,5.98682596277798));
#43428=CARTESIAN_POINT('Ctrl Pts',(1.34886869654328,-1.95500813275285,5.99858631979095));
#43429=CARTESIAN_POINT('Ctrl Pts',(1.4521548723051,-1.87956196080577,6.00635029065062));
#43430=CARTESIAN_POINT('Ctrl Pts',(1.6393249270639,-1.71816137194626,6.02160326949658));
#43431=CARTESIAN_POINT('Ctrl Pts',(1.72374965589472,-1.6334463780326,6.02905635080786));
#43432=CARTESIAN_POINT('Ctrl Pts',(1.82260905504624,-1.51801001942559,6.03888845338173));
#43433=CARTESIAN_POINT('Ctrl Pts',(1.84327554027202,-1.4928473819201,6.04101314710745));
#43434=CARTESIAN_POINT('Ctrl Pts',(1.87660997110012,-1.45051297104119,6.04456308041927));
#43435=CARTESIAN_POINT('Ctrl Pts',(1.88957624011359,-1.43358098713145,6.04597658301143));
#43436=CARTESIAN_POINT('Ctrl Pts',(1.91472281446972,-1.39980942889336,6.04878491875366));
#43437=CARTESIAN_POINT('Ctrl Pts',(1.92691361402352,-1.38298003281408,6.05017918180063));
#43438=CARTESIAN_POINT('Ctrl Pts',(1.95598218358289,-1.34172030039274,6.05358610134248));
#43439=CARTESIAN_POINT('Ctrl Pts',(1.97262498039105,-1.31712953724282,6.05560722078294));
#43440=CARTESIAN_POINT('Ctrl Pts',(2.03562316987075,-1.22017271995127,6.06354366745498));
#43441=CARTESIAN_POINT('Ctrl Pts',(2.07848883169563,-1.14562836532599,6.06957977513489));
#43442=CARTESIAN_POINT('Ctrl Pts',(2.20075018980182,-0.903467327831151,
6.08896743849208));
#43443=CARTESIAN_POINT('Ctrl Pts',(2.2645975261339,-0.728797575729085,6.10268820066702));
#43444=CARTESIAN_POINT('Ctrl Pts',(2.31765368782206,-0.505591909030072,
6.1190323471743));
#43445=CARTESIAN_POINT('Ctrl Pts',(2.32665210039277,-0.462420106924175,
6.12213736251942));
#43446=CARTESIAN_POINT('Ctrl Pts',(2.33742399838102,-0.402407704592652,
6.12635494040289));
#43447=CARTESIAN_POINT('Ctrl Pts',(2.34022845188182,-0.385763842731493,
6.12751423091057));
#43448=CARTESIAN_POINT('Ctrl Pts',(2.34466216184429,-0.357620259491832,
6.12945540294883));
#43449=CARTESIAN_POINT('Ctrl Pts',(2.34638502772495,-0.346136141516994,
6.13024213465479));
#43450=CARTESIAN_POINT('Ctrl Pts',(2.34984485052009,-0.321860009875625,
6.13189338091179));
#43451=CARTESIAN_POINT('Ctrl Pts',(2.35156183072193,-0.309065790492221,
6.13275684437723));
#43452=CARTESIAN_POINT('Ctrl Pts',(2.35607302652082,-0.273233386574049,
6.13515774469181));
#43453=CARTESIAN_POINT('Ctrl Pts',(2.35863378989579,-0.250166607445443,
6.13668325287829));
#43454=CARTESIAN_POINT('Ctrl Pts',(2.36372520486561,-0.197229787110296,
6.14014593105574));
#43455=CARTESIAN_POINT('Ctrl Pts',(2.36602903818142,-0.167341531977288,
6.14207316375314));
#43456=CARTESIAN_POINT('Ctrl Pts',(2.3720253511006,-0.0640214471063062,
6.1486638558142));
#43457=CARTESIAN_POINT('Ctrl Pts',(2.37287029338955,0.0095365984689538,
6.15323237955966));
#43458=CARTESIAN_POINT('Ctrl Pts',(2.36370367440257,0.271254507750847,6.16939603012114));
#43459=CARTESIAN_POINT('Ctrl Pts',(2.33471398869007,0.458015739130436,6.18082237169589));
#43460=CARTESIAN_POINT('Ctrl Pts',(2.27451404202174,0.673058116066307,6.19523085799782));
#43461=CARTESIAN_POINT('Ctrl Pts',(2.26434185218677,0.706524685358358,6.19750839231698));
#43462=CARTESIAN_POINT('Ctrl Pts',(2.2466309445949,0.760475625057775,6.20124413888627));
#43463=CARTESIAN_POINT('Ctrl Pts',(2.23954275452551,0.781103050839649,6.20268791127723));
#43464=CARTESIAN_POINT('Ctrl Pts',(2.22524124113493,0.820926233492554,6.20550687672391));
#43465=CARTESIAN_POINT('Ctrl Pts',(2.21806145041506,0.840132025201788,6.20688087539652));
#43466=CARTESIAN_POINT('Ctrl Pts',(2.20046784449994,0.885396371048065,6.21015475619988));
#43467=CARTESIAN_POINT('Ctrl Pts',(2.18983897349617,0.911367447255657,6.21206153180158));
#43468=CARTESIAN_POINT('Ctrl Pts',(2.15039853163296,1.00306205236417,6.21889821077395));
#43469=CARTESIAN_POINT('Ctrl Pts',(2.11907061418222,1.06765409603407,6.22390929128145));
#43470=CARTESIAN_POINT('Ctrl Pts',(2.02643388872319,1.2384610813929,6.2376982681088));
#43471=CARTESIAN_POINT('Ctrl Pts',(1.95974261250118,1.3415007431432,6.24661906463699));
#43472=CARTESIAN_POINT('Ctrl Pts',(1.8201674945745,1.5243844138546,6.2633680955525));
#43473=CARTESIAN_POINT('Ctrl Pts',(1.74919737943121,1.60532551075475,6.2711738241074));
#43474=CARTESIAN_POINT('Ctrl Pts',(1.6546643992218,1.6993972515994,6.28052183685177));
#43475=CARTESIAN_POINT('Ctrl Pts',(1.63605729532713,1.71731824382338,6.28231603270985));
#43476=CARTESIAN_POINT('Ctrl Pts',(1.60721113372758,1.74420624372959,6.28502379709278));
#43477=CARTESIAN_POINT('Ctrl Pts',(1.59718214650736,1.75339449700382,6.2859520226483));
#43478=CARTESIAN_POINT('Ctrl Pts',(1.57865939725611,1.77007367058003,6.28764151114012));
#43479=CARTESIAN_POINT('Ctrl Pts',(1.57019055350955,1.77759048295065,6.28840453490789));
#43480=CARTESIAN_POINT('Ctrl Pts',(1.55001067157273,1.79524507238569,6.29020096571449));
#43481=CARTESIAN_POINT('Ctrl Pts',(1.53825368606332,1.80532921670585,6.29123062253935));
#43482=CARTESIAN_POINT('Ctrl Pts',(1.49774405497266,1.83939185665732,6.29472429450027));
#43483=CARTESIAN_POINT('Ctrl Pts',(1.46852141247816,1.86280564631288,6.29715284943029));
#43484=CARTESIAN_POINT('Ctrl Pts',(1.39238493534334,1.92090196670928,6.30328552197746));
#43485=CARTESIAN_POINT('Ctrl Pts',(1.34472263082007,1.95456441453259,6.30694355982376));
#43486=CARTESIAN_POINT('Ctrl Pts',(1.13865851763053,2.08899165612909,6.32222644741322));
#43487=CARTESIAN_POINT('Ctrl Pts',(0.969842481153402,2.17251792697489,6.33352967809068));
#43488=CARTESIAN_POINT('Ctrl Pts',(0.746912031149507,2.25160081181676,6.34860470527262));
#43489=CARTESIAN_POINT('Ctrl Pts',(0.700387945400513,2.26650391863106,6.35175428550142));
#43490=CARTESIAN_POINT('Ctrl Pts',(0.629868117452508,2.28671499231276,6.35655273269274));
#43491=CARTESIAN_POINT('Ctrl Pts',(0.606194315205028,2.29310437635411,6.35816758295036));
#43492=CARTESIAN_POINT('Ctrl Pts',(0.562920112567481,2.30406682250814,6.36112884622699));
#43493=CARTESIAN_POINT('Ctrl Pts',(0.543352245829095,2.30875968236557,6.36247134559364));
#43494=CARTESIAN_POINT('Ctrl Pts',(0.500507481816747,2.31846007770791,6.36541948990815));
#43495=CARTESIAN_POINT('Ctrl Pts',(0.477210342804884,2.32336718791008,6.367028119285));
#43496=CARTESIAN_POINT('Ctrl Pts',(0.409660330319795,2.33653651174923,6.37171015517303));
#43497=CARTESIAN_POINT('Ctrl Pts',(0.365243127551471,2.34389023856262,6.37481097677845));
#43498=CARTESIAN_POINT('Ctrl Pts',(0.0987837685891144,2.38024769832461,
6.39355490890545));
#43499=CARTESIAN_POINT('Ctrl Pts',(-0.126231365591026,2.37894307121585,
6.41011984683565));
#43500=CARTESIAN_POINT('Ctrl Pts',(-0.405926009450226,2.33749691633769,
6.43043225221606));
#43501=CARTESIAN_POINT('Ctrl Pts',(-0.463857150945083,2.32669410936557,
6.43461410323573));
#43502=CARTESIAN_POINT('Ctrl Pts',(-0.53946059936844,2.30965922075857,6.43999100972916));
#43503=CARTESIAN_POINT('Ctrl Pts',(-0.557542855714967,2.30536102839415,
6.44127082646511));
#43504=CARTESIAN_POINT('Ctrl Pts',(-0.586004036519302,2.29824127069845,
6.4432735024244));
#43505=CARTESIAN_POINT('Ctrl Pts',(-0.596417069123826,2.29556101207306,
6.4440037214249));
#43506=CARTESIAN_POINT('Ctrl Pts',(-0.618410323064428,2.28974030932096,
6.44554020519186));
#43507=CARTESIAN_POINT('Ctrl Pts',(-0.629985659677364,2.2865826231699,6.44634542696884));
#43508=CARTESIAN_POINT('Ctrl Pts',(-0.659742191036129,2.27822209291788,
6.4484076679363));
#43509=CARTESIAN_POINT('Ctrl Pts',(-0.677886469452383,2.27288927414737,
6.44965766974099));
#43510=CARTESIAN_POINT('Ctrl Pts',(-0.761123500867893,2.24733945605914,
6.45536584572576));
#43511=CARTESIAN_POINT('Ctrl Pts',(-0.825395227103285,2.22453772459901,
6.45969956387093));
#43512=CARTESIAN_POINT('Ctrl Pts',(-1.05685522379626,2.13100617379443,6.47533223031337));
#43513=CARTESIAN_POINT('Ctrl Pts',(-1.21675038561398,2.04393069876013,6.48622809597149));
#43514=CARTESIAN_POINT('Ctrl Pts',(-1.41897166053197,1.90159103785509,6.50180018988613));
#43515=CARTESIAN_POINT('Ctrl Pts',(-1.47118327011399,1.86149071875855,6.50600114561125));
#43516=CARTESIAN_POINT('Ctrl Pts',(-1.54088922189402,1.80318803933655,6.51191467227363));
#43517=CARTESIAN_POINT('Ctrl Pts',(-1.55986453326166,1.78679860672471,6.51355747045079));
#43518=CARTESIAN_POINT('Ctrl Pts',(-1.59394938573373,1.75640192619069,6.51657187867528));
#43519=CARTESIAN_POINT('Ctrl Pts',(-1.60914319962626,1.74249260813757,6.51793945006947));
#43520=CARTESIAN_POINT('Ctrl Pts',(-1.63963690349021,1.7138378900879,6.52073442165589));
#43521=CARTESIAN_POINT('Ctrl Pts',(-1.65492362770187,1.69908128869193,6.52216221998327));
#43522=CARTESIAN_POINT('Ctrl Pts',(-1.69284366259746,1.66147900421524,6.52577315716763));
#43523=CARTESIAN_POINT('Ctrl Pts',(-1.71521383316145,1.63837525670508,6.52796727161902));
#43524=CARTESIAN_POINT('Ctrl Pts',(-1.81766149058534,1.52816980820141,6.53832586627115));
#43525=CARTESIAN_POINT('Ctrl Pts',(-1.8916079551903,1.43562124678482,6.54673204854011));
#43526=CARTESIAN_POINT('Ctrl Pts',(-2.05124613376433,1.20196260382582,6.56719200454078));
#43527=CARTESIAN_POINT('Ctrl Pts',(-2.12974029781669,1.05666139043118,6.57934505506317));
#43528=CARTESIAN_POINT('Ctrl Pts',(-2.20370183449107,0.877355121311782,
6.59302765788477));
#43529=CARTESIAN_POINT('Ctrl Pts',(-2.21435584019639,0.850107155447432,
6.5950721369387));
#43530=CARTESIAN_POINT('Ctrl Pts',(-2.22946695725954,0.809246509110479,
6.5980797211005));
#43531=CARTESIAN_POINT('Ctrl Pts',(-2.23430897500204,0.795780280657911,
6.59906161154154));
#43532=CARTESIAN_POINT('Ctrl Pts',(-2.24283046609485,0.771389917398216,
6.60082227597204));
#43533=CARTESIAN_POINT('Ctrl Pts',(-2.24655273910661,0.760481240816587,
6.60160335985199));
#43534=CARTESIAN_POINT('Ctrl Pts',(-2.25423928076437,0.737405621940138,
6.60324168706354));
#43535=CARTESIAN_POINT('Ctrl Pts',(-2.2581848446999,0.725233074271705,6.60409790349739));
#43536=CARTESIAN_POINT('Ctrl Pts',(-2.26884603345972,0.691411233443826,
6.60645632720292));
#43537=CARTESIAN_POINT('Ctrl Pts',(-2.27535031370248,0.669696093468538,
6.60794727717495));
#43538=CARTESIAN_POINT('Ctrl Pts',(-2.28947863487125,0.619943263563181,
6.61131748002293));
#43539=CARTESIAN_POINT('Ctrl Pts',(-2.29690091104665,0.591851692970257,
6.61318754583698));
#43540=CARTESIAN_POINT('Ctrl Pts',(-2.33523019469976,0.435182823143709,
6.62347137079951));
#43541=CARTESIAN_POINT('Ctrl Pts',(-2.35583463309604,0.304427903160431,
6.63152390776219));
#43542=CARTESIAN_POINT('Ctrl Pts',(-2.36545136499509,0.172736511319546,
6.63965300722759));
#43543=CARTESIAN_POINT('Origin',(0.,0.,-1.84858989190501));
#43544=CARTESIAN_POINT('',(-2.36545134965667,0.17273672136364,7.83525515262476));
#43545=CARTESIAN_POINT('',(-2.36545135498545,0.17273664839138,7.63805096494753));
#43546=CARTESIAN_POINT('',(-2.36545134966535,0.172736721244682,-1.84858989190501));
#43547=CARTESIAN_POINT('',(-2.37174965797748,-0.00127372827735513,6.85023264105921));
#43548=CARTESIAN_POINT('Ctrl Pts',(-2.36545134965667,0.17273672136364,7.83525515262476));
#43549=CARTESIAN_POINT('Ctrl Pts',(-2.36502652455963,0.178554263176551,
7.83488542092976));
#43550=CARTESIAN_POINT('Ctrl Pts',(-2.36458022850928,0.18437036980467,7.83451633788331));
#43551=CARTESIAN_POINT('Ctrl Pts',(-2.35550714366389,0.297154247534622,
7.82736904092432));
#43552=CARTESIAN_POINT('Ctrl Pts',(-2.33965115124067,0.40342258231143,7.82080147884784));
#43553=CARTESIAN_POINT('Ctrl Pts',(-2.28759914925481,0.640677282685825,
7.80586554411087));
#43554=CARTESIAN_POINT('Ctrl Pts',(-2.24725031471078,0.770349262957642,
7.79749654101737));
#43555=CARTESIAN_POINT('Ctrl Pts',(-2.18176354461517,0.930879425497304,
7.78634965453539));
#43556=CARTESIAN_POINT('Ctrl Pts',(-2.16664185855844,0.965552420234006,
7.78389396821056));
#43557=CARTESIAN_POINT('Ctrl Pts',(-2.14135567965776,1.01994365098656,7.77995616145276));
#43558=CARTESIAN_POINT('Ctrl Pts',(-2.13173219075743,1.03990721237562,7.77849213719076));
#43559=CARTESIAN_POINT('Ctrl Pts',(-2.11307879457354,1.07725564628182,7.77571614500148));
#43560=CARTESIAN_POINT('Ctrl Pts',(-2.10411045567512,1.09466929757376,7.77440637293124));
#43561=CARTESIAN_POINT('Ctrl Pts',(-2.08321827336733,1.13402974176567,7.77140941538428));
#43562=CARTESIAN_POINT('Ctrl Pts',(-2.07116153442144,1.15590295733346,7.76971772650803));
#43563=CARTESIAN_POINT('Ctrl Pts',(-2.03192983396312,1.2244916439511,7.76432721529079));
#43564=CARTESIAN_POINT('Ctrl Pts',(-2.00350414842023,1.2704680119567,7.7605852442756));
#43565=CARTESIAN_POINT('Ctrl Pts',(-1.93053267203484,1.37994681545583,7.7513511037216));
#43566=CARTESIAN_POINT('Ctrl Pts',(-1.88439616626324,1.44231025367349,7.74580982055011));
#43567=CARTESIAN_POINT('Ctrl Pts',(-1.73778474911568,1.62141906489628,7.72908408716959));
#43568=CARTESIAN_POINT('Ctrl Pts',(-1.62891287360248,1.73076254010812,7.71773699370195));
#43569=CARTESIAN_POINT('Ctrl Pts',(-1.47771302094563,1.85562357425548,7.70378464303611));
#43570=CARTESIAN_POINT('Ctrl Pts',(-1.44450099422281,1.88159294108815,7.70081955550987));
#43571=CARTESIAN_POINT('Ctrl Pts',(-1.39748614446874,1.91637604276122,7.69677637242602));
#43572=CARTESIAN_POINT('Ctrl Pts',(-1.38425969005128,1.92595166310529,7.69565527838919));
#43573=CARTESIAN_POINT('Ctrl Pts',(-1.36174978660769,1.94189656793928,7.69377614437337));
#43574=CARTESIAN_POINT('Ctrl Pts',(-1.35251812426689,1.94833762654464,7.69301355595475));
#43575=CARTESIAN_POINT('Ctrl Pts',(-1.33295763944737,1.96177920802411,7.69141513230602));
#43576=CARTESIAN_POINT('Ctrl Pts',(-1.32261892901348,1.96876431183186,7.69058025965388));
#43577=CARTESIAN_POINT('Ctrl Pts',(-1.29367996658551,1.98798537743181,7.68826956531754));
#43578=CARTESIAN_POINT('Ctrl Pts',(-1.27496131501434,2.00004186161467,7.68680471895894));
#43579=CARTESIAN_POINT('Ctrl Pts',(-1.23183460711029,2.02696773499214,7.68349049866248));
#43580=CARTESIAN_POINT('Ctrl Pts',(-1.20732170416249,2.04166332849617,7.68165011538188));
#43581=CARTESIAN_POINT('Ctrl Pts',(-1.12301494123781,2.09015604542276,7.67544574871097));
#43582=CARTESIAN_POINT('Ctrl Pts',(-1.06201855043906,2.12179938929066,7.67116656782923));
#43583=CARTESIAN_POINT('Ctrl Pts',(-0.839718853935663,2.22513064609199,
7.65601442700783));
#43584=CARTESIAN_POINT('Ctrl Pts',(-0.671917555688727,2.28141571668127,
7.64533474098238));
#43585=CARTESIAN_POINT('Ctrl Pts',(-0.454635120436417,2.32821918001872,
7.63114425278071));
#43586=CARTESIAN_POINT('Ctrl Pts',(-0.409573633211008,2.33656728002393,
7.62818576568138));
#43587=CARTESIAN_POINT('Ctrl Pts',(-0.340779987955371,2.34726088445391,
7.62362989651485));
#43588=CARTESIAN_POINT('Ctrl Pts',(-0.317206170593052,2.35056266419589,
7.6220618304207));
#43589=CARTESIAN_POINT('Ctrl Pts',(-0.274228745217447,2.35592386214044,
7.61918860047817));
#43590=CARTESIAN_POINT('Ctrl Pts',(-0.254841606014832,2.35809973635284,
7.61788715058258));
#43591=CARTESIAN_POINT('Ctrl Pts',(-0.212524061570712,2.36232121086805,
7.61503374652679));
#43592=CARTESIAN_POINT('Ctrl Pts',(-0.189586479206702,2.36427259074841,
7.61347902896167));
#43593=CARTESIAN_POINT('Ctrl Pts',(-0.123543484042322,2.36892386445819,
7.6089777725126));
#43594=CARTESIAN_POINT('Ctrl Pts',(-0.0803898966371576,2.3707805297001,
7.60600604212888));
#43595=CARTESIAN_POINT('Ctrl Pts',(0.0951811649743621,2.3735355199686,7.59378483158364));
#43596=CARTESIAN_POINT('Ctrl Pts',(0.227498054114296,2.36452238703567,7.58425457583065));
#43597=CARTESIAN_POINT('Ctrl Pts',(0.500002728637081,2.32287071039141,7.56419731460912));
#43598=CARTESIAN_POINT('Ctrl Pts',(0.639407217365449,2.2884264054405,7.55369336343553));
#43599=CARTESIAN_POINT('Ctrl Pts',(0.797386034651848,2.23381775534014,7.54200242891027));
#43600=CARTESIAN_POINT('Ctrl Pts',(0.819797161344559,2.22569067304343,7.54034966757875));
#43601=CARTESIAN_POINT('Ctrl Pts',(0.854184397856357,2.21263070689497,7.53782653875786));
#43602=CARTESIAN_POINT('Ctrl Pts',(0.866248355835281,2.2079355597409,7.5369438273306));
#43603=CARTESIAN_POINT('Ctrl Pts',(0.888600472627781,2.19902497811122,7.53531372767464));
#43604=CARTESIAN_POINT('Ctrl Pts',(0.898897885530266,2.19483581427227,7.53456499503793));
#43605=CARTESIAN_POINT('Ctrl Pts',(0.923367744427714,2.18467995360969,7.53279059130465));
#43606=CARTESIAN_POINT('Ctrl Pts',(0.937512212813359,2.17864760178998,7.53176872099825));
#43607=CARTESIAN_POINT('Ctrl Pts',(0.986862817021009,2.15703085268392,7.52821335089255));
#43608=CARTESIAN_POINT('Ctrl Pts',(1.02174915284601,2.14072636644534,7.5257179311656));
#43609=CARTESIAN_POINT('Ctrl Pts',(1.11110614338163,2.09628199944897,7.51933411173979));
#43610=CARTESIAN_POINT('Ctrl Pts',(1.16491179486983,2.06686635498482,7.51549765071626));
#43611=CARTESIAN_POINT('Ctrl Pts',(1.39513820214338,1.92915106693704,7.4988621003276));
#43612=CARTESIAN_POINT('Ctrl Pts',(1.55807184632938,1.80012315219386,7.486414631567));
#43613=CARTESIAN_POINT('Ctrl Pts',(1.72680459033591,1.62622055048095,7.47079111774733));
#43614=CARTESIAN_POINT('Ctrl Pts',(1.75084654811235,1.60030732363766,7.46849083972407));
#43615=CARTESIAN_POINT('Ctrl Pts',(1.78853420159905,1.55782014943282,7.46475610930128));
#43616=CARTESIAN_POINT('Ctrl Pts',(1.80255009508627,1.54158078389952,7.46333691732641));
#43617=CARTESIAN_POINT('Ctrl Pts',(1.82904653956851,1.5100255156513,7.46059354316046));
#43618=CARTESIAN_POINT('Ctrl Pts',(1.84155981555945,1.49473934438962,7.45927082961816));
#43619=CARTESIAN_POINT('Ctrl Pts',(1.87032128859955,1.45869502252313,7.45616527904333));
#43620=CARTESIAN_POINT('Ctrl Pts',(1.88641698018401,1.43781910290772,7.45437670669));
#43621=CARTESIAN_POINT('Ctrl Pts',(1.93973224032869,1.36623327951279,7.44827465914509));
#43622=CARTESIAN_POINT('Ctrl Pts',(1.97527871842204,1.31431628266825,7.44390009380195));
#43623=CARTESIAN_POINT('Ctrl Pts',(2.06089650031195,1.17793654025632,7.43253206979626));
#43624=CARTESIAN_POINT('Ctrl Pts',(2.10786203055443,1.09166999551216,7.42545220692885));
#43625=CARTESIAN_POINT('Ctrl Pts',(2.21220364138674,0.868018848592198,7.4075054997557));
#43626=CARTESIAN_POINT('Ctrl Pts',(2.2622573509093,0.727667117731736,7.39659262622969));
#43627=CARTESIAN_POINT('Ctrl Pts',(2.30461273177817,0.560810456796328,7.38455785794993));
#43628=CARTESIAN_POINT('Ctrl Pts',(2.31004636646847,0.537990796917997,7.38293218271559));
#43629=CARTESIAN_POINT('Ctrl Pts',(2.31793436907612,0.502537340288836,7.38044145371097));
#43630=CARTESIAN_POINT('Ctrl Pts',(2.32062581485954,0.489958533062745,7.3795645204982));
#43631=CARTESIAN_POINT('Ctrl Pts',(2.3254561461057,0.466450191074961,7.37793901921239));
#43632=CARTESIAN_POINT('Ctrl Pts',(2.32762049887429,0.455527043098023,7.37718919129556));
#43633=CARTESIAN_POINT('Ctrl Pts',(2.33261762788357,0.42934135973239,7.37540413838447));
#43634=CARTESIAN_POINT('Ctrl Pts',(2.33537763532172,0.414065614550607,7.37437284979324));
#43635=CARTESIAN_POINT('Ctrl Pts',(2.3446283891367,0.359827566007707,7.37074316731238));
#43636=CARTESIAN_POINT('Ctrl Pts',(2.35029600013696,0.320729306923126,7.36818500186079));
#43637=CARTESIAN_POINT('Ctrl Pts',(2.36254740546877,0.218237873021053,7.3615884837741));
#43638=CARTESIAN_POINT('Ctrl Pts',(2.36755799393233,0.154687352375816,7.35760649938418));
#43639=CARTESIAN_POINT('Ctrl Pts',(2.37770207794855,-0.109480267277751,
7.34123238647913));
#43640=CARTESIAN_POINT('Ctrl Pts',(2.35993123053883,-0.310119249543331,
7.32914322231165));
#43641=CARTESIAN_POINT('Ctrl Pts',(2.30928631048834,-0.541979388920817,
7.31386149591503));
#43642=CARTESIAN_POINT('Ctrl Pts',(2.30062394135968,-0.577645368834535,
7.31147565560392));
#43643=CARTESIAN_POINT('Ctrl Pts',(2.28552141397073,-0.63408360184742,7.30763631237744));
#43644=CARTESIAN_POINT('Ctrl Pts',(2.2796168797703,-0.654993876142164,7.30619969757301));
#43645=CARTESIAN_POINT('Ctrl Pts',(2.26781986744159,-0.694678487705738,
7.30344467837641));
#43646=CARTESIAN_POINT('Ctrl Pts',(2.26197937924298,-0.713466468001206,
7.30212803471927));
#43647=CARTESIAN_POINT('Ctrl Pts',(2.24795348540473,-0.756681435072762,
7.29906994611166));
#43648=CARTESIAN_POINT('Ctrl Pts',(2.23960261226199,-0.781051673525601,
7.2973233018715));
#43649=CARTESIAN_POINT('Ctrl Pts',(2.21085153094412,-0.860700394717117,
7.29153942721779));
#43650=CARTESIAN_POINT('Ctrl Pts',(2.1887897464905,-0.915351346143952,7.28744953641931));
#43651=CARTESIAN_POINT('Ctrl Pts',(2.12858840463606,-1.04982267197795,7.27707473340755));
#43652=CARTESIAN_POINT('Ctrl Pts',(2.08797742180165,-1.12843432337487,7.27072234248427));
#43653=CARTESIAN_POINT('Ctrl Pts',(1.97214517912684,-1.32489475388003,7.25417675618632));
#43654=CARTESIAN_POINT('Ctrl Pts',(1.89072500883904,-1.43870216521157,7.2439116346261));
#43655=CARTESIAN_POINT('Ctrl Pts',(1.77406184532892,-1.57463003708838,7.2311918316787));
#43656=CARTESIAN_POINT('Ctrl Pts',(1.74761680341099,-1.60392989561684,7.22842079782599));
#43657=CARTESIAN_POINT('Ctrl Pts',(1.70950746875328,-1.64409094963024,7.2245963900735));
#43658=CARTESIAN_POINT('Ctrl Pts',(1.69844766447122,-1.65551393882935,7.22350552779009));
#43659=CARTESIAN_POINT('Ctrl Pts',(1.67941050553304,-1.67478464129566,7.22166123813357));
#43660=CARTESIAN_POINT('Ctrl Pts',(1.67149111330934,-1.68268853921893,7.2209036587945));
#43661=CARTESIAN_POINT('Ctrl Pts',(1.65448497387235,-1.69942285885851,7.21929761758497));
#43662=CARTESIAN_POINT('Ctrl Pts',(1.64538299935255,-1.70823692311428,7.21845033289346));
#43663=CARTESIAN_POINT('Ctrl Pts',(1.61942281726809,-1.73297592829163,7.21606675039528));
#43664=CARTESIAN_POINT('Ctrl Pts',(1.60240057334283,-1.74872763121118,7.21454257657119));
#43665=CARTESIAN_POINT('Ctrl Pts',(1.48916451222402,-1.85046962749401,7.20463260142641));
#43666=CARTESIAN_POINT('Ctrl Pts',(1.38628928050044,-1.92874545377028,7.19668854330215));
#43667=CARTESIAN_POINT('Ctrl Pts',(1.14495016434149,-2.08303973603129,7.179073930088));
#43668=CARTESIAN_POINT('Ctrl Pts',(1.00426198499473,-2.15439482266694,7.16943299927251));
#43669=CARTESIAN_POINT('Ctrl Pts',(0.822214251241414,-2.22499399662373,
7.15687471378871));
#43670=CARTESIAN_POINT('Ctrl Pts',(0.786555542845042,-2.23784822674097,
7.1544130174151));
#43671=CARTESIAN_POINT('Ctrl Pts',(0.729763237336152,-2.2567956129927,7.15048090220939));
#43672=CARTESIAN_POINT('Ctrl Pts',(0.708825789978955,-2.26345902716322,
7.14902887132021));
#43673=CARTESIAN_POINT('Ctrl Pts',(0.669022042889277,-2.27552027687866,
7.14626240193886));
#43674=CARTESIAN_POINT('Ctrl Pts',(0.650175345426807,-2.28097676567459,
7.14494997195391));
#43675=CARTESIAN_POINT('Ctrl Pts',(0.60687759104082,-2.29293211152929,7.14192801984534));
#43676=CARTESIAN_POINT('Ctrl Pts',(0.582386263141423,-2.29927471926238,
7.1402137085369));
#43677=CARTESIAN_POINT('Ctrl Pts',(0.503362477921157,-2.31839623701822,
7.13466426577325));
#43678=CARTESIAN_POINT('Ctrl Pts',(0.44848069450325,-2.3296349675031,7.13078226199609));
#43679=CARTESIAN_POINT('Ctrl Pts',(0.312590049861713,-2.3524830526908,7.12109774144653));
#43680=CARTESIAN_POINT('Ctrl Pts',(0.231283038478646,-2.36186263858594,
7.11523927237148));
#43681=CARTESIAN_POINT('Ctrl Pts',(-0.0238050714686189,-2.3779911496083,
7.09673771199558));
#43682=CARTESIAN_POINT('Ctrl Pts',(-0.1979536189631,-2.36985809530594,7.08389502069377));
#43683=CARTESIAN_POINT('Ctrl Pts',(-0.39339543047754,-2.33902026264831,
7.07005285486293));
#43684=CARTESIAN_POINT('Ctrl Pts',(-0.417079734285967,-2.33491335106683,
7.06838599657265));
#43685=CARTESIAN_POINT('Ctrl Pts',(-0.4534596149512,-2.32803374274299,7.06584602458951));
#43686=CARTESIAN_POINT('Ctrl Pts',(-0.466200978853671,-2.32551572700607,
7.06496032236766));
#43687=CARTESIAN_POINT('Ctrl Pts',(-0.488706542044473,-2.32087565323569,
7.06340349336342));
#43688=CARTESIAN_POINT('Ctrl Pts',(-0.498478558587589,-2.31879645804281,
7.06273013286214));
#43689=CARTESIAN_POINT('Ctrl Pts',(-0.52247188885008,-2.31353269949699,
7.06108294523542));
#43690=CARTESIAN_POINT('Ctrl Pts',(-0.536677441331674,-2.3102787227508,
7.0601129327441));
#43691=CARTESIAN_POINT('Ctrl Pts',(-0.58332129217467,-2.29914085311653,
7.05694242168998));
#43692=CARTESIAN_POINT('Ctrl Pts',(-0.615624681335829,-2.29070271038756,
7.05476986066242));
#43693=CARTESIAN_POINT('Ctrl Pts',(-0.695569750735475,-2.2680063381689,
7.04942670692641));
#43694=CARTESIAN_POINT('Ctrl Pts',(-0.742962582434193,-2.25292636570427,
7.0462891462356));
#43695=CARTESIAN_POINT('Ctrl Pts',(-0.902053865927786,-2.19673787518309,
7.03575278108852));
#43696=CARTESIAN_POINT('Ctrl Pts',(-1.01112019036126,-2.14871967439778,
7.02851515494955));
#43697=CARTESIAN_POINT('Ctrl Pts',(-1.2162681898329,-2.03930654329121,7.01415073348884));
#43698=CARTESIAN_POINT('Ctrl Pts',(-1.31243809561989,-1.97878280750758,
7.00705239116125));
#43699=CARTESIAN_POINT('Ctrl Pts',(-1.42954271130414,-1.89278046901822,
6.99764872658452));
#43700=CARTESIAN_POINT('Ctrl Pts',(-1.4548029416123,-1.87343495083563,6.99557194117343));
#43701=CARTESIAN_POINT('Ctrl Pts',(-1.49586970238984,-1.84065254625775,
6.99210959383941));
#43702=CARTESIAN_POINT('Ctrl Pts',(-1.5119031578588,-1.82750561113263,6.99073535058864));
#43703=CARTESIAN_POINT('Ctrl Pts',(-1.54313467557989,-1.80120441992518,
6.98801249400454));
#43704=CARTESIAN_POINT('Ctrl Pts',(-1.55834198242689,-1.78806381682842,
6.98666449887356));
#43705=CARTESIAN_POINT('Ctrl Pts',(-1.59469381131914,-1.75583627649624,
6.98338692998539));
#43706=CARTESIAN_POINT('Ctrl Pts',(-1.61566460230753,-1.73655899818807,
6.98144966235478));
#43707=CARTESIAN_POINT('Ctrl Pts',(-1.69379104523058,-1.66210141715531,
6.97405011895024));
#43708=CARTESIAN_POINT('Ctrl Pts',(-1.74850357869881,-1.60444447094203,
6.96848520026739));
#43709=CARTESIAN_POINT('Ctrl Pts',(-1.89926682210155,-1.4286809857887,6.95198649834393));
#43710=CARTESIAN_POINT('Ctrl Pts',(-1.98697214206719,-1.3039474333246,6.94081496752217));
#43711=CARTESIAN_POINT('Ctrl Pts',(-2.10167674345068,-1.10207271876522,
6.92400195498985));
#43712=CARTESIAN_POINT('Ctrl Pts',(-2.13768650193864,-1.03048936230543,
6.91826418302858));
#43713=CARTESIAN_POINT('Ctrl Pts',(-2.17797508272193,-0.939155061384799,
6.91132318639994));
#43714=CARTESIAN_POINT('Ctrl Pts',(-2.18571610268048,-0.920995587069111,
6.90996133191355));
#43715=CARTESIAN_POINT('Ctrl Pts',(-2.19777437034843,-0.891699747116969,
6.90779569794099));
#43716=CARTESIAN_POINT('Ctrl Pts',(-2.20223561929945,-0.880624161910472,
6.90698407590782));
#43717=CARTESIAN_POINT('Ctrl Pts',(-2.21084994231891,-0.858763150688833,
6.90539671412672));
#43718=CARTESIAN_POINT('Ctrl Pts',(-2.21500815750429,-0.847980240364823,
6.90462072703593));
#43719=CARTESIAN_POINT('Ctrl Pts',(-2.22541634180217,-0.820391161040172,
6.90265201305297));
#43720=CARTESIAN_POINT('Ctrl Pts',(-2.23155500676116,-0.803543309651698,
6.90146550077109));
#43721=CARTESIAN_POINT('Ctrl Pts',(-2.25753518886798,-0.729644591788346,
6.89632288177082));
#43722=CARTESIAN_POINT('Ctrl Pts',(-2.27538590249599,-0.671912676666023,
6.89246473897535));
#43723=CARTESIAN_POINT('Ctrl Pts',(-2.34449771414989,-0.413850179482464,
6.87566109412968));
#43724=CARTESIAN_POINT('Ctrl Pts',(-2.37163862822805,-0.208017014815944,
6.86333732876224));
#43725=CARTESIAN_POINT('Ctrl Pts',(-2.37174965797748,-0.00127372827735513,
6.85023264105921));
#43726=CARTESIAN_POINT('Ctrl Pts',(-2.37174965943354,-0.00127101411488308,
6.85023246901852));
#43727=CARTESIAN_POINT('Ctrl Pts',(-2.37176696530802,0.0310222558120081,
6.84818551792834));
#43728=CARTESIAN_POINT('Ctrl Pts',(-2.37112472272847,0.0633116873235132,
6.84612333680678));
#43729=CARTESIAN_POINT('Ctrl Pts',(-2.36878519694936,0.121319892465059,
6.84238328321564));
#43730=CARTESIAN_POINT('Ctrl Pts',(-2.36732762140969,0.147043113666593,
6.84071228654366));
#43731=CARTESIAN_POINT('Ctrl Pts',(-2.36545134966532,0.172736721245143,
6.83902895557496));
#43732=CARTESIAN_POINT('',(-2.37174939424271,0.00169511337750838,6.6502503165247));
#43733=CARTESIAN_POINT('Ctrl Pts',(-2.36545136499509,0.172736511319545,
6.6396530072276));
#43734=CARTESIAN_POINT('Ctrl Pts',(-2.36960469570264,0.115860858821994,
6.64316385049418));
#43735=CARTESIAN_POINT('Ctrl Pts',(-2.37170857335039,0.0588104238426276,
6.64668720588036));
#43736=CARTESIAN_POINT('Ctrl Pts',(-2.37174939424271,0.00169511337380844,
6.65025031652493));
#43737=CARTESIAN_POINT('Ctrl Pts',(-2.37174939604129,0.00169259498356675,
6.65025047363349));
#43738=CARTESIAN_POINT('Ctrl Pts',(-2.37180198521626,-0.0719980074205978,
6.65484762707334));
#43739=CARTESIAN_POINT('Ctrl Pts',(-2.36842022635197,-0.145646969305529,
6.65950247976216));
#43740=CARTESIAN_POINT('Ctrl Pts',(-2.35920558020346,-0.245006984224481,
6.66593854475818));
#43741=CARTESIAN_POINT('Ctrl Pts',(-2.3563663772406,-0.270955358027443,
6.6676336889454));
#43742=CARTESIAN_POINT('Ctrl Pts',(-2.35061731969685,-0.316527421877923,
6.6706392077535));
#43743=CARTESIAN_POINT('Ctrl Pts',(-2.34788841388856,-0.336171607927287,
6.6719440911275));
#43744=CARTESIAN_POINT('Ctrl Pts',(-2.34186715063314,-0.375857339753646,
6.67460047600724));
#43745=CARTESIAN_POINT('Ctrl Pts',(-2.3385630816661,-0.395895392017766,
6.67595223138285));
#43746=CARTESIAN_POINT('Ctrl Pts',(-2.33107903663843,-0.437914541218356,
6.67881010480298));
#43747=CARTESIAN_POINT('Ctrl Pts',(-2.32684453395074,-0.459883764824666,
6.68031779259894));
#43748=CARTESIAN_POINT('Ctrl Pts',(-2.31463236085752,-0.518748369904315,
6.68439533682385));
#43749=CARTESIAN_POINT('Ctrl Pts',(-2.30608391989405,-0.555517339905188,
6.68698259608619));
#43750=CARTESIAN_POINT('Ctrl Pts',(-2.25656111397816,-0.74761983246704,
6.70072008158761));
#43751=CARTESIAN_POINT('Ctrl Pts',(-2.20076624756007,-0.898674411720307,
6.71232638877071));
#43752=CARTESIAN_POINT('Ctrl Pts',(-2.08388196602773,-1.13741193789532,
6.73168224039077));
#43753=CARTESIAN_POINT('Ctrl Pts',(-2.031372598892,-1.22873838423062,6.73934972224757));
#43754=CARTESIAN_POINT('Ctrl Pts',(-1.95263335928461,-1.34676040707862,
6.74939565463265));
#43755=CARTESIAN_POINT('Ctrl Pts',(-1.93159326687341,-1.37676738192395,
6.75196203189213));
#43756=CARTESIAN_POINT('Ctrl Pts',(-1.90075508417639,-1.41864873502436,
6.75554877399874));
#43757=CARTESIAN_POINT('Ctrl Pts',(-1.89152486940883,-1.43093250118447,
6.75660135769242));
#43758=CARTESIAN_POINT('Ctrl Pts',(-1.8752308407721,-1.45218374436709,6.75842218244956));
#43759=CARTESIAN_POINT('Ctrl Pts',(-1.86822069960764,-1.46119121621274,
6.75919383448859));
#43760=CARTESIAN_POINT('Ctrl Pts',(-1.85263232830738,-1.48092543239047,
6.76088400285217));
#43761=CARTESIAN_POINT('Ctrl Pts',(-1.84402560900503,-1.4916287259647,6.76180057017437));
#43762=CARTESIAN_POINT('Ctrl Pts',(-1.81802606981801,-1.52339268839907,
6.7645223098142));
#43763=CARTESIAN_POINT('Ctrl Pts',(-1.80036130275517,-1.54422906475486,
6.7663099200441));
#43764=CARTESIAN_POINT('Ctrl Pts',(-1.68255144531188,-1.67842065160567,
6.77787258430705));
#43765=CARTESIAN_POINT('Ctrl Pts',(-1.57210708097827,-1.7822921917115,6.78707690287077));
#43766=CARTESIAN_POINT('Ctrl Pts',(-1.37976973431109,-1.93129489222645,
6.8020523833101));
#43767=CARTESIAN_POINT('Ctrl Pts',(-1.30381632331299,-1.9833622745904,6.80773911319795));
#43768=CARTESIAN_POINT('Ctrl Pts',(-1.17305019504164,-2.06224075702158,
6.81739152855389));
#43769=CARTESIAN_POINT('Ctrl Pts',(-1.1198847529526,-2.09158813233912,6.82128003510613));
#43770=CARTESIAN_POINT('Ctrl Pts',(-1.0419762392597,-2.13077124550669,6.82696589349813));
#43771=CARTESIAN_POINT('Ctrl Pts',(-1.01810006535693,-2.14228213590605,
6.8287066685625));
#43772=CARTESIAN_POINT('Ctrl Pts',(-0.975620461835801,-2.1618913496205,
6.83180354819913));
#43773=CARTESIAN_POINT('Ctrl Pts',(-0.957096369004242,-2.17015575270161,
6.83315391779767));
#43774=CARTESIAN_POINT('Ctrl Pts',(-0.917831749074079,-2.18707290686811,
6.83601722267429));
#43775=CARTESIAN_POINT('Ctrl Pts',(-0.897069778186781,-2.19567046109229,
6.83753183138862));
#43776=CARTESIAN_POINT('Ctrl Pts',(-0.840662867369621,-2.218095041622,6.84164985841201));
#43777=CARTESIAN_POINT('Ctrl Pts',(-0.804801929362138,-2.2313568153584,
6.84427128799778));
#43778=CARTESIAN_POINT('Ctrl Pts',(-0.618462371374257,-2.2951909874728,
6.85791729898134));
#43779=CARTESIAN_POINT('Ctrl Pts',(-0.463524097536502,-2.33142181138276,
6.86938432423666));
#43780=CARTESIAN_POINT('Ctrl Pts',(-0.181278161257841,-2.36816282244178,
6.89010962258279));
#43781=CARTESIAN_POINT('Ctrl Pts',(-0.0552927285863765,-2.37444836370118,
6.89929122107597));
#43782=CARTESIAN_POINT('Ctrl Pts',(0.0943690088880997,-2.36999109482885,
6.90975666730572));
#43783=CARTESIAN_POINT('Ctrl Pts',(0.11812231988628,-2.36892602708971,6.91140402418232));
#43784=CARTESIAN_POINT('Ctrl Pts',(0.154859543466095,-2.36672479727579,
6.9139267869522));
#43785=CARTESIAN_POINT('Ctrl Pts',(0.167856158971682,-2.36583855616849,
6.91481440474648));
#43786=CARTESIAN_POINT('Ctrl Pts',(0.192381409982752,-2.36396305350721,
6.91647937823283));
#43787=CARTESIAN_POINT('Ctrl Pts',(0.203910598789635,-2.36299648715318,
6.91725779312367));
#43788=CARTESIAN_POINT('Ctrl Pts',(0.231974714817298,-2.36043676085089,
6.91914293124431));
#43789=CARTESIAN_POINT('Ctrl Pts',(0.248500788826079,-2.35875419796759,
6.92024490765104));
#43790=CARTESIAN_POINT('Ctrl Pts',(0.306983653290963,-2.35217841528138,
6.9241201202622));
#43791=CARTESIAN_POINT('Ctrl Pts',(0.34882828697458,-2.34633790810091,6.92684813995306));
#43792=CARTESIAN_POINT('Ctrl Pts',(0.575351928240905,-2.3085258416957,6.94147992913852));
#43793=CARTESIAN_POINT('Ctrl Pts',(0.755909757123629,-2.25586650789915,
6.95269558792164));
#43794=CARTESIAN_POINT('Ctrl Pts',(1.00775729147412,-2.1487347731389,6.96976494623298));
#43795=CARTESIAN_POINT('Ctrl Pts',(1.08521054818543,-2.1106756387633,6.97522233134478));
#43796=CARTESIAN_POINT('Ctrl Pts',(1.18633683261385,-2.05394411854507,6.98274902332448));
#43797=CARTESIAN_POINT('Ctrl Pts',(1.21198271470016,-2.03891620613159,6.9846939781063));
#43798=CARTESIAN_POINT('Ctrl Pts',(1.25507182883062,-2.01256672723371,6.98802793674009));
#43799=CARTESIAN_POINT('Ctrl Pts',(1.27266131727835,-2.00149025805052,6.98940813735224));
#43800=CARTESIAN_POINT('Ctrl Pts',(1.30799110614294,-1.97858833461649,6.99222093674746));
#43801=CARTESIAN_POINT('Ctrl Pts',(1.32572204509235,-1.96675202824174,6.993653840464));
#43802=CARTESIAN_POINT('Ctrl Pts',(1.37009215329695,-1.93626008666731,6.9972949959974));
#43803=CARTESIAN_POINT('Ctrl Pts',(1.39651091487895,-1.9172930705407,6.99951460923388));
#43804=CARTESIAN_POINT('Ctrl Pts',(1.51670479841012,-1.82719908155595,7.00985978346458));
#43805=CARTESIAN_POINT('Ctrl Pts',(1.60548089632023,-1.74970680780491,7.01822344438646));
#43806=CARTESIAN_POINT('Ctrl Pts',(1.77885265421624,-1.57402765574,7.03606937157826));
#43807=CARTESIAN_POINT('Ctrl Pts',(1.86191309703049,-1.47484210491552,7.04555326479193));
#43808=CARTESIAN_POINT('Ctrl Pts',(1.97079570438408,-1.32086854337817,7.05909895334066));
#43809=CARTESIAN_POINT('Ctrl Pts',(2.00327374292448,-1.27107235959096,7.06331648460182));
#43810=CARTESIAN_POINT('Ctrl Pts',(2.04319360101439,-1.20452808898838,7.06869661625635));
#43811=CARTESIAN_POINT('Ctrl Pts',(2.05235906457722,-1.18884411428124,7.06994674663879));
#43812=CARTESIAN_POINT('Ctrl Pts',(2.06720310304069,-1.16275953589027,7.07199457110828));
#43813=CARTESIAN_POINT('Ctrl Pts',(2.07298542874829,-1.15241912595429,7.07279835290198));
#43814=CARTESIAN_POINT('Ctrl Pts',(2.08468595348291,-1.13112226675523,7.07443680397979));
#43815=CARTESIAN_POINT('Ctrl Pts',(2.09059577249829,-1.12016179203454,7.07527098408579));
#43816=CARTESIAN_POINT('Ctrl Pts',(2.10625965468208,-1.0905554129311,7.07750140193677));
#43817=CARTESIAN_POINT('Ctrl Pts',(2.11585259812095,-1.07182493823015,7.07888830523962));
#43818=CARTESIAN_POINT('Ctrl Pts',(2.17727687734194,-0.947852954328027,
7.0879262831967));
#43819=CARTESIAN_POINT('Ctrl Pts',(2.22149455582226,-0.839004508869037,
7.09520168162207));
#43820=CARTESIAN_POINT('Ctrl Pts',(2.29411099697318,-0.613614930047822,
7.10979214429349));
#43821=CARTESIAN_POINT('Ctrl Pts',(2.32210018457666,-0.497310733101545,
7.11708789160099));
#43822=CARTESIAN_POINT('Ctrl Pts',(2.3492019533226,-0.330068581422661,7.12771874318987));
#43823=CARTESIAN_POINT('Ctrl Pts',(2.35563412103115,-0.280504037258696,
7.13088485540283));
#43824=CARTESIAN_POINT('Ctrl Pts',(2.36436205228061,-0.191230062449223,
7.13664548924809));
#43825=CARTESIAN_POINT('Ctrl Pts',(2.3672336850891,-0.151595659633722,7.13922326185328));
#43826=CARTESIAN_POINT('Ctrl Pts',(2.37018290714522,-0.0891610743582391,
7.14332574169825));
#43827=CARTESIAN_POINT('Ctrl Pts',(2.37092973915779,-0.0663989722919966,
7.14483009044519));
#43828=CARTESIAN_POINT('Ctrl Pts',(2.371720650477,-0.0234121593118154,7.14768920420574));
#43829=CARTESIAN_POINT('Ctrl Pts',(2.3718340477862,-0.00319065843857204,
7.14904172448005));
#43830=CARTESIAN_POINT('Ctrl Pts',(2.37150252947546,0.0429802358461522,
7.1521482748376));
#43831=CARTESIAN_POINT('Ctrl Pts',(2.37089028436428,0.0689254424510486,
7.15390725021403));
#43832=CARTESIAN_POINT('Ctrl Pts',(2.36765349567127,0.149793606831992,7.15943350070163));
#43833=CARTESIAN_POINT('Ctrl Pts',(2.36354494104859,0.204635484961782,7.16324466725661));
#43834=CARTESIAN_POINT('Ctrl Pts',(2.33667004538567,0.44899732504346,7.18051768991606));
#43835=CARTESIAN_POINT('Ctrl Pts',(2.29298155620036,0.635486233604201,7.1945638618519));
#43836=CARTESIAN_POINT('Ctrl Pts',(2.2102367491011,0.861718859319863,7.21196711979585));
#43837=CARTESIAN_POINT('Ctrl Pts',(2.19154884742905,0.908196065474832,7.21555789822041));
#43838=CARTESIAN_POINT('Ctrl Pts',(2.15783587409957,0.984926319749766,7.22147746198748));
#43839=CARTESIAN_POINT('Ctrl Pts',(2.14361145098473,1.01551254839014,7.22383469733135));
#43840=CARTESIAN_POINT('Ctrl Pts',(2.12217279471738,1.05915174836047,7.2271841724712));
#43841=CARTESIAN_POINT('Ctrl Pts',(2.11548101709301,1.07245507670386,7.22820337096737));
#43842=CARTESIAN_POINT('Ctrl Pts',(2.10345418748732,1.09581388985866,7.22998848121508));
#43843=CARTESIAN_POINT('Ctrl Pts',(2.09817145079525,1.10589519377805,7.2307573489492));
#43844=CARTESIAN_POINT('Ctrl Pts',(2.08618319772416,1.12837779655447,7.2324684956133));
#43845=CARTESIAN_POINT('Ctrl Pts',(2.07943943523042,1.14075783832828,7.23340845672332));
#43846=CARTESIAN_POINT('Ctrl Pts',(2.0583741778565,1.17862133910602,7.23627850810315));
#43847=CARTESIAN_POINT('Ctrl Pts',(2.04369108887535,1.20390175373111,7.23818808431925));
#43848=CARTESIAN_POINT('Ctrl Pts',(1.9227208720392,1.40358622631312,7.25327031806348));
#43849=CARTESIAN_POINT('Ctrl Pts',(1.79476796198041,1.56388570780492,7.26543469150203));
#43850=CARTESIAN_POINT('Ctrl Pts',(1.58424896289906,1.76724955621327,7.28367356558749));
#43851=CARTESIAN_POINT('Ctrl Pts',(1.51727742858009,1.82507055542942,7.28926329330823));
#43852=CARTESIAN_POINT('Ctrl Pts',(1.42352014445897,1.89728353834959,7.29694308398936));
#43853=CARTESIAN_POINT('Ctrl Pts',(1.39945786377047,1.91510103788407,7.29890175394842));
#43854=CARTESIAN_POINT('Ctrl Pts',(1.35809752047,1.94453153258822,7.30225203436734));
#43855=CARTESIAN_POINT('Ctrl Pts',(1.34097161861238,1.95638105405066,7.30363462632279));
#43856=CARTESIAN_POINT('Ctrl Pts',(1.30604659163203,1.97987186461351,7.30644614922014));
#43857=CARTESIAN_POINT('Ctrl Pts',(1.2882425193718,1.99150231264457,7.30787531068201));
#43858=CARTESIAN_POINT('Ctrl Pts',(1.24304684877533,2.02016656164038,7.31149433004567));
#43859=CARTESIAN_POINT('Ctrl Pts',(1.2154603996522,2.03688346454973,7.31369526636055));
#43860=CARTESIAN_POINT('Ctrl Pts',(1.09267511731122,2.1079066026822,7.32346140793998));
#43861=CARTESIAN_POINT('Ctrl Pts',(0.994131036750746,2.15613237182062,7.33123018050427));
#43862=CARTESIAN_POINT('Ctrl Pts',(0.766529143583916,2.24858914800888,7.3489531170373));
#43863=CARTESIAN_POINT('Ctrl Pts',(0.636269155954512,2.2888601143306,7.35895459966368));
#43864=CARTESIAN_POINT('Ctrl Pts',(0.44379539544784,2.33065409868693,7.37311151533002));
#43865=CARTESIAN_POINT('Ctrl Pts',(0.383833733594456,2.34127653985938,7.37743444396681));
#43866=CARTESIAN_POINT('Ctrl Pts',(0.305397991580051,2.3520767304602,7.38292507937804));
#43867=CARTESIAN_POINT('Ctrl Pts',(0.287242056744769,2.35436295645328,7.38418464375798));
#43868=CARTESIAN_POINT('Ctrl Pts',(0.257264310327961,2.35778584878636,7.38624367247878));
#43869=CARTESIAN_POINT('Ctrl Pts',(0.245457431606833,2.3590442355135,7.38704935472446));
#43870=CARTESIAN_POINT('Ctrl Pts',(0.222825498280978,2.36128460459393,7.38858302410748));
#43871=CARTESIAN_POINT('Ctrl Pts',(0.212002374865882,2.36228092978478,7.38931183003946));
#43872=CARTESIAN_POINT('Ctrl Pts',(0.182036159217526,2.36483186575039,7.39131782995691));
#43873=CARTESIAN_POINT('Ctrl Pts',(0.162879974216491,2.36622845212401,7.39258680935211));
#43874=CARTESIAN_POINT('Ctrl Pts',(0.078392821779802,2.37135708978973,7.39813296952163));
#43875=CARTESIAN_POINT('Ctrl Pts',(0.0129351781399842,2.37261756846035,
7.40229709889186));
#43876=CARTESIAN_POINT('Ctrl Pts',(-0.216141432622983,2.3675459414839,7.41665978937104));
#43877=CARTESIAN_POINT('Ctrl Pts',(-0.378974394102621,2.34699236951005,
7.42652249433897));
#43878=CARTESIAN_POINT('Ctrl Pts',(-0.618419801082092,2.29118013842813,
7.44188401620058));
#43879=CARTESIAN_POINT('Ctrl Pts',(-0.697411234680339,2.26838378804286,
7.44709285580397));
#43880=CARTESIAN_POINT('Ctrl Pts',(-0.802742258754739,2.23196351633728,
7.4543312233458));
#43881=CARTESIAN_POINT('Ctrl Pts',(-0.830248340535593,2.22187844947369,
7.45624904365158));
#43882=CARTESIAN_POINT('Ctrl Pts',(-0.876868581217198,2.2037986438129,7.45955081676203));
#43883=CARTESIAN_POINT('Ctrl Pts',(-0.896078093182024,2.19605805411751,
7.46092638835456));
#43884=CARTESIAN_POINT('Ctrl Pts',(-0.932615286225015,2.1807759687145,7.46357298923735));
#43885=CARTESIAN_POINT('Ctrl Pts',(-0.949959095499659,2.17327696802719,
7.46484252469831));
#43886=CARTESIAN_POINT('Ctrl Pts',(-0.995365651144746,2.15299700157365,
7.46820214049723));
#43887=CARTESIAN_POINT('Ctrl Pts',(-1.02327117354341,2.13987495467771,7.47030345822871));
#43888=CARTESIAN_POINT('Ctrl Pts',(-1.13335386894207,2.08546497570741,7.47874385890637));
#43889=CARTESIAN_POINT('Ctrl Pts',(-1.21334634119102,2.03996132895333,7.48522199544609));
#43890=CARTESIAN_POINT('Ctrl Pts',(-1.41894074867014,1.90663176628679,7.50278828029663));
#43891=CARTESIAN_POINT('Ctrl Pts',(-1.5390172086522,1.81109347798263,7.5140561621131));
#43892=CARTESIAN_POINT('Ctrl Pts',(-1.69504775177748,1.66015293673796,7.52968179971005));
#43893=CARTESIAN_POINT('Ctrl Pts',(-1.73923401380762,1.61380332180321,7.53423438264327));
#43894=CARTESIAN_POINT('Ctrl Pts',(-1.79375612377239,1.55176738751399,7.53996441974279));
#43895=CARTESIAN_POINT('Ctrl Pts',(-1.80585398661713,1.53767177523308,7.5412434802507));
#43896=CARTESIAN_POINT('Ctrl Pts',(-1.82544752818523,1.51429246742133,7.54332571911559));
#43897=CARTESIAN_POINT('Ctrl Pts',(-1.83304078757346,1.50509197289964,7.54413538570502));
#43898=CARTESIAN_POINT('Ctrl Pts',(-1.84834513663975,1.48626057949663,7.54577220607711));
#43899=CARTESIAN_POINT('Ctrl Pts',(-1.85605108658666,1.47662609864,7.54659902476091));
#43900=CARTESIAN_POINT('Ctrl Pts',(-1.87636310386161,1.45082044162099,7.54878689925829));
#43901=CARTESIAN_POINT('Ctrl Pts',(-1.88883555220949,1.43454479767433,7.55013922732561));
#43902=CARTESIAN_POINT('Ctrl Pts',(-1.95508579336583,1.34573069567163,7.55738359929408));
#43903=CARTESIAN_POINT('Ctrl Pts',(-2.00490446456094,1.27032012268282,7.56305592137044));
#43904=CARTESIAN_POINT('Ctrl Pts',(-2.12187220143662,1.06917043995233,7.5774847273837));
#43905=CARTESIAN_POINT('Ctrl Pts',(-2.18221118109443,0.939905061466952,
7.58611883632595));
#43906=CARTESIAN_POINT('Ctrl Pts',(-2.25688000149102,0.733262381041774,
7.59987803540204));
#43907=CARTESIAN_POINT('Ctrl Pts',(-2.27958971348356,0.659279948761734,
7.60479220512656));
#43908=CARTESIAN_POINT('Ctrl Pts',(-2.30572665257823,0.556461351126819,
7.61168729140122));
#43909=CARTESIAN_POINT('Ctrl Pts',(-2.31230229604116,0.528471956392537,
7.61357053296406));
#43910=CARTESIAN_POINT('Ctrl Pts',(-2.32271676591039,0.480218616516357,
7.61683152153846));
#43911=CARTESIAN_POINT('Ctrl Pts',(-2.32680314934294,0.460011036823562,
7.61820141802409));
#43912=CARTESIAN_POINT('Ctrl Pts',(-2.33414954083864,0.421076278769923,
7.62085017904811));
#43913=CARTESIAN_POINT('Ctrl Pts',(-2.33744887736892,0.402358076404976,
7.62212770554261));
#43914=CARTESIAN_POINT('Ctrl Pts',(-2.34561434226197,0.352537110139717,
7.62553989138193));
#43915=CARTESIAN_POINT('Ctrl Pts',(-2.35008665308357,0.321374575849296,
7.62768646840528));
#43916=CARTESIAN_POINT('Ctrl Pts',(-2.3587493140946,0.251091891849367,7.63255767963198));
#43917=CARTESIAN_POINT('Ctrl Pts',(-2.36258799030857,0.21194749286373,7.63529150187935));
#43918=CARTESIAN_POINT('Ctrl Pts',(-2.36545135498545,0.17273664839138,7.63805096494753));
#43919=CARTESIAN_POINT('Origin',(0.,0.,-1.84858989190501));
#43920=CARTESIAN_POINT('',(-2.36545132340078,0.172737080910542,8.8374806621729));
#43921=CARTESIAN_POINT('',(-2.36545134966571,0.172736721239843,8.64191454572571));
#43922=CARTESIAN_POINT('',(-2.36545134966535,0.172736721244682,-1.84858989190501));
#43923=CARTESIAN_POINT('Ctrl Pts',(-2.36545132340079,0.172737080910402,
8.8374806621729));
#43924=CARTESIAN_POINT('Ctrl Pts',(-2.3549239636921,0.31689811931398,8.82699267314082));
#43925=CARTESIAN_POINT('Ctrl Pts',(-2.33123218326878,0.459910024350676,
8.81635530687031));
#43926=CARTESIAN_POINT('Ctrl Pts',(-2.28553067457795,0.634692462460707,
8.80356992920104));
#43927=CARTESIAN_POINT('Ctrl Pts',(-2.2756687819126,0.669191233137263,8.8010584792055));
#43928=CARTESIAN_POINT('Ctrl Pts',(-2.26058560740237,0.717756955937051,
8.79755235779571));
#43929=CARTESIAN_POINT('Ctrl Pts',(-2.25600832838802,0.732016931087265,
8.79652652657968));
#43930=CARTESIAN_POINT('Ctrl Pts',(-2.24784333586149,0.756649740162565,
8.79476195436269));
#43931=CARTESIAN_POINT('Ctrl Pts',(-2.24431823953607,0.767042469089523,
8.79401983804858));
#43932=CARTESIAN_POINT('Ctrl Pts',(-2.23641162508261,0.789831593948998,
8.79239793566709));
#43933=CARTESIAN_POINT('Ctrl Pts',(-2.23199901587458,0.802216502404582,
8.79151991009927));
#43934=CARTESIAN_POINT('Ctrl Pts',(-2.2189697023577,0.837846073199519,8.78900207671265));
#43935=CARTESIAN_POINT('Ctrl Pts',(-2.21009099287284,0.860993903107094,
8.78737631896165));
#43936=CARTESIAN_POINT('Ctrl Pts',(-2.1376765042439,1.04128076720594,8.77476147587883));
#43937=CARTESIAN_POINT('Ctrl Pts',(-2.05781649567719,1.19135749774416,8.76451846399258));
#43938=CARTESIAN_POINT('Ctrl Pts',(-1.91567153528225,1.40085495720134,8.74891279280651));
#43939=CARTESIAN_POINT('Ctrl Pts',(-1.86509141385393,1.46752331187729,8.74372370211467));
#43940=CARTESIAN_POINT('Ctrl Pts',(-1.77440518435404,1.57477426443807,8.73482465831089));
#43941=CARTESIAN_POINT('Ctrl Pts',(-1.73616592633438,1.61683482192931,8.73117710804433));
#43942=CARTESIAN_POINT('Ctrl Pts',(-1.67868294991811,1.67566952560035,8.72580889181701));
#43943=CARTESIAN_POINT('Ctrl Pts',(-1.66061975758213,1.69357218483052,8.72413742800565));
#43944=CARTESIAN_POINT('Ctrl Pts',(-1.62810622060584,1.72477643174437,8.72115324375087));
#43945=CARTESIAN_POINT('Ctrl Pts',(-1.61377178187576,1.73819567435074,8.71984568720397));
#43946=CARTESIAN_POINT('Ctrl Pts',(-1.58310158214334,1.76620128826421,8.71706388210865));
#43947=CARTESIAN_POINT('Ctrl Pts',(-1.56672717869249,1.78074240217377,8.71558793436397));
#43948=CARTESIAN_POINT('Ctrl Pts',(-1.52174187602038,1.8195903398038,8.71155635937749));
#43949=CARTESIAN_POINT('Ctrl Pts',(-1.49275245705256,1.84344708923602,8.70898315832546));
#43950=CARTESIAN_POINT('Ctrl Pts',(-1.33413554991997,1.96778509864692,8.69502692453214));
#43951=CARTESIAN_POINT('Ctrl Pts',(-1.19493382305038,2.05528886884725,8.6831640713442));
#43952=CARTESIAN_POINT('Ctrl Pts',(-0.934262530268304,2.18366260055691,
8.66199792930429));
#43953=CARTESIAN_POINT('Ctrl Pts',(-0.816369126214726,2.23042064923685,
8.65277380803439));
#43954=CARTESIAN_POINT('Ctrl Pts',(-0.675033431480264,2.27375837176499,
8.64247333794866));
#43955=CARTESIAN_POINT('Ctrl Pts',(-0.654686938590233,2.27970005825391,
8.64100852100713));
#43956=CARTESIAN_POINT('Ctrl Pts',(-0.622457960550302,2.28864462833137,
8.63871942921143));
#43957=CARTESIAN_POINT('Ctrl Pts',(-0.610627699683309,2.29182939513999,
8.63788575307213));
#43958=CARTESIAN_POINT('Ctrl Pts',(-0.587909569632947,2.29775682953183,
8.63629808038055));
#43959=CARTESIAN_POINT('Ctrl Pts',(-0.577026128529414,2.30051406476027,
8.63554335624783));
#43960=CARTESIAN_POINT('Ctrl Pts',(-0.549805271056664,2.30720493100135,
8.63366948628896));
#43961=CARTESIAN_POINT('Ctrl Pts',(-0.533444466712569,2.31104250719786,
8.63255554070836));
#43962=CARTESIAN_POINT('Ctrl Pts',(-0.472441950473886,2.3246688451108,8.62844313687188));
#43963=CARTESIAN_POINT('Ctrl Pts',(-0.427558243811104,2.33334120847606,
8.62549868628831));
#43964=CARTESIAN_POINT('Ctrl Pts',(-0.234070547347241,2.36495515761656,
8.61304479302822));
#43965=CARTESIAN_POINT('Ctrl Pts',(-0.0837129401427739,2.37503703492672,
8.60394898112043));
#43966=CARTESIAN_POINT('Ctrl Pts',(0.143484614799508,2.36865503969153,8.58990906930768));
#43967=CARTESIAN_POINT('Ctrl Pts',(0.220218085022321,2.36275629812587,8.58511970448396));
#43968=CARTESIAN_POINT('Ctrl Pts',(0.349856788706824,2.34642018651598,8.57682335268715));
#43969=CARTESIAN_POINT('Ctrl Pts',(0.402940885513851,2.33788909908419,8.57336742155193));
#43970=CARTESIAN_POINT('Ctrl Pts',(0.480149098939338,2.32277339864573,8.56822880630346));
#43971=CARTESIAN_POINT('Ctrl Pts',(0.504533898614867,2.31759894879552,8.56658937387015));
#43972=CARTESIAN_POINT('Ctrl Pts',(0.547921447470655,2.30767493946582,8.56364051039771));
#43973=CARTESIAN_POINT('Ctrl Pts',(0.566955703985426,2.30307245436562,8.56233579394326));
#43974=CARTESIAN_POINT('Ctrl Pts',(0.60743389508692,2.2927526218239,8.55953651715485));
#43975=CARTESIAN_POINT('Ctrl Pts',(0.62885882114427,2.28696896522647,8.55803996922111));
#43976=CARTESIAN_POINT('Ctrl Pts',(0.686708241039703,2.27047816717114,8.55395714302827));
#43977=CARTESIAN_POINT('Ctrl Pts',(0.722960594875283,2.25919609863791,8.55135294905878));
#43978=CARTESIAN_POINT('Ctrl Pts',(0.881296621431954,2.20571923768995,8.53977058932203));
#43979=CARTESIAN_POINT('Ctrl Pts',(1.00007044574214,2.15446779905382,8.53051346576622));
#43980=CARTESIAN_POINT('Ctrl Pts',(1.21293423404048,2.04120810170904,8.51299556497496));
#43981=CARTESIAN_POINT('Ctrl Pts',(1.30795261672392,1.98166621610205,8.50479141178066));
#43982=CARTESIAN_POINT('Ctrl Pts',(1.44295753867741,1.88311274959956,8.49280944908056));
#43983=CARTESIAN_POINT('Ctrl Pts',(1.48636111024231,1.84904617275752,8.4889034448089));
#43984=CARTESIAN_POINT('Ctrl Pts',(1.54186615601031,1.80226261772794,8.48387484124514));
#43985=CARTESIAN_POINT('Ctrl Pts',(1.55506804389848,1.79088391845794,8.48267619875846));
#43986=CARTESIAN_POINT('Ctrl Pts',(1.57673849069261,1.7717858325653,8.48070602054185));
#43987=CARTESIAN_POINT('Ctrl Pts',(1.58527852375643,1.76414889595256,8.47992890976153));
#43988=CARTESIAN_POINT('Ctrl Pts',(1.60271146803955,1.74833063479896,8.47834171563353));
#43989=CARTESIAN_POINT('Ctrl Pts',(1.61159776495678,1.74014272927273,8.4775321246025));
#43990=CARTESIAN_POINT('Ctrl Pts',(1.63532250405768,1.71794493434399,8.47536796377216));
#43991=CARTESIAN_POINT('Ctrl Pts',(1.65004371824213,1.7038105191779,8.47402221006071));
#43992=CARTESIAN_POINT('Ctrl Pts',(1.73789322719995,1.61725606757282,8.4659600169087));
#43993=CARTESIAN_POINT('Ctrl Pts',(1.80643500266684,1.54032062372601,8.4595336504411));
#43994=CARTESIAN_POINT('Ctrl Pts',(1.95213913459416,1.35361620638187,8.44490343944075));
#43995=CARTESIAN_POINT('Ctrl Pts',(2.025422849414,1.24128380287203,8.43676329805829));
#43996=CARTESIAN_POINT('Ctrl Pts',(2.12427582032535,1.05747273986883,8.42367815060364));
#43997=CARTESIAN_POINT('Ctrl Pts',(2.15657378134703,0.989941547357563,8.41891878753288));
#43998=CARTESIAN_POINT('Ctrl Pts',(2.19647657751588,0.895248398487564,8.41223656984106));
#43999=CARTESIAN_POINT('Ctrl Pts',(2.20687226907676,0.869306466451068,8.41040530223374));
#44000=CARTESIAN_POINT('Ctrl Pts',(2.22391858549152,0.824490362279526,8.40723732987511));
#44001=CARTESIAN_POINT('Ctrl Pts',(2.23079332975739,0.805704233271185,8.40590808825291));
#44002=CARTESIAN_POINT('Ctrl Pts',(2.24435791059479,0.767132186225706,8.40317511875583));
#44003=CARTESIAN_POINT('Ctrl Pts',(2.25102565022031,0.747340415529887,8.40177081084249));
#44004=CARTESIAN_POINT('Ctrl Pts',(2.26741899436637,0.696469364474807,8.39815499235762));
#44005=CARTESIAN_POINT('Ctrl Pts',(2.27676718014668,0.665274003552024,8.39593167391743));
#44006=CARTESIAN_POINT('Ctrl Pts',(2.32161157723521,0.503590861911816,8.38437194764615));
#44007=CARTESIAN_POINT('Ctrl Pts',(2.34653754531588,0.370452639471144,8.37471104340073));
#44008=CARTESIAN_POINT('Ctrl Pts',(2.37151250747135,0.120636910462846,8.35648580319882));
#44009=CARTESIAN_POINT('Ctrl Pts',(2.37457451519073,0.00464695727427692,
8.34799130147554));
#44010=CARTESIAN_POINT('Ctrl Pts',(2.36651718712373,-0.167165538839918,
8.33565535932213));
#44011=CARTESIAN_POINT('Ctrl Pts',(2.36189877342919,-0.223121396098586,
8.3316787461218));
#44012=CARTESIAN_POINT('Ctrl Pts',(2.35323823682515,-0.296268439618266,
8.32657539763777));
#44013=CARTESIAN_POINT('Ctrl Pts',(2.35098478340419,-0.313649136299329,
8.3253698905354));
#44014=CARTESIAN_POINT('Ctrl Pts',(2.34693731432067,-0.342366739715257,
8.32339156730443));
#44015=CARTESIAN_POINT('Ctrl Pts',(2.34525332783633,-0.353718235736791,
8.32261308425144));
#44016=CARTESIAN_POINT('Ctrl Pts',(2.34163166304584,-0.376967514673342,
8.32102642918691));
#44017=CARTESIAN_POINT('Ctrl Pts',(2.3396855633769,-0.388863514376001,8.32021871231131));
#44018=CARTESIAN_POINT('Ctrl Pts',(2.33422388136751,-0.420722953448914,
8.31806535125519));
#44019=CARTESIAN_POINT('Ctrl Pts',(2.33054284642996,-0.440657507894412,
8.31672837171676));
#44020=CARTESIAN_POINT('Ctrl Pts',(2.30838064065158,-0.552618191179682,
8.30926548353026));
#44021=CARTESIAN_POINT('Ctrl Pts',(2.28470285653747,-0.643540877982558,
8.30337939804438));
#44022=CARTESIAN_POINT('Ctrl Pts',(2.2121850261031,-0.866755244311674,8.28884503313311));
#44023=CARTESIAN_POINT('Ctrl Pts',(2.15683586539921,-0.996537053381276,
8.28030319476529));
#44024=CARTESIAN_POINT('Ctrl Pts',(2.05406847825948,-1.18822603650397,8.26667954228969));
#44025=CARTESIAN_POINT('Ctrl Pts',(2.01458260883726,-1.25400702508516,8.26180594314104));
#44026=CARTESIAN_POINT('Ctrl Pts',(1.95633299401079,-1.34117586354337,8.25499027545934));
#44027=CARTESIAN_POINT('Ctrl Pts',(1.94026748779738,-1.36431427752057,8.25314493797997));
#44028=CARTESIAN_POINT('Ctrl Pts',(1.91207208446215,-1.40341729520979,8.24996037325855));
#44029=CARTESIAN_POINT('Ctrl Pts',(1.90014463649585,-1.41952459649963,8.2486288182691));
#44030=CARTESIAN_POINT('Ctrl Pts',(1.87690799595753,-1.45008661740033,8.24606303112605));
#44031=CARTESIAN_POINT('Ctrl Pts',(1.86563231263638,-1.46456507714444,8.24483015319904));
#44032=CARTESIAN_POINT('Ctrl Pts',(1.83545485539225,-1.50240017601154,8.24156131892143));
#44033=CARTESIAN_POINT('Ctrl Pts',(1.8162758070753,-1.52553035582997,8.23951461028934));
#44034=CARTESIAN_POINT('Ctrl Pts',(1.7385900946876,-1.61567829220736,8.2313395845881));
#44035=CARTESIAN_POINT('Ctrl Pts',(1.67677829675948,-1.67973900204807,8.22508081442414));
#44036=CARTESIAN_POINT('Ctrl Pts',(1.46866786457907,-1.87246396015657,8.20477264528074));
#44037=CARTESIAN_POINT('Ctrl Pts',(1.31007976439556,-1.98665348513427,8.19032081085633));
#44038=CARTESIAN_POINT('Ctrl Pts',(1.10850144091213,-2.09705933987949,8.17406528418838));
#44039=CARTESIAN_POINT('Ctrl Pts',(1.07730251507111,-2.1132564723877,8.17160603655951));
#44040=CARTESIAN_POINT('Ctrl Pts',(1.03241526907004,-2.13530738030571,8.1681589028466));
#44041=CARTESIAN_POINT('Ctrl Pts',(1.01901558864048,-2.1417343800413,8.16714119275506));
#44042=CARTESIAN_POINT('Ctrl Pts',(0.995537648664411,-2.15272506696177,
8.16537880652056));
#44043=CARTESIAN_POINT('Ctrl Pts',(0.985486566507586,-2.15734481914038,
8.16463093807182));
#44044=CARTESIAN_POINT('Ctrl Pts',(0.963305912992754,-2.1673522801188,8.16299522505074));
#44045=CARTESIAN_POINT('Ctrl Pts',(0.951162986656204,-2.1727087198867,8.16210918475372));
#44046=CARTESIAN_POINT('Ctrl Pts',(0.915665308598253,-2.18801267333933,
8.15954458590526));
#44047=CARTESIAN_POINT('Ctrl Pts',(0.892194273293991,-2.19768785731821,
8.15788088410781));
#44048=CARTESIAN_POINT('Ctrl Pts',(0.770420468177783,-2.2456126254546,8.14939070322152));
#44049=CARTESIAN_POINT('Ctrl Pts',(0.669791046594585,-2.27765416237008,
8.14284256141661));
#44050=CARTESIAN_POINT('Ctrl Pts',(0.447954197665646,-2.33230711158163,
8.12876218495918));
#44051=CARTESIAN_POINT('Ctrl Pts',(0.32645304234203,-2.3523916752934,8.12126271370613));
#44052=CARTESIAN_POINT('Ctrl Pts',(0.130006047252304,-2.36934677131047,
8.10889655596297));
#44053=CARTESIAN_POINT('Ctrl Pts',(0.0558148960734866,-2.37225395170327,
8.10417455127448));
#44054=CARTESIAN_POINT('Ctrl Pts',(-0.0462571224614121,-2.37146267247415,
8.09753603246053));
#44055=CARTESIAN_POINT('Ctrl Pts',(-0.0741216301720457,-2.37075532417822,
8.09570945600553));
#44056=CARTESIAN_POINT('Ctrl Pts',(-0.121939470981536,-2.36869763681544,
8.09254700521294));
#44057=CARTESIAN_POINT('Ctrl Pts',(-0.141900460704218,-2.3675856790782,
8.09121852456685));
#44058=CARTESIAN_POINT('Ctrl Pts',(-0.182702282129724,-2.3647949214371,
8.08848477690679));
#44059=CARTESIAN_POINT('Ctrl Pts',(-0.203539688850077,-2.36309261179102,
8.08707890231843));
#44060=CARTESIAN_POINT('Ctrl Pts',(-0.256878037826373,-2.35802444347678,
8.08345396220832));
#44061=CARTESIAN_POINT('Ctrl Pts',(-0.289335961161488,-2.35426211855619,
8.08122297132652));
#44062=CARTESIAN_POINT('Ctrl Pts',(-0.451879636089599,-2.3320090136016,
8.06991866394156));
#44063=CARTESIAN_POINT('Ctrl Pts',(-0.580328744695812,-2.30340403304197,
8.06054109373206));
#44064=CARTESIAN_POINT('Ctrl Pts',(-0.81723435082639,-2.22956647540326,
8.04253914554753));
#44065=CARTESIAN_POINT('Ctrl Pts',(-0.926018120435991,-2.18662519113367,
8.03397489551933));
#44066=CARTESIAN_POINT('Ctrl Pts',(-1.08375095666906,-2.1104709633366,8.02139871354414));
#44067=CARTESIAN_POINT('Ctrl Pts',(-1.13535549606405,-2.08316415344802,
8.01725903610057));
#44068=CARTESIAN_POINT('Ctrl Pts',(-1.20126854733559,-2.04510799275429,
8.01198380868001));
#44069=CARTESIAN_POINT('Ctrl Pts',(-1.21653360218727,-2.03606455351805,
8.01076302271101));
#44070=CARTESIAN_POINT('Ctrl Pts',(-1.24153952980891,-2.0208687062072,8.00876653307164));
#44071=CARTESIAN_POINT('Ctrl Pts',(-1.251339411356,-2.0148152344421,8.00798495725191));
#44072=CARTESIAN_POINT('Ctrl Pts',(-1.27125085489501,-2.00231444003762,
8.00639928493538));
#44073=CARTESIAN_POINT('Ctrl Pts',(-1.28135830893275,-1.99586140614889,
8.0055955629847));
#44074=CARTESIAN_POINT('Ctrl Pts',(-1.3081741193088,-1.97845335791459,8.00346521360673));
#44075=CARTESIAN_POINT('Ctrl Pts',(-1.32479412848804,-1.96736315833756,
8.0021469315357));
#44076=CARTESIAN_POINT('Ctrl Pts',(-1.4123836204893,-1.90730305701429,7.9951992642605));
#44077=CARTESIAN_POINT('Ctrl Pts',(-1.48079066010414,-1.85469530162944,
7.98977149843507));
#44078=CARTESIAN_POINT('Ctrl Pts',(-1.657677160601,-1.70262210404672,7.97528800677892));
#44079=CARTESIAN_POINT('Ctrl Pts',(-1.7600119922211,-1.59661327712456,7.96638697135753));
#44080=CARTESIAN_POINT('Ctrl Pts',(-1.90075606520653,-1.42072024839448,
7.95228721270071));
#44081=CARTESIAN_POINT('Ctrl Pts',(-1.94658175324105,-1.3572535909807,7.94731819457777));
#44082=CARTESIAN_POINT('Ctrl Pts',(-2.0046229189592,-1.26786774288802,7.94039125364936));
#44083=CARTESIAN_POINT('Ctrl Pts',(-2.01963293949227,-1.24381845139883,
7.93853447550187));
#44084=CARTESIAN_POINT('Ctrl Pts',(-2.04452942573839,-1.20228967052306,
7.93533638401601));
#44085=CARTESIAN_POINT('Ctrl Pts',(-2.05463176318525,-1.18494274169053,
7.93400291392176));
#44086=CARTESIAN_POINT('Ctrl Pts',(-2.0747364642462,-1.1493903062716,7.93127367229954));
#44087=CARTESIAN_POINT('Ctrl Pts',(-2.08472226152706,-1.13117749179517,
7.92987746644388));
#44088=CARTESIAN_POINT('Ctrl Pts',(-2.10948045144842,-1.08458014703557,
7.92630893298248));
#44089=CARTESIAN_POINT('Ctrl Pts',(-2.12391959767011,-1.05602426243711,
7.92412540050455));
#44090=CARTESIAN_POINT('Ctrl Pts',(-2.18876632437205,-0.921065493166437,
7.91381623221288));
#44091=CARTESIAN_POINT('Ctrl Pts',(-2.2317767355564,-0.811310732808078,
7.90545059117616));
#44092=CARTESIAN_POINT('Ctrl Pts',(-2.29950494995012,-0.591653742871962,
7.88882900923301));
#44093=CARTESIAN_POINT('Ctrl Pts',(-2.32490698880058,-0.482269670790919,
7.88060883849695));
#44094=CARTESIAN_POINT('Ctrl Pts',(-2.35047194887738,-0.321071218875139,
7.86880966527242));
#44095=CARTESIAN_POINT('Ctrl Pts',(-2.35683956364091,-0.270394110919458,
7.86514610975072));
#44096=CARTESIAN_POINT('Ctrl Pts',(-2.36471438586219,-0.185688753493123,
7.85913521416989));
#44097=CARTESIAN_POINT('Ctrl Pts',(-2.36713384013129,-0.15176331578463,
7.85675775115089));
#44098=CARTESIAN_POINT('Ctrl Pts',(-2.3695518587865,-0.103137917685317,
7.85340336897334));
#44099=CARTESIAN_POINT('Ctrl Pts',(-2.37014470908978,-0.0884733117476614,
7.85239866694298));
#44100=CARTESIAN_POINT('Ctrl Pts',(-2.37094516634511,-0.0627623326196688,
7.85065035756887));
#44101=CARTESIAN_POINT('Ctrl Pts',(-2.37121177635398,-0.0517186674172914,
7.84990372975537));
#44102=CARTESIAN_POINT('Ctrl Pts',(-2.37163109951675,-0.02727032137788,
7.84826053263253));
#44103=CARTESIAN_POINT('Ctrl Pts',(-2.37174735285992,-0.0138657098153779,
7.84736590041356));
#44104=CARTESIAN_POINT('Ctrl Pts',(-2.37175517113766,0.0264064460216114,
7.84469512404593));
#44105=CARTESIAN_POINT('Ctrl Pts',(-2.37130386950719,0.0532728415598212,
7.84293613589667));
#44106=CARTESIAN_POINT('Ctrl Pts',(-2.36935164355241,0.111025454414777,
7.83919283371531));
#44107=CARTESIAN_POINT('Ctrl Pts',(-2.36770310529822,0.141901248863294,
7.83721488955153));
#44108=CARTESIAN_POINT('Ctrl Pts',(-2.36545134965667,0.17273672136364,7.83525515262476));
#44109=CARTESIAN_POINT('Ctrl Pts',(-2.36545135498545,0.17273664839138,7.63805096494753));
#44110=CARTESIAN_POINT('Ctrl Pts',(-2.36969564154637,0.114615494079465,
7.64214124101686));
#44111=CARTESIAN_POINT('Ctrl Pts',(-2.37179705249545,0.056348380075055,
7.64628826398058));
#44112=CARTESIAN_POINT('Ctrl Pts',(-2.37164596878255,-0.127709886715962,
7.65951362959449));
#44113=CARTESIAN_POINT('Ctrl Pts',(-2.36153974571113,-0.253262801395892,
7.66873160391074));
#44114=CARTESIAN_POINT('Ctrl Pts',(-2.32862128519816,-0.457493503369781,
7.68371260501258));
#44115=CARTESIAN_POINT('Ctrl Pts',(-2.31161296451896,-0.536866318069673,
7.68952725375746));
#44116=CARTESIAN_POINT('Ctrl Pts',(-2.2853469329064,-0.63465950711383,7.69656973278061));
#44117=CARTESIAN_POINT('Ctrl Pts',(-2.27987771712292,-0.654034368172074,
7.69795881473493));
#44118=CARTESIAN_POINT('Ctrl Pts',(-2.27068255376979,-0.685090528620246,
7.70017291413598));
#44119=CARTESIAN_POINT('Ctrl Pts',(-2.26711170098149,-0.696816219943959,
7.70100599286095));
#44120=CARTESIAN_POINT('Ctrl Pts',(-2.25986743485643,-0.719959070578163,
7.70264379638817));
#44121=CARTESIAN_POINT('Ctrl Pts',(-2.25619803265587,-0.731377013514615,
7.70344868636484));
#44122=CARTESIAN_POINT('Ctrl Pts',(-2.2465278037122,-0.760702003015854,
7.70550894812826));
#44123=CARTESIAN_POINT('Ctrl Pts',(-2.2403992745425,-0.778566538826394,
7.7067573287942));
#44124=CARTESIAN_POINT('Ctrl Pts',(-2.21128176719794,-0.860251289797022,
7.71244275993688));
#44125=CARTESIAN_POINT('Ctrl Pts',(-2.18577290446614,-0.923145643361853,
7.71675657017447));
#44126=CARTESIAN_POINT('Ctrl Pts',(-2.0833080386943,-1.14762124926618,7.73221111153484));
#44127=CARTESIAN_POINT('Ctrl Pts',(-1.99083931699805,-1.30144906977679,
7.74295817418495));
#44128=CARTESIAN_POINT('Ctrl Pts',(-1.84064497204438,-1.49727434987451,
7.75847953829163));
#44129=CARTESIAN_POINT('Ctrl Pts',(-1.79705069694095,-1.54932628928999,
7.76280725902116));
#44130=CARTESIAN_POINT('Ctrl Pts',(-1.73227507276655,-1.62025182338726,
7.76905481266415));
#44131=CARTESIAN_POINT('Ctrl Pts',(-1.71289370930519,-1.64072786623663,
7.7709026961637));
#44132=CARTESIAN_POINT('Ctrl Pts',(-1.6787799150183,-1.67550509418278,7.77412229560732));
#44133=CARTESIAN_POINT('Ctrl Pts',(-1.66421802662226,-1.6899697155902,7.77548669593648));
#44134=CARTESIAN_POINT('Ctrl Pts',(-1.63383118982182,-1.71937995215943,
7.77831488589928));
#44135=CARTESIAN_POINT('Ctrl Pts',(-1.61798460226904,-1.73430030561914,
7.77977955919315));
#44136=CARTESIAN_POINT('Ctrl Pts',(-1.57631045750859,-1.77247027935652,
7.78360665372633));
#44137=CARTESIAN_POINT('Ctrl Pts',(-1.55017407632125,-1.7953734057534,7.78598289899113));
#44138=CARTESIAN_POINT('Ctrl Pts',(-1.49151540171793,-1.84453964673008,
7.79126698198328));
#44139=CARTESIAN_POINT('Ctrl Pts',(-1.45878340663383,-1.87053343220083,
7.79418401962525));
#44140=CARTESIAN_POINT('Ctrl Pts',(-1.3522332289137,-1.95065109124007,7.80358101733291));
#44141=CARTESIAN_POINT('Ctrl Pts',(-1.27596693791155,-2.00136955097843,
7.81016544377079));
#44142=CARTESIAN_POINT('Ctrl Pts',(-1.06765653125559,-2.12314467568511,
7.82768284562853));
#44143=CARTESIAN_POINT('Ctrl Pts',(-0.931469977135592,-2.18632156072484,
7.83869204615108));
#44144=CARTESIAN_POINT('Ctrl Pts',(-0.76312138283965,-2.24581174228092,
7.8512430068759));
#44145=CARTESIAN_POINT('Ctrl Pts',(-0.735840658237784,-2.25489763171209,
7.85324445091814));
#44146=CARTESIAN_POINT('Ctrl Pts',(-0.695032199689592,-2.26766939983407,
7.85618383034018));
#44147=CARTESIAN_POINT('Ctrl Pts',(-0.681627130546451,-2.2717347434363,
7.8571407255897));
#44148=CARTESIAN_POINT('Ctrl Pts',(-0.658355832589169,-2.27856767124094,
7.85878603650097));
#44149=CARTESIAN_POINT('Ctrl Pts',(-0.648506815866914,-2.28139035537146,
7.85947741973397));
#44150=CARTESIAN_POINT('Ctrl Pts',(-0.62483371581712,-2.28800926160929,
7.86112750599793));
#44151=CARTESIAN_POINT('Ctrl Pts',(-0.610993078232762,-2.29174410382166,
7.86208280696937));
#44152=CARTESIAN_POINT('Ctrl Pts',(-0.567569975762216,-2.30304029914023,
7.86505293303561));
#44153=CARTESIAN_POINT('Ctrl Pts',(-0.537873624393566,-2.31015637273775,
7.86704512408355));
#44154=CARTESIAN_POINT('Ctrl Pts',(-0.465553636509587,-2.32601598385394,
7.87182080459903));
#44155=CARTESIAN_POINT('Ctrl Pts',(-0.422809985104372,-2.33416423601922,
7.87458017118019));
#44156=CARTESIAN_POINT('Ctrl Pts',(-0.228598621890613,-2.36567630713049,
7.88692918202547));
#44157=CARTESIAN_POINT('Ctrl Pts',(-0.0753064098572458,-2.37550301558115,
7.89618393851273));
#44158=CARTESIAN_POINT('Ctrl Pts',(0.169624694623,-2.36745728356231,7.91142775911565));
#44159=CARTESIAN_POINT('Ctrl Pts',(0.261120681090563,-2.35911845059136,
7.91721977463129));
#44160=CARTESIAN_POINT('Ctrl Pts',(0.382374839465579,-2.34092660205461,
7.92516792191327));
#44161=CARTESIAN_POINT('Ctrl Pts',(0.412759534363085,-2.33576054016204,
7.9271823585518));
#44162=CARTESIAN_POINT('Ctrl Pts',(0.461593961683418,-2.32647501784464,
7.93046107111855));
#44163=CARTESIAN_POINT('Ctrl Pts',(0.480110772177981,-2.32272439314004,
7.93171387591075));
#44164=CARTESIAN_POINT('Ctrl Pts',(0.518830169912526,-2.31439891338066,
7.93435472685092));
#44165=CARTESIAN_POINT('Ctrl Pts',(0.539021503823726,-2.30977982672711,
7.93574405480011));
#44166=CARTESIAN_POINT('Ctrl Pts',(0.587632648502854,-2.2979871593182,7.93911960994225));
#44167=CARTESIAN_POINT('Ctrl Pts',(0.615984399798945,-2.29055019645612,
7.94111392619501));
#44168=CARTESIAN_POINT('Ctrl Pts',(0.723396450476649,-2.26023648735781,
7.94877082302968));
#44169=CARTESIAN_POINT('Ctrl Pts',(0.801377070980714,-2.23377786586226,
7.95454327675886));
#44170=CARTESIAN_POINT('Ctrl Pts',(1.03050788939765,-2.14249068864575,7.97214102712916));
#44171=CARTESIAN_POINT('Ctrl Pts',(1.17645690242371,-2.06595140668785,7.98424676714448));
#44172=CARTESIAN_POINT('Ctrl Pts',(1.36724121885025,-1.93908362014461,8.00074901433664));
#44173=CARTESIAN_POINT('Ctrl Pts',(1.41969205063714,-1.901018097494,8.00536054786745));
#44174=CARTESIAN_POINT('Ctrl Pts',(1.48552602775419,-1.848993281622,8.01118725734341));
#44175=CARTESIAN_POINT('Ctrl Pts',(1.50038603632138,-1.83695550678193,8.01250507750834));
#44176=CARTESIAN_POINT('Ctrl Pts',(1.52344906943512,-1.81780603378863,8.01455241612257));
#44177=CARTESIAN_POINT('Ctrl Pts',(1.53175127055003,-1.81081581074017,8.01528984005131));
#44178=CARTESIAN_POINT('Ctrl Pts',(1.54904699417004,-1.79604922335944,8.01682646742827));
#44179=CARTESIAN_POINT('Ctrl Pts',(1.55803055117504,-1.78826178557081,8.01762477042755));
#44180=CARTESIAN_POINT('Ctrl Pts',(1.58074856809176,-1.76826741458194,8.0196450823013));
#44181=CARTESIAN_POINT('Ctrl Pts',(1.59440078030569,-1.75596750746494,8.02086062626168));
#44182=CARTESIAN_POINT('Ctrl Pts',(1.65327649140403,-1.70167082384261,8.02611630101895));
#44183=CARTESIAN_POINT('Ctrl Pts',(1.69699766427537,-1.65807328959127,8.03005495040019));
#44184=CARTESIAN_POINT('Ctrl Pts',(1.83444423949544,-1.50987553642086,8.04275863462969));
#44185=CARTESIAN_POINT('Ctrl Pts',(1.9205914413677,-1.39865721942861,8.05126477026736));
#44186=CARTESIAN_POINT('Ctrl Pts',(2.05297347683027,-1.19225820742046,8.06645018202768));
#44187=CARTESIAN_POINT('Ctrl Pts',(2.10363565199946,-1.1004059149044,8.07302526204957));
#44188=CARTESIAN_POINT('Ctrl Pts',(2.16162641335428,-0.976521331857155,
8.08187980187649));
#44189=CARTESIAN_POINT('Ctrl Pts',(2.17460807708232,-0.947260374851391,
8.08396965671568));
#44190=CARTESIAN_POINT('Ctrl Pts',(2.19520336613113,-0.898181741613311,
8.08747744411587));
#44191=CARTESIAN_POINT('Ctrl Pts',(2.20315045301142,-0.878507992455981,
8.08888422817985));
#44192=CARTESIAN_POINT('Ctrl Pts',(2.21838615907276,-0.839283136580403,
8.09169167190216));
#44193=CARTESIAN_POINT('Ctrl Pts',(2.22568286020632,-0.819737209675419,
8.09309191665765));
#44194=CARTESIAN_POINT('Ctrl Pts',(2.24289023843927,-0.771719012735865,
8.0965362357175));
#44195=CARTESIAN_POINT('Ctrl Pts',(2.25251749986396,-0.74314980117693,8.09858922262866));
#44196=CARTESIAN_POINT('Ctrl Pts',(2.28888139776308,-0.628032488437149,
8.10688030335095));
#44197=CARTESIAN_POINT('Ctrl Pts',(2.31119190450171,-0.540177178709601,
8.113253870805));
#44198=CARTESIAN_POINT('Ctrl Pts',(2.34725336902153,-0.354110555470342,
8.1268268760525));
#44199=CARTESIAN_POINT('Ctrl Pts',(2.35998307784072,-0.255872143085667,
8.13403580336733));
#44200=CARTESIAN_POINT('Ctrl Pts',(2.37365226604275,-0.0500026144207975,
8.1490565709741));
#44201=CARTESIAN_POINT('Ctrl Pts',(2.37348341625518,0.0574954306504039,
8.15685102237765));
#44202=CARTESIAN_POINT('Ctrl Pts',(2.36423809050983,0.19037564767072,8.16618749915465));
#44203=CARTESIAN_POINT('Ctrl Pts',(2.36202556894763,0.216101778496226,8.16798078966887));
#44204=CARTESIAN_POINT('Ctrl Pts',(2.35800700727463,0.255315355196695,8.1706874783744));
#44205=CARTESIAN_POINT('Ctrl Pts',(2.35650437183402,0.268831070883973,8.17161551683453));
#44206=CARTESIAN_POINT('Ctrl Pts',(2.35353748697392,0.293577244666079,8.1733048440311));
#44207=CARTESIAN_POINT('Ctrl Pts',(2.35210898807194,0.304810788808532,8.17406789085659));
#44208=CARTESIAN_POINT('Ctrl Pts',(2.34853564084595,0.331388624277617,8.17586460805309));
#44209=CARTESIAN_POINT('Ctrl Pts',(2.34632082826278,0.34672276961846,8.1768945243763));
#44210=CARTESIAN_POINT('Ctrl Pts',(2.338237176191,0.399059543457767,8.1803901523937));
#44211=CARTESIAN_POINT('Ctrl Pts',(2.33164167447187,0.435946180381342,8.18282035037303));
#44212=CARTESIAN_POINT('Ctrl Pts',(2.31253846050477,0.529880276566465,8.18895841514605));
#44213=CARTESIAN_POINT('Ctrl Pts',(2.29879271471612,0.586651622366909,8.19262009966908));
#44214=CARTESIAN_POINT('Ctrl Pts',(2.23196759388967,0.82396484566138,8.2079340137591));
#44215=CARTESIAN_POINT('Ctrl Pts',(2.15960578153703,0.998348361724775,8.21926382848418));
#44216=CARTESIAN_POINT('Ctrl Pts',(2.04391987270714,1.20411168568955,8.23431180150085));
#44217=CARTESIAN_POINT('Ctrl Pts',(2.01918161697424,1.24514999614181,8.23740135351489));
#44218=CARTESIAN_POINT('Ctrl Pts',(1.97986172581403,1.30612136649654,8.24214586537232));
#44219=CARTESIAN_POINT('Ctrl Pts',(1.96618292678252,1.3266235720469,8.24376867896861));
#44220=CARTESIAN_POINT('Ctrl Pts',(1.94075773319689,1.3634744446508,8.246738088072));
#44221=CARTESIAN_POINT('Ctrl Pts',(1.92911784237151,1.37989399906621,8.24808065421761));
#44222=CARTESIAN_POINT('Ctrl Pts',(1.90332025748293,1.41532034457926,8.25102129431766));
#44223=CARTESIAN_POINT('Ctrl Pts',(1.88908392829844,1.43426689391887,8.25262225017362));
#44224=CARTESIAN_POINT('Ctrl Pts',(1.84733917537291,1.48812340554284,8.2572569771218));
#44225=CARTESIAN_POINT('Ctrl Pts',(1.81913152916892,1.52247605279063,8.26031730590236));
#44226=CARTESIAN_POINT('Ctrl Pts',(1.7316249197129,1.62314018892497,8.26960939772909));
#44227=CARTESIAN_POINT('Ctrl Pts',(1.6695490139937,1.68692385870969,8.2759436405587));
#44228=CARTESIAN_POINT('Ctrl Pts',(1.49951662797459,1.84303671834431,8.29260454631807));
#44229=CARTESIAN_POINT('Ctrl Pts',(1.38658980552346,1.92943062739906,8.30304223665321));
#44230=CARTESIAN_POINT('Ctrl Pts',(1.22122503182619,2.03388551334105,8.31705703773592));
#44231=CARTESIAN_POINT('Ctrl Pts',(1.17486664278883,2.06101192626047,8.32085894779784));
#44232=CARTESIAN_POINT('Ctrl Pts',(1.11171657682316,2.09513991433022,8.325835015011));
#44233=CARTESIAN_POINT('Ctrl Pts',(1.09571090099525,2.10355477186613,8.32707929961259));
#44234=CARTESIAN_POINT('Ctrl Pts',(1.07011744393479,2.11663893401677,8.32904040339933));
#44235=CARTESIAN_POINT('Ctrl Pts',(1.06059207646055,2.12142786331329,8.32976408273877));
#44236=CARTESIAN_POINT('Ctrl Pts',(1.04017066586785,2.13152290924386,8.33130185936936));
#44237=CARTESIAN_POINT('Ctrl Pts',(1.02926552123848,2.13681010613103,8.33211477302627));
#44238=CARTESIAN_POINT('Ctrl Pts',(1.00072291320443,2.15037935197861,8.33422220943636));
#44239=CARTESIAN_POINT('Ctrl Pts',(0.983022682825529,2.15852824186288,8.33550910942496));
#44240=CARTESIAN_POINT('Ctrl Pts',(0.895491942198271,2.19752585908194,8.34178496142611));
#44241=CARTESIAN_POINT('Ctrl Pts',(0.824293947352781,2.2252117998703,8.34661698852776));
#44242=CARTESIAN_POINT('Ctrl Pts',(0.659231984353985,2.28038450036551,8.35747102218209));
#44243=CARTESIAN_POINT('Ctrl Pts',(0.564759026287859,2.30559941016724,8.36343987920138));
#44244=CARTESIAN_POINT('Ctrl Pts',(0.342743285740497,2.35038593267697,8.37739521789696));
#44245=CARTESIAN_POINT('Ctrl Pts',(0.214638188783183,2.36552571928469,8.38540338346822));
#44246=CARTESIAN_POINT('Ctrl Pts',(0.0530895617267232,2.37138367532796,
8.3958574474851));
#44247=CARTESIAN_POINT('Ctrl Pts',(0.0202131137512774,2.37189171318549,
8.39800231243557));
#44248=CARTESIAN_POINT('Ctrl Pts',(-0.0340509465410546,2.37160201001303,
8.40157669179009));
#44249=CARTESIAN_POINT('Ctrl Pts',(-0.0554367298047564,2.37119849032336,
8.40299412389574));
#44250=CARTESIAN_POINT('Ctrl Pts',(-0.0975391702519295,2.36983420820918,
8.40580327672186));
#44251=CARTESIAN_POINT('Ctrl Pts',(-0.118254496977509,2.36889085691657,
8.40719433997542));
#44252=CARTESIAN_POINT('Ctrl Pts',(-0.168348492904814,2.36595093883005,
8.41058098127354));
#44253=CARTESIAN_POINT('Ctrl Pts',(-0.197706879876495,2.36367868314668,
8.41258478020899));
#44254=CARTESIAN_POINT('Ctrl Pts',(-0.310191774486386,2.35286242537215,
8.42033879799712));
#44255=CARTESIAN_POINT('Ctrl Pts',(-0.392879290725077,2.34047508799632,
8.42620261286005));
#44256=CARTESIAN_POINT('Ctrl Pts',(-0.642290695004911,2.28952134777254,
8.44437604281266));
#44257=CARTESIAN_POINT('Ctrl Pts',(-0.805638282673186,2.2372718671673,8.45699196158704));
#44258=CARTESIAN_POINT('Ctrl Pts',(-1.01481840393372,2.14445522883268,8.47342399092133));
#44259=CARTESIAN_POINT('Ctrl Pts',(-1.06682468527166,2.11906366958451,8.47752887289035));
#44260=CARTESIAN_POINT('Ctrl Pts',(-1.13416242524371,2.08307838648856,8.48282524513304));
#44261=CARTESIAN_POINT('Ctrl Pts',(-1.15036873754758,2.07417255572273,8.48409842526894));
#44262=CARTESIAN_POINT('Ctrl Pts',(-1.17581661301567,2.05979819183878,8.4860933211656));
#44263=CARTESIAN_POINT('Ctrl Pts',(-1.18512766426841,2.05445509301553,8.48682230262149));
#44264=CARTESIAN_POINT('Ctrl Pts',(-1.204786015868,2.0429961268592,8.48835891448365));
#44265=CARTESIAN_POINT('Ctrl Pts',(-1.21512375788213,2.03686444915694,8.48916547620686));
#44266=CARTESIAN_POINT('Ctrl Pts',(-1.24169223016957,2.02083149093699,8.49123568267977));
#44267=CARTESIAN_POINT('Ctrl Pts',(-1.25785171772501,2.0108129254032,8.49249220413479));
#44268=CARTESIAN_POINT('Ctrl Pts',(-1.33250806980285,1.96327522922821,8.49829351115728));
#44269=CARTESIAN_POINT('Ctrl Pts',(-1.38946352294843,1.92338772608136,8.50270879454897));
#44270=CARTESIAN_POINT('Ctrl Pts',(-1.59750112761593,1.76362133168454,8.51912281044851));
#44271=CARTESIAN_POINT('Ctrl Pts',(-1.73552178128846,1.62798585545978,8.5306763992787));
#44272=CARTESIAN_POINT('Ctrl Pts',(-1.8915570573266,1.4319714809327,8.54654239017726));
#44273=CARTESIAN_POINT('Ctrl Pts',(-1.92584612712206,1.38551301357996,8.55024574556285));
#44274=CARTESIAN_POINT('Ctrl Pts',(-1.97309190083853,1.31635268208284,8.55571060995324));
#44275=CARTESIAN_POINT('Ctrl Pts',(-1.98742375584441,1.29461297731719,8.55742173148907));
#44276=CARTESIAN_POINT('Ctrl Pts',(-2.01224972916017,1.25557093158282,8.56048559855389));
#44277=CARTESIAN_POINT('Ctrl Pts',(-2.02288594145161,1.23836172515876,8.56183303899265));
#44278=CARTESIAN_POINT('Ctrl Pts',(-2.0449990397418,1.20153791443017,8.56471095382916));
#44279=CARTESIAN_POINT('Ctrl Pts',(-2.05641670523636,1.18189031040987,8.56624336222025));
#44280=CARTESIAN_POINT('Ctrl Pts',(-2.08689607778864,1.12766211278627,8.57046597611491));
#44281=CARTESIAN_POINT('Ctrl Pts',(-2.10537858929404,1.09276610484775,8.57317580482938));
#44282=CARTESIAN_POINT('Ctrl Pts',(-2.14507135880974,1.01307549683747,8.5793509761318));
#44283=CARTESIAN_POINT('Ctrl Pts',(-2.16576548676149,0.968045653083784,
8.58283138115136));
#44284=CARTESIAN_POINT('Ctrl Pts',(-2.24980899744515,0.768959355722094,
8.59817463541804));
#44285=CARTESIAN_POINT('Ctrl Pts',(-2.29823741565605,0.609126018053348,
8.61042233149373));
#44286=CARTESIAN_POINT('Ctrl Pts',(-2.34337050149059,0.37315810509811,8.62778232674803));
#44287=CARTESIAN_POINT('Ctrl Pts',(-2.35383734973825,0.300140048069965,
8.63305077103258));
#44288=CARTESIAN_POINT('Ctrl Pts',(-2.36261357647977,0.208762033060345,
8.639431095488));
#44289=CARTESIAN_POINT('Ctrl Pts',(-2.36413538571208,0.190757491159955,
8.64067795450908));
#44290=CARTESIAN_POINT('Ctrl Pts',(-2.36545134966571,0.172736721239843,
8.64191454572571));
#44291=CARTESIAN_POINT('Origin',(0.,0.,-1.84858989190501));
#44292=CARTESIAN_POINT('',(-2.36545134562115,0.172736776625918,9.83860221205714));
#44293=CARTESIAN_POINT('',(-2.36545135066153,0.172736707603127,9.6385666740965));
#44294=CARTESIAN_POINT('',(-2.36545134966535,0.172736721244682,-1.84858989190501));
#44295=CARTESIAN_POINT('',(-2.37174928960774,0.00183568656896266,8.84980289335711));
#44296=CARTESIAN_POINT('Ctrl Pts',(-2.36545134562115,0.172736776625918,
9.83860221205714));
#44297=CARTESIAN_POINT('Ctrl Pts',(-2.36270050744156,0.210406657936654,
9.83620215240312));
#44298=CARTESIAN_POINT('Ctrl Pts',(-2.35904970563618,0.248012573239168,
9.8337801285158));
#44299=CARTESIAN_POINT('Ctrl Pts',(-2.35079058754754,0.316119639036604,
9.82933468224037));
#44300=CARTESIAN_POINT('Ctrl Pts',(-2.34648425556052,0.346640319302553,
9.82732090913839));
#44301=CARTESIAN_POINT('Ctrl Pts',(-2.33864538914113,0.395319605638881,
9.82407000408802));
#44302=CARTESIAN_POINT('Ctrl Pts',(-2.33549297178358,0.413536447631834,
9.82284465584872));
#44303=CARTESIAN_POINT('Ctrl Pts',(-2.32849878827973,0.451319158251563,
9.82028395987052));
#44304=CARTESIAN_POINT('Ctrl Pts',(-2.32462261746062,0.470877091142648,
9.81894763308492));
#44305=CARTESIAN_POINT('Ctrl Pts',(-2.31480510587413,0.517333685648665,
9.81574654021211));
#44306=CARTESIAN_POINT('Ctrl Pts',(-2.30864092691927,0.544181754669804,
9.81387495945927));
#44307=CARTESIAN_POINT('Ctrl Pts',(-2.28477943873297,0.640394606301797,
9.80708697444798));
#44308=CARTESIAN_POINT('Ctrl Pts',(-2.26441311991512,0.709051318997952,
9.80208899537439));
#44309=CARTESIAN_POINT('Ctrl Pts',(-2.20072850434366,0.892803063625451,
9.78828985711847));
#44310=CARTESIAN_POINT('Ctrl Pts',(-2.15151896239858,1.00561647988228,9.77934296383663));
#44311=CARTESIAN_POINT('Ctrl Pts',(-2.03857427984995,1.21788058930933,9.7618318409391));
#44312=CARTESIAN_POINT('Ctrl Pts',(-1.9757069980223,1.31742382282463,9.75329419851088));
#44313=CARTESIAN_POINT('Ctrl Pts',(-1.89339139947278,1.42852906700827,9.74366631357741));
#44314=CARTESIAN_POINT('Ctrl Pts',(-1.88085491333681,1.44499520874845,9.74223695077601));
#44315=CARTESIAN_POINT('Ctrl Pts',(-1.86062117095188,1.47086179543048,9.73999027065234));
#44316=CARTESIAN_POINT('Ctrl Pts',(-1.85306476463591,1.48037041220486,9.73916410196991));
#44317=CARTESIAN_POINT('Ctrl Pts',(-1.83826240761646,1.49870603613134,9.73757111125329));
#44318=CARTESIAN_POINT('Ctrl Pts',(-1.83102523376705,1.50753940638888,9.73680379237504));
#44319=CARTESIAN_POINT('Ctrl Pts',(-1.81270633540309,1.52957210109908,9.73488927583652));
#44320=CARTESIAN_POINT('Ctrl Pts',(-1.80154373987051,1.54270388166164,9.73374760731058));
#44321=CARTESIAN_POINT('Ctrl Pts',(-1.75528770810446,1.59593305605895,9.72911187892828));
#44322=CARTESIAN_POINT('Ctrl Pts',(-1.71898843840322,1.63496695209525,9.72569339917936));
#44323=CARTESIAN_POINT('Ctrl Pts',(-1.60743111652266,1.74710144017612,9.71569727336568));
#44324=CARTESIAN_POINT('Ctrl Pts',(-1.52860509433746,1.81647112432048,9.70927274410999));
#44325=CARTESIAN_POINT('Ctrl Pts',(-1.33537542780856,1.96500467536336,9.69428831203965));
#44326=CARTESIAN_POINT('Ctrl Pts',(-1.21810517814577,2.03977577559265,9.68572804350183));
#44327=CARTESIAN_POINT('Ctrl Pts',(-1.06143646155453,2.1213157141372,9.67437244120528));
#44328=CARTESIAN_POINT('Ctrl Pts',(-1.02748532640278,2.13796664503385,9.67191754482246));
#44329=CARTESIAN_POINT('Ctrl Pts',(-0.973029592836558,2.16307708760159,
9.66798071826503));
#44330=CARTESIAN_POINT('Ctrl Pts',(-0.952778597555091,2.17207319512371,
9.66651686859763));
#44331=CARTESIAN_POINT('Ctrl Pts',(-0.914394760430712,2.18848439615754,
9.66374102914066));
#44332=CARTESIAN_POINT('Ctrl Pts',(-0.896290215716101,2.19596118830619,
9.66243123263873));
#44333=CARTESIAN_POINT('Ctrl Pts',(-0.854891246715128,2.21246084451294,
9.65943396945349));
#44334=CARTESIAN_POINT('Ctrl Pts',(-0.831543039991164,2.22134151439018,
9.65774199565556));
#44335=CARTESIAN_POINT('Ctrl Pts',(-0.757227346005807,2.24827223840126,
9.65234948064842));
#44336=CARTESIAN_POINT('Ctrl Pts',(-0.705783781283619,2.26494807233927,
9.64860574404602));
#44337=CARTESIAN_POINT('Ctrl Pts',(-0.579238666376462,2.3012388555889,9.63936603286962));
#44338=CARTESIAN_POINT('Ctrl Pts',(-0.503660228994815,2.31895283300851,
9.63382086267452));
#44339=CARTESIAN_POINT('Ctrl Pts',(-0.275644278827654,2.36072169090191,
9.61706958517277));
#44340=CARTESIAN_POINT('Ctrl Pts',(-0.121586092798391,2.37364783199222,
9.60570019123308));
#44341=CARTESIAN_POINT('Ctrl Pts',(0.0745043209719084,2.37094926265457,
9.59174929891972));
#44342=CARTESIAN_POINT('Ctrl Pts',(0.116352444014803,2.36926442102748,9.58880424929518));
#44343=CARTESIAN_POINT('Ctrl Pts',(0.174386803344021,2.36538634230217,9.58478344614116));
#44344=CARTESIAN_POINT('Ctrl Pts',(0.190625796520028,2.36413306474882,9.58366528033896));
#44345=CARTESIAN_POINT('Ctrl Pts',(0.218057287231003,2.36173148816722,9.58178955411183));
#44346=CARTESIAN_POINT('Ctrl Pts',(0.229256670591841,2.36067066810648,9.5810274834417));
#44347=CARTESIAN_POINT('Ctrl Pts',(0.252878045339787,2.35826352434265,9.57942846014892));
#44348=CARTESIAN_POINT('Ctrl Pts',(0.26529755923328,2.3568986780344,9.57859248976774));
#44349=CARTESIAN_POINT('Ctrl Pts',(0.299897820725673,2.35281930454158,9.576275332844));
#44350=CARTESIAN_POINT('Ctrl Pts',(0.322052476829829,2.34988928929035,9.57480522194572));
#44351=CARTESIAN_POINT('Ctrl Pts',(0.372575813571147,2.34247944643263,9.57147695196925));
#44352=CARTESIAN_POINT('Ctrl Pts',(0.400911531880738,2.33779656633737,9.56962789498759));
#44353=CARTESIAN_POINT('Ctrl Pts',(0.497248445979401,2.32007230685416,9.56338035238693));
#44354=CARTESIAN_POINT('Ctrl Pts',(0.564763735187445,2.30456821714492,9.5590679320742));
#44355=CARTESIAN_POINT('Ctrl Pts',(0.803746270857736,2.23855305867927,9.54374650529064));
#44356=CARTESIAN_POINT('Ctrl Pts',(0.970043926634828,2.17166733256299,9.53293075161675));
#44357=CARTESIAN_POINT('Ctrl Pts',(1.16253735612875,2.06768309354584,9.51894100399682));
#44358=CARTESIAN_POINT('Ctrl Pts',(1.1973322815509,2.04773084155132,9.51635086817113));
#44359=CARTESIAN_POINT('Ctrl Pts',(1.25269665527534,2.01408995877829,9.51211782517234));
#44360=CARTESIAN_POINT('Ctrl Pts',(1.27358810668015,2.00094490990692,9.51049394907116));
#44361=CARTESIAN_POINT('Ctrl Pts',(1.31066127777069,1.97680239039825,9.50756198936938));
#44362=CARTESIAN_POINT('Ctrl Pts',(1.32691946359158,1.96592608571232,9.50625840288692));
#44363=CARTESIAN_POINT('Ctrl Pts',(1.36146103620129,1.9421949867402,9.5034493650615));
#44364=CARTESIAN_POINT('Ctrl Pts',(1.37970085826088,1.92928043662882,9.50194177480713));
#44365=CARTESIAN_POINT('Ctrl Pts',(1.42988779852772,1.89267031093537,9.49772401081248));
#44366=CARTESIAN_POINT('Ctrl Pts',(1.46142418337214,1.86842689305581,9.49499338920738));
#44367=CARTESIAN_POINT('Ctrl Pts',(1.53151363736918,1.81168569083562,9.48873578259558));
#44368=CARTESIAN_POINT('Ctrl Pts',(1.56966907965354,1.7787291664496,9.48519260472642));
#44369=CARTESIAN_POINT('Ctrl Pts',(1.69723382146595,1.6612433823564,9.47286948261818));
#44370=CARTESIAN_POINT('Ctrl Pts',(1.78109613134552,1.57099462126244,9.46390578762221));
#44371=CARTESIAN_POINT('Ctrl Pts',(1.9231243329933,1.39208685928815,9.44727246873413));
#44372=CARTESIAN_POINT('Ctrl Pts',(1.98310221828972,1.30522889538571,9.43962257802322));
#44373=CARTESIAN_POINT('Ctrl Pts',(2.05010164696505,1.19286433184417,9.43045558052956));
#44374=CARTESIAN_POINT('Ctrl Pts',(2.06274834906272,1.17085927889165,9.42869331467381));
#44375=CARTESIAN_POINT('Ctrl Pts',(2.08146663801651,1.13704475877193,9.4260397119296));
#44376=CARTESIAN_POINT('Ctrl Pts',(2.0877959088263,1.12538100766158,9.4251340797626));
#44377=CARTESIAN_POINT('Ctrl Pts',(2.09922141537343,1.10389758724809,9.42348450798587));
#44378=CARTESIAN_POINT('Ctrl Pts',(2.10434713881205,1.09409485922022,9.42273889499029));
#44379=CARTESIAN_POINT('Ctrl Pts',(2.11619884701865,1.07103753188662,9.42100124563398));
#44380=CARTESIAN_POINT('Ctrl Pts',(2.12286909686738,1.05775506637138,9.42001253282783));
#44381=CARTESIAN_POINT('Ctrl Pts',(2.14489632760124,1.0128444631606,9.4167077014125));
#44382=CARTESIAN_POINT('Ctrl Pts',(2.15967555931199,0.980936259162319,9.41442287419263));
#44383=CARTESIAN_POINT('Ctrl Pts',(2.25162658892635,0.770252448630054,9.39967037301248));
#44384=CARTESIAN_POINT('Ctrl Pts',(2.30724774696957,0.582867953444738,9.38804546966571));
#44385=CARTESIAN_POINT('Ctrl Pts',(2.35398489395921,0.303081012668453,9.37038258339995));
#44386=CARTESIAN_POINT('Ctrl Pts',(2.36368990795524,0.214640460521849,9.36476610209));
#44387=CARTESIAN_POINT('Ctrl Pts',(2.37000197749197,0.0958706998814639,
9.35705220257052));
#44388=CARTESIAN_POINT('Ctrl Pts',(2.37102612379592,0.0658449271813441,
9.35508789110941));
#44389=CARTESIAN_POINT('Ctrl Pts',(2.37175671902164,0.0174604707631053,
9.351895736216));
#44390=CARTESIAN_POINT('Ctrl Pts',(2.37182081505484,-0.000890064131993465,
9.35067886859219));
#44391=CARTESIAN_POINT('Ctrl Pts',(2.37150938071795,-0.0392817225884852,
9.34811913561296));
#44392=CARTESIAN_POINT('Ctrl Pts',(2.37109273929517,-0.0593209616367282,
9.34677511187267));
#44393=CARTESIAN_POINT('Ctrl Pts',(2.36947963077305,-0.107508127718996,
9.3435230524556));
#44394=CARTESIAN_POINT('Ctrl Pts',(2.36803552972143,-0.13564413609758,9.34160761734316));
#44395=CARTESIAN_POINT('Ctrl Pts',(2.36079395430166,-0.240282697912474,
9.33441911486086));
#44396=CARTESIAN_POINT('Ctrl Pts',(2.35178739339884,-0.31650869089915,9.32905097784582));
#44397=CARTESIAN_POINT('Ctrl Pts',(2.31579802713164,-0.531174582923423,
9.31356420449228));
#44398=CARTESIAN_POINT('Ctrl Pts',(2.28014605224576,-0.667828467604391,
9.30324597625646));
#44399=CARTESIAN_POINT('Ctrl Pts',(2.20095577962291,-0.888690206711893,
9.2862031748829));
#44400=CARTESIAN_POINT('Ctrl Pts',(2.16413116120363,-0.974944346914091,
9.27945422654761));
#44401=CARTESIAN_POINT('Ctrl Pts',(2.11324919574331,-1.07693386461123,9.27152307729709));
#44402=CARTESIAN_POINT('Ctrl Pts',(2.10397028471449,-1.0949510584915,9.27012406548367));
#44403=CARTESIAN_POINT('Ctrl Pts',(2.08880602639335,-1.1234913044795,9.26791382446343));
#44404=CARTESIAN_POINT('Ctrl Pts',(2.08306963689263,-1.13409180883961,9.26709420235118));
#44405=CARTESIAN_POINT('Ctrl Pts',(2.07171387091418,-1.15469970331739,9.26550405715009));
#44406=CARTESIAN_POINT('Ctrl Pts',(2.0661022637037,-1.16471078439809,9.26473314711422));
#44407=CARTESIAN_POINT('Ctrl Pts',(2.05173624496531,-1.18990912131953,9.26279572665168));
#44408=CARTESIAN_POINT('Ctrl Pts',(2.04288549987597,-1.20504116719562,9.26163503396239));
#44409=CARTESIAN_POINT('Ctrl Pts',(2.00497463911275,-1.26823868811787,9.25679317361903));
#44410=CARTESIAN_POINT('Ctrl Pts',(1.97437751565054,-1.31536579168252,9.25319631211771));
#44411=CARTESIAN_POINT('Ctrl Pts',(1.875525925207,-1.45638812724973,9.24233437402656));
#44412=CARTESIAN_POINT('Ctrl Pts',(1.80203098960492,-1.54639944790171,9.23525463550883));
#44413=CARTESIAN_POINT('Ctrl Pts',(1.6293174172416,-1.72881122447544,9.21979336805014));
#44414=CARTESIAN_POINT('Ctrl Pts',(1.52818960089582,-1.81881663940329,9.21141018122371));
#44415=CARTESIAN_POINT('Ctrl Pts',(1.39393444562791,-1.91916654685332,9.20056995388185));
#44416=CARTESIAN_POINT('Ctrl Pts',(1.3675172362166,-1.93807892489162,9.19845058952825));
#44417=CARTESIAN_POINT('Ctrl Pts',(1.32350627133017,-1.96823899044793,9.19493652423275));
#44418=CARTESIAN_POINT('Ctrl Pts',(1.30613715882049,-1.97980788213726,9.19355385942387));
#44419=CARTESIAN_POINT('Ctrl Pts',(1.27181650266675,-2.00201932400792,9.19082857177794));
#44420=CARTESIAN_POINT('Ctrl Pts',(1.25487840794817,-2.01267949010304,9.18948674154045));
#44421=CARTESIAN_POINT('Ctrl Pts',(1.2139248055203,-2.0377361338441,9.18624884619042));
#44422=CARTESIAN_POINT('Ctrl Pts',(1.1897857828507,-2.05192389264015,9.18434554383304));
#44423=CARTESIAN_POINT('Ctrl Pts',(1.09985562970788,-2.10266009807007,9.17727062619719));
#44424=CARTESIAN_POINT('Ctrl Pts',(1.0325928457344,-2.1364952259127,9.17200788030211));
#44425=CARTESIAN_POINT('Ctrl Pts',(0.840061338669288,-2.22212677658948,
9.15702668573074));
#44426=CARTESIAN_POINT('Ctrl Pts',(0.71180009157355,-2.2664698008437,9.14712598959486));
#44427=CARTESIAN_POINT('Ctrl Pts',(0.482730480164854,-2.32429149206015,
9.12994584922038));
#44428=CARTESIAN_POINT('Ctrl Pts',(0.383507563603569,-2.3427090560478,9.12266645747431));
#44429=CARTESIAN_POINT('Ctrl Pts',(0.263154416729208,-2.357194059464,9.11422958443261));
#44430=CARTESIAN_POINT('Ctrl Pts',(0.242872578004368,-2.35937005586239,
9.11282123186898));
#44431=CARTESIAN_POINT('Ctrl Pts',(0.210536987005296,-2.36241786795112,
9.11059979628028));
#44432=CARTESIAN_POINT('Ctrl Pts',(0.198500781770552,-2.36345963818564,
9.10977817956339));
#44433=CARTESIAN_POINT('Ctrl Pts',(0.175034580057199,-2.36531017778293,
9.10818724699811));
#44434=CARTESIAN_POINT('Ctrl Pts',(0.163605842878579,-2.36612816152204,
9.10741750993013));
#44435=CARTESIAN_POINT('Ctrl Pts',(0.134772797036977,-2.36798190863626,
9.10548745284677));
#44436=CARTESIAN_POINT('Ctrl Pts',(0.117361725280073,-2.36890867184927,
9.10433285788303));
#44437=CARTESIAN_POINT('Ctrl Pts',(0.0447678396191601,-2.37197037068075,
9.09955833901055));
#44438=CARTESIAN_POINT('Ctrl Pts',(-0.0104748885017752,-2.37236989014969,
9.09601981523516));
#44439=CARTESIAN_POINT('Ctrl Pts',(-0.177896848822243,-2.36773136469762,
9.08544953002196));
#44440=CARTESIAN_POINT('Ctrl Pts',(-0.289752313701264,-2.35665984568789,
9.07859192665172));
#44441=CARTESIAN_POINT('Ctrl Pts',(-0.527318272950489,-2.31596894895503,
9.06376438725667));
#44442=CARTESIAN_POINT('Ctrl Pts',(-0.652234487547055,-2.28393565129467,
9.05579795693928));
#44443=CARTESIAN_POINT('Ctrl Pts',(-0.809837273814174,-2.22953019097822,
9.04507998303646));
#44444=CARTESIAN_POINT('Ctrl Pts',(-0.84544283577815,-2.21627332269943,
9.04261380548274));
#44445=CARTESIAN_POINT('Ctrl Pts',(-0.901322996518006,-2.19392516319354,
9.03866306388553));
#44446=CARTESIAN_POINT('Ctrl Pts',(-0.921815492790863,-2.18539399381889,
9.03719680538935));
#44447=CARTESIAN_POINT('Ctrl Pts',(-0.958357186485925,-2.16957602425655,
9.03454924420304));
#44448=CARTESIAN_POINT('Ctrl Pts',(-0.974450789235,-2.16239548950957,9.03337156109689));
#44449=CARTESIAN_POINT('Ctrl Pts',(-1.0121996299569,-2.14504598613897,9.03058081650466));
#44450=CARTESIAN_POINT('Ctrl Pts',(-1.03378363103694,-2.13472754850017,
9.02896280660588));
#44451=CARTESIAN_POINT('Ctrl Pts',(-1.09819935279767,-2.10272697265849,
9.0240645511428));
#44452=CARTESIAN_POINT('Ctrl Pts',(-1.14053032554868,-2.08007032434139,
9.02075168815866));
#44453=CARTESIAN_POINT('Ctrl Pts',(-1.37258617161447,-1.94665421909629,
9.00204869593388));
#44454=CARTESIAN_POINT('Ctrl Pts',(-1.54688001653122,-1.81123930582838,
8.98579199854102));
#44455=CARTESIAN_POINT('Ctrl Pts',(-1.74126217921008,-1.61142898912077,
8.96576133403349));
#44456=CARTESIAN_POINT('Ctrl Pts',(-1.78091403174461,-1.56749602011773,
8.96156117454602));
#44457=CARTESIAN_POINT('Ctrl Pts',(-1.83061712209207,-1.50810252738383,
8.95618849039318));
#44458=CARTESIAN_POINT('Ctrl Pts',(-1.8421877198278,-1.49394669793652,8.95492958640676));
#44459=CARTESIAN_POINT('Ctrl Pts',(-1.86013185161236,-1.47146776427559,
8.95296602716394));
#44460=CARTESIAN_POINT('Ctrl Pts',(-1.866615601405,-1.46323412131904,8.95225416216658));
#44461=CARTESIAN_POINT('Ctrl Pts',(-1.88012729557723,-1.4458397946568,8.95076612831986));
#44462=CARTESIAN_POINT('Ctrl Pts',(-1.88714331607727,-1.43667027293165,
8.94999084636571));
#44463=CARTESIAN_POINT('Ctrl Pts',(-1.90485056480025,-1.41317441048455,
8.94802642209817));
#44464=CARTESIAN_POINT('Ctrl Pts',(-1.91544756830534,-1.39877741208341,
8.94684343973901));
#44465=CARTESIAN_POINT('Ctrl Pts',(-1.96078173005553,-1.33570536164168,
8.94174353341617));
#44466=CARTESIAN_POINT('Ctrl Pts',(-1.99383663185622,-1.28584234999697,
8.93792256592909));
#44467=CARTESIAN_POINT('Ctrl Pts',(-2.07225254057941,-1.15724429647089,
8.92844524260235));
#44468=CARTESIAN_POINT('Ctrl Pts',(-2.11504147136868,-1.07705438838185,
8.92287064418814));
#44469=CARTESIAN_POINT('Ctrl Pts',(-2.21585241640659,-0.858818090973323,
8.90809257166433));
#44470=CARTESIAN_POINT('Ctrl Pts',(-2.26558509578718,-0.717417723420512,
8.89888880217024));
#44471=CARTESIAN_POINT('Ctrl Pts',(-2.31030672126261,-0.53755170271021,
8.88694363773667));
#44472=CARTESIAN_POINT('Ctrl Pts',(-2.31815487282011,-0.502629834645124,
8.88461527215623));
#44473=CARTESIAN_POINT('Ctrl Pts',(-2.32945614205047,-0.446426025598749,
8.88084620698829));
#44474=CARTESIAN_POINT('Ctrl Pts',(-2.33341466301461,-0.425250601657645,
8.87942129469152));
#44475=CARTESIAN_POINT('Ctrl Pts',(-2.34030328579034,-0.385403313807903,
8.87672939529146));
#44476=CARTESIAN_POINT('Ctrl Pts',(-2.34329972388754,-0.366744533584877,
8.87546458485171));
#44477=CARTESIAN_POINT('Ctrl Pts',(-2.34888497990102,-0.329096702985042,
8.87290310592351));
#44478=CARTESIAN_POINT('Ctrl Pts',(-2.35146724466143,-0.310108125147207,
8.8716063360082));
#44479=CARTESIAN_POINT('Ctrl Pts',(-2.35689798317458,-0.266194076338138,
8.86859550506835));
#44480=CARTESIAN_POINT('Ctrl Pts',(-2.35958159577236,-0.241250908077913,
8.86687656214506));
#44481=CARTESIAN_POINT('Ctrl Pts',(-2.36850940866389,-0.143751205703641,
8.86012153730056));
#44482=CARTESIAN_POINT('Ctrl Pts',(-2.37180564160149,-0.0709723861126348,
8.85500019683922));
#44483=CARTESIAN_POINT('Ctrl Pts',(-2.37174928960774,0.00183568656896266,
8.84980289335711));
#44484=CARTESIAN_POINT('Ctrl Pts',(-2.37174929161342,0.00183309335181954,
8.8498030784703));
#44485=CARTESIAN_POINT('Ctrl Pts',(-2.37170518086058,0.0589058260080911,
8.84572902179415));
#44486=CARTESIAN_POINT('Ctrl Pts',(-2.3696010754449,0.11591062296176,8.84161489479427));
#44487=CARTESIAN_POINT('Ctrl Pts',(-2.36545132340079,0.172737080910408,
8.8374806621729));
#44488=CARTESIAN_POINT('',(-2.37175040066033,0.000883970845875868,8.65336333906485));
#44489=CARTESIAN_POINT('Ctrl Pts',(-2.36545134966571,0.172736721239843,
8.64191454572571));
#44490=CARTESIAN_POINT('Ctrl Pts',(-2.36557018947359,0.171109332564596,
8.64202621767707));
#44491=CARTESIAN_POINT('Ctrl Pts',(-2.36568735056825,0.169481811544686,
8.6421378058687));
#44492=CARTESIAN_POINT('Ctrl Pts',(-2.36666375034735,0.15572004744893,8.64308056562317));
#44493=CARTESIAN_POINT('Ctrl Pts',(-2.3674313260975,0.1435791522688,8.64390708121543));
#44494=CARTESIAN_POINT('Ctrl Pts',(-2.3686911561697,0.120879978181028,8.64544199252111));
#44495=CARTESIAN_POINT('Ctrl Pts',(-2.36920630706136,0.110323373530993,
8.64615162813759));
#44496=CARTESIAN_POINT('Ctrl Pts',(-2.37029459880395,0.0844735103778954,
8.64787979921009));
#44497=CARTESIAN_POINT('Ctrl Pts',(-2.37079033270636,0.0691772150860396,
8.64889428094819));
#44498=CARTESIAN_POINT('Ctrl Pts',(-2.3715392963827,0.0362149919024032,
8.65106492675962));
#44499=CARTESIAN_POINT('Ctrl Pts',(-2.37174326919453,0.0185488449211695,
8.65221871811156));
#44500=CARTESIAN_POINT('Ctrl Pts',(-2.37174983615641,0.000881584965583026,
8.65336447339507));
#44501=CARTESIAN_POINT('Ctrl Pts',(-2.37174983524487,0.000884033889070948,
8.65336431457769));
#44502=CARTESIAN_POINT('Ctrl Pts',(-2.37179372306343,-0.116861368983434,
8.66100033204862));
#44503=CARTESIAN_POINT('Ctrl Pts',(-2.36306931368071,-0.234464575574185,
8.66827214436893));
#44504=CARTESIAN_POINT('Ctrl Pts',(-2.32974670086994,-0.457183799256998,
8.68213251040277));
#44505=CARTESIAN_POINT('Ctrl Pts',(-2.30665348437395,-0.562214556911442,
8.68870951212139));
#44506=CARTESIAN_POINT('Ctrl Pts',(-2.25533256558931,-0.737820610276738,
8.70017655204398));
#44507=CARTESIAN_POINT('Ctrl Pts',(-2.23069258861883,-0.809267053886955,
8.70497970519907));
#44508=CARTESIAN_POINT('Ctrl Pts',(-2.19210784323786,-0.905911386254933,
8.7117450238051));
#44509=CARTESIAN_POINT('Ctrl Pts',(-2.1810509698559,-0.932217137115946,
8.71361453659954));
#44510=CARTESIAN_POINT('Ctrl Pts',(-2.16120708480675,-0.977141515638886,
8.71685941333449));
#44511=CARTESIAN_POINT('Ctrl Pts',(-2.15264713529207,-0.995857355066325,
8.71822713532883));
#44512=CARTESIAN_POINT('Ctrl Pts',(-2.13569477445129,-1.03168259252301,
8.72087710551277));
#44513=CARTESIAN_POINT('Ctrl Pts',(-2.12733755885752,-1.04880694894374,
8.72215807955269));
#44514=CARTESIAN_POINT('Ctrl Pts',(-2.10450477690648,-1.09419655689606,
8.72559273890156));
#44515=CARTESIAN_POINT('Ctrl Pts',(-2.08966676137337,-1.12227408491665,
8.7277586362397));
#44516=CARTESIAN_POINT('Ctrl Pts',(-2.02534606750555,-1.23828571285982,
8.73688629157932));
#44517=CARTESIAN_POINT('Ctrl Pts',(-1.97084741425494,-1.32330420913838,
8.7440179199265));
#44518=CARTESIAN_POINT('Ctrl Pts',(-1.82580459678857,-1.52065241319603,
8.76163722084073));
#44519=CARTESIAN_POINT('Ctrl Pts',(-1.73010907691664,-1.62870087703635,
8.77223096655667));
#44520=CARTESIAN_POINT('Ctrl Pts',(-1.57975788007769,-1.77015732066095,
8.78707924861977));
#44521=CARTESIAN_POINT('Ctrl Pts',(-1.53263614208144,-1.8111100818324,8.79151436243348));
#44522=CARTESIAN_POINT('Ctrl Pts',(-1.46956886898191,-1.86169419190209,
8.79712217679343));
#44523=CARTESIAN_POINT('Ctrl Pts',(-1.45505322777612,-1.87306115247112,
8.79839144269398));
#44524=CARTESIAN_POINT('Ctrl Pts',(-1.43095142528555,-1.89148558168181,
8.80046201231934));
#44525=CARTESIAN_POINT('Ctrl Pts',(-1.42144226626367,-1.89864203898062,
8.8012696682457));
#44526=CARTESIAN_POINT('Ctrl Pts',(-1.40193643119075,-1.91309315699462,
8.80290693580885));
#44527=CARTESIAN_POINT('Ctrl Pts',(-1.39193581805137,-1.92038170161609,
8.80373616127631));
#44528=CARTESIAN_POINT('Ctrl Pts',(-1.36507154225771,-1.93964053019555,
8.80593793641216));
#44529=CARTESIAN_POINT('Ctrl Pts',(-1.34810719074599,-1.95146938849341,
8.80730156187858));
#44530=CARTESIAN_POINT('Ctrl Pts',(-1.25178032569586,-2.01678020694889,
8.81490849064949));
#44531=CARTESIAN_POINT('Ctrl Pts',(-1.16938383968617,-2.06564806790555,
8.82090428927282));
#44532=CARTESIAN_POINT('Ctrl Pts',(-0.961455990256574,-2.17252454134085,
8.83537702358837));
#44533=CARTESIAN_POINT('Ctrl Pts',(-0.833387212095843,-2.22479794335441,
8.84376176089531));
#44534=CARTESIAN_POINT('Ctrl Pts',(-0.628678541069258,-2.28818105717448,
8.85718879052238));
#44535=CARTESIAN_POINT('Ctrl Pts',(-0.554819532077321,-2.307202388462,8.8620343896621));
#44536=CARTESIAN_POINT('Ctrl Pts',(-0.452153228605651,-2.32842746618177,
8.86884935434976));
#44537=CARTESIAN_POINT('Ctrl Pts',(-0.424027102977316,-2.33371333074984,
8.87072416419694));
#44538=CARTESIAN_POINT('Ctrl Pts',(-0.375507928059135,-2.34192569762119,
8.8739752535841));
#44539=CARTESIAN_POINT('Ctrl Pts',(-0.355159340236062,-2.34509786062143,
8.8753438108793));
#44540=CARTESIAN_POINT('Ctrl Pts',(-0.315927280468617,-2.3506914683562,
8.87799329472398));
#44541=CARTESIAN_POINT('Ctrl Pts',(-0.297050832954015,-2.35315133232896,
8.87927292233956));
#44542=CARTESIAN_POINT('Ctrl Pts',(-0.24671780393453,-2.35909516017397,
8.88269880868327));
#44543=CARTESIAN_POINT('Ctrl Pts',(-0.215218554301381,-2.36217705923991,
8.8848571642157));
#44544=CARTESIAN_POINT('Ctrl Pts',(-0.0838762823906145,-2.37237884054155,
8.89392096761391));
#44545=CARTESIAN_POINT('Ctrl Pts',(0.0162936412259015,-2.37380424034094,
8.90099343632069));
#44546=CARTESIAN_POINT('Ctrl Pts',(0.260961529613066,-2.36179824181781,
8.91861049124884));
#44547=CARTESIAN_POINT('Ctrl Pts',(0.404717249582548,-2.34145113839692,
8.92926756455896));
#44548=CARTESIAN_POINT('Ctrl Pts',(0.606593221353358,-2.29372103237233,
8.94418929212688));
#44549=CARTESIAN_POINT('Ctrl Pts',(0.6668846373904,-2.2769228736431,8.94863589387079));
#44550=CARTESIAN_POINT('Ctrl Pts',(0.744008509792408,-2.25210785072657,
8.9542556831629));
#44551=CARTESIAN_POINT('Ctrl Pts',(0.761505107755759,-2.24625209106925,
8.95552592393854));
#44552=CARTESIAN_POINT('Ctrl Pts',(0.790175382134453,-2.23628321527518,
8.95759765456637));
#44553=CARTESIAN_POINT('Ctrl Pts',(0.80138933509745,-2.23228916322732,8.95840551013263));
#44554=CARTESIAN_POINT('Ctrl Pts',(0.82419491735044,-2.22397253302153,8.960042726459));
#44555=CARTESIAN_POINT('Ctrl Pts',(0.835783647940387,-2.21964339484492,
8.96087170620349));
#44556=CARTESIAN_POINT('Ctrl Pts',(0.866636296614415,-2.20784204438973,
8.9630720696475));
#44557=CARTESIAN_POINT('Ctrl Pts',(0.885837808127657,-2.20020826541884,
8.96443454910261));
#44558=CARTESIAN_POINT('Ctrl Pts',(0.992939094369361,-2.15599947078173,
8.97200812964924));
#44559=CARTESIAN_POINT('Ctrl Pts',(1.0786836597914,-2.11440473670555,8.97797432928183));
#44560=CARTESIAN_POINT('Ctrl Pts',(1.2824185670099,-1.99994307935794,8.9924429385108));
#44561=CARTESIAN_POINT('Ctrl Pts',(1.39696015664093,-1.92168459733474,9.00085057921141));
#44562=CARTESIAN_POINT('Ctrl Pts',(1.56304481093426,-1.78547365322691,9.01430822075435));
#44563=CARTESIAN_POINT('Ctrl Pts',(1.61969281526299,-1.73424875426698,9.01916024509753));
#44564=CARTESIAN_POINT('Ctrl Pts',(1.69405320708211,-1.66018115116672,9.02598271818351));
#44565=CARTESIAN_POINT('Ctrl Pts',(1.71396913253943,-1.63961197313436,9.02785832085443));
#44566=CARTESIAN_POINT('Ctrl Pts',(1.74756373403812,-1.60363438986966,9.03111033678072));
#44567=CARTESIAN_POINT('Ctrl Pts',(1.76142321988089,-1.58839870844333,9.03247901567897));
#44568=CARTESIAN_POINT('Ctrl Pts',(1.78770516075917,-1.5587400599745,9.03512841865597));
#44569=CARTESIAN_POINT('Ctrl Pts',(1.80015590011304,-1.54434420254431,9.03640784007747));
#44570=CARTESIAN_POINT('Ctrl Pts',(1.83283443706518,-1.50562829084868,9.03983239979772));
#44571=CARTESIAN_POINT('Ctrl Pts',(1.85275064788113,-1.48105148347431,9.04198961763356));
#44572=CARTESIAN_POINT('Ctrl Pts',(1.93332650582873,-1.37745064778358,9.05101943219595));
#44573=CARTESIAN_POINT('Ctrl Pts',(1.98946184425113,-1.29505164227659,9.05805728880425));
#44574=CARTESIAN_POINT('Ctrl Pts',(2.11434220414787,-1.0843757392714,9.07566759371563));
#44575=CARTESIAN_POINT('Ctrl Pts',(2.17679015512256,-0.952835703272854,
9.08635593936601));
#44576=CARTESIAN_POINT('Ctrl Pts',(2.24836738241969,-0.757604949658079,
9.10131389948319));
#44577=CARTESIAN_POINT('Ctrl Pts',(2.26759166227018,-0.697961736111654,
9.10576613665012));
#44578=CARTESIAN_POINT('Ctrl Pts',(2.28939501658166,-0.619846061076553,
9.11139179506727));
#44579=CARTESIAN_POINT('Ctrl Pts',(2.29414923065706,-0.602011661625137,
9.11266250966497));
#44580=CARTESIAN_POINT('Ctrl Pts',(2.30162688783925,-0.572584888065648,
9.11473480246667));
#44581=CARTESIAN_POINT('Ctrl Pts',(2.30447201778613,-0.561024531815689,
9.11554275299629));
#44582=CARTESIAN_POINT('Ctrl Pts',(2.31009538771382,-0.537410775497299,
9.11717993898898));
#44583=CARTESIAN_POINT('Ctrl Pts',(2.31286660472596,-0.525356191280125,
9.11800879596065));
#44584=CARTESIAN_POINT('Ctrl Pts',(2.32001301190973,-0.4931168447722,9.12020845899542));
#44585=CARTESIAN_POINT('Ctrl Pts',(2.32421918116902,-0.472895195337293,
9.12157037066672));
#44586=CARTESIAN_POINT('Ctrl Pts',(2.34626273956681,-0.359508893452298,
9.12912068675838));
#44587=CARTESIAN_POINT('Ctrl Pts',(2.35876464196294,-0.26538439971447,9.13506603029884));
#44588=CARTESIAN_POINT('Ctrl Pts',(2.37558356834476,-0.0323788539098895,
9.14953148894067));
#44589=CARTESIAN_POINT('Ctrl Pts',(2.37341128534998,0.106603224990083,9.15795502267828));
#44590=CARTESIAN_POINT('Ctrl Pts',(2.35122358668863,0.320599429235769,9.17143390718812));
#44591=CARTESIAN_POINT('Ctrl Pts',(2.33967620201412,0.396169060316314,9.17629038752998));
#44592=CARTESIAN_POINT('Ctrl Pts',(2.31881537652723,0.499112683783822,9.18311807043744));
#44593=CARTESIAN_POINT('Ctrl Pts',(2.31261990620061,0.527074261853204,9.1849942253064));
#44594=CARTESIAN_POINT('Ctrl Pts',(2.30110068735885,0.574941690245038,9.18824688892575));
#44595=CARTESIAN_POINT('Ctrl Pts',(2.29602096949749,0.594903339868322,9.18961565491708));
#44596=CARTESIAN_POINT('Ctrl Pts',(2.28574889139593,0.633176316492555,9.19226500806614));
#44597=CARTESIAN_POINT('Ctrl Pts',(2.28059481982479,0.651496334873831,9.1935442899917));
#44598=CARTESIAN_POINT('Ctrl Pts',(2.26629173182967,0.700085499829344,9.19696794194264));
#44599=CARTESIAN_POINT('Ctrl Pts',(2.25675715943362,0.730236181229485,9.19912437961339));
#44600=CARTESIAN_POINT('Ctrl Pts',(2.21479559465308,0.854247690298336,9.20813151502607));
#44601=CARTESIAN_POINT('Ctrl Pts',(2.17709641091932,0.946205802471104,9.21514630375487));
#44602=CARTESIAN_POINT('Ctrl Pts',(2.07018457269287,1.16650370500511,9.23275207975238));
#44603=CARTESIAN_POINT('Ctrl Pts',(1.99469629829437,1.29134783978998,9.24346124788048));
#44604=CARTESIAN_POINT('Ctrl Pts',(1.88293945247744,1.44275855791601,9.25699879074772));
#44605=CARTESIAN_POINT('Ctrl Pts',(1.85671778152915,1.47635114754548,9.26003905496627));
#44606=CARTESIAN_POINT('Ctrl Pts',(1.81046376490667,1.53242414630268,9.26515549960008));
#44607=CARTESIAN_POINT('Ctrl Pts',(1.79088277782216,1.55526264173026,9.26725180693668));
#44608=CARTESIAN_POINT('Ctrl Pts',(1.76139038974623,1.5883655434728,9.27030135519299));
#44609=CARTESIAN_POINT('Ctrl Pts',(1.75181318207251,1.59892207601551,9.27127557035272));
#44610=CARTESIAN_POINT('Ctrl Pts',(1.73519140684872,1.61691488234794,9.27293805111133));
#44611=CARTESIAN_POINT('Ctrl Pts',(1.72819313902993,1.62439263724029,9.27362951982974));
#44612=CARTESIAN_POINT('Ctrl Pts',(1.71145629477165,1.64204560329323,9.27526326004018));
#44613=CARTESIAN_POINT('Ctrl Pts',(1.70167522968684,1.65217972663099,9.27620236640042));
#44614=CARTESIAN_POINT('Ctrl Pts',(1.67136831838386,1.68302592076169,9.27906686687213));
#44615=CARTESIAN_POINT('Ctrl Pts',(1.65054953055276,1.70344789586658,9.28097186207313));
#44616=CARTESIAN_POINT('Ctrl Pts',(1.52082225668994,1.82609045261793,9.29250554138645));
#44617=CARTESIAN_POINT('Ctrl Pts',(1.40282373501614,1.91822897164638,9.30159404090192));
#44618=CARTESIAN_POINT('Ctrl Pts',(1.19992450246832,2.04785973213286,9.31641544467116));
#44619=CARTESIAN_POINT('Ctrl Pts',(1.12014419618952,2.09256391138063,9.32206467321359));
#44620=CARTESIAN_POINT('Ctrl Pts',(0.983638335424083,2.15900611353173,9.33166200283295));
#44621=CARTESIAN_POINT('Ctrl Pts',(0.928300954092049,2.18337083378392,9.33553417123717));
#44622=CARTESIAN_POINT('Ctrl Pts',(0.847485857200007,2.21532529709751,9.34120057415677));
#44623=CARTESIAN_POINT('Ctrl Pts',(0.822714730877479,2.22464352900618,9.34293879377814));
#44624=CARTESIAN_POINT('Ctrl Pts',(0.778696262658941,2.24036636150025,9.34603282140109));
#44625=CARTESIAN_POINT('Ctrl Pts',(0.75951269160746,2.24694230721723,9.34738293179338));
#44626=CARTESIAN_POINT('Ctrl Pts',(0.718878956443703,2.26029135522454,9.35024743744187));
#44627=CARTESIAN_POINT('Ctrl Pts',(0.69741214219613,2.26700688339401,9.35176352790779));
#44628=CARTESIAN_POINT('Ctrl Pts',(0.639108837106248,2.28433961300818,9.35589018287369));
#44629=CARTESIAN_POINT('Ctrl Pts',(0.60210649530224,2.29437029529611,9.35851888894639));
#44630=CARTESIAN_POINT('Ctrl Pts',(0.412817780964479,2.34078890277546,9.37202261613574));
#44631=CARTESIAN_POINT('Ctrl Pts',(0.257460687460128,2.36292417204575,9.38332623428927));
#44632=CARTESIAN_POINT('Ctrl Pts',(-0.0282386144223951,2.37511159089061,
9.40414739207685));
#44633=CARTESIAN_POINT('Ctrl Pts',(-0.157805640889021,2.37003283343738,
9.41359046922257));
#44634=CARTESIAN_POINT('Ctrl Pts',(-0.309053741926881,2.35163949504515,
9.42422816095906));
#44635=CARTESIAN_POINT('Ctrl Pts',(-0.331747316249773,2.34854558030169,
9.4258135312875));
#44636=CARTESIAN_POINT('Ctrl Pts',(-0.367094058144187,2.34320400362349,
9.42826252557851));
#44637=CARTESIAN_POINT('Ctrl Pts',(-0.379779172827328,2.341181507056,9.42913730598617));
#44638=CARTESIAN_POINT('Ctrl Pts',(-0.403794872948664,2.33715214493119,
9.43078488082172));
#44639=CARTESIAN_POINT('Ctrl Pts',(-0.415128152612725,2.33516574788753,
9.43155866692182));
#44640=CARTESIAN_POINT('Ctrl Pts',(-0.443095402285866,2.33005385449331,
9.43345976999947));
#44641=CARTESIAN_POINT('Ctrl Pts',(-0.459711590970065,2.32683256675571,
9.4345819738873));
#44642=CARTESIAN_POINT('Ctrl Pts',(-0.5198423245129,2.31450606222062,9.4386211606779));
#44643=CARTESIAN_POINT('Ctrl Pts',(-0.563135752546555,2.30435523368947,
9.44148772379871));
#44644=CARTESIAN_POINT('Ctrl Pts',(-0.752024240275808,2.25442514980073,
9.4539118565018));
#44645=CARTESIAN_POINT('Ctrl Pts',(-0.893923667037494,2.20201742940164,
9.46304575106073));
#44646=CARTESIAN_POINT('Ctrl Pts',(-1.11259142243794,2.09660857354435,9.47804454533811));
#44647=CARTESIAN_POINT('Ctrl Pts',(-1.19290316324345,2.05197638749887,9.48377096393206));
#44648=CARTESIAN_POINT('Ctrl Pts',(-1.30789038000232,1.97903754157429,9.4924803630756));
#44649=CARTESIAN_POINT('Ctrl Pts',(-1.34468264219999,1.95422491990727,9.49534967173548));
#44650=CARTESIAN_POINT('Ctrl Pts',(-1.40001262852944,1.91460796245393,9.49980780081128));
#44651=CARTESIAN_POINT('Ctrl Pts',(-1.4190614144967,1.90053246377956,9.50136969980118));
#44652=CARTESIAN_POINT('Ctrl Pts',(-1.45390187939598,1.87397237895215,9.50427900686337));
#44653=CARTESIAN_POINT('Ctrl Pts',(-1.46975168775729,1.86156737360077,9.50562328073469));
#44654=CARTESIAN_POINT('Ctrl Pts',(-1.50466691632841,1.83351676496829,9.50863232706772));
#44655=CARTESIAN_POINT('Ctrl Pts',(-1.52364981087767,1.81777265694587,9.51030087207649));
#44656=CARTESIAN_POINT('Ctrl Pts',(-1.57171738282024,1.77662422136479,9.51461222496199));
#44657=CARTESIAN_POINT('Ctrl Pts',(-1.60043242356906,1.75080122218608,9.5172714780035));
#44658=CARTESIAN_POINT('Ctrl Pts',(-1.75980516826424,1.6002818864886,9.53252235407453));
#44659=CARTESIAN_POINT('Ctrl Pts',(-1.87649555236717,1.46169794568453,9.54569198610676));
#44660=CARTESIAN_POINT('Ctrl Pts',(-2.0145653845745,1.25359926660599,9.5638493504636));
#44661=CARTESIAN_POINT('Ctrl Pts',(-2.05027710838781,1.19429880409366,9.56885668814467));
#44662=CARTESIAN_POINT('Ctrl Pts',(-2.1033595398428,1.09673615524912,9.57675286767496));
#44663=CARTESIAN_POINT('Ctrl Pts',(-2.12239628268073,1.05942723080523,9.57969602322076));
#44664=CARTESIAN_POINT('Ctrl Pts',(-2.1473884429696,1.00706574991752,9.58370371718454));
#44665=CARTESIAN_POINT('Ctrl Pts',(-2.1541919649714,0.992429122613123,9.58481097094586));
#44666=CARTESIAN_POINT('Ctrl Pts',(-2.16558682494587,0.967245591501632,
9.58669251750971));
#44667=CARTESIAN_POINT('Ctrl Pts',(-2.17025171679305,0.95673289831598,9.58747095952193));
#44668=CARTESIAN_POINT('Ctrl Pts',(-2.18012977117355,0.934027860484056,
9.58913685060091));
#44669=CARTESIAN_POINT('Ctrl Pts',(-2.18531742133855,0.921825174228508,
9.59002285352634));
#44670=CARTESIAN_POINT('Ctrl Pts',(-2.19968876111952,0.887216843486742,
9.59251117304434));
#44671=CARTESIAN_POINT('Ctrl Pts',(-2.20863233727088,0.864712484018269,
9.5941004253458));
#44672=CARTESIAN_POINT('Ctrl Pts',(-2.26708116695001,0.710813311491544,
9.6047997574685));
#44673=CARTESIAN_POINT('Ctrl Pts',(-2.30518410320021,0.575368198759008,
9.61339651281581));
#44674=CARTESIAN_POINT('Ctrl Pts',(-2.34749610666244,0.349836134732319,
9.62750854484987));
#44675=CARTESIAN_POINT('Ctrl Pts',(-2.35896962915478,0.261497209672887,
9.6329851523993));
#44676=CARTESIAN_POINT('Ctrl Pts',(-2.36545135066152,0.172736707603127,
9.6385666740965));
#44677=CARTESIAN_POINT('Origin',(0.,0.,-1.84858989190501));
#44678=CARTESIAN_POINT('',(-2.36545134966486,0.172736721251459,10.8348238720555));
#44679=CARTESIAN_POINT('',(-2.36545136240482,0.172736546790724,10.6389210243916));
#44680=CARTESIAN_POINT('',(-2.36545134966535,0.172736721244682,-1.84858989190501));
#44681=CARTESIAN_POINT('Ctrl Pts',(-2.36545134966486,0.172736721251459,
10.8348238720555));
#44682=CARTESIAN_POINT('Ctrl Pts',(-2.3648141310891,0.18146277283564,10.8342459745555));
#44683=CARTESIAN_POINT('Ctrl Pts',(-2.3641286153735,0.190185463792282,10.8336704060082));
#44684=CARTESIAN_POINT('Ctrl Pts',(-2.35774171655097,0.266075007693205,
10.8286796145128));
#44685=CARTESIAN_POINT('Ctrl Pts',(-2.34922700958003,0.332980587207781,
10.8243938670154));
#44686=CARTESIAN_POINT('Ctrl Pts',(-2.30931187874156,0.566599868191367,
10.8095534952512));
#44687=CARTESIAN_POINT('Ctrl Pts',(-2.26290578278085,0.730217755192301,
10.799351455385));
#44688=CARTESIAN_POINT('Ctrl Pts',(-2.17056280845768,0.959068574332726,
10.7838965278587));
#44689=CARTESIAN_POINT('Ctrl Pts',(-2.13820686814942,1.02918660912107,10.7789918880586));
#44690=CARTESIAN_POINT('Ctrl Pts',(-2.08940851850851,1.12266178918704,10.7721370901271));
#44691=CARTESIAN_POINT('Ctrl Pts',(-2.07587748434274,1.14748856672506,10.7702848726713));
#44692=CARTESIAN_POINT('Ctrl Pts',(-2.05197197303922,1.18954327629968,10.7670893754009));
#44693=CARTESIAN_POINT('Ctrl Pts',(-2.04181609014105,1.20689237179421,10.7657538211073));
#44694=CARTESIAN_POINT('Ctrl Pts',(-2.02066802775424,1.24198811468645,10.763015454579));
#44695=CARTESIAN_POINT('Ctrl Pts',(-2.0096596602795,1.25972288941445,10.7616121501886));
#44696=CARTESIAN_POINT('Ctrl Pts',(-1.98101498902868,1.30453900453872,10.7580145626201));
#44697=CARTESIAN_POINT('Ctrl Pts',(-1.96305710380138,1.33140866517373,10.7558088039106));
#44698=CARTESIAN_POINT('Ctrl Pts',(-1.8710470939999,1.4631697756384,10.7447411160274));
#44699=CARTESIAN_POINT('Ctrl Pts',(-1.78912234796644,1.56227885267622,10.735590339397));
#44700=CARTESIAN_POINT('Ctrl Pts',(-1.61550699902938,1.74065198449498,10.7175537602029));
#44701=CARTESIAN_POINT('Ctrl Pts',(-1.52495534534345,1.82050650707048,10.708714496717));
#44702=CARTESIAN_POINT('Ctrl Pts',(-1.38304871472863,1.92760183507202,10.6959616385389));
#44703=CARTESIAN_POINT('Ctrl Pts',(-1.33613639479233,1.96041149267173,10.6919059437773));
#44704=CARTESIAN_POINT('Ctrl Pts',(-1.27323768544861,2.00109377160363,10.6867157281602));
#44705=CARTESIAN_POINT('Ctrl Pts',(-1.25828863512325,2.01052735442731,10.6854998211298));
#44706=CARTESIAN_POINT('Ctrl Pts',(-1.23340926665106,2.02584124900257,10.6835069184944));
#44707=CARTESIAN_POINT('Ctrl Pts',(-1.22353921032068,2.03181766040372,10.6827241646119));
#44708=CARTESIAN_POINT('Ctrl Pts',(-1.20326641684351,2.04389172163566,10.6811330192878));
#44709=CARTESIAN_POINT('Ctrl Pts',(-1.19286008859937,2.04998250345789,10.6803250443467));
#44710=CARTESIAN_POINT('Ctrl Pts',(-1.16486247531842,2.06608400485279,10.6781734100825));
#44711=CARTESIAN_POINT('Ctrl Pts',(-1.14718831923316,2.07594959663167,10.6768383609062));
#44712=CARTESIAN_POINT('Ctrl Pts',(-1.04808750146148,2.12961475008131,10.6694687091436));
#44713=CARTESIAN_POINT('Ctrl Pts',(-0.96427132847863,2.16885476744213,10.6636662253407));
#44714=CARTESIAN_POINT('Ctrl Pts',(-0.74667557557877,2.25560939722666,10.6491513370789));
#44715=CARTESIAN_POINT('Ctrl Pts',(-0.610542022154624,2.29620045458269,
10.6405527020144));
#44716=CARTESIAN_POINT('Ctrl Pts',(-0.396224604427038,2.33968356900343,
10.6268550999262));
#44717=CARTESIAN_POINT('Ctrl Pts',(-0.320158015855828,2.35129969454769,
10.6219673329604));
#44718=CARTESIAN_POINT('Ctrl Pts',(-0.215617203381814,2.36209704448768,
10.615134888227));
#44719=CARTESIAN_POINT('Ctrl Pts',(-0.187519346495358,2.3644935212483,10.6132874998247));
#44720=CARTESIAN_POINT('Ctrl Pts',(-0.139378520658169,2.3677360116027,10.610100124849));
#44721=CARTESIAN_POINT('Ctrl Pts',(-0.119354913118796,2.36882978627102,
10.6087678321376));
#44722=CARTESIAN_POINT('Ctrl Pts',(-0.0809829145337113,2.37043807808947,
10.6062011137326));
#44723=CARTESIAN_POINT('Ctrl Pts',(-0.0626376342545772,2.37099375983227,
10.6049680485464));
#44724=CARTESIAN_POINT('Ctrl Pts',(-0.0142604907776587,2.37189727382489,
10.6016998656697));
#44725=CARTESIAN_POINT('Ctrl Pts',(0.0157739053772274,2.37188766220675,
10.5996540141048));
#44726=CARTESIAN_POINT('Ctrl Pts',(0.134472654783052,2.36959514221939,10.5914982985479));
#44727=CARTESIAN_POINT('Ctrl Pts',(0.222970232197642,2.36291029130619,10.5852588485014));
#44728=CARTESIAN_POINT('Ctrl Pts',(0.504326148275779,2.32571062461546,10.5649401243395));
#44729=CARTESIAN_POINT('Ctrl Pts',(0.693864280823634,2.2763614459825,10.5504535969875));
#44730=CARTESIAN_POINT('Ctrl Pts',(0.908068546570374,2.19131452540714,10.5341491846981));
#44731=CARTESIAN_POINT('Ctrl Pts',(0.940631960859903,2.17753522624725,10.5316750467083));
#44732=CARTESIAN_POINT('Ctrl Pts',(0.986457265934111,2.15692416528568,10.5282112610055));
#44733=CARTESIAN_POINT('Ctrl Pts',(0.999980082003424,2.15068818205457,10.527191388972));
#44734=CARTESIAN_POINT('Ctrl Pts',(1.02344169457039,2.1395998336077,10.5254270371241));
#44735=CARTESIAN_POINT('Ctrl Pts',(1.03340662243669,2.13480470318847,10.5246793290169));
#44736=CARTESIAN_POINT('Ctrl Pts',(1.05522078656389,2.12411916504763,10.5230463799002));
#44737=CARTESIAN_POINT('Ctrl Pts',(1.06705472855796,2.11819908468151,10.5221629115309));
#44738=CARTESIAN_POINT('Ctrl Pts',(1.10130511691628,2.10070500383746,10.519611108604));
#44739=CARTESIAN_POINT('Ctrl Pts',(1.1235879509367,2.08887163599751,10.5179574375262));
#44740=CARTESIAN_POINT('Ctrl Pts',(1.23582887752474,2.02694983129745,10.5096393431796));
#44741=CARTESIAN_POINT('Ctrl Pts',(1.32265484723054,1.9713922231618,10.5032403605874));
#44742=CARTESIAN_POINT('Ctrl Pts',(1.47744407124267,1.85750166541294,10.4913920741543));
#44743=CARTESIAN_POINT('Ctrl Pts',(1.54624610457917,1.80063218823078,10.4859398222646));
#44744=CARTESIAN_POINT('Ctrl Pts',(1.66291419243344,1.69256938183855,10.4760884550932));
#44745=CARTESIAN_POINT('Ctrl Pts',(1.71202307151968,1.64287879355183,10.4717232198946));
#44746=CARTESIAN_POINT('Ctrl Pts',(1.792611234361,1.5537931981403,10.4640772630206));
#44747=CARTESIAN_POINT('Ctrl Pts',(1.82515909854651,1.51542800838617,10.4608369381118));
#44748=CARTESIAN_POINT('Ctrl Pts',(1.8715967231593,1.45702273188902,10.4559587524949));
#44749=CARTESIAN_POINT('Ctrl Pts',(1.88643824095814,1.4377552737608,10.454357953188));
#44750=CARTESIAN_POINT('Ctrl Pts',(1.91265093136617,1.4026208936315,10.4514518467481));
#44751=CARTESIAN_POINT('Ctrl Pts',(1.92412762198314,1.386835178612,10.4501507309009));
#44752=CARTESIAN_POINT('Ctrl Pts',(1.94844993226337,1.35249770111347,10.4473292647408));
#44753=CARTESIAN_POINT('Ctrl Pts',(1.96122814167697,1.33390077832656,10.4458065543122));
#44754=CARTESIAN_POINT('Ctrl Pts',(1.99580075672399,1.28201421743131,10.441571270367));
#44755=CARTESIAN_POINT('Ctrl Pts',(2.01702491864424,1.24835542519301,10.4388384109042));
#44756=CARTESIAN_POINT('Ctrl Pts',(2.1315680743255,1.05615231855416,10.4233051830074));
#44757=CARTESIAN_POINT('Ctrl Pts',(2.20702545692803,0.887725761489421,10.4098941541254));
#44758=CARTESIAN_POINT('Ctrl Pts',(2.28344453173726,0.645023878770619,10.39138324805));
#44759=CARTESIAN_POINT('Ctrl Pts',(2.301620107805,0.576819475705937,10.386273753754));
#44760=CARTESIAN_POINT('Ctrl Pts',(2.32294711951267,0.479539264592612,10.3791909449151));
#44761=CARTESIAN_POINT('Ctrl Pts',(2.32864424771602,0.451062466477919,10.3771421003303));
#44762=CARTESIAN_POINT('Ctrl Pts',(2.33783063240883,0.400316894994948,10.3735422212544));
#44763=CARTESIAN_POINT('Ctrl Pts',(2.34152811505399,0.37808975031402,10.3719827202543));
#44764=CARTESIAN_POINT('Ctrl Pts',(2.34678744748623,0.34342919410319,10.3695810749327));
#44765=CARTESIAN_POINT('Ctrl Pts',(2.34856837556704,0.331031022692462,10.3687279874603));
#44766=CARTESIAN_POINT('Ctrl Pts',(2.3517599125972,0.307489069047457,10.3671201949803));
#44767=CARTESIAN_POINT('Ctrl Pts',(2.3531896923688,0.296348596491448,10.3663645563449));
#44768=CARTESIAN_POINT('Ctrl Pts',(2.35648660710815,0.269129912239733,10.3645302932968));
#44769=CARTESIAN_POINT('Ctrl Pts',(2.35826843566734,0.253041617117834,10.3634562009092));
#44770=CARTESIAN_POINT('Ctrl Pts',(2.36400432916913,0.195911999072798,10.3596738600485));
#44771=CARTESIAN_POINT('Ctrl Pts',(2.36705303451665,0.154784930732243,10.3570089964869));
#44772=CARTESIAN_POINT('Ctrl Pts',(2.37644775935924,-0.0411396795073466,
10.34450146443));
#44773=CARTESIAN_POINT('Ctrl Pts',(2.36869021113247,-0.196243010957284,
10.3351351007388));
#44774=CARTESIAN_POINT('Ctrl Pts',(2.33440778276043,-0.426353287744361,
10.3207677746636));
#44775=CARTESIAN_POINT('Ctrl Pts',(2.31918688695937,-0.502601015078118,
10.31593114651));
#44776=CARTESIAN_POINT('Ctrl Pts',(2.28706120515446,-0.630459586801942,
10.3075626595756));
#44777=CARTESIAN_POINT('Ctrl Pts',(2.27207766100117,-0.682488585136529,
10.3040831143584));
#44778=CARTESIAN_POINT('Ctrl Pts',(2.24759278377427,-0.757726592283991,
10.298915719759));
#44779=CARTESIAN_POINT('Ctrl Pts',(2.23948222970795,-0.781371983244245,
10.297271813723));
#44780=CARTESIAN_POINT('Ctrl Pts',(2.22434916611074,-0.823318223939019,
10.2943175244825));
#44781=CARTESIAN_POINT('Ctrl Pts',(2.21747057464733,-0.841668772533344,
10.2930119105771));
#44782=CARTESIAN_POINT('Ctrl Pts',(2.20232873042736,-0.880589325818423,
10.2902135091187));
#44783=CARTESIAN_POINT('Ctrl Pts',(2.19400295642084,-0.901132824899221,
10.288718767672));
#44784=CARTESIAN_POINT('Ctrl Pts',(2.17069707417738,-0.956400715814385,
10.2846479963427));
#44785=CARTESIAN_POINT('Ctrl Pts',(2.15517294739815,-0.990887180850716,
10.2820542495652));
#44786=CARTESIAN_POINT('Ctrl Pts',(2.07974775404617,-1.14827642455878,10.269960546378));
#44787=CARTESIAN_POINT('Ctrl Pts',(2.01012276805081,-1.26620921364307,10.2601431563836));
#44788=CARTESIAN_POINT('Ctrl Pts',(1.86898575226593,-1.46403442175285,10.242471663215));
#44789=CARTESIAN_POINT('Ctrl Pts',(1.80147730257742,-1.54634579389781,10.2346912839414));
#44790=CARTESIAN_POINT('Ctrl Pts',(1.69192278767077,-1.66297212317622,10.2232306794748));
#44791=CARTESIAN_POINT('Ctrl Pts',(1.65385333285412,-1.70083776383401,10.2194325867183));
#44792=CARTESIAN_POINT('Ctrl Pts',(1.60186958416066,-1.74914566083241,10.2145180945304));
#44793=CARTESIAN_POINT('Ctrl Pts',(1.58908179283713,-1.76077136684891,10.2133298044658));
#44794=CARTESIAN_POINT('Ctrl Pts',(1.56762475138897,-1.77985432161889,10.2113715603265));
#44795=CARTESIAN_POINT('Ctrl Pts',(1.55902675260742,-1.78739038062069,10.2105961761196));
#44796=CARTESIAN_POINT('Ctrl Pts',(1.54119063240015,-1.80279692760646,10.2090072859227));
#44797=CARTESIAN_POINT('Ctrl Pts',(1.5319460424184,-1.81065918018273,10.208194331883));
#44798=CARTESIAN_POINT('Ctrl Pts',(1.50681161680059,-1.83170496440405,10.2060111584463));
#44799=CARTESIAN_POINT('Ctrl Pts',(1.49080892291326,-1.84475286973174,10.2046500205725));
#44800=CARTESIAN_POINT('Ctrl Pts',(1.38334282867479,-1.9300641855689,10.1956834633304));
#44801=CARTESIAN_POINT('Ctrl Pts',(1.28681788630652,-1.99571832487647,10.1884518772964));
#44802=CARTESIAN_POINT('Ctrl Pts',(1.08083871268706,-2.11463642461871,10.1737993064892));
#44803=CARTESIAN_POINT('Ctrl Pts',(0.971342583306341,-2.16711601016415,
10.1664001503345));
#44804=CARTESIAN_POINT('Ctrl Pts',(0.789641824565459,-2.23765296125633,
10.1541725078488));
#44805=CARTESIAN_POINT('Ctrl Pts',(0.719768256692264,-2.26109643578134,
10.1494840027605));
#44806=CARTESIAN_POINT('Ctrl Pts',(0.622177418744681,-2.28885701956249,
10.1428847059099));
#44807=CARTESIAN_POINT('Ctrl Pts',(0.595302356795183,-2.2959935095681,10.1410623794665));
#44808=CARTESIAN_POINT('Ctrl Pts',(0.548910660374062,-2.30744325243948,
10.137904921298));
#44809=CARTESIAN_POINT('Ctrl Pts',(0.529453185160148,-2.31198541525999,
10.1365771201438));
#44810=CARTESIAN_POINT('Ctrl Pts',(0.489503681551775,-2.32078050281092,
10.1338426264221));
#44811=CARTESIAN_POINT('Ctrl Pts',(0.469008155770108,-2.3250090964655,10.132435301074));
#44812=CARTESIAN_POINT('Ctrl Pts',(0.416277359050632,-2.33516280838918,
10.1288019527366));
#44813=CARTESIAN_POINT('Ctrl Pts',(0.38397127387502,-2.3406917907855,10.1265638956521));
#44814=CARTESIAN_POINT('Ctrl Pts',(0.21775659539949,-2.36560485353525,10.1149818512508));
#44815=CARTESIAN_POINT('Ctrl Pts',(0.0825010830535566,-2.37417088071727,
10.1053134787959));
#44816=CARTESIAN_POINT('Ctrl Pts',(-0.168241020979051,-2.36859516527716,
10.0871049815437));
#44817=CARTESIAN_POINT('Ctrl Pts',(-0.28341381764386,-2.35758894018879,
10.0786350637776));
#44818=CARTESIAN_POINT('Ctrl Pts',(-0.452579406046273,-2.32884325429845,
10.0663288918297));
#44819=CARTESIAN_POINT('Ctrl Pts',(-0.50748633557062,-2.31749815459589,
10.0623580114539));
#44820=CARTESIAN_POINT('Ctrl Pts',(-0.578961329777634,-2.30006709812867,
10.0572608026467));
#44821=CARTESIAN_POINT('Ctrl Pts',(-0.595932840175838,-2.29572841863876,
10.0560559108339));
#44822=CARTESIAN_POINT('Ctrl Pts',(-0.62393818688567,-2.2882374918552,10.0540783804432));
#44823=CARTESIAN_POINT('Ctrl Pts',(-0.634999784714441,-2.28519254633209,
10.0533000817387));
#44824=CARTESIAN_POINT('Ctrl Pts',(-0.65763716674221,-2.27878404195903,
10.0517136101878));
#44825=CARTESIAN_POINT('Ctrl Pts',(-0.669210150471104,-2.27541230181822,
10.0509058946002));
#44826=CARTESIAN_POINT('Ctrl Pts',(-0.700178890948696,-2.26613297256069,
10.048752217557));
#44827=CARTESIAN_POINT('Ctrl Pts',(-0.7195259122602,-2.26006452489786,10.0474149282273));
#44828=CARTESIAN_POINT('Ctrl Pts',(-0.828193461994642,-2.22444259066834,
10.0399374670984));
#44829=CARTESIAN_POINT('Ctrl Pts',(-0.915781017700501,-2.18983980194483,
10.0340383114291));
#44830=CARTESIAN_POINT('Ctrl Pts',(-1.1285963660017,-2.09075362488835,10.0195017973996));
#44831=CARTESIAN_POINT('Ctrl Pts',(-1.25056690711633,-2.02016402201288,
10.0109697039868));
#44832=CARTESIAN_POINT('Ctrl Pts',(-1.42822612332949,-1.89505721795778,
9.99735904815005));
#44833=CARTESIAN_POINT('Ctrl Pts',(-1.48870715734687,-1.84792342922087,
9.99248817102497));
#44834=CARTESIAN_POINT('Ctrl Pts',(-1.56814445432427,-1.77958254919911,
9.98567580007995));
#44835=CARTESIAN_POINT('Ctrl Pts',(-1.58916251857746,-1.76083885131525,
9.98383092800014));
#44836=CARTESIAN_POINT('Ctrl Pts',(-1.62455728823117,-1.72812420052886,
9.98064704182713));
#44837=CARTESIAN_POINT('Ctrl Pts',(-1.63910003194645,-1.71433680456435,
9.97931569550324));
#44838=CARTESIAN_POINT('Ctrl Pts',(-1.66662109221823,-1.68757485677465,
9.97675023058455));
#44839=CARTESIAN_POINT('Ctrl Pts',(-1.67962700254257,-1.67463066449613,
9.97551746507842));
#44840=CARTESIAN_POINT('Ctrl Pts',(-1.71352971008069,-1.64009656373993,
9.97224875510829));
#44841=CARTESIAN_POINT('Ctrl Pts',(-1.73416812655504,-1.61825880915578,
9.97020205607362));
#44842=CARTESIAN_POINT('Ctrl Pts',(-1.81426320576979,-1.53021714923285,
9.96202562341005));
#44843=CARTESIAN_POINT('Ctrl Pts',(-1.87038274324857,-1.46108884227429,
9.95576535214964));
#44844=CARTESIAN_POINT('Ctrl Pts',(-2.03649625447272,-1.23117160498902,
9.93545655850457));
#44845=CARTESIAN_POINT('Ctrl Pts',(-2.13063912030509,-1.0599395923189,9.92100575524482));
#44846=CARTESIAN_POINT('Ctrl Pts',(-2.21582609706409,-0.846491663826748,
9.9047511244005));
#44847=CARTESIAN_POINT('Ctrl Pts',(-2.22812789102517,-0.813559978279359,
9.90229175700462));
#44848=CARTESIAN_POINT('Ctrl Pts',(-2.24458304096902,-0.766332724797668,
9.89884456317377));
#44849=CARTESIAN_POINT('Ctrl Pts',(-2.24934042632534,-0.752254310552646,
9.89782690529501));
#44850=CARTESIAN_POINT('Ctrl Pts',(-2.25740774013701,-0.727619890423506,
9.89606461250593));
#44851=CARTESIAN_POINT('Ctrl Pts',(-2.26077660489127,-0.717084074930183,
9.8953167855619));
#44852=CARTESIAN_POINT('Ctrl Pts',(-2.26802511500451,-0.693856076639133,
9.89368113967146));
#44853=CARTESIAN_POINT('Ctrl Pts',(-2.27187210272346,-0.681154422108647,
9.89279512512651));
#44854=CARTESIAN_POINT('Ctrl Pts',(-2.28276537955258,-0.644068687399322,
9.89023076260137));
#44855=CARTESIAN_POINT('Ctrl Pts',(-2.28952735818247,-0.619602172120532,
9.88856726612624));
#44856=CARTESIAN_POINT('Ctrl Pts',(-2.32234578774264,-0.492973930230632,
9.88008048405161));
#44857=CARTESIAN_POINT('Ctrl Pts',(-2.34196457564742,-0.389255626507347,
9.87353526268328));
#44858=CARTESIAN_POINT('Ctrl Pts',(-2.36595613954081,-0.190739644980454,
9.86121175177847));
#44859=CARTESIAN_POINT('Ctrl Pts',(-2.37167706481602,-0.0963206531594225,
9.85543516074478));
#44860=CARTESIAN_POINT('Ctrl Pts',(-2.37179383901357,0.0564438951617469,
9.84594930673836));
#44861=CARTESIAN_POINT('Ctrl Pts',(-2.36969193076758,0.114666352731385,
9.84230205067175));
#44862=CARTESIAN_POINT('Ctrl Pts',(-2.36545134562115,0.172736776625918,
9.83860221205714));
#44863=CARTESIAN_POINT('Ctrl Pts',(-2.36545135066152,0.172736707603127,
9.6385666740965));
#44864=CARTESIAN_POINT('Ctrl Pts',(-2.36639360499426,0.159833504717226,
9.63937806548334));
#44865=CARTESIAN_POINT('Ctrl Pts',(-2.3672303695368,0.146921388370306,9.64019160353449));
#44866=CARTESIAN_POINT('Ctrl Pts',(-2.37047125625906,0.089651233376424,
9.64380842025643));
#44867=CARTESIAN_POINT('Ctrl Pts',(-2.37173443215917,0.0452411583139775,
9.64663578726132));
#44868=CARTESIAN_POINT('Ctrl Pts',(-2.37176249280153,-0.0355626031238575,
9.65184189280179));
#44869=CARTESIAN_POINT('Ctrl Pts',(-2.37093779965913,-0.0719426650288141,
9.65420854366404));
#44870=CARTESIAN_POINT('Ctrl Pts',(-2.36826774342647,-0.130361960128773,
9.65805303530838));
#44871=CARTESIAN_POINT('Ctrl Pts',(-2.36695043613609,-0.152420221659169,
9.65951476531774));
#44872=CARTESIAN_POINT('Ctrl Pts',(-2.36382526246912,-0.194792171052408,
9.66234362817504));
#44873=CARTESIAN_POINT('Ctrl Pts',(-2.36206321913186,-0.21510733712454,
9.66370923523363));
#44874=CARTESIAN_POINT('Ctrl Pts',(-2.35732846829581,-0.262576979943863,
9.6669231681066));
#44875=CARTESIAN_POINT('Ctrl Pts',(-2.35414819498047,-0.289707348872911,
9.66877769041165));
#44876=CARTESIAN_POINT('Ctrl Pts',(-2.34165493301826,-0.382408287116409,
9.67517770567363));
#44877=CARTESIAN_POINT('Ctrl Pts',(-2.33006541988164,-0.447635610921445,
9.67979103325344));
#44878=CARTESIAN_POINT('Ctrl Pts',(-2.29282793492771,-0.61596525676266,
9.69198644334059));
#44879=CARTESIAN_POINT('Ctrl Pts',(-2.26295795769526,-0.71797683906012,
9.69967098386616));
#44880=CARTESIAN_POINT('Ctrl Pts',(-2.18059222158132,-0.942252356629987,
9.71706106564632));
#44881=CARTESIAN_POINT('Ctrl Pts',(-2.12444095959257,-1.06281603295799,
9.72676515016147));
#44882=CARTESIAN_POINT('Ctrl Pts',(-2.04609033152589,-1.19972319162559,
9.7378106293349));
#44883=CARTESIAN_POINT('Ctrl Pts',(-2.03334749892793,-1.221195909545,9.73954332027444));
#44884=CARTESIAN_POINT('Ctrl Pts',(-2.01323739071232,-1.25389527339919,
9.74217789292613));
#44885=CARTESIAN_POINT('Ctrl Pts',(-2.00611030562084,-1.26526661660371,
9.74309331055332));
#44886=CARTESIAN_POINT('Ctrl Pts',(-1.993336312459,-1.28526835842575,9.74470130233207));
#44887=CARTESIAN_POINT('Ctrl Pts',(-1.98772930226305,-1.29392296304453,
9.74539625733571));
#44888=CARTESIAN_POINT('Ctrl Pts',(-1.97377705560849,-1.31515397589286,
9.74709944800765));
#44889=CARTESIAN_POINT('Ctrl Pts',(-1.96536794705419,-1.32768772967732,
9.74810358619174));
#44890=CARTESIAN_POINT('Ctrl Pts',(-1.93709729653372,-1.36896781556788,
9.75140928311966));
#44891=CARTESIAN_POINT('Ctrl Pts',(-1.91671929569221,-1.39735688167427,
9.75368033294478));
#44892=CARTESIAN_POINT('Ctrl Pts',(-1.76482359039027,-1.59938760735871,
9.76990653054075));
#44893=CARTESIAN_POINT('Ctrl Pts',(-1.61055830996404,-1.75464117308747,
9.78281547696509));
#44894=CARTESIAN_POINT('Ctrl Pts',(-1.38173225494166,-1.92895962212783,
9.80088738321199));
#44895=CARTESIAN_POINT('Ctrl Pts',(-1.32437757469801,-1.96877930735889,
9.8053334114941));
#44896=CARTESIAN_POINT('Ctrl Pts',(-1.24124523755315,-2.02121766462845,
9.81172370164513));
#44897=CARTESIAN_POINT('Ctrl Pts',(-1.21686472698057,-2.03598887812035,
9.81359138805103));
#44898=CARTESIAN_POINT('Ctrl Pts',(-1.17443686846665,-2.06065996654257,
9.81683420300584));
#44899=CARTESIAN_POINT('Ctrl Pts',(-1.15651563028311,-2.0707711144347,9.81820171888499));
#44900=CARTESIAN_POINT('Ctrl Pts',(-1.1194605353785,-2.09104650870954,9.82102598159974));
#44901=CARTESIAN_POINT('Ctrl Pts',(-1.10031447758006,-2.10118428262918,
9.82248348654896));
#44902=CARTESIAN_POINT('Ctrl Pts',(-1.05055258037578,-2.12666640527462,
9.82626848847833));
#44903=CARTESIAN_POINT('Ctrl Pts',(-1.01973937174752,-2.14161203995885,
9.82860923540437));
#44904=CARTESIAN_POINT('Ctrl Pts',(-0.850880303116009,-2.21904501163313,
9.84142734029265));
#44905=CARTESIAN_POINT('Ctrl Pts',(-0.707432316130912,-2.26885071822584,
9.85231569664025));
#44906=CARTESIAN_POINT('Ctrl Pts',(-0.424767738568074,-2.33756445858952,
9.87347981575511));
#44907=CARTESIAN_POINT('Ctrl Pts',(-0.286646392333594,-2.35848994046285,
9.88368695588045));
#44908=CARTESIAN_POINT('Ctrl Pts',(-0.123245512745035,-2.36867011652855,
9.89514135227839));
#44909=CARTESIAN_POINT('Ctrl Pts',(-0.0989896574277021,-2.36980774237117,
9.89682524168229));
#44910=CARTESIAN_POINT('Ctrl Pts',(-0.0614524736573346,-2.37099089937664,
9.89940156381164));
#44911=CARTESIAN_POINT('Ctrl Pts',(-0.048181773143534,-2.37129770145853,
9.90030666883464));
#44912=CARTESIAN_POINT('Ctrl Pts',(-0.0234128799076648,-2.37166230408445,
9.90198447805365));
#44913=CARTESIAN_POINT('Ctrl Pts',(-0.0119163092021866,-2.37174793246545,
9.90275851053423));
#44914=CARTESIAN_POINT('Ctrl Pts',(0.0156932799462805,-2.37175280855637,
9.90460667181672));
#44915=CARTESIAN_POINT('Ctrl Pts',(0.0318055874955957,-2.37159147064463,
9.90567653172282));
#44916=CARTESIAN_POINT('Ctrl Pts',(0.0895918935778713,-2.37042379813828,
9.9094863911435));
#44917=CARTESIAN_POINT('Ctrl Pts',(0.13124172156159,-2.36848301235794,9.91218172025578));
#44918=CARTESIAN_POINT('Ctrl Pts',(0.241336667800836,-2.36043937877468,
9.91922261929333));
#44919=CARTESIAN_POINT('Ctrl Pts',(0.309606469528001,-2.35245881317323,
9.92350311508977));
#44920=CARTESIAN_POINT('Ctrl Pts',(0.55373968521195,-2.31310626125181,9.9387906450863));
#44921=CARTESIAN_POINT('Ctrl Pts',(0.726255724265185,-2.26487024704045,
9.94960382151006));
#44922=CARTESIAN_POINT('Ctrl Pts',(0.928881109966353,-2.18265573504321,
9.96358857293454));
#44923=CARTESIAN_POINT('Ctrl Pts',(0.96564996926563,-2.1666393387325,9.96617880212663));
#44924=CARTESIAN_POINT('Ctrl Pts',(1.02472157724201,-2.13910554670781,9.97043770533736));
#44925=CARTESIAN_POINT('Ctrl Pts',(1.04727939818361,-2.12815239946008,9.97208776570118));
#44926=CARTESIAN_POINT('Ctrl Pts',(1.08763922339423,-2.10775824852671,9.97508541547286));
#44927=CARTESIAN_POINT('Ctrl Pts',(1.10550283439582,-2.09844403208524,9.97642857870606));
#44928=CARTESIAN_POINT('Ctrl Pts',(1.1438100635774,-2.07784547024858,9.97934562592108));
#44929=CARTESIAN_POINT('Ctrl Pts',(1.16420988063791,-2.06648458678929,9.98092206282418));
#44930=CARTESIAN_POINT('Ctrl Pts',(1.22138876535772,-2.03352564593499,9.98540796363083));
#44931=CARTESIAN_POINT('Ctrl Pts',(1.25775609430766,-2.01123501352887,9.98834137837533));
#44932=CARTESIAN_POINT('Ctrl Pts',(1.42934802394508,-1.89958670169278,10.0025813366958));
#44933=CARTESIAN_POINT('Ctrl Pts',(1.55575843956376,-1.79751661791073,10.0143353943163));
#44934=CARTESIAN_POINT('Ctrl Pts',(1.74975203220688,-1.60497749846737,10.034236821544));
#44935=CARTESIAN_POINT('Ctrl Pts',(1.8231363199652,-1.52110587796986,10.0423250622157));
#44936=CARTESIAN_POINT('Ctrl Pts',(1.90580893265975,-1.41200015440256,10.0519174248317));
#44937=CARTESIAN_POINT('Ctrl Pts',(1.92092441448219,-1.39136682636255,10.053693400758));
#44938=CARTESIAN_POINT('Ctrl Pts',(1.94353156266508,-1.35943614521977,10.0563794347307));
#44939=CARTESIAN_POINT('Ctrl Pts',(1.95126459898187,-1.34831304033031,10.0573038162807));
#44940=CARTESIAN_POINT('Ctrl Pts',(1.96529013481159,-1.32776546740986,10.0589898947209));
#44941=CARTESIAN_POINT('Ctrl Pts',(1.97161076734034,-1.31836164985411,10.0597532975408));
#44942=CARTESIAN_POINT('Ctrl Pts',(1.98645513001782,-1.29593071006068,10.0615552410154));
#44943=CARTESIAN_POINT('Ctrl Pts',(1.99491836446462,-1.28286442771054,10.0625899553305));
#44944=CARTESIAN_POINT('Ctrl Pts',(2.02357220881625,-1.23765674464989,10.0661223500924));
#44945=CARTESIAN_POINT('Ctrl Pts',(2.04312064333208,-1.20511290368074,10.0685834956661));
#44946=CARTESIAN_POINT('Ctrl Pts',(2.09130284835018,-1.12035481403923,10.0748235211222));
#44947=CARTESIAN_POINT('Ctrl Pts',(2.11876764923243,-1.06750504966171,10.0785542480441));
#44948=CARTESIAN_POINT('Ctrl Pts',(2.22831860070386,-0.835773023645834,
10.0944656166325));
#44949=CARTESIAN_POINT('Ctrl Pts',(2.28995066449202,-0.648108395524297,
10.1063090792218));
#44950=CARTESIAN_POINT('Ctrl Pts',(2.33569536007661,-0.414080435520385,
10.1215894055156));
#44951=CARTESIAN_POINT('Ctrl Pts',(2.34261124873455,-0.372971355377189,
10.1242884867938));
#44952=CARTESIAN_POINT('Ctrl Pts',(2.35171252700854,-0.308534823812108,
10.1285541584056));
#44953=CARTESIAN_POINT('Ctrl Pts',(2.35464180164886,-0.285319942218089,
10.130097968569));
#44954=CARTESIAN_POINT('Ctrl Pts',(2.35945291851521,-0.242045015064398,
10.132990659529));
#44955=CARTESIAN_POINT('Ctrl Pts',(2.36142355876905,-0.221996842522349,
10.134336679354));
#44956=CARTESIAN_POINT('Ctrl Pts',(2.36526851300837,-0.176999483583623,
10.137372132063));
#44957=CARTESIAN_POINT('Ctrl Pts',(2.36700387791533,-0.152041166589389,
10.1390656618073));
#44958=CARTESIAN_POINT('Ctrl Pts',(2.37111039744496,-0.0754979156906682,
10.1442917880726));
#44959=CARTESIAN_POINT('Ctrl Pts',(2.37219188992352,-0.0238620303363823,
10.1478626068129));
#44960=CARTESIAN_POINT('Ctrl Pts',(2.37074469235968,0.0997532523843913,
10.1565236720387));
#44961=CARTESIAN_POINT('Ctrl Pts',(2.36662467502378,0.171660252464469,10.1616541110278));
#44962=CARTESIAN_POINT('Ctrl Pts',(2.35044142080663,0.328610265406669,10.1730251913194));
#44963=CARTESIAN_POINT('Ctrl Pts',(2.33701675852122,0.413414253722766,10.179282683062));
#44964=CARTESIAN_POINT('Ctrl Pts',(2.29780771385445,0.596254905614223,10.1928903195935));
#44965=CARTESIAN_POINT('Ctrl Pts',(2.2702739150326,0.693757956272299,10.2002224021083));
#44966=CARTESIAN_POINT('Ctrl Pts',(2.22812497186673,0.813206406142454,10.2090969099169));
#44967=CARTESIAN_POINT('Ctrl Pts',(2.21927174254811,0.837065474140007,10.2108636905687));
#44968=CARTESIAN_POINT('Ctrl Pts',(2.20512839486497,0.873378303476749,10.213538940998));
#44969=CARTESIAN_POINT('Ctrl Pts',(2.20011316108581,0.885936227436829,10.2144615609834));
#44970=CARTESIAN_POINT('Ctrl Pts',(2.19108861313925,0.907983951431249,10.2160760331935));
#44971=CARTESIAN_POINT('Ctrl Pts',(2.18712463254486,0.917491152261432,10.2167703653121));
#44972=CARTESIAN_POINT('Ctrl Pts',(2.17725282851906,0.94074007816281,10.2184640872232));
#44973=CARTESIAN_POINT('Ctrl Pts',(2.17127676513124,0.954452205043743,10.2194595080588));
#44974=CARTESIAN_POINT('Ctrl Pts',(2.15125714420827,0.999226070389373,10.2227011282124));
#44975=CARTESIAN_POINT('Ctrl Pts',(2.13667299484858,1.03004312083716,10.2249184481402));
#44976=CARTESIAN_POINT('Ctrl Pts',(2.09869231990535,1.10601718521974,10.2303761210652));
#44977=CARTESIAN_POINT('Ctrl Pts',(2.07449790283775,1.15075737007607,10.2335823071362));
#44978=CARTESIAN_POINT('Ctrl Pts',(1.98783787901939,1.29937882642102,10.2443194272543));
#44979=CARTESIAN_POINT('Ctrl Pts',(1.91885772736134,1.39923960234297,10.2516900207509));
#44980=CARTESIAN_POINT('Ctrl Pts',(1.77447471032154,1.57737912387246,10.2658789603067));
#44981=CARTESIAN_POINT('Ctrl Pts',(1.70074824901947,1.65660403889973,10.272653631145));
#44982=CARTESIAN_POINT('Ctrl Pts',(1.59839434067211,1.75253239646334,10.2817327830896));
#44983=CARTESIAN_POINT('Ctrl Pts',(1.57446240837882,1.77406376303652,10.2838341393073));
#44984=CARTESIAN_POINT('Ctrl Pts',(1.53400958624207,1.80899547784127,10.2873562767059));
#44985=CARTESIAN_POINT('Ctrl Pts',(1.51773294158545,1.82267295999115,10.2887657285559));
#44986=CARTESIAN_POINT('Ctrl Pts',(1.4851357454157,1.84932541527664,10.2915747026501));
#44987=CARTESIAN_POINT('Ctrl Pts',(1.46882360354959,1.86230766757743,10.2929737627064));
#44988=CARTESIAN_POINT('Ctrl Pts',(1.4286082108599,1.89345661131758,10.2964082767619));
#44989=CARTESIAN_POINT('Ctrl Pts',(1.40452760876528,1.91138730114274,10.2984525098614));
#44990=CARTESIAN_POINT('Ctrl Pts',(1.30758576481174,1.98075009579461,10.3066376482886));
#44991=CARTESIAN_POINT('Ctrl Pts',(1.23219671829373,2.02850669567647,10.3129094529943));
#44992=CARTESIAN_POINT('Ctrl Pts',(0.989780091523776,2.1635627868354,10.3327703199869));
#44993=CARTESIAN_POINT('Ctrl Pts',(0.814935718426447,2.23529477751987,10.3467249850365));
#44994=CARTESIAN_POINT('Ctrl Pts',(0.595947395346577,2.29598773703518,10.3628536728971));
#44995=CARTESIAN_POINT('Ctrl Pts',(0.558186515639164,2.30545899981303,10.3655859323603));
#44996=CARTESIAN_POINT('Ctrl Pts',(0.506019520548593,2.31718660707905,10.3692791209043));
#44997=CARTESIAN_POINT('Ctrl Pts',(0.491802319326017,2.32024568351708,10.3702773975033));
#44998=CARTESIAN_POINT('Ctrl Pts',(0.46621508008337,2.32550546058195,10.3720582054168));
#44999=CARTESIAN_POINT('Ctrl Pts',(0.454855371541248,2.32775401656357,10.3728432238834));
#45000=CARTESIAN_POINT('Ctrl Pts',(0.431040604373656,2.33228694238738,10.37447671837));
#45001=CARTESIAN_POINT('Ctrl Pts',(0.418582987263027,2.33455492228331,10.37532431861));
#45002=CARTESIAN_POINT('Ctrl Pts',(0.384364718018118,2.34050183754267,10.3776351009658));
#45003=CARTESIAN_POINT('Ctrl Pts',(0.362569358446222,2.34397709723222,10.3790877328344));
#45004=CARTESIAN_POINT('Ctrl Pts',(0.312968571991182,2.35117748061079,10.3823564854415));
#45005=CARTESIAN_POINT('Ctrl Pts',(0.285138860795388,2.35471459873277,10.3841641893994));
#45006=CARTESIAN_POINT('Ctrl Pts',(0.191778442823405,2.36490102928783,10.3901600171776));
#45007=CARTESIAN_POINT('Ctrl Pts',(0.126031722727445,2.36931486718475,10.3942703640904));
#45008=CARTESIAN_POINT('Ctrl Pts',(-0.133674627215506,2.37590700097228,
10.4103473933092));
#45009=CARTESIAN_POINT('Ctrl Pts',(-0.327387855482908,2.35703543831419,
10.4220572208828));
#45010=CARTESIAN_POINT('Ctrl Pts',(-0.553949739640424,2.30646895790663,
10.4369855217963));
#45011=CARTESIAN_POINT('Ctrl Pts',(-0.591050259319969,2.29724154170777,
10.439468189087));
#45012=CARTESIAN_POINT('Ctrl Pts',(-0.649565601167914,2.2811766488887,10.4434535441794));
#45013=CARTESIAN_POINT('Ctrl Pts',(-0.67113500886909,2.27492420023726,10.4449378061231));
#45014=CARTESIAN_POINT('Ctrl Pts',(-0.711990826386118,2.26244948777299,
10.4477799348037));
#45015=CARTESIAN_POINT('Ctrl Pts',(-0.73129271505082,2.25628445538158,10.4491358638286));
#45016=CARTESIAN_POINT('Ctrl Pts',(-0.775616143406512,2.24149904405615,
10.452281213657));
#45017=CARTESIAN_POINT('Ctrl Pts',(-0.800576718113202,2.23270579978593,
10.4540760650354));
#45018=CARTESIAN_POINT('Ctrl Pts',(-0.882132910821974,2.20243133413291,
10.4600209516387));
#45019=CARTESIAN_POINT('Ctrl Pts',(-0.938049772733661,2.17920255559462,
10.464226381512));
#45020=CARTESIAN_POINT('Ctrl Pts',(-1.07620637779581,2.11550706600887,10.4749506164428));
#45021=CARTESIAN_POINT('Ctrl Pts',(-1.15710042642071,2.07236730063999,10.4815418509632));
#45022=CARTESIAN_POINT('Ctrl Pts',(-1.36350671292189,1.9464342658207,10.4990968383773));
#45023=CARTESIAN_POINT('Ctrl Pts',(-1.48400733116188,1.85620142546291,10.5101374063558));
#45024=CARTESIAN_POINT('Ctrl Pts',(-1.6162020083751,1.73605787626332,10.5226905445083));
#45025=CARTESIAN_POINT('Ctrl Pts',(-1.63689117564138,1.71656439799656,10.5246686937491));
#45026=CARTESIAN_POINT('Ctrl Pts',(-1.66719699994388,1.68696369126029,10.5275804108877));
#45027=CARTESIAN_POINT('Ctrl Pts',(-1.67708228052583,1.67713666120871,10.5285324762579));
#45028=CARTESIAN_POINT('Ctrl Pts',(-1.69480662440035,1.65920333311865,10.5302427976604));
#45029=CARTESIAN_POINT('Ctrl Pts',(-1.70267509328861,1.65112771498011,10.5310031669544));
#45030=CARTESIAN_POINT('Ctrl Pts',(-1.72087248490399,1.63218281696118,10.5327645593599));
#45031=CARTESIAN_POINT('Ctrl Pts',(-1.73115634698567,1.62127128770843,10.5337622977637));
#45032=CARTESIAN_POINT('Ctrl Pts',(-1.76466334700609,1.58503685182561,10.5370238241358));
#45033=CARTESIAN_POINT('Ctrl Pts',(-1.78744084120629,1.5593056380903,10.5392581842554));
#45034=CARTESIAN_POINT('Ctrl Pts',(-1.84289675431923,1.49384560388232,10.5447689368369));
#45035=CARTESIAN_POINT('Ctrl Pts',(-1.87485784171472,1.45353081576012,10.5480102347343));
#45036=CARTESIAN_POINT('Ctrl Pts',(-2.01735215698087,1.26126380576498,10.5629381770528));
#45037=CARTESIAN_POINT('Ctrl Pts',(-2.11088653623396,1.09756826182258,10.574220843688));
#45038=CARTESIAN_POINT('Ctrl Pts',(-2.20612426412014,0.872581375981715,
10.5897062650098));
#45039=CARTESIAN_POINT('Ctrl Pts',(-2.22625891694627,0.819849377514655,
10.5933291373229));
#45040=CARTESIAN_POINT('Ctrl Pts',(-2.25284165486595,0.742004023144325,
10.5986980916821));
#45041=CARTESIAN_POINT('Ctrl Pts',(-2.26079006270558,0.717421563725073,
10.6003963670633));
#45042=CARTESIAN_POINT('Ctrl Pts',(-2.27423951853357,0.673380542939109,
10.6034465341006));
#45043=CARTESIAN_POINT('Ctrl Pts',(-2.27989634816886,0.653971973923773,
10.6047933124285));
#45044=CARTESIAN_POINT('Ctrl Pts',(-2.29141892940331,0.612470232885562,
10.607679811952));
#45045=CARTESIAN_POINT('Ctrl Pts',(-2.29721474009163,0.590359951306312,
10.6092215939715));
#45046=CARTESIAN_POINT('Ctrl Pts',(-2.30842545787716,0.54492494591839,10.6123991557904));
#45047=CARTESIAN_POINT('Ctrl Pts',(-2.31380849312682,0.521595127925753,
10.6140357351284));
#45048=CARTESIAN_POINT('Ctrl Pts',(-2.32902548512657,0.45076706446286,10.6190205451965));
#45049=CARTESIAN_POINT('Ctrl Pts',(-2.33775597571351,0.403047266101511,
10.6224012594135));
#45050=CARTESIAN_POINT('Ctrl Pts',(-2.35418213593451,0.294570640936105,
10.6301365372826));
#45051=CARTESIAN_POINT('Ctrl Pts',(-2.3609967220633,0.2337383165994,10.6345099255067));
#45052=CARTESIAN_POINT('Ctrl Pts',(-2.36545136240482,0.172736546790724,
10.6389210243916));
#45053=CARTESIAN_POINT('Origin',(0.,0.,0.));
#45054=CARTESIAN_POINT('',(-2.94199911155216,0.00228640028720795,0.322176117089596));
#45055=CARTESIAN_POINT('',(1.29074626225713,2.64842276394507,7.39067040906624E-5));
#45056=CARTESIAN_POINT('Ctrl Pts',(-2.94437861999191,0.00228824954296311,
0.322176117089596));
#45057=CARTESIAN_POINT('Ctrl Pts',(-2.94551635113874,0.142778583613822,
0.314557432409286));
#45058=CARTESIAN_POINT('Ctrl Pts',(-2.87303612132235,1.24792270671419,0.254559243224474));
#45059=CARTESIAN_POINT('Ctrl Pts',(-1.53809074754619,3.05021726920943,0.147191839762635));
#45060=CARTESIAN_POINT('Ctrl Pts',(0.503747753874156,3.02562475113786,0.0474431209811117));
#45061=CARTESIAN_POINT('Ctrl Pts',(1.29074626225713,2.64842276394507,7.39067040906624E-5));
#45062=CARTESIAN_POINT('',(-1.28892185405326,2.64462557919716,0.));
#45063=CARTESIAN_POINT('Origin',(0.,0.,0.));
#45064=CARTESIAN_POINT('',(-2.94208929002299,0.0031237281129026,0.177823882910396));
#45065=CARTESIAN_POINT('Ctrl Pts',(-1.28892185405326,2.64462557919716,1.87350135405495E-15));
#45066=CARTESIAN_POINT('Ctrl Pts',(-2.16038499609478,2.21989706654312,0.0524451052237091));
#45067=CARTESIAN_POINT('Ctrl Pts',(-2.88156023630951,1.21946533172,0.111719732860507));
#45068=CARTESIAN_POINT('Ctrl Pts',(-2.94535953294187,0.128940758021734,
0.170994360497305));
#45069=CARTESIAN_POINT('Ctrl Pts',(-2.94436911647834,0.00312614869137163,
0.177823882910396));
#45070=CARTESIAN_POINT('',(-2.94199999091258,0.000231236646814539,1.17782388286648));
#45071=CARTESIAN_POINT('Ctrl Pts',(-2.94199834176125,0.00312363154967357,
0.177823882910396));
#45072=CARTESIAN_POINT('Ctrl Pts',(-2.94209484212644,-0.087765421741547,
0.182761583941182));
#45073=CARTESIAN_POINT('Ctrl Pts',(-2.93797538754606,-0.178839988680605,
0.187699284971969));
#45074=CARTESIAN_POINT('Ctrl Pts',(-2.92961510475039,-0.269665233240012,
0.192636986002755));
#45075=CARTESIAN_POINT('Ctrl Pts',(-2.92100587058736,-0.363195059615083,
0.197721721225234));
#45076=CARTESIAN_POINT('Ctrl Pts',(-2.90789915985505,-0.456459991579172,
0.202806456447713));
#45077=CARTESIAN_POINT('Ctrl Pts',(-2.89032562029103,-0.54898252129668,
0.207891191670192));
#45078=CARTESIAN_POINT('Ctrl Pts',(-2.87329698184751,-0.638636213468393,
0.212818264976582));
#45079=CARTESIAN_POINT('Ctrl Pts',(-2.85207453592643,-0.727592368507746,
0.217745338282971));
#45080=CARTESIAN_POINT('Ctrl Pts',(-2.82673878856991,-0.815421253827921,
0.222672411589361));
#45081=CARTESIAN_POINT('Ctrl Pts',(-2.80141446685841,-0.903210531014497,
0.227597262936801));
#45082=CARTESIAN_POINT('Ctrl Pts',(-2.77198065287895,-0.989873101288184,
0.232522114284241));
#45083=CARTESIAN_POINT('Ctrl Pts',(-2.73856850990087,-1.07499140302578,
0.237446965631682));
#45084=CARTESIAN_POINT('Ctrl Pts',(-2.70516121687009,-1.1600973493967,0.242371102111192));
#45085=CARTESIAN_POINT('Ctrl Pts',(-2.6677769119081,-1.24365903992741,0.247295238590702));
#45086=CARTESIAN_POINT('Ctrl Pts',(-2.62659549866888,-1.32527736205383,
0.252219375070212));
#45087=CARTESIAN_POINT('Ctrl Pts',(-2.58540746886886,-1.40690879768337,
0.257144302703932));
#45088=CARTESIAN_POINT('Ctrl Pts',(-2.54042133172357,-1.4865958314944,0.262069230337652));
#45089=CARTESIAN_POINT('Ctrl Pts',(-2.49186301833919,-1.5639637776603,0.266994157971371));
#45090=CARTESIAN_POINT('Ctrl Pts',(-2.4432540951925,-1.64141236034535,0.271924218596738));
#45091=CARTESIAN_POINT('Ctrl Pts',(-2.39106581805803,-1.71653664093556,
0.276854279222104));
#45092=CARTESIAN_POINT('Ctrl Pts',(-2.33556715859271,-1.7889913492533,0.281784339847471));
#45093=CARTESIAN_POINT('Ctrl Pts',(-2.2800335455957,-1.86149169016772,0.2867175054673));
#45094=CARTESIAN_POINT('Ctrl Pts',(-2.22118570578933,-1.93131876318205,
0.291650671087129));
#45095=CARTESIAN_POINT('Ctrl Pts',(-2.15933097659477,-1.9981625893601,0.296583836706958));
#45096=CARTESIAN_POINT('Ctrl Pts',(-2.09738264979832,-2.06510756256303,
0.301524467115298));
#45097=CARTESIAN_POINT('Ctrl Pts',(-2.03241869343511,-2.1290599663488,0.306465097523638));
#45098=CARTESIAN_POINT('Ctrl Pts',(-1.96478059555267,-2.18974912063909,
0.311405727931977));
#45099=CARTESIAN_POINT('Ctrl Pts',(-1.94988156188092,-2.20311747045361,
0.312494029068734));
#45100=CARTESIAN_POINT('Ctrl Pts',(-1.93485288848935,-2.21632764836611,
0.31358233020549));
#45101=CARTESIAN_POINT('Ctrl Pts',(-1.91969840995316,-2.22937704635697,
0.314670631342247));
#45102=CARTESIAN_POINT('Ctrl Pts',(-1.84914814332196,-2.29012730611899,
0.319737116156612));
#45103=CARTESIAN_POINT('Ctrl Pts',(-1.77559096880863,-2.3476290234709,0.324803600970976));
#45104=CARTESIAN_POINT('Ctrl Pts',(-1.69935779057415,-2.40157179772227,
0.329870085785341));
#45105=CARTESIAN_POINT('Ctrl Pts',(-1.62322724574283,-2.45544194833881,
0.334929749546319));
#45106=CARTESIAN_POINT('Ctrl Pts',(-1.54442821490432,-2.50576242592437,
0.339989413307297));
#45107=CARTESIAN_POINT('Ctrl Pts',(-1.46332566611215,-2.552262132873,0.345049077068274));
#45108=CARTESIAN_POINT('Ctrl Pts',(-1.3785330937065,-2.60087749486843,0.35033894664932));
#45109=CARTESIAN_POINT('Ctrl Pts',(-1.29122277624355,-2.64531582486387,
0.355628816230366));
#45110=CARTESIAN_POINT('Ctrl Pts',(-1.20184727105266,-2.6853169528127,0.360918685811411));
#45111=CARTESIAN_POINT('Ctrl Pts',(-1.11651204589616,-2.72350980277463,
0.365969423267753));
#45112=CARTESIAN_POINT('Ctrl Pts',(-1.0292947386691,-2.75765769436651,0.371020160724095));
#45113=CARTESIAN_POINT('Ctrl Pts',(-0.94061438002265,-2.78758113569715,
0.376070898180437));
#45114=CARTESIAN_POINT('Ctrl Pts',(-0.851963908520084,-2.81749449219942,
0.381119933432149));
#45115=CARTESIAN_POINT('Ctrl Pts',(-0.761851783158,-2.84318608660473,0.38616896868386));
#45116=CARTESIAN_POINT('Ctrl Pts',(-0.670715073634204,-2.86452531669732,
0.391218003935572));
#45117=CARTESIAN_POINT('Ctrl Pts',(-0.579584009289163,-2.88586322499796,
0.396266726440568));
#45118=CARTESIAN_POINT('Ctrl Pts',(-0.48742891675585,-2.90284920499647,
0.401315448945565));
#45119=CARTESIAN_POINT('Ctrl Pts',(-0.394698937554703,-2.91540335951875,
0.406364171450561));
#45120=CARTESIAN_POINT('Ctrl Pts',(-0.301949194876519,-2.92796018969939,
0.411413969986332));
#45121=CARTESIAN_POINT('Ctrl Pts',(-0.208624759428889,-2.93608325943364,
0.416463768522102));
#45122=CARTESIAN_POINT('Ctrl Pts',(-0.115180699757438,-2.93974444576453,
0.421513567057873));
#45123=CARTESIAN_POINT('Ctrl Pts',(-0.0216371349240405,-2.94340953075885,
0.426568742939435));
#45124=CARTESIAN_POINT('Ctrl Pts',(0.0720258668843346,-2.94260323236971,
0.431623918820998));
#45125=CARTESIAN_POINT('Ctrl Pts',(0.165352752788341,-2.93734956502377,
0.436679094702561));
#45126=CARTESIAN_POINT('Ctrl Pts',(0.258737808413396,-2.93209262311915,
0.441737421425042));
#45127=CARTESIAN_POINT('Ctrl Pts',(0.351785892563366,-2.92238283867174,
0.446795748147523));
#45128=CARTESIAN_POINT('Ctrl Pts',(0.444048176176827,-2.90829593013401,
0.451854074870004));
#45129=CARTESIAN_POINT('Ctrl Pts',(0.536449344569062,-2.89418781621202,
0.456920016021267));
#45130=CARTESIAN_POINT('Ctrl Pts',(0.62806191986878,-2.87568951449999,0.46198595717253));
#45131=CARTESIAN_POINT('Ctrl Pts',(0.718449120449233,-2.85292741956849,
0.467051898323793));
#45132=CARTESIAN_POINT('Ctrl Pts',(0.747912720546424,-2.84550763824847,
0.468703247886986));
#45133=CARTESIAN_POINT('Ctrl Pts',(0.777246254132491,-2.83763518819118,
0.470354597450178));
#45134=CARTESIAN_POINT('Ctrl Pts',(0.806435029787981,-2.82931556082577,
0.47200594701337));
#45135=CARTESIAN_POINT('Ctrl Pts',(0.895996558094848,-2.80378798986549,
0.477072873848329));
#45136=CARTESIAN_POINT('Ctrl Pts',(0.984494601690804,-2.77396099009945,
0.482139800683287));
#45137=CARTESIAN_POINT('Ctrl Pts',(1.07148797004047,-2.73994115448828,0.487206727518246));
#45138=CARTESIAN_POINT('Ctrl Pts',(1.15836681946443,-2.7059661029233,0.492266984200884));
#45139=CARTESIAN_POINT('Ctrl Pts',(1.24374452278692,-2.6678093451109,0.497327240883522));
#45140=CARTESIAN_POINT('Ctrl Pts',(1.32719410318614,-2.62562750832404,0.50238749756616));
#45141=CARTESIAN_POINT('Ctrl Pts',(1.41442813673475,-2.58153271781937,0.507677237779424));
#45142=CARTESIAN_POINT('Ctrl Pts',(1.4995545525342,-2.53303925475134,0.512966977992688));
#45143=CARTESIAN_POINT('Ctrl Pts',(1.58210772607098,-2.48038286220223,0.518256718205952));
#45144=CARTESIAN_POINT('Ctrl Pts',(1.66094607775778,-2.43009596205664,0.523308424656453));
#45145=CARTESIAN_POINT('Ctrl Pts',(1.73743734516003,-2.37601294348077,0.528360131106955));
#45146=CARTESIAN_POINT('Ctrl Pts',(1.81120153325415,-2.31838586217605,0.533411837557456));
#45147=CARTESIAN_POINT('Ctrl Pts',(1.8849428630771,-2.26077663852673,0.538461978569783));
#45148=CARTESIAN_POINT('Ctrl Pts',(1.95595844546941,-2.1996258058906,0.54351211958211));
#45149=CARTESIAN_POINT('Ctrl Pts',(2.02389929647884,-2.13522730352355,0.548562260594437));
#45150=CARTESIAN_POINT('Ctrl Pts',(2.09183776955575,-2.07083105510668,0.553612224851625));
#45151=CARTESIAN_POINT('Ctrl Pts',(2.15670140547223,-2.00318766693933,0.558662189108813));
#45152=CARTESIAN_POINT('Ctrl Pts',(2.21817701801937,-1.93262896509669,0.563712153366002));
#45153=CARTESIAN_POINT('Ctrl Pts',(2.27966737706337,-1.86205333794606,0.568763328986185));
#45154=CARTESIAN_POINT('Ctrl Pts',(2.33776780880627,-1.78856134071885,0.573814504606368));
#45155=CARTESIAN_POINT('Ctrl Pts',(2.392205184704,-1.71251813253912,0.578865680226551));
#45156=CARTESIAN_POINT('Ctrl Pts',(2.44670262226623,-1.63639102461989,0.583922428893017));
#45157=CARTESIAN_POINT('Ctrl Pts',(2.49752868096425,-1.55770744722914,0.588979177559483));
#45158=CARTESIAN_POINT('Ctrl Pts',(2.5444535663963,-1.47686155358353,0.59403592622595));
#45159=CARTESIAN_POINT('Ctrl Pts',(2.59140876108098,-1.39596344076695,0.599095941096936));
#45160=CARTESIAN_POINT('Ctrl Pts',(2.63445756290023,-1.31290062220285,0.604155955967922));
#45161=CARTESIAN_POINT('Ctrl Pts',(2.67341711042726,-1.22808996155605,0.609215970838908));
#45162=CARTESIAN_POINT('Ctrl Pts',(2.71243650719976,-1.14314901566804,0.6142837588513));
#45163=CARTESIAN_POINT('Ctrl Pts',(2.74735394768481,-1.05645527715427,0.619351546863693));
#45164=CARTESIAN_POINT('Ctrl Pts',(2.77803555508529,-0.968443315161994,
0.624419334876086));
#45165=CARTESIAN_POINT('Ctrl Pts',(2.78796839996764,-0.939950376221435,
0.626059977478889));
#45166=CARTESIAN_POINT('Ctrl Pts',(2.79745769571003,-0.911319374307146,
0.627700620081692));
#45167=CARTESIAN_POINT('Ctrl Pts',(2.80650004517479,-0.882565293014582,
0.629341262684495));
#45168=CARTESIAN_POINT('Ctrl Pts',(2.83434355154955,-0.794024759507225,
0.634393184527139));
#45169=CARTESIAN_POINT('Ctrl Pts',(2.8580426961888,-0.704007223986515,0.639445106369783));
#45170=CARTESIAN_POINT('Ctrl Pts',(2.87744208044141,-0.612936435289163,
0.644497028212428));
#45171=CARTESIAN_POINT('Ctrl Pts',(2.89681485382117,-0.521990571854782,
0.649542020141828));
#45172=CARTESIAN_POINT('Ctrl Pts',(2.9118994955391,-0.429994757065229,0.654587012071229));
#45173=CARTESIAN_POINT('Ctrl Pts',(2.92259009067868,-0.337388739982193,
0.65963200400063));
#45174=CARTESIAN_POINT('Ctrl Pts',(2.93380733780313,-0.240220662315065,
0.664925527932088));
#45175=CARTESIAN_POINT('Ctrl Pts',(2.94018634157949,-0.14238118685994,0.670219051863546));
#45176=CARTESIAN_POINT('Ctrl Pts',(2.94166506875022,-0.0443917029946411,
0.675512575795003));
#45177=CARTESIAN_POINT('Ctrl Pts',(2.94307183060904,0.0488289202518063,
0.680548479451143));
#45178=CARTESIAN_POINT('Ctrl Pts',(2.94004407342124,0.142184790760255,0.685584383107282));
#45179=CARTESIAN_POINT('Ctrl Pts',(2.93258153638806,0.235222304290782,0.690620286763422));
#45180=CARTESIAN_POINT('Ctrl Pts',(2.92512156149596,0.328227874899626,0.695654461423697));
#45181=CARTESIAN_POINT('Ctrl Pts',(2.91322986727545,0.420914863234052,0.700688636083973));
#45182=CARTESIAN_POINT('Ctrl Pts',(2.89695823735506,0.512832303019893,0.705722810744248));
#45183=CARTESIAN_POINT('Ctrl Pts',(2.88068764156459,0.604743901069218,0.710756665461736));
#45184=CARTESIAN_POINT('Ctrl Pts',(2.86003774144722,0.695885610416984,0.715790520179223));
#45185=CARTESIAN_POINT('Ctrl Pts',(2.83511168149093,0.785815343114191,0.720824374896711));
#45186=CARTESIAN_POINT('Ctrl Pts',(2.81018023198376,0.875764520556002,0.725859318041979));
#45187=CARTESIAN_POINT('Ctrl Pts',(2.78097090544223,0.964500772946039,0.730894261187247));
#45188=CARTESIAN_POINT('Ctrl Pts',(2.74763675774148,1.05159699862061,0.735929204332515));
#45189=CARTESIAN_POINT('Ctrl Pts',(2.7142663279024,1.13878802309839,0.740969627699006));
#45190=CARTESIAN_POINT('Ctrl Pts',(2.67676227588859,1.2243350429165,0.746010051065497));
#45191=CARTESIAN_POINT('Ctrl Pts',(2.63532574672929,1.30783110860146,0.751050474431987));
#45192=CARTESIAN_POINT('Ctrl Pts',(2.59386296360743,1.39138007694564,0.756094091383679));
#45193=CARTESIAN_POINT('Ctrl Pts',(2.54846295945311,1.47287511674493,0.76113770833537));
#45194=CARTESIAN_POINT('Ctrl Pts',(2.49937169266774,1.5519359335653,0.766181325287062));
#45195=CARTESIAN_POINT('Ctrl Pts',(2.45020449602868,1.63111903438132,0.7712327432413));
#45196=CARTESIAN_POINT('Ctrl Pts',(2.39733489394231,1.70786003317449,0.776284161195538));
#45197=CARTESIAN_POINT('Ctrl Pts',(2.34105060003791,1.7818097788659,0.781335579149776));
#45198=CARTESIAN_POINT('Ctrl Pts',(2.32121363730996,1.80787279302601,0.78311591221839));
#45199=CARTESIAN_POINT('Ctrl Pts',(2.30095286381563,1.83358941222552,0.784896245287003));
#45200=CARTESIAN_POINT('Ctrl Pts',(2.28028196720395,1.85894544030869,0.786676578355616));
#45201=CARTESIAN_POINT('Ctrl Pts',(2.22152962691378,1.93101420531368,0.791736771739677));
#45202=CARTESIAN_POINT('Ctrl Pts',(2.15925557718462,2.00041973759941,0.796796965123737));
#45203=CARTESIAN_POINT('Ctrl Pts',(2.09373019662748,2.0667989412931,0.801857158507798));
#45204=CARTESIAN_POINT('Ctrl Pts',(2.02829324392291,2.13308856488227,0.806910523056516));
#45205=CARTESIAN_POINT('Ctrl Pts',(1.95961398874799,2.19635966400071,0.811963887605234));
#45206=CARTESIAN_POINT('Ctrl Pts',(1.88800327535986,2.25628181578242,0.817017252153952));
#45207=CARTESIAN_POINT('Ctrl Pts',(1.81301877070208,2.31902707632783,0.822308695565318));
#45208=CARTESIAN_POINT('Ctrl Pts',(1.73482010442831,2.37809969142808,0.827600138976684));
#45209=CARTESIAN_POINT('Ctrl Pts',(1.65380805324627,2.43316315174667,0.83289158238805));
#45210=CARTESIAN_POINT('Ctrl Pts',(1.57657718863523,2.48565655966353,0.837936051003985));
#45211=CARTESIAN_POINT('Ctrl Pts',(1.49679007148308,2.53450636709367,0.842980519619919));
#45212=CARTESIAN_POINT('Ctrl Pts',(1.41482693862869,2.57946287698245,0.848024988235853));
#45213=CARTESIAN_POINT('Ctrl Pts',(1.33289104795545,2.6244044446241,0.853067780215926));
#45214=CARTESIAN_POINT('Ctrl Pts',(1.24878096634701,2.66545507322319,0.858110572195999));
#45215=CARTESIAN_POINT('Ctrl Pts',(1.16290326250868,2.70241003588402,0.863153364176072));
#45216=CARTESIAN_POINT('Ctrl Pts',(1.0770303008776,2.73936295787441,0.868195877690797));
#45217=CARTESIAN_POINT('Ctrl Pts',(0.989390317856509,2.77222048917931,0.873238391205521));
#45218=CARTESIAN_POINT('Ctrl Pts',(0.900410641304936,2.80082571343253,0.878280904720246));
#45219=CARTESIAN_POINT('Ctrl Pts',(0.811411218019824,2.82943728587404,0.883324537290182));
#45220=CARTESIAN_POINT('Ctrl Pts',(0.721071932073303,2.85379454182169,0.888368169860118));
#45221=CARTESIAN_POINT('Ctrl Pts',(0.629834990614495,2.87379050812644,0.893411802430054));
#45222=CARTESIAN_POINT('Ctrl Pts',(0.53849896313161,2.89380819064358,0.898460912534531));
#45223=CARTESIAN_POINT('Ctrl Pts',(0.446263767364402,2.9094550357618,0.903510022639008));
#45224=CARTESIAN_POINT('Ctrl Pts',(0.35358118898701,2.92067532307077,0.908559132743485));
#45225=CARTESIAN_POINT('Ctrl Pts',(0.260839829542242,2.93190272650097,0.913611445090352));
#45226=CARTESIAN_POINT('Ctrl Pts',(0.167650963502087,2.93869795083421,0.918663757437218));
#45227=CARTESIAN_POINT('Ctrl Pts',(0.0744687496395253,2.94105736178795,
0.923716069784084));
#45228=CARTESIAN_POINT('Ctrl Pts',(-0.018856247074606,2.94342038806065,
0.928776123775349));
#45229=CARTESIAN_POINT('Ctrl Pts',(-0.112174129778242,2.9413340453754,0.933836177766613));
#45230=CARTESIAN_POINT('Ctrl Pts',(-0.205033788460614,2.93484669882253,
0.938896231757877));
#45231=CARTESIAN_POINT('Ctrl Pts',(-0.236327173408762,2.93266048539194,
0.940601452514165));
#45232=CARTESIAN_POINT('Ctrl Pts',(-0.267568591902607,2.92997489653949,
0.942306673270454));
#45233=CARTESIAN_POINT('Ctrl Pts',(-0.298741044927317,2.92679308938567,
0.944011894026742));
#45234=CARTESIAN_POINT('Ctrl Pts',(-0.39123235943881,2.9173523974406,0.949071428775464));
#45235=CARTESIAN_POINT('Ctrl Pts',(-0.483435904631205,2.90350675974296,
0.954130963524185));
#45236=CARTESIAN_POINT('Ctrl Pts',(-0.574899822984667,2.88528234208235,
0.959190498272906));
#45237=CARTESIAN_POINT('Ctrl Pts',(-0.666240499171527,2.86708248073594,
0.964243215600773));
#45238=CARTESIAN_POINT('Ctrl Pts',(-0.756843098468711,2.84451565082106,
0.969295932928639));
#45239=CARTESIAN_POINT('Ctrl Pts',(-0.846260802748927,2.81765978317659,
0.974348650256506));
#45240=CARTESIAN_POINT('Ctrl Pts',(-0.939906120169776,2.78953418690432,
0.979640256899896));
#45241=CARTESIAN_POINT('Ctrl Pts',(-1.03225124784787,2.75670402781351,0.984931863543286));
#45242=CARTESIAN_POINT('Ctrl Pts',(-1.12279461453534,2.71931907902887,0.990223470186676));
#45243=CARTESIAN_POINT('Ctrl Pts',(-1.20909876630351,2.68368448301378,0.99526732529784));
#45244=CARTESIAN_POINT('Ctrl Pts',(-1.29376560658863,2.64391217426158,1.000311180409));
#45245=CARTESIAN_POINT('Ctrl Pts',(-1.37637759321857,2.60018243992337,1.00535503552017));
#45246=CARTESIAN_POINT('Ctrl Pts',(-1.4589623444017,2.55646712236537,1.01039722777763));
#45247=CARTESIAN_POINT('Ctrl Pts',(-1.53949319701646,2.5087971784811,1.0154394200351));
#45248=CARTESIAN_POINT('Ctrl Pts',(-1.61757569704293,2.45739961429477,1.02048161229256));
#45249=CARTESIAN_POINT('Ctrl Pts',(-1.69565411141169,2.40600473948,1.02552354071791));
#45250=CARTESIAN_POINT('Ctrl Pts',(-1.77128405842607,2.350882876062,1.03056546914325));
#45251=CARTESIAN_POINT('Ctrl Pts',(-1.84409960994581,2.29230465440301,1.03560739756859));
#45252=CARTESIAN_POINT('Ctrl Pts',(-1.91693154667289,2.23371325126991,1.04065046054611));
#45253=CARTESIAN_POINT('Ctrl Pts',(-1.98694748536537,2.17166422283282,1.04569352352363));
#45254=CARTESIAN_POINT('Ctrl Pts',(-2.05381503892687,2.10646808328012,1.05073658650115));
#45255=CARTESIAN_POINT('Ctrl Pts',(-2.12075557248106,2.04120078793458,1.05578515353378));
#45256=CARTESIAN_POINT('Ctrl Pts',(-2.18454054577324,1.97277983592785,1.0608337205664));
#45257=CARTESIAN_POINT('Ctrl Pts',(-2.244875119947,1.90155191773534,1.06588228759902));
#45258=CARTESIAN_POINT('Ctrl Pts',(-2.30524813984925,1.83027861247842,1.07093407162356));
#45259=CARTESIAN_POINT('Ctrl Pts',(-2.36216611417598,1.75619513085989,1.0759858556481));
#45260=CARTESIAN_POINT('Ctrl Pts',(-2.41537641249584,1.67967877463482,1.08103763967264));
#45261=CARTESIAN_POINT('Ctrl Pts',(-2.46866853256563,1.60304475881447,1.0860971918515));
#45262=CARTESIAN_POINT('Ctrl Pts',(-2.51824136337206,1.52397077629439,1.09115674403037));
#45263=CARTESIAN_POINT('Ctrl Pts',(-2.56388738984611,1.44286016376782,1.09621629620923));
#45264=CARTESIAN_POINT('Ctrl Pts',(-2.57931733335747,1.41544195749376,1.09792660070545));
#45265=CARTESIAN_POINT('Ctrl Pts',(-2.59429897366065,1.38779120837025,1.09963690520166));
#45266=CARTESIAN_POINT('Ctrl Pts',(-2.60882554488161,1.35992399654289,1.10134720969787));
#45267=CARTESIAN_POINT('Ctrl Pts',(-2.65422890282685,1.27282395247274,1.10669283228531));
#45268=CARTESIAN_POINT('Ctrl Pts',(-2.69532627336188,1.18333337786699,1.11203845487275));
#45269=CARTESIAN_POINT('Ctrl Pts',(-2.73187469153183,1.09189041106143,1.11738407746019));
#45270=CARTESIAN_POINT('Ctrl Pts',(-2.76831966707044,1.00070625439259,1.12271457038418));
#45271=CARTESIAN_POINT('Ctrl Pts',(-2.80024121316959,0.907581057944109,
1.12804506330817));
#45272=CARTESIAN_POINT('Ctrl Pts',(-2.8274432620727,0.812975153224073,1.13337555623216));
#45273=CARTESIAN_POINT('Ctrl Pts',(-2.85459889591541,0.718530675269989,
1.13869695369602));
#45274=CARTESIAN_POINT('Ctrl Pts',(-2.87705096140675,0.622610869338626,
1.14401835115989));
#45275=CARTESIAN_POINT('Ctrl Pts',(-2.89465180269297,0.525694722406793,
1.14933974862376));
#45276=CARTESIAN_POINT('Ctrl Pts',(-2.91221171667489,0.429003934966152,
1.15464877222153));
#45277=CARTESIAN_POINT('Ctrl Pts',(-2.92494282082446,0.33132178351378,1.1599577958193));
#45278=CARTESIAN_POINT('Ctrl Pts',(-2.93274783360769,0.233139753086851,
1.16526681941707));
#45279=CARTESIAN_POINT('Ctrl Pts',(-2.93890138450316,0.155732048829,1.16945250723354));
#45280=CARTESIAN_POINT('Ctrl Pts',(-2.94199387730798,0.0780139969306237,
1.17363819505001));
#45281=CARTESIAN_POINT('Ctrl Pts',(-2.94199999091258,0.0002312366468149,
1.17782388286648));
#45282=CARTESIAN_POINT('',(-2.94199916389813,-0.00221802224694258,2.1778238829104));
#45283=CARTESIAN_POINT('Ctrl Pts',(-2.94199999091264,0.000231235830579614,
1.1778238829104));
#45284=CARTESIAN_POINT('Ctrl Pts',(-2.94200765316831,-0.0972551962378792,
1.18306987533197));
#45285=CARTESIAN_POINT('Ctrl Pts',(-2.93716551547198,-0.194662940964098,
1.18831586775354));
#45286=CARTESIAN_POINT('Ctrl Pts',(-2.92752287042165,-0.291502732677018,
1.19356186017511));
#45287=CARTESIAN_POINT('Ctrl Pts',(-2.91754802661955,-0.391678751925135,
1.1989885822746));
#45288=CARTESIAN_POINT('Ctrl Pts',(-2.90243600485248,-0.491246522856216,
1.20441530437409));
#45289=CARTESIAN_POINT('Ctrl Pts',(-2.88229873438933,-0.589676187188932,
1.20984202647358));
#45290=CARTESIAN_POINT('Ctrl Pts',(-2.86276374898589,-0.685161921440928,
1.2151064408934));
#45291=CARTESIAN_POINT('Ctrl Pts',(-2.83850002950619,-0.779576312685586,
1.22037085531322));
#45292=CARTESIAN_POINT('Ctrl Pts',(-2.80966034937286,-0.872452131157923,
1.22563526973304));
#45293=CARTESIAN_POINT('Ctrl Pts',(-2.77948693070997,-0.969623144895513,
1.23114314567237));
#45294=CARTESIAN_POINT('Ctrl Pts',(-2.74430432737846,-1.06510939896652,
1.23665102161169));
#45295=CARTESIAN_POINT('Ctrl Pts',(-2.70434292712315,-1.15840119670129,
1.24215889755102));
#45296=CARTESIAN_POINT('Ctrl Pts',(-2.66438152686785,-1.25169299443606,
1.24766677349034));
#45297=CARTESIAN_POINT('Ctrl Pts',(-2.61964160962512,-1.34278994127986,
1.25317464942966));
#45298=CARTESIAN_POINT('Ctrl Pts',(-2.57040644515614,-1.43121441674537,
1.25868252536899));
#45299=CARTESIAN_POINT('Ctrl Pts',(-2.52518458599781,-1.5124311491109,1.26374143788967));
#45300=CARTESIAN_POINT('Ctrl Pts',(-2.47603107530938,-1.59164364202472,
1.26880035041034));
#45301=CARTESIAN_POINT('Ctrl Pts',(-2.42314835223583,-1.66844720115945,
1.27385926293102));
#45302=CARTESIAN_POINT('Ctrl Pts',(-2.37033708093894,-1.74514698820312,
1.2789113401704));
#45303=CARTESIAN_POINT('Ctrl Pts',(-2.31380685980803,-1.819443948046,1.28396341740979));
#45304=CARTESIAN_POINT('Ctrl Pts',(-2.25380569606738,-1.89095845654373,
1.28901549464918));
#45305=CARTESIAN_POINT('Ctrl Pts',(-2.19095787938252,-1.96586584900366,
1.29430725908213));
#45306=CARTESIAN_POINT('Ctrl Pts',(-2.12430185730173,-2.03771980690957,
1.29959902351509));
#45307=CARTESIAN_POINT('Ctrl Pts',(-2.05417342114962,-2.10611859966206,
1.30489078794804));
#45308=CARTESIAN_POINT('Ctrl Pts',(-1.9873393864957,-2.17130424383058,1.30993396282685));
#45309=CARTESIAN_POINT('Ctrl Pts',(-1.91735215473173,-2.23335165073221,
1.31497713770566));
#45310=CARTESIAN_POINT('Ctrl Pts',(-1.84454221207067,-2.2919485220854,1.32002031258447));
#45311=CARTESIAN_POINT('Ctrl Pts',(-1.77175646859857,-2.35052591812093,
1.32506181130838));
#45312=CARTESIAN_POINT('Ctrl Pts',(-1.69615022297717,-2.40565477984259,
1.3301033100323));
#45313=CARTESIAN_POINT('Ctrl Pts',(-1.61808776203471,-2.45706247261918,
1.33514480875621));
#45314=CARTESIAN_POINT('Ctrl Pts',(-1.54002957896282,-2.5084673482228,1.34018603120291));
#45315=CARTESIAN_POINT('Ctrl Pts',(-1.4595158183549,-2.55615121723485,1.34522725364962));
#45316=CARTESIAN_POINT('Ctrl Pts',(-1.37693957557334,-2.59988488307077,
1.35026847609632));
#45317=CARTESIAN_POINT('Ctrl Pts',(-1.29434493859787,-2.64362829075862,
1.35531082149582));
#45318=CARTESIAN_POINT('Ctrl Pts',(-1.20968729840001,-2.68341954067785,
1.36035316689533));
#45319=CARTESIAN_POINT('Ctrl Pts',(-1.12338314000202,-2.71907600496183,
1.36539551229483));
#45320=CARTESIAN_POINT('Ctrl Pts',(-1.0369850038881,-2.75477129603162,1.37044334836955));
#45321=CARTESIAN_POINT('Ctrl Pts',(-0.948937181157173,-2.7863226464533,
1.37549118444428));
#45322=CARTESIAN_POINT('Ctrl Pts',(-0.859674555171333,-2.81359621466744,
1.380539020519));
#45323=CARTESIAN_POINT('Ctrl Pts',(-0.770355194027269,-2.84088711791057,
1.38559006498889));
#45324=CARTESIAN_POINT('Ctrl Pts',(-0.679819921165122,-2.86389471709149,
1.39064110945879));
#45325=CARTESIAN_POINT('Ctrl Pts',(-0.588515064254157,-2.88253603952248,
1.39569215392868));
#45326=CARTESIAN_POINT('Ctrl Pts',(-0.497069908538492,-2.90120600616083,
1.40075095982032));
#45327=CARTESIAN_POINT('Ctrl Pts',(-0.40485324530817,-2.9154962382094,1.40580976571195));
#45328=CARTESIAN_POINT('Ctrl Pts',(-0.312317492516556,-2.92537549450804,
1.41086857160359));
#45329=CARTESIAN_POINT('Ctrl Pts',(-0.280920654748795,-2.92872746818219,
1.4125849947491));
#45330=CARTESIAN_POINT('Ctrl Pts',(-0.249487087405726,-2.93157209130842,
1.4143014178946));
#45331=CARTESIAN_POINT('Ctrl Pts',(-0.218034427519059,-2.93390950583286,
1.41601784104011));
#45332=CARTESIAN_POINT('Ctrl Pts',(-0.12533607140344,-2.9407984139493,1.42107654210261));
#45333=CARTESIAN_POINT('Ctrl Pts',(-0.032149715563284,-2.94330172661396,
1.42613524316511));
#45334=CARTESIAN_POINT('Ctrl Pts',(0.061075339909064,-2.9413659756744,1.43119394422761));
#45335=CARTESIAN_POINT('Ctrl Pts',(0.154174426977337,-2.93943284037775,
1.43624580982623));
#45336=CARTESIAN_POINT('Ctrl Pts',(0.24731167059882,-2.93307257090482,1.44129767542485));
#45337=CARTESIAN_POINT('Ctrl Pts',(0.340033650333316,-2.92228354487394,
1.44634954102347));
#45338=CARTESIAN_POINT('Ctrl Pts',(0.437159705798388,-2.91098206550853,
1.4516413583438));
#45339=CARTESIAN_POINT('Ctrl Pts',(0.533829582463102,-2.89482065294382,
1.45693317566412));
#45340=CARTESIAN_POINT('Ctrl Pts',(0.629523046017409,-2.87385885779608,
1.46222499298444));
#45341=CARTESIAN_POINT('Ctrl Pts',(0.720716429955741,-2.85388281176384,
1.46726795736989));
#45342=CARTESIAN_POINT('Ctrl Pts',(0.811022666097952,-2.82954774423491,
1.47231092175533));
#45343=CARTESIAN_POINT('Ctrl Pts',(0.899999209849383,-2.80095794725135,
1.47735388614077));
#45344=CARTESIAN_POINT('Ctrl Pts',(0.988946195632898,-2.77237764778552,
1.4823951752557));
#45345=CARTESIAN_POINT('Ctrl Pts',(1.0765639453971,-2.73954556257775,1.48743646437063));
#45346=CARTESIAN_POINT('Ctrl Pts',(1.16242445608337,-2.70261602598284,1.49247775348557));
#45347=CARTESIAN_POINT('Ctrl Pts',(1.24828028117491,-2.66568850471303,1.49751876748639));
#45348=CARTESIAN_POINT('Ctrl Pts',(1.33237865122145,-2.62466415215104,1.50255978148722));
#45349=CARTESIAN_POINT('Ctrl Pts',(1.41431200286067,-2.57974525071067,1.50760079548805));
#45350=CARTESIAN_POINT('Ctrl Pts',(1.49626362969372,-2.53481633013139,1.51264293388457));
#45351=CARTESIAN_POINT('Ctrl Pts',(1.57604889086872,-2.48599134852284,1.51768507228109));
#45352=CARTESIAN_POINT('Ctrl Pts',(1.65328625784548,-2.43351773151939,1.52272721067762));
#45353=CARTESIAN_POINT('Ctrl Pts',(1.73060778418476,-2.38098693822513,1.52777484308785));
#45354=CARTESIAN_POINT('Ctrl Pts',(1.80537550886616,-2.32479982438058,1.53282247549809));
#45355=CARTESIAN_POINT('Ctrl Pts',(1.8772385351632,-2.26524600917832,1.53787010790832));
#45356=CARTESIAN_POINT('Ctrl Pts',(1.94914726350187,-2.20565432010571,1.54292095041307));
#45357=CARTESIAN_POINT('Ctrl Pts',(2.01814728913691,-2.14269196536669,1.54797179291781));
#45358=CARTESIAN_POINT('Ctrl Pts',(2.08392391124165,-2.0766860937935,1.55302263542256));
#45359=CARTESIAN_POINT('Ctrl Pts',(2.14980166466098,-2.0105787384355,1.55808124357909));
#45360=CARTESIAN_POINT('Ctrl Pts',(2.21244582682778,-1.941418854671,1.56313985173561));
#45361=CARTESIAN_POINT('Ctrl Pts',(2.27158155730201,-1.86956712330031,1.56819845989214));
#45362=CARTESIAN_POINT('Ctrl Pts',(2.29166789675473,-1.84516160306739,1.56991669216517));
#45363=CARTESIAN_POINT('Ctrl Pts',(2.31134982887331,-1.82044576576877,1.5716349244382));
#45364=CARTESIAN_POINT('Ctrl Pts',(2.33061774403031,-1.79543446864849,1.57335315671124));
#45365=CARTESIAN_POINT('Ctrl Pts',(2.38734249612612,-1.72180119710962,1.57841163340354));
#45366=CARTESIAN_POINT('Ctrl Pts',(2.44067303442736,-1.64534888832417,1.58347011009584));
#45367=CARTESIAN_POINT('Ctrl Pts',(2.49031762523661,-1.56642335447218,1.58852858678814));
#45368=CARTESIAN_POINT('Ctrl Pts',(2.53989508790734,-1.48760454169661,1.59358022353839));
#45369=CARTESIAN_POINT('Ctrl Pts',(2.58579627403676,-1.40631952173164,1.59863186028864));
#45370=CARTESIAN_POINT('Ctrl Pts',(2.62777048391585,-1.3229460623399,1.6036834970389));
#45371=CARTESIAN_POINT('Ctrl Pts',(2.67174083249057,-1.23560766855251,1.60897537101154));
#45372=CARTESIAN_POINT('Ctrl Pts',(2.71140113034999,-1.14597765671579,1.61426724498419));
#45373=CARTESIAN_POINT('Ctrl Pts',(2.74651498733101,-1.05452331617947,1.61955911895683));
#45374=CARTESIAN_POINT('Ctrl Pts',(2.77997564038546,-0.967374759395649,
1.62460184494111));
#45375=CARTESIAN_POINT('Ctrl Pts',(2.80930806479646,-0.878570225485862,
1.62964457092539));
#45376=CARTESIAN_POINT('Ctrl Pts',(2.83435600314663,-0.788536649387113,
1.63468729690967));
#45377=CARTESIAN_POINT('Ctrl Pts',(2.85939560529548,-0.698533037351899,
1.63972834462493));
#45378=CARTESIAN_POINT('Ctrl Pts',(2.88015343593823,-0.607301622209397,
1.64476939234019));
#45379=CARTESIAN_POINT('Ctrl Pts',(2.89652302991949,-0.515284714644266,
1.64981044005545));
#45380=CARTESIAN_POINT('Ctrl Pts',(2.9128917217824,-0.423272878074804,1.65485120996164));
#45381=CARTESIAN_POINT('Ctrl Pts',(2.92487258077865,-0.330476071339442,
1.65989197986783));
#45382=CARTESIAN_POINT('Ctrl Pts',(2.93241042874529,-0.237345902399574,
1.66493274977402));
#45383=CARTESIAN_POINT('Ctrl Pts',(2.93994995452725,-0.144195004038615,
1.66997464168228));
#45384=CARTESIAN_POINT('Ctrl Pts',(2.94304446969761,-0.0507110375434266,
1.67501653359054));
#45385=CARTESIAN_POINT('Ctrl Pts',(2.94169081752702,0.0426513080366752,
1.6800584254988));
#45386=CARTESIAN_POINT('Ctrl Pts',(2.94033569091073,0.136115347176504,1.68510580921355));
#45387=CARTESIAN_POINT('Ctrl Pts',(2.93452273378389,0.229457057583668,1.69015319292831));
#45388=CARTESIAN_POINT('Ctrl Pts',(2.92430087528032,0.322224131366271,1.69520057664306));
#45389=CARTESIAN_POINT('Ctrl Pts',(2.91407251893188,0.415050175448054,1.70025116888554));
#45390=CARTESIAN_POINT('Ctrl Pts',(2.89942975104263,0.507300418757901,1.70530176112801));
#45391=CARTESIAN_POINT('Ctrl Pts',(2.88047275094337,0.598532147067083,1.71035235337049));
#45392=CARTESIAN_POINT('Ctrl Pts',(2.8614866040822,0.689904145959685,1.71541071099824));
#45393=CARTESIAN_POINT('Ctrl Pts',(2.83817309694171,0.780254076555261,1.720469068626));
#45394=CARTESIAN_POINT('Ctrl Pts',(2.81068233516932,0.869154077691133,1.72552742625376));
#45395=CARTESIAN_POINT('Ctrl Pts',(2.8013327201323,0.89938899057909,1.72724777496329));
#45396=CARTESIAN_POINT('Ctrl Pts',(2.7915003401192,0.929456364812504,1.72896812367282));
#45397=CARTESIAN_POINT('Ctrl Pts',(2.78119234739785,0.959339943281655,1.73068847238236));
#45398=CARTESIAN_POINT('Ctrl Pts',(2.75088182548335,1.04721222691228,1.7357471359525));
#45399=CARTESIAN_POINT('Ctrl Pts',(2.71634999530264,1.1337994539328,1.74080579952265));
#45400=CARTESIAN_POINT('Ctrl Pts',(2.67772531176649,1.21866777865219,1.74586446309279));
#45401=CARTESIAN_POINT('Ctrl Pts',(2.63915283356409,1.30342139487921,1.75091628934556));
#45402=CARTESIAN_POINT('Ctrl Pts',(2.59649867763927,1.38646032609095,1.75596811559833));
#45403=CARTESIAN_POINT('Ctrl Pts',(2.54994055222832,1.46736743186617,1.76101994185109));
#45404=CARTESIAN_POINT('Ctrl Pts',(2.50117055712073,1.55211824857107,1.76631176877619));
#45405=CARTESIAN_POINT('Ctrl Pts',(2.44811661779715,1.63452919777494,1.77160359570129));
#45406=CARTESIAN_POINT('Ctrl Pts',(2.39103904914586,1.71414592886943,1.77689542262639));
#45407=CARTESIAN_POINT('Ctrl Pts',(2.33664617980532,1.79001780908566,1.78193834329227));
#45408=CARTESIAN_POINT('Ctrl Pts',(2.27859990313235,1.86335196543142,1.78698126395815));
#45409=CARTESIAN_POINT('Ctrl Pts',(2.21717092098241,1.93378310757696,1.79202418462403));
#45410=CARTESIAN_POINT('Ctrl Pts',(2.15576236415779,2.00419083115133,1.79706542850329));
#45411=CARTESIAN_POINT('Ctrl Pts',(2.090973627524,2.0716971249235,1.80210667238255));
#45412=CARTESIAN_POINT('Ctrl Pts',(2.02311563396547,2.13596983396407,1.80714791626181));
#45413=CARTESIAN_POINT('Ctrl Pts',(1.95526136329416,2.20023901681657,1.81218888356375));
#45414=CARTESIAN_POINT('Ctrl Pts',(1.8843384924389,2.26127466350019,1.81722985086568));
#45415=CARTESIAN_POINT('Ctrl Pts',(1.81069391041864,2.31878234484672,1.82227081816762));
#45416=CARTESIAN_POINT('Ctrl Pts',(1.73703292248094,2.37630283726837,1.82731290845363));
#45417=CARTESIAN_POINT('Ctrl Pts',(1.66064936836453,2.43029353110668,1.83235499873965));
#45418=CARTESIAN_POINT('Ctrl Pts',(1.58192131534117,2.48050175409518,1.83739708902567));
#45419=CARTESIAN_POINT('Ctrl Pts',(1.50310750675042,2.53076466705103,1.84244467147486));
#45420=CARTESIAN_POINT('Ctrl Pts',(1.42194447643817,2.57723664802215,1.84749225392405));
#45421=CARTESIAN_POINT('Ctrl Pts',(1.33883694336503,2.61970983871897,1.85253983637324));
#45422=CARTESIAN_POINT('Ctrl Pts',(1.25567657527345,2.66221003144234,1.85759062778679));
#45423=CARTESIAN_POINT('Ctrl Pts',(1.17056964643962,2.70070619055931,1.86264141920034));
#45424=CARTESIAN_POINT('Ctrl Pts',(1.0839410443022,2.73503853948661,1.86769221061389));
#45425=CARTESIAN_POINT('Ctrl Pts',(0.997179271437195,2.76942366617753,1.87275076640953));
#45426=CARTESIAN_POINT('Ctrl Pts',(0.908891574806107,2.79963206485873,1.87780932220518));
#45427=CARTESIAN_POINT('Ctrl Pts',(0.819517889678413,2.82555382686245,1.88286787800082));
#45428=CARTESIAN_POINT('Ctrl Pts',(0.789153315268341,2.83436070631559,1.88458651468504));
#45429=CARTESIAN_POINT('Ctrl Pts',(0.758663468110167,2.84267322009762,1.88630515136926));
#45430=CARTESIAN_POINT('Ctrl Pts',(0.728065806503105,2.85048841102731,1.88802378805348));
#45431=CARTESIAN_POINT('Ctrl Pts',(0.638004965636491,2.87349156321913,1.89308240550317));
#45432=CARTESIAN_POINT('Ctrl Pts',(0.546696209144975,2.89226236604903,1.89814102295285));
#45433=CARTESIAN_POINT('Ctrl Pts',(0.454572528752249,2.9066695402305,1.90319964040254));
#45434=CARTESIAN_POINT('Ctrl Pts',(0.362573369558742,2.92105724060677,1.90825142024968));
#45435=CARTESIAN_POINT('Ctrl Pts',(0.269761909506563,2.93109296605129,1.91330320009683));
#45436=CARTESIAN_POINT('Ctrl Pts',(0.176584271950763,2.9366957613787,1.91835497994397));
#45437=CARTESIAN_POINT('Ctrl Pts',(0.0789788687414522,2.94256479939443,
1.92364681843483));
#45438=CARTESIAN_POINT('Ctrl Pts',(-0.0190279012904845,2.9435690350207,
1.92893865692569));
#45439=CARTESIAN_POINT('Ctrl Pts',(-0.116913393579505,2.9396760465061,1.93423049541655));
#45440=CARTESIAN_POINT('Ctrl Pts',(-0.21019367688271,2.93596621103358,1.93927336931011));
#45441=CARTESIAN_POINT('Ctrl Pts',(-0.303363336766012,2.9278095227097,1.94431624320366));
#45442=CARTESIAN_POINT('Ctrl Pts',(-0.395968419911317,2.91523121045878,
1.94935911709722));
#45443=CARTESIAN_POINT('Ctrl Pts',(-0.48854271069598,2.90265708065566,1.95440031417147));
#45444=CARTESIAN_POINT('Ctrl Pts',(-0.580552359244172,2.88566430773528,
1.95944151124571));
#45445=CARTESIAN_POINT('Ctrl Pts',(-0.671548970857717,2.86432993555909,
1.96448270831996));
#45446=CARTESIAN_POINT('Ctrl Pts',(-0.76254059060031,2.84299673373893,1.96952362884539));
#45447=CARTESIAN_POINT('Ctrl Pts',(-0.852518852812673,2.81732250785056,
1.97456454937082));
#45448=CARTESIAN_POINT('Ctrl Pts',(-0.941047095307283,2.7874350870314,1.97960546989625));
#45449=CARTESIAN_POINT('Ctrl Pts',(-1.02959506113424,2.75754100755148,1.98464751349549));
#45450=CARTESIAN_POINT('Ctrl Pts',(-1.11669194615718,2.72343201078684,1.98968955709474));
#45451=CARTESIAN_POINT('Ctrl Pts',(-1.20191882058613,2.68528492877774,1.99473160069398));
#45452=CARTESIAN_POINT('Ctrl Pts',(-1.28723853710523,2.64709629115779,1.99977913685492));
#45453=CARTESIAN_POINT('Ctrl Pts',(-1.3706837727355,2.60486097036844,2.00482667301587));
#45454=CARTESIAN_POINT('Ctrl Pts',(-1.45185837263565,2.55880270161804,2.00987420917681));
#45455=CARTESIAN_POINT('Ctrl Pts',(-1.53308458203182,2.51271514976626,2.0149249544795));
#45456=CARTESIAN_POINT('Ctrl Pts',(-1.61203690779445,2.46280004757637,2.0199756997822));
#45457=CARTESIAN_POINT('Ctrl Pts',(-1.68834826456665,2.40932441517011,2.02502644508489));
#45458=CARTESIAN_POINT('Ctrl Pts',(-1.7647769426638,2.35576656915486,2.03008495541963));
#45459=CARTESIAN_POINT('Ctrl Pts',(-1.8385561989998,2.29863753859219,2.03514346575437));
#45460=CARTESIAN_POINT('Ctrl Pts',(-1.90935232539742,2.23824433373559,2.0402019760891));
#45461=CARTESIAN_POINT('Ctrl Pts',(-1.93341109868383,2.21772080374012,2.04192101863427));
#45462=CARTESIAN_POINT('Ctrl Pts',(-1.95712568315988,2.19682061711989,2.04364006117944));
#45463=CARTESIAN_POINT('Ctrl Pts',(-1.9804840002322,2.17555673904963,2.0453591037246));
#45464=CARTESIAN_POINT('Ctrl Pts',(-2.04821780767799,2.11389632840008,2.05034393616715));
#45465=CARTESIAN_POINT('Ctrl Pts',(-2.11320397033815,2.04894673415118,2.0553287686097));
#45466=CARTESIAN_POINT('Ctrl Pts',(-2.17509965886792,1.98098598530951,2.06031360105224));
#45467=CARTESIAN_POINT('Ctrl Pts',(-2.23689675946619,1.91313348487431,2.06529049361511));
#45468=CARTESIAN_POINT('Ctrl Pts',(-2.29561286624946,1.84227969896945,2.07026738617798));
#45469=CARTESIAN_POINT('Ctrl Pts',(-2.35093969040451,1.76874152212265,2.07524427874085));
#45470=CARTESIAN_POINT('Ctrl Pts',(-2.4062167139959,1.69526953817076,2.08021669152274));
#45471=CARTESIAN_POINT('Ctrl Pts',(-2.45811023643264,1.6191183219238,2.08518910430462));
#45472=CARTESIAN_POINT('Ctrl Pts',(-2.5063507344052,1.540639476369,2.09016151708651));
#45473=CARTESIAN_POINT('Ctrl Pts',(-2.55456216243829,1.46220792251692,2.09513093347025));
#45474=CARTESIAN_POINT('Ctrl Pts',(-2.59912469775304,1.38145191262434,2.10010034985399));
#45475=CARTESIAN_POINT('Ctrl Pts',(-2.63981161566819,1.29875272233913,2.10506976623773));
#45476=CARTESIAN_POINT('Ctrl Pts',(-2.68048611712413,1.21607876943182,2.1100376661007));
#45477=CARTESIAN_POINT('Ctrl Pts',(-2.71728714955538,1.13146322434496,2.11500556596368));
#45478=CARTESIAN_POINT('Ctrl Pts',(-2.75003414804036,1.04531152515026,2.11997346582666));
#45479=CARTESIAN_POINT('Ctrl Pts',(-2.7827967723525,0.959118717102081,2.1249437362136));
#45480=CARTESIAN_POINT('Ctrl Pts',(-2.81150132898006,0.871388716150235,
2.12991400660054));
#45481=CARTESIAN_POINT('Ctrl Pts',(-2.8360158662163,0.782545849499835,2.13488427698748));
#45482=CARTESIAN_POINT('Ctrl Pts',(-2.86053553442199,0.693684387759097,
2.13985558766759));
#45483=CARTESIAN_POINT('Ctrl Pts',(-2.88086332994899,0.603710041624636,
2.14482689834769));
#45484=CARTESIAN_POINT('Ctrl Pts',(-2.89691807202127,0.513059142786233,
2.1497982090278));
#45485=CARTESIAN_POINT('Ctrl Pts',(-2.91299333472207,0.422292377033777,
2.15477587386914));
#45486=CARTESIAN_POINT('Ctrl Pts',(-2.92478456986051,0.330847784809518,
2.15975353871048));
#45487=CARTESIAN_POINT('Ctrl Pts',(-2.93226235225871,0.239168345577429,
2.16473120355182));
#45488=CARTESIAN_POINT('Ctrl Pts',(-2.93881858631446,0.158787314183534,
2.16909543000468));
#45489=CARTESIAN_POINT('Ctrl Pts',(-2.94205981200293,0.0782260192227659,
2.17345965645754));
#45490=CARTESIAN_POINT('Ctrl Pts',(-2.94199916389813,-0.00221802224694258,
2.1778238829104));
#45491=CARTESIAN_POINT('',(-2.94199896327432,0.00246983659489641,3.17782388291039));
#45492=CARTESIAN_POINT('Ctrl Pts',(-2.94409804542743,-0.00221960462873976,
2.1778238829104));
#45493=CARTESIAN_POINT('Ctrl Pts',(-2.94538405566721,-0.155139230593375,
2.18611406173884));
#45494=CARTESIAN_POINT('Ctrl Pts',(-2.86548296735221,-1.27410865528918,
2.24684934579097));
#45495=CARTESIAN_POINT('Ctrl Pts',(-1.43246863664449,-3.15699631612263,
2.36002973506688));
#45496=CARTESIAN_POINT('Ctrl Pts',(1.84914966771388,-2.93244645384978,2.51736505073795));
#45497=CARTESIAN_POINT('Ctrl Pts',(3.46611704321809,-0.0680333465830152,
2.67470036640911));
#45498=CARTESIAN_POINT('Ctrl Pts',(1.96279813083212,2.85762464397294,2.8320356820802));
#45499=CARTESIAN_POINT('Ctrl Pts',(-1.30748115680007,3.21077697834342,2.98937099775136));
#45500=CARTESIAN_POINT('Ctrl Pts',(-2.84098251749962,1.35199077004515,3.1046337313614));
#45501=CARTESIAN_POINT('Ctrl Pts',(-2.94470877622731,0.1939857347123,3.16745135974775));
#45502=CARTESIAN_POINT('Ctrl Pts',(-2.94300132914192,0.00247067809074119,
3.17782388291039));
#45503=CARTESIAN_POINT('',(-2.9419998880025,-0.000811784004742896,4.17782388295008));
#45504=CARTESIAN_POINT('Ctrl Pts',(-2.94199896327432,0.00246983659489641,
3.17782388291039));
#45505=CARTESIAN_POINT('Ctrl Pts',(-2.94207609672993,-0.0894093374798007,
3.18280182766136));
#45506=CARTESIAN_POINT('Ctrl Pts',(-2.93784490838638,-0.181424757288704,
3.18777977241232));
#45507=CARTESIAN_POINT('Ctrl Pts',(-2.92929377041212,-0.273133679037821,
3.19275771716329));
#45508=CARTESIAN_POINT('Ctrl Pts',(-2.92075064746702,-0.364756641504857,
3.19773099605897));
#45509=CARTESIAN_POINT('Ctrl Pts',(-2.907895662613,-0.456073223823022,3.20270427495465));
#45510=CARTESIAN_POINT('Ctrl Pts',(-2.89076924187452,-0.546641738465148,
3.20767755385033));
#45511=CARTESIAN_POINT('Ctrl Pts',(-2.87365122672512,-0.637165802388218,
3.21264839187764));
#45512=CARTESIAN_POINT('Ctrl Pts',(-2.85226602192575,-0.72694207935163,
3.21761922990495));
#45513=CARTESIAN_POINT('Ctrl Pts',(-2.82670563595407,-0.815536171892771,
3.22259006793226));
#45514=CARTESIAN_POINT('Ctrl Pts',(-2.80115020374067,-0.904113094359864,
3.22755994258092));
#45515=CARTESIAN_POINT('Ctrl Pts',(-2.77142132448528,-0.991507848683996,
3.23252981722959));
#45516=CARTESIAN_POINT('Ctrl Pts',(-2.73766131238054,-1.07729965130174,
3.23749969187825));
#45517=CARTESIAN_POINT('Ctrl Pts',(-2.70389781671987,-1.16310030642056,
3.24247007934771));
#45518=CARTESIAN_POINT('Ctrl Pts',(-2.66610253151236,-1.24729725700392,
3.24744046681717));
#45519=CARTESIAN_POINT('Ctrl Pts',(-2.62446600623389,-1.32948944415619,
3.25241085428663));
#45520=CARTESIAN_POINT('Ctrl Pts',(-2.58278806857674,-1.41176338102114,
3.25738618538591));
#45521=CARTESIAN_POINT('Ctrl Pts',(-2.53726147319968,-1.49202816704452,
3.26236151648519));
#45522=CARTESIAN_POINT('Ctrl Pts',(-2.48812260874791,-1.56990760359885,
3.26733684758447));
#45523=CARTESIAN_POINT('Ctrl Pts',(-2.43895604182231,-1.6478309453813,3.27231498357111));
#45524=CARTESIAN_POINT('Ctrl Pts',(-2.38617341628882,-1.72336588853971,
3.27729311955775));
#45525=CARTESIAN_POINT('Ctrl Pts',(-2.33005296738425,-1.79616735556124,
3.28227125554439));
#45526=CARTESIAN_POINT('Ctrl Pts',(-2.27384547617015,-1.86908173700078,
3.28725711257499));
#45527=CARTESIAN_POINT('Ctrl Pts',(-2.21429012675598,-1.93925383529866,
3.2922429696056));
#45528=CARTESIAN_POINT('Ctrl Pts',(-2.15170342491838,-2.00637393603349,
3.2972288266362));
#45529=CARTESIAN_POINT('Ctrl Pts',(-2.12319673533208,-2.03694547632034,
3.29949976078867));
#45530=CARTESIAN_POINT('Ctrl Pts',(-2.0940616444288,-2.06688439207575,3.30177069494113));
#45531=CARTESIAN_POINT('Ctrl Pts',(-2.06433029953457,-2.09616421456515,
3.3040416290936));
#45532=CARTESIAN_POINT('Ctrl Pts',(-1.99810235268668,-2.16138637435783,
3.30910024002693));
#45533=CARTESIAN_POINT('Ctrl Pts',(-1.92866513756462,-2.22358024361117,
3.31415885096025));
#45534=CARTESIAN_POINT('Ctrl Pts',(-1.85632664537554,-2.28241437641564,
3.31921746189358));
#45535=CARTESIAN_POINT('Ctrl Pts',(-1.78408593506831,-2.34116898154338,
3.32426923496671));
#45536=CARTESIAN_POINT('Ctrl Pts',(-1.70895208219965,-2.39657259833702,
3.32932100803984));
#45537=CARTESIAN_POINT('Ctrl Pts',(-1.63126976314557,-2.44833064757336,
3.33437278111297));
#45538=CARTESIAN_POINT('Ctrl Pts',(-1.54989587537742,-2.50254830921043,
3.33966462126512));
#45539=CARTESIAN_POINT('Ctrl Pts',(-1.46572565031327,-2.55276498127177,
3.34495646141728));
#45540=CARTESIAN_POINT('Ctrl Pts',(-1.37919431714492,-2.5986894842507,3.35024830156943));
#45541=CARTESIAN_POINT('Ctrl Pts',(-1.29673416140652,-2.64245330400467,
3.35529116809087));
#45542=CARTESIAN_POINT('Ctrl Pts',(-1.21213047463835,-2.68231944494002,
3.3603340346123));
#45543=CARTESIAN_POINT('Ctrl Pts',(-1.12578816507906,-2.7180811259725,3.36537690113373));
#45544=CARTESIAN_POINT('Ctrl Pts',(-1.03947456896874,-2.75383091432793,
3.37041809063157));
#45545=CARTESIAN_POINT('Ctrl Pts',(-0.951423907716638,-2.78547878548452,
3.3754592801294));
#45546=CARTESIAN_POINT('Ctrl Pts',(-0.862062377406132,-2.81286552424052,
3.38050046962724));
#45547=CARTESIAN_POINT('Ctrl Pts',(-0.772705752737703,-2.84025075955832,
3.38554138238103));
#45548=CARTESIAN_POINT('Ctrl Pts',(-0.68203882572377,-2.86337519832434,
3.39058229513482));
#45549=CARTESIAN_POINT('Ctrl Pts',(-0.590503227705854,-2.88212941036119,
3.39562320788861));
#45550=CARTESIAN_POINT('Ctrl Pts',(-0.498947239694171,-2.90088779998879,
3.40066524352991));
#45551=CARTESIAN_POINT('Ctrl Pts',(-0.406522630247812,-2.91527394084624,
3.40570727917121));
#45552=CARTESIAN_POINT('Ctrl Pts',(-0.313680384700831,-2.9252296689754,
3.41074931481251));
#45553=CARTESIAN_POINT('Ctrl Pts',(-0.220737005413307,-2.93519624195239,
3.4157968427803));
#45554=CARTESIAN_POINT('Ctrl Pts',(-0.127375523015461,-2.94072272327685,
3.42084437074808));
#45555=CARTESIAN_POINT('Ctrl Pts',(-0.0340508628673662,-2.94180294016067,
3.42589189871587));
#45556=CARTESIAN_POINT('Ctrl Pts',(0.0593331289896063,-2.94288384379882,
3.43094263567965));
#45557=CARTESIAN_POINT('Ctrl Pts',(0.152679809900273,-2.93951287148972,
3.43599337264342));
#45558=CARTESIAN_POINT('Ctrl Pts',(0.24553757471319,-2.93173588500123,3.4410441096072));
#45559=CARTESIAN_POINT('Ctrl Pts',(0.33853809684408,-2.92394694235879,3.44610261145379));
#45560=CARTESIAN_POINT('Ctrl Pts',(0.43104776463672,-2.91173852448358,3.45116111330039));
#45561=CARTESIAN_POINT('Ctrl Pts',(0.522623673943699,-2.89520785012641,
3.45621961514698));
#45562=CARTESIAN_POINT('Ctrl Pts',(0.553745348809922,-2.88958997227451,
3.45793872501956));
#45563=CARTESIAN_POINT('Ctrl Pts',(0.584759300125497,-2.88347332283188,
3.45965783489214));
#45564=CARTESIAN_POINT('Ctrl Pts',(0.615648561873941,-2.87686302215843,
3.46137694476471));
#45565=CARTESIAN_POINT('Ctrl Pts',(0.706542552901808,-2.85741171202365,
3.46643555570228));
#45566=CARTESIAN_POINT('Ctrl Pts',(0.79667193421986,-2.83361467773313,3.47149416663984));
#45567=CARTESIAN_POINT('Ctrl Pts',(0.885590508863522,-2.80554690757628,
3.47655277757741));
#45568=CARTESIAN_POINT('Ctrl Pts',(0.974388889872346,-2.77751707738114,
3.48160455065418));
#45569=CARTESIAN_POINT('Ctrl Pts',(1.06197929791018,-2.74522811605334,3.48665632373094));
#45570=CARTESIAN_POINT('Ctrl Pts',(1.14792615578853,-2.70880592528453,3.49170809680771));
#45571=CARTESIAN_POINT('Ctrl Pts',(1.23795732434584,-2.67065290285555,3.49699993695888));
#45572=CARTESIAN_POINT('Ctrl Pts',(1.32618438167442,-2.6279641773414,3.50229177711006));
#45573=CARTESIAN_POINT('Ctrl Pts',(1.4121247963118,-2.58094315312084,3.50758361726123));
#45574=CARTESIAN_POINT('Ctrl Pts',(1.49402183545367,-2.5361344018793,3.51262648378476));
#45575=CARTESIAN_POINT('Ctrl Pts',(1.57384208259694,-2.48739200595837,3.51766935030828));
#45576=CARTESIAN_POINT('Ctrl Pts',(1.65119017222557,-2.43494045412731,3.52271221683181));
#45577=CARTESIAN_POINT('Ctrl Pts',(1.72851253945697,-2.38250634525648,3.52775340633117));
#45578=CARTESIAN_POINT('Ctrl Pts',(1.80336401640768,-2.32636577968637,3.53279459583053));
#45579=CARTESIAN_POINT('Ctrl Pts',(1.87537726051578,-2.26678718249869,3.53783578532989));
#45580=CARTESIAN_POINT('Ctrl Pts',(1.94738655133499,-2.2072118559789,3.54287669808462));
#45581=CARTESIAN_POINT('Ctrl Pts',(2.01655757819793,-2.14419915586197,3.54791761083935));
#45582=CARTESIAN_POINT('Ctrl Pts',(2.08255609327364,-2.07805777551271,3.55295852359408));
#45583=CARTESIAN_POINT('Ctrl Pts',(2.1485693098279,-2.01190166186099,3.55800055923575));
#45584=CARTESIAN_POINT('Ctrl Pts',(2.211408298451,-1.94261579748505,3.56304259487742));
#45585=CARTESIAN_POINT('Ctrl Pts',(2.27077648720559,-1.87054487921414,3.5680846305191));
#45586=CARTESIAN_POINT('Ctrl Pts',(2.33020934615421,-1.79839545357478,3.57313215848637));
#45587=CARTESIAN_POINT('Ctrl Pts',(2.38616357782505,-1.72345526165858,3.57817968645365));
#45588=CARTESIAN_POINT('Ctrl Pts',(2.43838386875336,-1.64610088044548,3.58322721442093));
#45589=CARTESIAN_POINT('Ctrl Pts',(2.49063735903756,-1.56869732073135,3.58827795138368));
#45590=CARTESIAN_POINT('Ctrl Pts',(2.53915195290377,-1.48887689420251,3.59332868834643));
#45591=CARTESIAN_POINT('Ctrl Pts',(2.58371762390874,-1.40704201781731,3.59837942530919));
#45592=CARTESIAN_POINT('Ctrl Pts',(2.62835180910919,-1.32508133045268,3.60343792715401));
#45593=CARTESIAN_POINT('Ctrl Pts',(2.66902476244129,-1.24110041006272,3.60849642899883));
#45594=CARTESIAN_POINT('Ctrl Pts',(2.7055741373795,-1.15552264674613,3.61355493084364));
#45595=CARTESIAN_POINT('Ctrl Pts',(2.71799528358231,-1.12643941586566,3.61527404070771));
#45596=CARTESIAN_POINT('Ctrl Pts',(2.72994060057553,-1.09717189167846,3.61699315057177));
#45597=CARTESIAN_POINT('Ctrl Pts',(2.7414050356843,-1.06773706048107,3.61871226043584));
#45598=CARTESIAN_POINT('Ctrl Pts',(2.77514000445211,-0.981122839919069,
3.62377087143782));
#45599=CARTESIAN_POINT('Ctrl Pts',(2.80482480636004,-0.892757592239818,
3.62882948243979));
#45600=CARTESIAN_POINT('Ctrl Pts',(2.83027671647024,-0.803055233596317,
3.63388809344177));
#45601=CARTESIAN_POINT('Ctrl Pts',(2.85569422255346,-0.713474128027892,
3.63893986658409));
#45602=CARTESIAN_POINT('Ctrl Pts',(2.87689008777899,-0.62255992597192,3.6439916397264));
#45603=CARTESIAN_POINT('Ctrl Pts',(2.89372995174022,-0.530745670167476,
3.64904341286872));
#45604=CARTESIAN_POINT('Ctrl Pts',(2.91137006848068,-0.434568278559255,
3.65433525300364));
#45605=CARTESIAN_POINT('Ctrl Pts',(2.92422973198416,-0.33740362490082,3.65962709313857));
#45606=CARTESIAN_POINT('Ctrl Pts',(2.93221349554032,-0.239766587687357,
3.6649189332735));
#45607=CARTESIAN_POINT('Ctrl Pts',(2.93982163438892,-0.146723234053386,
3.66996179986491));
#45608=CARTESIAN_POINT('Ctrl Pts',(2.94300223870384,-0.053251436215734,
3.67500466645633));
#45609=CARTESIAN_POINT('Ctrl Pts',(2.94172540372301,0.040195137650254,3.68004753304774));
#45610=CARTESIAN_POINT('Ctrl Pts',(2.94044899335824,0.133610635521468,3.68508872261571));
#45611=CARTESIAN_POINT('Ctrl Pts',(2.93471809501812,0.227000483602088,3.69012991218367));
#45612=CARTESIAN_POINT('Ctrl Pts',(2.92455491072272,0.319910259553554,3.69517110175163));
#45613=CARTESIAN_POINT('Ctrl Pts',(2.91439228435121,0.412814935077624,3.70021201457561));
#45614=CARTESIAN_POINT('Ctrl Pts',(2.8997979045185,0.505239150647992,3.70525292739959));
#45615=CARTESIAN_POINT('Ctrl Pts',(2.88084580525227,0.596733982910627,3.71029384022357));
#45616=CARTESIAN_POINT('Ctrl Pts',(2.86188948431516,0.688249196085401,3.71533587593503));
#45617=CARTESIAN_POINT('Ctrl Pts',(2.83857360614135,0.778834181212185,3.72037791164649));
#45618=CARTESIAN_POINT('Ctrl Pts',(2.81102299374745,0.86805168545608,3.72541994735795));
#45619=CARTESIAN_POINT('Ctrl Pts',(2.78344237027186,0.957366374973706,3.73046747539544));
#45620=CARTESIAN_POINT('Ctrl Pts',(2.75161793717882,1.04531018701869,3.73551500343292));
#45621=CARTESIAN_POINT('Ctrl Pts',(2.71572383253706,1.13146279894224,3.74056253147041));
#45622=CARTESIAN_POINT('Ctrl Pts',(2.67980690800608,1.21767018289814,3.74561326850368));
#45623=CARTESIAN_POINT('Ctrl Pts',(2.63981535049567,1.30208369989305,3.75066400553696));
#45624=CARTESIAN_POINT('Ctrl Pts',(2.59596978338854,1.38430664367893,3.75571474257024));
#45625=CARTESIAN_POINT('Ctrl Pts',(2.55205680915813,1.46665599504657,3.7607732444855));
#45626=CARTESIAN_POINT('Ctrl Pts',(2.5042782264363,1.54680767233615,3.76583174640075));
#45627=CARTESIAN_POINT('Ctrl Pts',(2.45289839477102,1.62439326055292,3.77089024831601));
#45628=CARTESIAN_POINT('Ctrl Pts',(2.43543718865496,1.65076037588944,3.77260935757966));
#45629=CARTESIAN_POINT('Ctrl Pts',(2.41756040143675,1.67683140096625,3.77432846684332));
#45630=CARTESIAN_POINT('Ctrl Pts',(2.39927944231628,1.70259277505764,3.77604757610697));
#45631=CARTESIAN_POINT('Ctrl Pts',(2.34548631689361,1.77839759571429,3.78110618707074));
#45632=CARTESIAN_POINT('Ctrl Pts',(2.28800353010066,1.85178242755046,3.78616479803451));
#45633=CARTESIAN_POINT('Ctrl Pts',(2.22707632263131,1.92236704434273,3.79122340899828));
#45634=CARTESIAN_POINT('Ctrl Pts',(2.16623147210298,1.99285625001469,3.79627518210189));
#45635=CARTESIAN_POINT('Ctrl Pts',(2.1019517406955,2.06055243035501,3.8013269552055));
#45636=CARTESIAN_POINT('Ctrl Pts',(2.03452493941518,2.12510523760534,3.80637872830911));
#45637=CARTESIAN_POINT('Ctrl Pts',(1.96389392600361,2.19272568093168,3.81167056845365));
#45638=CARTESIAN_POINT('Ctrl Pts',(1.88980960211925,2.25689618708895,3.81696240859819));
#45639=CARTESIAN_POINT('Ctrl Pts',(1.81264952932897,2.31725391008916,3.82225424874273));
#45640=CARTESIAN_POINT('Ctrl Pts',(1.73911972880963,2.37477188760673,3.82729711529453));
#45641=CARTESIAN_POINT('Ctrl Pts',(1.6627974297708,2.42882741253796,3.83233998184632));
#45642=CARTESIAN_POINT('Ctrl Pts',(1.58404510922458,2.47914604086603,3.83738284839812));
#45643=CARTESIAN_POINT('Ctrl Pts',(1.50531897805058,2.52944793555021,3.8424240379262));
#45644=CARTESIAN_POINT('Ctrl Pts',(1.42416480392375,2.5760151645365,3.84746522745428));
#45645=CARTESIAN_POINT('Ctrl Pts',(1.34097434662436,2.61861639071006,3.85250641698236));
#45646=CARTESIAN_POINT('Ctrl Pts',(1.25778845619858,2.66121527822096,3.85754732976625));
#45647=CARTESIAN_POINT('Ctrl Pts',(1.17256689933829,2.69984839441936,3.86258824255015));
#45648=CARTESIAN_POINT('Ctrl Pts',(1.08572534462498,2.73433071811713,3.86762915533404));
#45649=CARTESIAN_POINT('Ctrl Pts',(0.998864445541836,2.76882072291671,3.87267119100526));
#45650=CARTESIAN_POINT('Ctrl Pts',(0.910383243580881,2.79915793569936,3.87771322667648));
#45651=CARTESIAN_POINT('Ctrl Pts',(0.820715587876747,2.82520617368293,3.8827552623477));
#45652=CARTESIAN_POINT('Ctrl Pts',(0.73095025654504,2.85128278620102,3.88780279034494));
#45653=CARTESIAN_POINT('Ctrl Pts',(0.639996317987379,2.87306097605417,3.89285031834218));
#45654=CARTESIAN_POINT('Ctrl Pts',(0.548300598314234,2.8904550600015,3.89789784633942));
#45655=CARTESIAN_POINT('Ctrl Pts',(0.456546582545437,2.90786020234048,3.90294858333241));
#45656=CARTESIAN_POINT('Ctrl Pts',(0.364050284881002,2.92087562833285,3.9079993203254));
#45657=CARTESIAN_POINT('Ctrl Pts',(0.271264367783776,2.92946746743685,3.91305005731839));
#45658=CARTESIAN_POINT('Ctrl Pts',(0.178335803837062,2.93807251542877,3.91810855919362));
#45659=CARTESIAN_POINT('Ctrl Pts',(0.0851171732932596,2.94224038400668,
3.92316706106885));
#45660=CARTESIAN_POINT('Ctrl Pts',(-0.00793844137284537,2.94198928977462,
3.92822556294408));
#45661=CARTESIAN_POINT('Ctrl Pts',(-0.0395629826910187,2.94190395650435,
3.92994467255541));
#45662=CARTESIAN_POINT('Ctrl Pts',(-0.0711687407238937,2.94130869726534,
3.93166378216675));
#45663=CARTESIAN_POINT('Ctrl Pts',(-0.10273811524122,2.94020558459382,3.93338289177808));
#45664=CARTESIAN_POINT('Ctrl Pts',(-0.195633404254339,2.93695959153877,
3.93844150274621));
#45665=CARTESIAN_POINT('Ctrl Pts',(-0.288536322850242,2.92930112879298,
3.94350011371434));
#45666=CARTESIAN_POINT('Ctrl Pts',(-0.380994436567301,2.91722594930608,
3.94855872468246));
#45667=CARTESIAN_POINT('Ctrl Pts',(-0.47332757217121,2.9051670921633,3.95361049779041));
#45668=CARTESIAN_POINT('Ctrl Pts',(-0.565216662209034,2.88870343982036,
3.95866227089836));
#45669=CARTESIAN_POINT('Ctrl Pts',(-0.656210818995895,2.86788273139484,
3.96371404400631));
#45670=CARTESIAN_POINT('Ctrl Pts',(-0.751529140190257,2.84607259497206,
3.96900588414976));
#45671=CARTESIAN_POINT('Ctrl Pts',(-0.845864871754567,2.81948104272493,
3.97429772429322));
#45672=CARTESIAN_POINT('Ctrl Pts',(-0.938707334299334,2.78822390430407,
3.97958956443667));
#45673=CARTESIAN_POINT('Ctrl Pts',(-1.02718169041233,2.75843736999724,3.98463243099269));
#45674=CARTESIAN_POINT('Ctrl Pts',(-1.11429963138459,2.72441447358109,3.9896752975487));
#45675=CARTESIAN_POINT('Ctrl Pts',(-1.19963260938906,2.68630705662819,3.99471816410471));
#45676=CARTESIAN_POINT('Ctrl Pts',(-1.28493720959873,2.64821231243656,3.99975935363696));
#45677=CARTESIAN_POINT('Ctrl Pts',(-1.36845762219716,2.60603592702048,4.00480054316921));
#45678=CARTESIAN_POINT('Ctrl Pts',(-1.44978520169076,2.5599779039981,4.00984173270145));
#45679=CARTESIAN_POINT('Ctrl Pts',(-1.53110831657547,2.5139224094053,4.01488264548945));
#45680=CARTESIAN_POINT('Ctrl Pts',(-1.61023845257691,2.4639859196289,4.01992355827746));
#45681=CARTESIAN_POINT('Ctrl Pts',(-1.68679250191346,2.41041387638898,4.02496447106546));
#45682=CARTESIAN_POINT('Ctrl Pts',(-1.76336360402821,2.3568298997219,4.03000650674073));
#45683=CARTESIAN_POINT('Ctrl Pts',(-1.8373571171338,2.29960901531408,4.03504854241601));
#45684=CARTESIAN_POINT('Ctrl Pts',(-1.90842072792448,2.2390387056119,4.04009057809128));
#45685=CARTESIAN_POINT('Ctrl Pts',(-1.97956174882022,2.1784024162334,4.04513810609247));
#45686=CARTESIAN_POINT('Ctrl Pts',(-2.04776616034983,2.11440970762616,4.05018563409367));
#45687=CARTESIAN_POINT('Ctrl Pts',(-2.11271669250956,2.04738667017041,4.05523316209486));
#45688=CARTESIAN_POINT('Ctrl Pts',(-2.17770851735284,1.98032102242365,4.06028389909172));
#45689=CARTESIAN_POINT('Ctrl Pts',(-2.23944205214108,1.91022154244694,4.06533463608858));
#45690=CARTESIAN_POINT('Ctrl Pts',(-2.29764009351157,1.8374476865174,4.07038537308545));
#45691=CARTESIAN_POINT('Ctrl Pts',(-2.35592760715734,1.76456194980429,4.07544387496443));
#45692=CARTESIAN_POINT('Ctrl Pts',(-2.41066852027046,1.68899398929134,4.08050237684342));
#45693=CARTESIAN_POINT('Ctrl Pts',(-2.46162890373495,1.61113225412958,4.0855608787224));
#45694=CARTESIAN_POINT('Ctrl Pts',(-2.47894756552178,1.58467128649691,4.087279988298));
#45695=CARTESIAN_POINT('Ctrl Pts',(-2.4958299886724,1.55794560555479,4.08899909787361));
#45696=CARTESIAN_POINT('Ctrl Pts',(-2.51226822610567,1.5309710513592,4.09071820744921));
#45697=CARTESIAN_POINT('Ctrl Pts',(-2.56203265636791,1.44930941783119,4.0959225676451));
#45698=CARTESIAN_POINT('Ctrl Pts',(-2.60788739691094,1.36509504662174,4.10112692784099));
#45699=CARTESIAN_POINT('Ctrl Pts',(-2.64957065136526,1.27872567950435,4.10633128803687));
#45700=CARTESIAN_POINT('Ctrl Pts',(-2.691186862575,1.19249522866591,4.11152727755254));
#45701=CARTESIAN_POINT('Ctrl Pts',(-2.72864475943488,1.10411704200888,4.11672326706821));
#45702=CARTESIAN_POINT('Ctrl Pts',(-2.76172698456252,1.01401580990595,4.12191925658388));
#45703=CARTESIAN_POINT('Ctrl Pts',(-2.79474985883382,0.924076223075112,
4.1271059242832));
#45704=CARTESIAN_POINT('Ctrl Pts',(-2.82341255694188,0.832420128498015,
4.13229259198251));
#45705=CARTESIAN_POINT('Ctrl Pts',(-2.84754514273931,0.739493515902438,
4.13747925968183));
#45706=CARTESIAN_POINT('Ctrl Pts',(-2.87165210534374,0.646665569755197,
4.14266042034644));
#45707=CARTESIAN_POINT('Ctrl Pts',(-2.89123842083447,0.552570181823066,
4.14784158101105));
#45708=CARTESIAN_POINT('Ctrl Pts',(-2.90618344854901,0.457669928419829,
4.15302274167566));
#45709=CARTESIAN_POINT('Ctrl Pts',(-2.92111279866343,0.36286922707175,4.1581984672105));
#45710=CARTESIAN_POINT('Ctrl Pts',(-2.93141049285336,0.267265743357151,
4.16337419274534));
#45711=CARTESIAN_POINT('Ctrl Pts',(-2.93700682387777,0.171332765387806,
4.16854991828018));
#45712=CARTESIAN_POINT('Ctrl Pts',(-2.94034936175837,0.114034579940489,
4.17164123982359));
#45713=CARTESIAN_POINT('Ctrl Pts',(-2.94201573484075,0.0566190577374391,
4.17473256136699));
#45714=CARTESIAN_POINT('Ctrl Pts',(-2.9419998880027,-0.000811783267522774,
4.1778238829104));
#45715=CARTESIAN_POINT('',(-2.94199963779692,-0.00145986396196984,5.17782388287747));
#45716=CARTESIAN_POINT('Ctrl Pts',(-2.9419998880025,-0.000811784004750149,
4.17782388295008));
#45717=CARTESIAN_POINT('Ctrl Pts',(-2.94197217039502,-0.10126362543284,
4.18323088963934));
#45718=CARTESIAN_POINT('Ctrl Pts',(-2.9367954789962,-0.20157521002038,4.1886378963286));
#45719=CARTESIAN_POINT('Ctrl Pts',(-2.92653799146242,-0.301229786918777,
4.19404490301786));
#45720=CARTESIAN_POINT('Ctrl Pts',(-2.91624122272408,-0.401265992535323,
4.19947261592148));
#45721=CARTESIAN_POINT('Ctrl Pts',(-2.90082476492119,-0.500639823046012,
4.20490032882511));
#45722=CARTESIAN_POINT('Ctrl Pts',(-2.88040829698104,-0.598842251918488,
4.21032804172873));
#45723=CARTESIAN_POINT('Ctrl Pts',(-2.85995051621559,-0.697243393898416,
4.21576673763664));
#45724=CARTESIAN_POINT('Ctrl Pts',(-2.83447260958186,-0.794468079685589,
4.22120543354456));
#45725=CARTESIAN_POINT('Ctrl Pts',(-2.80414401228342,-0.890022672955613,
4.22664412945247));
#45726=CARTESIAN_POINT('Ctrl Pts',(-2.77372602620075,-0.985858898403873,
4.23209885506364));
#45727=CARTESIAN_POINT('Ctrl Pts',(-2.73842887446513,-1.08001487435536,
4.23755358067482));
#45728=CARTESIAN_POINT('Ctrl Pts',(-2.69847051350961,-1.1720157369759,4.24300830628599));
#45729=CARTESIAN_POINT('Ctrl Pts',(-2.68615100624589,-1.20038039629173,
4.24469004523077));
#45730=CARTESIAN_POINT('Ctrl Pts',(-2.67338875796325,-1.22854038584006,
4.24637178417555));
#45731=CARTESIAN_POINT('Ctrl Pts',(-2.66019101498198,-1.25648229745156,
4.24805352312033));
#45732=CARTESIAN_POINT('Ctrl Pts',(-2.62049267319382,-1.34053057441395,
4.25311213409063));
#45733=CARTESIAN_POINT('Ctrl Pts',(-2.57673813346106,-1.42284184093946,
4.25817074506094));
#45734=CARTESIAN_POINT('Ctrl Pts',(-2.52910231826078,-1.5029988236083,4.26322935603124));
#45735=CARTESIAN_POINT('Ctrl Pts',(-2.4815308936694,-1.58304745593404,4.26828112914144));
#45736=CARTESIAN_POINT('Ctrl Pts',(-2.43008884431785,-1.66094721385083,
4.27333290225164));
#45737=CARTESIAN_POINT('Ctrl Pts',(-2.37499823449402,-1.73630279218524,
4.27838467536184));
#45738=CARTESIAN_POINT('Ctrl Pts',(-2.31728964501402,-1.81523936865509,
4.28367651550474));
#45739=CARTESIAN_POINT('Ctrl Pts',(-2.25557733499436,-1.89138351938762,
4.28896835564764));
#45740=CARTESIAN_POINT('Ctrl Pts',(-2.19016954749073,-1.96431192870284,
4.29426019579054));
#45741=CARTESIAN_POINT('Ctrl Pts',(-2.12783910375923,-2.03380915964032,
4.29930306234897));
#45742=CARTESIAN_POINT('Ctrl Pts',(-2.06215336565251,-2.10038600949863,
4.30434592890741));
#45743=CARTESIAN_POINT('Ctrl Pts',(-1.99342119354542,-2.16370884019176,
4.30938879546584));
#45744=CARTESIAN_POINT('Ctrl Pts',(-1.92471187857332,-2.22701061264614,
4.31442998500057));
#45745=CARTESIAN_POINT('Ctrl Pts',(-1.85295846800584,-2.2870602161998,4.3194711745353));
#45746=CARTESIAN_POINT('Ctrl Pts',(-1.77850619629435,-2.34356133048457,
4.32451236407003));
#45747=CARTESIAN_POINT('Ctrl Pts',(-1.70405801175985,-2.40005934304996,
4.32955327686057));
#45748=CARTESIAN_POINT('Ctrl Pts',(-1.62691161381304,-2.45300898635414,
4.33459418965111));
#45749=CARTESIAN_POINT('Ctrl Pts',(-1.54744388146588,-2.50215535762946,
4.33963510244165));
#45750=CARTESIAN_POINT('Ctrl Pts',(-1.46795844730319,-2.55131267649284,
4.3446771381195));
#45751=CARTESIAN_POINT('Ctrl Pts',(-1.38615102853373,-2.59666480803702,
4.34971917379735));
#45752=CARTESIAN_POINT('Ctrl Pts',(-1.30242495026298,-2.63800175301922,
4.35476120947519));
#45753=CARTESIAN_POINT('Ctrl Pts',(-1.21860766856898,-2.67938372663487,
4.35980873747901));
#45754=CARTESIAN_POINT('Ctrl Pts',(-1.1328679538705,-2.71674158842498,4.36485626548283));
#45755=CARTESIAN_POINT('Ctrl Pts',(-1.0456307447518,-2.74991278873163,4.36990379348665));
#45756=CARTESIAN_POINT('Ctrl Pts',(-0.958338074062372,-2.78310507782472,
4.37495453048619));
#45757=CARTESIAN_POINT('Ctrl Pts',(-0.869546434149082,-2.81210526918745,
4.38000526748574));
#45758=CARTESIAN_POINT('Ctrl Pts',(-0.779695576409692,-2.83680080515484,
4.38505600448528));
#45759=CARTESIAN_POINT('Ctrl Pts',(-0.689706584112763,-2.86153430744798,
4.39011450636697));
#45760=CARTESIAN_POINT('Ctrl Pts',(-0.598655555219479,-2.8819498497887,
4.39517300824865));
#45761=CARTESIAN_POINT('Ctrl Pts',(-0.506991769194499,-2.89798608450231,
4.40023151013034));
#45762=CARTESIAN_POINT('Ctrl Pts',(-0.4758402358018,-2.90343592814109,4.40195061968405));
#45763=CARTESIAN_POINT('Ctrl Pts',(-0.44461796584669,-2.90838042674006,
4.40366972923775));
#45764=CARTESIAN_POINT('Ctrl Pts',(-0.413342650666822,-2.91281854105945,
4.40538883879146));
#45765=CARTESIAN_POINT('Ctrl Pts',(-0.321312650505731,-2.92587803092167,
4.41044744976291));
#45766=CARTESIAN_POINT('Ctrl Pts',(-0.228503016871154,-2.93459446671002,
4.41550606073436));
#45767=CARTESIAN_POINT('Ctrl Pts',(-0.135358460381505,-2.93888449708442,
4.42056467170581));
#45768=CARTESIAN_POINT('Ctrl Pts',(-0.0423398098866227,-2.94316872850973,
4.42561644481716));
#45769=CARTESIAN_POINT('Ctrl Pts',(0.0510124249545995,-2.94303842499226,
4.43066821792851));
#45770=CARTESIAN_POINT('Ctrl Pts',(0.144245959569578,-2.93846168992346,
4.43571999103986));
#45771=CARTESIAN_POINT('Ctrl Pts',(0.241910076749521,-2.93366746226807,
4.44101183118247));
#45772=CARTESIAN_POINT('Ctrl Pts',(0.339443446913503,-2.92399365216437,
4.44630367132509));
#45773=CARTESIAN_POINT('Ctrl Pts',(0.436323001411083,-2.90946494023207,
4.4515955114677));
#45774=CARTESIAN_POINT('Ctrl Pts',(0.528644510095479,-2.89561978361686,
4.45663837802728));
#45775=CARTESIAN_POINT('Ctrl Pts',(0.620371837137919,-2.87736627422707,
4.46168124458686));
#45776=CARTESIAN_POINT('Ctrl Pts',(0.711056476639062,-2.85477892086754,
4.46672411114644));
#45777=CARTESIAN_POINT('Ctrl Pts',(0.801710958631962,-2.83219907901491,
4.47176530068231));
#45778=CARTESIAN_POINT('Ctrl Pts',(0.891323012636902,-2.80528836375621,
4.47680649021819));
#45779=CARTESIAN_POINT('Ctrl Pts',(0.979455300315797,-2.77417218547863,
4.48184767975407));
#45780=CARTESIAN_POINT('Ctrl Pts',(1.06758274983116,-2.74305771537365,4.48688859254574));
#45781=CARTESIAN_POINT('Ctrl Pts',(1.15423017707609,-2.70773838925117,4.49192950533742));
#45782=CARTESIAN_POINT('Ctrl Pts',(1.238977436356,-2.66838882327908,4.4969704181291));
#45783=CARTESIAN_POINT('Ctrl Pts',(1.32374357349118,-2.62903049200392,4.50201245380809));
#45784=CARTESIAN_POINT('Ctrl Pts',(1.40660830047679,-2.58564032460755,4.50705448948708));
#45785=CARTESIAN_POINT('Ctrl Pts',(1.48717443441246,-2.53843971794289,4.51209652516606));
#45786=CARTESIAN_POINT('Ctrl Pts',(1.56782832962084,-2.49118769531582,4.51714405317101));
#45787=CARTESIAN_POINT('Ctrl Pts',(1.64617825205445,-2.44011717375445,4.52219158117595));
#45788=CARTESIAN_POINT('Ctrl Pts',(1.72185476556907,-2.38549369445553,4.52723910918089));
#45789=CARTESIAN_POINT('Ctrl Pts',(1.79757939087379,-2.33083548795726,4.53228984618155));
#45790=CARTESIAN_POINT('Ctrl Pts',(1.87062687767098,-2.2726201025847,4.53734058318221));
#45791=CARTESIAN_POINT('Ctrl Pts',(1.94066139969039,-2.2111529417369,4.54239132018287));
#45792=CARTESIAN_POINT('Ctrl Pts',(2.01080359110695,-2.14959128274786,4.54744982206565));
#45793=CARTESIAN_POINT('Ctrl Pts',(2.07792325526939,-2.08476817792938,4.55250832394844));
#45794=CARTESIAN_POINT('Ctrl Pts',(2.14172209911554,-2.01702514861867,4.55756682583122));
#45795=CARTESIAN_POINT('Ctrl Pts',(2.16340385467871,-1.99400297902942,4.55928593537501));
#45796=CARTESIAN_POINT('Ctrl Pts',(2.18470242359527,-1.97064384466696,4.56100504491879));
#45797=CARTESIAN_POINT('Ctrl Pts',(2.20560720960889,-1.94696195055817,4.56272415446258));
#45798=CARTESIAN_POINT('Ctrl Pts',(2.26712113714525,-1.87727617060409,4.56778276543495));
#45799=CARTESIAN_POINT('Ctrl Pts',(2.32543628793261,-1.80455101993097,4.57284137640732));
#45800=CARTESIAN_POINT('Ctrl Pts',(2.38023850294436,-1.72911210426079,4.57789998737968));
#45801=CARTESIAN_POINT('Ctrl Pts',(2.43496664033275,-1.65377516139557,4.58295176049197));
#45802=CARTESIAN_POINT('Ctrl Pts',(2.48619102059477,-1.57573209892987,4.58800353360426));
#45803=CARTESIAN_POINT('Ctrl Pts',(2.53363629687119,-1.4953431429531,4.59305530671655));
#45804=CARTESIAN_POINT('Ctrl Pts',(2.58333623627569,-1.41113399602856,4.59834714685893));
#45805=CARTESIAN_POINT('Ctrl Pts',(2.62888866287606,-1.32435083333337,4.60363898700131));
#45806=CARTESIAN_POINT('Ctrl Pts',(2.67002656204015,-1.23544411366927,4.60893082714369));
#45807=CARTESIAN_POINT('Ctrl Pts',(2.70922898132806,-1.15072032921247,4.61397369370425));
#45808=CARTESIAN_POINT('Ctrl Pts',(2.74442264027815,-1.06406873081819,4.61901656026481));
#45809=CARTESIAN_POINT('Ctrl Pts',(2.77542314380754,-0.975904899474069,
4.62405942682536));
#45810=CARTESIAN_POINT('Ctrl Pts',(2.80641333800627,-0.887770387333999,
4.62910061636223));
#45811=CARTESIAN_POINT('Ctrl Pts',(2.83321300063944,-0.79812505893049,4.6341418058991));
#45812=CARTESIAN_POINT('Ctrl Pts',(2.85568639250246,-0.707403157807695,
4.63918299543597));
#45813=CARTESIAN_POINT('Ctrl Pts',(2.87815855065257,-0.616686237009219,
4.64422390822865));
#45814=CARTESIAN_POINT('Ctrl Pts',(2.89630480428302,-0.52489329104853,4.64926482102133));
#45815=CARTESIAN_POINT('Ctrl Pts',(2.91003996678476,-0.432471261143845,
4.65430573381401));
#45816=CARTESIAN_POINT('Ctrl Pts',(2.92377818885934,-0.340028643792029,
4.65934776949402));
#45817=CARTESIAN_POINT('Ctrl Pts',(2.93310330347559,-0.246957102247369,
4.66438980517402));
#45818=CARTESIAN_POINT('Ctrl Pts',(2.937981824019,-0.153710122418809,4.66943184085402));
#45819=CARTESIAN_POINT('Ctrl Pts',(2.94286565877014,-0.0603615679801721,
4.67447936885999));
#45820=CARTESIAN_POINT('Ctrl Pts',(2.94329320945978,0.0331623632958987,
4.67952689686595));
#45821=CARTESIAN_POINT('Ctrl Pts',(2.93928311813365,0.126407086251162,4.68457442487192));
#45822=CARTESIAN_POINT('Ctrl Pts',(2.93527047736829,0.219711090089497,4.68962516187361));
#45823=CARTESIAN_POINT('Ctrl Pts',(2.92681461807625,0.312735091659688,4.6946758988753));
#45824=CARTESIAN_POINT('Ctrl Pts',(2.91398595840712,0.405030658353332,4.69972663587699));
#45825=CARTESIAN_POINT('Ctrl Pts',(2.9011375762638,0.497468118041193,4.70478513776081));
#45826=CARTESIAN_POINT('Ctrl Pts',(2.88390305840322,0.589174473506708,4.70984363964463));
#45827=CARTESIAN_POINT('Ctrl Pts',(2.86240362911597,0.679712780535806,4.71490214152845));
#45828=CARTESIAN_POINT('Ctrl Pts',(2.85509714297926,0.710481824509529,4.71662125106353));
#45829=CARTESIAN_POINT('Ctrl Pts',(2.84729850129208,0.741116108795763,4.71834036059862));
#45830=CARTESIAN_POINT('Ctrl Pts',(2.83901374189667,0.771598971825321,4.72005947013371));
#45831=CARTESIAN_POINT('Ctrl Pts',(2.81463520526548,0.861297122069784,4.72511808110523));
#45832=CARTESIAN_POINT('Ctrl Pts',(2.78595910130138,0.949994841375823,4.73017669207676));
#45833=CARTESIAN_POINT('Ctrl Pts',(2.75308463646161,1.03725068545604,4.73523530304829));
#45834=CARTESIAN_POINT('Ctrl Pts',(2.72025460891749,1.12438858347209,4.74028707615972));
#45835=CARTESIAN_POINT('Ctrl Pts',(2.683237653453,1.21008806851943,4.74533884927116));
#45836=CARTESIAN_POINT('Ctrl Pts',(2.64218323512074,1.29392107643663,4.75039062238259));
#45837=CARTESIAN_POINT('Ctrl Pts',(2.59917785578772,1.38173794128485,4.75568246252518));
#45838=CARTESIAN_POINT('Ctrl Pts',(2.55174189366301,1.46750606120558,4.76097430266778));
#45839=CARTESIAN_POINT('Ctrl Pts',(2.50010476144967,1.55075471360776,4.76626614281037));
#45840=CARTESIAN_POINT('Ctrl Pts',(2.4508970831639,1.63008663483463,4.77130900937005));
#45841=CARTESIAN_POINT('Ctrl Pts',(2.39787485317142,1.70713036435466,4.77635187592973));
#45842=CARTESIAN_POINT('Ctrl Pts',(2.34128378431755,1.78150336550109,4.78139474248941));
#45843=CARTESIAN_POINT('Ctrl Pts',(2.28471153503033,1.85585163363432,4.7864359320254));
#45844=CARTESIAN_POINT('Ctrl Pts',(2.22457307297802,1.92753058592167,4.79147712156138));
#45845=CARTESIAN_POINT('Ctrl Pts',(2.16115645395047,1.99618806267051,4.79651831109737));
#45846=CARTESIAN_POINT('Ctrl Pts',(2.09774331628004,2.06484177035692,4.80155922388916));
#45847=CARTESIAN_POINT('Ctrl Pts',(2.03105268037183,2.13047400731676,4.80660013668095));
#45848=CARTESIAN_POINT('Ctrl Pts',(1.96141100583973,2.19276785505689,4.81164104947274));
#45849=CARTESIAN_POINT('Ctrl Pts',(1.89175381829319,2.25507557904807,4.81668308515185));
#45850=CARTESIAN_POINT('Ctrl Pts',(1.81914461679895,2.31404314185766,4.82172512083095));
#45851=CARTESIAN_POINT('Ctrl Pts',(1.74394375652461,2.36939320799204,4.82676715651006));
#45852=CARTESIAN_POINT('Ctrl Pts',(1.66866097940884,2.42480356735412,4.83181468451513));
#45853=CARTESIAN_POINT('Ctrl Pts',(1.59078126643307,2.47658830279768,4.83686221252019));
#45854=CARTESIAN_POINT('Ctrl Pts',(1.51069455579244,2.52451301424633,4.84190974052526));
#45855=CARTESIAN_POINT('Ctrl Pts',(1.43055692955278,2.57246819411318,4.84696047752605));
#45856=CARTESIAN_POINT('Ctrl Pts',(1.348209902331,2.61655825568513,4.85201121452685));
#45857=CARTESIAN_POINT('Ctrl Pts',(1.26406674449931,2.65659542750697,4.85706195152764));
#45858=CARTESIAN_POINT('Ctrl Pts',(1.17979422699146,2.69669415151812,4.86212045341056));
#45859=CARTESIAN_POINT('Ctrl Pts',(1.09372047547981,2.73272737974587,4.86717895529349));
#45860=CARTESIAN_POINT('Ctrl Pts',(1.00627710243888,2.764556093319,4.87223745717641));
#45861=CARTESIAN_POINT('Ctrl Pts',(0.976559857980167,2.7753729411734,4.87395656671921));
#45862=CARTESIAN_POINT('Ctrl Pts',(0.946684539921142,2.7857046189537,4.87567567626202));
#45863=CARTESIAN_POINT('Ctrl Pts',(0.916668384784554,2.7955470077136,4.87739478580483));
#45864=CARTESIAN_POINT('Ctrl Pts',(0.82834355851648,2.82450898746502,4.88245339677659));
#45865=CARTESIAN_POINT('Ctrl Pts',(0.738491153007888,2.84933134782435,4.88751200774835));
#45866=CARTESIAN_POINT('Ctrl Pts',(0.647534432040966,2.86985420523785,4.89257061872011));
#45867=CARTESIAN_POINT('Ctrl Pts',(0.556700659712732,2.89034932135467,4.89762239183178));
#45868=CARTESIAN_POINT('Ctrl Pts',(0.464765966952342,2.90655638762517,4.90267416494344));
#45869=CARTESIAN_POINT('Ctrl Pts',(0.37217007850815,2.91836485598755,4.90772593805511));
#45870=CARTESIAN_POINT('Ctrl Pts',(0.275173909307494,2.93073447859739,4.91301777819765));
#45871=CARTESIAN_POINT('Ctrl Pts',(0.177452609881884,2.93827692751991,4.91830961834018));
#45872=CARTESIAN_POINT('Ctrl Pts',(0.0795254971590513,2.94092497274269,
4.92360145848272));
#45873=CARTESIAN_POINT('Ctrl Pts',(-0.0137942836275936,2.9434484311888,
4.92864432504264));
#45874=CARTESIAN_POINT('Ctrl Pts',(-0.107300451681992,2.94152758026219,
4.93368719160255));
#45875=CARTESIAN_POINT('Ctrl Pts',(-0.200538383141079,2.93515729678788,
4.93873005816247));
#45876=CARTESIAN_POINT('Ctrl Pts',(-0.293745307985457,2.92878913177462,
4.94377124769869));
#45877=CARTESIAN_POINT('Ctrl Pts',(-0.386683731975325,2.91797450436237,
4.94881243723492));
#45878=CARTESIAN_POINT('Ctrl Pts',(-0.478901119425166,2.90276036176143,
4.95385362677114));
#45879=CARTESIAN_POINT('Ctrl Pts',(-0.57111344445348,2.88754705436527,4.95889453956317));
#45880=CARTESIAN_POINT('Ctrl Pts',(-0.66260437472947,2.86793478462953,4.9639354523552));
#45881=CARTESIAN_POINT('Ctrl Pts',(-0.752929691607653,2.84402195481955,
4.96897636514722));
#45882=CARTESIAN_POINT('Ctrl Pts',(-0.843275128880084,2.82010379831291,
4.97401840082657));
#45883=CARTESIAN_POINT('Ctrl Pts',(-0.932454009061602,2.79188329272425,
4.97906043650592));
#45884=CARTESIAN_POINT('Ctrl Pts',(-1.02003653602754,2.75950891739254,4.98410247218527));
#45885=CARTESIAN_POINT('Ctrl Pts',(-1.10771446727399,2.72709927641946,4.98915000019057));
#45886=CARTESIAN_POINT('Ctrl Pts',(-1.19379215891537,2.69052688901294,4.99419752819588));
#45887=CARTESIAN_POINT('Ctrl Pts',(-1.27785940882091,2.64998855304846,4.99924505620118));
#45888=CARTESIAN_POINT('Ctrl Pts',(-1.36198010497682,2.6094244445976,5.00429579320221));
#45889=CARTESIAN_POINT('Ctrl Pts',(-1.44408742599362,2.5648895789537,5.00934653020324));
#45890=CARTESIAN_POINT('Ctrl Pts',(-1.52379728570548,2.51662588242206,5.01439726720427));
#45891=CARTESIAN_POINT('Ctrl Pts',(-1.603629689447,2.46828798643905,5.01945576908742));
#45892=CARTESIAN_POINT('Ctrl Pts',(-1.6810569091271,2.41621006511714,5.02451427097058));
#45893=CARTESIAN_POINT('Ctrl Pts',(-1.75572549254014,2.36067617322764,5.02957277285373));
#45894=CARTESIAN_POINT('Ctrl Pts',(-1.78110128108464,2.34180322515193,5.03129188239447));
#45895=CARTESIAN_POINT('Ctrl Pts',(-1.80615875942737,2.32253145897469,5.03301099193521));
#45896=CARTESIAN_POINT('Ctrl Pts',(-1.83088500911839,2.30287300635219,5.03473010147595));
#45897=CARTESIAN_POINT('Ctrl Pts',(-1.90280242283027,2.24569550924469,5.03973020919962));
#45898=CARTESIAN_POINT('Ctrl Pts',(-1.97217831547442,2.18503475459089,5.04473031692329));
#45899=CARTESIAN_POINT('Ctrl Pts',(-2.03865087933601,2.12114747063529,5.04973042464695));
#45900=CARTESIAN_POINT('Ctrl Pts',(-2.10503315455134,2.05734696378061,5.05472374080232));
#45901=CARTESIAN_POINT('Ctrl Pts',(-2.16851960902195,1.99032894428582,5.05971705695769));
#45902=CARTESIAN_POINT('Ctrl Pts',(-2.22878016815274,1.92039135648155,5.06471037311306));
#45903=CARTESIAN_POINT('Ctrl Pts',(-2.28897401414869,1.85053119503695,5.06969816127833));
#45904=CARTESIAN_POINT('Ctrl Pts',(-2.34594876853345,1.777758232264,5.0746859494436));
#45905=CARTESIAN_POINT('Ctrl Pts',(-2.39941098219119,1.70240739499695,5.07967373760888));
#45906=CARTESIAN_POINT('Ctrl Pts',(-2.45284117464076,1.62710168913545,5.084658538337));
#45907=CARTESIAN_POINT('Ctrl Pts',(-2.50276274098691,1.54922154370341,5.08964333906513));
#45908=CARTESIAN_POINT('Ctrl Pts',(-2.54892297361249,1.46913432830032,5.09462813979326));
#45909=CARTESIAN_POINT('Ctrl Pts',(-2.59506912288116,1.38907154728101,5.09961141967272));
#45910=CARTESIAN_POINT('Ctrl Pts',(-2.63745599128222,1.30680342723575,5.10459469955219));
#45911=CARTESIAN_POINT('Ctrl Pts',(-2.67587531393081,1.22272454146291,5.10957797943166));
#45912=CARTESIAN_POINT('Ctrl Pts',(-2.71429420418152,1.13864660197256,5.11456120322581));
#45913=CARTESIAN_POINT('Ctrl Pts',(-2.74874545046826,1.05275835133024,5.11954442701997));
#45914=CARTESIAN_POINT('Ctrl Pts',(-2.77906824043815,0.965475900780554,
5.12452765081413));
#45915=CARTESIAN_POINT('Ctrl Pts',(-2.80941650208858,0.878120131426771,
5.12951506060451));
#45916=CARTESIAN_POINT('Ctrl Pts',(-2.83562923411632,0.789368253785789,
5.1345024703949));
#45917=CARTESIAN_POINT('Ctrl Pts',(-2.85759517427401,0.699652642363268,
5.13948988018529));
#45918=CARTESIAN_POINT('Ctrl Pts',(-2.87957120535488,0.609895816527108,
5.14447958113958));
#45919=CARTESIAN_POINT('Ctrl Pts',(-2.89729647349492,0.519174821433264,
5.14946928209386));
#45920=CARTESIAN_POINT('Ctrl Pts',(-2.91071106298119,0.427931195215936,
5.15445898304815));
#45921=CARTESIAN_POINT('Ctrl Pts',(-2.924145156996,0.336554902701618,5.15945593892178));
#45922=CARTESIAN_POINT('Ctrl Pts',(-2.9332560154029,0.244654913917933,5.16445289479541));
#45923=CARTESIAN_POINT('Ctrl Pts',(-2.93803572033691,0.152676475019436,
5.16944985066904));
#45924=CARTESIAN_POINT('Ctrl Pts',(-2.94070570609601,0.101296499604001,
5.17224119473852));
#45925=CARTESIAN_POINT('Ctrl Pts',(-2.94202511937368,0.0498920369940975,
5.17503253880799));
#45926=CARTESIAN_POINT('Ctrl Pts',(-2.94199963779692,-0.00145986396196948,
5.17782388287747));
#45927=CARTESIAN_POINT('',(-2.94199890533048,0.00253791927304355,6.17782385433891));
#45928=CARTESIAN_POINT('Ctrl Pts',(-2.94199963779662,-0.00145986456779249,
5.1778238829104));
#45929=CARTESIAN_POINT('Ctrl Pts',(-2.9419563018159,-0.0887929243620846,
5.18257106098929));
#45930=CARTESIAN_POINT('Ctrl Pts',(-2.93802453262175,-0.176025039555883,
5.18731823906819));
#45931=CARTESIAN_POINT('Ctrl Pts',(-2.93022946613174,-0.262905450330198,
5.19206541714709));
#45932=CARTESIAN_POINT('Ctrl Pts',(-2.92192301370534,-0.355485545677367,
5.19712402811885));
#45933=CARTESIAN_POINT('Ctrl Pts',(-2.90921023997664,-0.447832661136409,
5.20218263909061));
#45934=CARTESIAN_POINT('Ctrl Pts',(-2.89211157404499,-0.539494803751654,
5.20724125006237));
#45935=CARTESIAN_POINT('Ctrl Pts',(-2.87503602083856,-0.631033044190861,
5.21229302317404));
#45936=CARTESIAN_POINT('Ctrl Pts',(-2.85358643783142,-0.721887720013586,
5.2173447962857));
#45937=CARTESIAN_POINT('Ctrl Pts',(-2.82783507861033,-0.811611217382376,
5.22239656939736));
#45938=CARTESIAN_POINT('Ctrl Pts',(-2.80085998027575,-0.905598495633074,
5.2276884095399));
#45939=CARTESIAN_POINT('Ctrl Pts',(-2.76916415693882,-0.998343930454374,
5.23298024968244));
#45940=CARTESIAN_POINT('Ctrl Pts',(-2.73289111167492,-1.08934391802048,
5.23827208982498));
#45941=CARTESIAN_POINT('Ctrl Pts',(-2.69832466180862,-1.17606248507637,
5.24331495638489));
#45942=CARTESIAN_POINT('Ctrl Pts',(-2.65960211330447,-1.26119565939655,
5.2483578229448));
#45943=CARTESIAN_POINT('Ctrl Pts',(-2.61689844920908,-1.34432381014661,
5.25340068950471));
#45944=CARTESIAN_POINT('Ctrl Pts',(-2.57420898637316,-1.42742431632652,
5.25844187904093));
#45945=CARTESIAN_POINT('Ctrl Pts',(-2.52754124069688,-1.50852073013917,
5.26348306857715));
#45946=CARTESIAN_POINT('Ctrl Pts',(-2.47711720041013,-1.58721591960019,
5.26852425811337));
#45947=CARTESIAN_POINT('Ctrl Pts',(-2.42669592823206,-1.66590678896239,
5.27356517090539));
#45948=CARTESIAN_POINT('Ctrl Pts',(-2.37251901085926,-1.74219632344063,
5.27860608369741));
#45949=CARTESIAN_POINT('Ctrl Pts',(-2.31485241453424,-1.81571536836725,
5.28364699648943));
#45950=CARTESIAN_POINT('Ctrl Pts',(-2.25717297270046,-1.88925079001099,
5.28868903216876));
#45951=CARTESIAN_POINT('Ctrl Pts',(-2.19600258157004,-1.96001414814933,
5.29373106784809));
#45952=CARTESIAN_POINT('Ctrl Pts',(-2.13164750644185,-2.02766932912649,
5.29877310352742));
#45953=CARTESIAN_POINT('Ctrl Pts',(-2.06722232886441,-2.09539820738208,
5.30382063153272));
#45954=CARTESIAN_POINT('Ctrl Pts',(-1.99960584947404,-2.16001183004599,
5.30886815953802));
#45955=CARTESIAN_POINT('Ctrl Pts',(-1.92914097326535,-2.22121117980007,
5.31391568754332));
#45956=CARTESIAN_POINT('Ctrl Pts',(-1.85863129859563,-2.28244943740203,
5.31896642454435));
#45957=CARTESIAN_POINT('Ctrl Pts',(-1.78526996943886,-2.34026882694231,
5.32401716154537));
#45958=CARTESIAN_POINT('Ctrl Pts',(-1.70943102234009,-2.39441215747443,
5.3290678985464));
#45959=CARTESIAN_POINT('Ctrl Pts',(-1.63347548226001,-2.44863872666643,
5.33412640042955));
#45960=CARTESIAN_POINT('Ctrl Pts',(-1.55503509370221,-2.49917771834094,
5.3391849023127));
#45961=CARTESIAN_POINT('Ctrl Pts',(-1.47451048334426,-2.54581673230967,
5.34424340419586));
#45962=CARTESIAN_POINT('Ctrl Pts',(-1.44714454988593,-2.56166679537929,
5.34596251373663));
#45963=CARTESIAN_POINT('Ctrl Pts',(-1.41953808366408,-2.5770668348358,5.3476816232774));
#45964=CARTESIAN_POINT('Ctrl Pts',(-1.39170733449789,-2.59200977912985,
5.34940073281817));
#45965=CARTESIAN_POINT('Ctrl Pts',(-1.30981323191402,-2.63598053268787,
5.35445934378994));
#45966=CARTESIAN_POINT('Ctrl Pts',(-1.22569074274824,-2.67614284295641,
5.35951795476172));
#45967=CARTESIAN_POINT('Ctrl Pts',(-1.13972862276579,-2.71226522789502,
5.36457656573349));
#45968=CARTESIAN_POINT('Ctrl Pts',(-1.05388270008591,-2.74833878523732,
5.36962833884518));
#45969=CARTESIAN_POINT('Ctrl Pts',(-0.966202493368399,-2.78038309955491,
5.37468011195686));
#45970=CARTESIAN_POINT('Ctrl Pts',(-0.877101598400064,-2.80821238265272,
5.37973188506854));
#45971=CARTESIAN_POINT('Ctrl Pts',(-0.783766509451114,-2.83736415059222,
5.38502372521107));
#45972=CARTESIAN_POINT('Ctrl Pts',(-0.688872789287524,-2.86189011174939,
5.39031556535361));
#45973=CARTESIAN_POINT('Ctrl Pts',(-0.592919977901535,-2.88163320008034,
5.39560740549614));
#45974=CARTESIAN_POINT('Ctrl Pts',(-0.501481610370096,-2.90044740407222,
5.40065027205608));
#45975=CARTESIAN_POINT('Ctrl Pts',(-0.409082038246236,-2.91491848571425,
5.40569313861601));
#45976=CARTESIAN_POINT('Ctrl Pts',(-0.316167974458782,-2.92496184794377,
5.41073600517595));
#45977=CARTESIAN_POINT('Ctrl Pts',(-0.223284809582627,-2.93500187021649,
5.4157771947122));
#45978=CARTESIAN_POINT('Ctrl Pts',(-0.129887932960033,-2.94061705115688,
5.42081838424845));
#45979=CARTESIAN_POINT('Ctrl Pts',(-0.0364311131634972,-2.94177442608941,
5.42585957378469));
#45980=CARTESIAN_POINT('Ctrl Pts',(0.0570205761708374,-2.94293173748598,
5.43090048657674));
#45981=CARTESIAN_POINT('Ctrl Pts',(0.150531759252712,-2.93963172451159,
5.43594139936879));
#45982=CARTESIAN_POINT('Ctrl Pts',(0.243647852296875,-2.93189353900702,
5.44098231216084));
#45983=CARTESIAN_POINT('Ctrl Pts',(0.336784687393946,-2.9241536297848,5.44602434784021));
#45984=CARTESIAN_POINT('Ctrl Pts',(0.429525816372355,-2.91197362149412,
5.45106638351958));
#45985=CARTESIAN_POINT('Ctrl Pts',(0.521422092640471,-2.895424494147,5.45610841919894));
#45986=CARTESIAN_POINT('Ctrl Pts',(0.613418472187497,-2.87885733971568,
5.46115594720427));
#45987=CARTESIAN_POINT('Ctrl Pts',(0.704567725897267,-2.85791164643231,
5.4662034752096));
#45988=CARTESIAN_POINT('Ctrl Pts',(0.794431543773405,-2.83270939601255,
5.47125100321493));
#45989=CARTESIAN_POINT('Ctrl Pts',(0.884352493102186,-2.80749112311333,
5.47630174021598));
#45990=CARTESIAN_POINT('Ctrl Pts',(0.972985959899025,-2.77801104533038,
5.48135247721703));
#45991=CARTESIAN_POINT('Ctrl Pts',(1.05991145033037,-2.7444401464522,5.48640321421808));
#45992=CARTESIAN_POINT('Ctrl Pts',(1.14697057792937,-2.7108176364779,5.49146171610126));
#45993=CARTESIAN_POINT('Ctrl Pts',(1.23231608443701,-2.67309193230147,5.49652021798444));
#45994=CARTESIAN_POINT('Ctrl Pts',(1.31555026542164,-2.63148085669439,5.50157871986762));
#45995=CARTESIAN_POINT('Ctrl Pts',(1.34383703449613,-2.61733951628935,5.5032978294082));
#45996=CARTESIAN_POINT('Ctrl Pts',(1.37188019230894,-2.60274981128296,5.50501693894877));
#45997=CARTESIAN_POINT('Ctrl Pts',(1.39966489685727,-2.58772142559927,5.50673604848934));
#45998=CARTESIAN_POINT('Ctrl Pts',(1.48142350965003,-2.54349925422885,5.51179465946113));
#45999=CARTESIAN_POINT('Ctrl Pts',(1.5612265244099,-2.4953216330254,5.51685327043291));
#46000=CARTESIAN_POINT('Ctrl Pts',(1.63866682646632,-2.44338597684419,5.5219118814047));
#46001=CARTESIAN_POINT('Ctrl Pts',(1.71600245038998,-2.39152052348202,5.52696365451639));
#46002=CARTESIAN_POINT('Ctrl Pts',(1.7909813437599,-2.3359073750442,5.53201542762808));
#46003=CARTESIAN_POINT('Ctrl Pts',(1.86322089796477,-2.27678982020461,5.53706720073978));
#46004=CARTESIAN_POINT('Ctrl Pts',(1.9388933726321,-2.21486291990417,5.5423590408823));
#46005=CARTESIAN_POINT('Ctrl Pts',(2.01155926553294,-2.14909051759071,5.54765088102483));
#46006=CARTESIAN_POINT('Ctrl Pts',(2.08081269827853,-2.07980347982275,5.55294272116736));
#46007=CARTESIAN_POINT('Ctrl Pts',(2.14680785511398,-2.01377629903364,5.55798558772731));
#46008=CARTESIAN_POINT('Ctrl Pts',(2.2097040218404,-1.94455805473551,5.56302845428725));
#46009=CARTESIAN_POINT('Ctrl Pts',(2.26918489791011,-1.87247534005035,5.5680713208472));
#46010=CARTESIAN_POINT('Ctrl Pts',(2.3286459933972,-1.80041659673527,5.57311251038345));
#46011=CARTESIAN_POINT('Ctrl Pts',(2.38469377324528,-1.72549561707018,5.5781536999197));
#46012=CARTESIAN_POINT('Ctrl Pts',(2.43705118247127,-1.64807327932206,5.58319488945595));
#46013=CARTESIAN_POINT('Ctrl Pts',(2.48940571745324,-1.57065519179744,5.588235802248));
#46014=CARTESIAN_POINT('Ctrl Pts',(2.53807003696105,-1.49073638641421,5.59327671504006));
#46015=CARTESIAN_POINT('Ctrl Pts',(2.58281016747385,-1.40870708055072,5.59831762783212));
#46016=CARTESIAN_POINT('Ctrl Pts',(2.62756026406366,-1.32665950226891,5.6033596635115));
#46017=CARTESIAN_POINT('Ctrl Pts',(2.66838422376378,-1.2425008787025,5.60840169919087));
#46018=CARTESIAN_POINT('Ctrl Pts',(2.70509435179791,-1.1566453855314,5.61344373487025));
#46019=CARTESIAN_POINT('Ctrl Pts',(2.7418444684402,-1.07069636935017,5.61849126287558));
#46020=CARTESIAN_POINT('Ctrl Pts',(2.77447163567374,-0.983047202341485,
5.62353879088092));
#46021=CARTESIAN_POINT('Ctrl Pts',(2.80283671623168,-0.894131054232894,
5.62858631888626));
#46022=CARTESIAN_POINT('Ctrl Pts',(2.83121983005702,-0.805158377158289,
5.63363705588731));
#46023=CARTESIAN_POINT('Ctrl Pts',(2.85533534863092,-0.714917542795669,
5.63868779288837));
#46024=CARTESIAN_POINT('Ctrl Pts',(2.87509486000279,-0.623853785742722,
5.64373852988943));
#46025=CARTESIAN_POINT('Ctrl Pts',(2.89488474917432,-0.532650029450143,
5.64879703177262));
#46026=CARTESIAN_POINT('Ctrl Pts',(2.91030519268119,-0.44062126134618,5.65385553365581));
#46027=CARTESIAN_POINT('Ctrl Pts',(2.92131943191379,-0.348219437600584,
5.658914035539));
#46028=CARTESIAN_POINT('Ctrl Pts',(2.92506257250821,-0.316817085594656,
5.66063314507947));
#46029=CARTESIAN_POINT('Ctrl Pts',(2.92829726282772,-0.285371657139726,
5.66235225461995));
#46030=CARTESIAN_POINT('Ctrl Pts',(2.93102342983173,-0.253900873920183,
5.66407136416043));
#46031=CARTESIAN_POINT('Ctrl Pts',(2.93904538421723,-0.161295693426321,
5.6691299751322));
#46032=CARTESIAN_POINT('Ctrl Pts',(2.94268823470643,-0.0681488524178615,
5.67418858610397));
#46033=CARTESIAN_POINT('Ctrl Pts',(2.9418930026344,0.0250910551940078,5.67924719707574));
#46034=CARTESIAN_POINT('Ctrl Pts',(2.94109884549889,0.118204927922627,5.68429897018742));
#46035=CARTESIAN_POINT('Ctrl Pts',(2.93587853159832,0.211411177996739,5.6893507432991));
#46036=CARTESIAN_POINT('Ctrl Pts',(2.9262248734342,0.304256454483673,5.69440251641078));
#46037=CARTESIAN_POINT('Ctrl Pts',(2.91611246049209,0.401513862980918,5.69969435655332));
#46038=CARTESIAN_POINT('Ctrl Pts',(2.9011348536606,0.498374650664969,5.70498619669585));
#46039=CARTESIAN_POINT('Ctrl Pts',(2.88134521813328,0.594317872809211,5.71027803683838));
#46040=CARTESIAN_POINT('Ctrl Pts',(2.8624866569247,0.685747102259055,5.71532090339832));
#46041=CARTESIAN_POINT('Ctrl Pts',(2.83925870008827,0.77634266039385,5.72036376995825));
#46042=CARTESIAN_POINT('Ctrl Pts',(2.81176020120084,0.865660771285745,5.72540663651818));
#46043=CARTESIAN_POINT('Ctrl Pts',(2.78427084703965,0.954949179113599,5.73044782605442));
#46044=CARTESIAN_POINT('Ctrl Pts',(2.75251390281918,1.04296056084126,5.73548901559066));
#46045=CARTESIAN_POINT('Ctrl Pts',(2.71663843904049,1.12926506699165,5.7405302051269));
#46046=CARTESIAN_POINT('Ctrl Pts',(2.68076494470297,1.21556483531763,5.74557111791895));
#46047=CARTESIAN_POINT('Ctrl Pts',(2.6407735508614,1.3001575056006,5.75061203071099));
#46048=CARTESIAN_POINT('Ctrl Pts',(2.59686152313343,1.38263307846627,5.75565294350304));
#46049=CARTESIAN_POINT('Ctrl Pts',(2.55293971379227,1.46512702315838,5.7606949791824));
#46050=CARTESIAN_POINT('Ctrl Pts',(2.50509574440028,1.54550254305695,5.76573701486176));
#46051=CARTESIAN_POINT('Ctrl Pts',(2.45357233957565,1.62337511822415,5.77077905054113));
#46052=CARTESIAN_POINT('Ctrl Pts',(2.40199280993323,1.7013325205511,5.77582657854645));
#46053=CARTESIAN_POINT('Ctrl Pts',(2.34672609052198,1.77678116695695,5.78087410655178));
#46054=CARTESIAN_POINT('Ctrl Pts',(2.28805747168708,1.84936665003371,5.7859216345571));
#46055=CARTESIAN_POINT('Ctrl Pts',(2.22935155393146,1.92199827975978,5.79097237155815));
#46056=CARTESIAN_POINT('Ctrl Pts',(2.16723972525796,1.99176279195139,5.79602310855919));
#46057=CARTESIAN_POINT('Ctrl Pts',(2.10204524627031,2.05834151263399,5.80107384556024));
#46058=CARTESIAN_POINT('Ctrl Pts',(2.03675053885168,2.12502258984761,5.80613234744341));
#46059=CARTESIAN_POINT('Ctrl Pts',(1.96836404656305,2.18850780000787,5.81119084932659));
#46060=CARTESIAN_POINT('Ctrl Pts',(1.89724304764583,2.24851791590807,5.81624935120976));
#46061=CARTESIAN_POINT('Ctrl Pts',(1.87307289003801,2.26891208895757,5.81796846075037));
#46062=CARTESIAN_POINT('Ctrl Pts',(1.84858716292389,2.28890527179614,5.81968757029097));
#46063=CARTESIAN_POINT('Ctrl Pts',(1.82380062797807,2.308487658487,5.82140667983157));
#46064=CARTESIAN_POINT('Ctrl Pts',(1.75086435796854,2.36611032523885,5.82646529080335));
#46065=CARTESIAN_POINT('Ctrl Pts',(1.67506765815133,2.42037324670824,5.83152390177514));
#46066=CARTESIAN_POINT('Ctrl Pts',(1.59675277995121,2.47098048549925,5.83658251274692));
#46067=CARTESIAN_POINT('Ctrl Pts',(1.51854376207185,2.52151931712862,5.84163428585861));
#46068=CARTESIAN_POINT('Ctrl Pts',(1.43782369934923,2.56841204795329,5.8466860589703));
#46069=CARTESIAN_POINT('Ctrl Pts',(1.3549672957654,2.61140338274388,5.85173783208199));
#46070=CARTESIAN_POINT('Ctrl Pts',(1.26817344480329,2.6564377233993,5.85702967222452));
#46071=CARTESIAN_POINT('Ctrl Pts',(1.17903555827229,2.69719036849075,5.86232151236705));
#46072=CARTESIAN_POINT('Ctrl Pts',(1.08801798429798,2.73341926272648,5.86761335250958));
#46073=CARTESIAN_POINT('Ctrl Pts',(1.00128265824887,2.7679436388082,5.87265621906952));
#46074=CARTESIAN_POINT('Ctrl Pts',(0.912840971376588,2.79836010072875,5.87769908562946));
#46075=CARTESIAN_POINT('Ctrl Pts',(0.823117940895417,2.82450718805531,5.8827419521894));
#46076=CARTESIAN_POINT('Ctrl Pts',(0.733424748135756,2.85064558007246,5.88778314172565));
#46077=CARTESIAN_POINT('Ctrl Pts',(0.64245148327543,2.87251729469475,5.8928243312619));
#46078=CARTESIAN_POINT('Ctrl Pts',(0.550639145268767,2.89001047259308,5.89786552079815));
#46079=CARTESIAN_POINT('Ctrl Pts',(0.458831847447836,2.90750269017532,5.9029064335902));
#46080=CARTESIAN_POINT('Ctrl Pts',(0.366186003252556,2.92061676659582,5.90794734638225));
#46081=CARTESIAN_POINT('Ctrl Pts',(0.273152533946754,2.92929201227847,5.91298825917431));
#46082=CARTESIAN_POINT('Ctrl Pts',(0.180098340992911,2.93796919041338,5.91803029485367));
#46083=CARTESIAN_POINT('Ctrl Pts',(0.0866567923861568,2.94220553319126,
5.92307233053304));
#46084=CARTESIAN_POINT('Ctrl Pts',(-0.00671747469381417,2.94199233097806,
5.92811436621241));
#46085=CARTESIAN_POINT('Ctrl Pts',(-0.100193455038841,2.94177889652216,
5.93316189421774));
#46086=CARTESIAN_POINT('Ctrl Pts',(-0.19360156413738,2.93710624485276,5.93820942222307));
#46087=CARTESIAN_POINT('Ctrl Pts',(-0.286488909607947,2.92801777738313,
5.9432569502284));
#46088=CARTESIAN_POINT('Ctrl Pts',(-0.379435308756739,2.91892353186666,
5.94830768722946));
#46089=CARTESIAN_POINT('Ctrl Pts',(-0.471859847441745,2.90540794562666,
5.95335842423052));
#46090=CARTESIAN_POINT('Ctrl Pts',(-0.563318599866555,2.88756578367392,
5.95840916123158));
#46091=CARTESIAN_POINT('Ctrl Pts',(-0.654917958787383,2.86969619160863,
5.96346766311476));
#46092=CARTESIAN_POINT('Ctrl Pts',(-0.745548138939165,2.8474868538804,5.96852616499795));
#46093=CARTESIAN_POINT('Ctrl Pts',(-0.83477945612792,2.82108263963089,5.97358466688113));
#46094=CARTESIAN_POINT('Ctrl Pts',(-0.865104325473564,2.81210928394684,
5.97530377642165));
#46095=CARTESIAN_POINT('Ctrl Pts',(-0.895267799915388,2.80265185290961,
5.97702288596217));
#46096=CARTESIAN_POINT('Ctrl Pts',(-0.92525357189597,2.79271728388209,5.97874199550269));
#46097=CARTESIAN_POINT('Ctrl Pts',(-1.01348899352736,2.76348405662225,5.98380060647447));
#46098=CARTESIAN_POINT('Ctrl Pts',(-1.10049113970499,2.73001420585981,5.98885921744625));
#46099=CARTESIAN_POINT('Ctrl Pts',(-1.18582463229285,2.69243086103386,5.99391782841803));
#46100=CARTESIAN_POINT('Ctrl Pts',(-1.27104277731053,2.65489831862292,5.99896960152971));
#46101=CARTESIAN_POINT('Ctrl Pts',(-1.35459634924793,2.61326350930902,6.00402137464139));
#46102=CARTESIAN_POINT('Ctrl Pts',(-1.43606607063285,2.56769901678081,6.00907314775307));
#46103=CARTESIAN_POINT('Ctrl Pts',(-1.52140734239911,2.51996923848232,6.0143649878956));
#46104=CARTESIAN_POINT('Ctrl Pts',(-1.6044613313798,2.46792718037965,6.01965682803813));
#46105=CARTESIAN_POINT('Ctrl Pts',(-1.68477052443031,2.41182758090433,6.02494866818066));
#46106=CARTESIAN_POINT('Ctrl Pts',(-1.76130128370913,2.35836738811688,6.0299915347406));
#46107=CARTESIAN_POINT('Ctrl Pts',(-1.83533925988745,2.30122308642386,6.03503440130054));
#46108=CARTESIAN_POINT('Ctrl Pts',(-1.9065158833466,2.24066088164789,6.04007726786048));
#46109=CARTESIAN_POINT('Ctrl Pts',(-1.97766883675966,2.18011881705433,6.04511845739672));
#46110=CARTESIAN_POINT('Ctrl Pts',(-2.04596199107264,2.11616139454657,6.05015964693297));
#46111=CARTESIAN_POINT('Ctrl Pts',(-2.11105941727713,2.04909544353735,6.05520083646921));
#46112=CARTESIAN_POINT('Ctrl Pts',(-2.17615326985392,1.98203317422116,6.06024174926127));
#46113=CARTESIAN_POINT('Ctrl Pts',(-2.23805143504587,1.91186303389857,6.06528266205332));
#46114=CARTESIAN_POINT('Ctrl Pts',(-2.29645526665579,1.83892827708121,6.07032357484537));
#46115=CARTESIAN_POINT('Ctrl Pts',(-2.35487210799712,1.76597727369972,6.07536561052474));
#46116=CARTESIAN_POINT('Ctrl Pts',(-2.40979279324933,1.69026077657013,6.0804076462041));
#46117=CARTESIAN_POINT('Ctrl Pts',(-2.46096004854542,1.61215372699483,6.08544968188347));
#46118=CARTESIAN_POINT('Ctrl Pts',(-2.51218304070308,1.53396159484504,6.0904972098888));
#46119=CARTESIAN_POINT('Ctrl Pts',(-2.55964420000958,1.45337408417339,6.09554473789412));
#46120=CARTESIAN_POINT('Ctrl Pts',(-2.60313073720987,1.37079333416574,6.10059226589945));
#46121=CARTESIAN_POINT('Ctrl Pts',(-2.64664492123288,1.28816008295881,6.1056430029005));
#46122=CARTESIAN_POINT('Ctrl Pts',(-2.68617926538312,1.20353147045019,6.11069373990156));
#46123=CARTESIAN_POINT('Ctrl Pts',(-2.72156881188788,1.11733039077938,6.11574447690261));
#46124=CARTESIAN_POINT('Ctrl Pts',(-2.75701276543406,1.03099678763269,6.12080297878579));
#46125=CARTESIAN_POINT('Ctrl Pts',(-2.78829905578336,0.943086308889602,
6.12586148066897));
#46126=CARTESIAN_POINT('Ctrl Pts',(-2.81531240535529,0.854037505179129,
6.13091998255216));
#46127=CARTESIAN_POINT('Ctrl Pts',(-2.82449277299058,0.823774662232998,
6.13263909209271));
#46128=CARTESIAN_POINT('Ctrl Pts',(-2.8331800730815,0.793380435653022,6.13435820163326));
#46129=CARTESIAN_POINT('Ctrl Pts',(-2.84137113266297,0.762872260912386,
6.13607731117381));
#46130=CARTESIAN_POINT('Ctrl Pts',(-2.8719532099979,0.648967173299931,6.14249576539131));
#46131=CARTESIAN_POINT('Ctrl Pts',(-2.89569962933492,0.53315563976223,6.1489142196088));
#46132=CARTESIAN_POINT('Ctrl Pts',(-2.91241724655161,0.416160764595568,
6.15533267382629));
#46133=CARTESIAN_POINT('Ctrl Pts',(-2.92884290384954,0.301209112084665,
6.16163903483411));
#46134=CARTESIAN_POINT('Ctrl Pts',(-2.93848311852094,0.185114923026029,
6.16794539584194));
#46135=CARTESIAN_POINT('Ctrl Pts',(-2.94120044838797,0.0685851470977758,
6.17425175684976));
#46136=CARTESIAN_POINT('Ctrl Pts',(-2.94171350534655,0.0465832498869957,
6.17544245601281));
#46137=CARTESIAN_POINT('Ctrl Pts',(-2.94197990287227,0.0245658899272368,
6.17663315517586));
#46138=CARTESIAN_POINT('Ctrl Pts',(-2.94199890533048,0.00253791927304354,
6.17782385433891));
#46139=CARTESIAN_POINT('',(-2.93846014819028,-0.00170708260597003,7.1778238829104));
#46140=CARTESIAN_POINT('Ctrl Pts',(-2.94109090649655,0.00253660757586993,
6.1778238829104));
#46141=CARTESIAN_POINT('Ctrl Pts',(-2.9349800243151,-0.710047628629508,
6.21635346422191));
#46142=CARTESIAN_POINT('Ctrl Pts',(-2.31871586625516,-2.40205366998755,
6.30732815075713));
#46143=CARTESIAN_POINT('Ctrl Pts',(0.49761738400481,-3.43088509381354,6.45074794251606));
#46144=CARTESIAN_POINT('Ctrl Pts',(3.13924192099676,-1.47097102258829,6.6080832581872));
#46145=CARTESIAN_POINT('Ctrl Pts',(2.9548415774069,1.81314832273499,6.76541857385831));
#46146=CARTESIAN_POINT('Ctrl Pts',(0.110418200862219,3.46502574430695,6.92275388952942));
#46147=CARTESIAN_POINT('Ctrl Pts',(-2.46168690535804,2.18289276465007,7.06022232588014));
#46148=CARTESIAN_POINT('Ctrl Pts',(-2.93520341737875,0.60217681128353,7.14524565700712));
#46149=CARTESIAN_POINT('Ctrl Pts',(-2.93846014819028,-0.00170708260597003,
7.1778238829104));
#46150=CARTESIAN_POINT('',(-2.94242797829922,-0.000395178309583312,8.17782384089891));
#46151=CARTESIAN_POINT('Ctrl Pts',(-2.93846014819028,-0.00170708260597003,
7.1778238829104));
#46152=CARTESIAN_POINT('Ctrl Pts',(-2.94044617033292,-0.369968033311824,
7.19769076223082));
#46153=CARTESIAN_POINT('Ctrl Pts',(-2.7064938607242,-1.70794280458433,7.27000274677496));
#46154=CARTESIAN_POINT('Ctrl Pts',(-0.715046473049612,-3.39224175569136,
7.39475983654279));
#46155=CARTESIAN_POINT('Ctrl Pts',(2.44013696723815,-2.46258546444226,7.55209515221394));
#46156=CARTESIAN_POINT('Ctrl Pts',(3.39864746673817,0.683952471759658,7.70943046788504));
#46157=CARTESIAN_POINT('Ctrl Pts',(1.297609660921,3.21477911452055,7.86676578355616));
#46158=CARTESIAN_POINT('Ctrl Pts',(-1.94654513937998,2.85436050058246,8.02289677247183));
#46159=CARTESIAN_POINT('Ctrl Pts',(-2.94475147365309,0.9427053576651,8.12658265616376));
#46160=CARTESIAN_POINT('Ctrl Pts',(-2.94656694648226,-0.000388257878349857,
8.17782343463199));
#46161=CARTESIAN_POINT('',(-2.94199919951374,0.00217026738102695,9.17782384908627));
#46162=CARTESIAN_POINT('Ctrl Pts',(-2.94199997336302,-0.000395893941740302,
8.1778238829104));
#46163=CARTESIAN_POINT('Ctrl Pts',(-2.94199699558754,-0.0225245866073216,
8.17902806023974));
#46164=CARTESIAN_POINT('Ctrl Pts',(-2.94174435529623,-0.0446513335979655,
8.18023223756908));
#46165=CARTESIAN_POINT('Ctrl Pts',(-2.94124216062025,-0.0667723939207123,
8.18143641489842));
#46166=CARTESIAN_POINT('Ctrl Pts',(-2.93913249832053,-0.159700434032431,
8.18649502590215));
#46167=CARTESIAN_POINT('Ctrl Pts',(-2.93261078956895,-0.252690066630103,
8.19155363690589));
#46168=CARTESIAN_POINT('Ctrl Pts',(-2.92166725446723,-0.345288943022986,
8.19661224790961));
#46169=CARTESIAN_POINT('Ctrl Pts',(-2.9107385120351,-0.437762651033725,
8.20166402105332));
#46170=CARTESIAN_POINT('Ctrl Pts',(-2.89539987318824,-0.529846216297979,
8.20671579419702));
#46171=CARTESIAN_POINT('Ctrl Pts',(-2.87569355922515,-0.621088201007697,
8.21176756734073));
#46172=CARTESIAN_POINT('Ctrl Pts',(-2.85505077496562,-0.716666126402669,
8.21705940747526));
#46173=CARTESIAN_POINT('Ctrl Pts',(-2.82961491564589,-0.811320011255229,
8.2223512476098));
#46174=CARTESIAN_POINT('Ctrl Pts',(-2.79949555676382,-0.904537797805956,
8.22764308774433));
#46175=CARTESIAN_POINT('Ctrl Pts',(-2.7707932708266,-0.993369820243381,
8.23268595433622));
#46176=CARTESIAN_POINT('Ctrl Pts',(-2.7378383509055,-1.08089733868883,8.2377288209281));
#46177=CARTESIAN_POINT('Ctrl Pts',(-2.70077738617931,-1.16668998037288,
8.24277168751999));
#46178=CARTESIAN_POINT('Ctrl Pts',(-2.66372874621288,-1.25245409139922,
8.24781287708809));
#46179=CARTESIAN_POINT('Ctrl Pts',(-2.6225769500208,-1.33648406574942,8.25285406665619));
#46180=CARTESIAN_POINT('Ctrl Pts',(-2.57751698862641,-1.41836884248853,
8.25789525622429));
#46181=CARTESIAN_POINT('Ctrl Pts',(-2.53245950087213,-1.50024912402921,
8.26293616904806));
#46182=CARTESIAN_POINT('Ctrl Pts',(-2.48349448850748,-1.57998405433466,
8.26797708187183));
#46183=CARTESIAN_POINT('Ctrl Pts',(-2.43086268957996,-1.65718755257456,
8.27301799469561));
#46184=CARTESIAN_POINT('Ctrl Pts',(-2.37821916667063,-1.73440824825837,
8.27806003040652));
#46185=CARTESIAN_POINT('Ctrl Pts',(-2.32190748464932,-1.80909602620733,
8.28310206611743));
#46186=CARTESIAN_POINT('Ctrl Pts',(-2.26221079575508,-1.88089508361556,
8.28814410182835));
#46187=CARTESIAN_POINT('Ctrl Pts',(-2.20244907883106,-1.95277235225007,
8.29319162986479));
#46188=CARTESIAN_POINT('Ctrl Pts',(-2.13929527959758,-2.02175427932885,
8.29823915790124));
#46189=CARTESIAN_POINT('Ctrl Pts',(-2.07307158391174,-2.08751963056103,
8.30328668593768));
#46190=CARTESIAN_POINT('Ctrl Pts',(-2.00680578612355,-2.1533267925004,8.30833742296963));
#46191=CARTESIAN_POINT('Ctrl Pts',(-1.93746653482207,-2.21591301108361,
8.31338816000158));
#46192=CARTESIAN_POINT('Ctrl Pts',(-1.86540986927196,-2.27499670760702,
8.31843889703353));
#46193=CARTESIAN_POINT('Ctrl Pts',(-1.79324242553851,-2.33417123798342,
8.32349739894704));
#46194=CARTESIAN_POINT('Ctrl Pts',(-1.71834958445942,-2.38983223599387,
8.32855590086054));
#46195=CARTESIAN_POINT('Ctrl Pts',(-1.64111690523925,-2.44174103936882,
8.33361440277404));
#46196=CARTESIAN_POINT('Ctrl Pts',(-1.61486972441552,-2.45938201417745,
8.33533351203921));
#46197=CARTESIAN_POINT('Ctrl Pts',(-1.58835251507917,-2.47659002051337,
8.33705262130437));
#46198=CARTESIAN_POINT('Ctrl Pts',(-1.56158101890186,-2.49335691817386,
8.33877173056953));
#46199=CARTESIAN_POINT('Ctrl Pts',(-1.48280383701224,-2.54269480119604,
8.34383034150308));
#46200=CARTESIAN_POINT('Ctrl Pts',(-1.40154908211522,-2.58838144079867,
8.34888895243663));
#46201=CARTESIAN_POINT('Ctrl Pts',(-1.31818919554193,-2.6301599276007,8.35394756337018));
#46202=CARTESIAN_POINT('Ctrl Pts',(-1.2349419887612,-2.67188194130255,8.35899933644377));
#46203=CARTESIAN_POINT('Ctrl Pts',(-1.14959569804075,-2.70970610388165,
8.36405110951736));
#46204=CARTESIAN_POINT('Ctrl Pts',(-1.06255059870906,-2.74341944025755,
8.36910288259095));
#46205=CARTESIAN_POINT('Ctrl Pts',(-0.971368998709515,-2.77873487990525,
8.37439472274302));
#46206=CARTESIAN_POINT('Ctrl Pts',(-0.878323541763301,-2.8095388389535,
8.37968656289509));
#46207=CARTESIAN_POINT('Ctrl Pts',(-0.783902172583036,-2.8356412650086,
8.38497840304716));
#46208=CARTESIAN_POINT('Ctrl Pts',(-0.693923195902074,-2.86051560866321,
8.39002126956961));
#46209=CARTESIAN_POINT('Ctrl Pts',(-0.602695321896114,-2.88112065717945,
8.39506413609205));
#46210=CARTESIAN_POINT('Ctrl Pts',(-0.510658622135931,-2.89734219098094,
8.4001070026145));
#46211=CARTESIAN_POINT('Ctrl Pts',(-0.418652529511199,-2.91355833025303,
8.40514819211355));
#46212=CARTESIAN_POINT('Ctrl Pts',(-0.325838581377534,-2.92539377442687,
8.4101893816126));
#46213=CARTESIAN_POINT('Ctrl Pts',(-0.232667334874957,-2.93278535035931,
8.41523057111165));
#46214=CARTESIAN_POINT('Ctrl Pts',(-0.139501203151212,-2.94017652051983,
8.42027148386685));
#46215=CARTESIAN_POINT('Ctrl Pts',(-0.0459782536247714,-2.94312427300938,
8.42531239662205));
#46216=CARTESIAN_POINT('Ctrl Pts',(0.0474466652067634,-2.94161738061917,
8.43035330937725));
#46217=CARTESIAN_POINT('Ctrl Pts',(0.14089239489094,-2.94011015256138,8.43539534502016));
#46218=CARTESIAN_POINT('Ctrl Pts',(0.234239607738917,-2.9341463162658,8.44043738066306));
#46219=CARTESIAN_POINT('Ctrl Pts',(0.3270354216065,-2.923766720006,8.44547941630597));
#46220=CARTESIAN_POINT('Ctrl Pts',(0.419932318640967,-2.91337581717517,
8.45052694427562));
#46221=CARTESIAN_POINT('Ctrl Pts',(0.512276177259232,-2.89855960388633,
8.45557447224527));
#46222=CARTESIAN_POINT('Ctrl Pts',(0.603621524189472,-2.87941053959577,
8.46062200021492));
#46223=CARTESIAN_POINT('Ctrl Pts',(0.695024944471082,-2.8602493011729,8.4656727371807));
#46224=CARTESIAN_POINT('Ctrl Pts',(0.785428161133795,-2.83674983911359,
8.47072347414649));
#46225=CARTESIAN_POINT('Ctrl Pts',(0.87440020723099,-2.80905469466054,8.47577421111227));
#46226=CARTESIAN_POINT('Ctrl Pts',(0.963509036838297,-2.78131697235031,
8.48083271296109));
#46227=CARTESIAN_POINT('Ctrl Pts',(1.05118188944844,-2.74937084542327,8.48589121480991));
#46228=CARTESIAN_POINT('Ctrl Pts',(1.13700741094499,-2.71340711052657,8.49094971665872));
#46229=CARTESIAN_POINT('Ctrl Pts',(1.16617484128498,-2.7011849915802,8.49266882651937));
#46230=CARTESIAN_POINT('Ctrl Pts',(1.19512912467167,-2.68849925012339,8.49438793638002));
#46231=CARTESIAN_POINT('Ctrl Pts',(1.22385480592929,-2.67535855802615,8.49610704624066));
#46232=CARTESIAN_POINT('Ctrl Pts',(1.30838229812822,-2.63669107652149,8.50116565717601));
#46233=CARTESIAN_POINT('Ctrl Pts',(1.39122251621103,-2.59394645723791,8.50622426811136));
#46234=CARTESIAN_POINT('Ctrl Pts',(1.47195607870599,-2.54729450640488,8.51128287904671));
#46235=CARTESIAN_POINT('Ctrl Pts',(1.55258051147071,-2.50070561626994,8.51633465212145));
#46236=CARTESIAN_POINT('Ctrl Pts',(1.63110356743534,-2.45022011065338,8.52138642519618));
#46237=CARTESIAN_POINT('Ctrl Pts',(1.70712725519738,-2.39605520273684,8.52643819827092));
#46238=CARTESIAN_POINT('Ctrl Pts',(1.78676369124228,-2.33931630526747,8.53173003842262));
#46239=CARTESIAN_POINT('Ctrl Pts',(1.8636568749786,-2.27853983593225,8.53702187857433));
#46240=CARTESIAN_POINT('Ctrl Pts',(1.93737975263415,-2.21402883768103,8.54231371872603));
#46241=CARTESIAN_POINT('Ctrl Pts',(2.00763407267695,-2.15255299108432,8.54735658524801));
#46242=CARTESIAN_POINT('Ctrl Pts',(2.07500926457794,-2.08768638549101,8.55239945176999));
#46243=CARTESIAN_POINT('Ctrl Pts',(2.13916793791325,-2.0197337778539,8.55744231829197));
#46244=CARTESIAN_POINT('Ctrl Pts',(2.20330527504356,-1.95180376810872,8.56248350778996));
#46245=CARTESIAN_POINT('Ctrl Pts',(2.26422791513643,-1.88079011717847,8.56752469728795));
#46246=CARTESIAN_POINT('Ctrl Pts',(2.32163533784804,-1.8070344097596,8.57256588678595));
#46247=CARTESIAN_POINT('Ctrl Pts',(2.37903960908429,-1.7332827512822,8.57760679953951));
#46248=CARTESIAN_POINT('Ctrl Pts',(2.43292877501671,-1.65678968546736,8.58264771229308));
#46249=CARTESIAN_POINT('Ctrl Pts',(2.48304334279859,-1.57792894573349,8.58768862504665));
#46250=CARTESIAN_POINT('Ctrl Pts',(2.53316907383721,-1.49905063939727,8.59273066068734));
#46251=CARTESIAN_POINT('Ctrl Pts',(2.57951829953034,-1.41780398556084,8.59777269632804));
#46252=CARTESIAN_POINT('Ctrl Pts',(2.62187610376823,-1.33458971091835,8.60281473196874));
#46253=CARTESIAN_POINT('Ctrl Pts',(2.66428004866875,-1.25128479036439,8.60786225993534));
#46254=CARTESIAN_POINT('Ctrl Pts',(2.70268369366719,-1.16600836662952,8.61290978790194));
#46255=CARTESIAN_POINT('Ctrl Pts',(2.73691930436214,-1.07918335856789,8.61795731586855));
#46256=CARTESIAN_POINT('Ctrl Pts',(2.77117668054832,-0.992303150995767,
8.6230080528308));
#46257=CARTESIAN_POINT('Ctrl Pts',(2.80126060462734,-0.903872817919549,
8.62805878979304));
#46258=CARTESIAN_POINT('Ctrl Pts',(2.82705314929468,-0.81433070128972,8.63310952675529));
#46259=CARTESIAN_POINT('Ctrl Pts',(2.852885346804,-0.724650924749004,8.63816802859988));
#46260=CARTESIAN_POINT('Ctrl Pts',(2.87441289581222,-0.633856383383457,
8.64322653044447));
#46261=CARTESIAN_POINT('Ctrl Pts',(2.89156895864927,-0.54239557278429,8.64828503228906));
#46262=CARTESIAN_POINT('Ctrl Pts',(2.89739937206662,-0.511313013671278,
8.65000414216331));
#46263=CARTESIAN_POINT('Ctrl Pts',(2.9027253431409,-0.480153543002247,8.65172325203756));
#46264=CARTESIAN_POINT('Ctrl Pts',(2.90754561634846,-0.448934838092175,
8.6534423619118));
#46265=CARTESIAN_POINT('Ctrl Pts',(2.92172963584773,-0.357071431160895,
8.65850097309995));
#46266=CARTESIAN_POINT('Ctrl Pts',(2.93158046042886,-0.264375334532386,
8.6635595842881));
#46267=CARTESIAN_POINT('Ctrl Pts',(2.93700930629233,-0.171290206235695,
8.66861819547625));
#46268=CARTESIAN_POINT('Ctrl Pts',(2.94243081384023,-0.0783309035864636,
8.67366996880491));
#46269=CARTESIAN_POINT('Ctrl Pts',(2.94344219588367,0.0150159471495223,
8.67872174213356));
#46270=CARTESIAN_POINT('Ctrl Pts',(2.94000602687925,0.108298485278775,8.68377351546222));
#46271=CARTESIAN_POINT('Ctrl Pts',(2.93640656670854,0.206013929480568,8.68906535555059));
#46272=CARTESIAN_POINT('Ctrl Pts',(2.92792629014359,0.303658312521264,8.69435719563895));
#46273=CARTESIAN_POINT('Ctrl Pts',(2.91458347896305,0.400708303078024,8.69964903572731));
#46274=CARTESIAN_POINT('Ctrl Pts',(2.90186842747084,0.493192233979073,8.70469190250415));
#46275=CARTESIAN_POINT('Ctrl Pts',(2.88473808584657,0.58513594071538,8.70973476928099));
#46276=CARTESIAN_POINT('Ctrl Pts',(2.86326147221195,0.6760900396742,8.71477763605784));
#46277=CARTESIAN_POINT('Ctrl Pts',(2.8417920007054,0.767013891507716,8.7198188258105));
#46278=CARTESIAN_POINT('Ctrl Pts',(2.81597923070519,0.856948358768648,8.72486001556315));
#46279=CARTESIAN_POINT('Ctrl Pts',(2.78594321468515,0.945454602056485,8.72990120531581));
#46280=CARTESIAN_POINT('Ctrl Pts',(2.75590884754489,1.03395598663885,8.73494211832352));
#46281=CARTESIAN_POINT('Ctrl Pts',(2.7216518382119,1.12102888389986,8.73998303133123));
#46282=CARTESIAN_POINT('Ctrl Pts',(2.68334165152275,1.20625104402158,8.74502394433894));
#46283=CARTESIAN_POINT('Ctrl Pts',(2.64502293106542,1.29149218776677,8.75006598023293));
#46284=CARTESIAN_POINT('Ctrl Pts',(2.60264942190965,1.37488137180379,8.75510801612691));
#46285=CARTESIAN_POINT('Ctrl Pts',(2.55643764690833,1.4560187352743,8.7601500520209));
#46286=CARTESIAN_POINT('Ctrl Pts',(2.51017553311329,1.53724448221424,8.76519758023811));
#46287=CARTESIAN_POINT('Ctrl Pts',(2.46006702862052,1.61621312783523,8.77024510845532));
#46288=CARTESIAN_POINT('Ctrl Pts',(2.40637313666205,1.69255201608436,8.77529263667252));
#46289=CARTESIAN_POINT('Ctrl Pts',(2.35264510851053,1.76893943720998,8.78034337388411));
#46290=CARTESIAN_POINT('Ctrl Pts',(2.29532742646195,1.84269342327889,8.7853941110957));
#46291=CARTESIAN_POINT('Ctrl Pts',(2.23472136401146,1.9134744380918,8.79044484830729));
#46292=CARTESIAN_POINT('Ctrl Pts',(2.17402212730053,1.9843642698851,8.79550335039727));
#46293=CARTESIAN_POINT('Ctrl Pts',(2.1100247236143,2.05227168693138,8.80056185248724));
#46294=CARTESIAN_POINT('Ctrl Pts',(2.04306700070858,2.11689424171725,8.80562035457722));
#46295=CARTESIAN_POINT('Ctrl Pts',(2.02031173978954,2.13885590695306,8.80733946224578));
#46296=CARTESIAN_POINT('Ctrl Pts',(1.99721485376002,2.16043853602434,8.80905856991435));
#46297=CARTESIAN_POINT('Ctrl Pts',(1.97379041694743,2.18163135977793,8.81077767758291));
#46298=CARTESIAN_POINT('Ctrl Pts',(1.90486215393261,2.24399292438677,8.81583628823288));
#46299=CARTESIAN_POINT('Ctrl Pts',(1.8328556274808,2.30319312272707,8.82089489888285));
#46300=CARTESIAN_POINT('Ctrl Pts',(1.75809257682032,2.35891383719908,8.82595350953281));
#46301=CARTESIAN_POINT('Ctrl Pts',(1.68343058537718,2.41455923248943,8.83100528232332));
#46302=CARTESIAN_POINT('Ctrl Pts',(1.60601982680215,2.46673422837125,8.83605705511383));
#46303=CARTESIAN_POINT('Ctrl Pts',(1.52621713276797,2.51515909310833,8.84110882790434));
#46304=CARTESIAN_POINT('Ctrl Pts',(1.44262210114271,2.56588517633318,8.84640066812725));
#46305=CARTESIAN_POINT('Ctrl Pts',(1.35640252290727,2.61249553642561,8.85169250835015));
#46306=CARTESIAN_POINT('Ctrl Pts',(1.26800555770157,2.6547176696662,8.85698434857305));
#46307=CARTESIAN_POINT('Ctrl Pts',(1.18376755107093,2.69495330820428,8.86202721481567));
#46308=CARTESIAN_POINT('Ctrl Pts',(1.09755284862545,2.73120406339136,8.86707008105828));
#46309=CARTESIAN_POINT('Ctrl Pts',(1.00977474512091,2.76328047148964,8.87211294730089));
#46310=CARTESIAN_POINT('Ctrl Pts',(0.922025832511028,2.79534621247377,8.87715413652189));
#46311=CARTESIAN_POINT('Ctrl Pts',(0.832714967510445,2.82324021269868,8.88219532574288));
#46312=CARTESIAN_POINT('Ctrl Pts',(0.742274701086023,2.84682143242734,8.88723651496388));
#46313=CARTESIAN_POINT('Ctrl Pts',(0.651839399481275,2.87040135763854,8.89227742744315));
#46314=CARTESIAN_POINT('Ctrl Pts',(0.560275248446931,2.88966886187587,8.89731833992241));
#46315=CARTESIAN_POINT('Ctrl Pts',(0.468028113920198,2.90453329892778,8.90235925240168));
#46316=CARTESIAN_POINT('Ctrl Pts',(0.375760430851592,2.91940104711243,8.90740128777112));
#46317=CARTESIAN_POINT('Ctrl Pts',(0.282809899369842,2.92986370997426,8.91244332314057));
#46318=CARTESIAN_POINT('Ctrl Pts',(0.189629561890907,2.93588225738994,8.91748535851001));
#46319=CARTESIAN_POINT('Ctrl Pts',(0.0963477222794635,2.94190736086041,
8.92253288621138));
#46320=CARTESIAN_POINT('Ctrl Pts',(0.00283601960583585,2.94347865885932,
8.92758041391275));
#46321=CARTESIAN_POINT('Ctrl Pts',(-0.0904507670271132,2.94060923258161,
8.93262794161412));
#46322=CARTESIAN_POINT('Ctrl Pts',(-0.183796861346238,2.93773798204733,
8.93767867831431));
#46323=CARTESIAN_POINT('Ctrl Pts',(-0.276917313935894,2.9304204214277,8.94272941501451));
#46324=CARTESIAN_POINT('Ctrl Pts',(-0.36936286457646,2.91872147939331,8.9477801517147));
#46325=CARTESIAN_POINT('Ctrl Pts',(-0.461950538931314,2.90700455166806,
8.95283865330412));
#46326=CARTESIAN_POINT('Ctrl Pts',(-0.553860805277309,2.89089287552825,
8.95789715489354));
#46327=CARTESIAN_POINT('Ctrl Pts',(-0.64465526958578,2.87050232248561,8.96295565648295));
#46328=CARTESIAN_POINT('Ctrl Pts',(-0.675511418131734,2.86357267167033,
8.96467476873998));
#46329=CARTESIAN_POINT('Ctrl Pts',(-0.706238835613273,2.85614925247111,
8.96639388099701));
#46330=CARTESIAN_POINT('Ctrl Pts',(-0.736820787785887,2.84823789854123,
8.96811299325404));
#46331=CARTESIAN_POINT('Ctrl Pts',(-0.826810370879999,2.82495817336733,
8.97317160411147));
#46332=CARTESIAN_POINT('Ctrl Pts',(-0.915852156281128,2.79736896745877,
8.97823021496891));
#46333=CARTESIAN_POINT('Ctrl Pts',(-1.00350351945997,2.76556408105678,8.98328882582634));
#46334=CARTESIAN_POINT('Ctrl Pts',(-1.09103640187716,2.7338021861957,8.98834059882016));
#46335=CARTESIAN_POINT('Ctrl Pts',(-1.17718218424931,2.69783608528959,8.99339237181398));
#46336=CARTESIAN_POINT('Ctrl Pts',(-1.26151100651736,2.65780999705313,8.99844414480779));
#46337=CARTESIAN_POINT('Ctrl Pts',(-1.34984725001926,2.61588181423509,9.00373598497935));
#46338=CARTESIAN_POINT('Ctrl Pts',(-1.43618908692142,2.56949832423015,9.00902782515091));
#46339=CARTESIAN_POINT('Ctrl Pts',(-1.5200630241403,2.51888316573863,9.01431966532246));
#46340=CARTESIAN_POINT('Ctrl Pts',(-1.59999080899302,2.47064938022265,9.01936253175669));
#46341=CARTESIAN_POINT('Ctrl Pts',(-1.67767722455368,2.41857334437907,9.02440539819091));
#46342=CARTESIAN_POINT('Ctrl Pts',(-1.75273675775916,2.36289607431218,9.02944826462513));
#46343=CARTESIAN_POINT('Ctrl Pts',(-1.82777132960363,2.3072373199538,9.03448945403308));
#46344=CARTESIAN_POINT('Ctrl Pts',(-1.900180399401,2.24797997455053,9.03953064344102));
#46345=CARTESIAN_POINT('Ctrl Pts',(-1.96960831094362,2.1854077654895,9.04457183284897));
#46346=CARTESIAN_POINT('Ctrl Pts',(-2.03903241109631,2.12283899146033,9.04961274551031));
#46347=CARTESIAN_POINT('Ctrl Pts',(-2.10547534975239,2.0569560125236,9.05465365817165));
#46348=CARTESIAN_POINT('Ctrl Pts',(-2.16861623959636,1.98808138801181,9.059694570833));
#46349=CARTESIAN_POINT('Ctrl Pts',(-2.23177119434668,1.91919142137947,9.06473660637944));
#46350=CARTESIAN_POINT('Ctrl Pts',(-2.29162234038641,1.84730881225314,9.06977864192589));
#46351=CARTESIAN_POINT('Ctrl Pts',(-2.34788795590304,1.7727904970767,9.07482067747234));
#46352=CARTESIAN_POINT('Ctrl Pts',(-2.40421486193528,1.69819100859542,9.07986820534221));
#46353=CARTESIAN_POINT('Ctrl Pts',(-2.45694817535026,1.62095043798711,9.08491573321209));
#46354=CARTESIAN_POINT('Ctrl Pts',(-2.50584874474712,1.54145582760236,9.08996326108197));
#46355=CARTESIAN_POINT('Ctrl Pts',(-2.55478040295481,1.46191067807391,9.09501399794595));
#46356=CARTESIAN_POINT('Ctrl Pts',(-2.59987425261999,1.38010902333081,9.10006473480993));
#46357=CARTESIAN_POINT('Ctrl Pts',(-2.64093748212801,1.29646180641443,9.10511547167391));
#46358=CARTESIAN_POINT('Ctrl Pts',(-2.68206384125354,1.21268599228655,9.11017397341879));
#46359=CARTESIAN_POINT('Ctrl Pts',(-2.71914703754702,1.1270593588051,9.11523247516368));
#46360=CARTESIAN_POINT('Ctrl Pts',(-2.75204278401172,1.04001178597601,9.12029097690856));
#46361=CARTESIAN_POINT('Ctrl Pts',(-2.76322226593535,1.01042903223055,9.12201008758076));
#46362=CARTESIAN_POINT('Ctrl Pts',(-2.77391854663788,0.980682282963654,
9.12372919825296));
#46363=CARTESIAN_POINT('Ctrl Pts',(-2.78412729667365,0.950788723069774,
9.12544830892516));
#46364=CARTESIAN_POINT('Ctrl Pts',(-2.81929552746703,0.847808082942463,
9.13137049143208));
#46365=CARTESIAN_POINT('Ctrl Pts',(-2.84877409654376,0.742792724543732,
9.137292673939));
#46366=CARTESIAN_POINT('Ctrl Pts',(-2.87235963900125,0.636328613403945,
9.14321485644592));
#46367=CARTESIAN_POINT('Ctrl Pts',(-2.89572986727888,0.530836421091849,
9.14908297490611));
#46368=CARTESIAN_POINT('Ctrl Pts',(-2.9133141094229,0.423921925118199,9.15495109336631));
#46369=CARTESIAN_POINT('Ctrl Pts',(-2.92496101254477,0.316175702882257,
9.1608192118265));
#46370=CARTESIAN_POINT('Ctrl Pts',(-2.93621114687264,0.212100013337014,
9.16648742424642));
#46371=CARTESIAN_POINT('Ctrl Pts',(-2.94192168493498,0.107248485242721,
9.17215563666635));
#46372=CARTESIAN_POINT('Ctrl Pts',(-2.94199919951374,0.00217026738102695,
9.17782384908627));
#46373=CARTESIAN_POINT('',(-2.93989309841074,-0.00232834448912937,10.1778238829104));
#46374=CARTESIAN_POINT('Ctrl Pts',(-2.93938212312892,0.00216771032458683,
9.1778238829104));
#46375=CARTESIAN_POINT('Ctrl Pts',(-2.93484702512206,-0.645845798130107,
9.21281046347236));
#46376=CARTESIAN_POINT('Ctrl Pts',(-2.40612385725697,-2.27196315558581,
9.30024214925803));
#46377=CARTESIAN_POINT('Ctrl Pts',(0.267550388642242,-3.45644520972621,
9.44011894026741));
#46378=CARTESIAN_POINT('Ctrl Pts',(3.03407913010763,-1.67718692077773,9.59745425593852));
#46379=CARTESIAN_POINT('Ctrl Pts',(3.06925466623265,1.61191643161126,9.75478957160967));
#46380=CARTESIAN_POINT('Ctrl Pts',(0.341406797652991,3.44993374993849,9.91212488728076));
#46381=CARTESIAN_POINT('Ctrl Pts',(-2.3788716582907,2.31375700223615,10.053136324381));
#46382=CARTESIAN_POINT('Ctrl Pts',(-2.93479827488144,0.666407318052135,
10.1417026562576));
#46383=CARTESIAN_POINT('Ctrl Pts',(-2.93989309841074,-0.00232834448912937,
10.1778238829104));
#46384=CARTESIAN_POINT('',(-2.14415473270596,2.01243073062332,11.058));
#46385=CARTESIAN_POINT('Ctrl Pts',(-2.93989309841074,-0.00232834448912937,
10.1778238829104));
#46386=CARTESIAN_POINT('Ctrl Pts',(-2.94219554736775,-0.304542880453153,
10.1941477614813));
#46387=CARTESIAN_POINT('Ctrl Pts',(-2.76120346070747,-1.57501837043084,
10.262916745276));
#46388=CARTESIAN_POINT('Ctrl Pts',(-0.93982089220685,-3.33696855340065,
10.384130834294));
#46389=CARTESIAN_POINT('Ctrl Pts',(2.27033791967618,-2.61992335659031,10.5414661499654));
#46390=CARTESIAN_POINT('Ctrl Pts',(3.43675322554089,0.455595550491127,10.6988014656364));
#46391=CARTESIAN_POINT('Ctrl Pts',(1.50917870869015,3.12106661837876,10.8561367813075));
#46392=CARTESIAN_POINT('Ctrl Pts',(-0.991414248907668,3.01120383063971,
10.9758696260954));
#46393=CARTESIAN_POINT('Ctrl Pts',(-1.95802372783935,2.21436813426865,11.0431573656595));
#46394=CARTESIAN_POINT('Ctrl Pts',(-2.14415473270596,2.01243073062332,11.058));
#46395=CARTESIAN_POINT('',(0.261592048850261,2.93034701016421,11.0579991307071));
#46396=CARTESIAN_POINT('Origin',(0.,0.,11.058));
#46397=CARTESIAN_POINT('',(-2.94199895080427,-0.00248464616942429,10.3221761170896));
#46398=CARTESIAN_POINT('Ctrl Pts',(0.261592048850261,2.93034701016421,11.0579991307071));
#46399=CARTESIAN_POINT('Ctrl Pts',(0.360090029576933,2.92155409639102,11.0526819206525));
#46400=CARTESIAN_POINT('Ctrl Pts',(0.458023157418216,2.90780150422239,11.0473647105979));
#46401=CARTESIAN_POINT('Ctrl Pts',(0.554897463885622,2.88919587507896,11.0420475005432));
#46402=CARTESIAN_POINT('Ctrl Pts',(0.652086440068712,2.87052981063286,11.0367130189846));
#46403=CARTESIAN_POINT('Ctrl Pts',(0.74820935947663,2.84697925549818,11.0313785374259));
#46404=CARTESIAN_POINT('Ctrl Pts',(0.842784692145053,2.8187014674644,11.0260440558672));
#46405=CARTESIAN_POINT('Ctrl Pts',(0.937521801343244,2.79037530865265,11.0207004493719));
#46406=CARTESIAN_POINT('Ctrl Pts',(1.03070570050046,2.75730590422185,11.0153568428766));
#46407=CARTESIAN_POINT('Ctrl Pts',(1.12187471940277,2.71969871749886,11.0100132363813));
#46408=CARTESIAN_POINT('Ctrl Pts',(1.21330895958217,2.68198212709674,11.0046540847134));
#46409=CARTESIAN_POINT('Ctrl Pts',(1.30271626992542,2.63970151287218,10.9992949330454));
#46410=CARTESIAN_POINT('Ctrl Pts',(1.38965816406483,2.59310898094314,10.9939357813775));
#46411=CARTESIAN_POINT('Ctrl Pts',(1.4393916051184,2.56645661773934,10.9908701815742));
#46412=CARTESIAN_POINT('Ctrl Pts',(1.48831883990037,2.53839411919676,10.9878045817709));
#46413=CARTESIAN_POINT('Ctrl Pts',(1.53636235385959,2.50897483399954,10.9847389819675));
#46414=CARTESIAN_POINT('Ctrl Pts',(1.61577682077707,2.46034565060939,10.9796716387593));
#46415=CARTESIAN_POINT('Ctrl Pts',(1.6930151158665,2.40785972230369,10.974604295551));
#46416=CARTESIAN_POINT('Ctrl Pts',(1.76768054498651,2.35173754719276,10.9695369523427));
#46417=CARTESIAN_POINT('Ctrl Pts',(1.84224573176959,2.29569071910725,10.964476412314));
#46418=CARTESIAN_POINT('Ctrl Pts',(1.91424456807512,2.23601760989157,10.9594158722854));
#46419=CARTESIAN_POINT('Ctrl Pts',(1.9833073995402,2.17298314741028,10.9543553322567));
#46420=CARTESIAN_POINT('Ctrl Pts',(2.05538509733032,2.10719698080364,10.9490738795982));
#46421=CARTESIAN_POINT('Ctrl Pts',(2.12426418350433,2.03774953659513,10.9437924269398));
#46422=CARTESIAN_POINT('Ctrl Pts',(2.1895606759417,1.96499059701814,10.9385109742814));
#46423=CARTESIAN_POINT('Ctrl Pts',(2.25201606205986,1.89539746122778,10.9334593221522));
#46424=CARTESIAN_POINT('Ctrl Pts',(2.31119377002267,1.82277534227604,10.928407670023));
#46425=CARTESIAN_POINT('Ctrl Pts',(2.36679481678367,1.74746853912909,10.9233560178939));
#46426=CARTESIAN_POINT('Ctrl Pts',(2.4223772273332,1.6721869771168,10.9183060589641));
#46427=CARTESIAN_POINT('Ctrl Pts',(2.4743850971487,1.59422287358881,10.9132561000343));
#46428=CARTESIAN_POINT('Ctrl Pts',(2.52256048898002,1.51395263447602,10.9082061411045));
#46429=CARTESIAN_POINT('Ctrl Pts',(2.57073297109809,1.43368724355169,10.9031564871838));
#46430=CARTESIAN_POINT('Ctrl Pts',(2.61507320902485,1.35111637250567,10.8981068332631));
#46431=CARTESIAN_POINT('Ctrl Pts',(2.65536786073502,1.26664340845225,10.8930571793424));
#46432=CARTESIAN_POINT('Ctrl Pts',(2.69567115051051,1.18215233571813,10.8880064429148));
#46433=CARTESIAN_POINT('Ctrl Pts',(2.73192694188803,1.09575875826061,10.8829557064872));
#46434=CARTESIAN_POINT('Ctrl Pts',(2.76396938171704,1.00788752196399,10.8779049700595));
#46435=CARTESIAN_POINT('Ctrl Pts',(2.79604586983052,0.919922913724862,10.8728488667213));
#46436=CARTESIAN_POINT('Ctrl Pts',(2.82389991975566,0.830477927843595,10.867792763383));
#46437=CARTESIAN_POINT('Ctrl Pts',(2.84741517562019,0.739993795682003,10.8627366600447));
#46438=CARTESIAN_POINT('Ctrl Pts',(2.87094510473528,0.649453202457388,10.8576774017558));
#46439=CARTESIAN_POINT('Ctrl Pts',(2.89013075876966,0.557872603141818,10.8526181434669));
#46440=CARTESIAN_POINT('Ctrl Pts',(2.90490706649581,0.465702625097528,10.8475588851781));
#46441=CARTESIAN_POINT('Ctrl Pts',(2.91970550359378,0.373394610965105,10.8424920500161));
#46442=CARTESIAN_POINT('Ctrl Pts',(2.9300813658763,0.280495893871383,10.8374252148542));
#46443=CARTESIAN_POINT('Ctrl Pts',(2.936021514527,0.18746110592485,10.8323583796922));
#46444=CARTESIAN_POINT('Ctrl Pts',(2.93788084085319,0.158340280731397,10.8307724092795));
#46445=CARTESIAN_POINT('Ctrl Pts',(2.93930596103553,0.129206111948713,10.8291864388668));
#46446=CARTESIAN_POINT('Ctrl Pts',(2.94029751889039,0.100072475771473,10.8276004684541));
#46447=CARTESIAN_POINT('Ctrl Pts',(2.94346584595508,0.00698170195448691,
10.8225328135939));
#46448=CARTESIAN_POINT('Ctrl Pts',(2.94221421656088,-0.0864148034031075,
10.8174651587337));
#46449=CARTESIAN_POINT('Ctrl Pts',(2.9365089388319,-0.179664276249695,10.8123975038735));
#46450=CARTESIAN_POINT('Ctrl Pts',(2.93081115286242,-0.272791300609757,
10.8073365034924));
#46451=CARTESIAN_POINT('Ctrl Pts',(2.92067136891433,-0.365771239389406,
10.8022755031113));
#46452=CARTESIAN_POINT('Ctrl Pts',(2.90610787884632,-0.458149535094561,
10.7972145027302));
#46453=CARTESIAN_POINT('Ctrl Pts',(2.89091029493816,-0.55454997851267,10.7919331465723));
#46454=CARTESIAN_POINT('Ctrl Pts',(2.87089499576309,-0.650294708301221,
10.7866517904144));
#46455=CARTESIAN_POINT('Ctrl Pts',(2.84614326728887,-0.744870795551974,
10.7813704342565));
#46456=CARTESIAN_POINT('Ctrl Pts',(2.82246417805881,-0.835348339832311,
10.7763179505946));
#46457=CARTESIAN_POINT('Ctrl Pts',(2.79445075226464,-0.924755946327105,
10.7712654669328));
#46458=CARTESIAN_POINT('Ctrl Pts',(2.76222642396159,-1.01265452290915,10.7662129832709));
#46459=CARTESIAN_POINT('Ctrl Pts',(2.73001203106244,-1.10052599860482,10.7611620573907));
#46460=CARTESIAN_POINT('Ctrl Pts',(2.69358946727219,-1.18688895518827,10.7561111315104));
#46461=CARTESIAN_POINT('Ctrl Pts',(2.65313154084007,-1.2713209771728,10.7510602056302));
#46462=CARTESIAN_POINT('Ctrl Pts',(2.61267497758725,-1.35575015432579,10.7460094499345));
#46463=CARTESIAN_POINT('Ctrl Pts',(2.56818351321817,-1.43824812881357,10.7409586942389));
#46464=CARTESIAN_POINT('Ctrl Pts',(2.51987699422717,-1.51841494130051,10.7359079385433));
#46465=CARTESIAN_POINT('Ctrl Pts',(2.47155883699479,-1.59860106796563,10.7308559659951));
#46466=CARTESIAN_POINT('Ctrl Pts',(2.41942402710974,-1.67645453945573,10.7258039934469));
#46467=CARTESIAN_POINT('Ctrl Pts',(2.36373642214545,-1.75160330172761,10.7207520208986));
#46468=CARTESIAN_POINT('Ctrl Pts',(2.30798751091064,-1.82683479498335,10.7156944866532));
#46469=CARTESIAN_POINT('Ctrl Pts',(2.24867826160286,-1.89935528174567,10.7106369524078));
#46470=CARTESIAN_POINT('Ctrl Pts',(2.18611341615223,-1.96882506376753,10.7055794181624));
#46471=CARTESIAN_POINT('Ctrl Pts',(2.12350812171701,-2.0383397589051,10.7005186141555));
#46472=CARTESIAN_POINT('Ctrl Pts',(2.05764335060496,-2.10479950960304,10.6954578101485));
#46473=CARTESIAN_POINT('Ctrl Pts',(1.98885985606428,-2.16790232089363,10.6903970061416));
#46474=CARTESIAN_POINT('Ctrl Pts',(1.9199712252722,-2.23110158545511,10.6853284666457));
#46475=CARTESIAN_POINT('Ctrl Pts',(1.8481553052694,-2.29093338834345,10.6802599271498));
#46476=CARTESIAN_POINT('Ctrl Pts',(1.77378471914451,-2.34713693041744,10.6751913876539));
#46477=CARTESIAN_POINT('Ctrl Pts',(1.75065309294903,-2.36461802602068,10.6736149100828));
#46478=CARTESIAN_POINT('Ctrl Pts',(1.72727452462674,-2.38174844474552,10.6720384325117));
#46479=CARTESIAN_POINT('Ctrl Pts',(1.70366073469359,-2.3985212321477,10.6704619549406));
#46480=CARTESIAN_POINT('Ctrl Pts',(1.62797700284765,-2.45227910615473,10.6654092418398));
#46481=CARTESIAN_POINT('Ctrl Pts',(1.54961172748861,-2.50254685608309,10.6603565287391));
#46482=CARTESIAN_POINT('Ctrl Pts',(1.46892045792133,-2.54904623110295,10.6553038156384));
#46483=CARTESIAN_POINT('Ctrl Pts',(1.38833960322827,-2.59548197814086,10.6502580164787));
#46484=CARTESIAN_POINT('Ctrl Pts',(1.30543946062863,-2.63815937727123,10.6452122173191));
#46485=CARTESIAN_POINT('Ctrl Pts',(1.22060601730583,-2.67684234696719,10.6401664181594));
#46486=CARTESIAN_POINT('Ctrl Pts',(1.13174887977234,-2.71736006997648,10.6348812941289));
#46487=CARTESIAN_POINT('Ctrl Pts',(1.04077090544082,-2.75349478101027,10.6295961700984));
#46488=CARTESIAN_POINT('Ctrl Pts',(0.948146751141357,-2.78502813958856,
10.6243110460678));
#46489=CARTESIAN_POINT('Ctrl Pts',(0.8598755379332,-2.81507956450342,10.619274300376));
#46490=CARTESIAN_POINT('Ctrl Pts',(0.7701098414749,-2.84095216925188,10.6142375546841));
#46491=CARTESIAN_POINT('Ctrl Pts',(0.679281289723433,-2.86250605753624,
10.6092008089923));
#46492=CARTESIAN_POINT('Ctrl Pts',(0.588483774261536,-2.88405258081582,
10.604165784366));
#46493=CARTESIAN_POINT('Ctrl Pts',(0.49662455678125,-2.90128321708858,10.5991307597398));
#46494=CARTESIAN_POINT('Ctrl Pts',(0.404148771699878,-2.91410840058044,
10.5940957351136));
#46495=CARTESIAN_POINT('Ctrl Pts',(0.311678736658876,-2.92693278661681,
10.5890610235595));
#46496=CARTESIAN_POINT('Ctrl Pts',(0.218592650212067,-2.93535220400183,
10.5840263120055));
#46497=CARTESIAN_POINT('Ctrl Pts',(0.125343007597342,-2.93932868703833,
10.5789916004514));
#46498=CARTESIAN_POINT('Ctrl Pts',(0.0320730981095047,-2.94330603432347,
10.5739557946534));
#46499=CARTESIAN_POINT('Ctrl Pts',(-0.0613599944895516,-2.94283851101469,
10.5689199888553));
#46500=CARTESIAN_POINT('Ctrl Pts',(-0.154502669429059,-2.93794025213912,
10.5638841830573));
#46501=CARTESIAN_POINT('Ctrl Pts',(-0.247746501442313,-2.93303667353729,
10.5588429081509));
#46502=CARTESIAN_POINT('Ctrl Pts',(-0.340698842298211,-2.92369277946677,
10.5538016332446));
#46503=CARTESIAN_POINT('Ctrl Pts',(-0.432910463523054,-2.90997466150004,
10.5487603583382));
#46504=CARTESIAN_POINT('Ctrl Pts',(-0.525180571250394,-2.8962478426263,
10.5437158859332));
#46505=CARTESIAN_POINT('Ctrl Pts',(-0.616708588991816,-2.87814136307095,
10.5386714135281));
#46506=CARTESIAN_POINT('Ctrl Pts',(-0.707056849449534,-2.85577215681617,
10.5336269411231));
#46507=CARTESIAN_POINT('Ctrl Pts',(-0.797544146141969,-2.83336852676402,
10.5285747058187));
#46508=CARTESIAN_POINT('Ctrl Pts',(-0.886847637795464,-2.80668920528993,
10.5235224705143));
#46509=CARTESIAN_POINT('Ctrl Pts',(-0.974546437944797,-2.77590043774792,
10.51847023521));
#46510=CARTESIAN_POINT('Ctrl Pts',(-1.00432649978491,-2.76544543266438,
10.5167546372823));
#46511=CARTESIAN_POINT('Ctrl Pts',(-1.03392171338596,-2.75451697308154,
10.5150390393547));
#46512=CARTESIAN_POINT('Ctrl Pts',(-1.06331621815642,-2.74312278620654,
10.513323441427));
#46513=CARTESIAN_POINT('Ctrl Pts',(-1.15002978885464,-2.70951001957381,
10.5082624402857));
#46514=CARTESIAN_POINT('Ctrl Pts',(-1.23529755708651,-2.6717235695059,10.5032014391445));
#46515=CARTESIAN_POINT('Ctrl Pts',(-1.31869056571622,-2.62990859002571,
10.4981404380032));
#46516=CARTESIAN_POINT('Ctrl Pts',(-1.4019713265358,-2.58814989391933,10.4930862490193));
#46517=CARTESIAN_POINT('Ctrl Pts',(-1.48338195050866,-2.54237364151342,
10.4880320600354));
#46518=CARTESIAN_POINT('Ctrl Pts',(-1.56251207205325,-2.49277356065244,
10.4829778710514));
#46519=CARTESIAN_POINT('Ctrl Pts',(-1.64522515283805,-2.44092762114034,
10.477694831754));
#46520=CARTESIAN_POINT('Ctrl Pts',(-1.72544586872966,-2.38490355231225,
10.4724117924566));
#46521=CARTESIAN_POINT('Ctrl Pts',(-1.80273259262423,-2.32497724709089,
10.4671287531592));
#46522=CARTESIAN_POINT('Ctrl Pts',(-1.87654180176376,-2.26774732489783,
10.4620834241202));
#46523=CARTESIAN_POINT('Ctrl Pts',(-1.94767494127508,-2.20695902974395,
10.4570380950812));
#46524=CARTESIAN_POINT('Ctrl Pts',(-2.01577695263679,-2.14289693574338,
10.4519927660422));
#46525=CARTESIAN_POINT('Ctrl Pts',(-2.08385644498234,-2.07885602489585,
10.4469491053217));
#46526=CARTESIAN_POINT('Ctrl Pts',(-2.14890647874785,-2.01154376905216,
10.4419054446012));
#46527=CARTESIAN_POINT('Ctrl Pts',(-2.21060663169751,-1.94128367836723,
10.4368617838807));
#46528=CARTESIAN_POINT('Ctrl Pts',(-2.27230346586229,-1.87102736689702,
10.4318183944532));
#46529=CARTESIAN_POINT('Ctrl Pts',(-2.33065048599045,-1.79782386866528,
10.4267750050258));
#46530=CARTESIAN_POINT('Ctrl Pts',(-2.38536632740192,-1.72203120880462,
10.4217316155984));
#46531=CARTESIAN_POINT('Ctrl Pts',(-2.44009437491711,-1.64622164098742,
10.416687101083));
#46532=CARTESIAN_POINT('Ctrl Pts',(-2.49118937616854,-1.56782212316922,
10.4116425865677));
#46533=CARTESIAN_POINT('Ctrl Pts',(-2.53841286756387,-1.48722026404502,
10.4065980720523));
#46534=CARTESIAN_POINT('Ctrl Pts',(-2.58568753408577,-1.40653105834352,
10.4015480909003));
#46535=CARTESIAN_POINT('Ctrl Pts',(-2.62908209378073,-1.32363513043131,
10.3964981097482));
#46536=CARTESIAN_POINT('Ctrl Pts',(-2.66840386797062,-1.23894503405092,
10.3914481285962));
#46537=CARTESIAN_POINT('Ctrl Pts',(-2.70775060717982,-1.15420116873627,
10.3863949412593));
#46538=CARTESIAN_POINT('Ctrl Pts',(-2.74301924617896,-1.06766127635864,
10.3813417539225));
#46539=CARTESIAN_POINT('Ctrl Pts',(-2.77406590736742,-0.979756266416189,
10.3762885665856));
#46540=CARTESIAN_POINT('Ctrl Pts',(-2.80515990044789,-0.891717241726933,
10.37122767546));
#46541=CARTESIAN_POINT('Ctrl Pts',(-2.83201894283078,-0.802309368669151,
10.3661667843344));
#46542=CARTESIAN_POINT('Ctrl Pts',(-2.85454955267706,-0.711976721045849,
10.3611058932088));
#46543=CARTESIAN_POINT('Ctrl Pts',(-2.86185211042732,-0.682698357943202,
10.3594655714437));
#46544=CARTESIAN_POINT('Ctrl Pts',(-2.86870036250045,-0.653322905436628,
10.3578252496786));
#46545=CARTESIAN_POINT('Ctrl Pts',(-2.87509229263909,-0.623865617587072,
10.3561849279135));
#46546=CARTESIAN_POINT('Ctrl Pts',(-2.90197412367268,-0.499980372050345,
10.3492864087535));
#46547=CARTESIAN_POINT('Ctrl Pts',(-2.92085641814638,-0.374303537995701,
10.3423878895935));
#46548=CARTESIAN_POINT('Ctrl Pts',(-2.9315534651542,-0.247706037355537,
10.3354893704335));
#46549=CARTESIAN_POINT('Ctrl Pts',(-2.93843477274814,-0.166267081175227,
10.3310516193189));
#46550=CARTESIAN_POINT('Ctrl Pts',(-2.94192972963076,-0.0844474714313159,
10.3266138682042));
#46551=CARTESIAN_POINT('Ctrl Pts',(-2.94199895080427,-0.00248464616942429,
10.3221761170896));
#46552=CARTESIAN_POINT('',(-2.93787859032851,0.00118007037484616,9.3221761170896));
#46553=CARTESIAN_POINT('Ctrl Pts',(-2.9424244111198,-0.00248111071493722,
10.3221759062437));
#46554=CARTESIAN_POINT('Ctrl Pts',(-2.93565894065101,0.755679485053147,
10.2811327422958));
#46555=CARTESIAN_POINT('Ctrl Pts',(-2.25296184349933,2.49216616011857,10.1877100738435));
#46556=CARTESIAN_POINT('Ctrl Pts',(0.655114493273779,3.40289939669596,10.0419079008864));
#46557=CARTESIAN_POINT('Ctrl Pts',(3.20077001198984,1.32799366090116,9.88476938737303));
#46558=CARTESIAN_POINT('Ctrl Pts',(2.87168850378309,-1.93961114588259,9.72763087385946));
#46559=CARTESIAN_POINT('Ctrl Pts',(-0.0366657672895371,-3.46516125435104,
9.57049236034596));
#46560=CARTESIAN_POINT('Ctrl Pts',(-2.50974118686153,-2.10044319083052,
9.43534077475601));
#46561=CARTESIAN_POINT('Ctrl Pts',(-2.93580007289335,-0.56247072784923,
9.35256869367055));
#46562=CARTESIAN_POINT('Ctrl Pts',(-2.93787859032851,0.00118007037484616,
9.3221761170896));
#46563=CARTESIAN_POINT('',(-2.94622250669394,0.000937675328142526,8.3221761170896));
#46564=CARTESIAN_POINT('Ctrl Pts',(-2.93787859032851,0.00118007037484616,
9.3221761170896));
#46565=CARTESIAN_POINT('Ctrl Pts',(-2.93938225399168,0.408942454113454,
9.30018918916604));
#46566=CARTESIAN_POINT('Ctrl Pts',(-2.67122390572782,1.78622760720654,9.22582275673799));
#46567=CARTESIAN_POINT('Ctrl Pts',(-0.582935293544531,3.41596954985009,
9.09907681980543));
#46568=CARTESIAN_POINT('Ctrl Pts',(2.52967359714472,2.36841856552379,8.9419383062919));
#46569=CARTESIAN_POINT('Ctrl Pts',(3.37023102179741,-0.80635131037091,8.7847997927784));
#46570=CARTESIAN_POINT('Ctrl Pts',(1.18377939294799,-3.25688886436588,8.62766127926488));
#46571=CARTESIAN_POINT('Ctrl Pts',(-2.00528952627767,-2.7910698384739,8.47345338736861));
#46572=CARTESIAN_POINT('Ctrl Pts',(-2.94237161798714,-0.909460413780999,
8.37162499997686));
#46573=CARTESIAN_POINT('Ctrl Pts',(-2.94622250669394,0.000937675328142526,
8.3221761170896));
#46574=CARTESIAN_POINT('',(-2.93998607517527,-0.0023358300504342,7.3221761170896));
#46575=CARTESIAN_POINT('Ctrl Pts',(-2.94622250669394,0.000937675328142526,
8.3221761170896));
#46576=CARTESIAN_POINT('Ctrl Pts',(-2.94645073222768,0.0548930361868928,
8.31924549547236));
#46577=CARTESIAN_POINT('Ctrl Pts',(-2.92084742177771,1.07298108248981,8.26393536935057));
#46578=CARTESIAN_POINT('Ctrl Pts',(-1.74654067132516,2.9930342700521,8.15624573872437));
#46579=CARTESIAN_POINT('Ctrl Pts',(1.53565755714061,3.10651158777757,7.99910722521081));
#46580=CARTESIAN_POINT('Ctrl Pts',(3.43858888024392,0.429842977951656,7.84196871169733));
#46581=CARTESIAN_POINT('Ctrl Pts',(2.25311553735072,-2.63289362024366,7.6848301981838));
#46582=CARTESIAN_POINT('Ctrl Pts',(-0.956017138014639,-3.33086920560932,
7.52769168467029));
#46583=CARTESIAN_POINT('Ctrl Pts',(-2.76420883197108,-1.56637023902252,
7.40680699097222));
#46584=CARTESIAN_POINT('Ctrl Pts',(-2.94227697960606,-0.300857412821767,
7.33830180177866));
#46585=CARTESIAN_POINT('Ctrl Pts',(-2.93998607517527,-0.0023358300504342,
7.3221761170896));
#46586=CARTESIAN_POINT('',(-2.93949980478958,0.00219056232359141,6.3221761170896));
#46587=CARTESIAN_POINT('Ctrl Pts',(-2.93998607517527,-0.0023358300504342,
7.3221761170896));
#46588=CARTESIAN_POINT('Ctrl Pts',(-2.93483565594967,0.668801419715884,
7.28592229727415));
#46589=CARTESIAN_POINT('Ctrl Pts',(-2.3759760729603,2.31735690151427,7.1972889729542));
#46590=CARTESIAN_POINT('Ctrl Pts',(0.345621576330101,3.44807252913396,7.05627614412975));
#46591=CARTESIAN_POINT('Ctrl Pts',(3.06802702248428,1.61116995727812,6.89913763061623));
#46592=CARTESIAN_POINT('Ctrl Pts',(3.03485183459052,-1.67282180255627,6.74199911710273));
#46593=CARTESIAN_POINT('Ctrl Pts',(0.275892655912197,-3.45435112336391,
6.5848606035892));
#46594=CARTESIAN_POINT('Ctrl Pts',(-2.40179787617368,-2.2778948585372,6.44491960358484));
#46595=CARTESIAN_POINT('Ctrl Pts',(-2.93486858555413,-0.649377666932483,
6.35735810808496));
#46596=CARTESIAN_POINT('Ctrl Pts',(-2.93949980478958,0.00219056232359141,
6.3221761170896));
#46597=CARTESIAN_POINT('',(-2.94644869531747,-0.000604754645607275,5.3221761170896));
#46598=CARTESIAN_POINT('Ctrl Pts',(-2.93949980478958,0.00219056232359141,
6.3221761170896));
#46599=CARTESIAN_POINT('Ctrl Pts',(-2.94176361798241,0.320687415620876,
6.30497860358046));
#46600=CARTESIAN_POINT('Ctrl Pts',(-2.74834588968967,1.60657553764138,6.23540158556681));
#46601=CARTESIAN_POINT('Ctrl Pts',(-0.88853140270286,3.34950300605666,6.11344506304867));
#46602=CARTESIAN_POINT('Ctrl Pts',(2.30584575575064,2.5868385708981,5.95630654953516));
#46603=CARTESIAN_POINT('Ctrl Pts',(3.42920337545963,-0.49922204570182,5.79916803602163));
#46604=CARTESIAN_POINT('Ctrl Pts',(1.47258603363213,-3.13690114838419,5.64202952250812));
#46605=CARTESIAN_POINT('Ctrl Pts',(-1.80664989208077,-2.95713959911128,
5.48489100899462));
#46606=CARTESIAN_POINT('Ctrl Pts',(-2.9306284478891,-1.03309719749912,5.37827320718843));
#46607=CARTESIAN_POINT('Ctrl Pts',(-2.94654631348559,-0.0348197596345374,
5.32403490988676));
#46608=CARTESIAN_POINT('Ctrl Pts',(-2.94644869531747,-0.000604754645607275,
5.3221761170896));
#46609=CARTESIAN_POINT('',(-2.93815144027097,-0.00144838940242836,4.32217611708959));
#46610=CARTESIAN_POINT('Ctrl Pts',(-2.94644869531747,-0.000604754645607275,
5.3221761170896));
#46611=CARTESIAN_POINT('Ctrl Pts',(-2.94379550054715,0.929335583914262,
5.27165540538226));
#46612=CARTESIAN_POINT('Ctrl Pts',(-1.9707214474043,2.82822213535154,5.16875518917042));
#46613=CARTESIAN_POINT('Ctrl Pts',(1.24933397805705,3.23230924456063,5.01347546845408));
#46614=CARTESIAN_POINT('Ctrl Pts',(3.38583301773346,0.738101088738995,4.85633695494055));
#46615=CARTESIAN_POINT('Ctrl Pts',(2.48131063733585,-2.41904029776208,4.69919844142705));
#46616=CARTESIAN_POINT('Ctrl Pts',(-0.651826904677944,-3.40349528097658,
4.54205992791354));
#46617=CARTESIAN_POINT('Ctrl Pts',(-2.68938574184905,-1.74603534949716,
4.41638581980104));
#46618=CARTESIAN_POINT('Ctrl Pts',(-2.93991718809614,-0.389242894153138,
4.34309121619307));
#46619=CARTESIAN_POINT('Ctrl Pts',(-2.93815144027097,-0.00144838940242836,
4.32217611708959));
#46620=CARTESIAN_POINT('',(-2.94188729812012,0.00254759896953657,3.32217611708959));
#46621=CARTESIAN_POINT('Ctrl Pts',(-2.93815144027097,-0.00144838940242836,
4.32217611708959));
#46622=CARTESIAN_POINT('Ctrl Pts',(-2.93549507201127,0.581944663119171,
4.29071171168856));
#46623=CARTESIAN_POINT('Ctrl Pts',(-2.48662477666494,2.1402933973268,4.20686780178306));
#46624=CARTESIAN_POINT('Ctrl Pts',(0.0333505152944463,3.46519064195022,
4.07064438737298));
#46625=CARTESIAN_POINT('Ctrl Pts',(2.91027678633436,1.88120904397026,3.91350587385948));
#46626=CARTESIAN_POINT('Ctrl Pts',(3.17330745213008,-1.39240017768036,3.75636736034596));
#46627=CARTESIAN_POINT('Ctrl Pts',(0.586198762341217,-3.41541058398189,
3.59922884683245));
#46628=CARTESIAN_POINT('Ctrl Pts',(-2.28155114480077,-2.45331685892863,
3.45449843241366));
#46629=CARTESIAN_POINT('Ctrl Pts',(-2.93534805643284,-0.736191897535303,
3.36214752249938));
#46630=CARTESIAN_POINT('Ctrl Pts',(-2.94188729812012,0.00254759896953657,
3.32217611708959));
#46631=CARTESIAN_POINT('',(-2.94199938418253,-0.00190354132858995,2.32217611708959));
#46632=CARTESIAN_POINT('Ctrl Pts',(-2.94188729812012,0.00254759896953657,
3.32217611708959));
#46633=CARTESIAN_POINT('Ctrl Pts',(-2.94391723822425,0.231870355671395,
3.30976801799487));
#46634=CARTESIAN_POINT('Ctrl Pts',(-2.8154264390555,1.42700723566272,3.24498041439567));
#46635=CARTESIAN_POINT('Ctrl Pts',(-1.18688998506612,3.25575653825376,3.1278133062919));
#46636=CARTESIAN_POINT('Ctrl Pts',(2.06323722577403,2.78418938435942,2.9706747927784));
#46637=CARTESIAN_POINT('Ctrl Pts',(3.4602462989487,-0.188026617557372,2.81353627926488));
#46638=CARTESIAN_POINT('Ctrl Pts',(1.74939887098719,-2.99136460950402,2.65639776575137));
#46639=CARTESIAN_POINT('Ctrl Pts',(-1.53268946892132,-3.1079769880761,2.49925925223785));
#46640=CARTESIAN_POINT('Ctrl Pts',(-2.88363156232728,-1.21157661749859,
2.38785203601727));
#46641=CARTESIAN_POINT('Ctrl Pts',(-2.94579921760659,-0.124453265927633,
2.32882432430118));
#46642=CARTESIAN_POINT('Ctrl Pts',(-2.94487182720719,-0.00190539986535287,
2.32217611708959));
#46643=CARTESIAN_POINT('',(-2.94199999670507,-0.000139238540415516,1.32217611711858));
#46644=CARTESIAN_POINT('Ctrl Pts',(-2.94199938418253,-0.00190354132858995,
2.32217611708959));
#46645=CARTESIAN_POINT('Ctrl Pts',(-2.94205878758215,0.0899067926258124,
2.31719052791049));
#46646=CARTESIAN_POINT('Ctrl Pts',(-2.93781632057424,0.181878623548529,
2.31220493873139));
#46647=CARTESIAN_POINT('Ctrl Pts',(-2.92925308992623,0.273569616656554,
2.30721934955229));
#46648=CARTESIAN_POINT('Ctrl Pts',(-2.92050500409423,0.367239950985021,
2.30212613603806));
#46649=CARTESIAN_POINT('Ctrl Pts',(-2.90724736516512,0.460616705008599,
2.29703292252383));
#46650=CARTESIAN_POINT('Ctrl Pts',(-2.88951627230318,0.553226637188741,
2.29193970900961));
#46651=CARTESIAN_POINT('Ctrl Pts',(-2.87219424854482,0.643699991424419,
2.28696399960541));
#46652=CARTESIAN_POINT('Ctrl Pts',(-2.85060304408045,0.73344104896173,2.28198829020122));
#46653=CARTESIAN_POINT('Ctrl Pts',(-2.82482866310374,0.822014004812291,
2.27701258079702));
#46654=CARTESIAN_POINT('Ctrl Pts',(-2.79906463001987,0.910551400411887,
2.27203886903955));
#46655=CARTESIAN_POINT('Ctrl Pts',(-2.76912088217163,0.997921187859738,
2.26706515728208));
#46656=CARTESIAN_POINT('Ctrl Pts',(-2.73513396050232,1.08370024365914,2.26209144552461));
#46657=CARTESIAN_POINT('Ctrl Pts',(-2.70115061564178,1.16947027200728,2.25711825720424));
#46658=CARTESIAN_POINT('Ctrl Pts',(-2.66312511112893,1.25364947741371,2.25214506888387));
#46659=CARTESIAN_POINT('Ctrl Pts',(-2.62124258581226,1.33583356235881,2.2471718805635));
#46660=CARTESIAN_POINT('Ctrl Pts',(-2.57759754955394,1.42147613859236,2.24198940928411));
#46661=CARTESIAN_POINT('Ctrl Pts',(-2.5297639388273,1.50495148822779,2.23680693800472));
#46662=CARTESIAN_POINT('Ctrl Pts',(-2.4780040829923,1.58583093823821,2.23162446672534));
#46663=CARTESIAN_POINT('Ctrl Pts',(-2.42827199765954,1.6635418136782,2.2266450265831));
#46664=CARTESIAN_POINT('Ctrl Pts',(-2.37491586195325,1.73885602980887,2.22166558644086));
#46665=CARTESIAN_POINT('Ctrl Pts',(-2.31821134187879,1.81142490166844,2.21668614629863));
#46666=CARTESIAN_POINT('Ctrl Pts',(-2.26146982595984,1.88404111978356,2.21170345741021));
#46667=CARTESIAN_POINT('Ctrl Pts',(-2.20137587817613,1.95390808672331,2.20672076852179));
#46668=CARTESIAN_POINT('Ctrl Pts',(-2.13824331096343,2.02071263249383,2.20173807963337));
#46669=CARTESIAN_POINT('Ctrl Pts',(-2.07501857247312,2.08761471049859,2.19674811619837));
#46670=CARTESIAN_POINT('Ctrl Pts',(-2.008746697179,2.15144513885915,2.19175815276337));
#46671=CARTESIAN_POINT('Ctrl Pts',(-1.93977543542689,2.21193021140235,2.18676818932838));
#46672=CARTESIAN_POINT('Ctrl Pts',(-1.9315469049486,2.21914630764678,2.18617286795586));
#46673=CARTESIAN_POINT('Ctrl Pts',(-1.92327998722939,2.22631483862489,2.18557754658335));
#46674=CARTESIAN_POINT('Ctrl Pts',(-1.91497529975521,2.23343538105033,2.18498222521083));
#46675=CARTESIAN_POINT('Ctrl Pts',(-1.84439708423493,2.2939500216658,2.17992282709816));
#46676=CARTESIAN_POINT('Ctrl Pts',(-1.77082529385272,2.3512207736073,2.17486342898548));
#46677=CARTESIAN_POINT('Ctrl Pts',(-1.69459024701272,2.40493823095924,2.1698040308728));
#46678=CARTESIAN_POINT('Ctrl Pts',(-1.61845798842576,2.45858326068338,2.1647514543824));
#46679=CARTESIAN_POINT('Ctrl Pts',(-1.53966996865168,2.50868426408285,2.15969887789199));
#46680=CARTESIAN_POINT('Ctrl Pts',(-1.45859054654746,2.55497115786507,2.15464630140159));
#46681=CARTESIAN_POINT('Ctrl Pts',(-1.37380640461788,2.60337301458856,2.14936286016391));
#46682=CARTESIAN_POINT('Ctrl Pts',(-1.2865168312337,2.64760356830585,2.14407941892623));
#46683=CARTESIAN_POINT('Ctrl Pts',(-1.19717389059228,2.68740370537888,2.13879597768856));
#46684=CARTESIAN_POINT('Ctrl Pts',(-1.11188488670734,2.72539791086476,2.13375227264582));
#46685=CARTESIAN_POINT('Ctrl Pts',(-1.02472524270107,2.75935477790647,2.12870856760308));
#46686=CARTESIAN_POINT('Ctrl Pts',(-0.936113283859184,2.78909589648373,
2.12366486256034));
#46687=CARTESIAN_POINT('Ctrl Pts',(-0.847530646881758,2.81882717366871,
2.11862282648912));
#46688=CARTESIAN_POINT('Ctrl Pts',(-0.75749706931278,2.84434533342064,2.1135807904179));
#46689=CARTESIAN_POINT('Ctrl Pts',(-0.666448831070414,2.86552088730215,
2.10853875434668));
#46690=CARTESIAN_POINT('Ctrl Pts',(-0.575405464769122,2.88669530809143,
2.10349698807204));
#46691=CARTESIAN_POINT('Ctrl Pts',(-0.483347977108855,2.90352748529881,
2.09845522179739));
#46692=CARTESIAN_POINT('Ctrl Pts',(-0.390724613048398,2.91593866135044,
2.09341345552275));
#46693=CARTESIAN_POINT('Ctrl Pts',(-0.298080512743564,2.92835261597939,
2.0883705605124));
#46694=CARTESIAN_POINT('Ctrl Pts',(-0.204870723203345,2.93634354517789,
2.08332766550206));
#46695=CARTESIAN_POINT('Ctrl Pts',(-0.111549287758481,2.93988448011152,
2.07828477049171));
#46696=CARTESIAN_POINT('Ctrl Pts',(-0.0181264186579392,2.94342926378551,
2.07323639421896));
#46697=CARTESIAN_POINT('Ctrl Pts',(0.0754078955767428,2.9425143834227,2.06818801794621));
#46698=CARTESIAN_POINT('Ctrl Pts',(0.168599266171156,2.93716500854932,2.06313964167345));
#46699=CARTESIAN_POINT('Ctrl Pts',(0.261849944904348,2.93181222926773,2.05808805255171));
#46700=CARTESIAN_POINT('Ctrl Pts',(0.354756805729905,2.92201938341522,2.05303646342997));
#46701=CARTESIAN_POINT('Ctrl Pts',(0.446872353772485,2.90786332200017,2.04798487430823));
#46702=CARTESIAN_POINT('Ctrl Pts',(0.539128802992504,2.89368560728375,2.04292555820803));
#46703=CARTESIAN_POINT('Ctrl Pts',(0.630591090874431,2.87513144513155,2.03786624210784));
#46704=CARTESIAN_POINT('Ctrl Pts',(0.720823945817723,2.85232831895905,2.03280692600764));
#46705=CARTESIAN_POINT('Ctrl Pts',(0.750330239293404,2.84487165881645,2.03115252123753));
#46706=CARTESIAN_POINT('Ctrl Pts',(0.779705209996882,2.83696104752962,2.02949811646742));
#46707=CARTESIAN_POINT('Ctrl Pts',(0.808934084771822,2.82860206577284,2.02784371169731));
#46708=CARTESIAN_POINT('Ctrl Pts',(0.898320175890856,2.80303910070057,2.02278430463265));
#46709=CARTESIAN_POINT('Ctrl Pts',(0.986648264179951,2.77319068607448,2.01772489756798));
#46710=CARTESIAN_POINT('Ctrl Pts',(1.07347815233169,2.73916203545291,2.01266549050331));
#46711=CARTESIAN_POINT('Ctrl Pts',(1.16019096843477,2.70517926539075,2.00761290499701));
#46712=CARTESIAN_POINT('Ctrl Pts',(1.24540918999726,2.6670276205544,2.00256031949071));
#46713=CARTESIAN_POINT('Ctrl Pts',(1.32870668331679,2.6248623868137,1.9975077339844));
#46714=CARTESIAN_POINT('Ctrl Pts',(1.41581005317874,2.58077061641979,1.99222429499271));
#46715=CARTESIAN_POINT('Ctrl Pts',(1.50081251730368,2.53228987076498,1.98694085600102));
#46716=CARTESIAN_POINT('Ctrl Pts',(1.5832487812635,2.47965467285823,1.98165741700933));
#46717=CARTESIAN_POINT('Ctrl Pts',(1.66194467455955,2.42940768543889,1.97661370285788));
#46718=CARTESIAN_POINT('Ctrl Pts',(1.73830173591452,2.37537527927245,1.97156998870644));
#46719=CARTESIAN_POINT('Ctrl Pts',(1.81194060728049,2.31780828277232,1.96652627455499));
#46720=CARTESIAN_POINT('Ctrl Pts',(1.88555511165802,2.26026033510215,1.96148422936075));
#46721=CARTESIAN_POINT('Ctrl Pts',(1.95645286468793,2.19918039345385,1.9564421841665));
#46722=CARTESIAN_POINT('Ctrl Pts',(2.02428544472045,2.13486122225613,1.95140013897226));
#46723=CARTESIAN_POINT('Ctrl Pts',(2.0921143951082,2.07054549270463,1.94635836357216));
#46724=CARTESIAN_POINT('Ctrl Pts',(2.15687817772981,2.0029911832811,1.94131658817205));
#46725=CARTESIAN_POINT('Ctrl Pts',(2.21826411704521,1.93252899254568,1.93627481277195));
#46726=CARTESIAN_POINT('Ctrl Pts',(2.2796637991228,1.86205102710451,1.93123190864562));
#46727=CARTESIAN_POINT('Ctrl Pts',(2.33768384541717,1.78866422134694,1.92618900451928));
#46728=CARTESIAN_POINT('Ctrl Pts',(2.3920516066775,1.71273264434108,1.92114610039294));
#46729=CARTESIAN_POINT('Ctrl Pts',(2.44647846095373,1.63671853633187,1.91609771506953));
#46730=CARTESIAN_POINT('Ctrl Pts',(2.4972448496801,1.55815449742095,1.91104932974613));
#46731=CARTESIAN_POINT('Ctrl Pts',(2.54412144579094,1.47743360902162,1.90600094442272));
#46732=CARTESIAN_POINT('Ctrl Pts',(2.59102787443685,1.39666134938516,1.90094934627789));
#46733=CARTESIAN_POINT('Ctrl Pts',(2.63403937864078,1.31372990014908,1.89589774813306));
#46734=CARTESIAN_POINT('Ctrl Pts',(2.67297356051088,1.22905506174856,1.89084614998823));
#46735=CARTESIAN_POINT('Ctrl Pts',(2.71196729562918,1.14425070575131,1.88578682498069));
#46736=CARTESIAN_POINT('Ctrl Pts',(2.74687109648308,1.05769804824939,1.88072749997314));
#46737=CARTESIAN_POINT('Ctrl Pts',(2.7775515549006,0.969830583075863,1.8756681749656));
#46738=CARTESIAN_POINT('Ctrl Pts',(2.78758361797581,0.941099201657635,1.87401384937167));
#46739=CARTESIAN_POINT('Ctrl Pts',(2.79716452718351,0.91222733972703,1.87235952377774));
#46740=CARTESIAN_POINT('Ctrl Pts',(2.80629080157345,0.883230398596102,1.87070519818381));
#46741=CARTESIAN_POINT('Ctrl Pts',(2.83420143639891,0.794549848310172,1.86564581956316));
#46742=CARTESIAN_POINT('Ctrl Pts',(2.85795278857554,0.704391329236729,1.86058644094251));
#46743=CARTESIAN_POINT('Ctrl Pts',(2.87739015045553,0.613180170962414,1.85552706232187));
#46744=CARTESIAN_POINT('Ctrl Pts',(2.89680130479238,0.52209199338784,1.85047450529997));
#46745=CARTESIAN_POINT('Ctrl Pts',(2.91190993682756,0.429954426689562,1.84542194827807));
#46746=CARTESIAN_POINT('Ctrl Pts',(2.92261087498168,0.337208649709403,1.84036939125617));
#46747=CARTESIAN_POINT('Ctrl Pts',(2.93380081896342,0.240224625130997,1.83508594514843));
#46748=CARTESIAN_POINT('Ctrl Pts',(2.9401704609242,0.142575941416614,1.82980249904068));
#46749=CARTESIAN_POINT('Ctrl Pts',(2.94165918157964,0.0447801231376263,
1.82451905293294));
#46750=CARTESIAN_POINT('Ctrl Pts',(2.9430803447815,-0.0485777662194173,
1.81947536716159));
#46751=CARTESIAN_POINT('Ctrl Pts',(2.94005389202632,-0.142069231699168,
1.81443168139025));
#46752=CARTESIAN_POINT('Ctrl Pts',(2.93258015749533,-0.235239494695669,
1.8093879956189));
#46753=CARTESIAN_POINT('Ctrl Pts',(2.92510889587937,-0.328378929443869,
1.80434597870618));
#46754=CARTESIAN_POINT('Ctrl Pts',(2.91319331168689,-0.421196931931897,
1.79930396179347));
#46755=CARTESIAN_POINT('Ctrl Pts',(2.89688578062519,-0.513241438322724,
1.79426194488075));
#46756=CARTESIAN_POINT('Ctrl Pts',(2.88057912173122,-0.605281021942152,
1.78922019762776));
#46757=CARTESIAN_POINT('Ctrl Pts',(2.85988106080887,-0.696546755862382,
1.78417845037477));
#46758=CARTESIAN_POINT('Ctrl Pts',(2.83489532504749,-0.786595509791323,
1.77913670312179));
#46759=CARTESIAN_POINT('Ctrl Pts',(2.80990399473482,-0.876664426519443,
1.77409382697214));
#46760=CARTESIAN_POINT('Ctrl Pts',(2.78062320144801,-0.965515395581965,
1.76905095082249));
#46761=CARTESIAN_POINT('Ctrl Pts',(2.74720657326158,-1.05272030655267,1.76400807467285));
#46762=CARTESIAN_POINT('Ctrl Pts',(2.71375362120272,-1.14002000925535,1.75895971691719));
#46763=CARTESIAN_POINT('Ctrl Pts',(2.67615602077653,-1.22566966905998,1.75391135916153));
#46764=CARTESIAN_POINT('Ctrl Pts',(2.63461547956147,-1.30926134704079,1.74886300140587));
#46765=CARTESIAN_POINT('Ctrl Pts',(2.59304849987271,-1.3929062269375,1.74381143062338));
#46766=CARTESIAN_POINT('Ctrl Pts',(2.54753379891838,-1.47449013126337,1.73875985984088));
#46767=CARTESIAN_POINT('Ctrl Pts',(2.49831789871698,-1.55363177006342,1.73370828905838));
#46768=CARTESIAN_POINT('Ctrl Pts',(2.44902671290464,-1.63289447190616,1.72864899088309));
#46769=CARTESIAN_POINT('Ctrl Pts',(2.39602327933239,-1.70970708867303,1.72358969270781));
#46770=CARTESIAN_POINT('Ctrl Pts',(2.33959587545587,-1.78371946772745,1.71853039453252));
#46771=CARTESIAN_POINT('Ctrl Pts',(2.32114211293664,-1.80792414086007,1.71687582457844));
#46772=CARTESIAN_POINT('Ctrl Pts',(2.30232245356334,-1.83182960538549,1.71522125462436));
#46773=CARTESIAN_POINT('Ctrl Pts',(2.28314783790605,-1.85542446633241,1.71356668467028));
#46774=CARTESIAN_POINT('Ctrl Pts',(2.22451498180353,-1.92757371361778,1.70850727885152));
#46775=CARTESIAN_POINT('Ctrl Pts',(2.16235721498671,-1.99706600845774,1.70344787303276));
#46776=CARTESIAN_POINT('Ctrl Pts',(2.09694427168874,-2.06353791373742,1.698388467214));
#46777=CARTESIAN_POINT('Ctrl Pts',(2.03161952660659,-2.12992019297136,1.69333588314249));
#46778=CARTESIAN_POINT('Ctrl Pts',(1.96304863557668,-2.19328986305016,1.68828329907098));
#46779=CARTESIAN_POINT('Ctrl Pts',(1.89154185024512,-2.25331609606181,1.68323071499948));
#46780=CARTESIAN_POINT('Ctrl Pts',(1.81676788183502,-2.31608495960644,1.6779472756727));
#46781=CARTESIAN_POINT('Ctrl Pts',(1.73878363591286,-2.37519718468404,1.67266383634592));
#46782=CARTESIAN_POINT('Ctrl Pts',(1.65798761618054,-2.43031707079385,1.66738039701914));
#46783=CARTESIAN_POINT('Ctrl Pts',(1.58085757829445,-2.48293598590886,1.66233668475716));
#46784=CARTESIAN_POINT('Ctrl Pts',(1.50116576355505,-2.53191666207956,1.65729297249517));
#46785=CARTESIAN_POINT('Ctrl Pts',(1.41929189825447,-2.57700882954429,1.65224926023319));
#46786=CARTESIAN_POINT('Ctrl Pts',(1.33744512751896,-2.62208607463225,1.64720721708979));
#46787=CARTESIAN_POINT('Ctrl Pts',(1.25341812848943,-2.66327715446222,1.64216517394639));
#46788=CARTESIAN_POINT('Ctrl Pts',(1.16761703258563,-2.70037672653575,1.63712313080299));
#46789=CARTESIAN_POINT('Ctrl Pts',(1.08182053048615,-2.73747431229229,1.63208135761138));
#46790=CARTESIAN_POINT('Ctrl Pts',(0.994250526977929,-2.77048065066324,
1.62703958441977));
#46791=CARTESIAN_POINT('Ctrl Pts',(0.905333988585948,-2.79923817656002,
1.62199781122817));
#46792=CARTESIAN_POINT('Ctrl Pts',(0.816397546733572,-2.82800213966508,
1.61695490946436));
#46793=CARTESIAN_POINT('Ctrl Pts',(0.726114392624978,-2.85251526541975,
1.61191200770056));
#46794=CARTESIAN_POINT('Ctrl Pts',(0.634926449410641,-2.87266990861094,
1.60686910593675));
#46795=CARTESIAN_POINT('Ctrl Pts',(0.543639396670226,-2.89284645729824,
1.60182072318954));
#46796=CARTESIAN_POINT('Ctrl Pts',(0.451446025075634,-2.90865497379437,
1.59677234044232));
#46797=CARTESIAN_POINT('Ctrl Pts',(0.358797911633199,-2.92003905087032,
1.59172395769511));
#46798=CARTESIAN_POINT('Ctrl Pts',(0.266090838691182,-2.93143037255669,
1.58667236225301));
#46799=CARTESIAN_POINT('Ctrl Pts',(0.172928888751452,-2.93839161647353,
1.58162076681091));
#46800=CARTESIAN_POINT('Ctrl Pts',(0.0797660882176299,-2.94091845707603,
1.5765691713688));
#46801=CARTESIAN_POINT('Ctrl Pts',(-0.0135392100561702,-2.94344916262326,
1.57150984922753));
#46802=CARTESIAN_POINT('Ctrl Pts',(-0.106844919901419,-2.94153193742826,
1.56645052708625));
#46803=CARTESIAN_POINT('Ctrl Pts',(-0.199699996586498,-2.93521445747382,
1.56139120494498));
#46804=CARTESIAN_POINT('Ctrl Pts',(-0.230062620282292,-2.933148708638,1.55973686034891));
#46805=CARTESIAN_POINT('Ctrl Pts',(-0.260377129848652,-2.9306128852774,
1.55808251575285));
#46806=CARTESIAN_POINT('Ctrl Pts',(-0.290627994539668,-2.92760983889415,
1.55642817115678));
#46807=CARTESIAN_POINT('Ctrl Pts',(-0.383143673011526,-2.91842567584738,
1.55136871866527));
#46808=CARTESIAN_POINT('Ctrl Pts',(-0.475383880833377,-2.90483591609127,
1.54630926617376));
#46809=CARTESIAN_POINT('Ctrl Pts',(-0.566896699361166,-2.88686545101316,
1.54124981368224));
#46810=CARTESIAN_POINT('Ctrl Pts',(-0.658286137903122,-2.86891921418812,
1.53619718247748));
#46811=CARTESIAN_POINT('Ctrl Pts',(-0.748949705218559,-2.84660409424142,
1.53114455127273));
#46812=CARTESIAN_POINT('Ctrl Pts',(-0.838440375979872,-2.81999676168728,
1.52609192006797));
#46813=CARTESIAN_POINT('Ctrl Pts',(-0.932018842480568,-2.7921740472422,
1.52080849246694));
#46814=CARTESIAN_POINT('Ctrl Pts',(-1.02431421614288,-2.75965768435425,
1.51552506486591));
#46815=CARTESIAN_POINT('Ctrl Pts',(-1.11482680265103,-2.72259530597018,
1.51024163726488));
#46816=CARTESIAN_POINT('Ctrl Pts',(-1.20123354750174,-2.68721415516963,
1.50519787707338));
#46817=CARTESIAN_POINT('Ctrl Pts',(-1.28601525677221,-2.64769060652783,
1.50015411688188));
#46818=CARTESIAN_POINT('Ctrl Pts',(-1.36875386174827,-2.60420369133238,
1.49511035669038));
#46819=CARTESIAN_POINT('Ctrl Pts',(-1.45146508932322,-2.56073116553497,
1.49006826543017));
#46820=CARTESIAN_POINT('Ctrl Pts',(-1.53213416430511,-2.5132980847454,1.48502617416995));
#46821=CARTESIAN_POINT('Ctrl Pts',(-1.61036596567334,-2.46213026799984,
1.47998408290973));
#46822=CARTESIAN_POINT('Ctrl Pts',(-1.68859358046111,-2.41096518950366,
1.47494226147738));
#46823=CARTESIAN_POINT('Ctrl Pts',(-1.76438381076976,-2.3560660152615,1.46990044004504));
#46824=CARTESIAN_POINT('Ctrl Pts',(-1.83736993038489,-2.29770227377644,
1.4648586186127));
#46825=CARTESIAN_POINT('Ctrl Pts',(-1.91037238824883,-2.23932546732321,
1.45981566854749));
#46826=CARTESIAN_POINT('Ctrl Pts',(-1.98056914318539,-2.17748282995883,
1.45477271848228));
#46827=CARTESIAN_POINT('Ctrl Pts',(-2.04762689024727,-2.11248387410089,
1.44972976841708));
#46828=CARTESIAN_POINT('Ctrl Pts',(-2.11475751728926,-2.04741427580687,
1.44468133755187));
#46829=CARTESIAN_POINT('Ctrl Pts',(-2.17874200966107,-1.97918182146721,
1.43963290668666));
#46830=CARTESIAN_POINT('Ctrl Pts',(-2.23928450504664,-1.90813230816367,
1.43458447582145));
#46831=CARTESIAN_POINT('Ctrl Pts',(-2.29986552754096,-1.83703758145578,
1.42953283231289));
#46832=CARTESIAN_POINT('Ctrl Pts',(-2.35699992200141,-1.76312257674857,
1.42448118880433));
#46833=CARTESIAN_POINT('Ctrl Pts',(-2.41043394182378,-1.68676382819405,
1.41942954529578));
#46834=CARTESIAN_POINT('Ctrl Pts',(-2.46394968616524,-1.61028829295524,
1.41437017556453));
#46835=CARTESIAN_POINT('Ctrl Pts',(-2.51375352515499,-1.5313619281524,1.40931080583329));
#46836=CARTESIAN_POINT('Ctrl Pts',(-2.55963675307689,-1.45038742834389,
1.40425143610204));
#46837=CARTESIAN_POINT('Ctrl Pts',(-2.57463614522885,-1.4239165732636,1.40259750994911));
#46838=CARTESIAN_POINT('Ctrl Pts',(-2.58921693702995,-1.39722701076762,
1.40094358379619));
#46839=CARTESIAN_POINT('Ctrl Pts',(-2.60337295665021,-1.3703332618682,1.39928965764326));
#46840=CARTESIAN_POINT('Ctrl Pts',(-2.64903858949363,-1.28357723185635,
1.39395428891139));
#46841=CARTESIAN_POINT('Ctrl Pts',(-2.69042405278558,-1.19442196979203,
1.38861892017953));
#46842=CARTESIAN_POINT('Ctrl Pts',(-2.72728553218514,-1.10330305262589,
1.38328355144766));
#46843=CARTESIAN_POINT('Ctrl Pts',(-2.76404544329879,-1.01243520493341,
1.37796288381477));
#46844=CARTESIAN_POINT('Ctrl Pts',(-2.796306074387,-0.919614827091285,1.37264221618187));
#46845=CARTESIAN_POINT('Ctrl Pts',(-2.82387039829454,-0.825299929501884,
1.36732154854897));
#46846=CARTESIAN_POINT('Ctrl Pts',(-2.85138911804932,-0.731141072416592,
1.36200968376357));
#46847=CARTESIAN_POINT('Ctrl Pts',(-2.87422689292036,-0.635492970896159,
1.35669781897816));
#46848=CARTESIAN_POINT('Ctrl Pts',(-2.89223504922506,-0.538832460078394,
1.35138595419276));
#46849=CARTESIAN_POINT('Ctrl Pts',(-2.91020301497016,-0.442387675954391,
1.34608594441431));
#46850=CARTESIAN_POINT('Ctrl Pts',(-2.92336277411057,-0.344935348068787,
1.34078593463586));
#46851=CARTESIAN_POINT('Ctrl Pts',(-2.93161598538492,-0.246965006095231,
1.3354859248574));
#46852=CARTESIAN_POINT('Ctrl Pts',(-2.93852469309688,-0.164954691002573,
1.3310493222778));
#46853=CARTESIAN_POINT('Ctrl Pts',(-2.94199609487689,-0.0825817753051015,
1.32661271969819));
#46854=CARTESIAN_POINT('Ctrl Pts',(-2.94199999670507,-0.000139238540423715,
1.32217611711858));
#46855=CARTESIAN_POINT('Ctrl Pts',(-2.94199999670509,-0.000139238001722604,
1.32217611708959));
#46856=CARTESIAN_POINT('Ctrl Pts',(-2.94200461971914,0.0975417624295902,
1.3169194644501));
#46857=CARTESIAN_POINT('Ctrl Pts',(-2.93714008660293,0.195140032597408,
1.3116628118106));
#46858=CARTESIAN_POINT('Ctrl Pts',(-2.9274568958829,0.292164547383291,1.30640615917111));
#46859=CARTESIAN_POINT('Ctrl Pts',(-2.91759330638285,0.390996638267333,
1.30105157458433));
#46860=CARTESIAN_POINT('Ctrl Pts',(-2.90272978303102,0.489232965131264,
1.29569698999755));
#46861=CARTESIAN_POINT('Ctrl Pts',(-2.88297400170303,0.586365846127163,
1.29034240541077));
#46862=CARTESIAN_POINT('Ctrl Pts',(-2.86350947736034,0.682066709344435,
1.28506676278727));
#46863=CARTESIAN_POINT('Ctrl Pts',(-2.83929615567487,0.776696093972239,
1.27979112016378));
#46864=CARTESIAN_POINT('Ctrl Pts',(-2.81048718761002,0.86978489770744,1.27451547754029));
#46865=CARTESIAN_POINT('Ctrl Pts',(-2.78103159599759,0.964963099867981,
1.26912142197186));
#46866=CARTESIAN_POINT('Ctrl Pts',(-2.74677175407064,1.05853033508138,1.26372736640344));
#46867=CARTESIAN_POINT('Ctrl Pts',(-2.7079224893435,1.15000860505811,1.25833331083501));
#46868=CARTESIAN_POINT('Ctrl Pts',(-2.66907322461637,1.24148687503483,1.25293925526659));
#46869=CARTESIAN_POINT('Ctrl Pts',(-2.6256347840461,1.33087583051891,1.24754519969817));
#46870=CARTESIAN_POINT('Ctrl Pts',(-2.57787031674964,1.41772657096534,1.24215114412974));
#46871=CARTESIAN_POINT('Ctrl Pts',(-2.53306833937824,1.49919057817427,1.23709164343404));
#46872=CARTESIAN_POINT('Ctrl Pts',(-2.484323403088,1.57866996854652,1.23203214273833));
#46873=CARTESIAN_POINT('Ctrl Pts',(-2.43183598902006,1.655758956644,1.22697264204262));
#46874=CARTESIAN_POINT('Ctrl Pts',(-2.37941935174519,1.73274399389049,1.22191996384408));
#46875=CARTESIAN_POINT('Ctrl Pts',(-2.32327051304004,1.80734467177867,1.21686728564554));
#46876=CARTESIAN_POINT('Ctrl Pts',(-2.26363564474575,1.87918005200047,1.211814607447));
#46877=CARTESIAN_POINT('Ctrl Pts',(-2.20127746812945,1.95429589371013,1.20653119174572));
#46878=CARTESIAN_POINT('Ctrl Pts',(-2.1351075099787,2.02638741982237,1.20124777604444));
#46879=CARTESIAN_POINT('Ctrl Pts',(-2.06545788195732,2.09505315871946,1.19596436034315));
#46880=CARTESIAN_POINT('Ctrl Pts',(-1.99896698228195,2.16060479030521,1.19092055647346));
#46881=CARTESIAN_POINT('Ctrl Pts',(-1.92930549514981,2.22303423457185,1.18587675260376));
#46882=CARTESIAN_POINT('Ctrl Pts',(-1.85680233912528,2.28202740417789,1.18083294873406));
#46883=CARTESIAN_POINT('Ctrl Pts',(-1.78432319216586,2.34100103848468,1.17579081509532));
#46884=CARTESIAN_POINT('Ctrl Pts',(-1.70900458915356,2.39654037991088,1.17074868145657));
#46885=CARTESIAN_POINT('Ctrl Pts',(-1.63120945504026,2.44837082848723,1.16570654781783));
#46886=CARTESIAN_POINT('Ctrl Pts',(-1.55341850486603,2.50019848954427,1.1606646853526));
#46887=CARTESIAN_POINT('Ctrl Pts',(-1.47315165717348,2.54831740936594,1.15562282288737));
#46888=CARTESIAN_POINT('Ctrl Pts',(-1.39080087224642,2.59249627458915,1.15058096042214));
#46889=CARTESIAN_POINT('Ctrl Pts',(-1.30843167565013,2.63668501715176,1.14553797071685));
#46890=CARTESIAN_POINT('Ctrl Pts',(-1.22397800664928,2.67693174654931,1.14049498101155));
#46891=CARTESIAN_POINT('Ctrl Pts',(-1.13785545991309,2.71305159411795,1.13545199130626));
#46892=CARTESIAN_POINT('Ctrl Pts',(-1.05163935271553,2.749210681,1.13040352307692));
#46893=CARTESIAN_POINT('Ctrl Pts',(-0.963751158273544,2.78123376718841,
1.12535505484758));
#46894=CARTESIAN_POINT('Ctrl Pts',(-0.874625123638633,2.80898467299131,
1.12030658661823));
#46895=CARTESIAN_POINT('Ctrl Pts',(-0.785442395262867,2.83675323135408,
1.11525490702029));
#46896=CARTESIAN_POINT('Ctrl Pts',(-0.695020687100776,2.86024408796144,
1.11020322742234));
#46897=CARTESIAN_POINT('Ctrl Pts',(-0.603805961307181,2.87937186919125,
1.10515154782439));
#46898=CARTESIAN_POINT('Ctrl Pts',(-0.512451767661679,2.898528896911,1.10009214417864));
#46899=CARTESIAN_POINT('Ctrl Pts',(-0.420302572603004,2.91330946531776,
1.0950327405329));
#46900=CARTESIAN_POINT('Ctrl Pts',(-0.327810695308905,2.92367989835431,
1.08997333688715));
#46901=CARTESIAN_POINT('Ctrl Pts',(-0.297581504424793,2.92706927490266,
1.08831976813018));
#46902=CARTESIAN_POINT('Ctrl Pts',(-0.267315714603243,2.92998798311205,
1.08666619937321));
#46903=CARTESIAN_POINT('Ctrl Pts',(-0.23702909370367,2.93243605364857,1.08501263061624));
#46904=CARTESIAN_POINT('Ctrl Pts',(-0.144355971888771,2.93992683117027,
1.07995292523173));
#46905=CARTESIAN_POINT('Ctrl Pts',(-0.0511669651402399,2.94303318993482,
1.07489321984723));
#46906=CARTESIAN_POINT('Ctrl Pts',(0.0420887859023279,2.94169891968931,
1.06983351446272));
#46907=CARTESIAN_POINT('Ctrl Pts',(0.13521885028736,2.94036644772397,1.06478062836229));
#46908=CARTESIAN_POINT('Ctrl Pts',(0.228415041169705,2.93460524712247,1.05972774226186));
#46909=CARTESIAN_POINT('Ctrl Pts',(0.321223787193121,2.9244109284677,1.05467485616143));
#46910=CARTESIAN_POINT('Ctrl Pts',(0.418265832018059,2.91375161487665,1.04939149203398));
#46911=CARTESIAN_POINT('Ctrl Pts',(0.514883757398431,2.89824508608974,1.04410812790654));
#46912=CARTESIAN_POINT('Ctrl Pts',(0.610559589537355,2.8779473566457,1.03882476377909));
#46913=CARTESIAN_POINT('Ctrl Pts',(0.701901133702176,2.85856915100056,1.03378074558769));
#46914=CARTESIAN_POINT('Ctrl Pts',(0.792383595393697,2.8348244836784,1.02873672739629));
#46915=CARTESIAN_POINT('Ctrl Pts',(0.881563614700024,2.80681484840683,1.02369270920489));
#46916=CARTESIAN_POINT('Ctrl Pts',(0.970714136927654,2.7788144775694,1.01865035936704));
#46917=CARTESIAN_POINT('Ctrl Pts',(1.05856265076265,2.7465520742627,1.01360800952919));
#46918=CARTESIAN_POINT('Ctrl Pts',(1.1446800186878,2.71017926617722,1.00856565969134));
#46919=CARTESIAN_POINT('Ctrl Pts',(1.23079278236441,2.67380840275694,1.00352357944175));
#46920=CARTESIAN_POINT('Ctrl Pts',(1.31517417658744,2.63332774428076,0.998481499192167));
#46921=CARTESIAN_POINT('Ctrl Pts',(1.39741519490234,2.58893699673361,0.993439418942582));
#46922=CARTESIAN_POINT('Ctrl Pts',(1.47967462066404,2.54453631350788,0.988396210158526));
#46923=CARTESIAN_POINT('Ctrl Pts',(1.55979232969195,2.49622401350885,0.983353001374471));
#46924=CARTESIAN_POINT('Ctrl Pts',(1.63738505705346,2.4442451135142,0.978309792590416));
#46925=CARTESIAN_POINT('Ctrl Pts',(1.71506208503325,2.39220974104389,0.9732611046122));
#46926=CARTESIAN_POINT('Ctrl Pts',(1.79020828831455,2.33650006511776,0.968212416633985));
#46927=CARTESIAN_POINT('Ctrl Pts',(1.86247076061764,2.27740349210331,0.963163728655769));
#46928=CARTESIAN_POINT('Ctrl Pts',(1.93477920673401,2.21826932149876,0.958111828672331));
#46929=CARTESIAN_POINT('Ctrl Pts',(2.00419994088024,2.15574425994461,0.953059928688893));
#46930=CARTESIAN_POINT('Ctrl Pts',(2.0704160035922,2.09015348050551,0.948008028705455));
#46931=CARTESIAN_POINT('Ctrl Pts',(2.13673329482258,2.02446242845653,0.942948405575554));
#46932=CARTESIAN_POINT('Ctrl Pts',(2.19983583847281,1.9556966303443,0.937888782445653));
#46933=CARTESIAN_POINT('Ctrl Pts',(2.25944631754215,1.88421504562117,0.932829159315752));
#46934=CARTESIAN_POINT('Ctrl Pts',(2.27890576689535,1.86088035180019,0.931177478578075));
#46935=CARTESIAN_POINT('Ctrl Pts',(2.29799342574526,1.83725648233511,0.929525797840397));
#46936=CARTESIAN_POINT('Ctrl Pts',(2.31670066257897,1.81335656725481,0.92787411710272));
#46937=CARTESIAN_POINT('Ctrl Pts',(2.37399274853932,1.74016157852416,0.922815741264366));
#46938=CARTESIAN_POINT('Ctrl Pts',(2.42791212019609,1.66412162110509,0.917757365426012));
#46939=CARTESIAN_POINT('Ctrl Pts',(2.47816445280402,1.58558031800932,0.912698989587657));
#46940=CARTESIAN_POINT('Ctrl Pts',(2.52834900067583,1.50714495828431,0.907647436928519));
#46941=CARTESIAN_POINT('Ctrl Pts',(2.57487610284079,1.42621532820593,0.902595884269381));
#46942=CARTESIAN_POINT('Ctrl Pts',(2.61749222992237,1.34316731135626,0.897544331610243));
#46943=CARTESIAN_POINT('Ctrl Pts',(2.66206678314268,1.25630281895836,0.892260634609366));
#46944=CARTESIAN_POINT('Ctrl Pts',(2.70236197047381,1.16712094851813,0.88697693760849));
#46945=CARTESIAN_POINT('Ctrl Pts',(2.73813896039309,1.07608504941639,0.881693240607613));
#46946=CARTESIAN_POINT('Ctrl Pts',(2.77228400676289,0.989201692175915,0.8766505559238));
#46947=CARTESIAN_POINT('Ctrl Pts',(2.80231381262609,0.900630195460668,0.871607871239987));
#46948=CARTESIAN_POINT('Ctrl Pts',(2.82806884408845,0.810796283351271,0.866565186556173));
#46949=CARTESIAN_POINT('Ctrl Pts',(2.85381536898689,0.720992042256478,0.861524167407873));
#46950=CARTESIAN_POINT('Ctrl Pts',(2.87528980285597,0.629926639656187,0.856483148259572));
#46951=CARTESIAN_POINT('Ctrl Pts',(2.89238228544692,0.538041554931251,0.851442129111271));
#46952=CARTESIAN_POINT('Ctrl Pts',(2.90947386925272,0.446161301859626,0.846401375038167));
#46953=CARTESIAN_POINT('Ctrl Pts',(2.92218387947666,0.353461887938309,0.841360620965063));
#46954=CARTESIAN_POINT('Ctrl Pts',(2.93045367039417,0.26039448088107,0.836319866891959));
#46955=CARTESIAN_POINT('Ctrl Pts',(2.93872532296153,0.167306123001053,0.831277978072023));
#46956=CARTESIAN_POINT('Ctrl Pts',(2.94255473209556,0.0738500486034947,
0.826236089252088));
#46957=CARTESIAN_POINT('Ctrl Pts',(2.94193524824454,-0.0195190967095212,
0.821194200432152));
#46958=CARTESIAN_POINT('Ctrl Pts',(2.94131508913938,-0.112990016912663,
0.816146815817231));
#46959=CARTESIAN_POINT('Ctrl Pts',(2.93623636193386,-0.206373375464665,
0.811099431202309));
#46960=CARTESIAN_POINT('Ctrl Pts',(2.92674451882024,-0.299216512839292,
0.806052046587388));
#46961=CARTESIAN_POINT('Ctrl Pts',(2.91724662010408,-0.392118882244111,
0.80100144184391));
#46962=CARTESIAN_POINT('Ctrl Pts',(2.90333006640131,-0.484479906895986,
0.795950837100432));
#46963=CARTESIAN_POINT('Ctrl Pts',(2.88509163073236,-0.575856129843267,
0.790900232356954));
#46964=CARTESIAN_POINT('Ctrl Pts',(2.86682522357148,-0.66737249251143,0.785841881721643));
#46965=CARTESIAN_POINT('Ctrl Pts',(2.84422381317679,-0.757900610476704,
0.780783531086332));
#46966=CARTESIAN_POINT('Ctrl Pts',(2.817434206504,-0.847011506427842,0.775725180451022));
#46967=CARTESIAN_POINT('Ctrl Pts',(2.8086257488842,-0.876311285257559,0.77406198816375));
#46968=CARTESIAN_POINT('Ctrl Pts',(2.79936489210506,-0.905458007307212,
0.77239879587648));
#46969=CARTESIAN_POINT('Ctrl Pts',(2.78965797630214,-0.934436929521649,
0.770735603589208));
#46970=CARTESIAN_POINT('Ctrl Pts',(2.76012371083481,-1.02260820853707,0.765675174145623));
#46971=CARTESIAN_POINT('Ctrl Pts',(2.72635407592158,-1.10953048163224,0.760614744702038));
#46972=CARTESIAN_POINT('Ctrl Pts',(2.68847392916613,-1.19476856846589,0.755554315258454));
#46973=CARTESIAN_POINT('Ctrl Pts',(2.6506448841658,-1.27989166588652,0.750500712526178));
#46974=CARTESIAN_POINT('Ctrl Pts',(2.60871652594505,-1.36333469126638,0.745447109793901));
#46975=CARTESIAN_POINT('Ctrl Pts',(2.5628631043721,-1.44467875607285,0.740393507061625));
#46976=CARTESIAN_POINT('Ctrl Pts',(2.51492659691061,-1.52971821955847,0.735110323020545));
#46977=CARTESIAN_POINT('Ctrl Pts',(2.46270008736353,-1.61246302272199,0.729827138979464));
#46978=CARTESIAN_POINT('Ctrl Pts',(2.40643854657599,-1.6924590162108,0.724543954938384));
#46979=CARTESIAN_POINT('Ctrl Pts',(2.35271654217843,-1.76884414633411,0.719499243536685));
#46980=CARTESIAN_POINT('Ctrl Pts',(2.29531614667676,-1.84272282308006,0.714454532134986));
#46981=CARTESIAN_POINT('Ctrl Pts',(2.23450495372136,-1.91372715186746,0.709409820733287));
#46982=CARTESIAN_POINT('Ctrl Pts',(2.17371399249588,-1.98470785769443,0.704366787694299));
#46983=CARTESIAN_POINT('Ctrl Pts',(2.10951477618156,-2.0528157798459,0.699323754655311));
#46984=CARTESIAN_POINT('Ctrl Pts',(2.04221541263933,-2.11771579971874,0.694280721616323));
#46985=CARTESIAN_POINT('Ctrl Pts',(1.97491979124556,-2.18261221085745,0.689237968992741));
#46986=CARTESIAN_POINT('Ctrl Pts',(1.90452468432683,-2.24430076759546,0.684195216369159));
#46987=CARTESIAN_POINT('Ctrl Pts',(1.83137450342477,-2.30248375199602,0.679152463745576));
#46988=CARTESIAN_POINT('Ctrl Pts',(1.75820812106062,-2.36067962289125,0.674108594242112));
#46989=CARTESIAN_POINT('Ctrl Pts',(1.68228579925905,-2.41536810418269,0.669064724738647));
#46990=CARTESIAN_POINT('Ctrl Pts',(1.60398350556405,-2.46629294972808,0.664020855235182));
#46991=CARTESIAN_POINT('Ctrl Pts',(1.52559647602039,-2.51727290425947,0.658971527442531));
#46992=CARTESIAN_POINT('Ctrl Pts',(1.44482470597328,-2.56448085311737,0.653922199649879));
#46993=CARTESIAN_POINT('Ctrl Pts',(1.36207121844092,-2.60770512057918,0.648872871857228));
#46994=CARTESIAN_POINT('Ctrl Pts',(1.27926527577715,-2.65095678670052,0.643820343436291));
#46995=CARTESIAN_POINT('Ctrl Pts',(1.19447551590553,-2.69021955848492,0.638767815015354));
#46996=CARTESIAN_POINT('Ctrl Pts',(1.10812557491149,-2.72532965166181,0.633715286594418));
#46997=CARTESIAN_POINT('Ctrl Pts',(1.0216440172149,-2.76049326050573,0.62865505698547));
#46998=CARTESIAN_POINT('Ctrl Pts',(0.933597948821291,-2.79149141171207,
0.623594827376522));
#46999=CARTESIAN_POINT('Ctrl Pts',(0.844426506240923,-2.81821004816138,
0.618534597767575));
#47000=CARTESIAN_POINT('Ctrl Pts',(0.815423561206037,-2.82690026469172,
0.616888761870281));
#47001=CARTESIAN_POINT('Ctrl Pts',(0.786301645408335,-2.8351381676959,0.615242925972988));
#47002=CARTESIAN_POINT('Ctrl Pts',(0.757076058362179,-2.84292100520834,
0.613597090075694));
#47003=CARTESIAN_POINT('Ctrl Pts',(0.667207001745775,-2.86685333080839,
0.608536123491804));
#47004=CARTESIAN_POINT('Ctrl Pts',(0.576047154021573,-2.88656138929389,
0.603475156907913));
#47005=CARTESIAN_POINT('Ctrl Pts',(0.484028648964702,-2.90190976203283,
0.598414190324023));
#47006=CARTESIAN_POINT('Ctrl Pts',(0.392133871894972,-2.91723749736558,
0.59336002871059));
#47007=CARTESIAN_POINT('Ctrl Pts',(0.299383164868472,-2.92821712480805,
0.588305867097157));
#47008=CARTESIAN_POINT('Ctrl Pts',(0.206222253901962,-2.93476342862514,
0.583251705483724));
#47009=CARTESIAN_POINT('Ctrl Pts',(0.108842408851515,-2.94160619180498,
0.577968658445326));
#47010=CARTESIAN_POINT('Ctrl Pts',(0.0110147984464832,-2.94360446042169,
0.572685611406928));
#47011=CARTESIAN_POINT('Ctrl Pts',(-0.0867411774537793,-2.94072099460896,
0.567402564368531));
#47012=CARTESIAN_POINT('Ctrl Pts',(-0.180098316403701,-2.93796727939046,
0.562357244612878));
#47013=CARTESIAN_POINT('Ctrl Pts',(-0.273389632933628,-2.93076167051084,
0.557311924857226));
#47014=CARTESIAN_POINT('Ctrl Pts',(-0.366160572951378,-2.91912494333763,
0.552266605101574));
#47015=CARTESIAN_POINT('Ctrl Pts',(-0.458900958962508,-2.90749204870766,
0.54722294701641));
#47016=CARTESIAN_POINT('Ctrl Pts',(-0.551120870401268,-2.89143099057585,
0.542179288931246));
#47017=CARTESIAN_POINT('Ctrl Pts',(-0.642370803818245,-2.87101441138875,
0.537135630846082));
#47018=CARTESIAN_POINT('Ctrl Pts',(-0.733615949180425,-2.85059890349778,
0.532092237411098));
#47019=CARTESIAN_POINT('Ctrl Pts',(-0.823890786108729,-2.8258284261362,
0.527048843976114));
#47020=CARTESIAN_POINT('Ctrl Pts',(-0.912757038905083,-2.79682652088563,
0.52200545054113));
#47021=CARTESIAN_POINT('Ctrl Pts',(-1.00164323318172,-2.7678181076424,0.516960925374724));
#47022=CARTESIAN_POINT('Ctrl Pts',(-1.08911979511789,-2.73457651811266,
0.511916400208317));
#47023=CARTESIAN_POINT('Ctrl Pts',(-1.17476568767022,-2.69727447232808,
0.50687187504191));
#47024=CARTESIAN_POINT('Ctrl Pts',(-1.26050455944576,-2.65993193055311,
0.501821873418695));
#47025=CARTESIAN_POINT('Ctrl Pts',(-1.34440838938401,-2.61852031194909,
0.496771871795479));
#47026=CARTESIAN_POINT('Ctrl Pts',(-1.42607844119853,-2.57325946603695,
0.491721870172263));
#47027=CARTESIAN_POINT('Ctrl Pts',(-1.50780043677,-2.52796983333789,0.486668656648834));
#47028=CARTESIAN_POINT('Ctrl Pts',(-1.58728544990138,-2.47882633170898,
0.481615443125405));
#47029=CARTESIAN_POINT('Ctrl Pts',(-1.66416336507436,-2.42609239196375,
0.476562229601975));
#47030=CARTESIAN_POINT('Ctrl Pts',(-1.74115860868422,-2.3732779714887,0.471501304037415));
#47031=CARTESIAN_POINT('Ctrl Pts',(-1.81553846179002,-2.31686244365307,
0.466440378472854));
#47032=CARTESIAN_POINT('Ctrl Pts',(-1.88696577597676,-2.2571495653351,0.461379452908294));
#47033=CARTESIAN_POINT('Ctrl Pts',(-1.91011601969959,-2.23779607707655,
0.459739160792923));
#47034=CARTESIAN_POINT('Ctrl Pts',(-1.93295640049665,-2.21809649974357,
0.458098868677552));
#47035=CARTESIAN_POINT('Ctrl Pts',(-1.95547630356216,-2.19806197051104,
0.456458576562181));
#47036=CARTESIAN_POINT('Ctrl Pts',(-2.02385521807488,-2.137229587809,0.451478031397016));
#47037=CARTESIAN_POINT('Ctrl Pts',(-2.08952991361327,-2.07308110044888,
0.446497486231852));
#47038=CARTESIAN_POINT('Ctrl Pts',(-2.15215463624812,-2.00588993259244,
0.441516941066687));
#47039=CARTESIAN_POINT('Ctrl Pts',(-2.21467995181695,-1.93880542032789,
0.43654430174703));
#47040=CARTESIAN_POINT('Ctrl Pts',(-2.27416460854903,-1.86868815980554,
0.431571662427372));
#47041=CARTESIAN_POINT('Ctrl Pts',(-2.33029690289864,-1.79585086918179,
0.426599023107715));
#47042=CARTESIAN_POINT('Ctrl Pts',(-2.38637883272966,-1.72307893158024,
0.421630845472519));
#47043=CARTESIAN_POINT('Ctrl Pts',(-2.43911409152223,-1.64759216767629,
0.416662667837323));
#47044=CARTESIAN_POINT('Ctrl Pts',(-2.48822931388568,-1.5697384755175,0.411694490202127));
#47045=CARTESIAN_POINT('Ctrl Pts',(-2.53731512223824,-1.49193140819799,
0.406729287897674));
#47046=CARTESIAN_POINT('Ctrl Pts',(-2.58278495436859,-1.41176061293751,
0.40176408559322));
#47047=CARTESIAN_POINT('Ctrl Pts',(-2.6244078838903,-1.32960417379551,0.396798883288767));
#47048=CARTESIAN_POINT('Ctrl Pts',(-2.66601830188986,-1.24747243022683,
0.391835173484704));
#47049=CARTESIAN_POINT('Ctrl Pts',(-2.70378390784644,-1.1633566367953,0.386871463680641));
#47050=CARTESIAN_POINT('Ctrl Pts',(-2.73751964702703,-1.07765958546333,
0.381907753876579));
#47051=CARTESIAN_POINT('Ctrl Pts',(-2.77135003798828,-0.991722095394787,
0.376930117477664));
#47052=CARTESIAN_POINT('Ctrl Pts',(-2.80112772804158,-0.904194884455238,
0.371952481078748));
#47053=CARTESIAN_POINT('Ctrl Pts',(-2.82671515886674,-0.815503164085203,
0.366974844679833));
#47054=CARTESIAN_POINT('Ctrl Pts',(-2.85224966434525,-0.726994894725836,
0.362007504083325));
#47055=CARTESIAN_POINT('Ctrl Pts',(-2.87361114176866,-0.637327381440443,
0.357040163486818));
#47056=CARTESIAN_POINT('Ctrl Pts',(-2.89071367265674,-0.546935519705347,
0.35207282289031));
#47057=CARTESIAN_POINT('Ctrl Pts',(-2.90786937614552,-0.456262625273901,
0.347090038590191));
#47058=CARTESIAN_POINT('Ctrl Pts',(-2.92073954449786,-0.364861329719361,
0.342107254290072));
#47059=CARTESIAN_POINT('Ctrl Pts',(-2.92928980875558,-0.27317616352954,
0.337124469989953));
#47060=CARTESIAN_POINT('Ctrl Pts',(-2.9378400730133,-0.181490997339719,
0.332141685689834));
#47061=CARTESIAN_POINT('Ctrl Pts',(-2.94207046158018,-0.0895224226019215,
0.327158901389715));
#47062=CARTESIAN_POINT('Ctrl Pts',(-2.94199911155216,0.00228640028720795,
0.322176117089596));
#47063=CARTESIAN_POINT('Origin',(0.,0.,-1.84858989190501));
#47064=CARTESIAN_POINT('',(-2.37174915417064,-0.00200304539514994,10.651410108095));
#47065=CARTESIAN_POINT('Ctrl Pts',(-2.36545136240482,0.172736546790724,
10.6389210243916));
#47066=CARTESIAN_POINT('Ctrl Pts',(-2.36969609595299,0.114609237074736,
10.643124268197));
#47067=CARTESIAN_POINT('Ctrl Pts',(-2.37179806469451,0.0563280682077159,
10.6473616493302));
#47068=CARTESIAN_POINT('Ctrl Pts',(-2.37174916623817,-0.00198870524203496,
10.6516070788671));
#47069=CARTESIAN_POINT('',(-2.34668236863852,0.343918483395543,11.62825));
#47070=CARTESIAN_POINT('Ctrl Pts',(-2.37174915417064,-0.00200304539514992,
10.651410108095));
#47071=CARTESIAN_POINT('Ctrl Pts',(-2.3716576055993,-0.11040310820655,10.6586904087473));
#47072=CARTESIAN_POINT('Ctrl Pts',(-2.36413081146793,-0.21849095763389,
10.6659707093996));
#47073=CARTESIAN_POINT('Ctrl Pts',(-2.34931805963096,-0.325426976742579,
10.6732510100519));
#47074=CARTESIAN_POINT('Ctrl Pts',(-2.34106564337189,-0.385002709360389,
10.6773069796742));
#47075=CARTESIAN_POINT('Ctrl Pts',(-2.33055266045321,-0.444221480602426,
10.6813629492966));
#47076=CARTESIAN_POINT('Ctrl Pts',(-2.31781106222524,-0.502941291132799,
10.6854189189189));
#47077=CARTESIAN_POINT('Ctrl Pts',(-2.30103244669589,-0.580265745037053,
10.6907599721898));
#47078=CARTESIAN_POINT('Ctrl Pts',(-2.28034966391946,-0.656890328392001,
10.6961010254607));
#47079=CARTESIAN_POINT('Ctrl Pts',(-2.25583677761288,-0.732392309673682,
10.7014420787316));
#47080=CARTESIAN_POINT('Ctrl Pts',(-2.23135845642761,-0.807787827150567,
10.7067756006922));
#47081=CARTESIAN_POINT('Ctrl Pts',(-2.20306090137613,-0.88206344593845,
10.7121091226527));
#47082=CARTESIAN_POINT('Ctrl Pts',(-2.17106897787264,-0.954807601466947,
10.7174426446133));
#47083=CARTESIAN_POINT('Ctrl Pts',(-2.13911306659992,-1.02746987134964,
10.7227701628078));
#47084=CARTESIAN_POINT('Ctrl Pts',(-2.10347123892394,-1.09860367880999,
10.7280976810023));
#47085=CARTESIAN_POINT('Ctrl Pts',(-2.06431736356217,-1.16781500461148,
10.7334251991968));
#47086=CARTESIAN_POINT('Ctrl Pts',(-2.02518748579086,-1.23698391047278,
10.7387494521309));
#47087=CARTESIAN_POINT('Ctrl Pts',(-1.9825500628117,-1.3042322684173,10.744073705065));
#47088=CARTESIAN_POINT('Ctrl Pts',(-1.93662550425837,-1.36918943859351,
10.7493979579991));
#47089=CARTESIAN_POINT('Ctrl Pts',(-1.89071493070968,-1.43412682793013,
10.754720589585));
#47090=CARTESIAN_POINT('Ctrl Pts',(-1.84151947905621,-1.49677403427864,
10.7600432211708));
#47091=CARTESIAN_POINT('Ctrl Pts',(-1.78930279570886,-1.55678950657064,
10.7653658527567));
#47092=CARTESIAN_POINT('Ctrl Pts',(-1.73708591124963,-1.61680521001145,
10.7706885048426));
#47093=CARTESIAN_POINT('Ctrl Pts',(-1.68184807965202,-1.67418880810358,
10.7760111569285));
#47094=CARTESIAN_POINT('Ctrl Pts',(-1.62389216613693,-1.72863307131939,
10.7813338090144));
#47095=CARTESIAN_POINT('Ctrl Pts',(-1.56587940826847,-1.78313073458964,
10.786661681667));
#47096=CARTESIAN_POINT('Ctrl Pts',(-1.50514358481335,-1.83468298449049,
10.7919895543197));
#47097=CARTESIAN_POINT('Ctrl Pts',(-1.44202280445052,-1.8830210550986,10.7973174269724));
#47098=CARTESIAN_POINT('Ctrl Pts',(-1.37887101516864,-1.93138287242388,
10.802647917013));
#47099=CARTESIAN_POINT('Ctrl Pts',(-1.31333231975803,-1.9765270996243,10.8079784070537));
#47100=CARTESIAN_POINT('Ctrl Pts',(-1.24577408566008,-2.01822818085513,
10.8133088970943));
#47101=CARTESIAN_POINT('Ctrl Pts',(-1.17809860777621,-2.06000163213389,
10.818648637922));
#47102=CARTESIAN_POINT('Ctrl Pts',(-1.10839699898012,-2.09831977402247,
10.8239883787496));
#47103=CARTESIAN_POINT('Ctrl Pts',(-1.0370612503182,-2.13300305334719,10.8293281195772));
#47104=CARTESIAN_POINT('Ctrl Pts',(-0.978149343837453,-2.16164588876071,
10.833737890529));
#47105=CARTESIAN_POINT('Ctrl Pts',(-0.918123466404,-2.18781053406727,10.8381476614807));
#47106=CARTESIAN_POINT('Ctrl Pts',(-0.857212862138923,-2.21142130121865,
10.8425574324324));
#47107=CARTESIAN_POINT('Ctrl Pts',(-0.783564483559484,-2.23996960965684,
10.8478893854547));
#47108=CARTESIAN_POINT('Ctrl Pts',(-0.708351392720743,-2.2648878699676,
10.853221338477));
#47109=CARTESIAN_POINT('Ctrl Pts',(-0.631965683600276,-2.28600468880789,
10.8585532914993));
#47110=CARTESIAN_POINT('Ctrl Pts',(-0.555688377193635,-2.30709153973276,
10.8638776776851));
#47111=CARTESIAN_POINT('Ctrl Pts',(-0.478242205414549,-2.32438753902868,
10.8692020638708));
#47112=CARTESIAN_POINT('Ctrl Pts',(-0.400038041337422,-2.33776979790203,
10.8745264500565));
#47113=CARTESIAN_POINT('Ctrl Pts',(-0.321922208961844,-2.35113694149719,
10.8798448223414));
#47114=CARTESIAN_POINT('Ctrl Pts',(-0.243050545349262,-2.36059905065694,
10.8851631946262));
#47115=CARTESIAN_POINT('Ctrl Pts',(-0.163846373361652,-2.36608377460229,
10.8904815669111));
#47116=CARTESIAN_POINT('Ctrl Pts',(-0.0846908540129318,-2.37156512945374,
10.8957966722866));
#47117=CARTESIAN_POINT('Ctrl Pts',(-0.00520369810401163,-2.37307391631134,
10.9011117776622));
#47118=CARTESIAN_POINT('Ctrl Pts',(0.0741855701400063,-2.37058949708358,
10.9064268830377));
#47119=CARTESIAN_POINT('Ctrl Pts',(0.153550788114269,-2.36810583048844,
10.9117403782496));
#47120=CARTESIAN_POINT('Ctrl Pts',(0.232817709169052,-2.36163137480067,
10.9170538734614));
#47121=CARTESIAN_POINT('Ctrl Pts',(0.31155721659169,-2.35119760192325,10.9223673686732));
#47122=CARTESIAN_POINT('Ctrl Pts',(0.390297383798681,-2.3407637416178,10.9276809084086));
#47123=CARTESIAN_POINT('Ctrl Pts',(0.468509664188686,-2.32637056139121,
10.932994448144));
#47124=CARTESIAN_POINT('Ctrl Pts',(0.545771953761925,-2.30810117563916,
10.9383079878794));
#47125=CARTESIAN_POINT('Ctrl Pts',(0.623111609465042,-2.28981349594736,
10.9436268482959));
#47126=CARTESIAN_POINT('Ctrl Pts',(0.699498917311407,-2.26764196667449,
10.9489457087124));
#47127=CARTESIAN_POINT('Ctrl Pts',(0.774524443417242,-2.24172031017458,
10.9542645691289));
#47128=CARTESIAN_POINT('Ctrl Pts',(0.849587474036689,-2.21578569569664,
10.9595860883907));
#47129=CARTESIAN_POINT('Ctrl Pts',(0.92328693181771,-2.18609739534769,10.9649076076526));
#47130=CARTESIAN_POINT('Ctrl Pts',(0.995233349937592,-2.15283734677565,
10.9702291269145));
#47131=CARTESIAN_POINT('Ctrl Pts',(1.06730714142768,-2.11951841487639,10.975560067352));
#47132=CARTESIAN_POINT('Ctrl Pts',(1.13762127719207,-2.08261532012154,10.9808910077895));
#47133=CARTESIAN_POINT('Ctrl Pts',(1.20581113914771,-2.04235588456256,10.986221948227));
#47134=CARTESIAN_POINT('Ctrl Pts',(1.26326129296913,-2.00843719490262,10.9907132808));
#47135=CARTESIAN_POINT('Ctrl Pts',(1.31920397143183,-1.97213701067979,10.995204613373));
#47136=CARTESIAN_POINT('Ctrl Pts',(1.37343893525149,-1.93361411704488,10.999695945946));
#47137=CARTESIAN_POINT('Ctrl Pts',(1.43803180442143,-1.8877340416588,11.0050450424854));
#47138=CARTESIAN_POINT('Ctrl Pts',(1.50043956590866,-1.838531201315,11.0103941390249));
#47139=CARTESIAN_POINT('Ctrl Pts',(1.56030198093737,-1.78624068668892,11.0157432355643));
#47140=CARTESIAN_POINT('Ctrl Pts',(1.62007956202568,-1.73402427549485,11.0210847516389));
#47141=CARTESIAN_POINT('Ctrl Pts',(1.67731861367735,-1.67872918518825,11.0264262677134));
#47142=CARTESIAN_POINT('Ctrl Pts',(1.73168916755986,-1.62063280525104,11.031767783788));
#47143=CARTESIAN_POINT('Ctrl Pts',(1.78599747919602,-1.5626029328061,11.0371031850092));
#47144=CARTESIAN_POINT('Ctrl Pts',(1.83744350365328,-1.50177848304249,11.0424385862305));
#47145=CARTESIAN_POINT('Ctrl Pts',(1.88573269170631,-1.43847498342171,11.0477739874517));
#47146=CARTESIAN_POINT('Ctrl Pts',(1.93399167314639,-1.37521108240235,11.0531060511889));
#47147=CARTESIAN_POINT('Ctrl Pts',(1.97909745714498,-1.30947157937917,11.058438114926));
#47148=CARTESIAN_POINT('Ctrl Pts',(2.0207952858779,-1.24160560367358,11.0637701786631));
#47149=CARTESIAN_POINT('Ctrl Pts',(2.06247978565975,-1.17376132171794,11.0691005379753));
#47150=CARTESIAN_POINT('Ctrl Pts',(2.10075825055903,-1.10379231349086,11.0744308972876));
#47151=CARTESIAN_POINT('Ctrl Pts',(2.1354196543779,-1.03207604477412,11.0797612565998));
#47152=CARTESIAN_POINT('Ctrl Pts',(2.17008058021416,-0.960360765028534,
11.0850915424061));
#47153=CARTESIAN_POINT('Ctrl Pts',(2.20112434301785,-0.886898692362133,
11.0904218282124));
#47154=CARTESIAN_POINT('Ctrl Pts',(2.22838687424989,-0.812089897222463,
11.0957521140187));
#47155=CARTESIAN_POINT('Ctrl Pts',(2.25567509291515,-0.737210615380259,
11.1010874221525));
#47156=CARTESIAN_POINT('Ctrl Pts',(2.27917480399258,-0.660982514702551,
11.1064227302863));
#47157=CARTESIAN_POINT('Ctrl Pts',(2.29877114623207,-0.583822986658526,
11.1117580384201));
#47158=CARTESIAN_POINT('Ctrl Pts',(2.3183767394164,-0.506627033524114,11.11709586522));
#47159=CARTESIAN_POINT('Ctrl Pts',(2.33407520004438,-0.428499233640839,
11.1224336920198));
#47160=CARTESIAN_POINT('Ctrl Pts',(2.34580288183145,-0.349866977709081,
11.1277715188196));
#47161=CARTESIAN_POINT('Ctrl Pts',(2.35755035012552,-0.271102056369778,
11.1331183514016));
#47162=CARTESIAN_POINT('Ctrl Pts',(2.36531360899113,-0.191831442605272,
11.1384651839836));
#47163=CARTESIAN_POINT('Ctrl Pts',(2.36908098257407,-0.112487157070807,
11.1438120165656));
#47164=CARTESIAN_POINT('Ctrl Pts',(2.37213951654979,-0.0480716729824705,
11.1481528308635));
#47165=CARTESIAN_POINT('Ctrl Pts',(2.37256537656481,0.016392218425755,11.1524936451615));
#47166=CARTESIAN_POINT('Ctrl Pts',(2.37037751204224,0.0806753550002586,
11.1568344594594));
#47167=CARTESIAN_POINT('Ctrl Pts',(2.36768235674937,0.159863546953882,11.1621817597652));
#47168=CARTESIAN_POINT('Ctrl Pts',(2.36100990357596,0.239056903868901,11.167529060071));
#47169=CARTESIAN_POINT('Ctrl Pts',(2.35035851903795,0.317825257784452,11.1728763603767));
#47170=CARTESIAN_POINT('Ctrl Pts',(2.33972192171891,0.396484258320294,11.1782162370748));
#47171=CARTESIAN_POINT('Ctrl Pts',(2.32511742713896,0.474718970005106,11.1835561137728));
#47172=CARTESIAN_POINT('Ctrl Pts',(2.30659537861471,0.552101278619481,11.1888959904709));
#47173=CARTESIAN_POINT('Ctrl Pts',(2.28809370973354,0.62939844417701,11.1942299917507));
#47174=CARTESIAN_POINT('Ctrl Pts',(2.26568316195647,0.705844620125849,11.1995639930305));
#47175=CARTESIAN_POINT('Ctrl Pts',(2.23946541145361,0.781020315614714,11.2048979943104));
#47176=CARTESIAN_POINT('Ctrl Pts',(2.21326334452963,0.856151040656937,11.2102288047661));
#47177=CARTESIAN_POINT('Ctrl Pts',(2.18325874939859,0.93001235560192,11.2155596152219));
#47178=CARTESIAN_POINT('Ctrl Pts',(2.14960324258805,1.00219956194111,11.2208904256776));
#47179=CARTESIAN_POINT('Ctrl Pts',(2.11595756843179,1.07436567836333,11.2262196787057));
#47180=CARTESIAN_POINT('Ctrl Pts',(2.07866329785775,1.14485823605629,11.2315489317338));
#47181=CARTESIAN_POINT('Ctrl Pts',(2.03791975049785,1.21329351478971,11.236878184762));
#47182=CARTESIAN_POINT('Ctrl Pts',(1.99717563763221,1.28172974338012,11.2422075117582));
#47183=CARTESIAN_POINT('Ctrl Pts',(1.95298239238847,1.34810823714408,11.2475368387544));
#47184=CARTESIAN_POINT('Ctrl Pts',(1.90558401794835,1.41207209909403,11.2528661657506));
#47185=CARTESIAN_POINT('Ctrl Pts',(1.85813890409124,1.47609903564625,11.2582007479827));
#47186=CARTESIAN_POINT('Ctrl Pts',(1.80748262627876,1.53770620995198,11.2635353302148));
#47187=CARTESIAN_POINT('Ctrl Pts',(1.75390070327161,1.59656831534493,11.2688699124469));
#47188=CARTESIAN_POINT('Ctrl Pts',(1.70029220062007,1.65545961964941,11.2742071409315));
#47189=CARTESIAN_POINT('Ctrl Pts',(1.6437554920223,1.71160281372472,11.2795443694161));
#47190=CARTESIAN_POINT('Ctrl Pts',(1.5846125787407,1.76470990188097,11.2848815979007));
#47191=CARTESIAN_POINT('Ctrl Pts',(1.5253674895908,1.81790873835573,11.2902280470327));
#47192=CARTESIAN_POINT('Ctrl Pts',(1.46350756252603,1.86806069585571,11.2955744961648));
#47193=CARTESIAN_POINT('Ctrl Pts',(1.39938722291788,1.91491865697585,11.3009209452969));
#47194=CARTESIAN_POINT('Ctrl Pts',(1.34720926165235,1.9530493483485,11.3052716211889));
#47195=CARTESIAN_POINT('Ctrl Pts',(1.2935351519869,1.98899953936095,11.309622297081));
#47196=CARTESIAN_POINT('Ctrl Pts',(1.23856812126655,2.02265841690639,11.313972972973));
#47197=CARTESIAN_POINT('Ctrl Pts',(1.17182834791455,2.06352629405431,11.3192554690285));
#47198=CARTESIAN_POINT('Ctrl Pts',(1.10292632796187,2.10117133881163,11.324537965084));
#47199=CARTESIAN_POINT('Ctrl Pts',(1.03220941490833,2.13535518972245,11.3298204611394));
#47200=CARTESIAN_POINT('Ctrl Pts',(0.961594100115952,2.16948992904649,11.3350953678872));
#47201=CARTESIAN_POINT('Ctrl Pts',(0.889169494008856,2.20017313813373,11.340370274635));
#47202=CARTESIAN_POINT('Ctrl Pts',(0.8153105507563,2.2272105352493,11.3456451813828));
#47203=CARTESIAN_POINT('Ctrl Pts',(0.741533284605296,2.25421803299002,11.3509142548614));
#47204=CARTESIAN_POINT('Ctrl Pts',(0.666325277816863,2.27758756180128,11.35618332834));
#47205=CARTESIAN_POINT('Ctrl Pts',(0.59008317191016,2.29717215565757,11.3614524018187));
#47206=CARTESIAN_POINT('Ctrl Pts',(0.513886564346098,2.31674506218504,11.3667183309178));
#47207=CARTESIAN_POINT('Ctrl Pts',(0.436657543679518,2.33253739536388,11.371984260017));
#47208=CARTESIAN_POINT('Ctrl Pts',(0.358808370350743,2.34445187962266,11.3772501891162));
#47209=CARTESIAN_POINT('Ctrl Pts',(0.280980323372962,2.35636313058345,11.3825146891718));
#47210=CARTESIAN_POINT('Ctrl Pts',(0.202532930124588,2.36439854875748,11.3877791892273));
#47211=CARTESIAN_POINT('Ctrl Pts',(0.123887518991857,2.36851217964739,11.3930436892829));
#47212=CARTESIAN_POINT('Ctrl Pts',(0.045237860004629,2.3726260327258,11.3983084736885));
#47213=CARTESIAN_POINT('Ctrl Pts',(-0.0336093604692796,2.37281765462148,
11.4035732580942));
#47214=CARTESIAN_POINT('Ctrl Pts',(-0.112230456956044,2.36909315710283,
11.4088380424998));
#47215=CARTESIAN_POINT('Ctrl Pts',(-0.190941448627036,2.36536440100212,
11.414108846648));
#47216=CARTESIAN_POINT('Ctrl Pts',(-0.269425321212711,2.35771060679778,
11.4193796507963));
#47217=CARTESIAN_POINT('Ctrl Pts',(-0.34726182368926,2.34618995145491,11.4246504549445));
#47218=CARTESIAN_POINT('Ctrl Pts',(-0.425141988134603,2.3346628336622,11.4299242157221));
#47219=CARTESIAN_POINT('Ctrl Pts',(-0.502373590799942,2.31926463273651,
11.4351979764997));
#47220=CARTESIAN_POINT('Ctrl Pts',(-0.578547654010976,2.30010449209126,
11.4404717372772));
#47221=CARTESIAN_POINT('Ctrl Pts',(-0.654872977533989,2.28090630478381,
11.4457559702637));
#47222=CARTESIAN_POINT('Ctrl Pts',(-0.73013610921208,2.25793139694226,11.4510402032501));
#47223=CARTESIAN_POINT('Ctrl Pts',(-0.803944534133875,2.23133844329727,
11.4563244362366));
#47224=CARTESIAN_POINT('Ctrl Pts',(-0.872791415727006,2.20653311880011,
11.4612534529866));
#47225=CARTESIAN_POINT('Ctrl Pts',(-0.940372510114562,2.17858045132383,
11.4661824697365));
#47226=CARTESIAN_POINT('Ctrl Pts',(-1.00638901194834,2.14764504030104,11.4711114864865));
#47227=CARTESIAN_POINT('Ctrl Pts',(-1.07985541228931,2.11321859800581,11.4765967380188));
#47228=CARTESIAN_POINT('Ctrl Pts',(-1.15166315267971,2.07496716452492,11.4820819895511));
#47229=CARTESIAN_POINT('Ctrl Pts',(-1.22140116858542,2.03307089101147,11.4875672410834));
#47230=CARTESIAN_POINT('Ctrl Pts',(-1.2910301291608,1.99124013430242,11.4930439148563));
#47231=CARTESIAN_POINT('Ctrl Pts',(-1.35859543081844,1.9457760960418,11.4985205886293));
#47232=CARTESIAN_POINT('Ctrl Pts',(-1.42370896548185,1.89690559704657,11.5039972624022));
#47233=CARTESIAN_POINT('Ctrl Pts',(-1.48872157623438,1.84811084577277,11.5094654475048));
#47234=CARTESIAN_POINT('Ctrl Pts',(-1.5512896385893,1.79592040565499,11.5149336326073));
#47235=CARTESIAN_POINT('Ctrl Pts',(-1.61105366257491,1.74060453831534,11.5204018177098));
#47236=CARTESIAN_POINT('Ctrl Pts',(-1.67076303528782,1.68533925462702,11.5258650024249));
#47237=CARTESIAN_POINT('Ctrl Pts',(-1.72767314955874,1.62695452169227,11.53132818714));
#47238=CARTESIAN_POINT('Ctrl Pts',(-1.78145770591508,1.56576067920221,11.5367913718551));
#47239=CARTESIAN_POINT('Ctrl Pts',(-1.83520615804759,1.50460791460396,11.5422508892712));
#47240=CARTESIAN_POINT('Ctrl Pts',(-1.88583293825317,1.44065011779986,11.5477104066874));
#47241=CARTESIAN_POINT('Ctrl Pts',(-1.93304949521141,1.37423349965096,11.5531699241036));
#47242=CARTESIAN_POINT('Ctrl Pts',(-1.98024582745808,1.30784533035628,11.5586271029934));
#47243=CARTESIAN_POINT('Ctrl Pts',(-2.02403459094754,1.23900079045998,11.5640842818832));
#47244=CARTESIAN_POINT('Ctrl Pts',(-2.06416899572855,1.16807723185283,11.569541460773));
#47245=CARTESIAN_POINT('Ctrl Pts',(-2.10430706105056,1.09714720451654,11.574999137396));
#47246=CARTESIAN_POINT('Ctrl Pts',(-2.14078987938564,1.0241381548064,11.580456814019));
#47247=CARTESIAN_POINT('Ctrl Pts',(-2.17341566996079,0.949453731399744,
11.5859144906421));
#47248=CARTESIAN_POINT('Ctrl Pts',(-2.2060417007892,0.874768758024002,11.5913722074549));
#47249=CARTESIAN_POINT('Ctrl Pts',(-2.2348104786237,0.798408788636254,11.5968299242678));
#47250=CARTESIAN_POINT('Ctrl Pts',(-2.25956822195664,0.72079783075681,11.6022876410806));
#47251=CARTESIAN_POINT('Ctrl Pts',(-2.28434270277559,0.643134403946534,
11.6077490475859));
#47252=CARTESIAN_POINT('Ctrl Pts',(-2.30510060547981,0.564218716888628,
11.6132104540912));
#47253=CARTESIAN_POINT('Ctrl Pts',(-2.32173806871777,0.484489837629956,
11.6186718605965));
#47254=CARTESIAN_POINT('Ctrl Pts',(-2.33146425323691,0.437880701364198,
11.621864573731));
#47255=CARTESIAN_POINT('Ctrl Pts',(-2.33978322345457,0.39099388975932,11.6250572868655));
#47256=CARTESIAN_POINT('Ctrl Pts',(-2.34668236863852,0.343918483395542,
11.62825));
#47257=CARTESIAN_POINT('',(-0.439445221994028,2.33068358199191,11.62825));
#47258=CARTESIAN_POINT('Origin',(0.,0.,11.62825));
#47259=CARTESIAN_POINT('',(-2.37174991248389,0.000644307893693102,10.8485898919608));
#47260=CARTESIAN_POINT('Ctrl Pts',(-2.37174991248389,0.00064430789369313,
10.8485898919608));
#47261=CARTESIAN_POINT('Ctrl Pts',(-2.37177122382654,-0.0778044827509494,
10.8538838529935));
#47262=CARTESIAN_POINT('Ctrl Pts',(-2.36789607083802,-0.156407906642089,
10.8591778140261));
#47263=CARTESIAN_POINT('Ctrl Pts',(-2.36010456354706,-0.234743501772307,
10.8644717750587));
#47264=CARTESIAN_POINT('Ctrl Pts',(-2.35232391937685,-0.312969879392242,
10.8697583551141));
#47265=CARTESIAN_POINT('Ctrl Pts',(-2.34063780741033,-0.390928699789423,
10.8750449351695));
#47266=CARTESIAN_POINT('Ctrl Pts',(-2.32507835604017,-0.46819728830222,
10.8803315152249));
#47267=CARTESIAN_POINT('Ctrl Pts',(-2.30953561317691,-0.545382901990649,
10.8856124182897));
#47268=CARTESIAN_POINT('Ctrl Pts',(-2.29012788664027,-0.621879291708473,
10.8908933213545));
#47269=CARTESIAN_POINT('Ctrl Pts',(-2.26693895282476,-0.697270282362413,
10.8961742244193));
#47270=CARTESIAN_POINT('Ctrl Pts',(-2.24376319966359,-0.772618420568053,
10.9014521258041));
#47271=CARTESIAN_POINT('Ctrl Pts',(-2.21681064342658,-0.846861952431962,
10.906730027189));
#47272=CARTESIAN_POINT('Ctrl Pts',(-2.18621553114936,-0.919597582566052,
10.9120079285738));
#47273=CARTESIAN_POINT('Ctrl Pts',(-2.15562794303006,-0.992315325059684,
10.9172845319813));
#47274=CARTESIAN_POINT('Ctrl Pts',(-2.12139976213312,-1.06352546359016,
10.9225611353887));
#47275=CARTESIAN_POINT('Ctrl Pts',(-2.08371365013264,-1.13284398164571,
10.9278377387962));
#47276=CARTESIAN_POINT('Ctrl Pts',(-2.04602465333876,-1.20216780588948,
10.9331147461166));
#47277=CARTESIAN_POINT('Ctrl Pts',(-2.00487742936107,-1.26959930511781,
10.9383917534371));
#47278=CARTESIAN_POINT('Ctrl Pts',(-1.96050016921421,-1.3347798129321,10.9436687607576));
#47279=CARTESIAN_POINT('Ctrl Pts',(-1.91607700733521,-1.40002774037078,
10.948951226364));
#47280=CARTESIAN_POINT('Ctrl Pts',(-1.86841741009435,-1.46301963567997,
10.9542336919704));
#47281=CARTESIAN_POINT('Ctrl Pts',(-1.81779196223019,-1.52342720356153,
10.9595161575769));
#47282=CARTESIAN_POINT('Ctrl Pts',(-1.76713708810984,-1.58386988359803,
10.9648016936388));
#47283=CARTESIAN_POINT('Ctrl Pts',(-1.71351325705018,-1.641724898701,10.9700872297008));
#47284=CARTESIAN_POINT('Ctrl Pts',(-1.65722850576611,-1.69670025112753,
10.9753727657628));
#47285=CARTESIAN_POINT('Ctrl Pts',(-1.60085049685053,-1.75176669165593,
10.9806670593756));
#47286=CARTESIAN_POINT('Ctrl Pts',(-1.54180312567185,-1.8039436332366,10.9859613529885));
#47287=CARTESIAN_POINT('Ctrl Pts',(-1.48042760659234,-1.85297926705597,
10.9912556466014));
#47288=CARTESIAN_POINT('Ctrl Pts',(-1.45085410415822,-1.87660685437197,
10.9938066768394));
#47289=CARTESIAN_POINT('Ctrl Pts',(-1.42074049814803,-1.89950575430157,
10.9963577070774));
#47290=CARTESIAN_POINT('Ctrl Pts',(-1.39012715941737,-1.92165151449221,
10.9989087373155));
#47291=CARTESIAN_POINT('Ctrl Pts',(-1.3259451246521,-1.96808094719684,11.0042570697161));
#47292=CARTESIAN_POINT('Ctrl Pts',(-1.25931844617298,-2.01137536844812,
11.0096054021168));
#47293=CARTESIAN_POINT('Ctrl Pts',(-1.1905852556703,-2.05126907339834,11.0149537345174));
#47294=CARTESIAN_POINT('Ctrl Pts',(-1.12194971603061,-2.09110610042211,
11.0202944684162));
#47295=CARTESIAN_POINT('Ctrl Pts',(-1.05121400829883,-2.12755177584933,
11.025635202315));
#47296=CARTESIAN_POINT('Ctrl Pts',(-0.978746618937616,-2.16038263240987,
11.0309759362138));
#47297=CARTESIAN_POINT('Ctrl Pts',(-0.906362475006621,-2.19317577519593,
11.0363105350539));
#47298=CARTESIAN_POINT('Ctrl Pts',(-0.832251025353797,-2.22236216150651,
11.0416451338939));
#47299=CARTESIAN_POINT('Ctrl Pts',(-0.756805516214812,-2.24776410531151,
11.0469797327339));
#47300=CARTESIAN_POINT('Ctrl Pts',(-0.681407392065659,-2.2731500949416,
11.0523109810775));
#47301=CARTESIAN_POINT('Ctrl Pts',(-0.604677311999744,-2.29475621279531,
11.0576422294211));
#47302=CARTESIAN_POINT('Ctrl Pts',(-0.527027582336053,-2.31245324059904,
11.0629734777647));
#47303=CARTESIAN_POINT('Ctrl Pts',(-0.449402848386129,-2.33014457166895,
11.0683030099612));
#47304=CARTESIAN_POINT('Ctrl Pts',(-0.370859506435195,-2.34392920874058,
11.0736325421577));
#47305=CARTESIAN_POINT('Ctrl Pts',(-0.291822669626693,-2.3537284448279,
11.0789620743542));
#47306=CARTESIAN_POINT('Ctrl Pts',(-0.212787077779679,-2.36352752656097,
11.0842915226017));
#47307=CARTESIAN_POINT('Ctrl Pts',(-0.133258468712647,-2.369341276333,11.0896209708492));
#47308=CARTESIAN_POINT('Ctrl Pts',(-0.0536682963514557,-2.37114271533089,
11.0949504190967));
#47309=CARTESIAN_POINT('Ctrl Pts',(0.0259969974664904,-2.37294585462314,
11.1002848975622));
#47310=CARTESIAN_POINT('Ctrl Pts',(0.105723504207312,-2.37072910816615,
11.1056193760277));
#47311=CARTESIAN_POINT('Ctrl Pts',(0.185079153489236,-2.36451766105557,
11.1109538544932));
#47312=CARTESIAN_POINT('Ctrl Pts',(0.264472156223381,-2.35830329015828,
11.116290843948));
#47313=CARTESIAN_POINT('Ctrl Pts',(0.343493491352376,-2.34809053137083,
11.1216278334028));
#47314=CARTESIAN_POINT('Ctrl Pts',(0.421718057243618,-2.33395628551493,
11.1269648228575));
#47315=CARTESIAN_POINT('Ctrl Pts',(0.500075292527004,-2.31979806788259,
11.1323108638825));
#47316=CARTESIAN_POINT('Ctrl Pts',(0.577632604273632,-2.30170518061197,
11.1376569049075));
#47317=CARTESIAN_POINT('Ctrl Pts',(0.653977177730247,-2.27980523587169,
11.1430029459324));
#47318=CARTESIAN_POINT('Ctrl Pts',(0.717007412965831,-2.26172459691953,
11.1474166482838));
#47319=CARTESIAN_POINT('Ctrl Pts',(0.77921117835256,-2.24104996791998,11.1518303506352));
#47320=CARTESIAN_POINT('Ctrl Pts',(0.840366763087148,-2.21787776173495,
11.1562440529866));
#47321=CARTESIAN_POINT('Ctrl Pts',(0.914445461652096,-2.18980891267537,
11.1615904383979));
#47322=CARTESIAN_POINT('Ctrl Pts',(0.987248208124766,-2.15797464747206,
11.1669368238092));
#47323=CARTESIAN_POINT('Ctrl Pts',(1.05836734865268,-2.12251186517435,11.1722832092205));
#47324=CARTESIAN_POINT('Ctrl Pts',(1.12938749829716,-2.08709844359898,11.1776221529866));
#47325=CARTESIAN_POINT('Ctrl Pts',(1.19872828307868,-2.04806674295669,11.1829610967526));
#47326=CARTESIAN_POINT('Ctrl Pts',(1.26600072393684,-2.00560221118032,11.1883000405187));
#47327=CARTESIAN_POINT('Ctrl Pts',(1.33319888874628,-1.96318456483862,11.1936330895135));
#47328=CARTESIAN_POINT('Ctrl Pts',(1.39833285649444,-1.91734186791345,11.1989661385083));
#47329=CARTESIAN_POINT('Ctrl Pts',(1.46103833856832,-1.86830539145332,11.2042991875032));
#47330=CARTESIAN_POINT('Ctrl Pts',(1.52370615624454,-1.81929836902636,11.2096290331724));
#47331=CARTESIAN_POINT('Ctrl Pts',(1.58394801820038,-1.76710166180247,11.2149588788416));
#47332=CARTESIAN_POINT('Ctrl Pts',(1.64142971969882,-1.71198905889887,11.2202887245108));
#47333=CARTESIAN_POINT('Ctrl Pts',(1.69889450588698,-1.6568926741439,11.2256170017506));
#47334=CARTESIAN_POINT('Ctrl Pts',(1.75360040901508,-1.59888242016868,11.2309452789903));
#47335=CARTESIAN_POINT('Ctrl Pts',(1.80524844651054,-1.53827049275193,11.2362735562301));
#47336=CARTESIAN_POINT('Ctrl Pts',(1.85689710878867,-1.47765783211697,11.2416018979256));
#47337=CARTESIAN_POINT('Ctrl Pts',(1.90548753113069,-1.41444379101006,11.2469302396212));
#47338=CARTESIAN_POINT('Ctrl Pts',(1.95076051625495,-1.34897422907953,11.2522585813167));
#47339=CARTESIAN_POINT('Ctrl Pts',(1.99607824377803,-1.28343996487143,11.2575921889074));
#47340=CARTESIAN_POINT('Ctrl Pts',(2.03807172035962,-1.21564611154979,11.262925796498));
#47341=CARTESIAN_POINT('Ctrl Pts',(2.07652502630167,-1.14596765994632,11.2682594040886));
#47342=CARTESIAN_POINT('Ctrl Pts',(2.11499736363482,-1.07625472293695,11.2735956513995));
#47343=CARTESIAN_POINT('Ctrl Pts',(2.14992583517356,-1.00465574837578,11.2789318987104));
#47344=CARTESIAN_POINT('Ctrl Pts',(2.18114159737732,-0.931568244784202,
11.2842681460214));
#47345=CARTESIAN_POINT('Ctrl Pts',(2.21241159031212,-0.858353767238774,
11.2896136639242));
#47346=CARTESIAN_POINT('Ctrl Pts',(2.23995582575665,-0.783646031814463,
11.294959181827));
#47347=CARTESIAN_POINT('Ctrl Pts',(2.26365460363261,-0.707860083599078,
11.3003046997298));
#47348=CARTESIAN_POINT('Ctrl Pts',(2.28327187527456,-0.645126319834312,
11.3047295893725));
#47349=CARTESIAN_POINT('Ctrl Pts',(2.30025508348975,-0.581654154374832,
11.3091544790151));
#47350=CARTESIAN_POINT('Ctrl Pts',(2.31456296300781,-0.51768364159252,11.3135793686578));
#47351=CARTESIAN_POINT('Ctrl Pts',(2.33164103473651,-0.441327602639413,
11.3188609746857));
#47352=CARTESIAN_POINT('Ctrl Pts',(2.34497176150638,-0.363967864181439,
11.3241425807135));
#47353=CARTESIAN_POINT('Ctrl Pts',(2.35444182868038,-0.286010031048158,
11.3294241867414));
#47354=CARTESIAN_POINT('Ctrl Pts',(2.36389825649962,-0.208164477429283,
11.3346981858857));
#47355=CARTESIAN_POINT('Ctrl Pts',(2.36950500365836,-0.129723009269663,
11.33997218503));
#47356=CARTESIAN_POINT('Ctrl Pts',(2.37119938729804,-0.0511031131870544,
11.3452461841743));
#47357=CARTESIAN_POINT('Ctrl Pts',(2.37289189060657,0.0274295349804628,
11.3505143305326));
#47358=CARTESIAN_POINT('Ctrl Pts',(2.37068064217068,0.106139742249119,11.3557824768908));
#47359=CARTESIAN_POINT('Ctrl Pts',(2.36455474368832,0.184604784881244,11.3610506232491));
#47360=CARTESIAN_POINT('Ctrl Pts',(2.35843251699248,0.26302279655361,11.3663156119467));
#47361=CARTESIAN_POINT('Ctrl Pts',(2.34840033150624,0.341195459410748,11.3715806006443));
#47362=CARTESIAN_POINT('Ctrl Pts',(2.33449936041767,0.418701323988221,11.3768455893419));
#47363=CARTESIAN_POINT('Ctrl Pts',(2.32060219488859,0.496185970394946,11.3821091366849));
#47364=CARTESIAN_POINT('Ctrl Pts',(2.3028384299805,0.573003710209475,11.387372684028));
#47365=CARTESIAN_POINT('Ctrl Pts',(2.28130073672659,0.648741097134066,11.3926362313711));
#47366=CARTESIAN_POINT('Ctrl Pts',(2.2597619264151,0.724482412196269,11.3979000517093));
#47367=CARTESIAN_POINT('Ctrl Pts',(2.23444893155355,0.799142803430474,11.4031638720475));
#47368=CARTESIAN_POINT('Ctrl Pts',(2.20550445712356,0.872323421735368,11.4084276923857));
#47369=CARTESIAN_POINT('Ctrl Pts',(2.17652683422226,0.945587849667984,11.4136975410799));
#47370=CARTESIAN_POINT('Ctrl Pts',(2.14390960310454,1.01736867458185,11.4189673897742));
#47371=CARTESIAN_POINT('Ctrl Pts',(2.10784363126702,1.0872871233612,11.4242372384684));
#47372=CARTESIAN_POINT('Ctrl Pts',(2.07175748752627,1.15724467792671,11.429510034619));
#47373=CARTESIAN_POINT('Ctrl Pts',(2.03221900575049,1.22533737006819,11.4347828307696));
#47374=CARTESIAN_POINT('Ctrl Pts',(1.98946363971034,1.29121357209816,11.4400556269202));
#47375=CARTESIAN_POINT('Ctrl Pts',(1.946622945094,1.3572212458718,11.4453389461988));
#47376=CARTESIAN_POINT('Ctrl Pts',(1.90055282321152,1.42100320556413,11.4506222654773));
#47377=CARTESIAN_POINT('Ctrl Pts',(1.85153028639175,1.48223940747575,11.4559055847559));
#47378=CARTESIAN_POINT('Ctrl Pts',(1.80510845082124,1.54022695933492,11.4609086179469));
#47379=CARTESIAN_POINT('Ctrl Pts',(1.75603972614395,1.59593174530661,11.4659116511379));
#47380=CARTESIAN_POINT('Ctrl Pts',(1.70458831036001,1.64911393017098,11.4709146843289));
#47381=CARTESIAN_POINT('Ctrl Pts',(1.64818248118368,1.70741718944924,11.4763994748101));
#47382=CARTESIAN_POINT('Ctrl Pts',(1.58869775148269,1.76291086987612,11.4818842652913));
#47383=CARTESIAN_POINT('Ctrl Pts',(1.52643780178982,1.81526463629055,11.4873690557724));
#47384=CARTESIAN_POINT('Ctrl Pts',(1.46427549351293,1.86753629701891,11.4928452445327));
#47385=CARTESIAN_POINT('Ctrl Pts',(1.39934695251003,1.91667755805281,11.498321433293));
#47386=CARTESIAN_POINT('Ctrl Pts',(1.33199256123157,1.96239493459491,11.5037976220533));
#47387=CARTESIAN_POINT('Ctrl Pts',(1.26474295129913,2.00804118989072,11.5092652916597));
#47388=CARTESIAN_POINT('Ctrl Pts',(1.19507536319021,2.05027392108357,11.514732961266));
#47389=CARTESIAN_POINT('Ctrl Pts',(1.12336198797659,2.08884080448206,11.5202006308724));
#47390=CARTESIAN_POINT('Ctrl Pts',(1.05171442543819,2.12737229434674,11.5256632826984));
#47391=CARTESIAN_POINT('Ctrl Pts',(0.978025191487546,2.16224442009277,11.5311259345244));
#47392=CARTESIAN_POINT('Ctrl Pts',(0.90269362279425,2.19324925301859,11.5365885863504));
#47393=CARTESIAN_POINT('Ctrl Pts',(0.827412842259987,2.22423318264434,11.5420475552844));
#47394=CARTESIAN_POINT('Ctrl Pts',(0.750492331645188,2.25135483974438,11.5475065242184));
#47395=CARTESIAN_POINT('Ctrl Pts',(0.67235311416707,2.27445363821069,11.5529654931525));
#47396=CARTESIAN_POINT('Ctrl Pts',(0.594247567815922,2.29754248312741,11.5584221097513));
#47397=CARTESIAN_POINT('Ctrl Pts',(0.514924777329727,2.31661179547297,11.56387872635));
#47398=CARTESIAN_POINT('Ctrl Pts',(0.434821674870552,2.33155059425327,11.5693353429488));
#47399=CARTESIAN_POINT('Ctrl Pts',(0.354711340293603,2.34649074178472,11.5747924521988));
#47400=CARTESIAN_POINT('Ctrl Pts',(0.273820980146343,2.35729954199481,11.5802495614489));
#47401=CARTESIAN_POINT('Ctrl Pts',(0.192597799839124,2.36391711995094,11.5857066706989));
#47402=CARTESIAN_POINT('Ctrl Pts',(0.111374163091576,2.37053473509509,11.5911638106156));
#47403=CARTESIAN_POINT('Ctrl Pts',(0.0298181378171431,2.372961052068,11.5966209505323));
#47404=CARTESIAN_POINT('Ctrl Pts',(-0.0516193872324029,2.37118820454256,
11.602078090449));
#47405=CARTESIAN_POINT('Ctrl Pts',(-0.133112285751584,2.36941415156891,
11.6075389409496));
#47406=CARTESIAN_POINT('Ctrl Pts',(-0.214486086717864,2.3634352459725,11.6129997914503));
#47407=CARTESIAN_POINT('Ctrl Pts',(-0.295291847603898,2.3532957288107,11.6184606419509));
#47408=CARTESIAN_POINT('Ctrl Pts',(-0.343577154422689,2.3472368823648,11.6217237613006));
#47409=CARTESIAN_POINT('Ctrl Pts',(-0.391659720980486,2.33969343226212,
11.6249868806503));
#47410=CARTESIAN_POINT('Ctrl Pts',(-0.439445221994028,2.33068358199191,
11.62825));
#47411=CARTESIAN_POINT('Ctrl Pts',(-2.37174994708504,0.000501001099097663,
10.846534127968));
#47412=CARTESIAN_POINT('Ctrl Pts',(-2.37174721579639,0.0134309801352372,
10.8456327823122));
#47413=CARTESIAN_POINT('Ctrl Pts',(-2.37163874962865,0.0263610865209047,
10.8447359062959));
#47414=CARTESIAN_POINT('Ctrl Pts',(-2.37122058518967,0.0516002056234556,
10.8429947803213));
#47415=CARTESIAN_POINT('Ctrl Pts',(-2.3709207720263,0.0639089482834945,
10.84215009231));
#47416=CARTESIAN_POINT('Ctrl Pts',(-2.37019595250979,0.086453069150876,
10.8406117875281));
#47417=CARTESIAN_POINT('Ctrl Pts',(-2.36980045945753,0.0966891034644412,
10.8399166518587));
#47418=CARTESIAN_POINT('Ctrl Pts',(-2.36880781812163,0.118685419646535,
10.8384304507506));
#47419=CARTESIAN_POINT('Ctrl Pts',(-2.36818938716719,0.13044443017894,10.8376405618378));
#47420=CARTESIAN_POINT('Ctrl Pts',(-2.36687173668857,0.152382158825592,
10.8361747513223));
#47421=CARTESIAN_POINT('Ctrl Pts',(-2.36619437722359,0.162561724707678,
10.835497728382));
#47422=CARTESIAN_POINT('Ctrl Pts',(-2.36545134966486,0.172736721251459,
10.8348238720555));
#47423=CARTESIAN_POINT('Origin',(0.,0.,11.5));
#47424=CARTESIAN_POINT('',(-2.86802679864211,0.000931424361933773,11.1319730730322));
#47425=CARTESIAN_POINT('Ctrl Pts',(-0.439445221994028,2.33068358199191,
11.62825));
#47426=CARTESIAN_POINT('Ctrl Pts',(-0.240507280203547,2.37702795048113,
11.6195679168283));
#47427=CARTESIAN_POINT('Ctrl Pts',(-0.0361575228823814,2.39677384679906,
11.6116630415941));
#47428=CARTESIAN_POINT('Ctrl Pts',(0.38478462472991,2.38385320910818,11.5950312564841));
#47429=CARTESIAN_POINT('Ctrl Pts',(0.600009392259926,2.347949842227,11.5862993207748));
#47430=CARTESIAN_POINT('Ctrl Pts',(1.11765369336044,2.18962607273897,11.5630931646838));
#47431=CARTESIAN_POINT('Ctrl Pts',(1.40746702139056,2.03397333167281,11.547868232976));
#47432=CARTESIAN_POINT('Ctrl Pts',(1.95712023912967,1.57686556379433,11.5171288884504));
#47433=CARTESIAN_POINT('Ctrl Pts',(2.14314882880409,1.29900143794958,11.506029731789));
#47434=CARTESIAN_POINT('Ctrl Pts',(2.39172992067706,0.825805923776539,11.4861578388178));
#47435=CARTESIAN_POINT('Ctrl Pts',(2.48167644349775,0.548774870720514,11.4747308319184));
#47436=CARTESIAN_POINT('Ctrl Pts',(2.56075430605598,0.0142339080762581,
11.4516318992604));
#47437=CARTESIAN_POINT('Ctrl Pts',(2.57530303238998,-0.333395071522134,
11.4358158642582));
#47438=CARTESIAN_POINT('Ctrl Pts',(2.43710470439177,-0.874911153872938,
11.4148550733305));
#47439=CARTESIAN_POINT('Ctrl Pts',(2.38775837133174,-1.01518848497531,11.4096305966607));
#47440=CARTESIAN_POINT('Ctrl Pts',(2.20245412277555,-1.42582454691614,11.3937382959454));
#47441=CARTESIAN_POINT('Ctrl Pts',(2.03065015867802,-1.67833993794217,11.3829065162613));
#47442=CARTESIAN_POINT('Ctrl Pts',(1.57762541566582,-2.14937217153313,11.3569961163812));
#47443=CARTESIAN_POINT('Ctrl Pts',(1.2855517434416,-2.35320921048462,11.3416110035159));
#47444=CARTESIAN_POINT('Ctrl Pts',(0.687481433266787,-2.61091912218133,
11.3167784573464));
#47445=CARTESIAN_POINT('Ctrl Pts',(0.39320028291873,-2.68074961248442,11.3071650484887));
#47446=CARTESIAN_POINT('Ctrl Pts',(-0.26155692159266,-2.7262052030806,11.2845788353831));
#47447=CARTESIAN_POINT('Ctrl Pts',(-0.620457783435796,-2.68111934069518,
11.2712031183861));
#47448=CARTESIAN_POINT('Ctrl Pts',(-1.18549877043465,-2.49567016439237,
11.2473229739679));
#47449=CARTESIAN_POINT('Ctrl Pts',(-1.49718036941518,-2.36307019900528,
11.2332600373849));
#47450=CARTESIAN_POINT('Ctrl Pts',(-2.0933840473706,-1.8819605586974,11.2071778307903));
#47451=CARTESIAN_POINT('Ctrl Pts',(-2.32305937208553,-1.60866780784321,
11.1964123534349));
#47452=CARTESIAN_POINT('Ctrl Pts',(-2.60441312869722,-1.11220399175858,
11.1764267582063));
#47453=CARTESIAN_POINT('Ctrl Pts',(-2.69005811846215,-0.910752895230764,
11.1683028423465));
#47454=CARTESIAN_POINT('Ctrl Pts',(-2.81977109542483,-0.473542869844156,
11.150669348876));
#47455=CARTESIAN_POINT('Ctrl Pts',(-2.85892360397332,-0.237243928705007,
11.1411444695169));
#47456=CARTESIAN_POINT('Ctrl Pts',(-2.86761958932067,0.000821401650878822,
11.1323802930381));
#47457=CARTESIAN_POINT('Ctrl Pts',(0.261350361647427,2.92782130397338,11.0605371920139));
#47458=CARTESIAN_POINT('Ctrl Pts',(0.163402798461412,2.92403748423913,11.0730146348275));
#47459=CARTESIAN_POINT('Ctrl Pts',(0.0658923488504137,2.91546186050777,
11.0854003458105));
#47460=CARTESIAN_POINT('Ctrl Pts',(-0.0307627309535459,2.90211667593812,
11.0977202846083));
#47461=CARTESIAN_POINT('Ctrl Pts',(-0.126342250004264,2.88891999423866,
11.1099031292909));
#47462=CARTESIAN_POINT('Ctrl Pts',(-0.221085044441188,2.87105918456392,
11.1220217004903));
#47463=CARTESIAN_POINT('Ctrl Pts',(-0.314574853355365,2.84854913007817,
11.1341337287248));
#47464=CARTESIAN_POINT('Ctrl Pts',(-0.39017932206751,2.83034542713084,11.1439286301192));
#47465=CARTESIAN_POINT('Ctrl Pts',(-0.464964087502808,2.80910118651745,
11.1537198864481));
#47466=CARTESIAN_POINT('Ctrl Pts',(-0.538705163844275,2.78482060950474,
11.1635534412447));
#47467=CARTESIAN_POINT('Ctrl Pts',(-0.594010971100378,2.7666101767452,11.1709286073421));
#47468=CARTESIAN_POINT('Ctrl Pts',(-0.648729636076866,2.74669177190032,
11.1783278575236));
#47469=CARTESIAN_POINT('Ctrl Pts',(-0.702765788630647,2.7250651160814,11.1857754814952));
#47470=CARTESIAN_POINT('Ctrl Pts',(-0.718629674298013,2.71871598167666,
11.1879619483252));
#47471=CARTESIAN_POINT('Ctrl Pts',(-0.734434730791572,2.71221960024673,
11.1901526111987));
#47472=CARTESIAN_POINT('Ctrl Pts',(-0.750178534250807,2.70557592300405,
11.1923481504307));
#47473=CARTESIAN_POINT('Ctrl Pts',(-0.763358987334736,2.7000139457837,11.1941862197331));
#47474=CARTESIAN_POINT('Ctrl Pts',(-0.776488354911949,2.69435215882939,
11.196026571624));
#47475=CARTESIAN_POINT('Ctrl Pts',(-0.78956312197429,2.688591939758,11.1978692853271));
#47476=CARTESIAN_POINT('Ctrl Pts',(-0.872801830852324,2.65192029612018,
11.2096006690485));
#47477=CARTESIAN_POINT('Ctrl Pts',(-0.95385898559835,2.61124905776464,11.2214310006084));
#47478=CARTESIAN_POINT('Ctrl Pts',(-1.03246252049652,2.5666448806666,11.2334778512215));
#47479=CARTESIAN_POINT('Ctrl Pts',(-1.07746886343747,2.54110568712176,11.2403755650553));
#47480=CARTESIAN_POINT('Ctrl Pts',(-1.1216710063815,2.51427636072537,11.2473445633387));
#47481=CARTESIAN_POINT('Ctrl Pts',(-1.16501856324264,2.48616221908335,11.2544088373727));
#47482=CARTESIAN_POINT('Ctrl Pts',(-1.24266078345783,2.43580541619539,11.2670620515309));
#47483=CARTESIAN_POINT('Ctrl Pts',(-1.31756840157884,2.38132606317727,11.2800208331917));
#47484=CARTESIAN_POINT('Ctrl Pts',(-1.38952099343943,2.32292969176299,11.2931991310621));
#47485=CARTESIAN_POINT('Ctrl Pts',(-1.46277813137534,2.26347455713851,11.3066163598219));
#47486=CARTESIAN_POINT('Ctrl Pts',(-1.53297200293144,2.19995698204504,11.3202605352119));
#47487=CARTESIAN_POINT('Ctrl Pts',(-1.59978151883497,2.13260008847238,11.3340510047343));
#47488=CARTESIAN_POINT('Ctrl Pts',(-1.61331518168127,2.11895554284653,11.3368445523672));
#47489=CARTESIAN_POINT('Ctrl Pts',(-1.6267132492287,2.10514961901921,11.3396449260006));
#47490=CARTESIAN_POINT('Ctrl Pts',(-1.63995148862121,2.09120707263336,11.3424470079295));
#47491=CARTESIAN_POINT('Ctrl Pts',(-1.70171752547037,2.02615493025203,11.3555207627199));
#47492=CARTESIAN_POINT('Ctrl Pts',(-1.76008871104665,1.95805043285538,11.3686460413715));
#47493=CARTESIAN_POINT('Ctrl Pts',(-1.81484660700543,1.88716888932194,11.3817802567806));
#47494=CARTESIAN_POINT('Ctrl Pts',(-1.86940990513711,1.81653924360364,11.394867796003));
#47495=CARTESIAN_POINT('Ctrl Pts',(-1.92038481010494,1.74315138575278,11.4079639534782));
#47496=CARTESIAN_POINT('Ctrl Pts',(-1.96751101622977,1.6672954795621,11.4210518006067));
#47497=CARTESIAN_POINT('Ctrl Pts',(-2.01384320160487,1.59271765553543,11.4339191330144));
#47498=CARTESIAN_POINT('Ctrl Pts',(-2.05645453396309,1.51575388926486,11.4467782845076));
#47499=CARTESIAN_POINT('Ctrl Pts',(-2.09506613628272,1.43670608847597,11.4596404781877));
#47500=CARTESIAN_POINT('Ctrl Pts',(-2.11584570714243,1.39416500550823,11.4665625132479));
#47501=CARTESIAN_POINT('Ctrl Pts',(-2.13546637970218,1.35102082416007,11.4734859152846));
#47502=CARTESIAN_POINT('Ctrl Pts',(-2.15388188633923,1.30732413101464,11.4804159938924));
#47503=CARTESIAN_POINT('Ctrl Pts',(-2.15933961437786,1.29437392160277,11.4824698328159));
#47504=CARTESIAN_POINT('Ctrl Pts',(-2.16469222289073,1.28137334258626,11.484524567937));
#47505=CARTESIAN_POINT('Ctrl Pts',(-2.16993611370384,1.26832965527801,11.4865794518199));
#47506=CARTESIAN_POINT('Ctrl Pts',(-2.20175895320132,1.18917332223087,11.4990496275584));
#47507=CARTESIAN_POINT('Ctrl Pts',(-2.22947962309921,1.1086815952271,11.511483675394));
#47508=CARTESIAN_POINT('Ctrl Pts',(-2.25295126705805,1.02716409885249,11.5239435592641));
#47509=CARTESIAN_POINT('Ctrl Pts',(-2.2760786989779,0.946842057883126,11.5362207187353));
#47510=CARTESIAN_POINT('Ctrl Pts',(-2.29508104728318,0.865524217715744,
11.5485231608414));
#47511=CARTESIAN_POINT('Ctrl Pts',(-2.30979972814699,0.783500714904634,
11.5609329335986));
#47512=CARTESIAN_POINT('Ctrl Pts',(-2.32408698795012,0.703881413048161,
11.5729789619839));
#47513=CARTESIAN_POINT('Ctrl Pts',(-2.33433845898191,0.623597301201896,
11.5851264291944));
#47514=CARTESIAN_POINT('Ctrl Pts',(-2.34038703160473,0.542906490436884,
11.5974682280848));
#47515=CARTESIAN_POINT('Ctrl Pts',(-2.34534204029777,0.476804338124139,
11.6075786664647));
#47516=CARTESIAN_POINT('Ctrl Pts',(-2.3474763612765,0.410429125649973,11.6178199429796));
#47517=CARTESIAN_POINT('Ctrl Pts',(-2.34668236863853,0.343918483395475,
11.62825));
#47518=CARTESIAN_POINT('Ctrl Pts',(-2.86819969387402,0.00077918580006163,
11.1318002002877));
#47519=CARTESIAN_POINT('Ctrl Pts',(-2.86975559680702,0.0427595453757233,
11.1302328928719));
#47520=CARTESIAN_POINT('Ctrl Pts',(-2.87035280117414,0.0847243061035006,
11.1287027854165));
#47521=CARTESIAN_POINT('Ctrl Pts',(-2.8699874816256,0.12665023816086,11.1272193909883));
#47522=CARTESIAN_POINT('Ctrl Pts',(-2.86921038481711,0.21583382585658,11.1240639587632));
#47523=CARTESIAN_POINT('Ctrl Pts',(-2.86408052121998,0.304845801774181,
11.12111909617));
#47524=CARTESIAN_POINT('Ctrl Pts',(-2.85472489574556,0.393465375926996,
11.1182871009688));
#47525=CARTESIAN_POINT('Ctrl Pts',(-2.85411091907604,0.399281165704107,
11.1181012471222));
#47526=CARTESIAN_POINT('Ctrl Pts',(-2.85347873052284,0.405095279363024,
11.1179158793767));
#47527=CARTESIAN_POINT('Ctrl Pts',(-2.8528283606803,0.410907660087458,11.1177309701174));
#47528=CARTESIAN_POINT('Ctrl Pts',(-2.84203922631273,0.50733057598794,11.1146634680387));
#47529=CARTESIAN_POINT('Ctrl Pts',(-2.82624903601188,0.603272528673326,
11.1117216154067));
#47530=CARTESIAN_POINT('Ctrl Pts',(-2.80558094060506,0.698407783990052,
11.1087964708405));
#47531=CARTESIAN_POINT('Ctrl Pts',(-2.79250101933245,0.758614669302825,
11.1069452765295));
#47532=CARTESIAN_POINT('Ctrl Pts',(-2.77746677601657,0.818497584311128,
11.1051011503189));
#47533=CARTESIAN_POINT('Ctrl Pts',(-2.76050507677153,0.877965201122309,
11.1032412642294));
#47534=CARTESIAN_POINT('Ctrl Pts',(-2.74977650746049,0.915579501405769,
11.1020648539811));
#47535=CARTESIAN_POINT('Ctrl Pts',(-2.73827675238308,0.953027514721806,
11.100882217146));
#47536=CARTESIAN_POINT('Ctrl Pts',(-2.72601228780754,0.990284803198791,
11.0996884676428));
#47537=CARTESIAN_POINT('Ctrl Pts',(-2.72123391409771,1.00480066295458,11.099223369374));
#47538=CARTESIAN_POINT('Ctrl Pts',(-2.71633888424499,1.019289212608,11.0987565384275));
#47539=CARTESIAN_POINT('Ctrl Pts',(-2.71132938212565,1.03374376926027,11.0982878849096));
#47540=CARTESIAN_POINT('Ctrl Pts',(-2.67885568285608,1.12744428372618,11.0952498757343));
#47541=CARTESIAN_POINT('Ctrl Pts',(-2.64168416110042,1.21939768587777,11.0921427423104));
#47542=CARTESIAN_POINT('Ctrl Pts',(-2.60005965515925,1.30923023475234,11.0889187544872));
#47543=CARTESIAN_POINT('Ctrl Pts',(-2.55796403279677,1.40007953056444,11.0856582767749));
#47544=CARTESIAN_POINT('Ctrl Pts',(-2.51131407129837,1.48875923668141,11.0822782090206));
#47545=CARTESIAN_POINT('Ctrl Pts',(-2.4603548397369,1.57488396663604,11.0787664513456));
#47546=CARTESIAN_POINT('Ctrl Pts',(-2.40966787183388,1.66054855162101,11.0752734561983));
#47547=CARTESIAN_POINT('Ctrl Pts',(-2.35471797004357,1.74368521769819,11.0716502887964));
#47548=CARTESIAN_POINT('Ctrl Pts',(-2.29573496237524,1.82392072310517,11.0679212456613));
#47549=CARTESIAN_POINT('Ctrl Pts',(-2.24798135631813,1.888880698333,11.0649021514529));
#47550=CARTESIAN_POINT('Ctrl Pts',(-2.19758411414171,1.95193923017891,11.0618143815443));
#47551=CARTESIAN_POINT('Ctrl Pts',(-2.14465592532941,2.01290113297903,11.058687366294));
#47552=CARTESIAN_POINT('',(-2.,-2.4492935982947E-16,12.));
#47553=CARTESIAN_POINT('',(-2.5,3.06161699786838E-16,11.5));
#47554=CARTESIAN_POINT('Origin',(0.,0.,12.));
#47555=CARTESIAN_POINT('Ctrl Pts',(1.70910432722271,-2.39912472810947,-0.331414121240076));
#47556=CARTESIAN_POINT('Ctrl Pts',(2.49908112321251,-1.83639873781273,-0.279009803491007));
#47557=CARTESIAN_POINT('Ctrl Pts',(3.46688794428796,0.119722171111187,-0.174225981237435));
#47558=CARTESIAN_POINT('Ctrl Pts',(1.80646906852251,2.96481187827153,-0.0170626544793579));
#47559=CARTESIAN_POINT('Ctrl Pts',(-1.47762516829172,3.13820676414614,0.140075859034155));
#47560=CARTESIAN_POINT('Ctrl Pts',(-3.43381835120548,0.497172601989588,
0.297214372547669));
#47561=CARTESIAN_POINT('Ctrl Pts',(-2.30628780313538,-2.59256922604425,
0.454352886061182));
#47562=CARTESIAN_POINT('Ctrl Pts',(0.89286661821801,-3.35263685283103,0.611491399574695));
#47563=CARTESIAN_POINT('Ctrl Pts',(3.2899750863192,-1.10208983694566,0.768629913088208));
#47564=CARTESIAN_POINT('Ctrl Pts',(2.73221466175904,2.13861997197995,0.925768426601723));
#47565=CARTESIAN_POINT('Ctrl Pts',(-0.279542673141038,3.45834407847404,
1.08290694011524));
#47566=CARTESIAN_POINT('Ctrl Pts',(-3.04021030694678,1.67200480266538,1.24004545362875));
#47567=CARTESIAN_POINT('Ctrl Pts',(-3.07028929888958,-1.61610736971899,
1.39718396714226));
#47568=CARTESIAN_POINT('Ctrl Pts',(-0.34275152402455,-3.45267261769994,
1.55432248065578));
#47569=CARTESIAN_POINT('Ctrl Pts',(2.6926299045483,-2.18819586596506,1.71146099416929));
#47570=CARTESIAN_POINT('Ctrl Pts',(3.30959871793033,1.04163827573356,1.8685995076828));
#47571=CARTESIAN_POINT('Ctrl Pts',(0.954016139202541,3.33591076751599,2.02573802119631));
#47572=CARTESIAN_POINT('Ctrl Pts',(-2.2584257185156,2.63400176430825,2.18287653470983));
#47573=CARTESIAN_POINT('Ctrl Pts',(-3.44243900729852,-0.433664443236683,
2.34001504822334));
#47574=CARTESIAN_POINT('Ctrl Pts',(-1.53458952609955,-3.11182991073641,
2.49715356173686));
#47575=CARTESIAN_POINT('Ctrl Pts',(1.75156758027233,-2.99507296916488,2.65429207525037));
#47576=CARTESIAN_POINT('Ctrl Pts',(3.46453592574662,-0.1882597119523,2.81143058876388));
#47577=CARTESIAN_POINT('Ctrl Pts',(2.06579499679089,2.78764091132087,2.96856910227739));
#47578=CARTESIAN_POINT('Ctrl Pts',(-1.18836135867558,3.25979266149099,3.12570761579091));
#47579=CARTESIAN_POINT('Ctrl Pts',(-3.3751785051291,0.804127440320037,3.28284612930442));
#47580=CARTESIAN_POINT('Ctrl Pts',(-2.5305436919165,-2.37377326169313,3.43998464281794));
#47581=CARTESIAN_POINT('Ctrl Pts',(0.586925466079213,-3.41964462846938,
3.59712315633145));
#47582=CARTESIAN_POINT('Ctrl Pts',(3.17724136420127,-1.39412631986779,3.75426166984497));
#47583=CARTESIAN_POINT('Ctrl Pts',(2.91388462237087,1.8835411567826,3.91140018335848));
#47584=CARTESIAN_POINT('Ctrl Pts',(0.0333918595374598,3.46948639819222,
4.06853869687199));
#47585=CARTESIAN_POINT('Ctrl Pts',(-2.87709215207102,1.93927605850991,4.22567721038551));
#47586=CARTESIAN_POINT('Ctrl Pts',(-3.20348568541843,-1.3327154032213,4.38281572389901));
#47587=CARTESIAN_POINT('Ctrl Pts',(-0.652634966855167,-3.4077145542025,
4.53995423741253));
#47588=CARTESIAN_POINT('Ctrl Pts',(2.48438668906291,-2.42203915367867,4.69709275092605));
#47589=CARTESIAN_POINT('Ctrl Pts',(3.39003039525862,0.739016104011381,4.85423126443955));
#47590=CARTESIAN_POINT('Ctrl Pts',(1.25088276275288,3.23631630046266,5.01136977795308));
#47591=CARTESIAN_POINT('Ctrl Pts',(-2.01175833668358,2.82688508389631,5.16850829146658));
#47592=CARTESIAN_POINT('Ctrl Pts',(-3.46751759586556,-0.121542606266135,
5.3256468049801));
#47593=CARTESIAN_POINT('Ctrl Pts',(-1.8088895747861,-2.96080553042772,5.48278531849362));
#47594=CARTESIAN_POINT('Ctrl Pts',(1.47441158128589,-3.14078992798711,5.63992383200712));
#47595=CARTESIAN_POINT('Ctrl Pts',(3.43345451870903,-0.499840925423201,
5.79706234552064));
#47596=CARTESIAN_POINT('Ctrl Pts',(2.3087042857198,2.59004544436804,5.95420085903415));
#47597=CARTESIAN_POINT('Ctrl Pts',(-0.889632904673123,3.35365534569197,
6.11133937254767));
#47598=CARTESIAN_POINT('Ctrl Pts',(-3.2889369753028,1.10514454042514,6.26847788606118));
#47599=CARTESIAN_POINT('Ctrl Pts',(-2.73424782219197,-2.13596341956599,
6.4256163995747));
#47600=CARTESIAN_POINT('Ctrl Pts',(0.276234676805524,-3.45863344198172,
6.5827549130882));
#47601=CARTESIAN_POINT('Ctrl Pts',(3.03861410485482,-1.67489558014692,6.73989342660173));
#47602=CARTESIAN_POINT('Ctrl Pts',(3.07183041964025,1.61316730579844,6.89703194011523));
#47603=CARTESIAN_POINT('Ctrl Pts',(0.346050039349144,3.45234706425207,7.05417045362875));
#47604=CARTESIAN_POINT('Ctrl Pts',(-2.69053881099474,2.19076511490178,7.21130896714225));
#47605=CARTESIAN_POINT('Ctrl Pts',(-3.31059202324357,-1.0384754900275,7.36844748065578));
#47606=CARTESIAN_POINT('Ctrl Pts',(-0.957202301260398,-3.33499844514049,
7.52558599416929));
#47607=CARTESIAN_POINT('Ctrl Pts',(2.25590869828579,-2.63615758761869,7.68272450768281));
#47608=CARTESIAN_POINT('Ctrl Pts',(3.4428516585937,0.430375849255442,7.83986302119631));
#47609=CARTESIAN_POINT('Ctrl Pts',(1.53756129382305,3.11036269379847,7.99700153470983));
#47610=CARTESIAN_POINT('Ctrl Pts',(-1.74870583733373,2.99674469957124,8.15414004822333));
#47611=CARTESIAN_POINT('Ctrl Pts',(-3.46435454290838,0.191568995177432,
8.31127856173687));
#47612=CARTESIAN_POINT('Ctrl Pts',(-2.06845679284888,-2.78566633017768,
8.46841707525036));
#47613=CARTESIAN_POINT('Ctrl Pts',(1.18524691039277,-3.2609263913346,8.62555558876389));
#47614=CARTESIAN_POINT('Ctrl Pts',(3.37440905771097,-0.807350934643548,
8.7826941022774));
#47615=CARTESIAN_POINT('Ctrl Pts',(2.5328096038664,2.37135466627205,8.93983261579091));
#47616=CARTESIAN_POINT('Ctrl Pts',(-0.583657951598417,3.42020428728099,
9.09697112930442));
#47617=CARTESIAN_POINT('Ctrl Pts',(-3.17590966926535,1.39715951965449,9.25410964281793));
#47618=CARTESIAN_POINT('Ctrl Pts',(-2.91567971810012,-1.88075479361231,
9.41124815633145));
#47619=CARTESIAN_POINT('Ctrl Pts',(-0.0367112214115904,-3.46945697416158,
9.56838666984496));
#47620=CARTESIAN_POINT('Ctrl Pts',(2.87524850237772,-1.94201565909655,9.72552518335847));
#47621=CARTESIAN_POINT('Ctrl Pts',(3.20473796907475,1.32963995908438,9.88266369687199));
#47622=CARTESIAN_POINT('Ctrl Pts',(0.655926631036102,3.4071179312111,10.0398022103855));
#47623=CARTESIAN_POINT('Ctrl Pts',(-2.48214247180021,2.42435699247973,10.196940723899));
#47624=CARTESIAN_POINT('Ctrl Pts',(-3.39060001386736,-0.735673984079567,
10.3540792374125));
#47625=CARTESIAN_POINT('Ctrl Pts',(-1.25423123682802,-3.2353180102252,10.511217750926));
#47626=CARTESIAN_POINT('Ctrl Pts',(2.00955017432607,-2.82842662307344,10.6683562644396));
#47627=CARTESIAN_POINT('Ctrl Pts',(3.46668582007914,0.117504286576653,10.8254947779531));
#47628=CARTESIAN_POINT('Ctrl Pts',(1.81355903899321,2.96048029568761,10.9826332914666));
#47629=CARTESIAN_POINT('Ctrl Pts',(-1.47574573937,3.13939893589932,11.139796701647));
#47630=CARTESIAN_POINT('Ctrl Pts',(-2.77455595124166,1.38549983595441,11.2445806073229));
#47631=CARTESIAN_POINT('Ctrl Pts',(-2.914713972712,0.425769325633511,11.2969850084943));
#47632=CARTESIAN_POINT('Ctrl Pts',(1.5973239975809,-2.24221508328063,-0.22018540887939));
#47633=CARTESIAN_POINT('Ctrl Pts',(2.33563404318066,-1.71629298827072,-0.167781091130323));
#47634=CARTESIAN_POINT('Ctrl Pts',(3.24014351969597,0.111891997411981,-0.0629972688767504));
#47635=CARTESIAN_POINT('Ctrl Pts',(1.68832080527672,2.77090466979952,0.0941660578813266));
#47636=CARTESIAN_POINT('Ctrl Pts',(-1.38098424019397,2.9329590323412,0.25130457139484));
#47637=CARTESIAN_POINT('Ctrl Pts',(-3.20923677294008,0.464656086494237,
0.408443084908354));
#47638=CARTESIAN_POINT('Ctrl Pts',(-2.15544995972395,-2.42300775569364,
0.565581598421868));
#47639=CARTESIAN_POINT('Ctrl Pts',(0.834470578069453,-3.13336477762204,
0.72272011193538));
#47640=CARTESIAN_POINT('Ctrl Pts',(3.07480127053478,-1.03000999763654,0.879858625448894));
#47641=CARTESIAN_POINT('Ctrl Pts',(2.55351997900672,1.99874808608113,1.03699713896241));
#47642=CARTESIAN_POINT('Ctrl Pts',(-0.261259779782845,3.23215844723473,
1.19413565247591));
#47643=CARTESIAN_POINT('Ctrl Pts',(-2.84137182477921,1.56265088843805,1.35127416598943));
#47644=CARTESIAN_POINT('Ctrl Pts',(-2.86948356429563,-1.51040930808146,
1.50841267950295));
#47645=CARTESIAN_POINT('Ctrl Pts',(-0.320334590353228,-3.22685791627738,
1.66555119301647));
#47646=CARTESIAN_POINT('Ctrl Pts',(2.51652417856085,-2.0450815742729,1.82268970652997));
#47647=CARTESIAN_POINT('Ctrl Pts',(3.09314146030137,0.973512142077214,1.97982822004348));
#47648=CARTESIAN_POINT('Ctrl Pts',(0.891620744828347,3.11773262630528,2.136966733557));
#47649=CARTESIAN_POINT('Ctrl Pts',(-2.11071819284485,2.46173048700712,2.29410524707052));
#47650=CARTESIAN_POINT('Ctrl Pts',(-3.21729361337571,-0.405301543648401,
2.45124376058402));
#47651=CARTESIAN_POINT('Ctrl Pts',(-1.43422296546303,-2.90830730086939,
2.60838227409754));
#47652=CARTESIAN_POINT('Ctrl Pts',(1.63701003197397,-2.79918659847233,2.76552078761105));
#47653=CARTESIAN_POINT('Ctrl Pts',(3.23794532991962,-0.17594698631868,2.92265930112457));
#47654=CARTESIAN_POINT('Ctrl Pts',(1.9306860733415,2.60532119272485,3.07979781463808));
#47655=CARTESIAN_POINT('Ctrl Pts',(-1.11063911416977,3.0465928629406,3.23693632815159));
#47656=CARTESIAN_POINT('Ctrl Pts',(-3.15443214114532,0.75153519716593,3.39407484166512));
#47657=CARTESIAN_POINT('Ctrl Pts',(-2.36503886956599,-2.21852167554908,
3.55121335517862));
#47658=CARTESIAN_POINT('Ctrl Pts',(0.548538855602305,-3.19599005236204,
3.70835186869213));
#47659=CARTESIAN_POINT('Ctrl Pts',(2.9694406574889,-1.30294645617249,3.86549038220565));
#47660=CARTESIAN_POINT('Ctrl Pts',(2.72330820264104,1.76035215769955,4.02262889571916));
#47661=CARTESIAN_POINT('Ctrl Pts',(0.0312079360595172,3.24257202725503,
4.17976740923268));
#47662=CARTESIAN_POINT('Ctrl Pts',(-2.68892206552574,1.81244183684538,4.33690592274618));
#47663=CARTESIAN_POINT('Ctrl Pts',(-2.99396852475403,-1.24555198977838,
4.4940444362597));
#47664=CARTESIAN_POINT('Ctrl Pts',(-0.609950766383085,-3.18484023920209,
4.65118294977321));
#47665=CARTESIAN_POINT('Ctrl Pts',(2.32190066721047,-2.26363083963293,4.80832146328674));
#47666=CARTESIAN_POINT('Ctrl Pts',(3.16831267502232,0.690682329179025,4.96545997680025));
#47667=CARTESIAN_POINT('Ctrl Pts',(1.16907143892864,3.02465192332146,5.12259849031377));
#47668=CARTESIAN_POINT('Ctrl Pts',(-1.88018356593827,2.64199868374835,5.27973700382728));
#47669=CARTESIAN_POINT('Ctrl Pts',(-3.24073199025274,-0.113593370881535,
5.43687551734079));
#47670=CARTESIAN_POINT('Ctrl Pts',(-1.69058300348168,-2.76716034860646,
5.59401403085429));
#47671=CARTESIAN_POINT('Ctrl Pts',(1.37798083100417,-2.93537324985099,5.75115254436782));
#47672=CARTESIAN_POINT('Ctrl Pts',(3.20889673613342,-0.467149893914844,
5.90829105788132));
#47673=CARTESIAN_POINT('Ctrl Pts',(2.1577083974099,2.42064903658454,6.06542957139485));
#47674=CARTESIAN_POINT('Ctrl Pts',(-0.831448358674023,3.13431665812589,
6.22256808490835));
#47675=CARTESIAN_POINT('Ctrl Pts',(-3.07383105495917,1.03286491473878,6.37970659842187));
#47676=CARTESIAN_POINT('Ctrl Pts',(-2.55542016491037,-1.99626527982169,
6.53684511193538));
#47677=CARTESIAN_POINT('Ctrl Pts',(0.258168135904549,-3.23242888553827,
6.6939836254489));
#47678=CARTESIAN_POINT('Ctrl Pts',(2.83988001888659,-1.56535260077321,6.85112213896242));
#47679=CARTESIAN_POINT('Ctrl Pts',(2.87092389132481,1.5076615327819,7.00826065247592));
#47680=CARTESIAN_POINT('Ctrl Pts',(0.323417373305934,3.22655365495962,7.16539916598943));
#47681=CARTESIAN_POINT('Ctrl Pts',(-2.51456984852899,2.04748278695315,7.32253767950295));
#47682=CARTESIAN_POINT('Ctrl Pts',(-3.09406980059545,-0.970556211636323,
7.47967619301647));
#47683=CARTESIAN_POINT('Ctrl Pts',(-0.894598522740514,-3.11687997243229,
7.63681470652998));
#47684=CARTESIAN_POINT('Ctrl Pts',(2.10836579296415,-2.46374531328394,7.7939532200435));
#47685=CARTESIAN_POINT('Ctrl Pts',(3.21767927609153,0.402228033154709,7.951091733557));
#47686=CARTESIAN_POINT('Ctrl Pts',(1.43700037104582,2.90693604413139,8.10823024707053));
#47687=CARTESIAN_POINT('Ctrl Pts',(-1.63433545523929,2.80074899291077,8.26536876058403));
#47688=CARTESIAN_POINT('Ctrl Pts',(-3.23777581003972,0.179039832920316,
8.42250727409755));
#47689=CARTESIAN_POINT('Ctrl Pts',(-1.93317378029559,-2.60347575485722,
8.57964578761106));
#47690=CARTESIAN_POINT('Ctrl Pts',(1.10772835974587,-3.04765244359763,8.73678430112457));
#47691=CARTESIAN_POINT('Ctrl Pts',(3.15371301779734,-0.754547865706401,
8.89392281463809));
#47692=CARTESIAN_POINT('Ctrl Pts',(2.36715658436919,2.21626126321204,9.05106132815159));
#47693=CARTESIAN_POINT('Ctrl Pts',(-0.545485045949209,3.19651310788066,
9.20819984166512));
#47694=CARTESIAN_POINT('Ctrl Pts',(-2.96819605922493,1.3057812759852,9.36533835517862));
#47695=CARTESIAN_POINT('Ctrl Pts',(-2.72498589395606,-1.75774803067992,
9.52247686869215));
#47696=CARTESIAN_POINT('Ctrl Pts',(-0.0343102021375739,-3.24254452764047,
9.67961538220565));
#47697=CARTESIAN_POINT('Ctrl Pts',(2.6871989958153,-1.81500225968858,9.83675389571918));
#47698=CARTESIAN_POINT('Ctrl Pts',(2.99513890546405,1.24267768851727,9.99389240923267));
#47699=CARTESIAN_POINT('Ctrl Pts',(0.613027146276597,3.18428263706717,10.1510309227462));
#47700=CARTESIAN_POINT('Ctrl Pts',(-2.31980322819965,2.26579708512215,10.3081694362597));
#47701=CARTESIAN_POINT('Ctrl Pts',(-3.16884503893873,-0.687558793485591,
10.4653079497732));
#47702=CARTESIAN_POINT('Ctrl Pts',(-1.17220091318618,-3.0237189241315,10.6224464632867));
#47703=CARTESIAN_POINT('Ctrl Pts',(1.87811982373831,-2.64343940183772,10.7795849768002));
#47704=CARTESIAN_POINT('Ctrl Pts',(3.23995461499069,0.109819168893298,10.9367234903137));
#47705=CARTESIAN_POINT('Ctrl Pts',(1.69494707132415,2.76685638515205,11.0938620038273));
#47706=CARTESIAN_POINT('Ctrl Pts',(-1.37922773131934,2.93407323263913,11.2510254140077));
#47707=CARTESIAN_POINT('Ctrl Pts',(-2.59309202660024,1.2948841690727,11.3558093196836));
#47708=CARTESIAN_POINT('Ctrl Pts',(-2.7240833110889,0.397922789402426,11.408213720855));
#47709=CARTESIAN_POINT('Ctrl Pts',(1.48554366793907,-2.08530543845179,-0.108956696518706));
#47710=CARTESIAN_POINT('Ctrl Pts',(2.17218696314881,-1.59618723872872,-0.0565523787696377));
#47711=CARTESIAN_POINT('Ctrl Pts',(3.01339909510398,0.104061823712772,0.0482314434839342));
#47712=CARTESIAN_POINT('Ctrl Pts',(1.57017254203093,2.57699746132752,0.205394770242011));
#47713=CARTESIAN_POINT('Ctrl Pts',(-1.28434331209622,2.72771130053625,0.362533283755524));
#47714=CARTESIAN_POINT('Ctrl Pts',(-2.98465519467468,0.43213957099889,0.519671797269038));
#47715=CARTESIAN_POINT('Ctrl Pts',(-2.00461211631251,-2.25344628534304,
0.676810310782551));
#47716=CARTESIAN_POINT('Ctrl Pts',(0.776074537920896,-2.91409270241304,
0.833948824296065));
#47717=CARTESIAN_POINT('Ctrl Pts',(2.85962745475038,-0.957930158327435,
0.991087337809578));
#47718=CARTESIAN_POINT('Ctrl Pts',(2.37482529625441,1.85887620018229,1.14822585132309));
#47719=CARTESIAN_POINT('Ctrl Pts',(-0.242976886424651,3.00597281599543,
1.30536436483661));
#47720=CARTESIAN_POINT('Ctrl Pts',(-2.64253334261165,1.45329697421072,1.46250287835012));
#47721=CARTESIAN_POINT('Ctrl Pts',(-2.66867782970167,-1.40471124644393,
1.61964139186363));
#47722=CARTESIAN_POINT('Ctrl Pts',(-0.297917656681901,-3.00104321485481,
1.77677990537715));
#47723=CARTESIAN_POINT('Ctrl Pts',(2.34041845257341,-1.90196728258075,1.93391841889066));
#47724=CARTESIAN_POINT('Ctrl Pts',(2.87668420267241,0.905386008420865,2.09105693240418));
#47725=CARTESIAN_POINT('Ctrl Pts',(0.829225350454149,2.89955448509455,2.24819544591769));
#47726=CARTESIAN_POINT('Ctrl Pts',(-1.9630106671741,2.28945920970598,2.4053339594312));
#47727=CARTESIAN_POINT('Ctrl Pts',(-2.99214821945292,-0.376938644060123,
2.56247247294471));
#47728=CARTESIAN_POINT('Ctrl Pts',(-1.33385640482652,-2.70478469100235,
2.71961098645823));
#47729=CARTESIAN_POINT('Ctrl Pts',(1.52245248367561,-2.60330022777978,2.87674949997174));
#47730=CARTESIAN_POINT('Ctrl Pts',(3.0113547340926,-0.163634260685059,3.03388801348526));
#47731=CARTESIAN_POINT('Ctrl Pts',(1.79557714989212,2.42300147412883,3.19102652699877));
#47732=CARTESIAN_POINT('Ctrl Pts',(-1.03291686966396,2.83339306439021,3.34816504051229));
#47733=CARTESIAN_POINT('Ctrl Pts',(-2.93368577716156,0.698942954011819,
3.50530355402579));
#47734=CARTESIAN_POINT('Ctrl Pts',(-2.19953404721547,-2.06327008940503,
3.66244206753931));
#47735=CARTESIAN_POINT('Ctrl Pts',(0.510152245125398,-2.9723354762547,3.81958058105282));
#47736=CARTESIAN_POINT('Ctrl Pts',(2.76163995077652,-1.21176659247721,3.97671909456634));
#47737=CARTESIAN_POINT('Ctrl Pts',(2.53273178291119,1.63716315861649,4.13385760807985));
#47738=CARTESIAN_POINT('Ctrl Pts',(0.0290240125815749,3.01565765631784,
4.29099612159337));
#47739=CARTESIAN_POINT('Ctrl Pts',(-2.50075197898047,1.68560761518086,4.44813463510687));
#47740=CARTESIAN_POINT('Ctrl Pts',(-2.78445136408961,-1.15838857633547,
4.60527314862039));
#47741=CARTESIAN_POINT('Ctrl Pts',(-0.567266565911004,-2.96196592420167,
4.76241166213391));
#47742=CARTESIAN_POINT('Ctrl Pts',(2.15941464535803,-2.10522252558719,4.91955017564741));
#47743=CARTESIAN_POINT('Ctrl Pts',(2.94659495478601,0.642348554346671,5.07668868916094));
#47744=CARTESIAN_POINT('Ctrl Pts',(1.08726011510442,2.81298754618025,5.23382720267444));
#47745=CARTESIAN_POINT('Ctrl Pts',(-1.74860879519294,2.45711228360039,5.39096571618796));
#47746=CARTESIAN_POINT('Ctrl Pts',(-3.01394638463993,-0.105644135496936,
5.54810422970147));
#47747=CARTESIAN_POINT('Ctrl Pts',(-1.57227643217725,-2.5735151667852,5.70524274321499));
#47748=CARTESIAN_POINT('Ctrl Pts',(1.28155008072244,-2.72995657171488,5.8623812567285));
#47749=CARTESIAN_POINT('Ctrl Pts',(2.98433895355781,-0.434458862406489,
6.01951977024201));
#47750=CARTESIAN_POINT('Ctrl Pts',(2.00671250910002,2.25125262880104,6.17665828375553));
#47751=CARTESIAN_POINT('Ctrl Pts',(-0.773263812674921,2.91497797055982,
6.33379679726904));
#47752=CARTESIAN_POINT('Ctrl Pts',(-2.85872513461553,0.960585289052411,
6.49093531078255));
#47753=CARTESIAN_POINT('Ctrl Pts',(-2.37659250762878,-1.85656714007738,
6.64807382429607));
#47754=CARTESIAN_POINT('Ctrl Pts',(0.240101595003575,-3.00622432909485,
6.80521233780957));
#47755=CARTESIAN_POINT('Ctrl Pts',(2.64114593291835,-1.45580962139949,6.9623508513231));
#47756=CARTESIAN_POINT('Ctrl Pts',(2.67001736300939,1.40215575976535,7.11948936483661));
#47757=CARTESIAN_POINT('Ctrl Pts',(0.300784707262725,3.00076024566717,7.27662787835012));
#47758=CARTESIAN_POINT('Ctrl Pts',(-2.33860088606324,1.90420045900452,7.43376639186363));
#47759=CARTESIAN_POINT('Ctrl Pts',(-2.87754757794732,-0.902636933245142,
7.59090490537715));
#47760=CARTESIAN_POINT('Ctrl Pts',(-0.831994744220631,-2.89876149972411,
7.74804341889066));
#47761=CARTESIAN_POINT('Ctrl Pts',(1.96082288764251,-2.29133303894919,7.90518193240418));
#47762=CARTESIAN_POINT('Ctrl Pts',(2.99250689358935,0.374080217053975,8.06232044591769));
#47763=CARTESIAN_POINT('Ctrl Pts',(1.33643944826859,2.70350939446431,8.2194589594312));
#47764=CARTESIAN_POINT('Ctrl Pts',(-1.51996507314484,2.6047532862503,8.37659747294471));
#47765=CARTESIAN_POINT('Ctrl Pts',(-3.01119707717106,0.166510670663201,
8.53373598645823));
#47766=CARTESIAN_POINT('Ctrl Pts',(-1.79789076774231,-2.42128517953676,
8.69087449997174));
#47767=CARTESIAN_POINT('Ctrl Pts',(1.03020980909898,-2.83437849586067,8.84801301348525));
#47768=CARTESIAN_POINT('Ctrl Pts',(2.93301697788372,-0.701744796769256,
9.00515152699877));
#47769=CARTESIAN_POINT('Ctrl Pts',(2.20150356487198,2.06116786015204,9.16229004051228));
#47770=CARTESIAN_POINT('Ctrl Pts',(-0.507312140300006,2.97282192848032,
9.3194285540258));
#47771=CARTESIAN_POINT('Ctrl Pts',(-2.7604824491845,1.21440303231589,9.47656706753931));
#47772=CARTESIAN_POINT('Ctrl Pts',(-2.53429206981202,-1.63474126774752,
9.63370558105282));
#47773=CARTESIAN_POINT('Ctrl Pts',(-0.0319091828635594,-3.01563208111935,
9.79084409456634));
#47774=CARTESIAN_POINT('Ctrl Pts',(2.49914948925288,-1.68798886028062,9.94798260807984));
#47775=CARTESIAN_POINT('Ctrl Pts',(2.78553984185336,1.15571541795015,10.1051211215933));
#47776=CARTESIAN_POINT('Ctrl Pts',(0.570127661517096,2.96144734292322,10.2622596351068));
#47777=CARTESIAN_POINT('Ctrl Pts',(-2.15746398459908,2.10723717776457,10.4193981486204));
#47778=CARTESIAN_POINT('Ctrl Pts',(-2.9470900640101,-0.639443602891618,
10.576536662134));
#47779=CARTESIAN_POINT('Ctrl Pts',(-1.09017058954435,-2.81211983803781,
10.7336751756475));
#47780=CARTESIAN_POINT('Ctrl Pts',(1.74668947315055,-2.45845218060199,10.890813689161));
#47781=CARTESIAN_POINT('Ctrl Pts',(3.01322340990224,0.102134051209937,11.0479522026745));
#47782=CARTESIAN_POINT('Ctrl Pts',(1.57633510365508,2.57323247461651,11.2050907161879));
#47783=CARTESIAN_POINT('Ctrl Pts',(-1.2827097232687,2.72874752937894,11.3622541263684));
#47784=CARTESIAN_POINT('Ctrl Pts',(-2.41162810195881,1.20426850219099,11.4670380320443));
#47785=CARTESIAN_POINT('Ctrl Pts',(-2.53345264946579,0.37007625317134,11.5194424332157));
#47786=CARTESIAN_POINT('Ctrl Pts',(1.37376333829725,-1.92839579362295,0.00227201584197912));
#47787=CARTESIAN_POINT('Ctrl Pts',(2.00873988311696,-1.47608148918673,0.0546763335910469));
#47788=CARTESIAN_POINT('Ctrl Pts',(2.786654670512,0.0962316500135649,0.159460155844619));
#47789=CARTESIAN_POINT('Ctrl Pts',(1.45202427878513,2.3830902528555,0.316623482602697));
#47790=CARTESIAN_POINT('Ctrl Pts',(-1.18770238399847,2.52246356873131,0.47376199611621));
#47791=CARTESIAN_POINT('Ctrl Pts',(-2.76007361640928,0.399623055503541,
0.630900509629723));
#47792=CARTESIAN_POINT('Ctrl Pts',(-1.85377427290108,-2.08388481499243,
0.788039023143237));
#47793=CARTESIAN_POINT('Ctrl Pts',(0.717678497772337,-2.69482062720405,
0.94517753665675));
#47794=CARTESIAN_POINT('Ctrl Pts',(2.64445363896598,-0.885850319018325,
1.10231605017026));
#47795=CARTESIAN_POINT('Ctrl Pts',(2.19613061350208,1.71900431428346,1.25945456368378));
#47796=CARTESIAN_POINT('Ctrl Pts',(-0.224693993066457,2.77978718475613,
1.41659307719729));
#47797=CARTESIAN_POINT('Ctrl Pts',(-2.44369486044408,1.34394305998338,1.57373159071081));
#47798=CARTESIAN_POINT('Ctrl Pts',(-2.46787209510772,-1.2990131848064,1.73087010422431));
#47799=CARTESIAN_POINT('Ctrl Pts',(-0.275500723010577,-2.77522851343225,
1.88800861773783));
#47800=CARTESIAN_POINT('Ctrl Pts',(2.16431272658597,-1.75885299088859,2.04514713125134));
#47801=CARTESIAN_POINT('Ctrl Pts',(2.66022694504343,0.837259874764513,2.20228564476486));
#47802=CARTESIAN_POINT('Ctrl Pts',(0.766829956079953,2.68137634388383,2.35942415827837));
#47803=CARTESIAN_POINT('Ctrl Pts',(-1.81530314150335,2.11718793240485,2.51656267179188));
#47804=CARTESIAN_POINT('Ctrl Pts',(-2.76700282553012,-0.348575744471842,
2.67370118530539));
#47805=CARTESIAN_POINT('Ctrl Pts',(-1.23348984419001,-2.50126208113532,
2.83083969881891));
#47806=CARTESIAN_POINT('Ctrl Pts',(1.40789493537724,-2.40741385708723,2.98797821233242));
#47807=CARTESIAN_POINT('Ctrl Pts',(2.7847641382656,-0.151321535051437,3.14511672584594));
#47808=CARTESIAN_POINT('Ctrl Pts',(1.66046822644274,2.24068175553282,3.30225523935945));
#47809=CARTESIAN_POINT('Ctrl Pts',(-0.955194625158153,2.62019326583982,
3.45939375287296));
#47810=CARTESIAN_POINT('Ctrl Pts',(-2.71293941317779,0.64635071085771,3.61653226638648));
#47811=CARTESIAN_POINT('Ctrl Pts',(-2.03402922486496,-1.90801850326096,
3.77367077989999));
#47812=CARTESIAN_POINT('Ctrl Pts',(0.471765634648494,-2.74868090014737,
3.9308092934135));
#47813=CARTESIAN_POINT('Ctrl Pts',(2.55383924406414,-1.12058672878193,4.08794780692702));
#47814=CARTESIAN_POINT('Ctrl Pts',(2.34215536318135,1.51397415953343,4.24508632044053));
#47815=CARTESIAN_POINT('Ctrl Pts',(0.0268400891036326,2.78874328538067,
4.40222483395405));
#47816=CARTESIAN_POINT('Ctrl Pts',(-2.3125818924352,1.55877339351634,4.55936334746756));
#47817=CARTESIAN_POINT('Ctrl Pts',(-2.57493420342521,-1.07122516289255,
4.71650186098107));
#47818=CARTESIAN_POINT('Ctrl Pts',(-0.524582365438923,-2.73909160920127,
4.87364037449459));
#47819=CARTESIAN_POINT('Ctrl Pts',(1.9969286235056,-1.94681421154145,5.0307788880081));
#47820=CARTESIAN_POINT('Ctrl Pts',(2.72487723454969,0.594014779514313,5.18791740152161));
#47821=CARTESIAN_POINT('Ctrl Pts',(1.00544879128018,2.60132316903906,5.34505591503514));
#47822=CARTESIAN_POINT('Ctrl Pts',(-1.61703402444763,2.27222588345243,5.50219442854863));
#47823=CARTESIAN_POINT('Ctrl Pts',(-2.7871607790271,-0.0976949001123346,
5.65933294206217));
#47824=CARTESIAN_POINT('Ctrl Pts',(-1.45396986087282,-2.37986998496394,
5.81647145557566));
#47825=CARTESIAN_POINT('Ctrl Pts',(1.18511933044069,-2.52453989357877,5.97360996908919));
#47826=CARTESIAN_POINT('Ctrl Pts',(2.7597811709822,-0.401767830898135,6.13074848260269));
#47827=CARTESIAN_POINT('Ctrl Pts',(1.85571662079012,2.08185622101755,6.28788699611621));
#47828=CARTESIAN_POINT('Ctrl Pts',(-0.715079266675815,2.69563928299374,
6.44502550962972));
#47829=CARTESIAN_POINT('Ctrl Pts',(-2.64361921427189,0.888305663366045,
6.60216402314323));
#47830=CARTESIAN_POINT('Ctrl Pts',(-2.19776485034718,-1.71686900033308,
6.75930253665675));
#47831=CARTESIAN_POINT('Ctrl Pts',(0.222035054102601,-2.78001977265141,
6.91644105017026));
#47832=CARTESIAN_POINT('Ctrl Pts',(2.44241184695011,-1.34626664202579,7.07357956368377));
#47833=CARTESIAN_POINT('Ctrl Pts',(2.46911083469396,1.29664998674881,7.23071807719729));
#47834=CARTESIAN_POINT('Ctrl Pts',(0.278152041219513,2.77496683637473,7.3878565907108));
#47835=CARTESIAN_POINT('Ctrl Pts',(-2.16263192359748,1.76091813105588,7.54499510422432));
#47836=CARTESIAN_POINT('Ctrl Pts',(-2.66102535529921,-0.83471765485396,
7.70213361773782));
#47837=CARTESIAN_POINT('Ctrl Pts',(-0.769390965700746,-2.68064302701591,
7.85927213125134));
#47838=CARTESIAN_POINT('Ctrl Pts',(1.81327998232086,-2.11892076461443,8.01641064476486));
#47839=CARTESIAN_POINT('Ctrl Pts',(2.76733451108718,0.345932400953242,8.17354915827837));
#47840=CARTESIAN_POINT('Ctrl Pts',(1.23587852549135,2.50008274479723,8.33068767179189));
#47841=CARTESIAN_POINT('Ctrl Pts',(-1.4055946910504,2.40875757958982,8.4878261853054));
#47842=CARTESIAN_POINT('Ctrl Pts',(-2.78461834430241,0.153981508406087,
8.64496469881891));
#47843=CARTESIAN_POINT('Ctrl Pts',(-1.66260775518902,-2.23909460421632,
8.80210321233243));
#47844=CARTESIAN_POINT('Ctrl Pts',(0.952691258452081,-2.6211045481237,8.95924172584593));
#47845=CARTESIAN_POINT('Ctrl Pts',(2.71232093797009,-0.648941727832109,
9.11638023935945));
#47846=CARTESIAN_POINT('Ctrl Pts',(2.03585054537477,1.90607445709202,9.27351875287297));
#47847=CARTESIAN_POINT('Ctrl Pts',(-0.469139234650799,2.74913074907999,
9.43065726638646));
#47848=CARTESIAN_POINT('Ctrl Pts',(-2.55276883914408,1.12302478864659,9.5877957799));
#47849=CARTESIAN_POINT('Ctrl Pts',(-2.34359824566799,-1.51173450481514,
9.74493429341351));
#47850=CARTESIAN_POINT('Ctrl Pts',(-0.0295081635895418,-2.78871963459825,
9.90207280692703));
#47851=CARTESIAN_POINT('Ctrl Pts',(2.31109998269045,-1.56097546087265,10.0592113204406));
#47852=CARTESIAN_POINT('Ctrl Pts',(2.57594077824267,1.06875314738303,10.2163498339541));
#47853=CARTESIAN_POINT('Ctrl Pts',(0.527228176757592,2.73861204877929,10.3734883474676));
#47854=CARTESIAN_POINT('Ctrl Pts',(-1.99512474099851,1.948677270407,10.5306268609811));
#47855=CARTESIAN_POINT('Ctrl Pts',(-2.72533508908147,-0.591328412297643,
10.6877653744946));
#47856=CARTESIAN_POINT('Ctrl Pts',(-1.00814026590252,-2.60052075194411,
10.8449038880081));
#47857=CARTESIAN_POINT('Ctrl Pts',(1.61525912256279,-2.27346495936627,11.0020424015217));
#47858=CARTESIAN_POINT('Ctrl Pts',(2.78649220481378,0.0944489335265817,
11.1591809150351));
#47859=CARTESIAN_POINT('Ctrl Pts',(1.45772313598602,2.37960856408097,11.3163194285487));
#47860=CARTESIAN_POINT('Ctrl Pts',(-1.18619171521805,2.52342182611875,11.4734828387291));
#47861=CARTESIAN_POINT('Ctrl Pts',(-2.23016417731738,1.11365283530928,11.578266744405));
#47862=CARTESIAN_POINT('Ctrl Pts',(-2.34282198784267,0.342229716940255,
11.6306711455764));
#47863=CARTESIAN_POINT('Ctrl Pts',(1.29197400994444,2.64783394680711,-8.8037216405823E-17));
#47864=CARTESIAN_POINT('Ctrl Pts',(1.37074936016223,2.60046826619745,1.38836964406048E-15));
#47865=CARTESIAN_POINT('Ctrl Pts',(1.44700091320012,2.54930204226795,5.54450672197035E-16));
#47866=CARTESIAN_POINT('Ctrl Pts',(1.5204041597113,2.49432533414619,7.28583859910259E-17));
#47867=CARTESIAN_POINT('Ctrl Pts',(1.59819384922954,2.43606331906114,-3.44654117973336E-16));
#47868=CARTESIAN_POINT('Ctrl Pts',(1.67278528785766,2.37352116391825,2.10927055586783E-15));
#47869=CARTESIAN_POINT('Ctrl Pts',(1.74400344302578,2.30706978985341,3.50414142147315E-15));
#47870=CARTESIAN_POINT('Ctrl Pts',(1.77507572754732,2.27807723876983,4.11271972997575E-15));
#47871=CARTESIAN_POINT('Ctrl Pts',(1.80550534467386,2.2483401837646,3.54603031729656E-15));
#47872=CARTESIAN_POINT('Ctrl Pts',(1.83527511247412,2.21788805045802,3.41393580072236E-15));
#47873=CARTESIAN_POINT('Ctrl Pts',(1.85158854668356,2.20120068908634,3.34154977406537E-15));
#47874=CARTESIAN_POINT('Ctrl Pts',(1.86770501691636,2.18429728937136,3.85069962828599E-15));
#47875=CARTESIAN_POINT('Ctrl Pts',(1.883618179848,2.16718615052119,3.69843045078255E-15));
#47876=CARTESIAN_POINT('Ctrl Pts',(1.89863325668145,2.15104070755384,3.55475484025806E-15));
#47877=CARTESIAN_POINT('Ctrl Pts',(1.91346219376733,2.1347157726636,4.15166473682132E-15));
#47878=CARTESIAN_POINT('Ctrl Pts',(1.92809660170213,2.11822316236597,4.33680868994202E-15));
#47879=CARTESIAN_POINT('Ctrl Pts',(1.99241597015465,2.04573684906905,5.15053085694606E-15));
#47880=CARTESIAN_POINT('Ctrl Pts',(2.05302114486396,1.96997093364048,5.27402816434403E-15));
#47881=CARTESIAN_POINT('Ctrl Pts',(2.1097435081236,1.89129938269064,3.91353616180368E-15));
#47882=CARTESIAN_POINT('Ctrl Pts',(2.16643862125782,1.81266562652767,2.55369775646138E-15));
#47883=CARTESIAN_POINT('Ctrl Pts',(2.21925498259858,1.73112805545147,4.69792942335234E-15));
#47884=CARTESIAN_POINT('Ctrl Pts',(2.26797565137533,1.64704303172464,4.76008121808036E-15));
#47885=CARTESIAN_POINT('Ctrl Pts',(2.27370375376251,1.63715713242915,4.76738842162842E-15));
#47886=CARTESIAN_POINT('Ctrl Pts',(2.27937518380796,1.62723601064538,5.31291259247108E-15));
#47887=CARTESIAN_POINT('Ctrl Pts',(2.28498954152194,1.61728023964544,5.759281940243E-15));
#47888=CARTESIAN_POINT('Ctrl Pts',(2.29543189661598,1.59876312668031,6.68580931231859E-15));
#47889=CARTESIAN_POINT('Ctrl Pts',(2.30567682494647,1.58012614919259,4.74072510815603E-15));
#47890=CARTESIAN_POINT('Ctrl Pts',(2.31572165746038,1.56137299470242,4.413136522885E-15));
#47891=CARTESIAN_POINT('Ctrl Pts',(2.32292320728395,1.54792809393149,4.17340296428537E-15));
#47892=CARTESIAN_POINT('Ctrl Pts',(2.33002152872364,1.53442403232929,7.07982753161834E-15));
#47893=CARTESIAN_POINT('Ctrl Pts',(2.33700969851763,1.52087413145422,6.73072708679001E-15));
#47894=CARTESIAN_POINT('Ctrl Pts',(2.38054570717361,1.43645880967822,4.52005977667776E-15));
#47895=CARTESIAN_POINT('Ctrl Pts',(2.41987517047016,1.35014619738548,5.21195039373243E-15));
#47896=CARTESIAN_POINT('Ctrl Pts',(2.45484083362543,1.26228524501801,4.74620343027254E-15));
#47897=CARTESIAN_POINT('Ctrl Pts',(2.489466389985,1.17527890555589,4.28498673145102E-15));
#47898=CARTESIAN_POINT('Ctrl Pts',(2.5198128252979,1.08675327428347,5.61314304544713E-15));
#47899=CARTESIAN_POINT('Ctrl Pts',(2.54567771304716,0.997038113744462,4.12170297892089E-15));
#47900=CARTESIAN_POINT('Ctrl Pts',(2.57079955722097,0.90990028020974,2.67310883426158E-15));
#47901=CARTESIAN_POINT('Ctrl Pts',(2.59169365537883,0.821639511860095,2.2335485000352E-15));
#47902=CARTESIAN_POINT('Ctrl Pts',(2.60812613872453,0.732561686781793,3.58046925441613E-15));
#47903=CARTESIAN_POINT('Ctrl Pts',(2.6179205585058,0.679467726869315,4.38328809822516E-15));
#47904=CARTESIAN_POINT('Ctrl Pts',(2.62612900003745,0.62608362232302,5.90836632262066E-15));
#47905=CARTESIAN_POINT('Ctrl Pts',(2.6326933508001,0.572476447093943,2.692290834716E-15));
#47906=CARTESIAN_POINT('Ctrl Pts',(2.6352683765624,0.551447732716798,1.47778125432564E-15));
#47907=CARTESIAN_POINT('Ctrl Pts',(2.63759088070415,0.530377846603741,4.89932062977248E-15));
#47908=CARTESIAN_POINT('Ctrl Pts',(2.63965388200594,0.509307581220653,4.55191440096314E-15));
#47909=CARTESIAN_POINT('Ctrl Pts',(2.64834931960692,0.420497565581757,3.58563629104739E-15));
#47910=CARTESIAN_POINT('Ctrl Pts',(2.65245297897981,0.331587017875098,1.12456554759877E-15));
#47911=CARTESIAN_POINT('Ctrl Pts',(2.65178792227643,0.242870082279381,1.77635683940025E-15));
#47912=CARTESIAN_POINT('Ctrl Pts',(2.65141677862464,0.193360428010837,1.70825926277529E-15));
#47913=CARTESIAN_POINT('Ctrl Pts',(2.64955959473766,0.143911103164861,4.17994550737481E-16));
#47914=CARTESIAN_POINT('Ctrl Pts',(2.64617859082989,0.0945743399740334,
4.16333634234434E-16));
#47915=CARTESIAN_POINT('Ctrl Pts',(2.63994540686809,0.00361759178976989,
4.69281982652766E-16));
#47916=CARTESIAN_POINT('Ctrl Pts',(2.62853563407678,-0.0869581494466769,
-2.6842679134847E-16));
#47917=CARTESIAN_POINT('Ctrl Pts',(2.61214758827663,-0.176810898454838,
-8.60422844084496E-16));
#47918=CARTESIAN_POINT('Ctrl Pts',(2.59575954247647,-0.266663647463,-1.45241889682052E-15));
#47919=CARTESIAN_POINT('Ctrl Pts',(2.5743925683296,-0.3557942617185,5.20804214904531E-17));
#47920=CARTESIAN_POINT('Ctrl Pts',(2.54820206281091,-0.443829678011399,
-1.72084568816899E-15));
#47921=CARTESIAN_POINT('Ctrl Pts',(2.5433159398537,-0.460253640057088,-1.94456528016881E-15));
#47922=CARTESIAN_POINT('Ctrl Pts',(2.53826078384047,-0.476642310793063,
1.09767773292823E-15));
#47923=CARTESIAN_POINT('Ctrl Pts',(2.53304532831964,-0.492969520416451,
7.49400541621981E-16));
#47924=CARTESIAN_POINT('Ctrl Pts',(2.50606165438058,-0.577443081556576,
-1.37861067859985E-15));
#47925=CARTESIAN_POINT('Ctrl Pts',(2.47475445780067,-0.660402252413519,
-4.29383913192097E-16));
#47926=CARTESIAN_POINT('Ctrl Pts',(2.43933995245441,-0.741546545884959,
-7.7715611723761E-16));
#47927=CARTESIAN_POINT('Ctrl Pts',(2.40390362452278,-0.822740840853054,
-1.12514262015681E-15));
#47928=CARTESIAN_POINT('Ctrl Pts',(2.36435426939278,-0.902118814440422,
1.6833566618084E-16));
#47929=CARTESIAN_POINT('Ctrl Pts',(2.32086575374546,-0.979349725934495,
-1.47104550762833E-15));
#47930=CARTESIAN_POINT('Ctrl Pts',(2.27822747361116,-1.05507071089561,-3.07837545888844E-15));
#47931=CARTESIAN_POINT('Ctrl Pts',(2.23180185773245,-1.12872835588638,-1.56235785302982E-15));
#47932=CARTESIAN_POINT('Ctrl Pts',(2.18172187678888,-1.1999723751995,-4.44089209850063E-16));
#47933=CARTESIAN_POINT('Ctrl Pts',(2.15328177937689,-1.24043139317656,1.90968323031924E-16));
#47934=CARTESIAN_POINT('Ctrl Pts',(2.1236626297252,-1.28011125530021,-1.24815247604854E-15));
#47935=CARTESIAN_POINT('Ctrl Pts',(2.09288546869145,-1.31894102140197,-2.05391259555654E-15));
#47936=CARTESIAN_POINT('Ctrl Pts',(2.08472665052523,-1.32923453095322,-2.69181282397187E-15));
#47937=CARTESIAN_POINT('Ctrl Pts',(2.07648733901943,-1.33946704131009,-3.53561961405176E-15));
#47938=CARTESIAN_POINT('Ctrl Pts',(2.06817568052717,-1.3496280615777,-3.71924713249427E-15));
#47939=CARTESIAN_POINT('Ctrl Pts',(2.01414238364663,-1.41568388247562,-3.61763159642546E-15));
#47940=CARTESIAN_POINT('Ctrl Pts',(1.95696807639177,-1.47883106713657,-2.1047465562029E-15));
#47941=CARTESIAN_POINT('Ctrl Pts',(1.8968144714638,-1.53877542768777,-2.27595720048157E-15));
#47942=CARTESIAN_POINT('Ctrl Pts',(1.83758356200986,-1.59780030236209,-1.96915150342469E-15));
#47943=CARTESIAN_POINT('Ctrl Pts',(1.77546340768274,-1.65372037610682,1.00684964781356E-15));
#47944=CARTESIAN_POINT('Ctrl Pts',(1.71058212136984,-1.70621256949937,0.));
#47945=CARTESIAN_POINT('Ctrl Pts',(1.64772546514904,-1.75706673626848,-1.47459711886327E-15));
#47946=CARTESIAN_POINT('Ctrl Pts',(1.58227673613707,-1.8047039083925,6.77258530541363E-16));
#47947=CARTESIAN_POINT('Ctrl Pts',(1.51433650217974,-1.84878472649022,1.66533453693773E-16));
#47948=CARTESIAN_POINT('Ctrl Pts',(1.46963595840449,-1.87778722507249,-6.32259699606435E-17));
#47949=CARTESIAN_POINT('Ctrl Pts',(1.4238565767745,-1.90524929950466,4.02804854125218E-16));
#47950=CARTESIAN_POINT('Ctrl Pts',(1.37702479013104,-1.93106208855763,-3.88578058618805E-16));
#47951=CARTESIAN_POINT('Ctrl Pts',(-1.03730518518318,2.12835542941762,-0.331584989410291));
#47952=CARTESIAN_POINT('Ctrl Pts',(-1.73864579252332,1.78654022387532,-0.279139884186583));
#47953=CARTESIAN_POINT('Ctrl Pts',(-2.7656846889405,0.361807027866601,-0.174249673739168));
#47954=CARTESIAN_POINT('Ctrl Pts',(-1.82129522076317,-2.11585284458798,
-0.0169143580680439));
#47955=CARTESIAN_POINT('Ctrl Pts',(0.764938575946876,-2.68229399094113,
0.140420957603079));
#47956=CARTESIAN_POINT('Ctrl Pts',(2.66139142426043,-0.837298121388289,
0.297756273274203));
#47957=CARTESIAN_POINT('Ctrl Pts',(2.16259871848842,1.76312751480994,0.455091588945326));
#47958=CARTESIAN_POINT('Ctrl Pts',(-0.283336766153592,2.77546827896293,
0.61242690461645));
#47959=CARTESIAN_POINT('Ctrl Pts',(-2.47403969246375,1.28971871163609,0.769762220287572));
#47960=CARTESIAN_POINT('Ctrl Pts',(-2.4376362160542,-1.35730685306026,0.927097535958697));
#47961=CARTESIAN_POINT('Ctrl Pts',(-0.206765733213128,-2.78232569956815,
1.08443285162982));
#47962=CARTESIAN_POINT('Ctrl Pts',(2.21021679152004,-1.70268993439413,1.24176816730094));
#47963=CARTESIAN_POINT('Ctrl Pts',(2.63751871827682,0.909784458804265,1.39910348297206));
#47964=CARTESIAN_POINT('Ctrl Pts',(0.690453185041018,2.70323004638949,1.55643879864319));
#47965=CARTESIAN_POINT('Ctrl Pts',(-1.87817235801244,2.06316899439893,1.71377411431431));
#47966=CARTESIAN_POINT('Ctrl Pts',(-2.75602147084388,-0.434213789166044,
1.87110942998544));
#47967=CARTESIAN_POINT('Ctrl Pts',(-1.15282950609521,-2.54070379675866,
2.02844474565656));
#47968=CARTESIAN_POINT('Ctrl Pts',(1.48816821785387,-2.35998939911264,2.18578006132768));
#47969=CARTESIAN_POINT('Ctrl Pts',(2.78947957168654,-0.0547522279601586,
2.34311537699881));
#47970=CARTESIAN_POINT('Ctrl Pts',(1.57963081483742,2.2997739166102,2.50045069266992));
#47971=CARTESIAN_POINT('Ctrl Pts',(-1.05224143668056,2.58398567580241,2.65778600834106));
#47972=CARTESIAN_POINT('Ctrl Pts',(-2.73685940153096,0.542028153256274,
2.81512132401217));
#47973=CARTESIAN_POINT('Ctrl Pts',(-1.9576873758141,-1.98787675326332,2.9724566396833));
#47974=CARTESIAN_POINT('Ctrl Pts',(0.583844270639632,-2.72824481623496,
3.12979195535442));
#47975=CARTESIAN_POINT('Ctrl Pts',(2.59978456082284,-1.01257796062119,3.28712727102555));
#47976=CARTESIAN_POINT('Ctrl Pts',(2.27533311107693,1.61463714733595,3.44446258669667));
#47977=CARTESIAN_POINT('Ctrl Pts',(-0.0974306831352009,2.78831511032893,
3.60179790236779));
#47978=CARTESIAN_POINT('Ctrl Pts',(-2.38248491584478,1.45188137075193,3.75913321803891));
#47979=CARTESIAN_POINT('Ctrl Pts',(-2.52276604076759,-1.19157265502464,
3.91646853371004));
#47980=CARTESIAN_POINT('Ctrl Pts',(-0.391989446068178,-2.76234287588842,
4.07380384938116));
#47981=CARTESIAN_POINT('Ctrl Pts',(2.09166595049596,-1.84638225748661,4.23113916505228));
#47982=CARTESIAN_POINT('Ctrl Pts',(2.69235081885991,0.731738312121609,4.38847448072341));
#47983=CARTESIAN_POINT('Ctrl Pts',(0.869313466150996,2.65112956811967,4.54580979639453));
#47984=CARTESIAN_POINT('Ctrl Pts',(-1.73630182933374,2.18390701421848,4.70314511206566));
#47985=CARTESIAN_POINT('Ctrl Pts',(-2.77885435571787,-0.24932380355531,
4.86048042773678));
#47986=CARTESIAN_POINT('Ctrl Pts',(-1.31981199187883,-2.45810703498086,
5.0178157434079));
#47987=CARTESIAN_POINT('Ctrl Pts',(1.32735846804311,-2.45404021699529,5.17515105907903));
#47988=CARTESIAN_POINT('Ctrl Pts',(2.77960730340162,-0.240784401894037,
5.33248637475015));
#47989=CARTESIAN_POINT('Ctrl Pts',(1.7295834260075,2.18923161447142,5.48982169042127));
#47990=CARTESIAN_POINT('Ctrl Pts',(-0.877455144085315,2.64844602728405,
5.6471570060924));
#47991=CARTESIAN_POINT('Ctrl Pts',(-2.6945864272668,0.723462421491616,5.80449232176352));
#47992=CARTESIAN_POINT('Ctrl Pts',(-2.08598293818204,-1.85280033218167,
5.96182763743465));
#47993=CARTESIAN_POINT('Ctrl Pts',(0.400475087797133,-2.76112542152107,
6.11916295310577));
#47994=CARTESIAN_POINT('Ctrl Pts',(2.52641532297249,-1.18381565506602,6.27649826877689));
#47995=CARTESIAN_POINT('Ctrl Pts',(2.37801266228852,1.45919486954518,6.43383358444801));
#47996=CARTESIAN_POINT('Ctrl Pts',(0.0888629298452703,2.78860131051387,
6.59116890011914));
#47997=CARTESIAN_POINT('Ctrl Pts',(-2.28028345691278,1.60763840633388,6.74850421579025));
#47998=CARTESIAN_POINT('Ctrl Pts',(-2.59666107137131,-1.02056120329308,
6.90583953146139));
#47999=CARTESIAN_POINT('Ctrl Pts',(-0.575458792795455,-2.73002583632828,
7.0631748471325));
#48000=CARTESIAN_POINT('Ctrl Pts',(1.96378602838758,-1.98185224588264,7.22051016280364));
#48001=CARTESIAN_POINT('Ctrl Pts',(2.73518105754109,0.550434801880421,7.37784547847475));
#48002=CARTESIAN_POINT('Ctrl Pts',(1.04429700325446,2.58720653562064,7.53518079414588));
#48003=CARTESIAN_POINT('Ctrl Pts',(-1.58668959526433,2.29490958880404,7.692516109817));
#48004=CARTESIAN_POINT('Ctrl Pts',(-2.78929813547626,-0.0633229448848314,
7.84985142548812));
#48005=CARTESIAN_POINT('Ctrl Pts',(-1.48091003456564,-2.36455056163985,
8.00718674115925));
#48006=CARTESIAN_POINT('Ctrl Pts',(1.1606306967401,-2.53715003408474,8.16452205683039));
#48007=CARTESIAN_POINT('Ctrl Pts',(2.7573423423768,-0.425742944184182,8.32185737250149));
#48008=CARTESIAN_POINT('Ctrl Pts',(1.87182477991027,2.06892868315578,8.47919268817262));
#48009=CARTESIAN_POINT('Ctrl Pts',(-0.698756781752635,2.70109847539371,
8.63652800384375));
#48010=CARTESIAN_POINT('Ctrl Pts',(-2.64029974777462,0.901671126634157,
8.79386331951485));
#48011=CARTESIAN_POINT('Ctrl Pts',(-2.2049783515218,-1.70946323641174,8.951198635186));
#48012=CARTESIAN_POINT('Ctrl Pts',(0.215320583295009,-2.78169582358745,
9.1085339508571));
#48013=CARTESIAN_POINT('Ctrl Pts',(2.44178186910215,-1.34977515042753,9.26586926652825));
#48014=CARTESIAN_POINT('Ctrl Pts',(2.4700906186972,1.29724642912539,9.42320458219936));
#48015=CARTESIAN_POINT('Ctrl Pts',(0.274759125503672,2.77645549735693,9.58053989787048));
#48016=CARTESIAN_POINT('Ctrl Pts',(-2.16791313571898,1.75622632949552,9.73787521354162));
#48017=CARTESIAN_POINT('Ctrl Pts',(-2.65898352045171,-0.844996679702688,
9.89521052921272));
#48018=CARTESIAN_POINT('Ctrl Pts',(-0.756353910490317,-2.68554278318001,
10.0525458448839));
#48019=CARTESIAN_POINT('Ctrl Pts',(1.82713427411632,-2.1084754471556,10.209881160555));
#48020=CARTESIAN_POINT('Ctrl Pts',(2.76584800687315,0.366656539637837,10.3672164762261));
#48021=CARTESIAN_POINT('Ctrl Pts',(1.21456463397637,2.5117881090817,10.5245517918972));
#48022=CARTESIAN_POINT('Ctrl Pts',(-1.42988853112819,2.3956048670705,10.6818871075684));
#48023=CARTESIAN_POINT('Ctrl Pts',(-2.78752525882336,0.123104760709679,
10.8392224232395));
#48024=CARTESIAN_POINT('Ctrl Pts',(-1.63498599745775,-2.26072847669162,
10.9965577389106));
#48025=CARTESIAN_POINT('Ctrl Pts',(0.987923826072495,-2.60841687478992,
11.1538930545817));
#48026=CARTESIAN_POINT('Ctrl Pts',(2.72434297818965,-0.609840043220031,
11.3112283702529));
#48027=CARTESIAN_POINT('Ctrl Pts',(2.00243986412736,1.94197408587787,11.4685886307918));
#48028=CARTESIAN_POINT('Ctrl Pts',(0.327206363769202,2.47149229332866,11.573503786107));
#48029=CARTESIAN_POINT('Ctrl Pts',(-0.439784697349138,2.32647548997369,
11.6259738361986));
#48030=CARTESIAN_POINT('Ctrl Pts',(-1.12171304089722,2.30154449716799,-0.22035079308787));
#48031=CARTESIAN_POINT('Ctrl Pts',(-1.88012331070157,1.93191501964248,-0.167905687864162));
#48032=CARTESIAN_POINT('Ctrl Pts',(-2.99073467182806,0.391248079391971,
-0.0630154774167469));
#48033=CARTESIAN_POINT('Ctrl Pts',(-1.96949810878762,-2.28802454889368,
0.094319838254377));
#48034=CARTESIAN_POINT('Ctrl Pts',(0.827183348142068,-2.90055828519513,
0.2516551539255));
#48035=CARTESIAN_POINT('Ctrl Pts',(2.87795482965583,-0.905430952525466,
0.408990469596625));
#48036=CARTESIAN_POINT('Ctrl Pts',(2.33857423968022,1.90659716578758,0.566325785267747));
#48037=CARTESIAN_POINT('Ctrl Pts',(-0.306392516011564,3.00131437457293,
0.723661100938869));
#48038=CARTESIAN_POINT('Ctrl Pts',(-2.67535786610753,1.39466602365043,0.880996416609994));
#48039=CARTESIAN_POINT('Ctrl Pts',(-2.63599215695478,-1.46775396414121,
1.03833173228112));
#48040=CARTESIAN_POINT('Ctrl Pts',(-0.223590725920167,-3.00872979891445,
1.19566704795224));
#48041=CARTESIAN_POINT('Ctrl Pts',(2.39006710240269,-1.84124164353529,1.35300236362336));
#48042=CARTESIAN_POINT('Ctrl Pts',(2.852139547899,0.983815666231478,1.51033767929448));
#48043=CARTESIAN_POINT('Ctrl Pts',(0.746636913468031,2.92319795455841,1.66767299496561));
#48044=CARTESIAN_POINT('Ctrl Pts',(-2.03100346660582,2.23105369533406,1.82500831063673));
#48045=CARTESIAN_POINT('Ctrl Pts',(-2.98028513594331,-0.469546741693888,
1.98234362630786));
#48046=CARTESIAN_POINT('Ctrl Pts',(-1.24663783560453,-2.74744657848983,
2.13967894197898));
#48047=CARTESIAN_POINT('Ctrl Pts',(1.60926381248222,-2.55202704389875,2.2970142576501));
#48048=CARTESIAN_POINT('Ctrl Pts',(3.01646579769545,-0.0592075398815808,
2.45434957332123));
#48049=CARTESIAN_POINT('Ctrl Pts',(1.70816892667258,2.48691169216645,2.61168488899235));
#48050=CARTESIAN_POINT('Ctrl Pts',(-1.13786468876907,2.794250401368,2.76902020466348));
#48051=CARTESIAN_POINT('Ctrl Pts',(-2.95956380595681,0.586134203053899,
2.92635552033459));
#48052=CARTESIAN_POINT('Ctrl Pts',(-2.11698880022736,-2.14963475521249,
3.08369083600572));
#48053=CARTESIAN_POINT('Ctrl Pts',(0.631352991948975,-2.95024823248193,
3.24102615167684));
#48054=CARTESIAN_POINT('Ctrl Pts',(2.81133487719265,-1.09497370646359,3.39836146734797));
#48055=CARTESIAN_POINT('Ctrl Pts',(2.46048208332205,1.74602380317224,3.55569678301909));
#48056=CARTESIAN_POINT('Ctrl Pts',(-0.105358836933763,3.01520658149842,
3.71303209869021));
#48057=CARTESIAN_POINT('Ctrl Pts',(-2.57635307141754,1.57002422302613,3.87036741436133));
#48058=CARTESIAN_POINT('Ctrl Pts',(-2.72804918695356,-1.28853360169179,
4.02770273003246));
#48059=CARTESIAN_POINT('Ctrl Pts',(-0.423886508839853,-2.98712092793252,
4.18503804570358));
#48060=CARTESIAN_POINT('Ctrl Pts',(2.26186951283549,-1.99662653410748,4.34237336137471));
#48061=CARTESIAN_POINT('Ctrl Pts',(2.91143345981847,0.79128150418526,4.49970867704583));
#48062=CARTESIAN_POINT('Ctrl Pts',(0.940051457890825,2.86685794320302,4.65704399271695));
#48063=CARTESIAN_POINT('Ctrl Pts',(-1.8775886139559,2.36161643935406,4.81437930838807));
#48064=CARTESIAN_POINT('Ctrl Pts',(-3.00497598400837,-0.269611842154904,
4.97171462405921));
#48065=CARTESIAN_POINT('Ctrl Pts',(-1.4272080617833,-2.6581287324543,5.12904993973032));
#48066=CARTESIAN_POINT('Ctrl Pts',(1.4353686116843,-2.65373098834339,5.28638525540146));
#48067=CARTESIAN_POINT('Ctrl Pts',(3.00579020073843,-0.260377570176227,
5.44372057107256));
#48068=CARTESIAN_POINT('Ctrl Pts',(1.87032351904202,2.36737431430406,5.6010558867437));
#48069=CARTESIAN_POINT('Ctrl Pts',(-0.94885564246845,2.86395603661459,5.75839120241481));
#48070=CARTESIAN_POINT('Ctrl Pts',(-2.91385098470907,0.782332185723086,
5.91572651808595));
#48071=CARTESIAN_POINT('Ctrl Pts',(-2.25572406102908,-2.00356686197406,
6.07306183375706));
#48072=CARTESIAN_POINT('Ctrl Pts',(0.43306264631962,-2.98580440656537,6.23039714942819));
#48073=CARTESIAN_POINT('Ctrl Pts',(2.73199541945832,-1.28014539720187,6.38773246509931));
#48074=CARTESIAN_POINT('Ctrl Pts',(2.57151690053176,1.57793283766349,6.54506778077043));
#48075=CARTESIAN_POINT('Ctrl Pts',(0.0960939062906457,3.01551607043604,
6.70240309644156));
#48076=CARTESIAN_POINT('Ctrl Pts',(-2.46583524993137,1.73845555887539,6.85973841211269));
#48077=CARTESIAN_POINT('Ctrl Pts',(-2.80795722238004,-1.10360656354518,
7.0170737277838));
#48078=CARTESIAN_POINT('Ctrl Pts',(-0.622285168914556,-2.95217417818558,
7.17440904345494));
#48079=CARTESIAN_POINT('Ctrl Pts',(2.123583713876,-2.14312002011776,7.33174435912604));
#48080=CARTESIAN_POINT('Ctrl Pts',(2.95774889134204,0.595224919582278,7.48907967479718));
#48081=CARTESIAN_POINT('Ctrl Pts',(1.12927379892889,2.79773334979303,7.64641499046829));
#48082=CARTESIAN_POINT('Ctrl Pts',(-1.7158020959373,2.48165154306736,7.80375030613943));
#48083=CARTESIAN_POINT('Ctrl Pts',(-3.01626959761271,-0.0684756753170684,
7.96108562181053));
#48084=CARTESIAN_POINT('Ctrl Pts',(-1.60141501449694,-2.55695935847839,
8.11842093748168));
#48085=CARTESIAN_POINT('Ctrl Pts',(1.25507382667628,-2.74360363815508,8.27575625315278));
#48086=CARTESIAN_POINT('Ctrl Pts',(2.98171348976335,-0.4603866050058,8.43309156882392));
#48087=CARTESIAN_POINT('Ctrl Pts',(2.02413937179845,2.23728206291798,8.59042688449505));
#48088=CARTESIAN_POINT('Ctrl Pts',(-0.755616192517999,2.92089293283704,
8.74776220016616));
#48089=CARTESIAN_POINT('Ctrl Pts',(-2.8551468760213,0.975042133976645,8.90509751583729));
#48090=CARTESIAN_POINT('Ctrl Pts',(-2.38440239876109,-1.84856610437053,
9.0624328315084));
#48091=CARTESIAN_POINT('Ctrl Pts',(0.232841703392179,-3.00804866850868,
9.21976814717955));
#48092=CARTESIAN_POINT('Ctrl Pts',(2.64047515111439,-1.45960938992725,9.37710346285064));
#48093=CARTESIAN_POINT('Ctrl Pts',(2.67108744732754,1.40280628844088,9.5344387785218));
#48094=CARTESIAN_POINT('Ctrl Pts',(0.297116893451739,3.00238192514779,9.69177409419289));
#48095=CARTESIAN_POINT('Ctrl Pts',(-2.34432110299241,1.89913441550408,9.84910940986404));
#48096=CARTESIAN_POINT('Ctrl Pts',(-2.87535098929907,-0.913755959843164,
10.0064447255352));
#48097=CARTESIAN_POINT('Ctrl Pts',(-0.817900129151285,-2.90407143896469,
10.1637800412063));
#48098=CARTESIAN_POINT('Ctrl Pts',(1.97581229904352,-2.28004683604122,10.3211153568773));
#48099=CARTESIAN_POINT('Ctrl Pts',(2.99091127930818,0.396492206842064,10.4784506725486));
#48100=CARTESIAN_POINT('Ctrl Pts',(1.31339648967752,2.71617795627811,10.6357859882197));
#48101=CARTESIAN_POINT('Ctrl Pts',(-1.54624177658248,2.59054062257996,10.7931213038908));
#48102=CARTESIAN_POINT('Ctrl Pts',(-3.01435245799954,0.133122071938945,
10.9504566195618));
#48103=CARTESIAN_POINT('Ctrl Pts',(-1.76802848499101,-2.44468903699242,
11.1077919352331));
#48104=CARTESIAN_POINT('Ctrl Pts',(1.06831340954195,-2.82066962196045,11.2651272509042));
#48105=CARTESIAN_POINT('Ctrl Pts',(2.94602889310002,-0.659464099006171,
11.4224625665753));
#48106=CARTESIAN_POINT('Ctrl Pts',(2.16538289915855,2.09999688455137,11.5798228271142));
#48107=CARTESIAN_POINT('Ctrl Pts',(0.353831881443529,2.67260317937598,11.6847379824294));
#48108=CARTESIAN_POINT('Ctrl Pts',(-0.475570967204255,2.51578603260372,
11.737208032521));
#48109=CARTESIAN_POINT('Ctrl Pts',(-1.20612089661124,2.47473356491836,-0.109116596765449));
#48110=CARTESIAN_POINT('Ctrl Pts',(-2.02160082887981,2.07728981540964,-0.0566714915417416));
#48111=CARTESIAN_POINT('Ctrl Pts',(-3.21578465471561,0.420689130917341,
0.0482187189056736));
#48112=CARTESIAN_POINT('Ctrl Pts',(-2.11770099681207,-2.46019625319938,
0.205554034576798));
#48113=CARTESIAN_POINT('Ctrl Pts',(0.88942812033726,-3.11882257944914,0.36288935024792));
#48114=CARTESIAN_POINT('Ctrl Pts',(3.09451823505123,-0.973563783662645,
0.520224665919045));
#48115=CARTESIAN_POINT('Ctrl Pts',(2.51454976087203,2.05006681676523,0.677559981590167));
#48116=CARTESIAN_POINT('Ctrl Pts',(-0.329448265869537,3.22716047018292,
0.834895297261292));
#48117=CARTESIAN_POINT('Ctrl Pts',(-2.87667603975131,1.49961333566476,0.992230612932414));
#48118=CARTESIAN_POINT('Ctrl Pts',(-2.83434809785535,-1.57820107522217,
1.14956592860354));
#48119=CARTESIAN_POINT('Ctrl Pts',(-0.240415718627206,-3.23513389826074,
1.30690124427466));
#48120=CARTESIAN_POINT('Ctrl Pts',(2.56991741328534,-1.97979335267645,1.46423655994578));
#48121=CARTESIAN_POINT('Ctrl Pts',(3.0667603775212,1.05784687365869,1.62157187561691));
#48122=CARTESIAN_POINT('Ctrl Pts',(0.802820641895047,3.14316586272734,1.77890719128803));
#48123=CARTESIAN_POINT('Ctrl Pts',(-2.18383457519921,2.3989383962692,1.93624250695915));
#48124=CARTESIAN_POINT('Ctrl Pts',(-3.20454880104273,-0.504879694221727,
2.09357782263028));
#48125=CARTESIAN_POINT('Ctrl Pts',(-1.34044616511386,-2.954189360221,2.2509131383014));
#48126=CARTESIAN_POINT('Ctrl Pts',(1.73035940711057,-2.74406468868485,2.40824845397252));
#48127=CARTESIAN_POINT('Ctrl Pts',(3.24345202370436,-0.0636628518030065,
2.56558376964365));
#48128=CARTESIAN_POINT('Ctrl Pts',(1.83670703850775,2.67404946772271,2.72291908531477));
#48129=CARTESIAN_POINT('Ctrl Pts',(-1.22348794085758,3.00451512693359,2.8802544009859));
#48130=CARTESIAN_POINT('Ctrl Pts',(-3.18226821038265,0.630240252851527,
3.03758971665701));
#48131=CARTESIAN_POINT('Ctrl Pts',(-2.27629022464062,-2.31139275716167,
3.19492503232815));
#48132=CARTESIAN_POINT('Ctrl Pts',(0.678861713258322,-3.1722516487289,3.35226034799926));
#48133=CARTESIAN_POINT('Ctrl Pts',(3.02288519356245,-1.17736945230598,3.50959566367039));
#48134=CARTESIAN_POINT('Ctrl Pts',(2.64563105556716,1.87741045900853,3.66693097934151));
#48135=CARTESIAN_POINT('Ctrl Pts',(-0.113286990732327,3.2420980526679,3.82426629501263));
#48136=CARTESIAN_POINT('Ctrl Pts',(-2.77022122699029,1.68816707530034,3.98160161068376));
#48137=CARTESIAN_POINT('Ctrl Pts',(-2.93333233313953,-1.38549454835895,
4.13893692635488));
#48138=CARTESIAN_POINT('Ctrl Pts',(-0.455783571611524,-3.21189897997662,
4.29627224202601));
#48139=CARTESIAN_POINT('Ctrl Pts',(2.43207307517502,-2.14687081072835,4.45360755769713));
#48140=CARTESIAN_POINT('Ctrl Pts',(3.13051610077702,0.850824696248917,4.61094287336825));
#48141=CARTESIAN_POINT('Ctrl Pts',(1.01078944963065,3.08258631828635,4.76827818903937));
#48142=CARTESIAN_POINT('Ctrl Pts',(-2.01887539857807,2.53932586448964,4.9256135047105));
#48143=CARTESIAN_POINT('Ctrl Pts',(-3.23109761229886,-0.289899880754502,
5.08294882038162));
#48144=CARTESIAN_POINT('Ctrl Pts',(-1.53460413168777,-2.85815042992774,
5.24028413605275));
#48145=CARTESIAN_POINT('Ctrl Pts',(1.54337875532549,-2.8534217596915,5.39761945172386));
#48146=CARTESIAN_POINT('Ctrl Pts',(3.23197309807526,-0.279970738458419,
5.554954767395));
#48147=CARTESIAN_POINT('Ctrl Pts',(2.01106361207652,2.5455170141367,5.71229008306611));
#48148=CARTESIAN_POINT('Ctrl Pts',(-1.02025614085158,3.07946604594513,5.86962539873724));
#48149=CARTESIAN_POINT('Ctrl Pts',(-3.13311554215134,0.841201949954562,
6.02696071440836));
#48150=CARTESIAN_POINT('Ctrl Pts',(-2.42546518387612,-2.15433339176646,
6.18429603007949));
#48151=CARTESIAN_POINT('Ctrl Pts',(0.465650204842104,-3.21048339160967,
6.34163134575061));
#48152=CARTESIAN_POINT('Ctrl Pts',(2.93757551594416,-1.3764751393377,6.49896666142173));
#48153=CARTESIAN_POINT('Ctrl Pts',(2.76502113877501,1.6966708057818,6.65630197709286));
#48154=CARTESIAN_POINT('Ctrl Pts',(0.103324882736022,3.24243083035821,6.81363729276398));
#48155=CARTESIAN_POINT('Ctrl Pts',(-2.65138704294996,1.86927271141691,6.9709726084351));
#48156=CARTESIAN_POINT('Ctrl Pts',(-3.01925337338877,-1.18665192379726,
7.12830792410623));
#48157=CARTESIAN_POINT('Ctrl Pts',(-0.66911154503365,-3.17432252004288,
7.28564323977735));
#48158=CARTESIAN_POINT('Ctrl Pts',(2.28338139936439,-2.30438779435288,7.44297855544847));
#48159=CARTESIAN_POINT('Ctrl Pts',(3.18031672514302,0.640015037284128,7.6003138711196));
#48160=CARTESIAN_POINT('Ctrl Pts',(1.21425059460331,3.0082601639654,7.75764918679072));
#48161=CARTESIAN_POINT('Ctrl Pts',(-1.84491459661027,2.66839349733066,7.91498450246185));
#48162=CARTESIAN_POINT('Ctrl Pts',(-3.24324105974916,-0.0736284057493019,
8.07231981813296));
#48163=CARTESIAN_POINT('Ctrl Pts',(-1.72191999442822,-2.74936815531691,
8.2296551338041));
#48164=CARTESIAN_POINT('Ctrl Pts',(1.34951695661245,-2.95005724222544,8.3869904494752));
#48165=CARTESIAN_POINT('Ctrl Pts',(3.20608463714991,-0.495030265827418,
8.54432576514635));
#48166=CARTESIAN_POINT('Ctrl Pts',(2.17645396368663,2.40563544268021,8.70166108081746));
#48167=CARTESIAN_POINT('Ctrl Pts',(-0.812475603283364,3.14068739028035,
8.85899639648857));
#48168=CARTESIAN_POINT('Ctrl Pts',(-3.06999400426798,1.04841314131914,9.01633171215972));
#48169=CARTESIAN_POINT('Ctrl Pts',(-2.56382644600038,-1.9876689723293,9.17366702783083));
#48170=CARTESIAN_POINT('Ctrl Pts',(0.250362823489351,-3.2344015134299,9.33100234350195));
#48171=CARTESIAN_POINT('Ctrl Pts',(2.83916843312661,-1.56944362942696,9.48833765917307));
#48172=CARTESIAN_POINT('Ctrl Pts',(2.87208427595788,1.50836614775637,9.64567297484422));
#48173=CARTESIAN_POINT('Ctrl Pts',(0.319474661399804,3.22830835293867,9.80300829051531));
#48174=CARTESIAN_POINT('Ctrl Pts',(-2.52072907026583,2.04204250151264,9.96034360618647));
#48175=CARTESIAN_POINT('Ctrl Pts',(-3.09171845814643,-0.982515239983637,
10.1176789218575));
#48176=CARTESIAN_POINT('Ctrl Pts',(-0.879446347812255,-3.12260009474938,
10.2750142375287));
#48177=CARTESIAN_POINT('Ctrl Pts',(2.12449032397074,-2.45161822492683,10.4323495531998));
#48178=CARTESIAN_POINT('Ctrl Pts',(3.2159745517432,0.42632787404629,10.5896848688709));
#48179=CARTESIAN_POINT('Ctrl Pts',(1.41222834537867,2.92056780347451,10.7470201845421));
#48180=CARTESIAN_POINT('Ctrl Pts',(-1.66259502203677,2.78547637808942,10.9043555002132));
#48181=CARTESIAN_POINT('Ctrl Pts',(-3.24117965717572,0.143139383168213,
11.0616908158843));
#48182=CARTESIAN_POINT('Ctrl Pts',(-1.90107097252427,-2.62864959729321,
11.2190261315554));
#48183=CARTESIAN_POINT('Ctrl Pts',(1.1487029930114,-3.03292236913098,11.3763614472266));
#48184=CARTESIAN_POINT('Ctrl Pts',(3.1677148080104,-0.709088154792314,11.5336967628977));
#48185=CARTESIAN_POINT('Ctrl Pts',(2.32832593418973,2.25801968322488,11.6910570234366));
#48186=CARTESIAN_POINT('Ctrl Pts',(0.380457399117856,2.8737140654233,11.7959721787519));
#48187=CARTESIAN_POINT('Ctrl Pts',(-0.511357237059373,2.70509657523375,
11.8484422288434));
#48188=CARTESIAN_POINT('Ctrl Pts',(-1.29052875232528,2.64792263266873,0.00211759955697117));
#48189=CARTESIAN_POINT('Ctrl Pts',(-2.16307834705805,2.22266461117681,0.054562704780679));
#48190=CARTESIAN_POINT('Ctrl Pts',(-3.44083463760316,0.45013018244271,0.159452915228094));
#48191=CARTESIAN_POINT('Ctrl Pts',(-2.26590388483652,-2.63236795750508,
0.316788230899218));
#48192=CARTESIAN_POINT('Ctrl Pts',(0.951672892532446,-3.33708687370315,
0.474123546570341));
#48193=CARTESIAN_POINT('Ctrl Pts',(3.31108164044663,-1.04169661479983,0.631458862241466));
#48194=CARTESIAN_POINT('Ctrl Pts',(2.69052528206383,2.19353646774287,0.788794177912587));
#48195=CARTESIAN_POINT('Ctrl Pts',(-0.352504015727509,3.45300656579291,
0.946129493583712));
#48196=CARTESIAN_POINT('Ctrl Pts',(-3.07799421339509,1.6045606476791,1.10346480925483));
#48197=CARTESIAN_POINT('Ctrl Pts',(-3.03270403875592,-1.68864818630313,
1.26080012492596));
#48198=CARTESIAN_POINT('Ctrl Pts',(-0.257240711334243,-3.46153799760704,
1.41813544059708));
#48199=CARTESIAN_POINT('Ctrl Pts',(2.74976772416799,-2.11834506181761,1.57547075626821));
#48200=CARTESIAN_POINT('Ctrl Pts',(3.2813812071434,1.13187808108589,1.73280607193933));
#48201=CARTESIAN_POINT('Ctrl Pts',(0.859004370322057,3.36313377089626,1.89014138761045));
#48202=CARTESIAN_POINT('Ctrl Pts',(-2.3366656837926,2.56682309720432,2.04747670328157));
#48203=CARTESIAN_POINT('Ctrl Pts',(-3.42881246614216,-0.540212646749566,
2.2048120189527));
#48204=CARTESIAN_POINT('Ctrl Pts',(-1.43425449462318,-3.16093214195217,
2.36214733462382));
#48205=CARTESIAN_POINT('Ctrl Pts',(1.85145500173891,-2.93610233347096,2.51948265029494));
#48206=CARTESIAN_POINT('Ctrl Pts',(3.47043824971327,-0.0681181637244305,
2.67681796596607));
#48207=CARTESIAN_POINT('Ctrl Pts',(1.96524515034292,2.86118724327898,2.83415328163719));
#48208=CARTESIAN_POINT('Ctrl Pts',(-1.30911119294609,3.21477985249918,2.99148859730832));
#48209=CARTESIAN_POINT('Ctrl Pts',(-3.40497261480849,0.674346302649153,
3.14882391297943));
#48210=CARTESIAN_POINT('Ctrl Pts',(-2.43559164905389,-2.47315075911084,
3.30615922865057));
#48211=CARTESIAN_POINT('Ctrl Pts',(0.726370434567669,-3.39425506497587,
3.46349454432168));
#48212=CARTESIAN_POINT('Ctrl Pts',(3.23443550993226,-1.25976519814839,3.62082985999281));
#48213=CARTESIAN_POINT('Ctrl Pts',(2.83078002781227,2.00879711484483,3.77816517566393));
#48214=CARTESIAN_POINT('Ctrl Pts',(-0.12121514453089,3.46898952383738,3.93550049133506));
#48215=CARTESIAN_POINT('Ctrl Pts',(-2.96408938256305,1.80630992757453,4.09283580700618));
#48216=CARTESIAN_POINT('Ctrl Pts',(-3.1386154793255,-1.48245549502611,4.2501711226773));
#48217=CARTESIAN_POINT('Ctrl Pts',(-0.4876806343832,-3.43667703202072,4.40750643834843));
#48218=CARTESIAN_POINT('Ctrl Pts',(2.60227663751455,-2.29711508734921,4.56484175401955));
#48219=CARTESIAN_POINT('Ctrl Pts',(3.34959874173558,0.91036788831257,4.72217706969067));
#48220=CARTESIAN_POINT('Ctrl Pts',(1.08152744137048,3.29831469336969,4.87951238536179));
#48221=CARTESIAN_POINT('Ctrl Pts',(-2.16016218320023,2.71703528962523,5.03684770103292));
#48222=CARTESIAN_POINT('Ctrl Pts',(-3.45721924058936,-0.310187919354095,
5.19418301670405));
#48223=CARTESIAN_POINT('Ctrl Pts',(-1.64200020159223,-3.05817212740119,
5.35151833237516));
#48224=CARTESIAN_POINT('Ctrl Pts',(1.65138889896668,-3.05311253103961,5.5088536480463));
#48225=CARTESIAN_POINT('Ctrl Pts',(3.45815599541208,-0.299563906740608,
5.66618896371741));
#48226=CARTESIAN_POINT('Ctrl Pts',(2.15180370511103,2.72365971396933,5.82352427938854));
#48227=CARTESIAN_POINT('Ctrl Pts',(-1.09165663923471,3.29497605527567,5.98085959505965));
#48228=CARTESIAN_POINT('Ctrl Pts',(-3.35238009959362,0.900071714186031,
6.13819491073079));
#48229=CARTESIAN_POINT('Ctrl Pts',(-2.59520630672316,-2.30509992155884,
6.2955302264019));
#48230=CARTESIAN_POINT('Ctrl Pts',(0.498237763364587,-3.43516237665397,
6.45286554207304));
#48231=CARTESIAN_POINT('Ctrl Pts',(3.14315561242999,-1.47280488147353,6.61020085774415));
#48232=CARTESIAN_POINT('Ctrl Pts',(2.95852537701825,1.8154087739001,6.76753617341528));
#48233=CARTESIAN_POINT('Ctrl Pts',(0.110555859181397,3.46934559028038,6.9248714890864));
#48234=CARTESIAN_POINT('Ctrl Pts',(-2.83693883596855,2.00008986395841,7.08220680475753));
#48235=CARTESIAN_POINT('Ctrl Pts',(-3.2305495243975,-1.26969728404936,7.23954212042865));
#48236=CARTESIAN_POINT('Ctrl Pts',(-0.715937921152747,-3.39647086190017,
7.39687743609977));
#48237=CARTESIAN_POINT('Ctrl Pts',(2.4431790848528,-2.465655568588,7.5542127517709));
#48238=CARTESIAN_POINT('Ctrl Pts',(3.40288455894398,0.684805154985982,7.71154806744202));
#48239=CARTESIAN_POINT('Ctrl Pts',(1.29922739027773,3.21878697813778,7.86888338311314));
#48240=CARTESIAN_POINT('Ctrl Pts',(-1.97402709728324,2.85513545159397,8.02621869878427));
#48241=CARTESIAN_POINT('Ctrl Pts',(-3.47021252188561,-0.0787811361815389,
8.18355401445539));
#48242=CARTESIAN_POINT('Ctrl Pts',(-1.84242497435951,-2.94177695215544,
8.34088933012651));
#48243=CARTESIAN_POINT('Ctrl Pts',(1.44396008654862,-3.15651084629578,8.49822464579763));
#48244=CARTESIAN_POINT('Ctrl Pts',(3.43045578453647,-0.529673926649034,
8.65555996146877));
#48245=CARTESIAN_POINT('Ctrl Pts',(2.32876855557479,2.57398882244243,8.81289527713988));
#48246=CARTESIAN_POINT('Ctrl Pts',(-0.869335014048728,3.36048184772367,
8.97023059281101));
#48247=CARTESIAN_POINT('Ctrl Pts',(-3.28484113251466,1.12178414866162,9.12756590848212));
#48248=CARTESIAN_POINT('Ctrl Pts',(-2.74325049323966,-2.12677184028809,
9.28490122415326));
#48249=CARTESIAN_POINT('Ctrl Pts',(0.26788394358652,-3.46075435835112,9.44223653982438));
#48250=CARTESIAN_POINT('Ctrl Pts',(3.03786171513884,-1.67927786892668,9.5995718554955));
#48251=CARTESIAN_POINT('Ctrl Pts',(3.07308110458822,1.61392600707186,9.75690717116663));
#48252=CARTESIAN_POINT('Ctrl Pts',(0.34183242934787,3.45423478072953,9.91424248683774));
#48253=CARTESIAN_POINT('Ctrl Pts',(-2.69713703753925,2.1849505875212,10.0715778025089));
#48254=CARTESIAN_POINT('Ctrl Pts',(-3.30808592699379,-1.05127452012411,
10.22891311818));
#48255=CARTESIAN_POINT('Ctrl Pts',(-0.940992566473223,-3.34112875053406,
10.3862484338511));
#48256=CARTESIAN_POINT('Ctrl Pts',(2.27316834889794,-2.62318961381246,10.5435837495223));
#48257=CARTESIAN_POINT('Ctrl Pts',(3.44103782417822,0.456163541250519,10.7009190651934));
#48258=CARTESIAN_POINT('Ctrl Pts',(1.51106020107982,3.12495765067091,10.8582543808645));
#48259=CARTESIAN_POINT('Ctrl Pts',(-1.77894826749106,2.9804121335989,11.0155896965356));
#48260=CARTESIAN_POINT('Ctrl Pts',(-3.4680068563519,0.15315669439748,11.1729250122068));
#48261=CARTESIAN_POINT('Ctrl Pts',(-2.03411346005753,-2.812610157594,11.3302603278779));
#48262=CARTESIAN_POINT('Ctrl Pts',(1.22909257648086,-3.24517511630151,11.487595643549));
#48263=CARTESIAN_POINT('Ctrl Pts',(3.38940072292078,-0.758712210578455,
11.6449309592201));
#48264=CARTESIAN_POINT('Ctrl Pts',(2.49126896922092,2.41604248189839,11.8022912197591));
#48265=CARTESIAN_POINT('Ctrl Pts',(0.407082916792181,3.07482495147061,11.9072063750743));
#48266=CARTESIAN_POINT('Ctrl Pts',(-0.54714350691449,2.89440711786378,11.9596764251658));
#48267=CARTESIAN_POINT('Ctrl Pts',(-1.37989654081095,-1.933266887693,-5.06105574116233E-16));
#48268=CARTESIAN_POINT('Ctrl Pts',(-1.44414345926609,-1.89839188587405,
-3.26328455905852E-15));
#48269=CARTESIAN_POINT('Ctrl Pts',(-1.5065284577229,-1.86047032724736,-1.75540264544042E-15));
#48270=CARTESIAN_POINT('Ctrl Pts',(-1.56680444439783,-1.81955553349441,
-1.38777878078145E-15));
#48271=CARTESIAN_POINT('Ctrl Pts',(-1.63482660542644,-1.77338270675787,
-7.7622414528857E-16));
#48272=CARTESIAN_POINT('Ctrl Pts',(-1.70016423572007,-1.72339917541855,
-2.57234059054026E-16));
#48273=CARTESIAN_POINT('Ctrl Pts',(-1.76273246655484,-1.66996621356204,
-6.59194920871187E-16));
#48274=CARTESIAN_POINT('Ctrl Pts',(-1.80339137476382,-1.63524370562994,
-9.20402398950369E-16));
#48275=CARTESIAN_POINT('Ctrl Pts',(-1.84288047050014,-1.59906346566465,
3.12793119993545E-15));
#48276=CARTESIAN_POINT('Ctrl Pts',(-1.88117141744704,-1.56151405921778,
3.25434124093249E-15));
#48277=CARTESIAN_POINT('Ctrl Pts',(-1.89157558896771,-1.55131137434519,
3.31815239224361E-15));
#48278=CARTESIAN_POINT('Ctrl Pts',(-1.90188938652621,-1.54100934347453,
8.33738107600677E-16));
#48279=CARTESIAN_POINT('Ctrl Pts',(-1.91210630257196,-1.53061605927471,
1.19348975147204E-15));
#48280=CARTESIAN_POINT('Ctrl Pts',(-1.97123493955355,-1.47046672206319,
2.12803477396886E-15));
#48281=CARTESIAN_POINT('Ctrl Pts',(-2.02717988586207,-1.40720695656129,
2.65582936227977E-16));
#48282=CARTESIAN_POINT('Ctrl Pts',(-2.0798563871476,-1.34121621912243,1.70696790036118E-15));
#48283=CARTESIAN_POINT('Ctrl Pts',(-2.13394121087249,-1.27346119905171,
3.18688873417464E-15));
#48284=CARTESIAN_POINT('Ctrl Pts',(-2.18458111819303,-1.20282670578501,
2.66863689364878E-15));
#48285=CARTESIAN_POINT('Ctrl Pts',(-2.23165714456555,-1.12967611923023,
1.9151347174784E-15));
#48286=CARTESIAN_POINT('Ctrl Pts',(-2.24684650541785,-1.10607364592577,
1.67201274354048E-15));
#48287=CARTESIAN_POINT('Ctrl Pts',(-2.26166459424814,-1.08220890431245,
1.49719989934545E-15));
#48288=CARTESIAN_POINT('Ctrl Pts',(-2.27610666055719,-1.05809323638609,
1.13797860024079E-15));
#48289=CARTESIAN_POINT('Ctrl Pts',(-2.28578146762193,-1.0419380388242,8.35160740259033E-16));
#48290=CARTESIAN_POINT('Ctrl Pts',(-2.29528887628369,-1.02566760843717,
3.28760802647304E-15));
#48291=CARTESIAN_POINT('Ctrl Pts',(-2.30461525834334,-1.0093071858719,3.5527136788005E-15));
#48292=CARTESIAN_POINT('Ctrl Pts',(-2.34873078931698,-0.931919328093436,
3.71885869706561E-15));
#48293=CARTESIAN_POINT('Ctrl Pts',(-2.38885771815723,-0.852425177482761,
5.32218017872543E-15));
#48294=CARTESIAN_POINT('Ctrl Pts',(-2.42490246723541,-0.771229500912766,
5.34294830600857E-15));
#48295=CARTESIAN_POINT('Ctrl Pts',(-2.46140438292463,-0.689003994666118,
5.36397984182167E-15));
#48296=CARTESIAN_POINT('Ctrl Pts',(-2.4937205277099,-0.605032771340319,
6.32528744906619E-15));
#48297=CARTESIAN_POINT('Ctrl Pts',(-2.52171972824353,-0.519694226037686,
4.57966997657877E-15));
#48298=CARTESIAN_POINT('Ctrl Pts',(-2.54960930028344,-0.43468981656746,
2.84088732117391E-15));
#48299=CARTESIAN_POINT('Ctrl Pts',(-2.57321620377506,-0.348327885492083,
5.7661356876764E-15));
#48300=CARTESIAN_POINT('Ctrl Pts',(-2.59236876994043,-0.260953527499912,
4.9960036108132E-15));
#48301=CARTESIAN_POINT('Ctrl Pts',(-2.60380936393625,-0.208761327937561,
4.53597291108992E-15));
#48302=CARTESIAN_POINT('Ctrl Pts',(-2.61365974280453,-0.156207387307918,
3.44984801162762E-15));
#48303=CARTESIAN_POINT('Ctrl Pts',(-2.62187489230509,-0.103362317982872,
3.33066907387547E-15));
#48304=CARTESIAN_POINT('Ctrl Pts',(-2.62397146608191,-0.0898758212887859,
3.70099194019195E-15));
#48305=CARTESIAN_POINT('Ctrl Pts',(-2.62596008221826,-0.0763794055641211,
1.98967329662049E-15));
#48306=CARTESIAN_POINT('Ctrl Pts',(-2.6278400946394,-0.0628763941457671,
2.3037127760972E-15));
#48307=CARTESIAN_POINT('Ctrl Pts',(-2.64060982150931,0.028840961438971,
3.74500870588478E-15));
#48308=CARTESIAN_POINT('Ctrl Pts',(-2.64837710874139,0.12089024961922,5.0717148189266E-15));
#48309=CARTESIAN_POINT('Ctrl Pts',(-2.65101366112899,0.212875307175297,
4.08006961549745E-15));
#48310=CARTESIAN_POINT('Ctrl Pts',(-2.65226659852155,0.25658827063111,2.79591952247038E-15));
#48311=CARTESIAN_POINT('Ctrl Pts',(-2.65236023741466,0.300287183231581,
5.31362288609455E-15));
#48312=CARTESIAN_POINT('Ctrl Pts',(-2.6512772014093,0.343931535522,4.69069227904129E-15));
#48313=CARTESIAN_POINT('Ctrl Pts',(-2.64905271560999,0.433574207982051,
3.47166984399289E-15));
#48314=CARTESIAN_POINT('Ctrl Pts',(-2.64186793473848,0.522986312811907,
3.91533376087034E-15));
#48315=CARTESIAN_POINT('Ctrl Pts',(-2.62997259694039,0.611899469403195,
3.21964677141295E-15));
#48316=CARTESIAN_POINT('Ctrl Pts',(-2.61807725914231,0.700812625994483,
2.52395978195556E-15));
#48317=CARTESIAN_POINT('Ctrl Pts',(-2.60147108990245,0.789227566327091,
1.47008262914315E-15));
#48318=CARTESIAN_POINT('Ctrl Pts',(-2.58035146554208,0.876878238745712,
1.99840144432528E-15));
#48319=CARTESIAN_POINT('Ctrl Pts',(-2.576583244582,0.892517110694274,2.02142778531884E-15));
#48320=CARTESIAN_POINT('Ctrl Pts',(-2.57267071394585,0.908133543901725,
1.70495023809932E-15));
#48321=CARTESIAN_POINT('Ctrl Pts',(-2.5686164135305,0.923719945234905,1.11022302462516E-15));
#48322=CARTESIAN_POINT('Ctrl Pts',(-2.56541851969971,0.936013966782737,
6.41122491330844E-16));
#48323=CARTESIAN_POINT('Ctrl Pts',(-2.5621335320974,0.948285079155145,1.04705546521683E-15));
#48324=CARTESIAN_POINT('Ctrl Pts',(-2.55876298044222,0.960529869852389,
1.19348975147204E-15));
#48325=CARTESIAN_POINT('Ctrl Pts',(-2.53423311716393,1.04964378128372,2.52665339019896E-15));
#48326=CARTESIAN_POINT('Ctrl Pts',(-2.50516230366703,1.13741448707249,-6.39640594898038E-16));
#48327=CARTESIAN_POINT('Ctrl Pts',(-2.47183958755925,1.22356204886004,-3.60822483003176E-16));
#48328=CARTESIAN_POINT('Ctrl Pts',(-2.43793696028359,1.31120882616785,-7.71521334824393E-17));
#48329=CARTESIAN_POINT('Ctrl Pts',(-2.39963296981527,1.39717624648555,1.01309199915213E-15));
#48330=CARTESIAN_POINT('Ctrl Pts',(-2.35717721896034,1.48117223771656,4.16333634234434E-16));
#48331=CARTESIAN_POINT('Ctrl Pts',(-2.31422125531256,1.56615786800741,-1.87455725598068E-16));
#48332=CARTESIAN_POINT('Ctrl Pts',(-2.2670148596246,1.64912621348914,-1.4666715423013E-16));
#48333=CARTESIAN_POINT('Ctrl Pts',(-2.2157644123274,1.72976499945915,-9.99200722162641E-16));
#48334=CARTESIAN_POINT('Ctrl Pts',(-2.18483496065362,1.77843020269588,-1.5137015154285E-15));
#48335=CARTESIAN_POINT('Ctrl Pts',(-2.15243164629588,1.82624671746825,-1.21876760202498E-15));
#48336=CARTESIAN_POINT('Ctrl Pts',(-2.11859145320912,1.87314213253736,-2.38697950294409E-15));
#48337=CARTESIAN_POINT('Ctrl Pts',(-2.10923966749503,1.88610174750099,-2.64989400742177E-15));
#48338=CARTESIAN_POINT('Ctrl Pts',(-2.09977706809611,1.89899226435558,1.01111077252232E-15));
#48339=CARTESIAN_POINT('Ctrl Pts',(-2.0902160744712,1.91179680016256,6.10622663543836E-16));
#48340=CARTESIAN_POINT('Ctrl Pts',(-2.0314089911467,1.99055403331987,-9.7705151409358E-16));
#48341=CARTESIAN_POINT('Ctrl Pts',(-1.96879105165622,2.06618994281066,-2.55502889276557E-15));
#48342=CARTESIAN_POINT('Ctrl Pts',(-1.90263522084903,2.13839704217646,-1.72084568816899E-15));
#48343=CARTESIAN_POINT('Ctrl Pts',(-1.83630675568986,2.21079256674463,-1.02855259101591E-15));
#48344=CARTESIAN_POINT('Ctrl Pts',(-1.76642150904308,2.27974226115181,4.77271459200463E-16));
#48345=CARTESIAN_POINT('Ctrl Pts',(-1.69320457635212,2.34492041918575,1.11022302462516E-16));
#48346=CARTESIAN_POINT('Ctrl Pts',(-1.62138195171819,2.40885735572148,9.39521111622811E-16));
#48347=CARTESIAN_POINT('Ctrl Pts',(-1.54635279516223,2.46916580376612,5.81652154789426E-16));
#48348=CARTESIAN_POINT('Ctrl Pts',(-1.46828869933216,2.52551090352265,-7.7715611723761E-16));
#48349=CARTESIAN_POINT('Ctrl Pts',(-1.4101637796635,2.56746430556038,-8.9644473153275E-16));
#48350=CARTESIAN_POINT('Ctrl Pts',(-1.35035542783317,2.60721994909749,-2.27967887895237E-16));
#48351=CARTESIAN_POINT('Ctrl Pts',(-1.28892185405326,2.64462557919715,5.55111512312578E-17));
#48352=CARTESIAN_POINT('Origin',(-1.44337567297407,-2.5,-6.));
#48353=CARTESIAN_POINT('',(-1.44337567297407,-2.5,-6.));
#48354=CARTESIAN_POINT('',(1.44337567297406,-2.5,-6.));
#48355=CARTESIAN_POINT('',(-0.721687836487033,-2.5,-6.));
#48356=CARTESIAN_POINT('',(-1.44337567297407,-2.5,-3.));
#48357=CARTESIAN_POINT('',(-1.44337567297407,-2.5,-6.));
#48358=CARTESIAN_POINT('',(1.44337567297406,-2.5,-3.));
#48359=CARTESIAN_POINT('',(-1.44337567297407,-2.5,-3.));
#48360=CARTESIAN_POINT('',(1.44337567297406,-2.5,-6.));
#48361=CARTESIAN_POINT('Origin',(-2.88675134594813,3.53525079574969E-16,
-6.));
#48362=CARTESIAN_POINT('',(-2.88675134594813,3.53525079574969E-16,-6.));
#48363=CARTESIAN_POINT('',(-2.52590742770461,-0.625,-6.));
#48364=CARTESIAN_POINT('',(-2.88675134594813,5.55111512312578E-16,-3.));
#48365=CARTESIAN_POINT('',(-2.88675134594813,3.53525079574969E-16,-6.));
#48366=CARTESIAN_POINT('',(-2.88675134594813,3.53525079574969E-16,-3.));
#48367=CARTESIAN_POINT('Origin',(-1.44337567297406,2.5,-6.));
#48368=CARTESIAN_POINT('',(-1.44337567297406,2.5,-6.));
#48369=CARTESIAN_POINT('',(-1.80421959121758,1.875,-6.));
#48370=CARTESIAN_POINT('',(-1.44337567297406,2.5,-3.));
#48371=CARTESIAN_POINT('',(-1.44337567297406,2.5,-6.));
#48372=CARTESIAN_POINT('',(-1.44337567297406,2.5,-3.));
#48373=CARTESIAN_POINT('Origin',(1.44337567297406,2.5,-6.));
#48374=CARTESIAN_POINT('',(1.44337567297406,2.5,-6.));
#48375=CARTESIAN_POINT('',(0.721687836487033,2.5,-6.));
#48376=CARTESIAN_POINT('',(1.44337567297406,2.5,-3.));
#48377=CARTESIAN_POINT('',(1.44337567297406,2.5,-6.));
#48378=CARTESIAN_POINT('',(1.44337567297406,2.5,-3.));
#48379=CARTESIAN_POINT('Origin',(2.88675134594813,0.,-6.));
#48380=CARTESIAN_POINT('',(2.88675134594813,0.,-6.));
#48381=CARTESIAN_POINT('',(2.52590742770461,0.625,-6.));
#48382=CARTESIAN_POINT('',(2.88675134594813,0.,-3.));
#48383=CARTESIAN_POINT('',(2.88675134594813,0.,-6.));
#48384=CARTESIAN_POINT('',(2.88675134594813,0.,-3.));
#48385=CARTESIAN_POINT('Origin',(1.44337567297406,-2.5,-6.));
#48386=CARTESIAN_POINT('',(1.80421959121758,-1.875,-6.));
#48387=CARTESIAN_POINT('',(1.44337567297406,-2.5,-3.));
#48388=CARTESIAN_POINT('Origin',(0.,0.,-3.));
#48389=CARTESIAN_POINT('Origin',(0.,0.,0.));
#48390=CARTESIAN_POINT('',(-5.,-6.12323399573677E-16,0.));
#48391=CARTESIAN_POINT('Origin',(0.,0.,0.));
#48392=CARTESIAN_POINT('Origin',(0.,0.,-6.));
#48393=CARTESIAN_POINT('',(-5.,-6.12323399573677E-16,-6.));
#48394=CARTESIAN_POINT('',(-5.,-6.12323399573677E-16,-6.));
#48395=CARTESIAN_POINT('Origin',(0.,0.,-6.));
#48396=CARTESIAN_POINT('Origin',(0.,0.,-6.));
#48397=CARTESIAN_POINT('Origin',(0.,0.,12.));
#48398=CARTESIAN_POINT('',(0.,0.,0.));
#48399=CARTESIAN_POINT('Origin',(0.,0.,18.5459252805377));
#48400=CARTESIAN_POINT('',(1.25206542099588,1.62921138715834,6.10605191404524));
#48401=CARTESIAN_POINT('',(1.24933779518059,1.62565558510666,6.04785047420624));
#48402=CARTESIAN_POINT('',(1.25206542099588,1.62921138715835,18.5459252805377));
#48403=CARTESIAN_POINT('',(1.81742788875953,0.958620587959108,6.));
#48404=CARTESIAN_POINT('Ctrl Pts',(1.24933779518059,1.62565558510666,6.04785047420624));
#48405=CARTESIAN_POINT('Ctrl Pts',(1.48318281877138,1.44625946904293,6.0319003161375));
#48406=CARTESIAN_POINT('Ctrl Pts',(1.68018382414042,1.21881862015088,6.01595015806875));
#48407=CARTESIAN_POINT('Ctrl Pts',(1.81742788875952,0.958620587959134,6.));
#48408=CARTESIAN_POINT('',(2.05337162055578,-0.0752499195754643,6.00000000147866));
#48409=CARTESIAN_POINT('Origin',(0.,0.,6.));
#48410=CARTESIAN_POINT('Ctrl Pts',(1.25206542099588,1.62921138715834,6.10605191404525));
#48411=CARTESIAN_POINT('Ctrl Pts',(1.30822134072944,1.58605499515372,6.10219269208269));
#48412=CARTESIAN_POINT('Ctrl Pts',(1.36224784768931,1.53991148578638,6.09833347012013));
#48413=CARTESIAN_POINT('Ctrl Pts',(1.4138096340505,1.49101974539776,6.09447424815757));
#48414=CARTESIAN_POINT('Ctrl Pts',(1.46640293060909,1.44114990994419,6.09053782121262));
#48415=CARTESIAN_POINT('Ctrl Pts',(1.5164313608693,1.38842093138857,6.08660139426767));
#48416=CARTESIAN_POINT('Ctrl Pts',(1.56357224503334,1.33313142527712,6.08266496732271));
#48417=CARTESIAN_POINT('Ctrl Pts',(1.6096779245744,1.27905606593749,6.0788149835458));
#48418=CARTESIAN_POINT('Ctrl Pts',(1.65302125352251,1.22253188410836,6.07496499976889));
#48419=CARTESIAN_POINT('Ctrl Pts',(1.69333715435579,1.1638757855451,6.07111501599197));
#48420=CARTESIAN_POINT('Ctrl Pts',(1.73363253838607,1.10524953713016,6.06726699147573));
#48421=CARTESIAN_POINT('Ctrl Pts',(1.77090327511889,1.04449392614358,6.06341896695949));
#48422=CARTESIAN_POINT('Ctrl Pts',(1.80492601849622,0.981957040941911,6.05957094244324));
#48423=CARTESIAN_POINT('Ctrl Pts',(1.83894295411342,0.919430830929606,6.05572357479358));
#48424=CARTESIAN_POINT('Ctrl Pts',(1.86971276468624,0.855124379387284,6.05187620714392));
#48425=CARTESIAN_POINT('Ctrl Pts',(1.89705760188735,0.789411184124871,6.04802883949426));
#48426=CARTESIAN_POINT('Ctrl Pts',(1.9255043408027,0.721049975931321,6.04402643632629));
#48427=CARTESIAN_POINT('Ctrl Pts',(1.95024395649681,0.651166749571664,6.04002403315833));
#48428=CARTESIAN_POINT('Ctrl Pts',(1.97113196590956,0.580203701702709,6.03602162999036));
#48429=CARTESIAN_POINT('Ctrl Pts',(1.99123710164174,0.51190031859027,6.03216923518544));
#48430=CARTESIAN_POINT('Ctrl Pts',(2.00777416259453,0.442597125760258,6.02831684038051));
#48431=CARTESIAN_POINT('Ctrl Pts',(2.02066619972994,0.372700512166221,6.02446444557559));
#48432=CARTESIAN_POINT('Ctrl Pts',(2.03356726706987,0.302754939613283,6.02060935236756));
#48433=CARTESIAN_POINT('Ctrl Pts',(2.04281816954012,0.232215602728014,6.01675425915953));
#48434=CARTESIAN_POINT('Ctrl Pts',(2.04839380242372,0.161494249718358,6.0128991659515));
#48435=CARTESIAN_POINT('Ctrl Pts',(2.05397836731133,0.090659603128962,6.00903789699469));
#48436=CARTESIAN_POINT('Ctrl Pts',(2.05587591160232,0.0196428450353519,
6.00517662803788));
#48437=CARTESIAN_POINT('Ctrl Pts',(2.05411337054193,-0.0511451215746277,
6.00131535908107));
#48438=CARTESIAN_POINT('Ctrl Pts',(2.05391323151947,-0.0591831949887535,
6.00087690654694));
#48439=CARTESIAN_POINT('Ctrl Pts',(2.05366595440477,-0.0672183259752531,
6.0004384540128));
#48440=CARTESIAN_POINT('Ctrl Pts',(2.05337162055578,-0.0752499195754648,
6.00000000147866));
#48441=CARTESIAN_POINT('Origin',(0.,0.,18.5459252805377));
#48442=CARTESIAN_POINT('',(1.25156703223363,1.62854649222322,6.80617425834606));
#48443=CARTESIAN_POINT('',(1.25206542099589,1.62921138715833,6.74786344002215));
#48444=CARTESIAN_POINT('',(1.25206542099588,1.62921138715835,18.5459252805377));
#48445=CARTESIAN_POINT('',(-2.05462925654524,-0.0015224618017469,6.29592530139563));
#48446=CARTESIAN_POINT('Ctrl Pts',(1.25206542099589,1.62921138715833,6.74786344002215));
#48447=CARTESIAN_POINT('Ctrl Pts',(1.30854725833057,1.58580452418249,6.74400537831042));
#48448=CARTESIAN_POINT('Ctrl Pts',(1.36281932984893,1.53941850059499,6.7401473165987));
#48449=CARTESIAN_POINT('Ctrl Pts',(1.41455660915229,1.49031109571243,6.73628925488698));
#48450=CARTESIAN_POINT('Ctrl Pts',(1.46627146229503,1.44122497703904,6.7324328654996));
#48451=CARTESIAN_POINT('Ctrl Pts',(1.515453352015,1.38942015202907,6.72857647611223));
#48452=CARTESIAN_POINT('Ctrl Pts',(1.56181186435802,1.3351933428723,6.72472008672485));
#48453=CARTESIAN_POINT('Ctrl Pts',(1.60816577128011,1.28097192080131,6.72086408044503));
#48454=CARTESIAN_POINT('Ctrl Pts',(1.65169654324184,1.22432936221296,6.71700807416521));
#48455=CARTESIAN_POINT('Ctrl Pts',(1.69215320353844,1.16559645600636,6.71315206788539));
#48456=CARTESIAN_POINT('Ctrl Pts',(1.73268093267178,1.10676037570454,6.70928928789072));
#48457=CARTESIAN_POINT('Ctrl Pts',(1.77012346576075,1.04582700106825,6.70542650789604));
#48458=CARTESIAN_POINT('Ctrl Pts',(1.8042724723433,0.983157366876838,6.70156372790137));
#48459=CARTESIAN_POINT('Ctrl Pts',(1.83840916765922,0.920510326097459,6.69770234050107));
#48460=CARTESIAN_POINT('Ctrl Pts',(1.86925451742048,0.856128725321618,6.69384095310078));
#48461=CARTESIAN_POINT('Ctrl Pts',(1.89664781037034,0.790395246643986,6.68997956570048));
#48462=CARTESIAN_POINT('Ctrl Pts',(1.92409242387181,0.724538618172293,6.68611094410122));
#48463=CARTESIAN_POINT('Ctrl Pts',(1.94807189147438,0.657325508925034,6.68224232250196));
#48464=CARTESIAN_POINT('Ctrl Pts',(1.96847472927211,0.589156008810146,6.6783737009027));
#48465=CARTESIAN_POINT('Ctrl Pts',(1.98882329509229,0.521167840998941,6.67451536991824));
#48466=CARTESIAN_POINT('Ctrl Pts',(2.00561420302378,0.452228846973817,6.67065703893378));
#48467=CARTESIAN_POINT('Ctrl Pts',(2.01878791325744,0.382743940233756,6.66679870794932));
#48468=CARTESIAN_POINT('Ctrl Pts',(2.0320020065519,0.313046032511898,6.66292854952885));
#48469=CARTESIAN_POINT('Ctrl Pts',(2.04162817079777,0.242527197504543,6.65905839110839));
#48470=CARTESIAN_POINT('Ctrl Pts',(2.04757284006439,0.171589705782855,6.65518823268792));
#48471=CARTESIAN_POINT('Ctrl Pts',(2.05350867604944,0.100757621243658,6.65132382499933));
#48472=CARTESIAN_POINT('Ctrl Pts',(2.05577383564748,0.0295085947020155,
6.64745941731074));
#48473=CARTESIAN_POINT('Ctrl Pts',(2.05432589106127,-0.0417456083355204,
6.64359500962215));
#48474=CARTESIAN_POINT('Ctrl Pts',(2.05287963868512,-0.112916536723224,
6.63973511825939));
#48475=CARTESIAN_POINT('Ctrl Pts',(2.04772891178417,-0.18409214656408,6.63587522689661));
#48476=CARTESIAN_POINT('Ctrl Pts',(2.03888326303558,-0.25485800402063,6.63201533553385));
#48477=CARTESIAN_POINT('Ctrl Pts',(2.03004316454245,-0.325579459014725,
6.62815786608311));
#48478=CARTESIAN_POINT('Ctrl Pts',(2.01751280404875,-0.395891191136253,
6.62430039663237));
#48479=CARTESIAN_POINT('Ctrl Pts',(2.00135366856377,-0.465382698245589,
6.62044292718163));
#48480=CARTESIAN_POINT('Ctrl Pts',(1.98519927542666,-0.534853811138811,
6.61658658981262));
#48481=CARTESIAN_POINT('Ctrl Pts',(1.96541833149422,-0.603504704330993,
6.61273025244361));
#48482=CARTESIAN_POINT('Ctrl Pts',(1.94212331801147,-0.670935600587797,
6.6088739150746));
#48483=CARTESIAN_POINT('Ctrl Pts',(1.91882736130922,-0.738369227134346,
6.60501742156176));
#48484=CARTESIAN_POINT('Ctrl Pts',(1.89201721316103,-0.804582300537594,
6.60116092804892));
#48485=CARTESIAN_POINT('Ctrl Pts',(1.86185450043045,-0.869192373256286,
6.59730443453608));
#48486=CARTESIAN_POINT('Ctrl Pts',(1.83166022187499,-0.933870061585644,
6.59344390513297));
#48487=CARTESIAN_POINT('Ctrl Pts',(1.79810658072365,-0.996940959639327,
6.58958337572986));
#48488=CARTESIAN_POINT('Ctrl Pts',(1.76140206117851,-1.05804552897127,6.58572284632675));
#48489=CARTESIAN_POINT('Ctrl Pts',(1.72467674727163,-1.11918471612506,6.58186012980211));
#48490=CARTESIAN_POINT('Ctrl Pts',(1.68479727279809,-1.17835495413582,6.57799741327746));
#48491=CARTESIAN_POINT('Ctrl Pts',(1.64201500142225,-1.23522641552239,6.57413469675282));
#48492=CARTESIAN_POINT('Ctrl Pts',(1.599158006467,-1.29219720868879,6.5702652336017));
#48493=CARTESIAN_POINT('Ctrl Pts',(1.5533884038574,-1.34686083670187,6.56639577045058));
#48494=CARTESIAN_POINT('Ctrl Pts',(1.5049968323029,-1.39892176237924,6.56252630729946));
#48495=CARTESIAN_POINT('Ctrl Pts',(1.47639674996706,-1.42969048331602,6.56023940151892));
#48496=CARTESIAN_POINT('Ctrl Pts',(1.4468815172348,-1.45955079845428,6.55795249573838));
#48497=CARTESIAN_POINT('Ctrl Pts',(1.41651657404932,-1.48844830543206,6.55566558995783));
#48498=CARTESIAN_POINT('Ctrl Pts',(1.36521646640748,-1.53726925034495,6.55180197289153));
#48499=CARTESIAN_POINT('Ctrl Pts',(1.31128724265687,-1.58353219853699,6.54793835582523));
#48500=CARTESIAN_POINT('Ctrl Pts',(1.255014660813,-1.62694061466435,6.54407473875893));
#48501=CARTESIAN_POINT('Ctrl Pts',(1.19882623299308,-1.67028411475675,6.54021689962058));
#48502=CARTESIAN_POINT('Ctrl Pts',(1.14030178525658,-1.71078126046051,6.53635906048222));
#48503=CARTESIAN_POINT('Ctrl Pts',(1.07976287558482,-1.74817324513584,6.53250122134386));
#48504=CARTESIAN_POINT('Ctrl Pts',(1.01929498024369,-1.78552136766076,6.52864790759035));
#48505=CARTESIAN_POINT('Ctrl Pts',(0.956817728828559,-1.81977130880502,
6.52479459383683));
#48506=CARTESIAN_POINT('Ctrl Pts',(0.892683194147317,-1.85070642658066,
6.52094128008331));
#48507=CARTESIAN_POINT('Ctrl Pts',(0.828589006849113,-1.8816220829062,6.51709039047034));
#48508=CARTESIAN_POINT('Ctrl Pts',(0.762840042435076,-1.90922684157126,
6.51323950085737));
#48509=CARTESIAN_POINT('Ctrl Pts',(0.695813303091591,-1.93334978980545,
6.5093886112444));
#48510=CARTESIAN_POINT('Ctrl Pts',(0.628806142268257,-1.957465691723,6.50553884647684));
#48511=CARTESIAN_POINT('Ctrl Pts',(0.5605224056806,-1.97810163717773,6.50168908170928));
#48512=CARTESIAN_POINT('Ctrl Pts',(0.491357788836919,-1.99513535527024,
6.49783931694172));
#48513=CARTESIAN_POINT('Ctrl Pts',(0.422190066630577,-2.012169838145,6.49398937932688));
#48514=CARTESIAN_POINT('Ctrl Pts',(0.352141859343161,-2.02560165820165,
6.49013944171204));
#48515=CARTESIAN_POINT('Ctrl Pts',(0.281620981923863,-2.0353592275174,6.4862895040972));
#48516=CARTESIAN_POINT('Ctrl Pts',(0.211024891169831,-2.04512720367087,
6.48243546036999));
#48517=CARTESIAN_POINT('Ctrl Pts',(0.139955607671059,-2.05121303969876,
6.47858141664279));
#48518=CARTESIAN_POINT('Ctrl Pts',(0.068827126234984,-2.05359693932238,
6.47472737291559));
#48519=CARTESIAN_POINT('Ctrl Pts',(-0.00234226611308243,-2.05598221009164,
6.47087111246113));
#48520=CARTESIAN_POINT('Ctrl Pts',(-0.0735704367650953,-2.05466131556808,
6.46701485200667));
#48521=CARTESIAN_POINT('Ctrl Pts',(-0.144445123139336,-2.04966659945008,
6.4631585915522));
#48522=CARTESIAN_POINT('Ctrl Pts',(-0.21544595536584,-2.0446629935189,6.45929546755751));
#48523=CARTESIAN_POINT('Ctrl Pts',(-0.286091563497953,-2.03597257107392,
6.45543234356281));
#48524=CARTESIAN_POINT('Ctrl Pts',(-0.355977220656732,-2.02367926828179,
6.45156921956811));
#48525=CARTESIAN_POINT('Ctrl Pts',(-0.398409867662541,-2.01621511327314,
6.44922363703414));
#48526=CARTESIAN_POINT('Ctrl Pts',(-0.440562574257773,-2.00742372133879,
6.44687805450017));
#48527=CARTESIAN_POINT('Ctrl Pts',(-0.482347616612758,-1.99733280633148,
6.4445324719662));
#48528=CARTESIAN_POINT('Ctrl Pts',(-0.551405647416069,-1.98065557734873,
6.44065593381395));
#48529=CARTESIAN_POINT('Ctrl Pts',(-0.61973077906983,-1.96036049456912,
6.4367793956617));
#48530=CARTESIAN_POINT('Ctrl Pts',(-0.686916947322909,-1.93652850998393,
6.43290285750945));
#48531=CARTESIAN_POINT('Ctrl Pts',(-0.754002799907351,-1.91273210893521,
6.42903210741636));
#48532=CARTESIAN_POINT('Ctrl Pts',(-0.819952612775803,-1.88540945021994,
6.42516135732327));
#48533=CARTESIAN_POINT('Ctrl Pts',(-0.884372772943357,-1.85469198547265,
6.42129060723018));
#48534=CARTESIAN_POINT('Ctrl Pts',(-0.948716347889046,-1.82401103885643,
6.41742445883715));
#48535=CARTESIAN_POINT('Ctrl Pts',(-1.01153344826937,-1.78994351123954,
6.41355831044411));
#48536=CARTESIAN_POINT('Ctrl Pts',(-1.07244946898083,-1.75266930679542,
6.40969216205108));
#48537=CARTESIAN_POINT('Ctrl Pts',(-1.13332644277837,-1.71541899496009,
6.40582849184296));
#48538=CARTESIAN_POINT('Ctrl Pts',(-1.19230434322614,-1.67496633677039,
6.40196482163484));
#48539=CARTESIAN_POINT('Ctrl Pts',(-1.24903353557167,-1.63153694089878,
6.39810115142672));
#48540=CARTESIAN_POINT('Ctrl Pts',(-1.30574514939581,-1.58812100237659,
6.39423867844363));
#48541=CARTESIAN_POINT('Ctrl Pts',(-1.36020905472129,-1.54173045150558,
6.39037620546055));
#48542=CARTESIAN_POINT('Ctrl Pts',(-1.41210637222193,-1.49263296092181,
6.38651373247746));
#48543=CARTESIAN_POINT('Ctrl Pts',(-1.46400479239372,-1.4435344271553,6.38265117742776));
#48544=CARTESIAN_POINT('Ctrl Pts',(-1.51333616654172,-1.39172917353487,
6.37878862237805));
#48545=CARTESIAN_POINT('Ctrl Pts',(-1.55981761405094,-1.3375225506123,6.37492606732835));
#48546=CARTESIAN_POINT('Ctrl Pts',(-1.6063457778695,-1.28326144717115,6.37105963020684));
#48547=CARTESIAN_POINT('Ctrl Pts',(-1.65001798132448,-1.22659452423105,
6.36719319308534));
#48548=CARTESIAN_POINT('Ctrl Pts',(-1.6905914870465,-1.16786043105583,6.36332675596384));
#48549=CARTESIAN_POINT('Ctrl Pts',(-1.73118712286992,-1.10909430240785,
6.35945820996256));
#48550=CARTESIAN_POINT('Ctrl Pts',(-1.76868044147491,-1.04825917046698,
6.35558966396129));
#48551=CARTESIAN_POINT('Ctrl Pts',(-1.80287338849916,-0.985720603184072,
6.35172111796001));
#48552=CARTESIAN_POINT('Ctrl Pts',(-1.83712432758889,-0.923075968977871,
6.34784601081111));
#48553=CARTESIAN_POINT('Ctrl Pts',(-1.86806350901278,-0.858722567140702,
6.34397090366222));
#48554=CARTESIAN_POINT('Ctrl Pts',(-1.8955402628438,-0.793047712586098,
6.34009579651332));
#48555=CARTESIAN_POINT('Ctrl Pts',(-1.91136748138743,-0.755217542317477,
6.33786364900045));
#48556=CARTESIAN_POINT('Ctrl Pts',(-1.92604677240116,-0.71694924401247,
6.33563150148759));
#48557=CARTESIAN_POINT('Ctrl Pts',(-1.93955690842656,-0.67831892312895,
6.33339935397472));
#48558=CARTESIAN_POINT('Ctrl Pts',(-1.96671951453605,-0.600651297276029,
6.3289115424859));
#48559=CARTESIAN_POINT('Ctrl Pts',(-1.98923851869651,-0.521277422665017,
6.32442373099708));
#48560=CARTESIAN_POINT('Ctrl Pts',(-2.00692889343075,-0.440719842091111,
6.31993591950826));
#48561=CARTESIAN_POINT('Ctrl Pts',(-2.02446373253168,-0.360870532229469,
6.31548756532957));
#48562=CARTESIAN_POINT('Ctrl Pts',(-2.03725438909028,-0.279858398211875,
6.31103921115088));
#48563=CARTESIAN_POINT('Ctrl Pts',(-2.04516728440973,-0.198212868603796,
6.30659085697219));
#48564=CARTESIAN_POINT('Ctrl Pts',(-2.05149137716537,-0.132960659206291,
6.30303567226416));
#48565=CARTESIAN_POINT('Ctrl Pts',(-2.05470069136051,-0.0673042961116859,
6.29948048755612));
#48566=CARTESIAN_POINT('Ctrl Pts',(-2.05474943588193,-0.00152257770586607,
6.29592530284809));
#48567=CARTESIAN_POINT('Ctrl Pts',(-2.05290342576851,-0.00152079736506813,
6.29592528053768));
#48568=CARTESIAN_POINT('Ctrl Pts',(-2.04996245021167,0.452378852210551,
6.27137226568616));
#48569=CARTESIAN_POINT('Ctrl Pts',(-1.67847430924827,1.59588320600937,6.20977487817079));
#48570=CARTESIAN_POINT('Ctrl Pts',(-0.0899020486618461,2.28520748800009,
6.1270832760603));
#48571=CARTESIAN_POINT('Ctrl Pts',(0.940075837502264,1.86290841692593,6.06894468880133));
#48572=CARTESIAN_POINT('Ctrl Pts',(1.24933779518059,1.62565558510666,6.04785047420624));
#48573=CARTESIAN_POINT('',(-2.05474920289297,0.00180989245198827,6.35407471946232));
#48574=CARTESIAN_POINT('Ctrl Pts',(-2.05474920289297,0.00180989245198827,
6.35407471946232));
#48575=CARTESIAN_POINT('Ctrl Pts',(-2.05466014208798,0.102919556662241,
6.34858528835285));
#48576=CARTESIAN_POINT('Ctrl Pts',(-2.04710452302201,0.203708660391641,
6.34309585724339));
#48577=CARTESIAN_POINT('Ctrl Pts',(-2.03224380207686,0.303286484071088,
6.33760642613394));
#48578=CARTESIAN_POINT('Ctrl Pts',(-2.02648140179202,0.341898828764958,
6.33547784169275));
#48579=CARTESIAN_POINT('Ctrl Pts',(-2.01962109224582,0.380329380421406,
6.33334925725156));
#48580=CARTESIAN_POINT('Ctrl Pts',(-2.01167405834273,0.418527233870032,
6.33122067281038));
#48581=CARTESIAN_POINT('Ctrl Pts',(-1.99724932624694,0.487860498248844,
6.32735706021204));
#48582=CARTESIAN_POINT('Ctrl Pts',(-1.97920723753694,0.55658526441417,6.3234934476137));
#48583=CARTESIAN_POINT('Ctrl Pts',(-1.95761415720994,0.624295101687676,
6.31962983501537));
#48584=CARTESIAN_POINT('Ctrl Pts',(-1.93605336879913,0.691903680578496,
6.31577200035387));
#48585=CARTESIAN_POINT('Ctrl Pts',(-1.91095227567684,0.758499882712945,
6.31191416569237));
#48586=CARTESIAN_POINT('Ctrl Pts',(-1.8824281473951,0.823687946005434,6.30805633103088));
#48587=CARTESIAN_POINT('Ctrl Pts',(-1.85393747893297,0.888799541375144,
6.304203021747));
#48588=CARTESIAN_POINT('Ctrl Pts',(-1.82203194472304,0.952505834385205,
6.30034971246313));
#48589=CARTESIAN_POINT('Ctrl Pts',(-1.78687789504914,1.01442838617851,6.29649640317925));
#48590=CARTESIAN_POINT('Ctrl Pts',(-1.7517459609449,1.07631198221794,6.29264551802946));
#48591=CARTESIAN_POINT('Ctrl Pts',(-1.71336980552832,1.13641364039341,6.28879463287967));
#48592=CARTESIAN_POINT('Ctrl Pts',(-1.67196229335458,1.19437835383119,6.28494374772987));
#48593=CARTESIAN_POINT('Ctrl Pts',(-1.63056687620076,1.2523261359363,6.28109398741299));
#48594=CARTESIAN_POINT('Ctrl Pts',(-1.5861421430789,1.3081378160752,6.27724422709611));
#48595=CARTESIAN_POINT('Ctrl Pts',(-1.53894400043637,1.36148776197985,6.27339446677923));
#48596=CARTESIAN_POINT('Ctrl Pts',(-1.49174373845498,1.41484010345786,6.26954453359651));
#48597=CARTESIAN_POINT('Ctrl Pts',(-1.44177014427008,1.46573012775092,6.26569460041379));
#48598=CARTESIAN_POINT('Ctrl Pts',(-1.38931792025673,1.51386699513316,6.26184466723107));
#48599=CARTESIAN_POINT('Ctrl Pts',(-1.33680975299792,1.56205520319043,6.25799062787819));
#48600=CARTESIAN_POINT('Ctrl Pts',(-1.28181803861058,1.60748406262357,6.25413658852532));
#48601=CARTESIAN_POINT('Ctrl Pts',(-1.22467202077841,1.64990181647955,6.25028254917244));
#48602=CARTESIAN_POINT('Ctrl Pts',(-1.16749313389932,1.69234396803103,6.24642629306667));
#48603=CARTESIAN_POINT('Ctrl Pts',(-1.10815788334922,1.73177129709322,6.24257003696089));
#48604=CARTESIAN_POINT('Ctrl Pts',(-1.04702374466157,1.76797591629945,6.23871378085512));
#48605=CARTESIAN_POINT('Ctrl Pts',(-0.985780795263479,1.80424497495672,
6.23485066112167));
#48606=CARTESIAN_POINT('Ctrl Pts',(-0.922732997265713,1.83727964592423,
6.23098754138821));
#48607=CARTESIAN_POINT('Ctrl Pts',(-0.858260973366345,1.86691876205052,
6.22712442165476));
#48608=CARTESIAN_POINT('Ctrl Pts',(-0.819114628949602,1.88491514215329,
6.2247787993761));
#48609=CARTESIAN_POINT('Ctrl Pts',(-0.779443596283827,1.90166062200296,
6.22243317709744));
#48610=CARTESIAN_POINT('Ctrl Pts',(-0.739335794758498,1.91712809824717,
6.22008755481877));
#48611=CARTESIAN_POINT('Ctrl Pts',(-0.673050825505878,1.94269073564617,
6.21621101472666));
#48612=CARTESIAN_POINT('Ctrl Pts',(-0.605310861272263,1.96486087863528,
6.21233447463455));
#48613=CARTESIAN_POINT('Ctrl Pts',(-0.536495928273019,1.98347414438567,
6.20845793454244));
#48614=CARTESIAN_POINT('Ctrl Pts',(-0.467783743147285,2.00205961858862,
6.20458718252907));
#48615=CARTESIAN_POINT('Ctrl Pts',(-0.398000238841365,2.01709863318447,
6.2007164305157));
#48616=CARTESIAN_POINT('Ctrl Pts',(-0.327543924189893,2.02847542263304,
6.19684567850233));
#48617=CARTESIAN_POINT('Ctrl Pts',(-0.257171371421285,2.03983868680272,
6.19297952822663));
#48618=CARTESIAN_POINT('Ctrl Pts',(-0.186128072653157,2.04754829854207,
6.18911337795092));
#48619=CARTESIAN_POINT('Ctrl Pts',(-0.114824462259788,2.0515391552117,6.18524722767522));
#48620=CARTESIAN_POINT('Ctrl Pts',(-0.0435665576071448,2.05552745373514,
6.1813835556087));
#48621=CARTESIAN_POINT('Ctrl Pts',(0.0279508457125155,2.05580170015229,
6.17751988354218));
#48622=CARTESIAN_POINT('Ctrl Pts',(0.0993118548629316,2.05234858588488,
6.17365621147566));
#48623=CARTESIAN_POINT('Ctrl Pts',(0.17065075108685,2.04889654164805,6.16979373666093));
#48624=CARTESIAN_POINT('Ctrl Pts',(0.241832866438303,2.04171945339401,6.16593126184621));
#48625=CARTESIAN_POINT('Ctrl Pts',(0.312443678438297,2.03085610280589,6.16206878703149));
#48626=CARTESIAN_POINT('Ctrl Pts',(0.383055990182576,2.01999252148473,6.1582062301794));
#48627=CARTESIAN_POINT('Ctrl Pts',(0.453096496670009,2.00544259809723,6.15434367332732));
#48628=CARTESIAN_POINT('Ctrl Pts',(0.522158853022968,1.98729657945404,6.15048111647524));
#48629=CARTESIAN_POINT('Ctrl Pts',(0.591290619653305,1.96913232337654,6.14661467760759));
#48630=CARTESIAN_POINT('Ctrl Pts',(0.659441804753107,1.9473648800184,6.14274823873994));
#48631=CARTESIAN_POINT('Ctrl Pts',(0.726220140700263,1.92213471685553,6.13888179987229));
#48632=CARTESIAN_POINT('Ctrl Pts',(0.793034899188124,1.89689079254346,6.13501325215414));
#48633=CARTESIAN_POINT('Ctrl Pts',(0.858474874195766,1.86818058209607,6.131144704436));
#48634=CARTESIAN_POINT('Ctrl Pts',(0.922169238106877,1.83619210835614,6.12727615671785));
#48635=CARTESIAN_POINT('Ctrl Pts',(0.985971628101802,1.80414938194246,6.12340104791589));
#48636=CARTESIAN_POINT('Ctrl Pts',(1.04802207512344,1.76881753034704,6.11952593911392));
#48637=CARTESIAN_POINT('Ctrl Pts',(1.1079763550629,1.73042941466028,6.11565083031196));
#48638=CARTESIAN_POINT('Ctrl Pts',(1.14251107998624,1.70831718152353,6.11341869915037));
#48639=CARTESIAN_POINT('Ctrl Pts',(1.17635086489013,1.68519168236722,6.11118656798877));
#48640=CARTESIAN_POINT('Ctrl Pts',(1.20943496396806,1.66110343760754,6.10895443682718));
#48641=CARTESIAN_POINT('Ctrl Pts',(1.22377512356468,1.65066249214178,6.1079869292332));
#48642=CARTESIAN_POINT('Ctrl Pts',(1.23798712249006,1.64003070187989,6.10701942163922));
#48643=CARTESIAN_POINT('Ctrl Pts',(1.25206542099588,1.62921138715834,6.10605191404525));
#48644=CARTESIAN_POINT('Ctrl Pts',(1.2515670322334,1.6285464922234,6.80617425834608));
#48645=CARTESIAN_POINT('Ctrl Pts',(1.40105728510831,1.51592380612735,6.79603388715624));
#48646=CARTESIAN_POINT('Ctrl Pts',(2.02408552329212,0.900327067227945,6.74884914330253));
#48647=CARTESIAN_POINT('Ctrl Pts',(2.27789949074807,-0.842191245823211,
6.664620026785));
#48648=CARTESIAN_POINT('Ctrl Pts',(0.527846155910302,-2.37052290404747,
6.55348690879344));
#48649=CARTESIAN_POINT('Ctrl Pts',(-1.55202449963455,-1.7731560393209,6.4499719160968));
#48650=CARTESIAN_POINT('Ctrl Pts',(-2.05038434453856,-0.540370480513924,
6.383501296064));
#48651=CARTESIAN_POINT('Ctrl Pts',(-2.05538931506001,0.00180439026243735,
6.35407504869506));
#48652=CARTESIAN_POINT('Origin',(0.,0.,18.5459252805377));
#48653=CARTESIAN_POINT('',(1.25017377660034,1.6267706489614,7.50603355970618));
#48654=CARTESIAN_POINT('',(1.25206542099588,1.62921138715835,7.44794391597819));
#48655=CARTESIAN_POINT('',(1.25206542099588,1.62921138715835,18.5459252805377));
#48656=CARTESIAN_POINT('',(-2.05474994334797,-0.000482505435243929,6.99592528050785));
#48657=CARTESIAN_POINT('Ctrl Pts',(1.25206542099588,1.62921138715835,7.44794391597819));
#48658=CARTESIAN_POINT('Ctrl Pts',(1.26764871117023,1.61723547112532,7.44687278861555));
#48659=CARTESIAN_POINT('Ctrl Pts',(1.28305223476815,1.60504204850324,7.44580166125291));
#48660=CARTESIAN_POINT('Ctrl Pts',(1.29826972672408,1.59263720889969,7.44473053389027));
#48661=CARTESIAN_POINT('Ctrl Pts',(1.35323787633299,1.54782883435431,7.44086144105353));
#48662=CARTESIAN_POINT('Ctrl Pts',(1.40599119458351,1.50008360802498,7.43699234821679));
#48663=CARTESIAN_POINT('Ctrl Pts',(1.45619913804349,1.44964879638532,7.43312325538005));
#48664=CARTESIAN_POINT('Ctrl Pts',(1.50633227283071,1.39928913144674,7.42925992740201));
#48665=CARTESIAN_POINT('Ctrl Pts',(1.55392722100258,1.34624817728394,7.42539659942398));
#48666=CARTESIAN_POINT('Ctrl Pts',(1.59868643162176,1.29081340861044,7.42153327144594));
#48667=CARTESIAN_POINT('Ctrl Pts',(1.64339313728927,1.23544366789005,7.41767447535857));
#48668=CARTESIAN_POINT('Ctrl Pts',(1.68527040921453,1.17768606656781,7.41381567927119));
#48669=CARTESIAN_POINT('Ctrl Pts',(1.724058735042,1.11786360555543,7.40995688318382));
#48670=CARTESIAN_POINT('Ctrl Pts',(1.76282262571665,1.05807883039171,7.40610051798951));
#48671=CARTESIAN_POINT('Ctrl Pts',(1.79850116730473,0.996232182905278,7.4022441527952));
#48672=CARTESIAN_POINT('Ctrl Pts',(1.83087710417188,0.932677110215103,7.39838778760088));
#48673=CARTESIAN_POINT('Ctrl Pts',(1.86324347560073,0.869140814807854,7.39453256176583));
#48674=CARTESIAN_POINT('Ctrl Pts',(1.89230895906421,0.803897528887979,7.39067733593077));
#48675=CARTESIAN_POINT('Ctrl Pts',(1.91790221462563,0.737325340425854,7.38682211009571));
#48676=CARTESIAN_POINT('Ctrl Pts',(1.94349646970277,0.670750552062018,7.38296673369916));
#48677=CARTESIAN_POINT('Ctrl Pts',(1.96561805539294,0.602847212335397,7.37911135730261));
#48678=CARTESIAN_POINT('Ctrl Pts',(1.98414438906916,0.534011803076818,7.37525598090605));
#48679=CARTESIAN_POINT('Ctrl Pts',(2.002690113212,0.465104347684967,7.37139656930488));
#48680=CARTESIAN_POINT('Ctrl Pts',(2.01763294714544,0.395263345404606,7.3675371577037));
#48681=CARTESIAN_POINT('Ctrl Pts',(2.02890090929962,0.324897926652613,7.36367774610253));
#48682=CARTESIAN_POINT('Ctrl Pts',(2.04017525097089,0.254492669517639,7.35981614944056));
#48683=CARTESIAN_POINT('Ctrl Pts',(2.04777052731898,0.183562888110837,7.35595455277859));
#48684=CARTESIAN_POINT('Ctrl Pts',(2.05166669540355,0.112522590940064,7.35209295611663));
#48685=CARTESIAN_POINT('Ctrl Pts',(2.05556967960491,0.0413580129498467,
7.34822460381854));
#48686=CARTESIAN_POINT('Ctrl Pts',(2.05576063396187,-0.0299169808821453,
7.34435625152046));
#48687=CARTESIAN_POINT('Ctrl Pts',(2.05227164517212,-0.10088933007269,7.34048789922238));
#48688=CARTESIAN_POINT('Ctrl Pts',(2.05020006385277,-0.143029044939606,
7.33819107144783));
#48689=CARTESIAN_POINT('Ctrl Pts',(2.04683216072677,-0.185062161817784,
7.33589424367327));
#48690=CARTESIAN_POINT('Ctrl Pts',(2.04218320150506,-0.226903798977777,
7.33359741589872));
#48691=CARTESIAN_POINT('Ctrl Pts',(2.03435179900029,-0.297388113085845,
7.32972829553675));
#48692=CARTESIAN_POINT('Ctrl Pts',(2.02285171200631,-0.367604541133105,
7.32585917517479));
#48693=CARTESIAN_POINT('Ctrl Pts',(2.00771140280094,-0.437141264996901,
7.32199005481283));
#48694=CARTESIAN_POINT('Ctrl Pts',(1.99259365061969,-0.506574388495813,
7.31812669891975));
#48695=CARTESIAN_POINT('Ctrl Pts',(1.97384654412021,-0.575329347144338,
7.31426334302667));
#48696=CARTESIAN_POINT('Ctrl Pts',(1.95155022025858,-0.643000233521494,
7.31039998713359));
#48697=CARTESIAN_POINT('Ctrl Pts',(1.92928004845726,-0.710591746585247,
7.30654116269229));
#48698=CARTESIAN_POINT('Ctrl Pts',(1.90346907968105,-0.777101253957358,
7.30268233825098));
#48699=CARTESIAN_POINT('Ctrl Pts',(1.87424792885537,-0.84213553759556,7.29882351380968));
#48700=CARTESIAN_POINT('Ctrl Pts',(1.84504518416558,-0.907128856732772,
7.29496712000663));
#48701=CARTESIAN_POINT('Ctrl Pts',(1.81243671773462,-0.970648353663312,
7.29111072620358));
#48702=CARTESIAN_POINT('Ctrl Pts',(1.77660164236917,-1.03231979872091,7.28725433240053));
#48703=CARTESIAN_POINT('Ctrl Pts',(1.74077715240483,-1.09397302651577,7.28339907774606));
#48704=CARTESIAN_POINT('Ctrl Pts',(1.70172818962766,-1.15377886641638,7.27954382309159));
#48705=CARTESIAN_POINT('Ctrl Pts',(1.65967947199295,-1.21138829973928,7.27568856843712));
#48706=CARTESIAN_POINT('Ctrl Pts',(1.61762911038624,-1.26899998540898,7.27183316305438));
#48707=CARTESIAN_POINT('Ctrl Pts',(1.57257904924475,-1.32441470293893,7.26797775767164));
#48708=CARTESIAN_POINT('Ctrl Pts',(1.52479590461656,-1.37731442008155,7.26412235228889));
#48709=CARTESIAN_POINT('Ctrl Pts',(1.47696274781209,-1.4302695046555,7.2602629116503));
#48710=CARTESIAN_POINT('Ctrl Pts',(1.42639112344778,-1.48070397291409,7.25640347101171));
#48711=CARTESIAN_POINT('Ctrl Pts',(1.37338571891157,-1.52833544406643,7.25254403037312));
#48712=CARTESIAN_POINT('Ctrl Pts',(1.32035030384078,-1.57599388314639,7.24868240460119));
#48713=CARTESIAN_POINT('Ctrl Pts',(1.26487874343397,-1.62084586032309,7.24482077882926));
#48714=CARTESIAN_POINT('Ctrl Pts',(1.20730799371582,-1.6626499844555,7.24095915305733));
#48715=CARTESIAN_POINT('Ctrl Pts',(1.14963653116646,-1.70452723967824,7.23709077185375));
#48716=CARTESIAN_POINT('Ctrl Pts',(1.08985895505129,-1.74334573204196,7.23322239065017));
#48717=CARTESIAN_POINT('Ctrl Pts',(1.02833969894506,-1.77890838046078,7.2293540094466));
#48718=CARTESIAN_POINT('Ctrl Pts',(0.991817106643526,-1.80002112127676,
7.22705743893343));
#48719=CARTESIAN_POINT('Ctrl Pts',(0.954681113454435,-1.81998721792624,
7.22476086842027));
#48720=CARTESIAN_POINT('Ctrl Pts',(0.917011283475248,-1.83877346850532,
7.22246429790711));
#48721=CARTESIAN_POINT('Ctrl Pts',(0.85354996579394,-1.87042214376343,7.21859532926579));
#48722=CARTESIAN_POINT('Ctrl Pts',(0.788323957946326,-1.89884362351522,
7.21472636062447));
#48723=CARTESIAN_POINT('Ctrl Pts',(0.721694646449377,-1.92383845470099,
7.21085739198316));
#48724=CARTESIAN_POINT('Ctrl Pts',(0.655164614492342,-1.94879604288839,
7.20699418821345));
#48725=CARTESIAN_POINT('Ctrl Pts',(0.58723588053482,-1.97033694812449,7.20313098444375));
#48726=CARTESIAN_POINT('Ctrl Pts',(0.51829289493829,-1.98830833563522,7.19926778067405));
#48727=CARTESIAN_POINT('Ctrl Pts',(0.449430775593098,-2.00625864371739,
7.19540910822547));
#48728=CARTESIAN_POINT('Ctrl Pts',(0.379557235495024,-2.02064762859855,
7.19155043577689));
#48729=CARTESIAN_POINT('Ctrl Pts',(0.309073444491057,-2.0313717454987,7.18769176332832));
#48730=CARTESIAN_POINT('Ctrl Pts',(0.238634049373333,-2.04208910755965,
7.18383552135603));
#48731=CARTESIAN_POINT('Ctrl Pts',(0.167585645105574,-2.04914610856388,
7.17997927938375));
#48732=CARTESIAN_POINT('Ctrl Pts',(0.0963397545169107,-2.05249024704129,
7.17612303741146));
#48733=CARTESIAN_POINT('Ctrl Pts',(0.0251149031738014,-2.05583339797893,
7.17226793420551));
#48734=CARTESIAN_POINT('Ctrl Pts',(-0.0463068336956827,-2.05546584032901,
7.16841283099957));
#48735=CARTESIAN_POINT('Ctrl Pts',(-0.117510377601777,-2.05138706090681,
7.16455772779362));
#48736=CARTESIAN_POINT('Ctrl Pts',(-0.188716716584823,-2.04730812137317,
7.16070247325657));
#48737=CARTESIAN_POINT('Ctrl Pts',(-0.259704360706126,-2.03951770081616,
7.15684721871953));
#48738=CARTESIAN_POINT('Ctrl Pts',(-0.330061539169524,-2.02806729248835,
7.15299196418249));
#48739=CARTESIAN_POINT('Ctrl Pts',(-0.400492395360941,-2.01660489334328,
7.14913267243984));
#48740=CARTESIAN_POINT('Ctrl Pts',(-0.470290987458039,-2.00147493365622,
7.1452733806972));
#48741=CARTESIAN_POINT('Ctrl Pts',(-0.539054847388912,-1.98278022836786,
7.14141408895455));
#48742=CARTESIAN_POINT('Ctrl Pts',(-0.60785765704541,-1.96407493388858,
7.13755261120381));
#48743=CARTESIAN_POINT('Ctrl Pts',(-0.675624106053599,-1.94180102604834,
7.13369113345307));
#48744=CARTESIAN_POINT('Ctrl Pts',(-0.74196866205707,-1.91611066147685,
7.12982965570232));
#48745=CARTESIAN_POINT('Ctrl Pts',(-0.808429335272795,-1.89037533325354,
7.12596141953675));
#48746=CARTESIAN_POINT('Ctrl Pts',(-0.873462703469705,-1.86121180885213,
7.12209318337116));
#48747=CARTESIAN_POINT('Ctrl Pts',(-0.936705558148894,-1.82881936227528,
7.11822494720559));
#48748=CARTESIAN_POINT('Ctrl Pts',(-0.974274922604166,-1.80957665672038,
7.1159270247756));
#48749=CARTESIAN_POINT('Ctrl Pts',(-1.01121292152412,-1.78919535023045,
7.11362910234561));
#48750=CARTESIAN_POINT('Ctrl Pts',(-1.0474483806814,-1.76772437113593,7.11133117991563));
#48751=CARTESIAN_POINT('Ctrl Pts',(-1.10846071388344,-1.73157208933364,
7.10746199729088));
#48752=CARTESIAN_POINT('Ctrl Pts',(-1.16771865797709,-1.69218657582534,
7.10359281466615));
#48753=CARTESIAN_POINT('Ctrl Pts',(-1.22485861391118,-1.64976329769685,
7.09972363204141));
#48754=CARTESIAN_POINT('Ctrl Pts',(-1.28191342573315,-1.60740323439396,
7.09586021487647));
#48755=CARTESIAN_POINT('Ctrl Pts',(-1.33685612715621,-1.56201467879785,
7.09199679771154));
#48756=CARTESIAN_POINT('Ctrl Pts',(-1.38934977746784,-1.51383775826542,
7.08813338054661));
#48757=CARTESIAN_POINT('Ctrl Pts',(-1.44178183362564,-1.46571736679197,
7.08427449657587));
#48758=CARTESIAN_POINT('Ctrl Pts',(-1.49177019053785,-1.41481543609068,
7.08041561260514));
#48759=CARTESIAN_POINT('Ctrl Pts',(-1.5390102509223,-1.36141287273776,7.07655672863441));
#48760=CARTESIAN_POINT('Ctrl Pts',(-1.58622054216656,-1.30804396193275,
7.07270027640608));
#48761=CARTESIAN_POINT('Ctrl Pts',(-1.63068565183867,-1.25217790785008,
7.06884382417774));
#48762=CARTESIAN_POINT('Ctrl Pts',(-1.67213825123546,-1.1941319990919,7.06498737194941));
#48763=CARTESIAN_POINT('Ctrl Pts',(-1.71357859336585,-1.13610325413473,
7.06113206004914));
#48764=CARTESIAN_POINT('Ctrl Pts',(-1.75200791152176,-1.07589632924174,
7.05727674814888));
#48765=CARTESIAN_POINT('Ctrl Pts',(-1.78720062565951,-1.01385969746423,
7.05342143624861));
#48766=CARTESIAN_POINT('Ctrl Pts',(-1.82239470423566,-0.951820660496772,
7.04956597487605));
#48767=CARTESIAN_POINT('Ctrl Pts',(-1.85435169189239,-0.88795219939876,
7.04571051350349));
#48768=CARTESIAN_POINT('Ctrl Pts',(-1.88289149465536,-0.82262821605783,
7.04185505213093));
#48769=CARTESIAN_POINT('Ctrl Pts',(-1.91146115126503,-0.757235901053905,
7.03799555778191));
#48770=CARTESIAN_POINT('Ctrl Pts',(-1.93660629255638,-0.690385470517167,
7.03413606343289));
#48771=CARTESIAN_POINT('Ctrl Pts',(-1.95819498690959,-0.622470847303041,
7.03027656908387));
#48772=CARTESIAN_POINT('Ctrl Pts',(-1.97979589741874,-0.554517793991437,
7.02641489080542));
#48773=CARTESIAN_POINT('Ctrl Pts',(-1.99783623190938,-0.485499819428284,
7.02255321252697));
#48774=CARTESIAN_POINT('Ctrl Pts',(-2.01223469734867,-0.415823382322472,
7.01869153424853));
#48775=CARTESIAN_POINT('Ctrl Pts',(-2.0266583416096,-0.346025100941707,
7.0148231029929));
#48776=CARTESIAN_POINT('Ctrl Pts',(-2.03742732831468,-0.275566538420227,
7.01095467173727));
#48777=CARTESIAN_POINT('Ctrl Pts',(-2.04451205699333,-0.204860956038284,
7.00708624048164));
#48778=CARTESIAN_POINT('Ctrl Pts',(-2.04871711006231,-0.162894532244804,
7.00479018096243));
#48779=CARTESIAN_POINT('Ctrl Pts',(-2.05162524471206,-0.120841139796805,
7.00249412144322));
#48780=CARTESIAN_POINT('Ctrl Pts',(-2.05323895034625,-0.0787868979021409,
7.000198061924));
#48781=CARTESIAN_POINT('Ctrl Pts',(-2.05423994231227,-0.0527003816366956,
6.9987738014619));
#48782=CARTESIAN_POINT('Ctrl Pts',(-2.05474381156835,-0.0265946663309218,
6.99734954099979));
#48783=CARTESIAN_POINT('Ctrl Pts',(-2.05474994334785,-0.000482505981838667,
6.99592528053767));
#48784=CARTESIAN_POINT('Ctrl Pts',(-2.05474994334797,-0.000482505435243929,
6.99592528050786));
#48785=CARTESIAN_POINT('Ctrl Pts',(-2.05476649816122,0.0700161855421443,
6.99208000317933));
#48786=CARTESIAN_POINT('Ctrl Pts',(-2.05115055191818,0.140660126107189,
6.98823472585081));
#48787=CARTESIAN_POINT('Ctrl Pts',(-2.04388336541941,0.211041112254987,
6.98438944852229));
#48788=CARTESIAN_POINT('Ctrl Pts',(-2.03637696109566,0.283738866581148,
6.98041759416438));
#48789=CARTESIAN_POINT('Ctrl Pts',(-2.0249746271749,0.356155527681318,6.97644573980647));
#48790=CARTESIAN_POINT('Ctrl Pts',(-2.0097141915556,0.427839258086527,6.97247388544856));
#48791=CARTESIAN_POINT('Ctrl Pts',(-1.99497874903466,0.497056907924543,
6.96863867175921));
#48792=CARTESIAN_POINT('Ctrl Pts',(-1.97664644609815,0.565590706630233,
6.96480345806987));
#48793=CARTESIAN_POINT('Ctrl Pts',(-1.95480391551666,0.633039662565255,
6.96096824438053));
#48794=CARTESIAN_POINT('Ctrl Pts',(-1.93297398344573,0.70044971474872,6.9571352427966));
#48795=CARTESIAN_POINT('Ctrl Pts',(-1.90763799081597,0.766775697756702,
6.95330224121267));
#48796=CARTESIAN_POINT('Ctrl Pts',(-1.87893281749727,0.831630344463081,
6.94946923962874));
#48797=CARTESIAN_POINT('Ctrl Pts',(-1.8502342985522,0.896469956700014,6.94563712660327));
#48798=CARTESIAN_POINT('Ctrl Pts',(-1.81816834880263,0.959838459735692,
6.9418050135778));
#48799=CARTESIAN_POINT('Ctrl Pts',(-1.78291984061563,1.02136888754217,6.93797290055234));
#48800=CARTESIAN_POINT('Ctrl Pts',(-1.7476673440786,1.08290627748397,6.93414035392531));
#48801=CARTESIAN_POINT('Ctrl Pts',(-1.70923182180326,1.14260475376583,6.93030780729828));
#48802=CARTESIAN_POINT('Ctrl Pts',(-1.66784300479209,1.20012385771889,6.92647526067126));
#48803=CARTESIAN_POINT('Ctrl Pts',(-1.62640938656058,1.25770522308064,6.92263856551382));
#48804=CARTESIAN_POINT('Ctrl Pts',(-1.58201638538156,1.31310211060008,6.91880187035639));
#48805=CARTESIAN_POINT('Ctrl Pts',(-1.53493515674473,1.36600572000597,6.91496517519895));
#48806=CARTESIAN_POINT('Ctrl Pts',(-1.48782324497298,1.41894380702921,6.91112597964298));
#48807=CARTESIAN_POINT('Ctrl Pts',(-1.43801996747691,1.46938503482276,6.90728678408701));
#48808=CARTESIAN_POINT('Ctrl Pts',(-1.38583263452308,1.51705816354905,6.90344758853104));
#48809=CARTESIAN_POINT('Ctrl Pts',(-1.33355967559132,1.5648095116063,6.89960209384354));
#48810=CARTESIAN_POINT('Ctrl Pts',(-1.27889524014262,1.60978339213117,6.89575659915605));
#48811=CARTESIAN_POINT('Ctrl Pts',(-1.22217805839316,1.65175008887008,6.89191110446856));
#48812=CARTESIAN_POINT('Ctrl Pts',(-1.20818538926298,1.66210367280781,6.89096238428987));
#48813=CARTESIAN_POINT('Ctrl Pts',(-1.19406790386411,1.67227443734968,6.89001366411119));
#48814=CARTESIAN_POINT('Ctrl Pts',(-1.17983092207496,1.68225936104269,6.8890649439325));
#48815=CARTESIAN_POINT('Ctrl Pts',(-1.12178147454127,1.7229715929349,6.88519666039794));
#48816=CARTESIAN_POINT('Ctrl Pts',(-1.0615083071561,1.76075557326182,6.88132837686337));
#48817=CARTESIAN_POINT('Ctrl Pts',(-0.999339045620557,1.79536041907974,
6.87746009332881));
#48818=CARTESIAN_POINT('Ctrl Pts',(-0.937262455615625,1.8299136817849,6.87359757598395));
#48819=CARTESIAN_POINT('Ctrl Pts',(-0.873295802853424,1.86129698204855,
6.8697350586391));
#48820=CARTESIAN_POINT('Ctrl Pts',(-0.807796451145422,1.8893021081915,6.86587254129424));
#48821=CARTESIAN_POINT('Ctrl Pts',(-0.742373917871417,1.9172743895829,6.86201455395657));
#48822=CARTESIAN_POINT('Ctrl Pts',(-0.675422700874369,1.94187617640339,
6.85815656661889));
#48823=CARTESIAN_POINT('Ctrl Pts',(-0.607324023697059,1.96294551446045,
6.85429857928122));
#48824=CARTESIAN_POINT('Ctrl Pts',(-0.5392682270093,1.98400158554131,6.8504430212475));
#48825=CARTESIAN_POINT('Ctrl Pts',(-0.470066866807601,2.00152947749453,
6.84658746321378));
#48826=CARTESIAN_POINT('Ctrl Pts',(-0.400118988439783,2.01541617478622,
6.84273190518006));
#48827=CARTESIAN_POINT('Ctrl Pts',(-0.330191730537803,2.02929877831305,
6.83887748375555));
#48828=CARTESIAN_POINT('Ctrl Pts',(-0.259518867808598,2.0395422235871,6.83502306233104));
#48829=CARTESIAN_POINT('Ctrl Pts',(-0.188510683422475,2.04608437869399,
6.83116864090653));
#48830=CARTESIAN_POINT('Ctrl Pts',(-0.1174996532212,2.0526267959927,6.82731406500728));
#48831=CARTESIAN_POINT('Ctrl Pts',(-0.046153758839543,2.05546758622967,
6.82345948910803));
#48832=CARTESIAN_POINT('Ctrl Pts',(0.0251122658282849,2.05459653864329,
6.81960491320877));
#48833=CARTESIAN_POINT('Ctrl Pts',(0.0964531072273813,2.05372457661087,
6.81574629068604));
#48834=CARTESIAN_POINT('Ctrl Pts',(0.167713424566388,2.04913300390706,6.8118876681633));
#48835=CARTESIAN_POINT('Ctrl Pts',(0.238480064451791,2.04086374394742,6.80802904564056));
#48836=CARTESIAN_POINT('Ctrl Pts',(0.309286874236735,2.03258979003392,6.80416823281348));
#48837=CARTESIAN_POINT('Ctrl Pts',(0.379598969382153,2.02063407471531,6.80030741998639));
#48838=CARTESIAN_POINT('Ctrl Pts',(0.449012623742548,2.0050898299627,6.7964466071593));
#48839=CARTESIAN_POINT('Ctrl Pts',(0.518548039110839,1.98951831848676,6.79257902194045));
#48840=CARTESIAN_POINT('Ctrl Pts',(0.587181398984335,1.97034584076531,6.7887114367216));
#48841=CARTESIAN_POINT('Ctrl Pts',(0.654524062957153,1.94771553711266,6.78484385150275));
#48842=CARTESIAN_POINT('Ctrl Pts',(0.694641620247931,1.93423415028099,6.78253984298213));
#48843=CARTESIAN_POINT('Ctrl Pts',(0.734301491181396,1.919526565114,6.78023583446152));
#48844=CARTESIAN_POINT('Ctrl Pts',(0.773425401480044,1.90363092821204,6.77793182594091));
#48845=CARTESIAN_POINT('Ctrl Pts',(0.839137179113808,1.87693291798056,6.77406205693221));
#48846=CARTESIAN_POINT('Ctrl Pts',(0.903593417992809,1.84677624309011,6.7701922879235));
#48847=CARTESIAN_POINT('Ctrl Pts',(0.966405487979356,1.81330030477673,6.7663225189148));
#48848=CARTESIAN_POINT('Ctrl Pts',(1.02911755148771,1.77987766530696,6.76245891117368));
#48849=CARTESIAN_POINT('Ctrl Pts',(1.09019021993631,1.7431464839298,6.75859530343255));
#48850=CARTESIAN_POINT('Ctrl Pts',(1.14925471029172,1.70329421221711,6.75473169569142));
#48851=CARTESIAN_POINT('Ctrl Pts',(1.18425395175351,1.67967935882414,6.752442277135));
#48852=CARTESIAN_POINT('Ctrl Pts',(1.21854844377853,1.65496952297849,6.75015285857857));
#48853=CARTESIAN_POINT('Ctrl Pts',(1.25206542099589,1.62921138715833,6.74786344002215));
#48854=CARTESIAN_POINT('',(-2.05138364312766,-4.97672492245568E-5,7.05407471946232));
#48855=CARTESIAN_POINT('Ctrl Pts',(-2.05138364312766,-4.97672492245568E-5,
7.05407471946232));
#48856=CARTESIAN_POINT('Ctrl Pts',(-2.05130984591811,0.345894061862528,
7.03538960656144));
#48857=CARTESIAN_POINT('Ctrl Pts',(-1.80422556460434,1.37779248996311,6.97966012099671));
#48858=CARTESIAN_POINT('Ctrl Pts',(-0.348743598875701,2.30840998533453,
6.89702663395796));
#48859=CARTESIAN_POINT('Ctrl Pts',(0.854945852554142,1.92735221205475,6.8330782598201));
#48860=CARTESIAN_POINT('Ctrl Pts',(1.2515670322334,1.6285464922234,6.80617425834608));
#48861=CARTESIAN_POINT('Ctrl Pts',(1.25017377660034,1.6267706489614,7.50603355970618));
#48862=CARTESIAN_POINT('Ctrl Pts',(1.5598047990933,1.38694935814498,7.48487299071277));
#48863=CARTESIAN_POINT('Ctrl Pts',(2.23443033275686,0.494010394005184,7.42666804905549));
#48864=CARTESIAN_POINT('Ctrl Pts',(1.93017314387361,-1.47391051494563,7.33141873473435));
#48865=CARTESIAN_POINT('Ctrl Pts',(-0.191394880396712,-2.42102228346136,
7.2202856167428));
#48866=CARTESIAN_POINT('Ctrl Pts',(-1.81053415964382,-1.36562854594273,
7.12783761165212));
#48867=CARTESIAN_POINT('Ctrl Pts',(-2.05145615337403,-0.339960617975842,
7.07243397922529));
#48868=CARTESIAN_POINT('Ctrl Pts',(-2.05138364312766,-4.97672492245568E-5,
7.05407471946232));
#48869=CARTESIAN_POINT('Origin',(0.,0.,18.5459252805377));
#48870=CARTESIAN_POINT('',(1.25206542099588,1.62921138715834,8.20601752898817));
#48871=CARTESIAN_POINT('',(1.25206542099587,1.62921138715835,8.14797786267567));
#48872=CARTESIAN_POINT('',(1.25206542099588,1.62921138715835,18.5459252805377));
#48873=CARTESIAN_POINT('',(-2.05474915274975,0.00186595128382746,7.69592528050275));
#48874=CARTESIAN_POINT('Ctrl Pts',(1.25206542099587,1.62921138715835,8.14797786267567));
#48875=CARTESIAN_POINT('Ctrl Pts',(1.30862937348997,1.58574141785237,8.14411762025649));
#48876=CARTESIAN_POINT('Ctrl Pts',(1.36288888657392,1.53935147309315,8.14025737783731));
#48877=CARTESIAN_POINT('Ctrl Pts',(1.41454133522346,1.49032559309844,8.13639713541813));
#48878=CARTESIAN_POINT('Ctrl Pts',(1.46623000761081,1.4412653313722,8.13253418582025));
#48879=CARTESIAN_POINT('Ctrl Pts',(1.51530764476965,1.38956580912633,8.12867123622236));
#48880=CARTESIAN_POINT('Ctrl Pts',(1.56151034420752,1.33554595856261,8.12480828662448));
#48881=CARTESIAN_POINT('Ctrl Pts',(1.60778777584696,1.28143873166783,8.12093908876119));
#48882=CARTESIAN_POINT('Ctrl Pts',(1.65118070213744,1.22500407644762,8.11706989089792));
#48883=CARTESIAN_POINT('Ctrl Pts',(1.69146772913563,1.1665909667886,8.11320069303463));
#48884=CARTESIAN_POINT('Ctrl Pts',(1.69726891427347,1.15817969177384,8.1126435426363));
#48885=CARTESIAN_POINT('Ctrl Pts',(1.70300577641057,1.14972743544356,8.11208639223796));
#48886=CARTESIAN_POINT('Ctrl Pts',(1.70867773369655,1.14123528024225,8.11152924183962));
#48887=CARTESIAN_POINT('Ctrl Pts',(1.74806615162049,1.08226224125779,8.10766015897639));
#48888=CARTESIAN_POINT('Ctrl Pts',(1.78447505278231,1.0211321340826,8.10379107611316));
#48889=CARTESIAN_POINT('Ctrl Pts',(1.81766106723981,0.958178379604047,8.09992199324993));
#48890=CARTESIAN_POINT('Ctrl Pts',(1.85079763616627,0.895318423126603,8.09605867513007));
#48891=CARTESIAN_POINT('Ctrl Pts',(1.88072062542548,0.830640639033089,8.09219535701021));
#48892=CARTESIAN_POINT('Ctrl Pts',(1.90723000933527,0.764507196820929,8.08833203889035));
#48893=CARTESIAN_POINT('Ctrl Pts',(1.93370829771863,0.698451329184138,8.08447325244542));
#48894=CARTESIAN_POINT('Ctrl Pts',(1.95678075450588,0.63094364379623,8.0806144660005));
#48895=CARTESIAN_POINT('Ctrl Pts',(1.97629414719287,0.562369101454931,8.07675567955558));
#48896=CARTESIAN_POINT('Ctrl Pts',(1.99579524785997,0.493837756093833,8.0728993238658));
#48897=CARTESIAN_POINT('Ctrl Pts',(2.0117415997834,0.424241353231035,8.06904296817602));
#48898=CARTESIAN_POINT('Ctrl Pts',(2.02402930427195,0.353981550293792,8.06518661248625));
#48899=CARTESIAN_POINT('Ctrl Pts',(2.0363133788412,0.283742502853662,8.06133139600518));
#48900=CARTESIAN_POINT('Ctrl Pts',(2.04494086802811,0.212840922664285,8.05747617952411));
#48901=CARTESIAN_POINT('Ctrl Pts',(2.04985900006653,0.141688539925573,8.05362096304304));
#48902=CARTESIAN_POINT('Ctrl Pts',(2.05477732438586,0.0705333753898392,
8.04976559583716));
#48903=CARTESIAN_POINT('Ctrl Pts',(2.05598597233378,-0.00087212638403536,
8.04591022863127));
#48904=CARTESIAN_POINT('Ctrl Pts',(2.0534841811616,-0.0721129684526676,
8.04205486142539));
#48905=CARTESIAN_POINT('Ctrl Pts',(2.05097977129884,-0.143428380183379,
8.03819545870531));
#48906=CARTESIAN_POINT('Ctrl Pts',(2.04475718643642,-0.214578301673897,
8.03433605598523));
#48907=CARTESIAN_POINT('Ctrl Pts',(2.03486774836884,-0.28515050262682,8.03047665326515));
#48908=CARTESIAN_POINT('Ctrl Pts',(2.02497271082948,-0.355762662073375,
8.02661506532316));
#48909=CARTESIAN_POINT('Ctrl Pts',(2.01140677943915,-0.425795972664315,
8.02275347738118));
#48910=CARTESIAN_POINT('Ctrl Pts',(1.99427235752724,-0.494848791554304,
8.0188918894392));
#48911=CARTESIAN_POINT('Ctrl Pts',(1.97710795834521,-0.564022420764869,
8.01502354551412));
#48912=CARTESIAN_POINT('Ctrl Pts',(1.95636274535452,-0.632211668522653,
8.01115520158904));
#48913=CARTESIAN_POINT('Ctrl Pts',(1.93218867531514,-0.699031104804307,
8.00728685766396));
#48914=CARTESIAN_POINT('Ctrl Pts',(1.91783480837926,-0.738706562662871,
8.004989946392));
#48915=CARTESIAN_POINT('Ctrl Pts',(1.90227297183507,-0.777899457293998,
8.00269303512003));
#48916=CARTESIAN_POINT('Ctrl Pts',(1.88554268645341,-0.816533122452525,
8.00039612384806));
#48917=CARTESIAN_POINT('Ctrl Pts',(1.85736098084715,-0.881610468902424,
7.99652703998047));
#48918=CARTESIAN_POINT('Ctrl Pts',(1.82575101799983,-0.945354574838809,
7.99265795611289));
#48919=CARTESIAN_POINT('Ctrl Pts',(1.79086091697388,-1.00738013607351,7.9887888722453));
#48920=CARTESIAN_POINT('Ctrl Pts',(1.75602280040168,-1.06931328241617,7.98492555311343));
#48921=CARTESIAN_POINT('Ctrl Pts',(1.71791448290529,-1.12953254671932,7.98106223398155));
#48922=CARTESIAN_POINT('Ctrl Pts',(1.67673174527057,-1.18767344708128,7.97719891484968));
#48923=CARTESIAN_POINT('Ctrl Pts',(1.63559731493566,-1.2457461482397,7.97334012738632));
#48924=CARTESIAN_POINT('Ctrl Pts',(1.59139590720388,-1.30174493350011,7.96948133992297));
#48925=CARTESIAN_POINT('Ctrl Pts',(1.54436783027611,-1.35533227192016,7.96562255245962));
#48926=CARTESIAN_POINT('Ctrl Pts',(1.4973693775712,-1.40888585426597,7.961766195748));
#48927=CARTESIAN_POINT('Ctrl Pts',(1.44754810800904,-1.46003063925531,7.95790983903638));
#48928=CARTESIAN_POINT('Ctrl Pts',(1.39518511486163,-1.50846148700208,7.95405348232477));
#48929=CARTESIAN_POINT('Ctrl Pts',(1.34283759027272,-1.55687802778593,7.95019826481998));
#48930=CARTESIAN_POINT('Ctrl Pts',(1.28795018918138,-1.60258189330383,7.94634304731519));
#48931=CARTESIAN_POINT('Ctrl Pts',(1.23084019755949,-1.64530543382428,7.94248782981041));
#48932=CARTESIAN_POINT('Ctrl Pts',(1.17372797314172,-1.68803064468196,7.93863246158044));
#48933=CARTESIAN_POINT('Ctrl Pts',(1.11439337597587,-1.7277750099764,7.93477709335047));
#48934=CARTESIAN_POINT('Ctrl Pts',(1.05318464519525,-1.76431280265857,7.93092172512051));
#48935=CARTESIAN_POINT('Ctrl Pts',(0.991911845747888,-1.80088884033673,
7.92706232138287));
#48936=CARTESIAN_POINT('Ctrl Pts',(0.928761414662859,-1.83425135577758,
7.92320291764524));
#48937=CARTESIAN_POINT('Ctrl Pts',(0.864107516350061,-1.86421988045599,
7.9193435139076));
#48938=CARTESIAN_POINT('Ctrl Pts',(0.799417010575119,-1.89420537351002,
7.91548192495021));
#48939=CARTESIAN_POINT('Ctrl Pts',(0.733221793944371,-1.9207928691467,7.91162033599281));
#48940=CARTESIAN_POINT('Ctrl Pts',(0.66591484161939,-1.9438505565529,7.90775874703542));
#48941=CARTESIAN_POINT('Ctrl Pts',(0.598490133711226,-1.96694858409238,
7.90389040210937));
#48942=CARTESIAN_POINT('Ctrl Pts',(0.529950274118068,-1.98650434049851,
7.90002205718333));
#48943=CARTESIAN_POINT('Ctrl Pts',(0.460701493880856,-2.00243643994908,
7.89615371225729));
#48944=CARTESIAN_POINT('Ctrl Pts',(0.41958373573966,-2.01189642191044,7.8938568101237));
#48945=CARTESIAN_POINT('Ctrl Pts',(0.37821621810489,-2.02007982598716,7.8915599079901));
#48946=CARTESIAN_POINT('Ctrl Pts',(0.336684785059664,-2.02697827270282,
7.88926300585651));
#48947=CARTESIAN_POINT('Ctrl Pts',(0.266726007745194,-2.03859855310758,
7.88539392518447));
#48948=CARTESIAN_POINT('Ctrl Pts',(0.196027910386645,-2.04661552383361,
7.88152484451243));
#48949=CARTESIAN_POINT('Ctrl Pts',(0.124994536013101,-2.05094464295526,
7.87765576384039));
#48950=CARTESIAN_POINT('Ctrl Pts',(0.0540669978723382,-2.05526731190242,
7.87379244790819));
#48951=CARTESIAN_POINT('Ctrl Pts',(-0.0171943447640447,-2.05591300679656,
7.86992913197598));
#48952=CARTESIAN_POINT('Ctrl Pts',(-0.0883770915285675,-2.05284852149226,
7.86606581604377));
#48953=CARTESIAN_POINT('Ctrl Pts',(-0.159476341118476,-2.04978763082116,
7.86220703177099));
#48954=CARTESIAN_POINT('Ctrl Pts',(-0.230496694983797,-2.0430252253523,
7.8583482474982));
#48955=CARTESIAN_POINT('Ctrl Pts',(-0.301024244314913,-2.03258012556323,
7.85448946322541));
#48956=CARTESIAN_POINT('Ctrl Pts',(-0.371507366584102,-2.02214160540297,
7.85063310969706));
#48957=CARTESIAN_POINT('Ctrl Pts',(-0.441497820800681,-2.00802506441071,
7.84677675616871));
#48958=CARTESIAN_POINT('Ctrl Pts',(-0.510586789906049,-1.99030115622572,
7.84292040264035));
#48959=CARTESIAN_POINT('Ctrl Pts',(-0.579655349626495,-1.97258248381236,
7.83906518830693));
#48960=CARTESIAN_POINT('Ctrl Pts',(-0.647822482635188,-1.95125868044958,
7.83520997397351));
#48961=CARTESIAN_POINT('Ctrl Pts',(-0.714691238369664,-1.92645114038681,
7.83135475964009));
#48962=CARTESIAN_POINT('Ctrl Pts',(-0.781562608720652,-1.90164263033136,
7.82749939456501));
#48963=CARTESIAN_POINT('Ctrl Pts',(-0.847135046320205,-1.87335028416826,
7.82364402948994));
#48964=CARTESIAN_POINT('Ctrl Pts',(-0.911030032849573,-1.84174423896102,
7.81978866441486));
#48965=CARTESIAN_POINT('Ctrl Pts',(-0.974991900642846,-1.81010511052824,
7.81592926378546));
#48966=CARTESIAN_POINT('Ctrl Pts',(-1.03727237597784,-1.77514557483067,
7.81206986315606));
#48967=CARTESIAN_POINT('Ctrl Pts',(-1.09751690236007,-1.73708209694705,
7.80821046252666));
#48968=CARTESIAN_POINT('Ctrl Pts',(-1.15779553995399,-1.69899706704154,
7.80434887665588));
#48969=CARTESIAN_POINT('Ctrl Pts',(-1.21603553697043,-1.65780487697403,
7.8004872907851));
#48970=CARTESIAN_POINT('Ctrl Pts',(-1.27191301330507,-1.61376418633121,
7.79662570491432));
#48971=CARTESIAN_POINT('Ctrl Pts',(-1.32788825005739,-1.56964644431466,
7.79275736300744));
#48972=CARTESIAN_POINT('Ctrl Pts',(-1.38149234832285,-1.5226705721095,7.78888902110056));
#48973=CARTESIAN_POINT('Ctrl Pts',(-1.43243660198821,-1.47313371551413,
7.78502067919368));
#48974=CARTESIAN_POINT('Ctrl Pts',(-1.46268610163228,-1.44371989514897,
7.78272374875077));
#48975=CARTESIAN_POINT('Ctrl Pts',(-1.49199854774675,-1.41340383043145,
7.78042681830785));
#48976=CARTESIAN_POINT('Ctrl Pts',(-1.52032033835932,-1.38225309957004,
7.77812988786494));
#48977=CARTESIAN_POINT('Ctrl Pts',(-1.56750900270051,-1.33035096517784,
7.77430283182995));
#48978=CARTESIAN_POINT('Ctrl Pts',(-1.61213921803362,-1.27591667902572,
7.77047577579496));
#48979=CARTESIAN_POINT('Ctrl Pts',(-1.65392332358744,-1.21923549907042,
7.76664871975997));
#48980=CARTESIAN_POINT('Ctrl Pts',(-1.69565022628001,-1.16263191622123,
7.76282690300322));
#48981=CARTESIAN_POINT('Ctrl Pts',(-1.73453845065562,-1.10378793291417,
7.75900508624648));
#48982=CARTESIAN_POINT('Ctrl Pts',(-1.77033843346293,-1.04302415767997,
7.75518326948973));
#48983=CARTESIAN_POINT('Ctrl Pts',(-1.80610200917414,-0.98232217668228,
7.75136533936195));
#48984=CARTESIAN_POINT('Ctrl Pts',(-1.83878332051712,-0.91970470131575,
7.74754740923417));
#48985=CARTESIAN_POINT('Ctrl Pts',(-1.8681753626088,-0.855522283194004,
7.74372947910639));
#48986=CARTESIAN_POINT('Ctrl Pts',(-1.89884344211489,-0.788553424898569,
7.73974579589233));
#48987=CARTESIAN_POINT('Ctrl Pts',(-1.92592979667686,-0.719881098031171,
7.73576211267827));
#48988=CARTESIAN_POINT('Ctrl Pts',(-1.94925262780642,-0.649932116062723,
7.73177842946421));
#48989=CARTESIAN_POINT('Ctrl Pts',(-1.97158882915295,-0.582942198048359,
7.72796326869424));
#48990=CARTESIAN_POINT('Ctrl Pts',(-1.99047337491429,-0.514781984415854,
7.72414810792428));
#48991=CARTESIAN_POINT('Ctrl Pts',(-2.00579666901848,-0.445844462850394,
7.72033294715431));
#48992=CARTESIAN_POINT('Ctrl Pts',(-2.02112012375057,-0.376906218640789,
7.71651774639156));
#48993=CARTESIAN_POINT('Ctrl Pts',(-2.03288215514213,-0.307191137845921,
7.71270254562881));
#48994=CARTESIAN_POINT('Ctrl Pts',(-2.04102422708131,-0.237102650696173,
7.70888734486606));
#48995=CARTESIAN_POINT('Ctrl Pts',(-2.04917190604306,-0.166965897241075,
7.70506951677245));
#48996=CARTESIAN_POINT('Ctrl Pts',(-2.05369461174166,-0.0964557197208807,
7.70125168867884));
#48997=CARTESIAN_POINT('Ctrl Pts',(-2.05458575673003,-0.0259794292098742,
7.69743386058524));
#48998=CARTESIAN_POINT('Ctrl Pts',(-2.05470313267573,-0.0166967408083679,
7.69693100056938));
#48999=CARTESIAN_POINT('Ctrl Pts',(-2.05475758060194,-0.0074146383491741,
7.69642814055353));
#49000=CARTESIAN_POINT('Ctrl Pts',(-2.05474915275033,0.00186595063910761,
7.69592528053768));
#49001=CARTESIAN_POINT('Ctrl Pts',(-2.05474915274975,0.00186595128382797,
7.69592528050275));
#49002=CARTESIAN_POINT('Ctrl Pts',(-2.05466653542133,0.0928425416364572,
7.69099579922465));
#49003=CARTESIAN_POINT('Ctrl Pts',(-2.04853795670126,0.183549917638068,
7.68606631794656));
#49004=CARTESIAN_POINT('Ctrl Pts',(-2.03649277600636,0.273303376806667,
7.68113683666846));
#49005=CARTESIAN_POINT('Ctrl Pts',(-2.0249756981114,0.359121730783211,7.67642348107011));
#49006=CARTESIAN_POINT('Ctrl Pts',(-2.00804990481639,0.444068412205174,
7.67171012547175));
#49007=CARTESIAN_POINT('Ctrl Pts',(-1.9858683953167,0.527564478506904,7.66699676987339));
#49008=CARTESIAN_POINT('Ctrl Pts',(-1.96766008569713,0.596104549112073,
7.66312768070779));
#49009=CARTESIAN_POINT('Ctrl Pts',(-1.9458635701162,0.663835094034513,7.65925859154218));
#49010=CARTESIAN_POINT('Ctrl Pts',(-1.92056812646636,0.730353088650609,
7.65538950237658));
#49011=CARTESIAN_POINT('Ctrl Pts',(-1.89531037146572,0.796771975561802,
7.65152617791494));
#49012=CARTESIAN_POINT('Ctrl Pts',(-1.86656420769144,0.861981447908525,
7.6476628534533));
#49013=CARTESIAN_POINT('Ctrl Pts',(-1.83446913779108,0.925591997044075,
7.64379952899166));
#49014=CARTESIAN_POINT('Ctrl Pts',(-1.80241171513912,0.989127931537845,
7.63994073617728));
#49015=CARTESIAN_POINT('Ctrl Pts',(-1.76701340693965,1.0510682366476,7.6360819433629));
#49016=CARTESIAN_POINT('Ctrl Pts',(-1.72846175085154,1.11104344574963,7.63222315054852));
#49017=CARTESIAN_POINT('Ctrl Pts',(-1.6899343793302,1.17098087510061,7.62836678847568));
#49018=CARTESIAN_POINT('Ctrl Pts',(-1.64825786288973,1.22895525666185,7.62451042640283));
#49019=CARTESIAN_POINT('Ctrl Pts',(-1.60366488094096,1.28462310119997,7.62065406432999));
#49020=CARTESIAN_POINT('Ctrl Pts',(-1.55908507216608,1.3402745009487,7.6167988414617));
#49021=CARTESIAN_POINT('Ctrl Pts',(-1.51159081184357,1.39362033745739,7.61294361859342));
#49022=CARTESIAN_POINT('Ctrl Pts',(-1.46145613665084,1.44434882322297,7.60908839572513));
#49023=CARTESIAN_POINT('Ctrl Pts',(-1.41131950144824,1.4950792922134,7.60523302213731));
#49024=CARTESIAN_POINT('Ctrl Pts',(-1.35854258947012,1.54319186334069,7.60137764854948));
#49025=CARTESIAN_POINT('Ctrl Pts',(-1.30343627122762,1.58841161206667,7.59752227496166));
#49026=CARTESIAN_POINT('Ctrl Pts',(-1.24827227259226,1.63367869280384,7.59366286591165));
#49027=CARTESIAN_POINT('Ctrl Pts',(-1.19077437676783,1.67604659788638,7.58980345686166));
#49028=CARTESIAN_POINT('Ctrl Pts',(-1.13128581116102,1.71528131102911,7.58594404781165));
#49029=CARTESIAN_POINT('Ctrl Pts',(-1.07176356305579,1.75453823891429,7.58208245355954));
#49030=CARTESIAN_POINT('Ctrl Pts',(-1.01024882052389,1.79065819725059,7.57822085930742));
#49031=CARTESIAN_POINT('Ctrl Pts',(-0.947110636835177,1.82345249570524,
7.57435926505531));
#49032=CARTESIAN_POINT('Ctrl Pts',(-0.883861992499758,1.85630416798986,
7.57049091491993));
#49033=CARTESIAN_POINT('Ctrl Pts',(-0.818984678742866,1.88581836284658,
7.56662256478455));
#49034=CARTESIAN_POINT('Ctrl Pts',(-0.752868343745366,1.91185428824639,
7.56275421464917));
#49035=CARTESIAN_POINT('Ctrl Pts',(-0.713611404714169,1.92731326273552,
7.56045736039339));
#49036=CARTESIAN_POINT('Ctrl Pts',(-0.673917976614465,1.94154693435799,
7.55816050613761));
#49037=CARTESIAN_POINT('Ctrl Pts',(-0.633871702905928,1.95453427361997,
7.55586365188183));
#49038=CARTESIAN_POINT('Ctrl Pts',(-0.56641216747749,1.97641196140288,7.55199450984455));
#49039=CARTESIAN_POINT('Ctrl Pts',(-0.497686524259488,1.99483591590095,
7.54812536780728));
#49040=CARTESIAN_POINT('Ctrl Pts',(-0.428081808244282,2.00966254081383,
7.54425622577));
#49041=CARTESIAN_POINT('Ctrl Pts',(-0.355888897998268,2.02504048160384,
7.54024321286201));
#49042=CARTESIAN_POINT('Ctrl Pts',(-0.282750718369647,2.03654804692583,
7.53623019995401));
#49043=CARTESIAN_POINT('Ctrl Pts',(-0.209119137405439,2.04408090565682,
7.53221718704602));
#49044=CARTESIAN_POINT('Ctrl Pts',(-0.138320348723011,2.05132395634901,
7.52835856484706));
#49045=CARTESIAN_POINT('Ctrl Pts',(-0.0670659642655545,2.05489247764792,
7.5244999426481));
#49046=CARTESIAN_POINT('Ctrl Pts',(0.00423168083114419,2.05474564250112,
7.52064132044915));
#49047=CARTESIAN_POINT('Ctrl Pts',(0.0754847679454185,2.05459889912001,
7.51678510972423));
#49048=CARTESIAN_POINT('Ctrl Pts',(0.14678057739818,2.05074140756313,7.51292889899931));
#49049=CARTESIAN_POINT('Ctrl Pts',(0.217704390364775,2.04318436782291,7.50907268827439));
#49050=CARTESIAN_POINT('Ctrl Pts',(0.288607604665075,2.03562952290179,7.50521759752307));
#49051=CARTESIAN_POINT('Ctrl Pts',(0.359138554266875,2.02437731495336,7.50136250677175));
#49052=CARTESIAN_POINT('Ctrl Pts',(0.428886997541334,2.00949085736661,7.49750741602043));
#49053=CARTESIAN_POINT('Ctrl Pts',(0.498638515149956,1.99460374362262,7.4936521553465));
#49054=CARTESIAN_POINT('Ctrl Pts',(0.567606983521711,1.97608216631118,7.48979689467257));
#49055=CARTESIAN_POINT('Ctrl Pts',(0.635393421224808,1.95404011288516,7.48594163399864));
#49056=CARTESIAN_POINT('Ctrl Pts',(0.703245154887088,1.93197682723231,7.48208265970659));
#49057=CARTESIAN_POINT('Ctrl Pts',(0.769912123410777,1.90638644967083,7.47822368541454));
#49058=CARTESIAN_POINT('Ctrl Pts',(0.835012522395941,1.87743219583078,7.47436471112249));
#49059=CARTESIAN_POINT('Ctrl Pts',(0.900150331727464,1.84846130324992,7.47050351924703));
#49060=CARTESIAN_POINT('Ctrl Pts',(0.96371934678332,1.81612290688363,7.46664232737156));
#49061=CARTESIAN_POINT('Ctrl Pts',(1.02536206200968,1.78062635167832,7.4627811354961));
#49062=CARTESIAN_POINT('Ctrl Pts',(1.08709925014214,1.74507539486669,7.45891402600302));
#49063=CARTESIAN_POINT('Ctrl Pts',(1.14690384139378,1.70635688624157,7.45504691650995));
#49064=CARTESIAN_POINT('Ctrl Pts',(1.20444782450804,1.66472310025958,7.45117980701687));
#49065=CARTESIAN_POINT('Ctrl Pts',(1.22049823284037,1.65311043062381,7.45010117667064));
#49066=CARTESIAN_POINT('Ctrl Pts',(1.2363729737087,1.64127119153606,7.44902254632442));
#49067=CARTESIAN_POINT('Ctrl Pts',(1.25206542099588,1.62921138715835,7.44794391597819));
#49068=CARTESIAN_POINT('',(-2.05474920663131,-0.0018056433735876,7.75407471946232));
#49069=CARTESIAN_POINT('Ctrl Pts',(-2.05549758983786,-0.00179924508355834,
7.75407433641555));
#49070=CARTESIAN_POINT('Ctrl Pts',(-2.05046538848476,0.546255807336168,
7.72432225384672));
#49071=CARTESIAN_POINT('Ctrl Pts',(-1.5430773566099,1.78491604847996,7.65752579861402));
#49072=CARTESIAN_POINT('Ctrl Pts',(0.122430998286581,2.24741296338508,7.57484553971088));
#49073=CARTESIAN_POINT('Ctrl Pts',(1.0177547725044,1.80678822318179,7.5219173633766));
#49074=CARTESIAN_POINT('Ctrl Pts',(1.25017377660034,1.6267706489614,7.50603355970618));
#49075=CARTESIAN_POINT('Ctrl Pts',(1.25206542099588,1.62921138715834,8.20601752898817));
#49076=CARTESIAN_POINT('Ctrl Pts',(1.31084998697262,1.58403485394241,8.2019897386418));
#49077=CARTESIAN_POINT('Ctrl Pts',(1.36727460896177,1.53560488054058,8.19796194829543));
#49078=CARTESIAN_POINT('Ctrl Pts',(1.42096375839729,1.48420334180376,8.19393415794906));
#49079=CARTESIAN_POINT('Ctrl Pts',(1.47238898730883,1.43496926147769,8.19007620820041));
#49080=CARTESIAN_POINT('Ctrl Pts',(1.52130440251306,1.38300955213352,8.18621825845176));
#49081=CARTESIAN_POINT('Ctrl Pts',(1.56741308865996,1.32861347727525,8.18236030870311));
#49082=CARTESIAN_POINT('Ctrl Pts',(1.61349719502314,1.27424640007159,8.17850441556415));
#49083=CARTESIAN_POINT('Ctrl Pts',(1.65677722761158,1.21744590438802,8.17464852242519));
#49084=CARTESIAN_POINT('Ctrl Pts',(1.69699459227755,1.15853654076198,8.17079262928623));
#49085=CARTESIAN_POINT('Ctrl Pts',(1.73720397099022,1.09963887475538,8.16693750181112));
#49086=CARTESIAN_POINT('Ctrl Pts',(1.77435161589447,1.03863357366415,8.16308237433602));
#49087=CARTESIAN_POINT('Ctrl Pts',(1.80822157548012,0.975875143893002,8.15922724686091));
#49088=CARTESIAN_POINT('Ctrl Pts',(1.84209613916057,0.913108183088351,8.15537159534112));
#49089=CARTESIAN_POINT('Ctrl Pts',(1.87269190463754,0.848588049220232,8.15151594382132));
#49090=CARTESIAN_POINT('Ctrl Pts',(1.89983912488471,0.782693338452113,8.14766029230153));
#49091=CARTESIAN_POINT('Ctrl Pts',(1.92701636873427,0.716725751102979,8.14380037660489));
#49092=CARTESIAN_POINT('Ctrl Pts',(1.95073727309514,0.649381003814497,8.13994046090824));
#49093=CARTESIAN_POINT('Ctrl Pts',(1.97088081729802,0.581056250725073,8.1360805452116));
#49094=CARTESIAN_POINT('Ctrl Pts',(1.99103751614682,0.512686878479993,8.13221810881533));
#49095=CARTESIAN_POINT('Ctrl Pts',(2.00761209388234,0.443336699235825,8.12835567241907));
#49096=CARTESIAN_POINT('Ctrl Pts',(2.02053448880331,0.373413901798468,8.1244932360228));
#49097=CARTESIAN_POINT('Ctrl Pts',(2.03347837417841,0.303374819981901,8.12062437624196));
#49098=CARTESIAN_POINT('Ctrl Pts',(2.0427578967901,0.232761700841292,8.11675551646111));
#49099=CARTESIAN_POINT('Ctrl Pts',(2.04835483194737,0.161987792558138,8.11288665668027));
#49100=CARTESIAN_POINT('Ctrl Pts',(2.05006001135172,0.140425596931635,8.11170795801194));
#49101=CARTESIAN_POINT('Ctrl Pts',(2.05142374079295,0.118848470036735,8.11052925934361));
#49102=CARTESIAN_POINT('Ctrl Pts',(2.05244646447078,0.0972680470730852,
8.10935056067527));
#49103=CARTESIAN_POINT('Ctrl Pts',(2.05580355895899,0.0264302239588488,
8.10548147766828));
#49104=CARTESIAN_POINT('Ctrl Pts',(2.0554955948121,-0.0447203466931932,
8.10161239466129));
#49105=CARTESIAN_POINT('Ctrl Pts',(2.05148587354752,-0.115772505954377,
8.0977433116543));
#49106=CARTESIAN_POINT('Ctrl Pts',(2.04748212656679,-0.186718801057286,
8.09387999338719));
#49107=CARTESIAN_POINT('Ctrl Pts',(2.03978759759765,-0.257566494761722,
8.09001667512007));
#49108=CARTESIAN_POINT('Ctrl Pts',(2.0284175491114,-0.32790213319968,8.08615335685296));
#49109=CARTESIAN_POINT('Ctrl Pts',(2.01706083768672,-0.398155267966526,
8.08229457025637));
#49110=CARTESIAN_POINT('Ctrl Pts',(2.00203724775699,-0.467897063312294,
8.07843578365979));
#49111=CARTESIAN_POINT('Ctrl Pts',(1.98341388769491,-0.536718653112556,
8.0745769970632));
#49112=CARTESIAN_POINT('Ctrl Pts',(1.96480225898364,-0.605496890359343,
8.07072064121913));
#49113=CARTESIAN_POINT('Ctrl Pts',(1.94259548559621,-0.673355604291606,
8.06686428537505));
#49114=CARTESIAN_POINT('Ctrl Pts',(1.9169115576161,-0.739897048769495,8.06300792953097));
#49115=CARTESIAN_POINT('Ctrl Pts',(1.89123521692681,-0.806418836234995,
8.05915271289322));
#49116=CARTESIAN_POINT('Ctrl Pts',(1.86208393572596,-0.871623673837934,
8.05529749625548));
#49117=CARTESIAN_POINT('Ctrl Pts',(1.82962470828325,-0.93513153584906,8.05144227961773));
#49118=CARTESIAN_POINT('Ctrl Pts',(1.79716421178593,-0.998641880819646,
8.04758691225303));
#49119=CARTESIAN_POINT('Ctrl Pts',(1.76139573532314,-1.06045468691979,8.04373154488833));
#49120=CARTESIAN_POINT('Ctrl Pts',(1.72253252524606,-1.12021393580397,8.03987617752363));
#49121=CARTESIAN_POINT('Ctrl Pts',(1.68362863600564,-1.18003573629524,8.0360167746426));
#49122=CARTESIAN_POINT('Ctrl Pts',(1.64162381208422,-1.23779928058551,8.03215737176157));
#49123=CARTESIAN_POINT('Ctrl Pts',(1.59677450687319,-1.29317776685955,8.02829796888054));
#49124=CARTESIAN_POINT('Ctrl Pts',(1.5518998076435,-1.34858760885489,8.02443638077617));
#49125=CARTESIAN_POINT('Ctrl Pts',(1.50417774611702,-1.40160934328618,8.02057479267179));
#49126=CARTESIAN_POINT('Ctrl Pts',(1.45390309217126,-1.45195156981039,8.01671320456742));
#49127=CARTESIAN_POINT('Ctrl Pts',(1.40354048095847,-1.50238187182222,8.01284486047948));
#49128=CARTESIAN_POINT('Ctrl Pts',(1.35061672195277,-1.55012298092874,8.00897651639153));
#49129=CARTESIAN_POINT('Ctrl Pts',(1.2954606925744,-1.59492293120848,8.00510817230359));
#49130=CARTESIAN_POINT('Ctrl Pts',(1.26271065132406,-1.62152383479437,8.0028112624303));
#49131=CARTESIAN_POINT('Ctrl Pts',(1.22917418557495,-1.64708859639868,8.000514352557));
#49132=CARTESIAN_POINT('Ctrl Pts',(1.19492467762601,-1.67157188816407,7.99821744268371));
#49133=CARTESIAN_POINT('Ctrl Pts',(1.13723230782943,-1.71281333094543,7.99434836012647));
#49134=CARTESIAN_POINT('Ctrl Pts',(1.07728933315006,-1.75114526561477,7.99047927756924));
#49135=CARTESIAN_POINT('Ctrl Pts',(1.01542127717664,-1.7863138560614,7.986610195012));
#49136=CARTESIAN_POINT('Ctrl Pts',(0.953645401522744,-1.82143004706128,
7.98274687719491));
#49137=CARTESIAN_POINT('Ctrl Pts',(0.889950556900871,-1.8533920113503,7.97888355937782));
#49138=CARTESIAN_POINT('Ctrl Pts',(0.824692377558463,-1.88198832219995,
7.97502024156073));
#49139=CARTESIAN_POINT('Ctrl Pts',(0.759510746009658,-1.91055108959921,
7.97116145541244));
#49140=CARTESIAN_POINT('Ctrl Pts',(0.692769865048533,-1.93575585141558,
7.96730266926414));
#49141=CARTESIAN_POINT('Ctrl Pts',(0.624849634808915,-1.95743722667655,
7.96344388311585));
#49142=CARTESIAN_POINT('Ctrl Pts',(0.556972189314334,-1.97910494426719,
7.95958752771876));
#49143=CARTESIAN_POINT('Ctrl Pts',(0.487917330132223,-1.99725353132691,
7.95573117232168));
#49144=CARTESIAN_POINT('Ctrl Pts',(0.418083212371424,-2.01176638555106,
7.95187481692459));
#49145=CARTESIAN_POINT('Ctrl Pts',(0.348269724278994,-2.02627495253885,
7.94801960073188));
#49146=CARTESIAN_POINT('Ctrl Pts',(0.277677909981633,-2.03714982015024,
7.94416438453917));
#49147=CARTESIAN_POINT('Ctrl Pts',(0.206717615993114,-2.04432516732004,
7.94030916834647));
#49148=CARTESIAN_POINT('Ctrl Pts',(0.135754547630296,-2.0515007950284,7.93645380142422));
#49149=CARTESIAN_POINT('Ctrl Pts',(0.0644234545139279,-2.05497656844665,
7.93259843450196));
#49150=CARTESIAN_POINT('Ctrl Pts',(-0.00686090002047612,-2.05473854554561,
7.92874306757971));
#49151=CARTESIAN_POINT('Ctrl Pts',(-0.0782198699361268,-2.05450027349917,
7.92488366513417));
#49152=CARTESIAN_POINT('Ctrl Pts',(-0.149531516833611,-2.05054044676251,
7.92102426268864));
#49153=CARTESIAN_POINT('Ctrl Pts',(-0.220382188502956,-2.04289726944128,
7.9171648602431));
#49154=CARTESIAN_POINT('Ctrl Pts',(-0.291272976427429,-2.03524976448781,
7.91330327257095));
#49155=CARTESIAN_POINT('Ctrl Pts',(-0.361701789698669,-2.02391483449982,
7.9094416848988));
#49156=CARTESIAN_POINT('Ctrl Pts',(-0.431263935949848,-2.00898207559178,
7.90558009722665));
#49157=CARTESIAN_POINT('Ctrl Pts',(-0.500947783801651,-1.99402319125835,
7.90171175356111));
#49158=CARTESIAN_POINT('Ctrl Pts',(-0.569761468208529,-1.97545403738304,
7.89784340989556));
#49159=CARTESIAN_POINT('Ctrl Pts',(-0.637314927708768,-1.95341425340852,
7.89397506623002));
#49160=CARTESIAN_POINT('Ctrl Pts',(-0.677426275066602,-1.94032764855906,
7.89167815238407));
#49161=CARTESIAN_POINT('Ctrl Pts',(-0.717093664948321,-1.92601835521994,
7.88938123853811));
#49162=CARTESIAN_POINT('Ctrl Pts',(-0.756239214398889,-1.91052343955926,
7.88708432469216));
#49163=CARTESIAN_POINT('Ctrl Pts',(-0.822178724847217,-1.88442271629842,
7.8832152418291));
#49164=CARTESIAN_POINT('Ctrl Pts',(-0.886894544863902,-1.85485312506099,
7.87934615896604));
#49165=CARTESIAN_POINT('Ctrl Pts',(-0.949996860707018,-1.8219504732969,
7.87547707610299));
#49166=CARTESIAN_POINT('Ctrl Pts',(-1.01300515719984,-1.78909684486739,
7.8716137579833));
#49167=CARTESIAN_POINT('Ctrl Pts',(-1.07440429424018,-1.75292023624344,
7.86775043986362));
#49168=CARTESIAN_POINT('Ctrl Pts',(-1.13382375618332,-1.71360475384913,
7.86388712174393));
#49169=CARTESIAN_POINT('Ctrl Pts',(-1.19317351905456,-1.67433538854415,
7.8600283352992));
#49170=CARTESIAN_POINT('Ctrl Pts',(-1.25054781626174,-1.63193472972845,
7.85616954885447));
#49171=CARTESIAN_POINT('Ctrl Pts',(-1.30560165538449,-1.58663224471119,
7.85231076240974));
#49172=CARTESIAN_POINT('Ctrl Pts',(-1.36062081458777,-1.54135829696867,
7.84845440672016));
#49173=CARTESIAN_POINT('Ctrl Pts',(-1.41332204151208,-1.4931864575685,7.84459805103058));
#49174=CARTESIAN_POINT('Ctrl Pts',(-1.46339142316949,-1.44238798701805,
7.840741695341));
#49175=CARTESIAN_POINT('Ctrl Pts',(-1.51344601379599,-1.39160452287917,
7.83688647886014));
#49176=CARTESIAN_POINT('Ctrl Pts',(-1.56086996183677,-1.33819631382218,
7.83303126237929));
#49177=CARTESIAN_POINT('Ctrl Pts',(-1.60538567611349,-1.28247198543657,
7.82917604589843));
#49178=CARTESIAN_POINT('Ctrl Pts',(-1.64990313079121,-1.2267454784343,7.82532067869276));
#49179=CARTESIAN_POINT('Ctrl Pts',(-1.69151182448562,-1.16870305324428,
7.8214653114871));
#49180=CARTESIAN_POINT('Ctrl Pts',(-1.72997508452341,-1.10868560441101,
7.81760994428143));
#49181=CARTESIAN_POINT('Ctrl Pts',(-1.7684786050665,-1.04860533373648,7.81375054156157));
#49182=CARTESIAN_POINT('Ctrl Pts',(-1.80382985691664,-0.986546322444212,
7.8098911388417));
#49183=CARTESIAN_POINT('Ctrl Pts',(-1.8358365797444,-0.922876814624989,
7.80603173612184));
#49184=CARTESIAN_POINT('Ctrl Pts',(-1.86786142501153,-0.859171256667153,
7.80217014818007));
#49185=CARTESIAN_POINT('Ctrl Pts',(-1.89653777611546,-0.793853831934715,
7.79830856023831));
#49186=CARTESIAN_POINT('Ctrl Pts',(-1.92172140849375,-0.727313131076846,
7.79444697229655));
#49187=CARTESIAN_POINT('Ctrl Pts',(-1.94694910051717,-0.6606560149369,7.7905786283717));
#49188=CARTESIAN_POINT('Ctrl Pts',(-1.96867172566271,-0.59277181259146,
7.78671028444685));
#49189=CARTESIAN_POINT('Ctrl Pts',(-1.98679503793688,-0.524063965303268,
7.782841940522));
#49190=CARTESIAN_POINT('Ctrl Pts',(-1.99755613909279,-0.483267223312214,
7.7805450292482));
#49191=CARTESIAN_POINT('Ctrl Pts',(-2.00704922822886,-0.44218030315848,
7.7782481179744));
#49192=CARTESIAN_POINT('Ctrl Pts',(-2.01526320370241,-0.400888740554147,
7.7759512067006));
#49193=CARTESIAN_POINT('Ctrl Pts',(-2.03523538600266,-0.300488804073767,
7.77036629463998));
#49194=CARTESIAN_POINT('Ctrl Pts',(-2.04770968318372,-0.198551497556471,
7.76478138257937));
#49195=CARTESIAN_POINT('Ctrl Pts',(-2.05250622663751,-0.0959987089196925,
7.75919647051875));
#49196=CARTESIAN_POINT('Ctrl Pts',(-2.05397248079007,-0.0646493729564441,
7.75748922016661));
#49197=CARTESIAN_POINT('Ctrl Pts',(-2.05472158081271,-0.0332427087908737,
7.75578196981447));
#49198=CARTESIAN_POINT('Ctrl Pts',(-2.05474920663131,-0.0018056433735876,
7.75407471946232));
#49199=CARTESIAN_POINT('Origin',(0.,0.,18.5459252805377));
#49200=CARTESIAN_POINT('',(1.25206542099588,1.62921138715834,8.90613916330362));
#49201=CARTESIAN_POINT('',(1.25051812704728,1.62722676461094,8.84785675763342));
#49202=CARTESIAN_POINT('',(1.25206542099588,1.62921138715835,18.5459252805377));
#49203=CARTESIAN_POINT('',(-2.05451192518334,-0.000653016369823574,8.39592531845778));
#49204=CARTESIAN_POINT('Ctrl Pts',(1.25051812704735,1.62722676461089,8.84785675763342));
#49205=CARTESIAN_POINT('Ctrl Pts',(1.58873501929067,1.36387014211555,8.82468048835194));
#49206=CARTESIAN_POINT('Ctrl Pts',(2.26673114618394,0.412739085322609,8.76445984640662));
#49207=CARTESIAN_POINT('Ctrl Pts',(1.84698007748907,-1.57690952787191,8.6671948317974));
#49208=CARTESIAN_POINT('Ctrl Pts',(-0.323048206860337,-2.40699375331995,
8.55606171380587));
#49209=CARTESIAN_POINT('Ctrl Pts',(-1.84811520434371,-1.28994634362903,
8.46563869868007));
#49210=CARTESIAN_POINT('Ctrl Pts',(-2.05243358460716,-0.303009497723999,
8.41226005621812));
#49211=CARTESIAN_POINT('Ctrl Pts',(-2.05157518345028,-0.000660745958733733,
8.39592578642004));
#49212=CARTESIAN_POINT('Ctrl Pts',(-2.05474989643199,-0.000652390022636229,
8.39592528053767));
#49213=CARTESIAN_POINT('Ctrl Pts',(-2.05477316158455,0.0726229026154983,
8.3919727248606));
#49214=CARTESIAN_POINT('Ctrl Pts',(-2.05087243556388,0.145865091084949,
8.38802016918352));
#49215=CARTESIAN_POINT('Ctrl Pts',(-2.04308448283436,0.218639791669856,
8.38406761350645));
#49216=CARTESIAN_POINT('Ctrl Pts',(-2.03529044046684,0.291471397015037,
8.38011196720542));
#49217=CARTESIAN_POINT('Ctrl Pts',(-2.02360317415942,0.3638343400088,8.37615632090438));
#49218=CARTESIAN_POINT('Ctrl Pts',(-2.00811093276723,0.43530224465388,8.37220067460335));
#49219=CARTESIAN_POINT('Ctrl Pts',(-1.99259007572178,0.506902157362047,
8.36823772184484));
#49220=CARTESIAN_POINT('Ctrl Pts',(-1.97325031090492,0.577603291101814,
8.36427476908632));
#49221=CARTESIAN_POINT('Ctrl Pts',(-1.95023029805764,0.646992540171847,
8.36031181632781));
#49222=CARTESIAN_POINT('Ctrl Pts',(-1.92718562648172,0.716456118073708,
8.35634461850752));
#49223=CARTESIAN_POINT('Ctrl Pts',(-1.90045301963665,0.784604594021689,
8.35237742068722));
#49224=CARTESIAN_POINT('Ctrl Pts',(-1.87021901282319,0.851045478558368,
8.34841022286693));
#49225=CARTESIAN_POINT('Ctrl Pts',(-1.83992267930305,0.917623329443823,
8.34443484675996));
#49226=CARTESIAN_POINT('Ctrl Pts',(-1.80611074383731,0.982486162956809,
8.34045947065301));
#49227=CARTESIAN_POINT('Ctrl Pts',(-1.76901511959829,1.04526698461811,8.33648409454604));
#49228=CARTESIAN_POINT('Ctrl Pts',(-1.76065231207126,1.05942024227889,8.33558788897161));
#49229=CARTESIAN_POINT('Ctrl Pts',(-1.75212278665681,1.0734678111016,8.33469168339718));
#49230=CARTESIAN_POINT('Ctrl Pts',(-1.74342948855721,1.0874057112822,8.33379547782275));
#49231=CARTESIAN_POINT('Ctrl Pts',(-1.70589893428835,1.14757816978168,8.32992639481628));
#49232=CARTESIAN_POINT('Ctrl Pts',(-1.66517604049293,1.20592321640611,8.32605731180981));
#49233=CARTESIAN_POINT('Ctrl Pts',(-1.62146448556,1.26208180581436,8.32218822880335));
#49234=CARTESIAN_POINT('Ctrl Pts',(-1.57781805865443,1.31815672173736,8.31832491053676));
#49235=CARTESIAN_POINT('Ctrl Pts',(-1.53119210555474,1.3720512666889,8.31446159227018));
#49236=CARTESIAN_POINT('Ctrl Pts',(-1.48183434704247,1.42343406254916,8.31059827400359));
#49237=CARTESIAN_POINT('Ctrl Pts',(-1.43253448515796,1.4747565864138,8.30673948740754));
#49238=CARTESIAN_POINT('Ctrl Pts',(-1.38050951779156,1.52357286486347,8.30288070081147));
#49239=CARTESIAN_POINT('Ctrl Pts',(-1.32604719870036,1.56958478245647,8.29902191421542));
#49240=CARTESIAN_POINT('Ctrl Pts',(-1.27161918687533,1.6155677159164,8.29516555837187));
#49241=CARTESIAN_POINT('Ctrl Pts',(-1.21475723964478,1.65874948054823,8.29130920252832));
#49242=CARTESIAN_POINT('Ctrl Pts',(-1.15578463524892,1.69887004783254,8.28745284668477));
#49243=CARTESIAN_POINT('Ctrl Pts',(-1.0968294519539,1.73897876309748,8.28359763004755));
#49244=CARTESIAN_POINT('Ctrl Pts',(-1.03576525076006,1.77602780321708,8.27974241341033));
#49245=CARTESIAN_POINT('Ctrl Pts',(-0.972945535912756,1.80979958742603,
8.27588719677311));
#49246=CARTESIAN_POINT('Ctrl Pts',(-0.91012336501046,1.84357269200645,8.27203182940893));
#49247=CARTESIAN_POINT('Ctrl Pts',(-0.845545973103761,1.87406805820691,
8.26817646204476));
#49248=CARTESIAN_POINT('Ctrl Pts',(-0.779591250925281,1.90111415858721,
8.26432109468059));
#49249=CARTESIAN_POINT('Ctrl Pts',(-0.713567492171636,1.92818856884556,
8.26046169180008));
#49250=CARTESIAN_POINT('Ctrl Pts',(-0.646163975594236,1.95180632135027,
8.25660228891957));
#49251=CARTESIAN_POINT('Ctrl Pts',(-0.577777511014386,1.97184449444322,
8.25274288603907));
#49252=CARTESIAN_POINT('Ctrl Pts',(-0.509352325496681,1.9918940133026,8.24888129793521));
#49253=CARTESIAN_POINT('Ctrl Pts',(-0.439943556940449,2.00835980586299,
8.24501970983135));
#49254=CARTESIAN_POINT('Ctrl Pts',(-0.369959393931269,2.02116986157572,
8.2411581217275));
#49255=CARTESIAN_POINT('Ctrl Pts',(-0.299852791178743,2.03400232892939,
8.23728977764006));
#49256=CARTESIAN_POINT('Ctrl Pts',(-0.229169266026279,2.04316622748358,
8.23342143355262));
#49257=CARTESIAN_POINT('Ctrl Pts',(-0.158322630141146,2.04864138083882,
8.22955308946518));
#49258=CARTESIAN_POINT('Ctrl Pts',(-0.116255964376895,2.05189236718878,
8.22725617958718));
#49259=CARTESIAN_POINT('Ctrl Pts',(-0.0741318222005703,2.05384383432988,
8.22495926970918));
#49260=CARTESIAN_POINT('Ctrl Pts',(-0.0320363413327623,2.05450023979897,
8.22266235983118));
#49261=CARTESIAN_POINT('Ctrl Pts',(0.0388583812382214,2.0556057191204,8.21879403987821));
#49262=CARTESIAN_POINT('Ctrl Pts',(0.109949219424514,2.05303950652832,8.21492571992523));
#49263=CARTESIAN_POINT('Ctrl Pts',(0.180824300462245,2.04677798865982,8.21105739997225));
#49264=CARTESIAN_POINT('Ctrl Pts',(0.251600846644332,2.04052517593493,8.20719445799334));
#49265=CARTESIAN_POINT('Ctrl Pts',(0.322161751218005,2.03058729266115,8.20333151601444));
#49266=CARTESIAN_POINT('Ctrl Pts',(0.392094373796085,2.01699270314433,8.19946857403553));
#49267=CARTESIAN_POINT('Ctrl Pts',(0.461953175883252,2.00341246400126,8.19560970975688));
#49268=CARTESIAN_POINT('Ctrl Pts',(0.53118453789183,1.98618327218889,8.19175084547824));
#49269=CARTESIAN_POINT('Ctrl Pts',(0.599381904191762,1.96538517737045,8.18789198119959));
#49270=CARTESIAN_POINT('Ctrl Pts',(0.667536212769918,1.94460021383007,8.18403555328929));
#49271=CARTESIAN_POINT('Ctrl Pts',(0.734657357271598,1.92025095925107,8.18017912537899));
#49272=CARTESIAN_POINT('Ctrl Pts',(0.800351513123296,1.89246797012294,8.17632269746868));
#49273=CARTESIAN_POINT('Ctrl Pts',(0.866021363619131,1.86469526007411,8.17246769634972));
#49274=CARTESIAN_POINT('Ctrl Pts',(0.930264828230893,1.83349153086389,8.16861269523076));
#49275=CARTESIAN_POINT('Ctrl Pts',(0.992707432808873,1.79903571819628,8.1647576941118));
#49276=CARTESIAN_POINT('Ctrl Pts',(1.05516574029779,1.76457124066658,8.16090172354674));
#49277=CARTESIAN_POINT('Ctrl Pts',(1.11582185755692,1.72685328081183,8.15704575298169));
#49278=CARTESIAN_POINT('Ctrl Pts',(1.17432654764215,1.6861063792071,8.15318978241663));
#49279=CARTESIAN_POINT('Ctrl Pts',(1.20068582122837,1.66774787281,8.15145247583631));
#49280=CARTESIAN_POINT('Ctrl Pts',(1.22660874853696,1.64877509728869,8.14971516925599));
#49281=CARTESIAN_POINT('Ctrl Pts',(1.25206542099587,1.62921138715835,8.14797786267567));
#49282=CARTESIAN_POINT('',(-2.05474966036672,0.00118140715606992,8.45407471951265));
#49283=CARTESIAN_POINT('Ctrl Pts',(-2.05474966036618,0.0011814080800246,
8.45407471946232));
#49284=CARTESIAN_POINT('Ctrl Pts',(-2.05470981683469,0.0704787865199796,
8.45029978452486));
#49285=CARTESIAN_POINT('Ctrl Pts',(-2.05116461443229,0.139673811090078,
8.4465248495874));
#49286=CARTESIAN_POINT('Ctrl Pts',(-2.04414330436285,0.208508306137984,
8.44274991464995));
#49287=CARTESIAN_POINT('Ctrl Pts',(-2.03694688085526,0.279059552756773,
8.43888083177868));
#49288=CARTESIAN_POINT('Ctrl Pts',(-2.02607958224214,0.349375980540898,
8.4350117489074));
#49289=CARTESIAN_POINT('Ctrl Pts',(-2.01156615579492,0.419045538528258,
8.43114266603613));
#49290=CARTESIAN_POINT('Ctrl Pts',(-1.9970743536289,0.488611292350709,8.42727934790527));
#49291=CARTESIAN_POINT('Ctrl Pts',(-1.97894730535087,0.557531617800781,
8.42341602977442));
#49292=CARTESIAN_POINT('Ctrl Pts',(-1.95726148410381,0.625399908333671,
8.41955271164356));
#49293=CARTESIAN_POINT('Ctrl Pts',(-1.93560110031659,0.693188589388313,
8.41569392518335));
#49294=CARTESIAN_POINT('Ctrl Pts',(-1.91039038254942,0.759927226251012,
8.41183513872315));
#49295=CARTESIAN_POINT('Ctrl Pts',(-1.88175639426221,0.825221446130244,
8.40797635226295));
#49296=CARTESIAN_POINT('Ctrl Pts',(-1.853140443288,0.890474535438722,8.40411999655527));
#49297=CARTESIAN_POINT('Ctrl Pts',(-1.82110569471359,0.954284569112658,
8.40026364084759));
#49298=CARTESIAN_POINT('Ctrl Pts',(-1.78582787905737,1.01627572483133,8.3964072851399));
#49299=CARTESIAN_POINT('Ctrl Pts',(-1.75056048482158,1.0782485677411,8.39255206863836));
#49300=CARTESIAN_POINT('Ctrl Pts',(-1.71205216560505,1.13840317743994,8.38869685213682));
#49301=CARTESIAN_POINT('Ctrl Pts',(-1.67052448239039,1.19638853063472,8.38484163563528));
#49302=CARTESIAN_POINT('Ctrl Pts',(-1.62899517556853,1.25437615088198,8.38098626840639));
#49303=CARTESIAN_POINT('Ctrl Pts',(-1.58444655502027,1.31019395258132,8.37713090117751));
#49304=CARTESIAN_POINT('Ctrl Pts',(-1.53714235724309,1.36352152020756,8.37327553394862));
#49305=CARTESIAN_POINT('Ctrl Pts',(-1.48978864487407,1.41690490725088,8.36941613120188));
#49306=CARTESIAN_POINT('Ctrl Pts',(-1.43967392051527,1.4677924927167,8.36555672845514));
#49307=CARTESIAN_POINT('Ctrl Pts',(-1.38710031154951,1.51589916821642,8.3616973257084));
#49308=CARTESIAN_POINT('Ctrl Pts',(-1.3344969349954,1.56403308209186,8.35783573773766));
#49309=CARTESIAN_POINT('Ctrl Pts',(-1.27943227747534,1.6093826425411,8.35397414976692));
#49310=CARTESIAN_POINT('Ctrl Pts',(-1.22224110270172,1.65170343868579,8.35011256179617));
#49311=CARTESIAN_POINT('Ctrl Pts',(-1.16494986992548,1.69409827657467,8.34624421783937));
#49312=CARTESIAN_POINT('Ctrl Pts',(-1.10552509712036,1.73345350237821,8.34237587388257));
#49313=CARTESIAN_POINT('Ctrl Pts',(-1.04432942330775,1.76956876614437,8.33850752992577));
#49314=CARTESIAN_POINT('Ctrl Pts',(-1.00799319691305,1.79101296830366,8.33621061883665));
#49315=CARTESIAN_POINT('Ctrl Pts',(-0.971033081498362,1.81131575915701,
8.33391370774752));
#49316=CARTESIAN_POINT('Ctrl Pts',(-0.933528375546205,1.83044320713593,
8.33161679665839));
#49317=CARTESIAN_POINT('Ctrl Pts',(-0.870352742076924,1.86266286096445,
8.3277477138488));
#49318=CARTESIAN_POINT('Ctrl Pts',(-0.805383377294136,1.89167113018795,
8.3238786310392));
#49319=CARTESIAN_POINT('Ctrl Pts',(-0.738979881261259,1.91726531747463,
8.32000954822961));
#49320=CARTESIAN_POINT('Ctrl Pts',(-0.672675323125341,1.94282137069887,
8.31614623016042));
#49321=CARTESIAN_POINT('Ctrl Pts',(-0.604941324782959,1.96497326588098,
8.31228291209123));
#49322=CARTESIAN_POINT('Ctrl Pts',(-0.536160967358015,1.98356471524922,
8.30841959402204));
#49323=CARTESIAN_POINT('Ctrl Pts',(-0.467461289261398,2.00213435685571,
8.3045608076232));
#49324=CARTESIAN_POINT('Ctrl Pts',(-0.397718156749575,2.01715172225172,
8.30070202122437));
#49325=CARTESIAN_POINT('Ctrl Pts',(-0.327331812158638,2.02850966161094,
8.29684323482554));
#49326=CARTESIAN_POINT('Ctrl Pts',(-0.256989805800319,2.03986044630174,
8.292986879179));
#49327=CARTESIAN_POINT('Ctrl Pts',(-0.186005869672279,2.04755630117204,
8.28913052353247));
#49328=CARTESIAN_POINT('Ctrl Pts',(-0.114791057301673,2.05154102461139,
8.28527416788593));
#49329=CARTESIAN_POINT('Ctrl Pts',(-0.0435972824952619,2.05552457092379,
8.28141895144523));
#49330=CARTESIAN_POINT('Ctrl Pts',(0.0278267483912949,2.05579913515123,
8.27756373500453));
#49331=CARTESIAN_POINT('Ctrl Pts',(0.0990659587721552,2.05236046987671,
8.27370851856382));
#49332=CARTESIAN_POINT('Ctrl Pts',(0.170307954398715,2.0489216701604,8.26985315139538));
#49333=CARTESIAN_POINT('Ctrl Pts',(0.241364630061478,2.04176937833479,8.26599778422694));
#49334=CARTESIAN_POINT('Ctrl Pts',(0.311823748603643,2.03095138107902,8.2621424170585));
#49335=CARTESIAN_POINT('Ctrl Pts',(0.382356618643337,2.02012206032794,8.25828301437119));
#49336=CARTESIAN_POINT('Ctrl Pts',(0.452290201824877,2.00561944851768,8.25442361168388));
#49337=CARTESIAN_POINT('Ctrl Pts',(0.521221101224195,1.98754273567605,8.25056420899658));
#49338=CARTESIAN_POINT('Ctrl Pts',(0.590191029846752,1.9694557876559,8.24670262108478));
#49339=CARTESIAN_POINT('Ctrl Pts',(0.658156681460076,1.94779085767811,8.24284103317299));
#49340=CARTESIAN_POINT('Ctrl Pts',(0.724731149162215,1.92269662815901,8.2389794452612));
#49341=CARTESIAN_POINT('Ctrl Pts',(0.791422091298898,1.89755849537947,8.23511110136196));
#49342=CARTESIAN_POINT('Ctrl Pts',(0.85671654495917,1.86897927936765,8.23124275746271));
#49343=CARTESIAN_POINT('Ctrl Pts',(0.920249501264119,1.83715497928812,8.22737441356347));
#49344=CARTESIAN_POINT('Ctrl Pts',(0.957973548082761,1.81825862287731,8.22507750193125));
#49345=CARTESIAN_POINT('Ctrl Pts',(0.995077042346118,1.79821903709245,8.22278059029904));
#49346=CARTESIAN_POINT('Ctrl Pts',(1.03148846703391,1.77708443943332,8.22048367866683));
#49347=CARTESIAN_POINT('Ctrl Pts',(1.09282082805986,1.74148476749291,8.21661470032612));
#49348=CARTESIAN_POINT('Ctrl Pts',(1.15242817648098,1.70263650639596,8.21274572198541));
#49349=CARTESIAN_POINT('Ctrl Pts',(1.20994520886422,1.66073181280017,8.20887674364469));
#49350=CARTESIAN_POINT('Ctrl Pts',(1.22411376771944,1.65040914674942,8.20792367209252));
#49351=CARTESIAN_POINT('Ctrl Pts',(1.23815558639144,1.63990123566865,8.20697060054034));
#49352=CARTESIAN_POINT('Ctrl Pts',(1.25206542099588,1.62921138715834,8.20601752898817));
#49353=CARTESIAN_POINT('Ctrl Pts',(1.25206542099588,1.62921138715834,8.90613916330362));
#49354=CARTESIAN_POINT('Ctrl Pts',(1.30858031424556,1.58577912037765,8.90227086778885));
#49355=CARTESIAN_POINT('Ctrl Pts',(1.36275963984382,1.53945896042727,8.89840257227408));
#49356=CARTESIAN_POINT('Ctrl Pts',(1.41431082657472,1.49054434631565,8.89453427675932));
#49357=CARTESIAN_POINT('Ctrl Pts',(1.44652514779997,1.45997761853446,8.89211698004494));
#49358=CARTESIAN_POINT('Ctrl Pts',(1.47771392678912,1.42839848807823,8.88969968333056));
#49359=CARTESIAN_POINT('Ctrl Pts',(1.50781381874179,1.39588504201144,8.88728238661619));
#49360=CARTESIAN_POINT('Ctrl Pts',(1.55599117939921,1.34384458884843,8.88341330377005));
#49361=CARTESIAN_POINT('Ctrl Pts',(1.60156556405218,1.289205101346,8.87954422092392));
#49362=CARTESIAN_POINT('Ctrl Pts',(1.64424416955661,1.23225755156099,8.87567513807778));
#49363=CARTESIAN_POINT('Ctrl Pts',(1.68685918606722,1.17539485078519,8.87181181997214));
#49364=CARTESIAN_POINT('Ctrl Pts',(1.72658669876803,1.11623129940836,8.8679485018665));
#49365=CARTESIAN_POINT('Ctrl Pts',(1.76317218510371,1.05509308033775,8.86408518376085));
#49366=CARTESIAN_POINT('Ctrl Pts',(1.79971475667791,0.994026576374739,8.86022639732587));
#49367=CARTESIAN_POINT('Ctrl Pts',(1.83312237449395,0.930990420468526,8.85636761089089));
#49368=CARTESIAN_POINT('Ctrl Pts',(1.86318313994246,0.866340665982001,8.85250882445591));
#49369=CARTESIAN_POINT('Ctrl Pts',(1.89322496931296,0.801731636100334,8.84865246877344));
#49370=CARTESIAN_POINT('Ctrl Pts',(1.91992392475803,0.73551146370853,8.84479611309096));
#49371=CARTESIAN_POINT('Ctrl Pts',(1.94311419961833,0.668060453657902,8.84093975740849));
#49372=CARTESIAN_POINT('Ctrl Pts',(1.9662976238392,0.60062936931113,8.8370845409321));
#49373=CARTESIAN_POINT('Ctrl Pts',(1.98597426735778,0.531968628295968,8.83322932445571));
#49374=CARTESIAN_POINT('Ctrl Pts',(2.00202722852745,0.462476527766211,8.82937410797933));
#49375=CARTESIAN_POINT('Ctrl Pts',(2.01808081731988,0.392981710303225,8.82551874077551));
#49376=CARTESIAN_POINT('Ctrl Pts',(2.03051033529391,0.322655942608069,8.82166337357169));
#49377=CARTESIAN_POINT('Ctrl Pts',(2.03924972787343,0.251908931695832,8.81780800636788));
#49378=CARTESIAN_POINT('Ctrl Pts',(2.04799826821387,0.181087867954917,8.8139486036459));
#49379=CARTESIAN_POINT('Ctrl Pts',(2.05304891295617,0.109845163914514,8.81008920092393));
#49380=CARTESIAN_POINT('Ctrl Pts',(2.05438747855597,0.0385959901084021,
8.80622979820195));
#49381=CARTESIAN_POINT('Ctrl Pts',(2.05572680206213,-0.0326935255395951,
8.80236821025584));
#49382=CARTESIAN_POINT('Ctrl Pts',(2.05334987856776,-0.103989032502454,
8.79850662230973));
#49383=CARTESIAN_POINT('Ctrl Pts',(2.04729463568034,-0.174877777932225,
8.79464503436362));
#49384=CARTESIAN_POINT('Ctrl Pts',(2.04122879892843,-0.245890545763207,
8.79077669043098));
#49385=CARTESIAN_POINT('Ctrl Pts',(2.03147186094257,-0.316494649881803,
8.78690834649833));
#49386=CARTESIAN_POINT('Ctrl Pts',(2.0181132365875,-0.386285550869183,8.78304000256569));
#49387=CARTESIAN_POINT('Ctrl Pts',(2.01018126984653,-0.427725379607586,
8.780743091252));
#49388=CARTESIAN_POINT('Ctrl Pts',(2.00098044883844,-0.468878735330665,
8.77844617993832));
#49389=CARTESIAN_POINT('Ctrl Pts',(1.99053773827548,-0.509663688132791,
8.77614926862464));
#49390=CARTESIAN_POINT('Ctrl Pts',(1.9729472844728,-0.578364800146326,8.7722801857741));
#49391=CARTESIAN_POINT('Ctrl Pts',(1.95176149298502,-0.6462887309913,8.76841110292356));
#49392=CARTESIAN_POINT('Ctrl Pts',(1.92706600839946,-0.713031669543074,
8.76454202007303));
#49393=CARTESIAN_POINT('Ctrl Pts',(1.90240731885422,-0.779675164445281,
8.76067870196297));
#49394=CARTESIAN_POINT('Ctrl Pts',(1.87424948336426,-0.845140707965953,
8.75681538385291));
#49395=CARTESIAN_POINT('Ctrl Pts',(1.84272849095502,-0.909037552097063,
8.75295206574285));
#49396=CARTESIAN_POINT('Ctrl Pts',(1.81124447265776,-0.97285944525458,8.74909327930345));
#49397=CARTESIAN_POINT('Ctrl Pts',(1.77640534738202,-1.0351158605092,8.74523449286404));
#49398=CARTESIAN_POINT('Ctrl Pts',(1.73839531770047,-1.09543565849258,8.74137570642464));
#49399=CARTESIAN_POINT('Ctrl Pts',(1.7004092315505,-1.15571745942624,8.73751935073774));
#49400=CARTESIAN_POINT('Ctrl Pts',(1.65925646224923,-1.21406465338534,8.73366299505084));
#49401=CARTESIAN_POINT('Ctrl Pts',(1.61516658621353,-1.27013167084335,8.72980663936394));
#49402=CARTESIAN_POINT('Ctrl Pts',(1.57108973476881,-1.32618212554286,8.72595142288314));
#49403=CARTESIAN_POINT('Ctrl Pts',(1.52407779923766,-1.37995335934943,8.72209620640234));
#49404=CARTESIAN_POINT('Ctrl Pts',(1.47440199708189,-1.43113113078465,8.71824098992154));
#49405=CARTESIAN_POINT('Ctrl Pts',(1.42472425275104,-1.48231090311744,8.71438562271332));
#49406=CARTESIAN_POINT('Ctrl Pts',(1.37238277494907,-1.53089666472608,8.71053025550509));
#49407=CARTESIAN_POINT('Ctrl Pts',(1.31768594539002,-1.57661070395377,8.70667488829687));
#49408=CARTESIAN_POINT('Ctrl Pts',(1.26293186316627,-1.6223725933143,8.70281548557055));
#49409=CARTESIAN_POINT('Ctrl Pts',(1.2058178811779,-1.66525644765854,8.69895608284422));
#49410=CARTESIAN_POINT('Ctrl Pts',(1.14668510504853,-1.70502517059422,8.69509668011789));
#49411=CARTESIAN_POINT('Ctrl Pts',(1.08751884747718,-1.74481641089297,8.69123509216745));
#49412=CARTESIAN_POINT('Ctrl Pts',(1.02633193716306,-1.78148875872548,8.687373504217));
#49413=CARTESIAN_POINT('Ctrl Pts',(0.963491712615178,-1.81485020930706,
8.68351191626656));
#49414=CARTESIAN_POINT('Ctrl Pts',(0.900541546843314,-1.84827002694154,
8.67964357232966));
#49415=CARTESIAN_POINT('Ctrl Pts',(0.835932732302552,-1.87836717717327,
8.67577522839276));
#49416=CARTESIAN_POINT('Ctrl Pts',(0.770053632803515,-1.90499736616776,
8.67190688445586));
#49417=CARTESIAN_POINT('Ctrl Pts',(0.730936519939146,-1.92080960580702,
8.6696099731816));
#49418=CARTESIAN_POINT('Ctrl Pts',(0.691371880962958,-1.93540046172162,
8.66731306190733));
#49419=CARTESIAN_POINT('Ctrl Pts',(0.651443173023543,-1.94874815069085,
8.66501615063306));
#49420=CARTESIAN_POINT('Ctrl Pts',(0.584184380516407,-1.97123195968846,
8.66114706779078));
#49421=CARTESIAN_POINT('Ctrl Pts',(0.515628483213545,-1.9902736788152,8.65727798494849));
#49422=CARTESIAN_POINT('Ctrl Pts',(0.446161188134982,-2.00572624171445,
8.6534089021062));
#49423=CARTESIAN_POINT('Ctrl Pts',(0.37679739586139,-2.02115578106568,8.64954558400438));
#49424=CARTESIAN_POINT('Ctrl Pts',(0.306525371609875,-2.0330066745322,8.64568226590255));
#49425=CARTESIAN_POINT('Ctrl Pts',(0.235747153476675,-2.04118123696247,
8.64181894780073));
#49426=CARTESIAN_POINT('Ctrl Pts',(0.165051958165386,-2.04934621063424,
8.63796016136951));
#49427=CARTESIAN_POINT('Ctrl Pts',(0.0938522286243621,-2.05384336356217,
8.63410137493829));
#49428=CARTESIAN_POINT('Ctrl Pts',(0.0225596791623202,-2.05462615173079,
8.63024258850707));
#49429=CARTESIAN_POINT('Ctrl Pts',(-0.0486879612217034,-2.05540844680028,
8.62638623282832));
#49430=CARTESIAN_POINT('Ctrl Pts',(-0.120027820918118,-2.0524810138713,
8.62252987714958));
#49431=CARTESIAN_POINT('Ctrl Pts',(-0.191045057807914,-2.04584929757477,
8.61867352147083));
#49432=CARTESIAN_POINT('Ctrl Pts',(-0.262041315495508,-2.03921954035357,
8.61481830499813));
#49433=CARTESIAN_POINT('Ctrl Pts',(-0.332714656170015,-2.02888771736128,
8.61096308852544));
#49434=CARTESIAN_POINT('Ctrl Pts',(-0.402653972158619,-2.0149112489648,
8.60710787205273));
#49435=CARTESIAN_POINT('Ctrl Pts',(-0.472596022566016,-2.00093423413006,
8.60325250485256));
#49436=CARTESIAN_POINT('Ctrl Pts',(-0.541803515378322,-1.98331238834194,
8.59939713765239));
#49437=CARTESIAN_POINT('Ctrl Pts',(-0.609875875675157,-1.96215416794131,
8.59554177045221));
#49438=CARTESIAN_POINT('Ctrl Pts',(-0.678019489172598,-1.94097380065293,
8.59168236773379));
#49439=CARTESIAN_POINT('Ctrl Pts',(-0.745025133450511,-1.91624981397103,
8.58782296501536));
#49440=CARTESIAN_POINT('Ctrl Pts',(-0.810508607011173,-1.88814018559555,
8.58396356229694));
#49441=CARTESIAN_POINT('Ctrl Pts',(-0.876029157829791,-1.86001464132732,
8.58010197435432));
#49442=CARTESIAN_POINT('Ctrl Pts',(-0.940025386211164,-1.82849985396889,
8.57624038641171));
#49443=CARTESIAN_POINT('Ctrl Pts',(-1.0021367454079,-1.79380029713546,8.5723787984691));
#49444=CARTESIAN_POINT('Ctrl Pts',(-1.06435677065593,-1.75904003218243,
8.56851045453984));
#49445=CARTESIAN_POINT('Ctrl Pts',(-1.12468493157216,-1.72108413213595,
8.56464211061058));
#49446=CARTESIAN_POINT('Ctrl Pts',(-1.18278936124687,-1.680180612143,8.56077376668132));
#49447=CARTESIAN_POINT('Ctrl Pts',(-1.21729010012848,-1.65589327862099,
8.55847685533471));
#49448=CARTESIAN_POINT('Ctrl Pts',(-1.25100744344955,-1.63056750904801,
8.55617994398811));
#49449=CARTESIAN_POINT('Ctrl Pts',(-1.28387782488486,-1.60426160375075,
8.55388303264151));
#49450=CARTESIAN_POINT('Ctrl Pts',(-1.33854910133951,-1.56050861525176,
8.55006272177992));
#49451=CARTESIAN_POINT('Ctrl Pts',(-1.39110142157108,-1.51386129057278,
8.54624241091833));
#49452=CARTESIAN_POINT('Ctrl Pts',(-1.44120640785681,-1.46455510393172,
8.54242210005673));
#49453=CARTESIAN_POINT('Ctrl Pts',(-1.49122604728079,-1.41533290350854,
8.53860829656232));
#49454=CARTESIAN_POINT('Ctrl Pts',(-1.53880627704515,-1.36346118031355,
8.5347944930679));
#49455=CARTESIAN_POINT('Ctrl Pts',(-1.58365108837674,-1.30921609858081,
8.53098068957349));
#49456=CARTESIAN_POINT('Ctrl Pts',(-1.62845321325744,-1.25502265113862,
8.52717051632593));
#49457=CARTESIAN_POINT('Ctrl Pts',(-1.67052476385377,-1.19846070522761,
8.52336034307837));
#49458=CARTESIAN_POINT('Ctrl Pts',(-1.70960699564656,-1.13984274482769,
8.51955016983081));
#49459=CARTESIAN_POINT('Ctrl Pts',(-1.74866589227533,-1.08125978395718,
8.51574227155614));
#49460=CARTESIAN_POINT('Ctrl Pts',(-1.78473873300152,-1.02062365730354,
8.51193437328147));
#49461=CARTESIAN_POINT('Ctrl Pts',(-1.81760863708442,-0.958277832831442,
8.5081264750068));
#49462=CARTESIAN_POINT('Ctrl Pts',(-1.85047057485056,-0.895947118430393,
8.50431949961052));
#49463=CARTESIAN_POINT('Ctrl Pts',(-1.88013088470096,-0.831907970450107,
8.50051252421422));
#49464=CARTESIAN_POINT('Ctrl Pts',(-1.90641836529415,-0.766528915938064,
8.49670554881793));
#49465=CARTESIAN_POINT('Ctrl Pts',(-1.93272464880456,-0.701103097075756,
8.49289585036711));
#49466=CARTESIAN_POINT('Ctrl Pts',(-1.95565309513118,-0.634335920452832,
8.48908615191628));
#49467=CARTESIAN_POINT('Ctrl Pts',(-1.97508093173989,-0.566615280042358,
8.48527645346546));
#49468=CARTESIAN_POINT('Ctrl Pts',(-1.99451568455286,-0.498870531451931,
8.48146539878269));
#49469=CARTESIAN_POINT('Ctrl Pts',(-2.01044723129373,-0.430172129688349,
8.47765434409992));
#49470=CARTESIAN_POINT('Ctrl Pts',(-2.02280361780844,-0.360919778179445,
8.47384328941715));
#49471=CARTESIAN_POINT('Ctrl Pts',(-2.0351795119928,-0.291558094383596,
8.47002621802426));
#49472=CARTESIAN_POINT('Ctrl Pts',(-2.04396891161403,-0.221641210370022,
8.46620914663137));
#49473=CARTESIAN_POINT('Ctrl Pts',(-2.04915169493153,-0.151574713126082,
8.46239207523848));
#49474=CARTESIAN_POINT('Ctrl Pts',(-2.05291610382554,-0.100683342748401,
8.45961962332987));
#49475=CARTESIAN_POINT('Ctrl Pts',(-2.05477892290776,-0.0497131519036452,
8.45684717142126));
#49476=CARTESIAN_POINT('Ctrl Pts',(-2.05474966036672,0.00118140715607104,
8.45407471951265));
#49477=CARTESIAN_POINT('Origin',(0.,0.,18.5459252805377));
#49478=CARTESIAN_POINT('',(1.25005255340789,1.62658210076147,9.60609423337355));
#49479=CARTESIAN_POINT('',(1.25206542099588,1.62921138715834,9.54788499192677));
#49480=CARTESIAN_POINT('',(1.25206542099588,1.62921138715835,18.5459252805377));
#49481=CARTESIAN_POINT('',(-2.0547494382537,-0.00151937358419461,9.09592528053767));
#49482=CARTESIAN_POINT('Ctrl Pts',(1.25206542099588,1.62921138715834,9.54788499192677));
#49483=CARTESIAN_POINT('Ctrl Pts',(1.30837948877059,1.58593345678534,9.54402021208199));
#49484=CARTESIAN_POINT('Ctrl Pts',(1.36254035296318,1.53966063449194,9.54015543223721));
#49485=CARTESIAN_POINT('Ctrl Pts',(1.41421380051509,1.49063640400088,9.53629065239243));
#49486=CARTESIAN_POINT('Ctrl Pts',(1.4658192534186,1.44167668217865,9.53243095802886));
#49487=CARTESIAN_POINT('Ctrl Pts',(1.51494344120504,1.38997307654059,9.5285712636653));
#49488=CARTESIAN_POINT('Ctrl Pts',(1.56128488797241,1.33580951527116,9.52471156930173));
#49489=CARTESIAN_POINT('Ctrl Pts',(1.60759282263362,1.28168512271877,9.52085466610021));
#49490=CARTESIAN_POINT('Ctrl Pts',(1.65112169351406,1.22510467151956,9.51699776289868));
#49491=CARTESIAN_POINT('Ctrl Pts',(1.69160760247761,1.16638813511625,9.51314085969715));
#49492=CARTESIAN_POINT('Ctrl Pts',(1.73207777713509,1.10769441810808,9.50928545542938));
#49493=CARTESIAN_POINT('Ctrl Pts',(1.76950706155502,1.0468666631196,9.50543005116161));
#49494=CARTESIAN_POINT('Ctrl Pts',(1.80367357484215,0.984255656786465,9.50157464689384));
#49495=CARTESIAN_POINT('Ctrl Pts',(1.83783823880112,0.921648039394291,9.49771945130723));
#49496=CARTESIAN_POINT('Ctrl Pts',(1.86874025100017,0.857257789492544,9.49386425572062));
#49497=CARTESIAN_POINT('Ctrl Pts',(1.8962034405214,0.791460722117526,9.49000906013401));
#49498=CARTESIAN_POINT('Ctrl Pts',(1.92369373512672,0.725598715634017,9.48615005962152));
#49499=CARTESIAN_POINT('Ctrl Pts',(1.94773824003505,0.658327567596629,9.48229105910902));
#49500=CARTESIAN_POINT('Ctrl Pts',(1.96820911877231,0.590042733436753,9.47843205859653));
#49501=CARTESIAN_POINT('Ctrl Pts',(1.98868987694765,0.521724944375491,9.4745711956942));
#49502=CARTESIAN_POINT('Ctrl Pts',(2.00559345799348,0.452392967291722,9.47071033279187));
#49503=CARTESIAN_POINT('Ctrl Pts',(2.01884279277754,0.382454364009832,9.46684946988954));
#49504=CARTESIAN_POINT('Ctrl Pts',(2.03211648364741,0.312387193471582,9.46298150961141));
#49505=CARTESIAN_POINT('Ctrl Pts',(2.0417224414168,0.241711651288871,9.45911354933328));
#49506=CARTESIAN_POINT('Ctrl Pts',(2.04763537173146,0.170841876992033,9.45524558905514));
#49507=CARTESIAN_POINT('Ctrl Pts',(2.05279162390166,0.109041313130481,9.45187261194954));
#49508=CARTESIAN_POINT('Ctrl Pts',(2.05514038457062,0.0470933095698247,
9.44849963484393));
#49509=CARTESIAN_POINT('Ctrl Pts',(2.05469720726044,-0.0147291878983883,
9.44512665773833));
#49510=CARTESIAN_POINT('Ctrl Pts',(2.05418884634507,-0.0856446898450993,
9.44125757489156));
#49511=CARTESIAN_POINT('Ctrl Pts',(2.05000382978784,-0.156672739017571,
9.43738849204479));
#49512=CARTESIAN_POINT('Ctrl Pts',(2.042127920654,-0.227400787565428,9.43351940919801));
#49513=CARTESIAN_POINT('Ctrl Pts',(2.03426374623198,-0.29802345484829,9.42965609109173));
#49514=CARTESIAN_POINT('Ctrl Pts',(2.02271964840836,-0.368346529895437,
9.42579277298544));
#49515=CARTESIAN_POINT('Ctrl Pts',(2.00753339905201,-0.437958005053798,
9.42192945487916));
#49516=CARTESIAN_POINT('Ctrl Pts',(1.99236496316031,-0.507487825978572,
9.41807066844352));
#49517=CARTESIAN_POINT('Ctrl Pts',(1.97356296489507,-0.576307232707317,
9.41421188200788));
#49518=CARTESIAN_POINT('Ctrl Pts',(1.9512166949604,-0.644011623969472,9.41035309557225));
#49519=CARTESIAN_POINT('Ctrl Pts',(1.92888450153722,-0.711673366429671,
9.40649673988912));
#49520=CARTESIAN_POINT('Ctrl Pts',(1.90301261784714,-0.778221026714865,
9.40264038420599));
#49521=CARTESIAN_POINT('Ctrl Pts',(1.87374053468269,-0.843263879925522,
9.39878402852285));
#49522=CARTESIAN_POINT('Ctrl Pts',(1.84447709878471,-0.908287518826033,
9.3949288120458));
#49523=CARTESIAN_POINT('Ctrl Pts',(1.81181565678583,-0.971806790429911,
9.39107359556876));
#49524=CARTESIAN_POINT('Ctrl Pts',(1.77594366512749,-1.03345133450662,9.38721837909171));
#49525=CARTESIAN_POINT('Ctrl Pts',(1.74007027098157,-1.09509828870065,9.38336301188723));
#49526=CARTESIAN_POINT('Ctrl Pts',(1.70098632419905,-1.15486995108761,9.37950764468274));
#49527=CARTESIAN_POINT('Ctrl Pts',(1.65892415623246,-1.21242245375464,9.37565227747826));
#49528=CARTESIAN_POINT('Ctrl Pts',(1.61681796064581,-1.27003519819815,9.37179287475562));
#49529=CARTESIAN_POINT('Ctrl Pts',(1.57172760810276,-1.3254237529768,9.36793347203299));
#49530=CARTESIAN_POINT('Ctrl Pts',(1.52392698066661,-1.37827577795459,9.36407406931035));
#49531=CARTESIAN_POINT('Ctrl Pts',(1.47609928813973,-1.43115772816408,9.36021248136357));
#49532=CARTESIAN_POINT('Ctrl Pts',(1.42555861018493,-1.48149994654887,9.3563508934168));
#49533=CARTESIAN_POINT('Ctrl Pts',(1.37261515912689,-1.52902752997945,9.35248930547002));
#49534=CARTESIAN_POINT('Ctrl Pts',(1.31957908160349,-1.57663826462085,9.34862096153672));
#49535=CARTESIAN_POINT('Ctrl Pts',(1.26413221611949,-1.62142422745431,9.34475261760341));
#49536=CARTESIAN_POINT('Ctrl Pts',(1.2066166827877,-1.66315174993697,9.34088427367011));
#49537=CARTESIAN_POINT('Ctrl Pts',(1.172465614227,-1.68792835198902,9.33858736236233));
#49538=CARTESIAN_POINT('Ctrl Pts',(1.13758575582091,-1.71162749254131,9.33629045105455));
#49539=CARTESIAN_POINT('Ctrl Pts',(1.10205285120755,-1.73420791015533,9.33399353974677));
#49540=CARTESIAN_POINT('Ctrl Pts',(1.04219866733299,-1.77224399199384,9.33012445689933));
#49541=CARTESIAN_POINT('Ctrl Pts',(0.98025578314655,-1.80725223721137,9.3262553740519));
#49542=CARTESIAN_POINT('Ctrl Pts',(0.916563071910391,-1.83899692705295,
9.32238629120446));
#49543=CARTESIAN_POINT('Ctrl Pts',(0.852965259637481,-1.87069431888984,
9.3185229730975));
#49544=CARTESIAN_POINT('Ctrl Pts',(0.787623226678478,-1.89913759241964,
9.31465965499054));
#49545=CARTESIAN_POINT('Ctrl Pts',(0.720903601009475,-1.924135016196,9.31079633688358));
#49546=CARTESIAN_POINT('Ctrl Pts',(0.65426223743565,-1.94910311800391,9.30693755044728));
#49547=CARTESIAN_POINT('Ctrl Pts',(0.586246943603025,-1.97063322919154,
9.30307876401097));
#49548=CARTESIAN_POINT('Ctrl Pts',(0.517246067943104,-1.9885809180663,9.29921997757466));
#49549=CARTESIAN_POINT('Ctrl Pts',(0.448288657775253,-2.0065173012131,9.29536362189086));
#49550=CARTESIAN_POINT('Ctrl Pts',(0.378347366553541,-2.02087561723382,
9.29150726620705));
#49551=CARTESIAN_POINT('Ctrl Pts',(0.307826112251187,-2.03156113546118,
9.28765091052325));
#49552=CARTESIAN_POINT('Ctrl Pts',(0.237325690633525,-2.04224349707946,
9.28379569404553));
#49553=CARTESIAN_POINT('Ctrl Pts',(0.166246126105861,-2.04925514215687,
9.27994047756781));
#49554=CARTESIAN_POINT('Ctrl Pts',(0.095000243233387,-2.05255268295009,
9.27608526109009));
#49555=CARTESIAN_POINT('Ctrl Pts',(0.0237515748600807,-2.05585035266728,
9.27222989388494));
#49556=CARTESIAN_POINT('Ctrl Pts',(-0.0476629394025676,-2.05543360954481,
9.2683745266798));
#49557=CARTESIAN_POINT('Ctrl Pts',(-0.118828392738864,-2.05131113573224,
9.26451915947465));
#49558=CARTESIAN_POINT('Ctrl Pts',(-0.190068336898829,-2.04718434681374,
9.26065975675135));
#49559=CARTESIAN_POINT('Ctrl Pts',(-0.261058213755417,-2.03934411222334,
9.25680035402806));
#49560=CARTESIAN_POINT('Ctrl Pts',(-0.331387067787583,-2.02785112219885,
9.25294095130476));
#49561=CARTESIAN_POINT('Ctrl Pts',(-0.401755742569288,-2.01635162475314,
9.24907936335732));
#49562=CARTESIAN_POINT('Ctrl Pts',(-0.47146217454117,-2.00119535794867,
9.24521777540989));
#49563=CARTESIAN_POINT('Ctrl Pts',(-0.54010715543086,-1.98249383937312,
9.24135618746246));
#49564=CARTESIAN_POINT('Ctrl Pts',(-0.60887223317487,-1.96375960182056,
9.23748784352851));
#49565=CARTESIAN_POINT('Ctrl Pts',(-0.676571690631472,-1.9414678809202,
9.23361949959456));
#49566=CARTESIAN_POINT('Ctrl Pts',(-0.742823655912128,-1.91577936587628,
9.22975115566061));
#49567=CARTESIAN_POINT('Ctrl Pts',(-0.78216216624574,-1.90052626492706,
9.22745424435881));
#49568=CARTESIAN_POINT('Ctrl Pts',(-0.820990746805723,-1.88407648961503,
9.22515733305701));
#49569=CARTESIAN_POINT('Ctrl Pts',(-0.859233650634652,-1.86647129528344,
9.22286042175521));
#49570=CARTESIAN_POINT('Ctrl Pts',(-0.923652752532163,-1.83681583782536,
9.21899133890884));
#49571=CARTESIAN_POINT('Ctrl Pts',(-0.986660938675525,-1.80376335515144,
9.21512225606246));
#49572=CARTESIAN_POINT('Ctrl Pts',(-1.04787637575334,-1.7674706966844,9.21125317321608));
#49573=CARTESIAN_POINT('Ctrl Pts',(-1.10900060488281,-1.73123211246852,
9.20738985511019));
#49574=CARTESIAN_POINT('Ctrl Pts',(-1.16833697255914,-1.69176318103148,
9.20352653700429));
#49575=CARTESIAN_POINT('Ctrl Pts',(-1.22552554705327,-1.6492679272998,9.1996632188984));
#49576=CARTESIAN_POINT('Ctrl Pts',(-1.28264703937168,-1.60682252048429,
9.19580443246315));
#49577=CARTESIAN_POINT('Ctrl Pts',(-1.33762535478415,-1.56135813095968,
9.19194564602789));
#49578=CARTESIAN_POINT('Ctrl Pts',(-1.39012851890175,-1.51312268618114,
9.18808685959264));
#49579=CARTESIAN_POINT('Ctrl Pts',(-1.44259860987588,-1.46491762619582,
9.18423050390989));
#49580=CARTESIAN_POINT('Ctrl Pts',(-1.49259628602557,-1.41394530200018,
9.18037414822714));
#49581=CARTESIAN_POINT('Ctrl Pts',(-1.53982288382424,-1.36049367839443,
9.17651779254438));
#49582=CARTESIAN_POINT('Ctrl Pts',(-1.58703553041312,-1.3070578449334,9.17266257606771));
#49583=CARTESIAN_POINT('Ctrl Pts',(-1.63147840233561,-1.25114452994511,
9.16880735959103));
#49584=CARTESIAN_POINT('Ctrl Pts',(-1.67289114019362,-1.19307702834381,
9.16495214311435));
#49585=CARTESIAN_POINT('Ctrl Pts',(-1.71430549716584,-1.13500725647684,
9.16109677591023));
#49586=CARTESIAN_POINT('Ctrl Pts',(-1.75268920459536,-1.07478352756789,
9.15724140870612));
#49587=CARTESIAN_POINT('Ctrl Pts',(-1.78782451935178,-1.01275912758393,
9.15338604150201));
#49588=CARTESIAN_POINT('Ctrl Pts',(-1.82299661120194,-0.950669804966202,
9.14952663877972));
#49589=CARTESIAN_POINT('Ctrl Pts',(-1.85491328292847,-0.886776472309764,
9.14566723605744));
#49590=CARTESIAN_POINT('Ctrl Pts',(-1.88340262822067,-0.821457304131785,
9.14180783333516));
#49591=CARTESIAN_POINT('Ctrl Pts',(-1.91190810440402,-0.756101151727558,
9.13794624538873));
#49592=CARTESIAN_POINT('Ctrl Pts',(-1.93698222022606,-0.689318011678123,
9.1340846574423));
#49593=CARTESIAN_POINT('Ctrl Pts',(-1.95850214259047,-0.621503757002758,
9.13022306949587));
#49594=CARTESIAN_POINT('Ctrl Pts',(-1.9800597148305,-0.553570858857855,
9.1263547255629));
#49595=CARTESIAN_POINT('Ctrl Pts',(-1.99805055616579,-0.484603714607712,
9.12248638162993));
#49596=CARTESIAN_POINT('Ctrl Pts',(-2.01240254711499,-0.415010302119222,
9.11861803769696));
#49597=CARTESIAN_POINT('Ctrl Pts',(-2.02092434634467,-0.373687736418489,
9.11632112638586));
#49598=CARTESIAN_POINT('Ctrl Pts',(-2.02816420397466,-0.332144526961971,
9.11402421507476));
#49599=CARTESIAN_POINT('Ctrl Pts',(-2.03411569632439,-0.290466687361487,
9.11172730376365));
#49600=CARTESIAN_POINT('Ctrl Pts',(-2.04776382455714,-0.194889903270089,
9.10645996268833));
#49601=CARTESIAN_POINT('Ctrl Pts',(-2.05467785275471,-0.0983291808467869,
9.101192621613));
#49602=CARTESIAN_POINT('Ctrl Pts',(-2.0547494382537,-0.00151937358419461,
9.09592528053767));
#49603=CARTESIAN_POINT('Ctrl Pts',(-2.05657619914637,-0.00150476774419542,
9.09592441312253));
#49604=CARTESIAN_POINT('Ctrl Pts',(-2.05172851349779,0.583051337434284,
9.06414767067239));
#49605=CARTESIAN_POINT('Ctrl Pts',(-1.48485246887974,1.85727103545833,8.99532655555841));
#49606=CARTESIAN_POINT('Ctrl Pts',(0.203568424281083,2.2283551924176,8.91263733706201));
#49607=CARTESIAN_POINT('Ctrl Pts',(1.0481375467077,1.78481282053903,8.86172486101579));
#49608=CARTESIAN_POINT('Ctrl Pts',(1.25051812704735,1.62722676461089,8.84785675763342));
#49609=CARTESIAN_POINT('',(-2.05468488894014,0.00105741319522436,9.15407467172219));
#49610=CARTESIAN_POINT('Ctrl Pts',(-2.05474972788973,0.00105746728722069,
9.15407467060216));
#49611=CARTESIAN_POINT('Ctrl Pts',(-2.05470909252753,0.0800154647999912,
9.14981306013524));
#49612=CARTESIAN_POINT('Ctrl Pts',(-2.05011312005515,0.158816114439893,
9.14555144966831));
#49613=CARTESIAN_POINT('Ctrl Pts',(-2.04104077392044,0.236960169003702,
9.14128983920139));
#49614=CARTESIAN_POINT('Ctrl Pts',(-2.03193556684571,0.315387269105138,
9.13701279275751));
#49615=CARTESIAN_POINT('Ctrl Pts',(-2.0183216354985,0.393152725894291,9.13273574631362));
#49616=CARTESIAN_POINT('Ctrl Pts',(-2.00032874250127,0.46976854345868,9.12845869986974));
#49617=CARTESIAN_POINT('Ctrl Pts',(-1.98224879419337,0.546755052595601,
9.12416095972158));
#49618=CARTESIAN_POINT('Ctrl Pts',(-1.95974754943351,0.622580496287309,
9.11986321957341));
#49619=CARTESIAN_POINT('Ctrl Pts',(-1.93300491868768,0.696770799351727,
9.11556547942525));
#49620=CARTESIAN_POINT('Ctrl Pts',(-1.92052498157348,0.731393059425061,
9.11355986048327));
#49621=CARTESIAN_POINT('Ctrl Pts',(-1.9071220283947,0.765659543230826,9.11155424154129));
#49622=CARTESIAN_POINT('Ctrl Pts',(-1.89281777540094,0.799523878083839,
9.10954862259931));
#49623=CARTESIAN_POINT('Ctrl Pts',(-1.86522313179983,0.864852298342182,
9.10567953975186));
#49624=CARTESIAN_POINT('Ctrl Pts',(-1.83418836795403,0.928878399016742,
9.10181045690442));
#49625=CARTESIAN_POINT('Ctrl Pts',(-1.7998581277094,0.991215558099463,9.09794137405698));
#49626=CARTESIAN_POINT('Ctrl Pts',(-1.76557903781057,1.0534598379241,9.09407805595001));
#49627=CARTESIAN_POINT('Ctrl Pts',(-1.72801445035035,1.11401974916303,9.09021473784305));
#49628=CARTESIAN_POINT('Ctrl Pts',(-1.68735685644335,1.17252906211898,9.08635141973609));
#49629=CARTESIAN_POINT('Ctrl Pts',(-1.64674695387837,1.23096974367333,9.08249263329978));
#49630=CARTESIAN_POINT('Ctrl Pts',(-1.60305152735594,1.28736420779808,9.07863384686347));
#49631=CARTESIAN_POINT('Ctrl Pts',(-1.55650783625712,1.34137277375463,9.07477506042716));
#49632=CARTESIAN_POINT('Ctrl Pts',(-1.50999346427081,1.39534731827487,9.07091870474335));
#49633=CARTESIAN_POINT('Ctrl Pts',(-1.46063470374567,1.4469385793191,9.06706234905955));
#49634=CARTESIAN_POINT('Ctrl Pts',(-1.40870988911519,1.49583889868163,9.06320599337574));
#49635=CARTESIAN_POINT('Ctrl Pts',(-1.35680041359492,1.54472477240014,9.05935077689802));
#49636=CARTESIAN_POINT('Ctrl Pts',(-1.3023267423383,1.59092094973071,9.0554955604203));
#49637=CARTESIAN_POINT('Ctrl Pts',(-1.24560373855348,1.63415693524264,9.05164034394258));
#49638=CARTESIAN_POINT('Ctrl Pts',(-1.18887851706889,1.67739461115225,9.04778497673743));
#49639=CARTESIAN_POINT('Ctrl Pts',(-1.12990417614052,1.71767157273418,9.04392960953228));
#49640=CARTESIAN_POINT('Ctrl Pts',(-1.06902690833012,1.75475896685731,9.04007424232713));
#49641=CARTESIAN_POINT('Ctrl Pts',(-1.00808591862087,1.79188518136878,9.03621483960383));
#49642=CARTESIAN_POINT('Ctrl Pts',(-0.945238441568808,1.82581491055631,
9.03235543688053));
#49643=CARTESIAN_POINT('Ctrl Pts',(-0.880857001440585,1.85636432456377,
9.02849603415723));
#49644=CARTESIAN_POINT('Ctrl Pts',(-0.816439108035306,1.88693103588938,
9.0246344462098));
#49645=CARTESIAN_POINT('Ctrl Pts',(-0.750485971899848,1.9141134367325,9.02077285826237));
#49646=CARTESIAN_POINT('Ctrl Pts',(-0.68338936536759,1.93777618361938,9.01691127031493));
#49647=CARTESIAN_POINT('Ctrl Pts',(-0.616175370917405,1.96148032933002,
9.01304292638098));
#49648=CARTESIAN_POINT('Ctrl Pts',(-0.54781437800007,1.98165238941271,9.00917458244703));
#49649=CARTESIAN_POINT('Ctrl Pts',(-0.478711868279485,1.99820732399528,
9.00530623851308));
#49650=CARTESIAN_POINT('Ctrl Pts',(-0.437680786692985,2.00803716771966,
9.0030093272113));
#49651=CARTESIAN_POINT('Ctrl Pts',(-0.3963884600947,2.01659272382017,9.00071241590952));
#49652=CARTESIAN_POINT('Ctrl Pts',(-0.3549206547011,2.02386484019229,8.99841550460774));
#49653=CARTESIAN_POINT('Ctrl Pts',(-0.285091861551083,2.03611055961465,
8.99454767165508));
#49654=CARTESIAN_POINT('Ctrl Pts',(-0.214491835897539,2.04476209373249,
8.99067983870242));
#49655=CARTESIAN_POINT('Ctrl Pts',(-0.143523450780166,2.04973134375609,
8.98681200574976));
#49656=CARTESIAN_POINT('Ctrl Pts',(-0.0726506121767563,2.05469390355396,
8.98294938015746));
#49657=CARTESIAN_POINT('Ctrl Pts',(-0.00141087773771996,2.05598397860889,
8.97908675456515));
#49658=CARTESIAN_POINT('Ctrl Pts',(0.0697838918775918,2.05356464980638,
8.97522412897285));
#49659=CARTESIAN_POINT('Ctrl Pts',(0.1409066324066,2.05114776868429,8.97136541127144));
#49660=CARTESIAN_POINT('Ctrl Pts',(0.21198401549772,2.04502894632438,8.96750669357003));
#49661=CARTESIAN_POINT('Ctrl Pts',(0.282602001321962,2.03522324852799,8.96364797586862));
#49662=CARTESIAN_POINT('Ctrl Pts',(0.353172167215793,2.02542419079334,8.95979187115044));
#49663=CARTESIAN_POINT('Ctrl Pts',(0.423283073477898,2.01194328047611,8.95593576643225));
#49664=CARTESIAN_POINT('Ctrl Pts',(0.49252535892379,1.99484744612639,8.95207966171406));
#49665=CARTESIAN_POINT('Ctrl Pts',(0.5617703014393,1.97775095574948,8.9482234090236));
#49666=CARTESIAN_POINT('Ctrl Pts',(0.630146080390361,1.95703936211572,8.94436715633313));
#49667=CARTESIAN_POINT('Ctrl Pts',(0.697254340464982,1.93283055315326,8.94051090364267));
#49668=CARTESIAN_POINT('Ctrl Pts',(0.76435907002111,1.90862301779927,8.93665485382695));
#49669=CARTESIAN_POINT('Ctrl Pts',(0.830195958385753,1.8809188049123,8.93279880401124));
#49670=CARTESIAN_POINT('Ctrl Pts',(0.894384763685532,1.84988471451255,8.92894275419552));
#49671=CARTESIAN_POINT('Ctrl Pts',(0.958639725066976,1.81881863888096,8.9250827301487));
#49672=CARTESIAN_POINT('Ctrl Pts',(1.0212427742253,1.78441604733185,8.92122270610188));
#49673=CARTESIAN_POINT('Ctrl Pts',(1.08183724595149,1.74689030444734,8.91736268205507));
#49674=CARTESIAN_POINT('Ctrl Pts',(1.14056599836375,1.71051998880353,8.91362150913791));
#49675=CARTESIAN_POINT('Ctrl Pts',(1.19740775918225,1.67121635280537,8.90988033622077));
#49676=CARTESIAN_POINT('Ctrl Pts',(1.25206542099588,1.62921138715834,8.90613916330362));
#49677=CARTESIAN_POINT('Ctrl Pts',(1.25005255340789,1.62658210076147,9.60609423337355));
#49678=CARTESIAN_POINT('Ctrl Pts',(1.50489202993141,1.43143452431908,9.58875652043754));
#49679=CARTESIAN_POINT('Ctrl Pts',(2.16745735673946,0.642365888481017,9.53437443483768));
#49680=CARTESIAN_POINT('Ctrl Pts',(2.07210355506776,-1.2666354657809,9.44294797657398));
#49681=CARTESIAN_POINT('Ctrl Pts',(0.0597258374687065,-2.4278408865574,
9.33181485858242));
#49682=CARTESIAN_POINT('Ctrl Pts',(-1.7312581697553,-1.50866925322773,9.23552377287854));
#49683=CARTESIAN_POINT('Ctrl Pts',(-2.05000971940957,-0.409738837837595,
9.1762770598385));
#49684=CARTESIAN_POINT('Ctrl Pts',(-2.0519211775981,0.00105510756466237,
9.15407471946233));
#49685=CARTESIAN_POINT('Origin',(0.,0.,18.5459252805377));
#49686=CARTESIAN_POINT('',(1.25206542099588,1.62921138715834,10.3060095422728));
#49687=CARTESIAN_POINT('',(1.25206542099587,1.62921138715835,10.2479916911084));
#49688=CARTESIAN_POINT('',(1.25206542099588,1.62921138715835,18.5459252805377));
#49689=CARTESIAN_POINT('',(-2.0547493654031,0.0016148918149348,9.79592528057681));
#49690=CARTESIAN_POINT('Ctrl Pts',(1.25206542099587,1.62921138715835,10.2479916911084));
#49691=CARTESIAN_POINT('Ctrl Pts',(1.30857145584848,1.58578592814536,10.2441287597561));
#49692=CARTESIAN_POINT('Ctrl Pts',(1.36275485896034,1.53946409868074,10.2402658284038));
#49693=CARTESIAN_POINT('Ctrl Pts',(1.41431998267322,1.49053565845008,10.2364028970515));
#49694=CARTESIAN_POINT('Ctrl Pts',(1.4659685929782,1.44152800055373,10.2325337114143));
#49695=CARTESIAN_POINT('Ctrl Pts',(1.51499013745528,1.38990566754411,10.2286645257772));
#49696=CARTESIAN_POINT('Ctrl Pts',(1.56112811870158,1.33599272434368,10.22479534014));
#49697=CARTESIAN_POINT('Ctrl Pts',(1.5680318152698,1.327925648349,10.2242163879864));
#49698=CARTESIAN_POINT('Ctrl Pts',(1.5748710286009,1.31980734010624,10.2236374358328));
#49699=CARTESIAN_POINT('Ctrl Pts',(1.58164498343667,1.31163893997915,10.2230584836792));
#49700=CARTESIAN_POINT('Ctrl Pts',(1.62691468715583,1.25705028939348,10.2191894008323));
#49701=CARTESIAN_POINT('Ctrl Pts',(1.66944364287453,1.2000083218721,10.2153203179854));
#49702=CARTESIAN_POINT('Ctrl Pts',(1.70895533975419,1.14081953403053,10.2114512351385));
#49703=CARTESIAN_POINT('Ctrl Pts',(1.74840816617605,1.08171893453096,10.207587917032));
#49704=CARTESIAN_POINT('Ctrl Pts',(1.78485238981659,1.0204782646924,10.2037245989256));
#49705=CARTESIAN_POINT('Ctrl Pts',(1.81805164243257,0.957437093467896,10.1998612808192));
#49706=CARTESIAN_POINT('Ctrl Pts',(1.851211952338,0.894469869512967,10.1960024943834));
#49707=CARTESIAN_POINT('Ctrl Pts',(1.88113462665997,0.829706767031211,10.1921437079476));
#49708=CARTESIAN_POINT('Ctrl Pts',(1.90762748561629,0.763514858153578,10.1882849215118));
#49709=CARTESIAN_POINT('Ctrl Pts',(1.9341036560141,0.697364645324893,10.1844285658285));
#49710=CARTESIAN_POINT('Ctrl Pts',(1.95715411742514,0.629787861706434,10.1805722101452));
#49711=CARTESIAN_POINT('Ctrl Pts',(1.97663403516038,0.561173282993416,10.176715854462));
#49712=CARTESIAN_POINT('Ctrl Pts',(1.99610819833286,0.492578973714011,10.1728606379848));
#49713=CARTESIAN_POINT('Ctrl Pts',(2.01201377924935,0.422947945037063,10.1690054215076));
#49714=CARTESIAN_POINT('Ctrl Pts',(2.02425575608784,0.352684273033582,10.1651502050304));
#49715=CARTESIAN_POINT('Ctrl Pts',(2.03649821155102,0.282417853930677,10.1612948378257));
#49716=CARTESIAN_POINT('Ctrl Pts',(2.04507669734875,0.211519221345956,10.1574394706211));
#49717=CARTESIAN_POINT('Ctrl Pts',(2.04994758497279,0.140401073230255,10.1535841034165));
#49718=CARTESIAN_POINT('Ctrl Pts',(2.05482357108796,0.0692084838064535,
10.1497247006937));
#49719=CARTESIAN_POINT('Ctrl Pts',(2.05598417873304,-0.00220359418590887,
10.1458652979709));
#49720=CARTESIAN_POINT('Ctrl Pts',(2.05343787109383,-0.073419834225099,
10.1420058952481));
#49721=CARTESIAN_POINT('Ctrl Pts',(2.05089012171523,-0.144676397458819,
10.1381443073012));
#49722=CARTESIAN_POINT('Ctrl Pts',(2.04463132146234,-0.215736417862735,
10.1342827193543));
#49723=CARTESIAN_POINT('Ctrl Pts',(2.03472183547422,-0.286189822922526,
10.1304211314073));
#49724=CARTESIAN_POINT('Ctrl Pts',(2.02479501248517,-0.356766488739775,
10.1265527874739));
#49725=CARTESIAN_POINT('Ctrl Pts',(2.0112048445784,-0.426733943285215,10.1226844435404));
#49726=CARTESIAN_POINT('Ctrl Pts',(1.99406266002678,-0.49569312118175,10.118816099607));
#49727=CARTESIAN_POINT('Ctrl Pts',(1.98388412414919,-0.536639096544201,
10.1165191883005));
#49728=CARTESIAN_POINT('Ctrl Pts',(1.97245423162198,-0.57722987554729,10.1142222769941));
#49729=CARTESIAN_POINT('Ctrl Pts',(1.95980437203989,-0.617385119543161,
10.1119253656877));
#49730=CARTESIAN_POINT('Ctrl Pts',(1.93849603741333,-0.685025504839332,
10.1080562828408));
#49731=CARTESIAN_POINT('Ctrl Pts',(1.91364006230091,-0.751693927907768,
10.1041871999939));
#49732=CARTESIAN_POINT('Ctrl Pts',(1.88534397061039,-0.816991845114166,
10.1003181171469));
#49733=CARTESIAN_POINT('Ctrl Pts',(1.85709003868528,-0.882192471680514,
10.0964547990405));
#49734=CARTESIAN_POINT('Ctrl Pts',(1.8254063559399,-0.946026203568283,10.0925914809341));
#49735=CARTESIAN_POINT('Ctrl Pts',(1.7904500040004,-1.00811028448031,10.0887281628276));
#49736=CARTESIAN_POINT('Ctrl Pts',(1.75553465584828,-1.0701215407893,10.0848693763919));
#49737=CARTESIAN_POINT('Ctrl Pts',(1.7173545009178,-1.13038680152145,10.0810105899561));
#49738=CARTESIAN_POINT('Ctrl Pts',(1.67611369411628,-1.18854551738496,10.0771518035203));
#49739=CARTESIAN_POINT('Ctrl Pts',(1.63489886599898,-1.24666759752208,10.073295447837));
#49740=CARTESIAN_POINT('Ctrl Pts',(1.59062749143636,-1.30268537014652,10.0694390921537));
#49741=CARTESIAN_POINT('Ctrl Pts',(1.54354763826478,-1.3562662905592,10.0655827364705));
#49742=CARTESIAN_POINT('Ctrl Pts',(1.49648169295327,-1.40983138263144,10.0617275199933));
#49743=CARTESIAN_POINT('Ctrl Pts',(1.44660923659695,-1.46096068690869,10.0578723035161));
#49744=CARTESIAN_POINT('Ctrl Pts',(1.39421820890273,-1.50935520950638,10.0540170870389));
#49745=CARTESIAN_POINT('Ctrl Pts',(1.34182513287606,-1.55775162418514,10.0501617198343));
#49746=CARTESIAN_POINT('Ctrl Pts',(1.28691364835081,-1.60341271690293,10.0463063526296));
#49747=CARTESIAN_POINT('Ctrl Pts',(1.22980681328235,-1.64607799466013,10.042450985425));
#49748=CARTESIAN_POINT('Ctrl Pts',(1.17264020292981,-1.68878793132891,10.0385915827022));
#49749=CARTESIAN_POINT('Ctrl Pts',(1.11327404480641,-1.72849550192885,10.0347321799794));
#49750=CARTESIAN_POINT('Ctrl Pts',(1.05206185872653,-1.76498255173044,10.0308727772566));
#49751=CARTESIAN_POINT('Ctrl Pts',(0.990815013826058,-1.80149026078623,
10.0270111893097));
#49752=CARTESIAN_POINT('Ctrl Pts',(0.927720490096649,-1.83477359228649,
10.0231496013628));
#49753=CARTESIAN_POINT('Ctrl Pts',(0.863155543885299,-1.86466084571969,
10.0192880134159));
#49754=CARTESIAN_POINT('Ctrl Pts',(0.798477638986301,-1.89460038797404,
10.0154196694824));
#49755=CARTESIAN_POINT('Ctrl Pts',(0.732324626438617,-1.92113180878327,
10.011551325549));
#49756=CARTESIAN_POINT('Ctrl Pts',(0.665092156530011,-1.94413219350492,
10.0076829816155));
#49757=CARTESIAN_POINT('Ctrl Pts',(0.625171450679649,-1.95778916005942,
10.0053860703091));
#49758=CARTESIAN_POINT('Ctrl Pts',(0.58487044581956,-1.97020216898538,10.0030891590026));
#49759=CARTESIAN_POINT('Ctrl Pts',(0.544273662203676,-1.9813540176181,10.0007922476961));
#49760=CARTESIAN_POINT('Ctrl Pts',(0.475889515769289,-2.00013899470224,
9.99692316484918));
#49761=CARTESIAN_POINT('Ctrl Pts',(0.406397776570062,-2.01541630848205,
9.99305408200225));
#49762=CARTESIAN_POINT('Ctrl Pts',(0.336191593147607,-2.02706013112509,
9.98918499915532));
#49763=CARTESIAN_POINT('Ctrl Pts',(0.266090013437113,-2.0386866050531,9.98532168104887));
#49764=CARTESIAN_POINT('Ctrl Pts',(0.195276577811771,-2.04669025509523,
9.98145836294242));
#49765=CARTESIAN_POINT('Ctrl Pts',(0.124158050480217,-2.05099545123848,
9.97759504483598));
#49766=CARTESIAN_POINT('Ctrl Pts',(0.0531229451538365,-2.05529559738832,
9.97373625840018));
#49767=CARTESIAN_POINT('Ctrl Pts',(-0.0182160584807071,-2.05590587773127,
9.96987747196439));
#49768=CARTESIAN_POINT('Ctrl Pts',(-0.0894453214332187,-2.05280225471761,
9.96601868552859));
#49769=CARTESIAN_POINT('Ctrl Pts',(-0.160629715173089,-2.04970058675887,
9.9621623298453));
#49770=CARTESIAN_POINT('Ctrl Pts',(-0.23170402120557,-2.04288967804532,
9.95830597416201));
#49771=CARTESIAN_POINT('Ctrl Pts',(-0.30225431061661,-2.03239757287143,
9.95444961847871));
#49772=CARTESIAN_POINT('Ctrl Pts',(-0.372783758765723,-2.02190856717046,
9.9505944020015));
#49773=CARTESIAN_POINT('Ctrl Pts',(-0.442789017377062,-2.00774059534358,
9.94673918552429));
#49774=CARTESIAN_POINT('Ctrl Pts',(-0.511862718967743,-1.98997339666412,
9.94288396904708));
#49775=CARTESIAN_POINT('Ctrl Pts',(-0.5809391211336,-1.97220550334033,9.93902860184243));
#49776=CARTESIAN_POINT('Ctrl Pts',(-0.649083424049654,-1.95083822693263,
9.93517323463779));
#49777=CARTESIAN_POINT('Ctrl Pts',(-0.715901558653159,-1.92600169283881,
9.93131786743315));
#49778=CARTESIAN_POINT('Ctrl Pts',(-0.78278963362311,-1.90113916166642,
9.92745846471035));
#49779=CARTESIAN_POINT('Ctrl Pts',(-0.848348312971446,-1.87280029338593,
9.92359906198755));
#49780=CARTESIAN_POINT('Ctrl Pts',(-0.912202575503724,-1.84116376885501,
9.91973965926475));
#49781=CARTESIAN_POINT('Ctrl Pts',(-0.976092992821027,-1.80950933147538,
9.91587807131782));
#49782=CARTESIAN_POINT('Ctrl Pts',(-1.03827664853373,-1.77455375906357,
9.91201648337088));
#49783=CARTESIAN_POINT('Ctrl Pts',(-1.09840467494435,-1.73652087017703,
9.90815489542395));
#49784=CARTESIAN_POINT('Ctrl Pts',(-1.15863789749239,-1.69842144138814,
9.90428655149049));
#49785=CARTESIAN_POINT('Ctrl Pts',(-1.21680791384032,-1.65723422786973,
9.90041820755702));
#49786=CARTESIAN_POINT('Ctrl Pts',(-1.27259686640149,-1.61322496203261,
9.89654986362356));
#49787=CARTESIAN_POINT('Ctrl Pts',(-1.30572274096442,-1.58709352645621,
9.89425295231723));
#49788=CARTESIAN_POINT('Ctrl Pts',(-1.33800979227511,-1.55996789096557,
9.8919560410109));
#49789=CARTESIAN_POINT('Ctrl Pts',(-1.36939772568353,-1.53190973343496,
9.88965912970457));
#49790=CARTESIAN_POINT('Ctrl Pts',(-1.42276852495404,-1.48420075323606,
9.88575355265758));
#49791=CARTESIAN_POINT('Ctrl Pts',(-1.47376547698587,-1.43358958402843,
9.88184797561058));
#49792=CARTESIAN_POINT('Ctrl Pts',(-1.52205085019631,-1.3803473374179,9.8779423985636));
#49793=CARTESIAN_POINT('Ctrl Pts',(-1.56909432278065,-1.32847448230223,
9.87413727302516));
#49794=CARTESIAN_POINT('Ctrl Pts',(-1.61356363799311,-1.27410464308286,
9.87033214748672));
#49795=CARTESIAN_POINT('Ctrl Pts',(-1.6551798379899,-1.2175291645015,9.86652702194828));
#49796=CARTESIAN_POINT('Ctrl Pts',(-1.69675650695488,-1.16100742670001,
9.86272551088062));
#49797=CARTESIAN_POINT('Ctrl Pts',(-1.73548513649758,-1.10228460370845,
9.85892399981296));
#49798=CARTESIAN_POINT('Ctrl Pts',(-1.77112604724776,-1.0416861750357,9.85512248874529));
#49799=CARTESIAN_POINT('Ctrl Pts',(-1.80674585565399,-0.981123625605609,
9.85132322848415));
#49800=CARTESIAN_POINT('Ctrl Pts',(-1.8392813171203,-0.918688104157346,
9.847523968223));
#49801=CARTESIAN_POINT('Ctrl Pts',(-1.86853633227469,-0.854733606142541,
9.84372470796185));
#49802=CARTESIAN_POINT('Ctrl Pts',(-1.89920837710276,-0.787681334259777,
9.83974142234643));
#49803=CARTESIAN_POINT('Ctrl Pts',(-1.92627380211056,-0.718959700575715,
9.83575813673102));
#49804=CARTESIAN_POINT('Ctrl Pts',(-1.94956209011008,-0.649003250612513,
9.8317748511156));
#49805=CARTESIAN_POINT('Ctrl Pts',(-1.9717826685226,-0.582254128397057,
9.82797418915372));
#49806=CARTESIAN_POINT('Ctrl Pts',(-1.99056476797815,-0.514381463802514,
9.82417352719185));
#49807=CARTESIAN_POINT('Ctrl Pts',(-2.00581132846463,-0.44577850677547,
9.82037286522998));
#49808=CARTESIAN_POINT('Ctrl Pts',(-2.02106384368285,-0.377148756019672,
9.81657071887282));
#49809=CARTESIAN_POINT('Ctrl Pts',(-2.03277798733833,-0.30778863949544,
9.81276857251567));
#49810=CARTESIAN_POINT('Ctrl Pts',(-2.04090813970047,-0.238099827392568,
9.80896642615852));
#49811=CARTESIAN_POINT('Ctrl Pts',(-2.04904829932559,-0.168325236544232,
9.80515959980561));
#49812=CARTESIAN_POINT('Ctrl Pts',(-2.05359564008046,-0.0982216428501038,
9.80135277345271));
#49813=CARTESIAN_POINT('Ctrl Pts',(-2.05455657900118,-0.0281926618634648,
9.7975459470998));
#49814=CARTESIAN_POINT('Ctrl Pts',(-2.05469294469403,-0.0182549329345308,
9.79700572492547));
#49815=CARTESIAN_POINT('Ctrl Pts',(-2.05475717252371,-0.0083187000115196,
9.79646550275115));
#49816=CARTESIAN_POINT('Ctrl Pts',(-2.0547493654031,0.00161489181494824,
9.79592528057682));
#49817=CARTESIAN_POINT('Ctrl Pts',(-2.05474936540253,0.00161489253451075,
9.79592528053768));
#49818=CARTESIAN_POINT('Ctrl Pts',(-2.05466554911524,0.108260665819365,
9.79012552426279));
#49819=CARTESIAN_POINT('Ctrl Pts',(-2.04627725539838,0.214587344483438,
9.7843257679879));
#49820=CARTESIAN_POINT('Ctrl Pts',(-2.02974241605634,0.319598634167586,
9.77852601171301));
#49821=CARTESIAN_POINT('Ctrl Pts',(-2.01871183817646,0.389652850308721,
9.77465692886612));
#49822=CARTESIAN_POINT('Ctrl Pts',(-2.00402863742738,0.45927254399467,9.77078784601923));
#49823=CARTESIAN_POINT('Ctrl Pts',(-1.98573997994474,0.528047625265998,
9.76691876317234));
#49824=CARTESIAN_POINT('Ctrl Pts',(-1.96747857164965,0.596720235096198,
9.76305544506593));
#49825=CARTESIAN_POINT('Ctrl Pts',(-1.9456224936184,0.664550264817994,9.75919212695952));
#49826=CARTESIAN_POINT('Ctrl Pts',(-1.92027026428373,0.731135879715741,
9.75532880885311));
#49827=CARTESIAN_POINT('Ctrl Pts',(-1.8949477731043,0.797643389712853,9.75147002241735));
#49828=CARTESIAN_POINT('Ctrl Pts',(-1.86613744858043,0.862908932554423,
9.7476112359816));
#49829=CARTESIAN_POINT('Ctrl Pts',(-1.83398765757475,0.926545646130553,
9.74375244954584));
#49830=CARTESIAN_POINT('Ctrl Pts',(-1.80185811857994,0.990142273243446,
9.73989609386258));
#49831=CARTESIAN_POINT('Ctrl Pts',(-1.76639350518624,1.05211167417853,9.73603973817932));
#49832=CARTESIAN_POINT('Ctrl Pts',(-1.7277897680421,1.11208816194986,9.73218338249606));
#49833=CARTESIAN_POINT('Ctrl Pts',(-1.6891974348285,1.17204693206609,9.72832816601889));
#49834=CARTESIAN_POINT('Ctrl Pts',(-1.64746808164534,1.23001354954329,9.72447294954172));
#49835=CARTESIAN_POINT('Ctrl Pts',(-1.60284207001888,1.28564958720391,9.72061773306455));
#49836=CARTESIAN_POINT('Ctrl Pts',(-1.55821431364881,1.34128780006724,9.71676236585994));
#49837=CARTESIAN_POINT('Ctrl Pts',(-1.51068997966217,1.39459487464493,9.71290699865533));
#49838=CARTESIAN_POINT('Ctrl Pts',(-1.46054987438482,1.44526524449129,9.70905163145072));
#49839=CARTESIAN_POINT('Ctrl Pts',(-1.41035728608979,1.49598865239775,9.70519222872796));
#49840=CARTESIAN_POINT('Ctrl Pts',(-1.35754380323296,1.54406950016236,9.7013328260052));
#49841=CARTESIAN_POINT('Ctrl Pts',(-1.3024266418318,1.58923956820447,9.69747342328243));
#49842=CARTESIAN_POINT('Ctrl Pts',(-1.2472782726609,1.63443521189393,9.69361183533553));
#49843=CARTESIAN_POINT('Ctrl Pts',(-1.18982401980682,1.6767165069229,9.68975024738863));
#49844=CARTESIAN_POINT('Ctrl Pts',(-1.13041146921395,1.71585764933154,9.68588865944173));
#49845=CARTESIAN_POINT('Ctrl Pts',(-1.07089497423428,1.75506727057177,9.6820203155083));
#49846=CARTESIAN_POINT('Ctrl Pts',(-1.00941376035066,1.79112552480892,9.67815197157487));
#49847=CARTESIAN_POINT('Ctrl Pts',(-0.94634084619215,1.82385212265916,9.67428362764144));
#49848=CARTESIAN_POINT('Ctrl Pts',(-0.908889964841267,1.84328423467522,
9.67198671633478));
#49849=CARTESIAN_POINT('Ctrl Pts',(-0.870878325287496,1.86154263115638,
9.66968980502811));
#49850=CARTESIAN_POINT('Ctrl Pts',(-0.832386957370501,1.87859775250038,
9.66739289372144));
#49851=CARTESIAN_POINT('Ctrl Pts',(-0.767549324792952,1.90732662733934,
9.66352381087445));
#49852=CARTESIAN_POINT('Ctrl Pts',(-0.701095638141634,1.9327511364569,9.65965472802746));
#49853=CARTESIAN_POINT('Ctrl Pts',(-0.633396009540079,1.95468848096025,
9.65578564518046));
#49854=CARTESIAN_POINT('Ctrl Pts',(-0.565797250008816,1.97659313991436,
9.65192232707395));
#49855=CARTESIAN_POINT('Ctrl Pts',(-0.496956691774747,1.9950207990505,9.64805900896744));
#49856=CARTESIAN_POINT('Ctrl Pts',(-0.427265363933371,2.00983627972103,
9.64419569086093));
#49857=CARTESIAN_POINT('Ctrl Pts',(-0.357655783992714,2.02463438183845,
9.64033690442507));
#49858=CARTESIAN_POINT('Ctrl Pts',(-0.287197889574732,2.03582862124997,
9.63647811798921));
#49859=CARTESIAN_POINT('Ctrl Pts',(-0.216297167600942,2.0433338194695,9.63261933155335));
#49860=CARTESIAN_POINT('Ctrl Pts',(-0.145441107883076,2.05083428996448,
9.62876297586999));
#49861=CARTESIAN_POINT('Ctrl Pts',(-0.0741432559817849,2.0546502786848,
9.62490662018664));
#49862=CARTESIAN_POINT('Ctrl Pts',(-0.00281711740553753,2.0547480688273,
9.62105026450328));
#49863=CARTESIAN_POINT('Ctrl Pts',(0.0684879507151712,2.05484583008161,
9.61719504802601));
#49864=CARTESIAN_POINT('Ctrl Pts',(0.139820803403486,2.05122757270765,9.61333983154874));
#49865=CARTESIAN_POINT('Ctrl Pts',(0.21076674943155,2.04391167613331,9.60948461507146));
#49866=CARTESIAN_POINT('Ctrl Pts',(0.281715469233902,2.03659549352929,9.60562924786676));
#49867=CARTESIAN_POINT('Ctrl Pts',(0.352276769348831,2.02558143672748,9.60177388066205));
#49868=CARTESIAN_POINT('Ctrl Pts',(0.422041629472952,2.01093968718403,9.59791851345734));
#49869=CARTESIAN_POINT('Ctrl Pts',(0.491879514381641,1.99628261172143,9.59405911073448));
#49870=CARTESIAN_POINT('Ctrl Pts',(0.560918818736848,1.97799036342823,9.59019970801162));
#49871=CARTESIAN_POINT('Ctrl Pts',(0.62876215067166,1.95618396895148,9.58634030528876));
#49872=CARTESIAN_POINT('Ctrl Pts',(0.696643896033928,1.93436522752288,9.58247871734177));
#49873=CARTESIAN_POINT('Ctrl Pts',(0.763327866616845,1.9090285515789,9.57861712939477));
#49874=CARTESIAN_POINT('Ctrl Pts',(0.828435833268841,1.88034348794473,9.57475554144777));
#49875=CARTESIAN_POINT('Ctrl Pts',(0.893657708642155,1.85160823876358,9.57088719751425));
#49876=CARTESIAN_POINT('Ctrl Pts',(0.957297641224268,1.8195131247985,9.56701885358073));
#49877=CARTESIAN_POINT('Ctrl Pts',(1.01900184597678,1.78427374592463,9.5631505096472));
#49878=CARTESIAN_POINT('Ctrl Pts',(1.05564002705512,1.76334961685681,9.56085359834143));
#49879=CARTESIAN_POINT('Ctrl Pts',(1.09159627510292,1.74131777606738,9.55855668703566));
#49880=CARTESIAN_POINT('Ctrl Pts',(1.12680180713025,1.71823026685832,9.55625977572989));
#49881=CARTESIAN_POINT('Ctrl Pts',(1.16958951638453,1.69017042584594,9.55346818112885));
#49882=CARTESIAN_POINT('Ctrl Pts',(1.21138883555603,1.66047175427513,9.55067658652781));
#49883=CARTESIAN_POINT('Ctrl Pts',(1.25206542099588,1.62921138715834,9.54788499192677));
#49884=CARTESIAN_POINT('',(-2.05474925034019,-0.0017551998270615,9.85407473953553));
#49885=CARTESIAN_POINT('Ctrl Pts',(-2.05341023593874,-0.00175368529942944,
9.85407471946233));
#49886=CARTESIAN_POINT('Ctrl Pts',(-2.04952255586939,0.476750142715482,
9.82816558982444));
#49887=CARTESIAN_POINT('Ctrl Pts',(-1.64442914339024,1.64534304864115,9.76521208752269));
#49888=CARTESIAN_POINT('Ctrl Pts',(-0.0359990651139381,2.27726163037769,
9.68255192549311));
#49889=CARTESIAN_POINT('Ctrl Pts',(0.960392961764501,1.84839376068804,9.6258008931014));
#49890=CARTESIAN_POINT('Ctrl Pts',(1.25005255340789,1.62658210076147,9.60609423337355));
#49891=CARTESIAN_POINT('Ctrl Pts',(1.25206542099588,1.62921138715834,10.3060095422728));
#49892=CARTESIAN_POINT('Ctrl Pts',(1.30851140146314,1.58583208054759,10.3021514635839));
#49893=CARTESIAN_POINT('Ctrl Pts',(1.36275851760942,1.53947116858342,10.2982933848949));
#49894=CARTESIAN_POINT('Ctrl Pts',(1.41448006564251,1.49038374467785,10.294435306206));
#49895=CARTESIAN_POINT('Ctrl Pts',(1.46617322566471,1.44132326301158,10.2905793450712));
#49896=CARTESIAN_POINT('Ctrl Pts',(1.51534321631979,1.38953957251344,10.2867233839364));
#49897=CARTESIAN_POINT('Ctrl Pts',(1.56169756025049,1.33532703590081,10.2828674228016));
#49898=CARTESIAN_POINT('Ctrl Pts',(1.60804196821539,1.28112611964272,10.2790122881848));
#49899=CARTESIAN_POINT('Ctrl Pts',(1.65157161248229,1.22449776034556,10.275157153568));
#49900=CARTESIAN_POINT('Ctrl Pts',(1.69203312206044,1.16577076492353,10.2713020189511));
#49901=CARTESIAN_POINT('Ctrl Pts',(1.73249949335545,1.10703671306623,10.2674464211145));
#49902=CARTESIAN_POINT('Ctrl Pts',(1.7698967246232,1.04620392594292,10.2635908232779));
#49903=CARTESIAN_POINT('Ctrl Pts',(1.80401473488021,0.983630214478525,10.2597352254412));
#49904=CARTESIAN_POINT('Ctrl Pts',(1.83817015564835,0.920987890732478,10.2558753999288));
#49905=CARTESIAN_POINT('Ctrl Pts',(1.86903894831024,0.856601261111506,10.2520155744164));
#49906=CARTESIAN_POINT('Ctrl Pts',(1.89645743256838,0.790851926062102,10.248155748904));
#49907=CARTESIAN_POINT('Ctrl Pts',(1.92389343440825,0.725060583973251,10.2442934573614));
#49908=CARTESIAN_POINT('Ctrl Pts',(1.94787457831404,0.657905261353421,10.2404311658188));
#49909=CARTESIAN_POINT('Ctrl Pts',(1.9682866322125,0.589784109614337,10.2365688742763));
#49910=CARTESIAN_POINT('Ctrl Pts',(1.98873291175794,0.52154873661644,10.2327001066864));
#49911=CARTESIAN_POINT('Ctrl Pts',(2.00559804624542,0.452344774535711,10.2288313390965));
#49912=CARTESIAN_POINT('Ctrl Pts',(2.01881877631864,0.38258111673645,10.2249625715066));
#49913=CARTESIAN_POINT('Ctrl Pts',(2.02346945516632,0.358040235418474,10.2236016485094));
#49914=CARTESIAN_POINT('Ctrl Pts',(2.02766963312196,0.33343014000644,10.2222407255122));
#49915=CARTESIAN_POINT('Ctrl Pts',(2.03141808692682,0.308768713775479,10.2208798025149));
#49916=CARTESIAN_POINT('Ctrl Pts',(2.04207488260764,0.23865666378834,10.217010719668));
#49917=CARTESIAN_POINT('Ctrl Pts',(2.04911853507526,0.167854932925696,10.2131416368211));
#49918=CARTESIAN_POINT('Ctrl Pts',(2.05247006878331,0.0967686894023167,
10.2092725539742));
#49919=CARTESIAN_POINT('Ctrl Pts',(2.05581660887328,0.0257883608366547,
10.2054092358677));
#49920=CARTESIAN_POINT('Ctrl Pts',(2.05548192698947,-0.0454751576497036,
10.2015459177613));
#49921=CARTESIAN_POINT('Ctrl Pts',(2.05143849348082,-0.116609047526893,
10.1976825996549));
#49922=CARTESIAN_POINT('Ctrl Pts',(2.04739980291812,-0.187659497378737,
10.1938238132191));
#49923=CARTESIAN_POINT('Ctrl Pts',(2.0396610294618,-0.258580138006337,10.1899650267833));
#49924=CARTESIAN_POINT('Ctrl Pts',(2.02824668591195,-0.328957358311389,
10.1861062403475));
#49925=CARTESIAN_POINT('Ctrl Pts',(2.01683953256154,-0.399290246128239,
10.1822498846642));
#49926=CARTESIAN_POINT('Ctrl Pts',(2.00176148030334,-0.469079914386366,
10.178393528981));
#49927=CARTESIAN_POINT('Ctrl Pts',(1.98308880014757,-0.53791855631617,10.1745371732977));
#49928=CARTESIAN_POINT('Ctrl Pts',(1.9644216360885,-0.606736862621825,10.1706819568205));
#49929=CARTESIAN_POINT('Ctrl Pts',(1.94216207938165,-0.674604231762789,
10.1668267403433));
#49930=CARTESIAN_POINT('Ctrl Pts',(1.91643697360225,-0.741125420364361,
10.1629715238661));
#49931=CARTESIAN_POINT('Ctrl Pts',(1.89071086204816,-0.807649209745421,
10.1591161566615));
#49932=CARTESIAN_POINT('Ctrl Pts',(1.86151910968989,-0.872826261805287,
10.1552607894568));
#49933=CARTESIAN_POINT('Ctrl Pts',(1.82903704474084,-0.936280434199973,
10.1514054222522));
#49934=CARTESIAN_POINT('Ctrl Pts',(1.79652097992722,-0.999801025810044,
10.1475460195294));
#49935=CARTESIAN_POINT('Ctrl Pts',(1.76070794921565,-1.06159470448789,10.1436866168066));
#49936=CARTESIAN_POINT('Ctrl Pts',(1.72181927482045,-1.12130992475621,10.1398272140838));
#49937=CARTESIAN_POINT('Ctrl Pts',(1.68290858135236,-1.18105895625128,10.1359656261369));
#49938=CARTESIAN_POINT('Ctrl Pts',(1.64091906358225,-1.23872679371579,10.13210403819));
#49939=CARTESIAN_POINT('Ctrl Pts',(1.59611381224928,-1.29399314559509,10.1282424502431));
#49940=CARTESIAN_POINT('Ctrl Pts',(1.55123017252307,-1.349356187938,10.1243741063096));
#49941=CARTESIAN_POINT('Ctrl Pts',(1.50352128915094,-1.40230899529215,10.1205057623762));
#49942=CARTESIAN_POINT('Ctrl Pts',(1.45328825158113,-1.45256697618948,10.1166374184427));
#49943=CARTESIAN_POINT('Ctrl Pts',(1.42346131945304,-1.48240871894766,10.1143405071363));
#49944=CARTESIAN_POINT('Ctrl Pts',(1.39274513387088,-1.51130110075618,10.1120435958298));
#49945=CARTESIAN_POINT('Ctrl Pts',(1.36120800223661,-1.53919145565034,10.1097466845234));
#49946=CARTESIAN_POINT('Ctrl Pts',(1.30808458614967,-1.58617197832557,10.1058776016765));
#49947=CARTESIAN_POINT('Ctrl Pts',(1.25242204857328,-1.63049104920695,10.1020085188295));
#49948=CARTESIAN_POINT('Ctrl Pts',(1.19451794994457,-1.6718625630596,10.0981394359826));
#49949=CARTESIAN_POINT('Ctrl Pts',(1.13670012553504,-1.71317243541989,10.0942761178762));
#49950=CARTESIAN_POINT('Ctrl Pts',(1.07664776155301,-1.75154318807345,10.0904127997698));
#49951=CARTESIAN_POINT('Ctrl Pts',(1.01469274895957,-1.78672778780341,10.0865494816633));
#49952=CARTESIAN_POINT('Ctrl Pts',(0.952810409571998,-1.82187111601146,
10.0826906952275));
#49953=CARTESIAN_POINT('Ctrl Pts',(0.88903027506293,-1.85383547622168,10.0788319087917));
#49954=CARTESIAN_POINT('Ctrl Pts',(0.823713129057717,-1.88241712792833,
10.074973122356));
#49955=CARTESIAN_POINT('Ctrl Pts',(0.758437128065021,-1.91098077529019,
10.0711167666727));
#49956=CARTESIAN_POINT('Ctrl Pts',(0.691626480467066,-1.93616574745647,
10.0672604109894));
#49957=CARTESIAN_POINT('Ctrl Pts',(0.623665166115261,-1.95781493585947,
10.0634040553061));
#49958=CARTESIAN_POINT('Ctrl Pts',(0.555723928216199,-1.97945772887545,
10.0595488388289));
#49959=CARTESIAN_POINT('Ctrl Pts',(0.486633161009463,-1.99756666439603,
10.0556936223517));
#49960=CARTESIAN_POINT('Ctrl Pts',(0.416793718986835,-2.01203393567632,
10.0518384058745));
#49961=CARTESIAN_POINT('Ctrl Pts',(0.346951546450887,-2.02650177258365,
10.0479830386699));
#49962=CARTESIAN_POINT('Ctrl Pts',(0.276361117116424,-2.03732756619642,
10.0441276714652));
#49963=CARTESIAN_POINT('Ctrl Pts',(0.205433535181078,-2.0444546033412,10.0402723042606));
#49964=CARTESIAN_POINT('Ctrl Pts',(0.134431711408507,-2.05158910055041,
10.0364129015378));
#49965=CARTESIAN_POINT('Ctrl Pts',(0.0630925148932319,-2.05501706406355,
10.032553498815));
#49966=CARTESIAN_POINT('Ctrl Pts',(-0.00816866856745738,-2.05473376264513,
10.0286940960922));
#49967=CARTESIAN_POINT('Ctrl Pts',(-0.0794702006701796,-2.05445030081923,
10.0248325081453));
#49968=CARTESIAN_POINT('Ctrl Pts',(-0.15069314653743,-2.05045141817204,
10.0209709201983));
#49969=CARTESIAN_POINT('Ctrl Pts',(-0.221425723400285,-2.04278442609999,
10.0171093322514));
#49970=CARTESIAN_POINT('Ctrl Pts',(-0.292282049441501,-2.03510402035051,
10.013240988318));
#49971=CARTESIAN_POINT('Ctrl Pts',(-0.362645813896895,-2.02374276993654,
10.0093726443845));
#49972=CARTESIAN_POINT('Ctrl Pts',(-0.432114617069166,-2.00879927325135,
10.005504300451));
#49973=CARTESIAN_POINT('Ctrl Pts',(-0.473363193254439,-1.99992625495615,
10.0032073891446));
#49974=CARTESIAN_POINT('Ctrl Pts',(-0.514296493476365,-1.9897912307239,
10.0009104778382));
#49975=CARTESIAN_POINT('Ctrl Pts',(-0.5548332227254,-1.97842302287962,9.99861356653179));
#49976=CARTESIAN_POINT('Ctrl Pts',(-0.623116209259948,-1.95927359475523,
9.99474448368487));
#49977=CARTESIAN_POINT('Ctrl Pts',(-0.690540391634209,-1.93654744760311,
9.99087540083796));
#49978=CARTESIAN_POINT('Ctrl Pts',(-0.756704012451471,-1.91033939394021,
9.98700631799105));
#49979=CARTESIAN_POINT('Ctrl Pts',(-0.822769052773433,-1.88417038897021,
9.98314299988462));
#49980=CARTESIAN_POINT('Ctrl Pts',(-0.887576811699232,-1.8545299527043,
9.97927968177818));
#49981=CARTESIAN_POINT('Ctrl Pts',(-0.950739737326332,-1.8215629317618,
9.97541636367175));
#49982=CARTESIAN_POINT('Ctrl Pts',(-1.0138285728661,-1.78863458112212,9.97155757723597));
#49983=CARTESIAN_POINT('Ctrl Pts',(-1.07527597896355,-1.7523876203456,9.96769879080019));
#49984=CARTESIAN_POINT('Ctrl Pts',(-1.13471510454231,-1.71301465084906,
9.96384000436441));
#49985=CARTESIAN_POINT('Ctrl Pts',(-1.19411678783038,-1.67366648343625,
9.95998364868113));
#49986=CARTESIAN_POINT('Ctrl Pts',(-1.25151229644495,-1.63119648171335,
9.95612729299785));
#49987=CARTESIAN_POINT('Ctrl Pts',(-1.30656137516673,-1.58584202725947,
9.95227093731457));
#49988=CARTESIAN_POINT('Ctrl Pts',(-1.36159419183955,-1.54050097096548,
9.94841572083736));
#49989=CARTESIAN_POINT('Ctrl Pts',(-1.41428158001253,-1.49227746231644,
9.94456050436016));
#49990=CARTESIAN_POINT('Ctrl Pts',(-1.46431555208567,-1.44144980017343,
9.94070528788295));
#49991=CARTESIAN_POINT('Ctrl Pts',(-1.51435148033746,-1.39062015082088,
9.93684992067832));
#49992=CARTESIAN_POINT('Ctrl Pts',(-1.56173344730898,-1.33718649357301,
9.93299455347368));
#49993=CARTESIAN_POINT('Ctrl Pts',(-1.60619083156095,-1.28146345055548,
9.92913918626905));
#49994=CARTESIAN_POINT('Ctrl Pts',(-1.65069475057122,-1.22568208070693,
9.92527978354626));
#49995=CARTESIAN_POINT('Ctrl Pts',(-1.69226767235597,-1.16760692192484,
9.92142038082348));
#49996=CARTESIAN_POINT('Ctrl Pts',(-1.73068032496605,-1.10758438742852,
9.91756097810069));
#49997=CARTESIAN_POINT('Ctrl Pts',(-1.76911472712186,-1.04752786770153,
9.91369939015376));
#49998=CARTESIAN_POINT('Ctrl Pts',(-1.80438505772054,-0.985522199735724,
9.90983780220683));
#49999=CARTESIAN_POINT('Ctrl Pts',(-1.8363077217611,-0.921938996626441,
9.9059762142599));
#50000=CARTESIAN_POINT('Ctrl Pts',(-1.86828623564657,-0.858244552424377,
9.90210787032644));
#50001=CARTESIAN_POINT('Ctrl Pts',(-1.89690519446484,-0.792967507795669,
9.89823952639299));
#50002=CARTESIAN_POINT('Ctrl Pts',(-1.92202918031085,-0.726499409864598,
9.89437118245954));
#50003=CARTESIAN_POINT('Ctrl Pts',(-1.93694708010085,-0.687032566098429,
9.8920742711531));
#50004=CARTESIAN_POINT('Ctrl Pts',(-1.95063372748089,-0.647146108913449,
9.88977735984666));
#50005=CARTESIAN_POINT('Ctrl Pts',(-1.96306924422631,-0.606923969598107,
9.88748044854022));
#50006=CARTESIAN_POINT('Ctrl Pts',(-1.98856453961245,-0.524460542954842,
9.88277132117284));
#50007=CARTESIAN_POINT('Ctrl Pts',(-2.00887960280738,-0.440324787035022,
9.87806219380546));
#50008=CARTESIAN_POINT('Ctrl Pts',(-2.02383211662245,-0.355107203851881,
9.87335306643807));
#50009=CARTESIAN_POINT('Ctrl Pts',(-2.03858220171866,-0.27104330535358,
9.86870769173674));
#50010=CARTESIAN_POINT('Ctrl Pts',(-2.04811390579993,-0.185926671662672,
9.86406231703542));
#50011=CARTESIAN_POINT('Ctrl Pts',(-2.05229833310357,-0.100344977155406,
9.85941694233409));
#50012=CARTESIAN_POINT('Ctrl Pts',(-2.05390237014321,-0.0675385264886835,
9.8576362080679));
#50013=CARTESIAN_POINT('Ctrl Pts',(-2.0547211391509,-0.0346639571255305,
9.85585547380171));
#50014=CARTESIAN_POINT('Ctrl Pts',(-2.05474925034019,-0.0017551998270615,
9.85407473953553));
#50015=CARTESIAN_POINT('Origin',(0.,0.,18.5459252805377));
#50016=CARTESIAN_POINT('',(1.25206542099588,1.62921138715834,11.006111809188));
#50017=CARTESIAN_POINT('',(1.2500265821584,1.62656556227503,10.9479122870705));
#50018=CARTESIAN_POINT('',(1.25206542099588,1.62921138715835,18.5459252805377));
#50019=CARTESIAN_POINT('',(-2.05447077626017,0.000498338557913886,10.4959252565846));
#50020=CARTESIAN_POINT('Ctrl Pts',(1.2500265821584,1.62656556227503,10.9479122870705));
#50021=CARTESIAN_POINT('Ctrl Pts',(1.53383714851955,1.40790651594786,10.9285605885899));
#50022=CARTESIAN_POINT('Ctrl Pts',(2.20363273241515,0.565166268200534,10.8721645174454));
#50023=CARTESIAN_POINT('Ctrl Pts',(1.99999618452663,-1.37767715104267,10.778724073637));
#50024=CARTESIAN_POINT('Ctrl Pts',(-0.0726735740554304,-2.42748792422539,
10.6675909556455));
#50025=CARTESIAN_POINT('Ctrl Pts',(-1.77435205970044,-1.43343066499739,
10.573324691279));
#50026=CARTESIAN_POINT('Ctrl Pts',(-2.05068411161783,-0.373027881039349,
10.5161027995764));
#50027=CARTESIAN_POINT('Ctrl Pts',(-2.05149284387169,0.000497172743597965,
10.4959252805377));
#50028=CARTESIAN_POINT('Ctrl Pts',(-2.05474993954246,0.000498447846006602,
10.4959252543392));
#50029=CARTESIAN_POINT('Ctrl Pts',(-2.05473097356229,0.0786818464106275,
10.4917085431161));
#50030=CARTESIAN_POINT('Ctrl Pts',(-2.05024504110033,0.156745944516384,
10.487491831893));
#50031=CARTESIAN_POINT('Ctrl Pts',(-2.04136052314416,0.234189617721592,
10.48327512067));
#50032=CARTESIAN_POINT('Ctrl Pts',(-2.03264332173962,0.310174842825331,
10.4791378201234));
#50033=CARTESIAN_POINT('Ctrl Pts',(-2.01969195736155,0.385562469206602,
10.4750005195768));
#50034=CARTESIAN_POINT('Ctrl Pts',(-2.00262219642564,0.459893358163985,
10.4708632190302));
#50035=CARTESIAN_POINT('Ctrl Pts',(-1.98506098415044,0.536364289683557,
10.4666068024689));
#50036=CARTESIAN_POINT('Ctrl Pts',(-1.96314076623114,0.611716290701171,
10.4623503859076));
#50037=CARTESIAN_POINT('Ctrl Pts',(-1.93704088653234,0.685470762616473,
10.4580939693463));
#50038=CARTESIAN_POINT('Ctrl Pts',(-1.91094100683353,0.759225234531785,
10.453837552785));
#50039=CARTESIAN_POINT('Ctrl Pts',(-1.88066170729429,0.831381822486739,
10.4495811362237));
#50040=CARTESIAN_POINT('Ctrl Pts',(-1.84643304563615,0.901489085060272,
10.4453247196624));
#50041=CARTESIAN_POINT('Ctrl Pts',(-1.8153191906393,0.965216589913511,10.4414556368155));
#50042=CARTESIAN_POINT('Ctrl Pts',(-1.78084130052563,1.02745623344192,10.4375865539685));
#50043=CARTESIAN_POINT('Ctrl Pts',(-1.74316487402478,1.08782985088026,10.4337174711216));
#50044=CARTESIAN_POINT('Ctrl Pts',(-1.70554458352043,1.14811351463955,10.4298541530152));
#50045=CARTESIAN_POINT('Ctrl Pts',(-1.66473547142074,1.20653626233826,10.4259908349087));
#50046=CARTESIAN_POINT('Ctrl Pts',(-1.62094970129442,1.26274289876187,10.4221275168023));
#50047=CARTESIAN_POINT('Ctrl Pts',(-1.57721529185957,1.31888360482263,10.4182687303665));
#50048=CARTESIAN_POINT('Ctrl Pts',(-1.53051145702339,1.37281298172646,10.4144099439307));
#50049=CARTESIAN_POINT('Ctrl Pts',(-1.48109361524659,1.42420478351106,10.4105511574949));
#50050=CARTESIAN_POINT('Ctrl Pts',(-1.43170690308646,1.47556421222893,10.4066948018117));
#50051=CARTESIAN_POINT('Ctrl Pts',(-1.37960991176963,1.52438888786751,10.4028384461284));
#50052=CARTESIAN_POINT('Ctrl Pts',(-1.32509732862853,1.57038677788675,10.3989820904451));
#50053=CARTESIAN_POINT('Ctrl Pts',(-1.27060084905034,1.6163710796687,10.3951268739679));
#50054=CARTESIAN_POINT('Ctrl Pts',(-1.21369056539008,1.65952994055047,10.3912716574907));
#50055=CARTESIAN_POINT('Ctrl Pts',(-1.15469561420114,1.69961042625792,10.3874164410135));
#50056=CARTESIAN_POINT('Ctrl Pts',(-1.09569835648608,1.73969247899248,10.3835610738089));
#50057=CARTESIAN_POINT('Ctrl Pts',(-1.03461667248542,1.77669564643269,10.3797057066042));
#50058=CARTESIAN_POINT('Ctrl Pts',(-0.971808712157427,1.81041028208385,
10.3758503393996));
#50059=CARTESIAN_POINT('Ctrl Pts',(-0.908935009021874,1.84416020776501,
10.3719909366768));
#50060=CARTESIAN_POINT('Ctrl Pts',(-0.84433185139397,1.87461450003715,10.368131533954));
#50061=CARTESIAN_POINT('Ctrl Pts',(-0.778381228161229,1.90160990377791,
10.3642721312312));
#50062=CARTESIAN_POINT('Ctrl Pts',(-0.712393263167531,1.92862059252832,
10.3604105432843));
#50063=CARTESIAN_POINT('Ctrl Pts',(-0.64505677254964,1.95216833364465,10.3565489553374));
#50064=CARTESIAN_POINT('Ctrl Pts',(-0.576770322283165,1.97213933529895,
10.3526873673904));
#50065=CARTESIAN_POINT('Ctrl Pts',(-0.508364402424352,1.99214527693647,
10.348819023457));
#50066=CARTESIAN_POINT('Ctrl Pts',(-0.439005677581511,2.00856187364456,
10.3449506795235));
#50067=CARTESIAN_POINT('Ctrl Pts',(-0.369103661279685,2.02132630956259,
10.3410823355901));
#50068=CARTESIAN_POINT('Ctrl Pts',(-0.327597855604687,2.02890546428221,
10.3387854242837));
#50069=CARTESIAN_POINT('Ctrl Pts',(-0.285900638318682,2.03519798793061,
10.3364885129772));
#50070=CARTESIAN_POINT('Ctrl Pts',(-0.244098146947801,2.04019941602694,
10.3341916016708));
#50071=CARTESIAN_POINT('Ctrl Pts',(-0.173703126748368,2.04862177604236,
10.3303236236506));
#50072=CARTESIAN_POINT('Ctrl Pts',(-0.102733850231292,2.05341298926354,
10.3264556456304));
#50073=CARTESIAN_POINT('Ctrl Pts',(-0.0315974388829441,2.0545070368232,
10.3225876676102));
#50074=CARTESIAN_POINT('Ctrl Pts',(0.0394421200313115,2.05559959483387,
10.3187249558535));
#50075=CARTESIAN_POINT('Ctrl Pts',(0.110647881218013,2.05300496468608,10.3148622440967));
#50076=CARTESIAN_POINT('Ctrl Pts',(0.181606556230323,2.04670872896809,10.31099953234));
#50077=CARTESIAN_POINT('Ctrl Pts',(0.252492365379201,2.04041895871259,10.3071407871149));
#50078=CARTESIAN_POINT('Ctrl Pts',(0.323131110541038,2.0304351683889,10.3032820418898));
#50079=CARTESIAN_POINT('Ctrl Pts',(0.393110179594325,2.01679496954929,10.2994232966647));
#50080=CARTESIAN_POINT('Ctrl Pts',(0.463040801360492,2.0031642139709,10.2955672228918));
#50081=CARTESIAN_POINT('Ctrl Pts',(0.532312178227357,1.98588216865933,10.2917111491189));
#50082=CARTESIAN_POINT('Ctrl Pts',(0.600519215173281,1.96503797284115,10.287855075346));
#50083=CARTESIAN_POINT('Ctrl Pts',(0.668720126930718,1.94419564889183,10.2839993478596));
#50084=CARTESIAN_POINT('Ctrl Pts',(0.735856420422147,1.91979193921891,10.2801436203733));
#50085=CARTESIAN_POINT('Ctrl Pts',(0.801536916561915,1.89196620844253,10.2762878928869));
#50086=CARTESIAN_POINT('Ctrl Pts',(0.86721356021688,1.8641421097824,10.2724323915579));
#50087=CARTESIAN_POINT('Ctrl Pts',(0.931434131880338,1.8328965857645,10.268576890229));
#50088=CARTESIAN_POINT('Ctrl Pts',(0.993828199404314,1.79841682392286,10.2647213889001));
#50089=CARTESIAN_POINT('Ctrl Pts',(1.05626662864416,1.76391254722814,10.2608631463385));
#50090=CARTESIAN_POINT('Ctrl Pts',(1.11687554065305,1.72616968602744,10.2570049037769));
#50091=CARTESIAN_POINT('Ctrl Pts',(1.17531089106955,1.68542038430574,10.2531466612153));
#50092=CARTESIAN_POINT('Ctrl Pts',(1.20133590805387,1.6672721014282,10.2514283378463));
#50093=CARTESIAN_POINT('Ctrl Pts',(1.22693019820243,1.64852805997119,10.2497100144773));
#50094=CARTESIAN_POINT('Ctrl Pts',(1.25206542099587,1.62921138715835,10.2479916911084));
#50095=CARTESIAN_POINT('',(-2.05474999986746,-2.33377752992841E-5,10.5540747194726));
#50096=CARTESIAN_POINT('Ctrl Pts',(-2.05474999986747,-2.33375873728629E-5,
10.5540747194623));
#50097=CARTESIAN_POINT('Ctrl Pts',(-2.05475080507059,0.0708704990450557,
10.5502069203748));
#50098=CARTESIAN_POINT('Ctrl Pts',(-2.05107828913696,0.141903688300347,
10.5463391212873));
#50099=CARTESIAN_POINT('Ctrl Pts',(-2.04371513948629,0.212664033476554,
10.5424713221998));
#50100=CARTESIAN_POINT('Ctrl Pts',(-2.03636296193386,0.283318936077959,
10.538609286661));
#50101=CARTESIAN_POINT('Ctrl Pts',(-2.02533111680999,0.353701322035903,
10.5347472511222));
#50102=CARTESIAN_POINT('Ctrl Pts',(-2.01065430302448,0.423399145286292,
10.5308852155834));
#50103=CARTESIAN_POINT('Ctrl Pts',(-1.99599469219053,0.493015274492245,
10.5270277068044));
#50104=CARTESIAN_POINT('Ctrl Pts',(-1.97769869852177,0.561947961368902,
10.5231701980254));
#50105=CARTESIAN_POINT('Ctrl Pts',(-1.95585259333795,0.629792184480901,
10.5193126892464));
#50106=CARTESIAN_POINT('Ctrl Pts',(-1.93402022515182,0.697593746627546,
10.5154576060983));
#50107=CARTESIAN_POINT('Ctrl Pts',(-1.90864232294593,0.764307741231233,
10.5116025229502));
#50108=CARTESIAN_POINT('Ctrl Pts',(-1.8798554581763,0.829542656446767,10.5077474398022));
#50109=CARTESIAN_POINT('Ctrl Pts',(-1.85107704745796,0.89475841364273,10.5038934888049));
#50110=CARTESIAN_POINT('Ctrl Pts',(-1.8188918578528,0.958495509261486,10.5000395378076));
#50111=CARTESIAN_POINT('Ctrl Pts',(-1.78348457188773,1.02038245003452,10.4961855868103));
#50112=CARTESIAN_POINT('Ctrl Pts',(-1.74807581851152,1.08227195563519,10.4923314760907));
#50113=CARTESIAN_POINT('Ctrl Pts',(-1.70944494702554,1.14231073330303,10.4884773653712));
#50114=CARTESIAN_POINT('Ctrl Pts',(-1.66782170192874,1.20015346230202,10.4846232546517));
#50115=CARTESIAN_POINT('Ctrl Pts',(-1.62615484911945,1.25805679179216,10.4807651060694));
#50116=CARTESIAN_POINT('Ctrl Pts',(-1.58148964919704,1.31375908455404,10.4769069574871));
#50117=CARTESIAN_POINT('Ctrl Pts',(-1.53409761489166,1.3669462573502,10.4730488089047));
#50118=CARTESIAN_POINT('Ctrl Pts',(-1.48667859361788,1.42016371710434,10.4691884633344));
#50119=CARTESIAN_POINT('Ctrl Pts',(-1.43652998905314,1.47086286017553,10.465328117764));
#50120=CARTESIAN_POINT('Ctrl Pts',(-1.383959901113,1.51876678743357,10.4614677721936));
#50121=CARTESIAN_POINT('Ctrl Pts',(-1.33129808653137,1.56675429960717,10.4576006909196));
#50122=CARTESIAN_POINT('Ctrl Pts',(-1.27620672940096,1.61193655060224,10.4537336096455));
#50123=CARTESIAN_POINT('Ctrl Pts',(-1.21902610721736,1.65407766214966,10.4498665283715));
#50124=CARTESIAN_POINT('Ctrl Pts',(-1.18590191827414,1.67848960605422,10.4476263650803));
#50125=CARTESIAN_POINT('Ctrl Pts',(-1.15207715688745,1.70188182604525,10.4453862017892));
#50126=CARTESIAN_POINT('Ctrl Pts',(-1.11762181697521,1.72421548442213,10.443146038498));
#50127=CARTESIAN_POINT('Ctrl Pts',(-1.05811251014641,1.76278891113464,10.4392769556511));
#50128=CARTESIAN_POINT('Ctrl Pts',(-0.996487327073619,1.79835342918964,
10.4354078728042));
#50129=CARTESIAN_POINT('Ctrl Pts',(-0.933083005032195,1.83067027840081,
10.4315387899573));
#50130=CARTESIAN_POINT('Ctrl Pts',(-0.869773152268525,1.86293897711835,
10.4276754718508));
#50131=CARTESIAN_POINT('Ctrl Pts',(-0.804689851637586,1.89196939320252,
10.4238121537444));
#50132=CARTESIAN_POINT('Ctrl Pts',(-0.73819799003566,1.91756650210816,10.419948835638));
#50133=CARTESIAN_POINT('Ctrl Pts',(-0.671784123361779,1.94313358561491,
10.4160900492022));
#50134=CARTESIAN_POINT('Ctrl Pts',(-0.603965428777979,1.96527518778353,
10.4122312627664));
#50135=CARTESIAN_POINT('Ctrl Pts',(-0.535128938610543,1.98384338634922,
10.4083724763306));
#50136=CARTESIAN_POINT('Ctrl Pts',(-0.466335810384357,2.00239988831137,
10.4045161206473));
#50137=CARTESIAN_POINT('Ctrl Pts',(-0.396526626490185,2.01738732636825,
10.4006597649641));
#50138=CARTESIAN_POINT('Ctrl Pts',(-0.326104435639335,2.02870733708841,
10.3968034092808));
#50139=CARTESIAN_POINT('Ctrl Pts',(-0.255703048208796,2.04002400376405,
10.3929481928036));
#50140=CARTESIAN_POINT('Ctrl Pts',(-0.184689492697166,2.04767531688683,
10.3890929763264));
#50141=CARTESIAN_POINT('Ctrl Pts',(-0.113476186303622,2.05161417367935,
10.3852377598492));
#50142=CARTESIAN_POINT('Ctrl Pts',(-0.0422600956828595,2.05555318446937,
10.3813823926445));
#50143=CARTESIAN_POINT('Ctrl Pts',(0.0291552761615211,2.05577942613248,
10.3775270254399));
#50144=CARTESIAN_POINT('Ctrl Pts',(0.100354961062196,2.05229784492656,10.3736716582353));
#50145=CARTESIAN_POINT('Ctrl Pts',(0.171629172617799,2.0488126194545,10.3698122555125));
#50146=CARTESIAN_POINT('Ctrl Pts',(0.242686760353929,2.04161184738354,10.3659528527897));
#50147=CARTESIAN_POINT('Ctrl Pts',(0.313116238992187,2.03075251652667,10.3620934500669));
#50148=CARTESIAN_POINT('Ctrl Pts',(0.383585595354432,2.01988703703137,10.35823186212));
#50149=CARTESIAN_POINT('Ctrl Pts',(0.453425658821506,2.00535897400424,10.3543702741731));
#50150=CARTESIAN_POINT('Ctrl Pts',(0.522236233272553,1.98727624631235,10.3505086862261));
#50151=CARTESIAN_POINT('Ctrl Pts',(0.591167194290042,1.9691618822402,10.3466403422927));
#50152=CARTESIAN_POINT('Ctrl Pts',(0.659064607380088,1.94748058488558,10.3427719983592));
#50153=CARTESIAN_POINT('Ctrl Pts',(0.725545169395101,1.92238959882419,10.3389036544258));
#50154=CARTESIAN_POINT('Ctrl Pts',(0.765019413975448,1.90749129335671,10.3366067431193));
#50155=CARTESIAN_POINT('Ctrl Pts',(0.803994523493019,1.89139177096154,10.3343098318129));
#50156=CARTESIAN_POINT('Ctrl Pts',(0.842394382624847,1.87413160333582,10.3320129205065));
#50157=CARTESIAN_POINT('Ctrl Pts',(0.907080692986367,1.84505606542574,10.3281436688738));
#50158=CARTESIAN_POINT('Ctrl Pts',(0.970386608737807,1.81257063920744,10.3242744172411));
#50159=CARTESIAN_POINT('Ctrl Pts',(1.03192885009436,1.7768287511302,10.3204051656084));
#50160=CARTESIAN_POINT('Ctrl Pts',(1.09337296593308,1.74114385141087,10.316542083272));
#50161=CARTESIAN_POINT('Ctrl Pts',(1.15305857523068,1.70221304314449,10.3126790009356));
#50162=CARTESIAN_POINT('Ctrl Pts',(1.21062399045595,1.66023706627472,10.3088159185992));
#50163=CARTESIAN_POINT('Ctrl Pts',(1.22456365524853,1.6500724380059,10.3078804598238));
#50164=CARTESIAN_POINT('Ctrl Pts',(1.23837910404261,1.63972946009415,10.3069450010483));
#50165=CARTESIAN_POINT('Ctrl Pts',(1.25206542099588,1.62921138715834,10.3060095422728));
#50166=CARTESIAN_POINT('Ctrl Pts',(1.25206542099588,1.62921138715834,11.006111809188));
#50167=CARTESIAN_POINT('Ctrl Pts',(1.28751164932299,1.60197060235723,11.0036784156106));
#50168=CARTESIAN_POINT('Ctrl Pts',(1.32203066489551,1.57360155165411,11.0012450220332));
#50169=CARTESIAN_POINT('Ctrl Pts',(1.3555499459167,1.54417677311415,10.9988116284558));
#50170=CARTESIAN_POINT('Ctrl Pts',(1.40884542448033,1.49739153172055,10.9949425456089));
#50171=CARTESIAN_POINT('Ctrl Pts',(1.45982033721477,1.44775226898479,10.991073462762));
#50172=CARTESIAN_POINT('Ctrl Pts',(1.50815338956561,1.39551815324694,10.9872043799151));
#50173=CARTESIAN_POINT('Ctrl Pts',(1.55641442807892,1.34336186373652,10.9833410618086));
#50174=CARTESIAN_POINT('Ctrl Pts',(1.60204109229655,1.28861874917948,10.9794777437022));
#50175=CARTESIAN_POINT('Ctrl Pts',(1.64474652611685,1.23158695483777,10.9756144255958));
#50176=CARTESIAN_POINT('Ctrl Pts',(1.68740186647972,1.17462205876885,10.97175563916));
#50177=CARTESIAN_POINT('Ctrl Pts',(1.72714249307915,1.11537420244368,10.9678968527242));
#50178=CARTESIAN_POINT('Ctrl Pts',(1.76372086005815,1.05417564489781,10.9640380662884));
#50179=CARTESIAN_POINT('Ctrl Pts',(1.80027618534813,0.993015637955712,10.9601817106051));
#50180=CARTESIAN_POINT('Ctrl Pts',(1.8336729544594,0.929907783702804,10.9563253549218));
#50181=CARTESIAN_POINT('Ctrl Pts',(1.86370696167862,0.865213224292507,10.9524689992386));
#50182=CARTESIAN_POINT('Ctrl Pts',(1.89373209655137,0.800537776302861,10.9486137827614));
#50183=CARTESIAN_POINT('Ctrl Pts',(1.92039623725209,0.734276994088983,10.9447585662842));
#50184=CARTESIAN_POINT('Ctrl Pts',(1.94354196280814,0.666814967816328,10.940903349807));
#50185=CARTESIAN_POINT('Ctrl Pts',(1.96668859329283,0.599350303980218,10.9370479826023));
#50186=CARTESIAN_POINT('Ctrl Pts',(1.98631637996209,0.530684763048594,10.9331926153977));
#50187=CARTESIAN_POINT('Ctrl Pts',(2.00231729822874,0.461219036591021,10.9293372481931));
#50188=CARTESIAN_POINT('Ctrl Pts',(2.01833496509358,0.39168059846024,10.9254778454703));
#50189=CARTESIAN_POINT('Ctrl Pts',(2.0307180759414,0.321340777170848,10.9216184427475));
#50190=CARTESIAN_POINT('Ctrl Pts',(2.03940963532042,0.250611056943251,10.9177590400247));
#50191=CARTESIAN_POINT('Ctrl Pts',(2.04810611592864,0.179841288992474,10.9138974520778));
#50192=CARTESIAN_POINT('Ctrl Pts',(2.053106850083,0.108681667448183,10.9100358641309));
#50193=CARTESIAN_POINT('Ctrl Pts',(2.05440692444374,0.0375466549457377,
10.9061742761839));
#50194=CARTESIAN_POINT('Ctrl Pts',(2.05570927333117,-0.0337128108108279,
10.9023059322505));
#50195=CARTESIAN_POINT('Ctrl Pts',(2.05329805246777,-0.104947095907617,
10.898437588317));
#50196=CARTESIAN_POINT('Ctrl Pts',(2.04722040877868,-0.175744588480139,
10.8945692443836));
#50197=CARTESIAN_POINT('Ctrl Pts',(2.04361167885547,-0.217782102195106,
10.8922723330771));
#50198=CARTESIAN_POINT('Ctrl Pts',(2.03871128981978,-0.259665750204335,
10.8899754217707));
#50199=CARTESIAN_POINT('Ctrl Pts',(2.03253759863262,-0.301311255423278,
10.8876785104643));
#50200=CARTESIAN_POINT('Ctrl Pts',(2.02213818851715,-0.371461944064481,
10.8838094276174));
#50201=CARTESIAN_POINT('Ctrl Pts',(2.00808239143017,-0.441211013602958,
10.8799403447704));
#50202=CARTESIAN_POINT('Ctrl Pts',(1.99041367942357,-0.510147966048595,
10.8760712619235));
#50203=CARTESIAN_POINT('Ctrl Pts',(1.97277129291668,-0.578982205873156,
10.8722079438171));
#50204=CARTESIAN_POINT('Ctrl Pts',(1.95152679634787,-0.647006263709907,
10.8683446257107));
#50205=CARTESIAN_POINT('Ctrl Pts',(1.92677508630939,-0.713817434136649,
10.8644813076042));
#50206=CARTESIAN_POINT('Ctrl Pts',(1.90205241001727,-0.780550235086181,
10.8606225211684));
#50207=CARTESIAN_POINT('Ctrl Pts',(1.87383085991449,-0.846072521305738,
10.8567637347326));
#50208=CARTESIAN_POINT('Ctrl Pts',(1.84225531380601,-0.90999611057054,10.8529049482969));
#50209=CARTESIAN_POINT('Ctrl Pts',(1.81069965797624,-0.973879432661422,
10.8490485926136));
#50210=CARTESIAN_POINT('Ctrl Pts',(1.77579441247878,-1.03616562127687,10.8451922369303));
#50211=CARTESIAN_POINT('Ctrl Pts',(1.73773222762227,-1.09648724004565,10.841335881247));
#50212=CARTESIAN_POINT('Ctrl Pts',(1.69968128671632,-1.15679103920421,10.8374806647698));
#50213=CARTESIAN_POINT('Ctrl Pts',(1.65847551699416,-1.21513101006899,10.8336254482926));
#50214=CARTESIAN_POINT('Ctrl Pts',(1.61435222327109,-1.27116657512683,10.8297702318154));
#50215=CARTESIAN_POINT('Ctrl Pts',(1.5702272044592,-1.32720433100768,10.8259148646108));
#50216=CARTESIAN_POINT('Ctrl Pts',(1.52318473744178,-1.38093712190746,10.8220594974061));
#50217=CARTESIAN_POINT('Ctrl Pts',(1.47350286605021,-1.43205686557546,10.8182041302015));
#50218=CARTESIAN_POINT('Ctrl Pts',(1.42376899128687,-1.48323011767541,10.8143447274787));
#50219=CARTESIAN_POINT('Ctrl Pts',(1.37139053636781,-1.53178451349683,10.8104853247559));
#50220=CARTESIAN_POINT('Ctrl Pts',(1.31668228958614,-1.57744898833218,10.8066259220331));
#50221=CARTESIAN_POINT('Ctrl Pts',(1.26194306656539,-1.62313931875188,10.8027643340862));
#50222=CARTESIAN_POINT('Ctrl Pts',(1.20487181450027,-1.66593617924574,10.7989027461393));
#50223=CARTESIAN_POINT('Ctrl Pts',(1.14581407226143,-1.70561064557761,10.7950411581924));
#50224=CARTESIAN_POINT('Ctrl Pts',(1.0866530063857,-1.74535452381041,10.7911728142589));
#50225=CARTESIAN_POINT('Ctrl Pts',(1.02549892846466,-1.78196485176482,10.7873044703255));
#50226=CARTESIAN_POINT('Ctrl Pts',(0.962723218805193,-1.81525798895732,
10.783436126392));
#50227=CARTESIAN_POINT('Ctrl Pts',(0.925448808937162,-1.83502649572909,
10.7811392150856));
#50228=CARTESIAN_POINT('Ctrl Pts',(0.887603096255043,-1.85362638322459,
10.7788423037791));
#50229=CARTESIAN_POINT('Ctrl Pts',(0.849266841179643,-1.87102736350187,
10.7765453924727));
#50230=CARTESIAN_POINT('Ctrl Pts',(0.784690491839525,-1.90033882804205,
10.7726763096258));
#50231=CARTESIAN_POINT('Ctrl Pts',(0.718468403655894,-1.92636061064501,
10.7688072267789));
#50232=CARTESIAN_POINT('Ctrl Pts',(0.650969027954004,-1.94890658758818,
10.7649381439319));
#50233=CARTESIAN_POINT('Ctrl Pts',(0.583570222955575,-1.97141897215013,
10.7610748258255));
#50234=CARTESIAN_POINT('Ctrl Pts',(0.514898365035326,-1.99046567813353,
10.7572115077191));
#50235=CARTESIAN_POINT('Ctrl Pts',(0.445343250383112,-2.00590801180867,
10.7533481896126));
#50236=CARTESIAN_POINT('Ctrl Pts',(0.375869723853611,-2.02133223163235,
10.7494894031768));
#50237=CARTESIAN_POINT('Ctrl Pts',(0.305515470492084,-2.03316037246611,
10.7456306167411));
#50238=CARTESIAN_POINT('Ctrl Pts',(0.234685193895992,-2.04130360854675,
10.7417718303053));
#50239=CARTESIAN_POINT('Ctrl Pts',(0.163899535180383,-2.04944171498578,
10.737915474622));
#50240=CARTESIAN_POINT('Ctrl Pts',(0.092638929610532,-2.05389946658242,
10.7340591189387));
#50241=CARTESIAN_POINT('Ctrl Pts',(0.0213165623719672,-2.05463942497671,
10.7302027632554));
#50242=CARTESIAN_POINT('Ctrl Pts',(-0.0499847355251396,-2.05537916477989,
10.7263475467782));
#50243=CARTESIAN_POINT('Ctrl Pts',(-0.121347273377171,-2.05240328672127,
10.722492330301));
#50244=CARTESIAN_POINT('Ctrl Pts',(-0.192356211288108,-2.04572643588503,
10.7186371138238));
#50245=CARTESIAN_POINT('Ctrl Pts',(-0.263367925436155,-2.0390493240039,
10.7147817466192));
#50246=CARTESIAN_POINT('Ctrl Pts',(-0.334025528752484,-2.02867099973832,
10.7109263794145));
#50247=CARTESIAN_POINT('Ctrl Pts',(-0.403919385645346,-2.0146579591583,
10.7070710122099));
#50248=CARTESIAN_POINT('Ctrl Pts',(-0.473886402347216,-2.00063025074597,
10.7032116094871));
#50249=CARTESIAN_POINT('Ctrl Pts',(-0.543087599495356,-1.98296032696125,
10.6993522067643));
#50250=CARTESIAN_POINT('Ctrl Pts',(-0.611124511687531,-1.96176563169882,
10.6954928040415));
#50251=CARTESIAN_POINT('Ctrl Pts',(-0.679199946913825,-1.94055893583344,
10.6916312160946));
#50252=CARTESIAN_POINT('Ctrl Pts',(-0.746109329005823,-1.91582366408486,
10.6877696281477));
#50253=CARTESIAN_POINT('Ctrl Pts',(-0.811472917657158,-1.88772595108744,
10.6839080402008));
#50254=CARTESIAN_POINT('Ctrl Pts',(-0.876950862249698,-1.85957908013401,
10.6800396962673));
#50255=CARTESIAN_POINT('Ctrl Pts',(-0.940877178113974,-1.8280582378337,
10.6761713523339));
#50256=CARTESIAN_POINT('Ctrl Pts',(-1.0028961534356,-1.7933758300825,10.6723030084004));
#50257=CARTESIAN_POINT('Ctrl Pts',(-1.0397212362307,-1.77278241443272,10.670006097094));
#50258=CARTESIAN_POINT('Ctrl Pts',(-1.07587438671979,-1.75107519229419,
10.6677091857875));
#50259=CARTESIAN_POINT('Ctrl Pts',(-1.11128635613807,-1.72830558558415,
10.6654122744811));
#50260=CARTESIAN_POINT('Ctrl Pts',(-1.17093682808642,-1.68995081998811,
10.6615431916342));
#50261=CARTESIAN_POINT('Ctrl Pts',(-1.22871614578505,-1.64842915600993,
10.6576741087873));
#50262=CARTESIAN_POINT('Ctrl Pts',(-1.28426809979031,-1.60394919195122,
10.6538050259404));
#50263=CARTESIAN_POINT('Ctrl Pts',(-1.33973728415463,-1.55953550082063,
10.6499417078339));
#50264=CARTESIAN_POINT('Ctrl Pts',(-1.39298531615975,-1.51217255996362,
10.6460783897275));
#50265=CARTESIAN_POINT('Ctrl Pts',(-1.4436842568334,-1.46211262530333,10.6422150716211));
#50266=CARTESIAN_POINT('Ctrl Pts',(-1.49432372766912,-1.41211141092715,
10.6383562851853));
#50267=CARTESIAN_POINT('Ctrl Pts',(-1.5424197024965,-1.35941982633297,10.6344974987495));
#50268=CARTESIAN_POINT('Ctrl Pts',(-1.58767805258693,-1.3043296990538,10.6306387123137));
#50269=CARTESIAN_POINT('Ctrl Pts',(-1.63290789323544,-1.24927427451525,
10.6267823566304));
#50270=CARTESIAN_POINT('Ctrl Pts',(-1.67530334787002,-1.19182367937645,
10.6229260009471));
#50271=CARTESIAN_POINT('Ctrl Pts',(-1.71460885977287,-1.13230473834935,
10.6190696452639));
#50272=CARTESIAN_POINT('Ctrl Pts',(-1.75390276043392,-1.0728033798134,10.6152144287867));
#50273=CARTESIAN_POINT('Ctrl Pts',(-1.79010826297151,-1.01123529356004,
10.6113592123095));
#50274=CARTESIAN_POINT('Ctrl Pts',(-1.82301267020963,-0.947956943513336,
10.6075039958323));
#50275=CARTESIAN_POINT('Ctrl Pts',(-1.85591836391165,-0.884676119472439,
10.6036486286276));
#50276=CARTESIAN_POINT('Ctrl Pts',(-1.88552248391556,-0.819685330896271,
10.599793261423));
#50277=CARTESIAN_POINT('Ctrl Pts',(-1.91165871748591,-0.753364792355016,
10.5959378942184));
#50278=CARTESIAN_POINT('Ctrl Pts',(-1.93782230856582,-0.686974834294604,
10.5920784914956));
#50279=CARTESIAN_POINT('Ctrl Pts',(-1.96051058858047,-0.619252800632963,
10.5882190887728));
#50280=CARTESIAN_POINT('Ctrl Pts',(-1.9796061062381,-0.550597154592022,
10.58435968605));
#50281=CARTESIAN_POINT('Ctrl Pts',(-1.99871243592782,-0.481902635184988,
10.5804980981031));
#50282=CARTESIAN_POINT('Ctrl Pts',(-2.01422184802851,-0.41227392546909,
10.5766365101562));
#50283=CARTESIAN_POINT('Ctrl Pts',(-2.02606795407287,-0.342120165992837,
10.5727749222093));
#50284=CARTESIAN_POINT('Ctrl Pts',(-2.03793478530437,-0.271843669999794,
10.5689065782758));
#50285=CARTESIAN_POINT('Ctrl Pts',(-2.04612545871765,-0.201040772966261,
10.5650382343423));
#50286=CARTESIAN_POINT('Ctrl Pts',(-2.05062549244402,-0.130125524931508,
10.5611698904089));
#50287=CARTESIAN_POINT('Ctrl Pts',(-2.05329748297105,-0.0880180914117523,
10.5588729791025));
#50288=CARTESIAN_POINT('Ctrl Pts',(-2.05466928496541,-0.0458710637282637,
10.556576067796));
#50289=CARTESIAN_POINT('Ctrl Pts',(-2.05474654051348,-0.00377051029486843,
10.5542791564896));
#50290=CARTESIAN_POINT('Ctrl Pts',(-2.05474883256118,-0.00252145467031257,
10.5542110108299));
#50291=CARTESIAN_POINT('Ctrl Pts',(-2.05474998568027,-0.00127239695515452,
10.5541428651703));
#50292=CARTESIAN_POINT('Ctrl Pts',(-2.05474999986746,-2.33384712630955E-5,
10.5540747195105));
#50293=CARTESIAN_POINT('Origin',(0.,0.,18.5459252805377));
#50294=CARTESIAN_POINT('',(1.25062491733535,1.62730785058777,11.7061482541083));
#50295=CARTESIAN_POINT('',(1.25206542099587,1.62921138715835,11.6478607732374));
#50296=CARTESIAN_POINT('',(1.25206542099588,1.62921138715835,18.5459252805377));
#50297=CARTESIAN_POINT('',(-2.05474914153225,-0.00187826315611485,11.1959252893731));
#50298=CARTESIAN_POINT('Ctrl Pts',(1.25206542099587,1.62921138715835,11.6478607732374));
#50299=CARTESIAN_POINT('Ctrl Pts',(1.30846798771459,1.58586544445223,11.644001066733));
#50300=CARTESIAN_POINT('Ctrl Pts',(1.36268721289643,1.53953314852563,11.6401413602286));
#50301=CARTESIAN_POINT('Ctrl Pts',(1.41439379402388,1.49046561782777,11.6362816537241));
#50302=CARTESIAN_POINT('Ctrl Pts',(1.46606292217753,1.44143362854267,11.6324247429467));
#50303=CARTESIAN_POINT('Ctrl Pts',(1.51522266547132,1.38967066815831,11.6285678321693));
#50304=CARTESIAN_POINT('Ctrl Pts',(1.56157735598458,1.33546760491455,11.6247109213919));
#50305=CARTESIAN_POINT('Ctrl Pts',(1.60791397665069,1.28128567094718,11.620855514104));
#50306=CARTESIAN_POINT('Ctrl Pts',(1.65144739933588,1.22466589084389,11.617000106816));
#50307=CARTESIAN_POINT('Ctrl Pts',(1.69192054918418,1.16593413954146,11.6131446995281));
#50308=CARTESIAN_POINT('Ctrl Pts',(1.73239146057176,1.10720563653375,11.6092895054723));
#50309=CARTESIAN_POINT('Ctrl Pts',(1.7698021608593,1.0463657951568,11.6054343114166));
#50310=CARTESIAN_POINT('Ctrl Pts',(1.80393844138186,0.983770126708874,11.6015791173608));
#50311=CARTESIAN_POINT('Ctrl Pts',(1.83810838664273,0.921112727259046,11.5977201213648));
#50312=CARTESIAN_POINT('Ctrl Pts',(1.86899722866235,0.856696469425504,11.5938611253687));
#50313=CARTESIAN_POINT('Ctrl Pts',(1.89643679424826,0.790901414792889,11.5900021293727));
#50314=CARTESIAN_POINT('Ctrl Pts',(1.92388957338067,0.725074676494898,11.5861412750738));
#50315=CARTESIAN_POINT('Ctrl Pts',(1.94788960352915,0.657868276882644,11.582280420775));
#50316=CARTESIAN_POINT('Ctrl Pts',(1.96831794880335,0.589679586655826,11.5784195664761));
#50317=CARTESIAN_POINT('Ctrl Pts',(1.98878387090947,0.521365467035805,11.5745516103454));
#50318=CARTESIAN_POINT('Ctrl Pts',(2.0056648664798,0.452065919930567,11.5706836542146));
#50319=CARTESIAN_POINT('Ctrl Pts',(2.01889281237227,0.382190233590036,11.5668156980839));
#50320=CARTESIAN_POINT('Ctrl Pts',(2.03047457634721,0.321010386517599,11.5634290985819));
#50321=CARTESIAN_POINT('Ctrl Pts',(2.03925671420953,0.259389223890336,11.56004249908));
#50322=CARTESIAN_POINT('Ctrl Pts',(2.04522628418895,0.197603160305332,11.556655899578));
#50323=CARTESIAN_POINT('Ctrl Pts',(2.05204632913298,0.127014536331309,11.5527868167311));
#50324=CARTESIAN_POINT('Ctrl Pts',(2.05522101457037,0.0559341627700564,
11.5489177338841));
#50325=CARTESIAN_POINT('Ctrl Pts',(2.05469356287205,-0.0152290903256963,
11.5450486510372));
#50326=CARTESIAN_POINT('Ctrl Pts',(2.05416689705046,-0.0862863137234158,
11.5411853329308));
#50327=CARTESIAN_POINT('Ctrl Pts',(2.04994904677113,-0.157425689726149,
11.5373220148244));
#50328=CARTESIAN_POINT('Ctrl Pts',(2.04203502076875,-0.228233512994843,
11.5334586967179));
#50329=CARTESIAN_POINT('Ctrl Pts',(2.03413027791583,-0.298958278714105,
11.5295999102821));
#50330=CARTESIAN_POINT('Ctrl Pts',(2.02253802503167,-0.36935178377467,11.5257411238463));
#50331=CARTESIAN_POINT('Ctrl Pts',(2.00730527915571,-0.439002367617327,
11.5218823374106));
#50332=CARTESIAN_POINT('Ctrl Pts',(1.99208212879268,-0.508609076699419,
11.5180259817273));
#50333=CARTESIAN_POINT('Ctrl Pts',(1.97322313874075,-0.577473319595851,
11.514169626044));
#50334=CARTESIAN_POINT('Ctrl Pts',(1.95082669101271,-0.64519205213052,11.5103132703607));
#50335=CARTESIAN_POINT('Ctrl Pts',(1.9284368594196,-0.712890779873512,11.5064580538835));
#50336=CARTESIAN_POINT('Ctrl Pts',(1.90251179721924,-0.779444208100835,
11.5026028374063));
#50337=CARTESIAN_POINT('Ctrl Pts',(1.87319969916412,-0.844464593426782,
11.4987476209291));
#50338=CARTESIAN_POINT('Ctrl Pts',(1.84388645509363,-0.909487520855325,
11.4948922537245));
#50339=CARTESIAN_POINT('Ctrl Pts',(1.81118611391614,-0.972976844428992,
11.4910368865198));
#50340=CARTESIAN_POINT('Ctrl Pts',(1.77529424201665,-1.03456653568657,11.4871815193152));
#50341=CARTESIAN_POINT('Ctrl Pts',(1.73936480111453,-1.0962206945562,11.4833221165924));
#50342=CARTESIAN_POINT('Ctrl Pts',(1.70023740587255,-1.15597083124951,11.4794627138696));
#50343=CARTESIAN_POINT('Ctrl Pts',(1.65815220786431,-1.21347798416564,11.4756033111468));
#50344=CARTESIAN_POINT('Ctrl Pts',(1.61604318088636,-1.2710176980835,11.4717417231999));
#50345=CARTESIAN_POINT('Ctrl Pts',(1.57097332433423,-1.32631152333354,11.467880135253));
#50346=CARTESIAN_POINT('Ctrl Pts',(1.52322279298218,-1.37905398206146,11.4640185473061));
#50347=CARTESIAN_POINT('Ctrl Pts',(1.47538872036398,-1.4318887156114,11.4601502033726));
#50348=CARTESIAN_POINT('Ctrl Pts',(1.42486495381398,-1.48216282796461,11.4562818594392));
#50349=CARTESIAN_POINT('Ctrl Pts',(1.37196764478991,-1.52960855912538,11.4524135155057));
#50350=CARTESIAN_POINT('Ctrl Pts',(1.34055874494356,-1.55778046891927,11.4501166041993));
#50351=CARTESIAN_POINT('Ctrl Pts',(1.30831365070504,-1.58495596672168,11.4478196928928));
#50352=CARTESIAN_POINT('Ctrl Pts',(1.2753034381163,-1.61108618739928,11.4455227815864));
#50353=CARTESIAN_POINT('Ctrl Pts',(1.2196986583659,-1.65510181322117,11.4416536987395));
#50354=CARTESIAN_POINT('Ctrl Pts',(1.16170357226489,-1.69632156723997,11.4377846158926));
#50355=CARTESIAN_POINT('Ctrl Pts',(1.10163089000041,-1.73447598562128,11.4339155330457));
#50356=CARTESIAN_POINT('Ctrl Pts',(1.04164771303652,-1.77257355582206,11.4300522149392));
#50357=CARTESIAN_POINT('Ctrl Pts',(0.979593491143668,-1.80761459782017,
11.4261888968328));
#50358=CARTESIAN_POINT('Ctrl Pts',(0.91581308469753,-1.83937053265425,11.4223255787264));
#50359=CARTESIAN_POINT('Ctrl Pts',(0.852107492643623,-1.87108921778899,
11.4184667922906));
#50360=CARTESIAN_POINT('Ctrl Pts',(0.786680170754984,-1.89953023450996,
11.4146080058548));
#50361=CARTESIAN_POINT('Ctrl Pts',(0.719902469801093,-1.92450980680128,
11.410749219419));
#50362=CARTESIAN_POINT('Ctrl Pts',(0.653166833902216,-1.94947364379372,
11.4068928637357));
#50363=CARTESIAN_POINT('Ctrl Pts',(0.58508296051036,-1.97098019255074,11.4030365080524));
#50364=CARTESIAN_POINT('Ctrl Pts',(0.516042820837258,-1.98889350382627,
11.3991801523692));
#50365=CARTESIAN_POINT('Ctrl Pts',(0.44702307631272,-2.00680152333027,11.395324935892));
#50366=CARTESIAN_POINT('Ctrl Pts',(0.377048096286477,-2.02111829074576,
11.3914697194148));
#50367=CARTESIAN_POINT('Ctrl Pts',(0.306524014719824,-2.03175800500454,
11.3876145029376));
#50368=CARTESIAN_POINT('Ctrl Pts',(0.23599717587256,-2.04239813524432,11.3837591357329));
#50369=CARTESIAN_POINT('Ctrl Pts',(0.164921673538474,-2.04936085661723,
11.3799037685283));
#50370=CARTESIAN_POINT('Ctrl Pts',(0.0937110916937221,-2.05261194427821,
11.3760484013237));
#50371=CARTESIAN_POINT('Ctrl Pts',(0.0224259717879226,-2.05586643494144,
11.3721889986009));
#50372=CARTESIAN_POINT('Ctrl Pts',(-0.0489940236056687,-2.0554015142251,
11.3683295958781));
#50373=CARTESIAN_POINT('Ctrl Pts',(-0.120133868146701,-2.05123509530822,
11.3644701931553));
#50374=CARTESIAN_POINT('Ctrl Pts',(-0.191313992626522,-2.04706631733221,
11.3606086052084));
#50375=CARTESIAN_POINT('Ctrl Pts',(-0.262213167440128,-2.03919192267871,
11.3567470172615));
#50376=CARTESIAN_POINT('Ctrl Pts',(-0.332422800101435,-2.027681593464,11.3528854293145));
#50377=CARTESIAN_POINT('Ctrl Pts',(-0.402755267031661,-2.01615112651577,
11.3490170853811));
#50378=CARTESIAN_POINT('Ctrl Pts',(-0.472395308450975,-2.00097212818192,
11.3451487414476));
#50379=CARTESIAN_POINT('Ctrl Pts',(-0.540946496001207,-1.98226498000747,
11.3412803975142));
#50380=CARTESIAN_POINT('Ctrl Pts',(-0.581650218436983,-1.97115721376637,
11.3389834862077));
#50381=CARTESIAN_POINT('Ctrl Pts',(-0.621970357581862,-1.95880649870203,
11.3366865749013));
#50382=CARTESIAN_POINT('Ctrl Pts',(-0.661827309974577,-1.94524604466166,
11.3343896635949));
#50383=CARTESIAN_POINT('Ctrl Pts',(-0.72896523140905,-1.92240383914107,
11.330520580748));
#50384=CARTESIAN_POINT('Ctrl Pts',(-0.795050703584486,-1.8960370323457,
11.326651497901));
#50385=CARTESIAN_POINT('Ctrl Pts',(-0.859687733168942,-1.86626219056671,
11.3227824150541));
#50386=CARTESIAN_POINT('Ctrl Pts',(-0.924228456802882,-1.83653171181704,
11.3189190969477));
#50387=CARTESIAN_POINT('Ctrl Pts',(-0.987324584002499,-1.80340347897189,
11.3150557788412));
#50388=CARTESIAN_POINT('Ctrl Pts',(-1.0485970325405,-1.7670432439098,11.3111924607348));
#50389=CARTESIAN_POINT('Ctrl Pts',(-1.10979760851999,-1.73072565938941,
11.307333674299));
#50390=CARTESIAN_POINT('Ctrl Pts',(-1.16917833922634,-1.69118384984025,
11.3034748878632));
#50391=CARTESIAN_POINT('Ctrl Pts',(-1.22638341500047,-1.64863012283283,
11.2996161014274));
#50392=CARTESIAN_POINT('Ctrl Pts',(-1.28355245577151,-1.60610320155311,
11.2957597457442));
#50393=CARTESIAN_POINT('Ctrl Pts',(-1.33854817181992,-1.56056841625879,
11.2919033900609));
#50394=CARTESIAN_POINT('Ctrl Pts',(-1.39104375021585,-1.51228133873476,
11.2880470343776));
#50395=CARTESIAN_POINT('Ctrl Pts',(-1.44352382089228,-1.46400852569694,
11.2841918179004));
#50396=CARTESIAN_POINT('Ctrl Pts',(-1.49350486283601,-1.41298536325948,
11.2803366014232));
#50397=CARTESIAN_POINT('Ctrl Pts',(-1.54069451266359,-1.35950652118639,
11.276481384946));
#50398=CARTESIAN_POINT('Ctrl Pts',(-1.58788600746534,-1.30602558825051,
11.2726260177414));
#50399=CARTESIAN_POINT('Ctrl Pts',(-1.63228557371542,-1.25008915077213,
11.2687706505367));
#50400=CARTESIAN_POINT('Ctrl Pts',(-1.67364013817998,-1.1920261114476,11.2649152833321));
#50401=CARTESIAN_POINT('Ctrl Pts',(-1.71503798959668,-1.13390229595394,
11.2610558806093));
#50402=CARTESIAN_POINT('Ctrl Pts',(-1.75338419429404,-1.07364783156664,
11.2571964778865));
#50403=CARTESIAN_POINT('Ctrl Pts',(-1.78846869960691,-1.01162111139813,
11.2533370751637));
#50404=CARTESIAN_POINT('Ctrl Pts',(-1.82357307004229,-0.949559271213391,
11.2494754872168));
#50405=CARTESIAN_POINT('Ctrl Pts',(-1.85541184776366,-0.885723612576363,
11.2456138992699));
#50406=CARTESIAN_POINT('Ctrl Pts',(-1.88382196249841,-0.820495201758459,
11.2417523113229));
#50407=CARTESIAN_POINT('Ctrl Pts',(-1.9122817817472,-0.755152671497825,
11.2378839673895));
#50408=CARTESIAN_POINT('Ctrl Pts',(-1.93730079112354,-0.688412979191603,
11.234015623456));
#50409=CARTESIAN_POINT('Ctrl Pts',(-1.95876511220552,-0.620674469997365,
11.2301472795226));
#50410=CARTESIAN_POINT('Ctrl Pts',(-1.97151000837456,-0.580453292582558,
11.2278503682161));
#50411=CARTESIAN_POINT('Ctrl Pts',(-1.98300261409516,-0.539880225197758,
11.2255534569097));
#50412=CARTESIAN_POINT('Ctrl Pts',(-1.99322765470765,-0.499040157711441,
11.2232565456033));
#50413=CARTESIAN_POINT('Ctrl Pts',(-2.01567775412989,-0.409371704526085,
11.2182134470819));
#50414=CARTESIAN_POINT('Ctrl Pts',(-2.03208632056842,-0.318134497274714,
11.2131703485606));
#50415=CARTESIAN_POINT('Ctrl Pts',(-2.0422798960547,-0.226031831100864,
11.2081272500393));
#50416=CARTESIAN_POINT('Ctrl Pts',(-2.05050113851806,-0.151749911949275,
11.2040599298172));
#50417=CARTESIAN_POINT('Ctrl Pts',(-2.05468055872562,-0.0769052702050597,
11.1999926095951));
#50418=CARTESIAN_POINT('Ctrl Pts',(-2.05474914153225,-0.00187826315611485,
11.1959252893731));
#50419=CARTESIAN_POINT('Ctrl Pts',(-2.05448230159788,-0.00187785627648217,
11.1959252805377));
#50420=CARTESIAN_POINT('Ctrl Pts',(-2.04980379711585,0.513337962037447,
11.1679913295624));
#50421=CARTESIAN_POINT('Ctrl Pts',(-1.59250349515915,1.71920574835467,11.1030130059232));
#50422=CARTESIAN_POINT('Ctrl Pts',(0.0481892737830568,2.26260148112704,
11.0203420081008));
#50423=CARTESIAN_POINT('Ctrl Pts',(0.990547142386969,1.82647893255362,10.9656049612537));
#50424=CARTESIAN_POINT('Ctrl Pts',(1.2500265821584,1.62656556227503,10.9479122870705));
#50425=CARTESIAN_POINT('',(-2.05474923773585,0.00176989376130956,11.2540747002055));
#50426=CARTESIAN_POINT('Ctrl Pts',(-2.05474923773585,0.00176989376130957,
11.2540747002055));
#50427=CARTESIAN_POINT('Ctrl Pts',(-2.05467509737831,0.0878427680056098,
11.2494166422338));
#50428=CARTESIAN_POINT('Ctrl Pts',(-2.04918878694341,0.173679370728022,
11.2447585842621));
#50429=CARTESIAN_POINT('Ctrl Pts',(-2.03840174561635,0.258681050655506,
11.2401005262904));
#50430=CARTESIAN_POINT('Ctrl Pts',(-2.02745814788226,0.344916392084481,
11.2353748641632));
#50431=CARTESIAN_POINT('Ctrl Pts',(-2.01105891234539,0.430292414196941,
11.2306492020359));
#50432=CARTESIAN_POINT('Ctrl Pts',(-1.98936916430093,0.514206077977125,
11.2259235399086));
#50433=CARTESIAN_POINT('Ctrl Pts',(-1.98195563668563,0.542887658900054,
11.2243083147521));
#50434=CARTESIAN_POINT('Ctrl Pts',(-1.9739244479774,0.571398584098788,11.2226930895955));
#50435=CARTESIAN_POINT('Ctrl Pts',(-1.96528345696356,0.599715346047911,
11.2210778644389));
#50436=CARTESIAN_POINT('Ctrl Pts',(-1.94458497416931,0.667544835634683,
11.217208781592));
#50437=CARTESIAN_POINT('Ctrl Pts',(-1.92033024378843,0.734434342938788,
11.2133396987451));
#50438=CARTESIAN_POINT('Ctrl Pts',(-1.89262319715387,0.799984372406787,
11.2094706158982));
#50439=CARTESIAN_POINT('Ctrl Pts',(-1.86495743263698,0.865436735599987,
11.2056072977917));
#50440=CARTESIAN_POINT('Ctrl Pts',(-1.83384974971676,0.929553138667919,
11.2017439796853));
#50441=CARTESIAN_POINT('Ctrl Pts',(-1.79945377757442,0.991949426570303,
11.1978806615789));
#50442=CARTESIAN_POINT('Ctrl Pts',(-1.76509815189415,1.05427252365101,11.1940218751431));
#50443=CARTESIAN_POINT('Ctrl Pts',(-1.72746213199957,1.11487909002906,11.1901630887073));
#50444=CARTESIAN_POINT('Ctrl Pts',(-1.68674661838198,1.17340675295353,11.1863043022715));
#50445=CARTESIAN_POINT('Ctrl Pts',(-1.64605675255243,1.231897547742,11.1824479465882));
#50446=CARTESIAN_POINT('Ctrl Pts',(-1.60229151840284,1.28831163937972,11.1785915909049));
#50447=CARTESIAN_POINT('Ctrl Pts',(-1.55569597970807,1.34231426321117,11.1747352352217));
#50448=CARTESIAN_POINT('Ctrl Pts',(-1.509114205802,1.39630093412681,11.1708800187445));
#50449=CARTESIAN_POINT('Ctrl Pts',(-1.45970410441845,1.44787718389519,11.1670248022673));
#50450=CARTESIAN_POINT('Ctrl Pts',(-1.40775091165561,1.49674143833622,11.1631695857901));
#50451=CARTESIAN_POINT('Ctrl Pts',(-1.35579568767834,1.54560760322345,11.1593142185854));
#50452=CARTESIAN_POINT('Ctrl Pts',(-1.30129753029019,1.5917612310577,11.1554588513808));
#50453=CARTESIAN_POINT('Ctrl Pts',(-1.24457713905028,1.63493893080244,11.1516034841762));
#50454=CARTESIAN_POINT('Ctrl Pts',(-1.18779737702768,1.6781618258248,11.1477440814534));
#50455=CARTESIAN_POINT('Ctrl Pts',(-1.12879112511406,1.71840227970392,11.1438846787306));
#50456=CARTESIAN_POINT('Ctrl Pts',(-1.06790992467806,1.75543896369942,11.1400252760078));
#50457=CARTESIAN_POINT('Ctrl Pts',(-1.00699425282815,1.79249661815632,11.1361636880609));
#50458=CARTESIAN_POINT('Ctrl Pts',(-0.944201946926682,1.82634666099208,
11.132302100114));
#50459=CARTESIAN_POINT('Ctrl Pts',(-0.879908702155135,1.85681400209382,
11.128440512167));
#50460=CARTESIAN_POINT('Ctrl Pts',(-0.815502974047321,1.88733464690089,
11.1245721682336));
#50461=CARTESIAN_POINT('Ctrl Pts',(-0.749591513662162,1.91446058926608,
11.1207038243001));
#50462=CARTESIAN_POINT('Ctrl Pts',(-0.682568848611284,1.93806535736168,
11.1168354803667));
#50463=CARTESIAN_POINT('Ctrl Pts',(-0.64277271884858,1.95208118937072,11.1145385690602));
#50464=CARTESIAN_POINT('Ctrl Pts',(-0.602585105738489,1.96485653812434,
11.1122416577538));
#50465=CARTESIAN_POINT('Ctrl Pts',(-0.562090371228137,1.97637344069197,
11.1099447464474));
#50466=CARTESIAN_POINT('Ctrl Pts',(-0.493875070548586,1.9957742092375,11.1060754904244));
#50467=CARTESIAN_POINT('Ctrl Pts',(-0.424520539258813,2.01167711519797,
11.1022062344015));
#50468=CARTESIAN_POINT('Ctrl Pts',(-0.354418830153114,2.02395277991679,
11.0983369783785));
#50469=CARTESIAN_POINT('Ctrl Pts',(-0.284439025878964,2.03620709761199,
11.0944744508791));
#50470=CARTESIAN_POINT('Ctrl Pts',(-0.21371510006283,2.04484662432041,11.0906119233798));
#50471=CARTESIAN_POINT('Ctrl Pts',(-0.142652869620053,2.04979211660333,
11.0867493958804));
#50472=CARTESIAN_POINT('Ctrl Pts',(-0.0716604748457906,2.05473274875511,
11.0828906642398));
#50473=CARTESIAN_POINT('Ctrl Pts',(-0.000330916901744124,2.05598651416958,
11.0790319325992));
#50474=CARTESIAN_POINT('Ctrl Pts',(0.0709224168760033,2.053525644662,11.0751732009586));
#50475=CARTESIAN_POINT('Ctrl Pts',(0.142129564120466,2.05106637029425,11.0713169705544));
#50476=CARTESIAN_POINT('Ctrl Pts',(0.213260100960262,2.04489725599101,11.0674607401503));
#50477=CARTESIAN_POINT('Ctrl Pts',(0.28389990271725,2.03504260587761,11.0636045097462));
#50478=CARTESIAN_POINT('Ctrl Pts',(0.35451754588503,2.02519104701218,11.0597494889806));
#50479=CARTESIAN_POINT('Ctrl Pts',(0.424644278966299,2.01165631567822,11.0558944682149));
#50480=CARTESIAN_POINT('Ctrl Pts',(0.493872093027739,1.99451445676094,11.0520394474493));
#50481=CARTESIAN_POINT('Ctrl Pts',(0.563141981578827,1.97736217956057,11.0481820837233));
#50482=CARTESIAN_POINT('Ctrl Pts',(0.631511385573021,1.95659850524197,11.0443247199972));
#50483=CARTESIAN_POINT('Ctrl Pts',(0.698584466233787,1.93235020274195,11.0404673562711));
#50484=CARTESIAN_POINT('Ctrl Pts',(0.765674913431462,1.90809562188054,11.0366089937979));
#50485=CARTESIAN_POINT('Ctrl Pts',(0.831467917351197,1.88035479749049,11.0327506313246));
#50486=CARTESIAN_POINT('Ctrl Pts',(0.895587170542185,1.84930289094573,11.0288922688514));
#50487=CARTESIAN_POINT('Ctrl Pts',(0.95980545125286,1.8182030269914,11.0250279474181));
#50488=CARTESIAN_POINT('Ctrl Pts',(1.02234438568784,1.78378209158101,11.0211636259849));
#50489=CARTESIAN_POINT('Ctrl Pts',(1.08285236991923,1.74626123688877,11.0172993045516));
#50490=CARTESIAN_POINT('Ctrl Pts',(1.14124406125458,1.71005269030342,11.0135701394304));
#50491=CARTESIAN_POINT('Ctrl Pts',(1.19774422955969,1.67095777191887,11.0098409743092));
#50492=CARTESIAN_POINT('Ctrl Pts',(1.25206542099588,1.62921138715834,11.006111809188));
#50493=CARTESIAN_POINT('Ctrl Pts',(1.25062491733525,1.62730785058785,11.7061482541084));
#50494=CARTESIAN_POINT('Ctrl Pts',(1.44978277724123,1.47638255877163,11.6926356148739));
#50495=CARTESIAN_POINT('Ctrl Pts',(2.09378666756174,0.782978067453363,11.6420786029757));
#50496=CARTESIAN_POINT('Ctrl Pts',(2.19186345478925,-1.04580741136612,11.5544772184136));
#50497=CARTESIAN_POINT('Ctrl Pts',(0.310206203218445,-2.40868234883592,
11.443344100422));
#50498=CARTESIAN_POINT('Ctrl Pts',(-1.64103540980871,-1.65033490605083,
11.343209934105));
#50499=CARTESIAN_POINT('Ctrl Pts',(-2.04952780599468,-0.479212094141424,
11.2801201404517));
#50500=CARTESIAN_POINT('Ctrl Pts',(-2.05347838646333,0.0017684434794585,
11.2540747194623));
#50501=CARTESIAN_POINT('Origin',(0.,0.,18.5459252805377));
#50502=CARTESIAN_POINT('',(1.25206542099587,1.62921138715835,12.4060251712286));
#50503=CARTESIAN_POINT('',(1.25206542099587,1.62921138715835,12.3479810351515));
#50504=CARTESIAN_POINT('',(1.25206542099588,1.62921138715835,18.5459252805377));
#50505=CARTESIAN_POINT('',(-2.0547498960994,0.000653436693597364,11.8959252805748));
#50506=CARTESIAN_POINT('Ctrl Pts',(1.25206542099587,1.62921138715835,12.3479810351515));
#50507=CARTESIAN_POINT('Ctrl Pts',(1.30851985569991,1.58582558338117,12.3441118588283));
#50508=CARTESIAN_POINT('Ctrl Pts',(1.36263268936519,1.53956655303378,12.340242682505));
#50509=CARTESIAN_POINT('Ctrl Pts',(1.41411515648718,1.49072998450197,12.3363735061818));
#50510=CARTESIAN_POINT('Ctrl Pts',(1.42203556698149,1.48321663691921,12.3357782459608));
#50511=CARTESIAN_POINT('Ctrl Pts',(1.42989379641613,1.47564234693037,12.3351829857399));
#50512=CARTESIAN_POINT('Ctrl Pts',(1.43768887830515,1.46800826009178,12.3345877255189));
#50513=CARTESIAN_POINT('Ctrl Pts',(1.48835548857877,1.41838808827663,12.330718642672));
#50514=CARTESIAN_POINT('Ctrl Pts',(1.53654944525446,1.3660446008768,12.326849559825));
#50515=CARTESIAN_POINT('Ctrl Pts',(1.58196405520874,1.31125409075721,12.3229804769781));
#50516=CARTESIAN_POINT('Ctrl Pts',(1.62731099965912,1.25654521576516,12.3191171588717));
#50517=CARTESIAN_POINT('Ctrl Pts',(1.66988650985259,1.19939692610743,12.3152538407653));
#50518=CARTESIAN_POINT('Ctrl Pts',(1.70942040407517,1.14012255684706,12.3113905226588));
#50519=CARTESIAN_POINT('Ctrl Pts',(1.74890792505505,1.080917716399,12.307531736223));
#50520=CARTESIAN_POINT('Ctrl Pts',(1.78536064871228,1.01959215223843,12.3036729497872));
#50521=CARTESIAN_POINT('Ctrl Pts',(1.81854950426628,0.956491120205974,12.2998141633515));
#50522=CARTESIAN_POINT('Ctrl Pts',(1.8517174532749,0.893429837196706,12.2959578076682));
#50523=CARTESIAN_POINT('Ctrl Pts',(1.88162538764864,0.828595734156922,12.2921014519849));
#50524=CARTESIAN_POINT('Ctrl Pts',(1.90808908639414,0.762360545203895,12.2882450963016));
#50525=CARTESIAN_POINT('Ctrl Pts',(1.93454496749805,0.696144922788906,12.2843898798244));
#50526=CARTESIAN_POINT('Ctrl Pts',(1.95755845277884,0.628529487020637,12.2805346633472));
#50527=CARTESIAN_POINT('Ctrl Pts',(1.9769932870616,0.559906336286134,12.27667944687));
#50528=CARTESIAN_POINT('Ctrl Pts',(1.99642888118825,0.491280502591688,12.2728240796654));
#50529=CARTESIAN_POINT('Ctrl Pts',(2.01228541628162,0.421647343710315,12.2689687124607));
#50530=CARTESIAN_POINT('Ctrl Pts',(2.02447686487614,0.351412842795018,12.2651133452561));
#50531=CARTESIAN_POINT('Ctrl Pts',(2.03668107459289,0.28110482550929,12.2612539425333));
#50532=CARTESIAN_POINT('Ctrl Pts',(2.04521245635311,0.210194689290596,12.2573945398105));
#50533=CARTESIAN_POINT('Ctrl Pts',(2.05003652416308,0.139096412956515,12.2535351370877));
#50534=CARTESIAN_POINT('Ctrl Pts',(2.05486332339813,0.0679578802198854,
12.2496735491408));
#50535=CARTESIAN_POINT('Ctrl Pts',(2.0559786224031,-0.00336851873967881,
12.2458119611939));
#50536=CARTESIAN_POINT('Ctrl Pts',(2.05340010221357,-0.0744686694476668,
12.241950373247));
#50537=CARTESIAN_POINT('Ctrl Pts',(2.05081707081054,-0.145693212417816,
12.2380820293135));
#50538=CARTESIAN_POINT('Ctrl Pts',(2.04452736059261,-0.216690232810768,
12.23421368538));
#50539=CARTESIAN_POINT('Ctrl Pts',(2.03460048013541,-0.287051299827666,
12.2303453414466));
#50540=CARTESIAN_POINT('Ctrl Pts',(2.0287061841907,-0.328829676606923,12.2280484301402));
#50541=CARTESIAN_POINT('Ctrl Pts',(2.02153053389919,-0.370384024467946,
12.2257515188337));
#50542=CARTESIAN_POINT('Ctrl Pts',(2.01309645181131,-0.411631191972505,
12.2234546075273));
#50543=CARTESIAN_POINT('Ctrl Pts',(1.99888947645081,-0.481110891876079,
12.2195855246804));
#50544=CARTESIAN_POINT('Ctrl Pts',(1.9810534349364,-0.549990306481095,12.2157164418335));
#50545=CARTESIAN_POINT('Ctrl Pts',(1.9596541057285,-0.617861916937283,12.2118473589865));
#50546=CARTESIAN_POINT('Ctrl Pts',(1.9382866604539,-0.685632402078804,12.2079840408801));
#50547=CARTESIAN_POINT('Ctrl Pts',(1.91336661082874,-0.752397604135835,
12.2041207227737));
#50548=CARTESIAN_POINT('Ctrl Pts',(1.88501065875936,-0.81776058774166,12.2002574046672));
#50549=CARTESIAN_POINT('Ctrl Pts',(1.85668796821084,-0.88304690059289,12.1963986182314));
#50550=CARTESIAN_POINT('Ctrl Pts',(1.82493757317916,-0.946933818635436,
12.1925398317957));
#50551=CARTESIAN_POINT('Ctrl Pts',(1.789925291033,-1.00904163195601,12.1886810453599));
#50552=CARTESIAN_POINT('Ctrl Pts',(1.75493506405724,-1.07111032190835,12.1848246896766));
#50553=CARTESIAN_POINT('Ctrl Pts',(1.71668726455152,-1.1314017084279,12.1809683339933));
#50554=CARTESIAN_POINT('Ctrl Pts',(1.6753942808025,-1.18955940009496,12.17711197831));
#50555=CARTESIAN_POINT('Ctrl Pts',(1.63411349541436,-1.24769991139755,12.1732567618328));
#50556=CARTESIAN_POINT('Ctrl Pts',(1.58978959277674,-1.30370758331733,12.1694015453556));
#50557=CARTESIAN_POINT('Ctrl Pts',(1.5426780855889,-1.3572552769261,12.1655463288784));
#50558=CARTESIAN_POINT('Ctrl Pts',(1.49556473648206,-1.41080506408953,12.1616909616738));
#50559=CARTESIAN_POINT('Ctrl Pts',(1.4456638889812,-1.46189431872944,12.1578355944691));
#50560=CARTESIAN_POINT('Ctrl Pts',(1.39326996335785,-1.51023056905388,12.1539802272645));
#50561=CARTESIAN_POINT('Ctrl Pts',(1.34082119558151,-1.55861741425176,12.1501208245417));
#50562=CARTESIAN_POINT('Ctrl Pts',(1.28587449816979,-1.60424517265427,12.1462614218189));
#50563=CARTESIAN_POINT('Ctrl Pts',(1.22875896389649,-1.64686033747371,12.1424020190961));
#50564=CARTESIAN_POINT('Ctrl Pts',(1.17161109035904,-1.68949963133423,12.1385404311492));
#50565=CARTESIAN_POINT('Ctrl Pts',(1.11229233951033,-1.72912266602566,12.1346788432023));
#50566=CARTESIAN_POINT('Ctrl Pts',(1.0511602124641,-1.76551968842956,12.1308172552554));
#50567=CARTESIAN_POINT('Ctrl Pts',(0.989921132570398,-1.80198038872877,
12.1269489113219));
#50568=CARTESIAN_POINT('Ctrl Pts',(0.926862772277252,-1.83520358177884,
12.1230805673885));
#50569=CARTESIAN_POINT('Ctrl Pts',(0.862365967892246,-1.8650261392059,12.119212223455));
#50570=CARTESIAN_POINT('Ctrl Pts',(0.824069621505006,-1.88273391558754,
12.1169153121486));
#50571=CARTESIAN_POINT('Ctrl Pts',(0.785266507841448,-1.89924367492176,
12.1146184008421));
#50572=CARTESIAN_POINT('Ctrl Pts',(0.746038917915524,-1.91452957549771,
12.1123214895357));
#50573=CARTESIAN_POINT('Ctrl Pts',(0.679961139951928,-1.94027824744361,
12.1084524066888));
#50574=CARTESIAN_POINT('Ctrl Pts',(0.612419347461162,-1.96265243793997,
12.1045833238419));
#50575=CARTESIAN_POINT('Ctrl Pts',(0.54379158745156,-1.98148637944269,12.100714240995));
#50576=CARTESIAN_POINT('Ctrl Pts',(0.475266079381733,-2.00029225931187,
12.0968509228885));
#50577=CARTESIAN_POINT('Ctrl Pts',(0.405658280198486,-2.01556823299288,
12.0929876047821));
#50578=CARTESIAN_POINT('Ctrl Pts',(0.335364965250433,-2.02719705568615,
12.0891242866757));
#50579=CARTESIAN_POINT('Ctrl Pts',(0.265154104333754,-2.03881223777487,
12.0852655002399));
#50580=CARTESIAN_POINT('Ctrl Pts',(0.194259801829534,-2.04678868774226,
12.0814067138041));
#50581=CARTESIAN_POINT('Ctrl Pts',(0.12309100067338,-2.05105976706025,12.0775479273683));
#50582=CARTESIAN_POINT('Ctrl Pts',(0.0519670306433579,-2.05532815591144,
12.073691571685));
#50583=CARTESIAN_POINT('Ctrl Pts',(-0.019430611215484,-2.0558957759222,
12.0698352160017));
#50584=CARTESIAN_POINT('Ctrl Pts',(-0.0906873134559301,-2.05274776182515,
12.0659788603185));
#50585=CARTESIAN_POINT('Ctrl Pts',(-0.161922965752997,-2.04960067768298,
12.0621236438413));
#50586=CARTESIAN_POINT('Ctrl Pts',(-0.233017276043263,-2.0427401599728,
12.0582684273641));
#50587=CARTESIAN_POINT('Ctrl Pts',(-0.303556819032513,-2.03220343964842,
12.0544132108869));
#50588=CARTESIAN_POINT('Ctrl Pts',(-0.374099119906884,-2.02166630736979,
12.0505578436822));
#50589=CARTESIAN_POINT('Ctrl Pts',(-0.444086130290927,-2.00745276106833,
12.0467024764776));
#50590=CARTESIAN_POINT('Ctrl Pts',(-0.513112447196806,-1.98965152200874,
12.042847109273));
#50591=CARTESIAN_POINT('Ctrl Pts',(-0.582211015833957,-1.97183164990601,
12.0389877065502));
#50592=CARTESIAN_POINT('Ctrl Pts',(-0.650346412265481,-1.95041671011129,
12.0351283038274));
#50593=CARTESIAN_POINT('Ctrl Pts',(-0.717127163609594,-1.9255456872568,
12.0312689011046));
#50594=CARTESIAN_POINT('Ctrl Pts',(-0.783945726739678,-1.90066058223381,
12.0274073131577));
#50595=CARTESIAN_POINT('Ctrl Pts',(-0.849407671902037,-1.87231569176008,
12.0235457252108));
#50596=CARTESIAN_POINT('Ctrl Pts',(-0.913142876995169,-1.84069759838301,
12.0196841372638));
#50597=CARTESIAN_POINT('Ctrl Pts',(-0.97698958911414,-1.80902418801826,
12.0158157933304));
#50598=CARTESIAN_POINT('Ctrl Pts',(-1.03910310618935,-1.7740663797939,12.0119474493969));
#50599=CARTESIAN_POINT('Ctrl Pts',(-1.09913982055953,-1.73605564926945,
12.0080791054635));
#50600=CARTESIAN_POINT('Ctrl Pts',(-1.13478789384623,-1.71348597133768,
12.005782194157));
#50601=CARTESIAN_POINT('Ctrl Pts',(-1.16970433398133,-1.68984076058459,
12.0034852828506));
#50602=CARTESIAN_POINT('Ctrl Pts',(-1.20382279746224,-1.66517513637761,
12.0011883715442));
#50603=CARTESIAN_POINT('Ctrl Pts',(-1.26083681927375,-1.62395738232141,
11.9973500934401));
#50604=CARTESIAN_POINT('Ctrl Pts',(-1.31585191288247,-1.5797208791892,11.993511815336));
#50605=CARTESIAN_POINT('Ctrl Pts',(-1.36852678994371,-1.53268783113404,
11.9896735372319));
#50606=CARTESIAN_POINT('Ctrl Pts',(-1.42213348718528,-1.48482276702558,
11.9857673598712));
#50607=CARTESIAN_POINT('Ctrl Pts',(-1.4733158971113,-1.43406148037154,11.9818611825105));
#50608=CARTESIAN_POINT('Ctrl Pts',(-1.5217450967034,-1.38068440389509,11.9779550051498));
#50609=CARTESIAN_POINT('Ctrl Pts',(-1.5692056384388,-1.32837495035961,11.974126957294));
#50610=CARTESIAN_POINT('Ctrl Pts',(-1.6140217352881,-1.27355376028476,11.9702989094383));
#50611=CARTESIAN_POINT('Ctrl Pts',(-1.6559188631244,-1.21652385149195,11.9664708615825));
#50612=CARTESIAN_POINT('Ctrl Pts',(-1.69779086095982,-1.15952814937945,
11.9626451097993));
#50613=CARTESIAN_POINT('Ctrl Pts',(-1.73674706992695,-1.10032675344736,
11.9588193580162));
#50614=CARTESIAN_POINT('Ctrl Pts',(-1.77255338645319,-1.03925552905593,
11.954993606233));
#50615=CARTESIAN_POINT('Ctrl Pts',(-1.80835068587627,-0.978199684228333,
11.9511688178887));
#50616=CARTESIAN_POINT('Ctrl Pts',(-1.84099941769869,-0.915275372082998,
11.9473440295444));
#50617=CARTESIAN_POINT('Ctrl Pts',(-1.87030994639299,-0.850845618736703,
11.9435192412002));
#50618=CARTESIAN_POINT('Ctrl Pts',(-1.90070387548185,-0.784034358699591,
11.9395530778147));
#50619=CARTESIAN_POINT('Ctrl Pts',(-1.92750771800191,-0.715604685579293,
11.9355869144293));
#50620=CARTESIAN_POINT('Ctrl Pts',(-1.95056426599362,-0.64598498955375,
11.9316207510438));
#50621=CARTESIAN_POINT('Ctrl Pts',(-1.97282450374,-0.578769767833822,11.9277915681179));
#50622=CARTESIAN_POINT('Ctrl Pts',(-1.99159199666899,-0.510445894525309,
11.9239623851919));
#50623=CARTESIAN_POINT('Ctrl Pts',(-2.00677657951126,-0.441412870706191,
11.920133202266));
#50624=CARTESIAN_POINT('Ctrl Pts',(-2.02197110779225,-0.37233463236159,
11.916301511342));
#50625=CARTESIAN_POINT('Ctrl Pts',(-2.03357797952057,-0.302546806993616,
11.912469820418));
#50626=CARTESIAN_POINT('Ctrl Pts',(-2.0415586573881,-0.232456040884489,
11.908638129494));
#50627=CARTESIAN_POINT('Ctrl Pts',(-2.04955171545767,-0.162256544933185,
11.9048004945752));
#50628=CARTESIAN_POINT('Ctrl Pts',(-2.05390733765599,-0.091753662965547,
11.9009628596564));
#50629=CARTESIAN_POINT('Ctrl Pts',(-2.0546390270676,-0.0213548811910643,
11.8971252247376));
#50630=CARTESIAN_POINT('Ctrl Pts',(-2.05471528813786,-0.0140174968341446,
11.89672524335));
#50631=CARTESIAN_POINT('Ctrl Pts',(-2.05475222861971,-0.0066812384315459,
11.8963252619624));
#50632=CARTESIAN_POINT('Ctrl Pts',(-2.0547498960994,0.000653436693603956,
11.8959252805748));
#50633=CARTESIAN_POINT('Ctrl Pts',(-2.05474989609918,0.000653437373812688,
11.8959252805377));
#50634=CARTESIAN_POINT('Ctrl Pts',(-2.05473848559207,0.0365340576922297,
11.893968604876));
#50635=CARTESIAN_POINT('Ctrl Pts',(-2.05378729851884,0.0723985335872527,
11.8920119292143));
#50636=CARTESIAN_POINT('Ctrl Pts',(-2.05189850659895,0.108213128210028,
11.8900552535526));
#50637=CARTESIAN_POINT('Ctrl Pts',(-2.04816365541142,0.179032036237403,
11.8861861707057));
#50638=CARTESIAN_POINT('Ctrl Pts',(-2.04075083573292,0.249796068327482,
11.8823170878588));
#50639=CARTESIAN_POINT('Ctrl Pts',(-2.02966459840712,0.320092456132394,
11.8784480050119));
#50640=CARTESIAN_POINT('Ctrl Pts',(-2.01859487902203,0.390284105825381,
11.8745846869055));
#50641=CARTESIAN_POINT('Ctrl Pts',(-2.00386268121796,0.460009018352436,
11.870721368799));
#50642=CARTESIAN_POINT('Ctrl Pts',(-1.9855244861849,0.528857331669124,11.8668580506926));
#50643=CARTESIAN_POINT('Ctrl Pts',(-1.96720780184756,0.597624885940748,
11.8629992642568));
#50644=CARTESIAN_POINT('Ctrl Pts',(-1.94529364658789,0.665517416317043,
11.859140477821));
#50645=CARTESIAN_POINT('Ctrl Pts',(-1.91988963003493,0.732134803833518,
11.8552816913852));
#50646=CARTESIAN_POINT('Ctrl Pts',(-1.89450161614958,0.798710227280726,
11.8514253357019));
#50647=CARTESIAN_POINT('Ctrl Pts',(-1.86562827515809,0.864011648670079,
11.8475689800187));
#50648=CARTESIAN_POINT('Ctrl Pts',(-1.83342673333031,0.927655095393628,
11.8437126243354));
#50649=CARTESIAN_POINT('Ctrl Pts',(-1.80123470416043,0.991279741205714,
11.8398574078582));
#50650=CARTESIAN_POINT('Ctrl Pts',(-1.7657166452435,1.05324695148401,11.836002191381));
#50651=CARTESIAN_POINT('Ctrl Pts',(-1.72707667211473,1.11319527987551,11.8321469749038));
#50652=CARTESIAN_POINT('Ctrl Pts',(-1.68843518827859,1.17314595206732,11.8282916076992));
#50653=CARTESIAN_POINT('Ctrl Pts',(-1.64667181293418,1.2310771785415,11.8244362404945));
#50654=CARTESIAN_POINT('Ctrl Pts',(-1.60203428460654,1.28665601986125,11.8205808732899));
#50655=CARTESIAN_POINT('Ctrl Pts',(-1.55735003295878,1.34229303707229,11.8167214705671));
#50656=CARTESIAN_POINT('Ctrl Pts',(-1.50978592759242,1.39557237428656,11.8128620678443));
#50657=CARTESIAN_POINT('Ctrl Pts',(-1.45962977992668,1.44619447794935,11.8090026651215));
#50658=CARTESIAN_POINT('Ctrl Pts',(-1.40944523345615,1.49684524424488,11.8051410771746));
#50659=CARTESIAN_POINT('Ctrl Pts',(-1.35666608266766,1.54483545493889,11.8012794892277));
#50660=CARTESIAN_POINT('Ctrl Pts',(-1.30161472803287,1.58990460791455,11.7974179012807));
#50661=CARTESIAN_POINT('Ctrl Pts',(-1.24646705907993,1.63505261098876,11.7935495573473));
#50662=CARTESIAN_POINT('Ctrl Pts',(-1.1890396410044,1.67726906527471,11.7896812134138));
#50663=CARTESIAN_POINT('Ctrl Pts',(-1.1296848726291,1.71633611249457,11.7858128694804));
#50664=CARTESIAN_POINT('Ctrl Pts',(-1.0944417192495,1.7395330008819,11.783515958174));
#50665=CARTESIAN_POINT('Ctrl Pts',(-1.05851956096535,1.76162038025266,11.7812190468675));
#50666=CARTESIAN_POINT('Ctrl Pts',(-1.02199594055809,1.78256047863257,11.7789221355611));
#50667=CARTESIAN_POINT('Ctrl Pts',(-0.960472923613762,1.81783348862112,
11.7750530527142));
#50668=CARTESIAN_POINT('Ctrl Pts',(-0.897001152031734,1.84998675199316,
11.7711839698673));
#50669=CARTESIAN_POINT('Ctrl Pts',(-0.831929874442541,1.87880021463433,
11.7673148870203));
#50670=CARTESIAN_POINT('Ctrl Pts',(-0.766955549811701,1.90757074665316,
11.7634515689139));
#50671=CARTESIAN_POINT('Ctrl Pts',(-0.700386890294981,1.9330111603523,11.7595882508075));
#50672=CARTESIAN_POINT('Ctrl Pts',(-0.632598868839114,1.95494660634082,
11.755724932701));
#50673=CARTESIAN_POINT('Ctrl Pts',(-0.564890362706312,1.97685632205963,
11.7518661462652));
#50674=CARTESIAN_POINT('Ctrl Pts',(-0.495965795661029,1.99526908771997,
11.7480073598295));
#50675=CARTESIAN_POINT('Ctrl Pts',(-0.426219686225407,2.01005829307857,
11.7441485733937));
#50676=CARTESIAN_POINT('Ctrl Pts',(-0.356517511724471,2.02483818232223,
11.7402922177104));
#50677=CARTESIAN_POINT('Ctrl Pts',(-0.285995295661607,2.03599893933331,
11.7364358620271));
#50678=CARTESIAN_POINT('Ctrl Pts',(-0.215060848322245,2.04346431190244,
11.7325795063438));
#50679=CARTESIAN_POINT('Ctrl Pts',(-0.144147355728934,2.05092747912576,
11.7287242898666));
#50680=CARTESIAN_POINT('Ctrl Pts',(-0.0728223564725586,2.0546973783256,
11.7248690733894));
#50681=CARTESIAN_POINT('Ctrl Pts',(-0.00150022183944837,2.05474945232611,
11.7210138569122));
#50682=CARTESIAN_POINT('Ctrl Pts',(0.0698247012758174,2.05480152836255,
11.7171584897076));
#50683=CARTESIAN_POINT('Ctrl Pts',(0.141146273760915,2.05113549246291,11.7133031225029));
#50684=CARTESIAN_POINT('Ctrl Pts',(0.212050413681591,2.04377889815838,11.7094477552983));
#50685=CARTESIAN_POINT('Ctrl Pts',(0.283028770902149,2.03641460350565,11.7055883525755));
#50686=CARTESIAN_POINT('Ctrl Pts',(0.353588339152754,2.0253520892534,11.7017289498527));
#50687=CARTESIAN_POINT('Ctrl Pts',(0.423321350333843,2.01067068334214,11.69786954713));
#50688=CARTESIAN_POINT('Ctrl Pts',(0.493093844893627,1.99598096470352,11.694007959183));
#50689=CARTESIAN_POINT('Ctrl Pts',(0.562038381008229,1.97766840015477,11.6901463712361));
#50690=CARTESIAN_POINT('Ctrl Pts',(0.629761238561418,1.95586255777485,11.6862847832892));
#50691=CARTESIAN_POINT('Ctrl Pts',(0.69760257968133,1.93401856529209,11.6824164393557));
#50692=CARTESIAN_POINT('Ctrl Pts',(0.764217520754356,1.90866926579212,11.6785480954223));
#50693=CARTESIAN_POINT('Ctrl Pts',(0.829231897648688,1.87999255914005,11.6746797514888));
#50694=CARTESIAN_POINT('Ctrl Pts',(0.867835563697562,1.86296515597387,11.6723828401824));
#50695=CARTESIAN_POINT('Ctrl Pts',(0.905875373419138,1.84476552247177,11.6700859288759));
#50696=CARTESIAN_POINT('Ctrl Pts',(0.943277535649769,1.8254383181139,11.6677890175695));
#50697=CARTESIAN_POINT('Ctrl Pts',(1.00626540384789,1.79288994849758,11.6639208576022));
#50698=CARTESIAN_POINT('Ctrl Pts',(1.06768998270875,1.75701386646393,11.6600526976348));
#50699=CARTESIAN_POINT('Ctrl Pts',(1.12717723733065,1.71798400404184,11.6561845376675));
#50700=CARTESIAN_POINT('Ctrl Pts',(1.16984678376852,1.68998831761005,11.6534099495242));
#50701=CARTESIAN_POINT('Ctrl Pts',(1.21151987881709,1.66037104620426,11.6506353613808));
#50702=CARTESIAN_POINT('Ctrl Pts',(1.25206542099587,1.62921138715835,11.6478607732374));
#50703=CARTESIAN_POINT('',(-2.05466569125301,-0.00102264302692682,11.9540747659024));
#50704=CARTESIAN_POINT('Ctrl Pts',(-2.05188276458647,-0.00102039859364231,
11.9540747194623));
#50705=CARTESIAN_POINT('Ctrl Pts',(-2.05004756599998,0.40727097526418,11.9320086704376));
#50706=CARTESIAN_POINT('Ctrl Pts',(-1.7342531973136,1.50361561120492,11.8728982487491));
#50707=CARTESIAN_POINT('Ctrl Pts',(-0.200040598667229,2.29813379067046,
11.7902560936311));
#50708=CARTESIAN_POINT('Ctrl Pts',(0.90379928332058,1.89013835121545,11.7296799875378));
#50709=CARTESIAN_POINT('Ctrl Pts',(1.25062491733525,1.62730785058785,11.7061482541084));
#50710=CARTESIAN_POINT('Ctrl Pts',(1.25206542099587,1.62921138715835,12.4060251712286));
#50711=CARTESIAN_POINT('Ctrl Pts',(1.30857348607413,1.58578436789642,12.402169202365));
#50712=CARTESIAN_POINT('Ctrl Pts',(1.36285495219622,1.5393867813656,12.3983132335015));
#50713=CARTESIAN_POINT('Ctrl Pts',(1.41458832701998,1.49028098946434,12.394457264638));
#50714=CARTESIAN_POINT('Ctrl Pts',(1.46631052222186,1.44118580936228,12.3906021290523));
#50715=CARTESIAN_POINT('Ctrl Pts',(1.51548536748826,1.3893839205327,12.3867469934665));
#50716=CARTESIAN_POINT('Ctrl Pts',(1.56182668300009,1.33517600891004,12.3828918578808));
#50717=CARTESIAN_POINT('Ctrl Pts',(1.60817348550792,1.28096167885511,12.3790362658318));
#50718=CARTESIAN_POINT('Ctrl Pts',(1.65168577852569,1.2243411313406,12.3751806737827));
#50719=CARTESIAN_POINT('Ctrl Pts',(1.69211742153164,1.16564840078349,12.3713250817336));
#50720=CARTESIAN_POINT('Ctrl Pts',(1.73259335532627,1.10689137535402,12.3674652660814));
#50721=CARTESIAN_POINT('Ctrl Pts',(1.76998162974679,1.0460580384509,12.3636054504292));
#50722=CARTESIAN_POINT('Ctrl Pts',(1.80407977935618,0.983510911082403,12.359745634777));
#50723=CARTESIAN_POINT('Ctrl Pts',(1.83819966057492,0.920923920854698,12.3558833591671));
#50724=CARTESIAN_POINT('Ctrl Pts',(1.86902503473518,0.856621404660003,12.3520210835572));
#50725=CARTESIAN_POINT('Ctrl Pts',(1.89640089579593,0.790987487211018,12.3481588079473));
#50726=CARTESIAN_POINT('Ctrl Pts',(1.92382270088975,0.72524341845512,12.3442900504037));
#50727=CARTESIAN_POINT('Ctrl Pts',(1.94778327885194,0.658163946893732,12.34042129286));
#50728=CARTESIAN_POINT('Ctrl Pts',(1.96817720266579,0.590149185720579,12.3365525353163));
#50729=CARTESIAN_POINT('Ctrl Pts',(1.97545792419331,0.565867613406076,12.3351713716624));
#50730=CARTESIAN_POINT('Ctrl Pts',(1.9822845424209,0.541466932141748,12.3337902080085));
#50731=CARTESIAN_POINT('Ctrl Pts',(1.98865384835457,0.516965602264348,12.3324090443545));
#50732=CARTESIAN_POINT('Ctrl Pts',(2.00649631927715,0.448329510599995,12.3285399615076));
#50733=CARTESIAN_POINT('Ctrl Pts',(2.0208162221759,0.378634184255975,12.3246708786607));
#50734=CARTESIAN_POINT('Ctrl Pts',(2.03149314948497,0.308274465526457,12.3208017958138));
#50735=CARTESIAN_POINT('Ctrl Pts',(2.04215416870484,0.23801957926887,12.3169384777073));
#50736=CARTESIAN_POINT('Ctrl Pts',(2.04918291418265,0.16710274194488,12.3130751596009));
#50737=CARTESIAN_POINT('Ctrl Pts',(2.05250935872637,0.0959317196794512,
12.3092118414945));
#50738=CARTESIAN_POINT('Ctrl Pts',(2.05583190135193,0.0248441809956648,
12.3053530550587));
#50739=CARTESIAN_POINT('Ctrl Pts',(2.05546074673972,-0.0464964674867899,
12.3014942686229));
#50740=CARTESIAN_POINT('Ctrl Pts',(2.05137754985214,-0.11767629524525,12.2976354821871));
#50741=CARTESIAN_POINT('Ctrl Pts',(2.04729692507919,-0.188811284931504,
12.2937791265038));
#50742=CARTESIAN_POINT('Ctrl Pts',(2.03950892496536,-0.259785171042465,
12.2899227708206));
#50743=CARTESIAN_POINT('Ctrl Pts',(2.02804728537728,-0.330184449624538,
12.2860664151373));
#50744=CARTESIAN_POINT('Ctrl Pts',(2.01658903167228,-0.400562931554911,
12.2822111986601));
#50745=CARTESIAN_POINT('Ctrl Pts',(2.00145937099513,-0.470366663738085,
12.2783559821829));
#50746=CARTESIAN_POINT('Ctrl Pts',(1.98274363903717,-0.53918941417433,12.2745007657057));
#50747=CARTESIAN_POINT('Ctrl Pts',(1.96402717535011,-0.608014855374075,
12.2706453985011));
#50748=CARTESIAN_POINT('Ctrl Pts',(1.94172449162492,-0.675858770499862,
12.2667900312964));
#50749=CARTESIAN_POINT('Ctrl Pts',(1.9159711219694,-0.742328917852,12.2629346640918));
#50750=CARTESIAN_POINT('Ctrl Pts',(1.89019079555839,-0.808868641323056,
12.259075261369));
#50751=CARTESIAN_POINT('Ctrl Pts',(1.86095274886154,-0.874031272628489,
12.2552158586462));
#50752=CARTESIAN_POINT('Ctrl Pts',(1.82844080481938,-0.937444284089179,
12.2513564559235));
#50753=CARTESIAN_POINT('Ctrl Pts',(1.79591045225908,-1.00089320049512,12.2474948679765));
#50754=CARTESIAN_POINT('Ctrl Pts',(1.76010275615705,-1.06259010463368,12.2436332800296));
#50755=CARTESIAN_POINT('Ctrl Pts',(1.72124631310105,-1.12218924078608,12.2397716920827));
#50756=CARTESIAN_POINT('Ctrl Pts',(1.6823218893052,-1.18189264776338,12.2359033481492));
#50757=CARTESIAN_POINT('Ctrl Pts',(1.64033835552297,-1.23949056656658,12.2320350042158));
#50758=CARTESIAN_POINT('Ctrl Pts',(1.59556579163784,-1.29466882524262,12.2281666602823));
#50759=CARTESIAN_POINT('Ctrl Pts',(1.56898113164501,-1.32743208735248,12.2258697489759));
#50760=CARTESIAN_POINT('Ctrl Pts',(1.54141390511254,-1.3593429288423,12.2235728376694));
#50761=CARTESIAN_POINT('Ctrl Pts',(1.5129266135236,-1.39034190924103,12.221275926363));
#50762=CARTESIAN_POINT('Ctrl Pts',(1.46494056768335,-1.4425588246249,12.2174068435161));
#50763=CARTESIAN_POINT('Ctrl Pts',(1.41415405217899,-1.49239082213816,12.2135377606691));
#50764=CARTESIAN_POINT('Ctrl Pts',(1.3608334803882,-1.53952258871201,12.2096686778222));
#50765=CARTESIAN_POINT('Ctrl Pts',(1.30759235359024,-1.58658413130417,12.2058053597158));
#50766=CARTESIAN_POINT('Ctrl Pts',(1.25182502601033,-1.63095310980967,12.2019420416094));
#50767=CARTESIAN_POINT('Ctrl Pts',(1.19383609408718,-1.67234952774672,12.1980787235029));
#50768=CARTESIAN_POINT('Ctrl Pts',(1.13591518315877,-1.71369738770151,12.1942199370671));
#50769=CARTESIAN_POINT('Ctrl Pts',(1.0757782376257,-1.75207933220145,12.1903611506314));
#50770=CARTESIAN_POINT('Ctrl Pts',(1.01376306422456,-1.7872554412042,12.1865023641956));
#50771=CARTESIAN_POINT('Ctrl Pts',(0.951786955835391,-1.82240939183757,
12.1826460085123));
#50772=CARTESIAN_POINT('Ctrl Pts',(0.887935388464297,-1.85436127440682,
12.178789652829));
#50773=CARTESIAN_POINT('Ctrl Pts',(0.822574058130612,-1.88291515512265,
12.1749332971457));
#50774=CARTESIAN_POINT('Ctrl Pts',(0.757232036188336,-1.91146060073621,
12.1710780806685));
#50775=CARTESIAN_POINT('Ctrl Pts',(0.690381581630985,-1.93660984295883,
12.1672228641913));
#50776=CARTESIAN_POINT('Ctrl Pts',(0.622410267798343,-1.95821424288539,
12.1633676477141));
#50777=CARTESIAN_POINT('Ctrl Pts',(0.55443629649076,-1.97981948747932,12.1595122805095));
#50778=CARTESIAN_POINT('Ctrl Pts',(0.485341842531987,-1.99787946956899,
12.1556569133049));
#50779=CARTESIAN_POINT('Ctrl Pts',(0.415529952181181,-2.01229531166285,
12.1518015461003));
#50780=CARTESIAN_POINT('Ctrl Pts',(0.345644987817769,-2.02672624321242,
12.1479421433775));
#50781=CARTESIAN_POINT('Ctrl Pts',(0.275041564697992,-2.03750532188664,
12.1440827406547));
#50782=CARTESIAN_POINT('Ctrl Pts',(0.204132357592777,-2.04458493173642,
12.1402233379319));
#50783=CARTESIAN_POINT('Ctrl Pts',(0.133183001137418,-2.05166855011691,
12.136361749985));
#50784=CARTESIAN_POINT('Ctrl Pts',(0.061928001500897,-2.05504850680639,
12.132500162038));
#50785=CARTESIAN_POINT('Ctrl Pts',(-0.00921817421015008,-2.05472932226224,
12.1286385740911));
#50786=CARTESIAN_POINT('Ctrl Pts',(-0.0804888227056832,-2.05440957929328,
12.1247702301576));
#50787=CARTESIAN_POINT('Ctrl Pts',(-0.151649781995328,-2.05037780148638,
12.1209018862242));
#50788=CARTESIAN_POINT('Ctrl Pts',(-0.222290619815562,-2.04269049120076,
12.1170335422907));
#50789=CARTESIAN_POINT('Ctrl Pts',(-0.264235116446928,-2.03812598757469,
12.1147366309843));
#50790=CARTESIAN_POINT('Ctrl Pts',(-0.305996391073655,-2.03227366112877,
12.1124397196778));
#50791=CARTESIAN_POINT('Ctrl Pts',(-0.347490606215405,-2.02515378208472,
12.1101428083714));
#50792=CARTESIAN_POINT('Ctrl Pts',(-0.41738645095297,-2.013160544991,12.1062737255245));
#50793=CARTESIAN_POINT('Ctrl Pts',(-0.486797566932928,-1.99752100818105,
12.1024046426776));
#50794=CARTESIAN_POINT('Ctrl Pts',(-0.555314551843232,-1.97828797474259,
12.0985355598307));
#50795=CARTESIAN_POINT('Ctrl Pts',(-0.623729449863567,-1.95908359756464,
12.0946722417242));
#50796=CARTESIAN_POINT('Ctrl Pts',(-0.691252397319804,-1.93629648177733,
12.0908089236178));
#50797=CARTESIAN_POINT('Ctrl Pts',(-0.757482952791989,-1.91003066434273,
12.0869456055113));
#50798=CARTESIAN_POINT('Ctrl Pts',(-0.823635819847797,-1.88379565670198,
12.0830868190755));
#50799=CARTESIAN_POINT('Ctrl Pts',(-0.888498856782718,-1.85409023091444,
12.0792280326397));
#50800=CARTESIAN_POINT('Ctrl Pts',(-0.951687279107213,-1.821068061684,12.0753692462039));
#50801=CARTESIAN_POINT('Ctrl Pts',(-1.01483589735908,-1.78806669399875,
12.0715128905207));
#50802=CARTESIAN_POINT('Ctrl Pts',(-1.0763115643563,-1.75175295248498,12.0676565348374));
#50803=CARTESIAN_POINT('Ctrl Pts',(-1.13575132331738,-1.71232779983355,
12.0638001791541));
#50804=CARTESIAN_POINT('Ctrl Pts',(-1.19517352317843,-1.67291429376703,
12.0599449626769));
#50805=CARTESIAN_POINT('Ctrl Pts',(-1.25256060439685,-1.63039146968246,
12.0560897461997));
#50806=CARTESIAN_POINT('Ctrl Pts',(-1.30757747835969,-1.58500432194569,
12.0522345297225));
#50807=CARTESIAN_POINT('Ctrl Pts',(-1.36259650331782,-1.53961539970714,
12.0483791625179));
#50808=CARTESIAN_POINT('Ctrl Pts',(-1.41524476371604,-1.49136224231808,
12.0445237953132));
#50809=CARTESIAN_POINT('Ctrl Pts',(-1.46522058494397,-1.44052983306714,
12.0406684281086));
#50810=CARTESIAN_POINT('Ctrl Pts',(-1.51524871722895,-1.38964421614508,
12.0368090253858));
#50811=CARTESIAN_POINT('Ctrl Pts',(-1.56259848500875,-1.336174305125,12.032949622663));
#50812=CARTESIAN_POINT('Ctrl Pts',(-1.60700605787508,-1.28044097577858,
12.0290902199402));
#50813=CARTESIAN_POINT('Ctrl Pts',(-1.65143877465797,-1.22467608978332,
12.0252286319933));
#50814=CARTESIAN_POINT('Ctrl Pts',(-1.69292569759206,-1.16664562962774,
12.0213670440464));
#50815=CARTESIAN_POINT('Ctrl Pts',(-1.73124582566109,-1.10670025464488,
12.0175054560994));
#50816=CARTESIAN_POINT('Ctrl Pts',(-1.76963299616775,-1.04665000307977,
12.013637112166));
#50817=CARTESIAN_POINT('Ctrl Pts',(-1.80484207015481,-0.984678570400846,
12.0097687682325));
#50818=CARTESIAN_POINT('Ctrl Pts',(-1.83669790674073,-0.921161420096516,
12.0059004242991));
#50819=CARTESIAN_POINT('Ctrl Pts',(-1.85561298577411,-0.88344676411059,
12.0036035129927));
#50820=CARTESIAN_POINT('Ctrl Pts',(-1.87334674624879,-0.845187549237961,
12.0013066016863));
#50821=CARTESIAN_POINT('Ctrl Pts',(-1.88987074604909,-0.806465204288353,
11.9990096903798));
#50822=CARTESIAN_POINT('Ctrl Pts',(-1.92069469607791,-0.734232352669482,
11.9947250207971));
#50823=CARTESIAN_POINT('Ctrl Pts',(-1.94740950840208,-0.660146193744584,
11.9904403512143));
#50824=CARTESIAN_POINT('Ctrl Pts',(-1.96981308826176,-0.584665682089075,
11.9861556816316));
#50825=CARTESIAN_POINT('Ctrl Pts',(-1.99214571435029,-0.509424222718199,
11.9818845819099));
#50826=CARTESIAN_POINT('Ctrl Pts',(-2.01019421233967,-0.432797493083545,
11.9776134821881));
#50827=CARTESIAN_POINT('Ctrl Pts',(-2.02380481117486,-0.355262788320802,
11.9733423824664));
#50828=CARTESIAN_POINT('Ctrl Pts',(-2.03734384291512,-0.278135775654815,
11.9690937409923));
#50829=CARTESIAN_POINT('Ctrl Pts',(-2.04649139620821,-0.200110594467843,
11.9648450995182));
#50830=CARTESIAN_POINT('Ctrl Pts',(-2.05114422938467,-0.121675440257956,
11.9605964580442));
#50831=CARTESIAN_POINT('Ctrl Pts',(-2.05352493854566,-0.08154262588682,
11.9584225611311));
#50832=CARTESIAN_POINT('Ctrl Pts',(-2.05472969689495,-0.0413027495048298,
11.9562486642181));
#50833=CARTESIAN_POINT('Ctrl Pts',(-2.05474974548303,-0.00102271081675177,
11.9540747673051));
#50834=CARTESIAN_POINT('Origin',(0.,0.,18.5459252805377));
#50835=CARTESIAN_POINT('',(1.25206542099588,1.62921138715834,13.1060515834985));
#50836=CARTESIAN_POINT('',(1.2502432481766,1.62681756561327,13.047972482772));
#50837=CARTESIAN_POINT('',(1.25206542099588,1.62921138715835,18.5459252805377));
#50838=CARTESIAN_POINT('',(-2.0547494773391,0.00146556292173476,12.5959252537175));
#50839=CARTESIAN_POINT('Ctrl Pts',(1.25024324817659,1.62681756561327,13.047972482772));
#50840=CARTESIAN_POINT('Ctrl Pts',(1.47885177013841,1.452673658258,13.0324437996707));
#50841=CARTESIAN_POINT('Ctrl Pts',(2.13338525759955,0.709856746996147,12.9798707439056));
#50842=CARTESIAN_POINT('Ctrl Pts',(2.1316126390019,-1.16370384027608,12.8902533154766));
#50843=CARTESIAN_POINT('Ctrl Pts',(0.178478656788241,-2.42200834839547,
12.7791201974851));
#50844=CARTESIAN_POINT('Ctrl Pts',(-1.68997359897976,-1.57591260505555,
12.6810108525054));
#50845=CARTESIAN_POINT('Ctrl Pts',(-2.04962979387723,-0.442629241759327,
12.6199458801896));
#50846=CARTESIAN_POINT('Ctrl Pts',(-2.05255322210627,0.00146350058043466,
12.5959252805377));
#50847=CARTESIAN_POINT('Ctrl Pts',(-2.0547494773391,0.00146556292173476,
12.5959252537175));
#50848=CARTESIAN_POINT('Ctrl Pts',(-2.05469114092328,0.0832544224373133,
12.5915060692206));
#50849=CARTESIAN_POINT('Ctrl Pts',(-2.04974540773188,0.164848037177314,
12.5870868847237));
#50850=CARTESIAN_POINT('Ctrl Pts',(-2.04000589565819,0.245710211793937,
12.5826677002268));
#50851=CARTESIAN_POINT('Ctrl Pts',(-2.03017754638782,0.327309956101516,
12.5782082069382));
#50852=CARTESIAN_POINT('Ctrl Pts',(-2.01546767759796,0.408164668537392,
12.5737487136497));
#50853=CARTESIAN_POINT('Ctrl Pts',(-1.99602219393391,0.487742722983417,
12.5692892203612));
#50854=CARTESIAN_POINT('Ctrl Pts',(-1.97794767235628,0.561710297513277,
12.5651441340748));
#50855=CARTESIAN_POINT('Ctrl Pts',(-1.95578233527752,0.634574984482566,
12.5609990477884));
#50856=CARTESIAN_POINT('Ctrl Pts',(-1.92968005290243,0.705926664697185,
12.556853961502));
#50857=CARTESIAN_POINT('Ctrl Pts',(-1.90531580906655,0.772527343897062,
12.5529848786551));
#50858=CARTESIAN_POINT('Ctrl Pts',(-1.87745182895922,0.837995631989894,
12.5491157958081));
#50859=CARTESIAN_POINT('Ctrl Pts',(-1.84621366087208,0.901938291076125,
12.5452467129612));
#50860=CARTESIAN_POINT('Ctrl Pts',(-1.81502203609748,0.965785678789267,
12.5413833948548));
#50861=CARTESIAN_POINT('Ctrl Pts',(-1.78046641403582,1.0281115166333,12.5375200767484));
#50862=CARTESIAN_POINT('Ctrl Pts',(-1.74272113095632,1.08854059282064,12.5336567586419));
#50863=CARTESIAN_POINT('Ctrl Pts',(-1.70502012307931,1.14889878572493,12.5297979722061));
#50864=CARTESIAN_POINT('Ctrl Pts',(-1.6641371421163,1.20736422636482,12.5259391857703));
#50865=CARTESIAN_POINT('Ctrl Pts',(-1.62029253832278,1.26358602902831,12.5220803993346));
#50866=CARTESIAN_POINT('Ctrl Pts',(-1.57647555341467,1.31977241607866,12.5182240436513));
#50867=CARTESIAN_POINT('Ctrl Pts',(-1.52970094503791,1.37371758700872,12.514367687968));
#50868=CARTESIAN_POINT('Ctrl Pts',(-1.48023165653616,1.42510062995152,12.5105113322847));
#50869=CARTESIAN_POINT('Ctrl Pts',(-1.43077698175754,1.47646849382896,12.5066561158075));
#50870=CARTESIAN_POINT('Ctrl Pts',(-1.37862954394352,1.5252753825675,12.5028008993303));
#50871=CARTESIAN_POINT('Ctrl Pts',(-1.32409059027219,1.57123571473304,12.4989456828531));
#50872=CARTESIAN_POINT('Ctrl Pts',(-1.26954950429088,1.61719784381012,12.4950903156485));
#50873=CARTESIAN_POINT('Ctrl Pts',(-1.21261708970847,1.66031288400247,12.4912349484438));
#50874=CARTESIAN_POINT('Ctrl Pts',(-1.1536279235862,1.70033531293748,12.4873795812392));
#50875=CARTESIAN_POINT('Ctrl Pts',(-1.09457701189259,1.74039963444197,12.4835201785164));
#50876=CARTESIAN_POINT('Ctrl Pts',(-1.03346545388818,1.77736460937187,12.4796607757936));
#50877=CARTESIAN_POINT('Ctrl Pts',(-0.970656330330856,1.81102839593658,
12.4758013730708));
#50878=CARTESIAN_POINT('Ctrl Pts',(-0.907811643754378,1.8447112432017,12.4719397851239));
#50879=CARTESIAN_POINT('Ctrl Pts',(-0.84326791796477,1.87508897421654,12.468078197177));
#50880=CARTESIAN_POINT('Ctrl Pts',(-0.777409831760266,1.90200723342012,
12.4642166092301));
#50881=CARTESIAN_POINT('Ctrl Pts',(-0.711436524473381,1.92897258708302,
12.4603482652966));
#50882=CARTESIAN_POINT('Ctrl Pts',(-0.644144724493293,1.95246622483331,
12.4564799213632));
#50883=CARTESIAN_POINT('Ctrl Pts',(-0.575935265499068,1.97238336346019,
12.4526115774297));
#50884=CARTESIAN_POINT('Ctrl Pts',(-0.535434451645713,1.98420958721146,
12.4503146661233));
#50885=CARTESIAN_POINT('Ctrl Pts',(-0.494610339145961,1.9947758363981,12.4480177548168));
#50886=CARTESIAN_POINT('Ctrl Pts',(-0.453548143508707,2.00406877227799,
12.4457208435104));
#50887=CARTESIAN_POINT('Ctrl Pts',(-0.380743650195929,2.02054542379707,
12.4416483514955));
#50888=CARTESIAN_POINT('Ctrl Pts',(-0.306889998070348,2.03308359131829,
12.4375758594805));
#50889=CARTESIAN_POINT('Ctrl Pts',(-0.23245234744894,2.04155907792684,12.4335033674655));
#50890=CARTESIAN_POINT('Ctrl Pts',(-0.16185603027104,2.04959718949886,12.4296410352238));
#50891=CARTESIAN_POINT('Ctrl Pts',(-0.0907350550844751,2.05398142394467,
12.4257787029821));
#50892=CARTESIAN_POINT('Ctrl Pts',(-0.0194993857400896,2.05465747424133,
12.4219163707404));
#50893=CARTESIAN_POINT('Ctrl Pts',(0.0516664469702679,2.05533286176501,
12.4180578249765));
#50894=CARTESIAN_POINT('Ctrl Pts',(0.122946267557767,2.05230727293557,12.4141992792127));
#50895=CARTESIAN_POINT('Ctrl Pts',(0.193925736297766,2.04557824863811,12.4103407334488));
#50896=CARTESIAN_POINT('Ctrl Pts',(0.264859365375091,2.0388535700509,12.4064846795948));
#50897=CARTESIAN_POINT('Ctrl Pts',(0.335492545182316,2.02843024911777,12.4026286257407));
#50898=CARTESIAN_POINT('Ctrl Pts',(0.405413417056765,2.01435784402135,12.3987725718867));
#50899=CARTESIAN_POINT('Ctrl Pts',(0.475312522755492,2.00028981962607,12.3949177184117));
#50900=CARTESIAN_POINT('Ctrl Pts',(0.544499285330755,1.98257506415181,12.3910628649366));
#50901=CARTESIAN_POINT('Ctrl Pts',(0.612571145518115,1.96131439452695,12.3872080114616));
#50902=CARTESIAN_POINT('Ctrl Pts',(0.680674715449567,1.94004382109762,12.3833513622898));
#50903=CARTESIAN_POINT('Ctrl Pts',(0.747661880423524,1.91522417591916,12.379494713118));
#50904=CARTESIAN_POINT('Ctrl Pts',(0.813145524332736,1.88700607279299,12.3756380639462));
#50905=CARTESIAN_POINT('Ctrl Pts',(0.878646757697546,1.85878039004782,12.3717803788462));
#50906=CARTESIAN_POINT('Ctrl Pts',(0.942643226698747,1.82715464010088,12.3679226937461));
#50907=CARTESIAN_POINT('Ctrl Pts',(1.00477027017304,1.79232649555721,12.364065008646));
#50908=CARTESIAN_POINT('Ctrl Pts',(1.06696943851605,1.75745791813258,12.360202845061));
#50909=CARTESIAN_POINT('Ctrl Pts',(1.12729443571184,1.71937978027434,12.3563406814759));
#50910=CARTESIAN_POINT('Ctrl Pts',(1.18540845321352,1.67833380516211,12.3524785178908));
#50911=CARTESIAN_POINT('Ctrl Pts',(1.20796634379055,1.66240114975445,12.3509793569777));
#50912=CARTESIAN_POINT('Ctrl Pts',(1.23019144193433,1.64602176119478,12.3494801960646));
#50913=CARTESIAN_POINT('Ctrl Pts',(1.25206542099587,1.62921138715835,12.3479810351515));
#50914=CARTESIAN_POINT('',(-2.05474964003203,-0.00121625993429837,12.6540747194125));
#50915=CARTESIAN_POINT('Ctrl Pts',(-2.05474964003203,-0.00121625993429152,
12.6540747194125));
#50916=CARTESIAN_POINT('Ctrl Pts',(-2.05479111887721,0.0688581047612897,
12.6502578388075));
#50917=CARTESIAN_POINT('Ctrl Pts',(-2.05124368555208,0.139075573134476,
12.6464409582024));
#50918=CARTESIAN_POINT('Ctrl Pts',(-2.044089796226,0.209032216332157,12.6426240775974));
#50919=CARTESIAN_POINT('Ctrl Pts',(-2.0369463642195,0.278886599215084,12.6388127763825));
#50920=CARTESIAN_POINT('Ctrl Pts',(-2.02620699185267,0.348480420599989,
12.6350014751677));
#50921=CARTESIAN_POINT('Ctrl Pts',(-2.01190615332121,0.41741010137304,12.6311901739529));
#50922=CARTESIAN_POINT('Ctrl Pts',(-1.99761679316685,0.486284456658215,
12.6273819318281));
#50923=CARTESIAN_POINT('Ctrl Pts',(-1.9797717334666,0.554495240735824,12.6235736897033));
#50924=CARTESIAN_POINT('Ctrl Pts',(-1.95845703300675,0.62164588984919,12.6197654475785));
#50925=CARTESIAN_POINT('Ctrl Pts',(-1.93715187206696,0.688766485292987,
12.615958909855));
#50926=CARTESIAN_POINT('Ctrl Pts',(-1.91238030076588,0.754827411188127,
12.6121523721315));
#50927=CARTESIAN_POINT('Ctrl Pts',(-1.88427857892226,0.819446032094063,
12.6083458344079));
#50928=CARTESIAN_POINT('Ctrl Pts',(-1.85617945689729,0.884058674836218,
12.6045396488446));
#50929=CARTESIAN_POINT('Ctrl Pts',(-1.82475099666655,0.947228820103455,
12.6007334632813));
#50930=CARTESIAN_POINT('Ctrl Pts',(-1.79017732801765,1.00859441637934,12.5969272777179));
#50931=CARTESIAN_POINT('Ctrl Pts',(-1.75557129150574,1.07001746311657,12.5931175288043));
#50932=CARTESIAN_POINT('Ctrl Pts',(-1.71781441294439,1.12963215146144,12.5893077798906));
#50933=CARTESIAN_POINT('Ctrl Pts',(-1.67713593618041,1.18710261311828,12.585498030977));
#50934=CARTESIAN_POINT('Ctrl Pts',(-1.63643771004458,1.24460097664382,12.5816864324329));
#50935=CARTESIAN_POINT('Ctrl Pts',(-1.59281537301402,1.2999526496942,12.5778748338888));
#50936=CARTESIAN_POINT('Ctrl Pts',(-1.54653873298482,1.35285457824472,12.5740632353447));
#50937=CARTESIAN_POINT('Ctrl Pts',(-1.50018078791144,1.40584945204009,12.5702449400701));
#50938=CARTESIAN_POINT('Ctrl Pts',(-1.45115957837219,1.45638563068069,12.5664266447955));
#50939=CARTESIAN_POINT('Ctrl Pts',(-1.39978145601897,1.50419727359326,12.5626083495209));
#50940=CARTESIAN_POINT('Ctrl Pts',(-1.3641995911793,1.53730917683064,12.5599639931265));
#50941=CARTESIAN_POINT('Ctrl Pts',(-1.32748803416161,1.56911514178964,12.5573196367321));
#50942=CARTESIAN_POINT('Ctrl Pts',(-1.28975687735514,1.59953892100665,12.5546752803376));
#50943=CARTESIAN_POINT('Ctrl Pts',(-1.23455063817286,1.64405339059733,12.5508061974907));
#50944=CARTESIAN_POINT('Ctrl Pts',(-1.17692901738585,1.68579362240212,12.5469371146438));
#50945=CARTESIAN_POINT('Ctrl Pts',(-1.11720228643712,1.72448734807759,12.5430680317969));
#50946=CARTESIAN_POINT('Ctrl Pts',(-1.05756454533888,1.7631234220315,12.5392047136905));
#50947=CARTESIAN_POINT('Ctrl Pts',(-0.995828324344066,1.79872173795106,
12.535341395584));
#50948=CARTESIAN_POINT('Ctrl Pts',(-0.932336411880873,1.8310506212503,12.5314780774776));
#50949=CARTESIAN_POINT('Ctrl Pts',(-0.868918975406488,1.8633415827819,12.5276192910418));
#50950=CARTESIAN_POINT('Ctrl Pts',(-0.803750368975177,1.89237051003465,
12.523760504606));
#50951=CARTESIAN_POINT('Ctrl Pts',(-0.737200273710599,1.91795029105058,
12.5199017181702));
#50952=CARTESIAN_POINT('Ctrl Pts',(-0.670692100126142,1.94351395868015,
12.5160453624869));
#50953=CARTESIAN_POINT('Ctrl Pts',(-0.602804616613449,1.96563261681741,
12.5121890068037));
#50954=CARTESIAN_POINT('Ctrl Pts',(-0.533928554502491,1.98416679268324,
12.5083326511204));
#50955=CARTESIAN_POINT('Ctrl Pts',(-0.465072839069948,2.00269549336793,
12.5044774346432));
#50956=CARTESIAN_POINT('Ctrl Pts',(-0.395229593652036,2.01764168781327,
12.500622218166));
#50957=CARTESIAN_POINT('Ctrl Pts',(-0.324804163254478,2.02891592187369,
12.4967670016888));
#50958=CARTESIAN_POINT('Ctrl Pts',(-0.254375979433294,2.04019059672293,
12.4929116344842));
#50959=CARTESIAN_POINT('Ctrl Pts',(-0.18336604546572,2.04779295154757,12.4890562672795));
#50960=CARTESIAN_POINT('Ctrl Pts',(-0.112187620427746,2.05168503925987,
12.4852009000749));
#50961=CARTESIAN_POINT('Ctrl Pts',(-0.0409346909881128,2.05558120092668,
12.4813414973521));
#50962=CARTESIAN_POINT('Ctrl Pts',(0.0304865955321654,2.05575931629186,
12.4774820946293));
#50963=CARTESIAN_POINT('Ctrl Pts',(0.101661068335935,2.05223356119249,12.4736226919065));
#50964=CARTESIAN_POINT('Ctrl Pts',(0.172875840685214,2.04870580978289,12.4697611039596));
#50965=CARTESIAN_POINT('Ctrl Pts',(0.243843037616678,2.04147006240673,12.4658995160127));
#50966=CARTESIAN_POINT('Ctrl Pts',(0.314153455834246,2.03059231966621,12.4620379280658));
#50967=CARTESIAN_POINT('Ctrl Pts',(0.384586884648705,2.01969554592486,12.4581695841323));
#50968=CARTESIAN_POINT('Ctrl Pts',(0.454360764920788,2.00514415454549,12.4543012401989));
#50969=CARTESIAN_POINT('Ctrl Pts',(0.523077600526005,1.98705495302167,12.4504328962654));
#50970=CARTESIAN_POINT('Ctrl Pts',(0.563879680009971,1.97631410571874,12.448135984959));
#50971=CARTESIAN_POINT('Ctrl Pts',(0.604309382418821,1.96432690644618,12.4458390736525));
#50972=CARTESIAN_POINT('Ctrl Pts',(0.644286808518715,1.95112584700956,12.4435421623461));
#50973=CARTESIAN_POINT('Ctrl Pts',(0.711614188174318,1.92889348171609,12.4396738537867));
#50974=CARTESIAN_POINT('Ctrl Pts',(0.777921303223199,1.90312859844738,12.4358055452274));
#50975=CARTESIAN_POINT('Ctrl Pts',(0.842811364020459,1.87394412061245,12.431937236668));
#50976=CARTESIAN_POINT('Ctrl Pts',(0.907616620856139,1.84479778358532,12.4280739835499));
#50977=CARTESIAN_POINT('Ctrl Pts',(0.971008056576276,1.8122409112598,12.4242107304318));
#50978=CARTESIAN_POINT('Ctrl Pts',(1.0326051273996,1.77643581740744,12.4203474773137));
#50979=CARTESIAN_POINT('Ctrl Pts',(1.09413108355865,1.74067206102771,12.4164886843744));
#50980=CARTESIAN_POINT('Ctrl Pts',(1.15386637137547,1.7016677742289,12.412629891435));
#50981=CARTESIAN_POINT('Ctrl Pts',(1.21145327695171,1.65963204363587,12.4087710984957));
#50982=CARTESIAN_POINT('Ctrl Pts',(1.22511294175184,1.64966113125946,12.4078557894067));
#50983=CARTESIAN_POINT('Ctrl Pts',(1.23865184132203,1.63951985873777,12.4069404803176));
#50984=CARTESIAN_POINT('Ctrl Pts',(1.25206542099587,1.62921138715835,12.4060251712286));
#50985=CARTESIAN_POINT('Ctrl Pts',(1.25206542099588,1.62921138715834,13.1060515834985));
#50986=CARTESIAN_POINT('Ctrl Pts',(1.30834031581923,1.58596356159447,13.1021847974854));
#50987=CARTESIAN_POINT('Ctrl Pts',(1.36247333019475,1.53971860876087,13.0983180114722));
#50988=CARTESIAN_POINT('Ctrl Pts',(1.41412862706877,1.49071720611409,13.0944512254591));
#50989=CARTESIAN_POINT('Ctrl Pts',(1.46714239897573,1.44042712280717,13.090482747411));
#50990=CARTESIAN_POINT('Ctrl Pts',(1.51754582996521,1.38723380459452,13.0865142693628));
#50991=CARTESIAN_POINT('Ctrl Pts',(1.56500993085928,1.33144338175223,13.0825457913147));
#50992=CARTESIAN_POINT('Ctrl Pts',(1.61114869445704,1.27721079160406,13.0786881248456));
#50993=CARTESIAN_POINT('Ctrl Pts',(1.65450979289494,1.22052463414179,13.0748304583765));
#50994=CARTESIAN_POINT('Ctrl Pts',(1.69482808368481,1.16170363228031,13.0709727919073));
#50995=CARTESIAN_POINT('Ctrl Pts',(1.73512633244712,1.10291187005467,13.0671170430656));
#50996=CARTESIAN_POINT('Ctrl Pts',(1.77238450077215,1.04198776935196,13.0632612942238));
#50997=CARTESIAN_POINT('Ctrl Pts',(1.80637926427822,0.979281122091948,13.0594055453821));
#50998=CARTESIAN_POINT('Ctrl Pts',(1.84036850083389,0.916584669829447,13.0555504234173));
#50999=CARTESIAN_POINT('Ctrl Pts',(1.87109515527224,0.852106673817415,13.0516953014524));
#51000=CARTESIAN_POINT('Ctrl Pts',(1.89838145671275,0.786222237862287,13.0478401794876));
#51001=CARTESIAN_POINT('Ctrl Pts',(1.92706621861358,0.716961133990656,13.0437874772223));
#51002=CARTESIAN_POINT('Ctrl Pts',(1.95194827002454,0.646146091395115,13.039734774957));
#51003=CARTESIAN_POINT('Ctrl Pts',(1.97287896198443,0.574235286149538,13.0356820726917));
#51004=CARTESIAN_POINT('Ctrl Pts',(1.99281564784182,0.505739550954497,13.0318218347171));
#51005=CARTESIAN_POINT('Ctrl Pts',(2.00916769123172,0.436250271976713,13.0279615967426));
#51006=CARTESIAN_POINT('Ctrl Pts',(2.02185882763527,0.366175427375082,13.024101358768));
#51007=CARTESIAN_POINT('Ctrl Pts',(2.0345588558355,0.296051486203185,13.0202384161932));
#51008=CARTESIAN_POINT('Ctrl Pts',(2.04359281349571,0.225341644505659,13.0163754736184));
#51009=CARTESIAN_POINT('Ctrl Pts',(2.04893629360516,0.154459144266526,13.0125125310435));
#51010=CARTESIAN_POINT('Ctrl Pts',(2.05428842000437,0.0834619489927554,
13.008643337838));
#51011=CARTESIAN_POINT('Ctrl Pts',(2.05593815011108,0.0122920220530018,
13.0047741446325));
#51012=CARTESIAN_POINT('Ctrl Pts',(2.05391312248099,-0.0586382793097567,
13.0009049514269));
#51013=CARTESIAN_POINT('Ctrl Pts',(2.05361703361221,-0.0690093341934075,
13.0003392183859));
#51014=CARTESIAN_POINT('Ctrl Pts',(2.05324247306339,-0.0793752786927251,
12.9997734853449));
#51015=CARTESIAN_POINT('Ctrl Pts',(2.05278961933086,-0.0897348386495988,
12.9992077523039));
#51016=CARTESIAN_POINT('Ctrl Pts',(2.04969252497423,-0.16058450240405,12.995338669457));
#51017=CARTESIAN_POINT('Ctrl Pts',(2.04291711713161,-0.231412406381142,
12.9914695866101));
#51018=CARTESIAN_POINT('Ctrl Pts',(2.03246423017578,-0.301805757990093,
12.9876005037631));
#51019=CARTESIAN_POINT('Ctrl Pts',(2.0220269175002,-0.37209422701583,12.9837371856567));
#51020=CARTESIAN_POINT('Ctrl Pts',(2.00792307266343,-0.441948952266497,
12.9798738675503));
#51021=CARTESIAN_POINT('Ctrl Pts',(1.99020548444614,-0.510959579791311,
12.9760105494438));
#51022=CARTESIAN_POINT('Ctrl Pts',(1.972508678953,-0.579889257876603,12.9721517630081));
#51023=CARTESIAN_POINT('Ctrl Pts',(1.9512066702235,-0.647976336722143,12.9682929765723));
#51024=CARTESIAN_POINT('Ctrl Pts',(1.92640346112517,-0.71481974473638,12.9644341901365));
#51025=CARTESIAN_POINT('Ctrl Pts',(1.90161587622982,-0.781621046304986,
12.9605778344532));
#51026=CARTESIAN_POINT('Ctrl Pts',(1.87333163524002,-0.847179776975268,
12.9567214787699));
#51027=CARTESIAN_POINT('Ctrl Pts',(1.84170440102805,-0.911110565043517,
12.9528651230867));
#51028=CARTESIAN_POINT('Ctrl Pts',(1.81008650981775,-0.975022467316813,
12.9490099066095));
#51029=CARTESIAN_POINT('Ctrl Pts',(1.77512780124049,-1.03730694655122,12.9451546901323));
#51030=CARTESIAN_POINT('Ctrl Pts',(1.73702912834051,-1.09760073332547,12.9412994736551));
#51031=CARTESIAN_POINT('Ctrl Pts',(1.69892896589637,-1.15789687740644,12.9374441064504));
#51032=CARTESIAN_POINT('Ctrl Pts',(1.65768885675581,-1.21620176501485,12.9335887392458));
#51033=CARTESIAN_POINT('Ctrl Pts',(1.61355353184179,-1.27218023973842,12.9297333720412));
#51034=CARTESIAN_POINT('Ctrl Pts',(1.5693720092777,-1.32821730866042,12.9258739693184));
#51035=CARTESIAN_POINT('Ctrl Pts',(1.52228952276467,-1.38192272139538,12.9220145665956));
#51036=CARTESIAN_POINT('Ctrl Pts',(1.47259117507951,-1.43299434527075,12.9181551638728));
#51037=CARTESIAN_POINT('Ctrl Pts',(1.42286468779949,-1.48409488630074,12.9142935759259));
#51038=CARTESIAN_POINT('Ctrl Pts',(1.37051974752311,-1.53255833962242,12.910431987979));
#51039=CARTESIAN_POINT('Ctrl Pts',(1.31587639627039,-1.57812131100193,12.9065704000321));
#51040=CARTESIAN_POINT('Ctrl Pts',(1.26113744451604,-1.623763996433,12.9027020560986));
#51041=CARTESIAN_POINT('Ctrl Pts',(1.20409244236039,-1.66649577720976,12.8988337121652));
#51042=CARTESIAN_POINT('Ctrl Pts',(1.14509181289497,-1.70609563112415,12.8949653682317));
#51043=CARTESIAN_POINT('Ctrl Pts',(1.1100589370082,-1.72960888479427,12.8926684569253));
#51044=CARTESIAN_POINT('Ctrl Pts',(1.07433709447014,-1.752018787717,12.8903715456188));
#51045=CARTESIAN_POINT('Ctrl Pts',(1.03800348484611,-1.77328687130632,12.8880746343123));
#51046=CARTESIAN_POINT('Ctrl Pts',(0.976800535752212,-1.80911236320516,
12.8842055514654));
#51047=CARTESIAN_POINT('Ctrl Pts',(0.913620822920747,-1.84183578019922,
12.8803364686185));
#51048=CARTESIAN_POINT('Ctrl Pts',(0.848811599608828,-1.87123393269508,
12.8764673857716));
#51049=CARTESIAN_POINT('Ctrl Pts',(0.784098938807428,-1.90058828340989,
12.8726040676651));
#51050=CARTESIAN_POINT('Ctrl Pts',(0.717762025611132,-1.92662700508797,
12.8687407495587));
#51051=CARTESIAN_POINT('Ctrl Pts',(0.650174243543331,-1.94917187942286,
12.8648774314523));
#51052=CARTESIAN_POINT('Ctrl Pts',(0.582665741917904,-1.97169030862884,
12.8610186450165));
#51053=CARTESIAN_POINT('Ctrl Pts',(0.513909744499352,-1.9907228780986,12.8571598585807));
#51054=CARTESIAN_POINT('Ctrl Pts',(0.444299613906862,-2.00613943074309,
12.8533010721449));
#51055=CARTESIAN_POINT('Ctrl Pts',(0.374733332592358,-2.02154627208987,
12.8494447164616));
#51056=CARTESIAN_POINT('Ctrl Pts',(0.304314458738831,-2.03334151098861,
12.8455883607783));
#51057=CARTESIAN_POINT('Ctrl Pts',(0.23345009957965,-2.04144522667307,12.8417320050951));
#51058=CARTESIAN_POINT('Ctrl Pts',(0.162606674461754,-2.04954654843877,
12.8378767886179));
#51059=CARTESIAN_POINT('Ctrl Pts',(0.0913185076770635,-2.05395845679896,
12.8340215721407));
#51060=CARTESIAN_POINT('Ctrl Pts',(0.0199997326209688,-2.05465266485484,
12.8301663556635));
#51061=CARTESIAN_POINT('Ctrl Pts',(-0.0513218307859419,-2.05534690005218,
12.8263109884588));
#51062=CARTESIAN_POINT('Ctrl Pts',(-0.122673519058635,-2.05232314384442,
12.8224556212542));
#51063=CARTESIAN_POINT('Ctrl Pts',(-0.193641018972577,-2.04560522053285,
12.8186002540496));
#51064=CARTESIAN_POINT('Ctrl Pts',(-0.264682802507017,-2.03888026538747,
12.8147408513268));
#51065=CARTESIAN_POINT('Ctrl Pts',(-0.335339110308355,-2.02845347004202,
12.810881448604));
#51066=CARTESIAN_POINT('Ctrl Pts',(-0.40520147658915,-2.01440048795416,
12.8070220458812));
#51067=CARTESIAN_POINT('Ctrl Pts',(-0.475103399490517,-2.00033954895746,
12.8031604579343));
#51068=CARTESIAN_POINT('Ctrl Pts',(-0.544210015153872,-1.98264845651046,
12.7992988699874));
#51069=CARTESIAN_POINT('Ctrl Pts',(-0.612126452877568,-1.96145322865153,
12.7954372820404));
#51070=CARTESIAN_POINT('Ctrl Pts',(-0.680161712843429,-1.94022091898176,
12.791568938107));
#51071=CARTESIAN_POINT('Ctrl Pts',(-0.747002181878165,-1.91547240269251,
12.7877005941735));
#51072=CARTESIAN_POINT('Ctrl Pts',(-0.812272109325285,-1.88738220371822,
12.7838322502401));
#51073=CARTESIAN_POINT('Ctrl Pts',(-0.851027513938246,-1.8707030519329,
12.7815353389336));
#51074=CARTESIAN_POINT('Ctrl Pts',(-0.889229639044953,-1.85284664074278,
12.7792384276272));
#51075=CARTESIAN_POINT('Ctrl Pts',(-0.926804294388877,-1.83385696345226,
12.7769415163208));
#51076=CARTESIAN_POINT('Ctrl Pts',(-0.990097750284713,-1.80186938323196,
12.7730724334739));
#51077=CARTESIAN_POINT('Ctrl Pts',(-1.05185720819241,-1.76653855402879,
12.7692033506269));
#51078=CARTESIAN_POINT('Ctrl Pts',(-1.11170681581917,-1.72803516114725,
12.76533426778));
#51079=CARTESIAN_POINT('Ctrl Pts',(-1.17146725051544,-1.68958913640083,
12.7614709496736));
#51080=CARTESIAN_POINT('Ctrl Pts',(-1.22932307811853,-1.64798019155231,
12.7576076315671));
#51081=CARTESIAN_POINT('Ctrl Pts',(-1.28492205565918,-1.60342535634827,
12.7537443134607));
#51082=CARTESIAN_POINT('Ctrl Pts',(-1.34045581562056,-1.55892278394878,
12.7498855270249));
#51083=CARTESIAN_POINT('Ctrl Pts',(-1.39373760668099,-1.51148148734931,
12.7460267405891));
#51084=CARTESIAN_POINT('Ctrl Pts',(-1.44444472742131,-1.46136134885414,
12.7421679541533));
#51085=CARTESIAN_POINT('Ctrl Pts',(-1.49511990639376,-1.41127278237106,
12.7383115984701));
#51086=CARTESIAN_POINT('Ctrl Pts',(-1.54322328810036,-1.35850906260196,
12.7344552427868));
#51087=CARTESIAN_POINT('Ctrl Pts',(-1.58846692151022,-1.30336886634899,
12.7305988871035));
#51088=CARTESIAN_POINT('Ctrl Pts',(-1.63369718949773,-1.24824495906213,
12.7267436706263));
#51089=CARTESIAN_POINT('Ctrl Pts',(-1.67606907837354,-1.19074634436575,
12.7228884541491));
#51090=CARTESIAN_POINT('Ctrl Pts',(-1.71533420557472,-1.13120560716669,
12.7190332376719));
#51091=CARTESIAN_POINT('Ctrl Pts',(-1.7546008679249,-1.07166254210292,12.7151778704672));
#51092=CARTESIAN_POINT('Ctrl Pts',(-1.79076026184735,-1.01007760277419,
12.7113225032626));
#51093=CARTESIAN_POINT('Ctrl Pts',(-1.82360768758627,-0.94681178925712,
12.707467136058));
#51094=CARTESIAN_POINT('Ctrl Pts',(-1.85648949562289,-0.883479753685019,
12.7036077333352));
#51095=CARTESIAN_POINT('Ctrl Pts',(-1.88605219080747,-0.818463763753936,
12.6997483306124));
#51096=CARTESIAN_POINT('Ctrl Pts',(-1.91213778830766,-0.752148018029615,
12.6958889278896));
#51097=CARTESIAN_POINT('Ctrl Pts',(-1.93823815567809,-0.685794723809099,
12.6920273399427));
#51098=CARTESIAN_POINT('Ctrl Pts',(-1.96085735206333,-0.618140669715462,
12.6881657519957));
#51099=CARTESIAN_POINT('Ctrl Pts',(-1.97988707928822,-0.549585949390586,
12.6843041640488));
#51100=CARTESIAN_POINT('Ctrl Pts',(-1.99895009970299,-0.480911290125275,
12.6804358201154));
#51101=CARTESIAN_POINT('Ctrl Pts',(-2.01441100754087,-0.411333292970025,
12.6765674761819));
#51102=CARTESIAN_POINT('Ctrl Pts',(-2.02621262637065,-0.341262296827762,
12.6726991322485));
#51103=CARTESIAN_POINT('Ctrl Pts',(-2.03322008801068,-0.299656155786641,
12.670402220942));
#51104=CARTESIAN_POINT('Ctrl Pts',(-2.03893840716793,-0.257876320827019,
12.6681053096356));
#51105=CARTESIAN_POINT('Ctrl Pts',(-2.04336430473757,-0.216008982739983,
12.6658083983292));
#51106=CARTESIAN_POINT('Ctrl Pts',(-2.05090081120964,-0.144716446142108,
12.6618971720403));
#51107=CARTESIAN_POINT('Ctrl Pts',(-2.05470713587996,-0.0730227242236319,
12.6579859457513));
#51108=CARTESIAN_POINT('Ctrl Pts',(-2.05474964003149,-0.00121626084838144,
12.6540747194623));
#51109=CARTESIAN_POINT('Origin',(0.,0.,18.5459252805377));
#51110=CARTESIAN_POINT('',(1.25171901745462,1.62874802847325,13.8061758215987));
#51111=CARTESIAN_POINT('',(1.25206542099588,1.62921138715834,13.7478651251903));
#51112=CARTESIAN_POINT('',(1.25206542099588,1.62921138715835,18.5459252805377));
#51113=CARTESIAN_POINT('',(-2.05474946769684,-0.00147901978776689,13.2959253072757));
#51114=CARTESIAN_POINT('Ctrl Pts',(1.25206542099588,1.62921138715834,13.7478651251903));
#51115=CARTESIAN_POINT('Ctrl Pts',(1.30854407481545,1.58580697074604,13.7440082043291));
#51116=CARTESIAN_POINT('Ctrl Pts',(1.36281046402495,1.53942583980054,13.740151283468));
#51117=CARTESIAN_POINT('Ctrl Pts',(1.41454030475051,1.49032657117034,13.7362943626069));
#51118=CARTESIAN_POINT('Ctrl Pts',(1.46624989922677,1.44124651922472,13.7324389512841));
#51119=CARTESIAN_POINT('Ctrl Pts',(1.51542456358849,1.38945077514556,13.7285835399614));
#51120=CARTESIAN_POINT('Ctrl Pts',(1.56177476026823,1.3352367433115,13.7247281286387));
#51121=CARTESIAN_POINT('Ctrl Pts',(1.60812232080023,1.28102579487747,13.7208729365908));
#51122=CARTESIAN_POINT('Ctrl Pts',(1.65164541814656,1.22439720203785,13.717017744543));
#51123=CARTESIAN_POINT('Ctrl Pts',(1.69209406918464,1.16568229956973,13.7131625524951));
#51124=CARTESIAN_POINT('Ctrl Pts',(1.73258256853702,1.10690955364262,13.7093035624738));
#51125=CARTESIAN_POINT('Ctrl Pts',(1.76999029517012,1.0460467934869,13.7054445724524));
#51126=CARTESIAN_POINT('Ctrl Pts',(1.80411050084976,0.983454555749083,13.7015855824311));
#51127=CARTESIAN_POINT('Ctrl Pts',(1.83824708918921,0.920832264636221,13.6977247395335));
#51128=CARTESIAN_POINT('Ctrl Pts',(1.86909280168606,0.856479280384039,13.6938638966358));
#51129=CARTESIAN_POINT('Ctrl Pts',(1.89648806240337,0.790778471925942,13.6900030537382));
#51130=CARTESIAN_POINT('Ctrl Pts',(1.92393375738292,0.724956709269307,13.6861351030869));
#51131=CARTESIAN_POINT('Ctrl Pts',(1.94791614522091,0.657782623450311,13.6822671524356));
#51132=CARTESIAN_POINT('Ctrl Pts',(1.96832494877896,0.589656220618669,13.6783992017844));
#51133=CARTESIAN_POINT('Ctrl Pts',(1.98628939303304,0.529689306712218,13.6749945149955));
#51134=CARTESIAN_POINT('Ctrl Pts',(2.00148572043799,0.468984962301845,13.6715898282065));
#51135=CARTESIAN_POINT('Ctrl Pts',(2.01387175448042,0.407821185087241,13.6681851414176));
#51136=CARTESIAN_POINT('Ctrl Pts',(2.02794723185223,0.338314726505752,13.6643160585706));
#51137=CARTESIAN_POINT('Ctrl Pts',(2.03844765063878,0.267942577620449,13.6604469757236));
#51138=CARTESIAN_POINT('Ctrl Pts',(2.04527430002851,0.197105555839729,13.6565778928766));
#51139=CARTESIAN_POINT('Ctrl Pts',(2.05209077805113,0.126374077688449,13.6527145747701));
#51140=CARTESIAN_POINT('Ctrl Pts',(2.05524430566592,0.0551795811115907,
13.6488512566636));
#51141=CARTESIAN_POINT('Ctrl Pts',(2.05468718187911,-0.0160669574493126,
13.6449879385571));
#51142=CARTESIAN_POINT('Ctrl Pts',(2.05413071159829,-0.0872299238477516,
13.6411291521212));
#51143=CARTESIAN_POINT('Ctrl Pts',(2.0498722394188,-0.158444327562999,13.6372703656854));
#51144=CARTESIAN_POINT('Ctrl Pts',(2.04191600564024,-0.229295853451868,
13.6334115792495));
#51145=CARTESIAN_POINT('Ctrl Pts',(2.03396478370555,-0.300102748074791,
13.6295552235662));
#51146=CARTESIAN_POINT('Ctrl Pts',(2.02232047558545,-0.370546736775478,
13.6256988678828));
#51147=CARTESIAN_POINT('Ctrl Pts',(2.00703930184062,-0.440216768611935,
13.6218425121994));
#51148=CARTESIAN_POINT('Ctrl Pts',(1.9917626423075,-0.509866219223458,13.6179872957222));
#51149=CARTESIAN_POINT('Ctrl Pts',(1.97285135408459,-0.578741692629017,
13.6141320792449));
#51150=CARTESIAN_POINT('Ctrl Pts',(1.95041278457433,-0.646442211082326,
13.6102768627676));
#51151=CARTESIAN_POINT('Ctrl Pts',(1.92797333778316,-0.714145376423281,
13.6064214955629));
#51152=CARTESIAN_POINT('Ctrl Pts',(1.9020064908327,-0.780673035187002,13.6025661283582));
#51153=CARTESIAN_POINT('Ctrl Pts',(1.87266895251019,-0.845640914812181,
13.5987107611535));
#51154=CARTESIAN_POINT('Ctrl Pts',(1.84330070578498,-0.910676798091525,
13.5948513584306));
#51155=CARTESIAN_POINT('Ctrl Pts',(1.81055492495604,-0.974149199427638,
13.5909919557078));
#51156=CARTESIAN_POINT('Ctrl Pts',(1.77463546152237,-1.03569616259176,13.5871325529849));
#51157=CARTESIAN_POINT('Ctrl Pts',(1.73869566020634,-1.09727797412989,13.5832709650379));
#51158=CARTESIAN_POINT('Ctrl Pts',(1.69957886559094,-1.1569317708205,13.5794093770909));
#51159=CARTESIAN_POINT('Ctrl Pts',(1.65753217728701,-1.21432476865054,13.5755477891439));
#51160=CARTESIAN_POINT('Ctrl Pts',(1.61541192679481,-1.27181817758742,13.5716794452104));
#51161=CARTESIAN_POINT('Ctrl Pts',(1.57035185571098,-1.32704251419185,13.5678111012768));
#51162=CARTESIAN_POINT('Ctrl Pts',(1.52263876406622,-1.37969879200603,13.5639427573433));
#51163=CARTESIAN_POINT('Ctrl Pts',(1.49430810331966,-1.41096457444656,13.5616458460375));
#51164=CARTESIAN_POINT('Ctrl Pts',(1.4650427907852,-1.44132565585821,13.5593489347318));
#51165=CARTESIAN_POINT('Ctrl Pts',(1.43490847440599,-1.47072609026218,13.557052023426));
#51166=CARTESIAN_POINT('Ctrl Pts',(1.38414806136217,-1.52025029964636,13.5531829405791));
#51167=CARTESIAN_POINT('Ctrl Pts',(1.33072131183898,-1.56724051744266,13.5493138577322));
#51168=CARTESIAN_POINT('Ctrl Pts',(1.27491142699772,-1.61139641795885,13.5454447748853));
#51169=CARTESIAN_POINT('Ctrl Pts',(1.2191846961016,-1.65548652838537,13.5415814567789));
#51170=CARTESIAN_POINT('Ctrl Pts',(1.16108225589559,-1.69675040509438,13.5377181386725));
#51171=CARTESIAN_POINT('Ctrl Pts',(1.1009235092021,-1.73492506736923,13.5338548205661));
#51172=CARTESIAN_POINT('Ctrl Pts',(1.04083532869523,-1.77305495077999,13.5299960341304));
#51173=CARTESIAN_POINT('Ctrl Pts',(0.978696041021966,-1.80810255853046,
13.5261372476946));
#51174=CARTESIAN_POINT('Ctrl Pts',(0.914856025893739,-1.83984673665659,
13.5222784612589));
#51175=CARTESIAN_POINT('Ctrl Pts',(0.851056225293838,-1.87157091827821,
13.5184221055756));
#51176=CARTESIAN_POINT('Ctrl Pts',(0.785558256695593,-1.89999558300651,
13.5145657498924));
#51177=CARTESIAN_POINT('Ctrl Pts',(0.718737950517666,-1.92494501765262,
13.5107093942091));
#51178=CARTESIAN_POINT('Ctrl Pts',(0.651937383727202,-1.94988708198595,
13.5068541777319));
#51179=CARTESIAN_POINT('Ctrl Pts',(0.583815709716312,-1.97135578452716,
13.5029989612548));
#51180=CARTESIAN_POINT('Ctrl Pts',(0.514768026271573,-1.98922382894145,
13.4991437447776));
#51181=CARTESIAN_POINT('Ctrl Pts',(0.445717643268803,-2.00709257194285,
13.495288377573));
#51182=CARTESIAN_POINT('Ctrl Pts',(0.375741649796778,-2.02136025775853,
13.4914330103683));
#51183=CARTESIAN_POINT('Ctrl Pts',(0.305247881707282,-2.03195012074933,
13.4875776431637));
#51184=CARTESIAN_POINT('Ctrl Pts',(0.234680325865516,-2.04255106843894,
13.483718240441));
#51185=CARTESIAN_POINT('Ctrl Pts',(0.163594394891996,-2.0494664361701,13.4798588377182));
#51186=CARTESIAN_POINT('Ctrl Pts',(0.0924047452284538,-2.0526711683948,
13.4759994349954));
#51187=CARTESIAN_POINT('Ctrl Pts',(0.0211747874261737,-2.05587771516405,
13.4721378470485));
#51188=CARTESIAN_POINT('Ctrl Pts',(-0.050158519971401,-2.05536944746468,
13.4682762591017));
#51189=CARTESIAN_POINT('Ctrl Pts',(-0.121181572141126,-2.05117346635369,
13.4644146711548));
#51190=CARTESIAN_POINT('Ctrl Pts',(-0.192328881686445,-2.04697014422334,
13.4605463272213));
#51191=CARTESIAN_POINT('Ctrl Pts',(-0.263164369343408,-2.03906628139337,
13.4566779832879));
#51192=CARTESIAN_POINT('Ctrl Pts',(-0.333281292006573,-2.02754066368555,
13.4528096393545));
#51193=CARTESIAN_POINT('Ctrl Pts',(-0.374914702899041,-2.02069708356831,
13.4505127280478));
#51194=CARTESIAN_POINT('Ctrl Pts',(-0.416294981267516,-2.01257757953319,
13.4482158167411));
#51195=CARTESIAN_POINT('Ctrl Pts',(-0.457339518892111,-2.00320696059083,
13.4459189054345));
#51196=CARTESIAN_POINT('Ctrl Pts',(-0.526477894423543,-1.98742241509723,
13.4420498225876));
#51197=CARTESIAN_POINT('Ctrl Pts',(-0.594933548236747,-1.96802340496217,
13.4381807397407));
#51198=CARTESIAN_POINT('Ctrl Pts',(-0.66230056404705,-1.94508496610378,
13.4343116568937));
#51199=CARTESIAN_POINT('Ctrl Pts',(-0.729567206363272,-1.9221807043754,
13.4304483387873));
#51200=CARTESIAN_POINT('Ctrl Pts',(-0.795747974224224,-1.8957476371241,
13.4265850206809));
#51201=CARTESIAN_POINT('Ctrl Pts',(-0.860448691025966,-1.86591146966079,
13.4227217025745));
#51202=CARTESIAN_POINT('Ctrl Pts',(-0.925073513912106,-1.8361103000103,
13.4188629161387));
#51203=CARTESIAN_POINT('Ctrl Pts',(-0.988221295223039,-1.8029141617238,
13.4150041297029));
#51204=CARTESIAN_POINT('Ctrl Pts',(-1.04951619713821,-1.7664974708288,13.4111453432672));
#51205=CARTESIAN_POINT('Ctrl Pts',(-1.11077248775972,-1.73010371977875,
13.4072889875839));
#51206=CARTESIAN_POINT('Ctrl Pts',(-1.17017779800132,-1.69049368859268,
13.4034326319006));
#51207=CARTESIAN_POINT('Ctrl Pts',(-1.22738066237806,-1.64788782146128,
13.3995762762173));
#51208=CARTESIAN_POINT('Ctrl Pts',(-1.2845666284559,-1.60529454052963,13.3957210597401));
#51209=CARTESIAN_POINT('Ctrl Pts',(-1.33955105095852,-1.55970747064193,
13.3918658432629));
#51210=CARTESIAN_POINT('Ctrl Pts',(-1.39201269076037,-1.51138950349077,
13.3880106267857));
#51211=CARTESIAN_POINT('Ctrl Pts',(-1.44447638165533,-1.4630696472517,13.3841552595811));
#51212=CARTESIAN_POINT('Ctrl Pts',(-1.49441673819649,-1.4120190124909,13.3802998923765));
#51213=CARTESIAN_POINT('Ctrl Pts',(-1.54154806489132,-1.35853859942581,
13.3764445251719));
#51214=CARTESIAN_POINT('Ctrl Pts',(-1.58872872523317,-1.30500220695156,
13.3725851224491));
#51215=CARTESIAN_POINT('Ctrl Pts',(-1.63309416441128,-1.24903132434447,
13.3687257197263));
#51216=CARTESIAN_POINT('Ctrl Pts',(-1.67439843093734,-1.19096072856101,
13.3648663170035));
#51217=CARTESIAN_POINT('Ctrl Pts',(-1.71572608426352,-1.13285725275011,
13.3610047290566));
#51218=CARTESIAN_POINT('Ctrl Pts',(-1.75398885386358,-1.07265210726469,
13.3571431411097));
#51219=CARTESIAN_POINT('Ctrl Pts',(-1.78898517711555,-1.01070747427772,
13.3532815531627));
#51220=CARTESIAN_POINT('Ctrl Pts',(-1.82404272768947,-0.94865446693497,
13.3494132092293));
#51221=CARTESIAN_POINT('Ctrl Pts',(-1.85582220556054,-0.884856331025426,
13.3455448652958));
#51222=CARTESIAN_POINT('Ctrl Pts',(-1.88416919184789,-0.819697516765346,
13.3416765213624));
#51223=CARTESIAN_POINT('Ctrl Pts',(-1.9010008165506,-0.78100808796392,13.3393796100559));
#51224=CARTESIAN_POINT('Ctrl Pts',(-1.916623201266,-0.741839288145892,13.3370826987494));
#51225=CARTESIAN_POINT('Ctrl Pts',(-1.93101238379182,-0.702273975128398,
13.3347857874429));
#51226=CARTESIAN_POINT('Ctrl Pts',(-1.95903836976884,-0.625212133302755,
13.330312065329));
#51227=CARTESIAN_POINT('Ctrl Pts',(-1.98247429587934,-0.546396960948768,
13.3258383432151));
#51228=CARTESIAN_POINT('Ctrl Pts',(-2.00112975528962,-0.466344577533057,
13.3213646211012));
#51229=CARTESIAN_POINT('Ctrl Pts',(-2.01962152623802,-0.3869945971632,13.3169301527347));
#51230=CARTESIAN_POINT('Ctrl Pts',(-2.03341626232235,-0.306429189566792,
13.3124956843683));
#51231=CARTESIAN_POINT('Ctrl Pts',(-2.04237487167497,-0.225172036564603,
13.3080612160018));
#51232=CARTESIAN_POINT('Ctrl Pts',(-2.05054728051348,-0.151045947430806,
13.3040159130931));
#51233=CARTESIAN_POINT('Ctrl Pts',(-2.05469557909877,-0.0763445280967105,
13.2999706101844));
#51234=CARTESIAN_POINT('Ctrl Pts',(-2.05474946769684,-0.00147901978776689,
13.2959253072757));
#51235=CARTESIAN_POINT('Ctrl Pts',(-2.05258179091604,-0.00147696517085403,
13.2959252805377));
#51236=CARTESIAN_POINT('Ctrl Pts',(-2.04962018460403,0.443899356040318,
13.2718344101756));
#51237=CARTESIAN_POINT('Ctrl Pts',(-1.68832798325332,1.5785041446152,13.2106991671496));
#51238=CARTESIAN_POINT('Ctrl Pts',(-0.112928914327977,2.28830665208722,
13.1280482345611));
#51239=CARTESIAN_POINT('Ctrl Pts',(0.93349584868275,1.86810178948702,13.0694881723346));
#51240=CARTESIAN_POINT('Ctrl Pts',(1.25024324817659,1.62681756561327,13.047972482772));
#51241=CARTESIAN_POINT('',(-2.0547492176368,0.001793075842144,13.3540747194623));
#51242=CARTESIAN_POINT('Ctrl Pts',(-2.0547492176368,0.001793075842144,13.3540747194623));
#51243=CARTESIAN_POINT('Ctrl Pts',(-2.05465860807767,0.105625784059886,
13.3484351428617));
#51244=CARTESIAN_POINT('Ctrl Pts',(-2.04669415459996,0.209126407407667,
13.3427955662611));
#51245=CARTESIAN_POINT('Ctrl Pts',(-2.03102549815175,0.31134063075262,13.3371559896605));
#51246=CARTESIAN_POINT('Ctrl Pts',(-2.02681271789171,0.338822633681565,
13.3356396951998));
#51247=CARTESIAN_POINT('Ctrl Pts',(-2.02204324664326,0.366211817300818,
13.3341234007392));
#51248=CARTESIAN_POINT('Ctrl Pts',(-2.01672090784174,0.393489952062285,
13.3326071062786));
#51249=CARTESIAN_POINT('Ctrl Pts',(-2.00314005643268,0.463094745880791,
13.3287380234317));
#51250=CARTESIAN_POINT('Ctrl Pts',(-1.98592488139643,0.532131952383038,
13.3248689405848));
#51251=CARTESIAN_POINT('Ctrl Pts',(-1.9651374895038,0.600193477011109,13.3209998577379));
#51252=CARTESIAN_POINT('Ctrl Pts',(-1.94438106978837,0.668153593361924,
13.3171365396314));
#51253=CARTESIAN_POINT('Ctrl Pts',(-1.92006313882444,0.735140452615142,
13.313273221525));
#51254=CARTESIAN_POINT('Ctrl Pts',(-1.89229682005128,0.800756084787251,
13.3094099034186));
#51255=CARTESIAN_POINT('Ctrl Pts',(-1.86456307115937,0.866294749848045,
13.3055511169828));
#51256=CARTESIAN_POINT('Ctrl Pts',(-1.8333891575092,0.930464937546923,13.3016923305471));
#51257=CARTESIAN_POINT('Ctrl Pts',(-1.79893747109799,0.992885460453303,
13.2978335441113));
#51258=CARTESIAN_POINT('Ctrl Pts',(-1.76450748672299,1.05526666300735,13.2939771884281));
#51259=CARTESIAN_POINT('Ctrl Pts',(-1.72680406021419,1.11589996313947,13.2901208327448));
#51260=CARTESIAN_POINT('Ctrl Pts',(-1.68603636254319,1.17442707167458,13.2862644770616));
#51261=CARTESIAN_POINT('Ctrl Pts',(-1.64528070805828,1.23293689071581,13.2824092605844));
#51262=CARTESIAN_POINT('Ctrl Pts',(-1.60146285702327,1.28934135498523,13.2785540441072));
#51263=CARTESIAN_POINT('Ctrl Pts',(-1.5548353664441,1.34331103835063,13.27469882763));
#51264=CARTESIAN_POINT('Ctrl Pts',(-1.50820605286951,1.39728283176923,13.2708434604254));
#51265=CARTESIAN_POINT('Ctrl Pts',(-1.4587672009129,1.448819289138,13.2669880932208));
#51266=CARTESIAN_POINT('Ctrl Pts',(-1.40681058569492,1.49762529975849,13.2631327260162));
#51267=CARTESIAN_POINT('Ctrl Pts',(-1.35479958606871,1.54648239696333,13.2592733232934));
#51268=CARTESIAN_POINT('Ctrl Pts',(-1.30026591710236,1.59260300886624,13.2554139205707));
#51269=CARTESIAN_POINT('Ctrl Pts',(-1.24353637582797,1.63573067602605,13.2515545178479));
#51270=CARTESIAN_POINT('Ctrl Pts',(-1.18677471384167,1.67888276240979,13.247692929901));
#51271=CARTESIAN_POINT('Ctrl Pts',(-1.1278151061779,1.71903825698381,13.2438313419541));
#51272=CARTESIAN_POINT('Ctrl Pts',(-1.06701315098567,1.75598419643333,13.2399697540072));
#51273=CARTESIAN_POINT('Ctrl Pts',(-1.00610482059348,1.7929947741282,13.2361014100738));
#51274=CARTESIAN_POINT('Ctrl Pts',(-0.943348135217372,1.82678435536032,
13.2322330661404));
#51275=CARTESIAN_POINT('Ctrl Pts',(-0.879122447032021,1.85718638957549,
13.2283647222069));
#51276=CARTESIAN_POINT('Ctrl Pts',(-0.840987081638146,1.87523824259988,
13.2260678109003));
#51277=CARTESIAN_POINT('Ctrl Pts',(-0.802334183373884,1.89209668972226,
13.2237708995936));
#51278=CARTESIAN_POINT('Ctrl Pts',(-0.763245807256644,1.90773514938661,
13.221473988287));
#51279=CARTESIAN_POINT('Ctrl Pts',(-0.697402531066169,1.93407769725264,
13.2176049054401));
#51280=CARTESIAN_POINT('Ctrl Pts',(-0.630064918141975,1.95705908143398,
13.2137358225932));
#51281=CARTESIAN_POINT('Ctrl Pts',(-0.561609507711247,1.97651013742615,
13.2098667397462));
#51282=CARTESIAN_POINT('Ctrl Pts',(-0.493256092428051,1.99593221231496,
13.2060034216398));
#51283=CARTESIAN_POINT('Ctrl Pts',(-0.423788649014342,2.01183426830099,
13.2021401035334));
#51284=CARTESIAN_POINT('Ctrl Pts',(-0.353602881144418,2.02409549304038,
13.1982767854269));
#51285=CARTESIAN_POINT('Ctrl Pts',(-0.283499441153164,2.03634233536786,
13.1944179989912));
#51286=CARTESIAN_POINT('Ctrl Pts',(-0.21267982659666,2.04495674629938,13.1905592125554));
#51287=CARTESIAN_POINT('Ctrl Pts',(-0.141552363867611,2.0498684081627,13.1867004261196));
#51288=CARTESIAN_POINT('Ctrl Pts',(-0.070469706224526,2.05477697603921,
13.1828440704363));
#51289=CARTESIAN_POINT('Ctrl Pts',(0.000919931369931917,2.05598738902582,
13.1789877147531));
#51290=CARTESIAN_POINT('Ctrl Pts',(0.072202088109846,2.05348104957718,13.1751313590698));
#51291=CARTESIAN_POINT('Ctrl Pts',(0.143463187386881,2.0509754505263,13.1712761425926));
#51292=CARTESIAN_POINT('Ctrl Pts',(0.214616383625109,2.04475529586794,13.1674209261154));
#51293=CARTESIAN_POINT('Ctrl Pts',(0.285247933084463,2.03485409284574,13.1635657096382));
#51294=CARTESIAN_POINT('Ctrl Pts',(0.355882244026187,2.0249525027161,13.1597103424336));
#51295=CARTESIAN_POINT('Ctrl Pts',(0.425994386924309,2.01136964811211,13.1558549752289));
#51296=CARTESIAN_POINT('Ctrl Pts',(0.495178176436132,1.99419059672875,13.1519996080243));
#51297=CARTESIAN_POINT('Ctrl Pts',(0.564434382510014,1.97699356356312,13.1481402053015));
#51298=CARTESIAN_POINT('Ctrl Pts',(0.632759822969506,1.9561929366664,13.1442808025787));
#51299=CARTESIAN_POINT('Ctrl Pts',(0.699761789476065,1.93192417048114,13.140421399856));
#51300=CARTESIAN_POINT('Ctrl Pts',(0.766801693022361,1.90764166312985,13.136559811909));
#51301=CARTESIAN_POINT('Ctrl Pts',(0.832516183149191,1.87988729648662,13.1326982239621));
#51302=CARTESIAN_POINT('Ctrl Pts',(0.89653347289356,1.84884431320796,13.1288366360152));
#51303=CARTESIAN_POINT('Ctrl Pts',(0.960662763180963,1.81774701911736,13.1249682920817));
#51304=CARTESIAN_POINT('Ctrl Pts',(1.0230884991648,1.78334985577258,13.1210999481483));
#51305=CARTESIAN_POINT('Ctrl Pts',(1.08346500306139,1.74588119574076,13.1172316042149));
#51306=CARTESIAN_POINT('Ctrl Pts',(1.11931483359134,1.72363338366761,13.1149346929084));
#51307=CARTESIAN_POINT('Ctrl Pts',(1.15444274399193,1.70030349523615,13.1126377816019));
#51308=CARTESIAN_POINT('Ctrl Pts',(1.18878189719209,1.67594605026784,13.1103408702954));
#51309=CARTESIAN_POINT('Ctrl Pts',(1.21015704796113,1.66078423030358,13.1089111080298));
#51310=CARTESIAN_POINT('Ctrl Pts',(1.23125751467611,1.64520247351562,13.1074813457642));
#51311=CARTESIAN_POINT('Ctrl Pts',(1.25206542099588,1.62921138715834,13.1060515834985));
#51312=CARTESIAN_POINT('Ctrl Pts',(1.2517190174544,1.62874802847342,13.8061758215988));
#51313=CARTESIAN_POINT('Ctrl Pts',(1.39438384162289,1.52131572678504,13.7964970738141));
#51314=CARTESIAN_POINT('Ctrl Pts',(2.01423952061842,0.915915198607634,13.7497739533656));
#51315=CARTESIAN_POINT('Ctrl Pts',(2.28817075268951,-0.813789378500904,
13.6660064602532));
#51316=CARTESIAN_POINT('Ctrl Pts',(0.55736741032268,-2.36375128050173,13.5548733422617));
#51317=CARTESIAN_POINT('Ctrl Pts',(-1.53926415431828,-1.78981496460753,
13.4508962354953));
#51318=CARTESIAN_POINT('Ctrl Pts',(-2.05053220286094,-0.548727178269576,
13.3839635013926));
#51319=CARTESIAN_POINT('Ctrl Pts',(-2.05557322758416,0.00178604994939961,
13.3540751399538));
#51320=CARTESIAN_POINT('Origin',(0.,0.,18.5459252805377));
#51321=CARTESIAN_POINT('',(1.25206542099588,1.62921138715834,14.5060551473646));
#51322=CARTESIAN_POINT('',(1.25206542099587,1.62921138715835,14.4479364137113));
#51323=CARTESIAN_POINT('',(1.25206542099588,1.62921138715835,18.5459252805377));
#51324=CARTESIAN_POINT('',(-2.05474990309271,-0.000631062987199567,13.9959252805008));
#51325=CARTESIAN_POINT('Ctrl Pts',(1.25206542099587,1.62921138715835,14.4479364137114));
#51326=CARTESIAN_POINT('Ctrl Pts',(1.26088488177545,1.62243354239187,14.4473299315937));
#51327=CARTESIAN_POINT('Ctrl Pts',(1.26964669655897,1.61558608613413,14.4467234494761));
#51328=CARTESIAN_POINT('Ctrl Pts',(1.27834972325942,1.60867011768808,14.4461169673585));
#51329=CARTESIAN_POINT('Ctrl Pts',(1.33387111508418,1.56454935290619,14.4422478845157));
#51330=CARTESIAN_POINT('Ctrl Pts',(1.38721440473503,1.51746441295354,14.438378801673));
#51331=CARTESIAN_POINT('Ctrl Pts',(1.43804599837291,1.46765843065192,14.4345097188302));
#51332=CARTESIAN_POINT('Ctrl Pts',(1.4888018554701,1.41792665678123,14.430646400728));
#51333=CARTESIAN_POINT('Ctrl Pts',(1.53705310076354,1.36548222528367,14.4267830826258));
#51334=CARTESIAN_POINT('Ctrl Pts',(1.58249862997129,1.31060888469406,14.4229197645236));
#51335=CARTESIAN_POINT('Ctrl Pts',(1.62789085158941,1.25579991051348,14.4190609780921));
#51336=CARTESIAN_POINT('Ctrl Pts',(1.67048358601886,1.19856805885492,14.4152021916607));
#51337=CARTESIAN_POINT('Ctrl Pts',(1.71001332250266,1.13923307508315,14.4113434052293));
#51338=CARTESIAN_POINT('Ctrl Pts',(1.74951815815035,1.07993546800138,14.4074870495504));
#51339=CARTESIAN_POINT('Ctrl Pts',(1.78596355517878,1.01853776055163,14.4036306938715));
#51340=CARTESIAN_POINT('Ctrl Pts',(1.81912787742638,0.955390667774294,14.3997743381926));
#51341=CARTESIAN_POINT('Ctrl Pts',(1.85228240260056,0.89226222928148,14.3959191217199));
#51342=CARTESIAN_POINT('Ctrl Pts',(1.88215755149882,0.827385861267853,14.3920639052472));
#51343=CARTESIAN_POINT('Ctrl Pts',(1.90857729350246,0.761137489043105,14.3882086887745));
#51344=CARTESIAN_POINT('Ctrl Pts',(1.93499806843862,0.694886526706072,14.3843533215744));
#51345=CARTESIAN_POINT('Ctrl Pts',(1.95796299036314,0.627263905701272,14.3804979543743));
#51346=CARTESIAN_POINT('Ctrl Pts',(1.9773445533335,0.558664550425702,14.3766425871741));
#51347=CARTESIAN_POINT('Ctrl Pts',(1.99674640351495,0.489993390332135,14.3727831844559));
#51348=CARTESIAN_POINT('Ctrl Pts',(2.01255727495578,0.420343923520013,14.3689237817377));
#51349=CARTESIAN_POINT('Ctrl Pts',(2.02470010147728,0.350124351592271,14.3650643790195));
#51350=CARTESIAN_POINT('Ctrl Pts',(2.03684980336243,0.279865020791915,14.3612027910772));
#51351=CARTESIAN_POINT('Ctrl Pts',(2.04532726815123,0.209035424853614,14.3573412031349));
#51352=CARTESIAN_POINT('Ctrl Pts',(2.05010730359109,0.138049289250118,14.3534796151926));
#51353=CARTESIAN_POINT('Ctrl Pts',(2.05489570187429,0.0669389608579706,
14.3496112712638));
#51354=CARTESIAN_POINT('Ctrl Pts',(2.05597374834625,-0.00432796811090772,
14.3457429273349));
#51355=CARTESIAN_POINT('Ctrl Pts',(2.05336838815399,-0.0753380715833479,
14.3418745834061));
#51356=CARTESIAN_POINT('Ctrl Pts',(2.0518214002188,-0.117501828316216,14.3395776720597));
#51357=CARTESIAN_POINT('Ctrl Pts',(2.04897677048839,-0.159575120644791,
14.3372807607133));
#51358=CARTESIAN_POINT('Ctrl Pts',(2.04484870920189,-0.201472874043492,
14.3349838493669));
#51359=CARTESIAN_POINT('Ctrl Pts',(2.03789510554898,-0.272048466522004,
14.3311147665166));
#51360=CARTESIAN_POINT('Ctrl Pts',(2.02726984051678,-0.342401873588419,
14.3272456836663));
#51361=CARTESIAN_POINT('Ctrl Pts',(2.01299624329973,-0.412120961564876,
14.3233766008159));
#51362=CARTESIAN_POINT('Ctrl Pts',(1.99874391303048,-0.481736171578308,
14.319513282706));
#51363=CARTESIAN_POINT('Ctrl Pts',(1.98085413719419,-0.550718466471994,
14.3156499645961));
#51364=CARTESIAN_POINT('Ctrl Pts',(1.95940198928566,-0.618660978956498,
14.3117866464862));
#51365=CARTESIAN_POINT('Ctrl Pts',(1.93797500473801,-0.686523794901137,
14.3079278600469));
#51366=CARTESIAN_POINT('Ctrl Pts',(1.91299409390747,-0.753348790110171,
14.3040690736076));
#51367=CARTESIAN_POINT('Ctrl Pts',(1.88458496240443,-0.81874115688604,14.3002102871683));
#51368=CARTESIAN_POINT('Ctrl Pts',(1.85619372657082,-0.88409233126648,14.2963539314815));
#51369=CARTESIAN_POINT('Ctrl Pts',(1.82437874764256,-0.948012223162581,
14.2924975757947));
#51370=CARTESIAN_POINT('Ctrl Pts',(1.78931446183537,-1.01012440776709,14.2886412201078));
#51371=CARTESIAN_POINT('Ctrl Pts',(1.75426053436903,-1.0722182438108,14.284786003627));
#51372=CARTESIAN_POINT('Ctrl Pts',(1.71595944433067,-1.13250500993205,14.2809307871463));
#51373=CARTESIAN_POINT('Ctrl Pts',(1.67463154346597,-1.19063292249492,14.2770755706655));
#51374=CARTESIAN_POINT('Ctrl Pts',(1.63330202680369,-1.24876310768569,14.2732202034572));
#51375=CARTESIAN_POINT('Ctrl Pts',(1.58894574765226,-1.30473387710441,14.269364836249));
#51376=CARTESIAN_POINT('Ctrl Pts',(1.54182533834839,-1.35822390956972,14.2655094690408));
#51377=CARTESIAN_POINT('Ctrl Pts',(1.494655606825,-1.41176993151312,14.2616500663143));
#51378=CARTESIAN_POINT('Ctrl Pts',(1.44471629126146,-1.4628296677331,14.2577906635879));
#51379=CARTESIAN_POINT('Ctrl Pts',(1.39230853614955,-1.5111169718672,14.2539312608615));
#51380=CARTESIAN_POINT('Ctrl Pts',(1.33987110735488,-1.55943161665233,14.250069672911));
#51381=CARTESIAN_POINT('Ctrl Pts',(1.28496283081743,-1.6049703941579,14.2462080849604));
#51382=CARTESIAN_POINT('Ctrl Pts',(1.22791762721129,-1.64748774298439,14.2423464970099));
#51383=CARTESIAN_POINT('Ctrl Pts',(1.17077262097713,-1.69007947743633,14.2384781530728));
#51384=CARTESIAN_POINT('Ctrl Pts',(1.11148362761128,-1.72963895965841,14.2346098091357));
#51385=CARTESIAN_POINT('Ctrl Pts',(1.05041259455181,-1.76596459299357,14.2307414651987));
#51386=CARTESIAN_POINT('Ctrl Pts',(1.01415037313166,-1.78753370838652,14.2284445539242));
#51387=CARTESIAN_POINT('Ctrl Pts',(0.977260338518683,-1.80796356594284,
14.2261476426498));
#51388=CARTESIAN_POINT('Ctrl Pts',(0.939821671982243,-1.82721996140927,
14.2238507313754));
#51389=CARTESIAN_POINT('Ctrl Pts',(0.876757284563182,-1.85965682138151,
14.2199816485293));
#51390=CARTESIAN_POINT('Ctrl Pts',(0.811888125585217,-1.88888848819301,
14.2161125656831));
#51391=CARTESIAN_POINT('Ctrl Pts',(0.745573095478381,-1.91471102827523,
14.212243482837));
#51392=CARTESIAN_POINT('Ctrl Pts',(0.679356871459215,-1.94049509406051,
14.2083801647314));
#51393=CARTESIAN_POINT('Ctrl Pts',(0.611699501476661,-1.96287994081013,
14.2045168466258));
#51394=CARTESIAN_POINT('Ctrl Pts',(0.54298352658394,-1.98170796343923,14.2006535285201));
#51395=CARTESIAN_POINT('Ctrl Pts',(0.474348155503365,-2.00051390080502,
14.1967947420852));
#51396=CARTESIAN_POINT('Ctrl Pts',(0.404657112275731,-2.01577117361054,
14.1929359556502));
#51397=CARTESIAN_POINT('Ctrl Pts',(0.334310268155385,-2.02737125537132,
14.1890771692152));
#51398=CARTESIAN_POINT('Ctrl Pts',(0.264007737388558,-2.03896402993118,
14.1852208135327));
#51399=CARTESIAN_POINT('Ctrl Pts',(0.193050703503013,-2.04690410522378,
14.1813644578503));
#51400=CARTESIAN_POINT('Ctrl Pts',(0.121850024200273,-2.05113386547597,
14.1775081021678));
#51401=CARTESIAN_POINT('Ctrl Pts',(0.0506703782911608,-2.05536237621463,
14.1736528856914));
#51402=CARTESIAN_POINT('Ctrl Pts',(-0.0207522854801669,-2.05588271911257,
14.169797669215));
#51403=CARTESIAN_POINT('Ctrl Pts',(-0.0920029075953569,-2.05268921843858,
14.1659424527386));
#51404=CARTESIAN_POINT('Ctrl Pts',(-0.163256315396763,-2.04949559290827,
14.1620870855348));
#51405=CARTESIAN_POINT('Ctrl Pts',(-0.234337182990594,-2.04258785948211,
14.158231718331));
#51406=CARTESIAN_POINT('Ctrl Pts',(-0.304833111213674,-2.03201238598779,
14.1543763511271));
#51407=CARTESIAN_POINT('Ctrl Pts',(-0.375402829450457,-2.02142584285649,
14.1505169484051));
#51408=CARTESIAN_POINT('Ctrl Pts',(-0.445385904692635,-2.00716396812194,
14.1466575456832));
#51409=CARTESIAN_POINT('Ctrl Pts',(-0.514378601070832,-1.98932456307673,
14.1427981429612));
#51410=CARTESIAN_POINT('Ctrl Pts',(-0.583410361655732,-1.97147505722023,
14.138936555015));
#51411=CARTESIAN_POINT('Ctrl Pts',(-0.651450163514077,-1.95004413466785,
14.1350749670689));
#51412=CARTESIAN_POINT('Ctrl Pts',(-0.718110590390047,-1.92517914555235,
14.1312133791228));
#51413=CARTESIAN_POINT('Ctrl Pts',(-0.784887642072441,-1.90027065424704,
14.1273450351901));
#51414=CARTESIAN_POINT('Ctrl Pts',(-0.850280054788644,-1.87191629450514,
14.1234766912574));
#51415=CARTESIAN_POINT('Ctrl Pts',(-0.913922147352021,-1.84031080828198,
14.1196083473248));
#51416=CARTESIAN_POINT('Ctrl Pts',(-0.951710990582568,-1.82154438002661,
14.1173114360111));
#51417=CARTESIAN_POINT('Ctrl Pts',(-0.988883219120611,-1.80163259407143,
14.1150145246975));
#51418=CARTESIAN_POINT('Ctrl Pts',(-1.02536715047564,-1.78062342150873,
14.1127176133838));
#51419=CARTESIAN_POINT('Ctrl Pts',(-1.08682331212073,-1.74523405810712,
14.1088485305374));
#51420=CARTESIAN_POINT('Ctrl Pts',(-1.14656555754676,-1.70659001272789,
14.1049794476909));
#51421=CARTESIAN_POINT('Ctrl Pts',(-1.20422789488691,-1.66488219993975,
14.1011103648445));
#51422=CARTESIAN_POINT('Ctrl Pts',(-1.26180431821997,-1.62323652971276,
14.0972470467386));
#51423=CARTESIAN_POINT('Ctrl Pts',(-1.31730659441153,-1.57853643558272,
14.0933837286326));
#51424=CARTESIAN_POINT('Ctrl Pts',(-1.37039483147761,-1.53101782104567,
14.0895204105267));
#51425=CARTESIAN_POINT('Ctrl Pts',(-1.4234207960619,-1.48355494582533,14.0856616240914));
#51426=CARTESIAN_POINT('Ctrl Pts',(-1.47403798596418,-1.43328043969418,
14.0818028376561));
#51427=CARTESIAN_POINT('Ctrl Pts',(-1.52193834219604,-1.38047138509045,
14.0779440512208));
#51428=CARTESIAN_POINT('Ctrl Pts',(-1.56980852471574,-1.32769559631895,
14.0740876955381));
#51429=CARTESIAN_POINT('Ctrl Pts',(-1.61496494336878,-1.27238878562944,
14.0702313398553));
#51430=CARTESIAN_POINT('Ctrl Pts',(-1.6571363521066,-1.21486487850576,14.0663749841725));
#51431=CARTESIAN_POINT('Ctrl Pts',(-1.69929530298793,-1.15735796452035,
14.0625197676959));
#51432=CARTESIAN_POINT('Ctrl Pts',(-1.73847070751407,-1.09763564592932,
14.0586645512192));
#51433=CARTESIAN_POINT('Ctrl Pts',(-1.77443267720094,-1.03604354955837,
14.0548093347425));
#51434=CARTESIAN_POINT('Ctrl Pts',(-1.81039605289318,-0.974449045120822,
14.0509539675384));
#51435=CARTESIAN_POINT('Ctrl Pts',(-1.84314550127443,-0.910985038388832,
14.0470986003343));
#51436=CARTESIAN_POINT('Ctrl Pts',(-1.87249630030024,-0.846023148537866,
14.0432432331302));
#51437=CARTESIAN_POINT('Ctrl Pts',(-1.90187782160901,-0.780993261302558,
14.0393838304079));
#51438=CARTESIAN_POINT('Ctrl Pts',(-1.92785339165058,-0.714462804719801,
14.0355244276857));
#51439=CARTESIAN_POINT('Ctrl Pts',(-1.95028619813571,-0.64682401614454,
14.0316650249634));
#51440=CARTESIAN_POINT('Ctrl Pts',(-1.97273170625206,-0.579146929955948,
14.0278034370171));
#51441=CARTESIAN_POINT('Ctrl Pts',(-1.99163032884486,-0.51036073117081,
14.0239418490707));
#51442=CARTESIAN_POINT('Ctrl Pts',(-2.00689573268168,-0.44087082081271,
14.0200802611243));
#51443=CARTESIAN_POINT('Ctrl Pts',(-2.02218784388967,-0.371259335365698,
14.0162119171914));
#51444=CARTESIAN_POINT('Ctrl Pts',(-2.03383396611622,-0.300942159688749,
14.0123435732585));
#51445=CARTESIAN_POINT('Ctrl Pts',(-2.04179937024044,-0.230332138846787,
14.0084752293256));
#51446=CARTESIAN_POINT('Ctrl Pts',(-2.0465289979953,-0.188405940359313,
14.0061783180145));
#51447=CARTESIAN_POINT('Ctrl Pts',(-2.04996193318919,-0.14637656079547,
14.0038814067033));
#51448=CARTESIAN_POINT('Ctrl Pts',(-2.05209959875135,-0.104330241562734,
14.0015844953922));
#51449=CARTESIAN_POINT('Ctrl Pts',(-2.0538552185185,-0.0697984838886084,
13.9996980904407));
#51450=CARTESIAN_POINT('Ctrl Pts',(-2.05473927936225,-0.035222040657156,
13.9978116854892));
#51451=CARTESIAN_POINT('Ctrl Pts',(-2.0547499030925,-0.000631063664673059,
13.9959252805377));
#51452=CARTESIAN_POINT('Ctrl Pts',(-2.05474990309271,-0.000631062987199567,
13.9959252805008));
#51453=CARTESIAN_POINT('Ctrl Pts',(-2.05477152045948,0.0697553852428013,
13.9920867839909));
#51454=CARTESIAN_POINT('Ctrl Pts',(-2.05117219117543,0.140288018046474,
13.988248287481));
#51455=CARTESIAN_POINT('Ctrl Pts',(-2.0439330102198,0.210559759293677,13.9844097909711));
#51456=CARTESIAN_POINT('Ctrl Pts',(-2.03654967279865,0.282230847498369,
13.9804948570723));
#51457=CARTESIAN_POINT('Ctrl Pts',(-2.02537985399478,0.353630025937492,
13.9765799231736));
#51458=CARTESIAN_POINT('Ctrl Pts',(-2.01045943330037,0.424323496348664,
13.9726649892748));
#51459=CARTESIAN_POINT('Ctrl Pts',(-1.99586784174531,0.493458962899926,
13.9688363360762));
#51460=CARTESIAN_POINT('Ctrl Pts',(-1.97768938082227,0.561918997872263,
13.9650076828776));
#51461=CARTESIAN_POINT('Ctrl Pts',(-1.95600985617612,0.629303587342279,
13.9611790296791));
#51462=CARTESIAN_POINT('Ctrl Pts',(-1.93434249883849,0.696650358220673,
13.9573525252547));
#51463=CARTESIAN_POINT('Ctrl Pts',(-1.90917812574259,0.762922411139088,
13.9535260208304));
#51464=CARTESIAN_POINT('Ctrl Pts',(-1.88065280528506,0.827733404227122,
13.9496995164061));
#51465=CARTESIAN_POINT('Ctrl Pts',(-1.85213357842264,0.892530552354134,
13.9458738294018));
#51466=CARTESIAN_POINT('Ctrl Pts',(-1.82025502876711,0.955866808207142,
13.9420481423976));
#51467=CARTESIAN_POINT('Ctrl Pts',(-1.7852012286889,1.01737610331068,13.9382224553933));
#51468=CARTESIAN_POINT('Ctrl Pts',(-1.74872503901803,1.08138128134311,13.9342415322272));
#51469=CARTESIAN_POINT('Ctrl Pts',(-1.70881064470608,1.14340753871887,13.9302606090612));
#51470=CARTESIAN_POINT('Ctrl Pts',(-1.66571685187883,1.20307311991703,13.9262796858951));
#51471=CARTESIAN_POINT('Ctrl Pts',(-1.62425181462367,1.26048360492933,13.9224492240917));
#51472=CARTESIAN_POINT('Ctrl Pts',(-1.57984378140074,1.31570830617255,13.9186187622883));
#51473=CARTESIAN_POINT('Ctrl Pts',(-1.53276463744932,1.36844076550096,13.9147883004848));
#51474=CARTESIAN_POINT('Ctrl Pts',(-1.48565311409644,1.42120949238497,13.9109552042227));
#51475=CARTESIAN_POINT('Ctrl Pts',(-1.43586717517302,1.47148221951872,13.9071221079605));
#51476=CARTESIAN_POINT('Ctrl Pts',(-1.3837146116892,1.51899026853295,13.9032890116984));
#51477=CARTESIAN_POINT('Ctrl Pts',(-1.33147845967571,1.56657446199147,13.8994497718671));
#51478=CARTESIAN_POINT('Ctrl Pts',(-1.27686850329514,1.61138483359032,13.8956105320358));
#51479=CARTESIAN_POINT('Ctrl Pts',(-1.22022357684515,1.6531944788836,13.8917712922045));
#51480=CARTESIAN_POINT('Ctrl Pts',(-1.21373214622642,1.65798580669748,13.8913313206032));
#51481=CARTESIAN_POINT('Ctrl Pts',(-1.20721401848556,1.66273777538411,13.890891349002));
#51482=CARTESIAN_POINT('Ctrl Pts',(-1.20066972439088,1.66745008184087,13.8904513774007));
#51483=CARTESIAN_POINT('Ctrl Pts',(-1.1431196098986,1.70888981119686,13.8865822945539));
#51484=CARTESIAN_POINT('Ctrl Pts',(-1.08330889157962,1.74742779385032,13.8827132117072));
#51485=CARTESIAN_POINT('Ctrl Pts',(-1.02156221766485,1.78280907501047,13.8788441288604));
#51486=CARTESIAN_POINT('Ctrl Pts',(-0.959907543214647,1.81813763982629,
13.8749808107541));
#51487=CARTESIAN_POINT('Ctrl Pts',(-0.896323056833569,1.85031859957462,
13.8711174926478));
#51488=CARTESIAN_POINT('Ctrl Pts',(-0.831163663166718,1.87913930498281,
13.8672541745415));
#51489=CARTESIAN_POINT('Ctrl Pts',(-0.766080701443692,1.90792620371459,
13.8633953881059));
#51490=CARTESIAN_POINT('Ctrl Pts',(-0.699426944037772,1.93336048186316,
13.8595366016702));
#51491=CARTESIAN_POINT('Ctrl Pts',(-0.631581719784205,1.95527545213825,
13.8556778152346));
#51492=CARTESIAN_POINT('Ctrl Pts',(-0.563779233047022,1.97717661758902,
13.8518214595515));
#51493=CARTESIAN_POINT('Ctrl Pts',(-0.494787229687997,1.99556272450761,
13.8479651038683));
#51494=CARTESIAN_POINT('Ctrl Pts',(-0.425003461262185,2.01031580116537,
13.8441087481852));
#51495=CARTESIAN_POINT('Ctrl Pts',(-0.355240307660369,2.02506451961655,
13.8402535317081));
#51496=CARTESIAN_POINT('Ctrl Pts',(-0.284686328358028,2.03618223804894,
13.8363983152311));
#51497=CARTESIAN_POINT('Ctrl Pts',(-0.213751140990927,2.04360172544091,
13.832543098754));
#51498=CARTESIAN_POINT('Ctrl Pts',(-0.142813180270208,2.05102150291265,
13.8286877315496));
#51499=CARTESIAN_POINT('Ctrl Pts',(-0.0714944652711667,2.05474271393595,
13.8248323643451));
#51500=CARTESIAN_POINT('Ctrl Pts',(-0.000209708945903632,2.05474998929849,
13.8209769971406));
#51501=CARTESIAN_POINT('Ctrl Pts',(0.0711496630808504,2.05475727227636,
13.817117594418));
#51502=CARTESIAN_POINT('Ctrl Pts',(0.142474518698766,2.05104285926674,13.8132581916953));
#51503=CARTESIAN_POINT('Ctrl Pts',(0.213351076631586,2.04364353070689,13.8093987889727));
#51504=CARTESIAN_POINT('Ctrl Pts',(0.284267765428198,2.0362400125891,13.8055372010259));
#51505=CARTESIAN_POINT('Ctrl Pts',(0.354735171141851,2.02514750106051,13.8016756130791));
#51506=CARTESIAN_POINT('Ctrl Pts',(0.424348295436333,2.01045419909539,13.7978140251324));
#51507=CARTESIAN_POINT('Ctrl Pts',(0.494083210387085,1.99573519067179,13.7939456811991));
#51508=CARTESIAN_POINT('Ctrl Pts',(0.562960390327175,1.97740293924371,13.7900773372657));
#51509=CARTESIAN_POINT('Ctrl Pts',(0.630589295530054,1.95559574116506,13.7862089933324));
#51510=CARTESIAN_POINT('Ctrl Pts',(0.670745393273935,1.94264725449446,13.7839120820247));
#51511=CARTESIAN_POINT('Ctrl Pts',(0.710461744569614,1.92847456155713,13.7816151707169));
#51512=CARTESIAN_POINT('Ctrl Pts',(0.749660339633757,1.91311446016181,13.7793182594091));
#51513=CARTESIAN_POINT('Ctrl Pts',(0.815683790416979,1.88724294877625,13.7754494980305));
#51514=CARTESIAN_POINT('Ctrl Pts',(0.880495696393577,1.85789895683121,13.7715807366518));
#51515=CARTESIAN_POINT('Ctrl Pts',(0.943705875462188,1.82521691399081,13.7677119752731));
#51516=CARTESIAN_POINT('Ctrl Pts',(1.00681605076683,1.79258657686216,13.7638493345969));
#51517=CARTESIAN_POINT('Ctrl Pts',(1.06832910357685,1.75662889722033,13.7599866939208));
#51518=CARTESIAN_POINT('Ctrl Pts',(1.12787407849864,1.71752660111884,13.7561240532446));
#51519=CARTESIAN_POINT('Ctrl Pts',(1.17031289217566,1.68965766573388,13.7533710772265));
#51520=CARTESIAN_POINT('Ctrl Pts',(1.2117523357401,1.66019240070899,13.7506181012084));
#51521=CARTESIAN_POINT('Ctrl Pts',(1.25206542099588,1.62921138715834,13.7478651251903));
#51522=CARTESIAN_POINT('',(-2.05441708793377,9.11445141410593E-5,14.0540747126079));
#51523=CARTESIAN_POINT('Ctrl Pts',(-2.05138530455185,9.21659133880177E-5,
14.0540746501851));
#51524=CARTESIAN_POINT('Ctrl Pts',(-2.05151822953231,0.337478339785075,
14.0358517048661));
#51525=CARTESIAN_POINT('Ctrl Pts',(-1.81315401936802,1.36054008639431,13.9805843868831));
#51526=CARTESIAN_POINT('Ctrl Pts',(-0.369385311720978,2.3091885410961,13.897951444021));
#51527=CARTESIAN_POINT('Ctrl Pts',(0.848349475390589,1.93250137893999,13.833541446478));
#51528=CARTESIAN_POINT('Ctrl Pts',(1.2517190174544,1.62874802847342,13.8061758215988));
#51529=CARTESIAN_POINT('Ctrl Pts',(1.25206542099588,1.62921138715834,14.5060551473646));
#51530=CARTESIAN_POINT('Ctrl Pts',(1.30860924608552,1.58575688596617,14.5022000106753));
#51531=CARTESIAN_POINT('Ctrl Pts',(1.36290092959432,1.53934552907356,14.4983448739859));
#51532=CARTESIAN_POINT('Ctrl Pts',(1.41462456046657,1.49024659550853,14.4944897372965));
#51533=CARTESIAN_POINT('Ctrl Pts',(1.46635421293839,1.44114194590786,14.490634151797));
#51534=CARTESIAN_POINT('Ctrl Pts',(1.51551486871162,1.38934943476757,14.4867785662975));
#51535=CARTESIAN_POINT('Ctrl Pts',(1.56182696774729,1.33517567582596,14.482922980798));
#51536=CARTESIAN_POINT('Ctrl Pts',(1.60818974392862,1.28094263709505,14.4790631763131));
#51537=CARTESIAN_POINT('Ctrl Pts',(1.65169742786638,1.22432352138397,14.4752033718283));
#51538=CARTESIAN_POINT('Ctrl Pts',(1.69211093219569,1.16565782099373,14.4713435673434));
#51539=CARTESIAN_POINT('Ctrl Pts',(1.73255012112508,1.10695483591169,14.4674813097791));
#51540=CARTESIAN_POINT('Ctrl Pts',(1.76989096323924,1.04620309167034,14.4636190522149));
#51541=CARTESIAN_POINT('Ctrl Pts',(1.80393932467075,0.983768507021053,14.4597567946506));
#51542=CARTESIAN_POINT('Ctrl Pts',(1.83804488750296,0.921229031988096,14.4558880484762));
#51543=CARTESIAN_POINT('Ctrl Pts',(1.86884672327517,0.857001512854926,14.4520193023018));
#51544=CARTESIAN_POINT('Ctrl Pts',(1.89619834296505,0.791472934873064,14.4481505561275));
#51545=CARTESIAN_POINT('Ctrl Pts',(1.90612510821433,0.767690547646272,14.4467464661497));
#51546=CARTESIAN_POINT('Ctrl Pts',(1.91559788850765,0.743736934848507,14.4453423761719));
#51547=CARTESIAN_POINT('Ctrl Pts',(1.92461131969351,0.719631037829523,14.4439382861942));
#51548=CARTESIAN_POINT('Ctrl Pts',(1.94944855431137,0.65320529966295,14.4400692033241));
#51549=CARTESIAN_POINT('Ctrl Pts',(1.97089148697944,0.58536210665846,14.4362001204539));
#51550=CARTESIAN_POINT('Ctrl Pts',(1.98877956645739,0.516481750443847,14.4323310375838));
#51551=CARTESIAN_POINT('Ctrl Pts',(2.00664099359071,0.44770402251835,14.4284677194539));
#51552=CARTESIAN_POINT('Ctrl Pts',(2.02095795993475,0.377892665158933,14.4246044013239));
#51553=CARTESIAN_POINT('Ctrl Pts',(2.03161869003943,0.307446029056242,14.4207410831939));
#51554=CARTESIAN_POINT('Ctrl Pts',(2.04226691511295,0.237082026823042,14.4168822967342));
#51555=CARTESIAN_POINT('Ctrl Pts',(2.04926735054969,0.166084704012999,14.4130235102745));
#51556=CARTESIAN_POINT('Ctrl Pts',(2.05255898976634,0.0948638815851162,
14.4091647238148));
#51557=CARTESIAN_POINT('Ctrl Pts',(2.05584855549185,0.02368792304854,14.4053083681074));
#51558=CARTESIAN_POINT('Ctrl Pts',(2.0554339377446,-0.0477107716659809,
14.4014520124));
#51559=CARTESIAN_POINT('Ctrl Pts',(2.05130597628203,-0.118917425845184,
14.3975956566925));
#51560=CARTESIAN_POINT('Ctrl Pts',(2.0471792342604,-0.190103044869233,14.393740440191));
#51561=CARTESIAN_POINT('Ctrl Pts',(2.03934135439014,-0.261096251279422,
14.3898852236895));
#51562=CARTESIAN_POINT('Ctrl Pts',(2.02783525140285,-0.331484171066937,
14.386030007188));
#51563=CARTESIAN_POINT('Ctrl Pts',(2.01632869856094,-0.401874842814094,
14.3821746399589));
#51564=CARTESIAN_POINT('Ctrl Pts',(2.00115371841039,-0.471659701890479,
14.3783192727298));
#51565=CARTESIAN_POINT('Ctrl Pts',(1.98240460076224,-0.5404346041629,14.3744639055007));
#51566=CARTESIAN_POINT('Ctrl Pts',(1.96363585790037,-0.609281495004617,
14.3706045027534));
#51567=CARTESIAN_POINT('Ctrl Pts',(1.94128563740345,-0.677115849095894,
14.3667451000061));
#51568=CARTESIAN_POINT('Ctrl Pts',(1.91549829606384,-0.74354814254123,14.3628856972587));
#51569=CARTESIAN_POINT('Ctrl Pts',(1.8896963537286,-0.810018050474006,14.3590241092872));
#51570=CARTESIAN_POINT('Ctrl Pts',(1.86045361564986,-0.875083874135089,
14.3551625213157));
#51571=CARTESIAN_POINT('Ctrl Pts',(1.82796173831847,-0.938378093171251,
14.3513009333442));
#51572=CARTESIAN_POINT('Ctrl Pts',(1.79541301528476,-1.00178304770901,14.3474325893863));
#51573=CARTESIAN_POINT('Ctrl Pts',(1.75960404789974,-1.06340978925443,14.3435642454284));
#51574=CARTESIAN_POINT('Ctrl Pts',(1.72077101667156,-1.12291792695777,14.3396959014705));
#51575=CARTESIAN_POINT('Ctrl Pts',(1.6977130825711,-1.15825214306729,14.3373989903812));
#51576=CARTESIAN_POINT('Ctrl Pts',(1.67358978236133,-1.19283999979394,14.3351020792919));
#51577=CARTESIAN_POINT('Ctrl Pts',(1.64845714283379,-1.22661591818314,14.3328051682026));
#51578=CARTESIAN_POINT('Ctrl Pts',(1.60612191059531,-1.2835105132577,14.3289360853596));
#51579=CARTESIAN_POINT('Ctrl Pts',(1.5607548251177,-1.33832224264501,14.3250670025165));
#51580=CARTESIAN_POINT('Ctrl Pts',(1.51258830213628,-1.39070995924401,14.3211979196735));
#51581=CARTESIAN_POINT('Ctrl Pts',(1.46449354487208,-1.4430196207578,14.3173346015709));
#51582=CARTESIAN_POINT('Ctrl Pts',(1.4136079555805,-1.49291208383262,14.3134712834684));
#51583=CARTESIAN_POINT('Ctrl Pts',(1.36020557704207,-1.54007738464132,14.3096079653658));
#51584=CARTESIAN_POINT('Ctrl Pts',(1.30686583947285,-1.58718736057056,14.3057491789339));
#51585=CARTESIAN_POINT('Ctrl Pts',(1.25101553904864,-1.63157620843339,14.3018903925019));
#51586=CARTESIAN_POINT('Ctrl Pts',(1.19296589113649,-1.67297039575867,14.29803160607));
#51587=CARTESIAN_POINT('Ctrl Pts',(1.13495281024579,-1.71433850778134,14.2941752503906));
#51588=CARTESIAN_POINT('Ctrl Pts',(1.07474352512187,-1.75271542051358,14.2903188947111));
#51589=CARTESIAN_POINT('Ctrl Pts',(1.01268153506013,-1.78786847140617,14.2864625390317));
#51590=CARTESIAN_POINT('Ctrl Pts',(0.950637878731437,-1.82301113773569,
14.2826073225583));
#51591=CARTESIAN_POINT('Ctrl Pts',(0.88674302647926,-1.8549315936393,14.278752106085));
#51592=CARTESIAN_POINT('Ctrl Pts',(0.821367123515611,-1.88344195846532,
14.2748968896116));
#51593=CARTESIAN_POINT('Ctrl Pts',(0.755988664549258,-1.91195343796153,
14.2710415224108));
#51594=CARTESIAN_POINT('Ctrl Pts',(0.689129486072411,-1.93705436951408,
14.2671861552099));
#51595=CARTESIAN_POINT('Ctrl Pts',(0.621180263872119,-1.95860476928751,
14.2633307880091));
#51596=CARTESIAN_POINT('Ctrl Pts',(0.553159917363878,-1.98017772645335,
14.2594713852901));
#51597=CARTESIAN_POINT('Ctrl Pts',(0.484047713484457,-1.99819258583566,
14.255611982571));
#51598=CARTESIAN_POINT('Ctrl Pts',(0.4142492004212,-2.01255935625521,14.251752579852));
#51599=CARTESIAN_POINT('Ctrl Pts',(0.344411166890853,-2.02693426125318,
14.2478909919087));
#51600=CARTESIAN_POINT('Ctrl Pts',(0.273886531097746,-2.03765689230798,
14.2440294039655));
#51601=CARTESIAN_POINT('Ctrl Pts',(0.203088009751233,-2.04468893056995,
14.2401678160223));
#51602=CARTESIAN_POINT('Ctrl Pts',(0.132165623852401,-2.05173327163507,
14.2362994720925));
#51603=CARTESIAN_POINT('Ctrl Pts',(0.0609688811211802,-2.05507410589783,
14.2324311281626));
#51604=CARTESIAN_POINT('Ctrl Pts',(-0.0100881451754699,-2.05472523511707,
14.2285627842328));
#51605=CARTESIAN_POINT('Ctrl Pts',(-0.0522797632143424,-2.05451808568381,
14.2262658728922));
#51606=CARTESIAN_POINT('Ctrl Pts',(-0.0944221736534997,-2.05301107601554,
14.2239689615516));
#51607=CARTESIAN_POINT('Ctrl Pts',(-0.136429893586073,-2.05021570734303,
14.221672050211));
#51608=CARTESIAN_POINT('Ctrl Pts',(-0.207190721651772,-2.04550698708082,
14.2178029673682));
#51609=CARTESIAN_POINT('Ctrl Pts',(-0.277846082889716,-2.03712140126886,
14.2139338845255));
#51610=CARTESIAN_POINT('Ctrl Pts',(-0.34798331061511,-2.02506917857967,
14.2100648016827));
#51611=CARTESIAN_POINT('Ctrl Pts',(-0.418016037367383,-2.01303491310152,
14.2062014835805));
#51612=CARTESIAN_POINT('Ctrl Pts',(-0.487531688126347,-1.99734493646067,
14.2023381654784));
#51613=CARTESIAN_POINT('Ctrl Pts',(-0.556121216616893,-1.97806136278138,
14.1984748473762));
#51614=CARTESIAN_POINT('Ctrl Pts',(-0.62463028961483,-1.95880040872719,
14.1946160609447));
#51615=CARTESIAN_POINT('Ctrl Pts',(-0.692214932802764,-1.93595436146375,
14.1907572745133));
#51616=CARTESIAN_POINT('Ctrl Pts',(-0.75847654541342,-1.90963632468534,
14.1868984880819));
#51617=CARTESIAN_POINT('Ctrl Pts',(-0.82469641806565,-1.88333486634077,
14.1830421324031));
#51618=CARTESIAN_POINT('Ctrl Pts',(-0.889594463209346,-1.85356593654599,
14.1791857767242));
#51619=CARTESIAN_POINT('Ctrl Pts',(-0.952788906082997,-1.82049192883274,
14.1753294210453));
#51620=CARTESIAN_POINT('Ctrl Pts',(-1.01596468068449,-1.78742769151305,
14.1714742045726));
#51621=CARTESIAN_POINT('Ctrl Pts',(-1.07743742196365,-1.7510605397422,14.1676189880999));
#51622=CARTESIAN_POINT('Ctrl Pts',(-1.13684852569153,-1.71159954198784,
14.1637637716272));
#51623=CARTESIAN_POINT('Ctrl Pts',(-1.19626195221509,-1.67213700142701,
14.1599084044271));
#51624=CARTESIAN_POINT('Ctrl Pts',(-1.25361317772226,-1.62958064534053,
14.156053037227));
#51625=CARTESIAN_POINT('Ctrl Pts',(-1.30857270230379,-1.5841827689018,14.1521976700269));
#51626=CARTESIAN_POINT('Ctrl Pts',(-1.36358975452008,-1.53873737326644,
14.1483382673087));
#51627=CARTESIAN_POINT('Ctrl Pts',(-1.41620973304714,-1.49044482992165,
14.1444788645905));
#51628=CARTESIAN_POINT('Ctrl Pts',(-1.46613707196258,-1.43959704386921,
14.1406194618724));
#51629=CARTESIAN_POINT('Ctrl Pts',(-1.51609268012903,-1.38872046740139,
14.1367578739301));
#51630=CARTESIAN_POINT('Ctrl Pts',(-1.56335229170375,-1.33528613214971,
14.1328962859878));
#51631=CARTESIAN_POINT('Ctrl Pts',(-1.60765986433228,-1.27961999168312,
14.1290346980455));
#51632=CARTESIAN_POINT('Ctrl Pts',(-1.6520449546473,-1.22385646130848,14.1251663541167));
#51633=CARTESIAN_POINT('Ctrl Pts',(-1.69346741214216,-1.16585372547734,
14.1212980101879));
#51634=CARTESIAN_POINT('Ctrl Pts',(-1.73171424693945,-1.10596714663996,
14.117429666259));
#51635=CARTESIAN_POINT('Ctrl Pts',(-1.75442411721769,-1.07040821884861,
14.1151327549125));
#51636=CARTESIAN_POINT('Ctrl Pts',(-1.7760152426764,-1.03418561337468,14.112835843566));
#51637=CARTESIAN_POINT('Ctrl Pts',(-1.79645092163318,-0.997377385277664,
14.1105389322194));
#51638=CARTESIAN_POINT('Ctrl Pts',(-1.8325132064301,-0.932422909954774,
14.1064856354679));
#51639=CARTESIAN_POINT('Ctrl Pts',(-1.86510495352398,-0.86540946720002,
14.1024323387163));
#51640=CARTESIAN_POINT('Ctrl Pts',(-1.89399792216641,-0.796724188994735,
14.0983790419647));
#51641=CARTESIAN_POINT('Ctrl Pts',(-1.92280997820391,-0.728231258791105,
14.0943370961685));
#51642=CARTESIAN_POINT('Ctrl Pts',(-1.94794371962189,-0.658076199843631,
14.0902951503723));
#51643=CARTESIAN_POINT('Ctrl Pts',(-1.96921717900164,-0.586669638233323,
14.0862532045761));
#51644=CARTESIAN_POINT('Ctrl Pts',(-1.99045484462435,-0.51538322206207,
14.0822180595745));
#51645=CARTESIAN_POINT('Ctrl Pts',(-2.00784502257861,-0.44284988883517,
14.0781829145728));
#51646=CARTESIAN_POINT('Ctrl Pts',(-2.02125400722186,-0.369499392136954,
14.0741477695712));
#51647=CARTESIAN_POINT('Ctrl Pts',(-2.03463537803434,-0.296299949993299,
14.0701209343569));
#51648=CARTESIAN_POINT('Ctrl Pts',(-2.04405180395157,-0.222287105409238,
14.0660940991425));
#51649=CARTESIAN_POINT('Ctrl Pts',(-2.04941996305247,-0.147903270896886,
14.0620672639282));
#51650=CARTESIAN_POINT('Ctrl Pts',(-2.05297157352164,-0.0986904214962947,
14.0594030824396));
#51651=CARTESIAN_POINT('Ctrl Pts',(-2.05475218685897,-0.0493154866282622,
14.0567389009509));
#51652=CARTESIAN_POINT('Ctrl Pts',(-2.05474999798348,9.10323576868401E-5,
14.0540747194623));
#51653=CARTESIAN_POINT('Origin',(0.,0.,18.5459252805377));
#51654=CARTESIAN_POINT('',(1.25206542099588,1.62921138715835,15.2060150049977));
#51655=CARTESIAN_POINT('',(1.25109478256769,1.6279226134271,15.1480161847457));
#51656=CARTESIAN_POINT('',(1.25206542099588,1.62921138715835,18.5459252805377));
#51657=CARTESIAN_POINT('',(-2.05474914219178,0.00187754151781767,14.6959252704371));
#51658=CARTESIAN_POINT('Ctrl Pts',(1.25109478256748,1.62792261342726,15.1480161847458));
#51659=CARTESIAN_POINT('Ctrl Pts',(1.42360946980995,1.49766989531232,15.1363160149331));
#51660=CARTESIAN_POINT('Ctrl Pts',(2.05683536821899,0.846821926034871,15.0875714724566));
#51661=CARTESIAN_POINT('Ctrl Pts',(2.24042116521983,-0.937279091896088,
15.0017825573163));
#51662=CARTESIAN_POINT('Ctrl Pts',(0.427721193935683,-2.39061364822391,
14.8906494393247));
#51663=CARTESIAN_POINT('Ctrl Pts',(-1.59436008174594,-1.71665379493215,
14.7886970137319));
#51664=CARTESIAN_POINT('Ctrl Pts',(-2.04978635669156,-0.51206744035561,
14.7237889608028));
#51665=CARTESIAN_POINT('Ctrl Pts',(-2.05444347718377,0.00187707591058038,
14.6959252805377));
#51666=CARTESIAN_POINT('Ctrl Pts',(-2.05474914219178,0.00187754151781767,
14.6959252704371));
#51667=CARTESIAN_POINT('Ctrl Pts',(-2.05466440026703,0.0946176463469028,
14.6908980355964));
#51668=CARTESIAN_POINT('Ctrl Pts',(-2.04829723603806,0.187078217758331,
14.6858708007558));
#51669=CARTESIAN_POINT('Ctrl Pts',(-2.03578285247768,0.278542169263164,
14.6808435659151));
#51670=CARTESIAN_POINT('Ctrl Pts',(-2.02544358636103,0.354108826632005,
14.6766901117239));
#51671=CARTESIAN_POINT('Ctrl Pts',(-2.01090920585382,0.428995861661035,
14.6725366575328));
#51672=CARTESIAN_POINT('Ctrl Pts',(-1.99227978030212,0.502810938126188,
14.6683832033416));
#51673=CARTESIAN_POINT('Ctrl Pts',(-1.9749258411557,0.571572175100983,14.6645141204716));
#51674=CARTESIAN_POINT('Ctrl Pts',(-1.95397391117961,0.639568607569909,
14.6606450376015));
#51675=CARTESIAN_POINT('Ctrl Pts',(-1.9295082448856,0.70639613208063,14.6567759547315));
#51676=CARTESIAN_POINT('Ctrl Pts',(-1.90507903121191,0.773124086918992,
14.6529126366016));
#51677=CARTESIAN_POINT('Ctrl Pts',(-1.8771466387746,0.838686138398381,14.6490493184717));
#51678=CARTESIAN_POINT('Ctrl Pts',(-1.84584571117744,0.902691072863716,
14.6451860003418));
#51679=CARTESIAN_POINT('Ctrl Pts',(-1.81458149955306,0.9666209295722,14.6413272138822));
#51680=CARTESIAN_POINT('Ctrl Pts',(-1.77995681374694,1.02899686303295,14.6374684274226));
#51681=CARTESIAN_POINT('Ctrl Pts',(-1.74215457810066,1.08944710220501,14.633609640963));
#51682=CARTESIAN_POINT('Ctrl Pts',(-1.70437615508864,1.14985926216268,14.6297532852556));
#51683=CARTESIAN_POINT('Ctrl Pts',(-1.66342441038333,1.20834772359031,14.6258969295483));
#51684=CARTESIAN_POINT('Ctrl Pts',(-1.61952772989123,1.26456612899972,14.622040573841));
#51685=CARTESIAN_POINT('Ctrl Pts',(-1.57564401691594,1.32076792693203,14.6181853573395));
#51686=CARTESIAN_POINT('Ctrl Pts',(-1.52881739407797,1.37470061748818,14.6143301408381));
#51687=CARTESIAN_POINT('Ctrl Pts',(-1.47931799588639,1.42604902774999,14.6104749243367));
#51688=CARTESIAN_POINT('Ctrl Pts',(-1.4298166624145,1.47739944558301,14.6066195571077));
#51689=CARTESIAN_POINT('Ctrl Pts',(-1.37764268485453,1.52616503431371,14.6027641898787));
#51690=CARTESIAN_POINT('Ctrl Pts',(-1.32310348745199,1.57206702274183,14.5989088226497));
#51691=CARTESIAN_POINT('Ctrl Pts',(-1.26850720238146,1.61801705803534,14.5950494199025));
#51692=CARTESIAN_POINT('Ctrl Pts',(-1.21154112776492,1.66109719607844,14.5911900171552));
#51693=CARTESIAN_POINT('Ctrl Pts',(-1.15254555132663,1.70106916808729,14.587330614408));
#51694=CARTESIAN_POINT('Ctrl Pts',(-1.09351657112867,1.74106377254127,14.5834690264366));
#51695=CARTESIAN_POINT('Ctrl Pts',(-1.03245621757575,1.77794645632113,14.5796074384652));
#51696=CARTESIAN_POINT('Ctrl Pts',(-0.969731166288907,1.81152395171247,
14.5757458504937));
#51697=CARTESIAN_POINT('Ctrl Pts',(-0.906896375279786,1.8451601921338,14.5718775065359));
#51698=CARTESIAN_POINT('Ctrl Pts',(-0.842391511530458,1.87547949244146,
14.5680091625781));
#51699=CARTESIAN_POINT('Ctrl Pts',(-0.776604440019373,1.90233622323768,
14.5641408186203));
#51700=CARTESIAN_POINT('Ctrl Pts',(-0.737541974068368,1.91828297551264,
14.5618439075302));
#51701=CARTESIAN_POINT('Ctrl Pts',(-0.698027781771188,1.93300989149292,
14.5595469964402));
#51702=CARTESIAN_POINT('Ctrl Pts',(-0.658145244802309,1.9464949009037,14.5572500853501));
#51703=CARTESIAN_POINT('Ctrl Pts',(-0.590963485530717,1.9692102727146,14.5533809601727));
#51704=CARTESIAN_POINT('Ctrl Pts',(-0.522472755723196,1.98848796324828,
14.5495118349954));
#51705=CARTESIAN_POINT('Ctrl Pts',(-0.453058266798325,2.00417957513435,
14.545642709818));
#51706=CARTESIAN_POINT('Ctrl Pts',(-0.383747422431103,2.01984775747137,
14.541779361731));
#51707=CARTESIAN_POINT('Ctrl Pts',(-0.313516026828389,2.0319403835457,14.5379160136439));
#51708=CARTESIAN_POINT('Ctrl Pts',(-0.242765789127639,2.04035838374763,
14.5340526655568));
#51709=CARTESIAN_POINT('Ctrl Pts',(-0.172099404093816,2.04876640699697,
14.5301938962817));
#51710=CARTESIAN_POINT('Ctrl Pts',(-0.100915878549273,2.05350839865137,
14.5263351270067));
#51711=CARTESIAN_POINT('Ctrl Pts',(-0.0296267588397955,2.05453639969231,
14.5224763577316));
#51712=CARTESIAN_POINT('Ctrl Pts',(0.0416171306537917,2.05556374850597,
14.5186200366979));
#51713=CARTESIAN_POINT('Ctrl Pts',(0.112965996818219,2.0528817750382,14.5147637156641));
#51714=CARTESIAN_POINT('Ctrl Pts',(0.184004992428342,2.04649449675816,14.5109073946304));
#51715=CARTESIAN_POINT('Ctrl Pts',(0.255022680246738,2.04010913431033,14.5070522302809));
#51716=CARTESIAN_POINT('Ctrl Pts',(0.325730198514623,2.0300207172167,14.5031970659314));
#51717=CARTESIAN_POINT('Ctrl Pts',(0.395716261069186,2.01628524847687,14.4993419015818));
#51718=CARTESIAN_POINT('Ctrl Pts',(0.465704742375029,2.00254930503276,14.495486603996));
#51719=CARTESIAN_POINT('Ctrl Pts',(0.534971242295313,1.9851661556892,14.4916313064102));
#51720=CARTESIAN_POINT('Ctrl Pts',(0.603114836539192,1.96424287104378,14.4877760088244));
#51721=CARTESIAN_POINT('Ctrl Pts',(0.671326171198658,1.9432987869085,14.4839168787513));
#51722=CARTESIAN_POINT('Ctrl Pts',(0.738411907158264,1.91880768673003,14.4800577486781));
#51723=CARTESIAN_POINT('Ctrl Pts',(0.803987381797254,1.89092618904356,14.476198618605));
#51724=CARTESIAN_POINT('Ctrl Pts',(0.869599866550078,1.86302895533064,14.4723373104791));
#51725=CARTESIAN_POINT('Ctrl Pts',(0.933699956603814,1.83173772811405,14.4684760023532));
#51726=CARTESIAN_POINT('Ctrl Pts',(0.995926478592241,1.79725568902671,14.4646146942273));
#51727=CARTESIAN_POINT('Ctrl Pts',(1.05825441429214,1.76271745281551,14.4607470931322));
#51728=CARTESIAN_POINT('Ctrl Pts',(1.11870227588255,1.72497828292203,14.4568794920371));
#51729=CARTESIAN_POINT('Ctrl Pts',(1.17693752772968,1.68428489820503,14.4530118909419));
#51730=CARTESIAN_POINT('Ctrl Pts',(1.20241169009358,1.66648417001142,14.4513200651984));
#51731=CARTESIAN_POINT('Ctrl Pts',(1.22746289710024,1.64811867548308,14.4496282394549));
#51732=CARTESIAN_POINT('Ctrl Pts',(1.25206542099587,1.62921138715835,14.4479364137114));
#51733=CARTESIAN_POINT('',(-2.0547491753793,-0.00184086341081391,14.7540747194092));
#51734=CARTESIAN_POINT('Ctrl Pts',(-2.0547491753793,-0.00184086341080706,
14.7540747194092));
#51735=CARTESIAN_POINT('Ctrl Pts',(-2.05481200415796,0.068287849233049,
14.7502679504067));
#51736=CARTESIAN_POINT('Ctrl Pts',(-2.05128035637574,0.138528733663465,
14.7464611814043));
#51737=CARTESIAN_POINT('Ctrl Pts',(-2.04414642809902,0.208477679836533,
14.7426544124019));
#51738=CARTESIAN_POINT('Ctrl Pts',(-2.03701831865898,0.278369571680172,
14.7388507484163));
#51739=CARTESIAN_POINT('Ctrl Pts',(-2.02629380219727,0.347969501103903,
14.7350470844307));
#51740=CARTESIAN_POINT('Ctrl Pts',(-2.01201710821451,0.416874943780628,
14.7312434204451));
#51741=CARTESIAN_POINT('Ctrl Pts',(-1.99774696631999,0.485748763272034,
14.7274415020976));
#51742=CARTESIAN_POINT('Ctrl Pts',(-1.97992798093516,0.553928238327332,
14.7236395837502));
#51743=CARTESIAN_POINT('Ctrl Pts',(-1.95865575939417,0.621019467240785,
14.7198376654028));
#51744=CARTESIAN_POINT('Ctrl Pts',(-1.93738571327467,0.688103835013735,
14.7160361358617));
#51745=CARTESIAN_POINT('Ctrl Pts',(-1.91266328488549,0.754099700744834,
14.7122346063206));
#51746=CARTESIAN_POINT('Ctrl Pts',(-1.88463382974959,0.818628664452574,
14.7084330767795));
#51747=CARTESIAN_POINT('Ctrl Pts',(-1.8565783874181,0.883217455466713,14.7046280226928));
#51748=CARTESIAN_POINT('Ctrl Pts',(-1.82520999617619,0.946336168563494,
14.7008229686062));
#51749=CARTESIAN_POINT('Ctrl Pts',(-1.79072159216291,1.00762777942131,14.6970179145196));
#51750=CARTESIAN_POINT('Ctrl Pts',(-1.75621664581928,1.06894878874228,14.6932110353423));
#51751=CARTESIAN_POINT('Ctrl Pts',(-1.71858897733662,1.1284405288387,14.6894041561651));
#51752=CARTESIAN_POINT('Ctrl Pts',(-1.67807525655495,1.18577442873341,14.6855972769878));
#51753=CARTESIAN_POINT('Ctrl Pts',(-1.63749044941838,1.24320892807632,14.6817837181683));
#51754=CARTESIAN_POINT('Ctrl Pts',(-1.59400979112279,1.29847763551897,14.6779701593487));
#51755=CARTESIAN_POINT('Ctrl Pts',(-1.54791012952976,1.35128523761608,14.6741566005291));
#51756=CARTESIAN_POINT('Ctrl Pts',(-1.51586760806649,1.38799025160423,14.6715059077452));
#51757=CARTESIAN_POINT('Ctrl Pts',(-1.48256060688962,1.42350698204244,14.6688552149612));
#51758=CARTESIAN_POINT('Ctrl Pts',(-1.44809173787727,1.45774753684977,14.6662045221772));
#51759=CARTESIAN_POINT('Ctrl Pts',(-1.39777926479025,1.50772675118406,14.6623354393446));
#51760=CARTESIAN_POINT('Ctrl Pts',(-1.34477774896543,1.55519608254071,14.658466356512));
#51761=CARTESIAN_POINT('Ctrl Pts',(-1.28936767615483,1.59985266765008,14.6545972736794));
#51762=CARTESIAN_POINT('Ctrl Pts',(-1.23404016158673,1.64444271667683,14.6507339555871));
#51763=CARTESIAN_POINT('Ctrl Pts',(-1.1763115885187,1.68622803583219,14.6468706374948));
#51764=CARTESIAN_POINT('Ctrl Pts',(-1.11649897912541,1.72494277937325,14.6430073194025));
#51765=CARTESIAN_POINT('Ctrl Pts',(-1.0567565298946,1.76361211053848,14.6391485329805));
#51766=CARTESIAN_POINT('Ctrl Pts',(-0.994935305920528,1.79921775777028,
14.6352897465584));
#51767=CARTESIAN_POINT('Ctrl Pts',(-0.931383681591147,1.83153542148814,
14.6314309601364));
#51768=CARTESIAN_POINT('Ctrl Pts',(-0.867872090121343,1.86383272744949,
14.6275746044666));
#51769=CARTESIAN_POINT('Ctrl Pts',(-0.802632692876482,1.89284593942531,
14.6237182487969));
#51770=CARTESIAN_POINT('Ctrl Pts',(-0.736039723038107,1.91839596762764,
14.6198618931271));
#51771=CARTESIAN_POINT('Ctrl Pts',(-0.669466425425528,1.94393844809745,
14.6160066766632));
#51772=CARTESIAN_POINT('Ctrl Pts',(-0.601540802349471,1.96601960193036,
14.6121514601993));
#51773=CARTESIAN_POINT('Ctrl Pts',(-0.532656789490892,1.98450858075979,
14.6082962437353));
#51774=CARTESIAN_POINT('Ctrl Pts',(-0.463770083468561,2.00299828245431,
14.6044408765437));
#51775=CARTESIAN_POINT('Ctrl Pts',(-0.39392538301915,2.01789540651023,14.6005855093521));
#51776=CARTESIAN_POINT('Ctrl Pts',(-0.323529816316513,2.02911951852379,
14.5967301421604));
#51777=CARTESIAN_POINT('Ctrl Pts',(-0.253060564641824,2.04035537912349,
14.5928707394501));
#51778=CARTESIAN_POINT('Ctrl Pts',(-0.182039776383841,2.0479104762673,14.5890113367398));
#51779=CARTESIAN_POINT('Ctrl Pts',(-0.110881865592379,2.05175602213878,
14.5851519340295));
#51780=CARTESIAN_POINT('Ctrl Pts',(-0.0396836646277538,2.05560374538881,
14.5812903460948));
#51781=CARTESIAN_POINT('Ctrl Pts',(0.0316513274151431,2.05573773525014,
14.5774287581601));
#51782=CARTESIAN_POINT('Ctrl Pts',(0.102709278480053,2.05218136786545,14.5735671702254));
#51783=CARTESIAN_POINT('Ctrl Pts',(0.173891547988154,2.048618778488,14.5696988263036));
#51784=CARTESIAN_POINT('Ctrl Pts',(0.244795325409388,2.04135299099028,14.5658304823818));
#51785=CARTESIAN_POINT('Ctrl Pts',(0.315013174792762,2.03045912596314,14.5619621384599));
#51786=CARTESIAN_POINT('Ctrl Pts',(0.356706515335843,2.02399066205552,14.5596652270352));
#51787=CARTESIAN_POINT('Ctrl Pts',(0.398158221144476,2.01624404678126,14.5573683156105));
#51788=CARTESIAN_POINT('Ctrl Pts',(0.439285463970684,2.00724334440149,14.5550714041857));
#51789=CARTESIAN_POINT('Ctrl Pts',(0.508568827310319,1.99208067142763,14.5512020042974));
#51790=CARTESIAN_POINT('Ctrl Pts',(0.577201932179294,1.97329693947935,14.547332604409));
#51791=CARTESIAN_POINT('Ctrl Pts',(0.644778103482944,1.95096354649925,14.5434632045207));
#51792=CARTESIAN_POINT('Ctrl Pts',(0.712237378025983,1.92866878697889,14.5396004981206));
#51793=CARTESIAN_POINT('Ctrl Pts',(0.778642894299039,1.90283671819843,14.5357377917206));
#51794=CARTESIAN_POINT('Ctrl Pts',(0.84359954762269,1.8735894336142,14.5318750853206));
#51795=CARTESIAN_POINT('Ctrl Pts',(0.90849154592418,1.84437126050257,14.5280162236902));
#51796=CARTESIAN_POINT('Ctrl Pts',(0.971937101666074,1.81174481386403,14.5241573620598));
#51797=CARTESIAN_POINT('Ctrl Pts',(1.0335587985445,1.77588112565319,14.5202985004294));
#51798=CARTESIAN_POINT('Ctrl Pts',(1.09513639691661,1.74004310267329,14.5164424003268));
#51799=CARTESIAN_POINT('Ctrl Pts',(1.15489230980045,1.70097268283746,14.5125863002243));
#51800=CARTESIAN_POINT('Ctrl Pts',(1.2124731690813,1.65888708981593,14.5087302001218));
#51801=CARTESIAN_POINT('Ctrl Pts',(1.22578816197413,1.64915522094542,14.5078385158694));
#51802=CARTESIAN_POINT('Ctrl Pts',(1.23898696426032,1.63926231337188,14.506946831617));
#51803=CARTESIAN_POINT('Ctrl Pts',(1.25206542099588,1.62921138715834,14.5060551473646));
#51804=CARTESIAN_POINT('Ctrl Pts',(1.25206542099588,1.62921138715835,15.2060150049977));
#51805=CARTESIAN_POINT('Ctrl Pts',(1.31002493594645,1.5846689139966,15.2020450878788));
#51806=CARTESIAN_POINT('Ctrl Pts',(1.3656874068559,1.53696607619391,15.1980751707598));
#51807=CARTESIAN_POINT('Ctrl Pts',(1.41869350001138,1.48637354508396,15.1941052536409));
#51808=CARTESIAN_POINT('Ctrl Pts',(1.47020089051233,1.43721147519384,15.190247582586));
#51809=CARTESIAN_POINT('Ctrl Pts',(1.51919974906799,1.38532131376408,15.1863899115311));
#51810=CARTESIAN_POINT('Ctrl Pts',(1.56539333322814,1.33099259005634,15.1825322404761));
#51811=CARTESIAN_POINT('Ctrl Pts',(1.61156391415845,1.276690920671,15.1786764904433));
#51812=CARTESIAN_POINT('Ctrl Pts',(1.6549316785281,1.21995346821481,15.1748207404104));
#51813=CARTESIAN_POINT('Ctrl Pts',(1.69523825658542,1.16110499779703,15.1709649903775));
#51814=CARTESIAN_POINT('Ctrl Pts',(1.73553824609788,1.10226614679635,15.1671098706086));
#51815=CARTESIAN_POINT('Ctrl Pts',(1.77277776903087,1.04131736415472,15.1632547508396));
#51816=CARTESIAN_POINT('Ctrl Pts',(1.80674114035724,0.978613311906503,15.1593996310707));
#51817=CARTESIAN_POINT('Ctrl Pts',(1.84246738032578,0.912654606096864,15.1553444113267));
#51818=CARTESIAN_POINT('Ctrl Pts',(1.8745678293376,0.844753972659132,15.1512891915828));
#51819=CARTESIAN_POINT('Ctrl Pts',(1.90284681176006,0.775352547861011,15.1472339718389));
#51820=CARTESIAN_POINT('Ctrl Pts',(1.92976604909418,0.709288168402204,15.1433737401976));
#51821=CARTESIAN_POINT('Ctrl Pts',(1.95322274739721,0.641864500279134,15.1395135085564));
#51822=CARTESIAN_POINT('Ctrl Pts',(1.97309880704926,0.573479433040795,15.1356532769152));
#51823=CARTESIAN_POINT('Ctrl Pts',(1.99298878077377,0.50504649339728,15.1317903429505));
#51824=CARTESIAN_POINT('Ctrl Pts',(2.00929301886529,0.435651288130338,15.1279274089858));
#51825=CARTESIAN_POINT('Ctrl Pts',(2.02194445546334,0.365702312709494,15.1240644750211));
#51826=CARTESIAN_POINT('Ctrl Pts',(2.03461637026184,0.295640114641596,15.1201952883328));
#51827=CARTESIAN_POINT('Ctrl Pts',(2.0436236323153,0.225022839254271,15.1163261016445));
#51828=CARTESIAN_POINT('Ctrl Pts',(2.04895103336775,0.154263493287422,15.1124569149562));
#51829=CARTESIAN_POINT('Ctrl Pts',(2.0497404075253,0.143778906420101,15.1118836080186));
#51830=CARTESIAN_POINT('Ctrl Pts',(2.05044908328428,0.13329119718587,15.1113103010811));
#51831=CARTESIAN_POINT('Ctrl Pts',(2.0510771082687,0.122801703718274,15.1107369941435));
#51832=CARTESIAN_POINT('Ctrl Pts',(2.05531546848585,0.0520111254545155,
15.1068679103067));
#51833=CARTESIAN_POINT('Ctrl Pts',(2.05589294399514,-0.0191377846633052,
15.1029988264699));
#51834=CARTESIAN_POINT('Ctrl Pts',(2.05276772273151,-0.0902343560496397,
15.0991297426331));
#51835=CARTESIAN_POINT('Ctrl Pts',(2.04964715788051,-0.161224997344817,
15.0952664235244));
#51836=CARTESIAN_POINT('Ctrl Pts',(2.04283486815184,-0.232162973339852,
15.0914031044157));
#51837=CARTESIAN_POINT('Ctrl Pts',(2.0323409698537,-0.302634672095116,15.087539785307));
#51838=CARTESIAN_POINT('Ctrl Pts',(2.02185938085436,-0.373023707842593,
15.0836809978554));
#51839=CARTESIAN_POINT('Ctrl Pts',(2.0077048325131,-0.442947074607792,15.0798222104038));
#51840=CARTESIAN_POINT('Ctrl Pts',(1.989939340115,-0.511995102674516,15.0759634229523));
#51841=CARTESIAN_POINT('Ctrl Pts',(1.97218503863566,-0.58099963569729,15.0721070662455));
#51842=CARTESIAN_POINT('Ctrl Pts',(1.95082442667367,-0.649129454636971,
15.0682507095386));
#51843=CARTESIAN_POINT('Ctrl Pts',(1.92597053566178,-0.715985375732399,
15.0643943528318));
#51844=CARTESIAN_POINT('Ctrl Pts',(1.90112398669591,-0.782821547032968,
15.0605391353248));
#51845=CARTESIAN_POINT('Ctrl Pts',(1.87278637655547,-0.848384112500162,
15.0566839178178));
#51846=CARTESIAN_POINT('Ctrl Pts',(1.8411199575779,-0.912290997603469,15.0528287003108));
#51847=CARTESIAN_POINT('Ctrl Pts',(1.80945230049949,-0.9762003813527,15.0489733320716));
#51848=CARTESIAN_POINT('Ctrl Pts',(1.77445579384431,-1.03845352191843,15.0451179638324));
#51849=CARTESIAN_POINT('Ctrl Pts',(1.73633923719926,-1.09869177473134,15.0412625955933));
#51850=CARTESIAN_POINT('Ctrl Pts',(1.69818278292289,-1.15899308055358,15.0374031918358));
#51851=CARTESIAN_POINT('Ctrl Pts',(1.65690001959088,-1.21727487716614,15.0335437880784));
#51852=CARTESIAN_POINT('Ctrl Pts',(1.61274331405848,-1.27320719659436,15.0296843843209));
#51853=CARTESIAN_POINT('Ctrl Pts',(1.56856160664066,-1.32917118535626,15.0258227953377));
#51854=CARTESIAN_POINT('Ctrl Pts',(1.52150303828498,-1.38278268347052,15.0219612063545));
#51855=CARTESIAN_POINT('Ctrl Pts',(1.47185872990816,-1.43374664487598,15.0180996173713));
#51856=CARTESIAN_POINT('Ctrl Pts',(1.42212756716924,-1.48479976942024,15.0142312724103));
#51857=CARTESIAN_POINT('Ctrl Pts',(1.36980198918227,-1.5331957794779,15.0103629274492));
#51858=CARTESIAN_POINT('Ctrl Pts',(1.31520771249558,-1.57867863591427,15.0064945824881));
#51859=CARTESIAN_POINT('Ctrl Pts',(1.28279134045791,-1.60568493190458,15.0041976803761));
#51860=CARTESIAN_POINT('Ctrl Pts',(1.24957571633715,-1.63166495949266,15.001900778264));
#51861=CARTESIAN_POINT('Ctrl Pts',(1.21563365191156,-1.65657248161382,14.999603876152));
#51862=CARTESIAN_POINT('Ctrl Pts',(1.15845896507748,-1.69852867376624,14.9957347933143));
#51863=CARTESIAN_POINT('Ctrl Pts',(1.09899764070911,-1.73760358972471,14.9918657104766));
#51864=CARTESIAN_POINT('Ctrl Pts',(1.03757201844991,-1.77353936213149,14.9879966276389));
#51865=CARTESIAN_POINT('Ctrl Pts',(0.976237917260044,-1.80942159205556,
14.9841333095388));
#51866=CARTESIAN_POINT('Ctrl Pts',(0.912945743490394,-1.84217371916727,
14.9802699914388));
#51867=CARTESIAN_POINT('Ctrl Pts',(0.848048472860544,-1.87157990750566,
14.9764066733388));
#51868=CARTESIAN_POINT('Ctrl Pts',(0.783227326633131,-1.90095160242864,
14.9725478869052));
#51869=CARTESIAN_POINT('Ctrl Pts',(0.71680526370732,-1.92698495500048,14.9686891004716));
#51870=CARTESIAN_POINT('Ctrl Pts',(0.649160096811672,-1.94950986948193,
14.9648303140379));
#51871=CARTESIAN_POINT('Ctrl Pts',(0.581557541365009,-1.97202059493424,
14.9609739583542));
#51872=CARTESIAN_POINT('Ctrl Pts',(0.512733870351755,-1.99102711390201,
14.9571176026705));
#51873=CARTESIAN_POINT('Ctrl Pts',(0.443085757073116,-2.00640787836844,
14.9532612469867));
#51874=CARTESIAN_POINT('Ctrl Pts',(0.373458218497088,-2.02178409921352,
14.9494060305065));
#51875=CARTESIAN_POINT('Ctrl Pts',(0.303007195261644,-2.03353658725471,
14.9455508140262));
#51876=CARTESIAN_POINT('Ctrl Pts',(0.232141683100166,-2.04159442629221,
14.9416955975459));
#51877=CARTESIAN_POINT('Ctrl Pts',(0.161273400260681,-2.04965258037263,
14.9378402303356));
#51878=CARTESIAN_POINT('Ctrl Pts',(0.0899910792428621,-2.05401574596433,
14.9339848631252));
#51879=CARTESIAN_POINT('Ctrl Pts',(0.0187092778158862,-2.05466482070035,
14.9301294959149));
#51880=CARTESIAN_POINT('Ctrl Pts',(-0.0526471362938743,-2.05531457484131,
14.9262700931823));
#51881=CARTESIAN_POINT('Ctrl Pts',(-0.124002542968951,-2.05224247308525,
14.9224106904498));
#51882=CARTESIAN_POINT('Ctrl Pts',(-0.194942846560374,-2.0454815689893,
14.9185512877173));
#51883=CARTESIAN_POINT('Ctrl Pts',(-0.265923317150839,-2.03871683681235,
14.9146896997583));
#51884=CARTESIAN_POINT('Ctrl Pts',(-0.336487736013471,-2.02825921572408,
14.9108281117994));
#51885=CARTESIAN_POINT('Ctrl Pts',(-0.406230327112479,-2.01419325880961,
14.9069665238404));
#51886=CARTESIAN_POINT('Ctrl Pts',(-0.476094935437547,-2.00010269298662,
14.9030981798914));
#51887=CARTESIAN_POINT('Ctrl Pts',(-0.545134374660318,-1.98239130817406,
14.8992298359424));
#51888=CARTESIAN_POINT('Ctrl Pts',(-0.612956875764157,-1.96119387898123,
14.8953614919934));
#51889=CARTESIAN_POINT('Ctrl Pts',(-0.653227924491973,-1.94860745574358,
14.8930645807158));
#51890=CARTESIAN_POINT('Ctrl Pts',(-0.693070266519139,-1.93479291673721,
14.8907676694381));
#51891=CARTESIAN_POINT('Ctrl Pts',(-0.73240556392774,-1.91978635593331,
14.8884707581604));
#51892=CARTESIAN_POINT('Ctrl Pts',(-0.798664768406605,-1.89450822544146,
14.8846016755795));
#51893=CARTESIAN_POINT('Ctrl Pts',(-0.863743545098733,-1.86574626808071,
14.8807325929986));
#51894=CARTESIAN_POINT('Ctrl Pts',(-0.927250420455131,-1.83363142977693,
14.8768635104177));
#51895=CARTESIAN_POINT('Ctrl Pts',(-0.990662673646188,-1.80156444102523,
14.8730001925823));
#51896=CARTESIAN_POINT('Ctrl Pts',(-1.05250724444457,-1.76615470495226,
14.8691368747469));
#51897=CARTESIAN_POINT('Ctrl Pts',(-1.11241135485258,-1.72758170287111,
14.8652735569115));
#51898=CARTESIAN_POINT('Ctrl Pts',(-1.17224519766254,-1.68905394697068,
14.8614147707528));
#51899=CARTESIAN_POINT('Ctrl Pts',(-1.23014269485957,-1.64737055712081,
14.8575559845942));
#51900=CARTESIAN_POINT('Ctrl Pts',(-1.28575602520601,-1.60275668962773,
14.8536971984355));
#51901=CARTESIAN_POINT('Ctrl Pts',(-1.34133432317754,-1.55817092564368,
14.8498408430329));
#51902=CARTESIAN_POINT('Ctrl Pts',(-1.39463093094656,-1.5106586496889,14.8459844876304));
#51903=CARTESIAN_POINT('Ctrl Pts',(-1.44532858421168,-1.46048719479517,
14.8421281322279));
#51904=CARTESIAN_POINT('Ctrl Pts',(-1.4960112608391,-1.41033056109442,14.8382729160346));
#51905=CARTESIAN_POINT('Ctrl Pts',(-1.54409616207844,-1.35751664950813,
14.8344176998414));
#51906=CARTESIAN_POINT('Ctrl Pts',(-1.58930187764166,-1.30235060725778,
14.8305624836481));
#51907=CARTESIAN_POINT('Ctrl Pts',(-1.63450936058051,-1.24718240821999,
14.8267071167302));
#51908=CARTESIAN_POINT('Ctrl Pts',(-1.67683712816198,-1.18966227308283,
14.8228517498124));
#51909=CARTESIAN_POINT('Ctrl Pts',(-1.71604428386948,-1.13012812472696,
14.8189963828945));
#51910=CARTESIAN_POINT('Ctrl Pts',(-1.75529247875725,-1.07053166038305,
14.8151369804607));
#51911=CARTESIAN_POINT('Ctrl Pts',(-1.79141327351683,-1.008917381075,14.811277578027));
#51912=CARTESIAN_POINT('Ctrl Pts',(-1.82420984019043,-0.945651109792833,
14.8074181755933));
#51913=CARTESIAN_POINT('Ctrl Pts',(-1.8570249765243,-0.882349016676732,
14.8035565879372));
#51914=CARTESIAN_POINT('Ctrl Pts',(-1.88651193698957,-0.817393512101275,
14.799695000281));
#51915=CARTESIAN_POINT('Ctrl Pts',(-1.91252167247767,-0.751171361809826,
14.7958334126249));
#51916=CARTESIAN_POINT('Ctrl Pts',(-1.93857691293627,-0.684833353477571,
14.7919650689819));
#51917=CARTESIAN_POINT('Ctrl Pts',(-1.96114262862931,-0.617224735977862,
14.7880967253389));
#51918=CARTESIAN_POINT('Ctrl Pts',(-1.98011956034221,-0.548747746464777,
14.7842283816958));
#51919=CARTESIAN_POINT('Ctrl Pts',(-1.9913875295711,-0.508088032745304,
14.7819314678535));
#51920=CARTESIAN_POINT('Ctrl Pts',(-2.00139119319373,-0.467122383110239,
14.7796345540112));
#51921=CARTESIAN_POINT('Ctrl Pts',(-2.01011838596074,-0.425936188791907,
14.7773376401688));
#51922=CARTESIAN_POINT('Ctrl Pts',(-2.03070219490438,-0.328795128934876,
14.7719201781105));
#51923=CARTESIAN_POINT('Ctrl Pts',(-2.04425025502673,-0.230114996413423,
14.7665027160522));
#51924=CARTESIAN_POINT('Ctrl Pts',(-2.05058606170274,-0.13074542458709,
14.7610852539939));
#51925=CARTESIAN_POINT('Ctrl Pts',(-2.05331903832598,-0.0878819455148026,
14.7587484091501));
#51926=CARTESIAN_POINT('Ctrl Pts',(-2.05471060692694,-0.0448904742936152,
14.7564115643062));
#51927=CARTESIAN_POINT('Ctrl Pts',(-2.05474917537842,-0.00184086438999942,
14.7540747194623));
#51928=CARTESIAN_POINT('Origin',(0.,0.,18.5459252805377));
#51929=CARTESIAN_POINT('',(1.25299305265164,1.63043997671401,15.9061636440672));
#51930=CARTESIAN_POINT('',(1.2504235345857,1.62710269720821,15.8478625066523));
#51931=CARTESIAN_POINT('',(1.25206542099588,1.62921138715835,18.5459252805377));
#51932=CARTESIAN_POINT('',(-2.05150243251667,-0.000517798691100392,15.3959252805377));
#51933=CARTESIAN_POINT('Ctrl Pts',(1.25042353458576,1.62710269720817,15.8478625066523));
#51934=CARTESIAN_POINT('Ctrl Pts',(1.58212812467986,1.36911001369144,15.8251464655206));
#51935=CARTESIAN_POINT('Ctrl Pts',(2.25955063105262,0.431477643030573,15.765386051725));
#51936=CARTESIAN_POINT('Ctrl Pts',(1.86646051514274,-1.55380379648575,15.6685812652657));
#51937=CARTESIAN_POINT('Ctrl Pts',(-0.2930698752374,-2.41082710471087,15.5574481472741));
#51938=CARTESIAN_POINT('Ctrl Pts',(-1.83978745574197,-1.30723126236958,
15.4665628190314));
#51939=CARTESIAN_POINT('Ctrl Pts',(-2.05220371074748,-0.311451552032415,
15.4127218634526));
#51940=CARTESIAN_POINT('Ctrl Pts',(-2.05150243251667,-0.000517798691100392,
15.3959252805377));
#51941=CARTESIAN_POINT('Ctrl Pts',(-2.05150243251667,-0.000517798691100392,
15.3959252805377));
#51942=CARTESIAN_POINT('Ctrl Pts',(-2.05065706210741,0.374303752535962,
15.3756774907888));
#51943=CARTESIAN_POINT('Ctrl Pts',(-1.77290639219337,1.43604706618453,15.318385328376));
#51944=CARTESIAN_POINT('Ctrl Pts',(-0.27952259961467,2.30464022739995,15.235748963112));
#51945=CARTESIAN_POINT('Ctrl Pts',(0.877403861982676,1.91006820299453,15.173360387597));
#51946=CARTESIAN_POINT('Ctrl Pts',(1.25109478256748,1.62792261342726,15.1480161847458));
#51947=CARTESIAN_POINT('',(-2.05474972764537,0.00105794200385854,15.4540747194623));
#51948=CARTESIAN_POINT('Ctrl Pts',(-2.05474972764537,0.00105794200385854,
15.4540747194623));
#51949=CARTESIAN_POINT('Ctrl Pts',(-2.05471842613035,0.0618521814117124,
15.4507619290143));
#51950=CARTESIAN_POINT('Ctrl Pts',(-2.05198927252303,0.122574948398337,
15.4474491385663));
#51951=CARTESIAN_POINT('Ctrl Pts',(-2.04657974197177,0.183054424286241,
15.4441363481182));
#51952=CARTESIAN_POINT('Ctrl Pts',(-2.04026181886476,0.253689884164068,
15.4402672590869));
#51953=CARTESIAN_POINT('Ctrl Pts',(-2.03027037040625,0.32413621977251,15.4363981700556));
#51954=CARTESIAN_POINT('Ctrl Pts',(-2.01662501546903,0.393981102953597,
15.4325290810243));
#51955=CARTESIAN_POINT('Ctrl Pts',(-2.0029999911493,0.463721922179577,15.4286657566631));
#51956=CARTESIAN_POINT('Ctrl Pts',(-1.98573195905279,0.532862594871243,
15.4248024323018));
#51957=CARTESIAN_POINT('Ctrl Pts',(-1.96489232765821,0.600995593336517,
15.4209391079406));
#51958=CARTESIAN_POINT('Ctrl Pts',(-1.94407714070403,0.669048673256756,
15.4170803151759));
#51959=CARTESIAN_POINT('Ctrl Pts',(-1.91969881743501,0.736095964480883,
15.4132215224112));
#51960=CARTESIAN_POINT('Ctrl Pts',(-1.89187950494207,0.80174154269325,15.4093627296466));
#51961=CARTESIAN_POINT('Ctrl Pts',(-1.86407771624265,0.867345769791767,
15.4055063675921));
#51962=CARTESIAN_POINT('Ctrl Pts',(-1.8328394277634,0.931549589438368,15.4016500055377));
#51963=CARTESIAN_POINT('Ctrl Pts',(-1.79833568069386,0.993975020834709,
15.3977936434833));
#51964=CARTESIAN_POINT('Ctrl Pts',(-1.76384212606679,1.05638201169423,15.3939384206022));
#51965=CARTESIAN_POINT('Ctrl Pts',(-1.72608526275411,1.11701123231624,15.390083197721));
#51966=CARTESIAN_POINT('Ctrl Pts',(-1.68528226742459,1.17550892876415,15.3862279748399));
#51967=CARTESIAN_POINT('Ctrl Pts',(-1.64447767657622,1.23400891264651,15.3823726012081));
#51968=CARTESIAN_POINT('Ctrl Pts',(-1.60062699694711,1.29037680970439,15.3785172275763));
#51969=CARTESIAN_POINT('Ctrl Pts',(-1.55398995830775,1.34428894661032,15.3746618539445));
#51970=CARTESIAN_POINT('Ctrl Pts',(-1.50730410359366,1.39825751460579,15.3708024448033));
#51971=CARTESIAN_POINT('Ctrl Pts',(-1.45782638625428,1.44976482300761,15.366943035662));
#51972=CARTESIAN_POINT('Ctrl Pts',(-1.40585536331072,1.4985220251803,15.3630836265208));
#51973=CARTESIAN_POINT('Ctrl Pts',(-1.35385491395087,1.5473068340778,15.3592220321507));
#51974=CARTESIAN_POINT('Ctrl Pts',(-1.29935871995349,1.59333812336112,15.3553604377807));
#51975=CARTESIAN_POINT('Ctrl Pts',(-1.24269847857761,1.63636733462902,15.3514988434106));
#51976=CARTESIAN_POINT('Ctrl Pts',(-1.18593910915725,1.67947182622516,15.3476304931162));
#51977=CARTESIAN_POINT('Ctrl Pts',(-1.12700853520048,1.71956348033388,15.3437621428219));
#51978=CARTESIAN_POINT('Ctrl Pts',(-1.06626687541195,1.75643744918492,15.3398937925276));
#51979=CARTESIAN_POINT('Ctrl Pts',(-1.03020118286736,1.7783315697623,15.3375969383939));
#51980=CARTESIAN_POINT('Ctrl Pts',(-0.99349747827102,1.7990921871023,15.3353000842603));
#51981=CARTESIAN_POINT('Ctrl Pts',(-0.956234625635777,1.81868438802207,
15.3330032301266));
#51982=CARTESIAN_POINT('Ctrl Pts',(-0.893464821043241,1.85168772878371,
15.3291341467111));
#51983=CARTESIAN_POINT('Ctrl Pts',(-0.828861460673923,1.88150225355187,
15.3252650632955));
#51984=CARTESIAN_POINT('Ctrl Pts',(-0.76278159456887,1.90792080587402,15.32139597988));
#51985=CARTESIAN_POINT('Ctrl Pts',(-0.696800183655339,1.93429999607603,
15.3175326611757));
#51986=CARTESIAN_POINT('Ctrl Pts',(-0.62934708115861,1.95729307853427,15.3136693424714));
#51987=CARTESIAN_POINT('Ctrl Pts',(-0.560803393863145,1.97673901057564,
15.3098060237672));
#51988=CARTESIAN_POINT('Ctrl Pts',(-0.492340107551227,1.99616213275482,
15.3059472366928));
#51989=CARTESIAN_POINT('Ctrl Pts',(-0.422789242523565,2.0120462372698,15.3020884496184));
#51990=CARTESIAN_POINT('Ctrl Pts',(-0.35254967690598,2.02427920204044,15.2982296625441));
#51991=CARTESIAN_POINT('Ctrl Pts',(-0.282354356604742,2.03650446102031,
15.2943733061974));
#51992=CARTESIAN_POINT('Ctrl Pts',(-0.211471673866081,2.04508306012134,
15.2905169498507));
#51993=CARTESIAN_POINT('Ctrl Pts',(-0.140311951151932,2.04995368700465,
15.286660593504));
#51994=CARTESIAN_POINT('Ctrl Pts',(-0.069173249287603,2.05482287508644,
15.2828053763394));
#51995=CARTESIAN_POINT('Ctrl Pts',(0.00224184569476071,2.05598623236786,
15.2789501591749));
#51996=CARTESIAN_POINT('Ctrl Pts',(0.0735183420835199,2.05343434661965,
15.2750949420104));
#51997=CARTESIAN_POINT('Ctrl Pts',(0.144797625594737,2.05088236108514,15.2712395740954));
#51998=CARTESIAN_POINT('Ctrl Pts',(0.215937814359383,2.04461486367519,15.2673842061804));
#51999=CARTESIAN_POINT('Ctrl Pts',(0.286526108375765,2.03467450756111,15.2635288382655));
#52000=CARTESIAN_POINT('Ctrl Pts',(0.357188289632059,2.02472374652809,15.2596694348019));
#52001=CARTESIAN_POINT('Ctrl Pts',(0.427296940924071,2.01109252016697,15.2558100313383));
#52002=CARTESIAN_POINT('Ctrl Pts',(0.496447462142931,1.99387499102422,15.2519506278747));
#52003=CARTESIAN_POINT('Ctrl Pts',(0.565637137250949,1.97664771310133,15.2480890391686));
#52004=CARTESIAN_POINT('Ctrl Pts',(0.633867137467881,1.95583023191119,15.2442274504625));
#52005=CARTESIAN_POINT('Ctrl Pts',(0.700748735555524,1.9315664037556,15.2403658617565));
#52006=CARTESIAN_POINT('Ctrl Pts',(0.767747345736748,1.90726012503943,15.2364975170429));
#52007=CARTESIAN_POINT('Ctrl Pts',(0.833392396257111,1.8794956505322,15.2326291723293));
#52008=CARTESIAN_POINT('Ctrl Pts',(0.897316467401261,1.84846442211651,15.2287608276157));
#52009=CARTESIAN_POINT('Ctrl Pts',(0.935272632051664,1.8300390247041,15.2264639224555));
#52010=CARTESIAN_POINT('Ctrl Pts',(0.972622522132005,1.81046277088973,15.2241670172953));
#52011=CARTESIAN_POINT('Ctrl Pts',(1.00929402677359,1.78978298405677,15.2218701121351));
#52012=CARTESIAN_POINT('Ctrl Pts',(1.07106081302598,1.75495147153661,15.2180013739565));
#52013=CARTESIAN_POINT('Ctrl Pts',(1.13114335760791,1.71685056090996,15.2141326357779));
#52014=CARTESIAN_POINT('Ctrl Pts',(1.18917406150476,1.67566781133501,15.2102638975993));
#52015=CARTESIAN_POINT('Ctrl Pts',(1.21041838950633,1.66059131249516,15.2088476000654));
#52016=CARTESIAN_POINT('Ctrl Pts',(1.23138793186196,1.64510224658988,15.2074313025316));
#52017=CARTESIAN_POINT('Ctrl Pts',(1.25206542099588,1.62921138715835,15.2060150049977));
#52018=CARTESIAN_POINT('Ctrl Pts',(1.25299305265161,1.63043997671403,15.9061636440672));
#52019=CARTESIAN_POINT('Ctrl Pts',(1.33870026031667,1.5658514984805,15.9003320360729));
#52020=CARTESIAN_POINT('Ctrl Pts',(1.92956475440913,1.0413794257925,15.8574560554148));
#52021=CARTESIAN_POINT('Ctrl Pts',(2.35999751615834,-0.573068146683373,
15.7775357020929));
#52022=CARTESIAN_POINT('Ctrl Pts',(0.798563541884426,-2.29352622680378,
15.6664025841013));
#52023=CARTESIAN_POINT('Ctrl Pts',(-1.42540407770296,-1.92615524732257,
15.5585825778216));
#52024=CARTESIAN_POINT('Ctrl Pts',(-2.05354142278375,-0.618786125786745,
15.4878069442056));
#52025=CARTESIAN_POINT('Ctrl Pts',(-2.05744064634435,0.00104161743516934,
15.4540756832536));
#52026=CARTESIAN_POINT('Origin',(0.,0.,18.5459252805377));
#52027=CARTESIAN_POINT('',(1.25005477124305,1.62658000731212,16.6061086772888));
#52028=CARTESIAN_POINT('',(1.25371187806425,1.63132526051507,16.5478693678287));
#52029=CARTESIAN_POINT('',(1.25206542099588,1.62921138715835,18.5459252805377));
#52030=CARTESIAN_POINT('',(-2.05269453305337,-0.0025315228670039,16.8540747194623));
#52031=CARTESIAN_POINT('Ctrl Pts',(-2.05269453305337,-0.0025315228670039,
16.8540747194623));
#52032=CARTESIAN_POINT('Ctrl Pts',(-2.04912705821622,0.467702877218055,
16.8286277343139));
#52033=CARTESIAN_POINT('Ctrl Pts',(-1.65656296491944,1.62962812348302,16.7661363765015));
#52034=CARTESIAN_POINT('Ctrl Pts',(-0.0552297434345721,2.27982805376088,
16.6834810291103));
#52035=CARTESIAN_POINT('Ctrl Pts',(0.953586651517499,1.85321350766304,16.6262726668676));
#52036=CARTESIAN_POINT('Ctrl Pts',(1.25005477124305,1.62658000731212,16.6061086772888));
#52037=CARTESIAN_POINT('',(-0.530170217188714,-1.9851743256717,17.));
#52038=CARTESIAN_POINT('Ctrl Pts',(-0.5301702171887,-1.9851743256717,17.));
#52039=CARTESIAN_POINT('Ctrl Pts',(-1.19025956241818,-1.80888768575364,
16.9629556273361));
#52040=CARTESIAN_POINT('Ctrl Pts',(-1.9249882932336,-1.11315381096668,16.9143138671569));
#52041=CARTESIAN_POINT('Ctrl Pts',(-2.05432039906053,-0.216839446930442,
16.8656721069777));
#52042=CARTESIAN_POINT('Ctrl Pts',(-2.05269453305337,-0.0025315228670039,
16.8540747194623));
#52043=CARTESIAN_POINT('',(0.530281684557416,-1.98514455330662,16.9999999985106));
#52044=CARTESIAN_POINT('Origin',(0.,0.,17.));
#52045=CARTESIAN_POINT('',(-2.05474946839643,0.00147804755778122,16.7959252805377));
#52046=CARTESIAN_POINT('Ctrl Pts',(0.530281684557416,-1.98514455330662,
16.9999999985106));
#52047=CARTESIAN_POINT('Ctrl Pts',(0.461903534585254,-2.00341006474949,
16.9961388750594));
#52048=CARTESIAN_POINT('Ctrl Pts',(0.392444315027901,-2.01817488207207,
16.9922777516081));
#52049=CARTESIAN_POINT('Ctrl Pts',(0.322296520861052,-2.02931577511753,
16.9884166281568));
#52050=CARTESIAN_POINT('Ctrl Pts',(0.248587777035769,-2.0410222192221,16.9843595004492));
#52051=CARTESIAN_POINT('Ctrl Pts',(0.174119182236965,-2.04872680208598,
16.9803023727415));
#52052=CARTESIAN_POINT('Ctrl Pts',(0.0993639973638922,-2.05234606207819,
16.9762452450338));
#52053=CARTESIAN_POINT('Ctrl Pts',(0.0284118419057885,-2.05578119902618,
16.9723945160668));
#52054=CARTESIAN_POINT('Ctrl Pts',(-0.042797896797022,-2.05553648246812,
16.9685437870997));
#52055=CARTESIAN_POINT('Ctrl Pts',(-0.113852662049382,-2.05159331589969,
16.9646930581327));
#52056=CARTESIAN_POINT('Ctrl Pts',(-0.184864600835995,-2.04765252597534,
16.9608446500953));
#52057=CARTESIAN_POINT('Ctrl Pts',(-0.255721265268953,-2.04001773536084,
16.9569962420579));
#52058=CARTESIAN_POINT('Ctrl Pts',(-0.326010522590318,-2.02872243090581,
16.9531478340205));
#52059=CARTESIAN_POINT('Ctrl Pts',(-0.396281187004936,-2.0174301142835,
16.9493004439636));
#52060=CARTESIAN_POINT('Ctrl Pts',(-0.465984260690645,-2.00247928372715,
16.9454530539067));
#52061=CARTESIAN_POINT('Ctrl Pts',(-0.53471491016292,-1.98395502150363,
16.9416056638498));
#52062=CARTESIAN_POINT('Ctrl Pts',(-0.603450623543465,-1.9654293944572,
16.9377579903265));
#52063=CARTESIAN_POINT('Ctrl Pts',(-0.671213300002006,-1.94332994266954,
16.9339103168031));
#52064=CARTESIAN_POINT('Ctrl Pts',(-0.737612151282778,-1.91779192739463,
16.9300626432798));
#52065=CARTESIAN_POINT('Ctrl Pts',(-0.804080286638563,-1.89222726440319,
16.9262109548903));
#52066=CARTESIAN_POINT('Ctrl Pts',(-0.869181301035828,-1.86321705420353,
16.9223592665009));
#52067=CARTESIAN_POINT('Ctrl Pts',(-0.932544247534814,-1.83094478040429,
16.9185075781114));
#52068=CARTESIAN_POINT('Ctrl Pts',(-0.995945525859085,-1.79865298328379,
16.9146535596181));
#52069=CARTESIAN_POINT('Ctrl Pts',(-1.05760622149396,-1.76309543961573,
16.9107995411247));
#52070=CARTESIAN_POINT('Ctrl Pts',(-1.11718225388515,-1.72450032592171,
16.9069455226314));
#52071=CARTESIAN_POINT('Ctrl Pts',(-1.17685661880791,-1.68584150950894,
16.9030851429324));
#52072=CARTESIAN_POINT('Ctrl Pts',(-1.23443906058148,-1.64413540551827,
16.8992247632333));
#52073=CARTESIAN_POINT('Ctrl Pts',(-1.28961731996744,-1.59965144032692,
16.8953643835343));
#52074=CARTESIAN_POINT('Ctrl Pts',(-1.31019431055133,-1.58306254928428,
16.8939247767472));
#52075=CARTESIAN_POINT('Ctrl Pts',(-1.33043731809827,-1.56608772108779,
16.89248516996));
#52076=CARTESIAN_POINT('Ctrl Pts',(-1.35033149230716,-1.54874220688387,
16.8910455631728));
#52077=CARTESIAN_POINT('Ctrl Pts',(-1.40510164118834,-1.50098870953365,
16.887082218063));
#52078=CARTESIAN_POINT('Ctrl Pts',(-1.45745853908989,-1.45021867236757,
16.8831188729532));
#52079=CARTESIAN_POINT('Ctrl Pts',(-1.50704767249473,-1.39671216624193,
16.8791555278434));
#52080=CARTESIAN_POINT('Ctrl Pts',(-1.55473296292161,-1.34525990020817,
16.8753443448352));
#52081=CARTESIAN_POINT('Ctrl Pts',(-1.59985872901899,-1.29127783962401,
16.8715331618271));
#52082=CARTESIAN_POINT('Ctrl Pts',(-1.64214309495677,-1.23505611944794,
16.8677219788189));
#52083=CARTESIAN_POINT('Ctrl Pts',(-1.68438888372789,-1.17888569186242,
16.8639142728557));
#52084=CARTESIAN_POINT('Ctrl Pts',(-1.72379811160458,-1.12048005229482,
16.8601065668925));
#52085=CARTESIAN_POINT('Ctrl Pts',(-1.76012795126868,-1.06016374096774,
16.8562988609293));
#52086=CARTESIAN_POINT('Ctrl Pts',(-1.79643756910928,-0.999881002753381,
16.8524932744018));
#52087=CARTESIAN_POINT('Ctrl Pts',(-1.82967094081488,-0.937690129505748,
16.8486876878742));
#52088=CARTESIAN_POINT('Ctrl Pts',(-1.85962861413517,-0.873944494799123,
16.8448821013467));
#52089=CARTESIAN_POINT('Ctrl Pts',(-1.8895802663825,-0.810211672072712,
16.8410772796888));
#52090=CARTESIAN_POINT('Ctrl Pts',(-1.91625731622662,-0.744925161216608,
16.8372724580309));
#52091=CARTESIAN_POINT('Ctrl Pts',(-1.93950719738421,-0.67846104810436,
16.833467636373));
#52092=CARTESIAN_POINT('Ctrl Pts',(-1.96277242162608,-0.611953073929635,
16.8296603038334));
#52093=CARTESIAN_POINT('Ctrl Pts',(-1.98260579677084,-0.544266418605556,
16.8258529712939));
#52094=CARTESIAN_POINT('Ctrl Pts',(-1.99890412464787,-0.475793929097164,
16.8220456387543));
#52095=CARTESIAN_POINT('Ctrl Pts',(-2.01520895611267,-0.407294116734022,
16.8182367869595));
#52096=CARTESIAN_POINT('Ctrl Pts',(-2.02797584107969,-0.338008337619496,
16.8144279351646));
#52097=CARTESIAN_POINT('Ctrl Pts',(-2.03715290029361,-0.268338635543442,
16.8106190833698));
#52098=CARTESIAN_POINT('Ctrl Pts',(-2.04634216010382,-0.198576309905946,
16.8068051678326));
#52099=CARTESIAN_POINT('Ctrl Pts',(-2.05193203507066,-0.128429540871885,
16.8029912522954));
#52100=CARTESIAN_POINT('Ctrl Pts',(-2.05392266042328,-0.0583032374721763,
16.7991773367582));
#52101=CARTESIAN_POINT('Ctrl Pts',(-2.05448845040103,-0.038371430822669,
16.7980933180181));
#52102=CARTESIAN_POINT('Ctrl Pts',(-2.05476379699637,-0.0184412594723448,
16.7970092992779));
#52103=CARTESIAN_POINT('Ctrl Pts',(-2.05474946839643,0.00147804755778125,
16.7959252805377));
#52104=CARTESIAN_POINT('Ctrl Pts',(-2.05654452918444,0.00147933880289632,
16.7959252805377));
#52105=CARTESIAN_POINT('Ctrl Pts',(-2.05736468201256,0.099646559291543,
16.7905876687522));
#52106=CARTESIAN_POINT('Ctrl Pts',(-2.00636216552464,0.87829705013526,16.7482056843029));
#52107=CARTESIAN_POINT('Ctrl Pts',(-1.01136481471932,2.20819937049432,16.6687793271897));
#52108=CARTESIAN_POINT('Ctrl Pts',(0.601793643796052,2.09609164757904,16.5914316347388));
#52109=CARTESIAN_POINT('Ctrl Pts',(1.20647580811204,1.66813506378572,16.5511283149519));
#52110=CARTESIAN_POINT('Ctrl Pts',(1.25371187806425,1.63132526051507,16.5478693678287));
#52111=CARTESIAN_POINT('Origin',(0.,0.,11.));
#52112=CARTESIAN_POINT('',(-1.56343130033213,0.575533291080357,6.73212871955268));
#52113=CARTESIAN_POINT('',(-1.56343130033213,0.575533291080354,6.53916105310504));
#52114=CARTESIAN_POINT('',(-1.56343130033213,0.575533291080363,11.));
#52115=CARTESIAN_POINT('',(-0.769902040670541,-1.47743251885537,6.));
#52116=CARTESIAN_POINT('Ctrl Pts',(-1.56343130033213,0.575533291080354,
6.53916105310504));
#52117=CARTESIAN_POINT('Ctrl Pts',(-1.54247217282036,0.6324685830737,6.5350982232025));
#52118=CARTESIAN_POINT('Ctrl Pts',(-1.51836822901476,0.688340720433169,
6.53103539329996));
#52119=CARTESIAN_POINT('Ctrl Pts',(-1.49125198995376,0.742780924942838,
6.52697256339742));
#52120=CARTESIAN_POINT('Ctrl Pts',(-1.46415901312368,0.79717442678827,6.52291321887821));
#52121=CARTESIAN_POINT('Ctrl Pts',(-1.43405909049039,0.850137972438081,
6.51885387435899));
#52122=CARTESIAN_POINT('Ctrl Pts',(-1.40113273296279,0.901322952453898,
6.51479452983978));
#52123=CARTESIAN_POINT('Ctrl Pts',(-1.36822229829313,0.95248317992415,6.51073714837906));
#52124=CARTESIAN_POINT('Ctrl Pts',(-1.33248841656539,1.00186611597768,6.50667976691835));
#52125=CARTESIAN_POINT('Ctrl Pts',(-1.29415635636569,1.04914981069354,6.50262238545764));
#52126=CARTESIAN_POINT('Ctrl Pts',(-1.25582848671796,1.09642833624345,6.49856544755951));
#52127=CARTESIAN_POINT('Ctrl Pts',(-1.21490332691312,1.14160767809269,6.49450850966139));
#52128=CARTESIAN_POINT('Ctrl Pts',(-1.17164677677384,1.18439850999378,6.49045157176326));
#52129=CARTESIAN_POINT('Ctrl Pts',(-1.12834727602848,1.22723183007663,6.48639060562107));
#52130=CARTESIAN_POINT('Ctrl Pts',(-1.08271212759999,1.26767154162889,6.48232963947888));
#52131=CARTESIAN_POINT('Ctrl Pts',(-1.0350435982904,1.30546572135697,6.47826867333669));
#52132=CARTESIAN_POINT('Ctrl Pts',(-0.987351235684329,1.34327879740729,
6.4742056767939));
#52133=CARTESIAN_POINT('Ctrl Pts',(-0.937623887328302,1.3784434103523,6.47014268025112));
#52134=CARTESIAN_POINT('Ctrl Pts',(-0.88619381793384,1.41075033831498,6.46607968370834));
#52135=CARTESIAN_POINT('Ctrl Pts',(-0.83466622959496,1.44311852494501,6.46200898312902));
#52136=CARTESIAN_POINT('Ctrl Pts',(-0.781429921829616,1.47261795464689,
6.45793828254969));
#52137=CARTESIAN_POINT('Ctrl Pts',(-0.726841985000047,1.49908529738677,
6.45386758197037));
#52138=CARTESIAN_POINT('Ctrl Pts',(-0.685114164012645,1.51931732306875,
6.45075587863566));
#52139=CARTESIAN_POINT('Ctrl Pts',(-0.642597072760685,1.53777855804026,
6.44764417530095));
#52140=CARTESIAN_POINT('Ctrl Pts',(-0.599456592805752,1.55441557935506,
6.44453247196624));
#52141=CARTESIAN_POINT('Ctrl Pts',(-0.542819354942529,1.5762575925762,6.44044725357943));
#52142=CARTESIAN_POINT('Ctrl Pts',(-0.484871782532727,1.59504445632831,
6.43636203519262));
#52143=CARTESIAN_POINT('Ctrl Pts',(-0.425975071864993,1.61062138261902,
6.43227681680581));
#52144=CARTESIAN_POINT('Ctrl Pts',(-0.366578437783686,1.62633052801121,
6.42815692252118));
#52145=CARTESIAN_POINT('Ctrl Pts',(-0.306216934237057,1.63877471927378,
6.42403702823655));
#52146=CARTESIAN_POINT('Ctrl Pts',(-0.245281539516207,1.64784494609552,
6.41991713395192));
#52147=CARTESIAN_POINT('Ctrl Pts',(-0.185026578161849,1.65681389048529,
6.41584324435062));
#52148=CARTESIAN_POINT('Ctrl Pts',(-0.124210992214787,1.66248375485769,
6.41176935474932));
#52149=CARTESIAN_POINT('Ctrl Pts',(-0.0632254082952299,1.66479985215818,
6.40769546514802));
#52150=CARTESIAN_POINT('Ctrl Pts',(-0.00227792857393501,1.66711450234568,
6.40362412094002));
#52151=CARTESIAN_POINT('Ctrl Pts',(0.0588388300897228,1.66607952143167,
6.39955277673203));
#52152=CARTESIAN_POINT('Ctrl Pts',(0.119729966205783,1.66169213008679,6.39548143252403));
#52153=CARTESIAN_POINT('Ctrl Pts',(0.180605449286772,1.65730586659063,6.39141113491982));
#52154=CARTESIAN_POINT('Ctrl Pts',(0.241254916691805,1.64956894018868,6.38734083731562));
#52155=CARTESIAN_POINT('Ctrl Pts',(0.301286393336598,1.63853059452371,6.38327053971141));
#52156=CARTESIAN_POINT('Ctrl Pts',(0.362580865570188,1.62726001432676,6.37911460756668));
#52157=CARTESIAN_POINT('Ctrl Pts',(0.423230495090953,1.61254755918519,6.37495867542195));
#52158=CARTESIAN_POINT('Ctrl Pts',(0.482829061560443,1.59450057927636,6.37080274327722));
#52159=CARTESIAN_POINT('Ctrl Pts',(0.541270234380646,1.57680406853438,6.36672751860175));
#52160=CARTESIAN_POINT('Ctrl Pts',(0.598700337090838,1.55590163855073,6.36265229392628));
#52161=CARTESIAN_POINT('Ctrl Pts',(0.654754249728767,1.53194414795779,6.35857706925082));
#52162=CARTESIAN_POINT('Ctrl Pts',(0.712473335378472,1.50727496098385,6.35438078337146));
#52163=CARTESIAN_POINT('Ctrl Pts',(0.768732632032523,1.47936654553491,6.3501844974921));
#52164=CARTESIAN_POINT('Ctrl Pts',(0.823160899611873,1.44843437315958,6.34598821161275));
#52165=CARTESIAN_POINT('Ctrl Pts',(0.877589167191229,1.41750220078424,6.34179192573339));
#52166=CARTESIAN_POINT('Ctrl Pts',(0.930185952300682,1.38354664391381,6.33759563985403));
#52167=CARTESIAN_POINT('Ctrl Pts',(0.980614989643535,1.34682970047679,6.33339935397468));
#52168=CARTESIAN_POINT('Ctrl Pts',(1.02968244606439,1.3111041122655,6.32931636755725));
#52169=CARTESIAN_POINT('Ctrl Pts',(1.07689333142065,1.27262204689111,6.32523338113982));
#52170=CARTESIAN_POINT('Ctrl Pts',(1.12192208578457,1.23160335880867,6.32115039472239));
#52171=CARTESIAN_POINT('Ctrl Pts',(1.16736095126946,1.19021108232949,6.31703022144159));
#52172=CARTESIAN_POINT('Ctrl Pts',(1.21057726258409,1.14623598390422,6.31291004816079));
#52173=CARTESIAN_POINT('Ctrl Pts',(1.25126733031905,1.09994821154281,6.30878987487998));
#52174=CARTESIAN_POINT('Ctrl Pts',(1.29148153737639,1.0542017636851,6.3047178860471));
#52175=CARTESIAN_POINT('Ctrl Pts',(1.32922792601312,1.00619683655384,6.30064589721421));
#52176=CARTESIAN_POINT('Ctrl Pts',(1.36424921820571,0.956232226305472,6.29657390838132));
#52177=CARTESIAN_POINT('Ctrl Pts',(1.39924971771825,0.906297280814998,6.29250433715085));
#52178=CARTESIAN_POINT('Ctrl Pts',(1.4315280368189,0.854405376351585,6.28843476592039));
#52179=CARTESIAN_POINT('Ctrl Pts',(1.46086825225904,0.800886976758657,6.28436519468992));
#52180=CARTESIAN_POINT('Ctrl Pts',(1.49020185549971,0.747380638233718,6.28029654059031));
#52181=CARTESIAN_POINT('Ctrl Pts',(1.51659842460062,0.692248979560936,6.2762278864907));
#52182=CARTESIAN_POINT('Ctrl Pts',(1.53988738324474,0.635848131965233,6.27215923239108));
#52183=CARTESIAN_POINT('Ctrl Pts',(1.56368632472775,0.578212215648232,6.26800148269042));
#52184=CARTESIAN_POINT('Ctrl Pts',(1.58423968049731,0.519251356928695,6.26384373298975));
#52185=CARTESIAN_POINT('Ctrl Pts',(1.60141775831342,0.459366045064748,6.25968598328909));
#52186=CARTESIAN_POINT('Ctrl Pts',(1.61824946449418,0.400688235787859,6.25561206872869));
#52187=CARTESIAN_POINT('Ctrl Pts',(1.63184070452812,0.341123435405091,6.25153815416829));
#52188=CARTESIAN_POINT('Ctrl Pts',(1.64212094537824,0.281060137248377,6.24746423960789));
#52189=CARTESIAN_POINT('Ctrl Pts',(1.65271851447157,0.219142818241058,6.2432645723371));
#52190=CARTESIAN_POINT('Ctrl Pts',(1.6597972102613,0.156696296827122,6.2390649050663));
#52191=CARTESIAN_POINT('Ctrl Pts',(1.66333751254052,0.0941505144729865,
6.2348652377955));
#52192=CARTESIAN_POINT('Ctrl Pts',(1.66687781481973,0.0316047321188593,
6.23066557052471));
#52193=CARTESIAN_POINT('Ctrl Pts',(1.66687979361413,-0.0310397249814722,
6.22646590325391));
#52194=CARTESIAN_POINT('Ctrl Pts',(1.66338222244431,-0.093357281752649,
6.22226623598312));
#52195=CARTESIAN_POINT('Ctrl Pts',(1.66002325794814,-0.153205230662976,
6.21823299903858));
#52196=CARTESIAN_POINT('Ctrl Pts',(1.6534222319083,-0.213010620528822,6.21419976209404));
#52197=CARTESIAN_POINT('Ctrl Pts',(1.64358156678773,-0.272388754018175,
6.2101665251495));
#52198=CARTESIAN_POINT('Ctrl Pts',(1.63351361341894,-0.333138334638226,
6.20604013318458));
#52199=CARTESIAN_POINT('Ctrl Pts',(1.62005441559245,-0.393440119787072,
6.20191374121967));
#52200=CARTESIAN_POINT('Ctrl Pts',(1.60326314871747,-0.452883291770124,
6.19778734925476));
#52201=CARTESIAN_POINT('Ctrl Pts',(1.58689626677036,-0.51082408835517,6.19376524832216));
#52202=CARTESIAN_POINT('Ctrl Pts',(1.56736391839693,-0.567948626115506,
6.18974314738957));
#52203=CARTESIAN_POINT('Ctrl Pts',(1.54477275985811,-0.623885502636782,
6.18572104645698));
#52204=CARTESIAN_POINT('Ctrl Pts',(1.52219478243197,-0.67978974204158,6.18170129227281));
#52205=CARTESIAN_POINT('Ctrl Pts',(1.4965617259929,-0.73450720808756,6.17768153808864));
#52206=CARTESIAN_POINT('Ctrl Pts',(1.46802939675063,-0.787683750166262,
6.17366178390447));
#52207=CARTESIAN_POINT('Ctrl Pts',(1.43950256879724,-0.840850039330887,
6.16964280476494));
#52208=CARTESIAN_POINT('Ctrl Pts',(1.40807782472183,-0.892475532430629,
6.16562382562542));
#52209=CARTESIAN_POINT('Ctrl Pts',(1.37395720126328,-0.94223012533923,6.16160484648589));
#52210=CARTESIAN_POINT('Ctrl Pts',(1.33824898649299,-0.994299739235551,
6.15739886911136));
#52211=CARTESIAN_POINT('Ctrl Pts',(1.29958818278729,-1.04431954101807,6.15319289173684));
#52212=CARTESIAN_POINT('Ctrl Pts',(1.25825577968416,-1.0919470650592,6.14898691436231));
#52213=CARTESIAN_POINT('Ctrl Pts',(1.21870051728244,-1.13752678144517,6.14496177848308));
#52214=CARTESIAN_POINT('Ctrl Pts',(1.1766991429464,-1.18091540677872,6.14093664260385));
#52215=CARTESIAN_POINT('Ctrl Pts',(1.13253587503068,-1.2218504375612,6.13691150672463));
#52216=CARTESIAN_POINT('Ctrl Pts',(1.08833659888746,-1.26281884444944,6.13288308897756));
#52217=CARTESIAN_POINT('Ctrl Pts',(1.04197233113928,-1.3013293507988,6.1288546712305));
#52218=CARTESIAN_POINT('Ctrl Pts',(0.993759007638126,-1.33716081109868,
6.12482625348344));
#52219=CARTESIAN_POINT('Ctrl Pts',(0.945455378020833,-1.37305938562717,
6.12079029029594));
#52220=CARTESIAN_POINT('Ctrl Pts',(0.895296228032955,-1.40626863101897,
6.11675432710843));
#52221=CARTESIAN_POINT('Ctrl Pts',(0.84362365034703,-1.4366123821599,6.11271836392093));
#52222=CARTESIAN_POINT('Ctrl Pts',(0.836858330675631,-1.44058518912428,
6.11218994861114));
#52223=CARTESIAN_POINT('Ctrl Pts',(0.830067096357697,-1.44450894389794,
6.11166153330135));
#52224=CARTESIAN_POINT('Ctrl Pts',(0.823250739277983,-1.44838331262075,
6.11113311799157));
#52225=CARTESIAN_POINT('Ctrl Pts',(0.769183237850171,-1.47911489460841,
6.10694171557788));
#52226=CARTESIAN_POINT('Ctrl Pts',(0.713301855134838,-1.50686694462979,
6.1027503131642));
#52227=CARTESIAN_POINT('Ctrl Pts',(0.655958678299715,-1.53142881400452,
6.09855891075051));
#52228=CARTESIAN_POINT('Ctrl Pts',(0.59873760766417,-1.5559383814893,6.09437643348273));
#52229=CARTESIAN_POINT('Ctrl Pts',(0.540061369584661,-1.57727109296317,
6.09019395621495));
#52230=CARTESIAN_POINT('Ctrl Pts',(0.480306060998282,-1.59526238837638,
6.08601147894716));
#52231=CARTESIAN_POINT('Ctrl Pts',(0.420626058013942,-1.61323101056834,
6.08183427257457));
#52232=CARTESIAN_POINT('Ctrl Pts',(0.35987013933105,-1.62786644215779,6.07765706620198));
#52233=CARTESIAN_POINT('Ctrl Pts',(0.298432871660621,-1.63905272066288,
6.07347985982939));
#52234=CARTESIAN_POINT('Ctrl Pts',(0.237054984453405,-1.65022818738509,
6.06930669081814));
#52235=CARTESIAN_POINT('Ctrl Pts',(0.174997524326245,-1.65796103802397,
6.06513352180688));
#52236=CARTESIAN_POINT('Ctrl Pts',(0.112667056339353,-1.66218595061318,
6.06096035279563));
#52237=CARTESIAN_POINT('Ctrl Pts',(0.0503785495936725,-1.66640801896613,
6.05678999318654));
#52238=CARTESIAN_POINT('Ctrl Pts',(-0.012182124448017,-1.66712681027999,
6.05261963357745));
#52239=CARTESIAN_POINT('Ctrl Pts',(-0.0746030895967543,-1.66432880736428,
6.04844927396836));
#52240=CARTESIAN_POINT('Ctrl Pts',(-0.137019316940818,-1.66153101681939,
6.04427923089314));
#52241=CARTESIAN_POINT('Ctrl Pts',(-0.199295379105893,-1.65521697056048,
6.04010918781791));
#52242=CARTESIAN_POINT('Ctrl Pts',(-0.261020497571679,-1.64542526413309,
6.03593914474268));
#52243=CARTESIAN_POINT('Ctrl Pts',(-0.322737670498844,-1.63563481813878,
6.03176963845441));
#52244=CARTESIAN_POINT('Ctrl Pts',(-0.383903569929177,-1.6223676827034,
6.02760013216614));
#52245=CARTESIAN_POINT('Ctrl Pts',(-0.444115707757167,-1.60571393408769,
6.02343062587786));
#52246=CARTESIAN_POINT('Ctrl Pts',(-0.504373373391242,-1.58904759318302,
6.01925796692834));
#52247=CARTESIAN_POINT('Ctrl Pts',(-0.563675376158753,-1.56898965280899,
6.01508530797882));
#52248=CARTESIAN_POINT('Ctrl Pts',(-0.621633450291989,-1.54568038529253,
6.01091264902929));
#52249=CARTESIAN_POINT('Ctrl Pts',(-0.672158876970822,-1.52536034007963,
6.00727509935286));
#52250=CARTESIAN_POINT('Ctrl Pts',(-0.721663027466453,-1.50257025897668,
6.00363754967643));
#52251=CARTESIAN_POINT('Ctrl Pts',(-0.769902040670518,-1.47743251885539,
6.));
#52252=CARTESIAN_POINT('',(-1.33524939639864,0.997598393459654,6.00000056028684));
#52253=CARTESIAN_POINT('Origin',(0.,0.,6.));
#52254=CARTESIAN_POINT('',(-1.56343130033213,0.575533291080356,6.03223733991315));
#52255=CARTESIAN_POINT('Ctrl Pts',(-1.33464070599239,0.99714100603081,6.00000056115665));
#52256=CARTESIAN_POINT('Ctrl Pts',(-1.37078624190903,0.948761385412975,
6.00406393220756));
#52257=CARTESIAN_POINT('Ctrl Pts',(-1.40437715109543,0.898307539445458,
6.00812730325847));
#52258=CARTESIAN_POINT('Ctrl Pts',(-1.43516660948121,0.846080848991512,
6.01219067430938));
#52259=CARTESIAN_POINT('Ctrl Pts',(-1.46590351276494,0.79394330525176,6.01624710951629));
#52260=CARTESIAN_POINT('Ctrl Pts',(-1.49384819256357,0.7400393601093,6.02030354472319));
#52261=CARTESIAN_POINT('Ctrl Pts',(-1.51879562492657,0.684701285016984,
6.0243599799301));
#52262=CARTESIAN_POINT('Ctrl Pts',(-1.53494444323233,0.64888018298719,6.02698576659112));
#52263=CARTESIAN_POINT('Ctrl Pts',(-1.54983820983774,0.612458806035863,
6.02961155325213));
#52264=CARTESIAN_POINT('Ctrl Pts',(-1.56343130033213,0.575533291080356,
6.03223733991315));
#52265=CARTESIAN_POINT('',(-1.56343130033213,0.575533291080363,5.));
#52266=CARTESIAN_POINT('',(-1.56343130033213,0.575533291080363,11.));
#52267=CARTESIAN_POINT('Origin',(0.,0.,5.));
#52268=CARTESIAN_POINT('',(-1.66599954285828,-0.001234178273358,6.07148036342561));
#52269=CARTESIAN_POINT('Ctrl Pts',(-1.56343130033213,0.575533291080356,
6.03223733991315));
#52270=CARTESIAN_POINT('Ctrl Pts',(-1.58439805255523,0.518577286623392,
6.03628750189324));
#52271=CARTESIAN_POINT('Ctrl Pts',(-1.60226784904869,0.460421099189002,
6.04033766387333));
#52272=CARTESIAN_POINT('Ctrl Pts',(-1.61691251877963,0.401434809917774,
6.04438782585341));
#52273=CARTESIAN_POINT('Ctrl Pts',(-1.63155002543007,0.342477372341142,
6.04843600679625));
#52274=CARTESIAN_POINT('Ctrl Pts',(-1.64296541408166,0.282691138748249,
6.05248418773908));
#52275=CARTESIAN_POINT('Ctrl Pts',(-1.65108070322902,0.222460134461837,
6.05653236868192));
#52276=CARTESIAN_POINT('Ctrl Pts',(-1.65919668658871,0.162223977788912,
6.06058089592137));
#52277=CARTESIAN_POINT('Ctrl Pts',(-1.66401193639875,0.101543484887501,
6.06462942316082));
#52278=CARTESIAN_POINT('Ctrl Pts',(-1.66550009488837,0.04080972833555,6.06867795040027));
#52279=CARTESIAN_POINT('Ctrl Pts',(-1.66584346540607,0.0267963140556828,
6.06961208806358));
#52280=CARTESIAN_POINT('Ctrl Pts',(-1.66600992466137,0.0127800747921988,
6.0705462257269));
#52281=CARTESIAN_POINT('Ctrl Pts',(-1.66599954285867,-0.00123417774222995,
6.07148036339021));
#52282=CARTESIAN_POINT('Ctrl Pts',(-1.66599954285828,-0.00123417827337041,
6.07148036342561));
#52283=CARTESIAN_POINT('Ctrl Pts',(-1.66594753062002,-0.0714447524100149,
6.07616033772347));
#52284=CARTESIAN_POINT('Ctrl Pts',(-1.66145315819263,-0.141478574425917,
6.08084031202132));
#52285=CARTESIAN_POINT('Ctrl Pts',(-1.6526070389996,-0.210822139845356,
6.08552028631918));
#52286=CARTESIAN_POINT('Ctrl Pts',(-1.64367765414105,-0.280818413870458,
6.09024431170498));
#52287=CARTESIAN_POINT('Ctrl Pts',(-1.63031432693859,-0.350111196841199,
6.09496833709077));
#52288=CARTESIAN_POINT('Ctrl Pts',(-1.61265978947049,-0.418191826109729,
6.09969236247657));
#52289=CARTESIAN_POINT('Ctrl Pts',(-1.60112177366817,-0.462685508130673,
6.10277972059345));
#52290=CARTESIAN_POINT('Ctrl Pts',(-1.58775190295344,-0.506661860727517,
6.10586707871033));
#52291=CARTESIAN_POINT('Ctrl Pts',(-1.57260095361437,-0.549983854936836,
6.10895443682722));
#52292=CARTESIAN_POINT('Ctrl Pts',(-1.55255693979627,-0.607296874149416,
6.11303887057267));
#52293=CARTESIAN_POINT('Ctrl Pts',(-1.52933597420523,-0.663626358690032,
6.11712330431812));
#52294=CARTESIAN_POINT('Ctrl Pts',(-1.50305498755847,-0.718597038941581,
6.12120773806358));
#52295=CARTESIAN_POINT('Ctrl Pts',(-1.47654520160721,-0.774046287733134,
6.12532773042838));
#52296=CARTESIAN_POINT('Ctrl Pts',(-1.44692195174979,-0.8281124372478,6.12944772279318));
#52297=CARTESIAN_POINT('Ctrl Pts',(-1.41435640680187,-0.880427143231349,
6.13356771515798));
#52298=CARTESIAN_POINT('Ctrl Pts',(-1.38215784537766,-0.93215231094141,
6.13764127902548));
#52299=CARTESIAN_POINT('Ctrl Pts',(-1.34708323540234,-0.982164862027837,
6.14171484289298));
#52300=CARTESIAN_POINT('Ctrl Pts',(-1.30934474178789,-1.03013219887178,
6.14578840676048));
#52301=CARTESIAN_POINT('Ctrl Pts',(-1.27162823510276,-1.07807158933143,
6.14985959731754));
#52302=CARTESIAN_POINT('Ctrl Pts',(-1.23125123711747,-1.12396772848948,
6.1539307878746));
#52303=CARTESIAN_POINT('Ctrl Pts',(-1.18846814411064,-1.16751850967521,
6.15800197843166));
#52304=CARTESIAN_POINT('Ctrl Pts',(-1.1456942440287,-1.21105993298069,6.16207229420042));
#52305=CARTESIAN_POINT('Ctrl Pts',(-1.10051563268515,-1.25225663541508,
6.16614260996919));
#52306=CARTESIAN_POINT('Ctrl Pts',(-1.0532243429506,-1.29084254787959,6.17021292573795));
#52307=CARTESIAN_POINT('Ctrl Pts',(-1.00493497859783,-1.33024280945719,
6.17436914482802));
#52308=CARTESIAN_POINT('Ctrl Pts',(-0.954443134280577,-1.3669204304962,
6.17852536391809));
#52309=CARTESIAN_POINT('Ctrl Pts',(-0.902094275076489,-1.40063625501921,
6.18268158300815));
#52310=CARTESIAN_POINT('Ctrl Pts',(-0.85076001401308,-1.43369861710975,
6.18675724843908));
#52311=CARTESIAN_POINT('Ctrl Pts',(-0.797640573016811,-1.46391277769745,
6.19083291387));
#52312=CARTESIAN_POINT('Ctrl Pts',(-0.743087775427189,-1.49109911072694,
6.19490857930092));
#52313=CARTESIAN_POINT('Ctrl Pts',(-0.686917661277731,-1.5190914318735,
6.19910507522056));
#52314=CARTESIAN_POINT('Ctrl Pts',(-0.629228375774907,-1.54387328901976,
6.2033015711402));
#52315=CARTESIAN_POINT('Ctrl Pts',(-0.570424688362431,-1.56530242282654,
6.20749806705984));
#52316=CARTESIAN_POINT('Ctrl Pts',(-0.511621000949956,-1.58673155663331,
6.21169456297949));
#52317=CARTESIAN_POINT('Ctrl Pts',(-0.451703489315339,-1.60480786594618,
6.21589105889913));
#52318=CARTESIAN_POINT('Ctrl Pts',(-0.39108948985327,-1.619445896264,6.22008755481877));
#52319=CARTESIAN_POINT('Ctrl Pts',(-0.332275257023779,-1.63364929037952,
6.22415944729041));
#52320=CARTESIAN_POINT('Ctrl Pts',(-0.272561676081544,-1.64467460318456,
6.22823133976206));
#52321=CARTESIAN_POINT('Ctrl Pts',(-0.212324570981963,-1.65241468056821,
6.2323032322337));
#52322=CARTESIAN_POINT('Ctrl Pts',(-0.151352714266586,-1.66024916876981,
6.23642479225773));
#52323=CARTESIAN_POINT('Ctrl Pts',(-0.0898449686004922,-1.66471751880863,
6.24054635228175));
#52324=CARTESIAN_POINT('Ctrl Pts',(-0.0282053183113921,-1.66576122539185,
6.24466791230578));
#52325=CARTESIAN_POINT('Ctrl Pts',(0.0325208065838762,-1.66678946380704,
6.24872838908669));
#52326=CARTESIAN_POINT('Ctrl Pts',(0.0933744219731093,-1.66449386898338,
6.2527888658676));
#52327=CARTESIAN_POINT('Ctrl Pts',(0.153963202056404,-1.65887049898795,
6.25684934264851));
#52328=CARTESIAN_POINT('Ctrl Pts',(0.214514070017212,-1.65325064769502,
6.26090727867365));
#52329=CARTESIAN_POINT('Ctrl Pts',(0.274799920958721,-1.64430719665915,
6.26496521469878));
#52330=CARTESIAN_POINT('Ctrl Pts',(0.334430872690372,-1.63208823027174,
6.26902315072391));
#52331=CARTESIAN_POINT('Ctrl Pts',(0.394046829711921,-1.61987233644738,
6.27308006634651));
#52332=CARTESIAN_POINT('Ctrl Pts',(0.453007711537243,-1.60438266514088,
6.27713698196911));
#52333=CARTESIAN_POINT('Ctrl Pts',(0.510933284968012,-1.58571850538227,
6.28119389759171));
#52334=CARTESIAN_POINT('Ctrl Pts',(0.570457767584166,-1.56653916217863,
6.2853627955266));
#52335=CARTESIAN_POINT('Ctrl Pts',(0.628888381830324,-1.54400760526379,
6.28953169346148));
#52336=CARTESIAN_POINT('Ctrl Pts',(0.685831073304624,-1.51828578959622,
6.29370059139637));
#52337=CARTESIAN_POINT('Ctrl Pts',(0.741314463005289,-1.49322316109128,
6.2977626506836));
#52338=CARTESIAN_POINT('Ctrl Pts',(0.795384852046118,-1.46513215726107,
6.30182470997084));
#52339=CARTESIAN_POINT('Ctrl Pts',(0.847702110907871,-1.43420958411326,
6.30588676925808));
#52340=CARTESIAN_POINT('Ctrl Pts',(0.902083410982519,-1.40206704136509,
6.31010908651679));
#52341=CARTESIAN_POINT('Ctrl Pts',(0.954569835289881,-1.36686515395936,
6.3143314037755));
#52342=CARTESIAN_POINT('Ctrl Pts',(1.00481450032127,-1.32887313914614,6.31855372103421));
#52343=CARTESIAN_POINT('Ctrl Pts',(1.05505916535267,-1.29088112433292,6.32277603829291));
#52344=CARTESIAN_POINT('Ctrl Pts',(1.10306165111379,-1.25009943725184,6.32699835555162));
#52345=CARTESIAN_POINT('Ctrl Pts',(1.14851763589996,-1.20684018827133,6.33122067281033));
#52346=CARTESIAN_POINT('Ctrl Pts',(1.19242570771038,-1.16505404680642,6.33529920746917));
#52347=CARTESIAN_POINT('Ctrl Pts',(1.23414067015834,-1.12078260523448,6.339377742128));
#52348=CARTESIAN_POINT('Ctrl Pts',(1.27336854985667,-1.07428512799718,6.34345627678683));
#52349=CARTESIAN_POINT('Ctrl Pts',(1.31300226746573,-1.02730660413791,6.34757700653746));
#52350=CARTESIAN_POINT('Ctrl Pts',(1.35009670262528,-0.97805601886764,6.35169773628809));
#52351=CARTESIAN_POINT('Ctrl Pts',(1.3843850598368,-0.926840874206924,6.35581846603871));
#52352=CARTESIAN_POINT('Ctrl Pts',(1.41822892632856,-0.876289647516156,
6.35988577747824));
#52353=CARTESIAN_POINT('Ctrl Pts',(1.4493387417139,-0.823824930299692,6.36395308891776));
#52354=CARTESIAN_POINT('Ctrl Pts',(1.47749842961004,-0.769775545532505,
6.36802040035728));
#52355=CARTESIAN_POINT('Ctrl Pts',(1.5056408939184,-0.715759219523877,6.37208522406697));
#52356=CARTESIAN_POINT('Ctrl Pts',(1.53083657254523,-0.660160600538697,
6.37615004777666));
#52357=CARTESIAN_POINT('Ctrl Pts',(1.55291447988775,-0.603334582263409,
6.38021487148635));
#52358=CARTESIAN_POINT('Ctrl Pts',(1.57498707235554,-0.546522243870179,
6.38427871665997));
#52359=CARTESIAN_POINT('Ctrl Pts',(1.59394319832293,-0.488483569435168,
6.38834256183358));
#52360=CARTESIAN_POINT('Ctrl Pts',(1.60966015635893,-0.429593041180322,
6.3924064070072));
#52361=CARTESIAN_POINT('Ctrl Pts',(1.62575781964685,-0.369276032474007,
6.39656868899009));
#52362=CARTESIAN_POINT('Ctrl Pts',(1.63845714538738,-0.308065888929439,
6.40073097097298));
#52363=CARTESIAN_POINT('Ctrl Pts',(1.64768127900689,-0.246378576199764,
6.40489325295587));
#52364=CARTESIAN_POINT('Ctrl Pts',(1.65669871766469,-0.186073556622871,
6.40896226626437));
#52365=CARTESIAN_POINT('Ctrl Pts',(1.66239512475955,-0.125313062025278,
6.41303127957287));
#52366=CARTESIAN_POINT('Ctrl Pts',(1.66475131859362,-0.064490675611387,
6.41710029288137));
#52367=CARTESIAN_POINT('Ctrl Pts',(1.66718852435571,-0.0015770610825209,
6.42130920920146));
#52368=CARTESIAN_POINT('Ctrl Pts',(1.66605160417627,0.0614021824037467,
6.42551812552154));
#52369=CARTESIAN_POINT('Ctrl Pts',(1.66137784548386,0.124014735154304,6.42972704184163));
#52370=CARTESIAN_POINT('Ctrl Pts',(1.65670408679146,0.18662728790487,6.43393595816171));
#52371=CARTESIAN_POINT('Ctrl Pts',(1.64849363888062,0.248872566572567,6.4381448744818));
#52372=CARTESIAN_POINT('Ctrl Pts',(1.63684178780226,0.310330407315007,6.44235379080188));
#52373=CARTESIAN_POINT('Ctrl Pts',(1.62555182528446,0.369879462116787,6.44643198465922));
#52374=CARTESIAN_POINT('Ctrl Pts',(1.61098479711917,0.42893395946793,6.45051017851655));
#52375=CARTESIAN_POINT('Ctrl Pts',(1.59319910883432,0.487106353489169,6.45458837237389));
#52376=CARTESIAN_POINT('Ctrl Pts',(1.57522772858898,0.545886097966566,6.4587091447247));
#52377=CARTESIAN_POINT('Ctrl Pts',(1.55397010000998,0.60376467875591,6.46282991707552));
#52378=CARTESIAN_POINT('Ctrl Pts',(1.52953992863024,0.660351123816555,6.46695068942633));
#52379=CARTESIAN_POINT('Ctrl Pts',(1.50542850256665,0.71619927424801,6.47101769723881));
#52380=CARTESIAN_POINT('Ctrl Pts',(1.47822703288719,0.770788321482814,6.47508470505129));
#52381=CARTESIAN_POINT('Ctrl Pts',(1.44809461484857,0.823758451517545,6.47915171286377));
#52382=CARTESIAN_POINT('Ctrl Pts',(1.41798051848918,0.87669637365809,6.48321624777771));
#52383=CARTESIAN_POINT('Ctrl Pts',(1.38493925978072,0.928016886466262,6.48728078269165));
#52384=CARTESIAN_POINT('Ctrl Pts',(1.34917628873037,0.977383927598429,6.49134531760559));
#52385=CARTESIAN_POINT('Ctrl Pts',(1.31342179239797,1.02673927026884,6.49540888935048));
#52386=CARTESIAN_POINT('Ctrl Pts',(1.2749471641762,1.07414164602324,6.49947246109536));
#52387=CARTESIAN_POINT('Ctrl Pts',(1.23400049281121,1.11928494305145,6.50353603284025));
#52388=CARTESIAN_POINT('Ctrl Pts',(1.19205623312917,1.16552807125536,6.50769860583635));
#52389=CARTESIAN_POINT('Ctrl Pts',(1.14751823004332,1.20940014664625,6.51186117883245));
#52390=CARTESIAN_POINT('Ctrl Pts',(1.10069440802769,1.25061097873663,6.51602375182855));
#52391=CARTESIAN_POINT('Ctrl Pts',(1.05492562545604,1.29089324388173,6.52009253327773));
#52392=CARTESIAN_POINT('Ctrl Pts',(1.00697342147985,1.32863267997271,6.52416131472692));
#52393=CARTESIAN_POINT('Ctrl Pts',(0.957158064882367,1.36359980889946,6.5282300961761));
#52394=CARTESIAN_POINT('Ctrl Pts',(0.905620229670406,1.3997760053889,6.53243956494566));
#52395=CARTESIAN_POINT('Ctrl Pts',(0.852088517331065,1.43298430956935,6.53664903371522));
#52396=CARTESIAN_POINT('Ctrl Pts',(0.796946566940896,1.46302158884998,6.54085850248478));
#52397=CARTESIAN_POINT('Ctrl Pts',(0.741804616550727,1.4930588681306,6.54506797125434));
#52398=CARTESIAN_POINT('Ctrl Pts',(0.685052999916675,1.5199249316788,6.54927744002389));
#52399=CARTESIAN_POINT('Ctrl Pts',(0.627096590274101,1.54347201674232,6.55348690879345));
#52400=CARTESIAN_POINT('Ctrl Pts',(0.570970011416014,1.56627566063341,6.55756347396204));
#52401=CARTESIAN_POINT('Ctrl Pts',(0.513481638667367,1.58606110557588,6.56164003913063));
#52402=CARTESIAN_POINT('Ctrl Pts',(0.454988330986168,1.60266703300044,6.56571660429921));
#52403=CARTESIAN_POINT('Ctrl Pts',(0.39585778763514,1.61945386811691,6.56983758023612));
#52404=CARTESIAN_POINT('Ctrl Pts',(0.335700735833276,1.63299120758289,6.57395855617303));
#52405=CARTESIAN_POINT('Ctrl Pts',(0.274907480839262,1.64316215784645,6.57807953210994));
#52406=CARTESIAN_POINT('Ctrl Pts',(0.214935497216141,1.65319570618496,6.58214483674651));
#52407=CARTESIAN_POINT('Ctrl Pts',(0.154344913616217,1.65995316979927,6.58621014138308));
#52408=CARTESIAN_POINT('Ctrl Pts',(0.0935239959668483,1.66337285723267,
6.59027544601966));
#52409=CARTESIAN_POINT('Ctrl Pts',(0.0327404210518218,1.6667904450516,6.59433825464668));
#52410=CARTESIAN_POINT('Ctrl Pts',(-0.0282726972042708,1.66687429113425,
6.59840106327371));
#52411=CARTESIAN_POINT('Ctrl Pts',(-0.0891218696325091,1.66361452637118,
6.60246387190073));
#52412=CARTESIAN_POINT('Ctrl Pts',(-0.149956312603149,1.66035555068321,
6.60652569706381));
#52413=CARTESIAN_POINT('Ctrl Pts',(-0.210626377302139,1.65375459821952,
6.61058752222689));
#52414=CARTESIAN_POINT('Ctrl Pts',(-0.27074058094533,1.64385386754096,6.61464934738997));
#52415=CARTESIAN_POINT('Ctrl Pts',(-0.332370256373181,1.63370354064252,
6.61881357067289));
#52416=CARTESIAN_POINT('Ctrl Pts',(-0.393415100212304,1.62008483939551,
6.62297779395581));
#52417=CARTESIAN_POINT('Ctrl Pts',(-0.453463527979288,1.60309913255312,
6.62714201723873));
#52418=CARTESIAN_POINT('Ctrl Pts',(-0.512110054751508,1.58650997696453,
6.63120902184366));
#52419=CARTESIAN_POINT('Ctrl Pts',(-0.569805714942126,1.56670957536178,
6.63527602644859));
#52420=CARTESIAN_POINT('Ctrl Pts',(-0.626184237321801,1.54384238215231,
6.63934303105352));
#52421=CARTESIAN_POINT('Ctrl Pts',(-0.684584288791703,1.52015525442995,
6.64355586367544));
#52422=CARTESIAN_POINT('Ctrl Pts',(-0.741570391087137,1.49317744674347,
6.64776869629735));
#52423=CARTESIAN_POINT('Ctrl Pts',(-0.796762667802162,1.46312174858991,
6.65198152891926));
#52424=CARTESIAN_POINT('Ctrl Pts',(-0.851954944517186,1.43306605043634,
6.65619436154118));
#52425=CARTESIAN_POINT('Ctrl Pts',(-0.905352921888731,1.3999328414526,6.66040719416309));
#52426=CARTESIAN_POINT('Ctrl Pts',(-0.95661190713044,1.36398301277408,6.664620026785));
#52427=CARTESIAN_POINT('Ctrl Pts',(-1.00591490356432,1.32940499163734,6.66867210215785));
#52428=CARTESIAN_POINT('Ctrl Pts',(-1.05344849322557,1.29207460725326,6.67272417753069));
#52429=CARTESIAN_POINT('Ctrl Pts',(-1.09888593881631,1.25220034078888,6.67677625290353));
#52430=CARTESIAN_POINT('Ctrl Pts',(-1.1442566087339,1.21238467425129,6.68082237327478));
#52431=CARTESIAN_POINT('Ctrl Pts',(-1.18753685284736,1.17003287360593,6.68486849364603));
#52432=CARTESIAN_POINT('Ctrl Pts',(-1.22842991906173,1.12539590098506,6.68891461401728));
#52433=CARTESIAN_POINT('Ctrl Pts',(-1.2692780118434,1.08080801927545,6.6929562845407));
#52434=CARTESIAN_POINT('Ctrl Pts',(-1.30774378443032,1.03394033042938,6.69699795506411));
#52435=CARTESIAN_POINT('Ctrl Pts',(-1.34356618508168,0.985081674941245,
6.70103962558753));
#52436=CARTESIAN_POINT('Ctrl Pts',(-1.37936537676592,0.93625467447647,6.70507867755394));
#52437=CARTESIAN_POINT('Ctrl Pts',(-1.41252428754029,0.885439683712039,
6.70911772952034));
#52438=CARTESIAN_POINT('Ctrl Pts',(-1.44282250171624,0.832958119320112,
6.71315678148675));
#52439=CARTESIAN_POINT('Ctrl Pts',(-1.4731207834657,0.78047643787958,6.71719584246137));
#52440=CARTESIAN_POINT('Ctrl Pts',(-1.50055808611293,0.726328618815754,
6.72123490343599));
#52441=CARTESIAN_POINT('Ctrl Pts',(-1.52495866950945,0.670862919148136,
6.72527396441062));
#52442=CARTESIAN_POINT('Ctrl Pts',(-1.5387622099493,0.639485676401743,6.7275588827913));
#52443=CARTESIAN_POINT('Ctrl Pts',(-1.55159476705925,0.607687133252561,
6.72984380117199));
#52444=CARTESIAN_POINT('Ctrl Pts',(-1.56343130033213,0.575533291080356,
6.73212871955268));
#52445=CARTESIAN_POINT('Origin',(0.,0.,11.));
#52446=CARTESIAN_POINT('',(-1.56542652693575,0.576282819883045,7.43212287682542));
#52447=CARTESIAN_POINT('',(-1.56343130033213,0.575533291080368,7.23929268604744));
#52448=CARTESIAN_POINT('',(-1.56343130033213,0.575533291080363,11.));
#52449=CARTESIAN_POINT('',(-1.66599935370279,0.00146746784764705,6.57851963665102));
#52450=CARTESIAN_POINT('Ctrl Pts',(-1.56343130033213,0.575533291080367,
7.23929268604743));
#52451=CARTESIAN_POINT('Ctrl Pts',(-1.54138234413752,0.635429093440622,
7.23501522736555));
#52452=CARTESIAN_POINT('Ctrl Pts',(-1.51591964574246,0.693968813501019,
7.23073776868366));
#52453=CARTESIAN_POINT('Ctrl Pts',(-1.4872440411031,0.750773709051744,7.22646031000177));
#52454=CARTESIAN_POINT('Ctrl Pts',(-1.47831443503859,0.768462798651881,
7.22512830597023));
#52455=CARTESIAN_POINT('Ctrl Pts',(-1.46907359443735,0.78598386460582,7.22379630193869));
#52456=CARTESIAN_POINT('Ctrl Pts',(-1.45952843832683,0.803326046954314,
7.22246429790715));
#52457=CARTESIAN_POINT('Ctrl Pts',(-1.43031089589254,0.856410139325714,
7.21838705874379));
#52458=CARTESIAN_POINT('Ctrl Pts',(-1.3981331718646,0.908007795322158,7.21430981958043));
#52459=CARTESIAN_POINT('Ctrl Pts',(-1.36317088397108,0.957768834893627,
7.21023258041707));
#52460=CARTESIAN_POINT('Ctrl Pts',(-1.32783427608864,1.00806263570309,7.20611168872951));
#52461=CARTESIAN_POINT('Ctrl Pts',(-1.28965329993057,1.05647975370382,7.20199079704195));
#52462=CARTESIAN_POINT('Ctrl Pts',(-1.2488573994866,1.10268363357201,7.19786990535439));
#52463=CARTESIAN_POINT('Ctrl Pts',(-1.20860484307088,1.14827214273051,7.19380389814946));
#52464=CARTESIAN_POINT('Ctrl Pts',(-1.16580694026357,1.19170561312127,7.18973789094453));
#52465=CARTESIAN_POINT('Ctrl Pts',(-1.12072644732855,1.2326914578508,7.18567188373961));
#52466=CARTESIAN_POINT('Ctrl Pts',(-1.07567353141141,1.27365223037505,7.18160836382677));
#52467=CARTESIAN_POINT('Ctrl Pts',(-1.02834117191007,1.31216800219547,7.17754484391393));
#52468=CARTESIAN_POINT('Ctrl Pts',(-0.979028826309048,1.34798314427738,
7.17348132400109));
#52469=CARTESIAN_POINT('Ctrl Pts',(-0.929728323804896,1.38378968481759,
7.16941878000329));
#52470=CARTESIAN_POINT('Ctrl Pts',(-0.878449193254686,1.41689658243843,
7.1653562360055));
#52471=CARTESIAN_POINT('Ctrl Pts',(-0.825522135047476,1.44708990893678,
7.1612936920077));
#52472=CARTESIAN_POINT('Ctrl Pts',(-0.77127926023977,1.47803387001745,7.15713014933336));
#52473=CARTESIAN_POINT('Ctrl Pts',(-0.715305882186241,1.50591712507302,
7.15296660665902));
#52474=CARTESIAN_POINT('Ctrl Pts',(-0.657985199821807,1.53055920395634,
7.14880306398467));
#52475=CARTESIAN_POINT('Ctrl Pts',(-0.601983544797386,1.55463423488382,
7.14473533012475));
#52476=CARTESIAN_POINT('Ctrl Pts',(-0.544696453213824,1.57561556209212,
7.14066759626482));
#52477=CARTESIAN_POINT('Ctrl Pts',(-0.486499465941723,1.5933845328854,7.13659986240489));
#52478=CARTESIAN_POINT('Ctrl Pts',(-0.426246376471802,1.61178128222209,
7.13238841532334));
#52479=CARTESIAN_POINT('Ctrl Pts',(-0.365018465458375,1.62673425465843,
7.12817696824179));
#52480=CARTESIAN_POINT('Ctrl Pts',(-0.303244253389687,1.63816938159219,
7.12396552116024));
#52481=CARTESIAN_POINT('Ctrl Pts',(-0.241470041321007,1.64960450852595,
7.11975407407868));
#52482=CARTESIAN_POINT('Ctrl Pts',(-0.179150133517697,1.65752178616255,
7.11554262699714));
#52483=CARTESIAN_POINT('Ctrl Pts',(-0.11671604163373,1.66190654539458,7.11133117991559));
#52484=CARTESIAN_POINT('Ctrl Pts',(-0.0562682154602125,1.66615180877349,
7.10725371496907));
#52485=CARTESIAN_POINT('Ctrl Pts',(0.00453631480646224,1.6671035694609,
7.10317625002255));
#52486=CARTESIAN_POINT('Ctrl Pts',(0.065308063584061,1.66471945289016,7.09909878507604));
#52487=CARTESIAN_POINT('Ctrl Pts',(0.126726636767738,1.662309960963,7.09497792161137));
#52488=CARTESIAN_POINT('Ctrl Pts',(0.188111206837704,1.65649303449352,7.0908570581467));
#52489=CARTESIAN_POINT('Ctrl Pts',(0.24905461762166,1.64727890699824,7.08673619468204));
#52490=CARTESIAN_POINT('Ctrl Pts',(0.309190061268199,1.63818693729034,7.08266996423207));
#52491=CARTESIAN_POINT('Ctrl Pts',(0.368895450941059,1.62578737574579,7.07860373378211));
#52492=CARTESIAN_POINT('Ctrl Pts',(0.427782428687343,1.61014228989439,7.07453750333214));
#52493=CARTESIAN_POINT('Ctrl Pts',(0.486633363102706,1.59450678003124,7.07047376172598));
#52494=CARTESIAN_POINT('Ctrl Pts',(0.544666385047516,1.57562981571251,7.06641002011981));
#52495=CARTESIAN_POINT('Ctrl Pts',(0.601504280451816,1.55362434346213,7.06234627851365));
#52496=CARTESIAN_POINT('Ctrl Pts',(0.658328499581683,1.53162416614528,7.05828351472071));
#52497=CARTESIAN_POINT('Ctrl Pts',(0.713957685855581,1.50649716001936,7.05422075092777));
#52498=CARTESIAN_POINT('Ctrl Pts',(0.768032713517711,1.47840513762859,7.05015798713482));
#52499=CARTESIAN_POINT('Ctrl Pts',(0.823446229936901,1.44961776920179,7.04599466003392));
#52500=CARTESIAN_POINT('Ctrl Pts',(0.877227099802084,1.41771685332561,7.04183133293302));
#52501=CARTESIAN_POINT('Ctrl Pts',(0.929015940646776,1.38292638344352,7.03766800583213));
#52502=CARTESIAN_POINT('Ctrl Pts',(0.979618314271451,1.34893295306668,7.03360005933931));
#52503=CARTESIAN_POINT('Ctrl Pts',(1.02831859242541,1.3121813429381,7.02953211284648));
#52504=CARTESIAN_POINT('Ctrl Pts',(1.07481336684084,1.27292271032465,7.02546416635366));
#52505=CARTESIAN_POINT('Ctrl Pts',(1.12294337657611,1.23228333969353,7.02125314894873));
#52506=CARTESIAN_POINT('Ctrl Pts',(1.16870938909863,1.18895769286279,7.01704213154379));
#52507=CARTESIAN_POINT('Ctrl Pts',(1.21181684266056,1.14326547216479,7.01283111413885));
#52508=CARTESIAN_POINT('Ctrl Pts',(1.25492429622248,1.09757325146681,7.00862009673391));
#52509=CARTESIAN_POINT('Ctrl Pts',(1.29537285953596,1.04951496289525,7.00440907932897));
#52510=CARTESIAN_POINT('Ctrl Pts',(1.3329162180352,0.999445023850107,7.00019806192404));
#52511=CARTESIAN_POINT('Ctrl Pts',(1.369269928637,0.950961666296099,6.99612048031712));
#52512=CARTESIAN_POINT('Ctrl Pts',(1.40304988782896,0.90039221972186,6.99204289871021));
#52513=CARTESIAN_POINT('Ctrl Pts',(1.43400925267186,0.848040956116805,6.9879653171033));
#52514=CARTESIAN_POINT('Ctrl Pts',(1.46529712776615,0.795134192524742,6.98384446822118));
#52515=CARTESIAN_POINT('Ctrl Pts',(1.49370380886418,0.74040794320345,6.97972361933906));
#52516=CARTESIAN_POINT('Ctrl Pts',(1.5190170897545,0.684209822374529,6.97560277045694));
#52517=CARTESIAN_POINT('Ctrl Pts',(1.54399562256727,0.628754877153322,6.97153641653528));
#52518=CARTESIAN_POINT('Ctrl Pts',(1.56596185831363,0.571867233513525,6.96747006261362));
#52519=CARTESIAN_POINT('Ctrl Pts',(1.5847573135943,0.513906856355669,6.96340370869196));
#52520=CARTESIAN_POINT('Ctrl Pts',(1.60354127503716,0.455981923254109,6.95933984143592));
#52521=CARTESIAN_POINT('Ctrl Pts',(1.61915814293015,0.396986043224092,6.95527597417988));
#52522=CARTESIAN_POINT('Ctrl Pts',(1.63149822433278,0.33729741178813,6.95121210692384));
#52523=CARTESIAN_POINT('Ctrl Pts',(1.64383534250147,0.277623113432597,6.9471492155276));
#52524=CARTESIAN_POINT('Ctrl Pts',(1.65289713262305,0.217256894970195,6.94308632413137));
#52525=CARTESIAN_POINT('Ctrl Pts',(1.6586247670321,0.156588256864011,6.93902343273513));
#52526=CARTESIAN_POINT('Ctrl Pts',(1.66449382126762,0.0944216620691974,
6.93486022533491));
#52527=CARTESIAN_POINT('Ctrl Pts',(1.66686177525296,0.0319380680069127,
6.93069701793469));
#52528=CARTESIAN_POINT('Ctrl Pts',(1.66572190280597,-0.0304391608371186,
6.92653381053446));
#52529=CARTESIAN_POINT('Ctrl Pts',(1.66460807664504,-0.0913910590218248,
6.92246573315618));
#52530=CARTESIAN_POINT('Ctrl Pts',(1.660145155455,-0.152240882502124,6.91839765577791));
#52531=CARTESIAN_POINT('Ctrl Pts',(1.65237958996264,-0.212597485109536,
6.91432957839963));
#52532=CARTESIAN_POINT('Ctrl Pts',(1.64434163348051,-0.275071202657193,
6.91011880598843));
#52533=CARTESIAN_POINT('Ctrl Pts',(1.63276509875916,-0.337015858767348,
6.90590803357724));
#52534=CARTESIAN_POINT('Ctrl Pts',(1.61775879022358,-0.398010674045737,
6.90169726116605));
#52535=CARTESIAN_POINT('Ctrl Pts',(1.60275248168799,-0.459005489324134,
6.89748648875485));
#52536=CARTESIAN_POINT('Ctrl Pts',(1.58431664462742,-0.519049911293533,
6.89327571634366));
#52537=CARTESIAN_POINT('Ctrl Pts',(1.56261539719853,-0.577744857560916,
6.88906494393246));
#52538=CARTESIAN_POINT('Ctrl Pts',(1.54160607127545,-0.63456837704797,6.88498842758176));
#52539=CARTESIAN_POINT('Ctrl Pts',(1.5174496925766,-0.690362018593101,6.88091191123105));
#52540=CARTESIAN_POINT('Ctrl Pts',(1.49026783765061,-0.744753497517247,
6.87683539488034));
#52541=CARTESIAN_POINT('Ctrl Pts',(1.4627894893984,-0.799738265992379,6.87271441284119));
#52542=CARTESIAN_POINT('Ctrl Pts',(1.43221936086653,-0.853289571210904,
6.86859343080205));
#52543=CARTESIAN_POINT('Ctrl Pts',(1.39873439205661,-0.90504038610331,6.86447244876291));
#52544=CARTESIAN_POINT('Ctrl Pts',(1.36570199812458,-0.956091749284591,
6.86040716493731));
#52545=CARTESIAN_POINT('Ctrl Pts',(1.32983335510675,-1.0053905476909,6.8563418811117));
#52546=CARTESIAN_POINT('Ctrl Pts',(1.29134477954824,-1.05260850287916,6.8522765972861));
#52547=CARTESIAN_POINT('Ctrl Pts',(1.25287973596075,-1.09979758894101,6.84821379898094));
#52548=CARTESIAN_POINT('Ctrl Pts',(1.21179825868441,-1.14490795801612,6.84415100067577));
#52549=CARTESIAN_POINT('Ctrl Pts',(1.16835844803008,-1.18764242805516,6.84008820237061));
#52550=CARTESIAN_POINT('Ctrl Pts',(1.12492904067245,-1.23036666371784,6.83602637705533));
#52551=CARTESIAN_POINT('Ctrl Pts',(1.07914278607903,-1.27071577083916,6.83196455174004));
#52552=CARTESIAN_POINT('Ctrl Pts',(1.03129487317033,-1.30842916681515,6.82790272642476));
#52553=CARTESIAN_POINT('Ctrl Pts',(0.982240504983445,-1.34709348254642,
6.82373848471777));
#52554=CARTESIAN_POINT('Ctrl Pts',(0.931019507188232,-1.38298697528364,
6.81957424301078));
#52555=CARTESIAN_POINT('Ctrl Pts',(0.877984313423429,-1.41587412766192,
6.8154100013038));
#52556=CARTESIAN_POINT('Ctrl Pts',(0.826187186692727,-1.44799355400178,
6.81134297071293));
#52557=CARTESIAN_POINT('Ctrl Pts',(0.772660150675267,-1.47724530121765,
6.80727594012206));
#52558=CARTESIAN_POINT('Ctrl Pts',(0.717756886887557,-1.50345636828126,
6.80320890953119));
#52559=CARTESIAN_POINT('Ctrl Pts',(0.660885157127391,-1.53060718992515,
6.79899606226615));
#52560=CARTESIAN_POINT('Ctrl Pts',(0.602537179699622,-1.55449488489614,
6.7947832150011));
#52561=CARTESIAN_POINT('Ctrl Pts',(0.543126256529309,-1.57498249814671,
6.79057036773605));
#52562=CARTESIAN_POINT('Ctrl Pts',(0.483715333358995,-1.59547011139728,
6.786357520471));
#52563=CARTESIAN_POINT('Ctrl Pts',(0.423242064269878,-1.61255754928539,
6.78214467320596));
#52564=CARTESIAN_POINT('Ctrl Pts',(0.362131530765831,-1.62616627514692,
6.77793182594091));
#52565=CARTESIAN_POINT('Ctrl Pts',(0.30297272154368,-1.63934037085245,6.77385352694163));
#52566=CARTESIAN_POINT('Ctrl Pts',(0.242972147781927,-1.64930917517476,
6.76977522794235));
#52567=CARTESIAN_POINT('Ctrl Pts',(0.182508823830435,-1.65597298565648,
6.76569692894307));
#52568=CARTESIAN_POINT('Ctrl Pts',(0.121416000825612,-1.66270617476504,
6.761576169735));
#52569=CARTESIAN_POINT('Ctrl Pts',(0.0598512310689139,-1.66606495194213,
6.75745541052693));
#52570=CARTESIAN_POINT('Ctrl Pts',(-0.00178146810142189,-1.66599904753016,
6.75333465131886));
#52571=CARTESIAN_POINT('Ctrl Pts',(-0.0626108826772973,-1.66593400207779,
6.74926759967891));
#52572=CARTESIAN_POINT('Ctrl Pts',(-0.123505940107628,-1.66253301251172,
6.74520054803896));
#52573=CARTESIAN_POINT('Ctrl Pts',(-0.184073250022131,-1.65579981840387,
6.74113349639901));
#52574=CARTESIAN_POINT('Ctrl Pts',(-0.244603391048747,-1.64907075631603,
6.73706894062336));
#52575=CARTESIAN_POINT('Ctrl Pts',(-0.304805675828415,-1.63901360062296,
6.73300438484771));
#52576=CARTESIAN_POINT('Ctrl Pts',(-0.364290181355777,-1.62568406025518,
6.72893982907206));
#52577=CARTESIAN_POINT('Ctrl Pts',(-0.423760255386181,-1.61235775375847,
6.72487625939563));
#52578=CARTESIAN_POINT('Ctrl Pts',(-0.482512396761071,-1.5957607504669,
6.7208126897192));
#52579=CARTESIAN_POINT('Ctrl Pts',(-0.540167313231385,-1.57599976958005,
6.71674912004276));
#52580=CARTESIAN_POINT('Ctrl Pts',(-0.599226364472407,-1.55575752738775,
6.71258658570165));
#52581=CARTESIAN_POINT('Ctrl Pts',(-0.657133497568174,-1.53219530111909,
6.70842405136053));
#52582=CARTESIAN_POINT('Ctrl Pts',(-0.713500365734518,-1.50548106201862,
6.70426151701941));
#52583=CARTESIAN_POINT('Ctrl Pts',(-0.768596887935652,-1.47936888450076,
6.70019279414729));
#52584=CARTESIAN_POINT('Ctrl Pts',(-0.822221423291491,-1.45024560818,6.69612407127516));
#52585=CARTESIAN_POINT('Ctrl Pts',(-0.874036493550831,-1.41831456593429,
6.69205534840304));
#52586=CARTESIAN_POINT('Ctrl Pts',(-0.927643593401453,-1.38527918527316,
6.68784590832743));
#52587=CARTESIAN_POINT('Ctrl Pts',(-0.979313256794647,-1.34923856743358,
6.68363646825181));
#52588=CARTESIAN_POINT('Ctrl Pts',(-1.0287071089368,-1.31046468247828,6.6794270281762));
#52589=CARTESIAN_POINT('Ctrl Pts',(-1.07810096107896,-1.27169079752297,
6.67521758810058));
#52590=CARTESIAN_POINT('Ctrl Pts',(-1.12521860026201,-1.23018409495752,
6.67100814802497));
#52591=CARTESIAN_POINT('Ctrl Pts',(-1.16976409477779,-1.1862579662825,6.66679870794936));
#52592=CARTESIAN_POINT('Ctrl Pts',(-1.21228423010985,-1.14432903595683,
6.66278065935358));
#52593=CARTESIAN_POINT('Ctrl Pts',(-1.25264669484434,-1.10001260281998,
6.6587626107578));
#52594=CARTESIAN_POINT('Ctrl Pts',(-1.29056624785872,-1.05356288843517,
6.65474456216203));
#52595=CARTESIAN_POINT('Ctrl Pts',(-1.3284330151471,-1.00717783414526,6.6507321068709));
#52596=CARTESIAN_POINT('Ctrl Pts',(-1.36386327246504,-0.958665782258545,
6.64671965157978));
#52597=CARTESIAN_POINT('Ctrl Pts',(-1.39660808940078,-0.908318140642536,
6.64270719628865));
#52598=CARTESIAN_POINT('Ctrl Pts',(-1.42932031439161,-0.858020611615776,
6.63869873472032));
#52599=CARTESIAN_POINT('Ctrl Pts',(-1.45935210695291,-0.805891551873217,
6.63469027315199));
#52600=CARTESIAN_POINT('Ctrl Pts',(-1.48649583580301,-0.752254032983745,
6.63068181158365));
#52601=CARTESIAN_POINT('Ctrl Pts',(-1.513623308913,-0.69864863634145,6.62667575058858));
#52602=CARTESIAN_POINT('Ctrl Pts',(-1.53786590946504,-0.64353704156858,
6.6226696895935));
#52603=CARTESIAN_POINT('Ctrl Pts',(-1.55906143185519,-0.587267785342983,
6.61866362859842));
#52604=CARTESIAN_POINT('Ctrl Pts',(-1.5802611282017,-0.530987448219456,
6.61465677870447));
#52605=CARTESIAN_POINT('Ctrl Pts',(-1.59841235068726,-0.473549484378439,
6.61064992881052));
#52606=CARTESIAN_POINT('Ctrl Pts',(-1.61340136598415,-0.415321600979855,
6.60664307891656));
#52607=CARTESIAN_POINT('Ctrl Pts',(-1.62839221593782,-0.357086590483304,
6.60263573858384));
#52608=CARTESIAN_POINT('Ctrl Pts',(-1.64021997286835,-0.298061983443024,
6.59862839825111));
#52609=CARTESIAN_POINT('Ctrl Pts',(-1.64882174457498,-0.238627019879811,
6.59462105791838));
#52610=CARTESIAN_POINT('Ctrl Pts',(-1.6574325906907,-0.17912935560886,6.59060949005593));
#52611=CARTESIAN_POINT('Ctrl Pts',(-1.66281060799695,-0.11922099634073,
6.58659792219348));
#52612=CARTESIAN_POINT('Ctrl Pts',(-1.66494479657224,-0.0592859542136217,
6.58258635433103));
#52613=CARTESIAN_POINT('Ctrl Pts',(-1.66566597282296,-0.0390329505810895,
6.58123078177103));
#52614=CARTESIAN_POINT('Ctrl Pts',(-1.66601718561314,-0.018776894683292,
6.57987520921102));
#52615=CARTESIAN_POINT('Ctrl Pts',(-1.66599935370279,0.00146746784765552,
6.57851963665101));
#52616=CARTESIAN_POINT('Ctrl Pts',(-1.66599935370225,0.00146746846315725,
6.5785196366098));
#52617=CARTESIAN_POINT('Ctrl Pts',(-1.6659232556358,0.0878606910078806,
6.57273470356118));
#52618=CARTESIAN_POINT('Ctrl Pts',(-1.65912355325152,0.173965024338304,
6.56694977051255));
#52619=CARTESIAN_POINT('Ctrl Pts',(-1.64575458441607,0.258935991846446,
6.56116483746393));
#52620=CARTESIAN_POINT('Ctrl Pts',(-1.64151833437882,0.285860900468906,
6.55933175496188));
#52621=CARTESIAN_POINT('Ctrl Pts',(-1.63662281188489,0.312672235995731,
6.55749867245984));
#52622=CARTESIAN_POINT('Ctrl Pts',(-1.63107384411665,0.33934365330522,6.55566558995779));
#52623=CARTESIAN_POINT('Ctrl Pts',(-1.61875004980614,0.398578645220827,
6.55159446670515));
#52624=CARTESIAN_POINT('Ctrl Pts',(-1.60316934486775,0.457265793435973,
6.54752334345252));
#52625=CARTESIAN_POINT('Ctrl Pts',(-1.58439600177926,0.515019717628247,
6.54345222019989));
#52626=CARTESIAN_POINT('Ctrl Pts',(-1.57779998825323,0.535311557145502,
6.54202183116827));
#52627=CARTESIAN_POINT('Ctrl Pts',(-1.57081032106996,0.555488243876114,
6.54059144213665));
#52628=CARTESIAN_POINT('Ctrl Pts',(-1.56343130033213,0.575533291080354,
6.53916105310504));
#52629=CARTESIAN_POINT('',(-1.66802315249176,-0.000391568300512965,6.77148035500218));
#52630=CARTESIAN_POINT('Ctrl Pts',(-1.56343130033213,0.575533291080356,
6.73212871955268));
#52631=CARTESIAN_POINT('Ctrl Pts',(-1.58437359469063,0.518643726204979,
6.7361714094358));
#52632=CARTESIAN_POINT('Ctrl Pts',(-1.60219502983243,0.460641333802882,
6.74021409931893));
#52633=CARTESIAN_POINT('Ctrl Pts',(-1.61679613988877,0.401903274483785,
6.74425678920205));
#52634=CARTESIAN_POINT('Ctrl Pts',(-1.63140630364826,0.343128793484995,
6.74830198583391));
#52635=CARTESIAN_POINT('Ctrl Pts',(-1.64279207437441,0.283618247859168,
6.75234718246577));
#52636=CARTESIAN_POINT('Ctrl Pts',(-1.65090535474822,0.22375770302644,6.75639237909763));
#52637=CARTESIAN_POINT('Ctrl Pts',(-1.65903219328059,0.163797124825988,
6.76044433568537));
#52638=CARTESIAN_POINT('Ctrl Pts',(-1.66387559686924,0.103485897178399,
6.76449629227311));
#52639=CARTESIAN_POINT('Ctrl Pts',(-1.66543948648741,0.0432124617274922,
6.76854824886085));
#52640=CARTESIAN_POINT('Ctrl Pts',(-1.66581670718901,0.0286741034288136,
6.76952560806134));
#52641=CARTESIAN_POINT('Ctrl Pts',(-1.66600336108037,0.0141379256247708,
6.77050296726184));
#52642=CARTESIAN_POINT('Ctrl Pts',(-1.66599995419501,-0.000390668954461738,
6.77148032646233));
#52643=CARTESIAN_POINT('Ctrl Pts',(-1.66861778291936,-0.000391832623850849,
6.77148036339021));
#52644=CARTESIAN_POINT('Ctrl Pts',(-1.6686848074759,-0.0215969675807088,
6.77290462385233));
#52645=CARTESIAN_POINT('Ctrl Pts',(-1.6587079728118,-0.594273333106494,
6.81137325697827));
#52646=CARTESIAN_POINT('Ctrl Pts',(-1.00379156239439,-1.69403691970776,
6.88688626276814));
#52647=CARTESIAN_POINT('Ctrl Pts',(0.878789376459558,-1.76212723743541,
6.99801938075967));
#52648=CARTESIAN_POINT('Ctrl Pts',(1.95705435814059,-0.217444966801504,
7.10915249875125));
#52649=CARTESIAN_POINT('Ctrl Pts',(1.24415313987909,1.52624920138375,7.2202856167428));
#52650=CARTESIAN_POINT('Ctrl Pts',(-0.54953016239235,1.86221269474568,7.32794240943418));
#52651=CARTESIAN_POINT('Ctrl Pts',(-1.38933594127079,1.04443851451104,7.39855482946173));
#52652=CARTESIAN_POINT('Ctrl Pts',(-1.56542652693575,0.576282819883045,
7.43212287682542));
#52653=CARTESIAN_POINT('Origin',(0.,0.,11.));
#52654=CARTESIAN_POINT('',(-1.56343125288101,0.575533419980911,8.13202453882405));
#52655=CARTESIAN_POINT('',(-1.56343130037338,0.575533290968306,7.93773948050229));
#52656=CARTESIAN_POINT('',(-1.56343130033213,0.575533291080363,11.));
#52657=CARTESIAN_POINT('',(-1.66599999908997,-4.79547439094931E-5,7.2784065460554));
#52658=CARTESIAN_POINT('Ctrl Pts',(-1.56343130037338,0.575533290968306,
7.93773948050229));
#52659=CARTESIAN_POINT('Ctrl Pts',(-1.56203167958964,0.579335348948783,
7.93747628670542));
#52660=CARTESIAN_POINT('Ctrl Pts',(-1.56061816780054,0.583132360757538,
7.93721352742289));
#52661=CARTESIAN_POINT('Ctrl Pts',(-1.52941980829979,0.666012212448588,
7.93147968907109));
#52662=CARTESIAN_POINT('Ctrl Pts',(-1.49367280698885,0.742725695065311,
7.92621285832387));
#52663=CARTESIAN_POINT('Ctrl Pts',(-1.41856412868489,0.876332300525138,
7.91679788001118));
#52664=CARTESIAN_POINT('Ctrl Pts',(-1.38119752976503,0.934117609802933,
7.91263118292001));
#52665=CARTESIAN_POINT('Ctrl Pts',(-1.29770071258179,1.04722985814079,7.90398608123366));
#52666=CARTESIAN_POINT('Ctrl Pts',(-1.25134409869333,1.10220362883284,7.89951043725754));
#52667=CARTESIAN_POINT('Ctrl Pts',(-1.19356861801233,1.16236144131602,7.89405453492981));
#52668=CARTESIAN_POINT('Ctrl Pts',(-1.18545864918019,1.17063142740574,7.89329119735067));
#52669=CARTESIAN_POINT('Ctrl Pts',(-1.17271635867476,1.18335693629053,7.89209439707652));
#52670=CARTESIAN_POINT('Ctrl Pts',(-1.1681431862635,1.18787153745432,7.89166536779943));
#52671=CARTESIAN_POINT('Ctrl Pts',(-1.15965868270193,1.196150998751,7.89087004844909));
#52672=CARTESIAN_POINT('Ctrl Pts',(-1.15575492822701,1.19992333712037,7.89050434613051));
#52673=CARTESIAN_POINT('Ctrl Pts',(-1.14664122884843,1.20864449944749,7.88965114894849));
#52674=CARTESIAN_POINT('Ctrl Pts',(-1.14141765726347,1.21357874101211,7.88916258463778));
#52675=CARTESIAN_POINT('Ctrl Pts',(-1.12461588725819,1.22924543813192,7.88759300970436));
#52676=CARTESIAN_POINT('Ctrl Pts',(-1.1129173822338,1.23984680349988,7.88650303301046));
#52677=CARTESIAN_POINT('Ctrl Pts',(-1.04739204974372,1.2975522956479,7.88042200299868));
#52678=CARTESIAN_POINT('Ctrl Pts',(-0.990730009531427,1.34131431840367,
7.87525506931943));
#52679=CARTESIAN_POINT('Ctrl Pts',(-0.822406924389784,1.45481826894151,
7.86049590815139));
#52680=CARTESIAN_POINT('Ctrl Pts',(-0.705032198314378,1.515186711633,7.85091798884808));
#52681=CARTESIAN_POINT('Ctrl Pts',(-0.555783209276239,1.57080545575826,
7.83990310376356));
#52682=CARTESIAN_POINT('Ctrl Pts',(-0.52956327293834,1.57983785723202,7.83800631379048));
#52683=CARTESIAN_POINT('Ctrl Pts',(-0.491113492200113,1.59201833851759,
7.83527845449046));
#52684=CARTESIAN_POINT('Ctrl Pts',(-0.479055226254828,1.59568823952241,
7.83443050877856));
#52685=CARTESIAN_POINT('Ctrl Pts',(-0.457555813789876,1.60196584800041,
7.83293166317161));
#52686=CARTESIAN_POINT('Ctrl Pts',(-0.448131259840776,1.60462777050816,
7.83227902719695));
#52687=CARTESIAN_POINT('Ctrl Pts',(-0.428355727259881,1.61002546024071,
7.83091855409284));
#52688=CARTESIAN_POINT('Ctrl Pts',(-0.418000718261679,1.61274487141033,
7.83021127212468));
#52689=CARTESIAN_POINT('Ctrl Pts',(-0.390644924277279,1.61964781505652,
7.82835571014951));
#52690=CARTESIAN_POINT('Ctrl Pts',(-0.373602876372885,1.62366358286086,
7.82721283622368));
#52691=CARTESIAN_POINT('Ctrl Pts',(-0.28704871716064,1.64262412082784,7.82146955298152));
#52692=CARTESIAN_POINT('Ctrl Pts',(-0.216689840352994,1.65337784495494,
7.81700390013926));
#52693=CARTESIAN_POINT('Ctrl Pts',(-0.0773918888731418,1.66561984045195,
7.80836330926929));
#52694=CARTESIAN_POINT('Ctrl Pts',(-0.00862510000589039,1.66739460781424,
7.80419147471088));
#52695=CARTESIAN_POINT('Ctrl Pts',(0.0816869642174986,1.66413694338963,
7.79866064156089));
#52696=CARTESIAN_POINT('Ctrl Pts',(0.103300792882507,1.66293518957471,7.79733277290003));
#52697=CARTESIAN_POINT('Ctrl Pts',(0.18986870854935,1.65642767884693,7.79197795655623));
#52698=CARTESIAN_POINT('Ctrl Pts',(0.254502549675237,1.64773456119734,7.78789849265241));
#52699=CARTESIAN_POINT('Ctrl Pts',(0.329698051633503,1.63309107067683,7.78288596728083));
#52700=CARTESIAN_POINT('Ctrl Pts',(0.340919994515537,1.63078532917877,7.78213080168778));
#52701=CARTESIAN_POINT('Ctrl Pts',(0.35837035369613,1.6270118696835,7.78094412531749));
#52702=CARTESIAN_POINT('Ctrl Pts',(0.364615854345756,1.62562363720488,7.78051692974959));
#52703=CARTESIAN_POINT('Ctrl Pts',(0.376149827627841,1.62299008790842,7.77972313974866));
#52704=CARTESIAN_POINT('Ctrl Pts',(0.381440394439455,1.62175483369005,7.77935711257207));
#52705=CARTESIAN_POINT('Ctrl Pts',(0.393755361359132,1.61881591280597,7.7785006751061));
#52706=CARTESIAN_POINT('Ctrl Pts',(0.400774785914,1.61709239385297,7.77800916726913));
#52707=CARTESIAN_POINT('Ctrl Pts',(0.423317443318386,1.61140158034417,7.77642041243889));
#52708=CARTESIAN_POINT('Ctrl Pts',(0.438794194949957,1.60725614582408,7.77531390044416));
#52709=CARTESIAN_POINT('Ctrl Pts',(0.47585049621588,1.59675555828877,7.77263041949507));
#52710=CARTESIAN_POINT('Ctrl Pts',(0.497365469345877,1.59018536498431,7.77104429182738));
#52711=CARTESIAN_POINT('Ctrl Pts',(0.58192220943867,1.5624798083997,7.76471538870989));
#52712=CARTESIAN_POINT('Ctrl Pts',(0.643805522566909,1.53801500333623,7.75987442210042));
#52713=CARTESIAN_POINT('Ctrl Pts',(0.813236180856755,1.45901146271352,7.74626611905016));
#52714=CARTESIAN_POINT('Ctrl Pts',(0.916590094540017,1.39640257164126,7.7375695493467));
#52715=CARTESIAN_POINT('Ctrl Pts',(1.02899247990305,1.31040920176224,7.72783379107058));
#52716=CARTESIAN_POINT('Ctrl Pts',(1.04544377789134,1.29732231034052,7.72639991075937));
#52717=CARTESIAN_POINT('Ctrl Pts',(1.07133086541784,1.27591699551742,7.72412824001751));
#52718=CARTESIAN_POINT('Ctrl Pts',(1.0809273083582,1.26779737013674,7.72328262027302));
#52719=CARTESIAN_POINT('Ctrl Pts',(1.09783149118202,1.25316312828287,7.72178642395067));
#52720=CARTESIAN_POINT('Ctrl Pts',(1.10517534132402,1.24669133352132,7.72113413246839));
#52721=CARTESIAN_POINT('Ctrl Pts',(1.12044350104216,1.23299526774308,7.71977292720715));
#52722=CARTESIAN_POINT('Ctrl Pts',(1.12835598383182,1.22575843954846,7.7190645812382));
#52723=CARTESIAN_POINT('Ctrl Pts',(1.14905912024425,1.20645280386827,7.71720292230378));
#52724=CARTESIAN_POINT('Ctrl Pts',(1.16172972827058,1.19425680093639,7.71605508152727));
#52725=CARTESIAN_POINT('Ctrl Pts',(1.22554333447997,1.13085661772156,7.71022516209965));
#52726=CARTESIAN_POINT('Ctrl Pts',(1.27350709887378,1.0765568814807,7.7056831018695));
#52727=CARTESIAN_POINT('Ctrl Pts',(1.37964267794661,0.939341072402296,7.69497088398202));
#52728=CARTESIAN_POINT('Ctrl Pts',(1.4340842280218,0.853918438366526,7.6888979597863));
#52729=CARTESIAN_POINT('Ctrl Pts',(1.50505037886791,0.71641980291791,7.67928742194019));
#52730=CARTESIAN_POINT('Ctrl Pts',(1.5273352979142,0.667592407638185,7.67590022567893));
#52731=CARTESIAN_POINT('Ctrl Pts',(1.55135082598887,0.607445850336167,7.67165945351622));
#52732=CARTESIAN_POINT('Ctrl Pts',(1.55537371361498,0.597069879449797,7.67092546576335));
#52733=CARTESIAN_POINT('Ctrl Pts',(1.56151927727198,0.580735349026155,7.66976504207432));
#52734=CARTESIAN_POINT('Ctrl Pts',(1.56371256478532,0.574803453645227,7.66934262138998));
#52735=CARTESIAN_POINT('Ctrl Pts',(1.56756095812982,0.564210164745555,7.66858620995175));
#52736=CARTESIAN_POINT('Ctrl Pts',(1.5692291541367,0.559553685416715,7.66825299769306));
#52737=CARTESIAN_POINT('Ctrl Pts',(1.57322455731473,0.548242819132305,7.66744190969106));
#52738=CARTESIAN_POINT('Ctrl Pts',(1.57553027143562,0.54158107031377,7.66696280455243));
#52739=CARTESIAN_POINT('Ctrl Pts',(1.58262490038349,0.520654253127307,7.66545383506735));
#52740=CARTESIAN_POINT('Ctrl Pts',(1.58726271509061,0.506339274031315,7.66441591719923));
#52741=CARTESIAN_POINT('Ctrl Pts',(1.61071308974657,0.430467683600849,7.65889182748528));
#52742=CARTESIAN_POINT('Ctrl Pts',(1.626138663875,0.367927275960877,7.65426105383625));
#52743=CARTESIAN_POINT('Ctrl Pts',(1.65815475690377,0.195802136858974,7.64155515371738));
#52744=CARTESIAN_POINT('Ctrl Pts',(1.66750240072857,0.0851847124579617,
7.63345142371556));
#52745=CARTESIAN_POINT('Ctrl Pts',(1.66505605876994,-0.0743218353707407,
7.62219024586661));
#52746=CARTESIAN_POINT('Ctrl Pts',(1.66216627484113,-0.123042768685657,
7.61880338032627));
#52747=CARTESIAN_POINT('Ctrl Pts',(1.65548151757932,-0.18760835178785,7.61438435887574));
#52748=CARTESIAN_POINT('Ctrl Pts',(1.65358835242325,-0.203621072538078,
7.61329401414415));
#52749=CARTESIAN_POINT('Ctrl Pts',(1.65009072614499,-0.229923838817994,
7.61151166329134));
#52750=CARTESIAN_POINT('Ctrl Pts',(1.64862175570864,-0.240230496126132,
7.61081545119238));
#52751=CARTESIAN_POINT('Ctrl Pts',(1.64556620760834,-0.260319116061852,
7.60946251370362));
#52752=CARTESIAN_POINT('Ctrl Pts',(1.64398877706552,-0.270102006497136,
7.608805530402));
#52753=CARTESIAN_POINT('Ctrl Pts',(1.64004434347754,-0.293248569707283,
7.60725523623124));
#52754=CARTESIAN_POINT('Ctrl Pts',(1.63760112436008,-0.306598675356894,
7.60636437089141));
#52755=CARTESIAN_POINT('Ctrl Pts',(1.62871706348561,-0.352002201990275,
7.60334439516172));
#52756=CARTESIAN_POINT('Ctrl Pts',(1.62149578239099,-0.383896442527733,
7.60123994943381));
#52757=CARTESIAN_POINT('Ctrl Pts',(1.60144971967129,-0.461721960612977,
7.59612839119122));
#52758=CARTESIAN_POINT('Ctrl Pts',(1.58758293839445,-0.507355191672065,
7.59315215536533));
#52759=CARTESIAN_POINT('Ctrl Pts',(1.54918887881588,-0.616613273432739,
7.58599864896742));
#52760=CARTESIAN_POINT('Ctrl Pts',(1.52267861091282,-0.679446950595287,
7.5818625136953));
#52761=CARTESIAN_POINT('Ctrl Pts',(1.48307617590744,-0.759263229096041,
7.57640920392172));
#52762=CARTESIAN_POINT('Ctrl Pts',(1.47340367045259,-0.777867079452008,
7.5751230087387));
#52763=CARTESIAN_POINT('Ctrl Pts',(1.43199202029695,-0.853972038806598,
7.56978006534775));
#52764=CARTESIAN_POINT('Ctrl Pts',(1.39722107955565,-0.909747521852442,
7.56567027712554));
#52765=CARTESIAN_POINT('Ctrl Pts',(1.35262264314003,-0.972676483095749,
7.56062373859525));
#52766=CARTESIAN_POINT('Ctrl Pts',(1.34589433159103,-0.981965368933563,
7.55986771350742));
#52767=CARTESIAN_POINT('Ctrl Pts',(1.33526260974925,-0.996328628491809,
7.55867997023001));
#52768=CARTESIAN_POINT('Ctrl Pts',(1.3314247994995,-1.00145143307113,7.55825257955836));
#52769=CARTESIAN_POINT('Ctrl Pts',(1.32427542905052,-1.01088085395981,7.55745862984345));
#52770=CARTESIAN_POINT('Ctrl Pts',(1.32097220893052,-1.0151935445841,7.55709264025634));
#52771=CARTESIAN_POINT('Ctrl Pts',(1.31322769511709,-1.02520300355487,7.55623655680515));
#52772=CARTESIAN_POINT('Ctrl Pts',(1.30877040104304,-1.03088709867353,7.55574536843683));
#52773=CARTESIAN_POINT('Ctrl Pts',(1.29432353097421,-1.04906553567565,7.55415868224063));
#52774=CARTESIAN_POINT('Ctrl Pts',(1.28419125981278,-1.06144461102018,7.55305395168622));
#52775=CARTESIAN_POINT('Ctrl Pts',(1.25941632729917,-1.09083930834098,7.55037563659613));
#52776=CARTESIAN_POINT('Ctrl Pts',(1.24460515595084,-1.10770834873514,7.54879293679362));
#52777=CARTESIAN_POINT('Ctrl Pts',(1.18475603471489,-1.17315692544292,7.5424852571565));
#52778=CARTESIAN_POINT('Ctrl Pts',(1.13718010090682,-1.21932954753163,7.5376626606121));
#52779=CARTESIAN_POINT('Ctrl Pts',(0.995415658981791,-1.34138128937493,
7.52404543084659));
#52780=CARTESIAN_POINT('Ctrl Pts',(0.895525107244398,-1.41003580619472,
7.51532113868231));
#52781=CARTESIAN_POINT('Ctrl Pts',(0.770575909994075,-1.47723041668697,
7.50556181072833));
#52782=CARTESIAN_POINT('Ctrl Pts',(0.75189497190746,-1.48682579946201,7.5041293623527));
#52783=CARTESIAN_POINT('Ctrl Pts',(0.721754392967581,-1.50159396992655,
7.5018595108875));
#52784=CARTESIAN_POINT('Ctrl Pts',(0.710409497078258,-1.50699443123085,
7.5010142979853));
#52785=CARTESIAN_POINT('Ctrl Pts',(0.690120194140464,-1.51637261523005,
7.49951857380165));
#52786=CARTESIAN_POINT('Ctrl Pts',(0.681199897062275,-1.52040076882696,
7.49886635121487));
#52787=CARTESIAN_POINT('Ctrl Pts',(0.662431304005329,-1.52867779268205,
7.49750504386035));
#52788=CARTESIAN_POINT('Ctrl Pts',(0.652576405337925,-1.53291065318148,
7.49679652903752));
#52789=CARTESIAN_POINT('Ctrl Pts',(0.626445373352033,-1.54383673968681,
7.49493386521295));
#52790=CARTESIAN_POINT('Ctrl Pts',(0.610102604430971,-1.55036787089468,
7.49378519957891));
#52791=CARTESIAN_POINT('Ctrl Pts',(0.5258374232313,-1.58250427075608,7.48794043496538));
#52792=CARTESIAN_POINT('Ctrl Pts',(0.456393440769253,-1.60391137502625,
7.4833852717658));
#52793=CARTESIAN_POINT('Ctrl Pts',(0.286466541623964,-1.64435767834013,
7.47260009139512));
#52794=CARTESIAN_POINT('Ctrl Pts',(0.185208745897852,-1.65881631187453,
7.46647023069352));
#52795=CARTESIAN_POINT('Ctrl Pts',(0.0308040314928705,-1.66654328678569,
7.45686034967894));
#52796=CARTESIAN_POINT('Ctrl Pts',(-0.0217498511324031,-1.66668568808929,
7.45354073293712));
#52797=CARTESIAN_POINT('Ctrl Pts',(-0.0852748826907004,-1.66385297487849,
7.44937636382131));
#52798=CARTESIAN_POINT('Ctrl Pts',(-0.0963275598338264,-1.66324968440033,
7.4486462154374));
#52799=CARTESIAN_POINT('Ctrl Pts',(-0.113670902098468,-1.66212958416681,
7.44749055956977));
#52800=CARTESIAN_POINT('Ctrl Pts',(-0.119966275335952,-1.6616870698292,
7.44706901411883));
#52801=CARTESIAN_POINT('Ctrl Pts',(-0.131193345854335,-1.66083376527879,
7.44631331683516));
#52802=CARTESIAN_POINT('Ctrl Pts',(-0.136125941544077,-1.66043675444058,
7.44597993390369));
#52803=CARTESIAN_POINT('Ctrl Pts',(-0.148100824991372,-1.65941921293976,
7.44516729831359));
#52804=CARTESIAN_POINT('Ctrl Pts',(-0.155140955413846,-1.6587758311529,
7.44468680337489));
#52805=CARTESIAN_POINT('Ctrl Pts',(-0.177260090386513,-1.65661237110843,
7.44316897997566));
#52806=CARTESIAN_POINT('Ctrl Pts',(-0.192322080930886,-1.65493137762875,
7.44212346717845));
#52807=CARTESIAN_POINT('Ctrl Pts',(-0.272226218972042,-1.64490818447049,
7.43652062529918));
#52808=CARTESIAN_POINT('Ctrl Pts',(-0.336552692460002,-1.63296069560572,
7.43181442663552));
#52809=CARTESIAN_POINT('Ctrl Pts',(-0.510208695556801,-1.59000979200692,
7.4188280656632));
#52810=CARTESIAN_POINT('Ctrl Pts',(-0.617353601413024,-1.55155545277638,
7.41052315312256));
#52811=CARTESIAN_POINT('Ctrl Pts',(-0.760836352732686,-1.48282111383551,
7.39932123578709));
#52812=CARTESIAN_POINT('Ctrl Pts',(-0.801091048262076,-1.46146646465998,
7.39616476751244));
#52813=CARTESIAN_POINT('Ctrl Pts',(-0.854045407294286,-1.4305283428751,
7.3919920129286));
#52814=CARTESIAN_POINT('Ctrl Pts',(-0.867554072470824,-1.42237648271265,
7.39092558755175));
#52815=CARTESIAN_POINT('Ctrl Pts',(-0.889719375952903,-1.408567462375,7.38917196515257));
#52816=CARTESIAN_POINT('Ctrl Pts',(-0.898442532904366,-1.40301956058863,
7.38848082738135));
#52817=CARTESIAN_POINT('Ctrl Pts',(-0.914858132597249,-1.39236340369709,
7.38717807356309));
#52818=CARTESIAN_POINT('Ctrl Pts',(-0.922560809386965,-1.38727171439515,
7.38656587525558));
#52819=CARTESIAN_POINT('Ctrl Pts',(-0.938274947918068,-1.37669545434223,
7.38531484280078));
#52820=CARTESIAN_POINT('Ctrl Pts',(-0.946281605075904,-1.37120435473242,
7.38467628300811));
#52821=CARTESIAN_POINT('Ctrl Pts',(-0.973836879576364,-1.35195017596629,
7.38247419769189));
#52822=CARTESIAN_POINT('Ctrl Pts',(-0.993137540343235,-1.3378361131102,
7.38092398699142));
#52823=CARTESIAN_POINT('Ctrl Pts',(-1.03693124984591,-1.30434068666832,
7.37738209402012));
#52824=CARTESIAN_POINT('Ctrl Pts',(-1.06119673481312,-1.284676110951,7.3754012877494));
#52825=CARTESIAN_POINT('Ctrl Pts',(-1.14720843019216,-1.21087178791761,
7.36828392343225));
#52826=CARTESIAN_POINT('Ctrl Pts',(-1.2054854172128,-1.15286760463915,7.36328005521498));
#52827=CARTESIAN_POINT('Ctrl Pts',(-1.32204604946778,-1.01830696537451,
7.35240806219065));
#52828=CARTESIAN_POINT('Ctrl Pts',(-1.37845725767284,-0.94053472457296,
7.34655577552778));
#52829=CARTESIAN_POINT('Ctrl Pts',(-1.4358570166171,-0.845051238605321,
7.33932418678922));
#52830=CARTESIAN_POINT('Ctrl Pts',(-1.4436681553688,-0.831636448739964,
7.33830703240984));
#52831=CARTESIAN_POINT('Ctrl Pts',(-1.4547582326804,-0.811963272076779,
7.33681071336021));
#52832=CARTESIAN_POINT('Ctrl Pts',(-1.45818687081421,-0.805789622686513,
7.33634049867003));
#52833=CARTESIAN_POINT('Ctrl Pts',(-1.46420523223495,-0.794788680261306,
7.33550111699643));
#52834=CARTESIAN_POINT('Ctrl Pts',(-1.46681054641897,-0.789970143705068,
7.33513293935582));
#52835=CARTESIAN_POINT('Ctrl Pts',(-1.47243214868636,-0.779449279424317,
7.33432783787045));
#52836=CARTESIAN_POINT('Ctrl Pts',(-1.47543905303211,-0.773742340152184,
7.33389037737111));
#52837=CARTESIAN_POINT('Ctrl Pts',(-1.48395726036867,-0.757345039123737,
7.33263164860389));
#52838=CARTESIAN_POINT('Ctrl Pts',(-1.48938590554173,-0.746612524929958,
7.33180558737968));
#52839=CARTESIAN_POINT('Ctrl Pts',(-1.50152197018099,-0.7219601857328,7.32990474100212));
#52840=CARTESIAN_POINT('Ctrl Pts',(-1.50815281999854,-0.708004075085849,
7.32882619685348));
#52841=CARTESIAN_POINT('Ctrl Pts',(-1.52969675251713,-0.660983688600064,
7.32518897326475));
#52842=CARTESIAN_POINT('Ctrl Pts',(-1.54372337272971,-0.62752642248085,
7.32259547314784));
#52843=CARTESIAN_POINT('Ctrl Pts',(-1.5975735351535,-0.486320312482772,
7.3116959148403));
#52844=CARTESIAN_POINT('Ctrl Pts',(-1.62729684335138,-0.375043273491927,
7.30324382829815));
#52845=CARTESIAN_POINT('Ctrl Pts',(-1.65472558481929,-0.202525010328851,
7.29081226443812));
#52846=CARTESIAN_POINT('Ctrl Pts',(-1.66093006189091,-0.142989399614902,
7.28663378098082));
#52847=CARTESIAN_POINT('Ctrl Pts',(-1.66470165887666,-0.0675995426412908,
7.28148533229496));
#52848=CARTESIAN_POINT('Ctrl Pts',(-1.66526362916107,-0.0519459883801228,
7.28042390530268));
#52849=CARTESIAN_POINT('Ctrl Pts',(-1.66576334716281,-0.0290080946149532,
7.27887919665032));
#52850=CARTESIAN_POINT('Ctrl Pts',(-1.66587420348213,-0.0217287688149204,
7.27839055247581));
#52851=CARTESIAN_POINT('Ctrl Pts',(-1.6659786942146,-0.0096810953192746,
7.27758434923517));
#52852=CARTESIAN_POINT('Ctrl Pts',(-1.6659995782681,-0.0049131518317435,
7.2772659444449));
#52853=CARTESIAN_POINT('Ctrl Pts',(-1.66599999367699,-0.000145149081000685,
7.2769481782774));
#52854=CARTESIAN_POINT('Ctrl Pts',(-1.66599999950973,-4.04177140652074E-5,
7.2785196366098));
#52855=CARTESIAN_POINT('Ctrl Pts',(-1.66600154979607,0.0638616881954464,
7.27426975137157));
#52856=CARTESIAN_POINT('Ctrl Pts',(-1.66232218862922,0.12769579053969,7.27001986613334));
#52857=CARTESIAN_POINT('Ctrl Pts',(-1.6550110968451,0.191034733280547,7.26576998089511));
#52858=CARTESIAN_POINT('Ctrl Pts',(-1.64741960037028,0.256802935176299,
7.2613570984205));
#52859=CARTESIAN_POINT('Ctrl Pts',(-1.63591224260331,0.322036701043425,
7.25694421594588));
#52860=CARTESIAN_POINT('Ctrl Pts',(-1.62060186852973,0.38627138609784,7.25253133347127));
#52861=CARTESIAN_POINT('Ctrl Pts',(-1.60529149445616,0.450506071152247,
7.24811845099666));
#52862=CARTESIAN_POINT('Ctrl Pts',(-1.58617832364918,0.513741195306885,
7.24370556852205));
#52863=CARTESIAN_POINT('Ctrl Pts',(-1.56343130033213,0.575533291080367,
7.23929268604743));
#52864=CARTESIAN_POINT('',(-1.66554611378498,0.00151667131590039,7.47148008516546));
#52865=CARTESIAN_POINT('Ctrl Pts',(-1.56542652693575,0.576282819883045,
7.43212287682542));
#52866=CARTESIAN_POINT('Ctrl Pts',(-1.58366256406465,0.527800360715211,
7.43559920212559));
#52867=CARTESIAN_POINT('Ctrl Pts',(-1.64345104496323,0.34162213868473,7.44871827157227));
#52868=CARTESIAN_POINT('Ctrl Pts',(-1.66683094149558,0.145771637880644,
7.46183734101896));
#52869=CARTESIAN_POINT('Ctrl Pts',(-1.66554611378498,0.00151667131590039,
7.47148008516546));
#52870=CARTESIAN_POINT('Ctrl Pts',(-1.66599929579717,0.00153179741720764,
7.47174074231814));
#52871=CARTESIAN_POINT('Ctrl Pts',(-1.66606511006422,-0.0700485051244551,
7.47693011686521));
#52872=CARTESIAN_POINT('Ctrl Pts',(-1.66151769774625,-0.141566932664853,
7.48206009460744));
#52873=CARTESIAN_POINT('Ctrl Pts',(-1.64823818144976,-0.2447886730157,7.48933257774257));
#52874=CARTESIAN_POINT('Ctrl Pts',(-1.64315337568767,-0.27687150814081,
7.49157503229734));
#52875=CARTESIAN_POINT('Ctrl Pts',(-1.63482770468238,-0.321012704599486,
7.49463648679051));
#52876=CARTESIAN_POINT('Ctrl Pts',(-1.63238487073116,-0.333212288034103,
7.495480086183));
#52877=CARTESIAN_POINT('Ctrl Pts',(-1.62782711951716,-0.354719525273596,
7.49696311147657));
#52878=CARTESIAN_POINT('Ctrl Pts',(-1.62576847419785,-0.364038387434114,
7.49760429138865));
#52879=CARTESIAN_POINT('Ctrl Pts',(-1.62143651622804,-0.382877812467173,
7.49889786597761));
#52880=CARTESIAN_POINT('Ctrl Pts',(-1.61915914774067,-0.392397065168229,
7.49955010240221));
#52881=CARTESIAN_POINT('Ctrl Pts',(-1.61421016497247,-0.412306464290104,
7.5009115777872));
#52882=CARTESIAN_POINT('Ctrl Pts',(-1.61152181008147,-0.422692017796528,
7.50162024551048));
#52883=CARTESIAN_POINT('Ctrl Pts',(-1.60415669725266,-0.45005253573993,
7.5034836324523));
#52884=CARTESIAN_POINT('Ctrl Pts',(-1.59931075845737,-0.466980867530226,
7.50463286115424));
#52885=CARTESIAN_POINT('Ctrl Pts',(-1.57534973076255,-0.545931375598749,
7.50997990966618));
#52886=CARTESIAN_POINT('Ctrl Pts',(-1.5528884182984,-0.606882888538146,
7.51406792988093));
#52887=CARTESIAN_POINT('Ctrl Pts',(-1.48857539560215,-0.754249346768935,
7.52403223824845));
#52888=CARTESIAN_POINT('Ctrl Pts',(-1.44271212550968,-0.838647834028354,
7.52980624492016));
#52889=CARTESIAN_POINT('Ctrl Pts',(-1.35609292016508,-0.969698368615669,
7.53949342533846));
#52890=CARTESIAN_POINT('Ctrl Pts',(-1.31955528573769,-1.01885973066696,
7.54332040886845));
#52891=CARTESIAN_POINT('Ctrl Pts',(-1.27144415378068,-1.07665302696314,
7.54821253474785));
#52892=CARTESIAN_POINT('Ctrl Pts',(-1.26235269870898,-1.08729830740719,
7.54913118695542));
#52893=CARTESIAN_POINT('Ctrl Pts',(-1.24849314072053,-1.10311847086727,
7.55052528639408));
#52894=CARTESIAN_POINT('Ctrl Pts',(-1.24382437297918,-1.10838008278235,
7.55099385483223));
#52895=CARTESIAN_POINT('Ctrl Pts',(-1.23581725166109,-1.117289654297,7.55179601271377));
#52896=CARTESIAN_POINT('Ctrl Pts',(-1.23249575323544,-1.12095257189561,
7.55212835212134));
#52897=CARTESIAN_POINT('Ctrl Pts',(-1.22488155081081,-1.1292746874441,7.55288935121086));
#52898=CARTESIAN_POINT('Ctrl Pts',(-1.22057864391408,-1.13392411734268,
7.55331876327008));
#52899=CARTESIAN_POINT('Ctrl Pts',(-1.20861243642717,-1.14670696241178,
7.55451089892751));
#52900=CARTESIAN_POINT('Ctrl Pts',(-1.20089382329424,-1.15478781055824,
7.55527758177055));
#52901=CARTESIAN_POINT('Ctrl Pts',(-1.15487091837059,-1.20201016484932,
7.55983240784822));
#52902=CARTESIAN_POINT('Ctrl Pts',(-1.11474024097672,-1.23931763818206,
7.56373630352562));
#52903=CARTESIAN_POINT('Ctrl Pts',(-0.997439410417934,-1.33805329595476,
7.57480339429999));
#52904=CARTESIAN_POINT('Ctrl Pts',(-0.916538433098431,-1.39471535802987,
7.58204266147443));
#52905=CARTESIAN_POINT('Ctrl Pts',(-0.788758415227319,-1.46826538871721,
7.59261552521869));
#52906=CARTESIAN_POINT('Ctrl Pts',(-0.745359576585088,-1.49076588542471,
7.59607547705864));
#52907=CARTESIAN_POINT('Ctrl Pts',(-0.670850722051404,-1.52532689174123,
7.60178956246781));
#52908=CARTESIAN_POINT('Ctrl Pts',(-0.640256278989966,-1.53841963994834,
7.60407507782804));
#52909=CARTESIAN_POINT('Ctrl Pts',(-0.596573425602765,-1.5555843844099,
7.60725573063867));
#52910=CARTESIAN_POINT('Ctrl Pts',(-0.583797286906614,-1.56042410141119,
7.60817627107882));
#52911=CARTESIAN_POINT('Ctrl Pts',(-0.561639111401972,-1.56850757324789,
7.60975650491541));
#52912=CARTESIAN_POINT('Ctrl Pts',(-0.552285121072503,-1.57182557911951,
7.61041863758606));
#52913=CARTESIAN_POINT('Ctrl Pts',(-0.533086408394691,-1.57844311608841,
7.61176776878495));
#52914=CARTESIAN_POINT('Ctrl Pts',(-0.5232393606658,-1.58173460771746,7.61245447729455));
#52915=CARTESIAN_POINT('Ctrl Pts',(-0.498152223758011,-1.58986036152993,
7.61419107243432));
#52916=CARTESIAN_POINT('Ctrl Pts',(-0.482871911270453,-1.59456776387087,
7.61523678324587));
#52917=CARTESIAN_POINT('Ctrl Pts',(-0.421930410728298,-1.61238561757823,
7.61936256625576));
#52918=CARTESIAN_POINT('Ctrl Pts',(-0.375782985554731,-1.62376120063554,
7.62238689377845));
#52919=CARTESIAN_POINT('Ctrl Pts',(-0.219578268366115,-1.65524881249659,
7.63238012978473));
#52920=CARTESIAN_POINT('Ctrl Pts',(-0.108003527894205,-1.66625294721515,
7.63910055494325));
#52921=CARTESIAN_POINT('Ctrl Pts',(0.068598553793225,-1.66584655313675,
7.64996751217847));
#52922=CARTESIAN_POINT('Ctrl Pts',(0.133292675444497,-1.66192108996138,
7.65400312423229));
#52923=CARTESIAN_POINT('Ctrl Pts',(0.212570255889303,-1.65245199854183,
7.65918983361039));
#52924=CARTESIAN_POINT('Ctrl Pts',(0.227528534815957,-1.65045885981114,
7.66017923108757));
#52925=CARTESIAN_POINT('Ctrl Pts',(0.249439629064571,-1.64723577037253,
7.66164706266171));
#52926=CARTESIAN_POINT('Ctrl Pts',(0.256415476590733,-1.64616430243042,
7.6621171474832));
#52927=CARTESIAN_POINT('Ctrl Pts',(0.26826948284579,-1.64426639048574,7.66292100090787));
#52928=CARTESIAN_POINT('Ctrl Pts',(0.273151108871079,-1.64346248790184,
7.66325350468476));
#52929=CARTESIAN_POINT('Ctrl Pts',(0.28426016300007,-1.64158219318261,7.66401360070536));
#52930=CARTESIAN_POINT('Ctrl Pts',(0.290484951880989,-1.64049212940773,
7.66444193424402));
#52931=CARTESIAN_POINT('Ctrl Pts',(0.3076318398711,-1.63738877399296,7.6656282419087));
#52932=CARTESIAN_POINT('Ctrl Pts',(0.31854000686592,-1.63530168272758,7.66639011512619));
#52933=CARTESIAN_POINT('Ctrl Pts',(0.381434247155825,-1.62261480967266,
7.6708214168247));
#52934=CARTESIAN_POINT('Ctrl Pts',(0.432906395382925,-1.609646479883,7.67459951834391));
#52935=CARTESIAN_POINT('Ctrl Pts',(0.580896059449537,-1.56474901394487,
7.68575316171334));
#52936=CARTESIAN_POINT('Ctrl Pts',(0.675230307468231,-1.52641591423025,
7.69322004956054));
#52937=CARTESIAN_POINT('Ctrl Pts',(0.829844510994807,-1.4464318111034,7.70569617432575));
#52938=CARTESIAN_POINT('Ctrl Pts',(0.891971775772876,-1.40896978086581,
7.71078730172887));
#52939=CARTESIAN_POINT('Ctrl Pts',(0.96590976818101,-1.35752855430949,7.71693396908457));
#52940=CARTESIAN_POINT('Ctrl Pts',(0.980190480101765,-1.34725354701966,
7.71812579945101));
#52941=CARTESIAN_POINT('Ctrl Pts',(1.00291102710601,-1.33035351654904,7.72003022192212));
#52942=CARTESIAN_POINT('Ctrl Pts',(1.0114539635248,-1.32387004507877,7.72074821123819));
#52943=CARTESIAN_POINT('Ctrl Pts',(1.02767359117478,-1.31131186363387,7.72211535666721));
#52944=CARTESIAN_POINT('Ctrl Pts',(1.03536048002467,-1.30525112414625,7.72276502356839));
#52945=CARTESIAN_POINT('Ctrl Pts',(1.05279423744326,-1.29125452799047,7.72424275283952));
#52946=CARTESIAN_POINT('Ctrl Pts',(1.06250568992183,-1.28327535460166,7.72506903919155));
#52947=CARTESIAN_POINT('Ctrl Pts',(1.08820921005548,-1.26166486225525,7.72726524559726));
#52948=CARTESIAN_POINT('Ctrl Pts',(1.10403556524397,-1.24783935000791,7.72862725978399));
#52949=CARTESIAN_POINT('Ctrl Pts',(1.20891877081953,-1.15265801280928,7.73773260738465));
#52950=CARTESIAN_POINT('Ctrl Pts',(1.28917566899573,-1.06213701075134,7.74505952567361));
#52951=CARTESIAN_POINT('Ctrl Pts',(1.39736577450619,-0.909578346912501,
7.75648755336661));
#52952=CARTESIAN_POINT('Ctrl Pts',(1.43249730270166,-0.853178810569795,
7.76055511720956));
#52953=CARTESIAN_POINT('Ctrl Pts',(1.47489113962575,-0.775085353679222,
7.76617887338437));
#52954=CARTESIAN_POINT('Ctrl Pts',(1.48521302963107,-0.755118093401091,
7.76761627428513));
#52955=CARTESIAN_POINT('Ctrl Pts',(1.5021911859108,-0.720578963195752,7.77011222299979));
#52956=CARTESIAN_POINT('Ctrl Pts',(1.50904719011356,-0.706108301199287,
7.77116074308462));
#52957=CARTESIAN_POINT('Ctrl Pts',(1.51869291824966,-0.684967183717754,
7.77269986958501));
#52958=CARTESIAN_POINT('Ctrl Pts',(1.52164970748667,-0.678373337915016,
7.77318093290749));
#52959=CARTESIAN_POINT('Ctrl Pts',(1.5267541726125,-0.666788733680777,7.77402823585026));
#52960=CARTESIAN_POINT('Ctrl Pts',(1.52892047576051,-0.661806389022384,
7.77439334468097));
#52961=CARTESIAN_POINT('Ctrl Pts',(1.53358546406429,-0.650932085669827,
7.77519183288542));
#52962=CARTESIAN_POINT('Ctrl Pts',(1.53607454376806,-0.645036392993356,
7.7756257416792));
#52963=CARTESIAN_POINT('Ctrl Pts',(1.54292705929785,-0.628540761202718,
7.77684225581128));
#52964=CARTESIAN_POINT('Ctrl Pts',(1.54721505556059,-0.617910149206278,
7.77762907620787));
#52965=CARTESIAN_POINT('Ctrl Pts',(1.57523461865982,-0.54632461459301,7.78294241944471));
#52966=CARTESIAN_POINT('Ctrl Pts',(1.59546577626695,-0.48406790667297,7.78763367454426));
#52967=CARTESIAN_POINT('Ctrl Pts',(1.61771076303218,-0.398850927820837,
7.79401726211858));
#52968=CARTESIAN_POINT('Ctrl Pts',(1.62298943890232,-0.376796277985399,
7.79566628882188));
#52969=CARTESIAN_POINT('Ctrl Pts',(1.64308349721544,-0.284563756947635,
7.80253647332678));
#52970=CARTESIAN_POINT('Ctrl Pts',(1.65381047470781,-0.213569617150863,
7.80775806731946));
#52971=CARTESIAN_POINT('Ctrl Pts',(1.66374192572034,-0.0975577914778334,
7.81607844163075));
#52972=CARTESIAN_POINT('Ctrl Pts',(1.66576093713112,-0.0528753081618404,
7.81923371606509));
#52973=CARTESIAN_POINT('Ctrl Pts',(1.66613298995081,0.0230628265894545,
7.82450558909996));
#52974=CARTESIAN_POINT('Ctrl Pts',(1.6654080870238,0.054287794878682,7.82664754018315));
#52975=CARTESIAN_POINT('Ctrl Pts',(1.66312159779956,0.0987948085461002,
7.82966563439978));
#52976=CARTESIAN_POINT('Ctrl Pts',(1.66227743114115,0.112105410858295,7.83056380139308));
#52977=CARTESIAN_POINT('Ctrl Pts',(1.66053052740909,0.135247150480129,7.83211799397676));
#52978=CARTESIAN_POINT('Ctrl Pts',(1.65970008871767,0.1450828966386,7.83277624422192));
#52979=CARTESIAN_POINT('Ctrl Pts',(1.65780669637593,0.165357301616044,7.83412855316087));
#52980=CARTESIAN_POINT('Ctrl Pts',(1.65673244299333,0.175794483970449,7.83482222713154));
#52981=CARTESIAN_POINT('Ctrl Pts',(1.65371464562638,0.202623589199555,7.83659935453581));
#52982=CARTESIAN_POINT('Ctrl Pts',(1.65162593555921,0.218998285259902,7.83767822574861));
#52983=CARTESIAN_POINT('Ctrl Pts',(1.64190307290537,0.287137484126922,7.8421468546488));
#52984=CARTESIAN_POINT('Ctrl Pts',(1.63207552142209,0.338561595253835,7.84546780095202));
#52985=CARTESIAN_POINT('Ctrl Pts',(1.59467024787864,0.494144848548483,7.85546623960446));
#52986=CARTESIAN_POINT('Ctrl Pts',(1.55940633075307,0.596157978015871,7.86193909882742));
#52987=CARTESIAN_POINT('Ctrl Pts',(1.48818739189425,0.751569623524272,7.87246651426145));
#52988=CARTESIAN_POINT('Ctrl Pts',(1.45857869869201,0.807530210017678,7.87641345202993));
#52989=CARTESIAN_POINT('Ctrl Pts',(1.41814319337051,0.874441957315413,7.88149384781326));
#52990=CARTESIAN_POINT('Ctrl Pts',(1.41025114293976,0.887113594496471,7.88247283845108));
#52991=CARTESIAN_POINT('Ctrl Pts',(1.39839527008229,0.905591548686593,7.88392808775406));
#52992=CARTESIAN_POINT('Ctrl Pts',(1.39456301548982,0.911481966806043,7.88439619942984));
#52993=CARTESIAN_POINT('Ctrl Pts',(1.38797138181079,0.921474843121538,7.88519784878901));
#52994=CARTESIAN_POINT('Ctrl Pts',(1.38523082334428,0.925589546375507,7.88553014090408));
#52995=CARTESIAN_POINT('Ctrl Pts',(1.37893404613295,0.934952988206817,7.88629142174874));
#52996=CARTESIAN_POINT('Ctrl Pts',(1.37536623627921,0.940193547355703,7.88672116625208));
#52997=CARTESIAN_POINT('Ctrl Pts',(1.36541516301137,0.954632277652354,7.88791509622616));
#52998=CARTESIAN_POINT('Ctrl Pts',(1.35896909261153,0.963786460406188,7.88868325951374));
#52999=CARTESIAN_POINT('Ctrl Pts',(1.3201883176416,1.01769714643317,7.8932707835948));
#53000=CARTESIAN_POINT('Ctrl Pts',(1.28574005451607,1.06088449037299,7.89720777732692));
#53001=CARTESIAN_POINT('Ctrl Pts',(1.18415309445877,1.17601344225458,7.90829282629937));
#53002=CARTESIAN_POINT('Ctrl Pts',(1.11268486692914,1.24384894619304,7.91551426822696));
#53003=CARTESIAN_POINT('Ctrl Pts',(0.978225838533326,1.35055717992816,7.92782250416336));
#53004=CARTESIAN_POINT('Ctrl Pts',(0.917849439885174,1.39229507478499,7.9329753580091));
#53005=CARTESIAN_POINT('Ctrl Pts',(0.839769310743625,1.43897697519207,7.9391838343735));
#53006=CARTESIAN_POINT('Ctrl Pts',(0.824484136871119,1.44778906613068,7.9403791481222));
#53007=CARTESIAN_POINT('Ctrl Pts',(0.799677254216944,1.46157022684732,7.94228775891121));
#53008=CARTESIAN_POINT('Ctrl Pts',(0.790242805539901,1.46669272737715,7.94300649599863));
#53009=CARTESIAN_POINT('Ctrl Pts',(0.772114941154748,1.47630968064932,7.94437420442719));
#53010=CARTESIAN_POINT('Ctrl Pts',(0.763430183813212,1.48081940726994,7.94502369469331));
#53011=CARTESIAN_POINT('Ctrl Pts',(0.743520514111501,1.49093617094463,7.94649985042159));
#53012=CARTESIAN_POINT('Ctrl Pts',(0.732270896683394,1.49649349110809,7.94732475343653));
#53013=CARTESIAN_POINT('Ctrl Pts',(0.702085366697778,1.5109832713449,7.94951466886502));
#53014=CARTESIAN_POINT('Ctrl Pts',(0.683041686408396,1.51968694988088,7.95087184867256));
#53015=CARTESIAN_POINT('Ctrl Pts',(0.55201534789171,1.57661012590779,7.96005686810696));
#53016=CARTESIAN_POINT('Ctrl Pts',(0.435196273092605,1.6127704412075,7.96745771566366));
#53017=CARTESIAN_POINT('Ctrl Pts',(0.251121831622821,1.64826819860151,7.97891427079205));
#53018=CARTESIAN_POINT('Ctrl Pts',(0.186105438951403,1.65686865926942,7.98293138870828));
#53019=CARTESIAN_POINT('Ctrl Pts',(0.0985059633013611,1.66323488824296,
7.98849165973565));
#53020=CARTESIAN_POINT('Ctrl Pts',(0.0762258996552658,1.66440476794962,
7.9899187609824));
#53021=CARTESIAN_POINT('Ctrl Pts',(0.0380151033733838,1.66564234100321,
7.99239853011503));
#53022=CARTESIAN_POINT('Ctrl Pts',(0.0220941387001687,1.66592957827388,
7.99344134258725));
#53023=CARTESIAN_POINT('Ctrl Pts',(-0.00103821408095545,1.66601528003028,
7.99497359976737));
#53024=CARTESIAN_POINT('Ctrl Pts',(-0.00824858698606781,1.66599518222658,
7.99545361992826));
#53025=CARTESIAN_POINT('Ctrl Pts',(-0.0209388103681587,1.66587742745875,
7.99630306105777));
#53026=CARTESIAN_POINT('Ctrl Pts',(-0.0264186483120638,1.66579953500555,
7.99667138867874));
#53027=CARTESIAN_POINT('Ctrl Pts',(-0.0383280102897689,1.66557147011582,
7.99747528711151));
#53028=CARTESIAN_POINT('Ctrl Pts',(-0.0447569819896575,1.66541111065887,
7.99791138045322));
#53029=CARTESIAN_POINT('Ctrl Pts',(-0.062782991543381,1.66485703374347,
7.99913980107847));
#53030=CARTESIAN_POINT('Ctrl Pts',(-0.0743768143983663,1.66437937908024,
7.99993647093503));
#53031=CARTESIAN_POINT('Ctrl Pts',(-0.162800902106664,1.65981067961432,
8.00605809366056));
#53032=CARTESIAN_POINT('Ctrl Pts',(-0.239261837122403,1.65052316392243,
8.01161001941356));
#53033=CARTESIAN_POINT('Ctrl Pts',(-0.370962064885207,1.62518133251421,
8.02135846209847));
#53034=CARTESIAN_POINT('Ctrl Pts',(-0.426533862560759,1.61148885966271,
8.02553217262946));
#53035=CARTESIAN_POINT('Ctrl Pts',(-0.560594142451048,1.57103522777936,
8.03565143890614));
#53036=CARTESIAN_POINT('Ctrl Pts',(-0.638010556336312,1.54122146878622,
8.04153408754734));
#53037=CARTESIAN_POINT('Ctrl Pts',(-0.73354501441931,1.49599117479983,8.04880092474296));
#53038=CARTESIAN_POINT('Ctrl Pts',(-0.75399019036319,1.48579162938118,8.050357183041));
#53039=CARTESIAN_POINT('Ctrl Pts',(-0.784686729930373,1.46968107550826,
8.05269656218836));
#53040=CARTESIAN_POINT('Ctrl Pts',(-0.795094897195819,1.464076447723,8.05349027702771));
#53041=CARTESIAN_POINT('Ctrl Pts',(-0.813109955617594,1.45412685729342,
8.05486527134638));
#53042=CARTESIAN_POINT('Ctrl Pts',(-0.82074375191862,1.44983185774776,8.05544829606758));
#53043=CARTESIAN_POINT('Ctrl Pts',(-0.837880413007715,1.44001154025976,
8.05675813951172));
#53044=CARTESIAN_POINT('Ctrl Pts',(-0.847363243212797,1.43445193937729,
8.05748369358947));
#53045=CARTESIAN_POINT('Ctrl Pts',(-0.872949652750901,1.41910884543205,
8.05944390576916));
#53046=CARTESIAN_POINT('Ctrl Pts',(-0.888943715400256,1.40914517674267,
8.06067197870439));
#53047=CARTESIAN_POINT('Ctrl Pts',(-0.991004454565223,1.34313596899242,
8.06853426372312));
#53048=CARTESIAN_POINT('Ctrl Pts',(-1.071905481377,1.27950247797303,8.07486795667081));
#53049=CARTESIAN_POINT('Ctrl Pts',(-1.20644973377773,1.15190084610111,8.086203684078));
#53050=CARTESIAN_POINT('Ctrl Pts',(-1.26213527408976,1.09060048063982,8.09121461222647));
#53051=CARTESIAN_POINT('Ctrl Pts',(-1.33015657412914,1.00350049434024,8.098151631981));
#53052=CARTESIAN_POINT('Ctrl Pts',(-1.34672490227348,0.981153207537279,
8.09991743457312));
#53053=CARTESIAN_POINT('Ctrl Pts',(-1.37350914885983,0.943069472644633,
8.10292277046554));
#53054=CARTESIAN_POINT('Ctrl Pts',(-1.384033072597,0.927555817286041,8.10414598338264));
#53055=CARTESIAN_POINT('Ctrl Pts',(-1.39850197875305,0.905432142642013,
8.10589397763756));
#53056=CARTESIAN_POINT('Ctrl Pts',(-1.40266677839476,0.898966658189607,
8.10640524145278));
#53057=CARTESIAN_POINT('Ctrl Pts',(-1.40975526387062,0.887793223078588,
8.10728994421615));
#53058=CARTESIAN_POINT('Ctrl Pts',(-1.41270047985367,0.883099124857069,
8.10766197210237));
#53059=CARTESIAN_POINT('Ctrl Pts',(-1.4188711704967,0.8731543801116,8.10845102923716));
#53060=CARTESIAN_POINT('Ctrl Pts',(-1.42209090337137,0.867900587294937,
8.10886838032628));
#53061=CARTESIAN_POINT('Ctrl Pts',(-1.43081062880921,0.853493397511852,
8.11001394647914));
#53062=CARTESIAN_POINT('Ctrl Pts',(-1.43625176299642,0.844304976610573,
8.11074573993166));
#53063=CARTESIAN_POINT('Ctrl Pts',(-1.46350786890851,0.797251749940602,
8.11449677463402));
#53064=CARTESIAN_POINT('Ctrl Pts',(-1.48391348165602,0.758594551600372,
8.11758981484491));
#53065=CARTESIAN_POINT('Ctrl Pts',(-1.52523331491813,0.672254511327853,
8.12445572478906));
#53066=CARTESIAN_POINT('Ctrl Pts',(-1.54547257826816,0.62431799473414,8.12824032484045));
#53067=CARTESIAN_POINT('Ctrl Pts',(-1.56343125288101,0.575533419980911,
8.13202453882405));
#53068=CARTESIAN_POINT('Origin',(0.,0.,11.));
#53069=CARTESIAN_POINT('',(-1.56343130032506,0.575533291099565,8.8337599051164));
#53070=CARTESIAN_POINT('',(-1.56343135626508,0.575533139138958,8.63893242883258));
#53071=CARTESIAN_POINT('',(-1.56343130033213,0.575533291080363,11.));
#53072=CARTESIAN_POINT('Ctrl Pts',(-1.56343135626508,0.575533139138958,
8.63893242883258));
#53073=CARTESIAN_POINT('Ctrl Pts',(-1.55156188686748,0.607776461680207,
8.63643887173292));
#53074=CARTESIAN_POINT('Ctrl Pts',(-1.53869262498737,0.639658940293697,
8.63395501622995));
#53075=CARTESIAN_POINT('Ctrl Pts',(-1.49568115629646,0.737382554005722,
8.62630314241373));
#53076=CARTESIAN_POINT('Ctrl Pts',(-1.46223319859508,0.801668143669378,
8.62121791917477));
#53077=CARTESIAN_POINT('Ctrl Pts',(-1.41558849877557,0.878620774696276,
8.61507721229518));
#53078=CARTESIAN_POINT('Ctrl Pts',(-1.40623490021235,0.893514806920478,
8.61388576009589));
#53079=CARTESIAN_POINT('Ctrl Pts',(-1.39080123691318,0.917247454825696,
8.61198181784619));
#53080=CARTESIAN_POINT('Ctrl Pts',(-1.38486880752784,0.926179987484857,
8.61126393498847));
#53081=CARTESIAN_POINT('Ctrl Pts',(-1.37335674799568,0.943155899618945,
8.60989691550737));
#53082=CARTESIAN_POINT('Ctrl Pts',(-1.36779168125296,0.95120856384015,8.60924726887195));
#53083=CARTESIAN_POINT('Ctrl Pts',(-1.35491887154762,0.969488960392166,
8.60776948208694));
#53084=CARTESIAN_POINT('Ctrl Pts',(-1.34756564359279,0.979684052848258,
8.60694311895826));
#53085=CARTESIAN_POINT('Ctrl Pts',(-1.32761066880631,1.00670137271282,8.60474648013369));
#53086=CARTESIAN_POINT('Ctrl Pts',(-1.31480454461364,1.02337032129826,8.60338411588049));
#53087=CARTESIAN_POINT('Ctrl Pts',(-1.22647076150574,1.133952748546,8.59428534249608));
#53088=CARTESIAN_POINT('Ctrl Pts',(-1.14126030176033,1.21967542138474,8.58696449180771));
#53089=CARTESIAN_POINT('Ctrl Pts',(-0.974072506182121,1.35486719525386,
8.57382689287283));
#53090=CARTESIAN_POINT('Ctrl Pts',(-0.895696222676206,1.40790822641409,
8.56803879409931));
#53091=CARTESIAN_POINT('Ctrl Pts',(-0.802347439618496,1.46012019333494,
8.56105446659527));
#53092=CARTESIAN_POINT('Ctrl Pts',(-0.791364982907873,1.46610157687595,
8.56023133112747));
#53093=CARTESIAN_POINT('Ctrl Pts',(-0.774529699467277,1.47502631996908,
8.5589657402088));
#53094=CARTESIAN_POINT('Ctrl Pts',(-0.768724841268209,1.47805988198134,
8.55852868288533));
#53095=CARTESIAN_POINT('Ctrl Pts',(-0.758042120202873,1.48356261538287,
8.55772284364967));
#53096=CARTESIAN_POINT('Ctrl Pts',(-0.753169806554804,1.48604210216211,
8.55735470865122));
#53097=CARTESIAN_POINT('Ctrl Pts',(-0.741990403733578,1.49166212056432,
8.55650868917207));
#53098=CARTESIAN_POINT('Ctrl Pts',(-0.735675558886848,1.49478664319922,
8.55602985656871));
#53099=CARTESIAN_POINT('Ctrl Pts',(-0.715830891650597,1.50444938088344,
8.55452258772285));
#53100=CARTESIAN_POINT('Ctrl Pts',(-0.702232746780959,1.51084444437967,
8.55348612262694));
#53101=CARTESIAN_POINT('Ctrl Pts',(-0.593353960392721,1.56026162376179,
8.54516902877113));
#53102=CARTESIAN_POINT('Ctrl Pts',(-0.494309997480233,1.59440878562947,
8.53750885228049));
#53103=CARTESIAN_POINT('Ctrl Pts',(-0.282741951109502,1.64572841889288,
8.52168002866059));
#53104=CARTESIAN_POINT('Ctrl Pts',(-0.170303755067803,1.66113532481739,
8.51357088298754));
#53105=CARTESIAN_POINT('Ctrl Pts',(-0.037798613936452,1.66568374548627,
8.50449900090682));
#53106=CARTESIAN_POINT('Ctrl Pts',(-0.0184323687750814,1.66601061758158,
8.50318424426596));
#53107=CARTESIAN_POINT('Ctrl Pts',(0.0120391746531707,1.66599349966595,
8.50113225953731));
#53108=CARTESIAN_POINT('Ctrl Pts',(0.0231423312824171,1.66587626356018,
8.50038804384748));
#53109=CARTESIAN_POINT('Ctrl Pts',(0.0439585446219458,1.66544830721385,
8.49899904255763));
#53110=CARTESIAN_POINT('Ctrl Pts',(0.053671604258126,1.66516359057669,8.49835347481421));
#53111=CARTESIAN_POINT('Ctrl Pts',(0.0754987265250821,1.66433259149579,
8.4969082330555));
#53112=CARTESIAN_POINT('Ctrl Pts',(0.0876105185073098,1.66373899480864,
8.49611006793661));
#53113=CARTESIAN_POINT('Ctrl Pts',(0.123281745811791,1.66160013190565,8.49376970856189));
#53114=CARTESIAN_POINT('Ctrl Pts',(0.14681665651005,1.65968621924105,8.49223899015564));
#53115=CARTESIAN_POINT('Ctrl Pts',(0.270937909627736,1.64693132568469,8.48422332523232));
#53116=CARTESIAN_POINT('Ctrl Pts',(0.370425168801974,1.62744541907731,8.47801431130899));
#53117=CARTESIAN_POINT('Ctrl Pts',(0.54480232960941,1.57646006844147,8.46691723177511));
#53118=CARTESIAN_POINT('Ctrl Pts',(0.620321168007714,1.54830093285588,8.46202790150696));
#53119=CARTESIAN_POINT('Ctrl Pts',(0.71620349224181,1.50440415780349,8.45538074387492));
#53120=CARTESIAN_POINT('Ctrl Pts',(0.738666157512167,1.49350309257644,8.45378980383227));
#53121=CARTESIAN_POINT('Ctrl Pts',(0.776278412946118,1.47419390006593,8.45105418433659));
#53122=CARTESIAN_POINT('Ctrl Pts',(0.791557687843593,1.46604645171927,8.4499222827935));
#53123=CARTESIAN_POINT('Ctrl Pts',(0.813228435922316,1.45405332608714,8.44828315737086));
#53124=CARTESIAN_POINT('Ctrl Pts',(0.819725959529565,1.4504002585851,8.44778729027167));
#53125=CARTESIAN_POINT('Ctrl Pts',(0.830981437879596,1.44397236338543,8.44692022653032));
#53126=CARTESIAN_POINT('Ctrl Pts',(0.835750498100171,1.44121734664197,8.44655028431256));
#53127=CARTESIAN_POINT('Ctrl Pts',(0.845929426493821,1.43526961315458,8.44575507504796));
#53128=CARTESIAN_POINT('Ctrl Pts',(0.851334836389783,1.43206998786148,8.44532939510462));
#53129=CARTESIAN_POINT('Ctrl Pts',(0.866103180307964,1.42321499754878,8.44415731940145));
#53130=CARTESIAN_POINT('Ctrl Pts',(0.875428517629792,1.41749798688334,8.44340716944171));
#53131=CARTESIAN_POINT('Ctrl Pts',(0.927476389524408,1.38487993222596,8.43916644187511));
#53132=CARTESIAN_POINT('Ctrl Pts',(0.969011275985883,1.35614195090091,8.43557725806078));
#53133=CARTESIAN_POINT('Ctrl Pts',(1.08575340343721,1.26726445246093,8.42500978774405));
#53134=CARTESIAN_POINT('Ctrl Pts',(1.15713811807773,1.20243586642979,8.41793932531378));
#53135=CARTESIAN_POINT('Ctrl Pts',(1.26599318918323,1.08485515245093,8.40641179137648));
#53136=CARTESIAN_POINT('Ctrl Pts',(1.30672176021917,1.03543679839453,8.40187931671649));
#53137=CARTESIAN_POINT('Ctrl Pts',(1.36082250757125,0.961499435942552,8.39554419973778));
#53138=CARTESIAN_POINT('Ctrl Pts',(1.37657836831889,0.938803076366341,8.39365460294419));
#53139=CARTESIAN_POINT('Ctrl Pts',(1.39875615255915,0.905096171127229,8.39092580189108));
#53140=CARTESIAN_POINT('Ctrl Pts',(1.40562713718082,0.894388182009055,8.39006996346471));
#53141=CARTESIAN_POINT('Ctrl Pts',(1.41756205944802,0.875311063455623,8.38856425959711));
#53142=CARTESIAN_POINT('Ctrl Pts',(1.42267614401365,0.866974190192241,8.38791256703512));
#53143=CARTESIAN_POINT('Ctrl Pts',(1.43325814280668,0.849377840899167,8.38655000421158));
#53144=CARTESIAN_POINT('Ctrl Pts',(1.43871043773465,0.840109460742561,8.38583972456393));
#53145=CARTESIAN_POINT('Ctrl Pts',(1.45291230253581,0.815423852669319,8.38396698645757));
#53146=CARTESIAN_POINT('Ctrl Pts',(1.4615063546662,0.799918391391817,8.38281012114899));
#53147=CARTESIAN_POINT('Ctrl Pts',(1.50146908179505,0.725022422332459,8.37730958972848));
#53148=CARTESIAN_POINT('Ctrl Pts',(1.5294766270699,0.663904911482516,8.37308427077122));
#53149=CARTESIAN_POINT('Ctrl Pts',(1.6057657928442,0.466764629046022,8.36000058633287));
#53150=CARTESIAN_POINT('Ctrl Pts',(1.64012150314167,0.326104098013765,8.35148227773574));
#53151=CARTESIAN_POINT('Ctrl Pts',(1.65832675345838,0.161186801075403,8.3408224937926));
#53152=CARTESIAN_POINT('Ctrl Pts',(1.66028910526352,0.139530584330247,8.33940861422835));
#53153=CARTESIAN_POINT('Ctrl Pts',(1.66240306244523,0.109719583436152,8.33743537121793));
#53154=CARTESIAN_POINT('Ctrl Pts',(1.66291954880702,0.101591812845439,8.33689463102627));
#53155=CARTESIAN_POINT('Ctrl Pts',(1.66369165108474,0.0878502565845365,
8.33597526722552));
#53156=CARTESIAN_POINT('Ctrl Pts',(1.66397850041224,0.0822382307008209,
8.33559835105518));
#53157=CARTESIAN_POINT('Ctrl Pts',(1.66451203273601,0.0706502957458508,
8.33481690544078));
#53158=CARTESIAN_POINT('Ctrl Pts',(1.66475493467458,0.0646743847377087,
8.33441219077767));
#53159=CARTESIAN_POINT('Ctrl Pts',(1.66531277369112,0.0488511530677596,
8.3333362426067));
#53160=CARTESIAN_POINT('Ctrl Pts',(1.66557253759491,0.0390023021518545,
8.33266210279372));
#53161=CARTESIAN_POINT('Ctrl Pts',(1.66633511834445,-0.00457150655297279,
8.32966159127403));
#53162=CARTESIAN_POINT('Ctrl Pts',(1.66590100919347,-0.0383025707807233,
8.32729142754564));
#53163=CARTESIAN_POINT('Ctrl Pts',(1.66351732034801,-0.093411286807257,
8.32336500713657));
#53164=CARTESIAN_POINT('Ctrl Pts',(1.66217769252649,-0.114807673716851,
8.32182713011855));
#53165=CARTESIAN_POINT('Ctrl Pts',(1.65209296933613,-0.237777097563427,
8.31293036702973));
#53166=CARTESIAN_POINT('Ctrl Pts',(1.63445069092764,-0.338410797238987,
8.3054376232841));
#53167=CARTESIAN_POINT('Ctrl Pts',(1.58869943149386,-0.506806506664729,
8.29293066540681));
#53168=CARTESIAN_POINT('Ctrl Pts',(1.56512511102975,-0.575503874427037,
8.28783360743431));
#53169=CARTESIAN_POINT('Ctrl Pts',(1.53035770083746,-0.658688784506944,
8.28168103794203));
#53170=CARTESIAN_POINT('Ctrl Pts',(1.52331535685741,-0.674815509710883,
8.28048890992875));
#53171=CARTESIAN_POINT('Ctrl Pts',(1.51157147464176,-0.700587393571792,
8.27858415480886));
#53172=CARTESIAN_POINT('Ctrl Pts',(1.50703012543485,-0.710303617699735,
8.2778661266026));
#53173=CARTESIAN_POINT('Ctrl Pts',(1.49816538750638,-0.728801940612003,
8.27649899761351));
#53174=CARTESIAN_POINT('Ctrl Pts',(1.49385782508153,-0.737591080735014,
8.27584938523861));
#53175=CARTESIAN_POINT('Ctrl Pts',(1.48384391006696,-0.757575829778588,
8.27437190451116));
#53176=CARTESIAN_POINT('Ctrl Pts',(1.47808780626389,-0.768745951967338,
8.27354581053486));
#53177=CARTESIAN_POINT('Ctrl Pts',(1.46237439906771,-0.798409815685436,
8.27135039724));
#53178=CARTESIAN_POINT('Ctrl Pts',(1.45219263678725,-0.816782544906711,
8.2699889750509));
#53179=CARTESIAN_POINT('Ctrl Pts',(1.38113324543105,-0.939475939905433,
8.26087372301941));
#53180=CARTESIAN_POINT('Ctrl Pts',(1.30941412785534,-1.03710297131947,8.25353761411919));
#53181=CARTESIAN_POINT('Ctrl Pts',(1.18295665543291,-1.17497374578399,8.24210602070799));
#53182=CARTESIAN_POINT('Ctrl Pts',(1.13527908506359,-1.22110191340699,8.23804468836693));
#53183=CARTESIAN_POINT('Ctrl Pts',(1.06794430597665,-1.27888826954697,8.23242878418181));
#53184=CARTESIAN_POINT('Ctrl Pts',(1.05061063753319,-1.29316566391574,8.2309926659195));
#53185=CARTESIAN_POINT('Ctrl Pts',(1.02044054254375,-1.31700916483767,8.22849874165069));
#53186=CARTESIAN_POINT('Ctrl Pts',(1.007744747727,-1.32674885281173,8.22745094208523));
#53187=CARTESIAN_POINT('Ctrl Pts',(0.989116611891225,-1.34061796131578,
8.22591269799433));
#53188=CARTESIAN_POINT('Ctrl Pts',(0.983294133596994,-1.34489435724001,
8.22543178173831));
#53189=CARTESIAN_POINT('Ctrl Pts',(0.973044789403469,-1.35231998854345,
8.22458465863413));
#53190=CARTESIAN_POINT('Ctrl Pts',(0.968630053211665,-1.35548564448661,
8.22421958123445));
#53191=CARTESIAN_POINT('Ctrl Pts',(0.958980170915469,-1.36233402591073,
8.22342106703799));
#53192=CARTESIAN_POINT('Ctrl Pts',(0.953739345277282,-1.36600813474385,
8.2229871000141));
#53193=CARTESIAN_POINT('Ctrl Pts',(0.939049880231659,-1.37618052135733,
8.22177020817909));
#53194=CARTESIAN_POINT('Ctrl Pts',(0.929555336050126,-1.38261142913146,
8.22098306402333));
#53195=CARTESIAN_POINT('Ctrl Pts',(0.865300432886657,-1.42517199251911,
8.21565597055711));
#53196=CARTESIAN_POINT('Ctrl Pts',(0.808518968618958,-1.45813415207656,
8.21095032686179));
#53197=CARTESIAN_POINT('Ctrl Pts',(0.731110498994364,-1.49715682063077,
8.2046666923073));
#53198=CARTESIAN_POINT('Ctrl Pts',(0.712092849761228,-1.50629507818682,
8.20313269654204));
#53199=CARTESIAN_POINT('Ctrl Pts',(0.630755548887342,-1.54349415124639,
8.19662382333867));
#53200=CARTESIAN_POINT('Ctrl Pts',(0.566910725692281,-1.56806884334495,
8.19164570591671));
#53201=CARTESIAN_POINT('Ctrl Pts',(0.433540686573515,-1.61019026881979,
8.18162694175109));
#53202=CARTESIAN_POINT('Ctrl Pts',(0.36402374556907,-1.62731663855451,8.17660487566422));
#53203=CARTESIAN_POINT('Ctrl Pts',(0.276353459710387,-1.64301313830792,
8.17052754982417));
#53204=CARTESIAN_POINT('Ctrl Pts',(0.259046607574322,-1.64583058157559,
8.16933975336315));
#53205=CARTESIAN_POINT('Ctrl Pts',(0.231099985752947,-1.64992834008624,
8.16744020801134));
#53206=CARTESIAN_POINT('Ctrl Pts',(0.220487110611126,-1.65138008167619,
8.16672311109309));
#53207=CARTESIAN_POINT('Ctrl Pts',(0.200147406788656,-1.65396278250553,
8.1653566802735));
#53208=CARTESIAN_POINT('Ctrl Pts',(0.190423202524032,-1.6551105344601,8.16470684492952));
#53209=CARTESIAN_POINT('Ctrl Pts',(0.168171140269557,-1.65753824578816,
8.16322738727057));
#53210=CARTESIAN_POINT('Ctrl Pts',(0.155637657767756,-1.65876203918161,
8.16239955639886));
#53211=CARTESIAN_POINT('Ctrl Pts',(0.115531171631399,-1.66221952493399,
8.15976700409098));
#53212=CARTESIAN_POINT('Ctrl Pts',(0.0879150538168917,-1.66390873719184,
8.15797921838882));
#53213=CARTESIAN_POINT('Ctrl Pts',(-0.0712410793702744,-1.66967005678191,
8.14779416195986));
#53214=CARTESIAN_POINT('Ctrl Pts',(-0.202849170166269,-1.65883336407098,
8.13988171730874));
#53215=CARTESIAN_POINT('Ctrl Pts',(-0.401934414469848,-1.61837084025625,
8.12741818286835));
#53216=CARTESIAN_POINT('Ctrl Pts',(-0.471052639345271,-1.59961948996927,
8.12298330791998));
#53217=CARTESIAN_POINT('Ctrl Pts',(-0.5536843387361,-1.57138122825364,8.11731785579805));
#53218=CARTESIAN_POINT('Ctrl Pts',(-0.568551570314844,-1.56606333809926,
8.11628362046686));
#53219=CARTESIAN_POINT('Ctrl Pts',(-0.590071468988671,-1.55801903105587,
8.11476170574093));
#53220=CARTESIAN_POINT('Ctrl Pts',(-0.596786128560097,-1.5554594021245,
8.11428327419583));
#53221=CARTESIAN_POINT('Ctrl Pts',(-0.608543988677916,-1.55088996574776,
8.11343888331453));
#53222=CARTESIAN_POINT('Ctrl Pts',(-0.61359424009795,-1.5488988279637,8.1130740283054));
#53223=CARTESIAN_POINT('Ctrl Pts',(-0.624601301424744,-1.54449684596546,
8.1122739827093));
#53224=CARTESIAN_POINT('Ctrl Pts',(-0.630553830633365,-1.5420762484801,
8.11183824344927));
#53225=CARTESIAN_POINT('Ctrl Pts',(-0.647195288523337,-1.53519653333726,
8.11061169382127));
#53226=CARTESIAN_POINT('Ctrl Pts',(-0.657851695603722,-1.53066040170428,
8.10981656075523));
#53227=CARTESIAN_POINT('Ctrl Pts',(-0.734151124163853,-1.49723797377155,
8.10405771924946));
#53228=CARTESIAN_POINT('Ctrl Pts',(-0.797908925452065,-1.46425354522437,
8.09889652745042));
#53229=CARTESIAN_POINT('Ctrl Pts',(-0.87114283990524,-1.42016058667957,
8.09268971650659));
#53230=CARTESIAN_POINT('Ctrl Pts',(-0.882861081963212,-1.41290560375266,
8.0916874773964));
#53231=CARTESIAN_POINT('Ctrl Pts',(-0.950653911779776,-1.36976109884206,
8.08584005816142));
#53232=CARTESIAN_POINT('Ctrl Pts',(-1.00462946544215,-1.33067980954118,
8.08098920105092));
#53233=CARTESIAN_POINT('Ctrl Pts',(-1.09414974125374,-1.25730262110943,
8.07268652091806));
#53234=CARTESIAN_POINT('Ctrl Pts',(-1.13078045578505,-1.22446308427605,
8.06920371910412));
#53235=CARTESIAN_POINT('Ctrl Pts',(-1.18977844442658,-1.1666619049471,8.06345679052604));
#53236=CARTESIAN_POINT('Ctrl Pts',(-1.21294155673913,-1.14256107243737,
8.06116080325297));
#53237=CARTESIAN_POINT('Ctrl Pts',(-1.2445464679894,-1.10763140820518,8.05796837551124));
#53238=CARTESIAN_POINT('Ctrl Pts',(-1.25360230672679,-1.09737164324671,
8.05704627643156));
#53239=CARTESIAN_POINT('Ctrl Pts',(-1.26900871066669,-1.0794774018588,8.05546424558195));
#53240=CARTESIAN_POINT('Ctrl Pts',(-1.2754192050423,-1.07189571676968,8.0548018592463));
#53241=CARTESIAN_POINT('Ctrl Pts',(-1.28760122431716,-1.05722403055176,
8.05353489849969));
#53242=CARTESIAN_POINT('Ctrl Pts',(-1.29338289778619,-1.05014296598103,
8.05292992646612));
#53243=CARTESIAN_POINT('Ctrl Pts',(-1.30691522231043,-1.03328804746564,
8.05150495096485));
#53244=CARTESIAN_POINT('Ctrl Pts',(-1.31461503802747,-1.02347393864395,
8.05068698698352));
#53245=CARTESIAN_POINT('Ctrl Pts',(-1.33753643360303,-0.993573052116878,
8.048229097795));
#53246=CARTESIAN_POINT('Ctrl Pts',(-1.35241357714633,-0.973225946984257,
8.04660244422627));
#53247=CARTESIAN_POINT('Ctrl Pts',(-1.44187733165743,-0.844853229815511,
8.03659917607584));
#53248=CARTESIAN_POINT('Ctrl Pts',(-1.50393918730732,-0.728667702234672,
8.02870669459865));
#53249=CARTESIAN_POINT('Ctrl Pts',(-1.5777268343713,-0.539850463990858,
8.01626920027877));
#53250=CARTESIAN_POINT('Ctrl Pts',(-1.59942140196838,-0.471708941985083,
8.01184045526884));
#53251=CARTESIAN_POINT('Ctrl Pts',(-1.62048516886904,-0.387082422159707,
8.00618235550722));
#53252=CARTESIAN_POINT('Ctrl Pts',(-1.62407847852099,-0.371717682298452,
8.00514878485045));
#53253=CARTESIAN_POINT('Ctrl Pts',(-1.62898933120278,-0.349286947217741,
8.00362767055483));
#53254=CARTESIAN_POINT('Ctrl Pts',(-1.63048035819566,-0.34225927228254,
8.00314936111851));
#53255=CARTESIAN_POINT('Ctrl Pts',(-1.63301816922033,-0.329904727329983,
8.00230510358389));
#53256=CARTESIAN_POINT('Ctrl Pts',(-1.63408444039237,-0.3245820551392,8.00194025857179));
#53257=CARTESIAN_POINT('Ctrl Pts',(-1.63635635258896,-0.312945996847856,
8.00114013371571));
#53258=CARTESIAN_POINT('Ctrl Pts',(-1.63755146141554,-0.306630913851365,
8.00070430426921));
#53259=CARTESIAN_POINT('Ctrl Pts',(-1.64079871836077,-0.288911469363451,
7.99947726563726));
#53260=CARTESIAN_POINT('Ctrl Pts',(-1.64276842137086,-0.277492641922035,
7.9986817285183));
#53261=CARTESIAN_POINT('Ctrl Pts',(-1.65618234371281,-0.194574367272832,
7.99287458640212));
#53262=CARTESIAN_POINT('Ctrl Pts',(-1.66307219549193,-0.122424018168786,
7.98766171063302));
#53263=CARTESIAN_POINT('Ctrl Pts',(-1.66573474981424,-0.0338603643184752,
7.98122730133518));
#53264=CARTESIAN_POINT('Ctrl Pts',(-1.66598535914898,-0.017651009351957,
7.98004801819825));
#53265=CARTESIAN_POINT('Ctrl Pts',(-1.6661107565004,0.127358288344095,7.96949372028456));
#53266=CARTESIAN_POINT('Ctrl Pts',(-1.65128543468728,0.255761016431306,
7.96016710179683));
#53267=CARTESIAN_POINT('Ctrl Pts',(-1.61713992253171,0.401036344385619,
7.94991017892582));
#53268=CARTESIAN_POINT('Ctrl Pts',(-1.61211089489218,0.420797106648802,
7.94852026987872));
#53269=CARTESIAN_POINT('Ctrl Pts',(-1.60340887862091,0.45254042544968,7.94629526479896));
#53270=CARTESIAN_POINT('Ctrl Pts',(-1.59996137674876,0.464582044946932,
7.94545302892488));
#53271=CARTESIAN_POINT('Ctrl Pts',(-1.59358748337374,0.485932209161064,
7.94396259707877));
#53272=CARTESIAN_POINT('Ctrl Pts',(-1.59071453219384,0.495255957145969,
7.94331270011679));
#53273=CARTESIAN_POINT('Ctrl Pts',(-1.58447198456338,0.514900364063271,
7.94194525931866));
#53274=CARTESIAN_POINT('Ctrl Pts',(-1.58108306386391,0.525214441293306,
7.94122838224518));
#53275=CARTESIAN_POINT('Ctrl Pts',(-1.57304313111398,0.54890046792219,7.93958415920245));
#53276=CARTESIAN_POINT('Ctrl Pts',(-1.56832202215773,0.562247686748594,
7.93865916364133));
#53277=CARTESIAN_POINT('Ctrl Pts',(-1.56343130037338,0.575533290968306,
7.93773948050229));
#53278=CARTESIAN_POINT('Ctrl Pts',(-1.56343125288101,0.575533419980911,
8.13202453882405));
#53279=CARTESIAN_POINT('Ctrl Pts',(-1.57647476592086,0.540100836527222,
8.13477304034238));
#53280=CARTESIAN_POINT('Ctrl Pts',(-1.58831519947266,0.504220896311646,
8.13752158935909));
#53281=CARTESIAN_POINT('Ctrl Pts',(-1.62278062997201,0.386457854613517,
8.14639622254069));
#53282=CARTESIAN_POINT('Ctrl Pts',(-1.64036942313108,0.303246857124685,
8.1524335310521));
#53283=CARTESIAN_POINT('Ctrl Pts',(-1.65457539086693,0.196138385182223,
8.15986415733841));
#53284=CARTESIAN_POINT('Ctrl Pts',(-1.65713685274032,0.17316909209299,8.16143874830773));
#53285=CARTESIAN_POINT('Ctrl Pts',(-1.66028981546747,0.138328221684353,
8.16379976903536));
#53286=CARTESIAN_POINT('Ctrl Pts',(-1.66123349042863,0.126492178388229,
8.16459709293344));
#53287=CARTESIAN_POINT('Ctrl Pts',(-1.66265368033757,0.105903485861357,
8.16597606859828));
#53288=CARTESIAN_POINT('Ctrl Pts',(-1.66318779402146,0.0971554214281328,
8.16655949774668));
#53289=CARTESIAN_POINT('Ctrl Pts',(-1.6642341778765,0.0774636514998475,
8.16786737254177));
#53290=CARTESIAN_POINT('Ctrl Pts',(-1.66470758768369,0.0665182176389728,
8.16859057878443));
#53291=CARTESIAN_POINT('Ctrl Pts',(-1.66569572471977,0.0369094502227332,
8.17053730486913));
#53292=CARTESIAN_POINT('Ctrl Pts',(-1.66600476746025,0.0182404851654997,
8.17175439696182));
#53293=CARTESIAN_POINT('Ctrl Pts',(-1.66597468525883,-0.0982129333982162,
8.17928915711391));
#53294=CARTESIAN_POINT('Ctrl Pts',(-1.6573412001664,-0.195809012424007,
8.18533701810807));
#53295=CARTESIAN_POINT('Ctrl Pts',(-1.622980312546,-0.388754856964475,8.19732910409969));
#53296=CARTESIAN_POINT('Ctrl Pts',(-1.59725732387335,-0.483695423463917,
8.20325270540061));
#53297=CARTESIAN_POINT('Ctrl Pts',(-1.55225470669452,-0.605877913944535,
8.21150088433053));
#53298=CARTESIAN_POINT('Ctrl Pts',(-1.54031573519923,-0.635617685131605,
8.21356123459514));
#53299=CARTESIAN_POINT('Ctrl Pts',(-1.52366349205209,-0.673868895149786,
8.21630363282603));
#53300=CARTESIAN_POINT('Ctrl Pts',(-1.51972202289346,-0.682711276391223,
8.21694414380728));
#53301=CARTESIAN_POINT('Ctrl Pts',(-1.51323680997241,-0.696925880171094,
8.21798522492591));
#53302=CARTESIAN_POINT('Ctrl Pts',(-1.51074091781395,-0.702319871544494,
8.21838296128972));
#53303=CARTESIAN_POINT('Ctrl Pts',(-1.50581976664892,-0.712807588427169,
8.21916175031152));
#53304=CARTESIAN_POINT('Ctrl Pts',(-1.50339741501869,-0.717902525844541,
8.21954263007709));
#53305=CARTESIAN_POINT('Ctrl Pts',(-1.49736493318513,-0.730426230018712,
8.22048497655383));
#53306=CARTESIAN_POINT('Ctrl Pts',(-1.49372537370854,-0.737840579962083,
8.22104820089348));
#53307=CARTESIAN_POINT('Ctrl Pts',(-1.47993756403112,-0.765408358409469,
8.2231614910417));
#53308=CARTESIAN_POINT('Ctrl Pts',(-1.46943583693606,-0.785381019987932,
8.22473093530008));
#53309=CARTESIAN_POINT('Ctrl Pts',(-1.44109507755261,-0.836721501734517,
8.22885457112118));
#53310=CARTESIAN_POINT('Ctrl Pts',(-1.42263717149119,-0.867733281178739,
8.23143414725975));
#53311=CARTESIAN_POINT('Ctrl Pts',(-1.36414810505131,-0.95911442993948,
8.23925817852516));
#53312=CARTESIAN_POINT('Ctrl Pts',(-1.32117271813111,-1.01749846749838,
8.24455824763871));
#53313=CARTESIAN_POINT('Ctrl Pts',(-1.21044257897313,-1.1490385437035,8.25702146033253));
#53314=CARTESIAN_POINT('Ctrl Pts',(-1.13964737971101,-1.21929116152939,
8.2641054818042));
#53315=CARTESIAN_POINT('Ctrl Pts',(-1.04847294431203,-1.29484206897693,
8.27220144075366));
#53316=CARTESIAN_POINT('Ctrl Pts',(-1.03375127060128,-1.30662537085953,
8.27348071092021));
#53317=CARTESIAN_POINT('Ctrl Pts',(-1.01013308025676,-1.32488038834047,
8.27549018031205));
#53318=CARTESIAN_POINT('Ctrl Pts',(-1.00136744372863,-1.33151798182014,
8.27622689103781));
#53319=CARTESIAN_POINT('Ctrl Pts',(-0.985502100851652,-1.34328638778345,
8.27754436172706));
#53320=CARTESIAN_POINT('Ctrl Pts',(-0.978426496230581,-1.34844885215257,
8.27812633899214));
#53321=CARTESIAN_POINT('Ctrl Pts',(-0.961709746217389,-1.36044478039167,
8.27948847004329));
#53322=CARTESIAN_POINT('Ctrl Pts',(-0.952035872788811,-1.36723200131673,
8.28026683063976));
#53323=CARTESIAN_POINT('Ctrl Pts',(-0.923466736818148,-1.38682593928159,
8.2825374573401));
#53324=CARTESIAN_POINT('Ctrl Pts',(-0.904379063350026,-1.39934827375732,
8.28401904348867));
#53325=CARTESIAN_POINT('Ctrl Pts',(-0.814985446772792,-1.45540089210671,
8.29080667277284));
#53326=CARTESIAN_POINT('Ctrl Pts',(-0.741754629720165,-1.49405335264897,
8.29593631653938));
#53327=CARTESIAN_POINT('Ctrl Pts',(-0.613422720170676,-1.55001684498241,
8.30451966143371));
#53328=CARTESIAN_POINT('Ctrl Pts',(-0.559750394507417,-1.57019714476803,
8.30800055651609));
#53329=CARTESIAN_POINT('Ctrl Pts',(-0.431754905911915,-1.61092370584721,
8.31624369254192));
#53330=CARTESIAN_POINT('Ctrl Pts',(-0.356842673349537,-1.6291555074469,
8.32102412673696));
#53331=CARTESIAN_POINT('Ctrl Pts',(-0.269511455405308,-1.64409678387728,
8.3268193473141));
#53332=CARTESIAN_POINT('Ctrl Pts',(-0.258053626905415,-1.64593407112163,
8.327584058195));
#53333=CARTESIAN_POINT('Ctrl Pts',(-0.240217596007902,-1.64860330781699,
8.32878257245176));
#53334=CARTESIAN_POINT('Ctrl Pts',(-0.233851928842736,-1.64951830298534,
8.32921192251728));
#53335=CARTESIAN_POINT('Ctrl Pts',(-0.222051936946935,-1.65114474678727,
8.330011036413));
#53336=CARTESIAN_POINT('Ctrl Pts',(-0.216619207043025,-1.65186626380461,
8.33038023817655));
#53337=CARTESIAN_POINT('Ctrl Pts',(-0.204030903755151,-1.65347494052239,
8.33123865906529));
#53338=CARTESIAN_POINT('Ctrl Pts',(-0.196873060447458,-1.65434246208436,
8.33172893639085));
#53339=CARTESIAN_POINT('Ctrl Pts',(-0.173891085071332,-1.65697658865389,
8.33330956472752));
#53340=CARTESIAN_POINT('Ctrl Pts',(-0.158047721611828,-1.65856275015164,
8.33440905302607));
#53341=CARTESIAN_POINT('Ctrl Pts',(-0.119958442970756,-1.66182538422732,
8.33707213914044));
#53342=CARTESIAN_POINT('Ctrl Pts',(-0.0976971786070598,-1.6632825366167,
8.33864472367392));
#53343=CARTESIAN_POINT('Ctrl Pts',(-0.00996217509476534,-1.66725809757432,
8.34488988679133));
#53344=CARTESIAN_POINT('Ctrl Pts',(0.0556047338421275,-1.66636011197354,
8.34965838622301));
#53345=CARTESIAN_POINT('Ctrl Pts',(0.242542409377467,-1.6527533267283,8.36330235997769));
#53346=CARTESIAN_POINT('Ctrl Pts',(0.36282327793294,-1.63057965136885,8.37210888261677));
#53347=CARTESIAN_POINT('Ctrl Pts',(0.49967003365011,-1.58944144503542,8.38193785222053));
#53348=CARTESIAN_POINT('Ctrl Pts',(0.519603540309516,-1.58303710621968,
8.38336583231438));
#53349=CARTESIAN_POINT('Ctrl Pts',(0.551282382118694,-1.57219628107933,
8.38563006041636));
#53350=CARTESIAN_POINT('Ctrl Pts',(0.563106917524571,-1.56800000811813,
8.38647405646144));
#53351=CARTESIAN_POINT('Ctrl Pts',(0.584067590274744,-1.56029381994299,
8.38796843509581));
#53352=CARTESIAN_POINT('Ctrl Pts',(0.593222209193225,-1.55683627016599,
8.38862051758036));
#53353=CARTESIAN_POINT('Ctrl Pts',(0.612354929654905,-1.5494168849323,8.38998233798931));
#53354=CARTESIAN_POINT('Ctrl Pts',(0.622326298831967,-1.54543884708144,
8.39069149885451));
#53355=CARTESIAN_POINT('Ctrl Pts',(0.648581508597556,-1.53466911416794,
8.39255770951409));
#53356=CARTESIAN_POINT('Ctrl Pts',(0.664797393625992,-1.52771454382787,
8.3937092380412));
#53357=CARTESIAN_POINT('Ctrl Pts',(0.747824927532054,-1.49053378705425,
8.39960461243109));
#53358=CARTESIAN_POINT('Ctrl Pts',(0.812702572530906,-1.45617635501,8.40420438695232));
#53359=CARTESIAN_POINT('Ctrl Pts',(0.958675282472613,-1.36606788449267,
8.41479245417914));
#53360=CARTESIAN_POINT('Ctrl Pts',(1.0375110088575,-1.30719912777315,8.42069732865638));
#53361=CARTESIAN_POINT('Ctrl Pts',(1.13329006273765,-1.22152697997433,8.42866961566388));
#53362=CARTESIAN_POINT('Ctrl Pts',(1.15532255246585,-1.20070985214336,8.4305671629239));
#53363=CARTESIAN_POINT('Ctrl Pts',(1.19714827946132,-1.15897387662775,8.43432480645616));
#53364=CARTESIAN_POINT('Ctrl Pts',(1.21699092596074,-1.13812007301849,8.43618135541146));
#53365=CARTESIAN_POINT('Ctrl Pts',(1.24252938369635,-1.10984845335819,8.43868820408379));
#53366=CARTESIAN_POINT('Ctrl Pts',(1.24871837709632,-1.1028804393618,8.4393052807529));
#53367=CARTESIAN_POINT('Ctrl Pts',(1.25870585023804,-1.0914439853123,8.44031753452339));
#53368=CARTESIAN_POINT('Ctrl Pts',(1.26253987070088,-1.08700665255807,8.44071015743864));
#53369=CARTESIAN_POINT('Ctrl Pts',(1.27005126576689,-1.07821993232242,8.44148758170891));
#53370=CARTESIAN_POINT('Ctrl Pts',(1.27372989938261,-1.0738717708539,8.44187228507094));
#53371=CARTESIAN_POINT('Ctrl Pts',(1.28286281182262,-1.06296368177307,8.44283717214751));
#53372=CARTESIAN_POINT('Ctrl Pts',(1.28828907797353,-1.05638062575749,8.4434192982104));
#53373=CARTESIAN_POINT('Ctrl Pts',(1.30917141330941,-1.03064633665681,8.44569325331029));
#53374=CARTESIAN_POINT('Ctrl Pts',(1.3242521066046,-1.011196253096,8.44740832258734));
#53375=CARTESIAN_POINT('Ctrl Pts',(1.36326334225511,-0.958512290178814,
8.45202933435846));
#53376=CARTESIAN_POINT('Ctrl Pts',(1.38640814417708,-0.924718757234221,
8.45496807318686));
#53377=CARTESIAN_POINT('Ctrl Pts',(1.47397007662694,-0.786182986782976,
8.46682376122934));
#53378=CARTESIAN_POINT('Ctrl Pts',(1.52796041133313,-0.675288889839493,
8.47585606659958));
#53379=CARTESIAN_POINT('Ctrl Pts',(1.58509984556531,-0.515015217807913,
8.48785241306181));
#53380=CARTESIAN_POINT('Ctrl Pts',(1.59905027440103,-0.469916133318926,
8.49112542052958));
#53381=CARTESIAN_POINT('Ctrl Pts',(1.61513126941199,-0.408853887837366,
8.49542294259421));
#53382=CARTESIAN_POINT('Ctrl Pts',(1.61897250401778,-0.393368251163257,
8.49650159860911));
#53383=CARTESIAN_POINT('Ctrl Pts',(1.62494376012842,-0.367724649216032,
8.49826992902559));
#53384=CARTESIAN_POINT('Ctrl Pts',(1.62720229830606,-0.357598000581008,
8.49896367889286));
#53385=CARTESIAN_POINT('Ctrl Pts',(1.6314367977714,-0.337740363894764,8.50031540979819));
#53386=CARTESIAN_POINT('Ctrl Pts',(1.63342065183233,-0.328011524121865,
8.500973617056));
#53387=CARTESIAN_POINT('Ctrl Pts',(1.6379316408381,-0.304833069161371,8.50253247658616));
#53388=CARTESIAN_POINT('Ctrl Pts',(1.64038029659371,-0.291368771715381,
8.50343060775144));
#53389=CARTESIAN_POINT('Ctrl Pts',(1.64823671670308,-0.244925491507286,
8.50650460064613));
#53390=CARTESIAN_POINT('Ctrl Pts',(1.65281820004663,-0.211813622389608,
8.50865454970477));
#53391=CARTESIAN_POINT('Ctrl Pts',(1.66167140356726,-0.1296986704086,8.51390372066582));
#53392=CARTESIAN_POINT('Ctrl Pts',(1.66477553413735,-0.0806012339867121,
8.51696970605745));
#53393=CARTESIAN_POINT('Ctrl Pts',(1.66695948734626,0.035122304287747,8.52411129432649));
#53394=CARTESIAN_POINT('Ctrl Pts',(1.66422524699041,0.101695572042797,8.528152580872));
#53395=CARTESIAN_POINT('Ctrl Pts',(1.65608437628265,0.182049508679997,8.53309681936171));
#53396=CARTESIAN_POINT('Ctrl Pts',(1.65447319944977,0.196152772534445,8.53396722491075));
#53397=CARTESIAN_POINT('Ctrl Pts',(1.64368205888767,0.280983762683923,8.53922673288243));
#53398=CARTESIAN_POINT('Ctrl Pts',(1.63014931032971,0.35107440394229,8.543671425714));
#53399=CARTESIAN_POINT('Ctrl Pts',(1.60925145291554,0.431276959934603,8.54909285122589));
#53400=CARTESIAN_POINT('Ctrl Pts',(1.60621545229925,0.442449948900418,8.54985587867052));
#53401=CARTESIAN_POINT('Ctrl Pts',(1.60131396227464,0.459772639037495,8.55105230811356));
#53402=CARTESIAN_POINT('Ctrl Pts',(1.59952885613828,0.465944975617436,8.55148128132113));
#53403=CARTESIAN_POINT('Ctrl Pts',(1.59616958556057,0.477313452032107,8.55227657763063));
#53404=CARTESIAN_POINT('Ctrl Pts',(1.59460567107145,0.482512412327739,8.55264231380213));
#53405=CARTESIAN_POINT('Ctrl Pts',(1.59091220213775,0.494576617973036,8.55349569892178));
#53406=CARTESIAN_POINT('Ctrl Pts',(1.58876361104147,0.501435787905343,8.55398441865805));
#53407=CARTESIAN_POINT('Ctrl Pts',(1.58175079549993,0.523325913759013,8.55555491547915));
#53408=CARTESIAN_POINT('Ctrl Pts',(1.57671728990582,0.538301155009011,8.55664567246056));
#53409=CARTESIAN_POINT('Ctrl Pts',(1.54768511648739,0.620772394225589,8.5627351340626));
#53410=CARTESIAN_POINT('Ctrl Pts',(1.51956728163363,0.686732002454029,8.56791020903149));
#53411=CARTESIAN_POINT('Ctrl Pts',(1.42788868427538,0.868373897026183,8.5827023901046));
#53412=CARTESIAN_POINT('Ctrl Pts',(1.35470673340794,0.978632185031502,8.59230420308492));
#53413=CARTESIAN_POINT('Ctrl Pts',(1.2515199717874,1.10000241085572,8.6033172295377));
#53414=CARTESIAN_POINT('Ctrl Pts',(1.23324927163831,1.12044809431157,8.6051921927104));
#53415=CARTESIAN_POINT('Ctrl Pts',(1.20589098823588,1.14958270926931,8.60789490363158));
#53416=CARTESIAN_POINT('Ctrl Pts',(1.19719738179014,1.15863364570196,8.60873909157199));
#53417=CARTESIAN_POINT('Ctrl Pts',(1.18154392371254,1.17456618303465,8.61023368833256));
#53418=CARTESIAN_POINT('Ctrl Pts',(1.17462422783988,1.18148622183495,8.61088579879288));
#53419=CARTESIAN_POINT('Ctrl Pts',(1.15998754313556,1.19586793283096,8.61224755647325));
#53420=CARTESIAN_POINT('Ctrl Pts',(1.15225858334036,1.20331682412339,8.61295662769277));
#53421=CARTESIAN_POINT('Ctrl Pts',(1.13164177113739,1.2228057629931,8.61482232467038));
#53422=CARTESIAN_POINT('Ctrl Pts',(1.11863357924766,1.23471696604904,8.61597343476391));
#53423=CARTESIAN_POINT('Ctrl Pts',(1.05066066614992,1.29500152160799,8.62186123004472));
#53424=CARTESIAN_POINT('Ctrl Pts',(0.992736350951805,1.33992285693488,8.62645431707515));
#53425=CARTESIAN_POINT('Ctrl Pts',(0.849088366953883,1.43687860847934,8.63715171826821));
#53426=CARTESIAN_POINT('Ctrl Pts',(0.761266730042087,1.48527535553097,8.64316550830717));
#53427=CARTESIAN_POINT('Ctrl Pts',(0.62045662220063,1.5470857425111,8.65271642471071));
#53428=CARTESIAN_POINT('Ctrl Pts',(0.570266633662561,1.56628076522474,8.65610741869753));
#53429=CARTESIAN_POINT('Ctrl Pts',(0.508666407649397,1.58648617841625,8.66035245457467));
#53430=CARTESIAN_POINT('Ctrl Pts',(0.498055284321168,1.5898493091763,8.66108662295507));
#53431=CARTESIAN_POINT('Ctrl Pts',(0.481363079497813,1.59495629877267,8.66224728353454));
#53432=CARTESIAN_POINT('Ctrl Pts',(0.475304181533148,1.59677235102676,8.66266975806586));
#53433=CARTESIAN_POINT('Ctrl Pts',(0.464488884128356,1.59994704451508,8.66342623188712));
#53434=CARTESIAN_POINT('Ctrl Pts',(0.459736568115057,1.60131906697927,8.66375945222289));
#53435=CARTESIAN_POINT('Ctrl Pts',(0.44819707652217,1.60459498655572,8.66457051801326));
#53436=CARTESIAN_POINT('Ctrl Pts',(0.441403907649292,1.60647697651082,8.66504959249903));
#53437=CARTESIAN_POINT('Ctrl Pts',(0.420075782227149,1.61224026353008,8.66655831031604));
#53438=CARTESIAN_POINT('Ctrl Pts',(0.405500538857981,1.61596769884155,8.66759600333793));
#53439=CARTESIAN_POINT('Ctrl Pts',(0.328338507959011,1.63459131952331,8.67311761376156));
#53440=CARTESIAN_POINT('Ctrl Pts',(0.264983670729051,1.6460488947685,8.67774600013249));
#53441=CARTESIAN_POINT('Ctrl Pts',(0.0913068380318652,1.66717097982994,
8.69044302900279));
#53442=CARTESIAN_POINT('Ctrl Pts',(-0.019589679162119,1.6695560050994,8.6985403900644));
#53443=CARTESIAN_POINT('Ctrl Pts',(-0.178644586390325,1.6571154786613,8.70980358869952));
#53444=CARTESIAN_POINT('Ctrl Pts',(-0.227191696465896,1.65116031026339,
8.71319790034189));
#53445=CARTESIAN_POINT('Ctrl Pts',(-0.291323627982365,1.64041057867587,
8.71762489934705));
#53446=CARTESIAN_POINT('Ctrl Pts',(-0.307197039254748,1.63751223926375,
8.71871604486558));
#53447=CARTESIAN_POINT('Ctrl Pts',(-0.333241859470873,1.63236463342919,
8.72049937769125));
#53448=CARTESIAN_POINT('Ctrl Pts',(-0.343438420736708,1.63024982534615,
8.72119577983131));
#53449=CARTESIAN_POINT('Ctrl Pts',(-0.363297034196302,1.62593647955193,
8.7225488597867));
#53450=CARTESIAN_POINT('Ctrl Pts',(-0.372960601221663,1.62374707628679,
8.72320579754822));
#53451=CARTESIAN_POINT('Ctrl Pts',(-0.395806258911788,1.61835638933508,
8.72475562897965));
#53452=CARTESIAN_POINT('Ctrl Pts',(-0.408970049457145,1.61508003335612,
8.7256460815658));
#53453=CARTESIAN_POINT('Ctrl Pts',(-0.453677157490325,1.60337114924446,
8.72866286307849));
#53454=CARTESIAN_POINT('Ctrl Pts',(-0.485013163240443,1.59417203083503,
8.73076460066791));
#53455=CARTESIAN_POINT('Ctrl Pts',(-0.56130059777619,1.56931881607465,8.73586798607704));
#53456=CARTESIAN_POINT('Ctrl Pts',(-0.605890847325255,1.55264828270955,
8.73883889454781));
#53457=CARTESIAN_POINT('Ctrl Pts',(-0.712264135150214,1.50759770288853,
8.74597509660745));
#53458=CARTESIAN_POINT('Ctrl Pts',(-0.773140527237406,1.47730327343718,
8.75009950125815));
#53459=CARTESIAN_POINT('Ctrl Pts',(-0.901620421702202,1.4032442704519,8.75917505766934));
#53460=CARTESIAN_POINT('Ctrl Pts',(-0.968239763119025,1.35813198581288,
8.76412748864292));
#53461=CARTESIAN_POINT('Ctrl Pts',(-1.04372586745412,1.29863051006517,8.77036363760252));
#53462=CARTESIAN_POINT('Ctrl Pts',(-1.05597583350396,1.28868921109926,8.77139701313872));
#53463=CARTESIAN_POINT('Ctrl Pts',(-1.07353696164069,1.2740191951908,8.77291285363845));
#53464=CARTESIAN_POINT('Ctrl Pts',(-1.07896235349659,1.2694277265242,8.77338603804226));
#53465=CARTESIAN_POINT('Ctrl Pts',(-1.08852024776686,1.26123341501842,8.77422867354346));
#53466=CARTESIAN_POINT('Ctrl Pts',(-1.09266458954541,1.25764468370361,8.77459710561739));
#53467=CARTESIAN_POINT('Ctrl Pts',(-1.10121634701381,1.25016523600842,8.77536382144691));
#53468=CARTESIAN_POINT('Ctrl Pts',(-1.10562084751053,1.2462716795018,8.77576228694144));
#53469=CARTESIAN_POINT('Ctrl Pts',(-1.11769482871709,1.23548396217376,8.77686426278881));
#53470=CARTESIAN_POINT('Ctrl Pts',(-1.12532089136046,1.22854191179195,8.77757113776083));
#53471=CARTESIAN_POINT('Ctrl Pts',(-1.14261038103281,1.21250714230473,8.77919777042599));
#53472=CARTESIAN_POINT('Ctrl Pts',(-1.15223051403372,1.20336896688996,8.78012040401094));
#53473=CARTESIAN_POINT('Ctrl Pts',(-1.18243774780598,1.1739807664499,8.7830709971131));
#53474=CARTESIAN_POINT('Ctrl Pts',(-1.20260717994132,1.15331073258552,8.78512179536587));
#53475=CARTESIAN_POINT('Ctrl Pts',(-1.29003666671746,1.05892322041055,8.79434198015223));
#53476=CARTESIAN_POINT('Ctrl Pts',(-1.35113093004777,0.979774794346314,
8.80168058502672));
#53477=CARTESIAN_POINT('Ctrl Pts',(-1.45006038387843,0.824606839956776,
8.81494968166443));
#53478=CARTESIAN_POINT('Ctrl Pts',(-1.48989844303489,0.75023871510445,8.82090514340464));
#53479=CARTESIAN_POINT('Ctrl Pts',(-1.53147013550008,0.656126636541299,
8.82793727613864));
#53480=CARTESIAN_POINT('Ctrl Pts',(-1.53871027605076,0.638962967915996,
8.82920073070951));
#53481=CARTESIAN_POINT('Ctrl Pts',(-1.54974587564725,0.611525579507465,
8.8311912210077));
#53482=CARTESIAN_POINT('Ctrl Pts',(-1.55373033580632,0.601330081544555,
8.83192456056937));
#53483=CARTESIAN_POINT('Ctrl Pts',(-1.5595790154709,0.585918053014193,8.83302386221438));
#53484=CARTESIAN_POINT('Ctrl Pts',(-1.56151810396754,0.580730472766154,
8.8333923134209));
#53485=CARTESIAN_POINT('Ctrl Pts',(-1.5634313003251,0.575533291099453,8.8337599051164));
#53486=CARTESIAN_POINT('Origin',(0.,0.,11.));
#53487=CARTESIAN_POINT('',(-1.56343129957118,0.575533293147481,9.53174555314795));
#53488=CARTESIAN_POINT('',(-1.56343130066142,0.575533290185854,9.34073387093129));
#53489=CARTESIAN_POINT('',(-1.56343130033213,0.575533291080363,11.));
#53490=CARTESIAN_POINT('',(-1.66599968073865,0.00103139649387118,8.67968830643497));
#53491=CARTESIAN_POINT('Ctrl Pts',(-1.56343130066142,0.575533290185854,
9.34073387093129));
#53492=CARTESIAN_POINT('Ctrl Pts',(-1.56097552924839,0.582204372397549,
9.34027245229963));
#53493=CARTESIAN_POINT('Ctrl Pts',(-1.55847696309133,0.588860000088225,
9.33980899614486));
#53494=CARTESIAN_POINT('Ctrl Pts',(-1.55200027408469,0.605782445108938,
9.33862218896235));
#53495=CARTESIAN_POINT('Ctrl Pts',(-1.54796309817374,0.616025528943391,
9.33789586382596));
#53496=CARTESIAN_POINT('Ctrl Pts',(-1.54145760786735,0.63206337039196,9.33674494641135));
#53497=CARTESIAN_POINT('Ctrl Pts',(-1.53905736201547,0.637885643511393,
9.33632426318373));
#53498=CARTESIAN_POINT('Ctrl Pts',(-1.53449753828293,0.648770839018133,
9.33553213366531));
#53499=CARTESIAN_POINT('Ctrl Pts',(-1.53234581057166,0.653836837337789,
9.33516115112599));
#53500=CARTESIAN_POINT('Ctrl Pts',(-1.52723243813707,0.665711809482304,
9.33428615771948));
#53501=CARTESIAN_POINT('Ctrl Pts',(-1.52425033589358,0.67251174090141,9.33378094558348));
#53502=CARTESIAN_POINT('Ctrl Pts',(-1.51423183143901,0.694947443890996,
9.33210076031209));
#53503=CARTESIAN_POINT('Ctrl Pts',(-1.50699976831262,0.710493934059471,
9.33091502970169));
#53504=CARTESIAN_POINT('Ctrl Pts',(-1.48879447707084,0.748100243127719,
9.32799888777758));
#53505=CARTESIAN_POINT('Ctrl Pts',(-1.47756951776062,0.770033219713634,
9.32625724334489));
#53506=CARTESIAN_POINT('Ctrl Pts',(-1.42856753016359,0.860761366010843,
9.31890259846772));
#53507=CARTESIAN_POINT('Ctrl Pts',(-1.38644076361716,0.927090318123248,
9.31316267056956));
#53508=CARTESIAN_POINT('Ctrl Pts',(-1.2781069325487,1.0736721897975,9.29991373636214));
#53509=CARTESIAN_POINT('Ctrl Pts',(-1.20874123586981,1.15120830842992,9.29247029469186));
#53510=CARTESIAN_POINT('Ctrl Pts',(-1.11530646220642,1.23782205251341,9.28369987138508));
#53511=CARTESIAN_POINT('Ctrl Pts',(-1.09767577778892,1.25348311669719,9.28209193535454));
#53512=CARTESIAN_POINT('Ctrl Pts',(-1.07048807889734,1.2766198152194,9.27968102249366));
#53513=CARTESIAN_POINT('Ctrl Pts',(-1.06117275153837,1.28437349884273,9.27886671592648));
#53514=CARTESIAN_POINT('Ctrl Pts',(-1.04423812922288,1.29815913411964,9.27740700976256));
#53515=CARTESIAN_POINT('Ctrl Pts',(-1.0366491803215,1.30422731600888,9.27676016691537));
#53516=CARTESIAN_POINT('Ctrl Pts',(-1.02027179096743,1.31708953866069,9.27537952859756));
#53517=CARTESIAN_POINT('Ctrl Pts',(-1.01146757718169,1.32386280658285,9.27464657710427));
#53518=CARTESIAN_POINT('Ctrl Pts',(-0.987112222542235,1.34221508688822,
9.27264364842932));
#53519=CARTESIAN_POINT('Ctrl Pts',(-0.971425365535203,1.35361172035039,
9.27138076641554));
#53520=CARTESIAN_POINT('Ctrl Pts',(-0.862298646727868,1.43001881210667,
9.26277053203902));
#53521=CARTESIAN_POINT('Ctrl Pts',(-0.762606194274532,1.4855803412894,9.25579963404698));
#53522=CARTESIAN_POINT('Ctrl Pts',(-0.562636883398401,1.57155153941522,
9.24250794712151));
#53523=CARTESIAN_POINT('Ctrl Pts',(-0.463647047354229,1.60354606590308,
9.23620333847865));
#53524=CARTESIAN_POINT('Ctrl Pts',(-0.347639635208347,1.62939544992755,
9.22848191372836));
#53525=CARTESIAN_POINT('Ctrl Pts',(-0.332895574326801,1.63247154521253,
9.22749437401704));
#53526=CARTESIAN_POINT('Ctrl Pts',(-0.311190102548794,1.63669375650073,
9.22602880201785));
#53527=CARTESIAN_POINT('Ctrl Pts',(-0.304259404611052,1.63799631950061,
9.22555908285078));
#53528=CARTESIAN_POINT('Ctrl Pts',(-0.291941038471274,1.64023057038641,
9.224720775648));
#53529=CARTESIAN_POINT('Ctrl Pts',(-0.286556757568334,1.64117979425906,
9.22435317613292));
#53530=CARTESIAN_POINT('Ctrl Pts',(-0.274716889527764,1.64320706691254,
9.22354217336283));
#53531=CARTESIAN_POINT('Ctrl Pts',(-0.268259674255998,1.6442735714106,9.22309816606549));
#53532=CARTESIAN_POINT('Ctrl Pts',(-0.249470187993634,1.64726330914392,
9.22180155440096));
#53533=CARTESIAN_POINT('Ctrl Pts',(-0.237122695424326,1.64908598576885,
9.22094371396321));
#53534=CARTESIAN_POINT('Ctrl Pts',(-0.131572455557443,1.66345691086724,
9.21356796444791));
#53535=CARTESIAN_POINT('Ctrl Pts',(-0.0374912177045608,1.66822988847935,
9.20672016951786));
#53536=CARTESIAN_POINT('Ctrl Pts',(0.177434499990076,1.66093951644877,9.19106593409819));
#53537=CARTESIAN_POINT('Ctrl Pts',(0.297604498869452,1.64366808734118,9.18232697768861));
#53538=CARTESIAN_POINT('Ctrl Pts',(0.435184276323533,1.6082944760408,9.17255518598844));
#53539=CARTESIAN_POINT('Ctrl Pts',(0.455410875248718,1.60268446061466,9.17112350317226));
#53540=CARTESIAN_POINT('Ctrl Pts',(0.487565367210759,1.59310821726686,9.16885461237128));
#53541=CARTESIAN_POINT('Ctrl Pts',(0.499563186286021,1.58938680538606,9.16800960530725));
#53542=CARTESIAN_POINT('Ctrl Pts',(0.520832334594986,1.58252502810981,9.16651410555765));
#53543=CARTESIAN_POINT('Ctrl Pts',(0.530120115213247,1.57943801898851,9.16586190354779));
#53544=CARTESIAN_POINT('Ctrl Pts',(0.549529416410091,1.57279639036083,9.16450049985308));
#53545=CARTESIAN_POINT('Ctrl Pts',(0.55964492280403,1.56922548873373,9.16379186934133));
#53546=CARTESIAN_POINT('Ctrl Pts',(0.586269681980587,1.55953641197448,9.16192858206297));
#53547=CARTESIAN_POINT('Ctrl Pts',(0.602717939829225,1.55325370875977,9.16077941518731));
#53548=CARTESIAN_POINT('Ctrl Pts',(0.686571720539284,1.5196916199843,9.15492592019439));
#53549=CARTESIAN_POINT('Ctrl Pts',(0.752242731717066,1.48827958963831,9.15036306338987));
#53550=CARTESIAN_POINT('Ctrl Pts',(0.904948374433367,1.40253730246508,9.13955036651063));
#53551=CARTESIAN_POINT('Ctrl Pts',(0.989422249527681,1.34427846541188,9.13340146475944));
#53552=CARTESIAN_POINT('Ctrl Pts',(1.10803223265887,1.24520675335075,9.1237919664712));
#53553=CARTESIAN_POINT('Ctrl Pts',(1.14645856650726,1.20992019887443,9.12049540293726));
#53554=CARTESIAN_POINT('Ctrl Pts',(1.1909214241194,1.16506806868546,9.11635886649541));
#53555=CARTESIAN_POINT('Ctrl Pts',(1.19860169207671,1.15716524786349,9.11563189137821));
#53556=CARTESIAN_POINT('Ctrl Pts',(1.21054838922388,1.14462582839083,9.11448016752217));
#53557=CARTESIAN_POINT('Ctrl Pts',(1.21486803951332,1.14004005761475,9.11405933679653));
#53558=CARTESIAN_POINT('Ctrl Pts',(1.22291244692144,1.13140242097695,9.11326709535505));
#53559=CARTESIAN_POINT('Ctrl Pts',(1.22664326107979,1.12735646428281,9.11289615010343));
#53560=CARTESIAN_POINT('Ctrl Pts',(1.23535760088315,1.11781155471716,9.11202146971247));
#53561=CARTESIAN_POINT('Ctrl Pts',(1.24032450030819,1.11229771311548,9.11151653596295));
#53562=CARTESIAN_POINT('Ctrl Pts',(1.25662920186507,1.09395257563365,9.10983824466035));
#53563=CARTESIAN_POINT('Ctrl Pts',(1.26780560005384,1.08098015352847,9.10865416169138));
#53564=CARTESIAN_POINT('Ctrl Pts',(1.29454165676154,1.04896264896547,9.10574291328339));
#53565=CARTESIAN_POINT('Ctrl Pts',(1.30988310620379,1.02974116128939,9.10400456056646));
#53566=CARTESIAN_POINT('Ctrl Pts',(1.37221485467599,0.94799734478871,9.09667301017118));
#53567=CARTESIAN_POINT('Ctrl Pts',(1.41519706964186,0.882546856674632,9.09095354822708));
#53568=CARTESIAN_POINT('Ctrl Pts',(1.5043302913488,0.72345979222794,9.07769768776108));
#53569=CARTESIAN_POINT('Ctrl Pts',(1.54661363699716,0.628010079243398,9.0702274884415));
#53570=CARTESIAN_POINT('Ctrl Pts',(1.58719767665577,0.506868136226347,9.06143270608923));
#53571=CARTESIAN_POINT('Ctrl Pts',(1.59421145315137,0.484357010439733,9.05982501537455));
#53572=CARTESIAN_POINT('Ctrl Pts',(1.60410387652259,0.450059568730554,9.05741439375198));
#53573=CARTESIAN_POINT('Ctrl Pts',(1.60733528397174,0.438379014601159,9.05660013720136));
#53574=CARTESIAN_POINT('Ctrl Pts',(1.61292738480809,0.417271683984568,9.05514048515498));
#53575=CARTESIAN_POINT('Ctrl Pts',(1.61533357395156,0.407857645076977,9.05449364687));
#53576=CARTESIAN_POINT('Ctrl Pts',(1.62031382454423,0.387637074500956,9.05311298040351));
#53577=CARTESIAN_POINT('Ctrl Pts',(1.6228624509457,0.376824716411446,9.05237999654675));
#53578=CARTESIAN_POINT('Ctrl Pts',(1.62956239874507,0.347071117380833,9.05037688107808));
#53579=CARTESIAN_POINT('Ctrl Pts',(1.63349157147053,0.328081253334003,9.0491138468986));
#53580=CARTESIAN_POINT('Ctrl Pts',(1.6583326146526,0.196484154927194,9.04045811069591));
#53581=CARTESIAN_POINT('Ctrl Pts',(1.66791659486275,0.082047197763266,9.03344709681004));
#53582=CARTESIAN_POINT('Ctrl Pts',(1.66367544293997,-0.135452022568592,
9.02016332853214));
#53583=CARTESIAN_POINT('Ctrl Pts',(1.65212362194959,-0.238002012864326,
9.013906030819));
#53584=CARTESIAN_POINT('Ctrl Pts',(1.62810468208955,-0.35363882288545,9.00623432632791));
#53585=CARTESIAN_POINT('Ctrl Pts',(1.62482347168012,-0.368420845372653,
9.00524163515093));
#53586=CARTESIAN_POINT('Ctrl Pts',(1.61971606279495,-0.390033100788841,
9.00376983753511));
#53587=CARTESIAN_POINT('Ctrl Pts',(1.61804702711595,-0.396900185563143,
9.00329914500659));
#53588=CARTESIAN_POINT('Ctrl Pts',(1.61500908333953,-0.409061811656605,
9.00245980126052));
#53589=CARTESIAN_POINT('Ctrl Pts',(1.61365772586271,-0.41436052808787,9.00209214850982));
#53590=CARTESIAN_POINT('Ctrl Pts',(1.6106345928296,-0.425975224798329,9.00128188432054));
#53591=CARTESIAN_POINT('Ctrl Pts',(1.60895176718415,-0.432287972285607,
9.00083867698818));
#53592=CARTESIAN_POINT('Ctrl Pts',(1.60396070169457,-0.450577924351016,
8.99954670646235));
#53593=CARTESIAN_POINT('Ctrl Pts',(1.60055562333102,-0.462527915054894,
8.99869276232351));
#53594=CARTESIAN_POINT('Ctrl Pts',(1.59242801200662,-0.489886451504286,
8.99671684147853));
#53595=CARTESIAN_POINT('Ctrl Pts',(1.58761497161418,-0.50526663081294,8.99559069233664));
#53596=CARTESIAN_POINT('Ctrl Pts',(1.5704945262345,-0.557313937750623,8.99173274178863));
#53597=CARTESIAN_POINT('Ctrl Pts',(1.55713426522695,-0.593619729288246,
8.98896183238573));
#53598=CARTESIAN_POINT('Ctrl Pts',(1.51578073043222,-0.694964263678368,
8.98105453118276));
#53599=CARTESIAN_POINT('Ctrl Pts',(1.48488803090735,-0.758731929874797,
8.97587514990361));
#53600=CARTESIAN_POINT('Ctrl Pts',(1.40234665327102,-0.904631813293935,
8.9637327054364));
#53601=CARTESIAN_POINT('Ctrl Pts',(1.34739485235949,-0.984615545305077,
8.9568459518891));
#53602=CARTESIAN_POINT('Ctrl Pts',(1.27385239428416,-1.07387557405443,8.9489366458727));
#53603=CARTESIAN_POINT('Ctrl Pts',(1.26166618345012,-1.08816688177825,8.94766214835548));
#53604=CARTESIAN_POINT('Ctrl Pts',(1.24190729945677,-1.11056071863938,8.94565115738551));
#53605=CARTESIAN_POINT('Ctrl Pts',(1.23449120327357,-1.1187986099156,8.94490828831998));
#53606=CARTESIAN_POINT('Ctrl Pts',(1.22048140781736,-1.13405194073626,8.94352667464085));
#53607=CARTESIAN_POINT('Ctrl Pts',(1.21390808395396,-1.14108537869739,8.94288711041903));
#53608=CARTESIAN_POINT('Ctrl Pts',(1.19893033492005,-1.1568356207399,8.9414489773473));
#53609=CARTESIAN_POINT('Ctrl Pts',(1.19049104403098,-1.16551863494706,8.94065195376826));
#53610=CARTESIAN_POINT('Ctrl Pts',(1.16482402121885,-1.19135723447147,8.93826663298664));
#53611=CARTESIAN_POINT('Ctrl Pts',(1.14731423111349,-1.20822895739783,8.93669076915745));
#53612=CARTESIAN_POINT('Ctrl Pts',(1.10597504261343,-1.24635233389343,8.93308005135195));
#53613=CARTESIAN_POINT('Ctrl Pts',(1.08189133964565,-1.26731458250074,8.93105670413246));
#53614=CARTESIAN_POINT('Ctrl Pts',(0.99116420409578,-1.34181013541919,8.92369102213435));
#53615=CARTESIAN_POINT('Ctrl Pts',(0.921032512604105,-1.39088502280146,
8.91849267303895));
#53616=CARTESIAN_POINT('Ctrl Pts',(0.769104541649145,-1.4806461231887,8.90771212627441));
#53617=CARTESIAN_POINT('Ctrl Pts',(0.687117499168477,-1.52042757835009,
8.90214308745717));
#53618=CARTESIAN_POINT('Ctrl Pts',(0.587693485241293,-1.55897979432685,
8.89522313080932));
#53619=CARTESIAN_POINT('Ctrl Pts',(0.573002340018647,-1.56443916677728,
8.89419639204224));
#53620=CARTESIAN_POINT('Ctrl Pts',(0.551558033299664,-1.57206551606703,
8.89268854670433));
#53621=CARTESIAN_POINT('Ctrl Pts',(0.544864100988161,-1.57439809381273,
8.89221658495496));
#53622=CARTESIAN_POINT('Ctrl Pts',(0.532969141386325,-1.57845808556889,
8.89137530998448));
#53623=CARTESIAN_POINT('Ctrl Pts',(0.527774180112019,-1.58020266012999,
8.89100700374369));
#53624=CARTESIAN_POINT('Ctrl Pts',(0.51646427182502,-1.58393876516903,8.89020314012698));
#53625=CARTESIAN_POINT('Ctrl Pts',(0.51034646557059,-1.5859205016214,8.88976706016531));
#53626=CARTESIAN_POINT('Ctrl Pts',(0.492842449315931,-1.5914787960523,8.88851610672083));
#53627=CARTESIAN_POINT('Ctrl Pts',(0.481429346634263,-1.59496840153855,
8.88769652774585));
#53628=CARTESIAN_POINT('Ctrl Pts',(0.378905464045456,-1.6251148923719,8.8803052397185));
#53629=CARTESIAN_POINT('Ctrl Pts',(0.285718067041004,-1.64405874460856,
8.87339291019169));
#53630=CARTESIAN_POINT('Ctrl Pts',(0.0711743520457735,-1.66887587811384,
8.85767133657317));
#53631=CARTESIAN_POINT('Ctrl Pts',(-0.0502672840653522,-1.66963943239142,
8.84892944568429));
#53632=CARTESIAN_POINT('Ctrl Pts',(-0.1916103146031,-1.65507760227345,8.83915516420808));
#53633=CARTESIAN_POINT('Ctrl Pts',(-0.212443391405547,-1.65253267961743,
8.83772363724082));
#53634=CARTESIAN_POINT('Ctrl Pts',(-0.245660378469093,-1.64783638199264,
8.83545494364769));
#53635=CARTESIAN_POINT('Ctrl Pts',(-0.258077087228843,-1.6459374214758,
8.83460998008349));
#53636=CARTESIAN_POINT('Ctrl Pts',(-0.280128509403378,-1.64230928934702,
8.83311452982333));
#53637=CARTESIAN_POINT('Ctrl Pts',(-0.289771568967215,-1.64063531246301,
8.83246233419867));
#53638=CARTESIAN_POINT('Ctrl Pts',(-0.309952005264837,-1.63694863274541,
8.83110091649332));
#53639=CARTESIAN_POINT('Ctrl Pts',(-0.320485850233733,-1.63491892786626,
8.83039226582443));
#53640=CARTESIAN_POINT('Ctrl Pts',(-0.348255723880426,-1.62928940429542,
8.82852886300906));
#53641=CARTESIAN_POINT('Ctrl Pts',(-0.365455850017631,-1.6255177859212,
8.82737960201135));
#53642=CARTESIAN_POINT('Ctrl Pts',(-0.453388308813637,-1.60476975934026,
8.82152442476425));
#53643=CARTESIAN_POINT('Ctrl Pts',(-0.523018036583001,-1.58344592300441,
8.81696008384436));
#53644=CARTESIAN_POINT('Ctrl Pts',(-0.686813788657039,-1.52129436653,8.80614379945562));
#53645=CARTESIAN_POINT('Ctrl Pts',(-0.779028959680981,-1.47619854320018,
8.79999284016884));
#53646=CARTESIAN_POINT('Ctrl Pts',(-0.910950862107429,-1.39586219744732,
8.79038821181619));
#53647=CARTESIAN_POINT('Ctrl Pts',(-0.954089843793724,-1.36673851579903,
8.78709917020588));
#53648=CARTESIAN_POINT('Ctrl Pts',(-1.00465158155621,-1.32904226666063,
8.78296873720241));
#53649=CARTESIAN_POINT('Ctrl Pts',(-1.01344583747821,-1.32234854152571,
8.78223970117197));
#53650=CARTESIAN_POINT('Ctrl Pts',(-1.02715305800251,-1.31169827929561,
8.78108542045471));
#53651=CARTESIAN_POINT('Ctrl Pts',(-1.03211144346079,-1.30780034617788,
8.78066412225704));
#53652=CARTESIAN_POINT('Ctrl Pts',(-1.04120919514806,-1.3005643730182,8.77988391453783));
#53653=CARTESIAN_POINT('Ctrl Pts',(-1.04535486635163,-1.29723454960941,
8.77952557802632));
#53654=CARTESIAN_POINT('Ctrl Pts',(-1.04953501971799,-1.29384398078787,
8.77916143284886));
#53655=CARTESIAN_POINT('Ctrl Pts',(-1.0495855613694,-1.29380298098293,8.77915702960156));
#53656=CARTESIAN_POINT('Ctrl Pts',(-1.04968630994534,-1.29372124311757,
8.7791482514342));
#53657=CARTESIAN_POINT('Ctrl Pts',(-1.04973651691065,-1.29368050508796,
8.77914387651603));
#53658=CARTESIAN_POINT('Ctrl Pts',(-1.04983661266962,-1.2935992775302,8.77913515358076));
#53659=CARTESIAN_POINT('Ctrl Pts',(-1.04988650148876,-1.29355878804173,
8.77913080556657));
#53660=CARTESIAN_POINT('Ctrl Pts',(-1.04998597705971,-1.29347804467536,
8.77912213505119));
#53661=CARTESIAN_POINT('Ctrl Pts',(-1.0500355638331,-1.29343779083686,8.77911781255297));
#53662=CARTESIAN_POINT('Ctrl Pts',(-1.05013445099716,-1.29335750620696,
8.7791091917169));
#53663=CARTESIAN_POINT('Ctrl Pts',(-1.05018375141232,-1.2933174754493,8.77910489338149));
#53664=CARTESIAN_POINT('Ctrl Pts',(-1.05028208112494,-1.29323762474549,
8.77909631955391));
#53665=CARTESIAN_POINT('Ctrl Pts',(-1.05033111046096,-1.29319780481849,
8.77909204406267));
#53666=CARTESIAN_POINT('Ctrl Pts',(-1.05042891297235,-1.29311836377819,
8.77908351463211));
#53667=CARTESIAN_POINT('Ctrl Pts',(-1.05047768616211,-1.2930787427006,8.77907926069557));
#53668=CARTESIAN_POINT('Ctrl Pts',(-1.05057499093478,-1.29299968767697,
8.7790707731172));
#53669=CARTESIAN_POINT('Ctrl Pts',(-1.05062352254225,-1.29296025375542,
8.77906653947701));
#53670=CARTESIAN_POINT('Ctrl Pts',(-1.05072035841133,-1.2928815615881,8.77905809125873));
#53671=CARTESIAN_POINT('Ctrl Pts',(-1.05076866268573,-1.29284230337352,
8.77905387668305));
#53672=CARTESIAN_POINT('Ctrl Pts',(-1.0508650577971,-1.29276395143976,8.77904546539097));
#53673=CARTESIAN_POINT('Ctrl Pts',(-1.05091314866018,-1.29272485773818,
8.77904126867559));
#53674=CARTESIAN_POINT('Ctrl Pts',(-1.05642564804173,-1.28824316284837,
8.77856016936964));
#53675=CARTESIAN_POINT('Ctrl Pts',(-1.06186171174713,-1.28376606011976,
8.7780808458362));
#53676=CARTESIAN_POINT('Ctrl Pts',(-1.07368732762639,-1.27390007005085,
8.77702767044892));
#53677=CARTESIAN_POINT('Ctrl Pts',(-1.08006500553454,-1.26849731685145,
8.77645291152172));
#53678=CARTESIAN_POINT('Ctrl Pts',(-1.0975202940165,-1.25348326413653,8.77486169912587));
#53679=CARTESIAN_POINT('Ctrl Pts',(-1.10851180189213,-1.24377354908376,
8.77383932311324));
#53680=CARTESIAN_POINT('Ctrl Pts',(-1.14420401343289,-1.21139471165152,
8.77045556758337));
#53681=CARTESIAN_POINT('Ctrl Pts',(-1.1683477020553,-1.18812597995056,8.76806402850452));
#53682=CARTESIAN_POINT('Ctrl Pts',(-1.27431055831504,-1.07964862868766,
8.75715023320554));
#53683=CARTESIAN_POINT('Ctrl Pts',(-1.34763812731492,-0.986602201158724,
8.7484466510455));
#53684=CARTESIAN_POINT('Ctrl Pts',(-1.44289449031585,-0.835054252666842,
8.73569995999773));
#53685=CARTESIAN_POINT('Ctrl Pts',(-1.47243781013309,-0.781785511323394,
8.73144593816837));
#53686=CARTESIAN_POINT('Ctrl Pts',(-1.50654843293209,-0.711454037462047,
8.7261142363581));
#53687=CARTESIAN_POINT('Ctrl Pts',(-1.51385207947257,-0.695777945047683,
8.72494307836006));
#53688=CARTESIAN_POINT('Ctrl Pts',(-1.52526138858008,-0.67025914716124,
8.72306354635118));
#53689=CARTESIAN_POINT('Ctrl Pts',(-1.5295187879798,-0.660486119609003,
8.72235002634016));
#53690=CARTESIAN_POINT('Ctrl Pts',(-1.53751230917677,-0.641644817431444,
8.72098621082228));
#53691=CARTESIAN_POINT('Ctrl Pts',(-1.54126271775386,-0.632583128515173,
8.72033545332679));
#53692=CARTESIAN_POINT('Ctrl Pts',(-1.54976800137927,-0.611508017821998,
8.71883359915874));
#53693=CARTESIAN_POINT('Ctrl Pts',(-1.55446362358281,-0.599471244126243,
8.71798452042175));
#53694=CARTESIAN_POINT('Ctrl Pts',(-1.56915415568843,-0.56047981383675,
8.71526082019183));
#53695=CARTESIAN_POINT('Ctrl Pts',(-1.57859193186306,-0.533319844770116,
8.71340460488623));
#53696=CARTESIAN_POINT('Ctrl Pts',(-1.61546779329547,-0.417623734153171,
8.70564836649682));
#53697=CARTESIAN_POINT('Ctrl Pts',(-1.63619676418024,-0.327121366869854,
8.69996022469041));
#53698=CARTESIAN_POINT('Ctrl Pts',(-1.66046624743968,-0.157049875223947,
8.68946586476894));
#53699=CARTESIAN_POINT('Ctrl Pts',(-1.66604864137761,-0.0780540079694674,
8.6846626029166));
#53700=CARTESIAN_POINT('Ctrl Pts',(-1.66599968073865,0.00103139649387118,
8.67968830643497));
#53701=CARTESIAN_POINT('Ctrl Pts',(-1.66599967925263,0.00103379404400243,
8.67968815563433));
#53702=CARTESIAN_POINT('Ctrl Pts',(-1.66597648224291,0.0384166857153259,
8.67733685306753));
#53703=CARTESIAN_POINT('Ctrl Pts',(-1.6646950543706,0.0757857438253784,
8.6749486588933));
#53704=CARTESIAN_POINT('Ctrl Pts',(-1.66161369494957,0.121079560033358,
8.6719742140175));
#53705=CARTESIAN_POINT('Ctrl Pts',(-1.66101153588352,0.129077506502333,
8.67144595417797));
#53706=CARTESIAN_POINT('Ctrl Pts',(-1.65988110049662,0.142770597757506,
8.67053585219587));
#53707=CARTESIAN_POINT('Ctrl Pts',(-1.65938119599999,0.148468028065719,
8.67015548892855));
#53708=CARTESIAN_POINT('Ctrl Pts',(-1.65837961712452,0.159245417429015,
8.66943259787395));
#53709=CARTESIAN_POINT('Ctrl Pts',(-1.65788390923652,0.164325893963225,
8.66909039944385));
#53710=CARTESIAN_POINT('Ctrl Pts',(-1.65684510346844,0.1744890590459,8.66840285312853));
#53711=CARTESIAN_POINT('Ctrl Pts',(-1.65630194728617,0.179571674368825,
8.66805750879186));
#53712=CARTESIAN_POINT('Ctrl Pts',(-1.65495319390699,0.1916656853521,8.66723231936529));
#53713=CARTESIAN_POINT('Ctrl Pts',(-1.65412642417294,0.198674551342065,
8.66675133369868));
#53714=CARTESIAN_POINT('Ctrl Pts',(-1.65102180449209,0.223629741822775,
8.66502942676835));
#53715=CARTESIAN_POINT('Ctrl Pts',(-1.64849630276128,0.241543234602649,
8.66377615091533));
#53716=CARTESIAN_POINT('Ctrl Pts',(-1.63808689301534,0.307579550393764,
8.659100681074));
#53717=CARTESIAN_POINT('Ctrl Pts',(-1.62838346383068,0.355387628171913,
8.65560720346379));
#53718=CARTESIAN_POINT('Ctrl Pts',(-1.60201257983422,0.461251642266212,
8.64771584932469));
#53719=CARTESIAN_POINT('Ctrl Pts',(-1.58426157560517,0.518948008136952,
8.64330847460035));
#53720=CARTESIAN_POINT('Ctrl Pts',(-1.56343135626508,0.575533139138958,
8.63893242883258));
#53721=CARTESIAN_POINT('',(-1.66599975036832,-0.00128669572401095,8.8706297405923));
#53722=CARTESIAN_POINT('Ctrl Pts',(-1.5634313003251,0.575533291099453,8.8337599051164));
#53723=CARTESIAN_POINT('Ctrl Pts',(-1.56488277523164,0.571590371835501,
8.8340387840301));
#53724=CARTESIAN_POINT('Ctrl Pts',(-1.56631934733467,0.567641926262001,
8.83431716827669));
#53725=CARTESIAN_POINT('Ctrl Pts',(-1.57192654351643,0.55204707472868,8.83541323209833));
#53726=CARTESIAN_POINT('Ctrl Pts',(-1.57598240674274,0.540359600935614,
8.83622710063096));
#53727=CARTESIAN_POINT('Ctrl Pts',(-1.58806055678282,0.504261679637931,
8.83871852670838));
#53728=CARTESIAN_POINT('Ctrl Pts',(-1.5956488675341,0.479709265922574,8.84038190946538));
#53729=CARTESIAN_POINT('Ctrl Pts',(-1.61204382517528,0.421959319299,8.84422996185352));
#53730=CARTESIAN_POINT('Ctrl Pts',(-1.62039813340751,0.388645180678364,
8.84640078825903));
#53731=CARTESIAN_POINT('Ctrl Pts',(-1.65325862731819,0.23801619464825,8.85604619456224));
#53732=CARTESIAN_POINT('Ctrl Pts',(-1.66609189323001,0.118533972871092,
8.86321239120117));
#53733=CARTESIAN_POINT('Ctrl Pts',(-1.66599950474116,-0.00128460196485134,
8.8706291825431));
#53734=CARTESIAN_POINT('Ctrl Pts',(-1.66599950310516,-0.00128672194783298,
8.87062931377045));
#53735=CARTESIAN_POINT('Ctrl Pts',(-1.66596827752896,-0.041716431351172,
8.87313192108214));
#53736=CARTESIAN_POINT('Ctrl Pts',(-1.66446536543592,-0.0821296462730489,
8.87566262957749));
#53737=CARTESIAN_POINT('Ctrl Pts',(-1.66002256804847,-0.142414878799788,
8.8795327181488));
#53738=CARTESIAN_POINT('Ctrl Pts',(-1.65819112512869,-0.162354659756153,
8.88082843616167));
#53739=CARTESIAN_POINT('Ctrl Pts',(-1.65515491289895,-0.189942131585233,
8.8826488498797));
#53740=CARTESIAN_POINT('Ctrl Pts',(-1.65425545900996,-0.197622543984168,
8.88315864842651));
#53741=CARTESIAN_POINT('Ctrl Pts',(-1.65261124523688,-0.210863813782305,
8.88404315577053));
#53742=CARTESIAN_POINT('Ctrl Pts',(-1.65189179360435,-0.21642776119652,
8.88441653300406));
#53743=CARTESIAN_POINT('Ctrl Pts',(-1.65040124799167,-0.227514429378216,
8.8851641229737));
#53744=CARTESIAN_POINT('Ctrl Pts',(-1.64963049834339,-0.233037149421823,
8.88553831843663));
#53745=CARTESIAN_POINT('Ctrl Pts',(-1.64796278557865,-0.2445639165712,8.88632323048602));
#53746=CARTESIAN_POINT('Ctrl Pts',(-1.64706072011261,-0.250567023437197,
8.88673420589282));
#53747=CARTESIAN_POINT('Ctrl Pts',(-1.64454581597392,-0.266702699382268,
8.88784453008086));
#53748=CARTESIAN_POINT('Ctrl Pts',(-1.6428721790373,-0.276825325393903,
8.88854710997405));
#53749=CARTESIAN_POINT('Ctrl Pts',(-1.63452887836497,-0.32454484399152,
8.8918856384151));
#53750=CARTESIAN_POINT('Ctrl Pts',(-1.62666192085239,-0.361917804472079,
8.89457787022709));
#53751=CARTESIAN_POINT('Ctrl Pts',(-1.60236290832557,-0.46042828696624,
8.90182702534621));
#53752=CARTESIAN_POINT('Ctrl Pts',(-1.58371867614595,-0.520956425430241,
8.9064386797093));
#53753=CARTESIAN_POINT('Ctrl Pts',(-1.54265689778955,-0.63146491765145,
8.9150194758297));
#53754=CARTESIAN_POINT('Ctrl Pts',(-1.52112975916639,-0.681691295193066,
8.91898544338394));
#53755=CARTESIAN_POINT('Ctrl Pts',(-1.46526640162141,-0.796141765248175,
8.92811444013505));
#53756=CARTESIAN_POINT('Ctrl Pts',(-1.42910869966066,-0.859359230160901,
8.93322584024351));
#53757=CARTESIAN_POINT('Ctrl Pts',(-1.37920481484813,-0.934697876844317,
8.93939281986397));
#53758=CARTESIAN_POINT('Ctrl Pts',(-1.3692486848802,-0.94922290456683,8.9405858022141));
#53759=CARTESIAN_POINT('Ctrl Pts',(-1.35285907409059,-0.972339143184272,
8.94249160935605));
#53760=CARTESIAN_POINT('Ctrl Pts',(-1.34656983465826,-0.981030465081007,
8.94320984552036));
#53761=CARTESIAN_POINT('Ctrl Pts',(-1.3343828779837,-0.997534024008357,
8.94457717549616));
#53762=CARTESIAN_POINT('Ctrl Pts',(-1.32849942968826,-1.0053561888223,8.94522678279268));
#53763=CARTESIAN_POINT('Ctrl Pts',(-1.31490861998533,-1.02309779741006,
8.94670398731371));
#53764=CARTESIAN_POINT('Ctrl Pts',(-1.30715726093793,-1.03298290959966,
8.94752981303348));
#53765=CARTESIAN_POINT('Ctrl Pts',(-1.28615868963339,-1.05914695290626,
8.9497239253404));
#53766=CARTESIAN_POINT('Ctrl Pts',(-1.27271417548612,-1.07526514558967,
8.95108433046532));
#53767=CARTESIAN_POINT('Ctrl Pts',(-1.17967520622907,-1.18261585190103,
8.96021730129166));
#53768=CARTESIAN_POINT('Ctrl Pts',(-1.09064493160751,-1.2651922104763,8.96756981279484));
#53769=CARTESIAN_POINT('Ctrl Pts',(-0.91714083881409,-1.3940742640748,8.98077707195054));
#53770=CARTESIAN_POINT('Ctrl Pts',(-0.836139311024954,-1.44411086642029,
8.9866020385928));
#53771=CARTESIAN_POINT('Ctrl Pts',(-0.740733417825566,-1.4923173029462,
8.99359176309791));
#53772=CARTESIAN_POINT('Ctrl Pts',(-0.730081271344885,-1.49755742674096,
8.99437396919977));
#53773=CARTESIAN_POINT('Ctrl Pts',(-0.713585826375973,-1.50545423557928,
8.99558941361581));
#53774=CARTESIAN_POINT('Ctrl Pts',(-0.70778139567752,-1.50819185765991,
8.99601788941611));
#53775=CARTESIAN_POINT('Ctrl Pts',(-0.696989250214719,-1.5132058828545,
8.99681626862363));
#53776=CARTESIAN_POINT('Ctrl Pts',(-0.692005941441851,-1.51549128423895,
8.99718561972599));
#53777=CARTESIAN_POINT('Ctrl Pts',(-0.680535372881636,-1.52068344485008,
8.99803733820598));
#53778=CARTESIAN_POINT('Ctrl Pts',(-0.674040715602689,-1.52357331371274,
8.99852069139764));
#53779=CARTESIAN_POINT('Ctrl Pts',(-0.653067894642985,-1.53274505543102,
9.00008465279578));
#53780=CARTESIAN_POINT('Ctrl Pts',(-0.638519394461202,-1.53886257270924,
9.00117427039388));
#53781=CARTESIAN_POINT('Ctrl Pts',(-0.55055313685452,-1.57438948868897,
9.00778155852132));
#53782=CARTESIAN_POINT('Ctrl Pts',(-0.475210441366305,-1.5987443886253,
9.01351478732295));
#53783=CARTESIAN_POINT('Ctrl Pts',(-0.334183109827049,-1.63347970724582,
9.02408374086524));
#53784=CARTESIAN_POINT('Ctrl Pts',(-0.269045756079804,-1.64546329554329,
9.02890492484022));
#53785=CARTESIAN_POINT('Ctrl Pts',(-0.154346706218855,-1.65956992508093,
9.03719564964192));
#53786=CARTESIAN_POINT('Ctrl Pts',(-0.105080082227951,-1.66341641620293,
9.04069465968755));
#53787=CARTESIAN_POINT('Ctrl Pts',(-0.0222065774932575,-1.66618927387045,
9.04646489783672));
#53788=CARTESIAN_POINT('Ctrl Pts',(0.011326341424732,-1.66629883936254,
9.04876832701811));
#53789=CARTESIAN_POINT('Ctrl Pts',(0.0585375289211347,-1.66502764647522,
9.05196916792454));
#53790=CARTESIAN_POINT('Ctrl Pts',(0.0722284151591141,-1.66448994630165,
9.05289242005591));
#53791=CARTESIAN_POINT('Ctrl Pts',(0.0958297647904633,-1.66327126199123,
9.05447582700435));
#53792=CARTESIAN_POINT('Ctrl Pts',(0.105743457963293,-1.66267043133611,
9.05513844733031));
#53793=CARTESIAN_POINT('Ctrl Pts',(0.125996365850009,-1.66126110316037,
9.05648728401805));
#53794=CARTESIAN_POINT('Ctrl Pts',(0.136334603932253,-1.66044464559428,
9.05717322129421));
#53795=CARTESIAN_POINT('Ctrl Pts',(0.162532665486372,-1.65812933456241,
9.05890529161773));
#53796=CARTESIAN_POINT('Ctrl Pts',(0.178380085756071,-1.65649942084418,
9.05994729348267));
#53797=CARTESIAN_POINT('Ctrl Pts',(0.24084040071879,-1.64916857553735,9.06403424964974));
#53798=CARTESIAN_POINT('Ctrl Pts',(0.287229185158592,-1.64172503859499,
9.0670248555627));
#53799=CARTESIAN_POINT('Ctrl Pts',(0.443283019040145,-1.60986620198611,
9.07701773753384));
#53800=CARTESIAN_POINT('Ctrl Pts',(0.550765196775811,-1.57633345343412,
9.08376637265435));
#53801=CARTESIAN_POINT('Ctrl Pts',(0.713778368484908,-1.50674910042821,
9.09467185701371));
#53802=CARTESIAN_POINT('Ctrl Pts',(0.771951086832096,-1.4777895876209,9.09871745373136));
#53803=CARTESIAN_POINT('Ctrl Pts',(0.841387873409657,-1.43800233467586,
9.10391613433313));
#53804=CARTESIAN_POINT('Ctrl Pts',(0.854393533742128,-1.4303132238541,9.10490669395065));
#53805=CARTESIAN_POINT('Ctrl Pts',(0.873321126875506,-1.418772733341,9.10637593050457));
#53806=CARTESIAN_POINT('Ctrl Pts',(0.879326425696656,-1.41505861789301,
9.10684623545486));
#53807=CARTESIAN_POINT('Ctrl Pts',(0.889499328596857,-1.40867719040407,
9.10765033560148));
#53808=CARTESIAN_POINT('Ctrl Pts',(0.893678954296769,-1.40602930556266,
9.10798286382665));
#53809=CARTESIAN_POINT('Ctrl Pts',(0.903168283078739,-1.39995819994274,
9.10874283107237));
#53810=CARTESIAN_POINT('Ctrl Pts',(0.908470229525741,-1.39652345053351,
9.10917100979413));
#53811=CARTESIAN_POINT('Ctrl Pts',(0.923030779722948,-1.38697271322956,
9.11035648323831));
#53812=CARTESIAN_POINT('Ctrl Pts',(0.932247814456555,-1.38079438130641,
9.11111766848605));
#53813=CARTESIAN_POINT('Ctrl Pts',(0.984964663819151,-1.34468898717841,
9.11553055201172));
#53814=CARTESIAN_POINT('Ctrl Pts',(1.02707989540479,-1.31280219196893,9.11928988104042));
#53815=CARTESIAN_POINT('Ctrl Pts',(1.1452619041665,-1.21415138715253,9.13039123268855));
#53816=CARTESIAN_POINT('Ctrl Pts',(1.21685824025075,-1.14238617258293,9.13782495381783));
#53817=CARTESIAN_POINT('Ctrl Pts',(1.32821983473003,-1.00833197065608,9.1503196514515));
#53818=CARTESIAN_POINT('Ctrl Pts',(1.37119046048659,-0.949073587826089,
9.15545798478568));
#53819=CARTESIAN_POINT('Ctrl Pts',(1.41952163983021,-0.87225290491955,9.16165193191844));
#53820=CARTESIAN_POINT('Ctrl Pts',(1.42867276334667,-0.857182006831354,
9.16284643317738));
#53821=CARTESIAN_POINT('Ctrl Pts',(1.44300723280871,-0.832707217998786,
9.1647540669951));
#53822=CARTESIAN_POINT('Ctrl Pts',(1.4483417072764,-0.823393886990113,9.16547262959952));
#53823=CARTESIAN_POINT('Ctrl Pts',(1.45836756766491,-0.805491034420518,
9.16684020614021));
#53824=CARTESIAN_POINT('Ctrl Pts',(1.46307397370014,-0.796910486442735,
9.16748973710673));
#53825=CARTESIAN_POINT('Ctrl Pts',(1.47364360378934,-0.777231030880079,
9.16896625766983));
#53826=CARTESIAN_POINT('Ctrl Pts',(1.47945759650534,-0.766106246439847,
9.16979148166983));
#53827=CARTESIAN_POINT('Ctrl Pts',(1.49464013563545,-0.736237675511792,
9.17198285646175));
#53828=CARTESIAN_POINT('Ctrl Pts',(1.5037819132853,-0.71738070082642,9.17334115767906));
#53829=CARTESIAN_POINT('Ctrl Pts',(1.56355141408682,-0.587926153673739,
9.18250854084999));
#53830=CARTESIAN_POINT('Ctrl Pts',(1.60229199090032,-0.472244024635995,
9.18989299383956));
#53831=CARTESIAN_POINT('Ctrl Pts',(1.6481244794471,-0.261075211193354,9.20309809971954));
#53832=CARTESIAN_POINT('Ctrl Pts',(1.66026885543512,-0.167262528521581,
9.20888764052188));
#53833=CARTESIAN_POINT('Ctrl Pts',(1.66492499714733,-0.0610181047416712,
9.21584062516424));
#53834=CARTESIAN_POINT('Ctrl Pts',(1.66531939335526,-0.0490892375292942,
9.21662696999309));
#53835=CARTESIAN_POINT('Ctrl Pts',(1.6657290151657,-0.0307279760604022,
9.21784749257201));
#53836=CARTESIAN_POINT('Ctrl Pts',(1.6658352192432,-0.0242977228723366,
9.21827684516681));
#53837=CARTESIAN_POINT('Ctrl Pts',(1.66596296602662,-0.012386820105187,
9.21907596119453));
#53838=CARTESIAN_POINT('Ctrl Pts',(1.66599469829919,-0.00690648494370706,
9.21944516253258));
#53839=CARTESIAN_POINT('Ctrl Pts',(1.66600545811108,0.00566307078343564,
9.22029539091038));
#53840=CARTESIAN_POINT('Ctrl Pts',(1.66596627718651,0.0127520784019295,
9.22077739101599));
#53841=CARTESIAN_POINT('Ctrl Pts',(1.66569519640985,0.0355130745999442,
9.22233249587555));
#53842=CARTESIAN_POINT('Ctrl Pts',(1.66528738272876,0.0511815829638037,
9.22341447316345));
#53843=CARTESIAN_POINT('Ctrl Pts',(1.66100514156942,0.15782929327989,9.23084673964826));
#53844=CARTESIAN_POINT('Ctrl Pts',(1.64989827418297,0.248356240164162,9.23748291685502));
#53845=CARTESIAN_POINT('Ctrl Pts',(1.61415134764611,0.421147951123315,9.25032683511329));
#53846=CARTESIAN_POINT('Ctrl Pts',(1.59044183670801,0.50333658274887,9.25651678434946));
#53847=CARTESIAN_POINT('Ctrl Pts',(1.54935820118495,0.613240047714823,9.26478690489164));
#53848=CARTESIAN_POINT('Ctrl Pts',(1.53732823011057,0.64280349490545,9.26701196158952));
#53849=CARTESIAN_POINT('Ctrl Pts',(1.51465189834327,0.694245183325159,9.27088403957266));
#53850=CARTESIAN_POINT('Ctrl Pts',(1.50436206658491,0.716269242928525,9.27254199350692));
#53851=CARTESIAN_POINT('Ctrl Pts',(1.48822989608377,0.748915454057452,9.2750010974797));
#53852=CARTESIAN_POINT('Ctrl Pts',(1.48274802130399,0.759711063277453,9.27581455352803));
#53853=CARTESIAN_POINT('Ctrl Pts',(1.4726968004174,0.778981907827375,9.27726742712968));
#53854=CARTESIAN_POINT('Ctrl Pts',(1.46817079921307,0.787479009051319,9.27790832869274));
#53855=CARTESIAN_POINT('Ctrl Pts',(1.45827522156715,0.805675036706466,9.27928163848624));
#53856=CARTESIAN_POINT('Ctrl Pts',(1.45288195594977,0.815360606526759,9.2800131685031));
#53857=CARTESIAN_POINT('Ctrl Pts',(1.43808997055515,0.841312143543874,9.28197521661461));
#53858=CARTESIAN_POINT('Ctrl Pts',(1.42851197624656,0.857474469820867,9.28319927027255));
#53859=CARTESIAN_POINT('Ctrl Pts',(1.3678818172197,0.955947843273953,9.29067774583326));
#53860=CARTESIAN_POINT('Ctrl Pts',(1.31000320731597,1.03384333305896,9.29666871022893));
#53861=CARTESIAN_POINT('Ctrl Pts',(1.1986497301295,1.15922830839413,9.30693048243229));
#53862=CARTESIAN_POINT('Ctrl Pts',(1.1482962230191,1.20912637986913,9.31122428115046));
#53863=CARTESIAN_POINT('Ctrl Pts',(1.06579495785619,1.28106620524842,9.31800975750277));
#53864=CARTESIAN_POINT('Ctrl Pts',(1.03579429938842,1.3054421821606,9.32043256191278));
#53865=CARTESIAN_POINT('Ctrl Pts',(0.992128740573799,1.33846778368993,9.32394018100295));
#53866=CARTESIAN_POINT('Ctrl Pts',(0.9791423008097,1.34799694326833,9.32498115635007));
#53867=CARTESIAN_POINT('Ctrl Pts',(0.955900562946801,1.36453816158531,9.32684429467267));
#53868=CARTESIAN_POINT('Ctrl Pts',(0.945700992093933,1.37162673191366,9.32766196584529));
#53869=CARTESIAN_POINT('Ctrl Pts',(0.930017899544425,1.38226820125471,9.32892088185917));
#53870=CARTESIAN_POINT('Ctrl Pts',(0.924590894567865,1.3859041625341,9.32935681560543));
#53871=CARTESIAN_POINT('Ctrl Pts',(0.914581413095402,1.39252531348341,9.33016166536108));
#53872=CARTESIAN_POINT('Ctrl Pts',(0.910005449860086,1.39551997054404,9.33052994684436));
#53873=CARTESIAN_POINT('Ctrl Pts',(0.899480896795459,1.40233380014066,9.33137771980889));
#53874=CARTESIAN_POINT('Ctrl Pts',(0.893522705263631,1.40613766798398,9.33185817494019));
#53875=CARTESIAN_POINT('Ctrl Pts',(0.874718789433595,1.41797481868144,9.33337563686172));
#53876=CARTESIAN_POINT('Ctrl Pts',(0.861788001082651,1.42587059298853,9.33442082193067));
#53877=CARTESIAN_POINT('Ctrl Pts',(0.760188292474761,1.48602240282723,9.3426354482507));
#53878=CARTESIAN_POINT('Ctrl Pts',(0.666964112237238,1.53013209657131,9.35017212228367));
#53879=CARTESIAN_POINT('Ctrl Pts',(0.462629659926865,1.60457330099689,9.36598732243035));
#53880=CARTESIAN_POINT('Ctrl Pts',(0.351206968569368,1.63258829555905,9.37420138646117));
#53881=CARTESIAN_POINT('Ctrl Pts',(0.218580504684241,1.65171261501591,9.38337040615611));
#53882=CARTESIAN_POINT('Ctrl Pts',(0.199340775993966,1.65414488778328,9.3846868157456));
#53883=CARTESIAN_POINT('Ctrl Pts',(0.169018615241091,1.65744143513433,9.38674080516317));
#53884=CARTESIAN_POINT('Ctrl Pts',(0.157963032168888,1.65853160778333,9.38748539486287));
#53885=CARTESIAN_POINT('Ctrl Pts',(0.137218127792181,1.66036791183671,9.38887477288967));
#53886=CARTESIAN_POINT('Ctrl Pts',(0.127531638575733,1.6611400017016,9.38952034674685));
#53887=CARTESIAN_POINT('Ctrl Pts',(0.105749685260113,1.66268454160339,9.39096518903091));
#53888=CARTESIAN_POINT('Ctrl Pts',(0.0936513480057222,1.66340984690926,
9.39176295281699));
#53889=CARTESIAN_POINT('Ctrl Pts',(0.0579973689619847,1.66515710078907,
9.39410082797416));
#53890=CARTESIAN_POINT('Ctrl Pts',(0.0344261075203546,1.66581115305704,
9.39562950151584));
#53891=CARTESIAN_POINT('Ctrl Pts',(-0.0931665243769141,1.666641971733,9.40382669167687));
#53892=CARTESIAN_POINT('Ctrl Pts',(-0.197019943145331,1.65757714399507,
9.41020115579815));
#53893=CARTESIAN_POINT('Ctrl Pts',(-0.376404831263378,1.62481058165997,
9.42133739974519));
#53894=CARTESIAN_POINT('Ctrl Pts',(-0.452356424515242,1.60532301222424,
9.42610032771416));
#53895=CARTESIAN_POINT('Ctrl Pts',(-0.549997666377681,1.57278867310622,
9.43259134415604));
#53896=CARTESIAN_POINT('Ctrl Pts',(-0.573169050380657,1.56449313046206,
9.43416035289995));
#53897=CARTESIAN_POINT('Ctrl Pts',(-0.612144930537602,1.54955738932823,
9.43686191641999));
#53898=CARTESIAN_POINT('Ctrl Pts',(-0.628046645861519,1.54318076501461,
9.43798210704558));
#53899=CARTESIAN_POINT('Ctrl Pts',(-0.650692765361467,1.53369163361736,
9.43960723724647));
#53900=CARTESIAN_POINT('Ctrl Pts',(-0.657519686942117,1.53077723983599,
9.44010108410668));
#53901=CARTESIAN_POINT('Ctrl Pts',(-0.669374350513616,1.52562258582735,
9.4409658846489));
#53902=CARTESIAN_POINT('Ctrl Pts',(-0.674410829330468,1.52340287769807,
9.4413356045612));
#53903=CARTESIAN_POINT('Ctrl Pts',(-0.685188176393028,1.51858909737181,
9.44213183274501));
#53904=CARTESIAN_POINT('Ctrl Pts',(-0.690925264065114,1.51598745374315,
9.4425587671352));
#53905=CARTESIAN_POINT('Ctrl Pts',(-0.706655043245815,1.50874650864917,
9.44373753369747));
#53906=CARTESIAN_POINT('Ctrl Pts',(-0.716616472934998,1.50404062179375,
9.44449318776226));
#53907=CARTESIAN_POINT('Ctrl Pts',(-0.773410038662576,1.47651845310577,
9.44885111666423));
#53908=CARTESIAN_POINT('Ctrl Pts',(-0.819193944520505,1.4516163380312,9.45255833517449));
#53909=CARTESIAN_POINT('Ctrl Pts',(-0.951108913733647,1.37163740928306,
9.46367847866774));
#53910=CARTESIAN_POINT('Ctrl Pts',(-1.03343357253797,1.31073039215437,9.47118957482571));
#53911=CARTESIAN_POINT('Ctrl Pts',(-1.16407225991808,1.19407440973592,9.48374538986823));
#53912=CARTESIAN_POINT('Ctrl Pts',(-1.21524228771502,1.14195742025453,9.4888720729303));
#53913=CARTESIAN_POINT('Ctrl Pts',(-1.27432957321312,1.07328962588066,9.49505435778117));
#53914=CARTESIAN_POINT('Ctrl Pts',(-1.28561026739359,1.05975127457879,9.49624820385952));
#53915=CARTESIAN_POINT('Ctrl Pts',(-1.30341175859014,1.03768440712373,9.49815504974702));
#53916=CARTESIAN_POINT('Ctrl Pts',(-1.31006836520651,1.02926771494205,9.49887347154413));
#53917=CARTESIAN_POINT('Ctrl Pts',(-1.32263981563531,1.01305266292917,9.50024094163243));
#53918=CARTESIAN_POINT('Ctrl Pts',(-1.32856814245789,1.00526537669971,9.50089050542535));
#53919=CARTESIAN_POINT('Ctrl Pts',(-1.34194470406696,0.987369261748859,
9.50236732053446));
#53920=CARTESIAN_POINT('Ctrl Pts',(-1.34934802866682,0.977227486159524,
9.50319280370947));
#53921=CARTESIAN_POINT('Ctrl Pts',(-1.36880659635929,0.949928497954312,
9.50538535745504));
#53922=CARTESIAN_POINT('Ctrl Pts',(-1.38065401681838,0.932625432944944,
9.50674456472587));
#53923=CARTESIAN_POINT('Ctrl Pts',(-1.4588509010499,0.813662260537325,9.515897348041));
#53924=CARTESIAN_POINT('Ctrl Pts',(-1.51424471650612,0.705236852634478,
9.52326824179325));
#53925=CARTESIAN_POINT('Ctrl Pts',(-1.55941714307736,0.586350974627343,
9.53103998379564));
#53926=CARTESIAN_POINT('Ctrl Pts',(-1.56143835103431,0.580947120910484,
9.53139267944501));
#53927=CARTESIAN_POINT('Ctrl Pts',(-1.56343129957118,0.575533293147481,
9.53174555314795));
#53928=CARTESIAN_POINT('Origin',(0.,0.,11.));
#53929=CARTESIAN_POINT('',(-1.56343128570986,0.575533330801617,10.2310772794004));
#53930=CARTESIAN_POINT('',(-1.56343130417499,0.575533280641269,10.0383108307813));
#53931=CARTESIAN_POINT('',(-1.56343130033213,0.575533291080363,11.));
#53932=CARTESIAN_POINT('Ctrl Pts',(-1.56343130417499,0.575533280641269,
10.0383108307813));
#53933=CARTESIAN_POINT('Ctrl Pts',(-1.53523060277161,0.652140248225498,
10.0332234667563));
#53934=CARTESIAN_POINT('Ctrl Pts',(-1.50143364965884,0.726581757822608,
10.0282692374323));
#53935=CARTESIAN_POINT('Ctrl Pts',(-1.43399751588061,0.850116516093578,
10.0196617533966));
#53936=CARTESIAN_POINT('Ctrl Pts',(-1.40295051330593,0.900430953212348,
10.016032026659));
#53937=CARTESIAN_POINT('Ctrl Pts',(-1.34951857765154,0.977528270062683,
10.0101044793621));
#53938=CARTESIAN_POINT('Ctrl Pts',(-1.32885187559289,1.00544229460194,10.0078755641635));
#53939=CARTESIAN_POINT('Ctrl Pts',(-1.30135426628126,1.04025285934982,10.0049591657919));
#53940=CARTESIAN_POINT('Ctrl Pts',(-1.29531317288898,1.04776558014819,10.0043212960743));
#53941=CARTESIAN_POINT('Ctrl Pts',(-1.28544862983115,1.05981745454892,10.0032834797046));
#53942=CARTESIAN_POINT('Ctrl Pts',(-1.28166542414749,1.06438947508603,10.0028863348848));
#53943=CARTESIAN_POINT('Ctrl Pts',(-1.27427723331173,1.07322163470143,10.002112218223));
#53944=CARTESIAN_POINT('Ctrl Pts',(-1.27067514265848,1.07748402440607,10.0017354490756));
#53945=CARTESIAN_POINT('Ctrl Pts',(-1.26256192767033,1.08698721046191,10.0008884182401));
#53946=CARTESIAN_POINT('Ctrl Pts',(-1.25803945541209,1.09221817478157,10.000417352455));
#53947=CARTESIAN_POINT('Ctrl Pts',(-1.24213630585236,1.11038290737068,9.99876508867047));
#53948=CARTESIAN_POINT('Ctrl Pts',(-1.2305881219801,1.12316767219214,9.99757275236365));
#53949=CARTESIAN_POINT('Ctrl Pts',(-1.11986467331639,1.24198979119828,9.98622853174259));
#53950=CARTESIAN_POINT('Ctrl Pts',(-1.00742779980078,1.33481321196356,9.97542540082165));
#53951=CARTESIAN_POINT('Ctrl Pts',(-0.823273821872255,1.45016389535073,
9.9598547236061));
#53952=CARTESIAN_POINT('Ctrl Pts',(-0.759740027865684,1.48443684902757,
9.95478966692114));
#53953=CARTESIAN_POINT('Ctrl Pts',(-0.678205154310113,1.52180893794462,
9.94866918414366));
#53954=CARTESIAN_POINT('Ctrl Pts',(-0.662118495821922,1.52887665083948,
9.94747889008192));
#53955=CARTESIAN_POINT('Ctrl Pts',(-0.636041914962719,1.53984466078429,
9.94557634071355));
#53956=CARTESIAN_POINT('Ctrl Pts',(-0.626121262975809,1.54390513642291,
9.94485870680185));
#53957=CARTESIAN_POINT('Ctrl Pts',(-0.607066858659145,1.55149014076746,
9.94349187424011));
#53958=CARTESIAN_POINT('Ctrl Pts',(-0.597939913649682,1.5550304480697,9.94284216828926));
#53959=CARTESIAN_POINT('Ctrl Pts',(-0.577016984100031,1.56293492329162,
9.94136385453368));
#53960=CARTESIAN_POINT('Ctrl Pts',(-0.565201630303103,1.56724640880432,
9.94053702829906));
#53961=CARTESIAN_POINT('Ctrl Pts',(-0.52733045803624,1.58058181247636,9.93791123280812));
#53962=CARTESIAN_POINT('Ctrl Pts',(-0.501098149736979,1.58909315731782,
9.93612907350848));
#53963=CARTESIAN_POINT('Ctrl Pts',(-0.348436678416387,1.63446910767721,
9.92594284870366));
#53964=CARTESIAN_POINT('Ctrl Pts',(-0.218207106765685,1.65689033470997,
9.91802481707132));
#53965=CARTESIAN_POINT('Ctrl Pts',(-0.0151991641739799,1.66746804601808,
9.90555361358077));
#53966=CARTESIAN_POINT('Ctrl Pts',(0.056448756214413,1.66658089685919,9.90111659037635));
#53967=CARTESIAN_POINT('Ctrl Pts',(0.143555110290162,1.65987871743349,9.89544856154274));
#53968=CARTESIAN_POINT('Ctrl Pts',(0.159283079482503,1.65844333108409,9.8944140932327));
#53969=CARTESIAN_POINT('Ctrl Pts',(0.182134536644928,1.65602978828887,9.89289189779298));
#53970=CARTESIAN_POINT('Ctrl Pts',(0.189276393771199,1.65522871264101,9.89241342329013));
#53971=CARTESIAN_POINT('Ctrl Pts',(0.201803699051694,1.65374143679908,9.89156898514514));
#53972=CARTESIAN_POINT('Ctrl Pts',(0.207191311404195,1.65307508357983,9.89120412626254));
#53973=CARTESIAN_POINT('Ctrl Pts',(0.218948698080024,1.65156251921965,9.89040410712124));
#53974=CARTESIAN_POINT('Ctrl Pts',(0.22531676469835,1.65070580036019,9.88996839850992));
#53975=CARTESIAN_POINT('Ctrl Pts',(0.243146848625318,1.64820196013231,9.88874201690379));
#53976=CARTESIAN_POINT('Ctrl Pts',(0.254596620620649,1.64647217815995,9.88794702302528));
#53977=CARTESIAN_POINT('Ctrl Pts',(0.336624969883425,1.63320363307294,9.88220231437036));
#53978=CARTESIAN_POINT('Ctrl Pts',(0.406406724201536,1.61725129170012,9.87705621534536));
#53979=CARTESIAN_POINT('Ctrl Pts',(0.488368702671291,1.59287423059785,9.87084774580007));
#53980=CARTESIAN_POINT('Ctrl Pts',(0.501747179166583,1.58871081946642,9.86982886028981));
#53981=CARTESIAN_POINT('Ctrl Pts',(0.578125058137468,1.56388086303582,9.86398469475561));
#53982=CARTESIAN_POINT('Ctrl Pts',(0.639901731610865,1.53963582958029,9.85915380254484));
#53983=CARTESIAN_POINT('Ctrl Pts',(0.74482431550036,1.49104831719172,9.85085900013973));
#53984=CARTESIAN_POINT('Ctrl Pts',(0.788638338862812,1.46834555478519,9.84736513427056));
#53985=CARTESIAN_POINT('Ctrl Pts',(0.860405631944635,1.42701776981962,9.84160230737337));
#53986=CARTESIAN_POINT('Ctrl Pts',(0.888918517919397,1.40943311801642,9.83930125306193));
#53987=CARTESIAN_POINT('Ctrl Pts',(0.928318136329917,1.38346268087776,9.83610311658611));
#53988=CARTESIAN_POINT('Ctrl Pts',(0.939659428771498,1.37578476841183,9.83518025184924));
#53989=CARTESIAN_POINT('Ctrl Pts',(0.959058769966445,1.36229985063522,9.83359732503261));
#53990=CARTESIAN_POINT('Ctrl Pts',(0.967161792476038,1.35655913318124,9.83293480097407));
#53991=CARTESIAN_POINT('Ctrl Pts',(0.983621630902639,1.34467544179991,9.83158600103814));
#53992=CARTESIAN_POINT('Ctrl Pts',(0.991973392292757,1.3385261871834,9.83090000556373));
#53993=CARTESIAN_POINT('Ctrl Pts',(1.01301137498834,1.3227312315117,9.82916747226311));
#53994=CARTESIAN_POINT('Ctrl Pts',(1.02561780625701,1.31298061712983,9.82812507063503));
#53995=CARTESIAN_POINT('Ctrl Pts',(1.07486057412706,1.27375107487701,9.82403362848397));
#53996=CARTESIAN_POINT('Ctrl Pts',(1.11038370858937,1.24290614872212,9.82103909834878));
#53997=CARTESIAN_POINT('Ctrl Pts',(1.23402523487795,1.12600949522512,9.81036410464119));
#53998=CARTESIAN_POINT('Ctrl Pts',(1.31383727533622,1.03176869387582,9.80300445802751));
#53999=CARTESIAN_POINT('Ctrl Pts',(1.40539899037475,0.895593910871602,9.79285348558973));
#54000=CARTESIAN_POINT('Ctrl Pts',(1.42699744694836,0.86076280754317,9.79029084338165));
#54001=CARTESIAN_POINT('Ctrl Pts',(1.45557544645789,0.810639276917036,9.78659919426446));
#54002=CARTESIAN_POINT('Ctrl Pts',(1.4636424704079,0.79598152641481,9.78551915654964));
#54003=CARTESIAN_POINT('Ctrl Pts',(1.477484620222,0.769908301111194,9.78359269159236));
#54004=CARTESIAN_POINT('Ctrl Pts',(1.48335167129145,0.758542938744251,9.7827512020552));
#54005=CARTESIAN_POINT('Ctrl Pts',(1.49205050349164,0.741205075418628,9.78146316294614));
#54006=CARTESIAN_POINT('Ctrl Pts',(1.49497871081137,0.735281115813086,9.78102230807849));
#54007=CARTESIAN_POINT('Ctrl Pts',(1.50026312052961,0.724428335657685,9.78021298350743));
#54008=CARTESIAN_POINT('Ctrl Pts',(1.5026304193599,0.719505152479736,9.77984520163599));
#54009=CARTESIAN_POINT('Ctrl Pts',(1.50796428221539,0.708271378946464,9.77900453633642));
#54010=CARTESIAN_POINT('Ctrl Pts',(1.51091545316733,0.701953781708727,9.77853075372782));
#54011=CARTESIAN_POINT('Ctrl Pts',(1.51994010725099,0.682314031831669,9.77705517760469));
#54012=CARTESIAN_POINT('Ctrl Pts',(1.5258775024823,0.668930623127372,9.77604581226147));
#54013=CARTESIAN_POINT('Ctrl Pts',(1.57510776346683,0.553894442801432,9.767347732446));
#54014=CARTESIAN_POINT('Ctrl Pts',(1.60836208156626,0.448253648302818,9.75923338228561));
#54015=CARTESIAN_POINT('Ctrl Pts',(1.64985693769546,0.24927449376688,9.74446825980225));
#54016=CARTESIAN_POINT('Ctrl Pts',(1.66118021813261,0.157005041596671,9.73781377185635));
#54017=CARTESIAN_POINT('Ctrl Pts',(1.66586796274518,0.0355629830142027,
9.72939964313074));
#54018=CARTESIAN_POINT('Ctrl Pts',(1.66623353372136,0.00683983295146041,
9.72743338258102));
#54019=CARTESIAN_POINT('Ctrl Pts',(1.66568670311698,-0.0347936409229971,
9.72461621330597));
#54020=CARTESIAN_POINT('Ctrl Pts',(1.66536693390361,-0.0477051585925001,
9.72374710724748));
#54021=CARTESIAN_POINT('Ctrl Pts',(1.66454028782187,-0.0704115730776858,
9.72222635029701));
#54022=CARTESIAN_POINT('Ctrl Pts',(1.66409700506371,-0.0802080059171749,
9.72157274859218));
#54023=CARTESIAN_POINT('Ctrl Pts',(1.66299127661127,-0.100646348550529,
9.72021414130691));
#54024=CARTESIAN_POINT('Ctrl Pts',(1.66231311388042,-0.111286988923718,
9.7195096572032));
#54025=CARTESIAN_POINT('Ctrl Pts',(1.66026661568557,-0.139176648228174,
9.71767014843599));
#54026=CARTESIAN_POINT('Ctrl Pts',(1.65873161288151,-0.156412427857145,
9.71654035719821));
#54027=CARTESIAN_POINT('Ctrl Pts',(1.65056980147356,-0.234303243945644,
9.71146235049359));
#54028=CARTESIAN_POINT('Ctrl Pts',(1.64088221572044,-0.294593729542408,
9.70761018691498));
#54029=CARTESIAN_POINT('Ctrl Pts',(1.60288466518596,-0.469219931848416,
9.6965091751641));
#54030=CARTESIAN_POINT('Ctrl Pts',(1.5657489940434,-0.581235370587503,9.68947837433791));
#54031=CARTESIAN_POINT('Ctrl Pts',(1.5031989080091,-0.719085969304435,9.68004642642688));
#54032=CARTESIAN_POINT('Ctrl Pts',(1.4883475129231,-0.749341702362119,9.67792243242184));
#54033=CARTESIAN_POINT('Ctrl Pts',(1.46253066189549,-0.798137040348437,
9.67437449457909));
#54034=CARTESIAN_POINT('Ctrl Pts',(1.45210464902936,-0.816952051602266,
9.67297548035268));
#54035=CARTESIAN_POINT('Ctrl Pts',(1.43725012043614,-0.842575738476188,
9.67101970995689));
#54036=CARTESIAN_POINT('Ctrl Pts',(1.43313121993803,-0.849562642484641,
9.67048115002742));
#54037=CARTESIAN_POINT('Ctrl Pts',(1.42607575830524,-0.86133352367105,9.66956438463691));
#54038=CARTESIAN_POINT('Ctrl Pts',(1.4231656650753,-0.866133359340258,9.66918786368616));
#54039=CARTESIAN_POINT('Ctrl Pts',(1.41748758901722,-0.875392759554953,
9.66845612499556));
#54040=CARTESIAN_POINT('Ctrl Pts',(1.41472271411045,-0.879854072417098,
9.66810113523642));
#54041=CARTESIAN_POINT('Ctrl Pts',(1.40708157093585,-0.892054440173599,
9.66712382615363));
#54042=CARTESIAN_POINT('Ctrl Pts',(1.40216266246531,-0.899766375198331,
9.66649882393458));
#54043=CARTESIAN_POINT('Ctrl Pts',(1.3822831231997,-0.930374893007171,9.66399038474938));
#54044=CARTESIAN_POINT('Ctrl Pts',(1.36682401083448,-0.952940706376796,
9.66207844084234));
#54045=CARTESIAN_POINT('Ctrl Pts',(1.33203063542401,-1.00113968310678,9.65787318211656));
#54046=CARTESIAN_POINT('Ctrl Pts',(1.312496332161,-1.02661553015282,9.65557217242202));
#54047=CARTESIAN_POINT('Ctrl Pts',(1.23026319599558,-1.12767488032464,9.64616521533027));
#54048=CARTESIAN_POINT('Ctrl Pts',(1.16166999925484,-1.19821643404209,9.63895449798669));
#54049=CARTESIAN_POINT('Ctrl Pts',(1.03171010310813,-1.31015493586151,9.62665584009421));
#54050=CARTESIAN_POINT('Ctrl Pts',(0.973053079221091,-1.3542902498476,9.62150239099507));
#54051=CARTESIAN_POINT('Ctrl Pts',(0.896904712187983,-1.40407591118448,
9.61529335958614));
#54052=CARTESIAN_POINT('Ctrl Pts',(0.881986000110136,-1.41349494667739,
9.61409805207719));
#54053=CARTESIAN_POINT('Ctrl Pts',(0.85775324022666,-1.42826139397155,9.6121894733294));
#54054=CARTESIAN_POINT('Ctrl Pts',(0.848532548751569,-1.43375861066889,
9.61147076190123));
#54055=CARTESIAN_POINT('Ctrl Pts',(0.830806538715489,-1.44409564762368,
9.61010311701836));
#54056=CARTESIAN_POINT('Ctrl Pts',(0.822310486501808,-1.44895038390453,
9.6094536645505));
#54057=CARTESIAN_POINT('Ctrl Pts',(0.802824801480943,-1.45985812056773,
9.60797761581559));
#54058=CARTESIAN_POINT('Ctrl Pts',(0.791808492673642,-1.46586244897312,
9.60715278155812));
#54059=CARTESIAN_POINT('Ctrl Pts',(0.762232743133817,-1.48155170234157,
9.6049630988651));
#54060=CARTESIAN_POINT('Ctrl Pts',(0.743556462428251,-1.49101242488798,
9.60360608081827));
#54061=CARTESIAN_POINT('Ctrl Pts',(0.614893823103221,-1.55316923111023,
9.59441891342092));
#54062=CARTESIAN_POINT('Ctrl Pts',(0.49958722395514,-1.59400299213205,9.58701604869924));
#54063=CARTESIAN_POINT('Ctrl Pts',(0.317072268125654,-1.63686056433288,
9.57555863192214));
#54064=CARTESIAN_POINT('Ctrl Pts',(0.252475363236973,-1.64806015717417,
9.57154280796395));
#54065=CARTESIAN_POINT('Ctrl Pts',(0.165228744745377,-1.65793636090247,
9.56598418066398));
#54066=CARTESIAN_POINT('Ctrl Pts',(0.143018188975949,-1.65999976314588,
9.56455736076963));
#54067=CARTESIAN_POINT('Ctrl Pts',(0.104895083261007,-1.66277072833362,
9.56207804377577));
#54068=CARTESIAN_POINT('Ctrl Pts',(0.0890011028865264,-1.66369715744989,
9.56103539762414));
#54069=CARTESIAN_POINT('Ctrl Pts',(0.0658941561173299,-1.66471196949202,
9.55950335552001));
#54070=CARTESIAN_POINT('Ctrl Pts',(0.0586894901106203,-1.66498153747689,
9.55902338082443));
#54071=CARTESIAN_POINT('Ctrl Pts',(0.0460057995549087,-1.66537368177267,
9.55817400703662));
#54072=CARTESIAN_POINT('Ctrl Pts',(0.0405275813848081,-1.66551600033975,
9.55780570097485));
#54073=CARTESIAN_POINT('Ctrl Pts',(0.0286191739297413,-1.66576657999992,
9.55700183601556));
#54074=CARTESIAN_POINT('Ctrl Pts',(0.0221891271735024,-1.66586463894967,
9.55656575451637));
#54075=CARTESIAN_POINT('Ctrl Pts',(0.00415546885231957,-1.66603522822074,
9.55533733756193));
#54076=CARTESIAN_POINT('Ctrl Pts',(-0.00744830262296705,-1.66602375540589,
9.55454065930492));
#54077=CARTESIAN_POINT('Ctrl Pts',(-0.0961155783210517,-1.6650097849429,
9.54840997492033));
#54078=CARTESIAN_POINT('Ctrl Pts',(-0.173018129402188,-1.65878202958086,
9.54284823106372));
#54079=CARTESIAN_POINT('Ctrl Pts',(-0.305936075797573,-1.63867365071669,
9.53307672794286));
#54080=CARTESIAN_POINT('Ctrl Pts',(-0.362188474146878,-1.62716563251421,
9.52888968303591));
#54081=CARTESIAN_POINT('Ctrl Pts',(-0.490021991707802,-1.59405468337534,
9.51934805735818));
#54082=CARTESIAN_POINT('Ctrl Pts',(-0.56097530831822,-1.57049073589869,
9.51403492647141));
#54083=CARTESIAN_POINT('Ctrl Pts',(-0.655937280379037,-1.53169197867999,
9.50693938659011));
#54084=CARTESIAN_POINT('Ctrl Pts',(-0.681490725202018,-1.52049484948237,
9.50503092937275));
#54085=CARTESIAN_POINT('Ctrl Pts',(-0.718316354431279,-1.50324338975327,
9.50228034772167));
#54086=CARTESIAN_POINT('Ctrl Pts',(-0.72981797471069,-1.49769316397992,
9.50142121058435));
#54087=CARTESIAN_POINT('Ctrl Pts',(-0.750019230915707,-1.48765685753566,
9.49991177753699));
#54088=CARTESIAN_POINT('Ctrl Pts',(-0.758745156572715,-1.48322539316136,
9.49925962382293));
#54089=CARTESIAN_POINT('Ctrl Pts',(-0.776954801381172,-1.47377486512518,
9.4978981137786));
#54090=CARTESIAN_POINT('Ctrl Pts',(-0.786430128919887,-1.46874054137442,
9.49718933043051));
#54091=CARTESIAN_POINT('Ctrl Pts',(-0.811333121270085,-1.45519927159909,
9.49532516718411));
#54092=CARTESIAN_POINT('Ctrl Pts',(-0.826675890298681,-1.4465384076084,
9.49417528671567));
#54093=CARTESIAN_POINT('Ctrl Pts',(-0.898058342427392,-1.40473686752708,
9.48881439695062));
#54094=CARTESIAN_POINT('Ctrl Pts',(-0.952264945552204,-1.36857129055036,
9.48471394691546));
#54095=CARTESIAN_POINT('Ctrl Pts',(-1.12038435284886,-1.24156746197831,
9.4716581067006));
#54096=CARTESIAN_POINT('Ctrl Pts',(-1.22452743782071,-1.13897885349182,
9.46306590274078));
#54097=CARTESIAN_POINT('Ctrl Pts',(-1.32341529378525,-1.01210786367338,
9.45274176381477));
#54098=CARTESIAN_POINT('Ctrl Pts',(-1.33265938474566,-0.999904643240284,
9.45175089442855));
#54099=CARTESIAN_POINT('Ctrl Pts',(-1.34881228980712,-0.977959101265534,
9.44996934556504));
#54100=CARTESIAN_POINT('Ctrl Pts',(-1.3557870899869,-0.96826646300144,9.44918261784184));
#54101=CARTESIAN_POINT('Ctrl Pts',(-1.36635751749659,-0.95323895653241,
9.44796163927423));
#54102=CARTESIAN_POINT('Ctrl Pts',(-1.37002760883425,-0.947956603136958,
9.44753221952318));
#54103=CARTESIAN_POINT('Ctrl Pts',(-1.37676771134362,-0.938134692382204,
9.44673307075046));
#54104=CARTESIAN_POINT('Ctrl Pts',(-1.37984602430724,-0.933601080798416,
9.44636390477225));
#54105=CARTESIAN_POINT('Ctrl Pts',(-1.38685387262408,-0.923169842751786,
9.4455138779107));
#54106=CARTESIAN_POINT('Ctrl Pts',(-1.39076818773196,-0.917262266734908,
9.44503204539511));
#54107=CARTESIAN_POINT('Ctrl Pts',(-1.40321172423004,-0.898219427833956,
9.44347795171718));
#54108=CARTESIAN_POINT('Ctrl Pts',(-1.41159316629549,-0.88498924977661,
9.44239683318875));
#54109=CARTESIAN_POINT('Ctrl Pts',(-1.46767532093192,-0.793639191331975,
9.43493282635992));
#54110=CARTESIAN_POINT('Ctrl Pts',(-1.50904991793798,-0.711828145844744,
9.42826106152325));
#54111=CARTESIAN_POINT('Ctrl Pts',(-1.57551671441283,-0.548217120506717,
9.41540670471501));
#54112=CARTESIAN_POINT('Ctrl Pts',(-1.60145715012973,-0.467046769708951,
9.40924127323501));
#54113=CARTESIAN_POINT('Ctrl Pts',(-1.6320556844945,-0.337954494045842,
9.39989084826688));
#54114=CARTESIAN_POINT('Ctrl Pts',(-1.64104061152726,-0.291213815799972,
9.39659266222447));
#54115=CARTESIAN_POINT('Ctrl Pts',(-1.65028934074554,-0.228784444790369,
9.39230056887076));
#54116=CARTESIAN_POINT('Ctrl Pts',(-1.65235056278314,-0.213389025977572,
9.39125104775207));
#54117=CARTESIAN_POINT('Ctrl Pts',(-1.65541857727395,-0.187752889084874,
9.38951769821789));
#54118=CARTESIAN_POINT('Ctrl Pts',(-1.65654630510596,-0.17752791492329,
9.38883011315607));
#54119=CARTESIAN_POINT('Ctrl Pts',(-1.65857026742687,-0.157474003506889,
9.38748869313677));
#54120=CARTESIAN_POINT('Ctrl Pts',(-1.65947400696748,-0.147646270185248,
9.38683464948917));
#54121=CARTESIAN_POINT('Ctrl Pts',(-1.66144079941945,-0.123951145187176,
9.3852654417029));
#54122=CARTESIAN_POINT('Ctrl Pts',(-1.66241765143314,-0.11007719080431,
9.38435300365112));
#54123=CARTESIAN_POINT('Ctrl Pts',(-1.66508787822284,-0.0639074084529993,
9.38133625781657));
#54124=CARTESIAN_POINT('Ctrl Pts',(-1.66601474697079,-0.0315734630314515,
9.37925566578851));
#54125=CARTESIAN_POINT('Ctrl Pts',(-1.6659775013047,0.04914121364185,9.37412372009076));
#54126=CARTESIAN_POINT('Ctrl Pts',(-1.66384846670606,0.0974920269668017,
9.37110538969817));
#54127=CARTESIAN_POINT('Ctrl Pts',(-1.6506564845205,0.24777324822732,9.36179169531954));
#54128=CARTESIAN_POINT('Ctrl Pts',(-1.63229499545893,0.34881223821726,9.35563829044878));
#54129=CARTESIAN_POINT('Ctrl Pts',(-1.59271662237536,0.490736904679573,
9.34647552258277));
#54130=CARTESIAN_POINT('Ctrl Pts',(-1.57892576694212,0.533442703970636,
9.34364514980345));
#54131=CARTESIAN_POINT('Ctrl Pts',(-1.56343130066142,0.575533290185854,
9.34073387093129));
#54132=CARTESIAN_POINT('Ctrl Pts',(-1.56343129957118,0.575533293147481,
9.53174555314795));
#54133=CARTESIAN_POINT('Ctrl Pts',(-1.58419289085892,0.519134606860111,
9.53542162378452));
#54134=CARTESIAN_POINT('Ctrl Pts',(-1.60188765055432,0.461653412997373,
9.53911575611647));
#54135=CARTESIAN_POINT('Ctrl Pts',(-1.62185532032787,0.381630777066599,
9.54433646674948));
#54136=CARTESIAN_POINT('Ctrl Pts',(-1.62683459671384,0.359813598003652,
9.54576773531309));
#54137=CARTESIAN_POINT('Ctrl Pts',(-1.63460968963582,0.322276075362092,
9.54825405230925));
#54138=CARTESIAN_POINT('Ctrl Pts',(-1.63762178126171,0.306603264746934,
9.54929917577935));
#54139=CARTESIAN_POINT('Ctrl Pts',(-1.64166824217043,0.283784191892934,
9.55083421448561));
#54140=CARTESIAN_POINT('Ctrl Pts',(-1.64288214023067,0.276670116609555,
9.55131465725133));
#54141=CARTESIAN_POINT('Ctrl Pts',(-1.64492863877413,0.264187966370889,
9.55216127572685));
#54142=CARTESIAN_POINT('Ctrl Pts',(-1.64578126493858,0.25882336639988,9.55252632691499));
#54143=CARTESIAN_POINT('Ctrl Pts',(-1.64758221701498,0.247123196194553,
9.55332518876194));
#54144=CARTESIAN_POINT('Ctrl Pts',(-1.64852022836828,0.240786397304346,
9.55375953339173));
#54145=CARTESIAN_POINT('Ctrl Pts',(-1.65103869681518,0.223067846765733,
9.55497841988917));
#54146=CARTESIAN_POINT('Ctrl Pts',(-1.65253794025133,0.211675176587708,
9.55576720208956));
#54147=CARTESIAN_POINT('Ctrl Pts',(-1.66191605512822,0.134225859657009,
9.56115974042736));
#54148=CARTESIAN_POINT('Ctrl Pts',(-1.6659491898134,0.0677707496558123,
9.56593378901129));
#54149=CARTESIAN_POINT('Ctrl Pts',(-1.66611356037785,-0.149427585103849,
9.58168203907383));
#54150=CARTESIAN_POINT('Ctrl Pts',(-1.6457815380196,-0.29947360437319,9.59270913271564));
#54151=CARTESIAN_POINT('Ctrl Pts',(-1.60002946606151,-0.464636920357443,
9.60449250556361));
#54152=CARTESIAN_POINT('Ctrl Pts',(-1.59415191821658,-0.48441871125564,
9.60589954043457));
#54153=CARTESIAN_POINT('Ctrl Pts',(-1.58413773354867,-0.515964070477924,
9.60813723806045));
#54154=CARTESIAN_POINT('Ctrl Pts',(-1.58023409313649,-0.527798736651318,
9.60897536426683));
#54155=CARTESIAN_POINT('Ctrl Pts',(-1.57303228967165,-0.548835993771317,
9.6104630867351));
#54156=CARTESIAN_POINT('Ctrl Pts',(-1.56978526461057,-0.558055339923406,
9.61111432958306));
#54157=CARTESIAN_POINT('Ctrl Pts',(-1.56278710066076,-0.577380869580575,
9.61247815168184));
#54158=CARTESIAN_POINT('Ctrl Pts',(-1.55901862204584,-0.587480328073059,
9.61319012095391));
#54159=CARTESIAN_POINT('Ctrl Pts',(-1.54875083651637,-0.614203054840307,
9.61507242382464));
#54160=CARTESIAN_POINT('Ctrl Pts',(-1.54208185885704,-0.630759959740643,
9.61623705948122));
#54161=CARTESIAN_POINT('Ctrl Pts',(-1.50523746668701,-0.718153309609106,
9.62238126117852));
#54162=CARTESIAN_POINT('Ctrl Pts',(-1.47044301419912,-0.78694570376569,
9.62720069765186));
#54163=CARTESIAN_POINT('Ctrl Pts',(-1.37983173973436,-0.938940741423909,
9.63810383654603));
#54164=CARTESIAN_POINT('Ctrl Pts',(-1.32103430896475,-1.02000593080992,
9.6441101105277));
#54165=CARTESIAN_POINT('Ctrl Pts',(-1.22242884563063,-1.13301723109962,
9.65345061340903));
#54166=CARTESIAN_POINT('Ctrl Pts',(-1.18784898071334,-1.16921943639785,
9.65661942741841));
#54167=CARTESIAN_POINT('Ctrl Pts',(-1.14380791337771,-1.21135405531006,
9.66061248257686));
#54168=CARTESIAN_POINT('Ctrl Pts',(-1.13584554207816,-1.21882323533717,
9.66133281881186));
#54169=CARTESIAN_POINT('Ctrl Pts',(-1.12319063377697,-1.23046259600355,
9.66247631809722));
#54170=CARTESIAN_POINT('Ctrl Pts',(-1.11854678303275,-1.23468558382038,
9.66289565438378));
#54171=CARTESIAN_POINT('Ctrl Pts',(-1.10978235844957,-1.24256568038021,
9.66368679984777));
#54172=CARTESIAN_POINT('Ctrl Pts',(-1.10566737330146,-1.24622871465662,
9.66405816120041));
#54173=CARTESIAN_POINT('Ctrl Pts',(-1.09593511349671,-1.25480593320086,
9.66493616700633));
#54174=CARTESIAN_POINT('Ctrl Pts',(-1.09030290399817,-1.25970285194015,
9.66544403797978));
#54175=CARTESIAN_POINT('Ctrl Pts',(-1.07145436670136,-1.27586959409184,
9.66714229833874));
#54176=CARTESIAN_POINT('Ctrl Pts',(-1.05809521873624,-1.28697013560504,
9.66834375313866));
#54177=CARTESIAN_POINT('Ctrl Pts',(-1.02503542702626,-1.3135778922235,9.67130669037306));
#54178=CARTESIAN_POINT('Ctrl Pts',(-1.00515391109514,-1.32885288324915,
9.67307984866249));
#54179=CARTESIAN_POINT('Ctrl Pts',(-0.919496277229146,-1.39164148562462,
9.68065890495535));
#54180=CARTESIAN_POINT('Ctrl Pts',(-0.850641653369231,-1.43476388016848,
9.6865982002319));
#54181=CARTESIAN_POINT('Ctrl Pts',(-0.690278589420767,-1.51958128412775,
9.69977672845188));
#54182=CARTESIAN_POINT('Ctrl Pts',(-0.597570605812225,-1.55837326176305,
9.70695788300536));
#54183=CARTESIAN_POINT('Ctrl Pts',(-0.479379413053165,-1.59571623279424,
9.71549117644586));
#54184=CARTESIAN_POINT('Ctrl Pts',(-0.45668642165241,-1.60235842712725,
9.71710350824116));
#54185=CARTESIAN_POINT('Ctrl Pts',(-0.422144563164161,-1.61167526870591,
9.71951966447463));
#54186=CARTESIAN_POINT('Ctrl Pts',(-0.410396007002416,-1.61470688823499,
9.72033489186031));
#54187=CARTESIAN_POINT('Ctrl Pts',(-0.389179464835656,-1.61993511654294,
9.72179562592394));
#54188=CARTESIAN_POINT('Ctrl Pts',(-0.379723492865078,-1.62217770712472,
9.72244258409009));
#54189=CARTESIAN_POINT('Ctrl Pts',(-0.359426392473754,-1.62680418797331,
9.72382280665389));
#54190=CARTESIAN_POINT('Ctrl Pts',(-0.348579925351779,-1.62916274303221,
9.72455523304445));
#54191=CARTESIAN_POINT('Ctrl Pts',(-0.318765045895209,-1.63533456980239,
9.72655501467582));
#54192=CARTESIAN_POINT('Ctrl Pts',(-0.299752135064599,-1.63892617826557,
9.72781531336956));
#54193=CARTESIAN_POINT('Ctrl Pts',(-0.161307539077506,-1.66258895126955,
9.7368937428627));
#54194=CARTESIAN_POINT('Ctrl Pts',(-0.0400629299417626,-1.66991668446338,
9.74427886431592));
#54195=CARTESIAN_POINT('Ctrl Pts',(0.176728174425355,-1.65937476916281,
9.75753389347799));
#54196=CARTESIAN_POINT('Ctrl Pts',(0.271945605355837,-1.64645018288157,
9.76338695716254));
#54197=CARTESIAN_POINT('Ctrl Pts',(0.380652660388352,-1.62200508794904,
9.7706194104116));
#54198=CARTESIAN_POINT('Ctrl Pts',(0.395748144568305,-1.61838818487052,
9.77163653388678));
#54199=CARTESIAN_POINT('Ctrl Pts',(0.417634142804322,-1.61281976493946,
9.77313282492087));
#54200=CARTESIAN_POINT('Ctrl Pts',(0.424466773500164,-1.61103501672081,
9.77360304298463));
#54201=CARTESIAN_POINT('Ctrl Pts',(0.436578935510371,-1.60778880495735,
9.77444242779257));
#54202=CARTESIAN_POINT('Ctrl Pts',(0.441862903541104,-1.60634466457602,
9.77481060509767));
#54203=CARTESIAN_POINT('Ctrl Pts',(0.453353598785978,-1.60314320110716,
9.77561569180437));
#54204=CARTESIAN_POINT('Ctrl Pts',(0.459557179861626,-1.60137590955471,
9.7760531377531));
#54205=CARTESIAN_POINT('Ctrl Pts',(0.477297898498818,-1.5962103153045,9.77731184140587));
#54206=CARTESIAN_POINT('Ctrl Pts',(0.488808427020847,-1.59272312577864,
9.77813789254889));
#54207=CARTESIAN_POINT('Ctrl Pts',(0.593983063841548,-1.55961233732092,
9.7857657102244));
#54208=CARTESIAN_POINT('Ctrl Pts',(0.684883904509433,-1.52188587723097,
9.79293049503105));
#54209=CARTESIAN_POINT('Ctrl Pts',(0.875841767945102,-1.42204385587322,
9.80861482788145));
#54210=CARTESIAN_POINT('Ctrl Pts',(0.973752164077067,-1.35688007668907,
9.81707010185451));
#54211=CARTESIAN_POINT('Ctrl Pts',(1.08030742321903,-1.26843999805208,9.82659818715554));
#54212=CARTESIAN_POINT('Ctrl Pts',(1.09633862057704,-1.25460984283107,9.82804257648998));
#54213=CARTESIAN_POINT('Ctrl Pts',(1.12149376283654,-1.23205796169355,9.83032756153957));
#54214=CARTESIAN_POINT('Ctrl Pts',(1.13078930922861,-1.22353203242732,9.83117613150749));
#54215=CARTESIAN_POINT('Ctrl Pts',(1.14712991819355,-1.20819902558158,9.83267571876962));
#54216=CARTESIAN_POINT('Ctrl Pts',(1.15421335904524,-1.20143391972935,9.83332847758013));
#54217=CARTESIAN_POINT('Ctrl Pts',(1.16891088844057,-1.18714694635202,9.83468885029143));
#54218=CARTESIAN_POINT('Ctrl Pts',(1.17651300667199,-1.17961336525955,9.8353959120697));
#54219=CARTESIAN_POINT('Ctrl Pts',(1.19634556427573,-1.15957714856435,9.83725009029404));
#54220=CARTESIAN_POINT('Ctrl Pts',(1.20845284692679,-1.14695406496431,9.83839181613675));
#54221=CARTESIAN_POINT('Ctrl Pts',(1.26855777960162,-1.08227996958015,9.84411482428737));
#54222=CARTESIAN_POINT('Ctrl Pts',(1.31340442751963,-1.02739446222141,9.84856256765901));
#54223=CARTESIAN_POINT('Ctrl Pts',(1.39478704717676,-0.913720233845686,
9.85720253928365));
#54224=CARTESIAN_POINT('Ctrl Pts',(1.43142444823527,-0.855184097794034,
9.8613904458194));
#54225=CARTESIAN_POINT('Ctrl Pts',(1.47477745111027,-0.775285479383363,
9.86695373920112));
#54226=CARTESIAN_POINT('Ctrl Pts',(1.48484621669684,-0.755822590656976,
9.86829792002095));
#54227=CARTESIAN_POINT('Ctrl Pts',(1.52323941239803,-0.677878728364892,
9.87365786097997));
#54228=CARTESIAN_POINT('Ctrl Pts',(1.54851289668559,-0.617967355228113,
9.8777259195766));
#54229=CARTESIAN_POINT('Ctrl Pts',(1.57404819299209,-0.545948193219906,
9.882725677946));
#54230=CARTESIAN_POINT('Ctrl Pts',(1.57776361754512,-0.535115962071062,
9.88348054244917));
#54231=CARTESIAN_POINT('Ctrl Pts',(1.58337997721785,-0.518174460621776,
9.88466685992084));
#54232=CARTESIAN_POINT('Ctrl Pts',(1.58535796896452,-0.512090842250893,
9.88509400215145));
#54233=CARTESIAN_POINT('Ctrl Pts',(1.58895111626634,-0.500819202829908,
9.88588777399612));
#54234=CARTESIAN_POINT('Ctrl Pts',(1.59057598861679,-0.495634487372464,
9.88625383716857));
#54235=CARTESIAN_POINT('Ctrl Pts',(1.59430393741137,-0.483532038852569,
9.88711046885706));
#54236=CARTESIAN_POINT('Ctrl Pts',(1.59638736377652,-0.476608494826912,
9.88760213628928));
#54237=CARTESIAN_POINT('Ctrl Pts',(1.60294575600934,-0.454288434898384,
9.88919184426562));
#54238=CARTESIAN_POINT('Ctrl Pts',(1.60724338808575,-0.438841341498262,
9.89029916431186));
#54239=CARTESIAN_POINT('Ctrl Pts',(1.61703854665122,-0.401558588527275,
9.89298496994333));
#54240=CARTESIAN_POINT('Ctrl Pts',(1.62231753936912,-0.379669145462246,
9.89457263350263));
#54241=CARTESIAN_POINT('Ctrl Pts',(1.6414489827899,-0.292636895273826,9.90091097752498));
#54242=CARTESIAN_POINT('Ctrl Pts',(1.65183322335965,-0.226797726728758,
9.90576010235927));
#54243=CARTESIAN_POINT('Ctrl Pts',(1.6698397421027,-0.040779018369514,9.91936424862656));
#54244=CARTESIAN_POINT('Ctrl Pts',(1.668429260666,0.079884076545479,9.92804832284216));
#54245=CARTESIAN_POINT('Ctrl Pts',(1.65151268583907,0.22023631857544,9.93777345061942));
#54246=CARTESIAN_POINT('Ctrl Pts',(1.64860123931839,0.241064744818895,9.93920797397614));
#54247=CARTESIAN_POINT('Ctrl Pts',(1.64332013023371,0.274249934266454,9.94148048195015));
#54248=CARTESIAN_POINT('Ctrl Pts',(1.64120360382886,0.286644069708899,9.94232630446582));
#54249=CARTESIAN_POINT('Ctrl Pts',(1.63718998237085,0.308643463200404,9.94382276076907));
#54250=CARTESIAN_POINT('Ctrl Pts',(1.63534816936109,0.318258067847762,9.94447511106323));
#54251=CARTESIAN_POINT('Ctrl Pts',(1.63131170833158,0.338368243603977,9.94583634188096));
#54252=CARTESIAN_POINT('Ctrl Pts',(1.62910025988252,0.348860015389673,9.94654465537609));
#54253=CARTESIAN_POINT('Ctrl Pts',(1.6229957505092,0.376496846832748,9.94840600944377));
#54254=CARTESIAN_POINT('Ctrl Pts',(1.61893225685895,0.393603185801709,9.94955358163528));
#54255=CARTESIAN_POINT('Ctrl Pts',(1.59678063806785,0.480700768755718,9.95537810683076));
#54256=CARTESIAN_POINT('Ctrl Pts',(1.57442066810132,0.549529876782667,9.95991537558045));
#54257=CARTESIAN_POINT('Ctrl Pts',(1.51040557830855,0.710181914892721,9.97059487075951));
#54258=CARTESIAN_POINT('Ctrl Pts',(1.46476198713227,0.800096519125323,9.97664129069514));
#54259=CARTESIAN_POINT('Ctrl Pts',(1.38250698943556,0.931216017803965,9.98625169062259));
#54260=CARTESIAN_POINT('Ctrl Pts',(1.3515109451724,0.975656568627253,9.98966969220912));
#54261=CARTESIAN_POINT('Ctrl Pts',(1.31159441334511,1.02732681714753,9.99394489749943));
#54262=CARTESIAN_POINT('Ctrl Pts',(1.30469050269491,1.03608058084558,9.99468018475039));
#54263=CARTESIAN_POINT('Ctrl Pts',(1.29373039560431,1.04969410884822,9.99584223304506));
#54264=CARTESIAN_POINT('Ctrl Pts',(1.28973332146283,1.05460135352278,9.99626496080528));
#54265=CARTESIAN_POINT('Ctrl Pts',(1.2825631425793,1.06330251914205,9.99702163908297));
#54266=CARTESIAN_POINT('Ctrl Pts',(1.27940096817029,1.06710525355877,9.99735480784343));
#54267=CARTESIAN_POINT('Ctrl Pts',(1.27169456170755,1.07628924989468,9.9981654185625));
#54268=CARTESIAN_POINT('Ctrl Pts',(1.26713312439175,1.08165579010145,9.99864408580436));
#54269=CARTESIAN_POINT('Ctrl Pts',(1.2527426071593,1.09837031483181,10.0001502305882));
#54270=CARTESIAN_POINT('Ctrl Pts',(1.24279439408224,1.10961409648543,10.0011857201749));
#54271=CARTESIAN_POINT('Ctrl Pts',(1.18961316946802,1.16810881660869,10.0066846736551));
#54272=CARTESIAN_POINT('Ctrl Pts',(1.14383771951679,1.21296798751377,10.0112913918291));
#54273=CARTESIAN_POINT('Ctrl Pts',(1.01285855911909,1.32730419149547,10.0239079553979));
#54274=CARTESIAN_POINT('Ctrl Pts',(0.923167634812829,1.39118122265691,10.031947513982));
#54275=CARTESIAN_POINT('Ctrl Pts',(0.78461644643187,1.4705146830061,10.0432271204965));
#54276=CARTESIAN_POINT('Ctrl Pts',(0.740305098230693,1.49331364696042,10.0466871884885));
#54277=CARTESIAN_POINT('Ctrl Pts',(0.680274488975569,1.52087027175961,10.051184893164));
#54278=CARTESIAN_POINT('Ctrl Pts',(0.66541579010376,1.5274297439159,10.05228337898));
#54279=CARTESIAN_POINT('Ctrl Pts',(0.640855737489063,1.53784551422447,10.05407553266));
#54280=CARTESIAN_POINT('Ctrl Pts',(0.631210141182511,1.5418296495147,10.0547734980039));
#54281=CARTESIAN_POINT('Ctrl Pts',(0.612345332118319,1.54941509583786,10.0561274201735));
#54282=CARTESIAN_POINT('Ctrl Pts',(0.603130229953526,1.55302539512075,10.0567836564511));
#54283=CARTESIAN_POINT('Ctrl Pts',(0.581273040672289,1.56136473004009,10.0583284057609));
#54284=CARTESIAN_POINT('Ctrl Pts',(0.56860445181398,1.56602272114599,10.0592145226758));
#54285=CARTESIAN_POINT('Ctrl Pts',(0.525504637368104,1.58127769562196,10.0621994089584));
#54286=CARTESIAN_POINT('Ctrl Pts',(0.494821960615776,1.59114603997098,10.0642743072812));
#54287=CARTESIAN_POINT('Ctrl Pts',(0.419009090516657,1.61312401207268,10.0692972662629));
#54288=CARTESIAN_POINT('Ctrl Pts',(0.373618344532987,1.6242375162892,10.0722159149512));
#54289=CARTESIAN_POINT('Ctrl Pts',(0.26025489865599,1.64698876606478,10.0793634043344));
#54290=CARTESIAN_POINT('Ctrl Pts',(0.191914593555625,1.65634345175939,10.0835470828311));
#54291=CARTESIAN_POINT('Ctrl Pts',(0.0998712587242807,1.6631682269327,10.089194858098));
#54292=CARTESIAN_POINT('Ctrl Pts',(0.0765176552312613,1.66440615004458,
10.0906292818935));
#54293=CARTESIAN_POINT('Ctrl Pts',(-0.0109887161014974,1.66719906392807,
10.0960325048454));
#54294=CARTESIAN_POINT('Ctrl Pts',(-0.0751808909474305,1.66553875170138,
10.1000523508879));
#54295=CARTESIAN_POINT('Ctrl Pts',(-0.150499097483795,1.65922773188982,
10.1049980510783));
#54296=CARTESIAN_POINT('Ctrl Pts',(-0.161878660853386,1.6581561826447,10.1057515074042));
#54297=CARTESIAN_POINT('Ctrl Pts',(-0.179603557902194,1.65630293834261,
10.1069360800195));
#54298=CARTESIAN_POINT('Ctrl Pts',(-0.185957196213266,1.6556016366683,10.1073629057951));
#54299=CARTESIAN_POINT('Ctrl Pts',(-0.19720946095798,1.65429404643678,10.1081229750402));
#54300=CARTESIAN_POINT('Ctrl Pts',(-0.20210965055095,1.65370252780854,10.1084553917751));
#54301=CARTESIAN_POINT('Ctrl Pts',(-0.213905823672248,1.65222535902512,
10.109259004576));
#54302=CARTESIAN_POINT('Ctrl Pts',(-0.220798896967757,1.65131831611712,
10.1097313678525));
#54303=CARTESIAN_POINT('Ctrl Pts',(-0.242082486150913,1.64838201744531,
10.1111980349608));
#54304=CARTESIAN_POINT('Ctrl Pts',(-0.256451832644973,1.64620765011811,
10.1121997841692));
#54305=CARTESIAN_POINT('Ctrl Pts',(-0.329716481184864,1.63413878354507,
10.1173603502247));
#54306=CARTESIAN_POINT('Ctrl Pts',(-0.388072555233054,1.62127135312826,
10.1216448258449));
#54307=CARTESIAN_POINT('Ctrl Pts',(-0.547978501957975,1.57688404350042,
10.1336697971635));
#54308=CARTESIAN_POINT('Ctrl Pts',(-0.647409003187102,1.53873615273816,
10.1414590855755));
#54309=CARTESIAN_POINT('Ctrl Pts',(-0.793482994309661,1.46600827584074,
10.15304878776));
#54310=CARTESIAN_POINT('Ctrl Pts',(-0.843105101802522,1.43804402387369,
10.1570190139605));
#54311=CARTESIAN_POINT('Ctrl Pts',(-0.905563333304984,1.3984991670277,10.1620589542337));
#54312=CARTESIAN_POINT('Ctrl Pts',(-0.919783767187433,1.38918779493509,
10.1632096327131));
#54313=CARTESIAN_POINT('Ctrl Pts',(-0.942634971547567,1.37372034890518,
10.1650645529685));
#54314=CARTESIAN_POINT('Ctrl Pts',(-0.951353553816348,1.36769686377908,
10.1657736958843));
#54315=CARTESIAN_POINT('Ctrl Pts',(-0.967488583018499,1.35632056660546,
10.1670889837075));
#54316=CARTESIAN_POINT('Ctrl Pts',(-0.974919520667993,1.3509891086082,10.1676959085347));
#54317=CARTESIAN_POINT('Ctrl Pts',(-0.98273468800006,1.34528391587296,10.1683355724489));
#54318=CARTESIAN_POINT('Ctrl Pts',(-0.983162918554376,1.34497098737698,
10.1683706270508));
#54319=CARTESIAN_POINT('Ctrl Pts',(-0.983986378641286,1.34436864238054,
10.1684380432185));
#54320=CARTESIAN_POINT('Ctrl Pts',(-0.9843816300402,1.34407925599942,10.1684704059325));
#54321=CARTESIAN_POINT('Ctrl Pts',(-0.985149338739101,1.34351665183348,
10.168533272283));
#54322=CARTESIAN_POINT('Ctrl Pts',(-0.985521810118118,1.34324345341943,
10.1685637766573));
#54323=CARTESIAN_POINT('Ctrl Pts',(-0.986251615317336,1.34270769265317,
10.1686235522407));
#54324=CARTESIAN_POINT('Ctrl Pts',(-0.986608958005362,1.34244514249569,
10.1686528239135));
#54325=CARTESIAN_POINT('Ctrl Pts',(-0.987314584874487,1.34192626380884,
10.1687106313533));
#54326=CARTESIAN_POINT('Ctrl Pts',(-0.987662874143681,1.34166994229008,
10.1687391673855));
#54327=CARTESIAN_POINT('Ctrl Pts',(-0.988355495524049,1.34115979564662,
10.1687959211219));
#54328=CARTESIAN_POINT('Ctrl Pts',(-0.988699829745768,1.34090597345702,
10.1688241389353));
#54329=CARTESIAN_POINT('Ctrl Pts',(-0.989389061443817,1.34039750406156,
10.1688806265481));
#54330=CARTESIAN_POINT('Ctrl Pts',(-0.989733958462559,1.34014285629023,
10.1689088963228));
#54331=CARTESIAN_POINT('Ctrl Pts',(-0.990428537942846,1.33962961313098,
10.1689658340318));
#54332=CARTESIAN_POINT('Ctrl Pts',(-0.990778217524352,1.33937101388261,
10.1689945018154));
#54333=CARTESIAN_POINT('Ctrl Pts',(-0.99940569619487,1.3329854896335,10.1697018834107));
#54334=CARTESIAN_POINT('Ctrl Pts',(-1.00762675740504,1.3267819665612,10.1703776433778));
#54335=CARTESIAN_POINT('Ctrl Pts',(-1.02728463730618,1.31166024102058,10.1719980522675));
#54336=CARTESIAN_POINT('Ctrl Pts',(-1.03866368408487,1.30266806451372,10.1729398084153));
#54337=CARTESIAN_POINT('Ctrl Pts',(-1.06935368047912,1.27775777032562,10.1754917784745));
#54338=CARTESIAN_POINT('Ctrl Pts',(-1.08842611848111,1.26155098800991,10.1770909060809));
#54339=CARTESIAN_POINT('Ctrl Pts',(-1.14953064317724,1.20720977262236,10.1822702198343));
#54340=CARTESIAN_POINT('Ctrl Pts',(-1.18998215605509,1.16735570037742,10.1857874385844));
#54341=CARTESIAN_POINT('Ctrl Pts',(-1.27182548869574,1.07803635798541,10.1932270069303));
#54342=CARTESIAN_POINT('Ctrl Pts',(-1.31253845308454,1.02807839318132,10.1971334290981));
#54343=CARTESIAN_POINT('Ctrl Pts',(-1.39439776626126,0.914816476774274,
10.2057147958404));
#54344=CARTESIAN_POINT('Ctrl Pts',(-1.43433810898828,0.850826391364902,
10.2103975638657));
#54345=CARTESIAN_POINT('Ctrl Pts',(-1.47526709663119,0.774130174487371,
10.2160838642322));
#54346=CARTESIAN_POINT('Ctrl Pts',(-1.48062070941544,0.763840840631683,
10.2168482248152));
#54347=CARTESIAN_POINT('Ctrl Pts',(-1.48877440603304,0.747762069374777,
10.2180463052736));
#54348=CARTESIAN_POINT('Ctrl Pts',(-1.49164925891114,0.742010666619104,
10.218475576946));
#54349=CARTESIAN_POINT('Ctrl Pts',(-1.49688972861089,0.731373099462795,
10.2192711245895));
#54350=CARTESIAN_POINT('Ctrl Pts',(-1.49926484533613,0.726491838009372,
10.2196368103054));
#54351=CARTESIAN_POINT('Ctrl Pts',(-1.50472643158455,0.715126516610433,
10.2204896788759));
#54352=CARTESIAN_POINT('Ctrl Pts',(-1.50779486180267,0.708634051262194,
10.2209779280245));
#54353=CARTESIAN_POINT('Ctrl Pts',(-1.51746354186941,0.687829056989506,
10.222545372486));
#54354=CARTESIAN_POINT('Ctrl Pts',(-1.52390247370742,0.673443106853239,
10.2236335005455));
#54355=CARTESIAN_POINT('Ctrl Pts',(-1.54198585812882,0.631453190263509,
10.2268174900613));
#54356=CARTESIAN_POINT('Ctrl Pts',(-1.55308786246816,0.603631150045019,
10.2289369329063));
#54357=CARTESIAN_POINT('Ctrl Pts',(-1.56343128570986,0.575533330801617,
10.2310772794004));
#54358=CARTESIAN_POINT('Origin',(0.,0.,11.));
#54359=CARTESIAN_POINT('',(-1.5634312473966,0.575533434879242,10.9335682035678));
#54360=CARTESIAN_POINT('',(-1.56343131785294,0.575533243485219,10.7380842620731));
#54361=CARTESIAN_POINT('',(-1.56343130033213,0.575533291080363,11.));
#54362=CARTESIAN_POINT('',(-1.66599935349477,-0.0014677039958931,10.0778956387897));
#54363=CARTESIAN_POINT('Ctrl Pts',(-1.56343131785294,0.575533243485219,
10.7380842620731));
#54364=CARTESIAN_POINT('Ctrl Pts',(-1.54669125760662,0.621007479331894,
10.7346561303571));
#54365=CARTESIAN_POINT('Ctrl Pts',(-1.52797002107001,0.665743709967646,
10.7312816482152));
#54366=CARTESIAN_POINT('Ctrl Pts',(-1.49964821480684,0.725903166842574,
10.7267411743421));
#54367=CARTESIAN_POINT('Ctrl Pts',(-1.49171542647364,0.742068262625956,
10.7255207355039));
#54368=CARTESIAN_POINT('Ctrl Pts',(-1.47860171470767,0.767730342795993,
10.7235819413168));
#54369=CARTESIAN_POINT('Ctrl Pts',(-1.47358784994133,0.777310599456636,
10.722857833018));
#54370=CARTESIAN_POINT('Ctrl Pts',(-1.46386878823258,0.795449266508267,
10.7214859929087));
#54371=CARTESIAN_POINT('Ctrl Pts',(-1.45918093310503,0.804016402907594,
10.7208376842958));
#54372=CARTESIAN_POINT('Ctrl Pts',(-1.44827002431254,0.823546497044163,
10.7193586301703));
#54373=CARTESIAN_POINT('Ctrl Pts',(-1.44199728264548,0.834481124707548,
10.7185297001952));
#54374=CARTESIAN_POINT('Ctrl Pts',(-1.42191432600201,0.868586907288862,
10.7159406018878));
#54375=CARTESIAN_POINT('Ctrl Pts',(-1.40766472694261,0.891495212758521,
10.7141963174113));
#54376=CARTESIAN_POINT('Ctrl Pts',(-1.34317483435546,0.989767548629385,
10.7066731886934));
#54377=CARTESIAN_POINT('Ctrl Pts',(-1.28739151468958,1.06131240460098,10.7011000723651));
#54378=CARTESIAN_POINT('Ctrl Pts',(-1.15153669320075,1.20898122959927,10.6888358693497));
#54379=CARTESIAN_POINT('Ctrl Pts',(-1.06917509285037,1.28239258027238,10.682193434787));
#54380=CARTESIAN_POINT('Ctrl Pts',(-0.965807212193965,1.35760409028809,
10.6739346038279));
#54381=CARTESIAN_POINT('Ctrl Pts',(-0.951257169435558,1.36783850397806,
10.6727733757274));
#54382=CARTESIAN_POINT('Ctrl Pts',(-0.930750785230871,1.38177714926392,
10.6711342925756));
#54383=CARTESIAN_POINT('Ctrl Pts',(-0.924930122562201,1.38568011405303,
10.6706687709231));
#54384=CARTESIAN_POINT('Ctrl Pts',(-0.914410206921661,1.39263828388022,
10.6698265874857));
#54385=CARTESIAN_POINT('Ctrl Pts',(-0.909719759761508,1.39570676489599,
10.6694507946015));
#54386=CARTESIAN_POINT('Ctrl Pts',(-0.900064069009622,1.40195414694521,
10.6686764014897));
#54387=CARTESIAN_POINT('Ctrl Pts',(-0.895097307360368,1.40513044450681,
10.6682776514722));
#54388=CARTESIAN_POINT('Ctrl Pts',(-0.882114152632687,1.41333654294391,
10.6672344602678));
#54389=CARTESIAN_POINT('Ctrl Pts',(-0.874071710082956,1.41832443291388,
10.6665874103323));
#54390=CARTESIAN_POINT('Ctrl Pts',(-0.837715798585621,1.44044557072019,
10.6636601581778));
#54391=CARTESIAN_POINT('Ctrl Pts',(-0.80894004755658,1.45680020939396,10.6613372308029));
#54392=CARTESIAN_POINT('Ctrl Pts',(-0.721885077965701,1.50290311988185,
10.6543325201173));
#54393=CARTESIAN_POINT('Ctrl Pts',(-0.66232106785631,1.53008684651151,10.6495714266148));
#54394=CARTESIAN_POINT('Ctrl Pts',(-0.487473540033794,1.5977569027983,10.635923552115));
#54395=CARTESIAN_POINT('Ctrl Pts',(-0.369111921603434,1.6291790415787,10.6271055177121));
#54396=CARTESIAN_POINT('Ctrl Pts',(-0.22767123015447,1.65050284664622,10.6172668745934));
#54397=CARTESIAN_POINT('Ctrl Pts',(-0.206922819459439,1.65323224368624,
10.6158395840411));
#54398=CARTESIAN_POINT('Ctrl Pts',(-0.173662958595634,1.65697148712657,
10.6135762519264));
#54399=CARTESIAN_POINT('Ctrl Pts',(-0.161182550992097,1.6582320502666,10.6127324715235));
#54400=CARTESIAN_POINT('Ctrl Pts',(-0.138943276844838,1.66022483523352,
10.6112383666309));
#54401=CARTESIAN_POINT('Ctrl Pts',(-0.129190080884934,1.661012241896,10.6105863439705));
#54402=CARTESIAN_POINT('Ctrl Pts',(-0.108722158101178,1.66248330807813,
10.6092245416772));
#54403=CARTESIAN_POINT('Ctrl Pts',(-0.0980065896434857,1.66314941445107,
10.6085153399706));
#54404=CARTESIAN_POINT('Ctrl Pts',(-0.0696619185256244,1.66463649156229,
10.6066487790653));
#54405=CARTESIAN_POINT('Ctrl Pts',(-0.0520246211011804,1.66528103018159,
10.6054969454387));
#54406=CARTESIAN_POINT('Ctrl Pts',(0.0390245101569303,1.66716033507488,
10.5995953880143));
#54407=CARTESIAN_POINT('Ctrl Pts',(0.112453783752614,1.66382168613298,10.5949901253429));
#54408=CARTESIAN_POINT('Ctrl Pts',(0.280956841043332,1.64494952259849,10.5845252302558));
#54409=CARTESIAN_POINT('Ctrl Pts',(0.375374010994471,1.62600402554265,10.5787414599683));
#54410=CARTESIAN_POINT('Ctrl Pts',(0.522473207396021,1.58298546039346,10.5692448169471));
#54411=CARTESIAN_POINT('Ctrl Pts',(0.576450684788773,1.56413693994342,10.5656467251638));
#54412=CARTESIAN_POINT('Ctrl Pts',(0.639804332264874,1.53828930197729,10.5611680420818));
#54413=CARTESIAN_POINT('Ctrl Pts',(0.650217718205162,1.53391670632844,10.5604233531644));
#54414=CARTESIAN_POINT('Ctrl Pts',(0.666425727905554,1.52691624539809,10.5592496604774));
#54415=CARTESIAN_POINT('Ctrl Pts',(0.672251347977826,1.52436038817974,10.5588248223568));
#54416=CARTESIAN_POINT('Ctrl Pts',(0.682574558086989,1.51976063179552,10.5580664390523));
#54417=CARTESIAN_POINT('Ctrl Pts',(0.6870778965152,1.51773000468157,10.5577336990412));
#54418=CARTESIAN_POINT('Ctrl Pts',(0.697935688195287,1.51277582639699,10.5569268622724));
#54419=CARTESIAN_POINT('Ctrl Pts',(0.704280772177505,1.50983228051747,10.5564515712062));
#54420=CARTESIAN_POINT('Ctrl Pts',(0.723953201491947,1.50055506273643,10.5549665725276));
#54421=CARTESIAN_POINT('Ctrl Pts',(0.737214645381597,1.49408442316629,10.553949158589));
#54422=CARTESIAN_POINT('Ctrl Pts',(0.805477781673791,1.45964682060626,10.5486332539399));
#54423=CARTESIAN_POINT('Ctrl Pts',(0.858975985885196,1.4288184068559,10.5442011523411));
#54424=CARTESIAN_POINT('Ctrl Pts',(1.03647726335709,1.31295630494219,10.5288309553361));
#54425=CARTESIAN_POINT('Ctrl Pts',(1.15065778877938,1.21414339287638,10.517835120579));
#54426=CARTESIAN_POINT('Ctrl Pts',(1.26373953107352,1.08579360466303,10.5060725850247));
#54427=CARTESIAN_POINT('Ctrl Pts',(1.27714671317399,1.06999144591394,10.5046594923316));
#54428=CARTESIAN_POINT('Ctrl Pts',(1.29815471631044,1.0442730585435,10.5024141405338));
#54429=CARTESIAN_POINT('Ctrl Pts',(1.30594452139081,1.03451477034371,10.5015743359043));
#54430=CARTESIAN_POINT('Ctrl Pts',(1.3196372919869,1.01696066979632,10.5000847423281));
#54431=CARTESIAN_POINT('Ctrl Pts',(1.32558263846188,1.00919882180214,10.499433291326));
#54432=CARTESIAN_POINT('Ctrl Pts',(1.33793021902309,0.992781256683607,10.4980701482177));
#54433=CARTESIAN_POINT('Ctrl Pts',(1.34431759315388,0.984114887860952,10.4973590562378));
#54434=CARTESIAN_POINT('Ctrl Pts',(1.36103348963873,0.960968348136668,10.4954816637705));
#54435=CARTESIAN_POINT('Ctrl Pts',(1.3712150868309,0.946383406090704,10.4943210075649));
#54436=CARTESIAN_POINT('Ctrl Pts',(1.42357907714352,0.868753310221009,10.4882541323983));
#54437=CARTESIAN_POINT('Ctrl Pts',(1.46165546770604,0.803041165726937,10.483502946441));
#54438=CARTESIAN_POINT('Ctrl Pts',(1.54149128500431,0.640630693427758,10.4723464447573));
#54439=CARTESIAN_POINT('Ctrl Pts',(1.57882549497222,0.542135612906083,10.4660408722851));
#54440=CARTESIAN_POINT('Ctrl Pts',(1.61892963417412,0.395958991533776,10.4565743676173));
#54441=CARTESIAN_POINT('Ctrl Pts',(1.62934537289206,0.350641533556574,10.4536226759825));
#54442=CARTESIAN_POINT('Ctrl Pts',(1.63984025591783,0.294275207549444,10.4498648335958));
#54443=CARTESIAN_POINT('Ctrl Pts',(1.64172379131339,0.283578808034988,10.4491479147204));
#54444=CARTESIAN_POINT('Ctrl Pts',(1.64451823989629,0.266747475550451,10.4480127400516));
#54445=CARTESIAN_POINT('Ctrl Pts',(1.64549974340452,0.260624343426591,10.4475983065123));
#54446=CARTESIAN_POINT('Ctrl Pts',(1.64729163037781,0.249031835206956,10.4468106756429));
#54447=CARTESIAN_POINT('Ctrl Pts',(1.64810900049549,0.243563727265705,10.4464378680942));
#54448=CARTESIAN_POINT('Ctrl Pts',(1.64998630900513,0.230562469279665,10.4455485069081));
#54449=CARTESIAN_POINT('Ctrl Pts',(1.65102188576581,0.223026005724653,10.4450306311319));
#54450=CARTESIAN_POINT('Ctrl Pts',(1.65436405447699,0.197403174146386,10.4432625954017));
#54451=CARTESIAN_POINT('Ctrl Pts',(1.65642524502749,0.179286858639511,10.4420001374996));
#54452=CARTESIAN_POINT('Ctrl Pts',(1.66077883916317,0.134487174555217,10.4388534931753));
#54453=CARTESIAN_POINT('Ctrl Pts',(1.66272587975138,0.107775887327628,10.4369558073158));
#54454=CARTESIAN_POINT('Ctrl Pts',(1.66853185680683,-0.0114541294322638,
10.428420284254));
#54455=CARTESIAN_POINT('Ctrl Pts',(1.66531735322964,-0.104151559382932,
10.4216210645194));
#54456=CARTESIAN_POINT('Ctrl Pts',(1.64328831539891,-0.290001190951868,
10.4080751717489));
#54457=CARTESIAN_POINT('Ctrl Pts',(1.6241827012998,-0.382796516104936,10.4013589210312));
#54458=CARTESIAN_POINT('Ctrl Pts',(1.59194549884264,-0.491549189958379,
10.3936035201721));
#54459=CARTESIAN_POINT('Ctrl Pts',(1.58628380419756,-0.509524111874708,
10.3923250235971));
#54460=CARTESIAN_POINT('Ctrl Pts',(1.57683847884317,-0.537826398018662,
10.3903165069736));
#54461=CARTESIAN_POINT('Ctrl Pts',(1.57325562463237,-0.548218544335189,
10.3895799854177));
#54462=CARTESIAN_POINT('Ctrl Pts',(1.56663364266792,-0.566826019985522,
10.3882627172603));
#54463=CARTESIAN_POINT('Ctrl Pts',(1.563632111927,-0.57505419816941,10.3876807549634));
#54464=CARTESIAN_POINT('Ctrl Pts',(1.55642795541582,-0.594329632513051,
10.3863184860453));
#54465=CARTESIAN_POINT('Ctrl Pts',(1.55217234317064,-0.605356689583083,
10.3855399742696));
#54466=CARTESIAN_POINT('Ctrl Pts',(1.53935026876353,-0.637556569767095,
10.3832683048517));
#54467=CARTESIAN_POINT('Ctrl Pts',(1.53046513894832,-0.658600159293423,
10.3817858431087));
#54468=CARTESIAN_POINT('Ctrl Pts',(1.48738175601694,-0.755054306929365,
10.3749902717327));
#54469=CARTESIAN_POINT('Ctrl Pts',(1.44802322456057,-0.82803536018141,10.369854072376));
#54470=CARTESIAN_POINT('Ctrl Pts',(1.37255838166571,-0.945999049889552,
10.3612689968606));
#54471=CARTESIAN_POINT('Ctrl Pts',(1.33925732218618,-0.99258272285283,10.3577927978951));
#54472=CARTESIAN_POINT('Ctrl Pts',(1.25570458371164,-1.09758144470337,10.3495576638826));
#54473=CARTESIAN_POINT('Ctrl Pts',(1.20367422713917,-1.15440212486887,10.3447804511836));
#54474=CARTESIAN_POINT('Ctrl Pts',(1.1395024236288,-1.21541140023655,10.3389888532485));
#54475=CARTESIAN_POINT('Ctrl Pts',(1.13100976875244,-1.22331824549376,10.3382241815778));
#54476=CARTESIAN_POINT('Ctrl Pts',(1.11768327242383,-1.23546811297546,10.337025729378));
#54477=CARTESIAN_POINT('Ctrl Pts',(1.11290608752657,-1.2397731213864,10.3365964017093));
#54478=CARTESIAN_POINT('Ctrl Pts',(1.10401186422665,-1.24769541069684,10.3357973307104));
#54479=CARTESIAN_POINT('Ctrl Pts',(1.09990175724881,-1.25132016504145,10.3354281493976));
#54480=CARTESIAN_POINT('Ctrl Pts',(1.09034300104577,-1.25966667103941,10.3345697801022));
#54481=CARTESIAN_POINT('Ctrl Pts',(1.08488153119255,-1.26437337859423,10.3340795340737));
#54482=CARTESIAN_POINT('Ctrl Pts',(1.06726214140492,-1.27935960772184,10.3324990251892));
#54483=CARTESIAN_POINT('Ctrl Pts',(1.05498777225002,-1.28949999551867,10.331399626505));
#54484=CARTESIAN_POINT('Ctrl Pts',(1.02517235629961,-1.31342117496283,10.3287367794479));
#54485=CARTESIAN_POINT('Ctrl Pts',(1.00749644154243,-1.32702839565862,10.3271643460276));
#54486=CARTESIAN_POINT('Ctrl Pts',(0.936851514025167,-1.37918701540653,
10.3209200153979));
#54487=CARTESIAN_POINT('Ctrl Pts',(0.881902963949549,-1.41495365485163,
10.3161522174584));
#54488=CARTESIAN_POINT('Ctrl Pts',(0.719059492045232,-1.50777243766725,
10.3025077605635));
#54489=CARTESIAN_POINT('Ctrl Pts',(0.606796047528954,-1.55635252708872,
10.2937000344992));
#54490=CARTESIAN_POINT('Ctrl Pts',(0.470211811428143,-1.59840390566161,
10.2838700771653));
#54491=CARTESIAN_POINT('Ctrl Pts',(0.450090416030545,-1.60418604895799,
10.2824421912624));
#54492=CARTESIAN_POINT('Ctrl Pts',(0.417743744655853,-1.61282471357215,
10.2801781055908));
#54493=CARTESIAN_POINT('Ctrl Pts',(0.405586462687128,-1.61592482162347,
10.2793341588286));
#54494=CARTESIAN_POINT('Ctrl Pts',(0.383886839600371,-1.62119790233165,
10.2778398648467));
#54495=CARTESIAN_POINT('Ctrl Pts',(0.37435831104621,-1.62342465366125,10.2771878179438));
#54496=CARTESIAN_POINT('Ctrl Pts',(0.354336484933997,-1.62791796063293,
10.275826070119));
#54497=CARTESIAN_POINT('Ctrl Pts',(0.343839755493118,-1.63016731127452,
10.2751169462049));
#54498=CARTESIAN_POINT('Ctrl Pts',(0.316036757655364,-1.63584473563991,
10.2732508311237));
#54499=CARTESIAN_POINT('Ctrl Pts',(0.298696221749054,-1.63909970323242,
10.2720993606642));
#54500=CARTESIAN_POINT('Ctrl Pts',(0.209036410039491,-1.65445944537256,
10.2662043979341));
#54501=CARTESIAN_POINT('Ctrl Pts',(0.136022668791075,-1.66205657727013,
10.2616049543371));
#54502=CARTESIAN_POINT('Ctrl Pts',(-0.0355262246515348,-1.66852135373109,
10.2510090765229));
#54503=CARTESIAN_POINT('Ctrl Pts',(-0.133921419902664,-1.66351722365645,
10.2450965467666));
#54504=CARTESIAN_POINT('Ctrl Pts',(-0.264249661837201,-1.64524626985364,
10.2369313986337));
#54505=CARTESIAN_POINT('Ctrl Pts',(-0.297054054106251,-1.63964075832284,
10.2348460701389));
#54506=CARTESIAN_POINT('Ctrl Pts',(-0.355457843579343,-1.6278507340082,
10.2310449034782));
#54507=CARTESIAN_POINT('Ctrl Pts',(-0.381120338374965,-1.6220343383052,
10.2293435483973));
#54508=CARTESIAN_POINT('Ctrl Pts',(-0.415376433943941,-1.613412444456,10.227017274837));
#54509=CARTESIAN_POINT('Ctrl Pts',(-0.424102012507536,-1.61114082926893,
10.2264198779463));
#54510=CARTESIAN_POINT('Ctrl Pts',(-0.43785222009138,-1.6074416673281,10.2254701539325));
#54511=CARTESIAN_POINT('Ctrl Pts',(-0.442889465352447,-1.60606108230223,
10.2251204614575));
#54512=CARTESIAN_POINT('Ctrl Pts',(-0.453345272968204,-1.60314247336473,
10.2243907587088));
#54513=CARTESIAN_POINT('Ctrl Pts',(-0.458762609777383,-1.6016006339314,
10.2240105162271));
#54514=CARTESIAN_POINT('Ctrl Pts',(-0.472060448823053,-1.59774290776513,
10.2230719594518));
#54515=CARTESIAN_POINT('Ctrl Pts',(-0.479931779706434,-1.59539617226091,
10.2225119182922));
#54516=CARTESIAN_POINT('Ctrl Pts',(-0.509047531882594,-1.58648072305025,
10.2204245024478));
#54517=CARTESIAN_POINT('Ctrl Pts',(-0.530176110913511,-1.57954539267471,
10.2188783366942));
#54518=CARTESIAN_POINT('Ctrl Pts',(-0.688136346235638,-1.52416970496632,
10.2071130849968));
#54519=CARTESIAN_POINT('Ctrl Pts',(-0.81825125996781,-1.45845578252264,
10.1963154800243));
#54520=CARTESIAN_POINT('Ctrl Pts',(-0.992426767600683,-1.3397574755361,
10.1812603762908));
#54521=CARTESIAN_POINT('Ctrl Pts',(-1.04442115794302,-1.29963355517777,
10.1766627759453));
#54522=CARTESIAN_POINT('Ctrl Pts',(-1.1072642679773,-1.24492365990061,10.1709759002014));
#54523=CARTESIAN_POINT('Ctrl Pts',(-1.12042405825076,-1.23309328509323,
10.1697769692047));
#54524=CARTESIAN_POINT('Ctrl Pts',(-1.14126920789528,-1.21374464662334,
10.1678640330061));
#54525=CARTESIAN_POINT('Ctrl Pts',(-1.14907432399157,-1.20635802289323,
10.1671445429376));
#54526=CARTESIAN_POINT('Ctrl Pts',(-1.16384689178002,-1.19210406343739,
10.165776305619));
#54527=CARTESIAN_POINT('Ctrl Pts',(-1.17082636543591,-1.18524989539507,
10.1651270309301));
#54528=CARTESIAN_POINT('Ctrl Pts',(-1.17804979590416,-1.17803007764691,
10.1644519459491));
#54529=CARTESIAN_POINT('Ctrl Pts',(-1.17835427897449,-1.1777255107595,10.1644234838322));
#54530=CARTESIAN_POINT('Ctrl Pts',(-1.17895143575263,-1.17712772619244,
10.1643676520178));
#54531=CARTESIAN_POINT('Ctrl Pts',(-1.17924411823485,-1.17683451735714,
10.1643402819368));
#54532=CARTESIAN_POINT('Ctrl Pts',(-1.17981941313689,-1.17625775774524,
10.1642864727945));
#54533=CARTESIAN_POINT('Ctrl Pts',(-1.18010203276548,-1.17597421422997,
10.1642600334187));
#54534=CARTESIAN_POINT('Ctrl Pts',(-1.18065873073384,-1.17541529362739,
10.1642079436958));
#54535=CARTESIAN_POINT('Ctrl Pts',(-1.18093281498866,-1.17513992249204,
10.1641822930911));
#54536=CARTESIAN_POINT('Ctrl Pts',(-1.18147379968419,-1.17459601736338,
10.1641316547117));
#54537=CARTESIAN_POINT('Ctrl Pts',(-1.18174070495256,-1.17432748822666,
10.164106666727));
#54538=CARTESIAN_POINT('Ctrl Pts',(-1.19026300994896,-1.16574748524836,
10.163308652557));
#54539=CARTESIAN_POINT('Ctrl Pts',(-1.19843077735734,-1.15734908981982,
10.1625394637603));
#54540=CARTESIAN_POINT('Ctrl Pts',(-1.22663276611044,-1.1277320640116,10.1598672343591));
#54541=CARTESIAN_POINT('Ctrl Pts',(-1.24619825585961,-1.10607306403677,
10.1579840837568));
#54542=CARTESIAN_POINT('Ctrl Pts',(-1.29193757900133,-1.0526841966272,10.1534967572877));
#54543=CARTESIAN_POINT('Ctrl Pts',(-1.31752553662098,-1.02047711461148,
10.150914488051));
#54544=CARTESIAN_POINT('Ctrl Pts',(-1.39298158149786,-0.917926056802289,
10.1430056288141));
#54545=CARTESIAN_POINT('Ctrl Pts',(-1.43860090400361,-0.844638211444959,
10.1377919984518));
#54546=CARTESIAN_POINT('Ctrl Pts',(-1.5150494001073,-0.697508779990399,
10.1276252951632));
#54547=CARTESIAN_POINT('Ctrl Pts',(-1.54663881374471,-0.624338186244144,
10.1226931331175));
#54548=CARTESIAN_POINT('Ctrl Pts',(-1.57670541841323,-0.538229587135547,
10.116727646752));
#54549=CARTESIAN_POINT('Ctrl Pts',(-1.5804215136236,-0.527218062670438,
10.1159618085966));
#54550=CARTESIAN_POINT('Ctrl Pts',(-1.58601565604507,-0.510050728955306,
10.114761911908));
#54551=CARTESIAN_POINT('Ctrl Pts',(-1.5879738305639,-0.503921141942606,
10.1143323232592));
#54552=CARTESIAN_POINT('Ctrl Pts',(-1.59153369951653,-0.492551024147773,
10.1135330316411));
#54553=CARTESIAN_POINT('Ctrl Pts',(-1.593145107703,-0.487313749764808,10.1131638935963));
#54554=CARTESIAN_POINT('Ctrl Pts',(-1.5968151420117,-0.475172914484262,
10.1123059765617));
#54555=CARTESIAN_POINT('Ctrl Pts',(-1.59885484861613,-0.46826388356232,
10.1118161434898));
#54556=CARTESIAN_POINT('Ctrl Pts',(-1.60524934620423,-0.446075075594156,
10.1102383249954));
#54557=CARTESIAN_POINT('Ctrl Pts',(-1.60943023850302,-0.430746674869565,
10.1091412456697));
#54558=CARTESIAN_POINT('Ctrl Pts',(-1.64820379414772,-0.28013834405567,
10.0983080807256));
#54559=CARTESIAN_POINT('Ctrl Pts',(-1.66587635268669,-0.141086637584619,
10.0879378005138));
#54560=CARTESIAN_POINT('Ctrl Pts',(-1.66599935349477,-0.0014677039958931,
10.0778956387897));
#54561=CARTESIAN_POINT('Ctrl Pts',(-1.66599935485773,-0.00146615606807475,
10.0778955274543));
#54562=CARTESIAN_POINT('Ctrl Pts',(-1.66604451061792,0.0498445256343925,
10.0742049818099));
#54563=CARTESIAN_POINT('Ctrl Pts',(-1.66371921130138,0.101134532714982,
10.0705587717341));
#54564=CARTESIAN_POINT('Ctrl Pts',(-1.65643808135581,0.180480131690436,
10.0649991798008));
#54565=CARTESIAN_POINT('Ctrl Pts',(-1.65312593791863,0.208650415156738,
10.0630410675269));
#54566=CARTESIAN_POINT('Ctrl Pts',(-1.64723819627737,0.249666341968592,
10.060212325594));
#54567=CARTESIAN_POINT('Ctrl Pts',(-1.64522800177558,0.262586741225869,
10.0593244752333));
#54568=CARTESIAN_POINT('Ctrl Pts',(-1.6414516794009,0.285109940362668,10.0577821230972));
#54569=CARTESIAN_POINT('Ctrl Pts',(-1.63975288551601,0.294723218267103,
10.0571255380111));
#54570=CARTESIAN_POINT('Ctrl Pts',(-1.63616171736016,0.314052218965795,
10.0558086504158));
#54571=CARTESIAN_POINT('Ctrl Pts',(-1.63426705928971,0.32376711968777,10.0551484494935));
#54572=CARTESIAN_POINT('Ctrl Pts',(-1.63019778812774,0.343685909006897,
10.0537980276507));
#54573=CARTESIAN_POINT('Ctrl Pts',(-1.62801367594708,0.35388742810494,10.0531081412161));
#54574=CARTESIAN_POINT('Ctrl Pts',(-1.62218781495125,0.379902624331914,
10.0513528795156));
#54575=CARTESIAN_POINT('Ctrl Pts',(-1.61841053607833,0.395685074290687,
10.0502918661254));
#54576=CARTESIAN_POINT('Ctrl Pts',(-1.60212869295147,0.459576182438404,
10.0460092657414));
#54577=CARTESIAN_POINT('Ctrl Pts',(-1.58770408784237,0.507171633669777,
10.0428492217377));
#54578=CARTESIAN_POINT('Ctrl Pts',(-1.5686401382185,0.561232615627931,10.0392603670108));
#54579=CARTESIAN_POINT('Ctrl Pts',(-1.56606003411924,0.568392357912186,
10.0387850497008));
#54580=CARTESIAN_POINT('Ctrl Pts',(-1.56343130417499,0.575533280641269,
10.0383108307813));
#54581=CARTESIAN_POINT('',(-1.66599992285883,0.000506985575740082,10.2730004785459));
#54582=CARTESIAN_POINT('Ctrl Pts',(-1.56343128570986,0.575533330801617,
10.2310772794004));
#54583=CARTESIAN_POINT('Ctrl Pts',(-1.57769043289253,0.536798481541238,
10.2340278998061));
#54584=CARTESIAN_POINT('Ctrl Pts',(-1.59050792609994,0.497539507700919,
10.2370180206381));
#54585=CARTESIAN_POINT('Ctrl Pts',(-1.6363410722794,0.337181098515292,10.2491421604763));
#54586=CARTESIAN_POINT('Ctrl Pts',(-1.65708987690961,0.212993145401417,
10.2582884449228));
#54587=CARTESIAN_POINT('Ctrl Pts',(-1.66522185482676,0.0586221925312235,
10.2690299316985));
#54588=CARTESIAN_POINT('Ctrl Pts',(-1.665991079245,0.0295678911884265,10.2710268732202));
#54589=CARTESIAN_POINT('Ctrl Pts',(-1.66599992285883,0.000506985575740082,
10.2730004785459));
#54590=CARTESIAN_POINT('Ctrl Pts',(-1.66599992316667,0.000505972977507134,
10.2730005473142));
#54591=CARTESIAN_POINT('Ctrl Pts',(-1.66600231739398,-0.00737741743330579,
10.2735359296996));
#54592=CARTESIAN_POINT('Ctrl Pts',(-1.66594875621251,-0.0152608683665852,
10.2740695753403));
#54593=CARTESIAN_POINT('Ctrl Pts',(-1.6657174916656,-0.0319067840115265,
10.2751927750027));
#54594=CARTESIAN_POINT('Ctrl Pts',(-1.66552660043235,-0.04066882409478,
10.2757818989175));
#54595=CARTESIAN_POINT('Ctrl Pts',(-1.66499291961764,-0.0586485338171585,
10.276986600463));
#54596=CARTESIAN_POINT('Ctrl Pts',(-1.66464270229388,-0.0678656944789535,
10.277601924675));
#54597=CARTESIAN_POINT('Ctrl Pts',(-1.66373873333539,-0.0873831661284348,
10.2789002997265));
#54598=CARTESIAN_POINT('Ctrl Pts',(-1.66316583041524,-0.0976822356759736,
10.2795827254178));
#54599=CARTESIAN_POINT('Ctrl Pts',(-1.66148205488959,-0.123607299753442,
10.2812941155429));
#54600=CARTESIAN_POINT('Ctrl Pts',(-1.66024636027905,-0.13922440104548,
10.2823191507774));
#54601=CARTESIAN_POINT('Ctrl Pts',(-1.65461640934936,-0.199544623175656,
10.2862580216255));
#54602=CARTESIAN_POINT('Ctrl Pts',(-1.64863511964054,-0.244082586298848,
10.2891225228046));
#54603=CARTESIAN_POINT('Ctrl Pts',(-1.6152777470171,-0.43391801524496,10.3012359628447));
#54604=CARTESIAN_POINT('Ctrl Pts',(-1.57043610681048,-0.575440724368906,
10.3099627622332));
#54605=CARTESIAN_POINT('Ctrl Pts',(-1.49591934339789,-0.733841893602513,
10.3209597415386));
#54606=CARTESIAN_POINT('Ctrl Pts',(-1.4837165807553,-0.758210754916007,
10.3226909143782));
#54607=CARTESIAN_POINT('Ctrl Pts',(-1.46225120392947,-0.798572759528369,
10.3256431019065));
#54608=CARTESIAN_POINT('Ctrl Pts',(-1.45330991405886,-0.81473140378043,
10.3268485324409));
#54609=CARTESIAN_POINT('Ctrl Pts',(-1.4402898165524,-0.837364737272315,
10.3285753807705));
#54610=CARTESIAN_POINT('Ctrl Pts',(-1.43643179415618,-0.843965730327751,
10.3290837162452));
#54611=CARTESIAN_POINT('Ctrl Pts',(-1.42970284416014,-0.855299019365696,
10.3299650364177));
#54612=CARTESIAN_POINT('Ctrl Pts',(-1.42685353924176,-0.860043959234143,
10.3303366399452));
#54613=CARTESIAN_POINT('Ctrl Pts',(-1.42077102197167,-0.87005973095406,
10.3311267377867));
#54614=CARTESIAN_POINT('Ctrl Pts',(-1.41753214669269,-0.87532670601818,
10.3315455703305));
#54615=CARTESIAN_POINT('Ctrl Pts',(-1.40856811430863,-0.889723552486969,
10.3326993605331));
#54616=CARTESIAN_POINT('Ctrl Pts',(-1.40278369205506,-0.898815904698617,
10.3334379797107));
#54617=CARTESIAN_POINT('Ctrl Pts',(-1.37231307019707,-0.945701084986023,
10.3372960347145));
#54618=CARTESIAN_POINT('Ctrl Pts',(-1.34618855269544,-0.982532087505519,
10.3404942129081));
#54619=CARTESIAN_POINT('Ctrl Pts',(-1.26433631065196,-1.08852799167126,
10.350109502701));
#54620=CARTESIAN_POINT('Ctrl Pts',(-1.20453844770308,-1.15435118152197,
10.3566255637043));
#54621=CARTESIAN_POINT('Ctrl Pts',(-1.07820786925432,-1.27285139244742,
10.3691507056581));
#54622=CARTESIAN_POINT('Ctrl Pts',(-1.01232742304659,-1.32585061739875,
10.3751512299512));
#54623=CARTESIAN_POINT('Ctrl Pts',(-0.923701412872644,-1.38667329308936,
10.3825429577679));
#54624=CARTESIAN_POINT('Ctrl Pts',(-0.904430381614241,-1.39931872671803,
10.3841132239525));
#54625=CARTESIAN_POINT('Ctrl Pts',(-0.87485304270165,-1.41786065235273,
10.3864691416193));
#54626=CARTESIAN_POINT('Ctrl Pts',(-0.864736570333892,-1.42405314239243,
10.3872656160984));
#54627=CARTESIAN_POINT('Ctrl Pts',(-0.847032371913599,-1.43463199039787,
10.3886436530887));
#54628=CARTESIAN_POINT('Ctrl Pts',(-0.839474679794697,-1.439067425092,10.3892269854162));
#54629=CARTESIAN_POINT('Ctrl Pts',(-0.822383113957587,-1.44891760188876,
10.3905353145224));
#54630=CARTESIAN_POINT('Ctrl Pts',(-0.812830015027769,-1.45429831174043,
10.3912590660205));
#54631=CARTESIAN_POINT('Ctrl Pts',(-0.786832817720502,-1.46860483632872,
10.3932089229169));
#54632=CARTESIAN_POINT('Ctrl Pts',(-0.77029003650322,-1.47734875838842,
10.3944285641664));
#54633=CARTESIAN_POINT('Ctrl Pts',(-0.666783350087545,-1.52984726864472,
10.4019373649262));
#54634=CARTESIAN_POINT('Ctrl Pts',(-0.576266493608423,-1.56619066123537,
10.4079594855773));
#54635=CARTESIAN_POINT('Ctrl Pts',(-0.415422537318817,-1.61492362266278,
10.4182441028165));
#54636=CARTESIAN_POINT('Ctrl Pts',(-0.346528060957935,-1.63109529875563,
10.4225305617474));
#54637=CARTESIAN_POINT('Ctrl Pts',(-0.238595163156672,-1.64928189056236,
10.4293148733688));
#54638=CARTESIAN_POINT('Ctrl Pts',(-0.200162399428393,-1.65438599627872,
10.4317445913411));
#54639=CARTESIAN_POINT('Ctrl Pts',(-0.137993412992661,-1.6604444806956,
10.4357462387257));
#54640=CARTESIAN_POINT('Ctrl Pts',(-0.114352530539566,-1.66223987906268,
10.4372844823368));
#54641=CARTESIAN_POINT('Ctrl Pts',(-0.0822813354591848,-1.66398815431015,
10.4394033849361));
#54642=CARTESIAN_POINT('Ctrl Pts',(-0.0738766537231008,-1.66438247661131,
10.4399616556576));
#54643=CARTESIAN_POINT('Ctrl Pts',(-0.0598021060484204,-1.66493599814267,
10.440902075835));
#54644=CARTESIAN_POINT('Ctrl Pts',(-0.0541336146227459,-1.66512994091761,
10.4412823311622));
#54645=CARTESIAN_POINT('Ctrl Pts',(-0.0425698921484775,-1.66546647451406,
10.4420613131198));
#54646=CARTESIAN_POINT('Ctrl Pts',(-0.0366747324390218,-1.66560671669856,
10.4424601514394));
#54647=CARTESIAN_POINT('Ctrl Pts',(-0.0213120945399635,-1.66589058729547,
10.4435037669758));
#54648=CARTESIAN_POINT('Ctrl Pts',(-0.0118440763266761,-1.6659848023095,
10.4441511564931));
#54649=CARTESIAN_POINT('Ctrl Pts',(0.0277042310925202,-1.66604120622537,
10.4468714940803));
#54650=CARTESIAN_POINT('Ctrl Pts',(0.0577779916927537,-1.66526942561437,
10.4489791126753));
#54651=CARTESIAN_POINT('Ctrl Pts',(0.113590959686809,-1.66232352407493,
10.4529439991073));
#54652=CARTESIAN_POINT('Ctrl Pts',(0.139333761767613,-1.66036393547833,
10.4547939485429));
#54653=CARTESIAN_POINT('Ctrl Pts',(0.266480985432943,-1.64770759362963,
10.4640074078436));
#54654=CARTESIAN_POINT('Ctrl Pts',(0.366808460838594,-1.62831378542954,
10.4715013816703));
#54655=CARTESIAN_POINT('Ctrl Pts',(0.534401804488663,-1.5796309995296,10.4840098652485));
#54656=CARTESIAN_POINT('Ctrl Pts',(0.602682416379695,-1.55486201721768,
10.4891072599739));
#54657=CARTESIAN_POINT('Ctrl Pts',(0.685253899559558,-1.51864832347157,
10.4952602072844));
#54658=CARTESIAN_POINT('Ctrl Pts',(0.701256240852304,-1.51132569724481,
10.4964523938551));
#54659=CARTESIAN_POINT('Ctrl Pts',(0.72682083540509,-1.49913391795845,10.4983572439567));
#54660=CARTESIAN_POINT('Ctrl Pts',(0.736456941472921,-1.49442370611996,
10.4990753090867));
#54661=CARTESIAN_POINT('Ctrl Pts',(0.754798944689003,-1.48523747612596,
10.5004425102007));
#54662=CARTESIAN_POINT('Ctrl Pts',(0.763512158371822,-1.48077716027341,
10.50109215781));
#54663=CARTESIAN_POINT('Ctrl Pts',(0.783320489724964,-1.47041589910944,
10.5025697222322));
#54664=CARTESIAN_POINT('Ctrl Pts',(0.79438925399797,-1.46446564776934,10.5033958644325));
#54665=CARTESIAN_POINT('Ctrl Pts',(0.823776648428824,-1.44823658637119,
10.5055914170822));
#54666=CARTESIAN_POINT('Ctrl Pts',(0.841970354458956,-1.4377354283724,10.5069529292663));
#54667=CARTESIAN_POINT('Ctrl Pts',(0.963391453077724,-1.36455722172156,
10.5160670344918));
#54668=CARTESIAN_POINT('Ctrl Pts',(1.05973955372423,-1.29116049709134,10.5234020613916));
#54669=CARTESIAN_POINT('Ctrl Pts',(1.19538407275145,-1.16232878033086,10.5348331747996));
#54670=CARTESIAN_POINT('Ctrl Pts',(1.24068317830539,-1.11384705307276,10.5388951779501));
#54671=CARTESIAN_POINT('Ctrl Pts',(1.29729686277346,-1.04550524030338,10.5445119402044));
#54672=CARTESIAN_POINT('Ctrl Pts',(1.31127167967211,-1.02792355703174,10.5459482107291));
#54673=CARTESIAN_POINT('Ctrl Pts',(1.33458833153797,-0.99733949774668,10.5484423841564));
#54674=CARTESIAN_POINT('Ctrl Pts',(1.34410621671358,-0.984474743453597,
10.5494902782853));
#54675=CARTESIAN_POINT('Ctrl Pts',(1.35764977824141,-0.965606170684461,
10.5510286510707));
#54676=CARTESIAN_POINT('Ctrl Pts',(1.36182435131569,-0.959709658472877,
10.5515095996445));
#54677=CARTESIAN_POINT('Ctrl Pts',(1.36907070962736,-0.949331822358583,
10.5523567755868));
#54678=CARTESIAN_POINT('Ctrl Pts',(1.37215912709303,-0.944862342160033,
10.5527218733202));
#54679=CARTESIAN_POINT('Ctrl Pts',(1.37883865700368,-0.935094074587906,
10.5535204291737));
#54680=CARTESIAN_POINT('Ctrl Pts',(1.38242105458173,-0.929789758374915,
10.5539544175496));
#54681=CARTESIAN_POINT('Ctrl Pts',(1.392336356158,-0.914924580279304,10.555171364952));
#54682=CARTESIAN_POINT('Ctrl Pts',(1.39860109487848,-0.90531899101855,10.5559585436493));
#54683=CARTESIAN_POINT('Ctrl Pts',(1.44003794386071,-0.840328106734557,
10.5612859709902));
#54684=CARTESIAN_POINT('Ctrl Pts',(1.4720073938494,-0.782976959801305,10.5659919335387));
#54685=CARTESIAN_POINT('Ctrl Pts',(1.50967435092355,-0.704900182846258,
10.5722755538515));
#54686=CARTESIAN_POINT('Ctrl Pts',(1.51847780466338,-0.68573030582163,10.573809216254));
#54687=CARTESIAN_POINT('Ctrl Pts',(1.5542528193068,-0.603759253145454,10.5803179177953));
#54688=CARTESIAN_POINT('Ctrl Pts',(1.5777117938742,-0.539493715143421,10.5852961966818));
#54689=CARTESIAN_POINT('Ctrl Pts',(1.61067252348948,-0.428423639548609,
10.5935953483652));
#54690=CARTESIAN_POINT('Ctrl Pts',(1.62223439333167,-0.382320608545958,
10.5969559058095));
#54691=CARTESIAN_POINT('Ctrl Pts',(1.63838388006684,-0.303838606504144,
10.6025265531334));
#54692=CARTESIAN_POINT('Ctrl Pts',(1.64401808229459,-0.271706533246437,
10.6047659871326));
#54693=CARTESIAN_POINT('Ctrl Pts',(1.65065426618434,-0.226009594290692,
10.6078946149127));
#54694=CARTESIAN_POINT('Ctrl Pts',(1.65243903747961,-0.212567846757036,
10.6088081023518));
#54695=CARTESIAN_POINT('Ctrl Pts',(1.65524357020508,-0.189269318118188,
10.6103801021523));
#54696=CARTESIAN_POINT('Ctrl Pts',(1.65633984319084,-0.179422636934863,
10.6110409857462));
#54697=CARTESIAN_POINT('Ctrl Pts',(1.65840828152017,-0.159205665583671,
10.6123909791254));
#54698=CARTESIAN_POINT('Ctrl Pts',(1.65937116652569,-0.14883484876422,10.6130797699055));
#54699=CARTESIAN_POINT('Ctrl Pts',(1.66157837221135,-0.122367973206287,
10.6148285276571));
#54700=CARTESIAN_POINT('Ctrl Pts',(1.66268612743982,-0.106261372987656,
10.6158841981877));
#54701=CARTESIAN_POINT('Ctrl Pts',(1.66620899337148,-0.0412464035442574,
10.620113959611));
#54702=CARTESIAN_POINT('Ctrl Pts',(1.66670165240875,0.00774397952933208,
10.6232284822794));
#54703=CARTESIAN_POINT('Ctrl Pts',(1.66127268200489,0.16720114244251,10.6332230751237));
#54704=CARTESIAN_POINT('Ctrl Pts',(1.64651757434476,0.27706195808729,10.6398682726536));
#54705=CARTESIAN_POINT('Ctrl Pts',(1.60613883295747,0.447224588114197,10.6506321884736));
#54706=CARTESIAN_POINT('Ctrl Pts',(1.58768161977321,0.508878212068735,10.6546409052297));
#54707=CARTESIAN_POINT('Ctrl Pts',(1.56057052943083,0.583439688656357,10.6597953694081));
#54708=CARTESIAN_POINT('Ctrl Pts',(1.55523956802041,0.597504891159565,10.6607816286632));
#54709=CARTESIAN_POINT('Ctrl Pts',(1.54713198203958,0.618052031154743,10.662245667467));
#54710=CARTESIAN_POINT('Ctrl Pts',(1.54450330162264,0.624592050738987,10.6627151590068));
#54711=CARTESIAN_POINT('Ctrl Pts',(1.53995943249461,0.635692861299592,10.6635183488665));
#54712=CARTESIAN_POINT('Ctrl Pts',(1.53806530504006,0.640262121453006,10.6638507881532));
#54713=CARTESIAN_POINT('Ctrl Pts',(1.53370248675802,0.650655589164751,10.6646112358927));
#54714=CARTESIAN_POINT('Ctrl Pts',(1.5312210122152,0.656474083277997,10.6650399899589));
#54715=CARTESIAN_POINT('Ctrl Pts',(1.52428088533716,0.672493661534344,10.6662285684006));
#54716=CARTESIAN_POINT('Ctrl Pts',(1.51975311804168,0.682664182231136,10.6669923152537));
#54717=CARTESIAN_POINT('Ctrl Pts',(1.49277333547937,0.741668814636968,10.6714735511826));
#54718=CARTESIAN_POINT('Ctrl Pts',(1.46807259050383,0.789434307082179,10.6753025602115));
#54719=CARTESIAN_POINT('Ctrl Pts',(1.39091888631392,0.922446227848898,10.6863963762827));
#54720=CARTESIAN_POINT('Ctrl Pts',(1.33303273924989,1.00428472022224,10.6937454565943));
#54721=CARTESIAN_POINT('Ctrl Pts',(1.22067696851961,1.13616164795766,10.7061672406998));
#54722=CARTESIAN_POINT('Ctrl Pts',(1.16957280121252,1.18870420461285,10.7113126707277));
#54723=CARTESIAN_POINT('Ctrl Pts',(1.10206806355061,1.2495251106592,10.7175137197659));
#54724=CARTESIAN_POINT('Ctrl Pts',(1.08877893056966,1.26112152496551,10.7187086187532));
#54725=CARTESIAN_POINT('Ctrl Pts',(1.06710925401079,1.27943309764039,10.7206167308812));
#54726=CARTESIAN_POINT('Ctrl Pts',(1.05884387393308,1.28628180088746,10.7213353789613));
#54727=CARTESIAN_POINT('Ctrl Pts',(1.04291753403978,1.29922083557553,10.7227030201961));
#54728=CARTESIAN_POINT('Ctrl Pts',(1.03526800200861,1.30532445521796,10.7233525313084));
#54729=CARTESIAN_POINT('Ctrl Pts',(1.01768705017753,1.31910066059491,10.7248288734215));
#54730=CARTESIAN_POINT('Ctrl Pts',(1.00772174952041,1.32672920174228,10.7256539403676));
#54731=CARTESIAN_POINT('Ctrl Pts',(0.980896928925395,1.34678725182318,10.7278446008576));
#54732=CARTESIAN_POINT('Ctrl Pts',(0.963887284568795,1.35901289624771,10.7292023531369));
#54733=CARTESIAN_POINT('Ctrl Pts',(0.846446264646202,1.44010884978967,10.7383784289865));
#54734=CARTESIAN_POINT('Ctrl Pts',(0.738956249855005,1.49810957425059,10.7457709604885));
#54735=CARTESIAN_POINT('Ctrl Pts',(0.538700003263964,1.57932015887205,10.7589769753229));
#54736=CARTESIAN_POINT('Ctrl Pts',(0.448466242992239,1.60727183898405,10.7647590000626));
#54737=CARTESIAN_POINT('Ctrl Pts',(0.344706560141308,1.62999260911108,10.771703561903));
#54738=CARTESIAN_POINT('Ctrl Pts',(0.333018072325539,1.63242073674257,10.7724900774257));
#54739=CARTESIAN_POINT('Ctrl Pts',(0.314993897449877,1.63596338962739,10.7737108094161));
#54740=CARTESIAN_POINT('Ctrl Pts',(0.308675880467755,1.63716723793832,10.7741401981372));
#54741=CARTESIAN_POINT('Ctrl Pts',(0.296961626055338,1.63932907900742,10.7749393446692));
#54742=CARTESIAN_POINT('Ctrl Pts',(0.29156744141781,1.64029706472519,10.7753085399827));
#54743=CARTESIAN_POINT('Ctrl Pts',(0.279185561107272,1.64245598663259,10.7761587075954));
#54744=CARTESIAN_POINT('Ctrl Pts',(0.272194964657453,1.64362895513929,10.7766406524396));
#54745=CARTESIAN_POINT('Ctrl Pts',(0.249727745455846,1.64725152309702,10.7781953963066));
#54746=CARTESIAN_POINT('Ctrl Pts',(0.234224500375187,1.64952731603788,10.7792770623071));
#54747=CARTESIAN_POINT('Ctrl Pts',(0.128487510135252,1.66352833135523,10.7867041415661));
#54748=CARTESIAN_POINT('Ctrl Pts',(0.0374642063310759,1.66806143651587,
10.7933350484026));
#54749=CARTESIAN_POINT('Ctrl Pts',(-0.138880849423573,1.66239935415567,
10.8061779287301));
#54750=CARTESIAN_POINT('Ctrl Pts',(-0.223967896481416,1.65308822197952,
10.8123720110889));
#54751=CARTESIAN_POINT('Ctrl Pts',(-0.339341631203659,1.63138657463041,
10.8206468781927));
#54752=CARTESIAN_POINT('Ctrl Pts',(-0.370537260164742,1.62458525970883,
10.8228727331643));
#54753=CARTESIAN_POINT('Ctrl Pts',(-0.42511510497349,1.61103203180071,10.8267460471704));
#54754=CARTESIAN_POINT('Ctrl Pts',(-0.448580123170537,1.60465667392301,
10.8284044486489));
#54755=CARTESIAN_POINT('Ctrl Pts',(-0.483510713401975,1.59433998913135,
10.83086407774));
#54756=CARTESIAN_POINT('Ctrl Pts',(-0.495085645133136,1.59078371513181,
10.8316776191502));
#54757=CARTESIAN_POINT('Ctrl Pts',(-0.515792207536282,1.58417394225279,
10.83313058553));
#54758=CARTESIAN_POINT('Ctrl Pts',(-0.524937980937905,1.58116691197144,
10.8337714952928));
#54759=CARTESIAN_POINT('Ctrl Pts',(-0.544556947626232,1.57452742066514,
10.8351447579746));
#54760=CARTESIAN_POINT('Ctrl Pts',(-0.55502103608637,1.57086935393278,10.8358762332698));
#54761=CARTESIAN_POINT('Ctrl Pts',(-0.583114639097111,1.56073253964241,
10.8378379793589));
#54762=CARTESIAN_POINT('Ctrl Pts',(-0.600672720115562,1.5540595459307,10.8390617891867));
#54763=CARTESIAN_POINT('Ctrl Pts',(-0.708017085899768,1.51117186319131,
10.8465372717711));
#54764=CARTESIAN_POINT('Ctrl Pts',(-0.794622663703553,1.46748318879487,
10.852525737974));
#54765=CARTESIAN_POINT('Ctrl Pts',(-0.937072908165522,1.3792933641321,10.8627782224018));
#54766=CARTESIAN_POINT('Ctrl Pts',(-0.994760852658286,1.3382847395058,10.86706537434));
#54767=CARTESIAN_POINT('Ctrl Pts',(-1.07975849744114,1.26932232134072,10.8738497976444));
#54768=CARTESIAN_POINT('Ctrl Pts',(-1.10898708882771,1.2438668778189,10.8762788648574));
#54769=CARTESIAN_POINT('Ctrl Pts',(-1.14909068465635,1.20640248530941,10.8797947452555));
#54770=CARTESIAN_POINT('Ctrl Pts',(-1.16072055394583,1.19521718194735,10.8808374947491));
#54771=CARTESIAN_POINT('Ctrl Pts',(-1.18102402996743,1.17511401172272,10.8827035146304));
#54772=CARTESIAN_POINT('Ctrl Pts',(-1.1897638022903,1.16626445202765,10.8835222734383));
#54773=CARTESIAN_POINT('Ctrl Pts',(-1.20294370476452,1.15261665892353,10.8847825210151));
#54774=CARTESIAN_POINT('Ctrl Pts',(-1.20745625485334,1.14788854347665,10.885218681442));
#54775=CARTESIAN_POINT('Ctrl Pts',(-1.21569313043718,1.13915588004169,10.8860237346351));
#54776=CARTESIAN_POINT('Ctrl Pts',(-1.21942570266535,1.13515939814867,10.8863919904103));
#54777=CARTESIAN_POINT('Ctrl Pts',(-1.22793498003955,1.1259580769118,10.8872394232869));
#54778=CARTESIAN_POINT('Ctrl Pts',(-1.23269828697405,1.12074119889272,10.8877195609718));
#54779=CARTESIAN_POINT('Ctrl Pts',(-1.24755617500255,1.10425920613157,10.8892350095249));
#54780=CARTESIAN_POINT('Ctrl Pts',(-1.25753027021177,1.09288717787126,10.8902784689742));
#54781=CARTESIAN_POINT('Ctrl Pts',(-1.33430095697377,1.0029141580135,10.8985069289534));
#54782=CARTESIAN_POINT('Ctrl Pts',(-1.39381639785012,0.918405265247922,
10.9060609482324));
#54783=CARTESIAN_POINT('Ctrl Pts',(-1.49160972963105,0.747918408494714,
10.9203537899979));
#54784=CARTESIAN_POINT('Ctrl Pts',(-1.53117834198928,0.663148153811631,
10.9270752438853));
#54785=CARTESIAN_POINT('Ctrl Pts',(-1.5634312473966,0.575533434879242,10.9335682035678));
#54786=CARTESIAN_POINT('Origin',(0.,0.,11.));
#54787=CARTESIAN_POINT('',(-1.56343130033056,0.575533291084625,11.6327248639491));
#54788=CARTESIAN_POINT('',(-1.56343130602848,0.57553327560628,11.4406228970922));
#54789=CARTESIAN_POINT('',(-1.56343130033213,0.575533291080363,11.));
#54790=CARTESIAN_POINT('Ctrl Pts',(-1.56343130602848,0.575533275606279,
11.4406228970922));
#54791=CARTESIAN_POINT('Ctrl Pts',(-1.52680415602541,0.675030620751227,
11.4331999282501));
#54792=CARTESIAN_POINT('Ctrl Pts',(-1.4807595962946,0.770812720066577,11.4254116886702));
#54793=CARTESIAN_POINT('Ctrl Pts',(-1.38901729314585,0.922647599030889,
11.4125310881713));
#54794=CARTESIAN_POINT('Ctrl Pts',(-1.34822687156867,0.981291912119414,
11.4073994728654));
#54795=CARTESIAN_POINT('Ctrl Pts',(-1.27719545497935,1.07058569585643,11.3993896440164));
#54796=CARTESIAN_POINT('Ctrl Pts',(-1.2493150986331,1.10299334354318,11.3964352948152));
#54797=CARTESIAN_POINT('Ctrl Pts',(-1.21122468512642,1.14396905522107,11.3926339048998));
#54798=CARTESIAN_POINT('Ctrl Pts',(-1.20211745493481,1.15353546939814,11.391741373696));
#54799=CARTESIAN_POINT('Ctrl Pts',(-1.18582658642031,1.17024522982793,11.3901730329286));
#54800=CARTESIAN_POINT('Ctrl Pts',(-1.17868985742044,1.17743314835424,11.3894952427524));
#54801=CARTESIAN_POINT('Ctrl Pts',(-1.16451042910342,1.19145615191932,11.3881664502302));
#54802=CARTESIAN_POINT('Ctrl Pts',(-1.1574720198851,1.19829496854766,11.3875152981215));
#54803=CARTESIAN_POINT('Ctrl Pts',(-1.14115476302766,1.21387158957363,11.3860246559792));
#54804=CARTESIAN_POINT('Ctrl Pts',(-1.13183517777627,1.22256597960806,11.3851870536404));
#54805=CARTESIAN_POINT('Ctrl Pts',(-1.10213430496782,1.24964365104814,11.3825596062455));
#54806=CARTESIAN_POINT('Ctrl Pts',(-1.08139739599307,1.26763129140331,11.3807862410512));
#54807=CARTESIAN_POINT('Ctrl Pts',(-0.958853784418267,1.36873145575102,
11.3706280493842));
#54808=CARTESIAN_POINT('Ctrl Pts',(-0.847946011875471,1.44007515277548,
11.3627263346979));
#54809=CARTESIAN_POINT('Ctrl Pts',(-0.665501442593592,1.52898003752134,
11.3502750842259));
#54810=CARTESIAN_POINT('Ctrl Pts',(-0.599258275396191,1.55613601526051,
11.3458415704982));
#54811=CARTESIAN_POINT('Ctrl Pts',(-0.516521726540974,1.58398565171396,
11.3401777510343));
#54812=CARTESIAN_POINT('Ctrl Pts',(-0.50148916581896,1.58880892840692,11.3391436631441));
#54813=CARTESIAN_POINT('Ctrl Pts',(-0.479518412867594,1.59551550459381,
11.3376219259028));
#54814=CARTESIAN_POINT('Ctrl Pts',(-0.472632468861314,1.59756883366874,
11.3371435213696));
#54815=CARTESIAN_POINT('Ctrl Pts',(-0.460521283147991,1.6010951312682,11.3362991599318));
#54816=CARTESIAN_POINT('Ctrl Pts',(-0.455301801929291,1.60258720183891,
11.335934307079));
#54817=CARTESIAN_POINT('Ctrl Pts',(-0.443887692550371,1.6057898408727,11.335134243773));
#54818=CARTESIAN_POINT('Ctrl Pts',(-0.437690527287485,1.60749006077306,
11.3346984844407));
#54819=CARTESIAN_POINT('Ctrl Pts',(-0.420295981326831,1.61215429016526,
11.3334718260548));
#54820=CARTESIAN_POINT('Ctrl Pts',(-0.409077553698217,1.6150373690936,11.3326766031399));
#54821=CARTESIAN_POINT('Ctrl Pts',(-0.328053294678667,1.63496186459302,
11.3269081042534));
#54822=CARTESIAN_POINT('Ctrl Pts',(-0.257246741716699,1.64758642932576,
11.3217365917514));
#54823=CARTESIAN_POINT('Ctrl Pts',(-0.172315049178187,1.65712074998418,
11.3155308954068));
#54824=CARTESIAN_POINT('Ctrl Pts',(-0.158756465695755,1.65847461139677,
11.3145400165099));
#54825=CARTESIAN_POINT('Ctrl Pts',(-0.0783239098896369,1.66551064060783,
11.3086647877825));
#54826=CARTESIAN_POINT('Ctrl Pts',(-0.0111693775689137,1.66731412506099,
11.3037747107781));
#54827=CARTESIAN_POINT('Ctrl Pts',(0.104740214183322,1.66342185065338,11.2954579894606));
#54828=CARTESIAN_POINT('Ctrl Pts',(0.15347488822052,1.65963518838055,11.291998283413));
#54829=CARTESIAN_POINT('Ctrl Pts',(0.234998124708908,1.64967832418225,11.2862845732992));
#54830=CARTESIAN_POINT('Ctrl Pts',(0.267893389389845,1.64465683265151,11.2839991919595));
#54831=CARTESIAN_POINT('Ctrl Pts',(0.314054636464036,1.63618834343614,11.280818718306));
#54832=CARTESIAN_POINT('Ctrl Pts',(0.32746043685702,1.63355816899194,11.2798982259755));
#54833=CARTESIAN_POINT('Ctrl Pts',(0.350546970495702,1.62873303832968,11.2783180740732));
#54834=CARTESIAN_POINT('Ctrl Pts',(0.360243057067358,1.62661594601923,11.2776559754844));
#54835=CARTESIAN_POINT('Ctrl Pts',(0.380042310638634,1.62210715441826,11.2763069139866));
#54836=CARTESIAN_POINT('Ctrl Pts',(0.390143211155946,1.6197073999143,11.2756202410596));
#54837=CARTESIAN_POINT('Ctrl Pts',(0.415739907847208,1.61337283609254,11.2738837381741));
#54838=CARTESIAN_POINT('Ctrl Pts',(0.431202937373876,1.60930905518004,11.2728380835525));
#54839=CARTESIAN_POINT('Ctrl Pts',(0.492367500966336,1.59228971733899,11.26871259214));
#54840=CARTESIAN_POINT('Ctrl Pts',(0.537566744035031,1.57760417506351,11.2656884909209));
#54841=CARTESIAN_POINT('Ctrl Pts',(0.68687195542736,1.52193008346564,11.2556951671206));
#54842=CARTESIAN_POINT('Ctrl Pts',(0.787460706370518,1.47240289906889,11.2489744714618));
#54843=CARTESIAN_POINT('Ctrl Pts',(0.937267060222162,1.37886949937426,11.2381071702515));
#54844=CARTESIAN_POINT('Ctrl Pts',(0.990151535062417,1.34139804771574,11.2340714925394));
#54845=CARTESIAN_POINT('Ctrl Pts',(1.05249865954227,1.2915224685893,11.2288847237947));
#54846=CARTESIAN_POINT('Ctrl Pts',(1.06415322615937,1.28193665497802,11.2278953388318));
#54847=CARTESIAN_POINT('Ctrl Pts',(1.08106472997162,1.26763751041616,11.2264275365377));
#54848=CARTESIAN_POINT('Ctrl Pts',(1.08642485530412,1.26304664896806,11.2259574683638));
#54849=CARTESIAN_POINT('Ctrl Pts',(1.09549250344564,1.25517992763709,11.2251536484357));
#54850=CARTESIAN_POINT('Ctrl Pts',(1.09921486510716,1.25192138542609,11.2248211614527));
#54851=CARTESIAN_POINT('Ctrl Pts',(1.10765885666109,1.24446285149135,11.2240611132963));
#54852=CARTESIAN_POINT('Ctrl Pts',(1.11237103269848,1.24025264110613,11.2236328109873));
#54853=CARTESIAN_POINT('Ctrl Pts',(1.1252979248929,1.22856986028904,11.2224466113756));
#54854=CARTESIAN_POINT('Ctrl Pts',(1.13346187702411,1.22104196411171,11.2216848158298));
#54855=CARTESIAN_POINT('Ctrl Pts',(1.18017906181246,1.17709229775537,11.2172549094665));
#54856=CARTESIAN_POINT('Ctrl Pts',(1.21704721143242,1.13893099589742,11.213478201823));
#54857=CARTESIAN_POINT('Ctrl Pts',(1.31907103785556,1.0227095699659,11.2023247677993));
#54858=CARTESIAN_POINT('Ctrl Pts',(1.37898936413965,0.940358125328246,11.1948565532927));
#54859=CARTESIAN_POINT('Ctrl Pts',(1.46813511871479,0.790813959349761,11.1823788814111));
#54860=CARTESIAN_POINT('Ctrl Pts',(1.50114435264857,0.726206357437456,11.1772874817726));
#54861=CARTESIAN_POINT('Ctrl Pts',(1.53680945967183,0.643492134973699,11.1711405835001));
#54862=CARTESIAN_POINT('Ctrl Pts',(1.54351848247649,0.62722896821404,11.1699487783287));
#54863=CARTESIAN_POINT('Ctrl Pts',(1.5539008833093,0.60088521559031,11.1680444115883));
#54864=CARTESIAN_POINT('Ctrl Pts',(1.55773652977485,0.590870468520734,11.1673264528803));
#54865=CARTESIAN_POINT('Ctrl Pts',(1.56488764334266,0.571645402353845,11.1659593763906));
#54866=CARTESIAN_POINT('Ctrl Pts',(1.56821914585558,0.562441570180001,11.1653097477712));
#54867=CARTESIAN_POINT('Ctrl Pts',(1.57564248484131,0.54135450266583,11.16383212123));
#54868=CARTESIAN_POINT('Ctrl Pts',(1.57968139197608,0.529453163017561,11.163005898946));
#54869=CARTESIAN_POINT('Ctrl Pts',(1.59011160202665,0.497536438770089,11.1608099012462));
#54870=CARTESIAN_POINT('Ctrl Pts',(1.59625973198114,0.477443552781406,11.1594480297858));
#54871=CARTESIAN_POINT('Ctrl Pts',(1.63514025446537,0.341218029154579,11.1503405848552));
#54872=CARTESIAN_POINT('Ctrl Pts',(1.65555405592692,0.221941455764129,11.1430117065387));
#54873=CARTESIAN_POINT('Ctrl Pts',(1.66694887180154,0.0352486599636227,
11.1315828566084));
#54874=CARTESIAN_POINT('Ctrl Pts',(1.66702963059881,-0.0311760937028539,
11.1275165565406));
#54875=CARTESIAN_POINT('Ctrl Pts',(1.66183494844437,-0.119856516986022,
11.1218944039437));
#54876=CARTESIAN_POINT('Ctrl Pts',(1.66006717219818,-0.142259845034495,
11.1204572759337));
#54877=CARTESIAN_POINT('Ctrl Pts',(1.65626496397208,-0.180551071752954,
11.1179617660694));
#54878=CARTESIAN_POINT('Ctrl Pts',(1.65445349808572,-0.196458384572196,
11.1169134076195));
#54879=CARTESIAN_POINT('Ctrl Pts',(1.65149220758552,-0.219503305305378,
11.115374491118));
#54880=CARTESIAN_POINT('Ctrl Pts',(1.65052465809985,-0.226663982444802,
11.1148934729786));
#54881=CARTESIAN_POINT('Ctrl Pts',(1.6487481033183,-0.239197004915987,11.1140462375138));
#54882=CARTESIAN_POINT('Ctrl Pts',(1.64795935499907,-0.244572031157596,
11.1136811506669));
#54883=CARTESIAN_POINT('Ctrl Pts',(1.64618422338066,-0.256270279034346,
11.1128826977338));
#54884=CARTESIAN_POINT('Ctrl Pts',(1.64518770943096,-0.262591604046556,
11.1124488021662));
#54885=CARTESIAN_POINT('Ctrl Pts',(1.64230460115243,-0.280219550505908,
11.1112322993519));
#54886=CARTESIAN_POINT('Ctrl Pts',(1.64033773656282,-0.291512420487836,
11.1104454769018));
#54887=CARTESIAN_POINT('Ctrl Pts',(1.62636357641658,-0.367121615552409,
11.1051310347302));
#54888=CARTESIAN_POINT('Ctrl Pts',(1.61069410804004,-0.43069634982824,11.1004386024904));
#54889=CARTESIAN_POINT('Ctrl Pts',(1.58462123779733,-0.51482538160596,11.094054689002));
#54890=CARTESIAN_POINT('Ctrl Pts',(1.57747126718797,-0.53633387036908,11.0924065178323));
#54891=CARTESIAN_POINT('Ctrl Pts',(1.54587439361479,-0.625278431057768,
11.0855367599596));
#54892=CARTESIAN_POINT('Ctrl Pts',(1.51752269974111,-0.691250150453006,
11.0803147437912));
#54893=CARTESIAN_POINT('Ctrl Pts',(1.46474236767866,-0.795037127142525,
11.0719943756124));
#54894=CARTESIAN_POINT('Ctrl Pts',(1.44288248100356,-0.8340533333331,11.0688394967384));
#54895=CARTESIAN_POINT('Ctrl Pts',(1.40313300937471,-0.89874835459799,11.0635682236071));
#54896=CARTESIAN_POINT('Ctrl Pts',(1.38604262743308,-0.924887511315888,
11.06142648367));
#54897=CARTESIAN_POINT('Ctrl Pts',(1.36061799401955,-0.961484536254143,
11.0584086580134));
#54898=CARTESIAN_POINT('Ctrl Pts',(1.35287796822737,-0.972345134275289,
11.0575105529012));
#54899=CARTESIAN_POINT('Ctrl Pts',(1.339183964611,-0.991080078548571,11.055956459253));
#54900=CARTESIAN_POINT('Ctrl Pts',(1.33328895953985,-0.998996481851152,
11.0552982464258));
#54901=CARTESIAN_POINT('Ctrl Pts',(1.32098328685084,-1.01521880652963,11.0539460078468));
#54902=CARTESIAN_POINT('Ctrl Pts',(1.31456379924634,-1.0235175110837,11.0532523668282));
#54903=CARTESIAN_POINT('Ctrl Pts',(1.29784442106834,-1.0447144521434,11.0514753121389));
#54904=CARTESIAN_POINT('Ctrl Pts',(1.2874303147992,-1.05752146278332,11.0503964804088));
#54905=CARTESIAN_POINT('Ctrl Pts',(1.24321814543559,-1.1102712127916,11.0459279575913));
#54906=CARTESIAN_POINT('Ctrl Pts',(1.20773655484132,-1.14876749734315,11.0426070753747));
#54907=CARTESIAN_POINT('Ctrl Pts',(1.09386779429036,-1.26119224913727,11.0326086012846));
#54908=CARTESIAN_POINT('Ctrl Pts',(1.01008361065357,-1.3292418322361,11.0261356558024));
#54909=CARTESIAN_POINT('Ctrl Pts',(0.867580219550214,-1.42367948567678,
11.0156081026858));
#54910=CARTESIAN_POINT('Ctrl Pts',(0.812900167325927,-1.45559275937939,
11.0116611147194));
#54911=CARTESIAN_POINT('Ctrl Pts',(0.743244896754736,-1.49109552685628,
11.0065806783263));
#54912=CARTESIAN_POINT('Ctrl Pts',(0.729854854169249,-1.49769512942274,
11.0056017023295));
#54913=CARTESIAN_POINT('Ctrl Pts',(0.710034204065723,-1.50713529911211,
11.0041464851551));
#54914=CARTESIAN_POINT('Ctrl Pts',(0.703670979873864,-1.51011672674677,
11.003678390824));
#54915=CARTESIAN_POINT('Ctrl Pts',(0.692799317502628,-1.51512690769399,
11.0028767758379));
#54916=CARTESIAN_POINT('Ctrl Pts',(0.688300404963809,-1.5171759925429,11.0025445006919));
#54917=CARTESIAN_POINT('Ctrl Pts',(0.678011511069755,-1.52180701106143,
11.0017832673895));
#54918=CARTESIAN_POINT('Ctrl Pts',(0.672216000650368,-1.52437588316461,
11.001353553614));
#54919=CARTESIAN_POINT('Ctrl Pts',(0.656145715460671,-1.53138960695786,
11.0001597305562));
#54920=CARTESIAN_POINT('Ctrl Pts',(0.645840806281897,-1.53576396760066,
10.9993916443118));
#54921=CARTESIAN_POINT('Ctrl Pts',(0.584467237533515,-1.56108968797728,
10.9948052768274));
#54922=CARTESIAN_POINT('Ctrl Pts',(0.532431721699831,-1.57959429665994,
10.9908694265627));
#54923=CARTESIAN_POINT('Ctrl Pts',(0.385388106416058,-1.62379362779525,
10.9797842684263));
#54924=CARTESIAN_POINT('Ctrl Pts',(0.2888673992686,-1.64371135266555,10.9725614598439));
#54925=CARTESIAN_POINT('Ctrl Pts',(0.118326635277756,-1.66340894264715,
10.9602519194087));
#54926=CARTESIAN_POINT('Ctrl Pts',(0.0450160413489503,-1.66700532130982,
10.955099061244));
#54927=CARTESIAN_POINT('Ctrl Pts',(-0.0459412770266675,-1.66545987923935,
10.9488906209917));
#54928=CARTESIAN_POINT('Ctrl Pts',(-0.0635745736514136,-1.66488003334527,
10.9476953464629));
#54929=CARTESIAN_POINT('Ctrl Pts',(-0.0919176337360897,-1.66349703247122,
10.9457868073769));
#54930=CARTESIAN_POINT('Ctrl Pts',(-0.102634232230457,-1.66287024512904,
10.9450681030364));
#54931=CARTESIAN_POINT('Ctrl Pts',(-0.123106500576227,-1.66147420513064,
10.9437004635255));
#54932=CARTESIAN_POINT('Ctrl Pts',(-0.132862874972388,-1.6607224958501,
10.9430510094189));
#54933=CARTESIAN_POINT('Ctrl Pts',(-0.155112072106176,-1.65881091274185,
10.9415749459233));
#54934=CARTESIAN_POINT('Ctrl Pts',(-0.167599648248697,-1.65759578045169,
10.9407500986715));
#54935=CARTESIAN_POINT('Ctrl Pts',(-0.200883931849875,-1.65397698815559,
10.9385603568907));
#54936=CARTESIAN_POINT('Ctrl Pts',(-0.221651471651399,-1.65132217302296,
10.9372032934373));
#54937=CARTESIAN_POINT('Ctrl Pts',(-0.363010652843222,-1.63053657821236,
10.9280168293121));
#54938=CARTESIAN_POINT('Ctrl Pts',(-0.481346589209406,-1.5996048221466,
10.9206146187411));
#54939=CARTESIAN_POINT('Ctrl Pts',(-0.656446875116323,-1.5326205730266,
10.9091574593696));
#54940=CARTESIAN_POINT('Ctrl Pts',(-0.716199669293584,-1.5056244932141,
10.9051411926259));
#54941=CARTESIAN_POINT('Ctrl Pts',(-0.793954798611089,-1.46481717569995,
10.8995820077205));
#54942=CARTESIAN_POINT('Ctrl Pts',(-0.813495263033446,-1.45405603007515,
10.8981550969396));
#54943=CARTESIAN_POINT('Ctrl Pts',(-0.846602371653801,-1.4349473589184,
10.8956756371163));
#54944=CARTESIAN_POINT('Ctrl Pts',(-0.860276528287626,-1.42679141711541,
10.8946329405356));
#54945=CARTESIAN_POINT('Ctrl Pts',(-0.879969658466467,-1.41465945845793,
10.8931008377304));
#54946=CARTESIAN_POINT('Ctrl Pts',(-0.88608348358604,-1.41083806248265,
10.8926208538071));
#54947=CARTESIAN_POINT('Ctrl Pts',(-0.896800415679471,-1.40404239541337,
10.8917714699259));
#54948=CARTESIAN_POINT('Ctrl Pts',(-0.901413938743539,-1.40108491656536,
10.8914031630923));
#54949=CARTESIAN_POINT('Ctrl Pts',(-0.911409599276173,-1.39460743482798,
10.8905993039523));
#54950=CARTESIAN_POINT('Ctrl Pts',(-0.916785892387817,-1.39107906998691,
10.8901632291134));
#54951=CARTESIAN_POINT('Ctrl Pts',(-0.931805368220433,-1.3810971708628,
10.8889348485243));
#54952=CARTESIAN_POINT('Ctrl Pts',(-0.941401531734948,-1.37457403469348,
10.8881382003642));
#54953=CARTESIAN_POINT('Ctrl Pts',(-1.01411976068916,-1.32402411731741,
10.8820151980566));
#54954=CARTESIAN_POINT('Ctrl Pts',(-1.07418446962033,-1.27577576066867,
10.8764617505525));
#54955=CARTESIAN_POINT('Ctrl Pts',(-1.17271831573672,-1.18472027527041,
10.866709789005));
#54956=CARTESIAN_POINT('Ctrl Pts',(-1.2127160994911,-1.14374398593016,10.8625340679763));
#54957=CARTESIAN_POINT('Ctrl Pts',(-1.30523270470012,-1.03864271114068,
10.8524157577727));
#54958=CARTESIAN_POINT('Ctrl Pts',(-1.35523646339031,-0.972496182516221,
10.8465359739544));
#54959=CARTESIAN_POINT('Ctrl Pts',(-1.41249751619161,-0.883701534918635,
10.8392722112035));
#54960=CARTESIAN_POINT('Ctrl Pts',(-1.42447989055803,-0.864253878928096,
10.8377163294764));
#54961=CARTESIAN_POINT('Ctrl Pts',(-1.44205075479366,-0.834377201235911,
10.8353774208782));
#54962=CARTESIAN_POINT('Ctrl Pts',(-1.44793394389673,-0.824125597186695,
10.8345838058823));
#54963=CARTESIAN_POINT('Ctrl Pts',(-1.45798593633717,-0.806169781612048,
10.8332089484065));
#54964=CARTESIAN_POINT('Ctrl Pts',(-1.46220393856249,-0.798493803620333,
10.8326259613752));
#54965=CARTESIAN_POINT('Ctrl Pts',(-1.47157871329896,-0.781110051626613,
10.8313161574842));
#54966=CARTESIAN_POINT('Ctrl Pts',(-1.47670037024429,-0.771383723224131,
10.8305906055266));
#54967=CARTESIAN_POINT('Ctrl Pts',(-1.49033970080047,-0.744848071586037,
10.8286302887352));
#54968=CARTESIAN_POINT('Ctrl Pts',(-1.49866922321161,-0.727943459207529,
10.827402110806));
#54969=CARTESIAN_POINT('Ctrl Pts',(-1.55032747202257,-0.618456952377694,
10.8195712382604));
#54970=CARTESIAN_POINT('Ctrl Pts',(-1.58534697505317,-0.522190676368287,
10.8132658863826));
#54971=CARTESIAN_POINT('Ctrl Pts',(-1.63137840859933,-0.346972750260619,
10.802190147954));
#54972=CARTESIAN_POINT('Ctrl Pts',(-1.64598176929133,-0.26931079204428,
10.7974061195732));
#54973=CARTESIAN_POINT('Ctrl Pts',(-1.65850626943725,-0.160734821567394,
10.7905689514215));
#54974=CARTESIAN_POINT('Ctrl Pts',(-1.66116101457131,-0.130470663733504,
10.7886468331598));
#54975=CARTESIAN_POINT('Ctrl Pts',(-1.66418791587085,-0.0802104585073211,
10.7854031531401));
#54976=CARTESIAN_POINT('Ctrl Pts',(-1.66503005317733,-0.0602492566000276,
10.7841014471221));
#54977=CARTESIAN_POINT('Ctrl Pts',(-1.66570362216151,-0.032397461746249,
10.782260418426));
#54978=CARTESIAN_POINT('Ctrl Pts',(-1.66583827534872,-0.0245150283787174,
10.7817366178689));
#54979=CARTESIAN_POINT('Ctrl Pts',(-1.6659726109324,-0.0110596327767957,
10.7808373124782));
#54980=CARTESIAN_POINT('Ctrl Pts',(-1.66600028457275,-0.00548696565446436,
10.7804633385582));
#54981=CARTESIAN_POINT('Ctrl Pts',(-1.66599968502267,0.00616352312797371,
10.779678150415));
#54982=CARTESIAN_POINT('Ctrl Pts',(-1.66596611339039,0.0122411424855048,
10.7792666713526));
#54983=CARTESIAN_POINT('Ctrl Pts',(-1.66578610194907,0.0286116915225238,
10.7781535096789));
#54984=CARTESIAN_POINT('Ctrl Pts',(-1.66557751929742,0.0389034723344217,
10.7774485682847));
#54985=CARTESIAN_POINT('Ctrl Pts',(-1.6639886650865,0.0926898451027791,
10.7737399160954));
#54986=CARTESIAN_POINT('Ctrl Pts',(-1.66100009117117,0.136116355026789,
10.7706620761982));
#54987=CARTESIAN_POINT('Ctrl Pts',(-1.6441454412181,0.291751984701615,10.7594389432007));
#54988=CARTESIAN_POINT('Ctrl Pts',(-1.62056971782624,0.402603097172142,
10.7511066252568));
#54989=CARTESIAN_POINT('Ctrl Pts',(-1.57889401068256,0.532146948207532,
10.741354356213));
#54990=CARTESIAN_POINT('Ctrl Pts',(-1.57138636178916,0.553923432122347,
10.7397133445268));
#54991=CARTESIAN_POINT('Ctrl Pts',(-1.56343131785294,0.575533243485219,
10.7380842620731));
#54992=CARTESIAN_POINT('Ctrl Pts',(-1.5634312473966,0.575533434879242,10.9335682035678));
#54993=CARTESIAN_POINT('Ctrl Pts',(-1.57071877584423,0.555736931321281,
10.9350352846818));
#54994=CARTESIAN_POINT('Ctrl Pts',(-1.57763279198976,0.535795252065528,
10.9364913948363));
#54995=CARTESIAN_POINT('Ctrl Pts',(-1.59014703553624,0.497354401049535,
10.9392573276825));
#54996=CARTESIAN_POINT('Ctrl Pts',(-1.59580591892224,0.478886749103904,
10.9405683569805));
#54997=CARTESIAN_POINT('Ctrl Pts',(-1.60420744729071,0.449663767309595,
10.9426159013899));
#54998=CARTESIAN_POINT('Ctrl Pts',(-1.60716580672233,0.438972798223727,
10.9433593532419));
#54999=CARTESIAN_POINT('Ctrl Pts',(-1.61251548064756,0.418860691160464,
10.9447477043977));
#55000=CARTESIAN_POINT('Ctrl Pts',(-1.61493153853463,0.409446683484319,
10.9453933779506));
#55001=CARTESIAN_POINT('Ctrl Pts',(-1.62018074961505,0.388223899812921,
10.9468398600334));
#55002=CARTESIAN_POINT('Ctrl Pts',(-1.6229674694414,0.37640412321985,10.947639148739));
#55003=CARTESIAN_POINT('Ctrl Pts',(-1.63080912829016,0.341436542247001,
10.949986006012));
#55004=CARTESIAN_POINT('Ctrl Pts',(-1.63549994704836,0.318209583739206,
10.9515220012339));
#55005=CARTESIAN_POINT('Ctrl Pts',(-1.65728489821288,0.197077252263585,
10.9594276681495));
#55006=CARTESIAN_POINT('Ctrl Pts',(-1.66608966735504,0.0978828953325324,
10.9655325939493));
#55007=CARTESIAN_POINT('Ctrl Pts',(-1.6658981856851,-0.112759820905185,
10.9784007705868));
#55008=CARTESIAN_POINT('Ctrl Pts',(-1.65465493934185,-0.223699563860263,
10.9851260456819));
#55009=CARTESIAN_POINT('Ctrl Pts',(-1.62953788689807,-0.346950391322927,
10.9933054270432));
#55010=CARTESIAN_POINT('Ctrl Pts',(-1.62644134714192,-0.36118805044362,
10.9942614427947));
#55011=CARTESIAN_POINT('Ctrl Pts',(-1.62159043659175,-0.382163438860362,
10.995688878288));
#55012=CARTESIAN_POINT('Ctrl Pts',(-1.61997982909137,-0.388934168013582,
10.9961525892672));
#55013=CARTESIAN_POINT('Ctrl Pts',(-1.61702944769712,-0.401000754908375,
10.9969845888326));
#55014=CARTESIAN_POINT('Ctrl Pts',(-1.61570598591677,-0.406300388195197,
10.9973519506303));
#55015=CARTESIAN_POINT('Ctrl Pts',(-1.61272094838418,-0.418008334236784,
10.9981678971318));
#55016=CARTESIAN_POINT('Ctrl Pts',(-1.61104725109372,-0.424413213506575,
10.9986171386645));
#55017=CARTESIAN_POINT('Ctrl Pts',(-1.60601331846817,-0.443218086920089,
10.9999442460219));
#55018=CARTESIAN_POINT('Ctrl Pts',(-1.60254785861527,-0.455589055315543,
11.0008277165885));
#55019=CARTESIAN_POINT('Ctrl Pts',(-1.59421373107115,-0.484067895332003,
11.0028837454387));
#55020=CARTESIAN_POINT('Ctrl Pts',(-1.58924344028509,-0.500144366576006,
11.0040609407974));
#55021=CARTESIAN_POINT('Ctrl Pts',(-1.57122404753477,-0.555445555352912,
11.0081616190516));
#55022=CARTESIAN_POINT('Ctrl Pts',(-1.55695977481508,-0.594256337775516,
11.0111291398076));
#55023=CARTESIAN_POINT('Ctrl Pts',(-1.49354422057804,-0.748788072819416,
11.0232153221401));
#55024=CARTESIAN_POINT('Ctrl Pts',(-1.43280319360239,-0.859325543723636,
11.0324490374598));
#55025=CARTESIAN_POINT('Ctrl Pts',(-1.33452346236187,-0.998288870543778,
11.0444224162866));
#55026=CARTESIAN_POINT('Ctrl Pts',(-1.30740062046708,-1.03355589882088,
11.0475023441914));
#55027=CARTESIAN_POINT('Ctrl Pts',(-1.26886397986868,-1.07971536313839,
11.0515926877636));
#55028=CARTESIAN_POINT('Ctrl Pts',(-1.25866220333435,-1.0915908353244,11.0526506948859));
#55029=CARTESIAN_POINT('Ctrl Pts',(-1.24146474006488,-1.11104799449976,
11.0543942439288));
#55030=CARTESIAN_POINT('Ctrl Pts',(-1.23456350768248,-1.11871144655892,
11.0550836343344));
#55031=CARTESIAN_POINT('Ctrl Pts',(-1.22085370597447,-1.13365407152389,
11.0564333893415));
#55032=CARTESIAN_POINT('Ctrl Pts',(-1.21405010425275,-1.14093719239031,
11.0570939227923));
#55033=CARTESIAN_POINT('Ctrl Pts',(-1.19760444729514,-1.15822825780232,
11.0586688508361));
#55034=CARTESIAN_POINT('Ctrl Pts',(-1.18790162510323,-1.16817757971492,
11.0595805813252));
#55035=CARTESIAN_POINT('Ctrl Pts',(-1.15345733722443,-1.20262393233005,
11.062758266647));
#55036=CARTESIAN_POINT('Ctrl Pts',(-1.12807253976171,-1.22646678244395,
11.0649958171087));
#55037=CARTESIAN_POINT('Ctrl Pts',(-1.0628586638089,-1.28398022448151,11.0705144053655));
#55038=CARTESIAN_POINT('Ctrl Pts',(-1.0221608785796,-1.31660985373681,11.073757275999));
#55039=CARTESIAN_POINT('Ctrl Pts',(-0.90025344298711,-1.40528410075077,
11.0830397046707));
#55040=CARTESIAN_POINT('Ctrl Pts',(-0.815521375226819,-1.45609167489788,
11.0889683104914));
#55041=CARTESIAN_POINT('Ctrl Pts',(-0.681969091694501,-1.52084061545234,
11.0982131396581));
#55042=CARTESIAN_POINT('Ctrl Pts',(-0.636192135361141,-1.5405507331665,
11.1013683615726));
#55043=CARTESIAN_POINT('Ctrl Pts',(-0.57940544221888,-1.56203850371185,
11.1053461791347));
#55044=CARTESIAN_POINT('Ctrl Pts',(-0.569167394054663,-1.56579801238063,
11.1060658148755));
#55045=CARTESIAN_POINT('Ctrl Pts',(-0.552982626069039,-1.57156151149899,
11.1072084448144));
#55046=CARTESIAN_POINT('Ctrl Pts',(-0.547060020292501,-1.57363296232603,
11.1076276218111));
#55047=CARTESIAN_POINT('Ctrl Pts',(-0.535914766197649,-1.57746052977105,
11.1084186492292));
#55048=CARTESIAN_POINT('Ctrl Pts',(-0.530694935239136,-1.57922425315533,
11.1087900536916));
#55049=CARTESIAN_POINT('Ctrl Pts',(-0.518379805478667,-1.58331744985111,
11.1096684103215));
#55050=CARTESIAN_POINT('Ctrl Pts',(-0.511277489692944,-1.58562514262265,
11.1101765919751));
#55051=CARTESIAN_POINT('Ctrl Pts',(-0.487580399527958,-1.59314906723114,
11.1118769844955));
#55052=CARTESIAN_POINT('Ctrl Pts',(-0.470920097836824,-1.59815293336517,
11.113080297446));
#55053=CARTESIAN_POINT('Ctrl Pts',(-0.430015462363119,-1.6097433922762,
11.1160487814468));
#55054=CARTESIAN_POINT('Ctrl Pts',(-0.405695028750299,-1.61604408804506,
11.1178256814515));
#55055=CARTESIAN_POINT('Ctrl Pts',(-0.301944554148621,-1.64043323263404,
11.1254318220529));
#55056=CARTESIAN_POINT('Ctrl Pts',(-0.221388769564987,-1.65323256412621,
11.1313952444484));
#55057=CARTESIAN_POINT('Ctrl Pts',(-0.0407492538871145,-1.66849066695665,
11.1445633330364));
#55058=CARTESIAN_POINT('Ctrl Pts',(0.0592922748583388,-1.66793644952417,
11.1517110401823));
#55059=CARTESIAN_POINT('Ctrl Pts',(0.182254356801667,-1.65617010868027,
11.1602152398388));
#55060=CARTESIAN_POINT('Ctrl Pts',(0.205763018494868,-1.65341397097984,
11.1618292834324));
#55061=CARTESIAN_POINT('Ctrl Pts',(0.241228459531508,-1.6484878395009,11.1642474711962));
#55062=CARTESIAN_POINT('Ctrl Pts',(0.253232517701558,-1.64668656160653,
11.1650630469841));
#55063=CARTESIAN_POINT('Ctrl Pts',(0.274810473112354,-1.64320712308749,
11.1665241585472));
#55064=CARTESIAN_POINT('Ctrl Pts',(0.284391296317817,-1.64157608503067,
11.1671711490236));
#55065=CARTESIAN_POINT('Ctrl Pts',(0.304879335289231,-1.6379034498421,11.1685511781591));
#55066=CARTESIAN_POINT('Ctrl Pts',(0.315781578301719,-1.63583652145177,
11.1692833812133));
#55067=CARTESIAN_POINT('Ctrl Pts',(0.345617973157832,-1.6298705131317,11.1712818744192));
#55068=CARTESIAN_POINT('Ctrl Pts',(0.364506565942917,-1.62575049955715,
11.172541123597));
#55069=CARTESIAN_POINT('Ctrl Pts',(0.406406977212751,-1.61584410742754,
11.1753241779941));
#55070=CARTESIAN_POINT('Ctrl Pts',(0.429375700771275,-1.60989297847586,
11.176842746633));
#55071=CARTESIAN_POINT('Ctrl Pts',(0.502462289296101,-1.58928089204364,
11.1816621023883));
#55072=CARTESIAN_POINT('Ctrl Pts',(0.552022549693937,-1.57275358056102,
11.1849097421345));
#55073=CARTESIAN_POINT('Ctrl Pts',(0.691895420096322,-1.51868049015584,
11.1941433219231));
#55074=CARTESIAN_POINT('Ctrl Pts',(0.779780028180677,-1.4754834137176,11.2000214587095));
#55075=CARTESIAN_POINT('Ctrl Pts',(0.906552665573704,-1.39866649981039,
11.2092497060903));
#55076=CARTESIAN_POINT('Ctrl Pts',(0.948521502198097,-1.37055157187994,
11.2124459724652));
#55077=CARTESIAN_POINT('Ctrl Pts',(0.997946899462727,-1.33408307474949,
11.2164698057187));
#55078=CARTESIAN_POINT('Ctrl Pts',(1.00668480134007,-1.32750192451012,11.2171915453012));
#55079=CARTESIAN_POINT('Ctrl Pts',(1.0203373446209,-1.3170068962905,11.2183367861368));
#55080=CARTESIAN_POINT('Ctrl Pts',(1.02529591862805,-1.313150310399,11.2187564414388));
#55081=CARTESIAN_POINT('Ctrl Pts',(1.03456122504432,-1.30585964486613,11.219547824224));
#55082=CARTESIAN_POINT('Ctrl Pts',(1.03887288149714,-1.30243213757523,11.219919100151));
#55083=CARTESIAN_POINT('Ctrl Pts',(1.04897971470817,-1.29431569884276,11.2207964074553));
#55084=CARTESIAN_POINT('Ctrl Pts',(1.05476050034396,-1.28960918565829,11.2213036594433));
#55085=CARTESIAN_POINT('Ctrl Pts',(1.07386438920556,-1.27384109603936,11.2229976776673));
#55086=CARTESIAN_POINT('Ctrl Pts',(1.08704609586862,-1.26261102130514,11.2241954365437));
#55087=CARTESIAN_POINT('Ctrl Pts',(1.11880073826701,-1.23469198631321,11.2271473499815));
#55088=CARTESIAN_POINT('Ctrl Pts',(1.13717781067257,-1.2177872909621,11.2289130752273));
#55089=CARTESIAN_POINT('Ctrl Pts',(1.2131757470624,-1.14465776625704,11.2364386001796));
#55090=CARTESIAN_POINT('Ctrl Pts',(1.26706010841115,-1.08470947627988,11.2423302485443));
#55091=CARTESIAN_POINT('Ctrl Pts',(1.37838783151862,-0.941186696358283,
11.2555272860077));
#55092=CARTESIAN_POINT('Ctrl Pts',(1.43298033683817,-0.855779733771383,
11.2627725523329));
#55093=CARTESIAN_POINT('Ctrl Pts',(1.49034833877706,-0.744966654909961,
11.2713628015766));
#55094=CARTESIAN_POINT('Ctrl Pts',(1.50075693265496,-0.723769449465426,
11.2729730255757));
#55095=CARTESIAN_POINT('Ctrl Pts',(1.5158242279257,-0.691360949786361,11.2753866800049));
#55096=CARTESIAN_POINT('Ctrl Pts',(1.52081647000792,-0.680308996631328,
11.2762014781242));
#55097=CARTESIAN_POINT('Ctrl Pts',(1.52959102711326,-0.660304261570677,
11.2776617473107));
#55098=CARTESIAN_POINT('Ctrl Pts',(1.53341647787516,-0.651371123339749,
11.2783086659074));
#55099=CARTESIAN_POINT('Ctrl Pts',(1.54144519839993,-0.632159785037457,
11.2796891279832));
#55100=CARTESIAN_POINT('Ctrl Pts',(1.54562433043445,-0.621871958442806,
11.2804218304875));
#55101=CARTESIAN_POINT('Ctrl Pts',(1.5568096386581,-0.593527460832807,11.2824232052748));
#55102=CARTESIAN_POINT('Ctrl Pts',(1.56360443582741,-0.575388839656622,
11.2836848017333));
#55103=CARTESIAN_POINT('Ctrl Pts',(1.60842018115751,-0.449092070961539,
11.292346721424));
#55104=CARTESIAN_POINT('Ctrl Pts',(1.63550625635248,-0.33737647683352,11.2993644250222));
#55105=CARTESIAN_POINT('Ctrl Pts',(1.66472655707294,-0.121781079564549,
11.312649761082));
#55106=CARTESIAN_POINT('Ctrl Pts',(1.66906779960012,-0.0187623355534116,
11.3189020300812));
#55107=CARTESIAN_POINT('Ctrl Pts',(1.66311812060077,0.0991145056551233,
11.3265685230733));
#55108=CARTESIAN_POINT('Ctrl Pts',(1.66214797711956,0.11423498116346,11.3275618398591));
#55109=CARTESIAN_POINT('Ctrl Pts',(1.6604229850146,0.136387255304573,11.3290344080363));
#55110=CARTESIAN_POINT('Ctrl Pts',(1.65982933562618,0.143431323765842,11.329505233388));
#55111=CARTESIAN_POINT('Ctrl Pts',(1.65869693862962,0.155917847918266,11.3303447371709));
#55112=CARTESIAN_POINT('Ctrl Pts',(1.65817619663891,0.161361732980802,11.3307124159305));
#55113=CARTESIAN_POINT('Ctrl Pts',(1.65697461111951,0.173302655689231,11.3315226458025));
#55114=CARTESIAN_POINT('Ctrl Pts',(1.65628236613275,0.179798198959596,11.331965791999));
#55115=CARTESIAN_POINT('Ctrl Pts',(1.6541631150953,0.198631964565432,11.3332573408261));
#55116=CARTESIAN_POINT('Ctrl Pts',(1.6526363438578,0.21095819672448,11.3341109191133));
#55117=CARTESIAN_POINT('Ctrl Pts',(1.64881347569599,0.239226967968099,11.3360858372393));
#55118=CARTESIAN_POINT('Ctrl Pts',(1.6464237279742,0.255155414175295,11.3372113436737));
#55119=CARTESIAN_POINT('Ctrl Pts',(1.63751661099934,0.309174098002841,11.3410662245656));
#55120=CARTESIAN_POINT('Ctrl Pts',(1.62990540172425,0.347069556616587,11.3438346452289));
#55121=CARTESIAN_POINT('Ctrl Pts',(1.60463244465315,0.453570587915134,11.3517418972522));
#55122=CARTESIAN_POINT('Ctrl Pts',(1.5839036070138,0.521364535189539,11.35692389511));
#55123=CARTESIAN_POINT('Ctrl Pts',(1.52475986563298,0.678265952061657,11.3690698922512));
#55124=CARTESIAN_POINT('Ctrl Pts',(1.48275295180678,0.765758997451002,11.3759576152573));
#55125=CARTESIAN_POINT('Ctrl Pts',(1.42379957556579,0.865276549473997,11.3838679462899));
#55126=CARTESIAN_POINT('Ctrl Pts',(1.41395432555655,0.881272916746876,11.3851425681699));
#55127=CARTESIAN_POINT('Ctrl Pts',(1.39787156684631,0.906440262667726,11.3871537340142));
#55128=CARTESIAN_POINT('Ctrl Pts',(1.39180962183681,0.915720947683956,11.3878966549857));
#55129=CARTESIAN_POINT('Ctrl Pts',(1.38031054826023,0.932947732230548,11.389278353703));
#55130=CARTESIAN_POINT('Ctrl Pts',(1.37489632535546,0.940908487520375,11.3899179512588));
#55131=CARTESIAN_POINT('Ctrl Pts',(1.36251735466579,0.958774775370628,11.3913561455047));
#55132=CARTESIAN_POINT('Ctrl Pts',(1.35551296069141,0.968652279186948,11.3921531969008));
#55133=CARTESIAN_POINT('Ctrl Pts',(1.33412278702271,0.998129981138125,11.3945385577487));
#55134=CARTESIAN_POINT('Ctrl Pts',(1.31941466489741,1.01749305158815,11.3961144338449));
#55135=CARTESIAN_POINT('Ctrl Pts',(1.28442739687989,1.06151834328147,11.3997251588363));
#55136=CARTESIAN_POINT('Ctrl Pts',(1.26385248940985,1.08593370088755,11.401748501344));
#55137=CARTESIAN_POINT('Ctrl Pts',(1.1856571824124,1.17348951001685,11.40911405457));
#55138=CARTESIAN_POINT('Ctrl Pts',(1.12390482189085,1.23276098760362,11.4143122881039));
#55139=CARTESIAN_POINT('Ctrl Pts',(0.987582775935279,1.34481045468046,11.4250927673246));
#55140=CARTESIAN_POINT('Ctrl Pts',(0.912685219320327,1.3967234262007,11.4306618544543));
#55141=CARTESIAN_POINT('Ctrl Pts',(0.820368580384159,1.45010242268945,11.4375818878878));
#55142=CARTESIAN_POINT('Ctrl Pts',(0.806690992839717,1.45775554965117,11.4386086515978));
#55143=CARTESIAN_POINT('Ctrl Pts',(0.786673382212309,1.46858818079766,11.4401165416515));
#55144=CARTESIAN_POINT('Ctrl Pts',(0.780417345423651,1.47192221855082,11.4405885228168));
#55145=CARTESIAN_POINT('Ctrl Pts',(0.76928740144223,1.47776281273496,11.4414298366642));
#55146=CARTESIAN_POINT('Ctrl Pts',(0.76442212667314,1.48028539399641,11.4417981623177));
#55147=CARTESIAN_POINT('Ctrl Pts',(0.753820348580666,1.48571607101186,11.4426020757118));
#55148=CARTESIAN_POINT('Ctrl Pts',(0.748079513365872,1.4886149266299,11.4430381861598));
#55149=CARTESIAN_POINT('Ctrl Pts',(0.731636610028338,1.49679869589307,11.4442892483032));
#55150=CARTESIAN_POINT('Ctrl Pts',(0.720894593532401,1.50200180750442,11.4451089064427));
#55151=CARTESIAN_POINT('Ctrl Pts',(0.624045348150771,1.54763445491757,11.4525138410255));
#55152=CARTESIAN_POINT('Ctrl Pts',(0.534687206007513,1.5807310934726,11.4594410883713));
#55153=CARTESIAN_POINT('Ctrl Pts',(0.326512974647072,1.6381539008925,11.4751607674641));
#55154=CARTESIAN_POINT('Ctrl Pts',(0.206849823337168,1.65752290284946,11.4838859404648));
#55155=CARTESIAN_POINT('Ctrl Pts',(0.0651569315275816,1.66485780232014,
11.4936460555163));
#55156=CARTESIAN_POINT('Ctrl Pts',(0.0441672989285181,1.66554683123939,
11.4950784885497));
#55157=CARTESIAN_POINT('Ctrl Pts',(0.0106062076012587,1.66601361714739,
11.4973483518401));
#55158=CARTESIAN_POINT('Ctrl Pts',(-0.00195884137095795,1.66604623048518,
11.4981935912387));
#55159=CARTESIAN_POINT('Ctrl Pts',(-0.0243108864459776,1.66585136903568,
11.4996893838935));
#55160=CARTESIAN_POINT('Ctrl Pts',(-0.0340976438810582,1.66567978934368,
11.5003416483516));
#55161=CARTESIAN_POINT('Ctrl Pts',(-0.0546048516140105,1.66513944123438,
11.5017030657081));
#55162=CARTESIAN_POINT('Ctrl Pts',(-0.0653244269441687,1.66475336818898,
11.5024116483862));
#55163=CARTESIAN_POINT('Ctrl Pts',(-0.0936217981824038,1.66346046930715,
11.5042745453528));
#55164=CARTESIAN_POINT('Ctrl Pts',(-0.111190540708841,1.6623785598202,11.5054233744802));
#55165=CARTESIAN_POINT('Ctrl Pts',(-0.201138235611418,1.65540704628226,
11.5112702134185));
#55166=CARTESIAN_POINT('Ctrl Pts',(-0.273097733343431,1.64506796748348,
11.5158271660273));
#55167=CARTESIAN_POINT('Ctrl Pts',(-0.444126025430088,1.60895826451098,
11.5266198914193));
#55168=CARTESIAN_POINT('Ctrl Pts',(-0.541933500201491,1.57870240203124,
11.5327552591224));
#55169=CARTESIAN_POINT('Ctrl Pts',(-0.684813868886588,1.51964993687359,
11.5423662780989));
#55170=CARTESIAN_POINT('Ctrl Pts',(-0.732300099447912,1.49734476944057,
11.5456805477235));
#55171=CARTESIAN_POINT('Ctrl Pts',(-0.788416693140658,1.46767747089229,
11.549837798198));
#55172=CARTESIAN_POINT('Ctrl Pts',(-0.798131138591723,1.46241741992534,
11.5505665234232));
#55173=CARTESIAN_POINT('Ctrl Pts',(-0.813307631085186,1.45400359921348,
11.5517204319693));
#55174=CARTESIAN_POINT('Ctrl Pts',(-0.818805509009888,1.45091464409118,
11.5521416732198));
#55175=CARTESIAN_POINT('Ctrl Pts',(-0.829067608600657,1.44507203294153,
11.552934253373));
#55176=CARTESIAN_POINT('Ctrl Pts',(-0.833835885294892,1.44232589691537,
11.5533051222678));
#55177=CARTESIAN_POINT('Ctrl Pts',(-0.844994237058272,1.4358257779647,11.5541790364662));
#55178=CARTESIAN_POINT('Ctrl Pts',(-0.851372954624263,1.4320527267639,11.5546832735889));
#55179=CARTESIAN_POINT('Ctrl Pts',(-0.872354061618967,1.41945254937007,
11.5563567410385));
#55180=CARTESIAN_POINT('Ctrl Pts',(-0.886845471993696,1.41044397309229,
11.5575366149008));
#55181=CARTESIAN_POINT('Ctrl Pts',(-0.921780841104532,1.38797519309314,
11.5604353497723));
#55182=CARTESIAN_POINT('Ctrl Pts',(-0.94207110789277,1.37428416131279,11.562165280873));
#55183=CARTESIAN_POINT('Ctrl Pts',(-1.02533432213211,1.31539111972873,11.5694379275501));
#55184=CARTESIAN_POINT('Ctrl Pts',(-1.08541377692279,1.26627023946867,11.5751052154449));
#55185=CARTESIAN_POINT('Ctrl Pts',(-1.21836055489277,1.14113652902151,11.5883788451767));
#55186=CARTESIAN_POINT('Ctrl Pts',(-1.28789587849737,1.06203864965379,11.5959174714854));
#55187=CARTESIAN_POINT('Ctrl Pts',(-1.36334154165655,0.957815814520947,
11.6047744259544));
#55188=CARTESIAN_POINT('Ctrl Pts',(-1.37675335546527,0.938435714612838,
11.6063814095401));
#55189=CARTESIAN_POINT('Ctrl Pts',(-1.39643244525766,0.908668942095237,
11.6087912171587));
#55190=CARTESIAN_POINT('Ctrl Pts',(-1.40300445911742,0.898488353653019,
11.6096053547727));
#55191=CARTESIAN_POINT('Ctrl Pts',(-1.4146454606119,0.880016269312702,11.6110649091812));
#55192=CARTESIAN_POINT('Ctrl Pts',(-1.41975402547408,0.87175049612799,11.6117117674137));
#55193=CARTESIAN_POINT('Ctrl Pts',(-1.43054829926958,0.853938525447834,
11.613092600602));
#55194=CARTESIAN_POINT('Ctrl Pts',(-1.43621144110945,0.84437914959494,11.6138257299991));
#55195=CARTESIAN_POINT('Ctrl Pts',(-1.45149864506568,0.817975550740554,
11.6158295684961));
#55196=CARTESIAN_POINT('Ctrl Pts',(-1.46092499291914,0.801018435680312,
11.6170931719142));
#55197=CARTESIAN_POINT('Ctrl Pts',(-1.48126649693276,0.762871863691643,
11.6198873021926));
#55198=CARTESIAN_POINT('Ctrl Pts',(-1.49202755603811,0.741604862674909,
11.6214125266085));
#55199=CARTESIAN_POINT('Ctrl Pts',(-1.52495553742761,0.67290921345574,11.6262464397793));
#55200=CARTESIAN_POINT('Ctrl Pts',(-1.54534568696583,0.624662706286318,
11.6295018139068));
#55201=CARTESIAN_POINT('Ctrl Pts',(-1.56343130033056,0.575533291084625,
11.6327248639491));
#55202=CARTESIAN_POINT('Origin',(0.,0.,11.));
#55203=CARTESIAN_POINT('',(-1.56343130033211,0.57553329108042,12.3306070045052));
#55204=CARTESIAN_POINT('',(-1.56343130033213,0.575533291080364,12.1392916035562));
#55205=CARTESIAN_POINT('',(-1.56343130033213,0.575533291080363,11.));
#55206=CARTESIAN_POINT('',(-1.66599938220149,0.00143474884533201,11.4785196366098));
#55207=CARTESIAN_POINT('Ctrl Pts',(-1.56343130033213,0.575533291080363,
12.1392916035562));
#55208=CARTESIAN_POINT('Ctrl Pts',(-1.54206084724692,0.633585945502796,
12.1351571376634));
#55209=CARTESIAN_POINT('Ctrl Pts',(-1.51747847922349,0.69037758855015,12.1310226717706));
#55210=CARTESIAN_POINT('Ctrl Pts',(-1.48986988536785,0.745549277160123,
12.1268882058779));
#55211=CARTESIAN_POINT('Ctrl Pts',(-1.46220722533534,0.800829009022508,
12.1227456434205));
#55212=CARTESIAN_POINT('Ctrl Pts',(-1.43150675994854,0.854482032851016,
12.1186030809631));
#55213=CARTESIAN_POINT('Ctrl Pts',(-1.3979984684239,0.906176738988833,12.1144605185057));
#55214=CARTESIAN_POINT('Ctrl Pts',(-1.39223108756224,0.91507432956307,12.113747508849));
#55215=CARTESIAN_POINT('Ctrl Pts',(-1.38638062297089,0.923913984412125,
12.1130344991924));
#55216=CARTESIAN_POINT('Ctrl Pts',(-1.38044836581346,0.93269411348145,12.1123214895357));
#55217=CARTESIAN_POINT('Ctrl Pts',(-1.34652463687341,0.98290345382218,12.1082441298256));
#55218=CARTESIAN_POINT('Ctrl Pts',(-1.30978799052863,1.03136324686654,12.1041667701154));
#55219=CARTESIAN_POINT('Ctrl Pts',(-1.27044517463845,1.07774071939306,12.1000894104053));
#55220=CARTESIAN_POINT('Ctrl Pts',(-1.2306824601219,1.12461317014033,12.095968533786));
#55221=CARTESIAN_POINT('Ctrl Pts',(-1.1882578366262,1.16935810112152,12.0918476571668));
#55222=CARTESIAN_POINT('Ctrl Pts',(-1.14343038978819,1.21166123306344,12.0877267805476));
#55223=CARTESIAN_POINT('Ctrl Pts',(-1.09919851005162,1.2534023353684,12.0836606529431));
#55224=CARTESIAN_POINT('Ctrl Pts',(-1.05262764816723,1.29276576409608,12.0795945253385));
#55225=CARTESIAN_POINT('Ctrl Pts',(-1.00400609036898,1.329484024162,12.0755283977339));
#55226=CARTESIAN_POINT('Ctrl Pts',(-0.955414279483092,1.36617981981268,
12.0714647578066));
#55227=CARTESIAN_POINT('Ctrl Pts',(-0.904774667943586,1.40023334757946,
12.0674011178792));
#55228=CARTESIAN_POINT('Ctrl Pts',(-0.852408730657561,1.43141725429686,
12.0633374779519));
#55229=CARTESIAN_POINT('Ctrl Pts',(-0.800055376895427,1.46259366752793,
12.0592748145164));
#55230=CARTESIAN_POINT('Ctrl Pts',(-0.745976960568927,1.49090156677985,
12.0552121510808));
#55231=CARTESIAN_POINT('Ctrl Pts',(-0.690522278667592,1.51615796758244,
12.0511494876453));
#55232=CARTESIAN_POINT('Ctrl Pts',(-0.633692199812496,1.54204078216175,
12.0469860613036));
#55233=CARTESIAN_POINT('Ctrl Pts',(-0.575417161880126,1.56471842482518,
12.0428226349618));
#55234=CARTESIAN_POINT('Ctrl Pts',(-0.516095133905195,1.58404602608617,
12.03865920862));
#55235=CARTESIAN_POINT('Ctrl Pts',(-0.458134905445043,1.60292994194196,
12.0345913581068));
#55236=CARTESIAN_POINT('Ctrl Pts',(-0.399175774768682,1.61861593101746,
12.0305235075935));
#55237=CARTESIAN_POINT('Ctrl Pts',(-0.339602531693703,1.63101996323381,
12.0264556570802));
#55238=CARTESIAN_POINT('Ctrl Pts',(-0.277929741679332,1.64386115224291,
12.0222444428242));
#55239=CARTESIAN_POINT('Ctrl Pts',(-0.215599329682191,1.65318459814998,
12.0180332285682));
#55240=CARTESIAN_POINT('Ctrl Pts',(-0.153044687118163,1.65895549179142,
12.0138220143122));
#55241=CARTESIAN_POINT('Ctrl Pts',(-0.0904900445541309,1.66472638543285,
12.0096108000562));
#55242=CARTESIAN_POINT('Ctrl Pts',(-0.0277117742953075,1.66694477799572,
12.0053995858002));
#55243=CARTESIAN_POINT('Ctrl Pts',(0.0348591494664867,1.66563526610674,
12.0011883715442));
#55244=CARTESIAN_POINT('Ctrl Pts',(0.0954412400614033,1.66436737739544,
11.997111011834));
#55245=CARTESIAN_POINT('Ctrl Pts',(0.156079149144275,1.65978734370476,11.9930336521239));
#55246=CARTESIAN_POINT('Ctrl Pts',(0.216381166954204,1.65188837110367,11.9889562924138));
#55247=CARTESIAN_POINT('Ctrl Pts',(0.277326777091683,1.64390509422312,11.9848354157945));
#55248=CARTESIAN_POINT('Ctrl Pts',(0.337928754544622,1.63253153470738,11.9807145391753));
#55249=CARTESIAN_POINT('Ctrl Pts',(0.397782539949318,1.6178149000771,11.9765936625561));
#55250=CARTESIAN_POINT('Ctrl Pts',(0.456841121790149,1.60329378725428,11.9725275349516));
#55251=CARTESIAN_POINT('Ctrl Pts',(0.515170759296967,1.58551801480475,11.968461407347));
#55252=CARTESIAN_POINT('Ctrl Pts',(0.572390360221283,1.56458469745992,11.9643952797424));
#55253=CARTESIAN_POINT('Ctrl Pts',(0.629574953907417,1.5436641872234,11.9603316398151));
#55254=CARTESIAN_POINT('Ctrl Pts',(0.685650377718311,1.51959013782031,11.9562679998877));
#55255=CARTESIAN_POINT('Ctrl Pts',(0.740251263076272,1.49250931907107,11.9522043599604));
#55256=CARTESIAN_POINT('Ctrl Pts',(0.794839027852877,1.46543500783692,11.9481416965249));
#55257=CARTESIAN_POINT('Ctrl Pts',(0.847952499137718,1.43535558895083,11.9440790330893));
#55258=CARTESIAN_POINT('Ctrl Pts',(0.899248765001825,1.40246485112558,11.9400163696538));
#55259=CARTESIAN_POINT('Ctrl Pts',(0.951817290040193,1.36875835132932,11.935852943312));
#55260=CARTESIAN_POINT('Ctrl Pts',(1.00247676149926,1.3320994714463,11.9316895169703));
#55261=CARTESIAN_POINT('Ctrl Pts',(1.05088961915896,1.29274398406798,11.9275260906285));
#55262=CARTESIAN_POINT('Ctrl Pts',(1.09819110877679,1.25429194327509,11.9234582401153));
#55263=CARTESIAN_POINT('Ctrl Pts',(1.14334769923026,1.21326619913791,11.919390389602));
#55264=CARTESIAN_POINT('Ctrl Pts',(1.18608009164613,1.16994445004911,11.9153225390887));
#55265=CARTESIAN_POINT('Ctrl Pts',(1.23031850688496,1.12509590736954,11.9111113248327));
#55266=CARTESIAN_POINT('Ctrl Pts',(1.27195823100646,1.07778692007959,11.9069001105767));
#55267=CARTESIAN_POINT('Ctrl Pts',(1.31073495670596,1.02836271483802,11.9026888963207));
#55268=CARTESIAN_POINT('Ctrl Pts',(1.34951168240545,0.978938509596461,11.8984776820647));
#55269=CARTESIAN_POINT('Ctrl Pts',(1.38542512570093,0.927399620658939,11.8942664678087));
#55270=CARTESIAN_POINT('Ctrl Pts',(1.41826219911196,0.874121464425921,11.8900552535526));
#55271=CARTESIAN_POINT('Ctrl Pts',(1.45005553756154,0.822536768314798,11.8859778938425));
#55272=CARTESIAN_POINT('Ctrl Pts',(1.47909650830513,0.769108734991152,11.8819005341324));
#55273=CARTESIAN_POINT('Ctrl Pts',(1.50516694787099,0.714162767887491,11.8778231744222));
#55274=CARTESIAN_POINT('Ctrl Pts',(1.53151563243573,0.658630372598905,11.873702297803));
#55275=CARTESIAN_POINT('Ctrl Pts',(1.55482964881038,0.601547851913972,11.8695814211838));
#55276=CARTESIAN_POINT('Ctrl Pts',(1.57492923255732,0.5432806939662,11.8654605445646));
#55277=CARTESIAN_POINT('Ctrl Pts',(1.59476177787856,0.485787660016459,11.86139441696));
#55278=CARTESIAN_POINT('Ctrl Pts',(1.61146461092941,0.427141772983075,11.8573282893554));
#55279=CARTESIAN_POINT('Ctrl Pts',(1.62491262407231,0.367715874188799,11.8532621617509));
#55280=CARTESIAN_POINT('Ctrl Pts',(1.63835240965349,0.308326332456741,11.8491985218235));
#55281=CARTESIAN_POINT('Ctrl Pts',(1.64854121075687,0.248158223442775,11.8451348818961));
#55282=CARTESIAN_POINT('Ctrl Pts',(1.65540416483726,0.18759811043677,11.8410712419688));
#55283=CARTESIAN_POINT('Ctrl Pts',(1.66226546975121,0.127052550013376,11.8370085785333));
#55284=CARTESIAN_POINT('Ctrl Pts',(1.66580245654855,0.0661156810681977,
11.8329459150977));
#55285=CARTESIAN_POINT('Ctrl Pts',(1.66599194485515,0.00518070243959675,
11.8288832516622));
#55286=CARTESIAN_POINT('Ctrl Pts',(1.66618613288467,-0.0572655964437612,
11.8247198253205));
#55287=CARTESIAN_POINT('Ctrl Pts',(1.66286449565371,-0.11970934912481,11.8205563989787));
#55288=CARTESIAN_POINT('Ctrl Pts',(1.65605883015649,-0.18172823407689,11.8163929726369));
#55289=CARTESIAN_POINT('Ctrl Pts',(1.64940939586525,-0.242323410327245,
11.8123251221237));
#55290=CARTESIAN_POINT('Ctrl Pts',(1.6394343571667,-0.302512511885207,11.8082572716104));
#55291=CARTESIAN_POINT('Ctrl Pts',(1.62621553145385,-0.361910272385679,
11.8041894210971));
#55292=CARTESIAN_POINT('Ctrl Pts',(1.6125308330835,-0.423401395272077,11.7999782068411));
#55293=CARTESIAN_POINT('Ctrl Pts',(1.5953695548898,-0.484043768527647,11.7957669925851));
#55294=CARTESIAN_POINT('Ctrl Pts',(1.57487837812754,-0.543428094697315,
11.7915557783291));
#55295=CARTESIAN_POINT('Ctrl Pts',(1.55438720136529,-0.602812420866984,
11.7873445640731));
#55296=CARTESIAN_POINT('Ctrl Pts',(1.53056642085407,-0.660938171598326,
11.7831333498171));
#55297=CARTESIAN_POINT('Ctrl Pts',(1.50361586187397,-0.717422706583087,
11.7789221355611));
#55298=CARTESIAN_POINT('Ctrl Pts',(1.47752193345548,-0.772111865859231,
11.7748447758509));
#55299=CARTESIAN_POINT('Ctrl Pts',(1.44838652639371,-0.825488459811084,
11.7707674161408));
#55300=CARTESIAN_POINT('Ctrl Pts',(1.41636469530226,-0.87719270967179,11.7666900564306));
#55301=CARTESIAN_POINT('Ctrl Pts',(1.3840011011065,-0.929448789466517,11.7625691798114));
#55302=CARTESIAN_POINT('Ctrl Pts',(1.34868925098605,-0.979996101643676,
11.7584483031922));
#55303=CARTESIAN_POINT('Ctrl Pts',(1.31063870291815,-1.02848538658215,11.754327426573));
#55304=CARTESIAN_POINT('Ctrl Pts',(1.27309368564042,-1.07633045408422,11.7502612989684));
#55305=CARTESIAN_POINT('Ctrl Pts',(1.23288262401006,-1.12217143160885,11.7461951713639));
#55306=CARTESIAN_POINT('Ctrl Pts',(1.19025089843454,-1.16570099029544,11.7421290437593));
#55307=CARTESIAN_POINT('Ctrl Pts',(1.14764525516199,-1.20920391738027,11.7380654038319));
#55308=CARTESIAN_POINT('Ctrl Pts',(1.10262224176067,-1.25039786444183,11.7340017639046));
#55309=CARTESIAN_POINT('Ctrl Pts',(1.0554660188658,-1.28901027265867,11.7299381239772));
#55310=CARTESIAN_POINT('Ctrl Pts',(1.00832112760153,-1.32761340232181,11.7258754605417));
#55311=CARTESIAN_POINT('Ctrl Pts',(0.959044440380017,-1.36363590041568,
11.7218127971062));
#55312=CARTESIAN_POINT('Ctrl Pts',(0.907953723972735,-1.39684502902936,
11.7177501336707));
#55313=CARTESIAN_POINT('Ctrl Pts',(0.855595846465663,-1.4308778163994,11.7135867073289));
#55314=CARTESIAN_POINT('Ctrl Pts',(0.801333193676861,-1.46195546166263,
11.7094232809872));
#55315=CARTESIAN_POINT('Ctrl Pts',(0.745537817954203,-1.48987561964081,
11.7052598546454));
#55316=CARTESIAN_POINT('Ctrl Pts',(0.691023283736475,-1.51715484104137,
11.7011920041321));
#55317=CARTESIAN_POINT('Ctrl Pts',(0.635046163916582,-1.54141986525428,
11.6971241536189));
#55318=CARTESIAN_POINT('Ctrl Pts',(0.577974509655393,-1.56253046888328,
11.6930563031056));
#55319=CARTESIAN_POINT('Ctrl Pts',(0.518891472248906,-1.58438507604392,
11.6888450888496));
#55320=CARTESIAN_POINT('Ctrl Pts',(0.458635869004211,-1.6028585484011,11.6846338745936));
#55321=CARTESIAN_POINT('Ctrl Pts',(0.397631121277882,-1.61785212284414,
11.6804226603376));
#55322=CARTESIAN_POINT('Ctrl Pts',(0.336626373551552,-1.63284569728718,
11.6762114460816));
#55323=CARTESIAN_POINT('Ctrl Pts',(0.274873085134287,-1.64435933493581,
11.6720002318256));
#55324=CARTESIAN_POINT('Ctrl Pts',(0.212801106105302,-1.65235337904468,
11.6677890175695));
#55325=CARTESIAN_POINT('Ctrl Pts',(0.152702101154361,-1.66009333037203,
11.6637116578594));
#55326=CARTESIAN_POINT('Ctrl Pts',(0.0920561875886168,-1.66456612528513,
11.6596342981493));
#55327=CARTESIAN_POINT('Ctrl Pts',(0.0312497260217383,-1.66570689337097,
11.6555569384391));
#55328=CARTESIAN_POINT('Ctrl Pts',(-0.0302057117079062,-1.66685983666444,
11.6514360618199));
#55329=CARTESIAN_POINT('Ctrl Pts',(-0.0918246332323487,-1.66460905070646,
11.6473151852007));
#55330=CARTESIAN_POINT('Ctrl Pts',(-0.15319995386838,-1.65894116054028,
11.6431943085815));
#55331=CARTESIAN_POINT('Ctrl Pts',(-0.213759856175037,-1.6533485726533,
11.6391281809769));
#55332=CARTESIAN_POINT('Ctrl Pts',(-0.274082066190559,-1.64442917375535,
11.6350620533723));
#55333=CARTESIAN_POINT('Ctrl Pts',(-0.33377529726945,-1.63222242691757,
11.6309959257678));
#55334=CARTESIAN_POINT('Ctrl Pts',(-0.393432007730964,-1.62002314822857,
11.6269322858404));
#55335=CARTESIAN_POINT('Ctrl Pts',(-0.452460001683601,-1.60454061160897,
11.622868645913));
#55336=CARTESIAN_POINT('Ctrl Pts',(-0.510476170309535,-1.58586571926696,
11.6188050059857));
#55337=CARTESIAN_POINT('Ctrl Pts',(-0.568478397662058,-1.56719531449774,
11.6147423425502));
#55338=CARTESIAN_POINT('Ctrl Pts',(-0.625468795245726,-1.54533423365308,
11.6106796791146));
#55339=CARTESIAN_POINT('Ctrl Pts',(-0.681079481799879,-1.52042321064604,
11.6066170156791));
#55340=CARTESIAN_POINT('Ctrl Pts',(-0.738069434563094,-1.49489433998425,
11.6024535893373));
#55341=CARTESIAN_POINT('Ctrl Pts',(-0.793609787320232,-1.46616239368055,
11.5982901629956));
#55342=CARTESIAN_POINT('Ctrl Pts',(-0.847328749322365,-1.43443019717649,
11.5941267366538));
#55343=CARTESIAN_POINT('Ctrl Pts',(-0.899814536079456,-1.40342644660179,
11.5900588861406));
#55344=CARTESIAN_POINT('Ctrl Pts',(-0.950561273723657,-1.36955908824795,
11.5859910356273));
#55345=CARTESIAN_POINT('Ctrl Pts',(-0.999251532235019,-1.33306127965895,
11.581923185114));
#55346=CARTESIAN_POINT('Ctrl Pts',(-1.04965778735748,-1.29527717443144,
11.577711970858));
#55347=CARTESIAN_POINT('Ctrl Pts',(-1.09785941592614,-1.25467409688016,
11.573500756602));
#55348=CARTESIAN_POINT('Ctrl Pts',(-1.14354378837388,-1.21155421012496,
11.569289542346));
#55349=CARTESIAN_POINT('Ctrl Pts',(-1.18922816082161,-1.16843432336977,
11.56507832809));
#55350=CARTESIAN_POINT('Ctrl Pts',(-1.23239491699965,-1.1227981135873,11.560867113834));
#55351=CARTESIAN_POINT('Ctrl Pts',(-1.27277759774085,-1.07498520300934,
11.5566558995779));
#55352=CARTESIAN_POINT('Ctrl Pts',(-1.3116212125385,-1.02899453951805,11.5526051832464));
#55353=CARTESIAN_POINT('Ctrl Pts',(-1.34805528098541,-0.980793330512334,
11.5485544669148));
#55354=CARTESIAN_POINT('Ctrl Pts',(-1.38181662139976,-0.930665796525989,
11.5445037505832));
#55355=CARTESIAN_POINT('Ctrl Pts',(-1.41552828728624,-0.880612017359611,
11.5404589942467));
#55356=CARTESIAN_POINT('Ctrl Pts',(-1.44657472963222,-0.828637955103961,
11.5364142379102));
#55357=CARTESIAN_POINT('Ctrl Pts',(-1.47473247479964,-0.775061370325818,
11.5323694815737));
#55358=CARTESIAN_POINT('Ctrl Pts',(-1.50285958738946,-0.721543071070213,
11.528329125494));
#55359=CARTESIAN_POINT('Ctrl Pts',(-1.52810399251593,-0.666426162304626,
11.5242887694144));
#55360=CARTESIAN_POINT('Ctrl Pts',(-1.55028629329074,-0.610056070238507,
11.5202484133348));
#55361=CARTESIAN_POINT('Ctrl Pts',(-1.57245652133952,-0.553716657617442,
11.5162102562205));
#55362=CARTESIAN_POINT('Ctrl Pts',(-1.59156775366362,-0.496125893490407,
11.5121720991063));
#55363=CARTESIAN_POINT('Ctrl Pts',(-1.60748808713347,-0.437650602334751,
11.5081339419921));
#55364=CARTESIAN_POINT('Ctrl Pts',(-1.62340334069714,-0.379193969644614,
11.5040970733847));
#55365=CARTESIAN_POINT('Ctrl Pts',(-1.63612958438953,-0.319853871896392,
11.5000602047774));
#55366=CARTESIAN_POINT('Ctrl Pts',(-1.64558501067163,-0.260011485617207,
11.4960233361701));
#55367=CARTESIAN_POINT('Ctrl Pts',(-1.6550445903921,-0.200142812668726,
11.4919846943074));
#55368=CARTESIAN_POINT('Ctrl Pts',(-1.66123040716838,-0.139771924292852,
11.4879460524447));
#55369=CARTESIAN_POINT('Ctrl Pts',(-1.66411221800991,-0.0792876148595837,
11.4839074105821));
#55370=CARTESIAN_POINT('Ctrl Pts',(-1.66539371692077,-0.0523911317368556,
11.4821114859246));
#55371=CARTESIAN_POINT('Ctrl Pts',(-1.66602255436523,-0.0254722673943331,
11.4803155612672));
#55372=CARTESIAN_POINT('Ctrl Pts',(-1.66599938220149,0.00143474884533201,
11.4785196366098));
#55373=CARTESIAN_POINT('Ctrl Pts',(-1.66599941321298,0.00139827537052137,
11.4779266028919));
#55374=CARTESIAN_POINT('Ctrl Pts',(-1.66589455998199,0.126327473850728,
11.4702430512039));
#55375=CARTESIAN_POINT('Ctrl Pts',(-1.65173819877438,0.250838710108895,
11.4627912325929));
#55376=CARTESIAN_POINT('Ctrl Pts',(-1.61997824373514,0.389254288929557,
11.453712034288));
#55377=CARTESIAN_POINT('Ctrl Pts',(-1.61589773461963,0.405860658420447,
11.4526088843924));
#55378=CARTESIAN_POINT('Ctrl Pts',(-1.60826460209374,0.434982944530017,
11.4506450534144));
#55379=CARTESIAN_POINT('Ctrl Pts',(-1.60481956514939,0.44752578699632,11.4497895839921));
#55380=CARTESIAN_POINT('Ctrl Pts',(-1.59939126133126,0.466420247224837,
11.4484844664259));
#55381=CARTESIAN_POINT('Ctrl Pts',(-1.59751613115846,0.472802771476853,
11.4480407437214));
#55382=CARTESIAN_POINT('Ctrl Pts',(-1.59403225077199,0.484403760595211,
11.4472287256181));
#55383=CARTESIAN_POINT('Ctrl Pts',(-1.59243600561464,0.489625760383796,
11.4468611486657));
#55384=CARTESIAN_POINT('Ctrl Pts',(-1.58875835588181,0.501448690897791,
11.4460242538234));
#55385=CARTESIAN_POINT('Ctrl Pts',(-1.58666148509883,0.508044516146688,
11.445554071794));
#55386=CARTESIAN_POINT('Ctrl Pts',(-1.5800847112575,0.528294240404594,11.4441008376607));
#55387=CARTESIAN_POINT('Ctrl Pts',(-1.57546933580326,0.54190297701641,11.4431105279836));
#55388=CARTESIAN_POINT('Ctrl Pts',(-1.56830545224653,0.562160722799511,
11.4416175787372));
#55389=CARTESIAN_POINT('Ctrl Pts',(-1.56588958929984,0.568855369760643,
11.4411211002045));
#55390=CARTESIAN_POINT('Ctrl Pts',(-1.56343130602848,0.57553327560628,11.4406228970922));
#55391=CARTESIAN_POINT('',(-1.66599994488069,0.000428552845177652,11.6700306692265));
#55392=CARTESIAN_POINT('Ctrl Pts',(-1.56343130033056,0.575533291084625,
11.6327248639491));
#55393=CARTESIAN_POINT('Ctrl Pts',(-1.56351122601218,0.575316173648889,
11.6327391075618));
#55394=CARTESIAN_POINT('Ctrl Pts',(-1.56359110668459,0.575099038970977,
11.6327533505678));
#55395=CARTESIAN_POINT('Ctrl Pts',(-1.60363162838075,0.466189362563932,
11.6398964400467));
#55396=CARTESIAN_POINT('Ctrl Pts',(-1.6321469700982,0.353636689900426,11.6468216608511));
#55397=CARTESIAN_POINT('Ctrl Pts',(-1.65364856931402,0.205335811496005,
11.6562926822567));
#55398=CARTESIAN_POINT('Ctrl Pts',(-1.65750085011162,0.171484535364838,
11.6584789615107));
#55399=CARTESIAN_POINT('Ctrl Pts',(-1.66112862429576,0.127692478015936,
11.6613659914878));
#55400=CARTESIAN_POINT('Ctrl Pts',(-1.66185686981429,0.117836360658527,
11.662019590846));
#55401=CARTESIAN_POINT('Ctrl Pts',(-1.66288543893601,0.101999370109436,
11.6630767880648));
#55402=CARTESIAN_POINT('Ctrl Pts',(-1.66324129210249,0.0960221637506752,
11.6634773912633));
#55403=CARTESIAN_POINT('Ctrl Pts',(-1.66384554950732,0.084858406409156,
11.6642288016679));
#55404=CARTESIAN_POINT('Ctrl Pts',(-1.66410193987922,0.079672407006859,
11.6645791617619));
#55405=CARTESIAN_POINT('Ctrl Pts',(-1.66458357073178,0.0689106409105714,
11.6653088109921));
#55406=CARTESIAN_POINT('Ctrl Pts',(-1.6648050480824,0.0633347457529103,
11.6656883000724));
#55407=CARTESIAN_POINT('Ctrl Pts',(-1.66529993332798,0.0490686009949908,
11.6666627492508));
#55408=CARTESIAN_POINT('Ctrl Pts',(-1.66553332743975,0.0403772563584407,
11.6672597434594));
#55409=CARTESIAN_POINT('Ctrl Pts',(-1.66589684342434,0.0212668390744461,
11.6685791600074));
#55410=CARTESIAN_POINT('Ctrl Pts',(-1.6659972647262,0.010847658152853,11.6693029296631));
#55411=CARTESIAN_POINT('Ctrl Pts',(-1.66599994488069,0.000428552845177652,
11.6700306692265));
#55412=CARTESIAN_POINT('Ctrl Pts',(-1.66599994441765,0.000430349150014435,
11.6700305437606));
#55413=CARTESIAN_POINT('Ctrl Pts',(-1.66603398663936,-0.131356455761258,
11.6792354043323));
#55414=CARTESIAN_POINT('Ctrl Pts',(-1.65043138951007,-0.262683581037981,
11.6890002640304));
#55415=CARTESIAN_POINT('Ctrl Pts',(-1.60343336664041,-0.457446627409522,
11.703442600239));
#55416=CARTESIAN_POINT('Ctrl Pts',(-1.58325195220095,-0.52304039504908,
11.7083083319204));
#55417=CARTESIAN_POINT('Ctrl Pts',(-1.54930763632162,-0.613164745409152,
11.7149684577475));
#55418=CARTESIAN_POINT('Ctrl Pts',(-1.53888539439045,-0.638871708300922,
11.7168657543864));
#55419=CARTESIAN_POINT('Ctrl Pts',(-1.52274474471149,-0.675993198741766,
11.7196034780031));
#55420=CARTESIAN_POINT('Ctrl Pts',(-1.5175298762557,-0.687620136864921,
11.7204606929069));
#55421=CARTESIAN_POINT('Ctrl Pts',(-1.50807622133212,-0.708066254024198,
11.7219679805535));
#55422=CARTESIAN_POINT('Ctrl Pts',(-1.50389223403985,-0.716909941936505,
11.722619892978));
#55423=CARTESIAN_POINT('Ctrl Pts',(-1.49495048662678,-0.735387293080214,
11.7239820993412));
#55424=CARTESIAN_POINT('Ctrl Pts',(-1.49017693360736,-0.745012848181586,
11.7246918097402));
#55425=CARTESIAN_POINT('Ctrl Pts',(-1.47730131768552,-0.770356734711056,
11.7265611697142));
#55426=CARTESIAN_POINT('Ctrl Pts',(-1.46904140783254,-0.785993678727426,
11.7277152636192));
#55427=CARTESIAN_POINT('Ctrl Pts',(-1.42861311348497,-0.859664469187664,
11.7331607037792));
#55428=CARTESIAN_POINT('Ctrl Pts',(-1.39324388539401,-0.91587740689338,
11.7373368070795));
#55429=CARTESIAN_POINT('Ctrl Pts',(-1.27035251924036,-1.08752511347798,
11.7504087997539));
#55430=CARTESIAN_POINT('Ctrl Pts',(-1.17112827482285,-1.1937145325723,11.7589556465323));
#55431=CARTESIAN_POINT('Ctrl Pts',(-1.04783918606911,-1.29530515211135,
11.7692150133112));
#55432=CARTESIAN_POINT('Ctrl Pts',(-1.03609839116646,-1.30471548094666,
11.7701893786152));
#55433=CARTESIAN_POINT('Ctrl Pts',(-1.01752458650463,-1.31919371058587,
11.7717296187688));
#55434=CARTESIAN_POINT('Ctrl Pts',(-1.01077719063821,-1.32437071619692,
11.7722889083239));
#55435=CARTESIAN_POINT('Ctrl Pts',(-0.998266884594302,-1.33381808025436,
11.7733260581721));
#55436=CARTESIAN_POINT('Ctrl Pts',(-0.992515424157479,-1.33810334885753,
11.7738029421152));
#55437=CARTESIAN_POINT('Ctrl Pts',(-0.986682520742523,-1.34239100405459,
11.7742868487018));
#55438=CARTESIAN_POINT('Ctrl Pts',(-0.986628435126881,-1.34243075631653,
11.7742913357505));
#55439=CARTESIAN_POINT('Ctrl Pts',(-0.986520182520877,-1.3425103105739,
11.7743003166458));
#55440=CARTESIAN_POINT('Ctrl Pts',(-0.986466015518797,-1.34255011256367,
11.7743048104935));
#55441=CARTESIAN_POINT('Ctrl Pts',(-0.986357584220192,-1.34262977793024,
11.7743138063081));
#55442=CARTESIAN_POINT('Ctrl Pts',(-0.986303319919582,-1.34266964129279,
11.7743183082755));
#55443=CARTESIAN_POINT('Ctrl Pts',(-0.986194677852247,-1.3427494412316,
11.7743273216717));
#55444=CARTESIAN_POINT('Ctrl Pts',(-0.986140300070534,-1.34278937779857,
11.7743318331018));
#55445=CARTESIAN_POINT('Ctrl Pts',(-0.986031414581058,-1.3428693361724,
11.7743408667899));
#55446=CARTESIAN_POINT('Ctrl Pts',(-0.985976906869207,-1.34290935795885,
11.7743453890482));
#55447=CARTESIAN_POINT('Ctrl Pts',(-0.985867744763561,-1.34298949900268,
11.7743544457834));
#55448=CARTESIAN_POINT('Ctrl Pts',(-0.985813090355817,-1.34302961824368,
11.7743589802616));
#55449=CARTESIAN_POINT('Ctrl Pts',(-0.985729207033549,-1.34309118518265,
11.7743659397949));
#55450=CARTESIAN_POINT('Ctrl Pts',(-0.985699979852384,-1.34311263527425,
11.7743683646886));
#55451=CARTESIAN_POINT('Ctrl Pts',(-0.985640794992522,-1.34315606860381,
11.7743732750975));
#55452=CARTESIAN_POINT('Ctrl Pts',(-0.985610837285705,-1.34317805178826,
11.7743757606155));
#55453=CARTESIAN_POINT('Ctrl Pts',(-0.985550154785851,-1.34322257792734,
11.7743807953099));
#55454=CARTESIAN_POINT('Ctrl Pts',(-0.985519429951186,-1.34324512083271,
11.7743833444901));
#55455=CARTESIAN_POINT('Ctrl Pts',(-0.985457174147864,-1.3432907948206,
11.7743885097501));
#55456=CARTESIAN_POINT('Ctrl Pts',(-0.985425643133429,-1.34331392585066,
11.774391125834));
#55457=CARTESIAN_POINT('Ctrl Pts',(-0.985361733237205,-1.34336080644189,
11.7743964283651));
#55458=CARTESIAN_POINT('Ctrl Pts',(-0.985329354312176,-1.34338455594189,
11.7743991148164));
#55459=CARTESIAN_POINT('Ctrl Pts',(-0.985263703952054,-1.34343270593545,
11.7744045617876));
#55460=CARTESIAN_POINT('Ctrl Pts',(-0.985230432458938,-1.34345710637115,
11.7744073223129));
#55461=CARTESIAN_POINT('Ctrl Pts',(-0.985162949113861,-1.3435065930218,
11.7744129214038));
#55462=CARTESIAN_POINT('Ctrl Pts',(-0.985128737227789,-1.34353167915303,
11.7744157599728));
#55463=CARTESIAN_POINT('Ctrl Pts',(-0.985059321787992,-1.34358257448658,
11.7744215194099));
#55464=CARTESIAN_POINT('Ctrl Pts',(-0.985024118168926,-1.34360838361888,
11.774424440284));
#55465=CARTESIAN_POINT('Ctrl Pts',(-0.984952664132694,-1.34366076501403,
11.7744303689075));
#55466=CARTESIAN_POINT('Ctrl Pts',(-0.984916413654861,-1.34368733719323,
11.7744333766625));
#55467=CARTESIAN_POINT('Ctrl Pts',(-0.984842806578718,-1.3437412877765,
11.7744394839719));
#55468=CARTESIAN_POINT('Ctrl Pts',(-0.98480544991269,-1.34376866609077,
11.7744425835325));
#55469=CARTESIAN_POINT('Ctrl Pts',(-0.984729566531095,-1.34382427537263,
11.7744488797597));
#55470=CARTESIAN_POINT('Ctrl Pts',(-0.984691039750174,-1.34385250623609,
11.7744520764325));
#55471=CARTESIAN_POINT('Ctrl Pts',(-0.984612747148914,-1.34390987070635,
11.7744585726106));
#55472=CARTESIAN_POINT('Ctrl Pts',(-0.984572981243418,-1.34393900420947,
11.7744618721238));
#55473=CARTESIAN_POINT('Ctrl Pts',(-0.984492135789026,-1.34399822810989,
11.7744685801758));
#55474=CARTESIAN_POINT('Ctrl Pts',(-0.984451056167939,-1.34402831837829,
11.7744719887214));
#55475=CARTESIAN_POINT('Ctrl Pts',(-0.984367502500312,-1.34408951442711,
11.7744789215439));
#55476=CARTESIAN_POINT('Ctrl Pts',(-0.984325028352428,-1.34412062008237,
11.7744824458302));
#55477=CARTESIAN_POINT('Ctrl Pts',(-0.984238597970242,-1.34418391049498,
11.7744896174109));
#55478=CARTESIAN_POINT('Ctrl Pts',(-0.984194641640596,-1.344216095103,11.7744932647144));
#55479=CARTESIAN_POINT('Ctrl Pts',(-0.984105151607308,-1.34428161252185,
11.7745006902395));
#55480=CARTESIAN_POINT('Ctrl Pts',(-0.984059617783356,-1.34431494517932,
11.7745044684725));
#55481=CARTESIAN_POINT('Ctrl Pts',(-0.983966868962051,-1.3443828339459,
11.7745121644736));
#55482=CARTESIAN_POINT('Ctrl Pts',(-0.983919653840739,-1.34441738987909,
11.7745160822535));
#55483=CARTESIAN_POINT('Ctrl Pts',(-0.98382342912629,-1.34448780730439,
11.7745240667539));
#55484=CARTESIAN_POINT('Ctrl Pts',(-0.983774419385979,-1.34452366860899,
11.7745281334883));
#55485=CARTESIAN_POINT('Ctrl Pts',(-0.983674481481536,-1.3445967865735,
11.774536426188));
#55486=CARTESIAN_POINT('Ctrl Pts',(-0.983623553165258,-1.34463404301702,
11.7745406521678));
#55487=CARTESIAN_POINT('Ctrl Pts',(-0.983519642200692,-1.3447100496814,
11.7745492746414));
#55488=CARTESIAN_POINT('Ctrl Pts',(-0.983466659376021,-1.34474879966651,
11.7745536711518));
#55489=CARTESIAN_POINT('Ctrl Pts',(-0.98335849000438,-1.34482790155846,
11.7745626470892));
#55490=CARTESIAN_POINT('Ctrl Pts',(-0.983303303267584,-1.3448682531969,
11.7745672265342));
#55491=CARTESIAN_POINT('Ctrl Pts',(-0.983190561451798,-1.34495067751751,
11.7745765820081));
#55492=CARTESIAN_POINT('Ctrl Pts',(-0.983133006146599,-1.34499274990903,
11.7745813580582));
#55493=CARTESIAN_POINT('Ctrl Pts',(-0.983015345271399,-1.34507874732413,
11.7745911218464));
#55494=CARTESIAN_POINT('Ctrl Pts',(-0.982955239470018,-1.3451226720045,
11.7745961096065));
#55495=CARTESIAN_POINT('Ctrl Pts',(-0.982832276008239,-1.34521251975161,
11.7746063135525));
#55496=CARTESIAN_POINT('Ctrl Pts',(-0.982769418077261,-1.34525844243851,
11.774611529764));
#55497=CARTESIAN_POINT('Ctrl Pts',(-0.98264072628005,-1.34535244813465,
11.7746222092176));
#55498=CARTESIAN_POINT('Ctrl Pts',(-0.982574892101502,-1.34540053071856,
11.7746276724892));
#55499=CARTESIAN_POINT('Ctrl Pts',(-0.982439997920563,-1.34549903671376,
11.7746388668118));
#55500=CARTESIAN_POINT('Ctrl Pts',(-0.982370937565766,-1.34554945964017,
11.774644597896));
#55501=CARTESIAN_POINT('Ctrl Pts',(-0.982229311403413,-1.34565284820831,
11.7746563510622));
#55502=CARTESIAN_POINT('Ctrl Pts',(-0.982156745193897,-1.34570581329698,
11.7746623731824));
#55503=CARTESIAN_POINT('Ctrl Pts',(-0.98200779326378,-1.34581451281754,
11.7746747344987));
#55504=CARTESIAN_POINT('Ctrl Pts',(-0.981931407084554,-1.34587024661445,
11.7746810737384));
#55505=CARTESIAN_POINT('Ctrl Pts',(-0.981774461103005,-1.34598473894333,
11.7746940986989));
#55506=CARTESIAN_POINT('Ctrl Pts',(-0.981693900772395,-1.34604349674471,
11.7747007844698));
#55507=CARTESIAN_POINT('Ctrl Pts',(-0.981528205529277,-1.34616432609519,
11.7747145357891));
#55508=CARTESIAN_POINT('Ctrl Pts',(-0.981443070009156,-1.34622639679655,
11.7747216013952));
#55509=CARTESIAN_POINT('Ctrl Pts',(-0.981267768335308,-1.34635418047198,
11.7747361502574));
#55510=CARTESIAN_POINT('Ctrl Pts',(-0.981177601469712,-1.34641989246381,
11.7747436335812));
#55511=CARTESIAN_POINT('Ctrl Pts',(-0.980991715854019,-1.34655533397261,
11.7747590611677));
#55512=CARTESIAN_POINT('Ctrl Pts',(-0.980895996271455,-1.34662506234026,
11.7747670055095));
#55513=CARTESIAN_POINT('Ctrl Pts',(-0.980698406307501,-1.34676896747204,
11.7747834048727));
#55514=CARTESIAN_POINT('Ctrl Pts',(-0.980596534945786,-1.34684314288341,
11.7747918599873));
#55515=CARTESIAN_POINT('Ctrl Pts',(-0.980414402392712,-1.34697572711404,
11.7748069768027));
#55516=CARTESIAN_POINT('Ctrl Pts',(-0.980334144381575,-1.34703414032945,
11.7748136382001));
#55517=CARTESIAN_POINT('Ctrl Pts',(-0.975982948706236,-1.35020042349244,
11.7751747900155));
#55518=CARTESIAN_POINT('Ctrl Pts',(-0.971697445285686,-1.35328783766756,
11.7755306943022));
#55519=CARTESIAN_POINT('Ctrl Pts',(-0.961601634330326,-1.36048850606521,
11.7763695572758));
#55520=CARTESIAN_POINT('Ctrl Pts',(-0.955779586134885,-1.36458493922316,
11.7768536194049));
#55521=CARTESIAN_POINT('Ctrl Pts',(-0.936919353971478,-1.37767521879511,
11.7784222346485));
#55522=CARTESIAN_POINT('Ctrl Pts',(-0.923779556000115,-1.38652016595796,
11.7795158694891));
#55523=CARTESIAN_POINT('Ctrl Pts',(-0.842741645057831,-1.4394069235811,
11.7862560411484));
#55524=CARTESIAN_POINT('Ctrl Pts',(-0.771840536400978,-1.4786363415004,
11.7921279719249));
#55525=CARTESIAN_POINT('Ctrl Pts',(-0.635225132019675,-1.5417144908593,
11.8030792897942));
#55526=CARTESIAN_POINT('Ctrl Pts',(-0.570304544354859,-1.5668912770405,
11.8081445063092));
#55527=CARTESIAN_POINT('Ctrl Pts',(-0.437679761108076,-1.60898523820064,
11.8181009063769));
#55528=CARTESIAN_POINT('Ctrl Pts',(-0.370101776274779,-1.62586102088633,
11.8229822940843));
#55529=CARTESIAN_POINT('Ctrl Pts',(-0.284534050029324,-1.64161491607919,
11.828918020116));
#55530=CARTESIAN_POINT('Ctrl Pts',(-0.267361496749432,-1.64449902047222,
11.8300974072706));
#55531=CARTESIAN_POINT('Ctrl Pts',(-0.23958190985519,-1.64871789249165,
11.8319868627773));
#55532=CARTESIAN_POINT('Ctrl Pts',(-0.229002117693853,-1.65022065792549,
11.8327021764599));
#55533=CARTESIAN_POINT('Ctrl Pts',(-0.208693432350862,-1.65290625323593,
11.8340673358782));
#55534=CARTESIAN_POINT('Ctrl Pts',(-0.198967163893991,-1.65410522802625,
11.834717663101));
#55535=CARTESIAN_POINT('Ctrl Pts',(-0.176665255871253,-1.65665486490992,
11.8362011677848));
#55536=CARTESIAN_POINT('Ctrl Pts',(-0.164083580604366,-1.65794829451888,
11.8370325194119));
#55537=CARTESIAN_POINT('Ctrl Pts',(-0.123630244531254,-1.66164198698757,
11.8396886943809));
#55538=CARTESIAN_POINT('Ctrl Pts',(-0.0957115400342689,-1.66348368723332,
11.8414961391643));
#55539=CARTESIAN_POINT('Ctrl Pts',(0.0633884750719321,-1.66995984489162,
11.8516757440964));
#55540=CARTESIAN_POINT('Ctrl Pts',(0.194704438299184,-1.65978210686203,
11.8595674751431));
#55541=CARTESIAN_POINT('Ctrl Pts',(0.393553145097003,-1.62042457267945,
11.8720039669014));
#55542=CARTESIAN_POINT('Ctrl Pts',(0.462662491482679,-1.60206146971411,
11.8764324582381));
#55543=CARTESIAN_POINT('Ctrl Pts',(0.545329691230732,-1.5743000060104,11.8820902736034));
#55544=CARTESIAN_POINT('Ctrl Pts',(0.560215102778949,-1.56906468169421,
11.8831238380227));
#55545=CARTESIAN_POINT('Ctrl Pts',(0.581766137854563,-1.56113925595726,
11.8846449596258));
#55546=CARTESIAN_POINT('Ctrl Pts',(0.588492770549207,-1.55861601105339,
11.8851232828879));
#55547=CARTESIAN_POINT('Ctrl Pts',(0.600273337117831,-1.55410983968561,
11.8859675726368));
#55548=CARTESIAN_POINT('Ctrl Pts',(0.605334214120422,-1.5521455991657,11.8863324360359));
#55549=CARTESIAN_POINT('Ctrl Pts',(0.61636631934651,-1.54780162690558,11.8871326126535));
#55550=CARTESIAN_POINT('Ctrl Pts',(0.622333311754694,-1.5454121008547,11.8875684756355));
#55551=CARTESIAN_POINT('Ctrl Pts',(0.63901938534665,-1.53861773258297,11.8887956389323));
#55552=CARTESIAN_POINT('Ctrl Pts',(0.649706306442231,-1.53413558673956,
11.8895912682762));
#55553=CARTESIAN_POINT('Ctrl Pts',(0.726949311234621,-1.50078767405729,
11.8954079626773));
#55554=CARTESIAN_POINT('Ctrl Pts',(0.791596867669645,-1.46771623997692,
11.9006310499472));
#55555=CARTESIAN_POINT('Ctrl Pts',(0.913746976415361,-1.39480611582528,
11.9109619629968));
#55556=CARTESIAN_POINT('Ctrl Pts',(0.971317722102258,-1.35534501075365,
11.9160563105154));
#55557=CARTESIAN_POINT('Ctrl Pts',(1.09158129590482,-1.26130286230433,11.9270547777676));
#55558=CARTESIAN_POINT('Ctrl Pts',(1.15301718221431,-1.20540026753727,11.9329115406124));
#55559=CARTESIAN_POINT('Ctrl Pts',(1.22250968953689,-1.13196957375865,11.9398166287807));
#55560=CARTESIAN_POINT('Ctrl Pts',(1.23476277469953,-1.11859107466111,11.9410464129022));
#55561=CARTESIAN_POINT('Ctrl Pts',(1.25398643962519,-1.09690088623189,11.9429964631351));
#55562=CARTESIAN_POINT('Ctrl Pts',(1.26109830432541,-1.08871696111644,11.9437226000039));
#55563=CARTESIAN_POINT('Ctrl Pts',(1.27445940930742,-1.07303516457316,11.9450961103957));
#55564=CARTESIAN_POINT('Ctrl Pts',(1.28072360982477,-1.06555069918825,11.9457440817464));
#55565=CARTESIAN_POINT('Ctrl Pts',(1.29489338579194,-1.04831516456348,11.9472193708277));
#55566=CARTESIAN_POINT('Ctrl Pts',(1.30275531252242,-1.03852885124719,11.9480449071877));
#55567=CARTESIAN_POINT('Ctrl Pts',(1.32315312210294,-1.01254203442473,11.9502062449185));
#55568=CARTESIAN_POINT('Ctrl Pts',(1.3355023758078,-0.996197279156565,11.9515347328452));
#55569=CARTESIAN_POINT('Ctrl Pts',(1.42269489460525,-0.876257853132006,
11.9610748167096));
#55570=CARTESIAN_POINT('Ctrl Pts',(1.48569974989495,-0.764584013101859,
11.9688091137676));
#55571=CARTESIAN_POINT('Ctrl Pts',(1.56974477611269,-0.565083332411271,
11.9820499852387));
#55572=CARTESIAN_POINT('Ctrl Pts',(1.59758536104025,-0.480764467601537,
11.9875057890123));
#55573=CARTESIAN_POINT('Ctrl Pts',(1.62147493628602,-0.382784617727158,
11.9940954894124));
#55574=CARTESIAN_POINT('Ctrl Pts',(1.62423620788779,-0.370893181551427,
11.9948994154069));
#55575=CARTESIAN_POINT('Ctrl Pts',(1.62826447606163,-0.352637056289172,
11.9961414951042));
#55576=CARTESIAN_POINT('Ctrl Pts',(1.62962544621324,-0.34629322686093,11.9965745535006));
#55577=CARTESIAN_POINT('Ctrl Pts',(1.63206614071279,-0.334583429377948,
11.9973768559177));
#55578=CARTESIAN_POINT('Ctrl Pts',(1.63315651948792,-0.32921989413831,11.9977454968429));
#55579=CARTESIAN_POINT('Ctrl Pts',(1.635583191509,-0.316974399285635,11.9985897405316));
#55580=CARTESIAN_POINT('Ctrl Pts',(1.63690248873875,-0.310089316252672,
11.9990662646382));
#55581=CARTESIAN_POINT('Ctrl Pts',(1.6409516813258,-0.288211410930166,12.0005858670875));
#55582=CARTESIAN_POINT('Ctrl Pts',(1.64351924256803,-0.273189853823298,
12.0016372798464));
#55583=CARTESIAN_POINT('Ctrl Pts',(1.66170828591985,-0.157216092594068,
12.0098058409452));
#55584=CARTESIAN_POINT('Ctrl Pts',(1.66821939069655,-0.055063232255153,
12.0172841914388));
#55585=CARTESIAN_POINT('Ctrl Pts',(1.66208384983329,0.162184241350495,12.0330906853072));
#55586=CARTESIAN_POINT('Ctrl Pts',(1.64689668242077,0.276707617527558,12.0413522611565));
#55587=CARTESIAN_POINT('Ctrl Pts',(1.61548033641506,0.407621595821442,12.0505645968275));
#55588=CARTESIAN_POINT('Ctrl Pts',(1.61062590548988,0.426399261760057,12.0518811549029));
#55589=CARTESIAN_POINT('Ctrl Pts',(1.60247660913864,0.45579395614083,12.053935322168));
#55590=CARTESIAN_POINT('Ctrl Pts',(1.59940162380001,0.466469580389054,12.054679943252));
#55591=CARTESIAN_POINT('Ctrl Pts',(1.59343729295197,0.486423693598618,12.0560693496815));
#55592=CARTESIAN_POINT('Ctrl Pts',(1.5905731230154,0.495709152068423,12.0567149208678));
#55593=CARTESIAN_POINT('Ctrl Pts',(1.58395458830252,0.516517886652601,12.0581597183115));
#55594=CARTESIAN_POINT('Ctrl Pts',(1.58015537018089,0.528026404720095,12.0589574403438));
#55595=CARTESIAN_POINT('Ctrl Pts',(1.5685970932728,0.561796115284195,12.0612950698144));
#55596=CARTESIAN_POINT('Ctrl Pts',(1.56049054784824,0.583935831772029,12.0628235431184));
#55597=CARTESIAN_POINT('Ctrl Pts',(1.51397534657671,0.703077720301254,12.0710403500499));
#55598=CARTESIAN_POINT('Ctrl Pts',(1.46698891716395,0.796483862879099,12.0774326370651));
#55599=CARTESIAN_POINT('Ctrl Pts',(1.37009380568516,0.951050105963993,12.0885732008225));
#55600=CARTESIAN_POINT('Ctrl Pts',(1.32402180554306,1.01420801253581,12.0933225075936));
#55601=CARTESIAN_POINT('Ctrl Pts',(1.25785695493157,1.09268275665934,12.0997966702496));
#55602=CARTESIAN_POINT('Ctrl Pts',(1.24160586941739,1.11111406418342,12.101363278968));
#55603=CARTESIAN_POINT('Ctrl Pts',(1.21335573224741,1.14176034996381,12.1040611110721));
#55604=CARTESIAN_POINT('Ctrl Pts',(1.20156479510996,1.15416238768577,12.1051800151383));
#55605=CARTESIAN_POINT('Ctrl Pts',(1.18439096655243,1.17167789474204,12.10680360542));
#55606=CARTESIAN_POINT('Ctrl Pts',(1.17916122379466,1.17694088797136,12.1072972277283));
#55607=CARTESIAN_POINT('Ctrl Pts',(1.16999127903623,1.18604666760592,12.1081617753799));
#55608=CARTESIAN_POINT('Ctrl Pts',(1.16606691271147,1.18990514110198,12.1085314692338));
#55609=CARTESIAN_POINT('Ctrl Pts',(1.15760818457584,1.19813980797576,12.109327806577));
#55610=CARTESIAN_POINT('Ctrl Pts',(1.15306816731345,1.20250967009976,12.109754877645));
#55611=CARTESIAN_POINT('Ctrl Pts',(1.14051643118753,1.2144545438741,12.1109343803344));
#55612=CARTESIAN_POINT('Ctrl Pts',(1.1324543028324,1.22197577909172,12.1116906413558));
#55613=CARTESIAN_POINT('Ctrl Pts',(1.08578159058867,1.26465863084304,12.1160580460715));
#55614=CARTESIAN_POINT('Ctrl Pts',(1.04561283865277,1.29806616987811,12.1197746346321));
#55615=CARTESIAN_POINT('Ctrl Pts',(0.922274046945783,1.39120107235297,12.1309161614006));
#55616=CARTESIAN_POINT('Ctrl Pts',(0.835086336067767,1.44522055309898,12.1384389192172));
#55617=CARTESIAN_POINT('Ctrl Pts',(0.678451414407801,1.52333259106065,12.1509848903164));
#55618=CARTESIAN_POINT('Ctrl Pts',(0.611349752946374,1.55148077716466,12.1560918686487));
#55619=CARTESIAN_POINT('Ctrl Pts',(0.525970440413315,1.58089247275333,12.1622544186653));
#55620=CARTESIAN_POINT('Ctrl Pts',(0.509235591179539,1.5863622122864,12.1634471502125));
#55621=CARTESIAN_POINT('Ctrl Pts',(0.482168946347427,1.59473639646233,12.1653526557288));
#55622=CARTESIAN_POINT('Ctrl Pts',(0.471890694364649,1.5978079511958,12.1660708379894));
#55623=CARTESIAN_POINT('Ctrl Pts',(0.452178784730743,1.60349185995082,12.1674381273289));
#55624=CARTESIAN_POINT('Ctrl Pts',(0.442750406742478,1.60612075591902,12.1680877473068));
#55625=CARTESIAN_POINT('Ctrl Pts',(0.421168881415953,1.6119338058194,12.1695650651406));
#55626=CARTESIAN_POINT('Ctrl Pts',(0.409001693086385,1.61506391528166,12.1703909905131));
#55627=CARTESIAN_POINT('Ctrl Pts',(0.376411860189157,1.62305600188474,12.1725855563133));
#55628=CARTESIAN_POINT('Ctrl Pts',(0.355930373959067,1.62767020791043,12.1739463099901));
#55629=CARTESIAN_POINT('Ctrl Pts',(0.216869048068561,1.65624830838414,12.1830734005652));
#55630=CARTESIAN_POINT('Ctrl Pts',(0.0960700514466558,1.66762257067173,
12.1904204602756));
#55631=CARTESIAN_POINT('Ctrl Pts',(-0.120037404404096,1.66439148513532,
12.2036273793222));
#55632=CARTESIAN_POINT('Ctrl Pts',(-0.214858783860496,1.65482278637109,
12.2094576746848));
#55633=CARTESIAN_POINT('Ctrl Pts',(-0.319992476927955,1.63502344014951,
12.2164532582019));
#55634=CARTESIAN_POINT('Ctrl Pts',(-0.331630655418141,1.63270264400285,
12.2172352091307));
#55635=CARTESIAN_POINT('Ctrl Pts',(-0.349521847394895,1.62893574290971,
12.2184503404108));
#55636=CARTESIAN_POINT('Ctrl Pts',(-0.35579323712848,1.62757744679036,12.2188787620984));
#55637=CARTESIAN_POINT('Ctrl Pts',(-0.367408172061214,1.62499147544707,
12.2196770960556));
#55638=CARTESIAN_POINT('Ctrl Pts',(-0.372753692315715,1.62377361162524,
12.2200464566257));
#55639=CARTESIAN_POINT('Ctrl Pts',(-0.385017427150709,1.62091583100708,
12.2208982680414));
#55640=CARTESIAN_POINT('Ctrl Pts',(-0.391931234238567,1.61925799470271,
12.2213817054945));
#55641=CARTESIAN_POINT('Ctrl Pts',(-0.414163985967001,1.61377615752227,
12.2229462195415));
#55642=CARTESIAN_POINT('Ctrl Pts',(-0.429438721486368,1.60977875284756,
12.2240363141017));
#55643=CARTESIAN_POINT('Ctrl Pts',(-0.526400270201027,1.58292571174338,
12.2310435701363));
#55644=CARTESIAN_POINT('Ctrl Pts',(-0.606290870467466,1.55407840913979,
12.2372085575747));
#55645=CARTESIAN_POINT('Ctrl Pts',(-0.75147822819113,1.48874846248248,12.2487975812908));
#55646=CARTESIAN_POINT('Ctrl Pts',(-0.817210142405856,1.45370579912225,
12.254207674579));
#55647=CARTESIAN_POINT('Ctrl Pts',(-0.915369574617103,1.39260650838689,
12.2624425815092));
#55648=CARTESIAN_POINT('Ctrl Pts',(-0.949538563852768,1.36953690210696,
12.26534230662));
#55649=CARTESIAN_POINT('Ctrl Pts',(-1.00658334860366,1.32785998509348,12.2702373418834));
#55650=CARTESIAN_POINT('Ctrl Pts',(-1.02988448278311,1.30987034483122,12.2722534438722));
#55651=CARTESIAN_POINT('Ctrl Pts',(-1.06280307663763,1.28303374696575,12.275127859017));
#55652=CARTESIAN_POINT('Ctrl Pts',(-1.07281125854004,1.27467721243081,12.2760054202603));
#55653=CARTESIAN_POINT('Ctrl Pts',(-1.09018721170492,1.25981917679213,12.2775358684295));
#55654=CARTESIAN_POINT('Ctrl Pts',(-1.09759737086515,1.25336847469488,12.2781907851928));
#55655=CARTESIAN_POINT('Ctrl Pts',(-1.11289024136472,1.23981606157601,12.2795473205956));
#55656=CARTESIAN_POINT('Ctrl Pts',(-1.12076306475678,1.23270382385122,12.2802484592181));
#55657=CARTESIAN_POINT('Ctrl Pts',(-1.14111368830597,1.21396311370241,12.2820686357315));
#55658=CARTESIAN_POINT('Ctrl Pts',(-1.15348201128652,1.2022171916083,12.2831826457114));
#55659=CARTESIAN_POINT('Ctrl Pts',(-1.20603984639188,1.15074624494546,12.2879543169931));
#55660=CARTESIAN_POINT('Ctrl Pts',(-1.24437656200537,1.10917853015273,12.2915308551066));
#55661=CARTESIAN_POINT('Ctrl Pts',(-1.34855371515168,0.984005354277316,
12.3016748695222));
#55662=CARTESIAN_POINT('Ctrl Pts',(-1.40859442624594,0.89594928338679,12.3080627300279));
#55663=CARTESIAN_POINT('Ctrl Pts',(-1.48869650157309,0.75028446684585,12.3183189307649));
#55664=CARTESIAN_POINT('Ctrl Pts',(-1.51470510814306,0.696283674936131,
12.322066071126));
#55665=CARTESIAN_POINT('Ctrl Pts',(-1.54334682177581,0.627573411891013,
12.3269069115109));
#55666=CARTESIAN_POINT('Ctrl Pts',(-1.54876984199068,0.614068189093516,
12.3278618260956));
#55667=CARTESIAN_POINT('Ctrl Pts',(-1.55652241791239,0.594005349406701,
12.3292879272482));
#55668=CARTESIAN_POINT('Ctrl Pts',(-1.55898909311836,0.587500975144137,
12.3297514257693));
#55669=CARTESIAN_POINT('Ctrl Pts',(-1.56209021298762,0.579166570564681,
12.3303470399816));
#55670=CARTESIAN_POINT('Ctrl Pts',(-1.56276234322638,0.577350507380284,
12.3304769274012));
#55671=CARTESIAN_POINT('Ctrl Pts',(-1.56343130033211,0.57553329108042,12.3306070045052));
#55672=CARTESIAN_POINT('Origin',(0.,0.,11.));
#55673=CARTESIAN_POINT('',(-1.56343129955154,0.575533293200813,13.0328805013286));
#55674=CARTESIAN_POINT('',(-1.56343130043543,0.575533290799732,12.8376620384731));
#55675=CARTESIAN_POINT('',(-1.56343130033213,0.575533291080363,11.));
#55676=CARTESIAN_POINT('',(-1.66599979399416,-0.000828499501219724,12.1785196366098));
#55677=CARTESIAN_POINT('Ctrl Pts',(-1.56343130043543,0.575533290799732,
12.8376620384731));
#55678=CARTESIAN_POINT('Ctrl Pts',(-1.56057559831165,0.583290781385264,
12.8371017145145));
#55679=CARTESIAN_POINT('Ctrl Pts',(-1.55766210304294,0.591027169998756,
12.8365432982622));
#55680=CARTESIAN_POINT('Ctrl Pts',(-1.55073987019112,0.609001417257086,
12.8352466917295));
#55681=CARTESIAN_POINT('Ctrl Pts',(-1.54668715783039,0.619221864160468,
12.8345100178133));
#55682=CARTESIAN_POINT('Ctrl Pts',(-1.53922479276641,0.637510579794046,
12.8331926154892));
#55683=CARTESIAN_POINT('Ctrl Pts',(-1.53585215848513,0.645593412530058,
12.8326106698783));
#55684=CARTESIAN_POINT('Ctrl Pts',(-1.52777989022075,0.664518040901161,
12.8312486170692));
#55685=CARTESIAN_POINT('Ctrl Pts',(-1.52302829944338,0.675337271868922,
12.8304703028192));
#55686=CARTESIAN_POINT('Ctrl Pts',(-1.50876244240094,0.706903682303832,
12.8281998300067));
#55687=CARTESIAN_POINT('Ctrl Pts',(-1.49893623451018,0.727507505204777,
12.8267183497455));
#55688=CARTESIAN_POINT('Ctrl Pts',(-1.45157381147596,0.821781581506401,
12.8199314107458));
#55689=CARTESIAN_POINT('Ctrl Pts',(-1.40900838731808,0.892798509151854,
12.8148023101353));
#55690=CARTESIAN_POINT('Ctrl Pts',(-1.32830444365616,1.00719797834112,12.8062190730838));
#55691=CARTESIAN_POINT('Ctrl Pts',(-1.29287377565974,1.05229168349336,12.8027377532157));
#55692=CARTESIAN_POINT('Ctrl Pts',(-1.20454490719384,1.15349898951133,12.7944938526621));
#55693=CARTESIAN_POINT('Ctrl Pts',(-1.14994279741213,1.20793906736155,12.7897130855228));
#55694=CARTESIAN_POINT('Ctrl Pts',(-1.08301538323613,1.26600486988038,12.783917516342));
#55695=CARTESIAN_POINT('Ctrl Pts',(-1.07417154403224,1.27351722656889,12.7831528290758));
#55696=CARTESIAN_POINT('Ctrl Pts',(-1.06030574833672,1.28504827783642,12.7819543575631));
#55697=CARTESIAN_POINT('Ctrl Pts',(-1.05533757187814,1.28913147593223,12.7815250264043));
#55698=CARTESIAN_POINT('Ctrl Pts',(-1.04609202335394,1.29664085729999,12.7807259524591));
#55699=CARTESIAN_POINT('Ctrl Pts',(-1.0418212358962,1.30007482222813,12.7803567717288));
#55700=CARTESIAN_POINT('Ctrl Pts',(-1.03189264308965,1.30797765808361,12.7794984084989));
#55701=CARTESIAN_POINT('Ctrl Pts',(-1.02622271557862,1.31243091784007,12.7790081680065));
#55702=CARTESIAN_POINT('Ctrl Pts',(-1.00794004544287,1.32659953831916,12.7774276952099));
#55703=CARTESIAN_POINT('Ctrl Pts',(-0.995217312512813,1.33617061966191,
12.7763283276406));
#55704=CARTESIAN_POINT('Ctrl Pts',(-0.964345296447192,1.35870955519144,
12.7736655707429));
#55705=CARTESIAN_POINT('Ctrl Pts',(-0.946069195009378,1.37149789794062,
12.772093197122));
#55706=CARTESIAN_POINT('Ctrl Pts',(-0.873128305739834,1.4203851549974,12.7658492339669));
#55707=CARTESIAN_POINT('Ctrl Pts',(-0.816612995169159,1.45361251486965,
12.7610817536197));
#55708=CARTESIAN_POINT('Ctrl Pts',(-0.649713390930293,1.5389276661131,12.7474371352029));
#55709=CARTESIAN_POINT('Ctrl Pts',(-0.535349698712847,1.5823517018954,12.7386289212694));
#55710=CARTESIAN_POINT('Ctrl Pts',(-0.396987483619256,1.61814557882303,
12.7287985526631));
#55711=CARTESIAN_POINT('Ctrl Pts',(-0.376624201347912,1.6230059939517,12.7273706947822));
#55712=CARTESIAN_POINT('Ctrl Pts',(-0.343918433953247,1.6301636423514,12.7251066445784));
#55713=CARTESIAN_POINT('Ctrl Pts',(-0.331632784990003,1.63270729186905,
12.7242627056457));
#55714=CARTESIAN_POINT('Ctrl Pts',(-0.309715813490914,1.6369874338899,12.7227684205637));
#55715=CARTESIAN_POINT('Ctrl Pts',(-0.30009584153034,1.63877827565464,12.7221163748024));
#55716=CARTESIAN_POINT('Ctrl Pts',(-0.27989024504765,1.64235583326689,12.720754624417));
#55717=CARTESIAN_POINT('Ctrl Pts',(-0.269301974878431,1.64412520440636,
12.7200454968439));
#55718=CARTESIAN_POINT('Ctrl Pts',(-0.241269103423719,1.64853160736399,
12.7181793607935));
#55719=CARTESIAN_POINT('Ctrl Pts',(-0.22379814631042,1.65099414570989,12.7170278732524));
#55720=CARTESIAN_POINT('Ctrl Pts',(-0.133527473468258,1.66225851132056,
12.7111326006945));
#55721=CARTESIAN_POINT('Ctrl Pts',(-0.0602390778271082,1.66652517346292,
12.706532883713));
#55722=CARTESIAN_POINT('Ctrl Pts',(0.111340547297109,1.66517601317831,12.6959423211969));
#55723=CARTESIAN_POINT('Ctrl Pts',(0.209316410812084,1.65571537404338,12.6900350446318));
#55724=CARTESIAN_POINT('Ctrl Pts',(0.336620595046811,1.63193756917198,12.6820004291875));
#55725=CARTESIAN_POINT('Ctrl Pts',(0.367187292189199,1.62533287293225,12.6800421494094));
#55726=CARTESIAN_POINT('Ctrl Pts',(0.42471792522947,1.61119627539996,12.6762708310402));
#55727=CARTESIAN_POINT('Ctrl Pts',(0.451713090547941,1.60383721744689,12.6744647713115));
#55728=CARTESIAN_POINT('Ctrl Pts',(0.487343324507959,1.59315333881851,12.6720165602298));
#55729=CARTESIAN_POINT('Ctrl Pts',(0.496155992159062,1.59043085317141,12.6714057178708));
#55730=CARTESIAN_POINT('Ctrl Pts',(0.509961453357943,1.58604004444888,12.6704397745767));
#55731=CARTESIAN_POINT('Ctrl Pts',(0.5149698822242,1.58442094311208,12.6700874664156));
#55732=CARTESIAN_POINT('Ctrl Pts',(0.525293349519783,1.58102950252258,12.6693572372349));
#55733=CARTESIAN_POINT('Ctrl Pts',(0.53060719267888,1.57925406258393,12.6689791215216));
#55734=CARTESIAN_POINT('Ctrl Pts',(0.543537145119363,1.57486133615667,12.6680537437906));
#55735=CARTESIAN_POINT('Ctrl Pts',(0.551143369018455,1.57221558203638,12.6675048627041));
#55736=CARTESIAN_POINT('Ctrl Pts',(0.578621066940668,1.56243382572882,12.6655063773052));
#55737=CARTESIAN_POINT('Ctrl Pts',(0.598374692312269,1.55497569889347,12.6640399318227));
#55738=CARTESIAN_POINT('Ctrl Pts',(0.648462494777282,1.53496899546784,12.6602543374306));
#55739=CARTESIAN_POINT('Ctrl Pts',(0.678576629772541,1.52189583096448,12.6579143257129));
#55740=CARTESIAN_POINT('Ctrl Pts',(0.773563509689639,1.47728034296331,12.650365946967));
#55741=CARTESIAN_POINT('Ctrl Pts',(0.836782745962807,1.44241189649882,12.645089282005));
#55742=CARTESIAN_POINT('Ctrl Pts',(0.985840585672479,1.34709283443898,12.6322469940775));
#55743=CARTESIAN_POINT('Ctrl Pts',(1.06862684113967,1.28241361246042,12.6247686914399));
#55744=CARTESIAN_POINT('Ctrl Pts',(1.15841197934364,1.19749275930731,12.6163175807843));
#55745=CARTESIAN_POINT('Ctrl Pts',(1.17180970316557,1.18438561787403,12.6150457582739));
#55746=CARTESIAN_POINT('Ctrl Pts',(1.19276877017959,1.16317725201868,12.6130380046328));
#55747=CARTESIAN_POINT('Ctrl Pts',(1.20047505464536,1.15522219168414,12.6122957327183));
#55748=CARTESIAN_POINT('Ctrl Pts',(1.2147310974028,1.14020921432831,12.6109146536075));
#55749=CARTESIAN_POINT('Ctrl Pts',(1.22130006555649,1.13317026432942,12.6102750327436));
#55750=CARTESIAN_POINT('Ctrl Pts',(1.23600017438321,1.11714210138051,12.6088360295651));
#55751=CARTESIAN_POINT('Ctrl Pts',(1.24409503467342,1.10812023869926,12.6080382005021));
#55752=CARTESIAN_POINT('Ctrl Pts',(1.2681716320533,1.08069003240263,12.6056478633689));
#55753=CARTESIAN_POINT('Ctrl Pts',(1.28384895068836,1.06201798710102,12.6040678684018));
#55754=CARTESIAN_POINT('Ctrl Pts',(1.31916609333923,1.01802895199933,12.6004460351622));
#55755=CARTESIAN_POINT('Ctrl Pts',(1.33849691329658,0.992475858893271,12.5984158074655));
#55756=CARTESIAN_POINT('Ctrl Pts',(1.40697996922379,0.896305644707766,12.5910091483143));
#55757=CARTESIAN_POINT('Ctrl Pts',(1.45137863982918,0.822470423455903,12.5857786008085));
#55758=CARTESIAN_POINT('Ctrl Pts',(1.53022645030923,0.664900465330985,12.5750134057199));
#55759=CARTESIAN_POINT('Ctrl Pts',(1.56395752351259,0.581135370906246,12.5694919535862));
#55760=CARTESIAN_POINT('Ctrl Pts',(1.59541098557232,0.480069234958713,12.5626236415821));
#55761=CARTESIAN_POINT('Ctrl Pts',(1.59986569041235,0.465007969949144,12.5615947547427));
#55762=CARTESIAN_POINT('Ctrl Pts',(1.60602248540584,0.443055428413562,12.560084326015));
#55763=CARTESIAN_POINT('Ctrl Pts',(1.60789466686261,0.436212186879269,12.559611972826));
#55764=CARTESIAN_POINT('Ctrl Pts',(1.61113555908841,0.42406161146778,12.5587702683391));
#55765=CARTESIAN_POINT('Ctrl Pts',(1.61252187288238,0.418759176941351,12.5584019279243));
#55766=CARTESIAN_POINT('Ctrl Pts',(1.61547692785096,0.407224259435909,12.5575983193294));
#55767=CARTESIAN_POINT('Ctrl Pts',(1.61703575545577,0.400989605828504,12.5571625315986));
#55768=CARTESIAN_POINT('Ctrl Pts',(1.62138155909899,0.38317072178033,12.5559132476047));
#55769=CARTESIAN_POINT('Ctrl Pts',(1.62408032073768,0.371565678825545,12.5550950647572));
#55770=CARTESIAN_POINT('Ctrl Pts',(1.6299522551859,0.345028505677191,12.5532152945406));
#55771=CARTESIAN_POINT('Ctrl Pts',(1.63304509380198,0.330079852204156,12.552150059365));
#55772=CARTESIAN_POINT('Ctrl Pts',(1.66343390912173,0.172303309547315,12.5408546389933));
#55773=CARTESIAN_POINT('Ctrl Pts',(1.67212456616911,0.0265298737222167,
12.5300370154238));
#55774=CARTESIAN_POINT('Ctrl Pts',(1.65713143432942,-0.183678472453655,
12.5149876719441));
#55775=CARTESIAN_POINT('Ctrl Pts',(1.6486565614359,-0.248507224866853,12.5104117126023));
#55776=CARTESIAN_POINT('Ctrl Pts',(1.63308638494221,-0.329993348806482,
12.5047500513115));
#55777=CARTESIAN_POINT('Ctrl Pts',(1.62950318735082,-0.347255172485597,
12.5035556776559));
#55778=CARTESIAN_POINT('Ctrl Pts',(1.62329888724151,-0.37492918146853,12.5016482219629));
#55779=CARTESIAN_POINT('Ctrl Pts',(1.62085003620628,-0.385378175157583,
12.5009297112279));
#55780=CARTESIAN_POINT('Ctrl Pts',(1.61597548857948,-0.405308499689075,
12.4995622183109));
#55781=CARTESIAN_POINT('Ctrl Pts',(1.61356689121204,-0.414793507863377,
12.4989127192926));
#55782=CARTESIAN_POINT('Ctrl Pts',(1.60782412232259,-0.436601120012205,
12.4974221321239));
#55783=CARTESIAN_POINT('Ctrl Pts',(1.60443158870425,-0.448907828584265,
12.4965829621367));
#55784=CARTESIAN_POINT('Ctrl Pts',(1.59318436874859,-0.487950849599055,
12.4939260728876));
#55785=CARTESIAN_POINT('Ctrl Pts',(1.58479998059536,-0.514530495347398,
12.4921254832463));
#55786=CARTESIAN_POINT('Ctrl Pts',(1.55184338920774,-0.610541811953956,
12.4856351875206));
#55787=CARTESIAN_POINT('Ctrl Pts',(1.52334121620919,-0.678536924626257,
12.4810697436467));
#55788=CARTESIAN_POINT('Ctrl Pts',(1.43231860924841,-0.860774525529232,
12.4685766669968));
#55789=CARTESIAN_POINT('Ctrl Pts',(1.36079280440545,-0.969898085276284,
12.4608133479951));
#55790=CARTESIAN_POINT('Ctrl Pts',(1.26754856362993,-1.08125319969806,12.4513805824067));
#55791=CARTESIAN_POINT('Ctrl Pts',(1.25761399258041,-1.0927922257186,12.4503824612273));
#55792=CARTESIAN_POINT('Ctrl Pts',(1.24282874878284,-1.10949667303317,12.4489041040428));
#55793=CARTESIAN_POINT('Ctrl Pts',(1.23810072629406,-1.11477026927804,12.448432388812));
#55794=CARTESIAN_POINT('Ctrl Pts',(1.2296622037612,-1.12406262361142,12.4475919526881));
#55795=CARTESIAN_POINT('Ctrl Pts',(1.2259653342221,-1.12809348678403,12.4472242407048));
#55796=CARTESIAN_POINT('Ctrl Pts',(1.21781710387063,-1.13689050910773,12.4464147379689));
#55797=CARTESIAN_POINT('Ctrl Pts',(1.21335764663822,-1.14164869635495,12.4459723597842));
#55798=CARTESIAN_POINT('Ctrl Pts',(1.20035988693036,-1.15535497288458,12.4446851914861));
#55799=CARTESIAN_POINT('Ctrl Pts',(1.19174994487353,-1.1642340906382,12.4438352771806));
#55800=CARTESIAN_POINT('Ctrl Pts',(1.1717634146485,-1.18439145099116,12.4418702398946));
#55801=CARTESIAN_POINT('Ctrl Pts',(1.16032153265617,-1.19560298934976,12.4407510056824));
#55802=CARTESIAN_POINT('Ctrl Pts',(1.12096389207017,-1.23307120188708,12.4369254454263));
#55803=CARTESIAN_POINT('Ctrl Pts',(1.09230574309102,-1.25852788137488,12.4341806519727));
#55804=CARTESIAN_POINT('Ctrl Pts',(1.00799976108115,-1.32836585757318,12.4262738327249));
#55805=CARTESIAN_POINT('Ctrl Pts',(0.950350454453864,-1.37020196613827,
12.4210669315802));
#55806=CARTESIAN_POINT('Ctrl Pts',(0.807994396116067,-1.46019174264913,
12.4088670573473));
#55807=CARTESIAN_POINT('Ctrl Pts',(0.721381755008904,-1.50486847168071,
12.4019509044062));
#55808=CARTESIAN_POINT('Ctrl Pts',(0.613886306307181,-1.54888856190578,
12.3940085432739));
#55809=CARTESIAN_POINT('Ctrl Pts',(0.596300533029561,-1.55574351980763,
12.3927280323966));
#55810=CARTESIAN_POINT('Ctrl Pts',(0.568287874932052,-1.56611808314776,
12.3907170993207));
#55811=CARTESIAN_POINT('Ctrl Pts',(0.557936541988382,-1.56983559149122,
12.3899801489876));
#55812=CARTESIAN_POINT('Ctrl Pts',(0.539278000104317,-1.57632862410038,
12.3886625029863));
#55813=CARTESIAN_POINT('Ctrl Pts',(0.53098436640402,-1.57914163398914,12.3880805873817));
#55814=CARTESIAN_POINT('Ctrl Pts',(0.511454572329717,-1.58559443376058,
12.3867189253395));
#55815=CARTESIAN_POINT('Ctrl Pts',(0.500201027098248,-1.58918042790537,
12.3859409684182));
#55816=CARTESIAN_POINT('Ctrl Pts',(0.467117947049906,-1.59933625980721,
12.3836726594754));
#55817=CARTESIAN_POINT('Ctrl Pts',(0.445190034989375,-1.60557826419364,
12.3821929539685));
#55818=CARTESIAN_POINT('Ctrl Pts',(0.343385113452899,-1.63231189911165,
12.3754216020902));
#55819=CARTESIAN_POINT('Ctrl Pts',(0.262180733524004,-1.64730660142348,
12.370305319463));
#55820=CARTESIAN_POINT('Ctrl Pts',(0.123064555626081,-1.66244195409447,
12.3617253778789));
#55821=CARTESIAN_POINT('Ctrl Pts',(0.0656546454323221,-1.66569731025476,
12.3582347937311));
#55822=CARTESIAN_POINT('Ctrl Pts',(-0.0689381260133705,-1.66635911481172,
12.3499750616312));
#55823=CARTESIAN_POINT('Ctrl Pts',(-0.145991509935956,-1.66138150591947,
12.3451878925344));
#55824=CARTESIAN_POINT('Ctrl Pts',(-0.233912265440251,-1.64953803028404,
12.3393851690594));
#55825=CARTESIAN_POINT('Ctrl Pts',(-0.245395861825237,-1.64786877929135,
12.3386204528906));
#55826=CARTESIAN_POINT('Ctrl Pts',(-0.263214778905215,-1.64508824619619,
12.3374219455859));
#55827=CARTESIAN_POINT('Ctrl Pts',(-0.269562944418963,-1.6440599664044,
12.3369926079593));
#55828=CARTESIAN_POINT('Ctrl Pts',(-0.281309516236458,-1.64208738807223,
12.3361935285534));
#55829=CARTESIAN_POINT('Ctrl Pts',(-0.286709408311424,-1.64115317566291,
12.3358243489025));
#55830=CARTESIAN_POINT('Ctrl Pts',(-0.299202503155856,-1.63892825983488,
12.3349659969122));
#55831=CARTESIAN_POINT('Ctrl Pts',(-0.306292006985218,-1.63761814242546,
12.3344757666785));
#55832=CARTESIAN_POINT('Ctrl Pts',(-0.32900837952904,-1.63326756240484,
12.3328953607541));
#55833=CARTESIAN_POINT('Ctrl Pts',(-0.344599713090734,-1.63004921264532,
12.3317960508413));
#55834=CARTESIAN_POINT('Ctrl Pts',(-0.381917767605521,-1.62178674822694,
12.3291334610089));
#55835=CARTESIAN_POINT('Ctrl Pts',(-0.403593648455485,-1.61652884432489,
12.3275611981952));
#55836=CARTESIAN_POINT('Ctrl Pts',(-0.488485698902753,-1.59412286814509,
12.3213179159231));
#55837=CARTESIAN_POINT('Ctrl Pts',(-0.550770955754018,-1.57368880392259,
12.3165510240262));
#55838=CARTESIAN_POINT('Ctrl Pts',(-0.725134649075396,-1.50486250417439,
12.3029053168529));
#55839=CARTESIAN_POINT('Ctrl Pts',(-0.833341213322183,-1.44775142919914,
12.2940954314001));
#55840=CARTESIAN_POINT('Ctrl Pts',(-0.951679353126265,-1.3675892298811,
12.2842640524843));
#55841=CARTESIAN_POINT('Ctrl Pts',(-0.968782440150438,-1.35552740491392,
12.2828366669265));
#55842=CARTESIAN_POINT('Ctrl Pts',(-0.995767213079444,-1.33572489658619,
12.2805732145575));
#55843=CARTESIAN_POINT('Ctrl Pts',(-1.00579609052524,-1.32818958783254,
12.2797294076052));
#55844=CARTESIAN_POINT('Ctrl Pts',(-1.02327447208066,-1.31474550010255,
12.2782538767596));
#55845=CARTESIAN_POINT('Ctrl Pts',(-1.03076017683544,-1.30888496039293,
12.2776203020706));
#55846=CARTESIAN_POINT('Ctrl Pts',(-1.04614409617535,-1.29662709516369,
12.2763146276187));
#55847=CARTESIAN_POINT('Ctrl Pts',(-1.05403477236289,-1.29022091141695,
12.2756429168749));
#55848=CARTESIAN_POINT('Ctrl Pts',(-1.07294992336873,-1.27457496983093,
12.2740274704699));
#55849=CARTESIAN_POINT('Ctrl Pts',(-1.08391444466818,-1.26526376285485,
12.2730866614192));
#55850=CARTESIAN_POINT('Ctrl Pts',(-1.10838038931192,-1.24393550483927,
12.2709761998746));
#55851=CARTESIAN_POINT('Ctrl Pts',(-1.12180972911259,-1.23183830049405,
12.2698098774782));
#55852=CARTESIAN_POINT('Ctrl Pts',(-1.16042215702941,-1.19590081336927,
12.266429461949));
#55853=CARTESIAN_POINT('Ctrl Pts',(-1.18506172067924,-1.17148934595956,
12.2642379928043));
#55854=CARTESIAN_POINT('Ctrl Pts',(-1.2698678103973,-1.0820522583828,12.25653001053));
#55855=CARTESIAN_POINT('Ctrl Pts',(-1.32559085351529,-1.01302078397566,
12.2511600030804));
#55856=CARTESIAN_POINT('Ctrl Pts',(-1.3802732333519,-0.932990624174738,
12.2452308882704));
#55857=CARTESIAN_POINT('Ctrl Pts',(-1.38493139246276,-0.926061952883341,
12.2447197628913));
#55858=CARTESIAN_POINT('Ctrl Pts',(-1.4339603460905,-0.851937633190046,
12.2392719570824));
#55859=CARTESIAN_POINT('Ctrl Pts',(-1.47345005913669,-0.781653017104703,
12.2342862640505));
#55860=CARTESIAN_POINT('Ctrl Pts',(-1.51264908651603,-0.698272213346401,
12.2282602124022));
#55861=CARTESIAN_POINT('Ctrl Pts',(-1.5174880631557,-0.687692738367644,
12.2274936026497));
#55862=CARTESIAN_POINT('Ctrl Pts',(-1.52483189046305,-0.671181903325557,
12.226292750525));
#55863=CARTESIAN_POINT('Ctrl Pts',(-1.52741393073529,-0.665284993248127,
12.2258629893137));
#55864=CARTESIAN_POINT('Ctrl Pts',(-1.53213033520592,-0.654341394089419,
12.2250635514958));
#55865=CARTESIAN_POINT('Ctrl Pts',(-1.53427405628802,-0.649298961271169,
12.224694441734));
#55866=CARTESIAN_POINT('Ctrl Pts',(-1.53917710858784,-0.637606201714705,
12.2238368222859));
#55867=CARTESIAN_POINT('Ctrl Pts',(-1.54191822992249,-0.630948498279305,
12.2233472611282));
#55868=CARTESIAN_POINT('Ctrl Pts',(-1.55056147758728,-0.609562837458039,
12.2217712124408));
#55869=CARTESIAN_POINT('Ctrl Pts',(-1.55629618887594,-0.594768757769509,
12.2206756585349));
#55870=CARTESIAN_POINT('Ctrl Pts',(-1.58699466918464,-0.512089318036046,
12.2145324142179));
#55871=CARTESIAN_POINT('Ctrl Pts',(-1.60772601932432,-0.442721744933113,
12.2093051861428));
#55872=CARTESIAN_POINT('Ctrl Pts',(-1.6517995721916,-0.250449698524759,
12.1949625177314));
#55873=CARTESIAN_POINT('Ctrl Pts',(-1.66593062834089,-0.125894015948298,
12.1858615843024));
#55874=CARTESIAN_POINT('Ctrl Pts',(-1.6659997452095,-0.000921391271100774,
12.1771821268692));
#55875=CARTESIAN_POINT('Ctrl Pts',(-1.66599979399416,-0.000828499501219724,
12.1785196366098));
#55876=CARTESIAN_POINT('Ctrl Pts',(-1.66603059434109,0.0611068083237465,
12.1743970351476));
#55877=CARTESIAN_POINT('Ctrl Pts',(-1.66260328405743,0.123036889626019,
12.1702744336855));
#55878=CARTESIAN_POINT('Ctrl Pts',(-1.65574596036209,0.18455707720003,12.1661518322233));
#55879=CARTESIAN_POINT('Ctrl Pts',(-1.64888676465322,0.246094059463739,
12.1620281053125));
#55880=CARTESIAN_POINT('Ctrl Pts',(-1.63859576107942,0.307220439264669,
12.1579043784017));
#55881=CARTESIAN_POINT('Ctrl Pts',(-1.62495263499754,0.367539023798209,
12.1537806514908));
#55882=CARTESIAN_POINT('Ctrl Pts',(-1.61129538063748,0.427920071856396,
12.1496526542126));
#55883=CARTESIAN_POINT('Ctrl Pts',(-1.59427920275196,0.487491181084654,
12.1455246569344));
#55884=CARTESIAN_POINT('Ctrl Pts',(-1.57403402702575,0.545868923611786,
12.1413966596562));
#55885=CARTESIAN_POINT('Ctrl Pts',(-1.57059271091171,0.555792090927155,
12.1406949742895));
#55886=CARTESIAN_POINT('Ctrl Pts',(-1.56705820997352,0.565680821823223,
12.1399932889229));
#55887=CARTESIAN_POINT('Ctrl Pts',(-1.56343130033213,0.575533291080363,
12.1392916035562));
#55888=CARTESIAN_POINT('Ctrl Pts',(-1.56343130033211,0.57553329108042,12.3306070045052));
#55889=CARTESIAN_POINT('Ctrl Pts',(-1.56446758603764,0.572718229756892,
12.3308085077741));
#55890=CARTESIAN_POINT('Ctrl Pts',(-1.56549625706293,0.569900401527806,
12.3310104699606));
#55891=CARTESIAN_POINT('Ctrl Pts',(-1.56869220479126,0.561071824407949,
12.3316440473536));
#55892=CARTESIAN_POINT('Ctrl Pts',(-1.57083245714038,0.555051541463941,
12.3320772473261));
#55893=CARTESIAN_POINT('Ctrl Pts',(-1.57670050032788,0.538239620125473,
12.3332899072989));
#55894=CARTESIAN_POINT('Ctrl Pts',(-1.58035198047519,0.527421990685742,
12.3340735414443));
#55895=CARTESIAN_POINT('Ctrl Pts',(-1.60364844798922,0.455990774229675,
12.3392661468574));
#55896=CARTESIAN_POINT('Ctrl Pts',(-1.61991141185927,0.394336341501583,
12.3438315550567));
#55897=CARTESIAN_POINT('Ctrl Pts',(-1.65472577035379,0.223091012756832,
12.3564903812482));
#55898=CARTESIAN_POINT('Ctrl Pts',(-1.66591584845416,0.112320009136745,
12.3646350425551));
#55899=CARTESIAN_POINT('Ctrl Pts',(-1.66603996118025,-0.0524117735343192,
12.3763075003104));
#55900=CARTESIAN_POINT('Ctrl Pts',(-1.66348724514481,-0.106053903022186,
12.3800442000452));
#55901=CARTESIAN_POINT('Ctrl Pts',(-1.6567543340318,-0.176063883185556,
12.3848366249681));
#55902=CARTESIAN_POINT('Ctrl Pts',(-1.65491131019478,-0.192618806661558,
12.3859637759678));
#55903=CARTESIAN_POINT('Ctrl Pts',(-1.65149915185674,-0.219584383903663,
12.387790395302));
#55904=CARTESIAN_POINT('Ctrl Pts',(-1.65007910939348,-0.2300123730685,12.3884944891604));
#55905=CARTESIAN_POINT('Ctrl Pts',(-1.64713786441424,-0.250179956294903,
12.3898520149602));
#55906=CARTESIAN_POINT('Ctrl Pts',(-1.64562884995618,-0.259920853771098,
12.3905058004801));
#55907=CARTESIAN_POINT('Ctrl Pts',(-1.64188875601092,-0.282724065010168,
12.3920321490832));
#55908=CARTESIAN_POINT('Ctrl Pts',(-1.63958808776659,-0.295774412888371,
12.3929024785311));
#55909=CARTESIAN_POINT('Ctrl Pts',(-1.63144104614049,-0.338967237042632,
12.3957736101069));
#55910=CARTESIAN_POINT('Ctrl Pts',(-1.62491697459146,-0.368976545595315,
12.3977530157594));
#55911=CARTESIAN_POINT('Ctrl Pts',(-1.60711224551937,-0.441195860488513,
12.4024938837271));
#55912=CARTESIAN_POINT('Ctrl Pts',(-1.59499364553735,-0.483176198129534,
12.405230313708));
#55913=CARTESIAN_POINT('Ctrl Pts',(-1.55831024370868,-0.593739349029494,
12.412449563597));
#55914=CARTESIAN_POINT('Ctrl Pts',(-1.53087599955039,-0.661268668922863,
12.4168694850393));
#55915=CARTESIAN_POINT('Ctrl Pts',(-1.49197226807926,-0.741513728241527,
12.4223249799457));
#55916=CARTESIAN_POINT('Ctrl Pts',(-1.48461594090737,-0.756134482598804,
12.4233278169476));
#55917=CARTESIAN_POINT('Ctrl Pts',(-1.44364627026296,-0.834658470757961,
12.4287732003365));
#55918=CARTESIAN_POINT('Ctrl Pts',(-1.40612496149368,-0.89642582148789,
12.4332700962649));
#55919=CARTESIAN_POINT('Ctrl Pts',(-1.35807678677339,-0.965048022709284,
12.4387496928834));
#55920=CARTESIAN_POINT('Ctrl Pts',(-1.35133264153374,-0.974469249592769,
12.4395132499669));
#55921=CARTESIAN_POINT('Ctrl Pts',(-1.34069557866648,-0.989005902002203,
12.4407103353552));
#55922=CARTESIAN_POINT('Ctrl Pts',(-1.33687023778565,-0.994170645669132,
12.4411394271612));
#55923=CARTESIAN_POINT('Ctrl Pts',(-1.32975869781132,-1.0036569534013,12.4419348232516));
#55924=CARTESIAN_POINT('Ctrl Pts',(-1.3264811421569,-1.00798474736811,12.4423005392839));
#55925=CARTESIAN_POINT('Ctrl Pts',(-1.31881663185041,-1.01800310352015,
12.4431537187448));
#55926=CARTESIAN_POINT('Ctrl Pts',(-1.3144139771517,-1.0236813562338,12.4436422511729));
#55927=CARTESIAN_POINT('Ctrl Pts',(-1.30022301681158,-1.04174144008166,
12.4452115325764));
#55928=CARTESIAN_POINT('Ctrl Pts',(-1.29029576155259,-1.05401229782464,
12.4463012426588));
#55929=CARTESIAN_POINT('Ctrl Pts',(-1.23445003931559,-1.12107056235004,
12.4523790691956));
#55930=CARTESIAN_POINT('Ctrl Pts',(-1.18522021283528,-1.1729949451118,12.4575428747315));
#55931=CARTESIAN_POINT('Ctrl Pts',(-1.03648388078091,-1.31092199938641,
12.4722894813691));
#55932=CARTESIAN_POINT('Ctrl Pts',(-0.929906078632625,-1.38856104739653,
12.4818583442618));
#55933=CARTESIAN_POINT('Ctrl Pts',(-0.791325093235982,-1.4663274900714,
12.4928494127712));
#55934=CARTESIAN_POINT('Ctrl Pts',(-0.767021162759265,-1.47918572286742,
12.4947304894388));
#55935=CARTESIAN_POINT('Ctrl Pts',(-0.730991711486161,-1.49712049200004,
12.4974534308588));
#55936=CARTESIAN_POINT('Ctrl Pts',(-0.719509436847579,-1.50267256440613,
12.4983116955461));
#55937=CARTESIAN_POINT('Ctrl Pts',(-0.699079505529343,-1.51226326414033,
12.4998223817845));
#55938=CARTESIAN_POINT('Ctrl Pts',(-0.690157910212084,-1.51635563149986,
12.5004766333418));
#55939=CARTESIAN_POINT('Ctrl Pts',(-0.671494076266293,-1.52471795218344,
12.5018342400799));
#55940=CARTESIAN_POINT('Ctrl Pts',(-0.661746039972998,-1.52897394209645,
12.5025370940772));
#55941=CARTESIAN_POINT('Ctrl Pts',(-0.636146653580155,-1.53985993886215,
12.5043671276162));
#55942=CARTESIAN_POINT('Ctrl Pts',(-0.620232066946704,-1.54633871294533,
12.505489175088));
#55943=CARTESIAN_POINT('Ctrl Pts',(-0.542555749103448,-1.5765682961704,
12.5108946335196));
#55944=CARTESIAN_POINT('Ctrl Pts',(-0.479512761874191,-1.59687299700896,
12.5150626776159));
#55945=CARTESIAN_POINT('Ctrl Pts',(-0.345211393460327,-1.63145381770276,
12.523655080517));
#55946=CARTESIAN_POINT('Ctrl Pts',(-0.273893291767488,-1.64493017053553,
12.5280562357795));
#55947=CARTESIAN_POINT('Ctrl Pts',(-0.183201766622668,-1.65600388313279,
12.5336457290519));
#55948=CARTESIAN_POINT('Ctrl Pts',(-0.164442267148961,-1.65797179487159,
12.5348017809404));
#55949=CARTESIAN_POINT('Ctrl Pts',(-0.0763489424746476,-1.66570314723546,
12.5402448789092));
#55950=CARTESIAN_POINT('Ctrl Pts',(-0.00673961622210144,-1.66743764353843,
12.5445860086788));
#55951=CARTESIAN_POINT('Ctrl Pts',(0.0743107810027824,-1.66438199013478,
12.54989178074));
#55952=CARTESIAN_POINT('Ctrl Pts',(0.0858516173689782,-1.66382660838408,
12.5506532629449));
#55953=CARTESIAN_POINT('Ctrl Pts',(0.103794408001332,-1.6627759734235,12.5518477785519));
#55954=CARTESIAN_POINT('Ctrl Pts',(0.110201114114792,-1.66236365694203,
12.5522764056177));
#55955=CARTESIAN_POINT('Ctrl Pts',(0.122021906417831,-1.66153427293247,
12.5530714114351));
#55956=CARTESIAN_POINT('Ctrl Pts',(0.127436532699472,-1.66112775330455,
12.5534372071176));
#55957=CARTESIAN_POINT('Ctrl Pts',(0.14002192729201,-1.66012097134327,12.5542911957228));
#55958=CARTESIAN_POINT('Ctrl Pts',(0.147190859989878,-1.65950071574014,
12.5547804646773));
#55959=CARTESIAN_POINT('Ctrl Pts',(0.170129346847267,-1.65736627746899,
12.5563545289229));
#55960=CARTESIAN_POINT('Ctrl Pts',(0.185880867914779,-1.65567364828763,
12.5574483593736));
#55961=CARTESIAN_POINT('Ctrl Pts',(0.273152607026711,-1.64503458079424,
12.5635720843458));
#55962=CARTESIAN_POINT('Ctrl Pts',(0.344051883962195,-1.63167931265417,
12.5687803620079));
#55963=CARTESIAN_POINT('Ctrl Pts',(0.542927146236723,-1.58067742148149,
12.5837078260743));
#55964=CARTESIAN_POINT('Ctrl Pts',(0.667587267516383,-1.53220455268447,
12.5934075863587));
#55965=CARTESIAN_POINT('Ctrl Pts',(0.80821909880595,-1.45705934765141,12.6044144112106));
#55966=CARTESIAN_POINT('Ctrl Pts',(0.830994490755951,-1.44419124248433,
12.6062013486946));
#55967=CARTESIAN_POINT('Ctrl Pts',(0.864156121751638,-1.42441052768645,
12.6088111500678));
#55968=CARTESIAN_POINT('Ctrl Pts',(0.874781985215312,-1.41790960470397,
12.6096486564339));
#55969=CARTESIAN_POINT('Ctrl Pts',(0.893592443344653,-1.40610937780125,
12.6111338497161));
#55970=CARTESIAN_POINT('Ctrl Pts',(0.901805207791379,-1.40085631357486,
12.6117831936628));
#55971=CARTESIAN_POINT('Ctrl Pts',(0.919098340835933,-1.38958013639452,
12.6131526373275));
#55972=CARTESIAN_POINT('Ctrl Pts',(0.92816671578582,-1.38353940052268,12.613872042054));
#55973=CARTESIAN_POINT('Ctrl Pts',(0.952380877821386,-1.36706433801552,
12.6157969559625));
#55974=CARTESIAN_POINT('Ctrl Pts',(0.967414506755512,-1.35646727071466,
12.6169962885753));
#55975=CARTESIAN_POINT('Ctrl Pts',(1.0542060815529,-1.29311166392279,12.6239517940272));
#55976=CARTESIAN_POINT('Ctrl Pts',(1.12182017033327,-1.23491325611185,12.6294881295165));
#55977=CARTESIAN_POINT('Ctrl Pts',(1.27605995464213,-1.0789773905794,12.6429400603205));
#55978=CARTESIAN_POINT('Ctrl Pts',(1.35646620014991,-0.97596648887954,12.6507144487269));
#55979=CARTESIAN_POINT('Ctrl Pts',(1.43192817028973,-0.851685563546782,
12.6601581807319));
#55980=CARTESIAN_POINT('Ctrl Pts',(1.43963111942049,-0.838599298970701,
12.6611536457715));
#55981=CARTESIAN_POINT('Ctrl Pts',(1.4506592312883,-0.819264215803973,12.662628809302));
#55982=CARTESIAN_POINT('Ctrl Pts',(1.45412540737038,-0.813096154040623,
12.6631000395227));
#55983=CARTESIAN_POINT('Ctrl Pts',(1.4602011441877,-0.802121270628105,12.6639399754963));
#55984=CARTESIAN_POINT('Ctrl Pts',(1.46282647380285,-0.797323410095747,
12.6643076774426));
#55985=CARTESIAN_POINT('Ctrl Pts',(1.46853338856125,-0.786770803510303,
12.6651176047101));
#55986=CARTESIAN_POINT('Ctrl Pts',(1.47160475180358,-0.78101092271485,12.6655604217574));
#55987=CARTESIAN_POINT('Ctrl Pts',(1.4804110650728,-0.764259628556052,12.6668500635657));
#55988=CARTESIAN_POINT('Ctrl Pts',(1.48605712722863,-0.7532223398701,12.6677020414222));
#55989=CARTESIAN_POINT('Ctrl Pts',(1.49873688770819,-0.727737540787147,
12.6696726361898));
#55990=CARTESIAN_POINT('Ctrl Pts',(1.50568571572696,-0.713249374451216,
12.6707953953461));
#55991=CARTESIAN_POINT('Ctrl Pts',(1.52857012660578,-0.663710620119195,
12.6746373982194));
#55992=CARTESIAN_POINT('Ctrl Pts',(1.5434991234233,-0.628210553659201,12.677395433115));
#55993=CARTESIAN_POINT('Ctrl Pts',(1.5824120914602,-0.525894072596553,12.6853025272015));
#55994=CARTESIAN_POINT('Ctrl Pts',(1.60337565580648,-0.458016548948634,
12.6904955002919));
#55995=CARTESIAN_POINT('Ctrl Pts',(1.64263487650365,-0.294529692479793,
12.7026747881614));
#55996=CARTESIAN_POINT('Ctrl Pts',(1.65701733547024,-0.198233437646106,
12.7095841718912));
#55997=CARTESIAN_POINT('Ctrl Pts',(1.66406909268071,-0.0823788135472152,
12.7175203561996));
#55998=CARTESIAN_POINT('Ctrl Pts',(1.66489558599313,-0.0635212777457633,
12.7188009401027));
#55999=CARTESIAN_POINT('Ctrl Pts',(1.66569627834598,-0.0336582903609436,
12.7208119855056));
#56000=CARTESIAN_POINT('Ctrl Pts',(1.6658821920898,-0.0226606338558027,
12.7215489758778));
#56001=CARTESIAN_POINT('Ctrl Pts',(1.66602048830805,-0.00290402437482544,
12.7228666931106));
#56002=CARTESIAN_POINT('Ctrl Pts',(1.66601273547824,0.00585414840646092,
12.7234486400382));
#56003=CARTESIAN_POINT('Ctrl Pts',(1.66583232787135,0.0264226917070504,
12.7248103758247));
#56004=CARTESIAN_POINT('Ctrl Pts',(1.66560313832769,0.0382321962668288,
12.7255883749658));
#56005=CARTESIAN_POINT('Ctrl Pts',(1.66456365857613,0.0728253820508035,
12.7278568127073));
#56006=CARTESIAN_POINT('Ctrl Pts',(1.66341127719024,0.0955966211118545,
12.7293366035104));
#56007=CARTESIAN_POINT('Ctrl Pts',(1.65593420860147,0.200595318176297,12.7361084636989));
#56008=CARTESIAN_POINT('Ctrl Pts',(1.64397703088971,0.282309070224945,12.7412251398327));
#56009=CARTESIAN_POINT('Ctrl Pts',(1.61350224552191,0.418889046400651,12.749805149775));
#56010=CARTESIAN_POINT('Ctrl Pts',(1.59809654389551,0.474283556633144,12.7532954166224));
#56011=CARTESIAN_POINT('Ctrl Pts',(1.55538074100362,0.601909665500186,12.7615545692918));
#56012=CARTESIAN_POINT('Ctrl Pts',(1.52585534103527,0.673250947316369,12.766341481159));
#56013=CARTESIAN_POINT('Ctrl Pts',(1.4863304897064,0.752670143702575,12.7721439405539));
#56014=CARTESIAN_POINT('Ctrl Pts',(1.48105180524546,0.763004719197057,12.7729086806488));
#56015=CARTESIAN_POINT('Ctrl Pts',(1.47268066488823,0.778979473758189,12.7741072310869));
#56016=CARTESIAN_POINT('Ctrl Pts',(1.46966265675198,0.784658545579505,12.7745365876939));
#56017=CARTESIAN_POINT('Ctrl Pts',(1.46401199251504,0.795144592612918,12.775335707109));
#56018=CARTESIAN_POINT('Ctrl Pts',(1.46138840695088,0.799956222695908,12.7757049077776));
#56019=CARTESIAN_POINT('Ctrl Pts',(1.45525830521939,0.811067969752821,12.7765633172911));
#56020=CARTESIAN_POINT('Ctrl Pts',(1.45173459718152,0.817358330830522,12.7770535842369));
#56021=CARTESIAN_POINT('Ctrl Pts',(1.44029902542701,0.837465352001482,12.77863414495));
#56022=CARTESIAN_POINT('Ctrl Pts',(1.43223015916051,0.851191061589421,12.77973357495));
#56023=CARTESIAN_POINT('Ctrl Pts',(1.41238735299022,0.883863978131697,12.7823964921449));
#56024=CARTESIAN_POINT('Ctrl Pts',(1.40042732984628,0.902694167579866,12.7839689646434));
#56025=CARTESIAN_POINT('Ctrl Pts',(1.35186641571567,0.97586113825294,12.7902134392875));
#56026=CARTESIAN_POINT('Ctrl Pts',(1.31245319359004,1.02825749797639,12.7949813437029));
#56027=CARTESIAN_POINT('Ctrl Pts',(1.1911489601694,1.17114793437916,12.8086256200138));
#56028=CARTESIAN_POINT('Ctrl Pts',(1.10225733378982,1.25517427220707,12.8174330566012));
#56029=CARTESIAN_POINT('Ctrl Pts',(0.988278330456608,1.34137994608991,12.8272627966982));
#56030=CARTESIAN_POINT('Ctrl Pts',(0.971345117600342,1.35369233940924,12.8286907243316));
#56031=CARTESIAN_POINT('Ctrl Pts',(0.943899110223326,1.37286848439712,12.8309548860188));
#56032=CARTESIAN_POINT('Ctrl Pts',(0.93353348679762,1.37993791516368,12.8317988673914));
#56033=CARTESIAN_POINT('Ctrl Pts',(0.914942723829558,1.39231159088029,12.833293229329));
#56034=CARTESIAN_POINT('Ctrl Pts',(0.906748949755013,1.39766165545498,12.8339453096561));
#56035=CARTESIAN_POINT('Ctrl Pts',(0.8894682065154,1.40872905666082,12.8353071348065));
#56036=CARTESIAN_POINT('Ctrl Pts',(0.880372128812226,1.41443139437494,12.8360163024898));
#56037=CARTESIAN_POINT('Ctrl Pts',(0.856182920587735,1.42927187315541,12.8378825522987));
#56038=CARTESIAN_POINT('Ctrl Pts',(0.840998397119315,1.43825902245204,12.8390341127294));
#56039=CARTESIAN_POINT('Ctrl Pts',(0.76197652369579,1.48334962765855,12.844930066255));
#56040=CARTESIAN_POINT('Ctrl Pts',(0.695944834037316,1.51545276559591,12.8495303518046));
#56041=CARTESIAN_POINT('Ctrl Pts',(0.537207197143363,1.5800551281359,12.8601082116231));
#56042=CARTESIAN_POINT('Ctrl Pts',(0.443328711433185,1.60892024035801,12.8660030087829));
#56043=CARTESIAN_POINT('Ctrl Pts',(0.321624669954097,1.63487351493144,12.8737223988559));
#56044=CARTESIAN_POINT('Ctrl Pts',(0.295662605808025,1.63976746736776,12.8753742495313));
#56045=CARTESIAN_POINT('Ctrl Pts',(0.237912932408908,1.64923748013971,12.8790810921117));
#56046=CARTESIAN_POINT('Ctrl Pts',(0.206088399131596,1.65351567395734,12.8811454363986));
#56047=CARTESIAN_POINT('Ctrl Pts',(0.164527922900877,1.65788431960283,12.8838924352525));
#56048=CARTESIAN_POINT('Ctrl Pts',(0.154884781049913,1.65881299370744,12.8845333804704));
#56049=CARTESIAN_POINT('Ctrl Pts',(0.139312011104854,1.66017574568347,12.8855749961719));
#56050=CARTESIAN_POINT('Ctrl Pts',(0.133387031678032,1.66066228956638,12.8859728275995));
#56051=CARTESIAN_POINT('Ctrl Pts',(0.121835508450726,1.66154865308232,12.8867516496581));
#56052=CARTESIAN_POINT('Ctrl Pts',(0.116209345184492,1.66195162448117,12.8871324660537));
#56053=CARTESIAN_POINT('Ctrl Pts',(0.102344652903931,1.66287393271677,12.8880744298977));
#56054=CARTESIAN_POINT('Ctrl Pts',(0.094104169108446,1.66336061704084,12.8886373318445));
#56055=CARTESIAN_POINT('Ctrl Pts',(0.0633597997430186,1.66494719775285,
12.890747975213));
#56056=CARTESIAN_POINT('Ctrl Pts',(0.0408390600815614,1.66565172952927,
12.8923150344996));
#56057=CARTESIAN_POINT('Ctrl Pts',(-0.0176901115778156,1.66629511057611,
12.8964307176475));
#56058=CARTESIAN_POINT('Ctrl Pts',(-0.0536938065023354,1.66552363755354,
12.8990046148275));
#56059=CARTESIAN_POINT('Ctrl Pts',(-0.162034491289828,1.65968573489037,
12.906828305595));
#56060=CARTESIAN_POINT('Ctrl Pts',(-0.234094610449637,1.6510637678514,12.9121341705021));
#56061=CARTESIAN_POINT('Ctrl Pts',(-0.395076733766986,1.6210486121683,12.924004206247));
#56062=CARTESIAN_POINT('Ctrl Pts',(-0.483275276334051,1.59697649060253,
12.930513595068));
#56063=CARTESIAN_POINT('Ctrl Pts',(-0.591086216962083,1.55779390330297,
12.9384086095892));
#56064=CARTESIAN_POINT('Ctrl Pts',(-0.612932587514291,1.54932840320655,
12.9400059079389));
#56065=CARTESIAN_POINT('Ctrl Pts',(-0.645771090704461,1.53580005992499,
12.9424042130378));
#56066=CARTESIAN_POINT('Ctrl Pts',(-0.656897835639443,1.53107392785202,
12.9432163723326));
#56067=CARTESIAN_POINT('Ctrl Pts',(-0.676871867716483,1.52233204185319,
12.9446737896956));
#56068=CARTESIAN_POINT('Ctrl Pts',(-0.685737240829575,1.51835925075639,
12.9453204709544));
#56069=CARTESIAN_POINT('Ctrl Pts',(-0.704684727462295,1.50966861481764,
12.9467024346316));
#56070=CARTESIAN_POINT('Ctrl Pts',(-0.714755375187231,1.50492679404536,
12.9474368576336));
#56071=CARTESIAN_POINT('Ctrl Pts',(-0.742330914489212,1.49160344755027,
12.9494481661858));
#56072=CARTESIAN_POINT('Ctrl Pts',(-0.759734233455017,1.48281488311805,
12.9507178551845));
#56073=CARTESIAN_POINT('Ctrl Pts',(-0.874977468800661,1.42205604085857,
12.9591369169189));
#56074=CARTESIAN_POINT('Ctrl Pts',(-0.967581614535266,1.36074208538991,
12.9659324284006));
#56075=CARTESIAN_POINT('Ctrl Pts',(-1.13625910694765,1.22307161813057,12.9792294424446));
#56076=CARTESIAN_POINT('Ctrl Pts',(-1.21238323939863,1.1476538812621,12.9857102706021));
#56077=CARTESIAN_POINT('Ctrl Pts',(-1.29015623642924,1.05416760272271,12.9936131451692));
#56078=CARTESIAN_POINT('Ctrl Pts',(-1.299414694512,1.04273384161376,12.9945779040289));
#56079=CARTESIAN_POINT('Ctrl Pts',(-1.31286032658278,1.02567194214856,12.9960174840741));
#56080=CARTESIAN_POINT('Ctrl Pts',(-1.31716561169085,1.0201372049804,12.9964844611958));
#56081=CARTESIAN_POINT('Ctrl Pts',(-1.32476907197542,1.01023406487874,12.9973203245247));
#56082=CARTESIAN_POINT('Ctrl Pts',(-1.32808084103939,1.00587635330449,12.9976882536763));
#56083=CARTESIAN_POINT('Ctrl Pts',(-1.3352707463399,0.996318279912363,12.9984956055479));
#56084=CARTESIAN_POINT('Ctrl Pts',(-1.33913994817879,0.991111636764372,
12.9989355909969));
#56085=CARTESIAN_POINT('Ctrl Pts',(-1.35019915862409,0.976046676796701,
13.0002088806265));
#56086=CARTESIAN_POINT('Ctrl Pts',(-1.3573112194442,0.966132038104315,13.0010471463176));
#56087=CARTESIAN_POINT('Ctrl Pts',(-1.37334739919323,0.943250071439848,
13.0029807794682));
#56088=CARTESIAN_POINT('Ctrl Pts',(-1.38219782330862,0.930232720082306,
13.004080083989));
#56089=CARTESIAN_POINT('Ctrl Pts',(-1.41140085906255,0.885943406134831,
13.0078128873333));
#56090=CARTESIAN_POINT('Ctrl Pts',(-1.4308861669804,0.854115057018459,13.0104830415073));
#56091=CARTESIAN_POINT('Ctrl Pts',(-1.49396270299068,0.7428577050065,13.0197138967315));
#56092=CARTESIAN_POINT('Ctrl Pts',(-1.53213819264634,0.660540752150257,
13.0263605310097));
#56093=CARTESIAN_POINT('Ctrl Pts',(-1.56343129955154,0.575533293200813,
13.0328805013286));
#56094=CARTESIAN_POINT('Origin',(0.,0.,11.));
#56095=CARTESIAN_POINT('',(-1.56343128722854,0.575533326676141,13.7334757494662));
#56096=CARTESIAN_POINT('',(-1.56343130308087,0.575533283613436,13.5398191707253));
#56097=CARTESIAN_POINT('',(-1.56343130033213,0.575533291080363,11.));
#56098=CARTESIAN_POINT('Ctrl Pts',(-1.56343130308087,0.575533283613436,
13.5398191707253));
#56099=CARTESIAN_POINT('Ctrl Pts',(-1.56078063958421,0.582733788610461,
13.539262439699));
#56100=CARTESIAN_POINT('Ctrl Pts',(-1.55808001184986,0.589916580831864,
13.5387050978713));
#56101=CARTESIAN_POINT('Ctrl Pts',(-1.51920569478185,0.691179829684495,
13.5308213929391));
#56102=CARTESIAN_POINT('Ctrl Pts',(-1.47461275565274,0.781816166493946,
13.5234617103585));
#56103=CARTESIAN_POINT('Ctrl Pts',(-1.4050123037459,0.895863785834677,13.5140118707061));
#56104=CARTESIAN_POINT('Ctrl Pts',(-1.3871047788544,0.92334829391982,13.5117168563318));
#56105=CARTESIAN_POINT('Ctrl Pts',(-1.35301290840937,0.97243994143396,13.5075859500054));
#56106=CARTESIAN_POINT('Ctrl Pts',(-1.33709294894636,0.994216255604684,
13.5057415119941));
#56107=CARTESIAN_POINT('Ctrl Pts',(-1.31288663661251,1.02569336596771,13.5030559264581));
#56108=CARTESIAN_POINT('Ctrl Pts',(-1.30500714666334,1.03570003590777,13.5021991455198));
#56109=CARTESIAN_POINT('Ctrl Pts',(-1.29087419197495,1.05323098385015,13.5006923770766));
#56110=CARTESIAN_POINT('Ctrl Pts',(-1.28466783429224,1.06079227344404,13.5000405536887));
#56111=CARTESIAN_POINT('Ctrl Pts',(-1.27150444843871,1.07654443136885,13.498678296485));
#56112=CARTESIAN_POINT('Ctrl Pts',(-1.2645340209572,1.08472355652462,13.4979684482144));
#56113=CARTESIAN_POINT('Ctrl Pts',(-1.24587774173042,1.10619065013814,13.4960981821036));
#56114=CARTESIAN_POINT('Ctrl Pts',(-1.23405829266994,1.11936109952817,13.4949433303307));
#56115=CARTESIAN_POINT('Ctrl Pts',(-1.17677516370477,1.18118147173559,13.4894820990634));
#56116=CARTESIAN_POINT('Ctrl Pts',(-1.12862917971982,1.22726817125945,13.4852918507597));
#56117=CARTESIAN_POINT('Ctrl Pts',(-0.967598779638467,1.36389662016979,
13.4722166900698));
#56118=CARTESIAN_POINT('Ctrl Pts',(-0.84565746427689,1.44267607924082,13.4636782140505));
#56119=CARTESIAN_POINT('Ctrl Pts',(-0.695280129621473,1.51414104592946,
13.4529846237284));
#56120=CARTESIAN_POINT('Ctrl Pts',(-0.675276858608457,1.52316729808642,
13.4515580273188));
#56121=CARTESIAN_POINT('Ctrl Pts',(-0.647587975310001,1.53500899270622,
13.4495698482882));
#56122=CARTESIAN_POINT('Ctrl Pts',(-0.640050249902359,1.53816724195143,
13.4490272581202));
#56123=CARTESIAN_POINT('Ctrl Pts',(-0.627286175390144,1.54340522601208,
13.4481056860776));
#56124=CARTESIAN_POINT('Ctrl Pts',(-0.622071845109108,1.54551423673817,
13.4477284311482));
#56125=CARTESIAN_POINT('Ctrl Pts',(-0.611985814380127,1.54953436488008,
13.4469970397734));
#56126=CARTESIAN_POINT('Ctrl Pts',(-0.607115649575051,1.55144899080622,
13.4466431449657));
#56127=CARTESIAN_POINT('Ctrl Pts',(-0.593782200643017,1.55661842456099,
13.4456724154139));
#56128=CARTESIAN_POINT('Ctrl Pts',(-0.58530138817499,1.55982707284114,13.4450529569165));
#56129=CARTESIAN_POINT('Ctrl Pts',(-0.551733935474446,1.57221476238125,
13.4425943311884));
#56130=CARTESIAN_POINT('Ctrl Pts',(-0.52645566784073,1.58085857356714,13.4407280152879));
#56131=CARTESIAN_POINT('Ctrl Pts',(-0.469636774464721,1.59877375708414,
13.4365163684573));
#56132=CARTESIAN_POINT('Ctrl Pts',(-0.438007177312401,1.60772687718784,
13.4341607017602));
#56133=CARTESIAN_POINT('Ctrl Pts',(-0.31086969184172,1.6396844174034,13.4246958855022));
#56134=CARTESIAN_POINT('Ctrl Pts',(-0.213666309556907,1.65515960133083,
13.417482567313));
#56135=CARTESIAN_POINT('Ctrl Pts',(-0.0425254251703389,1.66707019277201,
13.4051815671385));
#56136=CARTESIAN_POINT('Ctrl Pts',(0.0308792862739422,1.66732737994433,
13.4000282438992));
#56137=CARTESIAN_POINT('Ctrl Pts',(0.121678815063038,1.66164421266878,13.3938193383965));
#56138=CARTESIAN_POINT('Ctrl Pts',(0.139267835052863,1.66026255008328,13.3926240379113));
#56139=CARTESIAN_POINT('Ctrl Pts',(0.167519056633602,1.65759120286808,13.3907154676102));
#56140=CARTESIAN_POINT('Ctrl Pts',(0.178196112571544,1.65647740248834,13.3899967576915));
#56141=CARTESIAN_POINT('Ctrl Pts',(0.198583706422165,1.65415121918064,13.3886291139528));
#56142=CARTESIAN_POINT('Ctrl Pts',(0.208295746665879,1.65295633132395,13.387979661136));
#56143=CARTESIAN_POINT('Ctrl Pts',(0.230434731083972,1.65003431172002,13.3865036092579));
#56144=CARTESIAN_POINT('Ctrl Pts',(0.24285392001679,1.64825222068555,13.3856787722332));
#56145=CARTESIAN_POINT('Ctrl Pts',(0.275938340243625,1.64312271002202,13.3834890769573));
#56146=CARTESIAN_POINT('Ctrl Pts',(0.296563008300342,1.63952574011155,13.3821320492411));
#56147=CARTESIAN_POINT('Ctrl Pts',(0.436838295541776,1.61232775207546,13.3729450315476));
#56148=CARTESIAN_POINT('Ctrl Pts',(0.553652594887798,1.57603970122121,13.3655423060756));
#56149=CARTESIAN_POINT('Ctrl Pts',(0.725525139122892,1.50115316127148,13.3540849441));
#56150=CARTESIAN_POINT('Ctrl Pts',(0.783981987973894,1.47146815935395,13.350069025891));
#56151=CARTESIAN_POINT('Ctrl Pts',(0.859793329183877,1.42716816105914,13.3445102798992));
#56152=CARTESIAN_POINT('Ctrl Pts',(0.878822846214977,1.41552952457611,13.3430834406582));
#56153=CARTESIAN_POINT('Ctrl Pts',(0.911024586985196,1.3949350095035,13.3406040932607));
#56154=CARTESIAN_POINT('Ctrl Pts',(0.92431291500871,1.38616559923526,13.3395614363744));
#56155=CARTESIAN_POINT('Ctrl Pts',(0.943432967883764,1.37315047126158,13.3380293813489));
#56156=CARTESIAN_POINT('Ctrl Pts',(0.949366473040456,1.36905488446975,13.3375494046891));
#56157=CARTESIAN_POINT('Ctrl Pts',(0.959762963440568,1.3617786485229,13.3367000287527));
#56158=CARTESIAN_POINT('Ctrl Pts',(0.96423711734629,1.35861429913119,13.3363317225267));
#56159=CARTESIAN_POINT('Ctrl Pts',(0.973927715458534,1.35168863314032,13.3355278588063));
#56160=CARTESIAN_POINT('Ctrl Pts',(0.979137940286179,1.34791922840272,13.335091778725));
#56161=CARTESIAN_POINT('Ctrl Pts',(0.993687959381296,1.33726395556338,13.3338633695121));
#56162=CARTESIAN_POINT('Ctrl Pts',(1.00297761217376,1.33031069233537,13.3330666976623));
#56163=CARTESIAN_POINT('Ctrl Pts',(1.07338986423151,1.27645070864256,13.3269376250523));
#56164=CARTESIAN_POINT('Ctrl Pts',(1.13125854920797,1.22545649252868,13.3213776218073));
#56165=CARTESIAN_POINT('Ctrl Pts',(1.22567950514986,1.12984698623709,13.3116102235553));
#56166=CARTESIAN_POINT('Ctrl Pts',(1.26384165218415,1.08699080449051,13.3074255594243));
#56167=CARTESIAN_POINT('Ctrl Pts',(1.35140611942951,0.977795346120671,13.2973117178933));
#56168=CARTESIAN_POINT('Ctrl Pts',(1.3982336997387,0.909575912711863,13.2914448819633));
#56169=CARTESIAN_POINT('Ctrl Pts',(1.45128979341069,0.818434207668401,13.2841948610304));
#56170=CARTESIAN_POINT('Ctrl Pts',(1.4623630391522,0.798480461866163,13.2826405325659));
#56171=CARTESIAN_POINT('Ctrl Pts',(1.47854286792671,0.767858434776805,13.2803034588139));
#56172=CARTESIAN_POINT('Ctrl Pts',(1.48395119894103,0.757353576465818,13.2795101506542));
#56173=CARTESIAN_POINT('Ctrl Pts',(1.49317318631019,0.738963148905957,13.2781356308063));
#56174=CARTESIAN_POINT('Ctrl Pts',(1.49703719751134,0.731103504334115,13.2775526772985));
#56175=CARTESIAN_POINT('Ctrl Pts',(1.50561210861306,0.713308538150928,13.2762427012624));
#56176=CARTESIAN_POINT('Ctrl Pts',(1.51028702174477,0.703356249639429,13.2755169458164));
#56177=CARTESIAN_POINT('Ctrl Pts',(1.52271164583514,0.676210677261127,13.2735554594478));
#56178=CARTESIAN_POINT('Ctrl Pts',(1.53026865779012,0.658930586916578,13.2723263291607));
#56179=CARTESIAN_POINT('Ctrl Pts',(1.57568503437986,0.550082066185779,13.2646973156984));
#56180=CARTESIAN_POINT('Ctrl Pts',(1.60560791153685,0.455412450130569,13.2585747852756));
#56181=CARTESIAN_POINT('Ctrl Pts',(1.64233484059112,0.288800724711676,13.2481384938311));
#56182=CARTESIAN_POINT('Ctrl Pts',(1.65321572748002,0.218051881689388,13.2438020376228));
#56183=CARTESIAN_POINT('Ctrl Pts',(1.66277342371212,0.11002480217375,13.2370682061555));
#56184=CARTESIAN_POINT('Ctrl Pts',(1.66480415103102,0.0731279813369949,
13.2347479146914));
#56185=CARTESIAN_POINT('Ctrl Pts',(1.66594652090965,0.0205613540279227,
13.2313757891008));
#56186=CARTESIAN_POINT('Ctrl Pts',(1.66606611797867,0.00492259779151108,
13.2303641947194));
#56187=CARTESIAN_POINT('Ctrl Pts',(1.66588746166219,-0.0228551018100175,
13.2285488546726));
#56188=CARTESIAN_POINT('Ctrl Pts',(1.6656766834191,-0.0349936539018341,
13.2277492798936));
#56189=CARTESIAN_POINT('Ctrl Pts',(1.66515013662737,-0.0535997655218569,
13.2265125469586));
#56190=CARTESIAN_POINT('Ctrl Pts',(1.66492928284331,-0.0600698923750112,
13.2260804167628));
#56191=CARTESIAN_POINT('Ctrl Pts',(1.66445207230846,-0.0720088335210612,
13.2252789464481));
#56192=CARTESIAN_POINT('Ctrl Pts',(1.66420646245664,-0.0774778701527156,
13.2249101994056));
#56193=CARTESIAN_POINT('Ctrl Pts',(1.6635839609758,-0.0899655931361387,
13.2240645887955));
#56194=CARTESIAN_POINT('Ctrl Pts',(1.66318960528338,-0.0969831714899934,
13.2235867916918));
#56195=CARTESIAN_POINT('Ctrl Pts',(1.66179323419462,-0.119308791606604,
13.2220589024835));
#56196=CARTESIAN_POINT('Ctrl Pts',(1.66062421189745,-0.134605074720966,
13.221000351478));
#56197=CARTESIAN_POINT('Ctrl Pts',(1.64759505101927,-0.278841944485463,
13.2109212176064));
#56198=CARTESIAN_POINT('Ctrl Pts',(1.62095247647327,-0.405996383736341,
13.2013389509523));
#56199=CARTESIAN_POINT('Ctrl Pts',(1.55143803924907,-0.613688483427946,
13.1855174709197));
#56200=CARTESIAN_POINT('Ctrl Pts',(1.51621567986653,-0.696181189724852,
13.1791746308323));
#56201=CARTESIAN_POINT('Ctrl Pts',(1.46595758784083,-0.791746943407482,
13.1717969717608));
#56202=CARTESIAN_POINT('Ctrl Pts',(1.45711947032206,-0.807897127205963,
13.1705485992364));
#56203=CARTESIAN_POINT('Ctrl Pts',(1.44262523044902,-0.833371005094781,
13.1685762425694));
#56204=CARTESIAN_POINT('Ctrl Pts',(1.43714235200819,-0.842790992770211,
13.167846149872));
#56205=CARTESIAN_POINT('Ctrl Pts',(1.42658151334173,-0.860532508537247,
13.1664694336762));
#56206=CARTESIAN_POINT('Ctrl Pts',(1.42152221475058,-0.868864553497879,
13.1658221707996));
#56207=CARTESIAN_POINT('Ctrl Pts',(1.40983576291534,-0.887735371601575,
13.1643543181588));
#56208=CARTESIAN_POINT('Ctrl Pts',(1.40316297802466,-0.898245311427428,
13.1635354435235));
#56209=CARTESIAN_POINT('Ctrl Pts',(1.38212838401984,-0.930569281940887,
13.1610117372549));
#56210=CARTESIAN_POINT('Ctrl Pts',(1.36737058064036,-0.952121774673777,
13.1593216345085));
#56211=CARTESIAN_POINT('Ctrl Pts',(1.2742265167525,-1.08151523042013,13.149107220142));
#56212=CARTESIAN_POINT('Ctrl Pts',(1.18363875495021,-1.17997054149023,13.1410900669583));
#56213=CARTESIAN_POINT('Ctrl Pts',(1.02747062876932,-1.31341441604048,13.12849043018));
#56214=CARTESIAN_POINT('Ctrl Pts',(0.969686058859638,-1.3566354993666,13.1240238088173));
#56215=CARTESIAN_POINT('Ctrl Pts',(0.896016987663439,-1.40462114582404,
13.1183202779933));
#56216=CARTESIAN_POINT('Ctrl Pts',(0.882619619151807,-1.413078047567,13.1172826106798));
#56217=CARTESIAN_POINT('Ctrl Pts',(0.862965249064118,-1.42509605220349,
13.1157565627056));
#56218=CARTESIAN_POINT('Ctrl Pts',(0.856802088325468,-1.42880997888933,
13.1152775004625));
#56219=CARTESIAN_POINT('Ctrl Pts',(0.845946506869366,-1.4352560711809,13.1144324174677));
#56220=CARTESIAN_POINT('Ctrl Pts',(0.841264498009107,-1.43800539828144,
13.1140675074197));
#56221=CARTESIAN_POINT('Ctrl Pts',(0.831017597381068,-1.4439553185029,13.1132678569433));
#56222=CARTESIAN_POINT('Ctrl Pts',(0.82544770846477,-1.44714660145552,13.1128325725695));
#56223=CARTESIAN_POINT('Ctrl Pts',(0.809802895970906,-1.45599063454264,
13.1116085050967));
#56224=CARTESIAN_POINT('Ctrl Pts',(0.799687643343507,-1.4615707689722,13.1108154259741));
#56225=CARTESIAN_POINT('Ctrl Pts',(0.728319681671741,-1.49997866525846,
13.1052126204907));
#56226=CARTESIAN_POINT('Ctrl Pts',(0.665129678011054,-1.52904738028681,
13.1002173113484));
#56227=CARTESIAN_POINT('Ctrl Pts',(0.585077707710549,-1.55997018917972,
13.0939897622467));
#56228=CARTESIAN_POINT('Ctrl Pts',(0.569752010605036,-1.56563263697475,
13.0928017591634));
#56229=CARTESIAN_POINT('Ctrl Pts',(0.499829501062926,-1.59030452887988,
13.0874060885637));
#56230=CARTESIAN_POINT('Ctrl Pts',(0.444347214891184,-1.60669039069399,
13.0831938179496));
#56231=CARTESIAN_POINT('Ctrl Pts',(0.308650461485002,-1.63919779272084,
13.0731468346497));
#56232=CARTESIAN_POINT('Ctrl Pts',(0.227874294767913,-1.65236541209983,
13.0673792546634));
#56233=CARTESIAN_POINT('Ctrl Pts',(0.128432718112406,-1.66114058803395,
13.0605616511355));
#56234=CARTESIAN_POINT('Ctrl Pts',(0.110393852130142,-1.6624368434493,13.0593357655432));
#56235=CARTESIAN_POINT('Ctrl Pts',(0.0815240961288447,-1.66403939166931,
13.0573904249872));
#56236=CARTESIAN_POINT('Ctrl Pts',(0.0707055612236025,-1.66453417161388,
13.0566651483949));
#56237=CARTESIAN_POINT('Ctrl Pts',(0.0501273633291889,-1.66527431315372,
13.0552923739536));
#56238=CARTESIAN_POINT('Ctrl Pts',(0.040368912603012,-1.6655394466729,13.0546442869696));
#56239=CARTESIAN_POINT('Ctrl Pts',(0.0180369109477417,-1.66594980969968,
13.0531675064122));
#56240=CARTESIAN_POINT('Ctrl Pts',(0.00546281731895583,-1.66603849614875,
13.0523406080641));
#56241=CARTESIAN_POINT('Ctrl Pts',(-0.0276690126860467,-1.66589707070504,
13.0501730990491));
#56242=CARTESIAN_POINT('Ctrl Pts',(-0.0482239536893625,-1.66542881389035,
13.048839871726));
#56243=CARTESIAN_POINT('Ctrl Pts',(-0.219716227839807,-1.65834427223022,
13.0377983868978));
#56244=CARTESIAN_POINT('Ctrl Pts',(-0.36910939800944,-1.6316068049493,13.0287900245318));
#56245=CARTESIAN_POINT('Ctrl Pts',(-0.57118261835091,-1.56622616859821,
13.0156970738585));
#56246=CARTESIAN_POINT('Ctrl Pts',(-0.628416089250399,-1.54415206187481,
13.0118665903021));
#56247=CARTESIAN_POINT('Ctrl Pts',(-0.697709480844861,-1.51293552264221,
13.0069258374521));
#56248=CARTESIAN_POINT('Ctrl Pts',(-0.71104112904732,-1.50671592935183,
13.0059607929047));
#56249=CARTESIAN_POINT('Ctrl Pts',(-0.730579569469668,-1.49728364048205,
13.0045224355632));
#56250=CARTESIAN_POINT('Ctrl Pts',(-0.736851728182095,-1.49420692465061,
13.0040570025248));
#56251=CARTESIAN_POINT('Ctrl Pts',(-0.747524862531159,-1.48888783179757,
13.003258344186));
#56252=CARTESIAN_POINT('Ctrl Pts',(-0.751935511858444,-1.48666518786077,
13.0029263384185));
#56253=CARTESIAN_POINT('Ctrl Pts',(-0.762009933595512,-1.48153211502753,
13.0021634291434));
#56254=CARTESIAN_POINT('Ctrl Pts',(-0.767666821414207,-1.47860887142577,
13.0017317499293));
#56255=CARTESIAN_POINT('Ctrl Pts',(-0.783333953774059,-1.47039861089681,
13.0005272852728));
#56256=CARTESIAN_POINT('Ctrl Pts',(-0.793307055207248,-1.46504199827002,
12.9997504118401));
#56257=CARTESIAN_POINT('Ctrl Pts',(-0.855947731648896,-1.43057018268568,
12.9948100204932));
#56258=CARTESIAN_POINT('Ctrl Pts',(-0.907054729155208,-1.39872359923603,
12.9905067810779));
#56259=CARTESIAN_POINT('Ctrl Pts',(-1.08004453067157,-1.277454402411,12.9752226578679));
#56260=CARTESIAN_POINT('Ctrl Pts',(-1.19142423807187,-1.17427059935779,
12.9641259278032));
#56261=CARTESIAN_POINT('Ctrl Pts',(-1.30443208684846,-1.03669465385404,
12.9518253194119));
#56262=CARTESIAN_POINT('Ctrl Pts',(-1.32099318626975,-1.01550776564639,
12.9499872596514));
#56263=CARTESIAN_POINT('Ctrl Pts',(-1.34454598337578,-0.983824474894265,
12.9473181119125));
#56264=CARTESIAN_POINT('Ctrl Pts',(-1.35194230553156,-0.973635720600104,
12.9464714040762));
#56265=CARTESIAN_POINT('Ctrl Pts',(-1.36486839297745,-0.955398135602065,
12.9449759714982));
#56266=CARTESIAN_POINT('Ctrl Pts',(-1.37044415117428,-0.947382796522105,
12.9443255043583));
#56267=CARTESIAN_POINT('Ctrl Pts',(-1.38205020898995,-0.930381809153599,
12.9429597681231));
#56268=CARTESIAN_POINT('Ctrl Pts',(-1.38806409381718,-0.921385463170396,
12.9422451401098));
#56269=CARTESIAN_POINT('Ctrl Pts',(-1.40387118522243,-0.897233123533381,
12.9403474884827));
#56270=CARTESIAN_POINT('Ctrl Pts',(-1.41350671485392,-0.881975278032113,
12.9391703338852));
#56271=CARTESIAN_POINT('Ctrl Pts',(-1.46040253022888,-0.804972583718597,
12.9333313256575));
#56272=CARTESIAN_POINT('Ctrl Pts',(-1.49387638226336,-0.741007171254946,
12.928807563864));
#56273=CARTESIAN_POINT('Ctrl Pts',(-1.56867733661043,-0.572239445837458,
12.9174113369234));
#56274=CARTESIAN_POINT('Ctrl Pts',(-1.60371910744669,-0.4650685563014,12.910681293389));
#56275=CARTESIAN_POINT('Ctrl Pts',(-1.63392286958697,-0.32665739931845,
12.9018055102691));
#56276=CARTESIAN_POINT('Ctrl Pts',(-1.63939785886919,-0.297965539809874,
12.8999547654432));
#56277=CARTESIAN_POINT('Ctrl Pts',(-1.64725312081612,-0.249980647800218,
12.8968196084319));
#56278=CARTESIAN_POINT('Ctrl Pts',(-1.6500550709274,-0.230762543971044,
12.8955533950085));
#56279=CARTESIAN_POINT('Ctrl Pts',(-1.65351021530464,-0.203766457521889,
12.8937543841654));
#56280=CARTESIAN_POINT('Ctrl Pts',(-1.65444578406096,-0.196025363012954,
12.8932361856761));
#56281=CARTESIAN_POINT('Ctrl Pts',(-1.6559551224938,-0.182755378027296,
12.8923434403922));
#56282=CARTESIAN_POINT('Ctrl Pts',(-1.65655563773657,-0.177229552129271,
12.891970366896));
#56283=CARTESIAN_POINT('Ctrl Pts',(-1.6577585841788,-0.165619608456608,
12.8911835975408));
#56284=CARTESIAN_POINT('Ctrl Pts',(-1.65835518725454,-0.159535099590306,
12.89076960832));
#56285=CARTESIAN_POINT('Ctrl Pts',(-1.65988156014858,-0.143033515998585,
12.8896425915346));
#56286=CARTESIAN_POINT('Ctrl Pts',(-1.66074673008251,-0.132610953280565,
12.8889261699202));
#56287=CARTESIAN_POINT('Ctrl Pts',(-1.66448157853897,-0.0818216500600575,
12.8854149250593));
#56288=CARTESIAN_POINT('Ctrl Pts',(-1.66597766395643,-0.0413707825729691,
12.8825568699521));
#56289=CARTESIAN_POINT('Ctrl Pts',(-1.66604677910934,0.085236454430287,
12.8734955076404));
#56290=CARTESIAN_POINT('Ctrl Pts',(-1.65941215201514,0.171254168355328,
12.8671784700656));
#56291=CARTESIAN_POINT('Ctrl Pts',(-1.63083730655712,0.354732671185672,
12.8537186085672));
#56292=CARTESIAN_POINT('Ctrl Pts',(-1.60673147312273,0.451537197537825,
12.8466328130717));
#56293=CARTESIAN_POINT('Ctrl Pts',(-1.57065155998457,0.555627367079107,
12.8391004744649));
#56294=CARTESIAN_POINT('Ctrl Pts',(-1.56708883221216,0.565597636766373,
12.8383796912937));
#56295=CARTESIAN_POINT('Ctrl Pts',(-1.56343130043543,0.575533290799732,
12.8376620384731));
#56296=CARTESIAN_POINT('',(-1.6659993171282,-0.00113364010792655,13.0724915839951));
#56297=CARTESIAN_POINT('Ctrl Pts',(-1.56343129955154,0.575533293200813,
13.0328805013286));
#56298=CARTESIAN_POINT('Ctrl Pts',(-1.56437182275508,0.57297836991185,13.0330764608858));
#56299=CARTESIAN_POINT('Ctrl Pts',(-1.56530612886598,0.57042101700076,13.0332723164847));
#56300=CARTESIAN_POINT('Ctrl Pts',(-1.59042310597543,0.501145171435164,
13.0385699050769));
#56301=CARTESIAN_POINT('Ctrl Pts',(-1.61032706365741,0.432944842177226,
13.0435817436763));
#56302=CARTESIAN_POINT('Ctrl Pts',(-1.63017709847875,0.344204408370925,
13.0498276822958));
#56303=CARTESIAN_POINT('Ctrl Pts',(-1.63418232908532,0.32465708416631,13.0511871468137));
#56304=CARTESIAN_POINT('Ctrl Pts',(-1.64010568145126,0.292853317024579,
13.0533733767878));
#56305=CARTESIAN_POINT('Ctrl Pts',(-1.64223966793376,0.28063962497421,13.0542068841866));
#56306=CARTESIAN_POINT('Ctrl Pts',(-1.64580673800576,0.258787745058411,
13.0556876428351));
#56307=CARTESIAN_POINT('Ctrl Pts',(-1.64729196723902,0.249158779600448,
13.0563365141801));
#56308=CARTESIAN_POINT('Ctrl Pts',(-1.65000269526167,0.230499751549097,
13.0575871235083));
#56309=CARTESIAN_POINT('Ctrl Pts',(-1.65123873696157,0.221471598543318,
13.0581891717326));
#56310=CARTESIAN_POINT('Ctrl Pts',(-1.65377085400944,0.201775694529071,
13.059496189771));
#56311=CARTESIAN_POINT('Ctrl Pts',(-1.65503792035683,0.191104577514267,
13.0602002335343));
#56312=CARTESIAN_POINT('Ctrl Pts',(-1.65874178780854,0.157104509034263,
13.0624311029811));
#56313=CARTESIAN_POINT('Ctrl Pts',(-1.66078929393574,0.133735383052599,
13.0639459438566));
#56314=CARTESIAN_POINT('Ctrl Pts',(-1.6648052270699,0.0732272208265782,
13.0678274033941));
#56315=CARTESIAN_POINT('Ctrl Pts',(-1.66602496239537,0.0360513616570116,
13.0701723343068));
#56316=CARTESIAN_POINT('Ctrl Pts',(-1.66599961292089,-0.00113567048074876,
13.0724922261414));
#56317=CARTESIAN_POINT('Ctrl Pts',(-1.66599961432537,-0.0011336082690304,
13.0724920974914));
#56318=CARTESIAN_POINT('Ctrl Pts',(-1.66594641663436,-0.0793152298434674,
13.0773694154298));
#56319=CARTESIAN_POINT('Ctrl Pts',(-1.66038991779439,-0.157401370556992,
13.0821227248742));
#56320=CARTESIAN_POINT('Ctrl Pts',(-1.63597659975319,-0.32888564353002,
13.0927072487401));
#56321=CARTESIAN_POINT('Ctrl Pts',(-1.61456184732864,-0.421627816383002,
13.0985306909447));
#56322=CARTESIAN_POINT('Ctrl Pts',(-1.58171934603026,-0.523317043441458,
13.1055184031541));
#56323=CARTESIAN_POINT('Ctrl Pts',(-1.57795185575317,-0.534569676197079,
13.1063003063003));
#56324=CARTESIAN_POINT('Ctrl Pts',(-1.57196250313768,-0.551843331990107,
13.1075153789434));
#56325=CARTESIAN_POINT('Ctrl Pts',(-1.56982542374298,-0.557893636686304,
13.1079437904974));
#56326=CARTESIAN_POINT('Ctrl Pts',(-1.56579761599185,-0.569090402467872,
13.1087421159837));
#56327=CARTESIAN_POINT('Ctrl Pts',(-1.56391637035455,-0.574240057585588,
13.1091114783297));
#56328=CARTESIAN_POINT('Ctrl Pts',(-1.55953709223092,-0.586046595080044,
13.1099633071619));
#56329=CARTESIAN_POINT('Ctrl Pts',(-1.5570218352854,-0.592696847852759,
13.1104467604043));
#56330=CARTESIAN_POINT('Ctrl Pts',(-1.54899056781344,-0.613527281740871,
13.1119720894485));
#56331=CARTESIAN_POINT('Ctrl Pts',(-1.54332299985029,-0.627647657641964,
13.1130221764799));
#56332=CARTESIAN_POINT('Ctrl Pts',(-1.49876753404505,-0.734401104769392,
13.1210737566866));
#56333=CARTESIAN_POINT('Ctrl Pts',(-1.45176845576423,-0.823416107200453,
13.1284238402932));
#56334=CARTESIAN_POINT('Ctrl Pts',(-1.35399540663144,-0.973907586420926,
13.1414783635447));
#56335=CARTESIAN_POINT('Ctrl Pts',(-1.30628361340923,-1.03702701586896,
13.1471857940558));
#56336=CARTESIAN_POINT('Ctrl Pts',(-1.2341514856595,-1.11953569386178,13.1548972205387));
#56337=CARTESIAN_POINT('Ctrl Pts',(-1.21340561366253,-1.14198821286013,
13.1570252923463));
#56338=CARTESIAN_POINT('Ctrl Pts',(-1.17577701945939,-1.18052834702326,
13.1607315374277));
#56339=CARTESIAN_POINT('Ctrl Pts',(-1.1591529016014,-1.19685564022498,13.16231977149));
#56340=CARTESIAN_POINT('Ctrl Pts',(-1.13369744131278,-1.22082850347254,
13.1646806177124));
#56341=CARTESIAN_POINT('Ctrl Pts',(-1.12511988253612,-1.22873812721237,
13.1654645016534));
#56342=CARTESIAN_POINT('Ctrl Pts',(-1.10936568983615,-1.24296223464047,
13.1668835715654));
#56343=CARTESIAN_POINT('Ctrl Pts',(-1.10221652132255,-1.24930624635725,
13.1675199867346));
#56344=CARTESIAN_POINT('Ctrl Pts',(-1.08672728158303,-1.26281458867568,
13.1688829519083));
#56345=CARTESIAN_POINT('Ctrl Pts',(-1.07837005149802,-1.26995862597754,
13.1696086435282));
#56346=CARTESIAN_POINT('Ctrl Pts',(-1.05549225782594,-1.28912663682244,
13.1715696467484));
#56347=CARTESIAN_POINT('Ctrl Pts',(-1.04083706187644,-1.30098795138861,
13.1727983638934));
#56348=CARTESIAN_POINT('Ctrl Pts',(-0.949119568113573,-1.37267827943915,
13.1803283512919));
#56349=CARTESIAN_POINT('Ctrl Pts',(-0.867123123995699,-1.42589433654383,
13.186361681104));
#56350=CARTESIAN_POINT('Ctrl Pts',(-0.701277990085902,-1.51390102374039,
13.1978497701251));
#56351=CARTESIAN_POINT('Ctrl Pts',(-0.618330773170805,-1.54962964597898,
13.2032987686595));
#56352=CARTESIAN_POINT('Ctrl Pts',(-0.507857656181761,-1.58692645798029,
13.2106322252125));
#56353=CARTESIAN_POINT('Ctrl Pts',(-0.482612029858826,-1.59478539530338,
13.2123135892961));
#56354=CARTESIAN_POINT('Ctrl Pts',(-0.439822678907821,-1.60699665786356,
13.2151891066286));
#56355=CARTESIAN_POINT('Ctrl Pts',(-0.422375198756701,-1.61167036761957,
13.216368704717));
#56356=CARTESIAN_POINT('Ctrl Pts',(-0.397503724534727,-1.61790118319616,
13.2180647897242));
#56357=CARTESIAN_POINT('Ctrl Pts',(-0.390139073065968,-1.61969285599178,
13.2185688141468));
#56358=CARTESIAN_POINT('Ctrl Pts',(-0.377385245666111,-1.62270357860465,
13.2194451797666));
#56359=CARTESIAN_POINT('Ctrl Pts',(-0.372001805314126,-1.6239461763282,
13.2198161837269));
#56360=CARTESIAN_POINT('Ctrl Pts',(-0.36054868794128,-1.62652982756921,
13.2206079284222));
#56361=CARTESIAN_POINT('Ctrl Pts',(-0.35447775569873,-1.62786367791967,
13.2210290323115));
#56362=CARTESIAN_POINT('Ctrl Pts',(-0.337714440099959,-1.63144854396684,
13.2221954617577));
#56363=CARTESIAN_POINT('Ctrl Pts',(-0.327007382752697,-1.63362833913063,
13.2229445781537));
#56364=CARTESIAN_POINT('Ctrl Pts',(-0.269445461659474,-1.6447585322237,
13.2269910443427));
#56365=CARTESIAN_POINT('Ctrl Pts',(-0.222247987086075,-1.65179793529914,
13.2303763251464));
#56366=CARTESIAN_POINT('Ctrl Pts',(-0.0714595543652354,-1.66770848083152,
13.2412797687857));
#56367=CARTESIAN_POINT('Ctrl Pts',(0.0326943170026807,-1.66891899136661,
13.2489255994165));
#56368=CARTESIAN_POINT('Ctrl Pts',(0.211723165289117,-1.65422441558984,
13.2618217550684));
#56369=CARTESIAN_POINT('Ctrl Pts',(0.286659223639609,-1.64289821350859,
13.2671481186679));
#56370=CARTESIAN_POINT('Ctrl Pts',(0.377930991826556,-1.62266453672199,
13.2735297012681));
#56371=CARTESIAN_POINT('Ctrl Pts',(0.395224816857861,-1.6185392858934,13.2747343954035));
#56372=CARTESIAN_POINT('Ctrl Pts',(0.422878856893835,-1.61147303326979,
13.2766542861866));
#56373=CARTESIAN_POINT('Ctrl Pts',(0.433281949989266,-1.60870712865462,
13.2773750388266));
#56374=CARTESIAN_POINT('Ctrl Pts',(0.453082494615455,-1.60323668230582,
13.2787442899798));
#56375=CARTESIAN_POINT('Ctrl Pts',(0.462484329673286,-1.60054986119791,
13.2793933291659));
#56376=CARTESIAN_POINT('Ctrl Pts',(0.483840697693467,-1.59424282321754,
13.2808653592859));
#56377=CARTESIAN_POINT('Ctrl Pts',(0.495779358229588,-1.59057060271246,
13.281686623469));
#56378=CARTESIAN_POINT('Ctrl Pts',(0.527425156434536,-1.58044571696831,
13.2838600152122));
#56379=CARTESIAN_POINT('Ctrl Pts',(0.547055417135793,-1.57375868270628,
13.2852045010952));
#56380=CARTESIAN_POINT('Ctrl Pts',(0.683914761284068,-1.52426725944938,
13.2945642432359));
#56381=CARTESIAN_POINT('Ctrl Pts',(0.796134499740034,-1.4687762973108,13.3021284080007));
#56382=CARTESIAN_POINT('Ctrl Pts',(0.977395699649095,-1.35221265081053,
13.3153035585825));
#56383=CARTESIAN_POINT('Ctrl Pts',(1.04953485736196,-1.29701711762812,13.3208742210172));
#56384=CARTESIAN_POINT('Ctrl Pts',(1.12610108313259,-1.22784729175888,13.3276119279827));
#56385=CARTESIAN_POINT('Ctrl Pts',(1.13529241728116,-1.21935381476108,13.3284356522641));
#56386=CARTESIAN_POINT('Ctrl Pts',(1.14914841703908,-1.20625737012636,13.3297019776696));
#56387=CARTESIAN_POINT('Ctrl Pts',(1.15388328721975,-1.20172887257747,13.3301391713918));
#56388=CARTESIAN_POINT('Ctrl Pts',(1.16251998067545,-1.19337051496657,13.3309451565939));
#56389=CARTESIAN_POINT('Ctrl Pts',(1.16642981393031,-1.18954923302104,13.3313132998701));
#56390=CARTESIAN_POINT('Ctrl Pts',(1.17533394019365,-1.18076066362978,13.332159203262));
#56391=CARTESIAN_POINT('Ctrl Pts',(1.18031556950598,-1.17578091819978,13.3326379101307));
#56392=CARTESIAN_POINT('Ctrl Pts',(1.19581773468374,-1.16008681796706,13.3341443051606));
#56393=CARTESIAN_POINT('Ctrl Pts',(1.20622474609754,-1.14926206866399,13.335180009024));
#56394=CARTESIAN_POINT('Ctrl Pts',(1.28782784918856,-1.06205399162405,13.3434875419961));
#56395=CARTESIAN_POINT('Ctrl Pts',(1.35183997685693,-0.97927749833731,13.3511381568114));
#56396=CARTESIAN_POINT('Ctrl Pts',(1.46826907879617,-0.795345781820444,
13.366965950129));
#56397=CARTESIAN_POINT('Ctrl Pts',(1.51894816544301,-0.693681763120602,
13.3750832464998));
#56398=CARTESIAN_POINT('Ctrl Pts',(1.56575804935059,-0.569502907082649,
13.3841639609022));
#56399=CARTESIAN_POINT('Ctrl Pts',(1.57227922068042,-0.551243990973118,
13.3854800678179));
#56400=CARTESIAN_POINT('Ctrl Pts',(1.58203330260813,-0.522350468616721,
13.3875336947073));
#56401=CARTESIAN_POINT('Ctrl Pts',(1.58548088521564,-0.511790734176277,
13.3882782204302));
#56402=CARTESIAN_POINT('Ctrl Pts',(1.59174590795364,-0.491930263128515,
13.389667540571));
#56403=CARTESIAN_POINT('Ctrl Pts',(1.59458806627149,-0.48263788186675,13.3903131198856));
#56404=CARTESIAN_POINT('Ctrl Pts',(1.60079240038472,-0.461699690150318,
13.3917580536405));
#56405=CARTESIAN_POINT('Ctrl Pts',(1.60410913329456,-0.450040903094354,
13.392555902592));
#56406=CARTESIAN_POINT('Ctrl Pts',(1.6135034708557,-0.415594415919144,13.3948942789194));
#56407=CARTESIAN_POINT('Ctrl Pts',(1.61922496018563,-0.392712091490457,
13.3964233609263));
#56408=CARTESIAN_POINT('Ctrl Pts',(1.64738569855396,-0.268979061725007,
13.4045756307217));
#56409=CARTESIAN_POINT('Ctrl Pts',(1.66089396345492,-0.166324894291564,
13.4109092970689));
#56410=CARTESIAN_POINT('Ctrl Pts',(1.66779110162462,0.0157310073905968,
13.4220358017062));
#56411=CARTESIAN_POINT('Ctrl Pts',(1.66517752952499,0.0946397567061671,
13.4268299820002));
#56412=CARTESIAN_POINT('Ctrl Pts',(1.65442138496804,0.197625694297063,13.4333596480732));
#56413=CARTESIAN_POINT('Ctrl Pts',(1.65130989158162,0.222129572903168,13.4349341376021));
#56414=CARTESIAN_POINT('Ctrl Pts',(1.6451128113114,0.263543036510313,13.4376442198349));
#56415=CARTESIAN_POINT('Ctrl Pts',(1.64230807570083,0.280491037616897,13.4387673457008));
#56416=CARTESIAN_POINT('Ctrl Pts',(1.63791546024065,0.304703403121771,13.4403959886441));
#56417=CARTESIAN_POINT('Ctrl Pts',(1.63654011832794,0.312005856758478,13.4408903471462));
#56418=CARTESIAN_POINT('Ctrl Pts',(1.63406091403176,0.324701764141206,13.4417557242885));
#56419=CARTESIAN_POINT('Ctrl Pts',(1.63297909758993,0.330099336912054,13.4421255039631));
#56420=CARTESIAN_POINT('Ctrl Pts',(1.63060284967423,0.34165768584096,13.4429214851699));
#56421=CARTESIAN_POINT('Ctrl Pts',(1.62930026879551,0.347816414900361,13.4433481095066));
#56422=CARTESIAN_POINT('Ctrl Pts',(1.62562626459965,0.364713849182281,13.4445252066675));
#56423=CARTESIAN_POINT('Ctrl Pts',(1.62318341322813,0.375436459107247,13.445279484383));
#56424=CARTESIAN_POINT('Ctrl Pts',(1.60864725719351,0.43644588743802,13.4496100475103));
#56425=CARTESIAN_POINT('Ctrl Pts',(1.5943246158628,0.486167595361645,13.4532897920663));
#56426=CARTESIAN_POINT('Ctrl Pts',(1.54682683042447,0.626202626085136,13.4639468386568));
#56427=CARTESIAN_POINT('Ctrl Pts',(1.50811234273667,0.714423706511268,13.4710098991774));
#56428=CARTESIAN_POINT('Ctrl Pts',(1.43689683467623,0.844763274976809,13.4816893558122));
#56429=CARTESIAN_POINT('Ctrl Pts',(1.40963756537154,0.889505659470023,13.4854073257522));
#56430=CARTESIAN_POINT('Ctrl Pts',(1.36700508834127,0.952584884773113,13.4907128411085));
#56431=CARTESIAN_POINT('Ctrl Pts',(1.35327607537385,0.971990142080068,13.492354550582));
#56432=CARTESIAN_POINT('Ctrl Pts',(1.32761973893876,1.00665613460049,13.4953054711994));
#56433=CARTESIAN_POINT('Ctrl Pts',(1.31583282988615,1.02201505037389,13.4966196360212));
#56434=CARTESIAN_POINT('Ctrl Pts',(1.29686903061903,1.04585370298794,13.4986709366427));
#56435=CARTESIAN_POINT('Ctrl Pts',(1.2898707932599,1.05447266330533,13.4994150517637));
#56436=CARTESIAN_POINT('Ctrl Pts',(1.27658626579411,1.07050359099232,13.5008040008145));
#56437=CARTESIAN_POINT('Ctrl Pts',(1.27032030044567,1.07793171094363,13.501449615573));
#56438=CARTESIAN_POINT('Ctrl Pts',(1.25608802108515,1.0945071966981,13.5028951384433));
#56439=CARTESIAN_POINT('Ctrl Pts',(1.24808602625913,1.10362330728539,13.5036935356074));
#56440=CARTESIAN_POINT('Ctrl Pts',(1.22420703832332,1.1302350443473,13.5060351393241));
#56441=CARTESIAN_POINT('Ctrl Pts',(1.20805624409073,1.14748173371283,13.5075668518917));
#56442=CARTESIAN_POINT('Ctrl Pts',(1.12121219356062,1.23635175424994,13.5155490781954));
#56443=CARTESIAN_POINT('Ctrl Pts',(1.04450200498592,1.30180691117526,13.521727007672));
#56444=CARTESIAN_POINT('Ctrl Pts',(0.89631194875483,1.40667150828439,13.5328161457826));
#56445=CARTESIAN_POINT('Ctrl Pts',(0.826967695998072,1.44852423567307,13.5377284413919));
#56446=CARTESIAN_POINT('Ctrl Pts',(0.732550372742284,1.49651343739044,13.5444039369826));
#56447=CARTESIAN_POINT('Ctrl Pts',(0.709985259653346,1.50734976517217,13.5459988188556));
#56448=CARTESIAN_POINT('Ctrl Pts',(0.671381817628897,1.52482898373729,13.5487405664365));
#56449=CARTESIAN_POINT('Ctrl Pts',(0.655467719797646,1.53173724413384,13.5498745794582));
#56450=CARTESIAN_POINT('Ctrl Pts',(0.632560827739368,1.54125872280368,13.5515162451771));
#56451=CARTESIAN_POINT('Ctrl Pts',(0.625653235402655,1.54407567015345,13.552012493366));
#56452=CARTESIAN_POINT('Ctrl Pts',(0.613612275240564,1.5488919662284,13.5528800047154));
#56453=CARTESIAN_POINT('Ctrl Pts',(0.608487534973512,1.55091239796915,13.5532500097162));
#56454=CARTESIAN_POINT('Ctrl Pts',(0.597500109804599,1.55518135362252,13.5540450994273));
#56455=CARTESIAN_POINT('Ctrl Pts',(0.591634803735674,1.55742212634069,13.5544705948436));
#56456=CARTESIAN_POINT('Ctrl Pts',(0.575528857615562,1.56347110869394,13.5556416194534));
#56457=CARTESIAN_POINT('Ctrl Pts',(0.565263415286893,1.56721173718473,13.556390891968));
#56458=CARTESIAN_POINT('Ctrl Pts',(0.507613028939983,1.58757890712265,13.5606120528637));
#56459=CARTESIAN_POINT('Ctrl Pts',(0.459536245180714,1.60215579474568,13.564181501569));
#56460=CARTESIAN_POINT('Ctrl Pts',(0.315826916027447,1.63872804396251,13.5748602014975));
#56461=CARTESIAN_POINT('Ctrl Pts',(0.218822535736473,1.65447697896201,13.5820675301847));
#56462=CARTESIAN_POINT('Ctrl Pts',(0.068947111650721,1.66539047284085,13.5928711562973));
#56463=CARTESIAN_POINT('Ctrl Pts',(0.0167481776930115,1.66673318255776,
13.5965761550655));
#56464=CARTESIAN_POINT('Ctrl Pts',(-0.0591421275863616,1.66511880452352,
13.6018653978931));
#56465=CARTESIAN_POINT('Ctrl Pts',(-0.0828397490805629,1.66410819901216,
13.6035034348538));
#56466=CARTESIAN_POINT('Ctrl Pts',(-0.125794721988943,1.66135642232413,
13.6064484371513));
#56467=CARTESIAN_POINT('Ctrl Pts',(-0.145058377989086,1.6597854064981,13.6077603259338));
#56468=CARTESIAN_POINT('Ctrl Pts',(-0.175331846431883,1.65678539334367,
13.609808900019));
#56469=CARTESIAN_POINT('Ctrl Pts',(-0.186361649179719,1.65558099831943,
13.6105525337237));
#56470=CARTESIAN_POINT('Ctrl Pts',(-0.207028819953206,1.65311509449884,
13.6119410486164));
#56471=CARTESIAN_POINT('Ctrl Pts',(-0.216668718088043,1.6518792696185,13.6125867058587));
#56472=CARTESIAN_POINT('Ctrl Pts',(-0.238324314348732,1.64891021167148,
13.6140329240105));
#56473=CARTESIAN_POINT('Ctrl Pts',(-0.250333076225962,1.6471298458022,13.6148319675367));
#56474=CARTESIAN_POINT('Ctrl Pts',(-0.285699984000059,1.64149077482557,
13.617177379437));
#56475=CARTESIAN_POINT('Ctrl Pts',(-0.30899716580376,1.63726518520925,13.618712196327));
#56476=CARTESIAN_POINT('Ctrl Pts',(-0.429844577385538,1.61267461848072,
13.6266339965178));
#56477=CARTESIAN_POINT('Ctrl Pts',(-0.525516618505373,1.58408372494524,
13.6327545570776));
#56478=CARTESIAN_POINT('Ctrl Pts',(-0.693845206382381,1.51683663228789,
13.6438277354306));
#56479=CARTESIAN_POINT('Ctrl Pts',(-0.767290094424702,1.48103970721281,
13.6487809528885));
#56480=CARTESIAN_POINT('Ctrl Pts',(-0.870126671251356,1.42120841083277,
13.6562784316146));
#56481=CARTESIAN_POINT('Ctrl Pts',(-0.901797213001384,1.40132618438397,
13.658672574052));
#56482=CARTESIAN_POINT('Ctrl Pts',(-0.940923431179376,1.37488761110621,
13.6617753954154));
#56483=CARTESIAN_POINT('Ctrl Pts',(-0.949028215208555,1.36930576630687,
13.6624262713061));
#56484=CARTESIAN_POINT('Ctrl Pts',(-0.961976456792547,1.36021801218715,
13.6634801144471));
#56485=CARTESIAN_POINT('Ctrl Pts',(-0.96685146412288,1.35675715866733,13.663880120796));
#56486=CARTESIAN_POINT('Ctrl Pts',(-0.976221083068241,1.3500293593988,13.6646554097535));
#56487=CARTESIAN_POINT('Ctrl Pts',(-0.980718135153803,1.34676605616228,
13.6650304507609));
#56488=CARTESIAN_POINT('Ctrl Pts',(-0.990696712075996,1.33944858385314,
13.6658690519785));
#56489=CARTESIAN_POINT('Ctrl Pts',(-0.996169840212795,1.3353831395923,13.6663333654091));
#56490=CARTESIAN_POINT('Ctrl Pts',(-1.01233882568955,1.3232180876719,13.6677176580756));
#56491=CARTESIAN_POINT('Ctrl Pts',(-1.02296167288394,1.31502296311746,13.6686436321306));
#56492=CARTESIAN_POINT('Ctrl Pts',(-1.11775078980674,1.24005321068179,13.6770478036626));
#56493=CARTESIAN_POINT('Ctrl Pts',(-1.19536602389239,1.16541636455799,13.684928987173));
#56494=CARTESIAN_POINT('Ctrl Pts',(-1.33707113643737,0.999992349300045,
13.7007595888945));
#56495=CARTESIAN_POINT('Ctrl Pts',(-1.40039247174524,0.909204679859933,
13.7086606587543));
#56496=CARTESIAN_POINT('Ctrl Pts',(-1.46375495978593,0.795836181745914,
13.7175480643725));
#56497=CARTESIAN_POINT('Ctrl Pts',(-1.47294066768611,0.778703830393552,
13.7188677062834));
#56498=CARTESIAN_POINT('Ctrl Pts',(-1.48690633516537,0.751524566049916,
13.7209255669042));
#56499=CARTESIAN_POINT('Ctrl Pts',(-1.49188885135243,0.741584309785389,
13.7216708395729));
#56500=CARTESIAN_POINT('Ctrl Pts',(-1.50103809508365,0.72286584727561,13.7230608366402));
#56501=CARTESIAN_POINT('Ctrl Pts',(-1.50522823850449,0.714099679943736,
13.7237063533248));
#56502=CARTESIAN_POINT('Ctrl Pts',(-1.51446629478674,0.694330167065318,
13.7251502244848));
#56503=CARTESIAN_POINT('Ctrl Pts',(-1.51947148242464,0.683307372969721,
13.725947083331));
#56504=CARTESIAN_POINT('Ctrl Pts',(-1.53384182147373,0.65072106960216,13.728279636644));
#56505=CARTESIAN_POINT('Ctrl Pts',(-1.54287146842955,0.62901221315323,13.7298039731925));
#56506=CARTESIAN_POINT('Ctrl Pts',(-1.55554398581049,0.596628693154489,
13.732038227184));
#56507=CARTESIAN_POINT('Ctrl Pts',(-1.55954156847558,0.586099713912162,
13.7327585704354));
#56508=CARTESIAN_POINT('Ctrl Pts',(-1.56343128722854,0.575533326676141,
13.7334757494662));
#56509=CARTESIAN_POINT('Origin',(0.,0.,11.));
#56510=CARTESIAN_POINT('',(-1.56343129324813,0.575533310323967,14.4309760522469));
#56511=CARTESIAN_POINT('',(-1.56343134771032,0.575533162377876,14.2401853336637));
#56512=CARTESIAN_POINT('',(-1.56343130033213,0.575533291080363,11.));
#56513=CARTESIAN_POINT('',(-1.66599934497354,0.00147734482691685,13.5789038102816));
#56514=CARTESIAN_POINT('Ctrl Pts',(-1.56343134771032,0.575533162377876,
14.2401853336637));
#56515=CARTESIAN_POINT('Ctrl Pts',(-1.54563346535971,0.6238809709991,14.2369930364229));
#56516=CARTESIAN_POINT('Ctrl Pts',(-1.52559334840805,0.671401985184517,
14.2337520000224));
#56517=CARTESIAN_POINT('Ctrl Pts',(-1.49757772934425,0.730066810385444,
14.2295271102982));
#56518=CARTESIAN_POINT('Ctrl Pts',(-1.49164013259726,0.74212282705374,14.228646527073));
#56519=CARTESIAN_POINT('Ctrl Pts',(-1.48246906387274,0.760189470780374,
14.2273062252057));
#56520=CARTESIAN_POINT('Ctrl Pts',(-1.47934327443169,0.766254545960231,
14.2268527173139));
#56521=CARTESIAN_POINT('Ctrl Pts',(-1.47360413945224,0.777224372697188,
14.2260256687841));
#56522=CARTESIAN_POINT('Ctrl Pts',(-1.47100330149631,0.782135647627981,
14.2256528981661));
#56523=CARTESIAN_POINT('Ctrl Pts',(-1.46555501330078,0.792300581227544,
14.2248760014611));
#56524=CARTESIAN_POINT('Ctrl Pts',(-1.46270381546158,0.797552038062961,
14.2244716572804));
#56525=CARTESIAN_POINT('Ctrl Pts',(-1.45508859430806,0.811399887267858,
14.223397743613));
#56526=CARTESIAN_POINT('Ctrl Pts',(-1.45027673178433,0.819969501785932,
14.2227252866415));
#56527=CARTESIAN_POINT('Ctrl Pts',(-1.42687306751663,0.860799414295964,
14.2194852746845));
#56528=CARTESIAN_POINT('Ctrl Pts',(-1.40728044634848,0.89247053052591,14.2168634912301));
#56529=CARTESIAN_POINT('Ctrl Pts',(-1.34176895398326,0.990841446508917,
14.2084295866173));
#56530=CARTESIAN_POINT('Ctrl Pts',(-1.29204199221702,1.05486367364607,14.2025035926654));
#56531=CARTESIAN_POINT('Ctrl Pts',(-1.17058137687715,1.18970600930494,14.1893195173065));
#56532=CARTESIAN_POINT('Ctrl Pts',(-1.09667125964575,1.25816508452776,14.1821201096597));
#56533=CARTESIAN_POINT('Ctrl Pts',(-0.998310974699384,1.33397510882556,
14.173570776052));
#56534=CARTESIAN_POINT('Ctrl Pts',(-0.979289064811212,1.3480012685526,14.1719592169296));
#56535=CARTESIAN_POINT('Ctrl Pts',(-0.950060400568612,1.36860818889356,
14.1695440033051));
#56536=CARTESIAN_POINT('Ctrl Pts',(-0.940070228643677,1.37548941041134,
14.1687289585216));
#56537=CARTESIAN_POINT('Ctrl Pts',(-0.921943290830429,1.38768548053969,
14.1672684532143));
#56538=CARTESIAN_POINT('Ctrl Pts',(-0.91383357649876,1.39303934823724,14.1666215426324));
#56539=CARTESIAN_POINT('Ctrl Pts',(-0.89636059495744,1.40435640019398,14.1652413177582));
#56540=CARTESIAN_POINT('Ctrl Pts',(-0.886983596277834,1.41029760154465,
14.1645088423294));
#56541=CARTESIAN_POINT('Ctrl Pts',(-0.861097574966405,1.42633848922139,
14.1625086608307));
#56542=CARTESIAN_POINT('Ctrl Pts',(-0.844470530302214,1.43624513699585,
14.1612480166618));
#56543=CARTESIAN_POINT('Ctrl Pts',(-0.730415548716905,1.50153523367751,
14.1527534439515));
#56544=CARTESIAN_POINT('Ctrl Pts',(-0.627784055215815,1.54725771660207,
14.1458831227031));
#56545=CARTESIAN_POINT('Ctrl Pts',(-0.420819140924783,1.61544596338825,
14.1325757690076));
#56546=CARTESIAN_POINT('Ctrl Pts',(-0.31739842629686,1.63890403047336,14.1261573608561));
#56547=CARTESIAN_POINT('Ctrl Pts',(-0.197829185084652,1.65427853961648,
14.1183236842443));
#56548=CARTESIAN_POINT('Ctrl Pts',(-0.183165430651324,1.65596626219152,
14.1173558245408));
#56549=CARTESIAN_POINT('Ctrl Pts',(-0.161496397614285,1.65816893402883,
14.1159124818691));
#56550=CARTESIAN_POINT('Ctrl Pts',(-0.154506720980915,1.65883482268614,
14.1154449017786));
#56551=CARTESIAN_POINT('Ctrl Pts',(-0.142060615607765,1.65994118784928,
14.1146084037009));
#56552=CARTESIAN_POINT('Ctrl Pts',(-0.136605928331721,1.66039898354506,
14.1142404489481));
#56553=CARTESIAN_POINT('Ctrl Pts',(-0.124689668753647,1.66133996192484,
14.1134335935092));
#56554=CARTESIAN_POINT('Ctrl Pts',(-0.118227595407533,1.66181232836255,
14.1129941353254));
#56555=CARTESIAN_POINT('Ctrl Pts',(-0.0996240660430227,1.66306315785753,
14.1117238138352));
#56556=CARTESIAN_POINT('Ctrl Pts',(-0.0874769232334655,1.66374631115576,
14.110888023148));
#56557=CARTESIAN_POINT('Ctrl Pts',(-0.0596576469455694,1.66500537460731,
14.1089610324874));
#56558=CARTESIAN_POINT('Ctrl Pts',(-0.0439828416268084,1.66549314092908,
14.107865931585));
#56559=CARTESIAN_POINT('Ctrl Pts',(0.00879052807203655,1.66638985170575,
14.1041525076836));
#56560=CARTESIAN_POINT('Ctrl Pts',(0.0458936552049288,1.66578084923985,
14.1014979024997));
#56561=CARTESIAN_POINT('Ctrl Pts',(0.154192615018678,1.66038241316854,14.0936727626892));
#56562=CARTESIAN_POINT('Ctrl Pts',(0.225139961452177,1.65225818079694,14.0884525567434));
#56563=CARTESIAN_POINT('Ctrl Pts',(0.392780698625073,1.62206057255451,14.0761072669606));
#56564=CARTESIAN_POINT('Ctrl Pts',(0.488469176903136,1.59585752020852,14.0690619385057));
#56565=CARTESIAN_POINT('Ctrl Pts',(0.598952188973332,1.55472439847301,14.0610013049357));
#56566=CARTESIAN_POINT('Ctrl Pts',(0.616514083691443,1.54784434463828,14.0597217016109));
#56567=CARTESIAN_POINT('Ctrl Pts',(0.644124184180432,1.53648330061058,14.0577118572541));
#56568=CARTESIAN_POINT('Ctrl Pts',(0.654250891343624,1.5321986421189,14.0569751000901));
#56569=CARTESIAN_POINT('Ctrl Pts',(0.672366042715144,1.52432168644296,14.0556576244148));
#56570=CARTESIAN_POINT('Ctrl Pts',(0.680369899815099,1.52076609101846,14.0550756878771));
#56571=CARTESIAN_POINT('Ctrl Pts',(0.699104290881365,1.51226610435816,14.0537137529317));
#56572=CARTESIAN_POINT('Ctrl Pts',(0.709811097704624,1.50727031335604,14.0529355464373));
#56573=CARTESIAN_POINT('Ctrl Pts',(0.741035689520064,1.4922944232628,14.0506657262689));
#56574=CARTESIAN_POINT('Ctrl Pts',(0.761403195200306,1.48200600359717,14.0491847813041));
#56575=CARTESIAN_POINT('Ctrl Pts',(0.854510586831767,1.43254747595464,14.0424025466643));
#56576=CARTESIAN_POINT('Ctrl Pts',(0.924488179485203,1.38841799612802,14.0372773146484));
#56577=CARTESIAN_POINT('Ctrl Pts',(1.0370176359957,1.30515907449163,14.0286950754777));
#56578=CARTESIAN_POINT('Ctrl Pts',(1.08133293829069,1.26868624512614,14.0252109619448));
#56579=CARTESIAN_POINT('Ctrl Pts',(1.18056782468595,1.17802930381744,14.0169622835631));
#56580=CARTESIAN_POINT('Ctrl Pts',(1.23377562680633,1.12218002308815,14.0121795820669));
#56581=CARTESIAN_POINT('Ctrl Pts',(1.29032435379716,1.05392301236079,14.006381851432));
#56582=CARTESIAN_POINT('Ctrl Pts',(1.29763357951774,1.04491039270479,14.0056171555454));
#56583=CARTESIAN_POINT('Ctrl Pts',(1.30884618423056,1.03078563374416,14.0044186733575));
#56584=CARTESIAN_POINT('Ctrl Pts',(1.31281527588576,1.0257257940794,14.0039893402696));
#56585=CARTESIAN_POINT('Ctrl Pts',(1.32011231479558,1.01631171912152,14.0031902646955));
#56586=CARTESIAN_POINT('Ctrl Pts',(1.32344819184896,1.01196388987053,14.002821084287));
#56587=CARTESIAN_POINT('Ctrl Pts',(1.33112299369749,1.00185805178356,14.001962724409));
#56588=CARTESIAN_POINT('Ctrl Pts',(1.33544603590394,0.996088279534443,14.001472486976));
#56589=CARTESIAN_POINT('Ctrl Pts',(1.34919473411293,0.977488123683293,13.9998920341239));
#56590=CARTESIAN_POINT('Ctrl Pts',(1.35847365012393,0.964551065583285,13.9987926837506));
#56591=CARTESIAN_POINT('Ctrl Pts',(1.38030376940767,0.933174683519973,13.9961299766807));
#56592=CARTESIAN_POINT('Ctrl Pts',(1.39267263102929,0.914612665691757,13.9945576361085));
#56593=CARTESIAN_POINT('Ctrl Pts',(1.43988580768317,0.840580502041863,13.9883138760368));
#56594=CARTESIAN_POINT('Ctrl Pts',(1.47181742078354,0.783325794241625,13.9835465712049));
#56595=CARTESIAN_POINT('Ctrl Pts',(1.55331359258663,0.614527139730089,13.969901863511));
#56596=CARTESIAN_POINT('Ctrl Pts',(1.59412513062366,0.499201510077962,13.9610933799439));
#56597=CARTESIAN_POINT('Ctrl Pts',(1.62676149294236,0.36005723460561,13.951262784045));
#56598=CARTESIAN_POINT('Ctrl Pts',(1.6311571553045,0.339588826138155,13.9498349416575));
#56599=CARTESIAN_POINT('Ctrl Pts',(1.63756855242655,0.306728910578537,13.9475709110637));
#56600=CARTESIAN_POINT('Ctrl Pts',(1.63983192631386,0.294388615384434,13.9467269764598));
#56601=CARTESIAN_POINT('Ctrl Pts',(1.64361214699959,0.272379980739625,13.9452326962979));
#56602=CARTESIAN_POINT('Ctrl Pts',(1.64518358605755,0.262721751784548,13.9445806511672));
#56603=CARTESIAN_POINT('Ctrl Pts',(1.6483003688112,0.242439945547055,13.9432188993649));
#56604=CARTESIAN_POINT('Ctrl Pts',(1.64982831132455,0.231814117928783,13.9425097697681));
#56605=CARTESIAN_POINT('Ctrl Pts',(1.65359560538315,0.203688045354073,13.9406436221211));
#56606=CARTESIAN_POINT('Ctrl Pts',(1.65565990477688,0.186165422120089,13.9394921251335));
#56607=CARTESIAN_POINT('Ctrl Pts',(1.66486715616074,0.0956591143175343,
13.9335966812282));
#56608=CARTESIAN_POINT('Ctrl Pts',(1.66746466905398,0.0222900669585823,
13.9289968130541));
#56609=CARTESIAN_POINT('Ctrl Pts',(1.66221157731468,-0.149166442099089,
13.9184092242576));
#56610=CARTESIAN_POINT('Ctrl Pts',(1.65053357868766,-0.246851681141567,
13.9125048852937));
#56611=CARTESIAN_POINT('Ctrl Pts',(1.62412326944738,-0.372406347329133,
13.9045451698716));
#56612=CARTESIAN_POINT('Ctrl Pts',(1.61712676958313,-0.401701029241101,
13.9026598110306));
#56613=CARTESIAN_POINT('Ctrl Pts',(1.60185589100986,-0.458750009173098,
13.8989048108138));
#56614=CARTESIAN_POINT('Ctrl Pts',(1.59364422586159,-0.486509721322128,
13.8970380384637));
#56615=CARTESIAN_POINT('Ctrl Pts',(1.58183292350379,-0.522922376135999,
13.894519352753));
#56616=CARTESIAN_POINT('Ctrl Pts',(1.57887697231132,-0.531780693187206,
13.893901057406));
#56617=CARTESIAN_POINT('Ctrl Pts',(1.57394255919479,-0.546164129779019,
13.892887319373));
#56618=CARTESIAN_POINT('Ctrl Pts',(1.57200904936928,-0.551704615093206,
13.89249444526));
#56619=CARTESIAN_POINT('Ctrl Pts',(1.56814248244164,-0.562598928924352,
13.891717013266));
#56620=CARTESIAN_POINT('Ctrl Pts',(1.56621118938815,-0.567953261247392,
13.8913325575065));
#56621=CARTESIAN_POINT('Ctrl Pts',(1.56132237414522,-0.581292482588408,
13.890369035037));
#56622=CARTESIAN_POINT('Ctrl Pts',(1.55833102945422,-0.589264712314062,
13.8897880369667));
#56623=CARTESIAN_POINT('Ctrl Pts',(1.54650137756292,-0.620071799448701,
13.8875238407525));
#56624=CARTESIAN_POINT('Ctrl Pts',(1.53722165269512,-0.64273243528617,13.8858176465327));
#56625=CARTESIAN_POINT('Ctrl Pts',(1.51121919480198,-0.702441739492555,
13.8812275890391));
#56626=CARTESIAN_POINT('Ctrl Pts',(1.49363464222281,-0.73909605995518,13.8783114153314));
#56627=CARTESIAN_POINT('Ctrl Pts',(1.41843721688195,-0.882174823563911,
13.8666206778354));
#56628=CARTESIAN_POINT('Ctrl Pts',(1.35063621685571,-0.98284507183653,13.8577305146817));
#56629=CARTESIAN_POINT('Ctrl Pts',(1.24079926080148,-1.1128293885765,13.845713901872));
#56630=CARTESIAN_POINT('Ctrl Pts',(1.20742575525371,-1.14895428628584,13.8423003242044));
#56631=CARTESIAN_POINT('Ctrl Pts',(1.16101762901055,-1.19492899975054,13.8378527771523));
#56632=CARTESIAN_POINT('Ctrl Pts',(1.14936975050277,-1.206136997994,13.8367596503541));
#56633=CARTESIAN_POINT('Ctrl Pts',(1.12994828453142,-1.22428813035644,13.8349739617505));
#56634=CARTESIAN_POINT('Ctrl Pts',(1.122269615377,-1.23133077228182,13.8342771626411));
#56635=CARTESIAN_POINT('Ctrl Pts',(1.10716354434819,-1.24492689836098,13.8329239249175));
#56636=CARTESIAN_POINT('Ctrl Pts',(1.09974278647722,-1.25148707823925,13.8322672209326));
#56637=CARTESIAN_POINT('Ctrl Pts',(1.08203627521113,-1.26686106612458,13.8307189041629));
#56638=CARTESIAN_POINT('Ctrl Pts',(1.07170056471045,-1.2756164702845,13.8298297195221));
#56639=CARTESIAN_POINT('Ctrl Pts',(1.0361853513146,-1.30496510445069,13.8268221174587));
#56640=CARTESIAN_POINT('Ctrl Pts',(1.01050909888216,-1.32494739206604,13.8247280838217));
#56641=CARTESIAN_POINT('Ctrl Pts',(0.946075914446345,-1.37212845246582,
13.8196477977291));
#56642=CARTESIAN_POINT('Ctrl Pts',(0.906713012574381,-1.39845204921205,
13.8166919006341));
#56643=CARTESIAN_POINT('Ctrl Pts',(0.807692499540422,-1.45873003779954,
13.8095293113601));
#56644=CARTESIAN_POINT('Ctrl Pts',(0.746958094718095,-1.4907428724512,13.8053656004681));
#56645=CARTESIAN_POINT('Ctrl Pts',(0.664818609608883,-1.52775474603952,
13.7998517172005));
#56646=CARTESIAN_POINT('Ctrl Pts',(0.645045718180894,-1.53620777951307,
13.7985326368586));
#56647=CARTESIAN_POINT('Ctrl Pts',(0.564611272681701,-1.56876724247348,
13.7931804330185));
#56648=CARTESIAN_POINT('Ctrl Pts',(0.502727428624714,-1.5896790948502,13.7890946793647));
#56649=CARTESIAN_POINT('Ctrl Pts',(0.428732256208436,-1.60993042299665,
13.7840750992329));
#56650=CARTESIAN_POINT('Ctrl Pts',(0.417648936072857,-1.61284117715866,
13.7833197531945));
#56651=CARTESIAN_POINT('Ctrl Pts',(0.400331639152728,-1.61719866476476,
13.7821328525658));
#56652=CARTESIAN_POINT('Ctrl Pts',(0.394117611889677,-1.61872426534024,
13.7817056157596));
#56653=CARTESIAN_POINT('Ctrl Pts',(0.382611398806776,-1.62147896530772,
13.7809117901695));
#56654=CARTESIAN_POINT('Ctrl Pts',(0.377321800387743,-1.62271802024248,
13.7805457690901));
#56655=CARTESIAN_POINT('Ctrl Pts',(0.364981670268074,-1.62554501980323,
13.779689400248));
#56656=CARTESIAN_POINT('Ctrl Pts',(0.357926796742602,-1.6271129752856,13.7791979555529));
#56657=CARTESIAN_POINT('Ctrl Pts',(0.335204284521835,-1.63200815983335,
13.7776096197283));
#56658=CARTESIAN_POINT('Ctrl Pts',(0.319499333643773,-1.63515524487017,
13.7765034702519));
#56659=CARTESIAN_POINT('Ctrl Pts',(0.281644111067665,-1.64217482879068,
13.7738210428304));
#56660=CARTESIAN_POINT('Ctrl Pts',(0.25945639203253,-1.64582619124666,13.7722356151435));
#56661=CARTESIAN_POINT('Ctrl Pts',(0.171442144395756,-1.6584865168876,13.765911054626));
#56662=CARTESIAN_POINT('Ctrl Pts',(0.105177976392292,-1.66400319144999,
13.7610738493845));
#56663=CARTESIAN_POINT('Ctrl Pts',(-0.0817395807860534,-1.66835366240431,
13.7474638294159));
#56664=CARTESIAN_POINT('Ctrl Pts',(-0.202214437460003,-1.65807257065349,
13.7387616953583));
#56665=CARTESIAN_POINT('Ctrl Pts',(-0.341162978413611,-1.63082968095876,
13.7290212042229));
#56666=CARTESIAN_POINT('Ctrl Pts',(-0.361707668032832,-1.62639640274447,
13.7275876120691));
#56667=CARTESIAN_POINT('Ctrl Pts',(-0.394397417196678,-1.61869226563308,
13.7253163054304));
#56668=CARTESIAN_POINT('Ctrl Pts',(-0.406598280424448,-1.61567070496945,
13.7244707656162));
#56669=CARTESIAN_POINT('Ctrl Pts',(-0.428237884255776,-1.6100509683455,
13.7229746596417));
#56670=CARTESIAN_POINT('Ctrl Pts',(-0.437689994314263,-1.6075071639306,
13.7223223793115));
#56671=CARTESIAN_POINT('Ctrl Pts',(-0.457448896860064,-1.6020023373628,
13.7209611465605));
#56672=CARTESIAN_POINT('Ctrl Pts',(-0.467750654004095,-1.59902480184126,
13.7202527623937));
#56673=CARTESIAN_POINT('Ctrl Pts',(-0.494871308041044,-1.59090154160773,
13.7183908870772));
#56674=CARTESIAN_POINT('Ctrl Pts',(-0.511638994089605,-1.5855885042182,
13.7172428704566));
#56675=CARTESIAN_POINT('Ctrl Pts',(-0.596996012848846,-1.55704704383942,
13.7114098519396));
#56676=CARTESIAN_POINT('Ctrl Pts',(-0.664106598019126,-1.52962873299698,
13.7068650589325));
#56677=CARTESIAN_POINT('Ctrl Pts',(-0.789909425776177,-1.46838490236284,
13.6982250950865));
#56678=CARTESIAN_POINT('Ctrl Pts',(-0.848741156108113,-1.43518283132511,
13.6941276729167));
#56679=CARTESIAN_POINT('Ctrl Pts',(-0.972486968042734,-1.35506923630702,
13.6851051377307));
#56680=CARTESIAN_POINT('Ctrl Pts',(-1.03635633275848,-1.30686877467561,
13.6801783319021));
#56681=CARTESIAN_POINT('Ctrl Pts',(-1.10838978117183,-1.24389588515171,
13.6739706539603));
#56682=CARTESIAN_POINT('Ctrl Pts',(-1.12011837726404,-1.23334490581664,
13.6729372944684));
#56683=CARTESIAN_POINT('Ctrl Pts',(-1.13691070342952,-1.21780152994364,
13.6714214880085));
#56684=CARTESIAN_POINT('Ctrl Pts',(-1.1420954897882,-1.21294039487503,13.6709483214237));
#56685=CARTESIAN_POINT('Ctrl Pts',(-1.15122409152189,-1.20427120904506,
13.6701057230189));
#56686=CARTESIAN_POINT('Ctrl Pts',(-1.15518044786978,-1.20047664926562,
13.6697373101891));
#56687=CARTESIAN_POINT('Ctrl Pts',(-1.16283254150445,-1.1930646346198,13.6690183625882));
#56688=CARTESIAN_POINT('Ctrl Pts',(-1.16653014622713,-1.18944951892796,
13.6686680367671));
#56689=CARTESIAN_POINT('Ctrl Pts',(-1.17693583912778,-1.17918077509708,
13.6676740257869));
#56690=CARTESIAN_POINT('Ctrl Pts',(-1.18360410971571,-1.17248734357653,
13.667027385642));
#56691=CARTESIAN_POINT('Ctrl Pts',(-1.21629711548992,-1.13910787880694,
13.6638105917625));
#56692=CARTESIAN_POINT('Ctrl Pts',(-1.24147608955379,-1.11161237426235,
13.6611857879259));
#56693=CARTESIAN_POINT('Ctrl Pts',(-1.31851935295915,-1.02159617019656,
13.6527303637501));
#56694=CARTESIAN_POINT('Ctrl Pts',(-1.36674463254303,-0.956117313027135,
13.6467852495804));
#56695=CARTESIAN_POINT('Ctrl Pts',(-1.46335756600952,-0.802605262317195,
13.6336090333831));
#56696=CARTESIAN_POINT('Ctrl Pts',(-1.5089664705099,-0.713173743223769,
13.6264357489282));
#56697=CARTESIAN_POINT('Ctrl Pts',(-1.55506955322967,-0.598225566857417,
13.6179093717365));
#56698=CARTESIAN_POINT('Ctrl Pts',(-1.56340403948772,-0.576092920493208,
13.6162967056883));
#56699=CARTESIAN_POINT('Ctrl Pts',(-1.5752981142217,-0.542345895267034,
13.6138801782969));
#56700=CARTESIAN_POINT('Ctrl Pts',(-1.5792062842643,-0.53085849718675,13.613064908146));
#56701=CARTESIAN_POINT('Ctrl Pts',(-1.58601785467818,-0.510095867559207,
13.6116041587127));
#56702=CARTESIAN_POINT('Ctrl Pts',(-1.58896622093097,-0.500836086025938,
13.6109572272941));
#56703=CARTESIAN_POINT('Ctrl Pts',(-1.59510789100386,-0.480946962539583,
13.6095771278574));
#56704=CARTESIAN_POINT('Ctrl Pts',(-1.59827635500801,-0.47031039512805,
13.6088447971468));
#56705=CARTESIAN_POINT('Ctrl Pts',(-1.60667469781162,-0.44105160928162,
13.606845450595));
#56706=CARTESIAN_POINT('Ctrl Pts',(-1.61168704269081,-0.422368362481585,
13.6055854865577));
#56707=CARTESIAN_POINT('Ctrl Pts',(-1.62212464255702,-0.380567083425392,
13.6028005949439));
#56708=CARTESIAN_POINT('Ctrl Pts',(-1.62738338033289,-0.357411637320071,
13.6012809151057));
#56709=CARTESIAN_POINT('Ctrl Pts',(-1.65475686652148,-0.223706991316348,
13.5926196156324));
#56710=CARTESIAN_POINT('Ctrl Pts',(-1.66609931397845,-0.11125753849907,
13.5858033966699));
#56711=CARTESIAN_POINT('Ctrl Pts',(-1.66599934497354,0.00147734482691685,
13.5789038102816));
#56712=CARTESIAN_POINT('Ctrl Pts',(-1.66599934402992,0.00147840856629485,
13.5789037451788));
#56713=CARTESIAN_POINT('Ctrl Pts',(-1.66592908092197,0.0806569891074675,
13.574057867085));
#56714=CARTESIAN_POINT('Ctrl Pts',(-1.6602143015703,0.159723172896025,13.5691777217738));
#56715=CARTESIAN_POINT('Ctrl Pts',(-1.64726516269832,0.249408511033996,
13.5633054302498));
#56716=CARTESIAN_POINT('Ctrl Pts',(-1.6455120615802,0.260724299713883,13.5625582417345));
#56717=CARTESIAN_POINT('Ctrl Pts',(-1.64248438447374,0.279018560692953,
13.5613387763251));
#56718=CARTESIAN_POINT('Ctrl Pts',(-1.64128160451835,0.286008742536837,
13.5608700963127));
#56719=CARTESIAN_POINT('Ctrl Pts',(-1.63908799017727,0.298287632070213,
13.5600416776263));
#56720=CARTESIAN_POINT('Ctrl Pts',(-1.63811609140399,0.303579676626428,
13.5596829558826));
#56721=CARTESIAN_POINT('Ctrl Pts',(-1.63611223900365,0.314200901439896,
13.5589594396421));
#56722=CARTESIAN_POINT('Ctrl Pts',(-1.6350798705893,0.319529780461453,13.5585946214091));
#56723=CARTESIAN_POINT('Ctrl Pts',(-1.63276757311799,0.331160690881833,
13.5577943014799));
#56724=CARTESIAN_POINT('Ctrl Pts',(-1.6314772142538,0.3374602893509,13.5573582478506));
#56725=CARTESIAN_POINT('Ctrl Pts',(-1.6277565484286,0.355104529492732,13.5561299830623));
#56726=CARTESIAN_POINT('Ctrl Pts',(-1.62524421130851,0.366431224965538,
13.5553334307419));
#56727=CARTESIAN_POINT('Ctrl Pts',(-1.60699162244934,0.444838754306764,
13.5497675594891));
#56728=CARTESIAN_POINT('Ctrl Pts',(-1.58722440750297,0.510899516444609,
13.5448165457068));
#56729=CARTESIAN_POINT('Ctrl Pts',(-1.56343130308087,0.575533283613436,
13.5398191707253));
#56730=CARTESIAN_POINT('Ctrl Pts',(-1.56343128722854,0.575533326676141,
13.7334757494662));
#56731=CARTESIAN_POINT('Ctrl Pts',(-1.59690734452391,0.484595907550651,
13.7396480019741));
#56732=CARTESIAN_POINT('Ctrl Pts',(-1.62239473420442,0.390886997980895,
13.7455715221201));
#56733=CARTESIAN_POINT('Ctrl Pts',(-1.65292263072649,0.221481194025369,
13.7560824791613));
#56734=CARTESIAN_POINT('Ctrl Pts',(-1.66123106262291,0.146686404472933,
13.7606625393582));
#56735=CARTESIAN_POINT('Ctrl Pts',(-1.66549569668114,0.0475373490342522,
13.7669268541262));
#56736=CARTESIAN_POINT('Ctrl Pts',(-1.66600871481831,0.0234639447436344,
13.7684630656757));
#56737=CARTESIAN_POINT('Ctrl Pts',(-1.66599370775538,-0.017467284978389,
13.7711135804174));
#56738=CARTESIAN_POINT('Ctrl Pts',(-1.66573169945979,-0.0343218927635916,
13.7722161249464));
#56739=CARTESIAN_POINT('Ctrl Pts',(-1.66498991816257,-0.058462075114235,
13.7738149067866));
#56740=CARTESIAN_POINT('Ctrl Pts',(-1.66471790388819,-0.0657536108263884,
13.7743003900498));
#56741=CARTESIAN_POINT('Ctrl Pts',(-1.66415667463459,-0.078542097544096,
13.7751567527131));
#56742=CARTESIAN_POINT('Ctrl Pts',(-1.66388810168304,-0.0840397696474318,
13.7755264907577));
#56743=CARTESIAN_POINT('Ctrl Pts',(-1.66325379827517,-0.0958252009860064,
13.7763226435167));
#56744=CARTESIAN_POINT('Ctrl Pts',(-1.66287966297194,-0.102112143263391,
13.7767494833393));
#56745=CARTESIAN_POINT('Ctrl Pts',(-1.66173409061338,-0.119681680786548,
13.7779480140864));
#56746=CARTESIAN_POINT('Ctrl Pts',(-1.6608834224287,-0.13095851331003,13.7787238328882));
#56747=CARTESIAN_POINT('Ctrl Pts',(-1.65440164952627,-0.206607521168572,
13.7839684999097));
#56748=CARTESIAN_POINT('Ctrl Pts',(-1.64514477056455,-0.270607275773206,
13.7885992513743));
#56749=CARTESIAN_POINT('Ctrl Pts',(-1.61097126101745,-0.437656990091769,
13.800952900476));
#56750=CARTESIAN_POINT('Ctrl Pts',(-1.57989789606257,-0.539164379848463,
13.8087181971043));
#56751=CARTESIAN_POINT('Ctrl Pts',(-1.51745878080532,-0.690047952664943,
13.8203210207799));
#56752=CARTESIAN_POINT('Ctrl Pts',(-1.49279640673099,-0.741894565033315,
13.824324417634));
#56753=CARTESIAN_POINT('Ctrl Pts',(-1.45735579329292,-0.807442670830319,
13.8294057940845));
#56754=CARTESIAN_POINT('Ctrl Pts',(-1.44897435276337,-0.822388556608074,
13.8305660001918));
#56755=CARTESIAN_POINT('Ctrl Pts',(-1.43502372122993,-0.846389882078534,
13.8324323821163));
#56756=CARTESIAN_POINT('Ctrl Pts',(-1.42959601266344,-0.855525664489342,
13.8331435723364));
#56757=CARTESIAN_POINT('Ctrl Pts',(-1.41898565994668,-0.873001774523313,
13.8345057892088));
#56758=CARTESIAN_POINT('Ctrl Pts',(-1.41381597911393,-0.88134941180789,
13.8351572513455));
#56759=CARTESIAN_POINT('Ctrl Pts',(-1.4016317106287,-0.900640603279529,
13.8366648967803));
#56760=CARTESIAN_POINT('Ctrl Pts',(-1.3945621835962,-0.911548836044693,
13.8375190114648));
#56761=CARTESIAN_POINT('Ctrl Pts',(-1.37119902967193,-0.946689953675526,
13.8402769861834));
#56762=CARTESIAN_POINT('Ctrl Pts',(-1.35439529193294,-0.97057828426904,
13.8421617669755));
#56763=CARTESIAN_POINT('Ctrl Pts',(-1.31264535720652,-1.02673290900314,
13.8466290331867));
#56764=CARTESIAN_POINT('Ctrl Pts',(-1.28712528665374,-1.05854954755507,
13.8491903354024));
#56765=CARTESIAN_POINT('Ctrl Pts',(-1.21288904200386,-1.14444271028742,
13.8562448222403));
#56766=CARTESIAN_POINT('Ctrl Pts',(-1.1617602368724,-1.19631207883954,13.8606671679549));
#56767=CARTESIAN_POINT('Ctrl Pts',(-1.04224443942692,-1.3026470017796,13.8704446402259));
#56768=CARTESIAN_POINT('Ctrl Pts',(-0.972640954062778,-1.35540710744694,
13.8757952959062));
#56769=CARTESIAN_POINT('Ctrl Pts',(-0.885925216762125,-1.41100766923844,
13.8824781461167));
#56770=CARTESIAN_POINT('Ctrl Pts',(-0.8724910691607,-1.41935387481402,13.8835140458672));
#56771=CARTESIAN_POINT('Ctrl Pts',(-0.852844605016776,-1.43117528541889,
13.8850329205947));
#56772=CARTESIAN_POINT('Ctrl Pts',(-0.846725163287895,-1.43480420655579,
13.8855065630757));
#56773=CARTESIAN_POINT('Ctrl Pts',(-0.835848762816267,-1.44116026538775,
13.8863497028104));
#56774=CARTESIAN_POINT('Ctrl Pts',(-0.831101308808723,-1.44390327864392,
13.886718176476));
#56775=CARTESIAN_POINT('Ctrl Pts',(-0.820771194398557,-1.44980404919066,
13.8875210206744));
#56776=CARTESIAN_POINT('Ctrl Pts',(-0.815183900759726,-1.45295297208106,
13.8879559011228));
#56777=CARTESIAN_POINT('Ctrl Pts',(-0.799220160707728,-1.46182885592752,
13.8891999427054));
#56778=CARTESIAN_POINT('Ctrl Pts',(-0.788800839435235,-1.46747732009287,
13.8900137309961));
#56779=CARTESIAN_POINT('Ctrl Pts',(-0.764917469109515,-1.48009700042222,
13.8918817392855));
#56780=CARTESIAN_POINT('Ctrl Pts',(-0.751416870193818,-1.48699647490331,
13.8929395452345));
#56781=CARTESIAN_POINT('Ctrl Pts',(-0.607749287548945,-1.55796167874946,
13.9042019219814));
#56782=CARTESIAN_POINT('Ctrl Pts',(-0.469839880225167,-1.60494788488956,
13.9149939478272));
#56783=CARTESIAN_POINT('Ctrl Pts',(-0.263141831534131,-1.64639967878009,
13.9300527313247));
#56784=CARTESIAN_POINT('Ctrl Pts',(-0.197987113674817,-1.65549949821642,
13.9346583385637));
#56785=CARTESIAN_POINT('Ctrl Pts',(-0.114812973027509,-1.66213335224514,
13.9403532567623));
#56786=CARTESIAN_POINT('Ctrl Pts',(-0.0971468685908385,-1.66325939868617,
13.9415526200734));
#56787=CARTESIAN_POINT('Ctrl Pts',(-0.068730293876874,-1.66461636888101,
13.9434661008017));
#56788=CARTESIAN_POINT('Ctrl Pts',(-0.0579901021721132,-1.66502512481235,
13.9441857082034));
#56789=CARTESIAN_POINT('Ctrl Pts',(-0.0374682900296803,-1.66560734187425,
13.9455540792577));
#56790=CARTESIAN_POINT('Ctrl Pts',(-0.0276876677031915,-1.66579863431472,
13.94620337125));
#56791=CARTESIAN_POINT('Ctrl Pts',(-0.00517194848982917,-1.66604064155266,
13.9476917751412));
#56792=CARTESIAN_POINT('Ctrl Pts',(0.00756328461740996,-1.66603150632131,
13.9485289887587));
#56793=CARTESIAN_POINT('Ctrl Pts',(0.0479863421841862,-1.66553898150288,
13.9511726802899));
#56794=CARTESIAN_POINT('Ctrl Pts',(0.0756636928236562,-1.66451132037318,
13.9529622757695));
#56795=CARTESIAN_POINT('Ctrl Pts',(0.169981547628219,-1.65865166371449,
13.9590055428783));
#56796=CARTESIAN_POINT('Ctrl Pts',(0.236353362100754,-1.65050217985981,
13.9631610528561));
#56797=CARTESIAN_POINT('Ctrl Pts',(0.368968746489921,-1.62605250914784,
13.9714504377125));
#56798=CARTESIAN_POINT('Ctrl Pts',(0.435056534029288,-1.60963052189566,
13.9755748475033));
#56799=CARTESIAN_POINT('Ctrl Pts',(0.571112886112889,-1.56682822395221,
13.984335735421));
#56800=CARTESIAN_POINT('Ctrl Pts',(0.640678368346614,-1.53969118887545,
13.9889738500163));
#56801=CARTESIAN_POINT('Ctrl Pts',(0.718679068260095,-1.5030605049748,13.9946104608379));
#56802=CARTESIAN_POINT('Ctrl Pts',(0.729123826646564,-1.49802166596762,
13.9953746859146));
#56803=CARTESIAN_POINT('Ctrl Pts',(0.745276134725738,-1.49002040974556,
13.9965725985625));
#56804=CARTESIAN_POINT('Ctrl Pts',(0.751020808986579,-1.48713317475332,
13.9970018399053));
#56805=CARTESIAN_POINT('Ctrl Pts',(0.761584862772429,-1.48174693107588,
13.9977973619751));
#56806=CARTESIAN_POINT('Ctrl Pts',(0.766408916516391,-1.47925753016715,
13.9981630527844));
#56807=CARTESIAN_POINT('Ctrl Pts',(0.777586659711129,-1.47342002333525,
13.9990159736937));
#56808=CARTESIAN_POINT('Ctrl Pts',(0.783930922955666,-1.47005438055086,
13.9995042705434));
#56809=CARTESIAN_POINT('Ctrl Pts',(0.804131556798847,-1.45916995965191,
14.0010720242152));
#56810=CARTESIAN_POINT('Ctrl Pts',(0.817902574273019,-1.45149573397758,
14.0021604185546));
#56811=CARTESIAN_POINT('Ctrl Pts',(0.893342255540834,-1.40804078040072,
14.0082236479097));
#56812=CARTESIAN_POINT('Ctrl Pts',(0.952768541965973,-1.36852816136779,
14.013373318905));
#56813=CARTESIAN_POINT('Ctrl Pts',(1.11351912187899,-1.24608845907502,14.0280629963583));
#56814=CARTESIAN_POINT('Ctrl Pts',(1.20788922694154,-1.1548490953192,14.0375907308053));
#56815=CARTESIAN_POINT('Ctrl Pts',(1.30857077993604,-1.03150584780667,14.0486098530869));
#56816=CARTESIAN_POINT('Ctrl Pts',(1.32595699847586,-1.00905897226283,14.0505528309424));
#56817=CARTESIAN_POINT('Ctrl Pts',(1.35029091686853,-0.975926334388468,
14.0533338785534));
#56818=CARTESIAN_POINT('Ctrl Pts',(1.35770231850719,-0.965589043137195,
14.0541897640057));
#56819=CARTESIAN_POINT('Ctrl Pts',(1.37061911500879,-0.947130126295397,
14.0556977193082));
#56820=CARTESIAN_POINT('Ctrl Pts',(1.37617243664457,-0.9390429522988,14.056351597411));
#56821=CARTESIAN_POINT('Ctrl Pts',(1.3876060593441,-0.922073146572204,14.0577098464854));
#56822=CARTESIAN_POINT('Ctrl Pts',(1.39347326710886,-0.91318219776115,14.0584137040025));
#56823=CARTESIAN_POINT('Ctrl Pts',(1.40862008826219,-0.889743319234936,
14.0602494997496));
#56824=CARTESIAN_POINT('Ctrl Pts',(1.417759825554,-0.875106188139725,14.0613762446505));
#56825=CARTESIAN_POINT('Ctrl Pts',(1.46138709288515,-0.802759759546435,
14.0668544369618));
#56826=CARTESIAN_POINT('Ctrl Pts',(1.49258943672587,-0.743137823823686,
14.0710864939885));
#56827=CARTESIAN_POINT('Ctrl Pts',(1.5494764243807,-0.61630317146352,14.0796939160186));
#56828=CARTESIAN_POINT('Ctrl Pts',(1.5745853162922,-0.548988321344521,14.0840504569113));
#56829=CARTESIAN_POINT('Ctrl Pts',(1.60171476774321,-0.458873435370217,
14.0898084522344));
#56830=CARTESIAN_POINT('Ctrl Pts',(1.60772351303908,-0.437355807994128,
14.0911783185495));
#56831=CARTESIAN_POINT('Ctrl Pts',(1.62970795671963,-0.352040950860208,
14.0966110233857));
#56832=CARTESIAN_POINT('Ctrl Pts',(1.64233116413986,-0.287449308485304,
14.1007260023808));
#56833=CARTESIAN_POINT('Ctrl Pts',(1.65263440578785,-0.210919736968887,
14.1057783854534));
#56834=CARTESIAN_POINT('Ctrl Pts',(1.65404759293201,-0.199534851672858,
14.1065345770714));
#56835=CARTESIAN_POINT('Ctrl Pts',(1.65606597753578,-0.181775852875196,
14.1077225388363));
#56836=CARTESIAN_POINT('Ctrl Pts',(1.65675222693959,-0.17541105365782,14.1081499791475));
#56837=CARTESIAN_POINT('Ctrl Pts',(1.65795301339992,-0.163637774595942,
14.1089439971056));
#56838=CARTESIAN_POINT('Ctrl Pts',(1.65847779879922,-0.158230539557421,
14.1093100049644));
#56839=CARTESIAN_POINT('Ctrl Pts',(1.65963871188628,-0.145628026669224,
14.1101660988646));
#56840=CARTESIAN_POINT('Ctrl Pts',(1.66025449844327,-0.138431108063503,
14.1106572791763));
#56841=CARTESIAN_POINT('Ctrl Pts',(1.66208334677203,-0.115285632797208,
14.1122438014421));
#56842=CARTESIAN_POINT('Ctrl Pts',(1.66311349816753,-0.0993240859317914,
14.1133483728752));
#56843=CARTESIAN_POINT('Ctrl Pts',(1.6650364676999,-0.0609363305812858,
14.1160261990991));
#56844=CARTESIAN_POINT('Ctrl Pts',(1.66570619735426,-0.0385024323218801,
14.1176085644583));
#56845=CARTESIAN_POINT('Ctrl Pts',(1.66656100022466,0.0501504940092083,
14.1239140517943));
#56846=CARTESIAN_POINT('Ctrl Pts',(1.66325127128114,0.116339770687247,14.1287347263514));
#56847=CARTESIAN_POINT('Ctrl Pts',(1.64279723960893,0.30229442939699,14.1423526692694));
#56848=CARTESIAN_POINT('Ctrl Pts',(1.6165449451845,0.42066285258121,14.1510796441945));
#56849=CARTESIAN_POINT('Ctrl Pts',(1.57096126496172,0.555047362847885,14.160841290152));
#56850=CARTESIAN_POINT('Ctrl Pts',(1.5638409425753,0.574802963632138,14.1622736291101));
#56851=CARTESIAN_POINT('Ctrl Pts',(1.55186599204742,0.606156578215076,14.1645433733652));
#56852=CARTESIAN_POINT('Ctrl Pts',(1.54725048896099,0.617842855432122,14.1653885865108));
#56853=CARTESIAN_POINT('Ctrl Pts',(1.53880490694127,0.638538378067501,14.1668843492923));
#56854=CARTESIAN_POINT('Ctrl Pts',(1.53502684296416,0.647568066151652,14.1675366098915));
#56855=CARTESIAN_POINT('Ctrl Pts',(1.52694217293726,0.666422278413724,14.1688980356776));
#56856=CARTESIAN_POINT('Ctrl Pts',(1.52261980791339,0.676239589412489,14.1696066305005));
#56857=CARTESIAN_POINT('Ctrl Pts',(1.51095510017821,0.702054478327146,14.1714695970835));
#56858=CARTESIAN_POINT('Ctrl Pts',(1.50345340713519,0.717978896851077,14.1726184829249));
#56859=CARTESIAN_POINT('Ctrl Pts',(1.46371062020843,0.798988394382672,14.1784663329392));
#56860=CARTESIAN_POINT('Ctrl Pts',(1.42748878356235,0.862037655032408,14.1830241775081));
#56861=CARTESIAN_POINT('Ctrl Pts',(1.33066376198011,1.00763955504913,14.19382042707));
#56862=CARTESIAN_POINT('Ctrl Pts',(1.26635479479252,1.08735809071863,14.1999583155859));
#56863=CARTESIAN_POINT('Ctrl Pts',(1.15864948543114,1.19826213614846,14.2095693458024));
#56864=CARTESIAN_POINT('Ctrl Pts',(1.12040092141735,1.23409942210474,14.2128806359686));
#56865=CARTESIAN_POINT('Ctrl Pts',(1.07212832918019,1.27523282470831,14.2170343202856));
#56866=CARTESIAN_POINT('Ctrl Pts',(1.06365352622961,1.28231005279961,14.2177626676304));
#56867=CARTESIAN_POINT('Ctrl Pts',(1.05022992805273,1.29329534557193,14.218916107369));
#56868=CARTESIAN_POINT('Ctrl Pts',(1.04532804091898,1.29726058918095,14.2193372629176));
#56869=CARTESIAN_POINT('Ctrl Pts',(1.03610584054368,1.3046344201951,14.2201297776281));
#56870=CARTESIAN_POINT('Ctrl Pts',(1.03179100376537,1.30804954195551,14.220500667775));
#56871=CARTESIAN_POINT('Ctrl Pts',(1.02162364722663,1.31601522899526,14.2213747619966));
#56872=CARTESIAN_POINT('Ctrl Pts',(1.01575759268414,1.32054816920395,14.2218791594218));
#56873=CARTESIAN_POINT('Ctrl Pts',(0.996279948621298,1.33539277766861,14.2235537149904));
#56874=CARTESIAN_POINT('Ctrl Pts',(0.98254057598484,1.34553393371724,14.2247345350109));
#56875=CARTESIAN_POINT('Ctrl Pts',(0.94871391290658,1.36970735488041,14.2276360762472));
#56876=CARTESIAN_POINT('Ctrl Pts',(0.928468573089017,1.3835108628743,14.2293678936929));
#56877=CARTESIAN_POINT('Ctrl Pts',(0.842806475686264,1.4391891992739,14.2366536703101));
#56878=CARTESIAN_POINT('Ctrl Pts',(0.774808085372231,1.47690888559529,14.2423325778821));
#56879=CARTESIAN_POINT('Ctrl Pts',(0.609402569674346,1.55408512573538,14.2556021897228));
#56880=CARTESIAN_POINT('Ctrl Pts',(0.510387408529094,1.58935949182553,14.2631255045931));
#56881=CARTESIAN_POINT('Ctrl Pts',(0.385850853920188,1.62087338626537,14.2719685751625));
#56882=CARTESIAN_POINT('Ctrl Pts',(0.362882682655123,1.62616963227339,14.273575739125));
#56883=CARTESIAN_POINT('Ctrl Pts',(0.327946063431739,1.63344856451324,14.2759857608915));
#56884=CARTESIAN_POINT('Ctrl Pts',(0.316056440094031,1.63579068757721,14.2767999352857));
#56885=CARTESIAN_POINT('Ctrl Pts',(0.294588630619136,1.63977679975059,14.2782595294737));
#56886=CARTESIAN_POINT('Ctrl Pts',(0.285019712736391,1.64146708297987,14.2789063910446));
#56887=CARTESIAN_POINT('Ctrl Pts',(0.264479204257985,1.64491038783715,14.2802872034649));
#56888=CARTESIAN_POINT('Ctrl Pts',(0.253503714716543,1.64663757705837,14.2810203090113));
#56889=CARTESIAN_POINT('Ctrl Pts',(0.223320981858193,1.65107843213516,14.283024009865));
#56890=CARTESIAN_POINT('Ctrl Pts',(0.204081958792875,1.65356670717591,14.2842875011597));
#56891=CARTESIAN_POINT('Ctrl Pts',(0.161122038762,1.65836168315444,14.2870813461343));
#56892=CARTESIAN_POINT('Ctrl Pts',(0.13738607460186,1.66049659288428,14.2886063990721));
#56893=CARTESIAN_POINT('Ctrl Pts',(0.0611651235402701,1.66570654906469,
14.293454237166));
#56894=CARTESIAN_POINT('Ctrl Pts',(0.00857596109655154,1.66680729428791,
14.2967231293628));
#56895=CARTESIAN_POINT('Ctrl Pts',(-0.139988420360405,1.66288400056109,
14.3058718144097));
#56896=CARTESIAN_POINT('Ctrl Pts',(-0.235592695276462,1.65205165053418,
14.3116506832653));
#56897=CARTESIAN_POINT('Ctrl Pts',(-0.38023238356863,1.62284752450269,14.3208300942808));
#56898=CARTESIAN_POINT('Ctrl Pts',(-0.430232065686764,1.61031363517197,
14.3240889071116));
#56899=CARTESIAN_POINT('Ctrl Pts',(-0.49008808860655,1.5923223297312,14.3281828946092));
#56900=CARTESIAN_POINT('Ctrl Pts',(-0.50057912825653,1.58905546059781,14.3289077941412));
#56901=CARTESIAN_POINT('Ctrl Pts',(-0.517026285111783,1.58375484886205,
14.330056956114));
#56902=CARTESIAN_POINT('Ctrl Pts',(-0.523004722428193,1.58179064918334,
14.3304773292493));
#56903=CARTESIAN_POINT('Ctrl Pts',(-0.534192553735803,1.57804455832385,
14.3312692504196));
#56904=CARTESIAN_POINT('Ctrl Pts',(-0.539404416768615,1.57627065701313,
14.3316403385264));
#56905=CARTESIAN_POINT('Ctrl Pts',(-0.551633579712859,1.57204060661297,
14.3325160938859));
#56906=CARTESIAN_POINT('Ctrl Pts',(-0.558643329468597,1.56956328329489,
14.3330219685981));
#56907=CARTESIAN_POINT('Ctrl Pts',(-0.581814836249913,1.56119933125588,
14.3347065757807));
#56908=CARTESIAN_POINT('Ctrl Pts',(-0.597901394769871,1.55510955245316,
14.3358961403127));
#56909=CARTESIAN_POINT('Ctrl Pts',(-0.636890889592165,1.53965520639481,
14.3388236547314));
#56910=CARTESIAN_POINT('Ctrl Pts',(-0.659684653274981,1.53002751191172,
14.340572944235));
#56911=CARTESIAN_POINT('Ctrl Pts',(-0.754432703746267,1.48749680646883,
14.3479813631546));
#56912=CARTESIAN_POINT('Ctrl Pts',(-0.824208677126646,1.44999815623618,
14.3537689631674));
#56913=CARTESIAN_POINT('Ctrl Pts',(-0.977898075333685,1.35271400981485,
14.3669885791716));
#56914=CARTESIAN_POINT('Ctrl Pts',(-1.0594817289804,1.28981578590912,14.3743570592595));
#56915=CARTESIAN_POINT('Ctrl Pts',(-1.15210803301264,1.20364641015806,14.3830672093403));
#56916=CARTESIAN_POINT('Ctrl Pts',(-1.1691133195215,1.18713594279958,14.3846834905366));
#56917=CARTESIAN_POINT('Ctrl Pts',(-1.19429208677732,1.16162381970452,14.3871043335213));
#56918=CARTESIAN_POINT('Ctrl Pts',(-1.20272825581565,1.15288691694172,14.3879203644517));
#56919=CARTESIAN_POINT('Ctrl Pts',(-1.21774235343396,1.13699341092075,14.3893819694509));
#56920=CARTESIAN_POINT('Ctrl Pts',(-1.22435454320049,1.12987008777023,14.3900290024176));
#56921=CARTESIAN_POINT('Ctrl Pts',(-1.23837845071978,1.11449442888469,14.3914087802236));
#56922=CARTESIAN_POINT('Ctrl Pts',(-1.24577088568864,1.10622508089439,14.3921406925872));
#56923=CARTESIAN_POINT('Ctrl Pts',(-1.26532010631377,1.08391235862654,14.3940891825104));
#56924=CARTESIAN_POINT('Ctrl Pts',(-1.27732577785194,1.06973822719028,14.3952995215685));
#56925=CARTESIAN_POINT('Ctrl Pts',(-1.33622300240261,0.997797334196229,
14.4013130821882));
#56926=CARTESIAN_POINT('Ctrl Pts',(-1.37944767345773,0.937132607897802,
14.4059695985546));
#56927=CARTESIAN_POINT('Ctrl Pts',(-1.45919537957205,0.807671111200176,
14.4153407664011));
#56928=CARTESIAN_POINT('Ctrl Pts',(-1.49524379293925,0.738802848579732,
14.4200377675521));
#56929=CARTESIAN_POINT('Ctrl Pts',(-1.53963306760386,0.637325035428461,
14.426848803303));
#56930=CARTESIAN_POINT('Ctrl Pts',(-1.55199565619263,0.60659812014485,14.4288983265017));
#56931=CARTESIAN_POINT('Ctrl Pts',(-1.56343129324813,0.575533310323967,
14.4309760522469));
#56932=CARTESIAN_POINT('Origin',(0.,0.,11.));
#56933=CARTESIAN_POINT('',(-1.56343130033034,0.575533291085225,15.1319018884674));
#56934=CARTESIAN_POINT('',(-1.56343130047997,0.575533290678746,14.9377828634576));
#56935=CARTESIAN_POINT('',(-1.56343130033213,0.575533291080363,11.));
#56936=CARTESIAN_POINT('Ctrl Pts',(-1.56343130047997,0.575533290678746,
14.9377828634576));
#56937=CARTESIAN_POINT('Ctrl Pts',(-1.56119071929035,0.581619810468057,
14.9373638967573));
#56938=CARTESIAN_POINT('Ctrl Pts',(-1.55891453933277,0.587693398516454,
14.9369460164377));
#56939=CARTESIAN_POINT('Ctrl Pts',(-1.5159297592197,0.700383605125528,14.9291951767874));
#56940=CARTESIAN_POINT('Ctrl Pts',(-1.46440746572649,0.802555128926979,
14.9222388432018));
#56941=CARTESIAN_POINT('Ctrl Pts',(-1.36459812965856,0.958359889818218,
14.9109387732747));
#56942=CARTESIAN_POINT('Ctrl Pts',(-1.32258914364437,1.01554825229322,14.9066081872519));
#56943=CARTESIAN_POINT('Ctrl Pts',(-1.26209494950135,1.08775735834899,14.9006547150445));
#56944=CARTESIAN_POINT('Ctrl Pts',(-1.2467475356055,1.10531452701706,14.8991653183197));
#56945=CARTESIAN_POINT('Ctrl Pts',(-1.22019586404586,1.1344324378979,14.8966117709185));
#56946=CARTESIAN_POINT('Ctrl Pts',(-1.20918299905693,1.14616374529065,14.895559007437));
#56947=CARTESIAN_POINT('Ctrl Pts',(-1.19310305825202,1.16280299257818,14.8940276352668));
#56948=CARTESIAN_POINT('Ctrl Pts',(-1.18817163436539,1.16784154318891,14.8935587504951));
#56949=CARTESIAN_POINT('Ctrl Pts',(-1.18316472569949,1.17289267869015,14.8930832570029));
#56950=CARTESIAN_POINT('Ctrl Pts',(-1.18312095950884,1.17293682653218,14.8930791006817));
#56951=CARTESIAN_POINT('Ctrl Pts',(-1.18303320412538,1.17302533725404,14.8930707669485));
#56952=CARTESIAN_POINT('Ctrl Pts',(-1.18298921490891,1.17306970010836,14.8930665895347));
#56953=CARTESIAN_POINT('Ctrl Pts',(-1.18290100108526,1.17315865319896,14.893058212441));
#56954=CARTESIAN_POINT('Ctrl Pts',(-1.18285677643809,1.17320324342315,14.8930540127577));
#56955=CARTESIAN_POINT('Ctrl Pts',(-1.18276807906039,1.17329266389225,14.8930455899209));
#56956=CARTESIAN_POINT('Ctrl Pts',(-1.18272360630839,1.17333749410324,14.8930413667657));
#56957=CARTESIAN_POINT('Ctrl Pts',(-1.18263439973514,1.17342740746785,14.8930328957531));
#56958=CARTESIAN_POINT('Ctrl Pts',(-1.18258966588265,1.17347249059412,14.8930286478932));
#56959=CARTESIAN_POINT('Ctrl Pts',(-1.18249992380736,1.17356292301601,14.8930201262093));
#56960=CARTESIAN_POINT('Ctrl Pts',(-1.18245491555522,1.17360827227896,14.8930158523831));
#56961=CARTESIAN_POINT('Ctrl Pts',(-1.18236461104836,1.17369925052128,14.8930072774734));
#56962=CARTESIAN_POINT('Ctrl Pts',(-1.18231931475618,1.17374487947263,14.893002976387));
#56963=CARTESIAN_POINT('Ctrl Pts',(-1.1822284201758,1.17383643098889,14.8929943456297));
#56964=CARTESIAN_POINT('Ctrl Pts',(-1.18218282186103,1.17388235351111,14.8929900159568));
#56965=CARTESIAN_POINT('Ctrl Pts',(-1.18209130887984,1.17397450641662,14.8929813266651));
#56966=CARTESIAN_POINT('Ctrl Pts',(-1.18204539417557,1.17402073676479,14.8929769670431));
#56967=CARTESIAN_POINT('Ctrl Pts',(-1.18195323366682,1.17411351995043,14.8929682164545));
#56968=CARTESIAN_POINT('Ctrl Pts',(-1.18190698782841,1.17416007274485,14.8929638254851));
#56969=CARTESIAN_POINT('Ctrl Pts',(-1.18181414989579,1.17425351584555,14.8929550107643));
#56970=CARTESIAN_POINT('Ctrl Pts',(-1.1817675577584,1.1743004061139,14.8929505870094));
#56971=CARTESIAN_POINT('Ctrl Pts',(-1.18167401163958,1.17439453960422,14.8929417052391));
#56972=CARTESIAN_POINT('Ctrl Pts',(-1.18162705761285,1.17444178278611,14.8929372472201));
#56973=CARTESIAN_POINT('Ctrl Pts',(-1.17775077340809,1.17834147038727,14.8925692199534));
#56974=CARTESIAN_POINT('Ctrl Pts',(-1.17390280303041,1.18217499251098,14.8922041882005));
#56975=CARTESIAN_POINT('Ctrl Pts',(-1.16547610263683,1.19048833884486,14.8914053733555));
#56976=CARTESIAN_POINT('Ctrl Pts',(-1.1608903355894,1.19496052488093,14.8909710563879));
#56977=CARTESIAN_POINT('Ctrl Pts',(-1.14800692105719,1.20738069019672,14.8897522600449));
#56978=CARTESIAN_POINT('Ctrl Pts',(-1.13965285726535,1.21526925761242,14.8889635410344));
#56979=CARTESIAN_POINT('Ctrl Pts',(-1.08239567901584,1.26822643349726,14.8835725626291));
#56980=CARTESIAN_POINT('Ctrl Pts',(-1.03091838467032,1.31041367479355,14.8788001175138));
#56981=CARTESIAN_POINT('Ctrl Pts',(-0.960908678429106,1.36110557287357,
14.8725330709332));
#56982=CARTESIAN_POINT('Ctrl Pts',(-0.944543885471565,1.37251255084979,
14.871082739937));
#56983=CARTESIAN_POINT('Ctrl Pts',(-0.872300961751523,1.42096496927852,
14.8647525158031));
#56984=CARTESIAN_POINT('Ctrl Pts',(-0.814417563714064,1.45491418242093,
14.8598688589706));
#56985=CARTESIAN_POINT('Ctrl Pts',(-0.689676328623525,1.51829275598098,
14.8498386804689));
#56986=CARTESIAN_POINT('Ctrl Pts',(-0.622606194331361,1.5470069473104,14.8447177880508));
#56987=CARTESIAN_POINT('Ctrl Pts',(-0.537248746449711,1.57709545681651,
14.8385413420599));
#56988=CARTESIAN_POINT('Ctrl Pts',(-0.520543116617423,1.58268796690588,
14.8373478623052));
#56989=CARTESIAN_POINT('Ctrl Pts',(-0.493524694113243,1.59125877380488,
14.8354414816637));
#56990=CARTESIAN_POINT('Ctrl Pts',(-0.483266730166625,1.59440408483508,
14.83472316307));
#56991=CARTESIAN_POINT('Ctrl Pts',(-0.463595124293845,1.60022852590215,
14.8333558154089));
#56992=CARTESIAN_POINT('Ctrl Pts',(-0.454186896777559,1.60292421659555,
14.8327062715908));
#56993=CARTESIAN_POINT('Ctrl Pts',(-0.432654068322825,1.60888909932573,
14.8312294021716));
#56994=CARTESIAN_POINT('Ctrl Pts',(-0.420515070017832,1.61210445288449,
14.8304038456708));
#56995=CARTESIAN_POINT('Ctrl Pts',(-0.388007222263089,1.62032288972042,
14.8282108778127));
#56996=CARTESIAN_POINT('Ctrl Pts',(-0.36757790448454,1.62507920377154,14.8268513350737));
#56997=CARTESIAN_POINT('Ctrl Pts',(-0.228427438951965,1.65471747580724,
14.8177044268828));
#56998=CARTESIAN_POINT('Ctrl Pts',(-0.107384922339684,1.6669557136625,14.8103389668518));
#56999=CARTESIAN_POINT('Ctrl Pts',(0.0798639467822497,1.6653906855874,14.7988961289787));
#57000=CARTESIAN_POINT('Ctrl Pts',(0.145708434319443,1.66092509836027,14.7948548845936));
#57001=CARTESIAN_POINT('Ctrl Pts',(0.233318455357688,1.64973324371481,14.7892642550525));
#57002=CARTESIAN_POINT('Ctrl Pts',(0.255466652901598,1.64644889578562,14.7878322305986));
#57003=CARTESIAN_POINT('Ctrl Pts',(0.2932835923487,1.64005964653999,14.7853447362173));
#57004=CARTESIAN_POINT('Ctrl Pts',(0.308986626402209,1.6371738235804,14.7842992041221));
#57005=CARTESIAN_POINT('Ctrl Pts',(0.33172458872782,1.63265639233715,14.7827636886263));
#57006=CARTESIAN_POINT('Ctrl Pts',(0.338794752024681,1.63120391410737,14.7822831863418));
#57007=CARTESIAN_POINT('Ctrl Pts',(0.351168740220887,1.62857791412775,14.7814365195677));
#57008=CARTESIAN_POINT('Ctrl Pts',(0.35647660217653,1.62742432616046,14.7810714803424));
#57009=CARTESIAN_POINT('Ctrl Pts',(0.368030709218323,1.62485396791104,14.7802727159857));
#57010=CARTESIAN_POINT('Ctrl Pts',(0.3742743563177,1.62342715349771,14.7798384575881));
#57011=CARTESIAN_POINT('Ctrl Pts',(0.391692190664877,1.61934096564819,14.7786199800375));
#57012=CARTESIAN_POINT('Ctrl Pts',(0.402847079646358,1.61660203742527,14.7778315246483));
#57013=CARTESIAN_POINT('Ctrl Pts',(0.478240548479853,1.59726146451807,14.7724515069581));
#57014=CARTESIAN_POINT('Ctrl Pts',(0.541459609394626,1.57695203859994,14.7676905341672));
#57015=CARTESIAN_POINT('Ctrl Pts',(0.623680596698855,1.54501033967742,14.7612952815514));
#57016=CARTESIAN_POINT('Ctrl Pts',(0.643911123140471,1.53668893507944,14.7597045007325));
#57017=CARTESIAN_POINT('Ctrl Pts',(0.729990828381493,1.49928347143604,14.7528735711166));
#57018=CARTESIAN_POINT('Ctrl Pts',(0.794085165422625,1.4663449345767,14.747633243334));
#57019=CARTESIAN_POINT('Ctrl Pts',(0.913254450216431,1.39499064206188,14.7377100375322));
#57020=CARTESIAN_POINT('Ctrl Pts',(0.968541415644979,1.35718907286088,14.733022336996));
#57021=CARTESIAN_POINT('Ctrl Pts',(1.03502487268179,1.30559429575693,14.727282732168));
#57022=CARTESIAN_POINT('Ctrl Pts',(1.04847427601915,1.2948183978652,14.726115731719));
#57023=CARTESIAN_POINT('Ctrl Pts',(1.06995899840976,1.27705015362701,14.7242412010459));
#57024=CARTESIAN_POINT('Ctrl Pts',(1.07809840911248,1.27018627867144,14.7235285748441));
#57025=CARTESIAN_POINT('Ctrl Pts',(1.09361072472019,1.25684837432017,14.7221653962301));
#57026=CARTESIAN_POINT('Ctrl Pts',(1.10099330754597,1.25038633910277,14.7215143918069));
#57027=CARTESIAN_POINT('Ctrl Pts',(1.11782159380567,1.23539179710259,14.720024968328));
#57028=CARTESIAN_POINT('Ctrl Pts',(1.12722753586224,1.2268154324332,14.7191884264979));
#57029=CARTESIAN_POINT('Ctrl Pts',(1.1573313490158,1.19872814443488,14.7164967653255));
#57030=CARTESIAN_POINT('Ctrl Pts',(1.17762879679031,1.17879412369778,14.7146597031325));
#57031=CARTESIAN_POINT('Ctrl Pts',(1.28831388571848,1.06437690692791,14.7044879638225));
#57032=CARTESIAN_POINT('Ctrl Pts',(1.36784186686909,0.960032240792337,14.6966271618862));
#57033=CARTESIAN_POINT('Ctrl Pts',(1.47061269457183,0.786088402341992,14.6842310485955));
#57034=CARTESIAN_POINT('Ctrl Pts',(1.50289085576768,0.722463439807858,14.6798120802158));
#57035=CARTESIAN_POINT('Ctrl Pts',(1.53720864387568,0.642490503140005,14.6741657065929));
#57036=CARTESIAN_POINT('Ctrl Pts',(1.54321837672034,0.627918353748305,14.673133197917));
#57037=CARTESIAN_POINT('Ctrl Pts',(1.55166361781409,0.606586833549017,14.6716133629124));
#57038=CARTESIAN_POINT('Ctrl Pts',(1.55426379402255,0.599893009906963,14.6711352490191));
#57039=CARTESIAN_POINT('Ctrl Pts',(1.55875332685467,0.588110136737703,14.670291206066));
#57040=CARTESIAN_POINT('Ctrl Pts',(1.56066120875769,0.583028350186222,14.6699263781181));
#57041=CARTESIAN_POINT('Ctrl Pts',(1.56477459095764,0.571907173541513,14.6691261307225));
#57042=CARTESIAN_POINT('Ctrl Pts',(1.56696994413406,0.565864406324,14.668690160204));
#57043=CARTESIAN_POINT('Ctrl Pts',(1.57302693945468,0.548886810765506,14.6674623491777));
#57044=CARTESIAN_POINT('Ctrl Pts',(1.57680937567146,0.53792439738774,14.6666661723987));
#57045=CARTESIAN_POINT('Ctrl Pts',(1.60410867830984,0.456041742701895,14.6606987128849));
#57046=CARTESIAN_POINT('Ctrl Pts',(1.62294263487886,0.38365791475213,14.6553132367539));
#57047=CARTESIAN_POINT('Ctrl Pts',(1.64950545813521,0.243520926872342,14.6449501419635));
#57048=CARTESIAN_POINT('Ctrl Pts',(1.65806294248567,0.176064029496761,14.6399890388297));
#57049=CARTESIAN_POINT('Ctrl Pts',(1.66681823323159,0.0416295507768519,
14.6302851313641));
#57050=CARTESIAN_POINT('Ctrl Pts',(1.66714782882214,-0.0252197761618907,
14.6255486597509));
#57051=CARTESIAN_POINT('Ctrl Pts',(1.66193482324454,-0.119563231094888,
14.6190145500985));
#57052=CARTESIAN_POINT('Ctrl Pts',(1.65971803046675,-0.147169770323015,
14.6171203253036));
#57053=CARTESIAN_POINT('Ctrl Pts',(1.65547858585899,-0.187373437147428,
14.6143861771779));
#57054=CARTESIAN_POINT('Ctrl Pts',(1.65399802776413,-0.200021731237748,
14.6135295271603));
#57055=CARTESIAN_POINT('Ctrl Pts',(1.65112401156462,-0.22235372374239,14.6120229066161));
#57056=CARTESIAN_POINT('Ctrl Pts',(1.64979002337648,-0.2320443186311,14.611371101424));
#57057=CARTESIAN_POINT('Ctrl Pts',(1.64681145788011,-0.252355934055075,
14.6100088019326));
#57058=CARTESIAN_POINT('Ctrl Pts',(1.64514929557366,-0.262973952437762,
14.6092988938812));
#57059=CARTESIAN_POINT('Ctrl Pts',(1.64047809545194,-0.291034146972347,
14.6074282852827));
#57060=CARTESIAN_POINT('Ctrl Pts',(1.63729360250342,-0.308446031978015,
14.6062731545515));
#57061=CARTESIAN_POINT('Ctrl Pts',(1.62098145371994,-0.390247601018884,
14.6008681961091));
#57062=CARTESIAN_POINT('Ctrl Pts',(1.60432849790091,-0.453878417222404,
14.596731117554));
#57063=CARTESIAN_POINT('Ctrl Pts',(1.53898268065541,-0.654327718377892,
14.5836720918014));
#57064=CARTESIAN_POINT('Ctrl Pts',(1.47618292509608,-0.785802678070321,
14.5751055504761));
#57065=CARTESIAN_POINT('Ctrl Pts',(1.38890212190533,-0.920183072215023,
14.5648178372127));
#57066=CARTESIAN_POINT('Ctrl Pts',(1.38046859518806,-0.932787442576402,
14.5638359939151));
#57067=CARTESIAN_POINT('Ctrl Pts',(1.36513844151433,-0.955035895427134,
14.5620691827171));
#57068=CARTESIAN_POINT('Ctrl Pts',(1.35830861327989,-0.964724943921282,
14.5612880730264));
#57069=CARTESIAN_POINT('Ctrl Pts',(1.34762510889843,-0.979542599537536,
14.5600739878309));
#57070=CARTESIAN_POINT('Ctrl Pts',(1.34384406736867,-0.984723442189037,
14.5596457584298));
#57071=CARTESIAN_POINT('Ctrl Pts',(1.33677558344973,-0.994292261168575,
14.5588476092693));
#57072=CARTESIAN_POINT('Ctrl Pts',(1.33349628260819,-0.998685997780765,
14.5584782392593));
#57073=CARTESIAN_POINT('Ctrl Pts',(1.3259126432943,-1.00874291108409,14.5576261863434));
#57074=CARTESIAN_POINT('Ctrl Pts',(1.3215936737399,-1.01439477285512,14.5571425144779));
#57075=CARTESIAN_POINT('Ctrl Pts',(1.3075595114807,-1.03251830603933,14.5555763780396));
#57076=CARTESIAN_POINT('Ctrl Pts',(1.29770328353408,-1.04487897427588,14.5544848699085));
#57077=CARTESIAN_POINT('Ctrl Pts',(1.23226323804921,-1.12459293804642,14.5473016490876));
#57078=CARTESIAN_POINT('Ctrl Pts',(1.17163737316485,-1.18762156472463,14.5409475611298));
#57079=CARTESIAN_POINT('Ctrl Pts',(1.01862569984769,-1.32352830155669,14.5260499413465));
#57080=CARTESIAN_POINT('Ctrl Pts',(0.922890444938109,-1.39197974819097,
14.5175642678565));
#57081=CARTESIAN_POINT('Ctrl Pts',(0.797592185649575,-1.46291159257379,
14.5076199060098));
#57082=CARTESIAN_POINT('Ctrl Pts',(0.774131366441445,-1.47546073854387,
14.5058017689212));
#57083=CARTESIAN_POINT('Ctrl Pts',(0.739184881645519,-1.49309038756018,
14.5031557354706));
#57084=CARTESIAN_POINT('Ctrl Pts',(0.727927259349844,-1.49861106184631,
14.5023126034722));
#57085=CARTESIAN_POINT('Ctrl Pts',(0.707799430191143,-1.50820130445134,
14.5008211718781));
#57086=CARTESIAN_POINT('Ctrl Pts',(0.698953886342473,-1.51232095794956,
14.5001711629913));
#57087=CARTESIAN_POINT('Ctrl Pts',(0.680198016468127,-1.52085645516787,
14.4988040741707));
#57088=CARTESIAN_POINT('Ctrl Pts',(0.670279687775431,-1.52525369967497,
14.498087655793));
#57089=CARTESIAN_POINT('Ctrl Pts',(0.643632682167299,-1.53675739529548,
14.4961797450383));
#57090=CARTESIAN_POINT('Ctrl Pts',(0.626829185090151,-1.54368764213444,
14.4949942368378));
#57091=CARTESIAN_POINT('Ctrl Pts',(0.540873073695879,-1.57750336658963,
14.489013326476));
#57092=CARTESIAN_POINT('Ctrl Pts',(0.470089132984541,-1.60002460979704,
14.4843647891147));
#57093=CARTESIAN_POINT('Ctrl Pts',(0.290731531638775,-1.64415374541834,
14.4729736319766));
#57094=CARTESIAN_POINT('Ctrl Pts',(0.181078439071984,-1.6598114896284,14.4663565762054));
#57095=CARTESIAN_POINT('Ctrl Pts',(0.0417232087857899,-1.66572979897458,
14.4576153558356));
#57096=CARTESIAN_POINT('Ctrl Pts',(0.012730862512881,-1.66620356511176,
14.455777631832));
#57097=CARTESIAN_POINT('Ctrl Pts',(-0.0355745694098858,-1.66573216374658,
14.4526623285535));
#57098=CARTESIAN_POINT('Ctrl Pts',(-0.0548860620305085,-1.66520768469757,
14.4514026535183));
#57099=CARTESIAN_POINT('Ctrl Pts',(-0.0819567641449366,-1.66400109366379,
14.4496113933152));
#57100=CARTESIAN_POINT('Ctrl Pts',(-0.0897277782912462,-1.66360015350894,
14.449094240045));
#57101=CARTESIAN_POINT('Ctrl Pts',(-0.103041778674237,-1.66281967112757,
14.448202714152));
#57102=CARTESIAN_POINT('Ctrl Pts',(-0.108586304897514,-1.66246680579926,
14.4478298041162));
#57103=CARTESIAN_POINT('Ctrl Pts',(-0.120235311393509,-1.66166691400585,
14.4470427185696));
#57104=CARTESIAN_POINT('Ctrl Pts',(-0.126339171814687,-1.66121397593284,
14.4466282442403));
#57105=CARTESIAN_POINT('Ctrl Pts',(-0.142897429857614,-1.65989348216293,
14.4454985460248));
#57106=CARTESIAN_POINT('Ctrl Pts',(-0.15334614435679,-1.65896081733869,
14.4447799016536));
#57107=CARTESIAN_POINT('Ctrl Pts',(-0.204492566660586,-1.65390811932029,
14.4412360681509));
#57108=CARTESIAN_POINT('Ctrl Pts',(-0.245034652740965,-1.64838911920957,
14.4383462639574));
#57109=CARTESIAN_POINT('Ctrl Pts',(-0.375753840304435,-1.62566566420576,
14.4288473142388));
#57110=CARTESIAN_POINT('Ctrl Pts',(-0.464723771855776,-1.60250161286187,
14.4221083930404));
#57111=CARTESIAN_POINT('Ctrl Pts',(-0.63999880388398,-1.54103410098925,
14.4086693362809));
#57112=CARTESIAN_POINT('Ctrl Pts',(-0.725887727091457,-1.50249024603493,
14.4019996520587));
#57113=CARTESIAN_POINT('Ctrl Pts',(-0.824309271557369,-1.44790007738957,
14.3943078786776));
#57114=CARTESIAN_POINT('Ctrl Pts',(-0.84038730672206,-1.43862769065992,
14.3930491349002));
#57115=CARTESIAN_POINT('Ctrl Pts',(-0.865684221334993,-1.42346981569469,
14.3910643245122));
#57116=CARTESIAN_POINT('Ctrl Pts',(-0.875005474744924,-1.41775911786363,
14.3903320151705));
#57117=CARTESIAN_POINT('Ctrl Pts',(-0.892526162237403,-1.40678639037462,
14.3889534388744));
#57118=CARTESIAN_POINT('Ctrl Pts',(-0.900736917818019,-1.40154340289076,
14.3883065097141));
#57119=CARTESIAN_POINT('Ctrl Pts',(-0.919288295974045,-1.38946703308628,
14.3868425402342));
#57120=CARTESIAN_POINT('Ctrl Pts',(-0.929599677992207,-1.38258962084153,
14.386027180012));
#57121=CARTESIAN_POINT('Ctrl Pts',(-0.956296068654092,-1.36435015586475,
14.3839110911912));
#57122=CARTESIAN_POINT('Ctrl Pts',(-0.972555847329067,-1.35280770878348,
14.3826171772229));
#57123=CARTESIAN_POINT('Ctrl Pts',(-1.09582719699795,-1.26192859892555,
14.3727562074008));
#57124=CARTESIAN_POINT('Ctrl Pts',(-1.19318199866672,-1.17030831958512,
14.3647163989273));
#57125=CARTESIAN_POINT('Ctrl Pts',(-1.3322484808992,-1.00383013736745,14.3514356915794));
#57126=CARTESIAN_POINT('Ctrl Pts',(-1.38098169462825,-0.935653117165252,
14.3462702150255));
#57127=CARTESIAN_POINT('Ctrl Pts',(-1.43088923417224,-0.853387043778903,
14.3399875984063));
#57128=CARTESIAN_POINT('Ctrl Pts',(-1.43727582983547,-0.842586264280778,
14.3391617500215));
#57129=CARTESIAN_POINT('Ctrl Pts',(-1.4468137621537,-0.82603205221215,14.3378928392095));
#57130=CARTESIAN_POINT('Ctrl Pts',(-1.45005428707857,-0.820330161884658,
14.3374552182932));
#57131=CARTESIAN_POINT('Ctrl Pts',(-1.45593387245327,-0.809840997406341,
14.3366488679771));
#57132=CARTESIAN_POINT('Ctrl Pts',(-1.4585831416257,-0.805059686090085,
14.3362807915933));
#57133=CARTESIAN_POINT('Ctrl Pts',(-1.46458789157623,-0.794095581678951,
14.3354355941896));
#57134=CARTESIAN_POINT('Ctrl Pts',(-1.46792776296666,-0.787904539393444,
14.3349575325043));
#57135=CARTESIAN_POINT('Ctrl Pts',(-1.4782510814726,-0.768474962626304,
14.3334551292887));
#57136=CARTESIAN_POINT('Ctrl Pts',(-1.48509516926469,-0.755163775220494,
14.3324228299294));
#57137=CARTESIAN_POINT('Ctrl Pts',(-1.53862939173661,-0.647501131951625,
14.3240600131066));
#57138=CARTESIAN_POINT('Ctrl Pts',(-1.57645633955487,-0.549017307145089,
14.316344318012));
#57139=CARTESIAN_POINT('Ctrl Pts',(-1.63446330171472,-0.341065839003679,
14.3006488236942));
#57140=CARTESIAN_POINT('Ctrl Pts',(-1.65350533917686,-0.231785534366187,
14.2927206925709));
#57141=CARTESIAN_POINT('Ctrl Pts',(-1.66305993220523,-0.101021954849681,
14.2837357873647));
#57142=CARTESIAN_POINT('Ctrl Pts',(-1.66417421190964,-0.0806103615335162,
14.2823466474091));
#57143=CARTESIAN_POINT('Ctrl Pts',(-1.66532187845883,-0.0488609195891628,
14.2802057277429));
#57144=CARTESIAN_POINT('Ctrl Pts',(-1.66561564446994,-0.0375351064723029,
14.2794459181799));
#57145=CARTESIAN_POINT('Ctrl Pts',(-1.66593112461483,-0.017482209441617,
14.278107286252));
#57146=CARTESIAN_POINT('Ctrl Pts',(-1.66599984091722,-0.00875640526475396,
14.2775270211396));
#57147=CARTESIAN_POINT('Ctrl Pts',(-1.66600020737263,0.0113795055583354,
14.2761929251591));
#57148=CARTESIAN_POINT('Ctrl Pts',(-1.66588320253356,0.0227892627417358,
14.2754406380613));
#57149=CARTESIAN_POINT('Ctrl Pts',(-1.66522147424093,0.0550202157232996,
14.2733252433562));
#57150=CARTESIAN_POINT('Ctrl Pts',(-1.6644035055733,0.0758341327895048,
14.2719706532173));
#57151=CARTESIAN_POINT('Ctrl Pts',(-1.65690917093362,0.204829257923058,
14.2636362407428));
#57152=CARTESIAN_POINT('Ctrl Pts',(-1.64007957644306,0.312163349893217,
14.2569890429078));
#57153=CARTESIAN_POINT('Ctrl Pts',(-1.59906991625028,0.470744190249016,
14.2469855902215));
#57154=CARTESIAN_POINT('Ctrl Pts',(-1.58254342204313,0.523615361484824,
14.2436133494779));
#57155=CARTESIAN_POINT('Ctrl Pts',(-1.56343134771032,0.575533162377876,
14.2401853336637));
#57156=CARTESIAN_POINT('',(-1.66599925405382,0.00153210873033471,14.4716226783165));
#57157=CARTESIAN_POINT('Ctrl Pts',(-1.56343129324813,0.575533310323967,
14.4309760522469));
#57158=CARTESIAN_POINT('Ctrl Pts',(-1.57677209618433,0.539293133754934,
14.4333999250567));
#57159=CARTESIAN_POINT('Ctrl Pts',(-1.58885135719543,0.502593098001554,
14.4358621957485));
#57160=CARTESIAN_POINT('Ctrl Pts',(-1.60288200634149,0.454378071893856,
14.439146856625));
#57161=CARTESIAN_POINT('Ctrl Pts',(-1.60600216048062,0.443223646242346,
14.4399101728418));
#57162=CARTESIAN_POINT('Ctrl Pts',(-1.61067217749139,0.425831462946423,
14.4411069599331));
#57163=CARTESIAN_POINT('Ctrl Pts',(-1.61230274453565,0.419615484318913,
14.4415359978152));
#57164=CARTESIAN_POINT('Ctrl Pts',(-1.61524443112633,0.408130988191647,
14.4423313485267));
#57165=CARTESIAN_POINT('Ctrl Pts',(-1.61656581024057,0.402865304878655,
14.4426970737048));
#57166=CARTESIAN_POINT('Ctrl Pts',(-1.61957647236361,0.390614509447594,
14.4435503466289));
#57167=CARTESIAN_POINT('Ctrl Pts',(-1.62124631214617,0.38362486283522,14.4440389641873));
#57168=CARTESIAN_POINT('Ctrl Pts',(-1.62467717231388,0.368841335600024,
14.4450758717672));
#57169=CARTESIAN_POINT('Ctrl Pts',(-1.62642744286349,0.361045166246974,
14.4456247079493));
#57170=CARTESIAN_POINT('Ctrl Pts',(-1.63298720533843,0.330810243027963,
14.4477602133763));
#57171=CARTESIAN_POINT('Ctrl Pts',(-1.63738871873334,0.30828670492056,14.4493659728305));
#57172=CARTESIAN_POINT('Ctrl Pts',(-1.65765738191466,0.191837047830531,
14.4577209459689));
#57173=CARTESIAN_POINT('Ctrl Pts',(-1.66591168597341,0.0967731178363305,
14.464706639791));
#57174=CARTESIAN_POINT('Ctrl Pts',(-1.66599929514542,0.00153250610393629,
14.4716227213688));
#57175=CARTESIAN_POINT('Ctrl Pts',(-1.6659992955061,0.00153211396245487,
14.4716227498449));
#57176=CARTESIAN_POINT('Ctrl Pts',(-1.66607010972176,-0.0754702737889355,
14.4772144272921));
#57177=CARTESIAN_POINT('Ctrl Pts',(-1.66080232591833,-0.152394421586609,
14.4827483996111));
#57178=CARTESIAN_POINT('Ctrl Pts',(-1.64568388868304,-0.261490397897914,
14.4904529449018));
#57179=CARTESIAN_POINT('Ctrl Pts',(-1.64016079294015,-0.294152219386785,
14.4927418217603));
#57180=CARTESIAN_POINT('Ctrl Pts',(-1.63117691918578,-0.339085851975443,
14.4958670201869));
#57181=CARTESIAN_POINT('Ctrl Pts',(-1.62854405384367,-0.351513352372362,
14.4967288697825));
#57182=CARTESIAN_POINT('Ctrl Pts',(-1.62317579314133,-0.375496087778437,
14.4983875187229));
#57183=CARTESIAN_POINT('Ctrl Pts',(-1.62045850316515,-0.387054543381548,
14.4991848400579));
#57184=CARTESIAN_POINT('Ctrl Pts',(-1.61552105335458,-0.407092784463793,
14.5005638129027));
#57185=CARTESIAN_POINT('Ctrl Pts',(-1.61335713857959,-0.415585800317818,
14.5011472417712));
#57186=CARTESIAN_POINT('Ctrl Pts',(-1.60833774361406,-0.434655862903503,
14.502455117978));
#57187=CARTESIAN_POINT('Ctrl Pts',(-1.60544473227513,-0.445222683556907,
14.5031783258944));
#57188=CARTESIAN_POINT('Ctrl Pts',(-1.59734023988666,-0.473717972479032,
14.5051250615301));
#57189=CARTESIAN_POINT('Ctrl Pts',(-1.59193118357728,-0.491588966312082,
14.5063421613897));
#57190=CARTESIAN_POINT('Ctrl Pts',(-1.5599033965559,-0.591327103316351,
14.5131199682385));
#57191=CARTESIAN_POINT('Ctrl Pts',(-1.52726977317752,-0.671130514199535,
14.5184774713513));
#57192=CARTESIAN_POINT('Ctrl Pts',(-1.44380304531921,-0.837225440257637,
14.5298868643198));
#57193=CARTESIAN_POINT('Ctrl Pts',(-1.39107945833932,-0.922176310024921,
14.535889535982));
#57194=CARTESIAN_POINT('Ctrl Pts',(-1.31356270904562,-1.02516201649674,
14.5439815501698));
#57195=CARTESIAN_POINT('Ctrl Pts',(-1.29544271213704,-1.04796570903423,
14.5458315163021));
#57196=CARTESIAN_POINT('Ctrl Pts',(-1.26553669003437,-1.08364051546153,
14.5488415248341));
#57197=CARTESIAN_POINT('Ctrl Pts',(-1.25412936494299,-1.09682239132879,
14.5499802779102));
#57198=CARTESIAN_POINT('Ctrl Pts',(-1.23743114165975,-1.11551713415926,
14.5516380902831));
#57199=CARTESIAN_POINT('Ctrl Pts',(-1.23230544303942,-1.12117688005384,
14.5521457791724));
#57200=CARTESIAN_POINT('Ctrl Pts',(-1.22339861173999,-1.13087685248107,
14.5530263542751));
#57201=CARTESIAN_POINT('Ctrl Pts',(-1.21963595220224,-1.13493381389021,
14.5533978659125));
#57202=CARTESIAN_POINT('Ctrl Pts',(-1.21162257271466,-1.14348809910577,
14.5541882018034));
#57203=CARTESIAN_POINT('Ctrl Pts',(-1.20736705408819,-1.14798043758478,
14.5546073679631));
#57204=CARTESIAN_POINT('Ctrl Pts',(-1.19561685918445,-1.16024692810146,
14.5557630124033));
#57205=CARTESIAN_POINT('Ctrl Pts',(-1.18807162549734,-1.16797191981294,
14.5565031710568));
#57206=CARTESIAN_POINT('Ctrl Pts',(-1.14843634436777,-1.20777001811595,
14.5603787522978));
#57207=CARTESIAN_POINT('Ctrl Pts',(-1.11512370828706,-1.23859306335655,
14.5635936987366));
#57208=CARTESIAN_POINT('Ctrl Pts',(-0.996874982331963,-1.33936423712399,
14.5747501486809));
#57209=CARTESIAN_POINT('Ctrl Pts',(-0.906290141437564,-1.40224691533985,
14.5828521166776));
#57210=CARTESIAN_POINT('Ctrl Pts',(-0.746775929912785,-1.49102119349974,
14.5959362552252));
#57211=CARTESIAN_POINT('Ctrl Pts',(-0.681144875635934,-1.52212442034724,
14.6010332013231));
#57212=CARTESIAN_POINT('Ctrl Pts',(-0.597327296600504,-1.55533460225163,
14.6071856990013));
#57213=CARTESIAN_POINT('Ctrl Pts',(-0.580866269635608,-1.56155692892208,
14.6083778599861));
#57214=CARTESIAN_POINT('Ctrl Pts',(-0.554218026583178,-1.57115034546383,
14.6102826792893));
#57215=CARTESIAN_POINT('Ctrl Pts',(-0.544091821678499,-1.57468572354225,
14.6110007388934));
#57216=CARTESIAN_POINT('Ctrl Pts',(-0.524660124979875,-1.58126011809069,
14.6123679357983));
#57217=CARTESIAN_POINT('Ctrl Pts',(-0.515360646064193,-1.58431537872759,
14.6130175846647));
#57218=CARTESIAN_POINT('Ctrl Pts',(-0.494062087273214,-1.59110545340586,
14.6144951605525));
#57219=CARTESIAN_POINT('Ctrl Pts',(-0.482046500779604,-1.5947868495233,
14.6153213128614));
#57220=CARTESIAN_POINT('Ctrl Pts',(-0.44983851909473,-1.60425761860508,
14.6175169116141));
#57221=CARTESIAN_POINT('Ctrl Pts',(-0.429575964593264,-1.60980177473706,
14.6188784592535));
#57222=CARTESIAN_POINT('Ctrl Pts',(-0.291734405852252,-1.64472928905196,
14.628020198793));
#57223=CARTESIAN_POINT('Ctrl Pts',(-0.171356548710252,-1.66159085754469,
14.6353794512661));
#57224=CARTESIAN_POINT('Ctrl Pts',(0.0446280021943476,-1.66810241068831,
14.6485837883545));
#57225=CARTESIAN_POINT('Ctrl Pts',(0.139517854804287,-1.66285503701495,
14.6543987134009));
#57226=CARTESIAN_POINT('Ctrl Pts',(0.245195739703589,-1.64790055934746,
14.6613776387719));
#57227=CARTESIAN_POINT('Ctrl Pts',(0.256942896019237,-1.64610981790285,
14.6621605931074));
#57228=CARTESIAN_POINT('Ctrl Pts',(0.275005595981684,-1.64315828226117,
14.6633769556955));
#57229=CARTESIAN_POINT('Ctrl Pts',(0.281335546297896,-1.64208633308998,
14.6638055901363));
#57230=CARTESIAN_POINT('Ctrl Pts',(0.293058904599432,-1.64003125986257,
14.6646041022298));
#57231=CARTESIAN_POINT('Ctrl Pts',(0.298453846172952,-1.63905806894606,
14.6649734258042));
#57232=CARTESIAN_POINT('Ctrl Pts',(0.310829805629302,-1.63676244908864,
14.6658248727309));
#57233=CARTESIAN_POINT('Ctrl Pts',(0.317807245887715,-1.63542197387879,
14.6663079795765));
#57234=CARTESIAN_POINT('Ctrl Pts',(0.340235789932005,-1.63096415120732,
14.6678703255545));
#57235=CARTESIAN_POINT('Ctrl Pts',(0.355650766555677,-1.62767224664835,
14.6689585490329));
#57236=CARTESIAN_POINT('Ctrl Pts',(0.454686699188658,-1.60504894353253,
14.6760334601717));
#57237=CARTESIAN_POINT('Ctrl Pts',(0.536747511112746,-1.57950037386838,
14.6822739848453));
#57238=CARTESIAN_POINT('Ctrl Pts',(0.684976868919276,-1.52046077225588,
14.6938884379796));
#57239=CARTESIAN_POINT('Ctrl Pts',(0.751604377672313,-1.48865260034702,
14.6992492185595));
#57240=CARTESIAN_POINT('Ctrl Pts',(0.851687623457646,-1.43243438213573,
14.7074235982992));
#57241=CARTESIAN_POINT('Ctrl Pts',(0.886714250555539,-1.41102032754759,
14.7103106604339));
#57242=CARTESIAN_POINT('Ctrl Pts',(0.945366705111057,-1.37211465523097,
14.7151868772352));
#57243=CARTESIAN_POINT('Ctrl Pts',(0.96938522592302,-1.35525248817611,14.7171966095338));
#57244=CARTESIAN_POINT('Ctrl Pts',(1.00340357305664,-1.33000257181772,14.7200637224803));
#57245=CARTESIAN_POINT('Ctrl Pts',(1.01376883397787,-1.32211888249016,14.7209402153563));
#57246=CARTESIAN_POINT('Ctrl Pts',(1.03178822823877,-1.3080770321896,14.7224694398955));
#57247=CARTESIAN_POINT('Ctrl Pts',(1.03948219938889,-1.3019712878299,14.7231241913594));
#57248=CARTESIAN_POINT('Ctrl Pts',(1.05537873580484,-1.28912544750986,14.7244809852469));
#57249=CARTESIAN_POINT('Ctrl Pts',(1.06357179766593,-1.28237425715964,14.7251825424673));
#57250=CARTESIAN_POINT('Ctrl Pts',(1.08478171138486,-1.26455390456639,14.72700512477));
#57251=CARTESIAN_POINT('Ctrl Pts',(1.0976940079385,-1.2533618149281,14.728121096596));
#57252=CARTESIAN_POINT('Ctrl Pts',(1.15280558425405,-1.20408724515266,14.7329161397536));
#57253=CARTESIAN_POINT('Ctrl Pts',(1.19321511787951,-1.16405563247742,14.7365130449766));
#57254=CARTESIAN_POINT('Ctrl Pts',(1.30299594852364,-1.04356418656821,14.746664105659));
#57255=CARTESIAN_POINT('Ctrl Pts',(1.36682418255457,-0.958444574142309,
14.7530409311685));
#57256=CARTESIAN_POINT('Ctrl Pts',(1.45322893397506,-0.816852665890636,
14.7632758235878));
#57257=CARTESIAN_POINT('Ctrl Pts',(1.48157122851813,-0.764243275375606,
14.7670122975575));
#57258=CARTESIAN_POINT('Ctrl Pts',(1.51322103877211,-0.697086288838903,
14.7718403478763));
#57259=CARTESIAN_POINT('Ctrl Pts',(1.51924403710868,-0.683860166143343,
14.7727939521289));
#57260=CARTESIAN_POINT('Ctrl Pts',(1.52789137805668,-0.664192950392203,
14.7742184653774));
#57261=CARTESIAN_POINT('Ctrl Pts',(1.53064983270592,-0.657811085194333,
14.7746817109449));
#57262=CARTESIAN_POINT('Ctrl Pts',(1.53529815767669,-0.646869330088177,
14.7754779692443));
#57263=CARTESIAN_POINT('Ctrl Pts',(1.53720783634039,-0.642318013160207,
14.7758097839184));
#57264=CARTESIAN_POINT('Ctrl Pts',(1.54154432496139,-0.631852795903634,
14.7765742015799));
#57265=CARTESIAN_POINT('Ctrl Pts',(1.54395729000703,-0.625933498633533,
14.7770075975889));
#57266=CARTESIAN_POINT('Ctrl Pts',(1.55058973455484,-0.609391597688285,
14.7782213233504));
#57267=CARTESIAN_POINT('Ctrl Pts',(1.55473395352052,-0.598739475897147,
14.7790058385461));
#57268=CARTESIAN_POINT('Ctrl Pts',(1.58142081902552,-0.527999024511015,
14.784231251723));
#57269=CARTESIAN_POINT('Ctrl Pts',(1.60058250564716,-0.466699680377038,
14.7888308202969));
#57270=CARTESIAN_POINT('Ctrl Pts',(1.62185328582796,-0.381704045948198,
14.7951788000757));
#57271=CARTESIAN_POINT('Ctrl Pts',(1.6270659334762,-0.358834895795534,14.7968841874953));
#57272=CARTESIAN_POINT('Ctrl Pts',(1.64314462818012,-0.280716527768322,
14.8026886661328));
#57273=CARTESIAN_POINT('Ctrl Pts',(1.65169277482749,-0.225027615424539,
14.8067897584466));
#57274=CARTESIAN_POINT('Ctrl Pts',(1.66568768263496,-0.0877869598424337,
14.8167223612981));
#57275=CARTESIAN_POINT('Ctrl Pts',(1.66798950416059,-0.00605385503372676,
14.8224843318956));
#57276=CARTESIAN_POINT('Ctrl Pts',(1.66346729498448,0.0935920234690066,
14.8292964695389));
#57277=CARTESIAN_POINT('Ctrl Pts',(1.6623535857015,0.111640087663716,14.8305221483701));
#57278=CARTESIAN_POINT('Ctrl Pts',(1.66010340728635,0.140463327788435,14.8324672649783));
#57279=CARTESIAN_POINT('Ctrl Pts',(1.65915530277145,0.151251314715752,14.8331925215497));
#57280=CARTESIAN_POINT('Ctrl Pts',(1.65715260023084,0.171745637690258,14.8345653222362));
#57281=CARTESIAN_POINT('Ctrl Pts',(1.65611774196164,0.181453399535798,14.8352134549247));
#57282=CARTESIAN_POINT('Ctrl Pts',(1.65355466122131,0.20364463730525,14.8366904292869));
#57283=CARTESIAN_POINT('Ctrl Pts',(1.65197028678698,0.216121127977426,14.8375174745102));
#57284=CARTESIAN_POINT('Ctrl Pts',(1.64742325238133,0.24894884672207,14.8396855622441));
#57285=CARTESIAN_POINT('Ctrl Pts',(1.6442247389431,0.269265608783011,14.8410192153679));
#57286=CARTESIAN_POINT('Ctrl Pts',(1.61440148967487,0.438268647032832,14.8520590300703));
#57287=CARTESIAN_POINT('Ctrl Pts',(1.56804810957986,0.58275060981159,14.8610656696918));
#57288=CARTESIAN_POINT('Ctrl Pts',(1.47639288644112,0.774325470044577,14.8741575439071));
#57289=CARTESIAN_POINT('Ctrl Pts',(1.44689846356851,0.828129881449129,14.877988942799));
#57290=CARTESIAN_POINT('Ctrl Pts',(1.40673678012072,0.892672452180107,14.8829308125711));
#57291=CARTESIAN_POINT('Ctrl Pts',(1.39879874257973,0.905060504493886,14.8838959881868));
#57292=CARTESIAN_POINT('Ctrl Pts',(1.38685089555989,0.92317355319401,14.8853345186604));
#57293=CARTESIAN_POINT('Ctrl Pts',(1.38296720620833,0.928981441149657,14.8857999914108));
#57294=CARTESIAN_POINT('Ctrl Pts',(1.37627571890856,0.93885331345002,14.8865987089707));
#57295=CARTESIAN_POINT('Ctrl Pts',(1.37348619677984,0.942929512160158,14.8869307339714));
#57296=CARTESIAN_POINT('Ctrl Pts',(1.36705889698197,0.952232388447557,14.8876936766206));
#57297=CARTESIAN_POINT('Ctrl Pts',(1.36340933394882,0.957450538738162,14.8881253699619));
#57298=CARTESIAN_POINT('Ctrl Pts',(1.35318867830356,0.971887112798959,14.8893298520007));
#57299=CARTESIAN_POINT('Ctrl Pts',(1.34655354777308,0.98105947045385,14.8901067286173));
#57300=CARTESIAN_POINT('Ctrl Pts',(1.30456944878151,1.03786967665884,14.8949877666505));
#57301=CARTESIAN_POINT('Ctrl Pts',(1.26679399989211,1.08365416496005,14.8992276229039));
#57302=CARTESIAN_POINT('Ctrl Pts',(1.12479950994088,1.23816136749632,14.9144043264441));
#57303=CARTESIAN_POINT('Ctrl Pts',(1.00835667963723,1.33471011059004,14.9254652015533));
#57304=CARTESIAN_POINT('Ctrl Pts',(0.856888718317735,1.4290109501614,14.9378058044863));
#57305=CARTESIAN_POINT('Ctrl Pts',(0.832896287738831,1.44312664259181,14.9397099163805));
#57306=CARTESIAN_POINT('Ctrl Pts',(0.797404173761675,1.46282787328466,14.9424555094821));
#57307=CARTESIAN_POINT('Ctrl Pts',(0.786177172158093,1.46889219239937,14.9433139155349));
#57308=CARTESIAN_POINT('Ctrl Pts',(0.766218821745587,1.47937840691593,14.9448225498853));
#57309=CARTESIAN_POINT('Ctrl Pts',(0.757516225975488,1.48385340517615,14.9454746289481));
#57310=CARTESIAN_POINT('Ctrl Pts',(0.739184617367353,1.49307647092038,14.9468364560966));
#57311=CARTESIAN_POINT('Ctrl Pts',(0.729548093566089,1.49780867764991,14.947545627002));
#57312=CARTESIAN_POINT('Ctrl Pts',(0.703954974341639,1.51007108562996,14.9494118959159));
#57313=CARTESIAN_POINT('Ctrl Pts',(0.687923069819701,1.51744165564607,14.9505634720172));
#57314=CARTESIAN_POINT('Ctrl Pts',(0.611746011949572,1.55100811763459,14.9559580423633));
#57315=CARTESIAN_POINT('Ctrl Pts',(0.550201463549296,1.5738930052545,14.9600886250358));
#57316=CARTESIAN_POINT('Ctrl Pts',(0.348572303948392,1.63558847049831,14.973150647575));
#57317=CARTESIAN_POINT('Ctrl Pts',(0.204742883871241,1.65973554132485,14.9817245848424));
#57318=CARTESIAN_POINT('Ctrl Pts',(0.0444306400704773,1.66547684905283,
14.9920227524561));
#57319=CARTESIAN_POINT('Ctrl Pts',(0.0292284189010689,1.66581297884413,
14.9930071325472));
#57320=CARTESIAN_POINT('Ctrl Pts',(0.00214577637284439,1.66604096752735,
14.994778094679));
#57321=CARTESIAN_POINT('Ctrl Pts',(-0.00973308183318889,1.66601391264209,
14.9955607924571));
#57322=CARTESIAN_POINT('Ctrl Pts',(-0.0280289915889216,1.66577657063434,
14.9967768402769));
#57323=CARTESIAN_POINT('Ctrl Pts',(-0.0344471001956311,1.66565620746902,
14.9972054203839));
#57324=CARTESIAN_POINT('Ctrl Pts',(-0.0463449329190276,1.66536428552764,
14.9980038874605));
#57325=CARTESIAN_POINT('Ctrl Pts',(-0.0518246988095145,1.66520276653938,
14.9983732209639));
#57326=CARTESIAN_POINT('Ctrl Pts',(-0.0644056767335511,1.66476977660643,
14.999224762513));
#57327=CARTESIAN_POINT('Ctrl Pts',(-0.0715060294726993,1.66447991379128,
14.9997079548539));
#57328=CARTESIAN_POINT('Ctrl Pts',(-0.0943558767970944,1.66340062495418,
15.0012708583614));
#57329=CARTESIAN_POINT('Ctrl Pts',(-0.110095547572428,1.66243303501844,
15.0023595624817));
#57330=CARTESIAN_POINT('Ctrl Pts',(-0.211658466737472,1.6547409105016,15.0094531284478));
#57331=CARTESIAN_POINT('Ctrl Pts',(-0.296857512588311,1.64159666458377,
15.0157133058776));
#57332=CARTESIAN_POINT('Ctrl Pts',(-0.452265443450762,1.60512403026894,
15.027333341642));
#57333=CARTESIAN_POINT('Ctrl Pts',(-0.522693418721993,1.58359092005621,
15.0326803090264));
#57334=CARTESIAN_POINT('Ctrl Pts',(-0.629789569983826,1.54291968285747,
15.0408377073797));
#57335=CARTESIAN_POINT('Ctrl Pts',(-0.66756018517107,1.52695772950736,15.0437211977033));
#57336=CARTESIAN_POINT('Ctrl Pts',(-0.731268861183344,1.49721781344463,
15.0485921042314));
#57337=CARTESIAN_POINT('Ctrl Pts',(-0.757500967938394,1.48411852627406,
15.0506000378084));
#57338=CARTESIAN_POINT('Ctrl Pts',(-0.794863927705322,1.46421200444325,
15.0534650888684));
#57339=CARTESIAN_POINT('Ctrl Pts',(-0.806280771680242,1.45795637501331,
15.0543412802621));
#57340=CARTESIAN_POINT('Ctrl Pts',(-0.826180589174423,1.44674741810042,
15.0558701603443));
#57341=CARTESIAN_POINT('Ctrl Pts',(-0.834695133932594,1.4418517601343,15.0565248659942));
#57342=CARTESIAN_POINT('Ctrl Pts',(-0.852323529573463,1.43150736511785,
15.0578817356757));
#57343=CARTESIAN_POINT('Ctrl Pts',(-0.86142960536506,1.42604620516515,15.0585834130294));
#57344=CARTESIAN_POINT('Ctrl Pts',(-0.885058895574051,1.41156614784214,
15.06040668276));
#57345=CARTESIAN_POINT('Ctrl Pts',(-0.899496837419093,1.40240996615437,
15.0615232146471));
#57346=CARTESIAN_POINT('Ctrl Pts',(-0.961399203605009,1.36180369540898,
15.0663249862226));
#57347=CARTESIAN_POINT('Ctrl Pts',(-1.00737760771395,1.32815252042373,15.0699277580662));
#57348=CARTESIAN_POINT('Ctrl Pts',(-1.1338423176092,1.22524081725169,15.0800808614251));
#57349=CARTESIAN_POINT('Ctrl Pts',(-1.20955033757919,1.15056556981926,15.0864545188659));
#57350=CARTESIAN_POINT('Ctrl Pts',(-1.31593705187389,1.0234383871181,15.0966832876255));
#57351=CARTESIAN_POINT('Ctrl Pts',(-1.35174151264472,0.975658659439617,
15.1004166933089));
#57352=CARTESIAN_POINT('Ctrl Pts',(-1.39297758113941,0.913991517523786,
15.1052410645524));
#57353=CARTESIAN_POINT('Ctrl Pts',(-1.40089400857755,0.901810943209442,
15.1061942916805));
#57354=CARTESIAN_POINT('Ctrl Pts',(-1.41236141940444,0.883651256967204,
15.10761834808));
#57355=CARTESIAN_POINT('Ctrl Pts',(-1.41603611859186,0.877750550830753,
15.1080815210105));
#57356=CARTESIAN_POINT('Ctrl Pts',(-1.4222566277471,0.867621142475052,15.1088776992591));
#57357=CARTESIAN_POINT('Ctrl Pts',(-1.4248207428189,0.863403852107385,15.1092095072288));
#57358=CARTESIAN_POINT('Ctrl Pts',(-1.43066312924325,0.853697769946753,
15.109973973578));
#57359=CARTESIAN_POINT('Ctrl Pts',(-1.43392850152452,0.848201580326376,
15.1104074255489));
#57360=CARTESIAN_POINT('Ctrl Pts',(-1.44294536763373,0.83282374672994,15.1116214574555));
#57361=CARTESIAN_POINT('Ctrl Pts',(-1.44862676022256,0.822901706542715,
15.1124062260964));
#57362=CARTESIAN_POINT('Ctrl Pts',(-1.48558600484684,0.756786739895782,
15.117641165683));
#57363=CARTESIAN_POINT('Ctrl Pts',(-1.51368652309156,0.698887130427848,
15.1222506589328));
#57364=CARTESIAN_POINT('Ctrl Pts',(-1.54716141035095,0.618362642153892,
15.128569107624));
#57365=CARTESIAN_POINT('Ctrl Pts',(-1.55551768061514,0.597030571873839,
15.1302347640674));
#57366=CARTESIAN_POINT('Ctrl Pts',(-1.56343130033034,0.575533291085225,
15.1319018884674));
#57367=CARTESIAN_POINT('Origin',(0.,0.,11.));
#57368=CARTESIAN_POINT('',(-1.5634313003304,0.575533291085054,15.8337663187435));
#57369=CARTESIAN_POINT('',(-1.56343131209646,0.575533259122642,15.6388155835246));
#57370=CARTESIAN_POINT('',(-1.56343130033213,0.575533291080363,11.));
#57371=CARTESIAN_POINT('',(-1.66599941198745,-0.00147660206947851,14.9787479457986));
#57372=CARTESIAN_POINT('Ctrl Pts',(-1.56343131209642,0.575533259122747,
15.6388155835246));
#57373=CARTESIAN_POINT('Ctrl Pts',(-1.55177222105231,0.607205082983509,
15.6363706320662));
#57374=CARTESIAN_POINT('Ctrl Pts',(-1.53914439133288,0.638539834474232,
15.6339365106143));
#57375=CARTESIAN_POINT('Ctrl Pts',(-1.49910450291894,0.729778033426274,
15.6268187785043));
#57376=CARTESIAN_POINT('Ctrl Pts',(-1.46909540592463,0.788448442551207,
15.62220506387));
#57377=CARTESIAN_POINT('Ctrl Pts',(-1.42670587109312,0.860453277364878,
15.6165020785214));
#57378=CARTESIAN_POINT('Ctrl Pts',(-1.417480561216,0.875567464976233,15.6153023522287));
#57379=CARTESIAN_POINT('Ctrl Pts',(-1.40227040247757,0.899616165400458,
15.6133884546029));
#57380=CARTESIAN_POINT('Ctrl Pts',(-1.39643717372203,0.908644460681454,
15.6126687886807));
#57381=CARTESIAN_POINT('Ctrl Pts',(-1.38512938178619,0.925779817708487,
15.611300407942));
#57382=CARTESIAN_POINT('Ctrl Pts',(-1.37967001471364,0.933896317921136,
15.6106511638684));
#57383=CARTESIAN_POINT('Ctrl Pts',(-1.36694101323808,0.95246540811069,15.6091630140976));
#57384=CARTESIAN_POINT('Ctrl Pts',(-1.3596223510197,0.962883775379662,15.6083260047986));
#57385=CARTESIAN_POINT('Ctrl Pts',(-1.33601814616774,0.995679371640372,
15.6056835536315));
#57386=CARTESIAN_POINT('Ctrl Pts',(-1.31929361415321,1.01773591836838,15.603894971513));
#57387=CARTESIAN_POINT('Ctrl Pts',(-1.26075086499363,1.09107309347279,15.5978938959737));
#57388=CARTESIAN_POINT('Ctrl Pts',(-1.21642957067679,1.14027786025765,15.5937772486746));
#57389=CARTESIAN_POINT('Ctrl Pts',(-1.12508377966516,1.23028242452983,15.585892447453));
#57390=CARTESIAN_POINT('Ctrl Pts',(-1.07847250180136,1.27134001546368,15.5821242435449));
#57391=CARTESIAN_POINT('Ctrl Pts',(-0.965883369033863,1.3598569092897,15.5733467078555));
#57392=CARTESIAN_POINT('Ctrl Pts',(-0.89851651284192,1.40527791427588,15.5683244154611));
#57393=CARTESIAN_POINT('Ctrl Pts',(-0.818016099911846,1.45139286509422,
15.5622567743807));
#57394=CARTESIAN_POINT('Ctrl Pts',(-0.807852211388698,1.45707459466636,
15.5614894830119));
#57395=CARTESIAN_POINT('Ctrl Pts',(-0.79197609607278,1.46573235472965,15.5602877832376));
#57396=CARTESIAN_POINT('Ctrl Pts',(-0.786304525505393,1.46878271440629,
15.5598578658583));
#57397=CARTESIAN_POINT('Ctrl Pts',(-0.775775068640214,1.47436734362632,
15.5590582918021));
#57398=CARTESIAN_POINT('Ctrl Pts',(-0.770922193799072,1.47691062323338,
15.558689203669));
#57399=CARTESIAN_POINT('Ctrl Pts',(-0.759666171328936,1.48273905322255,
15.5578318365845));
#57400=CARTESIAN_POINT('Ctrl Pts',(-0.75325422162104,1.48600668390545,15.557342508434));
#57401=CARTESIAN_POINT('Ctrl Pts',(-0.732654983581548,1.4963368049058,15.5557679788455));
#57402=CARTESIAN_POINT('Ctrl Pts',(-0.718388500173889,1.50323819662533,
15.5546737346606));
#57403=CARTESIAN_POINT('Ctrl Pts',(-0.638644111847153,1.54042003960233,
15.548545157333));
#57404=CARTESIAN_POINT('Ctrl Pts',(-0.571356938738306,1.5666235683454,15.5433321522475));
#57405=CARTESIAN_POINT('Ctrl Pts',(-0.375360212018787,1.6286402808487,15.5283853722561));
#57406=CARTESIAN_POINT('Ctrl Pts',(-0.243726813805456,1.6534734145658,15.5186716264791));
#57407=CARTESIAN_POINT('Ctrl Pts',(-0.0846055884013189,1.66405309198635,
15.5076655187007));
#57408=CARTESIAN_POINT('Ctrl Pts',(-0.0586479894757322,1.66517006442747,
15.5058909770305));
#57409=CARTESIAN_POINT('Ctrl Pts',(-0.020253121680027,1.66592320889176,
15.5032956296234));
#57410=CARTESIAN_POINT('Ctrl Pts',(-0.00783005576397834,1.66602792041299,
15.5024604136669));
#57411=CARTESIAN_POINT('Ctrl Pts',(0.0143379179613808,1.6659668010121,15.5009777929786));
#57412=CARTESIAN_POINT('Ctrl Pts',(0.0240822686485433,1.66585443818851,
15.5003287521227));
#57413=CARTESIAN_POINT('Ctrl Pts',(0.0447369180402899,1.66543499473685,
15.498958433904));
#57414=CARTESIAN_POINT('Ctrl Pts',(0.0556463542761696,1.66510618470226,
15.4982378649583));
#57415=CARTESIAN_POINT('Ctrl Pts',(0.0850155802516916,1.66393202986098,
15.4963061553773));
#57416=CARTESIAN_POINT('Ctrl Pts',(0.103466176324512,1.66288671999325,15.4951012696376));
#57417=CARTESIAN_POINT('Ctrl Pts',(0.213170929633009,1.65483838318132,15.4879820355488));
#57418=CARTESIAN_POINT('Ctrl Pts',(0.303744371465109,1.64063233264572,15.482301009781));
#57419=CARTESIAN_POINT('Ctrl Pts',(0.477586682812849,1.5984668254241,15.4713379173617));
#57420=CARTESIAN_POINT('Ctrl Pts',(0.560715860005859,1.57123566220749,15.4660639019779));
#57421=CARTESIAN_POINT('Ctrl Pts',(0.684874659348441,1.51945037555949,15.4576672169387));
#57422=CARTESIAN_POINT('Ctrl Pts',(0.727630959862287,1.49944491071121,15.4546724292722));
#57423=CARTESIAN_POINT('Ctrl Pts',(0.77914325382367,1.47262031195348,15.4508662246192));
#57424=CARTESIAN_POINT('Ctrl Pts',(0.788760346589713,1.46749170126251,15.4501468372356));
#57425=CARTESIAN_POINT('Ctrl Pts',(0.803776381540334,1.45929369490174,15.4490086248032));
#57426=CARTESIAN_POINT('Ctrl Pts',(0.809209862197859,1.45628773093741,15.4485936559644));
#57427=CARTESIAN_POINT('Ctrl Pts',(0.819447164821849,1.45054916756653,15.4478056614391));
#57428=CARTESIAN_POINT('Ctrl Pts',(0.824254351564816,1.44782295315993,15.4474330320016));
#57429=CARTESIAN_POINT('Ctrl Pts',(0.835631869106725,1.4412955968682,15.4465449991739));
#57430=CARTESIAN_POINT('Ctrl Pts',(0.842189891359466,1.43747340827862,15.4460282847164));
#57431=CARTESIAN_POINT('Ctrl Pts',(0.864323501526135,1.42436990535316,15.4442684418211));
#57432=CARTESIAN_POINT('Ctrl Pts',(0.87977299415682,1.41487955477236,15.443013163481));
#57433=CARTESIAN_POINT('Ctrl Pts',(0.917478723021633,1.39086127692496,15.4398883065606));
#57434=CARTESIAN_POINT('Ctrl Pts',(0.939547653743055,1.37604954436624,15.4380054516535));
#57435=CARTESIAN_POINT('Ctrl Pts',(1.03569190375755,1.30813035111853,15.4295903083518));
#57436=CARTESIAN_POINT('Ctrl Pts',(1.10568968850922,1.24952496514812,15.4229001777864));
#57437=CARTESIAN_POINT('Ctrl Pts',(1.23897747256315,1.11791780119275,15.409335103788));
#57438=CARTESIAN_POINT('Ctrl Pts',(1.30144265605379,1.04453726580949,15.4024985045623));
#57439=CARTESIAN_POINT('Ctrl Pts',(1.36809146079988,0.950911287168516,15.3946396863951));
#57440=CARTESIAN_POINT('Ctrl Pts',(1.37869152558984,0.935476481840212,15.3933691609651));
#57441=CARTESIAN_POINT('Ctrl Pts',(1.3951422524286,0.910635306285139,15.3913629782561));
#57442=CARTESIAN_POINT('Ctrl Pts',(1.40116292582691,0.901344013735505,15.3906209970282));
#57443=CARTESIAN_POINT('Ctrl Pts',(1.41224566449318,0.883861348935565,15.3892401792337));
#57444=CARTESIAN_POINT('Ctrl Pts',(1.41733016613232,0.875684822208499,15.3886005318789));
#57445=CARTESIAN_POINT('Ctrl Pts',(1.42865773017875,0.857111511584895,15.3871611082498));
#57446=CARTESIAN_POINT('Ctrl Pts',(1.43485877840326,0.846689643441299,15.3863628891065));
#57447=CARTESIAN_POINT('Ctrl Pts',(1.45319682672366,0.815089420620319,15.3839701146297));
#57448=CARTESIAN_POINT('Ctrl Pts',(1.46498307457946,0.793710571305735,15.3823881112902));
#57449=CARTESIAN_POINT('Ctrl Pts',(1.49116642231064,0.743645306132968,15.3787608699421));
#57450=CARTESIAN_POINT('Ctrl Pts',(1.50521310275329,0.71478622326705,15.3767272932658));
#57451=CARTESIAN_POINT('Ctrl Pts',(1.55392885379468,0.606884288466213,15.3693005980556));
#57452=CARTESIAN_POINT('Ctrl Pts',(1.58327531897998,0.525588997670174,15.3640542976308));
#57453=CARTESIAN_POINT('Ctrl Pts',(1.63002277261097,0.355859360144928,15.3532976158503));
#57454=CARTESIAN_POINT('Ctrl Pts',(1.6468199975481,0.267562899889985,15.3478005009654));
#57455=CARTESIAN_POINT('Ctrl Pts',(1.65810979065067,0.162712899987816,15.3409579379313));
#57456=CARTESIAN_POINT('Ctrl Pts',(1.65957247012197,0.147046720814122,15.3399272521456));
#57457=CARTESIAN_POINT('Ctrl Pts',(1.66137280831201,0.124285153722511,15.3384146607224));
#57458=CARTESIAN_POINT('Ctrl Pts',(1.66188736283359,0.117204079752066,15.3379419806333));
#57459=CARTESIAN_POINT('Ctrl Pts',(1.66271894086449,0.104650701030899,15.3370999173494));
#57460=CARTESIAN_POINT('Ctrl Pts',(1.66305424164536,0.0991798044272329,
15.3367315482994));
#57461=CARTESIAN_POINT('Ctrl Pts',(1.66372382786011,0.0872942244005637,
15.3359281517071));
#57462=CARTESIAN_POINT('Ctrl Pts',(1.66404801236243,0.0808793303274497,
15.3354926071388));
#57463=CARTESIAN_POINT('Ctrl Pts',(1.66486688344881,0.0625765696376846,
15.3342447127187));
#57464=CARTESIAN_POINT('Ctrl Pts',(1.66527131189861,0.0506853449523531,
15.3334276920026));
#57465=CARTESIAN_POINT('Ctrl Pts',(1.66590312541228,0.0235576766965499,
15.3315510303681));
#57466=CARTESIAN_POINT('Ctrl Pts',(1.66604889464,0.00832054946410637,15.3304877580062));
#57467=CARTESIAN_POINT('Ctrl Pts',(1.66538239538062,-0.152235772448115,
15.3192012849236));
#57468=CARTESIAN_POINT('Ctrl Pts',(1.64576940446321,-0.296851605038883,
15.3083906614042));
#57469=CARTESIAN_POINT('Ctrl Pts',(1.59046774197011,-0.500252120552606,
15.2933371410284));
#57470=CARTESIAN_POINT('Ctrl Pts',(1.56958736964694,-0.562349756946722,
15.2887515387907));
#57471=CARTESIAN_POINT('Ctrl Pts',(1.53850861289902,-0.639420241636941,
15.2830802278255));
#57472=CARTESIAN_POINT('Ctrl Pts',(1.53165379754557,-0.65567040756555,15.2818853707825));
#57473=CARTESIAN_POINT('Ctrl Pts',(1.52021390206232,-0.681631053313367,
15.2799773330015));
#57474=CARTESIAN_POINT('Ctrl Pts',(1.51579088730033,-0.691411018257144,
15.2792587176339));
#57475=CARTESIAN_POINT('Ctrl Pts',(1.50715536638607,-0.710024262663021,
15.2778911441648));
#57476=CARTESIAN_POINT('Ctrl Pts',(1.50295895894282,-0.71886447032848,15.2772416681038));
#57477=CARTESIAN_POINT('Ctrl Pts',(1.49311071067528,-0.739147667269043,
15.2757513016974));
#57478=CARTESIAN_POINT('Ctrl Pts',(1.4874047377871,-0.75056380770618,15.2749123275373));
#57479=CARTESIAN_POINT('Ctrl Pts',(1.46883234885912,-0.786678480135729,
15.2722567509974));
#57480=CARTESIAN_POINT('Ctrl Pts',(1.45547720843322,-0.811121285830036,
15.2704572535854));
#57481=CARTESIAN_POINT('Ctrl Pts',(1.40491734491293,-0.898383188327327,
15.2640089691905));
#57482=CARTESIAN_POINT('Ctrl Pts',(1.3642058792517,-0.959077159396175,15.25948187035));
#57483=CARTESIAN_POINT('Ctrl Pts',(1.23965898809748,-1.12070126200046,15.2469654666995));
#57484=CARTESIAN_POINT('Ctrl Pts',(1.14772461936356,-1.21467841656095,15.2391475890823));
#57485=CARTESIAN_POINT('Ctrl Pts',(1.0340588926637,-1.30633220382947,15.229660795745));
#57486=CARTESIAN_POINT('Ctrl Pts',(1.02223952680406,-1.31560173742588,15.2286758756794));
#57487=CARTESIAN_POINT('Ctrl Pts',(1.00469556309671,-1.32898173447869,15.227213469946));
#57488=CARTESIAN_POINT('Ctrl Pts',(0.999067253605341,-1.33321800294267,
15.2267442463408));
#57489=CARTESIAN_POINT('Ctrl Pts',(0.989023581819373,-1.34067827729617,
15.2259064652248));
#57490=CARTESIAN_POINT('Ctrl Pts',(0.984618977322235,-1.34391642467398,
15.2255388911628));
#57491=CARTESIAN_POINT('Ctrl Pts',(0.974901499512459,-1.35098703843999,
15.2247275055846));
#57492=CARTESIAN_POINT('Ctrl Pts',(0.969582002964589,-1.35480981972763,
15.2242830858361));
#57493=CARTESIAN_POINT('Ctrl Pts',(0.954038403877937,-1.36584158166964,
15.2229840784848));
#57494=CARTESIAN_POINT('Ctrl Pts',(0.943755737530097,-1.37296671001649,
15.2221242262529));
#57495=CARTESIAN_POINT('Ctrl Pts',(0.8596195262646,-1.42987516570604,15.2150907605256));
#57496=CARTESIAN_POINT('Ctrl Pts',(0.781969825852857,-1.47377356927853,
15.2086205781583));
#57497=CARTESIAN_POINT('Ctrl Pts',(0.58626384852657,-1.56457767545267,15.1929165860141));
#57498=CARTESIAN_POINT('Ctrl Pts',(0.465603492474386,-1.60462878300476,
15.1837488367089));
#57499=CARTESIAN_POINT('Ctrl Pts',(0.321410008702082,-1.63483181811235,
15.1736205306028));
#57500=CARTESIAN_POINT('Ctrl Pts',(0.301191611579758,-1.63867725496382,
15.1722173732211));
#57501=CARTESIAN_POINT('Ctrl Pts',(0.268506812889848,-1.64426832933593,
15.1699755121219));
#57502=CARTESIAN_POINT('Ctrl Pts',(0.256083365696785,-1.64624893995544,
15.1691294924123));
#57503=CARTESIAN_POINT('Ctrl Pts',(0.233980938909702,-1.64951636079465,
15.1676348309199));
#57504=CARTESIAN_POINT('Ctrl Pts',(0.224310968791953,-1.65085914013045,
15.1669844531109));
#57505=CARTESIAN_POINT('Ctrl Pts',(0.203893602002611,-1.65351159821838,
15.1656184620696));
#57506=CARTESIAN_POINT('Ctrl Pts',(0.193144081939528,-1.65480167371155,
15.1649034938252));
#57507=CARTESIAN_POINT('Ctrl Pts',(0.164422349999496,-1.65796494886197,
15.1630038921315));
#57508=CARTESIAN_POINT('Ctrl Pts',(0.146430633537744,-1.65965074395051,
15.1618251495231));
#57509=CARTESIAN_POINT('Ctrl Pts',(0.0472475442518117,-1.66731853994715,
15.1553827849607));
#57510=CARTESIAN_POINT('Ctrl Pts',(-0.0342755666667078,-1.66763638566252,
15.1502999042185));
#57511=CARTESIAN_POINT('Ctrl Pts',(-0.16602539576011,-1.6584801190757,15.1421777622315));
#57512=CARTESIAN_POINT('Ctrl Pts',(-0.21636093555196,-1.65266716942266,
15.1390947927211));
#57513=CARTESIAN_POINT('Ctrl Pts',(-0.351979994730006,-1.63070238828391,
15.1306972645686));
#57514=CARTESIAN_POINT('Ctrl Pts',(-0.436382153565351,-1.61016987802433,
15.1253742762429));
#57515=CARTESIAN_POINT('Ctrl Pts',(-0.533860854200183,-1.57822688011173,
15.1187199027992));
#57516=CARTESIAN_POINT('Ctrl Pts',(-0.548859047682911,-1.5730738055022,
15.1176812424208));
#57517=CARTESIAN_POINT('Ctrl Pts',(-0.570482611465693,-1.56529751618548,
15.1161590648939));
#57518=CARTESIAN_POINT('Ctrl Pts',(-0.577168828538687,-1.56284447815699,
15.1156849373639));
#57519=CARTESIAN_POINT('Ctrl Pts',(-0.588974858963148,-1.55842699089454,
15.1148412806736));
#57520=CARTESIAN_POINT('Ctrl Pts',(-0.59410100479565,-1.55648002406102,
15.1144727800796));
#57521=CARTESIAN_POINT('Ctrl Pts',(-0.605196632161427,-1.5522029820382,
15.1136703039472));
#57522=CARTESIAN_POINT('Ctrl Pts',(-0.611162218560856,-1.54986380052357,
15.1132358224526));
#57523=CARTESIAN_POINT('Ctrl Pts',(-0.62809858031899,-1.54310985417194,
15.1119939889164));
#57524=CARTESIAN_POINT('Ctrl Pts',(-0.639035786828177,-1.53861271666942,
15.111182034248));
#57525=CARTESIAN_POINT('Ctrl Pts',(-0.736029689118294,-1.49751841560116,
15.1038977632658));
#57526=CARTESIAN_POINT('Ctrl Pts',(-0.818901942218588,-1.45385590038076,
15.097093661109));
#57527=CARTESIAN_POINT('Ctrl Pts',(-1.00134058761238,-1.33716823178392,
15.0813290763024));
#57528=CARTESIAN_POINT('Ctrl Pts',(-1.09736863966334,-1.25956125883623,
15.072436700925));
#57529=CARTESIAN_POINT('Ctrl Pts',(-1.19858732368091,-1.15731391661627,
15.0625428972173));
#57530=CARTESIAN_POINT('Ctrl Pts',(-1.21291753097372,-1.14228639338515,
15.0611269147318));
#57531=CARTESIAN_POINT('Ctrl Pts',(-1.23541766086807,-1.11779040312,15.0588779019051));
#57532=CARTESIAN_POINT('Ctrl Pts',(-1.2437680257883,-1.10849145007598,15.0580372868624));
#57533=CARTESIAN_POINT('Ctrl Pts',(-1.25846419328916,-1.09175065420514,
15.0565467750719));
#57534=CARTESIAN_POINT('Ctrl Pts',(-1.26485051368203,-1.08434533327415,
15.0558952089094));
#57535=CARTESIAN_POINT('Ctrl Pts',(-1.27812608494293,-1.06867463420606,
15.0545323457399));
#57536=CARTESIAN_POINT('Ctrl Pts',(-1.28500122979276,-1.06039785524023,
15.0538216442932));
#57537=CARTESIAN_POINT('Ctrl Pts',(-1.3004985727496,-1.04136899700575,15.0522079146647));
#57538=CARTESIAN_POINT('Ctrl Pts',(-1.30906857449013,-1.03057528183028,
15.0513069913391));
#57539=CARTESIAN_POINT('Ctrl Pts',(-1.34775275171899,-0.980592205532774,
15.0471984674815));
#57540=CARTESIAN_POINT('Ctrl Pts',(-1.37624941168536,-0.94017914460346,
15.0440537276212));
#57541=CARTESIAN_POINT('Ctrl Pts',(-1.45222990873424,-0.821551267728504,
15.0352272624263));
#57542=CARTESIAN_POINT('Ctrl Pts',(-1.4951275765765,-0.740616453615575,
15.0296841960466));
#57543=CARTESIAN_POINT('Ctrl Pts',(-1.53305135900488,-0.652175104969901,
15.0237979377102));
#57544=CARTESIAN_POINT('Ctrl Pts',(-1.53491576265105,-0.647774990462892,
15.0235054848448));
#57545=CARTESIAN_POINT('Ctrl Pts',(-1.56681858847348,-0.571571158424203,
15.0184466161955));
#57546=CARTESIAN_POINT('Ctrl Pts',(-1.59180421959823,-0.497765513129217,
15.0136420231226));
#57547=CARTESIAN_POINT('Ctrl Pts',(-1.61554026550909,-0.407228099627312,
15.0075694629696));
#57548=CARTESIAN_POINT('Ctrl Pts',(-1.61932526842642,-0.391906500674153,
15.0065357084898));
#57549=CARTESIAN_POINT('Ctrl Pts',(-1.62449845592095,-0.369609653937734,
15.0050194272483));
#57550=CARTESIAN_POINT('Ctrl Pts',(-1.62606066465718,-0.362675116095122,
15.0045461889907));
#57551=CARTESIAN_POINT('Ctrl Pts',(-1.62874900461103,-0.35037513473146,
15.0037035117437));
#57552=CARTESIAN_POINT('Ctrl Pts',(-1.62989310038275,-0.345013818742599,
15.003335092459));
#57553=CARTESIAN_POINT('Ctrl Pts',(-1.63231902194102,-0.333364352626106,
15.0025320533508));
#57554=CARTESIAN_POINT('Ctrl Pts',(-1.63359096533703,-0.327074510607255,
15.0020969207898));
#57555=CARTESIAN_POINT('Ctrl Pts',(-1.63615204349318,-0.31402210817978,
15.0011909610798));
#57556=CARTESIAN_POINT('Ctrl Pts',(-1.63743566122322,-0.307258596595455,
15.000719850296));
#57557=CARTESIAN_POINT('Ctrl Pts',(-1.64064908818197,-0.289734505427428,
14.999495259328));
#57558=CARTESIAN_POINT('Ctrl Pts',(-1.64251493148324,-0.278962720389059,
14.9987386739575));
#57559=CARTESIAN_POINT('Ctrl Pts',(-1.65865690094451,-0.179990185347439,
14.9917564806084));
#57560=CARTESIAN_POINT('Ctrl Pts',(-1.66592020868823,-0.0908032192984881,
14.9852504582999));
#57561=CARTESIAN_POINT('Ctrl Pts',(-1.66599934620511,-0.00147595533024592,
14.9787480137938));
#57562=CARTESIAN_POINT('Ctrl Pts',(-1.66599934563946,-0.00147659367806648,
14.9787480602614));
#57563=CARTESIAN_POINT('Ctrl Pts',(-1.66610314052083,0.115632267753273,
14.970223295913));
#57564=CARTESIAN_POINT('Ctrl Pts',(-1.65385865480111,0.232450507843818,
14.9617624831313));
#57565=CARTESIAN_POINT('Ctrl Pts',(-1.62572354081887,0.364554152468414,
14.9524446927836));
#57566=CARTESIAN_POINT('Ctrl Pts',(-1.62171048484689,0.38201035004935,14.95121779562));
#57567=CARTESIAN_POINT('Ctrl Pts',(-1.61462003461837,0.410724018759949,
14.9492064580283));
#57568=CARTESIAN_POINT('Ctrl Pts',(-1.6117045585485,0.422019553761331,14.9484169717574));
#57569=CARTESIAN_POINT('Ctrl Pts',(-1.60577249778044,0.444043760741052,
14.9468807894801));
#57570=CARTESIAN_POINT('Ctrl Pts',(-1.60276643538076,0.454774603673521,
14.9461337994409));
#57571=CARTESIAN_POINT('Ctrl Pts',(-1.59693920745817,0.474800486290135,
14.9447422749769));
#57572=CARTESIAN_POINT('Ctrl Pts',(-1.59414399926716,0.484102520681658,
14.9440969310153));
#57573=CARTESIAN_POINT('Ctrl Pts',(-1.58769339545456,0.504907258900075,
14.9426555927583));
#57574=CARTESIAN_POINT('Ctrl Pts',(-1.58399400653956,0.516395834712217,
14.9418610710722));
#57575=CARTESIAN_POINT('Ctrl Pts',(-1.57483194207221,0.543823700837499,
14.9399669358166));
#57576=CARTESIAN_POINT('Ctrl Pts',(-1.56925173545991,0.559722128444655,
14.9388712276951));
#57577=CARTESIAN_POINT('Ctrl Pts',(-1.56343130047997,0.575533290678746,
14.9377828634576));
#57578=CARTESIAN_POINT('Ctrl Pts',(-1.56343130033034,0.575533291085225,
15.1319018884674));
#57579=CARTESIAN_POINT('Ctrl Pts',(-1.56361616135984,0.57503111766761,15.131940832256));
#57580=CARTESIAN_POINT('Ctrl Pts',(-1.56380078084195,0.574528854099077,
15.1319797768693));
#57581=CARTESIAN_POINT('Ctrl Pts',(-1.58799554347857,0.508608117607534,
15.1370903380066));
#57582=CARTESIAN_POINT('Ctrl Pts',(-1.60787910392355,0.441744119318942,
15.1421646437731));
#57583=CARTESIAN_POINT('Ctrl Pts',(-1.63386700579967,0.328880053710135,
15.1504511840247));
#57584=CARTESIAN_POINT('Ctrl Pts',(-1.64234636377242,0.283518137176467,
15.153710363797));
#57585=CARTESIAN_POINT('Ctrl Pts',(-1.65349195996309,0.206252539600368,
15.1591338921667));
#57586=CARTESIAN_POINT('Ctrl Pts',(-1.65714180010835,0.174519535944458,
15.161325577219));
#57587=CARTESIAN_POINT('Ctrl Pts',(-1.66102950745032,0.129297731720683,
15.1644001437324));
#57588=CARTESIAN_POINT('Ctrl Pts',(-1.66201931706476,0.115882423954891,
15.1653061940844));
#57589=CARTESIAN_POINT('Ctrl Pts',(-1.66345473009269,0.0925859279795217,
15.1668695338818));
#57590=CARTESIAN_POINT('Ctrl Pts',(-1.66397500639951,0.0827102077369872,
15.1675291232221));
#57591=CARTESIAN_POINT('Ctrl Pts',(-1.66480936250623,0.063642466787182,
15.1687968193843));
#57592=CARTESIAN_POINT('Ctrl Pts',(-1.6651353196239,0.0544513558431828,
15.1694052734281));
#57593=CARTESIAN_POINT('Ctrl Pts',(-1.66579791750518,0.0300692769474208,
15.1710127574103));
#57594=CARTESIAN_POINT('Ctrl Pts',(-1.66600288474831,0.0148753640508772,
15.1720076618229));
#57595=CARTESIAN_POINT('Ctrl Pts',(-1.66599141262338,-0.0449168762953361,
15.1758984239819));
#57596=CARTESIAN_POINT('Ctrl Pts',(-1.66419214261104,-0.0894984125453231,
15.1787452250402));
#57597=CARTESIAN_POINT('Ctrl Pts',(-1.65447971146818,-0.209898876319166,
15.1863433868392));
#57598=CARTESIAN_POINT('Ctrl Pts',(-1.64315124127635,-0.285334476225436,
15.1910031942807));
#57599=CARTESIAN_POINT('Ctrl Pts',(-1.60398435113785,-0.462445840440378,
15.2020801555452));
#57600=CARTESIAN_POINT('Ctrl Pts',(-1.57159591876881,-0.562762903924878,
15.2084629755019));
#57601=CARTESIAN_POINT('Ctrl Pts',(-1.52404955292086,-0.673092222856647,
15.2162692432924));
#57602=CARTESIAN_POINT('Ctrl Pts',(-1.51793908235321,-0.686761300788102,
15.2172510817204));
#57603=CARTESIAN_POINT('Ctrl Pts',(-1.50868784009518,-0.706729440802907,
15.2187097746519));
#57604=CARTESIAN_POINT('Ctrl Pts',(-1.50568985276522,-0.713094358522818,
15.2191784270216));
#57605=CARTESIAN_POINT('Ctrl Pts',(-1.50029097012475,-0.724370685617352,
15.2200156191681));
#57606=CARTESIAN_POINT('Ctrl Pts',(-1.49790609030435,-0.729289536626178,
15.220383181474));
#57607=CARTESIAN_POINT('Ctrl Pts',(-1.49260683036372,-0.74008368449563,
15.2211950715736));
#57608=CARTESIAN_POINT('Ctrl Pts',(-1.48968199070575,-0.745953465692557,
15.2216400127325));
#57609=CARTESIAN_POINT('Ctrl Pts',(-1.48106128491802,-0.763001219460017,
15.2229419892763));
#57610=CARTESIAN_POINT('Ctrl Pts',(-1.47527386582907,-0.774132022226061,
15.2238043245399));
#57611=CARTESIAN_POINT('Ctrl Pts',(-1.42995469326256,-0.858939191178976,
15.230463056535));
#57612=CARTESIAN_POINT('Ctrl Pts',(-1.38505648227977,-0.929603388047205,
15.2365212459306));
#57613=CARTESIAN_POINT('Ctrl Pts',(-1.25531384855932,-1.10340888526968,
15.2523031532071));
#57614=CARTESIAN_POINT('Ctrl Pts',(-1.16302820362113,-1.20029279239507,
15.2619704010721));
#57615=CARTESIAN_POINT('Ctrl Pts',(-1.044793441589,-1.29782885296469,15.2724979066783));
#57616=CARTESIAN_POINT('Ctrl Pts',(-1.02919534293735,-1.31023283155317,
15.273855660094));
#57617=CARTESIAN_POINT('Ctrl Pts',(-1.0035428472475,-1.32989145701371,15.2760397065342));
#57618=CARTESIAN_POINT('Ctrl Pts',(-0.993623837151769,-1.33731866746045,
15.2768727194598));
#57619=CARTESIAN_POINT('Ctrl Pts',(-0.975760075226436,-1.35038630644674,
15.2783529303569));
#57620=CARTESIAN_POINT('Ctrl Pts',(-0.967847063925048,-1.35606893955259,
15.2790017438661));
#57621=CARTESIAN_POINT('Ctrl Pts',(-0.950947963222408,-1.36798154894886,
15.2803731168512));
#57622=CARTESIAN_POINT('Ctrl Pts',(-0.941949436799228,-1.3741931505919,
15.2810949541027));
#57623=CARTESIAN_POINT('Ctrl Pts',(-0.917505101561957,-1.39071392125247,
15.2830338245257));
#57624=CARTESIAN_POINT('Ctrl Pts',(-0.901946728412277,-1.40085437008657,
15.2842445208855));
#57625=CARTESIAN_POINT('Ctrl Pts',(-0.80636672785814,-1.46089766725242,
15.2915488419405));
#57626=CARTESIAN_POINT('Ctrl Pts',(-0.722392148678671,-1.50419488081408,
15.2973933048079));
#57627=CARTESIAN_POINT('Ctrl Pts',(-0.54980268009964,-1.57537459087858,
15.3088263182101));
#57628=CARTESIAN_POINT('Ctrl Pts',(-0.461635419337567,-1.60342716694281,
15.3144007079377));
#57629=CARTESIAN_POINT('Ctrl Pts',(-0.332536864355155,-1.63296706330143,
15.3227190177802));
#57630=CARTESIAN_POINT('Ctrl Pts',(-0.293162758188266,-1.64049297987491,
15.3252774797753));
#57631=CARTESIAN_POINT('Ctrl Pts',(-0.243251161177065,-1.64817888946851,
15.3285907958126));
#57632=CARTESIAN_POINT('Ctrl Pts',(-0.232928588017561,-1.64966937241577,
15.3292798018988));
#57633=CARTESIAN_POINT('Ctrl Pts',(-0.21654010206061,-1.65187883576524,
15.3303806159117));
#57634=CARTESIAN_POINT('Ctrl Pts',(-0.210482855429853,-1.65266157104735,
15.3307889766175));
#57635=CARTESIAN_POINT('Ctrl Pts',(-0.198902204518846,-1.65409335952586,
15.331572799926));
#57636=CARTESIAN_POINT('Ctrl Pts',(-0.193379675546292,-1.65474808543996,
15.3319479480327));
#57637=CARTESIAN_POINT('Ctrl Pts',(-0.180090778258695,-1.65625612659678,
15.3328538176313));
#57638=CARTESIAN_POINT('Ctrl Pts',(-0.172321547705302,-1.65708247332934,
15.3333859977557));
#57639=CARTESIAN_POINT('Ctrl Pts',(-0.145123392740526,-1.65978197168793,
15.3352573525776));
#57640=CARTESIAN_POINT('Ctrl Pts',(-0.125668443500807,-1.66136821710382,
15.3366107707493));
#57641=CARTESIAN_POINT('Ctrl Pts',(-0.076840719859529,-1.66448684848598,
15.3400374689082));
#57642=CARTESIAN_POINT('Ctrl Pts',(-0.0474473920416858,-1.66558383425887,
15.3421272809172));
#57643=CARTESIAN_POINT('Ctrl Pts',(0.0963539027338841,-1.6671412476357,
15.3524388117315));
#57644=CARTESIAN_POINT('Ctrl Pts',(0.210574837179333,-1.65659424850831,
15.3608733439559));
#57645=CARTESIAN_POINT('Ctrl Pts',(0.391573247987135,-1.62084482159528,
15.3740845559402));
#57646=CARTESIAN_POINT('Ctrl Pts',(0.459409253531182,-1.60293887422585,
15.3790058446962));
#57647=CARTESIAN_POINT('Ctrl Pts',(0.542921182261424,-1.57515506310888,
15.3850149435742));
#57648=CARTESIAN_POINT('Ctrl Pts',(0.559826647023912,-1.56922625894704,
15.3862290386469));
#57649=CARTESIAN_POINT('Ctrl Pts',(0.586759934676838,-1.55928999024948,
15.3881602369433));
#57650=CARTESIAN_POINT('Ctrl Pts',(0.596849736355327,-1.55545584840314,
15.3888830132001));
#57651=CARTESIAN_POINT('Ctrl Pts',(0.616001174482712,-1.54796447673093,
15.3902538509961));
#57652=CARTESIAN_POINT('Ctrl Pts',(0.625069247711218,-1.54432506639398,
15.3909024747662));
#57653=CARTESIAN_POINT('Ctrl Pts',(0.64579758603769,-1.5357933966104,15.3923843670322));
#57654=CARTESIAN_POINT('Ctrl Pts',(0.657435317248927,-1.5308477055225,15.393215795302));
#57655=CARTESIAN_POINT('Ctrl Pts',(0.69391401204112,-1.51485261569091,15.3958211418802));
#57656=CARTESIAN_POINT('Ctrl Pts',(0.718542229232651,-1.50332707785994,
15.3975788833002));
#57657=CARTESIAN_POINT('Ctrl Pts',(0.813063371919907,-1.45623911801496,
15.4043359912983));
#57658=CARTESIAN_POINT('Ctrl Pts',(0.880696079452157,-1.41636178492724,
15.4091891916242));
#57659=CARTESIAN_POINT('Ctrl Pts',(1.01902951311069,-1.32104408387472,15.4194814262418));
#57660=CARTESIAN_POINT('Ctrl Pts',(1.08856215675058,-1.26436122821991,15.4248882478937));
#57661=CARTESIAN_POINT('Ctrl Pts',(1.18499499386729,-1.171871986873,15.4332504183841));
#57662=CARTESIAN_POINT('Ctrl Pts',(1.21556672089116,-1.14012889386062,15.436053697404));
#57663=CARTESIAN_POINT('Ctrl Pts',(1.25195208085808,-1.09922083844663,15.4396433894396));
#57664=CARTESIAN_POINT('Ctrl Pts',(1.25898505224871,-1.09115859888617,15.4403498111022));
#57665=CARTESIAN_POINT('Ctrl Pts',(1.26994827796263,-1.07834382058579,15.4414720759996));
#57666=CARTESIAN_POINT('Ctrl Pts',(1.2739307697762,-1.07363607187405,15.4418842400137));
#57667=CARTESIAN_POINT('Ctrl Pts',(1.28144163280502,-1.06465676956197,15.442670392491));
#57668=CARTESIAN_POINT('Ctrl Pts',(1.28497494707483,-1.06038958731908,15.4430440190084));
#57669=CARTESIAN_POINT('Ctrl Pts',(1.29335619278066,-1.05016415963807,15.4439392943375));
#57670=CARTESIAN_POINT('Ctrl Pts',(1.29818428276112,-1.0441899088713,15.4444623142954));
#57671=CARTESIAN_POINT('Ctrl Pts',(1.3146160015383,-1.02356728570179,15.4462669497862));
#57672=CARTESIAN_POINT('Ctrl Pts',(1.32601390710347,-1.00875778326753,15.4475615359026));
#57673=CARTESIAN_POINT('Ctrl Pts',(1.35368100202988,-0.971530177355729,
15.4508062309763));
#57674=CARTESIAN_POINT('Ctrl Pts',(1.36964445898344,-0.948892524567445,
15.452770866562));
#57675=CARTESIAN_POINT('Ctrl Pts',(1.4331485099955,-0.853894889023707,15.4609497533487));
#57676=CARTESIAN_POINT('Ctrl Pts',(1.47557720258271,-0.778281844100804,
15.4672988997019));
#57677=CARTESIAN_POINT('Ctrl Pts',(1.55351359134398,-0.609877807786816,
15.4807476175074));
#57678=CARTESIAN_POINT('Ctrl Pts',(1.58700629749733,-0.516500350930187,
15.4877922953916));
#57679=CARTESIAN_POINT('Ctrl Pts',(1.61677329856461,-0.402437323488599,
15.4958523597803));
#57680=CARTESIAN_POINT('Ctrl Pts',(1.6212256194518,-0.384108369944496,15.4971319966596));
#57681=CARTESIAN_POINT('Ctrl Pts',(1.62777959314886,-0.35497957903697,15.4991418974932));
#57682=CARTESIAN_POINT('Ctrl Pts',(1.63008706800584,-0.344228218134433,
15.4998786779808));
#57683=CARTESIAN_POINT('Ctrl Pts',(1.63404094310774,-0.324873669350474,
15.5011961979069));
#57684=CARTESIAN_POINT('Ctrl Pts',(1.63572624309877,-0.316278939288609,
15.5017781554477));
#57685=CARTESIAN_POINT('Ctrl Pts',(1.63952565043933,-0.296059509554514,
15.5031401434138));
#57686=CARTESIAN_POINT('Ctrl Pts',(1.64158404701692,-0.284424718083948,
15.503918381723));
#57687=CARTESIAN_POINT('Ctrl Pts',(1.64725422119827,-0.250260114800376,
15.5061883109003));
#57688=CARTESIAN_POINT('Ctrl Pts',(1.65052724552913,-0.227676278102937,
15.5076693316686));
#57689=CARTESIAN_POINT('Ctrl Pts',(1.66350310555647,-0.123041340112761,
15.5144520701939));
#57690=CARTESIAN_POINT('Ctrl Pts',(1.66755857594905,-0.0404037355153956,
15.5195776968399));
#57691=CARTESIAN_POINT('Ctrl Pts',(1.66401260858061,0.0995352561302625,
15.528160021742));
#57692=CARTESIAN_POINT('Ctrl Pts',(1.6596002720334,0.156754874360539,15.5316438346879));
#57693=CARTESIAN_POINT('Ctrl Pts',(1.64236578164872,0.290047389158333,15.5398919773014));
#57694=CARTESIAN_POINT('Ctrl Pts',(1.62719742072614,0.365675095095598,15.5446744492416));
#57695=CARTESIAN_POINT('Ctrl Pts',(1.60378997397939,0.451163361594568,15.5504719451597));
#57696=CARTESIAN_POINT('Ctrl Pts',(1.60060866897334,0.462322971283944,15.5512366563818));
#57697=CARTESIAN_POINT('Ctrl Pts',(1.59548355475557,0.479613996381464,15.5524351662606));
#57698=CARTESIAN_POINT('Ctrl Pts',(1.59362030021713,0.485769177991499,15.5528645114519));
#57699=CARTESIAN_POINT('Ctrl Pts',(1.59010328075809,0.497149467173237,15.5536636122648));
#57700=CARTESIAN_POINT('Ctrl Pts',(1.58845931419022,0.502377388186974,15.5540328057851));
#57701=CARTESIAN_POINT('Ctrl Pts',(1.58459283676959,0.514464310178104,15.5548912005595));
#57702=CARTESIAN_POINT('Ctrl Pts',(1.5823515728622,0.521317062651944,15.5553814599198));
#57703=CARTESIAN_POINT('Ctrl Pts',(1.57501853837099,0.543255093207375,15.5569620011035));
#57704=CARTESIAN_POINT('Ctrl Pts',(1.56975514904773,0.558281486560275,15.558061419231));
#57705=CARTESIAN_POINT('Ctrl Pts',(1.55660255824174,0.594173400221159,15.5607243063574));
#57706=CARTESIAN_POINT('Ctrl Pts',(1.54850816914736,0.614960082912384,15.5622967607548));
#57707=CARTESIAN_POINT('Ctrl Pts',(1.51500737247164,0.696132328839791,15.5685411125132));
#57708=CARTESIAN_POINT('Ctrl Pts',(1.48646674771988,0.755157775666766,15.5733089133505));
#57709=CARTESIAN_POINT('Ctrl Pts',(1.39506810007054,0.918809440581174,15.5869538678157));
#57710=CARTESIAN_POINT('Ctrl Pts',(1.32408918593116,1.01844193569244,15.5957620859157));
#57711=CARTESIAN_POINT('Ctrl Pts',(1.22891548996442,1.12506041555669,15.6055925319363));
#57712=CARTESIAN_POINT('Ctrl Pts',(1.21468142841152,1.14041366031784,15.6070204635948));
#57713=CARTESIAN_POINT('Ctrl Pts',(1.1914595094393,1.16453322974893,15.6092846298786));
#57714=CARTESIAN_POINT('Ctrl Pts',(1.18265580447379,1.17347290932298,15.6101286119361));
#57715=CARTESIAN_POINT('Ctrl Pts',(1.16680733683392,1.18920662306649,15.6116229736571));
#57716=CARTESIAN_POINT('Ctrl Pts',(1.15980220485253,1.19603955046502,15.6122750531022));
#57717=CARTESIAN_POINT('Ctrl Pts',(1.14498659836475,1.21023837904477,15.6136368748456));
#57718=CARTESIAN_POINT('Ctrl Pts',(1.13716428832194,1.21759132512249,15.61434604002));
#57719=CARTESIAN_POINT('Ctrl Pts',(1.11629987648073,1.23682733723651,15.6162122795394));
#57720=CARTESIAN_POINT('Ctrl Pts',(1.10313892233263,1.24857992660578,15.6173638323033));
#57721=CARTESIAN_POINT('Ctrl Pts',(1.03432386149207,1.30809338485769,15.6232596993818));
#57722=CARTESIAN_POINT('Ctrl Pts',(0.975743681172082,1.352353644106,15.6278599126304));
#57723=CARTESIAN_POINT('Ctrl Pts',(0.83249976794347,1.44641180458262,15.6384368342263));
#57724=CARTESIAN_POINT('Ctrl Pts',(0.745984384011499,1.49287279354739,15.6443308149655));
#57725=CARTESIAN_POINT('Ctrl Pts',(0.631770903264547,1.54178790590093,15.6520381779966));
#57726=CARTESIAN_POINT('Ctrl Pts',(0.607412321536898,1.55154586800623,15.6536787455991));
#57727=CARTESIAN_POINT('Ctrl Pts',(0.552608276617389,1.5720118097666,15.6573836339149));
#57728=CARTESIAN_POINT('Ctrl Pts',(0.522062788756211,1.58241813713555,15.6594578675558));
#57729=CARTESIAN_POINT('Ctrl Pts',(0.481963888388505,1.59479183204463,15.6622162615394));
#57730=CARTESIAN_POINT('Ctrl Pts',(0.472666298186928,1.59757213817262,15.6628582854483));
#57731=CARTESIAN_POINT('Ctrl Pts',(0.457631191862638,1.60192542886301,15.6639012343168));
#57732=CARTESIAN_POINT('Ctrl Pts',(0.451908449527273,1.60354923150448,15.664299307197));
#57733=CARTESIAN_POINT('Ctrl Pts',(0.440744141300227,1.60665254530285,15.6650782568018));
#57734=CARTESIAN_POINT('Ctrl Pts',(0.435303573703352,1.60813512942125,15.6654589562031));
#57735=CARTESIAN_POINT('Ctrl Pts',(0.421890245721668,1.61171728124755,15.6664000921706));
#57736=CARTESIAN_POINT('Ctrl Pts',(0.413909289399275,1.61378532251391,15.666962275919));
#57737=CARTESIAN_POINT('Ctrl Pts',(0.384137323976427,1.62126452064838,15.6690667986451));
#57738=CARTESIAN_POINT('Ctrl Pts',(0.362254040495224,1.62629395199782,15.6706283123874));
#57739=CARTESIAN_POINT('Ctrl Pts',(0.197699965571217,1.66062757513977,15.6824467648954));
#57740=CARTESIAN_POINT('Ctrl Pts',(0.0518380313566741,1.67155189733355,
15.6932822599853));
#57741=CARTESIAN_POINT('Ctrl Pts',(-0.158463322462585,1.65971893832539,
15.708320737297));
#57742=CARTESIAN_POINT('Ctrl Pts',(-0.223071719129287,1.65227675781392,
15.7128718494041));
#57743=CARTESIAN_POINT('Ctrl Pts',(-0.304435615465388,1.63804307392182,
15.7185087287761));
#57744=CARTESIAN_POINT('Ctrl Pts',(-0.321734750386793,1.63473329559382,
15.7197019335164));
#57745=CARTESIAN_POINT('Ctrl Pts',(-0.349483187294076,1.62896673095832,
15.7216080406818));
#57746=CARTESIAN_POINT('Ctrl Pts',(-0.35996650451912,1.62668227804572,15.7223263565386));
#57747=CARTESIAN_POINT('Ctrl Pts',(-0.379970243891386,1.6221203466728,15.7236938051796));
#57748=CARTESIAN_POINT('Ctrl Pts',(-0.389494054462821,1.61985993031703,
15.724343451796));
#57749=CARTESIAN_POINT('Ctrl Pts',(-0.41140094225353,1.61445609090268,15.7258348440392));
#57750=CARTESIAN_POINT('Ctrl Pts',(-0.423768992529285,1.61125387845079,
15.726674665631));
#57751=CARTESIAN_POINT('Ctrl Pts',(-0.463042919572187,1.6006019545044,15.7293355606454));
#57752=CARTESIAN_POINT('Ctrl Pts',(-0.48979978363936,1.59261786990147,15.7311394320014));
#57753=CARTESIAN_POINT('Ctrl Pts',(-0.588095900884025,1.56057506312904,
15.7377493515085));
#57754=CARTESIAN_POINT('Ctrl Pts',(-0.658178849962615,1.53233599965577,
15.7424236854143));
#57755=CARTESIAN_POINT('Ctrl Pts',(-0.80342682049788,1.4619989098313,15.7523158338598));
#57756=CARTESIAN_POINT('Ctrl Pts',(-0.87772689360696,1.41863655468647,15.7575040189252));
#57757=CARTESIAN_POINT('Ctrl Pts',(-0.988666687139947,1.34182672204963,
15.7659139182053));
#57758=CARTESIAN_POINT('Ctrl Pts',(-1.02772865427485,1.31214846722543,15.7690215649535));
#57759=CARTESIAN_POINT('Ctrl Pts',(-1.07377636659147,1.27384396065812,15.772946060816));
#57760=CARTESIAN_POINT('Ctrl Pts',(-1.08206331582573,1.26681217500199,15.7736632262553));
#57761=CARTESIAN_POINT('Ctrl Pts',(-1.095018414601,1.25559943197579,15.7748027970607));
#57762=CARTESIAN_POINT('Ctrl Pts',(-1.09973295692987,1.251472205888,15.7752214190555));
#57763=CARTESIAN_POINT('Ctrl Pts',(-1.10855045474257,1.24366485295932,15.7760120057806));
#57764=CARTESIAN_POINT('Ctrl Pts',(-1.11265856675455,1.23999084167605,15.7763835308096));
#57765=CARTESIAN_POINT('Ctrl Pts',(-1.11679516490339,1.23625424716575,15.7767608329646));
#57766=CARTESIAN_POINT('Ctrl Pts',(-1.11684201880059,1.23621191914185,15.776765106959));
#57767=CARTESIAN_POINT('Ctrl Pts',(-1.11693545101566,1.23612750240639,15.7767736306393));
#57768=CARTESIAN_POINT('Ctrl Pts',(-1.11698202936455,1.23608541372255,15.7767778803231));
#57769=CARTESIAN_POINT('Ctrl Pts',(-1.11707492429919,1.23600146334848,15.7767863566281));
#57770=CARTESIAN_POINT('Ctrl Pts',(-1.11712124090509,1.23595960169267,15.7767905832467));
#57771=CARTESIAN_POINT('Ctrl Pts',(-1.11721362582353,1.23587609335685,15.7767990146368));
#57772=CARTESIAN_POINT('Ctrl Pts',(-1.11725969415998,1.23583444670485,15.7768032194062));
#57773=CARTESIAN_POINT('Ctrl Pts',(-1.11735159571182,1.23575135661608,15.7768116082875));
#57774=CARTESIAN_POINT('Ctrl Pts',(-1.11739742894896,1.23570991320637,15.7768157923974));
#57775=CARTESIAN_POINT('Ctrl Pts',(-1.12265460424378,1.2309557293336,15.7772957648682));
#57776=CARTESIAN_POINT('Ctrl Pts',(-1.12783596631153,1.22621017637931,15.7777739638914));
#57777=CARTESIAN_POINT('Ctrl Pts',(-1.14488711497387,1.21039371762603,15.7793643304808));
#57778=CARTESIAN_POINT('Ctrl Pts',(-1.15662469990001,1.19918251846607,15.7804861450412));
#57779=CARTESIAN_POINT('Ctrl Pts',(-1.18490100450508,1.17137294811743,15.7832515650871));
#57780=CARTESIAN_POINT('Ctrl Pts',(-1.20125666179133,1.15459399472173,15.7849055649239));
#57781=CARTESIAN_POINT('Ctrl Pts',(-1.2660765272628,1.08522806737833,15.7916666894247));
#57782=CARTESIAN_POINT('Ctrl Pts',(-1.31148390390257,1.02989260290088,15.7968839343634));
#57783=CARTESIAN_POINT('Ctrl Pts',(-1.41925806813393,0.87982346978274,15.8103289024379));
#57784=CARTESIAN_POINT('Ctrl Pts',(-1.47578078979527,0.781320870746174,
15.8184820032896));
#57785=CARTESIAN_POINT('Ctrl Pts',(-1.53138047687393,0.656487360804334,
15.827886659614));
#57786=CARTESIAN_POINT('Ctrl Pts',(-1.54043628712573,0.634947211320445,
15.8294795787709));
#57787=CARTESIAN_POINT('Ctrl Pts',(-1.55348075342465,0.601996127229037,
15.8318726135231));
#57788=CARTESIAN_POINT('Ctrl Pts',(-1.5578029886287,0.590721296717067,15.8326838112989));
#57789=CARTESIAN_POINT('Ctrl Pts',(-1.56248027293879,0.578111827419007,
15.8335827743951));
#57790=CARTESIAN_POINT('Ctrl Pts',(-1.56295658424666,0.576822853297328,
15.8336745732498));
#57791=CARTESIAN_POINT('Ctrl Pts',(-1.5634313003304,0.575533291085054,15.8337663187435));
#57792=CARTESIAN_POINT('Origin',(0.,0.,11.));
#57793=CARTESIAN_POINT('',(-1.56343130033213,0.57553329108036,16.5321096688871));
#57794=CARTESIAN_POINT('',(-1.5634313003322,0.575533291080154,16.3407718992107));
#57795=CARTESIAN_POINT('',(-1.56343130033213,0.575533291080363,11.));
#57796=CARTESIAN_POINT('',(-1.66599956897413,0.00119840644346202,16.5714803634422));
#57797=CARTESIAN_POINT('Ctrl Pts',(-1.56343130033213,0.575533291080358,
16.5321096688871));
#57798=CARTESIAN_POINT('Ctrl Pts',(-1.58445950918258,0.518410340216824,
16.5361801898729));
#57799=CARTESIAN_POINT('Ctrl Pts',(-1.60232716192958,0.460203709933027,
16.5402507108586));
#57800=CARTESIAN_POINT('Ctrl Pts',(-1.61694683874032,0.40129654955867,16.5443212318443));
#57801=CARTESIAN_POINT('Ctrl Pts',(-1.63029117873162,0.347528112257761,
16.5480366639075));
#57802=CARTESIAN_POINT('Ctrl Pts',(-1.64093007365734,0.293176473642386,
16.5517520959706));
#57803=CARTESIAN_POINT('Ctrl Pts',(-1.64883476380889,0.238537044618418,
16.5554675280337));
#57804=CARTESIAN_POINT('Ctrl Pts',(-1.66019068866406,0.160041716119839,
16.5608051398192));
#57805=CARTESIAN_POINT('Ctrl Pts',(-1.6659423645046,0.0807228119652788,
16.5661427516047));
#57806=CARTESIAN_POINT('Ctrl Pts',(-1.66599956897358,0.00119840721805856,
16.5714803633902));
#57807=CARTESIAN_POINT('',(1.26907087985246,1.07935865304843,17.));
#57808=CARTESIAN_POINT('Ctrl Pts',(-1.66599956897413,0.00119840644346203,
16.5714803634422));
#57809=CARTESIAN_POINT('Ctrl Pts',(-1.66604263708935,-0.058673986420678,
16.5754989485644));
#57810=CARTESIAN_POINT('Ctrl Pts',(-1.66285394991176,-0.118667824823123,
16.5795175336867));
#57811=CARTESIAN_POINT('Ctrl Pts',(-1.65642067872897,-0.178399930154282,
16.5835361188089));
#57812=CARTESIAN_POINT('Ctrl Pts',(-1.64999457545002,-0.238065482409234,
16.5875502264529));
#57813=CARTESIAN_POINT('Ctrl Pts',(-1.64033110092478,-0.297469358720189,
16.5915643340969));
#57814=CARTESIAN_POINT('Ctrl Pts',(-1.62746943601073,-0.356229188656582,
16.5955784417409));
#57815=CARTESIAN_POINT('Ctrl Pts',(-1.61461702011814,-0.414946763493643,
16.5995896627782));
#57816=CARTESIAN_POINT('Ctrl Pts',(-1.59857108150669,-0.473020696127689,
16.6036008838155));
#57817=CARTESIAN_POINT('Ctrl Pts',(-1.57942222074496,-0.530076832748849,
16.6076121048528));
#57818=CARTESIAN_POINT('Ctrl Pts',(-1.56027956710547,-0.587114474566646,
16.6116220256488));
#57819=CARTESIAN_POINT('Ctrl Pts',(-1.53803615354127,-0.64313447551882,
16.6156319464449));
#57820=CARTESIAN_POINT('Ctrl Pts',(-1.51283233092265,-0.697778144194223,
16.6196418672409));
#57821=CARTESIAN_POINT('Ctrl Pts',(-1.48760918706544,-0.752463702680382,
16.6236548620403));
#57822=CARTESIAN_POINT('Ctrl Pts',(-1.45942131712902,-0.805770339496956,
16.6276678568398));
#57823=CARTESIAN_POINT('Ctrl Pts',(-1.42845651654735,-0.857361055992991,
16.6316808516392));
#57824=CARTESIAN_POINT('Ctrl Pts',(-1.39748096695344,-0.908969681509355,
16.6356952394956));
#57825=CARTESIAN_POINT('Ctrl Pts',(-1.36372686056116,-0.958860761762857,
16.6397096273519));
#57826=CARTESIAN_POINT('Ctrl Pts',(-1.32742536695106,-1.00672632585765,
16.6437240152083));
#57827=CARTESIAN_POINT('Ctrl Pts',(-1.29105750900536,-1.05467939506706,
16.6477457419413));
#57828=CARTESIAN_POINT('Ctrl Pts',(-1.25213330206962,-1.10059914757466,
16.6517674686743));
#57829=CARTESIAN_POINT('Ctrl Pts',(-1.21092354286444,-1.14421159465224,
16.6557891954073));
#57830=CARTESIAN_POINT('Ctrl Pts',(-1.17399601511252,-1.18329213966994,
16.65939301228));
#57831=CARTESIAN_POINT('Ctrl Pts',(-1.13523397431683,-1.2205203066986,16.6629968291527));
#57832=CARTESIAN_POINT('Ctrl Pts',(-1.09485449139006,-1.25572673885803,
16.6666006460254));
#57833=CARTESIAN_POINT('Ctrl Pts',(-1.04910619660825,-1.29561417970431,
16.6706836224451));
#57834=CARTESIAN_POINT('Ctrl Pts',(-1.00108366919819,-1.33307823890073,
16.6747665988648));
#57835=CARTESIAN_POINT('Ctrl Pts',(-0.951073693211118,-1.36785044141593,
16.6788495752846));
#57836=CARTESIAN_POINT('Ctrl Pts',(-0.900608099450398,-1.40293943739448,
16.6829697498151));
#57837=CARTESIAN_POINT('Ctrl Pts',(-0.848119000144949,-1.43528687187874,
16.6870899243456));
#57838=CARTESIAN_POINT('Ctrl Pts',(-0.793937348164885,-1.46465678136173,
16.6912100988761));
#57839=CARTESIAN_POINT('Ctrl Pts',(-0.740389486995609,-1.49368313582077,
16.6952820775938));
#57840=CARTESIAN_POINT('Ctrl Pts',(-0.685188917555343,-1.51980100130237,
16.6993540563115));
#57841=CARTESIAN_POINT('Ctrl Pts',(-0.628684192549413,-1.5428260388127,
16.7034260350292));
#57842=CARTESIAN_POINT('Ctrl Pts',(-0.57221301555606,-1.56583740588666,
16.7074955961298));
#57843=CARTESIAN_POINT('Ctrl Pts',(-0.51443968997464,-1.58575939410111,
16.7115651572303));
#57844=CARTESIAN_POINT('Ctrl Pts',(-0.455734440004197,-1.60245502907073,
16.7156347183309));
#57845=CARTESIAN_POINT('Ctrl Pts',(-0.397042420022204,-1.61914690146275,
16.7197033623031));
#57846=CARTESIAN_POINT('Ctrl Pts',(-0.337419383184623,-1.63261372476495,
16.7237720062753));
#57847=CARTESIAN_POINT('Ctrl Pts',(-0.277250486948461,-1.64276844609544,
16.7278406502476));
#57848=CARTESIAN_POINT('Ctrl Pts',(-0.215763711383714,-1.65314558628628,
16.7319984097283));
#57849=CARTESIAN_POINT('Ctrl Pts',(-0.15370741766246,-1.66006366939857,
16.7361561692091));
#57850=CARTESIAN_POINT('Ctrl Pts',(-0.0915009175646956,-1.66348537176761,
16.7403139286899));
#57851=CARTESIAN_POINT('Ctrl Pts',(-0.030549016544634,-1.66683806423206,
16.7443878332487));
#57852=CARTESIAN_POINT('Ctrl Pts',(0.0305465650727917,-1.66683417686648,
16.7484617378075));
#57853=CARTESIAN_POINT('Ctrl Pts',(0.0913913808401572,-1.66349139327744,
16.7525356423664));
#57854=CARTESIAN_POINT('Ctrl Pts',(0.154114788951663,-1.66004540076947,
16.7567353293081));
#57855=CARTESIAN_POINT('Ctrl Pts',(0.216571105926717,-1.65305096757422,
16.7609350162499));
#57856=CARTESIAN_POINT('Ctrl Pts',(0.27833681905625,-1.64258473606619,16.7651347031916));
#57857=CARTESIAN_POINT('Ctrl Pts',(0.340102532185782,-1.63211850455817,
16.7693343901334));
#57858=CARTESIAN_POINT('Ctrl Pts',(0.401177085533186,-1.61818067345858,
16.7735340770751));
#57859=CARTESIAN_POINT('Ctrl Pts',(0.461154195597915,-1.60090374722606,
16.7777337640169));
#57860=CARTESIAN_POINT('Ctrl Pts',(0.518754461466997,-1.58431149155853,
16.7817670207735));
#57861=CARTESIAN_POINT('Ctrl Pts',(0.575591792928433,-1.56456790261253,
16.7858002775301));
#57862=CARTESIAN_POINT('Ctrl Pts',(0.631291674499274,-1.54176094830162,
16.7898335342867));
#57863=CARTESIAN_POINT('Ctrl Pts',(0.688277733083706,-1.51842735408488,
16.7939599237751));
#57864=CARTESIAN_POINT('Ctrl Pts',(0.744072594574505,-1.49188719483812,
16.7980863132635));
#57865=CARTESIAN_POINT('Ctrl Pts',(0.798288913299178,-1.46228957833379,
16.8022127027519));
#57866=CARTESIAN_POINT('Ctrl Pts',(0.851135254615892,-1.43343985594869,
16.806234823627));
#57867=CARTESIAN_POINT('Ctrl Pts',(0.902481401571002,-1.40168564426234,
16.810256944502));
#57868=CARTESIAN_POINT('Ctrl Pts',(0.951988994920911,-1.36721357276377,
16.814279065377));
#57869=CARTESIAN_POINT('Ctrl Pts',(1.00146770267854,-1.33276161426474,16.8182988395142));
#57870=CARTESIAN_POINT('Ctrl Pts',(1.04910955271808,-1.29559523597842,16.8223186136514));
#57871=CARTESIAN_POINT('Ctrl Pts',(1.09460394209619,-1.25594514607425,16.8263383877886));
#57872=CARTESIAN_POINT('Ctrl Pts',(1.14008955967749,-1.21630270112449,16.830357386871));
#57873=CARTESIAN_POINT('Ctrl Pts',(1.18342814320243,-1.17417783877431,16.8343763859534));
#57874=CARTESIAN_POINT('Ctrl Pts',(1.22434282064919,-1.12984098771676,16.8383953850359));
#57875=CARTESIAN_POINT('Ctrl Pts',(1.26716079963126,-1.08344163972767,16.8426013431169));
#57876=CARTESIAN_POINT('Ctrl Pts',(1.30732337160491,-1.03461988625231,16.846807301198));
#57877=CARTESIAN_POINT('Ctrl Pts',(1.34455918892583,-0.983725870085312,
16.851013259279));
#57878=CARTESIAN_POINT('Ctrl Pts',(1.3801943417479,-0.93501964649934,16.855038414889));
#57879=CARTESIAN_POINT('Ctrl Pts',(1.41314900460982,-0.884416188042298,
16.859063570499));
#57880=CARTESIAN_POINT('Ctrl Pts',(1.44323049791081,-0.832251001741727,
16.8630887261089));
#57881=CARTESIAN_POINT('Ctrl Pts',(1.47333651729113,-0.780043284058683,
16.8671171635136));
#57882=CARTESIAN_POINT('Ctrl Pts',(1.50056447979353,-0.726271776394919,
16.8711456009183));
#57883=CARTESIAN_POINT('Ctrl Pts',(1.52476908460097,-0.671293705202969,
16.875174038323));
#57884=CARTESIAN_POINT('Ctrl Pts',(1.54901902426344,-0.616212660923562,
16.8792100209294));
#57885=CARTESIAN_POINT('Ctrl Pts',(1.57023414275995,-0.559921038899605,
16.8832460035358));
#57886=CARTESIAN_POINT('Ctrl Pts',(1.58831881229225,-0.502791557724004,
16.8872819861422));
#57887=CARTESIAN_POINT('Ctrl Pts',(1.59068604399918,-0.495313471436753,
16.8878102847643));
#57888=CARTESIAN_POINT('Ctrl Pts',(1.59299971048392,-0.48782104170286,16.8883385833864));
#57889=CARTESIAN_POINT('Ctrl Pts',(1.59525966256195,-0.480315114276783,
16.8888668820084));
#57890=CARTESIAN_POINT('Ctrl Pts',(1.61318955219974,-0.42076497970229,16.8930582699947));
#57891=CARTESIAN_POINT('Ctrl Pts',(1.62781101013488,-0.360109450417287,
16.897249657981));
#57892=CARTESIAN_POINT('Ctrl Pts',(1.6389970149018,-0.298738656927739,16.9014410459673));
#57893=CARTESIAN_POINT('Ctrl Pts',(1.65015919995767,-0.237498547681441,
16.9056235087249));
#57894=CARTESIAN_POINT('Ctrl Pts',(1.65790039706353,-0.175546669803257,
16.9098059714826));
#57895=CARTESIAN_POINT('Ctrl Pts',(1.66214386045146,-0.11328630616063,16.9139884342402));
#57896=CARTESIAN_POINT('Ctrl Pts',(1.66638197605736,-0.0511044055146698,
16.9181656260912));
#57897=CARTESIAN_POINT('Ctrl Pts',(1.66713107917674,0.0113847355010989,
16.9223428179422));
#57898=CARTESIAN_POINT('Ctrl Pts',(1.66436591304727,0.0737706410865663,
16.9265200097932));
#57899=CARTESIAN_POINT('Ctrl Pts',(1.66160341949632,0.136096249668811,16.9306931643196));
#57900=CARTESIAN_POINT('Ctrl Pts',(1.65533342493368,0.198318345883009,16.934866318846));
#57901=CARTESIAN_POINT('Ctrl Pts',(1.64558271333189,0.260026024819162,16.9390394733724));
#57902=CARTESIAN_POINT('Ctrl Pts',(1.63583856579119,0.321692162892365,16.9432098185817));
#57903=CARTESIAN_POINT('Ctrl Pts',(1.62261843225166,0.38284410133519,16.947380163791));
#57904=CARTESIAN_POINT('Ctrl Pts',(1.60600078445904,0.443077284812664,16.9515505090003));
#57905=CARTESIAN_POINT('Ctrl Pts',(1.58938439684669,0.503305900575694,16.9557205379562));
#57906=CARTESIAN_POINT('Ctrl Pts',(1.56937112107116,0.562615436229024,16.9598905669121));
#57907=CARTESIAN_POINT('Ctrl Pts',(1.5460899908123,0.620614002669949,16.964060595868));
#57908=CARTESIAN_POINT('Ctrl Pts',(1.52281185651521,0.678605105491798,16.9682300881985));
#57909=CARTESIAN_POINT('Ctrl Pts',(1.49626688725886,0.735285133471823,16.972399580529));
#57910=CARTESIAN_POINT('Ctrl Pts',(1.46663246192064,0.790281735611163,16.9765690728594));
#57911=CARTESIAN_POINT('Ctrl Pts',(1.43697562604361,0.845319928011596,16.9807417182988));
#57912=CARTESIAN_POINT('Ctrl Pts',(1.40422489523102,0.898671731071445,16.9849143637381));
#57913=CARTESIAN_POINT('Ctrl Pts',(1.3686034211478,0.949989829220572,16.9890870091775));
#57914=CARTESIAN_POINT('Ctrl Pts',(1.33754903567419,0.994728348406303,16.992724672785));
#57915=CARTESIAN_POINT('Ctrl Pts',(1.30431365841565,1.03792146822267,16.9963623363925));
#57916=CARTESIAN_POINT('Ctrl Pts',(1.26907087985245,1.07935865304843,17.));
#57917=CARTESIAN_POINT('',(-1.26912595136393,1.07929389860899,16.9999994389445));
#57918=CARTESIAN_POINT('Origin',(0.,0.,17.));
#57919=CARTESIAN_POINT('',(-1.66599973263063,0.000943861575540272,16.3785196366098));
#57920=CARTESIAN_POINT('Ctrl Pts',(-1.26912595136393,1.07929389860899,16.9999994389445));
#57921=CARTESIAN_POINT('Ctrl Pts',(-1.22994842185412,1.12536218406424,16.9959304579992));
#57922=CARTESIAN_POINT('Ctrl Pts',(-1.18817697004422,1.16939124983374,16.9918614770539));
#57923=CARTESIAN_POINT('Ctrl Pts',(-1.14405250554583,1.2110738476882,16.9877924961086));
#57924=CARTESIAN_POINT('Ctrl Pts',(-1.10000544393575,1.25268332616314,16.9837306529468));
#57925=CARTESIAN_POINT('Ctrl Pts',(-1.05361393425504,1.29195415756655,16.9796688097851));
#57926=CARTESIAN_POINT('Ctrl Pts',(-1.00515803396106,1.3286133097194,16.9756069666233));
#57927=CARTESIAN_POINT('Ctrl Pts',(-0.956749692797827,1.36523648116815,
16.9715491101325));
#57928=CARTESIAN_POINT('Ctrl Pts',(-0.906281384132347,1.39925274411531,
16.9674912536418));
#57929=CARTESIAN_POINT('Ctrl Pts',(-0.854067547829918,1.43042812603213,
16.963433397151));
#57930=CARTESIAN_POINT('Ctrl Pts',(-0.801885346769847,1.46158461945439,
16.9593779992283));
#57931=CARTESIAN_POINT('Ctrl Pts',(-0.747960155455131,1.48990338113144,
16.9553226013056));
#57932=CARTESIAN_POINT('Ctrl Pts',(-0.692635054495748,1.51519394180536,
16.951267203383));
#57933=CARTESIAN_POINT('Ctrl Pts',(-0.637322693849749,1.54047867854651,
16.9472127393409));
#57934=CARTESIAN_POINT('Ctrl Pts',(-0.580611531137159,1.56273638502247,
16.9431582752989));
#57935=CARTESIAN_POINT('Ctrl Pts',(-0.522866967902763,1.58182367344662,
16.9391038112569));
#57936=CARTESIAN_POINT('Ctrl Pts',(-0.465072383772699,1.60092749612456,
16.9350458350587));
#57937=CARTESIAN_POINT('Ctrl Pts',(-0.406243099257206,1.6168552492843,16.9309878588605));
#57938=CARTESIAN_POINT('Ctrl Pts',(-0.346760899012902,1.62951308031441,
16.9269298826623));
#57939=CARTESIAN_POINT('Ctrl Pts',(-0.287255151962042,1.64217592211241,
16.9228703000612));
#57940=CARTESIAN_POINT('Ctrl Pts',(-0.22709648298635,1.65156618061866,16.9188107174601));
#57941=CARTESIAN_POINT('Ctrl Pts',(-0.166675032253898,1.65764152747908,
16.914751134859));
#57942=CARTESIAN_POINT('Ctrl Pts',(-0.10613950514824,1.66372834466215,16.9106838877206));
#57943=CARTESIAN_POINT('Ctrl Pts',(-0.0453407203907892,1.66648771915369,
16.9066166405823));
#57944=CARTESIAN_POINT('Ctrl Pts',(0.0153287726306612,1.66592947891849,
16.9025493934439));
#57945=CARTESIAN_POINT('Ctrl Pts',(0.0725281121846614,1.66540316872245,
16.8987147833536));
#57946=CARTESIAN_POINT('Ctrl Pts',(0.12961217485131,1.66192841223509,16.8948801732632));
#57947=CARTESIAN_POINT('Ctrl Pts',(0.186257995909159,1.65555548350392,16.8910455631728));
#57948=CARTESIAN_POINT('Ctrl Pts',(0.246594300095448,1.64876735757865,16.8869611277012));
#57949=CARTESIAN_POINT('Ctrl Pts',(0.306678665411954,1.63866307257685,16.8828766922296));
#57950=CARTESIAN_POINT('Ctrl Pts',(0.366119211224653,1.62527312263885,16.878792256758));
#57951=CARTESIAN_POINT('Ctrl Pts',(0.426077211242961,1.61176660772296,16.874672264609));
#57952=CARTESIAN_POINT('Ctrl Pts',(0.485379598637478,1.59491692193667,16.8705522724599));
#57953=CARTESIAN_POINT('Ctrl Pts',(0.543629176032988,1.57480897856397,16.8664322803109));
#57954=CARTESIAN_POINT('Ctrl Pts',(0.601222363844623,1.55492762300826,16.8623587145919));
#57955=CARTESIAN_POINT('Ctrl Pts',(0.657785852831911,1.53186123201388,16.858285148873));
#57956=CARTESIAN_POINT('Ctrl Pts',(0.712948172994938,1.50574264156368,16.854211583154));
#57957=CARTESIAN_POINT('Ctrl Pts',(0.768078355465295,1.47963926786345,16.8501403907037));
#57958=CARTESIAN_POINT('Ctrl Pts',(0.82180852794464,1.45048743872728,16.8460691982534));
#57959=CARTESIAN_POINT('Ctrl Pts',(0.873787549594841,1.41846794753108,16.841998005803));
#57960=CARTESIAN_POINT('Ctrl Pts',(0.925755402865265,1.38645533614575,16.8379276881022));
#57961=CARTESIAN_POINT('Ctrl Pts',(0.975972418486816,1.35157655348069,16.8338573704014));
#57962=CARTESIAN_POINT('Ctrl Pts',(1.02411421476585,1.3140571049671,16.8297870527005));
#57963=CARTESIAN_POINT('Ctrl Pts',(1.07327199087348,1.27574584962835,16.8256308354073));
#57964=CARTESIAN_POINT('Ctrl Pts',(1.12026548795328,1.23468149423282,16.821474618114));
#57965=CARTESIAN_POINT('Ctrl Pts',(1.16478467374162,1.19114762469504,16.8173184008207));
#57966=CARTESIAN_POINT('Ctrl Pts',(1.2084410523779,1.14845746631973,16.8132427333835));
#57967=CARTESIAN_POINT('Ctrl Pts',(1.24971787740482,1.10339310045069,16.8091670659462));
#57968=CARTESIAN_POINT('Ctrl Pts',(1.28836173824702,1.05625755922555,16.805091398509));
#57969=CARTESIAN_POINT('Ctrl Pts',(1.32815121173139,1.00772466611202,16.8008949062877));
#57970=CARTESIAN_POINT('Ctrl Pts',(1.36514876678207,0.956996299983976,16.7966984140664));
#57971=CARTESIAN_POINT('Ctrl Pts',(1.39912564197979,0.904435424977723,16.7925019218451));
#57972=CARTESIAN_POINT('Ctrl Pts',(1.43310251717751,0.851874549971471,16.7883054296238));
#57973=CARTESIAN_POINT('Ctrl Pts',(1.46405848535841,0.797481706777552,16.7841089374025));
#57974=CARTESIAN_POINT('Ctrl Pts',(1.49181736902974,0.74164475152272,16.7799124451812));
#57975=CARTESIAN_POINT('Ctrl Pts',(1.51875202292534,0.687465733296311,16.7758405571725));
#57976=CARTESIAN_POINT('Ctrl Pts',(1.54278840870396,0.631702727019054,16.7717686691638));
#57977=CARTESIAN_POINT('Ctrl Pts',(1.5637384297878,0.574698288847972,16.7676967811551));
#57978=CARTESIAN_POINT('Ctrl Pts',(1.58494401817936,0.516998458976165,16.7635752205732));
#57979=CARTESIAN_POINT('Ctrl Pts',(1.60298711135448,0.458027136740834,16.7594536599913));
#57980=CARTESIAN_POINT('Ctrl Pts',(1.61772077496127,0.398165159523934,16.7553320994094));
#57981=CARTESIAN_POINT('Ctrl Pts',(1.63223606105954,0.339190436813987,16.7512716272408));
#57982=CARTESIAN_POINT('Ctrl Pts',(1.64353922624071,0.279351797244359,16.7472111550721));
#57983=CARTESIAN_POINT('Ctrl Pts',(1.65153912632907,0.219030852174293,16.7431506829035));
#57984=CARTESIAN_POINT('Ctrl Pts',(1.65953402056102,0.158747652324369,16.7390927515342));
#57985=CARTESIAN_POINT('Ctrl Pts',(1.66422968007249,0.0979832532653026,
16.7350348201648));
#57986=CARTESIAN_POINT('Ctrl Pts',(1.6655862263422,0.0371284610395597,16.7309768887955));
#57987=CARTESIAN_POINT('Ctrl Pts',(1.66694243148425,-0.0237110281677983,
16.7269199778651));
#57988=CARTESIAN_POINT('Ctrl Pts',(1.66496117857875,-0.084640352251613,
16.7228630669347));
#57989=CARTESIAN_POINT('Ctrl Pts',(1.65965465703569,-0.145266718073181,
16.7188061560042));
#57990=CARTESIAN_POINT('Ctrl Pts',(1.65420164838393,-0.20756668136684,16.714637253603));
#57991=CARTESIAN_POINT('Ctrl Pts',(1.64523705565621,-0.269546140949339,
16.7104683512018));
#57992=CARTESIAN_POINT('Ctrl Pts',(1.63283108802485,-0.33078488172765,16.7062994488006));
#57993=CARTESIAN_POINT('Ctrl Pts',(1.62074308199887,-0.390454090091595,
16.7022373942439));
#57994=CARTESIAN_POINT('Ctrl Pts',(1.60538821254725,-0.449419604041255,
16.6981753396871));
#57995=CARTESIAN_POINT('Ctrl Pts',(1.58688266513795,-0.507306029024575,
16.6941132851304));
#57996=CARTESIAN_POINT('Ctrl Pts',(1.5676469658471,-0.567476411417106,16.6898909588069));
#57997=CARTESIAN_POINT('Ctrl Pts',(1.5450069606227,-0.626480190402658,16.6856686324835));
#57998=CARTESIAN_POINT('Ctrl Pts',(1.51914792966687,-0.683919269935332,
16.68144630616));
#57999=CARTESIAN_POINT('Ctrl Pts',(1.49328889871103,-0.741358349468007,
16.6772239798366));
#58000=CARTESIAN_POINT('Ctrl Pts',(1.46421119230165,-0.797232218796164,
16.6730016535131));
#58001=CARTESIAN_POINT('Ctrl Pts',(1.43215137988136,-0.851174732416276,
16.6687793271897));
#58002=CARTESIAN_POINT('Ctrl Pts',(1.40118335205646,-0.903280254458425,
16.664700790567));
#58003=CARTESIAN_POINT('Ctrl Pts',(1.3673043206305,-0.953800681650137,16.6606222539444));
#58004=CARTESIAN_POINT('Ctrl Pts',(1.33070163494553,-1.00239171921624,16.6565437173218));
#58005=CARTESIAN_POINT('Ctrl Pts',(1.29372029069739,-1.0514854360837,16.6524229878166));
#58006=CARTESIAN_POINT('Ctrl Pts',(1.25395880785184,-1.0986091161508,16.6483022583115));
#58007=CARTESIAN_POINT('Ctrl Pts',(1.21165761114675,-1.14343422781993,16.6441815288063));
#58008=CARTESIAN_POINT('Ctrl Pts',(1.16990475502701,-1.18767828198039,16.6401142153604));
#58009=CARTESIAN_POINT('Ctrl Pts',(1.12567799822337,-1.22968262235875,16.6360469019145));
#58010=CARTESIAN_POINT('Ctrl Pts',(1.07924983827964,-1.26916341996347,16.6319795884686));
#58011=CARTESIAN_POINT('Ctrl Pts',(1.03285007551824,-1.30862006965,16.6279147627422));
#58012=CARTESIAN_POINT('Ctrl Pts',(0.984251968266631,-1.34555590618184,
16.6238499370159));
#58013=CARTESIAN_POINT('Ctrl Pts',(0.933763464755579,-1.37972525956716,
16.6197851112895));
#58014=CARTESIAN_POINT('Ctrl Pts',(0.883287115387296,-1.41388638733337,
16.6157212640923));
#58015=CARTESIAN_POINT('Ctrl Pts',(0.830921696685062,-1.44528206742015,
16.6116574168951));
#58016=CARTESIAN_POINT('Ctrl Pts',(0.777004998512594,-1.47370934457458,
16.6075935696979));
#58017=CARTESIAN_POINT('Ctrl Pts',(0.721782352132463,-1.50282517560763,
16.6034312896562));
#58018=CARTESIAN_POINT('Ctrl Pts',(0.664932764798376,-1.52882661656567,
16.5992690096146));
#58019=CARTESIAN_POINT('Ctrl Pts',(0.60684467049248,-1.55154617910485,16.5951067295729));
#58020=CARTESIAN_POINT('Ctrl Pts',(0.550058163190383,-1.57375666163915,
16.5910377142471));
#58021=CARTESIAN_POINT('Ctrl Pts',(0.492088600762408,-1.59283072759248,
16.5869686989213));
#58022=CARTESIAN_POINT('Ctrl Pts',(0.433315430431083,-1.60866209557829,
16.5828996835955));
#58023=CARTESIAN_POINT('Ctrl Pts',(0.372521576006573,-1.62503776282993,
16.5786907711959));
#58024=CARTESIAN_POINT('Ctrl Pts',(0.310868422187777,-1.63794352541022,
16.5744818587964));
#58025=CARTESIAN_POINT('Ctrl Pts',(0.248785745245518,-1.64731953578006,
16.5702729463968));
#58026=CARTESIAN_POINT('Ctrl Pts',(0.186703068303259,-1.6566955461499,16.5660640339973));
#58027=CARTESIAN_POINT('Ctrl Pts',(0.124191470175191,-1.66254182005321,
16.5618551215977));
#58028=CARTESIAN_POINT('Ctrl Pts',(0.0616817819915773,-1.66485775902037,
16.5576462091981));
#58029=CARTESIAN_POINT('Ctrl Pts',(0.00111348529636081,-1.66710177082986,
16.5535680148832));
#58030=CARTESIAN_POINT('Ctrl Pts',(-0.0597018689058509,-1.66604082959472,
16.5494898205682));
#58031=CARTESIAN_POINT('Ctrl Pts',(-0.120373454774682,-1.66164563953498,
16.5454116262532));
#58032=CARTESIAN_POINT('Ctrl Pts',(-0.181678476249575,-1.65720456193432,
16.5412908539596));
#58033=CARTESIAN_POINT('Ctrl Pts',(-0.242836186736639,-1.64935910138759,
16.537170081666));
#58034=CARTESIAN_POINT('Ctrl Pts',(-0.303440114899917,-1.63813311323272,
16.5330493093724));
#58035=CARTESIAN_POINT('Ctrl Pts',(-0.363253339565518,-1.62705359129494,
16.5289823010701));
#58036=CARTESIAN_POINT('Ctrl Pts',(-0.4225266283128,-1.61268132204695,16.5249152927678));
#58037=CARTESIAN_POINT('Ctrl Pts',(-0.480873786340675,-1.59509134585151,
16.5208482844654));
#58038=CARTESIAN_POINT('Ctrl Pts',(-0.539185467190902,-1.57751206499636,
16.5167837490509));
#58039=CARTESIAN_POINT('Ctrl Pts',(-0.596571644913312,-1.55671910379626,
16.5127192136364));
#58040=CARTESIAN_POINT('Ctrl Pts',(-0.652658965974062,-1.53283798039247,
16.5086546782219));
#58041=CARTESIAN_POINT('Ctrl Pts',(-0.708732996213481,-1.50896251601711,
16.5045911059665));
#58042=CARTESIAN_POINT('Ctrl Pts',(-0.763508310206096,-1.48200054257006,
16.5005275337111));
#58043=CARTESIAN_POINT('Ctrl Pts',(-0.816631266028351,-1.45212581250556,
16.4964639614557));
#58044=CARTESIAN_POINT('Ctrl Pts',(-0.871048449291931,-1.42152324840296,
16.4923013889349));
#58045=CARTESIAN_POINT('Ctrl Pts',(-0.923731189381291,-1.38786436356937,
16.4881388164141));
#58046=CARTESIAN_POINT('Ctrl Pts',(-0.974328052070879,-1.35138478863267,
16.4839762438934));
#58047=CARTESIAN_POINT('Ctrl Pts',(-1.02378487283793,-1.3157271667289,16.4799074619147));
#58048=CARTESIAN_POINT('Ctrl Pts',(-1.07124847497301,-1.27737503321648,
16.475838679936));
#58049=CARTESIAN_POINT('Ctrl Pts',(-1.11642386732308,-1.23658956346533,
16.4717698979574));
#58050=CARTESIAN_POINT('Ctrl Pts',(-1.16316128409206,-1.19439385915121,
16.4675604301656));
#58051=CARTESIAN_POINT('Ctrl Pts',(-1.20744890033411,-1.14959385170369,
16.4633509623737));
#58052=CARTESIAN_POINT('Ctrl Pts',(-1.24900330896305,-1.10251836002824,
16.4591414945819));
#58053=CARTESIAN_POINT('Ctrl Pts',(-1.29055771759198,-1.05544286835279,
16.4549320267901));
#58054=CARTESIAN_POINT('Ctrl Pts',(-1.32937860532145,-1.00609240745467,
16.4507225589984));
#58055=CARTESIAN_POINT('Ctrl Pts',(-1.36523182155122,-0.95482881891151,
16.4465130912066));
#58056=CARTESIAN_POINT('Ctrl Pts',(-1.40035050925344,-0.904615472778063,
16.4423898632142));
#58057=CARTESIAN_POINT('Ctrl Pts',(-1.43276572108851,-0.852361594770622,
16.4382666352219));
#58058=CARTESIAN_POINT('Ctrl Pts',(-1.4622365877862,-0.798385972659444,
16.4341434072296));
#58059=CARTESIAN_POINT('Ctrl Pts',(-1.49165868478443,-0.744499671805606,
16.4300270025382));
#58060=CARTESIAN_POINT('Ctrl Pts',(-1.5181458679218,-0.688897712197785,
16.4259105978467));
#58061=CARTESIAN_POINT('Ctrl Pts',(-1.54150011838769,-0.631928306859823,
16.4217941931553));
#58062=CARTESIAN_POINT('Ctrl Pts',(-1.56481949600417,-0.575043968927322,
16.4176839351291));
#58063=CARTESIAN_POINT('Ctrl Pts',(-1.58501504776261,-0.51679669915394,
16.413573677103));
#58064=CARTESIAN_POINT('Ctrl Pts',(-1.60193531728544,-0.457557908065854,
16.4094634190768));
#58065=CARTESIAN_POINT('Ctrl Pts',(-1.61884077099301,-0.398370987959132,
16.4053567600964));
#58066=CARTESIAN_POINT('Ctrl Pts',(-1.63247649805755,-0.338194745709455,
16.401250101116));
#58067=CARTESIAN_POINT('Ctrl Pts',(-1.64274022962142,-0.277417623779323,
16.3971434421355));
#58068=CARTESIAN_POINT('Ctrl Pts',(-1.65299927914237,-0.216668226764991,
16.3930386565043));
#58069=CARTESIAN_POINT('Ctrl Pts',(-1.65988930117611,-0.155318983035484,
16.3889338708731));
#58070=CARTESIAN_POINT('Ctrl Pts',(-1.66335908145097,-0.0937686842958181,
16.3848290852419));
#58071=CARTESIAN_POINT('Ctrl Pts',(-1.66513687631255,-0.0622324496759222,
16.3827259356979));
#58072=CARTESIAN_POINT('Ctrl Pts',(-1.66601762828668,-0.030643564989622,
16.3806227861538));
#58073=CARTESIAN_POINT('Ctrl Pts',(-1.66599973263063,0.000943861575540161,
16.3785196366098));
#58074=CARTESIAN_POINT('Ctrl Pts',(-1.66599977577897,0.000864352024730958,
16.3772626675068));
#58075=CARTESIAN_POINT('Ctrl Pts',(-1.66598176046584,0.0355880603993911,
16.3750662024614));
#58076=CARTESIAN_POINT('Ctrl Pts',(-1.66487815818066,0.0703044066738621,
16.3728974757554));
#58077=CARTESIAN_POINT('Ctrl Pts',(-1.65355857415653,0.249615190627302,
16.3617715086377));
#58078=CARTESIAN_POINT('Ctrl Pts',(-1.62559135098946,0.392435847117513,
16.353215676586));
#58079=CARTESIAN_POINT('Ctrl Pts',(-1.57468444189208,0.544201338787872,
16.3429390992582));
#58080=CARTESIAN_POINT('Ctrl Pts',(-1.56966340724548,0.558518523640452,
16.3419568924473));
#58081=CARTESIAN_POINT('Ctrl Pts',(-1.56410974302841,0.573687788191105,
16.3409005954565));
#58082=CARTESIAN_POINT('Ctrl Pts',(-1.56377092917891,0.5746106922007,16.3408362679555));
#58083=CARTESIAN_POINT('Ctrl Pts',(-1.5634313003322,0.575533291080154,16.3407718992107));
#58084=CARTESIAN_POINT('Origin',(0.,0.,11.));
#58085=CARTESIAN_POINT('Ctrl Pts',(-1.5634313003322,0.575533291080154,16.3407718992107));
#58086=CARTESIAN_POINT('Ctrl Pts',(-1.5596751818211,0.585736755135203,16.3400600143508));
#58087=CARTESIAN_POINT('Ctrl Pts',(-1.55581937928052,0.595902898087225,
16.3393430849936));
#58088=CARTESIAN_POINT('Ctrl Pts',(-1.54953271929507,0.612001177017325,
16.3381945028787));
#58089=CARTESIAN_POINT('Ctrl Pts',(-1.54716658128151,0.617958457471911,
16.337766540049));
#58090=CARTESIAN_POINT('Ctrl Pts',(-1.54271375868244,0.628983541257041,
16.3369688152863));
#58091=CARTESIAN_POINT('Ctrl Pts',(-1.5406363744731,0.63405488308338,16.3365996022725));
#58092=CARTESIAN_POINT('Ctrl Pts',(-1.53580697175768,0.645680632261762,
16.3357480258034));
#58093=CARTESIAN_POINT('Ctrl Pts',(-1.5330379906436,0.652227757754035,16.3352646742868));
#58094=CARTESIAN_POINT('Ctrl Pts',(-1.52398741590083,0.673251352442413,
16.3337008347677));
#58095=CARTESIAN_POINT('Ctrl Pts',(-1.51754222414108,0.687655858829796,
16.3326113405556));
#58096=CARTESIAN_POINT('Ctrl Pts',(-1.47506563651353,0.779081385328623,
16.3255903036547));
#58097=CARTESIAN_POINT('Ctrl Pts',(-1.43338959935601,0.853333434232536,
16.3194096914169));
#58098=CARTESIAN_POINT('Ctrl Pts',(-1.33810517651707,0.996272953350723,
16.3069050407079));
#58099=CARTESIAN_POINT('Ctrl Pts',(-1.28440454911611,1.06460927430752,16.3006011100336));
#58100=CARTESIAN_POINT('Ctrl Pts',(-1.20238508189192,1.15369095019632,16.2920412026584));
#58101=CARTESIAN_POINT('Ctrl Pts',(-1.17837503721039,1.17820424602859,16.2896433181791));
#58102=CARTESIAN_POINT('Ctrl Pts',(-1.1406777197705,1.21438557640963,16.2860384808385));
#58103=CARTESIAN_POINT('Ctrl Pts',(-1.1275314136631,1.22660137899651,16.2848091794439));
#58104=CARTESIAN_POINT('Ctrl Pts',(-1.10366785957624,1.24806792941671,16.2826262602532));
#58105=CARTESIAN_POINT('Ctrl Pts',(-1.0930254053607,1.2573988171632,16.2816693704768));
#58106=CARTESIAN_POINT('Ctrl Pts',(-1.07452386928761,1.2732078122323,16.2800337175353));
#58107=CARTESIAN_POINT('Ctrl Pts',(-1.06672206724027,1.27975142821405,16.2793522830947));
#58108=CARTESIAN_POINT('Ctrl Pts',(-1.05128618179399,1.29245874889821,16.2780199932486));
#58109=CARTESIAN_POINT('Ctrl Pts',(-1.04365668530581,1.29862734603498,16.2773689563997));
#58110=CARTESIAN_POINT('Ctrl Pts',(-1.02602338943884,1.31262843609015,16.2758810190201));
#58111=CARTESIAN_POINT('Ctrl Pts',(-1.01598351460997,1.3204146772117,16.2750459779494));
#58112=CARTESIAN_POINT('Ctrl Pts',(-0.983305106142277,1.34516440240364,
16.2723658183722));
#58113=CARTESIAN_POINT('Ctrl Pts',(-0.960322586195843,1.36166694997056,
16.270538518761));
#58114=CARTESIAN_POINT('Ctrl Pts',(-0.828766951679072,1.45114172645287,
16.2603706945963));
#58115=CARTESIAN_POINT('Ctrl Pts',(-0.712318860826929,1.51171136037505,
16.2525049832914));
#58116=CARTESIAN_POINT('Ctrl Pts',(-0.5232989193757,1.58328704946123,16.2401028110993));
#58117=CARTESIAN_POINT('Ctrl Pts',(-0.455074915546771,1.60422695859791,
16.2356823671256));
#58118=CARTESIAN_POINT('Ctrl Pts',(-0.370389081873657,1.62438189899929,
16.2300342330036));
#58119=CARTESIAN_POINT('Ctrl Pts',(-0.35499928173187,1.62781451385597,16.2290013757046));
#58120=CARTESIAN_POINT('Ctrl Pts',(-0.332529616665705,1.6324924741088,16.2274809407806));
#58121=CARTESIAN_POINT('Ctrl Pts',(-0.325486219314668,1.63391136242929,
16.2270025738289));
#58122=CARTESIAN_POINT('Ctrl Pts',(-0.313103139612887,1.63632268208565,
16.226158097851));
#58123=CARTESIAN_POINT('Ctrl Pts',(-0.307767451668835,1.63733462993636,
16.2257930906287));
#58124=CARTESIAN_POINT('Ctrl Pts',(-0.296101873344028,1.63948804455173,
16.2249924947713));
#58125=CARTESIAN_POINT('Ctrl Pts',(-0.289770390740234,1.64061893344611,
16.2245563552223));
#58126=CARTESIAN_POINT('Ctrl Pts',(-0.271997035398465,1.64368740457005,
16.2233278209827));
#58127=CARTESIAN_POINT('Ctrl Pts',(-0.260541495744583,1.64554209347455,
16.2225310837502));
#58128=CARTESIAN_POINT('Ctrl Pts',(-0.172913650200842,1.65879140546173,
16.216403845967));
#58129=CARTESIAN_POINT('Ctrl Pts',(-0.0960608530939728,1.66500981384815,
16.2108459440849));
#58130=CARTESIAN_POINT('Ctrl Pts',(0.0382465198165494,1.66654675091026,
16.201082994383));
#58131=CARTESIAN_POINT('Ctrl Pts',(0.0955535879539751,1.66424476838058,
16.1969006866591));
#58132=CARTESIAN_POINT('Ctrl Pts',(0.234929027541468,1.65142212402918,16.1867871594149));
#58133=CARTESIAN_POINT('Ctrl Pts',(0.316561551960156,1.6377359516911,16.1809183473741));
#58134=CARTESIAN_POINT('Ctrl Pts',(0.419014875669339,1.61260760863278,16.1736662188044));
#58135=CARTESIAN_POINT('Ctrl Pts',(0.441065139923292,1.60671665123273,16.1721116609777));
#58136=CARTESIAN_POINT('Ctrl Pts',(0.474338544037795,1.5970906529115,16.1697743013292));
#58137=CARTESIAN_POINT('Ctrl Pts',(0.485653688611424,1.59368632898281,16.1689809336961));
#58138=CARTESIAN_POINT('Ctrl Pts',(0.50529136332725,1.58754947731895,16.1676063333909));
#58139=CARTESIAN_POINT('Ctrl Pts',(0.513630214831017,1.5848711973619,16.1670233585435));
#58140=CARTESIAN_POINT('Ctrl Pts',(0.532389195516748,1.57868256314659,16.1657133631261));
#58141=CARTESIAN_POINT('Ctrl Pts',(0.542796542188667,1.57513453845384,16.1649876094402));
#58142=CARTESIAN_POINT('Ctrl Pts',(0.570955478127548,1.56522248614719,16.1630262024345));
#58143=CARTESIAN_POINT('Ctrl Pts',(0.588635713278688,1.55865956294998,16.1617971485567));
#58144=CARTESIAN_POINT('Ctrl Pts',(0.698772396141887,1.51563526677497,16.1541487860599));
#58145=CARTESIAN_POINT('Ctrl Pts',(0.787927247882166,1.47126049869444,16.1480087233898));
#58146=CARTESIAN_POINT('Ctrl Pts',(0.934029298937868,1.38142852256875,16.1375182314248));
#58147=CARTESIAN_POINT('Ctrl Pts',(0.992935519331589,1.33971406897554,16.1331457893078));
#58148=CARTESIAN_POINT('Ctrl Pts',(1.0772338415564,1.27139627062114,16.1264047918402));
#58149=CARTESIAN_POINT('Ctrl Pts',(1.10475525404588,1.24755629712246,16.1241171670876));
#58150=CARTESIAN_POINT('Ctrl Pts',(1.14813637325292,1.20741638597222,16.1203253707562));
#58151=CARTESIAN_POINT('Ctrl Pts',(1.1644828967793,1.19165889448185,16.1188506610842));
#58152=CARTESIAN_POINT('Ctrl Pts',(1.18634261120009,1.16970754298156,16.1168060870542));
#58153=CARTESIAN_POINT('Ctrl Pts',(1.19213991773492,1.16379849488765,16.1162566467879));
#58154=CARTESIAN_POINT('Ctrl Pts',(1.20181563649455,1.15378812444936,16.1153268962671));
#58155=CARTESIAN_POINT('Ctrl Pts',(1.20571777840392,1.14970974505162,16.1149483859604));
#58156=CARTESIAN_POINT('Ctrl Pts',(1.21317965095335,1.14183109410893,16.1142175427461));
#58157=CARTESIAN_POINT('Ctrl Pts',(1.21674240481423,1.13803384457583,16.1138654742685));
#58158=CARTESIAN_POINT('Ctrl Pts',(1.22637132325721,1.12767426173673,16.1129055922749));
#58159=CARTESIAN_POINT('Ctrl Pts',(1.23240247398457,1.12107983492308,16.1122952507489));
#58160=CARTESIAN_POINT('Ctrl Pts',(1.2555711095759,1.09533448785564,16.1099161056688));
#58161=CARTESIAN_POINT('Ctrl Pts',(1.27231668311415,1.07583759655167,16.1081222449568));
#58162=CARTESIAN_POINT('Ctrl Pts',(1.30944843376566,1.03052528691497,16.1039854241299));
#58163=CARTESIAN_POINT('Ctrl Pts',(1.32953449900069,1.0044776504301,16.1016301935625));
#58164=CARTESIAN_POINT('Ctrl Pts',(1.40791337936918,0.896363157284946,16.0919941636001));
#58165=CARTESIAN_POINT('Ctrl Pts',(1.45948876182478,0.809679781911558,16.0845993433231));
#58166=CARTESIAN_POINT('Ctrl Pts',(1.53411461682059,0.653661612804416,16.0722053704864));
#58167=CARTESIAN_POINT('Ctrl Pts',(1.56103175088294,0.586484110963284,16.0671271700023));
#58168=CARTESIAN_POINT('Ctrl Pts',(1.58896530001192,0.501053174593697,16.060993625145));
#58169=CARTESIAN_POINT('Ctrl Pts',(1.59416379785365,0.484259057889517,16.0598026750488));
#58170=CARTESIAN_POINT('Ctrl Pts',(1.60210314870812,0.457095637132175,16.0578994014729));
#58171=CARTESIAN_POINT('Ctrl Pts',(1.60501127650194,0.446777049745986,16.0571816900023));
#58172=CARTESIAN_POINT('Ctrl Pts',(1.61038352746254,0.426985575868721,16.0558149154284));
#58173=CARTESIAN_POINT('Ctrl Pts',(1.61286415561316,0.417517676315472,16.0551653431425));
#58174=CARTESIAN_POINT('Ctrl Pts',(1.61833978438064,0.39584130934438,16.0536876171827));
#58175=CARTESIAN_POINT('Ctrl Pts',(1.6212803614347,0.383619608362693,16.0528612415448));
#58176=CARTESIAN_POINT('Ctrl Pts',(1.63022116991452,0.344519020885195,16.0502380834013));
#58177=CARTESIAN_POINT('Ctrl Pts',(1.6356935876534,0.317523299662902,16.0484580664242));
#58178=CARTESIAN_POINT('Ctrl Pts',(1.66345772601487,0.160682930608727,16.0382704817449));
#58179=CARTESIAN_POINT('Ctrl Pts',(1.67095466772995,0.0286993695304271,
16.0303496073671));
#58180=CARTESIAN_POINT('Ctrl Pts',(1.6584078496364,-0.1742573439718,16.0178749314143));
#58181=CARTESIAN_POINT('Ctrl Pts',(1.6493885162593,-0.245351559196319,16.0134373434482));
#58182=CARTESIAN_POINT('Ctrl Pts',(1.63283471860549,-0.331143800783455,
16.0077686461894));
#58183=CARTESIAN_POINT('Ctrl Pts',(1.62962228781726,-0.346607255649431,
16.0067341646853));
#58184=CARTESIAN_POINT('Ctrl Pts',(1.62462909819665,-0.36903649523775,16.0052119904229));
#58185=CARTESIAN_POINT('Ctrl Pts',(1.62302220252905,-0.376040645242056,
16.0047335524248));
#58186=CARTESIAN_POINT('Ctrl Pts',(1.62012200309603,-0.388317091618687,
16.003889177361));
#58187=CARTESIAN_POINT('Ctrl Pts',(1.61884816913838,-0.393593791318744,
16.0035243449801));
#58188=CARTESIAN_POINT('Ctrl Pts',(1.61601022311097,-0.405102756810232,
16.0027243667008));
#58189=CARTESIAN_POINT('Ctrl Pts',(1.61443586365921,-0.411332132735254,
16.0022886723204));
#58190=CARTESIAN_POINT('Ctrl Pts',(1.60992362620736,-0.428760979550803,
16.0010623999002));
#58191=CARTESIAN_POINT('Ctrl Pts',(1.60690503843422,-0.439938903227747,
16.0002675023798));
#58192=CARTESIAN_POINT('Ctrl Pts',(1.58444817028227,-0.51978135681164,15.994533467335));
#58193=CARTESIAN_POINT('Ctrl Pts',(1.5607341073769,-0.587158758958952,15.989398778818));
#58194=CARTESIAN_POINT('Ctrl Pts',(1.50512389920432,-0.717731764814795,
15.9790949468929));
#58195=CARTESIAN_POINT('Ctrl Pts',(1.47337094637055,-0.780842794460663,
15.9739373366074));
#58196=CARTESIAN_POINT('Ctrl Pts',(1.39564020274277,-0.913606965214696,
15.9628523993985));
#58197=CARTESIAN_POINT('Ctrl Pts',(1.34823689778213,-0.982217065223451,
15.9569715181899));
#58198=CARTESIAN_POINT('Ctrl Pts',(1.28448399660806,-1.06112509274721,15.9500427957919));
#58199=CARTESIAN_POINT('Ctrl Pts',(1.27284405116492,-1.07505984330685,15.948811976492));
#58200=CARTESIAN_POINT('Ctrl Pts',(1.25389048461862,-1.09701060592593,15.9468606740721));
#58201=CARTESIAN_POINT('Ctrl Pts',(1.24672260254013,-1.10514993501778,15.9461343075227));
#58202=CARTESIAN_POINT('Ctrl Pts',(1.23295457486604,-1.12047947623846,15.9447605974681));
#58203=CARTESIAN_POINT('Ctrl Pts',(1.22636976049133,-1.1276827824464,15.944112653882));
#58204=CARTESIAN_POINT('Ctrl Pts',(1.21117532206315,-1.14401388314916,15.9426377502655));
#58205=CARTESIAN_POINT('Ctrl Pts',(1.20252504840967,-1.15310318180862,15.941812567842));
#58206=CARTESIAN_POINT('Ctrl Pts',(1.17518414830009,-1.18118939320463,15.9392481609189));
#58207=CARTESIAN_POINT('Ctrl Pts',(1.15613932053274,-1.19983672384999,15.9375243764412));
#58208=CARTESIAN_POINT('Ctrl Pts',(1.03963477330174,-1.30855859217155,15.9273213014175));
#58209=CARTESIAN_POINT('Ctrl Pts',(0.932147522466384,-1.38718049697853,
15.9193412140275));
#58210=CARTESIAN_POINT('Ctrl Pts',(0.753791854511078,-1.48745527859235,
15.9067898586047));
#58211=CARTESIAN_POINT('Ctrl Pts',(0.688911179517107,-1.51859289395451,
15.9023345646746));
#58212=CARTESIAN_POINT('Ctrl Pts',(0.607551768587619,-1.55135014199792,
15.8966446220115));
#58213=CARTESIAN_POINT('Ctrl Pts',(0.592789604758586,-1.5570506910133,15.8956081481134));
#58214=CARTESIAN_POINT('Ctrl Pts',(0.5712030121663,-1.56503509722877,15.8940835102819));
#58215=CARTESIAN_POINT('Ctrl Pts',(0.564440938953634,-1.56748657357542,
15.8936046388506));
#58216=CARTESIAN_POINT('Ctrl Pts',(0.552546779376451,-1.57171165911844,
15.8927597427969));
#58217=CARTESIAN_POINT('Ctrl Pts',(0.54742157821759,-1.57350408237768,15.8923948266762));
#58218=CARTESIAN_POINT('Ctrl Pts',(0.536215203118022,-1.57736187971095,
15.8915949845681));
#58219=CARTESIAN_POINT('Ctrl Pts',(0.530130916038701,-1.57941712413163,
15.8911595129657));
#58220=CARTESIAN_POINT('Ctrl Pts',(0.513057847479166,-1.58507456443021,
15.8899344480605));
#58221=CARTESIAN_POINT('Ctrl Pts',(0.502043469565574,-1.58859751532859,
15.889140548208));
#58222=CARTESIAN_POINT('Ctrl Pts',(0.423874931369722,-1.61270563703923,
15.883485408586));
#58223=CARTESIAN_POINT('Ctrl Pts',(0.355521480077651,-1.62913832481023,
15.8784346555065));
#58224=CARTESIAN_POINT('Ctrl Pts',(0.271100589546626,-1.6438673618563,15.8722146725655));
#58225=CARTESIAN_POINT('Ctrl Pts',(0.255821020050752,-1.64631437835075,
15.871089465356));
#58226=CARTESIAN_POINT('Ctrl Pts',(0.174602686720234,-1.6581634686579,15.865116755596));
#58227=CARTESIAN_POINT('Ctrl Pts',(0.108175231053316,-1.66381823013292,
15.860264030974));
#58228=CARTESIAN_POINT('Ctrl Pts',(-0.00743803082426778,-1.66670497116444,
15.8519694479799));
#58229=CARTESIAN_POINT('Ctrl Pts',(-0.0564949334702686,-1.66576404364807,
15.8484962016657));
#58230=CARTESIAN_POINT('Ctrl Pts',(-0.13873123792393,-1.66054877147338,
15.8427630185521));
#58231=CARTESIAN_POINT('Ctrl Pts',(-0.171950692152674,-1.65743832880728,
15.840471421896));
#58232=CARTESIAN_POINT('Ctrl Pts',(-0.218626712773681,-1.65164927982663,
15.8372839430274));
#58233=CARTESIAN_POINT('Ctrl Pts',(-0.23217601851265,-1.6497991692572,15.8363625095072));
#58234=CARTESIAN_POINT('Ctrl Pts',(-0.255519316212987,-1.64631844255846,
15.8347812580321));
#58235=CARTESIAN_POINT('Ctrl Pts',(-0.265324161874314,-1.64476674082864,
15.8341189919467));
#58236=CARTESIAN_POINT('Ctrl Pts',(-0.285349607611146,-1.64141380846098,
15.8327700388727));
#58237=CARTESIAN_POINT('Ctrl Pts',(-0.295568432132762,-1.63960452528795,
15.8320836380471));
#58238=CARTESIAN_POINT('Ctrl Pts',(-0.321465166518379,-1.63476942593702,
15.8303487245423));
#58239=CARTESIAN_POINT('Ctrl Pts',(-0.337117938792999,-1.63161345102511,
15.8293043715621));
#58240=CARTESIAN_POINT('Ctrl Pts',(-0.398959644253236,-1.61821670908877,
15.8251925211805));
#58241=CARTESIAN_POINT('Ctrl Pts',(-0.444751099002573,-1.60623510291768,
15.8221802675393));
#58242=CARTESIAN_POINT('Ctrl Pts',(-0.597031061031835,-1.55937691448192,
15.8121867814665));
#58243=CARTESIAN_POINT('Ctrl Pts',(-0.700490841514293,-1.51572274581293,
15.8054559209477));
#58244=CARTESIAN_POINT('Ctrl Pts',(-0.855679547479872,-1.43093368257201,
15.7945746612931));
#58245=CARTESIAN_POINT('Ctrl Pts',(-0.910701405319029,-1.39655998232127,
15.7905353160295));
#58246=CARTESIAN_POINT('Ctrl Pts',(-0.975890149919765,-1.35034156031706,
15.7853441489989));
#58247=CARTESIAN_POINT('Ctrl Pts',(-0.988085911639198,-1.34144329224654,
15.7843543409962));
#58248=CARTESIAN_POINT('Ctrl Pts',(-1.00580367672783,-1.32814336134475,
15.78288603253));
#58249=CARTESIAN_POINT('Ctrl Pts',(-1.01142169752578,-1.32387007280344,
15.7824158897241));
#58250=CARTESIAN_POINT('Ctrl Pts',(-1.0209308402924,-1.31654118648524,15.7816119918));
#58251=CARTESIAN_POINT('Ctrl Pts',(-1.02483578152973,-1.31350374814129,
15.7812795022457));
#58252=CARTESIAN_POINT('Ctrl Pts',(-1.03369696882739,-1.30654754810783,
15.7805195201553));
#58253=CARTESIAN_POINT('Ctrl Pts',(-1.03864437624081,-1.30261804655469,
15.7800912871219));
#58254=CARTESIAN_POINT('Ctrl Pts',(-1.05222245870807,-1.29170705951089,
15.7789054396665));
#58255=CARTESIAN_POINT('Ctrl Pts',(-1.0608057052323,-1.28466745478105,15.7781439304664));
#58256=CARTESIAN_POINT('Ctrl Pts',(-1.10990894679043,-1.24356749158952,
15.7737214589439));
#58257=CARTESIAN_POINT('Ctrl Pts',(-1.14885389302696,-1.20768023382744,
15.7699523183217));
#58258=CARTESIAN_POINT('Ctrl Pts',(-1.25745139389566,-1.0975961631655,15.7588004514543));
#58259=CARTESIAN_POINT('Ctrl Pts',(-1.3221060570547,-1.01879277679609,15.7513254851513));
#58260=CARTESIAN_POINT('Ctrl Pts',(-1.41983244181991,-0.874577733071923,
15.7388398444594));
#58261=CARTESIAN_POINT('Ctrl Pts',(-1.45654070032965,-0.811974236279621,
15.7337469722107));
#58262=CARTESIAN_POINT('Ctrl Pts',(-1.49694752205679,-0.731446235566926,
15.7275986137052));
#58263=CARTESIAN_POINT('Ctrl Pts',(-1.50458792349412,-0.715598142119026,
15.7264067374085));
#58264=CARTESIAN_POINT('Ctrl Pts',(-1.51647955078934,-0.68989910249403,
15.7245022936193));
#58265=CARTESIAN_POINT('Ctrl Pts',(-1.52088898600338,-0.680123298482586,
15.7237843279372));
#58266=CARTESIAN_POINT('Ctrl Pts',(-1.52914180125275,-0.661344954599427,
15.7224172613965));
#58267=CARTESIAN_POINT('Ctrl Pts',(-1.53300081982786,-0.652349822330814,
15.7217676494886));
#58268=CARTESIAN_POINT('Ctrl Pts',(-1.54163293519527,-0.631729222264729,
15.7202900929988));
#58269=CARTESIAN_POINT('Ctrl Pts',(-1.54635425325742,-0.620082619465765,
15.719463923651));
#58270=CARTESIAN_POINT('Ctrl Pts',(-1.5586148499656,-0.588826850632073,
15.7172681394584));
#58271=CARTESIAN_POINT('Ctrl Pts',(-1.56591592464048,-0.569126252011633,
15.7159064263993));
#58272=CARTESIAN_POINT('Ctrl Pts',(-1.61263746205119,-0.435343827427019,
15.7067963386614));
#58273=CARTESIAN_POINT('Ctrl Pts',(-1.63993309944968,-0.31740685036405,
15.6994650151364));
#58274=CARTESIAN_POINT('Ctrl Pts',(-1.66211310840186,-0.131671155714307,
15.6880352115809));
#58275=CARTESIAN_POINT('Ctrl Pts',(-1.66603723902746,-0.0653905900801613,
15.6839705638318));
#58276=CARTESIAN_POINT('Ctrl Pts',(-1.66598117318228,0.0337685101358439,
15.6776947913277));
#58277=CARTESIAN_POINT('Ctrl Pts',(-1.66499240476525,0.066584818794768,
15.6755855692984));
#58278=CARTESIAN_POINT('Ctrl Pts',(-1.66245306059566,0.109092223704411,
15.6727869395628));
#58279=CARTESIAN_POINT('Ctrl Pts',(-1.6617853260804,0.118831017128423,15.672141204225));
#58280=CARTESIAN_POINT('Ctrl Pts',(-1.66057206892032,0.134506271009967,
15.6710937088581));
#58281=CARTESIAN_POINT('Ctrl Pts',(-1.66008018471304,0.140446824583748,
15.6706948466149));
#58282=CARTESIAN_POINT('Ctrl Pts',(-1.65906169397268,0.151993422414892,
15.6699156890247));
#58283=CARTESIAN_POINT('Ctrl Pts',(-1.65853853093764,0.15759962742323,15.6695355827035));
#58284=CARTESIAN_POINT('Ctrl Pts',(-1.65718333082297,0.171367175554307,
15.6685978579932));
#58285=CARTESIAN_POINT('Ctrl Pts',(-1.65631941608769,0.179525167346422,
15.6680385195485));
#58286=CARTESIAN_POINT('Ctrl Pts',(-1.65289846811972,0.209699586210951,
15.665956817768));
#58287=CARTESIAN_POINT('Ctrl Pts',(-1.6499625220703,0.231669637581411,15.6644157921083));
#58288=CARTESIAN_POINT('Ctrl Pts',(-1.62966381919829,0.363480196932044,
15.6550426844342));
#58289=CARTESIAN_POINT('Ctrl Pts',(-1.60179071974468,0.471330247254834,
15.6468596831304));
#58290=CARTESIAN_POINT('Ctrl Pts',(-1.56343131209642,0.575533259122747,
15.6388155835246));
#58291=CARTESIAN_POINT('',(-1.66599949106555,-0.00130221707574717,15.8714803633902));
#58292=CARTESIAN_POINT('Ctrl Pts',(-1.5634313003304,0.575533291085054,15.8337663187435));
#58293=CARTESIAN_POINT('Ctrl Pts',(-1.56631175684939,0.567708555399402,
15.8343230070768));
#58294=CARTESIAN_POINT('Ctrl Pts',(-1.56913348118854,0.55986216761892,15.8348777298986));
#58295=CARTESIAN_POINT('Ctrl Pts',(-1.57558654127743,0.541486014195911,
15.8361688898208));
#58296=CARTESIAN_POINT('Ctrl Pts',(-1.57917144943652,0.530940294232612,
15.8369037696465));
#58297=CARTESIAN_POINT('Ctrl Pts',(-1.58875133243229,0.501803486817436,
15.8389180224672));
#58298=CARTESIAN_POINT('Ctrl Pts',(-1.59452565195486,0.483141317813025,
15.8401901606427));
#58299=CARTESIAN_POINT('Ctrl Pts',(-1.63175448761917,0.354873772701569,
15.8488207696302));
#58300=CARTESIAN_POINT('Ctrl Pts',(-1.65221372937049,0.242388691633483,
15.8558017586991));
#58301=CARTESIAN_POINT('Ctrl Pts',(-1.66437451528092,0.0854194373601954,
15.8654154696456));
#58302=CARTESIAN_POINT('Ctrl Pts',(-1.66603456238488,0.0420425528584947,
15.8680623906035));
#58303=CARTESIAN_POINT('Ctrl Pts',(-1.6659994546692,-0.00134797697576474,
15.8707383599279));
#58304=CARTESIAN_POINT('Ctrl Pts',(-1.66599949106555,-0.00130221707574717,
15.8714803633902));
#58305=CARTESIAN_POINT('Ctrl Pts',(-1.66593272647584,-0.0867179089486909,
15.8772098489549));
#58306=CARTESIAN_POINT('Ctrl Pts',(-1.65929579363609,-0.171882669676792,
15.8829393345197));
#58307=CARTESIAN_POINT('Ctrl Pts',(-1.64621084163618,-0.256019266617736,
15.8886688200845));
#58308=CARTESIAN_POINT('Ctrl Pts',(-1.63689876093366,-0.315896198589341,
15.8927462849436));
#58309=CARTESIAN_POINT('Ctrl Pts',(-1.62429637850684,-0.375388018068356,
15.8968237498028));
#58310=CARTESIAN_POINT('Ctrl Pts',(-1.60844905090086,-0.434105575472282,
15.9009012146619));
#58311=CARTESIAN_POINT('Ctrl Pts',(-1.59243305180001,-0.493448094915775,
15.9050220781375));
#58312=CARTESIAN_POINT('Ctrl Pts',(-1.57310261600574,-0.551999238257112,
15.9091429416131));
#58313=CARTESIAN_POINT('Ctrl Pts',(-1.55055832123582,-0.609364334734442,
15.9132638050887));
#58314=CARTESIAN_POINT('Ctrl Pts',(-1.52831291162266,-0.665968902837409,
15.9173300354548));
#58315=CARTESIAN_POINT('Ctrl Pts',(-1.50293853451633,-0.721418190930063,
15.9213962658208));
#58316=CARTESIAN_POINT('Ctrl Pts',(-1.4745821190571,-0.775347389340462,
15.9254624961868));
#58317=CARTESIAN_POINT('Ctrl Pts',(-1.44624305988114,-0.829243578979172,
15.9295262377106));
#58318=CARTESIAN_POINT('Ctrl Pts',(-1.41492581902222,-0.881621071495188,
15.9335899792343));
#58319=CARTESIAN_POINT('Ctrl Pts',(-1.38082444922466,-0.932137243341034,
15.9376537207581));
#58320=CARTESIAN_POINT('Ctrl Pts',(-1.34673128484919,-0.982641260058941,
15.9417164844702));
#58321=CARTESIAN_POINT('Ctrl Pts',(-1.30985560770955,-1.03128442108076,
15.9457792481824));
#58322=CARTESIAN_POINT('Ctrl Pts',(-1.27043508636807,-1.07775261137468,
15.9498420118945));
#58323=CARTESIAN_POINT('Ctrl Pts',(-1.23003880943716,-1.12537100452913,
15.9540053390763));
#58324=CARTESIAN_POINT('Ctrl Pts',(-1.18697034611114,-1.17070485539578,
15.9581686662581));
#58325=CARTESIAN_POINT('Ctrl Pts',(-1.14152804400468,-1.21345363518795,
15.9623319934399));
#58326=CARTESIAN_POINT('Ctrl Pts',(-1.09712681346015,-1.25522305132806,
15.9663999398568));
#58327=CARTESIAN_POINT('Ctrl Pts',(-1.05045981264175,-1.29452430883724,
15.9704678862737));
#58328=CARTESIAN_POINT('Ctrl Pts',(-1.00183941646775,-1.3311174942925,15.9745358326906));
#58329=CARTESIAN_POINT('Ctrl Pts',(-0.95150902336914,-1.36899767531988,
15.9787468502548));
#58330=CARTESIAN_POINT('Ctrl Pts',(-0.899085743350763,-1.40397537655519,
15.982957867819));
#58331=CARTESIAN_POINT('Ctrl Pts',(-0.84494680935439,-1.43583456197496,
15.9871688853832));
#58332=CARTESIAN_POINT('Ctrl Pts',(-0.790807875358018,-1.46769374739474,
15.9913799029474));
#58333=CARTESIAN_POINT('Ctrl Pts',(-0.734953854409687,-1.49643420661138,
15.9955909205116));
#58334=CARTESIAN_POINT('Ctrl Pts',(-0.677785088133018,-1.52189466596888,
15.9998019380759));
#58335=CARTESIAN_POINT('Ctrl Pts',(-0.622427853944392,-1.54654834844266,
16.0038795192562));
#58336=CARTESIAN_POINT('Ctrl Pts',(-0.565609547040969,-1.56822861107888,
16.0079571004366));
#58337=CARTESIAN_POINT('Ctrl Pts',(-0.507681738310143,-1.58676250667401,
16.012034681617));
#58338=CARTESIAN_POINT('Ctrl Pts',(-0.449139249913106,-1.60549306789499,
16.0161555305524));
#58339=CARTESIAN_POINT('Ctrl Pts',(-0.389464019847529,-1.62100979897185,
16.0202763794878));
#58340=CARTESIAN_POINT('Ctrl Pts',(-0.329042167298717,-1.63318316552044,
16.0243972284233));
#58341=CARTESIAN_POINT('Ctrl Pts',(-0.269419352970688,-1.64519554751232,
16.0284635819127));
#58342=CARTESIAN_POINT('Ctrl Pts',(-0.209070060128925,-1.65395235230431,
16.0325299354022));
#58343=CARTESIAN_POINT('Ctrl Pts',(-0.148380494402508,-1.65937916971404,
16.0365962888917));
#58344=CARTESIAN_POINT('Ctrl Pts',(-0.0877280417093517,-1.66480266850298,
16.0406601557146));
#58345=CARTESIAN_POINT('Ctrl Pts',(-0.0267362375120464,-1.66690017194147,
16.0447240225375));
#58346=CARTESIAN_POINT('Ctrl Pts',(0.0342017959122454,-1.66564889372172,
16.0487878893604));
#58347=CARTESIAN_POINT('Ctrl Pts',(0.0951251962315448,-1.66439791597253,
16.0528507803234));
#58348=CARTESIAN_POINT('Ctrl Pts',(0.155994339855136,-1.65979976342375,
16.0569136712863));
#58349=CARTESIAN_POINT('Ctrl Pts',(0.216416401589541,-1.65188375532997,
16.0609765622492));
#58350=CARTESIAN_POINT('Ctrl Pts',(0.278330344666112,-1.64377229305206,
16.0651397700674));
#58351=CARTESIAN_POINT('Ctrl Pts',(0.339774271096009,-1.63217697065474,
16.0693029778856));
#58352=CARTESIAN_POINT('Ctrl Pts',(0.400333934123755,-1.61718543809577,
16.0734661857038));
#58353=CARTESIAN_POINT('Ctrl Pts',(0.459509786011684,-1.60253646770971,
16.0775342626532));
#58354=CARTESIAN_POINT('Ctrl Pts',(0.517840878854687,-1.58464508547898,
16.0816023396027));
#58355=CARTESIAN_POINT('Ctrl Pts',(0.574956209664161,-1.56364361571575,
16.0856704165521));
#58356=CARTESIAN_POINT('Ctrl Pts',(0.634074980099093,-1.54190547549784,
16.0898811898047));
#58357=CARTESIAN_POINT('Ctrl Pts',(0.691890545514775,-1.51683520244987,
16.0940919630573));
#58358=CARTESIAN_POINT('Ctrl Pts',(0.748016887330044,-1.48863250544554,
16.0983027363099));
#58359=CARTESIAN_POINT('Ctrl Pts',(0.804143229145313,-1.46042980844121,
16.1025135095624));
#58360=CARTESIAN_POINT('Ctrl Pts',(0.858579863315902,-1.42909504955832,
16.106724282815));
#58361=CARTESIAN_POINT('Ctrl Pts',(0.910974232784795,-1.39487703658859,
16.1109350560676));
#58362=CARTESIAN_POINT('Ctrl Pts',(0.961698065301025,-1.36175002739831,
16.1150115734375));
#58363=CARTESIAN_POINT('Ctrl Pts',(1.01071755477704,-1.32578403686299,16.1190880908075));
#58364=CARTESIAN_POINT('Ctrl Pts',(1.05769680373141,-1.28718043466189,16.1231646081774));
#58365=CARTESIAN_POINT('Ctrl Pts',(1.10518847802066,-1.24815576434612,16.1272855900892));
#58366=CARTESIAN_POINT('Ctrl Pts',(1.15059464303148,-1.20643580723475,16.1314065720009));
#58367=CARTESIAN_POINT('Ctrl Pts',(1.19359684687473,-1.16227473823133,16.1355275539127));
#58368=CARTESIAN_POINT('Ctrl Pts',(1.23601785510366,-1.11871052746619,16.1395928387577));
#58369=CARTESIAN_POINT('Ctrl Pts',(1.27609911298653,-1.07277115976455,16.1436581236028));
#58370=CARTESIAN_POINT('Ctrl Pts',(1.31356870759362,-1.02474057713688,16.1477234084479));
#58371=CARTESIAN_POINT('Ctrl Pts',(1.35101539321729,-0.976739360501363,
16.1517862077699));
#58372=CARTESIAN_POINT('Ctrl Pts',(1.38585326705964,-0.926649866940003,
16.1558490070918));
#58373=CARTESIAN_POINT('Ctrl Pts',(1.41785003069954,-0.874789855019663,
16.1599118064138));
#58374=CARTESIAN_POINT('Ctrl Pts',(1.44983913147913,-0.82294226298126,16.1639736327416));
#58375=CARTESIAN_POINT('Ctrl Pts',(1.47898820393723,-0.769325430017754,
16.1680354590695));
#58376=CARTESIAN_POINT('Ctrl Pts',(1.50510888446671,-0.714285129272178,
16.1720972853973));
#58377=CARTESIAN_POINT('Ctrl Pts',(1.53188816865151,-0.657857049091822,
16.1762615261191));
#58378=CARTESIAN_POINT('Ctrl Pts',(1.55548398130981,-0.599933228332241,
16.1804257668409));
#58379=CARTESIAN_POINT('Ctrl Pts',(1.57574513398437,-0.540909671502153,
16.1845900075627));
#58380=CARTESIAN_POINT('Ctrl Pts',(1.595533314666,-0.483263947895697,16.1886570391442));
#58381=CARTESIAN_POINT('Ctrl Pts',(1.61214077248512,-0.424569805596175,
16.1927240707257));
#58382=CARTESIAN_POINT('Ctrl Pts',(1.62547754535728,-0.365210555076479,
16.1967911023072));
#58383=CARTESIAN_POINT('Ctrl Pts',(1.63929247638957,-0.303723120303577,
16.2010039475992));
#58384=CARTESIAN_POINT('Ctrl Pts',(1.64959760152643,-0.241522565118642,
16.2052167928912));
#58385=CARTESIAN_POINT('Ctrl Pts',(1.65635136775985,-0.179042303716351,
16.2094296381831));
#58386=CARTESIAN_POINT('Ctrl Pts',(1.66310513399328,-0.116562042314061,
16.2136424834751));
#58387=CARTESIAN_POINT('Ctrl Pts',(1.66630758350186,-0.0538026803141964,
16.2178553287671));
#58388=CARTESIAN_POINT('Ctrl Pts',(1.66597673802543,0.00880388312825253,
16.222068174059));
#58389=CARTESIAN_POINT('Ctrl Pts',(1.66565645885457,0.0694109630445556,
16.2261464725192));
#58390=CARTESIAN_POINT('Ctrl Pts',(1.6620239421295,0.130125458370124,16.2302247709794));
#58391=CARTESIAN_POINT('Ctrl Pts',(1.65506632374988,0.190555671626562,16.2343030694396));
#58392=CARTESIAN_POINT('Ctrl Pts',(1.64803626679041,0.251615048281927,16.2384238287151));
#58393=CARTESIAN_POINT('Ctrl Pts',(1.63761138311908,0.312383661791834,16.2425445879905));
#58394=CARTESIAN_POINT('Ctrl Pts',(1.62383256576161,0.372456438220727,16.246665347266));
#58395=CARTESIAN_POINT('Ctrl Pts',(1.61023333543289,0.431746252574764,16.2507323983824));
#58396=CARTESIAN_POINT('Ctrl Pts',(1.59336719382399,0.490357746760353,16.2547994494988));
#58397=CARTESIAN_POINT('Ctrl Pts',(1.57332532432983,0.547908225729845,16.2588665006152));
#58398=CARTESIAN_POINT('Ctrl Pts',(1.553295754077,0.605423387273993,16.2629310558744));
#58399=CARTESIAN_POINT('Ctrl Pts',(1.53009448798927,0.661878342362491,16.2669956111336));
#58400=CARTESIAN_POINT('Ctrl Pts',(1.50386260427813,0.716905340650921,16.2710601663929));
#58401=CARTESIAN_POINT('Ctrl Pts',(1.47763708461695,0.77191898898055,16.2751237355608));
#58402=CARTESIAN_POINT('Ctrl Pts',(1.44838262701719,0.82550490653593,16.2791873047287));
#58403=CARTESIAN_POINT('Ctrl Pts',(1.41628767545806,0.877317058050051,16.2832508738967));
#58404=CARTESIAN_POINT('Ctrl Pts',(1.38341107148504,0.930391062015504,16.2874134087428));
#58405=CARTESIAN_POINT('Ctrl Pts',(1.34755404742959,0.981603262365005,16.291575943589));
#58406=CARTESIAN_POINT('Ctrl Pts',(1.30896677860741,1.03061242594011,16.2957384784352));
#58407=CARTESIAN_POINT('Ctrl Pts',(1.27124916413082,1.07851705339804,16.2998072008238));
#58408=CARTESIAN_POINT('Ctrl Pts',(1.23092349388916,1.12431656765481,16.3038759232124));
#58409=CARTESIAN_POINT('Ctrl Pts',(1.18826309874579,1.16772719766178,16.3079446456011));
#58410=CARTESIAN_POINT('Ctrl Pts',(1.14412727367919,1.21263920481925,16.312154086676));
#58411=CARTESIAN_POINT('Ctrl Pts',(1.09749267804143,1.25499362159577,16.316363527751));
#58412=CARTESIAN_POINT('Ctrl Pts',(1.04869975885901,1.29452107583038,16.3205729688259));
#58413=CARTESIAN_POINT('Ctrl Pts',(0.999906839676595,1.334048530065,16.3247824099008));
#58414=CARTESIAN_POINT('Ctrl Pts',(0.948956124574717,1.37074873014535,16.3289918509758));
#58415=CARTESIAN_POINT('Ctrl Pts',(0.896218999045746,1.40440290007869,16.3332012920507));
#58416=CARTESIAN_POINT('Ctrl Pts',(0.845122427522264,1.43701015130473,16.3372797852337));
#58417=CARTESIAN_POINT('Ctrl Pts',(0.792139052839318,1.46689216301999,16.3413582784166));
#58418=CARTESIAN_POINT('Ctrl Pts',(0.737591101952586,1.49382574831216,16.3454367715996));
#58419=CARTESIAN_POINT('Ctrl Pts',(0.682478187262265,1.5210382900187,16.3495575065347));
#58420=CARTESIAN_POINT('Ctrl Pts',(0.625768496803139,1.54524062067916,16.3536782414698));
#58421=CARTESIAN_POINT('Ctrl Pts',(0.567824574566224,1.5662475067877,16.3577989764049));
#58422=CARTESIAN_POINT('Ctrl Pts',(0.510632110943244,1.58698196043208,16.3618662706746));
#58423=CARTESIAN_POINT('Ctrl Pts',(0.452237732746338,1.60460317900944,16.3659335649443));
#58424=CARTESIAN_POINT('Ctrl Pts',(0.393012503723287,1.6189802876864,16.3700008592139));
#58425=CARTESIAN_POINT('Ctrl Pts',(0.333823366799519,1.63334863489394,16.3740656748577));
#58426=CARTESIAN_POINT('Ctrl Pts',(0.273804879129351,1.64447667161387,16.3781304905014));
#58427=CARTESIAN_POINT('Ctrl Pts',(0.21334259394841,1.65228355242294,16.3821953061451));
#58428=CARTESIAN_POINT('Ctrl Pts',(0.152894728844761,1.66008857131388,16.3862591523423));
#58429=CARTESIAN_POINT('Ctrl Pts',(0.0920037835339048,1.66457394125964,
16.3903229985394));
#58430=CARTESIAN_POINT('Ctrl Pts',(0.0310627416359322,1.6657103908189,16.3943868447366));
#58431=CARTESIAN_POINT('Ctrl Pts',(-0.0313546605475901,1.66687437205375,
16.3985491418454));
#58432=CARTESIAN_POINT('Ctrl Pts',(-0.0938240599465998,1.66452498517886,
16.4027114389542));
#58433=CARTESIAN_POINT('Ctrl Pts',(-0.15592320112893,1.65868741942227,16.406873736063));
#58434=CARTESIAN_POINT('Ctrl Pts',(-0.21663094967383,1.65298065009635,16.410942772791));
#58435=CARTESIAN_POINT('Ctrl Pts',(-0.276984351890128,1.64394055084883,
16.4150118095191));
#58436=CARTESIAN_POINT('Ctrl Pts',(-0.336596719878015,1.63164292912615,
16.4190808462471));
#58437=CARTESIAN_POINT('Ctrl Pts',(-0.398258518422286,1.61892252396808,
16.4232897735463));
#58438=CARTESIAN_POINT('Ctrl Pts',(-0.459126813983947,1.60271663974591,
16.4274987008455));
#58439=CARTESIAN_POINT('Ctrl Pts',(-0.518790870360076,1.58316519442256,
16.4317076281447));
#58440=CARTESIAN_POINT('Ctrl Pts',(-0.578454926736205,1.56361374909921,
16.4359165554439));
#58441=CARTESIAN_POINT('Ctrl Pts',(-0.63691421349331,1.54071702763948,16.440125482743));
#58442=CARTESIAN_POINT('Ctrl Pts',(-0.693783714101098,1.51466833268808,
16.4443344100422));
#58443=CARTESIAN_POINT('Ctrl Pts',(-0.748781390671607,1.489477014236,16.4484048031323));
#58444=CARTESIAN_POINT('Ctrl Pts',(-0.802520678716739,1.46123344702838,
16.4524751962224));
#58445=CARTESIAN_POINT('Ctrl Pts',(-0.854640355774557,1.4300859632489,16.4565455893124));
#58446=CARTESIAN_POINT('Ctrl Pts',(-0.906685706697143,1.39898289785846,
16.4606101777505));
#58447=CARTESIAN_POINT('Ctrl Pts',(-0.957115587177322,1.36498438372882,
16.4646747661886));
#58448=CARTESIAN_POINT('Ctrl Pts',(-1.00559068253998,1.32828588006829,16.4687393546267));
#58449=CARTESIAN_POINT('Ctrl Pts',(-1.05401479805827,1.291625971154,16.4727996684556));
#58450=CARTESIAN_POINT('Ctrl Pts',(-1.10048779713101,1.25227201095724,16.4768599822845));
#58451=CARTESIAN_POINT('Ctrl Pts',(-1.14469864655802,1.21046313804603,16.4809202961134));
#58452=CARTESIAN_POINT('Ctrl Pts',(-1.1911467321681,1.16653857804753,16.4851860771779));
#58453=CARTESIAN_POINT('Ctrl Pts',(-1.23509713265109,1.11990436848361,16.4894518582424));
#58454=CARTESIAN_POINT('Ctrl Pts',(-1.27622915987716,1.07088520929147,16.4937176393069));
#58455=CARTESIAN_POINT('Ctrl Pts',(-1.31535296308151,1.02425935428716,16.4977751485067));
#58456=CARTESIAN_POINT('Ctrl Pts',(-1.3519268586612,0.975476465052506,16.5018326577066));
#58457=CARTESIAN_POINT('Ctrl Pts',(-1.3857150905121,0.924851170690201,16.5058901669065));
#58458=CARTESIAN_POINT('Ctrl Pts',(-1.41950462859003,0.874223919192992,
16.5099478329665));
#58459=CARTESIAN_POINT('Ctrl Pts',(-1.45050801328961,0.821754554449825,
16.5140054990266));
#58460=CARTESIAN_POINT('Ctrl Pts',(-1.47853337019028,0.76778582510604,16.5180631650867));
#58461=CARTESIAN_POINT('Ctrl Pts',(-1.50658065762251,0.713774863903229,
16.5221240063703));
#58462=CARTESIAN_POINT('Ctrl Pts',(-1.53164504722335,0.658262660893737,
16.5261848476539));
#58463=CARTESIAN_POINT('Ctrl Pts',(-1.55358182078835,0.601614100662496,
16.5302456889375));
#58464=CARTESIAN_POINT('Ctrl Pts',(-1.55693824402091,0.592946620775924,
16.5308670155874));
#58465=CARTESIAN_POINT('Ctrl Pts',(-1.56022154251401,0.584252570950185,
16.5314883422372));
#58466=CARTESIAN_POINT('Ctrl Pts',(-1.56343130033213,0.575533291080358,
16.5321096688871));
#58467=CARTESIAN_POINT('Origin',(0.,0.,18.5459252805377));
#58468=CARTESIAN_POINT('',(-2.0563417111099,-0.00160732539486083,16.0959252805377));
#58469=CARTESIAN_POINT('Ctrl Pts',(1.25371187806425,1.63132526051507,16.5478693678287));
#58470=CARTESIAN_POINT('Ctrl Pts',(1.74340706608286,1.24971892553013,16.514083942288));
#58471=CARTESIAN_POINT('Ctrl Pts',(2.39627136046535,-0.0471270964805914,
16.4432541440835));
#58472=CARTESIAN_POINT('Ctrl Pts',(1.32795615156593,-2.03338265732308,16.335379973215));
#58473=CARTESIAN_POINT('Ctrl Pts',(-0.988023685722461,-2.21849194904435,
16.2242468552235));
#58474=CARTESIAN_POINT('Ctrl Pts',(-2.00194149072845,-0.89317243655016,
16.144428624331));
#58475=CARTESIAN_POINT('Ctrl Pts',(-2.05724731722716,-0.107036611257045,
16.1016547661024));
#58476=CARTESIAN_POINT('Ctrl Pts',(-2.0563417111099,-0.00160732539486083,
16.0959252805377));
#58477=CARTESIAN_POINT('Ctrl Pts',(-2.0563417111099,-0.00160732539486083,
16.0959252805377));
#58478=CARTESIAN_POINT('Ctrl Pts',(-2.05139206022102,0.574623497846713,
16.0646103934386));
#58479=CARTESIAN_POINT('Ctrl Pts',(-1.49844555770996,1.84084369321786,15.9962511336756));
#58480=CARTESIAN_POINT('Ctrl Pts',(0.185193239695499,2.23289701273988,15.9135635423805));
#58481=CARTESIAN_POINT('Ctrl Pts',(1.04119811057559,1.78983372418912,15.8621908381845));
#58482=CARTESIAN_POINT('Ctrl Pts',(1.25042353458576,1.62710269720817,15.8478625066523));
#58483=CARTESIAN_POINT('',(-2.05205730519564,0.00116258004336799,16.1540747194623));
#58484=CARTESIAN_POINT('Ctrl Pts',(-2.05205730519564,0.00116258004336799,
16.1540747194623));
#58485=CARTESIAN_POINT('Ctrl Pts',(-2.05343779045931,0.267183359675191,
16.1396948316641));
#58486=CARTESIAN_POINT('Ctrl Pts',(-1.8817826354213,1.21679945356641,16.0882705712019));
#58487=CARTESIAN_POINT('Ctrl Pts',(-0.543648734454531,2.30953699739386,
16.0056335460702));
#58488=CARTESIAN_POINT('Ctrl Pts',(0.794258702541205,1.97613964882179,15.9373764087368));
#58489=CARTESIAN_POINT('Ctrl Pts',(1.25299305265161,1.63043997671403,15.9061636440672));
#58490=CARTESIAN_POINT('Ctrl Pts',(1.25005477124305,1.62658000731212,16.6061086772888));
#58491=CARTESIAN_POINT('Ctrl Pts',(1.49824451632764,1.43685265743115,16.5892282942038));
#58492=CARTESIAN_POINT('Ctrl Pts',(2.15876687313033,0.660018185534583,16.535303538455));
#58493=CARTESIAN_POINT('Ctrl Pts',(2.08782894295346,-1.24095677525917,16.4443344100422));
#58494=CARTESIAN_POINT('Ctrl Pts',(0.0898693055670313,-2.42680223738284,
16.3332012920507));
#58495=CARTESIAN_POINT('Ctrl Pts',(-1.72097869929178,-1.52582752830307,
16.2364480618573));
#58496=CARTESIAN_POINT('Ctrl Pts',(-2.04988148937533,-0.418119129138231,
16.1767392043279));
#58497=CARTESIAN_POINT('Ctrl Pts',(-2.05205730519564,0.00116258004336799,
16.1540747194623));
#58498=CARTESIAN_POINT('Origin',(-4.61329551933804E-17,0.,6.));
#58499=CARTESIAN_POINT('Ctrl Pts',(-0.769902040670523,-1.47743251885539,
6.));
#58500=CARTESIAN_POINT('Ctrl Pts',(-0.717792690454589,-1.5127546675874,
6.));
#58501=CARTESIAN_POINT('Ctrl Pts',(-0.663680270308176,-1.54477770941651,
6.00000000000001));
#58502=CARTESIAN_POINT('Ctrl Pts',(-0.607902703315375,-1.57356639043324,
6.00000000000001));
#58503=CARTESIAN_POINT('Ctrl Pts',(-0.573141437544782,-1.59150785052124,
6.));
#58504=CARTESIAN_POINT('Ctrl Pts',(-0.53773253874008,-1.60819244673183,
6.00000000000001));
#58505=CARTESIAN_POINT('Ctrl Pts',(-0.501750440668204,-1.62362886153923,
6.00000000000001));
#58506=CARTESIAN_POINT('Ctrl Pts',(-0.479711493700921,-1.63308362781289,
6.00000000000001));
#58507=CARTESIAN_POINT('Ctrl Pts',(-0.457457406962398,-1.64207002758286,
6.00000000000001));
#58508=CARTESIAN_POINT('Ctrl Pts',(-0.435004451876358,-1.65058900058075,
6.00000000000001));
#58509=CARTESIAN_POINT('Ctrl Pts',(-0.418606024085174,-1.65681079913802,
6.00000000000001));
#58510=CARTESIAN_POINT('Ctrl Pts',(-0.402098744685564,-1.66278403922844,
6.00000000000001));
#58511=CARTESIAN_POINT('Ctrl Pts',(-0.385511599491679,-1.66850143620088,
6.00000000000001));
#58512=CARTESIAN_POINT('Ctrl Pts',(-0.323111145475881,-1.69001015049128,
6.00000000000001));
#58513=CARTESIAN_POINT('Ctrl Pts',(-0.259519986062337,-1.70792667113092,
6.00000000000001));
#58514=CARTESIAN_POINT('Ctrl Pts',(-0.195088121265483,-1.72229690513172,
6.00000000000002));
#58515=CARTESIAN_POINT('Ctrl Pts',(-0.148683978642291,-1.7326464176005,
6.00000000000002));
#58516=CARTESIAN_POINT('Ctrl Pts',(-0.101842867286457,-1.74115566058215,
6.00000000000001));
#58517=CARTESIAN_POINT('Ctrl Pts',(-0.054686471152061,-1.74782780182351,
6.00000000000001));
#58518=CARTESIAN_POINT('Ctrl Pts',(-0.0415571896974309,-1.74968545905442,
6.00000000000002));
#58519=CARTESIAN_POINT('Ctrl Pts',(-0.0284034339604797,-1.75140063593638,
6.00000000000001));
#58520=CARTESIAN_POINT('Ctrl Pts',(-0.0152277599227589,-1.75297323080655,
6.00000000000001));
#58521=CARTESIAN_POINT('Ctrl Pts',(-0.0022440902626824,-1.75452290881506,
6.00000000000001));
#58522=CARTESIAN_POINT('Ctrl Pts',(0.0107521937013583,-1.75593306946262,
6.00000000000001));
#58523=CARTESIAN_POINT('Ctrl Pts',(0.0237549906381194,-1.75720382375573,
6.00000000000001));
#58524=CARTESIAN_POINT('Ctrl Pts',(0.0916321708382992,-1.76383741332595,
6.00000000000001));
#58525=CARTESIAN_POINT('Ctrl Pts',(0.159714737884047,-1.76667936393847,
6.00000000000001));
#58526=CARTESIAN_POINT('Ctrl Pts',(0.227642895266991,-1.76577762622816,
6.00000000000002));
#58527=CARTESIAN_POINT('Ctrl Pts',(0.29621450048859,-1.76486734682906,6.00000000000002));
#58528=CARTESIAN_POINT('Ctrl Pts',(0.364629792877382,-1.76014241722597,
6.00000000000003));
#58529=CARTESIAN_POINT('Ctrl Pts',(0.432540137812221,-1.75160369638492,
6.00000000000002));
#58530=CARTESIAN_POINT('Ctrl Pts',(0.499749119582646,-1.74315316158202,
6.00000000000001));
#58531=CARTESIAN_POINT('Ctrl Pts',(0.566464616270658,-1.73096734546305,
6.00000000000001));
#58532=CARTESIAN_POINT('Ctrl Pts',(0.632353683799982,-1.71499680905896,
6.));
#58533=CARTESIAN_POINT('Ctrl Pts',(0.641114946675616,-1.71287320839276,
6.));
#58534=CARTESIAN_POINT('Ctrl Pts',(0.64986159083715,-1.71068261477665,6.));
#58535=CARTESIAN_POINT('Ctrl Pts',(0.658592824186962,-1.70842484195969,
6.));
#58536=CARTESIAN_POINT('Ctrl Pts',(0.673329590642755,-1.70461412365901,
6.));
#58537=CARTESIAN_POINT('Ctrl Pts',(0.688024362203397,-1.70061130221074,
6.));
#58538=CARTESIAN_POINT('Ctrl Pts',(0.702647425019036,-1.69642335099993,
6.));
#58539=CARTESIAN_POINT('Ctrl Pts',(0.7693973145121,-1.67730661163773,6.));
#58540=CARTESIAN_POINT('Ctrl Pts',(0.834774763838756,-1.65430615406101,
5.99999999999999));
#58541=CARTESIAN_POINT('Ctrl Pts',(0.898433301540374,-1.62743891355796,
5.99999999999999));
#58542=CARTESIAN_POINT('Ctrl Pts',(0.90557737680475,-1.62442373923524,5.99999999999999));
#58543=CARTESIAN_POINT('Ctrl Pts',(0.912699810919337,-1.62135981461256,
5.99999999999998));
#58544=CARTESIAN_POINT('Ctrl Pts',(0.919800118172371,-1.61824712514219,
5.99999999999999));
#58545=CARTESIAN_POINT('Ctrl Pts',(0.981482004348972,-1.591206526648,5.99999999999998));
#58546=CARTESIAN_POINT('Ctrl Pts',(1.04149484275984,-1.56049006590522,5.99999999999998));
#58547=CARTESIAN_POINT('Ctrl Pts',(1.09969687621398,-1.52640741779604,5.99999999999998));
#58548=CARTESIAN_POINT('Ctrl Pts',(1.15948995750665,-1.49139306472077,5.99999999999998));
#58549=CARTESIAN_POINT('Ctrl Pts',(1.21737260446499,-1.45282558408269,5.99999999999998));
#58550=CARTESIAN_POINT('Ctrl Pts',(1.27317445221614,-1.410988847483,5.99999999999998));
#58551=CARTESIAN_POINT('Ctrl Pts',(1.28645120926298,-1.40103476513892,5.99999999999998));
#58552=CARTESIAN_POINT('Ctrl Pts',(1.29961007313401,-1.3908954029497,5.99999999999997));
#58553=CARTESIAN_POINT('Ctrl Pts',(1.31264854265785,-1.38057420752588,5.99999999999997));
#58554=CARTESIAN_POINT('Ctrl Pts',(1.32186339391781,-1.37327977158908,5.99999999999997));
#58555=CARTESIAN_POINT('Ctrl Pts',(1.33101119979217,-1.36589995544344,5.99999999999997));
#58556=CARTESIAN_POINT('Ctrl Pts',(1.34008906352326,-1.35843826611053,5.99999999999997));
#58557=CARTESIAN_POINT('Ctrl Pts',(1.3948324733697,-1.31344108071559,5.99999999999997));
#58558=CARTESIAN_POINT('Ctrl Pts',(1.447059982822,-1.26544976553847,5.99999999999997));
#58559=CARTESIAN_POINT('Ctrl Pts',(1.49662261989952,-1.21481178342751,5.99999999999997));
#58560=CARTESIAN_POINT('Ctrl Pts',(1.5476087031021,-1.16271947112618,5.99999999999997));
#58561=CARTESIAN_POINT('Ctrl Pts',(1.59577544363691,-1.10782579891501,5.99999999999997));
#58562=CARTESIAN_POINT('Ctrl Pts',(1.6409401980567,-1.05045698070005,5.99999999999997));
#58563=CARTESIAN_POINT('Ctrl Pts',(1.68610495247649,-0.993088162485092,
5.99999999999997));
#58564=CARTESIAN_POINT('Ctrl Pts',(1.72826847776074,-0.9332434256593,5.99999999999997));
#58565=CARTESIAN_POINT('Ctrl Pts',(1.76721630323826,-0.871207567283829,
5.99999999999997));
#58566=CARTESIAN_POINT('Ctrl Pts',(1.77683707359166,-0.855883663066091,
5.99999999999997));
#58567=CARTESIAN_POINT('Ctrl Pts',(1.78626144751713,-0.840425896263523,
5.99999999999997));
#58568=CARTESIAN_POINT('Ctrl Pts',(1.79548580943118,-0.824838255363802,
5.99999999999997));
#58569=CARTESIAN_POINT('Ctrl Pts',(1.80275062876371,-0.812561916250909,
5.99999999999997));
#58570=CARTESIAN_POINT('Ctrl Pts',(1.8098921539507,-0.800203421397945,5.99999999999997));
#58571=CARTESIAN_POINT('Ctrl Pts',(1.81689809304296,-0.787783901963097,
5.99999999999998));
#58572=CARTESIAN_POINT('Ctrl Pts',(1.85392217059638,-0.722150837690512,
5.99999999999998));
#58573=CARTESIAN_POINT('Ctrl Pts',(1.8872321068448,-0.654701280967435,5.99999999999997));
#58574=CARTESIAN_POINT('Ctrl Pts',(1.91664683208078,-0.585782110438423,
5.99999999999998));
#58575=CARTESIAN_POINT('Ctrl Pts',(1.94609438539803,-0.516786023191269,
5.99999999999998));
#58576=CARTESIAN_POINT('Ctrl Pts',(1.97163879432696,-0.446316209639087,
5.99999999999998));
#58577=CARTESIAN_POINT('Ctrl Pts',(1.99306265208051,-0.37468298955617,5.99999999999999));
#58578=CARTESIAN_POINT('Ctrl Pts',(2.01399848774479,-0.304681529454561,
5.99999999999999));
#58579=CARTESIAN_POINT('Ctrl Pts',(2.03099991890157,-0.233568183954131,
5.99999999999999));
#58580=CARTESIAN_POINT('Ctrl Pts',(2.04382045531739,-0.161609345165651,
5.99999999999999));
#58581=CARTESIAN_POINT('Ctrl Pts',(2.04657337095263,-0.146157837836297,
6.));
#58582=CARTESIAN_POINT('Ctrl Pts',(2.04913333444925,-0.130667287270638,
6.));
#58583=CARTESIAN_POINT('Ctrl Pts',(2.05149759654652,-0.11514024651189,6.));
#58584=CARTESIAN_POINT('Ctrl Pts',(2.05348812665688,-0.102067650968936,
6.));
#58585=CARTESIAN_POINT('Ctrl Pts',(2.05533993402975,-0.0889691892837262,
6.));
#58586=CARTESIAN_POINT('Ctrl Pts',(2.05705381956725,-0.0758464997591838,
6.));
#58587=CARTESIAN_POINT('Ctrl Pts',(1.81742788875951,0.95862058795916,6.));
#58588=CARTESIAN_POINT('Ctrl Pts',(1.77621084984922,1.02166717021418,6.));
#58589=CARTESIAN_POINT('Ctrl Pts',(1.73133475147209,1.08211786795308,6.));
#58590=CARTESIAN_POINT('Ctrl Pts',(1.68313661090665,1.13981832064103,5.99999999999999));
#58591=CARTESIAN_POINT('Ctrl Pts',(1.63705290425077,1.19498747663728,5.99999999999999));
#58592=CARTESIAN_POINT('Ctrl Pts',(1.58793118040593,1.24764248850107,6.));
#58593=CARTESIAN_POINT('Ctrl Pts',(1.53604072926498,1.29761177692827,5.99999999999999));
#58594=CARTESIAN_POINT('Ctrl Pts',(1.5243500726217,1.30886960531223,5.99999999999999));
#58595=CARTESIAN_POINT('Ctrl Pts',(1.51251721040882,1.31999241970392,5.99999999999999));
#58596=CARTESIAN_POINT('Ctrl Pts',(1.50055023090591,1.33097329770719,5.99999999999999));
#58597=CARTESIAN_POINT('Ctrl Pts',(1.44563988718906,1.38135892637195,5.99999999999999));
#58598=CARTESIAN_POINT('Ctrl Pts',(1.38801753538455,1.42866081625881,5.99999999999999));
#58599=CARTESIAN_POINT('Ctrl Pts',(1.32799860875722,1.47270620083035,5.99999999999998));
#58600=CARTESIAN_POINT('Ctrl Pts',(1.28586226841847,1.50362830188993,5.99999999999998));
#58601=CARTESIAN_POINT('Ctrl Pts',(1.24254403319794,1.53294445717117,5.99999999999998));
#58602=CARTESIAN_POINT('Ctrl Pts',(1.19814772472919,1.56058048211627,5.99999999999998));
#58603=CARTESIAN_POINT('Ctrl Pts',(1.18126768766072,1.57108804775828,5.99999999999998));
#58604=CARTESIAN_POINT('Ctrl Pts',(1.1642317740111,1.58135260171141,5.99999999999998));
#58605=CARTESIAN_POINT('Ctrl Pts',(1.14704561463724,1.59136957843244,5.99999999999998));
#58606=CARTESIAN_POINT('Ctrl Pts',(1.12886559876529,1.60196582578565,5.99999999999998));
#58607=CARTESIAN_POINT('Ctrl Pts',(1.11051220777787,1.61228760763449,5.99999999999998));
#58608=CARTESIAN_POINT('Ctrl Pts',(1.09202852306591,1.62231025051435,5.99999999999998));
#58609=CARTESIAN_POINT('Ctrl Pts',(1.02830389374007,1.65686446480318,5.99999999999998));
#58610=CARTESIAN_POINT('Ctrl Pts',(0.96295266441871,1.68791557464673,5.99999999999997));
#58611=CARTESIAN_POINT('Ctrl Pts',(0.896264420566148,1.71530083655865,5.99999999999998));
#58612=CARTESIAN_POINT('Ctrl Pts',(0.83112333229346,1.74205076518954,5.99999999999998));
#58613=CARTESIAN_POINT('Ctrl Pts',(0.764705634417287,1.76530310424274,5.99999999999997));
#58614=CARTESIAN_POINT('Ctrl Pts',(0.697273056338519,1.78485829517618,5.99999999999998));
#58615=CARTESIAN_POINT('Ctrl Pts',(0.632855923422684,1.80353901849189,5.99999999999998));
#58616=CARTESIAN_POINT('Ctrl Pts',(0.567511973039543,1.81884577856428,5.99999999999998));
#58617=CARTESIAN_POINT('Ctrl Pts',(0.501473119004981,1.83056029517611,5.99999999999998));
#58618=CARTESIAN_POINT('Ctrl Pts',(0.479400442364202,1.83447572861231,5.99999999999998));
#58619=CARTESIAN_POINT('Ctrl Pts',(0.457250209367251,1.83798948017187,5.99999999999998));
#58620=CARTESIAN_POINT('Ctrl Pts',(0.43503136941093,1.84109224547236,5.99999999999998));
#58621=CARTESIAN_POINT('Ctrl Pts',(0.422554411239721,1.84283459894111,5.99999999999998));
#58622=CARTESIAN_POINT('Ctrl Pts',(0.410054540378993,1.84444739607236,5.99999999999998));
#58623=CARTESIAN_POINT('Ctrl Pts',(0.397551021819996,1.84592711205622,5.99999999999998));
#58624=CARTESIAN_POINT('Ctrl Pts',(0.329729122828692,1.85395342461138,5.99999999999999));
#58625=CARTESIAN_POINT('Ctrl Pts',(0.261681552305431,1.85808602681896,5.99999999999998));
#58626=CARTESIAN_POINT('Ctrl Pts',(0.193653405621123,1.8581466652395,5.99999999999998));
#58627=CARTESIAN_POINT('Ctrl Pts',(0.183851896072672,1.85815540203576,5.99999999999998));
#58628=CARTESIAN_POINT('Ctrl Pts',(0.174050795898627,1.85807952026247,5.99999999999999));
#58629=CARTESIAN_POINT('Ctrl Pts',(0.16425084754495,1.85791839663518,5.99999999999999));
#58630=CARTESIAN_POINT('Ctrl Pts',(0.094541628531198,1.8567722883275,5.99999999999999));
#58631=CARTESIAN_POINT('Ctrl Pts',(0.0248892021213018,1.85131723329971,
6.));
#58632=CARTESIAN_POINT('Ctrl Pts',(-0.0443759064452823,1.84172919357483,
6.));
#58633=CARTESIAN_POINT('Ctrl Pts',(-0.108331243473457,1.83287616028383,
6.));
#58634=CARTESIAN_POINT('Ctrl Pts',(-0.171956842007351,1.82049853882197,
6.));
#58635=CARTESIAN_POINT('Ctrl Pts',(-0.23497231125761,1.8047009628164,6.));
#58636=CARTESIAN_POINT('Ctrl Pts',(-0.248832415923801,1.80122632302535,
6.));
#58637=CARTESIAN_POINT('Ctrl Pts',(-0.262662907057445,1.79758612674387,
6.00000000000001));
#58638=CARTESIAN_POINT('Ctrl Pts',(-0.276460624295276,1.79378131032826,
6.00000000000001));
#58639=CARTESIAN_POINT('Ctrl Pts',(-0.287524089711141,1.79073048285425,
6.00000000000001));
#58640=CARTESIAN_POINT('Ctrl Pts',(-0.2985659500238,1.78757387230117,6.00000000000001));
#58641=CARTESIAN_POINT('Ctrl Pts',(-0.309571502178386,1.78431609244398,
6.00000000000001));
#58642=CARTESIAN_POINT('Ctrl Pts',(-0.375122573183307,1.7649121628876,6.00000000000001));
#58643=CARTESIAN_POINT('Ctrl Pts',(-0.4395095308677,1.74189006878232,6.00000000000002));
#58644=CARTESIAN_POINT('Ctrl Pts',(-0.502429647359492,1.71543190874701,
6.00000000000002));
#58645=CARTESIAN_POINT('Ctrl Pts',(-0.56468103391033,1.68925495232009,6.00000000000002));
#58646=CARTESIAN_POINT('Ctrl Pts',(-0.625497437618468,1.6597138520638,6.00000000000002));
#58647=CARTESIAN_POINT('Ctrl Pts',(-0.684556584297603,1.62694431289946,
6.00000000000002));
#58648=CARTESIAN_POINT('Ctrl Pts',(-0.743113515046717,1.5944534331048,6.00000000000002));
#58649=CARTESIAN_POINT('Ctrl Pts',(-0.799943720377945,1.55878814071636,
6.00000000000003));
#58650=CARTESIAN_POINT('Ctrl Pts',(-0.854692340605141,1.52005068559395,
6.00000000000003));
#58651=CARTESIAN_POINT('Ctrl Pts',(-0.866175085382049,1.51192605508031,
6.00000000000003));
#58652=CARTESIAN_POINT('Ctrl Pts',(-0.877566096038144,1.50366619624473,
6.00000000000003));
#58653=CARTESIAN_POINT('Ctrl Pts',(-0.888861820035535,1.49527192360063,
6.00000000000004));
#58654=CARTESIAN_POINT('Ctrl Pts',(-0.899513606118717,1.48735618517168,
6.00000000000004));
#58655=CARTESIAN_POINT('Ctrl Pts',(-0.91008193062578,1.47931977959631,6.00000000000003));
#58656=CARTESIAN_POINT('Ctrl Pts',(-0.920547148745782,1.4711767155375,6.00000000000004));
#58657=CARTESIAN_POINT('Ctrl Pts',(-0.972167074707126,1.43101086720119,
6.00000000000004));
#58658=CARTESIAN_POINT('Ctrl Pts',(-1.02137633331925,1.38818383327732,6.00000000000004));
#58659=CARTESIAN_POINT('Ctrl Pts',(-1.06788265822317,1.34282814309811,6.00000000000004));
#58660=CARTESIAN_POINT('Ctrl Pts',(-1.11284005981166,1.29898305359853,6.00000000000005));
#58661=CARTESIAN_POINT('Ctrl Pts',(-1.15527203055497,1.2527742460767,6.00000000000005));
#58662=CARTESIAN_POINT('Ctrl Pts',(-1.19487404980438,1.20429687549393,6.00000000000005));
#58663=CARTESIAN_POINT('Ctrl Pts',(-1.23424035546928,1.15610804511705,6.00000000000005));
#58664=CARTESIAN_POINT('Ctrl Pts',(-1.27081086720789,1.10567706111428,6.00000000000005));
#58665=CARTESIAN_POINT('Ctrl Pts',(-1.30423797357443,1.05308139435648,6.00000000000005));
#58666=CARTESIAN_POINT('Ctrl Pts',(-1.30970780350955,1.04447492542271,6.00000000000005));
#58667=CARTESIAN_POINT('Ctrl Pts',(-1.31509334809115,1.03581046919314,6.00000000000005));
#58668=CARTESIAN_POINT('Ctrl Pts',(-1.32039294356288,1.02708833860433,6.00000000000005));
#58669=CARTESIAN_POINT('Ctrl Pts',(-1.32604932595056,1.0177790043148,6.00000000000004));
#58670=CARTESIAN_POINT('Ctrl Pts',(-1.33160779623118,1.00840396758307,6.00000000000005));
#58671=CARTESIAN_POINT('Ctrl Pts',(-1.33706795287322,0.998964888140392,
6.00000000000005));
#58672=CARTESIAN_POINT('Ctrl Pts',(1.26643921716274,1.07786902174452,16.998323674252));
#58673=CARTESIAN_POINT('Ctrl Pts',(1.62497761725199,0.656628334916694,16.9612665673906));
#58674=CARTESIAN_POINT('Ctrl Pts',(1.8823477456886,-0.564254992005215,16.8871650878655));
#58675=CARTESIAN_POINT('Ctrl Pts',(0.544110383007705,-1.8901268562736,16.7760192356764));
#58676=CARTESIAN_POINT('Ctrl Pts',(-1.29159322672144,-1.4809162453331,16.6648861176848));
#58677=CARTESIAN_POINT('Ctrl Pts',(-1.94534454504545,0.281174607083069,
16.5537529996932));
#58678=CARTESIAN_POINT('Ctrl Pts',(-0.81855718778506,1.78722597471637,16.4426198817017));
#58679=CARTESIAN_POINT('Ctrl Pts',(1.05736298279991,1.65685741880359,16.3314867637101));
#58680=CARTESIAN_POINT('Ctrl Pts',(1.96556536740795,0.0104236887533924,
16.2203536457186));
#58681=CARTESIAN_POINT('Ctrl Pts',(1.07479322704078,-1.64573649927818,16.109220527727));
#58682=CARTESIAN_POINT('Ctrl Pts',(-0.799665835591146,-1.7955563655213,
15.9980874097355));
#58683=CARTESIAN_POINT('Ctrl Pts',(-1.94224246594592,-0.302063406572706,
15.8869542917439));
#58684=CARTESIAN_POINT('Ctrl Pts',(-1.30720066280732,1.46791658208971,15.7758211737524));
#58685=CARTESIAN_POINT('Ctrl Pts',(0.524241757093383,1.89438755754002,15.6646880557608));
#58686=CARTESIAN_POINT('Ctrl Pts',(1.87587794794047,0.587047795516583,15.5535549377692));
#58687=CARTESIAN_POINT('Ctrl Pts',(1.51063656570958,-1.25758504499101,15.4424218197777));
#58688=CARTESIAN_POINT('Ctrl Pts',(-0.23719873324387,-1.95122454958629,
15.3312887017861));
#58689=CARTESIAN_POINT('Ctrl Pts',(-1.76794048158266,-0.859027596207237,
15.2201555837946));
#58690=CARTESIAN_POINT('Ctrl Pts',(-1.68059348111992,1.01938577340468,15.109022465803));
#58691=CARTESIAN_POINT('Ctrl Pts',(-0.055101197330089,1.9648168731157,14.9978893478114));
#58692=CARTESIAN_POINT('Ctrl Pts',(1.62082188049643,1.11197038656462,14.8867562298199));
#58693=CARTESIAN_POINT('Ctrl Pts',(1.81330497340411,-0.758595243245752,
14.7756231118283));
#58694=CARTESIAN_POINT('Ctrl Pts',(0.346179986260669,-1.93486460720292,
14.6644899938368));
#58695=CARTESIAN_POINT('Ctrl Pts',(-1.43778255117909,-1.34026974869229,
14.5533568758452));
#58696=CARTESIAN_POINT('Ctrl Pts',(-1.90582990649864,0.48099274761629,14.4422237578536));
#58697=CARTESIAN_POINT('Ctrl Pts',(-0.629586719028806,1.86203174370634,
14.3310906398621));
#58698=CARTESIAN_POINT('Ctrl Pts',(1.22287901418285,1.53886600219443,14.2199575218705));
#58699=CARTESIAN_POINT('Ctrl Pts',(1.95611774146339,-0.192730475320511,
14.108824403879));
#58700=CARTESIAN_POINT('Ctrl Pts',(0.899040519765985,-1.74793243517711,
13.9976912858874));
#58701=CARTESIAN_POINT('Ctrl Pts',(-0.980873971539237,-1.70335783285293,
13.8865581678959));
#58702=CARTESIAN_POINT('Ctrl Pts',(-1.96305399725381,-0.0998030981586012,
13.7754250499043));
#58703=CARTESIAN_POINT('Ctrl Pts',(-1.14856973963694,1.59509536006063,13.6642919319127));
#58704=CARTESIAN_POINT('Ctrl Pts',(0.71713075096409,1.83009976247439,13.5531588139212));
#58705=CARTESIAN_POINT('Ctrl Pts',(1.92648495228938,0.390124830213576,13.4420256959296));
#58706=CARTESIAN_POINT('Ctrl Pts',(1.3726442995717,-1.40690770180496,13.330892577938));
#58707=CARTESIAN_POINT('Ctrl Pts',(-0.437494442867744,-1.91628292979319,
13.2197594599465));
#58708=CARTESIAN_POINT('Ctrl Pts',(-1.84722105158085,-0.671800596268771,
13.1086263419549));
#58709=CARTESIAN_POINT('Ctrl Pts',(-1.56629824797523,1.18754008477213,12.9974932239634));
#58710=CARTESIAN_POINT('Ctrl Pts',(0.148162361075704,1.95999733910862,12.8863601059718));
#58711=CARTESIAN_POINT('Ctrl Pts',(1.7270189456564,0.938587883948701,12.7752269879802));
#58712=CARTESIAN_POINT('Ctrl Pts',(1.72523981636906,-0.941854145059837,
12.6640938699887));
#58713=CARTESIAN_POINT('Ctrl Pts',(0.144453302363285,-1.9602741894919,12.5529607519971));
#58714=CARTESIAN_POINT('Ctrl Pts',(-1.56854255959194,-1.18457414006062,
12.4418276340056));
#58715=CARTESIAN_POINT('Ctrl Pts',(-1.84594653377508,0.675294786737895,
12.330694516014));
#58716=CARTESIAN_POINT('Ctrl Pts',(-0.433867584499705,1.91710734537012,
12.2195613980225));
#58717=CARTESIAN_POINT('Ctrl Pts',(1.37530405497152,1.40430780490978,12.1084282800309));
#58718=CARTESIAN_POINT('Ctrl Pts',(1.9257432918927,-0.393769511620569,11.9972951620393));
#58719=CARTESIAN_POINT('Ctrl Pts',(0.713666471556317,-1.83145347249883,
11.8861620440478));
#58720=CARTESIAN_POINT('Ctrl Pts',(-1.15158599318701,-1.59291913003992,
11.7750289260562));
#58721=CARTESIAN_POINT('Ctrl Pts',(-1.96286163098258,0.103517496917523,
11.6638958080646));
#58722=CARTESIAN_POINT('Ctrl Pts',(-0.977649046621936,1.70521083628707,
11.5527626900731));
#58723=CARTESIAN_POINT('Ctrl Pts',(0.902346425098597,1.7462281018422,11.4416295720815));
#58724=CARTESIAN_POINT('Ctrl Pts',(1.9564789325597,0.189028677723019,11.33049645409));
#58725=CARTESIAN_POINT('Ctrl Pts',(1.21996491468177,-1.54117723234452,11.2193633360984));
#58726=CARTESIAN_POINT('Ctrl Pts',(-0.633109010464032,-1.86083707922561,
11.1082302181069));
#58727=CARTESIAN_POINT('Ctrl Pts',(-1.90673665030534,-0.477385589365701,
10.9970971001153));
#58728=CARTESIAN_POINT('Ctrl Pts',(-1.43524385936396,1.3429879815954,10.8859639821237));
#58729=CARTESIAN_POINT('Ctrl Pts',(0.349840602315146,1.93420609230853,10.7748308641322));
#58730=CARTESIAN_POINT('Ctrl Pts',(1.8147371751635,0.755162657730938,10.6636977461406));
#58731=CARTESIAN_POINT('Ctrl Pts',(1.61871485794303,-1.11503536411457,10.5525646281491));
#58732=CARTESIAN_POINT('Ctrl Pts',(-0.0588190092628553,-1.96470913335817,
10.4414315101575));
#58733=CARTESIAN_POINT('Ctrl Pts',(-1.68251940409772,-1.01620377355444,
10.330298392166));
#58734=CARTESIAN_POINT('Ctrl Pts',(-1.76631181698397,0.862371277197082,
10.2191652741744));
#58735=CARTESIAN_POINT('Ctrl Pts',(-0.23350613361075,1.9516701924551,10.1080321561828));
#58736=CARTESIAN_POINT('Ctrl Pts',(1.51301355395472,1.25472373058804,9.99689903819129));
#58737=CARTESIAN_POINT('Ctrl Pts',(1.87476368530798,-0.590595274958111,
9.88576592019971));
#58738=CARTESIAN_POINT('Ctrl Pts',(0.520656301887133,-1.89537823925887,
9.77463280220817));
#58739=CARTESIAN_POINT('Ctrl Pts',(-1.30997622185192,-1.4654364376298,9.6634996842166));
#58740=CARTESIAN_POINT('Ctrl Pts',(-1.94166694719282,0.305730470734983,
9.55236656622504));
#58741=CARTESIAN_POINT('Ctrl Pts',(-0.796267659191974,1.79708081884754,
9.44123344823349));
#58742=CARTESIAN_POINT('Ctrl Pts',(1.07790713128235,1.6436720691419,9.33010033024192));
#58743=CARTESIAN_POINT('Ctrl Pts',(1.96553888921238,-0.0140900525500748,
9.21896721225038));
#58744=CARTESIAN_POINT('Ctrl Pts',(1.05423209284676,-1.65895640355874,9.10783409425879));
#58745=CARTESIAN_POINT('Ctrl Pts',(-0.821949409002516,-1.78548055816259,
8.99670097626726));
#58746=CARTESIAN_POINT('Ctrl Pts',(-1.94585046023486,-0.277862630068061,
8.88556785827569));
#58747=CARTESIAN_POINT('Ctrl Pts',(-1.2888325821115,1.48406611355865,8.77443474028413));
#58748=CARTESIAN_POINT('Ctrl Pts',(0.547775602694242,1.88771913792229,8.66330162229257));
#58749=CARTESIAN_POINT('Ctrl Pts',(1.88303799648319,0.563657307092937,8.55216850430101));
#58750=CARTESIAN_POINT('Ctrl Pts',(1.49486989869632,-1.27628587601649,8.44103538630945));
#58751=CARTESIAN_POINT('Ctrl Pts',(-0.261461964938926,-1.94812199224134,
8.32990226831789));
#58752=CARTESIAN_POINT('Ctrl Pts',(-1.77849355284479,-0.836960181982545,
8.21876915032633));
#58753=CARTESIAN_POINT('Ctrl Pts',(-1.66777782961535,1.04022052572397,8.10763603233478));
#58754=CARTESIAN_POINT('Ctrl Pts',(-0.0306462141602966,1.96535047235978,
7.99650291434321));
#58755=CARTESIAN_POINT('Ctrl Pts',(1.63453406194913,1.0917142983495,7.88536979635166));
#58756=CARTESIAN_POINT('Ctrl Pts',(1.80372435497444,-0.781101746316954,
7.77423667836009));
#58757=CARTESIAN_POINT('Ctrl Pts',(0.322075267633636,-1.93902277598313,
7.66310356036854));
#58758=CARTESIAN_POINT('Ctrl Pts',(-1.45435005500721,-1.32227375190043,
7.55197044237697));
#58759=CARTESIAN_POINT('Ctrl Pts',(-1.89969644190983,0.50467208220374,7.44083732438543));
#58760=CARTESIAN_POINT('Ctrl Pts',(-0.60636687257194,1.86972249141181,7.32970420639386));
#58761=CARTESIAN_POINT('Ctrl Pts',(1.24193543302636,1.52352865742128,7.2185710884023));
#58762=CARTESIAN_POINT('Ctrl Pts',(1.95356590264256,-0.217057370469622,
7.10743797041074));
#58763=CARTESIAN_POINT('Ctrl Pts',(0.877222931654791,-1.75898624013855,
6.99630485241919));
#58764=CARTESIAN_POINT('Ctrl Pts',(-1.00200230080329,-1.6910172936132,6.88517173442762));
#58765=CARTESIAN_POINT('Ctrl Pts',(-1.96413016477178,-0.075371123179428,
6.77403861643607));
#58766=CARTESIAN_POINT('Ctrl Pts',(-1.12865736944011,1.6092736399872,6.6629054984445));
#58767=CARTESIAN_POINT('Ctrl Pts',(0.739899879799323,1.82101730763706,6.55177238045295));
#58768=CARTESIAN_POINT('Ctrl Pts',(1.93109432141268,0.366152571270065,6.44063926246139));
#58769=CARTESIAN_POINT('Ctrl Pts',(1.35521404062397,-1.42394081986265,6.32950614446983));
#58770=CARTESIAN_POINT('Ctrl Pts',(-0.461659097576337,-1.91057463508532,
6.21837302647827));
#58771=CARTESIAN_POINT('Ctrl Pts',(-1.85476354891606,-0.648982408557044,
6.10723990848671));
#58772=CARTESIAN_POINT('Ctrl Pts',(-1.55270934033744,1.20736462849148,5.99610679049515));
#58773=CARTESIAN_POINT('Ctrl Pts',(0.175237007265808,1.95716707999619,5.8849736725036));
#58774=CARTESIAN_POINT('Ctrl Pts',(1.21296802187357,1.26497356239067,5.81088492717589));
#58775=CARTESIAN_POINT('Ctrl Pts',(1.47095156957581,0.775868174581949,5.77384055451203));
#58776=CARTESIAN_POINT('Ctrl Pts',(1.36652085687194,1.16304871108613,17.0742005794842));
#58777=CARTESIAN_POINT('Ctrl Pts',(1.753393116568,0.708519053039916,17.0371434726228));
#58778=CARTESIAN_POINT('Ctrl Pts',(2.03110217964673,-0.608845813300611,
16.9630419930976));
#58779=CARTESIAN_POINT('Ctrl Pts',(0.587109256207644,-2.03949604231164,
16.8518961409086));
#58780=CARTESIAN_POINT('Ctrl Pts',(-1.39366268747075,-1.5979471490641,16.740763022917));
#58781=CARTESIAN_POINT('Ctrl Pts',(-2.09907736477262,0.30339471472038,16.6296299049255));
#58782=CARTESIAN_POINT('Ctrl Pts',(-0.883244497242211,1.92846331454007,
16.5184967869339));
#58783=CARTESIAN_POINT('Ctrl Pts',(1.14092216167901,1.7877922516728,16.4073636689423));
#58784=CARTESIAN_POINT('Ctrl Pts',(2.1208961580688,0.0112474312971465,16.2962305509508));
#58785=CARTESIAN_POINT('Ctrl Pts',(1.1597298485958,-1.77579249023686,16.1850974329592));
#58786=CARTESIAN_POINT('Ctrl Pts',(-0.862860236838991,-1.93745202290173,
16.0739643149677));
#58787=CARTESIAN_POINT('Ctrl Pts',(-2.09573014073555,-0.325934272711604,
15.9628311969761));
#58788=CARTESIAN_POINT('Ctrl Pts',(-1.41050351697493,1.58392017428815,15.8516980789846));
#58789=CARTESIAN_POINT('Ctrl Pts',(0.56567049204008,2.0440934498039,15.740564960993));
#58790=CARTESIAN_POINT('Ctrl Pts',(2.02412109958957,0.633439841156638,15.6294318430014));
#58791=CARTESIAN_POINT('Ctrl Pts',(1.63001614781033,-1.35696697479136,15.5182987250099));
#58792=CARTESIAN_POINT('Ctrl Pts',(-0.255943602984384,-2.10542204261793,
15.4071656070183));
#58793=CARTESIAN_POINT('Ctrl Pts',(-1.90765376581075,-0.926913120612018,
15.2960324890267));
#58794=CARTESIAN_POINT('Ctrl Pts',(-1.81340408031464,1.0999437649103,15.1848993710352));
#58795=CARTESIAN_POINT('Ctrl Pts',(-0.0594556251652374,2.12008851325826,
15.0737662530436));
#58796=CARTESIAN_POINT('Ctrl Pts',(1.7489089685132,1.19984497074307,14.9626331350521));
#58797=CARTESIAN_POINT('Ctrl Pts',(1.95660323246916,-0.818543999404555,
14.8515000170605));
#58798=CARTESIAN_POINT('Ctrl Pts',(0.37353720971834,-2.08776923924519,14.7403668990689));
#58799=CARTESIAN_POINT('Ctrl Pts',(-1.55140477111448,-1.44618592081011,
14.6292337810774));
#58800=CARTESIAN_POINT('Ctrl Pts',(-2.05644004195902,0.519003685857384,
14.5181006630858));
#58801=CARTESIAN_POINT('Ctrl Pts',(-0.679340446113083,2.0091806850651,14.4069675450943));
#58802=CARTESIAN_POINT('Ctrl Pts',(1.31951826480522,1.66047644405789,14.2958344271027));
#58803=CARTESIAN_POINT('Ctrl Pts',(2.11070192393092,-0.207961196014097,
14.1847013091112));
#58804=CARTESIAN_POINT('Ctrl Pts',(0.97008810591447,-1.88606456330667,14.0735681911196));
#58805=CARTESIAN_POINT('Ctrl Pts',(-1.05838852896084,-1.83796740796175,
13.962435073128));
#58806=CARTESIAN_POINT('Ctrl Pts',(-2.11818632434884,-0.107690138907505,
13.8513019551365));
#58807=CARTESIAN_POINT('Ctrl Pts',(-1.23933662469974,1.72114938378634,13.7401688371449));
#58808=CARTESIAN_POINT('Ctrl Pts',(0.77380273369309,1.97472524672794,13.6290357191534));
#58809=CARTESIAN_POINT('Ctrl Pts',(2.07872737362893,0.420954839399902,13.5179026011618));
#58810=CARTESIAN_POINT('Ctrl Pts',(1.48111890330862,-1.51809000554917,13.4067694831702));
#58811=CARTESIAN_POINT('Ctrl Pts',(-0.472067883592329,-2.0677191259891,
13.2956363651787));
#58812=CARTESIAN_POINT('Ctrl Pts',(-1.9931995630184,-0.724890317686927,
13.1845032471871));
#58813=CARTESIAN_POINT('Ctrl Pts',(-1.69007655079989,1.2813866407645,13.0733701291956));
#58814=CARTESIAN_POINT('Ctrl Pts',(0.159871041475593,2.11488811070296,12.962237011204));
#58815=CARTESIAN_POINT('Ctrl Pts',(1.86349836412969,1.01276074054045,12.8511038932124));
#58816=CARTESIAN_POINT('Ctrl Pts',(1.86157863735144,-1.0162851212386,12.7399707752209));
#58817=CARTESIAN_POINT('Ctrl Pts',(0.155868870647972,-2.11518683946771,
12.6288376572293));
#58818=CARTESIAN_POINT('Ctrl Pts',(-1.69249822141149,-1.27818630927312,
12.5177045392378));
#58819=CARTESIAN_POINT('Ctrl Pts',(-1.99182432515431,0.728660640091058,
12.4065714212462));
#58820=CARTESIAN_POINT('Ctrl Pts',(-0.468154409074422,2.06860869184061,
12.2954383032546));
#58821=CARTESIAN_POINT('Ctrl Pts',(1.48398884856836,1.51528464917292,12.1843051852631));
#58822=CARTESIAN_POINT('Ctrl Pts',(2.07792710276947,-0.424887545440438,
12.0731720672715));
#58823=CARTESIAN_POINT('Ctrl Pts',(0.770064686102175,-1.97618593505588,
11.96203894928));
#58824=CARTESIAN_POINT('Ctrl Pts',(-1.24259124073652,-1.71880117498774,
11.8509058312884));
#58825=CARTESIAN_POINT('Ctrl Pts',(-2.11797875613851,0.111698071784202,
11.7397727132969));
#58826=CARTESIAN_POINT('Ctrl Pts',(-1.05490875109103,1.83996684686597,11.6286395953053));
#58827=CARTESIAN_POINT('Ctrl Pts',(0.973655263758793,1.88422554330662,11.5175064773137));
#58828=CARTESIAN_POINT('Ctrl Pts',(2.11109165851883,0.203966860118353,11.4063733593222));
#58829=CARTESIAN_POINT('Ctrl Pts',(1.31637387564445,-1.66297032150761,11.2952402413306));
#58830=CARTESIAN_POINT('Ctrl Pts',(-0.683141090190578,-2.00789161101578,
11.1841071233391));
#58831=CARTESIAN_POINT('Ctrl Pts',(-2.05741844211191,-0.515111468278627,
11.0729740053475));
#58832=CARTESIAN_POINT('Ctrl Pts',(-1.54866545661165,1.44911896481696,10.961840887356));
#58833=CARTESIAN_POINT('Ctrl Pts',(0.377487109657989,2.08705868454541,10.8507077693644));
#58834=CARTESIAN_POINT('Ctrl Pts',(1.95814861542077,0.814840150348541,10.7395746513728));
#58835=CARTESIAN_POINT('Ctrl Pts',(1.746635436372,-1.20315216124309,10.6284415333813));
#58836=CARTESIAN_POINT('Ctrl Pts',(-0.0634672409452934,-2.11997225925744,
10.5173084153897));
#58837=CARTESIAN_POINT('Ctrl Pts',(-1.81548220130316,-1.09651030430438,
10.4061752973981));
#58838=CARTESIAN_POINT('Ctrl Pts',(-1.90589639434532,0.930521039373084,
10.2950421794066));
#58839=CARTESIAN_POINT('Ctrl Pts',(-0.251959191931444,2.10590290286506,
10.183909061415));
#58840=CARTESIAN_POINT('Ctrl Pts',(1.63258097995506,1.35387954212443,10.0727759434235));
#58841=CARTESIAN_POINT('Ctrl Pts',(2.02291878122584,-0.637267663748103,
9.96164282543193));
#58842=CARTESIAN_POINT('Ctrl Pts',(0.561801692610688,-2.04516242114731,
9.85050970744037));
#58843=CARTESIAN_POINT('Ctrl Pts',(-1.41349841737958,-1.58124403390446,
9.73937658944881));
#58844=CARTESIAN_POINT('Ctrl Pts',(-2.09510914103105,0.329891130327294,
9.62824347145725));
#58845=CARTESIAN_POINT('Ctrl Pts',(-0.859193516113775,1.93909694769355,
9.5171103534657));
#58846=CARTESIAN_POINT('Ctrl Pts',(1.16308983226872,1.7735649164216,9.40597723547412));
#58847=CARTESIAN_POINT('Ctrl Pts',(2.12086758740706,-0.0152035332001427,
9.29484411748258));
#58848=CARTESIAN_POINT('Ctrl Pts',(1.13754384998149,-1.79005711082064,9.18371099949101));
#58849=CARTESIAN_POINT('Ctrl Pts',(-0.886904792171455,-1.92657996467825,
9.07257788149945));
#58850=CARTESIAN_POINT('Ctrl Pts',(-2.09962326042144,-0.29982100537282,
8.9614447635079));
#58851=CARTESIAN_POINT('Ctrl Pts',(-1.39068388012905,1.6013459388112,8.85031164551634));
#58852=CARTESIAN_POINT('Ctrl Pts',(0.591064123586032,2.03689805158304,8.73917852752478));
#58853=CARTESIAN_POINT('Ctrl Pts',(2.03184697820833,0.608200895733785,8.62804540953321));
#58854=CARTESIAN_POINT('Ctrl Pts',(1.61300350399372,-1.37714565789816,8.51691229154166));
#58855=CARTESIAN_POINT('Ctrl Pts',(-0.282124261098154,-2.1020743025416,
8.40577917355011));
#58856=CARTESIAN_POINT('Ctrl Pts',(-1.91904080420022,-0.90310180666453,
8.29464605555853));
#58857=CARTESIAN_POINT('Ctrl Pts',(-1.79957565899125,1.12242500459889,8.183512937567));
#58858=CARTESIAN_POINT('Ctrl Pts',(-0.0330680622225432,2.12066428072216,
8.07237981957541));
#58859=CARTESIAN_POINT('Ctrl Pts',(1.76370476897043,1.1779881246746,7.96124670158388));
#58860=CARTESIAN_POINT('Ctrl Pts',(1.94626549598055,-0.842829101638638,
7.85011358359229));
#58861=CARTESIAN_POINT('Ctrl Pts',(0.347527591328071,-2.09225601151783,
7.73898046560075));
#58862=CARTESIAN_POINT('Ctrl Pts',(-1.56928153868503,-1.42676777217493,
7.62784734760918));
#58863=CARTESIAN_POINT('Ctrl Pts',(-2.04982187412916,0.544554303804206,
7.51671422961763));
#58864=CARTESIAN_POINT('Ctrl Pts',(-0.65428562781098,2.01747920188457,7.40558111162607));
#58865=CARTESIAN_POINT('Ctrl Pts',(1.34008063641694,1.64392705010552,7.29444799363451));
#58866=CARTESIAN_POINT('Ctrl Pts',(2.10794842346695,-0.234210548650754,
7.18331487564295));
#58867=CARTESIAN_POINT('Ctrl Pts',(0.946546360841719,-1.89799190638236,
7.07218175765139));
#58868=CARTESIAN_POINT('Ctrl Pts',(-1.0811865458091,-1.82465164513035,6.96104863965984));
#58869=CARTESIAN_POINT('Ctrl Pts',(-2.11934753709309,-0.0813274024009634,
6.84991552166827));
#58870=CARTESIAN_POINT('Ctrl Pts',(-1.21785065931351,1.73644811662063,6.73878240367672));
#58871=CARTESIAN_POINT('Ctrl Pts',(0.798371215957767,1.96492504171328,6.62764928568515));
#58872=CARTESIAN_POINT('Ctrl Pts',(2.08370100280802,0.395088148453585,6.5165161676936));
#58873=CARTESIAN_POINT('Ctrl Pts',(1.46231120052276,-1.53646918298456,6.40538304970203));
#58874=CARTESIAN_POINT('Ctrl Pts',(-0.498142174573606,-2.06155972751995,
6.29424993171048));
#58875=CARTESIAN_POINT('Ctrl Pts',(-2.00133811383221,-0.700268899618438,
6.18311681371891));
#58876=CARTESIAN_POINT('Ctrl Pts',(-1.67541376599547,1.30277783909705,6.07198369572737));
#58877=CARTESIAN_POINT('Ctrl Pts',(0.189085288957672,2.11183418750232,5.9608505777358));
#58878=CARTESIAN_POINT('Ctrl Pts',(1.3088240463071,1.3649393772495,5.88676183240809));
#58879=CARTESIAN_POINT('Ctrl Pts',(1.5871950047292,0.837181941605297,5.84971745974424));
#58880=CARTESIAN_POINT('Ctrl Pts',(1.46660249658114,1.24822840042773,17.1500774847164));
#58881=CARTESIAN_POINT('Ctrl Pts',(1.88180861588401,0.760409771163138,17.113020377855));
#58882=CARTESIAN_POINT('Ctrl Pts',(2.17985661360488,-0.653436634596006,
17.0389188983298));
#58883=CARTESIAN_POINT('Ctrl Pts',(0.630108129407586,-2.18886522834968,
16.9277730461408));
#58884=CARTESIAN_POINT('Ctrl Pts',(-1.49573214822006,-1.71497805279509,
16.8166399281492));
#58885=CARTESIAN_POINT('Ctrl Pts',(-2.2528101844998,0.325614822357685,16.7055068101576));
#58886=CARTESIAN_POINT('Ctrl Pts',(-0.947931806699366,2.06970065436379,
16.5943736921661));
#58887=CARTESIAN_POINT('Ctrl Pts',(1.22448134055812,1.91872708454201,16.4832405741745));
#58888=CARTESIAN_POINT('Ctrl Pts',(2.27622694872966,0.0120711738409036,
16.372107456183));
#58889=CARTESIAN_POINT('Ctrl Pts',(1.24466647015081,-1.90584848119554,16.2609743381914));
#58890=CARTESIAN_POINT('Ctrl Pts',(-0.926054638086837,-2.07934768028216,
16.1498412201999));
#58891=CARTESIAN_POINT('Ctrl Pts',(-2.24921781552518,-0.349805138850504,
16.0387081022083));
#58892=CARTESIAN_POINT('Ctrl Pts',(-1.51380637114255,1.6999237664866,15.9275749842167));
#58893=CARTESIAN_POINT('Ctrl Pts',(0.607099226986776,2.19379934206778,15.8164418662252));
#58894=CARTESIAN_POINT('Ctrl Pts',(2.17236425123866,0.679831886796696,15.7053087482336));
#58895=CARTESIAN_POINT('Ctrl Pts',(1.74939572991108,-1.45634890459171,15.5941756302421));
#58896=CARTESIAN_POINT('Ctrl Pts',(-0.274688472724895,-2.25961953564957,
15.4830425122505));
#58897=CARTESIAN_POINT('Ctrl Pts',(-2.04736705003885,-0.994798645016798,
15.3719093942589));
#58898=CARTESIAN_POINT('Ctrl Pts',(-1.94621467950935,1.18050175641591,15.2607762762674));
#58899=CARTESIAN_POINT('Ctrl Pts',(-0.063810053000384,2.27536015340083,
15.1496431582758));
#58900=CARTESIAN_POINT('Ctrl Pts',(1.87699605653,1.28771955492152,15.0385100402842));
#58901=CARTESIAN_POINT('Ctrl Pts',(2.09990149153423,-0.878492755563357,
14.9273769222927));
#58902=CARTESIAN_POINT('Ctrl Pts',(0.400894433176008,-2.24067387128746,
14.8162438043011));
#58903=CARTESIAN_POINT('Ctrl Pts',(-1.66502699104989,-1.55210209292793,
14.7051106863096));
#58904=CARTESIAN_POINT('Ctrl Pts',(-2.2070501774194,0.557014624098477,14.593977568318));
#58905=CARTESIAN_POINT('Ctrl Pts',(-0.729094173197359,2.15632962642386,
14.4828444503265));
#58906=CARTESIAN_POINT('Ctrl Pts',(1.4161575154276,1.78208688592133,14.3717113323349));
#58907=CARTESIAN_POINT('Ctrl Pts',(2.26528610639844,-0.223191916707685,
14.2605782143433));
#58908=CARTESIAN_POINT('Ctrl Pts',(1.04113569206295,-2.02419669143622,14.1494450963518));
#58909=CARTESIAN_POINT('Ctrl Pts',(-1.13590308638243,-1.97257698307058,
14.0383119783602));
#58910=CARTESIAN_POINT('Ctrl Pts',(-2.27331865144387,-0.115577179656406,
13.9271788603687));
#58911=CARTESIAN_POINT('Ctrl Pts',(-1.33010350976255,1.84720340751205,13.8160457423771));
#58912=CARTESIAN_POINT('Ctrl Pts',(0.830474716422089,2.11935073098151,13.7049126243855));
#58913=CARTESIAN_POINT('Ctrl Pts',(2.23096979496849,0.451784848586225,13.593779506394));
#58914=CARTESIAN_POINT('Ctrl Pts',(1.58959350704553,-1.62927230929336,13.4826463884024));
#58915=CARTESIAN_POINT('Ctrl Pts',(-0.506641324316914,-2.21915532218502,
13.3715132704109));
#58916=CARTESIAN_POINT('Ctrl Pts',(-2.13917807445597,-0.777980039105083,
13.2603801524193));
#58917=CARTESIAN_POINT('Ctrl Pts',(-1.81385485362456,1.37523319675687,13.1492470344277));
#58918=CARTESIAN_POINT('Ctrl Pts',(0.17157972187548,2.2697788822973,13.0381139164362));
#58919=CARTESIAN_POINT('Ctrl Pts',(1.99997778260299,1.08693359713219,12.9269807984446));
#58920=CARTESIAN_POINT('Ctrl Pts',(1.99791745833382,-1.09071609741737,12.8158476804531));
#58921=CARTESIAN_POINT('Ctrl Pts',(0.167284438932658,-2.27009948944352,
12.7047145624615));
#58922=CARTESIAN_POINT('Ctrl Pts',(-1.81645388323103,-1.37179847848562,
12.59358144447));
#58923=CARTESIAN_POINT('Ctrl Pts',(-2.13770211653352,0.782026493444224,
12.4824483264784));
#58924=CARTESIAN_POINT('Ctrl Pts',(-0.50244123364914,2.2201100383111,12.3713152084868));
#58925=CARTESIAN_POINT('Ctrl Pts',(1.59267364216519,1.62626149343605,12.2601820904953));
#58926=CARTESIAN_POINT('Ctrl Pts',(2.23011091364624,-0.456005579260306,
12.1490489725037));
#58927=CARTESIAN_POINT('Ctrl Pts',(0.826462900648038,-2.12091839761294,
12.0379158545121));
#58928=CARTESIAN_POINT('Ctrl Pts',(-1.33359648828603,-1.84468321993554,
11.9267827365206));
#58929=CARTESIAN_POINT('Ctrl Pts',(-2.27309588129444,0.119878646650881,
11.815649618529));
#58930=CARTESIAN_POINT('Ctrl Pts',(-1.13216845556012,1.97472285744486,11.7045165005375));
#58931=CARTESIAN_POINT('Ctrl Pts',(1.04496410241899,2.02222298477103,11.5933833825459));
#58932=CARTESIAN_POINT('Ctrl Pts',(2.26570438447796,0.218905042513688,11.4822502645544));
#58933=CARTESIAN_POINT('Ctrl Pts',(1.41278283660713,-1.78476341067069,11.3711171465628));
#58934=CARTESIAN_POINT('Ctrl Pts',(-0.733173169917125,-2.15494614280595,
11.2599840285712));
#58935=CARTESIAN_POINT('Ctrl Pts',(-2.20810023391847,-0.552837347191554,
11.1488509105797));
#58936=CARTESIAN_POINT('Ctrl Pts',(-1.66208705385933,1.55524994803851,11.0377177925881));
#58937=CARTESIAN_POINT('Ctrl Pts',(0.405133617000831,2.23991127678228,10.9265846745966));
#58938=CARTESIAN_POINT('Ctrl Pts',(2.10156005567805,0.874517642966142,10.815451556605));
#58939=CARTESIAN_POINT('Ctrl Pts',(1.87455601480096,-1.29126895837161,10.7043184386134));
#58940=CARTESIAN_POINT('Ctrl Pts',(-0.0681154726277299,-2.27523538515673,
10.5931853206219));
#58941=CARTESIAN_POINT('Ctrl Pts',(-1.94844499850862,-1.17681683505431,
10.4820522026303));
#58942=CARTESIAN_POINT('Ctrl Pts',(-2.04548097170666,0.998670801549088,
10.3709190846388));
#58943=CARTESIAN_POINT('Ctrl Pts',(-0.270412250252138,2.26013561327502,
10.2597859666472));
#58944=CARTESIAN_POINT('Ctrl Pts',(1.75214840595539,1.45303535366084,10.1486528486557));
#58945=CARTESIAN_POINT('Ctrl Pts',(2.17107387714371,-0.683940052538099,
10.0375197306641));
#58946=CARTESIAN_POINT('Ctrl Pts',(0.602947083334242,-2.19494660303576,
9.92638661267257));
#58947=CARTESIAN_POINT('Ctrl Pts',(-1.51702061290722,-1.69705163017914,
9.81525349468102));
#58948=CARTESIAN_POINT('Ctrl Pts',(-2.24855133486928,0.354051789919607,
9.70412037668947));
#58949=CARTESIAN_POINT('Ctrl Pts',(-0.922119373035574,2.08111307653956,
9.5929872586979));
#58950=CARTESIAN_POINT('Ctrl Pts',(1.24827253325508,1.90345776370129,9.48185414070634));
#58951=CARTESIAN_POINT('Ctrl Pts',(2.27619628560175,-0.0163170138502123,
9.37072102271479));
#58952=CARTESIAN_POINT('Ctrl Pts',(1.22085560711622,-1.92115781808254,9.25958790472321));
#58953=CARTESIAN_POINT('Ctrl Pts',(-0.951860175340397,-2.06767937119391,
9.14845478673168));
#58954=CARTESIAN_POINT('Ctrl Pts',(-2.25339606060801,-0.321779380677577,
9.03732166874011));
#58955=CARTESIAN_POINT('Ctrl Pts',(-1.49253517814661,1.71862576406373,8.92618855074854));
#58956=CARTESIAN_POINT('Ctrl Pts',(0.634352644477827,2.18607696524379,8.815055432757));
#58957=CARTESIAN_POINT('Ctrl Pts',(2.18065595993346,0.652744484374632,8.70392231476542));
#58958=CARTESIAN_POINT('Ctrl Pts',(1.73113710929113,-1.47800543977982,8.59278919677388));
#58959=CARTESIAN_POINT('Ctrl Pts',(-0.302786557257382,-2.25602661284187,
8.48165607878231));
#58960=CARTESIAN_POINT('Ctrl Pts',(-2.05958805555566,-0.969243431346512,
8.37052296079076));
#58961=CARTESIAN_POINT('Ctrl Pts',(-1.93137348836714,1.20462948347381,8.25938984279919));
#58962=CARTESIAN_POINT('Ctrl Pts',(-0.0354899102847957,2.27597808908455,
8.14825672480764));
#58963=CARTESIAN_POINT('Ctrl Pts',(1.89287547599173,1.2642619509997,8.03712360681607));
#58964=CARTESIAN_POINT('Ctrl Pts',(2.08880663698666,-0.904556456960322,
7.92599048882451));
#58965=CARTESIAN_POINT('Ctrl Pts',(0.372979915022507,-2.24548924705253,
7.81485737083296));
#58966=CARTESIAN_POINT('Ctrl Pts',(-1.68421302236285,-1.53126179244943,
7.70372425284139));
#58967=CARTESIAN_POINT('Ctrl Pts',(-2.1999473063485,0.584436525404674,7.59259113484984));
#58968=CARTESIAN_POINT('Ctrl Pts',(-0.702204383050016,2.16523591235734,
7.48145801685828));
#58969=CARTESIAN_POINT('Ctrl Pts',(1.43822583980751,1.76432544278975,7.37032489886673));
#58970=CARTESIAN_POINT('Ctrl Pts',(2.26233094429135,-0.251363726831888,
7.25919178087516));
#58971=CARTESIAN_POINT('Ctrl Pts',(1.01586979002864,-2.03699757262616,7.1480586628836));
#58972=CARTESIAN_POINT('Ctrl Pts',(-1.16037079081492,-1.95828599664749,
7.03692554489204));
#58973=CARTESIAN_POINT('Ctrl Pts',(-2.2745649094144,-0.0872836816224959,
6.92579242690049));
#58974=CARTESIAN_POINT('Ctrl Pts',(-1.30704394918692,1.86362259325405,6.81465930890892));
#58975=CARTESIAN_POINT('Ctrl Pts',(0.85684255211621,2.10883277578949,6.70352619091737));
#58976=CARTESIAN_POINT('Ctrl Pts',(2.23630768420334,0.424023725637105,6.59239307292581));
#58977=CARTESIAN_POINT('Ctrl Pts',(1.56940836042156,-1.64899754610648,6.48125995493424));
#58978=CARTESIAN_POINT('Ctrl Pts',(-0.534625251570878,-2.21254481995457,
6.37012683694269));
#58979=CARTESIAN_POINT('Ctrl Pts',(-2.14791267874834,-0.751555390679831,
6.25899371895112));
#58980=CARTESIAN_POINT('Ctrl Pts',(-1.79811819165351,1.39819104970264,6.14786060095958));
#58981=CARTESIAN_POINT('Ctrl Pts',(0.202933570649542,2.26650129500845,6.03672748296801));
#58982=CARTESIAN_POINT('Ctrl Pts',(1.40468007074062,1.46490519210833,5.9626387376403));
#58983=CARTESIAN_POINT('Ctrl Pts',(1.7034384398826,0.898495708628642,5.92559436497645));
#58984=CARTESIAN_POINT('Ctrl Pts',(1.56668413629034,1.33340808976933,17.2259543899486));
#58985=CARTESIAN_POINT('Ctrl Pts',(2.01022411520002,0.81230048928636,17.1888972830873));
#58986=CARTESIAN_POINT('Ctrl Pts',(2.32861104756301,-0.698027455891402,
17.1147958035621));
#58987=CARTESIAN_POINT('Ctrl Pts',(0.673107002607527,-2.33823441438773,
17.003649951373));
#58988=CARTESIAN_POINT('Ctrl Pts',(-1.59780160896937,-1.83200895652609,
16.8925168333815));
#58989=CARTESIAN_POINT('Ctrl Pts',(-2.40654300422696,0.347834929994993,
16.7813837153899));
#58990=CARTESIAN_POINT('Ctrl Pts',(-1.01261911615652,2.2109379941875,16.6702505973984));
#58991=CARTESIAN_POINT('Ctrl Pts',(1.30804051943724,2.04966191741122,16.5591174794068));
#58992=CARTESIAN_POINT('Ctrl Pts',(2.43155773939052,0.0128949163846598,
16.4479843614153));
#58993=CARTESIAN_POINT('Ctrl Pts',(1.32960309170584,-2.03590447215423,16.3368512434237));
#58994=CARTESIAN_POINT('Ctrl Pts',(-0.989249039334683,-2.22124333766259,
16.2257181254322));
#58995=CARTESIAN_POINT('Ctrl Pts',(-2.40270549031482,-0.373676004989402,
16.1145850074406));
#58996=CARTESIAN_POINT('Ctrl Pts',(-1.61710922531016,1.81592735868504,16.003451889449));
#58997=CARTESIAN_POINT('Ctrl Pts',(0.648527961933474,2.34350523433166,15.8923187714575));
#58998=CARTESIAN_POINT('Ctrl Pts',(2.32060740288776,0.726223932436752,15.7811856534659));
#58999=CARTESIAN_POINT('Ctrl Pts',(1.86877531201183,-1.55573083439205,15.6700525354744));
#59000=CARTESIAN_POINT('Ctrl Pts',(-0.293433342465408,-2.4138170286812,
15.5589194174828));
#59001=CARTESIAN_POINT('Ctrl Pts',(-2.18708033426694,-1.06268416942158,
15.4477862994912));
#59002=CARTESIAN_POINT('Ctrl Pts',(-2.07902527870407,1.26105974792152,15.3366531814997));
#59003=CARTESIAN_POINT('Ctrl Pts',(-0.0681644808355317,2.43063179354339,
15.2255200635081));
#59004=CARTESIAN_POINT('Ctrl Pts',(2.00508314454678,1.37559413909997,15.1143869455165));
#59005=CARTESIAN_POINT('Ctrl Pts',(2.24319975059928,-0.938441511722162,
15.003253827525));
#59006=CARTESIAN_POINT('Ctrl Pts',(0.42825165663368,-2.39357850332972,14.8921207095334));
#59007=CARTESIAN_POINT('Ctrl Pts',(-1.77864921098529,-1.65801826504575,
14.7809875915419));
#59008=CARTESIAN_POINT('Ctrl Pts',(-2.35766031287977,0.595025562339573,
14.6698544735503));
#59009=CARTESIAN_POINT('Ctrl Pts',(-0.778847900281635,2.30347856778261,
14.5587213555588));
#59010=CARTESIAN_POINT('Ctrl Pts',(1.51279676604996,1.90369732778478,14.4475882375672));
#59011=CARTESIAN_POINT('Ctrl Pts',(2.41987028886597,-0.238422637401272,
14.3364551195756));
#59012=CARTESIAN_POINT('Ctrl Pts',(1.11218327821145,-2.16232881956578,14.2253220015841));
#59013=CARTESIAN_POINT('Ctrl Pts',(-1.21341764380403,-2.10718655817941,
14.1141888835925));
#59014=CARTESIAN_POINT('Ctrl Pts',(-2.42845097853889,-0.123464220405309,
14.003055765601));
#59015=CARTESIAN_POINT('Ctrl Pts',(-1.42087039482534,1.97325743123777,13.8919226476094));
#59016=CARTESIAN_POINT('Ctrl Pts',(0.887146699151091,2.26397621523506,13.7807895296178));
#59017=CARTESIAN_POINT('Ctrl Pts',(2.38321221630804,0.482614857772549,13.6696564116263));
#59018=CARTESIAN_POINT('Ctrl Pts',(1.69806811078246,-1.74045461303755,13.5585232936347));
#59019=CARTESIAN_POINT('Ctrl Pts',(-0.541214765041502,-2.37059151838093,
13.4473901756432));
#59020=CARTESIAN_POINT('Ctrl Pts',(-2.28515658589353,-0.831069760523239,
13.3362570576516));
#59021=CARTESIAN_POINT('Ctrl Pts',(-1.93763315644923,1.46907975274924,13.22512393966));
#59022=CARTESIAN_POINT('Ctrl Pts',(0.183288402275368,2.42466965389163,13.1139908216685));
#59023=CARTESIAN_POINT('Ctrl Pts',(2.13645720107629,1.16110645372394,13.0028577036769));
#59024=CARTESIAN_POINT('Ctrl Pts',(2.1342562793162,-1.16514707359613,12.8917245856853));
#59025=CARTESIAN_POINT('Ctrl Pts',(0.178700007217345,-2.42501213941933,
12.7805914676938));
#59026=CARTESIAN_POINT('Ctrl Pts',(-1.94040954505056,-1.46541064769812,
12.6694583497022));
#59027=CARTESIAN_POINT('Ctrl Pts',(-2.28357990791274,0.835392346797389,
12.5583252317107));
#59028=CARTESIAN_POINT('Ctrl Pts',(-0.536728058223856,2.3716113847816,12.4471921137191));
#59029=CARTESIAN_POINT('Ctrl Pts',(1.70135843576202,1.7372383376992,12.3360589957276));
#59030=CARTESIAN_POINT('Ctrl Pts',(2.38229472452301,-0.487123613080176,
12.224925877736));
#59031=CARTESIAN_POINT('Ctrl Pts',(0.882861115193896,-2.26565086016999,
12.1137927597444));
#59032=CARTESIAN_POINT('Ctrl Pts',(-1.42460173583554,-1.97056526488335,
12.0026596417529));
#59033=CARTESIAN_POINT('Ctrl Pts',(-2.42821300645037,0.128059221517559,
11.8915265237613));
#59034=CARTESIAN_POINT('Ctrl Pts',(-1.20942816002921,2.10947886802376,11.7803934057698));
#59035=CARTESIAN_POINT('Ctrl Pts',(1.11627294107919,2.16022042623544,11.6692602877782));
#59036=CARTESIAN_POINT('Ctrl Pts',(2.4203171104371,0.233843224909024,11.5581271697867));
#59037=CARTESIAN_POINT('Ctrl Pts',(1.50919179756981,-1.90655649983379,11.4469940517951));
#59038=CARTESIAN_POINT('Ctrl Pts',(-0.783205249643668,-2.30200067459613,
11.3358609338036));
#59039=CARTESIAN_POINT('Ctrl Pts',(-2.35878202572504,-0.590563226104481,
11.224727815812));
#59040=CARTESIAN_POINT('Ctrl Pts',(-1.77550865110702,1.66138093126007,11.1135946978204));
#59041=CARTESIAN_POINT('Ctrl Pts',(0.432780124343675,2.39276386901915,11.0024615798289));
#59042=CARTESIAN_POINT('Ctrl Pts',(2.24497149593532,0.934195135583745,10.8913284618373));
#59043=CARTESIAN_POINT('Ctrl Pts',(2.00247659322994,-1.37938575550013,10.7801953438457));
#59044=CARTESIAN_POINT('Ctrl Pts',(-0.0727637043101689,-2.43049851105601,
10.6690622258542));
#59045=CARTESIAN_POINT('Ctrl Pts',(-2.08140779571408,-1.25712336580426,
10.5579291078626));
#59046=CARTESIAN_POINT('Ctrl Pts',(-2.18506554906801,1.06682056372509,10.4467959898711));
#59047=CARTESIAN_POINT('Ctrl Pts',(-0.288865308572835,2.41436832368498,
10.3356628718795));
#59048=CARTESIAN_POINT('Ctrl Pts',(1.87171583195574,1.55219116519724,10.2245297538879));
#59049=CARTESIAN_POINT('Ctrl Pts',(2.31922897306156,-0.730612441328091,
10.1133966358964));
#59050=CARTESIAN_POINT('Ctrl Pts',(0.644092474057795,-2.3447307849242,10.0022635179048));
#59051=CARTESIAN_POINT('Ctrl Pts',(-1.62054280843487,-1.81285922645382,
9.89113039991323));
#59052=CARTESIAN_POINT('Ctrl Pts',(-2.4019935287075,0.378212449511917,9.77999728192169));
#59053=CARTESIAN_POINT('Ctrl Pts',(-0.985045229957374,2.22312920538556,
9.66886416393011));
#59054=CARTESIAN_POINT('Ctrl Pts',(1.33345523424144,2.03335061098098,9.55773104593856));
#59055=CARTESIAN_POINT('Ctrl Pts',(2.43152498379642,-0.0174304945002811,
9.44659792794699));
#59056=CARTESIAN_POINT('Ctrl Pts',(1.30416736425096,-2.05225852534442,9.33546480995544));
#59057=CARTESIAN_POINT('Ctrl Pts',(-1.01681555850934,-2.20877877770956,
9.22433169196388));
#59058=CARTESIAN_POINT('Ctrl Pts',(-2.40716886079459,-0.343737755982333,
9.11319857397231));
#59059=CARTESIAN_POINT('Ctrl Pts',(-1.59438647616416,1.83590558931627,9.00206545598079));
#59060=CARTESIAN_POINT('Ctrl Pts',(0.67764116536962,2.33525587890453,8.89093233798919));
#59061=CARTESIAN_POINT('Ctrl Pts',(2.32946494165861,0.697288073015479,8.77979921999766));
#59062=CARTESIAN_POINT('Ctrl Pts',(1.84927071458852,-1.57886522166149,8.66866610200607));
#59063=CARTESIAN_POINT('Ctrl Pts',(-0.323448853416607,-2.40997892314214,
8.55753298401454));
#59064=CARTESIAN_POINT('Ctrl Pts',(-2.2001353069111,-1.0353850560285,8.44639986602296));
#59065=CARTESIAN_POINT('Ctrl Pts',(-2.06317131774303,1.28683396234873,8.33526674803142));
#59066=CARTESIAN_POINT('Ctrl Pts',(-0.0379117583470447,2.43129189744692,
8.22413363003985));
#59067=CARTESIAN_POINT('Ctrl Pts',(2.02204618301303,1.3505357773248,8.1130005120483));
#59068=CARTESIAN_POINT('Ctrl Pts',(2.23134777799278,-0.966283812282007,
8.00186739405672));
#59069=CARTESIAN_POINT('Ctrl Pts',(0.398432238716943,-2.39872248258723,
7.89073427606518));
#59070=CARTESIAN_POINT('Ctrl Pts',(-1.79914450604067,-1.63575581272393,
7.7796011580736));
#59071=CARTESIAN_POINT('Ctrl Pts',(-2.35007273856783,0.624318747005141,
7.66846804008207));
#59072=CARTESIAN_POINT('Ctrl Pts',(-0.750123138289054,2.3129926228301,7.55733492209049));
#59073=CARTESIAN_POINT('Ctrl Pts',(1.53637104319808,1.884723835474,7.44620180409894));
#59074=CARTESIAN_POINT('Ctrl Pts',(2.41671346511573,-0.26851690501302,7.33506868610738));
#59075=CARTESIAN_POINT('Ctrl Pts',(1.08519321921556,-2.17600323886998,7.22393556811581));
#59076=CARTESIAN_POINT('Ctrl Pts',(-1.23955503582072,-2.09192034816464,
7.11280245012427));
#59077=CARTESIAN_POINT('Ctrl Pts',(-2.42978228173572,-0.0932399608440297,
7.00166933213269));
#59078=CARTESIAN_POINT('Ctrl Pts',(-1.39623723906031,1.99079706988747,6.89053621414115));
#59079=CARTESIAN_POINT('Ctrl Pts',(0.915313888274649,2.25274050986571,6.77940309614957));
#59080=CARTESIAN_POINT('Ctrl Pts',(2.38891436559868,0.452959302820622,6.66826997815803));
#59081=CARTESIAN_POINT('Ctrl Pts',(1.67650552032034,-1.76152590922838,6.55713686016647));
#59082=CARTESIAN_POINT('Ctrl Pts',(-0.571108328568143,-2.36352991238919,
6.4460037421749));
#59083=CARTESIAN_POINT('Ctrl Pts',(-2.2944872436645,-0.802841881741225,
6.33487062418334));
#59084=CARTESIAN_POINT('Ctrl Pts',(-1.92082261731153,1.49360426030822,6.2237375061918));
#59085=CARTESIAN_POINT('Ctrl Pts',(0.216781852341404,2.42116840251458,6.11260438820022));
#59086=CARTESIAN_POINT('Ctrl Pts',(1.50053609517415,1.56487100696715,6.03851564287252));
#59087=CARTESIAN_POINT('Ctrl Pts',(1.81968187503599,0.95980947565199,6.00147127020867));
#59088=CARTESIAN_POINT('Ctrl Pts',(1.26907087985245,1.07935865304843,17.));
#59089=CARTESIAN_POINT('Ctrl Pts',(1.31463335343697,1.03685370088427,17.));
#59090=CARTESIAN_POINT('Ctrl Pts',(1.35743963235178,0.991755207691644,17.));
#59091=CARTESIAN_POINT('Ctrl Pts',(1.39749071248986,0.944412965608489,17.));
#59092=CARTESIAN_POINT('Ctrl Pts',(1.43900564122184,0.895340386309302,17.));
#59093=CARTESIAN_POINT('Ctrl Pts',(1.47756084223886,0.843856601716214,17.));
#59094=CARTESIAN_POINT('Ctrl Pts',(1.51313081159997,0.790300559584653,17.));
#59095=CARTESIAN_POINT('Ctrl Pts',(1.54562908903941,0.74136942056454,17.));
#59096=CARTESIAN_POINT('Ctrl Pts',(1.5756353908389,0.690707426732232,17.));
#59097=CARTESIAN_POINT('Ctrl Pts',(1.60310603850295,0.638543833142686,17.));
#59098=CARTESIAN_POINT('Ctrl Pts',(1.61661334372111,0.612895017413743,17.));
#59099=CARTESIAN_POINT('Ctrl Pts',(1.62950722716312,0.586882786829157,17.));
#59100=CARTESIAN_POINT('Ctrl Pts',(1.64178012375449,0.560532523386325,17.));
#59101=CARTESIAN_POINT('Ctrl Pts',(1.64738432617045,0.548500138940798,17.));
#59102=CARTESIAN_POINT('Ctrl Pts',(1.65285961119358,0.536395613146207,17.));
#59103=CARTESIAN_POINT('Ctrl Pts',(1.65819677046436,0.524241257566197,17.));
#59104=CARTESIAN_POINT('Ctrl Pts',(1.68515739063045,0.462843621196213,17.));
#59105=CARTESIAN_POINT('Ctrl Pts',(1.70864881961265,0.400067692729951,17.));
#59106=CARTESIAN_POINT('Ctrl Pts',(1.72864695641584,0.336272032400955,17.));
#59107=CARTESIAN_POINT('Ctrl Pts',(1.74902990067328,0.271248805429877,17.));
#59108=CARTESIAN_POINT('Ctrl Pts',(1.76578439667341,0.205165384088333,17.));
#59109=CARTESIAN_POINT('Ctrl Pts',(1.77884521789635,0.138364590989932,17.));
#59110=CARTESIAN_POINT('Ctrl Pts',(1.7896907150818,0.0828942801137585,17.));
#59111=CARTESIAN_POINT('Ctrl Pts',(1.79798870333448,0.0269283684180995,
17.));
#59112=CARTESIAN_POINT('Ctrl Pts',(1.80367735161904,-0.029348946606401,
17.));
#59113=CARTESIAN_POINT('Ctrl Pts',(1.80631029137596,-0.0553963963218251,
17.));
#59114=CARTESIAN_POINT('Ctrl Pts',(1.80838392210809,-0.0815106672623466,
17.));
#59115=CARTESIAN_POINT('Ctrl Pts',(1.80989031432926,-0.107673896123635,
17.));
#59116=CARTESIAN_POINT('Ctrl Pts',(1.81054780481405,-0.119093281981834,
17.));
#59117=CARTESIAN_POINT('Ctrl Pts',(1.81109711555612,-0.130521751152742,
17.));
#59118=CARTESIAN_POINT('Ctrl Pts',(1.81153725496673,-0.141943752396311,
17.));
#59119=CARTESIAN_POINT('Ctrl Pts',(1.81423915749931,-0.212060477559016,
17.));
#59120=CARTESIAN_POINT('Ctrl Pts',(1.8128391711499,-0.28206475899935,17.));
#59121=CARTESIAN_POINT('Ctrl Pts',(1.80728215470532,-0.351596341136129,
17.));
#59122=CARTESIAN_POINT('Ctrl Pts',(1.80231577265823,-0.413737672671453,
17.));
#59123=CARTESIAN_POINT('Ctrl Pts',(1.79402871946725,-0.475502410193276,
17.));
#59124=CARTESIAN_POINT('Ctrl Pts',(1.78234854127328,-0.536645515067971,
17.));
#59125=CARTESIAN_POINT('Ctrl Pts',(1.76958920689471,-0.603437759765362,
17.));
#59126=CARTESIAN_POINT('Ctrl Pts',(1.75278190243293,-0.669489034899465,
17.));
#59127=CARTESIAN_POINT('Ctrl Pts',(1.73217389519949,-0.734583882594501,
17.));
#59128=CARTESIAN_POINT('Ctrl Pts',(1.7242846189666,-0.759503867772431,17.));
#59129=CARTESIAN_POINT('Ctrl Pts',(1.7158377768979,-0.78428363611299,17.));
#59130=CARTESIAN_POINT('Ctrl Pts',(1.70684526783583,-0.808910785136196,
17.));
#59131=CARTESIAN_POINT('Ctrl Pts',(1.7028767076987,-0.819779200305976,17.));
#59132=CARTESIAN_POINT('Ctrl Pts',(1.69880197156565,-0.830617330567754,
17.));
#59133=CARTESIAN_POINT('Ctrl Pts',(1.69462717263472,-0.841411562228869,
17.));
#59134=CARTESIAN_POINT('Ctrl Pts',(1.66964189956069,-0.906012715515375,
17.));
#59135=CARTESIAN_POINT('Ctrl Pts',(1.64103489494096,-0.969158501636665,
17.));
#59136=CARTESIAN_POINT('Ctrl Pts',(1.60911056531399,-1.03063593785474,17.));
#59137=CARTESIAN_POINT('Ctrl Pts',(1.57635918906639,-1.09370603730061,17.));
#59138=CARTESIAN_POINT('Ctrl Pts',(1.54011611570736,-1.15502101490558,17.));
#59139=CARTESIAN_POINT('Ctrl Pts',(1.50065541627137,-1.21434743041401,17.));
#59140=CARTESIAN_POINT('Ctrl Pts',(1.46751534688147,-1.26417121850455,17.));
#59141=CARTESIAN_POINT('Ctrl Pts',(1.43210475062568,-1.31259265519435,17.));
#59142=CARTESIAN_POINT('Ctrl Pts',(1.39455982747634,-1.3594652647581,17.));
#59143=CARTESIAN_POINT('Ctrl Pts',(1.37456954356258,-1.38442194849485,17.));
#59144=CARTESIAN_POINT('Ctrl Pts',(1.35397457645813,-1.40893853932649,17.));
#59145=CARTESIAN_POINT('Ctrl Pts',(1.33279075072117,-1.43299413795622,17.));
#59146=CARTESIAN_POINT('Ctrl Pts',(1.31937221833251,-1.44823174580618,17.));
#59147=CARTESIAN_POINT('Ctrl Pts',(1.3057160205887,-1.46328534776906,17.));
#59148=CARTESIAN_POINT('Ctrl Pts',(1.29185135791409,-1.47812325485253,17.));
#59149=CARTESIAN_POINT('Ctrl Pts',(1.24079790013097,-1.53276046317518,17.));
#59150=CARTESIAN_POINT('Ctrl Pts',(1.1868605733564,-1.58454679540276,17.));
#59151=CARTESIAN_POINT('Ctrl Pts',(1.1303228346641,-1.63321750971738,17.));
#59152=CARTESIAN_POINT('Ctrl Pts',(1.08987767577489,-1.66803486922337,17.));
#59153=CARTESIAN_POINT('Ctrl Pts',(1.04810062967973,-1.70125755846181,17.));
#59154=CARTESIAN_POINT('Ctrl Pts',(1.00508147489063,-1.73278020099862,17.));
#59155=CARTESIAN_POINT('Ctrl Pts',(0.991017431819989,-1.7430857452268,17.));
#59156=CARTESIAN_POINT('Ctrl Pts',(0.976820548550378,-1.75320951848906,
17.));
#59157=CARTESIAN_POINT('Ctrl Pts',(0.962493729450331,-1.76314761869876,
17.));
#59158=CARTESIAN_POINT('Ctrl Pts',(0.948700205378558,-1.77271578756534,
17.));
#59159=CARTESIAN_POINT('Ctrl Pts',(0.934793273211275,-1.78210690615323,
17.));
#59160=CARTESIAN_POINT('Ctrl Pts',(0.920780914430478,-1.79131474048402,
17.));
#59161=CARTESIAN_POINT('Ctrl Pts',(0.857817216437198,-1.83268959457145,
17.));
#59162=CARTESIAN_POINT('Ctrl Pts',(0.792697129221742,-1.87038775038027,
17.));
#59163=CARTESIAN_POINT('Ctrl Pts',(0.725682411188942,-1.90412957333601,
17.));
#59164=CARTESIAN_POINT('Ctrl Pts',(0.674447265301284,-1.92992640233717,
17.));
#59165=CARTESIAN_POINT('Ctrl Pts',(0.622103705214267,-1.95341028870243,
17.));
#59166=CARTESIAN_POINT('Ctrl Pts',(0.56875484042429,-1.97444100905915,17.));
#59167=CARTESIAN_POINT('Ctrl Pts',(0.556450338865399,-1.97929158146463,
17.));
#59168=CARTESIAN_POINT('Ctrl Pts',(0.544092316022985,-1.98401158984533,
17.));
#59169=CARTESIAN_POINT('Ctrl Pts',(0.531682642424069,-1.98860160490479,
17.));
#59170=CARTESIAN_POINT('Ctrl Pts',(-0.530822314817812,-1.98761604614028,
16.9985408643923));
#59171=CARTESIAN_POINT('Ctrl Pts',(-1.19172355532747,-1.81111257755813,
16.9614964917284));
#59172=CARTESIAN_POINT('Ctrl Pts',(-2.31220282305949,-0.750101418116348,
16.8874077464009));
#59173=CARTESIAN_POINT('Ctrl Pts',(-1.88356022517535,1.54029064361322,16.7762746284092));
#59174=CARTESIAN_POINT('Ctrl Pts',(0.272138683002673,2.41558334409046,16.6651415104176));
#59175=CARTESIAN_POINT('Ctrl Pts',(2.17716537292403,1.08271362067439,16.5540083924261));
#59176=CARTESIAN_POINT('Ctrl Pts',(2.09039692632852,-1.24248312461781,16.4428752744345));
#59177=CARTESIAN_POINT('Ctrl Pts',(0.0899798428231618,-2.42978715040514,
16.331742156443));
#59178=CARTESIAN_POINT('Ctrl Pts',(-1.99256263878865,-1.39363276224998,
16.2206090384514));
#59179=CARTESIAN_POINT('Ctrl Pts',(-2.25155255412213,0.918227258501085,
16.1094759204598));
#59180=CARTESIAN_POINT('Ctrl Pts',(-0.449770559963355,2.38958586423339,
15.9983428024683));
#59181=CARTESIAN_POINT('Ctrl Pts',(1.76362649251955,1.67395571200075,15.8872096844767));
#59182=CARTESIAN_POINT('Ctrl Pts',(2.36290026085259,-0.573773007815998,
15.7760765664852));
#59183=CARTESIAN_POINT('Ctrl Pts',(0.799545757360654,-2.29634721328381,
15.6649434484936));
#59184=CARTESIAN_POINT('Ctrl Pts',(-1.4955798077745,-1.91722185216344,15.553810330502));
#59185=CARTESIAN_POINT('Ctrl Pts',(-2.42189432006925,0.216624485203865,
15.4426772125105));
#59186=CARTESIAN_POINT('Ctrl Pts',(-1.13159454186566,2.15220543372035,15.3315440945189));
#59187=CARTESIAN_POINT('Ctrl Pts',(1.19438442805909,2.11800437629149,15.2204109765274));
#59188=CARTESIAN_POINT('Ctrl Pts',(2.42721611075584,0.145321765122002,15.1092778585358));
#59189=CARTESIAN_POINT('Ctrl Pts',(1.43856389040869,-1.96036473920531,14.9981447405443));
#59190=CARTESIAN_POINT('Ctrl Pts',(-0.86671852734562,-2.27184843524121,
14.8870116225527));
#59191=CARTESIAN_POINT('Ctrl Pts',(-2.37874608563758,-0.504046940381654,
14.7758785045611));
#59192=CARTESIAN_POINT('Ctrl Pts',(-1.71365157339857,1.72507810949981,14.6647453865696));
#59193=CARTESIAN_POINT('Ctrl Pts',(0.519844293652045,2.37534379814029,14.553612268578));
#59194=CARTESIAN_POINT('Ctrl Pts',(2.27755820952083,0.851601338069138,14.4424791505865));
#59195=CARTESIAN_POINT('Ctrl Pts',(1.95076120442826,-1.45156017900596,14.3313460325949));
#59196=CARTESIAN_POINT('Ctrl Pts',(-0.161449234185697,-2.4261966907003,
14.2202129146033));
#59197=CARTESIAN_POINT('Ctrl Pts',(-2.12589498013164,-1.18028249516839,
14.1090797966117));
#59198=CARTESIAN_POINT('Ctrl Pts',(-2.14463796530634,1.14587269450434,13.9979466786202));
#59199=CARTESIAN_POINT('Ctrl Pts',(-0.200523872789563,2.42328009352997,
13.8868135606286));
#59200=CARTESIAN_POINT('Ctrl Pts',(1.92711756079595,1.4828061713343,13.7756804426371));
#59201=CARTESIAN_POINT('Ctrl Pts',(2.29098515205495,-0.814790321419068,
13.6645473246455));
#59202=CARTESIAN_POINT('Ctrl Pts',(0.558052959897197,-2.36665864224302,
13.553414206654));
#59203=CARTESIAN_POINT('Ctrl Pts',(-1.68563126593031,-1.7524678228742,13.4422810886624));
#59204=CARTESIAN_POINT('Ctrl Pts',(-2.38655941136709,0.465650524431861,
13.3311479706708));
#59205=CARTESIAN_POINT('Ctrl Pts',(-0.903214449463494,2.25758718396156,
13.2200148526793));
#59206=CARTESIAN_POINT('Ctrl Pts',(1.40678792676647,1.98329119495888,13.1088817346877));
#59207=CARTESIAN_POINT('Ctrl Pts',(2.42924262178492,-0.106190957248261,
12.9977486166962));
#59208=CARTESIAN_POINT('Ctrl Pts',(1.22835885528878,-2.09848296574785,12.8866154987046));
#59209=CARTESIAN_POINT('Ctrl Pts',(-1.09676728330151,-2.17016076850958,
12.7754823807131));
#59210=CARTESIAN_POINT('Ctrl Pts',(-2.41808883587442,-0.255622019236254,
12.6643492627215));
#59211=CARTESIAN_POINT('Ctrl Pts',(-1.52628031080604,1.89287206322695,12.5532161447299));
#59212=CARTESIAN_POINT('Ctrl Pts',(0.762440028519717,2.30893513070632,12.4420830267384));
#59213=CARTESIAN_POINT('Ctrl Pts',(2.35334524439711,0.611769887762175,12.3309499087468));
#59214=CARTESIAN_POINT('Ctrl Pts',(1.79037626583608,-1.64531123549009,12.2198167907553));
#59215=CARTESIAN_POINT('Ctrl Pts',(-0.411215539741278,-2.39653875720262,
12.1086836727637));
#59216=CARTESIAN_POINT('Ctrl Pts',(-2.23644669806148,-0.954359681477023,
11.9975505547722));
#59217=CARTESIAN_POINT('Ctrl Pts',(-2.01479381263157,1.36128693796739,11.8864174367806));
#59218=CARTESIAN_POINT('Ctrl Pts',(0.0508776716304708,2.43103017205227,
11.775284318789));
#59219=CARTESIAN_POINT('Ctrl Pts',(2.06998390829065,1.27579890825976,11.6641512007974));
#59220=CARTESIAN_POINT('Ctrl Pts',(2.19455939831053,-1.0470937313278,11.5530180828059));
#59221=CARTESIAN_POINT('Ctrl Pts',(0.310587749980402,-2.41164497479648,
11.4418849648143));
#59222=CARTESIAN_POINT('Ctrl Pts',(-1.8576460317465,-1.5689638159102,11.3307518468228));
#59223=CARTESIAN_POINT('Ctrl Pts',(-2.3256890489837,0.709694781111127,11.2196187288312));
#59224=CARTESIAN_POINT('Ctrl Pts',(-0.665169910362038,2.33881278114516,
11.1084856108397));
#59225=CARTESIAN_POINT('Ctrl Pts',(1.6041389110555,1.82735726910112,10.9973524928481));
#59226=CARTESIAN_POINT('Ctrl Pts',(2.40527666278277,-0.3565675397055,10.8862193748566));
#59227=CARTESIAN_POINT('Ctrl Pts',(1.00501054196433,-2.21414770181206,10.775086256865));
#59228=CARTESIAN_POINT('Ctrl Pts',(-1.31508078368933,-2.04525273921589,
10.6639531388734));
#59229=CARTESIAN_POINT('Ctrl Pts',(-2.43155841503526,-0.00446196932597716,
10.5528200208819));
#59230=CARTESIAN_POINT('Ctrl Pts',(-1.32257807973431,2.04041257051249,10.4416869028903));
#59231=CARTESIAN_POINT('Ctrl Pts',(0.996877770305409,2.21782121596171,10.3305537848988));
#59232=CARTESIAN_POINT('Ctrl Pts',(2.40395184823498,0.365392591970382,10.2194206669072));
#59233=CARTESIAN_POINT('Ctrl Pts',(1.61083457603706,-1.82145771390455,10.1082875489157));
#59234=CARTESIAN_POINT('Ctrl Pts',(-0.656581901980842,-2.34123822813698,
9.99715443092411));
#59235=CARTESIAN_POINT('Ctrl Pts',(-2.32306878049448,-0.718225365739856,
9.88602131293258));
#59236=CARTESIAN_POINT('Ctrl Pts',(-1.86339167600253,1.56213562045755,9.77488819494099));
#59237=CARTESIAN_POINT('Ctrl Pts',(0.301734832747034,2.41276860175285,9.66375507694945));
#59238=CARTESIAN_POINT('Ctrl Pts',(2.19070174640221,1.05514079307809,9.55262195895788));
#59239=CARTESIAN_POINT('Ctrl Pts',(2.07465219656388,-1.26819339936035,9.44148884096632));
#59240=CARTESIAN_POINT('Ctrl Pts',(0.059799298926456,-2.43082707709519,
9.33035572297477));
#59241=CARTESIAN_POINT('Ctrl Pts',(-2.00978427078675,-1.36867213745724,
9.21922260498321));
#59242=CARTESIAN_POINT('Ctrl Pts',(-2.23993417149811,0.946145412803733,
9.10808948699165));
#59243=CARTESIAN_POINT('Ctrl Pts',(-0.420008155580443,2.39501344132368,
8.99695636900008));
#59244=CARTESIAN_POINT('Ctrl Pts',(1.78432585582941,1.65187090157668,8.88582325100852));
#59245=CARTESIAN_POINT('Ctrl Pts',(2.35557461332577,-0.603128904380432,
8.77469013301699));
#59246=CARTESIAN_POINT('Ctrl Pts',(0.770908770722433,-2.30612139796956,
8.6635570150254));
#59247=CARTESIAN_POINT('Ctrl Pts',(-1.51932312253082,-1.8984608203825,8.55242389703386));
#59248=CARTESIAN_POINT('Ctrl Pts',(-2.41901069213679,0.246745823280066,
8.44129077904229));
#59249=CARTESIAN_POINT('Ctrl Pts',(-1.10472446865624,2.16612097656366,8.33015766105073));
#59250=CARTESIAN_POINT('Ctrl Pts',(1.22064907711907,2.10297695649155,8.21902454305917));
#59251=CARTESIAN_POINT('Ctrl Pts',(2.42883652976957,0.115105649486712,8.10789142506762));
#59252=CARTESIAN_POINT('Ctrl Pts',(1.41405721802439,-1.97811487082963,7.99675830707606));
#59253=CARTESIAN_POINT('Ctrl Pts',(-0.89492296554583,-2.26088681806294,
7.88562518908451));
#59254=CARTESIAN_POINT('Ctrl Pts',(-2.38483433335392,-0.474406133986129,
7.77449207109293));
#59255=CARTESIAN_POINT('Ctrl Pts',(-1.69205163242953,1.74626966328898,7.66335895310138));
#59256=CARTESIAN_POINT('Ctrl Pts',(0.549363663544479,2.368690833595,7.55222583510981));
#59257=CARTESIAN_POINT('Ctrl Pts',(2.28797905753948,0.823192728573481,7.44109271711826));
#59258=CARTESIAN_POINT('Ctrl Pts',(1.93254721410632,-1.47572339224646,7.32995959912669));
#59259=CARTESIAN_POINT('Ctrl Pts',(-0.191630291862095,-2.4240000872683,
7.21882648113514));
#59260=CARTESIAN_POINT('Ctrl Pts',(-2.14041565072953,-1.15373514472855,
7.10769336314358));
#59261=CARTESIAN_POINT('Ctrl Pts',(-2.13021707383623,1.17247103400131,6.99656024515202));
#59262=CARTESIAN_POINT('Ctrl Pts',(-0.170343340793051,2.42559050070374,
6.88542712716047));
#59263=CARTESIAN_POINT('Ctrl Pts',(1.94540352455545,1.45870466023832,6.77429400916891));
#59264=CARTESIAN_POINT('Ctrl Pts',(2.28070125668873,-0.843227122409361,
6.66316089117734));
#59265=CARTESIAN_POINT('Ctrl Pts',(0.528495394995496,-2.37343859473579,
6.55202777318578));
#59266=CARTESIAN_POINT('Ctrl Pts',(-1.70718858770076,-1.73132004390081,
6.44089465519424));
#59267=CARTESIAN_POINT('Ctrl Pts',(-2.38080986332144,0.495245413179216,
6.32976153720266));
#59268=CARTESIAN_POINT('Ctrl Pts',(-0.874610928483785,2.26878239794609,
6.21862841921112));
#59269=CARTESIAN_POINT('Ctrl Pts',(1.43051727062736,1.96538105553873,6.10749530121955));
#59270=CARTESIAN_POINT('Ctrl Pts',(2.42936606799034,-0.135922390952342,
5.99636218322799));
#59271=CARTESIAN_POINT('Ctrl Pts',(1.19867795027514,-2.1148820515815,5.88521633177802));
#59272=CARTESIAN_POINT('Ctrl Pts',(-0.344613920714289,-2.14055559361498,
5.81111485299191));
#59273=CARTESIAN_POINT('Ctrl Pts',(-0.951346992282116,-1.82409669095297,
5.77405774686964));
#59274=CARTESIAN_POINT('Ctrl Pts',(-0.496914232204698,-1.8606503040938,
17.0744136915879));
#59275=CARTESIAN_POINT('Ctrl Pts',(-1.11559815585193,-1.69542159549652,
17.037369318924));
#59276=CARTESIAN_POINT('Ctrl Pts',(-2.16450299553907,-0.702186136215599,
16.9632805735963));
#59277=CARTESIAN_POINT('Ctrl Pts',(-1.76324140296468,1.44189933463109,16.8521474556048));
#59278=CARTESIAN_POINT('Ctrl Pts',(0.25475489809407,2.26127973381666,16.7410143376132));
#59279=CARTESIAN_POINT('Ctrl Pts',(2.03809152228371,1.01355160191342,16.6298812196215));
#59280=CARTESIAN_POINT('Ctrl Pts',(1.95686570562903,-1.16311528483624,16.51874810163));
#59281=CARTESIAN_POINT('Ctrl Pts',(0.0842320740146667,-2.27457622364427,
16.4076149836385));
#59282=CARTESIAN_POINT('Ctrl Pts',(-1.86528091629542,-1.30460972475591,
16.296481865647));
#59283=CARTESIAN_POINT('Ctrl Pts',(-2.10772696902188,0.859572366139308,
16.1853487476554));
#59284=CARTESIAN_POINT('Ctrl Pts',(-0.421039934142888,2.23694293149729,
16.0742156296637));
#59285=CARTESIAN_POINT('Ctrl Pts',(1.65096884581237,1.56702609169514,15.9630825116722));
#59286=CARTESIAN_POINT('Ctrl Pts',(2.21196196188707,-0.537121303456362,
15.8519493936807));
#59287=CARTESIAN_POINT('Ctrl Pts',(0.748472049950942,-2.14966021682032,
15.7408162756892));
#59288=CARTESIAN_POINT('Ctrl Pts',(-1.40004455565548,-1.79475277892349,
15.6296831576976));
#59289=CARTESIAN_POINT('Ctrl Pts',(-2.26718757471825,0.202786858685022,
15.518550039706));
#59290=CARTESIAN_POINT('Ctrl Pts',(-1.0593100878421,2.01472598417605,15.4074169217145));
#59291=CARTESIAN_POINT('Ctrl Pts',(1.11808905627853,1.98270963573244,15.296283803723));
#59292=CARTESIAN_POINT('Ctrl Pts',(2.272169417906,0.136038842607842,15.1851506857314));
#59293=CARTESIAN_POINT('Ctrl Pts',(1.34667072412956,-1.83513976716994,15.0740175677399));
#59294=CARTESIAN_POINT('Ctrl Pts',(-0.811353930554621,-2.12672638163449,
14.9628844497482));
#59295=CARTESIAN_POINT('Ctrl Pts',(-2.22679558066473,-0.471849225970919,
14.8517513317567));
#59296=CARTESIAN_POINT('Ctrl Pts',(-1.60418624479641,1.61488287200104,14.740618213765));
#59297=CARTESIAN_POINT('Ctrl Pts',(0.486637469517006,2.22361062586486,14.6294850957736));
#59298=CARTESIAN_POINT('Ctrl Pts',(2.13207142464232,0.79720240321163,14.518351977782));
#59299=CARTESIAN_POINT('Ctrl Pts',(1.82614969087327,-1.35883683054512,14.4072188597905));
#59300=CARTESIAN_POINT('Ctrl Pts',(-0.151136114677013,-2.27121511677727,
14.2960857417988));
#59301=CARTESIAN_POINT('Ctrl Pts',(-1.99009620038771,-1.10488793236309,
14.1849526238074));
#59302=CARTESIAN_POINT('Ctrl Pts',(-2.00764191357142,1.07267617486913,14.0738195058158));
#59303=CARTESIAN_POINT('Ctrl Pts',(-0.187714727705331,2.26848482718112,
13.9626863878241));
#59304=CARTESIAN_POINT('Ctrl Pts',(1.80401636547585,1.38808687873242,13.8515532698327));
#59305=CARTESIAN_POINT('Ctrl Pts',(2.14464067550829,-0.76274281557801,13.7404201518411));
#59306=CARTESIAN_POINT('Ctrl Pts',(0.522405427119336,-2.21548026387029,
13.6292870338496));
#59307=CARTESIAN_POINT('Ctrl Pts',(-1.57795582986649,-1.64052297418177,
13.518153915858));
#59308=CARTESIAN_POINT('Ctrl Pts',(-2.23410980361178,0.435905511815549,
13.4070207978665));
#59309=CARTESIAN_POINT('Ctrl Pts',(-0.845518551392067,2.11337611633463,
13.2958876798749));
#59310=CARTESIAN_POINT('Ctrl Pts',(1.31692455835042,1.85660171750613,13.1847545618833));
#59311=CARTESIAN_POINT('Ctrl Pts',(2.27406647864359,-0.0994076483130035,
13.0736214438918));
#59312=CARTESIAN_POINT('Ctrl Pts',(1.14989325129853,-1.96443522175046,12.9624883259002));
#59313=CARTESIAN_POINT('Ctrl Pts',(-1.02670753899269,-2.03153436082434,
12.8513552079086));
#59314=CARTESIAN_POINT('Ctrl Pts',(-2.26362517878265,-0.239293292458876,
12.7402220899171));
#59315=CARTESIAN_POINT('Ctrl Pts',(-1.42878395953199,1.77195841565734,12.6290889719255));
#59316=CARTESIAN_POINT('Ctrl Pts',(0.713736575871035,2.16144403816025,12.517955853934));
#59317=CARTESIAN_POINT('Ctrl Pts',(2.20301730463899,0.572691003330619,12.4068227359424));
#59318=CARTESIAN_POINT('Ctrl Pts',(1.6760098862852,-1.54021137864547,12.2956896179507));
#59319=CARTESIAN_POINT('Ctrl Pts',(-0.384947747103115,-2.24345168475608,
12.1845564999592));
#59320=CARTESIAN_POINT('Ctrl Pts',(-2.09358605094697,-0.893396707580089,
12.0734233819677));
#59321=CARTESIAN_POINT('Ctrl Pts',(-1.88609199822018,1.27433010012496,11.9622902639762));
#59322=CARTESIAN_POINT('Ctrl Pts',(0.0476276871353746,2.27573984305167,
11.8511571459845));
#59323=CARTESIAN_POINT('Ctrl Pts',(1.93775663861714,1.19430290937011,11.740024027993));
#59324=CARTESIAN_POINT('Ctrl Pts',(2.05437444507841,-0.980207054271423,
11.6288909100015));
#59325=CARTESIAN_POINT('Ctrl Pts',(0.29074790001371,-2.25759294127003,11.5177577920098));
#59326=CARTESIAN_POINT('Ctrl Pts',(-1.73898256686937,-1.46874091042604,
11.4066246740184));
#59327=CARTESIAN_POINT('Ctrl Pts',(-2.17712774286675,0.664360610718776,
11.2954915560267));
#59328=CARTESIAN_POINT('Ctrl Pts',(-0.622679917679542,2.18941315195494,
11.1843584380353));
#59329=CARTESIAN_POINT('Ctrl Pts',(1.5016690766107,1.71062860206002,11.0732253200437));
#59330=CARTESIAN_POINT('Ctrl Pts',(2.25163142686794,-0.333790574125898,
10.962092202052));
#59331=CARTESIAN_POINT('Ctrl Pts',(0.940812071906275,-2.07271147900283,
10.8509590840606));
#59332=CARTESIAN_POINT('Ctrl Pts',(-1.23107552126632,-1.91460525716752,
10.7398259660689));
#59333=CARTESIAN_POINT('Ctrl Pts',(-2.27623434271564,-0.00417694584392041,
10.6286928480775));
#59334=CARTESIAN_POINT('Ctrl Pts',(-1.2380939020009,1.91007427071903,10.5175597300858));
#59335=CARTESIAN_POINT('Ctrl Pts',(0.933198808726156,2.07615033492922,10.4064266120944));
#59336=CARTESIAN_POINT('Ctrl Pts',(2.2503912393599,0.342051896131316,10.2952934941028));
#59337=CARTESIAN_POINT('Ctrl Pts',(1.50793703319531,-1.70510590103744,10.1841603761111));
#59338=CARTESIAN_POINT('Ctrl Pts',(-0.614640497572694,-2.19168366526239,
10.0730272581197));
#59339=CARTESIAN_POINT('Ctrl Pts',(-2.17467485294833,-0.672346275210854,
9.96189414012807));
#59340=CARTESIAN_POINT('Ctrl Pts',(-1.74436118853674,1.46234888920541,9.85076102213649));
#59341=CARTESIAN_POINT('Ctrl Pts',(0.28246049300954,2.25864479272903,9.73962790414495));
#59342=CARTESIAN_POINT('Ctrl Pts',(2.05076321381961,0.987740082555135,9.62849478615337));
#59343=CARTESIAN_POINT('Ctrl Pts',(1.94212672408311,-1.18718322824561,9.51736166816183));
#59344=CARTESIAN_POINT('Ctrl Pts',(0.0559794151129784,-2.27554972147643,
9.40622855017026));
#59345=CARTESIAN_POINT('Ctrl Pts',(-1.88140245791634,-1.28124354485353,
9.29509543217871));
#59346=CARTESIAN_POINT('Ctrl Pts',(-2.09685075014427,0.885707153284858,
9.18396231418714));
#59347=CARTESIAN_POINT('Ctrl Pts',(-0.393178704669941,2.24202380362205,
9.07282919619558));
#59348=CARTESIAN_POINT('Ctrl Pts',(1.67034596681712,1.54635202372753,8.96169607820403));
#59349=CARTESIAN_POINT('Ctrl Pts',(2.20510426503715,-0.564601992181745,
8.85056296021247));
#59350=CARTESIAN_POINT('Ctrl Pts',(0.721664348332612,-2.15881004218177,
8.73942984222091));
#59351=CARTESIAN_POINT('Ctrl Pts',(-1.42227118534451,-1.77719017192194,
8.62829672422935));
#59352=CARTESIAN_POINT('Ctrl Pts',(-2.26448814833767,0.230984093739564,
8.5171636062378));
#59353=CARTESIAN_POINT('Ctrl Pts',(-1.0341564320416,2.02775262434295,8.40603048824622));
#59354=CARTESIAN_POINT('Ctrl Pts',(1.14267596145836,1.96864214353504,8.29489737025468));
#59355=CARTESIAN_POINT('Ctrl Pts',(2.27368632713831,0.107752884233482,8.1837642522631));
#59356=CARTESIAN_POINT('Ctrl Pts',(1.32372949887998,-1.85175604870411,8.07263113427156));
#59357=CARTESIAN_POINT('Ctrl Pts',(-0.837756714239087,-2.11646497507375,
7.96149801627999));
#59358=CARTESIAN_POINT('Ctrl Pts',(-2.23249492082995,-0.44410182699992,
7.85036489828844));
#59359=CARTESIAN_POINT('Ctrl Pts',(-1.5839660735966,1.6347207431425,7.73923178029686));
#59360=CARTESIAN_POINT('Ctrl Pts',(0.514271189154998,2.21738264208079,7.62809866230533));
#59361=CARTESIAN_POINT('Ctrl Pts',(2.14182660551464,0.770608490368339,7.51696554431375));
#59362=CARTESIAN_POINT('Ctrl Pts',(1.80909918119506,-1.38145653627306,7.4058324263222));
#59363=CARTESIAN_POINT('Ctrl Pts',(-0.179389254538965,-2.26915882886811,
7.29469930833064));
#59364=CARTESIAN_POINT('Ctrl Pts',(-2.00368931371364,-1.08003638431653,
7.18356619033908));
#59365=CARTESIAN_POINT('Ctrl Pts',(-1.99414220564178,1.09757545487321,7.07243307234752));
#59366=CARTESIAN_POINT('Ctrl Pts',(-0.159462079943669,2.27064764923059,
6.96129995435596));
#59367=CARTESIAN_POINT('Ctrl Pts',(1.82113425104325,1.36552493371444,6.85016683636441));
#59368=CARTESIAN_POINT('Ctrl Pts',(2.13501369897146,-0.789363119088234,
6.73903371837284));
#59369=CARTESIAN_POINT('Ctrl Pts',(0.494735952308336,-2.22182712381435,
6.62790060038128));
#59370=CARTESIAN_POINT('Ctrl Pts',(-1.59813610431413,-1.62072608159068,
6.51676748238972));
#59371=CARTESIAN_POINT('Ctrl Pts',(-2.22872752752264,0.463609926284491,
6.40563436439817));
#59372=CARTESIAN_POINT('Ctrl Pts',(-0.818742177699371,2.12385619791032,
6.29450124640661));
#59373=CARTESIAN_POINT('Ctrl Pts',(1.33913810958254,1.83983564921886,6.18336812841505));
#59374=CARTESIAN_POINT('Ctrl Pts',(2.27418203930235,-0.127239885464669,
6.07223501042349));
#59375=CARTESIAN_POINT('Ctrl Pts',(1.12210831514517,-1.97978676014366,5.96108915897352));
#59376=CARTESIAN_POINT('Ctrl Pts',(-0.322600533245414,-2.00382031727082,
5.8869876801874));
#59377=CARTESIAN_POINT('Ctrl Pts',(-0.890576464164601,-1.70757630444214,
5.84993057406514));
#59378=CARTESIAN_POINT('Ctrl Pts',(-0.463006149591583,-1.73368456204731,
17.1502865187834));
#59379=CARTESIAN_POINT('Ctrl Pts',(-1.03947275637638,-1.5797306134349,17.1132421461195));
#59380=CARTESIAN_POINT('Ctrl Pts',(-2.01680316801866,-0.65427085431485,
17.0391534007918));
#59381=CARTESIAN_POINT('Ctrl Pts',(-1.64292258075401,1.34350802564897,16.9280202828002));
#59382=CARTESIAN_POINT('Ctrl Pts',(0.237371113185469,2.10697612354286,16.8168871648087));
#59383=CARTESIAN_POINT('Ctrl Pts',(1.89901767164339,0.944389583152448,16.7057540468171));
#59384=CARTESIAN_POINT('Ctrl Pts',(1.82333448492954,-1.08374744505468,16.5946209288256));
#59385=CARTESIAN_POINT('Ctrl Pts',(0.0784843052061702,-2.11936529688341,
16.483487810834));
#59386=CARTESIAN_POINT('Ctrl Pts',(-1.7379991938022,-1.21558668726184,16.3723546928424));
#59387=CARTESIAN_POINT('Ctrl Pts',(-1.96390138392162,0.80091747377753,16.2612215748509));
#59388=CARTESIAN_POINT('Ctrl Pts',(-0.39230930832242,2.08429999876119,16.1500884568593));
#59389=CARTESIAN_POINT('Ctrl Pts',(1.5383111991052,1.46009647138952,16.0389553388678));
#59390=CARTESIAN_POINT('Ctrl Pts',(2.06102366292156,-0.500469599096727,
15.9278222208762));
#59391=CARTESIAN_POINT('Ctrl Pts',(0.697398342541232,-2.00297322035683,
15.8166891028847));
#59392=CARTESIAN_POINT('Ctrl Pts',(-1.30450930353645,-1.67228370568353,
15.7055559848931));
#59393=CARTESIAN_POINT('Ctrl Pts',(-2.11248082936726,0.188949232166182,
15.5944228669016));
#59394=CARTESIAN_POINT('Ctrl Pts',(-0.987025633818535,1.87724653463175,
15.48328974891));
#59395=CARTESIAN_POINT('Ctrl Pts',(1.04179368449796,1.84741489517339,15.3721566309185));
#59396=CARTESIAN_POINT('Ctrl Pts',(2.11712272505618,0.126755920093683,15.2610235129269));
#59397=CARTESIAN_POINT('Ctrl Pts',(1.25477755785045,-1.70991479513458,15.1498903949353));
#59398=CARTESIAN_POINT('Ctrl Pts',(-0.755989333763624,-1.98160432802777,
15.0387572769437));
#59399=CARTESIAN_POINT('Ctrl Pts',(-2.07484507569188,-0.439651511560185,
14.9276241589522));
#59400=CARTESIAN_POINT('Ctrl Pts',(-1.49472091619425,1.50468763450227,14.8164910409607));
#59401=CARTESIAN_POINT('Ctrl Pts',(0.453430645381966,2.07187745358944,14.705357922969));
#59402=CARTESIAN_POINT('Ctrl Pts',(1.98658463976382,0.742803468354118,14.5942248049775));
#59403=CARTESIAN_POINT('Ctrl Pts',(1.70153817731828,-1.26611348208428,14.4830916869859));
#59404=CARTESIAN_POINT('Ctrl Pts',(-0.140822995168328,-2.11623354285424,
14.3719585689944));
#59405=CARTESIAN_POINT('Ctrl Pts',(-1.85429742064377,-1.02949336955781,
14.2608254510028));
#59406=CARTESIAN_POINT('Ctrl Pts',(-1.87064586183651,0.999479655233932,
14.1496923330113));
#59407=CARTESIAN_POINT('Ctrl Pts',(-0.174905582621096,2.11368956083228,
14.0385592150197));
#59408=CARTESIAN_POINT('Ctrl Pts',(1.68091517015576,1.29336758613053,13.9274260970282));
#59409=CARTESIAN_POINT('Ctrl Pts',(1.99829619896164,-0.710695309736953,
13.8162929790366));
#59410=CARTESIAN_POINT('Ctrl Pts',(0.486757894341478,-2.06430188549755,
13.7051598610451));
#59411=CARTESIAN_POINT('Ctrl Pts',(-1.47028039380267,-1.52857812548934,
13.5940267430535));
#59412=CARTESIAN_POINT('Ctrl Pts',(-2.08166019585647,0.406160499199236,
13.4828936250619));
#59413=CARTESIAN_POINT('Ctrl Pts',(-0.787822653320641,1.96916504870769,
13.3717605070704));
#59414=CARTESIAN_POINT('Ctrl Pts',(1.22706118993438,1.72991224005338,13.2606273890788));
#59415=CARTESIAN_POINT('Ctrl Pts',(2.11889033550226,-0.0926243393777398,
13.1494942710872));
#59416=CARTESIAN_POINT('Ctrl Pts',(1.07142764730828,-1.83038747775309,13.0383611530957));
#59417=CARTESIAN_POINT('Ctrl Pts',(-0.956647794683878,-1.89290795313909,
12.9272280351041));
#59418=CARTESIAN_POINT('Ctrl Pts',(-2.10916152169086,-0.222964565681501,
12.8160949171126));
#59419=CARTESIAN_POINT('Ctrl Pts',(-1.33128760825794,1.65104476808775,12.704961799121));
#59420=CARTESIAN_POINT('Ctrl Pts',(0.665033123222356,2.01395294561419,12.5938286811294));
#59421=CARTESIAN_POINT('Ctrl Pts',(2.05268936488087,0.533612118899064,12.4826955631379));
#59422=CARTESIAN_POINT('Ctrl Pts',(1.56164350673432,-1.43511152180085,12.3715624451463));
#59423=CARTESIAN_POINT('Ctrl Pts',(-0.358679954464953,-2.09036461230954,
12.2604293271548));
#59424=CARTESIAN_POINT('Ctrl Pts',(-1.95072540383246,-0.832433733683153,
12.1492962091632));
#59425=CARTESIAN_POINT('Ctrl Pts',(-1.7573901838088,1.18737326228254,12.0381630911717));
#59426=CARTESIAN_POINT('Ctrl Pts',(0.0443777026402783,2.12044951405105,
11.9270299731801));
#59427=CARTESIAN_POINT('Ctrl Pts',(1.80552936894361,1.11280691048046,11.8158968551885));
#59428=CARTESIAN_POINT('Ctrl Pts',(1.91418949184629,-0.913320377215045,
11.704763737197));
#59429=CARTESIAN_POINT('Ctrl Pts',(0.270908050047019,-2.10354090774357,
11.5936306192054));
#59430=CARTESIAN_POINT('Ctrl Pts',(-1.62031910199222,-1.36851800494188,
11.4824975012139));
#59431=CARTESIAN_POINT('Ctrl Pts',(-2.0285664367498,0.619026440326427,11.3713643832223));
#59432=CARTESIAN_POINT('Ctrl Pts',(-0.580189924997046,2.04001352276471,
11.2602312652308));
#59433=CARTESIAN_POINT('Ctrl Pts',(1.39919924216592,1.59389993501891,11.1490981472392));
#59434=CARTESIAN_POINT('Ctrl Pts',(2.09798619095311,-0.311013608546298,
11.0379650292476));
#59435=CARTESIAN_POINT('Ctrl Pts',(0.876613601848224,-1.93127525619361,
10.9268319112561));
#59436=CARTESIAN_POINT('Ctrl Pts',(-1.14707025884331,-1.78395777511916,
10.8156987932645));
#59437=CARTESIAN_POINT('Ctrl Pts',(-2.12091027039602,-0.00389192236186189,
10.704565675273));
#59438=CARTESIAN_POINT('Ctrl Pts',(-1.15360972426749,1.77973597092559,10.5934325572814));
#59439=CARTESIAN_POINT('Ctrl Pts',(0.869519847146903,1.93447945389672,10.4822994392899));
#59440=CARTESIAN_POINT('Ctrl Pts',(2.09683063048482,0.318711200292248,10.3711663212983));
#59441=CARTESIAN_POINT('Ctrl Pts',(1.40503949035355,-1.58875408817032,10.2600332033067));
#59442=CARTESIAN_POINT('Ctrl Pts',(-0.572699093164549,-2.04212910238781,
10.1489000853151));
#59443=CARTESIAN_POINT('Ctrl Pts',(-2.02628092540217,-0.62646718468185,
10.0377669673236));
#59444=CARTESIAN_POINT('Ctrl Pts',(-1.62533070107094,1.36256215795326,9.926633849332));
#59445=CARTESIAN_POINT('Ctrl Pts',(0.263186153272049,2.1045209837052,9.81550073134043));
#59446=CARTESIAN_POINT('Ctrl Pts',(1.91082468123702,0.92033937203218,9.70436761334888));
#59447=CARTESIAN_POINT('Ctrl Pts',(1.80960125160234,-1.10617305713086,9.59323449535732));
#59448=CARTESIAN_POINT('Ctrl Pts',(0.0521595312995029,-2.12027236585766,
9.48210137736577));
#59449=CARTESIAN_POINT('Ctrl Pts',(-1.75302064504595,-1.19381495224981,
9.3709682593742));
#59450=CARTESIAN_POINT('Ctrl Pts',(-1.95376732879043,0.825268893765985,
9.25983514138264));
#59451=CARTESIAN_POINT('Ctrl Pts',(-0.36634925375944,2.0890341659204,9.14870202339108));
#59452=CARTESIAN_POINT('Ctrl Pts',(1.55636607780483,1.44083314587839,9.03756890539953));
#59453=CARTESIAN_POINT('Ctrl Pts',(2.05463391674853,-0.52607507998306,8.92643578740797));
#59454=CARTESIAN_POINT('Ctrl Pts',(0.672419925942791,-2.01149868639398,
8.8153026694164));
#59455=CARTESIAN_POINT('Ctrl Pts',(-1.32521924815821,-1.65591952346139,
8.70416955142485));
#59456=CARTESIAN_POINT('Ctrl Pts',(-2.10996560453856,0.215222364199064,
8.59303643343329));
#59457=CARTESIAN_POINT('Ctrl Pts',(-0.963588395426978,1.88938427212225,
8.48190331544173));
#59458=CARTESIAN_POINT('Ctrl Pts',(1.06470284579765,1.83430733057853,8.37077019745017));
#59459=CARTESIAN_POINT('Ctrl Pts',(2.11853612450705,0.100400118980249,8.2596370794586));
#59460=CARTESIAN_POINT('Ctrl Pts',(1.23340177973559,-1.72539722657859,8.14850396146706));
#59461=CARTESIAN_POINT('Ctrl Pts',(-0.780590462932345,-1.97204313208455,
8.03737084347548));
#59462=CARTESIAN_POINT('Ctrl Pts',(-2.08015550830599,-0.413797520013708,
7.92623772548394));
#59463=CARTESIAN_POINT('Ctrl Pts',(-1.47588051476366,1.52317182299603,7.81510460749237));
#59464=CARTESIAN_POINT('Ctrl Pts',(0.479178714765514,2.06607445056659,7.70397148950082));
#59465=CARTESIAN_POINT('Ctrl Pts',(1.9956741534898,0.718024252163197,7.59283837150925));
#59466=CARTESIAN_POINT('Ctrl Pts',(1.6856511482838,-1.28718968029966,7.4817052535177));
#59467=CARTESIAN_POINT('Ctrl Pts',(-0.167148217215834,-2.11431757046793,
7.37057213552614));
#59468=CARTESIAN_POINT('Ctrl Pts',(-1.86696297669774,-1.00633762390452,
7.25943901753458));
#59469=CARTESIAN_POINT('Ctrl Pts',(-1.85806733744734,1.0226798757451,7.14830589954301));
#59470=CARTESIAN_POINT('Ctrl Pts',(-0.14858081909429,2.11570479775745,7.03717278155147));
#59471=CARTESIAN_POINT('Ctrl Pts',(1.69686497753106,1.27234520719057,6.9260396635599));
#59472=CARTESIAN_POINT('Ctrl Pts',(1.98932614125418,-0.735499115767105,
6.81490654556834));
#59473=CARTESIAN_POINT('Ctrl Pts',(0.460976509621175,-2.0702156528929,6.70377342757679));
#59474=CARTESIAN_POINT('Ctrl Pts',(-1.48908362092749,-1.51013211928057,
6.59264030958522));
#59475=CARTESIAN_POINT('Ctrl Pts',(-2.07664519172384,0.431974439389764,
6.48150719159367));
#59476=CARTESIAN_POINT('Ctrl Pts',(-0.762873426914959,1.97892999787455,
6.3703740736021));
#59477=CARTESIAN_POINT('Ctrl Pts',(1.24775894853773,1.71429024289899,6.25924095561055));
#59478=CARTESIAN_POINT('Ctrl Pts',(2.11899801061436,-0.118557379976997,
6.14810783761898));
#59479=CARTESIAN_POINT('Ctrl Pts',(1.04553868001519,-1.84469146870582,6.03696198616902));
#59480=CARTESIAN_POINT('Ctrl Pts',(-0.300587145776539,-1.86708504092665,
5.9628605073829));
#59481=CARTESIAN_POINT('Ctrl Pts',(-0.829805936047086,-1.59105591793132,
5.92580340126064));
#59482=CARTESIAN_POINT('Ctrl Pts',(-0.429098066978468,-1.60671882000083,
17.2261593459789));
#59483=CARTESIAN_POINT('Ctrl Pts',(-0.963347356900843,-1.46403963137329,
17.189114973315));
#59484=CARTESIAN_POINT('Ctrl Pts',(-1.86910334049824,-0.606355572414101,
17.1150262279873));
#59485=CARTESIAN_POINT('Ctrl Pts',(-1.52260375854332,1.24511671666685,17.0038931099958));
#59486=CARTESIAN_POINT('Ctrl Pts',(0.219987328276866,1.95267251326906,16.8927599920042));
#59487=CARTESIAN_POINT('Ctrl Pts',(1.75994382100308,0.875227564391478,16.7816268740126));
#59488=CARTESIAN_POINT('Ctrl Pts',(1.68980326423006,-1.00437960527311,16.6704937560211));
#59489=CARTESIAN_POINT('Ctrl Pts',(0.0727365363976771,-1.96415437012253,
16.5593606380295));
#59490=CARTESIAN_POINT('Ctrl Pts',(-1.61071747130897,-1.12656364976777,
16.448227520038));
#59491=CARTESIAN_POINT('Ctrl Pts',(-1.82007579882138,0.742262581415753,
16.3370944020464));
#59492=CARTESIAN_POINT('Ctrl Pts',(-0.363578682501955,1.93165706602509,
16.2259612840548));
#59493=CARTESIAN_POINT('Ctrl Pts',(1.42565355239802,1.3531668510839,16.1148281660633));
#59494=CARTESIAN_POINT('Ctrl Pts',(1.91008536395604,-0.46381789473709,16.0036950480717));
#59495=CARTESIAN_POINT('Ctrl Pts',(0.646324635131519,-1.85628622389334,
15.8925619300802));
#59496=CARTESIAN_POINT('Ctrl Pts',(-1.20897405141744,-1.54981463244357,
15.7814288120886));
#59497=CARTESIAN_POINT('Ctrl Pts',(-1.95777408401628,0.17511160564734,15.6702956940971));
#59498=CARTESIAN_POINT('Ctrl Pts',(-0.914741179794969,1.73976708508744,
15.5591625761055));
#59499=CARTESIAN_POINT('Ctrl Pts',(0.965498312717399,1.71212015461434,15.4480294581139));
#59500=CARTESIAN_POINT('Ctrl Pts',(1.96207603220635,0.117472997579524,15.3368963401224));
#59501=CARTESIAN_POINT('Ctrl Pts',(1.16288439157133,-1.5846898230992,15.2257632221308));
#59502=CARTESIAN_POINT('Ctrl Pts',(-0.700624736972627,-1.83648227442104,
15.1146301041392));
#59503=CARTESIAN_POINT('Ctrl Pts',(-1.92289457071904,-0.407453797149452,
15.0034969861477));
#59504=CARTESIAN_POINT('Ctrl Pts',(-1.38525558759209,1.3944923970035,14.8923638681561));
#59505=CARTESIAN_POINT('Ctrl Pts',(0.420223821246926,1.92014428131401,14.7812307501646));
#59506=CARTESIAN_POINT('Ctrl Pts',(1.84109785488531,0.688404533496607,14.670097632173));
#59507=CARTESIAN_POINT('Ctrl Pts',(1.57692666376329,-1.17339013362344,14.5589645141814));
#59508=CARTESIAN_POINT('Ctrl Pts',(-0.130509875659643,-1.9612519689312,
14.4478313961899));
#59509=CARTESIAN_POINT('Ctrl Pts',(-1.71849864089984,-0.954098806752508,
14.3366982781983));
#59510=CARTESIAN_POINT('Ctrl Pts',(-1.73364981010159,0.926283135598728,
14.2255651602068));
#59511=CARTESIAN_POINT('Ctrl Pts',(-0.162096437536863,1.95889429448345,
14.1144320422152));
#59512=CARTESIAN_POINT('Ctrl Pts',(1.55781397483566,1.19864829352863,14.0032989242236));
#59513=CARTESIAN_POINT('Ctrl Pts',(1.85195172241498,-0.658647803895892,
13.8921658062321));
#59514=CARTESIAN_POINT('Ctrl Pts',(0.451110361563619,-1.91312350712482,
13.7810326882405));
#59515=CARTESIAN_POINT('Ctrl Pts',(-1.36260495773885,-1.41663327679692,
13.669899570249));
#59516=CARTESIAN_POINT('Ctrl Pts',(-1.92921058810115,0.376415486582924,
13.5587664522574));
#59517=CARTESIAN_POINT('Ctrl Pts',(-0.730126755249216,1.82495398108075,
13.4476333342658));
#59518=CARTESIAN_POINT('Ctrl Pts',(1.13719782151834,1.60322276260062,13.3365002162743));
#59519=CARTESIAN_POINT('Ctrl Pts',(1.96371419236092,-0.0858410304424767,
13.2253670982827));
#59520=CARTESIAN_POINT('Ctrl Pts',(0.992962043318029,-1.69633973375572,
13.1142339802912));
#59521=CARTESIAN_POINT('Ctrl Pts',(-0.886588050375063,-1.75428154545383,
13.0031008622996));
#59522=CARTESIAN_POINT('Ctrl Pts',(-1.95469786459909,-0.206635838904127,
12.8919677443081));
#59523=CARTESIAN_POINT('Ctrl Pts',(-1.23379125698389,1.53013112051816,12.7808346263165));
#59524=CARTESIAN_POINT('Ctrl Pts',(0.616329670573675,1.86646185306811,12.6697015083249));
#59525=CARTESIAN_POINT('Ctrl Pts',(1.90236142512275,0.49453323446751,12.5585683903334));
#59526=CARTESIAN_POINT('Ctrl Pts',(1.44727712718345,-1.33001166495622,12.4474352723418));
#59527=CARTESIAN_POINT('Ctrl Pts',(-0.332412161826789,-1.93727753986298,
12.3363021543503));
#59528=CARTESIAN_POINT('Ctrl Pts',(-1.80786475671794,-0.77147075978622,
12.2251690363587));
#59529=CARTESIAN_POINT('Ctrl Pts',(-1.62868836939741,1.10041642444011,12.1140359183672));
#59530=CARTESIAN_POINT('Ctrl Pts',(0.0411277181451806,1.96515918505044,
12.0029028003756));
#59531=CARTESIAN_POINT('Ctrl Pts',(1.67330209927009,1.03131091159081,11.891769682384));
#59532=CARTESIAN_POINT('Ctrl Pts',(1.77400453861417,-0.846433700158669,
11.7806365643925));
#59533=CARTESIAN_POINT('Ctrl Pts',(0.25106820008033,-1.94948887421713,11.6695034464009));
#59534=CARTESIAN_POINT('Ctrl Pts',(-1.50165563711509,-1.26829509945771,
11.5583703284093));
#59535=CARTESIAN_POINT('Ctrl Pts',(-1.88000513063285,0.573692269934076,
11.4472372104178));
#59536=CARTESIAN_POINT('Ctrl Pts',(-0.537699932314552,1.89061389357449,
11.3361040924262));
#59537=CARTESIAN_POINT('Ctrl Pts',(1.29672940772112,1.47717126797781,11.2249709744347));
#59538=CARTESIAN_POINT('Ctrl Pts',(1.94434095503829,-0.288236642966698,
11.1138378564431));
#59539=CARTESIAN_POINT('Ctrl Pts',(0.81241513179017,-1.78983903338438,11.0027047384516));
#59540=CARTESIAN_POINT('Ctrl Pts',(-1.0630649964203,-1.65331029307079,10.89157162046));
#59541=CARTESIAN_POINT('Ctrl Pts',(-1.9655861980764,-0.00360689887980824,
10.7804385024684));
#59542=CARTESIAN_POINT('Ctrl Pts',(-1.0691255465341,1.64939767113214,10.6693053844769));
#59543=CARTESIAN_POINT('Ctrl Pts',(0.80584088556765,1.79280857286422,10.5581722664853));
#59544=CARTESIAN_POINT('Ctrl Pts',(1.94327002160974,0.295370504453181,10.4470391484938));
#59545=CARTESIAN_POINT('Ctrl Pts',(1.30214194751179,-1.47240227530321,10.3359060305022));
#59546=CARTESIAN_POINT('Ctrl Pts',(-0.530757688756401,-1.89257453951323,
10.2247729125106));
#59547=CARTESIAN_POINT('Ctrl Pts',(-1.87788699785602,-0.580588094152845,
10.1136397945191));
#59548=CARTESIAN_POINT('Ctrl Pts',(-1.50630021360515,1.26277542670112,10.0025066765275));
#59549=CARTESIAN_POINT('Ctrl Pts',(0.243911813534555,1.95039717468138,9.89137355853593));
#59550=CARTESIAN_POINT('Ctrl Pts',(1.77088614865442,0.852938661509229,9.78024044054438));
#59551=CARTESIAN_POINT('Ctrl Pts',(1.67707577912157,-1.02516288601611,9.66910732255282));
#59552=CARTESIAN_POINT('Ctrl Pts',(0.0483396474860255,-1.9649950102389,
9.55797420456127));
#59553=CARTESIAN_POINT('Ctrl Pts',(-1.62463883217554,-1.10638635964609,
9.44684108656969));
#59554=CARTESIAN_POINT('Ctrl Pts',(-1.8106839074366,0.76483063424711,9.33570796857815));
#59555=CARTESIAN_POINT('Ctrl Pts',(-0.339519802848938,1.93604452821876,
9.22457485058658));
#59556=CARTESIAN_POINT('Ctrl Pts',(1.44238618879254,1.33531426802924,9.11344173259502));
#59557=CARTESIAN_POINT('Ctrl Pts',(1.90416356845991,-0.487548167784373,
9.00230861460347));
#59558=CARTESIAN_POINT('Ctrl Pts',(0.62317550355297,-1.8641873306062,8.8911754966119));
#59559=CARTESIAN_POINT('Ctrl Pts',(-1.22816731097189,-1.53464887500082,
8.78004237862035));
#59560=CARTESIAN_POINT('Ctrl Pts',(-1.95544306073944,0.19946063465856,8.66890926062879));
#59561=CARTESIAN_POINT('Ctrl Pts',(-0.893020358812349,1.75101591990155,
8.55777614263723));
#59562=CARTESIAN_POINT('Ctrl Pts',(0.986729730136937,1.69997251762203,8.44664302464568));
#59563=CARTESIAN_POINT('Ctrl Pts',(1.96338592187579,0.0930473537270221,
8.33550990665409));
#59564=CARTESIAN_POINT('Ctrl Pts',(1.1430740605912,-1.59903840445307,8.22437678866256));
#59565=CARTESIAN_POINT('Ctrl Pts',(-0.723424211625604,-1.82762128909535,
8.11324367067098));
#59566=CARTESIAN_POINT('Ctrl Pts',(-1.92781609578202,-0.383493213027498,
8.00211055267944));
#59567=CARTESIAN_POINT('Ctrl Pts',(-1.36779495593073,1.41162290284956,7.89097743468786));
#59568=CARTESIAN_POINT('Ctrl Pts',(0.444086240376034,1.91476625905239,7.77984431669632));
#59569=CARTESIAN_POINT('Ctrl Pts',(1.84952170146496,0.665440013958054,7.66871119870474));
#59570=CARTESIAN_POINT('Ctrl Pts',(1.56220311537253,-1.19292282432625,7.5575780807132));
#59571=CARTESIAN_POINT('Ctrl Pts',(-0.154907179892704,-1.95947631206774,
7.44644496272163));
#59572=CARTESIAN_POINT('Ctrl Pts',(-1.73023663968183,-0.932638863492504,
7.33531184473009));
#59573=CARTESIAN_POINT('Ctrl Pts',(-1.72199246925288,0.947784296617001,
7.22417872673851));
#59574=CARTESIAN_POINT('Ctrl Pts',(-0.13769955824491,1.9607619462843,7.11304560874695));
#59575=CARTESIAN_POINT('Ctrl Pts',(1.57259570401887,1.17916548066668,7.00191249075541));
#59576=CARTESIAN_POINT('Ctrl Pts',(1.84363858353691,-0.681635112445974,
6.89077937276383));
#59577=CARTESIAN_POINT('Ctrl Pts',(0.427217066934015,-1.91860418197146,
6.77964625477228));
#59578=CARTESIAN_POINT('Ctrl Pts',(-1.38003113754085,-1.39953815697045,
6.66851313678072));
#59579=CARTESIAN_POINT('Ctrl Pts',(-1.92456285592503,0.400338952495038,
6.55738001878916));
#59580=CARTESIAN_POINT('Ctrl Pts',(-0.707004676130548,1.83400379783878,
6.44624690079761));
#59581=CARTESIAN_POINT('Ctrl Pts',(1.15637978749291,1.58874483657911,6.33511378280605));
#59582=CARTESIAN_POINT('Ctrl Pts',(1.96381398192635,-0.109874874489327,
6.22398066481448));
#59583=CARTESIAN_POINT('Ctrl Pts',(0.968969044885222,-1.70959617726799,
6.11283481336452));
#59584=CARTESIAN_POINT('Ctrl Pts',(-0.278573758307664,-1.7303497645825,
6.0387333345784));
#59585=CARTESIAN_POINT('Ctrl Pts',(-0.769035407929571,-1.47453553142049,
6.00167622845614));
#59586=CARTESIAN_POINT('Ctrl Pts',(-0.530170217188721,-1.98517432567169,
17.));
#59587=CARTESIAN_POINT('Ctrl Pts',(-0.59958638778647,-1.95947209126774,
17.));
#59588=CARTESIAN_POINT('Ctrl Pts',(-0.667262296603072,-1.92979787875034,
17.));
#59589=CARTESIAN_POINT('Ctrl Pts',(-0.733002470738773,-1.89645448736446,
17.));
#59590=CARTESIAN_POINT('Ctrl Pts',(-0.799702571694335,-1.86262422145966,
17.));
#59591=CARTESIAN_POINT('Ctrl Pts',(-0.864410706066083,-1.82501605153519,
17.));
#59592=CARTESIAN_POINT('Ctrl Pts',(-0.926891494234642,-1.78390179589663,
17.));
#59593=CARTESIAN_POINT('Ctrl Pts',(-0.977240315226614,-1.75077074300754,
17.));
#59594=CARTESIAN_POINT('Ctrl Pts',(-1.0261423231337,-1.71536194678685,17.));
#59595=CARTESIAN_POINT('Ctrl Pts',(-1.0734552151732,-1.6778024578881,17.));
#59596=CARTESIAN_POINT('Ctrl Pts',(-1.09711166119295,-1.65902271343873,
17.));
#59597=CARTESIAN_POINT('Ctrl Pts',(-1.12037053740919,-1.63970511721008,
17.));
#59598=CARTESIAN_POINT('Ctrl Pts',(-1.14321217455345,-1.61986466499212,
17.));
#59599=CARTESIAN_POINT('Ctrl Pts',(-1.15783918687559,-1.60715951004916,
17.));
#59600=CARTESIAN_POINT('Ctrl Pts',(-1.17229538706437,-1.59423965238433,
17.));
#59601=CARTESIAN_POINT('Ctrl Pts',(-1.18657442194043,-1.58110975612116,
17.));
#59602=CARTESIAN_POINT('Ctrl Pts',(-1.19459362037587,-1.57373592137077,
17.));
#59603=CARTESIAN_POINT('Ctrl Pts',(-1.20255571179842,-1.56629689983921,
17.));
#59604=CARTESIAN_POINT('Ctrl Pts',(-1.21045281961469,-1.55880022777578,
17.));
#59605=CARTESIAN_POINT('Ctrl Pts',(-1.26354014875506,-1.50840477838492,
17.));
#59606=CARTESIAN_POINT('Ctrl Pts',(-1.31378747767688,-1.45532141233497,
17.));
#59607=CARTESIAN_POINT('Ctrl Pts',(-1.36097600959484,-1.3998088981192,17.));
#59608=CARTESIAN_POINT('Ctrl Pts',(-1.40742908231333,-1.34516157694095,
17.));
#59609=CARTESIAN_POINT('Ctrl Pts',(-1.45091839778076,-1.28815934728008,
17.));
#59610=CARTESIAN_POINT('Ctrl Pts',(-1.49119167764656,-1.22902545012624,
17.));
#59611=CARTESIAN_POINT('Ctrl Pts',(-1.52524153022102,-1.17902951021394,
17.));
#59612=CARTESIAN_POINT('Ctrl Pts',(-1.55699193038151,-1.12750916897208,
17.));
#59613=CARTESIAN_POINT('Ctrl Pts',(-1.58626203451582,-1.07459264749954,
17.));
#59614=CARTESIAN_POINT('Ctrl Pts',(-1.59836979258552,-1.05270340388976,
17.));
#59615=CARTESIAN_POINT('Ctrl Pts',(-1.61005281462832,-1.03057521758956,
17.));
#59616=CARTESIAN_POINT('Ctrl Pts',(-1.62129684910972,-1.00821707885185,
17.));
#59617=CARTESIAN_POINT('Ctrl Pts',(-1.62649913652706,-0.997872618949778,
17.));
#59618=CARTESIAN_POINT('Ctrl Pts',(-1.63160743994957,-0.987478934463243,
17.));
#59619=CARTESIAN_POINT('Ctrl Pts',(-1.63662028259746,-0.977036917721011,
17.));
#59620=CARTESIAN_POINT('Ctrl Pts',(-1.64185147465901,-0.966140067585173,
17.));
#59621=CARTESIAN_POINT('Ctrl Pts',(-1.64697509598823,-0.955198041348551,
17.));
#59622=CARTESIAN_POINT('Ctrl Pts',(-1.65198809526169,-0.94421612686998,
17.));
#59623=CARTESIAN_POINT('Ctrl Pts',(-1.68052781084573,-0.881694530777598,
17.));
#59624=CARTESIAN_POINT('Ctrl Pts',(-1.70550660071472,-0.817838180873781,
17.));
#59625=CARTESIAN_POINT('Ctrl Pts',(-1.72670093437665,-0.752850869832327,
17.));
#59626=CARTESIAN_POINT('Ctrl Pts',(-1.74590469391102,-0.693967174127041,
17.));
#59627=CARTESIAN_POINT('Ctrl Pts',(-1.76200116624391,-0.634154383630976,
17.));
#59628=CARTESIAN_POINT('Ctrl Pts',(-1.77478736554882,-0.573559243480358,
17.));
#59629=CARTESIAN_POINT('Ctrl Pts',(-1.78927486034487,-0.504901485481765,
17.));
#59630=CARTESIAN_POINT('Ctrl Pts',(-1.799512747065,-0.435238075154566,17.));
#59631=CARTESIAN_POINT('Ctrl Pts',(-1.80556817728997,-0.364940578178376,
17.));
#59632=CARTESIAN_POINT('Ctrl Pts',(-1.80722934559513,-0.345656073267864,
17.));
#59633=CARTESIAN_POINT('Ctrl Pts',(-1.80857547625591,-0.326323949543816,
17.));
#59634=CARTESIAN_POINT('Ctrl Pts',(-1.80960732651783,-0.30695215324635,
17.));
#59635=CARTESIAN_POINT('Ctrl Pts',(-1.81050226718635,-0.290150676356872,
17.));
#59636=CARTESIAN_POINT('Ctrl Pts',(-1.81116079923754,-0.273313162210314,
17.));
#59637=CARTESIAN_POINT('Ctrl Pts',(-1.81158284306408,-0.256479086675087,
17.));
#59638=CARTESIAN_POINT('Ctrl Pts',(-1.81330048651302,-0.187967387785159,
17.));
#59639=CARTESIAN_POINT('Ctrl Pts',(-1.81111278941556,-0.11942609791947,
17.));
#59640=CARTESIAN_POINT('Ctrl Pts',(-1.80514016974053,-0.05119331079533,
17.));
#59641=CARTESIAN_POINT('Ctrl Pts',(-1.79915254414877,0.0172109078911375,
17.));
#59642=CARTESIAN_POINT('Ctrl Pts',(-1.78936051943155,0.085306157363821,
17.));
#59643=CARTESIAN_POINT('Ctrl Pts',(-1.77583551231836,0.152736676162679,
17.));
#59644=CARTESIAN_POINT('Ctrl Pts',(-1.76259194094567,0.218764063870252,
17.));
#59645=CARTESIAN_POINT('Ctrl Pts',(-1.74576857726395,0.284154971652147,
17.));
#59646=CARTESIAN_POINT('Ctrl Pts',(-1.72539221768325,0.348546576029075,
17.));
#59647=CARTESIAN_POINT('Ctrl Pts',(-1.71949214477078,0.367191474754506,
17.));
#59648=CARTESIAN_POINT('Ctrl Pts',(-1.71329394772695,0.385752356812901,
17.));
#59649=CARTESIAN_POINT('Ctrl Pts',(-1.70679772648935,0.404219792736258,
17.));
#59650=CARTESIAN_POINT('Ctrl Pts',(-1.70266287321327,0.415974339746853,
17.));
#59651=CARTESIAN_POINT('Ctrl Pts',(-1.698410480872,0.427681900514319,17.));
#59652=CARTESIAN_POINT('Ctrl Pts',(-1.69404123115752,0.439339805259342,
17.));
#59653=CARTESIAN_POINT('Ctrl Pts',(-1.67085891425587,0.501194187560434,
17.));
#59654=CARTESIAN_POINT('Ctrl Pts',(-1.64438824791585,0.561658220290148,
17.));
#59655=CARTESIAN_POINT('Ctrl Pts',(-1.6146796577165,0.62039476474356,17.));
#59656=CARTESIAN_POINT('Ctrl Pts',(-1.59391160861621,0.661455058450027,
17.));
#59657=CARTESIAN_POINT('Ctrl Pts',(-1.5715603802492,0.70167061883402,17.));
#59658=CARTESIAN_POINT('Ctrl Pts',(-1.54763291644676,0.740915041686162,
17.));
#59659=CARTESIAN_POINT('Ctrl Pts',(-1.53991882725148,0.753567238375207,
17.));
#59660=CARTESIAN_POINT('Ctrl Pts',(-1.53203975915063,0.766120089974338,
17.));
#59661=CARTESIAN_POINT('Ctrl Pts',(-1.52399923812354,0.778563773820041,
17.));
#59662=CARTESIAN_POINT('Ctrl Pts',(-1.48975784779894,0.83155648837186,17.));
#59663=CARTESIAN_POINT('Ctrl Pts',(-1.45266161665523,0.88246473729788,17.));
#59664=CARTESIAN_POINT('Ctrl Pts',(-1.41274488079971,0.930972884647871,
17.));
#59665=CARTESIAN_POINT('Ctrl Pts',(-1.37594347516523,0.975695178917259,
17.));
#59666=CARTESIAN_POINT('Ctrl Pts',(-1.33674405604559,1.01837748510076,17.));
#59667=CARTESIAN_POINT('Ctrl Pts',(-1.29515206733999,1.05873948677329,17.));
#59668=CARTESIAN_POINT('Ctrl Pts',(-1.28733353636727,1.06632680274491,17.));
#59669=CARTESIAN_POINT('Ctrl Pts',(-1.2794304058483,1.07383202241508,17.));
#59670=CARTESIAN_POINT('Ctrl Pts',(-1.27144426759649,1.08125448192165,17.));
#59671=CARTESIAN_POINT('Origin',(0.,0.,5.));
#59672=CARTESIAN_POINT('Origin',(0.,0.,0.));
#59673=CARTESIAN_POINT('',(-5.,-6.12323399573677E-16,17.));
#59674=CARTESIAN_POINT('Origin',(0.,0.,17.));
#59675=CARTESIAN_POINT('',(-5.,-6.12323399573677E-16,0.));
#59676=CARTESIAN_POINT('',(-5.,-6.12323399573677E-16,0.));
#59677=CARTESIAN_POINT('Origin',(0.,0.,0.));
#59678=CARTESIAN_POINT('Origin',(0.,0.,17.));
#59679=CARTESIAN_POINT('Origin',(0.,0.,0.));
#59680=CARTESIAN_POINT('',(0.,0.,0.));
#59681=CARTESIAN_POINT('',(0.,-108.5,3.));
#59682=CARTESIAN_POINT('',(0.,108.5,3.));
#59683=CARTESIAN_POINT('',(-148.5,0.,3.));
#59684=CARTESIAN_POINT('',(-130.,-90.,3.));
#59685=CARTESIAN_POINT('',(-130.,-90.,0.));
#59686=CARTESIAN_POINT('',(-100.,-55.,3.));
#59687=CARTESIAN_POINT('',(148.5,0.,3.));
#59688=CARTESIAN_POINT('',(-130.,90.,3.));
#59689=CARTESIAN_POINT('',(130.,-90.,3.));
#59690=CARTESIAN_POINT('',(130.,90.,3.));
#59691=CARTESIAN_POINT('',(-130.,90.,0.));
#59692=CARTESIAN_POINT('',(130.,-90.,0.));
#59693=CARTESIAN_POINT('',(130.,90.,0.));
#59694=CARTESIAN_POINT('',(-100.,55.,3.));
#59695=CARTESIAN_POINT('',(100.,-55.,3.));
#59696=CARTESIAN_POINT('',(100.,55.,3.));
#59697=CARTESIAN_POINT('',(0.,0.,0.));
#59698=CARTESIAN_POINT('Origin',(145.417424305044,-110.,-2.));
#59699=CARTESIAN_POINT('',(150.,110.,0.));
#59700=CARTESIAN_POINT('',(145.417424305044,110.,3.));
#59701=CARTESIAN_POINT('Origin',(145.417424305044,110.,-2.));
#59702=CARTESIAN_POINT('',(145.417424305044,-110.,3.));
#59703=CARTESIAN_POINT('',(145.417424305044,-110.,3.));
#59704=CARTESIAN_POINT('',(150.,-110.,0.));
#59705=CARTESIAN_POINT('Origin',(145.417424305044,-110.,-2.));
#59706=CARTESIAN_POINT('',(150.,-110.,0.));
#59707=CARTESIAN_POINT('Origin',(0.,0.,3.));
#59708=CARTESIAN_POINT('',(-150.,110.,3.));
#59709=CARTESIAN_POINT('',(150.,110.,3.));
#59710=CARTESIAN_POINT('',(-150.,-110.,3.));
#59711=CARTESIAN_POINT('',(-150.,110.,3.));
#59712=CARTESIAN_POINT('',(-150.,-110.,3.));
#59713=CARTESIAN_POINT('',(126.5,90.,3.));
#59714=CARTESIAN_POINT('Origin',(130.,90.,3.));
#59715=CARTESIAN_POINT('',(-133.5,90.,3.));
#59716=CARTESIAN_POINT('Origin',(-130.,90.,3.));
#59717=CARTESIAN_POINT('',(-133.5,-90.,3.));
#59718=CARTESIAN_POINT('Origin',(-130.,-90.,3.));
#59719=CARTESIAN_POINT('',(126.5,-90.,3.));
#59720=CARTESIAN_POINT('Origin',(130.,-90.,3.));
#59721=CARTESIAN_POINT('Origin',(150.,110.,0.));
#59722=CARTESIAN_POINT('',(-150.,110.,0.));
#59723=CARTESIAN_POINT('',(150.,110.,0.));
#59724=CARTESIAN_POINT('',(-150.,110.,0.));
#59725=CARTESIAN_POINT('Origin',(130.,-90.,1.5));
#59726=CARTESIAN_POINT('',(126.5,-90.,0.));
#59727=CARTESIAN_POINT('',(126.5,-90.,1.5));
#59728=CARTESIAN_POINT('Origin',(130.,-90.,0.));
#59729=CARTESIAN_POINT('Origin',(-130.,-90.,1.5));
#59730=CARTESIAN_POINT('',(-133.5,-90.,0.));
#59731=CARTESIAN_POINT('',(-133.5,-90.,1.5));
#59732=CARTESIAN_POINT('Origin',(-130.,-90.,0.));
#59733=CARTESIAN_POINT('Origin',(-130.,90.,1.5));
#59734=CARTESIAN_POINT('',(-133.5,90.,0.));
#59735=CARTESIAN_POINT('',(-133.5,90.,1.5));
#59736=CARTESIAN_POINT('Origin',(-130.,90.,0.));
#59737=CARTESIAN_POINT('Origin',(130.,90.,1.5));
#59738=CARTESIAN_POINT('',(126.5,90.,0.));
#59739=CARTESIAN_POINT('',(126.5,90.,1.5));
#59740=CARTESIAN_POINT('Origin',(130.,90.,0.));
#59741=CARTESIAN_POINT('Origin',(-150.,-110.,0.));
#59742=CARTESIAN_POINT('',(-150.,-110.,0.));
#59743=CARTESIAN_POINT('',(-150.,-110.,0.));
#59744=CARTESIAN_POINT('',(-150.,-110.,0.));
#59745=CARTESIAN_POINT('Origin',(-150.,110.,0.));
#59746=CARTESIAN_POINT('',(-150.,110.,0.));
#59747=CARTESIAN_POINT('Origin',(0.,0.,0.));
#59748=CARTESIAN_POINT('',(0.,0.,0.));
#59749=CARTESIAN_POINT('Origin',(130.,-90.,1.5));
#59750=CARTESIAN_POINT('',(126.5,-90.,3.));
#59751=CARTESIAN_POINT('Origin',(130.,-90.,3.));
#59752=CARTESIAN_POINT('',(126.5,-90.,0.));
#59753=CARTESIAN_POINT('',(126.5,-90.,1.5));
#59754=CARTESIAN_POINT('Origin',(130.,-90.,0.));
#59755=CARTESIAN_POINT('Origin',(-130.,-90.,1.5));
#59756=CARTESIAN_POINT('',(-133.5,-90.,3.));
#59757=CARTESIAN_POINT('Origin',(-130.,-90.,3.));
#59758=CARTESIAN_POINT('',(-133.5,-90.,0.));
#59759=CARTESIAN_POINT('',(-133.5,-90.,1.5));
#59760=CARTESIAN_POINT('Origin',(-130.,-90.,0.));
#59761=CARTESIAN_POINT('Origin',(-130.,90.,1.5));
#59762=CARTESIAN_POINT('',(-133.5,90.,3.));
#59763=CARTESIAN_POINT('Origin',(-130.,90.,3.));
#59764=CARTESIAN_POINT('',(-133.5,90.,0.));
#59765=CARTESIAN_POINT('',(-133.5,90.,1.5));
#59766=CARTESIAN_POINT('Origin',(-130.,90.,0.));
#59767=CARTESIAN_POINT('Origin',(130.,90.,1.5));
#59768=CARTESIAN_POINT('',(126.5,90.,3.));
#59769=CARTESIAN_POINT('Origin',(130.,90.,3.));
#59770=CARTESIAN_POINT('',(126.5,90.,0.));
#59771=CARTESIAN_POINT('',(126.5,90.,1.5));
#59772=CARTESIAN_POINT('Origin',(130.,90.,0.));
#59773=CARTESIAN_POINT('Origin',(125.,-85.,0.));
#59774=CARTESIAN_POINT('',(125.,-85.,0.));
#59775=CARTESIAN_POINT('',(-125.,-85.,0.));
#59776=CARTESIAN_POINT('',(-125.,-85.,0.));
#59777=CARTESIAN_POINT('',(-125.,-85.,3.));
#59778=CARTESIAN_POINT('',(-125.,-85.,0.));
#59779=CARTESIAN_POINT('',(125.,-85.,3.));
#59780=CARTESIAN_POINT('',(-125.,-85.,3.));
#59781=CARTESIAN_POINT('',(125.,-85.,0.));
#59782=CARTESIAN_POINT('Origin',(125.,85.,0.));
#59783=CARTESIAN_POINT('',(125.,85.,0.));
#59784=CARTESIAN_POINT('',(125.,-85.,0.));
#59785=CARTESIAN_POINT('',(125.,85.,3.));
#59786=CARTESIAN_POINT('',(125.,-85.,3.));
#59787=CARTESIAN_POINT('',(125.,85.,0.));
#59788=CARTESIAN_POINT('Origin',(-125.,85.,0.));
#59789=CARTESIAN_POINT('',(-125.,85.,0.));
#59790=CARTESIAN_POINT('',(125.,85.,0.));
#59791=CARTESIAN_POINT('',(-125.,85.,3.));
#59792=CARTESIAN_POINT('',(125.,85.,3.));
#59793=CARTESIAN_POINT('',(-125.,85.,0.));
#59794=CARTESIAN_POINT('Origin',(-125.,-85.,0.));
#59795=CARTESIAN_POINT('',(-125.,85.,0.));
#59796=CARTESIAN_POINT('',(-125.,85.,3.));
#59797=CARTESIAN_POINT('Origin',(150.,110.,0.));
#59798=CARTESIAN_POINT('',(150.,110.,0.));
#59799=CARTESIAN_POINT('',(-150.,110.,0.));
#59800=CARTESIAN_POINT('',(150.,110.,0.));
#59801=CARTESIAN_POINT('',(-150.,110.,3.));
#59802=CARTESIAN_POINT('',(-150.,110.,0.));
#59803=CARTESIAN_POINT('',(150.,110.,3.));
#59804=CARTESIAN_POINT('',(150.,110.,3.));
#59805=CARTESIAN_POINT('',(150.,110.,0.));
#59806=CARTESIAN_POINT('Origin',(150.,-110.,0.));
#59807=CARTESIAN_POINT('',(150.,-110.,0.));
#59808=CARTESIAN_POINT('',(150.,-110.,0.));
#59809=CARTESIAN_POINT('',(150.,-110.,3.));
#59810=CARTESIAN_POINT('',(150.,-110.,3.));
#59811=CARTESIAN_POINT('',(150.,-110.,0.));
#59812=CARTESIAN_POINT('Origin',(-150.,-110.,0.));
#59813=CARTESIAN_POINT('',(-150.,-110.,0.));
#59814=CARTESIAN_POINT('',(-150.,-110.,0.));
#59815=CARTESIAN_POINT('',(-150.,-110.,3.));
#59816=CARTESIAN_POINT('',(-150.,-110.,3.));
#59817=CARTESIAN_POINT('',(-150.,-110.,0.));
#59818=CARTESIAN_POINT('Origin',(-150.,110.,0.));
#59819=CARTESIAN_POINT('',(-150.,110.,0.));
#59820=CARTESIAN_POINT('',(-150.,110.,3.));
#59821=CARTESIAN_POINT('Origin',(0.,0.,3.));
#59822=CARTESIAN_POINT('Origin',(0.,0.,0.));
#59823=CARTESIAN_POINT('',(0.,0.,0.));
#59824=CARTESIAN_POINT('Origin',(100.,-55.,1.5));
#59825=CARTESIAN_POINT('',(97.5,-55.,3.));
#59826=CARTESIAN_POINT('Origin',(100.,-55.,3.));
#59827=CARTESIAN_POINT('',(97.5,-55.,0.));
#59828=CARTESIAN_POINT('',(97.5,-55.,1.5));
#59829=CARTESIAN_POINT('Origin',(100.,-55.,0.));
#59830=CARTESIAN_POINT('Origin',(-100.,-55.,1.5));
#59831=CARTESIAN_POINT('',(-102.5,-55.,3.));
#59832=CARTESIAN_POINT('Origin',(-100.,-55.,3.));
#59833=CARTESIAN_POINT('',(-102.5,-55.,0.));
#59834=CARTESIAN_POINT('',(-102.5,-55.,1.5));
#59835=CARTESIAN_POINT('Origin',(-100.,-55.,0.));
#59836=CARTESIAN_POINT('Origin',(-100.,55.,1.5));
#59837=CARTESIAN_POINT('',(-102.5,55.,3.));
#59838=CARTESIAN_POINT('Origin',(-100.,55.,3.));
#59839=CARTESIAN_POINT('',(-102.5,55.,0.));
#59840=CARTESIAN_POINT('',(-102.5,55.,1.5));
#59841=CARTESIAN_POINT('Origin',(-100.,55.,0.));
#59842=CARTESIAN_POINT('Origin',(100.,55.,1.5));
#59843=CARTESIAN_POINT('',(97.5,55.,3.));
#59844=CARTESIAN_POINT('Origin',(100.,55.,3.));
#59845=CARTESIAN_POINT('',(97.5,55.,0.));
#59846=CARTESIAN_POINT('',(97.5,55.,1.5));
#59847=CARTESIAN_POINT('Origin',(100.,55.,0.));
#59848=CARTESIAN_POINT('Origin',(120.,75.,0.));
#59849=CARTESIAN_POINT('',(120.,75.,0.));
#59850=CARTESIAN_POINT('',(-120.,75.,0.));
#59851=CARTESIAN_POINT('',(120.,75.,0.));
#59852=CARTESIAN_POINT('',(-120.,75.,3.));
#59853=CARTESIAN_POINT('',(-120.,75.,0.));
#59854=CARTESIAN_POINT('',(120.,75.,3.));
#59855=CARTESIAN_POINT('',(120.,75.,3.));
#59856=CARTESIAN_POINT('',(120.,75.,0.));
#59857=CARTESIAN_POINT('Origin',(120.,-75.,0.));
#59858=CARTESIAN_POINT('',(120.,-75.,0.));
#59859=CARTESIAN_POINT('',(120.,-75.,0.));
#59860=CARTESIAN_POINT('',(120.,-75.,3.));
#59861=CARTESIAN_POINT('',(120.,-75.,3.));
#59862=CARTESIAN_POINT('',(120.,-75.,0.));
#59863=CARTESIAN_POINT('Origin',(-120.,-75.,0.));
#59864=CARTESIAN_POINT('',(-120.,-75.,0.));
#59865=CARTESIAN_POINT('',(-120.,-75.,0.));
#59866=CARTESIAN_POINT('',(-120.,-75.,3.));
#59867=CARTESIAN_POINT('',(-120.,-75.,3.));
#59868=CARTESIAN_POINT('',(-120.,-75.,0.));
#59869=CARTESIAN_POINT('Origin',(-120.,75.,0.));
#59870=CARTESIAN_POINT('',(-120.,75.,0.));
#59871=CARTESIAN_POINT('',(-120.,75.,3.));
#59872=CARTESIAN_POINT('Origin',(0.,0.,3.));
#59873=CARTESIAN_POINT('Origin',(0.,0.,0.));
#59874=CARTESIAN_POINT('',(0.,0.,0.));
#59875=CARTESIAN_POINT('Origin',(0.,0.,-1.84858989190501));
#59876=CARTESIAN_POINT('',(-2.3654410179195,0.172878145651696,0.838781724910481));
#59877=CARTESIAN_POINT('',(-2.36544101854889,0.172878137039861,0.639858258416768));
#59878=CARTESIAN_POINT('',(-2.36544101854889,0.172878137039864,-1.84858989190501));
#59879=CARTESIAN_POINT('',(-1.35356952483514,-1.9475748006014,6.39245600897453E-15));
#59880=CARTESIAN_POINT('Ctrl Pts',(-2.3654410179195,0.172878145651696,0.838781724910481));
#59881=CARTESIAN_POINT('Ctrl Pts',(-2.36186465939432,0.221812411566921,
0.835334615307093));
#59882=CARTESIAN_POINT('Ctrl Pts',(-2.35677062881215,0.270624944567347,
0.83184711542494));
#59883=CARTESIAN_POINT('Ctrl Pts',(-2.33694122097281,0.416601558032087,
0.821281086510961));
#59884=CARTESIAN_POINT('Ctrl Pts',(-2.31768037501523,0.513036883753267,
0.814113668653049));
#59885=CARTESIAN_POINT('Ctrl Pts',(-2.28597334870978,0.632591079542157,
0.805094650590239));
#59886=CARTESIAN_POINT('Ctrl Pts',(-2.27905450086233,0.657081597685872,
0.803240261822677));
#59887=CARTESIAN_POINT('Ctrl Pts',(-2.24368658420091,0.774986184855901,
0.79428990008055));
#59888=CARTESIAN_POINT('Ctrl Pts',(-2.20987773177701,0.866705066958452,
0.787253905998845));
#59889=CARTESIAN_POINT('Ctrl Pts',(-2.16370961226913,0.971515839898839,
0.779308765321606));
#59890=CARTESIAN_POINT('Ctrl Pts',(-2.15674863856911,0.986872668338088,
0.778147236898505));
#59891=CARTESIAN_POINT('Ctrl Pts',(-2.14562043767858,1.01074269110853,0.776347313985111));
#59892=CARTESIAN_POINT('Ctrl Pts',(-2.1415651017538,1.01930700623228,0.775702640310355));
#59893=CARTESIAN_POINT('Ctrl Pts',(-2.1342657730286,1.03448632025165,0.774562320316757));
#59894=CARTESIAN_POINT('Ctrl Pts',(-2.13104224434626,1.04111060490884,0.774065492034439));
#59895=CARTESIAN_POINT('Ctrl Pts',(-2.12315470361223,1.05712920905827,0.772865916939248));
#59896=CARTESIAN_POINT('Ctrl Pts',(-2.11845917407976,1.06650775813566,0.772165100716468));
#59897=CARTESIAN_POINT('Ctrl Pts',(-2.10354419647061,1.09581078519145,0.769979200043173));
#59898=CARTESIAN_POINT('Ctrl Pts',(-2.09310436995499,1.11562253840262,0.768506828631546));
#59899=CARTESIAN_POINT('Ctrl Pts',(-2.03585578615508,1.22063023879177,0.760716543072306));
#59900=CARTESIAN_POINT('Ctrl Pts',(-1.98411825460355,1.30304485762746,0.754649036969893));
#59901=CARTESIAN_POINT('Ctrl Pts',(-1.82523675449555,1.52462596590747,0.73781782639295));
#59902=CARTESIAN_POINT('Ctrl Pts',(-1.70751693198461,1.65540217462058,0.727216805660831));
#59903=CARTESIAN_POINT('Ctrl Pts',(-1.54014420431978,1.80430483693017,0.71294069687559));
#59904=CARTESIAN_POINT('Ctrl Pts',(-1.50285088494264,1.83548326581983,0.709806324549395));
#59905=CARTESIAN_POINT('Ctrl Pts',(-1.44830866409291,1.87830523736781,0.705269145107943));
#59906=CARTESIAN_POINT('Ctrl Pts',(-1.43182222859937,1.89090285637174,0.703903594004995));
#59907=CARTESIAN_POINT('Ctrl Pts',(-1.40335800852905,1.91206724097651,0.701554667561739));
#59908=CARTESIAN_POINT('Ctrl Pts',(-1.39146164491344,1.92074186406775,0.700575504311545));
#59909=CARTESIAN_POINT('Ctrl Pts',(-1.3669883754162,1.93824066317396,0.698565893624467));
#59910=CARTESIAN_POINT('Ctrl Pts',(-1.35440497340061,1.94705450255701,0.697535116827317));
#59911=CARTESIAN_POINT('Ctrl Pts',(-1.32255276290548,1.96890667932377,0.694931662709459));
#59912=CARTESIAN_POINT('Ctrl Pts',(-1.30317644214468,1.98178465450931,0.693353118980663));
#59913=CARTESIAN_POINT('Ctrl Pts',(-1.22251483217302,2.03369986455857,0.686800868590589));
#59914=CARTESIAN_POINT('Ctrl Pts',(-1.15964659263396,2.0701921476143,0.681736995118589));
#59915=CARTESIAN_POINT('Ctrl Pts',(-0.974025572717844,2.16682660700429,
0.666903549043471));
#59916=CARTESIAN_POINT('Ctrl Pts',(-0.847628386542998,2.21932032730963,
0.656928480850742));
#59917=CARTESIAN_POINT('Ctrl Pts',(-0.608857015404388,2.29509626347655,
0.638676939884996));
#59918=CARTESIAN_POINT('Ctrl Pts',(-0.497928917510556,2.32169037878113,
0.63042264113472));
#59919=CARTESIAN_POINT('Ctrl Pts',(-0.368722491334158,2.34297486041688,
0.621337489821968));
#59920=CARTESIAN_POINT('Ctrl Pts',(-0.351906811332879,2.34555944485181,
0.620165382005684));
#59921=CARTESIAN_POINT('Ctrl Pts',(-0.325636997874695,2.34930825775137,
0.618351786208036));
#59922=CARTESIAN_POINT('Ctrl Pts',(-0.316201580846568,2.35059679921502,
0.617703900088474));
#59923=CARTESIAN_POINT('Ctrl Pts',(-0.299426413398389,2.35278485180953,
0.616558557540844));
#59924=CARTESIAN_POINT('Ctrl Pts',(-0.292090115237561,2.35370688542672,
0.616059906008229));
#59925=CARTESIAN_POINT('Ctrl Pts',(-0.274312432938551,2.35585680236328,
0.614856832197766));
#59926=CARTESIAN_POINT('Ctrl Pts',(-0.263867029304125,2.35704959329835,
0.614154336940135));
#59927=CARTESIAN_POINT('Ctrl Pts',(-0.231173137377478,2.36056294180309,
0.611968257993204));
#59928=CARTESIAN_POINT('Ctrl Pts',(-0.208898801954638,2.36263831335565,
0.610497273355312));
#59929=CARTESIAN_POINT('Ctrl Pts',(-0.0901970347951604,2.3720062147553,
0.602740154966611));
#59930=CARTESIAN_POINT('Ctrl Pts',(0.00658955635311563,2.37371221252312,
0.596700305590679));
#59931=CARTESIAN_POINT('Ctrl Pts',(0.277620911008778,2.3619056561937,0.579940780284691));
#59932=CARTESIAN_POINT('Ctrl Pts',(0.45063895407541,2.33507883443648,0.569381696653995));
#59933=CARTESIAN_POINT('Ctrl Pts',(0.665760870418325,2.27690415666136,0.555174641919089));
#59934=CARTESIAN_POINT('Ctrl Pts',(0.711978684101656,2.26287779766201,0.552059447160011));
#59935=CARTESIAN_POINT('Ctrl Pts',(0.777384766086199,2.24082597310604,0.547542726857982));
#59936=CARTESIAN_POINT('Ctrl Pts',(0.796947413607959,2.23394335017341,0.546177747699829));
#59937=CARTESIAN_POINT('Ctrl Pts',(0.830262568694626,2.22172896717452,0.543827785225058));
#59938=CARTESIAN_POINT('Ctrl Pts',(0.844060421028905,2.21652374805786,0.542846979719771));
#59939=CARTESIAN_POINT('Ctrl Pts',(0.872181368903933,2.20561451497476,0.540832104435277));
#59940=CARTESIAN_POINT('Ctrl Pts',(0.886499157016149,2.19989885094293,0.53979768831023));
#59941=CARTESIAN_POINT('Ctrl Pts',(0.922411289486603,2.18515520503335,0.537181033875542));
#59942=CARTESIAN_POINT('Ctrl Pts',(0.94392919767036,2.17594656630374,0.535592847532929));
#59943=CARTESIAN_POINT('Ctrl Pts',(1.03261188561223,2.13643163428384,0.528960334959937));
#59944=CARTESIAN_POINT('Ctrl Pts',(1.09847615585474,2.10332488825453,0.523823248821254));
#59945=CARTESIAN_POINT('Ctrl Pts',(1.28479577714394,1.99853074367456,0.50866291455141));
#59946=CARTESIAN_POINT('Ctrl Pts',(1.400568999181,1.91917292343225,0.498422231341662));
#59947=CARTESIAN_POINT('Ctrl Pts',(1.59343553547025,1.76018036745042,0.480216392171473));
#59948=CARTESIAN_POINT('Ctrl Pts',(1.67327078380359,1.68447082225648,0.472264799607404));
#59949=CARTESIAN_POINT('Ctrl Pts',(1.75904547110874,1.59098867026052,0.46346266878034));
#59950=CARTESIAN_POINT('Ctrl Pts',(1.77038197576315,1.57836422253609,0.462293725146222));
#59951=CARTESIAN_POINT('Ctrl Pts',(1.78785822205109,1.55847727827402,0.460484314870678));
#59952=CARTESIAN_POINT('Ctrl Pts',(1.79409116127325,1.55129796040275,0.459837482885743));
#59953=CARTESIAN_POINT('Ctrl Pts',(1.8055348617662,1.53795547858139,0.458647411994184));
#59954=CARTESIAN_POINT('Ctrl Pts',(1.81075742223906,1.53180310505493,0.458103359185067));
#59955=CARTESIAN_POINT('Ctrl Pts',(1.82289788713066,1.51735232074527,0.456836317763363));
#59956=CARTESIAN_POINT('Ctrl Pts',(1.82979061394445,1.5090331648348,0.456115119859604));
#59957=CARTESIAN_POINT('Ctrl Pts',(1.85207183462001,1.48176377159186,0.453776654939211));
#59958=CARTESIAN_POINT('Ctrl Pts',(1.86722522808072,1.46262230823132,0.452174989712506));
#59959=CARTESIAN_POINT('Ctrl Pts',(1.90323310391704,1.41566594541722,0.448331753756019));
#59960=CARTESIAN_POINT('Ctrl Pts',(1.92377729464535,1.3876193606771,0.446107150673477));
#59961=CARTESIAN_POINT('Ctrl Pts',(2.00580677077071,1.27030858976154,0.437044047431806));
#59962=CARTESIAN_POINT('Ctrl Pts',(2.0617580284874,1.17732824700928,0.430418002240968));
#59963=CARTESIAN_POINT('Ctrl Pts',(2.17949645139178,0.947355357133899,0.414575239300669));
#59964=CARTESIAN_POINT('Ctrl Pts',(2.23501525973239,0.807704694744713,0.405358809755413));
#59965=CARTESIAN_POINT('Ctrl Pts',(2.28564882371701,0.634009141522768,0.393697410790794));
#59966=CARTESIAN_POINT('Ctrl Pts',(2.29373617921035,0.604096296483124,0.391683546812165));
#59967=CARTESIAN_POINT('Ctrl Pts',(2.30572646189051,0.556028716525917,0.388433843836277));
#59968=CARTESIAN_POINT('Ctrl Pts',(2.31000638695124,0.537971105572854,0.387210004757949));
#59969=CARTESIAN_POINT('Ctrl Pts',(2.31724914193221,0.505731481000089,0.385018734083788));
#59970=CARTESIAN_POINT('Ctrl Pts',(2.3202947920383,0.491568895307345,0.384053993826783));
#59971=CARTESIAN_POINT('Ctrl Pts',(2.3264145786531,0.461786404806506,0.382020351837113));
#59972=CARTESIAN_POINT('Ctrl Pts',(2.32946156243208,0.446161723188248,0.380950640249393));
#59973=CARTESIAN_POINT('Ctrl Pts',(2.3371181763739,0.404680691314672,0.378102723669877));
#59974=CARTESIAN_POINT('Ctrl Pts',(2.34145589000034,0.37877704702966,0.376316059820126));
#59975=CARTESIAN_POINT('Ctrl Pts',(2.36240761185764,0.239496083503416,0.36666180589382));
#59976=CARTESIAN_POINT('Ctrl Pts',(2.37121640096425,0.125115428188706,0.358554181236972));
#59977=CARTESIAN_POINT('Ctrl Pts',(2.37208590174046,-0.0701559832253248,
0.344460763667022));
#59978=CARTESIAN_POINT('Ctrl Pts',(2.36832452413327,-0.15083597370437,0.338567564366654));
#59979=CARTESIAN_POINT('Ctrl Pts',(2.3583160822561,-0.253033992601144,0.331077217486314));
#59980=CARTESIAN_POINT('Ctrl Pts',(2.35587046312243,-0.274873276325728,
0.329475255686216));
#59981=CARTESIAN_POINT('Ctrl Pts',(2.34058849647143,-0.396084236037446,
0.320584684156407));
#59982=CARTESIAN_POINT('Ctrl Pts',(2.32176704570386,-0.494610412207226,
0.313355661202691));
#59983=CARTESIAN_POINT('Ctrl Pts',(2.29256371229504,-0.607974945883795,
0.305232625040322));
#59984=CARTESIAN_POINT('Ctrl Pts',(2.28818697311984,-0.62424540525134,0.304071677629845));
#59985=CARTESIAN_POINT('Ctrl Pts',(2.28108675276386,-0.649561761547126,
0.302274392641359));
#59986=CARTESIAN_POINT('Ctrl Pts',(2.27848208575926,-0.658639999028936,
0.301631742024198));
#59987=CARTESIAN_POINT('Ctrl Pts',(2.27375202965481,-0.674762103304527,
0.300494032106262));
#59988=CARTESIAN_POINT('Ctrl Pts',(2.27164807206643,-0.681811723835021,
0.299997801779754));
#59989=CARTESIAN_POINT('Ctrl Pts',(2.26647084315136,-0.698868775290624,
0.298800006210314));
#59990=CARTESIAN_POINT('Ctrl Pts',(2.26336406876574,-0.708865819725888,
0.298100362408445));
#59991=CARTESIAN_POINT('Ctrl Pts',(2.25344844462857,-0.740042628486866,
0.295924944364));
#59992=CARTESIAN_POINT('Ctrl Pts',(2.24640750639646,-0.761148071253899,
0.294461675014972));
#59993=CARTESIAN_POINT('Ctrl Pts',(2.20754460552579,-0.872401054242493,
0.286782909472146));
#59994=CARTESIAN_POINT('Ctrl Pts',(2.17058763224998,-0.960671714941174,
0.280809617470508));
#59995=CARTESIAN_POINT('Ctrl Pts',(2.05321737489586,-1.19938722330217,0.264379801525432));
#59996=CARTESIAN_POINT('Ctrl Pts',(1.96178249514218,-1.34374047907669,0.254085718735529));
#59997=CARTESIAN_POINT('Ctrl Pts',(1.82146627338783,-1.52002483927286,0.239783986318725));
#59998=CARTESIAN_POINT('Ctrl Pts',(1.78578007342064,-1.56179502658402,0.236252038611432));
#59999=CARTESIAN_POINT('Ctrl Pts',(1.73398202190576,-1.61832556601315,0.231240622171423));
#60000=CARTESIAN_POINT('Ctrl Pts',(1.71906622591561,-1.63416111497828,0.22981005575489));
#60001=CARTESIAN_POINT('Ctrl Pts',(1.69447570596016,-1.65955869886622,0.227470265242845));
#60002=CARTESIAN_POINT('Ctrl Pts',(1.68493261901047,-1.66924685099942,0.226566669843765));
#60003=CARTESIAN_POINT('Ctrl Pts',(1.66470238026997,-1.68943436842655,0.22466001872677));
#60004=CARTESIAN_POINT('Ctrl Pts',(1.65399803861146,-1.69991557756897,0.223656236176726));
#60005=CARTESIAN_POINT('Ctrl Pts',(1.62799686676017,-1.7248966581399,0.221229656098395));
#60006=CARTESIAN_POINT('Ctrl Pts',(1.61260487707393,-1.73929518507195,0.219802663854785));
#60007=CARTESIAN_POINT('Ctrl Pts',(1.55691336642268,-1.79001736624349,0.214671506218182));
#60008=CARTESIAN_POINT('Ctrl Pts',(1.51556466329592,-1.82515871740052,0.210919954734751));
#60009=CARTESIAN_POINT('Ctrl Pts',(1.40732622083025,-1.91093256998107,0.20123776794873));
#60010=CARTESIAN_POINT('Ctrl Pts',(1.33889205141778,-1.95948874306921,0.195240521769358));
#60011=CARTESIAN_POINT('Ctrl Pts',(1.11509172694683,-2.10107668246895,0.176082573805482));
#60012=CARTESIAN_POINT('Ctrl Pts',(0.951572376105325,-2.18001548031892,
0.162689781931049));
#60013=CARTESIAN_POINT('Ctrl Pts',(0.760226426510909,-2.24671364647345,
0.148548789202375));
#60014=CARTESIAN_POINT('Ctrl Pts',(0.739693156082017,-2.25355730876224,
0.147050772190553));
#60015=CARTESIAN_POINT('Ctrl Pts',(0.709067926405305,-2.2633008786137,0.144848072967571));
#60016=CARTESIAN_POINT('Ctrl Pts',(0.699046384328166,-2.26641619174735,
0.144132259535063));
#60017=CARTESIAN_POINT('Ctrl Pts',(0.68127301687442,-2.27181214462059,0.142871943229718));
#60018=CARTESIAN_POINT('Ctrl Pts',(0.673529949131877,-2.27411977604542,
0.142325983721347));
#60019=CARTESIAN_POINT('Ctrl Pts',(0.665525343622258,-2.276460881958,0.141764746676507));
#60020=CARTESIAN_POINT('Ctrl Pts',(0.665275806655039,-2.27653381946505,
0.141747253714633));
#60021=CARTESIAN_POINT('Ctrl Pts',(0.664825098788998,-2.27666547706024,
0.141715663995405));
#60022=CARTESIAN_POINT('Ctrl Pts',(0.664623932141617,-2.27672421150266,
0.141701566438231));
#60023=CARTESIAN_POINT('Ctrl Pts',(0.664259113498333,-2.27683067479652,
0.141676004002107));
#60024=CARTESIAN_POINT('Ctrl Pts',(0.664095464169348,-2.27687841265838,
0.141664538621842));
#60025=CARTESIAN_POINT('Ctrl Pts',(0.663797721166953,-2.27696523192209,
0.141643680996446));
#60026=CARTESIAN_POINT('Ctrl Pts',(0.663663629200559,-2.27700431911861,
0.14163428842895));
#60027=CARTESIAN_POINT('Ctrl Pts',(0.663419024160122,-2.27707559692949,
0.141617156539464));
#60028=CARTESIAN_POINT('Ctrl Pts',(0.663308512208448,-2.27710779133997,
0.141609417006726));
#60029=CARTESIAN_POINT('Ctrl Pts',(0.663012027299088,-2.27719414009332,
0.141588654789123));
#60030=CARTESIAN_POINT('Ctrl Pts',(0.662826049999859,-2.27724827971398,
0.141575632921399));
#60031=CARTESIAN_POINT('Ctrl Pts',(0.662460926474542,-2.2773545218526,0.141550070886846));
#60032=CARTESIAN_POINT('Ctrl Pts',(0.662281780735279,-2.27740662601438,
0.141537530629021));
#60033=CARTESIAN_POINT('Ctrl Pts',(0.661929771916511,-2.27750896199234,
0.141512893053815));
#60034=CARTESIAN_POINT('Ctrl Pts',(0.661756909271774,-2.27755919526496,
0.141500795656101));
#60035=CARTESIAN_POINT('Ctrl Pts',(0.661416971848513,-2.27765793790856,
0.141477008845056));
#60036=CARTESIAN_POINT('Ctrl Pts',(0.661249897450439,-2.27770644857693,
0.141465319359927));
#60037=CARTESIAN_POINT('Ctrl Pts',(0.660921088649673,-2.27780188019891,
0.141442316745847));
#60038=CARTESIAN_POINT('Ctrl Pts',(0.660759354592563,-2.27784880230845,
0.141431003553344));
#60039=CARTESIAN_POINT('Ctrl Pts',(0.660440819886888,-2.27794117847227,
0.141408724823067));
#60040=CARTESIAN_POINT('Ctrl Pts',(0.660284019537088,-2.27798663356405,
0.141397759227762));
#60041=CARTESIAN_POINT('Ctrl Pts',(0.659974982005834,-2.27807618633512,
0.14137614956625));
#60042=CARTESIAN_POINT('Ctrl Pts',(0.659822745097611,-2.27812028494385,
0.141365505448848));
#60043=CARTESIAN_POINT('Ctrl Pts',(0.659522496367177,-2.27820722565541,
0.141344514895681));
#60044=CARTESIAN_POINT('Ctrl Pts',(0.659374484794813,-2.27825006859312,
0.14133416841421));
#60045=CARTESIAN_POINT('Ctrl Pts',(0.659082377178886,-2.27833459024196,
0.141313751305601));
#60046=CARTESIAN_POINT('Ctrl Pts',(0.658938281357462,-2.27837626970667,
0.14130368063709));
#60047=CARTESIAN_POINT('Ctrl Pts',(0.658653721032273,-2.27845854903023,
0.14128379512159));
#60048=CARTESIAN_POINT('Ctrl Pts',(0.658513256728526,-2.27849914957005,
0.141273980237223));
#60049=CARTESIAN_POINT('Ctrl Pts',(0.658235697815475,-2.27857934884532,
0.141254587855974));
#60050=CARTESIAN_POINT('Ctrl Pts',(0.658098603388054,-2.27861894819685,
0.141245010325362));
#60051=CARTESIAN_POINT('Ctrl Pts',(0.657827542788207,-2.27869721680865,
0.14122607564583));
#60052=CARTESIAN_POINT('Ctrl Pts',(0.657693576778667,-2.27873588662801,
0.141216718466227));
#60053=CARTESIAN_POINT('Ctrl Pts',(0.657428549634764,-2.27881236244484,
0.141198208760571));
#60054=CARTESIAN_POINT('Ctrl Pts',(0.657297488648413,-2.27885016894986,
0.1411890562067));
#60055=CARTESIAN_POINT('Ctrl Pts',(0.657038064372579,-2.27892497952696,
0.141170941170318));
#60056=CARTESIAN_POINT('Ctrl Pts',(0.656909701217583,-2.27896198406044,
0.141161978662544));
#60057=CARTESIAN_POINT('Ctrl Pts',(0.656655479978541,-2.27903524770222,
0.141144230165295));
#60058=CARTESIAN_POINT('Ctrl Pts',(0.656529622019303,-2.27907150722968,
0.141135444153025));
#60059=CARTESIAN_POINT('Ctrl Pts',(0.656280231644268,-2.27914333392576,
0.14111803601988));
#60060=CARTESIAN_POINT('Ctrl Pts',(0.656156699343588,-2.27917890147566,
0.14110941387837));
#60061=CARTESIAN_POINT('Ctrl Pts',(0.655911792584199,-2.27924939372603,
0.141092321695904));
#60062=CARTESIAN_POINT('Ctrl Pts',(0.655790418221921,-2.27928431877636,
0.141083851635575));
#60063=CARTESIAN_POINT('Ctrl Pts',(0.655549670267695,-2.27935357234028,
0.141067052576089));
#60064=CARTESIAN_POINT('Ctrl Pts',(0.655430296770329,-2.27938790117085,
0.141058723559758));
#60065=CARTESIAN_POINT('Ctrl Pts',(0.655193403125064,-2.27945600570688,
0.141042196231044));
#60066=CARTESIAN_POINT('Ctrl Pts',(0.655075883056496,-2.27948978170325,
0.141033997902541));
#60067=CARTESIAN_POINT('Ctrl Pts',(0.654842557535596,-2.27955682137068,
0.141017722206349));
#60068=CARTESIAN_POINT('Ctrl Pts',(0.654726752161155,-2.27959008530523,
0.141009644824376));
#60069=CARTESIAN_POINT('Ctrl Pts',(0.654496725180476,-2.27965613927842,
0.140993601835456));
#60070=CARTESIAN_POINT('Ctrl Pts',(0.654382503647127,-2.27968892955646,
0.140985636215651));
#60071=CARTESIAN_POINT('Ctrl Pts',(0.654155520629878,-2.2797540725024,0.140969808069232));
#60072=CARTESIAN_POINT('Ctrl Pts',(0.654042759215101,-2.27978642538729,
0.140961945531126));
#60073=CARTESIAN_POINT('Ctrl Pts',(0.65381857920301,-2.27985072788195,0.140946315324815));
#60074=CARTESIAN_POINT('Ctrl Pts',(0.653707160658574,-2.27988267769168,
0.140938547645489));
#60075=CARTESIAN_POINT('Ctrl Pts',(0.642773200295821,-2.28301717661147,
0.140176332963112));
#60076=CARTESIAN_POINT('Ctrl Pts',(0.631928448548873,-2.28604270820098,
0.139426072922503));
#60077=CARTESIAN_POINT('Ctrl Pts',(0.592529711468753,-2.29673260205386,
0.136719772349793));
#60078=CARTESIAN_POINT('Ctrl Pts',(0.56385333062162,-2.30394047482028,0.134786759720534));
#60079=CARTESIAN_POINT('Ctrl Pts',(0.491264066821116,-2.32074934483806,
0.129968638040957));
#60080=CARTESIAN_POINT('Ctrl Pts',(0.447198071601828,-2.32964208558751,
0.127112106876457));
#60081=CARTESIAN_POINT('Ctrl Pts',(0.206461101231627,-2.3711407062007,0.111748819003527));
#60082=CARTESIAN_POINT('Ctrl Pts',(0.00653527505048171,-2.38010438082522,
0.0997909555847822));
#60083=CARTESIAN_POINT('Ctrl Pts',(-0.246381698433964,-2.35954515023386,
0.0836589002354788));
#60084=CARTESIAN_POINT('Ctrl Pts',(-0.300430197833493,-2.35327394798437,
0.0801577623923198));
#60085=CARTESIAN_POINT('Ctrl Pts',(-0.375793933479163,-2.34189098148609,
0.0751743064046654));
#60086=CARTESIAN_POINT('Ctrl Pts',(-0.397328822786406,-2.33833363864016,
0.0737386488176271));
#60087=CARTESIAN_POINT('Ctrl Pts',(-0.433679534887422,-2.33181223780764,
0.0712939858783489));
#60088=CARTESIAN_POINT('Ctrl Pts',(-0.448521963182565,-2.32900285154338,
0.0702897638987183));
#60089=CARTESIAN_POINT('Ctrl Pts',(-0.478492233631729,-2.32303294478006,
0.068249272422422));
#60090=CARTESIAN_POINT('Ctrl Pts',(-0.493618024999703,-2.31986596737215,
0.0672128480493124));
#60091=CARTESIAN_POINT('Ctrl Pts',(-0.531003292032719,-2.31165621452894,
0.0646342634396861));
#60092=CARTESIAN_POINT('Ctrl Pts',(-0.553222583331075,-2.30643960723948,
0.0630867719150712));
#60093=CARTESIAN_POINT('Ctrl Pts',(-0.639877970586715,-2.28477061351907,
0.0569907455003847));
#60094=CARTESIAN_POINT('Ctrl Pts',(-0.703680470963905,-2.26593312002907,
0.052368842208252));
#60095=CARTESIAN_POINT('Ctrl Pts',(-0.875354877752572,-2.20729670813393,
0.0395571363453451));
#60096=CARTESIAN_POINT('Ctrl Pts',(-0.981253416593894,-2.16230011210438,
0.0312298997291111));
#60097=CARTESIAN_POINT('Ctrl Pts',(-1.17700219292696,-2.06177611854969,
0.0151851737384018));
#60098=CARTESIAN_POINT('Ctrl Pts',(-1.26723605846899,-2.00757678307237,
0.0074963326966278));
#60099=CARTESIAN_POINT('Ctrl Pts',(-1.35356952483514,-1.9475748006014,6.39245600897453E-15));
#60100=CARTESIAN_POINT('',(1.37702479013102,-1.93106208855765,0.));
#60101=CARTESIAN_POINT('Origin',(0.,0.,0.));
#60102=CARTESIAN_POINT('Ctrl Pts',(1.37702479013102,-1.93106208855765,-3.33066907387547E-15));
#60103=CARTESIAN_POINT('Ctrl Pts',(1.44326778530957,-1.88382474332991,0.00545963808742537));
#60104=CARTESIAN_POINT('Ctrl Pts',(1.50712417061229,-1.83314207740384,0.0109192761748538));
#60105=CARTESIAN_POINT('Ctrl Pts',(1.56823230173022,-1.77928230202797,0.0163789142622826));
#60106=CARTESIAN_POINT('Ctrl Pts',(1.62930377606925,-1.7254548353783,0.0218352772905245));
#60107=CARTESIAN_POINT('Ctrl Pts',(1.68762994983901,-1.66845433970544,0.027291640318767));
#60108=CARTESIAN_POINT('Ctrl Pts',(1.74288236953678,-1.60858916708334,0.0327480033470089));
#60109=CARTESIAN_POINT('Ctrl Pts',(1.79812957679123,-1.54872964206582,0.0382038516288718));
#60110=CARTESIAN_POINT('Ctrl Pts',(1.85030330341389,-1.48600629137094,0.0436596999107342));
#60111=CARTESIAN_POINT('Ctrl Pts',(1.89911260932967,-1.42076365366836,0.0491155481925971));
#60112=CARTESIAN_POINT('Ctrl Pts',(1.94792122166181,-1.3555219430682,0.0545713189464766));
#60113=CARTESIAN_POINT('Ctrl Pts',(1.99336524640357,-1.28776136609834,0.060027089700356));
#60114=CARTESIAN_POINT('Ctrl Pts',(2.0351954503436,-1.21785776731141,0.0654828604542355));
#60115=CARTESIAN_POINT('Ctrl Pts',(2.07703526430301,-1.14793810895803,0.0709398846101495));
#60116=CARTESIAN_POINT('Ctrl Pts',(2.11525938183687,-1.07587482429233,0.0763969087660638));
#60117=CARTESIAN_POINT('Ctrl Pts',(2.14966370056128,-1.00206987630064,0.0818539329219778));
#60118=CARTESIAN_POINT('Ctrl Pts',(2.18408431909924,-0.92822996156826,0.0873135424648312));
#60119=CARTESIAN_POINT('Ctrl Pts',(2.21468135480373,-0.852647137883284,
0.092773152007684));
#60120=CARTESIAN_POINT('Ctrl Pts',(2.24129860351498,-0.77574392191096,0.0982327615505374));
#60121=CARTESIAN_POINT('Ctrl Pts',(2.26795510942114,-0.698727283076209,
0.103700423351469));
#60122=CARTESIAN_POINT('Ctrl Pts',(2.290619963958,-0.620386776580873,0.109168085152402));
#60123=CARTESIAN_POINT('Ctrl Pts',(2.30918670871589,-0.541160610900181,
0.114635746953334));
#60124=CARTESIAN_POINT('Ctrl Pts',(2.3277679904902,-0.461872414309592,0.120107689714143));
#60125=CARTESIAN_POINT('Ctrl Pts',(2.34224469032866,-0.381697606332208,
0.125579632474952));
#60126=CARTESIAN_POINT('Ctrl Pts',(2.35256183899474,-0.301082806227277,
0.131051575235762));
#60127=CARTESIAN_POINT('Ctrl Pts',(2.36289859025774,-0.220314837889131,
0.136533914695488));
#60128=CARTESIAN_POINT('Ctrl Pts',(2.36905996623431,-0.139105642971568,
0.142016254155214));
#60129=CARTESIAN_POINT('Ctrl Pts',(2.37104302952243,-0.0579052212937533,
0.147498593614941));
#60130=CARTESIAN_POINT('Ctrl Pts',(2.37229246741722,-0.00674453241181939,
0.150952766113663));
#60131=CARTESIAN_POINT('Ctrl Pts',(2.37188429523822,0.0444126803724593,
0.154406938612386));
#60132=CARTESIAN_POINT('Ctrl Pts',(2.36982835395112,0.0954548862516559,
0.157861111111109));
#60133=CARTESIAN_POINT('Ctrl Pts',(2.36668417853294,0.173514337668007,0.163143618120815));
#60134=CARTESIAN_POINT('Ctrl Pts',(2.35967183891541,0.251594288586149,0.168426125130522));
#60135=CARTESIAN_POINT('Ctrl Pts',(2.3487818857182,0.329274529567723,0.173708632140229));
#60136=CARTESIAN_POINT('Ctrl Pts',(2.33790926945034,0.406831102722223,0.1789827293387));
#60137=CARTESIAN_POINT('Ctrl Pts',(2.32317135634299,0.48398875988057,0.184256826537171));
#60138=CARTESIAN_POINT('Ctrl Pts',(2.30461067786112,0.56032819488984,0.189530923735642));
#60139=CARTESIAN_POINT('Ctrl Pts',(2.28607482777778,0.636565511546182,0.194797965837111));
#60140=CARTESIAN_POINT('Ctrl Pts',(2.26372648220335,0.711986318125151,0.200065007938579));
#60141=CARTESIAN_POINT('Ctrl Pts',(2.23765962166701,0.786179038171995,0.205332050040048));
#60142=CARTESIAN_POINT('Ctrl Pts',(2.21161201755268,0.86031694968811,0.210595201209378));
#60143=CARTESIAN_POINT('Ctrl Pts',(2.18185150513484,0.933228124097077,0.215858352378709));
#60144=CARTESIAN_POINT('Ctrl Pts',(2.14852221092795,1.00451499324265,0.221121503548039));
#60145=CARTESIAN_POINT('Ctrl Pts',(2.11520666201045,1.07577246306641,0.226382484148276));
#60146=CARTESIAN_POINT('Ctrl Pts',(2.0783254543951,1.14540652368449,0.231643464748513));
#60147=CARTESIAN_POINT('Ctrl Pts',(2.03807065845716,1.21304000496109,0.236904445348749));
#60148=CARTESIAN_POINT('Ctrl Pts',(1.99781932847753,1.2806676629607,0.242164972975893));
#60149=CARTESIAN_POINT('Ctrl Pts',(1.9541952328856,1.34629467288068,0.247425500603037));
#60150=CARTESIAN_POINT('Ctrl Pts',(1.90743535172774,1.40957030384415,0.252686028230181));
#60151=CARTESIAN_POINT('Ctrl Pts',(1.86063139824614,1.47290557362668,0.257951514032385));
#60152=CARTESIAN_POINT('Ctrl Pts',(1.81068603974131,1.53388465079858,0.263216999834587));
#60153=CARTESIAN_POINT('Ctrl Pts',(1.757877954138,1.59218816754038,0.268482485636791));
#60154=CARTESIAN_POINT('Ctrl Pts',(1.70504654917932,1.6505174303476,0.273750296608203));
#60155=CARTESIAN_POINT('Ctrl Pts',(1.64935023909496,1.70616844123663,0.279018107579616));
#60156=CARTESIAN_POINT('Ctrl Pts',(1.59110425956814,1.758859089775,0.284285918551029));
#60157=CARTESIAN_POINT('Ctrl Pts',(1.53275141754399,1.81164640857858,0.289563394248496));
#60158=CARTESIAN_POINT('Ctrl Pts',(1.47183993167519,1.86146220983978,0.294840869945963));
#60159=CARTESIAN_POINT('Ctrl Pts',(1.40871752970107,1.90806524626725,0.30011834564343));
#60160=CARTESIAN_POINT('Ctrl Pts',(1.3465063371901,1.95399554011085,0.305319637836361));
#60161=CARTESIAN_POINT('Ctrl Pts',(1.28214806856191,1.99680506618771,0.310520930029293));
#60162=CARTESIAN_POINT('Ctrl Pts',(1.21599894108394,2.03630661683911,0.315722222222224));
#60163=CARTESIAN_POINT('Ctrl Pts',(1.14802781677833,2.07689618939975,0.321066777648344));
#60164=CARTESIAN_POINT('Ctrl Pts',(1.07789839973257,2.1141527057923,0.326411333074464));
#60165=CARTESIAN_POINT('Ctrl Pts',(1.00597032896329,2.14784118587606,0.331755888500584));
#60166=CARTESIAN_POINT('Ctrl Pts',(0.934144558695706,2.18148175214291,0.337092842573081));
#60167=CARTESIAN_POINT('Ctrl Pts',(0.860525634521335,2.21156416519094,0.342429796645578));
#60168=CARTESIAN_POINT('Ctrl Pts',(0.785499756332435,2.23789816464058,0.347766750718074));
#60169=CARTESIAN_POINT('Ctrl Pts',(0.710559857948801,2.26420198527461,0.353097588630614));
#60170=CARTESIAN_POINT('Ctrl Pts',(0.634216647943832,2.28676577651481,0.358428426543155));
#60171=CARTESIAN_POINT('Ctrl Pts',(0.556877001243562,2.30544704298016,0.363759264455695));
#60172=CARTESIAN_POINT('Ctrl Pts',(0.479585816847761,2.32411660345433,0.369086761976844));
#60173=CARTESIAN_POINT('Ctrl Pts',(0.401299887304215,2.33890835972766,0.374414259497993));
#60174=CARTESIAN_POINT('Ctrl Pts',(0.322440839336424,2.34972976480872,0.379741757019143));
#60175=CARTESIAN_POINT('Ctrl Pts',(0.243606977598816,2.3605477137182,0.385067553028768));
#60176=CARTESIAN_POINT('Ctrl Pts',(0.164200822520171,2.36739776666325,0.390393349038394));
#60177=CARTESIAN_POINT('Ctrl Pts',(0.0846523363143929,2.37023881591213,
0.39571914504802));
#60178=CARTESIAN_POINT('Ctrl Pts',(0.00510481752400763,2.37307983061006,
0.401044876288883));
#60179=CARTESIAN_POINT('Ctrl Pts',(-0.0745845630179324,2.37191192337,0.406370607529746));
#60180=CARTESIAN_POINT('Ctrl Pts',(-0.153984063945952,2.36674607225843,
0.411696338770609));
#60181=CARTESIAN_POINT('Ctrl Pts',(-0.233460080683629,2.36157524291304,
0.417027202318768));
#60182=CARTESIAN_POINT('Ctrl Pts',(-0.312645193559593,2.35239880416356,
0.422358065866927));
#60183=CARTESIAN_POINT('Ctrl Pts',(-0.391111612601996,2.33927975432351,
0.427688929415086));
#60184=CARTESIAN_POINT('Ctrl Pts',(-0.469615311879154,2.3261544714826,0.433022325713522));
#60185=CARTESIAN_POINT('Ctrl Pts',(-0.547399181006083,2.30908294519053,
0.438355722011956));
#60186=CARTESIAN_POINT('Ctrl Pts',(-0.624046927172358,2.2881790784785,0.443689118310392));
#60187=CARTESIAN_POINT('Ctrl Pts',(-0.700827728124772,2.26723892420874,
0.449031772988093));
#60188=CARTESIAN_POINT('Ctrl Pts',(-0.776468021395321,2.24245328232575,
0.454374427665795));
#60189=CARTESIAN_POINT('Ctrl Pts',(-0.850568189023652,2.21398550544511,
0.459717082343496));
#60190=CARTESIAN_POINT('Ctrl Pts',(-0.914674367487779,2.18935721587982,
0.464339166006773));
#60191=CARTESIAN_POINT('Ctrl Pts',(-0.977627989544473,2.16197390682528,
0.468961249670049));
#60192=CARTESIAN_POINT('Ctrl Pts',(-1.03918531674208,2.13196902884814,0.473583333333325));
#60193=CARTESIAN_POINT('Ctrl Pts',(-1.11037453998178,2.09726927735084,0.478928636008362));
#60194=CARTESIAN_POINT('Ctrl Pts',(-1.1799508286317,2.05893811340978,0.4842739386834));
#60195=CARTESIAN_POINT('Ctrl Pts',(-1.24752088426758,2.01714890521653,0.489619241358437));
#60196=CARTESIAN_POINT('Ctrl Pts',(-1.3149970487025,1.9754177647414,0.494957116529044));
#60197=CARTESIAN_POINT('Ctrl Pts',(-1.38047212392445,1.93023836733986,0.50029499169965));
#60198=CARTESIAN_POINT('Ctrl Pts',(-1.44357582915885,1.88183072776707,0.505632866870257));
#60199=CARTESIAN_POINT('Ctrl Pts',(-1.50661029432368,1.83347620311549,0.510964885097174));
#60200=CARTESIAN_POINT('Ctrl Pts',(-1.56727819271147,1.78190075845812,0.516296903324091));
#60201=CARTESIAN_POINT('Ctrl Pts',(-1.62523800314883,1.72736779396306,0.521628921551007));
#60202=CARTESIAN_POINT('Ctrl Pts',(-1.68316321911901,1.67286737855393,0.526957757256653));
#60203=CARTESIAN_POINT('Ctrl Pts',(-1.73838321742658,1.61541326635611,0.532286592962297));
#60204=CARTESIAN_POINT('Ctrl Pts',(-1.79059031382657,1.55530845510801,0.537615428667943));
#60205=CARTESIAN_POINT('Ctrl Pts',(-1.84278227267436,1.49522107137036,0.542942719266998));
#60206=CARTESIAN_POINT('Ctrl Pts',(-1.89196275933862,1.43248486673609,0.548270009866054));
#60207=CARTESIAN_POINT('Ctrl Pts',(-1.9378626713541,1.36743787042495,0.553597300465109));
#60208=CARTESIAN_POINT('Ctrl Pts',(-1.98376336156647,1.30238977129319,0.558924681384183));
#60209=CARTESIAN_POINT('Ctrl Pts',(-2.02638309921908,1.23503118430805,0.564252062303258));
#60210=CARTESIAN_POINT('Ctrl Pts',(-2.06549547725366,1.16573002704086,0.569579443222332));
#60211=CARTESIAN_POINT('Ctrl Pts',(-2.10464725042194,1.09635906761656,0.574912190035637));
#60212=CARTESIAN_POINT('Ctrl Pts',(-2.14028437834377,1.02504203662645,0.580244936848942));
#60213=CARTESIAN_POINT('Ctrl Pts',(-2.17222620810871,0.952171918986102,
0.585577683662246));
#60214=CARTESIAN_POINT('Ctrl Pts',(-2.20418399500941,0.879265397721765,
0.590913094548508));
#60215=CARTESIAN_POINT('Ctrl Pts',(-2.23244264048258,0.804804680306168,
0.59624850543477));
#60216=CARTESIAN_POINT('Ctrl Pts',(-2.25687043503204,0.729200865316473,
0.601583916321033));
#60217=CARTESIAN_POINT('Ctrl Pts',(-2.28134152996764,0.653463036002394,
0.606928784686197));
#60218=CARTESIAN_POINT('Ctrl Pts',(-2.30196808540654,0.576578511717898,
0.612273653051362));
#60219=CARTESIAN_POINT('Ctrl Pts',(-2.31866893201719,0.498971388155922,
0.617618521416527));
#60220=CARTESIAN_POINT('Ctrl Pts',(-2.33306932531436,0.43205423551041,0.622227162425831));
#60221=CARTESIAN_POINT('Ctrl Pts',(-2.34455183302236,0.364600187711573,
0.626835803435136));
#60222=CARTESIAN_POINT('Ctrl Pts',(-2.35309545095156,0.296883581915646,
0.63144444444444));
#60223=CARTESIAN_POINT('Ctrl Pts',(-2.35829469962102,0.255674403848179,
0.634249049101883));
#60224=CARTESIAN_POINT('Ctrl Pts',(-2.36241188740593,0.214324853083953,
0.637053653759326));
#60225=CARTESIAN_POINT('Ctrl Pts',(-2.36544101854889,0.172878137039861,
0.639858258416768));
#60226=CARTESIAN_POINT('Origin',(0.,0.,-1.84858989190501));
#60227=CARTESIAN_POINT('',(-2.36544098584031,0.172878584581258,1.83759047784057));
#60228=CARTESIAN_POINT('',(-2.3654410189124,0.172878132066172,1.63813797379334));
#60229=CARTESIAN_POINT('',(-2.36544101854889,0.172878137039864,-1.84858989190501));
#60230=CARTESIAN_POINT('Ctrl Pts',(-2.36544098584031,0.172878584581292,
1.83759047784057));
#60231=CARTESIAN_POINT('Ctrl Pts',(-2.35722714105123,0.285265929505931,
1.83063249560928));
#60232=CARTESIAN_POINT('Ctrl Pts',(-2.34100928488915,0.396994903760292,
1.82357843620098));
#60233=CARTESIAN_POINT('Ctrl Pts',(-2.31227652442218,0.52824094054548,1.8148787327713));
#60234=CARTESIAN_POINT('Ctrl Pts',(-2.30738827607898,0.549199883895431,
1.81347699129859));
#60235=CARTESIAN_POINT('Ctrl Pts',(-2.29752545332533,0.589029365526151,
1.81078751172885));
#60236=CARTESIAN_POINT('Ctrl Pts',(-2.29260185398925,0.607910769652914,
1.80950144430633));
#60237=CARTESIAN_POINT('Ctrl Pts',(-2.28357172865025,0.640869081213229,
1.80723600928146));
#60238=CARTESIAN_POINT('Ctrl Pts',(-2.27956653457981,0.65497283704039,1.8062599236483));
#60239=CARTESIAN_POINT('Ctrl Pts',(-2.27097111447355,0.684206267933738,
1.80422246971128));
#60240=CARTESIAN_POINT('Ctrl Pts',(-2.26635986087931,0.699328949850444,
1.80316046570306));
#60241=CARTESIAN_POINT('Ctrl Pts',(-2.25394441030967,0.738632695028761,
1.80037880936328));
#60242=CARTESIAN_POINT('Ctrl Pts',(-2.24590238571254,0.762735898173374,
1.79865154530968));
#60243=CARTESIAN_POINT('Ctrl Pts',(-2.20814253065937,0.87012912299293,1.7908564441645));
#60244=CARTESIAN_POINT('Ctrl Pts',(-2.17417092653295,0.951837996609212,
1.78465223068797));
#60245=CARTESIAN_POINT('Ctrl Pts',(-2.08172617652505,1.14325385041396,1.76945955502235));
#60246=CARTESIAN_POINT('Ctrl Pts',(-2.01903828739529,1.2506373141881,1.76037551377554));
#60247=CARTESIAN_POINT('Ctrl Pts',(-1.88761543876851,1.43993272900011,1.74359744154145));
#60248=CARTESIAN_POINT('Ctrl Pts',(-1.8211818356568,1.5230889692512,1.73591354639221));
#60249=CARTESIAN_POINT('Ctrl Pts',(-1.73814036513874,1.61379784220138,1.72737990089503));
#60250=CARTESIAN_POINT('Ctrl Pts',(-1.72676564206465,1.62596305624391,1.72623214380853));
#60251=CARTESIAN_POINT('Ctrl Pts',(-1.70976545426397,1.64376504579486,1.72454897917922));
#60252=CARTESIAN_POINT('Ctrl Pts',(-1.70423852282264,1.64949461844379,1.72400669198597));
#60253=CARTESIAN_POINT('Ctrl Pts',(-1.69353818286094,1.66047608467419,1.72296643431434));
#60254=CARTESIAN_POINT('Ctrl Pts',(-1.68836899431332,1.66573183587551,1.72246818024996));
#60255=CARTESIAN_POINT('Ctrl Pts',(-1.67649671226384,1.67769088152275,1.72133361594357));
#60256=CARTESIAN_POINT('Ctrl Pts',(-1.66977784756702,1.68437818428432,1.72069854002105));
#60257=CARTESIAN_POINT('Ctrl Pts',(-1.65100253843425,1.70284254248132,1.71894258893228));
#60258=CARTESIAN_POINT('Ctrl Pts',(-1.6388601144059,1.71453191023563,1.71782814421354));
#60259=CARTESIAN_POINT('Ctrl Pts',(-1.55610667644027,1.79251516904905,1.71036567796915));
#60260=CARTESIAN_POINT('Ctrl Pts',(-1.48160808908416,1.85456750822954,1.7042889607379));
#60261=CARTESIAN_POINT('Ctrl Pts',(-1.38190249563347,1.92776096707279,1.69663401602998));
#60262=CARTESIAN_POINT('Ctrl Pts',(-1.3600226948554,1.94325890111906,1.69498167754051));
#60263=CARTESIAN_POINT('Ctrl Pts',(-1.25600581148036,2.01431885573764,1.68723283380043));
#60264=CARTESIAN_POINT('Ctrl Pts',(-1.17070152113985,2.06506379246464,1.68117968707572));
#60265=CARTESIAN_POINT('Ctrl Pts',(-1.02530954692287,2.13964150449271,1.67101943787669));
#60266=CARTESIAN_POINT('Ctrl Pts',(-0.966982132491316,2.16662643473258,
1.66698306976667));
#60267=CARTESIAN_POINT('Ctrl Pts',(-0.865969100204142,2.20846766216718,
1.65999314870265));
#60268=CARTESIAN_POINT('Ctrl Pts',(-0.823822533234024,2.22453318997038,
1.65707703022371));
#60269=CARTESIAN_POINT('Ctrl Pts',(-0.762725631891272,2.24584781549101,
1.65283637414099));
#60270=CARTESIAN_POINT('Ctrl Pts',(-0.744126607086938,2.25207867415585,
1.6515437360367));
#60271=CARTESIAN_POINT('Ctrl Pts',(-0.71147943220595,2.26256723456253,1.64927072063327));
#60272=CARTESIAN_POINT('Ctrl Pts',(-0.697464879150606,2.26692659770059,
1.64829369425624));
#60273=CARTESIAN_POINT('Ctrl Pts',(-0.668311197724116,2.27569920143619,
1.64625815145276));
#60274=CARTESIAN_POINT('Ctrl Pts',(-0.653166749350483,2.28009207914493,
1.64519903366324));
#60275=CARTESIAN_POINT('Ctrl Pts',(-0.613695568138675,2.2911157852552,1.64243363732617));
#60276=CARTESIAN_POINT('Ctrl Pts',(-0.589305441430633,2.29751013143529,
1.64071991203987));
#60277=CARTESIAN_POINT('Ctrl Pts',(-0.483816048245487,2.32337599829674,
1.63328412701791));
#60278=CARTESIAN_POINT('Ctrl Pts',(-0.401831269856879,2.33894908193943,
1.62744204829056));
#60279=CARTESIAN_POINT('Ctrl Pts',(-0.17174776317778,2.37019944214391,1.61088154295688));
#60280=CARTESIAN_POINT('Ctrl Pts',(-0.0227404602583429,2.37630367796558,
1.59994901974875));
#60281=CARTESIAN_POINT('Ctrl Pts',(0.185791845559624,2.36522386247665,1.5847982339267));
#60282=CARTESIAN_POINT('Ctrl Pts',(0.245605832468564,2.35976295507623,1.58047398159062));
#60283=CARTESIAN_POINT('Ctrl Pts',(0.329462113747185,2.34888350770507,1.57449178450488));
#60284=CARTESIAN_POINT('Ctrl Pts',(0.353723429490974,2.34535260763826,1.57277063107814));
#60285=CARTESIAN_POINT('Ctrl Pts',(0.396454823485551,2.33845544601771,1.56976097179854));
#60286=CARTESIAN_POINT('Ctrl Pts',(0.414947592733761,2.33524492287473,1.56846574669954));
#60287=CARTESIAN_POINT('Ctrl Pts',(0.443017285872127,2.33002777115706,1.56651275317212));
#60288=CARTESIAN_POINT('Ctrl Pts',(0.452622637003993,2.32818093947422,1.56584677116821));
#60289=CARTESIAN_POINT('Ctrl Pts',(0.470214826024624,2.32468547952722,1.56463163238418));
#60290=CARTESIAN_POINT('Ctrl Pts',(0.478204731948126,2.32305505731711,1.56408153280828));
#60291=CARTESIAN_POINT('Ctrl Pts',(0.496513982854802,2.31922039995022,1.56282492822785));
#60292=CARTESIAN_POINT('Ctrl Pts',(0.506827199798709,2.31698847617451,1.56211997180643));
#60293=CARTESIAN_POINT('Ctrl Pts',(0.538520564101027,2.30990784755526,1.55996143902869));
#60294=CARTESIAN_POINT('Ctrl Pts',(0.559849333984127,2.30483133183948,1.55851983863276));
#60295=CARTESIAN_POINT('Ctrl Pts',(0.717259587323752,2.26505156234966,1.54794172717568));
#60296=CARTESIAN_POINT('Ctrl Pts',(0.850107205491825,2.21861398032677,1.53934359629095));
#60297=CARTESIAN_POINT('Ctrl Pts',(1.02039547770398,2.14152956179533,1.5278678166501));
#60298=CARTESIAN_POINT('Ctrl Pts',(1.06214085299248,2.12113472626287,1.52501700945994));
#60299=CARTESIAN_POINT('Ctrl Pts',(1.17488916859823,2.06188772611835,1.51715773494356));
#60300=CARTESIAN_POINT('Ctrl Pts',(1.24454096549887,2.02060928815572,1.51212144239303));
#60301=CARTESIAN_POINT('Ctrl Pts',(1.35607655238759,1.94655102578013,1.50360905416926));
#60302=CARTESIAN_POINT('Ctrl Pts',(1.3992126373164,1.91577865398202,1.50019764934463));
#60303=CARTESIAN_POINT('Ctrl Pts',(1.45782661280982,1.87092857254056,1.49536931809172));
#60304=CARTESIAN_POINT('Ctrl Pts',(1.4742052332523,1.85805033344258,1.49399823369769));
#60305=CARTESIAN_POINT('Ctrl Pts',(1.50198860296427,1.83560610934965,1.49163324786386));
#60306=CARTESIAN_POINT('Ctrl Pts',(1.51347704636193,1.82614532971459,1.49064353872654));
#60307=CARTESIAN_POINT('Ctrl Pts',(1.535259276613,1.80786083949195,1.48874391459932));
#60308=CARTESIAN_POINT('Ctrl Pts',(1.54556796274832,1.79905573033828,1.48783477526325));
#60309=CARTESIAN_POINT('Ctrl Pts',(1.57224742187303,1.77586906168157,1.48545492341814));
#60310=CARTESIAN_POINT('Ctrl Pts',(1.58849617293463,1.76134969095868,1.48397859767628));
#60311=CARTESIAN_POINT('Ctrl Pts',(1.64548479942085,1.70899644201354,1.47870243595983));
#60312=CARTESIAN_POINT('Ctrl Pts',(1.68508914509912,1.66995891020658,1.47485273911037));
#60313=CARTESIAN_POINT('Ctrl Pts',(1.83899512925561,1.50720201689521,1.4591221784128));
#60314=CARTESIAN_POINT('Ctrl Pts',(1.94133221807234,1.37287138593709,1.44679758164857));
#60315=CARTESIAN_POINT('Ctrl Pts',(2.07766343437612,1.1478201046207,1.42765017478009));
#60316=CARTESIAN_POINT('Ctrl Pts',(2.12186195971634,1.06389926357105,1.42080585024223));
#60317=CARTESIAN_POINT('Ctrl Pts',(2.17004694041861,0.957384090435737,1.41264330451139));
#60318=CARTESIAN_POINT('Ctrl Pts',(2.17888783742548,0.937089056085034,1.41111076392095));
#60319=CARTESIAN_POINT('Ctrl Pts',(2.19147944336146,0.907041865247635,1.40887809186221));
#60320=CARTESIAN_POINT('Ctrl Pts',(2.19545165433309,0.897384610812732,1.40816595864972));
#60321=CARTESIAN_POINT('Ctrl Pts',(2.20211670982261,0.880871332978508,1.4069579136309));
#60322=CARTESIAN_POINT('Ctrl Pts',(2.20484155890789,0.874028611861918,1.40646015305633));
#60323=CARTESIAN_POINT('Ctrl Pts',(2.2110149531686,0.858313199521728,1.40532348104106));
#60324=CARTESIAN_POINT('Ctrl Pts',(2.21444200813456,0.849432323408591,1.40468583332721));
#60325=CARTESIAN_POINT('Ctrl Pts',(2.22385210444035,0.82460294586158,1.40291549840315));
#60326=CARTESIAN_POINT('Ctrl Pts',(2.22971708258325,0.80860990161976,1.40178941354801));
#60327=CARTESIAN_POINT('Ctrl Pts',(2.27408239626158,0.683477004093835,1.39307879589059));
#60328=CARTESIAN_POINT('Ctrl Pts',(2.30472511693814,0.571699924214598,1.38588439733219));
#60329=CARTESIAN_POINT('Ctrl Pts',(2.34433034938688,0.370519105607558,1.37325544362029));
#60330=CARTESIAN_POINT('Ctrl Pts',(2.35661537045364,0.282016126448506,1.36780542369962));
#60331=CARTESIAN_POINT('Ctrl Pts',(2.36995951427631,0.118602623711337,1.35766390741791));
#60332=CARTESIAN_POINT('Ctrl Pts',(2.37251835609022,0.0439329213658409,
1.35300050716303));
#60333=CARTESIAN_POINT('Ctrl Pts',(2.37110747847136,-0.064952209819849,
1.34606382877371));
#60334=CARTESIAN_POINT('Ctrl Pts',(2.36992332403909,-0.0991601109507234,
1.34386521466893));
#60335=CARTESIAN_POINT('Ctrl Pts',(2.36642314971465,-0.161325126519403,
1.33982614468255));
#60336=CARTESIAN_POINT('Ctrl Pts',(2.36435055432993,-0.18928990745626,1.33799309353948));
#60337=CARTESIAN_POINT('Ctrl Pts',(2.36028353797204,-0.233511578513536,
1.33506574764054));
#60338=CARTESIAN_POINT('Ctrl Pts',(2.35861564770367,-0.24979639893873,1.33398156687636));
#60339=CARTESIAN_POINT('Ctrl Pts',(2.35515049221901,-0.280490737932346,
1.33192578644221));
#60340=CARTESIAN_POINT('Ctrl Pts',(2.35338920180665,-0.294903618020155,
1.33095535002486));
#60341=CARTESIAN_POINT('Ctrl Pts',(2.34909597992227,-0.327543516644778,
1.32874561706829));
#60342=CARTESIAN_POINT('Ctrl Pts',(2.34648405947798,-0.345758881250932,
1.32750388109208));
#60343=CARTESIAN_POINT('Ctrl Pts',(2.33913153662566,-0.393106638576622,
1.3242531182976));
#60344=CARTESIAN_POINT('Ctrl Pts',(2.33405873737489,-0.422183432552812,
1.32223391206511));
#60345=CARTESIAN_POINT('Ctrl Pts',(2.29408248164245,-0.628503021377255,
1.30773756136826));
#60346=CARTESIAN_POINT('Ctrl Pts',(2.23957705021871,-0.801312713206304,
1.29463731563116));
#60347=CARTESIAN_POINT('Ctrl Pts',(2.11584767113732,-1.07867882313158,1.27249052091164));
#60348=CARTESIAN_POINT('Ctrl Pts',(2.05699900424848,-1.18706392674639,1.2635321868307));
#60349=CARTESIAN_POINT('Ctrl Pts',(1.97994558575719,-1.30589225498314,1.25368860738171));
#60350=CARTESIAN_POINT('Ctrl Pts',(1.96971706077336,-1.32126978952174,1.25241452320485));
#60351=CARTESIAN_POINT('Ctrl Pts',(1.95383317693645,-1.34455510223488,1.25048674429816));
#60352=CARTESIAN_POINT('Ctrl Pts',(1.94830736053536,-1.35254979334937,1.24982514168341));
#60353=CARTESIAN_POINT('Ctrl Pts',(1.93805222333603,-1.36719355255494,1.24861413085931));
#60354=CARTESIAN_POINT('Ctrl Pts',(1.93333766282671,-1.37385229025253,1.24806382482572));
#60355=CARTESIAN_POINT('Ctrl Pts',(1.92250399042443,-1.38898731060532,1.2468136891501));
#60356=CARTESIAN_POINT('Ctrl Pts',(1.91636309994222,-1.39744760959839,1.24611533474814));
#60357=CARTESIAN_POINT('Ctrl Pts',(1.8966488747823,-1.42423353108166,1.24390478237288));
#60358=CARTESIAN_POINT('Ctrl Pts',(1.8828666275923,-1.4424047493233,1.24240590526639));
#60359=CARTESIAN_POINT('Ctrl Pts',(1.79161041667228,-1.55918418160259,1.23275745516874));
#60360=CARTESIAN_POINT('Ctrl Pts',(1.70667211832771,-1.65172675898231,1.22503098673496));
#60361=CARTESIAN_POINT('Ctrl Pts',(1.52561312465911,-1.8200361549536,1.20984467067568));
#60362=CARTESIAN_POINT('Ctrl Pts',(1.43017505512048,-1.89594942000968,1.20240340108188));
#60363=CARTESIAN_POINT('Ctrl Pts',(1.27274617037463,-2.00249445076763,1.19042861772049));
#60364=CARTESIAN_POINT('Ctrl Pts',(1.21453509175683,-2.03832530050755,1.18606045651479));
#60365=CARTESIAN_POINT('Ctrl Pts',(1.13495443083451,-2.08268960768377,1.18011513547858));
#60366=CARTESIAN_POINT('Ctrl Pts',(1.11488806527567,-2.09349996541952,1.17861830051763));
#60367=CARTESIAN_POINT('Ctrl Pts',(1.0811305049346,-2.11106319627428,1.17610228673514));
#60368=CARTESIAN_POINT('Ctrl Pts',(1.0675240366116,-2.11797625112552,1.17508873679286));
#60369=CARTESIAN_POINT('Ctrl Pts',(1.04060926264119,-2.13132562942958,1.17308446435479));
#60370=CARTESIAN_POINT('Ctrl Pts',(1.02730561190618,-2.13776980495989,1.17209406940381));
#60371=CARTESIAN_POINT('Ctrl Pts',(0.99486657594864,-2.15311027226794,1.16967938558323));
#60372=CARTESIAN_POINT('Ctrl Pts',(0.975671314050858,-2.16187621890714,
1.16825073997559));
#60373=CARTESIAN_POINT('Ctrl Pts',(0.909539128102713,-2.19101682348607,
1.16332800091282));
#60374=CARTESIAN_POINT('Ctrl Pts',(0.862064033008021,-2.21012693362633,
1.15979244659638));
#60375=CARTESIAN_POINT('Ctrl Pts',(0.651803798343957,-2.28695741254817,
1.14411833223436));
#60376=CARTESIAN_POINT('Ctrl Pts',(0.483626682876532,-2.32832801224491,
1.13148938972811));
#60377=CARTESIAN_POINT('Ctrl Pts',(0.217087657648068,-2.363753747955,1.11191829219545));
#60378=CARTESIAN_POINT('Ctrl Pts',(0.121000722839993,-2.370616215204,1.10496314684639));
#60379=CARTESIAN_POINT('Ctrl Pts',(0.0024641159692989,-2.37185347444286,
1.09668494617114));
#60380=CARTESIAN_POINT('Ctrl Pts',(-0.0198294107899865,-2.37177188177341,
1.09514135820286));
#60381=CARTESIAN_POINT('Ctrl Pts',(-0.0525898389896183,-2.37119000401645,
1.09289572903689));
#60382=CARTESIAN_POINT('Ctrl Pts',(-0.0630591383815335,-2.37093468524795,
1.09218149660046));
#60383=CARTESIAN_POINT('Ctrl Pts',(-0.0808943114277315,-2.37038151097527,
1.0909709412764));
#60384=CARTESIAN_POINT('Ctrl Pts',(-0.088260910713815,-2.37011864980122,
1.09047275216746));
#60385=CARTESIAN_POINT('Ctrl Pts',(-0.105126233550873,-2.36943810421742,
1.08933639109983));
#60386=CARTESIAN_POINT('Ctrl Pts',(-0.114623797917891,-2.36899764614722,
1.08869947147881));
#60387=CARTESIAN_POINT('Ctrl Pts',(-0.141057145050599,-2.36761243544618,
1.08693456521219));
#60388=CARTESIAN_POINT('Ctrl Pts',(-0.157986211095145,-2.36654308218753,
1.08581310422719));
#60389=CARTESIAN_POINT('Ctrl Pts',(-0.283956293560617,-2.3572281497173,
1.07752458613099));
#60390=CARTESIAN_POINT('Ctrl Pts',(-0.392336216701509,-2.34163066935196,
1.07070497611412));
#60391=CARTESIAN_POINT('Ctrl Pts',(-0.588875322105803,-2.29930996560503,
1.05830382807689));
#60392=CARTESIAN_POINT('Ctrl Pts',(-0.677291713564731,-2.27483548045842,
1.05271113445951));
#60393=CARTESIAN_POINT('Ctrl Pts',(-0.873746232327288,-2.20798267310153,
1.03988680254655));
#60394=CARTESIAN_POINT('Ctrl Pts',(-0.980527711062764,-2.16267899830609,
1.03262502884645));
#60395=CARTESIAN_POINT('Ctrl Pts',(-1.10708865651824,-2.09767779686214,
1.02337968054841));
#60396=CARTESIAN_POINT('Ctrl Pts',(-1.13040849121314,-2.08520358370078,
1.02164861153288));
#60397=CARTESIAN_POINT('Ctrl Pts',(-1.16752584057593,-2.06454320128883,
1.01884605116049));
#60398=CARTESIAN_POINT('Ctrl Pts',(-1.18145778590585,-2.05660222148821,
1.01778319770985));
#60399=CARTESIAN_POINT('Ctrl Pts',(-1.20791865551661,-2.04116235567341,
1.01574297939982));
#60400=CARTESIAN_POINT('Ctrl Pts',(-1.22046099428596,-2.03368782898244,
1.01476652014516));
#60401=CARTESIAN_POINT('Ctrl Pts',(-1.24892416837596,-2.01636724884487,
1.01252856722221));
#60402=CARTESIAN_POINT('Ctrl Pts',(-1.26479888151332,-2.0064476607514,1.01126445309901));
#60403=CARTESIAN_POINT('Ctrl Pts',(-1.30690261543567,-1.97944020139196,
1.00786795665786));
#60404=CARTESIAN_POINT('Ctrl Pts',(-1.33291277430861,-1.96201970757236,
1.00572355125666));
#60405=CARTESIAN_POINT('Ctrl Pts',(-1.47216311538605,-1.86470875723151,
0.993984702995008));
#60406=CARTESIAN_POINT('Ctrl Pts',(-1.57856315593311,-1.77553662127184,
0.984046110716758));
#60407=CARTESIAN_POINT('Ctrl Pts',(-1.75837430822803,-1.59583753871045,
0.965549759989945));
#60408=CARTESIAN_POINT('Ctrl Pts',(-1.83410167163593,-1.50819435381047,
0.95706534680311));
#60409=CARTESIAN_POINT('Ctrl Pts',(-1.93502778995027,-1.37248751380129,
0.944961901987382));
#60410=CARTESIAN_POINT('Ctrl Pts',(-1.96546643445939,-1.32853197026797,
0.941185821270263));
#60411=CARTESIAN_POINT('Ctrl Pts',(-2.00220433016033,-1.27144958344077,
0.936495923685183));
#60412=CARTESIAN_POINT('Ctrl Pts',(-2.00990195840806,-1.25924595146886,
0.935505288100589));
#60413=CARTESIAN_POINT('Ctrl Pts',(-2.02214279624241,-1.23944138970281,
0.933917862388022));
#60414=CARTESIAN_POINT('Ctrl Pts',(-2.02675550552619,-1.23188415614345,
0.933316806956642));
#60415=CARTESIAN_POINT('Ctrl Pts',(-2.03562233701832,-1.2171725594088,0.932156073891346));
#60416=CARTESIAN_POINT('Ctrl Pts',(-2.03988126613385,-1.21002138867156,
0.931596114676016));
#60417=CARTESIAN_POINT('Ctrl Pts',(-2.0503636154985,-1.19220783350347,0.930211449886934));
#60418=CARTESIAN_POINT('Ctrl Pts',(-2.05654171318131,-1.18151879896961,
0.929389576069711));
#60419=CARTESIAN_POINT('Ctrl Pts',(-2.07824100601197,-1.14328985623197,
0.92648026688112));
#60420=CARTESIAN_POINT('Ctrl Pts',(-2.09329549230765,-1.11548715223054,
0.924419572581565));
#60421=CARTESIAN_POINT('Ctrl Pts',(-2.2069236663899,-0.895231001562671,
0.908456322006391));
#60422=CARTESIAN_POINT('Ctrl Pts',(-2.27932482143577,-0.690399886668755,
0.895663885715221));
#60423=CARTESIAN_POINT('Ctrl Pts',(-2.33944284874626,-0.398589840733198,
0.877036953899787));
#60424=CARTESIAN_POINT('Ctrl Pts',(-2.35177732393919,-0.317817602165625,
0.871852055914454));
#60425=CARTESIAN_POINT('Ctrl Pts',(-2.36241924832637,-0.211660932493143,
0.864909099738889));
#60426=CARTESIAN_POINT('Ctrl Pts',(-2.36452210844591,-0.186708801712192,
0.86326818950181));
#60427=CARTESIAN_POINT('Ctrl Pts',(-2.36730150719752,-0.146043841907032,
0.860577149244879));
#60428=CARTESIAN_POINT('Ctrl Pts',(-2.36821755008672,-0.13034893653533,
0.859534462298416));
#60429=CARTESIAN_POINT('Ctrl Pts',(-2.36968681167995,-0.0999890842487386,
0.857509125154726));
#60430=CARTESIAN_POINT('Ctrl Pts',(-2.37026009007793,-0.0853257949025577,
0.856527144055823));
#60431=CARTESIAN_POINT('Ctrl Pts',(-2.37128337384001,-0.0509930647768157,
0.8542186455999));
#60432=CARTESIAN_POINT('Ctrl Pts',(-2.37162476824478,-0.0313217203434785,
0.852888834174311));
#60433=CARTESIAN_POINT('Ctrl Pts',(-2.37194500005966,0.033877598813773,
0.848456482579792));
#60434=CARTESIAN_POINT('Ctrl Pts',(-2.37085769533092,0.0793982044377964,
0.845321642107885));
#60435=CARTESIAN_POINT('Ctrl Pts',(-2.3676168457696,0.140875261515083,0.841030930904592));
#60436=CARTESIAN_POINT('Ctrl Pts',(-2.36661000737738,0.156883205384554,
0.839908467310091));
#60437=CARTESIAN_POINT('Ctrl Pts',(-2.3654410179195,0.172878145651696,0.838781724910481));
#60438=CARTESIAN_POINT('',(-2.37174937133752,0.00172686423176496,0.651410108094986));
#60439=CARTESIAN_POINT('Ctrl Pts',(-2.36544101854889,0.172878137039861,
0.639858258416768));
#60440=CARTESIAN_POINT('Ctrl Pts',(-2.36959990151614,0.115973356999348,
0.643708874976174));
#60441=CARTESIAN_POINT('Ctrl Pts',(-2.37170775441788,0.0588853258924011,
0.64755949153558));
#60442=CARTESIAN_POINT('Ctrl Pts',(-2.37174937133752,0.00172686423176496,
0.651410108094986));
#60443=CARTESIAN_POINT('Ctrl Pts',(-2.37174930856301,0.00181103033629052,
0.65275631368545));
#60444=CARTESIAN_POINT('Ctrl Pts',(-2.37175145119913,-0.000994994296776971,
0.652931750428388));
#60445=CARTESIAN_POINT('Ctrl Pts',(-2.37174861411466,-0.0038010296480299,
0.65310707081996));
#60446=CARTESIAN_POINT('Ctrl Pts',(-2.37112535322287,-0.227533331300736,
0.667076921649127));
#60447=CARTESIAN_POINT('Ctrl Pts',(-2.3396475745453,-0.447280622863168,
0.680222654294109));
#60448=CARTESIAN_POINT('Ctrl Pts',(-2.26701041577751,-0.698201160524075,
0.696978619706972));
#60449=CARTESIAN_POINT('Ctrl Pts',(-2.25482443388412,-0.736605426184959,
0.699589963336822));
#60450=CARTESIAN_POINT('Ctrl Pts',(-2.23547414284124,-0.79259881954743,
0.703476454847408));
#60451=CARTESIAN_POINT('Ctrl Pts',(-2.22906688871707,-0.810443275725124,
0.704727032771976));
#60452=CARTESIAN_POINT('Ctrl Pts',(-2.21728559275687,-0.842057655345016,
0.706965036564985));
#60453=CARTESIAN_POINT('Ctrl Pts',(-2.21199541292227,-0.855857915296851,
0.707949648076686));
#60454=CARTESIAN_POINT('Ctrl Pts',(-2.20053398961831,-0.884940584850265,
0.710041373015548));
#60455=CARTESIAN_POINT('Ctrl Pts',(-2.19433175983725,-0.900209854596918,
0.711149478850414));
#60456=CARTESIAN_POINT('Ctrl Pts',(-2.1772431631345,-0.941054105058062,
0.714140902870466));
#60457=CARTESIAN_POINT('Ctrl Pts',(-2.16606579647482,-0.96650373606868,
0.716033903290692));
#60458=CARTESIAN_POINT('Ctrl Pts',(-2.09592106749537,-1.11888374959912,
0.72754969047471));
#60459=CARTESIAN_POINT('Ctrl Pts',(-2.02626992352521,-1.24056600855936,
0.737538388265311));
#60460=CARTESIAN_POINT('Ctrl Pts',(-1.88610855465222,-1.44183616444756,
0.755361002526343));
#60461=CARTESIAN_POINT('Ctrl Pts',(-1.82021019388062,-1.52418242029779,
0.763091497800347));
#60462=CARTESIAN_POINT('Ctrl Pts',(-1.71597217196654,-1.63799784157414,
0.774239643714896));
#60463=CARTESIAN_POINT('Ctrl Pts',(-1.68177576093693,-1.67308944643683,
0.777748092669314));
#60464=CARTESIAN_POINT('Ctrl Pts',(-1.63100221906363,-1.7220610750296,0.782721029860509));
#60465=CARTESIAN_POINT('Ctrl Pts',(-1.61528547457365,-1.7368118760284,0.784229542336085));
#60466=CARTESIAN_POINT('Ctrl Pts',(-1.58723310654433,-1.76242992664603,
0.786865083629891));
#60467=CARTESIAN_POINT('Ctrl Pts',(-1.57498167654345,-1.7733868547831,0.787997558657892));
#60468=CARTESIAN_POINT('Ctrl Pts',(-1.55543372395288,-1.79050695851107,
0.78977407154451));
#60469=CARTESIAN_POINT('Ctrl Pts',(-1.54821244273485,-1.79675470731068,
0.790423903869768));
#60470=CARTESIAN_POINT('Ctrl Pts',(-1.53460640982889,-1.80838351629775,
0.791635967312343));
#60471=CARTESIAN_POINT('Ctrl Pts',(-1.52823093181423,-1.81377451641353,
0.792198873503901));
#60472=CARTESIAN_POINT('Ctrl Pts',(-1.51345564143206,-1.82613504532349,
0.79349209079308));
#60473=CARTESIAN_POINT('Ctrl Pts',(-1.50503600681029,-1.83308041613884,
0.794220696915092));
#60474=CARTESIAN_POINT('Ctrl Pts',(-1.47750783631063,-1.8554709157772,0.79657709530287));
#60475=CARTESIAN_POINT('Ctrl Pts',(-1.45820648725909,-1.87067786653943,
0.79818930663787));
#60476=CARTESIAN_POINT('Ctrl Pts',(-1.29570412667248,-1.99466472928793,
0.811467235141947));
#60477=CARTESIAN_POINT('Ctrl Pts',(-1.14077572060438,-2.08714754920945,
0.822279528123996));
#60478=CARTESIAN_POINT('Ctrl Pts',(-0.901402159325332,-2.19534279964806,
0.838480786284841));
#60479=CARTESIAN_POINT('Ctrl Pts',(-0.824210523956122,-2.22547329304567,
0.843630086845949));
#60480=CARTESIAN_POINT('Ctrl Pts',(-0.71070527866864,-2.26306157493698,
0.851227276449663));
#60481=CARTESIAN_POINT('Ctrl Pts',(-0.675542240663434,-2.27380565457656,
0.853583816804143));
#60482=CARTESIAN_POINT('Ctrl Pts',(-0.611462431899902,-2.291767677618,0.857894237503964));
#60483=CARTESIAN_POINT('Ctrl Pts',(-0.582632010190856,-2.29926623238359,
0.859839279339637));
#60484=CARTESIAN_POINT('Ctrl Pts',(-0.537132610243582,-2.31018956688958,
0.862921663067962));
#60485=CARTESIAN_POINT('Ctrl Pts',(-0.52055435672148,-2.31398150655587,
0.864047393429071));
#60486=CARTESIAN_POINT('Ctrl Pts',(-0.489403537832321,-2.32075493128074,
0.866168253421457));
#60487=CARTESIAN_POINT('Ctrl Pts',(-0.474840849986072,-2.32377826481472,
0.867162009843196));
#60488=CARTESIAN_POINT('Ctrl Pts',(-0.44202294155307,-2.33027016550626,
0.86940706460838));
#60489=CARTESIAN_POINT('Ctrl Pts',(-0.423753631734454,-2.3336615331005,
0.870660714478425));
#60490=CARTESIAN_POINT('Ctrl Pts',(-0.368349914117364,-2.34327420698001,
0.874475125812053));
#60491=CARTESIAN_POINT('Ctrl Pts',(-0.331106960801865,-2.34882599866167,
0.877056346144162));
#60492=CARTESIAN_POINT('Ctrl Pts',(-0.108508777858752,-2.37660946758394,
0.89259391120447));
#60493=CARTESIAN_POINT('Ctrl Pts',(0.0787862494267347,-2.37777541526812,
0.906194176431287));
#60494=CARTESIAN_POINT('Ctrl Pts',(0.338701600130435,-2.34863653959509,
0.925228823579191));
#60495=CARTESIAN_POINT('Ctrl Pts',(0.412730920049532,-2.33676418864128,
0.930658280309585));
#60496=CARTESIAN_POINT('Ctrl Pts',(0.513791275463868,-2.31560322649303,
0.9379919636375));
#60497=CARTESIAN_POINT('Ctrl Pts',(0.541399989981951,-2.30930421884901,
0.939987080227885));
#60498=CARTESIAN_POINT('Ctrl Pts',(0.589329175876271,-2.29746217065792,
0.943428813460818));
#60499=CARTESIAN_POINT('Ctrl Pts',(0.609700583562067,-2.29214017379983,
0.944884702820515));
#60500=CARTESIAN_POINT('Ctrl Pts',(0.64002627596649,-2.28378471009155,0.947038914525128));
#60501=CARTESIAN_POINT('Ctrl Pts',(0.650035245989951,-2.2809560331226,0.947747764708422));
#60502=CARTESIAN_POINT('Ctrl Pts',(0.668051382498788,-2.27573619618193,
0.949019421197831));
#60503=CARTESIAN_POINT('Ctrl Pts',(0.676064835806887,-2.27336847605512,
0.949583480546604));
#60504=CARTESIAN_POINT('Ctrl Pts',(0.694073563047986,-2.26794382423523,
0.95084759754205));
#60505=CARTESIAN_POINT('Ctrl Pts',(0.704061309954511,-2.26486312672848,
0.951546302645843));
#60506=CARTESIAN_POINT('Ctrl Pts',(0.734448791757013,-2.25526973532177,
0.953665748998557));
#60507=CARTESIAN_POINT('Ctrl Pts',(0.754781608827425,-2.24854650991014,
0.955075153725061));
#60508=CARTESIAN_POINT('Ctrl Pts',(0.920177439180745,-2.19136045754968,
0.966489355638334));
#60509=CARTESIAN_POINT('Ctrl Pts',(1.06013575415447,-2.12718412074107,0.975844663725485));
#60510=CARTESIAN_POINT('Ctrl Pts',(1.32540086451254,-1.97281678311415,0.994700298363149));
#60511=CARTESIAN_POINT('Ctrl Pts',(1.45008064551625,-1.88306970722863,1.00416530319755));
#60512=CARTESIAN_POINT('Ctrl Pts',(1.58624245144136,-1.76346692311956,1.01592490926147));
#60513=CARTESIAN_POINT('Ctrl Pts',(1.60693195699883,-1.74463471338083,1.01775413549386));
#60514=CARTESIAN_POINT('Ctrl Pts',(1.63935811861069,-1.71405324532737,1.02069279639434));
#60515=CARTESIAN_POINT('Ctrl Pts',(1.65131325205398,-1.70253871884271,1.02179235589651));
#60516=CARTESIAN_POINT('Ctrl Pts',(1.67376568906253,-1.68045480513513,1.02388890427318));
#60517=CARTESIAN_POINT('Ctrl Pts',(1.68428623817782,-1.66991011275184,1.02488479768518));
#60518=CARTESIAN_POINT('Ctrl Pts',(1.70808782140226,-1.64560016510896,1.02716951056766));
#60519=CARTESIAN_POINT('Ctrl Pts',(1.72130291198352,-1.63177209114302,1.02846107307362));
#60520=CARTESIAN_POINT('Ctrl Pts',(1.76213870827008,-1.58799403877477,1.03252619501467));
#60521=CARTESIAN_POINT('Ctrl Pts',(1.78915461323599,-1.55749263669784,1.03532449500998));
#60522=CARTESIAN_POINT('Ctrl Pts',(1.96098850704832,-1.35311626841625,1.05386768113877));
#60523=CARTESIAN_POINT('Ctrl Pts',(2.08105502521308,-1.15998796730692,1.07059680633053));
#60524=CARTESIAN_POINT('Ctrl Pts',(2.19082625303358,-0.909775230626747,
1.09030199113213));
#60525=CARTESIAN_POINT('Ctrl Pts',(2.20843932542779,-0.866144855839831,
1.09366573769639));
#60526=CARTESIAN_POINT('Ctrl Pts',(2.23533767686969,-0.793345947717991,
1.09913120919846));
#60527=CARTESIAN_POINT('Ctrl Pts',(2.24537671694182,-0.764471016807144,
1.10126176680796));
#60528=CARTESIAN_POINT('Ctrl Pts',(2.25857867154093,-0.72399215680235,1.10418951621238));
#60529=CARTESIAN_POINT('Ctrl Pts',(2.26221538892767,-0.712547407553803,
1.10501079124258));
#60530=CARTESIAN_POINT('Ctrl Pts',(2.26827457703349,-0.692965062538959,
1.10640437699663));
#60531=CARTESIAN_POINT('Ctrl Pts',(2.27074053361962,-0.684841275819829,
1.10697910006482));
#60532=CARTESIAN_POINT('Ctrl Pts',(2.27582330671087,-0.667767385879586,
1.10817966718811));
#60533=CARTESIAN_POINT('Ctrl Pts',(2.27843103380718,-0.658814872792653,
1.10880500419741));
#60534=CARTESIAN_POINT('Ctrl Pts',(2.28537541982347,-0.634439833165862,
1.11049689161909));
#60535=CARTESIAN_POINT('Ctrl Pts',(2.28960881789367,-0.618988050506459,
1.11155778868104));
#60536=CARTESIAN_POINT('Ctrl Pts',(2.31029520318116,-0.540365798363026,
1.11690264325927));
#60537=CARTESIAN_POINT('Ctrl Pts',(2.32429331732944,-0.476572486717228,
1.12106599940257));
#60538=CARTESIAN_POINT('Ctrl Pts',(2.35711028523803,-0.290656993342265,
1.13291324646778));
#60539=CARTESIAN_POINT('Ctrl Pts',(2.36904694510039,-0.167540627655701,
1.14041529987787));
#60540=CARTESIAN_POINT('Ctrl Pts',(2.37331650557341,0.0623029918453421,
1.15457924796031));
#60541=CARTESIAN_POINT('Ctrl Pts',(2.36813512602746,0.168658437822752,1.16119618343337));
#60542=CARTESIAN_POINT('Ctrl Pts',(2.35114024660654,0.314619171190187,1.17062268103334));
#60543=CARTESIAN_POINT('Ctrl Pts',(2.34541175956555,0.354808470624256,1.17325394703149));
#60544=CARTESIAN_POINT('Ctrl Pts',(2.33547819809848,0.413647013762072,1.17716896028009));
#60545=CARTESIAN_POINT('Ctrl Pts',(2.33207430500875,0.43242533077708,1.17842788247742));
#60546=CARTESIAN_POINT('Ctrl Pts',(2.32561513168213,0.465761225338047,1.18068058186839));
#60547=CARTESIAN_POINT('Ctrl Pts',(2.32264878815785,0.480335142972431,1.18167152057143));
#60548=CARTESIAN_POINT('Ctrl Pts',(2.31608532724853,0.51109866029067,1.1837766253785));
#60549=CARTESIAN_POINT('Ctrl Pts',(2.31245509137365,0.527280295558261,1.18489178941482));
#60550=CARTESIAN_POINT('Ctrl Pts',(2.30224575422273,0.570653281422498,1.18790272057808));
#60551=CARTESIAN_POINT('Ctrl Pts',(2.29535492624418,0.597767787649016,1.18980823700607));
#60552=CARTESIAN_POINT('Ctrl Pts',(2.25236548060049,0.755204805825151,1.20101305092277));
#60553=CARTESIAN_POINT('Ctrl Pts',(2.20565929593438,0.882349537132457,1.2106493263401));
#60554=CARTESIAN_POINT('Ctrl Pts',(2.10602163479816,1.09538605110796,1.22771497423976));
#60555=CARTESIAN_POINT('Ctrl Pts',(2.05797104977608,1.18319599497077,1.23504329626426));
#60556=CARTESIAN_POINT('Ctrl Pts',(1.97546824325865,1.31365059042779,1.2462162935932));
#60557=CARTESIAN_POINT('Ctrl Pts',(1.94484207762595,1.35858112456882,1.25011999086455));
#60558=CARTESIAN_POINT('Ctrl Pts',(1.89271151206976,1.42967954289466,1.25634602099076));
#60559=CARTESIAN_POINT('Ctrl Pts',(1.87214417518171,1.45650847356269,1.25870722562996));
#60560=CARTESIAN_POINT('Ctrl Pts',(1.84321257030297,1.49262218317863,1.26189214982886));
#60561=CARTESIAN_POINT('Ctrl Pts',(1.8353391612079,1.50229282810518,1.26274567825644));
#60562=CARTESIAN_POINT('Ctrl Pts',(1.82192727040874,1.51850337839297,1.26417689962928));
#60563=CARTESIAN_POINT('Ctrl Pts',(1.81642902016666,1.52507610068707,1.26475733239305));
#60564=CARTESIAN_POINT('Ctrl Pts',(1.80571843012323,1.53773966336289,1.26587568955951));
#60565=CARTESIAN_POINT('Ctrl Pts',(1.80051070095198,1.54383403954897,1.26641395052481));
#60566=CARTESIAN_POINT('Ctrl Pts',(1.78609781030232,1.56052868218542,1.26788894907222));
#60567=CARTESIAN_POINT('Ctrl Pts',(1.77682909768598,1.5710740074874,1.2688212190783));
#60568=CARTESIAN_POINT('Ctrl Pts',(1.73881299221089,1.61355940269632,1.27258253134564));
#60569=CARTESIAN_POINT('Ctrl Pts',(1.70929187990182,1.64479979659607,1.27536077511873));
#60570=CARTESIAN_POINT('Ctrl Pts',(1.56896881864915,1.78543388897563,1.28802358061695));
#60571=CARTESIAN_POINT('Ctrl Pts',(1.44840802975891,1.88455828856604,1.29742458676366));
#60572=CARTESIAN_POINT('Ctrl Pts',(1.25095296966123,2.01668462593621,1.31208166062832));
#60573=CARTESIAN_POINT('Ctrl Pts',(1.18060613597337,2.05865681985602,1.31717442538939));
#60574=CARTESIAN_POINT('Ctrl Pts',(1.07598602026902,2.11394952103229,1.32469497210036));
#60575=CARTESIAN_POINT('Ctrl Pts',(1.043350237628,2.13024612847815,1.32703343007177));
#60576=CARTESIAN_POINT('Ctrl Pts',(0.983582086034664,2.15838826618867,1.33131285083499));
#60577=CARTESIAN_POINT('Ctrl Pts',(0.956578760293498,2.17049086109374,1.33324513966153));
#60578=CARTESIAN_POINT('Ctrl Pts',(0.913771316919989,2.18872269142306,1.3363102914883));
#60579=CARTESIAN_POINT('Ctrl Pts',(0.898115292716805,2.19519337094388,1.33743170823019));
#60580=CARTESIAN_POINT('Ctrl Pts',(0.86861530878883,2.20701739560162,1.33954616141698));
#60581=CARTESIAN_POINT('Ctrl Pts',(0.854787737307872,2.2124096018377,1.34053784776935));
#60582=CARTESIAN_POINT('Ctrl Pts',(0.823542505097351,2.22425736656804,1.34278044063124));
#60583=CARTESIAN_POINT('Ctrl Pts',(0.806097950028428,2.23063873178006,1.34403371803809));
#60584=CARTESIAN_POINT('Ctrl Pts',(0.760906815053217,2.24657069964286,1.34728432434011));
#60585=CARTESIAN_POINT('Ctrl Pts',(0.733055415140581,2.25581220761512,1.34929148513945));
#60586=CARTESIAN_POINT('Ctrl Pts',(0.501028944814056,2.32805139670054,1.36605033321133));
#60587=CARTESIAN_POINT('Ctrl Pts',(0.289399634212843,2.36369736878585,1.38170565954516));
#60588=CARTESIAN_POINT('Ctrl Pts',(0.0129065280083569,2.37255274745297,
1.40179246940914));
#60589=CARTESIAN_POINT('Ctrl Pts',(-0.0501686818238375,2.37205758837739,
1.40633980092114));
#60590=CARTESIAN_POINT('Ctrl Pts',(-0.138549892540939,2.36783624402563,
1.41260575429781));
#60591=CARTESIAN_POINT('Ctrl Pts',(-0.163927051732747,2.36621482211109,
1.41439254081993));
#60592=CARTESIAN_POINT('Ctrl Pts',(-0.208595446698214,2.36263871595097,
1.41751047450307));
#60593=CARTESIAN_POINT('Ctrl Pts',(-0.22789769611826,2.3608550277577,1.41884884466261));
#60594=CARTESIAN_POINT('Ctrl Pts',(-0.257166003484129,2.35778807188474,
1.42086249922082));
#60595=CARTESIAN_POINT('Ctrl Pts',(-0.267148829524415,2.35667784334923,
1.42154652871749));
#60596=CARTESIAN_POINT('Ctrl Pts',(-0.285414330981306,2.35452891131814,
1.42279262155435));
#60597=CARTESIAN_POINT('Ctrl Pts',(-0.293698756828221,2.35350988501504,
1.42335569120835));
#60598=CARTESIAN_POINT('Ctrl Pts',(-0.312684798195064,2.35107269199345,
1.42464141640278));
#60599=CARTESIAN_POINT('Ctrl Pts',(-0.323382300967351,2.34962517960746,
1.42536245910796));
#60600=CARTESIAN_POINT('Ctrl Pts',(-0.356296458515065,2.34494241295582,
1.42757156306101));
#60601=CARTESIAN_POINT('Ctrl Pts',(-0.378478072361685,2.3414646107761,1.42904710907445));
#60602=CARTESIAN_POINT('Ctrl Pts',(-0.527857820217949,2.315865337619,1.43891493182303));
#60603=CARTESIAN_POINT('Ctrl Pts',(-0.653131419620313,2.28370178563684,
1.44685848978369));
#60604=CARTESIAN_POINT('Ctrl Pts',(-0.83701416943505,2.22010958420151,1.45881150154125));
#60605=CARTESIAN_POINT('Ctrl Pts',(-0.897939740785599,2.19617470235712,
1.46282173611685));
#60606=CARTESIAN_POINT('Ctrl Pts',(-1.02650860820612,2.13942035309998,1.47151402142603));
#60607=CARTESIAN_POINT('Ctrl Pts',(-1.0937363537981,2.10584399320494,1.47620317707526));
#60608=CARTESIAN_POINT('Ctrl Pts',(-1.18938284589454,2.05225708376759,1.48318523328244));
#60609=CARTESIAN_POINT('Ctrl Pts',(-1.21913757012021,2.03472211830085,1.48540315433815));
#60610=CARTESIAN_POINT('Ctrl Pts',(-1.27260704927299,2.00161770177533,1.48948198991082));
#60611=CARTESIAN_POINT('Ctrl Pts',(-1.29644581715873,1.9862603703108,1.49133545102009));
#60612=CARTESIAN_POINT('Ctrl Pts',(-1.33385653720017,1.96119934133804,1.4943035706306));
#60613=CARTESIAN_POINT('Ctrl Pts',(-1.34761178097542,1.95177318929354,1.49540798514837));
#60614=CARTESIAN_POINT('Ctrl Pts',(-1.37344587871876,1.93366638762244,1.49750780499589));
#60615=CARTESIAN_POINT('Ctrl Pts',(-1.38554474548066,1.92501558994655,1.49850205205797));
#60616=CARTESIAN_POINT('Ctrl Pts',(-1.41289086437254,1.9050715113429,1.50077455982046));
#60617=CARTESIAN_POINT('Ctrl Pts',(-1.4280854046399,1.89370802899853,1.50205546394941));
#60618=CARTESIAN_POINT('Ctrl Pts',(-1.46752713953218,1.8634662349006,1.5054293972987));
#60619=CARTESIAN_POINT('Ctrl Pts',(-1.49154597110368,1.84429736715957,1.50753355964401));
#60620=CARTESIAN_POINT('Ctrl Pts',(-1.6430602872611,1.71848151000432,1.52113441313658));
#60621=CARTESIAN_POINT('Ctrl Pts',(-1.75939799465173,1.59916427142744,1.53314498467794));
#60622=CARTESIAN_POINT('Ctrl Pts',(-1.92099104389118,1.39426563647308,1.552170670839));
#60623=CARTESIAN_POINT('Ctrl Pts',(-1.9751774817936,1.31638098276282,1.55908778748221));
#60624=CARTESIAN_POINT('Ctrl Pts',(-2.04147834108255,1.20773309595234,1.56816851417481));
#60625=CARTESIAN_POINT('Ctrl Pts',(-2.05782718896163,1.17966118857975,1.5704664715147));
#60626=CARTESIAN_POINT('Ctrl Pts',(-2.08492124358308,1.13086070089689,1.57436877392988));
#60627=CARTESIAN_POINT('Ctrl Pts',(-2.09594634355981,1.11029344871243,1.5759859582585));
#60628=CARTESIAN_POINT('Ctrl Pts',(-2.11163009397244,1.07996904804094,1.57832694160497));
#60629=CARTESIAN_POINT('Ctrl Pts',(-2.11652806775114,1.07033814666915,1.57906411690521));
#60630=CARTESIAN_POINT('Ctrl Pts',(-2.12473609464031,1.05392199683107,1.58030955096247));
#60631=CARTESIAN_POINT('Ctrl Pts',(-2.128079791182,1.04715397890926,1.5808198210157));
#60632=CARTESIAN_POINT('Ctrl Pts',(-2.13563697569309,1.03167167948198,1.58197975587104));
#60633=CARTESIAN_POINT('Ctrl Pts',(-2.13982949879235,1.02294744269284,1.58262814843581));
#60634=CARTESIAN_POINT('Ctrl Pts',(-2.15131280325997,0.99867224798369,1.5844185112618));
#60635=CARTESIAN_POINT('Ctrl Pts',(-2.15848842343937,0.98306703929463,1.58555383592393));
#60636=CARTESIAN_POINT('Ctrl Pts',(-2.20845847513104,0.871208900056178,
1.5935907474126));
#60637=CARTESIAN_POINT('Ctrl Pts',(-2.24497356370835,0.772264898072949,
1.60017195110047));
#60638=CARTESIAN_POINT('Ctrl Pts',(-2.2794488463323,0.655424946887912,1.60769393027819));
#60639=CARTESIAN_POINT('Ctrl Pts',(-2.28394189547846,0.63959231471769,1.60870797867424));
#60640=CARTESIAN_POINT('Ctrl Pts',(-2.31658584853866,0.519828833390991,
1.61634705046536));
#60641=CARTESIAN_POINT('Ctrl Pts',(-2.3377939046557,0.414138771475803,1.62291648441333));
#60642=CARTESIAN_POINT('Ctrl Pts',(-2.35759003868515,0.262677186163501,
1.63244055125887));
#60643=CARTESIAN_POINT('Ctrl Pts',(-2.36215595308437,0.2178267288989,1.63527322863562));
#60644=CARTESIAN_POINT('Ctrl Pts',(-2.3654410189124,0.172878132066172,1.63813797379334));
#60645=CARTESIAN_POINT('Origin',(0.,0.,-1.84858989190501));
#60646=CARTESIAN_POINT('',(-2.36906969114779,0.173130678776567,2.83701751404115));
#60647=CARTESIAN_POINT('',(-2.36544104518992,0.172877772518167,2.63906222572513));
#60648=CARTESIAN_POINT('',(-2.36544101854889,0.172878137039864,-1.84858989190501));
#60649=CARTESIAN_POINT('',(-2.37214954248261,-0.00208751672060286,1.84858989190502));
#60650=CARTESIAN_POINT('Ctrl Pts',(-2.37214954248261,-0.00208751672060286,
1.84858989190502));
#60651=CARTESIAN_POINT('Ctrl Pts',(-2.37368814589582,-0.171375740131997,
1.85995808893514));
#60652=CARTESIAN_POINT('Ctrl Pts',(-2.28019409230745,-1.12323247312203,
1.92399124963194));
#60653=CARTESIAN_POINT('Ctrl Pts',(-0.995855715555496,-2.61553061219188,
2.04068937399542));
#60654=CARTESIAN_POINT('Ctrl Pts',(1.64637781974439,-2.26322161422709,2.19868426499547));
#60655=CARTESIAN_POINT('Ctrl Pts',(2.79508756969503,0.142186649832604,2.35667915599553));
#60656=CARTESIAN_POINT('Ctrl Pts',(1.40821242874264,2.41860884498944,2.51467404699558));
#60657=CARTESIAN_POINT('Ctrl Pts',(-1.25613315819632,2.50097199645567,2.67266893799564));
#60658=CARTESIAN_POINT('Ctrl Pts',(-2.29312995726813,1.01405513820569,2.78011676034415));
#60659=CARTESIAN_POINT('Ctrl Pts',(-2.36688836699276,0.204481261054058,
2.83489961902599));
#60660=CARTESIAN_POINT('Ctrl Pts',(-2.36906969114779,0.173130678776576,
2.83701751404115));
#60661=CARTESIAN_POINT('Ctrl Pts',(-2.37174906936557,-0.00210106248464756,
1.84835957816189));
#60662=CARTESIAN_POINT('Ctrl Pts',(-2.3718008254975,0.0563229770868639,
1.84477173666528));
#60663=CARTESIAN_POINT('Ctrl Pts',(-2.36969378183979,0.114688971414575,
1.8411930390963));
#60664=CARTESIAN_POINT('Ctrl Pts',(-2.36544098584031,0.172878584581292,
1.83759047784057));
#60665=CARTESIAN_POINT('Ctrl Pts',(-2.3654410189124,0.172878132066172,1.63813797379334));
#60666=CARTESIAN_POINT('Ctrl Pts',(-2.36650722285482,0.158289574740896,
1.63906775807807));
#60667=CARTESIAN_POINT('Ctrl Pts',(-2.36743850206663,0.143690677903543,
1.64000089714618));
#60668=CARTESIAN_POINT('Ctrl Pts',(-2.37057162816117,0.0862085864060536,
1.6436872167648));
#60669=CARTESIAN_POINT('Ctrl Pts',(-2.37174370262375,0.043280608190179,
1.64646696461456));
#60670=CARTESIAN_POINT('Ctrl Pts',(-2.37175279409662,-0.0189531630133541,
1.65054751451175));
#60671=CARTESIAN_POINT('Ctrl Pts',(-2.37152004312492,-0.0382516358593104,
1.65181990760461));
#60672=CARTESIAN_POINT('Ctrl Pts',(-2.37068903727249,-0.0724921348320239,
1.65409095565325));
#60673=CARTESIAN_POINT('Ctrl Pts',(-2.37018493560669,-0.0874355465879592,
1.65508666046218));
#60674=CARTESIAN_POINT('Ctrl Pts',(-2.36883482135379,-0.118685505063106,
1.65717890899175));
#60675=CARTESIAN_POINT('Ctrl Pts',(-2.36796164018241,-0.134990028426079,
1.65827624007328));
#60676=CARTESIAN_POINT('Ctrl Pts',(-2.36521514840107,-0.177960411516417,
1.66118392719267));
#60677=CARTESIAN_POINT('Ctrl Pts',(-2.36305929083378,-0.204605214837943,
1.66300288021788));
#60678=CARTESIAN_POINT('Ctrl Pts',(-2.34930136124216,-0.345063581175934,
1.67267964128663));
#60679=CARTESIAN_POINT('Ctrl Pts',(-2.32992773745585,-0.457947168149107,
1.68077369546693));
#60680=CARTESIAN_POINT('Ctrl Pts',(-2.28206810369801,-0.651621110046698,
1.69516658157102));
#60681=CARTESIAN_POINT('Ctrl Pts',(-2.25721196628489,-0.733101716672578,
1.70138214880325));
#60682=CARTESIAN_POINT('Ctrl Pts',(-2.18816697038893,-0.922304390653416,
1.7160585732042));
#60683=CARTESIAN_POINT('Ctrl Pts',(-2.14031895910505,-1.02847493746381,
1.72449265393572));
#60684=CARTESIAN_POINT('Ctrl Pts',(-2.0766287312908,-1.14591009468153,1.7337645618215));
#60685=CARTESIAN_POINT('Ctrl Pts',(-2.06822208430992,-1.16101433479644,
1.73495578440575));
#60686=CARTESIAN_POINT('Ctrl Pts',(-2.05483921263766,-1.18445263069519,
1.7368006808796));
#60687=CARTESIAN_POINT('Ctrl Pts',(-2.04997588534783,-1.19284999139944,
1.73746092872973));
#60688=CARTESIAN_POINT('Ctrl Pts',(-2.04123949529479,-1.20772361065788,
1.73862875053818));
#60689=CARTESIAN_POINT('Ctrl Pts',(-2.03738700580321,-1.21421134394877,
1.73913755885768));
#60690=CARTESIAN_POINT('Ctrl Pts',(-2.02796060001715,-1.22991457094225,
1.74036781969376));
#60691=CARTESIAN_POINT('Ctrl Pts',(-2.02235478740453,-1.23911063751104,
1.74108723303817));
#60692=CARTESIAN_POINT('Ctrl Pts',(-2.0045078157739,-1.26794397522642,1.74334061983464));
#60693=CARTESIAN_POINT('Ctrl Pts',(-1.9920413936179,-1.2874411405809,1.74486103753852));
#60694=CARTESIAN_POINT('Ctrl Pts',(-1.92276550832126,-1.39237074713954,
1.75304329595376));
#60695=CARTESIAN_POINT('Ctrl Pts',(-1.86073758110891,-1.47424009859307,
1.75942883148912));
#60696=CARTESIAN_POINT('Ctrl Pts',(-1.66497211251407,-1.70050282960164,
1.77787529660315));
#60697=CARTESIAN_POINT('Ctrl Pts',(-1.51838104454189,-1.83258123097054,
1.78977095423047));
#60698=CARTESIAN_POINT('Ctrl Pts',(-1.33211247178348,-1.96255160862391,
1.80446468675414));
#60699=CARTESIAN_POINT('Ctrl Pts',(-1.30670912094453,-1.97955641251372,
1.80645862279762));
#60700=CARTESIAN_POINT('Ctrl Pts',(-1.2664079672809,-2.00541988919985,1.80961065409293));
#60701=CARTESIAN_POINT('Ctrl Pts',(-1.25172909603453,-2.01461468160752,
1.8107564278356));
#60702=CARTESIAN_POINT('Ctrl Pts',(-1.22444052572031,-2.03129477310934,
1.81288298982044));
#60703=CARTESIAN_POINT('Ctrl Pts',(-1.21185950215961,-2.03882554107477,
1.81386207170541));
#60704=CARTESIAN_POINT('Ctrl Pts',(-1.18368629670252,-2.0553366038865,1.81605204221856));
#60705=CARTESIAN_POINT('Ctrl Pts',(-1.16806025376419,-2.06425701336986,
1.8172649941684));
#60706=CARTESIAN_POINT('Ctrl Pts',(-1.12195538575618,-2.0898857017594,1.8208397329011));
#60707=CARTESIAN_POINT('Ctrl Pts',(-1.09121010184416,-2.10610218851039,
1.82321846071209));
#60708=CARTESIAN_POINT('Ctrl Pts',(-1.01989030276269,-2.14173864684127,
1.82872758292421));
#60709=CARTESIAN_POINT('Ctrl Pts',(-0.979098407183258,-2.16069121512166,
1.83187231751021));
#60710=CARTESIAN_POINT('Ctrl Pts',(-0.830576121562144,-2.22462750021829,
1.84329896870486));
#60711=CARTESIAN_POINT('Ctrl Pts',(-0.720106475424665,-2.26280045639512,
1.8517651200716));
#60712=CARTESIAN_POINT('Ctrl Pts',(-0.480166277638578,-2.32635594391503,
1.86985963073218));
#60713=CARTESIAN_POINT('Ctrl Pts',(-0.350453921239645,-2.34939985246926,
1.87946992782941));
#60714=CARTESIAN_POINT('Ctrl Pts',(-0.197163516641058,-2.36364705789476,
1.89022514801687));
#60715=CARTESIAN_POINT('Ctrl Pts',(-0.174807133522279,-2.36540555132379,
1.89177852776345));
#60716=CARTESIAN_POINT('Ctrl Pts',(-0.14166168391293,-2.36754016407954,
1.89405589825042));
#60717=CARTESIAN_POINT('Ctrl Pts',(-0.130890296634255,-2.36816008806694,
1.8947919753747));
#60718=CARTESIAN_POINT('Ctrl Pts',(-0.111781702529406,-2.36912906623916,
1.89609024697721));
#60719=CARTESIAN_POINT('Ctrl Pts',(-0.103446432340889,-2.36950765438207,
1.89665399116552));
#60720=CARTESIAN_POINT('Ctrl Pts',(-0.0850765978253238,-2.37024489128089,
1.89789071701065));
#60721=CARTESIAN_POINT('Ctrl Pts',(-0.0750415913657593,-2.37058381855894,
1.89856262722164));
#60722=CARTESIAN_POINT('Ctrl Pts',(-0.0456270833055152,-2.37139030922434,
1.90052212175037));
#60723=CARTESIAN_POINT('Ctrl Pts',(-0.0262431140405828,-2.37168404029352,
1.90180069868994));
#60724=CARTESIAN_POINT('Ctrl Pts',(0.0739099002708013,-2.37197359425699,
1.90835119281824));
#60725=CARTESIAN_POINT('Ctrl Pts',(0.154644763099063,-2.36808131734941,
1.91344549821364));
#60726=CARTESIAN_POINT('Ctrl Pts',(0.409343641714807,-2.34271680135929,
1.92935658329961));
#60727=CARTESIAN_POINT('Ctrl Pts',(0.581191867306626,-2.30610086432765,
1.93989315444686));
#60728=CARTESIAN_POINT('Ctrl Pts',(0.808024438819154,-2.23077775345193,
1.95497703000433));
#60729=CARTESIAN_POINT('Ctrl Pts',(0.867764560154263,-2.20822473082563,
1.95906254299357));
#60730=CARTESIAN_POINT('Ctrl Pts',(0.947927506989698,-2.17420614907816,
1.96474296683036));
#60731=CARTESIAN_POINT('Ctrl Pts',(0.969200816938654,-2.16480683929959,
1.96626990901411));
#60732=CARTESIAN_POINT('Ctrl Pts',(1.00309067814366,-2.14923342531369,1.96873561568744));
#60733=CARTESIAN_POINT('Ctrl Pts',(1.01579693047782,-2.14325728901133,1.96966766686124));
#60734=CARTESIAN_POINT('Ctrl Pts',(1.04205032239121,-2.13062362216693,1.97160966886287));
#60735=CARTESIAN_POINT('Ctrl Pts',(1.05558843459342,-2.12394890064327,1.97262017396673));
#60736=CARTESIAN_POINT('Ctrl Pts',(1.08741410856206,-2.10787839111442,1.97501769598573));
#60737=CARTESIAN_POINT('Ctrl Pts',(1.10564477550843,-2.0983732603837,1.97640843997294));
#60738=CARTESIAN_POINT('Ctrl Pts',(1.16717112620376,-2.06527017601494,1.98116279699018));
#60739=CARTESIAN_POINT('Ctrl Pts',(1.20985108058,-2.04056097312134,1.98456471940501));
#60740=CARTESIAN_POINT('Ctrl Pts',(1.31329521226092,-1.97628635806193,1.99307606533235));
#60741=CARTESIAN_POINT('Ctrl Pts',(1.37307170333304,-1.93523243100975,1.99823270050377));
#60742=CARTESIAN_POINT('Ctrl Pts',(1.54550823622632,-1.80478933377107,2.01380375854382));
#60743=CARTESIAN_POINT('Ctrl Pts',(1.65201948031217,-1.70783183530549,2.0243887758945));
#60744=CARTESIAN_POINT('Ctrl Pts',(1.79376765309942,-1.55305205325193,2.03950710441214));
#60745=CARTESIAN_POINT('Ctrl Pts',(1.83638420011413,-1.50242064882401,2.0442122215492));
#60746=CARTESIAN_POINT('Ctrl Pts',(1.88668385765034,-1.43731755481127,2.0499105828646));
#60747=CARTESIAN_POINT('Ctrl Pts',(1.89640611804759,-1.42446537436496,2.05101924858662));
#60748=CARTESIAN_POINT('Ctrl Pts',(1.91156143615865,-1.40400084024771,2.05275779948194));
#60749=CARTESIAN_POINT('Ctrl Pts',(1.91708155730352,-1.39645400704104,2.05339327428123));
#60750=CARTESIAN_POINT('Ctrl Pts',(1.92752700819558,-1.38199483596361,2.05459973613502));
#60751=CARTESIAN_POINT('Ctrl Pts',(1.93246002570753,-1.37508848628665,2.05517120318125));
#60752=CARTESIAN_POINT('Ctrl Pts',(1.9442632199243,-1.35837475369387,2.05654298993827));
#60753=CARTESIAN_POINT('Ctrl Pts',(1.95109650770349,-1.34854138698825,2.05734088021646));
#60754=CARTESIAN_POINT('Ctrl Pts',(1.97497264494,-1.31362128471925,2.0601436685427));
#60755=CARTESIAN_POINT('Ctrl Pts',(1.9916092857163,-1.28825870336095,2.06212395566854));
#60756=CARTESIAN_POINT('Ctrl Pts',(2.03252255310066,-1.22319852539074,2.06708400758758));
#60757=CARTESIAN_POINT('Ctrl Pts',(2.05612665688058,-1.18309181836247,2.07003186619664));
#60758=CARTESIAN_POINT('Ctrl Pts',(2.18308825035769,-0.95207454479456,2.08654820420345));
#60759=CARTESIAN_POINT('Ctrl Pts',(2.26102693710006,-0.748387278041042,
2.09946127208388));
#60760=CARTESIAN_POINT('Ctrl Pts',(2.32064384756769,-0.491883416028774,
2.1162702325225));
#60761=CARTESIAN_POINT('Ctrl Pts',(2.32979376655162,-0.446539721317087,
2.11925645290524));
#60762=CARTESIAN_POINT('Ctrl Pts',(2.3407538491598,-0.382641990822375,2.12350009450854));
#60763=CARTESIAN_POINT('Ctrl Pts',(2.3436803195018,-0.364288352075148,2.12472304457366));
#60764=CARTESIAN_POINT('Ctrl Pts',(2.34840882212246,-0.332213098388674,
2.12686823929053));
#60765=CARTESIAN_POINT('Ctrl Pts',(2.35030704136993,-0.318506414750984,
2.12778745934583));
#60766=CARTESIAN_POINT('Ctrl Pts',(2.35404628870528,-0.289649834210623,
2.12972835949216));
#60767=CARTESIAN_POINT('Ctrl Pts',(2.35586124224451,-0.274497257825233,
2.13075080354843));
#60768=CARTESIAN_POINT('Ctrl Pts',(2.35988206230597,-0.237944381955068,
2.13322565482779));
#60769=CARTESIAN_POINT('Ctrl Pts',(2.36194319240294,-0.216529860221301,
2.13468246550038));
#60770=CARTESIAN_POINT('Ctrl Pts',(2.36829912274163,-0.139521672987643,
2.1399476304263));
#60771=CARTESIAN_POINT('Ctrl Pts',(2.37092421625406,-0.083812353207781,
2.14380637099085));
#60772=CARTESIAN_POINT('Ctrl Pts',(2.37261213971251,0.0588174204132735,
2.15381835638895));
#60773=CARTESIAN_POINT('Ctrl Pts',(2.36886503509941,0.145683725439771,2.16004402054196));
#60774=CARTESIAN_POINT('Ctrl Pts',(2.34795669888371,0.3582749801262,2.17552368244949));
#60775=CARTESIAN_POINT('Ctrl Pts',(2.32546121546305,0.48321001142874,2.18483933680214));
#60776=CARTESIAN_POINT('Ctrl Pts',(2.2776057435873,0.664369024038535,2.19830362552081));
#60777=CARTESIAN_POINT('Ctrl Pts',(2.25987701094352,0.722378953942853,2.20260550700941));
#60778=CARTESIAN_POINT('Ctrl Pts',(2.23477184592509,0.794506321767673,2.2078921405661));
#60779=CARTESIAN_POINT('Ctrl Pts',(2.22945314942921,0.809310932877813,2.20897386102416));
#60780=CARTESIAN_POINT('Ctrl Pts',(2.22076778582128,0.83275108506334,2.21067994120251));
#60781=CARTESIAN_POINT('Ctrl Pts',(2.21749723010272,0.84142139860191,2.21130955714423));
#60782=CARTESIAN_POINT('Ctrl Pts',(2.2111215323019,0.858028118825069,2.21251240726086));
#60783=CARTESIAN_POINT('Ctrl Pts',(2.20802433273991,0.865967223137882,2.2130860509396));
#60784=CARTESIAN_POINT('Ctrl Pts',(2.20039719867509,0.885211014543394,2.21447346106541));
#60785=CARTESIAN_POINT('Ctrl Pts',(2.19582277882416,0.896498026716529,2.21528465316774));
#60786=CARTESIAN_POINT('Ctrl Pts',(2.17903014924088,0.937032733036599,2.21819034212709));
#60787=CARTESIAN_POINT('Ctrl Pts',(2.16631228801756,0.966071445361223,2.22025777556173));
#60788=CARTESIAN_POINT('Ctrl Pts',(2.06267174775505,1.19036666658164,2.23618113030257));
#60789=CARTESIAN_POINT('Ctrl Pts',(1.94610863667187,1.37268773231333,2.24893413652057));
#60790=CARTESIAN_POINT('Ctrl Pts',(1.75338574569002,1.59923739335471,2.26752828031237));
#60791=CARTESIAN_POINT('Ctrl Pts',(1.69705640283385,1.65889097788463,2.27273353050838));
#60792=CARTESIAN_POINT('Ctrl Pts',(1.61937051417628,1.73305605138435,2.27972164372801));
#60793=CARTESIAN_POINT('Ctrl Pts',(1.60070509083984,1.75031062132554,2.28138713359509));
#60794=CARTESIAN_POINT('Ctrl Pts',(1.56980699861919,1.77796559605334,2.28412474896665));
#60795=CARTESIAN_POINT('Ctrl Pts',(1.55773936931983,1.78854793331922,2.28518928346335));
#60796=CARTESIAN_POINT('Ctrl Pts',(1.53414733249378,1.80881636095374,2.28726203110273));
#60797=CARTESIAN_POINT('Ctrl Pts',(1.52263625611515,1.8185168350131,2.288269589531));
#60798=CARTESIAN_POINT('Ctrl Pts',(1.495382159341,1.8410438889784,2.29064679455069));
#60799=CARTESIAN_POINT('Ctrl Pts',(1.47956541345178,1.85377899084149,2.29201999202037));
#60800=CARTESIAN_POINT('Ctrl Pts',(1.42604878679015,1.89574752987011,2.29664633392032));
#60801=CARTESIAN_POINT('Ctrl Pts',(1.38763292796508,1.92404473386648,2.29993503479337));
#60802=CARTESIAN_POINT('Ctrl Pts',(1.29150721130187,1.99047444130965,2.30809188003879));
#60803=CARTESIAN_POINT('Ctrl Pts',(1.23293486661149,2.02727638982289,2.31300218648632));
#60804=CARTESIAN_POINT('Ctrl Pts',(1.09118004450687,2.10792590973622,2.3247264753537));
#60805=CARTESIAN_POINT('Ctrl Pts',(1.00683175670646,2.14949152870335,2.33158314192042));
#60806=CARTESIAN_POINT('Ctrl Pts',(0.818738021908449,2.22867581720257,2.34645711017889));
#60807=CARTESIAN_POINT('Ctrl Pts',(0.714367718196973,2.26429043566019,2.35445456779312));
#60808=CARTESIAN_POINT('Ctrl Pts',(0.585672881320951,2.29841547776209,2.36375910320478));
#60809=CARTESIAN_POINT('Ctrl Pts',(0.563368915810369,2.30398393948334,2.36535172390611));
#60810=CARTESIAN_POINT('Ctrl Pts',(0.530528557705808,2.31167750424403,2.36766415938219));
#60811=CARTESIAN_POINT('Ctrl Pts',(0.520053811472902,2.31405649854322,2.36839690676218));
#60812=CARTESIAN_POINT('Ctrl Pts',(0.501417289955651,2.31815623452871,2.3696916096472));
#60813=CARTESIAN_POINT('Ctrl Pts',(0.493262176902826,2.31990518298289,2.3702550812083));
#60814=CARTESIAN_POINT('Ctrl Pts',(0.475233376679526,2.32367227708012,2.37149396182267));
#60815=CARTESIAN_POINT('Ctrl Pts',(0.465355895043343,2.32567055141762,2.37216827167205));
#60816=CARTESIAN_POINT('Ctrl Pts',(0.436263396578076,2.33136336952561,2.37414210426682));
#60817=CARTESIAN_POINT('Ctrl Pts',(0.417014519108134,2.33488326538684,2.37543241850249));
#60818=CARTESIAN_POINT('Ctrl Pts',(0.267001230920364,2.36040063644657,2.3853823207734));
#60819=CARTESIAN_POINT('Ctrl Pts',(0.134625913696415,2.3716378619941,2.39354585699655));
#60820=CARTESIAN_POINT('Ctrl Pts',(-0.164800082457489,2.37188912922675,
2.4119421846848));
#60821=CARTESIAN_POINT('Ctrl Pts',(-0.331121029983698,2.35443594925894,
2.42213921139802));
#60822=CARTESIAN_POINT('Ctrl Pts',(-0.524251091600474,2.31328794722317,
2.43487672094202));
#60823=CARTESIAN_POINT('Ctrl Pts',(-0.554145508291139,2.30630937928264,
2.43687307521349));
#60824=CARTESIAN_POINT('Ctrl Pts',(-0.602275439247987,2.29408412975374,
2.44013195577816));
#60825=CARTESIAN_POINT('Ctrl Pts',(-0.620598743577357,2.28919524379991,
2.4413832258896));
#60826=CARTESIAN_POINT('Ctrl Pts',(-0.653183564977096,2.28008124337408,
2.44362831775515));
#60827=CARTESIAN_POINT('Ctrl Pts',(-0.667467826403133,2.27594066918248,
2.44461939185791));
#60828=CARTESIAN_POINT('Ctrl Pts',(-0.697688281726195,2.26687171097754,
2.44673126621278));
#60829=CARTESIAN_POINT('Ctrl Pts',(-0.713613249026269,2.26190901650747,
2.4478531258937));
#60830=CARTESIAN_POINT('Ctrl Pts',(-0.756489667696547,2.24804958588336,
2.45089864073422));
#60831=CARTESIAN_POINT('Ctrl Pts',(-0.783335211578066,2.23883661401164,
2.45283241264343));
#60832=CARTESIAN_POINT('Ctrl Pts',(-0.842502914985661,2.21733674538441,
2.45715631128878));
#60833=CARTESIAN_POINT('Ctrl Pts',(-0.874734247176489,2.20482044436274,
2.45955342125923));
#60834=CARTESIAN_POINT('Ctrl Pts',(-0.976205886801671,2.1628410583344,2.46723480880692));
#60835=CARTESIAN_POINT('Ctrl Pts',(-1.04431852684647,2.13078774389948,2.47259532172554));
#60836=CARTESIAN_POINT('Ctrl Pts',(-1.22934198965628,2.03271261063227,2.48769677888344));
#60837=CARTESIAN_POINT('Ctrl Pts',(-1.34234470561332,1.95992633849734,2.49756488809204));
#60838=CARTESIAN_POINT('Ctrl Pts',(-1.50456002505023,1.8348009886683,2.51234834003741));
#60839=CARTESIAN_POINT('Ctrl Pts',(-1.55858274656376,1.78913870953042,2.51738707575922));
#60840=CARTESIAN_POINT('Ctrl Pts',(-1.62249603759713,1.73002085921584,2.52341950897839));
#60841=CARTESIAN_POINT('Ctrl Pts',(-1.63438801055534,1.71879068913576,2.52454510010271));
#60842=CARTESIAN_POINT('Ctrl Pts',(-1.65293207110211,1.70091211854387,2.52630403641596));
#60843=CARTESIAN_POINT('Ctrl Pts',(-1.65966216411146,1.69434588420771,2.52694318444354));
#60844=CARTESIAN_POINT('Ctrl Pts',(-1.67237924130797,1.68178995366011,2.52815210284693));
#60845=CARTESIAN_POINT('Ctrl Pts',(-1.67837323685405,1.67580817963298,2.52872238208247));
#60846=CARTESIAN_POINT('Ctrl Pts',(-1.68438613384638,1.66974292027718,2.52929506774057));
#60847=CARTESIAN_POINT('Ctrl Pts',(-1.68443694764035,1.66969165929934,2.52929990743776));
#60848=CARTESIAN_POINT('Ctrl Pts',(-1.68453737238546,1.66959034152202,2.52930947235767));
#60849=CARTESIAN_POINT('Ctrl Pts',(-1.68458698344294,1.66954028483338,2.52931419758844));
#60850=CARTESIAN_POINT('Ctrl Pts',(-1.68468505886197,1.66944131963004,2.52932353891723));
#60851=CARTESIAN_POINT('Ctrl Pts',(-1.684733523341,1.66939241119992,2.52932815502448));
#60852=CARTESIAN_POINT('Ctrl Pts',(-1.68482935847505,1.66929568975979,2.52933728313654));
#60853=CARTESIAN_POINT('Ctrl Pts',(-1.68487672922794,1.66924787684041,2.52934179514882));
#60854=CARTESIAN_POINT('Ctrl Pts',(-1.6849704267261,1.6691532967022,2.52935071981064));
#60855=CARTESIAN_POINT('Ctrl Pts',(-1.68501675354766,1.66910652958314,2.52935513246572));
#60856=CARTESIAN_POINT('Ctrl Pts',(-1.69275121881801,1.66129790453169,2.53009185080793));
#60857=CARTESIAN_POINT('Ctrl Pts',(-1.70038582126558,1.65348283530524,2.53082009581914));
#60858=CARTESIAN_POINT('Ctrl Pts',(-1.72620911450056,1.62668111522474,2.53328806396711));
#60859=CARTESIAN_POINT('Ctrl Pts',(-1.74413670366934,1.60744413708869,2.53500956635476));
#60860=CARTESIAN_POINT('Ctrl Pts',(-1.78797017729644,1.55881219237146,2.53925135948999));
#60861=CARTESIAN_POINT('Ctrl Pts',(-1.81347524889252,1.52906529142509,2.54174919284464));
#60862=CARTESIAN_POINT('Ctrl Pts',(-1.92441892772621,1.39298701020566,2.55282155417023));
#60863=CARTESIAN_POINT('Ctrl Pts',(-2.00133024481161,1.280032310735,2.56108727189952));
#60864=CARTESIAN_POINT('Ctrl Pts',(-2.12884680834715,1.05290190120611,2.57714961082586));
#60865=CARTESIAN_POINT('Ctrl Pts',(-2.18099497152325,0.940131094760641,
2.58489645022722));
#60866=CARTESIAN_POINT('Ctrl Pts',(-2.23368168852974,0.797889780500425,
2.59474186846515));
#60867=CARTESIAN_POINT('Ctrl Pts',(-2.24282780723674,0.771806525001884,
2.59654950174099));
#60868=CARTESIAN_POINT('Ctrl Pts',(-2.25670967017767,0.729885280115304,
2.59946136659405));
#60869=CARTESIAN_POINT('Ctrl Pts',(-2.26173945592868,0.7141468113005,2.6005560299086));
#60870=CARTESIAN_POINT('Ctrl Pts',(-2.27099276224718,0.68411407480358,2.60264831038471));
#60871=CARTESIAN_POINT('Ctrl Pts',(-2.27524679299409,0.669829983843014,
2.60364488571619));
#60872=CARTESIAN_POINT('Ctrl Pts',(-2.28468512286114,0.637010493029739,
2.60593841808241));
#60873=CARTESIAN_POINT('Ctrl Pts',(-2.28977893222255,0.618450388397305,
2.60723820241515));
#60874=CARTESIAN_POINT('Ctrl Pts',(-2.29995844813261,0.579508761910597,
2.6099717508555));
#60875=CARTESIAN_POINT('Ctrl Pts',(-2.30500036937791,0.559117623483894,
2.61140677763455));
#60876=CARTESIAN_POINT('Ctrl Pts',(-2.3178181405796,0.504155383295277,2.61528529455615));
#60877=CARTESIAN_POINT('Ctrl Pts',(-2.32509093595485,0.469473639692089,
2.61774388493411));
#60878=CARTESIAN_POINT('Ctrl Pts',(-2.34772955812159,0.34803193996765,2.62639308156394));
#60879=CARTESIAN_POINT('Ctrl Pts',(-2.35902693891148,0.260640299986158,
2.63269147581119));
#60880=CARTESIAN_POINT('Ctrl Pts',(-2.36544104518992,0.172877772518167,
2.63906222572513));
#60881=CARTESIAN_POINT('Origin',(0.,0.,-1.84858989190501));
#60882=CARTESIAN_POINT('',(-2.36544101854889,0.172878137039867,3.83707348408299));
#60883=CARTESIAN_POINT('',(-2.36544101877862,0.172878133896551,3.6418462952528));
#60884=CARTESIAN_POINT('',(-2.36544101854889,0.172878137039864,-1.84858989190501));
#60885=CARTESIAN_POINT('',(-2.37174955725825,0.00144918780827443,2.84858993475468));
#60886=CARTESIAN_POINT('Ctrl Pts',(-2.37174955725825,0.00144918780827443,
2.84858993475469));
#60887=CARTESIAN_POINT('Ctrl Pts',(-2.37179726134704,-0.0766236132632544,
2.85385139941758));
#60888=CARTESIAN_POINT('Ctrl Pts',(-2.36798576321773,-0.154846589518332,
2.85911286408048));
#60889=CARTESIAN_POINT('Ctrl Pts',(-2.36029698198233,-0.232800814743257,
2.86437432874338));
#60890=CARTESIAN_POINT('Ctrl Pts',(-2.35261882788851,-0.310647294596898,
2.86962852120952));
#60891=CARTESIAN_POINT('Ctrl Pts',(-2.34107408131574,-0.388225285324987,
2.87488271367567));
#60892=CARTESIAN_POINT('Ctrl Pts',(-2.32569668339652,-0.465116113823676,
2.88013690614181));
#60893=CARTESIAN_POINT('Ctrl Pts',(-2.31033102347183,-0.541948249419353,
2.88538708793705));
#60894=CARTESIAN_POINT('Ctrl Pts',(-2.29113860801431,-0.618093792558647,
2.89063726973229));
#60895=CARTESIAN_POINT('Ctrl Pts',(-2.26820501046763,-0.693140745440315,
2.89588745152753));
#60896=CARTESIAN_POINT('Ctrl Pts',(-2.24528134677732,-0.768155191182627,
2.90113535916792));
#60897=CARTESIAN_POINT('Ctrl Pts',(-2.21861985678342,-0.842071530751637,
2.90638326680832));
#60898=CARTESIAN_POINT('Ctrl Pts',(-2.18835647317101,-0.914491120148553,
2.91163117444872));
#60899=CARTESIAN_POINT('Ctrl Pts',(-2.15809620728109,-0.986903248906358,
2.91687854145162));
#60900=CARTESIAN_POINT('Ctrl Pts',(-2.12423497147806,-1.05781848976263,
2.92212590845453));
#60901=CARTESIAN_POINT('Ctrl Pts',(-2.08695690071309,-1.12685800217509,
2.92737327545744));
#60902=CARTESIAN_POINT('Ctrl Pts',(-2.04964530915196,-1.19595959557442,
2.93262536094271));
#60903=CARTESIAN_POINT('Ctrl Pts',(-2.00891097447246,-1.26318166641551,
2.93787744642799));
#60904=CARTESIAN_POINT('Ctrl Pts',(-1.9649837094817,-1.32817057788958,2.94312953191326));
#60905=CARTESIAN_POINT('Ctrl Pts',(-1.92103736272031,-1.39318772020167,
2.94838389887658));
#60906=CARTESIAN_POINT('Ctrl Pts',(-1.87389561400849,-1.45596938633539,
2.9536382658399));
#60907=CARTESIAN_POINT('Ctrl Pts',(-1.82382969244265,-1.51619369325444,
2.95889263280322));
#60908=CARTESIAN_POINT('Ctrl Pts',(-1.77367591830687,-1.57652367804719,
2.96415621980338));
#60909=CARTESIAN_POINT('Ctrl Pts',(-1.72058804887877,-1.63428698509946,
2.96941980680354));
#60910=CARTESIAN_POINT('Ctrl Pts',(-1.66487510562834,-1.68919772234012,
2.9746833938037));
#60911=CARTESIAN_POINT('Ctrl Pts',(-1.61556737720283,-1.73779547290835,
2.97934183586771));
#60912=CARTESIAN_POINT('Ctrl Pts',(-1.56420417740737,-1.7841592771669,2.98400027793172));
#60913=CARTESIAN_POINT('Ctrl Pts',(-1.51101990214086,-1.82811840913936,
2.98865871999573));
#60914=CARTESIAN_POINT('Ctrl Pts',(-1.45010266434992,-1.87846917319566,
2.99399449681185));
#60915=CARTESIAN_POINT('Ctrl Pts',(-1.38655261703524,-1.92586544674143,
2.99933027362796));
#60916=CARTESIAN_POINT('Ctrl Pts',(-1.32068805983314,-1.97002058646964,
3.00466605044407));
#60917=CARTESIAN_POINT('Ctrl Pts',(-1.25491766702395,-2.01411259904565,
3.00999419887542));
#60918=CARTESIAN_POINT('Ctrl Pts',(-1.18683972146185,-2.05497242184816,
3.01532234730677));
#60919=CARTESIAN_POINT('Ctrl Pts',(-1.1168056515261,-2.0923535072304,3.02065049573812));
#60920=CARTESIAN_POINT('Ctrl Pts',(-1.04685189699581,-2.12969172380563,
3.02597253382343));
#60921=CARTESIAN_POINT('Ctrl Pts',(-0.974946887030453,-2.16355891193964,
3.03129457190874));
#60922=CARTESIAN_POINT('Ctrl Pts',(-0.90146981626064,-2.19375254595203,
3.03661660999406));
#60923=CARTESIAN_POINT('Ctrl Pts',(-0.828038758435314,-2.22392727205218,
3.04193531530303));
#60924=CARTESIAN_POINT('Ctrl Pts',(-0.753038025698316,-2.25043283296074,
3.047254020612));
#60925=CARTESIAN_POINT('Ctrl Pts',(-0.676869037026495,-2.27311380472136,
3.05257272592098));
#60926=CARTESIAN_POINT('Ctrl Pts',(-0.600724117037506,-2.29578760950859,
3.05788975056918));
#60927=CARTESIAN_POINT('Ctrl Pts',(-0.523412122448103,-2.31463909170633,
3.06320677521738));
#60928=CARTESIAN_POINT('Ctrl Pts',(-0.445350561000367,-2.32956239244985,
3.06852379986559));
#60929=CARTESIAN_POINT('Ctrl Pts',(-0.367289449785087,-2.34448560712086,
3.07384079384701));
#60930=CARTESIAN_POINT('Ctrl Pts',(-0.288479240262441,-2.35548059896049,
3.07915778782843));
#60931=CARTESIAN_POINT('Ctrl Pts',(-0.209347124003659,-2.36249271833193,
3.08447478180984));
#60932=CARTESIAN_POINT('Ctrl Pts',(-0.130136702035626,-2.36951177659249,
3.08979703725784));
#60933=CARTESIAN_POINT('Ctrl Pts',(-0.0506042042954726,-2.37254004843377,
3.09511929270583));
#60934=CARTESIAN_POINT('Ctrl Pts',(0.0288191732936541,-2.37157490241204,
3.10044154815383));
#60935=CARTESIAN_POINT('Ctrl Pts',(0.108281098580519,-2.37060928796201,
3.10576638672912));
#60936=CARTESIAN_POINT('Ctrl Pts',(0.187633330540198,-2.36564642374603,
3.1110912253044));
#60937=CARTESIAN_POINT('Ctrl Pts',(0.266448342489727,-2.35673573895855,
3.11641606387969));
#60938=CARTESIAN_POINT('Ctrl Pts',(0.345403638790127,-2.34780919387236,
3.12175038023725));
#60939=CARTESIAN_POINT('Ctrl Pts',(0.42381934167684,-2.33492086440187,3.12708469659481));
#60940=CARTESIAN_POINT('Ctrl Pts',(0.501276921251674,-2.31817158785118,
3.13241901295237));
#60941=CARTESIAN_POINT('Ctrl Pts',(0.570175316519782,-2.30327313268928,
3.13716387896684));
#60942=CARTESIAN_POINT('Ctrl Pts',(0.63831559260771,-2.28532066239902,3.14190874498132));
#60943=CARTESIAN_POINT('Ctrl Pts',(0.705415006637884,-2.2644177465543,3.1466536109958));
#60944=CARTESIAN_POINT('Ctrl Pts',(0.780870772090863,-2.24091164686538,
3.15198938780203));
#60945=CARTESIAN_POINT('Ctrl Pts',(0.855290743765986,-2.21358614523013,
3.15732516460827));
#60946=CARTESIAN_POINT('Ctrl Pts',(0.928260929205188,-2.18255119294167,
3.1626609414145));
#60947=CARTESIAN_POINT('Ctrl Pts',(1.00112679155559,-2.15156061031,3.16798908983506));
#60948=CARTESIAN_POINT('Ctrl Pts',(1.07254655687529,-2.11687129091511,3.17331723825561));
#60949=CARTESIAN_POINT('Ctrl Pts',(1.14212171099343,-2.0786428408405,3.17864538667617));
#60950=CARTESIAN_POINT('Ctrl Pts',(1.21161707597577,-2.04045823134421,3.18396742474939));
#60951=CARTESIAN_POINT('Ctrl Pts',(1.27927162561687,-1.99874278130691,3.1892894628226));
#60952=CARTESIAN_POINT('Ctrl Pts',(1.3447085425351,-1.95370340587642,3.19461150089582));
#60953=CARTESIAN_POINT('Ctrl Pts',(1.41010448141865,-1.9086922350921,3.1999302061919));
#60954=CARTESIAN_POINT('Ctrl Pts',(1.47328515965246,-1.86036153533037,3.20524891148798));
#60955=CARTESIAN_POINT('Ctrl Pts',(1.5339010641881,-1.80896257224483,3.21056761678406));
#60956=CARTESIAN_POINT('Ctrl Pts',(1.59449781466011,-1.7575798507549,3.2158846414186));
#60957=CARTESIAN_POINT('Ctrl Pts',(1.65253104419497,-1.70313109381767,3.22120166605313));
#60958=CARTESIAN_POINT('Ctrl Pts',(1.70768395978545,-1.64590812501533,3.22651869068767));
#60959=CARTESIAN_POINT('Ctrl Pts',(1.76283655726462,-1.58868548626397,3.23183568465464));
#60960=CARTESIAN_POINT('Ctrl Pts',(1.81510855012025,-1.52868900545532,3.23715267862161));
#60961=CARTESIAN_POINT('Ctrl Pts',(1.86422074216089,-1.46624659829003,3.24246967258858));
#60962=CARTESIAN_POINT('Ctrl Pts',(1.9133815334861,-1.40374240084032,3.24779192802102));
#60963=CARTESIAN_POINT('Ctrl Pts',(1.95937598834536,-1.33878781111464,3.25311418345347));
#60964=CARTESIAN_POINT('Ctrl Pts',(2.00196628826689,-1.27174252234597,3.25843643888592));
#60965=CARTESIAN_POINT('Ctrl Pts',(2.04457725915028,-1.20466469352454,3.26376127744502));
#60966=CARTESIAN_POINT('Ctrl Pts',(2.08378055264218,-1.13549455186852,3.26908611600412));
#60967=CARTESIAN_POINT('Ctrl Pts',(2.11938395655237,-1.0646171646223,3.27441095456322));
#60968=CARTESIAN_POINT('Ctrl Pts',(2.15505073163808,-0.993613621366983,
3.27974527090371));
#60969=CARTESIAN_POINT('Ctrl Pts',(2.18710462542536,-0.920897190148557,
3.2850795872442));
#60970=CARTESIAN_POINT('Ctrl Pts',(2.21540139658963,-0.846873493792748,
3.29041390358468));
#60971=CARTESIAN_POINT('Ctrl Pts',(2.24057133078837,-0.78102953033815,3.29515876972174));
#60972=CARTESIAN_POINT('Ctrl Pts',(2.26276924267427,-0.714151720879358,
3.2999036358588));
#60973=CARTESIAN_POINT('Ctrl Pts',(2.28192737613385,-0.646533458183634,
3.30464850199585));
#60974=CARTESIAN_POINT('Ctrl Pts',(2.30347140343113,-0.570494229185414,
3.30998427887591));
#60975=CARTESIAN_POINT('Ctrl Pts',(2.32125066165164,-0.493235486043965,
3.31532005575597));
#60976=CARTESIAN_POINT('Ctrl Pts',(2.33513102189741,-0.415164031525341,
3.32065583263602));
#60977=CARTESIAN_POINT('Ctrl Pts',(2.34899153784952,-0.337204193192593,
3.3259839811317));
#60978=CARTESIAN_POINT('Ctrl Pts',(2.35896414468065,-0.258434408031037,
3.33131212962738));
#60979=CARTESIAN_POINT('Ctrl Pts',(2.36496475756639,-0.179275648008737,
3.33664027812306));
#60980=CARTESIAN_POINT('Ctrl Pts',(2.3709584889211,-0.100207667624079,3.34196231627303));
#60981=CARTESIAN_POINT('Ctrl Pts',(2.37298924354505,-0.0207520632132589,
3.347284354423));
#60982=CARTESIAN_POINT('Ctrl Pts',(2.3710244140385,0.0586625138686694,3.35260639257297));
#60983=CARTESIAN_POINT('Ctrl Pts',(2.36906081495098,0.138027359813093,3.35792509794676));
#60984=CARTESIAN_POINT('Ctrl Pts',(2.36310660992711,0.217350762769891,3.36324380332054));
#60985=CARTESIAN_POINT('Ctrl Pts',(2.35318125524889,0.296202704993171,3.36856250869433));
#60986=CARTESIAN_POINT('Ctrl Pts',(2.34325903688908,0.375029730746759,3.3738795334074));
#60987=CARTESIAN_POINT('Ctrl Pts',(2.3293682192789,0.453385127608195,3.37919655812048));
#60988=CARTESIAN_POINT('Ctrl Pts',(2.31158010531648,0.530844119497464,3.38451358283356));
#60989=CARTESIAN_POINT('Ctrl Pts',(2.29379209394997,0.608302664629148,3.38983057687981));
#60990=CARTESIAN_POINT('Ctrl Pts',(2.2721069371148,0.684864359270751,3.39514757092607));
#60991=CARTESIAN_POINT('Ctrl Pts',(2.24664670893548,0.760116193571344,3.40046456497232));
#60992=CARTESIAN_POINT('Ctrl Pts',(2.22116128642164,0.835442493814362,3.40578682048464));
#60993=CARTESIAN_POINT('Ctrl Pts',(2.19189348108999,0.909455900312832,3.41110907599696));
#60994=CARTESIAN_POINT('Ctrl Pts',(2.15901459074628,0.981760693572873,3.41643133150928));
#60995=CARTESIAN_POINT('Ctrl Pts',(2.126119742816,1.05410057956219,3.42175617014871));
#60996=CARTESIAN_POINT('Ctrl Pts',(2.0896105335621,1.12472978403073,3.42708100878814));
#60997=CARTESIAN_POINT('Ctrl Pts',(2.04970443203159,1.1932769183262,3.43240584742757));
#60998=CARTESIAN_POINT('Ctrl Pts',(2.00972730087455,1.26194606096529,3.43774016384823));
#60999=CARTESIAN_POINT('Ctrl Pts',(1.96634145294465,1.32852533584444,3.44307448026888));
#61000=CARTESIAN_POINT('Ctrl Pts',(1.91980778510332,1.39267229840932,3.44840879668954));
#61001=CARTESIAN_POINT('Ctrl Pts',(1.87841616625029,1.44973091313356,3.453153662125));
#61002=CARTESIAN_POINT('Ctrl Pts',(1.83453471518382,1.50486534392455,3.45789852756045));
#61003=CARTESIAN_POINT('Ctrl Pts',(1.78837212794992,1.5578585283882,3.46264339299591));
#61004=CARTESIAN_POINT('Ctrl Pts',(1.73646058963283,1.61745132616385,3.46797916983645));
#61005=CARTESIAN_POINT('Ctrl Pts',(1.68147054569493,1.67455745878579,3.47331494667699));
#61006=CARTESIAN_POINT('Ctrl Pts',(1.62366940683842,1.72884230622604,3.47865072351753));
#61007=CARTESIAN_POINT('Ctrl Pts',(1.56595090437147,1.78304954440306,3.48397887197319));
#61008=CARTESIAN_POINT('Ctrl Pts',(1.50542962686771,1.8344431900713,3.48930702042885));
#61009=CARTESIAN_POINT('Ctrl Pts',(1.44241219702958,1.88272279328644,3.49463516888451));
#61010=CARTESIAN_POINT('Ctrl Pts',(1.37946703588314,1.93094702922037,3.49995720699389));
#61011=CARTESIAN_POINT('Ctrl Pts',(1.31403178093854,1.976064036589,3.50527924510327));
#61012=CARTESIAN_POINT('Ctrl Pts',(1.24644761482377,2.01781228215118,3.51060128321265));
#61013=CARTESIAN_POINT('Ctrl Pts',(1.17890577139001,2.0595343840501,3.51591998854552));
#61014=CARTESIAN_POINT('Ctrl Pts',(1.10921808509587,2.09789166630804,3.5212386938784));
#61015=CARTESIAN_POINT('Ctrl Pts',(1.0377553316376,2.13266545293859,3.52655739921127));
#61016=CARTESIAN_POINT('Ctrl Pts',(0.966315159738883,2.16742825137884,3.53187442388316));
#61017=CARTESIAN_POINT('Ctrl Pts',(0.893101455105723,2.19860959829671,3.53719144855505));
#61018=CARTESIAN_POINT('Ctrl Pts',(0.818508933576427,2.22603710394854,3.54250847322694));
#61019=CARTESIAN_POINT('Ctrl Pts',(0.743916842274842,2.25346445140658,3.5478254672318));
#61020=CARTESIAN_POINT('Ctrl Pts',(0.667946389649167,2.27713784052501,3.55314246123665));
#61021=CARTESIAN_POINT('Ctrl Pts',(0.591010179673689,2.29693383231256,3.55845945524151));
#61022=CARTESIAN_POINT('Ctrl Pts',(0.513997836970756,2.31674941335267,3.5637817107124));
#61023=CARTESIAN_POINT('Ctrl Pts',(0.436018282280889,2.33267981610995,3.56910396618329));
#61024=CARTESIAN_POINT('Ctrl Pts',(0.357496535587641,2.34465227476119,3.57442622165418));
#61025=CARTESIAN_POINT('Ctrl Pts',(0.278936678802386,2.3566305441785,3.57975106025209));
#61026=CARTESIAN_POINT('Ctrl Pts',(0.199834571975749,2.36464699539121,3.58507589885001));
#61027=CARTESIAN_POINT('Ctrl Pts',(0.120620086702649,2.36868082636387,3.59040073744792));
#61028=CARTESIAN_POINT('Ctrl Pts',(0.0412646060595808,2.37272183722906,
3.59573505382739));
#61029=CARTESIAN_POINT('Ctrl Pts',(-0.0382031836249495,2.37276606394699,
3.60106937020687));
#61030=CARTESIAN_POINT('Ctrl Pts',(-0.117353921861988,2.36884489140248,
3.60640368658634));
#61031=CARTESIAN_POINT('Ctrl Pts',(-0.187758375674292,2.36535701475787,
3.61114855238954));
#61032=CARTESIAN_POINT('Ctrl Pts',(-0.25791180239772,2.35873246204575,3.61589341819275));
#61033=CARTESIAN_POINT('Ctrl Pts',(-0.327518373976074,2.34902741091033,
3.62063828399595));
#61034=CARTESIAN_POINT('Ctrl Pts',(-0.405793534570179,2.33811372246147,
3.62597406083887));
#61035=CARTESIAN_POINT('Ctrl Pts',(-0.483668247821571,2.32326298659204,
3.63130983768179));
#61036=CARTESIAN_POINT('Ctrl Pts',(-0.56071614705779,2.30451631908491,3.63664561452472));
#61037=CARTESIAN_POINT('Ctrl Pts',(-0.63765389344232,2.28579645307278,3.64197376298269));
#61038=CARTESIAN_POINT('Ctrl Pts',(-0.71376672234596,2.26319182685123,3.64730191144066));
#61039=CARTESIAN_POINT('Ctrl Pts',(-0.788635458630563,2.23679506792432,
3.65263005989863));
#61040=CARTESIAN_POINT('Ctrl Pts',(-0.863418335086616,2.2104285809281,3.6579520980102));
#61041=CARTESIAN_POINT('Ctrl Pts',(-0.936959515113458,2.18027875856735,
3.66327413612177));
#61042=CARTESIAN_POINT('Ctrl Pts',(-1.00885353244335,2.14648843755949,3.66859617423334));
#61043=CARTESIAN_POINT('Ctrl Pts',(-1.08070252816821,2.11271927678919,3.67391487956832));
#61044=CARTESIAN_POINT('Ctrl Pts',(-1.15090598621153,2.07531434119648,3.6792335849033));
#61045=CARTESIAN_POINT('Ctrl Pts',(-1.21907816342561,2.03446467011813,3.68455229023828));
#61046=CARTESIAN_POINT('Ctrl Pts',(-1.28722879887042,1.99362790715309,3.68986931491221));
#61047=CARTESIAN_POINT('Ctrl Pts',(-1.35334902700049,1.94934881074585,3.69518633958615));
#61048=CARTESIAN_POINT('Ctrl Pts',(-1.41707878848044,1.90186376213934,3.70050336426008));
#61049=CARTESIAN_POINT('Ctrl Pts',(-1.48080818238509,1.8543789874132,3.70582035826691));
#61050=CARTESIAN_POINT('Ctrl Pts',(-1.5421467626551,1.80368857806275,3.71113735227374));
#61051=CARTESIAN_POINT('Ctrl Pts',(-1.60076569226688,1.75007064456305,3.71645434628057));
#61052=CARTESIAN_POINT('Ctrl Pts',(-1.65944262862038,1.69639965308975,3.72177660175328));
#61053=CARTESIAN_POINT('Ctrl Pts',(-1.71539419253147,1.63979566751615,3.72709885722599));
#61054=CARTESIAN_POINT('Ctrl Pts',(-1.76832720191574,1.58057488575039,3.7324211126987));
#61055=CARTESIAN_POINT('Ctrl Pts',(-1.82128590204025,1.52132536150921,3.73774595129836));
#61056=CARTESIAN_POINT('Ctrl Pts',(-1.871222834753,1.45945687557879,3.74307078989801));
#61057=CARTESIAN_POINT('Ctrl Pts',(-1.91788568716399,1.3953180832597,3.74839562849767));
#61058=CARTESIAN_POINT('Ctrl Pts',(-1.96463159567272,1.33106512908532,3.75372994487874));
#61059=CARTESIAN_POINT('Ctrl Pts',(-2.00809152353448,1.26453418719018,3.75906426125981));
#61060=CARTESIAN_POINT('Ctrl Pts',(-2.04805714423203,1.19610200085951,3.76439857764088));
#61061=CARTESIAN_POINT('Ctrl Pts',(-2.08360649914073,1.13523168190572,3.76914344342592));
#61062=CARTESIAN_POINT('Ctrl Pts',(-2.11639168839733,1.0728576543847,3.77388830921096));
#61063=CARTESIAN_POINT('Ctrl Pts',(-2.14629811463882,1.00925837405387,3.77863317499601));
#61064=CARTESIAN_POINT('Ctrl Pts',(-2.18263941226135,0.931974637226914,
3.7843989785822));
#61065=CARTESIAN_POINT('Ctrl Pts',(-2.21484794111681,0.85262973882922,3.79016478216839));
#61066=CARTESIAN_POINT('Ctrl Pts',(-2.24270515369829,0.771668099687384,
3.79593058575458));
#61067=CARTESIAN_POINT('Ctrl Pts',(-2.27049771914493,0.690894345029207,
3.80168300886773));
#61068=CARTESIAN_POINT('Ctrl Pts',(-2.29395896027847,0.608511644250268,
3.80743543198088));
#61069=CARTESIAN_POINT('Ctrl Pts',(-2.31291772532025,0.524985388748469,
3.81318785509404));
#61070=CARTESIAN_POINT('Ctrl Pts',(-2.33181254437535,0.441740858813186,
3.81892087586896));
#61071=CARTESIAN_POINT('Ctrl Pts',(-2.34623506616155,0.357360794564243,
3.82465389664388));
#61072=CARTESIAN_POINT('Ctrl Pts',(-2.35606389049652,0.27232518502411,3.8303869174188));
#61073=CARTESIAN_POINT('Ctrl Pts',(-2.35988509236819,0.239265459948207,
3.83261577297353));
#61074=CARTESIAN_POINT('Ctrl Pts',(-2.36301250100132,0.206106832811691,
3.83484462852826));
#61075=CARTESIAN_POINT('Ctrl Pts',(-2.36544101854889,0.172878137039867,
3.83707348408299));
#61076=CARTESIAN_POINT('Ctrl Pts',(-2.36906969114779,0.173130678776576,
2.83701751404115));
#61077=CARTESIAN_POINT('Ctrl Pts',(-2.37304267803412,0.116029833869745,
2.8408749733291));
#61078=CARTESIAN_POINT('Ctrl Pts',(-2.37479248963291,0.0587544673927994,
2.84473243261706));
#61079=CARTESIAN_POINT('Ctrl Pts',(-2.37437841508221,0.00145143062880148,
2.84858989190502));
#61080=CARTESIAN_POINT('',(-2.37174914026029,-0.00201944907760664,2.65179578499715));
#61081=CARTESIAN_POINT('Ctrl Pts',(-2.36544104518992,0.172877772518167,
2.63906222572513));
#61082=CARTESIAN_POINT('Ctrl Pts',(-2.36969278946239,0.114702275059686,
2.64328523019093));
#61083=CARTESIAN_POINT('Ctrl Pts',(-2.37179885119879,0.0563637395522385,
2.6475390334268));
#61084=CARTESIAN_POINT('Ctrl Pts',(-2.3717491402603,-0.00201944906437184,
2.65179578499619));
#61085=CARTESIAN_POINT('Ctrl Pts',(-2.37174913936198,-0.00202050382956093,
2.65179586189972));
#61086=CARTESIAN_POINT('Ctrl Pts',(-2.37166453571845,-0.101331683442273,
2.65903669660693));
#61087=CARTESIAN_POINT('Ctrl Pts',(-2.36534239168155,-0.200547931638166,
2.66627265898347));
#61088=CARTESIAN_POINT('Ctrl Pts',(-2.34848290809305,-0.333177612601596,
2.67575133944222));
#61089=CARTESIAN_POINT('Ctrl Pts',(-2.34340804703312,-0.36717611268781,
2.6781632165284));
#61090=CARTESIAN_POINT('Ctrl Pts',(-2.33568000408453,-0.412219996206787,
2.68132484123119));
#61091=CARTESIAN_POINT('Ctrl Pts',(-2.33368430366111,-0.423372164611656,
2.68210483314665));
#61092=CARTESIAN_POINT('Ctrl Pts',(-2.33007339056013,-0.442748563509511,
2.68345470913304));
#61093=CARTESIAN_POINT('Ctrl Pts',(-2.32849437259453,-0.4509792212025,2.68402642878467));
#61094=CARTESIAN_POINT('Ctrl Pts',(-2.325242245973,-0.467458439313042,2.68516751588963));
#61095=CARTESIAN_POINT('Ctrl Pts',(-2.32356879468021,-0.475706800675879,
2.68573683866824));
#61096=CARTESIAN_POINT('Ctrl Pts',(-2.31989725724312,-0.493321898956267,
2.68694862933164));
#61097=CARTESIAN_POINT('Ctrl Pts',(-2.31788631035481,-0.502685627807307,
2.68759038368554));
#61098=CARTESIAN_POINT('Ctrl Pts',(-2.31220975293191,-0.528359308527758,
2.6893440006925));
#61099=CARTESIAN_POINT('Ctrl Pts',(-2.30842826483674,-0.544643447591906,
2.69044965248019));
#61100=CARTESIAN_POINT('Ctrl Pts',(-2.28536479591067,-0.639402644780134,
2.69685211272984));
#61101=CARTESIAN_POINT('Ctrl Pts',(-2.26225242380764,-0.716899442474599,
2.70196271518307));
#61102=CARTESIAN_POINT('Ctrl Pts',(-2.19733986671101,-0.899851464508593,
2.71404999186243));
#61103=CARTESIAN_POINT('Ctrl Pts',(-2.15185054296296,-1.00378074622129,
2.72094008662029));
#61104=CARTESIAN_POINT('Ctrl Pts',(-2.04284984697178,-1.21101896549969,
2.73538850854864));
#61105=CARTESIAN_POINT('Ctrl Pts',(-1.9785088706946,-1.31350667611797,2.74294251414993));
#61106=CARTESIAN_POINT('Ctrl Pts',(-1.89047562978078,-1.43249399692652,
2.75254888714955));
#61107=CARTESIAN_POINT('Ctrl Pts',(-1.87393209068782,-1.45406862974567,
2.75432655394988));
#61108=CARTESIAN_POINT('Ctrl Pts',(-1.84665564650964,-1.48840138863509,
2.75721695251851));
#61109=CARTESIAN_POINT('Ctrl Pts',(-1.8361524018056,-1.50133943671476,2.75832069538014));
#61110=CARTESIAN_POINT('Ctrl Pts',(-1.8160173654448,-1.52561471568281,2.76041996748123));
#61111=CARTESIAN_POINT('Ctrl Pts',(-1.80641351121026,-1.53697415127627,
2.76141434622753));
#61112=CARTESIAN_POINT('Ctrl Pts',(-1.78430657918546,-1.56262879548297,
2.76368817914601));
#61113=CARTESIAN_POINT('Ctrl Pts',(-1.77173751121983,-1.57686552258463,
2.76497028855934));
#61114=CARTESIAN_POINT('Ctrl Pts',(-1.73834562075071,-1.61378455068332,
2.76834964052941));
#61115=CARTESIAN_POINT('Ctrl Pts',(-1.71725027135635,-1.63621435832771,
2.77045807458388));
#61116=CARTESIAN_POINT('Ctrl Pts',(-1.58060609254344,-1.77594858184031,
2.78395602370275));
#61117=CARTESIAN_POINT('Ctrl Pts',(-1.45356019928084,-1.88134368605657,
2.79584863206657));
#61118=CARTESIAN_POINT('Ctrl Pts',(-1.2058179797959,-2.04669431722735,2.81756344679459));
#61119=CARTESIAN_POINT('Ctrl Pts',(-1.08893579591564,-2.11120345832247,
2.82729705161046));
#61120=CARTESIAN_POINT('Ctrl Pts',(-0.948629568679176,-2.17387111707438,
2.83800288245232));
#61121=CARTESIAN_POINT('Ctrl Pts',(-0.929907749476828,-2.1819453105832,
2.83941201723572));
#61122=CARTESIAN_POINT('Ctrl Pts',(-0.901627251860468,-2.19371175379784,
2.84150918321944));
#61123=CARTESIAN_POINT('Ctrl Pts',(-0.892145509892006,-2.1975848923158,
2.84220706046038));
#61124=CARTESIAN_POINT('Ctrl Pts',(-0.874904986726808,-2.20449739237499,
2.84346612342719));
#61125=CARTESIAN_POINT('Ctrl Pts',(-0.867155050661275,-2.20755738583396,
2.84402846474413));
#61126=CARTESIAN_POINT('Ctrl Pts',(-0.849557506330287,-2.21439864687001,
2.8452972231283));
#61127=CARTESIAN_POINT('Ctrl Pts',(-0.839700636960674,-2.21815512860845,
2.8460021995197));
#61128=CARTESIAN_POINT('Ctrl Pts',(-0.809246984323049,-2.22952901128098,
2.84816375918392));
#61129=CARTESIAN_POINT('Ctrl Pts',(-0.788568558226539,-2.23692646416329,
2.84960830611528));
#61130=CARTESIAN_POINT('Ctrl Pts',(-0.629834987532405,-2.29123663097842,
2.86054242576756));
#61131=CARTESIAN_POINT('Ctrl Pts',(-0.487802681198767,-2.32562191554701,
2.86945081499974));
#61132=CARTESIAN_POINT('Ctrl Pts',(-0.185556086462792,-2.36986208987159,
2.88820972579896));
#61133=CARTESIAN_POINT('Ctrl Pts',(-0.0257068585975406,-2.37697456937508,
2.8980371786083));
#61134=CARTESIAN_POINT('Ctrl Pts',(0.162007784731706,-2.36638101001443,
2.91023067338174));
#61135=CARTESIAN_POINT('Ctrl Pts',(0.190347867848262,-2.36427011674935,
2.9120880442439));
#61136=CARTESIAN_POINT('Ctrl Pts',(0.235259078202485,-2.36011222500127,
2.91506095313287));
#61137=CARTESIAN_POINT('Ctrl Pts',(0.25185885337257,-2.35839853349126,2.91616618794845));
#61138=CARTESIAN_POINT('Ctrl Pts',(0.283214153234367,-2.35482673446843,
2.91826664366234));
#61139=CARTESIAN_POINT('Ctrl Pts',(0.29797304011469,-2.35300472932154,2.91926069643645));
#61140=CARTESIAN_POINT('Ctrl Pts',(0.331499227975257,-2.3485453945005,2.92153146857095));
#61141=CARTESIAN_POINT('Ctrl Pts',(0.350253812158593,-2.34582169813812,
2.92281081636011));
#61142=CARTESIAN_POINT('Ctrl Pts',(0.39925165192219,-2.33810515132208,2.92617785743884));
#61143=CARTESIAN_POINT('Ctrl Pts',(0.429433456606923,-2.33275038018007,
2.92827660984285));
#61144=CARTESIAN_POINT('Ctrl Pts',(0.624031994540121,-2.2943208159619,2.94197405122998));
#61145=CARTESIAN_POINT('Ctrl Pts',(0.784624612047842,-2.24447534336406,
2.95409702900155));
#61146=CARTESIAN_POINT('Ctrl Pts',(1.05843989599386,-2.12648399221279,2.97583526038778));
#61147=CARTESIAN_POINT('Ctrl Pts',(1.1738338386256,-2.06503019974873,2.98535973460226));
#61148=CARTESIAN_POINT('Ctrl Pts',(1.30071312692411,-1.98337033561466,2.99587157269382));
#61149=CARTESIAN_POINT('Ctrl Pts',(1.3176905062577,-1.9721319238037,2.99727869131485));
#61150=CARTESIAN_POINT('Ctrl Pts',(1.34298384387888,-1.95491617169873,2.99937347463077));
#61151=CARTESIAN_POINT('Ctrl Pts',(1.351408756389,-1.94910164592195,3.00007095353421));
#61152=CARTESIAN_POINT('Ctrl Pts',(1.36662289829965,-1.93845540195784,3.00132962642542));
#61153=CARTESIAN_POINT('Ctrl Pts',(1.37342451441274,-1.93364231427944,3.00189197182804));
#61154=CARTESIAN_POINT('Ctrl Pts',(1.38878412204666,-1.92265132524841,3.00316114727992));
#61155=CARTESIAN_POINT('Ctrl Pts',(1.39732638564255,-1.91645204442879,3.00386653217528));
#61156=CARTESIAN_POINT('Ctrl Pts',(1.42353998628357,-1.89715989004291,3.00603066029356));
#61157=CARTESIAN_POINT('Ctrl Pts',(1.44107138510319,-1.88387767321635,3.00747732587617));
#61158=CARTESIAN_POINT('Ctrl Pts',(1.57255892680883,-1.78134966314566,3.01834376197554));
#61159=CARTESIAN_POINT('Ctrl Pts',(1.67833030230401,-1.68207215486069,3.02719118274639));
#61160=CARTESIAN_POINT('Ctrl Pts',(1.88102388917087,-1.45353674525177,3.04595007909564));
#61161=CARTESIAN_POINT('Ctrl Pts',(1.97514295908593,-1.3228082725533,3.05583942088915));
#61162=CARTESIAN_POINT('Ctrl Pts',(2.06948631094064,-1.15897813553268,3.06810070947339));
#61163=CARTESIAN_POINT('Ctrl Pts',(2.08320923435577,-1.13412657359018,3.06995617130182));
#61164=CARTESIAN_POINT('Ctrl Pts',(2.10428269235227,-1.09429003822757,3.07292673732268));
#61165=CARTESIAN_POINT('Ctrl Pts',(2.11192707352632,-1.07946299128262,3.07403156693486));
#61166=CARTESIAN_POINT('Ctrl Pts',(2.12608954213736,-1.05126709186429,3.07613169967825));
#61167=CARTESIAN_POINT('Ctrl Pts',(2.13263955064154,-1.03791510709839,3.07712583946221));
#61168=CARTESIAN_POINT('Ctrl Pts',(2.14725422183462,-1.00740107335586,3.07939743601935));
#61169=CARTESIAN_POINT('Ctrl Pts',(2.15523941853019,-0.990202317078247,
3.08067752845397));
#61170=CARTESIAN_POINT('Ctrl Pts',(2.17560613224354,-0.944922125510865,
3.08404788834286));
#61171=CARTESIAN_POINT('Ctrl Pts',(2.18764998694002,-0.916693650963465,
3.08614925053638));
#61172=CARTESIAN_POINT('Ctrl Pts',(2.26166578770966,-0.733442301421913,
3.09979731541105));
#61173=CARTESIAN_POINT('Ctrl Pts',(2.30765989744538,-0.572500818307961,
3.11186297917274));
#61174=CARTESIAN_POINT('Ctrl Pts',(2.35904897518861,-0.278295532692503,
3.13363767897881));
#61175=CARTESIAN_POINT('Ctrl Pts',(2.37086724139451,-0.146818167714574,
3.14325649730304));
#61176=CARTESIAN_POINT('Ctrl Pts',(2.37182913393468,0.00497294922744031,
3.15382687299924));
#61177=CARTESIAN_POINT('Ctrl Pts',(2.37170284630969,0.0249768833519108,
3.15520892442808));
#61178=CARTESIAN_POINT('Ctrl Pts',(2.37113071400462,0.0551410130007561,
3.1572740696992));
#61179=CARTESIAN_POINT('Ctrl Pts',(2.37087259952802,0.0653032963990511,
3.15796658518657));
#61180=CARTESIAN_POINT('Ctrl Pts',(2.37028393970051,0.0837948958401544,
3.15922045115297));
#61181=CARTESIAN_POINT('Ctrl Pts',(2.36997482015665,0.0921243492102253,
3.15978290072399));
#61182=CARTESIAN_POINT('Ctrl Pts',(2.36917134274281,0.111077975085575,3.16105750119646));
#61183=CARTESIAN_POINT('Ctrl Pts',(2.36864943261805,0.121700632243204,3.16176814951743));
#61184=CARTESIAN_POINT('Ctrl Pts',(2.36680530349489,0.154704048760214,3.16396552482737));
#61185=CARTESIAN_POINT('Ctrl Pts',(2.36523715385412,0.177070555720267,3.16543963335945));
#61186=CARTESIAN_POINT('Ctrl Pts',(2.35150418927784,0.339827858317348,3.17607853896595));
#61187=CARTESIAN_POINT('Ctrl Pts',(2.32716438876703,0.478927133189543,3.18470459370553));
#61188=CARTESIAN_POINT('Ctrl Pts',(2.2479750258018,0.773846644428364,3.20345668953966));
#61189=CARTESIAN_POINT('Ctrl Pts',(2.18894875000501,0.927752632783989,3.21356258072216));
#61190=CARTESIAN_POINT('Ctrl Pts',(2.10176293994524,1.09935423735365,3.22604993979178));
#61191=CARTESIAN_POINT('Ctrl Pts',(2.0885951057883,1.12416972540307,3.22788648813877));
#61192=CARTESIAN_POINT('Ctrl Pts',(2.06694085704888,1.16328403187454,3.23083384157158));
#61193=CARTESIAN_POINT('Ctrl Pts',(2.05873923588458,1.17773807809033,3.23193465391899));
#61194=CARTESIAN_POINT('Ctrl Pts',(2.04290556004708,1.20497156127583,3.23403162470707));
#61195=CARTESIAN_POINT('Ctrl Pts',(2.03530374886283,1.21776772147098,3.2350266674232));
#61196=CARTESIAN_POINT('Ctrl Pts',(2.01768799607393,1.24679465369323,3.23730663709432));
#61197=CARTESIAN_POINT('Ctrl Pts',(2.00759782214453,1.26297771398559,3.23859427303348));
#61198=CARTESIAN_POINT('Ctrl Pts',(1.98055987773673,1.30519952862996,3.24199832377279));
#61199=CARTESIAN_POINT('Ctrl Pts',(1.96329420080058,1.33102928724237,3.24412619804061));
#61200=CARTESIAN_POINT('Ctrl Pts',(1.85625475913446,1.48454668379774,3.25705502584972));
#61201=CARTESIAN_POINT('Ctrl Pts',(1.75457638646392,1.60343600905729,3.26830255431575));
#61202=CARTESIAN_POINT('Ctrl Pts',(1.5401057842388,1.80919968824234,3.28996226398094));
#61203=CARTESIAN_POINT('Ctrl Pts',(1.42969920166433,1.89765552071005,3.30029993218363));
#61204=CARTESIAN_POINT('Ctrl Pts',(1.2950196791271,1.98709362431834,3.31156470294395));
#61205=CARTESIAN_POINT('Ctrl Pts',(1.27782155411741,1.99819648344215,3.31297961613056));
#61206=CARTESIAN_POINT('Ctrl Pts',(1.25179156430458,2.01452753091751,3.31508360477274));
#61207=CARTESIAN_POINT('Ctrl Pts',(1.24306650281883,2.0199230115549,3.31578261789045));
#61208=CARTESIAN_POINT('Ctrl Pts',(1.22719193146805,2.02959785280089,3.3170427924258));
#61209=CARTESIAN_POINT('Ctrl Pts',(1.22005466474621,2.03389628563111,3.31760512136554));
#61210=CARTESIAN_POINT('Ctrl Pts',(1.20384546618367,2.04354227760208,3.31887268921134));
#61211=CARTESIAN_POINT('Ctrl Pts',(1.19476042414047,2.04886712261145,3.31957650018949));
#61212=CARTESIAN_POINT('Ctrl Pts',(1.16670220549042,2.0650622630127,3.32173074617748));
#61213=CARTESIAN_POINT('Ctrl Pts',(1.14761332809395,2.07573117669822,3.32316926201546));
#61214=CARTESIAN_POINT('Ctrl Pts',(0.999959514516119,2.15559630259737,3.33411135948907));
#61215=CARTESIAN_POINT('Ctrl Pts',(0.865382772913855,2.21306088995876,3.34303140298237));
#61216=CARTESIAN_POINT('Ctrl Pts',(0.578911483076773,2.30522248790353,3.36151177117991));
#61217=CARTESIAN_POINT('Ctrl Pts',(0.427189429310361,2.33809554939542,3.37104601028774));
#61218=CARTESIAN_POINT('Ctrl Pts',(0.242538495689467,2.3595202049885,3.38307070299426));
#61219=CARTESIAN_POINT('Ctrl Pts',(0.211655769213763,2.36249067973927,3.38509442718464));
#61220=CARTESIAN_POINT('Ctrl Pts',(0.163539723890257,2.36616776072085,3.38827136197865));
#61221=CARTESIAN_POINT('Ctrl Pts',(0.146341258491917,2.36729367067556,3.38941164375629));
#61222=CARTESIAN_POINT('Ctrl Pts',(0.114346405112707,2.36903825177073,3.39154244233865));
#61223=CARTESIAN_POINT('Ctrl Pts',(0.0995534574451802,2.3697059798536,3.39253139279111));
#61224=CARTESIAN_POINT('Ctrl Pts',(0.0666083012848616,2.37088404162967,
3.39474270413428));
#61225=CARTESIAN_POINT('Ctrl Pts',(0.0484546893818588,2.37132450673931,
3.39596716048946));
#61226=CARTESIAN_POINT('Ctrl Pts',(0.00235233804396185,2.37191349537953,
3.39909264994207));
#61227=CARTESIAN_POINT('Ctrl Pts',(-0.0255966113182181,2.37177652030432,
3.40100229129329));
#61228=CARTESIAN_POINT('Ctrl Pts',(-0.249432814631122,2.36672275643254,
3.41642052159575));
#61229=CARTESIAN_POINT('Ctrl Pts',(-0.443993706923091,2.3380405970847,3.43067946292181));
#61230=CARTESIAN_POINT('Ctrl Pts',(-0.732052942945985,2.2582979636334,3.45245168288398));
#61231=CARTESIAN_POINT('Ctrl Pts',(-0.829452489929389,2.22437042359602,
3.45991648798485));
#61232=CARTESIAN_POINT('Ctrl Pts',(-0.945693140785667,2.1751781375895,3.46873928221864));
#61233=CARTESIAN_POINT('Ctrl Pts',(-0.966909089703273,2.1658306392081,3.47034570740838));
#61234=CARTESIAN_POINT('Ctrl Pts',(-0.997783078708247,2.15168379109401,
3.4726742153637));
#61235=CARTESIAN_POINT('Ctrl Pts',(-1.00755016112144,2.14712759123717,3.47340947806434));
#61236=CARTESIAN_POINT('Ctrl Pts',(-1.0241030810991,2.13926807345349,3.47465282699743));
#61237=CARTESIAN_POINT('Ctrl Pts',(-1.03090464680746,2.1359987420046,3.47516290530994));
#61238=CARTESIAN_POINT('Ctrl Pts',(-1.04641282702203,2.12845303962702,3.47632400736059));
#61239=CARTESIAN_POINT('Ctrl Pts',(-1.0551089413061,2.12415566206872,3.47697374399987));
#61240=CARTESIAN_POINT('Ctrl Pts',(-1.07920848677103,2.112061822259,3.47877128973083));
#61241=CARTESIAN_POINT('Ctrl Pts',(-1.09455388052996,2.10415017137319,3.47991236933233));
#61242=CARTESIAN_POINT('Ctrl Pts',(-1.21170642635877,2.04212112591012,3.48860725875878));
#61243=CARTESIAN_POINT('Ctrl Pts',(-1.30954532108287,1.98080519080484,3.49577605428415));
#61244=CARTESIAN_POINT('Ctrl Pts',(-1.47464001851495,1.8597385624952,3.50838902616582));
#61245=CARTESIAN_POINT('Ctrl Pts',(-1.54368698249952,1.8028369606035,3.51384799308044));
#61246=CARTESIAN_POINT('Ctrl Pts',(-1.66380590988287,1.69187546378425,3.52396621626858));
#61247=CARTESIAN_POINT('Ctrl Pts',(-1.71586372671038,1.63905556964233,3.52859646960668));
#61248=CARTESIAN_POINT('Ctrl Pts',(-1.79880521309339,1.54661112068368,3.53650843350266));
#61249=CARTESIAN_POINT('Ctrl Pts',(-1.83105878846296,1.50828687827062,3.53973800000726));
#61250=CARTESIAN_POINT('Ctrl Pts',(-1.87488154557976,1.45273703382052,3.54436915877928));
#61251=CARTESIAN_POINT('Ctrl Pts',(-1.88747634768317,1.43633516010049,3.54573063422613));
#61252=CARTESIAN_POINT('Ctrl Pts',(-1.90890230195197,1.40766419983463,3.54810160937212));
#61253=CARTESIAN_POINT('Ctrl Pts',(-1.91783373911453,1.39547132869362,3.5491071812765));
#61254=CARTESIAN_POINT('Ctrl Pts',(-1.93593151511913,1.37026297948856,3.55118108078306));
#61255=CARTESIAN_POINT('Ctrl Pts',(-1.9450845494038,1.35723893944155,3.55224984412771));
#61256=CARTESIAN_POINT('Ctrl Pts',(-1.96815724513777,1.32369554359574,3.55499608475645));
#61257=CARTESIAN_POINT('Ctrl Pts',(-1.98188720607198,1.30304867751405,3.55668049550362));
#61258=CARTESIAN_POINT('Ctrl Pts',(-2.03744874723032,1.21658619620018,3.56371224121628));
#61259=CARTESIAN_POINT('Ctrl Pts',(-2.0763412523535,1.14894910766037,3.5691631557414));
#61260=CARTESIAN_POINT('Ctrl Pts',(-2.19383857373315,0.919094233418538,
3.58752407035314));
#61261=CARTESIAN_POINT('Ctrl Pts',(-2.2572960728765,0.749843854805076,3.60083851056522));
#61262=CARTESIAN_POINT('Ctrl Pts',(-2.31162296755825,0.532471099831156,
3.6169654277794));
#61263=CARTESIAN_POINT('Ctrl Pts',(-2.32108540255774,0.489580652901819,
3.62009898901766));
#61264=CARTESIAN_POINT('Ctrl Pts',(-2.33483045129457,0.417865870720783,
3.62523409357893));
#61265=CARTESIAN_POINT('Ctrl Pts',(-2.33978264259073,0.389181826825073,
3.62726054756144));
#61266=CARTESIAN_POINT('Ctrl Pts',(-2.34599674811093,0.348763839767802,
3.63007101161806));
#61267=CARTESIAN_POINT('Ctrl Pts',(-2.34770086165767,0.337101819498761,
3.63087669578817));
#61268=CARTESIAN_POINT('Ctrl Pts',(-2.35047841630775,0.317050153393801,
3.63225245957036));
#61269=CARTESIAN_POINT('Ctrl Pts',(-2.35159402653814,0.308666695474465,
3.6328247911001));
#61270=CARTESIAN_POINT('Ctrl Pts',(-2.35385932033755,0.290918165297765,
3.63403024016599));
#61271=CARTESIAN_POINT('Ctrl Pts',(-2.35499799602778,0.281551993777993,
3.6346627613146));
#61272=CARTESIAN_POINT('Ctrl Pts',(-2.3579749418256,0.255782471514389,3.63639373260987));
#61273=CARTESIAN_POINT('Ctrl Pts',(-2.35969796028263,0.239365980109384,
3.63748609457126));
#61274=CARTESIAN_POINT('Ctrl Pts',(-2.36282343523366,0.206261639698165,
3.63967045633817));
#61275=CARTESIAN_POINT('Ctrl Pts',(-2.36422065732617,0.189575983256105,
3.64076204671802));
#61276=CARTESIAN_POINT('Ctrl Pts',(-2.36544101877862,0.172878133896551,
3.6418462952528));
#61277=CARTESIAN_POINT('Origin',(0.,0.,-1.84858989190501));
#61278=CARTESIAN_POINT('',(-2.36544099470095,0.17287846334401,4.83774038296924));
#61279=CARTESIAN_POINT('',(-2.36544101871062,0.172878134827039,4.63810474394384));
#61280=CARTESIAN_POINT('',(-2.36544101854889,0.172878137039864,-1.84858989190501));
#61281=CARTESIAN_POINT('',(-2.37174988974127,0.00072227238077198,3.84873773164287));
#61282=CARTESIAN_POINT('Ctrl Pts',(-2.36544099470095,0.17287846334401,4.83774038296924));
#61283=CARTESIAN_POINT('Ctrl Pts',(-2.35845789403178,0.268426007401591,
4.83181080292367));
#61284=CARTESIAN_POINT('Ctrl Pts',(-2.34568866385242,0.36351075498014,4.82580135690754));
#61285=CARTESIAN_POINT('Ctrl Pts',(-2.3212245766169,0.487922993545994,4.81762457349267));
#61286=CARTESIAN_POINT('Ctrl Pts',(-2.3146727700282,0.518114090840626,4.81561589105462));
#61287=CARTESIAN_POINT('Ctrl Pts',(-2.30323476294297,0.566262842874677,
4.8123685283912));
#61288=CARTESIAN_POINT('Ctrl Pts',(-2.29872352692894,0.584306507532516,
4.81114161496601));
#61289=CARTESIAN_POINT('Ctrl Pts',(-2.2902983252808,0.616396136938661,4.80894087874079));
#61290=CARTESIAN_POINT('Ctrl Pts',(-2.28646612701277,0.630462727196739,
4.80796970529589));
#61291=CARTESIAN_POINT('Ctrl Pts',(-2.27813325548061,0.659974020912009,
4.80591813255358));
#61292=CARTESIAN_POINT('Ctrl Pts',(-2.27360465954054,0.675410000111424,
4.80483687897286));
#61293=CARTESIAN_POINT('Ctrl Pts',(-2.26114186226874,0.716343916098403,
4.80194716149905));
#61294=CARTESIAN_POINT('Ctrl Pts',(-2.25293365914112,0.741755319964089,
4.80012995772897));
#61295=CARTESIAN_POINT('Ctrl Pts',(-2.20495541253557,0.882139200335281,
4.78995695452051));
#61296=CARTESIAN_POINT('Ctrl Pts',(-2.15681995077656,0.994040958670789,
4.7813307000172));
#61297=CARTESIAN_POINT('Ctrl Pts',(-2.07968406714421,1.14108999831635,4.76932471665483));
#61298=CARTESIAN_POINT('Ctrl Pts',(-2.05794337717007,1.1798479103429,4.76609389117295));
#61299=CARTESIAN_POINT('Ctrl Pts',(-1.96198624137587,1.34018417860742,4.75247721082198));
#61300=CARTESIAN_POINT('Ctrl Pts',(-1.87797948599761,1.45556974013896,4.74203532983824));
#61301=CARTESIAN_POINT('Ctrl Pts',(-1.76969488421872,1.57919516943305,4.73056032611397));
#61302=CARTESIAN_POINT('Ctrl Pts',(-1.75504178266853,1.59546413041297,4.72904433915943));
#61303=CARTESIAN_POINT('Ctrl Pts',(-1.73299980593201,1.6192655540833,4.72682058500436));
#61304=CARTESIAN_POINT('Ctrl Pts',(-1.72578304381654,1.62695487282724,4.72610124638695));
#61305=CARTESIAN_POINT('Ctrl Pts',(-1.71289563352824,1.64050391429979,4.72483247642879));
#61306=CARTESIAN_POINT('Ctrl Pts',(-1.70724576759697,1.64638283513615,4.72428155819449));
#61307=CARTESIAN_POINT('Ctrl Pts',(-1.69474901234744,1.65925272050383,4.72307466066358));
#61308=CARTESIAN_POINT('Ctrl Pts',(-1.68788907825854,1.66623055826905,4.72241968954665));
#61309=CARTESIAN_POINT('Ctrl Pts',(-1.66773234870903,1.68648149715284,4.72051631798583));
#61310=CARTESIAN_POINT('Ctrl Pts',(-1.65432043859211,1.6996396580964,4.7192763805575));
#61311=CARTESIAN_POINT('Ctrl Pts',(-1.62302745897077,1.72961917868486,4.71643972880632));
#61312=CARTESIAN_POINT('Ctrl Pts',(-1.60503852439135,1.74632530506812,4.71485032134242));
#61313=CARTESIAN_POINT('Ctrl Pts',(-1.54207755816471,1.80300152926619,4.70941422412766));
#61314=CARTESIAN_POINT('Ctrl Pts',(-1.49584391310177,1.84154002401672,4.70563968335683));
#61315=CARTESIAN_POINT('Ctrl Pts',(-1.33032824362677,1.96915589106222,4.69266465441261));
#61316=CARTESIAN_POINT('Ctrl Pts',(-1.20417405850344,2.04873471784786,4.68367366123366));
#61317=CARTESIAN_POINT('Ctrl Pts',(-0.997149374780716,2.15355901505117,
4.66917485786519));
#61318=CARTESIAN_POINT('Ctrl Pts',(-0.920986004189636,2.18721418513263,
4.66389425793215));
#61319=CARTESIAN_POINT('Ctrl Pts',(-0.819666053969448,2.22575392393162,
4.65684065919758));
#61320=CARTESIAN_POINT('Ctrl Pts',(-0.795974413765612,2.23433605887255,
4.65518957553623));
#61321=CARTESIAN_POINT('Ctrl Pts',(-0.757244906739538,2.24767140747357,
4.65248539432111));
#61322=CARTESIAN_POINT('Ctrl Pts',(-0.742288066988935,2.25265510237962,
4.65143985887729));
#61323=CARTESIAN_POINT('Ctrl Pts',(-0.713311807731035,2.26199022530392,
4.64941143401917));
#61324=CARTESIAN_POINT('Ctrl Pts',(-0.699299456547478,2.26636134982266,
4.6484292378752));
#61325=CARTESIAN_POINT('Ctrl Pts',(-0.66646102967369,2.27627169782476,4.64612398009258));
#61326=CARTESIAN_POINT('Ctrl Pts',(-0.647605222470179,2.28170782143175,
4.64479766855683));
#61327=CARTESIAN_POINT('Ctrl Pts',(-0.585148346867495,2.29887757887209,
4.64039465720854));
#61328=CARTESIAN_POINT('Ctrl Pts',(-0.541281944014829,2.30959955213128,
4.63728630136688));
#61329=CARTESIAN_POINT('Ctrl Pts',(-0.43421692983303,2.33255113885727,4.62965689799795));
#61330=CARTESIAN_POINT('Ctrl Pts',(-0.370777175498944,2.34347226418801,
4.62509998918338));
#61331=CARTESIAN_POINT('Ctrl Pts',(-0.208562413869567,2.36464586969637,
4.61337272413455));
#61332=CARTESIAN_POINT('Ctrl Pts',(-0.10944417106953,2.37130096920578,4.60613354795731));
#61333=CARTESIAN_POINT('Ctrl Pts',(0.0159847305790551,2.37184075278795,
4.59698800652647));
#61334=CARTESIAN_POINT('Ctrl Pts',(0.0421764701777665,2.37151960445827,
4.59507948702687));
#61335=CARTESIAN_POINT('Ctrl Pts',(0.165502411761317,2.36796367281134,4.5861100154732));
#61336=CARTESIAN_POINT('Ctrl Pts',(0.262394352952177,2.35919400419603,4.57910899415974));
#61337=CARTESIAN_POINT('Ctrl Pts',(0.375150272313595,2.34195315826303,4.57119626828872));
#61338=CARTESIAN_POINT('Ctrl Pts',(0.391789525015507,2.33922707971141,4.57003476787374));
#61339=CARTESIAN_POINT('Ctrl Pts',(0.417738144042488,2.33469115576377,4.56823452908552));
#61340=CARTESIAN_POINT('Ctrl Pts',(0.427067751631594,2.33300259174809,4.56758951938854));
#61341=CARTESIAN_POINT('Ctrl Pts',(0.443633123965498,2.32990172694089,4.56644856285664));
#61342=CARTESIAN_POINT('Ctrl Pts',(0.450872536074295,2.32851161995794,4.56595143382581));
#61343=CARTESIAN_POINT('Ctrl Pts',(0.468406170674319,2.32505998503571,4.56475089698214));
#61344=CARTESIAN_POINT('Ctrl Pts',(0.478693345768431,2.32296383221399,4.56404942396354));
#61345=CARTESIAN_POINT('Ctrl Pts',(0.510921991991115,2.31617361652859,4.56185990680654));
#61346=CARTESIAN_POINT('Ctrl Pts',(0.532811705332697,2.31123630968462,4.56038462934856));
#61347=CARTESIAN_POINT('Ctrl Pts',(0.649570798466337,2.28315378937986,4.55256300541919));
#61348=CARTESIAN_POINT('Ctrl Pts',(0.743022769986403,2.25447440445754,4.54646917062328));
#61349=CARTESIAN_POINT('Ctrl Pts',(0.999996153721674,2.1578886009422,4.52952392502141));
#61350=CARTESIAN_POINT('Ctrl Pts',(1.15805291858275,2.07735061850423,4.51883506625677));
#61351=CARTESIAN_POINT('Ctrl Pts',(1.3448213058204,1.95418810934944,4.50456151357855));
#61352=CARTESIAN_POINT('Ctrl Pts',(1.38317938631754,1.92722853683288,4.5015357655861));
#61353=CARTESIAN_POINT('Ctrl Pts',(1.4354836397085,1.88810092727864,4.49726046696396));
#61354=CARTESIAN_POINT('Ctrl Pts',(1.4501258829477,1.87687860121356,4.49604668584982));
#61355=CARTESIAN_POINT('Ctrl Pts',(1.47532735031823,1.8570923664218,4.493927011705));
#61356=CARTESIAN_POINT('Ctrl Pts',(1.48594675019473,1.84860625625839,4.49302417787153));
#61357=CARTESIAN_POINT('Ctrl Pts',(1.50801167414376,1.83066089605524,4.4911275910862));
#61358=CARTESIAN_POINT('Ctrl Pts',(1.51944245696827,1.82118453994611,4.49013318180053));
#61359=CARTESIAN_POINT('Ctrl Pts',(1.54655385162029,1.7982757124639,4.48774558136999));
#61360=CARTESIAN_POINT('Ctrl Pts',(1.56214928487663,1.78474477708923,4.48634844001489));
#61361=CARTESIAN_POINT('Ctrl Pts',(1.61616741925779,1.73662701245878,4.48142377068412));
#61362=CARTESIAN_POINT('Ctrl Pts',(1.65363186088829,1.70099131893692,4.4778533197269));
#61363=CARTESIAN_POINT('Ctrl Pts',(1.74466797548432,1.60854726663301,4.46877142174846));
#61364=CARTESIAN_POINT('Ctrl Pts',(1.79665242060521,1.55026732056716,4.46320305573679));
#61365=CARTESIAN_POINT('Ctrl Pts',(1.90321196875481,1.41823067705923,4.45095103701813));
#61366=CARTESIAN_POINT('Ctrl Pts',(1.95657638519192,1.34365245889521,4.44425093270349));
#61367=CARTESIAN_POINT('Ctrl Pts',(2.06315775429619,1.17483885456498,4.42971264681733));
#61368=CARTESIAN_POINT('Ctrl Pts',(2.11452414790608,1.07965690774899,4.42190065623915));
#61369=CARTESIAN_POINT('Ctrl Pts',(2.16624008016026,0.965861972001209,4.41322864503305));
#61370=CARTESIAN_POINT('Ctrl Pts',(2.17308845319953,0.950353644228385,4.41206068155645));
#61371=CARTESIAN_POINT('Ctrl Pts',(2.18351497952661,0.926040319995402,4.410252626388));
#61372=CARTESIAN_POINT('Ctrl Pts',(2.18720733988164,0.917285342893548,4.40960617908199));
#61373=CARTESIAN_POINT('Ctrl Pts',(2.19366958342968,0.901701788512333,4.40846399769113));
#61374=CARTESIAN_POINT('Ctrl Pts',(2.19646030406429,0.894882389807685,4.40796706626231));
#61375=CARTESIAN_POINT('Ctrl Pts',(2.20313895757089,0.87834297525935,4.40676869411586));
#61376=CARTESIAN_POINT('Ctrl Pts',(2.20699437960985,0.868610077744394,4.40606916853241));
#61377=CARTESIAN_POINT('Ctrl Pts',(2.21885229884336,0.838086400145388,4.40389211388469));
#61378=CARTESIAN_POINT('Ctrl Pts',(2.22662666443721,0.817207514879115,4.40242714575856));
#61379=CARTESIAN_POINT('Ctrl Pts',(2.26637032313686,0.705691345979062,4.39471478986543));
#61380=CARTESIAN_POINT('Ctrl Pts',(2.29310583908683,0.613273512243121,4.38871220791078));
#61381=CARTESIAN_POINT('Ctrl Pts',(2.35190250016047,0.351347744039928,4.37213475522055));
#61382=CARTESIAN_POINT('Ctrl Pts',(2.37120780076013,0.179614940895584,4.36172154529799));
#61383=CARTESIAN_POINT('Ctrl Pts',(2.37189757378398,-0.0442382673390364,
4.3474844876419));
#61384=CARTESIAN_POINT('Ctrl Pts',(2.37037593223402,-0.0957729588965799,
4.3441651283401));
#61385=CARTESIAN_POINT('Ctrl Pts',(2.36586265613288,-0.168345491211155,
4.33941043632361));
#61386=CARTESIAN_POINT('Ctrl Pts',(2.36426566607077,-0.189457448937834,
4.33801769942444));
#61387=CARTESIAN_POINT('Ctrl Pts',(2.36107292456982,-0.225281150232464,
4.33563685937602));
#61388=CARTESIAN_POINT('Ctrl Pts',(2.35962171899245,-0.240004746497715,
4.33465327321344));
#61389=CARTESIAN_POINT('Ctrl Pts',(2.35639571671077,-0.269869746572138,
4.33264746229202));
#61390=CARTESIAN_POINT('Ctrl Pts',(2.35461249657588,-0.285009519575753,
4.33162502017097));
#61391=CARTESIAN_POINT('Ctrl Pts',(2.34981001686762,-0.322655494175157,
4.32906816008474));
#61392=CARTESIAN_POINT('Ctrl Pts',(2.34661330435842,-0.345137105172466,
4.32752829690175));
#61393=CARTESIAN_POINT('Ctrl Pts',(2.33262165099824,-0.434327955169522,
4.32136573094173));
#61394=CARTESIAN_POINT('Ctrl Pts',(2.31930156868292,-0.500602861913786,
4.31666584621332));
#61395=CARTESIAN_POINT('Ctrl Pts',(2.27466302471612,-0.682177886188146,
4.30344862022022));
#61396=CARTESIAN_POINT('Ctrl Pts',(2.23743948392025,-0.795812691469167,
4.29477952852381));
#61397=CARTESIAN_POINT('Ctrl Pts',(2.14255598133254,-1.02531973278421,4.2766692049156));
#61398=CARTESIAN_POINT('Ctrl Pts',(2.08364740383289,-1.14028333751504,4.26725119025549));
#61399=CARTESIAN_POINT('Ctrl Pts',(2.00377091230396,-1.26909839936587,4.25666283393892));
#61400=CARTESIAN_POINT('Ctrl Pts',(1.99158892105191,-1.28813131236185,4.2550977695728));
#61401=CARTESIAN_POINT('Ctrl Pts',(1.97333490729165,-1.31577286588697,4.25282716542868));
#61402=CARTESIAN_POINT('Ctrl Pts',(1.96747500355845,-1.32451916249002,4.25210905594809));
#61403=CARTESIAN_POINT('Ctrl Pts',(1.9569741758644,-1.33996888048981,4.25084159771245));
#61404=CARTESIAN_POINT('Ctrl Pts',(1.95235669777415,-1.34668773548087,4.25029077432447));
#61405=CARTESIAN_POINT('Ctrl Pts',(1.94211313216427,-1.36142963676411,4.24908306791377));
#61406=CARTESIAN_POINT('Ctrl Pts',(1.93647188904811,-1.36944174954849,4.24842720308254));
#61407=CARTESIAN_POINT('Ctrl Pts',(1.91983115396502,-1.39276770858054,4.2465185352256));
#61408=CARTESIAN_POINT('Ctrl Pts',(1.90869822401609,-1.40798604173824,4.24527426702636));
#61409=CARTESIAN_POINT('Ctrl Pts',(1.88258756946727,-1.44279946160086,4.24242604634609));
#61410=CARTESIAN_POINT('Ctrl Pts',(1.86748313310406,-1.46229719687333,4.24082948511135));
#61411=CARTESIAN_POINT('Ctrl Pts',(1.81422139748642,-1.52887907505249,4.23535892285664));
#61412=CARTESIAN_POINT('Ctrl Pts',(1.77456366399939,-1.57473657679957,4.23155805754317));
#61413=CARTESIAN_POINT('Ctrl Pts',(1.63120539536901,-1.72820351593248,4.21852356336183));
#61414=CARTESIAN_POINT('Ctrl Pts',(1.51913434336749,-1.82749832796879,4.20949822421794));
#61415=CARTESIAN_POINT('Ctrl Pts',(1.33209471739352,-1.96404548753282,4.19502204936909));
#61416=CARTESIAN_POINT('Ctrl Pts',(1.26325618140182,-2.00901286902285,4.18980526248348));
#61417=CARTESIAN_POINT('Ctrl Pts',(1.17052819686494,-2.06293284123708,4.18282489399736));
#61418=CARTESIAN_POINT('Ctrl Pts',(1.14863003527273,-2.07520532272388,4.1811799296383));
#61419=CARTESIAN_POINT('Ctrl Pts',(1.11268643216556,-2.09460613681363,4.17848324347907));
#61420=CARTESIAN_POINT('Ctrl Pts',(1.09875715505498,-2.10194639772447,4.17743900321718));
#61421=CARTESIAN_POINT('Ctrl Pts',(1.07169605474444,-2.1158641994673,4.17541132145039));
#61422=CARTESIAN_POINT('Ctrl Pts',(1.0585741576185,-2.12245953568389,4.17442855622038));
#61423=CARTESIAN_POINT('Ctrl Pts',(1.02773161935617,-2.13760447173287,4.17211921938208));
#61424=CARTESIAN_POINT('Ctrl Pts',(1.00996438650176,-2.14605616348765,4.17078936336591));
#61425=CARTESIAN_POINT('Ctrl Pts',(0.950800729540961,-2.17330229040582,
4.16636140601271));
#61426=CARTESIAN_POINT('Ctrl Pts',(0.908971334312819,-2.19112653675992,
4.16323115098714));
#61427=CARTESIAN_POINT('Ctrl Pts',(0.80618083444961,-2.23147745306819,4.15553523603898));
#61428=CARTESIAN_POINT('Ctrl Pts',(0.744758537213033,-2.25272116811427,
4.15093287237395));
#61429=CARTESIAN_POINT('Ctrl Pts',(0.58827374188585,-2.29974386013181,4.1392150810796));
#61430=CARTESIAN_POINT('Ctrl Pts',(0.492333892617951,-2.32217423507779,
4.13203464139189));
#61431=CARTESIAN_POINT('Ctrl Pts',(0.370267598890551,-2.34280679262582,
4.12300822057258));
#61432=CARTESIAN_POINT('Ctrl Pts',(0.34518477999019,-2.34663359917616,4.12115949797622));
#61433=CARTESIAN_POINT('Ctrl Pts',(0.223203318384627,-2.3632457835402,4.11220871919175));
#61434=CARTESIAN_POINT('Ctrl Pts',(0.125627582437506,-2.3704371448102,4.10516657274025));
#61435=CARTESIAN_POINT('Ctrl Pts',(0.0110075317138,-2.37178445840316,4.09721476815244));
#61436=CARTESIAN_POINT('Ctrl Pts',(-0.00586423581657563,-2.37180276029429,
4.09605251703333));
#61437=CARTESIAN_POINT('Ctrl Pts',(-0.0322181906673156,-2.37155012245268,
4.09425137018612));
#61438=CARTESIAN_POINT('Ctrl Pts',(-0.0417006121300469,-2.37140234078195,
4.09360619336722));
#61439=CARTESIAN_POINT('Ctrl Pts',(-0.0585517794148577,-2.37103860980113,
4.09246509497976));
#61440=CARTESIAN_POINT('Ctrl Pts',(-0.0659205130694228,-2.37084518435683,
4.09196798945262));
#61441=CARTESIAN_POINT('Ctrl Pts',(-0.0837782321403945,-2.37029310615626,
4.09076770661422));
#61442=CARTESIAN_POINT('Ctrl Pts',(-0.0942659001028998,-2.36989918596927,
4.09006646179363));
#61443=CARTESIAN_POINT('Ctrl Pts',(-0.127147659085825,-2.36844550974648,
4.08787840735119));
#61444=CARTESIAN_POINT('Ctrl Pts',(-0.149530292015629,-2.36713781604501,
4.08640434017427));
#61445=CARTESIAN_POINT('Ctrl Pts',(-0.269102929512568,-2.35844896950068,
4.078595610074));
#61446=CARTESIAN_POINT('Ctrl Pts',(-0.365797296301814,-2.34539857523862,
4.07251254326013));
#61447=CARTESIAN_POINT('Ctrl Pts',(-0.63436775037423,-2.29213044491303,
4.05561104291321));
#61448=CARTESIAN_POINT('Ctrl Pts',(-0.802936027419543,-2.2386547026024,
4.04495508880096));
#61449=CARTESIAN_POINT('Ctrl Pts',(-1.00733947850798,-2.14772280654071,
4.03068723882586));
#61450=CARTESIAN_POINT('Ctrl Pts',(-1.05006934938803,-2.12715771904762,
4.02762774263896));
#61451=CARTESIAN_POINT('Ctrl Pts',(-1.10859749909969,-2.09679586015655,
4.02331273995464));
#61452=CARTESIAN_POINT('Ctrl Pts',(-1.12494197748666,-2.08807251064354,
4.02209391797285));
#61453=CARTESIAN_POINT('Ctrl Pts',(-1.15311563121957,-2.07260891407359,
4.019967950112));
#61454=CARTESIAN_POINT('Ctrl Pts',(-1.16499222382804,-2.06595655208449,
4.01906390952175));
#61455=CARTESIAN_POINT('Ctrl Pts',(-1.18968797524339,-2.05184321203258,
4.01716725282294));
#61456=CARTESIAN_POINT('Ctrl Pts',(-1.20249569141502,-2.04436350492416,
4.01617399996849));
#61457=CARTESIAN_POINT('Ctrl Pts',(-1.23288414477396,-2.02623228280788,
4.01379383632225));
#61458=CARTESIAN_POINT('Ctrl Pts',(-1.25039796334513,-2.01547152443161,
4.01240303903997));
#61459=CARTESIAN_POINT('Ctrl Pts',(-1.31093871659444,-1.97718153296033,
4.00752720830551));
#61460=CARTESIAN_POINT('Ctrl Pts',(-1.35321182773701,-1.94849280155184,
4.00400038419033));
#61461=CARTESIAN_POINT('Ctrl Pts',(-1.45656370327992,-1.87336675142013,
3.99506029683457));
#61462=CARTESIAN_POINT('Ctrl Pts',(-1.51637462466789,-1.82529091446302,
3.98959242311701));
#61463=CARTESIAN_POINT('Ctrl Pts',(-1.64030347625462,-1.71537657887789,
3.97763838214814));
#61464=CARTESIAN_POINT('Ctrl Pts',(-1.70348390795264,-1.65265056421737,
3.97113763530534));
#61465=CARTESIAN_POINT('Ctrl Pts',(-1.83846496284148,-1.50265614753404,
3.9564353808969));
#61466=CARTESIAN_POINT('Ctrl Pts',(-1.90786819837947,-1.41349689189942,
3.94826156076083));
#61467=CARTESIAN_POINT('Ctrl Pts',(-1.98011516267886,-1.30561496058001,
3.93925310703173));
#61468=CARTESIAN_POINT('Ctrl Pts',(-1.98941357740214,-1.29140239340679,
3.93808297256903));
#61469=CARTESIAN_POINT('Ctrl Pts',(-2.003678704858,-1.26907845261888,3.93627229254215));
#61470=CARTESIAN_POINT('Ctrl Pts',(-2.00875044729849,-1.26103533635753,
3.93562536294709));
#61471=CARTESIAN_POINT('Ctrl Pts',(-2.01766586928946,-1.24670637304252,
3.93448276834022));
#61472=CARTESIAN_POINT('Ctrl Pts',(-2.02152869395997,-1.24043302215224,
3.93398590090995));
#61473=CARTESIAN_POINT('Ctrl Pts',(-2.03080444394315,-1.22521049286998,
3.93278824481496));
#61474=CARTESIAN_POINT('Ctrl Pts',(-2.03618749146496,-1.21624337662611,
3.93208936476674));
#61475=CARTESIAN_POINT('Ctrl Pts',(-2.05282351834494,-1.18811093072897,
3.92991643108976));
#61476=CARTESIAN_POINT('Ctrl Pts',(-2.06386692145194,-1.16882222690597,
3.92845487073881));
#61477=CARTESIAN_POINT('Ctrl Pts',(-2.12096811369601,-1.06575424811521,
3.92077835534359));
#61478=CARTESIAN_POINT('Ctrl Pts',(-2.16220483257843,-0.97939376186528,
3.91480570476036));
#61479=CARTESIAN_POINT('Ctrl Pts',(-2.25591523234802,-0.748148465755502,
3.89939502201402));
#61480=CARTESIAN_POINT('Ctrl Pts',(-2.29969200259628,-0.600245810281099,
3.89007972928553));
#61481=CARTESIAN_POINT('Ctrl Pts',(-2.34134467674219,-0.384275792330606,
3.87621504777191));
#61482=CARTESIAN_POINT('Ctrl Pts',(-2.35113892366926,-0.318915889244687,
3.87199024757244));
#61483=CARTESIAN_POINT('Ctrl Pts',(-2.36066405767634,-0.230215841739212,
3.86617158441218));
#61484=CARTESIAN_POINT('Ctrl Pts',(-2.36279885865572,-0.207160853132173,
3.86465161021022));
#61485=CARTESIAN_POINT('Ctrl Pts',(-2.36566705718336,-0.170317259552894,
3.86220880151603));
#61486=CARTESIAN_POINT('Ctrl Pts',(-2.36661819953601,-0.156546729317892,
3.86129272594805));
#61487=CARTESIAN_POINT('Ctrl Pts',(-2.36828596455728,-0.128891209416927,
3.85944644787649));
#61488=CARTESIAN_POINT('Ctrl Pts',(-2.36900080342762,-0.115006665483295,
3.85851622788222));
#61489=CARTESIAN_POINT('Ctrl Pts',(-2.37030257836427,-0.0845006092579927,
3.85646484375004));
#61490=CARTESIAN_POINT('Ctrl Pts',(-2.37083682662562,-0.0678777079366085,
3.85534209807801));
#61491=CARTESIAN_POINT('Ctrl Pts',(-2.37157155047331,-0.0338846715542729,
3.85303559976754));
#61492=CARTESIAN_POINT('Ctrl Pts',(-2.37175610092984,-0.0165153028660104,
3.85185143007632));
#61493=CARTESIAN_POINT('Ctrl Pts',(-2.37174984622549,0.000854066367404124,
3.85066146066936));
#61494=CARTESIAN_POINT('Ctrl Pts',(-2.36544101854889,0.172878137039867,
3.83707348408299));
#61495=CARTESIAN_POINT('Ctrl Pts',(-2.36962370299618,0.115647688304842,
3.84091228667815));
#61496=CARTESIAN_POINT('Ctrl Pts',(-2.37173262894057,0.0582092763231678,
3.84475108927331));
#61497=CARTESIAN_POINT('Ctrl Pts',(-2.37174989308549,0.000712143930775687,
3.84858989186847));
#61498=CARTESIAN_POINT('Ctrl Pts',(-2.36544101877862,0.172878133896551,
3.6418462952528));
#61499=CARTESIAN_POINT('Ctrl Pts',(-2.36960373216792,0.115920942269559,
3.64554472073481));
#61500=CARTESIAN_POINT('Ctrl Pts',(-2.37170862035855,0.0588218952681139,
3.6491579191629));
#61501=CARTESIAN_POINT('Ctrl Pts',(-2.37182237577473,-0.100556551570478,
3.6591144445237));
#61502=CARTESIAN_POINT('Ctrl Pts',(-2.36528314127671,-0.202707173211117,
3.66535159178271));
#61503=CARTESIAN_POINT('Ctrl Pts',(-2.33431192864043,-0.442249481340446,
3.68020778777026));
#61504=CARTESIAN_POINT('Ctrl Pts',(-2.30432302065855,-0.578519835038019,
3.68885420376579));
#61505=CARTESIAN_POINT('Ctrl Pts',(-2.25419661921153,-0.737951563018058,
3.69969918411873));
#61506=CARTESIAN_POINT('Ctrl Pts',(-2.24536920043085,-0.764389924131961,
3.70152169769104));
#61507=CARTESIAN_POINT('Ctrl Pts',(-2.23055360967836,-0.806289830611636,
3.70445182595685));
#61508=CARTESIAN_POINT('Ctrl Pts',(-2.22486552183372,-0.821855268976713,
3.705549654916));
#61509=CARTESIAN_POINT('Ctrl Pts',(-2.21375673553023,-0.851293714938383,
3.70764432718616));
#61510=CARTESIAN_POINT('Ctrl Pts',(-2.20836754204316,-0.865177817128302,
3.70864009047137));
#61511=CARTESIAN_POINT('Ctrl Pts',(-2.19574904883458,-0.896800465124892,
3.71092652551209));
#61512=CARTESIAN_POINT('Ctrl Pts',(-2.18843497853554,-0.914503836771113,
3.71221996270711));
#61513=CARTESIAN_POINT('Ctrl Pts',(-2.16482515182747,-0.969744637267543,
3.71629927681385));
#61514=CARTESIAN_POINT('Ctrl Pts',(-2.14777261681502,-1.00694837526237,
3.71911015748796));
#61515=CARTESIAN_POINT('Ctrl Pts',(-2.07892292666634,-1.14744386373356,
3.72997687826846));
#61516=CARTESIAN_POINT('Ctrl Pts',(-2.02057178792455,-1.24732964837458,
3.73824448739884));
#61517=CARTESIAN_POINT('Ctrl Pts',(-1.87647698814062,-1.45717708624776,
3.75672085480706));
#61518=CARTESIAN_POINT('Ctrl Pts',(-1.78784244632585,-1.56465722476262,
3.766951691505));
#61519=CARTESIAN_POINT('Ctrl Pts',(-1.65961926930181,-1.69492623233866,
3.77996216420211));
#61520=CARTESIAN_POINT('Ctrl Pts',(-1.62807903049174,-1.7252449938275,3.78303824535418));
#61521=CARTESIAN_POINT('Ctrl Pts',(-1.58526480940449,-1.76418057721875,
3.78703365527381));
#61522=CARTESIAN_POINT('Ctrl Pts',(-1.57472854975662,-1.77359173537276,
3.78800303914029));
#61523=CARTESIAN_POINT('Ctrl Pts',(-1.55740601791513,-1.78878843222804,
3.78957347697477));
#61524=CARTESIAN_POINT('Ctrl Pts',(-1.55067027790634,-1.79463067390134,
3.79017848176432));
#61525=CARTESIAN_POINT('Ctrl Pts',(-1.53726889079682,-1.80612257680302,
3.79137078963198));
#61526=CARTESIAN_POINT('Ctrl Pts',(-1.53060468937429,-1.81177363228175,
3.79195818021095));
#61527=CARTESIAN_POINT('Ctrl Pts',(-1.51372287944996,-1.82592930503251,
3.79343276296195));
#61528=CARTESIAN_POINT('Ctrl Pts',(-1.50346453024742,-1.83438524011886,
3.7943165606353));
#61529=CARTESIAN_POINT('Ctrl Pts',(-1.46191181147329,-1.86805430750717,
3.79785010427348));
#61530=CARTESIAN_POINT('Ctrl Pts',(-1.4300481238227,-1.89255801807241,3.80045509588657));
#61531=CARTESIAN_POINT('Ctrl Pts',(-1.34059995990195,-1.9577953576976,3.80753269189188));
#61532=CARTESIAN_POINT('Ctrl Pts',(-1.28179600352902,-1.99679024544941,
3.81192823862155));
#61533=CARTESIAN_POINT('Ctrl Pts',(-1.07608650476142,-2.12036494675952,
3.82675526953262));
#61534=CARTESIAN_POINT('Ctrl Pts',(-0.921911437537798,-2.19179988184697,
3.83699808164418));
#61535=CARTESIAN_POINT('Ctrl Pts',(-0.710339041339512,-2.26352119270964,
3.85118257011784));
#61536=CARTESIAN_POINT('Ctrl Pts',(-0.658662532730912,-2.279094716536,3.85465268105317));
#61537=CARTESIAN_POINT('Ctrl Pts',(-0.585369056277798,-2.29848189356178,
3.85960692999845));
#61538=CARTESIAN_POINT('Ctrl Pts',(-0.564159647413503,-2.30377945719161,
3.86104426684483));
#61539=CARTESIAN_POINT('Ctrl Pts',(-0.528110413886234,-2.31225597060964,
3.86349499251605));
#61540=CARTESIAN_POINT('Ctrl Pts',(-0.513307533194915,-2.31558710509237,
3.86450351509957));
#61541=CARTESIAN_POINT('Ctrl Pts',(-0.483264784661054,-2.32204548200769,
3.86655522940651));
#61542=CARTESIAN_POINT('Ctrl Pts',(-0.468024093897173,-2.32516526303998,
3.86759860130792));
#61543=CARTESIAN_POINT('Ctrl Pts',(-0.430136834202159,-2.33253322675051,
3.87019915988852));
#61544=CARTESIAN_POINT('Ctrl Pts',(-0.4074573698885,-2.33660167281496,3.8717618857363));
#61545=CARTESIAN_POINT('Ctrl Pts',(-0.317823210964544,-2.3513364247715,
3.87796378307435));
#61546=CARTESIAN_POINT('Ctrl Pts',(-0.250489025047789,-2.35945931665607,
3.8826802032051));
#61547=CARTESIAN_POINT('Ctrl Pts',(-0.0638319271176766,-2.37389694802061,
3.89591650184541));
#61548=CARTESIAN_POINT('Ctrl Pts',(0.0557555377632189,-2.37409927154267,
3.9045867423562));
#61549=CARTESIAN_POINT('Ctrl Pts',(0.301957369246828,-2.35590059003178,
3.92258574050193));
#61550=CARTESIAN_POINT('Ctrl Pts',(0.42812431333008,-2.33627077933483,3.93189051339065));
#61551=CARTESIAN_POINT('Ctrl Pts',(0.574359523544318,-2.30126759588808,
3.94239742209559));
#61552=CARTESIAN_POINT('Ctrl Pts',(0.596530656273767,-2.29562032605396,
3.94398230327808));
#61553=CARTESIAN_POINT('Ctrl Pts',(0.628967189899483,-2.28685663518021,
3.94628571041083));
#61554=CARTESIAN_POINT('Ctrl Pts',(0.639297966425779,-2.28399017445573,
3.9470170316191));
#61555=CARTESIAN_POINT('Ctrl Pts',(0.65762959210004,-2.27876960789954,3.94831022000159));
#61556=CARTESIAN_POINT('Ctrl Pts',(0.665637873394858,-2.27644324211311,
3.94887358871724));
#61557=CARTESIAN_POINT('Ctrl Pts',(0.683312070433236,-2.27120773122983,
3.95011344532317));
#61558=CARTESIAN_POINT('Ctrl Pts',(0.692971842172196,-2.26827907877277,
3.95078882181577));
#61559=CARTESIAN_POINT('Ctrl Pts',(0.72137837333316,-2.25946837272362,3.9527690331935));
#61560=CARTESIAN_POINT('Ctrl Pts',(0.740071599563027,-2.25341478056034,
3.95406456951641));
#61561=CARTESIAN_POINT('Ctrl Pts',(0.858913919426857,-2.21329058306258,
3.96226538897946));
#61562=CARTESIAN_POINT('Ctrl Pts',(0.956776237648073,-2.17278001089318,
3.9688591417187));
#61563=CARTESIAN_POINT('Ctrl Pts',(1.21914071544413,-2.04299434809594,3.98691472218457));
#61564=CARTESIAN_POINT('Ctrl Pts',(1.37626784177599,-1.94062144287982,3.99822060707618));
#61565=CARTESIAN_POINT('Ctrl Pts',(1.54907314261894,-1.79639349247608,4.01268839277248));
#61566=CARTESIAN_POINT('Ctrl Pts',(1.57780231699497,-1.77121336080525,4.01516826308633));
#61567=CARTESIAN_POINT('Ctrl Pts',(1.61963773597091,-1.73272031031374,4.01890103934084));
#61568=CARTESIAN_POINT('Ctrl Pts',(1.6332159220035,-1.7199278441055,4.02013245013286));
#61569=CARTESIAN_POINT('Ctrl Pts',(1.65732373511459,-1.6966721535124,4.02235581977527));
#61570=CARTESIAN_POINT('Ctrl Pts',(1.6679088150969,-1.68626763210078,4.0233452399468));
#61571=CARTESIAN_POINT('Ctrl Pts',(1.69031696490801,-1.66382430484322,4.02546871441459));
#61572=CARTESIAN_POINT('Ctrl Pts',(1.7021105580445,-1.65175736179064,4.02660397093101));
#61573=CARTESIAN_POINT('Ctrl Pts',(1.73402365170021,-1.61839985202185,4.02972545169917));
#61574=CARTESIAN_POINT('Ctrl Pts',(1.75387848902808,-1.59686136516933,4.03172267533304));
#61575=CARTESIAN_POINT('Ctrl Pts',(1.87376773244004,-1.46187201748468,4.04413458710343));
#61576=CARTESIAN_POINT('Ctrl Pts',(1.96314144056444,-1.33945373199465,4.05497540280774));
#61577=CARTESIAN_POINT('Ctrl Pts',(2.11847212772815,-1.07740949034975,4.07714530327044));
#61578=CARTESIAN_POINT('Ctrl Pts',(2.18371769189735,-0.93814673163701,4.0884232732239));
#61579=CARTESIAN_POINT('Ctrl Pts',(2.24222617527117,-0.773355684348227,
4.10062182614449));
#61580=CARTESIAN_POINT('Ctrl Pts',(2.24912206391935,-0.753065240368606,
4.10210440717391));
#61581=CARTESIAN_POINT('Ctrl Pts',(2.2589692899577,-0.722748178192925,4.10428808619995));
#61582=CARTESIAN_POINT('Ctrl Pts',(2.26213069229004,-0.712791640886172,
4.10500022173271));
#61583=CARTESIAN_POINT('Ctrl Pts',(2.26769476123474,-0.694858205213966,
4.10627350452493));
#61584=CARTESIAN_POINT('Ctrl Pts',(2.27012128503816,-0.686889228627869,
4.10683595607547));
#61585=CARTESIAN_POINT('Ctrl Pts',(2.2754649100563,-0.669002514741316,4.10809094143575));
#61586=CARTESIAN_POINT('Ctrl Pts',(2.27835920849477,-0.659078332658007,
4.10878218577872));
#61587=CARTESIAN_POINT('Ctrl Pts',(2.28690057009943,-0.629062315652003,
4.11085850311069));
#61588=CARTESIAN_POINT('Ctrl Pts',(2.29234758987992,-0.608913962599894,
4.11223286994105));
#61589=CARTESIAN_POINT('Ctrl Pts',(2.30448160260397,-0.561558011167402,
4.11542360382502));
#61590=CARTESIAN_POINT('Ctrl Pts',(2.31095400754689,-0.534298206414138,
4.11723001445656));
#61591=CARTESIAN_POINT('Ctrl Pts',(2.33269242551105,-0.434941757797497,
4.12372555979368));
#61592=CARTESIAN_POINT('Ctrl Pts',(2.34508027030422,-0.362254482681901,
4.12831043431692));
#61593=CARTESIAN_POINT('Ctrl Pts',(2.37615340116676,-0.109237659319397,
4.14404250816702));
#61594=CARTESIAN_POINT('Ctrl Pts',(2.37755541494182,0.0725530699381401,
4.15500091254152));
#61595=CARTESIAN_POINT('Ctrl Pts',(2.35368716776626,0.295272103271014,4.1693400533406));
#61596=CARTESIAN_POINT('Ctrl Pts',(2.34797753559637,0.337683332490251,4.17210908079347));
#61597=CARTESIAN_POINT('Ctrl Pts',(2.33798897570018,0.399235158617621,4.17619598556813));
#61598=CARTESIAN_POINT('Ctrl Pts',(2.33461475566494,0.418515313216202,4.1774859431454));
#61599=CARTESIAN_POINT('Ctrl Pts',(2.32823503460333,0.452487008944127,4.1797772538756));
#61600=CARTESIAN_POINT('Ctrl Pts',(2.32532807168639,0.467196116464522,4.18077547506145));
#61601=CARTESIAN_POINT('Ctrl Pts',(2.31898938680194,0.49774381159621,4.18286180723362));
#61602=CARTESIAN_POINT('Ctrl Pts',(2.31553441070921,0.513576721242177,4.18395060376919));
#61603=CARTESIAN_POINT('Ctrl Pts',(2.30608096832637,0.554862531998601,4.18680985523015));
#61604=CARTESIAN_POINT('Ctrl Pts',(2.29982346335846,0.580253225161831,4.188588392458));
#61605=CARTESIAN_POINT('Ctrl Pts',(2.26660510211341,0.706050544341082,4.1975038301838));
#61606=CARTESIAN_POINT('Ctrl Pts',(2.23348616480765,0.80469891273897,4.20483346058679));
#61607=CARTESIAN_POINT('Ctrl Pts',(2.15832209104737,0.987760876724163,4.2190595290515));
#61608=CARTESIAN_POINT('Ctrl Pts',(2.11750370050633,1.07247487818202,4.22591631181305));
#61609=CARTESIAN_POINT('Ctrl Pts',(2.01815769334302,1.25074684114226,4.24079050600832));
#61610=CARTESIAN_POINT('Ctrl Pts',(1.95790302393165,1.34311148162399,4.24878807269437));
#61611=CARTESIAN_POINT('Ctrl Pts',(1.87757276406196,1.44929187799698,4.25809270484753));
#61612=CARTESIAN_POINT('Ctrl Pts',(1.86343792138482,1.46742142600187,4.25968532571127));
#61613=CARTESIAN_POINT('Ctrl Pts',(1.84231438009874,1.49371722793525,4.26199775483745));
#61614=CARTESIAN_POINT('Ctrl Pts',(1.83553068430216,1.50204545545152,4.26273049597324));
#61615=CARTESIAN_POINT('Ctrl Pts',(1.8233793143044,1.51675822108982,4.2640251875543));
#61616=CARTESIAN_POINT('Ctrl Pts',(1.81803426817176,1.52316086861205,4.26458865403766));
#61617=CARTESIAN_POINT('Ctrl Pts',(1.80615655186901,1.53723717164261,4.26582752360302));
#61618=CARTESIAN_POINT('Ctrl Pts',(1.79960864862018,1.54489751529094,4.26650182749112));
#61619=CARTESIAN_POINT('Ctrl Pts',(1.78020423330311,1.56730781413396,4.26847562822554));
#61620=CARTESIAN_POINT('Ctrl Pts',(1.76721343980189,1.5819410908333,4.26976591697229));
#61621=CARTESIAN_POINT('Ctrl Pts',(1.66502024174839,1.6942248627772,4.27969344865641));
#61622=CARTESIAN_POINT('Ctrl Pts',(1.56795969961087,1.78443326465879,4.28783723443293));
#61623=CARTESIAN_POINT('Ctrl Pts',(1.33234479367039,1.96926387833958,4.30623615426188));
#61624=CARTESIAN_POINT('Ctrl Pts',(1.19029418389439,2.05823596475885,4.31645481621377));
#61625=CARTESIAN_POINT('Ctrl Pts',(1.01250670250646,2.14498704125831,4.3292156858405));
#61626=CARTESIAN_POINT('Ctrl Pts',(0.984678062614286,2.1579036601609,4.33121089777562));
#61627=CARTESIAN_POINT('Ctrl Pts',(0.939259284668015,2.17792320782464,4.33446828650197));
#61628=CARTESIAN_POINT('Ctrl Pts',(0.921820239631107,2.18536150659485,4.33571922441971));
#61629=CARTESIAN_POINT('Ctrl Pts',(0.890545985524313,2.19826001148066,4.33796395122685));
#61630=CARTESIAN_POINT('Ctrl Pts',(0.876744913067595,2.20380071031838,4.33895499597927));
#61631=CARTESIAN_POINT('Ctrl Pts',(0.847352914695435,2.21528089271755,4.34106705365825));
#61632=CARTESIAN_POINT('Ctrl Pts',(0.831749661643027,2.22118636581461,4.34218912831756));
#61633=CARTESIAN_POINT('Ctrl Pts',(0.78942388685468,2.23669718737106,4.3452358535863));
#61634=CARTESIAN_POINT('Ctrl Pts',(0.76258976112885,2.24598778206482,4.3471706347175));
#61635=CARTESIAN_POINT('Ctrl Pts',(0.58370959232814,2.3043450348951,4.36009444920802));
#61636=CARTESIAN_POINT('Ctrl Pts',(0.427232053849851,2.33841366935678,4.37156607975096));
#61637=CARTESIAN_POINT('Ctrl Pts',(0.123641458017868,2.37301105248853,4.39382105527679));
#61638=CARTESIAN_POINT('Ctrl Pts',(-0.0224902270683318,2.37612490106955,
4.40452075403554));
#61639=CARTESIAN_POINT('Ctrl Pts',(-0.189818035341091,2.36424321649236,
4.41622888168404));
#61640=CARTESIAN_POINT('Ctrl Pts',(-0.211623299379721,2.36239127502634,
4.41774346910772));
#61641=CARTESIAN_POINT('Ctrl Pts',(-0.243882774834674,2.35920117881856,
4.41996470345987));
#61642=CARTESIAN_POINT('Ctrl Pts',(-0.254358038094077,2.35809478371122,
4.42068292560049));
#61643=CARTESIAN_POINT('Ctrl Pts',(-0.273105517132446,2.35598829745526,
4.42196243634705));
#61644=CARTESIAN_POINT('Ctrl Pts',(-0.281380188187089,2.35501436874272,
4.42252509212732));
#61645=CARTESIAN_POINT('Ctrl Pts',(-0.299828667998173,2.3527443564465,4.42377489344016));
#61646=CARTESIAN_POINT('Ctrl Pts',(-0.309999365756123,2.35142587377134,
4.42446080884023));
#61647=CARTESIAN_POINT('Ctrl Pts',(-0.34042932692158,2.34728020230701,4.42650457728493));
#61648=CARTESIAN_POINT('Ctrl Pts',(-0.360661489414601,2.34425677625829,
4.42785221174127));
#61649=CARTESIAN_POINT('Ctrl Pts',(-0.518866454472196,2.31851840323123,
4.43831981837334));
#61650=CARTESIAN_POINT('Ctrl Pts',(-0.654643601409779,2.28390067787529,
4.44689431564035));
#61651=CARTESIAN_POINT('Ctrl Pts',(-0.934854572738278,2.18539308545424,
4.46513509942551));
#61652=CARTESIAN_POINT('Ctrl Pts',(-1.07755166740775,2.11867208953042,4.47477547046208));
#61653=CARTESIAN_POINT('Ctrl Pts',(-1.23942986016123,2.02237152506852,4.4869191703135));
#61654=CARTESIAN_POINT('Ctrl Pts',(-1.26594506163832,2.00588033573256,4.48894897991668));
#61655=CARTESIAN_POINT('Ctrl Pts',(-1.30815575669471,1.97845697060891,4.49225156112831));
#61656=CARTESIAN_POINT('Ctrl Pts',(-1.32405857191477,1.96784967193015,4.49351256481133));
#61657=CARTESIAN_POINT('Ctrl Pts',(-1.35163394769947,1.94897109673667,4.49572963594782));
#61658=CARTESIAN_POINT('Ctrl Pts',(-1.36336327075376,1.94078418205506,4.49668252559138));
#61659=CARTESIAN_POINT('Ctrl Pts',(-1.38790595311149,1.92332143263944,4.4986976435483));
#61660=CARTESIAN_POINT('Ctrl Pts',(-1.40070195983474,1.91402253563031,4.49976071468466));
#61661=CARTESIAN_POINT('Ctrl Pts',(-1.42685422316272,1.89461490461995,4.50195962318708));
#61662=CARTESIAN_POINT('Ctrl Pts',(-1.44019829076275,1.88449130258461,4.5030959933871));
#61663=CARTESIAN_POINT('Ctrl Pts',(-1.49956907625671,1.83845019765496,4.50821787184103));
#61664=CARTESIAN_POINT('Ctrl Pts',(-1.54436394055369,1.80098460680724,4.5122630007033));
#61665=CARTESIAN_POINT('Ctrl Pts',(-1.65701062699657,1.69947399305766,4.52292423399785));
#61666=CARTESIAN_POINT('Ctrl Pts',(-1.72254385661214,1.63301430173476,4.52962570077938));
#61667=CARTESIAN_POINT('Ctrl Pts',(-1.87795491040315,1.45561588080458,4.5467508536347));
#61668=CARTESIAN_POINT('Ctrl Pts',(-1.96205789598359,1.34009836122726,4.55724541564508));
#61669=CARTESIAN_POINT('Ctrl Pts',(-2.05540245718138,1.18408420749316,4.57014498711645));
#61670=CARTESIAN_POINT('Ctrl Pts',(-2.0746930028049,1.1499495800197,4.57289450358811));
#61671=CARTESIAN_POINT('Ctrl Pts',(-2.09951373352872,1.10336958265515,4.57653488918519));
#61672=CARTESIAN_POINT('Ctrl Pts',(-2.10579496058023,1.09133402715711,4.57746569521676));
#61673=CARTESIAN_POINT('Ctrl Pts',(-2.11557888794184,1.07218787397129,4.57893017838993));
#61674=CARTESIAN_POINT('Ctrl Pts',(-2.11914976800319,1.06511273280841,4.57946787428792));
#61675=CARTESIAN_POINT('Ctrl Pts',(-2.1265442834618,1.05027725437029,4.58058787513904));
#61676=CARTESIAN_POINT('Ctrl Pts',(-2.130361031667,1.04251368274627,4.58116972030882));
#61677=CARTESIAN_POINT('Ctrl Pts',(-2.13974951608967,1.02314987841658,4.58261078683348));
#61678=CARTESIAN_POINT('Ctrl Pts',(-2.14526958637589,1.01152463412428,4.58346693222359));
#61679=CARTESIAN_POINT('Ctrl Pts',(-2.16617979731744,0.966546615213636,
4.58674694458278));
#61680=CARTESIAN_POINT('Ctrl Pts',(-2.18088983625737,0.932881099418687,
4.58913376975468));
#61681=CARTESIAN_POINT('Ctrl Pts',(-2.21810468336384,0.842013421677471,
4.59543075903007));
#61682=CARTESIAN_POINT('Ctrl Pts',(-2.23917887005602,0.784253772634774,
4.59928297783405));
#61683=CARTESIAN_POINT('Ctrl Pts',(-2.31566055517881,0.546296231661375,
4.61479023688534));
#61684=CARTESIAN_POINT('Ctrl Pts',(-2.35171383526137,0.360703176060175,
4.62611511055786));
#61685=CARTESIAN_POINT('Ctrl Pts',(-2.36544101871061,0.17287813482709,4.63810474394384));
#61686=CARTESIAN_POINT('Origin',(0.,0.,-1.84858989190501));
#61687=CARTESIAN_POINT('',(-2.36544101854819,0.172878137049535,5.83485941057446));
#61688=CARTESIAN_POINT('',(-2.36449584214975,0.172800370348396,5.63966122007073));
#61689=CARTESIAN_POINT('',(-2.36544101854889,0.172878137039864,-1.84858989190501));
#61690=CARTESIAN_POINT('Ctrl Pts',(-2.36544101854819,0.172878137049535,
5.83485941057446));
#61691=CARTESIAN_POINT('Ctrl Pts',(-2.3652981630827,0.174832786628508,5.83472426691884));
#61692=CARTESIAN_POINT('Ctrl Pts',(-2.36515288377511,0.176787273442486,
5.83458923813668));
#61693=CARTESIAN_POINT('Ctrl Pts',(-2.36428940002551,0.18821239004539,5.833800530386));
#61694=CARTESIAN_POINT('Ctrl Pts',(-2.36351672128189,0.197678998633314,
5.83314949174867));
#61695=CARTESIAN_POINT('Ctrl Pts',(-2.36201461348199,0.214812316023825,
5.83197596993832));
#61696=CARTESIAN_POINT('Ctrl Pts',(-2.36130467689932,0.222480544027811,
5.83145247919523));
#61697=CARTESIAN_POINT('Ctrl Pts',(-2.35976308180321,0.238292396343194,
5.83037680667898));
#61698=CARTESIAN_POINT('Ctrl Pts',(-2.35892662326193,0.246435097312728,
5.82982496239602));
#61699=CARTESIAN_POINT('Ctrl Pts',(-2.35689706009234,0.265234398327371,
5.82855557255112));
#61700=CARTESIAN_POINT('Ctrl Pts',(-2.35567382524878,0.27588743699874,5.82783968257873));
#61701=CARTESIAN_POINT('Ctrl Pts',(-2.35144113758588,0.310666609810523,
5.82551266801943));
#61702=CARTESIAN_POINT('Ctrl Pts',(-2.34813285296849,0.334755704981761,
5.82391691158141));
#61703=CARTESIAN_POINT('Ctrl Pts',(-2.333313581828,0.431589597217501,5.81755143098955));
#61704=CARTESIAN_POINT('Ctrl Pts',(-2.31878680031268,0.503836880407571,
5.81291382130682));
#61705=CARTESIAN_POINT('Ctrl Pts',(-2.27547228552324,0.677074775104708,
5.80181754294908));
#61706=CARTESIAN_POINT('Ctrl Pts',(-2.24329946016118,0.777054009232324,
5.79543025349959));
#61707=CARTESIAN_POINT('Ctrl Pts',(-2.17357425332955,0.952815698519893,
5.78377520704926));
#61708=CARTESIAN_POINT('Ctrl Pts',(-2.13839541039005,1.02934265702245,5.77854518477113));
#61709=CARTESIAN_POINT('Ctrl Pts',(-2.07390923761444,1.15197982358111,5.76974385018016));
#61710=CARTESIAN_POINT('Ctrl Pts',(-2.046945456575,1.19923752065692,5.76624346743483));
#61711=CARTESIAN_POINT('Ctrl Pts',(-2.00733491089914,1.26342676080899,5.76131037827371));
#61712=CARTESIAN_POINT('Ctrl Pts',(-1.99604985044595,1.28118131912445,5.75992630082692));
#61713=CARTESIAN_POINT('Ctrl Pts',(-1.97636083657577,1.31126598132529,5.75754592825429));
#61714=CARTESIAN_POINT('Ctrl Pts',(-1.96807383953829,1.32367139997946,5.75655396937008));
#61715=CARTESIAN_POINT('Ctrl Pts',(-1.95205588501542,1.34716688659854,5.75465482810676));
#61716=CARTESIAN_POINT('Ctrl Pts',(-1.944346040109,1.35827068802221,5.75374846317746));
#61717=CARTESIAN_POINT('Ctrl Pts',(-1.92408916587008,1.38691894726582,5.75138654882944));
#61718=CARTESIAN_POINT('Ctrl Pts',(-1.91139721180828,1.40435890365694,5.74992555067283));
#61719=CARTESIAN_POINT('Ctrl Pts',(-1.86603712327907,1.46493386236972,5.74476744932677));
#61720=CARTESIAN_POINT('Ctrl Pts',(-1.83213455788877,1.50711907949305,5.74102339401878));
#61721=CARTESIAN_POINT('Ctrl Pts',(-1.68596654338915,1.67677020325248,5.72531277353773));
#61722=CARTESIAN_POINT('Ctrl Pts',(-1.56162420310305,1.79314147399814,5.71288703647184));
#61723=CARTESIAN_POINT('Ctrl Pts',(-1.36929726689747,1.93784654386613,5.69537099228855));
#61724=CARTESIAN_POINT('Ctrl Pts',(-1.31075967405018,1.97791166165294,5.69023947562557));
#61725=CARTESIAN_POINT('Ctrl Pts',(-1.22738382822378,2.02964722521763,5.68327588209299));
#61726=CARTESIAN_POINT('Ctrl Pts',(-1.20400945848729,2.04359983326879,5.68135951949691));
#61727=CARTESIAN_POINT('Ctrl Pts',(-1.16276246966077,2.06726751150561,5.67804631629346));
#61728=CARTESIAN_POINT('Ctrl Pts',(-1.14499572833956,2.0771606522856,5.67664083845206));
#61729=CARTESIAN_POINT('Ctrl Pts',(-1.11822052172634,2.09162206115305,5.67455730604109));
#61730=CARTESIAN_POINT('Ctrl Pts',(-1.10930706651258,2.09636299896061,5.67386935512712));
#61731=CARTESIAN_POINT('Ctrl Pts',(-1.09315269787907,2.10482338860201,5.6726330888083));
#61732=CARTESIAN_POINT('Ctrl Pts',(-1.08592268450922,2.10856260193877,5.67208360288256));
#61733=CARTESIAN_POINT('Ctrl Pts',(-1.06960093446685,2.11689765311899,5.67085165395637));
#61734=CARTESIAN_POINT('Ctrl Pts',(-1.06049870366577,2.12147221094061,5.67017048638989));
#61735=CARTESIAN_POINT('Ctrl Pts',(-1.03272227467651,2.13520851693974,5.66810873788662));
#61736=CARTESIAN_POINT('Ctrl Pts',(-1.01395621266517,2.14418366234985,5.66673889412827));
#61737=CARTESIAN_POINT('Ctrl Pts',(-0.851983897161047,2.21904713208814,
5.65509187739822));
#61738=CARTESIAN_POINT('Ctrl Pts',(-0.702636285996771,2.27076264096107,
5.64550775631935));
#61739=CARTESIAN_POINT('Ctrl Pts',(-0.40193321266248,2.34234450758117,5.62652227180799));
#61740=CARTESIAN_POINT('Ctrl Pts',(-0.25162267459038,2.36321942364835,5.61716492363531));
#61741=CARTESIAN_POINT('Ctrl Pts',(-0.0728094653995724,2.37079251387567,
5.60554912862823));
#61742=CARTESIAN_POINT('Ctrl Pts',(-0.0452433520591043,2.37147871573019,
5.60374591454108));
#61743=CARTESIAN_POINT('Ctrl Pts',(-0.00140084380394981,2.37180540508297,
5.60085510525446));
#61744=CARTESIAN_POINT('Ctrl Pts',(0.0148712176391393,2.37175919241675,
5.59977718294867));
#61745=CARTESIAN_POINT('Ctrl Pts',(0.0456792490888016,2.37135464671611,
5.59772627023614));
#61746=CARTESIAN_POINT('Ctrl Pts',(0.0602149690143406,2.37103007061824,
5.59675436961611));
#61747=CARTESIAN_POINT('Ctrl Pts',(0.0933088821955444,2.36998658625858,
5.59453151179002));
#61748=CARTESIAN_POINT('Ctrl Pts',(0.111863264907208,2.36918330712374,5.5932780044235));
#61749=CARTESIAN_POINT('Ctrl Pts',(0.160457345085561,2.36650741247831,5.58997526291353));
#61750=CARTESIAN_POINT('Ctrl Pts',(0.190473364226601,2.3642807886782,5.58791530968564));
#61751=CARTESIAN_POINT('Ctrl Pts',(0.429685760111566,2.34195099634652,5.57133338897994));
#61752=CARTESIAN_POINT('Ctrl Pts',(0.635377674367417,2.29469504398765,5.55594167216778));
#61753=CARTESIAN_POINT('Ctrl Pts',(0.893047341279078,2.19815840643455,5.53594574169321));
#61754=CARTESIAN_POINT('Ctrl Pts',(0.953032197343802,2.17282411141126,5.53124676581123));
#61755=CARTESIAN_POINT('Ctrl Pts',(1.03523985700263,2.1340436610381,5.5248064050044));
#61756=CARTESIAN_POINT('Ctrl Pts',(1.05839727220288,2.12265381994892,5.52299224255321));
#61757=CARTESIAN_POINT('Ctrl Pts',(1.09873925563241,2.10198743731354,5.51983745033577));
#61758=CARTESIAN_POINT('Ctrl Pts',(1.11600350124328,2.09287251990842,5.51848921491388));
#61759=CARTESIAN_POINT('Ctrl Pts',(1.14188058911878,2.07879904341009,5.5164733282726));
#61760=CARTESIAN_POINT('Ctrl Pts',(1.15057756203222,2.07399807746633,5.51579667111589));
#61761=CARTESIAN_POINT('Ctrl Pts',(1.16634931940817,2.06516189535902,5.51457148536338));
#61762=CARTESIAN_POINT('Ctrl Pts',(1.17343365954732,2.0611447886668,5.51402190231649));
#61763=CARTESIAN_POINT('Ctrl Pts',(1.1894858889286,2.05193293743101,5.51277822630914));
#61764=CARTESIAN_POINT('Ctrl Pts',(1.19844056514836,2.04671582820594,5.51208555200552));
#61765=CARTESIAN_POINT('Ctrl Pts',(1.22605519974177,2.03038381224104,5.50995198202931));
#61766=CARTESIAN_POINT('Ctrl Pts',(1.24459748956698,2.0190708129608,5.50852294264353));
#61767=CARTESIAN_POINT('Ctrl Pts',(1.38679911980856,1.9296074011854,5.49757035896489));
#61768=CARTESIAN_POINT('Ctrl Pts',(1.50316085553991,1.84041176953142,5.48863532489169));
#61769=CARTESIAN_POINT('Ctrl Pts',(1.72821612349001,1.63222258639811,5.46981310634935));
#61770=CARTESIAN_POINT('Ctrl Pts',(1.83451215049238,1.51176656786397,5.4599490771709));
#61771=CARTESIAN_POINT('Ctrl Pts',(1.944252560164,1.3586291946268,5.4477290081568));
#61772=CARTESIAN_POINT('Ctrl Pts',(1.96024849047158,1.33544638728331,5.44588799831982));
#61773=CARTESIAN_POINT('Ctrl Pts',(1.98489798545891,1.29832466371339,5.44295079437928));
#61774=CARTESIAN_POINT('Ctrl Pts',(1.99382659044595,1.28457092050305,5.44186483033838));
#61775=CARTESIAN_POINT('Ctrl Pts',(2.01039006568428,1.25846756746148,5.43980742768117));
#61776=CARTESIAN_POINT('Ctrl Pts',(2.01805558247382,1.24613822854737,5.43883717110611));
#61777=CARTESIAN_POINT('Ctrl Pts',(2.03515929948378,1.21805660100813,5.4366302663616));
#61778=CARTESIAN_POINT('Ctrl Pts',(2.04452862363098,1.2022636699432,5.43539120548939));
#61779=CARTESIAN_POINT('Ctrl Pts',(2.06840828539195,1.16092561098876,5.43215256908947));
#61780=CARTESIAN_POINT('Ctrl Pts',(2.0826286711716,1.13521750978203,5.43014294213169));
#61781=CARTESIAN_POINT('Ctrl Pts',(2.18152427802634,0.948315562040573,5.41555916008675));
#61782=CARTESIAN_POINT('Ctrl Pts',(2.24785087046105,0.778134607647297,5.40235055184386));
#61783=CARTESIAN_POINT('Ctrl Pts',(2.32458491401091,0.485762832607977,5.38030984705614));
#61784=CARTESIAN_POINT('Ctrl Pts',(2.34622556603806,0.367276497671959,5.37156367947194));
#61785=CARTESIAN_POINT('Ctrl Pts',(2.36082076241201,0.228261731792622,5.36183539373392));
#61786=CARTESIAN_POINT('Ctrl Pts',(2.3626172586553,0.208848845309161,5.36048904969874));
#61787=CARTESIAN_POINT('Ctrl Pts',(2.36496716956883,0.179518584567353,5.35847540310722));
#61788=CARTESIAN_POINT('Ctrl Pts',(2.36569794845537,0.16961680606868,5.35779912341425));
#61789=CARTESIAN_POINT('Ctrl Pts',(2.36691497295297,0.151584642381062,5.3565743011276));
#61790=CARTESIAN_POINT('Ctrl Pts',(2.36742153652131,0.143456145451489,5.35602470798875));
#61791=CARTESIAN_POINT('Ctrl Pts',(2.36847789615951,0.124972175922791,5.35478060972845));
#61792=CARTESIAN_POINT('Ctrl Pts',(2.36900166236205,0.114615544500593,5.35408752760864));
#61793=CARTESIAN_POINT('Ctrl Pts',(2.37041365644713,0.0825245981244625,
5.35195138467514));
#61794=CARTESIAN_POINT('Ctrl Pts',(2.37107085863046,0.0607805612814262,
5.35052022127107));
#61795=CARTESIAN_POINT('Ctrl Pts',(2.37383034879061,-0.106885211152354,
5.33958861474284));
#61796=CARTESIAN_POINT('Ctrl Pts',(2.36275974514105,-0.252730697895482,
5.33067358259826));
#61797=CARTESIAN_POINT('Ctrl Pts',(2.31146507372993,-0.555126139779607,
5.3118433003837));
#61798=CARTESIAN_POINT('Ctrl Pts',(2.26854638195518,-0.710439670629666,
5.30195077076225));
#61799=CARTESIAN_POINT('Ctrl Pts',(2.20007801831038,-0.886364708090971,
5.28970476914955));
#61800=CARTESIAN_POINT('Ctrl Pts',(2.18943622845295,-0.912334684508902,
5.28787015368775));
#61801=CARTESIAN_POINT('Ctrl Pts',(2.17185904416167,-0.953149800327596,
5.28494079845569));
#61802=CARTESIAN_POINT('Ctrl Pts',(2.16522613825512,-0.968122924715021,
5.28385619355425));
#61803=CARTESIAN_POINT('Ctrl Pts',(2.15242015739865,-0.996241133839447,
5.28179990791864));
#61804=CARTESIAN_POINT('Ctrl Pts',(2.14628034848585,-1.00940060455088,5.28082939376168));
#61805=CARTESIAN_POINT('Ctrl Pts',(2.13208893729212,-1.03910214861662,5.27861989222144));
#61806=CARTESIAN_POINT('Ctrl Pts',(2.12396500553494,-1.05560841898881,5.277378469678));
#61807=CARTESIAN_POINT('Ctrl Pts',(2.10231856712259,-1.09832811564316,5.2741293841941));
#61808=CARTESIAN_POINT('Ctrl Pts',(2.08849798705697,-1.12438606845454,5.27211156236119));
#61809=CARTESIAN_POINT('Ctrl Pts',(1.98648720663364,-1.30834908178088,5.25760195107445));
#61810=CARTESIAN_POINT('Ctrl Pts',(1.88098923744897,-1.45594131183394,5.24448543434291));
#61811=CARTESIAN_POINT('Ctrl Pts',(1.67734628204884,-1.6813164779206,5.22233620840792));
#61812=CARTESIAN_POINT('Ctrl Pts',(1.58793661111369,-1.76600658334652,5.21339144794867));
#61813=CARTESIAN_POINT('Ctrl Pts',(1.478003763277,-1.85500507579957,5.20356061779455));
#61814=CARTESIAN_POINT('Ctrl Pts',(1.46351787916972,-1.86645504227541,5.20228682431552));
#61815=CARTESIAN_POINT('Ctrl Pts',(1.44120525051743,-1.88367192775855,5.20035933772398));
#61816=CARTESIAN_POINT('Ctrl Pts',(1.43347469438542,-1.88956154026869,5.19969774223817));
#61817=CARTESIAN_POINT('Ctrl Pts',(1.41918679323507,-1.90030878944935,5.19848666369345));
#61818=CARTESIAN_POINT('Ctrl Pts',(1.41264047963194,-1.90518018257248,5.19793628361086));
#61819=CARTESIAN_POINT('Ctrl Pts',(1.39764765189411,-1.91621722445493,5.1966858609638));
#61820=CARTESIAN_POINT('Ctrl Pts',(1.38918536357089,-1.92236090419131,5.19598729516338));
#61821=CARTESIAN_POINT('Ctrl Pts',(1.36212866676027,-1.94173228346285,5.19377558464823));
#61822=CARTESIAN_POINT('Ctrl Pts',(1.34338323805886,-1.95474815109517,5.19227577796469));
#61823=CARTESIAN_POINT('Ctrl Pts',(1.22223227320997,-2.03630306585041,5.18276828875893));
#61824=CARTESIAN_POINT('Ctrl Pts',(1.11479213393869,-2.09705218913936,5.17516855675224));
#61825=CARTESIAN_POINT('Ctrl Pts',(0.945379235625385,-2.17612370770374,
5.16368088096112));
#61826=CARTESIAN_POINT('Ctrl Pts',(0.886591354429019,-2.20072986871388,
5.15977966306666));
#61827=CARTESIAN_POINT('Ctrl Pts',(0.751620642816595,-2.25093602605472,
5.15089184486527));
#61828=CARTESIAN_POINT('Ctrl Pts',(0.674988086665912,-2.27509038153553,
5.14589223014156));
#61829=CARTESIAN_POINT('Ctrl Pts',(0.546276860842511,-2.30858340583356,
5.1374346946491));
#61830=CARTESIAN_POINT('Ctrl Pts',(0.494846738765258,-2.32015124687534,
5.13404036366586));
#61831=CARTESIAN_POINT('Ctrl Pts',(0.422648284155725,-2.33388065400993,
5.12923221876156));
#61832=CARTESIAN_POINT('Ctrl Pts',(0.402170081182587,-2.3374964513562,5.12786372808805));
#61833=CARTESIAN_POINT('Ctrl Pts',(0.366966882564049,-2.34323592901909,
5.12550187172242));
#61834=CARTESIAN_POINT('Ctrl Pts',(0.352264361810375,-2.34549123092685,
5.1245126707273));
#61835=CARTESIAN_POINT('Ctrl Pts',(0.324116109565076,-2.34953842011654,
5.12261309467419));
#61836=CARTESIAN_POINT('Ctrl Pts',(0.310674273850211,-2.35135355116424,
5.12170348714916));
#61837=CARTESIAN_POINT('Ctrl Pts',(0.275558193711459,-2.35578911827115,
5.11932032703938));
#61838=CARTESIAN_POINT('Ctrl Pts',(0.253862449704423,-2.35822570795184,
5.11784112932851));
#61839=CARTESIAN_POINT('Ctrl Pts',(0.176527516144385,-2.36583143911257,
5.11254270950452));
#61840=CARTESIAN_POINT('Ctrl Pts',(0.120746687765224,-2.3693331786405,5.10867306486535));
#61841=CARTESIAN_POINT('Ctrl Pts',(-0.103178546333948,-2.37546272277441,
5.09293911122627));
#61842=CARTESIAN_POINT('Ctrl Pts',(-0.271250090448635,-2.36217655614269,
5.08063398237339));
#61843=CARTESIAN_POINT('Ctrl Pts',(-0.529518501311077,-2.31382120385999,
5.06151362631611));
#61844=CARTESIAN_POINT('Ctrl Pts',(-0.621443989771581,-2.290844658127,5.05467638259956));
#61845=CARTESIAN_POINT('Ctrl Pts',(-0.732862488046355,-2.25579257394576,
5.04652125382848));
#61846=CARTESIAN_POINT('Ctrl Pts',(-0.753874397545816,-2.24885771949728,
5.04498944050483));
#61847=CARTESIAN_POINT('Ctrl Pts',(-0.784654115750265,-2.2382191514835,
5.04275763140437));
#61848=CARTESIAN_POINT('Ctrl Pts',(-0.794498746923263,-2.23474356533645,
5.04204564603436));
#61849=CARTESIAN_POINT('Ctrl Pts',(-0.811249105518429,-2.22870527387681,
5.04083774844552));
#61850=CARTESIAN_POINT('Ctrl Pts',(-0.818166239288852,-2.22617526694883,
5.04033998914812));
#61851=CARTESIAN_POINT('Ctrl Pts',(-0.833998536931158,-2.22030069161058,
5.0392031457014));
#61852=CARTESIAN_POINT('Ctrl Pts',(-0.842905466013555,-2.21693461878631,
5.03856532685785));
#61853=CARTESIAN_POINT('Ctrl Pts',(-0.867696864975055,-2.20739453531885,
5.0367942713596));
#61854=CARTESIAN_POINT('Ctrl Pts',(-0.883535786400458,-2.20110268703148,
5.03566764365087));
#61855=CARTESIAN_POINT('Ctrl Pts',(-1.00668284353969,-2.15064025459855,
5.02693608509348));
#61856=CARTESIAN_POINT('Ctrl Pts',(-1.11070066680025,-2.09881276778849,
5.01972333614952));
#61857=CARTESIAN_POINT('Ctrl Pts',(-1.28769825776428,-1.9937619301061,5.00704677436244));
#61858=CARTESIAN_POINT('Ctrl Pts',(-1.36221653708385,-1.94360989732643,
5.00156804588226));
#61859=CARTESIAN_POINT('Ctrl Pts',(-1.49280769753586,-1.84451249259589,
4.99142566107865));
#61860=CARTESIAN_POINT('Ctrl Pts',(-1.54976213834342,-1.79692438871535,
4.98679178318952));
#61861=CARTESIAN_POINT('Ctrl Pts',(-1.62949049096849,-1.72369380374607,
4.97989462267737));
#61862=CARTESIAN_POINT('Ctrl Pts',(-1.65408978781575,-1.70010187651077,
4.97770498499979));
#61863=CARTESIAN_POINT('Ctrl Pts',(-1.69792110029346,-1.65621348917713,
4.97368083338071));
#61864=CARTESIAN_POINT('Ctrl Pts',(-1.71731905625329,-1.63609117639608,
4.97185363526228));
#61865=CARTESIAN_POINT('Ctrl Pts',(-1.74749507321233,-1.60366031706711,
4.9689333846657));
#61866=CARTESIAN_POINT('Ctrl Pts',(-1.75850954035204,-1.59157457179876,
4.96785035710913));
#61867=CARTESIAN_POINT('Ctrl Pts',(-1.77907049449402,-1.56853983762533,
4.96579535782261));
#61868=CARTESIAN_POINT('Ctrl Pts',(-1.78864311734304,-1.55761510951789,
4.96482453466022));
#61869=CARTESIAN_POINT('Ctrl Pts',(-1.81013736893641,-1.53262542620302,
4.96261197007417));
#61870=CARTESIAN_POINT('Ctrl Pts',(-1.82199642763213,-1.51850814161053,
4.96136776704467));
#61871=CARTESIAN_POINT('Ctrl Pts',(-1.85248378237576,-1.48134398854073,
4.95810636426919));
#61872=CARTESIAN_POINT('Ctrl Pts',(-1.8708463669378,-1.45808432931162,4.95607887827389));
#61873=CARTESIAN_POINT('Ctrl Pts',(-1.99725136090337,-1.29164882871519,
4.94166095743455));
#61874=CARTESIAN_POINT('Ctrl Pts',(-2.08916325645431,-1.13698900617608,
4.92865761031279));
#61875=CARTESIAN_POINT('Ctrl Pts',(-2.21370757501617,-0.860293800848927,
4.90653067278365));
#61876=CARTESIAN_POINT('Ctrl Pts',(-2.25569782886252,-0.743263297334418,
4.89749655228345));
#61877=CARTESIAN_POINT('Ctrl Pts',(-2.29319862305957,-0.605623952511441,
4.88758085445317));
#61878=CARTESIAN_POINT('Ctrl Pts',(-2.29785288088542,-0.587718033360064,
4.88630450918909));
#61879=CARTESIAN_POINT('Ctrl Pts',(-2.30463369035238,-0.560317949411029,
4.884373984422));
#61880=CARTESIAN_POINT('Ctrl Pts',(-2.30691202010398,-0.550862588145834,
4.88371186573602));
#61881=CARTESIAN_POINT('Ctrl Pts',(-2.31099467408976,-0.533449391215215,
4.88250031183981));
#61882=CARTESIAN_POINT('Ctrl Pts',(-2.31281613072446,-0.525496132773104,
4.88194997407838));
#61883=CARTESIAN_POINT('Ctrl Pts',(-2.31687624121119,-0.507337844474354,
4.88070023853457));
#61884=CARTESIAN_POINT('Ctrl Pts',(-2.31908855145077,-0.497127253536078,
4.88000231090401));
#61885=CARTESIAN_POINT('Ctrl Pts',(-2.3257420416033,-0.465407731117818,
4.87784813625195));
#61886=CARTESIAN_POINT('Ctrl Pts',(-2.32995213459907,-0.443850801518335,
4.87640399157544));
#61887=CARTESIAN_POINT('Ctrl Pts',(-2.35894128111667,-0.283617131047518,
4.86579545824992));
#61888=CARTESIAN_POINT('Ctrl Pts',(-2.37162363284765,-0.143018943548074,
4.85717261551335));
#61889=CARTESIAN_POINT('Ctrl Pts',(-2.37180106459394,0.0563113734359232,
4.84493532920882));
#61890=CARTESIAN_POINT('Ctrl Pts',(-2.36969438103518,0.114680731789333,
4.84135207295172));
#61891=CARTESIAN_POINT('Ctrl Pts',(-2.36544099470095,0.17287846334401,4.83774038296924));
#61892=CARTESIAN_POINT('',(-2.36824990783039,0.000427589681932447,4.65128666940576));
#61893=CARTESIAN_POINT('Ctrl Pts',(-2.36544101871061,0.172878134827089,
4.63810474394384));
#61894=CARTESIAN_POINT('Ctrl Pts',(-2.36696574558802,0.152015742357601,
4.63943647498258));
#61895=CARTESIAN_POINT('Ctrl Pts',(-2.36821501678678,0.131125760271669,
4.64077559292494));
#61896=CARTESIAN_POINT('Ctrl Pts',(-2.37023193297686,0.0877694335960402,
4.64356885572076));
#61897=CARTESIAN_POINT('Ctrl Pts',(-2.37095701087706,0.0653122499247474,
4.64502343606539));
#61898=CARTESIAN_POINT('Ctrl Pts',(-2.37161918842369,0.0286655714961145,
4.64741167205354));
#61899=CARTESIAN_POINT('Ctrl Pts',(-2.37174821222471,0.01448071021935,4.64833964750865));
#61900=CARTESIAN_POINT('Ctrl Pts',(-2.37174998154971,0.000295836006343133,
4.64927143992648));
#61901=CARTESIAN_POINT('Ctrl Pts',(-2.36803551809634,0.000435659979227676,
4.65141010809499));
#61902=CARTESIAN_POINT('Ctrl Pts',(-2.36733685507668,-0.420470574046625,
4.67955118317444));
#61903=CARTESIAN_POINT('Ctrl Pts',(-2.06020439223756,-1.62937224150312,
4.76031262862425));
#61904=CARTESIAN_POINT('Ctrl Pts',(-0.135586668767159,-2.79462423533096,
4.89369444444444));
#61905=CARTESIAN_POINT('Ctrl Pts',(2.2650598786042,-1.64250178316317,5.05155555555556));
#61906=CARTESIAN_POINT('Ctrl Pts',(2.61412853009539,0.997316594419356,5.20941666666666));
#61907=CARTESIAN_POINT('Ctrl Pts',(0.595450368366912,2.73381550588105,5.36727777777778));
#61908=CARTESIAN_POINT('Ctrl Pts',(-1.72846737744239,2.061848728322,5.51069262891245));
#61909=CARTESIAN_POINT('Ctrl Pts',(-2.31767164028317,0.740184958633683,
5.60148710967678));
#61910=CARTESIAN_POINT('Ctrl Pts',(-2.36449584214975,0.172800370348396,
5.63966122007073));
#61911=CARTESIAN_POINT('Origin',(0.,0.,-1.84858989190501));
#61912=CARTESIAN_POINT('',(-2.36285989125428,0.172707701180992,6.83708460818679));
#61913=CARTESIAN_POINT('',(-2.36544101887183,0.172878132621275,6.64182320144908));
#61914=CARTESIAN_POINT('',(-2.36544101854889,0.172878137039864,-1.84858989190501));
#61915=CARTESIAN_POINT('',(-2.37459233302104,0.00130583459664112,5.84859123935915));
#61916=CARTESIAN_POINT('Ctrl Pts',(-2.37459233302104,0.00130583459664112,
5.84859123935915));
#61917=CARTESIAN_POINT('Ctrl Pts',(-2.36985292963545,-0.701523551850097,
5.89591470923835));
#61918=CARTESIAN_POINT('Ctrl Pts',(-1.66848328383473,-2.19471928883836,
5.99590314278425));
#61919=CARTESIAN_POINT('Ctrl Pts',(0.864288593995119,-2.66190468356086,
6.14855653999681));
#61920=CARTESIAN_POINT('Ctrl Pts',(2.70163876039796,-0.730670463607777,
6.30655143099686));
#61921=CARTESIAN_POINT('Ctrl Pts',(2.08817696449889,1.86339697407977,6.46454632199692));
#61922=CARTESIAN_POINT('Ctrl Pts',(-0.419590302218696,2.76706980330411,
6.62254121299697));
#61923=CARTESIAN_POINT('Ctrl Pts',(-2.09145531965774,1.50441074284138,6.74672064172692));
#61924=CARTESIAN_POINT('Ctrl Pts',(-2.34427764227796,0.453694740318712,
6.8182351067902));
#61925=CARTESIAN_POINT('Ctrl Pts',(-2.36285989125428,0.172707701180992,
6.83708460818679));
#61926=CARTESIAN_POINT('Ctrl Pts',(-2.37174969264697,0.00120744731113393,
5.84695890962807));
#61927=CARTESIAN_POINT('Ctrl Pts',(-2.37173086567736,0.0381886546764642,
5.84431029447727));
#61928=CARTESIAN_POINT('Ctrl Pts',(-2.37084710102938,0.0751666995482175,
5.84168447192852));
#61929=CARTESIAN_POINT('Ctrl Pts',(-2.36813959604457,0.132380889107501,
5.83767047856927));
#61930=CARTESIAN_POINT('Ctrl Pts',(-2.36692025046112,0.152638239149765,
5.83625878866294));
#61931=CARTESIAN_POINT('Ctrl Pts',(-2.36544101854819,0.172878137049535,
5.83485941057446));
#61932=CARTESIAN_POINT('',(-2.37251493491373,-0.00202804545912198,5.65140963369938));
#61933=CARTESIAN_POINT('Ctrl Pts',(-2.36449584214975,0.172800370348396,
5.63966122007073));
#61934=CARTESIAN_POINT('Ctrl Pts',(-2.36929936025563,0.114594527340226,
5.64357735794695));
#61935=CARTESIAN_POINT('Ctrl Pts',(-2.37198857858181,0.056265582705663,
5.64749349582317));
#61936=CARTESIAN_POINT('Ctrl Pts',(-2.37251493491373,-0.00202804545912198,
5.65140963369939));
#61937=CARTESIAN_POINT('Ctrl Pts',(-2.37174915472122,-0.00200239336298696,
5.65184980432678));
#61938=CARTESIAN_POINT('Ctrl Pts',(-2.37166794312654,-0.0981940481058294,
5.65886281514045));
#61939=CARTESIAN_POINT('Ctrl Pts',(-2.36573489179878,-0.194299783852276,
5.66586596605852));
#61940=CARTESIAN_POINT('Ctrl Pts',(-2.3497986979236,-0.323751847410071,
5.67511270209506));
#61941=CARTESIAN_POINT('Ctrl Pts',(-2.34488253083876,-0.357624627038201,
5.67751425362095));
#61942=CARTESIAN_POINT('Ctrl Pts',(-2.33735999376333,-0.402585872055809,
5.68066812323276));
#61943=CARTESIAN_POINT('Ctrl Pts',(-2.33540477226843,-0.413777339585329,
5.68145035057679));
#61944=CARTESIAN_POINT('Ctrl Pts',(-2.33186555464311,-0.43321071317438,
5.68280325624251));
#61945=CARTESIAN_POINT('Ctrl Pts',(-2.33031810765848,-0.441458955457005,
5.68337578586718));
#61946=CARTESIAN_POINT('Ctrl Pts',(-2.32713019967211,-0.457967259067173,
5.68451803759382));
#61947=CARTESIAN_POINT('Ctrl Pts',(-2.32548946222107,-0.466227140607921,
5.68508771958931));
#61948=CARTESIAN_POINT('Ctrl Pts',(-2.32189257884279,-0.483843228240834,
5.68629862105365));
#61949=CARTESIAN_POINT('Ctrl Pts',(-2.31992383518342,-0.493196536974783,
5.6869391423792));
#61950=CARTESIAN_POINT('Ctrl Pts',(-2.3143744281283,-0.518792542470743,
5.68868600205301));
#61951=CARTESIAN_POINT('Ctrl Pts',(-2.31067929090371,-0.535010231847836,
5.68978620766974));
#61952=CARTESIAN_POINT('Ctrl Pts',(-2.28839528053491,-0.628272489029095,
5.69608199438093));
#61953=CARTESIAN_POINT('Ctrl Pts',(-2.26612256851991,-0.704393706809874,
5.70109852589671));
#61954=CARTESIAN_POINT('Ctrl Pts',(-2.20294805643682,-0.885995548806609,
5.71307902927118));
#61955=CARTESIAN_POINT('Ctrl Pts',(-2.15823755304937,-0.989939599355856,
5.71995216633633));
#61956=CARTESIAN_POINT('Ctrl Pts',(-2.05095933236282,-1.1971835582713,5.73434570236838));
#61957=CARTESIAN_POINT('Ctrl Pts',(-1.9875847909272,-1.29968620325887,5.74186106462762));
#61958=CARTESIAN_POINT('Ctrl Pts',(-1.89989583690999,-1.42000316492679,
5.75151037429319));
#61959=CARTESIAN_POINT('Ctrl Pts',(-1.88266547412633,-1.44276948252377,
5.75337524915367));
#61960=CARTESIAN_POINT('Ctrl Pts',(-1.85455393447574,-1.47855174696766,
5.75637277602015));
#61961=CARTESIAN_POINT('Ctrl Pts',(-1.84393649331933,-1.49177201614181,
5.75749516343398));
#61962=CARTESIAN_POINT('Ctrl Pts',(-1.82376738348017,-1.5163411846726,5.7596099266484));
#61963=CARTESIAN_POINT('Ctrl Pts',(-1.81424918020712,-1.52771658121852,
5.76060093619527));
#61964=CARTESIAN_POINT('Ctrl Pts',(-1.79259963651647,-1.55310271869043,
5.76283993916535));
#61965=CARTESIAN_POINT('Ctrl Pts',(-1.78040962704136,-1.56706191266333,
5.76409027952431));
#61966=CARTESIAN_POINT('Ctrl Pts',(-1.74858607135156,-1.60265348425514,
5.7673289357105));
#61967=CARTESIAN_POINT('Ctrl Pts',(-1.7287146750491,-1.62406800395068,5.7693269732948));
#61968=CARTESIAN_POINT('Ctrl Pts',(-1.58063178415813,-1.77785277088925,
5.78404817766247));
#61969=CARTESIAN_POINT('Ctrl Pts',(-1.43779618794092,-1.89522429238506,
5.79742202102943));
#61970=CARTESIAN_POINT('Ctrl Pts',(-1.18456463126363,-2.05807213279846,
5.81936802902516));
#61971=CARTESIAN_POINT('Ctrl Pts',(-1.08172724905443,-2.11393611482528,
5.82785934724171));
#61972=CARTESIAN_POINT('Ctrl Pts',(-0.956752551750246,-2.17030673506258,
5.83740901699846));
#61973=CARTESIAN_POINT('Ctrl Pts',(-0.938217684610245,-2.17838344028346,
5.83880613460741));
#61974=CARTESIAN_POINT('Ctrl Pts',(-0.910171579756127,-2.1901803489787,
5.84088910000979));
#61975=CARTESIAN_POINT('Ctrl Pts',(-0.900736422135724,-2.19407752212689,
5.84158460455654));
#61976=CARTESIAN_POINT('Ctrl Pts',(-0.883553561026318,-2.20104534553064,
5.84284135633981));
#61977=CARTESIAN_POINT('Ctrl Pts',(-0.8758146192241,-2.2041361722323,5.84340373421265));
#61978=CARTESIAN_POINT('Ctrl Pts',(-0.85820768060397,-2.21106076408846,
5.84467502784564));
#61979=CARTESIAN_POINT('Ctrl Pts',(-0.848330143529769,-2.21486931977632,
5.84538247591548));
#61980=CARTESIAN_POINT('Ctrl Pts',(-0.817698653911014,-2.22644515083145,
5.84755959837781));
#61981=CARTESIAN_POINT('Ctrl Pts',(-0.796860432302053,-2.23398805618294,
5.84901698517874));
#61982=CARTESIAN_POINT('Ctrl Pts',(-0.641225565782021,-2.28786898746856,
5.85974823718837));
#61983=CARTESIAN_POINT('Ctrl Pts',(-0.502584568826552,-2.3222691889155,
5.86846862559448));
#61984=CARTESIAN_POINT('Ctrl Pts',(-0.200484376636533,-2.36888287304801,
5.88723970182822));
#61985=CARTESIAN_POINT('Ctrl Pts',(-0.0371763193537273,-2.37705895602669,
5.89726972323087));
#61986=CARTESIAN_POINT('Ctrl Pts',(0.153769447917697,-2.36692730583829,
5.90967436473727));
#61987=CARTESIAN_POINT('Ctrl Pts',(0.181840008248037,-2.36493636650573,
5.91151400393899));
#61988=CARTESIAN_POINT('Ctrl Pts',(0.226431364426487,-2.36097510024288,
5.91446515068847));
#61989=CARTESIAN_POINT('Ctrl Pts',(0.242978858837109,-2.35932953134603,
5.91556661966193));
#61990=CARTESIAN_POINT('Ctrl Pts',(0.27429980513601,-2.35588181959543,5.91766410185168));
#61991=CARTESIAN_POINT('Ctrl Pts',(0.289076325572834,-2.35411435402693,
5.91865899152265));
#61992=CARTESIAN_POINT('Ctrl Pts',(0.322730659542994,-2.34976722015807,
5.9209375659714));
#61993=CARTESIAN_POINT('Ctrl Pts',(0.34159577959488,-2.34709892303891,5.9222239475366));
#61994=CARTESIAN_POINT('Ctrl Pts',(0.391070384778924,-2.3394920985684,5.92562238761362));
#61995=CARTESIAN_POINT('Ctrl Pts',(0.421617885048203,-2.33418026909222,
5.92774584447236));
#61996=CARTESIAN_POINT('Ctrl Pts',(0.607481495457014,-2.29809345997478,
5.94082479006268));
#61997=CARTESIAN_POINT('Ctrl Pts',(0.759473790852414,-2.25243224387335,
5.95224128414857));
#61998=CARTESIAN_POINT('Ctrl Pts',(1.03485026984828,-2.13864274578075,5.97395822250262));
#61999=CARTESIAN_POINT('Ctrl Pts',(1.15898801540537,-2.07399653816928,5.98417970654474));
#62000=CARTESIAN_POINT('Ctrl Pts',(1.29364213274884,-1.98798671299195,5.99530717374739));
#62001=CARTESIAN_POINT('Ctrl Pts',(1.31042462640827,-1.97696446678553,5.99669444299449));
#62002=CARTESIAN_POINT('Ctrl Pts',(1.33550313641406,-1.96003394582676,5.99876576210146));
#62003=CARTESIAN_POINT('Ctrl Pts',(1.34390390814573,-1.95428349821039,5.99945931474755));
#62004=CARTESIAN_POINT('Ctrl Pts',(1.35911474806026,-1.94372699455734,6.00071417881865));
#62005=CARTESIAN_POINT('Ctrl Pts',(1.36593669637092,-1.9389390072561,6.00127660029417));
#62006=CARTESIAN_POINT('Ctrl Pts',(1.38139228425708,-1.92796943935018,6.00255003912493));
#62007=CARTESIAN_POINT('Ctrl Pts',(1.39000980042788,-1.92176574208364,6.00325956611506));
#62008=CARTESIAN_POINT('Ctrl Pts',(1.41661840509883,-1.90233774513479,6.00544983191101));
#62009=CARTESIAN_POINT('Ctrl Pts',(1.43446521057047,-1.88891668667636,6.00691806890733));
#62010=CARTESIAN_POINT('Ctrl Pts',(1.56440607940641,-1.78829526939246,6.01762398864826));
#62011=CARTESIAN_POINT('Ctrl Pts',(1.66867043826281,-1.69142422172829,6.02631362159911));
#62012=CARTESIAN_POINT('Ctrl Pts',(1.87255311146014,-1.46467491947559,6.04503903001394));
#62013=CARTESIAN_POINT('Ctrl Pts',(1.96867757303984,-1.33267691942787,6.05505415970181));
#62014=CARTESIAN_POINT('Ctrl Pts',(2.06478852906705,-1.16732727622128,6.06745799708827));
#62015=CARTESIAN_POINT('Ctrl Pts',(2.07861790555876,-1.14252007918357,6.06931428010355));
#62016=CARTESIAN_POINT('Ctrl Pts',(2.09985899735469,-1.10275501329495,6.07228585413338));
#62017=CARTESIAN_POINT('Ctrl Pts',(2.10756427569611,-1.08795644593969,6.07339085826053));
#62018=CARTESIAN_POINT('Ctrl Pts',(2.12184112361499,-1.05981577237725,6.07549113037718));
#62019=CARTESIAN_POINT('Ctrl Pts',(2.12844460552388,-1.04649069242988,6.07648523296498));
#62020=CARTESIAN_POINT('Ctrl Pts',(2.14317976182847,-1.01604032845627,6.07875647537248));
#62021=CARTESIAN_POINT('Ctrl Pts',(2.15123221052809,-0.99887806118754,6.08003624774184));
#62022=CARTESIAN_POINT('Ctrl Pts',(2.17177274193197,-0.953699134860895,
6.08340518033409));
#62023=CARTESIAN_POINT('Ctrl Pts',(2.18392422570758,-0.925534282549245,
6.0855054199611));
#62024=CARTESIAN_POINT('Ctrl Pts',(2.25880126029705,-0.742292049572722,
6.09917507062049));
#62025=CARTESIAN_POINT('Ctrl Pts',(2.30550651396125,-0.581207258801752,
6.11126576478187));
#62026=CARTESIAN_POINT('Ctrl Pts',(2.35139354153301,-0.324017641551093,
6.13031318824199));
#62027=CARTESIAN_POINT('Ctrl Pts',(2.36239035490912,-0.230548353423396,
6.13717293743749));
#62028=CARTESIAN_POINT('Ctrl Pts',(2.36967215289794,-0.104390336391882,
6.14618724693443));
#62029=CARTESIAN_POINT('Ctrl Pts',(2.37087512005553,-0.072075158327642,
6.14847441463289));
#62030=CARTESIAN_POINT('Ctrl Pts',(2.37180665194257,-0.0164930959482848,
6.15236043475196));
#62031=CARTESIAN_POINT('Ctrl Pts',(2.3718543744367,0.00676331707411645,
6.15397199079599));
#62032=CARTESIAN_POINT('Ctrl Pts',(2.37142346659216,0.0408073455603119,
6.15630647100209));
#62033=CARTESIAN_POINT('Ctrl Pts',(2.3712132637851,0.0515961845427436,6.1570426674515));
#62034=CARTESIAN_POINT('Ctrl Pts',(2.37073089880731,0.0699288182410932,
6.15828705818149));
#62035=CARTESIAN_POINT('Ctrl Pts',(2.3704963484424,0.0774732345676194,6.15879725358695));
#62036=CARTESIAN_POINT('Ctrl Pts',(2.36987840497654,0.0947012026120704,
6.15995788123622));
#62037=CARTESIAN_POINT('Ctrl Pts',(2.36947167751313,0.10438366663914,6.16060703320101));
#62038=CARTESIAN_POINT('Ctrl Pts',(2.36817728492117,0.131267123853438,6.16240135066376));
#62039=CARTESIAN_POINT('Ctrl Pts',(2.36716156245559,0.148461744861513,6.16353982541141));
#62040=CARTESIAN_POINT('Ctrl Pts',(2.35805772577831,0.278495139973572,6.17209036885216));
#62041=CARTESIAN_POINT('Ctrl Pts',(2.34209176644544,0.3906515282706,6.17913186592397));
#62042=CARTESIAN_POINT('Ctrl Pts',(2.31562194557889,0.513068438372429,6.18685153373076));
#62043=CARTESIAN_POINT('Ctrl Pts',(2.31297660886462,0.524865150709604,6.18759574457694));
#62044=CARTESIAN_POINT('Ctrl Pts',(2.2814148673633,0.660738504601893,6.19617569045349));
#62045=CARTESIAN_POINT('Ctrl Pts',(2.24263809764807,0.782305326129489,6.20394463107483));
#62046=CARTESIAN_POINT('Ctrl Pts',(2.16761985853045,0.965173117035017,6.21638260139341));
#62047=CARTESIAN_POINT('Ctrl Pts',(2.13807902265709,1.0289565946446,6.22087010455547));
#62048=CARTESIAN_POINT('Ctrl Pts',(2.09502335796077,1.11203368889986,6.22697333188627));
#62049=CARTESIAN_POINT('Ctrl Pts',(2.08398942813815,1.13257661834035,6.22850421071076));
#62050=CARTESIAN_POINT('Ctrl Pts',(2.06506507766063,1.16659677877985,6.23107774091571));
#62051=CARTESIAN_POINT('Ctrl Pts',(2.05734106109059,1.18016505542708,6.23211451179386));
#62052=CARTESIAN_POINT('Ctrl Pts',(2.04186932841817,1.20672971922513,6.23416540886358));
#62053=CARTESIAN_POINT('Ctrl Pts',(2.03413008477298,1.21973019546412,6.23517919624074));
#62054=CARTESIAN_POINT('Ctrl Pts',(2.01502784637667,1.25113088968851,6.23765300620252));
#62055=CARTESIAN_POINT('Ctrl Pts',(2.0035367252948,1.26945116565578,6.23911760440889));
#62056=CARTESIAN_POINT('Ctrl Pts',(1.96320934194487,1.33183331897786,6.24417993860481));
#62057=CARTESIAN_POINT('Ctrl Pts',(1.93315896656321,1.37508784267071,6.24782152875939));
#62058=CARTESIAN_POINT('Ctrl Pts',(1.79963732491798,1.5542432063077,6.26348319573832));
#62059=CARTESIAN_POINT('Ctrl Pts',(1.68309694255494,1.67974274988152,6.27597317026033));
#62060=CARTESIAN_POINT('Ctrl Pts',(1.50057186855107,1.83807146027089,6.29355498997769));
#62061=CARTESIAN_POINT('Ctrl Pts',(1.44496712732386,1.88209825588017,6.29868542273145));
#62062=CARTESIAN_POINT('Ctrl Pts',(1.36528505362854,1.93957290831984,6.30565854747292));
#62063=CARTESIAN_POINT('Ctrl Pts',(1.34282320786524,1.95519111906169,6.30758471133477));
#62064=CARTESIAN_POINT('Ctrl Pts',(1.30306828536725,1.98182520638829,6.31091900388936));
#62065=CARTESIAN_POINT('Ctrl Pts',(1.28589350464133,1.99301180865828,6.31233574800345));
#62066=CARTESIAN_POINT('Ctrl Pts',(1.25990330910869,2.00946436907164,6.31444189797018));
#62067=CARTESIAN_POINT('Ctrl Pts',(1.25119570016981,2.01489769678574,6.31514127058831));
#62068=CARTESIAN_POINT('Ctrl Pts',(1.2353559568882,2.02463901429807,6.31640179781952));
#62069=CARTESIAN_POINT('Ctrl Pts',(1.22823617740633,2.02896608544545,6.31696412372678));
#62070=CARTESIAN_POINT('Ctrl Pts',(1.21207089210003,2.0386743195224,6.3182313186339));
#62071=CARTESIAN_POINT('Ctrl Pts',(1.20301222255233,2.04403288411482,6.31893476371194));
#62072=CARTESIAN_POINT('Ctrl Pts',(1.17504981067659,2.06032348065511,6.32108671648624));
#62073=CARTESIAN_POINT('Ctrl Pts',(1.15602992510676,2.07105523750016,6.32252334163217));
#62074=CARTESIAN_POINT('Ctrl Pts',(1.00841092271245,2.15168017927849,6.33348752082668));
#62075=CARTESIAN_POINT('Ctrl Pts',(0.873721809573873,2.20980584028212,6.34242836118869));
#62076=CARTESIAN_POINT('Ctrl Pts',(0.583487503549271,2.30433726137325,6.36117352513113));
#62077=CARTESIAN_POINT('Ctrl Pts',(0.427917875657047,2.33822706952737,6.37095396050662));
#62078=CARTESIAN_POINT('Ctrl Pts',(0.241681792298568,2.35957801538512,6.38310849996914));
#62079=CARTESIAN_POINT('Ctrl Pts',(0.213169196996673,2.36232454992421,6.38498030710498));
#62080=CARTESIAN_POINT('Ctrl Pts',(0.167929800115494,2.36585665908776,6.38797093359657));
#62081=CARTESIAN_POINT('Ctrl Pts',(0.151231834886828,2.36698269054815,6.3890792321497));
#62082=CARTESIAN_POINT('Ctrl Pts',(0.119684918883122,2.36877489069326,6.39118215537347));
#62083=CARTESIAN_POINT('Ctrl Pts',(0.104838835965593,2.36947837381484,6.39217557597353));
#62084=CARTESIAN_POINT('Ctrl Pts',(0.0711297031559081,2.37075826548578,
6.39444023879082));
#62085=CARTESIAN_POINT('Ctrl Pts',(0.0522646125744744,2.37124915666286,
6.39571405572123));
#62086=CARTESIAN_POINT('Ctrl Pts',(0.00302386918786248,2.37194257433258,
6.39905648113215));
#62087=CARTESIAN_POINT('Ctrl Pts',(-0.0273525361268728,2.37178675520128,
6.40113588612477));
#62088=CARTESIAN_POINT('Ctrl Pts',(-0.26650507321228,2.36596526740108,6.41765082735151));
#62089=CARTESIAN_POINT('Ctrl Pts',(-0.473676394463343,2.33332678581228,
6.43294090165484));
#62090=CARTESIAN_POINT('Ctrl Pts',(-0.758236246628948,2.24900496389794,
6.45450603596177));
#62091=CARTESIAN_POINT('Ctrl Pts',(-0.841179760054879,2.21931636515862,
6.46084645882629));
#62092=CARTESIAN_POINT('Ctrl Pts',(-0.942183816947739,2.17668419956558,
6.46849574397388));
#62093=CARTESIAN_POINT('Ctrl Pts',(-0.961965353313174,2.16801457315593,
6.46999015892612));
#62094=CARTESIAN_POINT('Ctrl Pts',(-0.991165323829755,2.15473876830929,
6.47218773379054));
#62095=CARTESIAN_POINT('Ctrl Pts',(-1.00067548523696,2.15033868086364,6.47290212873397));
#62096=CARTESIAN_POINT('Ctrl Pts',(-1.01769368528513,2.14232747856053,6.47417771323426));
#62097=CARTESIAN_POINT('Ctrl Pts',(-1.02521216477358,2.13873969559181,6.47474023046216));
#62098=CARTESIAN_POINT('Ctrl Pts',(-1.04199003476132,2.13062456835668,6.47599324657539));
#62099=CARTESIAN_POINT('Ctrl Pts',(-1.05123896914347,2.1260764152266,6.47668247835339));
#62100=CARTESIAN_POINT('Ctrl Pts',(-1.07898516150538,2.11220692658176,6.4787464694199));
#62101=CARTESIAN_POINT('Ctrl Pts',(-1.09739080255681,2.10270315940521,6.48011070850734));
#62102=CARTESIAN_POINT('Ctrl Pts',(-1.25726881501884,2.01747877350479,6.49193834297783));
#62103=CARTESIAN_POINT('Ctrl Pts',(-1.39086250400372,1.92781262917818,6.50168438669642));
#62104=CARTESIAN_POINT('Ctrl Pts',(-1.61100020577519,1.74517466684006,6.51926163015064));
#62105=CARTESIAN_POINT('Ctrl Pts',(-1.70108575256117,1.65748577807768,6.52701750948861));
#62106=CARTESIAN_POINT('Ctrl Pts',(-1.81110409040156,1.53193206389676,6.53771988382237));
#62107=CARTESIAN_POINT('Ctrl Pts',(-1.83758098174724,1.50006989261944,6.54040385598605));
#62108=CARTESIAN_POINT('Ctrl Pts',(-1.87511626406298,1.45241433384362,6.54438308900106));
#62109=CARTESIAN_POINT('Ctrl Pts',(-1.88683895878102,1.43715243057007,6.54565235426911));
#62110=CARTESIAN_POINT('Ctrl Pts',(-1.90730849595032,1.40982072915163,6.54791744813605));
#62111=CARTESIAN_POINT('Ctrl Pts',(-1.9161298147236,1.39780782050987,6.54891033929669));
#62112=CARTESIAN_POINT('Ctrl Pts',(-1.93449125404957,1.37230269361937,6.55101326012844));
#62113=CARTESIAN_POINT('Ctrl Pts',(-1.94400472687026,1.35879236572654,6.55212422997065));
#62114=CARTESIAN_POINT('Ctrl Pts',(-1.96905512816116,1.32241603864394,6.55510826510037));
#62115=CARTESIAN_POINT('Ctrl Pts',(-1.98433434223131,1.2993765367708,6.5569907555173));
#62116=CARTESIAN_POINT('Ctrl Pts',(-2.06610586074821,1.17126647757892,6.56742170154033));
#62117=CARTESIAN_POINT('Ctrl Pts',(-2.12464894754521,1.06137495115133,6.57625134991567));
#62118=CARTESIAN_POINT('Ctrl Pts',(-2.24341076832004,0.788819037881383,
6.59776737571126));
#62119=CARTESIAN_POINT('Ctrl Pts',(-2.29495825635376,0.623134794124575,
6.61056644981406));
#62120=CARTESIAN_POINT('Ctrl Pts',(-2.33347219714566,0.42534408358896,6.62472907394182));
#62121=CARTESIAN_POINT('Ctrl Pts',(-2.3384144303431,0.397275990065826,6.62671227495847));
#62122=CARTESIAN_POINT('Ctrl Pts',(-2.34466907916963,0.357577416564442,
6.62947372682879));
#62123=CARTESIAN_POINT('Ctrl Pts',(-2.34640297078246,0.346017069639293,
6.63027269063599));
#62124=CARTESIAN_POINT('Ctrl Pts',(-2.3492418767404,0.326085794439408,6.63164074259073));
#62125=CARTESIAN_POINT('Ctrl Pts',(-2.35038777459285,0.317721039527598,
6.63221201510996));
#62126=CARTESIAN_POINT('Ctrl Pts',(-2.35272563345256,0.299950068680857,
6.63341943561299));
#62127=CARTESIAN_POINT('Ctrl Pts',(-2.35390589037828,0.290542625114165,
6.63405494874092));
#62128=CARTESIAN_POINT('Ctrl Pts',(-2.35701148363441,0.264526858563489,
6.63580294536797));
#62129=CARTESIAN_POINT('Ctrl Pts',(-2.35881771050953,0.247904497812455,
6.63690914094991));
#62130=CARTESIAN_POINT('Ctrl Pts',(-2.36235291397937,0.211821625798301,
6.63929002479679));
#62131=CARTESIAN_POINT('Ctrl Pts',(-2.36401731734834,0.192358224933772,
6.64056147713844));
#62132=CARTESIAN_POINT('Ctrl Pts',(-2.36544101887183,0.172878132621275,
6.64182320144908));
#62133=CARTESIAN_POINT('Origin',(0.,0.,-1.84858989190501));
#62134=CARTESIAN_POINT('',(-2.36544101854889,0.172878137039867,7.83684641963031));
#62135=CARTESIAN_POINT('',(-2.36544101891311,0.172878132056353,7.63807246982441));
#62136=CARTESIAN_POINT('',(-2.36544101854889,0.172878137039864,-1.84858989190501));
#62137=CARTESIAN_POINT('',(-2.37167361653571,0.000854563641824859,6.84858987464153));
#62138=CARTESIAN_POINT('Ctrl Pts',(-2.37174984612948,0.000854332948242326,
6.84858989190503));
#62139=CARTESIAN_POINT('Ctrl Pts',(-2.37177915559275,-0.0805129081841288,
6.85402314595505));
#62140=CARTESIAN_POINT('Ctrl Pts',(-2.36761694184918,-0.161853312165533,
6.85945640000507));
#62141=CARTESIAN_POINT('Ctrl Pts',(-2.35929771545254,-0.242718669163329,
6.86488965405509));
#62142=CARTESIAN_POINT('Ctrl Pts',(-2.35097324343856,-0.323635015123228,
6.87032633399717));
#62143=CARTESIAN_POINT('Ctrl Pts',(-2.33848658967688,-0.404075282207293,
6.87576301393926));
#62144=CARTESIAN_POINT('Ctrl Pts',(-2.32192384517465,-0.483598717646512,
6.88119969388134));
#62145=CARTESIAN_POINT('Ctrl Pts',(-2.30533317653517,-0.563256226477143,
6.88664553985245));
#62146=CARTESIAN_POINT('Ctrl Pts',(-2.28465278577067,-0.641993387252711,
6.89209138582357));
#62147=CARTESIAN_POINT('Ctrl Pts',(-2.26001938753787,-0.71938197812632,
6.89753723179468));
#62148=CARTESIAN_POINT('Ctrl Pts',(-2.23536311814162,-0.796842421332077,
6.90298813402447));
#62149=CARTESIAN_POINT('Ctrl Pts',(-2.20674668417494,-0.87295139022043,
6.90843903625425));
#62150=CARTESIAN_POINT('Ctrl Pts',(-2.17435507022211,-0.947300422832917,
6.91388993848403));
#62151=CARTESIAN_POINT('Ctrl Pts',(-2.14189739854026,-1.0218010788951,6.91935195699296));
#62152=CARTESIAN_POINT('Ctrl Pts',(-2.10564936477121,-1.09453423738812,
6.92481397550188));
#62153=CARTESIAN_POINT('Ctrl Pts',(-2.06584201697569,-1.16511579827835,
6.9302759940108));
#62154=CARTESIAN_POINT('Ctrl Pts',(-2.04578778886831,-1.20067352318729,
6.93302766100623));
#62155=CARTESIAN_POINT('Ctrl Pts',(-2.02483090688869,-1.2356856397051,6.93577932800166));
#62156=CARTESIAN_POINT('Ctrl Pts',(-2.00300491013283,-1.27010605560473,
6.93853099499709));
#62157=CARTESIAN_POINT('Ctrl Pts',(-1.96068196612791,-1.33685092645943,
6.94386677184479));
#62158=CARTESIAN_POINT('Ctrl Pts',(-1.91494048268382,-1.40160223551842,
6.94920254869248));
#62159=CARTESIAN_POINT('Ctrl Pts',(-1.8659943053119,-1.46398883706248,6.95453832554018));
#62160=CARTESIAN_POINT('Ctrl Pts',(-1.81711810468153,-1.52628624653219,
6.95986647400304));
#62161=CARTESIAN_POINT('Ctrl Pts',(-1.76504659571131,-1.5862252973756,6.96519462246589));
#62162=CARTESIAN_POINT('Ctrl Pts',(-1.71003754383265,-1.64346270453053,
6.97052277092875));
#62163=CARTESIAN_POINT('Ctrl Pts',(-1.65509157659909,-1.70063447155181,
6.97584480904534));
#62164=CARTESIAN_POINT('Ctrl Pts',(-1.59721508397275,-1.75511041634507,
6.98116684716193));
#62165=CARTESIAN_POINT('Ctrl Pts',(-1.53670586889553,-1.80658050886254,
6.98648888527852));
#62166=CARTESIAN_POINT('Ctrl Pts',(-1.47623454601038,-1.85801836968392,
6.9918075906186));
#62167=CARTESIAN_POINT('Ctrl Pts',(-1.41313412880433,-1.90645381215827,
6.99712629595868));
#62168=CARTESIAN_POINT('Ctrl Pts',(-1.34773814248875,-1.95161470628323,
7.00244500129877));
#62169=CARTESIAN_POINT('Ctrl Pts',(-1.28236282069116,-1.99676132998944,
7.00776202597787));
#62170=CARTESIAN_POINT('Ctrl Pts',(-1.21469375514147,-2.038635194455,7.01307905065698));
#62171=CARTESIAN_POINT('Ctrl Pts',(-1.14509512266201,-2.07700631259409,
7.01839607533609));
#62172=CARTESIAN_POINT('Ctrl Pts',(-1.07549689160726,-2.1153772094197,7.02371306934814));
#62173=CARTESIAN_POINT('Ctrl Pts',(-1.00396952630723,-2.15024517542969,
7.02903006336019));
#62174=CARTESIAN_POINT('Ctrl Pts',(-0.930902274650232,-2.18142591383504,
7.03434705737224));
#62175=CARTESIAN_POINT('Ctrl Pts',(-0.857762718819599,-2.21263750734267,
7.03966931285026));
#62176=CARTESIAN_POINT('Ctrl Pts',(-0.783080664326686,-2.24015440096073,
7.04499156832829));
#62177=CARTESIAN_POINT('Ctrl Pts',(-0.707265280633499,-2.26384051675696,
7.05031382380631));
#62178=CARTESIAN_POINT('Ctrl Pts',(-0.63141310036695,-2.2875381284773,7.05563866241132));
#62179=CARTESIAN_POINT('Ctrl Pts',(-0.554426948833437,-2.30740114141282,
7.06096350101634));
#62180=CARTESIAN_POINT('Ctrl Pts',(-0.47672863410306,-2.32334411397155,
7.06628833962136));
#62181=CARTESIAN_POINT('Ctrl Pts',(-0.398892022665602,-2.33931546373013,
7.07162265600781));
#62182=CARTESIAN_POINT('Ctrl Pts',(-0.320341178971256,-2.35135276097182,
7.07695697239425));
#62183=CARTESIAN_POINT('Ctrl Pts',(-0.241505282084628,-2.35942223038294,
7.08229128878071));
#62184=CARTESIAN_POINT('Ctrl Pts',(-0.171380880188349,-2.366600010283,7.08703615451951));
#62185=CARTESIAN_POINT('Ctrl Pts',(-0.101031231045985,-2.37063915759974,
7.09178102025832));
#62186=CARTESIAN_POINT('Ctrl Pts',(-0.0307572526518399,-2.37155055900339,
7.09652588599712));
#62187=CARTESIAN_POINT('Ctrl Pts',(0.0482684326998375,-2.3725754635584,
7.10186166284482));
#62188=CARTESIAN_POINT('Ctrl Pts',(0.127492451646572,-2.36964798094668,
7.10719743969251));
#62189=CARTESIAN_POINT('Ctrl Pts',(0.206487116023799,-2.36274440712832,
7.11253321654021));
#62190=CARTESIAN_POINT('Ctrl Pts',(0.285368844324812,-2.35585070312263,
7.11786136500305));
#62191=CARTESIAN_POINT('Ctrl Pts',(0.36402140683267,-2.34499223760633,7.1231895134659));
#62192=CARTESIAN_POINT('Ctrl Pts',(0.442016450198779,-2.3301973135882,7.12851766192875));
#62193=CARTESIAN_POINT('Ctrl Pts',(0.519922048474432,-2.31541935646002,
7.13383970004534));
#62194=CARTESIAN_POINT('Ctrl Pts',(0.597171168623043,-2.29671399904263,
7.13916173816193));
#62195=CARTESIAN_POINT('Ctrl Pts',(0.673341431373987,-2.27416124742623,
7.14448377627852));
#62196=CARTESIAN_POINT('Ctrl Pts',(0.749463994642761,-2.25162261883547,
7.1498024816186));
#62197=CARTESIAN_POINT('Ctrl Pts',(0.824508593977999,-2.2252415110142,7.15512118695869));
#62198=CARTESIAN_POINT('Ctrl Pts',(0.898065072388576,-2.19514855721787,
7.16043989229877));
#62199=CARTESIAN_POINT('Ctrl Pts',(0.971598307642224,-2.16506511251255,
7.16575691697788));
#62200=CARTESIAN_POINT('Ctrl Pts',(1.0436439229545,-2.13127232819516,7.17107394165699));
#62201=CARTESIAN_POINT('Ctrl Pts',(1.11381030777835,-2.09394953635151,7.17639096633609));
#62202=CARTESIAN_POINT('Ctrl Pts',(1.18397628790289,-2.05662695977488,7.18170796034815));
#62203=CARTESIAN_POINT('Ctrl Pts',(1.25226264659941,-2.01577463724099,7.1870249543602));
#62204=CARTESIAN_POINT('Ctrl Pts',(1.31830234006142,-1.97161786426493,7.19234194837225));
#62205=CARTESIAN_POINT('Ctrl Pts',(1.38440738353117,-1.92741739566726,7.19766420385028));
#62206=CARTESIAN_POINT('Ctrl Pts',(1.44826093106839,-1.87990620577915,7.2029864593283));
#62207=CARTESIAN_POINT('Ctrl Pts',(1.50952543709459,-1.82935262244992,7.20830871480632));
#62208=CARTESIAN_POINT('Ctrl Pts',(1.57081967750687,-1.77877450322115,7.21363355341134));
#62209=CARTESIAN_POINT('Ctrl Pts',(1.62952202715037,-1.72515136495837,7.21895839201636));
#62210=CARTESIAN_POINT('Ctrl Pts',(1.68533044290944,-1.66878978924928,7.22428323062138));
#62211=CARTESIAN_POINT('Ctrl Pts',(1.74123819312836,-1.61232789450045,7.22961754700782));
#62212=CARTESIAN_POINT('Ctrl Pts',(1.79424140472672,-1.55311817291498,7.23495186339427));
#62213=CARTESIAN_POINT('Ctrl Pts',(1.84407727797157,-1.49150161091732,7.24028617978072));
#62214=CARTESIAN_POINT('Ctrl Pts',(1.88840620606527,-1.43669377936282,7.24503104551954));
#62215=CARTESIAN_POINT('Ctrl Pts',(1.9302295762927,-1.37998228539239,7.24977591125837));
#62216=CARTESIAN_POINT('Ctrl Pts',(1.96939207837337,-1.32162509969363,7.25452077699719));
#62217=CARTESIAN_POINT('Ctrl Pts',(2.01343175903073,-1.25600028805771,7.25985655384489));
#62218=CARTESIAN_POINT('Ctrl Pts',(2.05426964762353,-1.18804970168938,7.26519233069258));
#62219=CARTESIAN_POINT('Ctrl Pts',(2.09165219387575,-1.11811858152647,7.27052810754028));
#62220=CARTESIAN_POINT('Ctrl Pts',(2.12898129552994,-1.0482874395882,7.27585625600314));
#62221=CARTESIAN_POINT('Ctrl Pts',(2.16286464673432,-0.976481796539616,
7.281184404466));
#62222=CARTESIAN_POINT('Ctrl Pts',(2.19309189019156,-0.903075868172765,
7.28651255292887));
#62223=CARTESIAN_POINT('Ctrl Pts',(2.2232844689007,-0.829754122077439,7.29183459104546));
#62224=CARTESIAN_POINT('Ctrl Pts',(2.24982909504344,-0.754836168402808,
7.29715662916205));
#62225=CARTESIAN_POINT('Ctrl Pts',(2.27256197755904,-0.678719471249317,
7.30247866727864));
#62226=CARTESIAN_POINT('Ctrl Pts',(2.2952806242471,-0.602650440034032,7.30779737261873));
#62227=CARTESIAN_POINT('Ctrl Pts',(2.31419213185353,-0.525384602697456,
7.31311607795882));
#62228=CARTESIAN_POINT('Ctrl Pts',(2.32918178861309,-0.447336850810598,
7.3184347832989));
#62229=CARTESIAN_POINT('Ctrl Pts',(2.34416670878176,-0.369313761280986,
7.32375180797801));
#62230=CARTESIAN_POINT('Ctrl Pts',(2.35523215095679,-0.290509707152289,
7.32906883265711));
#62231=CARTESIAN_POINT('Ctrl Pts',(2.36231432332553,-0.211350657228775,
7.33438585733622));
#62232=CARTESIAN_POINT('Ctrl Pts',(2.36939645484637,-0.132192063871593,
7.33970285134828));
#62233=CARTESIAN_POINT('Ctrl Pts',(2.37249532201,-0.0526789450624656,7.34501984536034));
#62234=CARTESIAN_POINT('Ctrl Pts',(2.37159905164703,0.0267581899038842,
7.35033683937239));
#62235=CARTESIAN_POINT('Ctrl Pts',(2.37070189437389,0.106273932403163,7.35565909485041));
#62236=CARTESIAN_POINT('Ctrl Pts',(2.36580170807694,0.185713071823991,7.36098135032843));
#62237=CARTESIAN_POINT('Ctrl Pts',(2.35693877807661,0.264646290166226,7.36630360580646));
#62238=CARTESIAN_POINT('Ctrl Pts',(2.34807154650266,0.343617818305553,7.37162844441148));
#62239=CARTESIAN_POINT('Ctrl Pts',(2.33523781536877,0.422082473762712,7.3769532830165));
#62240=CARTESIAN_POINT('Ctrl Pts',(2.31852930720246,0.499619769568116,7.38227812162152));
#62241=CARTESIAN_POINT('Ctrl Pts',(2.30179105924491,0.577295075479918,7.38761243800797));
#62242=CARTESIAN_POINT('Ctrl Pts',(2.28116437588896,0.654039270724346,7.39294675439442));
#62243=CARTESIAN_POINT('Ctrl Pts',(2.25679123749161,0.729445935543599,7.39828107078087));
#62244=CARTESIAN_POINT('Ctrl Pts',(2.23511137057895,0.796520041100205,7.40302593651966));
#62245=CARTESIAN_POINT('Ctrl Pts',(2.21046807638914,0.86253591719785,7.40777080225845));
#62246=CARTESIAN_POINT('Ctrl Pts',(2.18299254324694,0.927222529185008,7.41251566799724));
#62247=CARTESIAN_POINT('Ctrl Pts',(2.15209529099812,0.999965014557204,7.41785144484493));
#62248=CARTESIAN_POINT('Ctrl Pts',(2.11750065082667,1.07129681815087,7.42318722169263));
#62249=CARTESIAN_POINT('Ctrl Pts',(2.07935922038889,1.14081694196908,7.42852299854032));
#62250=CARTESIAN_POINT('Ctrl Pts',(2.04127231950099,1.21023767515052,7.43385114700318));
#62251=CARTESIAN_POINT('Ctrl Pts',(1.99964892199597,1.27785146547898,7.43917929546604));
#62252=CARTESIAN_POINT('Ctrl Pts',(1.95468749383537,1.34327765705516,7.44450744392889));
#62253=CARTESIAN_POINT('Ctrl Pts',(1.90977762765667,1.40862881756041,7.44982948204548));
#62254=CARTESIAN_POINT('Ctrl Pts',(1.8615376021355,1.47179698119973,7.45515152016207));
#62255=CARTESIAN_POINT('Ctrl Pts',(1.81021079871614,1.53242778841662,7.46047355827866));
#62256=CARTESIAN_POINT('Ctrl Pts',(1.75891613726213,1.59302062729779,7.46579226361875));
#62257=CARTESIAN_POINT('Ctrl Pts',(1.70453883648867,1.65107890749843,7.47111096895883));
#62258=CARTESIAN_POINT('Ctrl Pts',(1.64736369149876,1.7062798511474,7.47642967429891));
#62259=CARTESIAN_POINT('Ctrl Pts',(1.59020661331815,1.76146335181617,7.48174669897802));
#62260=CARTESIAN_POINT('Ctrl Pts',(1.53025378309257,1.81379098414925,7.48706372365712));
#62261=CARTESIAN_POINT('Ctrl Pts',(1.4678270969674,1.86297656343505,7.49238074833623));
#62262=CARTESIAN_POINT('Ctrl Pts',(1.40540077090118,1.91216185903273,7.49769774234828));
#62263=CARTESIAN_POINT('Ctrl Pts',(1.34050098582996,1.95820484914146,7.50301473636034));
#62264=CARTESIAN_POINT('Ctrl Pts',(1.27348181005652,2.00086035043807,7.50833173037239));
#62265=CARTESIAN_POINT('Ctrl Pts',(1.20639631502228,2.04355806176312,7.51365398585042));
#62266=CARTESIAN_POINT('Ctrl Pts',(1.13718763582058,2.08286133670076,7.51897624132844));
#62267=CARTESIAN_POINT('Ctrl Pts',(1.06623734353874,2.11856932615939,7.52429849680646));
#62268=CARTESIAN_POINT('Ctrl Pts',(0.995252615928549,2.15429464629141,7.52962333541147));
#62269=CARTESIAN_POINT('Ctrl Pts',(0.92252501993645,2.18642101539873,7.53494817401649));
#62270=CARTESIAN_POINT('Ctrl Pts',(0.84845683695102,2.21479548905335,7.5402730126215));
#62271=CARTESIAN_POINT('Ctrl Pts',(0.774256818598921,2.24322046697293,7.54560732900795));
#62272=CARTESIAN_POINT('Ctrl Pts',(0.698711891547283,2.26788006078031,7.5509416453944));
#62273=CARTESIAN_POINT('Ctrl Pts',(0.622240017692211,2.2886711041306,7.55627596178086));
#62274=CARTESIAN_POINT('Ctrl Pts',(0.554218410432574,2.30716470333247,7.56102082751967));
#62275=CARTESIAN_POINT('Ctrl Pts',(0.485463801873102,2.3225981620295,7.56576569325849));
#62276=CARTESIAN_POINT('Ctrl Pts',(0.416274870466302,2.33493325273299,7.5705105589973));
#62277=CARTESIAN_POINT('Ctrl Pts',(0.338469360544844,2.34880451801486,7.575846335845));
#62278=CARTESIAN_POINT('Ctrl Pts',(0.259824980161947,2.3588083556142,7.5811821126927));
#62279=CARTESIAN_POINT('Ctrl Pts',(0.180759859107338,2.36485177883002,7.5865178895404));
#62280=CARTESIAN_POINT('Ctrl Pts',(0.101807774858563,2.37088656196222,7.59184603800324));
#62281=CARTESIAN_POINT('Ctrl Pts',(0.022436607384243,2.37297214010521,7.59717418646609));
#62282=CARTESIAN_POINT('Ctrl Pts',(-0.0569263939879318,2.37106673212028,
7.60250233492894));
#62283=CARTESIAN_POINT('Ctrl Pts',(-0.13619838148887,2.36916350926638,7.60782437304554));
#62284=CARTESIAN_POINT('Ctrl Pts',(-0.215461755963201,2.36327840716033,
7.61314641116213));
#62285=CARTESIAN_POINT('Ctrl Pts',(-0.294286748773025,2.35342163073186,
7.61846844927873));
#62286=CARTESIAN_POINT('Ctrl Pts',(-0.373062379650736,2.34357102683207,
7.62378715461882));
#62287=CARTESIAN_POINT('Ctrl Pts',(-0.451399710594871,2.32975374345857,
7.62910585995891));
#62288=CARTESIAN_POINT('Ctrl Pts',(-0.528872793658224,2.31203192681852,
7.63442456529899));
#62289=CARTESIAN_POINT('Ctrl Pts',(-0.606321395954214,2.29431571010625,
7.6397415899781));
#62290=CARTESIAN_POINT('Ctrl Pts',(-0.682905836808822,2.27269751460741,
7.6450586146572));
#62291=CARTESIAN_POINT('Ctrl Pts',(-0.758210542632892,2.24729055432099,
7.6503756393363));
#62292=CARTESIAN_POINT('Ctrl Pts',(-0.833514814121615,2.22188374057443,
7.65569263334838));
#62293=CARTESIAN_POINT('Ctrl Pts',(-0.907538922285617,2.19268835650416,
7.66100962736044));
#62294=CARTESIAN_POINT('Ctrl Pts',(-0.979884053079207,2.15986696465802,
7.66632662137252));
#62295=CARTESIAN_POINT('Ctrl Pts',(-1.05230077346679,2.12701309419044,7.67164887685054));
#62296=CARTESIAN_POINT('Ctrl Pts',(-1.12303477064667,2.09052624257737,7.67697113232857));
#62297=CARTESIAN_POINT('Ctrl Pts',(-1.19170933285217,2.0506162314029,7.68229338780659));
#62298=CARTESIAN_POINT('Ctrl Pts',(-1.26041722587316,2.01068685012725,7.68761822641161));
#62299=CARTESIAN_POINT('Ctrl Pts',(-1.3270632999103,1.9673312550298,7.69294306501663));
#62300=CARTESIAN_POINT('Ctrl Pts',(-1.39129964730741,1.92080278891465,7.69826790362165));
#62301=CARTESIAN_POINT('Ctrl Pts',(-1.45565033020007,1.87419150589837,7.7036022200081));
#62302=CARTESIAN_POINT('Ctrl Pts',(-1.51758235103075,1.82439636190014,7.70893653639454));
#62303=CARTESIAN_POINT('Ctrl Pts',(-1.57678092364827,1.77171103211526,7.71427085278099));
#62304=CARTESIAN_POINT('Ctrl Pts',(-1.62943795758635,1.72484751706995,7.71901571851978));
#62305=CARTESIAN_POINT('Ctrl Pts',(-1.67993261919358,1.67569797999556,7.72376058425856));
#62306=CARTESIAN_POINT('Ctrl Pts',(-1.72806968829886,1.62449167892072,7.72850544999735));
#62307=CARTESIAN_POINT('Ctrl Pts',(-1.78152787162293,1.56762498800901,7.73377481739396));
#62308=CARTESIAN_POINT('Ctrl Pts',(-1.83228762165757,1.50799773269415,7.73904418479058));
#62309=CARTESIAN_POINT('Ctrl Pts',(-1.88004585703971,1.44589959469108,7.74431355218719));
#62310=CARTESIAN_POINT('Ctrl Pts',(-1.92774098637691,1.38388351097364,7.7495759568279));
#62311=CARTESIAN_POINT('Ctrl Pts',(-1.97244217725324,1.31940339730663,7.7548383614686));
#62312=CARTESIAN_POINT('Ctrl Pts',(-2.01388372529189,1.25278505878083,7.7601007661093));
#62313=CARTESIAN_POINT('Ctrl Pts',(-2.05528415322878,1.1862328218605,7.76535794916383));
#62314=CARTESIAN_POINT('Ctrl Pts',(-2.0934311035362,1.11754697568823,7.77061513221836));
#62315=CARTESIAN_POINT('Ctrl Pts',(-2.12810067786589,1.04708431721937,7.77587231527289));
#62316=CARTESIAN_POINT('Ctrl Pts',(-2.16275317801482,0.976656360421645,
7.78112690925342));
#62317=CARTESIAN_POINT('Ctrl Pts',(-2.19393148153228,0.90445375435945,7.78638150323394));
#62318=CARTESIAN_POINT('Ctrl Pts',(-2.22145711368449,0.830858805430019,
7.79163609721447));
#62319=CARTESIAN_POINT('Ctrl Pts',(-2.24897367615864,0.757288105988838,
7.79688895980966));
#62320=CARTESIAN_POINT('Ctrl Pts',(-2.27283979226548,0.682326426055847,
7.80214182240485));
#62321=CARTESIAN_POINT('Ctrl Pts',(-2.29292544290108,0.606375276373366,
7.80739468500005));
#62322=CARTESIAN_POINT('Ctrl Pts',(-2.31302103634047,0.530386529333843,
7.81265014786859));
#62323=CARTESIAN_POINT('Ctrl Pts',(-2.32933230031485,0.453407798864271,
7.81790561073714));
#62324=CARTESIAN_POINT('Ctrl Pts',(-2.34177963671045,0.375853955131875,
7.82316107360568));
#62325=CARTESIAN_POINT('Ctrl Pts',(-2.35258402000454,0.308536624983187,
7.82772285561389));
#62326=CARTESIAN_POINT('Ctrl Pts',(-2.3604779488569,0.240786368979323,7.8322846376221));
#62327=CARTESIAN_POINT('Ctrl Pts',(-2.36544101854889,0.172878137039867,
7.83684641963031));
#62328=CARTESIAN_POINT('Ctrl Pts',(-2.36285989125428,0.172707701180992,
6.83708460818679));
#62329=CARTESIAN_POINT('Ctrl Pts',(-2.3666403501721,0.115542394696668,6.84091943817652));
#62330=CARTESIAN_POINT('Ctrl Pts',(-2.36843179856191,0.0582097310194607,
6.84475426816626));
#62331=CARTESIAN_POINT('Ctrl Pts',(-2.36824492703387,0.000864939883196495,
6.848589098156));
#62332=CARTESIAN_POINT('Ctrl Pts',(-2.36544101887183,0.172878132621275,
6.64182320144908));
#62333=CARTESIAN_POINT('Ctrl Pts',(-2.3696028942636,0.115932406647306,6.6455115724124));
#62334=CARTESIAN_POINT('Ctrl Pts',(-2.3717078335312,0.0588440556893744,
6.649117014029));
#62335=CARTESIAN_POINT('Ctrl Pts',(-2.37182241343598,-0.0987107308918925,
6.6589457848745));
#62336=CARTESIAN_POINT('Ctrl Pts',(-2.36551574960962,-0.199052636883313,
6.66507245937646));
#62337=CARTESIAN_POINT('Ctrl Pts',(-2.33549906223717,-0.435498516360033,
6.6797348662378));
#62338=CARTESIAN_POINT('Ctrl Pts',(-2.30623659196225,-0.570509188646735,
6.68830004755357));
#62339=CARTESIAN_POINT('Ctrl Pts',(-2.25715959474339,-0.728838943472387,
6.69905632790079));
#62340=CARTESIAN_POINT('Ctrl Pts',(-2.24843486114649,-0.755325235666134,
6.70087968329226));
#62341=CARTESIAN_POINT('Ctrl Pts',(-2.2337829333825,-0.797299564727317,
6.7038108446944));
#62342=CARTESIAN_POINT('Ctrl Pts',(-2.22815662326822,-0.812890415955453,
6.70490885260466));
#62343=CARTESIAN_POINT('Ctrl Pts',(-2.21716565087573,-0.842375410527281,
6.70700366143278));
#62344=CARTESIAN_POINT('Ctrl Pts',(-2.21183260335262,-0.856280545869361,
6.70799938017444));
#62345=CARTESIAN_POINT('Ctrl Pts',(-2.19934361038919,-0.887948448863229,
6.7102854209587));
#62346=CARTESIAN_POINT('Ctrl Pts',(-2.19210285774203,-0.905676425964556,
6.71157850500284));
#62347=CARTESIAN_POINT('Ctrl Pts',(-2.16872901781536,-0.960981125305863,
6.71565551079747));
#62348=CARTESIAN_POINT('Ctrl Pts',(-2.1518390454007,-0.998227751475453,
6.71846439584239));
#62349=CARTESIAN_POINT('Ctrl Pts',(-2.0838998956203,-1.13830449049972,6.72927701819808));
#62350=CARTESIAN_POINT('Ctrl Pts',(-2.02637815012396,-1.23780500804915,
6.73748938227872));
#62351=CARTESIAN_POINT('Ctrl Pts',(-1.88448336932091,-1.44668425086851,
6.75581480762632));
#62352=CARTESIAN_POINT('Ctrl Pts',(-1.79729884355684,-1.55367030911945,
6.76594959572496));
#62353=CARTESIAN_POINT('Ctrl Pts',(-1.66966416242216,-1.68507682140923,
6.77900317946093));
#62354=CARTESIAN_POINT('Ctrl Pts',(-1.63707618817158,-1.71675405646577,
6.78220163287787));
#62355=CARTESIAN_POINT('Ctrl Pts',(-1.59304679130593,-1.75715821104158,
6.78632873058291));
#62356=CARTESIAN_POINT('Ctrl Pts',(-1.58240993682746,-1.76674329627262,
6.78731148563113));
#62357=CARTESIAN_POINT('Ctrl Pts',(-1.56497805070622,-1.78216778236279,
6.7888980762533));
#62358=CARTESIAN_POINT('Ctrl Pts',(-1.55823577411518,-1.78806587759391,
6.78950601099475));
#62359=CARTESIAN_POINT('Ctrl Pts',(-1.54487658720046,-1.79961944690007,
6.79069906659249));
#62360=CARTESIAN_POINT('Ctrl Pts',(-1.53826169253364,-1.80527692966612,
6.79128431618931));
#62361=CARTESIAN_POINT('Ctrl Pts',(-1.52158884797871,-1.81937843692709,
6.79274613828125));
#62362=CARTESIAN_POINT('Ctrl Pts',(-1.51149144480041,-1.82777573864787,
6.79361943816486));
#62363=CARTESIAN_POINT('Ctrl Pts',(-1.47125703817624,-1.86067441761021,
6.79705441129358));
#62364=CARTESIAN_POINT('Ctrl Pts',(-1.44058811093905,-1.88451926582055,
6.79957442141113));
#62365=CARTESIAN_POINT('Ctrl Pts',(-1.3555449256559,-1.94734958384348,6.80634203326719));
#62366=CARTESIAN_POINT('Ctrl Pts',(-1.30008328969004,-1.98480656522978,
6.81052051454161));
#62367=CARTESIAN_POINT('Ctrl Pts',(-1.10981909712928,-2.1019027092626,6.82434498460179));
#62368=CARTESIAN_POINT('Ctrl Pts',(-0.968741844165485,-2.17053725949386,
6.83380780514352));
#62369=CARTESIAN_POINT('Ctrl Pts',(-0.758149723052398,-2.24833952044726,
6.84794352022592));
#62370=CARTESIAN_POINT('Ctrl Pts',(-0.693388028410569,-2.26914815654295,
6.8522872965909));
#62371=CARTESIAN_POINT('Ctrl Pts',(-0.604934630307132,-2.29342880016947,
6.85826705130769));
#62372=CARTESIAN_POINT('Ctrl Pts',(-0.581950793738913,-2.29936834284573,
6.85982488139079));
#62373=CARTESIAN_POINT('Ctrl Pts',(-0.543625745317512,-2.30866098842447,
6.86243112964569));
#62374=CARTESIAN_POINT('Ctrl Pts',(-0.528333121618525,-2.31220859854863,
6.86347333685002));
#62375=CARTESIAN_POINT('Ctrl Pts',(-0.498124045824823,-2.31890121876107,
6.86553707858791));
#62376=CARTESIAN_POINT('Ctrl Pts',(-0.483210246131083,-2.32205475106376,
6.86655828832828));
#62377=CARTESIAN_POINT('Ctrl Pts',(-0.44727151231933,-2.32929280336112,
6.86902534493162));
#62378=CARTESIAN_POINT('Ctrl Pts',(-0.426219949576982,-2.33323665160871,
6.87047552616544));
#62379=CARTESIAN_POINT('Ctrl Pts',(-0.350850603343726,-2.3463024998168,
6.87568710122809));
#62380=CARTESIAN_POINT('Ctrl Pts',(-0.29627569461842,-2.3538163539585,6.87949752965821));
#62381=CARTESIAN_POINT('Ctrl Pts',(-0.156647771769953,-2.3681075898587,
6.88934496853297));
#62382=CARTESIAN_POINT('Ctrl Pts',(-0.0714042844503148,-2.37220805810313,
6.89545131762471));
#62383=CARTESIAN_POINT('Ctrl Pts',(0.0938088628072688,-2.37124202659616,
6.90741669484149));
#62384=CARTESIAN_POINT('Ctrl Pts',(0.173673970260044,-2.36673313615369,
6.91325942787623));
#62385=CARTESIAN_POINT('Ctrl Pts',(0.359484437566331,-2.34678607061269,
6.92686391936632));
#62386=CARTESIAN_POINT('Ctrl Pts',(0.464930602485518,-2.32819210286688,
6.93459460465086));
#62387=CARTESIAN_POINT('Ctrl Pts',(0.585450773473143,-2.29842133445283,
6.94320921632534));
#62388=CARTESIAN_POINT('Ctrl Pts',(0.602085472828304,-2.29411995423426,
6.94439310884151));
#62389=CARTESIAN_POINT('Ctrl Pts',(0.628018514899812,-2.28711270642982,
6.94622919340903));
#62390=CARTESIAN_POINT('Ctrl Pts',(0.637349143619226,-2.28453011894731,
6.94688786126991));
#62391=CARTESIAN_POINT('Ctrl Pts',(0.653927657307026,-2.27983194138786,
6.94805437885535));
#62392=CARTESIAN_POINT('Ctrl Pts',(0.661181370154349,-2.27773884806067,
6.94856344561814));
#62393=CARTESIAN_POINT('Ctrl Pts',(0.678792133937286,-2.27256596069434,
6.94979628319067));
#62394=CARTESIAN_POINT('Ctrl Pts',(0.689138306711379,-2.26944998010988,
6.9505179912615));
#62395=CARTESIAN_POINT('Ctrl Pts',(0.721757411035039,-2.25938236855589,
6.95278628826473));
#62396=CARTESIAN_POINT('Ctrl Pts',(0.743950017063917,-2.25217248865375,
6.95431906506496));
#62397=CARTESIAN_POINT('Ctrl Pts',(0.796770387086757,-2.23414632356999,
6.95795013535149));
#62398=CARTESIAN_POINT('Ctrl Pts',(0.827290014210964,-2.22302593013655,
6.96003428440339));
#62399=CARTESIAN_POINT('Ctrl Pts',(0.945934746429238,-2.17701346200874,
6.96811683093034));
#62400=CARTESIAN_POINT('Ctrl Pts',(1.03216932058011,-2.13747728404483,6.9739510531906));
#62401=CARTESIAN_POINT('Ctrl Pts',(1.26242978010615,-2.01471497116616,6.98998226599722));
#62402=CARTESIAN_POINT('Ctrl Pts',(1.4004118987679,-1.92136528535204,7.00014274218385));
#62403=CARTESIAN_POINT('Ctrl Pts',(1.55100694858399,-1.79458061730114,7.01284075786388));
#62404=CARTESIAN_POINT('Ctrl Pts',(1.5741243849488,-1.77433774417279,7.01483898618652));
#62405=CARTESIAN_POINT('Ctrl Pts',(1.61086944380141,-1.74087841552257,7.01810031701388));
#62406=CARTESIAN_POINT('Ctrl Pts',(1.62474351091385,-1.72793706828704,7.0193521349625));
#62407=CARTESIAN_POINT('Ctrl Pts',(1.64921414687152,-1.704556238788,7.02159783301899));
#62408=CARTESIAN_POINT('Ctrl Pts',(1.65987069285566,-1.6941807871086,7.02258895972179));
#62409=CARTESIAN_POINT('Ctrl Pts',(1.68226652790765,-1.67196155944354,7.02470054566282));
#62410=CARTESIAN_POINT('Ctrl Pts',(1.69397985287178,-1.66009287719607,7.02582206058283));
#62411=CARTESIAN_POINT('Ctrl Pts',(1.72527231413255,-1.62770933203581,7.02886562047749));
#62412=CARTESIAN_POINT('Ctrl Pts',(1.74460973630826,-1.60696576684072,7.03079775985279));
#62413=CARTESIAN_POINT('Ctrl Pts',(1.87108150618424,-1.46632357893424,7.04378872692781));
#62414=CARTESIAN_POINT('Ctrl Pts',(1.96613768300477,-1.33616463509958,7.05533702008942));
#62415=CARTESIAN_POINT('Ctrl Pts',(2.12034581783549,-1.0725075358376,7.07758578855422));
#62416=CARTESIAN_POINT('Ctrl Pts',(2.18182507985484,-0.941161387785913,
7.0881991744085));
#62417=CARTESIAN_POINT('Ctrl Pts',(2.23841745355933,-0.78432733609461,7.09983793475331));
#62418=CARTESIAN_POINT('Ctrl Pts',(2.2455967817933,-0.763529465914965,7.1013608786973));
#62419=CARTESIAN_POINT('Ctrl Pts',(2.25579114984286,-0.732608882176843,
7.10359190384237));
#62420=CARTESIAN_POINT('Ctrl Pts',(2.25902943875635,-0.722561756086708,
7.10431170247714));
#62421=CARTESIAN_POINT('Ctrl Pts',(2.26470373884189,-0.704545574605662,
7.10559284019789));
#62422=CARTESIAN_POINT('Ctrl Pts',(2.26716494702284,-0.696584955734328,
7.10615556269561));
#62423=CARTESIAN_POINT('Ctrl Pts',(2.27255588861011,-0.678817022944849,
7.10740408249667));
#62424=CARTESIAN_POINT('Ctrl Pts',(2.27546414251413,-0.669003559961076,
7.10808866458126));
#62425=CARTESIAN_POINT('Ctrl Pts',(2.28396520799075,-0.639621135265913,
7.11012433346575));
#62426=CARTESIAN_POINT('Ctrl Pts',(2.28936992662831,-0.61999812442002,7.11146532127249));
#62427=CARTESIAN_POINT('Ctrl Pts',(2.32739653088577,-0.474651097669245,
7.12127826543412));
#62428=CARTESIAN_POINT('Ctrl Pts',(2.34989833898823,-0.346489452995756,
7.12928008233079));
#62429=CARTESIAN_POINT('Ctrl Pts',(2.37720545198774,-0.0494414544196821,
7.14760929545741));
#62430=CARTESIAN_POINT('Ctrl Pts',(2.37471928981639,0.119378172044436,7.15789767836298));
#62431=CARTESIAN_POINT('Ctrl Pts',(2.35068326201323,0.316896903420457,7.1707336660732));
#62432=CARTESIAN_POINT('Ctrl Pts',(2.34639679030516,0.347213785266757,7.17272495750371));
#62433=CARTESIAN_POINT('Ctrl Pts',(2.33851055651111,0.396137861007947,7.17597722197912));
#62434=CARTESIAN_POINT('Ctrl Pts',(2.33527246206423,0.414800339368095,7.17722701539976));
#62435=CARTESIAN_POINT('Ctrl Pts',(2.32909389986666,0.448041047810954,7.17947048015268));
#62436=CARTESIAN_POINT('Ctrl Pts',(2.32623916086342,0.462634331164522,7.18046141939979));
#62437=CARTESIAN_POINT('Ctrl Pts',(2.31988861408223,0.493551988515321,7.18257409584109));
#62438=CARTESIAN_POINT('Ctrl Pts',(2.31635730883444,0.509868159939565,7.18369690267167));
#62439=CARTESIAN_POINT('Ctrl Pts',(2.30634384967794,0.553881982349753,7.18674776940844));
#62440=CARTESIAN_POINT('Ctrl Pts',(2.29953533989399,0.581501765347872,7.18868600717747));
#62441=CARTESIAN_POINT('Ctrl Pts',(2.25081620746351,0.764879642677311,7.20171904912304));
#62442=CARTESIAN_POINT('Ctrl Pts',(2.19361389118331,0.916108566889364,7.21330647354243));
#62443=CARTESIAN_POINT('Ctrl Pts',(2.05720142096442,1.18904290086975,7.23553349990947));
#62444=CARTESIAN_POINT('Ctrl Pts',(1.98129183426437,1.31163636877934,7.24608424605006));
#62445=CARTESIAN_POINT('Ctrl Pts',(1.88143878534284,1.44425572347289,7.25767378523139));
#62446=CARTESIAN_POINT('Ctrl Pts',(1.86789863484344,1.4617254441259,7.25920382494491));
#62447=CARTESIAN_POINT('Ctrl Pts',(1.84752129772089,1.48727097199259,7.2614431590431));
#62448=CARTESIAN_POINT('Ctrl Pts',(1.84087154258191,1.49549385288059,7.26216429222363));
#62449=CARTESIAN_POINT('Ctrl Pts',(1.82888380371679,1.51011639737894,7.26344681150377));
#62450=CARTESIAN_POINT('Ctrl Pts',(1.82356685908338,1.51653269592234,7.26400959474538));
#62451=CARTESIAN_POINT('Ctrl Pts',(1.81165494779065,1.53075432965639,7.26525704861679));
#62452=CARTESIAN_POINT('Ctrl Pts',(1.80504325576535,1.53854519660589,7.26594051651285));
#62453=CARTESIAN_POINT('Ctrl Pts',(1.78516852306887,1.56166005310812,7.2679694303066));
#62454=CARTESIAN_POINT('Ctrl Pts',(1.7717588243932,1.57685747988189,7.26930487642771));
#62455=CARTESIAN_POINT('Ctrl Pts',(1.67651827873663,1.68204599781137,7.27857420177716));
#62456=CARTESIAN_POINT('Ctrl Pts',(1.58805513640682,1.76580880417996,7.28609653806636));
#62457=CARTESIAN_POINT('Ctrl Pts',(1.35522057316574,1.95455429770869,7.30452970151637));
#62458=CARTESIAN_POINT('Ctrl Pts',(1.20472447806156,2.05074054312495,7.31537289045612));
#62459=CARTESIAN_POINT('Ctrl Pts',(1.01802605995908,2.14236235361175,7.32879829177989));
#62460=CARTESIAN_POINT('Ctrl Pts',(0.990916385407184,2.15503552248849,7.33074558170127));
#62461=CARTESIAN_POINT('Ctrl Pts',(0.946451114429461,2.17480563504929,7.33394029118139));
#62462=CARTESIAN_POINT('Ctrl Pts',(0.929237882064308,2.18221588932124,7.33517718633303));
#62463=CARTESIAN_POINT('Ctrl Pts',(0.898230569055258,2.1951310740017,7.33740651521236));
#62464=CARTESIAN_POINT('Ctrl Pts',(0.884469043556387,2.20071194872723,7.33839635258057));
#62465=CARTESIAN_POINT('Ctrl Pts',(0.855012935228019,2.21233672179498,7.34051642941176));
#62466=CARTESIAN_POINT('Ctrl Pts',(0.839304728604938,2.21834362477832,7.34164783037931));
#62467=CARTESIAN_POINT('Ctrl Pts',(0.796311002216604,2.23426264372641,7.34474740083008));
#62468=CARTESIAN_POINT('Ctrl Pts',(0.768906020756085,2.24384138840245,7.34672631188091));
#62469=CARTESIAN_POINT('Ctrl Pts',(0.589652009753747,2.3028258492445,7.35969626420056));
#62470=CARTESIAN_POINT('Ctrl Pts',(0.433345000726604,2.33728291154694,7.37116771494721));
#62471=CARTESIAN_POINT('Ctrl Pts',(0.131213378561963,2.37252530053532,7.39332478450898));
#62472=CARTESIAN_POINT('Ctrl Pts',(-0.0136061789618504,2.37611337086567,
7.40392620990931));
#62473=CARTESIAN_POINT('Ctrl Pts',(-0.179829903316131,2.36502517623719,
7.41555551566093));
#62474=CARTESIAN_POINT('Ctrl Pts',(-0.201779121588205,2.36325372100239,
7.41707976194162));
#62475=CARTESIAN_POINT('Ctrl Pts',(-0.234213596287553,2.36018083023182,
7.41931231241066));
#62476=CARTESIAN_POINT('Ctrl Pts',(-0.244719247619747,2.35911467726927,
7.42003235626606));
#62477=CARTESIAN_POINT('Ctrl Pts',(-0.263501796326132,2.35708173308941,
7.42131374755409));
#62478=CARTESIAN_POINT('Ctrl Pts',(-0.27178108341004,2.35614145203311,7.42187648092241));
#62479=CARTESIAN_POINT('Ctrl Pts',(-0.290215911158583,2.35394933627779,
7.42312480357085));
#62480=CARTESIAN_POINT('Ctrl Pts',(-0.300368469263164,2.35267540156487,
7.42380917993586));
#62481=CARTESIAN_POINT('Ctrl Pts',(-0.330673815942261,2.34867333812875,
7.42584360067606));
#62482=CARTESIAN_POINT('Ctrl Pts',(-0.350800678673438,2.3457516008146,7.4271835644265));
#62483=CARTESIAN_POINT('Ctrl Pts',(-0.497668738454781,2.32249867215093,
7.43689602851683));
#62484=CARTESIAN_POINT('Ctrl Pts',(-0.622627905629938,2.29216434121425,
7.44480949288075));
#62485=CARTESIAN_POINT('Ctrl Pts',(-0.905971725192098,2.19848255461361,
7.46314905448098));
#62486=CARTESIAN_POINT('Ctrl Pts',(-1.06118657362328,2.1279064789699,7.47353213792594));
#62487=CARTESIAN_POINT('Ctrl Pts',(-1.2338205645033,2.02578845683034,7.48647204132157));
#62488=CARTESIAN_POINT('Ctrl Pts',(-1.25982027544244,2.00972256693065,7.48845981518635));
#62489=CARTESIAN_POINT('Ctrl Pts',(-1.30140558394444,1.98290184534547,7.49170748152236));
#62490=CARTESIAN_POINT('Ctrl Pts',(-1.31718603580137,1.97245459647306,7.49295624740771));
#62491=CARTESIAN_POINT('Ctrl Pts',(-1.34458946251215,1.95383700182474,7.49515459183675));
#62492=CARTESIAN_POINT('Ctrl Pts',(-1.35626734123795,1.94574888838764,7.49610107924194));
#62493=CARTESIAN_POINT('Ctrl Pts',(-1.38102182846849,1.92827277290675,7.49812857621854));
#62494=CARTESIAN_POINT('Ctrl Pts',(-1.39407686900362,1.91885560657373,7.49921065641467));
#62495=CARTESIAN_POINT('Ctrl Pts',(-1.42066314855186,1.89926324663761,7.50144123238396));
#62496=CARTESIAN_POINT('Ctrl Pts',(-1.43418329336556,1.88907461927215,7.50259020258912));
#62497=CARTESIAN_POINT('Ctrl Pts',(-1.49569639889367,1.84167805341126,7.50788628647372));
#62498=CARTESIAN_POINT('Ctrl Pts',(-1.54235459523769,1.80278310986801,7.51209819253961));
#62499=CARTESIAN_POINT('Ctrl Pts',(-1.66120912669775,1.69571040312451,7.52336172220979));
#62500=CARTESIAN_POINT('Ctrl Pts',(-1.73070257644153,1.62471986270786,7.53051189332773));
#62501=CARTESIAN_POINT('Ctrl Pts',(-1.90003827368715,1.42850765006668,7.54936016177648));
#62502=CARTESIAN_POINT('Ctrl Pts',(-1.99202732439295,1.29715600336247,7.56113686158805));
#62503=CARTESIAN_POINT('Ctrl Pts',(-2.08023707081611,1.1394048306588,7.57373487372417));
#62504=CARTESIAN_POINT('Ctrl Pts',(-2.09013782533608,1.12113941259399,7.57517132401714));
#62505=CARTESIAN_POINT('Ctrl Pts',(-2.10459530074865,1.09361014734234,7.57730071914553));
#62506=CARTESIAN_POINT('Ctrl Pts',(-2.10933334190351,1.08444335811109,7.5780039462687));
#62507=CARTESIAN_POINT('Ctrl Pts',(-2.11778819313102,1.06782050400462,7.5792682793152));
#62508=CARTESIAN_POINT('Ctrl Pts',(-2.12152567489906,1.0603755352024,7.57983059687707));
#62509=CARTESIAN_POINT('Ctrl Pts',(-2.12987011299709,1.04353289006254,7.58109389960709));
#62510=CARTESIAN_POINT('Ctrl Pts',(-2.13445417226877,1.03412426119809,7.58179350300568));
#62511=CARTESIAN_POINT('Ctrl Pts',(-2.14827750379485,1.0052687961514,7.58392146781022));
#62512=CARTESIAN_POINT('Ctrl Pts',(-2.15731468306736,0.98572563264348,7.58533832636668));
#62513=CARTESIAN_POINT('Ctrl Pts',(-2.20169701805067,0.886212377915345,
7.59244386638894));
#62514=CARTESIAN_POINT('Ctrl Pts',(-2.2328705999432,0.80444654839222,7.59793024137301));
#62515=CARTESIAN_POINT('Ctrl Pts',(-2.31627508780185,0.54312473178222,7.614921824028));
#62516=CARTESIAN_POINT('Ctrl Pts',(-2.35183113479429,0.359098203816666,
7.62616644971573));
#62517=CARTESIAN_POINT('Ctrl Pts',(-2.36544101891311,0.172878132056388,
7.63807246982441));
#62518=CARTESIAN_POINT('Origin',(0.,0.,-1.84858989190501));
#62519=CARTESIAN_POINT('',(-2.36544101854848,0.172878137045581,8.83481520889907));
#62520=CARTESIAN_POINT('',(-2.36544103037033,0.172877975290513,8.63916402106918));
#62521=CARTESIAN_POINT('',(-2.36544101854889,0.172878137039864,-1.84858989190501));
#62522=CARTESIAN_POINT('',(-2.37174905777015,-0.00211411125499902,7.84858989190503));
#62523=CARTESIAN_POINT('Ctrl Pts',(-2.36544101854848,0.172878137045581,
8.83481520889907));
#62524=CARTESIAN_POINT('Ctrl Pts',(-2.36522450343307,0.175840650084406,
8.83461214175899));
#62525=CARTESIAN_POINT('Ctrl Pts',(-2.3650024209695,0.178802782450663,8.83440935971078));
#62526=CARTESIAN_POINT('Ctrl Pts',(-2.36410014521746,0.190541481262514,
8.83360679734256));
#62527=CARTESIAN_POINT('Ctrl Pts',(-2.3633766456752,0.199314800527096,8.83300929497062));
#62528=CARTESIAN_POINT('Ctrl Pts',(-2.36186181322496,0.216514337868644,
8.83184274600605));
#62529=CARTESIAN_POINT('Ctrl Pts',(-2.36107420171444,0.224940660154587,
8.83127352558446));
#62530=CARTESIAN_POINT('Ctrl Pts',(-2.3590011093727,0.245908015463755,8.82986243955776));
#62531=CARTESIAN_POINT('Ctrl Pts',(-2.35766068704253,0.25844358802887,8.82902354076649));
#62532=CARTESIAN_POINT('Ctrl Pts',(-2.35210421230338,0.306760246587437,
8.82580633671276));
#62533=CARTESIAN_POINT('Ctrl Pts',(-2.34717280660752,0.342456162550787,
8.82346384134261));
#62534=CARTESIAN_POINT('Ctrl Pts',(-2.33185541045421,0.437329024720731,
8.81729671325565));
#62535=CARTESIAN_POINT('Ctrl Pts',(-2.32003109877927,0.496248920226127,
8.81352787248409));
#62536=CARTESIAN_POINT('Ctrl Pts',(-2.27120500380131,0.699241929876785,
8.80056570211307));
#62537=CARTESIAN_POINT('Ctrl Pts',(-2.22290870527848,0.840231695052893,
8.79158212610435));
#62538=CARTESIAN_POINT('Ctrl Pts',(-2.12739746066221,1.05182749343225,8.77707835176978));
#62539=CARTESIAN_POINT('Ctrl Pts',(-2.08908072762203,1.1260108944087,8.77178389100937));
#62540=CARTESIAN_POINT('Ctrl Pts',(-2.03420015004174,1.21978020202948,8.76471440933066));
#62541=CARTESIAN_POINT('Ctrl Pts',(-2.02111635563053,1.2413390310197,8.76306202687768));
#62542=CARTESIAN_POINT('Ctrl Pts',(-1.99929622471128,1.27603344259689,8.76035625467828));
#62543=CARTESIAN_POINT('Ctrl Pts',(-1.99076800753314,1.28929804965762,8.75931044418509));
#62544=CARTESIAN_POINT('Ctrl Pts',(-1.97404845384651,1.31474186374438,8.7572818596292));
#62545=CARTESIAN_POINT('Ctrl Pts',(-1.96587507144712,1.32693204549555,8.7562997824317));
#62546=CARTESIAN_POINT('Ctrl Pts',(-1.94651621994868,1.35523331184055,8.75399538133016));
#62547=CARTESIAN_POINT('Ctrl Pts',(-1.93524313552712,1.37128286311329,8.75266981477617));
#62548=CARTESIAN_POINT('Ctrl Pts',(-1.89740250655503,1.42376071119182,8.74827203217096));
#62549=CARTESIAN_POINT('Ctrl Pts',(-1.86999666409134,1.45956940107746,8.74516826388431));
#62550=CARTESIAN_POINT('Ctrl Pts',(-1.80111860798629,1.54443980171655,8.73755276639764));
#62551=CARTESIAN_POINT('Ctrl Pts',(-1.75864311121558,1.59263798907632,8.7330053506173));
#62552=CARTESIAN_POINT('Ctrl Pts',(-1.64557086036521,1.7108992094521,8.72127702110117));
#62553=CARTESIAN_POINT('Ctrl Pts',(-1.57242868832636,1.77835471967077,8.71402651703346));
#62554=CARTESIAN_POINT('Ctrl Pts',(-1.47481048283427,1.85764021923475,8.70485691316441));
#62555=CARTESIAN_POINT('Ctrl Pts',(-1.45406980998814,1.87391946285739,8.7029358044755));
#62556=CARTESIAN_POINT('Ctrl Pts',(-1.3557057095739,1.94850838306494,8.69396148001873));
#62557=CARTESIAN_POINT('Ctrl Pts',(-1.27481196478586,2.00236896616912,8.68696818903353));
#62558=CARTESIAN_POINT('Ctrl Pts',(-1.17625706659223,2.05958771732764,8.67906281579098));
#62559=CARTESIAN_POINT('Ctrl Pts',(-1.1615877440449,2.06789656535271,8.67790146167291));
#62560=CARTESIAN_POINT('Ctrl Pts',(-1.13853212877622,2.08063272412531,8.67610139985186));
#62561=CARTESIAN_POINT('Ctrl Pts',(-1.13020609757778,2.0851671697375,8.67545642272779));
#62562=CARTESIAN_POINT('Ctrl Pts',(-1.11535786594808,2.09313860933563,8.6743154938278));
#62563=CARTESIAN_POINT('Ctrl Pts',(-1.10884673773102,2.09659517347276,8.67381836019959));
#62564=CARTESIAN_POINT('Ctrl Pts',(-1.09302327933246,2.10490104278499,8.67261777377626));
#62565=CARTESIAN_POINT('Ctrl Pts',(-1.08369472387583,2.10971894925435,8.67191625622493));
#62566=CARTESIAN_POINT('Ctrl Pts',(-1.0543273968431,2.12464006572886,8.66972645354584));
#62567=CARTESIAN_POINT('Ctrl Pts',(-1.03417637749854,2.13452125256227,8.66825093983201));
#62568=CARTESIAN_POINT('Ctrl Pts',(-0.925577947587826,2.18587416356705,
8.66042679686366));
#62569=CARTESIAN_POINT('Ctrl Pts',(-0.834762813857075,2.22214213612493,
8.6543308583523));
#62570=CARTESIAN_POINT('Ctrl Pts',(-0.573882021064348,2.30806681387092,
8.63737705458315));
#62571=CARTESIAN_POINT('Ctrl Pts',(-0.400148476741573,2.34443827029624,
8.62668175452108));
#62572=CARTESIAN_POINT('Ctrl Pts',(-0.177424114017925,2.36556684892325,
8.61240698104738));
#62573=CARTESIAN_POINT('Ctrl Pts',(-0.130741758282932,2.36860548953888,
8.60938773498955));
#62574=CARTESIAN_POINT('Ctrl Pts',(-0.0655818506414271,2.3709147658194,
8.60512013221767));
#62575=CARTESIAN_POINT('Ctrl Pts',(-0.0471547398900403,2.37135282172969,
8.60390737059215));
#62576=CARTESIAN_POINT('Ctrl Pts',(-0.0151360867046855,2.37174063545921,
8.60178896826439));
#62577=CARTESIAN_POINT('Ctrl Pts',(-0.00154644273461836,2.37178842618969,
8.60088637745654));
#62578=CARTESIAN_POINT('Ctrl Pts',(0.0268937806436004,2.3716440182913,8.59898979918228));
#62579=CARTESIAN_POINT('Ctrl Pts',(0.0417436014420987,2.37142912176135,
8.59799515139003));
#62580=CARTESIAN_POINT('Ctrl Pts',(0.0772498838415376,2.37058169782121,
8.5956060241282));
#62581=CARTESIAN_POINT('Ctrl Pts',(0.0979017153081718,2.36981862981113,
8.59420758135082));
#62582=CARTESIAN_POINT('Ctrl Pts',(0.170298611195169,2.36619569516256,8.58927283794836));
#62583=CARTESIAN_POINT('Ctrl Pts',(0.221954290254871,2.36191008797139,8.585693378759));
#62584=CARTESIAN_POINT('Ctrl Pts',(0.351239397644735,2.34690553736394,8.57658206813842));
#62585=CARTESIAN_POINT('Ctrl Pts',(0.428551784349948,2.3340257277654,8.5709928118362));
#62586=CARTESIAN_POINT('Ctrl Pts',(0.593272769837011,2.29812381549023,8.55881752016145));
#62587=CARTESIAN_POINT('Ctrl Pts',(0.68029485049825,2.27388294270118,8.55221817955544));
#62588=CARTESIAN_POINT('Ctrl Pts',(0.868812085910096,2.20957647639467,8.53771182038727));
#62589=CARTESIAN_POINT('Ctrl Pts',(0.969370758663379,2.1673458932066,8.52983184972568));
#62590=CARTESIAN_POINT('Ctrl Pts',(1.08182285689192,2.11072140477582,8.52109675662066));
#62591=CARTESIAN_POINT('Ctrl Pts',(1.09688488749237,2.10293345747359,8.51992856855779));
#62592=CARTESIAN_POINT('Ctrl Pts',(1.12025595959787,2.09052982246708,8.5181202418336));
#62593=CARTESIAN_POINT('Ctrl Pts',(1.1286226299633,2.08602476510235,8.51747374462084));
#62594=CARTESIAN_POINT('Ctrl Pts',(1.14342870561117,2.07793723441988,8.51633152052423));
#62595=CARTESIAN_POINT('Ctrl Pts',(1.14987859225252,2.07437498546742,8.51583459577112));
#62596=CARTESIAN_POINT('Ctrl Pts',(1.16545109200853,2.06567939893509,8.5146362979563));
#62597=CARTESIAN_POINT('Ctrl Pts',(1.17455646312786,2.0605156520165,8.51393683935252));
#62598=CARTESIAN_POINT('Ctrl Pts',(1.20292762902248,2.0441769034375,8.51176021252081));
#62599=CARTESIAN_POINT('Ctrl Pts',(1.22207102978549,2.03279034292229,8.51029559819831));
#62600=CARTESIAN_POINT('Ctrl Pts',(1.32290721839901,1.97087318452317,8.50258696973562));
#62601=CARTESIAN_POINT('Ctrl Pts',(1.4016428748682,1.91567897537897,8.49658750066281));
#62602=CARTESIAN_POINT('Ctrl Pts',(1.61153487136253,1.74865468825113,8.48002248623198));
#62603=CARTESIAN_POINT('Ctrl Pts',(1.73416844896571,1.62711248166638,8.46961856041105));
#62604=CARTESIAN_POINT('Ctrl Pts',(1.87511476060403,1.45320853084984,8.45538332487945));
#62605=CARTESIAN_POINT('Ctrl Pts',(1.9063404750766,1.41199709021595,8.45205471097492));
#62606=CARTESIAN_POINT('Ctrl Pts',(1.94843710648818,1.35249411567479,8.44728870621528));
#62607=CARTESIAN_POINT('Ctrl Pts',(1.96044804945538,1.33502467718915,8.44589418158319));
#62608=CARTESIAN_POINT('Ctrl Pts',(1.98044361621967,1.30509010653594,8.44351121409396));
#62609=CARTESIAN_POINT('Ctrl Pts',(1.98854880600868,1.29270674656078,8.44252730817855));
#62610=CARTESIAN_POINT('Ctrl Pts',(2.00476255860354,1.26742152898944,8.44052164388082));
#62611=CARTESIAN_POINT('Ctrl Pts',(2.01286372749634,1.25451578089376,8.43949967509763));
#62612=CARTESIAN_POINT('Ctrl Pts',(2.03270896549492,1.22221374523139,8.43694556304038));
#62613=CARTESIAN_POINT('Ctrl Pts',(2.04430009125479,1.20272575962581,8.43540799964329));
#62614=CARTESIAN_POINT('Ctrl Pts',(2.08917208247737,1.12476004464512,8.42926788902468));
#62615=CARTESIAN_POINT('Ctrl Pts',(2.12023466188495,1.06504863671246,8.42458887911569));
#62616=CARTESIAN_POINT('Ctrl Pts',(2.19888708545887,0.896737495981399,8.41145862750961));
#62617=CARTESIAN_POINT('Ctrl Pts',(2.24093685424168,0.785773114316431,8.40285823962442));
#62618=CARTESIAN_POINT('Ctrl Pts',(2.3114478150972,0.547165774077421,8.38471499241365));
#62619=CARTESIAN_POINT('Ctrl Pts',(2.33801974314791,0.419345989834354,8.3751934093175));
#62620=CARTESIAN_POINT('Ctrl Pts',(2.35671102505075,0.267617134542715,8.36451461947616));
#62621=CARTESIAN_POINT('Ctrl Pts',(2.35914726529833,0.245214310936882,8.36295398526356));
#62622=CARTESIAN_POINT('Ctrl Pts',(2.36225172205368,0.212309792661528,8.36068854443314));
#62623=CARTESIAN_POINT('Ctrl Pts',(2.36316986619369,0.201833694850995,8.35997124610218));
#62624=CARTESIAN_POINT('Ctrl Pts',(2.36467600348764,0.183226396494269,8.35870465200194));
#62625=CARTESIAN_POINT('Ctrl Pts',(2.36529179137303,0.175097864132252,8.35815388969546));
#62626=CARTESIAN_POINT('Ctrl Pts',(2.3665561245411,0.157182576707728,8.35694564274529));
#62627=CARTESIAN_POINT('Ctrl Pts',(2.3671858875695,0.147394827700926,8.35628918294804));
#62628=CARTESIAN_POINT('Ctrl Pts',(2.36885140783511,0.118736026631401,8.35437698533906));
#62629=CARTESIAN_POINT('Ctrl Pts',(2.36972237578679,0.0998556597063659,
8.35312983037368));
#62630=CARTESIAN_POINT('Ctrl Pts',(2.37121207371819,0.0562432340600832,
8.35027389255599));
#62631=CARTESIAN_POINT('Ctrl Pts',(2.37166974445286,0.0315075437582258,
8.34867255753801));
#62632=CARTESIAN_POINT('Ctrl Pts',(2.37191411308031,-0.0541249708904168,
8.34317893529605));
#62633=CARTESIAN_POINT('Ctrl Pts',(2.36974272322408,-0.115006467625612,
8.339360447559));
#62634=CARTESIAN_POINT('Ctrl Pts',(2.35050445200808,-0.373927493967537,
8.32324840626464));
#62635=CARTESIAN_POINT('Ctrl Pts',(2.3109305833944,-0.569466351606306,8.31132645191904));
#62636=CARTESIAN_POINT('Ctrl Pts',(2.23338867465496,-0.799441032081753,
8.29580891030043));
#62637=CARTESIAN_POINT('Ctrl Pts',(2.21818702988349,-0.840700213819528,
8.29296653520742));
#62638=CARTESIAN_POINT('Ctrl Pts',(2.19516774341166,-0.898198042199665,
8.28890975906897));
#62639=CARTESIAN_POINT('Ctrl Pts',(2.18829782121302,-0.914808046156683,
8.28772638639143));
#62640=CARTESIAN_POINT('Ctrl Pts',(2.17541718153855,-0.944975145147703,
8.28555528996647));
#62641=CARTESIAN_POINT('Ctrl Pts',(2.16946679310329,-0.958557121662552,
8.28456962007275));
#62642=CARTESIAN_POINT('Ctrl Pts',(2.15715898200056,-0.985948417582597,
8.28256467815422));
#62643=CARTESIAN_POINT('Ctrl Pts',(2.15079537093093,-0.999754174651041,
8.28154523335808));
#62644=CARTESIAN_POINT('Ctrl Pts',(2.1346863681327,-1.0338366733664,8.27900581621406));
#62645=CARTESIAN_POINT('Ctrl Pts',(2.12478452997909,-1.05403738008532,8.27748055742196));
#62646=CARTESIAN_POINT('Ctrl Pts',(2.08482351369028,-1.13270971422044,8.27145896364283));
#62647=CARTESIAN_POINT('Ctrl Pts',(2.05262829280513,-1.19005715929661,8.266889900931));
#62648=CARTESIAN_POINT('Ctrl Pts',(1.95828903181032,-1.3428559664986,8.25420939913357));
#62649=CARTESIAN_POINT('Ctrl Pts',(1.89159161789649,-1.43528201554369,8.24596182080934));
#62650=CARTESIAN_POINT('Ctrl Pts',(1.73036274840799,-1.62785226054613,8.22765312878666));
#62651=CARTESIAN_POINT('Ctrl Pts',(1.63321534326675,-1.72530352243292,8.2175994000662));
#62652=CARTESIAN_POINT('Ctrl Pts',(1.51114707343403,-1.82814884274172,8.206453115561));
#62653=CARTESIAN_POINT('Ctrl Pts',(1.49392007381084,-1.84225312325041,8.20491158833296));
#62654=CARTESIAN_POINT('Ctrl Pts',(1.46830603961633,-1.86262850934513,8.20266843586979));
#62655=CARTESIAN_POINT('Ctrl Pts',(1.46007256951136,-1.86908953554275,8.20195465282239));
#62656=CARTESIAN_POINT('Ctrl Pts',(1.44535259522795,-1.88048407107331,8.20069178935787));
#62657=CARTESIAN_POINT('Ctrl Pts',(1.43888312655781,-1.8854388933468,8.20014127753173));
#62658=CARTESIAN_POINT('Ctrl Pts',(1.42453876318168,-1.89630808618116,8.19893062469174));
#62659=CARTESIAN_POINT('Ctrl Pts',(1.4166524543515,-1.90220684409439,8.19827153781574));
#62660=CARTESIAN_POINT('Ctrl Pts',(1.39336614327712,-1.91939926654922,8.19634371691687));
#62661=CARTESIAN_POINT('Ctrl Pts',(1.37786579882295,-1.93055656492797,8.19508377983455));
#62662=CARTESIAN_POINT('Ctrl Pts',(1.34170524456011,-1.95592787613369,8.1921936176166));
#62663=CARTESIAN_POINT('Ctrl Pts',(1.32095072354095,-1.97000408928778,8.19057109414517));
#62664=CARTESIAN_POINT('Ctrl Pts',(1.24794922003068,-2.01784290332449,8.18497452303515));
#62665=CARTESIAN_POINT('Ctrl Pts',(1.19459769589462,-2.04987917258099,8.18107727318176));
#62666=CARTESIAN_POINT('Ctrl Pts',(0.955018527770854,-2.18120589196073,
8.16413441409012));
#62667=CARTESIAN_POINT('Ctrl Pts',(0.757300459264175,-2.25747941330803,
8.15148606117072));
#62668=CARTESIAN_POINT('Ctrl Pts',(0.517978059911723,-2.31476302733993,
8.13563367842031));
#62669=CARTESIAN_POINT('Ctrl Pts',(0.483679640576045,-2.32217203166779,
8.13335229361054));
#62670=CARTESIAN_POINT('Ctrl Pts',(0.431516783128349,-2.33223429212277,
8.12986190819428));
#62671=CARTESIAN_POINT('Ctrl Pts',(0.413764709319992,-2.3354490495559,8.12867047352132));
#62672=CARTESIAN_POINT('Ctrl Pts',(0.381691025755587,-2.34088017555615,
8.12651056788367));
#62673=CARTESIAN_POINT('Ctrl Pts',(0.367382370088271,-2.3431684134538,8.12554439898229));
#62674=CARTESIAN_POINT('Ctrl Pts',(0.336626289043042,-2.34779828480732,
8.12346165910674));
#62675=CARTESIAN_POINT('Ctrl Pts',(0.320173509679108,-2.35009849670347,
8.12234384871914));
#62676=CARTESIAN_POINT('Ctrl Pts',(0.274756070910216,-2.35596238905125,
8.11924742589648));
#62677=CARTESIAN_POINT('Ctrl Pts',(0.245748532917796,-2.35916451419739,
8.11725774251436));
#62678=CARTESIAN_POINT('Ctrl Pts',(0.0591210187654135,-2.37628699024479,
8.10437404035668));
#62679=CARTESIAN_POINT('Ctrl Pts',(-0.09947168399798,-2.37493659998389,
8.09300851852358));
#62680=CARTESIAN_POINT('Ctrl Pts',(-0.402375771350924,-2.34195616925058,
8.07081159269121));
#62681=CARTESIAN_POINT('Ctrl Pts',(-0.546258892797123,-2.31263334205272,
8.06005903640391));
#62682=CARTESIAN_POINT('Ctrl Pts',(-0.707295762208248,-2.26393499483603,
8.04831837123785));
#62683=CARTESIAN_POINT('Ctrl Pts',(-0.727980609219806,-2.25736866081363,
8.04681653139063));
#62684=CARTESIAN_POINT('Ctrl Pts',(-0.758403439035173,-2.24724934285205,
8.04461977516528));
#62685=CARTESIAN_POINT('Ctrl Pts',(-0.768212282890147,-2.2439151685677,
8.04391338172618));
#62686=CARTESIAN_POINT('Ctrl Pts',(-0.785692470000997,-2.23784533158747,
8.04265828092084));
#62687=CARTESIAN_POINT('Ctrl Pts',(-0.793371903728572,-2.23513431673883,
8.04210821624337));
#62688=CARTESIAN_POINT('Ctrl Pts',(-0.810390599576168,-2.22902756390045,
8.04089215288714));
#62689=CARTESIAN_POINT('Ctrl Pts',(-0.81972262433329,-2.22561264206116,
8.0402272724433));
#62690=CARTESIAN_POINT('Ctrl Pts',(-0.847337384001219,-2.21531015901738,
8.03826477397155));
#62691=CARTESIAN_POINT('Ctrl Pts',(-0.865557295347477,-2.20825505127425,
8.03697643716299));
#62692=CARTESIAN_POINT('Ctrl Pts',(-0.907659460200483,-2.19135108834415,
8.03400991573589));
#62693=CARTESIAN_POINT('Ctrl Pts',(-0.931472478570623,-2.18133546810302,
8.0323400160753));
#62694=CARTESIAN_POINT('Ctrl Pts',(-1.01478852177506,-2.14467994504452,
8.02650964257522));
#62695=CARTESIAN_POINT('Ctrl Pts',(-1.07335540150549,-2.115976641658,8.02243298681323));
#62696=CARTESIAN_POINT('Ctrl Pts',(-1.31506949936308,-1.98489157082227,
8.00540628000545));
#62697=CARTESIAN_POINT('Ctrl Pts',(-1.48537359650764,-1.86087721654588,
7.99281027195385));
#62698=CARTESIAN_POINT('Ctrl Pts',(-1.65900313125208,-1.69523420656825,
7.97732462592896));
#62699=CARTESIAN_POINT('Ctrl Pts',(-1.68045690164503,-1.673969795345,7.97535959163726));
#62700=CARTESIAN_POINT('Ctrl Pts',(-1.71445780075216,-1.63895655077891,
7.9721560204747));
#62701=CARTESIAN_POINT('Ctrl Pts',(-1.72725982599742,-1.62545919262608,
7.9709284486055));
#62702=CARTESIAN_POINT('Ctrl Pts',(-1.74978451575416,-1.6011444974019,7.96872915234497));
#62703=CARTESIAN_POINT('Ctrl Pts',(-1.75956904977996,-1.59038558099717,
7.96776010198917));
#62704=CARTESIAN_POINT('Ctrl Pts',(-1.78007875157388,-1.56741248460543,
7.96569912445809));
#62705=CARTESIAN_POINT('Ctrl Pts',(-1.79077849484654,-1.55517671617345,
7.96460621675112));
#62706=CARTESIAN_POINT('Ctrl Pts',(-1.81852355427765,-1.52278265416788,
7.96172462349407));
#62707=CARTESIAN_POINT('Ctrl Pts',(-1.83535914732937,-1.50244854579761,
7.9599276204616));
#62708=CARTESIAN_POINT('Ctrl Pts',(-1.92021413417696,-1.39640539046586,
7.95061261952489));
#62709=CARTESIAN_POINT('Ctrl Pts',(-1.98257335796383,-1.3063564356396,7.9428795273893));
#62710=CARTESIAN_POINT('Ctrl Pts',(-2.09630194528895,-1.1151270540726,7.92684681226009));
#62711=CARTESIAN_POINT('Ctrl Pts',(-2.14708599253335,-1.01390836739786,
7.91855684364855));
#62712=CARTESIAN_POINT('Ctrl Pts',(-2.22648796364629,-0.822666879990042,
7.90351253933223));
#62713=CARTESIAN_POINT('Ctrl Pts',(-2.257337138877,-0.733799932419877,7.89675096671677));
#62714=CARTESIAN_POINT('Ctrl Pts',(-2.2873862596507,-0.627171368670858,
7.88906692167713));
#62715=CARTESIAN_POINT('Ctrl Pts',(-2.29176786362082,-0.610966386429781,
7.88791063045272));
#62716=CARTESIAN_POINT('Ctrl Pts',(-2.29835036979,-0.585553766115996,7.88611669392574));
#62717=CARTESIAN_POINT('Ctrl Pts',(-2.30066872901587,-0.576377517269646,
7.88547284490305));
#62718=CARTESIAN_POINT('Ctrl Pts',(-2.30469573223073,-0.560026811119789,
7.88433286964282));
#62719=CARTESIAN_POINT('Ctrl Pts',(-2.30642587166939,-0.55285816260873,
7.88383557346393));
#62720=CARTESIAN_POINT('Ctrl Pts',(-2.31054363709618,-0.535440838022192,
7.88263325517533));
#62721=CARTESIAN_POINT('Ctrl Pts',(-2.31289653340099,-0.525184183039262,
7.88193018399214));
#62722=CARTESIAN_POINT('Ctrl Pts',(-2.3177110549547,-0.503536813787723,
7.88045605554141));
#62723=CARTESIAN_POINT('Ctrl Pts',(-2.32015715841289,-0.49214289625118,
7.87968582548661));
#62724=CARTESIAN_POINT('Ctrl Pts',(-2.32931266135115,-0.447910621972815,
7.87671600705543));
#62725=CARTESIAN_POINT('Ctrl Pts',(-2.33541000664873,-0.414947895937856,
7.87454605676779));
#62726=CARTESIAN_POINT('Ctrl Pts',(-2.36128728269817,-0.256321997131525,
7.86426222955652));
#62727=CARTESIAN_POINT('Ctrl Pts',(-2.3716359730428,-0.12932670716072,7.85649532889853));
#62728=CARTESIAN_POINT('Ctrl Pts',(-2.37174906289902,-0.00210834949801023,
7.84868373744261));
#62729=CARTESIAN_POINT('Ctrl Pts',(-2.36544101854889,0.172878137039867,
7.83684641963031));
#62730=CARTESIAN_POINT('Ctrl Pts',(-2.36969985652205,0.114605701869349,
7.84076091038855));
#62731=CARTESIAN_POINT('Ctrl Pts',(-2.37180105257304,0.0562170784915722,
7.84467540114679));
#62732=CARTESIAN_POINT('Ctrl Pts',(-2.37174905777015,-0.00211411125499902,
7.84858989190503));
#62733=CARTESIAN_POINT('',(-2.37174998736518,0.000244812681607679,7.64926189700123));
#62734=CARTESIAN_POINT('Ctrl Pts',(-2.36544101891311,0.172878132056386,
7.63807246982441));
#62735=CARTESIAN_POINT('Ctrl Pts',(-2.36683982265571,0.153738708748238,
7.63929615294632));
#62736=CARTESIAN_POINT('Ctrl Pts',(-2.36800678971193,0.134576069779931,
7.64052614156132));
#62737=CARTESIAN_POINT('Ctrl Pts',(-2.37008903249588,0.0918295100026025,
7.64328254293788));
#62738=CARTESIAN_POINT('Ctrl Pts',(-2.37088519743952,0.0682495467476106,
7.64481159244682));
#62739=CARTESIAN_POINT('Ctrl Pts',(-2.37160827875137,0.0298577568740206,
7.64731723586861));
#62740=CARTESIAN_POINT('Ctrl Pts',(-2.37174845903576,0.0150512976496863,
7.6482874755401));
#62741=CARTESIAN_POINT('Ctrl Pts',(-2.37174998736518,0.000244812681607679,
7.64926189700123));
#62742=CARTESIAN_POINT('Ctrl Pts',(-2.37174998746501,0.000243843695986532,
7.64926196077062));
#62743=CARTESIAN_POINT('Ctrl Pts',(-2.37175104793131,-0.0100708004041009,
7.64994077228303));
#62744=CARTESIAN_POINT('Ctrl Pts',(-2.37168482144786,-0.0203852376566066,
7.65062159798491));
#62745=CARTESIAN_POINT('Ctrl Pts',(-2.37138670818907,-0.0434151458843365,
7.65214645450117));
#62746=CARTESIAN_POINT('Ctrl Pts',(-2.37111982763709,-0.0561297343481302,
7.65299152717104));
#62747=CARTESIAN_POINT('Ctrl Pts',(-2.37031804331917,-0.0837414902881062,
7.65483402903007));
#62748=CARTESIAN_POINT('Ctrl Pts',(-2.36974492408593,-0.0986369157752481,
7.65583259857848));
#62749=CARTESIAN_POINT('Ctrl Pts',(-2.36804869582846,-0.134033476588653,
7.65821696919595));
#62750=CARTESIAN_POINT('Ctrl Pts',(-2.36679972368118,-0.154527088572115,
7.65960658558108));
#62751=CARTESIAN_POINT('Ctrl Pts',(-2.36170347148804,-0.223407056852555,
7.66430918087067));
#62752=CARTESIAN_POINT('Ctrl Pts',(-2.35663721639544,-0.271688137133943,
7.66765901622017));
#62753=CARTESIAN_POINT('Ctrl Pts',(-2.34370905362379,-0.366699345244975,
7.67436090788512));
#62754=CARTESIAN_POINT('Ctrl Pts',(-2.33592084255079,-0.413417317870091,
7.6777094133968));
#62755=CARTESIAN_POINT('Ctrl Pts',(-2.30104722842467,-0.589863052739477,
7.69054991057742));
#62756=CARTESIAN_POINT('Ctrl Pts',(-2.26450673015186,-0.717468680115592,
7.70025457385694));
#62757=CARTESIAN_POINT('Ctrl Pts',(-2.1931890865448,-0.905438696381539,
7.71487583134441));
#62758=CARTESIAN_POINT('Ctrl Pts',(-2.16610180842508,-0.968453254887932,
7.71983270889984));
#62759=CARTESIAN_POINT('Ctrl Pts',(-2.12468236338812,-1.05434380345765,
7.72659638762268));
#62760=CARTESIAN_POINT('Ctrl Pts',(-2.112635098113,-1.07828060889541,7.7284820391519));
#62761=CARTESIAN_POINT('Ctrl Pts',(-2.09081062957852,-1.11987319050323,
7.73175360898754));
#62762=CARTESIAN_POINT('Ctrl Pts',(-2.08120906876835,-1.13761765559537,
7.73314772895018));
#62763=CARTESIAN_POINT('Ctrl Pts',(-2.06641387352654,-1.16414595118647,
7.73522715033727));
#62764=CARTESIAN_POINT('Ctrl Pts',(-2.06138834858849,-1.17302181491389,
7.73592206153771));
#62765=CARTESIAN_POINT('Ctrl Pts',(-2.05215282107977,-1.18909054021136,
7.73717823822132));
#62766=CARTESIAN_POINT('Ctrl Pts',(-2.04796205438064,-1.19629383613383,
7.73774062808807));
#62767=CARTESIAN_POINT('Ctrl Pts',(-2.03835675822992,-1.2126054823266,7.73901256824784));
#62768=CARTESIAN_POINT('Ctrl Pts',(-2.03291907270906,-1.22169979291215,
7.73972064400058));
#62769=CARTESIAN_POINT('Ctrl Pts',(-2.01589510681606,-1.2497432827057,7.74190172958407));
#62770=CARTESIAN_POINT('Ctrl Pts',(-2.00410309549641,-1.26856699586418,
7.74336238742602));
#62771=CARTESIAN_POINT('Ctrl Pts',(-1.91444306773753,-1.40732077547722,
7.75412574517736));
#62772=CARTESIAN_POINT('Ctrl Pts',(-1.82612578710931,-1.52017084870762,
7.7628717943006));
#62773=CARTESIAN_POINT('Ctrl Pts',(-1.61705746750953,-1.74259640166611,
7.78161731740108));
#62774=CARTESIAN_POINT('Ctrl Pts',(-1.49412683980813,-1.84907908301282,
7.79159582261825));
#62775=CARTESIAN_POINT('Ctrl Pts',(-1.33810842607101,-1.95843458488203,
7.80395352541111));
#62776=CARTESIAN_POINT('Ctrl Pts',(-1.31462784998292,-1.97427295204799,
7.8058047879604));
#62777=CARTESIAN_POINT('Ctrl Pts',(-1.27688742162115,-1.99875821068158,
7.80877020031037));
#62778=CARTESIAN_POINT('Ctrl Pts',(-1.26280983825666,-2.0076820368439,7.80987413839438));
#62779=CARTESIAN_POINT('Ctrl Pts',(-1.23599335115478,-2.02428746740166,
7.81197356307449));
#62780=CARTESIAN_POINT('Ctrl Pts',(-1.22327390427851,-2.03199907794294,
7.81296789685022));
#62781=CARTESIAN_POINT('Ctrl Pts',(-1.19415622648995,-2.04928022137772,
7.81524131996426));
#62782=CARTESIAN_POINT('Ctrl Pts',(-1.17771410983524,-2.05877341116072,
7.81652306098004));
#62783=CARTESIAN_POINT('Ctrl Pts',(-1.13432883227761,-2.08313298667806,
7.81990077277483));
#62784=CARTESIAN_POINT('Ctrl Pts',(-1.10720796216833,-2.09767378692851,
7.82200791740675));
#62785=CARTESIAN_POINT('Ctrl Pts',(-0.931416305383729,-2.18756520041128,
7.83564376912977));
#62786=CARTESIAN_POINT('Ctrl Pts',(-0.775458739050126,-2.24758166178981,
7.84768929423007));
#62787=CARTESIAN_POINT('Ctrl Pts',(-0.52341126050802,-2.31519740855457,
7.86671529496087));
#62788=CARTESIAN_POINT('Ctrl Pts',(-0.430909845994576,-2.33418439900242,
7.87359865419005));
#62789=CARTESIAN_POINT('Ctrl Pts',(-0.305455623747408,-2.35222113461249,
7.88264031079023));
#62790=CARTESIAN_POINT('Ctrl Pts',(-0.273299043263232,-2.35617385753945,
7.88493191582932));
#62791=CARTESIAN_POINT('Ctrl Pts',(-0.217903690123094,-2.36183367887303,
7.88882464079312));
#62792=CARTESIAN_POINT('Ctrl Pts',(-0.194702647581203,-2.36385941287312,
7.8904385189752));
#62793=CARTESIAN_POINT('Ctrl Pts',(-0.160706206545447,-2.36632376122687,
7.89277570137009));
#62794=CARTESIAN_POINT('Ctrl Pts',(-0.149932454659455,-2.36703081899685,
7.89351231976217));
#62795=CARTESIAN_POINT('Ctrl Pts',(-0.131618332410639,-2.36810718917024,
7.89475718163007));
#62796=CARTESIAN_POINT('Ctrl Pts',(-0.124080539978081,-2.36851410599818,
7.89526743031774));
#62797=CARTESIAN_POINT('Ctrl Pts',(-0.106865646805108,-2.36936101668786,
7.89642784542258));
#62798=CARTESIAN_POINT('Ctrl Pts',(-0.0971876511047162,-2.36977772429777,
7.89707673462868));
#62799=CARTESIAN_POINT('Ctrl Pts',(-0.0703134833379145,-2.37076993867694,
7.89886960189225));
#62800=CARTESIAN_POINT('Ctrl Pts',(-0.053112798728508,-2.37121765352606,
7.90000690656921));
#62801=CARTESIAN_POINT('Ctrl Pts',(0.075658706849736,-2.37316747054677,
7.90845500545173));
#62802=CARTESIAN_POINT('Ctrl Pts',(0.187220952049796,-2.36698180242157,
7.91540543526459));
#62803=CARTESIAN_POINT('Ctrl Pts',(0.385550877352111,-2.34186813535702,
7.92773142044119));
#62804=CARTESIAN_POINT('Ctrl Pts',(0.472468110367663,-2.32589117207989,
7.93312277505396));
#62805=CARTESIAN_POINT('Ctrl Pts',(0.633251191678771,-2.28694982202508,
7.94334614415156));
#62806=CARTESIAN_POINT('Ctrl Pts',(0.707275425986675,-2.26515048701398,
7.94815594274821));
#62807=CARTESIAN_POINT('Ctrl Pts',(0.828707032653938,-2.2228566493564,7.95633965407458));
#62808=CARTESIAN_POINT('Ctrl Pts',(0.876744479901385,-2.20435150165048,
7.95965629790721));
#62809=CARTESIAN_POINT('Ctrl Pts',(0.943378917228261,-2.17615962116963,
7.96439064099154));
#62810=CARTESIAN_POINT('Ctrl Pts',(0.962509498593233,-2.16776610774485,
7.96576568239927));
#62811=CARTESIAN_POINT('Ctrl Pts',(0.995318013290381,-2.1528515130751,7.96815258762281));
#62812=CARTESIAN_POINT('Ctrl Pts',(1.00904913808842,-2.14644995374487,7.96916037439106));
#62813=CARTESIAN_POINT('Ctrl Pts',(1.03531649933598,-2.13389615334149,7.97110570974525));
#62814=CARTESIAN_POINT('Ctrl Pts',(1.04786161372329,-2.12776386642913,7.97204254258729));
#62815=CARTESIAN_POINT('Ctrl Pts',(1.08077060550112,-2.11131571515383,7.97452101023074));
#62816=CARTESIAN_POINT('Ctrl Pts',(1.10104054891598,-2.10081622181181,7.97606892068383));
#62817=CARTESIAN_POINT('Ctrl Pts',(1.174635342519,-2.06133767887945,7.98176936904308));
#62818=CARTESIAN_POINT('Ctrl Pts',(1.22699016722261,-2.03060956797838,7.98598193802389));
#62819=CARTESIAN_POINT('Ctrl Pts',(1.42857460566665,-1.90165173056859,8.00284243729954));
#62820=CARTESIAN_POINT('Ctrl Pts',(1.56767509570022,-1.78871026071855,8.01597479239079));
#62821=CARTESIAN_POINT('Ctrl Pts',(1.73367315373764,-1.61956393454659,8.03315698938038));
#62822=CARTESIAN_POINT('Ctrl Pts',(1.77303497408888,-1.57637488109569,8.03736062896923));
#62823=CARTESIAN_POINT('Ctrl Pts',(1.83369206723989,-1.5046699923059,8.04400220543952));
#62824=CARTESIAN_POINT('Ctrl Pts',(1.85601014446657,-1.47705282584351,8.04648499509374));
#62825=CARTESIAN_POINT('Ctrl Pts',(1.88546471992215,-1.43888232631621,8.04980495012984));
#62826=CARTESIAN_POINT('Ctrl Pts',(1.89314756706856,-1.4287588551893,8.0506751111582));
#62827=CARTESIAN_POINT('Ctrl Pts',(1.90590417313046,-1.41166626262207,8.0521263706434));
#62828=CARTESIAN_POINT('Ctrl Pts',(1.91102191345115,-1.40473044014356,8.0527103737348));
#62829=CARTESIAN_POINT('Ctrl Pts',(1.92145332455339,-1.39043073807732,8.05390418486546));
#62830=CARTESIAN_POINT('Ctrl Pts',(1.9267626932921,-1.38306400663559,8.05451371437129));
#62831=CARTESIAN_POINT('Ctrl Pts',(1.94065974795882,-1.36354654600783,8.05611472685101));
#62832=CARTESIAN_POINT('Ctrl Pts',(1.94917579079016,-1.35134496143176,8.05710155675881));
#62833=CARTESIAN_POINT('Ctrl Pts',(1.98629388330938,-1.29708203477689,8.06143234451782));
#62834=CARTESIAN_POINT('Ctrl Pts',(2.01365552263569,-1.25418398747864,8.06470418220121));
#62835=CARTESIAN_POINT('Ctrl Pts',(2.11677153463526,-1.08043060282398,8.07750325440686));
#62836=CARTESIAN_POINT('Ctrl Pts',(2.18132326108089,-0.943338418588722,
8.0866329687639));
#62837=CARTESIAN_POINT('Ctrl Pts',(2.25896486338486,-0.72695815522344,8.10083109307866));
#62838=CARTESIAN_POINT('Ctrl Pts',(2.28183747897087,-0.651618582400698,
8.10573437923005));
#62839=CARTESIAN_POINT('Ctrl Pts',(2.31357889990477,-0.524664984486468,
8.11405891259849));
#62840=CARTESIAN_POINT('Ctrl Pts',(2.32456049313992,-0.473643915337655,
8.11742011879281));
#62841=CARTESIAN_POINT('Ctrl Pts',(2.33758877497483,-0.401643683845031,
8.12220718185949));
#62842=CARTESIAN_POINT('Ctrl Pts',(2.34105275907137,-0.38093419735971,8.12358904942655));
#62843=CARTESIAN_POINT('Ctrl Pts',(2.34654477234757,-0.345189477301149,
8.12598399626081));
#62844=CARTESIAN_POINT('Ctrl Pts',(2.34870437684061,-0.330175523164932,
8.12699292296573));
#62845=CARTESIAN_POINT('Ctrl Pts',(2.35257208377099,-0.301325385395171,
8.12893777833687));
#62846=CARTESIAN_POINT('Ctrl Pts',(2.35430250346827,-0.287492791581175,
8.12987296774164));
#62847=CARTESIAN_POINT('Ctrl Pts',(2.35852961179169,-0.251100187496578,
8.13234088113243));
#62848=CARTESIAN_POINT('Ctrl Pts',(2.3608245166847,-0.228518650783053,8.13387977929147));
#62849=CARTESIAN_POINT('Ctrl Pts',(2.36798421088701,-0.146361263384634,
8.13950789423378));
#62850=CARTESIAN_POINT('Ctrl Pts',(2.37092018767185,-0.0866442644387087,
8.14365517117644));
#62851=CARTESIAN_POINT('Ctrl Pts',(2.37363386820713,0.152742235553974,8.16051305208115));
#62852=CARTESIAN_POINT('Ctrl Pts',(2.3552549731757,0.332003595872032,8.17371929308276));
#62853=CARTESIAN_POINT('Ctrl Pts',(2.30430581762809,0.564623405310789,8.19098502197735));
#62854=CARTESIAN_POINT('Ctrl Pts',(2.28966766152932,0.621327399653343,8.19519813350487));
#62855=CARTESIAN_POINT('Ctrl Pts',(2.26279028055774,0.711507028324684,8.20185273378364));
#62856=CARTESIAN_POINT('Ctrl Pts',(2.25186977110335,0.745348887392009,8.20433927125092));
#62857=CARTESIAN_POINT('Ctrl Pts',(2.23601586026846,0.790944250913351,8.20766335722722));
#62858=CARTESIAN_POINT('Ctrl Pts',(2.23174332786445,0.802920588793549,8.2085340031808));
#62859=CARTESIAN_POINT('Ctrl Pts',(2.22441278644027,0.822958159861634,8.20998583848492));
#62860=CARTESIAN_POINT('Ctrl Pts',(2.22140680512468,0.83103802107498,8.21056993743034));
#62861=CARTESIAN_POINT('Ctrl Pts',(2.21514495737823,0.847592646330202,8.21176370141507));
#62862=CARTESIAN_POINT('Ctrl Pts',(2.21188438689456,0.856065384304466,8.21237309002592));
#62863=CARTESIAN_POINT('Ctrl Pts',(2.20315538768663,0.878365232877269,8.21397330748037));
#62864=CARTESIAN_POINT('Ctrl Pts',(2.19760534318609,0.892160259078836,8.21495949156517));
#62865=CARTESIAN_POINT('Ctrl Pts',(2.17253914976547,0.952810526192658,8.21928260919121));
#62866=CARTESIAN_POINT('Ctrl Pts',(2.15165015710305,0.999087931669876,8.22254773850242));
#62867=CARTESIAN_POINT('Ctrl Pts',(2.06267822881898,1.1804355062056,8.23534464334201));
#62868=CARTESIAN_POINT('Ctrl Pts',(1.98322852628405,1.30953450504377,8.24447781274483));
#62869=CARTESIAN_POINT('Ctrl Pts',(1.84454225789204,1.49300403029087,8.25868192825093));
#62870=CARTESIAN_POINT('Ctrl Pts',(1.79396941336661,1.55340579437019,8.26358777893927));
#62871=CARTESIAN_POINT('Ctrl Pts',(1.71631535254533,1.63729227873551,8.27085941053797));
#62872=CARTESIAN_POINT('Ctrl Pts',(1.69155767902533,1.66285802770128,8.27314262891968));
#62873=CARTESIAN_POINT('Ctrl Pts',(1.64557935119972,1.70824738362576,8.27733015674813));
#62874=CARTESIAN_POINT('Ctrl Pts',(1.62455175200325,1.72825692872703,8.27922636046222));
#62875=CARTESIAN_POINT('Ctrl Pts',(1.59076988728,1.75924188943857,8.28224692581897));
#62876=CARTESIAN_POINT('Ctrl Pts',(1.57825654192364,1.77047652441155,8.28336039453712));
#62877=CARTESIAN_POINT('Ctrl Pts',(1.55447008533641,1.79137973218446,8.28546757197581));
#62878=CARTESIAN_POINT('Ctrl Pts',(1.54322352293435,1.80107738098956,8.28646001654407));
#62879=CARTESIAN_POINT('Ctrl Pts',(1.51757882069618,1.82277366612269,8.28871481616));
#62880=CARTESIAN_POINT('Ctrl Pts',(1.50312817914012,1.8347084120912,8.28997965882692));
#62881=CARTESIAN_POINT('Ctrl Pts',(1.46523747993118,1.86525411996823,8.29328228312747));
#62882=CARTESIAN_POINT('Ctrl Pts',(1.44158449807153,1.88359438296152,8.29533044290969));
#62883=CARTESIAN_POINT('Ctrl Pts',(1.24839831843216,2.02761846612328,8.31195815579918));
#62884=CARTESIAN_POINT('Ctrl Pts',(1.06315109295959,2.13058917605791,8.32741447140575));
#62885=CARTESIAN_POINT('Ctrl Pts',(0.80702706284224,2.23114931548736,8.34740251456449));
#62886=CARTESIAN_POINT('Ctrl Pts',(0.746334343286624,2.25217806002468,8.35203582257617));
#62887=CARTESIAN_POINT('Ctrl Pts',(0.660238702723952,2.27814491495189,8.35840649756832));
#62888=CARTESIAN_POINT('Ctrl Pts',(0.635497476423738,2.28517011850271,8.36021429525033));
#62889=CARTESIAN_POINT('Ctrl Pts',(0.591754601202301,2.29682536779215,8.36336484504061));
#62890=CARTESIAN_POINT('Ctrl Pts',(0.572801079892815,2.30162535223692,8.36471502984957));
#62891=CARTESIAN_POINT('Ctrl Pts',(0.543994135296906,2.30854281483105,8.36674241938423));
#62892=CARTESIAN_POINT('Ctrl Pts',(0.53418352674584,2.31083264564142,8.36742855669106));
#62893=CARTESIAN_POINT('Ctrl Pts',(0.516224045974578,2.31490396453901,8.3686763633121));
#62894=CARTESIAN_POINT('Ctrl Pts',(0.508080183135024,2.31670502272567,8.36923906401294));
#62895=CARTESIAN_POINT('Ctrl Pts',(0.48942298130101,2.32072804592323,8.37052115535057));
#62896=CARTESIAN_POINT('Ctrl Pts',(0.478903861111284,2.32292157004819,8.3712389656026));
#62897=CARTESIAN_POINT('Ctrl Pts',(0.445815240669384,2.32958712914599,8.37348210010128));
#62898=CARTESIAN_POINT('Ctrl Pts',(0.423194598073375,2.33380244413997,8.37499404197863));
#62899=CARTESIAN_POINT('Ctrl Pts',(0.290843859099948,2.35647804493942,8.3837337524287));
#62900=CARTESIAN_POINT('Ctrl Pts',(0.179972709486823,2.36752920512794,8.39063323555376));
#62901=CARTESIAN_POINT('Ctrl Pts',(-0.0265363382539642,2.37351554953665,
8.40335013819423));
#62902=CARTESIAN_POINT('Ctrl Pts',(-0.121874997163298,2.37053293151438,
8.40916897789272));
#62903=CARTESIAN_POINT('Ctrl Pts',(-0.318069480469154,2.35252564811557,
8.42139720165957));
#62904=CARTESIAN_POINT('Ctrl Pts',(-0.418650117422634,2.3367228257694,8.42780831070464));
#62905=CARTESIAN_POINT('Ctrl Pts',(-0.543279363520799,2.30883564606645,
8.43611221546574));
#62906=CARTESIAN_POINT('Ctrl Pts',(-0.568564297047864,2.30273946887195,
8.43781551918868));
#62907=CARTESIAN_POINT('Ctrl Pts',(-0.609403473070009,2.29217955545606,
8.44059942945652));
#62908=CARTESIAN_POINT('Ctrl Pts',(-0.625021689852114,2.28797018621753,
8.44167193645631));
#62909=CARTESIAN_POINT('Ctrl Pts',(-0.655041812495071,2.27954894897275,
8.44374918634264));
#62910=CARTESIAN_POINT('Ctrl Pts',(-0.669449242239081,2.27535950595442,
8.44475316704247));
#62911=CARTESIAN_POINT('Ctrl Pts',(-0.702623583775113,2.26537060332344,
8.44708171946393));
#62912=CARTESIAN_POINT('Ctrl Pts',(-0.721359913133924,2.25947421023918,
8.4484093576213));
#62913=CARTESIAN_POINT('Ctrl Pts',(-0.78273816590162,2.23931700455241,8.45280100880603));
#62914=CARTESIAN_POINT('Ctrl Pts',(-0.825045717980147,2.22407706187215,
8.45589626532447));
#62915=CARTESIAN_POINT('Ctrl Pts',(-1.0339909561512,2.14202898626124,8.47153540447672));
#62916=CARTESIAN_POINT('Ctrl Pts',(-1.19307743526602,2.05766179960348,8.48464331104332));
#62917=CARTESIAN_POINT('Ctrl Pts',(-1.40150453032509,1.91477077908679,8.50303971272681));
#62918=CARTESIAN_POINT('Ctrl Pts',(-1.45996445986056,1.87057936132581,8.50834565794288));
#62919=CARTESIAN_POINT('Ctrl Pts',(-1.53774925555721,1.80590814140734,8.51552966696886));
#62920=CARTESIAN_POINT('Ctrl Pts',(-1.55889438197209,1.78768717527148,8.51749594556425));
#62921=CARTESIAN_POINT('Ctrl Pts',(-1.5952364426701,1.75523554765958,8.52089217870456));
#62922=CARTESIAN_POINT('Ctrl Pts',(-1.6105765616182,1.74117039595729,8.52233116748917));
#62923=CARTESIAN_POINT('Ctrl Pts',(-1.63324840008679,1.71982683546863,8.5244635545474));
#62924=CARTESIAN_POINT('Ctrl Pts',(-1.64072048606587,1.7126999086007,8.52516727606303));
#62925=CARTESIAN_POINT('Ctrl Pts',(-1.65413634948671,1.69973538982177,8.52643210028336));
#62926=CARTESIAN_POINT('Ctrl Pts',(-1.66009611935743,1.69391509167485,8.52699441978956));
#62927=CARTESIAN_POINT('Ctrl Pts',(-1.67346887482924,1.68071691872532,8.52825723663176));
#62928=CARTESIAN_POINT('Ctrl Pts',(-1.68086385122312,1.67332129603862,8.5289563575037));
#62929=CARTESIAN_POINT('Ctrl Pts',(-1.70330488962462,1.65057940950423,8.53108132074057));
#62930=CARTESIAN_POINT('Ctrl Pts',(-1.71819196493604,1.63507687407473,8.53249570733397));
#62931=CARTESIAN_POINT('Ctrl Pts',(-1.8370517548105,1.50788682375964,8.54384847515719));
#62932=CARTESIAN_POINT('Ctrl Pts',(-1.93024923217312,1.38659022980856,8.55314549380267));
#62933=CARTESIAN_POINT('Ctrl Pts',(-2.09167677948846,1.12834593644778,8.57185183086385));
#62934=CARTESIAN_POINT('Ctrl Pts',(-2.15962830449452,0.992105902265263,
8.58122612207079));
#62935=CARTESIAN_POINT('Ctrl Pts',(-2.22459448335393,0.822944109772677,
8.59296753734976));
#62936=CARTESIAN_POINT('Ctrl Pts',(-2.23459680753082,0.79538330969721,8.59488245600698));
#62937=CARTESIAN_POINT('Ctrl Pts',(-2.24954824514856,0.751675220080702,
8.59792598459038));
#62938=CARTESIAN_POINT('Ctrl Pts',(-2.2548403984496,0.735647807567967,8.59904341237464));
#62939=CARTESIAN_POINT('Ctrl Pts',(-2.26446374840526,0.705423468798896,
8.60115392024307));
#62940=CARTESIAN_POINT('Ctrl Pts',(-2.26883363597871,0.691239649774912,
8.60214569062537));
#62941=CARTESIAN_POINT('Ctrl Pts',(-2.27839272861406,0.659145155211388,
8.60439329619397));
#62942=CARTESIAN_POINT('Ctrl Pts',(-2.28350435452909,0.641212593606924,
8.60565155513117));
#62943=CARTESIAN_POINT('Ctrl Pts',(-2.29618263350691,0.594659326431703,
8.60892508674917));
#62944=CARTESIAN_POINT('Ctrl Pts',(-2.30342562779406,0.565954629436567,
8.61095043661536));
#62945=CARTESIAN_POINT('Ctrl Pts',(-2.33800615071406,0.417226160865794,
8.62148371565086));
#62946=CARTESIAN_POINT('Ctrl Pts',(-2.35648357902692,0.2954402791331,8.63025421109628));
#62947=CARTESIAN_POINT('Ctrl Pts',(-2.36544103037033,0.172877975290479,
8.63916402106918));
#62948=CARTESIAN_POINT('Origin',(0.,0.,-1.84858989190501));
#62949=CARTESIAN_POINT('',(-2.36544098814976,0.172878552981809,9.83847008213854));
#62950=CARTESIAN_POINT('',(-2.36544101901418,0.172878130673515,9.64179857564526));
#62951=CARTESIAN_POINT('',(-2.36544101854889,0.172878137039864,-1.84858989190501));
#62952=CARTESIAN_POINT('Ctrl Pts',(-2.36544098814985,0.172878552980627,
9.83847008213863));
#62953=CARTESIAN_POINT('Ctrl Pts',(-2.35148711096064,0.36380491416238,9.82484861518335));
#62954=CARTESIAN_POINT('Ctrl Pts',(-2.31445237025283,0.55253567477952,9.8106434709485));
#62955=CARTESIAN_POINT('Ctrl Pts',(-2.23794170651039,0.787307871903176,
9.7929557917114));
#62956=CARTESIAN_POINT('Ctrl Pts',(-2.21903757596194,0.839112664346452,
9.78905776136071));
#62957=CARTESIAN_POINT('Ctrl Pts',(-2.1928766108117,0.903715870097693,9.78424123912396));
#62958=CARTESIAN_POINT('Ctrl Pts',(-2.18728531968704,0.917165830621656,
9.78324098386449));
#62959=CARTESIAN_POINT('Ctrl Pts',(-2.17808512853153,0.938734328061768,
9.78164198851849));
#62960=CARTESIAN_POINT('Ctrl Pts',(-2.17455400606125,0.946885339958971,
9.78103887316123));
#62961=CARTESIAN_POINT('Ctrl Pts',(-2.16762966264957,0.962626001179744,
9.77987670827261));
#62962=CARTESIAN_POINT('Ctrl Pts',(-2.16424221786804,0.970217912399061,
9.77931735336366));
#62963=CARTESIAN_POINT('Ctrl Pts',(-2.15656846452531,0.987176080711072,
9.77807022063541));
#62964=CARTESIAN_POINT('Ctrl Pts',(-2.15226086240516,0.996532661901697,
9.77738370216783));
#62965=CARTESIAN_POINT('Ctrl Pts',(-2.13699632842712,1.02912819213788,9.77499659573381));
#62966=CARTESIAN_POINT('Ctrl Pts',(-2.125722433982,1.05221785109319,9.77331371025024));
#62967=CARTESIAN_POINT('Ctrl Pts',(-2.0439129998954,1.21308467798131,9.76161433437499));
#62968=CARTESIAN_POINT('Ctrl Pts',(-1.96040531853024,1.34386673884254,9.7522175609079));
#62969=CARTESIAN_POINT('Ctrl Pts',(-1.80428914859166,1.54250058301034,9.73669321773066));
#62970=CARTESIAN_POINT('Ctrl Pts',(-1.73914371988262,1.615594176294,9.73065469331309));
#62971=CARTESIAN_POINT('Ctrl Pts',(-1.64093522793271,1.71294110253295,9.72190171273114));
#62972=CARTESIAN_POINT('Ctrl Pts',(-1.61147184054409,1.74068775928852,9.71931623468367));
#62973=CARTESIAN_POINT('Ctrl Pts',(-1.56432940170174,1.78286032489152,9.71522843926986));
#62974=CARTESIAN_POINT('Ctrl Pts',(-1.54712688814872,1.79780859689002,9.71374654372105));
#62975=CARTESIAN_POINT('Ctrl Pts',(-1.51557579985745,1.82443696347632,9.71104395242591));
#62976=CARTESIAN_POINT('Ctrl Pts',(-1.50130075098538,1.83620158540842,9.70982670402882));
#62977=CARTESIAN_POINT('Ctrl Pts',(-1.48667747145421,1.84796867741251,9.70858477716191));
#62978=CARTESIAN_POINT('Ctrl Pts',(-1.48646503961248,1.84813955718636,9.70856673680146));
#62979=CARTESIAN_POINT('Ctrl Pts',(-1.48602988534387,1.8484894708987,9.70852978435111));
#62980=CARTESIAN_POINT('Ctrl Pts',(-1.48580716002368,1.84866850121398,9.7085108721204));
#62981=CARTESIAN_POINT('Ctrl Pts',(-1.48534938349809,1.84903633342807,9.70847200343065));
#62982=CARTESIAN_POINT('Ctrl Pts',(-1.48511432864625,1.84922513076281,9.70845204679392));
#62983=CARTESIAN_POINT('Ctrl Pts',(-1.48462944364324,1.8496144409547,9.70841088174035));
#62984=CARTESIAN_POINT('Ctrl Pts',(-1.48437960886694,1.84981494801519,9.70838967309801));
#62985=CARTESIAN_POINT('Ctrl Pts',(-1.48386216936193,1.85023005123698,9.70834575033391));
#62986=CARTESIAN_POINT('Ctrl Pts',(-1.48359455869878,1.85044463996172,9.70832303592245));
#62987=CARTESIAN_POINT('Ctrl Pts',(-1.48303784424433,1.85089085368922,9.70827578626848));
#62988=CARTESIAN_POINT('Ctrl Pts',(-1.4827487327451,1.85112246901003,9.70825125064959));
#62989=CARTESIAN_POINT('Ctrl Pts',(-1.48214430274669,1.85160646236075,9.70819995940289));
#62990=CARTESIAN_POINT('Ctrl Pts',(-1.48182897404411,1.85185882758476,9.70817320327594));
#62991=CARTESIAN_POINT('Ctrl Pts',(-1.48116601963447,1.85238912836158,9.70811695541674));
#62992=CARTESIAN_POINT('Ctrl Pts',(-1.48081838015965,1.85266704660413,9.70808746301048));
#62993=CARTESIAN_POINT('Ctrl Pts',(-1.48008275391455,1.85325479915633,9.70802506119342));
#62994=CARTESIAN_POINT('Ctrl Pts',(-1.47969474808779,1.85356460947873,9.70799215084859));
#62995=CARTESIAN_POINT('Ctrl Pts',(-1.47886746035172,1.85422474714124,9.7079219883459));
#62996=CARTESIAN_POINT('Ctrl Pts',(-1.47842815125135,1.854575040214,9.70788473485352));
#62997=CARTESIAN_POINT('Ctrl Pts',(-1.46712066230866,1.86358475192356,9.70692597145883));
#62998=CARTESIAN_POINT('Ctrl Pts',(-1.45617691199566,1.87214848568603,9.70600075008007));
#62999=CARTESIAN_POINT('Ctrl Pts',(-1.43267453005572,1.89020888890415,9.70401911832907));
#63000=CARTESIAN_POINT('Ctrl Pts',(-1.42009537486021,1.89967761964359,9.70296168208276));
#63001=CARTESIAN_POINT('Ctrl Pts',(-1.38722006069915,1.92391491023237,9.70020575582528));
#63002=CARTESIAN_POINT('Ctrl Pts',(-1.36678251426728,1.93848743973094,9.69849991446179));
#63003=CARTESIAN_POINT('Ctrl Pts',(-1.2771135363642,2.00030084697416,9.69104482019084));
#63004=CARTESIAN_POINT('Ctrl Pts',(-1.20564389511275,2.04417279079857,9.68517408335815));
#63005=CARTESIAN_POINT('Ctrl Pts',(-1.00131563043175,2.15515313382224,9.6685890935545));
#63006=CARTESIAN_POINT('Ctrl Pts',(-0.864240406150317,2.21368475219605,
9.65766246877988));
#63007=CARTESIAN_POINT('Ctrl Pts',(-0.665480470696995,2.27726387852573,
9.64252253836906));
#63008=CARTESIAN_POINT('Ctrl Pts',(-0.607680832715585,2.29336432617498,
9.63820291478292));
#63009=CARTESIAN_POINT('Ctrl Pts',(-0.525497889041362,2.31293107984241,
9.63222641491523));
#63010=CARTESIAN_POINT('Ctrl Pts',(-0.501578594032632,2.31823580053441,
9.63050644420239));
#63011=CARTESIAN_POINT('Ctrl Pts',(-0.45920639861616,2.32694637196008,9.62749864111949));
#63012=CARTESIAN_POINT('Ctrl Pts',(-0.440787490615252,2.33050560544254,
9.62620410026929));
#63013=CARTESIAN_POINT('Ctrl Pts',(-0.412705011742257,2.33558734839377,
9.62425192786481));
#63014=CARTESIAN_POINT('Ctrl Pts',(-0.403071534776486,2.33726914048361,
9.62358609255653));
#63015=CARTESIAN_POINT('Ctrl Pts',(-0.385386426734616,2.34024397373358,
9.62237112969533));
#63016=CARTESIAN_POINT('Ctrl Pts',(-0.377338384388984,2.34155510330733,
9.62182106045599));
#63017=CARTESIAN_POINT('Ctrl Pts',(-0.35885921704808,2.34446784730728,9.62056440624811));
#63018=CARTESIAN_POINT('Ctrl Pts',(-0.34842399171355,2.3460413801096,9.61985937110377));
#63019=CARTESIAN_POINT('Ctrl Pts',(-0.316270310105425,2.35067057685119,
9.6177001515864));
#63020=CARTESIAN_POINT('Ctrl Pts',(-0.29451900707349,2.35349478591801,9.6162579564743));
#63021=CARTESIAN_POINT('Ctrl Pts',(-0.131703921679352,2.37234213629051,
9.60557945547388));
#63022=CARTESIAN_POINT('Ctrl Pts',(0.0105232603289849,2.37597412133972,
9.5968935442722));
#63023=CARTESIAN_POINT('Ctrl Pts',(0.196983066990513,2.36398102361645,9.58542279486496));
#63024=CARTESIAN_POINT('Ctrl Pts',(0.241638704094815,2.35983458609864,9.58267045296649));
#63025=CARTESIAN_POINT('Ctrl Pts',(0.366532928588348,2.34465533006828,9.57490731471129));
#63026=CARTESIAN_POINT('Ctrl Pts',(0.446358526545137,2.3307761850153,9.56986758619594));
#63027=CARTESIAN_POINT('Ctrl Pts',(0.576998983451227,2.3011039576171,9.56135003850568));
#63028=CARTESIAN_POINT('Ctrl Pts',(0.62827298326351,2.28763625862558,9.5579370272949));
#63029=CARTESIAN_POINT('Ctrl Pts',(0.699015558183576,2.2664971932997,9.55310685203236));
#63030=CARTESIAN_POINT('Ctrl Pts',(0.718901041158526,2.26026846317124,9.55173558474785));
#63031=CARTESIAN_POINT('Ctrl Pts',(0.752843381958993,2.24914347841472,9.54937043530725));
#63032=CARTESIAN_POINT('Ctrl Pts',(0.766941178466973,2.24437535987474,9.54838074829018));
#63033=CARTESIAN_POINT('Ctrl Pts',(0.795498563013189,2.23441627798508,9.54636057078262));
#63034=CARTESIAN_POINT('Ctrl Pts',(0.809954431395487,2.22921687305942,9.54532984388606));
#63035=CARTESIAN_POINT('Ctrl Pts',(0.84618993467659,2.21578490818336,9.54272522441529));
#63036=CARTESIAN_POINT('Ctrl Pts',(0.867900338501009,2.20737153663911,9.54114544548773));
#63037=CARTESIAN_POINT('Ctrl Pts',(0.951315592386749,2.17362502927501,9.53499894183274));
#63038=CARTESIAN_POINT('Ctrl Pts',(1.01205998159402,2.1460149655055,9.5303579142361));
#63039=CARTESIAN_POINT('Ctrl Pts',(1.21268036011542,2.04441400655871,9.51445905386734));
#63040=CARTESIAN_POINT('Ctrl Pts',(1.34628882035849,1.95900952645719,9.50286599063631));
#63041=CARTESIAN_POINT('Ctrl Pts',(1.52344307442583,1.81903598766663,9.48644729432043));
#63042=CARTESIAN_POINT('Ctrl Pts',(1.57468751898544,1.77486086093433,9.48155956001868));
#63043=CARTESIAN_POINT('Ctrl Pts',(1.64323979885341,1.71045596652806,9.4748901458056));
#63044=CARTESIAN_POINT('Ctrl Pts',(1.66219982478415,1.69203679525596,9.47303072381381));
#63045=CARTESIAN_POINT('Ctrl Pts',(1.69487649721588,1.65921278116701,9.46980564328797));
#63046=CARTESIAN_POINT('Ctrl Pts',(1.70872703141753,1.64494540646239,9.46843192967085));
#63047=CARTESIAN_POINT('Ctrl Pts',(1.7292760149873,1.62323832224529,9.46638589875089));
#63048=CARTESIAN_POINT('Ctrl Pts',(1.73610908038843,1.61592804817882,9.46570418368012));
#63049=CARTESIAN_POINT('Ctrl Pts',(1.74841753056706,1.60259180210318,9.46447408334904));
#63050=CARTESIAN_POINT('Ctrl Pts',(1.75390830782466,1.5965807206913,9.46392459147162));
#63051=CARTESIAN_POINT('Ctrl Pts',(1.76626342866086,1.58291417242978,9.46268637846542));
#63052=CARTESIAN_POINT('Ctrl Pts',(1.77310905229181,1.57524222744087,9.46199901923663));
#63053=CARTESIAN_POINT('Ctrl Pts',(1.79397675247366,1.55154723154073,9.4598988083296));
#63054=CARTESIAN_POINT('Ctrl Pts',(1.80783357313211,1.53537918721192,9.45849728624363));
#63055=CARTESIAN_POINT('Ctrl Pts',(1.91982800644748,1.40108613008783,9.44709098360785));
#63056=CARTESIAN_POINT('Ctrl Pts',(2.00651131288746,1.27385528842763,9.437739319127));
#63057=CARTESIAN_POINT('Ctrl Pts',(2.09671773686658,1.10911802167004,9.42620574617628));
#63058=CARTESIAN_POINT('Ctrl Pts',(2.11249491857299,1.07876467913218,9.42410355613875));
#63059=CARTESIAN_POINT('Ctrl Pts',(2.16351929548914,0.975184926706866,9.41697962961143));
#63060=CARTESIAN_POINT('Ctrl Pts',(2.19565642594743,0.900495856184954,9.41192286251095));
#63061=CARTESIAN_POINT('Ctrl Pts',(2.2423605662312,0.774493212381704,9.40337983031205));
#63062=CARTESIAN_POINT('Ctrl Pts',(2.25914512369835,0.724074093809713,9.39995890903668));
#63063=CARTESIAN_POINT('Ctrl Pts',(2.28014109210763,0.65313829929521,9.39511940802262));
#63064=CARTESIAN_POINT('Ctrl Pts',(2.28579613997125,0.633063187263666,9.39374696903231));
#63065=CARTESIAN_POINT('Ctrl Pts',(2.29503234694673,0.598536689844454,9.39138042922393));
#63066=CARTESIAN_POINT('Ctrl Pts',(2.29874359372843,0.584121148298664,9.39039053640619));
#63067=CARTESIAN_POINT('Ctrl Pts',(2.30557386243002,0.556516739073323,9.38849110059571));
#63068=CARTESIAN_POINT('Ctrl Pts',(2.308716026696,0.543334161472777,9.38758233790412));
#63069=CARTESIAN_POINT('Ctrl Pts',(2.31660952799268,0.50891257963218,9.38520468906432));
#63070=CARTESIAN_POINT('Ctrl Pts',(2.32118170813522,0.48763423008766,9.38373020890018));
#63071=CARTESIAN_POINT('Ctrl Pts',(2.33635735266499,0.411952011816685,9.37846766349362));
#63072=CARTESIAN_POINT('Ctrl Pts',(2.34534524198157,0.357246368536955,9.37463007053426));
#63073=CARTESIAN_POINT('Ctrl Pts',(2.37389291516638,0.13508206490017,9.35890200215186));
#63074=CARTESIAN_POINT('Ctrl Pts',(2.37748822584853,-0.0339119585594604,
9.3465660316688));
#63075=CARTESIAN_POINT('Ctrl Pts',(2.35507867162033,-0.296296172675962,
9.32740272814821));
#63076=CARTESIAN_POINT('Ctrl Pts',(2.34135262247255,-0.390202963455172,
9.32055418549568));
#63077=CARTESIAN_POINT('Ctrl Pts',(2.31753010546241,-0.504720199178202,
9.31238726450181));
#63078=CARTESIAN_POINT('Ctrl Pts',(2.31271731398419,-0.526333527072715,
9.31085432474736));
#63079=CARTESIAN_POINT('Ctrl Pts',(2.30519005896671,-0.558037548864441,
9.30862119984535));
#63080=CARTESIAN_POINT('Ctrl Pts',(2.30271063214854,-0.568182073585557,
9.30790900565085));
#63081=CARTESIAN_POINT('Ctrl Pts',(2.29836826453691,-0.58545335791376,9.30670087679319));
#63082=CARTESIAN_POINT('Ctrl Pts',(2.29653903018043,-0.592588222853283,
9.30620309306734));
#63083=CARTESIAN_POINT('Ctrl Pts',(2.29226946753881,-0.608924764427316,
9.30506636427981));
#63084=CARTESIAN_POINT('Ctrl Pts',(2.28980694963943,-0.618120394228029,
9.30442868296862));
#63085=CARTESIAN_POINT('Ctrl Pts',(2.28278423371278,-0.643726885693345,
9.30265838774089));
#63086=CARTESIAN_POINT('Ctrl Pts',(2.27810242281787,-0.660104198444361,
9.30153237371654));
#63087=CARTESIAN_POINT('Ctrl Pts',(2.24026524832242,-0.787261654335602,
9.29282808508605));
#63088=CARTESIAN_POINT('Ctrl Pts',(2.19922021800222,-0.895548334966029,
9.28563923534048));
#63089=CARTESIAN_POINT('Ctrl Pts',(2.11397473538188,-1.07878601617863,9.27319129731505));
#63090=CARTESIAN_POINT('Ctrl Pts',(2.07326119708041,-1.15510016887345,9.26791370880281));
#63091=CARTESIAN_POINT('Ctrl Pts',(1.98884516503763,-1.2944269891429,9.25784473318693));
#63092=CARTESIAN_POINT('Ctrl Pts',(1.94607946948904,-1.35787323693729,9.25307374877631));
#63093=CARTESIAN_POINT('Ctrl Pts',(1.86982443788483,-1.4599839827616,9.24496009623301));
#63094=CARTESIAN_POINT('Ctrl Pts',(1.8380156683664,-1.49983148107835,9.24167412807066));
#63095=CARTESIAN_POINT('Ctrl Pts',(1.79162477340676,-1.55425243141779,9.23699397390853));
#63096=CARTESIAN_POINT('Ctrl Pts',(1.77809783518523,-1.56970952548147,9.23564185770807));
#63097=CARTESIAN_POINT('Ctrl Pts',(1.75446220637669,-1.59602015397974,9.23329937049808));
#63098=CARTESIAN_POINT('Ctrl Pts',(1.74444917781166,-1.60695831143951,9.23231298566059));
#63099=CARTESIAN_POINT('Ctrl Pts',(1.72504676233704,-1.62775831317476,9.23041259565368));
#63100=CARTESIAN_POINT('Ctrl Pts',(1.715673702457,-1.63763463318999,9.22949930410942));
#63101=CARTESIAN_POINT('Ctrl Pts',(1.69333844260084,-1.66076690291513,9.22733380888859));
#63102=CARTESIAN_POINT('Ctrl Pts',(1.68030498020774,-1.67395248644821,9.22607856577313));
#63103=CARTESIAN_POINT('Ctrl Pts',(1.64049010737506,-1.71329852070843,9.22226825102614));
#63104=CARTESIAN_POINT('Ctrl Pts',(1.61324368154949,-1.73897790821269,9.21969298702677));
#63105=CARTESIAN_POINT('Ctrl Pts',(1.43439512744109,-1.89971872952771,9.20298380336546));
#63106=CARTESIAN_POINT('Ctrl Pts',(1.26660425165898,-2.01546671432156,9.18807757817609));
#63107=CARTESIAN_POINT('Ctrl Pts',(1.03162676163839,-2.13651808003215,9.168891356934));
#63108=CARTESIAN_POINT('Ctrl Pts',(0.976004717201496,-2.16249370260018,
9.16446885523825));
#63109=CARTESIAN_POINT('Ctrl Pts',(0.896520059949574,-2.19592071483974,
9.15836608020356));
#63110=CARTESIAN_POINT('Ctrl Pts',(0.873454428309954,-2.20519692336756,
9.15662012720267));
#63111=CARTESIAN_POINT('Ctrl Pts',(0.832537062710284,-2.2209097156853,9.15357168092312));
#63112=CARTESIAN_POINT('Ctrl Pts',(0.814746206923005,-2.22749783399454,
9.15226223685996));
#63113=CARTESIAN_POINT('Ctrl Pts',(0.787626362086828,-2.2371721550558,9.15029235507755));
#63114=CARTESIAN_POINT('Ctrl Pts',(0.778354565483334,-2.24041485368655,
9.14962349416447));
#63115=CARTESIAN_POINT('Ctrl Pts',(0.7613523158724,-2.24624289619348,9.14840571604894));
#63116=CARTESIAN_POINT('Ctrl Pts',(0.753628529272592,-2.24884604659254,
9.14785582546228));
#63117=CARTESIAN_POINT('Ctrl Pts',(0.735926133014581,-2.25471084375293,
9.14660298911896));
#63118=CARTESIAN_POINT('Ctrl Pts',(0.725939126502567,-2.25794611475101,
9.14590155507408));
#63119=CARTESIAN_POINT('Ctrl Pts',(0.694542943237828,-2.26788700326566,
9.14371228777933));
#63120=CARTESIAN_POINT('Ctrl Pts',(0.673059197512471,-2.27435546142892,
9.14223721706842));
#63121=CARTESIAN_POINT('Ctrl Pts',(0.52236135636481,-2.31740599318907,9.1320292638117));
#63122=CARTESIAN_POINT('Ctrl Pts',(0.390319733023683,-2.34326517904431,
9.12378589617284));
#63123=CARTESIAN_POINT('Ctrl Pts',(0.141675797779439,-2.37034453767382,
9.10842866581614));
#63124=CARTESIAN_POINT('Ctrl Pts',(0.0258078210196054,-2.37443404509145,
9.10133597575133));
#63125=CARTESIAN_POINT('Ctrl Pts',(-0.156236704289563,-2.36752961991268,
9.08984765738798));
#63126=CARTESIAN_POINT('Ctrl Pts',(-0.222444214608251,-2.36222855776211,
9.08559936600194));
#63127=CARTESIAN_POINT('Ctrl Pts',(-0.310742829760694,-2.35141371596325,
9.07979294479662));
#63128=CARTESIAN_POINT('Ctrl Pts',(-0.333106702136198,-2.34834993937831,
9.07831025484754));
#63129=CARTESIAN_POINT('Ctrl Pts',(-0.370468028076421,-2.34268714530822,
9.07581139182127));
#63130=CARTESIAN_POINT('Ctrl Pts',(-0.385490629303042,-2.34026207447042,
9.0748006801923));
#63131=CARTESIAN_POINT('Ctrl Pts',(-0.415091836924292,-2.33519085814491,
9.07279689314523));
#63132=CARTESIAN_POINT('Ctrl Pts',(-0.429671054061224,-2.33255232424078,
9.07180409904083));
#63133=CARTESIAN_POINT('Ctrl Pts',(-0.465133949345981,-2.32579052791769,
9.06937437220082));
#63134=CARTESIAN_POINT('Ctrl Pts',(-0.485988352777718,-2.32152244027249,
9.0679329507757));
#63135=CARTESIAN_POINT('Ctrl Pts',(-0.557735312622603,-2.30582953392651,
9.06292892076605));
#63136=CARTESIAN_POINT('Ctrl Pts',(-0.608303510587483,-2.29300776955365,
9.059323060125));
#63137=CARTESIAN_POINT('Ctrl Pts',(-0.823356595925388,-2.23086597162423,
9.04363832515264));
#63138=CARTESIAN_POINT('Ctrl Pts',(-0.982625874559098,-2.16543520297995,
9.03107990166978));
#63139=CARTESIAN_POINT('Ctrl Pts',(-1.19614029231164,-2.04927937633003,
9.01338872448353));
#63140=CARTESIAN_POINT('Ctrl Pts',(-1.25730007813356,-2.01233578751767,
9.00821881329493));
#63141=CARTESIAN_POINT('Ctrl Pts',(-1.33944313510384,-1.9575080231577,9.0012090523693));
#63142=CARTESIAN_POINT('Ctrl Pts',(-1.36192041597794,-1.94193678812602,
8.99928387345556));
#63143=CARTESIAN_POINT('Ctrl Pts',(-1.40069277935262,-1.91407264469806,
8.99595705600795));
#63144=CARTESIAN_POINT('Ctrl Pts',(-1.41710752370737,-1.90195180973846,
8.99454668844659));
#63145=CARTESIAN_POINT('Ctrl Pts',(-1.44141864018205,-1.88351070116848,
8.99245739103078));
#63146=CARTESIAN_POINT('Ctrl Pts',(-1.44943385285639,-1.8773496672767,8.99176848709025));
#63147=CARTESIAN_POINT('Ctrl Pts',(-1.46383119453235,-1.86613572664205,
8.99053126864363));
#63148=CARTESIAN_POINT('Ctrl Pts',(-1.47022691318475,-1.86110105719123,
8.98998177388721));
#63149=CARTESIAN_POINT('Ctrl Pts',(-1.48455768547101,-1.84969998272741,
8.98875073919286));
#63150=CARTESIAN_POINT('Ctrl Pts',(-1.49247782027438,-1.84331535908052,
8.98807048484977));
#63151=CARTESIAN_POINT('Ctrl Pts',(-1.5164104116554,-1.82376730487328,8.98601437392899));
#63152=CARTESIAN_POINT('Ctrl Pts',(-1.53229209125323,-1.81044434793005,
8.98464916902821));
#63153=CARTESIAN_POINT('Ctrl Pts',(-1.66879189941941,-1.69285310562152,
8.97288809503347));
#63154=CARTESIAN_POINT('Ctrl Pts',(-1.77880288974573,-1.57686166355601,
8.96320197064748));
#63155=CARTESIAN_POINT('Ctrl Pts',(-1.96797081049228,-1.33218852471019,
8.94420386499854));
#63156=CARTESIAN_POINT('Ctrl Pts',(-2.04814739152945,-1.2052882129219,8.93494150105376));
#63157=CARTESIAN_POINT('Ctrl Pts',(-2.12826538272142,-1.04711186545144,
8.92343336652158));
#63158=CARTESIAN_POINT('Ctrl Pts',(-2.14028231036323,-1.02232496216988,
8.92163196743653));
#63159=CARTESIAN_POINT('Ctrl Pts',(-2.15870439118753,-0.982577221843002,
8.91874338617778));
#63160=CARTESIAN_POINT('Ctrl Pts',(-2.16539219677101,-0.96774958413176,
8.91766585047418));
#63161=CARTESIAN_POINT('Ctrl Pts',(-2.17776847267248,-0.939539231070214,
8.9156152422617));
#63162=CARTESIAN_POINT('Ctrl Pts',(-2.18348743879779,-0.926170651588775,
8.91464325505616));
#63163=CARTESIAN_POINT('Ctrl Pts',(-2.19623418181204,-0.895599672843647,
8.91241959323735));
#63164=CARTESIAN_POINT('Ctrl Pts',(-2.20318336293789,-0.878365750027235,
8.91116536156537));
#63165=CARTESIAN_POINT('Ctrl Pts',(-2.22086888988578,-0.83297505921796,
8.90785939404667));
#63166=CARTESIAN_POINT('Ctrl Pts',(-2.23127208802867,-0.804692985741374,
8.90579690498634));
#63167=CARTESIAN_POINT('Ctrl Pts',(-2.29777435372505,-0.612685363880377,
8.89177191727566));
#63168=CARTESIAN_POINT('Ctrl Pts',(-2.33633596332856,-0.44346836933917,
8.87924453169628));
#63169=CARTESIAN_POINT('Ctrl Pts',(-2.36658112276971,-0.181087885413271,
8.85998287512962));
#63170=CARTESIAN_POINT('Ctrl Pts',(-2.37179094824305,-0.0900468686838555,
8.85334087044894));
#63171=CARTESIAN_POINT('Ctrl Pts',(-2.37172892309297,0.0471615849229897,
8.84355947082574));
#63172=CARTESIAN_POINT('Ctrl Pts',(-2.37036462550106,0.0932442653156125,
8.8403138512315));
#63173=CARTESIAN_POINT('Ctrl Pts',(-2.36699861119947,0.150471749008194,
8.83635476923397));
#63174=CARTESIAN_POINT('Ctrl Pts',(-2.36625960457586,0.161677663697427,
8.83558295171082));
#63175=CARTESIAN_POINT('Ctrl Pts',(-2.36544101854848,0.172878137045581,
8.83481520889907));
#63176=CARTESIAN_POINT('Ctrl Pts',(-2.36544103037033,0.172877975290479,
8.63916402106918));
#63177=CARTESIAN_POINT('Ctrl Pts',(-2.36969110373298,0.114725409024034,
8.64339148986364));
#63178=CARTESIAN_POINT('Ctrl Pts',(-2.37179807639038,0.0563978649742825,
8.64764768427651));
#63179=CARTESIAN_POINT('Ctrl Pts',(-2.37172922193285,-0.0257972780762,8.65363963955622));
#63180=CARTESIAN_POINT('Ctrl Pts',(-2.37135071963491,-0.0496062506427067,
8.65537450011653));
#63181=CARTESIAN_POINT('Ctrl Pts',(-2.36752241566682,-0.173240244889286,
8.66436993795079));
#63182=CARTESIAN_POINT('Ctrl Pts',(-2.35812718016877,-0.272791361719819,
8.67157241560903));
#63183=CARTESIAN_POINT('Ctrl Pts',(-2.33979591461862,-0.388390117061927,
8.67969388238334));
#63184=CARTESIAN_POINT('Ctrl Pts',(-2.33692812120695,-0.40528854325954,
8.68087483945892));
#63185=CARTESIAN_POINT('Ctrl Pts',(-2.33215578260783,-0.431672343114279,
8.68270737349088));
#63186=CARTESIAN_POINT('Ctrl Pts',(-2.33037603146268,-0.441179290541376,
8.68336538761148));
#63187=CARTESIAN_POINT('Ctrl Pts',(-2.32710321772572,-0.458089184916654,
8.68453135861992));
#63188=CARTESIAN_POINT('Ctrl Pts',(-2.32563293743243,-0.465496004095176,
8.68504052548217));
#63189=CARTESIAN_POINT('Ctrl Pts',(-2.32197008549597,-0.48349770857284,
8.68627439277048));
#63190=CARTESIAN_POINT('Ctrl Pts',(-2.31974036097812,-0.494084791326151,
8.68699702096028));
#63191=CARTESIAN_POINT('Ctrl Pts',(-2.31245728566126,-0.527529475203023,
8.68927128501116));
#63192=CARTESIAN_POINT('Ctrl Pts',(-2.30713776898514,-0.550328501778816,
8.69080900581221));
#63193=CARTESIAN_POINT('Ctrl Pts',(-2.29359972583681,-0.604700316003327,
8.69445405567242));
#63194=CARTESIAN_POINT('Ctrl Pts',(-2.285065516087,-0.636190201856579,8.69654709393603));
#63195=CARTESIAN_POINT('Ctrl Pts',(-2.24900109106115,-0.759154993822237,
8.70468480811763));
#63196=CARTESIAN_POINT('Ctrl Pts',(-2.21660355898122,-0.849113301685393,
8.71056300510052));
#63197=CARTESIAN_POINT('Ctrl Pts',(-2.11366517557661,-1.08851380876652,
8.72657174633265));
#63198=CARTESIAN_POINT('Ctrl Pts',(-2.03282120082926,-1.23291259183521,
8.73666928093543));
#63199=CARTESIAN_POINT('Ctrl Pts',(-1.91990059253567,-1.39288434100355,
8.74929915538806));
#63200=CARTESIAN_POINT('Ctrl Pts',(-1.90166713696624,-1.41767663285545,
8.75130040492403));
#63201=CARTESIAN_POINT('Ctrl Pts',(-1.8714127756611,-1.45717973023777,8.75456568377653));
#63202=CARTESIAN_POINT('Ctrl Pts',(-1.85968813330553,-1.47211363539139,
8.75581838269655));
#63203=CARTESIAN_POINT('Ctrl Pts',(-1.8384604931022,-1.498493354043,8.75806505374931));
#63204=CARTESIAN_POINT('Ctrl Pts',(-1.82902662392166,-1.50999367838631,
8.75905626319781));
#63205=CARTESIAN_POINT('Ctrl Pts',(-1.80879385440372,-1.53419055274483,
8.76116738037484));
#63206=CARTESIAN_POINT('Ctrl Pts',(-1.797968082871,-1.54686347443788,8.76228833775034));
#63207=CARTESIAN_POINT('Ctrl Pts',(-1.76838952118473,-1.58075886430365,
8.76532874533101));
#63208=CARTESIAN_POINT('Ctrl Pts',(-1.74938921009142,-1.60176070563365,
8.76725825401839));
#63209=CARTESIAN_POINT('Ctrl Pts',(-1.6197929068788,-1.73995206569927,8.78026989254322));
#63210=CARTESIAN_POINT('Ctrl Pts',(-1.49789679410241,-1.84592790123689,
8.79184388857896));
#63211=CARTESIAN_POINT('Ctrl Pts',(-1.24821512516698,-2.02188035806493,
8.81409382046256));
#63212=CARTESIAN_POINT('Ctrl Pts',(-1.1228471065884,-2.09410175812764,8.8246815597713));
#63213=CARTESIAN_POINT('Ctrl Pts',(-0.971659512126865,-2.16369166523987,
8.83630008420685));
#63214=CARTESIAN_POINT('Ctrl Pts',(-0.951510080256589,-2.17262801291885,
8.83782585534649));
#63215=CARTESIAN_POINT('Ctrl Pts',(-0.921523094717212,-2.18543012534301,
8.84006019157753));
#63216=CARTESIAN_POINT('Ctrl Pts',(-0.911780220517392,-2.1895128423743,
8.8407805223917));
#63217=CARTESIAN_POINT('Ctrl Pts',(-0.894303673782871,-2.19669944103258,
8.84206221057335));
#63218=CARTESIAN_POINT('Ctrl Pts',(-0.886580583446402,-2.19982780471648,
8.84262495682947));
#63219=CARTESIAN_POINT('Ctrl Pts',(-0.869340728826177,-2.20670554778219,
8.84387304950858));
#63220=CARTESIAN_POINT('Ctrl Pts',(-0.859816047487276,-2.21043413190396,
8.84455718570671));
#63221=CARTESIAN_POINT('Ctrl Pts',(-0.83130020326974,-2.22138489244577,
8.84659014982574));
#63222=CARTESIAN_POINT('Ctrl Pts',(-0.812239496907764,-2.22842498974693,
8.84792891853767));
#63223=CARTESIAN_POINT('Ctrl Pts',(-0.673796550087457,-2.277546653924,8.8575241768069));
#63224=CARTESIAN_POINT('Ctrl Pts',(-0.551289798213978,-2.31026155370225,
8.86533442631666));
#63225=CARTESIAN_POINT('Ctrl Pts',(-0.257386274511344,-2.36402025350706,
8.88369868649895));
#63226=CARTESIAN_POINT('Ctrl Pts',(-0.0851790809236598,-2.37646303448863,
8.89420424301676));
#63227=CARTESIAN_POINT('Ctrl Pts',(0.117218371160872,-2.36904650700781,
8.90727269603405));
#63228=CARTESIAN_POINT('Ctrl Pts',(0.14756074138742,-2.36735024740952,8.90924946709203));
#63229=CARTESIAN_POINT('Ctrl Pts',(0.196682960348062,-2.36365609634398,
8.91248274732521));
#63230=CARTESIAN_POINT('Ctrl Pts',(0.215486795199738,-2.36201603209922,
8.91372829507624));
#63231=CARTESIAN_POINT('Ctrl Pts',(0.249059014345419,-2.35868365430675,
8.91596708881466));
#63232=CARTESIAN_POINT('Ctrl Pts',(0.263834994614235,-2.35707659025862,
8.91695764741032));
#63233=CARTESIAN_POINT('Ctrl Pts',(0.295212293031634,-2.35336520227598,
8.91907267189971));
#63234=CARTESIAN_POINT('Ctrl Pts',(0.311808328060308,-2.35122385476407,
8.92019823709332));
#63235=CARTESIAN_POINT('Ctrl Pts',(0.356736790576114,-2.34494280325636,
8.92326471678894));
#63236=CARTESIAN_POINT('Ctrl Pts',(0.385018389970618,-2.34046546748684,
8.92521598845843));
#63237=CARTESIAN_POINT('Ctrl Pts',(0.566627292253324,-2.30833379650326,
8.937886718477));
#63238=CARTESIAN_POINT('Ctrl Pts',(0.716968722902595,-2.26614457234044,
8.94906243748415));
#63239=CARTESIAN_POINT('Ctrl Pts',(1.00153815751344,-2.1551180028078,8.97130230461971));
#63240=CARTESIAN_POINT('Ctrl Pts',(1.13555647389969,-2.08761361022277,8.98229720666778));
#63241=CARTESIAN_POINT('Ctrl Pts',(1.28066162070134,-1.99639001492484,8.99425690028263));
#63242=CARTESIAN_POINT('Ctrl Pts',(1.29884212010733,-1.98460991305389,8.99575593134402));
#63243=CARTESIAN_POINT('Ctrl Pts',(1.3255847528977,-1.96675702246259,8.99795892334738));
#63244=CARTESIAN_POINT('Ctrl Pts',(1.3342715277231,-1.96087419872322,8.99867419677291));
#63245=CARTESIAN_POINT('Ctrl Pts',(1.34978597597072,-1.95021672772141,8.99995067948742));
#63246=CARTESIAN_POINT('Ctrl Pts',(1.35662781040202,-1.94546355811187,9.00051322552578));
#63247=CARTESIAN_POINT('Ctrl Pts',(1.37186825897043,-1.93475619133123,9.00176549047198));
#63248=CARTESIAN_POINT('Ctrl Pts',(1.38025328877524,-1.92878327151087,9.00245395085806));
#63249=CARTESIAN_POINT('Ctrl Pts',(1.4053422714649,-1.91066420249992,9.00451322830024));
#63250=CARTESIAN_POINT('Ctrl Pts',(1.42192722808726,-1.89835392453265,9.00587359584243));
#63251=CARTESIAN_POINT('Ctrl Pts',(1.46032030898519,-1.86907093409941,9.00902610570363));
#63252=CARTESIAN_POINT('Ctrl Pts',(1.48199716105387,-1.85193037472327,9.01080861712011));
#63253=CARTESIAN_POINT('Ctrl Pts',(1.5590991940925,-1.7887423981917,9.01717836782274));
#63254=CARTESIAN_POINT('Ctrl Pts',(1.61272173268814,-1.74055155225078,9.02166555640838));
#63255=CARTESIAN_POINT('Ctrl Pts',(1.78881180502335,-1.567162324042,9.03692570653259));
#63256=CARTESIAN_POINT('Ctrl Pts',(1.89956320930316,-1.4309094780823,9.0475093584347));
#63257=CARTESIAN_POINT('Ctrl Pts',(2.02040849530408,-1.24317025477864,9.06174042270349));
#63258=CARTESIAN_POINT('Ctrl Pts',(2.04526116988756,-1.20184400705704,9.06485015871237));
#63259=CARTESIAN_POINT('Ctrl Pts',(2.07807619458399,-1.14330855506922,9.0692405821331));
#63260=CARTESIAN_POINT('Ctrl Pts',(2.08711886449137,-1.1267164392501,9.07048347262085));
#63261=CARTESIAN_POINT('Ctrl Pts',(2.10247328876188,-1.09772386524254,9.07265348747314));
#63262=CARTESIAN_POINT('Ctrl Pts',(2.1088760491729,-1.08537247508891,9.07357740239453));
#63263=CARTESIAN_POINT('Ctrl Pts',(2.12204237441756,-1.05941730051279,9.0755181584421));
#63264=CARTESIAN_POINT('Ctrl Pts',(2.12878461544259,-1.04580347016109,9.07653568206859));
#63265=CARTESIAN_POINT('Ctrl Pts',(2.14459076840625,-1.01310166329334,9.07897934956259));
#63266=CARTESIAN_POINT('Ctrl Pts',(2.15353115172818,-0.993955770140758,
9.08040962233996));
#63267=CARTESIAN_POINT('Ctrl Pts',(2.18402890161604,-0.926300993892744,
9.08546369969597));
#63268=CARTESIAN_POINT('Ctrl Pts',(2.20421115454798,-0.877193363210987,
9.08913268420984));
#63269=CARTESIAN_POINT('Ctrl Pts',(2.25088625676115,-0.751813408810636,
9.09850675869672));
#63270=CARTESIAN_POINT('Ctrl Pts',(2.27516275698209,-0.674792296983518,
9.10427277130544));
#63271=CARTESIAN_POINT('Ctrl Pts',(2.33424262951194,-0.447512162946366,
9.12124935201723));
#63272=CARTESIAN_POINT('Ctrl Pts',(2.35838562298804,-0.294912238489469,
9.13262263793216));
#63273=CARTESIAN_POINT('Ctrl Pts',(2.37027110054534,-0.0954107725242537,
9.14686640411079));
#63274=CARTESIAN_POINT('Ctrl Pts',(2.37167005911244,-0.0496998372567961,
9.15008544845627));
#63275=CARTESIAN_POINT('Ctrl Pts',(2.37177071217618,0.0103752464815843,
9.15423463620473));
#63276=CARTESIAN_POINT('Ctrl Pts',(2.37166453690988,0.0247246146822026,
9.15521958679712));
#63277=CARTESIAN_POINT('Ctrl Pts',(2.37128045049076,0.0480359387389798,
9.15680882991398));
#63278=CARTESIAN_POINT('Ctrl Pts',(2.37108194591365,0.0569985853377878,
9.1574172461428));
#63279=CARTESIAN_POINT('Ctrl Pts',(2.37059070320885,0.0746555425380767,
9.15861044060898));
#63280=CARTESIAN_POINT('Ctrl Pts',(2.37030094293751,0.0833497220091635,
9.15919535427092));
#63281=CARTESIAN_POINT('Ctrl Pts',(2.369454711778,0.105139032489686,9.16065515535903));
#63282=CARTESIAN_POINT('Ctrl Pts',(2.36883750353173,0.118231757663547,9.16152678940569));
#63283=CARTESIAN_POINT('Ctrl Pts',(2.36597292280751,0.169889509056894,9.16494638937481));
#63284=CARTESIAN_POINT('Ctrl Pts',(2.36289192527264,0.208404577931597,9.1674531636235));
#63285=CARTESIAN_POINT('Ctrl Pts',(2.35196738337655,0.312806873967035,9.17417319520786));
#63286=CARTESIAN_POINT('Ctrl Pts',(2.34229809410907,0.378470003194304,9.1783185098135));
#63287=CARTESIAN_POINT('Ctrl Pts',(2.30097554920606,0.595483189855097,9.19199181287162));
#63288=CARTESIAN_POINT('Ctrl Pts',(2.25729131104077,0.744126445343541,9.201337930195));
#63289=CARTESIAN_POINT('Ctrl Pts',(2.17316880613711,0.952612701511904,9.21547654532826));
#63290=CARTESIAN_POINT('Ctrl Pts',(2.1440017754646,1.01655722927408,9.21996008780387));
#63291=CARTESIAN_POINT('Ctrl Pts',(2.10113432665654,1.10045779208825,9.22610055730908));
#63292=CARTESIAN_POINT('Ctrl Pts',(2.08990384524729,1.12163927380636,9.22767349731689));
#63293=CARTESIAN_POINT('Ctrl Pts',(2.07076790264729,1.15644556001664,9.23029812410213));
#63294=CARTESIAN_POINT('Ctrl Pts',(2.06304418638892,1.17016866515129,9.23134341206431));
#63295=CARTESIAN_POINT('Ctrl Pts',(2.04759205729515,1.19699466014047,9.23340799325484));
#63296=CARTESIAN_POINT('Ctrl Pts',(2.03987309711524,1.21010213568609,9.23442691281994));
#63297=CARTESIAN_POINT('Ctrl Pts',(2.02107518299485,1.24133166206136,9.23687949603385));
#63298=CARTESIAN_POINT('Ctrl Pts',(2.00987799385751,1.25938063743353,9.23831736675421));
#63299=CARTESIAN_POINT('Ctrl Pts',(1.96944765578644,1.32263837838641,9.24343100964493));
#63300=CARTESIAN_POINT('Ctrl Pts',(1.93892119410322,1.3669967650531,9.24715339965342));
#63301=CARTESIAN_POINT('Ctrl Pts',(1.85790595105463,1.47654211669806,9.25670478737249));
#63302=CARTESIAN_POINT('Ctrl Pts',(1.8054813240699,1.54020326325481,9.26259778430103));
#63303=CARTESIAN_POINT('Ctrl Pts',(1.6297996334736,1.73221887539952,9.28142553029935));
#63304=CARTESIAN_POINT('Ctrl Pts',(1.49536649525984,1.84951652990295,9.29459465223122));
#63305=CARTESIAN_POINT('Ctrl Pts',(1.32808994357103,1.96520396407011,9.30885609830946));
#63306=CARTESIAN_POINT('Ctrl Pts',(1.30686355317677,1.97938306056233,9.31062959341449));
#63307=CARTESIAN_POINT('Ctrl Pts',(1.27666754142965,1.99885624859202,9.31309768649173));
#63308=CARTESIAN_POINT('Ctrl Pts',(1.26788648379674,2.00443762387957,9.31380900791315));
#63309=CARTESIAN_POINT('Ctrl Pts',(1.25189033752674,2.01445784158312,9.3150928281774));
#63310=CARTESIAN_POINT('Ctrl Pts',(1.24468766128208,2.01891615663986,9.31566654168909));
#63311=CARTESIAN_POINT('Ctrl Pts',(1.22963952105555,2.0281195154152,9.31685590251305));
#63312=CARTESIAN_POINT('Ctrl Pts',(1.22179020862177,2.03285779476494,9.31747112850516));
#63313=CARTESIAN_POINT('Ctrl Pts',(1.20078591549016,2.04537154277977,9.31910427150307));
#63314=CARTESIAN_POINT('Ctrl Pts',(1.18758268057096,2.0530657489581,9.32011719501711));
#63315=CARTESIAN_POINT('Ctrl Pts',(1.1206229276701,2.09122453215934,9.32519047295354));
#63316=CARTESIAN_POINT('Ctrl Pts',(1.06576013446699,2.11971048827659,9.32914198925722));
#63317=CARTESIAN_POINT('Ctrl Pts',(0.868104849406729,2.21272005143675,9.34288640433982));
#63318=CARTESIAN_POINT('Ctrl Pts',(0.720102892398409,2.26521369056948,9.35232418308173));
#63319=CARTESIAN_POINT('Ctrl Pts',(0.469402536932037,2.32705223044951,9.36834515896069));
#63320=CARTESIAN_POINT('Ctrl Pts',(0.369356448200614,2.34501237798579,9.37474192578317));
#63321=CARTESIAN_POINT('Ctrl Pts',(0.241984795319236,2.35952373528033,9.38307137193066));
#63322=CARTESIAN_POINT('Ctrl Pts',(0.21544655113751,2.36209474613533,9.38481646850575));
#63323=CARTESIAN_POINT('Ctrl Pts',(0.172608860409931,2.36551694207414,9.38765161016746));
#63324=CARTESIAN_POINT('Ctrl Pts',(0.156333655671251,2.36664826027426,9.3887329791187));
#63325=CARTESIAN_POINT('Ctrl Pts',(0.125116053418824,2.36849483661091,9.39081585160927));
#63326=CARTESIAN_POINT('Ctrl Pts',(0.110175976349677,2.36923680848318,9.39181647825584));
#63327=CARTESIAN_POINT('Ctrl Pts',(0.0755782586266434,2.37062709223273,
9.39414297296713));
#63328=CARTESIAN_POINT('Ctrl Pts',(0.0559178148986994,2.37117229267772,
9.39547195401794));
#63329=CARTESIAN_POINT('Ctrl Pts',(-0.00759176972708754,2.37214318125126,
9.3997885073408));
#63330=CARTESIAN_POINT('Ctrl Pts',(-0.0514443800924831,2.37159734085096,
9.40280542318398));
#63331=CARTESIAN_POINT('Ctrl Pts',(-0.314738314500225,2.36101438413367,
9.42114844721092));
#63332=CARTESIAN_POINT('Ctrl Pts',(-0.531911557557401,2.32174203550533,
9.43737740328743));
#63333=CARTESIAN_POINT('Ctrl Pts',(-0.807335969270521,2.23122237939522,
9.45829548987956));
#63334=CARTESIAN_POINT('Ctrl Pts',(-0.873149099615852,2.20629944966075,
9.46330773665482));
#63335=CARTESIAN_POINT('Ctrl Pts',(-0.952769312213094,2.17202569596862,
9.46931378367047));
#63336=CARTESIAN_POINT('Ctrl Pts',(-0.967709183547159,2.16541080605382,
9.47043813163747));
#63337=CARTESIAN_POINT('Ctrl Pts',(-0.991134066135066,2.15474816579871,
9.47219557354606));
#63338=CARTESIAN_POINT('Ctrl Pts',(-0.999665088160347,2.15080359730926,
9.47283445450126));
#63339=CARTESIAN_POINT('Ctrl Pts',(-1.0158390312485,2.14320807688906,9.47404319462444));
#63340=CARTESIAN_POINT('Ctrl Pts',(-1.02348589576222,2.13956687709165,9.47461355948928));
#63341=CARTESIAN_POINT('Ctrl Pts',(-1.04179792388996,2.13072661603665,9.47597703956171));
#63342=CARTESIAN_POINT('Ctrl Pts',(-1.05244385886684,2.12548835918394,9.47676778860926));
#63343=CARTESIAN_POINT('Ctrl Pts',(-1.08952073235049,2.10689806862577,9.47951654661126));
#63344=CARTESIAN_POINT('Ctrl Pts',(-1.11574174014033,2.09313054052115,9.48145118469449));
#63345=CARTESIAN_POINT('Ctrl Pts',(-1.1811297912143,2.05722000819529,9.48626937657015));
#63346=CARTESIAN_POINT('Ctrl Pts',(-1.21993845281494,2.03444645896966,9.48912330004573));
#63347=CARTESIAN_POINT('Ctrl Pts',(-1.42214459709699,1.90792032730895,9.50408729962109));
#63348=CARTESIAN_POINT('Ctrl Pts',(-1.57302976684585,1.78556392645479,9.51564900818305));
#63349=CARTESIAN_POINT('Ctrl Pts',(-1.7529378803204,1.59897336871174,9.53199001684069));
#63350=CARTESIAN_POINT('Ctrl Pts',(-1.7965155368893,1.54985089642644,9.53618780621946));
#63351=CARTESIAN_POINT('Ctrl Pts',(-1.85283569250154,1.48079342399289,9.54199901086684));
#63352=CARTESIAN_POINT('Ctrl Pts',(-1.86740263087196,1.46238046289781,9.54354013243447));
#63353=CARTESIAN_POINT('Ctrl Pts',(-1.89026557830815,1.43258242695924,9.54602275896612));
#63354=CARTESIAN_POINT('Ctrl Pts',(-1.89873790866833,1.4213341290635,9.54695737318403));
#63355=CARTESIAN_POINT('Ctrl Pts',(-1.91606753494523,1.3978949590008,9.54890011003865));
#63356=CARTESIAN_POINT('Ctrl Pts',(-1.92490980056579,1.38569381780829,9.54990874947502));
#63357=CARTESIAN_POINT('Ctrl Pts',(-1.94544837205442,1.35677738625094,9.55229350503431));
#63358=CARTESIAN_POINT('Ctrl Pts',(-1.95704629843104,1.33999402435167,9.5536732375475));
#63359=CARTESIAN_POINT('Ctrl Pts',(-1.99536836053763,1.28297927189882,9.55834693565643));
#63360=CARTESIAN_POINT('Ctrl Pts',(-2.02107826053437,1.24208405186535,9.56167746367964));
#63361=CARTESIAN_POINT('Ctrl Pts',(-2.11990997075654,1.07367652851818,9.57531440363025));
#63362=CARTESIAN_POINT('Ctrl Pts',(-2.18234618852898,0.940294325538168,
9.58596604376384));
#63363=CARTESIAN_POINT('Ctrl Pts',(-2.26345742274058,0.714558909791934,
9.60345463387719));
#63364=CARTESIAN_POINT('Ctrl Pts',(-2.289716188443,0.625328240950382,9.61023252754985));
#63365=CARTESIAN_POINT('Ctrl Pts',(-2.32126694420569,0.48900484363474,9.62021316956104));
#63366=CARTESIAN_POINT('Ctrl Pts',(-2.33049997824004,0.44291816469533,9.62352390107418));
#63367=CARTESIAN_POINT('Ctrl Pts',(-2.34078042033313,0.382302146062441,
9.62777121849047));
#63368=CARTESIAN_POINT('Ctrl Pts',(-2.34307182890227,0.367997741472551,
9.62876576136883));
#63369=CARTESIAN_POINT('Ctrl Pts',(-2.34657335094488,0.344778874157576,
9.63036659347512));
#63370=CARTESIAN_POINT('Ctrl Pts',(-2.3478640242078,0.335877200775326,9.63097711420203));
#63371=CARTESIAN_POINT('Ctrl Pts',(-2.35018518307835,0.319200828476313,
9.63211459384491));
#63372=CARTESIAN_POINT('Ctrl Pts',(-2.35122779282664,0.311428053561827,
9.63264220855057));
#63373=CARTESIAN_POINT('Ctrl Pts',(-2.35333889442491,0.29507436395037,9.63374717934676));
#63374=CARTESIAN_POINT('Ctrl Pts',(-2.35439905964234,0.286492418602906,
9.63432408236932));
#63375=CARTESIAN_POINT('Ctrl Pts',(-2.35682411179554,0.265938618886863,
9.63569911596267));
#63376=CARTESIAN_POINT('Ctrl Pts',(-2.35814476549191,0.253961654898472,
9.63649497337361));
#63377=CARTESIAN_POINT('Ctrl Pts',(-2.36173336889086,0.218971002775416,
9.63880570166824));
#63378=CARTESIAN_POINT('Ctrl Pts',(-2.36375581492573,0.195936286500906,
9.64030877126689));
#63379=CARTESIAN_POINT('Ctrl Pts',(-2.36544101901418,0.172878130673515,
9.64179857564526));
#63380=CARTESIAN_POINT('Origin',(0.,0.,-1.84858989190501));
#63381=CARTESIAN_POINT('',(-2.36342245950295,0.172714633282403,10.8368568258743));
#63382=CARTESIAN_POINT('',(-2.36544102832235,0.172878003312457,10.6380411716245));
#63383=CARTESIAN_POINT('',(-2.36544101854889,0.172878137039864,-1.84858989190501));
#63384=CARTESIAN_POINT('',(-2.36840389010906,0.000992657309442972,9.8486171864275));
#63385=CARTESIAN_POINT('Ctrl Pts',(-2.36835645684558,0.00099074781327764,
9.84858989190503));
#63386=CARTESIAN_POINT('Ctrl Pts',(-2.36661646666674,-0.456757128880904,
9.87920456926939));
#63387=CARTESIAN_POINT('Ctrl Pts',(-2.01853982608692,-1.70439405627733,
9.96248421030043));
#63388=CARTESIAN_POINT('Ctrl Pts',(-0.00283249851198579,-2.79870028674429,
10.0984288149982));
#63389=CARTESIAN_POINT('Ctrl Pts',(2.34239313895008,-1.53164150527581,10.2564237059982));
#63390=CARTESIAN_POINT('Ctrl Pts',(2.56269918704329,1.12485741087042,10.4144185969983));
#63391=CARTESIAN_POINT('Ctrl Pts',(0.458233353927178,2.76093344928963,10.5724134879983));
#63392=CARTESIAN_POINT('Ctrl Pts',(-1.78785214186282,1.98686117431254,10.713226230957));
#63393=CARTESIAN_POINT('Ctrl Pts',(-2.32054658323031,0.700757067499405,
10.8013740102491));
#63394=CARTESIAN_POINT('Ctrl Pts',(-2.36342245950295,0.172714633282403,
10.8368568258743));
#63395=CARTESIAN_POINT('Ctrl Pts',(-2.37174973207207,0.00112734912545944,
9.85054248424486));
#63396=CARTESIAN_POINT('Ctrl Pts',(-2.37172246228312,0.0584983207034222,
9.84657087381565));
#63397=CARTESIAN_POINT('Ctrl Pts',(-2.36961357827909,0.11578635994523,9.84254327253529));
#63398=CARTESIAN_POINT('Ctrl Pts',(-2.36544098814985,0.172878552980629,
9.83847008213863));
#63399=CARTESIAN_POINT('',(-2.37174935477677,0.00174946163004134,9.65263340565988));
#63400=CARTESIAN_POINT('Ctrl Pts',(-2.36544101901418,0.172878130673515,
9.64179857564526));
#63401=CARTESIAN_POINT('Ctrl Pts',(-2.36960227195145,0.115940920917956,
9.64547733057349));
#63402=CARTESIAN_POINT('Ctrl Pts',(-2.3717072280224,0.0588608042184611,
9.6490754070573));
#63403=CARTESIAN_POINT('Ctrl Pts',(-2.37174935477677,0.00174946162997413,
9.65263340565988));
#63404=CARTESIAN_POINT('Ctrl Pts',(-2.37174935259837,0.0017524123925753,
9.6526332218293));
#63405=CARTESIAN_POINT('Ctrl Pts',(-2.37189696828361,-0.198033555437239,
9.66507975964639));
#63406=CARTESIAN_POINT('Ctrl Pts',(-2.34680234990767,-0.397041953603912,
9.67703688754385));
#63407=CARTESIAN_POINT('Ctrl Pts',(-2.28444680226741,-0.639579868005419,
9.69298420833203));
#63408=CARTESIAN_POINT('Ctrl Pts',(-2.27027959600028,-0.688178450613413,
9.69624710276722));
#63409=CARTESIAN_POINT('Ctrl Pts',(-2.24812457344293,-0.756019162610858,
9.7009177805947));
#63410=CARTESIAN_POINT('Ctrl Pts',(-2.24142094803958,-0.775668202873776,
9.7022844840852));
#63411=CARTESIAN_POINT('Ctrl Pts',(-2.22938819730055,-0.809478337383775,
9.7046615899808));
#63412=CARTESIAN_POINT('Ctrl Pts',(-2.22417984286543,-0.823681322903598,
9.70566800719936));
#63413=CARTESIAN_POINT('Ctrl Pts',(-2.21322217939644,-0.852700533225414,
9.7077409082246));
#63414=CARTESIAN_POINT('Ctrl Pts',(-2.20745911926852,-0.86751070914359,
9.70880780316681));
#63415=CARTESIAN_POINT('Ctrl Pts',(-2.1923718049639,-0.905158777718782,
9.7115434511026));
#63416=CARTESIAN_POINT('Ctrl Pts',(-2.18283948693289,-0.927910685051638,
9.71321903300169));
#63417=CARTESIAN_POINT('Ctrl Pts',(-2.14219244083099,-1.02083370810906,
9.720157291347));
#63418=CARTESIAN_POINT('Ctrl Pts',(-2.10803802273787,-1.08961616571965,
9.72552008268168));
#63419=CARTESIAN_POINT('Ctrl Pts',(-1.99153094959514,-1.29819103162955,
9.74250231450349));
#63420=CARTESIAN_POINT('Ctrl Pts',(-1.89814132261071,-1.43127430452756,
9.75443100791042));
#63421=CARTESIAN_POINT('Ctrl Pts',(-1.75518481734824,-1.59614192310762,
9.77023714630915));
#63422=CARTESIAN_POINT('Ctrl Pts',(-1.71695385698451,-1.63719669212105,
9.77426797587678));
#63423=CARTESIAN_POINT('Ctrl Pts',(-1.66062531935576,-1.69354005801802,
9.77989754426118));
#63424=CARTESIAN_POINT('Ctrl Pts',(-1.64370084065891,-1.70997134979475,
9.78155180578109));
#63425=CARTESIAN_POINT('Ctrl Pts',(-1.61364265102402,-1.7382949040952,9.78442138122552));
#63426=CARTESIAN_POINT('Ctrl Pts',(-1.60061577677476,-1.75029739179488,
9.78564329703428));
#63427=CARTESIAN_POINT('Ctrl Pts',(-1.58040473826532,-1.76850472888952,
9.78750442533477));
#63428=CARTESIAN_POINT('Ctrl Pts',(-1.5733160709537,-1.77481397939371,9.78815077141662));
#63429=CARTESIAN_POINT('Ctrl Pts',(-1.5599322125769,-1.78658304751176,9.78935882124527));
#63430=CARTESIAN_POINT('Ctrl Pts',(-1.55364599731484,-1.79205234670469,
9.78992117026506));
#63431=CARTESIAN_POINT('Ctrl Pts',(-1.53932901511499,-1.80437682326645,
9.79119060200072));
#63432=CARTESIAN_POINT('Ctrl Pts',(-1.53128116589691,-1.81121162169856,
9.79189623683382));
#63433=CARTESIAN_POINT('Ctrl Pts',(-1.50631449331585,-1.83212971000257,
9.79406193584163));
#63434=CARTESIAN_POINT('Ctrl Pts',(-1.48924450155775,-1.84603183220491,
9.79550989709972));
#63435=CARTESIAN_POINT('Ctrl Pts',(-1.35898877087792,-1.94913163910465,
9.80633594102442));
#63436=CARTESIAN_POINT('Ctrl Pts',(-1.23806316720064,-2.0280964565922,9.81514692234843));
#63437=CARTESIAN_POINT('Ctrl Pts',(-0.968094416981237,-2.17118428167353,
9.83391011966802));
#63438=CARTESIAN_POINT('Ctrl Pts',(-0.818162954298518,-2.23200555721507,
9.8438406924624));
#63439=CARTESIAN_POINT('Ctrl Pts',(-0.636025910893141,-2.28505400205844,
9.85614499011183));
#63440=CARTESIAN_POINT('Ctrl Pts',(-0.608685618214998,-2.2924882681643,
9.85799689387449));
#63441=CARTESIAN_POINT('Ctrl Pts',(-0.565058162149105,-2.30351583815349,
9.86096309319629));
#63442=CARTESIAN_POINT('Ctrl Pts',(-0.548854435514508,-2.30743033009552,
9.86206716745091));
#63443=CARTESIAN_POINT('Ctrl Pts',(-0.518116864625605,-2.31451381888413,
9.86416670008757));
#63444=CARTESIAN_POINT('Ctrl Pts',(-0.503591787347632,-2.31771754055666,
9.86516100404022));
#63445=CARTESIAN_POINT('Ctrl Pts',(-0.470463666611901,-2.32469832858261,
9.86743414716486));
#63446=CARTESIAN_POINT('Ctrl Pts',(-0.451843681657343,-2.32838906368685,
9.86871563555951));
#63447=CARTESIAN_POINT('Ctrl Pts',(-0.402940520373667,-2.33747365721108,
9.87209222031347));
#63448=CARTESIAN_POINT('Ctrl Pts',(-0.372594041330407,-2.3425024417487,
9.87419847837966));
#63449=CARTESIAN_POINT('Ctrl Pts',(-0.178488731972618,-2.37080099062955,
9.88774546478855));
#63450=CARTESIAN_POINT('Ctrl Pts',(-0.0127978964774504,-2.3774721637237,
9.89969441778271));
#63451=CARTESIAN_POINT('Ctrl Pts',(0.247311519571186,-2.36074503467751,
9.91869703591491));
#63452=CARTESIAN_POINT('Ctrl Pts',(0.341964252868863,-2.34890235623918,
9.9256521829863));
#63453=CARTESIAN_POINT('Ctrl Pts',(0.467675137770763,-2.32541165297936,
9.93477691163778));
#63454=CARTESIAN_POINT('Ctrl Pts',(0.499573820109125,-2.31876812153278,
9.93708193359391));
#63455=CARTESIAN_POINT('Ctrl Pts',(0.554118736770761,-2.30623012680582,
9.940994920712));
#63456=CARTESIAN_POINT('Ctrl Pts',(0.576832790482701,-2.30065403857896,
9.9426158099575));
#63457=CARTESIAN_POINT('Ctrl Pts',(0.6099252771058,-2.29200920102225,9.94496114813725));
#63458=CARTESIAN_POINT('Ctrl Pts',(0.62037031996651,-2.2892041627286,9.94569903808636));
#63459=CARTESIAN_POINT('Ctrl Pts',(0.638074917294891,-2.28431947791222,
9.94694532121363));
#63460=CARTESIAN_POINT('Ctrl Pts',(0.645344204936719,-2.28227648200979,
9.94745573191827));
#63461=CARTESIAN_POINT('Ctrl Pts',(0.661905050982908,-2.27753668758164,
9.94861551355769));
#63462=CARTESIAN_POINT('Ctrl Pts',(0.671190004016461,-2.27481771720609,
9.9492636164745));
#63463=CARTESIAN_POINT('Ctrl Pts',(0.696888540505749,-2.26712121252731,
9.9510521462279));
#63464=CARTESIAN_POINT('Ctrl Pts',(0.713265537282157,-2.26202222465746,
9.95218595151629));
#63465=CARTESIAN_POINT('Ctrl Pts',(0.825583057221632,-2.22571094517473,
9.95992986188339));
#63466=CARTESIAN_POINT('Ctrl Pts',(0.919514131052333,-2.18857839074197,
9.96624676617244));
#63467=CARTESIAN_POINT('Ctrl Pts',(1.03179075061727,-2.13568352032923,9.97391954991515));
#63468=CARTESIAN_POINT('Ctrl Pts',(1.05263133129648,-2.12548901492121,9.97534902856974));
#63469=CARTESIAN_POINT('Ctrl Pts',(1.18774129844156,-2.05692316014143,9.98467001472017));
#63470=CARTESIAN_POINT('Ctrl Pts',(1.29725706456724,-1.98966944818795,9.99249186079622));
#63471=CARTESIAN_POINT('Ctrl Pts',(1.45771111815406,-1.87223165718302,10.0050024211273));
#63472=CARTESIAN_POINT('Ctrl Pts',(1.51273723112318,-1.82805845665418,10.0095066563379));
#63473=CARTESIAN_POINT('Ctrl Pts',(1.58324729280076,-1.76608923666427,10.01562923608));
#63474=CARTESIAN_POINT('Ctrl Pts',(1.60055554172562,-1.75041854337613,10.0171620206678));
#63475=CARTESIAN_POINT('Ctrl Pts',(1.62905135931443,-1.72384270645276,10.0197378614953));
#63476=CARTESIAN_POINT('Ctrl Pts',(1.64036783860305,-1.71307773974128,10.0207750140567));
#63477=CARTESIAN_POINT('Ctrl Pts',(1.66243229935759,-1.69166949634559,10.0228259821768));
#63478=CARTESIAN_POINT('Ctrl Pts',(1.67318643037672,-1.68103360642867,10.0238394526183));
#63479=CARTESIAN_POINT('Ctrl Pts',(1.69905037083895,-1.65495997136972,10.0263112715902));
#63480=CARTESIAN_POINT('Ctrl Pts',(1.71405218430938,-1.63941749591492,10.0277741779942));
#63481=CARTESIAN_POINT('Ctrl Pts',(1.76479964833593,-1.585383081048,10.0328258730662));
#63482=CARTESIAN_POINT('Ctrl Pts',(1.79947552136426,-1.54591216470964,10.0364582794382));
#63483=CARTESIAN_POINT('Ctrl Pts',(1.94129249893621,-1.37324275081368,10.0521188421248));
#63484=CARTESIAN_POINT('Ctrl Pts',(2.03516643270432,-1.22983508180745,10.064618333903));
#63485=CARTESIAN_POINT('Ctrl Pts',(2.14502800773871,-1.0144371271919,10.0822127012073));
#63486=CARTESIAN_POINT('Ctrl Pts',(2.1744032986397,-0.949841751574492,10.0873458723951));
#63487=CARTESIAN_POINT('Ctrl Pts',(2.21104009186348,-0.858631780811633,
10.0943222945228));
#63488=CARTESIAN_POINT('Ctrl Pts',(2.22079957839519,-0.833064337761657,
10.096249090814));
#63489=CARTESIAN_POINT('Ctrl Pts',(2.23709290343086,-0.788056883134659,
10.0995843611732));
#63490=CARTESIAN_POINT('Ctrl Pts',(2.24382107317067,-0.768690686169711,
10.1010014571952));
#63491=CARTESIAN_POINT('Ctrl Pts',(2.2535400834804,-0.739500176684509,10.1031080225628));
#63492=CARTESIAN_POINT('Ctrl Pts',(2.25671942301165,-0.729740278961135,
10.103807464271));
#63493=CARTESIAN_POINT('Ctrl Pts',(2.26236448246739,-0.712021366587215,
10.1050680593437));
#63494=CARTESIAN_POINT('Ctrl Pts',(2.26485170806518,-0.704069757499664,
10.1056303847271));
#63495=CARTESIAN_POINT('Ctrl Pts',(2.27038572663566,-0.686044793136716,
10.1068975082129));
#63496=CARTESIAN_POINT('Ctrl Pts',(2.2734074316233,-0.675964101217361,10.1076008831616));
#63497=CARTESIAN_POINT('Ctrl Pts',(2.28249102437409,-0.644910366171897,
10.1097523965818));
#63498=CARTESIAN_POINT('Ctrl Pts',(2.2883307141886,-0.623872808507573,10.1111886595128));
#63499=CARTESIAN_POINT('Ctrl Pts',(2.33109489386882,-0.461127435375906,
10.1221573914015));
#63500=CARTESIAN_POINT('Ctrl Pts',(2.35511886311573,-0.316336120004382,
10.131102497151));
#63501=CARTESIAN_POINT('Ctrl Pts',(2.37691494453227,-0.0134562447597651,
10.1497507797876));
#63502=CARTESIAN_POINT('Ctrl Pts',(2.37258311042138,0.144038363818025,10.1594289844395));
#63503=CARTESIAN_POINT('Ctrl Pts',(2.34897565927689,0.329214987849362,10.1715222979813));
#63504=CARTESIAN_POINT('Ctrl Pts',(2.34469717691383,0.358419001594101,10.1734497324591));
#63505=CARTESIAN_POINT('Ctrl Pts',(2.33711038642924,0.404226892874554,10.1765086158826));
#63506=CARTESIAN_POINT('Ctrl Pts',(2.33416729165211,0.420888784848467,10.1776286874421));
#63507=CARTESIAN_POINT('Ctrl Pts',(2.32830935124672,0.452099268480903,10.1797414524958));
#63508=CARTESIAN_POINT('Ctrl Pts',(2.32543575071495,0.466654836014901,10.1807328060753));
#63509=CARTESIAN_POINT('Ctrl Pts',(2.31865527081592,0.499380820835648,10.1829757710508));
#63510=CARTESIAN_POINT('Ctrl Pts',(2.31467102813681,0.517534024829609,10.1842297648244));
#63511=CARTESIAN_POINT('Ctrl Pts',(2.30383592185284,0.564271236033883,10.1874844960903));
#63512=CARTESIAN_POINT('Ctrl Pts',(2.29666646803133,0.59277734818792,10.1894951184429));
#63513=CARTESIAN_POINT('Ctrl Pts',(2.24089316067131,0.798307538488215,10.2041826415171));
#63514=CARTESIAN_POINT('Ctrl Pts',(2.17241863239951,0.969262788708023,10.2175040804772));
#63515=CARTESIAN_POINT('Ctrl Pts',(2.029065362032,1.23362584189697,10.2394253353511));
#63516=CARTESIAN_POINT('Ctrl Pts',(1.9656191104642,1.33239857826465,10.2479439564619));
#63517=CARTESIAN_POINT('Ctrl Pts',(1.88296421062956,1.44223878139379,10.2575191368997));
#63518=CARTESIAN_POINT('Ctrl Pts',(1.87059958548463,1.45824009647451,10.2589165186127));
#63519=CARTESIAN_POINT('Ctrl Pts',(1.85168643000596,1.48207950051417,10.2609997962191));
#63520=CARTESIAN_POINT('Ctrl Pts',(1.84528981056551,1.49003617592114,10.2616953530094));
#63521=CARTESIAN_POINT('Ctrl Pts',(1.83357866390065,1.50441244048723,10.2629521554821));
#63522=CARTESIAN_POINT('Ctrl Pts',(1.82828153294526,1.51084550792069,10.2635145323511));
#63523=CARTESIAN_POINT('Ctrl Pts',(1.81617883535609,1.5253866872513,10.264785769289));
#63524=CARTESIAN_POINT('Ctrl Pts',(1.80935278444664,1.53347729674108,10.265493162269));
#63525=CARTESIAN_POINT('Ctrl Pts',(1.78807304939942,1.55835928805388,10.2676699371144));
#63526=CARTESIAN_POINT('Ctrl Pts',(1.77343762327078,1.57499459759057,10.2691270370286));
#63527=CARTESIAN_POINT('Ctrl Pts',(1.66233599385471,1.69776525548381,10.279915728994));
#63528=CARTESIAN_POINT('Ctrl Pts',(1.55664058149877,1.79517374732517,10.2886868068831));
#63529=CARTESIAN_POINT('Ctrl Pts',(1.31430550141054,1.98090883246258,10.3074365109161));
#63530=CARTESIAN_POINT('Ctrl Pts',(1.17610804970284,2.06595257120173,10.3173939329292));
#63531=CARTESIAN_POINT('Ctrl Pts',(1.00481904177262,2.14856682916893,10.3297284572614));
#63532=CARTESIAN_POINT('Ctrl Pts',(0.979083180604796,2.16041587233054,10.3315803322242));
#63533=CARTESIAN_POINT('Ctrl Pts',(0.937877769959852,2.17849976558698,10.3345464961994));
#63534=CARTESIAN_POINT('Ctrl Pts',(0.922543571243064,2.18503759134694,10.335650564338));
#63535=CARTESIAN_POINT('Ctrl Pts',(0.89339883359168,2.19710214324928,10.337750092124));
#63536=CARTESIAN_POINT('Ctrl Pts',(0.879602677463094,2.20266166634965,10.3387443974142));
#63537=CARTESIAN_POINT('Ctrl Pts',(0.848083034370927,2.21501998942308,10.3410175531051));
#63538=CARTESIAN_POINT('Ctrl Pts',(0.830328573856182,2.22173644031019,10.3422990528386));
#63539=CARTESIAN_POINT('Ctrl Pts',(0.783597756079672,2.23877617298577,10.3456756881765));
#63540=CARTESIAN_POINT('Ctrl Pts',(0.75449864286222,2.24874983982022,10.3477819860328));
#63541=CARTESIAN_POINT('Ctrl Pts',(0.567748495047655,2.30872536457436,10.3613281002155));
#63542=CARTESIAN_POINT('Ctrl Pts',(0.405450364494166,2.34267865474243,10.3732760495036));
#63543=CARTESIAN_POINT('Ctrl Pts',(0.146156633887866,2.36916020515457,10.3922783545669));
#63544=CARTESIAN_POINT('Ctrl Pts',(0.0508390205520596,2.37312008888871,
10.3992341827757));
#63545=CARTESIAN_POINT('Ctrl Pts',(-0.0770361610597585,2.37072244975007,
10.4083596990675));
#63546=CARTESIAN_POINT('Ctrl Pts',(-0.109595841219814,2.36944053910416,
10.4106648477868));
#63547=CARTESIAN_POINT('Ctrl Pts',(-0.165465339254681,2.36608669272603,
10.414578026264));
#63548=CARTESIAN_POINT('Ctrl Pts',(-0.188789443928183,2.36434000580312,
10.4161989816768));
#63549=CARTESIAN_POINT('Ctrl Pts',(-0.222856535826352,2.36128142951531,
10.4185443968077));
#63550=CARTESIAN_POINT('Ctrl Pts',(-0.233621649172559,2.36024065749635,
10.4192822987401));
#63551=CARTESIAN_POINT('Ctrl Pts',(-0.251890166376688,2.3583482401123,10.4205285952718));
#63552=CARTESIAN_POINT('Ctrl Pts',(-0.259397114464808,2.35753435192281,
10.4210390075136));
#63553=CARTESIAN_POINT('Ctrl Pts',(-0.276513377142015,2.35559589273409,
10.4221987832332));
#63554=CARTESIAN_POINT('Ctrl Pts',(-0.286119840559264,2.3544483648302,10.4228468787794));
#63555=CARTESIAN_POINT('Ctrl Pts',(-0.312736197410932,2.35110363098444,
10.4246353678878));
#63556=CARTESIAN_POINT('Ctrl Pts',(-0.329730074791131,2.34878060531698,
10.4257691403868));
#63557=CARTESIAN_POINT('Ctrl Pts',(-0.446456614498282,2.33153247007922,
10.4335099576443));
#63558=CARTESIAN_POINT('Ctrl Pts',(-0.545186597271174,2.31044232772754,
10.4398240793893));
#63559=CARTESIAN_POINT('Ctrl Pts',(-0.663414950866502,2.27718257967988,
10.4474169113792));
#63560=CARTESIAN_POINT('Ctrl Pts',(-0.684462145524698,2.27094506470677,
10.4487697368993));
#63561=CARTESIAN_POINT('Ctrl Pts',(-0.800337493661663,2.23484711805594,
10.4562376646973));
#63562=CARTESIAN_POINT('Ctrl Pts',(-0.893299901973538,2.19934001456066,
10.4623078060687));
#63563=CARTESIAN_POINT('Ctrl Pts',(-1.04187266082449,2.1316140374058,10.4724630956405));
#63564=CARTESIAN_POINT('Ctrl Pts',(-1.09888925499292,2.10278828842802,10.4764764716026));
#63565=CARTESIAN_POINT('Ctrl Pts',(-1.19404951007999,2.0497502928577,10.4834414070272));
#63566=CARTESIAN_POINT('Ctrl Pts',(-1.23279261940857,2.02668508578709,10.486356464352));
#63567=CARTESIAN_POINT('Ctrl Pts',(-1.2876351910465,1.99188070576603,10.4906130051567));
#63568=CARTESIAN_POINT('Ctrl Pts',(-1.30428232660842,1.98102011709773,10.4919228874475));
#63569=CARTESIAN_POINT('Ctrl Pts',(-1.33323941820297,1.96160530036622,10.4942340205658));
#63570=CARTESIAN_POINT('Ctrl Pts',(-1.34560860219892,1.95314110421553,10.4952319022128));
#63571=CARTESIAN_POINT('Ctrl Pts',(-1.37119656429182,1.93527289912736,10.4973190295664));
#63572=CARTESIAN_POINT('Ctrl Pts',(-1.3844007053726,1.92584939094815,10.4984089744894));
#63573=CARTESIAN_POINT('Ctrl Pts',(-1.41869733937242,1.90083765099661,10.5012746867894));
#63574=CARTESIAN_POINT('Ctrl Pts',(-1.43962925860995,1.88503406312493,10.5030586040423));
#63575=CARTESIAN_POINT('Ctrl Pts',(-1.53460997740724,1.81081888955236,10.51131884108));
#63576=CARTESIAN_POINT('Ctrl Pts',(-1.60538674456188,1.74837703192024,10.517950779524));
#63577=CARTESIAN_POINT('Ctrl Pts',(-1.7882257216775,1.56658637890967,10.5364257575791));
#63578=CARTESIAN_POINT('Ctrl Pts',(-1.8919531697296,1.43960138715518,10.548497385358));
#63579=CARTESIAN_POINT('Ctrl Pts',(-2.01632472267099,1.25043375420406,10.5647754803677));
#63580=CARTESIAN_POINT('Ctrl Pts',(-2.04876151676514,1.1965482384832,10.569237858778));
#63581=CARTESIAN_POINT('Ctrl Pts',(-2.08641154346434,1.12797195932742,10.5746500680487));
#63582=CARTESIAN_POINT('Ctrl Pts',(-2.09367114818095,1.11443933156233,10.5757055620591));
#63583=CARTESIAN_POINT('Ctrl Pts',(-2.10506210914811,1.09270121228457,10.5773800075954));
#63584=CARTESIAN_POINT('Ctrl Pts',(-2.10927797914548,1.08454084134036,10.5780038983954));
#63585=CARTESIAN_POINT('Ctrl Pts',(-2.11728695816243,1.0688150518666,10.5791969222604));
#63586=CARTESIAN_POINT('Ctrl Pts',(-2.12108711662803,1.06125356269191,10.5797664538227));
#63587=CARTESIAN_POINT('Ctrl Pts',(-2.13032041645303,1.04263358315963,10.5811591892522));
#63588=CARTESIAN_POINT('Ctrl Pts',(-2.1357081120458,1.03155258802487,10.5819796674777));
#63589=CARTESIAN_POINT('Ctrl Pts',(-2.15112252146199,0.999210927459784,
10.5843516083496));
#63590=CARTESIAN_POINT('Ctrl Pts',(-2.16092013987067,0.977841923262025,
10.5858904402346));
#63591=CARTESIAN_POINT('Ctrl Pts',(-2.23275512167892,0.814811811758568,
10.5974432430522));
#63592=CARTESIAN_POINT('Ctrl Pts',(-2.28112866501053,0.667516115389473,
10.6068356159993));
#63593=CARTESIAN_POINT('Ctrl Pts',(-2.34008065616195,0.403330972762036,
10.6234726127201));
#63594=CARTESIAN_POINT('Ctrl Pts',(-2.35699311800545,0.288468380828906,
10.6306390066344));
#63595=CARTESIAN_POINT('Ctrl Pts',(-2.36544102832235,0.172878003312455,
10.6380411716245));
#63596=CARTESIAN_POINT('Origin',(0.,0.,-1.84858989190501));
#63597=CARTESIAN_POINT('',(-2.36544101854889,0.172878137039869,11.8369824012687));
#63598=CARTESIAN_POINT('',(-2.3654410511783,0.172877690580661,11.6392156713196));
#63599=CARTESIAN_POINT('',(-2.36544101854889,0.172878137039864,-1.84858989190501));
#63600=CARTESIAN_POINT('',(-2.37174906171763,-0.00210967806991183,10.848589891905));
#63601=CARTESIAN_POINT('Ctrl Pts',(-2.37174906171763,-0.00210967806991183,
10.848589891905));
#63602=CARTESIAN_POINT('Ctrl Pts',(-2.37165805342341,-0.104423315161401,
10.8554530893873));
#63603=CARTESIAN_POINT('Ctrl Pts',(-2.3649427778268,-0.20644680868023,10.8623162868697));
#63604=CARTESIAN_POINT('Ctrl Pts',(-2.35173784392009,-0.307452721526542,
10.869179484352));
#63605=CARTESIAN_POINT('Ctrl Pts',(-2.33940885685767,-0.401758425857108,
10.8755874129008));
#63606=CARTESIAN_POINT('Ctrl Pts',(-2.3214231975442,-0.495177584694326,
10.8819953414496));
#63607=CARTESIAN_POINT('Ctrl Pts',(-2.29792715611661,-0.587136140670828,
10.8884032699985));
#63608=CARTESIAN_POINT('Ctrl Pts',(-2.27836238835693,-0.663708519756064,
10.8937390468469));
#63609=CARTESIAN_POINT('Ctrl Pts',(-2.25492967935947,-0.739444399516909,
10.8990748236953));
#63610=CARTESIAN_POINT('Ctrl Pts',(-2.2277173816223,-0.813924646461752,
10.9044106005437));
#63611=CARTESIAN_POINT('Ctrl Pts',(-2.20054398841307,-0.888298411444805,
10.9097387490072));
#63612=CARTESIAN_POINT('Ctrl Pts',(-2.16960189711789,-0.961419672718621,
10.9150668974708));
#63613=CARTESIAN_POINT('Ctrl Pts',(-2.13502985033385,-1.03288218141442,
10.9203950459344));
#63614=CARTESIAN_POINT('Ctrl Pts',(-2.10049745093925,-1.10426273656173,
10.9257170840517));
#63615=CARTESIAN_POINT('Ctrl Pts',(-2.06234357174016,-1.17398790033652,
10.9310391221689));
#63616=CARTESIAN_POINT('Ctrl Pts',(-2.02075532507061,-1.24167064018554,
10.9363611602862));
#63617=CARTESIAN_POINT('Ctrl Pts',(-1.97919312186946,-1.30931099562459,
10.941679865627));
#63618=CARTESIAN_POINT('Ctrl Pts',(-1.93420106461656,-1.37491106822296,
10.9469985709678));
#63619=CARTESIAN_POINT('Ctrl Pts',(-1.88601197135451,-1.43810879505254,
10.9523172763086));
#63620=CARTESIAN_POINT('Ctrl Pts',(-1.83783810539373,-1.50128655199349,
10.9576343009884));
#63621=CARTESIAN_POINT('Ctrl Pts',(-1.78646949321897,-1.56206309880546,
10.9629513256682));
#63622=CARTESIAN_POINT('Ctrl Pts',(-1.7321811517149,-1.62010694713147,10.968268350348));
#63623=CARTESIAN_POINT('Ctrl Pts',(-1.67789312333021,-1.67815046067743,
10.9735853443608));
#63624=CARTESIAN_POINT('Ctrl Pts',(-1.62068571986508,-1.73346096628657,
10.9789023383735));
#63625=CARTESIAN_POINT('Ctrl Pts',(-1.5608719499261,-1.78574265179334,10.9842193323863));
#63626=CARTESIAN_POINT('Ctrl Pts',(-1.50099899088266,-1.8380760729815,10.989541587865));
#63627=CARTESIAN_POINT('Ctrl Pts',(-1.43851486679859,-1.88737437859769,
10.9948638433437));
#63628=CARTESIAN_POINT('Ctrl Pts',(-1.37376646512047,-1.9333814320538,11.0001860988224));
#63629=CARTESIAN_POINT('Ctrl Pts',(-1.30898663816695,-1.97941081477655,
11.0055109374281));
#63630=CARTESIAN_POINT('Ctrl Pts',(-1.24194073947866,-2.02214551123571,
11.0108357760338));
#63631=CARTESIAN_POINT('Ctrl Pts',(-1.17300335952702,-2.06137361510191,
11.0161606146395));
#63632=CARTESIAN_POINT('Ctrl Pts',(-1.1039432766229,-2.10067154181557,11.0214949310267));
#63633=CARTESIAN_POINT('Ctrl Pts',(-1.03298540449351,-2.13645019403203,
11.0268292474138));
#63634=CARTESIAN_POINT('Ctrl Pts',(-0.960527347199169,-2.16854450675621,
11.0321635638009));
#63635=CARTESIAN_POINT('Ctrl Pts',(-0.896076023327083,-2.19709234561746,
11.0369084295334));
#63636=CARTESIAN_POINT('Ctrl Pts',(-0.830438246495536,-2.22272572395615,
11.041653295266));
#63637=CARTESIAN_POINT('Ctrl Pts',(-0.763903504479376,-2.24536177449072,
11.0463981609985));
#63638=CARTESIAN_POINT('Ctrl Pts',(-0.689082728510087,-2.2708168497575,
11.0517339378456));
#63639=CARTESIAN_POINT('Ctrl Pts',(-0.612849004292881,-2.29257540263513,
11.0570697146927));
#63640=CARTESIAN_POINT('Ctrl Pts',(-0.535601638208493,-2.31048240582965,
11.0624054915398));
#63641=CARTESIAN_POINT('Ctrl Pts',(-0.458464710145092,-2.32836380797013,
11.0677336400021));
#63642=CARTESIAN_POINT('Ctrl Pts',(-0.380317470439179,-2.34240449127473,
11.0730617884644));
#63643=CARTESIAN_POINT('Ctrl Pts',(-0.301575968684563,-2.352498671118,11.0783899369267));
#63644=CARTESIAN_POINT('Ctrl Pts',(-0.222924768062563,-2.36258127490732,
11.0837119750427));
#63645=CARTESIAN_POINT('Ctrl Pts',(-0.143681121640871,-2.368726310344,11.0890340131587));
#63646=CARTESIAN_POINT('Ctrl Pts',(-0.0642714153984966,-2.37087900316795,
11.0943560512748));
#63647=CARTESIAN_POINT('Ctrl Pts',(0.0150885627515715,-2.37303034792865,
11.0996747566143));
#63648=CARTESIAN_POINT('Ctrl Pts',(0.0946139276757409,-2.3711943000465,
11.1049934619538));
#63649=CARTESIAN_POINT('Ctrl Pts',(0.173874231148637,-2.36536800820559,
11.1103121672934));
#63650=CARTESIAN_POINT('Ctrl Pts',(0.253109489109495,-2.35954355741822,
11.1156291919719));
#63651=CARTESIAN_POINT('Ctrl Pts',(0.332079385536634,-2.34973140093729,
11.1209462166505));
#63652=CARTESIAN_POINT('Ctrl Pts',(0.410356020385786,-2.33598073601499,
11.126263241329));
#63653=CARTESIAN_POINT('Ctrl Pts',(0.488632203758231,-2.3222301504025,11.1315802353405));
#63654=CARTESIAN_POINT('Ctrl Pts',(0.566214672815223,-2.30454118394526,
11.136897229352));
#63655=CARTESIAN_POINT('Ctrl Pts',(0.642684647213917,-2.28301434658995,
11.1422142233636));
#63656=CARTESIAN_POINT('Ctrl Pts',(0.719230292972739,-2.26146620721283,
11.1475364788411));
#63657=CARTESIAN_POINT('Ctrl Pts',(0.794660793590124,-2.23607273810929,
11.1528587343185));
#63658=CARTESIAN_POINT('Ctrl Pts',(0.868572085318437,-2.20698450268813,
11.158180989796));
#63659=CARTESIAN_POINT('Ctrl Pts',(0.942519249479862,-2.17788214945419,
11.1635058284005));
#63660=CARTESIAN_POINT('Ctrl Pts',(1.01494530901105,-2.14508165082385,11.168830667005));
#63661=CARTESIAN_POINT('Ctrl Pts',(1.08546810594951,-2.10878094013257,11.1741555056095));
#63662=CARTESIAN_POINT('Ctrl Pts',(1.15611642775475,-2.07241561711631,11.1794898219955));
#63663=CARTESIAN_POINT('Ctrl Pts',(1.22485431254362,-2.03253786939297,11.1848241383814));
#63664=CARTESIAN_POINT('Ctrl Pts',(1.29132625734933,-1.98939049951993,11.1901584547674));
#63665=CARTESIAN_POINT('Ctrl Pts',(1.35045294407114,-1.95101098424007,11.1949033205111));
#63666=CARTESIAN_POINT('Ctrl Pts',(1.40778704258294,-1.91004527902808,11.1996481862548));
#63667=CARTESIAN_POINT('Ctrl Pts',(1.46310096839824,-1.86669055249448,11.2043930519985));
#63668=CARTESIAN_POINT('Ctrl Pts',(1.52530352176559,-1.8179365605985,11.2097288288448));
#63669=CARTESIAN_POINT('Ctrl Pts',(1.58518226374215,-1.76597935139275,11.2150646056912));
#63670=CARTESIAN_POINT('Ctrl Pts',(1.64238916785706,-1.71106863795869,11.2204003825375));
#63671=CARTESIAN_POINT('Ctrl Pts',(1.69951428514076,-1.65623642856746,11.225728530999));
#63672=CARTESIAN_POINT('Ctrl Pts',(1.75397481580564,-1.59845942225094,11.2310566794604));
#63673=CARTESIAN_POINT('Ctrl Pts',(1.80545482578562,-1.5380282619469,11.2363848279219));
#63674=CARTESIAN_POINT('Ctrl Pts',(1.85687579824254,-1.47766640438818,11.2417068660371));
#63675=CARTESIAN_POINT('Ctrl Pts',(1.90532274082491,-1.41465679630268,11.2470289041523));
#63676=CARTESIAN_POINT('Ctrl Pts',(1.95051679316291,-1.349326610606,11.2523509422675));
#63677=CARTESIAN_POINT('Ctrl Pts',(1.99568254399822,-1.28403733609853,11.2576696476062));
#63678=CARTESIAN_POINT('Ctrl Pts',(2.03759918247399,-1.21643075243213,11.2629883529449));
#63679=CARTESIAN_POINT('Ctrl Pts',(2.07602911453367,-1.14686580649549,11.2683070582836));
#63680=CARTESIAN_POINT('Ctrl Pts',(2.1144469030954,-1.07732284242905,11.2736240829613));
#63681=CARTESIAN_POINT('Ctrl Pts',(2.14937994709338,-1.00582315437657,11.278941107639));
#63682=CARTESIAN_POINT('Ctrl Pts',(2.18063563607361,-0.932751995541057,
11.2842581323167));
#63683=CARTESIAN_POINT('Ctrl Pts',(2.21189114478014,-0.859681258158691,
11.2895751263273));
#63684=CARTESIAN_POINT('Ctrl Pts',(2.23946915794707,-0.785039498887169,
11.294892120338));
#63685=CARTESIAN_POINT('Ctrl Pts',(2.26322502323928,-0.709232371429521,
11.3002091143486));
#63686=CARTESIAN_POINT('Ctrl Pts',(2.28700439630235,-0.633350228536371,
11.3055313698253));
#63687=CARTESIAN_POINT('Ctrl Pts',(2.30695392636338,-0.556300861602376,
11.3108536253019));
#63688=CARTESIAN_POINT('Ctrl Pts',(2.32297892284745,-0.478504949301994,
11.3161758807785));
#63689=CARTESIAN_POINT('Ctrl Pts',(2.33901169697415,-0.400671279189647,
11.3215007193821));
#63690=CARTESIAN_POINT('Ctrl Pts',(2.35111607163671,-0.322090805013658,
11.3268255579857));
#63691=CARTESIAN_POINT('Ctrl Pts',(2.35924899885723,-0.243191743057085,
11.3321503965894));
#63692=CARTESIAN_POINT('Ctrl Pts',(2.36739640202951,-0.164152247160374,
11.3374847129744));
#63693=CARTESIAN_POINT('Ctrl Pts',(2.37155820928297,-0.0847934988890727,
11.3428190293595));
#63694=CARTESIAN_POINT('Ctrl Pts',(2.37174351593979,-0.00554590818296819,
11.3481533457446));
#63695=CARTESIAN_POINT('Ctrl Pts',(2.37190834590974,0.0649446948997903,
11.3528982114959));
#63696=CARTESIAN_POINT('Ctrl Pts',(2.36892770638879,0.135347135622957,11.3576430772473));
#63697=CARTESIAN_POINT('Ctrl Pts',(2.36284237116327,0.205363072472949,11.3623879429986));
#63698=CARTESIAN_POINT('Ctrl Pts',(2.35599918685866,0.284098580438945,11.3677237198513));
#63699=CARTESIAN_POINT('Ctrl Pts',(2.34520349453185,0.362638177910462,11.3730594967039));
#63700=CARTESIAN_POINT('Ctrl Pts',(2.33047426245826,0.440553940533523,11.3783952735566));
#63701=CARTESIAN_POINT('Ctrl Pts',(2.31576608828375,0.51835830955121,11.3837234220245));
#63702=CARTESIAN_POINT('Ctrl Pts',(2.29713562905319,0.595540158857205,11.3890515704923));
#63703=CARTESIAN_POINT('Ctrl Pts',(2.27465366819779,0.671676076881063,11.3943797189602));
#63704=CARTESIAN_POINT('Ctrl Pts',(2.2521974897632,0.74772468186805,11.3997017570817));
#63705=CARTESIAN_POINT('Ctrl Pts',(2.22589871938598,0.822729292707825,11.4050237952033));
#63706=CARTESIAN_POINT('Ctrl Pts',(2.19587899259207,0.896277586684419,11.4103458333249));
#63707=CARTESIAN_POINT('Ctrl Pts',(2.16587806480675,0.969779823112926,11.4156645386699));
#63708=CARTESIAN_POINT('Ctrl Pts',(2.13216098228431,1.04182712074477,11.420983244015));
#63709=CARTESIAN_POINT('Ctrl Pts',(2.0948985403765,1.11202435586116,11.42630194936));
#63710=CARTESIAN_POINT('Ctrl Pts',(2.05764787305077,1.18219940930977,11.4316189740441));
#63711=CARTESIAN_POINT('Ctrl Pts',(2.0168542904177,1.2505251481216,11.4369359987282));
#63712=CARTESIAN_POINT('Ctrl Pts',(1.97273519963897,1.31662974848869,11.4422530234122));
#63713=CARTESIAN_POINT('Ctrl Pts',(1.92861636332647,1.38273396758345,11.4475700174292));
#63714=CARTESIAN_POINT('Ctrl Pts',(1.88117231803757,1.44661668525981,11.4528870114462));
#63715=CARTESIAN_POINT('Ctrl Pts',(1.83066376190132,1.5079350958716,11.4582040054632));
#63716=CARTESIAN_POINT('Ctrl Pts',(1.78010522469597,1.56931418451406,11.4635262609461));
#63717=CARTESIAN_POINT('Ctrl Pts',(1.7264764175646,1.62812353542051,11.468848516429));
#63718=CARTESIAN_POINT('Ctrl Pts',(1.67007792237415,1.68405397648011,11.4741707719119));
#63719=CARTESIAN_POINT('Ctrl Pts',(1.6136520544891,1.74001156306684,11.4794956105217));
#63720=CARTESIAN_POINT('Ctrl Pts',(1.5544541694805,1.79308714344333,11.4848204491316));
#63721=CARTESIAN_POINT('Ctrl Pts',(1.49281938065313,1.84301067800662,11.4901452877414));
#63722=CARTESIAN_POINT('Ctrl Pts',(1.4310748868951,1.89302307241677,11.4954796041326));
#63723=CARTESIAN_POINT('Ctrl Pts',(1.36688520168584,1.93987193466428,11.5008139205238));
#63724=CARTESIAN_POINT('Ctrl Pts',(1.30061576774694,1.98332969704687,11.5061482369149));
#63725=CARTESIAN_POINT('Ctrl Pts',(1.24166921477974,2.02198530552065,11.5108931026095));
#63726=CARTESIAN_POINT('Ctrl Pts',(1.18107774744107,2.05795837654709,11.5156379683041));
#63727=CARTESIAN_POINT('Ctrl Pts',(1.11911350953335,2.09112003846741,11.5203828339987));
#63728=CARTESIAN_POINT('Ctrl Pts',(1.04943243382725,2.12841155294148,11.525718610841));
#63729=CARTESIAN_POINT('Ctrl Pts',(0.977755700919738,2.16228575080617,11.5310543876833));
#63730=CARTESIAN_POINT('Ctrl Pts',(0.904452066617334,2.19252469123876,11.5363901645256));
#63731=CARTESIAN_POINT('Ctrl Pts',(0.831253232111973,2.22272040005194,11.5417183129831));
#63732=CARTESIAN_POINT('Ctrl Pts',(0.756432544572834,2.2492909959733,11.5470464614406));
#63733=CARTESIAN_POINT('Ctrl Pts',(0.680383293204182,2.27206439979782,11.5523746098981));
#63734=CARTESIAN_POINT('Ctrl Pts',(0.604421255481801,2.2948116869736,11.5576966480094));
#63735=CARTESIAN_POINT('Ctrl Pts',(0.527233899998554,2.31377030249646,11.5630186861207));
#63736=CARTESIAN_POINT('Ctrl Pts',(0.449233015590976,2.32881681551019,11.568340724232));
#63737=CARTESIAN_POINT('Ctrl Pts',(0.37128097704024,2.34385390606896,11.5736594295669));
#63738=CARTESIAN_POINT('Ctrl Pts',(0.292516879159635,2.35498366858037,11.5789781349017));
#63739=CARTESIAN_POINT('Ctrl Pts',(0.213364968417591,2.3621332419557,11.5842968402365));
#63740=CARTESIAN_POINT('Ctrl Pts',(0.134238068935938,2.369280556133,11.5896138649104));
#63741=CARTESIAN_POINT('Ctrl Pts',(0.0547240657327129,2.37245013677191,
11.5949308895843));
#63742=CARTESIAN_POINT('Ctrl Pts',(-0.0247468389610155,2.37162089222992,
11.6002479142582));
#63743=CARTESIAN_POINT('Ctrl Pts',(-0.104217285290536,2.37079165247077,
11.6055649082651));
#63744=CARTESIAN_POINT('Ctrl Pts',(-0.183644165643882,2.36596363975148,
11.610881902272));
#63745=CARTESIAN_POINT('Ctrl Pts',(-0.262597925701454,2.357167875209,11.6161988962789));
#63746=CARTESIAN_POINT('Ctrl Pts',(-0.341629814967029,2.34836340676036,
11.6215211517519));
#63747=CARTESIAN_POINT('Ctrl Pts',(-0.420187182575315,2.33558339576522,
11.6268434072249));
#63748=CARTESIAN_POINT('Ctrl Pts',(-0.497846849324561,2.31891064448754,
11.6321656626979));
#63749=CARTESIAN_POINT('Ctrl Pts',(-0.575544207760615,2.30222980118287,
11.637490501298));
#63750=CARTESIAN_POINT('Ctrl Pts',(-0.652342544751022,2.28165257506089,
11.642815339898));
#63751=CARTESIAN_POINT('Ctrl Pts',(-0.727832586269522,2.2573120716605,11.648140178498));
#63752=CARTESIAN_POINT('Ctrl Pts',(-0.803456993949874,2.23292824413478,
11.6534744948797));
#63753=CARTESIAN_POINT('Ctrl Pts',(-0.877768014758273,2.20476792196589,
11.6588088112613));
#63754=CARTESIAN_POINT('Ctrl Pts',(-0.950375372694002,2.17301281944602,
11.6641431276429));
#63755=CARTESIAN_POINT('Ctrl Pts',(-1.01495950002739,2.14476670716573,11.6688879934282));
#63756=CARTESIAN_POINT('Ctrl Pts',(-1.07819579016902,2.11367716630258,11.6736328592135));
#63757=CARTESIAN_POINT('Ctrl Pts',(-1.13982760658501,2.07990170194812,11.6783777249987));
#63758=CARTESIAN_POINT('Ctrl Pts',(-1.20913486069273,2.04191994468787,11.6837135018395));
#63759=CARTESIAN_POINT('Ctrl Pts',(-1.2766705457286,2.00039950921893,11.6890492786802));
#63760=CARTESIAN_POINT('Ctrl Pts',(-1.34205063796326,1.95553014490762,11.694385055521));
#63761=CARTESIAN_POINT('Ctrl Pts',(-1.40733725842716,1.91072492885293,11.6997132039768));
#63762=CARTESIAN_POINT('Ctrl Pts',(-1.47047402371722,1.86258055520362,11.7050413524327));
#63763=CARTESIAN_POINT('Ctrl Pts',(-1.53110191412093,1.8113323800659,11.7103695008885));
#63764=CARTESIAN_POINT('Ctrl Pts',(-1.59166027616738,1.76014297658273,11.715691538998));
#63765=CARTESIAN_POINT('Ctrl Pts',(-1.64971512556803,1.70585714597935,11.7210135771075));
#63766=CARTESIAN_POINT('Ctrl Pts',(-1.70493807752139,1.64875232048894,11.726335615217));
#63767=CARTESIAN_POINT('Ctrl Pts',(-1.76012644765555,1.59168325528806,11.7316543205499));
#63768=CARTESIAN_POINT('Ctrl Pts',(-1.81248611598677,1.53179903486834,11.7369730258828));
#63769=CARTESIAN_POINT('Ctrl Pts',(-1.86172424331017,1.46941515725515,11.7422917312158));
#63770=CARTESIAN_POINT('Ctrl Pts',(-1.91094681184696,1.40705099236242,11.7476087558877));
#63771=CARTESIAN_POINT('Ctrl Pts',(-1.95704950847581,1.34218910597912,11.7529257805596));
#63772=CARTESIAN_POINT('Ctrl Pts',(-1.99977959709141,1.27517827206902,11.7582428052315));
#63773=CARTESIAN_POINT('Ctrl Pts',(-2.04250943925208,1.20816782465824,11.7635597992363));
#63774=CARTESIAN_POINT('Ctrl Pts',(-2.08186646170133,1.13900884976351,11.7688767932411));
#63775=CARTESIAN_POINT('Ctrl Pts',(-2.11764192736636,1.06807805424515,11.7741937872459));
#63776=CARTESIAN_POINT('Ctrl Pts',(-2.15345279487587,0.997077068697235,
11.7795160427167));
#63777=CARTESIAN_POINT('Ctrl Pts',(-2.18567481505506,0.924301179164118,
11.7848382981875));
#63778=CARTESIAN_POINT('Ctrl Pts',(-2.21414610156846,0.850150047585235,
11.7901605536583));
#63779=CARTESIAN_POINT('Ctrl Pts',(-2.24263120646184,0.775962927168565,
11.7954853922561));
#63780=CARTESIAN_POINT('Ctrl Pts',(-2.26736180543186,0.700399680352984,
11.8008102308538));
#63781=CARTESIAN_POINT('Ctrl Pts',(-2.28822573974705,0.623875810124956,
11.8061350694516));
#63782=CARTESIAN_POINT('Ctrl Pts',(-2.30912681017575,0.547215733604843,
11.8114693858309));
#63783=CARTESIAN_POINT('Ctrl Pts',(-2.32614736421891,0.469592075524575,
11.8168037022101));
#63784=CARTESIAN_POINT('Ctrl Pts',(-2.33922633441086,0.391430988679662,
11.8221380185894));
#63785=CARTESIAN_POINT('Ctrl Pts',(-2.3508600572708,0.321906828180753,11.8268828843925));
#63786=CARTESIAN_POINT('Ctrl Pts',(-2.35937589195445,0.251957785728667,
11.8316277501956));
#63787=CARTESIAN_POINT('Ctrl Pts',(-2.36476551897855,0.181884861244936,
11.8363726159987));
#63788=CARTESIAN_POINT('Ctrl Pts',(-2.36499640117885,0.178883059652061,
11.8365758777554));
#63789=CARTESIAN_POINT('Ctrl Pts',(-2.3652215681227,0.175880813078295,11.8367791395121));
#63790=CARTESIAN_POINT('Ctrl Pts',(-2.36544101854889,0.172878137039869,
11.8369824012687));
#63791=CARTESIAN_POINT('Ctrl Pts',(-2.36342245950295,0.172714633282403,
10.8368568258743));
#63792=CARTESIAN_POINT('Ctrl Pts',(-2.36814836675846,0.114512217657902,
10.8407678478846));
#63793=CARTESIAN_POINT('Ctrl Pts',(-2.37079004863033,0.0561842181634697,
10.8446788698948));
#63794=CARTESIAN_POINT('Ctrl Pts',(-2.37130727717011,-0.00210928510120129,
10.848589891905));
#63795=CARTESIAN_POINT('Ctrl Pts',(-2.36544102832235,0.172878003312457,
10.6380411716245));
#63796=CARTESIAN_POINT('Ctrl Pts',(-2.36761077134982,0.143190020574595,
10.6399423276824));
#63797=CARTESIAN_POINT('Ctrl Pts',(-2.36922213530041,0.113453987121819,
10.6418583939412));
#63798=CARTESIAN_POINT('Ctrl Pts',(-2.37125543553081,0.0558635986214012,
10.6455979483888));
#63799=CARTESIAN_POINT('Ctrl Pts',(-2.37174775862709,0.0280276099855107,
10.647418367514));
#63800=CARTESIAN_POINT('Ctrl Pts',(-2.3717513215929,-0.0163748061093179,
10.6503459252659));
#63801=CARTESIAN_POINT('Ctrl Pts',(-2.37157910610943,-0.0329391262577879,
10.6514433088954));
#63802=CARTESIAN_POINT('Ctrl Pts',(-2.37092253239266,-0.0643914778828075,
10.6535376418931));
#63803=CARTESIAN_POINT('Ctrl Pts',(-2.37047140185951,-0.0792794600979941,
10.6545335165904));
#63804=CARTESIAN_POINT('Ctrl Pts',(-2.36911911123579,-0.113314094809938,
10.6568209357159));
#63805=CARTESIAN_POINT('Ctrl Pts',(-2.36812602299492,-0.13245583975935,
10.6581152541651));
#63806=CARTESIAN_POINT('Ctrl Pts',(-2.36428118966396,-0.19249121106912,
10.6622003329518));
#63807=CARTESIAN_POINT('Ctrl Pts',(-2.36060135304912,-0.233322319521807,
10.6650161982669));
#63808=CARTESIAN_POINT('Ctrl Pts',(-2.34230835635987,-0.390586038447003,
10.6760131053646));
#63809=CARTESIAN_POINT('Ctrl Pts',(-2.32012269553777,-0.505954487331847,
10.6844135510187));
#63810=CARTESIAN_POINT('Ctrl Pts',(-2.25236810346385,-0.75647991857096,
10.7032574373893));
#63811=CARTESIAN_POINT('Ctrl Pts',(-2.20296585817177,-0.890150470362178,
10.7137238106242));
#63812=CARTESIAN_POINT('Ctrl Pts',(-2.12484445951778,-1.05442319004706,
10.726634683633));
#63813=CARTESIAN_POINT('Ctrl Pts',(-2.10690726831195,-1.08982312265966,
10.7294184178092));
#63814=CARTESIAN_POINT('Ctrl Pts',(-2.08162241119225,-1.13676389103889,
10.7330962606637));
#63815=CARTESIAN_POINT('Ctrl Pts',(-2.07505211827638,-1.14871351306282,
10.7340313179125));
#63816=CARTESIAN_POINT('Ctrl Pts',(-2.06449511933105,-1.16752771136826,
10.7355008359058));
#63817=CARTESIAN_POINT('Ctrl Pts',(-2.06057651099288,-1.1744298623332,10.7360393619083));
#63818=CARTESIAN_POINT('Ctrl Pts',(-2.05231975665899,-1.18880458139498,
10.7371595004205));
#63819=CARTESIAN_POINT('Ctrl Pts',(-2.04797530950731,-1.19627331794074,
10.7377406648065));
#63820=CARTESIAN_POINT('Ctrl Pts',(-2.03708631554236,-1.21475990338113,
10.739177499455));
#63821=CARTESIAN_POINT('Ctrl Pts',(-2.03049298046604,-1.22574897685172,
10.7400301336276));
#63822=CARTESIAN_POINT('Ctrl Pts',(-2.00487588430864,-1.26767087300146,
10.7432793128472));
#63823=CARTESIAN_POINT('Ctrl Pts',(-1.98523066488482,-1.29822043580283,
10.7456397010797));
#63824=CARTESIAN_POINT('Ctrl Pts',(-1.93105609487217,-1.37835775045932,
10.7518453519994));
#63825=CARTESIAN_POINT('Ctrl Pts',(-1.89531960939131,-1.42709925120586,
10.7556347162636));
#63826=CARTESIAN_POINT('Ctrl Pts',(-1.73637989334765,-1.62736136242325,
10.771505895477));
#63827=CARTESIAN_POINT('Ctrl Pts',(-1.59658873820786,-1.76471638290985,
10.7832267961463));
#63828=CARTESIAN_POINT('Ctrl Pts',(-1.40484857468159,-1.91147430753635,
10.7986394693922));
#63829=CARTESIAN_POINT('Ctrl Pts',(-1.36734161650525,-1.93848136595417,
10.8016232323118));
#63830=CARTESIAN_POINT('Ctrl Pts',(-1.31368368177447,-1.97478566701633,
10.8058639566675));
#63831=CARTESIAN_POINT('Ctrl Pts',(-1.29817430171207,-1.98501554069485,
10.8070865122338));
#63832=CARTESIAN_POINT('Ctrl Pts',(-1.27090800807103,-2.00254396643393,
10.809231228289));
#63833=CARTESIAN_POINT('Ctrl Pts',(-1.25920428893038,-2.00992389099941,
10.8101503679546));
#63834=CARTESIAN_POINT('Ctrl Pts',(-1.23445581852363,-2.02522834338775,
10.8120913134238));
#63835=CARTESIAN_POINT('Ctrl Pts',(-1.2213978454651,-2.03313017174818,10.813113884953));
#63836=CARTESIAN_POINT('Ctrl Pts',(-1.18974505492012,-2.05186938146257,
10.8155894653238));
#63837=CARTESIAN_POINT('Ctrl Pts',(-1.17107750343702,-2.0625805881903,10.817046883762));
#63838=CARTESIAN_POINT('Ctrl Pts',(-1.10347823765448,-2.10015466966398,
10.8223168767987));
#63839=CARTESIAN_POINT('Ctrl Pts',(-1.05375083457926,-2.12554043740749,
10.8261799589875));
#63840=CARTESIAN_POINT('Ctrl Pts',(-0.924312301932151,-2.18595968829431,
10.8362067745672));
#63841=CARTESIAN_POINT('Ctrl Pts',(-0.843487664042719,-2.21840009660104,
10.8424432069615));
#63842=CARTESIAN_POINT('Ctrl Pts',(-0.640680912583949,-2.28711244447997,
10.8579608773524));
#63843=CARTESIAN_POINT('Ctrl Pts',(-0.517208556455046,-2.31815678329798,
10.8673040560055));
#63844=CARTESIAN_POINT('Ctrl Pts',(-0.332564843551434,-2.34908731494332,
10.8807537646472));
#63845=CARTESIAN_POINT('Ctrl Pts',(-0.272924869608937,-2.35676131774492,
10.8850172485117));
#63846=CARTESIAN_POINT('Ctrl Pts',(-0.197423086596382,-2.36357112465351,
10.8902645798494));
#63847=CARTESIAN_POINT('Ctrl Pts',(-0.18177928371521,-2.36482571474434,
10.8913437065873));
#63848=CARTESIAN_POINT('Ctrl Pts',(-0.15688801513545,-2.36657345777885,
10.8930466647778));
#63849=CARTESIAN_POINT('Ctrl Pts',(-0.147648444124111,-2.36716786996808,
10.8936757206684));
#63850=CARTESIAN_POINT('Ctrl Pts',(-0.129894574831891,-2.36820568029223,
10.8948782447475));
#63851=CARTESIAN_POINT('Ctrl Pts',(-0.121381083391091,-2.3686572946643,
10.8954521155643));
#63852=CARTESIAN_POINT('Ctrl Pts',(-0.100680069077297,-2.36964351774111,
10.8968411175852));
#63853=CARTESIAN_POINT('Ctrl Pts',(-0.088490294262907,-2.37013003041661,
10.8976536596307));
#63854=CARTESIAN_POINT('Ctrl Pts',(-0.0444747156983343,-2.37154670376562,
10.9005700042944));
#63855=CARTESIAN_POINT('Ctrl Pts',(-0.0126331809773593,-2.37193010158469,
10.9026464820383));
#63856=CARTESIAN_POINT('Ctrl Pts',(0.234909305702097,-2.3699252497085,10.9185976786031));
#63857=CARTESIAN_POINT('Ctrl Pts',(0.449385021978406,-2.33876122690857,
10.9313684147293));
#63858=CARTESIAN_POINT('Ctrl Pts',(0.735429006861394,-2.2563362729168,10.9499817859639));
#63859=CARTESIAN_POINT('Ctrl Pts',(0.812912209166751,-2.22959207883852,
10.9551834577116));
#63860=CARTESIAN_POINT('Ctrl Pts',(0.912215256774717,-2.18945117654963,
10.9621541304073));
#63861=CARTESIAN_POINT('Ctrl Pts',(0.935426394144762,-2.17963540800888,
10.9638056863942));
#63862=CARTESIAN_POINT('Ctrl Pts',(0.973115105759387,-2.1629843241158,10.9665262485121));
#63863=CARTESIAN_POINT('Ctrl Pts',(0.98768804011086,-2.15636882510184,10.9675878476797));
#63864=CARTESIAN_POINT('Ctrl Pts',(1.01585407474009,-2.14323721608009,10.9696590619744));
#63865=CARTESIAN_POINT('Ctrl Pts',(1.02945423087269,-2.13673798913953,10.9706680629007));
#63866=CARTESIAN_POINT('Ctrl Pts',(1.06134117481704,-2.12112480094123,10.9730553065989));
#63867=CARTESIAN_POINT('Ctrl Pts',(1.07957371991653,-2.11190341846424,10.9744371872994));
#63868=CARTESIAN_POINT('Ctrl Pts',(1.14067138262331,-2.08000443512069,10.9791265242894));
#63869=CARTESIAN_POINT('Ctrl Pts',(1.1829570542001,-2.05624941945276,10.9824708782442));
#63870=CARTESIAN_POINT('Ctrl Pts',(1.28509771722023,-1.99467575258601,10.9908012014855));
#63871=CARTESIAN_POINT('Ctrl Pts',(1.34404188475828,-1.95544301648385,10.9958317623906));
#63872=CARTESIAN_POINT('Ctrl Pts',(1.51486902019203,-1.83036563751252,11.0110654913835));
#63873=CARTESIAN_POINT('Ctrl Pts',(1.62094253909181,-1.73712668850761,11.0214378693496));
#63874=CARTESIAN_POINT('Ctrl Pts',(1.76723933350045,-1.58339593837949,11.0367549985814));
#63875=CARTESIAN_POINT('Ctrl Pts',(1.81402443566845,-1.5295734402061,11.0418361765889));
#63876=CARTESIAN_POINT('Ctrl Pts',(1.86849836130648,-1.4608834176921,11.0479108587597));
#63877=CARTESIAN_POINT('Ctrl Pts',(1.87854563774639,-1.44794088627373,11.0490384236365));
#63878=CARTESIAN_POINT('Ctrl Pts',(1.89415039470531,-1.42740353928194,11.0507997369866));
#63879=CARTESIAN_POINT('Ctrl Pts',(1.89979795836684,-1.4198782718048,11.0514393133437));
#63880=CARTESIAN_POINT('Ctrl Pts',(1.91044215978607,-1.40551787396807,11.0526485263231));
#63881=CARTESIAN_POINT('Ctrl Pts',(1.91544701612256,-1.39868955472059,11.0532186768001));
#63882=CARTESIAN_POINT('Ctrl Pts',(1.92736505835354,-1.38224536155758,11.0545805014306));
#63883=CARTESIAN_POINT('Ctrl Pts',(1.93424296748527,-1.37260426378177,11.0553698248556));
#63884=CARTESIAN_POINT('Ctrl Pts',(1.95798344764781,-1.33879325382507,11.0581079151122));
#63885=CARTESIAN_POINT('Ctrl Pts',(1.97446827870506,-1.31435983054275,11.0600335517433));
#63886=CARTESIAN_POINT('Ctrl Pts',(2.01479148050235,-1.25212223920481,11.0648239532593));
#63887=CARTESIAN_POINT('Ctrl Pts',(2.03802544404504,-1.21393886611671,11.0676595226463));
#63888=CARTESIAN_POINT('Ctrl Pts',(2.1541080301262,-1.01042800271325,11.0823612869461));
#63889=CARTESIAN_POINT('Ctrl Pts',(2.2279627070365,-0.835065408478117,11.0936966926515));
#63890=CARTESIAN_POINT('Ctrl Pts',(2.29920364538345,-0.586219332223322,
11.1099838615966));
#63891=CARTESIAN_POINT('Ctrl Pts',(2.31533249142618,-0.518868587837711,
11.1144038952656));
#63892=CARTESIAN_POINT('Ctrl Pts',(2.33302969587434,-0.427481175567841,
11.1204713484972));
#63893=CARTESIAN_POINT('Ctrl Pts',(2.33721323425537,-0.40398260840325,11.1220374615554));
#63894=CARTESIAN_POINT('Ctrl Pts',(2.3435636306448,-0.364903900029264,11.1246537816613));
#63895=CARTESIAN_POINT('Ctrl Pts',(2.34593146247775,-0.349357840263814,
11.1256976749986));
#63896=CARTESIAN_POINT('Ctrl Pts',(2.35028727496787,-0.318715560680419,
11.1277618571478));
#63897=CARTESIAN_POINT('Ctrl Pts',(2.35228482079826,-0.303621453306717,
11.1287817942581));
#63898=CARTESIAN_POINT('Ctrl Pts',(2.35673019692726,-0.267348729313647,
11.1312408306455));
#63899=CARTESIAN_POINT('Ctrl Pts',(2.35903802805765,-0.24615461678996,11.1326841936868));
#63900=CARTESIAN_POINT('Ctrl Pts',(2.36621770004242,-0.170791527576243,
11.1378413086496));
#63901=CARTESIAN_POINT('Ctrl Pts',(2.36951145418653,-0.116492909905071,
11.1416027431029));
#63902=CARTESIAN_POINT('Ctrl Pts',(2.37312828622778,0.021522725271247,11.1512848411506));
#63903=CARTESIAN_POINT('Ctrl Pts',(2.3708913620756,0.105227906048028,11.1572718299163));
#63904=CARTESIAN_POINT('Ctrl Pts',(2.34977445630342,0.369897151067537,11.1764891291856));
#63905=CARTESIAN_POINT('Ctrl Pts',(2.31451467985329,0.548899113046853,11.1899595373143));
#63906=CARTESIAN_POINT('Ctrl Pts',(2.25241475606172,0.743178785510291,11.2041990487165));
#63907=CARTESIAN_POINT('Ctrl Pts',(2.24538834530105,0.764145408762086,11.2057297957282));
#63908=CARTESIAN_POINT('Ctrl Pts',(2.23456871303429,0.794992199088426,11.2079699578168));
#63909=CARTESIAN_POINT('Ctrl Pts',(2.23100117392993,0.804949503036919,11.2086912238168));
#63910=CARTESIAN_POINT('Ctrl Pts',(2.2245040019162,0.822708604311988,11.2099738808063));
#63911=CARTESIAN_POINT('Ctrl Pts',(2.22159973937641,0.830519178814453,11.2105366703035));
#63912=CARTESIAN_POINT('Ctrl Pts',(2.21504322617145,0.847871416691498,11.2117840190212));
#63913=CARTESIAN_POINT('Ctrl Pts',(2.21137043624777,0.857404943012496,11.2124673767437));
#63914=CARTESIAN_POINT('Ctrl Pts',(2.20023157663559,0.885770536000592,11.2144956232393));
#63915=CARTESIAN_POINT('Ctrl Pts',(2.19258550364321,0.904531541103641,11.215830522011));
#63916=CARTESIAN_POINT('Ctrl Pts',(2.13767282300085,1.0344802222361,11.225046094202));
#63917=CARTESIAN_POINT('Ctrl Pts',(2.0822049834673,1.14202639380956,11.2325208211302));
#63918=CARTESIAN_POINT('Ctrl Pts',(1.92478727761452,1.3973031746124,11.2509672519315));
#63919=CARTESIAN_POINT('Ctrl Pts',(1.81385292076667,1.53856827820668,11.2618675513927));
#63920=CARTESIAN_POINT('Ctrl Pts',(1.66712983933618,1.68723626408464,11.2753528739307));
#63921=CARTESIAN_POINT('Ctrl Pts',(1.64577558268649,1.70807222262501,11.2772944201427));
#63922=CARTESIAN_POINT('Ctrl Pts',(1.61039621403862,1.74131338657186,11.2804816109504));
#63923=CARTESIAN_POINT('Ctrl Pts',(1.59660684952368,1.75396545332463,11.2817168153476));
#63924=CARTESIAN_POINT('Ctrl Pts',(1.57161115605591,1.77636057423984,11.2839443036673));
#63925=CARTESIAN_POINT('Ctrl Pts',(1.56046020912751,1.78616416780128,11.2849340090133));
#63926=CARTESIAN_POINT('Ctrl Pts',(1.53647135246248,1.80685839018196,11.2870551166591));
#63927=CARTESIAN_POINT('Ctrl Pts',(1.52360812240843,1.81771827393775,11.2881876929057));
#63928=CARTESIAN_POINT('Ctrl Pts',(1.4881893830893,1.8469807224303,11.2912939379937));
#63929=CARTESIAN_POINT('Ctrl Pts',(1.46540957983616,1.8651059119781,11.2932784266632));
#63930=CARTESIAN_POINT('Ctrl Pts',(1.31362172298315,1.98138129192633,11.306420999138));
#63931=CARTESIAN_POINT('Ctrl Pts',(1.17519698880692,2.066486899303,11.3180753149664));
#63932=CARTESIAN_POINT('Ctrl Pts',(0.90179295237735,2.19817372794707,11.3401852438487));
#63933=CARTESIAN_POINT('Ctrl Pts',(0.769136605695957,2.24802882554433,11.3505491621864));
#63934=CARTESIAN_POINT('Ctrl Pts',(0.6112428012686,2.29174203047535,11.3619907041922));
#63935=CARTESIAN_POINT('Ctrl Pts',(0.589581697081399,2.29741002180713,11.3635410637796));
#63936=CARTESIAN_POINT('Ctrl Pts',(0.557522524435657,2.30531552682975,11.3658041680821));
#63937=CARTESIAN_POINT('Ctrl Pts',(0.547185171992227,2.30779103079777,11.3665291021671));
#63938=CARTESIAN_POINT('Ctrl Pts',(0.528712634281577,2.31208358076373,11.3678155771344));
#63939=CARTESIAN_POINT('Ctrl Pts',(0.520584132205729,2.31392733287147,11.3683785541912));
#63940=CARTESIAN_POINT('Ctrl Pts',(0.502515649423265,2.31792569304389,11.3696230644751));
#63941=CARTESIAN_POINT('Ctrl Pts',(0.492571371706077,2.32005925562388,11.3703034298462));
#63942=CARTESIAN_POINT('Ctrl Pts',(0.463004703721785,2.32620416518914,11.3723135966938));
#63943=CARTESIAN_POINT('Ctrl Pts',(0.443344334692556,2.33003112403478,11.3736336712399));
#63944=CARTESIAN_POINT('Ctrl Pts',(0.397523497086638,2.3383493159859,11.376676772031));
#63945=CARTESIAN_POINT('Ctrl Pts',(0.371331042469932,2.34265145380631,11.3783910661869));
#63946=CARTESIAN_POINT('Ctrl Pts',(0.278277250044224,2.35633564891823,11.3844097795754));
#63947=CARTESIAN_POINT('Ctrl Pts',(0.211090062245934,2.3633023808543,11.388625463039));
#63948=CARTESIAN_POINT('Ctrl Pts',(-0.0147137151474146,2.37700793182493,
11.4026199782668));
#63949=CARTESIAN_POINT('Ctrl Pts',(-0.173679367568807,2.37069984916276,
11.412214325951));
#63950=CARTESIAN_POINT('Ctrl Pts',(-0.395677426188681,2.33942876304294,
11.4263494876972));
#63951=CARTESIAN_POINT('Ctrl Pts',(-0.460120206294244,2.32761160746172,
11.4305380562791));
#63952=CARTESIAN_POINT('Ctrl Pts',(-0.546868208946277,2.30796092207109,
11.4363385691125));
#63953=CARTESIAN_POINT('Ctrl Pts',(-0.569670106830477,2.3024387855898,11.4378785807993));
#63954=CARTESIAN_POINT('Ctrl Pts',(-0.606018341044855,2.29306302731454,
11.4403598823669));
#63955=CARTESIAN_POINT('Ctrl Pts',(-0.619619154701768,2.28942533526242,
11.4412942954518));
#63956=CARTESIAN_POINT('Ctrl Pts',(-0.64770977849127,2.28164353414745,11.4432369703262));
#63957=CARTESIAN_POINT('Ctrl Pts',(-0.662194053312797,2.2774819849947,11.4442457518201));
#63958=CARTESIAN_POINT('Ctrl Pts',(-0.69620181060596,2.26735920867427,11.4466314862691));
#63959=CARTESIAN_POINT('Ctrl Pts',(-0.715689673645624,2.26128348256856,
11.4480120640872));
#63960=CARTESIAN_POINT('Ctrl Pts',(-0.7810884612337,2.23996405351457,11.4526919107012));
#63961=CARTESIAN_POINT('Ctrl Pts',(-0.826608184854206,2.22356840957802,
11.4560278735314));
#63962=CARTESIAN_POINT('Ctrl Pts',(-0.937187266862924,2.1798744485167,11.4643319443174));
#63963=CARTESIAN_POINT('Ctrl Pts',(-1.0015881620851,2.15104445090205,11.4693442712427));
#63964=CARTESIAN_POINT('Ctrl Pts',(-1.14670359972957,2.07815060360049,11.4810272672697));
#63965=CARTESIAN_POINT('Ctrl Pts',(-1.22633412951655,2.03217674291938,11.4877326025311));
#63966=CARTESIAN_POINT('Ctrl Pts',(-1.39500302750715,1.92126637996043,11.5024449495047));
#63967=CARTESIAN_POINT('Ctrl Pts',(-1.48260568405541,1.8545034109025,11.5104319205716));
#63968=CARTESIAN_POINT('Ctrl Pts',(-1.58248008890892,1.76677104990736,11.5197212673895));
#63969=CARTESIAN_POINT('Ctrl Pts',(-1.59947707349315,1.75139840170692,11.5213088720311));
#63970=CARTESIAN_POINT('Ctrl Pts',(-1.62410058739057,1.72847054689037,11.5236154544296));
#63971=CARTESIAN_POINT('Ctrl Pts',(-1.63190234091686,1.72110659466795,11.5243472757942));
#63972=CARTESIAN_POINT('Ctrl Pts',(-1.64567981851533,1.70792433899507,11.5256409932386));
#63973=CARTESIAN_POINT('Ctrl Pts',(-1.65167513402508,1.70212716071313,11.5262043959674));
#63974=CARTESIAN_POINT('Ctrl Pts',(-1.65776914061374,1.69617203476208,11.526777512244));
#63975=CARTESIAN_POINT('Ctrl Pts',(-1.65789822136299,1.69604586691564,11.5267896519781));
#63976=CARTESIAN_POINT('Ctrl Pts',(-1.65815019483043,1.69579952336018,11.5268133499097));
#63977=CARTESIAN_POINT('Ctrl Pts',(-1.65827308888625,1.69567934902814,11.5268249082123));
#63978=CARTESIAN_POINT('Ctrl Pts',(-1.65851316707359,1.69544453286398,11.5268474881894));
#63979=CARTESIAN_POINT('Ctrl Pts',(-1.65863035238019,1.69532989224459,11.5268585099559));
#63980=CARTESIAN_POINT('Ctrl Pts',(-1.65885944312666,1.69510572973115,11.5268800572581));
#63981=CARTESIAN_POINT('Ctrl Pts',(-1.65897134959819,1.69499620891324,11.5268905828744));
#63982=CARTESIAN_POINT('Ctrl Pts',(-1.65919027053181,1.6947819125488,11.5269111743109));
#63983=CARTESIAN_POINT('Ctrl Pts',(-1.65929728591611,1.69467713794736,11.5269212402034));
#63984=CARTESIAN_POINT('Ctrl Pts',(-1.65950677542559,1.69447199604805,11.526940945143));
#63985=CARTESIAN_POINT('Ctrl Pts',(-1.65960925036564,1.69437162959469,11.5269505842539));
#63986=CARTESIAN_POINT('Ctrl Pts',(-1.65980997692845,1.69417499742773,11.5269694655003));
#63987=CARTESIAN_POINT('Ctrl Pts',(-1.65990822928521,1.69407873245954,11.5269787076932));
#63988=CARTESIAN_POINT('Ctrl Pts',(-1.6601007996036,1.69389002449895,11.5269968222487));
#63989=CARTESIAN_POINT('Ctrl Pts',(-1.66019511821752,1.6937975821769,11.5270056946621));
#63990=CARTESIAN_POINT('Ctrl Pts',(-1.6603800841846,1.69361626546828,11.5270230943815));
#63991=CARTESIAN_POINT('Ctrl Pts',(-1.66047073211945,1.69352739168586,11.5270316217328));
#63992=CARTESIAN_POINT('Ctrl Pts',(-1.66064859689912,1.69335298004889,11.5270483538946));
#63993=CARTESIAN_POINT('Ctrl Pts',(-1.66073581426663,1.69326744273775,11.5270565587457));
#63994=CARTESIAN_POINT('Ctrl Pts',(-1.66090703756157,1.69309949173918,11.5270726665461));
#63995=CARTESIAN_POINT('Ctrl Pts',(-1.66099104397026,1.69301707853158,11.5270805695329));
#63996=CARTESIAN_POINT('Ctrl Pts',(-1.66115604667892,1.69285518103593,11.5270960925235));
#63997=CARTESIAN_POINT('Ctrl Pts',(-1.66123704340525,1.69277569718978,11.5271037125603));
#63998=CARTESIAN_POINT('Ctrl Pts',(-1.66139621161197,1.6926194795465,11.5271186870225));
#63999=CARTESIAN_POINT('Ctrl Pts',(-1.66147438347757,1.69254274615051,11.5271260414777));
#64000=CARTESIAN_POINT('Ctrl Pts',(-1.66162807201355,1.692391864787,11.527140500757));
#64001=CARTESIAN_POINT('Ctrl Pts',(-1.6617035890396,1.69231771717772,11.5271476056089));
#64002=CARTESIAN_POINT('Ctrl Pts',(-1.66185212461924,1.69217185559656,11.5271615804098));
#64003=CARTESIAN_POINT('Ctrl Pts',(-1.66192514349472,1.6921001419522,11.5271684503839));
#64004=CARTESIAN_POINT('Ctrl Pts',(-1.66206882746833,1.6919590080941,11.5271819690281));
#64005=CARTESIAN_POINT('Ctrl Pts',(-1.66213949285173,1.69188958818693,11.5271886177201));
#64006=CARTESIAN_POINT('Ctrl Pts',(-1.66227860359914,1.69175291213719,11.5272017063711));
#64007=CARTESIAN_POINT('Ctrl Pts',(-1.66234704923766,1.69168565626094,11.5272081463515));
#64008=CARTESIAN_POINT('Ctrl Pts',(-1.66248184440961,1.69155318809765,11.5272208292255));
#64009=CARTESIAN_POINT('Ctrl Pts',(-1.66254819418398,1.69148797606442,11.5272270721378));
#64010=CARTESIAN_POINT('Ctrl Pts',(-1.66267891255589,1.69135948408067,11.5272393716776));
#64011=CARTESIAN_POINT('Ctrl Pts',(-1.66274328137291,1.69129620436425,11.5272454283221));
#64012=CARTESIAN_POINT('Ctrl Pts',(-1.66287014457589,1.69117147340533,11.5272573653597));
#64013=CARTESIAN_POINT('Ctrl Pts',(-1.6629326391694,1.69111002237196,11.5272632457689));
#64014=CARTESIAN_POINT('Ctrl Pts',(-1.66305585324881,1.69098885233702,11.5272748396719));
#64015=CARTESIAN_POINT('Ctrl Pts',(-1.66311657291818,1.6909291335352,11.5272805531797));
#64016=CARTESIAN_POINT('Ctrl Pts',(-1.66323632965187,1.69081133811092,11.527291821975));
#64017=CARTESIAN_POINT('Ctrl Pts',(-1.66329536689234,1.69075326166556,11.5272973772761));
#64018=CARTESIAN_POINT('Ctrl Pts',(-1.66341184505365,1.69063866711044,11.5273083377688));
#64019=CARTESIAN_POINT('Ctrl Pts',(-1.66346928614063,1.69058214916062,11.5273137429733));
#64020=CARTESIAN_POINT('Ctrl Pts',(-1.66358265260062,1.69047059324412,11.5273244108499));
#64021=CARTESIAN_POINT('Ctrl Pts',(-1.66363857812016,1.6904155554322,11.5273296735333));
#64022=CARTESIAN_POINT('Ctrl Pts',(-1.66374898881376,1.69030688650497,11.5273400634528));
#64023=CARTESIAN_POINT('Ctrl Pts',(-1.66380347412451,1.69025325553189,11.5273451906995));
#64024=CARTESIAN_POINT('Ctrl Pts',(-1.6639110749565,1.69014733165275,11.5273553163783));
#64025=CARTESIAN_POINT('Ctrl Pts',(-1.66396419060955,1.69009503887353,11.5273603148207));
#64026=CARTESIAN_POINT('Ctrl Pts',(-1.66406911828847,1.68999172700522,11.527370189111));
#64027=CARTESIAN_POINT('Ctrl Pts',(-1.66412093042876,1.68994070804166,11.5273750649676));
#64028=CARTESIAN_POINT('Ctrl Pts',(-1.66422331313304,1.68983988340981,11.5273846999199));
#64029=CARTESIAN_POINT('Ctrl Pts',(-1.66427388381735,1.68979007784443,11.527389459025));
#64030=CARTESIAN_POINT('Ctrl Pts',(-1.66437384194789,1.68969162320983,11.5273988659589));
#64031=CARTESIAN_POINT('Ctrl Pts',(-1.66442322949193,1.68964297425033,11.5274035137951));
#64032=CARTESIAN_POINT('Ctrl Pts',(-1.66452087619098,1.68954677940979,11.5274127033481));
#64033=CARTESIAN_POINT('Ctrl Pts',(-1.66456913543723,1.68949923363087,11.5274172450717));
#64034=CARTESIAN_POINT('Ctrl Pts',(-1.66466457717607,1.68940519484906,11.5274262272541));
#64035=CARTESIAN_POINT('Ctrl Pts',(-1.66471175975834,1.68935870193694,11.5274306677198));
#64036=CARTESIAN_POINT('Ctrl Pts',(-1.67252159931882,1.6816623742972,11.5281656759792));
#64037=CARTESIAN_POINT('Ctrl Pts',(-1.6802316227727,1.67395894408148,11.5288922017329));
#64038=CARTESIAN_POINT('Ctrl Pts',(-1.70631987731404,1.6475311451034,11.5313548386357));
#64039=CARTESIAN_POINT('Ctrl Pts',(-1.72444114075359,1.62855435476854,11.5330727974936));
#64040=CARTESIAN_POINT('Ctrl Pts',(-1.76871060836043,1.58062717568079,11.5373003135647));
#64041=CARTESIAN_POINT('Ctrl Pts',(-1.79446718892364,1.55132437826418,11.5397876671384));
#64042=CARTESIAN_POINT('Ctrl Pts',(-1.90616184075693,1.41774502401846,11.5507704828611));
#64043=CARTESIAN_POINT('Ctrl Pts',(-1.98382205172522,1.30686968575048,11.5589620211415));
#64044=CARTESIAN_POINT('Ctrl Pts',(-2.11463327291961,1.0813403608795,11.5750343610985));
#64045=CARTESIAN_POINT('Ctrl Pts',(-2.16890960460965,0.967882344875475,
11.5828716916835));
#64046=CARTESIAN_POINT('Ctrl Pts',(-2.22386900861041,0.824845476334893,
11.5928172274308));
#64047=CARTESIAN_POINT('Ctrl Pts',(-2.23333867670243,0.79885022351086,11.5946265254691));
#64048=CARTESIAN_POINT('Ctrl Pts',(-2.24773589165326,0.757069747605381,
11.5975404347685));
#64049=CARTESIAN_POINT('Ctrl Pts',(-2.25295700637494,0.741387851102285,
11.598635453568));
#64050=CARTESIAN_POINT('Ctrl Pts',(-2.26257331235674,0.711464801394712,
11.6007280023598));
#64051=CARTESIAN_POINT('Ctrl Pts',(-2.26699902113685,0.697234234919124,
11.6017244862371));
#64052=CARTESIAN_POINT('Ctrl Pts',(-2.27682935038138,0.664542090379139,
11.6040172174803));
#64053=CARTESIAN_POINT('Ctrl Pts',(-2.28214400558302,0.646054781726542,
11.6053162851375));
#64054=CARTESIAN_POINT('Ctrl Pts',(-2.2927865396314,0.607263149794055,11.6080480848004));
#64055=CARTESIAN_POINT('Ctrl Pts',(-2.29807088805373,0.5869487153479,11.609482075427));
#64056=CARTESIAN_POINT('Ctrl Pts',(-2.3115401225282,0.53219655220293,11.6133568907369));
#64057=CARTESIAN_POINT('Ctrl Pts',(-2.31922459673377,0.497642396052019,
11.6158127786441));
#64058=CARTESIAN_POINT('Ctrl Pts',(-2.34520742514599,0.367083970263016,
11.6251326921883));
#64059=CARTESIAN_POINT('Ctrl Pts',(-2.35832728678283,0.270213502234134,
11.6321350057906));
#64060=CARTESIAN_POINT('Ctrl Pts',(-2.3654410511783,0.172877690580661,11.6392156713196));
#64061=CARTESIAN_POINT('Origin',(0.,0.,-1.84858989190501));
#64062=CARTESIAN_POINT('',(-2.3654409861093,0.172878580900717,12.8383513775306));
#64063=CARTESIAN_POINT('',(-2.3654410188404,0.172878133051282,12.6417724606485));
#64064=CARTESIAN_POINT('',(-2.36544101854889,0.172878137039864,-1.84858989190501));
#64065=CARTESIAN_POINT('',(-2.37174976881083,0.001047208561118,11.848589891905));
#64066=CARTESIAN_POINT('Ctrl Pts',(-2.36544098610933,0.172878580900381,
12.8383513775307));
#64067=CARTESIAN_POINT('Ctrl Pts',(-2.35368532029865,0.333727504941463,
12.8268323824084));
#64068=CARTESIAN_POINT('Ctrl Pts',(-2.32554364816744,0.49308856543647,12.8149340599441));
#64069=CARTESIAN_POINT('Ctrl Pts',(-2.26150281083728,0.718392965099194,
12.7980181616257));
#64070=CARTESIAN_POINT('Ctrl Pts',(-2.23841878234253,0.78737976057016,12.7928320854961));
#64071=CARTESIAN_POINT('Ctrl Pts',(-2.20634816523779,0.870338527495156,
12.7866697169524));
#64072=CARTESIAN_POINT('Ctrl Pts',(-2.20034166505561,0.885414011477231,
12.7855529926201));
#64073=CARTESIAN_POINT('Ctrl Pts',(-2.19067082483952,0.908980127465351,
12.7838135283743));
#64074=CARTESIAN_POINT('Ctrl Pts',(-2.18711088689246,0.917512676005192,
12.7831850124943));
#64075=CARTESIAN_POINT('Ctrl Pts',(-2.18027890830946,0.933622006436859,
12.7820011238744));
#64076=CARTESIAN_POINT('Ctrl Pts',(-2.17701720325093,0.941202564651642,
12.7814452152662));
#64077=CARTESIAN_POINT('Ctrl Pts',(-2.16914548539114,0.959237436417395,
12.7801252439033));
#64078=CARTESIAN_POINT('Ctrl Pts',(-2.16449939473682,0.969675708424831,
12.779363329515));
#64079=CARTESIAN_POINT('Ctrl Pts',(-2.14828857028532,1.00539908994135,12.7767615291189));
#64080=CARTESIAN_POINT('Ctrl Pts',(-2.13635426851358,1.03051526562823,12.7749421896048));
#64081=CARTESIAN_POINT('Ctrl Pts',(-2.10553822376845,1.09253120133172,12.7704605957774));
#64082=CARTESIAN_POINT('Ctrl Pts',(-2.0861253111776,1.12915774582066,12.7678233119092));
#64083=CARTESIAN_POINT('Ctrl Pts',(-1.98888111531938,1.30155148936724,12.7553678304165));
#64084=CARTESIAN_POINT('Ctrl Pts',(-1.89869843969871,1.42990695370422,12.7459422120141));
#64085=CARTESIAN_POINT('Ctrl Pts',(-1.72929980948198,1.62644484348827,12.7298519306799));
#64086=CARTESIAN_POINT('Ctrl Pts',(-1.65707394369871,1.69997143375175,12.7233688064913));
#64087=CARTESIAN_POINT('Ctrl Pts',(-1.56061726833879,1.78616038658732,12.7149630512803));
#64088=CARTESIAN_POINT('Ctrl Pts',(-1.54063728172853,1.80342226364561,12.7132347377168));
#64089=CARTESIAN_POINT('Ctrl Pts',(-1.50807652429115,1.83061737590564,12.7104358615175));
#64090=CARTESIAN_POINT('Ctrl Pts',(-1.495675631454,1.84076320163941,12.7093739064254));
#64091=CARTESIAN_POINT('Ctrl Pts',(-1.47178349728129,1.85990979161744,12.7073349171214));
#64092=CARTESIAN_POINT('Ctrl Pts',(-1.46031006244873,1.86893167373904,12.7063587831407));
#64093=CARTESIAN_POINT('Ctrl Pts',(-1.43367806708608,1.88947819304339,12.7040994795357));
#64094=CARTESIAN_POINT('Ctrl Pts',(-1.4184626978491,1.90092718967656,12.7028134490074));
#64095=CARTESIAN_POINT('Ctrl Pts',(-1.36946747856372,1.93687848270104,12.6986862716378));
#64096=CARTESIAN_POINT('Ctrl Pts',(-1.33517974749175,1.96067184809507,12.6958187016042));
#64097=CARTESIAN_POINT('Ctrl Pts',(-1.19849640655294,2.05027252305485,12.6844605512025));
#64098=CARTESIAN_POINT('Ctrl Pts',(-1.09173740694761,2.10905504589217,12.6757321868461));
#64099=CARTESIAN_POINT('Ctrl Pts',(-0.842299405949466,2.22236861898381,
12.655816883615));
#64100=CARTESIAN_POINT('Ctrl Pts',(-0.697894923088279,2.27185782186304,
12.6446014806088));
#64101=CARTESIAN_POINT('Ctrl Pts',(-0.522127663977529,2.31373859353405,
12.6318960163141));
#64102=CARTESIAN_POINT('Ctrl Pts',(-0.49440162142858,2.31982128340238,12.62991970416));
#64103=CARTESIAN_POINT('Ctrl Pts',(-0.454952763714559,2.3277363420113,12.6271532658853));
#64104=CARTESIAN_POINT('Ctrl Pts',(-0.443316283008119,2.32998051130195,
12.6263428059367));
#64105=CARTESIAN_POINT('Ctrl Pts',(-0.423561780313416,2.33363693873078,
12.6249769266042));
#64106=CARTESIAN_POINT('Ctrl Pts',(-0.41545242661444,2.33509426646395,12.6244190737827));
#64107=CARTESIAN_POINT('Ctrl Pts',(-0.398438393101934,2.33806040787042,
12.623254813285));
#64108=CARTESIAN_POINT('Ctrl Pts',(-0.389532473530618,2.33956066020504,
12.6226488748526));
#64109=CARTESIAN_POINT('Ctrl Pts',(-0.365572673081522,2.34345621452128,
12.6210275432804));
#64110=CARTESIAN_POINT('Ctrl Pts',(-0.350503614549928,2.34575737334082,
12.6200171957994));
#64111=CARTESIAN_POINT('Ctrl Pts',(-0.271644435512103,2.35702286198107,
12.6147737477271));
#64112=CARTESIAN_POINT('Ctrl Pts',(-0.207524935239054,2.36353178006703,
12.6106598601183));
#64113=CARTESIAN_POINT('Ctrl Pts',(0.0323455344874606,2.37804243515194,
12.5955636758481));
#64114=CARTESIAN_POINT('Ctrl Pts',(0.208545808667721,2.36910247484388,12.585020887531));
#64115=CARTESIAN_POINT('Ctrl Pts',(0.463872134455581,2.3274187607184,12.5688536040343));
#64116=CARTESIAN_POINT('Ctrl Pts',(0.544836975535693,2.3098064739618,12.5635980380843));
#64117=CARTESIAN_POINT('Ctrl Pts',(0.648981343053251,2.28137114932725,12.556573147168));
#64118=CARTESIAN_POINT('Ctrl Pts',(0.67314542774841,2.2743584281003,12.5549244373256));
#64119=CARTESIAN_POINT('Ctrl Pts',(0.712253810154569,2.26233084807667,12.5522231639617));
#64120=CARTESIAN_POINT('Ctrl Pts',(0.727268120722198,2.2575489843552,12.5511781312591));
#64121=CARTESIAN_POINT('Ctrl Pts',(0.756177224827359,2.24802348906941,12.5491499969445));
#64122=CARTESIAN_POINT('Ctrl Pts',(0.770077843566041,2.24329973500468,12.5481675820223));
#64123=CARTESIAN_POINT('Ctrl Pts',(0.802472724444302,2.23195462517863,12.5458607511447));
#64124=CARTESIAN_POINT('Ctrl Pts',(0.820930126365432,2.22523203509207,12.5445330719799));
#64125=CARTESIAN_POINT('Ctrl Pts',(0.881643202165655,2.20226083877156,12.5401204476021));
#64126=CARTESIAN_POINT('Ctrl Pts',(0.923514936174089,2.18503254449068,12.5370036550561));
#64127=CARTESIAN_POINT('Ctrl Pts',(1.02386875026566,2.1403417082127,12.5293486531496));
#64128=CARTESIAN_POINT('Ctrl Pts',(1.08176915624401,2.11166856676646,12.52477425959));
#64129=CARTESIAN_POINT('Ctrl Pts',(1.22522830575137,2.03317596098664,12.5130497465472));
#64130=CARTESIAN_POINT('Ctrl Pts',(1.30897160389477,1.98029800870965,12.505832247627));
#64131=CARTESIAN_POINT('Ctrl Pts',(1.41012696802889,1.90719925165595,12.4967324586226));
#64132=CARTESIAN_POINT('Ctrl Pts',(1.43084184121407,1.89170787831256,12.4948477653999));
#64133=CARTESIAN_POINT('Ctrl Pts',(1.52833192470601,1.81628341550561,12.4858864199982));
#64134=CARTESIAN_POINT('Ctrl Pts',(1.60162924079109,1.75199082577809,12.4788696989353));
#64135=CARTESIAN_POINT('Ctrl Pts',(1.68274088301113,1.67148604037625,12.4709420472858));
#64136=CARTESIAN_POINT('Ctrl Pts',(1.69458371924528,1.65947838825293,12.4697802548858));
#64137=CARTESIAN_POINT('Ctrl Pts',(1.71288365923934,1.64052355585521,12.4679796629568));
#64138=CARTESIAN_POINT('Ctrl Pts',(1.71942861923611,1.63366251060502,12.4673345883049));
#64139=CARTESIAN_POINT('Ctrl Pts',(1.73098854127184,1.62139787640107,12.4661935766336));
#64140=CARTESIAN_POINT('Ctrl Pts',(1.73601953380098,1.61601008167037,12.4656964567333));
#64141=CARTESIAN_POINT('Ctrl Pts',(1.74815369405448,1.60289329280881,12.4644960186554));
#64142=CARTESIAN_POINT('Ctrl Pts',(1.75523078227935,1.59514048203293,12.4637946343759));
#64143=CARTESIAN_POINT('Ctrl Pts',(1.77726816945934,1.57067470503781,12.4616056864818));
#64144=CARTESIAN_POINT('Ctrl Pts',(1.79204349565567,1.55379579532073,12.4601308801083));
#64145=CARTESIAN_POINT('Ctrl Pts',(1.86980097058446,1.46238296476312,12.4523142780117));
#64146=CARTESIAN_POINT('Ctrl Pts',(1.92838435086007,1.38421733200816,12.4462246371086));
#64147=CARTESIAN_POINT('Ctrl Pts',(2.07900939374692,1.15504151312781,12.4292964407797));
#64148=CARTESIAN_POINT('Ctrl Pts',(2.1592282462606,0.997061184076536,12.4186204101356));
#64149=CARTESIAN_POINT('Ctrl Pts',(2.23767390085516,0.787547144207726,12.4043491932527));
#64150=CARTESIAN_POINT('Ctrl Pts',(2.25286608628951,0.742973027089248,12.4013104008901));
#64151=CARTESIAN_POINT('Ctrl Pts',(2.27215918249905,0.680317713848536,12.3970197048892));
#64152=CARTESIAN_POINT('Ctrl Pts',(2.27739067092952,0.662594327493564,12.3958039224706));
#64153=CARTESIAN_POINT('Ctrl Pts',(2.28611218479078,0.631723146044363,12.3936817505051));
#64154=CARTESIAN_POINT('Ctrl Pts',(2.28969723843485,0.618602940546634,12.3927784384338));
#64155=CARTESIAN_POINT('Ctrl Pts',(2.29695787914994,0.591103065859568,12.3908818289405));
#64156=CARTESIAN_POINT('Ctrl Pts',(2.3006117219288,0.576718320223502,12.3898878829898));
#64157=CARTESIAN_POINT('Ctrl Pts',(2.30901656719768,0.542277913208629,12.3875032563217));
#64158=CARTESIAN_POINT('Ctrl Pts',(2.31364154954401,0.522193045536226,12.3861086508924));
#64159=CARTESIAN_POINT('Ctrl Pts',(2.32889464825206,0.451768435767889,12.381203558638));
#64160=CARTESIAN_POINT('Ctrl Pts',(2.33814546612742,0.401148454201618,12.3776506046863));
#64161=CARTESIAN_POINT('Ctrl Pts',(2.3571895640957,0.273611310385184,12.3686257073142));
#64162=CARTESIAN_POINT('Ctrl Pts',(2.36487078730657,0.196443417582445,12.3630977796077));
#64163=CARTESIAN_POINT('Ctrl Pts',(2.37340848897089,0.02655862949043,12.3508179698316));
#64164=CARTESIAN_POINT('Ctrl Pts',(2.37263581298928,-0.0661172918759338,
12.3440465442837));
#64165=CARTESIAN_POINT('Ctrl Pts',(2.3592343941836,-0.266195358355569,12.3294441449788));
#64166=CARTESIAN_POINT('Ctrl Pts',(2.34467808124429,-0.373278367396632,
12.3216388838325));
#64167=CARTESIAN_POINT('Ctrl Pts',(2.31945173486574,-0.495609799991988,
12.3129731164611));
#64168=CARTESIAN_POINT('Ctrl Pts',(2.31585007807841,-0.512175634678752,
12.3118051729443));
#64169=CARTESIAN_POINT('Ctrl Pts',(2.30995297241232,-0.537964314934816,
12.3099971417989));
#64170=CARTESIAN_POINT('Ctrl Pts',(2.30777927145049,-0.547214017554594,
12.3093506988199));
#64171=CARTESIAN_POINT('Ctrl Pts',(2.30382123515826,-0.563613407636575,
12.3082085210499));
#64172=CARTESIAN_POINT('Ctrl Pts',(2.30205914411235,-0.570767952927958,
12.3077115889613));
#64173=CARTESIAN_POINT('Ctrl Pts',(2.29771286406004,-0.588067381207843,
12.3065132100097));
#64174=CARTESIAN_POINT('Ctrl Pts',(2.29509481447099,-0.598203521663688,
12.3058136783417));
#64175=CARTESIAN_POINT('Ctrl Pts',(2.28669573221546,-0.629854736198219,
12.3036365848373));
#64176=CARTESIAN_POINT('Ctrl Pts',(2.28067843902456,-0.651306613803576,
12.3021715845777));
#64177=CARTESIAN_POINT('Ctrl Pts',(2.24710031706686,-0.764837106980526,
12.2944588900615));
#64178=CARTESIAN_POINT('Ctrl Pts',(2.21426078692,-0.85527122940738,12.2884560253101));
#64179=CARTESIAN_POINT('Ctrl Pts',(2.10746758559104,-1.10157876651784,12.2718774423619));
#64180=CARTESIAN_POINT('Ctrl Pts',(2.02189348217914,-1.25173459712863,12.261463388681));
#64181=CARTESIAN_POINT('Ctrl Pts',(1.89057804057558,-1.43302770738922,12.2472261660712));
#64182=CARTESIAN_POINT('Ctrl Pts',(1.85899783180382,-1.4737639547733,12.2439076486273));
#64183=CARTESIAN_POINT('Ctrl Pts',(1.81260931044947,-1.52973647821582,12.2391539853959));
#64184=CARTESIAN_POINT('Ctrl Pts',(1.79888367453573,-1.54585370693393,12.2377614108665));
#64185=CARTESIAN_POINT('Ctrl Pts',(1.77520242778473,-1.57291871322669,12.235380764051));
#64186=CARTESIAN_POINT('Ctrl Pts',(1.76535659331639,-1.58396118000503,12.234397206941));
#64187=CARTESIAN_POINT('Ctrl Pts',(1.74515660347387,-1.60619391789739,12.2323913826264));
#64188=CARTESIAN_POINT('Ctrl Pts',(1.73479658690927,-1.61737789524186,12.2313688974264));
#64189=CARTESIAN_POINT('Ctrl Pts',(1.70873661193864,-1.64497203974724,12.2288117871193));
#64190=CARTESIAN_POINT('Ctrl Pts',(1.69290769110749,-1.66125774886385,12.2272717145065));
#64191=CARTESIAN_POINT('Ctrl Pts',(1.62903907429867,-1.72510864579499,12.2211070983148));
#64192=CARTESIAN_POINT('Ctrl Pts',(1.57921323242279,-1.77083374788939,12.2164053069193));
#64193=CARTESIAN_POINT('Ctrl Pts',(1.43609012774958,-1.89132852362624,12.2031801109847));
#64194=CARTESIAN_POINT('Ctrl Pts',(1.33899600834075,-1.96126562739898,12.1945047158915));
#64195=CARTESIAN_POINT('Ctrl Pts',(1.12713663128748,-2.09077947933883,12.1763970009083));
#64196=CARTESIAN_POINT('Ctrl Pts',(1.01191440422633,-2.14891390102675,12.1669880622536));
#64197=CARTESIAN_POINT('Ctrl Pts',(0.87159487385442,-2.20590822281858,12.1564078992929));
#64198=CARTESIAN_POINT('Ctrl Pts',(0.850537031371892,-2.21411281600388,
12.1548426858484));
#64199=CARTESIAN_POINT('Ctrl Pts',(0.819500968268428,-2.22569698345398,
12.1525719080389));
#64200=CARTESIAN_POINT('Ctrl Pts',(0.809613084207701,-2.22931280073484,
12.1518537713408));
#64201=CARTESIAN_POINT('Ctrl Pts',(0.79202610336444,-2.23561158917672,12.1505862841361));
#64202=CARTESIAN_POINT('Ctrl Pts',(0.784336862511593,-2.2383208480322,12.1500354587246));
#64203=CARTESIAN_POINT('Ctrl Pts',(0.767375387368757,-2.24419898467767,
12.1488277705183));
#64204=CARTESIAN_POINT('Ctrl Pts',(0.758097348306255,-2.24735010333356,
12.1481719256916));
#64205=CARTESIAN_POINT('Ctrl Pts',(0.730911226940141,-2.25639585879313,
12.146263376365));
#64206=CARTESIAN_POINT('Ctrl Pts',(0.712951592034295,-2.2621347384588,12.1450192050823));
#64207=CARTESIAN_POINT('Ctrl Pts',(0.67134820903718,-2.27488410682514,12.1421712433914));
#64208=CARTESIAN_POINT('Ctrl Pts',(0.647659428560118,-2.28174132695525,
12.1405748423353));
#64209=CARTESIAN_POINT('Ctrl Pts',(0.565409896985093,-2.30416600205678,
12.1351050529145));
#64210=CARTESIAN_POINT('Ctrl Pts',(0.506359434364415,-2.31785901602653,
12.1313047780662));
#64211=CARTESIAN_POINT('Ctrl Pts',(0.300133764570324,-2.3574211173756,12.1182716193439));
#64212=CARTESIAN_POINT('Ctrl Pts',(0.151092572164565,-2.37164215166157,
12.1092470524373));
#64213=CARTESIAN_POINT('Ctrl Pts',(-0.0804971057218945,-2.37180839463319,
12.0947703755599));
#64214=CARTESIAN_POINT('Ctrl Pts',(-0.162636564098529,-2.36759415143137,
12.0895521603162));
#64215=CARTESIAN_POINT('Ctrl Pts',(-0.269356245101135,-2.35653887927567,
12.0825701508277));
#64216=CARTESIAN_POINT('Ctrl Pts',(-0.294283230403527,-2.35355594343502,
12.0809250470722));
#64217=CARTESIAN_POINT('Ctrl Pts',(-0.334759586720019,-2.3480591982231,
12.0782281902113));
#64218=CARTESIAN_POINT('Ctrl Pts',(-0.350339938890633,-2.34578513220333,
12.0771839204764));
#64219=CARTESIAN_POINT('Ctrl Pts',(-0.380406299027762,-2.34109051227903,
12.0751562220014));
#64220=CARTESIAN_POINT('Ctrl Pts',(-0.394894770862997,-2.33869019804239,
12.0741734699246));
#64221=CARTESIAN_POINT('Ctrl Pts',(-0.428738079874039,-2.33275990439674,
12.0718642268873));
#64222=CARTESIAN_POINT('Ctrl Pts',(-0.448072895481977,-2.32912338721785,
12.0705344523123));
#64223=CARTESIAN_POINT('Ctrl Pts',(-0.511923530421011,-2.31628981801075,
12.0661070692974));
#64224=CARTESIAN_POINT('Ctrl Pts',(-0.556217784749888,-2.30605409999189,
12.0629773186715));
#64225=CARTESIAN_POINT('Ctrl Pts',(-0.663029625108726,-2.27811523462277,
12.0552829380522));
#64226=CARTESIAN_POINT('Ctrl Pts',(-0.725164353940703,-2.25910441217664,
12.050681623877));
#64227=CARTESIAN_POINT('Ctrl Pts',(-0.879322709689901,-2.2049225193488,
12.0389635274988));
#64228=CARTESIAN_POINT('Ctrl Pts',(-0.97008154028637,-2.1665252294242,12.0317816429962));
#64229=CARTESIAN_POINT('Ctrl Pts',(-1.16005427195128,-2.07181762736532,
12.0163043676642));
#64230=CARTESIAN_POINT('Ctrl Pts',(-1.25814406690428,-2.01376080469628,
12.0080285677111));
#64231=CARTESIAN_POINT('Ctrl Pts',(-1.37047279748793,-1.93585246179476,
11.9984760667337));
#64232=CARTESIAN_POINT('Ctrl Pts',(-1.38906498154816,-1.92255533460683,
11.9968926174823));
#64233=CARTESIAN_POINT('Ctrl Pts',(-1.41588488353937,-1.90278152875475,
11.9946082751795));
#64234=CARTESIAN_POINT('Ctrl Pts',(-1.42426592222551,-1.89651631753648,
11.9938944118124));
#64235=CARTESIAN_POINT('Ctrl Pts',(-1.43885556712512,-1.88545862423564,
11.992652078047));
#64236=CARTESIAN_POINT('Ctrl Pts',(-1.44508222439617,-1.88069054815789,
11.9921220005331));
#64237=CARTESIAN_POINT('Ctrl Pts',(-1.45139280023392,-1.87580836451055,
11.991584943202));
#64238=CARTESIAN_POINT('Ctrl Pts',(-1.45150019277676,-1.87572526541273,
11.9915758036702));
#64239=CARTESIAN_POINT('Ctrl Pts',(-1.45175595634967,-1.87552732342296,
11.9915540372653));
#64240=CARTESIAN_POINT('Ctrl Pts',(-1.45190432092828,-1.87541247211718,
11.9915414109756));
#64241=CARTESIAN_POINT('Ctrl Pts',(-1.45219308286609,-1.87518888224929,
11.9915168365695));
#64242=CARTESIAN_POINT('Ctrl Pts',(-1.45233348163533,-1.87508014552885,
11.9915048883256));
#64243=CARTESIAN_POINT('Ctrl Pts',(-1.45260701429589,-1.87486824947377,
11.9914816102156));
#64244=CARTESIAN_POINT('Ctrl Pts',(-1.45274014940653,-1.87476509172984,
11.9914702802395));
#64245=CARTESIAN_POINT('Ctrl Pts',(-1.45299977556276,-1.87456388003426,
11.9914481858123));
#64246=CARTESIAN_POINT('Ctrl Pts',(-1.45312626767412,-1.8744658274586,11.9914374212653));
#64247=CARTESIAN_POINT('Ctrl Pts',(-1.45337315879328,-1.87427440547349,
11.9914164107914));
#64248=CARTESIAN_POINT('Ctrl Pts',(-1.45349355872528,-1.87418103726879,
11.9914061647814));
#64249=CARTESIAN_POINT('Ctrl Pts',(-1.45372875626543,-1.87399860907556,
11.9913861496014));
#64250=CARTESIAN_POINT('Ctrl Pts',(-1.45384355468032,-1.87390955014501,
11.9913763803589));
#64251=CARTESIAN_POINT('Ctrl Pts',(-1.45406798788894,-1.87373540510821,
11.9913572813675));
#64252=CARTESIAN_POINT('Ctrl Pts',(-1.45417762339537,-1.87365031993049,
11.9913479515547));
#64253=CARTESIAN_POINT('Ctrl Pts',(-1.45439212423638,-1.87348382140975,
11.9913296979298));
#64254=CARTESIAN_POINT('Ctrl Pts',(-1.4544969902062,-1.8734024088823,11.9913207740608));
#64255=CARTESIAN_POINT('Ctrl Pts',(-1.4547023059679,-1.87324298468929,11.9913033021895));
#64256=CARTESIAN_POINT('Ctrl Pts',(-1.45480275631614,-1.8731649737519,11.9912947541374));
#64257=CARTESIAN_POINT('Ctrl Pts',(-1.45499956024397,-1.87301210809677,
11.9912780067108));
#64258=CARTESIAN_POINT('Ctrl Pts',(-1.45509591431884,-1.87293725402638,
11.9912698072919));
#64259=CARTESIAN_POINT('Ctrl Pts',(-1.45528481472938,-1.87279048060783,
11.9912537325288));
#64260=CARTESIAN_POINT('Ctrl Pts',(-1.45537736150449,-1.8727185618393,11.9912458571453));
#64261=CARTESIAN_POINT('Ctrl Pts',(-1.45555890951743,-1.8725774579793,11.9912304081341));
#64262=CARTESIAN_POINT('Ctrl Pts',(-1.4556479111605,-1.87250827339745,11.9912228344703));
#64263=CARTESIAN_POINT('Ctrl Pts',(-1.45582260741477,-1.87237245494151,
11.9912079685969));
#64264=CARTESIAN_POINT('Ctrl Pts',(-1.45590830238647,-1.87230582152751,
11.9912006763552));
#64265=CARTESIAN_POINT('Ctrl Pts',(-1.45607660277043,-1.87217493849164,
11.9911863548153));
#64266=CARTESIAN_POINT('Ctrl Pts',(-1.45615920849617,-1.87211068929257,
11.991179325489));
#64267=CARTESIAN_POINT('Ctrl Pts',(-1.45632152908978,-1.87198442210673,
11.991165512867));
#64268=CARTESIAN_POINT('Ctrl Pts',(-1.45640124424951,-1.87192240449469,
11.9911587295452));
#64269=CARTESIAN_POINT('Ctrl Pts',(-1.4565579657066,-1.87180046066822,11.9911453934413));
#64270=CARTESIAN_POINT('Ctrl Pts',(-1.45663497226408,-1.87174053479598,
11.991138840636));
#64271=CARTESIAN_POINT('Ctrl Pts',(-1.45678644353232,-1.87162264608685,
11.9911259513495));
#64272=CARTESIAN_POINT('Ctrl Pts',(-1.45686090848133,-1.87156468355855,
11.9911196148472));
#64273=CARTESIAN_POINT('Ctrl Pts',(-1.45700745011316,-1.8714506034515,11.9911071450946));
#64274=CARTESIAN_POINT('Ctrl Pts',(-1.45707952701537,-1.87139448615114,
11.991101011825));
#64275=CARTESIAN_POINT('Ctrl Pts',(-1.45722143405187,-1.87128398766017,
11.9910889364945));
#64276=CARTESIAN_POINT('Ctrl Pts',(-1.45729126438516,-1.87122960672395,
11.991082994416));
#64277=CARTESIAN_POINT('Ctrl Pts',(-1.45742880891731,-1.87112248043925,
11.9910712903492));
#64278=CARTESIAN_POINT('Ctrl Pts',(-1.45749652328378,-1.87106973533404,
11.991065528346));
#64279=CARTESIAN_POINT('Ctrl Pts',(-1.45762995661824,-1.87096578777106,
11.9910541741539));
#64280=CARTESIAN_POINT('Ctrl Pts',(-1.45769567575834,-1.87091458552124,
11.9910485819497));
#64281=CARTESIAN_POINT('Ctrl Pts',(-1.45782523050553,-1.87081363752543,
11.9910375578346));
#64282=CARTESIAN_POINT('Ctrl Pts',(-1.45788906626306,-1.87076389197575,
11.9910321259103));
#64283=CARTESIAN_POINT('Ctrl Pts',(-1.45801495799662,-1.87066577745695,
11.9910214135246));
#64284=CARTESIAN_POINT('Ctrl Pts',(-1.45807701411725,-1.8706174086631,11.9910161330505));
#64285=CARTESIAN_POINT('Ctrl Pts',(-1.45819944302822,-1.87052197333053,
11.9910057153562));
#64286=CARTESIAN_POINT('Ctrl Pts',(-1.45825981593289,-1.87047490696762,
11.991000578126));
#64287=CARTESIAN_POINT('Ctrl Pts',(-1.45837896808324,-1.87038200737393,
11.9909904392876));
#64288=CARTESIAN_POINT('Ctrl Pts',(-1.45843774746246,-1.8703361742832,11.9909854376678));
#64289=CARTESIAN_POINT('Ctrl Pts',(-1.45855379622822,-1.87024567671815,
11.9909755629297));
#64290=CARTESIAN_POINT('Ctrl Pts',(-1.45861106570686,-1.87020101239739,
11.9909706898032));
#64291=CARTESIAN_POINT('Ctrl Pts',(-1.45872417265534,-1.87011279222028,
11.9909610654147));
#64292=CARTESIAN_POINT('Ctrl Pts',(-1.45878001023926,-1.87006923648332,
11.9909563141427));
#64293=CARTESIAN_POINT('Ctrl Pts',(-1.45889032634701,-1.86998317718785,
11.9909469272547));
#64294=CARTESIAN_POINT('Ctrl Pts',(-1.45894480495845,-1.86994067375391,
11.990942291631));
#64295=CARTESIAN_POINT('Ctrl Pts',(-1.45905247134113,-1.86985666641185,
11.9909331302338));
#64296=CARTESIAN_POINT('Ctrl Pts',(-1.45910565920336,-1.8698151626116,11.9909286044522));
#64297=CARTESIAN_POINT('Ctrl Pts',(-1.45921080801912,-1.86973310517965,
11.9909196572982));
#64298=CARTESIAN_POINT('Ctrl Pts',(-1.45926276905571,-1.86969255164918,
11.9909152359185));
#64299=CARTESIAN_POINT('Ctrl Pts',(-1.4593655241983,-1.86961234843846,11.9909064924639));
#64300=CARTESIAN_POINT('Ctrl Pts',(-1.45941631837631,-1.86957269885637,
11.9909021703825));
#64301=CARTESIAN_POINT('Ctrl Pts',(-1.4595167961498,-1.86949426001518,11.9908936207292));
#64302=CARTESIAN_POINT('Ctrl Pts',(-1.45956647980392,-1.86945547085397,
11.9908893931519));
#64303=CARTESIAN_POINT('Ctrl Pts',(-1.45966478945822,-1.86937871195809,
11.9908810280022));
#64304=CARTESIAN_POINT('Ctrl Pts',(-1.45971341553625,-1.86934074229652,
11.9908768904229));
#64305=CARTESIAN_POINT('Ctrl Pts',(-1.4598096599376,-1.86926558383323,11.9908687010226));
#64306=CARTESIAN_POINT('Ctrl Pts',(-1.4598572783116,-1.86922839511686,11.990864649197));
#64307=CARTESIAN_POINT('Ctrl Pts',(-1.45995155428373,-1.86915476222533,
11.9908566273061));
#64308=CARTESIAN_POINT('Ctrl Pts',(-1.45999821194105,-1.86911831812062,
11.9908526572355));
#64309=CARTESIAN_POINT('Ctrl Pts',(-1.46009061081547,-1.86904614016821,
11.9908447950813));
#64310=CARTESIAN_POINT('Ctrl Pts',(-1.46013635208901,-1.86901040638552,
11.9908409029928));
#64311=CARTESIAN_POINT('Ctrl Pts',(-1.46022696008722,-1.86893961667475,
11.9908331932378));
#64312=CARTESIAN_POINT('Ctrl Pts',(-1.46027182685854,-1.86890456081234,
11.9908293755671));
#64313=CARTESIAN_POINT('Ctrl Pts',(-1.4687285525005,-1.862296556564,11.9901098015401));
#64314=CARTESIAN_POINT('Ctrl Pts',(-1.47709613636665,-1.85566673736044,
11.9893979360074));
#64315=CARTESIAN_POINT('Ctrl Pts',(-1.49538883683277,-1.84097089686564,
11.9878412569181));
#64316=CARTESIAN_POINT('Ctrl Pts',(-1.50529411804956,-1.83288058841192,
11.9869980432305));
#64317=CARTESIAN_POINT('Ctrl Pts',(-1.5326543267251,-1.81016225672793,11.9846665662472));
#64318=CARTESIAN_POINT('Ctrl Pts',(-1.54996518159996,-1.79536199651148,
11.983188718568));
#64319=CARTESIAN_POINT('Ctrl Pts',(-1.60727462691208,-1.74491731003007,
11.9782764228534));
#64320=CARTESIAN_POINT('Ctrl Pts',(-1.64628019526784,-1.70816579910932,
11.9748999217458));
#64321=CARTESIAN_POINT('Ctrl Pts',(-1.75404302393251,-1.59950690725286,
11.9653611689266));
#64322=CARTESIAN_POINT('Ctrl Pts',(-1.81956733866899,-1.52455411286104,
11.9592956704791));
#64323=CARTESIAN_POINT('Ctrl Pts',(-1.96445427157441,-1.33612342304257,
11.9446764098377));
#64324=CARTESIAN_POINT('Ctrl Pts',(-2.03896259118745,-1.21939779014186,
11.9360909821371));
#64325=CARTESIAN_POINT('Ctrl Pts',(-2.11561349903799,-1.07244384190076,
11.92533343761));
#64326=CARTESIAN_POINT('Ctrl Pts',(-2.12792124447116,-1.04781074008785,
11.923532650185));
#64327=CARTESIAN_POINT('Ctrl Pts',(-2.14681182692223,-1.00829636466461,
11.9206448197545));
#64328=CARTESIAN_POINT('Ctrl Pts',(-2.15367544310135,-0.993551530121191,
11.9195674143209));
#64329=CARTESIAN_POINT('Ctrl Pts',(-2.16638722206217,-0.965492569921478,
11.9175169085102));
#64330=CARTESIAN_POINT('Ctrl Pts',(-2.17226566500195,-0.952192923259751,
11.9165448919243));
#64331=CARTESIAN_POINT('Ctrl Pts',(-2.18537830895178,-0.921772821031553,
11.9143209582364));
#64332=CARTESIAN_POINT('Ctrl Pts',(-2.19253422637532,-0.904619875512886,
11.9130664817441));
#64333=CARTESIAN_POINT('Ctrl Pts',(-2.21414692200013,-0.851050279136837,
11.9091462701112));
#64334=CARTESIAN_POINT('Ctrl Pts',(-2.22790279728864,-0.814359860423141,
11.9064577176621));
#64335=CARTESIAN_POINT('Ctrl Pts',(-2.31373562872294,-0.566942400451359,
11.8882942262351));
#64336=CARTESIAN_POINT('Ctrl Pts',(-2.35671860544731,-0.34732802550277,
11.8718600667347));
#64337=CARTESIAN_POINT('Ctrl Pts',(-2.37066663023684,-0.0830754162589632,
11.8527358073335));
#64338=CARTESIAN_POINT('Ctrl Pts',(-2.37176604780075,-0.0410838677914949,
11.8497212300524));
#64339=CARTESIAN_POINT('Ctrl Pts',(-2.37174982303164,0.00091621470674144,
11.8467427388015));
#64340=CARTESIAN_POINT('Ctrl Pts',(-2.36544101854889,0.172878137039869,
11.8369824012687));
#64341=CARTESIAN_POINT('Ctrl Pts',(-2.36961833947221,0.115721075835709,
11.8408515648142));
#64342=CARTESIAN_POINT('Ctrl Pts',(-2.37172444190719,0.058408349480251,
11.8447207283596));
#64343=CARTESIAN_POINT('Ctrl Pts',(-2.37174976881083,0.001047208561118,
11.848589891905));
#64344=CARTESIAN_POINT('',(-2.37174934418356,-0.00196579904219032,11.65195718999));
#64345=CARTESIAN_POINT('Ctrl Pts',(-2.3654410511783,0.172877690580661,11.6392156713196));
#64346=CARTESIAN_POINT('Ctrl Pts',(-2.36969121283375,0.114723819944284,
11.6434460578567));
#64347=CARTESIAN_POINT('Ctrl Pts',(-2.37179752731082,0.0564037460590684,
11.6477030248798));
#64348=CARTESIAN_POINT('Ctrl Pts',(-2.37174918657996,-0.00196429562807089,
11.6519573558634));
#64349=CARTESIAN_POINT('Ctrl Pts',(-2.37174918535101,-0.0019657789382381,
11.6519574639789));
#64350=CARTESIAN_POINT('Ctrl Pts',(-2.37167497384227,-0.0915033571298152,
11.6584836805817));
#64351=CARTESIAN_POINT('Ctrl Pts',(-2.36653051349874,-0.180972548701005,
11.6649920740709));
#64352=CARTESIAN_POINT('Ctrl Pts',(-2.35248817208768,-0.303548324308444,
11.6737404926746));
#64353=CARTESIAN_POINT('Ctrl Pts',(-2.34791967395338,-0.337069216544892,
11.6761150148799));
#64354=CARTESIAN_POINT('Ctrl Pts',(-2.34082399987725,-0.381936558039573,
11.6792596032624));
#64355=CARTESIAN_POINT('Ctrl Pts',(-2.33892858794854,-0.393377180619818,
11.680058473185));
#64356=CARTESIAN_POINT('Ctrl Pts',(-2.33550234516674,-0.413157027951826,
11.6814339978809));
#64357=CARTESIAN_POINT('Ctrl Pts',(-2.33401058861634,-0.421502682903235,
11.6820126217831));
#64358=CARTESIAN_POINT('Ctrl Pts',(-2.3309408428091,-0.43816027009921,11.6831637992376));
#64359=CARTESIAN_POINT('Ctrl Pts',(-2.32936306051245,-0.44647214532998,
11.6837363451214));
#64360=CARTESIAN_POINT('Ctrl Pts',(-2.32593336843323,-0.464026806104101,
11.6849414236367));
#64361=CARTESIAN_POINT('Ctrl Pts',(-2.32407079820625,-0.473267201202765,
11.6855733673658));
#64362=CARTESIAN_POINT('Ctrl Pts',(-2.31880369261213,-0.498616664358954,
11.6873010575767));
#64363=CARTESIAN_POINT('Ctrl Pts',(-2.3152863554122,-0.514702119883485,
11.688390754045));
#64364=CARTESIAN_POINT('Ctrl Pts',(-2.29550587306111,-0.600853001049982,
11.6941978272971));
#64365=CARTESIAN_POINT('Ctrl Pts',(-2.27622773060333,-0.670194724058452,
11.6987684459377));
#64366=CARTESIAN_POINT('Ctrl Pts',(-2.22202953050266,-0.835588715945488,
11.7096514363538));
#64367=CARTESIAN_POINT('Ctrl Pts',(-2.18400002231236,-0.930467229131064,
11.7158817334689));
#64368=CARTESIAN_POINT('Ctrl Pts',(-2.10204868021794,-1.10196460729585,
11.7275694528838));
#64369=CARTESIAN_POINT('Ctrl Pts',(-2.05974125457172,-1.1791518860656,11.7330046471257));
#64370=CARTESIAN_POINT('Ctrl Pts',(-2.00736387867571,-1.26325459984847,
11.7392607087811));
#64371=CARTESIAN_POINT('Ctrl Pts',(-2.00141406039578,-1.27266007997351,
11.7399651984782));
#64372=CARTESIAN_POINT('Ctrl Pts',(-1.97243146645444,-1.31776988584319,
11.7433684149852));
#64373=CARTESIAN_POINT('Ctrl Pts',(-1.94850931087567,-1.35289116354973,
11.7460924093145));
#64374=CARTESIAN_POINT('Ctrl Pts',(-1.90772646410503,-1.40943945436466,
11.7506171927791));
#64375=CARTESIAN_POINT('Ctrl Pts',(-1.89141633536604,-1.43125259324117,
11.7523980077808));
#64376=CARTESIAN_POINT('Ctrl Pts',(-1.86452043772451,-1.46596032342567,
11.7552922937405));
#64377=CARTESIAN_POINT('Ctrl Pts',(-1.85416765304805,-1.47903293516779,
11.7563967311374));
#64378=CARTESIAN_POINT('Ctrl Pts',(-1.83432186664118,-1.50355663748159,
11.758496552076));
#64379=CARTESIAN_POINT('Ctrl Pts',(-1.82485727614539,-1.51502976113639,
11.7594907769));
#64380=CARTESIAN_POINT('Ctrl Pts',(-1.8030753480022,-1.54093390567706,11.7617631753499));
#64381=CARTESIAN_POINT('Ctrl Pts',(-1.79069163034447,-1.55530751343312,
11.7630439916683));
#64382=CARTESIAN_POINT('Ctrl Pts',(-1.75780448053989,-1.59256569708522,
11.766417578738));
#64383=CARTESIAN_POINT('Ctrl Pts',(-1.7370270191405,-1.6152024872212,11.768521478921));
#64384=CARTESIAN_POINT('Ctrl Pts',(-1.60109620869237,-1.7576406707858,11.7821186431199));
#64385=CARTESIAN_POINT('Ctrl Pts',(-1.4740792983213,-1.86544415627209,11.7941254336972));
#64386=CARTESIAN_POINT('Ctrl Pts',(-1.2585822710186,-2.01249882590599,11.8131461888694));
#64387=CARTESIAN_POINT('Ctrl Pts',(-1.17715995538558,-2.06118340178794,
11.820062216178));
#64388=CARTESIAN_POINT('Ctrl Pts',(-1.06421613217573,-2.11983416497274,
11.8291416905219));
#64389=CARTESIAN_POINT('Ctrl Pts',(-1.03508714139557,-2.13420891289673,
11.8314394151011));
#64390=CARTESIAN_POINT('Ctrl Pts',(-0.98453981984614,-2.15787483358758,
11.8353413837852));
#64391=CARTESIAN_POINT('Ctrl Pts',(-0.963263117133661,-2.16745627914078,
11.8369584616639));
#64392=CARTESIAN_POINT('Ctrl Pts',(-0.931931147594175,-2.18101332951712,
11.8392993666904));
#64393=CARTESIAN_POINT('Ctrl Pts',(-0.921985322390353,-2.185236345108,11.8400365658365));
#64394=CARTESIAN_POINT('Ctrl Pts',(-0.905041581319549,-2.19229441354389,
11.8412820765689));
#64395=CARTESIAN_POINT('Ctrl Pts',(-0.89805853691285,-2.19516421475892,
11.8417923989916));
#64396=CARTESIAN_POINT('Ctrl Pts',(-0.882089699840957,-2.20163792392421,
11.8429525234988));
#64397=CARTESIAN_POINT('Ctrl Pts',(-0.873095413329371,-2.20522021441734,
11.8436010525805));
#64398=CARTESIAN_POINT('Ctrl Pts',(-0.848079395640629,-2.21500667603205,
11.8453919327832));
#64399=CARTESIAN_POINT('Ctrl Pts',(-0.832011440220698,-2.22109212799873,
11.8465276342917));
#64400=CARTESIAN_POINT('Ctrl Pts',(-0.71554194041701,-2.26376155528429,
11.8546646811357));
#64401=CARTESIAN_POINT('Ctrl Pts',(-0.612822725794605,-2.29370241073513,
11.8613361363706));
#64402=CARTESIAN_POINT('Ctrl Pts',(-0.370568688761269,-2.34686938907974,
11.8766448927312));
#64403=CARTESIAN_POINT('Ctrl Pts',(-0.230294523961769,-2.36475800737835,
11.885208242189));
#64404=CARTESIAN_POINT('Ctrl Pts',(-0.015215546199552,-2.37285849549867,
11.8987249824446));
#64405=CARTESIAN_POINT('Ctrl Pts',(0.0589161247387191,-2.37217541749953,
11.9034495321975));
#64406=CARTESIAN_POINT('Ctrl Pts',(0.156579348232306,-2.36669473265056,
11.9098264853198));
#64407=CARTESIAN_POINT('Ctrl Pts',(0.180247420646461,-2.3650099051179,11.9113836147958));
#64408=CARTESIAN_POINT('Ctrl Pts',(0.219523866893952,-2.36162099240057,
11.9139890114895));
#64409=CARTESIAN_POINT('Ctrl Pts',(0.235148071145408,-2.36011648116872,
11.9150310764083));
#64410=CARTESIAN_POINT('Ctrl Pts',(0.265742772822165,-2.35686359111583,
11.9170831978626));
#64411=CARTESIAN_POINT('Ctrl Pts',(0.280713831725573,-2.35512737134034,
11.9180928301899));
#64412=CARTESIAN_POINT('Ctrl Pts',(0.316802596939105,-2.35059310403269,
11.920540284206));
#64413=CARTESIAN_POINT('Ctrl Pts',(0.337900806670581,-2.34765304509489,
11.9219824474648));
#64414=CARTESIAN_POINT('Ctrl Pts',(0.40899151441259,-2.33676833445001,11.9268815948784));
#64415=CARTESIAN_POINT('Ctrl Pts',(0.458765455680081,-2.3275080882638,11.9303787147761));
#64416=CARTESIAN_POINT('Ctrl Pts',(0.676992314021041,-2.27963607908064,
11.9460171415026));
#64417=CARTESIAN_POINT('Ctrl Pts',(0.841210715220259,-2.22427683493749,
11.9586502487233));
#64418=CARTESIAN_POINT('Ctrl Pts',(1.06273544759074,-2.12153116639698,11.9764207887479));
#64419=CARTESIAN_POINT('Ctrl Pts',(1.12615304829603,-2.08855971127362,11.9815923084801));
#64420=CARTESIAN_POINT('Ctrl Pts',(1.21177794851088,-2.03900655370253,11.9886148829339));
#64421=CARTESIAN_POINT('Ctrl Pts',(1.23532703183532,-2.02482611202863,11.9905505137406));
#64422=CARTESIAN_POINT('Ctrl Pts',(1.27605961554106,-1.99932314258323,11.9938994389281));
#64423=CARTESIAN_POINT('Ctrl Pts',(1.29335191225893,-1.98818059350367,11.9953214467544));
#64424=CARTESIAN_POINT('Ctrl Pts',(1.31906440387144,-1.97113490173564,11.9974338090302));
#64425=CARTESIAN_POINT('Ctrl Pts',(1.32759424463532,-1.965400018779,11.9981342141073));
#64426=CARTESIAN_POINT('Ctrl Pts',(1.3429702619161,-1.95491645549979,11.9993957565948));
#64427=CARTESIAN_POINT('Ctrl Pts',(1.34982891669337,-1.95018700975994,11.9999580761221));
#64428=CARTESIAN_POINT('Ctrl Pts',(1.36528245175797,-1.93941030180508,12.0012242101416));
#64429=CARTESIAN_POINT('Ctrl Pts',(1.37386220627893,-1.93334196156205,12.001926612142));
#64430=CARTESIAN_POINT('Ctrl Pts',(1.40007744911805,-1.91453764493427,12.0040720357569));
#64431=CARTESIAN_POINT('Ctrl Pts',(1.41757884566627,-1.90161551183372,12.00550327878));
#64432=CARTESIAN_POINT('Ctrl Pts',(1.55251136731188,-1.79908996166132,12.0165510143658));
#64433=CARTESIAN_POINT('Ctrl Pts',(1.66153306121014,-1.69892197049655,12.0255691063844));
#64434=CARTESIAN_POINT('Ctrl Pts',(1.86331984497369,-1.47538678445643,12.0440630153602));
#64435=CARTESIAN_POINT('Ctrl Pts',(1.9548032712851,-1.35183713609888,12.053510569405));
#64436=CARTESIAN_POINT('Ctrl Pts',(2.04966696774308,-1.19374395171846,12.0654372298339));
#64437=CARTESIAN_POINT('Ctrl Pts',(2.06509583259137,-1.1668497590746,12.067459701207));
#64438=CARTESIAN_POINT('Ctrl Pts',(2.0882723392337,-1.12455040344599,12.0706351011929));
#64439=CARTESIAN_POINT('Ctrl Pts',(2.0963870229493,-1.10934953766589,12.0717751217301));
#64440=CARTESIAN_POINT('Ctrl Pts',(2.11116605487177,-1.08092332521409,12.0739056793087));
#64441=CARTESIAN_POINT('Ctrl Pts',(2.11787359498922,-1.0677212955679,12.0748946528817));
#64442=CARTESIAN_POINT('Ctrl Pts',(2.1325324233703,-1.03818758023562,12.0771063346396));
#64443=CARTESIAN_POINT('Ctrl Pts',(2.14042053630489,-1.02182576046515,12.0783311417036));
#64444=CARTESIAN_POINT('Ctrl Pts',(2.15997409230534,-0.980046955587586,
12.0814581563107));
#64445=CARTESIAN_POINT('Ctrl Pts',(2.17137907569643,-0.954511869872516,
12.0833689867123));
#64446=CARTESIAN_POINT('Ctrl Pts',(2.2590104290717,-0.748607270073845,12.0987794598873));
#64447=CARTESIAN_POINT('Ctrl Pts',(2.31306992452865,-0.559660126662052,
12.1130282552086));
#64448=CARTESIAN_POINT('Ctrl Pts',(2.35922076886864,-0.264398485667585,
12.1347973142268));
#64449=CARTESIAN_POINT('Ctrl Pts',(2.36848527963057,-0.161588031708222,
12.1422686867567));
#64450=CARTESIAN_POINT('Ctrl Pts',(2.37160053456625,-0.0353093846962169,
12.1510982735963));
#64451=CARTESIAN_POINT('Ctrl Pts',(2.37183243525361,-0.0121180069424332,
12.152705310845));
#64452=CARTESIAN_POINT('Ctrl Pts',(2.37167381896125,0.0218526859785101,
12.1550345313741));
#64453=CARTESIAN_POINT('Ctrl Pts',(2.37155001354541,0.0326310879798007,
12.1557699055898));
#64454=CARTESIAN_POINT('Ctrl Pts',(2.37121460813197,0.0509538592425347,
12.15701337888));
#64455=CARTESIAN_POINT('Ctrl Pts',(2.37104047617629,0.0584985450088929,
12.1575234711148));
#64456=CARTESIAN_POINT('Ctrl Pts',(2.37056026376969,0.0757374503522885,
12.1586845161773));
#64457=CARTESIAN_POINT('Ctrl Pts',(2.37023073098655,0.0854307655534443,
12.159334182723));
#64458=CARTESIAN_POINT('Ctrl Pts',(2.36914954893606,0.112367019877441,12.1611313414907));
#64459=CARTESIAN_POINT('Ctrl Pts',(2.3682691204173,0.129604582230312,12.1622721088702));
#64460=CARTESIAN_POINT('Ctrl Pts',(2.36007604591103,0.261692297545161,12.170952695441));
#64461=CARTESIAN_POINT('Ctrl Pts',(2.34460005619444,0.375898046438222,12.1781089334486));
#64462=CARTESIAN_POINT('Ctrl Pts',(2.30254473525346,0.575688206585353,12.1906879991891));
#64463=CARTESIAN_POINT('Ctrl Pts',(2.27930684793615,0.661732101267775,12.1961260056565));
#64464=CARTESIAN_POINT('Ctrl Pts',(2.22785364384537,0.816952889794791,12.2062427079913));
#64465=CARTESIAN_POINT('Ctrl Pts',(2.20110704587178,0.886493339973293,12.2108935938381));
#64466=CARTESIAN_POINT('Ctrl Pts',(2.1573101261585,0.986098775526492,12.2178244176621));
#64467=CARTESIAN_POINT('Ctrl Pts',(2.14280426729861,1.01723520966622,12.2200306646666));
#64468=CARTESIAN_POINT('Ctrl Pts',(2.11515070134807,1.07337452049931,12.2240900542522));
#64469=CARTESIAN_POINT('Ctrl Pts',(2.10222256874422,1.09847872671453,12.2259358564495));
#64470=CARTESIAN_POINT('Ctrl Pts',(2.08096397692257,1.13800887291864,12.228894567147));
#64471=CARTESIAN_POINT('Ctrl Pts',(2.07292416993712,1.15258866481411,12.2299973454221));
#64472=CARTESIAN_POINT('Ctrl Pts',(2.0574106250297,1.18003429389195,12.2320958539988));
#64473=CARTESIAN_POINT('Ctrl Pts',(2.04996799200713,1.19291685768597,12.2330904452065));
#64474=CARTESIAN_POINT('Ctrl Pts',(2.03273712719069,1.22210452857911,12.2353662700093));
#64475=CARTESIAN_POINT('Ctrl Pts',(2.02287310479298,1.23836346553517,12.2366501763271));
#64476=CARTESIAN_POINT('Ctrl Pts',(1.99648138951181,1.28070827863653,12.2400375542884));
#64477=CARTESIAN_POINT('Ctrl Pts',(1.97963834608529,1.30659232306072,12.2421523042127));
#64478=CARTESIAN_POINT('Ctrl Pts',(1.87116441259609,1.46637886098409,12.2554916578287));
#64479=CARTESIAN_POINT('Ctrl Pts',(1.76651416460043,1.59089093361851,12.2672030799314));
#64480=CARTESIAN_POINT('Ctrl Pts',(1.55245579894765,1.79819861378936,12.2889260311413));
#64481=CARTESIAN_POINT('Ctrl Pts',(1.4469695547581,1.88412397004255,12.2988518671792));
#64482=CARTESIAN_POINT('Ctrl Pts',(1.31800242342718,1.97192183331187,12.3097189272458));
#64483=CARTESIAN_POINT('Ctrl Pts',(1.30115925694379,1.98307608523859,12.3111148857916));
#64484=CARTESIAN_POINT('Ctrl Pts',(1.27559549682919,1.99953952877235,12.3131964809662));
#64485=CARTESIAN_POINT('Ctrl Pts',(1.26698026413232,2.00500953079047,12.3138917561725));
#64486=CARTESIAN_POINT('Ctrl Pts',(1.25126583485465,2.01484523499068,12.3151482856301));
#64487=CARTESIAN_POINT('Ctrl Pts',(1.24417873794932,2.01922925473189,12.3157106681003));
#64488=CARTESIAN_POINT('Ctrl Pts',(1.22803319238963,2.02909947580363,12.3169822113783));
#64489=CARTESIAN_POINT('Ctrl Pts',(1.21896095781306,2.03456245866863,12.3176899018509));
#64490=CARTESIAN_POINT('Ctrl Pts',(1.19077590306894,2.0512783128576,12.3198685536537));
#64491=CARTESIAN_POINT('Ctrl Pts',(1.17154098961669,2.06232435942036,12.3213272025687));
#64492=CARTESIAN_POINT('Ctrl Pts',(1.02695536630034,2.14267978077985,12.3321048848252));
#64493=CARTESIAN_POINT('Ctrl Pts',(0.895694664394937,2.20078528271987,12.340865085487));
#64494=CARTESIAN_POINT('Ctrl Pts',(0.606598915363746,2.29857621266965,12.3596062804192));
#64495=CARTESIAN_POINT('Ctrl Pts',(0.448330855646171,2.33461040037506,12.369566117304));
#64496=CARTESIAN_POINT('Ctrl Pts',(0.259459930672364,2.35768623107378,12.3819067149446));
#64497=CARTESIAN_POINT('Ctrl Pts',(0.231225076976445,2.36062251807222,12.3837620755276));
#64498=CARTESIAN_POINT('Ctrl Pts',(0.186325213078974,2.36447864042204,12.386732517611));
#64499=CARTESIAN_POINT('Ctrl Pts',(0.169690928763128,2.36573060408042,12.3878373260575));
#64500=CARTESIAN_POINT('Ctrl Pts',(0.13820407173097,2.3677666431033,12.389937442526));
#64501=CARTESIAN_POINT('Ctrl Pts',(0.123354571519996,2.36858668285574,12.3909315874561));
#64502=CARTESIAN_POINT('Ctrl Pts',(0.0895559997636695,2.37013446050989,
12.3932032293259));
#64503=CARTESIAN_POINT('Ctrl Pts',(0.0706041426167315,2.37077469557539,
12.3944833623162));
#64504=CARTESIAN_POINT('Ctrl Pts',(0.020963555476188,2.37185592288384,12.3978539019316));
#64505=CARTESIAN_POINT('Ctrl Pts',(-0.00972878240669629,2.37192858018127,
12.3999554052154));
#64506=CARTESIAN_POINT('Ctrl Pts',(-0.207294558031061,2.3685617305641,12.4136007322531));
#64507=CARTESIAN_POINT('Ctrl Pts',(-0.373382413760315,2.34811050327965,
12.4256632230052));
#64508=CARTESIAN_POINT('Ctrl Pts',(-0.627757951115977,2.28910601890843,
12.4447016328042));
#64509=CARTESIAN_POINT('Ctrl Pts',(-0.718250184669095,2.26234497776169,
12.4515802350739));
#64510=CARTESIAN_POINT('Ctrl Pts',(-0.837362368212341,2.21925006998316,
12.4606163829121));
#64511=CARTESIAN_POINT('Ctrl Pts',(-0.867584732140789,2.20761037118771,
12.4629070949889));
#64512=CARTESIAN_POINT('Ctrl Pts',(-0.919109598390386,2.18654466758929,
12.4667984708824));
#64513=CARTESIAN_POINT('Ctrl Pts',(-0.940528634475465,2.17741728312332,
12.4684118819509));
#64514=CARTESIAN_POINT('Ctrl Pts',(-0.971678581013751,2.16359777610425,
12.470748520895));
#64515=CARTESIAN_POINT('Ctrl Pts',(-0.981516637414081,2.15915254285377,
12.4714850545158));
#64516=CARTESIAN_POINT('Ctrl Pts',(-0.998181765352541,2.15148511638033,
12.4727298217306));
#64517=CARTESIAN_POINT('Ctrl Pts',(-1.00502425055415,2.14829730353386,12.4732400597154));
#64518=CARTESIAN_POINT('Ctrl Pts',(-1.0206133142889,2.14094380408955,12.4744005174537));
#64519=CARTESIAN_POINT('Ctrl Pts',(-1.02934972025902,2.13675713903471,12.4750494593805));
#64520=CARTESIAN_POINT('Ctrl Pts',(-1.05353360908341,2.12498497584489,12.4768426178083));
#64521=CARTESIAN_POINT('Ctrl Pts',(-1.06892491043338,2.11728453227802,12.4779801574411));
#64522=CARTESIAN_POINT('Ctrl Pts',(-1.18379779517616,2.05824034632913,12.4864526450614));
#64523=CARTESIAN_POINT('Ctrl Pts',(-1.27962930665314,2.00007147080152,12.4934248034534));
#64524=CARTESIAN_POINT('Ctrl Pts',(-1.48300257376349,1.85600118054244,12.5087903979374));
#64525=CARTESIAN_POINT('Ctrl Pts',(-1.58789939250964,1.76709115416447,12.5171298934038));
#64526=CARTESIAN_POINT('Ctrl Pts',(-1.73595384741521,1.61771479228139,12.5303450339128));
#64527=CARTESIAN_POINT('Ctrl Pts',(-1.78496020370499,1.56347446698995,12.5350058273635));
#64528=CARTESIAN_POINT('Ctrl Pts',(-1.8463905117887,1.48882437875424,12.5413092503845));
#64529=CARTESIAN_POINT('Ctrl Pts',(-1.86112525479835,1.47036344953181,12.5428594756417));
#64530=CARTESIAN_POINT('Ctrl Pts',(-1.88517523844693,1.43929082063817,12.5454564830382));
#64531=CARTESIAN_POINT('Ctrl Pts',(-1.89464575431619,1.4268010344555,12.54649714805));
#64532=CARTESIAN_POINT('Ctrl Pts',(-1.91298706008569,1.40210775621875,12.548548897046));
#64533=CARTESIAN_POINT('Ctrl Pts',(-1.92186659237952,1.38991166455625,12.5495595789913));
#64534=CARTESIAN_POINT('Ctrl Pts',(-1.94305009503871,1.3602248638427,12.5520137464494));
#64535=CARTESIAN_POINT('Ctrl Pts',(-1.95523484029815,1.34265111621546,12.5534616329772));
#64536=CARTESIAN_POINT('Ctrl Pts',(-1.99579951207146,1.28242236230203,12.5584087662337));
#64537=CARTESIAN_POINT('Ctrl Pts',(-2.02303267927108,1.23901610117099,12.5619492658185));
#64538=CARTESIAN_POINT('Ctrl Pts',(-2.15506681764593,1.0125979207379,12.580303066425));
#64539=CARTESIAN_POINT('Ctrl Pts',(-2.23651645768568,0.81708958512084,12.5958956052405));
#64540=CARTESIAN_POINT('Ctrl Pts',(-2.30298201998029,0.568860631470241,
12.6144171164765));
#64541=CARTESIAN_POINT('Ctrl Pts',(-2.3136172064994,0.523931794267859,12.6177158551158));
#64542=CARTESIAN_POINT('Ctrl Pts',(-2.32902205938667,0.449181281508012,
12.6230883587012));
#64543=CARTESIAN_POINT('Ctrl Pts',(-2.33454566095764,0.4195287115111,12.6251898078999));
#64544=CARTESIAN_POINT('Ctrl Pts',(-2.34146607873374,0.377991307388502,
12.6280849400354));
#64545=CARTESIAN_POINT('Ctrl Pts',(-2.34334065659209,0.366190399276157,
12.6289020099896));
#64546=CARTESIAN_POINT('Ctrl Pts',(-2.34639349027772,0.345987876029962,
12.6302909197348));
#64547=CARTESIAN_POINT('Ctrl Pts',(-2.34761598249118,0.337593290355653,
12.6308651259901));
#64548=CARTESIAN_POINT('Ctrl Pts',(-2.35009278510104,0.31992123849544,12.6320676145371));
#64549=CARTESIAN_POINT('Ctrl Pts',(-2.35133724216032,0.310642686289107,
12.6326953629443));
#64550=CARTESIAN_POINT('Ctrl Pts',(-2.35458085988286,0.285321548060174,
12.6343992542525));
#64551=CARTESIAN_POINT('Ctrl Pts',(-2.35647103066586,0.269265163371451,
12.6354696209421));
#64552=CARTESIAN_POINT('Ctrl Pts',(-2.36106678317317,0.226460620983871,
12.6382992727383));
#64553=CARTESIAN_POINT('Ctrl Pts',(-2.36348176316326,0.199686056432405,
12.6400445342361));
#64554=CARTESIAN_POINT('Ctrl Pts',(-2.3654410188404,0.172878133051282,12.6417724606485));
#64555=CARTESIAN_POINT('Origin',(0.,0.,-1.84858989190501));
#64556=CARTESIAN_POINT('',(-2.36544101497364,0.172878185958964,13.8381597463488));
#64557=CARTESIAN_POINT('',(-2.3654410187889,0.172878133755955,13.6380106975316));
#64558=CARTESIAN_POINT('',(-2.36544101854889,0.172878137039864,-1.84858989190501));
#64559=CARTESIAN_POINT('Ctrl Pts',(-2.36544101497364,0.172878185958964,
13.8381597463488));
#64560=CARTESIAN_POINT('Ctrl Pts',(-2.36276108291472,0.20954690257207,13.8358629187249));
#64561=CARTESIAN_POINT('Ctrl Pts',(-2.35922832534139,0.246155734497383,
13.8335498568797));
#64562=CARTESIAN_POINT('Ctrl Pts',(-2.34943075770665,0.327775080991724,
13.8283318218708));
#64563=CARTESIAN_POINT('Ctrl Pts',(-2.34272273041678,0.372707920858889,
13.8254173289339));
#64564=CARTESIAN_POINT('Ctrl Pts',(-2.3313675139366,0.436220587174823,13.8212225507192));
#64565=CARTESIAN_POINT('Ctrl Pts',(-2.32777900537393,0.454981047943001,
13.819974129542));
#64566=CARTESIAN_POINT('Ctrl Pts',(-2.32108537077806,0.487820207276247,
13.8177712569735));
#64567=CARTESIAN_POINT('Ctrl Pts',(-2.31807770452967,0.501917915292993,
13.8168198548091));
#64568=CARTESIAN_POINT('Ctrl Pts',(-2.31174678358148,0.530321171818991,
13.8148909845316));
#64569=CARTESIAN_POINT('Ctrl Pts',(-2.3084187938634,0.544625001659661,13.8139134058292));
#64570=CARTESIAN_POINT('Ctrl Pts',(-2.30124693043164,0.574202640406508,
13.8118786355917));
#64571=CARTESIAN_POINT('Ctrl Pts',(-2.29738333245326,0.58947087318232,13.8108208596796));
#64572=CARTESIAN_POINT('Ctrl Pts',(-2.28696353669542,0.628988747778604,
13.8080632497421));
#64573=CARTESIAN_POINT('Ctrl Pts',(-2.28017377773735,0.653174190257341,
13.8063560489414));
#64574=CARTESIAN_POINT('Ctrl Pts',(-2.24901281768177,0.75775783947841,13.7988859445409));
#64575=CARTESIAN_POINT('Ctrl Pts',(-2.22076635737281,0.836928612087447,
13.7930009567286));
#64576=CARTESIAN_POINT('Ctrl Pts',(-2.13519938762358,1.04170530817572,13.7771697356733));
#64577=CARTESIAN_POINT('Ctrl Pts',(-2.07101572650728,1.16409398572356,13.7670585861267));
#64578=CARTESIAN_POINT('Ctrl Pts',(-1.95689686009889,1.34207103573256,13.7516866178795));
#64579=CARTESIAN_POINT('Ctrl Pts',(-1.914367453418,1.40206946177415,13.7463788282227));
#64580=CARTESIAN_POINT('Ctrl Pts',(-1.84860173026452,1.48626391194827,13.7388351630916));
#64581=CARTESIAN_POINT('Ctrl Pts',(-1.82753352662377,1.51209465773799,13.7365070339046));
#64582=CARTESIAN_POINT('Ctrl Pts',(-1.79786161812875,1.54694746208743,13.7333560489755));
#64583=CARTESIAN_POINT('Ctrl Pts',(-1.78972197703129,1.55635732086554,13.7325043225996));
#64584=CARTESIAN_POINT('Ctrl Pts',(-1.7759429784471,1.57203551987203,13.7310841677081));
#64585=CARTESIAN_POINT('Ctrl Pts',(-1.77034363402645,1.57833854549753,13.7305129423225));
#64586=CARTESIAN_POINT('Ctrl Pts',(-1.75879600369852,1.59119862025627,13.7293471033848));
#64587=CARTESIAN_POINT('Ctrl Pts',(-1.7528444320212,1.59775243240796,13.7287527398659));
#64588=CARTESIAN_POINT('Ctrl Pts',(-1.73709755496473,1.61489884779452,13.7271966582382));
#64589=CARTESIAN_POINT('Ctrl Pts',(-1.72724187719481,1.62543585759475,13.7262393032648));
#64590=CARTESIAN_POINT('Ctrl Pts',(-1.68399671261342,1.67083306674584,13.7221063918393));
#64591=CARTESIAN_POINT('Ctrl Pts',(-1.64964116954359,1.70476180499079,13.7189959727027));
#64592=CARTESIAN_POINT('Ctrl Pts',(-1.50059241295543,1.84322995517101,13.7060830834404));
#64593=CARTESIAN_POINT('Ctrl Pts',(-1.37681631989302,1.93743606687906,13.6967229276606));
#64594=CARTESIAN_POINT('Ctrl Pts',(-1.17760731229289,2.06025595884288,13.6822713203688));
#64595=CARTESIAN_POINT('Ctrl Pts',(-1.10848145045337,2.09825668096637,13.6773590490224));
#64596=CARTESIAN_POINT('Ctrl Pts',(-0.990791265609828,2.15551382549267,
13.6690325845493));
#64597=CARTESIAN_POINT('Ctrl Pts',(-0.943253273120034,2.17673604777566,
13.6656792976149));
#64598=CARTESIAN_POINT('Ctrl Pts',(-0.875889899825235,2.20418769407958,
13.6609195960509));
#64599=CARTESIAN_POINT('Ctrl Pts',(-0.856620603374425,2.21174763588929,
13.659557257492));
#64600=CARTESIAN_POINT('Ctrl Pts',(-0.823354614845609,2.22429898570321,
13.6572026922286));
#64601=CARTESIAN_POINT('Ctrl Pts',(-0.809405214337752,2.22941292309398,
13.6562145629784));
#64602=CARTESIAN_POINT('Ctrl Pts',(-0.782612725164148,2.23895061995955,
13.6543147350375));
#64603=CARTESIAN_POINT('Ctrl Pts',(-0.769777837705112,2.24339577953811,
13.6534037838277));
#64604=CARTESIAN_POINT('Ctrl Pts',(-0.739464041401159,2.25360371442001,
13.6512499603246));
#64605=CARTESIAN_POINT('Ctrl Pts',(-0.721955046812446,2.25927369915118,
13.6500041280289));
#64606=CARTESIAN_POINT('Ctrl Pts',(-0.659890299322825,2.27857716095646,
13.6455806728019));
#64607=CARTESIAN_POINT('Ctrl Pts',(-0.615003115657367,2.29110011385842,
13.6423680046136));
#64608=CARTESIAN_POINT('Ctrl Pts',(-0.397796932936669,2.34485501004911,
13.6267491743822));
#64609=CARTESIAN_POINT('Ctrl Pts',(-0.221609048674075,2.36800726341303,
13.6138032128394));
#64610=CARTESIAN_POINT('Ctrl Pts',(0.0532131251998344,2.37316706764431,
13.5937911028067));
#64611=CARTESIAN_POINT('Ctrl Pts',(0.150978027962253,2.36895818706504,13.5867218428623));
#64612=CARTESIAN_POINT('Ctrl Pts',(0.27053684975708,2.35637683342352,13.5783250202505));
#64613=CARTESIAN_POINT('Ctrl Pts',(0.292827966065009,2.35371065359643,13.5767703803196));
#64614=CARTESIAN_POINT('Ctrl Pts',(0.32548576232331,2.34933338007757,13.5745119381951));
#64615=CARTESIAN_POINT('Ctrl Pts',(0.3358835532825,2.34786936631262,13.573795749026));
#64616=CARTESIAN_POINT('Ctrl Pts',(0.353564247253944,2.34526005546162,13.5725831923355));
#64617=CARTESIAN_POINT('Ctrl Pts',(0.360851966552392,2.34414979648057,13.5720849376955));
#64618=CARTESIAN_POINT('Ctrl Pts',(0.377499095017051,2.34153418775725,13.5709503762176));
#64619=CARTESIAN_POINT('Ctrl Pts',(0.386854783468157,2.34000668875643,13.5703153036658));
#64620=CARTESIAN_POINT('Ctrl Pts',(0.412817733444255,2.33560776131276,13.5685593766704));
#64621=CARTESIAN_POINT('Ctrl Pts',(0.429404301207037,2.33261528788169,13.5674449523658));
#64622=CARTESIAN_POINT('Ctrl Pts',(0.541072625177116,2.31123707450552,13.5599832545991));
#64623=CARTESIAN_POINT('Ctrl Pts',(0.634994675150038,2.28721724239256,13.5539072192625));
#64624=CARTESIAN_POINT('Ctrl Pts',(0.752763202386717,2.24928148800337,13.5462497207829));
#64625=CARTESIAN_POINT('Ctrl Pts',(0.778190347992261,2.24061140479784,13.5445941767885));
#64626=CARTESIAN_POINT('Ctrl Pts',(0.89746754378451,2.19766514761424,13.5367961068051));
#64627=CARTESIAN_POINT('Ctrl Pts',(0.989235361902849,2.157914024441,13.5306975304384));
#64628=CARTESIAN_POINT('Ctrl Pts',(1.16364308231315,2.06889596386664,13.5185189138606));
#64629=CARTESIAN_POINT('Ctrl Pts',(1.2463322226425,2.02016052602677,13.5124593168942));
#64630=CARTESIAN_POINT('Ctrl Pts',(1.34678813917956,1.95243390240448,13.5045765917239));
#64631=CARTESIAN_POINT('Ctrl Pts',(1.36750999009039,1.93797646603168,13.5029211090723));
#64632=CARTESIAN_POINT('Ctrl Pts',(1.40079162581702,1.91395660384901,13.5002115505319));
#64633=CARTESIAN_POINT('Ctrl Pts',(1.41349420843968,1.90459475031936,13.4991650951147));
#64634=CARTESIAN_POINT('Ctrl Pts',(1.43782598667334,1.88628464889105,13.4971361580608));
#64635=CARTESIAN_POINT('Ctrl Pts',(1.44946744639308,1.87735384249763,13.4961543819207));
#64636=CARTESIAN_POINT('Ctrl Pts',(1.47618735296003,1.85645884487857,13.4938748396358));
#64637=CARTESIAN_POINT('Ctrl Pts',(1.4912043355533,1.84441810222092,13.4925741035197));
#64638=CARTESIAN_POINT('Ctrl Pts',(1.54018547728282,1.80415540479429,13.4882651976858));
#64639=CARTESIAN_POINT('Ctrl Pts',(1.57350635300837,1.77516910179508,13.4852267765631));
#64640=CARTESIAN_POINT('Ctrl Pts',(1.75296568613457,1.61003079356689,13.4682467245569));
#64641=CARTESIAN_POINT('Ctrl Pts',(1.88224455140966,1.45678315504625,13.4535789826234));
#64642=CARTESIAN_POINT('Ctrl Pts',(2.02392927071146,1.23799410808772,13.434661184738));
#64643=CARTESIAN_POINT('Ctrl Pts',(2.05510129259139,1.18552887387326,13.4302654724022));
#64644=CARTESIAN_POINT('Ctrl Pts',(2.09603637601082,1.11015443708886,13.4241955516293));
#64645=CARTESIAN_POINT('Ctrl Pts',(2.10751435959628,1.0882070998676,13.4224563385966));
#64646=CARTESIAN_POINT('Ctrl Pts',(2.12714916505769,1.04918648279608,13.4194184320745));
#64647=CARTESIAN_POINT('Ctrl Pts',(2.13544928551196,1.03218808885265,13.418112850886));
#64648=CARTESIAN_POINT('Ctrl Pts',(2.14774445456061,1.00622466370559,13.4161475635831));
#64649=CARTESIAN_POINT('Ctrl Pts',(2.15188847690972,0.997331593542218,13.4154794912224));
#64650=CARTESIAN_POINT('Ctrl Pts',(2.1593744176129,0.981002872365718,13.4142624524404));
#64651=CARTESIAN_POINT('Ctrl Pts',(2.16273325517824,0.973575565507571,13.4137125208669));
#64652=CARTESIAN_POINT('Ctrl Pts',(2.17033582878251,0.956530683535731,13.4124587149267));
#64653=CARTESIAN_POINT('Ctrl Pts',(2.17455399201601,0.946902056394619,13.4117563620212));
#64654=CARTESIAN_POINT('Ctrl Pts',(2.18760335821565,0.916567677119023,13.4095612122662));
#64655=CARTESIAN_POINT('Ctrl Pts',(2.19620418741125,0.895763370741718,13.4080812754844));
#64656=CARTESIAN_POINT('Ctrl Pts',(2.25334194099725,0.751781850841294,13.3979929702021));
#64657=CARTESIAN_POINT('Ctrl Pts',(2.29179304771167,0.624835519677969,13.389859547353));
#64658=CARTESIAN_POINT('Ctrl Pts',(2.33254490601527,0.434009183669126,13.3778774738183));
#64659=CARTESIAN_POINT('Ctrl Pts',(2.34320310696718,0.372194480841895,13.3740339847284));
#64660=CARTESIAN_POINT('Ctrl Pts',(2.36127416211096,0.235136382124309,13.3654859635678));
#64661=CARTESIAN_POINT('Ctrl Pts',(2.36756454390981,0.159817576288654,13.3607706665713));
#64662=CARTESIAN_POINT('Ctrl Pts',(2.3714762831625,0.0498719840989109,13.3537644492922));
#64663=CARTESIAN_POINT('Ctrl Pts',(2.37195065036051,0.0153918972247291,
13.3515499613032));
#64664=CARTESIAN_POINT('Ctrl Pts',(2.3714462627868,-0.0472877138775438,
13.347484410659));
#64665=CARTESIAN_POINT('Ctrl Pts',(2.3707162842125,-0.0754830842777611,
13.3456409061781));
#64666=CARTESIAN_POINT('Ctrl Pts',(2.36876669650036,-0.120048147461304,
13.3427006328884));
#64667=CARTESIAN_POINT('Ctrl Pts',(2.36787963828969,-0.136430261247075,
13.3416141312154));
#64668=CARTESIAN_POINT('Ctrl Pts',(2.36588745321069,-0.167288259135244,
13.3395562715876));
#64669=CARTESIAN_POINT('Ctrl Pts',(2.3648192258425,-0.181765827482735,13.3385861016556));
#64670=CARTESIAN_POINT('Ctrl Pts',(2.36209994905798,-0.214519500125747,
13.3363801655352));
#64671=CARTESIAN_POINT('Ctrl Pts',(2.36036957833212,-0.232787900038322,
13.3351419952159));
#64672=CARTESIAN_POINT('Ctrl Pts',(2.35532272406598,-0.280202361761902,
13.3319073193338));
#64673=CARTESIAN_POINT('Ctrl Pts',(2.35167727542628,-0.309309485877959,
13.3299008031946));
#64674=CARTESIAN_POINT('Ctrl Pts',(2.32145481303518,-0.519000715961252,
13.3152897984617));
#64675=CARTESIAN_POINT('Ctrl Pts',(2.27465286048027,-0.696020697804163,
13.3020472537032));
#64676=CARTESIAN_POINT('Ctrl Pts',(2.16362472731613,-0.979145516434845,
13.2798725412824));
#64677=CARTESIAN_POINT('Ctrl Pts',(2.1105575749877,-1.08883001911628,13.27102629108));
#64678=CARTESIAN_POINT('Ctrl Pts',(2.04002817664888,-1.20988532455299,13.2612891067581));
#64679=CARTESIAN_POINT('Ctrl Pts',(2.03056843600912,-1.22569545093014,13.2600181648935));
#64680=CARTESIAN_POINT('Ctrl Pts',(2.01584283715474,-1.24966795606068,13.2580940681641));
#64681=CARTESIAN_POINT('Ctrl Pts',(2.01070972275329,-1.25791047522443,13.257433052148));
#64682=CARTESIAN_POINT('Ctrl Pts',(2.0011693805951,-1.27302229954661,13.2562224938037));
#64683=CARTESIAN_POINT('Ctrl Pts',(1.9967772539878,-1.27990049078457,13.2556720606271));
#64684=CARTESIAN_POINT('Ctrl Pts',(1.98667020532569,-1.29554974371605,13.2544208513494));
#64685=CARTESIAN_POINT('Ctrl Pts',(1.98093262397,-1.30430578955758,13.2537215594881));
#64686=CARTESIAN_POINT('Ctrl Pts',(1.96247041277676,-1.33207786782794,13.2515051008533));
#64687=CARTESIAN_POINT('Ctrl Pts',(1.94952807285545,-1.35094853857973,13.2500013527538));
#64688=CARTESIAN_POINT('Ctrl Pts',(1.86762807893217,-1.46673465403492,13.2407692874927));
#64689=CARTESIAN_POINT('Ctrl Pts',(1.79172595625999,-1.55854744537032,13.2334198121188));
#64690=CARTESIAN_POINT('Ctrl Pts',(1.62167193288928,-1.73531974947297,13.2183409291342));
#64691=CARTESIAN_POINT('Ctrl Pts',(1.52696977510027,-1.8192074619561,13.2106354271467));
#64692=CARTESIAN_POINT('Ctrl Pts',(1.37033005973527,-1.9370737213977,13.1982958981603));
#64693=CARTESIAN_POINT('Ctrl Pts',(1.31280257796597,-1.97651386864463,13.1938414955082));
#64694=CARTESIAN_POINT('Ctrl Pts',(1.23414662316862,-2.02548925008237,13.1877964634833));
#64695=CARTESIAN_POINT('Ctrl Pts',(1.21449337606589,-2.03733413295289,13.1862897686535));
#64696=CARTESIAN_POINT('Ctrl Pts',(1.18146061079586,-2.05659494466532,13.1837618046922));
#64697=CARTESIAN_POINT('Ctrl Pts',(1.16817538238523,-2.06417009930813,13.1827462821234));
#64698=CARTESIAN_POINT('Ctrl Pts',(1.14192640862472,-2.07880253508793,13.1807416280576));
#64699=CARTESIAN_POINT('Ctrl Pts',(1.12896819037678,-2.08586833498525,13.1797528558857));
#64700=CARTESIAN_POINT('Ctrl Pts',(1.09743504360342,-2.10268267428213,13.1773483400488));
#64701=CARTESIAN_POINT('Ctrl Pts',(1.07879537409456,-2.11230646351584,13.1759283278761));
#64702=CARTESIAN_POINT('Ctrl Pts',(1.01493590948249,-2.14421182400213,13.1710664772113));
#64703=CARTESIAN_POINT('Ctrl Pts',(0.969137145392655,-2.16529715804273,
13.1675845334342));
#64704=CARTESIAN_POINT('Ctrl Pts',(0.76289046654408,-2.25239686541711,13.1519167606892));
#64705=CARTESIAN_POINT('Ctrl Pts',(0.596172939465782,-2.30214132199112,
13.1392320196889));
#64706=CARTESIAN_POINT('Ctrl Pts',(0.330618992596286,-2.35057478795073,
13.119583194056));
#64707=CARTESIAN_POINT('Ctrl Pts',(0.23470488584106,-2.36208127946849,13.1126077479123));
#64708=CARTESIAN_POINT('Ctrl Pts',(0.116068011500286,-2.36901337800748,
13.1043085360878));
#64709=CARTESIAN_POINT('Ctrl Pts',(0.0937694494648238,-2.37000074846898,
13.1027630484942));
#64710=CARTESIAN_POINT('Ctrl Pts',(0.0609880869604961,-2.37098887845012,
13.1005152755374));
#64711=CARTESIAN_POINT('Ctrl Pts',(0.0505146464855438,-2.37123514003166,
13.0998007634007));
#64712=CARTESIAN_POINT('Ctrl Pts',(0.0326715872010758,-2.37153640791543,
13.0985900646363));
#64713=CARTESIAN_POINT('Ctrl Pts',(0.0253029142285122,-2.37162647450572,
13.0980920069092));
#64714=CARTESIAN_POINT('Ctrl Pts',(0.00843780228341203,-2.37175400110903,
13.0969565352849));
#64715=CARTESIAN_POINT('Ctrl Pts',(-0.00105856972606136,-2.37176877572306,
13.096320368005));
#64716=CARTESIAN_POINT('Ctrl Pts',(-0.0274829177625788,-2.37165117851174,
13.0945584306821));
#64717=CARTESIAN_POINT('Ctrl Pts',(-0.0444101559562398,-2.37139461103667,
13.0934391614116));
#64718=CARTESIAN_POINT('Ctrl Pts',(-0.163171860820531,-2.36832238964647,
13.0856433428351));
#64719=CARTESIAN_POINT('Ctrl Pts',(-0.264747740045853,-2.35912903464265,
13.0792675432846));
#64720=CARTESIAN_POINT('Ctrl Pts',(-0.398032333988223,-2.33834496628121,
13.070931468768));
#64721=CARTESIAN_POINT('Ctrl Pts',(-0.430526881505042,-2.33258088271208,
13.0689017925701));
#64722=CARTESIAN_POINT('Ctrl Pts',(-0.58201546543949,-2.30243537538697,
13.0594131921702));
#64723=CARTESIAN_POINT('Ctrl Pts',(-0.699136499344073,-2.26961597894804,
13.0519901050512));
#64724=CARTESIAN_POINT('Ctrl Pts',(-0.877315031907168,-2.20457957383278,
13.0400408777054));
#64725=CARTESIAN_POINT('Ctrl Pts',(-0.940360124192913,-2.17843390654501,
13.0356791065165));
#64726=CARTESIAN_POINT('Ctrl Pts',(-1.02283359773433,-2.13998328209318,
13.0297412162558));
#64727=CARTESIAN_POINT('Ctrl Pts',(-1.04334013740576,-2.13006063654149,
13.0282451537603));
#64728=CARTESIAN_POINT('Ctrl Pts',(-1.07733857292259,-2.11300082989485,
13.0257300896777));
#64729=CARTESIAN_POINT('Ctrl Pts',(-1.0909105056597,-2.10602591584364,13.0247167078207));
#64730=CARTESIAN_POINT('Ctrl Pts',(-1.11749704804048,-2.09203656014731,
13.0227124988813));
#64731=CARTESIAN_POINT('Ctrl Pts',(-1.13051525674968,-2.08503042153271,
13.0217219969079));
#64732=CARTESIAN_POINT('Ctrl Pts',(-1.16196239482079,-2.06772511057704,
13.0193065737755));
#64733=CARTESIAN_POINT('Ctrl Pts',(-1.18032066910222,-2.05730085509232,
13.0178772890568));
#64734=CARTESIAN_POINT('Ctrl Pts',(-1.24273495558209,-2.02075018165785,
13.0129503254845));
#64735=CARTESIAN_POINT('Ctrl Pts',(-1.28607988100212,-1.99344408435901,
13.0094110898422));
#64736=CARTESIAN_POINT('Ctrl Pts',(-1.47154385160806,-1.86803949707763,
12.9937346775241));
#64737=CARTESIAN_POINT('Ctrl Pts',(-1.60357683029832,-1.7560005506902,12.9811074481034));
#64738=CARTESIAN_POINT('Ctrl Pts',(-1.78841747518489,-1.56077551703415,
12.9615386626739));
#64739=CARTESIAN_POINT('Ctrl Pts',(-1.85026800854569,-1.48693280262806,
12.9545840306608));
#64740=CARTESIAN_POINT('Ctrl Pts',(-1.92071197005659,-1.3916035373627,12.9463064964809));
#64741=CARTESIAN_POINT('Ctrl Pts',(-1.93370575283272,-1.37349081801791,
12.944763053749));
#64742=CARTESIAN_POINT('Ctrl Pts',(-1.95242561740281,-1.34660384084437,
12.9425176661053));
#64743=CARTESIAN_POINT('Ctrl Pts',(-1.95835158985206,-1.33797113441267,
12.9418035300652));
#64744=CARTESIAN_POINT('Ctrl Pts',(-1.9683502080345,-1.32319681708584,12.9405932477136));
#64745=CARTESIAN_POINT('Ctrl Pts',(-1.97245164549792,-1.31707511924756,
12.9400952338928));
#64746=CARTESIAN_POINT('Ctrl Pts',(-1.98177552176051,-1.30301730292257,
12.9389595563739));
#64747=CARTESIAN_POINT('Ctrl Pts',(-1.9869788820073,-1.29506881694029,12.9383231420749));
#64748=CARTESIAN_POINT('Ctrl Pts',(-2.00133008231086,-1.27285627518941,
12.9365598476668));
#64749=CARTESIAN_POINT('Ctrl Pts',(-2.01037323685284,-1.25852480476586,
12.9354394843266));
#64750=CARTESIAN_POINT('Ctrl Pts',(-2.07460506315104,-1.15427176704404,
12.9274043463363));
#64751=CARTESIAN_POINT('Ctrl Pts',(-2.12389974386801,-1.06084164991093,
12.920812726887));
#64752=CARTESIAN_POINT('Ctrl Pts',(-2.17330310257412,-0.949845497337405,
12.913312109175));
#64753=CARTESIAN_POINT('Ctrl Pts',(-2.17964637370493,-0.935197592217239,
12.9123287025405));
#64754=CARTESIAN_POINT('Ctrl Pts',(-2.22325952109642,-0.83163127010402,
12.9054140620019));
#64755=CARTESIAN_POINT('Ctrl Pts',(-2.25522424853189,-0.740578601250993,
12.8995290600494));
#64756=CARTESIAN_POINT('Ctrl Pts',(-2.30909958737916,-0.550839106575901,
12.8872837562639));
#64757=CARTESIAN_POINT('Ctrl Pts',(-2.33042460006533,-0.452197111838367,
12.8809257199156));
#64758=CARTESIAN_POINT('Ctrl Pts',(-2.34921242200156,-0.327191553254358,
12.8727040766289));
#64759=CARTESIAN_POINT('Ctrl Pts',(-2.35260677218798,-0.30181883540353,
12.8710273276736));
#64760=CARTESIAN_POINT('Ctrl Pts',(-2.35743687358524,-0.26065435011963,
12.8682916945888));
#64761=CARTESIAN_POINT('Ctrl Pts',(-2.35912615581418,-0.244893984667378,
12.8672407140727));
#64762=CARTESIAN_POINT('Ctrl Pts',(-2.36207231405805,-0.214539039336571,
12.8652090077865));
#64763=CARTESIAN_POINT('Ctrl Pts',(-2.36335220466617,-0.199947384392037,
12.8642290455479));
#64764=CARTESIAN_POINT('Ctrl Pts',(-2.3659882613244,-0.166318504377655,
12.8619624894185));
#64765=CARTESIAN_POINT('Ctrl Pts',(-2.36724994513088,-0.147275110785489,
12.8606730324435));
#64766=CARTESIAN_POINT('Ctrl Pts',(-2.37061613006155,-0.0850996774214071,
12.8564425883442));
#64767=CARTESIAN_POINT('Ctrl Pts',(-2.37177243490227,-0.04192720419408,
12.8534728544509));
#64768=CARTESIAN_POINT('Ctrl Pts',(-2.37171944942813,0.0585716059263682,
12.846480727164));
#64769=CARTESIAN_POINT('Ctrl Pts',(-2.36961122643535,0.115818548722168,
12.8424376605832));
#64770=CARTESIAN_POINT('Ctrl Pts',(-2.36544098610933,0.17287858090038,12.8383513775307));
#64771=CARTESIAN_POINT('Ctrl Pts',(-2.3654410188404,0.172878133051282,12.6417724606485));
#64772=CARTESIAN_POINT('Ctrl Pts',(-2.36840946129808,0.132261801607106,
12.6443904191857));
#64773=CARTESIAN_POINT('Ctrl Pts',(-2.37033179351654,0.0915688979090119,
12.6469686252575));
#64774=CARTESIAN_POINT('Ctrl Pts',(-2.37155557740686,0.0344908708101321,
12.6505468214597));
#64775=CARTESIAN_POINT('Ctrl Pts',(-2.3717370196609,0.0181383935128824,
12.6515675627952));
#64776=CARTESIAN_POINT('Ctrl Pts',(-2.37187300748867,-0.162536444707336,
12.6628090630617));
#64777=CARTESIAN_POINT('Ctrl Pts',(-2.35492008404575,-0.326423957580101,
12.6727066142147));
#64778=CARTESIAN_POINT('Ctrl Pts',(-2.30585543483136,-0.560160392558652,
12.6876935499561));
#64779=CARTESIAN_POINT('Ctrl Pts',(-2.28712362018204,-0.632307563801859,
12.6924394762415));
#64780=CARTESIAN_POINT('Ctrl Pts',(-2.25778087046183,-0.726788042997782,
12.6988836597969));
#64781=CARTESIAN_POINT('Ctrl Pts',(-2.25017236855946,-0.750013038853927,
12.7004864050573));
#64782=CARTESIAN_POINT('Ctrl Pts',(-2.23704191239831,-0.788094269532373,
12.7031473477744));
#64783=CARTESIAN_POINT('Ctrl Pts',(-2.23172740660467,-0.803020459096754,
12.7041987703312));
#64784=CARTESIAN_POINT('Ctrl Pts',(-2.22103815400418,-0.832116106440198,
12.7062654487943));
#64785=CARTESIAN_POINT('Ctrl Pts',(-2.21567635457738,-0.84628953068378,
12.7072802373006));
#64786=CARTESIAN_POINT('Ctrl Pts',(-2.20259291891659,-0.879897608825033,
12.7097062041929));
#64787=CARTESIAN_POINT('Ctrl Pts',(-2.19474944749005,-0.899283149570606,
12.7111213568444));
#64788=CARTESIAN_POINT('Ctrl Pts',(-2.16666264788104,-0.96614421099116,
12.7160588191024));
#64789=CARTESIAN_POINT('Ctrl Pts',(-2.14512808256747,-1.01305798049471,
12.7196235633563));
#64790=CARTESIAN_POINT('Ctrl Pts',(-2.08749767102967,-1.12851596004621,
12.7286562824752));
#64791=CARTESIAN_POINT('Ctrl Pts',(-2.04954386228103,-1.19606138550838,
12.7341795082623));
#64792=CARTESIAN_POINT('Ctrl Pts',(-1.96183689698446,-1.33568055303906,
12.746082098946));
#64793=CARTESIAN_POINT('Ctrl Pts',(-1.91125660761959,-1.40710476898585,
12.752471505137));
#64794=CARTESIAN_POINT('Ctrl Pts',(-1.78721622481081,-1.56319655725212,
12.7669940221214));
#64795=CARTESIAN_POINT('Ctrl Pts',(-1.7114592033492,-1.6457940881261,12.7750993442954));
#64796=CARTESIAN_POINT('Ctrl Pts',(-1.61764470502298,-1.73456616440675,
12.7840622917513));
#64797=CARTESIAN_POINT('Ctrl Pts',(-1.60501689916595,-1.74625741692137,
12.7852480878166));
#64798=CARTESIAN_POINT('Ctrl Pts',(-1.58508290657565,-1.76431405467799,
12.7870864745226));
#64799=CARTESIAN_POINT('Ctrl Pts',(-1.57786335410403,-1.77077360165624,
12.7877455660819));
#64800=CARTESIAN_POINT('Ctrl Pts',(-1.56494787997788,-1.78218775075735,
12.7889124398645));
#64801=CARTESIAN_POINT('Ctrl Pts',(-1.5592677939541,-1.78715947665374,12.7894214436933));
#64802=CARTESIAN_POINT('Ctrl Pts',(-1.5454064951305,-1.79917574901716,12.7906536217159));
#64803=CARTESIAN_POINT('Ctrl Pts',(-1.53720078707583,-1.80619167377828,
12.791374739274));
#64804=CARTESIAN_POINT('Ctrl Pts',(-1.51114815912431,-1.82816065673567,
12.7936392074242));
#64805=CARTESIAN_POINT('Ctrl Pts',(-1.4931281998876,-1.84290760012197,12.7951688117805));
#64806=CARTESIAN_POINT('Ctrl Pts',(-1.44953110248083,-1.87752668962281,
12.7987909185952));
#64807=CARTESIAN_POINT('Ctrl Pts',(-1.42375790559918,-1.8971453610175,12.8008693700763));
#64808=CARTESIAN_POINT('Ctrl Pts',(-1.32140260834384,-1.97179748699354,
12.8089167159968));
#64809=CARTESIAN_POINT('Ctrl Pts',(-1.2419639118952,-2.0227748982854,12.8147228981608));
#64810=CARTESIAN_POINT('Ctrl Pts',(-1.01414552366624,-2.15047627957305,
12.8307687889671));
#64811=CARTESIAN_POINT('Ctrl Pts',(-0.860408968650429,-2.21646756000236,
12.8409696508369));
#64812=CARTESIAN_POINT('Ctrl Pts',(-0.671706066392747,-2.27485188619683,
12.8537113053155));
#64813=CARTESIAN_POINT('Ctrl Pts',(-0.64221188979384,-2.28335365108502,
12.8557074631192));
#64814=CARTESIAN_POINT('Ctrl Pts',(-0.594242234073739,-2.29617809277502,
12.8589660890472));
#64815=CARTESIAN_POINT('Ctrl Pts',(-0.575864770778239,-2.30085579685789,
12.8602173040168));
#64816=CARTESIAN_POINT('Ctrl Pts',(-0.542978031122819,-2.30880793966486,
12.8624623379565));
#64817=CARTESIAN_POINT('Ctrl Pts',(-0.528490169099001,-2.31216724496456,
12.8634534098897));
#64818=CARTESIAN_POINT('Ctrl Pts',(-0.497687503886618,-2.31900484282395,
12.8655653233746));
#64819=CARTESIAN_POINT('Ctrl Pts',(-0.481365746859044,-2.32244769714399,
12.8666872247679));
#64820=CARTESIAN_POINT('Ctrl Pts',(-0.437176345450544,-2.33128302714323,
12.8697329647625));
#64821=CARTESIAN_POINT('Ctrl Pts',(-0.409246743096404,-2.33634772517161,
12.8716669225954));
#64822=CARTESIAN_POINT('Ctrl Pts',(-0.223276815545454,-2.36663426442617,
12.8846085288236));
#64823=CARTESIAN_POINT('Ctrl Pts',(-0.0631498173451738,-2.3763007143207,
12.8961006065482));
#64824=CARTESIAN_POINT('Ctrl Pts',(0.242130365687578,-2.36384343476796,
12.9183545657598));
#64825=CARTESIAN_POINT('Ctrl Pts',(0.386715371032393,-2.34453423882222,
12.9290318715257));
#64826=CARTESIAN_POINT('Ctrl Pts',(0.549985073679765,-2.30720491429947,
12.9407217903089));
#64827=CARTESIAN_POINT('Ctrl Pts',(0.571275899405755,-2.30202563599738,
12.9422383520892));
#64828=CARTESIAN_POINT('Ctrl Pts',(0.602697180513232,-2.29391918585775,
12.9444619006601));
#64829=CARTESIAN_POINT('Ctrl Pts',(0.612884140030201,-2.29121848894177,
12.9451804961823));
#64830=CARTESIAN_POINT('Ctrl Pts',(0.6310922926893,-2.28626114029126,12.946460391651));
#64831=CARTESIAN_POINT('Ctrl Pts',(0.639119942504405,-2.28403003234786,
12.9470230626226));
#64832=CARTESIAN_POINT('Ctrl Pts',(0.656997706323036,-2.27895966413714,
12.9482725576811));
#64833=CARTESIAN_POINT('Ctrl Pts',(0.666841329599441,-2.27609880885453,
12.9489581551867));
#64834=CARTESIAN_POINT('Ctrl Pts',(0.696247748937998,-2.26734526328648,
12.9509999940704));
#64835=CARTESIAN_POINT('Ctrl Pts',(0.715753843541684,-2.26126335801083,
12.9523460453813));
#64836=CARTESIAN_POINT('Ctrl Pts',(0.865863382007861,-2.21232281913067,
12.9626573447264));
#64837=CARTESIAN_POINT('Ctrl Pts',(0.992614154654155,-2.15842973952103,
12.9710955722125));
#64838=CARTESIAN_POINT('Ctrl Pts',(1.25530444528176,-2.01867018343394,12.9893705191329));
#64839=CARTESIAN_POINT('Ctrl Pts',(1.38862444655848,-1.92938683600411,12.9991802526417));
#64840=CARTESIAN_POINT('Ctrl Pts',(1.53577984665586,-1.80763281003834,13.0114972490739));
#64841=CARTESIAN_POINT('Ctrl Pts',(1.55923830393702,-1.78743723948182,13.0135098550013));
#64842=CARTESIAN_POINT('Ctrl Pts',(1.59647583808682,-1.75408819568557,13.0167899692906));
#64843=CARTESIAN_POINT('Ctrl Pts',(1.61050387876314,-1.74121731027292,13.0180459741507));
#64844=CARTESIAN_POINT('Ctrl Pts',(1.63521757458232,-1.71798805738148,13.0202963009484));
#64845=CARTESIAN_POINT('Ctrl Pts',(1.64596366008834,-1.70769525798722,13.0212878253483));
#64846=CARTESIAN_POINT('Ctrl Pts',(1.66851829685136,-1.68568133432917,13.0233972083325));
#64847=CARTESIAN_POINT('Ctrl Pts',(1.68030173998804,-1.67393575332826,13.0245160940969));
#64848=CARTESIAN_POINT('Ctrl Pts',(1.71170811942719,-1.64196451739063,13.0275448010512));
#64849=CARTESIAN_POINT('Ctrl Pts',(1.73109524371255,-1.62151204195831,13.0294645479227));
#64850=CARTESIAN_POINT('Ctrl Pts',(1.86015380971549,-1.48040862044347,13.0425959401033));
#64851=CARTESIAN_POINT('Ctrl Pts',(1.95747589028711,-1.34909294981243,13.0543126512743));
#64852=CARTESIAN_POINT('Ctrl Pts',(2.11309377871672,-1.08641146176599,13.0765560869538));
#64853=CARTESIAN_POINT('Ctrl Pts',(2.17447308091316,-0.957668263108391,
13.0869887401408));
#64854=CARTESIAN_POINT('Ctrl Pts',(2.23168820749158,-0.803282596906085,
13.0984858734064));
#64855=CARTESIAN_POINT('Ctrl Pts',(2.23914137381111,-0.782266695243478,
13.1000297351353));
#64856=CARTESIAN_POINT('Ctrl Pts',(2.24970297438995,-0.751097331600258,
13.1022852408903));
#64857=CARTESIAN_POINT('Ctrl Pts',(2.25304115524079,-0.741023776973954,
13.1030089617295));
#64858=CARTESIAN_POINT('Ctrl Pts',(2.25888014592064,-0.722999314383953,
13.1042941687939));
#64859=CARTESIAN_POINT('Ctrl Pts',(2.26140678265523,-0.715057264809579,
13.1048570787688));
#64860=CARTESIAN_POINT('Ctrl Pts',(2.26692819258393,-0.697379645861272,
13.106102506855));
#64861=CARTESIAN_POINT('Ctrl Pts',(2.26990216980819,-0.687637949632474,
13.1067838461194));
#64862=CARTESIAN_POINT('Ctrl Pts',(2.2785589414793,-0.658613183684788,13.108799896842));
#64863=CARTESIAN_POINT('Ctrl Pts',(2.28405959854197,-0.639276145941719,
13.110124796041));
#64864=CARTESIAN_POINT('Ctrl Pts',(2.29628436772607,-0.594127483823742,
13.1131809513696));
#64865=CARTESIAN_POINT('Ctrl Pts',(2.30282038132163,-0.56826734930511,13.1149033706462));
#64866=CARTESIAN_POINT('Ctrl Pts',(2.32447708730503,-0.476061087632978,
13.1209632938333));
#64867=CARTESIAN_POINT('Ctrl Pts',(2.33717844807057,-0.409177286231348,
13.1252107660865));
#64868=CARTESIAN_POINT('Ctrl Pts',(2.37013013059669,-0.182936568363289,
13.1393510471256));
#64869=CARTESIAN_POINT('Ctrl Pts',(2.3770765442375,-0.0221045916504001,
13.1490583632207));
#64870=CARTESIAN_POINT('Ctrl Pts',(2.36402588730863,0.201494965036854,13.1631970952294));
#64871=CARTESIAN_POINT('Ctrl Pts',(2.35779463704632,0.2646167048838,13.1672561260194));
#64872=CARTESIAN_POINT('Ctrl Pts',(2.34583997113291,0.350387124139192,13.1729054396145));
#64873=CARTESIAN_POINT('Ctrl Pts',(2.34230042325414,0.373316182912867,13.1744287490258));
#64874=CARTESIAN_POINT('Ctrl Pts',(2.33608135038002,0.410022999767895,13.1768901275722));
#64875=CARTESIAN_POINT('Ctrl Pts',(2.33361484278695,0.423835684305044,13.17782152859));
#64876=CARTESIAN_POINT('Ctrl Pts',(2.32823957619533,0.452467215399191,13.1797633747636));
#64877=CARTESIAN_POINT('Ctrl Pts',(2.32531155966412,0.467281754083812,13.1807743839614));
#64878=CARTESIAN_POINT('Ctrl Pts',(2.31805498045391,0.502238584117538,13.1831752957166));
#64879=CARTESIAN_POINT('Ctrl Pts',(2.31360510513128,0.522354151211805,13.1845689546825));
#64880=CARTESIAN_POINT('Ctrl Pts',(2.29755555855379,0.590672933837754,13.1893448506171));
#64881=CARTESIAN_POINT('Ctrl Pts',(2.28470748160061,0.638566486290968,13.192765870189));
#64882=CARTESIAN_POINT('Ctrl Pts',(2.2492376553112,0.755953244806758,13.2013376824374));
#64883=CARTESIAN_POINT('Ctrl Pts',(2.22488816760373,0.824867460799703,13.2065365808122));
#64884=CARTESIAN_POINT('Ctrl Pts',(2.14306287386725,1.02631751120825,13.2221998015429));
#64885=CARTESIAN_POINT('Ctrl Pts',(2.07662676769961,1.15484423705883,13.2328341078078));
#64886=CARTESIAN_POINT('Ctrl Pts',(1.96406528930488,1.33110433832273,13.2478897109991));
#64887=CARTESIAN_POINT('Ctrl Pts',(1.92698902791874,1.38423483697416,13.2524929420564));
#64888=CARTESIAN_POINT('Ctrl Pts',(1.87809706872479,1.44851833535258,13.2580859192617));
#64889=CARTESIAN_POINT('Ctrl Pts',(1.86828405012235,1.46115321235797,13.2591863595671));
#64890=CARTESIAN_POINT('Ctrl Pts',(1.85254977401225,1.4809943772317,13.2609150112656));
#64891=CARTESIAN_POINT('Ctrl Pts',(1.84671277023413,1.48826642853051,13.2615487094573));
#64892=CARTESIAN_POINT('Ctrl Pts',(1.83547486344484,1.50209929579979,13.2627540619901));
#64893=CARTESIAN_POINT('Ctrl Pts',(1.83008141844705,1.50866572598866,13.263326174956));
#64894=CARTESIAN_POINT('Ctrl Pts',(1.81696413502696,1.52446194921286,13.2647026194063));
#64895=CARTESIAN_POINT('Ctrl Pts',(1.80920498867873,1.53366235746264,13.2655044785323));
#64896=CARTESIAN_POINT('Ctrl Pts',(1.78138661044474,1.56614306928139,13.2683375463508));
#64897=CARTESIAN_POINT('Ctrl Pts',(1.7609444287249,1.58909323255431,13.2703434364619));
#64898=CARTESIAN_POINT('Ctrl Pts',(1.70785313724778,1.64641498386317,13.2753837011017));
#64899=CARTESIAN_POINT('Ctrl Pts',(1.67460825682304,1.68021795200097,13.2783848442467));
#64900=CARTESIAN_POINT('Ctrl Pts',(1.47116415658264,1.87503582381759,13.2960214023276));
#64901=CARTESIAN_POINT('Ctrl Pts',(1.2788936983792,2.01109927157288,13.3099220162397));
#64902=CARTESIAN_POINT('Ctrl Pts',(1.04165564399438,2.13099634566499,13.3270544861575));
#64903=CARTESIAN_POINT('Ctrl Pts',(1.01323985779057,2.14465306033068,13.3291034543336));
#64904=CARTESIAN_POINT('Ctrl Pts',(0.967091970049809,2.16571002258847,13.3324310458546));
#64905=CARTESIAN_POINT('Ctrl Pts',(0.949526882590109,2.17346852843598,13.3336976037676));
#64906=CARTESIAN_POINT('Ctrl Pts',(0.918169143497226,2.18686658625315,13.3359596806725));
#64907=CARTESIAN_POINT('Ctrl Pts',(0.904413761317703,2.19259110948139,13.336952290945));
#64908=CARTESIAN_POINT('Ctrl Pts',(0.875269932601788,2.20439887413349,13.3390565046697));
#64909=CARTESIAN_POINT('Ctrl Pts',(0.859869988747321,2.21045140862487,13.3401690657902));
#64910=CARTESIAN_POINT('Ctrl Pts',(0.818475309363497,2.2262224440055,13.3431620356483));
#64911=CARTESIAN_POINT('Ctrl Pts',(0.792371894677743,2.23564640999891,13.3450519685062));
#64912=CARTESIAN_POINT('Ctrl Pts',(0.631775327267986,2.29045978657781,13.3566997173279));
#64913=CARTESIAN_POINT('Ctrl Pts',(0.49361882114513,2.32415017957269,13.3668320034302));
#64914=CARTESIAN_POINT('Ctrl Pts',(0.208149752466547,2.36715422716738,13.3878034996021));
#64915=CARTESIAN_POINT('Ctrl Pts',(0.0612764048750438,2.37549870898118,
13.3986086049959));
#64916=CARTESIAN_POINT('Ctrl Pts',(-0.119512532297057,2.36898246446797,
13.4113934682666));
#64917=CARTESIAN_POINT('Ctrl Pts',(-0.153566352071415,2.36701897447235,
13.4137778375838));
#64918=CARTESIAN_POINT('Ctrl Pts',(-0.200410867308527,2.36330267303301,
13.4170147551339));
#64919=CARTESIAN_POINT('Ctrl Pts',(-0.213245594425363,2.36217915814911,
13.4178971564725));
#64920=CARTESIAN_POINT('Ctrl Pts',(-0.233830949630623,2.36020802478089,
13.4193045783921));
#64921=CARTESIAN_POINT('Ctrl Pts',(-0.241587445752562,2.35942669810265,
13.4198330999844));
#64922=CARTESIAN_POINT('Ctrl Pts',(-0.258087931508426,2.35768234969891,
13.4209534185395));
#64923=CARTESIAN_POINT('Ctrl Pts',(-0.26683072612777,2.3567088941761,13.4215446152658));
#64924=CARTESIAN_POINT('Ctrl Pts',(-0.289050397931817,2.35410963862184,
13.4230414743531));
#64925=CARTESIAN_POINT('Ctrl Pts',(-0.302519331985634,2.3524167144305,13.4239435272546));
#64926=CARTESIAN_POINT('Ctrl Pts',(-0.358237426548172,2.34492697857831,
13.4276559171999));
#64927=CARTESIAN_POINT('Ctrl Pts',(-0.400343674750294,2.33810651117025,
13.4304155863227));
#64928=CARTESIAN_POINT('Ctrl Pts',(-0.518360279303401,2.31570782880167,
13.4380787316155));
#64929=CARTESIAN_POINT('Ctrl Pts',(-0.593726521661219,2.29754012201324,
13.4428889035842));
#64930=CARTESIAN_POINT('Ctrl Pts',(-0.855378932721612,2.22072782047201,
13.4596976516556));
#64931=CARTESIAN_POINT('Ctrl Pts',(-1.03516035886966,2.14283482619258,13.471515828387));
#64932=CARTESIAN_POINT('Ctrl Pts',(-1.22752141257753,2.02957513379975,13.4859544124786));
#64933=CARTESIAN_POINT('Ctrl Pts',(-1.25142523327983,2.01492402397062,13.4877815667973));
#64934=CARTESIAN_POINT('Ctrl Pts',(-1.29039613613172,1.99007702179657,13.4908187469689));
#64935=CARTESIAN_POINT('Ctrl Pts',(-1.30561600623997,1.98012513611661,13.4920199464396));
#64936=CARTESIAN_POINT('Ctrl Pts',(-1.33302014770862,1.96175295502885,13.494211107932));
#64937=CARTESIAN_POINT('Ctrl Pts',(-1.34524295406418,1.95339160141212,13.495198849232));
#64938=CARTESIAN_POINT('Ctrl Pts',(-1.36136779109533,1.94213783549373,13.4965161435903));
#64939=CARTESIAN_POINT('Ctrl Pts',(-1.36534058910176,1.93934698025914,13.4968418540968));
#64940=CARTESIAN_POINT('Ctrl Pts',(-1.37132372985496,1.93511638013127,13.4973341452362));
#64941=CARTESIAN_POINT('Ctrl Pts',(-1.37334045470343,1.93368564459462,13.4975003843192));
#64942=CARTESIAN_POINT('Ctrl Pts',(-1.377406463844,1.9307915053146,13.4978361613133));
#64943=CARTESIAN_POINT('Ctrl Pts',(-1.37945566204042,1.92932798663551,13.4980057034387));
#64944=CARTESIAN_POINT('Ctrl Pts',(-1.40023502014631,1.91443752907382,13.4997281243367));
#64945=CARTESIAN_POINT('Ctrl Pts',(-1.41877028355022,1.90074195578745,13.5012911726827));
#64946=CARTESIAN_POINT('Ctrl Pts',(-1.49107076552093,1.8456728620222,13.5074963261497));
#64947=CARTESIAN_POINT('Ctrl Pts',(-1.54324548457178,1.80227416217043,13.5122157864676));
#64948=CARTESIAN_POINT('Ctrl Pts',(-1.6820412019242,1.67637418663608,13.5254648155077));
#64949=CARTESIAN_POINT('Ctrl Pts',(-1.76438873548279,1.58947167111063,13.5341451307449));
#64950=CARTESIAN_POINT('Ctrl Pts',(-1.92000926340729,1.39817960703495,13.552124114471));
#64951=CARTESIAN_POINT('Ctrl Pts',(-1.99214913740489,1.29332489655779,13.5613985112742));
#64952=CARTESIAN_POINT('Ctrl Pts',(-2.06703141223117,1.16323227623332,13.571888920859));
#64953=CARTESIAN_POINT('Ctrl Pts',(-2.07822689018659,1.14311035222473,13.5734842405068));
#64954=CARTESIAN_POINT('Ctrl Pts',(-2.09421633577458,1.11336046291501,13.5757998058157));
#64955=CARTESIAN_POINT('Ctrl Pts',(-2.09924032387422,1.10385853040896,13.5765330327748));
#64956=CARTESIAN_POINT('Ctrl Pts',(-2.10804802681143,1.08692278727384,13.577828228231));
#64957=CARTESIAN_POINT('Ctrl Pts',(-2.11185732770483,1.07950278514011,13.5783917178547));
#64958=CARTESIAN_POINT('Ctrl Pts',(-2.12017987403082,1.06307892070894,13.5796302123124));
#64959=CARTESIAN_POINT('Ctrl Pts',(-2.1246749895009,1.05406626360807,13.5803041222944));
#64960=CARTESIAN_POINT('Ctrl Pts',(-2.13772093839215,1.02748671402799,13.5822756175935));
#64961=CARTESIAN_POINT('Ctrl Pts',(-2.14611252144664,1.00984199910224,13.5835640267986));
#64962=CARTESIAN_POINT('Ctrl Pts',(-2.16503301813163,0.968757068978621,
13.5865217774907));
#64963=CARTESIAN_POINT('Ctrl Pts',(-2.17540111867858,0.945245107796463,
13.5881830541251));
#64964=CARTESIAN_POINT('Ctrl Pts',(-2.21029677456371,0.862494367268822,
13.5939367358987));
#64965=CARTESIAN_POINT('Ctrl Pts',(-2.2328042368885,0.802430501282534,13.5979485190075));
#64966=CARTESIAN_POINT('Ctrl Pts',(-2.31350866745295,0.557239622330448,
13.613942060782));
#64967=CARTESIAN_POINT('Ctrl Pts',(-2.35130711032184,0.366268275802427,
13.6256063379384));
#64968=CARTESIAN_POINT('Ctrl Pts',(-2.3654410187889,0.172878133755955,13.6380106975316));
#64969=CARTESIAN_POINT('Origin',(0.,0.,-1.84858989190501));
#64970=CARTESIAN_POINT('',(-2.36929349484951,0.173162376944888,14.8369729823432));
#64971=CARTESIAN_POINT('',(-2.36544101854889,0.172878137039872,14.63965844111));
#64972=CARTESIAN_POINT('',(-2.36544101854889,0.172878137039864,-1.84858989190501));
#64973=CARTESIAN_POINT('',(-2.37103408855011,-0.00209831677342502,13.8485903224414));
#64974=CARTESIAN_POINT('Ctrl Pts',(-2.37103408855011,-0.00209831677342502,
13.8485903224414));
#64975=CARTESIAN_POINT('Ctrl Pts',(-2.37284029274397,-0.209416860088268,
13.8624956146275));
#64976=CARTESIAN_POINT('Ctrl Pts',(-2.25333046601257,-1.19988580892436,
13.9290658704801));
#64977=CARTESIAN_POINT('Ctrl Pts',(-0.869666078203209,-2.66015561356989,
14.0483010899995));
#64978=CARTESIAN_POINT('Ctrl Pts',(1.75267763866885,-2.18191305067097,14.2062959809995));
#64979=CARTESIAN_POINT('Ctrl Pts',(2.78512620401791,0.275629071355557,14.3642908719996));
#64980=CARTESIAN_POINT('Ctrl Pts',(1.29091271455523,2.48320730756548,14.5222857629997));
#64981=CARTESIAN_POINT('Ctrl Pts',(-1.36682061392716,2.43810610823687,14.6798464664475));
#64982=CARTESIAN_POINT('Ctrl Pts',(-2.3122698979759,0.94596955261334,14.7847422062287));
#64983=CARTESIAN_POINT('Ctrl Pts',(-2.36929349484953,0.173162376944586,
14.8369729823432));
#64984=CARTESIAN_POINT('Ctrl Pts',(-2.3717490991011,-0.00206722352871417,
13.8490012910668));
#64985=CARTESIAN_POINT('Ctrl Pts',(-2.37179998906972,0.0563194170761172,
13.8454099352406));
#64986=CARTESIAN_POINT('Ctrl Pts',(-2.36969484767437,0.114674253025937,
13.8418054807329));
#64987=CARTESIAN_POINT('Ctrl Pts',(-2.36544101497364,0.172878185958964,
13.8381597463488));
#64988=CARTESIAN_POINT('',(-2.37174998280982,0.000285554948450898,13.651410108095));
#64989=CARTESIAN_POINT('Ctrl Pts',(-2.3654410187889,0.172878133755955,13.6380106975316));
#64990=CARTESIAN_POINT('Ctrl Pts',(-2.36637511213128,0.160097207334322,
13.6388304870286));
#64991=CARTESIAN_POINT('Ctrl Pts',(-2.3672058393811,0.147305694585705,13.6396531778704));
#64992=CARTESIAN_POINT('Ctrl Pts',(-2.36952297024855,0.10651302519473,13.6422846450463));
#64993=CARTESIAN_POINT('Ctrl Pts',(-2.3706164545265,0.0784962032887724,
13.6441037981315));
#64994=CARTESIAN_POINT('Ctrl Pts',(-2.37156998763884,0.0336944680560588,
13.6470352721048));
#64995=CARTESIAN_POINT('Ctrl Pts',(-2.37174898697047,0.0169185798481951,
13.648137976221));
#64996=CARTESIAN_POINT('Ctrl Pts',(-2.37174999571231,0.000142613750890254,
13.6492461020341));
#64997=CARTESIAN_POINT('Ctrl Pts',(-2.37174998280982,0.000285554948450898,
13.651410108095));
#64998=CARTESIAN_POINT('Ctrl Pts',(-2.37175993590189,-0.082382408167183,
13.6569281379447));
#64999=CARTESIAN_POINT('Ctrl Pts',(-2.36744344666263,-0.164985957670592,
13.6624461677945));
#65000=CARTESIAN_POINT('Ctrl Pts',(-2.35884659186433,-0.247064401624429,
13.6679641976442));
#65001=CARTESIAN_POINT('Ctrl Pts',(-2.35023020288839,-0.329329348077393,
13.6734947658208));
#65002=CARTESIAN_POINT('Ctrl Pts',(-2.33731405720822,-0.411066390836204,
13.6790253339974));
#65003=CARTESIAN_POINT('Ctrl Pts',(-2.32019591278182,-0.491822110941082,
13.6845559021739));
#65004=CARTESIAN_POINT('Ctrl Pts',(-2.30305844536776,-0.572668988226546,
13.6900927132644));
#65005=CARTESIAN_POINT('Ctrl Pts',(-2.28170963114255,-0.652531933827544,
13.6956295243548));
#65006=CARTESIAN_POINT('Ctrl Pts',(-2.25629726319919,-0.730972449945869,
13.7011663354452));
#65007=CARTESIAN_POINT('Ctrl Pts',(-2.23081935718109,-0.809615262852067,
13.7067174258794));
#65008=CARTESIAN_POINT('Ctrl Pts',(-2.20125709223112,-0.886827922498776,
13.7122685163137));
#65009=CARTESIAN_POINT('Ctrl Pts',(-2.16780691071137,-0.962190864835064,
13.7178196067479));
#65010=CARTESIAN_POINT('Ctrl Pts',(-2.13547394943128,-1.0350367205466,13.7231852933875));
#65011=CARTESIAN_POINT('Ctrl Pts',(-2.0995088878053,-1.10615419575088,13.7285509800271));
#65012=CARTESIAN_POINT('Ctrl Pts',(-2.06012841898357,-1.17518890387727,
13.7339166666667));
#65013=CARTESIAN_POINT('Ctrl Pts',(-2.02096290085725,-1.24384679936117,
13.7392530657404));
#65014=CARTESIAN_POINT('Ctrl Pts',(-1.97828872257431,-1.31067205434257,
13.7445894648141));
#65015=CARTESIAN_POINT('Ctrl Pts',(-1.93230231440578,-1.37528390823207,
13.7499258638878));
#65016=CARTESIAN_POINT('Ctrl Pts',(-1.88638153493216,-1.43980355244885,
13.7552546472133));
#65017=CARTESIAN_POINT('Ctrl Pts',(-1.83715818247681,-1.50211569089093,
13.7605834305388));
#65018=CARTESIAN_POINT('Ctrl Pts',(-1.7848738524587,-1.56186535697199,13.7659122138643));
#65019=CARTESIAN_POINT('Ctrl Pts',(-1.73264933883228,-1.62154666587168,
13.7712349007438));
#65020=CARTESIAN_POINT('Ctrl Pts',(-1.6773711137276,-1.67867097815146,13.7765575876234));
#65021=CARTESIAN_POINT('Ctrl Pts',(-1.61932231096069,-1.73291468795349,
13.781880274503));
#65022=CARTESIAN_POINT('Ctrl Pts',(-1.56130975717306,-1.78712452489304,
13.7871996375936));
#65023=CARTESIAN_POINT('Ctrl Pts',(-1.50053040095659,-1.83845701136883,
13.7925190006843));
#65024=CARTESIAN_POINT('Ctrl Pts',(-1.43730482004822,-1.88662474190448,
13.7978383637749));
#65025=CARTESIAN_POINT('Ctrl Pts',(-1.37409911990853,-1.93477732648979,
13.8031560542352));
#65026=CARTESIAN_POINT('Ctrl Pts',(-1.30844909455567,-1.97976684805962,
13.8084737446955));
#65027=CARTESIAN_POINT('Ctrl Pts',(-1.24070789877305,-2.02134657404963,
13.8137914351558));
#65028=CARTESIAN_POINT('Ctrl Pts',(-1.17296700344431,-2.06292611562025,
13.8191091020304));
#65029=CARTESIAN_POINT('Ctrl Pts',(-1.10313535565988,-2.10109564821282,
13.8244267689051));
#65030=CARTESIAN_POINT('Ctrl Pts',(-1.03159327904617,-2.13565291401173,
13.8297444357797));
#65031=CARTESIAN_POINT('Ctrl Pts',(-0.959980502109187,-2.17024433048082,
13.8350673577543));
#65032=CARTESIAN_POINT('Ctrl Pts',(-0.886654342325077,-2.20121614581692,
13.8403902797289));
#65033=CARTESIAN_POINT('Ctrl Pts',(-0.812017264618513,-2.22841334237198,
13.8457132017036));
#65034=CARTESIAN_POINT('Ctrl Pts',(-0.73734389526598,-2.25562376333318,
13.8510387119039));
#65035=CARTESIAN_POINT('Ctrl Pts',(-0.661358785788709,-2.27905577112385,
13.8563642221041));
#65036=CARTESIAN_POINT('Ctrl Pts',(-0.584479384209729,-2.29860434001457,
13.8616897323044));
#65037=CARTESIAN_POINT('Ctrl Pts',(-0.50746364867594,-2.31818757532638,
13.8670246864891));
#65038=CARTESIAN_POINT('Ctrl Pts',(-0.429550912080691,-2.33387351945313,
13.8723596406738));
#65039=CARTESIAN_POINT('Ctrl Pts',(-0.35116838442565,-2.34560841324375,
13.8776945948584));
#65040=CARTESIAN_POINT('Ctrl Pts',(-0.282197128288541,-2.35593431608957,
13.8823889891649));
#65041=CARTESIAN_POINT('Ctrl Pts',(-0.212862435259374,-2.36320177056976,
13.8870833834713));
#65042=CARTESIAN_POINT('Ctrl Pts',(-0.143455852460942,-2.3674075443182,
13.8917777777778));
#65043=CARTESIAN_POINT('Ctrl Pts',(-0.064560343655558,-2.37218831073004,
13.8971139665427));
#65044=CARTESIAN_POINT('Ctrl Pts',(0.0147208745263364,-2.37302977826968,
13.9024501553077));
#65045=CARTESIAN_POINT('Ctrl Pts',(0.0939616444336405,-2.36988802939618,
13.9077863440726));
#65046=CARTESIAN_POINT('Ctrl Pts',(0.173089315342885,-2.36675076468721,
13.9131149165864));
#65047=CARTESIAN_POINT('Ctrl Pts',(0.252176188878941,-2.35964159268616,
13.9184434891002));
#65048=CARTESIAN_POINT('Ctrl Pts',(0.330792984760269,-2.34856851374053,
13.923772061614));
#65049=CARTESIAN_POINT('Ctrl Pts',(0.40931983826296,-2.33750810306824,13.929094537918));
#65050=CARTESIAN_POINT('Ctrl Pts',(0.487377221848571,-2.32249286279898,
13.9344170142219));
#65051=CARTESIAN_POINT('Ctrl Pts',(0.564539376960543,-2.30358272140616,
13.9397394905259));
#65052=CARTESIAN_POINT('Ctrl Pts',(0.64165334927425,-2.28468438817923,13.945058643286));
#65053=CARTESIAN_POINT('Ctrl Pts',(0.717872749447858,-2.2618960926493,13.9503777960462));
#65054=CARTESIAN_POINT('Ctrl Pts',(0.792781632525433,-2.23532891218056,
13.9556969488063));
#65055=CARTESIAN_POINT('Ctrl Pts',(0.867666967735637,-2.2087700831972,13.9610144294723));
#65056=CARTESIAN_POINT('Ctrl Pts',(0.941242163291927,-2.17843488466003,
13.9663319101384));
#65057=CARTESIAN_POINT('Ctrl Pts',(1.01310749493875,-2.14448391605042,13.9716493908044));
#65058=CARTESIAN_POINT('Ctrl Pts',(1.08497251901454,-2.110533092745,13.9769668487125));
#65059=CARTESIAN_POINT('Ctrl Pts',(1.15512727130074,-2.07296673136787,13.9822843066206));
#65060=CARTESIAN_POINT('Ctrl Pts',(1.22319439008194,-2.03199250652459,13.9876017645288));
#65061=CARTESIAN_POINT('Ctrl Pts',(1.29132881283307,-1.99097776684762,13.992924480277));
#65062=CARTESIAN_POINT('Ctrl Pts',(1.35737107712532,-1.94654867490852,13.9982471960253));
#65063=CARTESIAN_POINT('Ctrl Pts',(1.42097124946717,-1.89895728511405,14.0035699117735));
#65064=CARTESIAN_POINT('Ctrl Pts',(1.48460236219264,-1.85134274293172,14.0088952169309));
#65065=CARTESIAN_POINT('Ctrl Pts',(1.54578865572984,-1.80056313736407,14.0142205220882));
#65066=CARTESIAN_POINT('Ctrl Pts',(1.60421384537677,-1.74691041579168,14.0195458272456));
#65067=CARTESIAN_POINT('Ctrl Pts',(1.66274269488672,-1.69316250182365,14.0248805807318));
#65068=CARTESIAN_POINT('Ctrl Pts',(1.71850032353031,-1.63653162096747,14.030215334218));
#65069=CARTESIAN_POINT('Ctrl Pts',(1.77120801884488,-1.57734594064828,14.0355500877042));
#65070=CARTESIAN_POINT('Ctrl Pts',(1.81760742868406,-1.52524385913339,14.0402463547658));
#65071=CARTESIAN_POINT('Ctrl Pts',(1.86164374629265,-1.47116260311739,14.0449426218273));
#65072=CARTESIAN_POINT('Ctrl Pts',(1.90315456387766,-1.41534475252203,14.0496388888889));
#65073=CARTESIAN_POINT('Ctrl Pts',(1.95032416329439,-1.35191777598767,14.0549753541511));
#65074=CARTESIAN_POINT('Ctrl Pts',(1.99440705959551,-1.28601247874764,14.0603118194133));
#65075=CARTESIAN_POINT('Ctrl Pts',(2.03513332155307,-1.21796158642397,14.0656482846755));
#65076=CARTESIAN_POINT('Ctrl Pts',(2.07580145221783,-1.15000782764891,14.0709771328472));
#65077=CARTESIAN_POINT('Ctrl Pts',(2.11312222544839,-1.07991495422045,14.0763059810188));
#65078=CARTESIAN_POINT('Ctrl Pts',(2.14686746081374,-1.00804670933403,14.0816348291905));
#65079=CARTESIAN_POINT('Ctrl Pts',(2.18057407555734,-0.936260715949818,
14.0869575786218));
#65080=CARTESIAN_POINT('Ctrl Pts',(2.21071308696344,-0.862703810504251,
14.0922803280531));
#65081=CARTESIAN_POINT('Ctrl Pts',(2.23710170881016,-0.787765197846848,
14.0976030774844));
#65082=CARTESIAN_POINT('Ctrl Pts',(2.26347384522741,-0.712873400639668,
14.1029225017018));
#65083=CARTESIAN_POINT('Ctrl Pts',(2.28610008780648,-0.636602049795984,
14.1082419259193));
#65084=CARTESIAN_POINT('Ctrl Pts',(2.30484583411056,-0.559360119675312,
14.1135613501368));
#65085=CARTESIAN_POINT('Ctrl Pts',(2.32358568075857,-0.482142499113462,
14.1188791002265));
#65086=CARTESIAN_POINT('Ctrl Pts',(2.33844734622214,-0.403955360241968,
14.1241968503162));
#65087=CARTESIAN_POINT('Ctrl Pts',(2.34934655535866,-0.32522119445757,14.129514600406));
#65088=CARTESIAN_POINT('Ctrl Pts',(2.36024571293403,-0.246487401142772,
14.1348323253389));
#65089=CARTESIAN_POINT('Ctrl Pts',(2.36718238878815,-0.167207049704571,
14.1401500502719));
#65090=CARTESIAN_POINT('Ctrl Pts',(2.37012394706579,-0.0878096694291725,
14.1454677752048));
#65091=CARTESIAN_POINT('Ctrl Pts',(2.37306841069168,-0.0083338691404468,
14.1507907524025));
#65092=CARTESIAN_POINT('Ctrl Pts',(2.37200985761628,0.0712587222624321,
14.1561137296001));
#65093=CARTESIAN_POINT('Ctrl Pts',(2.36696780673544,0.150537252459319,14.1614367067978));
#65094=CARTESIAN_POINT('Ctrl Pts',(2.36192330561845,0.22985430886828,14.1667622707506));
#65095=CARTESIAN_POINT('Ctrl Pts',(2.35289150344097,0.308856534625879,14.1720878347035));
#65096=CARTESIAN_POINT('Ctrl Pts',(2.33994372181595,0.387119414695437,14.1774133986563));
#65097=CARTESIAN_POINT('Ctrl Pts',(2.32697298694027,0.465521035713479,14.1827484035318));
#65098=CARTESIAN_POINT('Ctrl Pts',(2.31007250191994,0.54318023410877,14.1880834084072));
#65099=CARTESIAN_POINT('Ctrl Pts',(2.28936446340997,0.619684126128467,14.1934184132827));
#65100=CARTESIAN_POINT('Ctrl Pts',(2.27114504613167,0.686994042103818,14.1981122755218));
#65101=CARTESIAN_POINT('Ctrl Pts',(2.24997907262273,0.753409670215016,14.2028061377609));
#65102=CARTESIAN_POINT('Ctrl Pts',(2.22598053518453,0.818662762973606,14.2075));
#65103=CARTESIAN_POINT('Ctrl Pts',(2.1986955606952,0.892851824530099,14.2128366548599));
#65104=CARTESIAN_POINT('Ctrl Pts',(2.16764701274257,0.96581289382715,14.2181733097198));
#65105=CARTESIAN_POINT('Ctrl Pts',(2.13296575399468,1.03713796323628,14.2235099645797));
#65106=CARTESIAN_POINT('Ctrl Pts',(2.09833397300293,1.10836127727327,14.2288390059412));
#65107=CARTESIAN_POINT('Ctrl Pts',(2.06007997676588,1.17795280942164,14.2341680473027));
#65108=CARTESIAN_POINT('Ctrl Pts',(2.01838343264649,1.24552253344456,14.2394970886642));
#65109=CARTESIAN_POINT('Ctrl Pts',(1.97673457284241,1.31301498449215,14.2448200357152));
#65110=CARTESIAN_POINT('Ctrl Pts',(1.93165123356707,1.3784898262756,14.2501429827661));
#65111=CARTESIAN_POINT('Ctrl Pts',(1.88335922953472,1.44158110247964,14.2554659298171));
#65112=CARTESIAN_POINT('Ctrl Pts',(1.8350973696749,1.5046329967124,14.260785554251));
#65113=CARTESIAN_POINT('Ctrl Pts',(1.78363110438294,1.5653039081915,14.266105178685));
#65114=CARTESIAN_POINT('Ctrl Pts',(1.72922915705936,1.62325739945203,14.2714248031189));
#65115=CARTESIAN_POINT('Ctrl Pts',(1.67484430700169,1.68119267727906,14.2767427557187));
#65116=CARTESIAN_POINT('Ctrl Pts',(1.61752592712794,1.73641189007495,14.2820607083185));
#65117=CARTESIAN_POINT('Ctrl Pts',(1.55758158864451,1.78861333362346,14.2873786609183));
#65118=CARTESIAN_POINT('Ctrl Pts',(1.49763751126917,1.84081454979072,14.292696590354));
#65119=CARTESIAN_POINT('Ctrl Pts',(1.4350678518109,1.88999771675696,14.2980145197896));
#65120=CARTESIAN_POINT('Ctrl Pts',(1.37021432386846,1.93590050600895,14.3033324492252));
#65121=CARTESIAN_POINT('Ctrl Pts',(1.30529672305414,1.9818486455083,14.3086556325772));
#65122=CARTESIAN_POINT('Ctrl Pts',(1.23809112950543,2.02450966293762,14.3139788159292));
#65123=CARTESIAN_POINT('Ctrl Pts',(1.16896889790373,2.06366416314131,14.3193019992812));
#65124=CARTESIAN_POINT('Ctrl Pts',(1.09981306102228,2.10283769915886,14.3246277706148));
#65125=CARTESIAN_POINT('Ctrl Pts',(1.02873914840437,2.13850111171075,14.3299535419485));
#65126=CARTESIAN_POINT('Ctrl Pts',(0.956141551439548,2.17048183501055,14.3352793132821));
#65127=CARTESIAN_POINT('Ctrl Pts',(0.883415266843213,2.20251924783877,14.340614525161));
#65128=CARTESIAN_POINT('Ctrl Pts',(0.809160339463884,2.23086076116328,14.3459497370398));
#65129=CARTESIAN_POINT('Ctrl Pts',(0.733789258690845,2.25538275827628,14.3512849489187));
#65130=CARTESIAN_POINT('Ctrl Pts',(0.667504133771765,2.2769486377254,14.3559770029829));
#65131=CARTESIAN_POINT('Ctrl Pts',(0.600356174241293,2.29556108606254,14.360669057047));
#65132=CARTESIAN_POINT('Ctrl Pts',(0.532631938092542,2.31116881274904,14.3653611111112));
#65133=CARTESIAN_POINT('Ctrl Pts',(0.455623932109421,2.32891607692514,14.37069636106));
#65134=CARTESIAN_POINT('Ctrl Pts',(0.377584696267147,2.3428433025856,14.3760316110088));
#65135=CARTESIAN_POINT('Ctrl Pts',(0.298927131925522,2.35283672028018,14.3813668609576));
#65136=CARTESIAN_POINT('Ctrl Pts',(0.220381878725929,2.36281586888107,14.3866944929739));
#65137=CARTESIAN_POINT('Ctrl Pts',(0.141220510988674,2.36887230598976,14.3920221249902));
#65138=CARTESIAN_POINT('Ctrl Pts',(0.0618675983092391,2.37094294802288,
14.3973497570065));
#65139=CARTESIAN_POINT('Ctrl Pts',(-0.0173945417789801,2.37301122142786,
14.4026712946912));
#65140=CARTESIAN_POINT('Ctrl Pts',(-0.0968473257635621,2.37110274848552,
14.407992832376));
#65141=CARTESIAN_POINT('Ctrl Pts',(-0.17606106878112,2.36520624101994,14.4133143700607));
#65142=CARTESIAN_POINT('Ctrl Pts',(-0.255225362854192,2.35931341443167,
14.4186325857913));
#65143=CARTESIAN_POINT('Ctrl Pts',(-0.334150446549355,2.34943752959353,
14.4239508015218));
#65144=CARTESIAN_POINT('Ctrl Pts',(-0.41240785669708,2.33561936587161,14.4292690172524));
#65145=CARTESIAN_POINT('Ctrl Pts',(-0.49064070436756,2.32180553922566,14.4345855637666));
#65146=CARTESIAN_POINT('Ctrl Pts',(-0.568205834015373,2.30405197229394,
14.4399021102808));
#65147=CARTESIAN_POINT('Ctrl Pts',(-0.644682594492096,2.28245096658372,
14.4452186567949));
#65148=CARTESIAN_POINT('Ctrl Pts',(-0.721159087558693,2.26085003640399,
14.4505351847192));
#65149=CARTESIAN_POINT('Ctrl Pts',(-0.79654676896273,2.23540182288431,14.4558517126434));
#65150=CARTESIAN_POINT('Ctrl Pts',(-0.870439263776206,2.20624875083857,
14.4611682405676));
#65151=CARTESIAN_POINT('Ctrl Pts',(-0.944405015211498,2.17706677659404,
14.4664900392691));
#65152=CARTESIAN_POINT('Ctrl Pts',(-1.01687218280534,2.1441727795042,14.4718118379705));
#65153=CARTESIAN_POINT('Ctrl Pts',(-1.08745411003328,2.10775748630428,14.4771336366719));
#65154=CARTESIAN_POINT('Ctrl Pts',(-1.15807045526469,2.07132443584358,14.4824580304524));
#65155=CARTESIAN_POINT('Ctrl Pts',(-1.22679932362353,2.031366904202,14.487782424233));
#65156=CARTESIAN_POINT('Ctrl Pts',(-1.29328065728895,1.9881205204872,14.4931068180135));
#65157=CARTESIAN_POINT('Ctrl Pts',(-1.35988021411545,1.94479723211501,14.4984406801159));
#65158=CARTESIAN_POINT('Ctrl Pts',(-1.42422387078254,1.89817368150386,14.5037745422183));
#65159=CARTESIAN_POINT('Ctrl Pts',(-1.48598264397024,1.84852742590399,14.5091084043207));
#65160=CARTESIAN_POINT('Ctrl Pts',(-1.54045549821504,1.8047381291692,14.5138130102879));
#65161=CARTESIAN_POINT('Ctrl Pts',(-1.59291773557545,1.75859800492949,14.5185176162551));
#65162=CARTESIAN_POINT('Ctrl Pts',(-1.64316804155503,1.71032068622005,14.5232222222222));
#65163=CARTESIAN_POINT('Ctrl Pts',(-1.69933498648107,1.65635903467842,14.5284807642173));
#65164=CARTESIAN_POINT('Ctrl Pts',(-1.75295966586774,1.59951330178753,14.5337393062124));
#65165=CARTESIAN_POINT('Ctrl Pts',(-1.80372544079536,1.54005603687904,14.5389978482074));
#65166=CARTESIAN_POINT('Ctrl Pts',(-1.8544254792806,1.48067576299599,14.544249580933));
#65167=CARTESIAN_POINT('Ctrl Pts',(-1.9022736438561,1.41869102593679,14.5495013136585));
#65168=CARTESIAN_POINT('Ctrl Pts',(-1.94698872974409,1.35441239980646,14.5547530463841));
#65169=CARTESIAN_POINT('Ctrl Pts',(-1.99166074834241,1.29019568356976,14.5599997209086));
#65170=CARTESIAN_POINT('Ctrl Pts',(-2.03320540028179,1.22368985496531,14.5652463954331));
#65171=CARTESIAN_POINT('Ctrl Pts',(-2.07138162539946,1.15523860066113,14.5704930699576));
#65172=CARTESIAN_POINT('Ctrl Pts',(-2.1095337380326,1.08683058085187,14.5757364306301));
#65173=CARTESIAN_POINT('Ctrl Pts',(-2.1443214124326,1.01647999482645,14.5809797913026));
#65174=CARTESIAN_POINT('Ctrl Pts',(-2.17554774381685,0.944558138429518,
14.5862231519752));
#65175=CARTESIAN_POINT('Ctrl Pts',(-2.20677350765612,0.872637589227062,
14.5914664173486));
#65176=CARTESIAN_POINT('Ctrl Pts',(-2.23443785121702,0.799146263057828,
14.596709682722));
#65177=CARTESIAN_POINT('Ctrl Pts',(-2.25839114180805,0.724477406896129,
14.6019529480953));
#65178=CARTESIAN_POINT('Ctrl Pts',(-2.28234418143799,0.649809333047704,
14.6071961585345));
#65179=CARTESIAN_POINT('Ctrl Pts',(-2.30258610691287,0.573964216339154,
14.6124393689737));
#65180=CARTESIAN_POINT('Ctrl Pts',(-2.31901714769678,0.497350511398446,
14.6176825794128));
#65181=CARTESIAN_POINT('Ctrl Pts',(-2.33546048118088,0.42067948876752,14.6229297125015));
#65182=CARTESIAN_POINT('Ctrl Pts',(-2.34808715120127,0.343239205000396,
14.6281768455901));
#65183=CARTESIAN_POINT('Ctrl Pts',(-2.3568487095738,0.265447212606071,14.6334239786788));
#65184=CARTESIAN_POINT('Ctrl Pts',(-2.3603187699915,0.234637292481815,14.6355021328225));
#65185=CARTESIAN_POINT('Ctrl Pts',(-2.36318312355598,0.203772254267595,
14.6375802869662));
#65186=CARTESIAN_POINT('Ctrl Pts',(-2.36544101854889,0.172878137039876,
14.63965844111));
#65187=CARTESIAN_POINT('Origin',(0.,0.,0.));
#65188=CARTESIAN_POINT('',(-2.94490570994055,0.00214417779480537,0.322176117089595));
#65189=CARTESIAN_POINT('',(1.29086451147292,2.64866566268225,6.84448539295995E-5));
#65190=CARTESIAN_POINT('Ctrl Pts',(-2.94490570994055,0.00214417779480537,
0.322176117089595));
#65191=CARTESIAN_POINT('Ctrl Pts',(-2.94584715833611,0.124808428590093,
0.315520895872749));
#65192=CARTESIAN_POINT('Ctrl Pts',(-2.88343765101094,1.21631589477965,0.256245304285532));
#65193=CARTESIAN_POINT('Ctrl Pts',(-1.5758107673324,3.04168494025884,0.148876080206978));
#65194=CARTESIAN_POINT('Ctrl Pts',(0.492178778194427,3.03189561568121,0.0481620773452684));
#65195=CARTESIAN_POINT('Ctrl Pts',(1.29086451147292,2.64866566268226,6.84448539295995E-5));
#65196=CARTESIAN_POINT('',(-1.28892185405328,2.64462557919715,0.));
#65197=CARTESIAN_POINT('Origin',(0.,0.,0.));
#65198=CARTESIAN_POINT('',(-2.94214443421968,0.0031336297816172,0.177823882910391));
#65199=CARTESIAN_POINT('Ctrl Pts',(-1.28892185405328,2.64462557919715,2.08166817117217E-15));
#65200=CARTESIAN_POINT('Ctrl Pts',(-2.16403831185616,2.21811653527939,0.0526649636666859));
#65201=CARTESIAN_POINT('Ctrl Pts',(-2.88384118710636,1.2152373497456,0.111939591303482));
#65202=CARTESIAN_POINT('Ctrl Pts',(-2.94548559297357,0.124877349165528,
0.171214218940278));
#65203=CARTESIAN_POINT('Ctrl Pts',(-2.94453111094736,0.00313617179185542,
0.177823882910391));
#65204=CARTESIAN_POINT('',(-2.94199991145336,0.000721809122472048,1.17782388287515));
#65205=CARTESIAN_POINT('Ctrl Pts',(-2.9419983312945,0.00313347416978786,
0.177823882910391));
#65206=CARTESIAN_POINT('Ctrl Pts',(-2.94209506616752,-0.0876902631826912,
0.182759245863396));
#65207=CARTESIAN_POINT('Ctrl Pts',(-2.93798190413056,-0.178703263263171,
0.1876946088164));
#65208=CARTESIAN_POINT('Ctrl Pts',(-2.92963295760384,-0.269471211303483,
0.192629971769405));
#65209=CARTESIAN_POINT('Ctrl Pts',(-2.92093784854289,-0.364002563842836,
0.197769963862351));
#65210=CARTESIAN_POINT('Ctrl Pts',(-2.90764798017833,-0.458267605499484,
0.202909955955296));
#65211=CARTESIAN_POINT('Ctrl Pts',(-2.88979424712816,-0.551772787717021,
0.208049948048242));
#65212=CARTESIAN_POINT('Ctrl Pts',(-2.87268923544769,-0.641356698797145,
0.212974387354032));
#65213=CARTESIAN_POINT('Ctrl Pts',(-2.85139553236819,-0.730242684954411,
0.217898826659821));
#65214=CARTESIAN_POINT('Ctrl Pts',(-2.82599323800431,-0.818001356205424,
0.22282326596561));
#65215=CARTESIAN_POINT('Ctrl Pts',(-2.80060282204545,-0.905718990492374,
0.227745402546939));
#65216=CARTESIAN_POINT('Ctrl Pts',(-2.77110775565445,-0.99230990960784,
0.232667539128269));
#65217=CARTESIAN_POINT('Ctrl Pts',(-2.73763880875135,-1.07735683634462,
0.237589675709598));
#65218=CARTESIAN_POINT('Ctrl Pts',(-2.70417526134609,-1.16239004258105,
0.242511018209598));
#65219=CARTESIAN_POINT('Ctrl Pts',(-2.66673927712545,-1.24587931828404,
0.247432360709598));
#65220=CARTESIAN_POINT('Ctrl Pts',(-2.62551038526634,-1.32742578581953,
0.252353703209598));
#65221=CARTESIAN_POINT('Ctrl Pts',(-2.58427551695018,-1.40898407416658,
0.257275759097486));
#65222=CARTESIAN_POINT('Ctrl Pts',(-2.53924686203539,-1.48859858140532,
0.262197814985374));
#65223=CARTESIAN_POINT('Ctrl Pts',(-2.49065000028613,-1.56589481641479,
0.267119870873263));
#65224=CARTESIAN_POINT('Ctrl Pts',(-2.44200245894562,-1.64327166036595,
0.272047059762985));
#65225=CARTESIAN_POINT('Ctrl Pts',(-2.38977953656764,-1.71832501562463,
0.276974248652708));
#65226=CARTESIAN_POINT('Ctrl Pts',(-2.33424989136487,-1.79070976002899,
0.281901437542431));
#65227=CARTESIAN_POINT('Ctrl Pts',(-2.27868603773292,-1.86313909626162,
0.286831661772854));
#65228=CARTESIAN_POINT('Ctrl Pts',(-2.21981171243828,-1.93289619995114,
0.291761886003278));
#65229=CARTESIAN_POINT('Ctrl Pts',(-2.15793396856311,-1.99967121980626,
0.296692110233701));
#65230=CARTESIAN_POINT('Ctrl Pts',(-2.09596038024424,-2.06654966965463,
0.301629971048285));
#65231=CARTESIAN_POINT('Ctrl Pts',(-2.03097442847363,-2.13043650193002,
0.306567831862868));
#65232=CARTESIAN_POINT('Ctrl Pts',(-1.96331739471672,-2.19106111452939,
0.311505692677451));
#65233=CARTESIAN_POINT('Ctrl Pts',(-1.94283752876775,-2.2094122580883,0.313000389118337));
#65234=CARTESIAN_POINT('Ctrl Pts',(-1.92211312278979,-2.22746478869269,
0.314495085559222));
#65235=CARTESIAN_POINT('Ctrl Pts',(-1.90115415235717,-2.24521199198986,
0.315989782000107));
#65236=CARTESIAN_POINT('Ctrl Pts',(-1.83014985636319,-2.30533554052147,
0.321053478656916));
#65237=CARTESIAN_POINT('Ctrl Pts',(-1.75616783242176,-2.36219158712132,
0.326117175313725));
#65238=CARTESIAN_POINT('Ctrl Pts',(-1.67954076700263,-2.41547237864071,
0.331180871970533));
#65239=CARTESIAN_POINT('Ctrl Pts',(-1.60301781255998,-2.46868077909042,
0.33623768872922));
#65240=CARTESIAN_POINT('Ctrl Pts',(-1.52385731868644,-2.51832332827906,
0.341294505487906));
#65241=CARTESIAN_POINT('Ctrl Pts',(-1.44242576961557,-2.56413180221863,
0.346351322246593));
#65242=CARTESIAN_POINT('Ctrl Pts',(-1.36108003456659,-2.60989200236958,
0.351402810041394));
#65243=CARTESIAN_POINT('Ctrl Pts',(-1.27746838515045,-2.65182594377412,
0.356454297836196));
#65244=CARTESIAN_POINT('Ctrl Pts',(-1.19198618132318,-2.68970870979268,
0.361505785630998));
#65245=CARTESIAN_POINT('Ctrl Pts',(-1.1065648040585,-2.72756451957549,0.366553678939173));
#65246=CARTESIAN_POINT('Ctrl Pts',(-1.01927592131206,-2.76137470613425,
0.371601572247347));
#65247=CARTESIAN_POINT('Ctrl Pts',(-0.930538472228052,-2.79096079365216,
0.376649465555521));
#65248=CARTESIAN_POINT('Ctrl Pts',(-0.841832764178936,-2.82053629834347,
0.381695553252206));
#65249=CARTESIAN_POINT('Ctrl Pts',(-0.751679938120826,-2.84589056656832,
0.38674164094889));
#65250=CARTESIAN_POINT('Ctrl Pts',(-0.660516895174555,-2.86689403905847,
0.391787728645575));
#65251=CARTESIAN_POINT('Ctrl Pts',(-0.569361295671956,-2.88789579661941,
0.396833404330239));
#65252=CARTESIAN_POINT('Ctrl Pts',(-0.477196073958768,-2.90454736594484,
0.401879080014903));
#65253=CARTESIAN_POINT('Ctrl Pts',(-0.384470115660988,-2.91676991381967,
0.406924755699566));
#65254=CARTESIAN_POINT('Ctrl Pts',(-0.291726132427484,-2.92899483762724,
0.411971412209682));
#65255=CARTESIAN_POINT('Ctrl Pts',(-0.198421634210417,-2.9367889726155,
0.417018068719797));
#65256=CARTESIAN_POINT('Ctrl Pts',(-0.105011336595889,-2.94012527270291,
0.422064725229913));
#65257=CARTESIAN_POINT('Ctrl Pts',(-0.0115016090678875,-2.94346512409074,
0.427116753616929));
#65258=CARTESIAN_POINT('Ctrl Pts',(0.0821137004248008,-2.94233765336725,
0.432168782003946));
#65259=CARTESIAN_POINT('Ctrl Pts',(0.175379475041113,-2.93676795810195,
0.437220810390963));
#65260=CARTESIAN_POINT('Ctrl Pts',(0.268701937369612,-2.93119487752963,
0.44227590944278));
#65261=CARTESIAN_POINT('Ctrl Pts',(0.361674002795658,-2.921174243566,0.447331008494597));
#65262=CARTESIAN_POINT('Ctrl Pts',(0.453847390536592,-2.90678285155653,
0.452386107546414));
#65263=CARTESIAN_POINT('Ctrl Pts',(0.546163258905372,-2.89236921348864,
0.45744902071578));
#65264=CARTESIAN_POINT('Ctrl Pts',(0.637677552843819,-2.87357141900821,
0.462511933885146));
#65265=CARTESIAN_POINT('Ctrl Pts',(0.727954087509513,-2.85051694372761,
0.467574847054513));
#65266=CARTESIAN_POINT('Ctrl Pts',(0.766051842354462,-2.84078768517142,
0.469711455703062));
#65267=CARTESIAN_POINT('Ctrl Pts',(0.803929369709169,-2.83030093979513,
0.471848064351611));
#65268=CARTESIAN_POINT('Ctrl Pts',(0.841554919396199,-2.81906887422781,
0.47398467300016));
#65269=CARTESIAN_POINT('Ctrl Pts',(0.930740388511047,-2.79244502301282,
0.479049168966884));
#65270=CARTESIAN_POINT('Ctrl Pts',(1.01881225662041,-2.76153967205838,0.484113664933607));
#65271=CARTESIAN_POINT('Ctrl Pts',(1.10533098686978,-2.72646426887745,0.48917816090033));
#65272=CARTESIAN_POINT('Ctrl Pts',(1.1917348781136,-2.69143542237171,0.494235934603807));
#65273=CARTESIAN_POINT('Ctrl Pts',(1.27658932259279,-2.65224768894435,0.499293708307284));
#65274=CARTESIAN_POINT('Ctrl Pts',(1.35946954869609,-2.60906238832421,0.504351482010761));
#65275=CARTESIAN_POINT('Ctrl Pts',(1.44661135021264,-2.56365656510189,0.509669318760322));
#65276=CARTESIAN_POINT('Ctrl Pts',(1.5315700051311,-2.51383121810154,0.514987155509882));
#65277=CARTESIAN_POINT('Ctrl Pts',(1.61387501033182,-2.45983158997247,0.520304992259443));
#65278=CARTESIAN_POINT('Ctrl Pts',(1.6920209146595,-2.40856071327166,0.525354103924619));
#65279=CARTESIAN_POINT('Ctrl Pts',(1.76777439658345,-2.35352740947702,0.530403215589796));
#65280=CARTESIAN_POINT('Ctrl Pts',(1.84075891398426,-2.29498815260286,0.535452327254972));
#65281=CARTESIAN_POINT('Ctrl Pts',(1.91372043576901,-2.23646734000049,0.540499848069961));
#65282=CARTESIAN_POINT('Ctrl Pts',(1.98391438227733,-2.17444304540529,0.545547368884949));
#65283=CARTESIAN_POINT('Ctrl Pts',(2.0509957297191,-2.10921324589858,0.550594889699937));
#65284=CARTESIAN_POINT('Ctrl Pts',(2.11807443805565,-2.04398601265374,0.55564221193605));
#65285=CARTESIAN_POINT('Ctrl Pts',(2.18204047452283,-1.97555383358849,0.560689534172162));
#65286=CARTESIAN_POINT('Ctrl Pts',(2.24258507684834,-1.90425212960289,0.565736856408275));
#65287=CARTESIAN_POINT('Ctrl Pts',(2.30314399100082,-1.83293357097441,0.570785371754917));
#65288=CARTESIAN_POINT('Ctrl Pts',(2.36027957882199,-1.75874447683552,0.575833887101558));
#65289=CARTESIAN_POINT('Ctrl Pts',(2.41372354800039,-1.68205310077548,0.5808824024482));
#65290=CARTESIAN_POINT('Ctrl Pts',(2.46722692088939,-1.6052764811907,0.585936529289444));
#65291=CARTESIAN_POINT('Ctrl Pts',(2.51703023276193,-1.52599239144779,0.590990656130688));
#65292=CARTESIAN_POINT('Ctrl Pts',(2.56290888110394,-1.44459754504794,0.596044782971933));
#65293=CARTESIAN_POINT('Ctrl Pts',(2.6088170703451,-1.36315028914965,0.601102164125514));
#65294=CARTESIAN_POINT('Ctrl Pts',(2.65079536683394,-1.27958996498174,0.606159545279095));
#65295=CARTESIAN_POINT('Ctrl Pts',(2.68866638945535,-1.1943353993804,0.611216926432676));
#65296=CARTESIAN_POINT('Ctrl Pts',(2.72659657450263,-1.10894764838904,0.616282208269072));
#65297=CARTESIAN_POINT('Ctrl Pts',(2.76040651923683,-1.02186078404611,0.621347490105469));
#65298=CARTESIAN_POINT('Ctrl Pts',(2.78996804485245,-0.933510743752968,
0.626412771941866));
#65299=CARTESIAN_POINT('Ctrl Pts',(2.80079750912478,-0.901144903868558,
0.628268369294649));
#65300=CARTESIAN_POINT('Ctrl Pts',(2.81105731798492,-0.868609657173925,
0.630123966647432));
#65301=CARTESIAN_POINT('Ctrl Pts',(2.82074288781733,-0.835926767622583,
0.631979564000215));
#65302=CARTESIAN_POINT('Ctrl Pts',(2.84709806122688,-0.746994135205994,
0.637028785765904));
#65303=CARTESIAN_POINT('Ctrl Pts',(2.86929096570047,-0.656653017668738,
0.642078007531594));
#65304=CARTESIAN_POINT('Ctrl Pts',(2.88717285259965,-0.565329036236088,
0.647127229297283));
#65305=CARTESIAN_POINT('Ctrl Pts',(2.9050300056007,-0.474131372460271,0.652169467071996));
#65306=CARTESIAN_POINT('Ctrl Pts',(2.91858790503137,-0.381953978906644,
0.657211704846709));
#65307=CARTESIAN_POINT('Ctrl Pts',(2.92774751912123,-0.289237729695639,
0.662253942621422));
#65308=CARTESIAN_POINT('Ctrl Pts',(2.93689730321423,-0.196620982541043,
0.667290769122148));
#65309=CARTESIAN_POINT('Ctrl Pts',(2.94165814031151,-0.1034669694437,0.672327595622874));
#65310=CARTESIAN_POINT('Ctrl Pts',(2.94198222867482,-0.0102257597046888,
0.6773644221236));
#65311=CARTESIAN_POINT('Ctrl Pts',(2.94230608195311,0.0829478153600106,
0.68239759504539));
#65312=CARTESIAN_POINT('Ctrl Pts',(2.93819958177322,0.176208017789602,0.687430767967179));
#65313=CARTESIAN_POINT('Ctrl Pts',(2.92966691956076,0.269101728778078,0.692463940888968));
#65314=CARTESIAN_POINT('Ctrl Pts',(2.92113736977366,0.361961555296011,0.697495277880232));
#65315=CARTESIAN_POINT('Ctrl Pts',(2.90818490597114,0.454454713415537,0.702526614871497));
#65316=CARTESIAN_POINT('Ctrl Pts',(2.89086573545834,0.54613121093095,0.707557951862761));
#65317=CARTESIAN_POINT('Ctrl Pts',(2.87354802183069,0.63779999663782,0.712588865618969));
#65318=CARTESIAN_POINT('Ctrl Pts',(2.85186441463844,0.728651821261133,0.717619779375176));
#65319=CARTESIAN_POINT('Ctrl Pts',(2.82592239528182,0.81824606069609,0.722650693131384));
#65320=CARTESIAN_POINT('Ctrl Pts',(2.79997527770826,0.907857907506256,0.727682595580467));
#65321=CARTESIAN_POINT('Ctrl Pts',(2.76976821013846,0.996211251182744,0.73271449802955));
#65322=CARTESIAN_POINT('Ctrl Pts',(2.73545843967439,1.08288093750613,0.737746400478632));
#65323=CARTESIAN_POINT('Ctrl Pts',(2.70111134687185,1.16964490354413,0.742783776656154));
#65324=CARTESIAN_POINT('Ctrl Pts',(2.66265280727058,1.25472114242027,0.747821152833675));
#65325=CARTESIAN_POINT('Ctrl Pts',(2.62028797139766,1.33770510462834,0.752858529011197));
#65326=CARTESIAN_POINT('Ctrl Pts',(2.57789699387572,1.42074027292682,0.757899013552468));
#65327=CARTESIAN_POINT('Ctrl Pts',(2.53159514237759,1.50168020867647,0.762939498093739));
#65328=CARTESIAN_POINT('Ctrl Pts',(2.48163212106294,1.58014746644376,0.76797998263501));
#65329=CARTESIAN_POINT('Ctrl Pts',(2.43158969263946,1.6587394336044,0.773028478107047));
#65330=CARTESIAN_POINT('Ctrl Pts',(2.37787473550395,1.73485051541562,0.778076973579084));
#65331=CARTESIAN_POINT('Ctrl Pts',(2.32077845266215,1.80813477751496,0.78312546905112));
#65332=CARTESIAN_POINT('Ctrl Pts',(2.29495877093069,1.84127487401779,0.785408464367503));
#65333=CARTESIAN_POINT('Ctrl Pts',(2.26844813894097,1.8738373779853,0.787691459683886));
#65334=CARTESIAN_POINT('Ctrl Pts',(2.24127592913026,1.90579280340264,0.789974455000268));
#65335=CARTESIAN_POINT('Ctrl Pts',(2.18108158057603,1.97658336586221,0.795031953701307));
#65336=CARTESIAN_POINT('Ctrl Pts',(2.11742442598073,2.04464353376129,0.800089452402345));
#65337=CARTESIAN_POINT('Ctrl Pts',(2.05058155168944,2.10961591287867,0.805146951103383));
#65338=CARTESIAN_POINT('Ctrl Pts',(1.9838296674296,2.17449984818088,0.810197565271541));
#65339=CARTESIAN_POINT('Ctrl Pts',(1.91390099653275,2.23630404141466,0.815248179439699));
#65340=CARTESIAN_POINT('Ctrl Pts',(1.84111245454658,2.29470454083167,0.820298793607857));
#65341=CARTESIAN_POINT('Ctrl Pts',(1.76840064344793,2.35304347668345,0.825344083612388));
#65342=CARTESIAN_POINT('Ctrl Pts',(1.69283529787275,2.40798557511709,0.83038937361692));
#65343=CARTESIAN_POINT('Ctrl Pts',(1.61476891579968,2.45924487364864,0.835434663621452));
#65344=CARTESIAN_POINT('Ctrl Pts',(1.53675761127843,2.51046800761618,0.840476394062772));
#65345=CARTESIAN_POINT('Ctrl Pts',(1.45624914716212,2.55801326391338,0.845518124504092));
#65346=CARTESIAN_POINT('Ctrl Pts',(1.37362688380007,2.60163663567795,0.850559854945412));
#65347=CARTESIAN_POINT('Ctrl Pts',(1.29103380369538,2.6452445991006,0.855599804582007));
#65348=CARTESIAN_POINT('Ctrl Pts',(1.20632879924938,2.68493322351417,0.860639754218602));
#65349=CARTESIAN_POINT('Ctrl Pts',(1.11992093775121,2.72050383076121,0.865679703855197));
#65350=CARTESIAN_POINT('Ctrl Pts',(1.0335195704517,2.75607176461043,0.870719274701789));
#65351=CARTESIAN_POINT('Ctrl Pts',(0.945416010489703,2.78752212828983,0.875758845548382));
#65352=CARTESIAN_POINT('Ctrl Pts',(0.856039414196785,2.81470433995147,0.880798416394974));
#65353=CARTESIAN_POINT('Ctrl Pts',(0.76664468403887,2.84189206668726,0.885839009734044));
#65354=CARTESIAN_POINT('Ctrl Pts',(0.67597682860988,2.8648097929073,0.890879603073113));
#65355=CARTESIAN_POINT('Ctrl Pts',(0.584479177086341,2.88335708706925,0.895920196412183));
#65356=CARTESIAN_POINT('Ctrl Pts',(0.492882185301544,2.90192451828408,0.90096626239291));
#65357=CARTESIAN_POINT('Ctrl Pts',(0.400454034134328,2.91611195822221,0.906012328373636));
#65358=CARTESIAN_POINT('Ctrl Pts',(0.307646922816162,2.92587036125693,0.911058394354362));
#65359=CARTESIAN_POINT('Ctrl Pts',(0.214782423521637,2.93563479847367,0.916107580607998));
#65360=CARTESIAN_POINT('Ctrl Pts',(0.121538939593842,2.94096472095991,0.921156766861633));
#65361=CARTESIAN_POINT('Ctrl Pts',(0.0283702941602265,2.94186320661061,
0.926205953115268));
#65362=CARTESIAN_POINT('Ctrl Pts',(-0.0649449852879284,2.94276310634818,
0.931263086060058));
#65363=CARTESIAN_POINT('Ctrl Pts',(-0.15818474898884,2.93921766386027,0.936320219004848));
#65364=CARTESIAN_POINT('Ctrl Pts',(-0.250898903538924,2.93128192779251,
0.941377351949637));
#65365=CARTESIAN_POINT('Ctrl Pts',(-0.291183333595817,2.92783383935204,
0.943574683299865));
#65366=CARTESIAN_POINT('Ctrl Pts',(-0.331368647522973,2.92355755823557,
0.945772014650093));
#65367=CARTESIAN_POINT('Ctrl Pts',(-0.371418589105699,2.91846059278976,
0.947969346000321));
#65368=CARTESIAN_POINT('Ctrl Pts',(-0.463589604632388,2.90673042633558,
0.953026288757175));
#65369=CARTESIAN_POINT('Ctrl Pts',(-0.555366086263561,2.89060897992472,
0.958083231514028));
#65370=CARTESIAN_POINT('Ctrl Pts',(-0.646297382647046,2.87013304450919,
0.963140174270881));
#65371=CARTESIAN_POINT('Ctrl Pts',(-0.737105123568885,2.84968493134797,
0.968190245764245));
#65372=CARTESIAN_POINT('Ctrl Pts',(-0.827069532619359,2.82489418394959,
0.973240317257609));
#65373=CARTESIAN_POINT('Ctrl Pts',(-0.915746207164976,2.79584922412904,
0.978290388750974));
#65374=CARTESIAN_POINT('Ctrl Pts',(-1.00432963801989,2.76683480513857,0.983335150084628));
#65375=CARTESIAN_POINT('Ctrl Pts',(-1.09162760686539,2.73357520298744,0.988379911418283));
#65376=CARTESIAN_POINT('Ctrl Pts',(-1.17720808957269,2.69620939725471,0.993424672751938));
#65377=CARTESIAN_POINT('Ctrl Pts',(-1.26272858078861,2.65886978476537,0.998465897733069));
#65378=CARTESIAN_POINT('Ctrl Pts',(-1.34653357386059,2.61742986709688,1.0035071227142));
#65379=CARTESIAN_POINT('Ctrl Pts',(-1.42820932323039,2.5720773956158,1.00854834769533));
#65380=CARTESIAN_POINT('Ctrl Pts',(-1.50985645895331,2.52674081256691,1.0135878065729));
#65381=CARTESIAN_POINT('Ctrl Pts',(-1.58937544583396,2.47749461396421,1.01862726545048));
#65382=CARTESIAN_POINT('Ctrl Pts',(-1.66637646224517,2.42457284610615,1.02366672432805));
#65383=CARTESIAN_POINT('Ctrl Pts',(-1.74337192617543,2.37165489439392,1.02870581981432));
#65384=CARTESIAN_POINT('Ctrl Pts',(-1.81784941553468,2.31506215176441,1.0337449153006));
#65385=CARTESIAN_POINT('Ctrl Pts',(-1.88944842091631,2.25507176486623,1.03878401078687));
#65386=CARTESIAN_POINT('Ctrl Pts',(-1.9610621834845,2.19506901342014,1.04382414487517));
#65387=CARTESIAN_POINT('Ctrl Pts',(-2.02979594425108,2.13166751179191,1.04886427896348));
#65388=CARTESIAN_POINT('Ctrl Pts',(-2.0953234593135,2.06518367242493,1.05390441305178));
#65389=CARTESIAN_POINT('Ctrl Pts',(-2.16092247946098,1.99862728441049,1.05895004704674));
#65390=CARTESIAN_POINT('Ctrl Pts',(-2.22330795890934,1.92898216128935,1.06399568104171));
#65391=CARTESIAN_POINT('Ctrl Pts',(-2.28219185000088,1.8566002153909,1.06904131503668));
#65392=CARTESIAN_POINT('Ctrl Pts',(-2.34111233073465,1.78417329234413,1.0740900843194));
#65393=CARTESIAN_POINT('Ctrl Pts',(-2.39652662849536,1.70900651726631,1.07913885360212));
#65394=CARTESIAN_POINT('Ctrl Pts',(-2.4481894708365,1.63148163179525,1.08418762288484));
#65395=CARTESIAN_POINT('Ctrl Pts',(-2.49993390695292,1.55383430729844,1.0892443659477));
#65396=CARTESIAN_POINT('Ctrl Pts',(-2.5479148330536,1.47382181766616,1.09430110901056));
#65397=CARTESIAN_POINT('Ctrl Pts',(-2.59193254713781,1.39185116700302,1.09935785207342));
#65398=CARTESIAN_POINT('Ctrl Pts',(-2.61110153655979,1.35615429886334,1.1015599803824));
#65399=CARTESIAN_POINT('Ctrl Pts',(-2.62951953427345,1.32008633759295,1.10376210869139));
#65400=CARTESIAN_POINT('Ctrl Pts',(-2.64717293912874,1.28368198177917,1.10596423700037));
#65401=CARTESIAN_POINT('Ctrl Pts',(-2.69070471588802,1.19391197404748,1.11139449585003));
#65402=CARTESIAN_POINT('Ctrl Pts',(-2.72971984887089,1.10181517866251,1.11682475469968));
#65403=CARTESIAN_POINT('Ctrl Pts',(-2.76398258188106,1.00785132190125,1.12225501354934));
#65404=CARTESIAN_POINT('Ctrl Pts',(-2.79813144968367,0.914199734860317,
1.12766722604084));
#65405=CARTESIAN_POINT('Ctrl Pts',(-2.82755928144001,0.818693772995606,
1.13307943853235));
#65406=CARTESIAN_POINT('Ctrl Pts',(-2.85207809395669,0.721813373367632,
1.13849165102385));
#65407=CARTESIAN_POINT('Ctrl Pts',(-2.87654556343054,0.625135843862536,
1.14389253019904));
#65408=CARTESIAN_POINT('Ctrl Pts',(-2.89612440031345,0.527089935859038,
1.14929340937424));
#65409=CARTESIAN_POINT('Ctrl Pts',(-2.91067553749488,0.428172763529981,
1.15469428854943));
#65410=CARTESIAN_POINT('Ctrl Pts',(-2.92518344663001,0.32954945112759,1.16007912296798));
#65411=CARTESIAN_POINT('Ctrl Pts',(-2.93469337094891,0.230060368059112,
1.16546395738653));
#65412=CARTESIAN_POINT('Ctrl Pts',(-2.93911694740661,0.130213553316331,
1.17084879180507));
#65413=CARTESIAN_POINT('Ctrl Pts',(-2.94102693177194,0.0871023158572045,
1.17317382216177));
#65414=CARTESIAN_POINT('Ctrl Pts',(-2.94198931181531,0.043924552416158,
1.17549885251846));
#65415=CARTESIAN_POINT('Ctrl Pts',(-2.94199991145336,0.000721809122473715,
1.17782388287515));
#65416=CARTESIAN_POINT('',(-2.9419988608317,-0.00258898917603258,2.17782388285735));
#65417=CARTESIAN_POINT('Ctrl Pts',(-2.94199991145352,0.000721808467689169,
1.17782388291039));
#65418=CARTESIAN_POINT('Ctrl Pts',(-2.94202355561543,-0.0956488013929025,
1.18301023396904));
#65419=CARTESIAN_POINT('Ctrl Pts',(-2.93730766573634,-0.191968159835166,
1.18819658502768));
#65420=CARTESIAN_POINT('Ctrl Pts',(-2.92789344151773,-0.287756833311465,
1.19338293608633));
#65421=CARTESIAN_POINT('Ctrl Pts',(-2.91847121359393,-0.383626943588707,
1.19857369643287));
#65422=CARTESIAN_POINT('Ctrl Pts',(-2.90434273592682,-0.478965067538306,
1.20376445677941));
#65423=CARTESIAN_POINT('Ctrl Pts',(-2.88560073246625,-0.573299583804366,
1.20895521712596));
#65424=CARTESIAN_POINT('Ctrl Pts',(-2.86682343567474,-0.667811742727869,
1.21415575226648));
#65425=CARTESIAN_POINT('Ctrl Pts',(-2.84341533879536,-0.761316120895031,
1.21935628740701));
#65426=CARTESIAN_POINT('Ctrl Pts',(-2.81551983296595,-0.8533534262985,1.22455682254754));
#65427=CARTESIAN_POINT('Ctrl Pts',(-2.78759562729326,-0.945485422805862,
1.22976270817514));
#65428=CARTESIAN_POINT('Ctrl Pts',(-2.75517494659144,-1.03614695707487,
1.23496859380275));
#65429=CARTESIAN_POINT('Ctrl Pts',(-2.71844963260622,-1.12489803759412,
1.24017447943036));
#65430=CARTESIAN_POINT('Ctrl Pts',(-2.68164772762766,-1.21383420934008,
1.24539122198219));
#65431=CARTESIAN_POINT('Ctrl Pts',(-2.64052342543697,-1.300851600445,1.25060796453403));
#65432=CARTESIAN_POINT('Ctrl Pts',(-2.59531509453087,-1.38553367339095,
1.25582470708587));
#65433=CARTESIAN_POINT('Ctrl Pts',(-2.57181744321684,-1.42954834464183,
1.25853618072406));
#65434=CARTESIAN_POINT('Ctrl Pts',(-2.54721719901399,-1.47293258280772,
1.26124765436224));
#65435=CARTESIAN_POINT('Ctrl Pts',(-2.52155234293504,-1.5156311496663,1.26395912800042));
#65436=CARTESIAN_POINT('Ctrl Pts',(-2.47369344260184,-1.5952539010805,1.26901538649674));
#65437=CARTESIAN_POINT('Ctrl Pts',(-2.42197520912676,-1.67274780387845,
1.27407164499306));
#65438=CARTESIAN_POINT('Ctrl Pts',(-2.36661265200757,-1.7477152386352,1.27912790348937));
#65439=CARTESIAN_POINT('Ctrl Pts',(-2.31132553580172,-1.82258051749376,
1.28417727197231));
#65440=CARTESIAN_POINT('Ctrl Pts',(-2.25240422582496,-1.89492581618144,
1.28922664045525));
#65441=CARTESIAN_POINT('Ctrl Pts',(-2.19010848152011,-1.96438001394172,
1.2942760089382));
#65442=CARTESIAN_POINT('Ctrl Pts',(-2.12787846816781,-2.0337609275535,1.29932004961257));
#65443=CARTESIAN_POINT('Ctrl Pts',(-2.0622813924961,-2.1002564756025,1.30436409028694));
#65444=CARTESIAN_POINT('Ctrl Pts',(-1.99361831361261,-2.16352721721461,
1.30940813096132));
#65445=CARTESIAN_POINT('Ctrl Pts',(-1.92500369041134,-2.2267533085285,1.31444861204536));
#65446=CARTESIAN_POINT('Ctrl Pts',(-1.85332769000155,-2.28675881734355,
1.3194890931294));
#65447=CARTESIAN_POINT('Ctrl Pts',(-1.77892865897807,-2.34324066759402,
1.32452957421344));
#65448=CARTESIAN_POINT('Ctrl Pts',(-1.70455590533159,-2.39970256872887,
1.329568275024));
#65449=CARTESIAN_POINT('Ctrl Pts',(-1.62746238469865,-2.45264301605041,
1.33460697583456));
#65450=CARTESIAN_POINT('Ctrl Pts',(-1.54801919157099,-2.50179946888793,
1.33964567664512));
#65451=CARTESIAN_POINT('Ctrl Pts',(-1.46858193675127,-2.55095224732436,
1.34468400081729));
#65452=CARTESIAN_POINT('Ctrl Pts',(-1.38679573589047,-2.59632136063284,
1.34972232498945));
#65453=CARTESIAN_POINT('Ctrl Pts',(-1.30305933650958,-2.63768845118889,
1.35476064916162));
#65454=CARTESIAN_POINT('Ctrl Pts',(-1.21930588068801,-2.67906396789331,
1.35979999960047));
#65455=CARTESIAN_POINT('Ctrl Pts',(-1.13360183506648,-2.71643564679005,
1.36483935003932));
#65456=CARTESIAN_POINT('Ctrl Pts',(-1.0463680943448,-2.74963230471589,1.36987870047817));
#65457=CARTESIAN_POINT('Ctrl Pts',(-0.959039389308916,-2.78286510115681,
1.37492353685004));
#65458=CARTESIAN_POINT('Ctrl Pts',(-0.870178080357952,-2.81191364693698,
1.37996837322192));
#65459=CARTESIAN_POINT('Ctrl Pts',(-0.780222177114766,-2.83665601621668,
1.38501320959379));
#65460=CARTESIAN_POINT('Ctrl Pts',(-0.690210530607099,-2.8614137176801,
1.39006117211567));
#65461=CARTESIAN_POINT('Ctrl Pts',(-0.599103371688591,-2.88185983316448,
1.39510913463755));
#65462=CARTESIAN_POINT('Ctrl Pts',(-0.507348789825996,-2.89792360241986,
1.40015709715944));
#65463=CARTESIAN_POINT('Ctrl Pts',(-0.415449388810102,-2.91401272562939,
1.40521302703994));
#65464=CARTESIAN_POINT('Ctrl Pts',(-0.322900964278842,-2.92570564006765,
1.41026895692043));
#65465=CARTESIAN_POINT('Ctrl Pts',(-0.230156378281364,-2.9329834710643,
1.41532488680093));
#65466=CARTESIAN_POINT('Ctrl Pts',(-0.189622052852163,-2.93616427096614,
1.41753459753412));
#65467=CARTESIAN_POINT('Ctrl Pts',(-0.149050251605291,-2.93850239437844,
1.4197443082673));
#65468=CARTESIAN_POINT('Ctrl Pts',(-0.108478607732732,-2.93999938633741,
1.42195401900049));
#65469=CARTESIAN_POINT('Ctrl Pts',(-0.0156461043132878,-2.94342467301267,
1.42701008672697));
#65470=CARTESIAN_POINT('Ctrl Pts',(0.0775123415620981,-2.94245481385698,
1.43206615445345));
#65471=CARTESIAN_POINT('Ctrl Pts',(0.170546264212455,-2.93705259942058,
1.43712222217993));
#65472=CARTESIAN_POINT('Ctrl Pts',(0.263453411334196,-2.9316577464774,1.44217140010062));
#65473=CARTESIAN_POINT('Ctrl Pts',(0.356235933449431,-2.92184256643932,
1.44722057802131));
#65474=CARTESIAN_POINT('Ctrl Pts',(0.448441103364991,-2.90762180773442,
1.45226975594201));
#65475=CARTESIAN_POINT('Ctrl Pts',(0.540548988733222,-2.89341605317815,
1.45731360653681));
#65476=CARTESIAN_POINT('Ctrl Pts',(0.632080296767727,-2.87481402687157,
1.46235745713162));
#65477=CARTESIAN_POINT('Ctrl Pts',(0.722586263894362,-2.85188237682258,
1.46740130772643));
#65478=CARTESIAN_POINT('Ctrl Pts',(0.813028386037383,-2.82896690328512,
1.47244160027342));
#65479=CARTESIAN_POINT('Ctrl Pts',(0.902446176311072,-2.80172798555608,
1.47748189282042));
#65480=CARTESIAN_POINT('Ctrl Pts',(0.990400951093039,-2.77028337107849,
1.48252218536741));
#65481=CARTESIAN_POINT('Ctrl Pts',(1.078324677722,-2.73884985659182,1.4875606986844));
#65482=CARTESIAN_POINT('Ctrl Pts',(1.16478599774774,-2.70321374407966,1.49259921200139));
#65483=CARTESIAN_POINT('Ctrl Pts',(1.24936228166699,-2.66354235730312,1.49763772531838));
#65484=CARTESIAN_POINT('Ctrl Pts',(1.33393226499431,-2.62387392588484,1.50267586328645));
#65485=CARTESIAN_POINT('Ctrl Pts',(1.4166170900887,-2.58017100652061,1.50771400125453));
#65486=CARTESIAN_POINT('Ctrl Pts',(1.4970160209526,-2.53264822527947,1.5127521392226));
#65487=CARTESIAN_POINT('Ctrl Pts',(1.57743135356895,-2.48511574917193,1.51779130499404));
#65488=CARTESIAN_POINT('Ctrl Pts',(1.65555948426003,-2.4337620894399,1.52283047076549));
#65489=CARTESIAN_POINT('Ctrl Pts',(1.73102708483011,-2.37884619754716,1.52786963653693));
#65490=CARTESIAN_POINT('Ctrl Pts',(1.8065768956395,-2.32387048331238,1.53291429169747));
#65491=CARTESIAN_POINT('Ctrl Pts',(1.87946003242905,-2.26532505280048,1.53795894685801));
#65492=CARTESIAN_POINT('Ctrl Pts',(1.94933506901085,-2.2035101063359,1.54300360201855));
#65493=CARTESIAN_POINT('Ctrl Pts',(2.01925343069665,-2.14165683232095,1.54805138505165));
#65494=CARTESIAN_POINT('Ctrl Pts',(2.08615966147826,-2.07653031548178,1.55309916808475));
#65495=CARTESIAN_POINT('Ctrl Pts',(2.14974968016417,-2.00846715498015,1.55814695111785));
#65496=CARTESIAN_POINT('Ctrl Pts',(2.21344012346541,-1.94029650564847,1.56320270586852));
#65497=CARTESIAN_POINT('Ctrl Pts',(2.27380361401271,-1.86918029259692,1.56825846061919));
#65498=CARTESIAN_POINT('Ctrl Pts',(2.33057691842516,-1.79548746230763,1.57331421536986));
#65499=CARTESIAN_POINT('Ctrl Pts',(2.35541155779665,-1.7632516274652,1.57552578024675));
#65500=CARTESIAN_POINT('Ctrl Pts',(2.37955978458651,-1.73052312151934,1.57773734512364));
#65501=CARTESIAN_POINT('Ctrl Pts',(2.40300228181253,-1.69733439062661,1.57994891000054));
#65502=CARTESIAN_POINT('Ctrl Pts',(2.45659386546322,-1.6214620707645,1.58500473929023));
#65503=CARTESIAN_POINT('Ctrl Pts',(2.50668306427918,-1.54291530114352,1.59006056857992));
#65504=CARTESIAN_POINT('Ctrl Pts',(2.5529925573868,-1.46205095736354,1.59511639786962));
#65505=CARTESIAN_POINT('Ctrl Pts',(2.59923890000525,-1.38129688520439,1.60016533271778));
#65506=CARTESIAN_POINT('Ctrl Pts',(2.64171556104463,-1.29823190093204,1.60521426756594));
#65507=CARTESIAN_POINT('Ctrl Pts',(2.68018749526955,-1.21324317026751,1.6102632024141));
#65508=CARTESIAN_POINT('Ctrl Pts',(2.71861880377871,-1.12834418627373,1.61530680567194));
#65509=CARTESIAN_POINT('Ctrl Pts',(2.75305360961187,-1.04152589584114,1.62035040892979));
#65510=CARTESIAN_POINT('Ctrl Pts',(2.78330249689689,-0.953200509214898,
1.62539401218763));
#65511=CARTESIAN_POINT('Ctrl Pts',(2.81353001308168,-0.864937525237457,
1.63043405209619));
#65512=CARTESIAN_POINT('Ctrl Pts',(2.83957734588901,-0.775169979961409,
1.63547409200476));
#65513=CARTESIAN_POINT('Ctrl Pts',(2.86130338179092,-0.684329567790158,
1.64051413191332));
#65514=CARTESIAN_POINT('Ctrl Pts',(2.88302173420405,-0.593521281649192,
1.6455523893941));
#65515=CARTESIAN_POINT('Ctrl Pts',(2.90042172289502,-0.501641313355758,
1.65059064687488));
#65516=CARTESIAN_POINT('Ctrl Pts',(2.91341252606591,-0.409135005789376,
1.65562890435566));
#65517=CARTESIAN_POINT('Ctrl Pts',(2.92640235399592,-0.316635642823058,
1.66066678360619));
#65518=CARTESIAN_POINT('Ctrl Pts',(2.93498359318536,-0.223510473307597,
1.66570466285673));
#65519=CARTESIAN_POINT('Ctrl Pts',(2.93911700049843,-0.130212354948023,
1.67074254210726));
#65520=CARTESIAN_POINT('Ctrl Pts',(2.94325124898259,-0.0368952499088041,
1.6757814465939));
#65521=CARTESIAN_POINT('Ctrl Pts',(2.94293584862796,0.0565944308396144,
1.68082035108054));
#65522=CARTESIAN_POINT('Ctrl Pts',(2.93818365541052,0.149802560320151,1.68585925556718));
#65523=CARTESIAN_POINT('Ctrl Pts',(2.93342628733005,0.243112188052422,1.69090364712881));
#65524=CARTESIAN_POINT('Ctrl Pts',(2.92422250559392,0.33613920900909,1.69594803869043));
#65525=CARTESIAN_POINT('Ctrl Pts',(2.91063714470086,0.428433672681843,1.70099243025206));
#65526=CARTESIAN_POINT('Ctrl Pts',(2.89704336452254,0.520785334203316,1.70603994798544));
#65527=CARTESIAN_POINT('Ctrl Pts',(2.87906268454813,0.612403099804473,1.71108746571883));
#65528=CARTESIAN_POINT('Ctrl Pts',(2.85681083026607,0.702848404760571,1.71613498345221));
#65529=CARTESIAN_POINT('Ctrl Pts',(2.8345238333228,0.793436551237681,1.72119047280016));
#65530=CARTESIAN_POINT('Ctrl Pts',(2.80795232305858,0.882848116377528,1.7262459621481));
#65531=CARTESIAN_POINT('Ctrl Pts',(2.77726143690243,0.970661069114589,1.73130145149605));
#65532=CARTESIAN_POINT('Ctrl Pts',(2.76381996906272,1.0091198797895,1.73351556799757));
#65533=CARTESIAN_POINT('Ctrl Pts',(2.74958897348094,1.04727233574671,1.73572968449908));
#65534=CARTESIAN_POINT('Ctrl Pts',(2.73458512827856,1.08508440971092,1.73794380100059));
#65535=CARTESIAN_POINT('Ctrl Pts',(2.70032328606808,1.17142969615842,1.74299981892048));
#65536=CARTESIAN_POINT('Ctrl Pts',(2.66190749143318,1.25630282867087,1.74805583684037));
#65537=CARTESIAN_POINT('Ctrl Pts',(2.61948513840147,1.33927652473037,1.75311185476026));
#65538=CARTESIAN_POINT('Ctrl Pts',(2.5771206111932,1.42213711951291,1.75816098083237));
#65539=CARTESIAN_POINT('Ctrl Pts',(2.53076057872994,1.50310303150586,1.76321010690448));
#65540=CARTESIAN_POINT('Ctrl Pts',(2.48060090216308,1.58176583734373,1.76825923297659));
#65541=CARTESIAN_POINT('Ctrl Pts',(2.43049416845524,1.66034561565582,1.77330302976454));
#65542=CARTESIAN_POINT('Ctrl Pts',(2.37659599970475,1.7366267478902,1.77834682655249));
#65543=CARTESIAN_POINT('Ctrl Pts',(2.3191481632378,1.81022534424606,1.78339062334044));
#65544=CARTESIAN_POINT('Ctrl Pts',(2.26174088289033,1.88377198262315,1.78843085938811));
#65545=CARTESIAN_POINT('Ctrl Pts',(2.20078918805151,1.95463950081475,1.79347109543578));
#65546=CARTESIAN_POINT('Ctrl Pts',(2.13657755592481,2.02247381874732,1.79851133148346));
#65547=CARTESIAN_POINT('Ctrl Pts',(2.07238861192725,2.09028416853402,1.80354978664622));
#65548=CARTESIAN_POINT('Ctrl Pts',(2.00494232364948,2.15506312558991,1.80858824180899));
#65549=CARTESIAN_POINT('Ctrl Pts',(1.93456207767309,2.21649127397993,1.81362669697176));
#65550=CARTESIAN_POINT('Ctrl Pts',(1.86418709696534,2.27791482682331,1.81866477519893));
#65551=CARTESIAN_POINT('Ctrl Pts',(1.79087892929389,2.33598777806775,1.8237028534261));
#65552=CARTESIAN_POINT('Ctrl Pts',(1.714995436969,2.39042980469528,1.82874093165327));
#65553=CARTESIAN_POINT('Ctrl Pts',(1.63909648677024,2.44488292145526,1.83378003616396));
#65554=CARTESIAN_POINT('Ctrl Pts',(1.56062153050848,2.49570338643916,1.83881914067465));
#65555=CARTESIAN_POINT('Ctrl Pts',(1.47995796014645,2.54265381760851,1.84385824518534));
#65556=CARTESIAN_POINT('Ctrl Pts',(1.39920654928022,2.58965537656117,1.84890283714816));
#65557=CARTESIAN_POINT('Ctrl Pts',(1.31626215101297,2.63277826650391,1.85394742911098));
#65558=CARTESIAN_POINT('Ctrl Pts',(1.23153706047447,2.67183092067554,1.85899202107381));
#65559=CARTESIAN_POINT('Ctrl Pts',(1.14675945673896,2.71090777995229,1.86403973970961));
#65560=CARTESIAN_POINT('Ctrl Pts',(1.06019937420788,2.74590921490711,1.86908745834541));
#65561=CARTESIAN_POINT('Ctrl Pts',(0.972287379531894,2.77669250216926,1.87413517698122));
#65562=CARTESIAN_POINT('Ctrl Pts',(0.884236569514481,2.80752439704801,1.87919086609691));
#65563=CARTESIAN_POINT('Ctrl Pts',(0.794830010497076,2.83412472241532,1.88424655521261));
#65564=CARTESIAN_POINT('Ctrl Pts',(0.704511421209433,2.85640117234703,1.8893022443283));
#65565=CARTESIAN_POINT('Ctrl Pts',(0.664991942728182,2.86614837600309,1.89151439355242));
#65566=CARTESIAN_POINT('Ctrl Pts',(0.625297954831822,2.87506841575694,1.89372654277653));
#65567=CARTESIAN_POINT('Ctrl Pts',(0.585466966754457,2.8831566781636,1.89593869200064));
#65568=CARTESIAN_POINT('Ctrl Pts',(0.494431293710531,2.9016427978279,1.90099466734074));
#65569=CARTESIAN_POINT('Ctrl Pts',(0.402358753236711,2.9158456024913,1.90605064268083));
#65570=CARTESIAN_POINT('Ctrl Pts',(0.309687730333526,2.92565505650972,1.91110661802092));
#65571=CARTESIAN_POINT('Ctrl Pts',(0.217143032101936,2.93545113875324,1.91615570129914));
#65572=CARTESIAN_POINT('Ctrl Pts',(0.12400190997247,2.94086572523229,1.92120478457735));
#65573=CARTESIAN_POINT('Ctrl Pts',(0.0307134383321627,2.94183967692086,
1.92625386785556));
#65574=CARTESIAN_POINT('Ctrl Pts',(-0.0624765649613562,2.94281260057873,
1.93129762169837));
#65575=CARTESIAN_POINT('Ctrl Pts',(-0.155813167463065,2.93935420188634,
1.93634137554119));
#65576=CARTESIAN_POINT('Ctrl Pts',(-0.248842757236273,2.93145719432692,
1.941385129384));
#65577=CARTESIAN_POINT('Ctrl Pts',(-0.341806670138463,2.92356576188342,
1.94642532244608));
#65578=CARTESIAN_POINT('Ctrl Pts',(-0.434463560481314,2.91124198663328,
1.95146551550816));
#65579=CARTESIAN_POINT('Ctrl Pts',(-0.526361444244065,2.89453064071074,
1.95650570857024));
#65580=CARTESIAN_POINT('Ctrl Pts',(-0.61822685699421,2.8778251995414,1.96154412074069));
#65581=CARTESIAN_POINT('Ctrl Pts',(-0.709333360089032,2.85673534703234,
1.96658253291114));
#65582=CARTESIAN_POINT('Ctrl Pts',(-0.799236739844116,2.83135738360302,
1.97162094508159));
#65583=CARTESIAN_POINT('Ctrl Pts',(-0.889133394581078,2.80598131851461,
1.97665898036506));
#65584=CARTESIAN_POINT('Ctrl Pts',(-0.977826678217004,2.7763179010643,1.98169701564853));
#65585=CARTESIAN_POINT('Ctrl Pts',(-1.06488627931391,2.7425136667169,1.98673505093199));
#65586=CARTESIAN_POINT('Ctrl Pts',(-1.15196361686693,2.70870254550911,1.99177411260303));
#65587=CARTESIAN_POINT('Ctrl Pts',(-1.23740619763973,2.67074909280154,1.99681317427406));
#65588=CARTESIAN_POINT('Ctrl Pts',(-1.32080353799129,2.62884803935672,2.00185223594509));
#65589=CARTESIAN_POINT('Ctrl Pts',(-1.40429170354303,2.58690135290309,2.00689678548639));
#65590=CARTESIAN_POINT('Ctrl Pts',(-1.4857297859912,2.54099868396863,2.0119413350277));
#65591=CARTESIAN_POINT('Ctrl Pts',(-1.56473206480836,2.49138065444857,2.016985884569));
#65592=CARTESIAN_POINT('Ctrl Pts',(-1.64378331300254,2.44173186930941,2.0220335609625));
#65593=CARTESIAN_POINT('Ctrl Pts',(-1.72039538815675,2.38836339198487,2.02708123735599));
#65594=CARTESIAN_POINT('Ctrl Pts',(-1.79421349276549,2.33155783594966,2.03212891374948));
#65595=CARTESIAN_POINT('Ctrl Pts',(-1.86814816897435,2.27466257408147,2.03718456130015));
#65596=CARTESIAN_POINT('Ctrl Pts',(-1.93927972961946,2.21431968527227,2.04224020885082));
#65597=CARTESIAN_POINT('Ctrl Pts',(-2.00728841587209,2.15085034707339,2.04729585640148));
#65598=CARTESIAN_POINT('Ctrl Pts',(-2.03705203244759,2.12307335047865,2.04950843193455));
#65599=CARTESIAN_POINT('Ctrl Pts',(-2.06621801832268,2.0946979882731,2.05172100746763));
#65600=CARTESIAN_POINT('Ctrl Pts',(-2.09476199980797,2.06575317116071,2.0539335830007));
#65601=CARTESIAN_POINT('Ctrl Pts',(-2.16135713544021,1.99822285754822,2.05909567882806));
#65602=CARTESIAN_POINT('Ctrl Pts',(-2.22482119968381,1.92732884677633,2.06425777465542));
#65603=CARTESIAN_POINT('Ctrl Pts',(-2.28479134284929,1.8534002588866,2.06941987048278));
#65604=CARTESIAN_POINT('Ctrl Pts',(-2.34263346067958,1.78209500820637,2.07439879064766));
#65605=CARTESIAN_POINT('Ctrl Pts',(-2.39722507039791,1.70796726967815,2.07937771081254));
#65606=CARTESIAN_POINT('Ctrl Pts',(-2.44827630613403,1.63135131986421,2.08435663097742));
#65607=CARTESIAN_POINT('Ctrl Pts',(-2.49928059877251,1.55480582064685,2.08933097288025));
#65608=CARTESIAN_POINT('Ctrl Pts',(-2.54675072770875,1.47577702963361,2.09430531478307));
#65609=CARTESIAN_POINT('Ctrl Pts',(-2.59043752705122,1.39463164256543,2.0992796566859));
#65610=CARTESIAN_POINT('Ctrl Pts',(-2.63409713182315,1.31353676764249,2.10425090211349));
#65611=CARTESIAN_POINT('Ctrl Pts',(-2.67397786788455,1.23032831423302,2.10922214754109));
#65612=CARTESIAN_POINT('Ctrl Pts',(-2.70987500029302,1.14540014090575,2.11419339296869));
#65613=CARTESIAN_POINT('Ctrl Pts',(-2.74576044686172,1.06049961482936,2.11916302007266));
#65614=CARTESIAN_POINT('Ctrl Pts',(-2.77766468977229,0.973880901981224,
2.12413264717664));
#65615=CARTESIAN_POINT('Ctrl Pts',(-2.80543045870139,0.885959333937228,
2.12910227428061));
#65616=CARTESIAN_POINT('Ctrl Pts',(-2.83320497738106,0.798010059410781,
2.13407346744953));
#65617=CARTESIAN_POINT('Ctrl Pts',(-2.85683827546653,0.708757544282162,
2.13904466061845));
#65618=CARTESIAN_POINT('Ctrl Pts',(-2.8762227310473,0.618633010278974,2.14401585378738));
#65619=CARTESIAN_POINT('Ctrl Pts',(-2.89561102794042,0.528490616786008,
2.14898803207067));
#65620=CARTESIAN_POINT('Ctrl Pts',(-2.91074872468526,0.437476310031793,
2.15396021035396));
#65621=CARTESIAN_POINT('Ctrl Pts',(-2.92157953159936,0.346030404068275,
2.15893238863725));
#65622=CARTESIAN_POINT('Ctrl Pts',(-2.93242016404137,0.254501539899681,
2.16390907759799));
#65623=CARTESIAN_POINT('Ctrl Pts',(-2.93894607405413,0.162540750341504,
2.16888576655873));
#65624=CARTESIAN_POINT('Ctrl Pts',(-2.94115297628147,0.0705915725185198,
2.17386245551947));
#65625=CARTESIAN_POINT('Ctrl Pts',(-2.94173853848186,0.0461944958277922,
2.17518293129876));
#65626=CARTESIAN_POINT('Ctrl Pts',(-2.94202032183177,0.0217982266268764,
2.17650340707806));
#65627=CARTESIAN_POINT('Ctrl Pts',(-2.9419988608317,-0.00258898917602336,
2.17782388285735));
#65628=CARTESIAN_POINT('',(-2.94199945032593,0.00179841093808543,3.17782388291039));
#65629=CARTESIAN_POINT('Ctrl Pts',(-2.94199886083084,-0.00258899015562637,
2.17782388291039));
#65630=CARTESIAN_POINT('Ctrl Pts',(-2.94188600231367,-0.130835761680184,
2.18476796201073));
#65631=CARTESIAN_POINT('Ctrl Pts',(-2.93338382342992,-0.258723098115673,
2.19171204111106));
#65632=CARTESIAN_POINT('Ctrl Pts',(-2.91665378210995,-0.385350120414867,
2.1986561202114));
#65633=CARTESIAN_POINT('Ctrl Pts',(-2.90599496404346,-0.466025019368996,
2.20308023814118));
#65634=CARTESIAN_POINT('Ctrl Pts',(-2.89199735598012,-0.546189033564816,
2.20750435607097));
#65635=CARTESIAN_POINT('Ctrl Pts',(-2.87471226218597,-0.625614425694941,
2.21192847400075));
#65636=CARTESIAN_POINT('Ctrl Pts',(-2.85495849231584,-0.716383439543999,
2.21698444931127));
#65637=CARTESIAN_POINT('Ctrl Pts',(-2.83086664751314,-0.806375944703539,
2.22204042462179));
#65638=CARTESIAN_POINT('Ctrl Pts',(-2.80251261705139,-0.895146374213621,
2.22709639993232));
#65639=CARTESIAN_POINT('Ctrl Pts',(-2.77419723852078,-0.983795792760766,
2.23214548298779));
#65640=CARTESIAN_POINT('Ctrl Pts',(-2.74163135430876,-1.07122602734494,
2.23719456604326));
#65641=CARTESIAN_POINT('Ctrl Pts',(-2.70494174390693,-1.15700223079722,
2.24224364909874));
#65642=CARTESIAN_POINT('Ctrl Pts',(-2.66829086171616,-1.24268789202583,
2.24728740252677));
#65643=CARTESIAN_POINT('Ctrl Pts',(-2.62752507927499,-1.32672258700668,
2.25233115595481));
#65644=CARTESIAN_POINT('Ctrl Pts',(-2.58282046295422,-1.40868820401996,
2.25737490938285));
#65645=CARTESIAN_POINT('Ctrl Pts',(-2.53814740965108,-1.49059595045009,
2.26241510174513));
#65646=CARTESIAN_POINT('Ctrl Pts',(-2.48954126199213,-1.57043713441029,
2.2674552941074));
#65647=CARTESIAN_POINT('Ctrl Pts',(-2.43722507816321,-1.64781610575098,
2.27249548646968));
#65648=CARTESIAN_POINT('Ctrl Pts',(-2.38492738147362,-1.72516773343395,
2.27753389776286));
#65649=CARTESIAN_POINT('Ctrl Pts',(-2.32892250146209,-1.80005851010918,
2.28257230905604));
#65650=CARTESIAN_POINT('Ctrl Pts',(-2.26947752827149,-1.8721206554789,2.28761072034922));
#65651=CARTESIAN_POINT('Ctrl Pts',(-2.21003700381689,-1.94417740787015,
2.29264875457836));
#65652=CARTESIAN_POINT('Ctrl Pts',(-2.14715718051741,-2.01340560796873,
2.2976867888075));
#65653=CARTESIAN_POINT('Ctrl Pts',(-2.08114552660342,-2.07947043669742,
2.30272482303664));
#65654=CARTESIAN_POINT('Ctrl Pts',(-2.01512042659782,-2.14554872234905,
2.30776388347654));
#65655=CARTESIAN_POINT('Ctrl Pts',(-1.94596254268457,-2.20846204348059,
2.31280294391645));
#65656=CARTESIAN_POINT('Ctrl Pts',(-1.87401546718772,-2.26791314400292,
2.31784200435635));
#65657=CARTESIAN_POINT('Ctrl Pts',(-1.80199004029304,-2.32742898762698,
2.3228865524054));
#65658=CARTESIAN_POINT('Ctrl Pts',(-1.72716970142457,-2.38347480208937,
2.32793110045444));
#65659=CARTESIAN_POINT('Ctrl Pts',(-1.64993006988533,-2.43579448322066,
2.33297564850348));
#65660=CARTESIAN_POINT('Ctrl Pts',(-1.57264256385075,-2.48814659301947,
2.338023323253));
#65661=CARTESIAN_POINT('Ctrl Pts',(-1.49293315807301,-2.53676774082672,
2.34307099800251));
#65662=CARTESIAN_POINT('Ctrl Pts',(-1.41120344823185,-2.58144704142823,
2.34811867275202));
#65663=CARTESIAN_POINT('Ctrl Pts',(-1.32934467648473,-2.62619689649155,
2.35317431844044));
#65664=CARTESIAN_POINT('Ctrl Pts',(-1.24545963043639,-2.66699228522441,
2.35822996412886));
#65665=CARTESIAN_POINT('Ctrl Pts',(-1.15997108707264,-2.7036699275532,2.36328560981727));
#65666=CARTESIAN_POINT('Ctrl Pts',(-1.12255733508012,-2.71972176514178,
2.36549819487845));
#65667=CARTESIAN_POINT('Ctrl Pts',(-1.08483666928519,-2.73498555357217,
2.36771077993963));
#65668=CARTESIAN_POINT('Ctrl Pts',(-1.04684537007887,-2.74945063078871,
2.36992336500081));
#65669=CARTESIAN_POINT('Ctrl Pts',(-0.960031640089006,-2.78250470722182,
2.37497933218523));
#65670=CARTESIAN_POINT('Ctrl Pts',(-0.871497829437372,-2.8115013151519,
2.38003529936965));
#65671=CARTESIAN_POINT('Ctrl Pts',(-0.781658570989003,-2.83626054487232,
2.38509126655407));
#65672=CARTESIAN_POINT('Ctrl Pts',(-0.691941781869693,-2.86098602268623,
2.3901403414186));
#65673=CARTESIAN_POINT('Ctrl Pts',(-0.600923505364346,-2.88148548455725,
2.39518941628312));
#65674=CARTESIAN_POINT('Ctrl Pts',(-0.509037204033009,-2.89762749933635,
2.40023849114764));
#65675=CARTESIAN_POINT('Ctrl Pts',(-0.417247895638188,-2.91375247499873,
2.405282236332));
#65676=CARTESIAN_POINT('Ctrl Pts',(-0.324592818251352,-2.92552907017723,
2.41032598151635));
#65677=CARTESIAN_POINT('Ctrl Pts',(-0.231518349837081,-2.93287627657368,
2.41536972670071));
#65678=CARTESIAN_POINT('Ctrl Pts',(-0.138509596146128,-2.94021829551493,
2.42040991077615));
#65679=CARTESIAN_POINT('Ctrl Pts',(-0.0450824808836744,-2.94313710717171,
2.42545009485159));
#65680=CARTESIAN_POINT('Ctrl Pts',(0.0483097523589236,-2.94160333284877,
2.43049027892703));
#65681=CARTESIAN_POINT('Ctrl Pts',(0.141668982798636,-2.94007010052863,
2.43552868191002));
#65682=CARTESIAN_POINT('Ctrl Pts',(0.23499291272157,-2.93408741556855,2.44056708489301));
#65683=CARTESIAN_POINT('Ctrl Pts',(0.32782757975047,-2.92367800517686,2.445605487876));
#65684=CARTESIAN_POINT('Ctrl Pts',(0.420655298983171,-2.91326937383103,
2.45064351378221));
#65685=CARTESIAN_POINT('Ctrl Pts',(0.512993387454905,-2.89843472551226,
2.45568153968842));
#65686=CARTESIAN_POINT('Ctrl Pts',(0.604393424651897,-2.87924861521848,
2.46071956559464));
#65687=CARTESIAN_POINT('Ctrl Pts',(0.695812079360467,-2.86005859685594,
2.46575861770946));
#65688=CARTESIAN_POINT('Ctrl Pts',(0.786291869415099,-2.83651544760013,
2.47079766982429));
#65689=CARTESIAN_POINT('Ctrl Pts',(0.875396094689752,-2.80874450197983,
2.47583672193912));
#65690=CARTESIAN_POINT('Ctrl Pts',(0.964597356741051,-2.78094331309061,
2.48088126171038));
#65691=CARTESIAN_POINT('Ctrl Pts',(1.052419639995,-2.74890527012251,2.48592580148163));
#65692=CARTESIAN_POINT('Ctrl Pts',(1.13844320924513,-2.71280501682735,2.49097034125289));
#65693=CARTESIAN_POINT('Ctrl Pts',(1.22452009777977,-2.67668238780781,2.49601800773992));
#65694=CARTESIAN_POINT('Ctrl Pts',(1.30879565281152,-2.63649272650979,2.50106567422696));
#65695=CARTESIAN_POINT('Ctrl Pts',(1.39087381644699,-2.59245714076861,2.50611334071399));
#65696=CARTESIAN_POINT('Ctrl Pts',(1.47308159411412,-2.54835201607151,2.51116897824198));
#65697=CARTESIAN_POINT('Ctrl Pts',(1.55308467393018,-2.5003890712952,2.51622461576997));
#65698=CARTESIAN_POINT('Ctrl Pts',(1.630515293901,-2.44883316629674,2.52128025329796));
#65699=CARTESIAN_POINT('Ctrl Pts',(1.66440384318929,-2.42626903303395,2.52349292086559));
#65700=CARTESIAN_POINT('Ctrl Pts',(1.69780006104988,-2.40301719778661,2.52570558843322));
#65701=CARTESIAN_POINT('Ctrl Pts',(1.73067519028839,-2.37910222262942,2.52791825600085));
#65702=CARTESIAN_POINT('Ctrl Pts',(1.80579514236009,-2.324456299428,2.53297422035692));
#65703=CARTESIAN_POINT('Ctrl Pts',(1.87845681597899,-2.26615270702094,2.53803018471299));
#65704=CARTESIAN_POINT('Ctrl Pts',(1.94828297072153,-2.20444039746972,2.54308614906906));
#65705=CARTESIAN_POINT('Ctrl Pts',(2.01801393706277,-2.14281221536486,2.54813522103407));
#65706=CARTESIAN_POINT('Ctrl Pts',(2.08491673656094,-2.07778484167878,2.55318429299909));
#65707=CARTESIAN_POINT('Ctrl Pts',(2.14864444107427,-2.00964948830402,2.55823336496411));
#65708=CARTESIAN_POINT('Ctrl Pts',(2.21230487529856,-1.9415860578857,2.5632771071823));
#65709=CARTESIAN_POINT('Ctrl Pts',(2.27279657535678,-1.87042149133203,2.5683208494005));
#65710=CARTESIAN_POINT('Ctrl Pts',(2.32980778546171,-1.79648536949289,2.57336459161869));
#65711=CARTESIAN_POINT('Ctrl Pts',(2.38677874210695,-1.72260145115364,2.57840477264123));
#65712=CARTESIAN_POINT('Ctrl Pts',(2.44027382346524,-1.6459502175064,2.58344495366376));
#65713=CARTESIAN_POINT('Ctrl Pts',(2.49002076251487,-1.56689521099685,2.5884851346863));
#65714=CARTESIAN_POINT('Ctrl Pts',(2.53975012153647,-1.4878681416681,2.59352353456359));
#65715=CARTESIAN_POINT('Ctrl Pts',(2.58573373385401,-1.40643936214698,2.59856193444088));
#65716=CARTESIAN_POINT('Ctrl Pts',(2.62774257888884,-1.32300148869707,2.60360033431818));
#65717=CARTESIAN_POINT('Ctrl Pts',(2.66974827954866,-1.23956986059769,2.60863835706969));
#65718=CARTESIAN_POINT('Ctrl Pts',(2.70777960533304,-1.15412983381828,2.6136763798212));
#65719=CARTESIAN_POINT('Ctrl Pts',(2.74165397014574,-1.06709770311069,2.61871440257271));
#65720=CARTESIAN_POINT('Ctrl Pts',(2.77553523461601,-0.980047845372544,
2.62375345148758));
#65721=CARTESIAN_POINT('Ctrl Pts',(2.80525769600541,-0.891405653015827,
2.62879250040244));
#65722=CARTESIAN_POINT('Ctrl Pts',(2.83068770085907,-0.801605351906549,
2.63383154931731));
#65723=CARTESIAN_POINT('Ctrl Pts',(2.85614539940599,-0.71170725679332,2.63887608583927));
#65724=CARTESIAN_POINT('Ctrl Pts',(2.8773011900834,-0.620648962894841,2.64392062236123));
#65725=CARTESIAN_POINT('Ctrl Pts',(2.89407198641106,-0.528877431425054,
2.64896515888319));
#65726=CARTESIAN_POINT('Ctrl Pts',(2.91085317754145,-0.437049018519976,
2.65401282208805));
#65727=CARTESIAN_POINT('Ctrl Pts',(2.9232439045966,-0.344506927092404,2.6590604852929));
#65728=CARTESIAN_POINT('Ctrl Pts',(2.93121293303732,-0.251703677356409,
2.66410814849776));
#65729=CARTESIAN_POINT('Ctrl Pts',(2.93919454577573,-0.15875387729379,2.66916378272404));
#65730=CARTESIAN_POINT('Ctrl Pts',(2.94274050481757,-0.065542538123331,
2.67421941695031));
#65731=CARTESIAN_POINT('Ctrl Pts',(2.94187167988244,0.0274776109886878,
2.67927505117659));
#65732=CARTESIAN_POINT('Ctrl Pts',(2.94149142141465,0.0681897244949632,
2.68148774978469));
#65733=CARTESIAN_POINT('Ctrl Pts',(2.94026616103632,0.108865279596634,2.68370044839281));
#65734=CARTESIAN_POINT('Ctrl Pts',(2.93820075641009,0.149466768986119,2.68591314700091));
#65735=CARTESIAN_POINT('Ctrl Pts',(2.93348135175555,0.242240289280005,2.69096911520086));
#65736=CARTESIAN_POINT('Ctrl Pts',(2.92435534782047,0.334953600743333,2.69602508340081));
#65737=CARTESIAN_POINT('Ctrl Pts',(2.91082511309175,0.427154727229405,2.70108105160076));
#65738=CARTESIAN_POINT('Ctrl Pts',(2.89731332287732,0.5192301644699,2.70613012746811));
#65739=CARTESIAN_POINT('Ctrl Pts',(2.87940929684365,0.610794369165965,2.71117920333547));
#65740=CARTESIAN_POINT('Ctrl Pts',(2.85716735980202,0.70139766044803,2.71622827920283));
#65741=CARTESIAN_POINT('Ctrl Pts',(2.83494890086353,0.791905312873912,2.72127202537594));
#65742=CARTESIAN_POINT('Ctrl Pts',(2.80840173806753,0.88145363966347,2.72631577154905));
#65743=CARTESIAN_POINT('Ctrl Pts',(2.77763154953919,0.969601451630791,2.73135951772215));
#65744=CARTESIAN_POINT('Ctrl Pts',(2.74688308628559,1.05768702688378,2.73639970276104));
#65745=CARTESIAN_POINT('Ctrl Pts',(2.71191766977773,1.14437363530412,2.74143988779993));
#65746=CARTESIAN_POINT('Ctrl Pts',(2.6728909988161,1.22923460268896,2.74648007283881));
#65747=CARTESIAN_POINT('Ctrl Pts',(2.63387811916186,1.31406558176944,2.75151847676905));
#65748=CARTESIAN_POINT('Ctrl Pts',(2.59080702151335,1.39707179904879,2.75655688069928));
#65749=CARTESIAN_POINT('Ctrl Pts',(2.54388138505031,1.47784691317962,2.76159528462952));
#65750=CARTESIAN_POINT('Ctrl Pts',(2.49695926068922,1.55861598177846,2.7666333114655));
#65751=CARTESIAN_POINT('Ctrl Pts',(2.44618339416343,1.63715389594888,2.77167133830147));
#65752=CARTESIAN_POINT('Ctrl Pts',(2.3918026683974,1.71308026532533,2.77670936513744));
#65753=CARTESIAN_POINT('Ctrl Pts',(2.33741086588451,1.78902210005574,2.78174841816325));
#65754=CARTESIAN_POINT('Ctrl Pts',(2.27941300431981,1.86235097323249,2.78678747118906));
#65755=CARTESIAN_POINT('Ctrl Pts',(2.21809972193437,1.93271767818134,2.79182652421486));
#65756=CARTESIAN_POINT('Ctrl Pts',(2.15671966824536,2.00316101377913,2.79687106486303));
#65757=CARTESIAN_POINT('Ctrl Pts',(2.09201727888038,2.07063540757098,2.8019156055112));
#65758=CARTESIAN_POINT('Ctrl Pts',(2.02432148890567,2.13482704441243,2.80696014615936));
#65759=CARTESIAN_POINT('Ctrl Pts',(1.95658373985626,2.19905846839112,2.81200781350504));
#65760=CARTESIAN_POINT('Ctrl Pts',(1.88584923210365,2.26000279538914,2.81705548085071));
#65761=CARTESIAN_POINT('Ctrl Pts',(1.81247988942131,2.31738659926291,2.82210314819639));
#65762=CARTESIAN_POINT('Ctrl Pts',(1.7389946858213,2.37486102055171,2.8271587865467));
#65763=CARTESIAN_POINT('Ctrl Pts',(1.66286670303201,2.42876343927813,2.83221442489702));
#65764=CARTESIAN_POINT('Ctrl Pts',(1.58448651068657,2.47886395299385,2.83727006324733));
#65765=CARTESIAN_POINT('Ctrl Pts',(1.55018251833043,2.50079101885213,2.83948272149854));
#65766=CARTESIAN_POINT('Ctrl Pts',(1.51544743317355,2.52199043688933,2.84169537974975));
#65767=CARTESIAN_POINT('Ctrl Pts',(1.48031532040129,2.54244578156255,2.84390803800096));
#65768=CARTESIAN_POINT('Ctrl Pts',(1.40003776517855,2.58918663863112,2.84896400477706));
#65769=CARTESIAN_POINT('Ctrl Pts',(1.31740277673951,2.63220402586784,2.85401997155316));
#65770=CARTESIAN_POINT('Ctrl Pts',(1.23279018373386,2.6712529574882,2.85907593832925));
#65771=CARTESIAN_POINT('Ctrl Pts',(1.14829293549576,2.71024865719849,2.86412501275881));
#65772=CARTESIAN_POINT('Ctrl Pts',(1.06182383933879,2.74528646765623,2.86917408718837));
#65773=CARTESIAN_POINT('Ctrl Pts',(0.97378919165651,2.7761661712176,2.87422316161793));
#65774=CARTESIAN_POINT('Ctrl Pts',(0.88584747165863,2.80701327875657,2.87926690634143));
#65775=CARTESIAN_POINT('Ctrl Pts',(0.796343901345705,2.83371085809587,2.88431065106493));
#65776=CARTESIAN_POINT('Ctrl Pts',(0.705705725800024,2.85610634055755,2.88935439578843));
#65777=CARTESIAN_POINT('Ctrl Pts',(0.615131545511419,2.87848601064604,2.89439457936632));
#65778=CARTESIAN_POINT('Ctrl Pts',(0.523424781669523,2.8965695154927,2.89943476294422));
#65779=CARTESIAN_POINT('Ctrl Pts',(0.431027855283761,2.91025411054937,2.90447494652212));
#65780=CARTESIAN_POINT('Ctrl Pts',(0.338663580399644,2.92393386970298,2.9095133489849));
#65781=CARTESIAN_POINT('Ctrl Pts',(0.245610065792039,2.93321774257587,2.91455175144768));
#65782=CARTESIAN_POINT('Ctrl Pts',(0.152318921004724,2.93805427899213,2.91959015391046));
#65783=CARTESIAN_POINT('Ctrl Pts',(0.0590347585864077,2.94289045341817,
2.92462817927438));
#65784=CARTESIAN_POINT('Ctrl Pts',(-0.0344865557569679,2.9432799305776,
2.92966620463829));
#65785=CARTESIAN_POINT('Ctrl Pts',(-0.127790446402868,2.93922329907208,
2.9347042300022));
#65786=CARTESIAN_POINT('Ctrl Pts',(-0.221113341964551,2.93516584127797,
2.9397432815532));
#65787=CARTESIAN_POINT('Ctrl Pts',(-0.314218282880421,2.92666049582177,
2.9447823331042));
#65788=CARTESIAN_POINT('Ctrl Pts',(-0.406653994202056,2.91375986124449,
2.9498213846552));
#65789=CARTESIAN_POINT('Ctrl Pts',(-0.499190369847777,2.90084517762014,
2.95486592383334));
#65790=CARTESIAN_POINT('Ctrl Pts',(-0.591055621380578,2.88352571237771,
2.95991046301148));
#65791=CARTESIAN_POINT('Ctrl Pts',(-0.681807188419884,2.86190547674429,
2.96495500218962));
#65792=CARTESIAN_POINT('Ctrl Pts',(-0.772615004949508,2.8402718404912,2.97000266806593));
#65793=CARTESIAN_POINT('Ctrl Pts',(-0.862307337098888,2.81433224992399,
2.97505033394223));
#65794=CARTESIAN_POINT('Ctrl Pts',(-0.950457424969032,2.78424041406651,
2.98009799981853));
#65795=CARTESIAN_POINT('Ctrl Pts',(-1.03874671501582,2.75410105869825,2.98515363671442));
#65796=CARTESIAN_POINT('Ctrl Pts',(-1.12548848753932,2.71979653200843,2.99020927361031));
#65797=CARTESIAN_POINT('Ctrl Pts',(-1.21027678148644,2.68152831650065,2.9952649105062));
#65798=CARTESIAN_POINT('Ctrl Pts',(-1.24738560838968,2.66477967681155,2.9974775833378));
#65799=CARTESIAN_POINT('Ctrl Pts',(-1.28412057603821,2.64727238009407,2.99969025616941));
#65800=CARTESIAN_POINT('Ctrl Pts',(-1.32044931328002,2.62902598143463,3.00190292900102));
#65801=CARTESIAN_POINT('Ctrl Pts',(-1.40346062756966,2.58733288531376,3.00695889553853));
#65802=CARTESIAN_POINT('Ctrl Pts',(-1.48464164879389,2.54163083150868,3.01201486207605));
#65803=CARTESIAN_POINT('Ctrl Pts',(-1.56357965235937,2.4921040649876,3.01707082861356));
#65804=CARTESIAN_POINT('Ctrl Pts',(-1.64241004668626,2.44264481395203,3.02211990279651));
#65805=CARTESIAN_POINT('Ctrl Pts',(-1.71900312724652,2.38937144515071,3.02716897697946));
#65806=CARTESIAN_POINT('Ctrl Pts',(-1.79296920068921,2.3325148328317,3.0322180511624));
#65807=CARTESIAN_POINT('Ctrl Pts',(-1.86685719684845,2.27571823735054,3.03726179563164));
#65808=CARTESIAN_POINT('Ctrl Pts',(-1.93812334822593,2.21534618574687,3.04230554010087));
#65809=CARTESIAN_POINT('Ctrl Pts',(-2.00640642116441,2.15167313342669,3.0473492845701));
#65810=CARTESIAN_POINT('Ctrl Pts',(-2.07464128256659,2.08804503771934,3.05238946788341));
#65811=CARTESIAN_POINT('Ctrl Pts',(-2.13989692866009,2.02112087565847,3.05742965119672));
#65812=CARTESIAN_POINT('Ctrl Pts',(-2.20184556156528,1.95121503761509,3.06246983451003));
#65813=CARTESIAN_POINT('Ctrl Pts',(-2.26377230279882,1.8813339031944,3.0675082367019));
#65814=CARTESIAN_POINT('Ctrl Pts',(-2.32239405882412,1.8084735177801,3.07254663889377));
#65815=CARTESIAN_POINT('Ctrl Pts',(-2.37742097052157,1.7329839955765,3.07758504108564));
#65816=CARTESIAN_POINT('Ctrl Pts',(-2.43244376366806,1.6575001234709,3.08262306617264));
#65817=CARTESIAN_POINT('Ctrl Pts',(-2.48387198649497,1.57938786439255,3.08766109125965));
#65818=CARTESIAN_POINT('Ctrl Pts',(-2.53145774217293,1.49902825176604,3.09269911634665));
#65819=CARTESIAN_POINT('Ctrl Pts',(-2.57905319046182,1.41865227091233,3.09773816761505));
#65820=CARTESIAN_POINT('Ctrl Pts',(-2.62280439156022,1.33602840910849,3.10277721888344));
#65821=CARTESIAN_POINT('Ctrl Pts',(-2.66250881106457,1.25156335477017,3.10781627015184));
#65822=CARTESIAN_POINT('Ctrl Pts',(-2.70225646941769,1.16700631642207,3.11286080904047));
#65823=CARTESIAN_POINT('Ctrl Pts',(-2.73794836091714,1.08060448532161,3.1179053479291));
#65824=CARTESIAN_POINT('Ctrl Pts',(-2.76942977164678,0.992785344330023,
3.12294988681773));
#65825=CARTESIAN_POINT('Ctrl Pts',(-2.80093069510763,0.904911771492653,
3.12799755240015));
#65826=CARTESIAN_POINT('Ctrl Pts',(-2.82821581271975,0.815619563584813,
3.13304521798257));
#65827=CARTESIAN_POINT('Ctrl Pts',(-2.85118066671101,0.725350126334424,
3.13809288356499));
#65828=CARTESIAN_POINT('Ctrl Pts',(-2.87418178562652,0.634938140200193,
3.14314852016303));
#65829=CARTESIAN_POINT('Ctrl Pts',(-2.89284893382899,0.54354627806371,3.14820415676108));
#65830=CARTESIAN_POINT('Ctrl Pts',(-2.90712902926765,0.45162463084879,3.15325979335912));
#65831=CARTESIAN_POINT('Ctrl Pts',(-2.91337892824233,0.411393736654406,
3.15547246890643));
#65832=CARTESIAN_POINT('Ctrl Pts',(-2.91878915727341,0.371061406909721,
3.15768514445375));
#65833=CARTESIAN_POINT('Ctrl Pts',(-2.92335840566048,0.33066543825171,3.15989782000106));
#65834=CARTESIAN_POINT('Ctrl Pts',(-2.93569771046495,0.221575686958495,
3.16587317430417));
#65835=CARTESIAN_POINT('Ctrl Pts',(-2.94193221819642,0.111782666421697,
3.17184852860728));
#65836=CARTESIAN_POINT('Ctrl Pts',(-2.94199945032593,0.00179841093808543,
3.17782388291039));
#65837=CARTESIAN_POINT('',(-2.93753500859377,0.000882026442511374,4.17782388291039));
#65838=CARTESIAN_POINT('Ctrl Pts',(-2.94526019727207,0.00177566248466101,
3.1778252256184));
#65839=CARTESIAN_POINT('Ctrl Pts',(-2.9390358564779,-0.858556525610316,
3.22451438741265));
#65840=CARTESIAN_POINT('Ctrl Pts',(-2.08902058352625,-2.70002933468896,
3.32386851287358));
#65841=CARTESIAN_POINT('Ctrl Pts',(1.03253827306806,-3.31449993698517,3.47588760200119));
#65842=CARTESIAN_POINT('Ctrl Pts',(3.34012933187308,-0.946351485827778,
3.63388249300123));
#65843=CARTESIAN_POINT('Ctrl Pts',(2.61769689100761,2.28028683820626,3.79187738400129));
#65844=CARTESIAN_POINT('Ctrl Pts',(-0.479399010889303,3.43834577670272,
3.94987227500133));
#65845=CARTESIAN_POINT('Ctrl Pts',(-2.64712497717356,1.84153222841377,4.07852110797104));
#65846=CARTESIAN_POINT('Ctrl Pts',(-2.9387088904313,0.433468688742346,4.15450497727406));
#65847=CARTESIAN_POINT('Ctrl Pts',(-2.93753500859377,0.000882026442511374,
4.17782388291039));
#65848=CARTESIAN_POINT('',(-2.94199883948398,-0.00261313506862708,5.1778238829104));
#65849=CARTESIAN_POINT('Ctrl Pts',(-2.93753500859377,0.000882026442511374,
4.17782388291039));
#65850=CARTESIAN_POINT('Ctrl Pts',(-2.93605771780397,-0.543513730930775,
4.20716994094074));
#65851=CARTESIAN_POINT('Ctrl Pts',(-2.53067828075829,-2.06693687065717,
4.28918096263777));
#65852=CARTESIAN_POINT('Ctrl Pts',(-0.0865207644540764,-3.47052722867771,
4.42385694800151));
#65853=CARTESIAN_POINT('Ctrl Pts',(2.85932621153643,-1.96883181171988,4.58185183900155));
#65854=CARTESIAN_POINT('Ctrl Pts',(3.21131386544662,1.31890422107431,4.73984673000161));
#65855=CARTESIAN_POINT('Ctrl Pts',(0.650133944399006,3.41018634994862,4.89784162100167));
#65856=CARTESIAN_POINT('Ctrl Pts',(-2.26144874453696,2.48403434461044,5.04383398224286));
#65857=CARTESIAN_POINT('Ctrl Pts',(-2.93533655136359,0.748725030981945,
5.13716137981739));
#65858=CARTESIAN_POINT('Ctrl Pts',(-2.94214528694468,-0.00261198679238441,
5.17782381372523));
#65859=CARTESIAN_POINT('',(-2.94199954141428,0.00164265582640845,6.1778238829446));
#65860=CARTESIAN_POINT('Ctrl Pts',(-2.94199883948398,-0.00261313506862708,
5.1778238829104));
#65861=CARTESIAN_POINT('Ctrl Pts',(-2.94188759074597,-0.127862557515314,
5.18460279148083));
#65862=CARTESIAN_POINT('Ctrl Pts',(-2.93377434766609,-0.252765317972737,
5.19138170005127));
#65863=CARTESIAN_POINT('Ctrl Pts',(-2.91781295978548,-0.376472484662446,
5.1981606086217));
#65864=CARTESIAN_POINT('Ctrl Pts',(-2.90551365305103,-0.471797051657878,
5.20338420674839));
#65865=CARTESIAN_POINT('Ctrl Pts',(-2.88855531595855,-0.566412456081979,
5.20860780487509));
#65866=CARTESIAN_POINT('Ctrl Pts',(-2.86702688068737,-0.659940046834597,
5.21383140300178));
#65867=CARTESIAN_POINT('Ctrl Pts',(-2.84618931765164,-0.750466229687144,
5.2188873698599));
#65868=CARTESIAN_POINT('Ctrl Pts',(-2.82102328837992,-0.840164100998177,
5.22394333671802));
#65869=CARTESIAN_POINT('Ctrl Pts',(-2.79161000243732,-0.928589034122145,
5.22899930357613));
#65870=CARTESIAN_POINT('Ctrl Pts',(-2.76223681300493,-1.01689342541886,
5.23404837808543));
#65871=CARTESIAN_POINT('Ctrl Pts',(-2.72862801161075,-1.10392790968113,
5.23909745259473));
#65872=CARTESIAN_POINT('Ctrl Pts',(-2.69091556626771,-1.18925918756936,
5.24414652710403));
#65873=CARTESIAN_POINT('Ctrl Pts',(-2.65324292947538,-1.27450039135944,
5.24919027190487));
#65874=CARTESIAN_POINT('Ctrl Pts',(-2.61147543751921,-1.3580415590014,5.25423401670572));
#65875=CARTESIAN_POINT('Ctrl Pts',(-2.56579414172501,-1.4394667145473,5.25927776150656));
#65876=CARTESIAN_POINT('Ctrl Pts',(-2.52014509933188,-1.52083437964436,
5.2643179451579));
#65877=CARTESIAN_POINT('Ctrl Pts',(-2.47058796226295,-1.60008861664314,
5.26935812880924));
#65878=CARTESIAN_POINT('Ctrl Pts',(-2.41735050179949,-1.67683647129044,
5.27439831246058));
#65879=CARTESIAN_POINT('Ctrl Pts',(-2.36413185457447,-1.75355720451464,
5.27943671499434));
#65880=CARTESIAN_POINT('Ctrl Pts',(-2.3072357203883,-1.82777295105162,5.28447511752809));
#65881=CARTESIAN_POINT('Ctrl Pts',(-2.24693356617299,-1.89911915087103,
5.28951352006185));
#65882=CARTESIAN_POINT('Ctrl Pts',(-2.18663592529874,-1.97046001075298,
5.29455154549417));
#65883=CARTESIAN_POINT('Ctrl Pts',(-2.12293305777881,-2.0389314124613,5.29958957092649));
#65884=CARTESIAN_POINT('Ctrl Pts',(-2.05613641171031,-2.10420223753304,
5.30462759635881));
#65885=CARTESIAN_POINT('Ctrl Pts',(-1.98932615997853,-2.1694863574769,5.30966664797555));
#65886=CARTESIAN_POINT('Ctrl Pts',(-1.91942119555477,-2.23156829638511,
5.31470569959229));
#65887=CARTESIAN_POINT('Ctrl Pts',(-1.84676863898251,-2.29015492796245,
5.31974475120903));
#65888=CARTESIAN_POINT('Ctrl Pts',(-1.77403696239967,-2.34880536149155,
5.32478929044845));
#65889=CARTESIAN_POINT('Ctrl Pts',(-1.69855206703457,-2.40395261129819,
5.32983382968787));
#65890=CARTESIAN_POINT('Ctrl Pts',(-1.62069260613675,-2.45534508295956,
5.3348783689273));
#65891=CARTESIAN_POINT('Ctrl Pts',(-1.54278488655175,-2.50676940859455,
5.33992603486241));
#65892=CARTESIAN_POINT('Ctrl Pts',(-1.46250005228599,-2.55443409661416,
5.34497370079753));
#65893=CARTESIAN_POINT('Ctrl Pts',(-1.38024219047631,-2.59813307889129,
5.35002136673264));
#65894=CARTESIAN_POINT('Ctrl Pts',(-1.29785443126904,-2.64190106836056,
5.35507700368298));
#65895=CARTESIAN_POINT('Ctrl Pts',(-1.21348782552278,-2.68169066238758,
5.36013264063332));
#65896=CARTESIAN_POINT('Ctrl Pts',(-1.12756707099972,-2.71734364782909,
5.36518827758366));
#65897=CARTESIAN_POINT('Ctrl Pts',(-1.0899626184658,-2.73294768908979,5.36740094972305));
#65898=CARTESIAN_POINT('Ctrl Pts',(-1.05206067194799,-2.74776000585019,
5.36961362186243));
#65899=CARTESIAN_POINT('Ctrl Pts',(-1.01389764111355,-2.76177036940879,
5.37182629400181));
#65900=CARTESIAN_POINT('Ctrl Pts',(-0.926694925595327,-2.79378411991534,
5.37688226085996));
#65901=CARTESIAN_POINT('Ctrl Pts',(-0.837820763837992,-2.82172012748783,
5.38193822771812));
#65902=CARTESIAN_POINT('Ctrl Pts',(-0.747691909956341,-2.84540345255042,
5.38699419457627));
#65903=CARTESIAN_POINT('Ctrl Pts',(-0.657685920705157,-2.86905449224759,
5.3920432690856));
#65904=CARTESIAN_POINT('Ctrl Pts',(-0.566429063623805,-2.88846425828712,
5.39709234359494));
#65905=CARTESIAN_POINT('Ctrl Pts',(-0.474356341582972,-2.90350651130663,
5.40214141810427));
#65906=CARTESIAN_POINT('Ctrl Pts',(-0.382380809782441,-2.91853288600569,
5.40718516290515));
#65907=CARTESIAN_POINT('Ctrl Pts',(-0.289591560303666,-2.92920084066322,
5.41222890770603));
#65908=CARTESIAN_POINT('Ctrl Pts',(-0.196435907659241,-2.93543470957575,
5.41727265250691));
#65909=CARTESIAN_POINT('Ctrl Pts',(-0.103346027812463,-2.94166417704847,
5.42231283615829));
#65910=CARTESIAN_POINT('Ctrl Pts',(-0.00989070028221488,-2.94346575221075,
5.42735301980967));
#65911=CARTESIAN_POINT('Ctrl Pts',(0.0834765125543756,-2.94081547735518,
5.43239320346105));
#65912=CARTESIAN_POINT('Ctrl Pts',(0.17681073096138,-2.93816613906293,5.43743160599484));
#65913=CARTESIAN_POINT('Ctrl Pts',(0.270056453670778,-2.93106808891615,
5.44247000852863));
#65914=CARTESIAN_POINT('Ctrl Pts',(0.362760022533932,-2.91954947997995,
5.44750841106243));
#65915=CARTESIAN_POINT('Ctrl Pts',(0.455456652958058,-2.90803173315906,
5.45254643649479));
#65916=CARTESIAN_POINT('Ctrl Pts',(0.54761077017085,-2.89209414039802,5.45758446192715));
#65917=CARTESIAN_POINT('Ctrl Pts',(0.638774877130006,-2.87181661258994,
5.46262248735951));
#65918=CARTESIAN_POINT('Ctrl Pts',(0.729957553107359,-2.85153495449643,
5.46766153897628));
#65919=CARTESIAN_POINT('Ctrl Pts',(0.820149385565806,-2.82691170232326,
5.47270059059306));
#65920=CARTESIAN_POINT('Ctrl Pts',(0.908915204120345,-2.79807740273904,
5.47773964220984));
#65921=CARTESIAN_POINT('Ctrl Pts',(0.997777690333067,-2.76921170205628,
5.4827841814493));
#65922=CARTESIAN_POINT('Ctrl Pts',(1.08521064059338,-2.73612593777001,5.48782872068876));
#65923=CARTESIAN_POINT('Ctrl Pts',(1.17079643775542,-2.69899975941815,5.49287325992821));
#65924=CARTESIAN_POINT('Ctrl Pts',(1.25643528252616,-2.66185056959655,5.49792092586337));
#65925=CARTESIAN_POINT('Ctrl Pts',(1.34022429725,-2.62065617545347,5.50296859179852));
#65926=CARTESIAN_POINT('Ctrl Pts',(1.42177009591575,-2.57564240420904,5.50801625773367));
#65927=CARTESIAN_POINT('Ctrl Pts',(1.50344466752548,-2.53055754952514,5.51307189468405));
#65928=CARTESIAN_POINT('Ctrl Pts',(1.58286857494277,-2.48164151034904,5.51812753163443));
#65929=CARTESIAN_POINT('Ctrl Pts',(1.65967724912457,-2.42916352449527,5.52318316858481));
#65930=CARTESIAN_POINT('Ctrl Pts',(1.69329366878947,-2.40619578010415,5.52539584072383));
#65931=CARTESIAN_POINT('Ctrl Pts',(1.7264095679016,-2.38254626630141,5.52760851286286));
#65932=CARTESIAN_POINT('Ctrl Pts',(1.75899648480085,-2.35823988738598,5.52982118500188));
#65933=CARTESIAN_POINT('Ctrl Pts',(1.83345775221901,-2.30269969050315,5.53487715186005));
#65934=CARTESIAN_POINT('Ctrl Pts',(1.90541718082672,-2.24353147452815,5.53993311871821));
#65935=CARTESIAN_POINT('Ctrl Pts',(1.97450053359559,-2.18098868470947,5.54498908557638));
#65936=CARTESIAN_POINT('Ctrl Pts',(2.04348971118917,-2.11853115389977,5.55003816008572));
#65937=CARTESIAN_POINT('Ctrl Pts',(2.10961027830197,-2.05270848617203,5.55508723459507));
#65938=CARTESIAN_POINT('Ctrl Pts',(2.17251881333806,-1.98381602113003,5.56013630910441));
#65939=CARTESIAN_POINT('Ctrl Pts',(2.23536094330328,-1.9149962776833,5.56518005390531));
#65940=CARTESIAN_POINT('Ctrl Pts',(2.2949974833367,-1.84311350388941,5.5702237987062));
#65941=CARTESIAN_POINT('Ctrl Pts',(2.35112064047022,-1.76850098500253,5.5752675435071));
#65942=CARTESIAN_POINT('Ctrl Pts',(2.40720417169855,-1.69394114648414,5.58030772715849));
#65943=CARTESIAN_POINT('Ctrl Pts',(2.45977898499771,-1.61665574732327,5.58534791080988));
#65944=CARTESIAN_POINT('Ctrl Pts',(2.50857717942338,-1.53701155977313,5.59038809446127));
#65945=CARTESIAN_POINT('Ctrl Pts',(2.55735812937383,-1.45739551716226,5.59542649699508));
#65946=CARTESIAN_POINT('Ctrl Pts',(2.60236488050688,-1.37542272001601,5.60046489952889));
#65947=CARTESIAN_POINT('Ctrl Pts',(2.64337312286579,-1.29148849522974,5.6055033020627));
#65948=CARTESIAN_POINT('Ctrl Pts',(2.68437829594491,-1.20756055253713,5.61054132749507));
#65949=CARTESIAN_POINT('Ctrl Pts',(2.72138536090392,-1.12167187269252,5.61557935292745));
#65950=CARTESIAN_POINT('Ctrl Pts',(2.7542167220698,-1.03424090417616,5.62061737835982));
#65951=CARTESIAN_POINT('Ctrl Pts',(2.78705477058403,-0.946792127036474,
5.62565642997661));
#65952=CARTESIAN_POINT('Ctrl Pts',(2.81571527053406,-0.857800852562817,
5.6306954815934));
#65953=CARTESIAN_POINT('Ctrl Pts',(2.84006976978777,-0.767702873993343,
5.63573453321018));
#65954=CARTESIAN_POINT('Ctrl Pts',(2.86445079155261,-0.677506777018114,
5.64077907244966));
#65955=CARTESIAN_POINT('Ctrl Pts',(2.88451633694319,-0.586201999060682,
5.64582361168913));
#65956=CARTESIAN_POINT('Ctrl Pts',(2.90018866945859,-0.494236463187442,
5.6508681509286));
#65957=CARTESIAN_POINT('Ctrl Pts',(2.91587071596613,-0.402213925429321,
5.65591581686377));
#65958=CARTESIAN_POINT('Ctrl Pts',(2.92715407496732,-0.309530254230438,
5.66096348279894));
#65959=CARTESIAN_POINT('Ctrl Pts',(2.93401292466136,-0.21663831129351,5.66601114873411));
#65960=CARTESIAN_POINT('Ctrl Pts',(2.94088260549915,-0.123599678163332,
5.6710667856845));
#65961=CARTESIAN_POINT('Ctrl Pts',(2.94331381839724,-0.030352559376767,
5.6761224226349));
#65962=CARTESIAN_POINT('Ctrl Pts',(2.94133284458672,0.0626505974064284,
5.68117805958529));
#65963=CARTESIAN_POINT('Ctrl Pts',(2.94046584294056,0.103354765023912,5.68339073172417));
#65964=CARTESIAN_POINT('Ctrl Pts',(2.93875435719679,0.144012274704711,5.68560340386305));
#65965=CARTESIAN_POINT('Ctrl Pts',(2.93620369291188,0.184585681271942,5.68781607600193));
#65966=CARTESIAN_POINT('Ctrl Pts',(2.93037541231659,0.277296117364836,5.69287204286007));
#65967=CARTESIAN_POINT('Ctrl Pts',(2.92014156979324,0.369893663846107,5.69792800971822));
#65968=CARTESIAN_POINT('Ctrl Pts',(2.90550993734058,0.461926405410154,5.70298397657637));
#65969=CARTESIAN_POINT('Ctrl Pts',(2.89089825088787,0.553833686943376,5.7080330510857));
#65970=CARTESIAN_POINT('Ctrl Pts',(2.87190075726029,0.645177259338613,5.71308212559503));
#65971=CARTESIAN_POINT('Ctrl Pts',(2.8485771536256,0.735508123573278,5.71813120010435));
#65972=CARTESIAN_POINT('Ctrl Pts',(2.82527816994991,0.825743636240132,5.72317494490523));
#65973=CARTESIAN_POINT('Ctrl Pts',(2.79766226379785,0.914968138495921,5.7282186897061));
#65974=CARTESIAN_POINT('Ctrl Pts',(2.76584038045652,1.00274173635895,5.73326243450698));
#65975=CARTESIAN_POINT('Ctrl Pts',(2.734040965041,1.09045336143851,5.73830261815835));
#65976=CARTESIAN_POINT('Ctrl Pts',(2.69804162599648,1.17671570261467,5.74334280180973));
#65977=CARTESIAN_POINT('Ctrl Pts',(2.65800315217212,1.26110397788727,5.7483829854611));
#65978=CARTESIAN_POINT('Ctrl Pts',(2.61797882728254,1.34546243173839,5.75342138799489));
#65979=CARTESIAN_POINT('Ctrl Pts',(2.57391839335713,1.42794773516738,5.75845979052868));
#65980=CARTESIAN_POINT('Ctrl Pts',(2.52603037309879,1.50815601122112,5.76349819306247));
#65981=CARTESIAN_POINT('Ctrl Pts',(2.47814593704021,1.58835828405145,5.76853621849482));
#65982=CARTESIAN_POINT('Ctrl Pts',(2.42643471186556,1.66628348776118,5.77357424392717));
#65983=CARTESIAN_POINT('Ctrl Pts',(2.37115011052428,1.74155423497539,5.77861226935953));
#65984=CARTESIAN_POINT('Ctrl Pts',(2.3158542483831,1.81684031392396,5.7836513209763));
#65985=CARTESIAN_POINT('Ctrl Pts',(2.25698382729643,1.88947050537935,5.78869037259306));
#65986=CARTESIAN_POINT('Ctrl Pts',(2.19483363970474,1.95909910265419,5.79372942420983));
#65987=CARTESIAN_POINT('Ctrl Pts',(2.13261576938121,2.0288035267907,5.79877396344929));
#65988=CARTESIAN_POINT('Ctrl Pts',(2.06711129917795,2.09549950097959,5.80381850268874));
#65989=CARTESIAN_POINT('Ctrl Pts',(1.99865289249164,2.15887716541141,5.8088630419282));
#65990=CARTESIAN_POINT('Ctrl Pts',(1.93015205405978,2.22229411245381,5.81391070786334));
#65991=CARTESIAN_POINT('Ctrl Pts',(1.85869397318406,2.28238836987287,5.81895837379849));
#65992=CARTESIAN_POINT('Ctrl Pts',(1.78464381671532,2.33889085838988,5.82400603973364));
#65993=CARTESIAN_POINT('Ctrl Pts',(1.71047672403643,2.39548257273959,5.82906167668401));
#65994=CARTESIAN_POINT('Ctrl Pts',(1.63370974931247,2.44847094457545,5.83411731363439));
#65995=CARTESIAN_POINT('Ctrl Pts',(1.55473618283181,2.4976307576969,5.83917295058476));
#65996=CARTESIAN_POINT('Ctrl Pts',(1.5201722669513,2.51914625612443,5.84138562272384));
#65997=CARTESIAN_POINT('Ctrl Pts',(1.48518598354178,2.53992899536583,5.84359829486291));
#65998=CARTESIAN_POINT('Ctrl Pts',(1.44981159240075,2.55996295804068,5.84581096700198));
#65999=CARTESIAN_POINT('Ctrl Pts',(1.36898093245885,2.60574066253328,5.85086693386014));
#66000=CARTESIAN_POINT('Ctrl Pts',(1.28583752617665,2.64776697737243,5.8559229007183));
#66001=CARTESIAN_POINT('Ctrl Pts',(1.20076410415281,2.68580147557077,5.86097886757645));
#66002=CARTESIAN_POINT('Ctrl Pts',(1.11580665513994,2.72378412472892,5.86602794208578));
#66003=CARTESIAN_POINT('Ctrl Pts',(1.02892482029024,2.75778559168595,5.87107701659512));
#66004=CARTESIAN_POINT('Ctrl Pts',(0.940527260799538,2.78761053084769,5.87612609110445));
#66005=CARTESIAN_POINT('Ctrl Pts',(0.852223012116351,2.81740398736247,5.88116983590533));
#66006=CARTESIAN_POINT('Ctrl Pts',(0.76240663717098,2.8430295384218,5.88621358070622));
#66007=CARTESIAN_POINT('Ctrl Pts',(0.67150717465237,2.86433973445721,5.8912573255071));
#66008=CARTESIAN_POINT('Ctrl Pts',(0.580671891942362,2.88563488437172,5.89629750915848));
#66009=CARTESIAN_POINT('Ctrl Pts',(0.488755472276119,2.90262063465239,5.90133769280986));
#66010=CARTESIAN_POINT('Ctrl Pts',(0.396201533479985,2.91519953774491,5.90637787646124));
#66011=CARTESIAN_POINT('Ctrl Pts',(0.303680301715806,2.92777399566101,5.91141627899504));
#66012=CARTESIAN_POINT('Ctrl Pts',(0.210522437427181,2.93594464071984,5.91645468152884));
#66013=CARTESIAN_POINT('Ctrl Pts',(0.117180133035207,2.93966542593232,5.92149308406263));
#66014=CARTESIAN_POINT('Ctrl Pts',(0.0238448148887003,2.94338593266101,
5.92653110949499));
#66015=CARTESIAN_POINT('Ctrl Pts',(-0.0696744727827794,2.9426572244103,
5.93156913492736));
#66016=CARTESIAN_POINT('Ctrl Pts',(-0.162923193874212,2.93748532471191,
5.93660716035972));
#66017=CARTESIAN_POINT('Ctrl Pts',(-0.256190908594257,2.93231237156055,
5.94164621197649));
#66018=CARTESIAN_POINT('Ctrl Pts',(-0.349187504554182,2.92269445444429,
5.94668526359326));
#66019=CARTESIAN_POINT('Ctrl Pts',(-0.441462367924965,2.90868956365338,
5.95172431521004));
#66020=CARTESIAN_POINT('Ctrl Pts',(-0.533837720370289,2.89466942127105,
5.9567688544495));
#66021=CARTESIAN_POINT('Ctrl Pts',(-0.625489332350595,2.87625283605432,
5.96181339368896));
#66022=CARTESIAN_POINT('Ctrl Pts',(-0.715975918679006,2.85354910311208,
5.96685793292842));
#66023=CARTESIAN_POINT('Ctrl Pts',(-0.806518590212959,2.83083129798986,
5.97190559886357));
#66024=CARTESIAN_POINT('Ctrl Pts',(-0.895894374358191,2.80382118311333,
5.97695326479873));
#66025=CARTESIAN_POINT('Ctrl Pts',(-0.98367837947304,2.77267755892338,5.98200093073389));
#66026=CARTESIAN_POINT('Ctrl Pts',(-1.07160100858761,2.741484754319,5.98705656768427));
#66027=CARTESIAN_POINT('Ctrl Pts',(-1.15792643126154,2.70614557834843,5.99211220463465));
#66028=CARTESIAN_POINT('Ctrl Pts',(-1.24225112439828,2.66686635284396,5.99716784158503));
#66029=CARTESIAN_POINT('Ctrl Pts',(-1.27915703773121,2.6496752355291,5.99938051372403));
#66030=CARTESIAN_POINT('Ctrl Pts',(-1.31568004813735,2.63172998579684,6.00159318586303));
#66031=CARTESIAN_POINT('Ctrl Pts',(-1.35178802061164,2.61305054435058,6.00380585800203));
#66032=CARTESIAN_POINT('Ctrl Pts',(-1.43429491755644,2.57036792761018,6.00886182486019));
#66033=CARTESIAN_POINT('Ctrl Pts',(-1.51492371998122,2.52369852257086,6.01391779171835));
#66034=CARTESIAN_POINT('Ctrl Pts',(-1.59326393563444,2.47323149571702,6.01897375857651));
#66035=CARTESIAN_POINT('Ctrl Pts',(-1.67149735705655,2.42283326606121,6.02402283308584));
#66036=CARTESIAN_POINT('Ctrl Pts',(-1.74744802186249,2.36864794057893,6.02907190759518));
#66037=CARTESIAN_POINT('Ctrl Pts',(-1.82072902491203,2.3109110363324,6.03412098210451));
#66038=CARTESIAN_POINT('Ctrl Pts',(-1.89393267390775,2.25323507808023,6.0391647269054));
#66039=CARTESIAN_POINT('Ctrl Pts',(-1.96447191621663,2.19201526617343,6.04420847170628));
#66040=CARTESIAN_POINT('Ctrl Pts',(-2.03198882542798,2.12753035544403,6.04925221650716));
#66041=CARTESIAN_POINT('Ctrl Pts',(-2.09945806414508,2.06309097445825,6.05429240015855));
#66042=CARTESIAN_POINT('Ctrl Pts',(-2.16390889160784,1.99539138246366,6.05933258380993));
#66043=CARTESIAN_POINT('Ctrl Pts',(-2.2250172922672,1.92474986663513,6.06437276746131));
#66044=CARTESIAN_POINT('Ctrl Pts',(-2.28610409822795,1.85413331435052,6.06941116999511));
#66045=CARTESIAN_POINT('Ctrl Pts',(-2.34385053420923,1.78057723879614,6.07444957252891));
#66046=CARTESIAN_POINT('Ctrl Pts',(-2.3979709478345,1.70443519482018,6.07948797506271));
#66047=CARTESIAN_POINT('Ctrl Pts',(-2.4520873107938,1.62829884972871,6.08452600049507));
#66048=CARTESIAN_POINT('Ctrl Pts',(-2.50257793434589,1.54957728269897,6.08956402592744));
#66049=CARTESIAN_POINT('Ctrl Pts',(-2.54919949508346,1.46865446387713,6.0946020513598));
#66050=CARTESIAN_POINT('Ctrl Pts',(-2.59583055206506,1.38771516206282,6.09964110297658));
#66051=CARTESIAN_POINT('Ctrl Pts',(-2.63859076000742,1.30457410237197,6.10468015459335));
#66052=CARTESIAN_POINT('Ctrl Pts',(-2.67728246142404,1.21964036574363,6.10971920621013));
#66053=CARTESIAN_POINT('Ctrl Pts',(-2.7160162988366,1.13461413466683,6.11476374544959));
#66054=CARTESIAN_POINT('Ctrl Pts',(-2.75067260205668,1.04779173411973,6.11980828468905));
#66055=CARTESIAN_POINT('Ctrl Pts',(-2.78110177929019,0.959602466247833,
6.12485282392852));
#66056=CARTESIAN_POINT('Ctrl Pts',(-2.81154981707233,0.871358537089423,
6.12990048986368));
#66057=CARTESIAN_POINT('Ctrl Pts',(-2.83776538832204,0.781746479188209,
6.13494815579885));
#66058=CARTESIAN_POINT('Ctrl Pts',(-2.85964932026176,0.691208915687925,
6.13999582173401));
#66059=CARTESIAN_POINT('Ctrl Pts',(-2.88156781018467,0.60052837990977,6.14505145868439));
#66060=CARTESIAN_POINT('Ctrl Pts',(-2.89914092304114,0.50891985594691,6.15010709563478));
#66061=CARTESIAN_POINT('Ctrl Pts',(-2.91232096194462,0.416834037259401,
6.15516273258516));
#66062=CARTESIAN_POINT('Ctrl Pts',(-2.9180893953109,0.376531355835743,6.15737540472414));
#66063=CARTESIAN_POINT('Ctrl Pts',(-2.92301700857039,0.336137285669298,
6.15958807686312));
#66064=CARTESIAN_POINT('Ctrl Pts',(-2.92710294302251,0.295689636187929,
6.1618007490021));
#66065=CARTESIAN_POINT('Ctrl Pts',(-2.93696575003513,0.198055333527562,
6.1671417936382));
#66066=CARTESIAN_POINT('Ctrl Pts',(-2.94194466883354,0.0999195090394462,
6.1724828382743));
#66067=CARTESIAN_POINT('Ctrl Pts',(-2.94199954141393,0.00164265645566952,
6.1778238829104));
#66068=CARTESIAN_POINT('',(-2.94171674527821,0.00106055427202949,7.17782383379665));
#66069=CARTESIAN_POINT('Ctrl Pts',(-2.94199954141428,0.00164265582640454,
6.1778238829446));
#66070=CARTESIAN_POINT('Ctrl Pts',(-2.94205080717708,-0.0901744176067026,
6.18281385845425));
#66071=CARTESIAN_POINT('Ctrl Pts',(-2.93779956711471,-0.182160903610382,
6.18780383396389));
#66072=CARTESIAN_POINT('Ctrl Pts',(-2.92922461152939,-0.273874378521423,
6.19279380947354));
#66073=CARTESIAN_POINT('Ctrl Pts',(-2.92066024317377,-0.365474617670936,
6.19777762401636));
#66074=CARTESIAN_POINT('Ctrl Pts',(-2.90778280444553,-0.456802064969237,
6.20276143855917));
#66075=CARTESIAN_POINT('Ctrl Pts',(-2.89062311501965,-0.547413926488978,
6.20774525310199));
#66076=CARTESIAN_POINT('Ctrl Pts',(-2.87347918866651,-0.637942550991512,
6.2127244894599));
#66077=CARTESIAN_POINT('Ctrl Pts',(-2.85206091248782,-0.727756450041725,
6.21770372581781));
#66078=CARTESIAN_POINT('Ctrl Pts',(-2.82645082215898,-0.816418856909155,
6.22268296217572));
#66079=CARTESIAN_POINT('Ctrl Pts',(-2.80085303484738,-0.905038670599187,
6.22765980652212));
#66080=CARTESIAN_POINT('Ctrl Pts',(-2.77106755726666,-0.992507653228784,
6.23263665086852));
#66081=CARTESIAN_POINT('Ctrl Pts',(-2.73722757790628,-1.07840121789125,
6.23761349521492));
#66082=CARTESIAN_POINT('Ctrl Pts',(-2.70339385391829,-1.16427890499577,
6.24258941958397));
#66083=CARTESIAN_POINT('Ctrl Pts',(-2.66550728414514,-1.24858132879256,
6.24756534395302));
#66084=CARTESIAN_POINT('Ctrl Pts',(-2.62374984100905,-1.33090223976256,
6.25254126832206));
#66085=CARTESIAN_POINT('Ctrl Pts',(-2.58198777541944,-1.41323226346925,
6.25751774351456));
#66086=CARTESIAN_POINT('Ctrl Pts',(-2.53635419345989,-1.4935799332287,6.26249421870706));
#66087=CARTESIAN_POINT('Ctrl Pts',(-2.48707721678308,-1.57156320832429,
6.26747069389957));
#66088=CARTESIAN_POINT('Ctrl Pts',(-2.43775032743971,-1.64962547270593,
6.27245220976549));
#66089=CARTESIAN_POINT('Ctrl Pts',(-2.3847729219904,-1.72531817690721,6.27743372563142));
#66090=CARTESIAN_POINT('Ctrl Pts',(-2.32841641952734,-1.79828834653274,
6.28241524149735));
#66091=CARTESIAN_POINT('Ctrl Pts',(-2.27202793949408,-1.87129992058581,
6.28739958395412));
#66092=CARTESIAN_POINT('Ctrl Pts',(-2.21225684298608,-1.94158553997426,
6.29238392641088));
#66093=CARTESIAN_POINT('Ctrl Pts',(-2.14941328097355,-2.00882715721749,
6.29736826886764));
#66094=CARTESIAN_POINT('Ctrl Pts',(-2.08647035740677,-2.07617508975199,
6.3023604920364));
#66095=CARTESIAN_POINT('Ctrl Pts',(-2.02044559977181,-2.1404690982592,6.30735271520517));
#66096=CARTESIAN_POINT('Ctrl Pts',(-1.95168397390846,-2.20142991393977,
6.31234493837394));
#66097=CARTESIAN_POINT('Ctrl Pts',(-1.91747594404155,-2.23175714046081,
6.31482850558334));
#66098=CARTESIAN_POINT('Ctrl Pts',(-1.88259104094524,-2.26126007576763,
6.31731207279274));
#66099=CARTESIAN_POINT('Ctrl Pts',(-1.84707437066062,-2.28990835389731,
6.31979564000214));
#66100=CARTESIAN_POINT('Ctrl Pts',(-1.77477066686261,-2.34822960416126,
6.3248516068603));
#66101=CARTESIAN_POINT('Ctrl Pts',(-1.69957457315796,-2.40322582802012,
6.32990757371846));
#66102=CARTESIAN_POINT('Ctrl Pts',(-1.62182459324367,-2.45459752072514,
6.33496354057661));
#66103=CARTESIAN_POINT('Ctrl Pts',(-1.54418060294483,-2.50589918298178,
6.34001261508594));
#66104=CARTESIAN_POINT('Ctrl Pts',(-1.46399001186172,-2.55358589060345,
6.34506168959526));
#66105=CARTESIAN_POINT('Ctrl Pts',(-1.38162424483441,-2.59739839956941,
6.35011076410459));
#66106=CARTESIAN_POINT('Ctrl Pts',(-1.29934542156755,-2.64116466087179,
6.35515450890547));
#66107=CARTESIAN_POINT('Ctrl Pts',(-1.21489637590213,-2.68106464535286,
6.36019825370634));
#66108=CARTESIAN_POINT('Ctrl Pts',(-1.12867643276995,-2.71688305050286,
6.36524199850721));
#66109=CARTESIAN_POINT('Ctrl Pts',(-1.042517365459,-2.75267616597218,6.3702821821586));
#66110=CARTESIAN_POINT('Ctrl Pts',(-0.954590294430732,-2.78439326068864,
6.37532236580998));
#66111=CARTESIAN_POINT('Ctrl Pts',(-0.86531706635547,-2.81186599514877,
6.38036254946136));
#66112=CARTESIAN_POINT('Ctrl Pts',(-0.776075385963216,-2.83932902119869,
6.38540095199516));
#66113=CARTESIAN_POINT('Ctrl Pts',(-0.685488917094498,-2.86255053659711,
6.39043935452896));
#66114=CARTESIAN_POINT('Ctrl Pts',(-0.593996331243704,-2.88141152188802,
6.39547775706276));
#66115=CARTESIAN_POINT('Ctrl Pts',(-0.5025105931954,-2.90027109552025,6.40051578249512));
#66116=CARTESIAN_POINT('Ctrl Pts',(-0.41011930741132,-2.91477069873775,
6.40555380792748));
#66117=CARTESIAN_POINT('Ctrl Pts',(-0.317271931378721,-2.92484230712687,
6.41059183335985));
#66118=CARTESIAN_POINT('Ctrl Pts',(-0.224405643466573,-2.93491596697994,
6.41563088497663));
#66119=CARTESIAN_POINT('Ctrl Pts',(-0.131083521679968,-2.94055979325709,
6.4206699365934));
#66120=CARTESIAN_POINT('Ctrl Pts',(-0.0377596101771619,-2.94175767388126,
6.42570898821018));
#66121=CARTESIAN_POINT('Ctrl Pts',(0.0556659328334915,-2.94295685902013,
6.43075352744964));
#66122=CARTESIAN_POINT('Ctrl Pts',(0.149092825385948,-2.9397004288215,6.43579806668911));
#66123=CARTESIAN_POINT('Ctrl Pts',(0.242067878670679,-2.93202441021828,
6.44084260592857));
#66124=CARTESIAN_POINT('Ctrl Pts',(0.335100559557109,-2.92434363388138,
6.44589027186372));
#66125=CARTESIAN_POINT('Ctrl Pts',(0.427680404283645,-2.912237872955,6.45093793779887));
#66126=CARTESIAN_POINT('Ctrl Pts',(0.519362342953723,-2.8957946675691,6.45598560373402));
#66127=CARTESIAN_POINT('Ctrl Pts',(0.61118906104042,-2.87932549591637,6.4610412406844));
#66128=CARTESIAN_POINT('Ctrl Pts',(0.70211461107622,-2.8585053059846,6.46609687763478));
#66129=CARTESIAN_POINT('Ctrl Pts',(0.791707273613052,-2.83347200319823,
6.47115251458516));
#66130=CARTESIAN_POINT('Ctrl Pts',(0.830918789432085,-2.82251581861328,
6.47336518672417));
#66131=CARTESIAN_POINT('Ctrl Pts',(0.869875227929949,-2.81075324335716,
6.47557785886319));
#66132=CARTESIAN_POINT('Ctrl Pts',(0.908541637458077,-2.79819872292963,
6.4777905310022));
#66133=CARTESIAN_POINT('Ctrl Pts',(0.996894575813124,-2.76951158122324,
6.48284649786035));
#66134=CARTESIAN_POINT('Ctrl Pts',(1.08404323289694,-2.73658516757626,6.4879024647185));
#66135=CARTESIAN_POINT('Ctrl Pts',(1.16955180473061,-2.69953932663545,6.49295843157666));
#66136=CARTESIAN_POINT('Ctrl Pts',(1.25494381035219,-2.66254398698661,6.49800750608598));
#66137=CARTESIAN_POINT('Ctrl Pts',(1.33869977024762,-2.62144055447741,6.5030565805953));
#66138=CARTESIAN_POINT('Ctrl Pts',(1.42039961040886,-2.57639844487423,6.50810565510463));
#66139=CARTESIAN_POINT('Ctrl Pts',(1.50201320975003,-2.53140388087777,6.51314939990553));
#66140=CARTESIAN_POINT('Ctrl Pts',(1.58157461725397,-2.48247911709228,6.51819314470643));
#66141=CARTESIAN_POINT('Ctrl Pts',(1.65868531518699,-2.4298409464784,6.52323688950733));
#66142=CARTESIAN_POINT('Ctrl Pts',(1.73574156890529,-2.37723994118581,6.52827707315871));
#66143=CARTESIAN_POINT('Ctrl Pts',(1.81035018721417,-2.32093098993557,6.53331725681009));
#66144=CARTESIAN_POINT('Ctrl Pts',(1.88213967803469,-2.26117540946461,6.53835744046147));
#66145=CARTESIAN_POINT('Ctrl Pts',(1.95390379963586,-2.20144094562801,6.54339584299526));
#66146=CARTESIAN_POINT('Ctrl Pts',(2.02285043250667,-2.13826255584747,6.54843424552905));
#66147=CARTESIAN_POINT('Ctrl Pts',(2.0886401971847,-2.07194259734778,6.55347264806285));
#66148=CARTESIAN_POINT('Ctrl Pts',(2.15442503779919,-2.00562760259421,6.55851067349521));
#66149=CARTESIAN_POINT('Ctrl Pts',(2.21705316792122,-1.93617182169925,6.56354869892758));
#66150=CARTESIAN_POINT('Ctrl Pts',(2.27622202327628,-1.86391451004386,6.56858672435995));
#66151=CARTESIAN_POINT('Ctrl Pts',(2.33540293060655,-1.79164248045412,6.57362577597674));
#66152=CARTESIAN_POINT('Ctrl Pts',(2.39112288311124,-1.71656813008922,6.57866482759353));
#66153=CARTESIAN_POINT('Ctrl Pts',(2.44312028738842,-1.63906292171812,6.58370387921032));
#66154=CARTESIAN_POINT('Ctrl Pts',(2.49517431782387,-1.56147330870688,6.58874841844977));
#66155=CARTESIAN_POINT('Ctrl Pts',(2.54349746104888,-1.48144792261921,6.59379295768923));
#66156=CARTESIAN_POINT('Ctrl Pts',(2.5878722580105,-1.39938599972261,6.59883749692869));
#66157=CARTESIAN_POINT('Ctrl Pts',(2.63227455926544,-1.31727321337756,6.60388516286385));
#66158=CARTESIAN_POINT('Ctrl Pts',(2.67272345017241,-1.23312177654122,6.608932828799));
#66159=CARTESIAN_POINT('Ctrl Pts',(2.70904905086834,-1.14735227371081,6.61398049473416));
#66160=CARTESIAN_POINT('Ctrl Pts',(2.74543201509027,-1.0614473280794,6.61903613168454));
#66161=CARTESIAN_POINT('Ctrl Pts',(2.77767853846176,-0.973919631385354,
6.62409176863493));
#66162=CARTESIAN_POINT('Ctrl Pts',(2.80566821755118,-0.885206107651309,
6.62914740558531));
#66163=CARTESIAN_POINT('Ctrl Pts',(2.81791830269533,-0.846379359559351,
6.63136007772429));
#66164=CARTESIAN_POINT('Ctrl Pts',(2.82935364752133,-0.807325612418335,
6.63357274986326));
#66165=CARTESIAN_POINT('Ctrl Pts',(2.83996725196405,-0.768082031928714,
6.63578542200224));
#66166=CARTESIAN_POINT('Ctrl Pts',(2.86421939097853,-0.678410255050615,
6.6408413888604));
#66167=CARTESIAN_POINT('Ctrl Pts',(2.88426305037514,-0.58743064818646,6.64589735571855));
#66168=CARTESIAN_POINT('Ctrl Pts',(2.89996046875691,-0.495573687403992,
6.6509533225767));
#66169=CARTESIAN_POINT('Ctrl Pts',(2.91563648824782,-0.403841947026036,
6.65600239708604));
#66170=CARTESIAN_POINT('Ctrl Pts',(2.92697796671261,-0.311235662961098,
6.66105147159537));
#66171=CARTESIAN_POINT('Ctrl Pts',(2.93389725427756,-0.218199223973404,
6.66610054610471));
#66172=CARTESIAN_POINT('Ctrl Pts',(2.94080923797221,-0.125260992507357,
6.6711442909056));
#66173=CARTESIAN_POINT('Ctrl Pts',(2.94330827688525,-0.0318939486430189,
6.6761880357065));
#66174=CARTESIAN_POINT('Ctrl Pts',(2.94135817884662,0.0614496845566321,
6.68123178050739));
#66175=CARTESIAN_POINT('Ctrl Pts',(2.93940945767992,0.154727412234268,6.68627196415877));
#66176=CARTESIAN_POINT('Ctrl Pts',(2.93301785288524,0.247981319954036,6.69131214781015));
#66177=CARTESIAN_POINT('Ctrl Pts',(2.92219922881418,0.340757490185938,6.69635233146153));
#66178=CARTESIAN_POINT('Ctrl Pts',(2.91138442786602,0.433500874852939,6.70139073399533));
#66179=CARTESIAN_POINT('Ctrl Pts',(2.89614576711634,0.525766417381258,6.70642913652912));
#66180=CARTESIAN_POINT('Ctrl Pts',(2.87655102977172,0.617104669500464,6.71146753906292));
#66181=CARTESIAN_POINT('Ctrl Pts',(2.8569577590038,0.708436085368164,6.71650556449527));
#66182=CARTESIAN_POINT('Ctrl Pts',(2.83300915322888,0.798839915285311,6.72154358992762));
#66183=CARTESIAN_POINT('Ctrl Pts',(2.80482401484709,0.88787738215198,6.72658161535997));
#66184=CARTESIAN_POINT('Ctrl Pts',(2.77663313549592,0.976932984866134,6.73162066697673));
#66185=CARTESIAN_POINT('Ctrl Pts',(2.74420414387257,1.06462124914391,6.7366597185935));
#66186=CARTESIAN_POINT('Ctrl Pts',(2.70770520375747,1.15052011262069,6.74169877021026));
#66187=CARTESIAN_POINT('Ctrl Pts',(2.67116651560502,1.23651252158737,6.74674330944972));
#66188=CARTESIAN_POINT('Ctrl Pts',(2.63054920594053,1.32071123146603,6.75178784868917));
#66189=CARTESIAN_POINT('Ctrl Pts',(2.58606881508641,1.40271596684346,6.75683238792862));
#66190=CARTESIAN_POINT('Ctrl Pts',(2.54156085448992,1.48477153022361,6.76188005386379));
#66191=CARTESIAN_POINT('Ctrl Pts',(2.4931852753493,1.56463003283944,6.76692771979894));
#66192=CARTESIAN_POINT('Ctrl Pts',(2.44120149563302,1.64191938222287,6.77197538573411));
#66193=CARTESIAN_POINT('Ctrl Pts',(2.38913562579732,1.71933078298377,6.77703102268449));
#66194=CARTESIAN_POINT('Ctrl Pts',(2.33345044580327,1.79416457673464,6.78208665963487));
#66195=CARTESIAN_POINT('Ctrl Pts',(2.27444609311608,1.86608117977462,6.78714229658525));
#66196=CARTESIAN_POINT('Ctrl Pts',(2.24862199052466,1.89755651422624,6.78935496872427));
#66197=CARTESIAN_POINT('Ctrl Pts',(2.22216258243794,1.92847353220668,6.79156764086329));
#66198=CARTESIAN_POINT('Ctrl Pts',(2.19509517053609,1.95880606296007,6.79378031300231));
#66199=CARTESIAN_POINT('Ctrl Pts',(2.13324599952761,2.02811604680667,6.79883627986046));
#66200=CARTESIAN_POINT('Ctrl Pts',(2.06800190455703,2.09461601085653,6.80389224671861));
#66201=CARTESIAN_POINT('Ctrl Pts',(1.99964813809884,2.15795535723004,6.80894821357677));
#66202=CARTESIAN_POINT('Ctrl Pts',(1.93138755223598,2.22120835872003,6.8139972880861));
#66203=CARTESIAN_POINT('Ctrl Pts',(1.86002604160601,2.281309005827,6.81904636259542));
#66204=CARTESIAN_POINT('Ctrl Pts',(1.78588789271304,2.33794106740546,6.82409543710475));
#66205=CARTESIAN_POINT('Ctrl Pts',(1.71182800266095,2.3945133492408,6.82913918190564));
#66206=CARTESIAN_POINT('Ctrl Pts',(1.63499765099952,2.44762405568488,6.83418292670652));
#66207=CARTESIAN_POINT('Ctrl Pts',(1.55575580312215,2.49699577113213,6.8392266715074));
#66208=CARTESIAN_POINT('Ctrl Pts',(1.4765699041633,2.54633262754772,6.84426685515878));
#66209=CARTESIAN_POINT('Ctrl Pts',(1.39497626872466,2.59193550654423,6.84930703881016));
#66210=CARTESIAN_POINT('Ctrl Pts',(1.31136372612226,2.63356966450685,6.85434722246154));
#66211=CARTESIAN_POINT('Ctrl Pts',(1.22778073081025,2.67518910964629,6.85938562499534));
#66212=CARTESIAN_POINT('Ctrl Pts',(1.14218064238477,2.71284242266176,6.86442402752913));
#66213=CARTESIAN_POINT('Ctrl Pts',(1.05497691667472,2.74634078462297,6.86946243006293));
#66214=CARTESIAN_POINT('Ctrl Pts',(0.967779717765627,2.77983663938464,6.87450045549528));
#66215=CARTESIAN_POINT('Ctrl Pts',(0.878979534310409,2.8091780026896,6.87953848092764));
#66216=CARTESIAN_POINT('Ctrl Pts',(0.7890087628912,2.83422461567197,6.88457650636));
#66217=CARTESIAN_POINT('Ctrl Pts',(0.699019665521892,2.85927633034428,6.88961555797676));
#66218=CARTESIAN_POINT('Ctrl Pts',(0.607859933921857,2.88003143873615,6.89465460959352));
#66219=CARTESIAN_POINT('Ctrl Pts',(0.515974938013121,2.89640015594226,6.89969366121029));
#66220=CARTESIAN_POINT('Ctrl Pts',(0.423989877602615,2.9127866989916,6.90473820044975));
#66221=CARTESIAN_POINT('Ctrl Pts',(0.331278413621512,2.92477723843429,6.90978273968921));
#66222=CARTESIAN_POINT('Ctrl Pts',(0.23829355673967,2.93233357256918,6.91482727892868));
#66223=CARTESIAN_POINT('Ctrl Pts',(0.145251066179789,2.93989459025518,6.91987494486382));
#66224=CARTESIAN_POINT('Ctrl Pts',(0.051935288190086,2.94301591615171,6.92492261079897));
#66225=CARTESIAN_POINT('Ctrl Pts',(-0.041200394394593,2.94171149630648,
6.92997027673411));
#66226=CARTESIAN_POINT('Ctrl Pts',(-0.134483152073845,2.94040501658832,
6.93502591368449));
#66227=CARTESIAN_POINT('Ctrl Pts',(-0.22758480473242,2.93465886741266,6.94008155063487));
#66228=CARTESIAN_POINT('Ctrl Pts',(-0.320056945971786,2.9245388613139,6.94513718758525));
#66229=CARTESIAN_POINT('Ctrl Pts',(-0.360528707011103,2.92010969526393,
6.94734985972429));
#66230=CARTESIAN_POINT('Ctrl Pts',(-0.400880016554807,2.91484337821709,
6.94956253186332));
#66231=CARTESIAN_POINT('Ctrl Pts',(-0.441074038102379,2.9087484753605,6.95177520400236));
#66232=CARTESIAN_POINT('Ctrl Pts',(-0.532917577529378,2.89482159197687,
6.95683117086051));
#66233=CARTESIAN_POINT('Ctrl Pts',(-0.624262754404763,2.87651596964992,
6.96188713771867));
#66234=CARTESIAN_POINT('Ctrl Pts',(-0.714660071314614,2.85387893619694,
6.96694310457682));
#66235=CARTESIAN_POINT('Ctrl Pts',(-0.80493415762276,2.8312727617932,6.97199217908619));
#66236=CARTESIAN_POINT('Ctrl Pts',(-0.894262525166504,2.80434701697255,
6.97704125359555));
#66237=CARTESIAN_POINT('Ctrl Pts',(-0.982203130010084,2.77320049967513,
6.98209032810491));
#66238=CARTESIAN_POINT('Ctrl Pts',(-1.07005090639836,2.74208686005798,6.98713407290579));
#66239=CARTESIAN_POINT('Ctrl Pts',(-1.15651341609533,2.70676145146423,6.99217781770668));
#66240=CARTESIAN_POINT('Ctrl Pts',(-1.24116217430607,2.66737332540307,6.99722156250756));
#66241=CARTESIAN_POINT('Ctrl Pts',(-1.32575116603479,2.62801300943361,7.00226174615894));
#66242=CARTESIAN_POINT('Ctrl Pts',(-1.40852855080163,2.58459586434057,7.00730192981032));
#66243=CARTESIAN_POINT('Ctrl Pts',(-1.48908526377058,2.53731926986363,7.01234211346171));
#66244=CARTESIAN_POINT('Ctrl Pts',(-1.56961350932878,2.49005938215369,7.0173805159955));
#66245=CARTESIAN_POINT('Ctrl Pts',(-1.64792226009275,2.43894297898139,7.02241891852929));
#66246=CARTESIAN_POINT('Ctrl Pts',(-1.72362745718247,2.38421315927219,7.02745732106309));
#66247=CARTESIAN_POINT('Ctrl Pts',(-1.79932698808367,2.32948743584025,7.03249534649545));
#66248=CARTESIAN_POINT('Ctrl Pts',(-1.87242299355824,2.27114909368057,7.03753337192781));
#66249=CARTESIAN_POINT('Ctrl Pts',(-1.94256173466028,2.20948362904857,7.04257139736016));
#66250=CARTESIAN_POINT('Ctrl Pts',(-2.01271476216936,2.14780560391272,7.04761044897692));
#66251=CARTESIAN_POINT('Ctrl Pts',(-2.07990899620287,2.08279940342091,7.05264950059368));
#66252=CARTESIAN_POINT('Ctrl Pts',(-2.14382588137846,2.01478896918061,7.05768855221044));
#66253=CARTESIAN_POINT('Ctrl Pts',(-2.20781237325329,1.94670447028857,7.0627330914499));
#66254=CARTESIAN_POINT('Ctrl Pts',(-2.26851408828369,1.87560953107339,7.06777763068936));
#66255=CARTESIAN_POINT('Ctrl Pts',(-2.32565149749558,1.80186267850704,7.07282216992883));
#66256=CARTESIAN_POINT('Ctrl Pts',(-2.38282432149591,1.72807011632212,7.07786983586396));
#66257=CARTESIAN_POINT('Ctrl Pts',(-2.43642818706021,1.65162273118897,7.08291750179909));
#66258=CARTESIAN_POINT('Ctrl Pts',(-2.48622703614279,1.57290785640883,7.08796516773422));
#66259=CARTESIAN_POINT('Ctrl Pts',(-2.53610452501461,1.49406867913423,7.0930208046846));
#66260=CARTESIAN_POINT('Ctrl Pts',(-2.58216478447112,1.41295524956243,7.09807644163498));
#66261=CARTESIAN_POINT('Ctrl Pts',(-2.62421791442431,1.32997907412655,7.10313207858535));
#66262=CARTESIAN_POINT('Ctrl Pts',(-2.64262307087035,1.29366335893743,7.10534475072438));
#66263=CARTESIAN_POINT('Ctrl Pts',(-2.66026128731189,1.25699108606173,7.1075574228634));
#66264=CARTESIAN_POINT('Ctrl Pts',(-2.67711960893711,1.21999778665553,7.10977009500242));
#66265=CARTESIAN_POINT('Ctrl Pts',(-2.72032798952284,1.12518285813541,7.11544123961691));
#66266=CARTESIAN_POINT('Ctrl Pts',(-2.75854574650834,1.02795888196169,7.1211123842314));
#66267=CARTESIAN_POINT('Ctrl Pts',(-2.79152320776205,0.928849923575334,
7.12678352884589));
#66268=CARTESIAN_POINT('Ctrl Pts',(-2.82342445984176,0.832975355168836,
7.13226959742272));
#66269=CARTESIAN_POINT('Ctrl Pts',(-2.85042193779947,0.735337238862226,
7.13775566599955));
#66270=CARTESIAN_POINT('Ctrl Pts',(-2.872336278233,0.636434053729535,7.14324173457637));
#66271=CARTESIAN_POINT('Ctrl Pts',(-2.89419608233716,0.537777000425265,
7.14871415044739));
#66272=CARTESIAN_POINT('Ctrl Pts',(-2.91099787708547,0.437861453721849,
7.15418656631841));
#66273=CARTESIAN_POINT('Ctrl Pts',(-2.92261169191948,0.337201569177166,
7.15965898218943));
#66274=CARTESIAN_POINT('Ctrl Pts',(-2.93418480596277,0.236894448728771,
7.1651122198958));
#66275=CARTESIAN_POINT('Ctrl Pts',(-2.94060613122474,0.135848499407986,
7.17056545760217));
#66276=CARTESIAN_POINT('Ctrl Pts',(-2.94179668125678,0.03458736975534,7.17601869530855));
#66277=CARTESIAN_POINT('Ctrl Pts',(-2.94192804686186,0.0234141899564756,
7.1766204069978));
#66278=CARTESIAN_POINT('Ctrl Pts',(-2.94199577873787,0.0122384025922069,
7.17722211868706));
#66279=CARTESIAN_POINT('Ctrl Pts',(-2.94199980878204,0.00106071977267785,
7.17782383037631));
#66280=CARTESIAN_POINT('',(-2.94179645842688,-0.00262223567938445,8.17782388291039));
#66281=CARTESIAN_POINT('Ctrl Pts',(-2.93765213932985,0.00105817779144944,
7.17782388291039));
#66282=CARTESIAN_POINT('Ctrl Pts',(-2.93583728528984,-0.555049110608679,
7.20780425060775));
#66283=CARTESIAN_POINT('Ctrl Pts',(-2.51737468444769,-2.09057369894412,
7.2904495819718));
#66284=CARTESIAN_POINT('Ctrl Pts',(-0.0450203642769795,-3.47131362076717,
7.42575987700252));
#66285=CARTESIAN_POINT('Ctrl Pts',(2.88266152300012,-1.93450449230245,7.58375476800256));
#66286=CARTESIAN_POINT('Ctrl Pts',(3.19531528460893,1.35720496568047,7.74174965900263));
#66287=CARTESIAN_POINT('Ctrl Pts',(0.609314704401834,3.41771571051832,7.89974455000268));
#66288=CARTESIAN_POINT('Ctrl Pts',(-2.27838582827551,2.4609932925897,8.04510262463861));
#66289=CARTESIAN_POINT('Ctrl Pts',(-2.93514585523751,0.737219387421443,
8.13779573560784));
#66290=CARTESIAN_POINT('Ctrl Pts',(-2.94179645842688,-0.00262223567938445,
8.17782388291039));
#66291=CARTESIAN_POINT('',(-2.94199962980641,0.00147587903620585,9.1778238829104));
#66292=CARTESIAN_POINT('Ctrl Pts',(-2.94179645842688,-0.00262223567938445,
8.17782388291039));
#66293=CARTESIAN_POINT('Ctrl Pts',(-2.94389604226671,-0.236188947098698,
8.19046069927452));
#66294=CARTESIAN_POINT('Ctrl Pts',(-2.81210260417286,-1.44082338645902,
8.25576247930533));
#66295=CARTESIAN_POINT('Ctrl Pts',(-1.15736505241686,-3.2730033947992,8.37372922300285));
#66296=CARTESIAN_POINT('Ctrl Pts',(2.10876587186763,-2.75774393020281,8.53172411400289));
#66297=CARTESIAN_POINT('Ctrl Pts',(3.46191394284634,0.259223724318882,8.68971900500295));
#66298=CARTESIAN_POINT('Ctrl Pts',(1.67456068997757,3.0410346236939,8.84771389600301));
#66299=CARTESIAN_POINT('Ctrl Pts',(-1.63188291307294,3.06414804553308,9.00570878700305));
#66300=CARTESIAN_POINT('Ctrl Pts',(-2.90366142307977,1.14432815538467,9.11574544930552));
#66301=CARTESIAN_POINT('Ctrl Pts',(-2.94630689264378,0.0881682471389342,
9.1731171479413));
#66302=CARTESIAN_POINT('Ctrl Pts',(-2.94577110767244,0.00147777103002609,
9.1778238829104));
#66303=CARTESIAN_POINT('',(-2.94199974257833,0.00123071890407352,10.177823882882));
#66304=CARTESIAN_POINT('Ctrl Pts',(-2.94199962980641,0.00147587903620585,
9.1778238829104));
#66305=CARTESIAN_POINT('Ctrl Pts',(-2.94204572414441,-0.090408023372339,
9.1828189994887));
#66306=CARTESIAN_POINT('Ctrl Pts',(-2.93778304636917,-0.182462980810345,
9.18781411606701));
#66307=CARTESIAN_POINT('Ctrl Pts',(-2.92918984160053,-0.274246006104506,
9.19280923264531));
#66308=CARTESIAN_POINT('Ctrl Pts',(-2.92060748250135,-0.365913190058677,
9.19779804477902));
#66309=CARTESIAN_POINT('Ctrl Pts',(-2.9077054945994,-0.457308674286831,
9.20278685691273));
#66310=CARTESIAN_POINT('Ctrl Pts',(-2.89051414762716,-0.547989016648372,
9.20777566904644));
#66311=CARTESIAN_POINT('Ctrl Pts',(-2.873339267682,-0.638582499285849,9.21275970256072));
#66312=CARTESIAN_POINT('Ctrl Pts',(-2.85188327766594,-0.728461756432582,
9.217743736075));
#66313=CARTESIAN_POINT('Ctrl Pts',(-2.82622816886955,-0.817189291099845,
9.22272776958929));
#66314=CARTESIAN_POINT('Ctrl Pts',(-2.80058607711949,-0.905871806646775,
9.2277092742741));
#66315=CARTESIAN_POINT('Ctrl Pts',(-2.77074922233177,-0.993403323725543,
9.23269077895892));
#66316=CARTESIAN_POINT('Ctrl Pts',(-2.73685027191682,-1.07935841549916,
9.23767228364374));
#66317=CARTESIAN_POINT('Ctrl Pts',(-2.70295853881579,-1.16529520685717,
9.24265272773279));
#66318=CARTESIAN_POINT('Ctrl Pts',(-2.66500659490321,-1.24965581662519,
9.24763317182184));
#66319=CARTESIAN_POINT('Ctrl Pts',(-2.62317593448274,-1.33203303891104,
9.25261361591089));
#66320=CARTESIAN_POINT('Ctrl Pts',(-2.58134186177172,-1.41441698102908,
9.25759446627424));
#66321=CARTESIAN_POINT('Ctrl Pts',(-2.53562865177555,-1.49481680959483,
9.2625753166376));
#66322=CARTESIAN_POINT('Ctrl Pts',(-2.48626401269523,-1.57284940766006,
9.26755616700095));
#66323=CARTESIAN_POINT('Ctrl Pts',(-2.43685013110183,-1.65095984527407,
9.27254198589226));
#66324=CARTESIAN_POINT('Ctrl Pts',(-2.38377779299346,-1.72669795348462,
9.27752780478357));
#66325=CARTESIAN_POINT('Ctrl Pts',(-2.32731810365292,-1.79970954445693,
9.28251362367488));
#66326=CARTESIAN_POINT('Ctrl Pts',(-2.2708279617166,-1.87276051560461,9.28750213176142));
#66327=CARTESIAN_POINT('Ctrl Pts',(-2.21094712780141,-1.94308169708971,
9.29249063984796));
#66328=CARTESIAN_POINT('Ctrl Pts',(-2.14798555653675,-2.01035371238733,
9.2974791479345));
#66329=CARTESIAN_POINT('Ctrl Pts',(-2.08492219063923,-2.07773449133175,
9.30247572131133));
#66330=CARTESIAN_POINT('Ctrl Pts',(-2.01876847020445,-2.14205594622441,
9.30747229468816));
#66331=CARTESIAN_POINT('Ctrl Pts',(-1.94986937444732,-2.20303731756692,
9.31246886806499));
#66332=CARTESIAN_POINT('Ctrl Pts',(-1.90744576391868,-2.24058570508794,
9.31554543504438));
#66333=CARTESIAN_POINT('Ctrl Pts',(-1.86398193743162,-2.27686857571756,
9.31862200202377));
#66334=CARTESIAN_POINT('Ctrl Pts',(-1.81956381119789,-2.3118286132365,9.32169856900316));
#66335=CARTESIAN_POINT('Ctrl Pts',(-1.74656797667083,-2.36928121941724,
9.32675453586132));
#66336=CARTESIAN_POINT('Ctrl Pts',(-1.67071971356128,-2.42337445495032,
9.33181050271948));
#66337=CARTESIAN_POINT('Ctrl Pts',(-1.5923610823007,-2.47381288370284,9.33686646957763));
#66338=CARTESIAN_POINT('Ctrl Pts',(-1.51410927037554,-2.5241825542426,9.34191554408697));
#66339=CARTESIAN_POINT('Ctrl Pts',(-1.43335426070549,-2.57090708094193,
9.3469646185963));
#66340=CARTESIAN_POINT('Ctrl Pts',(-1.35047055114782,-2.613731679129,9.35201369310564));
#66341=CARTESIAN_POINT('Ctrl Pts',(-1.26767433208128,-2.65651107247247,
9.35705743790651));
#66342=CARTESIAN_POINT('Ctrl Pts',(-1.18275427160391,-2.6953985177973,9.36210118270738));
#66343=CARTESIAN_POINT('Ctrl Pts',(-1.09611224029828,-2.73018350238007,
9.36714492750825));
#66344=CARTESIAN_POINT('Ctrl Pts',(-1.00953138283035,-2.76494392693152,
9.37218511115963));
#66345=CARTESIAN_POINT('Ctrl Pts',(-0.921231381617468,-2.79560748351997,
9.37722529481101));
#66346=CARTESIAN_POINT('Ctrl Pts',(-0.831636065873206,-2.82201088834521,
9.38226547846238));
#66347=CARTESIAN_POINT('Ctrl Pts',(-0.74207241163243,-2.84840496264367,
9.38730388099618));
#66348=CARTESIAN_POINT('Ctrl Pts',(-0.651214777262631,-2.87054175094294,
9.39234228352997));
#66349=CARTESIAN_POINT('Ctrl Pts',(-0.559503225919944,-2.88830748712549,
9.39738068606376));
#66350=CARTESIAN_POINT('Ctrl Pts',(-0.467798538768296,-2.90607189362377,
9.40241871149612));
#66351=CARTESIAN_POINT('Ctrl Pts',(-0.37524049715759,-2.91946581446411,
9.40745673692848));
#66352=CARTESIAN_POINT('Ctrl Pts',(-0.282279339760464,-2.92842660388551,
9.41249476236084));
#66353=CARTESIAN_POINT('Ctrl Pts',(-0.189299247307974,-2.93738921851055,
9.41753381397761));
#66354=CARTESIAN_POINT('Ctrl Pts',(-0.0959163174091777,-2.9419168661658,
9.42257286559438));
#66355=CARTESIAN_POINT('Ctrl Pts',(-0.00258475440709994,-2.9419988645553,
9.42761191721115));
#66356=CARTESIAN_POINT('Ctrl Pts',(0.0908484484355715,-2.94208095224259,
9.43265645645062));
#66357=CARTESIAN_POINT('Ctrl Pts',(0.184229728626193,-2.93770772693357,
9.43770099569008));
#66358=CARTESIAN_POINT('Ctrl Pts',(0.277106360492218,-2.92892063138876,
9.44274553492954));
#66359=CARTESIAN_POINT('Ctrl Pts',(0.370040558956836,-2.92012808944488,
9.4477932008647));
#66360=CARTESIAN_POINT('Ctrl Pts',(0.462469047758238,-2.90691629338502,
9.45284086679987));
#66361=CARTESIAN_POINT('Ctrl Pts',(0.553947835457103,-2.88937809841363,
9.45788853273503));
#66362=CARTESIAN_POINT('Ctrl Pts',(0.645571081766846,-2.87181220802404,
9.46294416968541));
#66363=CARTESIAN_POINT('Ctrl Pts',(0.736241202921866,-2.8499063848746,9.4679998066358));
#66364=CARTESIAN_POINT('Ctrl Pts',(0.825528159153147,-2.823803686244,9.47305544358618));
#66365=CARTESIAN_POINT('Ctrl Pts',(0.864605878215817,-2.81237946520524,
9.47526811572519));
#66366=CARTESIAN_POINT('Ctrl Pts',(0.903418896845142,-2.80015196088214,
9.4774807878642));
#66367=CARTESIAN_POINT('Ctrl Pts',(0.941932438603662,-2.78713603562979,
9.47969346000321));
#66368=CARTESIAN_POINT('Ctrl Pts',(1.02993607334383,-2.7573945816006,9.48474942686136));
#66369=CARTESIAN_POINT('Ctrl Pts',(1.11668482743304,-2.72342855723606,9.48980539371952));
#66370=CARTESIAN_POINT('Ctrl Pts',(1.20174436092563,-2.68536300916346,9.49486136057767));
#66371=CARTESIAN_POINT('Ctrl Pts',(1.28668794034038,-2.64734935245851,9.49991043508701));
#66372=CARTESIAN_POINT('Ctrl Pts',(1.36994647391018,-2.60524745737157,9.50495950959635));
#66373=CARTESIAN_POINT('Ctrl Pts',(1.45110194321668,-2.55923175003609,9.5100085841057));
#66374=CARTESIAN_POINT('Ctrl Pts',(1.53217174633044,-2.51326461601905,9.51505232890659));
#66375=CARTESIAN_POINT('Ctrl Pts',(1.61114251415322,-2.46339209948992,9.52009607370749));
#66376=CARTESIAN_POINT('Ctrl Pts',(1.68761834945002,-2.40983574265957,9.52513981850839));
#66377=CARTESIAN_POINT('Ctrl Pts',(1.76404018877863,-2.3563171994383,9.53018000215977));
#66378=CARTESIAN_POINT('Ctrl Pts',(1.83797023481414,-2.29912023964101,9.53522018581115));
#66379=CARTESIAN_POINT('Ctrl Pts',(1.90904014637848,-2.23851060294903,9.54026036946253));
#66380=CARTESIAN_POINT('Ctrl Pts',(1.98008494301095,-2.1779223847007,9.54529877199633));
#66381=CARTESIAN_POINT('Ctrl Pts',(2.04827127613392,-2.11392417304796,9.55033717453013));
#66382=CARTESIAN_POINT('Ctrl Pts',(2.11326340557759,-2.04682236128263,9.55537557706393));
#66383=CARTESIAN_POINT('Ctrl Pts',(2.17825067065679,-1.97972557178187,9.56041360249628));
#66384=CARTESIAN_POINT('Ctrl Pts',(2.24004389910237,-1.90952596280487,9.56545162792863));
#66385=CARTESIAN_POINT('Ctrl Pts',(2.29834460446165,-1.83656638299355,9.57048965336099));
#66386=CARTESIAN_POINT('Ctrl Pts',(2.35665718496453,-1.76359194220445,9.57552870497775));
#66387=CARTESIAN_POINT('Ctrl Pts',(2.41147555299702,-1.68785676070982,9.58056775659452));
#66388=CARTESIAN_POINT('Ctrl Pts',(2.46254257512752,-1.60973540238275,9.58560680821129));
#66389=CARTESIAN_POINT('Ctrl Pts',(2.51366521021272,-1.53152896841622,9.59065134745075));
#66390=CARTESIAN_POINT('Ctrl Pts',(2.5610281022436,-1.45093154260062,9.59569588669021));
#66391=CARTESIAN_POINT('Ctrl Pts',(2.6044185810476,-1.36834493264454,9.60074042592966));
#66392=CARTESIAN_POINT('Ctrl Pts',(2.64783595404679,-1.28570713402981,9.60578809186481));
#66393=CARTESIAN_POINT('Ctrl Pts',(2.68727582482498,-1.2010780982904,9.61083575779996));
#66394=CARTESIAN_POINT('Ctrl Pts',(2.72257335424169,-1.11488041097381,9.61588342373511));
#66395=CARTESIAN_POINT('Ctrl Pts',(2.75792662370707,-1.02854660468899,9.62093906068549));
#66396=CARTESIAN_POINT('Ctrl Pts',(2.78912434609606,-0.940639619324569,
9.62599469763587));
#66397=CARTESIAN_POINT('Ctrl Pts',(2.81605135052136,-0.851597787236908,
9.63105033458626));
#66398=CARTESIAN_POINT('Ctrl Pts',(2.82783634083285,-0.812627350277191,
9.63326300672526));
#66399=CARTESIAN_POINT('Ctrl Pts',(2.83880393502246,-0.773439671668044,
9.63547567886426));
#66400=CARTESIAN_POINT('Ctrl Pts',(2.84894757788484,-0.734071998147376,
9.63768835100327));
#66401=CARTESIAN_POINT('Ctrl Pts',(2.87212585234727,-0.644116668076289,
9.64274431786142));
#66402=CARTESIAN_POINT('Ctrl Pts',(2.89108031136519,-0.552903918800198,
9.64780028471957));
#66403=CARTESIAN_POINT('Ctrl Pts',(2.90567835023381,-0.460865842716244,
9.65285625157773));
#66404=CARTESIAN_POINT('Ctrl Pts',(2.92025648889761,-0.368953233935213,
9.65790532608706));
#66405=CARTESIAN_POINT('Ctrl Pts',(2.93048994016416,-0.276217968489724,
9.66295440059639));
#66406=CARTESIAN_POINT('Ctrl Pts',(2.93629637361263,-0.183105451337015,
9.66800347510572));
#66407=CARTESIAN_POINT('Ctrl Pts',(2.94209667789873,-0.0900912220130057,
9.67304721990659));
#66408=CARTESIAN_POINT('Ctrl Pts',(2.94347922587559,0.00329902713788016,
9.67809096470747));
#66409=CARTESIAN_POINT('Ctrl Pts',(2.94041323481618,0.0966126726567079,
9.68313470950834));
#66410=CARTESIAN_POINT('Ctrl Pts',(2.93734940850794,0.18986043382687,9.68817489315972));
#66411=CARTESIAN_POINT('Ctrl Pts',(2.9298433009337,0.283031256866857,9.6932150768111));
#66412=CARTESIAN_POINT('Ctrl Pts',(2.91791620242656,0.37567144636848,9.69825526046248));
#66413=CARTESIAN_POINT('Ctrl Pts',(2.90599331875885,0.468278898358642,9.70329366299628));
#66414=CARTESIAN_POINT('Ctrl Pts',(2.88965260465848,0.560355649942324,9.70833206553008));
#66415=CARTESIAN_POINT('Ctrl Pts',(2.86896721216729,0.651453095402149,9.71337046806389));
#66416=CARTESIAN_POINT('Ctrl Pts',(2.84828336788339,0.742543722633653,9.71840849349624));
#66417=CARTESIAN_POINT('Ctrl Pts',(2.82325559027714,0.832654757087544,9.72344651892859));
#66418=CARTESIAN_POINT('Ctrl Pts',(2.79400791935088,0.921348873448373,9.72848454436094));
#66419=CARTESIAN_POINT('Ctrl Pts',(2.7647542910301,1.01006105572096,9.73352359597774));
#66420=CARTESIAN_POINT('Ctrl Pts',(2.73127920149873,1.09735532569753,9.73856264759454));
#66421=CARTESIAN_POINT('Ctrl Pts',(2.6937558487669,1.18281166177633,9.74360169921134));
#66422=CARTESIAN_POINT('Ctrl Pts',(2.65619163239318,1.26836106142387,9.7486462384508));
#66423=CARTESIAN_POINT('Ctrl Pts',(2.61457053180976,1.35206812549773,9.75369077769027));
#66424=CARTESIAN_POINT('Ctrl Pts',(2.56911285769389,1.43353518423231,9.75873531692973));
#66425=CARTESIAN_POINT('Ctrl Pts',(2.52362700809808,1.51505273770784,9.76378298286489));
#66426=CARTESIAN_POINT('Ctrl Pts',(2.47430008483955,1.59432714555223,9.76883064880005));
#66427=CARTESIAN_POINT('Ctrl Pts',(2.42139593614525,1.67098944353914,9.77387831473521));
#66428=CARTESIAN_POINT('Ctrl Pts',(2.36840824393209,1.74777280269605,9.77893395168559));
#66429=CARTESIAN_POINT('Ctrl Pts',(2.31183231856937,1.82193546599406,9.78398958863597));
#66430=CARTESIAN_POINT('Ctrl Pts',(2.2519723361899,1.89314146249968,9.78904522558635));
#66431=CARTESIAN_POINT('Ctrl Pts',(2.22577375497221,1.92430578979287,9.79125789772534));
#66432=CARTESIAN_POINT('Ctrl Pts',(2.19894658899634,1.95490424470108,9.79347056986433));
#66433=CARTESIAN_POINT('Ctrl Pts',(2.17151845089302,1.98491098476259,9.79568324200333));
#66434=CARTESIAN_POINT('Ctrl Pts',(2.10884501871682,2.05347653525637,9.80073920886148));
#66435=CARTESIAN_POINT('Ctrl Pts',(2.04281050231568,2.1191916765165,9.80579517571964));
#66436=CARTESIAN_POINT('Ctrl Pts',(1.97370432558301,2.1817092462505,9.81085114257779));
#66437=CARTESIAN_POINT('Ctrl Pts',(1.90469235513961,2.24414159135571,9.81590021708712));
#66438=CARTESIAN_POINT('Ctrl Pts',(1.83261737166266,2.30338473221478,9.82094929159644));
#66439=CARTESIAN_POINT('Ctrl Pts',(1.7578074193906,2.35912633751043,9.82599836610577));
#66440=CARTESIAN_POINT('Ctrl Pts',(1.68307643510208,2.41480910301223,9.83104211090667));
#66441=CARTESIAN_POINT('Ctrl Pts',(1.6056165744162,2.46699741643588,9.83608585570757));
#66442=CARTESIAN_POINT('Ctrl Pts',(1.52579009389671,2.51541817385632,9.84112960050847));
#66443=CARTESIAN_POINT('Ctrl Pts',(1.44601997507753,2.56380474367134,9.84616978415985));
#66444=CARTESIAN_POINT('Ctrl Pts',(1.36388693594899,2.60842881565462,9.85120996781123));
#66445=CARTESIAN_POINT('Ctrl Pts',(1.27978258466925,2.64906031187991,9.85625015146261));
#66446=CARTESIAN_POINT('Ctrl Pts',(1.19570795447693,2.68967744960611,9.86128855399641));
#66447=CARTESIAN_POINT('Ctrl Pts',(1.1096637951006,2.72630462198829,9.86632695653021));
#66448=CARTESIAN_POINT('Ctrl Pts',(1.0220657903677,2.75875796694093,9.871365359064));
#66449=CARTESIAN_POINT('Ctrl Pts',(0.934474341945591,2.79120888290884,9.87640338449637));
#66450=CARTESIAN_POINT('Ctrl Pts',(0.845329695363665,2.81948643881613,9.88144140992873));
#66451=CARTESIAN_POINT('Ctrl Pts',(0.755065893256345,2.84345555562963,9.8864794353611));
#66452=CARTESIAN_POINT('Ctrl Pts',(0.664783705512163,2.86742955466022,9.89151848697787));
#66453=CARTESIAN_POINT('Ctrl Pts',(0.57338233816931,2.88709325821866,9.89655753859464));
#66454=CARTESIAN_POINT('Ctrl Pts',(0.481308202799502,2.90236221273602,9.90159659021141));
#66455=CARTESIAN_POINT('Ctrl Pts',(0.389133796951625,2.91764779543416,9.90664112945088));
#66456=CARTESIAN_POINT('Ctrl Pts',(0.296285598824076,2.92852900373624,9.91168566869033));
#66457=CARTESIAN_POINT('Ctrl Pts',(0.203217043452678,2.93497305494452,9.9167302079298));
#66458=CARTESIAN_POINT('Ctrl Pts',(0.110090802525321,2.94142110029105,9.92177787386495));
#66459=CARTESIAN_POINT('Ctrl Pts',(0.0167443754147969,2.94342650371529,
9.9268255398001));
#66460=CARTESIAN_POINT('Ctrl Pts',(-0.076369054192065,2.9410086309907,9.93187320573525));
#66461=CARTESIAN_POINT('Ctrl Pts',(-0.169629523752704,2.93858694008548,
9.93692884268563));
#66462=CARTESIAN_POINT('Ctrl Pts',(-0.262655819791868,2.93172806238203,
9.94198447963601));
#66463=CARTESIAN_POINT('Ctrl Pts',(-0.355000354827928,2.92050316693409,
9.94704011658639));
#66464=CARTESIAN_POINT('Ctrl Pts',(-0.395416267178388,2.91559043018805,
9.94925278872538));
#66465=CARTESIAN_POINT('Ctrl Pts',(-0.435701727522635,2.90984204242133,
9.95146546086437));
#66466=CARTESIAN_POINT('Ctrl Pts',(-0.475820004399961,2.90326700863231,
9.95367813300336));
#66467=CARTESIAN_POINT('Ctrl Pts',(-0.567490466880002,2.88824302367643,
9.95873409986152));
#66468=CARTESIAN_POINT('Ctrl Pts',(-0.658610249480061,2.86884657126655,
9.96379006671967));
#66469=CARTESIAN_POINT('Ctrl Pts',(-0.748730452774665,2.84513035010487,
9.96884603357783));
#66470=CARTESIAN_POINT('Ctrl Pts',(-0.838727803231509,2.82144645915288,
9.97389510808717));
#66471=CARTESIAN_POINT('Ctrl Pts',(-0.927727857000532,2.79345461371134,
9.97894418259651));
#66472=CARTESIAN_POINT('Ctrl Pts',(-1.01528978298722,2.76125888981127,9.98399325710585));
#66473=CARTESIAN_POINT('Ctrl Pts',(-1.1027592802453,2.72909715111417,9.98903700190674));
#66474=CARTESIAN_POINT('Ctrl Pts',(-1.18879325319887,2.69274050697242,9.99408074670762));
#66475=CARTESIAN_POINT('Ctrl Pts',(-1.27296502976534,2.65234312127872,9.9991244915085));
#66476=CARTESIAN_POINT('Ctrl Pts',(-1.35707737662388,2.61197425826721,10.0041646751599));
#66477=CARTESIAN_POINT('Ctrl Pts',(-1.43932974186841,2.56757051598641,10.0092048588113));
#66478=CARTESIAN_POINT('Ctrl Pts',(-1.51931544980777,2.51933415091675,10.0142450424626));
#66479=CARTESIAN_POINT('Ctrl Pts',(-1.59927289212015,2.47111483178113,10.0192834449964));
#66480=CARTESIAN_POINT('Ctrl Pts',(-1.67696488912535,2.41906580949601,10.0243218475302));
#66481=CARTESIAN_POINT('Ctrl Pts',(-1.75201031592716,2.36343475748429,10.029360250064));
#66482=CARTESIAN_POINT('Ctrl Pts',(-1.82705012592134,2.30780786920286,10.0343982754964));
#66483=CARTESIAN_POINT('Ctrl Pts',(-1.89944340349649,2.2485997486092,10.0394363009288));
#66484=CARTESIAN_POINT('Ctrl Pts',(-1.96883984843305,2.18610010091535,10.0444743263611));
#66485=CARTESIAN_POINT('Ctrl Pts',(-2.03825042858016,2.12358772280455,10.0495133779779));
#66486=CARTESIAN_POINT('Ctrl Pts',(-2.10466263450646,2.05778278306738,10.0545524295947));
#66487=CARTESIAN_POINT('Ctrl Pts',(-2.16776180670031,1.98901300885927,10.0595914812115));
#66488=CARTESIAN_POINT('Ctrl Pts',(-2.23092969508812,1.92016834306418,10.0646360204509));
#66489=CARTESIAN_POINT('Ctrl Pts',(-2.29077704808106,1.84835272547744,10.0696805596904));
#66490=CARTESIAN_POINT('Ctrl Pts',(-2.34702864329479,1.77392799954052,10.0747250989298));
#66491=CARTESIAN_POINT('Ctrl Pts',(-2.40331510425386,1.69945714382662,10.079772764865));
#66492=CARTESIAN_POINT('Ctrl Pts',(-2.45600112036106,1.62237432600091,10.0848204308001));
#66493=CARTESIAN_POINT('Ctrl Pts',(-2.50485528146661,1.54306967402927,10.0898680967353));
#66494=CARTESIAN_POINT('Ctrl Pts',(-2.55378659055836,1.46363978821765,10.0949237336857));
#66495=CARTESIAN_POINT('Ctrl Pts',(-2.59887375173245,1.38198145211319,10.0999793706361));
#66496=CARTESIAN_POINT('Ctrl Pts',(-2.63993179851563,1.29850841321343,10.1050350075864));
#66497=CARTESIAN_POINT('Ctrl Pts',(-2.65790144251704,1.26197523859199,10.1072476797254));
#66498=CARTESIAN_POINT('Ctrl Pts',(-2.67509993826843,1.22509470143544,10.1094603518644));
#66499=CARTESIAN_POINT('Ctrl Pts',(-2.69151475670051,1.18790248525012,10.1116730240034));
#66500=CARTESIAN_POINT('Ctrl Pts',(-2.73261802804903,1.09477189350805,10.117213631334));
#66501=CARTESIAN_POINT('Ctrl Pts',(-2.7689288940169,0.999403769174305,10.1227542386645));
#66502=CARTESIAN_POINT('Ctrl Pts',(-2.80022210883355,0.902286063950788,
10.1282948459951));
#66503=CARTESIAN_POINT('Ctrl Pts',(-2.83143484581624,0.805418119661116,
10.1338212043557));
#66504=CARTESIAN_POINT('Ctrl Pts',(-2.85765555046733,0.706809841115378,
10.1393475627163));
#66505=CARTESIAN_POINT('Ctrl Pts',(-2.87870681400129,0.606968762806256,
10.1448739210769));
#66506=CARTESIAN_POINT('Ctrl Pts',(-2.89966358194114,0.507575854365658,
10.150375472541));
#66507=CARTESIAN_POINT('Ctrl Pts',(-2.91549709249138,0.406961465818858,
10.1558770240051));
#66508=CARTESIAN_POINT('Ctrl Pts',(-2.92608011603149,0.305645472018067,
10.1613785754692));
#66509=CARTESIAN_POINT('Ctrl Pts',(-2.93662508542849,0.204693787463402,
10.1668603446068));
#66510=CARTESIAN_POINT('Ctrl Pts',(-2.94195715053947,0.103045818157862,
10.1723421137444));
#66511=CARTESIAN_POINT('Ctrl Pts',(-2.94199974257833,0.0012307189040667,
10.177823882882));
#66512=CARTESIAN_POINT('',(-2.94199883612238,-0.00261691699413304,11.1778238829104));
#66513=CARTESIAN_POINT('Ctrl Pts',(-2.94199974257855,0.00123071837608816,
10.1778238829104));
#66514=CARTESIAN_POINT('Ctrl Pts',(-2.9420396062843,-0.0940624163727975,
10.1829545066481));
#66515=CARTESIAN_POINT('Ctrl Pts',(-2.93744522033648,-0.189336333036378,
10.1880851303858));
#66516=CARTESIAN_POINT('Ctrl Pts',(-2.92824851849128,-0.284120773534126,
10.1932157541235));
#66517=CARTESIAN_POINT('Ctrl Pts',(-2.91904744884976,-0.378950230075376,
10.1983488145521));
#66518=CARTESIAN_POINT('Ctrl Pts',(-2.9052397544149,-0.473289329612877,
10.2034818749807));
#66519=CARTESIAN_POINT('Ctrl Pts',(-2.88690905912501,-0.566674584167986,
10.2086149354093));
#66520=CARTESIAN_POINT('Ctrl Pts',(-2.86855028875814,-0.660202866478942,
10.2137558575728));
#66521=CARTESIAN_POINT('Ctrl Pts',(-2.84565476095613,-0.752773972174129,
10.2188967797363));
#66522=CARTESIAN_POINT('Ctrl Pts',(-2.81835699241197,-0.843935935555881,
10.2240377018997));
#66523=CARTESIAN_POINT('Ctrl Pts',(-2.7910382169181,-0.935168052465979,
10.2291825802508));
#66524=CARTESIAN_POINT('Ctrl Pts',(-2.75931058979704,-1.02498846973067,
10.2343274586019));
#66525=CARTESIAN_POINT('Ctrl Pts',(-2.72335740126719,-1.11296382015015,
10.2394723369529));
#66526=CARTESIAN_POINT('Ctrl Pts',(-2.68732964970811,-1.20112162194304,
10.2446278852259));
#66527=CARTESIAN_POINT('Ctrl Pts',(-2.64705899886438,-1.28742632684711,
10.2497834334989));
#66528=CARTESIAN_POINT('Ctrl Pts',(-2.60277572787018,-1.37146728375482,
10.2549389817719));
#66529=CARTESIAN_POINT('Ctrl Pts',(-2.56060463327417,-1.45149974441383,
10.2598486261824));
#66530=CARTESIAN_POINT('Ctrl Pts',(-2.51479509137513,-1.52947919320769,
10.2647582705929));
#66531=CARTESIAN_POINT('Ctrl Pts',(-2.46558161295246,-1.60507673021285,
10.2696679150034));
#66532=CARTESIAN_POINT('Ctrl Pts',(-2.41490142207189,-1.68292730546819,
10.2747238818616));
#66533=CARTESIAN_POINT('Ctrl Pts',(-2.36044109596539,-1.75851242323328,
10.2797798487197));
#66534=CARTESIAN_POINT('Ctrl Pts',(-2.30242970610783,-1.83144245021027,
10.2848358155779));
#66535=CARTESIAN_POINT('Ctrl Pts',(-2.2444973980057,-1.90427305818402,10.2898848900872));
#66536=CARTESIAN_POINT('Ctrl Pts',(-2.18302391981014,-1.97445542392243,
10.2949339645966));
#66537=CARTESIAN_POINT('Ctrl Pts',(-2.11828211666327,-2.04162799604251,
10.2999830391059));
#66538=CARTESIAN_POINT('Ctrl Pts',(-2.05360865375081,-2.108729662054,10.3050267839068));
#66539=CARTESIAN_POINT('Ctrl Pts',(-1.98567402978589,-2.17282753208236,
10.3100705287077));
#66540=CARTESIAN_POINT('Ctrl Pts',(-1.91479122975435,-2.23359319180011,
10.3151142735086));
#66541=CARTESIAN_POINT('Ctrl Pts',(-1.84395847671322,-2.29431594776142,
10.32015445716));
#66542=CARTESIAN_POINT('Ctrl Pts',(-1.77018202094336,-2.35171088212786,
10.3251946408114));
#66543=CARTESIAN_POINT('Ctrl Pts',(-1.69381080949119,-2.40548725659705,
10.3302348244628));
#66544=CARTESIAN_POINT('Ctrl Pts',(-1.61746658636276,-2.4592446273844,10.3352732269966));
#66545=CARTESIAN_POINT('Ctrl Pts',(-1.53852979155112,-2.50938572374625,
10.3403116295304));
#66546=CARTESIAN_POINT('Ctrl Pts',(-1.4573806476547,-2.55566148929031,10.3453500320642));
#66547=CARTESIAN_POINT('Ctrl Pts',(-1.37623757740107,-2.60193379130467,
10.3503880574965));
#66548=CARTESIAN_POINT('Ctrl Pts',(-1.29288287268842,-2.64434111832053,
10.3554260829289));
#66549=CARTESIAN_POINT('Ctrl Pts',(-1.20772280877705,-2.68267955916462,
10.3604641083613));
#66550=CARTESIAN_POINT('Ctrl Pts',(-1.12254539879805,-2.72102580908208,
10.3655031599781));
#66551=CARTESIAN_POINT('Ctrl Pts',(-1.03556230377543,-2.75530134511192,
10.3705422115949));
#66552=CARTESIAN_POINT('Ctrl Pts',(-0.947200241424677,-2.78535019389753,
10.3755812632117));
#66553=CARTESIAN_POINT('Ctrl Pts',(-0.858741951113913,-2.81543176644879,
10.3806258024512));
#66554=CARTESIAN_POINT('Ctrl Pts',(-0.768902116520257,-2.84127732138304,
10.3856703416906));
#66555=CARTESIAN_POINT('Ctrl Pts',(-0.678122793716223,-2.86278072451288,
10.3907148809301));
#66556=CARTESIAN_POINT('Ctrl Pts',(-0.587287204263457,-2.88429745583678,
10.3957625468653));
#66557=CARTESIAN_POINT('Ctrl Pts',(-0.495511402822684,-2.90146659580192,
10.4008102128005));
#66558=CARTESIAN_POINT('Ctrl Pts',(-0.403245683702458,-2.91423350446997,
10.4058578787356));
#66559=CARTESIAN_POINT('Ctrl Pts',(-0.310834263289522,-2.92702057398557,
10.410913515686));
#66560=CARTESIAN_POINT('Ctrl Pts',(-0.217931821828598,-2.93539149560384,
10.4159691526364));
#66561=CARTESIAN_POINT('Ctrl Pts',(-0.124991562079888,-2.93934365282606,
10.4210247895868));
#66562=CARTESIAN_POINT('Ctrl Pts',(-0.0843149222526134,-2.94107337120971,
10.4232374617257));
#66563=CARTESIAN_POINT('Ctrl Pts',(-0.0436310082262822,-2.94195734882917,
10.4254501338646));
#66564=CARTESIAN_POINT('Ctrl Pts',(-0.0029775272444785,-2.94199849325786,
10.4276628060035));
#66565=CARTESIAN_POINT('Ctrl Pts',(0.0899158792836095,-2.94209250848234,
10.4327187728617));
#66566=CARTESIAN_POINT('Ctrl Pts',(0.182977487522895,-2.93778272669165,
10.4377747397198));
#66567=CARTESIAN_POINT('Ctrl Pts',(0.275755805977844,-2.92904809374471,
10.442830706578));
#66568=CARTESIAN_POINT('Ctrl Pts',(0.368407648023413,-2.92032536794407,
10.4478797810873));
#66569=CARTESIAN_POINT('Ctrl Pts',(0.460776529914912,-2.90718981922397,
10.4529288555966));
#66570=CARTESIAN_POINT('Ctrl Pts',(0.552410560194182,-2.88967239890371,
10.457977930106));
#66571=CARTESIAN_POINT('Ctrl Pts',(0.643947863307934,-2.87217346964415,
10.4630216749068));
#66572=CARTESIAN_POINT('Ctrl Pts',(0.734751423385491,-2.85030194586016,
10.4680654197077));
#66573=CARTESIAN_POINT('Ctrl Pts',(0.824375168337771,-2.82414050320236,
10.4731091645086));
#66574=CARTESIAN_POINT('Ctrl Pts',(0.91393563420547,-2.79799753190105,10.47814934816));
#66575=CARTESIAN_POINT('Ctrl Pts',(1.00231751621661,-2.76757078628082,10.4831895318114));
#66576=CARTESIAN_POINT('Ctrl Pts',(1.08908664591529,-2.73299364757567,10.4882297154627));
#66577=CARTESIAN_POINT('Ctrl Pts',(1.17582511283777,-2.6984287278598,10.4932681179965));
#66578=CARTESIAN_POINT('Ctrl Pts',(1.26095154817089,-2.65971649301147,10.4983065205303));
#66579=CARTESIAN_POINT('Ctrl Pts',(1.34404960287046,-2.61703929374852,10.5033449230641));
#66580=CARTESIAN_POINT('Ctrl Pts',(1.42714143805984,-2.57436528867919,10.5083829484965));
#66581=CARTESIAN_POINT('Ctrl Pts',(1.50820480013138,-2.52772711212906,10.5134209739288));
#66582=CARTESIAN_POINT('Ctrl Pts',(1.58684691390828,-2.47735360250001,10.5184589993612));
#66583=CARTESIAN_POINT('Ctrl Pts',(1.6655050461258,-2.42696983240066,10.5234980509779));
#66584=CARTESIAN_POINT('Ctrl Pts',(1.74174057736602,-2.37284945762111,10.5285371025947));
#66585=CARTESIAN_POINT('Ctrl Pts',(1.81518971068537,-2.31526463157496,10.5335761542115));
#66586=CARTESIAN_POINT('Ctrl Pts',(1.88871883150269,-2.25761709456208,10.5386206934509));
#66587=CARTESIAN_POINT('Ctrl Pts',(1.95945514821674,-2.19649784974213,10.5436652326904));
#66588=CARTESIAN_POINT('Ctrl Pts',(2.02706822350752,-2.13221912974395,10.5487097719299));
#66589=CARTESIAN_POINT('Ctrl Pts',(2.09472320659242,-2.06790056864475,10.553757437865));
#66590=CARTESIAN_POINT('Ctrl Pts',(2.15925078805762,-2.00041895390797,10.5588051038002));
#66591=CARTESIAN_POINT('Ctrl Pts',(2.22035915601031,-1.93012155532267,10.5638527697353));
#66592=CARTESIAN_POINT('Ctrl Pts',(2.28156402316422,-1.85971314669015,10.5689084066857));
#66593=CARTESIAN_POINT('Ctrl Pts',(2.33933862441082,-1.78648042580054,10.5739640436361));
#66594=CARTESIAN_POINT('Ctrl Pts',(2.39343312879448,-1.71080152501366,10.5790196805865));
#66595=CARTESIAN_POINT('Ctrl Pts',(2.4171083657428,-1.67767956690475,10.5812323527255));
#66596=CARTESIAN_POINT('Ctrl Pts',(2.44007926069762,-1.64408938586755,10.5834450248646));
#66597=CARTESIAN_POINT('Ctrl Pts',(2.46232764474373,-1.61006415087437,10.5856576970036));
#66598=CARTESIAN_POINT('Ctrl Pts',(2.51316531309907,-1.53231631944934,10.5907136638617));
#66599=CARTESIAN_POINT('Ctrl Pts',(2.56040666420099,-1.45202128913561,10.5957696307198));
#66600=CARTESIAN_POINT('Ctrl Pts',(2.60378736044614,-1.36954568437162,10.6008255975779));
#66601=CARTESIAN_POINT('Ctrl Pts',(2.64710891965606,-1.28718251124581,10.6058746720872));
#66602=CARTESIAN_POINT('Ctrl Pts',(2.68658007790076,-1.20264506008488,10.6109237465965));
#66603=CARTESIAN_POINT('Ctrl Pts',(2.72197983414798,-1.11632870718787,10.6159728211058));
#66604=CARTESIAN_POINT('Ctrl Pts',(2.75734222307558,-1.03010346821619,10.6210165659067));
#66605=CARTESIAN_POINT('Ctrl Pts',(2.78864158540353,-0.942103468255528,
10.6260603107075));
#66606=CARTESIAN_POINT('Ctrl Pts',(2.81570341959696,-0.85274747309505,10.6311040555083));
#66607=CARTESIAN_POINT('Ctrl Pts',(2.8427461467101,-0.763454567973511,10.6361442391596));
#66608=CARTESIAN_POINT('Ctrl Pts',(2.86555716460931,-0.672807993966921,
10.641184422811));
#66609=CARTESIAN_POINT('Ctrl Pts',(2.88401094261607,-0.581244254054003,
10.6462246064623));
#66610=CARTESIAN_POINT('Ctrl Pts',(2.90245819936272,-0.489712871253188,
10.6512630089961));
#66611=CARTESIAN_POINT('Ctrl Pts',(2.91655118785282,-0.39726540079145,10.6563014115298));
#66612=CARTESIAN_POINT('Ctrl Pts',(2.92621512676966,-0.304350179668779,
10.6613398140636));
#66613=CARTESIAN_POINT('Ctrl Pts',(2.93587834238477,-0.211441912826502,
10.6663778394959));
#66614=CARTESIAN_POINT('Ctrl Pts',(2.94111312198164,-0.118066406055722,
10.6714158649282));
#66615=CARTESIAN_POINT('Ctrl Pts',(2.94189649942872,-0.0246776548525677,
10.6764538903605));
#66616=CARTESIAN_POINT('Ctrl Pts',(2.94268003644025,0.0687301185018934,
10.6814929419773));
#66617=CARTESIAN_POINT('Ctrl Pts',(2.93901036718802,0.162150698232739,10.686531993594));
#66618=CARTESIAN_POINT('Ctrl Pts',(2.93091663663948,0.255130690176428,10.6915710452107));
#66619=CARTESIAN_POINT('Ctrl Pts',(2.92281409186503,0.348211939093015,10.6966155844502));
#66620=CARTESIAN_POINT('Ctrl Pts',(2.91027790789137,0.440851200105211,10.7016601236896));
#66621=CARTESIAN_POINT('Ctrl Pts',(2.89338902485617,0.532601117950279,10.706704662929));
#66622=CARTESIAN_POINT('Ctrl Pts',(2.87648967378904,0.624407904036254,10.7117523288641));
#66623=CARTESIAN_POINT('Ctrl Pts',(2.85523235344346,0.715323818093096,10.7167999947992));
#66624=CARTESIAN_POINT('Ctrl Pts',(2.82974845370013,0.804914709010681,10.7218476607343));
#66625=CARTESIAN_POINT('Ctrl Pts',(2.80422431108897,0.894647077269552,10.7269032976847));
#66626=CARTESIAN_POINT('Ctrl Pts',(2.77446040718515,0.983049825995977,10.731958934635));
#66627=CARTESIAN_POINT('Ctrl Pts',(2.74063691887184,1.0697070995916,10.7370145715854));
#66628=CARTESIAN_POINT('Ctrl Pts',(2.72583358331108,1.10763390027916,10.7392272437248));
#66629=CARTESIAN_POINT('Ctrl Pts',(2.71025323871163,1.14522665410072,10.7414399158642));
#66630=CARTESIAN_POINT('Ctrl Pts',(2.69391373655503,1.18245202016831,10.7436525880037));
#66631=CARTESIAN_POINT('Ctrl Pts',(2.65657789275248,1.26751216702421,10.7487085548619));
#66632=CARTESIAN_POINT('Ctrl Pts',(2.61514363903161,1.3509522039735,10.7537645217202));
#66633=CARTESIAN_POINT('Ctrl Pts',(2.56977358753034,1.4323504141206,10.7588204885784));
#66634=CARTESIAN_POINT('Ctrl Pts',(2.52446538497513,1.51363766134519,10.7638695630879));
#66635=CARTESIAN_POINT('Ctrl Pts',(2.47523226089738,1.59288822901452,10.7689186375973));
#66636=CARTESIAN_POINT('Ctrl Pts',(2.42228458744273,1.66970098443925,10.7739677121067));
#66637=CARTESIAN_POINT('Ctrl Pts',(2.3693928045601,1.74643265775859,10.7790114569077));
#66638=CARTESIAN_POINT('Ctrl Pts',(2.31279451671488,1.82073127072479,10.7840552017087));
#66639=CARTESIAN_POINT('Ctrl Pts',(2.25274509330889,1.89222185395178,10.7890989465096));
#66640=CARTESIAN_POINT('Ctrl Pts',(2.19273806795893,1.96366196106125,10.7941391301611));
#66641=CARTESIAN_POINT('Ctrl Pts',(2.12928503494304,2.03229764069085,10.7991793138126));
#66642=CARTESIAN_POINT('Ctrl Pts',(2.06268297746117,2.09778524508395,10.804219497464));
#66643=CARTESIAN_POINT('Ctrl Pts',(1.99610445604537,2.16324970724028,10.8092578999979));
#66644=CARTESIAN_POINT('Ctrl Pts',(1.92637943697039,2.22556799376019,10.8142963025318));
#66645=CARTESIAN_POINT('Ctrl Pts',(1.85384254508205,2.28443249364995,10.8193347050657));
#66646=CARTESIAN_POINT('Ctrl Pts',(1.78131108224913,2.34329258780045,10.8243727304982));
#66647=CARTESIAN_POINT('Ctrl Pts',(1.70596850960611,2.39869913010453,10.8294107559306));
#66648=CARTESIAN_POINT('Ctrl Pts',(1.62818250396606,2.45038481340764,10.834448781363));
#66649=CARTESIAN_POINT('Ctrl Pts',(1.55038065426389,2.50208102445504,10.8394878329799));
#66650=CARTESIAN_POINT('Ctrl Pts',(1.47013475263499,2.55005462617398,10.8445268845968));
#66651=CARTESIAN_POINT('Ctrl Pts',(1.38784044688097,2.5940822835834,10.8495659362137));
#66652=CARTESIAN_POINT('Ctrl Pts',(1.30545652106893,2.63815788794581,10.8546104754532));
#66653=CARTESIAN_POINT('Ctrl Pts',(1.22102013017517,2.67827876135069,10.8596550146928));
#66654=CARTESIAN_POINT('Ctrl Pts',(1.13495016633914,2.71426824759948,10.8646995539323));
#66655=CARTESIAN_POINT('Ctrl Pts',(1.04882685479923,2.75028004077591,10.8697472198676));
#66656=CARTESIAN_POINT('Ctrl Pts',(0.961068370996616,2.78215519753157,10.8747948858028));
#66657=CARTESIAN_POINT('Ctrl Pts',(0.872110115265059,2.80976652888676,10.8798425517381));
#66658=CARTESIAN_POINT('Ctrl Pts',(0.783011381217533,2.83742146264062,10.8848981886885));
#66659=CARTESIAN_POINT('Ctrl Pts',(0.692709521901368,2.86079901945179,10.889953825639));
#66660=CARTESIAN_POINT('Ctrl Pts',(0.601651273221105,2.8798228670235,10.8950094625895));
#66661=CARTESIAN_POINT('Ctrl Pts',(0.561798322589845,2.88814892720014,10.8972221347275));
#66662=CARTESIAN_POINT('Ctrl Pts',(0.521800565480502,2.89564170384939,10.8994348068656));
#66663=CARTESIAN_POINT('Ctrl Pts',(0.48169567966528,2.9022979296054,10.9016474790037));
#66664=CARTESIAN_POINT('Ctrl Pts',(0.390055815791504,2.91750743861646,10.9067034458618));
#66665=CARTESIAN_POINT('Ctrl Pts',(0.297533352779683,2.92839922383743,10.9117594127199));
#66666=CARTESIAN_POINT('Ctrl Pts',(0.204570337682543,2.93487903957564,10.916815379578));
#66667=CARTESIAN_POINT('Ctrl Pts',(0.111734050775317,2.94135002195881,10.9218644540873));
#66668=CARTESIAN_POINT('Ctrl Pts',(0.0184588439276381,2.94342095640441,
10.9269135285966));
#66669=CARTESIAN_POINT('Ctrl Pts',(-0.0748043782143797,2.94104884437507,
10.9319626031059));
#66670=CARTESIAN_POINT('Ctrl Pts',(-0.167969153446333,2.93867923630276,
10.9370063479067));
#66671=CARTESIAN_POINT('Ctrl Pts',(-0.261121528092837,2.93187591557138,
10.9420500927076));
#66672=CARTESIAN_POINT('Ctrl Pts',(-0.35380792209284,2.92064786550251,10.9470938375084));
#66673=CARTESIAN_POINT('Ctrl Pts',(-0.446428874616717,2.90942774302838,
10.9521340211597));
#66674=CARTESIAN_POINT('Ctrl Pts',(-0.538584061433512,2.89378915423348,
10.9571742048111));
#66675=CARTESIAN_POINT('Ctrl Pts',(-0.629823396012821,2.87379304923561,
10.9622143884624));
#66676=CARTESIAN_POINT('Ctrl Pts',(-0.721030488119714,2.85380401053064,
10.9672527909962));
#66677=CARTESIAN_POINT('Ctrl Pts',(-0.811321938223273,2.82946060983173,
10.9722911935299));
#66678=CARTESIAN_POINT('Ctrl Pts',(-0.900257272765933,2.80087501378267,
10.9773295960637));
#66679=CARTESIAN_POINT('Ctrl Pts',(-0.989185950904777,2.77229155723498,
10.982367621496));
#66680=CARTESIAN_POINT('Ctrl Pts',(-1.07675829319537,2.73946667265119,10.9874056469283));
#66681=CARTESIAN_POINT('Ctrl Pts',(-1.16254952067202,2.70256223091814,10.9924436723607));
#66682=CARTESIAN_POINT('Ctrl Pts',(-1.24835822277642,2.66565027219996,10.9974827239774));
#66683=CARTESIAN_POINT('Ctrl Pts',(-1.33238468234558,2.62465728155637,11.0025217755941));
#66684=CARTESIAN_POINT('Ctrl Pts',(-1.41422566362877,2.57979258320001,11.0075608272108));
#66685=CARTESIAN_POINT('Ctrl Pts',(-1.49615577129122,2.53487902633708,11.0126053664503));
#66686=CARTESIAN_POINT('Ctrl Pts',(-1.57589526075064,2.48608555945655,11.0176499056897));
#66687=CARTESIAN_POINT('Ctrl Pts',(-1.65306728902706,2.43366648042593,11.0226944449291));
#66688=CARTESIAN_POINT('Ctrl Pts',(-1.73028714990762,2.38121491111207,11.0277421108642));
#66689=CARTESIAN_POINT('Ctrl Pts',(-1.80493602719354,2.3251335218908,11.0327897767993));
#66690=CARTESIAN_POINT('Ctrl Pts',(-1.87666948679219,2.26571746635435,11.0378374427344));
#66691=CARTESIAN_POINT('Ctrl Pts',(-1.94851622419222,2.20620758402945,11.0428930796847));
#66692=CARTESIAN_POINT('Ctrl Pts',(-2.01743802668207,2.14335282208175,11.0479487166351));
#66693=CARTESIAN_POINT('Ctrl Pts',(-2.0831268591785,2.07748561693436,11.0530043535854));
#66694=CARTESIAN_POINT('Ctrl Pts',(-2.11187652039143,2.04865788836827,11.0552170257249));
#66695=CARTESIAN_POINT('Ctrl Pts',(-2.14000742323412,2.01925355904415,11.0574296978643));
#66696=CARTESIAN_POINT('Ctrl Pts',(-2.16749624331862,1.98930239913385,11.0596423700038));
#66697=CARTESIAN_POINT('Ctrl Pts',(-2.22958430090055,1.92165273881957,11.0646400568736));
#66698=CARTESIAN_POINT('Ctrl Pts',(-2.28862416138595,1.8509604081968,11.0696377437435));
#66699=CARTESIAN_POINT('Ctrl Pts',(-2.34429841515415,1.77753451181847,11.0746354306133));
#66700=CARTESIAN_POINT('Ctrl Pts',(-2.39990319760607,1.70420023756933,11.0796268812813));
#66701=CARTESIAN_POINT('Ctrl Pts',(-2.4521504371219,1.62813952602512,11.0846183319493));
#66702=CARTESIAN_POINT('Ctrl Pts',(-2.50076027439732,1.54969740594615,11.0896097826173));
#66703=CARTESIAN_POINT('Ctrl Pts',(-2.5493237596314,1.4713300845622,11.094596473674));
#66704=CARTESIAN_POINT('Ctrl Pts',(-2.5942564910186,1.39058624708043,11.0995831647308));
#66705=CARTESIAN_POINT('Ctrl Pts',(-2.63532034526617,1.30784199268343,11.1045698557875));
#66706=CARTESIAN_POINT('Ctrl Pts',(-2.67635712129754,1.22515230127989,11.1095532585339));
#66707=CARTESIAN_POINT('Ctrl Pts',(-2.71352988621776,1.14046521899455,11.1145366612802));
#66708=CARTESIAN_POINT('Ctrl Pts',(-2.74664579315571,1.05418256812566,11.1195200640266));
#66709=CARTESIAN_POINT('Ctrl Pts',(-2.77975901597079,0.967906910670452,
11.1245030628563));
#66710=CARTESIAN_POINT('Ctrl Pts',(-2.80881585622071,0.880036359803671,
11.1294860616861));
#66711=CARTESIAN_POINT('Ctrl Pts',(-2.83367146361466,0.790993069688948,
11.1344690605158));
#66712=CARTESIAN_POINT('Ctrl Pts',(-2.85852459050563,0.701958665784222,
11.1394515620596));
#66713=CARTESIAN_POINT('Ctrl Pts',(-2.87917720172363,0.611752195000438,
11.1444340636035));
#66714=CARTESIAN_POINT('Ctrl Pts',(-2.89553471140255,0.520809691790528,
11.1494165651473));
#66715=CARTESIAN_POINT('Ctrl Pts',(-2.91190491411364,0.429796619396097,
11.1544029329919));
#66716=CARTESIAN_POINT('Ctrl Pts',(-2.92397328119532,0.338046822642366,
11.1593893008365));
#66717=CARTESIAN_POINT('Ctrl Pts',(-2.93169672481608,0.246004702602807,
11.1643756686811));
#66718=CARTESIAN_POINT('Ctrl Pts',(-2.93864009038374,0.163258958807896,
11.1688584067575));
#66719=CARTESIAN_POINT('Ctrl Pts',(-2.94207257076881,0.0802772842537297,
11.173341144834));
#66720=CARTESIAN_POINT('Ctrl Pts',(-2.94199883612238,-0.00261691699413304,
11.1778238829104));
#66721=CARTESIAN_POINT('',(-2.94599368555865,0.00130075687149912,12.1778238829104));
#66722=CARTESIAN_POINT('Ctrl Pts',(-2.94145087575173,-0.00262142569101594,
11.1778241531392));
#66723=CARTESIAN_POINT('Ctrl Pts',(-2.94362752589749,-0.247984084398526,
11.1910951890941));
#66724=CARTESIAN_POINT('Ctrl Pts',(-2.80368830243438,-1.46459917676703,
11.2570311887159));
#66725=CARTESIAN_POINT('Ctrl Pts',(-1.11814973965556,-3.2866071025494,11.3756321520037));
#66726=CARTESIAN_POINT('Ctrl Pts',(2.14158719959913,-2.73233404879197,11.533627043004));
#66727=CARTESIAN_POINT('Ctrl Pts',(3.45856717040371,0.300596429689326,11.691621934004));
#66728=CARTESIAN_POINT('Ctrl Pts',(1.63808186784714,3.06083859111985,11.849616825004));
#66729=CARTESIAN_POINT('Ctrl Pts',(-1.66840174770122,3.04441795752147,12.0076117160041));
#66730=CARTESIAN_POINT('Ctrl Pts',(-2.90993729409171,1.12068341154196,12.1170140686395));
#66731=CARTESIAN_POINT('Ctrl Pts',(-2.94641083929854,0.0762932715455572,
12.1737514576083));
#66732=CARTESIAN_POINT('Ctrl Pts',(-2.94599368555865,0.00130075687149912,
12.1778238829104));
#66733=CARTESIAN_POINT('',(-2.94186551558604,0.00139596930223792,13.1778238494248));
#66734=CARTESIAN_POINT('Ctrl Pts',(-2.94599368555865,0.00130075687149912,
12.1778238829104));
#66735=CARTESIAN_POINT('Ctrl Pts',(-2.94101617029297,-0.893516551252978,
12.226416421275));
#66736=CARTESIAN_POINT('Ctrl Pts',(-2.03018396278169,-2.76692136029347,
12.3276739233063));
#66737=CARTESIAN_POINT('Ctrl Pts',(1.15073763387882,-3.27533937411075,12.4815963890041));
#66738=CARTESIAN_POINT('Ctrl Pts',(3.37191857800937,-0.825960120600501,
12.6395912800043));
#66739=CARTESIAN_POINT('Ctrl Pts',(2.53423820298509,2.37269506052472,12.7975861710044));
#66740=CARTESIAN_POINT('Ctrl Pts',(-0.60239551675097,3.41894207513383,12.9555810620044));
#66741=CARTESIAN_POINT('Ctrl Pts',(-2.68026052099427,1.77017590350058,13.0823266290105));
#66742=CARTESIAN_POINT('Ctrl Pts',(-2.93966479896272,0.398551205875977,
13.1564072323499));
#66743=CARTESIAN_POINT('Ctrl Pts',(-2.93794974228868,0.001412237267097,
13.1778228720226));
#66744=CARTESIAN_POINT('',(-2.94199885496721,-0.00259564473995637,14.1778238829374));
#66745=CARTESIAN_POINT('Ctrl Pts',(-2.94199966907297,0.0013954119655268,
13.1778238829104));
#66746=CARTESIAN_POINT('Ctrl Pts',(-2.94204471264643,-0.0935716525962874,
13.1829379245465));
#66747=CARTESIAN_POINT('Ctrl Pts',(-2.93748713814666,-0.188529989784559,
13.1880519661827));
#66748=CARTESIAN_POINT('Ctrl Pts',(-2.92835588116753,-0.28301207258969,
13.1931660078188));
#66749=CARTESIAN_POINT('Ctrl Pts',(-2.91922127699117,-0.377528789199093,
13.1982819240825));
#66750=CARTESIAN_POINT('Ctrl Pts',(-2.90550969590064,-0.471568481542718,
13.2033978403461));
#66751=CARTESIAN_POINT('Ctrl Pts',(-2.88730181220689,-0.564670032166427,
13.2085137566098));
#66752=CARTESIAN_POINT('Ctrl Pts',(-2.86859978416063,-0.660298268824794,
13.2137685138927));
#66753=CARTESIAN_POINT('Ctrl Pts',(-2.84515397675717,-0.754936240875184,
13.2190232711756));
#66754=CARTESIAN_POINT('Ctrl Pts',(-2.81710711756315,-0.848098749070564,
13.2242780284585));
#66755=CARTESIAN_POINT('Ctrl Pts',(-2.78974280920771,-0.938994046251209,
13.2294049055048));
#66756=CARTESIAN_POINT('Ctrl Pts',(-2.75799905007121,-1.02848449562343,
13.234531782551));
#66757=CARTESIAN_POINT('Ctrl Pts',(-2.72205758840463,-1.1161390976974,13.2396586595973));
#66758=CARTESIAN_POINT('Ctrl Pts',(-2.68477138921636,-1.20707326679207,
13.2449773569985));
#66759=CARTESIAN_POINT('Ctrl Pts',(-2.64296744073451,-1.29603105910162,
13.2502960543997));
#66760=CARTESIAN_POINT('Ctrl Pts',(-2.59690049794005,-1.38255987349508,
13.2556147518009));
#66761=CARTESIAN_POINT('Ctrl Pts',(-2.55083355514558,-1.46908868788855,
13.2609334492021));
#66762=CARTESIAN_POINT('Ctrl Pts',(-2.50050393867054,-1.55318813126393,
13.2662521466033));
#66763=CARTESIAN_POINT('Ctrl Pts',(-2.44621482673287,-1.63444088956201,
13.2715708440045));
#66764=CARTESIAN_POINT('Ctrl Pts',(-2.39460749082002,-1.71167992040394,
13.2766268081491));
#66765=CARTESIAN_POINT('Ctrl Pts',(-2.33924737933322,-1.78660846295203,
13.2816827722938));
#66766=CARTESIAN_POINT('Ctrl Pts',(-2.28036820549469,-1.85883965079533,
13.2867387364384));
#66767=CARTESIAN_POINT('Ctrl Pts',(-2.22156929641021,-1.93097237226847,
13.2917878082357));
#66768=CARTESIAN_POINT('Ctrl Pts',(-2.15926113603735,-2.00041470538282,
13.296836880033));
#66769=CARTESIAN_POINT('Ctrl Pts',(-2.09372087240025,-2.06680838697629,
13.3018859518303));
#66770=CARTESIAN_POINT('Ctrl Pts',(-2.02824979180801,-2.13313198467328,
13.3069296939243));
#66771=CARTESIAN_POINT('Ctrl Pts',(-1.95955369962162,-2.19641301369781,
13.3119734360183));
#66772=CARTESIAN_POINT('Ctrl Pts',(-1.88794948466174,-2.25632682547664,
13.3170171781123));
#66773=CARTESIAN_POINT('Ctrl Pts',(-1.81639582581118,-2.31619833514768,
13.3220573590754));
#66774=CARTESIAN_POINT('Ctrl Pts',(-1.74193846471106,-2.37270706943091,
13.3270975400386));
#66775=CARTESIAN_POINT('Ctrl Pts',(-1.66492979922436,-2.42556648304159,
13.3321377210018));
#66776=CARTESIAN_POINT('Ctrl Pts',(-1.58794834714745,-2.47840721713257,
13.33717612086));
#66777=CARTESIAN_POINT('Ctrl Pts',(-1.50841774718876,-2.52760094195155,
13.3422145207183));
#66778=CARTESIAN_POINT('Ctrl Pts',(-1.42672117217879,-2.57290316507574,
13.3472529205766));
#66779=CARTESIAN_POINT('Ctrl Pts',(-1.34503071152868,-2.61820199767721,
13.3522909433495));
#66780=CARTESIAN_POINT('Ctrl Pts',(-1.26117498613445,-2.65960969289675,
13.3573289661223));
#66781=CARTESIAN_POINT('Ctrl Pts',(-1.17556267986372,-2.69692721179338,
13.3623669888951));
#66782=CARTESIAN_POINT('Ctrl Pts',(-1.08993293507243,-2.73425233196077,
13.3674060378716));
#66783=CARTESIAN_POINT('Ctrl Pts',(-1.00254630542262,-2.76748544429363,
13.3724450868481));
#66784=CARTESIAN_POINT('Ctrl Pts',(-0.913831342618127,-2.79647568865684,
13.3774841358246));
#66785=CARTESIAN_POINT('Ctrl Pts',(-0.825019766700395,-2.82549750421924,
13.3825286724686));
#66786=CARTESIAN_POINT('Ctrl Pts',(-0.734877392389711,-2.85026709122484,
13.3875732091125));
#66787=CARTESIAN_POINT('Ctrl Pts',(-0.64384751275842,-2.87068360853557,
13.3926177457564));
#66788=CARTESIAN_POINT('Ctrl Pts',(-0.552761210754769,-2.89111278046418,
13.3976654091179));
#66789=CARTESIAN_POINT('Ctrl Pts',(-0.460786744733421,-2.9071834348439,
13.4027130724794));
#66790=CARTESIAN_POINT('Ctrl Pts',(-0.36837502971951,-2.91884631960628,
13.4077607358409));
#66791=CARTESIAN_POINT('Ctrl Pts',(-0.275817381732566,-2.93052762194102,
13.4128163702753));
#66792=CARTESIAN_POINT('Ctrl Pts',(-0.182821547841941,-2.93778722576749,
13.4178720047097));
#66793=CARTESIAN_POINT('Ctrl Pts',(-0.0898407292960799,-2.94062793351344,
13.4229276391442));
#66794=CARTESIAN_POINT('Ctrl Pts',(-0.0491458310464539,-2.94187122556536,
13.4251403377643));
#66795=CARTESIAN_POINT('Ctrl Pts',(-0.00845377089998635,-2.94226873013071,
13.4273530363844));
#66796=CARTESIAN_POINT('Ctrl Pts',(0.0321977799876051,-2.94182380556074,
13.4295657350046));
#66797=CARTESIAN_POINT('Ctrl Pts',(0.125085675168177,-2.94080716275335,
13.4346217024402));
#66798=CARTESIAN_POINT('Ctrl Pts',(0.218089107719228,-2.93538502623224,
13.4396776698758));
#66799=CARTESIAN_POINT('Ctrl Pts',(0.310756366649291,-2.92554174138516,
13.4447336373114));
#66800=CARTESIAN_POINT('Ctrl Pts',(0.403297300160726,-2.9157118750539,13.4497827123752));
#66801=CARTESIAN_POINT('Ctrl Pts',(0.495502533472043,-2.90147288387257,
13.454831787439));
#66802=CARTESIAN_POINT('Ctrl Pts',(0.586920577431533,-2.88286111975368,
13.4598808625028));
#66803=CARTESIAN_POINT('Ctrl Pts',(0.67824212180384,-2.86426900194833,13.4649246078347));
#66804=CARTESIAN_POINT('Ctrl Pts',(0.768777696246268,-2.84131337440413,
13.4699683531667));
#66805=CARTESIAN_POINT('Ctrl Pts',(0.858082248971938,-2.81408224009165,
13.4750120984986));
#66806=CARTESIAN_POINT('Ctrl Pts',(0.947323747340353,-2.78687033258923,
13.4800522826446));
#66807=CARTESIAN_POINT('Ctrl Pts',(1.0353355286556,-2.75538904777478,13.4850924667906));
#66808=CARTESIAN_POINT('Ctrl Pts',(1.12168505014706,-2.71977694825818,13.4901326509366));
#66809=CARTESIAN_POINT('Ctrl Pts',(1.20800405675712,-2.68417743362885,13.4951710539422));
#66810=CARTESIAN_POINT('Ctrl Pts',(1.29266156103043,-2.64445017345002,13.5002094569478));
#66811=CARTESIAN_POINT('Ctrl Pts',(1.37524342380712,-2.60078248326831,13.5052478599533));
#66812=CARTESIAN_POINT('Ctrl Pts',(1.45781910532763,-2.55711806161519,13.5102858858342));
#66813=CARTESIAN_POINT('Ctrl Pts',(1.53831906237339,-2.50951400397826,13.5153239117151));
#66814=CARTESIAN_POINT('Ctrl Pts',(1.61635328376672,-2.45820382841955,13.520361937596));
#66815=CARTESIAN_POINT('Ctrl Pts',(1.6944033994116,-2.4068832018456,13.5254009896376));
#66816=CARTESIAN_POINT('Ctrl Pts',(1.76998641163778,-2.35185520204692,13.5304400416792));
#66817=CARTESIAN_POINT('Ctrl Pts',(1.84274180329659,-2.29339631254243,13.5354790937207));
#66818=CARTESIAN_POINT('Ctrl Pts',(1.9155764264014,-2.23487376064481,13.5405236333471));
#66819=CARTESIAN_POINT('Ctrl Pts',(1.98557693649643,-2.17291313966353,13.5455681729735));
#66820=CARTESIAN_POINT('Ctrl Pts',(2.05241665285454,-2.10783061062443,13.5506127125998));
#66821=CARTESIAN_POINT('Ctrl Pts',(2.11929779738181,-2.04270774254487,13.5556603789007));
#66822=CARTESIAN_POINT('Ctrl Pts',(2.18301394551469,-1.97445943796929,13.5607080452017));
#66823=CARTESIAN_POINT('Ctrl Pts',(2.24327745808883,-1.90343643078264,13.5657557115026));
#66824=CARTESIAN_POINT('Ctrl Pts',(2.30363613528146,-1.83230126821215,13.5708113487832));
#66825=CARTESIAN_POINT('Ctrl Pts',(2.36053102339126,-1.75838300741313,13.5758669860639));
#66826=CARTESIAN_POINT('Ctrl Pts',(2.41371683017811,-1.68206274071894,13.5809226233446));
#66827=CARTESIAN_POINT('Ctrl Pts',(2.43699431280634,-1.64866015101536,13.5831352908979));
#66828=CARTESIAN_POINT('Ctrl Pts',(2.45956190856083,-1.6147977949142,13.5853479584512));
#66829=CARTESIAN_POINT('Ctrl Pts',(2.48140184649713,-1.58050905603247,13.5875606260046));
#66830=CARTESIAN_POINT('Ctrl Pts',(2.53130640275208,-1.50215881971651,13.5926166015623));
#66831=CARTESIAN_POINT('Ctrl Pts',(2.57758442902489,-1.42130455947248,13.5976725771201));
#66832=CARTESIAN_POINT('Ctrl Pts',(2.61997599008422,-1.33831603568897,13.6027285526779));
#66833=CARTESIAN_POINT('Ctrl Pts',(2.66230976296541,-1.25544064186519,13.6077776359295));
#66834=CARTESIAN_POINT('Ctrl Pts',(2.70076739903187,-1.17043715783292,13.6128267191811));
#66835=CARTESIAN_POINT('Ctrl Pts',(2.73513264036075,-1.08370357553771,13.6178758024328));
#66836=CARTESIAN_POINT('Ctrl Pts',(2.7694616066527,-0.997061546910688,13.6229195560061));
#66837=CARTESIAN_POINT('Ctrl Pts',(2.79970660248309,-0.908693460310509,
13.6279633095794));
#66838=CARTESIAN_POINT('Ctrl Pts',(2.82569814580013,-0.819020139448189,
13.6330070631527));
#66839=CARTESIAN_POINT('Ctrl Pts',(2.85167133779114,-0.729410132423238,
13.6380472555844));
#66840=CARTESIAN_POINT('Ctrl Pts',(2.87339692358576,-0.638497147704853,
13.6430874480162));
#66841=CARTESIAN_POINT('Ctrl Pts',(2.89075460058646,-0.546719159338895,
13.6481276404479));
#66842=CARTESIAN_POINT('Ctrl Pts',(2.90810614368617,-0.454973603716871,
13.6531660517633));
#66843=CARTESIAN_POINT('Ctrl Pts',(2.92109276231074,-0.362364087082582,
13.6582044630787));
#66844=CARTESIAN_POINT('Ctrl Pts',(2.92964504110006,-0.269339809827301,
13.6632428743942));
#66845=CARTESIAN_POINT('Ctrl Pts',(2.93819667977488,-0.176322495182945,
13.6682809085984));
#66846=CARTESIAN_POINT('Ctrl Pts',(2.94231459825068,-0.0828909232772339,
13.6733189428026));
#66847=CARTESIAN_POINT('Ctrl Pts',(2.9419812603063,0.010500666957926,13.6783569770068));
#66848=CARTESIAN_POINT('Ctrl Pts',(2.94164785446653,0.103911279503686,13.6833960373746));
#66849=CARTESIAN_POINT('Ctrl Pts',(2.93686139349325,0.197281450784621,13.6884350977425));
#66850=CARTESIAN_POINT('Ctrl Pts',(2.92765644134919,0.290158166224171,13.6934741581103));
#66851=CARTESIAN_POINT('Ctrl Pts',(2.91844146500886,0.383136024440997,13.6985187060167));
#66852=CARTESIAN_POINT('Ctrl Pts',(2.90479843715336,0.475618912294044,13.7035632539231));
#66853=CARTESIAN_POINT('Ctrl Pts',(2.88681364100954,0.567160472953867,13.7086078018296));
#66854=CARTESIAN_POINT('Ctrl Pts',(2.86881769771396,0.658758771964252,13.7136554763959));
#66855=CARTESIAN_POINT('Ctrl Pts',(2.84647473462245,0.749414152026579,13.7187031509622));
#66856=CARTESIAN_POINT('Ctrl Pts',(2.81992132323482,0.838694062674587,13.7237508255285));
#66857=CARTESIAN_POINT('Ctrl Pts',(2.79332598085164,0.928114956922829,13.7288064709735));
#66858=CARTESIAN_POINT('Ctrl Pts',(2.76250706438297,1.01615562814751,13.7338621164185));
#66859=CARTESIAN_POINT('Ctrl Pts',(2.72764971011007,1.10240240336115,13.7389177618635));
#66860=CARTESIAN_POINT('Ctrl Pts',(2.71239451437209,1.14014799435907,13.7411303469105));
#66861=CARTESIAN_POINT('Ctrl Pts',(2.69636642006694,1.1775502988612,13.7433429319576));
#66862=CARTESIAN_POINT('Ctrl Pts',(2.67958367377214,1.21457619573816,13.7455555170047));
#66863=CARTESIAN_POINT('Ctrl Pts',(2.64123365918508,1.29918354547628,13.7506114635905));
#66864=CARTESIAN_POINT('Ctrl Pts',(2.59880492609599,1.38212191993738,13.7556674101764));
#66865=CARTESIAN_POINT('Ctrl Pts',(2.55246511434818,1.46297157868345,13.7607233567623));
#66866=CARTESIAN_POINT('Ctrl Pts',(2.50618847383475,1.54371102177369,13.7657724109941));
#66867=CARTESIAN_POINT('Ctrl Pts',(2.45601156858285,1.62236702602864,13.770821465226));
#66868=CARTESIAN_POINT('Ctrl Pts',(2.40214954901253,1.69854100456212,13.7758705194578));
#66869=CARTESIAN_POINT('Ctrl Pts',(2.3483443851696,1.77463457528705,13.7809142440037));
#66870=CARTESIAN_POINT('Ctrl Pts',(2.29086209398443,1.84825096796688,13.7859579685496));
#66871=CARTESIAN_POINT('Ctrl Pts',(2.22996250719433,1.91901829499033,13.7910016930954));
#66872=CARTESIAN_POINT('Ctrl Pts',(2.16910591748539,1.98973565798833,13.7960418566084));
#66873=CARTESIAN_POINT('Ctrl Pts',(2.10483711646537,2.05760761848628,13.8010820201213));
#66874=CARTESIAN_POINT('Ctrl Pts',(2.03745717229748,2.12229410569166,13.8061221836343));
#66875=CARTESIAN_POINT('Ctrl Pts',(1.97010103810533,2.18695773470518,13.8111605661102));
#66876=CARTESIAN_POINT('Ctrl Pts',(1.89963626457905,2.2484378199862,13.8161989485862));
#66877=CARTESIAN_POINT('Ctrl Pts',(1.82640112802997,2.3064307749271,13.8212373310622));
#66878=CARTESIAN_POINT('Ctrl Pts',(1.75317147128809,2.36441939055458,13.826275336542));
#66879=CARTESIAN_POINT('Ctrl Pts',(1.67717221155185,2.41892111958122,13.8313133420219));
#66880=CARTESIAN_POINT('Ctrl Pts',(1.59877419287678,2.46967307152004,13.8363513475017));
#66881=CARTESIAN_POINT('Ctrl Pts',(1.52036020339346,2.52043536236418,13.841390379296));
#66882=CARTESIAN_POINT('Ctrl Pts',(1.43954685689406,2.56744611832926,13.8464294110903));
#66883=CARTESIAN_POINT('Ctrl Pts',(1.35673244065961,2.61048675240114,13.8514684428845));
#66884=CARTESIAN_POINT('Ctrl Pts',(1.27382783244256,2.65357426140488,13.8565129626154));
#66885=CARTESIAN_POINT('Ctrl Pts',(1.18891819863695,2.69268281348045,13.8615574823463));
#66886=CARTESIAN_POINT('Ctrl Pts',(1.10242451106388,2.72764077499321,13.8666020020773));
#66887=CARTESIAN_POINT('Ctrl Pts',(1.01587721034462,2.76262040521214,13.8716496486557));
#66888=CARTESIAN_POINT('Ctrl Pts',(0.927744319322681,2.79344417662816,13.8766972952341));
#66889=CARTESIAN_POINT('Ctrl Pts',(0.838462725260018,2.81999011671132,13.8817449418126));
#66890=CARTESIAN_POINT('Ctrl Pts',(0.749040134406092,2.84657797912363,13.8868005598209));
#66891=CARTESIAN_POINT('Ctrl Pts',(0.658465649250251,2.8688744188892,13.8918561778293));
#66892=CARTESIAN_POINT('Ctrl Pts',(0.567186883632633,2.88680845208599,13.8969117958377));
#66893=CARTESIAN_POINT('Ctrl Pts',(0.527233685493236,2.89465827320158,13.89912466656));
#66894=CARTESIAN_POINT('Ctrl Pts',(0.487145629108541,2.90167298955917,13.9013375372823));
#66895=CARTESIAN_POINT('Ctrl Pts',(0.446960438952583,2.90784978394884,13.9035504080047));
#66896=CARTESIAN_POINT('Ctrl Pts',(0.355145127557181,2.92196255281,13.9086063854347));
#66897=CARTESIAN_POINT('Ctrl Pts',(0.262498902156857,2.93174733982606,13.9136623628647));
#66898=CARTESIAN_POINT('Ctrl Pts',(0.169464906306277,2.93711519105578,13.9187183402947));
#66899=CARTESIAN_POINT('Ctrl Pts',(0.0765577378091241,2.94247572463393,
13.9237674252309));
#66900=CARTESIAN_POINT('Ctrl Pts',(-0.01673571162763,2.94343126289967,13.9288165101671));
#66901=CARTESIAN_POINT('Ctrl Pts',(-0.109964054207938,2.93994420130419,
13.9338655951033));
#66902=CARTESIAN_POINT('Ctrl Pts',(-0.203093984001307,2.93646082068641,
13.9389093501741));
#66903=CARTESIAN_POINT('Ctrl Pts',(-0.296158502692968,2.9285441786145,13.9439531052449));
#66904=CARTESIAN_POINT('Ctrl Pts',(-0.388704168742802,2.91620868066776,
13.9489968603157));
#66905=CARTESIAN_POINT('Ctrl Pts',(-0.481184487815518,2.9038818928804,13.9540370539648));
#66906=CARTESIAN_POINT('Ctrl Pts',(-0.573146244111906,2.88714250970049,
13.9590772476138));
#66907=CARTESIAN_POINT('Ctrl Pts',(-0.664140110676326,2.8660568580178,13.9641174412629));
#66908=CARTESIAN_POINT('Ctrl Pts',(-0.755101818452255,2.84497865836498,
13.9691558536213));
#66909=CARTESIAN_POINT('Ctrl Pts',(-0.845095884496893,2.81955734197982,
13.9741942659798));
#66910=CARTESIAN_POINT('Ctrl Pts',(-0.933683206420332,2.7899103336933,13.9792326783382));
#66911=CARTESIAN_POINT('Ctrl Pts',(-1.0222638947614,2.76026554542954,13.984270713411));
#66912=CARTESIAN_POINT('Ctrl Pts',(-1.10943762798828,2.72639583546516,13.9893087484838));
#66913=CARTESIAN_POINT('Ctrl Pts',(-1.19478159135926,2.68846814170245,13.9943467835566));
#66914=CARTESIAN_POINT('Ctrl Pts',(-1.28014293491138,2.6505327240169,13.9993858446184));
#66915=CARTESIAN_POINT('Ctrl Pts',(-1.36367336347592,2.60853786165571,14.0044249056801));
#66916=CARTESIAN_POINT('Ctrl Pts',(-1.44497217123477,2.56269768493224,14.0094639667418));
#66917=CARTESIAN_POINT('Ctrl Pts',(-1.52635950914418,2.5168075906533,14.0145085150776));
#66918=CARTESIAN_POINT('Ctrl Pts',(-1.60550998893169,2.46706404226412,14.0195530634133));
#66919=CARTESIAN_POINT('Ctrl Pts',(-1.6820498332811,2.41372582501804,14.0245976117491));
#66920=CARTESIAN_POINT('Ctrl Pts',(-1.75863711548155,2.36035454982122,14.0296452865941));
#66921=CARTESIAN_POINT('Ctrl Pts',(-1.83261018996262,2.30338444068044,14.0346929614391));
#66922=CARTESIAN_POINT('Ctrl Pts',(-1.90362817431552,2.24311474828021,14.0397406362841));
#66923=CARTESIAN_POINT('Ctrl Pts',(-1.97475830126131,2.18274988562641,14.044796281777));
#66924=CARTESIAN_POINT('Ctrl Pts',(-2.0429236998364,2.11907534138202,14.0498519272699));
#66925=CARTESIAN_POINT('Ctrl Pts',(-2.10782032968545,2.0524272113195,14.0549075727627));
#66926=CARTESIAN_POINT('Ctrl Pts',(-2.13622198242389,2.02325902415623,14.0571201481768));
#66927=CARTESIAN_POINT('Ctrl Pts',(-2.16399808150058,1.9935217248477,14.0593327235908));
#66928=CARTESIAN_POINT('Ctrl Pts',(-2.19112566304988,1.96324535622123,14.0615452990048));
#66929=CARTESIAN_POINT('Ctrl Pts',(-2.25247103055659,1.89477943135491,14.0665487399368));
#66930=CARTESIAN_POINT('Ctrl Pts',(-2.31072385919334,1.82330178025768,14.0715521808688));
#66931=CARTESIAN_POINT('Ctrl Pts',(-2.36557007798156,1.74912612642952,14.0765556218008));
#66932=CARTESIAN_POINT('Ctrl Pts',(-2.42034738467949,1.67504367135719,14.0815527761085));
#66933=CARTESIAN_POINT('Ctrl Pts',(-2.47172631103157,1.59827030322655,14.0865499304161));
#66934=CARTESIAN_POINT('Ctrl Pts',(-2.51943079147653,1.51915518857026,14.0915470847238));
#66935=CARTESIAN_POINT('Ctrl Pts',(-2.56708930283369,1.44011631098056,14.0965394236635));
#66936=CARTESIAN_POINT('Ctrl Pts',(-2.6110801661733,1.35874055337824,14.1015317626033));
#66937=CARTESIAN_POINT('Ctrl Pts',(-2.65116943561575,1.27540763038992,14.106524101543));
#66938=CARTESIAN_POINT('Ctrl Pts',(-2.69123180915622,1.19213061548275,14.1115130911212));
#66939=CARTESIAN_POINT('Ctrl Pts',(-2.72739759264673,1.10689945089866,14.1165020806993));
#66940=CARTESIAN_POINT('Ctrl Pts',(-2.75947842570916,1.0201190215096,14.1214910702775));
#66941=CARTESIAN_POINT('Ctrl Pts',(-2.79155519502114,0.933349584790464,
14.1264794278892));
#66942=CARTESIAN_POINT('Ctrl Pts',(-2.81954787202627,0.845031693356858,
14.131467785501));
#66943=CARTESIAN_POINT('Ctrl Pts',(-2.84331634284331,0.755589951309676,
14.1364561431128));
#66944=CARTESIAN_POINT('Ctrl Pts',(-2.86708219185211,0.666158075235707,
14.1414439504781));
#66945=CARTESIAN_POINT('Ctrl Pts',(-2.88662465035953,0.575603034936791,
14.1464317578433));
#66946=CARTESIAN_POINT('Ctrl Pts',(-2.90185401778846,0.484362735400811,
14.1514195652086));
#66947=CARTESIAN_POINT('Ctrl Pts',(-2.91709378833748,0.393060109980562,
14.1564107797252));
#66948=CARTESIAN_POINT('Ctrl Pts',(-2.92801451324544,0.301071739064547,
14.1614019942418));
#66949=CARTESIAN_POINT('Ctrl Pts',(-2.93457808096583,0.208843210842305,
14.1663932087584));
#66950=CARTESIAN_POINT('Ctrl Pts',(-2.93958861855725,0.13843721712899,14.1702034334757));
#66951=CARTESIAN_POINT('Ctrl Pts',(-2.94206104379116,0.0678914605600493,
14.1740136581931));
#66952=CARTESIAN_POINT('Ctrl Pts',(-2.94199885496765,-0.00259564423991444,
14.1778238829104));
#66953=CARTESIAN_POINT('',(-2.14520543675184,2.01332005258239,15.058));
#66954=CARTESIAN_POINT('Ctrl Pts',(-2.94199885496721,-0.00259564473995252,
14.1778238829374));
#66955=CARTESIAN_POINT('Ctrl Pts',(-2.94189565643288,-0.119564644835924,
14.1841467156966));
#66956=CARTESIAN_POINT('Ctrl Pts',(-2.93481305925187,-0.236228347809689,
14.1904695484559));
#66957=CARTESIAN_POINT('Ctrl Pts',(-2.92088173825648,-0.351871952732533,
14.1967923812151));
#66958=CARTESIAN_POINT('Ctrl Pts',(-2.90668755319215,-0.469697586807298,
14.2032345167703));
#66959=CARTESIAN_POINT('Ctrl Pts',(-2.88538377477223,-0.58646445157355,
14.2096766523255));
#66960=CARTESIAN_POINT('Ctrl Pts',(-2.85715701480589,-0.701439799801467,
14.2161187878807));
#66961=CARTESIAN_POINT('Ctrl Pts',(-2.85215996086937,-0.721794173351571,
14.2172592552554));
#66962=CARTESIAN_POINT('Ctrl Pts',(-2.84694605760728,-0.742092453460343,
14.2183997226302));
#66963=CARTESIAN_POINT('Ctrl Pts',(-2.84151649525502,-0.762330641646823,
14.2195401900049));
#66964=CARTESIAN_POINT('Ctrl Pts',(-2.81744663606155,-0.852048800933916,
14.2245960098561));
#66965=CARTESIAN_POINT('Ctrl Pts',(-2.78908102661924,-0.940784068631668,
14.2296518297074));
#66966=CARTESIAN_POINT('Ctrl Pts',(-2.75651675117941,-1.028095034745,14.2347076495587));
#66967=CARTESIAN_POINT('Ctrl Pts',(-2.72399686991963,-1.11528697168611,
14.2397565769189));
#66968=CARTESIAN_POINT('Ctrl Pts',(-2.68728985116877,-1.20105805364865,
14.2448055042791));
#66969=CARTESIAN_POINT('Ctrl Pts',(-2.6465430991831,-1.28498000924774,14.2498544316393));
#66970=CARTESIAN_POINT('Ctrl Pts',(-2.6058393594745,-1.36881337681881,14.2548980293511));
#66971=CARTESIAN_POINT('Ctrl Pts',(-2.56110455572065,-1.45080110112108,
14.2599416270629));
#66972=CARTESIAN_POINT('Ctrl Pts',(-2.5125345231665,-1.53053398194763,14.2649852247747));
#66973=CARTESIAN_POINT('Ctrl Pts',(-2.46399877791862,-1.61021057650958,
14.2700252620322));
#66974=CARTESIAN_POINT('Ctrl Pts',(-2.41163341555522,-1.68763511388406,
14.2750652992898));
#66975=CARTESIAN_POINT('Ctrl Pts',(-2.35568013616085,-1.76242307522831,
14.2801053365473));
#66976=CARTESIAN_POINT('Ctrl Pts',(-2.29974662484673,-1.83718461427098,
14.2851435931789));
#66977=CARTESIAN_POINT('Ctrl Pts',(-2.24022798033645,-1.90931107315869,
14.2901818498104));
#66978=CARTESIAN_POINT('Ctrl Pts',(-2.17740855236688,-1.9784478755023,14.295220106442));
#66979=CARTESIAN_POINT('Ctrl Pts',(-2.11459381790793,-2.04757951233699,
14.3002579866437));
#66980=CARTESIAN_POINT('Ctrl Pts',(-2.04847908882045,-2.11372160873315,
14.3052958668454));
#66981=CARTESIAN_POINT('Ctrl Pts',(-1.97938747119111,-2.17655444197743,
14.310333747047));
#66982=CARTESIAN_POINT('Ctrl Pts',(-1.91028176834968,-2.23940008450034,
14.3153726542852));
#66983=CARTESIAN_POINT('Ctrl Pts',(-1.83819829999229,-2.29893482591311,
14.3204115615233));
#66984=CARTESIAN_POINT('Ctrl Pts',(-1.76349445914154,-2.35487819060288,
14.3254504687615));
#66985=CARTESIAN_POINT('Ctrl Pts',(-1.6887092302608,-2.41088250423706,14.3304948657673));
#66986=CARTESIAN_POINT('Ctrl Pts',(-1.61129828619155,-2.46328736521615,
14.3355392627732));
#66987=CARTESIAN_POINT('Ctrl Pts',(-1.5316490427886,-2.51185493405267,14.340583659779));
#66988=CARTESIAN_POINT('Ctrl Pts',(-1.45195041378729,-2.56045261665231,
14.3456311845053));
#66989=CARTESIAN_POINT('Ctrl Pts',(-1.3700111113627,-2.60520805793399,14.3506787092316));
#66990=CARTESIAN_POINT('Ctrl Pts',(-1.28624233540467,-2.64592982798349,
14.3557262339578));
#66991=CARTESIAN_POINT('Ctrl Pts',(-1.20234122426813,-2.68671592895638,
14.3607817325989));
#66992=CARTESIAN_POINT('Ctrl Pts',(-1.1166052773998,-2.7234554642434,14.3658372312401));
#66993=CARTESIAN_POINT('Ctrl Pts',(-1.02946457505551,-2.75600556761153,
14.3708927298812));
#66994=CARTESIAN_POINT('Ctrl Pts',(-0.991300245927731,-2.7702612807819,
14.3731068469224));
#66995=CARTESIAN_POINT('Ctrl Pts',(-0.952866649820146,-2.78371406631994,
14.3753209639636));
#66996=CARTESIAN_POINT('Ctrl Pts',(-0.914200613338942,-2.79635499151497,
14.3775350810048));
#66997=CARTESIAN_POINT('Ctrl Pts',(-0.825904134260677,-2.82522138922698,
14.3825911652792));
#66998=CARTESIAN_POINT('Ctrl Pts',(-0.736083485315032,-2.84995255267627,
14.3876472495537));
#66999=CARTESIAN_POINT('Ctrl Pts',(-0.645161442640455,-2.8703885996377,
14.3927033338281));
#67000=CARTESIAN_POINT('Ctrl Pts',(-0.554363358769105,-2.89079678506138,
14.3977525248769));
#67001=CARTESIAN_POINT('Ctrl Pts',(-0.462467294202034,-2.90692139435603,
14.4028017159257));
#67002=CARTESIAN_POINT('Ctrl Pts',(-0.369912515066137,-2.91865186879104,
14.4078509069745));
#67003=CARTESIAN_POINT('Ctrl Pts',(-0.277455451504325,-2.93036995866791,
14.4128947672926));
#67004=CARTESIAN_POINT('Ctrl Pts',(-0.184341493399725,-2.937703079752,14.4179386276107));
#67005=CARTESIAN_POINT('Ctrl Pts',(-0.0910203966399159,-2.94059165600998,
14.4229824879288));
#67006=CARTESIAN_POINT('Ctrl Pts',(0.00223477549366748,-2.9434781916971,
14.4280227851232));
#67007=CARTESIAN_POINT('Ctrl Pts',(0.0956963534091555,-2.94192640984882,
14.4330630823177));
#67008=CARTESIAN_POINT('Ctrl Pts',(0.188910191959557,-2.93592863322217,
14.4381033795121));
#67009=CARTESIAN_POINT('Ctrl Pts',(0.282091067504582,-2.92993297757612,
14.4431418943174));
#67010=CARTESIAN_POINT('Ctrl Pts',(0.375023935629332,-2.91949447924339,
14.4481804091226));
#67011=CARTESIAN_POINT('Ctrl Pts',(0.467256423995743,-2.90465754164492,
14.4532189239278));
#67012=CARTESIAN_POINT('Ctrl Pts',(0.559481983632671,-2.88982171863339,
14.4582570602275));
#67013=CARTESIAN_POINT('Ctrl Pts',(0.651006830355907,-2.87058818408287,
14.4632951965272));
#67014=CARTESIAN_POINT('Ctrl Pts',(0.741386604551002,-2.84705284506493,
14.4683333328268));
#67015=CARTESIAN_POINT('Ctrl Pts',(0.831784760014276,-2.82351271947409,
14.4733724937732));
#67016=CARTESIAN_POINT('Ctrl Pts',(0.921036951425746,-2.79566916391259,
14.4784116547196));
#67017=CARTESIAN_POINT('Ctrl Pts',(1.00871295298068,-2.76366824682142,14.4834508156659));
#67018=CARTESIAN_POINT('Ctrl Pts',(1.0964843818845,-2.7316324996442,14.4884954612804));
#67019=CARTESIAN_POINT('Ctrl Pts',(1.18267577958268,-2.69543051155382,14.4935401068949));
#67020=CARTESIAN_POINT('Ctrl Pts',(1.2668762223947,-2.65525679306747,14.4985847525093));
#67021=CARTESIAN_POINT('Ctrl Pts',(1.35112882736926,-2.61505818696814,14.5036325232811));
#67022=CARTESIAN_POINT('Ctrl Pts',(1.43338763160374,-2.5708831616033,14.5086802940528));
#67023=CARTESIAN_POINT('Ctrl Pts',(1.51326758167948,-2.5229715072188,14.5137280648245));
#67024=CARTESIAN_POINT('Ctrl Pts',(1.59327361875479,-2.47498422638813,14.5187838032811));
#67025=CARTESIAN_POINT('Ctrl Pts',(1.6708929378474,-2.42324878851226,14.5238395417377));
#67026=CARTESIAN_POINT('Ctrl Pts',(1.74577083965426,-2.36804733386241,14.5288952801943));
#67027=CARTESIAN_POINT('Ctrl Pts',(1.77852515808371,-2.3439002092804,14.5311068441312));
#67028=CARTESIAN_POINT('Ctrl Pts',(1.81075535040236,-2.31909036610409,14.5333184080681));
#67029=CARTESIAN_POINT('Ctrl Pts',(1.84243390724532,-2.29364367272529,14.5355299720049));
#67030=CARTESIAN_POINT('Ctrl Pts',(1.91486001573722,-2.23546536035615,14.5405862304204));
#67031=CARTESIAN_POINT('Ctrl Pts',(1.98465534059067,-2.17375074658722,14.5456424888359));
#67032=CARTESIAN_POINT('Ctrl Pts',(2.05145495982987,-2.1087665939571,14.5506987472514));
#67033=CARTESIAN_POINT('Ctrl Pts',(2.11816355342989,-2.04387099308966,14.5557481156702));
#67034=CARTESIAN_POINT('Ctrl Pts',(2.1818842384775,-1.97571501370655,14.560797484089));
#67035=CARTESIAN_POINT('Ctrl Pts',(2.24228439509932,-1.90460617753227,14.5658468525078));
#67036=CARTESIAN_POINT('Ctrl Pts',(2.30262082108396,-1.83357237115413,14.5708908931347));
#67037=CARTESIAN_POINT('Ctrl Pts',(2.35964339746632,-1.75959223743332,14.5759349337616));
#67038=CARTESIAN_POINT('Ctrl Pts',(2.41305647398855,-1.68300993857492,14.5809789743885));
#67039=CARTESIAN_POINT('Ctrl Pts',(2.46643185705006,-1.60648168363351,14.5860194554499));
#67040=CARTESIAN_POINT('Ctrl Pts',(2.51620255046604,-1.52735527639034,14.5910599365112));
#67041=CARTESIAN_POINT('Ctrl Pts',(2.56211397344786,-1.44600691113951,14.5961004175726));
#67042=CARTESIAN_POINT('Ctrl Pts',(2.60800918087819,-1.36468727748791,14.6011391183759));
#67043=CARTESIAN_POINT('Ctrl Pts',(2.65004760823598,-1.28114763078779,14.6061778191791));
#67044=CARTESIAN_POINT('Ctrl Pts',(2.68801926317368,-1.19579113594609,14.6112165199824));
#67045=CARTESIAN_POINT('Ctrl Pts',(2.72598807988017,-1.11044102116521,14.6162548441628));
#67046=CARTESIAN_POINT('Ctrl Pts',(2.75989054863299,-1.02327473352243,14.6212931683431));
#67047=CARTESIAN_POINT('Ctrl Pts',(2.78956419132914,-0.934716867534871,
14.6263314925234));
#67048=CARTESIAN_POINT('Ctrl Pts',(2.81924387840178,-0.846140962741329,
14.6313708429858));
#67049=CARTESIAN_POINT('Ctrl Pts',(2.84469288811306,-0.756173337145417,
14.6364101934482));
#67050=CARTESIAN_POINT('Ctrl Pts',(2.86579847665913,-0.665254155325767,
14.6414495439106));
#67051=CARTESIAN_POINT('Ctrl Pts',(2.88692704124803,-0.574235996734604,
14.6464943803291));
#67052=CARTESIAN_POINT('Ctrl Pts',(2.90370264655347,-0.482264646847366,
14.6515392167476));
#67053=CARTESIAN_POINT('Ctrl Pts',(2.91606366689416,-0.38979057276928,14.6565840531661));
#67054=CARTESIAN_POINT('Ctrl Pts',(2.92843234706057,-0.297259194741166,
14.6616320157479));
#67055=CARTESIAN_POINT('Ctrl Pts',(2.93638095831432,-0.204224913726281,
14.6666799783297));
#67056=CARTESIAN_POINT('Ctrl Pts',(2.93989993331261,-0.111141270950566,
14.6717279409115));
#67057=CARTESIAN_POINT('Ctrl Pts',(2.9434244624339,-0.0179107109612863,
14.6767838708715));
#67058=CARTESIAN_POINT('Ctrl Pts',(2.94250540358311,0.075368923634541,14.6818398008316));
#67059=CARTESIAN_POINT('Ctrl Pts',(2.93718524404744,0.168246373363566,14.6868957307917));
#67060=CARTESIAN_POINT('Ctrl Pts',(2.93486005090881,0.20883876676735,14.6891054415295));
#67061=CARTESIAN_POINT('Ctrl Pts',(2.93169484525421,0.24935443342959,14.6913151522672));
#67062=CARTESIAN_POINT('Ctrl Pts',(2.92769624279459,0.289756294023833,14.693524863005));
#67063=CARTESIAN_POINT('Ctrl Pts',(2.91854904743635,0.382179513242121,14.6985797930731));
#67064=CARTESIAN_POINT('Ctrl Pts',(2.90500489782404,0.474332466220693,14.7036347231412));
#67065=CARTESIAN_POINT('Ctrl Pts',(2.88708765809673,0.565763956492032,14.7086896532093));
#67066=CARTESIAN_POINT('Ctrl Pts',(2.86919485437241,0.65707075009114,14.7137376892307));
#67067=CARTESIAN_POINT('Ctrl Pts',(2.84694089715092,0.747657604582368,14.7187857252522));
#67068=CARTESIAN_POINT('Ctrl Pts',(2.82040143879216,0.837078087193264,14.7238337612737));
#67069=CARTESIAN_POINT('Ctrl Pts',(2.79389000213786,0.926404155129092,14.728876467323));
#67070=CARTESIAN_POINT('Ctrl Pts',(2.76310218415545,1.01456587599627,14.7339191733723));
#67071=CARTESIAN_POINT('Ctrl Pts',(2.72816452790847,1.10112774402517,14.7389618794216));
#67072=CARTESIAN_POINT('Ctrl Pts',(2.69325151757845,1.18762854909678,14.7440010282171));
#67073=CARTESIAN_POINT('Ctrl Pts',(2.65419465335663,1.27253133430926,14.7490401770125));
#67074=CARTESIAN_POINT('Ctrl Pts',(2.61116975058343,1.35541747577565,14.7540793258079));
#67075=CARTESIAN_POINT('Ctrl Pts',(2.56816003098295,1.43827436733049,14.7591166963246));
#67076=CARTESIAN_POINT('Ctrl Pts',(2.52118525904805,1.51911563561082,14.7641540668414));
#67077=CARTESIAN_POINT('Ctrl Pts',(2.47046820581466,1.59754525571544,14.7691914373581));
#67078=CARTESIAN_POINT('Ctrl Pts',(2.4197549078974,1.67596906854225,14.7742284348856));
#67079=CARTESIAN_POINT('Ctrl Pts',(2.36530012081552,1.75198121585167,14.779265432413));
#67080=CARTESIAN_POINT('Ctrl Pts',(2.30737052829664,1.82521375327606,14.7843024299404));
#67081=CARTESIAN_POINT('Ctrl Pts',(2.2494290718373,1.89846128867344,14.7893404590415));
#67082=CARTESIAN_POINT('Ctrl Pts',(2.18801167210225,1.96892773589567,14.7943784881425));
#67083=CARTESIAN_POINT('Ctrl Pts',(2.12342522929933,2.0362782952178,14.7994165172436));
#67084=CARTESIAN_POINT('Ctrl Pts',(2.05876825398377,2.103702405644,14.8044600481935));
#67085=CARTESIAN_POINT('Ctrl Pts',(1.9909356354547,2.16800351568651,14.8095035791435));
#67086=CARTESIAN_POINT('Ctrl Pts',(1.92027083415288,2.22888400853472,14.8145471100935));
#67087=CARTESIAN_POINT('Ctrl Pts',(1.84956213092389,2.28980232461195,14.8195937744384));
#67088=CARTESIAN_POINT('Ctrl Pts',(1.77601809119875,2.34729551974612,14.8246404387832));
#67089=CARTESIAN_POINT('Ctrl Pts',(1.70001319058036,2.4011079009184,14.8296871031281));
#67090=CARTESIAN_POINT('Ctrl Pts',(1.62388794625745,2.45500548687679,14.8347417581983));
#67091=CARTESIAN_POINT('Ctrl Pts',(1.54529443642721,2.505210386688,14.8397964132685));
#67092=CARTESIAN_POINT('Ctrl Pts',(1.46463366396149,2.55151175391977,14.8448510683387));
#67093=CARTESIAN_POINT('Ctrl Pts',(1.42916132346781,2.57187379377584,14.8470739635608));
#67094=CARTESIAN_POINT('Ctrl Pts',(1.39328946144843,2.59148150978898,14.8492968587829));
#67095=CARTESIAN_POINT('Ctrl Pts',(1.35705338672014,2.61031992399235,14.8515197540051));
#67096=CARTESIAN_POINT('Ctrl Pts',(1.27461660312295,2.65317716740632,14.8565768230657));
#67097=CARTESIAN_POINT('Ctrl Pts',(1.19000253446716,2.69220084533978,14.8616338921263));
#67098=CARTESIAN_POINT('Ctrl Pts',(1.10360245323297,2.7271643927747,14.8666909611869));
#67099=CARTESIAN_POINT('Ctrl Pts',(1.01732021364868,2.76208025319291,14.8717411328771));
#67100=CARTESIAN_POINT('Ctrl Pts',(0.929257209804122,2.79294682294084,14.8767913045673));
#67101=CARTESIAN_POINT('Ctrl Pts',(0.839829004222327,2.81958352308757,14.8818414762576));
#67102=CARTESIAN_POINT('Ctrl Pts',(0.750495290970565,2.84619207815586,14.8868863117959));
#67103=CARTESIAN_POINT('Ctrl Pts',(0.659799665997159,2.86857952193179,14.8919311473342));
#67104=CARTESIAN_POINT('Ctrl Pts',(0.56817633346858,2.88661387339668,14.8969759828725));
#67105=CARTESIAN_POINT('Ctrl Pts',(0.47661793118525,2.90463544454862,14.9020172433126));
#67106=CARTESIAN_POINT('Ctrl Pts',(0.384133561889784,2.91830997004826,14.9070585037528));
#67107=CARTESIAN_POINT('Ctrl Pts',(0.291170202025931,2.92755596248,14.9120997641929));
#67108=CARTESIAN_POINT('Ctrl Pts',(0.198239854739045,2.93679867153173,14.9171392344116));
#67109=CARTESIAN_POINT('Ctrl Pts',(0.10483129549399,2.94161592817868,14.9221787046303));
#67110=CARTESIAN_POINT('Ctrl Pts',(0.0113982264469119,2.94197791977334,
14.927218174849));
#67111=CARTESIAN_POINT('Ctrl Pts',(-0.0820276584529391,2.94233988353416,
14.9322572575786));
#67112=CARTESIAN_POINT('Ctrl Pts',(-0.175477606146424,2.93824726198362,
14.9372963403083));
#67113=CARTESIAN_POINT('Ctrl Pts',(-0.268497436916809,2.92972236335956,
14.9423354230379));
#67114=CARTESIAN_POINT('Ctrl Pts',(-0.361535995095789,2.92119574844276,
14.9473755202712));
#67115=CARTESIAN_POINT('Ctrl Pts',(-0.454143823029988,2.90823512502494,
14.9524156175045));
#67116=CARTESIAN_POINT('Ctrl Pts',(-0.545872518920582,2.89091459456818,
14.9574557147378));
#67117=CARTESIAN_POINT('Ctrl Pts',(-0.637700656134728,2.87357528725587,
14.962501275844));
#67118=CARTESIAN_POINT('Ctrl Pts',(-0.72864732283676,2.85186672123159,14.9675468369502));
#67119=CARTESIAN_POINT('Ctrl Pts',(-0.818275274387837,2.82591393629132,
14.9725923980565));
#67120=CARTESIAN_POINT('Ctrl Pts',(-0.907958552103803,2.79994513103558,
14.9776410737218));
#67121=CARTESIAN_POINT('Ctrl Pts',(-0.996321074966273,2.76972703420609,
14.982689749387));
#67122=CARTESIAN_POINT('Ctrl Pts',(-1.08294374574899,2.73543357505591,14.9877384250523));
#67123=CARTESIAN_POINT('Ctrl Pts',(-1.16970269872328,2.70108616250383,14.9927950437258));
#67124=CARTESIAN_POINT('Ctrl Pts',(-1.25471593226287,2.66265077107231,14.9978516623992));
#67125=CARTESIAN_POINT('Ctrl Pts',(-1.33758739858879,2.62034805915865,15.0029082810727));
#67126=CARTESIAN_POINT('Ctrl Pts',(-1.37367733018883,2.60192553030587,15.0051104023835));
#67127=CARTESIAN_POINT('Ctrl Pts',(-1.40936142196231,2.58277011622747,15.0073125236943));
#67128=CARTESIAN_POINT('Ctrl Pts',(-1.44460872073146,2.56290258183697,15.0095146450051));
#67129=CARTESIAN_POINT('Ctrl Pts',(-1.54202772550784,2.50799126961531,15.0156010253516));
#67130=CARTESIAN_POINT('Ctrl Pts',(-1.63638431559853,2.44748194167846,15.021687405698));
#67131=CARTESIAN_POINT('Ctrl Pts',(-1.72710266414602,2.38169695542899,15.0277737860445));
#67132=CARTESIAN_POINT('Ctrl Pts',(-1.81676908628711,2.31667478028982,15.0337895916472));
#67133=CARTESIAN_POINT('Ctrl Pts',(-1.90288109881628,2.24649858300431,15.0398053972498));
#67134=CARTESIAN_POINT('Ctrl Pts',(-1.98490247403207,2.17152623023103,15.0458212028525));
#67135=CARTESIAN_POINT('Ctrl Pts',(-2.0402523172333,2.12093322371886,15.0498808019017));
#67136=CARTESIAN_POINT('Ctrl Pts',(-2.09373974757189,2.06815707469092,15.0539404009508));
#67137=CARTESIAN_POINT('Ctrl Pts',(-2.14520543675184,2.01332005258239,15.058));
#67138=CARTESIAN_POINT('',(0.261483065272176,2.93035673708439,15.0579981933191));
#67139=CARTESIAN_POINT('Origin',(0.,0.,15.058));
#67140=CARTESIAN_POINT('',(-2.94199899580993,-0.00243077217840307,14.3221761170896));
#67141=CARTESIAN_POINT('Ctrl Pts',(0.261483065272176,2.93035673708439,15.0579981933191));
#67142=CARTESIAN_POINT('Ctrl Pts',(0.359661773013358,2.92159600528688,15.0526990630625));
#67143=CARTESIAN_POINT('Ctrl Pts',(0.45728330298564,2.90790733319514,15.0473999328059));
#67144=CARTESIAN_POINT('Ctrl Pts',(0.553856556304756,2.88939559683998,15.0421008025493));
#67145=CARTESIAN_POINT('Ctrl Pts',(0.650732804101302,2.87082578069884,15.0367850464967));
#67146=CARTESIAN_POINT('Ctrl Pts',(0.74655383536055,2.84740271291704,15.0314692904441));
#67147=CARTESIAN_POINT('Ctrl Pts',(0.84084094592112,2.8192819127683,15.0261535343916));
#67148=CARTESIAN_POINT('Ctrl Pts',(0.935282325557894,2.79111510240846,15.020829080896));
#67149=CARTESIAN_POINT('Ctrl Pts',(1.02818443064924,2.75823534881844,15.0155046274004));
#67150=CARTESIAN_POINT('Ctrl Pts',(1.11908839081021,2.72084640756398,15.0101801739048));
#67151=CARTESIAN_POINT('Ctrl Pts',(1.210258016484,2.68334819766782,15.0048401597706));
#67152=CARTESIAN_POINT('Ctrl Pts',(1.29941748571425,2.64131460587378,14.9995001456364));
#67153=CARTESIAN_POINT('Ctrl Pts',(1.3861310604502,2.59499608540267,14.9941601315022));
#67154=CARTESIAN_POINT('Ctrl Pts',(1.44494860738031,2.56357837762349,14.9905380165923));
#67155=CARTESIAN_POINT('Ctrl Pts',(1.50264140027149,2.53019016395851,14.9869159016824));
#67156=CARTESIAN_POINT('Ctrl Pts',(1.55908161262863,2.49492054485976,14.9832937867725));
#67157=CARTESIAN_POINT('Ctrl Pts',(1.63799388701391,2.44560808228123,14.9782295016876));
#67158=CARTESIAN_POINT('Ctrl Pts',(1.71470044723877,2.39246299705959,14.9731652166027));
#67159=CARTESIAN_POINT('Ctrl Pts',(1.78880676794263,2.33570853210812,14.9681009315178));
#67160=CARTESIAN_POINT('Ctrl Pts',(1.86281259231978,2.27903103245727,14.9630435141609));
#67161=CARTESIAN_POINT('Ctrl Pts',(1.93422483739239,2.2187541473552,14.9579860968039));
#67162=CARTESIAN_POINT('Ctrl Pts',(2.00267634239024,2.15514534721685,14.952928679447));
#67163=CARTESIAN_POINT('Ctrl Pts',(2.07457810505856,2.08833038308557,14.9476163459559));
#67164=CARTESIAN_POINT('Ctrl Pts',(2.14321240660558,2.01783906022885,14.9423040124648));
#67165=CARTESIAN_POINT('Ctrl Pts',(2.20819115000048,1.94403082410222,14.9369916789738));
#67166=CARTESIAN_POINT('Ctrl Pts',(2.26994142235796,1.87388975265451,14.9319432889497));
#67167=CARTESIAN_POINT('Ctrl Pts',(2.32839034435918,1.80075383929931,14.9268948989257));
#67168=CARTESIAN_POINT('Ctrl Pts',(2.38324229469831,1.7249696127066,14.9218465089017));
#67169=CARTESIAN_POINT('Ctrl Pts',(2.43807549335941,1.64921129369617,14.9167998447194));
#67170=CARTESIAN_POINT('Ctrl Pts',(2.48931390495793,1.57080681794917,14.9117531805371));
#67171=CARTESIAN_POINT('Ctrl Pts',(2.53670323007296,1.49013446458278,14.9067065163548));
#67172=CARTESIAN_POINT('Ctrl Pts',(2.58408942671674,1.40946743691236,14.901660185335));
#67173=CARTESIAN_POINT('Ctrl Pts',(2.62762681880991,1.32653321046229,14.8966138543152));
#67174=CARTESIAN_POINT('Ctrl Pts',(2.66710593886766,1.24173665116919,14.8915675232953));
#67175=CARTESIAN_POINT('Ctrl Pts',(2.70659334242671,1.15692229987847,14.8865201334553));
#67176=CARTESIAN_POINT('Ctrl Pts',(2.74202059656648,1.07024524019156,14.8814727436153));
#67177=CARTESIAN_POINT('Ctrl Pts',(2.77322591465876,0.982131369148298,14.8764253537752));
#67178=CARTESIAN_POINT('Ctrl Pts',(2.8044646487814,0.893923141887225,14.8713725589676));
#67179=CARTESIAN_POINT('Ctrl Pts',(2.83147227578439,0.804275449368773,14.86631976416));
#67180=CARTESIAN_POINT('Ctrl Pts',(2.85413665238589,0.713630134949094,14.8612669693524));
#67181=CARTESIAN_POINT('Ctrl Pts',(2.87681511196177,0.622928496207644,14.8562110348873));
#67182=CARTESIAN_POINT('Ctrl Pts',(2.895144861223,0.531228434084276,14.8511551004222));
#67183=CARTESIAN_POINT('Ctrl Pts',(2.90906513108331,0.438980709274588,14.8460991659571));
#67184=CARTESIAN_POINT('Ctrl Pts',(2.92300664127415,0.346592227699102,14.8410355168629));
#67185=CARTESIAN_POINT('Ctrl Pts',(2.93252519769504,0.25365485410448,14.8359718677687));
#67186=CARTESIAN_POINT('Ctrl Pts',(2.93761200366519,0.160622899744075,14.8309082186745));
#67187=CARTESIAN_POINT('Ctrl Pts',(2.93944553151384,0.127089739616721,14.8290830376701));
#67188=CARTESIAN_POINT('Ctrl Pts',(2.94070376646984,0.0935442727577978,
14.8272578566656));
#67189=CARTESIAN_POINT('Ctrl Pts',(2.94138795159684,0.0600076511867527,
14.8254326756612));
#67190=CARTESIAN_POINT('Ctrl Pts',(2.94328660875558,-0.0330586025407972,
14.8203676825134));
#67191=CARTESIAN_POINT('Ctrl Pts',(2.94076720379232,-0.126372285094918,
14.8153026893656));
#67192=CARTESIAN_POINT('Ctrl Pts',(2.93380166489366,-0.21948073051458,14.8102376962178));
#67193=CARTESIAN_POINT('Ctrl Pts',(2.92684535599062,-0.312465798467389,
14.8051794146633));
#67194=CARTESIAN_POINT('Ctrl Pts',(2.91545465513211,-0.405245732896898,
14.8001211331089));
#67195=CARTESIAN_POINT('Ctrl Pts',(2.8996534899233,-0.497366704128502,14.7950628515544));
#67196=CARTESIAN_POINT('Ctrl Pts',(2.8830593259192,-0.59411086727295,14.7897507145959));
#67197=CARTESIAN_POINT('Ctrl Pts',(2.8616004292145,-0.690127704461536,14.7844385776374));
#67198=CARTESIAN_POINT('Ctrl Pts',(2.8353663274954,-0.784896037004432,14.7791264406789));
#67199=CARTESIAN_POINT('Ctrl Pts',(2.81042856039029,-0.874981477367452,
14.7740767982051));
#67200=CARTESIAN_POINT('Ctrl Pts',(2.78117639119523,-0.963938376115757,
14.7690271557314));
#67201=CARTESIAN_POINT('Ctrl Pts',(2.74773902194529,-1.05132976143509,14.7639775132576));
#67202=CARTESIAN_POINT('Ctrl Pts',(2.71431215219443,-1.13869370542782,14.7589294563965));
#67203=CARTESIAN_POINT('Ctrl Pts',(2.67670285138473,-1.22449270066437,14.7538813995354));
#67204=CARTESIAN_POINT('Ctrl Pts',(2.63508946894432,-1.3083071086938,14.7488333426744));
#67205=CARTESIAN_POINT('Ctrl Pts',(2.59347768630801,-1.39211829452341,14.7437854798831));
#67206=CARTESIAN_POINT('Ctrl Pts',(2.54786232501567,-1.47394464957085,14.7387376170918));
#67207=CARTESIAN_POINT('Ctrl Pts',(2.49846846617174,-1.55338962386951,14.7336897543006));
#67208=CARTESIAN_POINT('Ctrl Pts',(2.44906289559007,-1.63285343530146,14.7286406946147));
#67209=CARTESIAN_POINT('Ctrl Pts',(2.39587728115249,-1.70993436955877,14.7235916349288));
#67210=CARTESIAN_POINT('Ctrl Pts',(2.33918033139902,-1.78426437984844,14.7185425752429));
#67211=CARTESIAN_POINT('Ctrl Pts',(2.28242045583138,-1.85867688622363,14.7134879117954));
#67212=CARTESIAN_POINT('Ctrl Pts',(2.22214173515893,-1.93033202352542,14.7084332483478));
#67213=CARTESIAN_POINT('Ctrl Pts',(2.15865332432241,-1.9988946508988,14.7033785849003));
#67214=CARTESIAN_POINT('Ctrl Pts',(2.09512400695069,-2.06750145420118,14.6983206646573));
#67215=CARTESIAN_POINT('Ctrl Pts',(2.02838119685972,-2.13301147158374,14.6932627444143));
#67216=CARTESIAN_POINT('Ctrl Pts',(1.95876953423314,-2.19512776661407,14.6882048241713));
#67217=CARTESIAN_POINT('Ctrl Pts',(1.88904949279933,-2.25734077086971,14.6831390292225));
#67218=CARTESIAN_POINT('Ctrl Pts',(1.8164520263333,-2.31614922946661,14.6780732342738));
#67219=CARTESIAN_POINT('Ctrl Pts',(1.7413530971558,-2.37129782841083,14.673007439325));
#67220=CARTESIAN_POINT('Ctrl Pts',(1.71449134568613,-2.3910236484054,14.6711954810667));
#67221=CARTESIAN_POINT('Ctrl Pts',(1.68730980978028,-2.4102816484538,14.6693835228084));
#67222=CARTESIAN_POINT('Ctrl Pts',(1.65982647247631,-2.42906156391041,14.6675715645502));
#67223=CARTESIAN_POINT('Ctrl Pts',(1.58323294978353,-2.48139945376653,14.6625218042376));
#67224=CARTESIAN_POINT('Ctrl Pts',(1.50402331994656,-2.53020547805049,14.6574720439251));
#67225=CARTESIAN_POINT('Ctrl Pts',(1.42255732262935,-2.57520769333924,14.6524222836126));
#67226=CARTESIAN_POINT('Ctrl Pts',(1.34120382081709,-2.62014776556095,14.6473794964589));
#67227=CARTESIAN_POINT('Ctrl Pts',(1.25760052876846,-2.66129425305727,14.6423367093051));
#67228=CARTESIAN_POINT('Ctrl Pts',(1.17213692290193,-2.69841787608406,14.6372939221514));
#67229=CARTESIAN_POINT('Ctrl Pts',(1.08676485621621,-2.73550173638371,14.6322565362746));
#67230=CARTESIAN_POINT('Ctrl Pts',(0.999536841876472,-2.76857112030728,
14.6272191503979));
#67231=CARTESIAN_POINT('Ctrl Pts',(0.910866790340188,-2.79744270544642,
14.6221817645211));
#67232=CARTESIAN_POINT('Ctrl Pts',(0.822260869946003,-2.8262934090399,14.6171480219636));
#67233=CARTESIAN_POINT('Ctrl Pts',(0.732215407066378,-2.85095221122863,
14.6121142794061));
#67234=CARTESIAN_POINT('Ctrl Pts',(0.64116313067073,-2.87128435371151,14.6070805368487));
#67235=CARTESIAN_POINT('Ctrl Pts',(0.550143932939321,-2.89160910966721,
14.6020486230152));
#67236=CARTESIAN_POINT('Ctrl Pts',(0.45811908193511,-2.90761023173326,14.5970167091816));
#67237=CARTESIAN_POINT('Ctrl Pts',(0.365534253305122,-2.9192034375255,14.5919847953481));
#67238=CARTESIAN_POINT('Ctrl Pts',(0.272957092441749,-2.93079568318207,
14.5869532982518));
#67239=CARTESIAN_POINT('Ctrl Pts',(0.179820487475819,-2.93798068339455,
14.5819218011555));
#67240=CARTESIAN_POINT('Ctrl Pts',(0.0865768933064366,-2.94072583583465,
14.5768903040592));
#67241=CARTESIAN_POINT('Ctrl Pts',(-0.00668513067810722,-2.94347153086057,
14.5718578124756));
#67242=CARTESIAN_POINT('Ctrl Pts',(-0.100053741348647,-2.94177562272804,
14.5668253208921));
#67243=CARTESIAN_POINT('Ctrl Pts',(-0.193075973589511,-2.93565762111702,
14.5617928293086));
#67244=CARTESIAN_POINT('Ctrl Pts',(-0.286199262361645,-2.92953297309465,
14.5567548705788));
#67245=CARTESIAN_POINT('Ctrl Pts',(-0.378974977231565,-2.91897667224081,
14.5517169118491));
#67246=CARTESIAN_POINT('Ctrl Pts',(-0.470955102753805,-2.90406013904502,
14.5466789531194));
#67247=CARTESIAN_POINT('Ctrl Pts',(-0.56299205820675,-2.88913438966754,
14.5416378816863));
#67248=CARTESIAN_POINT('Ctrl Pts',(-0.654232011064526,-2.86984313698716,
14.5365968102532));
#67249=CARTESIAN_POINT('Ctrl Pts',(-0.744239103737049,-2.8463085139297,
14.5315557388201));
#67250=CARTESIAN_POINT('Ctrl Pts',(-0.834388722700486,-2.82273662378102,
14.5265066848471));
#67251=CARTESIAN_POINT('Ctrl Pts',(-0.923301160924991,-2.79490808336421,
14.521457630874));
#67252=CARTESIAN_POINT('Ctrl Pts',(-1.01055785568057,-2.7629941766718,14.516408576901));
#67253=CARTESIAN_POINT('Ctrl Pts',(-1.04914304526776,-2.74888174502809,
14.5141758690803));
#67254=CARTESIAN_POINT('Ctrl Pts',(-1.08740475570698,-2.73397106640143,
14.5119431612597));
#67255=CARTESIAN_POINT('Ctrl Pts',(-1.12530831193825,-2.71827982427908,
14.509710453439));
#67256=CARTESIAN_POINT('Ctrl Pts',(-1.21117629085882,-2.68273236167218,
14.5046524027667));
#67257=CARTESIAN_POINT('Ctrl Pts',(-1.29550855517803,-2.6430499600766,14.4995943520943));
#67258=CARTESIAN_POINT('Ctrl Pts',(-1.37787983046257,-2.59938669166487,
14.494536301422));
#67259=CARTESIAN_POINT('Ctrl Pts',(-1.46013917454961,-2.55578275561024,
14.4894851239426));
#67260=CARTESIAN_POINT('Ctrl Pts',(-1.54044243695998,-2.50820890864038,
14.4844339464632));
#67261=CARTESIAN_POINT('Ctrl Pts',(-1.61838395162,-2.45686739266466,14.4793827689838));
#67262=CARTESIAN_POINT('Ctrl Pts',(-1.6962434735779,-2.40557988679695,14.4743369052283));
#67263=CARTESIAN_POINT('Ctrl Pts',(-1.7717458184305,-2.35053283308713,14.4692910414728));
#67264=CARTESIAN_POINT('Ctrl Pts',(-1.8445105575821,-2.29197399700961,14.4642451777173));
#67265=CARTESIAN_POINT('Ctrl Pts',(-1.91722412050728,-2.23345634599354,
14.4592028627722));
#67266=CARTESIAN_POINT('Ctrl Pts',(-1.98720356076137,-2.17143209917494,
14.4541605478272));
#67267=CARTESIAN_POINT('Ctrl Pts',(-2.0540989090585,-2.10619127141974,14.4491182328822));
#67268=CARTESIAN_POINT('Ctrl Pts',(-2.12097073098796,-2.04097338815528,
14.4440776912645));
#67269=CARTESIAN_POINT('Ctrl Pts',(-2.18476029907851,-1.9725414805608,14.4390371496469));
#67270=CARTESIAN_POINT('Ctrl Pts',(-2.24515289510571,-1.90122394199065,
14.4339966080293));
#67271=CARTESIAN_POINT('Ctrl Pts',(-2.30554103308762,-1.82991166792041,
14.4289564384931));
#67272=CARTESIAN_POINT('Ctrl Pts',(-2.36253241155492,-1.75571452473796,
14.4239162689569));
#67273=CARTESIAN_POINT('Ctrl Pts',(-2.4158519204632,-1.67899478807835,14.4188760994207));
#67274=CARTESIAN_POINT('Ctrl Pts',(-2.46918230912261,-1.60225939689269,
14.4138349014468));
#67275=CARTESIAN_POINT('Ctrl Pts',(-2.51883908763949,-1.52300075389714,
14.4087937034729));
#67276=CARTESIAN_POINT('Ctrl Pts',(-2.56459052396015,-1.44161001814423,
14.4037525054991));
#67277=CARTESIAN_POINT('Ctrl Pts',(-2.61039156885869,-1.36013102989089,
14.3987058413217));
#67278=CARTESIAN_POINT('Ctrl Pts',(-2.65227860204805,-1.27651572125823,
14.3936591771443));
#67279=CARTESIAN_POINT('Ctrl Pts',(-2.69006607358686,-1.19117946579724,
14.388612512967));
#67280=CARTESIAN_POINT('Ctrl Pts',(-2.72787694116127,-1.10579037456846,
14.3835627241578));
#67281=CARTESIAN_POINT('Ctrl Pts',(-2.76158303393655,-1.01867862796998,
14.3785129353487));
#67282=CARTESIAN_POINT('Ctrl Pts',(-2.79104790841499,-0.930277148452167,
14.3734631465395));
#67283=CARTESIAN_POINT('Ctrl Pts',(-2.82055898625829,-0.841737048088894,
14.368405439243));
#67284=CARTESIAN_POINT('Ctrl Pts',(-2.84581545058168,-0.75190360359488,
14.3633477319465));
#67285=CARTESIAN_POINT('Ctrl Pts',(-2.86673146364986,-0.661222137651145,
14.3582900246501));
#67286=CARTESIAN_POINT('Ctrl Pts',(-2.87560988673235,-0.622729695627666,
14.3561431305427));
#67287=CARTESIAN_POINT('Ctrl Pts',(-2.88370687142123,-0.584084543517024,
14.3539962364353));
#67288=CARTESIAN_POINT('Ctrl Pts',(-2.89101867841434,-0.54532100735198,
14.351849342328));
#67289=CARTESIAN_POINT('Ctrl Pts',(-2.9162676760388,-0.411463476174145,
14.344435727025));
#67290=CARTESIAN_POINT('Ctrl Pts',(-2.93222540650343,-0.27580307450041,
14.337022111722));
#67291=CARTESIAN_POINT('Ctrl Pts',(-2.93869582950559,-0.13939448212346,
14.329608496419));
#67292=CARTESIAN_POINT('Ctrl Pts',(-2.94085809610147,-0.0938098669305718,
14.3271310366425));
#67293=CARTESIAN_POINT('Ctrl Pts',(-2.9419612278275,-0.0481419117786443,
14.3246535768661));
#67294=CARTESIAN_POINT('Ctrl Pts',(-2.94199899580993,-0.00243077217840307,
14.3221761170896));
#67295=CARTESIAN_POINT('',(-2.94154465770424,0.000354470811248017,13.3221761002206));
#67296=CARTESIAN_POINT('Ctrl Pts',(-2.94325255946896,-0.00241996395558216,
14.3221754754428));
#67297=CARTESIAN_POINT('Ctrl Pts',(-2.9361986618122,0.786308567410447,14.2794463940342));
#67298=CARTESIAN_POINT('Ctrl Pts',(-2.20502853201952,2.55780260563958,14.1840969422552));
#67299=CARTESIAN_POINT('Ctrl Pts',(0.779438885227077,3.38200690959716,14.0361271201057));
#67300=CARTESIAN_POINT('Ctrl Pts',(3.25729747472218,1.19795113049604,13.8782660089947));
#67301=CARTESIAN_POINT('Ctrl Pts',(2.78492903121012,-2.07109504482707,13.7204048978835));
#67302=CARTESIAN_POINT('Ctrl Pts',(-0.209925428309956,-3.4642751230223,
13.5625437867724));
#67303=CARTESIAN_POINT('Ctrl Pts',(-2.5683496391778,-1.99726696188011,13.4298008598411));
#67304=CARTESIAN_POINT('Ctrl Pts',(-2.9367843178467,-0.509922711901109,
13.3496783032802));
#67305=CARTESIAN_POINT('Ctrl Pts',(-2.93733773658367,0.000353650820144602,
13.3221761170896));
#67306=CARTESIAN_POINT('',(-2.94199923889461,0.0021162097116246,12.3221761170896));
#67307=CARTESIAN_POINT('Ctrl Pts',(-2.94199997863486,0.0003545595600269,
13.3221760983949));
#67308=CARTESIAN_POINT('Ctrl Pts',(-2.9419880493624,0.0993391119192297,
13.3168496162708));
#67309=CARTESIAN_POINT('Ctrl Pts',(-2.93697629515374,0.198210372559447,
13.3115231341467));
#67310=CARTESIAN_POINT('Ctrl Pts',(-2.92702446251479,0.296465505312221,
13.3061966520225));
#67311=CARTESIAN_POINT('Ctrl Pts',(-2.91704196021071,0.395023441792436,
13.3008537546884));
#67312=CARTESIAN_POINT('Ctrl Pts',(-2.90208897278557,0.492961091822583,
13.2955108573543));
#67313=CARTESIAN_POINT('Ctrl Pts',(-2.88227683628384,0.589783213580746,
13.2901679600201));
#67314=CARTESIAN_POINT('Ctrl Pts',(-2.86243333684518,0.686758606345156,
13.2848166047919));
#67315=CARTESIAN_POINT('Ctrl Pts',(-2.83771543063832,0.782614597196314,
13.2794652495637));
#67316=CARTESIAN_POINT('Ctrl Pts',(-2.808284369287,0.876871085860581,13.2741138943355));
#67317=CARTESIAN_POINT('Ctrl Pts',(-2.77877089374446,0.971391515814227,
13.2687475539999));
#67318=CARTESIAN_POINT('Ctrl Pts',(-2.74451799497217,1.06430314579817,13.2633812136644));
#67319=CARTESIAN_POINT('Ctrl Pts',(-2.70573563698505,1.15514443371775,13.2580148733288));
#67320=CARTESIAN_POINT('Ctrl Pts',(-2.67877108380303,1.21830445972866,13.2542837704026));
#67321=CARTESIAN_POINT('Ctrl Pts',(-2.64961792582727,1.28046412723049,13.2505526674764));
#67322=CARTESIAN_POINT('Ctrl Pts',(-2.61835946279969,1.34147594967906,13.2468215645502));
#67323=CARTESIAN_POINT('Ctrl Pts',(-2.5759972019918,1.42416071676599,13.2417650793634));
#67324=CARTESIAN_POINT('Ctrl Pts',(-2.52963999234658,1.50498226700905,13.2367085941766));
#67325=CARTESIAN_POINT('Ctrl Pts',(-2.47947552240893,1.58352932835959,13.2316521089898));
#67326=CARTESIAN_POINT('Ctrl Pts',(-2.42937932357179,1.6619694914547,13.2266025054029));
#67327=CARTESIAN_POINT('Ctrl Pts',(-2.37548639797535,1.73814094657396,13.2215529018159));
#67328=CARTESIAN_POINT('Ctrl Pts',(-2.31803087083851,1.81165583978847,13.2165032982289));
#67329=CARTESIAN_POINT('Ctrl Pts',(-2.2606358735758,1.88509328445355,13.2114590144412));
#67330=CARTESIAN_POINT('Ctrl Pts',(-2.19968600696845,1.9558793829046,13.2064147306535));
#67331=CARTESIAN_POINT('Ctrl Pts',(-2.13545874046757,2.02365510098946,13.2013704468658));
#67332=CARTESIAN_POINT('Ctrl Pts',(-2.07127668804704,2.09138310698987,13.1963297141035));
#67333=CARTESIAN_POINT('Ctrl Pts',(-2.00382212594782,2.15610462414014,13.1912889813411));
#67334=CARTESIAN_POINT('Ctrl Pts',(-1.93341218163038,2.21749438238821,13.1862482485788));
#67335=CARTESIAN_POINT('Ctrl Pts',(-1.86302701698762,2.27886253547449,13.1812092898232));
#67336=CARTESIAN_POINT('Ctrl Pts',(-1.78968887043984,2.33690096819232,13.1761703310676));
#67337=CARTESIAN_POINT('Ctrl Pts',(-1.71375027989472,2.39132264200396,13.171131372312));
#67338=CARTESIAN_POINT('Ctrl Pts',(-1.63781727600902,2.4457403121153,13.1660927842632));
#67339=CARTESIAN_POINT('Ctrl Pts',(-1.55928456908114,2.49654149438389,13.1610541962143));
#67340=CARTESIAN_POINT('Ctrl Pts',(-1.47853527103567,2.5434813646464,13.1560156081655));
#67341=CARTESIAN_POINT('Ctrl Pts',(-1.39776943609134,2.59043084787032,13.1509759882486));
#67342=CARTESIAN_POINT('Ctrl Pts',(-1.31478649191079,2.63351722608229,13.1459363683317));
#67343=CARTESIAN_POINT('Ctrl Pts',(-1.22999483376291,2.67254124550334,13.1408967484148));
#67344=CARTESIAN_POINT('Ctrl Pts',(-1.14511095785756,2.71160770668856,13.1358516475053));
#67345=CARTESIAN_POINT('Ctrl Pts',(-1.05841484500098,2.74660280501691,13.1308065465959));
#67346=CARTESIAN_POINT('Ctrl Pts',(-0.970335291761442,2.77737527560865,
13.1257614456864));
#67347=CARTESIAN_POINT('Ctrl Pts',(-0.882201077622042,2.80816684315164,
13.1207132138601));
#67348=CARTESIAN_POINT('Ctrl Pts',(-0.792682138512077,2.8347304398849,13.1156649820338));
#67349=CARTESIAN_POINT('Ctrl Pts',(-0.702220785372583,2.85696516754943,
13.1106167502075));
#67350=CARTESIAN_POINT('Ctrl Pts',(-0.611617100800494,2.87923487922128,
13.105560575519));
#67351=CARTESIAN_POINT('Ctrl Pts',(-0.520068476729443,2.89716204108954,
13.1005044008304));
#67352=CARTESIAN_POINT('Ctrl Pts',(-0.428025485042737,2.91069719898067,
13.0954482261419));
#67353=CARTESIAN_POINT('Ctrl Pts',(-0.3886575144761,2.91648635997716,13.0932856352409));
#67354=CARTESIAN_POINT('Ctrl Pts',(-0.349199142779485,2.92147270529838,
13.09112304434));
#67355=CARTESIAN_POINT('Ctrl Pts',(-0.309685661186744,2.92565527553321,
13.088960453439));
#67356=CARTESIAN_POINT('Ctrl Pts',(-0.217296290305112,2.93543484992374,
13.0839039409587));
#67357=CARTESIAN_POINT('Ctrl Pts',(-0.124280802336355,2.94085098155313,
13.0788474284784));
#67358=CARTESIAN_POINT('Ctrl Pts',(-0.0310861472398973,2.94183576214747,
13.0737909159981));
#67359=CARTESIAN_POINT('Ctrl Pts',(0.0619816830295821,2.94281920259383,
13.0687412847206));
#67360=CARTESIAN_POINT('Ctrl Pts',(0.155227756270759,2.93938327137785,13.0636916534431));
#67361=CARTESIAN_POINT('Ctrl Pts',(0.248199318647507,2.93151174280829,13.0586420221656));
#67362=CARTESIAN_POINT('Ctrl Pts',(0.34107294178894,2.92364850636021,13.0535977103322));
#67363=CARTESIAN_POINT('Ctrl Pts',(0.433672189396265,2.91135899786555,13.0485533984987));
#67364=CARTESIAN_POINT('Ctrl Pts',(0.525544717101477,2.89467904098654,13.0435090866653));
#67365=CARTESIAN_POINT('Ctrl Pts',(0.617352577095301,2.8780108248821,13.0384683254482));
#67366=CARTESIAN_POINT('Ctrl Pts',(0.708434298944026,2.85695838221765,13.0334275642312));
#67367=CARTESIAN_POINT('Ctrl Pts',(0.798344103119171,2.83160920556048,13.0283868030141));
#67368=CARTESIAN_POINT('Ctrl Pts',(0.888222269458715,2.80626894887695,13.023347815561));
#67369=CARTESIAN_POINT('Ctrl Pts',(0.976928911119476,2.7766350823183,13.018308828108));
#67370=CARTESIAN_POINT('Ctrl Pts',(1.06403087676328,2.74284565611964,13.0132698406549));
#67371=CARTESIAN_POINT('Ctrl Pts',(1.15112643808778,2.70905871434567,13.008231223702));
#67372=CARTESIAN_POINT('Ctrl Pts',(1.23661714477252,2.671116981117,13.003192606749));
#67373=CARTESIAN_POINT('Ctrl Pts',(1.32008845357155,2.62920719509647,12.998153989796));
#67374=CARTESIAN_POINT('Ctrl Pts',(1.40357685944841,2.58728882487039,12.9931143408043));
#67375=CARTESIAN_POINT('Ctrl Pts',(1.48504464993766,2.54140098688932,12.9880746918125));
#67376=CARTESIAN_POINT('Ctrl Pts',(1.564101593611,2.49177651583434,12.9830350428208));
#67377=CARTESIAN_POINT('Ctrl Pts',(1.64324451888058,2.44209807366645,12.9779899127537));
#67378=CARTESIAN_POINT('Ctrl Pts',(1.71997098785871,2.38867512301693,12.9729447826866));
#67379=CARTESIAN_POINT('Ctrl Pts',(1.79391977637422,2.33178383130458,12.9678996526195));
#67380=CARTESIAN_POINT('Ctrl Pts',(1.8679144574754,2.27485723288158,12.9628513915469));
#67381=CARTESIAN_POINT('Ctrl Pts',(1.93912768839629,2.21445829466963,12.9578031304743));
#67382=CARTESIAN_POINT('Ctrl Pts',(2.00723301042557,2.15090205306004,12.9527548694018));
#67383=CARTESIAN_POINT('Ctrl Pts',(2.07544548651093,2.08724581472664,12.947698665607));
#67384=CARTESIAN_POINT('Ctrl Pts',(2.14053998407788,2.02042267413597,12.9426424618123));
#67385=CARTESIAN_POINT('Ctrl Pts',(2.20222858602172,1.95078272878063,12.9375862580175));
#67386=CARTESIAN_POINT('Ctrl Pts',(2.22860995671424,1.92100093513422,12.9354239527877));
#67387=CARTESIAN_POINT('Ctrl Pts',(2.25436895385661,1.89070436916235,12.9332616475578));
#67388=CARTESIAN_POINT('Ctrl Pts',(2.27948547368887,1.8599220347212,12.9310993423279));
#67389=CARTESIAN_POINT('Ctrl Pts',(2.33821991426747,1.78793820873022,12.9260428381273));
#67390=CARTESIAN_POINT('Ctrl Pts',(2.39364451016909,1.71304294853357,12.9209863339267));
#67391=CARTESIAN_POINT('Ctrl Pts',(2.44545788122685,1.63557321791031,12.9159298297262));
#67392=CARTESIAN_POINT('Ctrl Pts',(2.49720074076032,1.55820891391113,12.910880206796));
#67393=CARTESIAN_POINT('Ctrl Pts',(2.54534189723609,1.47827746733343,12.9058305838658));
#67394=CARTESIAN_POINT('Ctrl Pts',(2.58962005589505,1.39614897704582,12.9007809609357));
#67395=CARTESIAN_POINT('Ctrl Pts',(2.63385156995547,1.31410700459398,12.8957366575048));
#67396=CARTESIAN_POINT('Ctrl Pts',(2.67422796606321,1.22987297731259,12.890692354074));
#67397=CARTESIAN_POINT('Ctrl Pts',(2.71053174137645,1.14384512893607,12.8856480506432));
#67398=CARTESIAN_POINT('Ctrl Pts',(2.74680996262532,1.05787783517558,12.8806072978748));
#67399=CARTESIAN_POINT('Ctrl Pts',(2.77902108941892,0.970119637511359,12.8755665451065));
#67400=CARTESIAN_POINT('Ctrl Pts',(2.8069944601598,0.880991544018547,12.8705257923382));
#67401=CARTESIAN_POINT('Ctrl Pts',(2.83495798735894,0.791894813786075,12.865486813359));
#67402=CARTESIAN_POINT('Ctrl Pts',(2.85868658860374,0.70142956806775,12.8604478343798));
#67403=CARTESIAN_POINT('Ctrl Pts',(2.87805883080864,0.610033905946551,12.8554088554006));
#67404=CARTESIAN_POINT('Ctrl Pts',(2.89742964857949,0.518644964115729,12.8503702469357));
#67405=CARTESIAN_POINT('Ctrl Pts',(2.9124446526143,0.426326175699014,12.8453316384708));
#67406=CARTESIAN_POINT('Ctrl Pts',(2.92303334545943,0.333526702577529,12.8402930300059));
#67407=CARTESIAN_POINT('Ctrl Pts',(2.93362420713858,0.240708221760124,12.8352533895056));
#67408=CARTESIAN_POINT('Ctrl Pts',(2.9397869071143,0.147409301188208,12.8302137490054));
#67409=CARTESIAN_POINT('Ctrl Pts',(2.9415028342468,0.0540839728388559,12.8251741085052));
#67410=CARTESIAN_POINT('Ctrl Pts',(2.94322062762461,-0.0393428562980931,
12.8201289868832));
#67411=CARTESIAN_POINT('Ctrl Pts',(2.94048198688949,-0.132795706635729,
12.8150838652613));
#67412=CARTESIAN_POINT('Ctrl Pts',(2.93332044320623,-0.225821118295903,
12.8100387436394));
#67413=CARTESIAN_POINT('Ctrl Pts',(2.92615445504389,-0.318904261852187,
12.8049904909973));
#67414=CARTESIAN_POINT('Ctrl Pts',(2.91456015427157,-0.41155899908982,12.7999422383553));
#67415=CARTESIAN_POINT('Ctrl Pts',(2.89862262841597,-0.503339704409327,
12.7948939857132));
#67416=CARTESIAN_POINT('Ctrl Pts',(2.88266002676136,-0.595264815738986,
12.7898377902468));
#67417=CARTESIAN_POINT('Ctrl Pts',(2.86234065578813,-0.686312718114918,
12.7847815947804));
#67418=CARTESIAN_POINT('Ctrl Pts',(2.83780003802596,-0.77605086442827,12.7797253993139));
#67419=CARTESIAN_POINT('Ctrl Pts',(2.82730472168999,-0.814429288398268,
12.7775630099482));
#67420=CARTESIAN_POINT('Ctrl Pts',(2.8160379383468,-0.852568380814664,12.7754006205825));
#67421=CARTESIAN_POINT('Ctrl Pts',(2.80401296805785,-0.890435441210312,
12.7732382312168));
#67422=CARTESIAN_POINT('Ctrl Pts',(2.7758939434078,-0.978983252897487,12.7681817297523));
#67423=CARTESIAN_POINT('Ctrl Pts',(2.74352700603293,-1.06635347859154,12.7631252282878));
#67424=CARTESIAN_POINT('Ctrl Pts',(2.70702931838185,-1.1521094867334,12.7580687268232));
#67425=CARTESIAN_POINT('Ctrl Pts',(2.67058130005601,-1.23774879041166,12.7530191066992));
#67426=CARTESIAN_POINT('Ctrl Pts',(2.63001387495199,-1.32177783754301,12.7479694865751));
#67427=CARTESIAN_POINT('Ctrl Pts',(2.58549387302857,-1.40377542097436,12.7429198664511));
#67428=CARTESIAN_POINT('Ctrl Pts',(2.54102077107732,-1.48568662335865,12.737875565892));
#67429=CARTESIAN_POINT('Ctrl Pts',(2.49260357962393,-1.56557022839382,12.7328312653329));
#67430=CARTESIAN_POINT('Ctrl Pts',(2.44045663862699,-1.64302629162818,12.7277869647739));
#67431=CARTESIAN_POINT('Ctrl Pts',(2.3883464045338,-1.72042783254151,12.722746214963));
#67432=CARTESIAN_POINT('Ctrl Pts',(2.33251188645847,-1.79540486148966,12.7177054651521));
#67433=CARTESIAN_POINT('Ctrl Pts',(2.27321211569137,-1.86758418205819,12.7126647153412));
#67434=CARTESIAN_POINT('Ctrl Pts',(2.21393321252999,-1.93973810270386,12.7076257393715));
#67435=CARTESIAN_POINT('Ctrl Pts',(2.15119176058289,-2.00909592874094,12.7025867634019));
#67436=CARTESIAN_POINT('Ctrl Pts',(2.08528803137386,-2.07531631955443,12.6975477874323));
#67437=CARTESIAN_POINT('Ctrl Pts',(2.01938914867922,-2.14153184056644,12.6925091820254));
#67438=CARTESIAN_POINT('Ctrl Pts',(1.95032876409864,-2.20461007109985,12.6874705766185));
#67439=CARTESIAN_POINT('Ctrl Pts',(1.8784442774801,-2.26424625348089,12.6824319712117));
#67440=CARTESIAN_POINT('Ctrl Pts',(1.80654506771829,-2.32389465034797,12.6773923338143));
#67441=CARTESIAN_POINT('Ctrl Pts',(1.73182094854209,-2.38009931613171,12.6723526964169));
#67442=CARTESIAN_POINT('Ctrl Pts',(1.65464178465762,-2.43259626006147,12.6673130590195));
#67443=CARTESIAN_POINT('Ctrl Pts',(1.57737868128386,-2.48515029928017,12.6622679405497));
#67444=CARTESIAN_POINT('Ctrl Pts',(1.49765557091017,-2.53398831824227,12.6572228220798));
#67445=CARTESIAN_POINT('Ctrl Pts',(1.41587036776032,-2.57889028492843,12.65217770361));
#67446=CARTESIAN_POINT('Ctrl Pts',(1.33403440892513,-2.62382011765888,12.6471294541527));
#67447=CARTESIAN_POINT('Ctrl Pts',(1.25013420754304,-2.66480884058395,12.6420812046954));
#67448=CARTESIAN_POINT('Ctrl Pts',(1.16458932795676,-2.70168386329882,12.6370329552381));
#67449=CARTESIAN_POINT('Ctrl Pts',(1.07890985394616,-2.73861690436005,12.6319767629766));
#67450=CARTESIAN_POINT('Ctrl Pts',(0.991580950691239,-2.77142316980094,
12.626920570715));
#67451=CARTESIAN_POINT('Ctrl Pts',(0.90303882945407,-2.79997944144207,12.6218643784535));
#67452=CARTESIAN_POINT('Ctrl Pts',(0.865171360192689,-2.81219231508323,
12.6197019590043));
#67453=CARTESIAN_POINT('Ctrl Pts',(0.827082128135142,-2.82362846559316,
12.617539539555));
#67454=CARTESIAN_POINT('Ctrl Pts',(0.788805772570232,-2.8342811175252,12.6153771201057));
#67455=CARTESIAN_POINT('Ctrl Pts',(0.69930204799943,-2.8591908042078,12.6103206148053));
#67456=CARTESIAN_POINT('Ctrl Pts',(0.60845988395492,-2.8799004770425,12.605264109505));
#67457=CARTESIAN_POINT('Ctrl Pts',(0.516708866610124,-2.89626931537219,
12.6002076042046));
#67458=CARTESIAN_POINT('Ctrl Pts',(0.425082711115756,-2.91261587772606,
12.595157980186));
#67459=CARTESIAN_POINT('Ctrl Pts',(0.332550593042832,-2.92463326773718,
12.5901083561675));
#67460=CARTESIAN_POINT('Ctrl Pts',(0.239556361801636,-2.93223067808799,
12.5850587321489));
#67461=CARTESIAN_POINT('Ctrl Pts',(0.146660095071974,-2.93982008496823,
12.5800144276426));
#67462=CARTESIAN_POINT('Ctrl Pts',(0.0533031224500042,-2.94299873179844,
12.5749701231362));
#67463=CARTESIAN_POINT('Ctrl Pts',(-0.0400625107877926,-2.9417272129192,
12.5699258186299));
#67464=CARTESIAN_POINT('Ctrl Pts',(-0.133362423946594,-2.94045658906224,
12.56488506481));
#67465=CARTESIAN_POINT('Ctrl Pts',(-0.226670543507126,-2.93474203204424,
12.5598443109902));
#67466=CARTESIAN_POINT('Ctrl Pts',(-0.319532761982364,-2.92459617964941,
12.5548035571703));
#67467=CARTESIAN_POINT('Ctrl Pts',(-0.4123623029202,-2.91445389750604,12.549764577155));
#67468=CARTESIAN_POINT('Ctrl Pts',(-0.504745814202936,-2.89988346616527,
12.5447255971396));
#67469=CARTESIAN_POINT('Ctrl Pts',(-0.596233289766803,-2.88094947268671,
12.5396866171243));
#67470=CARTESIAN_POINT('Ctrl Pts',(-0.687714037985619,-2.86201687148078,
12.53464800764));
#67471=CARTESIAN_POINT('Ctrl Pts',(-0.778298447406953,-2.83872143630571,
12.5296093981558));
#67472=CARTESIAN_POINT('Ctrl Pts',(-0.86754681996549,-2.81117884795112,
12.5245707886716));
#67473=CARTESIAN_POINT('Ctrl Pts',(-0.956813472537783,-2.78363061827356,
12.5195311471702));
#67474=CARTESIAN_POINT('Ctrl Pts',(-1.04474312126971,-2.75183363878216,
12.5144915056688));
#67475=CARTESIAN_POINT('Ctrl Pts',(-1.13091242977066,-2.71595306958538,
12.5094518641674));
#67476=CARTESIAN_POINT('Ctrl Pts',(-1.21717545556445,-2.6800334768677,12.5044067415781));
#67477=CARTESIAN_POINT('Ctrl Pts',(-1.30167390991871,-2.64002160046159,
12.4993616189888));
#67478=CARTESIAN_POINT('Ctrl Pts',(-1.38400590558996,-2.5961301302693,12.4943164963995));
#67479=CARTESIAN_POINT('Ctrl Pts',(-1.46638899648283,-2.55221142103855,
12.489268242808));
#67480=CARTESIAN_POINT('Ctrl Pts',(-1.54660257146044,-2.50440855142868,
12.4842199892165));
#67481=CARTESIAN_POINT('Ctrl Pts',(-1.62427260901957,-2.45297829007694,
12.479171735625));
#67482=CARTESIAN_POINT('Ctrl Pts',(-1.70206485054719,-2.40146710972174,
12.4741155392457));
#67483=CARTESIAN_POINT('Ctrl Pts',(-1.77730520929182,-2.34631740689808,
12.4690593428665));
#67484=CARTESIAN_POINT('Ctrl Pts',(-1.84965188288115,-2.28782689733166,
12.4640031464873));
#67485=CARTESIAN_POINT('Ctrl Pts',(-1.88059232265756,-2.2628123113259,12.4618407673231));
#67486=CARTESIAN_POINT('Ctrl Pts',(-1.91100395709612,-2.23718715700358,
12.4596783881588));
#67487=CARTESIAN_POINT('Ctrl Pts',(-1.94086216417454,-2.21097672074487,
12.4575160089946));
#67488=CARTESIAN_POINT('Ctrl Pts',(-2.00967785375516,-2.15056822935034,
12.4525322665707));
#67489=CARTESIAN_POINT('Ctrl Pts',(-2.07580853770669,-2.08682247606317,
12.4475485241467));
#67490=CARTESIAN_POINT('Ctrl Pts',(-2.1389063411806,-2.02001080780708,12.4425647817228));
#67491=CARTESIAN_POINT('Ctrl Pts',(-2.20241500976163,-1.95276409139205,
12.4375485873631));
#67492=CARTESIAN_POINT('Ctrl Pts',(-2.26285075439455,-1.8824116313411,12.4325323930033));
#67493=CARTESIAN_POINT('Ctrl Pts',(-2.31989191581895,-1.80927209090227,
12.4275161986436));
#67494=CARTESIAN_POINT('Ctrl Pts',(-2.37642201481953,-1.73678784691744,
12.4225449470653));
#67495=CARTESIAN_POINT('Ctrl Pts',(-2.42961780913018,-1.66156661640815,
12.417573695487));
#67496=CARTESIAN_POINT('Ctrl Pts',(-2.47920362591192,-1.58395498082022,
12.4126024439086));
#67497=CARTESIAN_POINT('Ctrl Pts',(-2.52875950177525,-1.50639020870657,
12.4076341940725));
#67498=CARTESIAN_POINT('Ctrl Pts',(-2.57470948191501,-1.4264382813823,12.4026659442363));
#67499=CARTESIAN_POINT('Ctrl Pts',(-2.6168201469361,-1.34447622462776,12.3976976944002));
#67500=CARTESIAN_POINT('Ctrl Pts',(-2.65891791987531,-1.26253926036575,
12.3927309655822));
#67501=CARTESIAN_POINT('Ctrl Pts',(-2.69717850398541,-1.17859379583,12.3877642367641));
#67502=CARTESIAN_POINT('Ctrl Pts',(-2.73141419640922,-1.09304185082464,
12.3827975079461));
#67503=CARTESIAN_POINT('Ctrl Pts',(-2.76623616488011,-1.00602485421419,
12.3777457253747));
#67504=CARTESIAN_POINT('Ctrl Pts',(-2.79689388932123,-0.91734627984373,
12.3726939428033));
#67505=CARTESIAN_POINT('Ctrl Pts',(-2.82324129385255,-0.827449452646961,
12.3676421602319));
#67506=CARTESIAN_POINT('Ctrl Pts',(-2.84916408591644,-0.739001394856118,
12.3626717917467));
#67507=CARTESIAN_POINT('Ctrl Pts',(-2.87091440004144,-0.649374526423084,
12.3577014232615));
#67508=CARTESIAN_POINT('Ctrl Pts',(-2.88840419500333,-0.559003762319318,
12.3527310547763));
#67509=CARTESIAN_POINT('Ctrl Pts',(-2.90632371132637,-0.466412603531484,
12.3476385651619));
#67510=CARTESIAN_POINT('Ctrl Pts',(-2.91977050802025,-0.373041016470945,
12.3425460755474));
#67511=CARTESIAN_POINT('Ctrl Pts',(-2.92870625322799,-0.279362993797054,
12.337453585933));
#67512=CARTESIAN_POINT('Ctrl Pts',(-2.93764199843573,-0.185684971123177,
12.3323610963185));
#67513=CARTESIAN_POINT('Ctrl Pts',(-2.94206672257804,-0.0917010259822679,
12.3272686067041));
#67514=CARTESIAN_POINT('Ctrl Pts',(-2.94199923889461,0.0021162097116246,
12.3221761170896));
#67515=CARTESIAN_POINT('',(-2.94199894961115,-0.00248605850196559,11.3221761170896));
#67516=CARTESIAN_POINT('Ctrl Pts',(-2.9445363666432,0.00211803469319205,
12.3221761170896));
#67517=CARTESIAN_POINT('Ctrl Pts',(-2.9456637214079,0.140538485345201,12.3146690440209));
#67518=CARTESIAN_POINT('Ctrl Pts',(-2.87416309229677,1.24803879024156,12.2545416005818));
#67519=CARTESIAN_POINT('Ctrl Pts',(-1.4701722548823,3.14385641459552,12.1417937867725));
#67520=CARTESIAN_POINT('Ctrl Pts',(1.82719979676511,2.95069151525937,11.9839326756612));
#67521=CARTESIAN_POINT('Ctrl Pts',(3.46958573405994,0.0849379149032947,
11.8260715645502));
#67522=CARTESIAN_POINT('Ctrl Pts',(1.96939451380668,-2.85774821044887,11.668210453439));
#67523=CARTESIAN_POINT('Ctrl Pts',(-1.31457570167652,-3.21202900045203,
11.5103493423279));
#67524=CARTESIAN_POINT('Ctrl Pts',(-2.84408765266999,-1.34515018134913,
11.3950045635448));
#67525=CARTESIAN_POINT('Ctrl Pts',(-2.94485546023631,-0.189014750280763,
11.332280155132));
#67526=CARTESIAN_POINT('Ctrl Pts',(-2.94318142996902,-0.00248705772575741,
11.3221761170896));
#67527=CARTESIAN_POINT('',(-2.94199997051088,0.000416550106448989,10.3221761170469));
#67528=CARTESIAN_POINT('Ctrl Pts',(-2.94199894961115,-0.00248605850196559,
11.3221761170896));
#67529=CARTESIAN_POINT('Ctrl Pts',(-2.94207652581505,0.089317537506325,
11.3172011584662));
#67530=CARTESIAN_POINT('Ctrl Pts',(-2.93785286391276,0.181261441456098,
11.3122261998427));
#67531=CARTESIAN_POINT('Ctrl Pts',(-2.92931522269092,0.272903510624668,
11.3072512412193));
#67532=CARTESIAN_POINT('Ctrl Pts',(-2.92078590003141,0.36445628929195,11.3022811298953));
#67533=CARTESIAN_POINT('Ctrl Pts',(-2.90795099198411,0.455707364124172,
11.2973110185713));
#67534=CARTESIAN_POINT('Ctrl Pts',(-2.89084981018168,0.546215502318019,
11.2923409072473));
#67535=CARTESIAN_POINT('Ctrl Pts',(-2.87375744361081,0.63667698583005,11.2873733578914));
#67536=CARTESIAN_POINT('Ctrl Pts',(-2.85240325316874,0.726395844222927,
11.2824058085355));
#67537=CARTESIAN_POINT('Ctrl Pts',(-2.82687815151478,0.81493798321612,11.2774382591796));
#67538=CARTESIAN_POINT('Ctrl Pts',(-2.80135860763729,0.903460843249249,
11.2724717914464));
#67539=CARTESIAN_POINT('Ctrl Pts',(-2.77167008307933,0.990807053319003,
11.2675053237131));
#67540=CARTESIAN_POINT('Ctrl Pts',(-2.73795383302997,1.07655599399032,11.2625388559799));
#67541=CARTESIAN_POINT('Ctrl Pts',(-2.70423488576364,1.16231179436574,11.2575719909415));
#67542=CARTESIAN_POINT('Ctrl Pts',(-2.66648774252331,1.246469646557,11.2526051259031));
#67543=CARTESIAN_POINT('Ctrl Pts',(-2.62490194595386,1.32862853127864,11.2476382608647));
#67544=CARTESIAN_POINT('Ctrl Pts',(-2.58327509075301,1.41086853339232,11.242666491924));
#67545=CARTESIAN_POINT('Ctrl Pts',(-2.53780222461493,1.49110521992984,11.2376947229834));
#67546=CARTESIAN_POINT('Ctrl Pts',(-2.48871880318195,1.56896230633135,11.2327229540427));
#67547=CARTESIAN_POINT('Ctrl Pts',(-2.43960868296054,1.64686174287508,11.2277484807224));
#67548=CARTESIAN_POINT('Ctrl Pts',(-2.38688436221856,1.72237862948383,11.2227740074021));
#67549=CARTESIAN_POINT('Ctrl Pts',(-2.33082322136789,1.79516771103209,11.2177995340818));
#67550=CARTESIAN_POINT('Ctrl Pts',(-2.27467308627105,1.86807234159245,11.2128171640349));
#67551=CARTESIAN_POINT('Ctrl Pts',(-2.21517585487161,1.93824017657899,11.2078347939879));
#67552=CARTESIAN_POINT('Ctrl Pts',(-2.15264731424576,2.0053611995026,11.202852423941));
#67553=CARTESIAN_POINT('Ctrl Pts',(-2.11823823849968,2.04229749033582,11.2001106559959));
#67554=CARTESIAN_POINT('Ctrl Pts',(-2.08291183600716,2.07831181353667,11.1973688880508));
#67555=CARTESIAN_POINT('Ctrl Pts',(-2.04672493224266,2.11335776709394,11.1946271201058));
#67556=CARTESIAN_POINT('Ctrl Pts',(-1.97998725583821,2.17799124673651,11.1895706161538));
#67557=CARTESIAN_POINT('Ctrl Pts',(-1.91006766593611,2.2395739985057,11.1845141122018));
#67558=CARTESIAN_POINT('Ctrl Pts',(-1.83727632392557,2.29777712355715,11.1794576082499));
#67559=CARTESIAN_POINT('Ctrl Pts',(-1.76458404224229,2.35590104110318,11.1744079855962));
#67560=CARTESIAN_POINT('Ctrl Pts',(-1.68902811823042,2.41065419727838,11.1693583629425));
#67561=CARTESIAN_POINT('Ctrl Pts',(-1.61095513182416,2.46174482090436,11.1643087402888));
#67562=CARTESIAN_POINT('Ctrl Pts',(-1.53296439143067,2.51278162309634,11.1592644371618));
#67563=CARTESIAN_POINT('Ctrl Pts',(-1.45246222850332,2.56016332066176,11.1542201340347));
#67564=CARTESIAN_POINT('Ctrl Pts',(-1.36982697401538,2.60363938771479,11.1491758309076));
#67565=CARTESIAN_POINT('Ctrl Pts',(-1.28724988676171,2.64708485181763,11.1441350784826));
#67566=CARTESIAN_POINT('Ctrl Pts',(-1.20254308380114,2.68662994420094,11.1390943260575));
#67567=CARTESIAN_POINT('Ctrl Pts',(-1.1161115648444,2.72206887767753,11.1340535736324));
#67568=CARTESIAN_POINT('Ctrl Pts',(-1.02971046067275,2.75749534038466,11.1290145950209));
#67569=CARTESIAN_POINT('Ctrl Pts',(-0.941586256143343,2.7888183469212,11.1239756164094));
#67570=CARTESIAN_POINT('Ctrl Pts',(-0.852165159560519,2.81587970993635,
11.1189366377978));
#67571=CARTESIAN_POINT('Ctrl Pts',(-0.762750638506969,2.84293908300962,
11.1138980297247));
#67572=CARTESIAN_POINT('Ctrl Pts',(-0.672039839466033,2.86573730756244,
11.1088594216516));
#67573=CARTESIAN_POINT('Ctrl Pts',(-0.580474317815216,2.88416600880687,
11.1038208135785));
#67574=CARTESIAN_POINT('Ctrl Pts',(-0.488890041643242,2.90259848463219,
11.0987811734938));
#67575=CARTESIAN_POINT('Ctrl Pts',(-0.396451129835384,2.91665957256184,
11.0937415334091));
#67576=CARTESIAN_POINT('Ctrl Pts',(-0.303608395204779,2.92629218335442,
11.0887018933244));
#67577=CARTESIAN_POINT('Ctrl Pts',(-0.2106646852654,2.93593527052787,11.0836567721515));
#67578=CARTESIAN_POINT('Ctrl Pts',(-0.117316717492807,2.94114022141322,
11.0786116509787));
#67579=CARTESIAN_POINT('Ctrl Pts',(-0.0240191613170752,2.94190194940104,
11.0735665298058));
#67580=CARTESIAN_POINT('Ctrl Pts',(0.0693362952866036,2.94266415011696,
11.0685182776326));
#67581=CARTESIAN_POINT('Ctrl Pts',(0.162640835401097,2.93897765568961,11.0634700254595));
#67582=CARTESIAN_POINT('Ctrl Pts',(0.255443218682719,2.93088941484134,11.0584217732863));
#67583=CARTESIAN_POINT('Ctrl Pts',(0.348391614996983,2.9227884481499,11.0533655783149));
#67584=CARTESIAN_POINT('Ctrl Pts',(0.440835838760165,2.91027197002818,11.0483093833435));
#67585=CARTESIAN_POINT('Ctrl Pts',(0.532333399195466,2.89343829243013,11.0432531883721));
#67586=CARTESIAN_POINT('Ctrl Pts',(0.571464345852351,2.88623899949823,11.0410907952462));
#67587=CARTESIAN_POINT('Ctrl Pts',(0.610422318321621,2.87825070366841,11.0389284021204));
#67588=CARTESIAN_POINT('Ctrl Pts',(0.64917360658853,2.86948386099466,11.0367660089946));
#67589=CARTESIAN_POINT('Ctrl Pts',(0.739788971436703,2.84898362260321,11.0317095050485));
#67590=CARTESIAN_POINT('Ctrl Pts',(0.829591626257177,2.82415083111023,11.0266530011023));
#67591=CARTESIAN_POINT('Ctrl Pts',(0.918136568920149,2.79506515859855,11.0215964971561));
#67592=CARTESIAN_POINT('Ctrl Pts',(1.00656101248464,2.76601906821557,11.0165468745083));
#67593=CARTESIAN_POINT('Ctrl Pts',(1.09373072757481,2.73273173556562,11.0114972518605));
#67594=CARTESIAN_POINT('Ctrl Pts',(1.17921186430988,2.69533363038248,11.0064476292127));
#67595=CARTESIAN_POINT('Ctrl Pts',(1.2646029509125,2.65797492224592,11.0014033260916));
#67596=CARTESIAN_POINT('Ctrl Pts',(1.34830859100062,2.61651422642895,10.9963590229704));
#67597=CARTESIAN_POINT('Ctrl Pts',(1.42991208731481,2.5711311562328,10.9913147198493));
#67598=CARTESIAN_POINT('Ctrl Pts',(1.51145814265147,2.52578003133352,10.9862739674302));
#67599=CARTESIAN_POINT('Ctrl Pts',(1.59090460907757,2.47651223503371,10.9812332150111));
#67600=CARTESIAN_POINT('Ctrl Pts',(1.66785764676815,2.42355418138671,10.9761924625921));
#67601=CARTESIAN_POINT('Ctrl Pts',(1.74478360509921,2.37061476339358,10.9711534839866));
#67602=CARTESIAN_POINT('Ctrl Pts',(1.81921751306633,2.31398791915949,10.9661145053812));
#67603=CARTESIAN_POINT('Ctrl Pts',(1.89079377057828,2.25394385847172,10.9610755267757));
#67604=CARTESIAN_POINT('Ctrl Pts',(1.96236476477056,2.19390421309003,10.9560369187087));
#67605=CARTESIAN_POINT('Ctrl Pts',(2.03107818687781,2.13044813608663,10.9509983106418));
#67606=CARTESIAN_POINT('Ctrl Pts',(2.09660173569173,2.06388593722968,10.9459597025748));
#67607=CARTESIAN_POINT('Ctrl Pts',(2.16213870508923,1.99731010505205,10.9409200624962));
#67608=CARTESIAN_POINT('Ctrl Pts',(2.22448419285335,1.92762720366024,10.9358804224176));
#67609=CARTESIAN_POINT('Ctrl Pts',(2.28334376141409,1.85518335137295,10.930840782339));
#67610=CARTESIAN_POINT('Ctrl Pts',(2.34226734535684,1.7826607095024,10.9257956611723));
#67611=CARTESIAN_POINT('Ctrl Pts',(2.39769716290024,1.70737146784726,10.9207505400056));
#67612=CARTESIAN_POINT('Ctrl Pts',(2.44938019527269,1.62969342485203,10.9157054188388));
#67613=CARTESIAN_POINT('Ctrl Pts',(2.5010953021154,1.5519671748928,10.9106571666718));
#67614=CARTESIAN_POINT('Ctrl Pts',(2.54905876699972,1.4718495522115,10.9056089145048));
#67615=CARTESIAN_POINT('Ctrl Pts',(2.59306300351438,1.38974395476468,10.9005606623378));
#67616=CARTESIAN_POINT('Ctrl Pts',(2.63713647523431,1.30750917434951,10.8955044673724));
#67617=CARTESIAN_POINT('Ctrl Pts',(2.67723809372118,1.22328057524653,10.8904482724071));
#67618=CARTESIAN_POINT('Ctrl Pts',(2.71320805331004,1.13748233368854,10.8853920774418));
#67619=CARTESIAN_POINT('Ctrl Pts',(2.72859139909721,1.10078882519136,10.8832296842557));
#67620=CARTESIAN_POINT('Ctrl Pts',(2.74321967074903,1.06380842165138,10.8810672910696));
#67621=CARTESIAN_POINT('Ctrl Pts',(2.75708317692166,1.02657506083851,10.8789048978835));
#67622=CARTESIAN_POINT('Ctrl Pts',(2.78950136716245,0.939509194591843,10.8738483939365));
#67623=CARTESIAN_POINT('Ctrl Pts',(2.81784833592938,0.85075315980588,10.8687918899894));
#67624=CARTESIAN_POINT('Ctrl Pts',(2.84194730101225,0.760723036504873,10.8637353860424));
#67625=CARTESIAN_POINT('Ctrl Pts',(2.86601347028002,0.670815433455974,10.8586857633936));
#67626=CARTESIAN_POINT('Ctrl Pts',(2.88584301053909,0.579637612249602,10.8536361407449));
#67627=CARTESIAN_POINT('Ctrl Pts',(2.90130776147331,0.4876241105757,10.8485865180962));
#67628=CARTESIAN_POINT('Ctrl Pts',(2.91675622106045,0.395707540556076,10.8435422149742));
#67629=CARTESIAN_POINT('Ctrl Pts',(2.92784895820001,0.30295747497166,10.8384979118521));
#67630=CARTESIAN_POINT('Ctrl Pts',(2.93450833287159,0.209820981570504,10.8334536087301));
#67631=CARTESIAN_POINT('Ctrl Pts',(2.94116301998676,0.116750047262867,10.8284128563101));
#67632=CARTESIAN_POINT('Ctrl Pts',(2.94339051614705,0.0232936668301138,
10.8233721038901));
#67633=CARTESIAN_POINT('Ctrl Pts',(2.94116486181815,-0.0700946189534286,
10.8183313514702));
#67634=CARTESIAN_POINT('Ctrl Pts',(2.93893999068502,-0.163450041902257,
10.8132923728638));
#67635=CARTESIAN_POINT('Ctrl Pts',(2.93226509298428,-0.256736974999994,
10.8082533942575));
#67636=CARTESIAN_POINT('Ctrl Pts',(2.92116631910506,-0.34950155382513,10.8032144156511));
#67637=CARTESIAN_POINT('Ctrl Pts',(2.91006836136792,-0.442259311259358,
10.7981758075832));
#67638=CARTESIAN_POINT('Ctrl Pts',(2.89454722727486,-0.534494350619572,
10.7931371995153));
#67639=CARTESIAN_POINT('Ctrl Pts',(2.8746808515922,-0.625758740641423,10.7880985914474));
#67640=CARTESIAN_POINT('Ctrl Pts',(2.85481040686323,-0.717041823505658,
10.783058951368));
#67641=CARTESIAN_POINT('Ctrl Pts',(2.8305930475925,-0.807353429093737,10.7780193112885));
#67642=CARTESIAN_POINT('Ctrl Pts',(2.8021573982697,-0.896257728179997,10.772979671209));
#67643=CARTESIAN_POINT('Ctrl Pts',(2.77369082247245,-0.98525871915126,10.7679345500414));
#67644=CARTESIAN_POINT('Ctrl Pts',(2.74099693481821,-1.07284892576681,10.7628894288738));
#67645=CARTESIAN_POINT('Ctrl Pts',(2.7042535389354,-1.1586098554541,10.7578443077062));
#67646=CARTESIAN_POINT('Ctrl Pts',(2.66748734011517,-1.24442400834152,10.7527960555383));
#67647=CARTESIAN_POINT('Ctrl Pts',(2.62666682341887,-1.32840622578979,10.7477478033704));
#67648=CARTESIAN_POINT('Ctrl Pts',(2.58201607775066,-1.41016203829102,10.7426995512026));
#67649=CARTESIAN_POINT('Ctrl Pts',(2.5372950796754,-1.49204648341714,10.7376433562364));
#67650=CARTESIAN_POINT('Ctrl Pts',(2.48873205358918,-1.57169715329904,10.7325871612703));
#67651=CARTESIAN_POINT('Ctrl Pts',(2.43659462291282,-1.64874820503082,10.7275309663041));
#67652=CARTESIAN_POINT('Ctrl Pts',(2.41429690197303,-1.68170078492101,10.7253685731269));
#67653=CARTESIAN_POINT('Ctrl Pts',(2.39134591533303,-1.71417829678479,10.7232061799497));
#67654=CARTESIAN_POINT('Ctrl Pts',(2.36776476825675,-1.74615406027134,10.7210437867724));
#67655=CARTESIAN_POINT('Ctrl Pts',(2.31262300932557,-1.82092564946127,10.7159872828243));
#67656=CARTESIAN_POINT('Ctrl Pts',(2.25383902616345,-1.89321415253696,10.7109307788762));
#67657=CARTESIAN_POINT('Ctrl Pts',(2.19166437696011,-1.96264394599837,10.705874274928));
#67658=CARTESIAN_POINT('Ctrl Pts',(2.12957434003321,-2.03197925379797,10.7008246522782));
#67659=CARTESIAN_POINT('Ctrl Pts',(2.06410310012087,-2.09846325559609,10.6957750296284));
#67660=CARTESIAN_POINT('Ctrl Pts',(1.99554426767324,-2.16175092824231,10.6907254069786));
#67661=CARTESIAN_POINT('Ctrl Pts',(1.92705765855026,-2.22497193046889,10.6856811038554));
#67662=CARTESIAN_POINT('Ctrl Pts',(1.85549024648217,-2.28500299756638,10.6806368007323));
#67663=CARTESIAN_POINT('Ctrl Pts',(1.78117377113338,-2.3415345389352,10.6755924976091));
#67664=CARTESIAN_POINT('Ctrl Pts',(1.70690960740335,-2.39802628756054,10.670551745188));
#67665=CARTESIAN_POINT('Ctrl Pts',(1.6299005787077,-2.45102313921977,10.6655109927669));
#67666=CARTESIAN_POINT('Ctrl Pts',(1.55051211865024,-2.5002552209562,10.6604702403458));
#67667=CARTESIAN_POINT('Ctrl Pts',(1.47115159496399,-2.54946997818842,10.6554312617383));
#67668=CARTESIAN_POINT('Ctrl Pts',(1.38941367989568,-2.59492236415437,10.6503922831308));
#67669=CARTESIAN_POINT('Ctrl Pts',(1.30569258860119,-2.63638594748036,10.6453533045233));
#67670=CARTESIAN_POINT('Ctrl Pts',(1.22197765368996,-2.67784648180512,10.6403146964543));
#67671=CARTESIAN_POINT('Ctrl Pts',(1.13628022996328,-2.71531860023218,10.6352760883852));
#67672=CARTESIAN_POINT('Ctrl Pts',(1.04901789875083,-2.74862246372622,10.6302374803162));
#67673=CARTESIAN_POINT('Ctrl Pts',(0.961737694400502,-2.78193314854322,
10.6251978402355));
#67674=CARTESIAN_POINT('Ctrl Pts',(0.872892360276499,-2.81107372509559,
10.6201582001549));
#67675=CARTESIAN_POINT('Ctrl Pts',(0.782917081301991,-2.83591340555483,
10.6151185600743));
#67676=CARTESIAN_POINT('Ctrl Pts',(0.692843945649627,-2.86078010153029,
10.6100734389055));
#67677=CARTESIAN_POINT('Ctrl Pts',(0.601638840232294,-2.88133644688177,
10.6050283177367));
#67678=CARTESIAN_POINT('Ctrl Pts',(0.509749345449273,-2.8975023045399,10.5999831965679));
#67679=CARTESIAN_POINT('Ctrl Pts',(0.417802824080872,-2.91367819472313,
10.5949349443989));
#67680=CARTESIAN_POINT('Ctrl Pts',(0.325171507177231,-2.9254581167554,10.5898866922298));
#67681=CARTESIAN_POINT('Ctrl Pts',(0.232308190442077,-2.9328138203189,10.5848384400608));
#67682=CARTESIAN_POINT('Ctrl Pts',(0.139298764802533,-2.9401810971691,10.5797822450934));
#67683=CARTESIAN_POINT('Ctrl Pts',(0.046057053095913,-2.94311024668023,
10.5747260501261));
#67684=CARTESIAN_POINT('Ctrl Pts',(-0.0469642920738009,-2.94162512147112,
10.5696698551587));
#67685=CARTESIAN_POINT('Ctrl Pts',(-0.0867469195964879,-2.94098997495813,
10.5675074619929));
#67686=CARTESIAN_POINT('Ctrl Pts',(-0.12648930900846,-2.93954809020669,
10.5653450688271));
#67687=CARTESIAN_POINT('Ctrl Pts',(-0.166156486030579,-2.93730421001128,
10.5631826756613));
#67688=CARTESIAN_POINT('Ctrl Pts',(-0.258913548142371,-2.93205715815928,
10.558126171714));
#67689=CARTESIAN_POINT('Ctrl Pts',(-0.351584892786728,-2.92240282069134,
10.5530696677668));
#67690=CARTESIAN_POINT('Ctrl Pts',(-0.443718470194708,-2.90834625160211,
10.5480131638195));
#67691=CARTESIAN_POINT('Ctrl Pts',(-0.53572666480091,-2.89430881182563,
10.5429635411705));
#67692=CARTESIAN_POINT('Ctrl Pts',(-0.627198111896935,-2.87588111218902,
10.5379139185216));
#67693=CARTESIAN_POINT('Ctrl Pts',(-0.717683367920239,-2.85312014878635,
10.5328642958726));
#67694=CARTESIAN_POINT('Ctrl Pts',(-0.808073302220233,-2.83038316292822,
10.5278199927503));
#67695=CARTESIAN_POINT('Ctrl Pts',(-0.897478682815411,-2.80332209486652,
10.522775689628));
#67696=CARTESIAN_POINT('Ctrl Pts',(-0.9854588635448,-2.77204524282361,10.5177313865058));
#67697=CARTESIAN_POINT('Ctrl Pts',(-1.07337711472662,-2.74079040666291,
10.5126906340856));
#67698=CARTESIAN_POINT('Ctrl Pts',(-1.15987174354931,-2.70532583323625,
10.5076498816653));
#67699=CARTESIAN_POINT('Ctrl Pts',(-1.2445169147434,-2.66580975482452,10.5026091292451));
#67700=CARTESIAN_POINT('Ctrl Pts',(-1.32913229975777,-2.62630758190789,
10.4975701506385));
#67701=CARTESIAN_POINT('Ctrl Pts',(-1.41189911881721,-2.58275692393808,
10.492531172032));
#67702=CARTESIAN_POINT('Ctrl Pts',(-1.49241215236125,-2.53536387279705,
10.4874921934254));
#67703=CARTESIAN_POINT('Ctrl Pts',(-1.57291926542495,-2.48797430667721,
10.4824535853572));
#67704=CARTESIAN_POINT('Ctrl Pts',(-1.65117254059657,-2.43674313438026,
10.4774149772891));
#67705=CARTESIAN_POINT('Ctrl Pts',(-1.72679297425622,-2.38192149829909,
10.4723763692209));
#67706=CARTESIAN_POINT('Ctrl Pts',(-1.80242889655112,-2.32708863360833,
10.4673367291412));
#67707=CARTESIAN_POINT('Ctrl Pts',(-1.87543054762043,-2.26866410506297,
10.4622970890615));
#67708=CARTESIAN_POINT('Ctrl Pts',(-1.94545035083473,-2.2069406273022,10.4572574489818));
#67709=CARTESIAN_POINT('Ctrl Pts',(-2.01554630724814,-2.14515001938573,
10.4522123278139));
#67710=CARTESIAN_POINT('Ctrl Pts',(-2.08265360976431,-2.08005359448698,
10.447167206646));
#67711=CARTESIAN_POINT('Ctrl Pts',(-2.14646029714233,-2.01198215518719,
10.4421220854781));
#67712=CARTESIAN_POINT('Ctrl Pts',(-2.21030658292621,-1.94386847077812,
10.43707383331));
#67713=CARTESIAN_POINT('Ctrl Pts',(-2.27084788837547,-1.87277643348794,
10.4320255811418));
#67714=CARTESIAN_POINT('Ctrl Pts',(-2.32781283067783,-1.79906959991315,
10.4269773289737));
#67715=CARTESIAN_POINT('Ctrl Pts',(-2.38486740024746,-1.72524679778287,
10.4219211340072));
#67716=CARTESIAN_POINT('Ctrl Pts',(-2.43833412084441,-1.64880134988332,
10.4168649390408));
#67717=CARTESIAN_POINT('Ctrl Pts',(-2.48798530075998,-1.57012519984944,
10.4118087440743));
#67718=CARTESIAN_POINT('Ctrl Pts',(-2.50921972175825,-1.53647761090627,
10.4096463508996));
#67719=CARTESIAN_POINT('Ctrl Pts',(-2.52975684650336,-1.50242231663193,
10.4074839577249));
#67720=CARTESIAN_POINT('Ctrl Pts',(-2.54958150965234,-1.46799118718026,
10.4053215645501));
#67721=CARTESIAN_POINT('Ctrl Pts',(-2.59775504666128,-1.38432422767455,
10.4000669921598));
#67722=CARTESIAN_POINT('Ctrl Pts',(-2.64187647244433,-1.29816218218148,
10.3948124197694));
#67723=CARTESIAN_POINT('Ctrl Pts',(-2.68169059492538,-1.20991716786265,
10.389557847379));
#67724=CARTESIAN_POINT('Ctrl Pts',(-2.72143509013441,-1.12182647716651,
10.384312464229));
#67725=CARTESIAN_POINT('Ctrl Pts',(-2.75688711194816,-1.0316604243227,10.379067081079));
#67726=CARTESIAN_POINT('Ctrl Pts',(-2.78783665101677,-0.939856801458403,
10.373821697929));
#67727=CARTESIAN_POINT('Ctrl Pts',(-2.81872219219728,-0.848243011404531,
10.3685871612554));
#67728=CARTESIAN_POINT('Ctrl Pts',(-2.84512367388878,-0.75499876941976,
10.3633526245818));
#67729=CARTESIAN_POINT('Ctrl Pts',(-2.86687908403034,-0.66058180231471,
10.3581180879081));
#67730=CARTESIAN_POINT('Ctrl Pts',(-2.88860740729712,-0.566282390362534,
10.3528900685669));
#67731=CARTESIAN_POINT('Ctrl Pts',(-2.90570108032047,-0.470813540940017,
10.3476620492256));
#67732=CARTESIAN_POINT('Ctrl Pts',(-2.91804772344475,-0.374648480176971,
10.3424340298844));
#67733=CARTESIAN_POINT('Ctrl Pts',(-2.93037738695065,-0.278615669614791,
10.3372132003333));
#67734=CARTESIAN_POINT('Ctrl Pts',(-2.93797297421279,-0.181888944945489,
10.3319923707823));
#67735=CARTESIAN_POINT('Ctrl Pts',(-2.94077325018523,-0.0849511094394904,
10.3267715412312));
#67736=CARTESIAN_POINT('Ctrl Pts',(-2.94159486008975,-0.0565092392245919,
10.325239733184));
#67737=CARTESIAN_POINT('Ctrl Pts',(-2.94200400090166,-0.0280492502006135,
10.3237079251368));
#67738=CARTESIAN_POINT('Ctrl Pts',(-2.94199997051099,0.000416549312712471,
10.3221761170896));
#67739=CARTESIAN_POINT('',(-2.94199926785449,0.00207555863534859,9.3221761170896));
#67740=CARTESIAN_POINT('Ctrl Pts',(-2.94199997051088,0.000416550106449056,
10.3221761170469));
#67741=CARTESIAN_POINT('Ctrl Pts',(-2.94198593005877,0.0995811140799426,
10.3168398510825));
#67742=CARTESIAN_POINT('Ctrl Pts',(-2.93695388461969,0.198628671924865,
10.3115035851181));
#67743=CARTESIAN_POINT('Ctrl Pts',(-2.9269647239196,0.297054717064461,10.3061673191537));
#67744=CARTESIAN_POINT('Ctrl Pts',(-2.91694385381805,0.395793203967011,
10.3008141138483));
#67745=CARTESIAN_POINT('Ctrl Pts',(-2.90193443700809,0.493905874428624,
10.2954609085429));
#67746=CARTESIAN_POINT('Ctrl Pts',(-2.88204893916369,0.59089585568477,10.2901077032374));
#67747=CARTESIAN_POINT('Ctrl Pts',(-2.86213087062913,0.688044697968832,
10.2847457298542));
#67748=CARTESIAN_POINT('Ctrl Pts',(-2.83732087392621,0.784066834855588,
10.279383756471));
#67749=CARTESIAN_POINT('Ctrl Pts',(-2.80778130463142,0.878480589064014,
10.2740217830878));
#67750=CARTESIAN_POINT('Ctrl Pts',(-2.77815835592025,0.973160838821047,
10.268644674812));
#67751=CARTESIAN_POINT('Ctrl Pts',(-2.74377926182703,1.06622328964424,10.2632675665361));
#67752=CARTESIAN_POINT('Ctrl Pts',(-2.70485505981839,1.15720486750395,10.2578904582602));
#67753=CARTESIAN_POINT('Ctrl Pts',(-2.67968790095532,1.2160306803774,10.2544137899865));
#67754=CARTESIAN_POINT('Ctrl Pts',(-2.65262161242553,1.27398705792399,10.2509371217127));
#67755=CARTESIAN_POINT('Ctrl Pts',(-2.62372318127054,1.33095479564996,10.247460453439));
#67756=CARTESIAN_POINT('Ctrl Pts',(-2.58169299037788,1.41380928967087,10.2424039494914));
#67757=CARTESIAN_POINT('Ctrl Pts',(-2.53566037629418,1.49481659052653,10.2373474455438));
#67758=CARTESIAN_POINT('Ctrl Pts',(-2.48581137957154,1.57356467461387,10.2322909415962));
#67759=CARTESIAN_POINT('Ctrl Pts',(-2.43603022138356,1.65220559195798,10.227241318947));
#67760=CARTESIAN_POINT('Ctrl Pts',(-2.38244323678257,1.72859303091348,10.2221916962977));
#67761=CARTESIAN_POINT('Ctrl Pts',(-2.32528299642955,1.8023381998159,10.2171420736484));
#67762=CARTESIAN_POINT('Ctrl Pts',(-2.26818297155094,1.87600568184535,10.2120977705259));
#67763=CARTESIAN_POINT('Ctrl Pts',(-2.2075174436185,1.94703607819576,10.2070534674033));
#67764=CARTESIAN_POINT('Ctrl Pts',(-2.14356244264622,2.01506924309726,10.2020091642807));
#67765=CARTESIAN_POINT('Ctrl Pts',(-2.07965245981562,2.08305451922369,10.1969684118602));
#67766=CARTESIAN_POINT('Ctrl Pts',(-2.01245790932483,2.14804643540509,10.1919276594396));
#67767=CARTESIAN_POINT('Ctrl Pts',(-1.94229461420281,2.20971845076217,10.1868869070191));
#67768=CARTESIAN_POINT('Ctrl Pts',(-1.87215600916627,2.27136876406936,10.1818479284122));
#67769=CARTESIAN_POINT('Ctrl Pts',(-1.79905106774777,2.32970120519855,10.1768089498053));
#67770=CARTESIAN_POINT('Ctrl Pts',(-1.72333117638428,2.3844273225456,10.1717699711983));
#67771=CARTESIAN_POINT('Ctrl Pts',(-1.64761685304031,2.43914941563846,10.1667313631299));
#67772=CARTESIAN_POINT('Ctrl Pts',(-1.5692883216123,2.49026545280252,10.1616927550614));
#67773=CARTESIAN_POINT('Ctrl Pts',(-1.48872771155874,2.53752907389001,10.1566541469929));
#67774=CARTESIAN_POINT('Ctrl Pts',(-1.40815060101888,2.58480237554883,10.1516145069129));
#67775=CARTESIAN_POINT('Ctrl Pts',(-1.32534088641352,2.62822146999654,10.1465748668328));
#67776=CARTESIAN_POINT('Ctrl Pts',(-1.24070616309238,2.6675854657095,10.1415352267527));
#67777=CARTESIAN_POINT('Ctrl Pts',(-1.15597939145598,2.7069922735136,10.1364901055845));
#67778=CARTESIAN_POINT('Ctrl Pts',(-1.06942405194301,2.74233499254364,10.1314449844163));
#67779=CARTESIAN_POINT('Ctrl Pts',(-0.981468333530933,2.77346063795324,
10.1263998632481));
#67780=CARTESIAN_POINT('Ctrl Pts',(-0.893458029833515,2.80460559992653,
10.1213516110796));
#67781=CARTESIAN_POINT('Ctrl Pts',(-0.804046041169711,2.83152815024812,
10.1163033589111));
#67782=CARTESIAN_POINT('Ctrl Pts',(-0.713674272862074,2.85412561606086,
10.1112551067427));
#67783=CARTESIAN_POINT('Ctrl Pts',(-0.623160315792424,2.87675863618165,
10.1061989117759));
#67784=CARTESIAN_POINT('Ctrl Pts',(-0.531683998757212,2.89505290136774,
10.1011427168091));
#67785=CARTESIAN_POINT('Ctrl Pts',(-0.439695694379682,2.90895714927944,
10.0960865218424));
#67786=CARTESIAN_POINT('Ctrl Pts',(-0.400354869401907,2.91490360722584,
10.0939241286709));
#67787=CARTESIAN_POINT('Ctrl Pts',(-0.360920440448954,2.92004776598015,
10.0917617354994));
#67788=CARTESIAN_POINT('Ctrl Pts',(-0.321427684744325,2.92438852471417,
10.0895993423279));
#67789=CARTESIAN_POINT('Ctrl Pts',(-0.229078486757704,2.93453888218069,
10.0845428383805));
#67790=CARTESIAN_POINT('Ctrl Pts',(-0.136085657609308,2.94032836210759,
10.079486334433));
#67791=CARTESIAN_POINT('Ctrl Pts',(-0.0428958694685178,2.9416872614849,
10.0744298304855));
#67792=CARTESIAN_POINT('Ctrl Pts',(0.0501670984936496,2.94304431156236,
10.0693802078364));
#67793=CARTESIAN_POINT('Ctrl Pts',(0.143426053188793,2.93998275679977,10.0643305851872));
#67794=CARTESIAN_POINT('Ctrl Pts',(0.236428310975977,2.93248455303162,10.0592809625381));
#67795=CARTESIAN_POINT('Ctrl Pts',(0.329332595503363,2.92499424824876,10.0542366594156));
#67796=CARTESIAN_POINT('Ctrl Pts',(0.421980281012603,2.91307662036411,10.0491923562932));
#67797=CARTESIAN_POINT('Ctrl Pts',(0.513918884235275,2.89676567578849,10.0441480531707));
#67798=CARTESIAN_POINT('Ctrl Pts',(0.605792771563805,2.88046621254199,10.0391073007503));
#67799=CARTESIAN_POINT('Ctrl Pts',(0.696958133395661,2.85977965685362,10.0340665483299));
#67800=CARTESIAN_POINT('Ctrl Pts',(0.786968843712302,2.83479170998966,10.0290257959095));
#67801=CARTESIAN_POINT('Ctrl Pts',(0.876947879744954,2.80981255624957,10.0239868173027));
#67802=CARTESIAN_POINT('Ctrl Pts',(0.965772644729208,2.78053513708429,10.0189478386959));
#67803=CARTESIAN_POINT('Ctrl Pts',(1.05300943767834,2.74709576173827,10.0139088600891));
#67804=CARTESIAN_POINT('Ctrl Pts',(1.14023981571905,2.71365884533787,10.0088702520208));
#67805=CARTESIAN_POINT('Ctrl Pts',(1.22588204004082,2.6760607402814,10.0038316439524));
#67806=CARTESIAN_POINT('Ctrl Pts',(1.30952082207223,2.63448651857611,9.99879303588408));
#67807=CARTESIAN_POINT('Ctrl Pts',(1.3931767350635,2.59290378160665,9.99375339580415));
#67808=CARTESIAN_POINT('Ctrl Pts',(1.47482799397496,2.54734350819388,9.98871375572421));
#67809=CARTESIAN_POINT('Ctrl Pts',(1.55408343676181,2.49803696361415,9.98367411564428));
#67810=CARTESIAN_POINT('Ctrl Pts',(1.63342507738448,2.44867679347527,9.9786289944762));
#67811=CARTESIAN_POINT('Ctrl Pts',(1.71036532406792,2.39556245429527,9.97358387330812));
#67812=CARTESIAN_POINT('Ctrl Pts',(1.78454184780575,2.33896866020689,9.96853875214004));
#67813=CARTESIAN_POINT('Ctrl Pts',(1.85876440546589,2.28233974403151,9.96349049997169));
#67814=CARTESIAN_POINT('Ctrl Pts',(1.93021948655862,2.22222735913253,9.95844224780333));
#67815=CARTESIAN_POINT('Ctrl Pts',(1.99857937121796,2.15894522786986,9.95339399563498));
#67816=CARTESIAN_POINT('Ctrl Pts',(2.06704681167218,2.0955635300271,9.94833780066834));
#67817=CARTESIAN_POINT('Ctrl Pts',(2.1324090246093,2.02900244652801,9.9432816057017));
#67818=CARTESIAN_POINT('Ctrl Pts',(2.19437669071125,1.95961091527454,9.93822541073506));
#67819=CARTESIAN_POINT('Ctrl Pts',(2.22087852835673,1.92993409813857,9.93606301756232));
#67820=CARTESIAN_POINT('Ctrl Pts',(2.24676001381569,1.89973997174884,9.93390062438958));
#67821=CARTESIAN_POINT('Ctrl Pts',(2.27200092458726,1.86905746264652,9.93173823121683));
#67822=CARTESIAN_POINT('Ctrl Pts',(2.33102384722868,1.79730999768455,9.92668172726932));
#67823=CARTESIAN_POINT('Ctrl Pts',(2.38674864010326,1.72263783546821,9.92162522332181));
#67824=CARTESIAN_POINT('Ctrl Pts',(2.43887257272417,1.64537672707918,9.9165687193743));
#67825=CARTESIAN_POINT('Ctrl Pts',(2.49092557089423,1.56822076183687,9.91151909672512));
#67826=CARTESIAN_POINT('Ctrl Pts',(2.53938720114163,1.4884832164628,9.90646947407594));
#67827=CARTESIAN_POINT('Ctrl Pts',(2.58399468503541,1.40653313779261,9.90141985142676));
#67828=CARTESIAN_POINT('Ctrl Pts',(2.62855517716029,1.32466938946035,9.89637554830426));
#67829=CARTESIAN_POINT('Ctrl Pts',(2.66926938274567,1.24059812832851,9.89133124518176));
#67830=CARTESIAN_POINT('Ctrl Pts',(2.70591820197124,1.15471671168331,9.88628694205926));
#67831=CARTESIAN_POINT('Ctrl Pts',(2.74254122396885,1.06889574725815,9.88124618963881));
#67832=CARTESIAN_POINT('Ctrl Pts',(2.77510437425366,0.981267566700582,9.87620543721836));
#67833=CARTESIAN_POINT('Ctrl Pts',(2.80343530244129,0.892252489503912,9.87116468479791));
#67834=CARTESIAN_POINT('Ctrl Pts',(2.83175626112793,0.803268736233301,9.86612570619108));
#67835=CARTESIAN_POINT('Ctrl Pts',(2.85584782229247,0.712899478029739,9.86108672758425));
#67836=CARTESIAN_POINT('Ctrl Pts',(2.87558679505007,0.621582322893509,9.85604774897742));
#67837=CARTESIAN_POINT('Ctrl Pts',(2.89532431631343,0.530271882712828,9.85100914090904));
#67838=CARTESIAN_POINT('Ctrl Pts',(2.91070979222329,0.43801411761001,9.84597053284066));
#67839=CARTESIAN_POINT('Ctrl Pts',(2.92167092270248,0.345257902784065,9.84093192477228));
#67840=CARTESIAN_POINT('Ctrl Pts',(2.93263429824887,0.252482689558648,9.83589228469231));
#67841=CARTESIAN_POINT('Ctrl Pts',(2.939171476924,0.159209264134449,9.83085264461234));
#67842=CARTESIAN_POINT('Ctrl Pts',(2.94126202499463,0.0658915800728639,
9.82581300453237));
#67843=CARTESIAN_POINT('Ctrl Pts',(2.94335484673521,-0.0275275958500429,
9.82076788336426));
#67844=CARTESIAN_POINT('Ctrl Pts',(2.94099137518667,-0.120990682620149,
9.81572276219614));
#67845=CARTESIAN_POINT('Ctrl Pts',(2.93420332079691,-0.214044089440471,
9.81067764102802));
#67846=CARTESIAN_POINT('Ctrl Pts',(2.92741105374318,-0.307155245169547,
9.80562938885963));
#67847=CARTESIAN_POINT('Ctrl Pts',(2.91618879038018,-0.399855775035067,
9.80058113669124));
#67848=CARTESIAN_POINT('Ctrl Pts',(2.90061982855417,-0.491699715475195,
9.79553288452285));
#67849=CARTESIAN_POINT('Ctrl Pts',(2.88502637089887,-0.583688160957556,
9.79047668955618));
#67850=CARTESIAN_POINT('Ctrl Pts',(2.86507265794508,-0.674816894385031,
9.7854204945895));
#67851=CARTESIAN_POINT('Ctrl Pts',(2.84089247464087,-0.76465282810494,9.78036429962283));
#67852=CARTESIAN_POINT('Ctrl Pts',(2.83055128652842,-0.803073144368351,
9.77820190645046));
#67853=CARTESIAN_POINT('Ctrl Pts',(2.81943767403642,-0.84125722711009,9.77603951327809));
#67854=CARTESIAN_POINT('Ctrl Pts',(2.80756478591604,-0.879172322633171,
9.77387712010573));
#67855=CARTESIAN_POINT('Ctrl Pts',(2.77980142335258,-0.967832346459148,
9.7688206161582));
#67856=CARTESIAN_POINT('Ctrl Pts',(2.74778545100014,-1.05533184283114,9.76376411221068));
#67857=CARTESIAN_POINT('Ctrl Pts',(2.71163227818096,-1.14123371310486,9.75870760826316));
#67858=CARTESIAN_POINT('Ctrl Pts',(2.6755283055148,-1.22701868118629,9.75365798561397));
#67859=CARTESIAN_POINT('Ctrl Pts',(2.6352984916249,-1.31120993858839,9.74860836296478));
#67860=CARTESIAN_POINT('Ctrl Pts',(2.59110797484379,-1.39338561163122,9.74355874031559));
#67861=CARTESIAN_POINT('Ctrl Pts',(2.54696401057743,-1.47547471668369,9.73851443719307));
#67862=CARTESIAN_POINT('Ctrl Pts',(2.49886784613195,-1.55555206960214,9.73347013407056));
#67863=CARTESIAN_POINT('Ctrl Pts',(2.44703221478881,-1.63321686857128,9.72842583094805));
#67864=CARTESIAN_POINT('Ctrl Pts',(2.39523307072211,-1.71082699902541,9.72338507852758));
#67865=CARTESIAN_POINT('Ctrl Pts',(2.33969993737056,-1.78602758336162,9.71834432610713));
#67866=CARTESIAN_POINT('Ctrl Pts',(2.28069034633778,-1.85844438822411,9.71330357368666));
#67867=CARTESIAN_POINT('Ctrl Pts',(2.22170152046214,-1.93083571000313,9.70826459507982));
#67868=CARTESIAN_POINT('Ctrl Pts',(2.15923894722988,-2.00044485518431,9.70322561647297));
#67869=CARTESIAN_POINT('Ctrl Pts',(2.09360152599711,-2.06692928044057,9.69818663786613));
#67870=CARTESIAN_POINT('Ctrl Pts',(2.02796893137513,-2.13340881680208,9.69314802979773));
#67871=CARTESIAN_POINT('Ctrl Pts',(1.95916226467271,-2.19676377484079,9.68810942172934));
#67872=CARTESIAN_POINT('Ctrl Pts',(1.88751770009901,-2.25668804485975,9.68307081366095));
#67873=CARTESIAN_POINT('Ctrl Pts',(1.81585846123038,-2.31662458861389,9.67803117358097));
#67874=CARTESIAN_POINT('Ctrl Pts',(1.74136051034097,-2.37312876464277,9.67299153350099));
#67875=CARTESIAN_POINT('Ctrl Pts',(1.66439264986219,-2.42593509952033,9.66795189342101));
#67876=CARTESIAN_POINT('Ctrl Pts',(1.58734107951099,-2.47879886631205,9.66290677225287));
#67877=CARTESIAN_POINT('Ctrl Pts',(1.50781460399198,-2.52795651350885,9.65786165108474));
#67878=CARTESIAN_POINT('Ctrl Pts',(1.42621025147046,-2.57318641349603,9.65281652991661));
#67879=CARTESIAN_POINT('Ctrl Pts',(1.34455525531888,-2.6184443831419,9.64776827774821));
#67880=CARTESIAN_POINT('Ctrl Pts',(1.26082021209893,-2.65976955669674,9.6427200255798));
#67881=CARTESIAN_POINT('Ctrl Pts',(1.17542399034816,-2.69698766087537,9.63767177341139));
#67882=CARTESIAN_POINT('Ctrl Pts',(1.08989340824036,-2.73426432312207,9.6326155784447));
#67883=CARTESIAN_POINT('Ctrl Pts',(1.0026968441177,-2.76742085976246,9.62755938347801));
#67884=CARTESIAN_POINT('Ctrl Pts',(0.914270011482932,-2.79633230251753,
9.62250318851132));
#67885=CARTESIAN_POINT('Ctrl Pts',(0.876452328345462,-2.80869691796943,
9.62034079533908));
#67886=CARTESIAN_POINT('Ctrl Pts',(0.838409771986596,-2.82028572562746,
9.61817840216685));
#67887=CARTESIAN_POINT('Ctrl Pts',(0.800176952928685,-2.83109181129856,
9.61601600899462));
#67888=CARTESIAN_POINT('Ctrl Pts',(0.710773969709414,-2.8563605808982,9.61095950504711));
#67889=CARTESIAN_POINT('Ctrl Pts',(0.620015697827995,-2.8774347460313,9.60590300109961));
#67890=CARTESIAN_POINT('Ctrl Pts',(0.528331154426677,-2.8941717625708,9.6008464971521));
#67891=CARTESIAN_POINT('Ctrl Pts',(0.4367713827455,-2.91088600202851,9.59579687450293));
#67892=CARTESIAN_POINT('Ctrl Pts',(0.344288277065512,-2.9232747433809,9.59074725185375));
#67893=CARTESIAN_POINT('Ctrl Pts',(0.251325318444532,-2.93124539817272,
9.58569762920458));
#67894=CARTESIAN_POINT('Ctrl Pts',(0.158460291683603,-2.93920765627557,
9.58065332608208));
#67895=CARTESIAN_POINT('Ctrl Pts',(0.0651168562606086,-2.94276104172703,
9.57560902295958));
#67896=CARTESIAN_POINT('Ctrl Pts',(-0.0282531046025607,-2.94186433441114,
9.57056471983709));
#67897=CARTESIAN_POINT('Ctrl Pts',(-0.121557342034083,-2.94096825829058,
9.56552396741664));
#67898=CARTESIAN_POINT('Ctrl Pts',(-0.214887625674755,-2.93562832010324,
9.56048321499619));
#67899=CARTESIAN_POINT('Ctrl Pts',(-0.307789801172765,-2.92585533447811,
9.55544246257575));
#67900=CARTESIAN_POINT('Ctrl Pts',(-0.400659284895781,-2.91608578791397,
9.55040348396892));
#67901=CARTESIAN_POINT('Ctrl Pts',(-0.493100519278439,-2.90188633956518,
9.54536450536209));
#67902=CARTESIAN_POINT('Ctrl Pts',(-0.584663242803674,-2.88331976938291,
9.54032552675526));
#67903=CARTESIAN_POINT('Ctrl Pts',(-0.676219233315614,-2.86475456448291,
9.53528691868688));
#67904=CARTESIAN_POINT('Ctrl Pts',(-0.76689640697302,-2.84182296470806,
9.53024831061851));
#67905=CARTESIAN_POINT('Ctrl Pts',(-0.856254605057123,-2.81463888470945,
9.52520970255013));
#67906=CARTESIAN_POINT('Ctrl Pts',(-0.945631105556222,-2.78744923684664,
9.52017006247016));
#67907=CARTESIAN_POINT('Ctrl Pts',(-1.03368766992456,-2.75600550826659,
9.51513042239021));
#67908=CARTESIAN_POINT('Ctrl Pts',(-1.12000030235379,-2.72047115822378,
9.51009078231024));
#67909=CARTESIAN_POINT('Ctrl Pts',(-1.20640680798421,-2.68489816119388,
9.50504566114213));
#67910=CARTESIAN_POINT('Ctrl Pts',(-1.29106518540278,-2.64522583180418,
9.500000539974));
#67911=CARTESIAN_POINT('Ctrl Pts',(-1.37357269697196,-2.60166524482555,
9.49495541880589));
#67912=CARTESIAN_POINT('Ctrl Pts',(-1.45613141267132,-2.55807762416326,
9.4899071666375));
#67913=CARTESIAN_POINT('Ctrl Pts',(-1.53653622364786,-2.51059716708712,
9.48485891446911));
#67914=CARTESIAN_POINT('Ctrl Pts',(-1.61441208083413,-2.45947913860981,
9.47981066230072));
#67915=CARTESIAN_POINT('Ctrl Pts',(-1.69241046601709,-2.40828068225855,
9.47475446733405));
#67916=CARTESIAN_POINT('Ctrl Pts',(-1.76787159678691,-2.35343349035532,
9.46969827236737));
#67917=CARTESIAN_POINT('Ctrl Pts',(-1.84045247857413,-2.29523390400855,
9.4646420774007));
#67918=CARTESIAN_POINT('Ctrl Pts',(-1.87149329172669,-2.27034356869074,
9.4624796842283));
#67919=CARTESIAN_POINT('Ctrl Pts',(-1.90200774803109,-2.24484053918549,
9.4603172910559));
#67920=CARTESIAN_POINT('Ctrl Pts',(-1.93197112367303,-2.21875000333376,
9.4581548978835));
#67921=CARTESIAN_POINT('Ctrl Pts',(-2.00103674140832,-2.15861128608182,
9.45317057895952));
#67922=CARTESIAN_POINT('Ctrl Pts',(-2.0674300095447,-2.09512390774132,9.44818626003554));
#67923=CARTESIAN_POINT('Ctrl Pts',(-2.13080192571592,-2.02855789992924,
9.44320194111156));
#67924=CARTESIAN_POINT('Ctrl Pts',(-2.19491665642982,-1.96121163799769,
9.43815919844398));
#67925=CARTESIAN_POINT('Ctrl Pts',(-2.25593833618249,-1.89071434632796,
9.4331164557764));
#67926=CARTESIAN_POINT('Ctrl Pts',(-2.31353904436894,-1.81738853583389,
9.42807371310882));
#67927=CARTESIAN_POINT('Ctrl Pts',(-2.37032961360863,-1.74509403375171,
9.42310189530244));
#67928=CARTESIAN_POINT('Ctrl Pts',(-2.42379451678455,-1.67005042725981,
9.41813007749606));
#67929=CARTESIAN_POINT('Ctrl Pts',(-2.4736568633579,-1.59260344165218,9.41315825968969));
#67930=CARTESIAN_POINT('Ctrl Pts',(-2.52348920478088,-1.51520306051883,
9.40818943372287));
#67931=CARTESIAN_POINT('Ctrl Pts',(-2.56972304646865,-1.4354025549002,9.40322060775605));
#67932=CARTESIAN_POINT('Ctrl Pts',(-2.61212364897492,-1.35357823655153,
9.39825178178923));
#67933=CARTESIAN_POINT('Ctrl Pts',(-2.65451135241786,-1.27177881070444,
9.39328446743303));
#67934=CARTESIAN_POINT('Ctrl Pts',(-2.69306792318456,-1.18795720101285,
9.38831715307682));
#67935=CARTESIAN_POINT('Ctrl Pts',(-2.72760425371636,-1.10251486842963,
9.38334983872062));
#67936=CARTESIAN_POINT('Ctrl Pts',(-2.76304788446274,-1.01482788954229,
9.3782520285847));
#67937=CARTESIAN_POINT('Ctrl Pts',(-2.79425685906639,-0.925434289069423,
9.37315421844878));
#67938=CARTESIAN_POINT('Ctrl Pts',(-2.82107978309542,-0.834789109542235,
9.36805640831286));
#67939=CARTESIAN_POINT('Ctrl Pts',(-2.847235644682,-0.746398195612121,9.36308537621489));
#67940=CARTESIAN_POINT('Ctrl Pts',(-2.86922100535572,-0.656817697940494,
9.35811434411692));
#67941=CARTESIAN_POINT('Ctrl Pts',(-2.88694677326747,-0.56648241660315,
9.35314331201895));
#67942=CARTESIAN_POINT('Ctrl Pts',(-2.90535064122947,-0.472691355007414,
9.34798211286406));
#67943=CARTESIAN_POINT('Ctrl Pts',(-2.91916237285942,-0.378087135627378,
9.34282091370917));
#67944=CARTESIAN_POINT('Ctrl Pts',(-2.92834128938451,-0.283163014685617,
9.33765971455428));
#67945=CARTESIAN_POINT('Ctrl Pts',(-2.93752020590961,-0.188238893743857,
9.33249851539938));
#67946=CARTESIAN_POINT('Ctrl Pts',(-2.94206633972349,-0.0929954194237398,
9.32733731624449));
#67947=CARTESIAN_POINT('Ctrl Pts',(-2.94199926785449,0.00207555863534859,
9.3221761170896));
#67948=CARTESIAN_POINT('',(-2.94199893297947,-0.00250566312373982,8.3221761170896));
#67949=CARTESIAN_POINT('Ctrl Pts',(-2.94464008512449,0.00207742171232136,
9.3221761170896));
#67950=CARTESIAN_POINT('Ctrl Pts',(-2.94572064417758,0.136558752036829,
9.31488200698387));
#67951=CARTESIAN_POINT('Ctrl Pts',(-2.87651233014906,1.2400826680256,9.25496752650772));
#67952=CARTESIAN_POINT('Ctrl Pts',(-1.48278064012933,3.13792943795001,9.14243267566131));
#67953=CARTESIAN_POINT('Ctrl Pts',(1.81534028008774,2.95800257805624,8.98457156455015));
#67954=CARTESIAN_POINT('Ctrl Pts',(3.46921681308081,0.0988649995372459,
8.82671045343907));
#67955=CARTESIAN_POINT('Ctrl Pts',(1.98085035420067,-2.84981954842035,8.66884934232795));
#67956=CARTESIAN_POINT('Ctrl Pts',(-1.30167123501552,-3.2172801525869,8.51098823121684));
#67957=CARTESIAN_POINT('Ctrl Pts',(-2.8415027498017,-1.35312072688065,8.39543048947073));
#67958=CARTESIAN_POINT('Ctrl Pts',(-2.94478032747652,-0.192985093804385,
8.33249311809497));
#67959=CARTESIAN_POINT('Ctrl Pts',(-2.94306537549688,-0.00250657139928612,
8.3221761170896));
#67960=CARTESIAN_POINT('',(-2.94199996099939,0.000479040305267797,7.32217611704064));
#67961=CARTESIAN_POINT('Ctrl Pts',(-2.94199893297947,-0.00250566312373982,
8.3221761170896));
#67962=CARTESIAN_POINT('Ctrl Pts',(-2.94207713595497,0.0893155670756921,
8.31720090487355));
#67963=CARTESIAN_POINT('Ctrl Pts',(-2.93785244836421,0.181275223426796,
8.31222569265751));
#67964=CARTESIAN_POINT('Ctrl Pts',(-2.92931265872361,0.272931030558297,
8.30725048044146));
#67965=CARTESIAN_POINT('Ctrl Pts',(-2.92078100783252,0.364499486163972,
8.3022800097949));
#67966=CARTESIAN_POINT('Ctrl Pts',(-2.90794246826347,0.455764214554573,
8.29730953914834));
#67967=CARTESIAN_POINT('Ctrl Pts',(-2.89083688222758,0.546283919178212,
8.29233906850178));
#67968=CARTESIAN_POINT('Ctrl Pts',(-2.87373987349475,0.636758234246803,
8.28737109021257));
#67969=CARTESIAN_POINT('Ctrl Pts',(-2.85238015013863,0.726487818501757,
8.28240311192336));
#67970=CARTESIAN_POINT('Ctrl Pts',(-2.82684914637299,0.815038590282867,
8.27743513363415));
#67971=CARTESIAN_POINT('Ctrl Pts',(-2.80132334617133,0.903571314218693,
8.27246816788612));
#67972=CARTESIAN_POINT('Ctrl Pts',(-2.77162808100322,0.990925263531778,
8.2675012021381));
#67973=CARTESIAN_POINT('Ctrl Pts',(-2.73790510853684,1.07667990445066,8.26253423639008));
#67974=CARTESIAN_POINT('Ctrl Pts',(-2.70417897265835,1.16244258965657,8.25756680471161));
#67975=CARTESIAN_POINT('Ctrl Pts',(-2.66642454858315,1.24660524362766,8.25259937303314));
#67976=CARTESIAN_POINT('Ctrl Pts',(-2.62483185301556,1.32876700116871,8.24763194135467));
#67977=CARTESIAN_POINT('Ctrl Pts',(-2.58319772789434,1.41101059819852,8.24265956172862));
#67978=CARTESIAN_POINT('Ctrl Pts',(-2.53771790793819,1.49124891238343,8.23768718210257));
#67979=CARTESIAN_POINT('Ctrl Pts',(-2.48862828313252,1.56910588182981,8.23271480247653));
#67980=CARTESIAN_POINT('Ctrl Pts',(-2.43951135879074,1.64700614879897,8.22773965762957));
#67981=CARTESIAN_POINT('Ctrl Pts',(-2.38678089793278,1.72252206200371,8.22276451278261));
#67982=CARTESIAN_POINT('Ctrl Pts',(-2.3307146686714,1.79530864567627,8.21778936793565));
#67983=CARTESIAN_POINT('Ctrl Pts',(-2.27456009386465,1.8682099217495,8.21280638357656));
#67984=CARTESIAN_POINT('Ctrl Pts',(-2.21505955674095,1.93837293788326,8.20782339921746));
#67985=CARTESIAN_POINT('Ctrl Pts',(-2.15252915667446,2.00548802780429,8.20284041485836));
#67986=CARTESIAN_POINT('Ctrl Pts',(-2.12084595943131,2.03949421726892,8.20031561290378));
#67987=CARTESIAN_POINT('Ctrl Pts',(-2.08838546529636,2.0727185323238,8.1977908109492));
#67988=CARTESIAN_POINT('Ctrl Pts',(-2.05519198062807,2.10512468104909,8.19526600899461));
#67989=CARTESIAN_POINT('Ctrl Pts',(-1.98871429672409,2.17002554135448,8.1902095050471));
#67990=CARTESIAN_POINT('Ctrl Pts',(-1.91904247858982,2.2318884713599,8.18515300109959));
#67991=CARTESIAN_POINT('Ctrl Pts',(-1.84648536483333,2.29038332980668,8.18009649715207));
#67992=CARTESIAN_POINT('Ctrl Pts',(-1.77402699264839,2.34879858373294,8.1750468745029));
#67993=CARTESIAN_POINT('Ctrl Pts',(-1.69869147014349,2.40385459882147,8.16999725185372));
#67994=CARTESIAN_POINT('Ctrl Pts',(-1.62082420321798,2.45525821498734,8.16494762920454));
#67995=CARTESIAN_POINT('Ctrl Pts',(-1.54303896559086,2.50660767999656,8.15990332608204));
#67996=CARTESIAN_POINT('Ctrl Pts',(-1.46272765317577,2.55431215130621,8.15485902295953));
#67997=CARTESIAN_POINT('Ctrl Pts',(-1.38026758822414,2.59811958633507,8.14981471983702));
#67998=CARTESIAN_POINT('Ctrl Pts',(-1.2978655671916,2.641896185162,8.14477396741658));
#67999=CARTESIAN_POINT('Ctrl Pts',(-1.21331819055915,2.68178099290725,8.13973321499613));
#68000=CARTESIAN_POINT('Ctrl Pts',(-1.12702962869304,2.71756659827281,8.13469246257568));
#68001=CARTESIAN_POINT('Ctrl Pts',(-1.04077143130685,2.75333961087668,8.12965348396884));
#68002=CARTESIAN_POINT('Ctrl Pts',(-0.952773675161863,2.78501611732971,
8.124614505362));
#68003=CARTESIAN_POINT('Ctrl Pts',(-0.863461930124583,2.81243622065026,
8.11957552675517));
#68004=CARTESIAN_POINT('Ctrl Pts',(-0.774156752576108,2.83985430764898,
8.11453691868678));
#68005=CARTESIAN_POINT('Ctrl Pts',(-0.683538202183492,2.8630164840472,8.1094983106184));
#68006=CARTESIAN_POINT('Ctrl Pts',(-0.592047395722709,2.88181260341785,
8.10445970255001));
#68007=CARTESIAN_POINT('Ctrl Pts',(-0.50053785004424,2.90061257262419,8.09942006247003));
#68008=CARTESIAN_POINT('Ctrl Pts',(-0.408156127785994,2.9150446198816,8.09438042239004));
#68009=CARTESIAN_POINT('Ctrl Pts',(-0.315352808957852,2.92504984673465,
8.08934078231006));
#68010=CARTESIAN_POINT('Ctrl Pts',(-0.222448557689706,2.93506595522396,
8.08429566114194));
#68011=CARTESIAN_POINT('Ctrl Pts',(-0.129122236070494,2.940645585982,8.07925053997382));
#68012=CARTESIAN_POINT('Ctrl Pts',(-0.0358284894473728,2.94178182728494,
8.07420541880569));
#68013=CARTESIAN_POINT('Ctrl Pts',(0.0575231552393617,2.9429187737388,8.0691571666373));
#68014=CARTESIAN_POINT('Ctrl Pts',(0.150841742008688,2.93960685650917,8.0641089144689));
#68015=CARTESIAN_POINT('Ctrl Pts',(0.243675845689539,2.93189121254993,8.0590606623005));
#68016=CARTESIAN_POINT('Ctrl Pts',(0.336656012311531,2.92416342898245,8.05400446733382));
#68017=CARTESIAN_POINT('Ctrl Pts',(0.429149735399227,2.91201814569531,8.04894827236714));
#68018=CARTESIAN_POINT('Ctrl Pts',(0.52071413309325,2.89555189758307,8.04389207740046));
#68019=CARTESIAN_POINT('Ctrl Pts',(0.559873665054721,2.88850974380414,8.04172968422814));
#68020=CARTESIAN_POINT('Ctrl Pts',(0.598863391467464,2.88067789908918,8.03956729105582));
#68021=CARTESIAN_POINT('Ctrl Pts',(0.637649560612953,2.87206668408833,8.0374048978835));
#68022=CARTESIAN_POINT('Ctrl Pts',(0.72834648839811,2.85193036327393,8.03234839393599));
#68023=CARTESIAN_POINT('Ctrl Pts',(0.818248104638546,2.82745826184522,8.02729188998847));
#68024=CARTESIAN_POINT('Ctrl Pts',(0.906909090966337,2.79872826489508,8.02223538604096));
#68025=CARTESIAN_POINT('Ctrl Pts',(0.99544942027428,2.77003736604158,8.01718576339178));
#68026=CARTESIAN_POINT('Ctrl Pts',(1.08275205660791,2.73710022230183,8.0121361407426));
#68027=CARTESIAN_POINT('Ctrl Pts',(1.16838262984417,2.70004556077827,8.00708651809342));
#68028=CARTESIAN_POINT('Ctrl Pts',(1.2539229955243,2.66302993450033,8.00204221497091));
#68029=CARTESIAN_POINT('Ctrl Pts',(1.33779439465786,2.62190558779252,7.99699791184841));
#68030=CARTESIAN_POINT('Ctrl Pts',(1.41957941233063,2.57685045978361,7.9919536087259));
#68031=CARTESIAN_POINT('Ctrl Pts',(1.5013068612524,2.53182704623194,7.98691285630545));
#68032=CARTESIAN_POINT('Ctrl Pts',(1.58095046066298,2.48287856456771,7.981872103885));
#68033=CARTESIAN_POINT('Ctrl Pts',(1.65811546502868,2.43022984605011,7.97683135146455));
#68034=CARTESIAN_POINT('Ctrl Pts',(1.73525331544513,2.37759965433286,7.97179237285772));
#68035=CARTESIAN_POINT('Ctrl Pts',(1.80991393781239,2.32127206237876,7.96675339425089));
#68036=CARTESIAN_POINT('Ctrl Pts',(1.88173065029614,2.26151581018928,7.96171441564405));
#68037=CARTESIAN_POINT('Ctrl Pts',(1.95354208177837,2.20176395214216,7.95667580757567));
#68038=CARTESIAN_POINT('Ctrl Pts',(2.02250967859608,2.1385842189999,7.9516371995073));
#68039=CARTESIAN_POINT('Ctrl Pts',(2.08829989655837,2.0722855840917,7.94659859143892));
#68040=CARTESIAN_POINT('Ctrl Pts',(2.15410358972397,2.00597336984585,7.94155895135894));
#68041=CARTESIAN_POINT('Ctrl Pts',(2.21672829950995,1.93654130002476,7.93651931127896));
#68042=CARTESIAN_POINT('Ctrl Pts',(2.27587820131431,1.86433430821361,7.93147967119898));
#68043=CARTESIAN_POINT('Ctrl Pts',(2.33509243426537,1.79204878442792,7.92643455003086));
#68044=CARTESIAN_POINT('Ctrl Pts',(2.39082403477812,1.71698265830804,7.92138942886275));
#68045=CARTESIAN_POINT('Ctrl Pts',(2.44281846954338,1.63951270957494,7.91634430769463));
#68046=CARTESIAN_POINT('Ctrl Pts',(2.49484517203511,1.56199468302106,7.91129605552623));
#68047=CARTESIAN_POINT('Ctrl Pts',(2.5431298623532,1.48207024299637,7.90624780335782));
#68048=CARTESIAN_POINT('Ctrl Pts',(2.58746333642,1.40014195090436,7.90119955118942));
#68049=CARTESIAN_POINT('Ctrl Pts',(2.63186656370626,1.31808475481242,7.89614335622274));
#68050=CARTESIAN_POINT('Ctrl Pts',(2.67230597343853,1.23401781209865,7.89108716125607));
#68051=CARTESIAN_POINT('Ctrl Pts',(2.70862005849138,1.14836465407908,7.88603096628939));
#68052=CARTESIAN_POINT('Ctrl Pts',(2.7241505770128,1.11173319399672,7.88386857311706));
#68053=CARTESIAN_POINT('Ctrl Pts',(2.73892717915958,1.07481181013318,7.88170617994472));
#68054=CARTESIAN_POINT('Ctrl Pts',(2.75294003743155,1.03763440108083,7.87954378677239));
#68055=CARTESIAN_POINT('Ctrl Pts',(2.78570747032704,0.9506993709316,7.87448728282488));
#68056=CARTESIAN_POINT('Ctrl Pts',(2.81441049930312,0.86205784297445,7.86943077887736));
#68057=CARTESIAN_POINT('Ctrl Pts',(2.83887067332622,0.772125184233966,7.86437427492985));
#68058=CARTESIAN_POINT('Ctrl Pts',(2.863297559972,0.682314913107818,7.85932465228068));
#68059=CARTESIAN_POINT('Ctrl Pts',(2.88349295071196,0.591217427185472,7.8542750296315));
#68060=CARTESIAN_POINT('Ctrl Pts',(2.89932694192119,0.499266746188751,7.84922540698233));
#68061=CARTESIAN_POINT('Ctrl Pts',(2.91514425280701,0.407412930668159,7.84418110385985));
#68062=CARTESIAN_POINT('Ctrl Pts',(2.92660922219562,0.314708141355005,7.83913680073737));
#68063=CARTESIAN_POINT('Ctrl Pts',(2.93364241605211,0.221599130729175,7.83409249761489));
#68064=CARTESIAN_POINT('Ctrl Pts',(2.94067065921967,0.128555659850846,7.82905174519444));
#68065=CARTESIAN_POINT('Ctrl Pts',(2.94327329437766,0.0351089741175195,
7.82401099277399));
#68066=CARTESIAN_POINT('Ctrl Pts',(2.94142254157655,-0.0582874935586067,
7.81897024035353));
#68067=CARTESIAN_POINT('Ctrl Pts',(2.93957244004538,-0.151651095520984,
7.8139312617467));
#68068=CARTESIAN_POINT('Ctrl Pts',(2.93327207286506,-0.24496407168727,7.80889228313987));
#68069=CARTESIAN_POINT('Ctrl Pts',(2.92254576829046,-0.337772456318622,
7.80385330453303));
#68070=CARTESIAN_POINT('Ctrl Pts',(2.9118202524686,-0.430574016337872,7.79881469646464));
#68071=CARTESIAN_POINT('Ctrl Pts',(2.89666949760899,-0.522870618214443,
7.79377608839625));
#68072=CARTESIAN_POINT('Ctrl Pts',(2.87716963974356,-0.614214021443608,
7.78873748032786));
#68073=CARTESIAN_POINT('Ctrl Pts',(2.85766578790226,-0.705576133698785,
7.78369784024789));
#68074=CARTESIAN_POINT('Ctrl Pts',(2.83381115679292,-0.795984226091077,
7.77865820016793));
#68075=CARTESIAN_POINT('Ctrl Pts',(2.80573262034301,-0.885001956575884,
7.77361856008796));
#68076=CARTESIAN_POINT('Ctrl Pts',(2.77762354581281,-0.974116502313364,
7.76857343891985));
#68077=CARTESIAN_POINT('Ctrl Pts',(2.74528153024882,-1.06183724453324,7.76352831775173));
#68078=CARTESIAN_POINT('Ctrl Pts',(2.70888269591461,-1.14774498028716,7.75848319658362));
#68079=CARTESIAN_POINT('Ctrl Pts',(2.67246127247764,-1.23370603034926,7.75343494441522));
#68080=CARTESIAN_POINT('Ctrl Pts',(2.63197820998977,-1.31785143476304,7.74838669224683));
#68081=CARTESIAN_POINT('Ctrl Pts',(2.58765601205185,-1.39978582765077,7.74333844007843));
#68082=CARTESIAN_POINT('Ctrl Pts',(2.543264078636,-1.48184913413737,7.73828224511175));
#68083=CARTESIAN_POINT('Ctrl Pts',(2.49502118123996,-1.56169410622437,7.73322605014507));
#68084=CARTESIAN_POINT('Ctrl Pts',(2.44319347254472,-1.63895382964709,7.7281698551784));
#68085=CARTESIAN_POINT('Ctrl Pts',(2.4210282110861,-1.6719956525059,7.72600746200602));
#68086=CARTESIAN_POINT('Ctrl Pts',(2.39820778215354,-1.70456503353761,7.72384506883365));
#68087=CARTESIAN_POINT('Ctrl Pts',(2.37475518372315,-1.73663519985633,7.72168267566128));
#68088=CARTESIAN_POINT('Ctrl Pts',(2.31991402067386,-1.81162753920514,7.71662617171377));
#68089=CARTESIAN_POINT('Ctrl Pts',(2.26142069502047,-1.88415143323315,7.71156966776626));
#68090=CARTESIAN_POINT('Ctrl Pts',(2.1995252550804,-1.95383025165021,7.70651316381875));
#68091=CARTESIAN_POINT('Ctrl Pts',(2.13771404744642,-2.02341424551207,7.70146354116958));
#68092=CARTESIAN_POINT('Ctrl Pts',(2.07251021822523,-2.09016052932911,7.69641391852041));
#68093=CARTESIAN_POINT('Ctrl Pts',(2.00420599049321,-2.15372290410608,7.69136429587124));
#68094=CARTESIAN_POINT('Ctrl Pts',(1.9359737178726,-2.21721831907821,7.68631999274873));
#68095=CARTESIAN_POINT('Ctrl Pts',(1.86464786194383,-2.27753619172648,7.68127568962622));
#68096=CARTESIAN_POINT('Ctrl Pts',(1.79055891692532,-2.33436560226097,7.67623138650371));
#68097=CARTESIAN_POINT('Ctrl Pts',(1.71652212336627,-2.39115501038081,7.67119063408326));
#68098=CARTESIAN_POINT('Ctrl Pts',(1.63972645757972,-2.44446056825905,7.66614988166281));
#68099=CARTESIAN_POINT('Ctrl Pts',(1.56053626688848,-2.49401093817284,7.66110912924236));
#68100=CARTESIAN_POINT('Ctrl Pts',(1.48137394279865,-2.54354387157844,7.65607015063552));
#68101=CARTESIAN_POINT('Ctrl Pts',(1.39981914339623,-2.58932400746781,7.65103117202868));
#68102=CARTESIAN_POINT('Ctrl Pts',(1.31626517170938,-2.63112333381483,7.64599219342185));
#68103=CARTESIAN_POINT('Ctrl Pts',(1.23271734411695,-2.67291958647185,7.64095358535348));
#68104=CARTESIAN_POINT('Ctrl Pts',(1.14717103319778,-2.71073541356624,7.63591497728511));
#68105=CARTESIAN_POINT('Ctrl Pts',(1.06004309499874,-2.74438930123725,7.63087636921674));
#68106=CARTESIAN_POINT('Ctrl Pts',(0.972897311187784,-2.77805008192365,
7.62583672913675));
#68107=CARTESIAN_POINT('Ctrl Pts',(0.884169670371078,-2.80754707076227,
7.62079708905677));
#68108=CARTESIAN_POINT('Ctrl Pts',(0.794294828950772,-2.83274773403882,
7.61575744897678));
#68109=CARTESIAN_POINT('Ctrl Pts',(0.704322240088413,-2.85797580543464,
7.61071232780866));
#68110=CARTESIAN_POINT('Ctrl Pts',(0.613200387771495,-2.87889810494226,
7.60566720664055));
#68111=CARTESIAN_POINT('Ctrl Pts',(0.521376527103044,-2.89543269943992,
7.60062208547243));
#68112=CARTESIAN_POINT('Ctrl Pts',(0.429495680581492,-2.91197755530066,
7.59557383330403));
#68113=CARTESIAN_POINT('Ctrl Pts',(0.336912397542223,-2.92412922736843,
7.59052558113563));
#68114=CARTESIAN_POINT('Ctrl Pts',(0.244079356636889,-2.93185764791944,
7.58547732896723));
#68115=CARTESIAN_POINT('Ctrl Pts',(0.151100254462614,-2.93959822818106,
7.58042113400055));
#68116=CARTESIAN_POINT('Ctrl Pts',(0.0578710523553916,-2.94290164931675,
7.57536493903387));
#68117=CARTESIAN_POINT('Ctrl Pts',(-0.0351555049776785,-2.94178994669398,
7.57030874406719));
#68118=CARTESIAN_POINT('Ctrl Pts',(-0.0749403617224944,-2.94131450257503,
7.56814635089485));
#68119=CARTESIAN_POINT('Ctrl Pts',(-0.114688219126788,-2.94003216518703,
7.56598395772251));
#68120=CARTESIAN_POINT('Ctrl Pts',(-0.154364084154138,-2.93794753689089,
7.56382156455017));
#68121=CARTESIAN_POINT('Ctrl Pts',(-0.247141461875206,-2.93307287702638,
7.55876506060266));
#68122=CARTESIAN_POINT('Ctrl Pts',(-0.339850814750179,-2.92379062296448,
7.55370855665515));
#68123=CARTESIAN_POINT('Ctrl Pts',(-0.432040076364305,-2.91010401401997,
7.54865205270765));
#68124=CARTESIAN_POINT('Ctrl Pts',(-0.524103879397204,-2.89643603091658,
7.54360243005846));
#68125=CARTESIAN_POINT('Ctrl Pts',(-0.615648562829644,-2.87837566868871,
7.53855280740927));
#68126=CARTESIAN_POINT('Ctrl Pts',(-0.706224457923897,-2.855978118794,7.53350318476009));
#68127=CARTESIAN_POINT('Ctrl Pts',(-0.796704935811239,-2.83360416360569,
7.52845888163757));
#68128=CARTESIAN_POINT('Ctrl Pts',(-0.886218225858062,-2.80690220881182,
7.52341457851505));
#68129=CARTESIAN_POINT('Ctrl Pts',(-0.974323250717918,-2.77597878289991,
7.51837027539253));
#68130=CARTESIAN_POINT('Ctrl Pts',(-1.06236625815215,-2.74507712409231,
7.51332952297207));
#68131=CARTESIAN_POINT('Ctrl Pts',(-1.14900255362035,-2.70996004716568,
7.50828877055162));
#68132=CARTESIAN_POINT('Ctrl Pts',(-1.23380567010069,-2.67078407371831,
7.50324801813116));
#68133=CARTESIAN_POINT('Ctrl Pts',(-1.31857894482114,-2.63162188608497,
7.49820903952433));
#68134=CARTESIAN_POINT('Ctrl Pts',(-1.40151992009744,-2.58840382541785,
7.4931700609175));
#68135=CARTESIAN_POINT('Ctrl Pts',(-1.48222255233038,-2.54133435528724,
7.48813108231067));
#68136=CARTESIAN_POINT('Ctrl Pts',(-1.56291925014091,-2.49426834638349,
7.48309247424227));
#68137=CARTESIAN_POINT('Ctrl Pts',(-1.64137754937265,-2.44335171479377,
7.47805386617388));
#68138=CARTESIAN_POINT('Ctrl Pts',(-1.71721744131187,-2.38883407947357,
7.47301525810549));
#68139=CARTESIAN_POINT('Ctrl Pts',(-1.7930728668365,-2.33430527780906,7.46797561802549));
#68140=CARTESIAN_POINT('Ctrl Pts',(-1.86630846018385,-2.27617426661408,
7.4629359779455));
#68141=CARTESIAN_POINT('Ctrl Pts',(-1.93657547249624,-2.21473236291114,
7.4578963378655));
#68142=CARTESIAN_POINT('Ctrl Pts',(-2.00691890687062,-2.15322363529156,
7.45285121669738));
#68143=CARTESIAN_POINT('Ctrl Pts',(-2.0742869817916,-2.08839712013141,7.44780609552925));
#68144=CARTESIAN_POINT('Ctrl Pts',(-2.13836641060864,-2.02058236505734,
7.44276097436113));
#68145=CARTESIAN_POINT('Ctrl Pts',(-2.20248560709479,-1.95272552417211,
7.43771272219273));
#68146=CARTESIAN_POINT('Ctrl Pts',(-2.2633118057172,-1.88187708739681,7.43266447002434));
#68147=CARTESIAN_POINT('Ctrl Pts',(-2.32057216644433,-1.80839951900123,
7.42761621785594));
#68148=CARTESIAN_POINT('Ctrl Pts',(-2.37792261924285,-1.7348063427706,7.42256002288926));
#68149=CARTESIAN_POINT('Ctrl Pts',(-2.43169577992265,-1.65857613939135,
7.41750382792259));
#68150=CARTESIAN_POINT('Ctrl Pts',(-2.48166238525116,-1.58009993532989,
7.41244763295591));
#68151=CARTESIAN_POINT('Ctrl Pts',(-2.50303170485151,-1.54653785772654,
7.41028523978362));
#68152=CARTESIAN_POINT('Ctrl Pts',(-2.52370537044815,-1.51256527895886,
7.40812284661134));
#68153=CARTESIAN_POINT('Ctrl Pts',(-2.54366808888571,-1.47821400804637,
7.40596045343906));
#68154=CARTESIAN_POINT('Ctrl Pts',(-2.59210151914144,-1.39487115626297,
7.40071406782164));
#68155=CARTESIAN_POINT('Ctrl Pts',(-2.63650617799513,-1.3090235510266,7.39546768220423));
#68156=CARTESIAN_POINT('Ctrl Pts',(-2.67662574138782,-1.22108093119993,
7.39022129658682));
#68157=CARTESIAN_POINT('Ctrl Pts',(-2.71667599687629,-1.13329023522677,
7.38498397427821));
#68158=CARTESIAN_POINT('Ctrl Pts',(-2.75245572483854,-1.04341208544652,
7.37974665196959));
#68159=CARTESIAN_POINT('Ctrl Pts',(-2.78375366163325,-0.951882110002848,
7.37450932966098));
#68160=CARTESIAN_POINT('Ctrl Pts',(-2.81498817722214,-0.860537608171982,
7.36928262010612));
#68161=CARTESIAN_POINT('Ctrl Pts',(-2.8417588666175,-0.767548322398948,
7.36405591055125));
#68162=CARTESIAN_POINT('Ctrl Pts',(-2.86390237024338,-0.673370042186563,
7.35882920099639));
#68163=CARTESIAN_POINT('Ctrl Pts',(-2.88601895663896,-0.579306243336356,
7.35360884493225));
#68164=CARTESIAN_POINT('Ctrl Pts',(-2.90351945760502,-0.484056709901852,
7.3483884888681));
#68165=CARTESIAN_POINT('Ctrl Pts',(-2.91629009012335,-0.388092914452626,
7.34316813280396));
#68166=CARTESIAN_POINT('Ctrl Pts',(-2.92904377630873,-0.292256460732716,
7.33795470403115));
#68167=CARTESIAN_POINT('Ctrl Pts',(-2.93708004351147,-0.195708024943747,
7.33274127525835));
#68168=CARTESIAN_POINT('Ctrl Pts',(-2.94033621960299,-0.098928841551814,
7.32752784648554));
#68169=CARTESIAN_POINT('Ctrl Pts',(-2.94145040466026,-0.0658133352158173,
7.32574393668689));
#68170=CARTESIAN_POINT('Ctrl Pts',(-2.94200535872909,-0.0326708858341013,
7.32396002688824));
#68171=CARTESIAN_POINT('Ctrl Pts',(-2.94199996099953,0.000479039395695414,
7.32217611708959));
#68172=CARTESIAN_POINT('',(-2.94199929728077,0.0020334206256296,6.3221761170896));
#68173=CARTESIAN_POINT('Ctrl Pts',(-2.94199996099939,0.000479040305269824,
7.32217611704064));
#68174=CARTESIAN_POINT('Ctrl Pts',(-2.94198378421545,0.0998278783730615,
7.31682981944008));
#68175=CARTESIAN_POINT('Ctrl Pts',(-2.93693095783807,0.199055979289579,
7.31148352183952));
#68176=CARTESIAN_POINT('Ctrl Pts',(-2.92690352421262,0.297657118093517,
7.30613722423896));
#68177=CARTESIAN_POINT('Ctrl Pts',(-2.91684329563174,0.39658073422059,7.30077344144746));
#68178=CARTESIAN_POINT('Ctrl Pts',(-2.90177595852271,0.494872932518549,
7.29540965865596));
#68179=CARTESIAN_POINT('Ctrl Pts',(-2.88181511798122,0.592035155860621,
7.29004587586446));
#68180=CARTESIAN_POINT('Ctrl Pts',(-2.86182045155733,0.689362031484373,
7.28467300354161));
#68181=CARTESIAN_POINT('Ctrl Pts',(-2.83691582196706,0.785554767436168,
7.27930013121876));
#68182=CARTESIAN_POINT('Ctrl Pts',(-2.80726469917522,0.880130052188105,
7.27392725889591));
#68183=CARTESIAN_POINT('Ctrl Pts',(-2.77752918840202,0.974974501026125,
7.2685390952179));
#68184=CARTESIAN_POINT('Ctrl Pts',(-2.74302029293948,1.06819195891079,7.26315093153989));
#68185=CARTESIAN_POINT('Ctrl Pts',(-2.70395013541805,1.15931775849967,7.25776276786188));
#68186=CARTESIAN_POINT('Ctrl Pts',(-2.6805932875586,1.21379441209139,7.25454162601724));
#68187=CARTESIAN_POINT('Ctrl Pts',(-2.65560720026491,1.26752399495668,7.25132048417259));
#68188=CARTESIAN_POINT('Ctrl Pts',(-2.62904482224712,1.32041180039244,7.24809934232795));
#68189=CARTESIAN_POINT('Ctrl Pts',(-2.58734756836014,1.40343434638977,7.24304283838044));
#68190=CARTESIAN_POINT('Ctrl Pts',(-2.54164050844154,1.48462578081831,7.23798633443293));
#68191=CARTESIAN_POINT('Ctrl Pts',(-2.49210802758016,1.56357333658211,7.23292983048542));
#68192=CARTESIAN_POINT('Ctrl Pts',(-2.44264295451304,1.64241345414569,7.22788020783624));
#68193=CARTESIAN_POINT('Ctrl Pts',(-2.38936303967928,1.71901538900267,7.22283058518707));
#68194=CARTESIAN_POINT('Ctrl Pts',(-2.33249929116039,1.79298941902519,7.21778096253789));
#68195=CARTESIAN_POINT('Ctrl Pts',(-2.27569544577662,1.86688552108075,7.21273665941539));
#68196=CARTESIAN_POINT('Ctrl Pts',(-2.21531554015483,1.93815887151289,7.2076923562929));
#68197=CARTESIAN_POINT('Ctrl Pts',(-2.1516341563711,2.00644821940094,7.20264805317041));
#68198=CARTESIAN_POINT('Ctrl Pts',(-2.08799759812901,2.07468949818583,7.19760730074996));
#68199=CARTESIAN_POINT('Ctrl Pts',(-2.02106448260628,2.13995062620793,7.19256654832952));
#68200=CARTESIAN_POINT('Ctrl Pts',(-1.95114931947164,2.20190379742743,7.18752579590907));
#68201=CARTESIAN_POINT('Ctrl Pts',(-1.88125875910622,2.26383516765978,7.18248681730224));
#68202=CARTESIAN_POINT('Ctrl Pts',(-1.80838856750224,2.32246060005221,7.17744783869541));
#68203=CARTESIAN_POINT('Ctrl Pts',(-1.73288897034967,2.37749023477289,7.17240886008858));
#68204=CARTESIAN_POINT('Ctrl Pts',(-1.65739492501744,2.43251582292039,7.1673702520202));
#68205=CARTESIAN_POINT('Ctrl Pts',(-1.57927221706682,2.4839458782693,7.16233164395183));
#68206=CARTESIAN_POINT('Ctrl Pts',(-1.49890198392706,2.53153250869498,7.15729303588345));
#68207=CARTESIAN_POINT('Ctrl Pts',(-1.41851528929414,2.57912888585102,7.15225339580348));
#68208=CARTESIAN_POINT('Ctrl Pts',(-1.33588053684632,2.62288004907297,7.14721375572351));
#68209=CARTESIAN_POINT('Ctrl Pts',(-1.25140451222114,2.6625834722676,7.14217411564354));
#68210=CARTESIAN_POINT('Ctrl Pts',(-1.16683661188062,2.70233007671304,7.13712899447543));
#68211=CARTESIAN_POINT('Ctrl Pts',(-1.08042384414241,2.73801996545164,7.13208387330731));
#68212=CARTESIAN_POINT('Ctrl Pts',(-0.99259378041509,2.76949843601351,7.12703875213919));
#68213=CARTESIAN_POINT('Ctrl Pts',(-0.90470920938366,2.80099644210223,7.1219904999708));
#68214=CARTESIAN_POINT('Ctrl Pts',(-0.815406014878199,2.82827769726885,
7.1169422478024));
#68215=CARTESIAN_POINT('Ctrl Pts',(-0.725125686506602,2.85123775556658,
7.11189399563401));
#68216=CARTESIAN_POINT('Ctrl Pts',(-0.634703313242367,2.87423393866663,
7.10683780066733));
#68217=CARTESIAN_POINT('Ctrl Pts',(-0.543301170934598,2.89289526494013,
7.10178160570066));
#68218=CARTESIAN_POINT('Ctrl Pts',(-0.451369422798152,2.90716866455369,
7.09672541073398));
#68219=CARTESIAN_POINT('Ctrl Pts',(-0.412052785325619,2.91327299836091,
7.0945630175616));
#68220=CARTESIAN_POINT('Ctrl Pts',(-0.372639324005275,2.91857541518902,
7.09240062438922));
#68221=CARTESIAN_POINT('Ctrl Pts',(-0.333164311357436,2.92307467260721,
7.09023823121684));
#68222=CARTESIAN_POINT('Ctrl Pts',(-0.24085660347553,2.93359566073579,7.08518172726933));
#68223=CARTESIAN_POINT('Ctrl Pts',(-0.147887763980285,2.93975839015493,
7.08012522332181));
#68224=CARTESIAN_POINT('Ctrl Pts',(-0.0547041816371323,2.94149136536408,
7.0750687193743));
#68225=CARTESIAN_POINT('Ctrl Pts',(0.038352588972679,2.94322198220081,7.07001909672512));
#68226=CARTESIAN_POINT('Ctrl Pts',(0.131623082105364,2.94053481653771,7.06496947407595));
#68227=CARTESIAN_POINT('Ctrl Pts',(0.224654690201034,2.93341000717095,7.05991985142677));
#68228=CARTESIAN_POINT('Ctrl Pts',(0.317588294117885,2.92629270343701,7.05487554830427));
#68229=CARTESIAN_POINT('Ctrl Pts',(0.410283073450271,2.914747082221,7.04983124518177));
#68230=CARTESIAN_POINT('Ctrl Pts',(0.50228641206536,2.89880533328033,7.04478694205927));
#68231=CARTESIAN_POINT('Ctrl Pts',(0.594224989218892,2.88287480579073,7.03974618963882));
#68232=CARTESIAN_POINT('Ctrl Pts',(0.685472657454865,2.86255437701052,7.03470543721837));
#68233=CARTESIAN_POINT('Ctrl Pts',(0.775582950323216,2.83792795665569,7.02966468479792));
#68234=CARTESIAN_POINT('Ctrl Pts',(0.865661533865007,2.8133102022055,7.02462570619108));
#68235=CARTESIAN_POINT('Ctrl Pts',(0.954603109955396,2.78438958343318,7.01958672758425));
#68236=CARTESIAN_POINT('Ctrl Pts',(1.04197343392313,2.75130066750227,7.01454774897741));
#68237=CARTESIAN_POINT('Ctrl Pts',(1.12933733316328,2.71821418474617,7.00950914090904));
#68238=CARTESIAN_POINT('Ctrl Pts',(1.2151297955174,2.68096017162062,7.00447053284066));
#68239=CARTESIAN_POINT('Ctrl Pts',(1.29893479283542,2.63972203157105,6.99943192477228));
#68240=CARTESIAN_POINT('Ctrl Pts',(1.38275695515762,2.59847544509384,6.99439228469231));
#68241=CARTESIAN_POINT('Ctrl Pts',(1.46459044636346,2.55324330704513,6.98935264461233));
#68242=CARTESIAN_POINT('Ctrl Pts',(1.54404317920392,2.50425531061708,6.98431300453236));
#68243=CARTESIAN_POINT('Ctrl Pts',(1.62358232445195,2.45521403508129,6.97926788336424));
#68244=CARTESIAN_POINT('Ctrl Pts',(1.70073516526895,2.40240898096491,6.97422276219612));
#68245=CARTESIAN_POINT('Ctrl Pts',(1.77513827279761,2.34611340570935,6.969177641028));
#68246=CARTESIAN_POINT('Ctrl Pts',(1.84958755486642,2.28978289344125,6.96412938885961));
#68247=CARTESIAN_POINT('Ctrl Pts',(1.92128336616778,2.22995783118312,6.95908113669121));
#68248=CARTESIAN_POINT('Ctrl Pts',(1.9898967301173,2.16695062321883,6.95403288452282));
#68249=CARTESIAN_POINT('Ctrl Pts',(2.05861804867987,2.10384428123219,6.94897668955614));
#68250=CARTESIAN_POINT('Ctrl Pts',(2.12424692758221,2.03754611405718,6.94392049458946));
#68251=CARTESIAN_POINT('Ctrl Pts',(2.18649264911458,1.96840389538527,6.93886429962278));
#68252=CARTESIAN_POINT('Ctrl Pts',(2.21311340328578,1.93883370227314,6.93670190645043));
#68253=CARTESIAN_POINT('Ctrl Pts',(2.2391158868758,1.90874371382886,6.93453951327808));
#68254=CARTESIAN_POINT('Ctrl Pts',(2.26447976142844,1.87816277518243,6.93237712010573));
#68255=CARTESIAN_POINT('Ctrl Pts',(2.32379022052512,1.8066528208589,6.92732061615821));
#68256=CARTESIAN_POINT('Ctrl Pts',(2.3798143168841,1.73220495333977,6.9222641122107));
#68257=CARTESIAN_POINT('Ctrl Pts',(2.43224797467008,1.65515370576672,6.91720760826319));
#68258=CARTESIAN_POINT('Ctrl Pts',(2.48461027650623,1.57820731574487,6.91215798561401));
#68259=CARTESIAN_POINT('Ctrl Pts',(2.5333916024548,1.49866494975525,6.90710836296483));
#68260=CARTESIAN_POINT('Ctrl Pts',(2.5783276947571,1.41689459680265,6.90205874031565));
#68261=CARTESIAN_POINT('Ctrl Pts',(2.62321644911784,1.33521038485588,6.89701443719315));
#68262=CARTESIAN_POINT('Ctrl Pts',(2.66426780942961,1.25130323795345,6.89197013407064));
#68263=CARTESIAN_POINT('Ctrl Pts',(2.7012610825473,1.16556963065935,6.88692583094814));
#68264=CARTESIAN_POINT('Ctrl Pts',(2.73822831597478,1.07989637154176,6.88188507852769));
#68265=CARTESIAN_POINT('Ctrl Pts',(2.77114296501136,0.992399613526902,6.87684432610724));
#68266=CARTESIAN_POINT('Ctrl Pts',(2.79983099339525,0.903498980864605,6.87180357368678));
#68267=CARTESIAN_POINT('Ctrl Pts',(2.82850892661651,0.814629631855959,6.86676459507995));
#68268=CARTESIAN_POINT('Ctrl Pts',(2.85296305815076,0.72435781123335,6.86172561647312));
#68269=CARTESIAN_POINT('Ctrl Pts',(2.87306844143933,0.633120628952623,6.85668663786628));
#68270=CARTESIAN_POINT('Ctrl Pts',(2.89317234628988,0.541890155746658,6.8516480297979));
#68271=CARTESIAN_POINT('Ctrl Pts',(2.90892804364763,0.449694895068448,6.84660942172951));
#68272=CARTESIAN_POINT('Ctrl Pts',(2.92026143212223,0.35698342827003,6.84157081366113));
#68273=CARTESIAN_POINT('Ctrl Pts',(2.9315971419102,0.264252972237484,6.83653117358116));
#68274=CARTESIAN_POINT('Ctrl Pts',(2.93850869043589,0.171006540175025,6.83149153350119));
#68275=CARTESIAN_POINT('Ctrl Pts',(2.94097382184918,0.0776979999604444,
6.82645189342121));
#68276=CARTESIAN_POINT('Ctrl Pts',(2.94344163432745,-0.0157120221706676,
6.82140677225309));
#68277=CARTESIAN_POINT('Ctrl Pts',(2.94145336569045,-0.109183843454912,
6.81636165108497));
#68278=CARTESIAN_POINT('Ctrl Pts',(2.93503890530532,-0.202263749456388,
6.81131652991685));
#68279=CARTESIAN_POINT('Ctrl Pts',(2.92862046410852,-0.295401420811999,
6.80626827774845));
#68280=CARTESIAN_POINT('Ctrl Pts',(2.91777041394201,-0.388146252709685,
6.80122002558006));
#68281=CARTESIAN_POINT('Ctrl Pts',(2.90257026177326,-0.480051950802704,
6.79617177341167));
#68282=CARTESIAN_POINT('Ctrl Pts',(2.88734619405146,-0.572102251105938,
6.79111557844499));
#68283=CARTESIAN_POINT('Ctrl Pts',(2.86775845506615,-0.663310349420649,
6.78605938347831));
#68284=CARTESIAN_POINT('Ctrl Pts',(2.8439390901669,-0.753242624537838,6.78100318851163));
#68285=CARTESIAN_POINT('Ctrl Pts',(2.83375221399479,-0.791704143321829,
6.77884079533929));
#68286=CARTESIAN_POINT('Ctrl Pts',(2.82279197136707,-0.829932531189377,
6.77667840216695));
#68287=CARTESIAN_POINT('Ctrl Pts',(2.81107137944757,-0.867894981925068,
6.77451600899461));
#68288=CARTESIAN_POINT('Ctrl Pts',(2.78366414376714,-0.956665740387302,
6.7694595050471));
#68289=CARTESIAN_POINT('Ctrl Pts',(2.75199967391826,-1.04429305177003,6.76440300109959));
#68290=CARTESIAN_POINT('Ctrl Pts',(2.71619162367162,-1.13033935766926,6.75934649715208));
#68291=CARTESIAN_POINT('Ctrl Pts',(2.68043230390734,-1.21626856481658,6.7542968745029));
#68292=CARTESIAN_POINT('Ctrl Pts',(2.64054077861423,-1.30062063626899,6.74924725185372));
#68293=CARTESIAN_POINT('Ctrl Pts',(2.59668049128932,-1.38297303883968,6.74419762920454));
#68294=CARTESIAN_POINT('Ctrl Pts',(2.55286640859885,-1.46523868724418,6.73915332608204));
#68295=CARTESIAN_POINT('Ctrl Pts',(2.50509208190367,-1.54550846482934,6.73410902295954));
#68296=CARTESIAN_POINT('Ctrl Pts',(2.45356863385393,-1.62338071904534,6.72906471983704));
#68297=CARTESIAN_POINT('Ctrl Pts',(2.40208145333375,-1.70119815871788,6.72402396741659));
#68298=CARTESIAN_POINT('Ctrl Pts',(2.34685064110187,-1.77662106083995,6.71898321499614));
#68299=CARTESIAN_POINT('Ctrl Pts',(2.28813222442199,-1.84927416127562,6.71394246257569));
#68300=CARTESIAN_POINT('Ctrl Pts',(2.22943447043659,-1.92190169547669,6.70890348396885));
#68301=CARTESIAN_POINT('Ctrl Pts',(2.16725182874029,-1.99176101997443,6.70386450536202));
#68302=CARTESIAN_POINT('Ctrl Pts',(2.10188182122762,-2.05850839434598,6.69882552675519));
#68303=CARTESIAN_POINT('Ctrl Pts',(2.03651662066159,-2.12525086048699,6.69378691868681));
#68304=CARTESIAN_POINT('Ctrl Pts',(1.96796483076143,-2.18888151498805,6.68874831061843));
#68305=CARTESIAN_POINT('Ctrl Pts',(1.89656139422789,-2.24909290113245,6.68370970255004));
#68306=CARTESIAN_POINT('Ctrl Pts',(1.82514333278744,-2.30931661981936,6.67867006247007));
#68307=CARTESIAN_POINT('Ctrl Pts',(1.75087280382795,-2.36611939372584,6.6736304223901));
#68308=CARTESIAN_POINT('Ctrl Pts',(1.67411754113354,-2.41923427110087,6.66859078231013));
#68309=CARTESIAN_POINT('Ctrl Pts',(1.59727879978707,-2.47240691595937,6.66354566114201));
#68310=CARTESIAN_POINT('Ctrl Pts',(1.51795029593581,-2.52188340596303,6.65850053997389));
#68311=CARTESIAN_POINT('Ctrl Pts',(1.43652816487824,-2.5674405215139,6.65345541880577));
#68312=CARTESIAN_POINT('Ctrl Pts',(1.35505550327721,-2.6130259097933,6.64840716663738));
#68313=CARTESIAN_POINT('Ctrl Pts',(1.27148702415407,-2.65468688349036,6.64335891446899));
#68314=CARTESIAN_POINT('Ctrl Pts',(1.18624089309556,-2.69224748928248,6.6383106623006));
#68315=CARTESIAN_POINT('Ctrl Pts',(1.1008606378291,-2.72986719202646,6.63325446733392));
#68316=CARTESIAN_POINT('Ctrl Pts',(1.01379787477102,-2.76337349002297,6.62819827236724));
#68317=CARTESIAN_POINT('Ctrl Pts',(0.925487812259978,-2.79263966693848,
6.62314207740057));
#68318=CARTESIAN_POINT('Ctrl Pts',(0.88772006843628,-2.8051559922701,6.62097968422821));
#68319=CARTESIAN_POINT('Ctrl Pts',(0.849724338919268,-2.81689741875508,
6.61881729105586));
#68320=CARTESIAN_POINT('Ctrl Pts',(0.811535206197165,-2.8278568933209,6.6166548978835));
#68321=CARTESIAN_POINT('Ctrl Pts',(0.722234378378193,-2.85348434493941,
6.61159839393599));
#68322=CARTESIAN_POINT('Ctrl Pts',(0.631561434640505,-2.87492266635056,
6.60654188998847));
#68323=CARTESIAN_POINT('Ctrl Pts',(0.539944816462444,-2.89202759239523,
6.60148538604096));
#68324=CARTESIAN_POINT('Ctrl Pts',(0.448452877566457,-2.90910924067718,
6.59643576339178));
#68325=CARTESIAN_POINT('Ctrl Pts',(0.356020248495451,-2.92186913219511,
6.5913861407426));
#68326=CARTESIAN_POINT('Ctrl Pts',(0.263090035061182,-2.93021289899753,
6.58633651809342));
#68327=CARTESIAN_POINT('Ctrl Pts',(0.170257718991431,-2.93854787605601,
6.58129221497091));
#68328=CARTESIAN_POINT('Ctrl Pts',(0.0769292998126101,-2.94247593643618,
6.57624791184841));
#68329=CARTESIAN_POINT('Ctrl Pts',(-0.0164435083619719,-2.94195404638359,
6.5712036087259));
#68330=CARTESIAN_POINT('Ctrl Pts',(-0.109750591100613,-2.94143252369117,
6.56616285630545));
#68331=CARTESIAN_POINT('Ctrl Pts',(-0.20310155859628,-2.9364672792926,6.561122103885));
#68332=CARTESIAN_POINT('Ctrl Pts',(-0.296042216743756,-2.92706730464222,
6.55608135146455));
#68333=CARTESIAN_POINT('Ctrl Pts',(-0.388950169574352,-2.91767063779227,
6.55104237285771));
#68334=CARTESIAN_POINT('Ctrl Pts',(-0.48144765923277,-2.9038423857515,6.54600339425088));
#68335=CARTESIAN_POINT('Ctrl Pts',(-0.573084175815556,-2.88564352050453,
6.54096441564405));
#68336=CARTESIAN_POINT('Ctrl Pts',(-0.664713953958702,-2.86744599350087,
6.53592580757567));
#68337=CARTESIAN_POINT('Ctrl Pts',(-0.755482450113381,-2.84487857901544,
6.53088719950729));
#68338=CARTESIAN_POINT('Ctrl Pts',(-0.844949051825742,-2.81805342387592,
6.52584859143891));
#68339=CARTESIAN_POINT('Ctrl Pts',(-0.934433978156555,-2.79122277438741,
6.52080895135893));
#68340=CARTESIAN_POINT('Ctrl Pts',(-1.0226160559201,-2.76013277990829,6.51576931127896));
#68341=CARTESIAN_POINT('Ctrl Pts',(-1.10907063655849,-2.72494519635235,
6.51072967119899));
#68342=CARTESIAN_POINT('Ctrl Pts',(-1.19561924478017,-2.68971934295091,
6.50568455003086));
#68343=CARTESIAN_POINT('Ctrl Pts',(-1.28043619460545,-2.65038717280091,
6.50063942886274));
#68344=CARTESIAN_POINT('Ctrl Pts',(-1.36311790433551,-2.60715814228442,
6.49559430769461));
#68345=CARTESIAN_POINT('Ctrl Pts',(-1.44585092630306,-2.5639022838481,6.49054605552622));
#68346=CARTESIAN_POINT('Ctrl Pts',(-1.52644568770699,-2.51674497405849,
6.48549780335783));
#68347=CARTESIAN_POINT('Ctrl Pts',(-1.60452611780499,-2.46593997033213,
6.48044955118943));
#68348=CARTESIAN_POINT('Ctrl Pts',(-1.68272939776976,-2.41505503123745,
6.47539335622275));
#68349=CARTESIAN_POINT('Ctrl Pts',(-1.75841009068825,-2.36051120082445,
6.47033716125607));
#68350=CARTESIAN_POINT('Ctrl Pts',(-1.8312240151683,-2.30260344094916,6.46528096628939));
#68351=CARTESIAN_POINT('Ctrl Pts',(-1.86236449416172,-2.27783791165198,
6.46311857311706));
#68352=CARTESIAN_POINT('Ctrl Pts',(-1.89298108005343,-2.25245758017783,
6.46095617994473));
#68353=CARTESIAN_POINT('Ctrl Pts',(-1.92304894811814,-2.22648753491721,
6.45879378677239));
#68354=CARTESIAN_POINT('Ctrl Pts',(-1.99236460879073,-2.16661861301485,
6.4538088070907));
#68355=CARTESIAN_POINT('Ctrl Pts',(-2.05902051282149,-2.10338958358544,
6.44882382740901));
#68356=CARTESIAN_POINT('Ctrl Pts',(-2.12266652911026,-2.03706917069475,
6.44383884772732));
#68357=CARTESIAN_POINT('Ctrl Pts',(-2.18738886024589,-1.96962721635957,
6.43876956728409));
#68358=CARTESIAN_POINT('Ctrl Pts',(-2.24899815107245,-1.89898859804056,
6.43370028684085));
#68359=CARTESIAN_POINT('Ctrl Pts',(-2.3071601469075,-1.82547967847406,6.42863100639761));
#68360=CARTESIAN_POINT('Ctrl Pts',(-2.36421136770326,-1.75337462876876,
6.42365853883197));
#68361=CARTESIAN_POINT('Ctrl Pts',(-2.41794548947623,-1.67850830759329,
6.41868607126633));
#68362=CARTESIAN_POINT('Ctrl Pts',(-2.46808440048347,-1.60122559063055,
6.41371360370068));
#68363=CARTESIAN_POINT('Ctrl Pts',(-2.51819323891477,-1.52398922669638,
6.40874411854741));
#68364=CARTESIAN_POINT('Ctrl Pts',(-2.56471089929148,-1.44433972671108,
6.40377463339414));
#68365=CARTESIAN_POINT('Ctrl Pts',(-2.60740131820889,-1.36265269449062,
6.39880514824087));
#68366=CARTESIAN_POINT('Ctrl Pts',(-2.650078827755,-1.28099036402424,6.3938371658353));
#68367=CARTESIAN_POINT('Ctrl Pts',(-2.68893118346864,-1.19729213026207,
6.38886918342974));
#68368=CARTESIAN_POINT('Ctrl Pts',(-2.72376786861293,-1.11195890117926,
6.38390120102417));
#68369=CARTESIAN_POINT('Ctrl Pts',(-2.75983712736816,-1.02360645583439,
6.37875744402963));
#68370=CARTESIAN_POINT('Ctrl Pts',(-2.79160102499696,-0.933501625967505,
6.37361368703508));
#68371=CARTESIAN_POINT('Ctrl Pts',(-2.81890271353629,-0.842111329705131,
6.36846993004053));
#68372=CARTESIAN_POINT('Ctrl Pts',(-2.84529157772194,-0.753776642549063,
6.36349815312872));
#68373=CARTESIAN_POINT('Ctrl Pts',(-2.86751181411504,-0.664241554947752,
6.35852637621692));
#68374=CARTESIAN_POINT('Ctrl Pts',(-2.88547327196091,-0.573940760705475,
6.35355459930512));
#68375=CARTESIAN_POINT('Ctrl Pts',(-2.90436669429192,-0.47895453758905,
6.3483248522692));
#68376=CARTESIAN_POINT('Ctrl Pts',(-2.91854736623395,-0.383121572191401,
6.34309510523328));
#68377=CARTESIAN_POINT('Ctrl Pts',(-2.9279721520141,-0.286954834477387,
6.33786535819736));
#68378=CARTESIAN_POINT('Ctrl Pts',(-2.93739693779424,-0.190788096763381,
6.33263561116144));
#68379=CARTESIAN_POINT('Ctrl Pts',(-2.94206587184204,-0.0942881716709648,
6.32740586412552));
#68380=CARTESIAN_POINT('Ctrl Pts',(-2.94199929728077,0.0020334206256296,
6.3221761170896));
#68381=CARTESIAN_POINT('',(-2.94199891764675,-0.00252360166277677,5.3221761170896));
#68382=CARTESIAN_POINT('Ctrl Pts',(-2.94474230559933,0.0020353165097306,
6.3221761170896));
#68383=CARTESIAN_POINT('Ctrl Pts',(-2.94577608567865,0.132578411608025,
6.31509496994683));
#68384=CARTESIAN_POINT('Ctrl Pts',(-2.87884406698728,1.23212772485676,6.25539345243361));
#68385=CARTESIAN_POINT('Ctrl Pts',(-1.49536511544646,3.13195190828347,6.14307156455023));
#68386=CARTESIAN_POINT('Ctrl Pts',(1.803451502182,2.96526596843762,5.98521045343903));
#68387=CARTESIAN_POINT('Ctrl Pts',(3.46879199270658,0.112790494414378,5.82734934232797));
#68388=CARTESIAN_POINT('Ctrl Pts',(1.99227427239527,-2.84184496548413,5.66948823121683));
#68389=CARTESIAN_POINT('Ctrl Pts',(-1.28874579170721,-3.22247945977241,
5.51162712010572));
#68390=CARTESIAN_POINT('Ctrl Pts',(-2.83889964018183,-1.36109225107598,
5.39585641539665));
#68391=CARTESIAN_POINT('Ctrl Pts',(-2.94470393564848,-0.196954622309047,
5.33270608105794));
#68392=CARTESIAN_POINT('Ctrl Pts',(-2.94294893056736,-0.00252441656932667,
5.3221761170896));
#68393=CARTESIAN_POINT('',(-2.94157989262999,0.000541900692576724,4.32217607813505));
#68394=CARTESIAN_POINT('Ctrl Pts',(-2.94199891764675,-0.00252360166277676,
5.3221761170896));
#68395=CARTESIAN_POINT('Ctrl Pts',(-2.94207769696413,0.0893168301654653,
5.31720056856825));
#68396=CARTESIAN_POINT('Ctrl Pts',(-2.93785178601327,0.181293760433016,
5.3122250200469));
#68397=CARTESIAN_POINT('Ctrl Pts',(-2.92930951506285,0.272964768719746,
5.30724947152555));
#68398=CARTESIAN_POINT('Ctrl Pts',(-2.92077520090699,0.364550389012694,
5.30227855753494));
#68399=CARTESIAN_POINT('Ctrl Pts',(-2.9079325573502,0.455830200173258,5.29730764354433));
#68400=CARTESIAN_POINT('Ctrl Pts',(-2.89082196906571,0.546362831062912,
5.29233672955373));
#68401=CARTESIAN_POINT('Ctrl Pts',(-2.87371971674413,0.636851356125155,
5.2873682373007));
#68402=CARTESIAN_POINT('Ctrl Pts',(-2.85235373180398,0.726592974961472,
5.28239974504768));
#68403=CARTESIAN_POINT('Ctrl Pts',(-2.8268159815655,0.815153609061427,5.27743125279465));
#68404=CARTESIAN_POINT('Ctrl Pts',(-2.80128307582474,0.903697443255923,
5.27246370306198));
#68405=CARTESIAN_POINT('Ctrl Pts',(-2.77158010358642,0.991060298465522,
5.2674961533293));
#68406=CARTESIAN_POINT('Ctrl Pts',(-2.73784933610354,1.07682171820474,5.26252860359663));
#68407=CARTESIAN_POINT('Ctrl Pts',(-2.70411493295863,1.16259238171637,5.2575605184379));
#68408=CARTESIAN_POINT('Ctrl Pts',(-2.66635204186074,1.24676084220454,5.25259243327916));
#68409=CARTESIAN_POINT('Ctrl Pts',(-2.62475116418239,1.32892638100205,5.24762434812043));
#68410=CARTESIAN_POINT('Ctrl Pts',(-2.58310848034422,1.41117449078935,5.24265127036121));
#68411=CARTESIAN_POINT('Ctrl Pts',(-2.53762031987618,1.49141525350977,5.23767819260199));
#68412=CARTESIAN_POINT('Ctrl Pts',(-2.48852301719977,1.56927282295557,5.23270511484277));
#68413=CARTESIAN_POINT('Ctrl Pts',(-2.43939780754102,1.64717464676357,5.22772921037851));
#68414=CARTESIAN_POINT('Ctrl Pts',(-2.38665963665628,1.7226902083042,5.22275330591424));
#68415=CARTESIAN_POINT('Ctrl Pts',(-2.33058667000846,1.79547480449571,5.21777740144998));
#68416=CARTESIAN_POINT('Ctrl Pts',(-2.27442599553133,1.86837324839887,5.21279371380952));
#68417=CARTESIAN_POINT('Ctrl Pts',(-2.21492041233414,1.93853185555798,5.20781002616905));
#68418=CARTESIAN_POINT('Ctrl Pts',(-2.15238634144226,2.0056413032177,5.20282633852859));
#68419=CARTESIAN_POINT('Ctrl Pts',(-2.12343683716622,2.03670893106088,5.20051919164689));
#68420=CARTESIAN_POINT('Ctrl Pts',(-2.093838775635,2.06712363248387,5.1982120447652));
#68421=CARTESIAN_POINT('Ctrl Pts',(-2.0636259110797,2.096857672595,5.1959048978835));
#68422=CARTESIAN_POINT('Ctrl Pts',(-1.99740929084564,2.16202486779619,5.19084839393599));
#68423=CARTESIAN_POINT('Ctrl Pts',(-1.92798636711574,2.22416697921654,5.18579188998848));
#68424=CARTESIAN_POINT('Ctrl Pts',(-1.85566465074133,2.28295262850306,5.18073538604096));
#68425=CARTESIAN_POINT('Ctrl Pts',(-1.78344135559066,2.3416582775375,5.17568576339178));
#68426=CARTESIAN_POINT('Ctrl Pts',(-1.70832744848884,2.39701626439059,5.17063614074261));
#68427=CARTESIAN_POINT('Ctrl Pts',(-1.63066715573537,2.448732044795,5.16558651809343));
#68428=CARTESIAN_POINT('Ctrl Pts',(-1.5530886742435,2.50039334519311,5.16054221497093));
#68429=CARTESIAN_POINT('Ctrl Pts',(-1.47296950641336,2.54841982154668,5.15549791184844));
#68430=CARTESIAN_POINT('Ctrl Pts',(-1.3906859596952,2.59255791864071,5.15045360872594));
#68431=CARTESIAN_POINT('Ctrl Pts',(-1.30846033264412,2.63666494677878,5.14541285630549));
#68432=CARTESIAN_POINT('Ctrl Pts',(-1.22407374466982,2.67688882717798,5.14037210388503));
#68433=CARTESIAN_POINT('Ctrl Pts',(-1.13792953028198,2.713020527772,5.13533135146458));
#68434=CARTESIAN_POINT('Ctrl Pts',(-1.05181562957913,2.74913951381521,5.13029237285775));
#68435=CARTESIAN_POINT('Ctrl Pts',(-0.963945739747836,2.78116900973128,
5.12525339425093));
#68436=CARTESIAN_POINT('Ctrl Pts',(-0.874744785359857,2.80894741148455,
5.1202144156441));
#68437=CARTESIAN_POINT('Ctrl Pts',(-0.785550390313629,2.83672377056874,
5.11517580757571));
#68438=CARTESIAN_POINT('Ctrl Pts',(-0.695025548731039,2.86024952554517,
5.11013719950733));
#68439=CARTESIAN_POINT('Ctrl Pts',(-0.603610931679016,2.87941276012273,
5.10509859143894));
#68440=CARTESIAN_POINT('Ctrl Pts',(-0.512177591014646,2.89857991972877,
5.10005895135896));
#68441=CARTESIAN_POINT('Ctrl Pts',(-0.41985454688234,2.91338269371054,5.09501931127899));
#68442=CARTESIAN_POINT('Ctrl Pts',(-0.32709213922869,2.92376037534795,5.08997967119902));
#68443=CARTESIAN_POINT('Ctrl Pts',(-0.234228843629678,2.93414934370166,
5.08493455003089));
#68444=CARTESIAN_POINT('Ctrl Pts',(-0.140925671965079,2.94010356436376,
5.07988942886277));
#68445=CARTESIAN_POINT('Ctrl Pts',(-0.0476372381735444,2.94161430060761,
5.07484430769465));
#68446=CARTESIAN_POINT('Ctrl Pts',(0.0457090903843088,2.9431259744138,5.06979605552626));
#68447=CARTESIAN_POINT('Ctrl Pts',(0.139040220126571,2.94018868767891,5.06474780335787));
#68448=CARTESIAN_POINT('Ctrl Pts',(0.231904548328501,2.93284576486125,5.05969955118948));
#68449=CARTESIAN_POINT('Ctrl Pts',(0.32491498702623,2.9254912888658,5.0546433562228));
#68450=CARTESIAN_POINT('Ctrl Pts',(0.417456719041778,2.91371739603875,5.04958716125613));
#68451=CARTESIAN_POINT('Ctrl Pts',(0.509086478569261,2.89761884265994,5.04453096628945));
#68452=CARTESIAN_POINT('Ctrl Pts',(0.548273963959443,2.89073394163447,5.04236857311709));
#68453=CARTESIAN_POINT('Ctrl Pts',(0.587294815183116,2.88305867439424,5.04020617994474));
#68454=CARTESIAN_POINT('Ctrl Pts',(0.62611523936405,2.87460322601852,5.03804378677239));
#68455=CARTESIAN_POINT('Ctrl Pts',(0.716892268547699,2.85483114726983,5.03298728282492));
#68456=CARTESIAN_POINT('Ctrl Pts',(0.80689139748673,2.83072013026423,5.02793077887745));
#68457=CARTESIAN_POINT('Ctrl Pts',(0.895666998751246,2.80234627184935,5.02287427492999));
#68458=CARTESIAN_POINT('Ctrl Pts',(0.984321787018764,2.77401102686904,5.01782465228084));
#68459=CARTESIAN_POINT('Ctrl Pts',(1.0717559377579,2.74142460281036,5.0127750296317));
#68460=CARTESIAN_POINT('Ctrl Pts',(1.15753456760308,2.70471398206981,5.00772540698256));
#68461=CARTESIAN_POINT('Ctrl Pts',(1.24322283392177,2.66804203414504,5.00268110386009));
#68462=CARTESIAN_POINT('Ctrl Pts',(1.3272586405576,2.6272546992518,4.99763680073763));
#68463=CARTESIAN_POINT('Ctrl Pts',(1.40922386166798,2.58252823947882,4.99259249761517));
#68464=CARTESIAN_POINT('Ctrl Pts',(1.49113138718159,2.53783326281237,4.98755174519476));
#68465=CARTESIAN_POINT('Ctrl Pts',(1.5709708361648,2.48920488457255,4.98251099277435));
#68466=CARTESIAN_POINT('Ctrl Pts',(1.64834656373636,2.43686634960117,4.97747024035394));
#68467=CARTESIAN_POINT('Ctrl Pts',(1.72569506320627,2.38454623227826,4.97243126174715));
#68468=CARTESIAN_POINT('Ctrl Pts',(1.80058119686232,2.32851880030492,4.96739228314035));
#68469=CARTESIAN_POINT('Ctrl Pts',(1.87263720703598,2.26905131956606,4.96235330453356));
#68470=CARTESIAN_POINT('Ctrl Pts',(1.94468791861156,2.20958821173488,4.95731469646522));
#68471=CARTESIAN_POINT('Ctrl Pts',(2.01390857877139,2.14668584057405,4.95227608839688));
#68472=CARTESIAN_POINT('Ctrl Pts',(2.07996440571687,2.08065183799474,4.94723748032854));
#68473=CARTESIAN_POINT('Ctrl Pts',(2.14603376226782,2.01460431028003,4.94219784024861));
#68474=CARTESIAN_POINT('Ctrl Pts',(2.20893668492199,1.94542419090428,4.93715820016867));
#68475=CARTESIAN_POINT('Ctrl Pts',(2.26837596681243,1.87345522316061,4.93211856008874));
#68476=CARTESIAN_POINT('Ctrl Pts',(2.32787989457801,1.80140798231614,4.92707343892066));
#68477=CARTESIAN_POINT('Ctrl Pts',(2.3839123799885,1.72656618139609,4.92202831775258));
#68478=CARTESIAN_POINT('Ctrl Pts',(2.43621737929887,1.64930557532622,4.91698319658449));
#68479=CARTESIAN_POINT('Ctrl Pts',(2.48855483907183,1.57199702135372,4.91193494441614));
#68480=CARTESIAN_POINT('Ctrl Pts',(2.53715997675792,1.49226705193994,4.90688669224779));
#68481=CARTESIAN_POINT('Ctrl Pts',(2.58182197398437,1.41051738544814,4.90183844007944));
#68482=CARTESIAN_POINT('Ctrl Pts',(2.62655424132081,1.32863909600141,4.8967822451128));
#68483=CARTESIAN_POINT('Ctrl Pts',(2.66733079065861,1.2447351643849,4.89172605014616));
#68484=CARTESIAN_POINT('Ctrl Pts',(2.70398841601454,1.1592284701728,4.88666985517952));
#68485=CARTESIAN_POINT('Ctrl Pts',(2.71966585711833,1.12265964855726,4.88450746200678));
#68486=CARTESIAN_POINT('Ctrl Pts',(2.73459055174711,1.08579787909022,4.88234506883403));
#68487=CARTESIAN_POINT('Ctrl Pts',(2.74875253640259,1.04867702064093,4.88018267566128));
#68488=CARTESIAN_POINT('Ctrl Pts',(2.78186868392787,0.961874227488885,4.87512617171368));
#68489=CARTESIAN_POINT('Ctrl Pts',(2.81092731058382,0.873348634759145,4.87006966776607));
#68490=CARTESIAN_POINT('Ctrl Pts',(2.83574829938907,0.783514889783219,4.86501316381847));
#68491=CARTESIAN_POINT('Ctrl Pts',(2.86053550979112,0.693803397811868,4.85996354116921));
#68492=CARTESIAN_POINT('Ctrl Pts',(2.88109642557836,0.602787715147935,4.85491391851994));
#68493=CARTESIAN_POINT('Ctrl Pts',(2.89729940191038,0.510901336551127,4.84986429587068));
#68494=CARTESIAN_POINT('Ctrl Pts',(2.91348530921158,0.419111755690579,4.84481999274808));
#68495=CARTESIAN_POINT('Ctrl Pts',(2.92532232610127,0.326453736522251,4.83977568962548));
#68496=CARTESIAN_POINT('Ctrl Pts',(2.93272922581001,0.233373709058706,4.83473138650289));
#68497=CARTESIAN_POINT('Ctrl Pts',(2.94013091177696,0.140359200941705,4.82969063408234));
#68498=CARTESIAN_POINT('Ctrl Pts',(2.94310864399567,0.0469237157370147,
4.8246498816618));
#68499=CARTESIAN_POINT('Ctrl Pts',(2.94163282254895,-0.0464794288120706,
4.81960912924125));
#68500=CARTESIAN_POINT('Ctrl Pts',(2.94015752043585,-0.139849705297845,
4.81457015063433));
#68501=CARTESIAN_POINT('Ctrl Pts',(2.93423178530535,-0.233187220858687,
4.8095311720274));
#68502=CARTESIAN_POINT('Ctrl Pts',(2.92387812288593,-0.326037915753797,
4.80449219342047));
#68503=CARTESIAN_POINT('Ctrl Pts',(2.91352522181726,-0.418881782925141,
4.79945358535201));
#68504=CARTESIAN_POINT('Ctrl Pts',(2.89874509033896,-0.511238460022593,
4.79441497728354));
#68505=CARTESIAN_POINT('Ctrl Pts',(2.87961206452165,-0.602659404524128,
4.78937636921508));
#68506=CARTESIAN_POINT('Ctrl Pts',(2.8604751198631,-0.694099073934688,4.78433672913499));
#68507=CARTESIAN_POINT('Ctrl Pts',(2.83698360132016,-0.784602196269378,
4.7792970890549));
#68508=CARTESIAN_POINT('Ctrl Pts',(2.80926263021356,-0.873731923696038,
4.77425744897481));
#68509=CARTESIAN_POINT('Ctrl Pts',(2.7815115099132,-0.962958588182086,4.7692123278066));
#68510=CARTESIAN_POINT('Ctrl Pts',(2.74952188761334,-1.05080845244922,4.7641672066384));
#68511=CARTESIAN_POINT('Ctrl Pts',(2.71346820137455,-1.13686160992847,4.75912208547019));
#68512=CARTESIAN_POINT('Ctrl Pts',(2.67739214023187,-1.22296817196435,4.75407383330172));
#68513=CARTESIAN_POINT('Ctrl Pts',(2.6372471843141,-1.30727540740105,4.74902558113325));
#68514=CARTESIAN_POINT('Ctrl Pts',(2.59325424833327,-1.38938706036202,4.74397732896477));
#68515=CARTESIAN_POINT('Ctrl Pts',(2.5491920949273,-1.47162790581872,4.73892113399801));
#68516=CARTESIAN_POINT('Ctrl Pts',(2.50127010362758,-1.55166589346778,4.73386493903125));
#68517=CARTESIAN_POINT('Ctrl Pts',(2.44975295208641,-1.62913304359832,4.72880874406449));
#68518=CARTESIAN_POINT('Ctrl Pts',(2.42772050724658,-1.66226357704378,4.72664635089305));
#68519=CARTESIAN_POINT('Ctrl Pts',(2.4050310037142,-1.69492430247281,4.72448395772161));
#68520=CARTESIAN_POINT('Ctrl Pts',(2.38170733180708,-1.72708835489572,4.72232156455017));
#68521=CARTESIAN_POINT('Ctrl Pts',(2.32716764835563,-1.80230023596858,4.7172650606027));
#68522=CARTESIAN_POINT('Ctrl Pts',(2.26896592277806,-1.87505835229019,4.71220855665523));
#68523=CARTESIAN_POINT('Ctrl Pts',(2.20735068949027,-1.94498507284936,4.70715205270776));
#68524=CARTESIAN_POINT('Ctrl Pts',(2.14581930718074,-2.01481663148815,4.70210243005863));
#68525=CARTESIAN_POINT('Ctrl Pts',(2.08088393935117,-2.08182412176524,4.6970528074095));
#68526=CARTESIAN_POINT('Ctrl Pts',(2.01283541699537,-2.1456601744193,4.69200318476036));
#68527=CARTESIAN_POINT('Ctrl Pts',(1.94485858037865,-2.20942897896193,4.68695888163793));
#68528=CARTESIAN_POINT('Ctrl Pts',(1.87377542994107,-2.2700326851886,4.6819145785155));
#68529=CARTESIAN_POINT('Ctrl Pts',(1.79991520912955,-2.32715904912924,4.67687027539307));
#68530=CARTESIAN_POINT('Ctrl Pts',(1.72610697877716,-2.38424520162919,4.67182952297266));
#68531=CARTESIAN_POINT('Ctrl Pts',(1.64952591339223,-2.43785860675055,4.66678877055225));
#68532=CARTESIAN_POINT('Ctrl Pts',(1.57053526814548,-2.48772646637672,4.66174801813184));
#68533=CARTESIAN_POINT('Ctrl Pts',(1.49157241928116,-2.5375767777718,4.65670903952505));
#68534=CARTESIAN_POINT('Ctrl Pts',(1.41020204972646,-2.58368392587307,4.65167006091826));
#68535=CARTESIAN_POINT('Ctrl Pts',(1.32681654404416,-2.62581832167626,4.64663108231146));
#68536=CARTESIAN_POINT('Ctrl Pts',(1.24343717006805,-2.66794961915038,4.64159247424312));
#68537=CARTESIAN_POINT('Ctrl Pts',(1.15804335045787,-2.70610854553738,4.63655386617478));
#68538=CARTESIAN_POINT('Ctrl Pts',(1.07105120926042,-2.74011191507606,4.63151525810644));
#68539=CARTESIAN_POINT('Ctrl Pts',(0.984041250265262,-2.77412224921122,
4.6264756180265));
#68540=CARTESIAN_POINT('Ctrl Pts',(0.895432732522731,-2.80397517501077,
4.62143597794655));
#68541=CARTESIAN_POINT('Ctrl Pts',(0.805659776909909,-2.82953641501032,
4.6163963378666));
#68542=CARTESIAN_POINT('Ctrl Pts',(0.715789184665435,-2.85512545529068,
4.61135121669852));
#68543=CARTESIAN_POINT('Ctrl Pts',(0.624752053796445,-2.87641337180181,
4.60630609553044));
#68544=CARTESIAN_POINT('Ctrl Pts',(0.532995306902624,-2.89331643668987,
4.60126097436235));
#68545=CARTESIAN_POINT('Ctrl Pts',(0.441181615806447,-2.9102299916136,4.59621272219398));
#68546=CARTESIAN_POINT('Ctrl Pts',(0.348647858529523,-2.92275321789415,
4.59116447002561));
#68547=CARTESIAN_POINT('Ctrl Pts',(0.25584658937695,-2.93085423088631,4.58611621785724));
#68548=CARTESIAN_POINT('Ctrl Pts',(0.162899308944509,-2.93896798981703,
4.5810600228906));
#68549=CARTESIAN_POINT('Ctrl Pts',(0.0696841187437275,-2.9426456293354,
4.57600382792396));
#68550=CARTESIAN_POINT('Ctrl Pts',(-0.0233461517107244,-2.94190736720249,
4.57094763295732));
#68551=CARTESIAN_POINT('Ctrl Pts',(-0.0631325964616277,-2.94159163313638,
4.56878523978457));
#68552=CARTESIAN_POINT('Ctrl Pts',(-0.102885281238585,-2.94046886377766,
4.56662284661181));
#68553=CARTESIAN_POINT('Ctrl Pts',(-0.142569194812085,-2.93854352097951,
4.56446045343906));
#68554=CARTESIAN_POINT('Ctrl Pts',(-0.235365393096446,-2.93404133165457,
4.55940394949179));
#68555=CARTESIAN_POINT('Ctrl Pts',(-0.328111260252495,-2.92513131057668,
4.55434744554452));
#68556=CARTESIAN_POINT('Ctrl Pts',(-0.420354720504467,-2.91181488232848,
4.54929094159725));
#68557=CARTESIAN_POINT('Ctrl Pts',(-0.512472648416987,-2.8985165761497,
4.54424131894832));
#68558=CARTESIAN_POINT('Ctrl Pts',(-0.604089093004346,-2.88082384236276,
4.53919169629939));
#68559=CARTESIAN_POINT('Ctrl Pts',(-0.69475416759977,-2.85879006689941,
4.53414207365046));
#68560=CARTESIAN_POINT('Ctrl Pts',(-0.785323731042124,-2.83677950292417,
4.5290977705282));
#68561=CARTESIAN_POINT('Ctrl Pts',(-0.874943488094165,-2.81043709168458,
4.52405346740593));
#68562=CARTESIAN_POINT('Ctrl Pts',(-0.9631719373317,-2.77986759021661,4.51900916428366));
#68563=CARTESIAN_POINT('Ctrl Pts',(-1.0513382822649,-2.74931960672429,4.51396841186346));
#68564=CARTESIAN_POINT('Ctrl Pts',(-1.13811484829377,-2.71455059218884,
4.50892765944325));
#68565=CARTESIAN_POINT('Ctrl Pts',(-1.22307454351632,-2.67571535500366,
4.50388690702304));
#68566=CARTESIAN_POINT('Ctrl Pts',(-1.30800434187964,-2.63689378372931,
4.49884792841646));
#68567=CARTESIAN_POINT('Ctrl Pts',(-1.39111813683626,-2.59400901679853,
4.49380894980989));
#68568=CARTESIAN_POINT('Ctrl Pts',(-1.47200906729136,-2.54726388617513,
4.48876997120331));
#68569=CARTESIAN_POINT('Ctrl Pts',(-1.5528940494777,-2.50052219292843,4.48373136313517));
#68570=CARTESIAN_POINT('Ctrl Pts',(-1.63155610846921,-2.44992092253735,
4.47869275506703));
#68571=CARTESIAN_POINT('Ctrl Pts',(-1.70761423658196,-2.39570816649746,
4.47365414699889));
#68572=CARTESIAN_POINT('Ctrl Pts',(-1.783687942979,-2.34148430655918,4.46861450691918));
#68573=CARTESIAN_POINT('Ctrl Pts',(-1.85715629846442,-2.28364774946203,
4.46357486683946));
#68574=CARTESIAN_POINT('Ctrl Pts',(-1.92766938757211,-2.22248840991744,
4.45853522675974));
#68575=CARTESIAN_POINT('Ctrl Pts',(-1.99825916637435,-2.16126255377108,
4.45349010559186));
#68576=CARTESIAN_POINT('Ctrl Pts',(-2.06588692811334,-2.09670699298994,
4.44844498442397));
#68577=CARTESIAN_POINT('Ctrl Pts',(-2.1302380657774,-2.02915001493555,4.44339986325609));
#68578=CARTESIAN_POINT('Ctrl Pts',(-2.1946291397329,-1.9615511110464,4.43835161108794));
#68579=CARTESIAN_POINT('Ctrl Pts',(-2.25573925136043,-1.89094741646589,
4.43330335891978));
#68580=CARTESIAN_POINT('Ctrl Pts',(-2.31329410780585,-1.81770029729621,
4.42825510675163));
#68581=CARTESIAN_POINT('Ctrl Pts',(-2.37093951967525,-1.74433793287459,
4.42319891178519));
#68582=CARTESIAN_POINT('Ctrl Pts',(-2.42501825392597,-1.668324202419,4.41814271681874));
#68583=CARTESIAN_POINT('Ctrl Pts',(-2.47529947949604,-1.59004920892613,
4.4130865218523));
#68584=CARTESIAN_POINT('Ctrl Pts',(-2.49680335340005,-1.55657318341515,
4.41092412867752));
#68585=CARTESIAN_POINT('Ctrl Pts',(-2.51761322675657,-1.52268386751969,
4.40876173550273));
#68586=CARTESIAN_POINT('Ctrl Pts',(-2.53771367884418,-1.48841300861257,
4.40659934232795));
#68587=CARTESIAN_POINT('Ctrl Pts',(-2.58640672226634,-1.40539236740483,
4.40136097732518));
#68588=CARTESIAN_POINT('Ctrl Pts',(-2.63109406438861,-1.3198572950255,4.39612261232242));
#68589=CARTESIAN_POINT('Ctrl Pts',(-2.67151824800373,-1.23221518030865,
4.39088424731965));
#68590=CARTESIAN_POINT('Ctrl Pts',(-2.71187342478902,-1.14472267664032,
4.3856548245621));
#68591=CARTESIAN_POINT('Ctrl Pts',(-2.74797975873238,-1.05513064776356,
4.38042540180455));
#68592=CARTESIAN_POINT('Ctrl Pts',(-2.77962473008703,-0.963872584882775,
4.37519597904699));
#68593=CARTESIAN_POINT('Ctrl Pts',(-2.81120685140212,-0.872795769530967,
4.36997694243969));
#68594=CARTESIAN_POINT('Ctrl Pts',(-2.83834513170718,-0.780059886798695,
4.36475790583239));
#68595=CARTESIAN_POINT('Ctrl Pts',(-2.86087486123827,-0.68611881502761,
4.35953886922509));
#68596=CARTESIAN_POINT('Ctrl Pts',(-2.88337783884318,-0.592289289407769,
4.35432602973089));
#68597=CARTESIAN_POINT('Ctrl Pts',(-2.90128305986531,-0.497257807785013,
4.34911319023669));
#68598=CARTESIAN_POINT('Ctrl Pts',(-2.91447533446412,-0.401494115523807,
4.34390035074249));
#68599=CARTESIAN_POINT('Ctrl Pts',(-2.92765073378575,-0.30585292214167,
4.33869417940174));
#68600=CARTESIAN_POINT('Ctrl Pts',(-2.9361251402031,-0.209481777646127,
4.33348800806098));
#68601=CARTESIAN_POINT('Ctrl Pts',(-2.93983444014366,-0.112860376329525,
4.32828183672023));
#68602=CARTESIAN_POINT('Ctrl Pts',(-2.94128451058126,-0.0750883331045788,
4.32624659684335));
#68603=CARTESIAN_POINT('Ctrl Pts',(-2.94200690804472,-0.0372781398498132,
4.32421135696648));
#68604=CARTESIAN_POINT('Ctrl Pts',(-2.94199995021121,0.000541255242094748,
4.3221761170896));
#68605=CARTESIAN_POINT('',(-2.94484294150901,0.00199174253909633,3.3221761170896));
#68606=CARTESIAN_POINT('Ctrl Pts',(-2.93739244246854,0.000548335028833932,
4.32217568980677));
#68607=CARTESIAN_POINT('Ctrl Pts',(-2.93814515251413,0.454714538465635,
4.29769653694346));
#68608=CARTESIAN_POINT('Ctrl Pts',(-2.62620581469539,1.88417429984043,4.22059701370977));
#68609=CARTESIAN_POINT('Ctrl Pts',(-0.406867188726433,3.44669387613551,
4.09087712010572));
#68610=CARTESIAN_POINT('Ctrl Pts',(2.66245099976357,2.22634100195606,3.93301600899463));
#68611=CARTESIAN_POINT('Ctrl Pts',(3.32025430017048,-1.01052014634335,3.77515489788349));
#68612=CARTESIAN_POINT('Ctrl Pts',(0.970737398643962,-3.33210271331847,
3.6172937867724));
#68613=CARTESIAN_POINT('Ctrl Pts',(-2.11754863214004,-2.66593520061748,
3.46630085984108));
#68614=CARTESIAN_POINT('Ctrl Pts',(-2.93826750108625,-0.841388295482023,
3.36792830328016));
#68615=CARTESIAN_POINT('Ctrl Pts',(-2.94484294150901,0.00199174253909633,
3.3221761170896));
#68616=CARTESIAN_POINT('',(-2.9419989036421,-0.00253987572311715,2.3221761170896));
#68617=CARTESIAN_POINT('Ctrl Pts',(-2.94484294150901,0.00199174253909633,
3.3221761170896));
#68618=CARTESIAN_POINT('Ctrl Pts',(-2.94583002736539,0.128597483532049,
3.31530793290979));
#68619=CARTESIAN_POINT('Ctrl Pts',(-2.88115833278038,1.22417398585304,3.25581937835959));
#68620=CARTESIAN_POINT('Ctrl Pts',(-1.50792549309295,3.12592391504645,3.14371045343908));
#68621=CARTESIAN_POINT('Ctrl Pts',(1.79153366111829,2.97248156539303,2.98584934232795));
#68622=CARTESIAN_POINT('Ctrl Pts',(3.46831127903085,0.126714191662369,2.82798823121682));
#68623=CARTESIAN_POINT('Ctrl Pts',(2.00366607964191,-2.83382462640087,2.67012712010574));
#68624=CARTESIAN_POINT('Ctrl Pts',(-1.2757995679391,-3.22762676650926,2.5122660089946));
#68625=CARTESIAN_POINT('Ctrl Pts',(-2.83627828908289,-1.36906481860164,
2.39628234132257));
#68626=CARTESIAN_POINT('Ctrl Pts',(-2.94462630681883,-0.200923340849699,
2.3329190440209));
#68627=CARTESIAN_POINT('Ctrl Pts',(-2.94283216929169,-0.00254059509496668,
2.3221761170896));
#68628=CARTESIAN_POINT('',(-2.94155351776559,0.000606762388042248,1.32217607092416));
#68629=CARTESIAN_POINT('Ctrl Pts',(-2.9419989036421,-0.00253987572311715,
2.3221761170896));
#68630=CARTESIAN_POINT('Ctrl Pts',(-2.94208233219418,0.0940974150397186,
2.31694143665972));
#68631=CARTESIAN_POINT('Ctrl Pts',(-2.93739914386076,0.190883610583203,
2.31170675622983));
#68632=CARTESIAN_POINT('Ctrl Pts',(-2.92793797328572,0.287303366829364,
2.30647207579995));
#68633=CARTESIAN_POINT('Ctrl Pts',(-2.91895287204066,0.378871451880253,
2.30150079520893));
#68634=CARTESIAN_POINT('Ctrl Pts',(-2.90565898929855,0.470108555172867,
2.2965295146179));
#68635=CARTESIAN_POINT('Ctrl Pts',(-2.88809996570594,0.560573445758306,
2.29155823402688));
#68636=CARTESIAN_POINT('Ctrl Pts',(-2.87054897094082,0.650996971458291,
2.28658922654369));
#68637=CARTESIAN_POINT('Ctrl Pts',(-2.84873679368341,0.740648537302737,
2.28162021906051));
#68638=CARTESIAN_POINT('Ctrl Pts',(-2.82275860045843,0.829094616758536,
2.27665121157733));
#68639=CARTESIAN_POINT('Ctrl Pts',(-2.79678456174355,0.917526551653617,
2.27168299875264));
#68640=CARTESIAN_POINT('Ctrl Pts',(-2.7666459596833,1.00475294463453,2.26671478592795));
#68641=CARTESIAN_POINT('Ctrl Pts',(-2.73248815572983,1.09035429049287,2.26174657310326));
#68642=CARTESIAN_POINT('Ctrl Pts',(-2.69832565821172,1.17596739868377,2.25677767760505));
#68643=CARTESIAN_POINT('Ctrl Pts',(-2.66014303362448,1.25995459257028,2.25180878210685));
#68644=CARTESIAN_POINT('Ctrl Pts',(-2.61813371460277,1.34191648490519,2.24683988660865));
#68645=CARTESIAN_POINT('Ctrl Pts',(-2.5760814180424,1.42396222816838,2.24186590769316));
#68646=CARTESIAN_POINT('Ctrl Pts',(-2.53019482458214,1.50397812834879,2.23689192877767));
#68647=CARTESIAN_POINT('Ctrl Pts',(-2.48071299062712,1.58159004110859,2.23191794986219));
#68648=CARTESIAN_POINT('Ctrl Pts',(-2.43120173070495,1.6592481082934,2.22694101300985));
#68649=CARTESIAN_POINT('Ctrl Pts',(-2.37809124117542,1.73449897176268,2.22196407615751));
#68650=CARTESIAN_POINT('Ctrl Pts',(-2.32166215487591,1.80699995534503,2.21698713930517));
#68651=CARTESIAN_POINT('Ctrl Pts',(-2.26514624234863,1.87961249463965,2.21200254454658));
#68652=CARTESIAN_POINT('Ctrl Pts',(-2.20530184332275,1.94946636739178,2.20701794978799));
#68653=CARTESIAN_POINT('Ctrl Pts',(-2.14244750736819,2.01625461640435,2.2020333550294));
#68654=CARTESIAN_POINT('Ctrl Pts',(-2.1193735375216,2.04077273469195,2.20020349894373));
#68655=CARTESIAN_POINT('Ctrl Pts',(-2.09589426644895,2.06487810247725,2.19837364285806));
#68656=CARTESIAN_POINT('Ctrl Pts',(-2.07202654684849,2.08855691546942,2.19654378677239));
#68657=CARTESIAN_POINT('Ctrl Pts',(-2.00607205389579,2.15398939627457,2.19148728232508));
#68658=CARTESIAN_POINT('Ctrl Pts',(-1.93689913945909,2.21640968854567,2.18643077787778));
#68659=CARTESIAN_POINT('Ctrl Pts',(-1.86481398163189,2.27548518208979,2.18137427343047));
#68660=CARTESIAN_POINT('Ctrl Pts',(-1.79282692342056,2.33448028067608,2.17632465030463));
#68661=CARTESIAN_POINT('Ctrl Pts',(-1.71793583779818,2.39013934760752,2.17127502717879));
#68662=CARTESIAN_POINT('Ctrl Pts',(-1.64048376588073,2.44216645908541,2.16622540405295));
#68663=CARTESIAN_POINT('Ctrl Pts',(-1.56311328622637,2.49413876234885,2.16118110047724));
#68664=CARTESIAN_POINT('Ctrl Pts',(-1.48318754920317,2.54248646965816,2.15613679690152));
#68665=CARTESIAN_POINT('Ctrl Pts',(-1.40108184137037,2.58695451714602,2.1510924933258));
#68666=CARTESIAN_POINT('Ctrl Pts',(-1.3190339286073,2.63139126310842,2.14605174048833));
#68667=CARTESIAN_POINT('Ctrl Pts',(-1.23480948400394,2.67195356706271,2.14101098765085));
#68668=CARTESIAN_POINT('Ctrl Pts',(-1.14881099969759,2.70843077943185,2.13597023481338));
#68669=CARTESIAN_POINT('Ctrl Pts',(-1.06284277817821,2.74489515550375,2.13093125581216));
#68670=CARTESIAN_POINT('Ctrl Pts',(-0.975102165040744,2.77727712311088,
2.12589227681094));
#68671=CARTESIAN_POINT('Ctrl Pts',(-0.886013432712717,2.80541337364971,
2.12085329780972));
#68672=CARTESIAN_POINT('Ctrl Pts',(-0.796931251880015,2.83354755507711,
2.11581468936992));
#68673=CARTESIAN_POINT('Ctrl Pts',(-0.706501571851507,2.85743650704494,
2.11077608093013));
#68674=CARTESIAN_POINT('Ctrl Pts',(-0.615164610897789,2.87696654507816,
2.10573747249033));
#68675=CARTESIAN_POINT('Ctrl Pts',(-0.523808942661735,2.89650058317808,
2.10069783206228));
#68676=CARTESIAN_POINT('Ctrl Pts',(-0.431546058022076,2.91167384188408,
2.09565819163423));
#68677=CARTESIAN_POINT('Ctrl Pts',(-0.338826049636303,2.92242380706287,
2.09061855120618));
#68678=CARTESIAN_POINT('Ctrl Pts',(-0.246005200103549,2.9331854637723,2.08557342972685));
#68679=CARTESIAN_POINT('Ctrl Pts',(-0.152726675531535,2.93951417380657,
2.08052830824751));
#68680=CARTESIAN_POINT('Ctrl Pts',(-0.0594450511706656,2.94139937544892,
2.07548318676818));
#68681=CARTESIAN_POINT('Ctrl Pts',(0.0338944633452301,2.94328574703891,
2.07043493430923));
#68682=CARTESIAN_POINT('Ctrl Pts',(0.127236638694068,2.94072313234364,2.06538668185028));
#68683=CARTESIAN_POINT('Ctrl Pts',(0.220129701808395,2.93375304250064,2.06033842939132));
#68684=CARTESIAN_POINT('Ctrl Pts',(0.313168919995696,2.92677198613381,2.05528223416806));
#68685=CARTESIAN_POINT('Ctrl Pts',(0.405757176148202,2.91536966639149,2.0502260389448));
#68686=CARTESIAN_POINT('Ctrl Pts',(0.497450827572616,2.89963905928778,2.04516984372153));
#68687=CARTESIAN_POINT('Ctrl Pts',(0.536665566494046,2.89291153081591,2.04300745436812));
#68688=CARTESIAN_POINT('Ctrl Pts',(0.575716845939192,2.8853929763205,2.0408450650147));
#68689=CARTESIAN_POINT('Ctrl Pts',(0.614570832594503,2.87709344508031,2.03868267566128));
#68690=CARTESIAN_POINT('Ctrl Pts',(0.705426662090724,2.85768589233814,2.03362616292447));
#68691=CARTESIAN_POINT('Ctrl Pts',(0.795522008345901,2.8339362990504,2.02856965018766));
#68692=CARTESIAN_POINT('Ctrl Pts',(0.884410940870408,2.80591897382457,2.02351313745085));
#68693=CARTESIAN_POINT('Ctrl Pts',(0.973178907124536,2.77793977653258,2.01846350596989));
#68694=CARTESIAN_POINT('Ctrl Pts',(1.0607433029531,2.74570452108668,2.01341387448892));
#68695=CARTESIAN_POINT('Ctrl Pts',(1.14666873770656,2.70933844433774,2.00836424300796));
#68696=CARTESIAN_POINT('Ctrl Pts',(1.2325036549473,2.67301067716296,2.00331993102388));
#68697=CARTESIAN_POINT('Ctrl Pts',(1.31670263693068,2.63256091057823,1.99827561903979));
#68698=CARTESIAN_POINT('Ctrl Pts',(1.3988468526778,2.58816372796495,1.99323130705571));
#68699=CARTESIAN_POINT('Ctrl Pts',(1.48093324704763,2.543797796563,1.98819054576675));
#68700=CARTESIAN_POINT('Ctrl Pts',(1.56096736118657,2.49549018245944,1.98314978447779));
#68701=CARTESIAN_POINT('Ctrl Pts',(1.63855265637552,2.44346254161686,1.97810902318883));
#68702=CARTESIAN_POINT('Ctrl Pts',(1.7161106497743,2.39145320898243,1.97307003571289));
#68703=CARTESIAN_POINT('Ctrl Pts',(1.79122116840698,2.33572669710995,1.96803104823695));
#68704=CARTESIAN_POINT('Ctrl Pts',(1.8635153838847,2.27654879456274,1.96299206076102));
#68705=CARTESIAN_POINT('Ctrl Pts',(1.93580428310543,2.21737524374596,1.95795344383412));
#68706=CARTESIAN_POINT('Ctrl Pts',(2.00527694809872,2.15475108798733,1.95291482690723));
#68707=CARTESIAN_POINT('Ctrl Pts',(2.07159736407132,2.08898261389911,1.94787620998034));
#68708=CARTESIAN_POINT('Ctrl Pts',(2.13793136353176,2.02320066936963,1.94283656106366));
#68709=CARTESIAN_POINT('Ctrl Pts',(2.20111151718236,1.9542734398753,1.93779691214698));
#68710=CARTESIAN_POINT('Ctrl Pts',(2.26083923990971,1.88254347394277,1.9327572632303));
#68711=CARTESIAN_POINT('Ctrl Pts',(2.32063192108609,1.81073549620727,1.92771213331147));
#68712=CARTESIAN_POINT('Ctrl Pts',(2.37696439284234,1.73611903914493,1.92266700339263));
#68713=CARTESIAN_POINT('Ctrl Pts',(2.42957910435542,1.65906882789097,1.91762187347379));
#68714=CARTESIAN_POINT('Ctrl Pts',(2.48222646809696,1.58197079995174,1.91257361259158));
#68715=CARTESIAN_POINT('Ctrl Pts',(2.53115124617158,1.50243638816991,1.90752535170937));
#68716=CARTESIAN_POINT('Ctrl Pts',(2.57614100852258,1.42086646248276,1.90247709082716));
#68717=CARTESIAN_POINT('Ctrl Pts',(2.6212015553242,1.33916819910108,1.89742088728523));
#68718=CARTESIAN_POINT('Ctrl Pts',(2.66231453302157,1.25542842638829,1.8923646837433));
#68719=CARTESIAN_POINT('Ctrl Pts',(2.69931503860233,1.17006936648016,1.88730848020137));
#68720=CARTESIAN_POINT('Ctrl Pts',(2.71513844950498,1.13356523071256,1.8851461749843));
#68721=CARTESIAN_POINT('Ctrl Pts',(2.73021035688101,1.0967651522541,1.88298386976724));
#68722=CARTESIAN_POINT('Ctrl Pts',(2.74452066257809,1.05970294549083,1.88082156455017));
#68723=CARTESIAN_POINT('Ctrl Pts',(2.77798486904029,0.973034123361867,1.87576508079993));
#68724=CARTESIAN_POINT('Ctrl Pts',(2.80739853700098,0.884626233625418,1.8707085970497));
#68725=CARTESIAN_POINT('Ctrl Pts',(2.83257988597991,0.794893193795283,1.86565211329946));
#68726=CARTESIAN_POINT('Ctrl Pts',(2.85772696598989,0.705282270487064,1.86060251085192));
#68727=CARTESIAN_POINT('Ctrl Pts',(2.87865305421882,0.614350204153821,1.85555290840438));
#68728=CARTESIAN_POINT('Ctrl Pts',(2.89522476619359,0.522529954375151,1.85050330595683));
#68729=CARTESIAN_POINT('Ctrl Pts',(2.91177902069943,0.430806432632733,1.84545902301267));
#68730=CARTESIAN_POINT('Ctrl Pts',(2.92398793878408,0.338197021380879,1.8404147400685));
#68731=CARTESIAN_POINT('Ctrl Pts',(2.93176850166836,0.245147817908464,1.83537045712433));
#68732=CARTESIAN_POINT('Ctrl Pts',(2.93954358794746,0.152164110179341,1.83032972476468));
#68733=CARTESIAN_POINT('Ctrl Pts',(2.94289647804148,0.0587416661613416,
1.82528899240502));
#68734=CARTESIAN_POINT('Ctrl Pts',(2.94179575194014,-0.0346663217969656,
1.82024826004537));
#68735=CARTESIAN_POINT('Ctrl Pts',(2.94069541316216,-0.128041441364473,
1.81520930141797));
#68736=CARTESIAN_POINT('Ctrl Pts',(2.93514457697084,-0.221401672070292,
1.81017034279057));
#68737=CARTESIAN_POINT('Ctrl Pts',(2.92516392560423,-0.3142928703354,1.80513138416317));
#68738=CARTESIAN_POINT('Ctrl Pts',(2.91518400795212,-0.40717723982588,1.8000927959682));
#68739=CARTESIAN_POINT('Ctrl Pts',(2.90077497032774,-0.499592204648292,
1.79505420777324));
#68740=CARTESIAN_POINT('Ctrl Pts',(2.88200934704536,-0.591088930316898,
1.79001561957828));
#68741=CARTESIAN_POINT('Ctrl Pts',(2.86323987967138,-0.682604398863855,
1.78497599924096));
#68742=CARTESIAN_POINT('Ctrl Pts',(2.84011214361872,-0.77320082047799,1.77993637890365));
#68743=CARTESIAN_POINT('Ctrl Pts',(2.81274950498193,-0.862440851434997,
1.77489675856633));
#68744=CARTESIAN_POINT('Ctrl Pts',(2.78535710504907,-0.951777945362338,
1.76985165682662));
#68745=CARTESIAN_POINT('Ctrl Pts',(2.75372073900004,-1.03975527952438,1.76480655508691));
#68746=CARTESIAN_POINT('Ctrl Pts',(2.71801315726655,-1.1259522533953,1.7597614533472));
#68747=CARTESIAN_POINT('Ctrl Pts',(2.68228341425677,-1.2122027238868,1.75471322045472));
#68748=CARTESIAN_POINT('Ctrl Pts',(2.64247761402116,-1.29667023359253,1.74966498756224));
#68749=CARTESIAN_POINT('Ctrl Pts',(2.59881507814656,-1.37895764604939,1.74461675466976));
#68750=CARTESIAN_POINT('Ctrl Pts',(2.55508384085064,-1.46137453477417,1.73956057856537));
#68751=CARTESIAN_POINT('Ctrl Pts',(2.50748398038528,-1.5416040982564,1.73450440246099));
#68752=CARTESIAN_POINT('Ctrl Pts',(2.45627869436139,-1.61927730041099,1.7294482263566));
#68753=CARTESIAN_POINT('Ctrl Pts',(2.4343775407991,-1.65249911909723,1.72728563538409));
#68754=CARTESIAN_POINT('Ctrl Pts',(2.41181732711787,-1.68525368649539,1.72512304441157));
#68755=CARTESIAN_POINT('Ctrl Pts',(2.38862084210658,-1.71751403856098,1.72296045343906));
#68756=CARTESIAN_POINT('Ctrl Pts',(2.33438342280857,-1.79294435659545,1.71790393934698));
#68757=CARTESIAN_POINT('Ctrl Pts',(2.27647413028142,-1.86593562161687,1.7128474252549));
#68758=CARTESIAN_POINT('Ctrl Pts',(2.21513998173545,-1.93610920697079,1.70779091116282));
#68759=CARTESIAN_POINT('Ctrl Pts',(2.1538893032477,-2.00618729261706,1.70274127851502));
#68760=CARTESIAN_POINT('Ctrl Pts',(2.08922332047284,-2.0734549878868,1.69769164586722));
#68761=CARTESIAN_POINT('Ctrl Pts',(2.02143146833816,-2.13756375783559,1.69264201321942));
#68762=CARTESIAN_POINT('Ctrl Pts',(1.95371103352441,-2.20160499051474,1.68759770025568));
#68763=CARTESIAN_POINT('Ctrl Pts',(1.88287159564746,-2.26249360987447,1.68255338729194));
#68764=CARTESIAN_POINT('Ctrl Pts',(1.80924114279776,-2.31991605175874,1.6775090743282));
#68765=CARTESIAN_POINT('Ctrl Pts',(1.73566252252895,-2.37729807078468,1.6724683123376));
#68766=CARTESIAN_POINT('Ctrl Pts',(1.65929714134141,-2.43121849058279,1.66742755034699));
#68767=CARTESIAN_POINT('Ctrl Pts',(1.58050715713632,-2.48140305598282,1.66238678835638));
#68768=CARTESIAN_POINT('Ctrl Pts',(1.50174490134216,-2.53156996002315,1.65734780035166));
#68769=CARTESIAN_POINT('Ctrl Pts',(1.42056011141324,-2.57800338384005,1.65230881234694));
#68770=CARTESIAN_POINT('Ctrl Pts',(1.33734424792106,-2.62047216404839,1.64726982434222));
#68771=CARTESIAN_POINT('Ctrl Pts',(1.25413450667023,-2.66293781980292,1.64223120705889));
#68772=CARTESIAN_POINT('Ctrl Pts',(1.16889438401989,-2.70143921067305,1.63719258977556));
#68773=CARTESIAN_POINT('Ctrl Pts',(1.08203926619567,-2.7357914807987,1.63215397249223));
#68774=CARTESIAN_POINT('Ctrl Pts',(0.995166362011864,-2.77015078564889,
1.62711432339107));
#68775=CARTESIAN_POINT('Ctrl Pts',(0.906678218184794,-2.80035911955002,
1.62207467428992));
#68776=CARTESIAN_POINT('Ctrl Pts',(0.817008414070304,-2.82628046225748,
1.61703502518876));
#68777=CARTESIAN_POINT('Ctrl Pts',(0.727241091791453,-2.85222999507624,
1.61198989534262));
#68778=CARTESIAN_POINT('Ctrl Pts',(0.636289970756585,-2.87388310780977,
1.60694476549647));
#68779=CARTESIAN_POINT('Ctrl Pts',(0.544601634966138,-2.89115427799905,
1.60189963565033));
#68780=CARTESIAN_POINT('Ctrl Pts',(0.452856400874139,-2.9084361660211,1.59685137498807));
#68781=CARTESIAN_POINT('Ctrl Pts',(0.360373479938316,-2.92133063663873,
1.59180311432582));
#68782=CARTESIAN_POINT('Ctrl Pts',(0.267605296108074,-2.9298039875553,1.58675485366356));
#68783=CARTESIAN_POINT('Ctrl Pts',(0.174691159895797,-2.93829066961298,
1.581698650562));
#68784=CARTESIAN_POINT('Ctrl Pts',(0.0814913071132577,-2.94234232815569,
1.57664244746044));
#68785=CARTESIAN_POINT('Ctrl Pts',(-0.0115413537709718,-2.94197736176761,
1.57158624435889));
#68786=CARTESIAN_POINT('Ctrl Pts',(-0.0513270549326549,-2.94182128277867,
1.56942394368191));
#68787=CARTESIAN_POINT('Ctrl Pts',(-0.0910822387100624,-2.94085810811356,
1.56726164300493));
#68788=CARTESIAN_POINT('Ctrl Pts',(-0.130771880773216,-2.93909215833717,
1.56509934232795));
#68789=CARTESIAN_POINT('Ctrl Pts',(-0.22358640832019,-2.93496247145547,
1.56004278587352));
#68790=CARTESIAN_POINT('Ctrl Pts',(-0.3163682720864,-2.92642469220872,1.55498622941909));
#68791=CARTESIAN_POINT('Ctrl Pts',(-0.408665385939188,-2.91347843690925,
1.54992967296466));
#68792=CARTESIAN_POINT('Ctrl Pts',(-0.500836901600221,-2.90054979891316,
1.54487999748755));
#68793=CARTESIAN_POINT('Ctrl Pts',(-0.592524542861914,-2.88322466760058,
1.53983032201044));
#68794=CARTESIAN_POINT('Ctrl Pts',(-0.683278204939454,-2.86155462898312,
1.53478064653333));
#68795=CARTESIAN_POINT('Ctrl Pts',(-0.773936267927405,-2.83990741738901,
1.52973629033885));
#68796=CARTESIAN_POINT('Ctrl Pts',(-0.863661878402266,-2.81392449876672,
1.52469193414437));
#68797=CARTESIAN_POINT('Ctrl Pts',(-0.952013111233592,-2.78370886337622,
1.51964757794989));
#68798=CARTESIAN_POINT('Ctrl Pts',(-1.04030215639899,-2.75351449582522,
1.51460677231977));
#68799=CARTESIAN_POINT('Ctrl Pts',(-1.12721832848165,-2.71909347659518,
1.50956596668964));
#68800=CARTESIAN_POINT('Ctrl Pts',(-1.21233391138896,-2.68059890459135,
1.50452516105951));
#68801=CARTESIAN_POINT('Ctrl Pts',(-1.29741954396359,-2.64211787799482,
1.49948612917986));
#68802=CARTESIAN_POINT('Ctrl Pts',(-1.38070544259646,-2.59956632899173,
1.49444709730021));
#68803=CARTESIAN_POINT('Ctrl Pts',(-1.46178392945742,-2.55314546071704,
1.48940806542056));
#68804=CARTESIAN_POINT('Ctrl Pts',(-1.5428564542476,-2.50672800598043,1.4843694040839));
#68805=CARTESIAN_POINT('Ctrl Pts',(-1.6217215054357,-2.45644201828579,1.47933074274723));
#68806=CARTESIAN_POINT('Ctrl Pts',(-1.69799707696022,-2.40253406357424,
1.47429208141057));
#68807=CARTESIAN_POINT('Ctrl Pts',(-1.77428827004858,-2.34861506828261,
1.46925238813448));
#68808=CARTESIAN_POINT('Ctrl Pts',(-1.84798856838221,-2.29107288886368,
1.46421269485838));
#68809=CARTESIAN_POINT('Ctrl Pts',(-1.91874689009342,-2.23019603886224,
1.45917300158229));
#68810=CARTESIAN_POINT('Ctrl Pts',(-1.98958216136788,-2.16925298538245,
1.45412782764771));
#68811=CARTESIAN_POINT('Ctrl Pts',(-2.05746873359588,-2.10496831261553,
1.44908265371313));
#68812=CARTESIAN_POINT('Ctrl Pts',(-2.12209067909298,-2.03766904812992,
1.44403747977855));
#68813=CARTESIAN_POINT('Ctrl Pts',(-2.18675272632632,-1.9703280204734,1.43898917501538));
#68814=CARTESIAN_POINT('Ctrl Pts',(-2.24814582232597,-1.89996901047082,
1.43394087025221));
#68815=CARTESIAN_POINT('Ctrl Pts',(-2.30599422035143,-1.82695228610542,
1.42889256548904));
#68816=CARTESIAN_POINT('Ctrl Pts',(-2.36393362600364,-1.75382069116408,
1.42383631868683));
#68817=CARTESIAN_POINT('Ctrl Pts',(-2.41831694414293,-1.67802339537995,
1.41878007188462));
#68818=CARTESIAN_POINT('Ctrl Pts',(-2.46891177401681,-1.59994957799338,
1.4137238250824));
#68819=CARTESIAN_POINT('Ctrl Pts',(-2.49054425696941,-1.56656809360318,
1.41156196046055));
#68820=CARTESIAN_POINT('Ctrl Pts',(-2.51148474069642,-1.53277074223601,
1.4094000958387));
#68821=CARTESIAN_POINT('Ctrl Pts',(-2.5317176883814,-1.49858918531289,1.40723823121684));
#68822=CARTESIAN_POINT('Ctrl Pts',(-2.58066863291028,-1.41589142308336,
1.40200788530626));
#68823=CARTESIAN_POINT('Ctrl Pts',(-2.62563695420144,-1.33066964034243,
1.39677753939567));
#68824=CARTESIAN_POINT('Ctrl Pts',(-2.66636406248024,-1.2433288729511,1.39154719348508));
#68825=CARTESIAN_POINT('Ctrl Pts',(-2.70702244659364,-1.15613548703612,
1.3863256734198));
#68826=CARTESIAN_POINT('Ctrl Pts',(-2.74345368984489,-1.06683059212917,
1.38110415335452));
#68827=CARTESIAN_POINT('Ctrl Pts',(-2.77544401528677,-0.975845540036365,
1.37588263328924));
#68828=CARTESIAN_POINT('Ctrl Pts',(-2.80737206235508,-0.885037616528062,
1.37067127841524));
#68829=CARTESIAN_POINT('Ctrl Pts',(-2.83487628148681,-0.792556427915325,
1.36545992354124));
#68830=CARTESIAN_POINT('Ctrl Pts',(-2.85779061008119,-0.698853939626707,
1.36024856866724));
#68831=CARTESIAN_POINT('Ctrl Pts',(-2.88067835069349,-0.605260176325145,
1.35504326063897));
#68832=CARTESIAN_POINT('Ctrl Pts',(-2.89898670081184,-0.510448320170043,
1.3498379526107));
#68833=CARTESIAN_POINT('Ctrl Pts',(-2.91259906001162,-0.414886388809551,
1.34463264458243));
#68834=CARTESIAN_POINT('Ctrl Pts',(-2.92619465701788,-0.319442131950787,
1.33943374634538));
#68835=CARTESIAN_POINT('Ctrl Pts',(-2.93510572388532,-0.223250035343443,
1.33423484810833));
#68836=CARTESIAN_POINT('Ctrl Pts',(-2.93926670076444,-0.126788255675884,
1.32903594987128));
#68837=CARTESIAN_POINT('Ctrl Pts',(-2.94109680683036,-0.0843618511973775,
1.32674933894406));
#68838=CARTESIAN_POINT('Ctrl Pts',(-2.94200868962107,-0.0418833966442406,
1.32446272801683));
#68839=CARTESIAN_POINT('Ctrl Pts',(-2.9419999375878,0.000605997841190852,
1.3221761170896));
#68840=CARTESIAN_POINT('Ctrl Pts',(-2.93741502701325,0.00061385004391417,
1.322175642952));
#68841=CARTESIAN_POINT('Ctrl Pts',(-2.93824669003836,0.450821023061646,
1.29790946866991));
#68842=CARTESIAN_POINT('Ctrl Pts',(-2.63011361001259,1.87620303645204,1.22102292401743));
#68843=CARTESIAN_POINT('Ctrl Pts',(-0.420704297245342,3.44500822120456,
1.09151600899461));
#68844=CARTESIAN_POINT('Ctrl Pts',(2.6535010782834,2.23705783115148,0.933654897883501));
#68845=CARTESIAN_POINT('Ctrl Pts',(3.3242675736315,-0.997273536182898,0.775793786772391));
#68846=CARTESIAN_POINT('Ctrl Pts',(0.984136888139677,-3.32800743087111,
0.61793267566128));
#68847=CARTESIAN_POINT('Ctrl Pts',(-2.11124554144075,-2.67379892134876,
0.466726785767013));
#68848=CARTESIAN_POINT('Ctrl Pts',(-2.93840347440061,-0.845052391620324,
0.368141266243119));
#68849=CARTESIAN_POINT('Ctrl Pts',(-2.94490570994055,0.00214417779480537,
0.322176117089595));
#68850=CARTESIAN_POINT('Origin',(0.,0.,-1.84858989190501));
#68851=CARTESIAN_POINT('',(-2.3717491904533,-0.00195961326026947,14.6514101080561));
#68852=CARTESIAN_POINT('Ctrl Pts',(-2.36544101854889,0.172878137039876,
14.63965844111));
#68853=CARTESIAN_POINT('Ctrl Pts',(-2.36969704386767,0.114644186597092,
14.6435756634253));
#68854=CARTESIAN_POINT('Ctrl Pts',(-2.37179733216257,0.0563070163347199,
14.6474928857407));
#68855=CARTESIAN_POINT('Ctrl Pts',(-2.3717491904533,-0.00195961326026254,
14.6514101080561));
#68856=CARTESIAN_POINT('',(-2.34668236863853,0.343918483395512,15.62825));
#68857=CARTESIAN_POINT('Ctrl Pts',(-2.37174919045282,-0.00195961383911467,
14.651410108095));
#68858=CARTESIAN_POINT('Ctrl Pts',(-2.37165303655356,-0.118336079531962,
14.6592340116152));
#68859=CARTESIAN_POINT('Ctrl Pts',(-2.36298799025286,-0.234362805409626,
14.6670579151354));
#68860=CARTESIAN_POINT('Ctrl Pts',(-2.34592725613449,-0.349032049281036,
14.6748818186556));
#68861=CARTESIAN_POINT('Ctrl Pts',(-2.34141960030033,-0.379329074165719,
14.6769489902149));
#68862=CARTESIAN_POINT('Ctrl Pts',(-2.33632609141068,-0.409531501361688,
14.6790161617741));
#68863=CARTESIAN_POINT('Ctrl Pts',(-2.33065042506097,-0.439621039832174,
14.6810833333333));
#68864=CARTESIAN_POINT('Ctrl Pts',(-2.31599449587478,-0.517319431156899,
14.6864212651497));
#68865=CARTESIAN_POINT('Ctrl Pts',(-2.29742185661224,-0.59442755062193,
14.6917591969661));
#68866=CARTESIAN_POINT('Ctrl Pts',(-2.27499436621545,-0.670521212332572,
14.6970971287826));
#68867=CARTESIAN_POINT('Ctrl Pts',(-2.2525987969661,-0.746506569594014,
14.7024274630968));
#68868=CARTESIAN_POINT('Ctrl Pts',(-2.22635940435725,-0.821479891836962,
14.707757797411));
#68869=CARTESIAN_POINT('Ctrl Pts',(-2.19638914799177,-0.895026688475827,
14.7130881317251));
#68870=CARTESIAN_POINT('Ctrl Pts',(-2.16645305795681,-0.968489641181807,
14.7184123894158));
#68871=CARTESIAN_POINT('Ctrl Pts',(-2.13279473239622,-1.04052886937477,
14.7237366471065));
#68872=CARTESIAN_POINT('Ctrl Pts',(-2.09557661492103,-1.11074601664652,
14.7290609047972));
#68873=CARTESIAN_POINT('Ctrl Pts',(-2.05838165286002,-1.18091947801374,
14.7343818499777));
#68874=CARTESIAN_POINT('Ctrl Pts',(-2.01763151364378,-1.24927269667142,
14.7397027951583));
#68875=CARTESIAN_POINT('Ctrl Pts',(-1.9735358295509,-1.315429356514,14.7450237403388));
#68876=CARTESIAN_POINT('Ctrl Pts',(-1.92945393263375,-1.38156533148656,
14.7503430218462));
#68877=CARTESIAN_POINT('Ctrl Pts',(-1.88202882737253,-1.4455057228044,14.7556623033536));
#68878=CARTESIAN_POINT('Ctrl Pts',(-1.83151419094341,-1.50690206412789,
14.7609815848609));
#68879=CARTESIAN_POINT('Ctrl Pts',(-1.78099971538943,-1.56829820992104,
14.7663008494279));
#68880=CARTESIAN_POINT('Ctrl Pts',(-1.72739602646039,-1.62714996174261,
14.7716201139948));
#68881=CARTESIAN_POINT('Ctrl Pts',(-1.67099697324794,-1.68314205517426,
14.7769393785617));
#68882=CARTESIAN_POINT('Ctrl Pts',(-1.614542210969,-1.73918945569137,14.7822638973173));
#68883=CARTESIAN_POINT('Ctrl Pts',(-1.55528690171925,-1.79237122556598,
14.7875884160728));
#68884=CARTESIAN_POINT('Ctrl Pts',(-1.49356121586978,-1.84240955190467,
14.7929129348284));
#68885=CARTESIAN_POINT('Ctrl Pts',(-1.43180550260319,-1.89247222016321,
14.7982400437787));
#68886=CARTESIAN_POINT('Ctrl Pts',(-1.36757739662557,-1.93938812234721,
14.8035671527289));
#68887=CARTESIAN_POINT('Ctrl Pts',(-1.30123752244291,-1.9829218271749,14.8088942616792));
#68888=CARTESIAN_POINT('Ctrl Pts',(-1.23478023064405,-2.02653258406077,
14.8142307992942));
#68889=CARTESIAN_POINT('Ctrl Pts',(-1.1662041068135,-2.06674894578569,14.8195673369093));
#68890=CARTESIAN_POINT('Ctrl Pts',(-1.09589570948668,-2.10338076829391,
14.8249038745243));
#68891=CARTESIAN_POINT('Ctrl Pts',(-1.03423463259541,-2.13550719572259,
14.8295840644977));
#68892=CARTESIAN_POINT('Ctrl Pts',(-0.971241734419387,-2.16487723257753,
14.8342642544711));
#68893=CARTESIAN_POINT('Ctrl Pts',(-0.907188983289324,-2.19139366867263,
14.8389444444445));
#68894=CARTESIAN_POINT('Ctrl Pts',(-0.834258870232282,-2.22158513817499,
14.8442732832198));
#68895=CARTESIAN_POINT('Ctrl Pts',(-0.759682288760601,-2.24818891298128,
14.8496021219951));
#68896=CARTESIAN_POINT('Ctrl Pts',(-0.683846636270297,-2.27102440333912,
14.8549309607704));
#68897=CARTESIAN_POINT('Ctrl Pts',(-0.608119617639673,-2.29382718207157,
14.8602521660343));
#68898=CARTESIAN_POINT('Ctrl Pts',(-0.531137555331562,-2.31287226173924,
14.8655733712981));
#68899=CARTESIAN_POINT('Ctrl Pts',(-0.453307800790021,-2.32802708322797,
14.870894576562));
#68900=CARTESIAN_POINT('Ctrl Pts',(-0.375567090829125,-2.34316456617141,
14.876209693865));
#68901=CARTESIAN_POINT('Ctrl Pts',(-0.296981074207135,-2.35442054610887,
14.8815248111681));
#68902=CARTESIAN_POINT('Ctrl Pts',(-0.217970767376855,-2.36171268512263,
14.8868399284712));
#68903=CARTESIAN_POINT('Ctrl Pts',(-0.139009742111534,-2.36900027576749,
14.8921517305448));
#68904=CARTESIAN_POINT('Ctrl Pts',(-0.0596254180553557,-2.37232888966095,
14.8974635326184));
#68905=CARTESIAN_POINT('Ctrl Pts',(0.0197537452978395,-2.371667736435,14.902775334692));
#68906=CARTESIAN_POINT('Ctrl Pts',(0.0991081939534888,-2.37100678905906,
14.9080854829364));
#68907=CARTESIAN_POINT('Ctrl Pts',(0.178457016093407,-2.36635854517191,
14.9133956311807));
#68908=CARTESIAN_POINT('Ctrl Pts',(0.257370915444152,-2.35774431912865,
14.9187057794251));
#68909=CARTESIAN_POINT('Ctrl Pts',(0.33628489608205,-2.34913008421211,14.9240159331393));
#68910=CARTESIAN_POINT('Ctrl Pts',(0.414763486632712,-2.33654991148123,
14.9293260868535));
#68911=CARTESIAN_POINT('Ctrl Pts',(0.492383177521609,-2.32007691014624,
14.9346362405677));
#68912=CARTESIAN_POINT('Ctrl Pts',(0.570081103006483,-2.3035873053104,14.9399517465028));
#68913=CARTESIAN_POINT('Ctrl Pts',(0.646917939504538,-2.283197132457,14.9452672524379));
#68914=CARTESIAN_POINT('Ctrl Pts',(0.722481638564208,-2.25903039918403,
14.950582758373));
#68915=CARTESIAN_POINT('Ctrl Pts',(0.798082721014159,-2.23485170997941,
14.9559008940315));
#68916=CARTESIAN_POINT('Ctrl Pts',(0.872408971671045,-2.2068929043621,14.9612190296901));
#68917=CARTESIAN_POINT('Ctrl Pts',(0.945067178850849,-2.17532666281616,
14.9665371653487));
#68918=CARTESIAN_POINT('Ctrl Pts',(1.01785652619065,-2.1437034476381,14.9718648996636));
#68919=CARTESIAN_POINT('Ctrl Pts',(1.08897139349092,-2.10845999664893,14.9771926339784));
#68920=CARTESIAN_POINT('Ctrl Pts',(1.15804230830806,-2.06981546874801,14.9825203682933));
#68921=CARTESIAN_POINT('Ctrl Pts',(1.2197753011225,-2.03527643926591,14.9872820973808));
#68922=CARTESIAN_POINT('Ctrl Pts',(1.27987573716285,-1.99802135198414,14.9920438264682));
#68923=CARTESIAN_POINT('Ctrl Pts',(1.3381010999646,-1.95823479408715,14.9968055555556));
#68924=CARTESIAN_POINT('Ctrl Pts',(1.40347453969688,-1.91356381189524,15.0021518616074));
#68925=CARTESIAN_POINT('Ctrl Pts',(1.46672801140548,-1.86553405579549,15.0074981676593));
#68926=CARTESIAN_POINT('Ctrl Pts',(1.52749715228343,-1.8143733111645,15.0128444737111));
#68927=CARTESIAN_POINT('Ctrl Pts',(1.58817937416269,-1.76328574250129,15.0181831328625));
#68928=CARTESIAN_POINT('Ctrl Pts',(1.64638396926533,-1.70907637782963,15.0235217920139));
#68929=CARTESIAN_POINT('Ctrl Pts',(1.70177600406537,-1.65201588808562,15.0288604511653));
#68930=CARTESIAN_POINT('Ctrl Pts',(1.7571038186477,-1.59502155292659,15.0341929208014));
#68931=CARTESIAN_POINT('Ctrl Pts',(1.80962523111407,-1.53518299546105,15.0395253904374));
#68932=CARTESIAN_POINT('Ctrl Pts',(1.8590399755671,-1.47280970656208,15.0448578600734));
#68933=CARTESIAN_POINT('Ctrl Pts',(1.90842334678594,-1.41047601822811,15.0501869441446));
#68934=CARTESIAN_POINT('Ctrl Pts',(1.95470367709152,-1.34561115761927,15.0555160282158));
#68935=CARTESIAN_POINT('Ctrl Pts',(1.99761983056691,-1.27855898378833,15.060845112287));
#68936=CARTESIAN_POINT('Ctrl Pts',(2.04052190853373,-1.21152880152399,15.0661724485416));
#68937=CARTESIAN_POINT('Ctrl Pts',(2.08006175013366,-1.14231312308764,15.0714997847961));
#68938=CARTESIAN_POINT('Ctrl Pts',(2.11602139654005,-1.07128498163873,15.0768271210507));
#68939=CARTESIAN_POINT('Ctrl Pts',(2.1519802852596,-1.0002583367865,15.0821543450557));
#68940=CARTESIAN_POINT('Ctrl Pts',(2.18435891954638,-0.927419721225917,
15.0874815690608));
#68941=CARTESIAN_POINT('Ctrl Pts',(2.21298585799553,-0.853165666686019,
15.0928087930658));
#68942=CARTESIAN_POINT('Ctrl Pts',(2.2416399377268,-0.778841211664881,15.0981410678272));
#68943=CARTESIAN_POINT('Ctrl Pts',(2.26653504833346,-0.703099072749055,
15.1034733425885));
#68944=CARTESIAN_POINT('Ctrl Pts',(2.28754861581706,-0.626354047463135,
15.1088056173499));
#68945=CARTESIAN_POINT('Ctrl Pts',(2.30857199613196,-0.549573184093736,
15.1141403821554));
#68946=CARTESIAN_POINT('Ctrl Pts',(2.32571012093138,-0.471788956798449,
15.119475146961));
#68947=CARTESIAN_POINT('Ctrl Pts',(2.33889143828093,-0.393427124682763,
15.1248099117666));
#68948=CARTESIAN_POINT('Ctrl Pts',(2.35209542360752,-0.314930533334536,
15.1301538507938));
#68949=CARTESIAN_POINT('Ctrl Pts',(2.36132895093892,-0.235854816316838,
15.1354977898209));
#68950=CARTESIAN_POINT('Ctrl Pts',(2.36657234708878,-0.156631377746257,
15.1408417288481));
#68951=CARTESIAN_POINT('Ctrl Pts',(2.37109395716964,-0.0883135378878964,
15.1454500414543));
#68952=CARTESIAN_POINT('Ctrl Pts',(2.37264921575342,-0.0198860738465293,
15.1500583540605));
#68953=CARTESIAN_POINT('Ctrl Pts',(2.37125658538404,0.0483763245071093,
15.1546666666666));
#68954=CARTESIAN_POINT('Ctrl Pts',(2.36964161779268,0.127537000213953,15.1600107089003));
#68955=CARTESIAN_POINT('Ctrl Pts',(2.36405545103476,0.206759138475579,15.165354751134));
#68956=CARTESIAN_POINT('Ctrl Pts',(2.35449000539771,0.285613159679849,15.1706987933677));
#68957=CARTESIAN_POINT('Ctrl Pts',(2.34493796483008,0.364356674414422,15.1760353464305));
#68958=CARTESIAN_POINT('Ctrl Pts',(2.33141777735698,0.442732637510022,15.1813718994932));
#68959=CARTESIAN_POINT('Ctrl Pts',(2.31397336310136,0.520312730343378,15.186708452556));
#68960=CARTESIAN_POINT('Ctrl Pts',(2.2965483857409,0.59780638197503,15.1920390595308));
#68961=CARTESIAN_POINT('Ctrl Pts',(2.27520797345393,0.674505473075603,15.1973696665055));
#68962=CARTESIAN_POINT('Ctrl Pts',(2.25004750123224,0.749989536392724,15.2027002734803));
#68963=CARTESIAN_POINT('Ctrl Pts',(2.22490230563315,0.825427768235062,15.2080276438834));
#68964=CARTESIAN_POINT('Ctrl Pts',(2.19594180171421,0.899651995628935,15.2133550142866));
#68965=CARTESIAN_POINT('Ctrl Pts',(2.16331151907301,0.972255796560776,15.2186823846897));
#68966=CARTESIAN_POINT('Ctrl Pts',(2.13069102338093,1.0448378211043,15.2240081572304));
#68967=CARTESIAN_POINT('Ctrl Pts',(2.09440312610934,1.11579995955118,15.229333929771));
#68968=CARTESIAN_POINT('Ctrl Pts',(2.05464136394079,1.1847560626912,15.2346597023117));
#68969=CARTESIAN_POINT('Ctrl Pts',(2.01487931203249,1.25371266830701,15.2399855136607));
#68970=CARTESIAN_POINT('Ctrl Pts',(1.9716435791553,1.32066280648512,15.2453113250098));
#68971=CARTESIAN_POINT('Ctrl Pts',(1.9251727719285,1.38524649818187,15.2506371363588));
#68972=CARTESIAN_POINT('Ctrl Pts',(1.87865577596628,1.44989438155564,15.2559682411922));
#68973=CARTESIAN_POINT('Ctrl Pts',(1.82889755604729,1.51217074113547,15.2612993460255));
#68974=CARTESIAN_POINT('Ctrl Pts',(1.77617869626716,1.57174657671861,15.2666304508589));
#68975=CARTESIAN_POINT('Ctrl Pts',(1.72343391037242,1.63135171054433,15.2719641774264));
#68976=CARTESIAN_POINT('Ctrl Pts',(1.66772591038729,1.6882533409391,15.277297903994));
#68977=CARTESIAN_POINT('Ctrl Pts',(1.60937229223899,1.74215926007739,15.2826316305615));
#68978=CARTESIAN_POINT('Ctrl Pts',(1.5509157973428,1.79616021472213,15.2879747604267));
#68979=CARTESIAN_POINT('Ctrl Pts',(1.4898047237546,1.84715460629835,15.293317890292));
#68980=CARTESIAN_POINT('Ctrl Pts',(1.42638970436655,1.89489062316987,15.2986610201572));
#68981=CARTESIAN_POINT('Ctrl Pts',(1.37153042865215,1.93618625528247,15.3032832726974));
#68982=CARTESIAN_POINT('Ctrl Pts',(1.31494760601248,1.97504400532842,15.3079055252376));
#68983=CARTESIAN_POINT('Ctrl Pts',(1.25688368958199,2.01132828085392,15.3125277777778));
#68984=CARTESIAN_POINT('Ctrl Pts',(1.19056964084797,2.0527680831166,15.3178067926817));
#68985=CARTESIAN_POINT('Ctrl Pts',(1.12206547864385,2.09101114118911,15.3230858075856));
#68986=CARTESIAN_POINT('Ctrl Pts',(1.05171556453074,2.12581571022132,15.3283648224894));
#68987=CARTESIAN_POINT('Ctrl Pts',(0.981467658141026,2.1605698124563,15.3336361827956));
#68988=CARTESIAN_POINT('Ctrl Pts',(0.909379736706693,2.19189511070529,15.3389075431017));
#68989=CARTESIAN_POINT('Ctrl Pts',(0.83582423970175,2.2195936346158,15.3441789034078));
#68990=CARTESIAN_POINT('Ctrl Pts',(0.762351145219771,2.24726112851027,15.3494443583309));
#68991=CARTESIAN_POINT('Ctrl Pts',(0.687414185600126,2.27130974851289,15.3547098132539));
#68992=CARTESIAN_POINT('Ctrl Pts',(0.611407990096484,2.29158860447205,15.359975268177));
#68993=CARTESIAN_POINT('Ctrl Pts',(0.535447891305022,2.311855161584,15.365237529674));
#68994=CARTESIAN_POINT('Ctrl Pts',(0.458420304264606,2.32835636625989,15.3704997911711));
#68995=CARTESIAN_POINT('Ctrl Pts',(0.380736000933961,2.34099085006602,15.3757620526681));
#68996=CARTESIAN_POINT('Ctrl Pts',(0.303073462940556,2.35362179398327,15.3810228398018));
#68997=CARTESIAN_POINT('Ctrl Pts',(0.224755046136807,2.36238808998572,15.3862836269354));
#68998=CARTESIAN_POINT('Ctrl Pts',(0.14620112273661,2.3672395937485,15.391544414069));
#68999=CARTESIAN_POINT('Ctrl Pts',(0.0676435753024226,2.37209132133224,
15.3968054439056));
#69000=CARTESIAN_POINT('Ctrl Pts',(-0.0111490222247413,2.37302787014035,
15.4020664737422));
#69001=CARTESIAN_POINT('Ctrl Pts',(-0.0897534095969474,2.37005113614996,
15.4073275035788));
#69002=CARTESIAN_POINT('Ctrl Pts',(-0.168448232980228,2.36707097736413,
15.4125945863416));
#69003=CARTESIAN_POINT('Ctrl Pts',(-0.246953934046379,2.36016856275869,
15.4178616691043));
#69004=CARTESIAN_POINT('Ctrl Pts',(-0.32485014880416,2.3493978895287,15.4231287518671));
#69005=CARTESIAN_POINT('Ctrl Pts',(-0.402789595570061,2.33862123862914,
15.4283987578343));
#69006=CARTESIAN_POINT('Ctrl Pts',(-0.480118412252643,2.32397214703836,
15.4336687638016));
#69007=CARTESIAN_POINT('Ctrl Pts',(-0.556427007255923,2.30555569182274,
15.4389387697688));
#69008=CARTESIAN_POINT('Ctrl Pts',(-0.632890005094257,2.28710197274586,
15.4442194390678));
#69009=CARTESIAN_POINT('Ctrl Pts',(-0.708328197589392,2.26486579866246,
15.4495001083668));
#69010=CARTESIAN_POINT('Ctrl Pts',(-0.782347930230338,2.23900196037527,
15.4547807776658));
#69011=CARTESIAN_POINT('Ctrl Pts',(-0.855274810918575,2.21351998439923,
15.4599834814068));
#69012=CARTESIAN_POINT('Ctrl Pts',(-0.926824476841342,2.18451701900297,
15.4651861851478));
#69013=CARTESIAN_POINT('Ctrl Pts',(-0.996644042858746,2.15218463760296,
15.4703888888888));
#69014=CARTESIAN_POINT('Ctrl Pts',(-1.07023465554323,2.11810594172304,15.4758725975075));
#69015=CARTESIAN_POINT('Ctrl Pts',(-1.14218689897926,2.08019728947419,15.4813563061261));
#69016=CARTESIAN_POINT('Ctrl Pts',(-1.21208900263023,2.03863638547998,15.4868400147447));
#69017=CARTESIAN_POINT('Ctrl Pts',(-1.28188065229525,1.99714115286424,15.4923150584242));
#69018=CARTESIAN_POINT('Ctrl Pts',(-1.34962823191753,1.95200536686404,15.4977901021036));
#69019=CARTESIAN_POINT('Ctrl Pts',(-1.41494265277655,1.90345353288533,15.5032651457831));
#69020=CARTESIAN_POINT('Ctrl Pts',(-1.48015447212883,1.85497796830098,15.5087315887933));
#69021=CARTESIAN_POINT('Ctrl Pts',(-1.5429403935587,1.80309729790061,15.5141980318035));
#69022=CARTESIAN_POINT('Ctrl Pts',(-1.60293970151325,1.74807962513514,15.5196644748137));
#69023=CARTESIAN_POINT('Ctrl Pts',(-1.66288342070942,1.69311292569291,15.5251258532192));
#69024=CARTESIAN_POINT('Ctrl Pts',(-1.72004533954628,1.63501529660287,15.5305872316247));
#69025=CARTESIAN_POINT('Ctrl Pts',(-1.77409770341292,1.5740951055273,15.5360486100302));
#69026=CARTESIAN_POINT('Ctrl Pts',(-1.82811319668854,1.51321646977493,15.5415062630805));
#69027=CARTESIAN_POINT('Ctrl Pts',(-1.87902306477552,1.44951942710436,15.5469639161309));
#69028=CARTESIAN_POINT('Ctrl Pts',(-1.92653709979407,1.38334842524111,15.5524215691813));
#69029=CARTESIAN_POINT('Ctrl Pts',(-1.97403032342431,1.31720640661226,15.5578768317519));
#69030=CARTESIAN_POINT('Ctrl Pts',(-2.01813041946052,1.24859293908361,15.5633320943226));
#69031=CARTESIAN_POINT('Ctrl Pts',(-2.05858877012042,1.17788383893918,15.5687873568932));
#69032=CARTESIAN_POINT('Ctrl Pts',(-2.09905065068051,1.10716856958462,15.5742430954233));
#69033=CARTESIAN_POINT('Ctrl Pts',(-2.13586992630258,1.03435767661531,15.5796988339534));
#69034=CARTESIAN_POINT('Ctrl Pts',(-2.1688428443841,0.959853519482995,15.5851545724834));
#69035=CARTESIAN_POINT('Ctrl Pts',(-2.20181578264016,0.885349316765168,
15.5906103143516));
#69036=CARTESIAN_POINT('Ctrl Pts',(-2.23094218778358,0.809152249651672,
15.5960660562197));
#69037=CARTESIAN_POINT('Ctrl Pts',(-2.2560662000637,0.731685289882293,15.6015217980879));
#69038=CARTESIAN_POINT('Ctrl Pts',(-2.28120754002064,0.654164902243658,
15.6069813027043));
#69039=CARTESIAN_POINT('Ctrl Pts',(-2.30234084338011,0.575373289754166,
15.6124408073206));
#69040=CARTESIAN_POINT('Ctrl Pts',(-2.31936008877542,0.495748768123185,
15.617900311937));
#69041=CARTESIAN_POINT('Ctrl Pts',(-2.33011465921646,0.445433521658159,
15.621350207958));
#69042=CARTESIAN_POINT('Ctrl Pts',(-2.33922747603912,0.394785958881003,
15.624800103979));
#69043=CARTESIAN_POINT('Ctrl Pts',(-2.34668236863853,0.343918483395496,
15.62825));
#69044=CARTESIAN_POINT('',(-0.439445221994505,2.33068358199182,15.62825));
#69045=CARTESIAN_POINT('Origin',(0.,0.,15.62825));
#69046=CARTESIAN_POINT('',(-2.37181912929798,0.000927365841751814,14.8485899293694));
#69047=CARTESIAN_POINT('Ctrl Pts',(-2.37174981871279,0.00092732725788483,
14.8485899301431));
#69048=CARTESIAN_POINT('Ctrl Pts',(-2.3717804010031,-0.0772905196480431,
14.8538670087384));
#69049=CARTESIAN_POINT('Ctrl Pts',(-2.36793742071335,-0.155665441830004,
14.8591440873337));
#69050=CARTESIAN_POINT('Ctrl Pts',(-2.36020048238129,-0.233777127767286,
14.864421165929));
#69051=CARTESIAN_POINT('Ctrl Pts',(-2.35214591793149,-0.315095548783754,
14.8699148855153));
#69052=CARTESIAN_POINT('Ctrl Pts',(-2.33987067538355,-0.396128138407514,
14.8754086051016));
#69053=CARTESIAN_POINT('Ctrl Pts',(-2.32341183915449,-0.476398455262787,
14.8809023246879));
#69054=CARTESIAN_POINT('Ctrl Pts',(-2.3076405835705,-0.553315417392622,
14.8861665398788));
#69055=CARTESIAN_POINT('Ctrl Pts',(-2.28802840003837,-0.629531996772985,
14.8914307550697));
#69056=CARTESIAN_POINT('Ctrl Pts',(-2.26466074652353,-0.704634490821663,
14.8966949702607));
#69057=CARTESIAN_POINT('Ctrl Pts',(-2.24130539769904,-0.779697438198127,
14.9019564134772));
#69058=CARTESIAN_POINT('Ctrl Pts',(-2.21419864424466,-0.853647007499199,
14.9072178566937));
#69059=CARTESIAN_POINT('Ctrl Pts',(-2.18347633982578,-0.926082683091,14.9124792999102));
#69060=CARTESIAN_POINT('Ctrl Pts',(-2.15276017382182,-0.998503885802566,
14.9177396918735));
#69061=CARTESIAN_POINT('Ctrl Pts',(-2.11843007850108,-1.06941135454287,
14.9230000838367));
#69062=CARTESIAN_POINT('Ctrl Pts',(-2.08067018877933,-1.1384241863317,14.9282604758));
#69063=CARTESIAN_POINT('Ctrl Pts',(-2.04290550487823,-1.20744578032549,
14.9335215356483));
#69064=CARTESIAN_POINT('Ctrl Pts',(-2.00171039456691,-1.27457184092691,
14.9387825954965));
#69065=CARTESIAN_POINT('Ctrl Pts',(-1.95731432203941,-1.33944716478084,
14.9440436553447));
#69066=CARTESIAN_POINT('Ctrl Pts',(-1.91287075215952,-1.40439189581299,
14.9493103437632));
#69067=CARTESIAN_POINT('Ctrl Pts',(-1.86521965965363,-1.46708069074338,
14.9545770321817));
#69068=CARTESIAN_POINT('Ctrl Pts',(-1.81463261526301,-1.52718909573232,
14.9598437206002));
#69069=CARTESIAN_POINT('Ctrl Pts',(-1.76401351139897,-1.58733559434456,
14.9651137467757));
#69070=CARTESIAN_POINT('Ctrl Pts',(-1.71045508175997,-1.64489810102531,
14.9703837729511));
#69071=CARTESIAN_POINT('Ctrl Pts',(-1.65426598936552,-1.69958880289573,
14.9756537991265));
#69072=CARTESIAN_POINT('Ctrl Pts',(-1.59798611215559,-1.75436786862941,
14.9809323400925));
#69073=CARTESIAN_POINT('Ctrl Pts',(-1.53906745394361,-1.80626556029958,
14.9862108810585));
#69074=CARTESIAN_POINT('Ctrl Pts',(-1.47785131589474,-1.85503464943601,
14.9914894220245));
#69075=CARTESIAN_POINT('Ctrl Pts',(-1.45936923827676,-1.8697587747975,14.9930830933496));
#69076=CARTESIAN_POINT('Ctrl Pts',(-1.44067793128034,-1.88419802432291,
14.9946767646747));
#69077=CARTESIAN_POINT('Ctrl Pts',(-1.42178725865968,-1.89834639979457,
14.9962704359998));
#69078=CARTESIAN_POINT('Ctrl Pts',(-1.35842070635087,-1.94580547086168,
15.0016162201026));
#69079=CARTESIAN_POINT('Ctrl Pts',(-1.29255927181258,-1.99017524410936,
15.0069620042054));
#69080=CARTESIAN_POINT('Ctrl Pts',(-1.22453598376717,-2.03118430649692,
15.0123077883082));
#69081=CARTESIAN_POINT('Ctrl Pts',(-1.15661015585879,-2.07213461328835,
15.0176459132567));
#69082=CARTESIAN_POINT('Ctrl Pts',(-1.08652902241226,-2.10973353404438,
15.0229840382053));
#69083=CARTESIAN_POINT('Ctrl Pts',(-1.01465672105759,-2.14375133840487,
15.0283221631539));
#69084=CARTESIAN_POINT('Ctrl Pts',(-0.942867940345527,-2.17772961169669,
15.0336540848279));
#69085=CARTESIAN_POINT('Ctrl Pts',(-0.869292548025791,-2.2081348415054,
15.0389860065018));
#69086=CARTESIAN_POINT('Ctrl Pts',(-0.794320251626988,-2.23478262933003,
15.0443179281757));
#69087=CARTESIAN_POINT('Ctrl Pts',(-0.719395684358074,-2.26141345254523,
15.0496464554227));
#69088=CARTESIAN_POINT('Ctrl Pts',(-0.643076416527853,-2.28429142689331,
15.0549749826697));
#69089=CARTESIAN_POINT('Ctrl Pts',(-0.565772072374481,-2.30328027487344,
15.0603035099167));
#69090=CARTESIAN_POINT('Ctrl Pts',(-0.488493200923583,-2.32226286580191,
15.0656302813505));
#69091=CARTESIAN_POINT('Ctrl Pts',(-0.410230350154702,-2.33735876452577,
15.0709570527843));
#69092=CARTESIAN_POINT('Ctrl Pts',(-0.331406838044755,-2.34848197144393,
15.076283824218));
#69093=CARTESIAN_POINT('Ctrl Pts',(-0.252585092592087,-2.35960492905965,
15.0816104762638));
#69094=CARTESIAN_POINT('Ctrl Pts',(-0.173203172501378,-2.36675530813906,
15.0869371283096));
#69095=CARTESIAN_POINT('Ctrl Pts',(-0.0936916385221681,-2.3698987192222,
15.0922637803554));
#69096=CARTESIAN_POINT('Ctrl Pts',(-0.0141046307164287,-2.37304511408959,
15.0975954885584));
#69097=CARTESIAN_POINT('Ctrl Pts',(0.0656117699587432,-2.37217692473355,
15.1029271967614));
#69098=CARTESIAN_POINT('Ctrl Pts',(0.14502546978225,-2.36731190923681,15.1082589049644));
#69099=CARTESIAN_POINT('Ctrl Pts',(0.224476179236341,-2.36244462646847,
15.1135930979345));
#69100=CARTESIAN_POINT('Ctrl Pts',(0.303623442888271,-2.35357685774052,
15.1189272909046));
#69101=CARTESIAN_POINT('Ctrl Pts',(0.382041247237252,-2.34077819280457,
15.1242614838747));
#69102=CARTESIAN_POINT('Ctrl Pts',(0.460594386535239,-2.32795743968748,
15.1296048826972));
#69103=CARTESIAN_POINT('Ctrl Pts',(0.538415094286813,-2.31119233319851,
15.1349482815197));
#69104=CARTESIAN_POINT('Ctrl Pts',(0.615088739328564,-2.29060339326807,
15.1402916803422));
#69105=CARTESIAN_POINT('Ctrl Pts',(0.681925750711367,-2.2726558545572,15.1449495625614));
#69106=CARTESIAN_POINT('Ctrl Pts',(0.747891177234452,-2.25180353856829,
15.1496074447807));
#69107=CARTESIAN_POINT('Ctrl Pts',(0.812722713330219,-2.22815615559978,
15.1542653269999));
#69108=CARTESIAN_POINT('Ctrl Pts',(0.887095955506878,-2.20102842353797,
15.1596087419979));
#69109=CARTESIAN_POINT('Ctrl Pts',(0.960243664981093,-2.17012395952759,
15.164952156996));
#69110=CARTESIAN_POINT('Ctrl Pts',(1.03175679799573,-2.13557392105485,15.170295571994));
#69111=CARTESIAN_POINT('Ctrl Pts',(1.10316953615153,-2.1010723862078,15.1756314855533));
#69112=CARTESIAN_POINT('Ctrl Pts',(1.17295183897759,-2.06293564331141,15.1809673991125));
#69113=CARTESIAN_POINT('Ctrl Pts',(1.24071265927342,-2.02134365203413,15.1863033126717));
#69114=CARTESIAN_POINT('Ctrl Pts',(1.30839780260162,-1.97979811172607,15.19163326695));
#69115=CARTESIAN_POINT('Ctrl Pts',(1.37406555478731,-1.9348052351937,15.1969632212284));
#69116=CARTESIAN_POINT('Ctrl Pts',(1.4373489279239,-1.8865911379777,15.2022931755067));
#69117=CARTESIAN_POINT('Ctrl Pts',(1.50059377146843,-1.83840639554173,15.2076198846837));
#69118=CARTESIAN_POINT('Ctrl Pts',(1.56145674785138,-1.78700460774479,15.2129465938606));
#69119=CARTESIAN_POINT('Ctrl Pts',(1.61960037055053,-1.73265481334644,15.2182733030376));
#69120=CARTESIAN_POINT('Ctrl Pts',(1.6777264696894,-1.67832139910905,15.2235984068294));
#69121=CARTESIAN_POINT('Ctrl Pts',(1.73313450246579,-1.62104206115198,15.2289235106211));
#69122=CARTESIAN_POINT('Ctrl Pts',(1.78552168443477,-1.56112471536172,15.2342486144129));
#69123=CARTESIAN_POINT('Ctrl Pts',(1.83790918402227,-1.50120700629828,15.2395737504903));
#69124=CARTESIAN_POINT('Ctrl Pts',(1.88727549062441,-1.43865160970255,15.2448988865677));
#69125=CARTESIAN_POINT('Ctrl Pts',(1.93335715456253,-1.37380063160631,15.2502240226451));
#69126=CARTESIAN_POINT('Ctrl Pts',(1.97948468935904,-1.30888509919976,15.2555544594981));
#69127=CARTESIAN_POINT('Ctrl Pts',(2.0223207799605,-1.24166980202093,15.2608848963512));
#69128=CARTESIAN_POINT('Ctrl Pts',(2.06164486190368,-1.17252655658034,15.2662153332042));
#69129=CARTESIAN_POINT('Ctrl Pts',(2.10098825176765,-1.10334936216396,15.2715483872742));
#69130=CARTESIAN_POINT('Ctrl Pts',(2.13681598740719,-1.03224275051682,15.2768814413441));
#69131=CARTESIAN_POINT('Ctrl Pts',(2.16895428834543,-0.959601666092737,
15.2822144954141));
#69132=CARTESIAN_POINT('Ctrl Pts',(2.20114946393685,-0.886832029867145,
15.2875569873072));
#69133=CARTESIAN_POINT('Ctrl Pts',(2.2296419918257,-0.812522931436238,15.2928994792003));
#69134=CARTESIAN_POINT('Ctrl Pts',(2.25430699883861,-0.737087523627462,
15.2982419710934));
#69135=CARTESIAN_POINT('Ctrl Pts',(2.27587996298933,-0.671108813485499,
15.3029147200623));
#69136=CARTESIAN_POINT('Ctrl Pts',(2.29452563020474,-0.604268919533596,
15.3075874690311));
#69137=CARTESIAN_POINT('Ctrl Pts',(2.31019260680153,-0.536850241668533,
15.3122602179999));
#69138=CARTESIAN_POINT('Ctrl Pts',(2.3278902754598,-0.460693019190823,15.3175386303638));
#69139=CARTESIAN_POINT('Ctrl Pts',(2.34185491885702,-0.383500328117279,
15.3228170427277));
#69140=CARTESIAN_POINT('Ctrl Pts',(2.35196941557815,-0.305676185995863,
15.3280954550917));
#69141=CARTESIAN_POINT('Ctrl Pts',(2.36206922168904,-0.227965078083739,
15.333366200925));
#69142=CARTESIAN_POINT('Ctrl Pts',(2.3683299184671,-0.149624809785199,15.3386369467583));
#69143=CARTESIAN_POINT('Ctrl Pts',(2.37068489347443,-0.071071783093953,
15.3439076925916));
#69144=CARTESIAN_POINT('Ctrl Pts',(2.37303722400934,0.0073930340362505,
15.3491725197455));
#69145=CARTESIAN_POINT('Ctrl Pts',(2.37149252781999,0.0860696590820804,
15.3544373468995));
#69146=CARTESIAN_POINT('Ctrl Pts',(2.3660359219475,0.164535949123724,15.3597021740534));
#69147=CARTESIAN_POINT('Ctrl Pts',(2.36058263520585,0.242954509882856,15.3649637987312));
#69148=CARTESIAN_POINT('Ctrl Pts',(2.3512221914708,0.321162512866807,15.370225423409));
#69149=CARTESIAN_POINT('Ctrl Pts',(2.33799178822351,0.39873858692059,15.3754870480869));
#69150=CARTESIAN_POINT('Ctrl Pts',(2.324765113418,0.476292799367432,15.3807471899934));
#69151=CARTESIAN_POINT('Ctrl Pts',(2.30767072365399,0.553214964383808,15.3860073319));
#69152=CARTESIAN_POINT('Ctrl Pts',(2.28679738776715,0.629091225341251,15.3912674738066));
#69153=CARTESIAN_POINT('Ctrl Pts',(2.26592311963945,0.704970875069427,15.3965278506406));
#69154=CARTESIAN_POINT('Ctrl Pts',(2.24126969884978,0.779804066555513,15.4017882274746));
#69155=CARTESIAN_POINT('Ctrl Pts',(2.21297606265564,0.85319107391789,15.4070486043086));
#69156=CARTESIAN_POINT('Ctrl Pts',(2.18464568023134,0.926673392319267,15.4123158130329));
#69157=CARTESIAN_POINT('Ctrl Pts',(2.15266580974587,0.998705325762675,15.4175830217572));
#69158=CARTESIAN_POINT('Ctrl Pts',(2.11722382701338,1.06890660435176,15.4228502304815));
#69159=CARTESIAN_POINT('Ctrl Pts',(2.08176741572692,1.13913646212462,15.4281195835047));
#69160=CARTESIAN_POINT('Ctrl Pts',(2.04284633207388,1.20753376939129,15.4333889365279));
#69161=CARTESIAN_POINT('Ctrl Pts',(2.00069270464125,1.27374517235406,15.4386582895511));
#69162=CARTESIAN_POINT('Ctrl Pts',(1.95845349473204,1.3400910011347,15.4439383406876));
#69163=CARTESIAN_POINT('Ctrl Pts',(1.91296890876711,1.40424166909597,15.449218391824));
#69164=CARTESIAN_POINT('Ctrl Pts',(1.86451294622471,1.46587500690217,15.4544984429605));
#69165=CARTESIAN_POINT('Ctrl Pts',(1.81631237646607,1.52718349903638,15.4597506649737));
#69166=CARTESIAN_POINT('Ctrl Pts',(1.76517206266093,1.58600085819359,15.4650028869868));
#69167=CARTESIAN_POINT('Ctrl Pts',(1.71139636532063,1.64204766778171,15.470255109));
#69168=CARTESIAN_POINT('Ctrl Pts',(1.65525380497527,1.70056130024199,15.4757385003069));
#69169=CARTESIAN_POINT('Ctrl Pts',(1.59602203841579,1.75628138880867,15.4812218916139));
#69170=CARTESIAN_POINT('Ctrl Pts',(1.53400284422592,1.80887626343174,15.4867052829208));
#69171=CARTESIAN_POINT('Ctrl Pts',(1.47208183857198,1.86138787006329,15.4921799929449));
#69172=CARTESIAN_POINT('Ctrl Pts',(1.40738251214331,1.910783822024,15.497654702969));
#69173=CARTESIAN_POINT('Ctrl Pts',(1.34024353999736,1.9567691013493,15.5031294129932));
#69174=CARTESIAN_POINT('Ctrl Pts',(1.2732102974973,2.00268196360976,15.5085955015098));
#69175=CARTESIAN_POINT('Ctrl Pts',(1.20374541608499,2.04519460060527,15.5140615900264));
#69176=CARTESIAN_POINT('Ctrl Pts',(1.13221958775623,2.08405299059336,15.5195276785431));
#69177=CARTESIAN_POINT('Ctrl Pts',(1.06076018696158,2.12287529198119,15.5249886905888));
#69178=CARTESIAN_POINT('Ctrl Pts',(0.98724402702801,2.15804988681664,15.5304497026346));
#69179=CARTESIAN_POINT('Ctrl Pts',(0.912069174297032,2.18936700527735,15.5359107146804));
#69180=CARTESIAN_POINT('Ctrl Pts',(0.836945750303487,2.22066269902217,15.5413679907301));
#69181=CARTESIAN_POINT('Ctrl Pts',(0.760166292428859,2.248105997647,15.5468252667799));
#69182=CARTESIAN_POINT('Ctrl Pts',(0.682150793644788,2.27153436188621,15.5522825428296));
#69183=CARTESIAN_POINT('Ctrl Pts',(0.604169603162241,2.29495242320616,15.5577374189732));
#69184=CARTESIAN_POINT('Ctrl Pts',(0.524953870931903,2.3143589380584,15.5631922951168));
#69185=CARTESIAN_POINT('Ctrl Pts',(0.444939746137389,2.32964089181298,15.5686471712604));
#69186=CARTESIAN_POINT('Ctrl Pts',(0.364918690462446,2.34492416930128,15.5741025199093));
#69187=CARTESIAN_POINT('Ctrl Pts',(0.284099531150378,2.35608208087988,15.5795578685581));
#69188=CARTESIAN_POINT('Ctrl Pts',(0.202928946101218,2.3630526666442,15.585013217207));
#69189=CARTESIAN_POINT('Ctrl Pts',(0.121758408129459,2.37002324836571,15.5904685626919));
#69190=CARTESIAN_POINT('Ctrl Pts',(0.0402368804729099,2.37280647805828,
15.5959239081767));
#69191=CARTESIAN_POINT('Ctrl Pts',(-0.0411850251413373,2.37139238764995,
15.6013792536616));
#69192=CARTESIAN_POINT('Ctrl Pts',(-0.122663307909011,2.36997731811454,
15.6068383764696));
#69193=CARTESIAN_POINT('Ctrl Pts',(-0.204041393925436,2.36435913591515,
15.6122974992776));
#69194=CARTESIAN_POINT('Ctrl Pts',(-0.284870348510406,2.35457999376525,
15.6177566220856));
#69195=CARTESIAN_POINT('Ctrl Pts',(-0.336659423831911,2.34831425975964,
15.6212544147238));
#69196=CARTESIAN_POINT('Ctrl Pts',(-0.388223137926654,2.34034139237763,
15.6247522073619));
#69197=CARTESIAN_POINT('Ctrl Pts',(-0.439445221994505,2.33068358199182,
15.62825));
#69198=CARTESIAN_POINT('Ctrl Pts',(-2.36929349484953,0.173162376944586,
14.8369729823432));
#69199=CARTESIAN_POINT('Ctrl Pts',(-2.36976752448848,0.166738132832525,
14.8374071698954));
#69200=CARTESIAN_POINT('Ctrl Pts',(-2.37374016789726,0.109425107004542,
14.8412794730826));
#69201=CARTESIAN_POINT('Ctrl Pts',(-2.37542909742077,0.0519633377314283,
14.8451517762699));
#69202=CARTESIAN_POINT('Ctrl Pts',(-2.37517539399571,0.000929234209626874,
14.848589891905));
#69203=CARTESIAN_POINT('Origin',(0.,0.,15.5));
#69204=CARTESIAN_POINT('',(-2.86750655814837,8.90676632684412E-12,15.1324934418516));
#69205=CARTESIAN_POINT('Ctrl Pts',(-0.439445221994173,2.33068358199189,
15.62825));
#69206=CARTESIAN_POINT('Ctrl Pts',(-0.147008436989358,2.39880934021625,
15.6154874245605));
#69207=CARTESIAN_POINT('Ctrl Pts',(0.156480113641278,2.40931707764128,15.6043391916112));
#69208=CARTESIAN_POINT('Ctrl Pts',(0.737928439613964,2.32205123249246,15.5805131341436));
#69209=CARTESIAN_POINT('Ctrl Pts',(1.01352850236858,2.22934105143109,15.5679821521404));
#69210=CARTESIAN_POINT('Ctrl Pts',(1.47507484108102,1.97772793770723,15.5442630334499));
#69211=CARTESIAN_POINT('Ctrl Pts',(1.74286514902497,1.79346046158376,15.5295935945513));
#69212=CARTESIAN_POINT('Ctrl Pts',(2.17583696066496,1.25931375699315,15.5037713171893));
#69213=CARTESIAN_POINT('Ctrl Pts',(2.3203740697325,0.994251451750397,15.4932862058718));
#69214=CARTESIAN_POINT('Ctrl Pts',(2.51613707821668,0.414921897144935,15.4691143190916));
#69215=CARTESIAN_POINT('Ctrl Pts',(2.56173394912988,0.10148589177416,15.4553705111695));
#69216=CARTESIAN_POINT('Ctrl Pts',(2.53656022337087,-0.536980409493823,
15.4277868133117));
#69217=CARTESIAN_POINT('Ctrl Pts',(2.46062401708309,-0.853728603629975,
15.4157681065155));
#69218=CARTESIAN_POINT('Ctrl Pts',(2.20286218964617,-1.42534776432417,15.3936829887307));
#69219=CARTESIAN_POINT('Ctrl Pts',(2.03089606467517,-1.67805785252003,15.3829262679689));
#69220=CARTESIAN_POINT('Ctrl Pts',(1.57719177316252,-2.14967050654236,15.357096870092));
#69221=CARTESIAN_POINT('Ctrl Pts',(1.28448753171242,-2.35379022866316,15.3416926900889));
#69222=CARTESIAN_POINT('Ctrl Pts',(0.688989948483511,-2.61018154805751,
15.3167193293302));
#69223=CARTESIAN_POINT('Ctrl Pts',(0.398757154749054,-2.67942819397912,
15.3071940127235));
#69224=CARTESIAN_POINT('Ctrl Pts',(-0.251140580273949,-2.72678822036303,
15.2849170067093));
#69225=CARTESIAN_POINT('Ctrl Pts',(-0.609715051811953,-2.68297212826165,
15.2717461797437));
#69226=CARTESIAN_POINT('Ctrl Pts',(-1.17927502173795,-2.49854219510547,
15.2477763655208));
#69227=CARTESIAN_POINT('Ctrl Pts',(-1.49930249907036,-2.36318439438247,
15.2331919507368));
#69228=CARTESIAN_POINT('Ctrl Pts',(-2.09484079639828,-1.87954071233988,
15.2068720036005));
#69229=CARTESIAN_POINT('Ctrl Pts',(-2.32001767675477,-1.61164092749457,
15.1963836430683));
#69230=CARTESIAN_POINT('Ctrl Pts',(-2.59888433046962,-1.12346182881195,
15.1769355703592));
#69231=CARTESIAN_POINT('Ctrl Pts',(-2.68470675960721,-0.92393846071841,
15.168981896123));
#69232=CARTESIAN_POINT('Ctrl Pts',(-2.81771204745999,-0.484244810756474,
15.1513296903239));
#69233=CARTESIAN_POINT('Ctrl Pts',(-2.85842499981825,-0.243042999797827,
15.1415750001833));
#69234=CARTESIAN_POINT('Ctrl Pts',(-2.86750655814837,1.78013159768398E-11,
15.1324934418516));
#69235=CARTESIAN_POINT('Ctrl Pts',(0.261217229955146,2.92775537770323,15.060614691318));
#69236=CARTESIAN_POINT('Ctrl Pts',(0.163263701748706,2.92398569950982,15.0730743864785));
#69237=CARTESIAN_POINT('Ctrl Pts',(0.0657522159450944,2.91542515906648,
15.0854400947226));
#69238=CARTESIAN_POINT('Ctrl Pts',(-0.0308985911385236,2.90209534740483,
15.0977401687025));
#69239=CARTESIAN_POINT('Ctrl Pts',(-0.131043112735575,2.88828369231249,
15.1104848633563));
#69240=CARTESIAN_POINT('Ctrl Pts',(-0.230263368948763,2.86935169178861,
15.1231588590619));
#69241=CARTESIAN_POINT('Ctrl Pts',(-0.328080927958953,2.84531552794264,
15.1358321367556));
#69242=CARTESIAN_POINT('Ctrl Pts',(-0.401444097216596,2.82728840505817,
15.1453370950259));
#69243=CARTESIAN_POINT('Ctrl Pts',(-0.474017960878834,2.80639013673891,
15.1548424738783));
#69244=CARTESIAN_POINT('Ctrl Pts',(-0.545597552831274,2.78262387417559,
15.1643920731548));
#69245=CARTESIAN_POINT('Ctrl Pts',(-0.599282246795606,2.7647991772531,15.1715542726122));
#69246=CARTESIAN_POINT('Ctrl Pts',(-0.652407612168172,2.74536119848702,
15.1787416045881));
#69247=CARTESIAN_POINT('Ctrl Pts',(-0.704886515140488,2.72430928904873,
15.1859768832463));
#69248=CARTESIAN_POINT('Ctrl Pts',(-0.720596781816833,2.71800711631664,
15.1881428613968));
#69249=CARTESIAN_POINT('Ctrl Pts',(-0.736249110096228,2.71156029066323,
15.1903131609141));
#69250=CARTESIAN_POINT('Ctrl Pts',(-0.751841153536472,2.70496875253283,
15.1924884555304));
#69251=CARTESIAN_POINT('Ctrl Pts',(-0.76457047729845,2.69958742947065,15.1942643631947));
#69252=CARTESIAN_POINT('Ctrl Pts',(-0.777250594925623,2.69411346937544,
15.1960423418424));
#69253=CARTESIAN_POINT('Ctrl Pts',(-0.789880380926013,2.68854724896585,
15.1978227525559));
#69254=CARTESIAN_POINT('Ctrl Pts',(-0.873086561955101,2.65187648169916,
15.2095522605717));
#69255=CARTESIAN_POINT('Ctrl Pts',(-0.954109753653407,2.61120393346883,
15.2213864180752));
#69256=CARTESIAN_POINT('Ctrl Pts',(-1.0326800470441,2.56659382923925,15.2334440248114));
#69257=CARTESIAN_POINT('Ctrl Pts',(-1.07396798549143,2.54315164571067,15.2397801819423));
#69258=CARTESIAN_POINT('Ctrl Pts',(-1.11457874886226,2.51862142780173,15.2461783007471));
#69259=CARTESIAN_POINT('Ctrl Pts',(-1.15447370792355,2.49300700336368,15.252657017934));
#69260=CARTESIAN_POINT('Ctrl Pts',(-1.23233138917397,2.44301874068001,15.2653006678968));
#69261=CARTESIAN_POINT('Ctrl Pts',(-1.30746996628184,2.38890091090125,15.2782511407249));
#69262=CARTESIAN_POINT('Ctrl Pts',(-1.37967108001291,2.33085874954981,15.2914219968078));
#69263=CARTESIAN_POINT('Ctrl Pts',(-1.45359796468599,2.27142924844285,15.3049076663268));
#69264=CARTESIAN_POINT('Ctrl Pts',(-1.52444526031354,2.20788342659833,15.318623759732));
#69265=CARTESIAN_POINT('Ctrl Pts',(-1.59188833385002,2.1404469597675,15.332487740417));
#69266=CARTESIAN_POINT('Ctrl Pts',(-1.60226264324965,2.13007366663248,15.3346203422928));
#69267=CARTESIAN_POINT('Ctrl Pts',(-1.61255750286032,2.11960704884808,15.3367567393357));
#69268=CARTESIAN_POINT('Ctrl Pts',(-1.6227675606002,2.10905212039588,15.3388958302459));
#69269=CARTESIAN_POINT('Ctrl Pts',(-1.68513439043447,2.04457869199203,15.3519621930614));
#69270=CARTESIAN_POINT('Ctrl Pts',(-1.74412898638654,1.97703074697555,15.365082540821));
#69271=CARTESIAN_POINT('Ctrl Pts',(-1.79953647467951,1.90668242393888,15.3782125582993));
#69272=CARTESIAN_POINT('Ctrl Pts',(-1.85482014934552,1.83649130133295,15.3913132354279));
#69273=CARTESIAN_POINT('Ctrl Pts',(-1.90653200235803,1.76351139803357,15.404423277528));
#69274=CARTESIAN_POINT('Ctrl Pts',(-1.95441360534623,1.68803174082651,15.41752372735));
#69275=CARTESIAN_POINT('Ctrl Pts',(-2.00152977687848,1.61375869535139,15.4304147544343));
#69276=CARTESIAN_POINT('Ctrl Pts',(-2.04493641973501,1.53706478161179,15.4432963377886));
#69277=CARTESIAN_POINT('Ctrl Pts',(-2.08435494788096,1.4582510974481,15.45617771612));
#69278=CARTESIAN_POINT('Ctrl Pts',(-2.1059680281026,1.41503775188416,15.4632405435856));
#69279=CARTESIAN_POINT('Ctrl Pts',(-2.12638166130199,1.37118763733681,15.470303805537));
#69280=CARTESIAN_POINT('Ctrl Pts',(-2.14554686211721,1.32675413515881,15.4773728232848));
#69281=CARTESIAN_POINT('Ctrl Pts',(-2.15238081888792,1.31090996864141,15.479893504501));
#69282=CARTESIAN_POINT('Ctrl Pts',(-2.15905601977847,1.29499164910449,15.4824149433682));
#69283=CARTESIAN_POINT('Ctrl Pts',(-2.16557018945707,1.27900167913697,15.484937467835));
#69284=CARTESIAN_POINT('Ctrl Pts',(-2.1701386561413,1.26778771808245,15.4867065450244));
#69285=CARTESIAN_POINT('Ctrl Pts',(-2.17462683200284,1.25654108535781,15.4884757499118));
#69286=CARTESIAN_POINT('Ctrl Pts',(-2.1790311425866,1.2452704312927,15.4902440024149));
#69287=CARTESIAN_POINT('Ctrl Pts',(-2.21002477719553,1.1659575564956,15.5026873964345));
#69288=CARTESIAN_POINT('Ctrl Pts',(-2.2369126125938,1.08534359103648,15.5150992820502));
#69289=CARTESIAN_POINT('Ctrl Pts',(-2.25954646256793,1.00373624547512,15.5275444054577));
#69290=CARTESIAN_POINT('Ctrl Pts',(-2.28183631964793,0.923369181483772,
15.5398003858769));
#69291=CARTESIAN_POINT('Ctrl Pts',(-2.30000078071459,0.842038814791743,
15.5520888107296));
#69292=CARTESIAN_POINT('Ctrl Pts',(-2.31387996442088,0.760032592464827,
15.5644938859947));
#69293=CARTESIAN_POINT('Ctrl Pts',(-2.32735702168778,0.680402365073205,
15.5765395446794));
#69294=CARTESIAN_POINT('Ctrl Pts',(-2.33679399591497,0.600134965111233,
15.588695508872));
#69295=CARTESIAN_POINT('Ctrl Pts',(-2.34202168375654,0.519485938537849,
15.601056230854));
#69296=CARTESIAN_POINT('Ctrl Pts',(-2.3458041924598,0.46113210139823,15.6099998671025));
#69297=CARTESIAN_POINT('Ctrl Pts',(-2.34738263953659,0.402578305857887,
15.6190510917899));
#69298=CARTESIAN_POINT('Ctrl Pts',(-2.34668236863854,0.343918483395395,
15.62825));
#69299=CARTESIAN_POINT('',(-2.86810422470753,0.00112209329583249,15.1318955557932));
#69300=CARTESIAN_POINT('Ctrl Pts',(-2.86810422470753,0.00112209329583249,
15.1318955557932));
#69301=CARTESIAN_POINT('Ctrl Pts',(-2.87043208924124,0.0628907887003932,
15.1295435255677));
#69302=CARTESIAN_POINT('Ctrl Pts',(-2.87069405598972,0.124617231014218,
15.1272626996305));
#69303=CARTESIAN_POINT('Ctrl Pts',(-2.86887882812214,0.18622628149455,15.1250833127955));
#69304=CARTESIAN_POINT('Ctrl Pts',(-2.86624429184131,0.27564275730815,15.121920253331));
#69305=CARTESIAN_POINT('Ctrl Pts',(-2.85923588778213,0.364817170574697,
15.1189701933795));
#69306=CARTESIAN_POINT('Ctrl Pts',(-2.84798023700843,0.453530392715298,
15.1161343222149));
#69307=CARTESIAN_POINT('Ctrl Pts',(-2.84725382473312,0.459255727912805,
15.1159513019998));
#69308=CARTESIAN_POINT('Ctrl Pts',(-2.84650970988206,0.464979155137534,
15.1157687573921));
#69309=CARTESIAN_POINT('Ctrl Pts',(-2.84574792123122,0.470700620581005,
15.115586661831));
#69310=CARTESIAN_POINT('Ctrl Pts',(-2.83292253676448,0.56702654240334,15.1125209223));
#69311=CARTESIAN_POINT('Ctrl Pts',(-2.81509017073285,0.662792526882216,
15.1095819301958));
#69312=CARTESIAN_POINT('Ctrl Pts',(-2.79237326851397,0.75767385608828,15.1066596911336));
#69313=CARTESIAN_POINT('Ctrl Pts',(-2.77861012505902,0.815158161495671,
15.1048892386733));
#69314=CARTESIAN_POINT('Ctrl Pts',(-2.76305343525744,0.87231684260555,15.1031252999957));
#69315=CARTESIAN_POINT('Ctrl Pts',(-2.74572684796513,0.929069661288577,
15.1013474925125));
#69316=CARTESIAN_POINT('Ctrl Pts',(-2.73593206408982,0.961152239579201,
15.1003424913674));
#69317=CARTESIAN_POINT('Ctrl Pts',(-2.72557164273762,0.993105009075931,
15.0993331185811));
#69318=CARTESIAN_POINT('Ctrl Pts',(-2.71464968609205,1.02491266185944,15.0983161987151));
#69319=CARTESIAN_POINT('Ctrl Pts',(-2.7095518477653,1.03975892766194,15.0978415499652));
#69320=CARTESIAN_POINT('Ctrl Pts',(-2.70433399449945,1.05456668921369,15.0973654813685));
#69321=CARTESIAN_POINT('Ctrl Pts',(-2.69899954771354,1.06932740672487,15.0968879351064));
#69322=CARTESIAN_POINT('Ctrl Pts',(-2.66530865040951,1.16255203483741,15.0938718843853));
#69323=CARTESIAN_POINT('Ctrl Pts',(-2.62693751439746,1.25398885395718,15.0907912075745));
#69324=CARTESIAN_POINT('Ctrl Pts',(-2.58413151251978,1.34326828686256,15.0875945741555));
#69325=CARTESIAN_POINT('Ctrl Pts',(-2.54084885367928,1.43354187155657,15.0843623453175));
#69326=CARTESIAN_POINT('Ctrl Pts',(-2.49303197702603,1.52160928443245,15.0810114657988));
#69327=CARTESIAN_POINT('Ctrl Pts',(-2.44092724967875,1.60708697826089,15.0775259806253));
#69328=CARTESIAN_POINT('Ctrl Pts',(-2.38908958411024,1.69212655781216,15.0740583602391));
#69329=CARTESIAN_POINT('Ctrl Pts',(-2.33300828307443,1.77460269145118,15.070457600858));
#69330=CARTESIAN_POINT('Ctrl Pts',(-2.27291614853868,1.85414146323808,15.0667444052748));
#69331=CARTESIAN_POINT('Ctrl Pts',(-2.23194216665565,1.90837518649277,15.0642125529829));
#69332=CARTESIAN_POINT('Ctrl Pts',(-2.18910328969542,1.96124339077654,15.0616291892213));
#69333=CARTESIAN_POINT('Ctrl Pts',(-2.14446881854968,2.0126287210334,15.0590102206127));
#69334=CARTESIAN_POINT('Ctrl Pts',(-2.86750655814837,1.78005205161276E-11,
15.1324934418516));
#69335=CARTESIAN_POINT('Ctrl Pts',(-2.8675210427035,0.000387639407476004,
15.1324789572965));
#69336=CARTESIAN_POINT('Ctrl Pts',(-2.8675354467886,0.0007752834867927,
15.1324644746078));
#69337=CARTESIAN_POINT('Ctrl Pts',(-2.8675497703958,0.00116293222919048,
15.1324499937912));
#69338=CARTESIAN_POINT('',(-2.,-2.44929359829471E-16,16.));
#69339=CARTESIAN_POINT('',(-2.5,3.06161699786838E-16,15.5));
#69340=CARTESIAN_POINT('Origin',(0.,0.,16.));
#69341=CARTESIAN_POINT('Ctrl Pts',(1.70912691251745,-2.39920179129963,-0.331459347220305));
#69342=CARTESIAN_POINT('Ctrl Pts',(2.50276811089229,-1.8338774509613,-0.278813689627446));
#69343=CARTESIAN_POINT('Ctrl Pts',(3.47164055573234,0.135559128113983,-0.173547661664216));
#69344=CARTESIAN_POINT('Ctrl Pts',(1.7822571658123,2.98575720466778,-0.0156612633306156));
#69345=CARTESIAN_POINT('Ctrl Pts',(-1.52260497856303,3.12258994484077,0.142199847780495));
#69346=CARTESIAN_POINT('Ctrl Pts',(-3.44759473877435,0.435419189166611,
0.300060958891607));
#69347=CARTESIAN_POINT('Ctrl Pts',(-2.25033077153724,-2.64835158515141,
0.457922070002716));
#69348=CARTESIAN_POINT('Ctrl Pts',(0.985382290881231,-3.33221894822028,
0.615783181113829));
#69349=CARTESIAN_POINT('Ctrl Pts',(3.32847435827679,-0.998535563052339,
0.77364429222494));
#69350=CARTESIAN_POINT('Ctrl Pts',(2.65685902325779,2.23988877671352,0.93150540333605));
#69351=CARTESIAN_POINT('Ctrl Pts',(-0.421236688919228,3.44936780038012,
1.08936651444716));
#69352=CARTESIAN_POINT('Ctrl Pts',(-3.11778136245101,1.534669043428,1.24722762555827));
#69353=CARTESIAN_POINT('Ctrl Pts',(-2.99040402529488,-1.77010166332876,
1.40508873666939));
#69354=CARTESIAN_POINT('Ctrl Pts',(-0.154463996640659,-3.47157902841105,
1.5629498477805));
#69355=CARTESIAN_POINT('Ctrl Pts',(2.82137950689542,-2.02868629898774,1.72081095889161));
#69356=CARTESIAN_POINT('Ctrl Pts',(3.24175982869864,1.25169549534852,1.87867207000272));
#69357=CARTESIAN_POINT('Ctrl Pts',(0.725915687453796,3.39835072617039,2.03653318111383));
#69358=CARTESIAN_POINT('Ctrl Pts',(-2.44742623153422,2.46695170965159,2.19439429222494));
#69359=CARTESIAN_POINT('Ctrl Pts',(-3.40401210913808,-0.698889657279975,
2.35225540333606));
#69360=CARTESIAN_POINT('Ctrl Pts',(-1.27741406313663,-3.23171125442164,
2.51011651444716));
#69361=CARTESIAN_POINT('Ctrl Pts',(2.00620167327619,-2.83741076670449,2.66797762555828));
#69362=CARTESIAN_POINT('Ctrl Pts',(3.47270034769341,0.126874545576242,2.82583873666938));
#69363=CARTESIAN_POINT('Ctrl Pts',(1.79380080602483,2.97624317288409,2.9836998477805));
#69364=CARTESIAN_POINT('Ctrl Pts',(-1.50983373834399,3.12987970032478,3.14156095889161));
#69365=CARTESIAN_POINT('Ctrl Pts',(-3.44593643717389,0.448627793146361,
3.29942207000272));
#69366=CARTESIAN_POINT('Ctrl Pts',(-2.26088234184521,-2.63896870992823,
3.45728318111383));
#69367=CARTESIAN_POINT('Ctrl Pts',(0.971965844637692,-3.33631941315407,
3.61514429222494));
#69368=CARTESIAN_POINT('Ctrl Pts',(3.32445600610991,-1.01179893649521,3.77300540333605));
#69369=CARTESIAN_POINT('Ctrl Pts',(2.66582027065906,2.22915838561566,3.93086651444717));
#69370=CARTESIAN_POINT('Ctrl Pts',(-0.40738206985568,3.45105558846889,4.08872762555827));
#69371=CARTESIAN_POINT('Ctrl Pts',(-3.11159811670885,1.54715932752985,4.24658873666939));
#69372=CARTESIAN_POINT('Ctrl Pts',(-2.99748429181114,-1.75807643320396,
4.4044498477805));
#69373=CARTESIAN_POINT('Ctrl Pts',(-0.168399187629091,-3.47093453388311,
4.56231095889161));
#69374=CARTESIAN_POINT('Ctrl Pts',(2.81321347412892,-2.03999381708313,4.72017207000272));
#69375=CARTESIAN_POINT('Ctrl Pts',(3.24675814243868,1.2386712192005,4.87803318111383));
#69376=CARTESIAN_POINT('Ctrl Pts',(0.739551751054495,3.39540984747235,5.03589429222495));
#69377=CARTESIAN_POINT('Ctrl Pts',(-2.43750360973441,2.47675614005708,5.19375540333605));
#69378=CARTESIAN_POINT('Ctrl Pts',(-3.40679017196424,-0.68521934370669,
5.35161651444717));
#69379=CARTESIAN_POINT('Ctrl Pts',(-1.290376670055,-3.2265574338858,5.50947762555827));
#69380=CARTESIAN_POINT('Ctrl Pts',(1.99479544995775,-2.84544125534347,5.66733873666938));
#69381=CARTESIAN_POINT('Ctrl Pts',(3.47318166970145,0.112933228207418,5.8251998477805));
#69382=CARTESIAN_POINT('Ctrl Pts',(1.80573372884392,2.96901844475568,5.98306095889161));
#69383=CARTESIAN_POINT('Ctrl Pts',(-1.49725746582663,3.13591532184942,6.14092207000272));
#69384=CARTESIAN_POINT('Ctrl Pts',(-3.44410776976812,0.462457019631576,
6.29878318111384));
#69385=CARTESIAN_POINT('Ctrl Pts',(-2.27145759682837,-2.62987170991179,
6.45664429222494));
#69386=CARTESIAN_POINT('Ctrl Pts',(0.958565205016858,-3.34019424173425,
6.61450540333606));
#69387=CARTESIAN_POINT('Ctrl Pts',(3.32036761015448,-1.02513597060133,6.77236651444716));
#69388=CARTESIAN_POINT('Ctrl Pts',(2.67474718310955,2.21843916554662,6.93022762555828));
#69389=CARTESIAN_POINT('Ctrl Pts',(-0.393525399738489,3.45266311483532,
7.08808873666939));
#69390=CARTESIAN_POINT('Ctrl Pts',(-3.10536236726555,1.55963758378497,7.2459498477805));
#69391=CARTESIAN_POINT('Ctrl Pts',(-3.00451749289248,-1.74602962737945,
7.4038109588916));
#69392=CARTESIAN_POINT('Ctrl Pts',(-0.182331017612658,-3.47023057228191,
7.56167207000273));
#69393=CARTESIAN_POINT('Ctrl Pts',(2.80500176969189,-2.05127031295465,7.71953318111383));
#69394=CARTESIAN_POINT('Ctrl Pts',(3.25170431452417,1.22562795157771,7.87739429222495));
#69395=CARTESIAN_POINT('Ctrl Pts',(0.753175804487954,3.39241374721859,8.03525540333604));
#69396=CARTESIAN_POINT('Ctrl Pts',(-2.42754166081253,2.48652092486737,8.19311651444717));
#69397=CARTESIAN_POINT('Ctrl Pts',(-3.4095133623985,-0.671538127294123,
8.35097762555827));
#69398=CARTESIAN_POINT('Ctrl Pts',(-1.30331847021638,-3.22135154709579,
8.50883873666939));
#69399=CARTESIAN_POINT('Ctrl Pts',(1.98335707505572,-2.85342592993231,8.6666998477805));
#69400=CARTESIAN_POINT('Ctrl Pts',(3.47360702767608,0.0989901109348193,
8.82456095889161));
#69401=CARTESIAN_POINT('Ctrl Pts',(1.81763755172645,2.96174586271981,8.98242207000272));
#69402=CARTESIAN_POINT('Ctrl Pts',(-1.48465706514355,3.14190041594302,9.14028318111382));
#69403=CARTESIAN_POINT('Ctrl Pts',(-3.44222360370688,0.476278791115081,
9.29814429222495));
#69404=CARTESIAN_POINT('Ctrl Pts',(-2.28199624872525,-2.62073233001576,
9.45600540333604));
#69405=CARTESIAN_POINT('Ctrl Pts',(0.945149118703501,-3.34401524640603,
9.61386651444717));
#69406=CARTESIAN_POINT('Ctrl Pts',(3.31622570907301,-1.03845648501127,9.77172762555827));
#69407=CARTESIAN_POINT('Ctrl Pts',(2.68363099400492,2.20768419680356,9.92958873666939));
#69408=CARTESIAN_POINT('Ctrl Pts',(-0.379662388241621,3.45421500426974,
10.0874498477804));
#69409=CARTESIAN_POINT('Ctrl Pts',(-3.09907657727214,1.57209070761236,10.2453109588916));
#69410=CARTESIAN_POINT('Ctrl Pts',(-3.01150227846558,-1.73395468559392,
10.4031720700027));
#69411=CARTESIAN_POINT('Ctrl Pts',(-0.19625990944859,-3.46947069054991,
10.5610331811138));
#69412=CARTESIAN_POINT('Ctrl Pts',(2.79674486473763,-2.06251375419229,10.7188942922249));
#69413=CARTESIAN_POINT('Ctrl Pts',(3.25659808795613,1.21256493395727,10.876755403336));
#69414=CARTESIAN_POINT('Ctrl Pts',(0.766787720893258,3.38936298066535,11.0346165144471));
#69415=CARTESIAN_POINT('Ctrl Pts',(-2.41754059357168,2.49624564153576,11.1924776255582));
#69416=CARTESIAN_POINT('Ctrl Pts',(-3.41218161174795,-0.657846090039483,
11.3503387366693));
#69417=CARTESIAN_POINT('Ctrl Pts',(-1.31623926718511,-3.21609374974792,
11.5081998477805));
#69418=CARTESIAN_POINT('Ctrl Pts',(1.97188673755754,-2.86136462550139,11.6660609588915));
#69419=CARTESIAN_POINT('Ctrl Pts',(3.47397641551634,0.0850454018936421,
11.8239220700027));
#69420=CARTESIAN_POINT('Ctrl Pts',(1.82951207635102,2.95442554793994,11.9817831811138));
#69421=CARTESIAN_POINT('Ctrl Pts',(-1.47203272427312,3.14783489304223,12.1396442922249));
#69422=CARTESIAN_POINT('Ctrl Pts',(-3.44028399952346,0.490092864148866,
12.297505403336));
#69423=CARTESIAN_POINT('Ctrl Pts',(-2.29249806934856,-2.61155067396514,
12.4553665144471));
#69424=CARTESIAN_POINT('Ctrl Pts',(0.931717690008006,-3.3477824508677,12.6132276255582));
#69425=CARTESIAN_POINT('Ctrl Pts',(3.3120305835413,-1.05176010108855,12.7710887366694));
#69426=CARTESIAN_POINT('Ctrl Pts',(2.69247115139201,2.19689333884833,12.9289498477804));
#69427=CARTESIAN_POINT('Ctrl Pts',(-0.365792477741649,3.45571183163002,
13.0868109588916));
#69428=CARTESIAN_POINT('Ctrl Pts',(-3.09274234008898,1.58451735220887,13.2446720700027));
#69429=CARTESIAN_POINT('Ctrl Pts',(-3.01843568553144,-1.72184961279198,
13.4025331811139));
#69430=CARTESIAN_POINT('Ctrl Pts',(-0.210191084142041,-3.4686590840217,
13.5603942922249));
#69431=CARTESIAN_POINT('Ctrl Pts',(2.78845329525541,-2.07371596827588,13.718255403336));
#69432=CARTESIAN_POINT('Ctrl Pts',(3.26141951023774,1.19946711027502,13.8761165144471));
#69433=CARTESIAN_POINT('Ctrl Pts',(0.780425247323911,3.38628676205265,14.0339776255582));
#69434=CARTESIAN_POINT('Ctrl Pts',(-2.40757310028838,2.50587441647701,14.1918387366693));
#69435=CARTESIAN_POINT('Ctrl Pts',(-3.41465630905069,-0.64403700912367,
14.3496998477805));
#69436=CARTESIAN_POINT('Ctrl Pts',(-1.3294036198624,-3.21098749848051,14.5075609588917));
#69437=CARTESIAN_POINT('Ctrl Pts',(1.96089086179741,-2.86886848447928,14.6654220700027));
#69438=CARTESIAN_POINT('Ctrl Pts',(3.47331888567816,0.0703548346390749,
14.8232831811138));
#69439=CARTESIAN_POINT('Ctrl Pts',(1.84324590483098,2.94849643456436,14.9811442922249));
#69440=CARTESIAN_POINT('Ctrl Pts',(-1.46382348530112,3.15085562308053,15.1390307759807));
#69441=CARTESIAN_POINT('Ctrl Pts',(-2.77399534817744,1.38993107123141,15.244296889366));
#69442=CARTESIAN_POINT('Ctrl Pts',(-2.91479286562129,0.42575414026495,15.2969426323811));
#69443=CARTESIAN_POINT('Ctrl Pts',(1.59731828398619,-2.24224945505684,-0.220201080228989));
#69444=CARTESIAN_POINT('Ctrl Pts',(2.33904061472963,-1.71390782133067,-0.16755542263613));
#69445=CARTESIAN_POINT('Ctrl Pts',(3.24453081540399,0.126691044598195,-0.0622893946728999));
#69446=CARTESIAN_POINT('Ctrl Pts',(1.66566446111606,2.79043325550034,0.0955970036607006));
#69447=CARTESIAN_POINT('Ctrl Pts',(-1.42299834712965,2.91831459428533,0.253458114771811));
#69448=CARTESIAN_POINT('Ctrl Pts',(-3.22205804126471,0.406934691017055,
0.411319225882923));
#69449=CARTESIAN_POINT('Ctrl Pts',(-2.10311736364774,-2.47510022714181,
0.569180336994034));
#69450=CARTESIAN_POINT('Ctrl Pts',(0.920919996293564,-3.11422996926394,
0.727041448105144));
#69451=CARTESIAN_POINT('Ctrl Pts',(3.11073034501781,-0.933212800285599,
0.884902559216257));
#69452=CARTESIAN_POINT('Ctrl Pts',(2.48305112086282,2.09335846913207,1.04276367032736));
#69453=CARTESIAN_POINT('Ctrl Pts',(-0.393679989571658,3.22371511172612,
1.20062478143848));
#69454=CARTESIAN_POINT('Ctrl Pts',(-2.91382058245102,1.43427319819356,1.35848589254958));
#69455=CARTESIAN_POINT('Ctrl Pts',(-2.79477608779421,-1.65430415415129,
1.5163470036607));
#69456=CARTESIAN_POINT('Ctrl Pts',(-0.144359183770769,-3.24447331311172,
1.67420811477181));
#69457=CARTESIAN_POINT('Ctrl Pts',(2.63680891069109,-1.89597255423958,1.83206922588292));
#69458=CARTESIAN_POINT('Ctrl Pts',(3.02968855545379,1.16981137331599,1.98993033699403));
#69459=CARTESIAN_POINT('Ctrl Pts',(0.678427325501767,3.17603550125726,2.14779144810514));
#69460=CARTESIAN_POINT('Ctrl Pts',(-2.28731912165539,2.30556727103035,2.30565255921625));
#69461=CARTESIAN_POINT('Ctrl Pts',(-3.18132652468021,-0.653169299416062,
2.46351367032736));
#69462=CARTESIAN_POINT('Ctrl Pts',(-1.1938474693279,-3.02029734447755,2.62137478143847));
#69463=CARTESIAN_POINT('Ctrl Pts',(1.87495884045709,-2.65179142850224,2.77923589254959));
#69464=CARTESIAN_POINT('Ctrl Pts',(3.2455212772967,0.118574594980136,2.9370970036607));
#69465=CARTESIAN_POINT('Ctrl Pts',(1.67645293296106,2.781541618015,3.09495811477181));
#69466=CARTESIAN_POINT('Ctrl Pts',(-1.41106258310788,2.92512746443273,3.25281922588292));
#69467=CARTESIAN_POINT('Ctrl Pts',(-3.22050822337385,0.419279207090299,
3.41068033699403));
#69468=CARTESIAN_POINT('Ctrl Pts',(-2.11297866537686,-2.46633116614313,
3.56854144810514));
#69469=CARTESIAN_POINT('Ctrl Pts',(0.908381234698991,-3.1180621876695,3.72640255921625));
#69470=CARTESIAN_POINT('Ctrl Pts',(3.10697486767988,-0.94560850288233,3.88426367032737));
#69471=CARTESIAN_POINT('Ctrl Pts',(2.4914261363263,2.08333004481237,4.04212478143847));
#69472=CARTESIAN_POINT('Ctrl Pts',(-0.380731719793802,3.22529248714156,
4.19998589254959));
#69473=CARTESIAN_POINT('Ctrl Pts',(-2.90804183576698,1.44594638584389,4.3578470036607));
#69474=CARTESIAN_POINT('Ctrl Pts',(-2.80139317344133,-1.64306559731458,
4.5157081147718));
#69475=CARTESIAN_POINT('Ctrl Pts',(-0.157382754573871,-3.24387098049039,
4.67356922588293));
#69476=CARTESIAN_POINT('Ctrl Pts',(2.62917708806279,-1.9065403507373,4.83143033699403));
#69477=CARTESIAN_POINT('Ctrl Pts',(3.03435988668589,1.15763912661238,4.98929144810515));
#69478=CARTESIAN_POINT('Ctrl Pts',(0.691171337401332,3.17328701062093,5.14715255921625));
#69479=CARTESIAN_POINT('Ctrl Pts',(-2.27804562352611,2.31473030967662,5.30501367032737));
#69480=CARTESIAN_POINT('Ctrl Pts',(-3.18392285062523,-0.64039327812794,
5.46287478143848));
#69481=CARTESIAN_POINT('Ctrl Pts',(-1.2059620811143,-3.01548067948094,5.62073589254959));
#69482=CARTESIAN_POINT('Ctrl Pts',(1.86429879589028,-2.6592965741052,5.77859700366071));
#69483=CARTESIAN_POINT('Ctrl Pts',(3.2459711119101,0.105545298575644,5.93645811477181));
#69484=CARTESIAN_POINT('Ctrl Pts',(1.68760522110346,2.77478952122698,6.09431922588292));
#69485=CARTESIAN_POINT('Ctrl Pts',(-1.39930903228071,2.93076824426359,6.25218033699404));
#69486=CARTESIAN_POINT('Ctrl Pts',(-3.21879918476404,0.43220374543584,6.41004144810514));
#69487=CARTESIAN_POINT('Ctrl Pts',(-2.12286210236372,-2.45782927880566,
6.56790255921625));
#69488=CARTESIAN_POINT('Ctrl Pts',(0.895857245680565,-3.12168353052771,
6.72576367032737));
#69489=CARTESIAN_POINT('Ctrl Pts',(3.10315392871742,-0.958073047367486,
6.88362478143849));
#69490=CARTESIAN_POINT('Ctrl Pts',(2.49976906298218,2.07331206072884,7.04148589254958));
#69491=CARTESIAN_POINT('Ctrl Pts',(-0.367781533139289,3.2267948514413,7.1993470036607));
#69492=CARTESIAN_POINT('Ctrl Pts',(-2.90221402009851,1.45760833249197,7.3572081147718));
#69493=CARTESIAN_POINT('Ctrl Pts',(-2.80796627260669,-1.63180687622944,
7.51506922588292));
#69494=CARTESIAN_POINT('Ctrl Pts',(-0.170403184244221,-3.24321307104634,
7.67293033699403));
#69495=CARTESIAN_POINT('Ctrl Pts',(2.62150258153908,-1.9170791544405,7.83079144810515));
#69496=CARTESIAN_POINT('Ctrl Pts',(3.03898248729561,1.14544913082903,7.98865255921625));
#69497=CARTESIAN_POINT('Ctrl Pts',(0.703904124821557,3.17048691094375,8.14651367032737));
#69498=CARTESIAN_POINT('Ctrl Pts',(-2.26873537099862,2.32385629628559,8.30437478143848));
#69499=CARTESIAN_POINT('Ctrl Pts',(-3.18646789385143,-0.627607067248622,
8.46223589254958));
#69500=CARTESIAN_POINT('Ctrl Pts',(-1.21805724729189,-3.01061535432976,
8.62009700366071));
#69501=CARTESIAN_POINT('Ctrl Pts',(1.85360870305031,-2.6667589027474,8.77795811477182));
#69502=CARTESIAN_POINT('Ctrl Pts',(3.24636864357678,0.0925143200145056,
8.93581922588293));
#69503=CARTESIAN_POINT('Ctrl Pts',(1.69873031298536,2.7679927010654,9.09368033699404));
#69504=CARTESIAN_POINT('Ctrl Pts',(-1.38753293171776,2.93636180209542,9.25154144810513));
#69505=CARTESIAN_POINT('Ctrl Pts',(-3.2170382781411,0.445121316475167,9.40940255921626));
#69506=CARTESIAN_POINT('Ctrl Pts',(-2.13271133078565,-2.44928778401944,
9.56726367032736));
#69507=CARTESIAN_POINT('Ctrl Pts',(0.883318820470059,-3.12525457056035,
9.72512478143848));
#69508=CARTESIAN_POINT('Ctrl Pts',(3.09928298485748,-0.970522152851265,
9.88298589254958));
#69509=CARTESIAN_POINT('Ctrl Pts',(2.50807170772477,2.06326066659819,10.0408470036607));
#69510=CARTESIAN_POINT('Ctrl Pts',(-0.354825419949051,3.22824521849724,
10.1987081147718));
#69511=CARTESIAN_POINT('Ctrl Pts',(-2.8963394374609,1.46924679083965,10.3565692258829));
#69512=CARTESIAN_POINT('Ctrl Pts',(-2.81449412353686,-1.62052185979746,
10.514430336994));
#69513=CARTESIAN_POINT('Ctrl Pts',(-0.183420867976338,-3.24250289968617,
10.6722914481051));
#69514=CARTESIAN_POINT('Ctrl Pts',(2.61378583145108,-1.92758706589651,10.8301525592163));
#69515=CARTESIAN_POINT('Ctrl Pts',(3.04355611709647,1.1332406770645,10.9880136703274));
#69516=CARTESIAN_POINT('Ctrl Pts',(0.716625569200582,3.16763572115793,11.1458747814385));
#69517=CARTESIAN_POINT('Ctrl Pts',(-2.25938855921644,2.33294483595297,11.3037358925496));
#69518=CARTESIAN_POINT('Ctrl Pts',(-3.18896159015968,-0.61481074341118,
11.4615970036607));
#69519=CARTESIAN_POINT('Ctrl Pts',(-1.23013278427552,-3.00570151453487,
11.6194581147718));
#69520=CARTESIAN_POINT('Ctrl Pts',(1.84288873856135,-2.67417826025129,11.7773192258829));
#69521=CARTESIAN_POINT('Ctrl Pts',(3.24671386659492,0.0794818538159997,
11.935180336994));
#69522=CARTESIAN_POINT('Ctrl Pts',(1.70982802325928,2.76115127076741,12.0930414481051));
#69523=CARTESIAN_POINT('Ctrl Pts',(-1.37573445710014,2.94190805422394,12.2509025592163));
#69524=CARTESIAN_POINT('Ctrl Pts',(-3.21522556007834,0.458031692686313,
12.4087636703274));
#69525=CARTESIAN_POINT('Ctrl Pts',(-2.14252613738304,-2.440706778724,12.5666247814385));
#69526=CARTESIAN_POINT('Ctrl Pts',(0.870766056554023,-3.12877532991534,
12.7244858925496));
#69527=CARTESIAN_POINT('Ctrl Pts',(3.09536229841439,-0.982955465467049,
12.8823470036607));
#69528=CARTESIAN_POINT('Ctrl Pts',(2.51633355470891,2.05317573107611,13.0402081147718));
#69529=CARTESIAN_POINT('Ctrl Pts',(-0.341862859078587,3.22964412556086,
13.1980692258829));
#69530=CARTESIAN_POINT('Ctrl Pts',(-2.89041957697911,1.48086050218972,13.355930336994));
#69531=CARTESIAN_POINT('Ctrl Pts',(-2.82097395706795,-1.6092086834769,13.5137914481051));
#69532=CARTESIAN_POINT('Ctrl Pts',(-0.196440685224712,-3.24174438729166,
13.6716525592163));
#69533=CARTESIAN_POINT('Ctrl Pts',(2.60603668453876,-1.93805644721967,13.8295136703274));
#69534=CARTESIAN_POINT('Ctrl Pts',(3.04806212885536,1.12099969420077,13.9873747814385));
#69535=CARTESIAN_POINT('Ctrl Pts',(0.729370948233867,3.1647607443498,14.1452358925496));
#69536=CARTESIAN_POINT('Ctrl Pts',(-2.2500731250317,2.34194371026325,14.3030970036607));
#69537=CARTESIAN_POINT('Ctrl Pts',(-3.19127439631823,-0.601905032740824,
14.4609581147718));
#69538=CARTESIAN_POINT('Ctrl Pts',(-1.24243594390296,-3.00092930689345,
14.6188192258829));
#69539=CARTESIAN_POINT('Ctrl Pts',(1.83261219720478,-2.68119122754943,14.776680336994));
#69540=CARTESIAN_POINT('Ctrl Pts',(3.24609935141463,0.0657523223774665,
14.9345414481051));
#69541=CARTESIAN_POINT('Ctrl Pts',(1.72266340440009,2.75561003147542,15.0924025592163));
#69542=CARTESIAN_POINT('Ctrl Pts',(-1.36806225475429,2.94473117244051,15.2502890429721));
#69543=CARTESIAN_POINT('Ctrl Pts',(-2.5925245555989,1.29900377631302,15.3555551563574));
#69544=CARTESIAN_POINT('Ctrl Pts',(-2.72411130161863,0.397901915736784,
15.4082008993725));
#69545=CARTESIAN_POINT('Ctrl Pts',(1.48550965545491,-2.08529711881406,-0.108942813237673));
#69546=CARTESIAN_POINT('Ctrl Pts',(2.17531311856699,-1.59393819170005,-0.0562971556448137));
#69547=CARTESIAN_POINT('Ctrl Pts',(3.01742107507566,0.117822961082407,0.0489688723184162));
#69548=CARTESIAN_POINT('Ctrl Pts',(1.54907175641981,2.59510930633288,0.206855270652017));
#69549=CARTESIAN_POINT('Ctrl Pts',(-1.32339171569626,2.71403924372989,0.364716381763127));
#69550=CARTESIAN_POINT('Ctrl Pts',(-2.99652134375508,0.378450192867501,
0.52257749287424));
#69551=CARTESIAN_POINT('Ctrl Pts',(-1.95590395575824,-2.30184886913221,
0.680438603985348));
#69552=CARTESIAN_POINT('Ctrl Pts',(0.856457701705894,-2.8962409903076,0.838299715096462));
#69553=CARTESIAN_POINT('Ctrl Pts',(2.89298633175884,-0.86789003751886,0.996160826207572));
#69554=CARTESIAN_POINT('Ctrl Pts',(2.30924321846785,1.94682816155061,1.15402193731868));
#69555=CARTESIAN_POINT('Ctrl Pts',(-0.366123290224087,2.99806242307211,
1.31188304842979));
#69556=CARTESIAN_POINT('Ctrl Pts',(-2.70985980245103,1.33387735295911,1.46974415954091));
#69557=CARTESIAN_POINT('Ctrl Pts',(-2.59914815029355,-1.53850664497382,
1.62760527065202));
#69558=CARTESIAN_POINT('Ctrl Pts',(-0.134254370900873,-3.0173675978124,
1.78546638176313));
#69559=CARTESIAN_POINT('Ctrl Pts',(2.45223831448674,-1.76325880949142,1.94332749287424));
#69560=CARTESIAN_POINT('Ctrl Pts',(2.81761728220894,1.08792725128345,2.10118860398535));
#69561=CARTESIAN_POINT('Ctrl Pts',(0.630938963549732,2.95372027634413,2.25904971509646));
#69562=CARTESIAN_POINT('Ctrl Pts',(-2.12721201177655,2.14418283240911,2.41691082620757));
#69563=CARTESIAN_POINT('Ctrl Pts',(-2.95864094022234,-0.607448941552151,
2.57477193731869));
#69564=CARTESIAN_POINT('Ctrl Pts',(-1.11028087551918,-2.80888343453346,
2.73263304842979));
#69565=CARTESIAN_POINT('Ctrl Pts',(1.743716007638,-2.46617209029998,2.8904941595409));
#69566=CARTESIAN_POINT('Ctrl Pts',(3.01834220689999,0.110274644384027,3.04835527065202));
#69567=CARTESIAN_POINT('Ctrl Pts',(1.55910505989728,2.5868400631459,3.20621638176313));
#69568=CARTESIAN_POINT('Ctrl Pts',(-1.31229142787177,2.72037522854068,3.36407749287424));
#69569=CARTESIAN_POINT('Ctrl Pts',(-2.99508000957381,0.389930621034239,
3.52193860398535));
#69570=CARTESIAN_POINT('Ctrl Pts',(-1.9650749889085,-2.29369362235803,3.67979971509646));
#69571=CARTESIAN_POINT('Ctrl Pts',(0.844796624760288,-2.89980496218494,
3.83766082620758));
#69572=CARTESIAN_POINT('Ctrl Pts',(2.88949372924982,-0.879418069269448,
3.99552193731869));
#69573=CARTESIAN_POINT('Ctrl Pts',(2.31703200199353,1.93750170400908,4.1533830484298));
#69574=CARTESIAN_POINT('Ctrl Pts',(-0.354081369731924,2.99952938581424,
4.31124415954091));
#69575=CARTESIAN_POINT('Ctrl Pts',(-2.7044855548251,1.34473344415793,4.46910527065202));
#69576=CARTESIAN_POINT('Ctrl Pts',(-2.60530205507152,-1.52805476142519,
4.62696638176313));
#69577=CARTESIAN_POINT('Ctrl Pts',(-0.146366321518651,-3.01680742709766,
4.78482749287424));
#69578=CARTESIAN_POINT('Ctrl Pts',(2.44514070199668,-1.77308688439148,4.94268860398535));
#69579=CARTESIAN_POINT('Ctrl Pts',(2.8219616309331,1.07660703402426,5.10054971509647));
#69580=CARTESIAN_POINT('Ctrl Pts',(0.642790923748172,2.95116417376951,5.25841082620757));
#69581=CARTESIAN_POINT('Ctrl Pts',(-2.11858763731782,2.15270447929615,5.41627193731869));
#69582=CARTESIAN_POINT('Ctrl Pts',(-2.96105552928621,-0.595567212549187,
5.57413304842979));
#69583=CARTESIAN_POINT('Ctrl Pts',(-1.1215474921736,-2.80440392507609,5.73199415954091));
#69584=CARTESIAN_POINT('Ctrl Pts',(1.73380214182281,-2.47315189286694,5.88985527065202));
#69585=CARTESIAN_POINT('Ctrl Pts',(3.01876055411874,0.0981573689438738,
6.04771638176313));
#69586=CARTESIAN_POINT('Ctrl Pts',(1.569476713363,2.58056059769827,6.20557749287424));
#69587=CARTESIAN_POINT('Ctrl Pts',(-1.30136059873477,2.72562116667776,6.36343860398535));
#69588=CARTESIAN_POINT('Ctrl Pts',(-2.99349059975995,0.4019504712401,6.52129971509647));
#69589=CARTESIAN_POINT('Ctrl Pts',(-1.97426660789908,-2.28578684769951,
6.67916082620757));
#69590=CARTESIAN_POINT('Ctrl Pts',(0.833149286344271,-2.90317281932119,
6.83702193731869));
#69591=CARTESIAN_POINT('Ctrl Pts',(2.88594024728037,-0.891010124133642,
6.9948830484298));
#69592=CARTESIAN_POINT('Ctrl Pts',(2.3247909428548,1.92818495591104,7.15274415954091));
#69593=CARTESIAN_POINT('Ctrl Pts',(-0.342037666540088,3.00092658804729,
7.31060527065203));
#69594=CARTESIAN_POINT('Ctrl Pts',(-2.69906567293149,1.35557908119896,7.46846638176313));
#69595=CARTESIAN_POINT('Ctrl Pts',(-2.6114150523209,-1.51758412507944,7.62632749287424));
#69596=CARTESIAN_POINT('Ctrl Pts',(-0.158475350875785,-3.01619556981077,
7.78418860398534));
#69597=CARTESIAN_POINT('Ctrl Pts',(2.43800339338629,-1.78288799592635,7.94204971509647));
#69598=CARTESIAN_POINT('Ctrl Pts',(2.82626066006705,1.06527031008035,8.09991082620757));
#69599=CARTESIAN_POINT('Ctrl Pts',(0.65463244515516,2.94856007466891,8.2577719373187));
#69600=CARTESIAN_POINT('Ctrl Pts',(-2.10992908118473,2.1611916677038,8.41563304842979));
#69601=CARTESIAN_POINT('Ctrl Pts',(-2.96342242530435,-0.583676007203117,
8.57349415954092));
#69602=CARTESIAN_POINT('Ctrl Pts',(-1.13279602436738,-2.79987916156373,
8.73135527065201));
#69603=CARTESIAN_POINT('Ctrl Pts',(1.72386033104489,-2.48009187556249,8.88921638176315));
#69604=CARTESIAN_POINT('Ctrl Pts',(3.01913025947748,0.0860385290941875,
9.04707749287423));
#69605=CARTESIAN_POINT('Ctrl Pts',(1.57982307424428,2.574239539411,9.20493860398536));
#69606=CARTESIAN_POINT('Ctrl Pts',(-1.29040879829197,2.7308231882478,9.36279971509646));
#69607=CARTESIAN_POINT('Ctrl Pts',(-2.99185295257532,0.413963841835261,
9.52066082620758));
#69608=CARTESIAN_POINT('Ctrl Pts',(-1.98342641284605,-2.27784323802312,
9.67852193731868));
#69609=CARTESIAN_POINT('Ctrl Pts',(0.821488522236616,-2.90649389471465,
9.8363830484298));
#69610=CARTESIAN_POINT('Ctrl Pts',(2.88234026064193,-0.902587820691261,
9.9942441595409));
#69611=CARTESIAN_POINT('Ctrl Pts',(2.33251242144462,1.91883713639282,10.1521052706521));
#69612=CARTESIAN_POINT('Ctrl Pts',(-0.329988451656481,3.00227543272473,
10.3099663817632));
#69613=CARTESIAN_POINT('Ctrl Pts',(-2.69360229764966,1.36640287406693,10.4678274928743));
#69614=CARTESIAN_POINT('Ctrl Pts',(-2.61748596860813,-1.50708903400101,
10.6256886039854));
#69615=CARTESIAN_POINT('Ctrl Pts',(-0.170581826504084,-3.0155351088224,
10.7835497150965));
#69616=CARTESIAN_POINT('Ctrl Pts',(2.43082679816454,-1.79266037760072,10.9414108262076));
#69617=CARTESIAN_POINT('Ctrl Pts',(2.83051414623682,1.05391642017174,11.0992719373187));
#69618=CARTESIAN_POINT('Ctrl Pts',(0.666463417507903,2.94590846165049,11.2571330484298));
#69619=CARTESIAN_POINT('Ctrl Pts',(-2.10123652486119,2.16964403037017,11.414994159541));
#69620=CARTESIAN_POINT('Ctrl Pts',(-2.96574156857143,-0.571775396782877,
11.5728552706521));
#69621=CARTESIAN_POINT('Ctrl Pts',(-1.14402630136591,-2.79530927932181,
11.7307163817632));
#69622=CARTESIAN_POINT('Ctrl Pts',(1.71389073956514,-2.48699189500119,11.8885774928743));
#69623=CARTESIAN_POINT('Ctrl Pts',(3.01945131767349,0.0739183057383534,
12.0464386039854));
#69624=CARTESIAN_POINT('Ctrl Pts',(1.59014397016754,2.56787699359488,12.2042997150965));
#69625=CARTESIAN_POINT('Ctrl Pts',(-1.27943618992718,2.73598121540565,12.3621608262076));
#69626=CARTESIAN_POINT('Ctrl Pts',(-2.99016712063321,0.42597052122376,12.5200219373187));
#69627=CARTESIAN_POINT('Ctrl Pts',(-1.99255420541753,-2.26986288348284,
12.6778830484298));
#69628=CARTESIAN_POINT('Ctrl Pts',(0.809814423100042,-2.90976820896299,
12.8357441595409));
#69629=CARTESIAN_POINT('Ctrl Pts',(2.87869401328747,-0.914150829845545,
12.9936052706521));
#69630=CARTESIAN_POINT('Ctrl Pts',(2.34019595802583,1.9094581233039,13.1514663817632));
#69631=CARTESIAN_POINT('Ctrl Pts',(-0.317933240415524,3.00357641949169,
13.3093274928743));
#69632=CARTESIAN_POINT('Ctrl Pts',(-2.68809681386924,1.37720365217055,13.4671886039854));
#69633=CARTESIAN_POINT('Ctrl Pts',(-2.62351222860445,-1.49656775416184,
13.6250497150965));
#69634=CARTESIAN_POINT('Ctrl Pts',(-0.182690286307381,-3.01482969056162,
13.7829108262076));
#69635=CARTESIAN_POINT('Ctrl Pts',(2.42362007382213,-1.80239692616347,13.9407719373187));
#69636=CARTESIAN_POINT('Ctrl Pts',(2.83470474747299,1.04253227812653,14.0986330484299));
#69637=CARTESIAN_POINT('Ctrl Pts',(0.678316649143826,2.94323472664697,14.2564941595409));
#69638=CARTESIAN_POINT('Ctrl Pts',(-2.09257314977501,2.17801300404947,14.4143552706521));
#69639=CARTESIAN_POINT('Ctrl Pts',(-2.96789248358577,-0.559773056357977,
14.5722163817632));
#69640=CARTESIAN_POINT('Ctrl Pts',(-1.15546826794353,-2.79087111530639,
14.7300774928743));
#69641=CARTESIAN_POINT('Ctrl Pts',(1.70433353261215,-2.49351397061956,14.8879386039854));
#69642=CARTESIAN_POINT('Ctrl Pts',(3.01887981715109,0.0611498101158578,
15.0457997150965));
#69643=CARTESIAN_POINT('Ctrl Pts',(1.6020809039692,2.56272362838647,15.2036608262076));
#69644=CARTESIAN_POINT('Ctrl Pts',(-1.27230102420747,2.73860672180048,15.3615473099633));
#69645=CARTESIAN_POINT('Ctrl Pts',(-2.41105376302034,1.20807648139464,15.4668134233488));
#69646=CARTESIAN_POINT('Ctrl Pts',(-2.53342973761595,0.370049691208616,
15.5194591663637));
#69647=CARTESIAN_POINT('Ctrl Pts',(1.37370102692364,-1.92834478257128,0.00231545375364296));
#69648=CARTESIAN_POINT('Ctrl Pts',(2.01158562240434,-1.47396856206942,0.0549611113465025));
#69649=CARTESIAN_POINT('Ctrl Pts',(2.79031133474731,0.108954877566618,0.160227139309733));
#69650=CARTESIAN_POINT('Ctrl Pts',(1.43247905172356,2.39978535716542,0.318113537643333));
#69651=CARTESIAN_POINT('Ctrl Pts',(-1.22378508426288,2.50976389317445,0.475974648754443));
#69652=CARTESIAN_POINT('Ctrl Pts',(-2.77098464624544,0.349965694717946,
0.633835759865555));
#69653=CARTESIAN_POINT('Ctrl Pts',(-1.80869054786874,-2.1285975111226,0.791696870976666));
#69654=CARTESIAN_POINT('Ctrl Pts',(0.791995407118226,-2.67825201135127,
0.949557982087777));
#69655=CARTESIAN_POINT('Ctrl Pts',(2.67524231849987,-0.802567274752119,
1.10741909319888));
#69656=CARTESIAN_POINT('Ctrl Pts',(2.13543531607289,1.80029785396915,1.26528020430999));
#69657=CARTESIAN_POINT('Ctrl Pts',(-0.338566590876518,2.77240973441811,
1.42314131542111));
#69658=CARTESIAN_POINT('Ctrl Pts',(-2.50589902245105,1.23348150772466,1.58100242653222));
#69659=CARTESIAN_POINT('Ctrl Pts',(-2.40352021279288,-1.42270913579635,
1.73886353764333));
#69660=CARTESIAN_POINT('Ctrl Pts',(-0.12414955803098,-2.79026188251307,
1.89672464875444));
#69661=CARTESIAN_POINT('Ctrl Pts',(2.26766771828241,-1.63054506474326,2.05458575986555));
#69662=CARTESIAN_POINT('Ctrl Pts',(2.60554600896408,1.00604312925092,2.21244687097666));
#69663=CARTESIAN_POINT('Ctrl Pts',(0.583450601597702,2.731405051431,2.37030798208778));
#69664=CARTESIAN_POINT('Ctrl Pts',(-1.96710490189772,1.98279839378788,2.52816909319888));
#69665=CARTESIAN_POINT('Ctrl Pts',(-2.73595535576447,-0.561728583688241,
2.68603020431));
#69666=CARTESIAN_POINT('Ctrl Pts',(-1.02671428171045,-2.59746952458937,
2.8438913154211));
#69667=CARTESIAN_POINT('Ctrl Pts',(1.61247317481889,-2.28055275209774,3.00175242653222));
#69668=CARTESIAN_POINT('Ctrl Pts',(2.79116313650327,0.101974693787918,3.15961353764333));
#69669=CARTESIAN_POINT('Ctrl Pts',(1.44175718683351,2.39213850827682,3.31747464875444));
#69670=CARTESIAN_POINT('Ctrl Pts',(-1.21352027263567,2.51562299264861,3.47533575986556));
#69671=CARTESIAN_POINT('Ctrl Pts',(-2.76965179577376,0.360582034978182,
3.63319687097666));
#69672=CARTESIAN_POINT('Ctrl Pts',(-1.81717131244015,-2.12105607857293,
3.79105798208778));
#69673=CARTESIAN_POINT('Ctrl Pts',(0.781212014821587,-2.68154773670037,
3.94891909319888));
#69674=CARTESIAN_POINT('Ctrl Pts',(2.67201259081977,-0.813227635656568,
4.10678020431));
#69675=CARTESIAN_POINT('Ctrl Pts',(2.14263786766077,1.79167336320579,4.26464131542111));
#69676=CARTESIAN_POINT('Ctrl Pts',(-0.327431019670046,2.77376628448691,
4.42250242653222));
#69677=CARTESIAN_POINT('Ctrl Pts',(-2.50092927388322,1.24352050247198,4.58036353764333));
#69678=CARTESIAN_POINT('Ctrl Pts',(-2.4092109367017,-1.4130439255358,4.73822464875444));
#69679=CARTESIAN_POINT('Ctrl Pts',(-0.135349888463429,-2.78974387370495,
4.89608575986555));
#69680=CARTESIAN_POINT('Ctrl Pts',(2.26110431593055,-1.63963341804565,5.05394687097667));
#69681=CARTESIAN_POINT('Ctrl Pts',(2.6095633751803,0.995574941436156,5.21180798208777));
#69682=CARTESIAN_POINT('Ctrl Pts',(0.594410510095007,2.72904133691807,5.36966909319889));
#69683=CARTESIAN_POINT('Ctrl Pts',(-1.95912965110952,1.99067864891568,5.52753020430999));
#69684=CARTESIAN_POINT('Ctrl Pts',(-2.7381882079472,-0.550741146970434,
5.68539131542111));
#69685=CARTESIAN_POINT('Ctrl Pts',(-1.03713290323291,-2.59332717067123,
5.84325242653222));
#69686=CARTESIAN_POINT('Ctrl Pts',(1.60330548775534,-2.28700721162866,6.00111353764333));
#69687=CARTESIAN_POINT('Ctrl Pts',(2.79154999632737,0.0907694393121017,
6.15897464875444));
#69688=CARTESIAN_POINT('Ctrl Pts',(1.45134820562253,2.38633167416956,6.31683575986555));
#69689=CARTESIAN_POINT('Ctrl Pts',(-1.20341216518885,2.52047408909194,6.47469687097668));
#69690=CARTESIAN_POINT('Ctrl Pts',(-2.76818201475586,0.371697197044361,
6.63255798208777));
#69691=CARTESIAN_POINT('Ctrl Pts',(-1.82567111343442,-2.11374441659337,
6.79041909319889));
#69692=CARTESIAN_POINT('Ctrl Pts',(0.770441327007976,-2.68466210811466,
6.94828020430999));
#69693=CARTESIAN_POINT('Ctrl Pts',(2.66872656584332,-0.823947200899797,
7.10614131542111));
#69694=CARTESIAN_POINT('Ctrl Pts',(2.14981282272741,1.78305785109325,7.26400242653222));
#69695=CARTESIAN_POINT('Ctrl Pts',(-0.316293799940889,2.77505832465327,
7.42186353764333));
#69696=CARTESIAN_POINT('Ctrl Pts',(-2.49591732576446,1.25354982990597,7.57972464875445));
#69697=CARTESIAN_POINT('Ctrl Pts',(-2.41486383203512,-1.40336137392943,
7.73758575986554));
#69698=CARTESIAN_POINT('Ctrl Pts',(-0.146547517507347,-2.7891780685752,
7.89544687097668));
#69699=CARTESIAN_POINT('Ctrl Pts',(2.25450420523348,-1.64869683741221,8.05330798208776));
#69700=CARTESIAN_POINT('Ctrl Pts',(2.61353883283848,0.98509148933167,8.21116909319889));
#69701=CARTESIAN_POINT('Ctrl Pts',(0.605360765488762,2.72663323839408,8.36903020430999));
#69702=CARTESIAN_POINT('Ctrl Pts',(-1.95112279137082,1.99852703912202,8.52689131542112));
#69703=CARTESIAN_POINT('Ctrl Pts',(-2.74037695675728,-0.539744947157614,
8.68475242653222));
#69704=CARTESIAN_POINT('Ctrl Pts',(-1.04753480144288,-2.58914296879769,
8.84261353764335));
#69705=CARTESIAN_POINT('Ctrl Pts',(1.59411195903949,-2.29342484837757,9.00047464875443));
#69706=CARTESIAN_POINT('Ctrl Pts',(2.79189187537818,0.0795627381738728,
9.15833575986557));
#69707=CARTESIAN_POINT('Ctrl Pts',(1.46091583550319,2.38048637775659,9.31619687097666));
#69708=CARTESIAN_POINT('Ctrl Pts',(-1.19328466486618,2.5252845744002,9.47405798208777));
#69709=CARTESIAN_POINT('Ctrl Pts',(-2.76666762700954,0.38280636719535,9.63191909319889));
#69710=CARTESIAN_POINT('Ctrl Pts',(-1.83414149490645,-2.10639869202682,
9.78978020431));
#69711=CARTESIAN_POINT('Ctrl Pts',(0.759658224003173,-2.68773321886896,
9.94764131542111));
#69712=CARTESIAN_POINT('Ctrl Pts',(2.66539753642639,-0.834653488531258,
10.1055024265322));
#69713=CARTESIAN_POINT('Ctrl Pts',(2.15695313516446,1.77441360618746,10.2633635376433));
#69714=CARTESIAN_POINT('Ctrl Pts',(-0.305151483363911,2.77630564695223,
10.4212246487544));
#69715=CARTESIAN_POINT('Ctrl Pts',(-2.49086515783842,1.26355895729423,10.5790857598655));
#69716=CARTESIAN_POINT('Ctrl Pts',(-2.42047781367941,-1.39365620820457,
10.7369468709767));
#69717=CARTESIAN_POINT('Ctrl Pts',(-0.157742785031831,-2.78856731795865,
10.8948079820878));
#69718=CARTESIAN_POINT('Ctrl Pts',(2.247867764878,-1.65773368930495,11.0526690931989));
#69719=CARTESIAN_POINT('Ctrl Pts',(2.61747217537717,0.974592163278993,11.21053020431));
#69720=CARTESIAN_POINT('Ctrl Pts',(0.616301265815223,2.72418120214306,11.3683913154211));
#69721=CARTESIAN_POINT('Ctrl Pts',(-1.94308449050595,2.00634322478738,11.5262524265322));
#69722=CARTESIAN_POINT('Ctrl Pts',(-2.74252154698318,-0.528740050154576,
11.6841135376433));
#69723=CARTESIAN_POINT('Ctrl Pts',(-1.05791981845631,-2.58491704410876,
11.8419746487544));
#69724=CARTESIAN_POINT('Ctrl Pts',(1.58489274056894,-2.2998055297511,11.9998357598655));
#69725=CARTESIAN_POINT('Ctrl Pts',(2.79218876875207,0.0683547576607113,
12.1576968709766));
#69726=CARTESIAN_POINT('Ctrl Pts',(1.4704599170758,2.37460271642234,12.3155579820878));
#69727=CARTESIAN_POINT('Ctrl Pts',(-1.18313792275421,2.53005437658735,12.4734190931989));
#69728=CARTESIAN_POINT('Ctrl Pts',(-2.7651086811881,0.393909349761204,12.63128020431));
#69729=CARTESIAN_POINT('Ctrl Pts',(-1.84258227345201,-2.09901898824168,
12.7891413154211));
#69730=CARTESIAN_POINT('Ctrl Pts',(0.74886278964606,-2.69076108801064,12.9470024265322));
#69731=CARTESIAN_POINT('Ctrl Pts',(2.66202572816055,-0.845346194224041,
13.1048635376433));
#69732=CARTESIAN_POINT('Ctrl Pts',(2.16405836134274,1.76574051553168,13.2627246487544));
#69733=CARTESIAN_POINT('Ctrl Pts',(-0.294003621752462,2.77750871342253,
13.4205857598655));
#69734=CARTESIAN_POINT('Ctrl Pts',(-2.48577405075937,1.2735468021514,13.5784468709767));
#69735=CARTESIAN_POINT('Ctrl Pts',(-2.42605050014095,-1.38392682484676,
13.7363079820877));
#69736=CARTESIAN_POINT('Ctrl Pts',(-0.168939887390049,-2.78791499383159,
13.8941690931989));
#69737=CARTESIAN_POINT('Ctrl Pts',(2.24120346310549,-1.66673740510728,14.05203020431));
#69738=CARTESIAN_POINT('Ctrl Pts',(2.62134736609061,0.964064862052277,14.2098913154211));
#69739=CARTESIAN_POINT('Ctrl Pts',(0.627262350053781,2.72170870894412,14.3677524265322));
#69740=CARTESIAN_POINT('Ctrl Pts',(-1.93507317451832,2.0140822978357,14.5256135376433));
#69741=CARTESIAN_POINT('Ctrl Pts',(-2.74451057085332,-0.517641079975128,
14.6834746487544));
#69742=CARTESIAN_POINT('Ctrl Pts',(-1.06850059198409,-2.58081292371933,
14.8413357598655));
#69743=CARTESIAN_POINT('Ctrl Pts',(1.57605486801951,-2.30583671368971,14.9991968709767));
#69744=CARTESIAN_POINT('Ctrl Pts',(2.79166028288756,0.0565472978542511,
15.1570579820878));
#69745=CARTESIAN_POINT('Ctrl Pts',(1.4814984035383,2.36983722529753,15.3149190931989));
#69746=CARTESIAN_POINT('Ctrl Pts',(-1.17653979366064,2.53248227116047,15.4728055769547));
#69747=CARTESIAN_POINT('Ctrl Pts',(-2.2295829704418,1.11714918647624,15.57807169034));
#69748=CARTESIAN_POINT('Ctrl Pts',(-2.34274817361327,0.34219746668045,15.6307174333551));
#69749=CARTESIAN_POINT('Ctrl Pts',(1.29200104020317,2.64812001020929,3.10255293678452E-15));
#69750=CARTESIAN_POINT('Ctrl Pts',(1.36315737313149,2.60529414881161,2.09107015119386E-15));
#69751=CARTESIAN_POINT('Ctrl Pts',(1.43224767624703,2.55934891308958,1.31609841305187E-15));
#69752=CARTESIAN_POINT('Ctrl Pts',(1.49903325513989,2.51027466650741,1.66186508998578E-15));
#69753=CARTESIAN_POINT('Ctrl Pts',(1.57400867069288,2.45518250302776,1.95949932089937E-15));
#69754=CARTESIAN_POINT('Ctrl Pts',(1.64608024297622,2.39614668551523,1.83946245349909E-15));
#69755=CARTESIAN_POINT('Ctrl Pts',(1.71509586361607,2.3334939900483,1.70696790036118E-15));
#69756=CARTESIAN_POINT('Ctrl Pts',(1.74960367393599,2.30216764231483,1.64072062379222E-15));
#69757=CARTESIAN_POINT('Ctrl Pts',(1.78334695259876,2.26993667275488,1.11913045518732E-15));
#69758=CARTESIAN_POINT('Ctrl Pts',(1.81630324354019,2.23683999242427,1.31838984174237E-15));
#69759=CARTESIAN_POINT('Ctrl Pts',(1.83676158255619,2.21629450362181,1.44208446773989E-15));
#69760=CARTESIAN_POINT('Ctrl Pts',(1.85691660316518,2.19541538445973,1.46191677087001E-15));
#69761=CARTESIAN_POINT('Ctrl Pts',(1.87676245786726,2.17421177399615,2.54657406273395E-15));
#69762=CARTESIAN_POINT('Ctrl Pts',(1.88888624454376,2.16125853746939,3.20918869037616E-15));
#69763=CARTESIAN_POINT('Ctrl Pts',(1.90089366672971,2.1481851241337,1.96170375495304E-15));
#69764=CARTESIAN_POINT('Ctrl Pts',(1.91277473204615,2.1350036118777,1.54737334057131E-15));
#69765=CARTESIAN_POINT('Ctrl Pts',(1.9776543595374,2.06302255780864,-1.97990253103911E-15));
#69766=CARTESIAN_POINT('Ctrl Pts',(2.03884298327229,1.98774253915799,-1.66382442733107E-15));
#69767=CARTESIAN_POINT('Ctrl Pts',(2.09617256623861,1.90953752585601,-9.71445146547012E-16));
#69768=CARTESIAN_POINT('Ctrl Pts',(2.1535084707902,1.83132388908891,-2.78989518885305E-16));
#69769=CARTESIAN_POINT('Ctrl Pts',(2.20698482442042,1.75018364400972,1.25908428358211E-15));
#69770=CARTESIAN_POINT('Ctrl Pts',(2.25638533273427,1.66647271728721,-1.98452365651747E-15));
#69771=CARTESIAN_POINT('Ctrl Pts',(2.26598195715652,1.65021089425715,-2.61463229783777E-15));
#69772=CARTESIAN_POINT('Ctrl Pts',(2.27542461416388,1.63385203033854,-2.47328191587402E-15));
#69773=CARTESIAN_POINT('Ctrl Pts',(2.28471149018554,1.61739870311764,-1.85962356624714E-15));
#69774=CARTESIAN_POINT('Ctrl Pts',(2.29658165337844,1.59636863027905,-1.51468754041748E-15));
#69775=CARTESIAN_POINT('Ctrl Pts',(2.30819775718845,1.57518341353175,-2.25374764460409E-15));
#69776=CARTESIAN_POINT('Ctrl Pts',(2.319554459588,1.55385101519017,-2.52575738102223E-15));
#69777=CARTESIAN_POINT('Ctrl Pts',(2.32539410160174,1.54288184780102,-2.66562540160156E-15));
#69778=CARTESIAN_POINT('Ctrl Pts',(2.33116442149476,1.53187508817643,-2.94361108551474E-15));
#69779=CARTESIAN_POINT('Ctrl Pts',(2.33686168047272,1.52083799385098,-2.56739074444567E-15));
#69780=CARTESIAN_POINT('Ctrl Pts',(2.38042908971752,1.43643642333951,-3.13104787203378E-16));
#69781=CARTESIAN_POINT('Ctrl Pts',(2.41979213021192,1.3501422097958,-1.59953211202993E-15));
#69782=CARTESIAN_POINT('Ctrl Pts',(2.45479061001924,1.26230270075925,-1.83186799063151E-15));
#69783=CARTESIAN_POINT('Ctrl Pts',(2.48943950316612,1.17534058756353,-2.06188315346638E-15));
#69784=CARTESIAN_POINT('Ctrl Pts',(2.51981079469772,1.08686297282194,-1.65071434113658E-15));
#69785=CARTESIAN_POINT('Ctrl Pts',(2.54569935642937,0.997197819015192,-3.8441472227646E-15));
#69786=CARTESIAN_POINT('Ctrl Pts',(2.57084179381203,0.910116870356819,-5.97436401313909E-15));
#69787=CARTESIAN_POINT('Ctrl Pts',(2.59175618069638,0.82191508220806,-3.21503687969247E-15));
#69788=CARTESIAN_POINT('Ctrl Pts',(2.60820620752898,0.732896562075562,-4.85722573273506E-15));
#69789=CARTESIAN_POINT('Ctrl Pts',(2.61778223009678,0.681076381694317,-5.8131899799285E-15));
#69790=CARTESIAN_POINT('Ctrl Pts',(2.62584449121432,0.628979560875543,-2.63541690974722E-15));
#69791=CARTESIAN_POINT('Ctrl Pts',(2.63233843305125,0.576668196894127,-3.19189119579733E-15));
#69792=CARTESIAN_POINT('Ctrl Pts',(2.63414224296016,0.562137768524487,-3.34548576625677E-15));
#69793=CARTESIAN_POINT('Ctrl Pts',(2.63582527555606,0.547588319420663,-4.76400556623387E-15));
#69794=CARTESIAN_POINT('Ctrl Pts',(2.63738542604938,0.53302926152673,-4.71844785465692E-15));
#69795=CARTESIAN_POINT('Ctrl Pts',(2.64690685377399,0.444176924480302,-4.60028352020783E-15));
#69796=CARTESIAN_POINT('Ctrl Pts',(2.65183263786071,0.355196731306933,-1.12077890731655E-15));
#69797=CARTESIAN_POINT('Ctrl Pts',(2.65198717743402,0.26638198029663,-3.05311331771918E-15));
#69798=CARTESIAN_POINT('Ctrl Pts',(2.65207998114263,0.213047173580212,-3.85426492076651E-15));
#69799=CARTESIAN_POINT('Ctrl Pts',(2.65045121279154,0.159772024913009,-2.51411300564142E-15));
#69800=CARTESIAN_POINT('Ctrl Pts',(2.64705383408491,0.106621318043218,-3.10862446895044E-15));
#69801=CARTESIAN_POINT('Ctrl Pts',(2.64122335367285,0.0154056538352043,
-4.35916179998321E-15));
#69802=CARTESIAN_POINT('Ctrl Pts',(2.6301863282489,-0.0754450034552312,
-4.42204053305948E-15));
#69803=CARTESIAN_POINT('Ctrl Pts',(2.61414363949405,-0.165586435036926,
-3.66373598126302E-15));
#69804=CARTESIAN_POINT('Ctrl Pts',(2.5981009507392,-0.255727866618621,-2.90543142946655E-15));
#69805=CARTESIAN_POINT('Ctrl Pts',(2.57705193629621,-0.345160943019199,
-4.87329601145403E-15));
#69806=CARTESIAN_POINT('Ctrl Pts',(2.55115372858487,-0.433510589178545,
-1.60982338570648E-15));
#69807=CARTESIAN_POINT('Ctrl Pts',(2.54730992415644,-0.446623417870877,
-1.20154213111825E-15));
#69808=CARTESIAN_POINT('Ctrl Pts',(2.54335838534963,-0.4597150170452,-1.8738946464181E-15));
#69809=CARTESIAN_POINT('Ctrl Pts',(2.53930241226215,-0.472774949708627,
-1.97064586870965E-15));
#69810=CARTESIAN_POINT('Ctrl Pts',(2.51300579541806,-0.557448106520195,
-3.25376286445461E-15));
#69811=CARTESIAN_POINT('Ctrl Pts',(2.48237490705924,-0.640633082256515,
-3.13037515801062E-15));
#69812=CARTESIAN_POINT('Ctrl Pts',(2.44762844889866,-0.722031078368415,
-1.77635683940025E-15));
#69813=CARTESIAN_POINT('Ctrl Pts',(2.41285997251622,-0.80348065496454,-3.32163561638838E-16));
#69814=CARTESIAN_POINT('Ctrl Pts',(2.37397005509929,-0.883141781461181,
-2.97904560551731E-15));
#69815=CARTESIAN_POINT('Ctrl Pts',(2.33113438836156,-0.96068640220217,-3.02535774210355E-15));
#69816=CARTESIAN_POINT('Ctrl Pts',(2.28891526221294,-1.03711491083859,-3.47404387143521E-15));
#69817=CARTESIAN_POINT('Ctrl Pts',(2.24286247134769,-1.11148803976047,-3.0687412209896E-15));
#69818=CARTESIAN_POINT('Ctrl Pts',(2.19311210718949,-1.18345333934342,-1.33226762955019E-15));
#69819=CARTESIAN_POINT('Ctrl Pts',(2.1665899473663,-1.22181838871659,1.22294838671581E-16));
#69820=CARTESIAN_POINT('Ctrl Pts',(2.13901644806922,-1.25949841971484,-1.28609992312022E-16));
#69821=CARTESIAN_POINT('Ctrl Pts',(2.11040940577999,-1.29643454214332,-1.88737914186277E-15));
#69822=CARTESIAN_POINT('Ctrl Pts',(2.09658409753436,-1.31428515643645,-2.18989034168364E-15));
#69823=CARTESIAN_POINT('Ctrl Pts',(2.08251135224091,-1.33196908693401,-1.95637260965346E-15));
#69824=CARTESIAN_POINT('Ctrl Pts',(2.06822143203954,-1.34944529769313,-1.60982338570648E-15));
#69825=CARTESIAN_POINT('Ctrl Pts',(2.01420303007452,-1.41550843620673,-2.99806603525348E-16));
#69826=CARTESIAN_POINT('Ctrl Pts',(1.95704446263552,-1.47866336737798,-6.19616046821105E-16));
#69827=CARTESIAN_POINT('Ctrl Pts',(1.8969065179103,-1.53861547303735,-1.0547118733939E-15));
#69828=CARTESIAN_POINT('Ctrl Pts',(1.83769520508206,-1.59764381028979,-1.48310355214476E-15));
#69829=CARTESIAN_POINT('Ctrl Pts',(1.77559497936228,-1.65356778346114,2.20446172603681E-16));
#69830=CARTESIAN_POINT('Ctrl Pts',(1.71073303306612,-1.70606397784894,8.88178419700125E-16));
#69831=CARTESIAN_POINT('Ctrl Pts',(1.64789827301082,-1.75691946348473,1.5350414560931E-15));
#69832=CARTESIAN_POINT('Ctrl Pts',(1.58247114995395,-1.80455837340375,-6.98079953837882E-16));
#69833=CARTESIAN_POINT('Ctrl Pts',(1.51455134937916,-1.8486411040293,-4.9960036108132E-16));
#69834=CARTESIAN_POINT('Ctrl Pts',(1.46978363624784,-1.87769718225669,-3.68777281570644E-16));
#69835=CARTESIAN_POINT('Ctrl Pts',(1.42393267971699,-1.90520735301187,1.69235332884175E-16));
#69836=CARTESIAN_POINT('Ctrl Pts',(1.37702479013106,-1.93106208855762,-2.22044604925031E-16));
#69837=CARTESIAN_POINT('Ctrl Pts',(-1.03727419333506,2.12829183996564,-0.33162583102735));
#69838=CARTESIAN_POINT('Ctrl Pts',(-1.74153389301133,1.78505394459699,-0.278960867360666));
#69839=CARTESIAN_POINT('Ctrl Pts',(-2.77088494568995,0.350890813503785,
-0.173630940027297));
#69840=CARTESIAN_POINT('Ctrl Pts',(-1.80617750337226,-2.13380867727772,
-0.0156360490272432));
#69841=CARTESIAN_POINT('Ctrl Pts',(0.799331096145292,-2.67619672977392,
0.14235884197281));
#69842=CARTESIAN_POINT('Ctrl Pts',(2.6785330878346,-0.794154761772425,0.300353732972864));
#69843=CARTESIAN_POINT('Ctrl Pts',(2.12850244685976,1.81002105660491,0.458348623972918));
#69844=CARTESIAN_POINT('Ctrl Pts',(-0.352738835506404,2.771329446129,0.616343514972972));
#69845=CARTESIAN_POINT('Ctrl Pts',(-2.51382108425654,1.21907270575297,0.774338405973023));
#69846=CARTESIAN_POINT('Ctrl Pts',(-2.39456021962358,-1.43931956546868,
0.932333296973079));
#69847=CARTESIAN_POINT('Ctrl Pts',(-0.103009617793377,-2.79189425785633,
1.09032818797313));
#69848=CARTESIAN_POINT('Ctrl Pts',(2.28196265616274,-1.61184802118412,1.24832307897318));
#69849=CARTESIAN_POINT('Ctrl Pts',(2.59684801618063,1.03043335678079,1.40631796997323));
#69850=CARTESIAN_POINT('Ctrl Pts',(0.555976476186501,2.73793099838751,1.56431286097329));
#69851=CARTESIAN_POINT('Ctrl Pts',(-1.98924983312574,1.96170350529848,1.72230775197334));
#69852=CARTESIAN_POINT('Ctrl Pts',(-2.72991498642861,-0.594103134059335,
1.8803026429734));
#69853=CARTESIAN_POINT('Ctrl Pts',(-0.994116232242361,-2.61096200673646,
2.03829753397345));
#69854=CARTESIAN_POINT('Ctrl Pts',(1.64350205501279,-2.25926839472914,2.1962924249735));
#69855=CARTESIAN_POINT('Ctrl Pts',(2.79020532811094,0.141938289250975,2.35428731597356));
#69856=CARTESIAN_POINT('Ctrl Pts',(1.40575267279317,2.41438420716175,2.51228220697361));
#69857=CARTESIAN_POINT('Ctrl Pts',(-1.25393904248897,2.49660349308063,2.67027709797367));
#69858=CARTESIAN_POINT('Ctrl Pts',(-2.77611054256664,0.314010001336946,
2.82827198897372));
#69859=CARTESIAN_POINT('Ctrl Pts',(-1.7799124222889,-2.15343997555266,2.98626687997377));
#69860=CARTESIAN_POINT('Ctrl Pts',(0.830946655855235,-2.66738067760568,
3.14426177097383));
#69861=CARTESIAN_POINT('Ctrl Pts',(2.68800621811034,-0.761586880528364,
3.30225666197388));
#69862=CARTESIAN_POINT('Ctrl Pts',(2.1066206787299,1.83508618713756,3.46025155297393));
#69863=CARTESIAN_POINT('Ctrl Pts',(-0.385801684362841,2.76704699413756,
3.61824644397398));
#69864=CARTESIAN_POINT('Ctrl Pts',(-2.52824114267486,1.1888602645272,3.77624133497404));
#69865=CARTESIAN_POINT('Ctrl Pts',(-2.37716759400457,-1.46781001274115,
3.93423622597408));
#69866=CARTESIAN_POINT('Ctrl Pts',(-0.0696285472027664,-2.7929453754341,
4.09223111697415));
#69867=CARTESIAN_POINT('Ctrl Pts',(2.30107456105757,-1.58443929156132,4.25022600797419));
#69868=CARTESIAN_POINT('Ctrl Pts',(2.58434053922803,1.0614028365637,4.40822089897426));
#69869=CARTESIAN_POINT('Ctrl Pts',(0.523202520475101,2.7443853823577,4.56621578997431));
#69870=CARTESIAN_POINT('Ctrl Pts',(-2.01256260784032,1.93777804553689,4.72421068097436));
#69871=CARTESIAN_POINT('Ctrl Pts',(-2.72261639883674,-0.626699249266954,
4.88220557197441));
#69872=CARTESIAN_POINT('Ctrl Pts',(-0.962828204728596,-2.62266159701306,
5.04020046297447));
#69873=CARTESIAN_POINT('Ctrl Pts',(1.67039685162278,-2.23945671142426,5.19819535397451));
#69874=CARTESIAN_POINT('Ctrl Pts',(2.78830881513536,0.175288207517705,5.3561902449746));
#69875=CARTESIAN_POINT('Ctrl Pts',(1.37678542300575,2.43101910795819,5.51418513597462));
#69876=CARTESIAN_POINT('Ctrl Pts',(-1.2836992416995,2.48143270332224,5.67218002697469));
#69877=CARTESIAN_POINT('Ctrl Pts',(-2.77966646474201,0.280795920636377,
5.83017491797473));
#69878=CARTESIAN_POINT('Ctrl Pts',(-1.7540383054339,-2.17456699766373,5.98816980897479));
#69879=CARTESIAN_POINT('Ctrl Pts',(0.862778921897542,-2.65725507548423,
6.14616469997484));
#69880=CARTESIAN_POINT('Ctrl Pts',(2.69691974792615,-0.729394185268462,
6.30415959097489));
#69881=CARTESIAN_POINT('Ctrl Pts',(2.08452949938132,1.86014213716763,6.46215448197495));
#69882=CARTESIAN_POINT('Ctrl Pts',(-0.418857394511624,2.76223650097533,
6.620149372975));
#69883=CARTESIAN_POINT('Ctrl Pts',(-2.5422746462691,1.15854720542358,6.77814426397505));
#69884=CARTESIAN_POINT('Ctrl Pts',(-2.35944829289878,-1.49612691887905,
6.93613915497512));
#69885=CARTESIAN_POINT('Ctrl Pts',(-0.0362306387250156,-2.79357823321186,
7.09413404597515));
#69886=CARTESIAN_POINT('Ctrl Pts',(2.3198539124191,-1.55681399958096,7.25212893697523));
#69887=CARTESIAN_POINT('Ctrl Pts',(2.5714655034136,1.09222578664457,7.41012382797526));
#69888=CARTESIAN_POINT('Ctrl Pts',(0.490352783225777,2.75044471899368,7.56811871897533));
#69889=CARTESIAN_POINT('Ctrl Pts',(-2.03558715979207,1.91357699587635,7.72611360997538));
#69890=CARTESIAN_POINT('Ctrl Pts',(-2.71492886967243,-0.659206520656943,
7.88410850097543));
#69891=CARTESIAN_POINT('Ctrl Pts',(-0.931402394462092,-2.63398587388918,
8.0421033919755));
#69892=CARTESIAN_POINT('Ctrl Pts',(1.69705278236641,-2.21932509067958,8.20009828297554));
#69893=CARTESIAN_POINT('Ctrl Pts',(2.78601373789173,0.208613174406663,8.3580931739756));
#69894=CARTESIAN_POINT('Ctrl Pts',(1.34762133439256,2.44730642612392,8.51608806497565));
#69895=CARTESIAN_POINT('Ctrl Pts',(-1.31327591890231,2.46590720934279,8.6740829559757));
#69896=CARTESIAN_POINT('Ctrl Pts',(-2.78282502490651,0.247541683382087,
8.83207784697575));
#69897=CARTESIAN_POINT('Ctrl Pts',(-1.72791343690234,-2.19538314624801,
8.99007273797581));
#69898=CARTESIAN_POINT('Ctrl Pts',(0.894487847747497,-2.64674960933017,
9.14806762897587));
#69899=CARTESIAN_POINT('Ctrl Pts',(2.70544774003657,-0.697097217171796,
9.30606251997591));
#69900=CARTESIAN_POINT('Ctrl Pts',(2.06214032543822,1.88493216919308,9.46405741097597));
#69901=CARTESIAN_POINT('Ctrl Pts',(-0.451853226630304,2.75703113254833,
9.62205230197602));
#69902=CARTESIAN_POINT('Ctrl Pts',(-2.55594471878539,1.12806852574304,9.78004719297607));
#69903=CARTESIAN_POINT('Ctrl Pts',(-2.34139169650468,-1.52422994583995,
9.93804208397613));
#69904=CARTESIAN_POINT('Ctrl Pts',(-0.00282755092387669,-2.79381173474703,
10.0960369749762));
#69905=CARTESIAN_POINT('Ctrl Pts',(2.33830162879016,-1.52896615301492,10.2540318659762));
#69906=CARTESIAN_POINT('Ctrl Pts',(2.55822286341245,1.12289259742877,10.4120267569763));
#69907=CARTESIAN_POINT('Ctrl Pts',(0.457432947542771,2.7561108654668,10.5700216479763));
#69908=CARTESIAN_POINT('Ctrl Pts',(-2.05832071413818,1.88910239057596,10.7280165389764));
#69909=CARTESIAN_POINT('Ctrl Pts',(-2.70685322748717,-0.691619555106155,
10.8860114299764));
#69910=CARTESIAN_POINT('Ctrl Pts',(-0.899843435489688,-2.64493360895804,
11.0440063209765));
#69911=CARTESIAN_POINT('Ctrl Pts',(1.72346611079269,-2.19887620608651,11.2020012119765));
#69912=CARTESIAN_POINT('Ctrl Pts',(2.78332038555639,0.241908319069164,11.3599961029766));
#69913=CARTESIAN_POINT('Ctrl Pts',(1.31826459668171,2.46324388910665,11.5179909939767));
#69914=CARTESIAN_POINT('Ctrl Pts',(-1.34266485711555,2.45002920164021,11.6759858849767));
#69915=CARTESIAN_POINT('Ctrl Pts',(-2.78558576494693,0.214252058101096,
11.8339807759768));
#69916=CARTESIAN_POINT('Ctrl Pts',(-1.70154155624011,-2.21588545226976,
11.9919756669768));
#69917=CARTESIAN_POINT('Ctrl Pts',(0.926068905704722,-2.63586577921336,
12.1499705579768));
#69918=CARTESIAN_POINT('Ctrl Pts',(2.71358896739729,-0.66470059075221,12.3079654489769));
#69919=CARTESIAN_POINT('Ctrl Pts',(2.03945637158195,1.90945273151837,12.465960339977));
#69920=CARTESIAN_POINT('Ctrl Pts',(-0.484784490030591,2.7514316495538,12.623955230977));
#69921=CARTESIAN_POINT('Ctrl Pts',(-2.56924935619517,1.09742855008785,12.7819501219771));
#69922=CARTESIAN_POINT('Ctrl Pts',(-2.32300048113579,-1.55211501365623,
12.9399450129771));
#69923=CARTESIAN_POINT('Ctrl Pts',(0.0305761225400629,-2.79364596629274,
13.0979399039772));
#69924=CARTESIAN_POINT('Ctrl Pts',(2.35641472627957,-1.50089950416469,13.2559347949772));
#69925=CARTESIAN_POINT('Ctrl Pts',(2.54461517470071,1.15339844793961,13.4139296859773));
#69926=CARTESIAN_POINT('Ctrl Pts',(0.424446453969621,2.76138384673405,13.5719245769773));
#69927=CARTESIAN_POINT('Ctrl Pts',(-2.08075760311621,1.86435613311354,13.7299194679774));
#69928=CARTESIAN_POINT('Ctrl Pts',(-2.69839524633484,-0.72393067103507,
13.8879143589774));
#69929=CARTESIAN_POINT('Ctrl Pts',(-0.86814701313444,-2.65550906063268,
14.0459092499775));
#69930=CARTESIAN_POINT('Ctrl Pts',(1.74961619768082,-2.17810185464822,14.2039041409775));
#69931=CARTESIAN_POINT('Ctrl Pts',(2.78026136217266,0.275147623930244,14.3618990319776));
#69932=CARTESIAN_POINT('Ctrl Pts',(1.28865784862374,2.47886983416738,14.5198939229777));
#69933=CARTESIAN_POINT('Ctrl Pts',(-1.37174423913667,2.4337233465313,14.6778888139777));
#69934=CARTESIAN_POINT('Ctrl Pts',(-2.78817303762162,0.181080103603136,
14.8358837049778));
#69935=CARTESIAN_POINT('Ctrl Pts',(-1.67449675827739,-2.23635459951884,
14.9938785959778));
#69936=CARTESIAN_POINT('Ctrl Pts',(0.956694219915353,-2.62406084291086,
15.1518734869779));
#69937=CARTESIAN_POINT('Ctrl Pts',(2.72293688569169,-0.633270369947463,
15.3098683779779));
#69938=CARTESIAN_POINT('Ctrl Pts',(2.01312970789309,1.93633043049701,15.4678886471889));
#69939=CARTESIAN_POINT('Ctrl Pts',(0.330396509531936,2.47203073808571,15.573243952733));
#69940=CARTESIAN_POINT('Ctrl Pts',(-0.439790560653197,2.32640238805053,
15.6259342946106));
#69941=CARTESIAN_POINT('Ctrl Pts',(-1.12170252862657,2.30152292796285,-0.22036464634795));
#69942=CARTESIAN_POINT('Ctrl Pts',(-1.88328504076518,1.93034738187355,-0.167699682681266));
#69943=CARTESIAN_POINT('Ctrl Pts',(-2.99641952926692,0.379451369086483,
-0.062369755347896));
#69944=CARTESIAN_POINT('Ctrl Pts',(-1.95319028054399,-2.30748880506914,
0.0956251356521572));
#69945=CARTESIAN_POINT('Ctrl Pts',(0.864392190143294,-2.89402422057555,
0.253620026652211));
#69946=CARTESIAN_POINT('Ctrl Pts',(2.89655074515435,-0.858794531016792,
0.411614917652264));
#69947=CARTESIAN_POINT('Ctrl Pts',(2.30175067708376,1.95734667757734,0.569609808652319));
#69948=CARTESIAN_POINT('Ctrl Pts',(-0.381449809775129,2.9969002095631,0.727604699652371));
#69949=CARTESIAN_POINT('Ctrl Pts',(-2.71843210295174,1.3182984262109,0.885599590652427));
#69950=CARTESIAN_POINT('Ctrl Pts',(-2.58946406895983,-1.55647215216739,
1.04359448165247));
#69951=CARTESIAN_POINT('Ctrl Pts',(-0.111394026279792,-3.01913888229157,
1.20158937265253));
#69952=CARTESIAN_POINT('Ctrl Pts',(2.46770169169952,-1.74304346212535,1.35958426365258));
#69953=CARTESIAN_POINT('Ctrl Pts',(2.80821696415988,1.11430488612263,1.51757915465264));
#69954=CARTESIAN_POINT('Ctrl Pts',(0.601229861113374,2.96078331441178,1.67557404565269));
#69955=CARTESIAN_POINT('Ctrl Pts',(-2.15116367709187,2.12137523178328,1.83356893665274));
#69956=CARTESIAN_POINT('Ctrl Pts',(-2.95211484377831,-0.642459816335227,
1.9915638276528));
#69957=CARTESIAN_POINT('Ctrl Pts',(-1.07503175015829,-2.82347975484453,
2.14955871865285));
#69958=CARTESIAN_POINT('Ctrl Pts',(1.77727395779847,-2.44316024393295,2.3075536096529));
#69959=CARTESIAN_POINT('Ctrl Pts',(3.01731248308272,0.153491274520022,2.46554850065296));
#69960=CARTESIAN_POINT('Ctrl Pts',(1.52017310160377,2.6109016185411,2.62354339165301));
#69961=CARTESIAN_POINT('Ctrl Pts',(-1.35600268833558,2.69981309586282,2.78153828265307));
#69962=CARTESIAN_POINT('Ctrl Pts',(-3.0020704605904,0.339568664463957,2.93953317365312));
#69963=CARTESIAN_POINT('Ctrl Pts',(-1.92478736831974,-2.32871798155565,
3.09752806465317));
#69964=CARTESIAN_POINT('Ctrl Pts',(0.898581080119023,-2.88449059092087,
3.25552295565323));
#69965=CARTESIAN_POINT('Ctrl Pts',(2.90679493541049,-0.823575805844403,
3.41351784665328));
#69966=CARTESIAN_POINT('Ctrl Pts',(2.2780878550452,1.9844519699672,3.57151273765333));
#69967=CARTESIAN_POINT('Ctrl Pts',(-0.417203790163499,2.99226918985935,
3.72950762865338));
#69968=CARTESIAN_POINT('Ctrl Pts',(-2.73402587371621,1.2856268607399,3.88750251965344));
#69969=CARTESIAN_POINT('Ctrl Pts',(-2.57065578060014,-1.58728156297948,
4.04549741065349));
#69970=CARTESIAN_POINT('Ctrl Pts',(-0.0752959226825514,-3.02027555497893,
4.20349230165355));
#69971=CARTESIAN_POINT('Ctrl Pts',(2.48836919908102,-1.71340381474775,4.3614871926536));
#69972=CARTESIAN_POINT('Ctrl Pts',(2.79469144832751,1.14779510886793,4.51948208365366));
#69973=CARTESIAN_POINT('Ctrl Pts',(0.565788288161118,2.96776304924624,4.67747697465371));
#69974=CARTESIAN_POINT('Ctrl Pts',(-2.17637398167157,2.09550237301017,4.83547186565376));
#69975=CARTESIAN_POINT('Ctrl Pts',(-2.94422219185483,-0.677709073558362,
4.99346675665382));
#69976=CARTESIAN_POINT('Ctrl Pts',(-1.04119705167313,-2.83613162653042,
5.15146164765387));
#69977=CARTESIAN_POINT('Ctrl Pts',(1.80635784088181,-2.4217360000809,5.30945653865392));
#69978=CARTESIAN_POINT('Ctrl Pts',(3.01526160452625,0.189555690167927,5.46745142965398));
#69979=CARTESIAN_POINT('Ctrl Pts',(1.48884807921076,2.62889050750288,5.62544632065403));
#69980=CARTESIAN_POINT('Ctrl Pts',(-1.38818520181308,2.68340748841342,5.78344121165409));
#69981=CARTESIAN_POINT('Ctrl Pts',(-3.00591581500234,0.303651142802643,
5.94143610265413));
#69982=CARTESIAN_POINT('Ctrl Pts',(-1.89680724263192,-2.35156462545811,
6.0994309936542));
#69983=CARTESIAN_POINT('Ctrl Pts',(0.933004315114162,-2.87354082124909,
6.25742588465425));
#69984=CARTESIAN_POINT('Ctrl Pts',(2.9164339768497,-0.78876280470318,6.4154207756543));
#69985=CARTESIAN_POINT('Ctrl Pts',(2.25419857688244,2.0115473346128,6.57341566665436));
#69986=CARTESIAN_POINT('Ctrl Pts',(-0.452950050793218,2.98706714937797,
6.73141055765441));
#69987=CARTESIAN_POINT('Ctrl Pts',(-2.74920162624943,1.25284648765685,6.88940544865445));
#69988=CARTESIAN_POINT('Ctrl Pts',(-2.55149422719067,-1.61790330737633,
7.04740033965452));
#69989=CARTESIAN_POINT('Ctrl Pts',(-0.0391796106880552,-3.02095992385085,
7.20539523065456));
#69990=CARTESIAN_POINT('Ctrl Pts',(2.50867708492601,-1.68352997804427,7.36339012165463));
#69991=CARTESIAN_POINT('Ctrl Pts',(2.78076845639151,1.18112687521052,7.52138501265468));
#69992=CARTESIAN_POINT('Ctrl Pts',(0.530264765476331,2.97431558209632,7.67937990365473));
#69993=CARTESIAN_POINT('Ctrl Pts',(-2.20127260376274,2.0693314928571,7.83737479465478));
#69994=CARTESIAN_POINT('Ctrl Pts',(-2.93590894068373,-0.712862255572524,
7.99536968565484));
#69995=CARTESIAN_POINT('Ctrl Pts',(-1.00721335568747,-2.84837763639784,
8.1533645766549));
#69996=CARTESIAN_POINT('Ctrl Pts',(1.83518341574924,-2.3999657776655,8.31135946765493));
#69997=CARTESIAN_POINT('Ctrl Pts',(3.0127797207928,0.225593123535039,8.469354358655));
#69998=CARTESIAN_POINT('Ctrl Pts',(1.45731019640918,2.646503522546,8.62734924965505));
#69999=CARTESIAN_POINT('Ctrl Pts',(-1.42016925561481,2.66661830579726,8.78534414065509));
#70000=CARTESIAN_POINT('Ctrl Pts',(-3.00933146435147,0.267690196068054,
8.94333903165517));
#70001=CARTESIAN_POINT('Ctrl Pts',(-1.86855595547932,-2.37407509246219,
9.1013339226552));
#70002=CARTESIAN_POINT('Ctrl Pts',(0.967294170713062,-2.86218026873064,
9.25932881365528));
#70003=CARTESIAN_POINT('Ctrl Pts',(2.92565609996415,-0.753837043497722,
9.41732370465531));
#70004=CARTESIAN_POINT('Ctrl Pts',(2.22998704902682,2.03835513701099,9.57531859565539));
#70005=CARTESIAN_POINT('Ctrl Pts',(-0.488631559655073,2.98143809298718,
9.73331348665541));
#70006=CARTESIAN_POINT('Ctrl Pts',(-2.76398436644151,1.21988701340545,9.89130837765549));
#70007=CARTESIAN_POINT('Ctrl Pts',(-2.53196792453725,-1.64829376402382,
10.0493032686556));
#70008=CARTESIAN_POINT('Ctrl Pts',(-0.00305769780212466,-3.02121243110894,
10.2072981596556));
#70009=CARTESIAN_POINT('Ctrl Pts',(2.52862634254158,-1.65341547205285,10.3652930506557));
#70010=CARTESIAN_POINT('Ctrl Pts',(2.76644793933786,1.21428979338836,10.5232879416557));
#70011=CARTESIAN_POINT('Ctrl Pts',(0.494665438736237,2.9804429212968,10.6812828326558));
#70012=CARTESIAN_POINT('Ctrl Pts',(-2.22585654266583,2.0428647911605,10.8392777236558));
#70013=CARTESIAN_POINT('Ctrl Pts',(-2.92717598625596,-0.74791353028442,
10.9972726146559));
#70014=CARTESIAN_POINT('Ctrl Pts',(-0.973085673433698,-2.86021645605457,
11.1552675056559));
#70015=CARTESIAN_POINT('Ctrl Pts',(1.86374664182347,-2.37785246789358,11.313262396656));
#70016=CARTESIAN_POINT('Ctrl Pts',(3.00986714459602,0.261598307312764,11.471257287656));
#70017=CARTESIAN_POINT('Ctrl Pts',(1.42556398394764,2.66373820614507,11.6292521786561));
#70018=CARTESIAN_POINT('Ctrl Pts',(-1.45195028952006,2.6494479168066,11.7872470696561));
#70019=CARTESIAN_POINT('Ctrl Pts',(-3.01231691323675,0.23169098091872,11.9452419606562));
#70020=CARTESIAN_POINT('Ctrl Pts',(-1.840037550786,-2.3962461718692,12.1032368516563));
#70021=CARTESIAN_POINT('Ctrl Pts',(1.00144575068579,-2.8504105555327,12.2612317426563));
#70022=CARTESIAN_POINT('Ctrl Pts',(2.93445997783494,-0.718803512337577,
12.4192266336564));
#70023=CARTESIAN_POINT('Ctrl Pts',(2.20545674781687,2.06487153637807,12.5772215246564));
#70024=CARTESIAN_POINT('Ctrl Pts',(-0.52424324426491,2.97538284330073,12.7352164156565));
#70025=CARTESIAN_POINT('Ctrl Pts',(-2.77837192714716,1.18675311458651,12.8932113066565));
#70026=CARTESIAN_POINT('Ctrl Pts',(-2.51207976679037,-1.67844852086771,
13.0512061976566));
#70027=CARTESIAN_POINT('Ctrl Pts',(0.0330648484162935,-3.02103317002684,
13.2092010886566));
#70028=CARTESIAN_POINT('Ctrl Pts',(2.54821374516441,-1.62306435449139,13.3671959796567));
#70029=CARTESIAN_POINT('Ctrl Pts',(2.75173266064415,1.24727865002413,13.5251908706567));
#70030=CARTESIAN_POINT('Ctrl Pts',(0.458994028525444,2.98614509383602,13.6831857616568));
#70031=CARTESIAN_POINT('Ctrl Pts',(-2.25011966929414,2.01610432633067,13.8411806526569));
#70032=CARTESIAN_POINT('Ctrl Pts',(-2.91802957260121,-0.782854590876773,
13.9991755436569));
#70033=CARTESIAN_POINT('Ctrl Pts',(-0.938809339044251,-2.87165269052473,
14.157170434657));
#70034=CARTESIAN_POINT('Ctrl Pts',(1.89202519996625,-2.35538720009011,14.315165325657));
#70035=CARTESIAN_POINT('Ctrl Pts',(3.00655913376658,0.297543106240599,14.4731602166571));
#70036=CARTESIAN_POINT('Ctrl Pts',(1.39354741169084,2.6806360160004,14.6311551076571));
#70037=CARTESIAN_POINT('Ctrl Pts',(-1.48339657108533,2.63181485601649,14.7891499986572));
#70038=CARTESIAN_POINT('Ctrl Pts',(-3.01511477548001,0.195819014298005,
14.9471448896572));
#70039=CARTESIAN_POINT('Ctrl Pts',(-1.81079145707627,-2.41838139356435,
15.1051397806573));
#70040=CARTESIAN_POINT('Ctrl Pts',(1.03456379470036,-2.83764476324185,15.2631346716573));
#70041=CARTESIAN_POINT('Ctrl Pts',(2.94456876455265,-0.68481504682045,15.4211295626574));
#70042=CARTESIAN_POINT('Ctrl Pts',(2.17698724050641,2.09393693017821,15.5791498318682));
#70043=CARTESIAN_POINT('Ctrl Pts',(0.357288943051609,2.67324025563383,15.6845051374125));
#70044=CARTESIAN_POINT('Ctrl Pts',(-0.475587059931246,2.51575856995826,
15.73719547929));
#70045=CARTESIAN_POINT('Ctrl Pts',(-1.20613086391808,2.47475401596006,-0.109103461668549));
#70046=CARTESIAN_POINT('Ctrl Pts',(-2.02503618851906,2.0756408191501,-0.0564384980018643));
#70047=CARTESIAN_POINT('Ctrl Pts',(-3.22195411284388,0.408011924669176,
0.0488914293315046));
#70048=CARTESIAN_POINT('Ctrl Pts',(-2.10020305771572,-2.48116893286055,
0.206886320331559));
#70049=CARTESIAN_POINT('Ctrl Pts',(0.929453284141298,-3.11185171137717,
0.364881211331612));
#70050=CARTESIAN_POINT('Ctrl Pts',(3.11456840247411,-0.923434300261156,
0.522876102331665));
#70051=CARTESIAN_POINT('Ctrl Pts',(2.47499890730776,2.10467229854974,0.68087099333172));
#70052=CARTESIAN_POINT('Ctrl Pts',(-0.410160784043849,3.22247097299719,
0.838865884331773));
#70053=CARTESIAN_POINT('Ctrl Pts',(-2.92304312164692,1.41752414666883,0.996860775331826));
#70054=CARTESIAN_POINT('Ctrl Pts',(-2.78436791829607,-1.6736247388661,1.15485566633188));
#70055=CARTESIAN_POINT('Ctrl Pts',(-0.119778434766208,-3.24638350672681,
1.31285055733193));
#70056=CARTESIAN_POINT('Ctrl Pts',(2.6534407272363,-1.87423890306657,1.47084544833198));
#70057=CARTESIAN_POINT('Ctrl Pts',(3.01958591213912,1.19817641546448,1.62884033933204));
#70058=CARTESIAN_POINT('Ctrl Pts',(0.646483246040247,3.18363563043606,1.78683523033209));
#70059=CARTESIAN_POINT('Ctrl Pts',(-2.31307752105799,2.28104695826807,1.94483012133214));
#70060=CARTESIAN_POINT('Ctrl Pts',(-3.17431470112801,-0.690816498611117,
2.1028250123322));
#70061=CARTESIAN_POINT('Ctrl Pts',(-1.15594726807422,-3.0359975029526,2.26081990333225));
#70062=CARTESIAN_POINT('Ctrl Pts',(1.91104586058415,-2.62705209313675,2.41881479433231));
#70063=CARTESIAN_POINT('Ctrl Pts',(3.24441963805449,0.165044259789067,2.57680968533236));
#70064=CARTESIAN_POINT('Ctrl Pts',(1.63459353041437,2.80741902992046,2.73480457633241));
#70065=CARTESIAN_POINT('Ctrl Pts',(-1.45806633418219,2.903022698645,2.89279946733247));
#70066=CARTESIAN_POINT('Ctrl Pts',(-3.22803037861418,0.365127327590972,
3.05079435833252));
#70067=CARTESIAN_POINT('Ctrl Pts',(-2.06966231435056,-2.50399598755864,
3.20878924933257));
#70068=CARTESIAN_POINT('Ctrl Pts',(0.9662155043828,-3.10160050423604,3.36678414033263));
#70069=CARTESIAN_POINT('Ctrl Pts',(3.12558365271064,-0.885564731160449,
3.52477903133268));
#70070=CARTESIAN_POINT('Ctrl Pts',(2.44955503136051,2.13381775279686,3.68277392233274));
#70071=CARTESIAN_POINT('Ctrl Pts',(-0.448605895964152,3.21749138558114,
3.84076881333278));
#70072=CARTESIAN_POINT('Ctrl Pts',(-2.93981060475756,1.3823934569526,3.99876370433284));
#70073=CARTESIAN_POINT('Ctrl Pts',(-2.76414396719572,-1.70675311321781,
4.15675859533289));
#70074=CARTESIAN_POINT('Ctrl Pts',(-0.0809632981623413,-3.24760573452376,
4.31475348633295));
#70075=CARTESIAN_POINT('Ctrl Pts',(2.67566383710448,-1.84236833793416,4.472748377333));
#70076=CARTESIAN_POINT('Ctrl Pts',(3.00504235742698,1.23418738117217,4.63074326833305));
#70077=CARTESIAN_POINT('Ctrl Pts',(0.60837405584714,3.19114071613476,4.78873815933311));
#70078=CARTESIAN_POINT('Ctrl Pts',(-2.34018535550283,2.25322670048346,4.94673305033316));
#70079=CARTESIAN_POINT('Ctrl Pts',(-3.16582798487292,-0.72871889784977,
5.10472794133323));
#70080=CARTESIAN_POINT('Ctrl Pts',(-1.11956589861766,-3.04960165604779,
5.26272283233327));
#70081=CARTESIAN_POINT('Ctrl Pts',(1.94231883014085,-2.60401528873755,5.42071772333333));
#70082=CARTESIAN_POINT('Ctrl Pts',(3.24221439391714,0.203823172818145,5.57871261433338));
#70083=CARTESIAN_POINT('Ctrl Pts',(1.60091073541578,2.82676190704757,5.73670750533343));
#70084=CARTESIAN_POINT('Ctrl Pts',(-1.49267116192667,2.88538227350458,5.8947023963335));
#70085=CARTESIAN_POINT('Ctrl Pts',(-3.23216516526265,0.326506364968914,
6.05269728733353));
#70086=CARTESIAN_POINT('Ctrl Pts',(-2.03957617982994,-2.52856225325249,
6.21069217833361));
#70087=CARTESIAN_POINT('Ctrl Pts',(1.00322970833078,-3.08982656701393,6.36868706933365));
#70088=CARTESIAN_POINT('Ctrl Pts',(3.13594820577326,-0.848131424137899,
6.5266819603337));
#70089=CARTESIAN_POINT('Ctrl Pts',(2.42386765438354,2.16295253205797,6.68467685133376));
#70090=CARTESIAN_POINT('Ctrl Pts',(-0.487042707074808,3.21189779778061,
6.84267174233381));
#70091=CARTESIAN_POINT('Ctrl Pts',(-2.95612860622976,1.34714576989012,7.00066663333385));
#70092=CARTESIAN_POINT('Ctrl Pts',(-2.74354016148256,-1.73967969587362,
7.15866152433392));
#70093=CARTESIAN_POINT('Ctrl Pts',(-0.0421285826510928,-3.24834161448985,
7.31665641533396));
#70094=CARTESIAN_POINT('Ctrl Pts',(2.69750025743292,-1.81024595650758,7.47465130633402));
#70095=CARTESIAN_POINT('Ctrl Pts',(2.99007140936943,1.27002796377647,7.63264619733409));
#70096=CARTESIAN_POINT('Ctrl Pts',(0.570176747726886,3.19818644519895,7.79064108833413));
#70097=CARTESIAN_POINT('Ctrl Pts',(-2.36695804773341,2.22508598983787,7.94863597933417));
#70098=CARTESIAN_POINT('Ctrl Pts',(-3.15688901169502,-0.766517990488109,
8.10663087033424));
#70099=CARTESIAN_POINT('Ctrl Pts',(-1.08302431691284,-3.06276939890652,
8.2646257613343));
#70100=CARTESIAN_POINT('Ctrl Pts',(1.97331404913207,-2.58060646465142,8.42262065233434));
#70101=CARTESIAN_POINT('Ctrl Pts',(3.23954570369386,0.24257307266342,8.5806155433344));
#70102=CARTESIAN_POINT('Ctrl Pts',(1.56699905842581,2.84570061896807,8.73861043433446));
#70103=CARTESIAN_POINT('Ctrl Pts',(-1.52706259232731,2.86732940225174,8.89660532533451));
#70104=CARTESIAN_POINT('Ctrl Pts',(-3.23583790379643,0.287838708754021,
9.05460021633457));
#70105=CARTESIAN_POINT('Ctrl Pts',(-2.0091984740563,-2.55276703867637,9.21259510733461));
#70106=CARTESIAN_POINT('Ctrl Pts',(1.04010049367863,-3.07761092813111,9.37058999833468));
#70107=CARTESIAN_POINT('Ctrl Pts',(3.14586445989173,-0.810576869823648,
9.52858488933471));
#70108=CARTESIAN_POINT('Ctrl Pts',(2.39783377261543,2.19177810482891,9.68657978033478));
#70109=CARTESIAN_POINT('Ctrl Pts',(-0.525409892679846,3.20584505342603,
9.84457467133482));
#70110=CARTESIAN_POINT('Ctrl Pts',(-2.97202401409764,1.31170550106787,10.0025695623349));
#70111=CARTESIAN_POINT('Ctrl Pts',(-2.72254415256981,-1.77235758220769,
10.1605644533349));
#70112=CARTESIAN_POINT('Ctrl Pts',(-0.00328784468036826,-3.24861312747085,
10.318559344335));
#70113=CARTESIAN_POINT('Ctrl Pts',(2.71895105629298,-1.77786479109078,10.476554235335));
#70114=CARTESIAN_POINT('Ctrl Pts',(2.97467301526326,1.30568698934795,10.6345491263351));
#70115=CARTESIAN_POINT('Ctrl Pts',(0.531897929929706,3.2047749771268,10.7925440173351));
#70116=CARTESIAN_POINT('Ctrl Pts',(-2.39339237119349,2.19662719174505,10.9505389083352));
#70117=CARTESIAN_POINT('Ctrl Pts',(-3.14749874502475,-0.804207505462682,
11.1085337993352));
#70118=CARTESIAN_POINT('Ctrl Pts',(-1.04632791137771,-3.0754993031511,11.2665286903353));
#70119=CARTESIAN_POINT('Ctrl Pts',(2.00402717285426,-2.55682872970066,11.4245235813353));
#70120=CARTESIAN_POINT('Ctrl Pts',(3.23641390363566,0.281288295556363,11.5825184723354));
#70121=CARTESIAN_POINT('Ctrl Pts',(1.53286337121357,2.86423252318349,11.7405133633355));
#70122=CARTESIAN_POINT('Ctrl Pts',(-1.56123572192459,2.84886663197299,11.8985082543355));
#70123=CARTESIAN_POINT('Ctrl Pts',(-3.23904806152655,0.249129903736346,
12.0565031453356));
#70124=CARTESIAN_POINT('Ctrl Pts',(-1.9785335453319,-2.57660689146864,12.2144980363356));
#70125=CARTESIAN_POINT('Ctrl Pts',(1.07682259566685,-3.06495533185205,12.3724929273357));
#70126=CARTESIAN_POINT('Ctrl Pts',(3.15533098827258,-0.772906433922943,
12.5304878183357));
#70127=CARTESIAN_POINT('Ctrl Pts',(2.37145712405178,2.22029034123777,12.6884827093358));
#70128=CARTESIAN_POINT('Ctrl Pts',(-0.56370199849923,3.19933403704765,12.8464776003358));
#70129=CARTESIAN_POINT('Ctrl Pts',(-2.98749449809915,1.27607767908515,13.0044724913359));
#70130=CARTESIAN_POINT('Ctrl Pts',(-2.70115905244496,-1.80478202807917,
13.1624673823359));
#70131=CARTESIAN_POINT('Ctrl Pts',(0.0355535742925287,-3.24842037376092,
13.320462273336));
#70132=CARTESIAN_POINT('Ctrl Pts',(2.74001276404922,-1.7452292048181,13.478457164336));
#70133=CARTESIAN_POINT('Ctrl Pts',(2.95885014658758,1.34115885210865,13.6364520553361));
#70134=CARTESIAN_POINT('Ctrl Pts',(0.493541603081266,3.21090634093799,13.7944469463361));
#70135=CARTESIAN_POINT('Ctrl Pts',(-2.41948173547208,2.1678525195478,13.9524418373362));
#70136=CARTESIAN_POINT('Ctrl Pts',(-3.13766389886759,-0.841778510718479,
14.1104367283363));
#70137=CARTESIAN_POINT('Ctrl Pts',(-1.00947166495406,-3.08779632041677,
14.2684316193363));
#70138=CARTESIAN_POINT('Ctrl Pts',(2.03443420225168,-2.53267254553199,14.4264265103364));
#70139=CARTESIAN_POINT('Ctrl Pts',(3.23285690536049,0.319938588550955,14.5844214013364));
#70140=CARTESIAN_POINT('Ctrl Pts',(1.49843697475794,2.88240219783341,14.7424162923365));
#70141=CARTESIAN_POINT('Ctrl Pts',(-1.595048903034,2.82990636550169,14.9004111833365));
#70142=CARTESIAN_POINT('Ctrl Pts',(-3.2420565133384,0.210557924992872,15.0584060743366));
#70143=CARTESIAN_POINT('Ctrl Pts',(-1.94708615587513,-2.60040818760985,
15.2164009653366));
#70144=CARTESIAN_POINT('Ctrl Pts',(1.11243336948536,-3.05122868357283,15.3743958563367));
#70145=CARTESIAN_POINT('Ctrl Pts',(3.16620064341362,-0.736359723693434,
15.5323907473367));
#70146=CARTESIAN_POINT('Ctrl Pts',(2.34084477311972,2.2515434298594,15.6904110165477));
#70147=CARTESIAN_POINT('Ctrl Pts',(0.384181376571284,2.87444977318196,15.7957663220919));
#70148=CARTESIAN_POINT('Ctrl Pts',(-0.511383559209293,2.70511475186599,
15.8484566639694));
#70149=CARTESIAN_POINT('Ctrl Pts',(-1.29055919920959,2.64798510395726,0.00215772301085195));
#70150=CARTESIAN_POINT('Ctrl Pts',(-2.16678733627292,2.22093425642666,0.0548226866775366));
#70151=CARTESIAN_POINT('Ctrl Pts',(-3.44748869642086,0.436572480251873,
0.160152614010905));
#70152=CARTESIAN_POINT('Ctrl Pts',(-2.24721583488744,-2.65484906065196,
0.318147505010959));
#70153=CARTESIAN_POINT('Ctrl Pts',(0.994514378139303,-3.32967920217881,
0.476142396011012));
#70154=CARTESIAN_POINT('Ctrl Pts',(3.33258605979387,-0.988074069505522,
0.634137287011066));
#70155=CARTESIAN_POINT('Ctrl Pts',(2.64824713753178,2.25199791952217,0.79213217801112));
#70156=CARTESIAN_POINT('Ctrl Pts',(-0.43887175831257,3.44804173643128,0.950127069011173));
#70157=CARTESIAN_POINT('Ctrl Pts',(-3.12765414034211,1.51674986712676,1.10812196001123));
#70158=CARTESIAN_POINT('Ctrl Pts',(-2.97927176763231,-1.79077732556482,
1.26611685101128));
#70159=CARTESIAN_POINT('Ctrl Pts',(-0.128162843252621,-3.47362813116205,
1.42411174201133));
#70160=CARTESIAN_POINT('Ctrl Pts',(2.83917976277308,-2.0054343440078,1.58210663301139));
#70161=CARTESIAN_POINT('Ctrl Pts',(3.23095486011837,1.28204794480633,1.74010152401144));
#70162=CARTESIAN_POINT('Ctrl Pts',(0.691736630967119,3.40648794646033,1.89809641501149));
#70163=CARTESIAN_POINT('Ctrl Pts',(-2.47499136502412,2.44071868475286,2.05609130601155));
#70164=CARTESIAN_POINT('Ctrl Pts',(-3.39651455847771,-0.73917318088701,
2.2140861970116));
#70165=CARTESIAN_POINT('Ctrl Pts',(-1.23686278599015,-3.24851525106067,
2.37208108801165));
#70166=CARTESIAN_POINT('Ctrl Pts',(2.04481776336984,-2.81094394234055,2.53007597901171));
#70167=CARTESIAN_POINT('Ctrl Pts',(3.47152679302626,0.176597245058115,2.68807087001176));
#70168=CARTESIAN_POINT('Ctrl Pts',(1.74901395922498,3.00393644129981,2.84606576101181));
#70169=CARTESIAN_POINT('Ctrl Pts',(-1.5601299800288,3.10623230142719,3.00406065201187));
#70170=CARTESIAN_POINT('Ctrl Pts',(-3.45399029663795,0.390685990717984,
3.16205554301192));
#70171=CARTESIAN_POINT('Ctrl Pts',(-2.21453726038139,-2.67927399356163,
3.32005043401198));
#70172=CARTESIAN_POINT('Ctrl Pts',(1.03384992864659,-3.31871041755122,3.47804532501203));
#70173=CARTESIAN_POINT('Ctrl Pts',(3.3443723700108,-0.947553656476489,3.63604021601208));
#70174=CARTESIAN_POINT('Ctrl Pts',(2.62102220767581,2.28318353562651,3.79403510701214));
#70175=CARTESIAN_POINT('Ctrl Pts',(-0.480008001764807,3.44271358130293,
3.95202999801219));
#70176=CARTESIAN_POINT('Ctrl Pts',(-3.1455953357989,1.47916005316529,4.11002488901225));
#70177=CARTESIAN_POINT('Ctrl Pts',(-2.9576321537913,-1.82622466345613,4.2680197800123));
#70178=CARTESIAN_POINT('Ctrl Pts',(-0.086630673642128,-3.47493591406859,
4.42601467101235));
#70179=CARTESIAN_POINT('Ctrl Pts',(2.86295847512794,-1.97133286112058,4.5840095620124));
#70180=CARTESIAN_POINT('Ctrl Pts',(3.21539326652644,1.3205796534764,4.74200445301246));
#70181=CARTESIAN_POINT('Ctrl Pts',(0.650959823533161,3.41451838302329,4.89999934401251));
#70182=CARTESIAN_POINT('Ctrl Pts',(-2.50399672933409,2.41095102795676,5.05799423501256));
#70183=CARTESIAN_POINT('Ctrl Pts',(-3.387433777891,-0.779728722141183,5.21598912601263));
#70184=CARTESIAN_POINT('Ctrl Pts',(-1.1979347455622,-3.26307168556515,5.37398401701266));
#70185=CARTESIAN_POINT('Ctrl Pts',(2.07827981939988,-2.7862945773942,5.53197890801273));
#70186=CARTESIAN_POINT('Ctrl Pts',(3.46916718330803,0.218090655468369,5.68997379901277));
#70187=CARTESIAN_POINT('Ctrl Pts',(1.7129733916208,3.02463330659226,5.84796869001284));
#70188=CARTESIAN_POINT('Ctrl Pts',(-1.59715712204027,3.08735705859576,6.00596358101288));
#70189=CARTESIAN_POINT('Ctrl Pts',(-3.45841451552297,0.349361587135177,
6.16395847201295));
#70190=CARTESIAN_POINT('Ctrl Pts',(-2.18234511702796,-2.70555988104687,
6.321953363013));
#70191=CARTESIAN_POINT('Ctrl Pts',(1.0734551015474,-3.30611231277879,6.47994825401305));
#70192=CARTESIAN_POINT('Ctrl Pts',(3.35546243469681,-0.907500043572617,
6.63794314501309));
#70193=CARTESIAN_POINT('Ctrl Pts',(2.59353673188465,2.31435772950313,6.79593803601317));
#70194=CARTESIAN_POINT('Ctrl Pts',(-0.521135363356403,3.43672844618325,
6.95393292701321));
#70195=CARTESIAN_POINT('Ctrl Pts',(-3.16305558621008,1.44144505212338,7.11192781801326));
#70196=CARTESIAN_POINT('Ctrl Pts',(-2.93558609577446,-1.86145608437091,
7.26992270901332));
#70197=CARTESIAN_POINT('Ctrl Pts',(-0.0450775546141294,-3.47572330512885,
7.42791760001339));
#70198=CARTESIAN_POINT('Ctrl Pts',(2.88632342993983,-1.93696193497089,7.58591249101342));
#70199=CARTESIAN_POINT('Ctrl Pts',(3.19937436234735,1.35892905234243,7.74390738201349));
#70200=CARTESIAN_POINT('Ctrl Pts',(0.610088729977438,3.42205730830159,7.90190227301353));
#70201=CARTESIAN_POINT('Ctrl Pts',(-2.53264349170409,2.38084048681862,8.0598971640136));
#70202=CARTESIAN_POINT('Ctrl Pts',(-3.37786908270631,-0.820173725403692,
8.21789205501364));
#70203=CARTESIAN_POINT('Ctrl Pts',(-1.15883527813821,-3.27716116141519,
8.3758869460137));
#70204=CARTESIAN_POINT('Ctrl Pts',(2.1114446825149,-2.76124715163735,8.53388183701374));
#70205=CARTESIAN_POINT('Ctrl Pts',(3.46631168659493,0.259553021791801,8.6918767280138));
#70206=CARTESIAN_POINT('Ctrl Pts',(1.67668792044244,3.04489771539016,8.84987161901386));
#70207=CARTESIAN_POINT('Ctrl Pts',(-1.63395592903981,3.06804049870621,9.0078665100139));
#70208=CARTESIAN_POINT('Ctrl Pts',(-3.46234434324138,0.307987221439991,
9.16586140101396));
#70209=CARTESIAN_POINT('Ctrl Pts',(-2.14984099263328,-2.73145898489056,
9.32385629201401));
#70210=CARTESIAN_POINT('Ctrl Pts',(1.1129068166442,-3.29304158753158,9.48185118301408));
#70211=CARTESIAN_POINT('Ctrl Pts',(3.3660728198193,-0.867316696149578,9.63984607401411));
#70212=CARTESIAN_POINT('Ctrl Pts',(2.56568049620403,2.34520107264683,9.79784096501418));
#70213=CARTESIAN_POINT('Ctrl Pts',(-0.562188225704613,3.43025201386488,
9.95583585601423));
#70214=CARTESIAN_POINT('Ctrl Pts',(-3.18006366175377,1.40352398873029,10.1138307470143));
#70215=CARTESIAN_POINT('Ctrl Pts',(-2.91312038060238,-1.89642140039157,
10.2718256380144));
#70216=CARTESIAN_POINT('Ctrl Pts',(-0.00351799155861674,-3.47601382383277,
10.4298205290144));
#70217=CARTESIAN_POINT('Ctrl Pts',(2.90927577004438,-1.90231411012871,10.5878154200145));
#70218=CARTESIAN_POINT('Ctrl Pts',(3.18289809118866,1.39708418530755,10.7458103110145));
#70219=CARTESIAN_POINT('Ctrl Pts',(0.569130421123177,3.42910703295679,10.9038052020146));
#70220=CARTESIAN_POINT('Ctrl Pts',(-2.56092819972115,2.35038959232959,11.0618000930147));
#70221=CARTESIAN_POINT('Ctrl Pts',(-3.36782150379354,-0.860501480640944,
11.2197949840147));
#70222=CARTESIAN_POINT('Ctrl Pts',(-1.11957014932173,-3.29078215024765,
11.3777898750148));
#70223=CARTESIAN_POINT('Ctrl Pts',(2.14430770388506,-2.73580499150773,11.5357847660148));
#70224=CARTESIAN_POINT('Ctrl Pts',(3.46296066267528,0.300978283799964,11.6937796570149));
#70225=CARTESIAN_POINT('Ctrl Pts',(1.64016275847952,3.06472684022192,11.8517745480149));
#70226=CARTESIAN_POINT('Ctrl Pts',(-1.67052115432913,3.04828534713938,12.009769439015));
#70227=CARTESIAN_POINT('Ctrl Pts',(-3.46577920981637,0.266568826553971,
12.167764330015));
#70228=CARTESIAN_POINT('Ctrl Pts',(-2.1170295398778,-2.75696761106808,12.3257592210151));
#70229=CARTESIAN_POINT('Ctrl Pts',(1.15219944064791,-3.2795001081714,12.4837541120151));
#70230=CARTESIAN_POINT('Ctrl Pts',(3.37620199871023,-0.82700935550831,12.6417490030152));
#70231=CARTESIAN_POINT('Ctrl Pts',(2.5374575002867,2.37570914609746,12.7997438940152));
#70232=CARTESIAN_POINT('Ctrl Pts',(-0.603160752733551,3.42328523079457,
12.9577387850153));
#70233=CARTESIAN_POINT('Ctrl Pts',(-3.19661706905115,1.36540224358379,13.1157336760154));
#70234=CARTESIAN_POINT('Ctrl Pts',(-2.89023833809954,-1.93111553529064,
13.2737285670154));
#70235=CARTESIAN_POINT('Ctrl Pts',(0.0380423001687606,-3.47580757749502,
13.4317234580155));
#70236=CARTESIAN_POINT('Ctrl Pts',(2.93181178293406,-1.8673940551448,13.5897183490155));
#70237=CARTESIAN_POINT('Ctrl Pts',(3.165967632531,1.43503905419316,13.7477132400156));
#70238=CARTESIAN_POINT('Ctrl Pts',(0.528089177637088,3.43566758803995,13.9057081310156));
#70239=CARTESIAN_POINT('Ctrl Pts',(-2.58884380165001,2.31960071276493,14.0637030220157));
#70240=CARTESIAN_POINT('Ctrl Pts',(-3.35729822513396,-0.90070243056019,
14.2216979130157));
#70241=CARTESIAN_POINT('Ctrl Pts',(-1.08013399086388,-3.30393995030882,
14.3796928040158));
#70242=CARTESIAN_POINT('Ctrl Pts',(2.1768432045371,-2.70995789097388,14.5376876950158));
#70243=CARTESIAN_POINT('Ctrl Pts',(3.45915467695442,0.342334070861309,14.6956825860159));
#70244=CARTESIAN_POINT('Ctrl Pts',(1.60332653782504,3.08416837966642,14.8536774770159));
#70245=CARTESIAN_POINT('Ctrl Pts',(-1.70670123498267,3.02799787498689,15.011672368016));
#70246=CARTESIAN_POINT('Ctrl Pts',(-3.4689982511968,0.225296835687742,15.1696672590161));
#70247=CARTESIAN_POINT('Ctrl Pts',(-2.083380854674,-2.78243498165535,15.3276621500161));
#70248=CARTESIAN_POINT('Ctrl Pts',(1.19030294427037,-3.26481260390381,15.4856570410162));
#70249=CARTESIAN_POINT('Ctrl Pts',(3.38783252227459,-0.787904400566419,
15.6436519320162));
#70250=CARTESIAN_POINT('Ctrl Pts',(2.50470230573304,2.4091499295406,15.8016722012271));
#70251=CARTESIAN_POINT('Ctrl Pts',(0.411073810090958,3.07565929073008,15.9070275067712));
#70252=CARTESIAN_POINT('Ctrl Pts',(-0.547180058487341,2.89447093377372,
15.9597178486488));
#70253=CARTESIAN_POINT('',(-1.37838761780672,-1.93231671732536,-0.00102187466432732));
#70254=CARTESIAN_POINT('Ctrl Pts',(-1.37994859234592,-1.93347131995892,
-3.54317269968263E-16));
#70255=CARTESIAN_POINT('Ctrl Pts',(-1.43831895271373,-1.90176082500493,
-3.157397654546E-15));
#70256=CARTESIAN_POINT('Ctrl Pts',(-1.49514575458196,-1.86752259046863,
-4.34169899202657E-15));
#70257=CARTESIAN_POINT('Ctrl Pts',(-1.55024291463986,-1.83079524515745,
-4.08700850940136E-15));
#70258=CARTESIAN_POINT('Ctrl Pts',(-1.61848165101461,-1.78530782562802,
-3.78829000146298E-15));
#70259=CARTESIAN_POINT('Ctrl Pts',(-1.68406861913595,-1.7360041391636,-3.23024659681305E-15));
#70260=CARTESIAN_POINT('Ctrl Pts',(-1.74691851112218,-1.68324606443273,
-1.38083988687754E-15));
#70261=CARTESIAN_POINT('Ctrl Pts',(-1.78341473484423,-1.65261004521818,
-3.06910260178252E-16));
#70262=CARTESIAN_POINT('Ctrl Pts',(-1.81898770098065,-1.6208082297802,-6.08222538088405E-16));
#70263=CARTESIAN_POINT('Ctrl Pts',(-1.8536174249306,-1.58790418430479,9.99200722162641E-16));
#70264=CARTESIAN_POINT('Ctrl Pts',(-1.86599100473682,-1.57614720832583,
1.20135119786233E-15));
#70265=CARTESIAN_POINT('Ctrl Pts',(-1.87824533378606,-1.56424827137885,
-1.41288533260964E-15));
#70266=CARTESIAN_POINT('Ctrl Pts',(-1.89037564784624,-1.55221386701802,
-9.99200722162641E-16));
#70267=CARTESIAN_POINT('Ctrl Pts',(-1.95007879268067,-1.49298277184718,
9.89920292723067E-16));
#70268=CARTESIAN_POINT('Ctrl Pts',(-2.00663609510422,-1.43061741633727,
-1.65749671126755E-16));
#70269=CARTESIAN_POINT('Ctrl Pts',(-2.05996340201355,-1.36549876184075,
-1.87350135405495E-16));
#70270=CARTESIAN_POINT('Ctrl Pts',(-2.1147730212604,-1.29857003684645,-2.09551016929213E-16));
#70271=CARTESIAN_POINT('Ctrl Pts',(-2.16617121071363,-1.22873232295192,
-1.7198130603224E-15));
#70272=CARTESIAN_POINT('Ctrl Pts',(-2.2140407003356,-1.15635106472184,1.94289029309402E-16));
#70273=CARTESIAN_POINT('Ctrl Pts',(-2.22834382104116,-1.13472397236174,
7.66211425954361E-16));
#70274=CARTESIAN_POINT('Ctrl Pts',(-2.24233169959178,-1.11286950794349,
1.53050669563487E-15));
#70275=CARTESIAN_POINT('Ctrl Pts',(-2.25600064404541,-1.09079672684346,
6.66133814775094E-16));
#70276=CARTESIAN_POINT('Ctrl Pts',(-2.26668277274188,-1.07354709288677,
8.73288649491799E-17));
#70277=CARTESIAN_POINT('Ctrl Pts',(-2.27717011522814,-1.05616412126237,
1.79116184180511E-15));
#70278=CARTESIAN_POINT('Ctrl Pts',(-2.28746078556243,-1.03865201740679,
1.04083408558608E-15));
#70279=CARTESIAN_POINT('Ctrl Pts',(-2.3043278418407,-1.00994857713634,-1.81981144522876E-16));
#70280=CARTESIAN_POINT('Ctrl Pts',(-2.32064206145016,-0.980939786561838,
8.03113917588522E-16));
#70281=CARTESIAN_POINT('Ctrl Pts',(-2.33639567929063,-0.951653513157818,
1.1518563880486E-15));
#70282=CARTESIAN_POINT('Ctrl Pts',(-2.37855893182263,-0.873271229560512,
2.08523670738533E-15));
#70283=CARTESIAN_POINT('Ctrl Pts',(-2.41671657812553,-0.792890901649699,
2.49401152098159E-15));
#70284=CARTESIAN_POINT('Ctrl Pts',(-2.45076495402598,-0.710905122334628,
2.48412401759879E-15));
#70285=CARTESIAN_POINT('Ctrl Pts',(-2.48531718185078,-0.62770610768645,
2.47409019776256E-15));
#70286=CARTESIAN_POINT('Ctrl Pts',(-2.51563826586878,-0.542853018948936,
3.90133880310071E-16));
#70287=CARTESIAN_POINT('Ctrl Pts',(-2.54158369978739,-0.456717097481997,
1.08246744900953E-15));
#70288=CARTESIAN_POINT('Ctrl Pts',(-2.56086666911763,-0.392699808848862,
1.59701837205101E-15));
#70289=CARTESIAN_POINT('Ctrl Pts',(-2.57773198353371,-0.327973042405811,
9.74482875872416E-16));
#70290=CARTESIAN_POINT('Ctrl Pts',(-2.59210443472119,-0.262679462931668,
1.36002320516582E-15));
#70291=CARTESIAN_POINT('Ctrl Pts',(-2.5985839551262,-0.233243211940112,
1.53383603625654E-15));
#70292=CARTESIAN_POINT('Ctrl Pts',(-2.60455661090768,-0.203691668580144,
2.53601366117178E-15));
#70293=CARTESIAN_POINT('Ctrl Pts',(-2.61001448404778,-0.174037544115253,
3.24740234702858E-15));
#70294=CARTESIAN_POINT('Ctrl Pts',(-2.61367527686472,-0.154147450841394,
3.72455645530154E-15));
#70295=CARTESIAN_POINT('Ctrl Pts',(-2.61710457712665,-0.134210532287337,
4.62273400142151E-15));
#70296=CARTESIAN_POINT('Ctrl Pts',(-2.62029962849891,-0.114231655457859,
4.24660306919122E-15));
#70297=CARTESIAN_POINT('Ctrl Pts',(-2.62289997143562,-0.0979715315368936,
3.94048297941976E-15));
#70298=CARTESIAN_POINT('Ctrl Pts',(-2.62534443718676,-0.0816875079929038,
3.10814855031425E-15));
#70299=CARTESIAN_POINT('Ctrl Pts',(-2.62763003749086,-0.0653963791800208,
2.80331313717852E-15));
#70300=CARTESIAN_POINT('Ctrl Pts',(-2.64049518650456,0.0263028559853445,
1.08746062892512E-15));
#70301=CARTESIAN_POINT('Ctrl Pts',(-2.64834915604118,0.118337335855572,
-1.43867851364987E-16));
#70302=CARTESIAN_POINT('Ctrl Pts',(-2.651061018059,0.210311484632908,1.11022302462516E-15));
#70303=CARTESIAN_POINT('Ctrl Pts',(-2.65226580187014,0.251172326652904,
1.66737098243456E-15));
#70304=CARTESIAN_POINT('Ctrl Pts',(-2.65245512561064,0.292021668535638,
3.00696151315835E-15));
#70305=CARTESIAN_POINT('Ctrl Pts',(-2.65161463128253,0.332826444242183,
2.4980018054066E-15));
#70306=CARTESIAN_POINT('Ctrl Pts',(-2.64976919202174,0.422419833034951,
1.50902187236961E-15));
#70307=CARTESIAN_POINT('Ctrl Pts',(-2.64296288001183,0.511797898314078,
2.96934449413589E-15));
#70308=CARTESIAN_POINT('Ctrl Pts',(-2.63144647848012,0.600691769744574,
1.72084568816899E-15));
#70309=CARTESIAN_POINT('Ctrl Pts',(-2.6199300769484,0.68958564117507,4.72346882202091E-16));
#70310=CARTESIAN_POINT('Ctrl Pts',(-2.60370331353105,0.777996048559996,
1.9168699501881E-15));
#70311=CARTESIAN_POINT('Ctrl Pts',(-2.58296460883121,0.865656938831558,
2.05391259555654E-15));
#70312=CARTESIAN_POINT('Ctrl Pts',(-2.57869408333521,0.88370811764552,1.96966790296377E-15));
#70313=CARTESIAN_POINT('Ctrl Pts',(-2.57423206760738,0.901727502426253,
-1.21291301995112E-15));
#70314=CARTESIAN_POINT('Ctrl Pts',(-2.56958003501042,0.919712740461558,
-3.05311331771918E-16));
#70315=CARTESIAN_POINT('Ctrl Pts',(-2.56604635272843,0.933374320783267,
4.12631142411499E-16));
#70316=CARTESIAN_POINT('Ctrl Pts',(-2.56240532303519,0.94700728407811,2.96072359195587E-16));
#70317=CARTESIAN_POINT('Ctrl Pts',(-2.5586586911495,0.960608258314246,4.16333634234434E-16));
#70318=CARTESIAN_POINT('Ctrl Pts',(-2.53410521411211,1.0497419706143,2.12171029893344E-15));
#70319=CARTESIAN_POINT('Ctrl Pts',(-2.5050122305201,1.13753405978208,1.37195759662732E-17));
#70320=CARTESIAN_POINT('Ctrl Pts',(-2.47166814999145,1.22370371724256,5.82867087928207E-16));
#70321=CARTESIAN_POINT('Ctrl Pts',(-2.43774488106874,1.31137014608583,1.16190072145076E-15));
#70322=CARTESIAN_POINT('Ctrl Pts',(-2.3994213674271,1.39735806555781,5.22902315393273E-16));
#70323=CARTESIAN_POINT('Ctrl Pts',(-2.35694651643052,1.48137454593671,-1.4432899320127E-15));
#70324=CARTESIAN_POINT('Ctrl Pts',(-2.31397714205714,1.56636920781853,-3.43237403205193E-15));
#70325=CARTESIAN_POINT('Ctrl Pts',(-2.26675893828999,1.64934713164981,-7.02071007117468E-16));
#70326=CARTESIAN_POINT('Ctrl Pts',(-2.21549747648264,1.72999528429546,-1.38777878078145E-15));
#70327=CARTESIAN_POINT('Ctrl Pts',(-2.1844953421251,1.77877003194907,-1.80248417113962E-15));
#70328=CARTESIAN_POINT('Ctrl Pts',(-2.15201333894673,1.82669238798436,3.6817056606625E-16));
#70329=CARTESIAN_POINT('Ctrl Pts',(-2.11808850376185,1.87368930169053,-5.55111512312578E-16));
#70330=CARTESIAN_POINT('Ctrl Pts',(-2.1089145366433,1.88639822536441,-8.91198155137096E-16));
#70331=CARTESIAN_POINT('Ctrl Pts',(-2.09963412322397,1.89904053530927,-2.70664328051753E-15));
#70332=CARTESIAN_POINT('Ctrl Pts',(-2.09025911328956,1.91160012317952,-2.4980018054066E-15));
#70333=CARTESIAN_POINT('Ctrl Pts',(-2.03145402967863,1.9903805852799,-9.44997988912952E-16));
#70334=CARTESIAN_POINT('Ctrl Pts',(-1.96883756375649,2.06603912302116,-8.89268907589407E-16));
#70335=CARTESIAN_POINT('Ctrl Pts',(-1.90268196527423,2.13826743811982,-1.4432899320127E-15));
#70336=CARTESIAN_POINT('Ctrl Pts',(-1.8363597619551,2.21067765145431,-1.96590601829329E-15));
#70337=CARTESIAN_POINT('Ctrl Pts',(-1.76648017671596,2.27964124288177,-1.24430221715273E-15));
#70338=CARTESIAN_POINT('Ctrl Pts',(-1.69326751955099,2.34483179094349,-1.4432899320127E-15));
#70339=CARTESIAN_POINT('Ctrl Pts',(-1.62146081065517,2.40877044429517,-8.49003099635195E-16));
#70340=CARTESIAN_POINT('Ctrl Pts',(-1.54644728359594,2.46908034426638,-2.45521957121142E-15));
#70341=CARTESIAN_POINT('Ctrl Pts',(-1.46839770083036,2.5254261196735,-1.99840144432528E-15));
#70342=CARTESIAN_POINT('Ctrl Pts',(-1.41023968234419,2.56741172077001,-9.78062777089129E-16));
#70343=CARTESIAN_POINT('Ctrl Pts',(-1.35039506896439,2.6071958124341,2.30014117106762E-15));
#70344=CARTESIAN_POINT('Ctrl Pts',(-1.28892185405328,2.64462557919714,7.7715611723761E-16));
#70345=CARTESIAN_POINT('Ctrl Pts',(-1.37733488469885,-1.93084092506131,
-0.00102187466432729));
#70346=CARTESIAN_POINT('Ctrl Pts',(-1.36944737626449,-1.93646735465424,
-0.000681249776216117));
#70347=CARTESIAN_POINT('Ctrl Pts',(-1.36152539135263,-1.94204545278975,
-0.000340624888104793));
#70348=CARTESIAN_POINT('Ctrl Pts',(-1.35356952483514,-1.9475748006014,6.38378239159465E-15));
#70349=CARTESIAN_POINT('Origin',(-1.44337567297407,-2.5,-6.));
#70350=CARTESIAN_POINT('',(-1.44337567297407,-2.5,-6.));
#70351=CARTESIAN_POINT('',(1.44337567297406,-2.5,-6.));
#70352=CARTESIAN_POINT('',(-0.721687836487033,-2.5,-6.));
#70353=CARTESIAN_POINT('',(-1.44337567297407,-2.5,-3.));
#70354=CARTESIAN_POINT('',(-1.44337567297407,-2.5,-6.));
#70355=CARTESIAN_POINT('',(1.44337567297406,-2.5,-3.));
#70356=CARTESIAN_POINT('',(-1.44337567297407,-2.5,-3.));
#70357=CARTESIAN_POINT('',(1.44337567297406,-2.5,-6.));
#70358=CARTESIAN_POINT('Origin',(-2.88675134594813,3.53525079574969E-16,
-6.));
#70359=CARTESIAN_POINT('',(-2.88675134594813,3.53525079574969E-16,-6.));
#70360=CARTESIAN_POINT('',(-2.52590742770461,-0.625,-6.));
#70361=CARTESIAN_POINT('',(-2.88675134594813,5.55111512312578E-16,-3.));
#70362=CARTESIAN_POINT('',(-2.88675134594813,3.53525079574969E-16,-6.));
#70363=CARTESIAN_POINT('',(-2.88675134594813,3.53525079574969E-16,-3.));
#70364=CARTESIAN_POINT('Origin',(-1.44337567297406,2.5,-6.));
#70365=CARTESIAN_POINT('',(-1.44337567297406,2.5,-6.));
#70366=CARTESIAN_POINT('',(-1.80421959121758,1.875,-6.));
#70367=CARTESIAN_POINT('',(-1.44337567297406,2.5,-3.));
#70368=CARTESIAN_POINT('',(-1.44337567297406,2.5,-6.));
#70369=CARTESIAN_POINT('',(-1.44337567297406,2.5,-3.));
#70370=CARTESIAN_POINT('Origin',(1.44337567297406,2.5,-6.));
#70371=CARTESIAN_POINT('',(1.44337567297406,2.5,-6.));
#70372=CARTESIAN_POINT('',(0.721687836487033,2.5,-6.));
#70373=CARTESIAN_POINT('',(1.44337567297406,2.5,-3.));
#70374=CARTESIAN_POINT('',(1.44337567297406,2.5,-6.));
#70375=CARTESIAN_POINT('',(1.44337567297406,2.5,-3.));
#70376=CARTESIAN_POINT('Origin',(2.88675134594813,0.,-6.));
#70377=CARTESIAN_POINT('',(2.88675134594813,0.,-6.));
#70378=CARTESIAN_POINT('',(2.52590742770461,0.625,-6.));
#70379=CARTESIAN_POINT('',(2.88675134594813,0.,-3.));
#70380=CARTESIAN_POINT('',(2.88675134594813,0.,-6.));
#70381=CARTESIAN_POINT('',(2.88675134594813,0.,-3.));
#70382=CARTESIAN_POINT('Origin',(1.44337567297406,-2.5,-6.));
#70383=CARTESIAN_POINT('',(1.80421959121758,-1.875,-6.));
#70384=CARTESIAN_POINT('',(1.44337567297406,-2.5,-3.));
#70385=CARTESIAN_POINT('Origin',(0.,0.,-3.));
#70386=CARTESIAN_POINT('Origin',(0.,0.,0.));
#70387=CARTESIAN_POINT('',(-5.,-6.12323399573677E-16,0.));
#70388=CARTESIAN_POINT('Origin',(0.,0.,0.));
#70389=CARTESIAN_POINT('Origin',(0.,0.,-6.));
#70390=CARTESIAN_POINT('',(-5.,-6.12323399573677E-16,-6.));
#70391=CARTESIAN_POINT('',(-5.,-6.12323399573677E-16,-6.));
#70392=CARTESIAN_POINT('Origin',(0.,0.,-6.));
#70393=CARTESIAN_POINT('Origin',(0.,0.,-6.));
#70394=CARTESIAN_POINT('Origin',(0.,0.,16.));
#70395=CARTESIAN_POINT('',(0.,0.,0.));
#70396=CARTESIAN_POINT('Origin',(0.,0.,-1.2940562256037));
#70397=CARTESIAN_POINT('',(-1.5555,7.45448211670055E-9,0.595401982137319));
#70398=CARTESIAN_POINT('',(-1.5554996707636,0.00101205451123986,0.455943774396298));
#70399=CARTESIAN_POINT('',(-1.5555,-1.46451138874614E-13,-1.2940562256037));
#70400=CARTESIAN_POINT('',(-0.88780425057628,-1.27725638094264,5.87637577487143E-16));
#70401=CARTESIAN_POINT('Ctrl Pts',(-1.5555,7.45448211670055E-9,0.595401982137319));
#70402=CARTESIAN_POINT('Ctrl Pts',(-1.55549999991128,0.018512536755729,
0.594032592656952));
#70403=CARTESIAN_POINT('Ctrl Pts',(-1.55516951495068,0.0370244920773043,
0.592653507332298));
#70404=CARTESIAN_POINT('Ctrl Pts',(-1.55237186799618,0.115346003264795,
0.586777551248481));
#70405=CARTESIAN_POINT('Ctrl Pts',(-1.54678433317852,0.174985822388469,
0.582198572384768));
#70406=CARTESIAN_POINT('Ctrl Pts',(-1.52375452305799,0.326233632272393,
0.570378927484362));
#70407=CARTESIAN_POINT('Ctrl Pts',(-1.50149047938202,0.416873764313208,
0.563089890526641));
#70408=CARTESIAN_POINT('Ctrl Pts',(-1.46287086095033,0.529391380345427,
0.554092311366315));
#70409=CARTESIAN_POINT('Ctrl Pts',(-1.45388505621647,0.553592655730208,
0.552161188814886));
#70410=CARTESIAN_POINT('Ctrl Pts',(-1.44064757834529,0.586695484464925,
0.549535696586906));
#70411=CARTESIAN_POINT('Ctrl Pts',(-1.43690799387877,0.595795658877528,
0.548815630057317));
#70412=CARTESIAN_POINT('Ctrl Pts',(-1.43050774584853,0.610959631805391,
0.547619323005683));
#70413=CARTESIAN_POINT('Ctrl Pts',(-1.42789429642329,0.617042922146608,
0.547140378815347));
#70414=CARTESIAN_POINT('Ctrl Pts',(-1.42237010685853,0.629678430730447,
0.546147849258026));
#70415=CARTESIAN_POINT('Ctrl Pts',(-1.41945279032853,0.636227497509268,
0.54563466220687));
#70416=CARTESIAN_POINT('Ctrl Pts',(-1.41147967660201,0.653798444662134,
0.544260540807749));
#70417=CARTESIAN_POINT('Ctrl Pts',(-1.40633998288666,0.664782039701448,
0.543404502975092));
#70418=CARTESIAN_POINT('Ctrl Pts',(-1.37662258287187,0.726400987288663,
0.538612318112056));
#70419=CARTESIAN_POINT('Ctrl Pts',(-1.34943636016353,0.775739114277784,
0.534814000768419));
#70420=CARTESIAN_POINT('Ctrl Pts',(-1.2575048081127,0.92305641873251,0.523260613003983));
#70421=CARTESIAN_POINT('Ctrl Pts',(-1.1843140339995,1.01525952376867,0.515692469820306));
#70422=CARTESIAN_POINT('Ctrl Pts',(-1.07406526773624,1.12581890886688,0.505129782754011));
#70423=CARTESIAN_POINT('Ctrl Pts',(-1.04566431181909,1.1522457006782,0.50247275350819));
#70424=CARTESIAN_POINT('Ctrl Pts',(-1.00396914072051,1.18823054923343,0.498636166169495));
#70425=CARTESIAN_POINT('Ctrl Pts',(-0.991464697438271,1.19868410853647,
0.497493362131378));
#70426=CARTESIAN_POINT('Ctrl Pts',(-0.969731759193258,1.21627984611124,
0.495518793479236));
#70427=CARTESIAN_POINT('Ctrl Pts',(-0.960582736146466,1.22351834574391,
0.4946909868274));
#70428=CARTESIAN_POINT('Ctrl Pts',(-0.94160356329022,1.23819014938679,0.492980195222397));
#70429=CARTESIAN_POINT('Ctrl Pts',(-0.93176478916661,1.24561088543581,0.492096792847722));
#70430=CARTESIAN_POINT('Ctrl Pts',(-0.90644772642809,1.26423807303257,0.489831747582821));
#70431=CARTESIAN_POINT('Ctrl Pts',(-0.890849618589299,1.27527733557657,
0.488443798170784));
#70432=CARTESIAN_POINT('Ctrl Pts',(-0.81716620132816,1.32541386096325,0.48191916643826));
#70433=CARTESIAN_POINT('Ctrl Pts',(-0.756695027176243,1.3608425814421,0.476649753070564));
#70434=CARTESIAN_POINT('Ctrl Pts',(-0.641075964976838,1.41848718470827,
0.46674807880466));
#70435=CARTESIAN_POINT('Ctrl Pts',(-0.586637715584596,1.44185294601319,
0.462152121432829));
#70436=CARTESIAN_POINT('Ctrl Pts',(-0.460195370473517,1.48777537284252,
0.451724442026016));
#70437=CARTESIAN_POINT('Ctrl Pts',(-0.38760459272556,1.50831713593063,0.445909124683959));
#70438=CARTESIAN_POINT('Ctrl Pts',(-0.30131759167514,1.52608992990789,0.439377069921943));
#70439=CARTESIAN_POINT('Ctrl Pts',(-0.288799865526645,1.52850823710081,
0.438438761604621));
#70440=CARTESIAN_POINT('Ctrl Pts',(-0.269058926096808,1.53207081720116,
0.436975061610269));
#70441=CARTESIAN_POINT('Ctrl Pts',(-0.261855295105846,1.53331846168122,
0.436444292094167));
#70442=CARTESIAN_POINT('Ctrl Pts',(-0.248061104849824,1.5356075187817,0.435434657553588));
#70443=CARTESIAN_POINT('Ctrl Pts',(-0.241472285230778,1.53665737914733,
0.43495536941656));
#70444=CARTESIAN_POINT('Ctrl Pts',(-0.225363062773822,1.53911804710218,
0.433790379706224));
#70445=CARTESIAN_POINT('Ctrl Pts',(-0.215835724210277,1.54048298454096,
0.433107183462439));
#70446=CARTESIAN_POINT('Ctrl Pts',(-0.180539056426624,1.5452058754826,0.430595463113567));
#70447=CARTESIAN_POINT('Ctrl Pts',(-0.15469786646918,1.54800656233667,0.428794695553193));
#70448=CARTESIAN_POINT('Ctrl Pts',(-0.0858993015172276,1.55372277386261,
0.424072194382331));
#70449=CARTESIAN_POINT('Ctrl Pts',(-0.0428691974083889,1.55550503236974,
0.421192210095358));
#70450=CARTESIAN_POINT('Ctrl Pts',(0.132688724120503,1.55548446751562,0.4095484119285));
#70451=CARTESIAN_POINT('Ctrl Pts',(0.264638307722797,1.53853916396096,0.400991220938502));
#70452=CARTESIAN_POINT('Ctrl Pts',(0.415506462100098,1.4991608657509,0.39025704443433));
#70453=CARTESIAN_POINT('Ctrl Pts',(0.438033282177534,1.49273429176367,0.388630102732755));
#70454=CARTESIAN_POINT('Ctrl Pts',(0.473175653277626,1.48184472478897,0.38604897608951));
#70455=CARTESIAN_POINT('Ctrl Pts',(0.485893958995597,1.47772325824553,0.385105867372256));
#70456=CARTESIAN_POINT('Ctrl Pts',(0.509500094666379,1.46973581296729,0.383337735438035));
#70457=CARTESIAN_POINT('Ctrl Pts',(0.520401108730382,1.46591144999129,0.382514134483903));
#70458=CARTESIAN_POINT('Ctrl Pts',(0.54471711145105,1.45707535118003,0.380660497474331));
#70459=CARTESIAN_POINT('Ctrl Pts',(0.558107361196416,1.45199912480921,0.379628374460689));
#70460=CARTESIAN_POINT('Ctrl Pts',(0.598375626252592,1.4360941803677,0.376488887218452));
#70461=CARTESIAN_POINT('Ctrl Pts',(0.625021551629308,1.42469917446781,0.37436284958701));
#70462=CARTESIAN_POINT('Ctrl Pts',(0.722136309462623,1.37991974350355,0.36642767293284));
#70463=CARTESIAN_POINT('Ctrl Pts',(0.79037583793247,1.34199936042264,0.360473755592434));
#70464=CARTESIAN_POINT('Ctrl Pts',(0.938568680933969,1.24441433692573,0.346753356577317));
#70465=CARTESIAN_POINT('Ctrl Pts',(1.01622283282754,1.18185090609348,0.338965801117648));
#70466=CARTESIAN_POINT('Ctrl Pts',(1.10105389802654,1.09892067214589,0.330072917079713));
#70467=CARTESIAN_POINT('Ctrl Pts',(1.11448842922287,1.08529348940666,0.328652143885256));
#70468=CARTESIAN_POINT('Ctrl Pts',(1.13349527551604,1.06528881641021,0.326628207776626));
#70469=CARTESIAN_POINT('Ctrl Pts',(1.13927174794241,1.05910891561717,0.326011190445906));
#70470=CARTESIAN_POINT('Ctrl Pts',(1.14939584061324,1.04809907534924,0.324926851646702));
#70471=CARTESIAN_POINT('Ctrl Pts',(1.15376405127621,1.0432885461509,0.324458030585922));
#70472=CARTESIAN_POINT('Ctrl Pts',(1.16328037687154,1.03267573604481,0.323434671989912));
#70473=CARTESIAN_POINT('Ctrl Pts',(1.16841539625678,1.02686215226696,0.322881087351371));
#70474=CARTESIAN_POINT('Ctrl Pts',(1.18342712058944,1.0096082982659,0.321257765399967));
#70475=CARTESIAN_POINT('Ctrl Pts',(1.19318116961843,0.998061825311609,0.3201965354114));
#70476=CARTESIAN_POINT('Ctrl Pts',(1.23919303860226,0.941955846171118,0.315148492212561));
#70477=CARTESIAN_POINT('Ctrl Pts',(1.27313597606693,0.895548151661867,0.311295152234127));
#70478=CARTESIAN_POINT('Ctrl Pts',(1.37878874923958,0.73290568892236,0.298443712833807));
#70479=CARTESIAN_POINT('Ctrl Pts',(1.43774765055429,0.609170710372294,0.289660951708166));
#70480=CARTESIAN_POINT('Ctrl Pts',(1.48686138503173,0.457545515182043,0.278687813794266));
#70481=CARTESIAN_POINT('Ctrl Pts',(1.49343589198353,0.435607413818198,0.277097145248795));
#70482=CARTESIAN_POINT('Ctrl Pts',(1.50302646506023,0.400830782301211,0.274566387022329));
#70483=CARTESIAN_POINT('Ctrl Pts',(1.50636782967047,0.388084801519073,0.273636930102327));
#70484=CARTESIAN_POINT('Ctrl Pts',(1.51230688445424,0.364196385176079,0.271890591354906));
#70485=CARTESIAN_POINT('Ctrl Pts',(1.51494436661361,0.353064686497044,0.27107506806126));
#70486=CARTESIAN_POINT('Ctrl Pts',(1.52058979791986,0.32800888237305,0.269235007957275));
#70487=CARTESIAN_POINT('Ctrl Pts',(1.52352969850585,0.314070681402649,0.268208346795258));
#70488=CARTESIAN_POINT('Ctrl Pts',(1.53187889563939,0.271606746280942,0.265070235771341));
#70489=CARTESIAN_POINT('Ctrl Pts',(1.53668106773495,0.24296967142752,0.262939763969736));
#70490=CARTESIAN_POINT('Ctrl Pts',(1.55132022252328,0.137682663825198,0.255050320854012));
#70491=CARTESIAN_POINT('Ctrl Pts',(1.55624257647875,0.0604726876665596,
0.249148574607311));
#70492=CARTESIAN_POINT('Ctrl Pts',(1.55434498185425,-0.115492583717271,
0.235537249635111));
#70493=CARTESIAN_POINT('Ctrl Pts',(1.54388465414917,-0.213890375967072,
0.227805643155988));
#70494=CARTESIAN_POINT('Ctrl Pts',(1.52019922850531,-0.330104994002925,
0.218902583673613));
#70495=CARTESIAN_POINT('Ctrl Pts',(1.5158585891988,-0.349496546515298,0.217425528013309));
#70496=CARTESIAN_POINT('Ctrl Pts',(1.50912003263549,-0.37710753046299,0.21533953110097));
#70497=CARTESIAN_POINT('Ctrl Pts',(1.50702421265426,-0.385397708914141,
0.21471544280655));
#70498=CARTESIAN_POINT('Ctrl Pts',(1.50321306886298,-0.399966336773176,
0.213623148259265));
#70499=CARTESIAN_POINT('Ctrl Pts',(1.50152656928863,-0.4062518530699,0.213153379347063));
#70500=CARTESIAN_POINT('Ctrl Pts',(1.49775147457336,-0.419976747098681,
0.212130911627952));
#70501=CARTESIAN_POINT('Ctrl Pts',(1.49564684797744,-0.427411348270103,
0.211579128792934));
#70502=CARTESIAN_POINT('Ctrl Pts',(1.48936534280459,-0.448986082588979,
0.209983097985466));
#70503=CARTESIAN_POINT('Ctrl Pts',(1.48504258151533,-0.463083361146562,
0.208946758638793));
#70504=CARTESIAN_POINT('Ctrl Pts',(1.45306499014261,-0.562311406876981,
0.201684382466008));
#70505=CARTESIAN_POINT('Ctrl Pts',(1.41830384723797,-0.644988908568745,
0.195796136088718));
#70506=CARTESIAN_POINT('Ctrl Pts',(1.32837295625108,-0.815930663028428,
0.183085549891426));
#70507=CARTESIAN_POINT('Ctrl Pts',(1.27109152562521,-0.902574474924967,
0.17628313238586));
#70508=CARTESIAN_POINT('Ctrl Pts',(1.19048746772787,-1.0014458786914,0.167506298012972));
#70509=CARTESIAN_POINT('Ctrl Pts',(1.17492252825074,-1.01966229960277,0.165842849505779));
#70510=CARTESIAN_POINT('Ctrl Pts',(1.14993525016314,-1.04757414413541,0.163215015903657));
#70511=CARTESIAN_POINT('Ctrl Pts',(1.14079626986148,-1.05751903870457,0.162262347650834));
#70512=CARTESIAN_POINT('Ctrl Pts',(1.1235866109884,-1.07576361831739,0.160482980427928));
#70513=CARTESIAN_POINT('Ctrl Pts',(1.11555048431325,-1.08409470923548,0.159657796531519));
#70514=CARTESIAN_POINT('Ctrl Pts',(1.0974314557056,-1.1024639954418,0.157809285018915));
#70515=CARTESIAN_POINT('Ctrl Pts',(1.08730241453723,-1.11245498591742,0.156783972140584));
#70516=CARTESIAN_POINT('Ctrl Pts',(1.05657317118804,-1.14194479017135,0.153696185763408));
#70517=CARTESIAN_POINT('Ctrl Pts',(1.03557625211531,-1.16101955304724,0.151616076757967));
#70518=CARTESIAN_POINT('Ctrl Pts',(0.961915534494003,-1.22434862727732,
0.144413579078096));
#70519=CARTESIAN_POINT('Ctrl Pts',(0.906850190899483,-1.26567436622153,
0.139184051067798));
#70520=CARTESIAN_POINT('Ctrl Pts',(0.77932044943164,-1.34877878841218,0.127455334698482));
#70521=CARTESIAN_POINT('Ctrl Pts',(0.705850183141632,-1.38863971415017,
0.12093952742659));
#70522=CARTESIAN_POINT('Ctrl Pts',(0.594824432243085,-1.43777784001647,
0.111664302209529));
#70523=CARTESIAN_POINT('Ctrl Pts',(0.559557982843611,-1.45186659868798,
0.108797965180966));
#70524=CARTESIAN_POINT('Ctrl Pts',(0.513165740206983,-1.46845800852058,
0.105158298394703));
#70525=CARTESIAN_POINT('Ctrl Pts',(0.502481638082137,-1.47214816607982,
0.104328928711061));
#70526=CARTESIAN_POINT('Ctrl Pts',(0.485733325520589,-1.47772924169189,
0.103043570040798));
#70527=CARTESIAN_POINT('Ctrl Pts',(0.479696407299655,-1.4796999480139,0.102583234316208));
#70528=CARTESIAN_POINT('Ctrl Pts',(0.467059967417248,-1.48373955475198,
0.101626097413697));
#70529=CARTESIAN_POINT('Ctrl Pts',(0.460458355077576,-1.48580153037768,
0.101129706915055));
#70530=CARTESIAN_POINT('Ctrl Pts',(0.443989228673884,-1.49082525710952,
0.0998998893963307));
#70531=CARTESIAN_POINT('Ctrl Pts',(0.434105455498511,-1.49373319261437,
0.0991694173315211));
#70532=CARTESIAN_POINT('Ctrl Pts',(0.395090628935827,-1.50479189613147,
0.0963130647560802));
#70533=CARTESIAN_POINT('Ctrl Pts',(0.365751302103199,-1.51219097026429,
0.0942241858870127));
#70534=CARTESIAN_POINT('Ctrl Pts',(0.282694260721605,-1.53057792609647,
0.0884274226344181));
#70535=CARTESIAN_POINT('Ctrl Pts',(0.228583271129527,-1.53958934235147,
0.0847853164299095));
#70536=CARTESIAN_POINT('Ctrl Pts',(0.0641370703332336,-1.55811210159829,
0.0738323779676044));
#70537=CARTESIAN_POINT('Ctrl Pts',(-0.0468280309652776,-1.55872737574299,
0.0665726339379135));
#70538=CARTESIAN_POINT('Ctrl Pts',(-0.17971458194017,-1.54525341050698,
0.0573627144330893));
#70539=CARTESIAN_POINT('Ctrl Pts',(-0.202459639548319,-1.54243814682873,
0.0557690687999702));
#70540=CARTESIAN_POINT('Ctrl Pts',(-0.23836807715185,-1.53718568105015,
0.0532210487949003));
#70541=CARTESIAN_POINT('Ctrl Pts',(-0.251577002390507,-1.53507920008026,
0.0522768509115466));
#70542=CARTESIAN_POINT('Ctrl Pts',(-0.275173619224738,-1.53100342177695,
0.0505768936094622));
#70543=CARTESIAN_POINT('Ctrl Pts',(-0.285571621136733,-1.52909804703773,
0.0498231723718662));
#70544=CARTESIAN_POINT('Ctrl Pts',(-0.309931777101898,-1.52437705312248,
0.0480460525134765));
#70545=CARTESIAN_POINT('Ctrl Pts',(-0.323876067252991,-1.52147539411363,
0.0470200117010014));
#70546=CARTESIAN_POINT('Ctrl Pts',(-0.365009537565507,-1.51232487739698,
0.0439662258590709));
#70547=CARTESIAN_POINT('Ctrl Pts',(-0.392071328181965,-1.50553591365357,
0.0419217438090517));
#70548=CARTESIAN_POINT('Ctrl Pts',(-0.478070805425748,-1.48148546069609,
0.0353059677852516));
#70549=CARTESIAN_POINT('Ctrl Pts',(-0.536168973236151,-1.46146230507891,
0.0306530148100327));
#70550=CARTESIAN_POINT('Ctrl Pts',(-0.696755658561653,-1.3952509070401,
0.0173030657599812));
#70551=CARTESIAN_POINT('Ctrl Pts',(-0.79562111359592,-1.34133167707247,
0.00847101705034995));
#70552=CARTESIAN_POINT('Ctrl Pts',(-0.88780425057628,-1.27725638094264,
5.87637577487143E-16));
#70553=CARTESIAN_POINT('',(0.903606778650208,-1.26612599672284,0.));
#70554=CARTESIAN_POINT('Origin',(0.,0.,0.));
#70555=CARTESIAN_POINT('Ctrl Pts',(0.903606778650205,-1.26612599672284,
-2.22044604925031E-15));
#70556=CARTESIAN_POINT('Ctrl Pts',(0.951852589186397,-1.23169400373413,
0.00424522636382672));
#70557=CARTESIAN_POINT('Ctrl Pts',(0.998166011006757,-1.19447361099769,
0.00849045272765591));
#70558=CARTESIAN_POINT('Ctrl Pts',(1.04222332457801,-1.15470809805143,0.0127356790914848));
#70559=CARTESIAN_POINT('Ctrl Pts',(1.08625940090756,-1.11496175354151,0.0169788591004388));
#70560=CARTESIAN_POINT('Ctrl Pts',(1.12804116560105,-1.07267304654868,0.0212220391093926));
#70561=CARTESIAN_POINT('Ctrl Pts',(1.16727847323326,-1.02812509741093,0.0254652191183466));
#70562=CARTESIAN_POINT('Ctrl Pts',(1.20650614422342,-0.983588089203271,
0.0297073570066925));
#70563=CARTESIAN_POINT('Ctrl Pts',(1.24319027816322,-0.936793305067274,
0.0339494948950384));
#70564=CARTESIAN_POINT('Ctrl Pts',(1.27707935615917,-0.888058876467136,
0.0381916327833842));
#70565=CARTESIAN_POINT('Ctrl Pts',(1.31097037158942,-0.839321661725895,
0.0424340131942152));
#70566=CARTESIAN_POINT('Ctrl Pts',(1.34206573671913,-0.788644981368028,
0.0466763936050461));
#70567=CARTESIAN_POINT('Ctrl Pts',(1.37015685435733,-0.736376564304986,
0.050918774015877));
#70568=CARTESIAN_POINT('Ctrl Pts',(1.39825808387485,-0.684089332329275,
0.0551626815442565));
#70569=CARTESIAN_POINT('Ctrl Pts',(1.42335268862159,-0.63020965371423,0.0594065890726361));
#70570=CARTESIAN_POINT('Ctrl Pts',(1.4452785167722,-0.575108910517601,0.0636504966010156));
#70571=CARTESIAN_POINT('Ctrl Pts',(1.46723749651958,-0.519924855639086,
0.067900820868144));
#70572=CARTESIAN_POINT('Ctrl Pts',(1.48601795394136,-0.463516502569013,
0.0721511451352726));
#70573=CARTESIAN_POINT('Ctrl Pts',(1.50150660304027,-0.406273517505732,
0.0764014694024009));
#70574=CARTESIAN_POINT('Ctrl Pts',(1.51700725558701,-0.348986170072261,
0.0806550876008007));
#70575=CARTESIAN_POINT('Ctrl Pts',(1.52921091674141,-0.29086337777291,0.0849087057992003));
#70576=CARTESIAN_POINT('Ctrl Pts',(1.5380554381532,-0.232305228454644,0.0891623239976));
#70577=CARTESIAN_POINT('Ctrl Pts',(1.54691876241006,-0.173622588532727,
0.0934249850961493));
#70578=CARTESIAN_POINT('Ctrl Pts',(1.55240863162362,-0.114503227054264,
0.0976876461946983));
#70579=CARTESIAN_POINT('Ctrl Pts',(1.55451484431141,-0.0553520443656737,
0.101950307293247));
#70580=CARTESIAN_POINT('Ctrl Pts',(1.5560237591571,-0.0129754609295238,
0.10500412643079));
#70581=CARTESIAN_POINT('Ctrl Pts',(1.55579713131465,0.0294173901035382,
0.108057945568333));
#70582=CARTESIAN_POINT('Ctrl Pts',(1.55384760097146,0.0716790273038469,
0.111111764705876));
#70583=CARTESIAN_POINT('Ctrl Pts',(1.55122671815316,0.128494146493297,0.115217216121782));
#70584=CARTESIAN_POINT('Ctrl Pts',(1.5454787588811,0.185310342956839,0.119322667537688));
#70585=CARTESIAN_POINT('Ctrl Pts',(1.53659924649562,0.241749882459346,0.123428118953594));
#70586=CARTESIAN_POINT('Ctrl Pts',(1.52769589071,0.298340974261668,0.127544594389351));
#70587=CARTESIAN_POINT('Ctrl Pts',(1.51564409042012,0.354552843155991,0.131661069825108));
#70588=CARTESIAN_POINT('Ctrl Pts',(1.50049208636959,0.410004571611382,0.135777545260865));
#70589=CARTESIAN_POINT('Ctrl Pts',(1.48542844675149,0.465132913107788,0.139870013970232));
#70590=CARTESIAN_POINT('Ctrl Pts',(1.46730077025642,0.519509429534535,0.143962482679598));
#70591=CARTESIAN_POINT('Ctrl Pts',(1.44620795176229,0.57276767564129,0.148054951388965));
#70592=CARTESIAN_POINT('Ctrl Pts',(1.42513055978693,0.625986970607685,0.152144427015856));
#70593=CARTESIAN_POINT('Ctrl Pts',(1.40109251607126,0.678089120794082,0.156233902642746));
#70594=CARTESIAN_POINT('Ctrl Pts',(1.37424213128275,0.72872410047112,0.160323378269637));
#70595=CARTESIAN_POINT('Ctrl Pts',(1.34740052506661,0.779342525345045,0.164411516866983));
#70596=CARTESIAN_POINT('Ctrl Pts',(1.31774865036365,0.82849426020466,0.168499655464329));
#70597=CARTESIAN_POINT('Ctrl Pts',(1.28548137744857,0.87585265783288,0.172587794061675));
#70598=CARTESIAN_POINT('Ctrl Pts',(1.25283388232855,0.923769104305707,0.176724105340849));
#70599=CARTESIAN_POINT('Ctrl Pts',(1.21750922328882,0.969849187380873,0.180860416620023));
#70600=CARTESIAN_POINT('Ctrl Pts',(1.17975365575837,1.01378575731008,0.184996727899197));
#70601=CARTESIAN_POINT('Ctrl Pts',(1.14239287771065,1.0572629063684,0.18908978801577));
#70602=CARTESIAN_POINT('Ctrl Pts',(1.10265221302859,1.0986408140825,0.193182848132343));
#70603=CARTESIAN_POINT('Ctrl Pts',(1.06080812131677,1.13765828777731,0.197275908248916));
#70604=CARTESIAN_POINT('Ctrl Pts',(1.01830078295221,1.17729420502692,0.201433845109391));
#70605=CARTESIAN_POINT('Ctrl Pts',(0.973623180597843,1.21449382674095,0.205591781969865));
#70606=CARTESIAN_POINT('Ctrl Pts',(0.927098415443284,1.24902713264467,0.20974971883034));
#70607=CARTESIAN_POINT('Ctrl Pts',(0.880573650288724,1.28356043854838,0.213907655690814));
#70608=CARTESIAN_POINT('Ctrl Pts',(0.832202237818035,1.31542717887904,0.218065592551289));
#70609=CARTESIAN_POINT('Ctrl Pts',(0.782333459475337,1.34444583683589,0.222223529411763));
#70610=CARTESIAN_POINT('Ctrl Pts',(0.732507149389121,1.3734397825008,0.226377925372803));
#70611=CARTESIAN_POINT('Ctrl Pts',(0.680964149283562,1.39971985823112,0.230532321333844));
#70612=CARTESIAN_POINT('Ctrl Pts',(0.628031163394784,1.42308014806089,0.234686717294884));
#70613=CARTESIAN_POINT('Ctrl Pts',(0.575192226704268,1.44639893226816,0.238833731892435));
#70614=CARTESIAN_POINT('Ctrl Pts',(0.520968677667857,1.46680802087634,0.242980746489986));
#70615=CARTESIAN_POINT('Ctrl Pts',(0.465712498432397,1.48414693302377,0.247127761087537));
#70616=CARTESIAN_POINT('Ctrl Pts',(0.410511312767616,1.50146858866335,0.251270648379445));
#70617=CARTESIAN_POINT('Ctrl Pts',(0.354280026066142,1.51572596806045,0.255413535671353));
#70618=CARTESIAN_POINT('Ctrl Pts',(0.297389711468627,1.52680699812144,0.259556422963261));
#70619=CARTESIAN_POINT('Ctrl Pts',(0.240534338057534,1.53788122237832,0.263696765755315));
#70620=CARTESIAN_POINT('Ctrl Pts',(0.183021247547025,1.54578286595004,0.267837108547369));
#70621=CARTESIAN_POINT('Ctrl Pts',(0.125233629452144,1.55045051132058,0.271977451339423));
#70622=CARTESIAN_POINT('Ctrl Pts',(0.0674594843894061,1.5551170684418,0.276116828821375));
#70623=CARTESIAN_POINT('Ctrl Pts',(0.00941145582046524,1.55655108260044,
0.280256206303327));
#70624=CARTESIAN_POINT('Ctrl Pts',(-0.0485223781685535,1.55474301053803,
0.284395583785279));
#70625=CARTESIAN_POINT('Ctrl Pts',(-0.10650706570377,1.55293335137411,0.288538594757534));
#70626=CARTESIAN_POINT('Ctrl Pts',(-0.164376838372728,1.54787593355955,
0.292681605729789));
#70627=CARTESIAN_POINT('Ctrl Pts',(-0.221745214900975,1.53961336369509,
0.296824616702044));
#70628=CARTESIAN_POINT('Ctrl Pts',(-0.279136622138923,1.53134747679677,
0.300969290898688));
#70629=CARTESIAN_POINT('Ctrl Pts',(-0.336025721732457,1.51987397337167,
0.305113965095331));
#70630=CARTESIAN_POINT('Ctrl Pts',(-0.39203592095745,1.50528671245017,0.309258639291975));
#70631=CARTESIAN_POINT('Ctrl Pts',(-0.448152991738652,1.49067161796805,
0.313411221830091));
#70632=CARTESIAN_POINT('Ctrl Pts',(-0.503387314396123,1.4729310505554,0.317563804368206));
#70633=CARTESIAN_POINT('Ctrl Pts',(-0.557378054162897,1.4522086471088,0.321716386906322));
#70634=CARTESIAN_POINT('Ctrl Pts',(-0.607733336276543,1.43288158331724,
0.325589355976764));
#70635=CARTESIAN_POINT('Ctrl Pts',(-0.657006753231046,1.41096136958093,
0.329462325047206));
#70636=CARTESIAN_POINT('Ctrl Pts',(-0.704925006136371,1.38660051410766,
0.333335294117649));
#70637=CARTESIAN_POINT('Ctrl Pts',(-0.756335755000233,1.36046413085264,
0.337490542445074));
#70638=CARTESIAN_POINT('Ctrl Pts',(-0.806394588382471,1.33141199988986,
0.3416457907725));
#70639=CARTESIAN_POINT('Ctrl Pts',(-0.854751427758667,1.29960772802585,
0.345801039099926));
#70640=CARTESIAN_POINT('Ctrl Pts',(-0.903025134232295,1.26785813263509,
0.349949143911381));
#70641=CARTESIAN_POINT('Ctrl Pts',(-0.949602224940859,1.23336607111526,
0.354097248722836));
#70642=CARTESIAN_POINT('Ctrl Pts',(-0.994157179600198,1.19634098494091,
0.358245353534292));
#70643=CARTESIAN_POINT('Ctrl Pts',(-1.03866934915577,1.15935145310986,0.362389475015585));
#70644=CARTESIAN_POINT('Ctrl Pts',(-1.08116283352943,1.11983404664001,0.366533596496878));
#70645=CARTESIAN_POINT('Ctrl Pts',(-1.12134253402106,1.07804043124329,0.370677717978171));
#70646=CARTESIAN_POINT('Ctrl Pts',(-1.16149894037202,1.03627104565278,0.374819436909231));
#70647=CARTESIAN_POINT('Ctrl Pts',(-1.19934386353526,0.992228440648924,
0.378961155840291));
#70648=CARTESIAN_POINT('Ctrl Pts',(-1.23461828262234,0.946201852785475,
0.383102874771351));
#70649=CARTESIAN_POINT('Ctrl Pts',(-1.2698856734745,0.900184435467712,0.387243768487585));
#70650=CARTESIAN_POINT('Ctrl Pts',(-1.30258326197006,0.852184231805444,
0.391384662203819));
#70651=CARTESIAN_POINT('Ctrl Pts',(-1.3324930326322,0.802522627710056,0.395525555920053));
#70652=CARTESIAN_POINT('Ctrl Pts',(-1.3624305653706,0.752814928000761,0.399670293189902));
#70653=CARTESIAN_POINT('Ctrl Pts',(-1.38957484055183,0.701443191304415,
0.403815030459752));
#70654=CARTESIAN_POINT('Ctrl Pts',(-1.4137525726554,0.648755665339603,0.407959767729602));
#70655=CARTESIAN_POINT('Ctrl Pts',(-1.43794069300726,0.596045501556706,
0.412106285834794));
#70656=CARTESIAN_POINT('Ctrl Pts',(-1.45915953825246,0.542018904870885,
0.416252803939985));
#70657=CARTESIAN_POINT('Ctrl Pts',(-1.47728429048435,0.487043504307524,
0.420399322045177));
#70658=CARTESIAN_POINT('Ctrl Pts',(-1.49544438670223,0.431960899531784,
0.424553926025197));
#70659=CARTESIAN_POINT('Ctrl Pts',(-1.51049819643063,0.375926295918723,
0.428708530005218));
#70660=CARTESIAN_POINT('Ctrl Pts',(-1.52237129403959,0.319320987541107,
0.432863133985238));
#70661=CARTESIAN_POINT('Ctrl Pts',(-1.53340620622867,0.266711750427474,
0.436724442264667));
#70662=CARTESIAN_POINT('Ctrl Pts',(-1.54169413920795,0.213609984417661,
0.440585750544096));
#70663=CARTESIAN_POINT('Ctrl Pts',(-1.54721562759394,0.160324831916597,
0.444447058823525));
#70664=CARTESIAN_POINT('Ctrl Pts',(-1.55269554760363,0.107440835248059,
0.448279297347783));
#70665=CARTESIAN_POINT('Ctrl Pts',(-1.55546502074381,0.054268172421782,
0.452111535872041));
#70666=CARTESIAN_POINT('Ctrl Pts',(-1.5554996707636,0.00101205451123986,
0.455943774396298));
#70667=CARTESIAN_POINT('Origin',(0.,0.,-1.2940562256037));
#70668=CARTESIAN_POINT('',(-1.5555,3.44063942631422E-11,1.29450125422325));
#70669=CARTESIAN_POINT('',(-1.55549984592209,0.000692341893093657,1.15469914294653));
#70670=CARTESIAN_POINT('',(-1.5555,-1.46451138874614E-13,-1.2940562256037));
#70671=CARTESIAN_POINT('Ctrl Pts',(-1.5555,3.44063942631422E-11,1.29450125422325));
#70672=CARTESIAN_POINT('Ctrl Pts',(-1.55549999999854,0.066173945636013,
1.29012001595974));
#70673=CARTESIAN_POINT('Ctrl Pts',(-1.55127736795033,0.132275922252037,
1.28568825759211));
#70674=CARTESIAN_POINT('Ctrl Pts',(-1.54073252750121,0.214482744420159,
1.27997892833963));
#70675=CARTESIAN_POINT('Ctrl Pts',(-1.53833920511577,0.231023858141827,
1.27882022788333));
#70676=CARTESIAN_POINT('Ctrl Pts',(-1.53377098061585,0.259366030837854,
1.27681583757398));
#70677=CARTESIAN_POINT('Ctrl Pts',(-1.53172516204335,0.27118660135864,1.27597415535806));
#70678=CARTESIAN_POINT('Ctrl Pts',(-1.52757693494643,0.293608134394578,
1.27436606438647));
#70679=CARTESIAN_POINT('Ctrl Pts',(-1.5255003593377,0.304213201128698,1.27360051127662));
#70680=CARTESIAN_POINT('Ctrl Pts',(-1.52094071828573,0.32627756375004,1.27199694126935));
#70681=CARTESIAN_POINT('Ctrl Pts',(-1.51843825394136,0.337732101226949,
1.27115834939666));
#70682=CARTESIAN_POINT('Ctrl Pts',(-1.51265106479368,0.362856215182116,
1.26930502282033));
#70683=CARTESIAN_POINT('Ctrl Pts',(-1.50931005894072,0.376511618066541,
1.26828854077887));
#70684=CARTESIAN_POINT('Ctrl Pts',(-1.49723031814387,0.423137046820157,
1.264785311714));
#70685=CARTESIAN_POINT('Ctrl Pts',(-1.48759311794438,0.455861785575783,
1.26227017677252));
#70686=CARTESIAN_POINT('Ctrl Pts',(-1.44502743237814,0.584619452469703,
1.25214220891536));
#70687=CARTESIAN_POINT('Ctrl Pts',(-1.40381235831859,0.677635212499371,
1.24428169122734));
#70688=CARTESIAN_POINT('Ctrl Pts',(-1.32515992381098,0.816654115623695,
1.23189669967755));
#70689=CARTESIAN_POINT('Ctrl Pts',(-1.29365199034441,0.865701003739014,
1.22739257785155));
#70690=CARTESIAN_POINT('Ctrl Pts',(-1.24464284452598,0.933317923564547,
1.22108303769413));
#70691=CARTESIAN_POINT('Ctrl Pts',(-1.22932352548615,0.953405481557837,
1.21919527835678));
#70692=CARTESIAN_POINT('Ctrl Pts',(-1.20754392395819,0.980565752913682,
1.2166336338176));
#70693=CARTESIAN_POINT('Ctrl Pts',(-1.20149840610152,0.987964127211284,
1.21593488078652));
#70694=CARTESIAN_POINT('Ctrl Pts',(-1.19113600430478,1.00040959770847,1.21475845516477));
#70695=CARTESIAN_POINT('Ctrl Pts',(-1.18685433748461,1.00548552090548,1.21427837182051));
#70696=CARTESIAN_POINT('Ctrl Pts',(-1.17779409009436,1.01608793944454,1.21327522601179));
#70697=CARTESIAN_POINT('Ctrl Pts',(-1.17300890288194,1.02160840782781,1.21275264885535));
#70698=CARTESIAN_POINT('Ctrl Pts',(-1.15976245927782,1.03667448580016,1.21132507732875));
#70699=CARTESIAN_POINT('Ctrl Pts',(-1.15122217873001,1.0461503115702,1.2104256514839));
#70700=CARTESIAN_POINT('Ctrl Pts',(-1.09111436901719,1.11121502799647,1.20422986280805));
#70701=CARTESIAN_POINT('Ctrl Pts',(-1.03565183073949,1.16308120668778,1.19918548515016));
#70702=CARTESIAN_POINT('Ctrl Pts',(-0.929738615780285,1.24851683725739,
1.19020616051433));
#70703=CARTESIAN_POINT('Ctrl Pts',(-0.880701311753465,1.28357831839745,
1.18626448535201));
#70704=CARTESIAN_POINT('Ctrl Pts',(-0.790913638996762,1.3402031655219,1.17922265348124));
#70705=CARTESIAN_POINT('Ctrl Pts',(-0.7510093689496,1.36296491309884,1.17614915979125));
#70706=CARTESIAN_POINT('Ctrl Pts',(-0.681231689241316,1.39877116195034,
1.17080726956671));
#70707=CARTESIAN_POINT('Ctrl Pts',(-0.651848040812775,1.4127035278664,1.16856731727388));
#70708=CARTESIAN_POINT('Ctrl Pts',(-0.608372292156527,1.43167249540638,
1.16525347927361));
#70709=CARTESIAN_POINT('Ctrl Pts',(-0.594608721960165,1.4374433624772,1.16420447782444));
#70710=CARTESIAN_POINT('Ctrl Pts',(-0.570023591896887,1.44733804374563,
1.1623296831578));
#70711=CARTESIAN_POINT('Ctrl Pts',(-0.559234863988521,1.45154078890057,
1.16150662349314));
#70712=CARTESIAN_POINT('Ctrl Pts',(-0.536314244002038,1.46017604856547,
1.15975677932745));
#70713=CARTESIAN_POINT('Ctrl Pts',(-0.524172109283518,1.46457865691336,
1.15882906697885));
#70714=CARTESIAN_POINT('Ctrl Pts',(-0.491223805595871,1.47606315587526,
1.15630893603045));
#70715=CARTESIAN_POINT('Ctrl Pts',(-0.4703207841585,1.48285587147171,1.15470716132368));
#70716=CARTESIAN_POINT('Ctrl Pts',(-0.328839710171484,1.52553968913687,
1.14384019863525));
#70717=CARTESIAN_POINT('Ctrl Pts',(-0.20445570935984,1.54712389381478,1.13410707864492));
#70718=CARTESIAN_POINT('Ctrl Pts',(-0.0114200659839933,1.55692327211328,
1.11912579359675));
#70719=CARTESIAN_POINT('Ctrl Pts',(0.0561809398123301,1.55595179554514,
1.11391509028815));
#70720=CARTESIAN_POINT('Ctrl Pts',(0.139731607269046,1.5492966534169,1.10765966348977));
#70721=CARTESIAN_POINT('Ctrl Pts',(0.155932262152015,1.54775005329729,1.10645558004929));
#70722=CARTESIAN_POINT('Ctrl Pts',(0.180080614039595,1.54506168071519,1.1046768685259));
#70723=CARTESIAN_POINT('Ctrl Pts',(0.188047989997336,1.54411223227,1.10409263194985));
#70724=CARTESIAN_POINT('Ctrl Pts',(0.201813506300838,1.54236370795235,1.10308816908085));
#70725=CARTESIAN_POINT('Ctrl Pts',(0.207614846360526,1.54159351894441,1.1026663974491));
#70726=CARTESIAN_POINT('Ctrl Pts',(0.221348387392079,1.53969131176186,1.10167156914738));
#70727=CARTESIAN_POINT('Ctrl Pts',(0.229276365890333,1.53853072757603,1.10110010912347));
#70728=CARTESIAN_POINT('Ctrl Pts',(0.253217737167928,1.53483675322822,1.09938195474112));
#70729=CARTESIAN_POINT('Ctrl Pts',(0.269201422364817,1.53211413736664,1.09824515059708));
#70730=CARTESIAN_POINT('Ctrl Pts',(0.359073598840509,1.51535559468211,1.09189612958587));
#70731=CARTESIAN_POINT('Ctrl Pts',(0.431919275167733,1.49622358005086,1.08691145468797));
#70732=CARTESIAN_POINT('Ctrl Pts',(0.580310450272275,1.44550253334568,1.07657555997579));
#70733=CARTESIAN_POINT('Ctrl Pts',(0.655318700204039,1.41307975129853,1.07124207902358));
#70734=CARTESIAN_POINT('Ctrl Pts',(0.755355148903462,1.36015312366644,1.06363217683254));
#70735=CARTESIAN_POINT('Ctrl Pts',(0.782816396694977,1.34453568583332,1.06148837013198));
#70736=CARTESIAN_POINT('Ctrl Pts',(0.830919075018346,1.31520592316116,1.05761592088477));
#70737=CARTESIAN_POINT('Ctrl Pts',(0.85174445395616,1.30181580789285,1.0558983234026));
#70738=CARTESIAN_POINT('Ctrl Pts',(0.883405250437868,1.28037386614156,1.05321697993251));
#70739=CARTESIAN_POINT('Ctrl Pts',(0.894470886126156,1.27266801917128,1.05226617375764));
#70740=CARTESIAN_POINT('Ctrl Pts',(0.914794916227206,1.25811884367658,1.05049343451662));
#70741=CARTESIAN_POINT('Ctrl Pts',(0.924080284731778,1.25131465980768,1.04967304896571));
#70742=CARTESIAN_POINT('Ctrl Pts',(0.944561091209134,1.23595433644441,1.04783949679965));
#70743=CARTESIAN_POINT('Ctrl Pts',(0.955717386008275,1.22734796638103,1.04682440442133));
#70744=CARTESIAN_POINT('Ctrl Pts',(0.983839068008911,1.20503796834503,1.04422280258073));
#70745=CARTESIAN_POINT('Ctrl Pts',(1.00063548309312,1.19112734737754,1.04262816237686));
#70746=CARTESIAN_POINT('Ctrl Pts',(1.09190984219276,1.11224160219564,1.0337293845014));
#70747=CARTESIAN_POINT('Ctrl Pts',(1.16034425149336,1.04064566170079,1.02615433406886));
#70748=CARTESIAN_POINT('Ctrl Pts',(1.26284734305497,0.910633504833359,1.0133218770693));
#70749=CARTESIAN_POINT('Ctrl Pts',(1.30076274982857,0.855601413603371,1.00812836319334));
#70750=CARTESIAN_POINT('Ctrl Pts',(1.34683281767853,0.778556907172249,1.00128978248354));
#70751=CARTESIAN_POINT('Ctrl Pts',(1.35820064344568,0.758551663580726,0.999551149736661));
#70752=CARTESIAN_POINT('Ctrl Pts',(1.37705959911517,0.723579192941432,0.996583524393833));
#70753=CARTESIAN_POINT('Ctrl Pts',(1.38476058822685,0.70872996351125,0.995345190632082));
#70754=CARTESIAN_POINT('Ctrl Pts',(1.39583807666929,0.686499881086753,0.99352635858116));
#70755=CARTESIAN_POINT('Ctrl Pts',(1.39939847609441,0.67921273248502,0.992935635391156));
#70756=CARTESIAN_POINT('Ctrl Pts',(1.40543105609367,0.666616893088735,0.991924422068322));
#70757=CARTESIAN_POINT('Ctrl Pts',(1.4079304361811,0.661321726472419,0.991502314175194));
#70758=CARTESIAN_POINT('Ctrl Pts',(1.41374361763505,0.648823620193149,0.990513038061281));
#70759=CARTESIAN_POINT('Ctrl Pts',(1.41703232810791,0.641609300853237,0.989947393961184));
#70760=CARTESIAN_POINT('Ctrl Pts',(1.42650514259419,0.62040099032651,0.988299382972986));
#70761=CARTESIAN_POINT('Ctrl Pts',(1.43253833737854,0.606340060173557,0.987225563230212));
#70762=CARTESIAN_POINT('Ctrl Pts',(1.47381100755128,0.506093644539667,0.979686236681375));
#70763=CARTESIAN_POINT('Ctrl Pts',(1.50146162238255,0.416974206890176,0.973581055212101));
#70764=CARTESIAN_POINT('Ctrl Pts',(1.53563626338026,0.257483984088193,0.962848208943956));
#70765=CARTESIAN_POINT('Ctrl Pts',(1.54566279089013,0.18815516542045,0.958244160154274));
#70766=CARTESIAN_POINT('Ctrl Pts',(1.55424527879838,0.0757185524093037,
0.950637991356019));
#70767=CARTESIAN_POINT('Ctrl Pts',(1.55573984246288,0.0329346859891965,
0.947712587502483));
#70768=CARTESIAN_POINT('Ctrl Pts',(1.55536441024355,-0.0263309600484623,
0.943585749178343));
#70769=CARTESIAN_POINT('Ctrl Pts',(1.55499821543606,-0.0428051589004132,
0.942430724169581));
#70770=CARTESIAN_POINT('Ctrl Pts',(1.55392047158784,-0.0710693084944344,
0.940433954213125));
#70771=CARTESIAN_POINT('Ctrl Pts',(1.55333621677948,-0.0828629125835807,
0.939596247208741));
#70772=CARTESIAN_POINT('Ctrl Pts',(1.55187017296961,-0.106911970931832,
0.937878212999806));
#70773=CARTESIAN_POINT('Ctrl Pts',(1.5509773302719,-0.119165885253095,0.936997597002927));
#70774=CARTESIAN_POINT('Ctrl Pts',(1.54833828902965,-0.150293107417539,
0.934746763264206));
#70775=CARTESIAN_POINT('Ctrl Pts',(1.54639216534164,-0.169146939979477,
0.933370381848849));
#70776=CARTESIAN_POINT('Ctrl Pts',(1.53657373629975,-0.249805999471025,
0.927423341283527));
#70777=CARTESIAN_POINT('Ctrl Pts',(1.52533753099491,-0.311135699364405,
0.922749905055785));
#70778=CARTESIAN_POINT('Ctrl Pts',(1.48568590045217,-0.472300638863577,
0.910077219739693));
#70779=CARTESIAN_POINT('Ctrl Pts',(1.45091322431365,-0.570244938439349,
0.901947840269197));
#70780=CARTESIAN_POINT('Ctrl Pts',(1.39456428372374,-0.689618261921028,
0.891832458899489));
#70781=CARTESIAN_POINT('Ctrl Pts',(1.38177220260347,-0.714904653519119,
0.889678711772563));
#70782=CARTESIAN_POINT('Ctrl Pts',(1.35903324482003,-0.756959808063756,
0.886093058320462));
#70783=CARTESIAN_POINT('Ctrl Pts',(1.34944922420061,-0.773916270808348,
0.884646331242522));
#70784=CARTESIAN_POINT('Ctrl Pts',(1.33517432258963,-0.798100140902384,
0.882586126061654));
#70785=CARTESIAN_POINT('Ctrl Pts',(1.33073836765728,-0.805474836808508,
0.881958317218233));
#70786=CARTESIAN_POINT('Ctrl Pts',(1.32283631764262,-0.81836836912185,0.880861964513523));
#70787=CARTESIAN_POINT('Ctrl Pts',(1.31939643941452,-0.823902756535837,
0.880391815074281));
#70788=CARTESIAN_POINT('Ctrl Pts',(1.31174903461766,-0.83603585902308,0.879362142896668));
#70789=CARTESIAN_POINT('Ctrl Pts',(1.30752637984319,-0.842624626073871,
0.878803611552494));
#70790=CARTESIAN_POINT('Ctrl Pts',(1.2951692328433,-0.861589362402017,0.877196902272928));
#70791=CARTESIAN_POINT('Ctrl Pts',(1.28690723169062,-0.873881794136387,
0.876156640225968));
#70792=CARTESIAN_POINT('Ctrl Pts',(1.22141787581551,-0.968375046143511,
0.868153293452749));
#70793=CARTESIAN_POINT('Ctrl Pts',(1.15653919864745,-1.04500466797491,0.861612810327628));
#70794=CARTESIAN_POINT('Ctrl Pts',(1.03754706242522,-1.16078013036358,0.850685718088348));
#70795=CARTESIAN_POINT('Ctrl Pts',(0.987497119244587,-1.20364570616782,
0.846342908330371));
#70796=CARTESIAN_POINT('Ctrl Pts',(0.912422323536318,-1.26010145516987,
0.839998408926332));
#70797=CARTESIAN_POINT('Ctrl Pts',(0.889506811781509,-1.27638068694012,
0.83808300540988));
#70798=CARTESIAN_POINT('Ctrl Pts',(0.847339647100369,-1.3046491408938,0.834583713781654));
#70799=CARTESIAN_POINT('Ctrl Pts',(0.828242705493292,-1.3168552646975,0.833007891812109));
#70800=CARTESIAN_POINT('Ctrl Pts',(0.797733448174011,-1.33542955594234,
0.830499946943618));
#70801=CARTESIAN_POINT('Ctrl Pts',(0.786495405086956,-1.34207887709794,
0.829578154626251));
#70802=CARTESIAN_POINT('Ctrl Pts',(0.765158916519037,-1.35434322035417,
0.827831012091375));
#70803=CARTESIAN_POINT('Ctrl Pts',(0.755078973249932,-1.35998877088987,
0.827006838760781));
#70804=CARTESIAN_POINT('Ctrl Pts',(0.732048652454525,-1.37255257678912,
0.825126024806289));
#70805=CARTESIAN_POINT('Ctrl Pts',(0.719061506810858,-1.37940071318173,
0.824066977559879));
#70806=CARTESIAN_POINT('Ctrl Pts',(0.678256088485306,-1.40018460535361,
0.820743195622856));
#70807=CARTESIAN_POINT('Ctrl Pts',(0.650116956007206,-1.41346946848273,
0.818456294662544));
#70808=CARTESIAN_POINT('Ctrl Pts',(0.505109638405407,-1.47668324460947,
0.80668956913138));
#70809=CARTESIAN_POINT('Ctrl Pts',(0.382849090961857,-1.51299213477604,
0.79677199893315));
#70810=CARTESIAN_POINT('Ctrl Pts',(0.200276156925776,-1.54364644407647,
0.782474536140982));
#70811=CARTESIAN_POINT('Ctrl Pts',(0.142485811906422,-1.5500497410089,0.778030836873473));
#70812=CARTESIAN_POINT('Ctrl Pts',(0.0722771104930077,-1.55386785097514,
0.772823130975401));
#70813=CARTESIAN_POINT('Ctrl Pts',(0.0600794839110052,-1.55438726172793,
0.771925382508288));
#70814=CARTESIAN_POINT('Ctrl Pts',(0.0406912623802615,-1.55498429184524,
0.770510817673444));
#70815=CARTESIAN_POINT('Ctrl Pts',(0.0335043722516422,-1.5551557444108,
0.769989170164399));
#70816=CARTESIAN_POINT('Ctrl Pts',(0.019694468714525,-1.5553894174391,0.768992330454731));
#70817=CARTESIAN_POINT('Ctrl Pts',(0.0130718858168326,-1.55545917331499,
0.768516766739881));
#70818=CARTESIAN_POINT('Ctrl Pts',(-0.00336274671031001,-1.55552731025794,
0.767342331540919));
#70819=CARTESIAN_POINT('Ctrl Pts',(-0.0131749458998763,-1.55547515412416,
0.766646194608348));
#70820=CARTESIAN_POINT('Ctrl Pts',(-0.0485207013566759,-1.55495277678717,
0.764154613184552));
#70821=CARTESIAN_POINT('Ctrl Pts',(-0.0740437748815334,-1.55394662214301,
0.762385633961577));
#70822=CARTESIAN_POINT('Ctrl Pts',(-0.204869799206001,-1.54555822445316,
0.753419844711295));
#70823=CARTESIAN_POINT('Ctrl Pts',(-0.309256457753484,-1.52809909361066,
0.746589414115095));
#70824=CARTESIAN_POINT('Ctrl Pts',(-0.472120577036149,-1.48347172064588,
0.735428391334662));
#70825=CARTESIAN_POINT('Ctrl Pts',(-0.532079558488635,-1.46303669022891,
0.731206452936639));
#70826=CARTESIAN_POINT('Ctrl Pts',(-0.616674170741491,-1.42831585439364,
0.724947530180732));
#70827=CARTESIAN_POINT('Ctrl Pts',(-0.642428242777043,-1.41691883934955,
0.723000153963644));
#70828=CARTESIAN_POINT('Ctrl Pts',(-0.680635374747506,-1.39875512908199,
0.720038968348202));
#70829=CARTESIAN_POINT('Ctrl Pts',(-0.693329369726769,-1.39250665566949,
0.719042881519532));
#70830=CARTESIAN_POINT('Ctrl Pts',(-0.716199741093375,-1.38085873654213,
0.717224875711715));
#70831=CARTESIAN_POINT('Ctrl Pts',(-0.72640484178124,-1.37551768879564,
0.716405052021045));
#70832=CARTESIAN_POINT('Ctrl Pts',(-0.748392457814292,-1.3636970971313,
0.714619404106716));
#70833=CARTESIAN_POINT('Ctrl Pts',(-0.760152066574892,-1.35717716537746,
0.713652191039164));
#70834=CARTESIAN_POINT('Ctrl Pts',(-0.792545644141668,-1.33866396523111,
0.710952936475932));
#70835=CARTESIAN_POINT('Ctrl Pts',(-0.812989548258128,-1.32634749868085,
0.709209413087034));
#70836=CARTESIAN_POINT('Ctrl Pts',(-0.918760733669823,-1.2592611867752,
0.699971078486175));
#70837=CARTESIAN_POINT('Ctrl Pts',(-0.998851292290241,-1.19672442878681,
0.692192415550732));
#70838=CARTESIAN_POINT('Ctrl Pts',(-1.11932734767826,-1.08208354350407,
0.679298953207176));
#70839=CARTESIAN_POINT('Ctrl Pts',(-1.16352957688896,-1.03440715295421,
0.674249426583443));
#70840=CARTESIAN_POINT('Ctrl Pts',(-1.22574374795021,-0.958252039711842,
0.666761307294949));
#70841=CARTESIAN_POINT('Ctrl Pts',(-1.24602837120463,-0.931723347663148,
0.664249040344013));
#70842=CARTESIAN_POINT('Ctrl Pts',(-1.27153936887439,-0.896034436492706,
0.661013006060535));
#70843=CARTESIAN_POINT('Ctrl Pts',(-1.27754758047765,-0.887447054050633,
0.660244896544388));
#70844=CARTESIAN_POINT('Ctrl Pts',(-1.28731987800289,-0.873174809320621,
0.658986417738811));
#70845=CARTESIAN_POINT('Ctrl Pts',(-1.2911341069374,-0.867524892915393,
0.658492839991736));
#70846=CARTESIAN_POINT('Ctrl Pts',(-1.29878653211309,-0.856027286412465,
0.657498001873287));
#70847=CARTESIAN_POINT('Ctrl Pts',(-1.302622656876,-0.850178446013116,0.656996876485008));
#70848=CARTESIAN_POINT('Ctrl Pts',(-1.31257278138028,-0.834782287554142,
0.65569009229947));
#70849=CARTESIAN_POINT('Ctrl Pts',(-1.31862222576262,-0.825193443812122,
0.654888541614257));
#70850=CARTESIAN_POINT('Ctrl Pts',(-1.34514093410318,-0.782122792873095,
0.651338690354689));
#70851=CARTESIAN_POINT('Ctrl Pts',(-1.36444548890473,-0.747936696834765,
0.648655699755602));
#70852=CARTESIAN_POINT('Ctrl Pts',(-1.42450778606151,-0.631490507014228,
0.639831350612569));
#70853=CARTESIAN_POINT('Ctrl Pts',(-1.45927906244556,-0.546360014322117,
0.633875920029916));
#70854=CARTESIAN_POINT('Ctrl Pts',(-1.5084705040553,-0.386947935828809,
0.622841825458153));
#70855=CARTESIAN_POINT('Ctrl Pts',(-1.52537744295723,-0.31374110894365,
0.617817409433293));
#70856=CARTESIAN_POINT('Ctrl Pts',(-1.53998347561593,-0.220051829075397,
0.611253665695753));
#70857=CARTESIAN_POINT('Ctrl Pts',(-1.54265837579021,-0.200441977704697,
0.609873001858645));
#70858=CARTESIAN_POINT('Ctrl Pts',(-1.54640551987449,-0.168419898296888,
0.607604506038478));
#70859=CARTESIAN_POINT('Ctrl Pts',(-1.54770411844452,-0.156036019908814,
0.606723843332135));
#70860=CARTESIAN_POINT('Ctrl Pts',(-1.54993484458716,-0.131982051576268,
0.605006075357329));
#70861=CARTESIAN_POINT('Ctrl Pts',(-1.55088417448401,-0.120314371102912,
0.604169573089886));
#70862=CARTESIAN_POINT('Ctrl Pts',(-1.5528133634839,-0.0927591598438819,
0.602185750767877));
#70863=CARTESIAN_POINT('Ctrl Pts',(-1.55368120297326,-0.0768653887194082,
0.601034997748598));
#70864=CARTESIAN_POINT('Ctrl Pts',(-1.55510168454109,-0.0406481588717827,
0.598397021803662));
#70865=CARTESIAN_POINT('Ctrl Pts',(-1.5555000000974,-0.0203237295583516,
0.596905348382645));
#70866=CARTESIAN_POINT('Ctrl Pts',(-1.5555,7.45448211670055E-9,0.595401982137319));
#70867=CARTESIAN_POINT('Ctrl Pts',(-1.55549962214825,0.00108420323222797,
0.45701132945449));
#70868=CARTESIAN_POINT('Ctrl Pts',(-1.55559222809785,-0.131776975675532,
0.465990612534344));
#70869=CARTESIAN_POINT('Ctrl Pts',(-1.53866326941148,-0.264113784066724,
0.474473953896888));
#70870=CARTESIAN_POINT('Ctrl Pts',(-1.49386726717658,-0.435803972088965,
0.486419820767815));
#70871=CARTESIAN_POINT('Ctrl Pts',(-1.48077610088256,-0.478399474189407,
0.489459784139951));
#70872=CARTESIAN_POINT('Ctrl Pts',(-1.46022645306863,-0.536287411661747,
0.493733536133207));
#70873=CARTESIAN_POINT('Ctrl Pts',(-1.45431789749139,-0.552109496244956,
0.49491660831121));
#70874=CARTESIAN_POINT('Ctrl Pts',(-1.44375505425784,-0.579048136409908,
0.496958435657103));
#70875=CARTESIAN_POINT('Ctrl Pts',(-1.43922696275649,-0.59021278852078,
0.497812891309869));
#70876=CARTESIAN_POINT('Ctrl Pts',(-1.42973896931268,-0.612848175116802,
0.499562673758938));
#70877=CARTESIAN_POINT('Ctrl Pts',(-1.42476961910855,-0.624313960766495,
0.500458271815235));
#70878=CARTESIAN_POINT('Ctrl Pts',(-1.41181107643544,-0.653252501987194,
0.502742967494973));
#70879=CARTESIAN_POINT('Ctrl Pts',(-1.40363552926885,-0.670638938646375,
0.504138396380045));
#70880=CARTESIAN_POINT('Ctrl Pts',(-1.36725250891238,-0.744431240597183,
0.510162070654917));
#70881=CARTESIAN_POINT('Ctrl Pts',(-1.33595455858357,-0.799237610854561,
0.514896133475867));
#70882=CARTESIAN_POINT('Ctrl Pts',(-1.24499532827392,-0.938178953378845,
0.527587555202891));
#70883=CARTESIAN_POINT('Ctrl Pts',(-1.18015101899143,-1.0185454145577,0.535669321779819));
#70884=CARTESIAN_POINT('Ctrl Pts',(-1.08792313130614,-1.11211900459493,
0.545742557369242));
#70885=CARTESIAN_POINT('Ctrl Pts',(-1.06745393217973,-1.13178077363924,
0.547900739243709));
#70886=CARTESIAN_POINT('Ctrl Pts',(-1.03198308789238,-1.16403344440843,
0.551497782500001));
#70887=CARTESIAN_POINT('Ctrl Pts',(-1.0172612049225,-1.17692085014791,0.552951506823508));
#70888=CARTESIAN_POINT('Ctrl Pts',(-0.995639225204317,-1.19513958630086,
0.555026143112321));
#70889=CARTESIAN_POINT('Ctrl Pts',(-0.988931983560631,-1.20069548140919,
0.555661548166732));
#70890=CARTESIAN_POINT('Ctrl Pts',(-0.977065314993787,-1.21035825081999,
0.556770966315458));
#70891=CARTESIAN_POINT('Ctrl Pts',(-0.971926028505627,-1.21448899752712,
0.557246621559516));
#70892=CARTESIAN_POINT('Ctrl Pts',(-0.960440653869167,-1.22360086432171,
0.558298987468403));
#70893=CARTESIAN_POINT('Ctrl Pts',(-0.954081912521708,-1.22856543849585,
0.558874554832622));
#70894=CARTESIAN_POINT('Ctrl Pts',(-0.935487546849195,-1.2428515138766,
0.560538195715148));
#70895=CARTESIAN_POINT('Ctrl Pts',(-0.923151516896774,-1.25204159646333,
0.561617730230413));
#70896=CARTESIAN_POINT('Ctrl Pts',(-0.834443992119293,-1.31610279440216,
0.569226789975005));
#70897=CARTESIAN_POINT('Ctrl Pts',(-0.753360876617966,-1.36413916058978,
0.575390220523253));
#70898=CARTESIAN_POINT('Ctrl Pts',(-0.60614640690851,-1.43419795321606,
0.58612089256293));
#70899=CARTESIAN_POINT('Ctrl Pts',(-0.541969828151479,-1.45965922560717,
0.590661972331486));
#70900=CARTESIAN_POINT('Ctrl Pts',(-0.435741462610644,-1.49382946295933,
0.598190459943658));
#70901=CARTESIAN_POINT('Ctrl Pts',(-0.394648655385648,-1.50520729431177,
0.601104513386016));
#70902=CARTESIAN_POINT('Ctrl Pts',(-0.336846680359906,-1.51868185493772,
0.605237084806839));
#70903=CARTESIAN_POINT('Ctrl Pts',(-0.320490387296837,-1.52221750620717,
0.606410071391811));
#70904=CARTESIAN_POINT('Ctrl Pts',(-0.292200495609419,-1.52785662599148,
0.608446722203742));
#70905=CARTESIAN_POINT('Ctrl Pts',(-0.28029326737502,-1.53008583695195,
0.609306323867898));
#70906=CARTESIAN_POINT('Ctrl Pts',(-0.255825916384155,-1.53437130855106,
0.611078133434445));
#70907=CARTESIAN_POINT('Ctrl Pts',(-0.243264198761912,-1.53641294053229,
0.611990733851619));
#70908=CARTESIAN_POINT('Ctrl Pts',(-0.210980316102215,-1.54125414113151,
0.614344370188822));
#70909=CARTESIAN_POINT('Ctrl Pts',(-0.191227416351517,-1.5438293391593,
0.615792314669233));
#70910=CARTESIAN_POINT('Ctrl Pts',(-0.100912577616179,-1.55384392442836,
0.622451611889749));
#70911=CARTESIAN_POINT('Ctrl Pts',(-0.0299519142444876,-1.55682834827152,
0.627797506409655));
#70912=CARTESIAN_POINT('Ctrl Pts',(0.134700830305024,-1.55249160655785,
0.640428994785667));
#70913=CARTESIAN_POINT('Ctrl Pts',(0.228026725137361,-1.54155038163138,
0.647765603871157));
#70914=CARTESIAN_POINT('Ctrl Pts',(0.346494571530747,-1.51666277175438,
0.657027971589266));
#70915=CARTESIAN_POINT('Ctrl Pts',(0.373041333769766,-1.51035253843597,
0.659098910664312));
#70916=CARTESIAN_POINT('Ctrl Pts',(0.417818956285551,-1.49845600077114,
0.662570475163492));
#70917=CARTESIAN_POINT('Ctrl Pts',(0.436137775119659,-1.49322703992496,
0.6639844547229));
#70918=CARTESIAN_POINT('Ctrl Pts',(0.46266215851283,-1.48512605104798,0.66601827279117));
#70919=CARTESIAN_POINT('Ctrl Pts',(0.47094623509352,-1.4825199201197,0.666651529664496));
#70920=CARTESIAN_POINT('Ctrl Pts',(0.484971186319934,-1.47797831233667,
0.66771982510586));
#70921=CARTESIAN_POINT('Ctrl Pts',(0.490723175654049,-1.47607849148383,
0.668156845773352));
#70922=CARTESIAN_POINT('Ctrl Pts',(0.503976228395926,-1.47161511326572,
0.669161126042264));
#70923=CARTESIAN_POINT('Ctrl Pts',(0.511468990133657,-1.46902776006226,
0.669726998119038));
#70924=CARTESIAN_POINT('Ctrl Pts',(0.532797491404099,-1.46147976549026,
0.671333210290149));
#70925=CARTESIAN_POINT('Ctrl Pts',(0.546583585810319,-1.45637999727997,
0.672365899101507));
#70926=CARTESIAN_POINT('Ctrl Pts',(0.655603763529275,-1.41428490882571,
0.680504131455665));
#70927=CARTESIAN_POINT('Ctrl Pts',(0.74706844026402,-1.368178689696,0.687170240203545));
#70928=CARTESIAN_POINT('Ctrl Pts',(0.85612686663686,-1.29898192507432,0.695676226158675));
#70929=CARTESIAN_POINT('Ctrl Pts',(0.878514028559614,-1.28394716241009,
0.6974540226012));
#70930=CARTESIAN_POINT('Ctrl Pts',(0.939197004647554,-1.24086327567092,
0.702386879951735));
#70931=CARTESIAN_POINT('Ctrl Pts',(0.97661497617679,-1.21163334327879,0.705559521268203));
#70932=CARTESIAN_POINT('Ctrl Pts',(1.03799619983705,-1.15899106544816,0.71106261919988));
#70933=CARTESIAN_POINT('Ctrl Pts',(1.06264704234687,-1.13643186922587,0.713362660632223));
#70934=CARTESIAN_POINT('Ctrl Pts',(1.09750695625718,-1.10240334469373,0.716764811806982));
#70935=CARTESIAN_POINT('Ctrl Pts',(1.10830393765384,-1.0915479859966,0.717840711788879));
#70936=CARTESIAN_POINT('Ctrl Pts',(1.12719648717863,-1.07198397756297,0.719764566217214));
#70937=CARTESIAN_POINT('Ctrl Pts',(1.13535585941975,-1.06333843485334,0.720609656162315));
#70938=CARTESIAN_POINT('Ctrl Pts',(1.15242066131286,-1.04483649601181,0.722408138872987));
#70939=CARTESIAN_POINT('Ctrl Pts',(1.16130048480583,-1.03495789659564,0.723362523171695));
#70940=CARTESIAN_POINT('Ctrl Pts',(1.18500763224571,-1.00789497227222,0.725962223662884));
#70941=CARTESIAN_POINT('Ctrl Pts',(1.19958659492175,-0.990498492767489,
0.727617530659071));
#70942=CARTESIAN_POINT('Ctrl Pts',(1.30039971917826,-0.864710968863832,
0.739482643387864));
#70943=CARTESIAN_POINT('Ctrl Pts',(1.37218219636709,-0.745563409998109,
0.750268706956153));
#70944=CARTESIAN_POINT('Ctrl Pts',(1.45116588071695,-0.563311225532864,
0.76561946739305));
#70945=CARTESIAN_POINT('Ctrl Pts',(1.47187425060517,-0.506744290007288,
0.770228891819041));
#70946=CARTESIAN_POINT('Ctrl Pts',(1.4928596724745,-0.437156966989877,0.775614632176288));
#70947=CARTESIAN_POINT('Ctrl Pts',(1.49632149209804,-0.425156717247051,
0.776533355658679));
#70948=CARTESIAN_POINT('Ctrl Pts',(1.501594232799,-0.406016298289001,0.777981440068602));
#70949=CARTESIAN_POINT('Ctrl Pts',(1.5034995369481,-0.398903024395469,0.778515833978629));
#70950=CARTESIAN_POINT('Ctrl Pts',(1.5070673596748,-0.385194085373924,0.779538154195339));
#70951=CARTESIAN_POINT('Ctrl Pts',(1.50873723574029,-0.378600667892621,
0.780026455637771));
#70952=CARTESIAN_POINT('Ctrl Pts',(1.51278907379748,-0.362149568528122,
0.781236821726823));
#70953=CARTESIAN_POINT('Ctrl Pts',(1.51511804048059,-0.35227890908491,0.781955939948439));
#70954=CARTESIAN_POINT('Ctrl Pts',(1.52329259849065,-0.31605174178774,0.784571698156795));
#70955=CARTESIAN_POINT('Ctrl Pts',(1.528548701326,-0.289565417157093,0.786438697744324));
#70956=CARTESIAN_POINT('Ctrl Pts',(1.54865968620811,-0.172311294572819,
0.794558890861106));
#70957=CARTESIAN_POINT('Ctrl Pts',(1.55613860216703,-0.0804602061068882,
0.80054836749639));
#70958=CARTESIAN_POINT('Ctrl Pts',(1.55491905320242,0.0841967079041952,
0.811401617338453));
#70959=CARTESIAN_POINT('Ctrl Pts',(1.54928814381692,0.156738856062114,0.816223034879309));
#70960=CARTESIAN_POINT('Ctrl Pts',(1.53427759584364,0.257760749117066,0.823202677273314));
#70961=CARTESIAN_POINT('Ctrl Pts',(1.52912035680635,0.286773583659468,0.825237737280817));
#70962=CARTESIAN_POINT('Ctrl Pts',(1.52018021177721,0.329917474840088,0.828319739719143));
#70963=CARTESIAN_POINT('Ctrl Pts',(1.51701668816986,0.344171118133979,0.829347130060704));
#70964=CARTESIAN_POINT('Ctrl Pts',(1.5109320704643,0.369870262939396,0.8312172583201));
#70965=CARTESIAN_POINT('Ctrl Pts',(1.50808032319764,0.381331165352149,0.832057711287271));
#70966=CARTESIAN_POINT('Ctrl Pts',(1.50163583492686,0.406027248325023,0.83388326014716));
#70967=CARTESIAN_POINT('Ctrl Pts',(1.49799803953429,0.41924951795191,0.834869753205673));
#70968=CARTESIAN_POINT('Ctrl Pts',(1.48746349982297,0.455650480893109,0.83761167867197));
#70969=CARTESIAN_POINT('Ctrl Pts',(1.48020059711373,0.478718178854514,0.839378813515945));
#70970=CARTESIAN_POINT('Ctrl Pts',(1.44561745438315,0.580232770910194,0.84729182666431));
#70971=CARTESIAN_POINT('Ctrl Pts',(1.41258085929661,0.656575422198195,0.853618566900436));
#70972=CARTESIAN_POINT('Ctrl Pts',(1.33697110850095,0.798865910015656,0.866070037158325));
#70973=CARTESIAN_POINT('Ctrl Pts',(1.29518614811871,0.864969230372958,0.872165185939581));
#70974=CARTESIAN_POINT('Ctrl Pts',(1.22656771051593,0.957328770611055,0.88095217671356));
#70975=CARTESIAN_POINT('Ctrl Pts',(1.20346945985135,0.986209151402802,0.883741917856108));
#70976=CARTESIAN_POINT('Ctrl Pts',(1.17219511628505,1.02257501996507,0.887283767590779));
#70977=CARTESIAN_POINT('Ctrl Pts',(1.16493988953768,1.0308327382976,0.888090045246842));
#70978=CARTESIAN_POINT('Ctrl Pts',(1.15289676090454,1.04425036922231,0.889402500673036));
#70979=CARTESIAN_POINT('Ctrl Pts',(1.14816041907011,1.04945577962064,0.889912268140033));
#70980=CARTESIAN_POINT('Ctrl Pts',(1.1385453918034,1.05988002714475,0.890934009704774));
#70981=CARTESIAN_POINT('Ctrl Pts',(1.13366577932167,1.06509773610221,0.891445899212164));
#70982=CARTESIAN_POINT('Ctrl Pts',(1.1208639580628,1.07859890871543,0.892772280668619));
#70983=CARTESIAN_POINT('Ctrl Pts',(1.11288565992149,1.08682894093078,0.893582638543893));
#70984=CARTESIAN_POINT('Ctrl Pts',(1.0776165971945,1.12241515870123,0.897098781588745));
#70985=CARTESIAN_POINT('Ctrl Pts',(1.04940052499586,1.14883960078862,0.899741852092821));
#70986=CARTESIAN_POINT('Ctrl Pts',(0.906744814047346,1.27279010744027,0.912477734325908));
#70987=CARTESIAN_POINT('Ctrl Pts',(0.779570311632964,1.35442067617543,0.92203587703761));
#70988=CARTESIAN_POINT('Ctrl Pts',(0.615756303871838,1.42873955618678,0.934329076352657));
#70989=CARTESIAN_POINT('Ctrl Pts',(0.588519711417521,1.44017252519928,0.936369049803746));
#70990=CARTESIAN_POINT('Ctrl Pts',(0.547333698359148,1.45609752368984,0.939457888815914));
#70991=CARTESIAN_POINT('Ctrl Pts',(0.533618472968219,1.46117948087086,0.94048712334576));
#70992=CARTESIAN_POINT('Ctrl Pts',(0.508685894298989,1.47002000567117,0.942360393314172));
#70993=CARTESIAN_POINT('Ctrl Pts',(0.497493325218803,1.47384549168836,0.943202136259653));
#70994=CARTESIAN_POINT('Ctrl Pts',(0.473215110276006,1.4818354380438,0.945030301710871));
#70995=CARTESIAN_POINT('Ctrl Pts',(0.460115859099777,1.48595497233822,0.946018121336703));
#70996=CARTESIAN_POINT('Ctrl Pts',(0.423774595164706,1.49685720612247,0.948763473124544));
#70997=CARTESIAN_POINT('Ctrl Pts',(0.400427045964196,1.50327125365992,0.950532715142734));
#70998=CARTESIAN_POINT('Ctrl Pts',(0.287446758967202,1.53149058065117,0.959125167818554));
#70999=CARTESIAN_POINT('Ctrl Pts',(0.19615670761787,1.54583517391963,0.966176765304142));
#71000=CARTESIAN_POINT('Ctrl Pts',(0.0334843880084227,1.55675141941361,
0.97879900278409));
#71001=CARTESIAN_POINT('Ctrl Pts',(-0.0374232788441268,1.55666191856376,
0.984314846594833));
#71002=CARTESIAN_POINT('Ctrl Pts',(-0.131880126116507,1.55008292680199,
0.991534843764174));
#71003=CARTESIAN_POINT('Ctrl Pts',(-0.155640418922857,1.54787778446996,
0.993339640488362));
#71004=CARTESIAN_POINT('Ctrl Pts',(-0.196489056925793,1.54313651001296,
0.996413303548926));
#71005=CARTESIAN_POINT('Ctrl Pts',(-0.213602905328831,1.54086083150488,
0.997692153280786));
#71006=CARTESIAN_POINT('Ctrl Pts',(-0.238922876000515,1.53706396930472,
0.999567673935903));
#71007=CARTESIAN_POINT('Ctrl Pts',(-0.247159697958938,1.53576100960163,
1.00017518830595));
#71008=CARTESIAN_POINT('Ctrl Pts',(-0.261319108792152,1.53340430143648,
1.00121457917991));
#71009=CARTESIAN_POINT('Ctrl Pts',(-0.267246509880269,1.53238237231014,
1.00164816269389));
#71010=CARTESIAN_POINT('Ctrl Pts',(-0.28120592498404,1.52989219849192,1.00266569714525));
#71011=CARTESIAN_POINT('Ctrl Pts',(-0.289232499173429,1.52839506693504,
1.00324802753633));
#71012=CARTESIAN_POINT('Ctrl Pts',(-0.313310747236021,1.52370746691639,
1.00498768038198));
#71013=CARTESIAN_POINT('Ctrl Pts',(-0.329324827126571,1.52032670267708,
1.00613501485091));
#71014=CARTESIAN_POINT('Ctrl Pts',(-0.415928134730588,1.50061099860013,
1.01230195857146));
#71015=CARTESIAN_POINT('Ctrl Pts',(-0.485371964030678,1.47961015371916,
1.01711245896106));
#71016=CARTESIAN_POINT('Ctrl Pts',(-0.613870513446562,1.43072360236324,
1.02618087146745));
#71017=CARTESIAN_POINT('Ctrl Pts',(-0.673124875431059,1.40381968665097,
1.03043598953591));
#71018=CARTESIAN_POINT('Ctrl Pts',(-0.767073201720941,1.35384380712579,
1.03752016919881));
#71019=CARTESIAN_POINT('Ctrl Pts',(-0.802831926286873,1.3329496867159,1.04030224056641));
#71020=CARTESIAN_POINT('Ctrl Pts',(-0.863280611184542,1.29431356272571,
1.04520045266843));
#71021=CARTESIAN_POINT('Ctrl Pts',(-0.888363127674324,1.27722815442603,
1.04729481949152));
#71022=CARTESIAN_POINT('Ctrl Pts',(-0.924887434124145,1.25075243075224,
1.0504491633037));
#71023=CARTESIAN_POINT('Ctrl Pts',(-0.936721772073318,1.24191412906317,
1.05148819933784));
#71024=CARTESIAN_POINT('Ctrl Pts',(-0.957806965145237,1.22569412320197,
1.05337151349873));
#71025=CARTESIAN_POINT('Ctrl Pts',(-0.96710294939559,1.21837274151374,1.05421337455123));
#71026=CARTESIAN_POINT('Ctrl Pts',(-0.986912342666978,1.20240159978864,
1.05603298124082));
#71027=CARTESIAN_POINT('Ctrl Pts',(-0.997397461981246,1.19371850126346,
1.05701202471686));
#71028=CARTESIAN_POINT('Ctrl Pts',(-1.02580090396011,1.1695611285888,1.05970913338976));
#71029=CARTESIAN_POINT('Ctrl Pts',(-1.04348136141507,1.15381422351143,1.06143825587099));
#71030=CARTESIAN_POINT('Ctrl Pts',(-1.14131694306618,1.06258970350716,1.07130132611706));
#71031=CARTESIAN_POINT('Ctrl Pts',(-1.21362659262786,0.979185027256165,
1.07977639651119));
#71032=CARTESIAN_POINT('Ctrl Pts',(-1.32470051676394,0.819669853337824,
1.09485004100646));
#71033=CARTESIAN_POINT('Ctrl Pts',(-1.36718278928739,0.746662120492023,
1.10138986949551));
#71034=CARTESIAN_POINT('Ctrl Pts',(-1.40933026401122,0.658444271783863,
1.10864840838774));
#71035=CARTESIAN_POINT('Ctrl Pts',(-1.41496347625935,0.646249986748281,
1.10963803485002));
#71036=CARTESIAN_POINT('Ctrl Pts',(-1.42352197205447,0.62707470753663,1.11117121190658));
#71037=CARTESIAN_POINT('Ctrl Pts',(-1.42655531089423,0.620143084458317,
1.11172079679926));
#71038=CARTESIAN_POINT('Ctrl Pts',(-1.43221718429254,0.606943470684567,
1.11275819686319));
#71039=CARTESIAN_POINT('Ctrl Pts',(-1.43485528551005,0.60068024038802,1.11324652107264));
#71040=CARTESIAN_POINT('Ctrl Pts',(-1.44115854644419,0.585436896212434,
1.1144258795316));
#71041=CARTESIAN_POINT('Ctrl Pts',(-1.44478092145409,0.576439430732838,
1.11511439915468));
#71042=CARTESIAN_POINT('Ctrl Pts',(-1.45706253830672,0.545090405231021,
1.11748904274888));
#71043=CARTESIAN_POINT('Ctrl Pts',(-1.46528962750255,0.522571771381402,
1.11915221299581));
#71044=CARTESIAN_POINT('Ctrl Pts',(-1.50336086093163,0.410385349732555,
1.12727193303035));
#71045=CARTESIAN_POINT('Ctrl Pts',(-1.52551390061082,0.318309759635744,
1.13342720236391));
#71046=CARTESIAN_POINT('Ctrl Pts',(-1.55001067948958,0.150572425861762,
1.14459839210316));
#71047=CARTESIAN_POINT('Ctrl Pts',(-1.55546646918372,0.0756807431247202,
1.1495710878573));
#71048=CARTESIAN_POINT('Ctrl Pts',(-1.55549984592239,0.000692340549475381,
1.15469914303843));
#71049=CARTESIAN_POINT('Origin',(0.,0.,-1.2940562256037));
#71050=CARTESIAN_POINT('',(-1.55549999695016,-9.74065728153838E-5,1.9925897317728));
#71051=CARTESIAN_POINT('',(-1.5555,-2.74013238336738E-11,1.8552873792152));
#71052=CARTESIAN_POINT('',(-1.5555,-1.46451138874614E-13,-1.2940562256037));
#71053=CARTESIAN_POINT('',(-1.55549944251185,-0.00131694544789358,1.29458843968849));
#71054=CARTESIAN_POINT('Ctrl Pts',(-1.55549999695016,-9.74065733091837E-5,
1.99258973177283));
#71055=CARTESIAN_POINT('Ctrl Pts',(-1.55550042240159,0.00669669026298216,
1.99209974652595));
#71056=CARTESIAN_POINT('Ctrl Pts',(-1.55545633515302,0.0134908251544085,
1.99161230739549));
#71057=CARTESIAN_POINT('Ctrl Pts',(-1.55523249795908,0.030654068342381,
1.99038689780355));
#71058=CARTESIAN_POINT('Ctrl Pts',(-1.5549935624627,0.0410223211014157,
1.98965211790128));
#71059=CARTESIAN_POINT('Ctrl Pts',(-1.55358192282881,0.0837291063027906,
1.98664527636159));
#71060=CARTESIAN_POINT('Ctrl Pts',(-1.55150387733412,0.116032038609492,
1.98441748339199));
#71061=CARTESIAN_POINT('Ctrl Pts',(-1.54256037562029,0.209444232643618,
1.9780492879162));
#71062=CARTESIAN_POINT('Ctrl Pts',(-1.53307841464066,0.270242600687175,
1.97399543916995));
#71063=CARTESIAN_POINT('Ctrl Pts',(-1.49743200941476,0.434273455668504,
1.9629455430482));
#71064=CARTESIAN_POINT('Ctrl Pts',(-1.46424194660417,0.535619591522633,
1.95597394652533));
#71065=CARTESIAN_POINT('Ctrl Pts',(-1.41133476944503,0.654427914580389,
1.94702542055528));
#71066=CARTESIAN_POINT('Ctrl Pts',(-1.40120248882616,0.675849990047823,
1.94538029727317));
#71067=CARTESIAN_POINT('Ctrl Pts',(-1.38457797880069,0.709016073637523,
1.94277822597506));
#71068=CARTESIAN_POINT('Ctrl Pts',(-1.37841611833844,0.720922295846305,
1.94183274415279));
#71069=CARTESIAN_POINT('Ctrl Pts',(-1.36667691411272,0.742904475360018,
1.94006500008127));
#71070=CARTESIAN_POINT('Ctrl Pts',(-1.36114003768344,0.753001083522817,
1.9392442195225));
#71071=CARTESIAN_POINT('Ctrl Pts',(-1.34853406815254,0.775394926802664,
1.93740338952845));
#71072=CARTESIAN_POINT('Ctrl Pts',(-1.34140792262617,0.787658673411109,
1.93638133735227));
#71073=CARTESIAN_POINT('Ctrl Pts',(-1.31952881339227,0.824153320517702,
1.93329673518592));
#71074=CARTESIAN_POINT('Ctrl Pts',(-1.30428044598937,0.848078597914033,
1.93121637744028));
#71075=CARTESIAN_POINT('Ctrl Pts',(-1.24984305865419,0.928549775038145,
1.92401222878502));
#71076=CARTESIAN_POINT('Ctrl Pts',(-1.20756654330442,0.982900391575368,
1.91878016273706));
#71077=CARTESIAN_POINT('Ctrl Pts',(-1.12693314945042,1.07347923964885,1.90942986312774));
#71078=CARTESIAN_POINT('Ctrl Pts',(-1.09006641680109,1.1108964928434,1.90534825770143));
#71079=CARTESIAN_POINT('Ctrl Pts',(-1.00185600507271,1.19179710344253,1.89608068486811));
#71080=CARTESIAN_POINT('Ctrl Pts',(-0.949435266784904,1.2339653672362,1.89091384742753));
#71081=CARTESIAN_POINT('Ctrl Pts',(-0.8840976239087,1.27988734630444,1.88499330068621));
#71082=CARTESIAN_POINT('Ctrl Pts',(-0.873660844490999,1.28703418138462,
1.8840624401335));
#71083=CARTESIAN_POINT('Ctrl Pts',(-0.85707909131719,1.29809426351719,1.88260815267143));
#71084=CARTESIAN_POINT('Ctrl Pts',(-0.850992100570774,1.30209282938476,
1.8820794410913));
#71085=CARTESIAN_POINT('Ctrl Pts',(-0.839293226527584,1.30966077943526,
1.88107341521404));
#71086=CARTESIAN_POINT('Ctrl Pts',(-0.833686247326268,1.31323711498445,
1.8805956860591));
#71087=CARTESIAN_POINT('Ctrl Pts',(-0.819920535842528,1.32189369206497,
1.87943322593413));
#71088=CARTESIAN_POINT('Ctrl Pts',(-0.811737154130547,1.32693459648706,
1.87875101196142));
#71089=CARTESIAN_POINT('Ctrl Pts',(-0.781185091089543,1.34536602146513,
1.87623457341919));
#71090=CARTESIAN_POINT('Ctrl Pts',(-0.758526195414836,1.35827025675906,
1.87442846067734));
#71091=CARTESIAN_POINT('Ctrl Pts',(-0.697421538640053,1.3910629471175,1.86968622527334));
#71092=CARTESIAN_POINT('Ctrl Pts',(-0.658450929898505,1.40992759909519,
1.86679261128791));
#71093=CARTESIAN_POINT('Ctrl Pts',(-0.496755171104799,1.48003120496167,
1.8551114163104));
#71094=CARTESIAN_POINT('Ctrl Pts',(-0.368502769447701,1.51705692645734,
1.8465321251534));
#71095=CARTESIAN_POINT('Ctrl Pts',(-0.213882348908616,1.54090452907775,
1.83576475283433));
#71096=CARTESIAN_POINT('Ctrl Pts',(-0.190581448328274,1.54395953243374,
1.83413296822417));
#71097=CARTESIAN_POINT('Ctrl Pts',(-0.15393487376396,1.54792212275118,1.8315473473044));
#71098=CARTESIAN_POINT('Ctrl Pts',(-0.140630856025979,1.54918745988524,
1.8306047349969));
#71099=CARTESIAN_POINT('Ctrl Pts',(-0.115833139937345,1.55122390364735,
1.82883960791086));
#71100=CARTESIAN_POINT('Ctrl Pts',(-0.104343906238084,1.55203906254514,
1.82801853869876));
#71101=CARTESIAN_POINT('Ctrl Pts',(-0.0786348425843992,1.55357636373879,
1.82617346295836));
#71102=CARTESIAN_POINT('Ctrl Pts',(-0.0644121854129839,1.55423100011759,
1.82514740990195));
#71103=CARTESIAN_POINT('Ctrl Pts',(-0.0215409314190439,1.55561481727486,
1.82203751776997));
#71104=CARTESIAN_POINT('Ctrl Pts',(0.00711931223707813,1.55574759709805,
1.81993543250216));
#71105=CARTESIAN_POINT('Ctrl Pts',(0.110600894710714,1.55336764378502,1.81225748584931));
#71106=CARTESIAN_POINT('Ctrl Pts',(0.18520459516661,1.54624709059672,1.80654937089049));
#71107=CARTESIAN_POINT('Ctrl Pts',(0.35108186265785,1.51823687986099,1.7935530488995));
#71108=CARTESIAN_POINT('Ctrl Pts',(0.441581636394824,1.49442582896406,1.78624540831788));
#71109=CARTESIAN_POINT('Ctrl Pts',(0.5533774719476,1.45396141400024,1.77725642090986));
#71110=CARTESIAN_POINT('Ctrl Pts',(0.577138477655064,1.44469435755366,1.77534921137645));
#71111=CARTESIAN_POINT('Ctrl Pts',(0.609704926740366,1.43106123081994,1.7727496259907));
#71112=CARTESIAN_POINT('Ctrl Pts',(0.618711659046347,1.42719033082052,1.77203223172054));
#71113=CARTESIAN_POINT('Ctrl Pts',(0.63373690278963,1.4205638274673,1.77083878944275));
#71114=CARTESIAN_POINT('Ctrl Pts',(0.639775405183407,1.41785453685955,1.77036007229562));
#71115=CARTESIAN_POINT('Ctrl Pts',(0.652335418883908,1.41212266124957,1.76936650272906));
#71116=CARTESIAN_POINT('Ctrl Pts',(0.658853555281885,1.40909329266088,1.76885206428689));
#71117=CARTESIAN_POINT('Ctrl Pts',(0.67638355853743,1.40079781393772,1.76747109696171));
#71118=CARTESIAN_POINT('Ctrl Pts',(0.68735510211705,1.39544696133576,1.76660954685675));
#71119=CARTESIAN_POINT('Ctrl Pts',(0.750160335241729,1.36389616965809,1.76168709577322));
#71120=CARTESIAN_POINT('Ctrl Pts',(0.800563480618143,1.33493560235412,1.75777304416725));
#71121=CARTESIAN_POINT('Ctrl Pts',(0.955618548785537,1.23389507517694,1.74547188316114));
#71122=CARTESIAN_POINT('Ctrl Pts',(1.05310874978011,1.15180957201234,1.73729255546327));
#71123=CARTESIAN_POINT('Ctrl Pts',(1.16077135661094,1.0359358906346,1.72650397885697));
#71124=CARTESIAN_POINT('Ctrl Pts',(1.18131070279753,1.01245153504198,1.72435256141543));
#71125=CARTESIAN_POINT('Ctrl Pts',(1.21046688852601,0.977019002578325,1.72114512266678));
#71126=CARTESIAN_POINT('Ctrl Pts',(1.21964310643819,0.965539686559332,1.72011169744114));
#71127=CARTESIAN_POINT('Ctrl Pts',(1.23574085882477,0.944805949004342,1.71825409328068));
#71128=CARTESIAN_POINT('Ctrl Pts',(1.24272459877097,0.935601042044511,1.71743246121537));
#71129=CARTESIAN_POINT('Ctrl Pts',(1.2573754703902,0.915837014798329,1.71567425670148));
#71130=CARTESIAN_POINT('Ctrl Pts',(1.26501353062137,0.905257565162052,1.71473663596056));
#71131=CARTESIAN_POINT('Ctrl Pts',(1.28552592735114,0.876079317055153,1.71215943502555));
#71132=CARTESIAN_POINT('Ctrl Pts',(1.29812863689277,0.85729447789019,1.71050975608045));
#71133=CARTESIAN_POINT('Ctrl Pts',(1.32542466723428,0.814626099995463,1.70678160612249));
#71134=CARTESIAN_POINT('Ctrl Pts',(1.33989048112244,0.790607077749816,1.70469572743318));
#71135=CARTESIAN_POINT('Ctrl Pts',(1.38598984211966,0.709161378820918,1.69766434437611));
#71136=CARTESIAN_POINT('Ctrl Pts',(1.41463909913779,0.650132541306723,1.69263183984459));
#71137=CARTESIAN_POINT('Ctrl Pts',(1.47761320598073,0.496352884787545,1.6797678566552));
#71138=CARTESIAN_POINT('Ctrl Pts',(1.50662473965882,0.399739869686322,1.67189971801405));
#71139=CARTESIAN_POINT('Ctrl Pts',(1.52895671009825,0.286512702427338,1.66330608376524));
#71140=CARTESIAN_POINT('Ctrl Pts',(1.53160694539565,0.271989626569737,1.66221571267937));
#71141=CARTESIAN_POINT('Ctrl Pts',(1.53534361392497,0.249722488311717,1.66056423800519));
#71142=CARTESIAN_POINT('Ctrl Pts',(1.53657900224458,0.242004774604928,1.65999555613959));
#71143=CARTESIAN_POINT('Ctrl Pts',(1.53873794463341,0.227833878964166,1.65895856983725));
#71144=CARTESIAN_POINT('Ctrl Pts',(1.53967914809701,0.221383970630543,1.65848935479183));
#71145=CARTESIAN_POINT('Ctrl Pts',(1.54177111077939,0.206389012378765,1.65740476614938));
#71146=CARTESIAN_POINT('Ctrl Pts',(1.54289140977704,0.197840060014053,1.65679107949262));
#71147=CARTESIAN_POINT('Ctrl Pts',(1.54632126300174,0.169863334843644,1.65479667149174));
#71148=CARTESIAN_POINT('Ctrl Pts',(1.5483355024413,0.150400346591329,1.65343105919379));
#71149=CARTESIAN_POINT('Ctrl Pts',(1.55238145260537,0.102493641838777,1.65011178396755));
#71150=CARTESIAN_POINT('Ctrl Pts',(1.55399940246688,0.0740214853586055,
1.64817531826315));
#71151=CARTESIAN_POINT('Ctrl Pts',(1.55791639385685,-0.0597739854922687,
1.63917876770213));
#71152=CARTESIAN_POINT('Ctrl Pts',(1.55029571732122,-0.165111385533724,
1.63237794902716));
#71153=CARTESIAN_POINT('Ctrl Pts',(1.52163349124112,-0.328433055147209,
1.62133646806496));
#71154=CARTESIAN_POINT('Ctrl Pts',(1.50771830971467,-0.387325391405457,
1.61725319240488));
#71155=CARTESIAN_POINT('Ctrl Pts',(1.4850068635085,-0.463348125058852,1.61175240737552));
#71156=CARTESIAN_POINT('Ctrl Pts',(1.47927246579131,-0.481341653742719,
1.61043333478162));
#71157=CARTESIAN_POINT('Ctrl Pts',(1.469273085226,-0.510849769315237,1.60823930132945));
#71158=CARTESIAN_POINT('Ctrl Pts',(1.46519670696532,-0.522426530785203,
1.6073705882895));
#71159=CARTESIAN_POINT('Ctrl Pts',(1.45692694211236,-0.545053954192963,
1.60565634690366));
#71160=CARTESIAN_POINT('Ctrl Pts',(1.45274374687497,-0.556107471000831,
1.60481120821579));
#71161=CARTESIAN_POINT('Ctrl Pts',(1.44240814363397,-0.582505169100086,
1.60277368091914));
#71162=CARTESIAN_POINT('Ctrl Pts',(1.43613640247646,-0.597800735251731,
1.60157734841902));
#71163=CARTESIAN_POINT('Ctrl Pts',(1.41260315075026,-0.652684994311897,
1.59722572760465));
#71164=CARTESIAN_POINT('Ctrl Pts',(1.39394004659215,-0.691647197437364,
1.5940237954592));
#71165=CARTESIAN_POINT('Ctrl Pts',(1.34034412812436,-0.792532141444396,
1.58542535729496));
#71166=CARTESIAN_POINT('Ctrl Pts',(1.30274868731775,-0.852920589182869,
1.5799529953886));
#71167=CARTESIAN_POINT('Ctrl Pts',(1.20787084878965,-0.984335611636769,
1.56738943898602));
#71168=CARTESIAN_POINT('Ctrl Pts',(1.1481981189719,-1.05333398858936,1.56029576845));
#71169=CARTESIAN_POINT('Ctrl Pts',(1.07150392429687,-1.12770048087016,1.55232942889065));
#71170=CARTESIAN_POINT('Ctrl Pts',(1.06001334522495,-1.13850814365394,1.5511630932229));
#71171=CARTESIAN_POINT('Ctrl Pts',(1.0425042943951,-1.15448164534395,1.54942875078616));
#71172=CARTESIAN_POINT('Ctrl Pts',(1.03660788913597,-1.15977892928544,1.54885179553724));
#71173=CARTESIAN_POINT('Ctrl Pts',(1.02628516539578,-1.16891116030012,1.54785439818787));
#71174=CARTESIAN_POINT('Ctrl Pts',(1.02187744487876,-1.17276640123739,1.54743249534417));
#71175=CARTESIAN_POINT('Ctrl Pts',(1.01131073451146,-1.18190383523552,1.5464304374402));
#71176=CARTESIAN_POINT('Ctrl Pts',(1.00513205217448,-1.18716285444679,1.54585196317003));
#71177=CARTESIAN_POINT('Ctrl Pts',(0.986077218852454,-1.20312606454267,
1.54408964291304));
#71178=CARTESIAN_POINT('Ctrl Pts',(0.973068654093634,-1.2136713156748,1.54291644901125));
#71179=CARTESIAN_POINT('Ctrl Pts',(0.941761815017421,-1.2382228280371,1.54015616641951));
#71180=CARTESIAN_POINT('Ctrl Pts',(0.923317285083143,-1.25203689947955,
1.53857960897408));
#71181=CARTESIAN_POINT('Ctrl Pts',(0.850111614545197,-1.30436647718886,
1.53248349762847));
#71182=CARTESIAN_POINT('Ctrl Pts',(0.793191335935832,-1.3397426743099,1.52808407595263));
#71183=CARTESIAN_POINT('Ctrl Pts',(0.647271099905978,-1.41786284018175,
1.51719273302274));
#71184=CARTESIAN_POINT('Ctrl Pts',(0.556162694338765,-1.45601337694449,
1.51070689246357));
#71185=CARTESIAN_POINT('Ctrl Pts',(0.44123597303963,-1.49176634374891,1.50242804825739));
#71186=CARTESIAN_POINT('Ctrl Pts',(0.420275595667262,-1.49780651353516,
1.50091525607307));
#71187=CARTESIAN_POINT('Ctrl Pts',(0.385577225897743,-1.5070199071476,1.49840202778982));
#71188=CARTESIAN_POINT('Ctrl Pts',(0.37191035792813,-1.51045074733249,1.49740989195976));
#71189=CARTESIAN_POINT('Ctrl Pts',(0.346997833771406,-1.51634601891086,
1.49559634807217));
#71190=CARTESIAN_POINT('Ctrl Pts',(0.335767716777587,-1.51887220430872,
1.49477699249018));
#71191=CARTESIAN_POINT('Ctrl Pts',(0.311325844056116,-1.52408602914984,
1.49298918127931));
#71192=CARTESIAN_POINT('Ctrl Pts',(0.298105210515063,-1.52672697874053,
1.49201930197494));
#71193=CARTESIAN_POINT('Ctrl Pts',(0.260523985397398,-1.53372745520851,
1.48925338129883));
#71194=CARTESIAN_POINT('Ctrl Pts',(0.236092369202305,-1.53767776749234,
1.48744461066454));
#71195=CARTESIAN_POINT('Ctrl Pts',(0.180301525189084,-1.54533759374342,
1.48328767599053));
#71196=CARTESIAN_POINT('Ctrl Pts',(0.148903490368004,-1.54867828173776,
1.48092923947184));
#71197=CARTESIAN_POINT('Ctrl Pts',(0.0361448519108882,-1.55721499115108,
1.47239293873807));
#71198=CARTESIAN_POINT('Ctrl Pts',(-0.0454882902225601,-1.55696927000366,
1.46608092289781));
#71199=CARTESIAN_POINT('Ctrl Pts',(-0.201811487278772,-1.54419207842826,
1.4539163793286));
#71200=CARTESIAN_POINT('Ctrl Pts',(-0.276367856641488,-1.53260564010354,
1.44808284438709));
#71201=CARTESIAN_POINT('Ctrl Pts',(-0.36559277444116,-1.51201355057665,
1.4412493200826));
#71202=CARTESIAN_POINT('Ctrl Pts',(-0.381331667675789,-1.50812110521511,
1.44004986295108));
#71203=CARTESIAN_POINT('Ctrl Pts',(-0.404753775105823,-1.50193835271276,
1.43827658676716));
#71204=CARTESIAN_POINT('Ctrl Pts',(-0.412484239437945,-1.4998337219893,
1.43769324099884));
#71205=CARTESIAN_POINT('Ctrl Pts',(-0.425832689426701,-1.49608857214347,
1.43668969785668));
#71206=CARTESIAN_POINT('Ctrl Pts',(-0.431458026469112,-1.49447598495009,
1.43626796496759));
#71207=CARTESIAN_POINT('Ctrl Pts',(-0.444774238752368,-1.49057723566151,
1.4352724121881));
#71208=CARTESIAN_POINT('Ctrl Pts',(-0.452456699423105,-1.48826327027236,
1.43470019850365));
#71209=CARTESIAN_POINT('Ctrl Pts',(-0.475663733470028,-1.48107697275505,
1.43297719427063));
#71210=CARTESIAN_POINT('Ctrl Pts',(-0.491130665509083,-1.47602022708121,
1.43183637779808));
#71211=CARTESIAN_POINT('Ctrl Pts',(-0.570348505492139,-1.44873761801244,
1.42601839445595));
#71212=CARTESIAN_POINT('Ctrl Pts',(-0.632689836800856,-1.42261865655347,
1.42152217420117));
#71213=CARTESIAN_POINT('Ctrl Pts',(-0.805837881249277,-1.33643271326311,
1.40875072909323));
#71214=CARTESIAN_POINT('Ctrl Pts',(-0.911294795102424,-1.26687235284656,
1.40057790419277));
#71215=CARTESIAN_POINT('Ctrl Pts',(-1.02393193334483,-1.17116390031802,
1.39037892928127));
#71216=CARTESIAN_POINT('Ctrl Pts',(-1.04034595860708,-1.15660783717111,
1.38885234592013));
#71217=CARTESIAN_POINT('Ctrl Pts',(-1.06591969417315,-1.13294397573777,
1.38640470642414));
#71218=CARTESIAN_POINT('Ctrl Pts',(-1.0752836360918,-1.124060465681,1.38549313448061));
#71219=CARTESIAN_POINT('Ctrl Pts',(-1.09283701789119,-1.10698762630689,
1.38375409753356));
#71220=CARTESIAN_POINT('Ctrl Pts',(-1.10104770441881,-1.09882131927994,
1.3829276725442));
#71221=CARTESIAN_POINT('Ctrl Pts',(-1.10953585517822,-1.09018838463639,
1.38205935470084));
#71222=CARTESIAN_POINT('Ctrl Pts',(-1.10990527288889,-1.08981228343891,
1.38202153614781));
#71223=CARTESIAN_POINT('Ctrl Pts',(-1.11100381338066,-1.08869273029426,
1.38190899142423));
#71224=CARTESIAN_POINT('Ctrl Pts',(-1.11173237965975,-1.0879487351655,1.38183424090737));
#71225=CARTESIAN_POINT('Ctrl Pts',(-1.11312712635291,-1.08652158794629,
1.38169093048727));
#71226=CARTESIAN_POINT('Ctrl Pts',(-1.11379342658473,-1.08583855309392,
1.38162237587091));
#71227=CARTESIAN_POINT('Ctrl Pts',(-1.11508251506942,-1.08451465327213,
1.38148956463998));
#71228=CARTESIAN_POINT('Ctrl Pts',(-1.11570538054872,-1.08387386368707,
1.38142531143358));
#71229=CARTESIAN_POINT('Ctrl Pts',(-1.1169218050378,-1.08262027473558,1.38129966937235));
#71230=CARTESIAN_POINT('Ctrl Pts',(-1.11751541288339,-1.08200752298683,
1.38123828267683));
#71231=CARTESIAN_POINT('Ctrl Pts',(-1.1186846087931,-1.08079863190838,1.38111722636629));
#71232=CARTESIAN_POINT('Ctrl Pts',(-1.11926022524283,-1.0802025203035,1.38105755801418));
#71233=CARTESIAN_POINT('Ctrl Pts',(-1.13216040008558,-1.06682164555934,
1.37971875127788));
#71234=CARTESIAN_POINT('Ctrl Pts',(-1.14426511282732,-1.05382773635198,
1.37843018740865));
#71235=CARTESIAN_POINT('Ctrl Pts',(-1.17030020272246,-1.02490264108695,
1.37558546007939));
#71236=CARTESIAN_POINT('Ctrl Pts',(-1.18413308080033,-1.00888887162499,
1.37402562893014));
#71237=CARTESIAN_POINT('Ctrl Pts',(-1.22410267252708,-0.96066297481476,
1.36937091883344));
#71238=CARTESIAN_POINT('Ctrl Pts',(-1.24928078478142,-0.9276840534824,1.36624188408179));
#71239=CARTESIAN_POINT('Ctrl Pts',(-1.32767018534053,-0.816020517526509,
1.35583114064007));
#71240=CARTESIAN_POINT('Ctrl Pts',(-1.37499774255554,-0.733469067908072,
1.34840530939154));
#71241=CARTESIAN_POINT('Ctrl Pts',(-1.4353620536622,-0.601523801398121,
1.33723289275254));
#71242=CARTESIAN_POINT('Ctrl Pts',(-1.45400983333373,-0.554933859497567,
1.33341324503986));
#71243=CARTESIAN_POINT('Ctrl Pts',(-1.47432505632885,-0.496077023277669,
1.32880261628201));
#71244=CARTESIAN_POINT('Ctrl Pts',(-1.47814111446276,-0.484588128944107,
1.32791256703494));
#71245=CARTESIAN_POINT('Ctrl Pts',(-1.48400202963421,-0.466229099546399,
1.32650732027827));
#71246=CARTESIAN_POINT('Ctrl Pts',(-1.48613411007386,-0.459387646398022,
1.32598739335756));
#71247=CARTESIAN_POINT('Ctrl Pts',(-1.49017028977825,-0.446114054117088,
1.32498618701739));
#71248=CARTESIAN_POINT('Ctrl Pts',(-1.49208017156295,-0.439683983852518,
1.32450461491047));
#71249=CARTESIAN_POINT('Ctrl Pts',(-1.49671384447043,-0.423705676292738,
1.32331601758002));
#71250=CARTESIAN_POINT('Ctrl Pts',(-1.49938798582166,-0.414143108185379,
1.32261178730915));
#71251=CARTESIAN_POINT('Ctrl Pts',(-1.50499488347232,-0.39332668194911,
1.32109283446394));
#71252=CARTESIAN_POINT('Ctrl Pts',(-1.50789339518977,-0.382064138797969,
1.32027987779891));
#71253=CARTESIAN_POINT('Ctrl Pts',(-1.5403387351931,-0.249868743657241,
1.31082954772173));
#71254=CARTESIAN_POINT('Ctrl Pts',(-1.55539402393791,-0.125831239692401,
1.30283100004325));
#71255=CARTESIAN_POINT('Ctrl Pts',(-1.55549944251185,-0.00131694544789358,
1.29458843968849));
#71256=CARTESIAN_POINT('Ctrl Pts',(-1.55549944365257,-0.00131559740958673,
1.29458835045145));
#71257=CARTESIAN_POINT('Ctrl Pts',(-1.55549981455353,-0.000877061857157378,
1.29455932040035));
#71258=CARTESIAN_POINT('Ctrl Pts',(-1.55550000000001,-0.000438529336851416,
1.29453028833394));
#71259=CARTESIAN_POINT('Ctrl Pts',(-1.5555,3.44063942631422E-11,1.29450125422325));
#71260=CARTESIAN_POINT('Ctrl Pts',(-1.55549984592239,0.000692340549475381,
1.15469914303843));
#71261=CARTESIAN_POINT('Ctrl Pts',(-1.55551257150503,-0.027898562953657,
1.1566543217835));
#71262=CARTESIAN_POINT('Ctrl Pts',(-1.55473702459326,-0.0564827265290557,
1.15862986850662));
#71263=CARTESIAN_POINT('Ctrl Pts',(-1.55237477829611,-0.0996330809139592,
1.1616526805757));
#71264=CARTESIAN_POINT('Ctrl Pts',(-1.55136927411398,-0.114225884010962,
1.16268195301729));
#71265=CARTESIAN_POINT('Ctrl Pts',(-1.54917927419936,-0.140582995622195,
1.16455478456607));
#71266=CARTESIAN_POINT('Ctrl Pts',(-1.54806614344282,-0.152352235574461,
1.16539604474447));
#71267=CARTESIAN_POINT('Ctrl Pts',(-1.54537199378593,-0.177746355919815,
1.16722255598176));
#71268=CARTESIAN_POINT('Ctrl Pts',(-1.54374470130584,-0.191365203346941,
1.16820919653007));
#71269=CARTESIAN_POINT('Ctrl Pts',(-1.53866421279967,-0.229586234511424,
1.17099902838866));
#71270=CARTESIAN_POINT('Ctrl Pts',(-1.53480156302857,-0.254128765242878,
1.172814870643));
#71271=CARTESIAN_POINT('Ctrl Pts',(-1.52470483006877,-0.309596804834773,
1.17697686031794));
#71272=CARTESIAN_POINT('Ctrl Pts',(-1.51811448268113,-0.340445546959844,
1.1793330596931));
#71273=CARTESIAN_POINT('Ctrl Pts',(-1.48004058039864,-0.495440521408541,
1.19138082780159));
#71274=CARTESIAN_POINT('Ctrl Pts',(-1.43424687375455,-0.6155572796414,1.20145975086901));
#71275=CARTESIAN_POINT('Ctrl Pts',(-1.35684646593193,-0.761531711890244,
1.21408418243729));
#71276=CARTESIAN_POINT('Ctrl Pts',(-1.33825356437203,-0.793751086447115,
1.21689229799129));
#71277=CARTESIAN_POINT('Ctrl Pts',(-1.31250936790574,-0.834881931413758,
1.22047830722698));
#71278=CARTESIAN_POINT('Ctrl Pts',(-1.3063917238745,-0.844422503343065,
1.22131017186896));
#71279=CARTESIAN_POINT('Ctrl Pts',(-1.29626455838588,-0.859842463322647,
1.22265372547877));
#71280=CARTESIAN_POINT('Ctrl Pts',(-1.29231813935291,-0.865762495861777,
1.22316931104151));
#71281=CARTESIAN_POINT('Ctrl Pts',(-1.28436899039843,-0.87751156100424,
1.22419176570673));
#71282=CARTESIAN_POINT('Ctrl Pts',(-1.28036686423132,-0.883340784289243,
1.22469865208484));
#71283=CARTESIAN_POINT('Ctrl Pts',(-1.26996638378299,-0.898270214723518,
1.22599640002921));
#71284=CARTESIAN_POINT('Ctrl Pts',(-1.26350976646733,-0.907329644355399,
1.22678345419836));
#71285=CARTESIAN_POINT('Ctrl Pts',(-1.23437541166623,-0.947294542114509,
1.2302573524832));
#71286=CARTESIAN_POINT('Ctrl Pts',(-1.21065506531935,-0.977427482498418,
1.23288177181989));
#71287=CARTESIAN_POINT('Ctrl Pts',(-1.13143761463001,-1.07074585326335,
1.24113752833254));
#71288=CARTESIAN_POINT('Ctrl Pts',(-1.07192267362721,-1.13032352718731,
1.24661343932134));
#71289=CARTESIAN_POINT('Ctrl Pts',(-0.944573608882746,-1.23865614171747,
1.2576475089124));
#71290=CARTESIAN_POINT('Ctrl Pts',(-0.877059837393692,-1.28734290569844,
1.26318774073735));
#71291=CARTESIAN_POINT('Ctrl Pts',(-0.788633023455372,-1.34091381355098,
1.27034088175279));
#71292=CARTESIAN_POINT('Ctrl Pts',(-0.771076631976693,-1.35108573467332,
1.27175581641909));
#71293=CARTESIAN_POINT('Ctrl Pts',(-0.742145474283537,-1.36710046495544,
1.27408209854847));
#71294=CARTESIAN_POINT('Ctrl Pts',(-0.730888403587942,-1.37315174334064,
1.2749859449404));
#71295=CARTESIAN_POINT('Ctrl Pts',(-0.708885840312691,-1.38463209095437,
1.27675077615059));
#71296=CARTESIAN_POINT('Ctrl Pts',(-0.69814933997256,-1.39007648925562,
1.27761114211641));
#71297=CARTESIAN_POINT('Ctrl Pts',(-0.672619022808428,-1.4026523417733,
1.27965570167936));
#71298=CARTESIAN_POINT('Ctrl Pts',(-0.657773593015741,-1.40967507023487,
1.2808435643331));
#71299=CARTESIAN_POINT('Ctrl Pts',(-0.605866449725281,-1.43323163787405,
1.28499507257164));
#71300=CARTESIAN_POINT('Ctrl Pts',(-0.568273906151289,-1.44854799615041,
1.2879989965888));
#71301=CARTESIAN_POINT('Ctrl Pts',(-0.470213808685758,-1.4840959402274,
1.29583206701084));
#71302=CARTESIAN_POINT('Ctrl Pts',(-0.409026695516784,-1.50211100029218,
1.30071944156057));
#71303=CARTESIAN_POINT('Ctrl Pts',(-0.246432125887757,-1.53931035147845,
1.31362272494032));
#71304=CARTESIAN_POINT('Ctrl Pts',(-0.143908487441227,-1.55225597248363,
1.32168746925037));
#71305=CARTESIAN_POINT('Ctrl Pts',(-0.0262605372461818,-1.55534680592977,
1.33044705839491));
#71306=CARTESIAN_POINT('Ctrl Pts',(-0.011663871183709,-1.55552476592351,
1.33152483795714));
#71307=CARTESIAN_POINT('Ctrl Pts',(0.0108322838024829,-1.55548233600033,
1.33316987070728));
#71308=CARTESIAN_POINT('Ctrl Pts',(0.0187307543558288,-1.55540727853855,
1.33374440185324));
#71309=CARTESIAN_POINT('Ctrl Pts',(0.0326658240077856,-1.55516868970386,
1.33475226496763));
#71310=CARTESIAN_POINT('Ctrl Pts',(0.0387022994507902,-1.55503017453997,
1.33518691171666));
#71311=CARTESIAN_POINT('Ctrl Pts',(0.0533941646873858,-1.55460744296237,
1.33624019030064));
#71312=CARTESIAN_POINT('Ctrl Pts',(0.0620482142251911,-1.5542860956146,
1.33685677870773));
#71313=CARTESIAN_POINT('Ctrl Pts',(0.0897163930256136,-1.5530272417345,
1.33881714514677));
#71314=CARTESIAN_POINT('Ctrl Pts',(0.108717018673513,-1.55181292015254,
1.34014684359232));
#71315=CARTESIAN_POINT('Ctrl Pts',(0.154876773261621,-1.54801081393482,
1.34334741189554));
#71316=CARTESIAN_POINT('Ctrl Pts',(0.181999974660383,-1.54505679005421,
1.34520291656093));
#71317=CARTESIAN_POINT('Ctrl Pts',(0.301853865953547,-1.52880301365944,
1.35334565183725));
#71318=CARTESIAN_POINT('Ctrl Pts',(0.393352308920886,-1.50785619871998,
1.35942162203061));
#71319=CARTESIAN_POINT('Ctrl Pts',(0.550756781489194,-1.45650781133415,
1.37038728987654));
#71320=CARTESIAN_POINT('Ctrl Pts',(0.617463816418402,-1.42950500001155,
1.37520862876884));
#71321=CARTESIAN_POINT('Ctrl Pts',(0.699991560594923,-1.38924085535629,
1.38156522741266));
#71322=CARTESIAN_POINT('Ctrl Pts',(0.71775263057027,-1.38014833886309,1.38295725327239));
#71323=CARTESIAN_POINT('Ctrl Pts',(0.74653352768383,-1.36470857363931,1.38525554956542));
#71324=CARTESIAN_POINT('Ctrl Pts',(0.757659457834445,-1.35856318498824,
1.38615466879788));
#71325=CARTESIAN_POINT('Ctrl Pts',(0.779202002284005,-1.34631726724444,
1.38791722402732));
#71326=CARTESIAN_POINT('Ctrl Pts',(0.789625397322583,-1.34023045078361,
1.38878011861224));
#71327=CARTESIAN_POINT('Ctrl Pts',(0.814234697877007,-1.32547293614791,
1.39084211302042));
#71328=CARTESIAN_POINT('Ctrl Pts',(0.828354232074695,-1.31669505734386,
1.39204505832186));
#71329=CARTESIAN_POINT('Ctrl Pts',(0.877666280145273,-1.28493147432753,
1.39631882515552));
#71330=CARTESIAN_POINT('Ctrl Pts',(0.912062229832128,-1.26074932862043,
1.39943321547664));
#71331=CARTESIAN_POINT('Ctrl Pts',(0.999023160485334,-1.1941889227265,1.40766800360979));
#71332=CARTESIAN_POINT('Ctrl Pts',(1.04988087345275,-1.14973167300025,1.41285496363954));
#71333=CARTESIAN_POINT('Ctrl Pts',(1.16594204046471,-1.03413708914863,1.42554079724708));
#71334=CARTESIAN_POINT('Ctrl Pts',(1.22773952772954,-0.959957803233155,
1.43306005944108));
#71335=CARTESIAN_POINT('Ctrl Pts',(1.29089633946304,-0.867985343697893,
1.44137365188863));
#71336=CARTESIAN_POINT('Ctrl Pts',(1.29932816584917,-0.855311802421614,
1.44249856602405));
#71337=CARTESIAN_POINT('Ctrl Pts',(1.31192292172241,-0.835764916296272,
1.44419991867356));
#71338=CARTESIAN_POINT('Ctrl Pts',(1.31622061783963,-0.828980120800091,
1.44478439106641));
#71339=CARTESIAN_POINT('Ctrl Pts',(1.32400347370087,-0.816480160460945,
1.44584968199021));
#71340=CARTESIAN_POINT('Ctrl Pts',(1.32750444140163,-0.810775562005542,
1.44633146119466));
#71341=CARTESIAN_POINT('Ctrl Pts',(1.33556365660579,-0.797451436410707,
1.4474467674408));
#71342=CARTESIAN_POINT('Ctrl Pts',(1.34009364045356,-0.789815243676535,
1.44807849773311));
#71343=CARTESIAN_POINT('Ctrl Pts',(1.35476716712116,-0.764590349720044,
1.45014235520998));
#71344=CARTESIAN_POINT('Ctrl Pts',(1.36463223592371,-0.746840974847227,
1.45155823997507));
#71345=CARTESIAN_POINT('Ctrl Pts',(1.38812950264298,-0.702543263330322,
1.45501610980875));
#71346=CARTESIAN_POINT('Ctrl Pts',(1.40135103580084,-0.675785507508407,
1.45703927776334));
#71347=CARTESIAN_POINT('Ctrl Pts',(1.4629273713598,-0.541576485620519,1.46694761101303));
#71348=CARTESIAN_POINT('Ctrl Pts',(1.4997347762154,-0.429254379257706,1.47452560104263));
#71349=CARTESIAN_POINT('Ctrl Pts',(1.53316489514631,-0.266975749424769,
1.48564912598903));
#71350=CARTESIAN_POINT('Ctrl Pts',(1.54065188686204,-0.219685456308865,
1.48890634097348));
#71351=CARTESIAN_POINT('Ctrl Pts',(1.54792193181771,-0.154390672883636,
1.49347069055151));
#71352=CARTESIAN_POINT('Ctrl Pts',(1.5495914081969,-0.136620674365634,1.49471949700427));
#71353=CARTESIAN_POINT('Ctrl Pts',(1.55179975548467,-0.107796746571169,
1.4967578160672));
#71354=CARTESIAN_POINT('Ctrl Pts',(1.55252709828289,-0.0967585518690566,
1.49754139472352));
#71355=CARTESIAN_POINT('Ctrl Pts',(1.55380743017729,-0.0735588971693167,
1.49919508457876));
#71356=CARTESIAN_POINT('Ctrl Pts',(1.55433550093533,-0.0613968762544586,
1.50006591919336));
#71357=CARTESIAN_POINT('Ctrl Pts',(1.55526574173982,-0.0320192986339642,
1.5021795079022));
#71358=CARTESIAN_POINT('Ctrl Pts',(1.5555248772087,-0.0148011832395994,
1.5034266309181));
#71359=CARTESIAN_POINT('Ctrl Pts',(1.55542572861681,0.0490058399249677,
1.50808108886355));
#71360=CARTESIAN_POINT('Ctrl Pts',(1.55326033473315,0.095562957666692,1.51154312652778));
#71361=CARTESIAN_POINT('Ctrl Pts',(1.53766015553395,0.265799421837773,1.52444773895408));
#71362=CARTESIAN_POINT('Ctrl Pts',(1.5114973187938,0.387837244620299,1.53422214620163));
#71363=CARTESIAN_POINT('Ctrl Pts',(1.45802138765674,0.543481681710278,1.54682386148311));
#71364=CARTESIAN_POINT('Ctrl Pts',(1.44347687063239,0.581011059182153,1.54986871499844));
#71365=CARTESIAN_POINT('Ctrl Pts',(1.42287269650239,0.628608582388586,1.55370439541757));
#71366=CARTESIAN_POINT('Ctrl Pts',(1.41813366400091,0.639227966347026,1.55455842492058));
#71367=CARTESIAN_POINT('Ctrl Pts',(1.41027692292235,0.65631607193709,1.55592871710326));
#71368=CARTESIAN_POINT('Ctrl Pts',(1.40723284337583,0.662817860162931,1.55644915529748));
#71369=CARTESIAN_POINT('Ctrl Pts',(1.40112559332492,0.675630464633236,1.55747254949708));
#71370=CARTESIAN_POINT('Ctrl Pts',(1.39806455405764,0.681942050096462,1.55797560217759));
#71371=CARTESIAN_POINT('Ctrl Pts',(1.39015684955491,0.697969966190883,1.55925086584494));
#71372=CARTESIAN_POINT('Ctrl Pts',(1.38525083952554,0.707656886710863,1.56001952369793));
#71373=CARTESIAN_POINT('Ctrl Pts',(1.36387219920556,0.748794570914391,1.56327829901729));
#71374=CARTESIAN_POINT('Ctrl Pts',(1.34642553425715,0.779730354962053,1.56571513538569));
#71375=CARTESIAN_POINT('Ctrl Pts',(1.2903384129393,0.871675893619082,1.5729993716271));
#71376=CARTESIAN_POINT('Ctrl Pts',(1.24849551460942,0.930619386303604,1.57772995021185));
#71377=CARTESIAN_POINT('Ctrl Pts',(1.14528698412185,1.05645452911,1.58844445020901));
#71378=CARTESIAN_POINT('Ctrl Pts',(1.08187098220137,1.12130770439264,1.59442727919992));
#71379=CARTESIAN_POINT('Ctrl Pts',(0.994802021677467,1.19605008474157,1.60231797567165));
#71380=CARTESIAN_POINT('Ctrl Pts',(0.976059315127333,1.21139381350646,1.6039987673587));
#71381=CARTESIAN_POINT('Ctrl Pts',(0.946142661906033,1.23473998391124,1.60665969638051));
#71382=CARTESIAN_POINT('Ctrl Pts',(0.93520739655663,1.24304298735971,1.60762790182591));
#71383=CARTESIAN_POINT('Ctrl Pts',(0.914654227584452,1.25822401300077,1.60944043382414));
#71384=CARTESIAN_POINT('Ctrl Pts',(0.90506497447117,1.26513928116891,1.61028322786175));
#71385=CARTESIAN_POINT('Ctrl Pts',(0.883448598878422,1.28035634638747,1.61217731387228));
#71386=CARTESIAN_POINT('Ctrl Pts',(0.871381578612699,1.28859920766093,1.61323075527442));
#71387=CARTESIAN_POINT('Ctrl Pts',(0.834620903696914,1.31295758678308,1.61642937380675));
#71388=CARTESIAN_POINT('Ctrl Pts',(0.809584740152224,1.32854130837422,1.6185938419179));
#71389=CARTESIAN_POINT('Ctrl Pts',(0.721856723471828,1.37974670813473,1.62613579498519));
#71390=CARTESIAN_POINT('Ctrl Pts',(0.657147802997672,1.41171257530011,1.63163162669835));
#71391=CARTESIAN_POINT('Ctrl Pts',(0.506220749502165,1.47363919492169,1.64422774132595));
#71392=CARTESIAN_POINT('Ctrl Pts',(0.419103963830437,1.50074138114655,1.65134993321597));
#71393=CARTESIAN_POINT('Ctrl Pts',(0.302649773761244,1.52603186864642,1.66038410610987));
#71394=CARTESIAN_POINT('Ctrl Pts',(0.275026020676002,1.53125147590902,1.66249126283635));
#71395=CARTESIAN_POINT('Ctrl Pts',(0.237105395459742,1.53735726550729,1.66532237734685));
#71396=CARTESIAN_POINT('Ctrl Pts',(0.226920450895822,1.53889358134582,1.66607675158115));
#71397=CARTESIAN_POINT('Ctrl Pts',(0.209952695918003,1.54128090470716,1.66732269243146));
#71398=CARTESIAN_POINT('Ctrl Pts',(0.203178314171763,1.54218855579942,1.66781727121354));
#71399=CARTESIAN_POINT('Ctrl Pts',(0.189139504293926,1.54397539989931,1.66883600407346));
#71400=CARTESIAN_POINT('Ctrl Pts',(0.181874495306422,1.54484803829491,1.66935979824651));
#71401=CARTESIAN_POINT('Ctrl Pts',(0.162414179944644,1.54704633323502,1.67075443368066));
#71402=CARTESIAN_POINT('Ctrl Pts',(0.150208594530881,1.54827908530454,1.67162032234984));
#71403=CARTESIAN_POINT('Ctrl Pts',(0.0830005288571901,1.55426474608517,
1.676346061959));
#71404=CARTESIAN_POINT('Ctrl Pts',(0.0277833220635295,1.5562318355235,1.68007429016936));
#71405=CARTESIAN_POINT('Ctrl Pts',(-0.140239859767713,1.55326868444381,
1.69126299485227));
#71406=CARTESIAN_POINT('Ctrl Pts',(-0.252497950296415,1.53901135578109,
1.69854799371766));
#71407=CARTESIAN_POINT('Ctrl Pts',(-0.403246828051388,1.50291427434431,
1.70900208242791));
#71408=CARTESIAN_POINT('Ctrl Pts',(-0.443846497152932,1.49142854308859,
1.71188403980153));
#71409=CARTESIAN_POINT('Ctrl Pts',(-0.500171001422126,1.47299062280338,
1.71600733469374));
#71410=CARTESIAN_POINT('Ctrl Pts',(-0.516325999066684,1.46740581562399,
1.71720469678339));
#71411=CARTESIAN_POINT('Ctrl Pts',(-0.543688776177104,1.45743867457308,
1.71925976410873));
#71412=CARTESIAN_POINT('Ctrl Pts',(-0.554943963526747,1.45319033786993,
1.7201129769381));
#71413=CARTESIAN_POINT('Ctrl Pts',(-0.577831255460509,1.44424673080798,
1.72186478539408));
#71414=CARTESIAN_POINT('Ctrl Pts',(-0.589458076228139,1.43954046089804,
1.72276369793834));
#71415=CARTESIAN_POINT('Ctrl Pts',(-0.618673774303046,1.42730133312625,
1.72504595951518));
#71416=CARTESIAN_POINT('Ctrl Pts',(-0.63618247323713,1.41958378923593,1.72643546846558));
#71417=CARTESIAN_POINT('Ctrl Pts',(-0.71369947185705,1.38369352512946,1.73268812983505));
#71418=CARTESIAN_POINT('Ctrl Pts',(-0.772004757824122,1.35202852354838,
1.73766877120883));
#71419=CARTESIAN_POINT('Ctrl Pts',(-0.880427981112995,1.28384077901513,
1.74746702913104));
#71420=CARTESIAN_POINT('Ctrl Pts',(-0.930739652452833,1.24784757436664,
1.75226387614408));
#71421=CARTESIAN_POINT('Ctrl Pts',(-1.03802670040422,1.16098791015851,1.76296460702661));
#71422=CARTESIAN_POINT('Ctrl Pts',(-1.09367941760893,1.10872011016489,1.76885292769043));
#71423=CARTESIAN_POINT('Ctrl Pts',(-1.15405160970268,1.04303077528815,1.77547029210355));
#71424=CARTESIAN_POINT('Ctrl Pts',(-1.16270482748837,1.03337593814659,1.77642473732977));
#71425=CARTESIAN_POINT('Ctrl Pts',(-1.1761503154436,1.01799137467532,1.77791578627785));
#71426=CARTESIAN_POINT('Ctrl Pts',(-1.18102353109491,1.01233365482285,1.77845791677759));
#71427=CARTESIAN_POINT('Ctrl Pts',(-1.19028084987463,1.00142823014288,1.77949070877013));
#71428=CARTESIAN_POINT('Ctrl Pts',(-1.1946713437654,0.996186420375517,1.77998179122058));
#71429=CARTESIAN_POINT('Ctrl Pts',(-1.20536009966606,0.983252818872716,
1.78118087611187));
#71430=CARTESIAN_POINT('Ctrl Pts',(-1.21161960069142,0.975529103969746,
1.78188616563002));
#71431=CARTESIAN_POINT('Ctrl Pts',(-1.23465144262714,0.946545983429047,
1.78449521453369));
#71432=CARTESIAN_POINT('Ctrl Pts',(-1.25094289736705,0.92490841334122,1.78636882566694));
#71433=CARTESIAN_POINT('Ctrl Pts',(-1.29922754135232,0.85716736673855,1.79204924855407));
#71434=CARTESIAN_POINT('Ctrl Pts',(-1.32929980899916,0.80974756851155,1.79577248435407));
#71435=CARTESIAN_POINT('Ctrl Pts',(-1.40762443979197,0.670070649317171,
1.80633762550688));
#71436=CARTESIAN_POINT('Ctrl Pts',(-1.44926962485242,0.574470986770568,
1.81311762730602));
#71437=CARTESIAN_POINT('Ctrl Pts',(-1.49104929188769,0.444319804641668,
1.82242663502483));
#71438=CARTESIAN_POINT('Ctrl Pts',(-1.50005353975116,0.412900959941094,
1.82467756808877));
#71439=CARTESIAN_POINT('Ctrl Pts',(-1.51178196458939,0.366505143153333,
1.8280204900524));
#71440=CARTESIAN_POINT('Ctrl Pts',(-1.51528687048223,0.351733421468968,
1.82908755968414));
#71441=CARTESIAN_POINT('Ctrl Pts',(-1.52114564853001,0.325326047490414,
1.83100126535571));
#71442=CARTESIAN_POINT('Ctrl Pts',(-1.52358362316759,0.313710137203169,
1.8318451398117));
#71443=CARTESIAN_POINT('Ctrl Pts',(-1.52804418057769,0.291177733102495,
1.83348663208431));
#71444=CARTESIAN_POINT('Ctrl Pts',(-1.53008329414758,0.280265215790429,
1.83428366605995));
#71445=CARTESIAN_POINT('Ctrl Pts',(-1.53428158358357,0.256384650306407,
1.83603273479997));
#71446=CARTESIAN_POINT('Ctrl Pts',(-1.53639349389318,0.243409282611066,
1.83698620286335));
#71447=CARTESIAN_POINT('Ctrl Pts',(-1.54251818793367,0.202517377611905,
1.84000154654074));
#71448=CARTESIAN_POINT('Ctrl Pts',(-1.54593614980552,0.174518998350778,
1.84208156461047));
#71449=CARTESIAN_POINT('Ctrl Pts',(-1.55319495060664,0.097760279318961,
1.84782834642718));
#71450=CARTESIAN_POINT('Ctrl Pts',(-1.55550000000086,0.0488912887219831,
1.85153659513319));
#71451=CARTESIAN_POINT('Ctrl Pts',(-1.5555,-2.74013238336738E-11,1.8552873792152));
#71452=CARTESIAN_POINT('Origin',(0.,0.,-1.2940562256037));
#71453=CARTESIAN_POINT('',(-1.55549941625285,0.00134760418419674,2.6940562256037));
#71454=CARTESIAN_POINT('',(-1.55549999398642,0.000136778062909979,2.55740452554329));
#71455=CARTESIAN_POINT('',(-1.5555,-1.46451138874614E-13,-1.2940562256037));
#71456=CARTESIAN_POINT('Ctrl Pts',(-1.55549937946843,0.0013894147425314,
2.69460090097471));
#71457=CARTESIAN_POINT('Ctrl Pts',(-1.55538731803193,0.126846191331773,
2.68497053713314));
#71458=CARTESIAN_POINT('Ctrl Pts',(-1.54009868858362,0.251831453706691,
2.67506939719058));
#71459=CARTESIAN_POINT('Ctrl Pts',(-1.50718157259488,0.384860815458307,
2.66484140237633));
#71460=CARTESIAN_POINT('Ctrl Pts',(-1.50427686849575,0.396062195069036,
2.66398304455757));
#71461=CARTESIAN_POINT('Ctrl Pts',(-1.49865793622203,0.416776279059666,
2.66240231052651));
#71462=CARTESIAN_POINT('Ctrl Pts',(-1.49597745984636,0.426297466496353,
2.66167832884848));
#71463=CARTESIAN_POINT('Ctrl Pts',(-1.4913290659897,0.442224786329797,2.66047233255536));
#71464=CARTESIAN_POINT('Ctrl Pts',(-1.48941027402812,0.448644834414615,
2.65998761956497));
#71465=CARTESIAN_POINT('Ctrl Pts',(-1.48534986958436,0.46191725370731,2.65898871930838));
#71466=CARTESIAN_POINT('Ctrl Pts',(-1.48320221671903,0.468767505521267,
2.65847487960452));
#71467=CARTESIAN_POINT('Ctrl Pts',(-1.47728743102513,0.487185898851621,
2.65709732565416));
#71468=CARTESIAN_POINT('Ctrl Pts',(-1.47343179155847,0.498725409237205,
2.65623854810703));
#71469=CARTESIAN_POINT('Ctrl Pts',(-1.45249565967407,0.559021895269329,
2.65176788787174));
#71470=CARTESIAN_POINT('Ctrl Pts',(-1.43312755540957,0.606956138145253,
2.64827081138505));
#71471=CARTESIAN_POINT('Ctrl Pts',(-1.37077081508216,0.741561594571889,
2.63837505717821));
#71472=CARTESIAN_POINT('Ctrl Pts',(-1.32204520338672,0.825302114826695,
2.63211279749097));
#71473=CARTESIAN_POINT('Ctrl Pts',(-1.24282707217797,0.936232842896575,
2.62302467603076));
#71474=CARTESIAN_POINT('Ctrl Pts',(-1.21857117371497,0.967592380453974,
2.62035694460501));
#71475=CARTESIAN_POINT('Ctrl Pts',(-1.17996201399898,1.01375151310462,2.61624350410729));
#71476=CARTESIAN_POINT('Ctrl Pts',(-1.16646794206675,1.02924970792222,2.61482838873042));
#71477=CARTESIAN_POINT('Ctrl Pts',(-1.14102586457854,1.05732729653718,2.61219661074604));
#71478=CARTESIAN_POINT('Ctrl Pts',(-1.12916670423239,1.06998296603336,2.61098360781891));
#71479=CARTESIAN_POINT('Ctrl Pts',(-1.11651372554014,1.08304111539856,2.60970235692377));
#71480=CARTESIAN_POINT('Ctrl Pts',(-1.11592813564962,1.08364447722668,2.6096430881903));
#71481=CARTESIAN_POINT('Ctrl Pts',(-1.11473285812393,1.0848740336368,2.60952216973579));
#71482=CARTESIAN_POINT('Ctrl Pts',(-1.11412313145297,1.08550018968049,2.6094605183518));
#71483=CARTESIAN_POINT('Ctrl Pts',(-1.10522359663464,1.09462412942643,2.60856110380358));
#71484=CARTESIAN_POINT('Ctrl Pts',(-1.09683751380288,1.10302703384602,2.60771920656324));
#71485=CARTESIAN_POINT('Ctrl Pts',(-1.08066647767016,1.11886373624548,2.60610581458366));
#71486=CARTESIAN_POINT('Ctrl Pts',(-1.07289890360038,1.1263143558157,2.60533512678551));
#71487=CARTESIAN_POINT('Ctrl Pts',(-1.05447583125259,1.14362216721686,2.60351677129868));
#71488=CARTESIAN_POINT('Ctrl Pts',(-1.04375860196292,1.15341184937758,2.60246630520392));
#71489=CARTESIAN_POINT('Ctrl Pts',(-1.0051450586133,1.18770459469041,2.59870612107435));
#71490=CARTESIAN_POINT('Ctrl Pts',(-0.976512357557173,1.2113554314497,2.59596213449223));
#71491=CARTESIAN_POINT('Ctrl Pts',(-0.860393500237104,1.30047671650134,
2.5849970225351));
#71492=CARTESIAN_POINT('Ctrl Pts',(-0.766966199039916,1.35767201562551,
2.57649439843529));
#71493=CARTESIAN_POINT('Ctrl Pts',(-0.613813654634173,1.43054494715563,
2.56336739180946));
#71494=CARTESIAN_POINT('Ctrl Pts',(-0.557820602450821,1.45329408370597,
2.55872669280604));
#71495=CARTESIAN_POINT('Ctrl Pts',(-0.485967510277927,1.47771987787638,
2.55307005043627));
#71496=CARTESIAN_POINT('Ctrl Pts',(-0.47121904885204,1.48248882456758,2.55192442637811));
#71497=CARTESIAN_POINT('Ctrl Pts',(-0.448875447652583,1.48934651847286,
2.55021448773321));
#71498=CARTESIAN_POINT('Ctrl Pts',(-0.441332203420827,1.49159917975371,
2.54964157845548));
#71499=CARTESIAN_POINT('Ctrl Pts',(-0.427517687808653,1.49561067491995,
2.54860073702107));
#71500=CARTESIAN_POINT('Ctrl Pts',(-0.421252225197364,1.49738746828486,
2.54813184290923));
#71501=CARTESIAN_POINT('Ctrl Pts',(-0.406877505106342,1.50136655967539,
2.5470631672131));
#71502=CARTESIAN_POINT('Ctrl Pts',(-0.398761332315587,1.50354256976768,
2.54646487882233));
#71503=CARTESIAN_POINT('Ctrl Pts',(-0.372413409347209,1.51037829458614,
2.54453790590667));
#71504=CARTESIAN_POINT('Ctrl Pts',(-0.354113827462144,1.51477319078226,
2.54322315409331));
#71505=CARTESIAN_POINT('Ctrl Pts',(-0.238387588028007,1.54035443349811,
2.53503032226885));
#71506=CARTESIAN_POINT('Ctrl Pts',(-0.139181094682225,1.5524671141496,2.52853618842363));
#71507=CARTESIAN_POINT('Ctrl Pts',(0.0383606594663556,1.55697556753864,
2.51684006157532));
#71508=CARTESIAN_POINT('Ctrl Pts',(0.116239512612371,1.5531036858916,2.51168478884959));
#71509=CARTESIAN_POINT('Ctrl Pts',(0.22227982715778,1.53980954575471,2.50437740128042));
#71510=CARTESIAN_POINT('Ctrl Pts',(0.250955007850187,1.53539674339928,2.50237288563666));
#71511=CARTESIAN_POINT('Ctrl Pts',(0.293558426393745,1.52761522161944,2.4993427387498));
#71512=CARTESIAN_POINT('Ctrl Pts',(0.307591735686541,1.52485150586117,2.49833614767991));
#71513=CARTESIAN_POINT('Ctrl Pts',(0.332857657336027,1.51951268093812,2.49650746870956));
#71514=CARTESIAN_POINT('Ctrl Pts',(0.344103679479624,1.51700548854042,2.49568760669109));
#71515=CARTESIAN_POINT('Ctrl Pts',(0.368283005257328,1.5113322446563,2.49391158695646));
#71516=CARTESIAN_POINT('Ctrl Pts',(0.381205499332206,1.5081246210074,2.49295414789157));
#71517=CARTESIAN_POINT('Ctrl Pts',(0.416593994985894,1.49885659938431,2.49030861601903));
#71518=CARTESIAN_POINT('Ctrl Pts',(0.438966827899616,1.49245759657769,2.48860976148115));
#71519=CARTESIAN_POINT('Ctrl Pts',(0.568836187261001,1.45214011829659,2.4785880684266));
#71520=CARTESIAN_POINT('Ctrl Pts',(0.672515419378876,1.40712454988079,2.46990361764407));
#71521=CARTESIAN_POINT('Ctrl Pts',(0.820318677154777,1.32286015823109,2.45670735443873));
#71522=CARTESIAN_POINT('Ctrl Pts',(0.868622464217616,1.29165686114389,2.4522533726896));
#71523=CARTESIAN_POINT('Ctrl Pts',(0.940247678765377,1.23954925415527,2.4455221429992));
#71524=CARTESIAN_POINT('Ctrl Pts',(0.964851773310903,1.22049556795271,2.44318526346992));
#71525=CARTESIAN_POINT('Ctrl Pts',(0.996768367475079,1.19421010551509,2.44013720841082));
#71526=CARTESIAN_POINT('Ctrl Pts',(1.00460292111922,1.18762702078202,2.43938762772936));
#71527=CARTESIAN_POINT('Ctrl Pts',(1.01750929331096,1.17656316031375,2.43815128775061));
#71528=CARTESIAN_POINT('Ctrl Pts',(1.02261775867184,1.17212582879304,2.43766153525754));
#71529=CARTESIAN_POINT('Ctrl Pts',(1.03234963440209,1.16356043808607,2.43672802485861));
#71530=CARTESIAN_POINT('Ctrl Pts',(1.03697756388193,1.15943787946948,2.43628385628941));
#71531=CARTESIAN_POINT('Ctrl Pts',(1.04958323065644,1.14807289976351,2.43507293719761));
#71532=CARTESIAN_POINT('Ctrl Pts',(1.05751074295105,1.1407749063971,2.43431020806476));
#71533=CARTESIAN_POINT('Ctrl Pts',(1.08957021177264,1.11063982860917,2.43121750546881));
#71534=CARTESIAN_POINT('Ctrl Pts',(1.11304524561238,1.08711303032182,2.42893367217328));
#71535=CARTESIAN_POINT('Ctrl Pts',(1.19538539273192,0.999125225509335,2.42076826750388));
#71536=CARTESIAN_POINT('Ctrl Pts',(1.24955549341899,0.930489550683917,2.41508510310124));
#71537=CARTESIAN_POINT('Ctrl Pts',(1.32944070314122,0.809620069684692,2.40553136922015));
#71538=CARTESIAN_POINT('Ctrl Pts',(1.35850125887831,0.759849217181745,2.40171121374538));
#71539=CARTESIAN_POINT('Ctrl Pts',(1.40199781615542,0.674847099985842,2.39524236315461));
#71540=CARTESIAN_POINT('Ctrl Pts',(1.41802154801234,0.640492770933341,2.39264249811136));
#71541=CARTESIAN_POINT('Ctrl Pts',(1.43891974784693,0.591049408493478,2.38889948765799));
#71542=CARTESIAN_POINT('Ctrl Pts',(1.44484362646754,0.57641678224768,2.38779167058978));
#71543=CARTESIAN_POINT('Ctrl Pts',(1.4547667579778,0.550790982212269,2.3858500182355));
#71544=CARTESIAN_POINT('Ctrl Pts',(1.45886667721435,0.539837967078563,2.38501963012689));
#71545=CARTESIAN_POINT('Ctrl Pts',(1.46709905332136,0.517066108313143,2.38329165773792));
#71546=CARTESIAN_POINT('Ctrl Pts',(1.47121308585006,0.505241557717529,2.38239353038934));
#71547=CARTESIAN_POINT('Ctrl Pts',(1.48155184089338,0.474328456558938,2.38004263559217));
#71548=CARTESIAN_POINT('Ctrl Pts',(1.48755032635559,0.455167330100504,2.37858257724474));
#71549=CARTESIAN_POINT('Ctrl Pts',(1.51704220779918,0.354141989310401,2.37086582298681));
#71550=CARTESIAN_POINT('Ctrl Pts',(1.5341498494065,0.270579713124991,2.36440730304874));
#71551=CARTESIAN_POINT('Ctrl Pts',(1.55427327142607,0.103542958193033,2.35142699245007));
#71552=CARTESIAN_POINT('Ctrl Pts',(1.5575852321844,0.0203718502983426,2.34493238733094));
#71553=CARTESIAN_POINT('Ctrl Pts',(1.55320140247792,-0.0883552993543667,
2.33661633755969));
#71554=CARTESIAN_POINT('Ctrl Pts',(1.55152881887798,-0.114016377704457,
2.33466721279431));
#71555=CARTESIAN_POINT('Ctrl Pts',(1.54759139744469,-0.157704170990874,
2.33138372148261));
#71556=CARTESIAN_POINT('Ctrl Pts',(1.54564562241275,-0.175753873677335,
2.33003736834424));
#71557=CARTESIAN_POINT('Ctrl Pts',(1.54234111524195,-0.202074870726715,
2.32809283802791));
#71558=CARTESIAN_POINT('Ctrl Pts',(1.54123090756904,-0.210375063372572,
2.32748238390657));
#71559=CARTESIAN_POINT('Ctrl Pts',(1.53913951238114,-0.225104645774646,
2.3264044191252));
#71560=CARTESIAN_POINT('Ctrl Pts',(1.53818497186468,-0.231537334833427,
2.32593550320462));
#71561=CARTESIAN_POINT('Ctrl Pts',(1.53596437888963,-0.245881814914582,
2.32489398764974));
#71562=CARTESIAN_POINT('Ctrl Pts',(1.53467751366932,-0.253790024817268,
2.32432254654461));
#71563=CARTESIAN_POINT('Ctrl Pts',(1.53060192905334,-0.277670410362816,
2.32260432535035));
#71564=CARTESIAN_POINT('Ctrl Pts',(1.52762443960365,-0.293609856442446,
2.32146743871919));
#71565=CARTESIAN_POINT('Ctrl Pts',(1.50974770917352,-0.381658959976725,
2.31522789121622));
#71566=CARTESIAN_POINT('Ctrl Pts',(1.48999037025805,-0.452695366466934,
2.31034289757394));
#71567=CARTESIAN_POINT('Ctrl Pts',(1.44282686400929,-0.585066636100503,
2.30107826171337));
#71568=CARTESIAN_POINT('Ctrl Pts',(1.41634372454438,-0.646546594597441,
2.29670279499597));
#71569=CARTESIAN_POINT('Ctrl Pts',(1.36776434477102,-0.74189776665953,2.28957135770917));
#71570=CARTESIAN_POINT('Ctrl Pts',(1.34816522475285,-0.776943864119547,
2.28687072576075));
#71571=CARTESIAN_POINT('Ctrl Pts',(1.31182505428172,-0.836401996948736,
2.28210893498225));
#71572=CARTESIAN_POINT('Ctrl Pts',(1.2957020762172,-0.861167353290425,2.28006820415153));
#71573=CARTESIAN_POINT('Ctrl Pts',(1.27068671733997,-0.897297560800229,
2.27699426400264));
#71574=CARTESIAN_POINT('Ctrl Pts',(1.26232512224383,-0.909023051010533,
2.27598094388079));
#71575=CARTESIAN_POINT('Ctrl Pts',(1.24697875331156,-0.929923197739378,
2.27414510532413));
#71576=CARTESIAN_POINT('Ctrl Pts',(1.24005240429697,-0.939139598993209,
2.27332489330736));
#71577=CARTESIAN_POINT('Ctrl Pts',(1.22495124452529,-0.958775296530983,
2.27155380197568));
#71578=CARTESIAN_POINT('Ctrl Pts',(1.21674458903061,-0.969168822037419,
2.27060170324061));
#71579=CARTESIAN_POINT('Ctrl Pts',(1.1939648351247,-0.997273404188338,2.26798602442701));
#71580=CARTESIAN_POINT('Ctrl Pts',(1.17913166831744,-1.01476828632398,2.26631207982835));
#71581=CARTESIAN_POINT('Ctrl Pts',(1.07392893634551,-1.13342708539449,2.25463055130822));
#71582=CARTESIAN_POINT('Ctrl Pts',(0.971063849893259,-1.22270215999018,
2.24407412871352));
#71583=CARTESIAN_POINT('Ctrl Pts',(0.82277362573525,-1.32075866088322,2.23032683404809));
#71584=CARTESIAN_POINT('Ctrl Pts',(0.78665092684456,-1.34258729850469,2.2270835643428));
#71585=CARTESIAN_POINT('Ctrl Pts',(0.727219688405929,-1.37527781461728,
2.22195719271888));
#71586=CARTESIAN_POINT('Ctrl Pts',(0.704452290761252,-1.38707775785196,
2.22004053039881));
#71587=CARTESIAN_POINT('Ctrl Pts',(0.672815076671022,-1.40249469406085,
2.21745098099835));
#71588=CARTESIAN_POINT('Ctrl Pts',(0.66418952089079,-1.40660008070629,2.21675234546226));
#71589=CARTESIAN_POINT('Ctrl Pts',(0.649504677449499,-1.41342421650912,
2.21557604913213));
#71590=CARTESIAN_POINT('Ctrl Pts',(0.643464902652125,-1.41618405163887,
2.21509597902856));
#71591=CARTESIAN_POINT('Ctrl Pts',(0.630742594695907,-1.42189922704868,
2.2140927826862));
#71592=CARTESIAN_POINT('Ctrl Pts',(0.624056657428621,-1.42484628181611,
2.21357014255493));
#71593=CARTESIAN_POINT('Ctrl Pts',(0.605638667570506,-1.43281012471862,
2.21214224019816));
#71594=CARTESIAN_POINT('Ctrl Pts',(0.593864950902522,-1.43772998056109,
2.2112425505208));
#71595=CARTESIAN_POINT('Ctrl Pts',(0.51161977071174,-1.4709148229566,2.20503926334067));
#71596=CARTESIAN_POINT('Ctrl Pts',(0.439212034146059,-1.49413560587586,
2.19998833393911));
#71597=CARTESIAN_POINT('Ctrl Pts',(0.306755854313112,-1.52614536433074,
2.19099654745206));
#71598=CARTESIAN_POINT('Ctrl Pts',(0.247349219848664,-1.53689202634323,
2.18704907088973));
#71599=CARTESIAN_POINT('Ctrl Pts',(0.142001991818524,-1.54968171085334,
2.18000869855851));
#71600=CARTESIAN_POINT('Ctrl Pts',(0.0963163463532044,-1.55319047515296,
2.17694287312981));
#71601=CARTESIAN_POINT('Ctrl Pts',(0.018107810677906,-1.55573314981053,
2.17161280567155));
#71602=CARTESIAN_POINT('Ctrl Pts',(-0.0143522159617565,-1.55577224857403,
2.16937682813084));
#71603=CARTESIAN_POINT('Ctrl Pts',(-0.0616951794880102,-1.55434757484017,
2.16606775977228));
#71604=CARTESIAN_POINT('Ctrl Pts',(-0.0765947715009059,-1.55368461800005,
2.16501944782693));
#71605=CARTESIAN_POINT('Ctrl Pts',(-0.103039274247553,-1.5521266669576,
2.16314541829147));
#71606=CARTESIAN_POINT('Ctrl Pts',(-0.114588211648479,-1.55131679898818,
2.16232242594881));
#71607=CARTESIAN_POINT('Ctrl Pts',(-0.139005380404212,-1.54933040728745,
2.16057223416413));
#71608=CARTESIAN_POINT('Ctrl Pts',(-0.151870079932455,-1.54812230357828,
2.15964410172136));
#71609=CARTESIAN_POINT('Ctrl Pts',(-0.186598870437028,-1.54442394400177,
2.15712156247851));
#71610=CARTESIAN_POINT('Ctrl Pts',(-0.208426849186091,-1.54162985625917,
2.15551776871427));
#71611=CARTESIAN_POINT('Ctrl Pts',(-0.354420788616174,-1.51978475107023,
2.14466217164243));
#71612=CARTESIAN_POINT('Ctrl Pts',(-0.475922905125124,-1.4862182913149,
2.13494408974712));
#71613=CARTESIAN_POINT('Ctrl Pts',(-0.654598557060875,-1.41267745780737,
2.11996763470592));
#71614=CARTESIAN_POINT('Ctrl Pts',(-0.715417583243432,-1.38287250046008,
2.11474723840267));
#71615=CARTESIAN_POINT('Ctrl Pts',(-0.788232551768143,-1.34109466083933,
2.10848170970822));
#71616=CARTESIAN_POINT('Ctrl Pts',(-0.802230172532691,-1.33276864117463,
2.10727669009433));
#71617=CARTESIAN_POINT('Ctrl Pts',(-0.822927552905985,-1.32001322114888,
2.10549688802283));
#71618=CARTESIAN_POINT('Ctrl Pts',(-0.829727455348345,-1.31574960338492,
2.10491248018596));
#71619=CARTESIAN_POINT('Ctrl Pts',(-0.841428013752229,-1.30828643393038,
2.10390786565032));
#71620=CARTESIAN_POINT('Ctrl Pts',(-0.846343925988586,-1.30511166481538,
2.10348611136737));
#71621=CARTESIAN_POINT('Ctrl Pts',(-0.85794516680684,-1.29752629284738,
2.10249153910797));
#71622=CARTESIAN_POINT('Ctrl Pts',(-0.864614499983425,-1.2930917074296,
2.10192031521566));
#71623=CARTESIAN_POINT('Ctrl Pts',(-0.884667456810305,-1.27953354259813,
2.10020344563143));
#71624=CARTESIAN_POINT('Ctrl Pts',(-0.897943611344265,-1.27025191231025,
2.09906767057882));
#71625=CARTESIAN_POINT('Ctrl Pts',(-0.969382346623749,-1.2186277392443,
2.09294642539172));
#71626=CARTESIAN_POINT('Ctrl Pts',(-1.02470574589138,-1.17249152587738,
2.08816833050163));
#71627=CARTESIAN_POINT('Ctrl Pts',(-1.12190979149695,-1.07927402318772,
2.07928552843029));
#71628=CARTESIAN_POINT('Ctrl Pts',(-1.16450997141931,-1.03316521502718,
2.07518124081249));
#71629=CARTESIAN_POINT('Ctrl Pts',(-1.24533709583144,-0.934311137469707,
2.06669487242445));
#71630=CARTESIAN_POINT('Ctrl Pts',(-1.28326786800508,-0.88148953936091,
2.06231608436082));
#71631=CARTESIAN_POINT('Ctrl Pts',(-1.32774473711978,-0.810571234795339,
2.0565111089062));
#71632=CARTESIAN_POINT('Ctrl Pts',(-1.33741843583963,-0.794508456979942,
2.05520118404223));
#71633=CARTESIAN_POINT('Ctrl Pts',(-1.352926216453,-0.767672369896671,2.05301826887636));
#71634=CARTESIAN_POINT('Ctrl Pts',(-1.35892776707444,-0.756997703453047,
2.05215139546252));
#71635=CARTESIAN_POINT('Ctrl Pts',(-1.37041631025434,-0.735986624449652,
2.05044725806438));
#71636=CARTESIAN_POINT('Ctrl Pts',(-1.37591393992763,-0.725656937446091,
2.04961044549914));
#71637=CARTESIAN_POINT('Ctrl Pts',(-1.38889634092822,-0.700585836960875,
2.04758124882784));
#71638=CARTESIAN_POINT('Ctrl Pts',(-1.39626350263485,-0.685785500525342,
2.04638483559864));
#71639=CARTESIAN_POINT('Ctrl Pts',(-1.42071587397855,-0.634633660818418,
2.0422533391069));
#71640=CARTESIAN_POINT('Ctrl Pts',(-1.43662701924741,-0.597742209261008,
2.03927903598984));
#71641=CARTESIAN_POINT('Ctrl Pts',(-1.49703788902239,-0.441281493234144,
2.02668054718635));
#71642=CARTESIAN_POINT('Ctrl Pts',(-1.52816783187321,-0.317091084462268,
2.01666570016941));
#71643=CARTESIAN_POINT('Ctrl Pts',(-1.54931440220941,-0.145742777560349,
2.00341007027543));
#71644=CARTESIAN_POINT('Ctrl Pts',(-1.55289043748145,-0.100738299445941,
1.9999858901203));
#71645=CARTESIAN_POINT('Ctrl Pts',(-1.55491545829476,-0.0441597243189167,
1.99579942571185));
#71646=CARTESIAN_POINT('Ctrl Pts',(-1.55519914969052,-0.0326770470229673,
1.99495590995198));
#71647=CARTESIAN_POINT('Ctrl Pts',(-1.55545143281546,-0.0141609537247806,
1.9936066933907));
#71648=CARTESIAN_POINT('Ctrl Pts',(-1.55549955660677,-0.00712931545088431,
1.99309686784853));
#71649=CARTESIAN_POINT('Ctrl Pts',(-1.55549999695016,-9.74065733091837E-5,
1.99258973177283));
#71650=CARTESIAN_POINT('',(-1.55549938663868,-0.00138136406952889,1.85539336356033));
#71651=CARTESIAN_POINT('Ctrl Pts',(-1.5555,-2.74013238336738E-11,1.8552873792152));
#71652=CARTESIAN_POINT('Ctrl Pts',(-1.55549999999999,-0.000460452766239691,
1.85532270368398));
#71653=CARTESIAN_POINT('Ctrl Pts',(-1.55549979554798,-0.000920907491934938,
1.85535803180706));
#71654=CARTESIAN_POINT('Ctrl Pts',(-1.55549938663868,-0.00138136406952337,
1.85539336356033));
#71655=CARTESIAN_POINT('Ctrl Pts',(-1.55549938786299,-0.00137998473721819,
1.85539325772142));
#71656=CARTESIAN_POINT('Ctrl Pts',(-1.55538895339302,-0.125860166144892,
1.86494486888977));
#71657=CARTESIAN_POINT('Ctrl Pts',(-1.54033730079042,-0.249879935971551,
1.87476439976426));
#71658=CARTESIAN_POINT('Ctrl Pts',(-1.50776464436006,-0.382588199128195,
1.88497621214416));
#71659=CARTESIAN_POINT('Ctrl Pts',(-1.50472931714602,-0.394357270960365,
1.88587878350894));
#71660=CARTESIAN_POINT('Ctrl Pts',(-1.49886077654995,-0.416056756393507,
1.88753581801422));
#71661=CARTESIAN_POINT('Ctrl Pts',(-1.49606603794035,-0.425996804714526,
1.88829208838697));
#71662=CARTESIAN_POINT('Ctrl Pts',(-1.49123663290028,-0.442539570210456,
1.8895452384819));
#71663=CARTESIAN_POINT('Ctrl Pts',(-1.48925661774329,-0.4491577680103,1.89004510407235));
#71664=CARTESIAN_POINT('Ctrl Pts',(-1.48508452641398,-0.462772019206191,
1.89107004065383));
#71665=CARTESIAN_POINT('Ctrl Pts',(-1.48288697859833,-0.469766119442804,
1.89159479668266));
#71666=CARTESIAN_POINT('Ctrl Pts',(-1.47686050901928,-0.488482706249938,
1.89299492924222));
#71667=CARTESIAN_POINT('Ctrl Pts',(-1.4729414056685,-0.500175927131773,
1.89386528496247));
#71668=CARTESIAN_POINT('Ctrl Pts',(-1.45207732788873,-0.560053994973987,
1.89830561736203));
#71669=CARTESIAN_POINT('Ctrl Pts',(-1.43290375404118,-0.607434815703687,
1.90176420414499));
#71670=CARTESIAN_POINT('Ctrl Pts',(-1.36879750231898,-0.745830041297932,
1.91194243722714));
#71671=CARTESIAN_POINT('Ctrl Pts',(-1.3172636407411,-0.833478532759328,
1.91850581248235));
#71672=CARTESIAN_POINT('Ctrl Pts',(-1.23576813988254,-0.945425090500928,
1.92776092931786));
#71673=CARTESIAN_POINT('Ctrl Pts',(-1.21291318763459,-0.974573138543642,
1.93025970686544));
#71674=CARTESIAN_POINT('Ctrl Pts',(-1.17117840361002,-1.02405518021531,
1.93469146115071));
#71675=CARTESIAN_POINT('Ctrl Pts',(-1.15275397548987,-1.04475163413647,
1.93660760361265));
#71676=CARTESIAN_POINT('Ctrl Pts',(-1.1243214114316,-1.0750222291773,1.93951409624123));
#71677=CARTESIAN_POINT('Ctrl Pts',(-1.11472149983761,-1.08497344915393,
1.94048726209598));
#71678=CARTESIAN_POINT('Ctrl Pts',(-1.09666547333496,-1.1031976240658,1.94230365227641));
#71679=CARTESIAN_POINT('Ctrl Pts',(-1.08824511798946,-1.11150470408145,
1.9431452721247));
#71680=CARTESIAN_POINT('Ctrl Pts',(-1.0698992049,-1.12919550631676,1.94496793051884));
#71681=CARTESIAN_POINT('Ctrl Pts',(-1.05994321362271,-1.13854607370604,
1.94595030674817));
#71682=CARTESIAN_POINT('Ctrl Pts',(-1.03224187762911,-1.16388462787798,
1.9486662123565));
#71683=CARTESIAN_POINT('Ctrl Pts',(-1.01425009016321,-1.17959626926235,
1.95041105639542));
#71684=CARTESIAN_POINT('Ctrl Pts',(-0.913570936574439,-1.26350952510231,
1.96007754882727));
#71685=CARTESIAN_POINT('Ctrl Pts',(-0.824379246614064,-1.32342707469424,
1.96831981862014));
#71686=CARTESIAN_POINT('Ctrl Pts',(-0.653479893284431,-1.41421513709615,
1.98332565504959));
#71687=CARTESIAN_POINT('Ctrl Pts',(-0.573952423149791,-1.4483169776219,
1.99003197518426));
#71688=CARTESIAN_POINT('Ctrl Pts',(-0.479021574910063,-1.479968135154,1.99746477994711));
#71689=CARTESIAN_POINT('Ctrl Pts',(-0.465988253622172,-1.48412342205631,
1.99847300502116));
#71690=CARTESIAN_POINT('Ctrl Pts',(-0.445612709828477,-1.49032466462937,
2.0000284568485));
#71691=CARTESIAN_POINT('Ctrl Pts',(-0.438307779542034,-1.49248939365378,
2.0005819916172));
#71692=CARTESIAN_POINT('Ctrl Pts',(-0.424473033983126,-1.49647881841761,
2.00162218217989));
#71693=CARTESIAN_POINT('Ctrl Pts',(-0.417947040954146,-1.49831454758053,
2.00210939938525));
#71694=CARTESIAN_POINT('Ctrl Pts',(-0.402163576260625,-1.50264320880102,
2.00327980011711));
#71695=CARTESIAN_POINT('Ctrl Pts',(-0.392894698115519,-1.50509332722969,
2.00396056830364));
#71696=CARTESIAN_POINT('Ctrl Pts',(-0.361161071179086,-1.51316859786325,
2.00627086512746));
#71697=CARTESIAN_POINT('Ctrl Pts',(-0.338592439014884,-1.5183780257571,
2.00787911439485));
#71698=CARTESIAN_POINT('Ctrl Pts',(-0.222722533241381,-1.54241151626245,
2.01599881315053));
#71699=CARTESIAN_POINT('Ctrl Pts',(-0.127943171529968,-1.55314940330456,
2.02219851355788));
#71700=CARTESIAN_POINT('Ctrl Pts',(0.0275662866768698,-1.55642610834329,
2.03244837243229));
#71701=CARTESIAN_POINT('Ctrl Pts',(0.0879203693184907,-1.55418511138195,
2.03644357891812));
#71702=CARTESIAN_POINT('Ctrl Pts',(0.174732533722277,-1.54588828315864,
2.04234449835434));
#71703=CARTESIAN_POINT('Ctrl Pts',(0.201404849295889,-1.54263994447678,
2.04417835725252));
#71704=CARTESIAN_POINT('Ctrl Pts',(0.249740767191859,-1.53547835907496,
2.04755026612022));
#71705=CARTESIAN_POINT('Ctrl Pts',(0.271431167863581,-1.53179283181913,
2.04908133579775));
#71706=CARTESIAN_POINT('Ctrl Pts',(0.305934563681394,-1.52517435345614,
2.0515495651768));
#71707=CARTESIAN_POINT('Ctrl Pts',(0.318801687986122,-1.52253677474816,
2.05247734732059));
#71708=CARTESIAN_POINT('Ctrl Pts',(0.34327365389699,-1.51719655721571,2.0542566899509));
#71709=CARTESIAN_POINT('Ctrl Pts',(0.354883911083687,-1.51452289180877,
2.05510726542497));
#71710=CARTESIAN_POINT('Ctrl Pts',(0.381341200355258,-1.5081092596013,2.05706078451662));
#71711=CARTESIAN_POINT('Ctrl Pts',(0.396165804548793,-1.50428297675511,
2.05816643444416));
#71712=CARTESIAN_POINT('Ctrl Pts',(0.444134347228622,-1.49114389166325,
2.06178134930234));
#71713=CARTESIAN_POINT('Ctrl Pts',(0.477023974661305,-1.48095010332295,
2.06431850993454));
#71714=CARTESIAN_POINT('Ctrl Pts',(0.637074778030712,-1.42545940099006,
2.07696415963508));
#71715=CARTESIAN_POINT('Ctrl Pts',(0.758294454130408,-1.36483596205011,
2.08755599361962));
#71716=CARTESIAN_POINT('Ctrl Pts',(0.895957060259923,-1.2719320463403,2.10031308382366));
#71717=CARTESIAN_POINT('Ctrl Pts',(0.921244745709634,-1.2537378289102,2.10268701357591));
#71718=CARTESIAN_POINT('Ctrl Pts',(0.962585255199995,-1.22206707633824,
2.10660037029232));
#71719=CARTESIAN_POINT('Ctrl Pts',(0.978942463008052,-1.20900375424844,
2.10815768705266));
#71720=CARTESIAN_POINT('Ctrl Pts',(1.00193667335043,-1.18986715515646,2.11035417749409));
#71721=CARTESIAN_POINT('Ctrl Pts',(1.00879165204961,-1.1840609602348,2.11100994111039));
#71722=CARTESIAN_POINT('Ctrl Pts',(1.02067296297553,-1.17381935464664,2.11214763870729));
#71723=CARTESIAN_POINT('Ctrl Pts',(1.02572148103765,-1.16941037475094,2.11263138761461));
#71724=CARTESIAN_POINT('Ctrl Pts',(1.03670203881312,-1.15969499015047,2.11368417373872));
#71725=CARTESIAN_POINT('Ctrl Pts',(1.04262204078994,-1.15437553462164,2.11425224329532));
#71726=CARTESIAN_POINT('Ctrl Pts',(1.05949151441324,-1.13898171646649,2.11587328420474));
#71727=CARTESIAN_POINT('Ctrl Pts',(1.07033797298595,-1.12879505917099,2.11691835845458));
#71728=CARTESIAN_POINT('Ctrl Pts',(1.15329314593588,-1.04861506785732,2.12494931511784));
#71729=CARTESIAN_POINT('Ctrl Pts',(1.21862217906004,-0.971928217588851,
2.13151123968312));
#71730=CARTESIAN_POINT('Ctrl Pts',(1.31333186829491,-0.836049552033223,
2.14241586659887));
#71731=CARTESIAN_POINT('Ctrl Pts',(1.34717019026984,-0.780353175971586,
2.14671284302865));
#71732=CARTESIAN_POINT('Ctrl Pts',(1.39652400543303,-0.686288624063325,
2.15388834069765));
#71733=CARTESIAN_POINT('Ctrl Pts',(1.41417726793712,-0.649132921379771,
2.1567026166598));
#71734=CARTESIAN_POINT('Ctrl Pts',(1.4368208200654,-0.596152986482158,2.16071586962058));
#71735=CARTESIAN_POINT('Ctrl Pts',(1.44306287758538,-0.580880320742302,
2.1618727409201));
#71736=CARTESIAN_POINT('Ctrl Pts',(1.45344132644151,-0.554286706428067,
2.16388870521874));
#71737=CARTESIAN_POINT('Ctrl Pts',(1.45769133138501,-0.543011427032976,
2.16474391518476));
#71738=CARTESIAN_POINT('Ctrl Pts',(1.46616875584323,-0.519703814812717,
2.16651333373831));
#71739=CARTESIAN_POINT('Ctrl Pts',(1.47038003700313,-0.507666627421351,
2.16742800329111));
#71740=CARTESIAN_POINT('Ctrl Pts',(1.48086483408395,-0.476472363747926,
2.16980127808126));
#71741=CARTESIAN_POINT('Ctrl Pts',(1.48691463419079,-0.457243228543902,
2.17126707616361));
#71742=CARTESIAN_POINT('Ctrl Pts',(1.5144007327763,-0.363557037144884,2.17842570562278));
#71743=CARTESIAN_POINT('Ctrl Pts',(1.5306240803864,-0.287697408101522,2.18428207894123));
#71744=CARTESIAN_POINT('Ctrl Pts',(1.55652738760939,-0.098461874207653,
2.1989765761342));
#71745=CARTESIAN_POINT('Ctrl Pts',(1.55956301776891,0.0153796263588531,
2.20790529566261));
#71746=CARTESIAN_POINT('Ctrl Pts',(1.54852402745033,0.148509800108015,2.21793150997985));
#71747=CARTESIAN_POINT('Ctrl Pts',(1.54648220304895,0.168447969809931,2.21942108444098));
#71748=CARTESIAN_POINT('Ctrl Pts',(1.5429859294184,0.197110892601732,2.22154013866877));
#71749=CARTESIAN_POINT('Ctrl Pts',(1.54184163492863,0.205870505797548,2.22218471586751));
#71750=CARTESIAN_POINT('Ctrl Pts',(1.53969971545498,0.221245993681795,2.2233102594707));
#71751=CARTESIAN_POINT('Ctrl Pts',(1.53873395162544,0.227865828319695,2.22379290989689));
#71752=CARTESIAN_POINT('Ctrl Pts',(1.53650984271501,0.242451610065509,2.22485200281617));
#71753=CARTESIAN_POINT('Ctrl Pts',(1.53523222850838,0.25041424125383,2.22542737811352));
#71754=CARTESIAN_POINT('Ctrl Pts',(1.53133861678548,0.273530146183861,2.22709052510622));
#71755=CARTESIAN_POINT('Ctrl Pts',(1.52855969292173,0.288655524553191,2.22816975820267));
#71756=CARTESIAN_POINT('Ctrl Pts',(1.50277060528302,0.418184017971041,2.23735396464956));
#71757=CARTESIAN_POINT('Ctrl Pts',(1.46717508273175,0.529719477436725,2.24489309309676));
#71758=CARTESIAN_POINT('Ctrl Pts',(1.38872008483013,0.704751246615246,2.25755873807192));
#71759=CARTESIAN_POINT('Ctrl Pts',(1.35309220528608,0.770945742191927,2.26256493559077));
#71760=CARTESIAN_POINT('Ctrl Pts',(1.30028940479976,0.85403405388403,2.26934507074808));
#71761=CARTESIAN_POINT('Ctrl Pts',(1.28730879893311,0.873477337068966,2.2709694313602));
#71762=CARTESIAN_POINT('Ctrl Pts',(1.26619530931275,0.903609290306081,2.2735518475855));
#71763=CARTESIAN_POINT('Ctrl Pts',(1.25835337942552,0.914498257607495,2.274498897505));
#71764=CARTESIAN_POINT('Ctrl Pts',(1.2433186903096,0.93481520745987,2.27629306513166));
#71765=CARTESIAN_POINT('Ctrl Pts',(1.23615704743023,0.944265099195209,2.27713892953889));
#71766=CARTESIAN_POINT('Ctrl Pts',(1.219654736508,0.965530636501451,2.27906899082795));
#71767=CARTESIAN_POINT('Ctrl Pts',(1.21024920931724,0.977294176806536,2.28015570944413));
#71768=CARTESIAN_POINT('Ctrl Pts',(1.18034183258107,1.01360557567902,2.2835715894737));
#71769=CARTESIAN_POINT('Ctrl Pts',(1.15925397644534,1.03765748019393,2.28592413217753));
#71770=CARTESIAN_POINT('Ctrl Pts',(1.05174425678653,1.15290845025216,2.29765932807919));
#71771=CARTESIAN_POINT('Ctrl Pts',(0.955242908549995,1.23404411774343,2.30746298039647));
#71772=CARTESIAN_POINT('Ctrl Pts',(0.817293234500351,1.32406311370377,2.3201816895712));
#71773=CARTESIAN_POINT('Ctrl Pts',(0.783726272767845,1.34420418108044,2.32318362421356));
#71774=CARTESIAN_POINT('Ctrl Pts',(0.734635837831378,1.37119495302055,2.32741201073855));
#71775=CARTESIAN_POINT('Ctrl Pts',(0.71970601770741,1.37908981385141,2.32867732168767));
#71776=CARTESIAN_POINT('Ctrl Pts',(0.692787766165383,1.39276789278243,2.33091839535678));
#71777=CARTESIAN_POINT('Ctrl Pts',(0.680848228462122,1.39864327599412,2.33189855421603));
#71778=CARTESIAN_POINT('Ctrl Pts',(0.662027113144578,1.40760690485269,2.3334204260006));
#71779=CARTESIAN_POINT('Ctrl Pts',(0.655196305437748,1.41079938506277,2.33396803417576));
#71780=CARTESIAN_POINT('Ctrl Pts',(0.642154512448631,1.41677950725701,2.33500422071643));
#71781=CARTESIAN_POINT('Ctrl Pts',(0.635948295355103,1.41957611900225,2.3354932803866));
#71782=CARTESIAN_POINT('Ctrl Pts',(0.620796744562882,1.42628431986702,2.33667785229888));
#71783=CARTESIAN_POINT('Ctrl Pts',(0.61183257624404,1.43015260406258,2.33737079449766));
#71784=CARTESIAN_POINT('Ctrl Pts',(0.58037540697374,1.44337731709365,2.33977705460789));
#71785=CARTESIAN_POINT('Ctrl Pts',(0.557698272922248,1.45229008614372,2.3414666131695));
#71786=CARTESIAN_POINT('Ctrl Pts',(0.446402948902243,1.49304059043542,2.34958533411337));
#71787=CARTESIAN_POINT('Ctrl Pts',(0.355220357095774,1.51732263070553,2.35571844497338));
#71788=CARTESIAN_POINT('Ctrl Pts',(0.203285018399969,1.54332484730588,2.36587707175755));
#71789=CARTESIAN_POINT('Ctrl Pts',(0.143644426684709,1.55001351257482,2.3698481304727));
#71790=CARTESIAN_POINT('Ctrl Pts',(0.0447726383139681,1.55534590614523,
2.37654898994093));
#71791=CARTESIAN_POINT('Ctrl Pts',(0.00571275325077085,1.55597957098679,
2.37922572645748));
#71792=CARTESIAN_POINT('Ctrl Pts',(-0.0495231557783744,1.55479585136106,
2.38307644808628));
#71793=CARTESIAN_POINT('Ctrl Pts',(-0.065712232184456,1.554195788892,2.3842129480116));
#71794=CARTESIAN_POINT('Ctrl Pts',(-0.093874162099351,1.55271116049058,
2.38620524099852));
#71795=CARTESIAN_POINT('Ctrl Pts',(-0.105851831056515,1.55194061787074,
2.38705740960886));
#71796=CARTESIAN_POINT('Ctrl Pts',(-0.130642781109732,1.55005745371851,
2.38883178575243));
#71797=CARTESIAN_POINT('Ctrl Pts',(-0.143453535061102,1.54892437225602,
2.38975457168524));
#71798=CARTESIAN_POINT('Ctrl Pts',(-0.176824166531395,1.54555528559057,
2.39217440274962));
#71799=CARTESIAN_POINT('Ctrl Pts',(-0.197355473352966,1.54306793998091,
2.39367918954526));
#71800=CARTESIAN_POINT('Ctrl Pts',(-0.308233837236498,1.52738614960515,
2.40189653002818));
#71801=CARTESIAN_POINT('Ctrl Pts',(-0.397320308485734,1.50666776780901,
2.40884220181864));
#71802=CARTESIAN_POINT('Ctrl Pts',(-0.557274061624737,1.45429040141275,
2.42185154414691));
#71803=CARTESIAN_POINT('Ctrl Pts',(-0.628604739612074,1.4249110537569,2.42786221698135));
#71804=CARTESIAN_POINT('Ctrl Pts',(-0.719722226644113,1.37920271984165,
2.43564526011264));
#71805=CARTESIAN_POINT('Ctrl Pts',(-0.741708254627189,1.36750474707354,
2.43753119524499));
#71806=CARTESIAN_POINT('Ctrl Pts',(-0.778924694583664,1.3465414390679,2.44072667019765));
#71807=CARTESIAN_POINT('Ctrl Pts',(-0.794293837946009,1.33753313871166,
2.44204721312236));
#71808=CARTESIAN_POINT('Ctrl Pts',(-0.816711093926893,1.3238710060714,2.44397107509786));
#71809=CARTESIAN_POINT('Ctrl Pts',(-0.823880879694541,1.31942099290638,
2.44458603964271));
#71810=CARTESIAN_POINT('Ctrl Pts',(-0.83665534650042,1.31134763211018,2.44568060993475));
#71811=CARTESIAN_POINT('Ctrl Pts',(-0.842273313293819,1.30774632535656,
2.44616154882484));
#71812=CARTESIAN_POINT('Ctrl Pts',(-0.854912911102718,1.29952867154592,
2.44724266204309));
#71813=CARTESIAN_POINT('Ctrl Pts',(-0.861920520228475,1.29489145458927,
2.44784146003915));
#71814=CARTESIAN_POINT('Ctrl Pts',(-0.883505862549115,1.28035469056066,
2.44968524167102));
#71815=CARTESIAN_POINT('Ctrl Pts',(-0.897953806441506,1.27026366260986,
2.45091839191383));
#71816=CARTESIAN_POINT('Ctrl Pts',(-0.993818641449694,1.20085451539209,
2.45911707311284));
#71817=CARTESIAN_POINT('Ctrl Pts',(-1.06948921135085,1.13398645770458,2.46568082264389));
#71818=CARTESIAN_POINT('Ctrl Pts',(-1.18063253729121,1.01467643010332,2.47642103133751));
#71819=CARTESIAN_POINT('Ctrl Pts',(-1.2203177894895,0.966584258016473,2.48054004427704));
#71820=CARTESIAN_POINT('Ctrl Pts',(-1.27313355837751,0.894125506974991,
2.48660283746285));
#71821=CARTESIAN_POINT('Ctrl Pts',(-1.28866922124142,0.871585326068368,
2.48847002155155));
#71822=CARTESIAN_POINT('Ctrl Pts',(-1.31577620498229,0.829946503707971,
2.49189702238606));
#71823=CARTESIAN_POINT('Ctrl Pts',(-1.32754652642819,0.810986038004548,
2.49344948364089));
#71824=CARTESIAN_POINT('Ctrl Pts',(-1.34562343665252,0.780417871368361,
2.49594389695653));
#71825=CARTESIAN_POINT('Ctrl Pts',(-1.35219735111069,0.768971255395661,
2.49687610783986));
#71826=CARTESIAN_POINT('Ctrl Pts',(-1.36441842097084,0.747050327296673,
2.49865866202314));
#71827=CARTESIAN_POINT('Ctrl Pts',(-1.37009264297018,0.736592122012945,
2.49950795709923));
#71828=CARTESIAN_POINT('Ctrl Pts',(-1.38273491576973,0.712639484286972,
2.50145111392439));
#71829=CARTESIAN_POINT('Ctrl Pts',(-1.38962633138911,0.699106222670906,
2.50254758089147));
#71830=CARTESIAN_POINT('Ctrl Pts',(-1.41115771808279,0.655246587514691,
2.50609783020888));
#71831=CARTESIAN_POINT('Ctrl Pts',(-1.42501052816707,0.6245469307339,2.5085781263187));
#71832=CARTESIAN_POINT('Ctrl Pts',(-1.48498723162047,0.479224498839212,
2.52030496068836));
#71833=CARTESIAN_POINT('Ctrl Pts',(-1.51834019358153,0.359829211161852,
2.52994815320353));
#71834=CARTESIAN_POINT('Ctrl Pts',(-1.54315895425967,0.19937522749374,2.54248287376783));
#71835=CARTESIAN_POINT('Ctrl Pts',(-1.54765799975354,0.16076423955664,2.54546324943519));
#71836=CARTESIAN_POINT('Ctrl Pts',(-1.55261918076152,0.0977160113661703,
2.550236099301));
#71837=CARTESIAN_POINT('Ctrl Pts',(-1.55396022927822,0.0733656160231017,
2.55205674173795));
#71838=CARTESIAN_POINT('Ctrl Pts',(-1.55502807326686,0.0394783775701928,
2.55455026825913));
#71839=CARTESIAN_POINT('Ctrl Pts',(-1.55524054590962,0.0299617693615345,
2.55524612591083));
#71840=CARTESIAN_POINT('Ctrl Pts',(-1.55545461412657,0.0136751995529757,
2.55642880848515));
#71841=CARTESIAN_POINT('Ctrl Pts',(-1.55549939873703,0.00690621489850628,
2.55691791433138));
#71842=CARTESIAN_POINT('Ctrl Pts',(-1.55549999398642,0.000136778059410365,
2.55740452554354));
#71843=CARTESIAN_POINT('Origin',(0.,0.,-1.2940562256037));
#71844=CARTESIAN_POINT('',(-1.55549982468662,-0.000738511954293953,3.3940562256037));
#71845=CARTESIAN_POINT('',(-1.5555,-2.78355693781297E-11,3.25542335925836));
#71846=CARTESIAN_POINT('',(-1.5555,-1.46451138874614E-13,-1.2940562256037));
#71847=CARTESIAN_POINT('Ctrl Pts',(-1.55549941625285,0.00134760418419674,
2.6940562256037));
#71848=CARTESIAN_POINT('Ctrl Pts',(-1.55554919476569,-0.0561102521829977,
2.69816386501832));
#71849=CARTESIAN_POINT('Ctrl Pts',(-1.55241106539883,-0.113626806645204,
2.70227150443293));
#71850=CARTESIAN_POINT('Ctrl Pts',(-1.54609216886034,-0.170819364794349,
2.70637914384755));
#71851=CARTESIAN_POINT('Ctrl Pts',(-1.53977588609704,-0.227988265570853,
2.71048508416075));
#71852=CARTESIAN_POINT('Ctrl Pts',(-1.53028150231367,-0.284832911193982,
2.71459102447395));
#71853=CARTESIAN_POINT('Ctrl Pts',(-1.51766808417958,-0.340974832300971,
2.71869696478716));
#71854=CARTESIAN_POINT('Ctrl Pts',(-1.50505487515628,-0.39711582266256,
2.72280283703028));
#71855=CARTESIAN_POINT('Ctrl Pts',(-1.48932285319747,-0.452553597006042,
2.7269087092734));
#71856=CARTESIAN_POINT('Ctrl Pts',(-1.470581879495,-0.506921281562494,2.73101458151653));
#71857=CARTESIAN_POINT('Ctrl Pts',(-1.45182095795932,-0.561346834910656,
2.7351248240371));
#71858=CARTESIAN_POINT('Ctrl Pts',(-1.43004486854431,-0.614699526164613,
2.73923506655766));
#71859=CARTESIAN_POINT('Ctrl Pts',(-1.40541240745189,-0.666630493587175,
2.74334530907823));
#71860=CARTESIAN_POINT('Ctrl Pts',(-1.38076460904644,-0.718593795639242,
2.74745811082648));
#71861=CARTESIAN_POINT('Ctrl Pts',(-1.35325715531117,-0.769133149955912,
2.75157091257473));
#71862=CARTESIAN_POINT('Ctrl Pts',(-1.32309423869949,-0.817925354491605,
2.75568371432297));
#71863=CARTESIAN_POINT('Ctrl Pts',(-1.29287728787355,-0.86680496597365,
2.7598038837941));
#71864=CARTESIAN_POINT('Ctrl Pts',(-1.25999568941062,-0.91393075368594,
2.76392405326522));
#71865=CARTESIAN_POINT('Ctrl Pts',(-1.22469538727744,-0.9590106664586,2.76804422273635));
#71866=CARTESIAN_POINT('Ctrl Pts',(-1.21231302893473,-0.97482343859588,
2.76948946291112));
#71867=CARTESIAN_POINT('Ctrl Pts',(-1.19963341132009,-0.990384807910173,
2.77093470308588));
#71868=CARTESIAN_POINT('Ctrl Pts',(-1.18666820409511,-1.00568326196158,
2.77237994326064));
#71869=CARTESIAN_POINT('Ctrl Pts',(-1.14946026765927,-1.04958721937883,
2.77652753640158));
#71870=CARTESIAN_POINT('Ctrl Pts',(-1.10973421380613,-1.09151588262236,
2.78067512954252));
#71871=CARTESIAN_POINT('Ctrl Pts',(-1.06772786924713,-1.13116641005335,
2.78482272268345));
#71872=CARTESIAN_POINT('Ctrl Pts',(-1.02579635357129,-1.17074630518545,
2.78896292742233));
#71873=CARTESIAN_POINT('Ctrl Pts',(-0.981592985373571,-1.20805576476433,
2.79310313216121));
#71874=CARTESIAN_POINT('Ctrl Pts',(-0.935394673694029,-1.24282623661751,
2.79724333690009));
#71875=CARTESIAN_POINT('Ctrl Pts',(-0.889242412098968,-1.27756204955983,
2.80137941471807));
#71876=CARTESIAN_POINT('Ctrl Pts',(-0.841099560958813,-1.30976357736525,
2.80551549253606));
#71877=CARTESIAN_POINT('Ctrl Pts',(-0.791277263798694,-1.33920145676267,
2.80965157035404));
#71878=CARTESIAN_POINT('Ctrl Pts',(-0.741485463799256,-1.36862131668308,
2.81378511640137));
#71879=CARTESIAN_POINT('Ctrl Pts',(-0.690016703152289,-1.39528061706911,
2.81791866244869));
#71880=CARTESIAN_POINT('Ctrl Pts',(-0.637210522527536,-1.41899365748413,
2.82205220849602));
#71881=CARTESIAN_POINT('Ctrl Pts',(-0.584416353486958,-1.4427013040006,
2.82618481430424));
#71882=CARTESIAN_POINT('Ctrl Pts',(-0.530285843394223,-1.46346380767148,
2.83031742011246));
#71883=CARTESIAN_POINT('Ctrl Pts',(-0.475180504680632,-1.48114271357336,
2.83445002592068));
#71884=CARTESIAN_POINT('Ctrl Pts',(-0.420025304777168,-1.49883761595225,
2.83858637105158));
#71885=CARTESIAN_POINT('Ctrl Pts',(-0.363894010408683,-1.5134431839856,
2.84272271618248));
#71886=CARTESIAN_POINT('Ctrl Pts',(-0.307164078818147,-1.5248706432625,
2.84685906131337));
#71887=CARTESIAN_POINT('Ctrl Pts',(-0.250410771305569,-1.53630281129525,
2.85099711085107));
#71888=CARTESIAN_POINT('Ctrl Pts',(-0.193058851394598,-1.5445541842286,
2.85513516038878));
#71889=CARTESIAN_POINT('Ctrl Pts',(-0.135493559801193,-1.54958760489764,
2.85927320992648));
#71890=CARTESIAN_POINT('Ctrl Pts',(-0.0778156612983488,-1.55463087174186,
2.86341935415035));
#71891=CARTESIAN_POINT('Ctrl Pts',(-0.019924079591581,-1.55644358914889,
2.86756549837421));
#71892=CARTESIAN_POINT('Ctrl Pts',(0.0377941783268421,-1.55504078727363,
2.87171164259808));
#71893=CARTESIAN_POINT('Ctrl Pts',(0.0928761285919074,-1.55370205901136,
2.87566840980082));
#71894=CARTESIAN_POINT('Ctrl Pts',(0.147799846995512,-1.54943528185692,
2.87962517700356));
#71895=CARTESIAN_POINT('Ctrl Pts',(0.20223592217179,-1.54229727412822,2.8835819442063));
#71896=CARTESIAN_POINT('Ctrl Pts',(0.259297326209693,-1.53481501642109,
2.88772953734758));
#71897=CARTESIAN_POINT('Ctrl Pts',(0.316063027217814,-1.52414602651293,
2.89187713048887));
#71898=CARTESIAN_POINT('Ctrl Pts',(0.372149627444133,-1.51032609220433,
2.89602472363015));
#71899=CARTESIAN_POINT('Ctrl Pts',(0.428136316628248,-1.49653077632569,
2.90016492836936));
#71900=CARTESIAN_POINT('Ctrl Pts',(0.483445804533315,-1.47959578054093,
2.90430513310856));
#71901=CARTESIAN_POINT('Ctrl Pts',(0.537702335435016,-1.45960832022421,
2.90844533784777));
#71902=CARTESIAN_POINT('Ctrl Pts',(0.591904783887736,-1.43964078323809,
2.91258141566608));
#71903=CARTESIAN_POINT('Ctrl Pts',(0.645055868486251,-1.41662698921405,
2.91671749348438));
#71904=CARTESIAN_POINT('Ctrl Pts',(0.696794220209838,-1.39070416145281,
2.92085357130269));
#71905=CARTESIAN_POINT('Ctrl Pts',(0.748500901919766,-1.36479720153973,
2.92498711735033));
#71906=CARTESIAN_POINT('Ctrl Pts',(0.79879610012921,-1.33598497050557,2.92912066339797));
#71907=CARTESIAN_POINT('Ctrl Pts',(0.847339755745634,-1.30445221772702,
2.93325420944561));
#71908=CARTESIAN_POINT('Ctrl Pts',(0.895872369355102,-1.27292663756188,
2.93738681525413));
#71909=CARTESIAN_POINT('Ctrl Pts',(0.942653794652543,-1.23868204778156,
2.94151942106265));
#71910=CARTESIAN_POINT('Ctrl Pts',(0.987371775264395,-1.20194726482123,
2.94565202687117));
#71911=CARTESIAN_POINT('Ctrl Pts',(1.03213021823005,-1.16517924297657,2.94978837200235));
#71912=CARTESIAN_POINT('Ctrl Pts',(1.07482108101088,-1.1259168556243,2.95392471713353));
#71913=CARTESIAN_POINT('Ctrl Pts',(1.11516522225963,-1.08442924022853,2.95806106226472));
#71914=CARTESIAN_POINT('Ctrl Pts',(1.15552598756321,-1.04292452960228,2.96219911180269));
#71915=CARTESIAN_POINT('Ctrl Pts',(1.19353776009774,-0.999193156172173,
2.96633716134066));
#71916=CARTESIAN_POINT('Ctrl Pts',(1.22896056361456,-0.953538768525005,
2.97047521087863));
#71917=CARTESIAN_POINT('Ctrl Pts',(1.26445265979554,-0.90779507360014,2.97462135510275));
#71918=CARTESIAN_POINT('Ctrl Pts',(1.29734536823604,-0.860121276720506,
2.97876749932687));
#71919=CARTESIAN_POINT('Ctrl Pts',(1.32744161739779,-0.810850789233342,
2.98291364355099));
#71920=CARTESIAN_POINT('Ctrl Pts',(1.35616320668628,-0.763830753678599,
2.98687041075131));
#71921=CARTESIAN_POINT('Ctrl Pts',(1.38233812416302,-0.715357112159338,
2.99082717795163));
#71922=CARTESIAN_POINT('Ctrl Pts',(1.40583562872532,-0.665737512092028,
2.99478394515196));
#71923=CARTESIAN_POINT('Ctrl Pts',(1.43046636484214,-0.61372487082453,2.99893153829439));
#71924=CARTESIAN_POINT('Ctrl Pts',(1.4522585237969,-0.560233993408507,3.00307913143682));
#71925=CARTESIAN_POINT('Ctrl Pts',(1.47103443589969,-0.50560650549342,3.00722672457926));
#71926=CARTESIAN_POINT('Ctrl Pts',(1.48977690113767,-0.451076329399633,
3.01136692931966));
#71927=CARTESIAN_POINT('Ctrl Pts',(1.50551361623966,-0.395414050122525,
3.01550713406006));
#71928=CARTESIAN_POINT('Ctrl Pts',(1.51811427567436,-0.338982737014302,
3.01964733880046));
#71929=CARTESIAN_POINT('Ctrl Pts',(1.53070237487886,-0.282607674159265,
3.02378341661997));
#71930=CARTESIAN_POINT('Ctrl Pts',(1.54016049888285,-0.225465602079293,
3.02791949443948));
#71931=CARTESIAN_POINT('Ctrl Pts',(1.54640816782067,-0.167934595892287,
3.032055572259));
#71932=CARTESIAN_POINT('Ctrl Pts',(1.55265201244341,-0.110438805510911,
3.03618911830786));
#71933=CARTESIAN_POINT('Ctrl Pts',(1.5556892413464,-0.052555069776979,3.04032266435673));
#71934=CARTESIAN_POINT('Ctrl Pts',(1.55549086583674,0.0053306939939586,
3.0444562104056));
#71935=CARTESIAN_POINT('Ctrl Pts',(1.55529253545068,0.0632032907508674,
3.04858881621536));
#71936=CARTESIAN_POINT('Ctrl Pts',(1.55186006351953,0.121077393943223,3.05272142202512));
#71937=CARTESIAN_POINT('Ctrl Pts',(1.54521656351735,0.178566575348327,3.05685402783489));
#71938=CARTESIAN_POINT('Ctrl Pts',(1.5385670522498,0.236107774925385,3.06099037296732));
#71939=CARTESIAN_POINT('Ctrl Pts',(1.52870076533746,0.293262837779958,3.06512671809976));
#71940=CARTESIAN_POINT('Ctrl Pts',(1.51569264853327,0.349651319434369,3.0692630632322));
#71941=CARTESIAN_POINT('Ctrl Pts',(1.50267917165344,0.406063036314289,3.07340111277144));
#71942=CARTESIAN_POINT('Ctrl Pts',(1.48652142831699,0.461707040531794,3.07753916231068));
#71943=CARTESIAN_POINT('Ctrl Pts',(1.46734459181078,0.516217104408279,3.08167721184993));
#71944=CARTESIAN_POINT('Ctrl Pts',(1.44813024234798,0.570833798680196,3.08582335607531));
#71945=CARTESIAN_POINT('Ctrl Pts',(1.42588519719966,0.624311636572228,3.0899695003007));
#71946=CARTESIAN_POINT('Ctrl Pts',(1.40078289268773,0.676304323181071,3.09411564452609));
#71947=CARTESIAN_POINT('Ctrl Pts',(1.37682714742183,0.725922220035861,3.09807241171659));
#71948=CARTESIAN_POINT('Ctrl Pts',(1.35026975093779,0.774187372099828,3.1020291789071));
#71949=CARTESIAN_POINT('Ctrl Pts',(1.32129842765043,0.820823193561499,3.10598594609761));
#71950=CARTESIAN_POINT('Ctrl Pts',(1.2909298828292,0.869708155435229,3.1101335392393));
#71951=CARTESIAN_POINT('Ctrl Pts',(1.25778081383162,0.917008381459534,3.11428113238098));
#71952=CARTESIAN_POINT('Ctrl Pts',(1.22204207394009,0.962389432361037,3.11842872552267));
#71953=CARTESIAN_POINT('Ctrl Pts',(1.1863669980026,1.00768964277551,3.1225689302623));
#71954=CARTESIAN_POINT('Ctrl Pts',(1.14811172718562,1.05107705788631,3.12670913500193));
#71955=CARTESIAN_POINT('Ctrl Pts',(1.10751080230268,1.09224542699106,3.13084933974157));
#71956=CARTESIAN_POINT('Ctrl Pts',(1.0669503480766,1.13337275981536,3.1349854175603));
#71957=CARTESIAN_POINT('Ctrl Pts',(1.02404923616821,1.17228506001833,3.13912149537904));
#71958=CARTESIAN_POINT('Ctrl Pts',(0.979081617834388,1.20870982275267,3.14325757319777));
#71959=CARTESIAN_POINT('Ctrl Pts',(0.934141525021421,1.24511228920797,3.14739111924586));
#71960=CARTESIAN_POINT('Ctrl Pts',(0.887137837190999,1.27902990927621,3.15152466529394));
#71961=CARTESIAN_POINT('Ctrl Pts',(0.838379197764765,1.31022920542755,3.15565821134203));
#71962=CARTESIAN_POINT('Ctrl Pts',(0.789631649246822,1.34142140481539,3.159790817151));
#71963=CARTESIAN_POINT('Ctrl Pts',(0.739130380193175,1.36989622714469,3.16392342295997));
#71964=CARTESIAN_POINT('Ctrl Pts',(0.687212695546969,1.39546370826298,3.16805602876893));
#71965=CARTESIAN_POINT('Ctrl Pts',(0.63524803400905,1.42105432371016,3.17219237390058));
#71966=CARTESIAN_POINT('Ctrl Pts',(0.581864863608335,1.44373210896724,3.17632871903223));
#71967=CARTESIAN_POINT('Ctrl Pts',(0.527423546018679,1.46335390562402,3.18046506416387));
#71968=CARTESIAN_POINT('Ctrl Pts',(0.472959795544747,1.48298378756443,3.18460311370231));
#71969=CARTESIAN_POINT('Ctrl Pts',(0.417437528561135,1.49955501995419,3.18874116324076));
#71970=CARTESIAN_POINT('Ctrl Pts',(0.361232374303376,1.51297436255713,3.1928792127792));
#71971=CARTESIAN_POINT('Ctrl Pts',(0.304917273782369,1.52641995553859,3.19702535700379));
#71972=CARTESIAN_POINT('Ctrl Pts',(0.247917130813764,1.53670124337833,3.20117150122839));
#71973=CARTESIAN_POINT('Ctrl Pts',(0.190616973613277,1.54377635017852,3.20531764545298));
#71974=CARTESIAN_POINT('Ctrl Pts',(0.135934027218097,1.55052829824982,3.20927441264974));
#71975=CARTESIAN_POINT('Ctrl Pts',(0.0809782871612533,1.55436064168982,
3.21323117984651));
#71976=CARTESIAN_POINT('Ctrl Pts',(0.0260839355377171,1.55528128591161,
3.21718794704327));
#71977=CARTESIAN_POINT('Ctrl Pts',(-0.0314578466786569,1.55624633072482,
3.22133554018506));
#71978=CARTESIAN_POINT('Ctrl Pts',(-0.0891743656713,1.55401572701735,3.22548313332686));
#71979=CARTESIAN_POINT('Ctrl Pts',(-0.146681119937474,1.54856866139474,
3.22963072646865));
#71980=CARTESIAN_POINT('Ctrl Pts',(-0.204085433340574,1.54313129901674,
3.23377093120839));
#71981=CARTESIAN_POINT('Ctrl Pts',(-0.261280209372237,1.53448889598676,
3.23791113594813));
#71982=CARTESIAN_POINT('Ctrl Pts',(-0.317880965569942,1.52267263117465,
3.24205134068788));
#71983=CARTESIAN_POINT('Ctrl Pts',(-0.374425302614842,1.51086814471489,
3.24618741850672));
#71984=CARTESIAN_POINT('Ctrl Pts',(-0.430376285603987,1.49589617047065,
3.25032349632556));
#71985=CARTESIAN_POINT('Ctrl Pts',(-0.485356331049852,1.47783946418744,
3.2544595741444));
#71986=CARTESIAN_POINT('Ctrl Pts',(-0.540302722180867,1.45979381075211,
3.2585931201926));
#71987=CARTESIAN_POINT('Ctrl Pts',(-0.594278859959502,1.43866733041535,
3.26272666624079));
#71988=CARTESIAN_POINT('Ctrl Pts',(-0.646921272169161,1.41459291586486,
3.26686021228899));
#71989=CARTESIAN_POINT('Ctrl Pts',(-0.699551710046281,1.39052397741307,
3.27099281809807));
#71990=CARTESIAN_POINT('Ctrl Pts',(-0.750848551095643,1.36350865247988,
3.27512542390715));
#71991=CARTESIAN_POINT('Ctrl Pts',(-0.800469364159435,1.33372750104442,
3.27925802971623));
#71992=CARTESIAN_POINT('Ctrl Pts',(-0.850135075827078,1.30391940260753,
3.28339437484798));
#71993=CARTESIAN_POINT('Ctrl Pts',(-0.898121280457421,1.27134074407872,
3.28753071997973));
#71994=CARTESIAN_POINT('Ctrl Pts',(-0.944112392095885,1.23621682608311,
3.29166706511148));
#71995=CARTESIAN_POINT('Ctrl Pts',(-0.990122454658598,1.20107843505813,
3.29580511465003));
#71996=CARTESIAN_POINT('Ctrl Pts',(-1.03413538790551,1.16339303229937,3.29994316418858));
#71997=CARTESIAN_POINT('Ctrl Pts',(-1.07586928763052,1.12342579903321,3.30408121372713));
#71998=CARTESIAN_POINT('Ctrl Pts',(-1.11768482553238,1.08338038347209,3.30822735795182));
#71999=CARTESIAN_POINT('Ctrl Pts',(-1.15721206300446,1.04104459865491,3.31237350217652));
#72000=CARTESIAN_POINT('Ctrl Pts',(-1.19420717299843,0.996719357672504,
3.31651964640121));
#72001=CARTESIAN_POINT('Ctrl Pts',(-1.22951251446752,0.954418692291638,
3.32047641359712));
#72002=CARTESIAN_POINT('Ctrl Pts',(-1.26251183707756,0.910306733284846,
3.32443318079302));
#72003=CARTESIAN_POINT('Ctrl Pts',(-1.29303070491053,0.864668633731202,
3.32838994798892));
#72004=CARTESIAN_POINT('Ctrl Pts',(-1.32557770694717,0.815997650022029,
3.33260966251727));
#72005=CARTESIAN_POINT('Ctrl Pts',(-1.35543705041063,0.765390969309646,
3.33682937704562));
#72006=CARTESIAN_POINT('Ctrl Pts',(-1.38237733416478,0.713171196829676,
3.34104909157397));
#72007=CARTESIAN_POINT('Ctrl Pts',(-1.41057883180484,0.658506746974681,
3.34546635274312));
#72008=CARTESIAN_POINT('Ctrl Pts',(-1.43558082164121,0.602074834659629,
3.34988361391226));
#72009=CARTESIAN_POINT('Ctrl Pts',(-1.45716801087107,0.544280844871521,
3.3543008750814));
#72010=CARTESIAN_POINT('Ctrl Pts',(-1.4777184304184,0.489262531703761,3.35850598809123));
#72011=CARTESIAN_POINT('Ctrl Pts',(-1.49517431711702,0.433010500479543,
3.36271110110106));
#72012=CARTESIAN_POINT('Ctrl Pts',(-1.50939742874429,0.375898459826751,
3.36691621411088));
#72013=CARTESIAN_POINT('Ctrl Pts',(-1.52360699435621,0.318840812375658,
3.3711173221936));
#72014=CARTESIAN_POINT('Ctrl Pts',(-1.53458977591059,0.26092526186512,3.37531843027631));
#72015=CARTESIAN_POINT('Ctrl Pts',(-1.5422572513629,0.202540910974892,3.37951953835902));
#72016=CARTESIAN_POINT('Ctrl Pts',(-1.54991969604829,0.14419486709509,3.38371789002005));
#72017=CARTESIAN_POINT('Ctrl Pts',(-1.55427109154466,0.0853811260470057,
3.38791624168107));
#72018=CARTESIAN_POINT('Ctrl Pts',(-1.55527429853346,0.0264972889417979,
3.3921145933421));
#72019=CARTESIAN_POINT('Ctrl Pts',(-1.55542895121716,0.0174198567301612,
3.39276180409596));
#72020=CARTESIAN_POINT('Ctrl Pts',(-1.5555041352991,0.00834076823806055,
3.39340901484983));
#72021=CARTESIAN_POINT('Ctrl Pts',(-1.55549982468662,-0.000738511954293953,
3.3940562256037));
#72022=CARTESIAN_POINT('',(-1.55549947476597,0.00127828118742131,3.25533856168564));
#72023=CARTESIAN_POINT('Ctrl Pts',(-1.55549999398642,0.000136778059410365,
2.55740452554354));
#72024=CARTESIAN_POINT('Ctrl Pts',(-1.55550066677956,-0.00751452008594075,
2.55795452808491));
#72025=CARTESIAN_POINT('Ctrl Pts',(-1.55544488600269,-0.0151659363071791,
2.55850137101385));
#72026=CARTESIAN_POINT('Ctrl Pts',(-1.55512972380064,-0.0366492764225271,
2.56002866939962));
#72027=CARTESIAN_POINT('Ctrl Pts',(-1.55474227162549,-0.0504790145162955,
2.5610024208821));
#72028=CARTESIAN_POINT('Ctrl Pts',(-1.5507605366209,-0.14671644808943,2.5677243704524));
#72029=CARTESIAN_POINT('Ctrl Pts',(-1.54080024390489,-0.228740829829826,
2.5731811021714));
#72030=CARTESIAN_POINT('Ctrl Pts',(-1.50221506830842,-0.418724185891338,
2.58595363659456));
#72031=CARTESIAN_POINT('Ctrl Pts',(-1.4684010507505,-0.525142967947681,
2.59323359772228));
#72032=CARTESIAN_POINT('Ctrl Pts',(-1.41401818085348,-0.648604910160357,
2.60251882338264));
#72033=CARTESIAN_POINT('Ctrl Pts',(-1.40402879760403,-0.669954311443345,
2.60415556407635));
#72034=CARTESIAN_POINT('Ctrl Pts',(-1.38752070105268,-0.703243386997612,
2.60676216209202));
#72035=CARTESIAN_POINT('Ctrl Pts',(-1.38132357394818,-0.715339164546512,
2.60772089505095));
#72036=CARTESIAN_POINT('Ctrl Pts',(-1.36943494295856,-0.737813154368939,
2.60952497419714));
#72037=CARTESIAN_POINT('Ctrl Pts',(-1.36378189974084,-0.748210685224179,
2.61036891130377));
#72038=CARTESIAN_POINT('Ctrl Pts',(-1.35079292373463,-0.771464718384139,
2.61227796885413));
#72039=CARTESIAN_POINT('Ctrl Pts',(-1.34339110705816,-0.784282882557667,
2.61334539532601));
#72040=CARTESIAN_POINT('Ctrl Pts',(-1.32017086496893,-0.823201387824557,
2.61663409906608));
#72041=CARTESIAN_POINT('Ctrl Pts',(-1.30376717518654,-0.848942017646318,
2.61887631537352));
#72042=CARTESIAN_POINT('Ctrl Pts',(-1.26316368376271,-0.908702099935163,
2.62424698580593));
#72043=CARTESIAN_POINT('Ctrl Pts',(-1.23833144776733,-0.942261479662191,
2.62739632774339));
#72044=CARTESIAN_POINT('Ctrl Pts',(-1.17192749556495,-1.02483776366739,
2.63548418697364));
#72045=CARTESIAN_POINT('Ctrl Pts',(-1.12861297157979,-1.07235179214764,
2.64046610377546));
#72046=CARTESIAN_POINT('Ctrl Pts',(-1.03031144500876,-1.16761191090088,
2.65107908546627));
#72047=CARTESIAN_POINT('Ctrl Pts',(-0.974650843652776,-1.21446161680688,
2.65669755866666));
#72048=CARTESIAN_POINT('Ctrl Pts',(-0.902685969855538,-1.26688836512334,
2.66334302505764));
#72049=CARTESIAN_POINT('Ctrl Pts',(-0.889306135304163,-1.27631608304539,
2.66455406797432));
#72050=CARTESIAN_POINT('Ctrl Pts',(-0.869032337807875,-1.29012778230562,
2.66634991564225));
#72051=CARTESIAN_POINT('Ctrl Pts',(-0.862249079867954,-1.29467116717456,
2.666944339601));
#72052=CARTESIAN_POINT('Ctrl Pts',(-0.85040903911395,-1.30246721974515,
2.66797035125066));
#72053=CARTESIAN_POINT('Ctrl Pts',(-0.845368866448033,-1.30574418438921,
2.66840349604331));
#72054=CARTESIAN_POINT('Ctrl Pts',(-0.833298791917207,-1.31349258802845,
2.66943225002405));
#72055=CARTESIAN_POINT('Ctrl Pts',(-0.826251799324381,-1.31793688314205,
2.67002609142558));
#72056=CARTESIAN_POINT('Ctrl Pts',(-0.804514817460219,-1.33140276606742,
2.67183823325247));
#72057=CARTESIAN_POINT('Ctrl Pts',(-0.789709712342323,-1.34023731161851,
2.67304527615289));
#72058=CARTESIAN_POINT('Ctrl Pts',(-0.754108225941177,-1.36068668109432,
2.67589132368899));
#72059=CARTESIAN_POINT('Ctrl Pts',(-0.733185544818253,-1.3720738120714,
2.67751909735938));
#72060=CARTESIAN_POINT('Ctrl Pts',(-0.649251437632802,-1.41528625398166,
2.68390676129007));
#72061=CARTESIAN_POINT('Ctrl Pts',(-0.584363617661553,-1.44328899831511,
2.68853614528891));
#72062=CARTESIAN_POINT('Ctrl Pts',(-0.430403580540948,-1.49763876101227,
2.6992837319135));
#72063=CARTESIAN_POINT('Ctrl Pts',(-0.340440968283687,-1.52061378958834,
2.7054006977874));
#72064=CARTESIAN_POINT('Ctrl Pts',(-0.225074329439661,-1.53932063899589,
2.71343753695664));
#72065=CARTESIAN_POINT('Ctrl Pts',(-0.201088200458417,-1.54263732278657,
2.71511779170382));
#72066=CARTESIAN_POINT('Ctrl Pts',(-0.163396438537252,-1.54695517694606,
2.71777805227307));
#72067=CARTESIAN_POINT('Ctrl Pts',(-0.149737681512893,-1.54833695325033,
2.71874613601522));
#72068=CARTESIAN_POINT('Ctrl Pts',(-0.124285577097147,-1.55057186802312,
2.72055854671853));
#72069=CARTESIAN_POINT('Ctrl Pts',(-0.112497248359295,-1.55147168118908,
2.72140134261587));
#72070=CARTESIAN_POINT('Ctrl Pts',(-0.0861154641478392,-1.55318317776514,
2.72329557210615));
#72071=CARTESIAN_POINT('Ctrl Pts',(-0.0715186968300371,-1.55392371298778,
2.72434915684566));
#72072=CARTESIAN_POINT('Ctrl Pts',(-0.0274368483683089,-1.55553770231681,
2.7275487263976));
#72073=CARTESIAN_POINT('Ctrl Pts',(0.00206316530907804,-1.55577821332288,
2.72971401967982));
#72074=CARTESIAN_POINT('Ctrl Pts',(0.103148066050718,-1.55372747290761,
2.73722096485802));
#72075=CARTESIAN_POINT('Ctrl Pts',(0.174550679077534,-1.54733261192267,
2.74267898537828));
#72076=CARTESIAN_POINT('Ctrl Pts',(0.334405274658064,-1.52180962946239,
2.75517629248939));
#72077=CARTESIAN_POINT('Ctrl Pts',(0.42215254603717,-1.49983981473869,2.76223737825773));
#72078=CARTESIAN_POINT('Ctrl Pts',(0.534978008388259,-1.46089826797665,
2.77129447765354));
#72079=CARTESIAN_POINT('Ctrl Pts',(0.562186723515036,-1.45064522697536,
2.77347568542298));
#72080=CARTESIAN_POINT('Ctrl Pts',(0.598745281613202,-1.43568557815522,
2.77638827694897));
#72081=CARTESIAN_POINT('Ctrl Pts',(0.608356855410751,-1.43163925064063,
2.77715227513264));
#72082=CARTESIAN_POINT('Ctrl Pts',(0.623655573244839,-1.42501681985392,
2.77836471086829));
#72083=CARTESIAN_POINT('Ctrl Pts',(0.629368953979372,-1.42250270103646,
2.77881668628916));
#72084=CARTESIAN_POINT('Ctrl Pts',(0.641545977332521,-1.41705659021329,
2.77977800648085));
#72085=CARTESIAN_POINT('Ctrl Pts',(0.648005038399275,-1.41411459808982,
2.7802867179991));
#72086=CARTESIAN_POINT('Ctrl Pts',(0.66464901454116,-1.40639556368957,2.7815950521461));
#72087=CARTESIAN_POINT('Ctrl Pts',(0.674802871338014,-1.4015519606559,2.78239074623073));
#72088=CARTESIAN_POINT('Ctrl Pts',(0.720607227504908,-1.379089117413,2.78597294660997));
#72089=CARTESIAN_POINT('Ctrl Pts',(0.755629815717988,-1.36021534078926,
2.78869212282522));
#72090=CARTESIAN_POINT('Ctrl Pts',(0.868272761519911,-1.29381627328179,
2.79749913649785));
#72091=CARTESIAN_POINT('Ctrl Pts',(0.942451140986418,-1.24082467600295,
2.80340733545588));
#72092=CARTESIAN_POINT('Ctrl Pts',(1.06849598321466,-1.13292145742947,2.81438416256689));
#72093=CARTESIAN_POINT('Ctrl Pts',(1.12181490289742,-1.08014994603771,2.81940104834758));
#72094=CARTESIAN_POINT('Ctrl Pts',(1.18433486489243,-1.00862992407715,2.8259756026149));
#72095=CARTESIAN_POINT('Ctrl Pts',(1.19725496627948,-0.993259219626242,
2.82737621466455));
#72096=CARTESIAN_POINT('Ctrl Pts',(1.2178782538717,-0.967737061446407,2.82968498058656));
#72097=CARTESIAN_POINT('Ctrl Pts',(1.22576087397562,-0.957733117215039,
2.83058585250302));
#72098=CARTESIAN_POINT('Ctrl Pts',(1.2408651223291,-0.938072161336295,2.83234918312583));
#72099=CARTESIAN_POINT('Ctrl Pts',(1.24809907014167,-0.928425725467489,
2.83321107102667));
#72100=CARTESIAN_POINT('Ctrl Pts',(1.26499258002281,-0.905344030031443,
2.83526628443137));
#72101=CARTESIAN_POINT('Ctrl Pts',(1.27455115790333,-0.891837062931261,
2.83646338717477));
#72102=CARTESIAN_POINT('Ctrl Pts',(1.30730244554708,-0.843954978902197,
2.8406894778553));
#72103=CARTESIAN_POINT('Ctrl Pts',(1.32933265301186,-0.808810113314039,
2.84376073671328));
#72104=CARTESIAN_POINT('Ctrl Pts',(1.38272092575624,-0.715554839641528,
2.85183698587778));
#72105=CARTESIAN_POINT('Ctrl Pts',(1.41182924184471,-0.656256404518643,
2.85690516928635));
#72106=CARTESIAN_POINT('Ctrl Pts',(1.47492623802638,-0.503935962714824,
2.86966857722658));
#72107=CARTESIAN_POINT('Ctrl Pts',(1.50397528371496,-0.40917017445148,2.87739430262341));
#72108=CARTESIAN_POINT('Ctrl Pts',(1.52684922231614,-0.297552931621444,
2.88588148259573));
#72109=CARTESIAN_POINT('Ctrl Pts',(1.52965405030364,-0.28278052526185,2.88699236380233));
#72110=CARTESIAN_POINT('Ctrl Pts',(1.53362113569536,-0.260096771705943,
2.8886769669872));
#72111=CARTESIAN_POINT('Ctrl Pts',(1.5349372466382,-0.252213748510286,2.88925849472302));
#72112=CARTESIAN_POINT('Ctrl Pts',(1.53724467080977,-0.237705571874942,
2.89032116725107));
#72113=CARTESIAN_POINT('Ctrl Pts',(1.53825399282406,-0.231083909729386,
2.89080323568961));
#72114=CARTESIAN_POINT('Ctrl Pts',(1.5405097763891,-0.21561470491729,2.89192275849157));
#72115=CARTESIAN_POINT('Ctrl Pts',(1.54172283011084,-0.206762659752222,
2.89255836727252));
#72116=CARTESIAN_POINT('Ctrl Pts',(1.54548509465893,-0.177431507639867,
2.89464932927137));
#72117=CARTESIAN_POINT('Ctrl Pts',(1.5477031746557,-0.156911142221963,2.89608784830627));
#72118=CARTESIAN_POINT('Ctrl Pts',(1.55218843318401,-0.105940194308941,
2.89961446193309));
#72119=CARTESIAN_POINT('Ctrl Pts',(1.5539688142981,-0.0754547455868742,
2.90168275320559));
#72120=CARTESIAN_POINT('Ctrl Pts',(1.55849862962008,0.0812875922889848,
2.91219620116184));
#72121=CARTESIAN_POINT('Ctrl Pts',(1.54676377354634,0.207483869094535,2.92029866090758));
#72122=CARTESIAN_POINT('Ctrl Pts',(1.51125711902438,0.370585557176765,2.93157176474556));
#72123=CARTESIAN_POINT('Ctrl Pts',(1.50106063534625,0.409936877928736,2.9343517461041));
#72124=CARTESIAN_POINT('Ctrl Pts',(1.48448020982984,0.464953700068905,2.93835155572542));
#72125=CARTESIAN_POINT('Ctrl Pts',(1.4793634549305,0.480985619414882,2.93953089575813));
#72126=CARTESIAN_POINT('Ctrl Pts',(1.47015904366596,0.508287587206274,2.94156473538278));
#72127=CARTESIAN_POINT('Ctrl Pts',(1.46619927875229,0.519599408557588,2.94241497815045));
#72128=CARTESIAN_POINT('Ctrl Pts',(1.45780303707786,0.542724392656266,2.94416936406522));
#72129=CARTESIAN_POINT('Ctrl Pts',(1.45335274509936,0.554531552081247,2.94507391356647));
#72130=CARTESIAN_POINT('Ctrl Pts',(1.44165981417089,0.584446356844289,2.94738887558736));
#72131=CARTESIAN_POINT('Ctrl Pts',(1.43421956947114,0.60247383859173,2.94880581323711));
#72132=CARTESIAN_POINT('Ctrl Pts',(1.39785350793337,0.686093739276635,2.95548442006801));
#72133=CARTESIAN_POINT('Ctrl Pts',(1.364758656916,0.7497666850119,2.96088506695034));
#72134=CARTESIAN_POINT('Ctrl Pts',(1.31268204102985,0.835010683626217,2.96854818384035));
#72135=CARTESIAN_POINT('Ctrl Pts',(1.29731434304312,0.85869225689098,2.9707264005899));
#72136=CARTESIAN_POINT('Ctrl Pts',(1.22462154754005,0.96430249328216,2.98064993055986));
#72137=CARTESIAN_POINT('Ctrl Pts',(1.16011906811862,1.04101106038503,2.98846446751961));
#72138=CARTESIAN_POINT('Ctrl Pts',(1.07803053308083,1.12145145076103,2.99702410884487));
#72139=CARTESIAN_POINT('Ctrl Pts',(1.06721572046666,1.1317481327949,2.99812715855436));
#72140=CARTESIAN_POINT('Ctrl Pts',(1.05040326888894,1.14729975980074,2.99980240142664));
#72141=CARTESIAN_POINT('Ctrl Pts',(1.04451105612193,1.1526666592142,3.00038227438098));
#72142=CARTESIAN_POINT('Ctrl Pts',(1.03358898230614,1.16246246041332,3.00144348733738));
#72143=CARTESIAN_POINT('Ctrl Pts',(1.0285715728754,1.16690431422159,3.00192573017348));
#72144=CARTESIAN_POINT('Ctrl Pts',(1.0167734474811,1.17721383083758,3.00304767886981));
#72145=CARTESIAN_POINT('Ctrl Pts',(1.00997048562823,1.18305548285214,3.00368551109597));
#72146=CARTESIAN_POINT('Ctrl Pts',(0.987197401696555,1.20227094226485,3.00579216531965));
#72147=CARTESIAN_POINT('Ctrl Pts',(0.971008416489164,1.21538343417404,3.00724380511885));
#72148=CARTESIAN_POINT('Ctrl Pts',(0.930136327124901,1.24715015686346,3.01081050752392));
#72149=CARTESIAN_POINT('Ctrl Pts',(0.905150316694884,1.26540122104497,3.01290517853364));
#72150=CARTESIAN_POINT('Ctrl Pts',(0.770903718344337,1.35744922297951,3.02381341498146));
#72151=CARTESIAN_POINT('Ctrl Pts',(0.653137773882393,1.4178765751256,3.03226054165568));
#72152=CARTESIAN_POINT('Ctrl Pts',(0.49511419470183,1.47504332771572,3.04365665765363));
#72153=CARTESIAN_POINT('Ctrl Pts',(0.460653535675166,1.48616582802963,3.04614157739441));
#72154=CARTESIAN_POINT('Ctrl Pts',(0.411885177842958,1.5000471042921,3.04967630261994));
#72155=CARTESIAN_POINT('Ctrl Pts',(0.397877545711802,1.50382317729253,3.0506935762601));
#72156=CARTESIAN_POINT('Ctrl Pts',(0.37214058149244,1.51037640310508,3.05256748583295));
#72157=CARTESIAN_POINT('Ctrl Pts',(0.360427753703246,1.51321423168955,3.05342210538286));
#72158=CARTESIAN_POINT('Ctrl Pts',(0.336490771335413,1.51872009825405,3.05517294093227));
#72159=CARTESIAN_POINT('Ctrl Pts',(0.324265064788769,1.52137731246451,3.05606943414939));
#72160=CARTESIAN_POINT('Ctrl Pts',(0.293420348508984,1.52769262964377,3.05833758590178));
#72161=CARTESIAN_POINT('Ctrl Pts',(0.274764457423025,1.53115796225464,3.05971524869403));
#72162=CARTESIAN_POINT('Ctrl Pts',(0.192727491827976,1.54484881348478,3.06580150307484));
#72163=CARTESIAN_POINT('Ctrl Pts',(0.128819709276032,1.55148483181308,3.070619759824));
#72164=CARTESIAN_POINT('Ctrl Pts',(-0.0340268311751895,1.55826338465152,
3.08307355389477));
#72165=CARTESIAN_POINT('Ctrl Pts',(-0.132905830901143,1.5529574776016,3.09081017326475));
#72166=CARTESIAN_POINT('Ctrl Pts',(-0.273817259753969,1.53183327443442,
3.10174400677911));
#72167=CARTESIAN_POINT('Ctrl Pts',(-0.316736965535675,1.52353783377184,
3.10505845832463));
#72168=CARTESIAN_POINT('Ctrl Pts',(-0.370831151647846,1.51069721702341,
3.10917265223417));
#72169=CARTESIAN_POINT('Ctrl Pts',(-0.382376537511689,1.5078163121503,3.1100469970095));
#72170=CARTESIAN_POINT('Ctrl Pts',(-0.40088967848638,1.5029704239286,3.11144175913816));
#72171=CARTESIAN_POINT('Ctrl Pts',(-0.407878485003016,1.50108886370351,
3.11196661411289));
#72172=CARTESIAN_POINT('Ctrl Pts',(-0.421571009292349,1.49729980497505,
3.11299128119691));
#72173=CARTESIAN_POINT('Ctrl Pts',(-0.428275460830389,1.49539591908275,
3.1134912599735));
#72174=CARTESIAN_POINT('Ctrl Pts',(-0.445179855151272,1.49047250773447,
3.11474800438157));
#72175=CARTESIAN_POINT('Ctrl Pts',(-0.455362292910664,1.48739322258794,
3.11550142380806));
#72176=CARTESIAN_POINT('Ctrl Pts',(-0.497334160288804,1.4742290187605,3.11859526534472));
#72177=CARTESIAN_POINT('Ctrl Pts',(-0.528829243104645,1.46322673847797,
3.12088889189161));
#72178=CARTESIAN_POINT('Ctrl Pts',(-0.619990830119003,1.42805230071179,
3.12751249065167));
#72179=CARTESIAN_POINT('Ctrl Pts',(-0.678541556288328,1.40117969116268,
3.13174881750846));
#72180=CARTESIAN_POINT('Ctrl Pts',(-0.824199000176661,1.32305015840969,
3.14262881113184));
#72181=CARTESIAN_POINT('Ctrl Pts',(-0.908271736794991,1.26680903863619,
3.14926055087571));
#72182=CARTESIAN_POINT('Ctrl Pts',(-1.00506785920549,1.18743750937835,3.15786773475718));
#72183=CARTESIAN_POINT('Ctrl Pts',(-1.02347086873527,1.17161278202752,3.15955183429557));
#72184=CARTESIAN_POINT('Ctrl Pts',(-1.05170116182092,1.14616478498989,3.1622168343793));
#72185=CARTESIAN_POINT('Ctrl Pts',(-1.06178433133578,1.13683026888804,3.16318574119065));
#72186=CARTESIAN_POINT('Ctrl Pts',(-1.08031010434405,1.11921851318366,3.16499890037722));
#72187=CARTESIAN_POINT('Ctrl Pts',(-1.08878461570736,1.11097616907149,3.16584161104774));
#72188=CARTESIAN_POINT('Ctrl Pts',(-1.10690567057418,1.09294507688949,3.16767318785373));
#72189=CARTESIAN_POINT('Ctrl Pts',(-1.11651801054958,1.08312354524126,3.16866346606241));
#72190=CARTESIAN_POINT('Ctrl Pts',(-1.14476824736488,1.05348281297292,3.17163127472119));
#72191=CARTESIAN_POINT('Ctrl Pts',(-1.16301677298507,1.03330159741598,3.17362504240296));
#72192=CARTESIAN_POINT('Ctrl Pts',(-1.20425022545421,0.985224537130244,
3.17831646419471));
#72193=CARTESIAN_POINT('Ctrl Pts',(-1.22681002964438,0.956986303982907,
3.18102900277771));
#72194=CARTESIAN_POINT('Ctrl Pts',(-1.30975983730283,0.845399322573014,
3.19158183578564));
#72195=CARTESIAN_POINT('Ctrl Pts',(-1.36280402610939,0.756923228062467,
3.19962943570454));
#72196=CARTESIAN_POINT('Ctrl Pts',(-1.4286109880124,0.617480513162525,3.21150716946423));
#72197=CARTESIAN_POINT('Ctrl Pts',(-1.44819793151959,0.570031066384954,
3.21541704128836));
#72198=CARTESIAN_POINT('Ctrl Pts',(-1.46954440868428,0.510070346638533,
3.22013153937928));
#72199=CARTESIAN_POINT('Ctrl Pts',(-1.47354481131869,0.498395668327471,
3.22103906356265));
#72200=CARTESIAN_POINT('Ctrl Pts',(-1.47970023587389,0.479709527938183,
3.2224737523592));
#72201=CARTESIAN_POINT('Ctrl Pts',(-1.481945244217,0.472728588445855,3.22300579498135));
#72202=CARTESIAN_POINT('Ctrl Pts',(-1.48620882975001,0.459141882683332,
3.22403330146045));
#72203=CARTESIAN_POINT('Ctrl Pts',(-1.48823290217871,0.452538159151741,
3.22452904114376));
#72204=CARTESIAN_POINT('Ctrl Pts',(-1.49317118369247,0.436035033926161,
3.22575926801548));
#72205=CARTESIAN_POINT('Ctrl Pts',(-1.49603106785679,0.426119459694168,
3.22649070193102));
#72206=CARTESIAN_POINT('Ctrl Pts',(-1.50204147877787,0.404473903453057,
3.22807215182909));
#72207=CARTESIAN_POINT('Ctrl Pts',(-1.50515375825844,0.392733915449799,
3.22892020866478));
#72208=CARTESIAN_POINT('Ctrl Pts',(-1.53948062599013,0.256841540014063,
3.23863820370184));
#72209=CARTESIAN_POINT('Ctrl Pts',(-1.55539425379136,0.129318318352997,
3.24684545811903));
#72210=CARTESIAN_POINT('Ctrl Pts',(-1.55549947476597,0.00127828118742131,
3.25533856168564));
#72211=CARTESIAN_POINT('Ctrl Pts',(-1.55549947598823,0.00127679299616906,
3.25533866039979));
#72212=CARTESIAN_POINT('Ctrl Pts',(-1.55549982533167,0.000851192647130529,
3.25536689116748));
#72213=CARTESIAN_POINT('Ctrl Pts',(-1.55550000000001,0.000425594936828899,
3.25539512411182));
#72214=CARTESIAN_POINT('Ctrl Pts',(-1.5555,-2.78355693781297E-11,3.25542335925836));
#72215=CARTESIAN_POINT('Origin',(0.,0.,-1.2940562256037));
#72216=CARTESIAN_POINT('',(-1.5555,3.27936543916168E-11,4.09298010292487));
#72217=CARTESIAN_POINT('',(-1.55549973205853,-0.000912999512362819,3.95473109552063));
#72218=CARTESIAN_POINT('',(-1.5555,-1.46451138874614E-13,-1.2940562256037));
#72219=CARTESIAN_POINT('Ctrl Pts',(-1.5555,3.27936543916168E-11,4.09298010292487));
#72220=CARTESIAN_POINT('Ctrl Pts',(-1.55549999999797,0.0961723718999923,
4.0865093943148));
#72221=CARTESIAN_POINT('Ctrl Pts',(-1.54658104654986,0.19214252460412,4.08027899656591));
#72222=CARTESIAN_POINT('Ctrl Pts',(-1.5160184056625,0.355132423876049,4.0692864656076));
#72223=CARTESIAN_POINT('Ctrl Pts',(-1.4986013139837,0.422638307704138,4.06460887058734));
#72224=CARTESIAN_POINT('Ctrl Pts',(-1.47058125802744,0.507299717203055,
4.05843293558878));
#72225=CARTESIAN_POINT('Ctrl Pts',(-1.46409136710595,0.525736291991427,
4.05706892840103));
#72226=CARTESIAN_POINT('Ctrl Pts',(-1.45291589980749,0.555670429162924,
4.05482015705476));
#72227=CARTESIAN_POINT('Ctrl Pts',(-1.44843687620198,0.567243190624775,
4.05394229765395));
#72228=CARTESIAN_POINT('Ctrl Pts',(-1.43945027808374,0.589661829440032,
4.05222449354026));
#72229=CARTESIAN_POINT('Ctrl Pts',(-1.43495736839511,0.600512708519122,
4.05138509259346));
#72230=CARTESIAN_POINT('Ctrl Pts',(-1.42401722826071,0.626110371663382,
4.04938538850006));
#72231=CARTESIAN_POINT('Ctrl Pts',(-1.41746325999352,0.640809748848823,
4.04822151416309));
#72232=CARTESIAN_POINT('Ctrl Pts',(-1.39382744592283,0.691683129952188,
4.04413732687073));
#72233=CARTESIAN_POINT('Ctrl Pts',(-1.37558060494067,0.727294966522605,
4.04117766697035));
#72234=CARTESIAN_POINT('Ctrl Pts',(-1.32527484197728,0.816795404353789,
4.03347186927593));
#72235=CARTESIAN_POINT('Ctrl Pts',(-1.29129572384702,0.869518282893116,
4.02866908328488));
#72236=CARTESIAN_POINT('Ctrl Pts',(-1.19446380387038,1.00152268546568,4.016007762852));
#72237=CARTESIAN_POINT('Ctrl Pts',(-1.12689419921254,1.07698813317372,4.00809764905098));
#72238=CARTESIAN_POINT('Ctrl Pts',(-1.03977283005922,1.15704383364694,3.99925028601655));
#72239=CARTESIAN_POINT('Ctrl Pts',(-1.02687358290104,1.16850703075635,3.99797142028373));
#72240=CARTESIAN_POINT('Ctrl Pts',(-1.00747199783853,1.18517919299813,3.99609662136178));
#72241=CARTESIAN_POINT('Ctrl Pts',(-1.00111477980536,1.19055396855765,3.99548985595854));
#72242=CARTESIAN_POINT('Ctrl Pts',(-0.989716231450383,1.2000351241053,3.99441572401816));
#72243=CARTESIAN_POINT('Ctrl Pts',(-0.984691950335508,1.20416123738632,
3.99394699498987));
#72244=CARTESIAN_POINT('Ctrl Pts',(-0.973384553336077,1.2133291595659,3.99290261887856));
#72245=CARTESIAN_POINT('Ctrl Pts',(-0.967087977612545,1.21835380301992,
3.99232816884416));
#72246=CARTESIAN_POINT('Ctrl Pts',(-0.947823887904936,1.23348302408408,
3.99059116742359));
#72247=CARTESIAN_POINT('Ctrl Pts',(-0.934734483940863,1.24343153977477,
3.98943882914256));
#72248=CARTESIAN_POINT('Ctrl Pts',(-0.90338067449584,1.26648680592147,3.98673721904535));
#72249=CARTESIAN_POINT('Ctrl Pts',(-0.884984700595165,1.27940910719654,
3.98519788141716));
#72250=CARTESIAN_POINT('Ctrl Pts',(-0.813195164333619,1.32754820574574,
3.9793368882468));
#72251=CARTESIAN_POINT('Ctrl Pts',(-0.757926064274728,1.35986023703415,
3.9751261010072));
#72252=CARTESIAN_POINT('Ctrl Pts',(-0.609082211501665,1.43497685278604,
3.96415378350199));
#72253=CARTESIAN_POINT('Ctrl Pts',(-0.51299250989561,1.47206496064522,3.95740658000145));
#72254=CARTESIAN_POINT('Ctrl Pts',(-0.390988362417942,1.5057476387048,3.94869955841954));
#72255=CARTESIAN_POINT('Ctrl Pts',(-0.367881609119759,1.51155908518508,
3.94704571324467));
#72256=CARTESIAN_POINT('Ctrl Pts',(-0.331551877907083,1.51981382502132,
3.94443288756169));
#72257=CARTESIAN_POINT('Ctrl Pts',(-0.318414589652544,1.52262038582644,
3.94348553286073));
#72258=CARTESIAN_POINT('Ctrl Pts',(-0.293953463955743,1.52751568510971,
3.94171606521265));
#72259=CARTESIAN_POINT('Ctrl Pts',(-0.282639519677632,1.5296495337313,3.94089545744011));
#72260=CARTESIAN_POINT('Ctrl Pts',(-0.257370779052741,1.53412539738197,
3.93905732226748));
#72261=CARTESIAN_POINT('Ctrl Pts',(-0.243405773758763,1.53640296064816,
3.93803782005983));
#72262=CARTESIAN_POINT('Ctrl Pts',(-0.201535766674934,1.54264641164664,
3.93496926788953));
#72263=CARTESIAN_POINT('Ctrl Pts',(-0.173553444326004,1.54604451009725,
3.93290268568777));
#72264=CARTESIAN_POINT('Ctrl Pts',(-0.081877620771733,1.55465729680042,
3.92607635915011));
#72265=CARTESIAN_POINT('Ctrl Pts',(-0.0179593145520292,1.55670771324327,
3.9212262033976));
#72266=CARTESIAN_POINT('Ctrl Pts',(0.153773987858308,1.55163828903036,3.90800325951898));
#72267=CARTESIAN_POINT('Ctrl Pts',(0.261025946268553,1.53723582719364,3.89952528091339));
#72268=CARTESIAN_POINT('Ctrl Pts',(0.388697071536212,1.50633456344946,3.88961783538915));
#72269=CARTESIAN_POINT('Ctrl Pts',(0.411344012874213,1.50030846299012,3.88786887178004));
#72270=CARTESIAN_POINT('Ctrl Pts',(0.442947721905521,1.49112955932365,3.88544791612991));
#72271=CARTESIAN_POINT('Ctrl Pts',(0.452023776008327,1.48840336102673,3.88475497358671));
#72272=CARTESIAN_POINT('Ctrl Pts',(0.467404321649869,1.48362979684451,3.88358528893068));
#72273=CARTESIAN_POINT('Ctrl Pts',(0.473721567440397,1.48162480328825,3.88310620216603));
#72274=CARTESIAN_POINT('Ctrl Pts',(0.487006278791073,1.47731478885378,3.88210174829763));
#72275=CARTESIAN_POINT('Ctrl Pts',(0.493970510288702,1.47500075994025,3.88157690080123));
#72276=CARTESIAN_POINT('Ctrl Pts',(0.513139613029507,1.46848038105032,3.88013631415919));
#72277=CARTESIAN_POINT('Ctrl Pts',(0.525309235761293,1.46417114009887,3.87922631281039));
#72278=CARTESIAN_POINT('Ctrl Pts',(0.618344789530839,1.42991807285091,3.87229424768459));
#72279=CARTESIAN_POINT('Ctrl Pts',(0.696660204834102,1.39344353793524,3.86659896100625));
#72280=CARTESIAN_POINT('Ctrl Pts',(0.866552692998655,1.29639329700604,3.85371511181484));
#72281=CARTESIAN_POINT('Ctrl Pts',(0.955547501503209,1.2322641084535,3.84655613748701));
#72282=CARTESIAN_POINT('Ctrl Pts',(1.05460928615685,1.14364896646002,3.83740891282686));
#72283=CARTESIAN_POINT('Ctrl Pts',(1.07178429223863,1.12756908207228,3.83577528834192));
#72284=CARTESIAN_POINT('Ctrl Pts',(1.09813740297661,1.10175008206707,3.83318739791945));
#72285=CARTESIAN_POINT('Ctrl Pts',(1.10756619464419,1.09227107609621,3.8322443892467));
#72286=CARTESIAN_POINT('Ctrl Pts',(1.12488796282642,1.07440214851652,3.83047890211347));
#72287=CARTESIAN_POINT('Ctrl Pts',(1.13281225259552,1.06604375749793,3.82965787421626));
#72288=CARTESIAN_POINT('Ctrl Pts',(1.15031788975076,1.04716354730411,3.82781339240678));
#72289=CARTESIAN_POINT('Ctrl Pts',(1.15984902449567,1.03659681536245,3.8267878980819));
#72290=CARTESIAN_POINT('Ctrl Pts',(1.18810701985886,1.00439079118751,3.82368154684059));
#72291=CARTESIAN_POINT('Ctrl Pts',(1.20638206321886,0.982365140601841,3.82158250544671));
#72292=CARTESIAN_POINT('Ctrl Pts',(1.26979367882918,0.90150011391547,3.81396027197312));
#72293=CARTESIAN_POINT('Ctrl Pts',(1.31131227227638,0.839961813950697,3.80830771229271));
#72294=CARTESIAN_POINT('Ctrl Pts',(1.39421044262462,0.695873714600873,3.79546804290782));
#72295=CARTESIAN_POINT('Ctrl Pts',(1.43296018313743,0.612118553094414,3.78826184291176));
#72296=CARTESIAN_POINT('Ctrl Pts',(1.47322287196129,0.499928416234718,3.77923481401478));
#72297=CARTESIAN_POINT('Ctrl Pts',(1.48170618626917,0.474195162606534,3.77720576194676));
#72298=CARTESIAN_POINT('Ctrl Pts',(1.4923986817236,0.438664630753659,3.77447208963765));
#72299=CARTESIAN_POINT('Ctrl Pts',(1.49519124327984,0.429049698406976,3.77373905151848));
#72300=CARTESIAN_POINT('Ctrl Pts',(1.49968567723108,0.412998098588867,3.77252719548992));
#72301=CARTESIAN_POINT('Ctrl Pts',(1.50143938020525,0.406576381749281,3.77204552893751));
#72302=CARTESIAN_POINT('Ctrl Pts',(1.5049826460929,0.393265984719415,3.77105394955424));
#72303=CARTESIAN_POINT('Ctrl Pts',(1.50676624714113,0.386375958996842,3.77054437219304));
#72304=CARTESIAN_POINT('Ctrl Pts',(1.5114006023796,0.367953244210156,3.7691911215732));
#72305=CARTESIAN_POINT('Ctrl Pts',(1.51416670922835,0.356399453117021,3.76835208934191));
#72306=CARTESIAN_POINT('Ctrl Pts',(1.52820287487348,0.294655961635023,3.76391400858891));
#72307=CARTESIAN_POINT('Ctrl Pts',(1.53711176539667,0.243956558049187,3.76042969817292));
#72308=CARTESIAN_POINT('Ctrl Pts',(1.55156672203716,0.128297067216008,3.75265086713397));
#72309=CARTESIAN_POINT('Ctrl Pts',(1.55557706746083,0.0632454462312255,
3.74839324341717));
#72310=CARTESIAN_POINT('Ctrl Pts',(1.5553939680873,-0.0892340033225456,
3.7383422055366));
#72311=CARTESIAN_POINT('Ctrl Pts',(1.54792911191298,-0.176424694897936,
3.73253316740635));
#72312=CARTESIAN_POINT('Ctrl Pts',(1.52976132969099,-0.282528868339989,
3.72508698312319));
#72313=CARTESIAN_POINT('Ctrl Pts',(1.52594436201107,-0.302466568221327,
3.7236716840226));
#72314=CARTESIAN_POINT('Ctrl Pts',(1.51913467717288,-0.334616171589868,
3.72136026318372));
#72315=CARTESIAN_POINT('Ctrl Pts',(1.51638205671683,-0.346876910515645,
3.7204718252204));
#72316=CARTESIAN_POINT('Ctrl Pts',(1.5107854714666,-0.370464392339823,3.71874850480573));
#72317=CARTESIAN_POINT('Ctrl Pts',(1.50796189180211,-0.381795136085018,
3.7179143316572));
#72318=CARTESIAN_POINT('Ctrl Pts',(1.50105165052053,-0.408251971148112,
3.7159511343197));
#72319=CARTESIAN_POINT('Ctrl Pts',(1.49686355076355,-0.423349981027338,
3.71481889572626));
#72320=CARTESIAN_POINT('Ctrl Pts',(1.48198735243904,-0.47399524870437,3.71097918483647));
#72321=CARTESIAN_POINT('Ctrl Pts',(1.47025596021202,-0.509219983615412,
3.70823845436778));
#72322=CARTESIAN_POINT('Ctrl Pts',(1.43776457389458,-0.59626027222761,3.70128436723927));
#72323=CARTESIAN_POINT('Ctrl Pts',(1.41545576459332,-0.647438920799612,
3.6970279551877));
#72324=CARTESIAN_POINT('Ctrl Pts',(1.36693300922773,-0.744194934353254,
3.6886823755887));
#72325=CARTESIAN_POINT('Ctrl Pts',(1.34106097370961,-0.789865320960806,
3.68460383020917));
#72326=CARTESIAN_POINT('Ctrl Pts',(1.27683647936504,-0.890954306381601,
3.67533029822414));
#72327=CARTESIAN_POINT('Ctrl Pts',(1.23708697992361,-0.945372331420556,
3.67015448970654));
#72328=CARTESIAN_POINT('Ctrl Pts',(1.18582446423293,-1.00675746025347,3.66422551982853));
#72329=CARTESIAN_POINT('Ctrl Pts',(1.17759828734018,-1.01636732770417,3.66329461198794));
#72330=CARTESIAN_POINT('Ctrl Pts',(1.16445239868656,-1.03135052185687,3.66184026763188));
#72331=CARTESIAN_POINT('Ctrl Pts',(1.15961082610881,-1.03679121597966,3.66131154579171));
#72332=CARTESIAN_POINT('Ctrl Pts',(1.15027532746898,-1.04713473230588,3.66030551328904));
#72333=CARTESIAN_POINT('Ctrl Pts',(1.14578794270035,-1.05204299760754,3.65982778763336));
#72334=CARTESIAN_POINT('Ctrl Pts',(1.13473903634854,-1.06397365162221,3.65866535382958));
#72335=CARTESIAN_POINT('Ctrl Pts',(1.12814350943214,-1.0709644469436,3.65798316239319));
#72336=CARTESIAN_POINT('Ctrl Pts',(1.10341992854202,-1.09668783710814,3.65546691670175));
#72337=CARTESIAN_POINT('Ctrl Pts',(1.08488554087559,-1.11502615000068,3.65366096864965));
#72338=CARTESIAN_POINT('Ctrl Pts',(1.03438481289924,-1.16254051382225,3.64891931005681));
#72339=CARTESIAN_POINT('Ctrl Pts',(1.00164628811219,-1.19086423959588,3.64602609538907));
#72340=CARTESIAN_POINT('Ctrl Pts',(0.863663916002498,-1.30051783274062,
3.63434428573772));
#72341=CARTESIAN_POINT('Ctrl Pts',(0.749392523045323,-1.36955130673227,
3.62576409737399));
#72342=CARTESIAN_POINT('Ctrl Pts',(0.606238571196468,-1.43269224747661,
3.61499587623665));
#72343=CARTESIAN_POINT('Ctrl Pts',(0.584530395116345,-1.44168526306604,
3.61336430152426));
#72344=CARTESIAN_POINT('Ctrl Pts',(0.550169381495906,-1.45501631517865,
3.61077893934143));
#72345=CARTESIAN_POINT('Ctrl Pts',(0.537649522632959,-1.45968893832079,
3.60983637207233));
#72346=CARTESIAN_POINT('Ctrl Pts',(0.514229308578519,-1.46808757742567,
3.60807128554323));
#72347=CARTESIAN_POINT('Ctrl Pts',(0.503344685431386,-1.47185496273268,
3.60725021127794));
#72348=CARTESIAN_POINT('Ctrl Pts',(0.478913398223881,-1.48000842503088,
3.60540506670967));
#72349=CARTESIAN_POINT('Ctrl Pts',(0.465346486850612,-1.4843300183086,3.60437894917613));
#72350=CARTESIAN_POINT('Ctrl Pts',(0.424296143791934,-1.49678806814361,
3.60126864939008));
#72351=CARTESIAN_POINT('Ctrl Pts',(0.396646704143519,-1.50435133183752,
3.59916621384345));
#72352=CARTESIAN_POINT('Ctrl Pts',(0.296009361989527,-1.5289125775164,3.59148212640709));
#72353=CARTESIAN_POINT('Ctrl Pts',(0.222034226977328,-1.54139327201333,
3.58576790247432));
#72354=CARTESIAN_POINT('Ctrl Pts',(0.0543470526105254,-1.5573614745651,
3.57275426770513));
#72355=CARTESIAN_POINT('Ctrl Pts',(-0.0393752239906029,-1.55781230544449,
3.5654353864327));
#72356=CARTESIAN_POINT('Ctrl Pts',(-0.157805989479645,-1.54768178052438,
3.55645039637803));
#72357=CARTESIAN_POINT('Ctrl Pts',(-0.18298460958476,-1.5449072601812,3.55455643455861));
#72358=CARTESIAN_POINT('Ctrl Pts',(-0.217776743347928,-1.5402107525119,
3.55197154456373));
#72359=CARTESIAN_POINT('Ctrl Pts',(-0.227455295180025,-1.53881122106602,
3.55125595487535));
#72360=CARTESIAN_POINT('Ctrl Pts',(-0.243656874047524,-1.53631224708758,
3.55006462847682));
#72361=CARTESIAN_POINT('Ctrl Pts',(-0.250187139087899,-1.53526232129158,
3.54958624326111));
#72362=CARTESIAN_POINT('Ctrl Pts',(-0.263808173778837,-1.53298313119613,
3.54859240233945));
#72363=CARTESIAN_POINT('Ctrl Pts',(-0.2708974121799,-1.53174626840134,3.54807737001296));
#72364=CARTESIAN_POINT('Ctrl Pts',(-0.290026757988819,-1.52827179890672,
3.54669300923794));
#72365=CARTESIAN_POINT('Ctrl Pts',(-0.302049748108351,-1.52594108211685,
3.54582870159898));
#72366=CARTESIAN_POINT('Ctrl Pts',(-0.371852740508876,-1.51155204681196,
3.54083768130732));
#72367=CARTESIAN_POINT('Ctrl Pts',(-0.428943380458982,-1.49635335222618,
3.53686271390149));
#72368=CARTESIAN_POINT('Ctrl Pts',(-0.610687498550401,-1.43670776867674,
3.52415530077221));
#72369=CARTESIAN_POINT('Ctrl Pts',(-0.730556903895627,-1.37962097910419,
3.51564119168497));
#72370=CARTESIAN_POINT('Ctrl Pts',(-0.862351647997895,-1.2948086667663,
3.5049014408981));
#72371=CARTESIAN_POINT('Ctrl Pts',(-0.882626353682912,-1.28107394683488,
3.50320820619611));
#72372=CARTESIAN_POINT('Ctrl Pts',(-0.91466378750058,-1.25824917737933,
3.50045959811465));
#72373=CARTESIAN_POINT('Ctrl Pts',(-0.926635598489587,-1.2494587936889,
3.49941550962772));
#72374=CARTESIAN_POINT('Ctrl Pts',(-0.947706641671402,-1.23351783341402,
3.49754616460189));
#72375=CARTESIAN_POINT('Ctrl Pts',(-0.9568555263783,-1.22643451208446,3.49672358265607));
#72376=CARTESIAN_POINT('Ctrl Pts',(-0.97607960686687,-1.21120465154065,
3.49497123847157));
#72377=CARTESIAN_POINT('Ctrl Pts',(-0.986133688616471,-1.20303301540983,
3.49404051140951));
#72378=CARTESIAN_POINT('Ctrl Pts',(-1.01311425080504,-1.18053859725922,
3.49150305238647));
#72379=CARTESIAN_POINT('Ctrl Pts',(-1.02983786772414,-1.16597844612327,
3.4898867413495));
#72380=CARTESIAN_POINT('Ctrl Pts',(-1.06645428953764,-1.13269652526368,
3.48624707481798));
#72381=CARTESIAN_POINT('Ctrl Pts',(-1.08617625269331,-1.11379852410176,
3.48421683990996));
#72382=CARTESIAN_POINT('Ctrl Pts',(-1.14947531658844,-1.04986338233452,
3.47746426964904));
#72383=CARTESIAN_POINT('Ctrl Pts',(-1.19082585791133,-1.00271578881269,
3.47266244576171));
#72384=CARTESIAN_POINT('Ctrl Pts',(-1.29111794189993,-0.873383294073018,
3.46000500492474));
#72385=CARTESIAN_POINT('Ctrl Pts',(-1.34509916989565,-0.787714822142316,
3.45209782458507));
#72386=CARTESIAN_POINT('Ctrl Pts',(-1.39814664451044,-0.681956878310091,
3.44325004227776));
#72387=CARTESIAN_POINT('Ctrl Pts',(-1.40564122936845,-0.666372285728577,
3.44196843057678));
#72388=CARTESIAN_POINT('Ctrl Pts',(-1.41635984390617,-0.643097548266357,
3.44009040630299));
#72389=CARTESIAN_POINT('Ctrl Pts',(-1.41978416174851,-0.635501854075211,
3.43948311047828));
#72390=CARTESIAN_POINT('Ctrl Pts',(-1.42577175900896,-0.621930391532003,
3.43840842944615));
#72391=CARTESIAN_POINT('Ctrl Pts',(-1.42835879869708,-0.615965638412577,
3.4379396755894));
#72392=CARTESIAN_POINT('Ctrl Pts',(-1.43406490147965,-0.602580197367621,
3.43689571987182));
#72393=CARTESIAN_POINT('Ctrl Pts',(-1.43716385493171,-0.59515132330036,
3.43632170944422));
#72394=CARTESIAN_POINT('Ctrl Pts',(-1.44640359618374,-0.572508552946962,
3.43458745949149));
#72395=CARTESIAN_POINT('Ctrl Pts',(-1.45236172086018,-0.557220687073791,
3.43343738592663));
#72396=CARTESIAN_POINT('Ctrl Pts',(-1.48205480727729,-0.477317467350164,
3.42751968035562));
#72397=CARTESIAN_POINT('Ctrl Pts',(-1.50172605748703,-0.411265767278821,
3.42293994475575));
#72398=CARTESIAN_POINT('Ctrl Pts',(-1.54252708223655,-0.231406233733472,
3.41076701841973));
#72399=CARTESIAN_POINT('Ctrl Pts',(-1.5554514956748,-0.116208668896937,
3.40325199989059));
#72400=CARTESIAN_POINT('Ctrl Pts',(-1.55549986374249,-0.000651073801188791,
3.39533201070811));
#72401=CARTESIAN_POINT('Ctrl Pts',(-1.5555,-2.78355693781297E-11,3.25542335925836));
#72402=CARTESIAN_POINT('Ctrl Pts',(-1.55549999999891,-0.0607860708812731,
3.25945607524617));
#72403=CARTESIAN_POINT('Ctrl Pts',(-1.55193697213556,-0.121515943941803,
3.26353655937556));
#72404=CARTESIAN_POINT('Ctrl Pts',(-1.54284580338691,-0.198733706385335,
3.26889097315067));
#72405=CARTESIAN_POINT('Ctrl Pts',(-1.54058583546237,-0.215553949602213,
3.27006729424422));
#72406=CARTESIAN_POINT('Ctrl Pts',(-1.53622297308072,-0.244436185471864,
3.27210645413131));
#72407=CARTESIAN_POINT('Ctrl Pts',(-1.53425200647297,-0.256516739104691,
3.27296521076461));
#72408=CARTESIAN_POINT('Ctrl Pts',(-1.53022115015054,-0.279511764896393,
3.27461171291426));
#72409=CARTESIAN_POINT('Ctrl Pts',(-1.5281865185639,-0.290429936450797,
3.27539862007994));
#72410=CARTESIAN_POINT('Ctrl Pts',(-1.52369387412355,-0.313182547425268,
3.27704972294765));
#72411=CARTESIAN_POINT('Ctrl Pts',(-1.52121449704045,-0.325011951823233,
3.27791454974933));
#72412=CARTESIAN_POINT('Ctrl Pts',(-1.5154255758991,-0.351112770075724,
3.27983746802952));
#72413=CARTESIAN_POINT('Ctrl Pts',(-1.51205179272346,-0.365368584095339,
3.28089754711258));
#72414=CARTESIAN_POINT('Ctrl Pts',(-1.49956986812762,-0.414973379702481,
3.28462173942229));
#72415=CARTESIAN_POINT('Ctrl Pts',(-1.48941990867522,-0.450045136977735,
3.2873185771476));
#72416=CARTESIAN_POINT('Ctrl Pts',(-1.4386366890612,-0.604895778239368,
3.2995197546192));
#72417=CARTESIAN_POINT('Ctrl Pts',(-1.38472089335823,-0.719801133176935,
3.30942524276129));
#72418=CARTESIAN_POINT('Ctrl Pts',(-1.29124933733976,-0.868732283639018,
3.32295827192875));
#72419=CARTESIAN_POINT('Ctrl Pts',(-1.26300733993977,-0.909304196565685,
3.32671924801125));
#72420=CARTESIAN_POINT('Ctrl Pts',(-1.22542628259493,-0.958154514751454,
3.33128341996175));
#72421=CARTESIAN_POINT('Ctrl Pts',(-1.21785914857268,-0.967754497448563,
3.33218213374262));
#72422=CARTESIAN_POINT('Ctrl Pts',(-1.20558831904237,-0.982949873518572,
3.33360622512833));
#72423=CARTESIAN_POINT('Ctrl Pts',(-1.20095717706635,-0.988602808821515,
3.33413636232796));
#72424=CARTESIAN_POINT('Ctrl Pts',(-1.19191418881416,-0.999483669430574,
3.33515711940426));
#72425=CARTESIAN_POINT('Ctrl Pts',(-1.18750743581047,-1.00471544800308,
3.33564804897284));
#72426=CARTESIAN_POINT('Ctrl Pts',(-1.17636009579729,-1.01777397417979,
3.33687420330828));
#72427=CARTESIAN_POINT('Ctrl Pts',(-1.16957562827719,-1.02556316362537,
3.33760631658791));
#72428=CARTESIAN_POINT('Ctrl Pts',(-1.14389903790712,-1.05445600736992,
3.34032734573549));
#72429=CARTESIAN_POINT('Ctrl Pts',(-1.12450801161479,-1.07511137160182,
3.34228349171483));
#72430=CARTESIAN_POINT('Ctrl Pts',(-1.04057578437535,-1.15975898687436,
3.35040658346888));
#72431=CARTESIAN_POINT('Ctrl Pts',(-0.971051608072913,-1.21856497727376,
3.35632563994744));
#72432=CARTESIAN_POINT('Ctrl Pts',(-0.837968091971192,-1.31246767562476,
3.36706354742693));
#72433=CARTESIAN_POINT('Ctrl Pts',(-0.776347310742355,-1.34983157507516,
3.37184074195209));
#72434=CARTESIAN_POINT('Ctrl Pts',(-0.686150698456772,-1.39629761831886,
3.37877486756192));
#72435=CARTESIAN_POINT('Ctrl Pts',(-0.659559173426035,-1.40905334368822,
3.38081170985634));
#72436=CARTESIAN_POINT('Ctrl Pts',(-0.619272052132952,-1.4269884151098,
3.38389648679915));
#72437=CARTESIAN_POINT('Ctrl Pts',(-0.605838826215595,-1.43274320876832,
3.38492485435898));
#72438=CARTESIAN_POINT('Ctrl Pts',(-0.58139516340195,-1.44280964942013,
3.38679684844014));
#72439=CARTESIAN_POINT('Ctrl Pts',(-0.570412732423084,-1.44718669184952,
3.38763818861054));
#72440=CARTESIAN_POINT('Ctrl Pts',(-0.546570760135594,-1.45637534750301,
3.38946580551102));
#72441=CARTESIAN_POINT('Ctrl Pts',(-0.533695360963547,-1.46114269936617,
3.39045348242595));
#72442=CARTESIAN_POINT('Ctrl Pts',(-0.497938469113249,-1.47384668153679,
3.39319924249326));
#72443=CARTESIAN_POINT('Ctrl Pts',(-0.474933044732482,-1.48142000821229,
3.3949690538451));
#72444=CARTESIAN_POINT('Ctrl Pts',(-0.364130450539393,-1.51504978086094,
3.40351321751441));
#72445=CARTESIAN_POINT('Ctrl Pts',(-0.274336258379674,-1.53385179761166,
3.4105124170346));
#72446=CARTESIAN_POINT('Ctrl Pts',(-0.112505898868495,-1.55306891692159,
3.42312866137376));
#72447=CARTESIAN_POINT('Ctrl Pts',(-0.0410895024410422,-1.55659658445065,
3.42869220018023));
#72448=CARTESIAN_POINT('Ctrl Pts',(0.0542747113740685,-1.55473747928889,
3.43596661321126));
#72449=CARTESIAN_POINT('Ctrl Pts',(0.0782184428484231,-1.55371695573676,
3.43777950301424));
#72450=CARTESIAN_POINT('Ctrl Pts',(0.119408719021244,-1.55100665489163,
3.44086523003329));
#72451=CARTESIAN_POINT('Ctrl Pts',(0.136667897161868,-1.54958124582316,
3.44214816058904));
#72452=CARTESIAN_POINT('Ctrl Pts',(0.162205181816856,-1.54704213807897,
3.44402819226639));
#72453=CARTESIAN_POINT('Ctrl Pts',(0.170503248063316,-1.54614958814523,
3.44463622413106));
#72454=CARTESIAN_POINT('Ctrl Pts',(0.18476670296111,-1.54449916365417,3.44567597910792));
#72455=CARTESIAN_POINT('Ctrl Pts',(0.190735330327972,-1.5437734414532,3.4461094174091));
#72456=CARTESIAN_POINT('Ctrl Pts',(0.204785124664938,-1.54198240429226,
3.44712582511819));
#72457=CARTESIAN_POINT('Ctrl Pts',(0.212862319282244,-1.54088816056889,
3.44770718398428));
#72458=CARTESIAN_POINT('Ctrl Pts',(0.237063211504203,-1.53741565536871,
3.44944115072805));
#72459=CARTESIAN_POINT('Ctrl Pts',(0.253159105872497,-1.53484734930616,
3.45058386281324));
#72460=CARTESIAN_POINT('Ctrl Pts',(0.34785296670199,-1.51820744736787,3.45726026693833));
#72461=CARTESIAN_POINT('Ctrl Pts',(0.425323236034948,-1.49835207651838,
3.4625371778767));
#72462=CARTESIAN_POINT('Ctrl Pts',(0.573085353210863,-1.44808893689026,
3.47281806006367));
#72463=CARTESIAN_POINT('Ctrl Pts',(0.643331526199665,-1.41827788145873,
3.47781075825616));
#72464=CARTESIAN_POINT('Ctrl Pts',(0.7527509524352,-1.36203471361566,3.48608225237901));
#72465=CARTESIAN_POINT('Ctrl Pts',(0.793402484442948,-1.33876225616569,
3.48927378454031));
#72466=CARTESIAN_POINT('Ctrl Pts',(0.847507031028264,-1.30445758564444,
3.49372954065074));
#72467=CARTESIAN_POINT('Ctrl Pts',(0.861919034635415,-1.29498003712624,
3.49493752954185));
#72468=CARTESIAN_POINT('Ctrl Pts',(0.886232945305602,-1.27840515456497,
3.49701371329313));
#72469=CARTESIAN_POINT('Ctrl Pts',(0.896214738556411,-1.27142742602964,
3.49787736163097));
#72470=CARTESIAN_POINT('Ctrl Pts',(0.915100626648279,-1.25789242418635,
3.49953372879897));
#72471=CARTESIAN_POINT('Ctrl Pts',(0.924018783896665,-1.25135597775206,
3.50032560859368));
#72472=CARTESIAN_POINT('Ctrl Pts',(0.944827186580309,-1.23576100308039,
3.50219675450528));
#72473=CARTESIAN_POINT('Ctrl Pts',(0.956657850512842,-1.22662520653967,
3.50327899760884));
#72474=CARTESIAN_POINT('Ctrl Pts',(0.998908138827007,-1.19301593207937,
3.50721237466657));
#72475=CARTESIAN_POINT('Ctrl Pts',(1.0285330681755,-1.1675717188049,3.51010155075974));
#72476=CARTESIAN_POINT('Ctrl Pts',(1.15121702971096,-1.05390590887231,3.52265216421355));
#72477=CARTESIAN_POINT('Ctrl Pts',(1.23412544244741,-0.955481174912032,
3.53271408168902));
#72478=CARTESIAN_POINT('Ctrl Pts',(1.32072768779213,-0.822313467803962,
3.54491123362982));
#72479=CARTESIAN_POINT('Ctrl Pts',(1.33668667053844,-0.796109315406132,
3.54724824359846));
#72480=CARTESIAN_POINT('Ctrl Pts',(1.36210342901551,-0.751454066336237,
3.55110816399502));
#72481=CARTESIAN_POINT('Ctrl Pts',(1.37198599152631,-0.733255420732715,
3.55264839672875));
#72482=CARTESIAN_POINT('Ctrl Pts',(1.38561405705907,-0.706918639022424,
3.55482539992706));
#72483=CARTESIAN_POINT('Ctrl Pts',(1.38965681095889,-0.698937933885297,
3.55547837807798));
#72484=CARTESIAN_POINT('Ctrl Pts',(1.39660623815778,-0.684920538374741,
3.5566130301217));
#72485=CARTESIAN_POINT('Ctrl Pts',(1.39954308625618,-0.678899318384618,
3.55709648640158));
#72486=CARTESIAN_POINT('Ctrl Pts',(1.40589466997023,-0.665660700793265,
3.55815075710846));
#72487=CARTESIAN_POINT('Ctrl Pts',(1.40929284983607,-0.658435769465999,
3.55872057981965));
#72488=CARTESIAN_POINT('Ctrl Pts',(1.4189137830434,-0.637564780612528,3.56035167931683));
#72489=CARTESIAN_POINT('Ctrl Pts',(1.42499521590975,-0.62385403039611,3.56140490790846));
#72490=CARTESIAN_POINT('Ctrl Pts',(1.46981602417088,-0.518727601458954,
3.56935818113446));
#72491=CARTESIAN_POINT('Ctrl Pts',(1.4999267326764,-0.423866626399561,3.57584564312699));
#72492=CARTESIAN_POINT('Ctrl Pts',(1.53460624281731,-0.262468337359891,
3.58671343910008));
#72493=CARTESIAN_POINT('Ctrl Pts',(1.5443299749483,-0.197357595802677,3.5910522198203));
#72494=CARTESIAN_POINT('Ctrl Pts',(1.55341046346989,-0.0906003373645394,
3.59828803159756));
#72495=CARTESIAN_POINT('Ctrl Pts',(1.55527054292207,-0.0492497805970797,
3.60111929965253));
#72496=CARTESIAN_POINT('Ctrl Pts',(1.55556378546693,0.00865730581965027,
3.60515258545369));
#72497=CARTESIAN_POINT('Ctrl Pts',(1.55538387593836,0.0251912934767595,
3.60631190726155));
#72498=CARTESIAN_POINT('Ctrl Pts',(1.55461711938295,0.0537698425695558,
3.60833073347586));
#72499=CARTESIAN_POINT('Ctrl Pts',(1.55415371220992,0.0658164706205951,
3.6091863235393));
#72500=CARTESIAN_POINT('Ctrl Pts',(1.55291266181557,0.0905805154546697,
3.61095522025259));
#72501=CARTESIAN_POINT('Ctrl Pts',(1.55211869723514,0.103296160748277,3.61186897426871));
#72502=CARTESIAN_POINT('Ctrl Pts',(1.54966983852326,0.136042573045771,3.61423698789709));
#72503=CARTESIAN_POINT('Ctrl Pts',(1.54778279293913,0.156053022352627,3.61569837921906));
#72504=CARTESIAN_POINT('Ctrl Pts',(1.53696557978105,0.251031171078054,3.62270656400717));
#72505=CARTESIAN_POINT('Ctrl Pts',(1.52297436257048,0.32530869355889,3.62840792686284));
#72506=CARTESIAN_POINT('Ctrl Pts',(1.48047849683495,0.48575091670956,3.64116681057139));
#72507=CARTESIAN_POINT('Ctrl Pts',(1.44971730180168,0.571042823307886,3.64824790371171));
#72508=CARTESIAN_POINT('Ctrl Pts',(1.39505828000717,0.689177979869859,3.65820734170105));
#72509=CARTESIAN_POINT('Ctrl Pts',(1.3770278473173,0.724533509919141,3.66120683221527));
#72510=CARTESIAN_POINT('Ctrl Pts',(1.35217737854268,0.768975256494281,3.66496895312808));
#72511=CARTESIAN_POINT('Ctrl Pts',(1.34658482737159,0.778727121975855,3.66579392654287));
#72512=CARTESIAN_POINT('Ctrl Pts',(1.33729043893774,0.794534377858817,3.66712922826534));
#72513=CARTESIAN_POINT('Ctrl Pts',(1.33365213614556,0.800626367832799,3.66764336658298));
#72514=CARTESIAN_POINT('Ctrl Pts',(1.32673447595282,0.812031314815556,3.66860469112551));
#72515=CARTESIAN_POINT('Ctrl Pts',(1.32346459254547,0.81734980386155,3.66905248844869));
#72516=CARTESIAN_POINT('Ctrl Pts',(1.31464416675451,0.831504568502812,3.6702433393182));
#72517=CARTESIAN_POINT('Ctrl Pts',(1.30903646123255,0.840305118141006,3.67098276162416));
#72518=CARTESIAN_POINT('Ctrl Pts',(1.28744571292995,0.873448197808177,3.67376643751292));
#72519=CARTESIAN_POINT('Ctrl Pts',(1.27086771106949,0.897398321508173,3.67577594679725));
#72520=CARTESIAN_POINT('Ctrl Pts',(1.20020472960121,0.99359525315292,3.68390172411251));
#72521=CARTESIAN_POINT('Ctrl Pts',(1.14055223864123,1.06153960941272,3.68977907762025));
#72522=CARTESIAN_POINT('Ctrl Pts',(1.02361707230754,1.17341916484714,3.70044913488262));
#72523=CARTESIAN_POINT('Ctrl Pts',(0.968544708676698,1.2192719618557,3.70520059978927));
#72524=CARTESIAN_POINT('Ctrl Pts',(0.886598805241418,1.27843376908419,3.71210790562896));
#72525=CARTESIAN_POINT('Ctrl Pts',(0.862198093567136,1.2950152892425,3.71414534474061));
#72526=CARTESIAN_POINT('Ctrl Pts',(0.825024984598602,1.31875988489306,3.71723084399427));
#72527=CARTESIAN_POINT('Ctrl Pts',(0.812598039994556,1.32645326295926,3.71825932300566));
#72528=CARTESIAN_POINT('Ctrl Pts',(0.789926083913295,1.34005104553896,3.72013143419495));
#72529=CARTESIAN_POINT('Ctrl Pts',(0.779718534316432,1.34601597903946,3.72097277865108));
#72530=CARTESIAN_POINT('Ctrl Pts',(0.757513231743672,1.35865463514754,3.7228003065987));
#72531=CARTESIAN_POINT('Ctrl Pts',(0.745493219111438,1.36528698511159,3.72378788916717));
#72532=CARTESIAN_POINT('Ctrl Pts',(0.712035335391271,1.38317466461226,3.72653311690271));
#72533=CARTESIAN_POINT('Ctrl Pts',(0.690420884575803,1.39408943468898,3.72830248283838));
#72534=CARTESIAN_POINT('Ctrl Pts',(0.584838874199675,1.44434813142377,3.73693069837145));
#72535=CARTESIAN_POINT('Ctrl Pts',(0.497734093839646,1.4766291095255,3.74402075881413));
#72536=CARTESIAN_POINT('Ctrl Pts',(0.340205353866142,1.51947980109964,3.75666163577891));
#72537=CARTESIAN_POINT('Ctrl Pts',(0.270939086164993,1.53334640972864,3.76215675698973));
#72538=CARTESIAN_POINT('Ctrl Pts',(0.17735770129943,1.54553920806934,3.76935283956779));
#72539=CARTESIAN_POINT('Ctrl Pts',(0.153677707322813,1.54807315321948,3.77115404507967));
#72540=CARTESIAN_POINT('Ctrl Pts',(0.112772285398751,1.5515024094248,3.77422215753199));
#72541=CARTESIAN_POINT('Ctrl Pts',(0.0955732645950326,1.55265679751913,
3.77549901539143));
#72542=CARTESIAN_POINT('Ctrl Pts',(0.0700378400900962,1.55394476963077,
3.77737195661427));
#72543=CARTESIAN_POINT('Ctrl Pts',(0.0617144909625686,1.55429758289432,
3.77797885715571));
#72544=CARTESIAN_POINT('Ctrl Pts',(0.047380211490857,1.55478985948599,3.77901741770781));
#72545=CARTESIAN_POINT('Ctrl Pts',(0.0413708629452457,1.55496136510556,
3.77945078012098));
#72546=CARTESIAN_POINT('Ctrl Pts',(0.0271980468000013,1.55528363118929,
3.78046807750647));
#72547=CARTESIAN_POINT('Ctrl Pts',(0.0190341925520919,1.55540496806032,
3.78105038955749));
#72548=CARTESIAN_POINT('Ctrl Pts',(-0.00549853325664263,1.55557640196247,
3.78279025334399));
#72549=CARTESIAN_POINT('Ctrl Pts',(-0.0218682241375157,1.55543241980869,
3.78393780957672));
#72550=CARTESIAN_POINT('Ctrl Pts',(-0.111198544749674,1.55323606069066,
3.79014205518946));
#72551=CARTESIAN_POINT('Ctrl Pts',(-0.183956303259965,1.54630853016511,
3.79498634205472));
#72552=CARTESIAN_POINT('Ctrl Pts',(-0.32046191274894,1.52353532527263,3.80411338942916));
#72553=CARTESIAN_POINT('Ctrl Pts',(-0.384213540820087,1.50871980034343,
3.80839311112881));
#72554=CARTESIAN_POINT('Ctrl Pts',(-0.486029259238781,1.47818452842605,
3.81547230877433));
#72555=CARTESIAN_POINT('Ctrl Pts',(-0.524734320829272,1.46489162121172,
3.8182226094687));
#72556=CARTESIAN_POINT('Ctrl Pts',(-0.590915582161795,1.43920262194015,
3.82307105588552));
#72557=CARTESIAN_POINT('Ctrl Pts',(-0.618639226485134,1.42750506735872,
3.82514806300027));
#72558=CARTESIAN_POINT('Ctrl Pts',(-0.659398207977537,1.4088970950988,3.82828141712173));
#72559=CARTESIAN_POINT('Ctrl Pts',(-0.672703696651877,1.40259286017864,
3.82931724115352));
#72560=CARTESIAN_POINT('Ctrl Pts',(-0.696534381742325,1.39088462388856,
3.83119711285093));
#72561=CARTESIAN_POINT('Ctrl Pts',(-0.707091339055635,1.38554754736967,
3.83203878252375));
#72562=CARTESIAN_POINT('Ctrl Pts',(-0.729694229951577,1.37379504373212,
3.83386065822316));
#72563=CARTESIAN_POINT('Ctrl Pts',(-0.741718575976136,1.36734049286904,
3.83484219197334));
#72564=CARTESIAN_POINT('Ctrl Pts',(-0.774503763128134,1.349182020093,3.83755336856953));
#72565=CARTESIAN_POINT('Ctrl Pts',(-0.795082187738909,1.33715833051186,
3.83929426122792));
#72566=CARTESIAN_POINT('Ctrl Pts',(-0.907056260347639,1.26823469007577,
3.84899121052981));
#72567=CARTESIAN_POINT('Ctrl Pts',(-0.992615230169811,1.20244641552962,
3.85727124457528));
#72568=CARTESIAN_POINT('Ctrl Pts',(-1.11422359903628,1.08705501331505,3.87027076716141));
#72569=CARTESIAN_POINT('Ctrl Pts',(-1.15533794183563,1.04325345832949,3.87492800745078));
#72570=CARTESIAN_POINT('Ctrl Pts',(-1.21436578555386,0.972585819178756,
3.88193121779223));
#72571=CARTESIAN_POINT('Ctrl Pts',(-1.23414858373607,0.94735688093723,3.88434067756427));
#72572=CARTESIAN_POINT('Ctrl Pts',(-1.25935734167289,0.913076940659836,
3.88747873809432));
#72573=CARTESIAN_POINT('Ctrl Pts',(-1.2654899594665,0.90455823046206,3.88824783097148));
#72574=CARTESIAN_POINT('Ctrl Pts',(-1.27553416094645,0.890303898549334,
3.88951619744513));
#72575=CARTESIAN_POINT('Ctrl Pts',(-1.27949434271589,0.88460310974975,3.89001860838951));
#72576=CARTESIAN_POINT('Ctrl Pts',(-1.28701911004849,0.873614742561962,
3.89097747143102));
#72577=CARTESIAN_POINT('Ctrl Pts',(-1.29058953553784,0.868331482058339,
3.89143434315744));
#72578=CARTESIAN_POINT('Ctrl Pts',(-1.30031456586995,0.853748578907524,
3.89268448026577));
#72579=CARTESIAN_POINT('Ctrl Pts',(-1.30640196328723,0.84440424888625,3.89347343034902));
#72580=CARTESIAN_POINT('Ctrl Pts',(-1.33129693310522,0.805276017497543,
3.896730705872));
#72581=CARTESIAN_POINT('Ctrl Pts',(-1.34919210545048,0.774920704266457,
3.8991473029384));
#72582=CARTESIAN_POINT('Ctrl Pts',(-1.40695071097731,0.668868691062298,
3.90731246306713));
#72583=CARTESIAN_POINT('Ctrl Pts',(-1.44159678355945,0.590505159647553,
3.91288389473558));
#72584=CARTESIAN_POINT('Ctrl Pts',(-1.49523176312639,0.435854322458862,
3.92368256333216));
#72585=CARTESIAN_POINT('Ctrl Pts',(-1.51523471972271,0.360206433021615,
3.9288826851764));
#72586=CARTESIAN_POINT('Ctrl Pts',(-1.53380238538461,0.259992883848979,
3.93589797543827));
#72587=CARTESIAN_POINT('Ctrl Pts',(-1.53759858512539,0.236509077635695,
3.93755012244972));
#72588=CARTESIAN_POINT('Ctrl Pts',(-1.54270321353632,0.199572961961079,
3.94016653464031));
#72589=CARTESIAN_POINT('Ctrl Pts',(-1.54437744070055,0.186174306275306,
3.94111928775718));
#72590=CARTESIAN_POINT('Ctrl Pts',(-1.54719252055082,0.160984043077589,
3.94291821874048));
#72591=CARTESIAN_POINT('Ctrl Pts',(-1.54837351793495,0.149197830003592,
3.94376306673269));
#72592=CARTESIAN_POINT('Ctrl Pts',(-1.55073858002753,0.122527630868944,
3.94568250085911));
#72593=CARTESIAN_POINT('Ctrl Pts',(-1.55184316274791,0.107637973202424,
3.94675950004294));
#72594=CARTESIAN_POINT('Ctrl Pts',(-1.55459560178378,0.0615518718819224,
3.95011086755889));
#72595=CARTESIAN_POINT('Ctrl Pts',(-1.55551806522174,0.0303217476106547,
3.95240736132449));
#72596=CARTESIAN_POINT('Ctrl Pts',(-1.55549973205925,-0.000912997037756428,
3.95473109533655));
#72597=CARTESIAN_POINT('Origin',(0.,0.,-1.2940562256037));
#72598=CARTESIAN_POINT('',(-1.5555,1.04251457910392E-10,4.79368285916456));
#72599=CARTESIAN_POINT('',(-1.55731034188284,-0.00109208591688013,4.65637838558307));
#72600=CARTESIAN_POINT('',(-1.5555,-1.46451138874614E-13,-1.2940562256037));
#72601=CARTESIAN_POINT('',(-1.55549960461727,0.00128691399081897,4.79358337162685));
#72602=CARTESIAN_POINT('Ctrl Pts',(-1.5555,1.04251457910392E-10,4.79368285916456));
#72603=CARTESIAN_POINT('Ctrl Pts',(-1.55549999999997,0.000428530864078361,
4.79364965059424));
#72604=CARTESIAN_POINT('Ctrl Pts',(-1.55549982291353,0.000857065800172565,
4.79361644270702));
#72605=CARTESIAN_POINT('Ctrl Pts',(-1.55549946873031,0.00128560480406378,
4.79358323553491));
#72606=CARTESIAN_POINT('Ctrl Pts',(-1.55549946766297,0.00128689557921172,
4.7935831355137));
#72607=CARTESIAN_POINT('Ctrl Pts',(-1.55544058013389,0.0724655689735681,
4.78806755282632));
#72608=CARTESIAN_POINT('Ctrl Pts',(-1.55049609564374,0.143566382762285,
4.78258209313387));
#72609=CARTESIAN_POINT('Ctrl Pts',(-1.53939498818184,0.223456484097864,
4.77659888361676));
#72610=CARTESIAN_POINT('Ctrl Pts',(-1.53800759084097,0.232814070963751,
4.77590096791649));
#72611=CARTESIAN_POINT('Ctrl Pts',(-1.53548389434461,0.248827319965951,
4.77471227496371));
#72612=CARTESIAN_POINT('Ctrl Pts',(-1.53438948968821,0.255489184388934,
4.77421942557452));
#72613=CARTESIAN_POINT('Ctrl Pts',(-1.53213016146775,0.26870375559159,4.77324540404521));
#72614=CARTESIAN_POINT('Ctrl Pts',(-1.53096647814555,0.275256589324356,
4.77276417957794));
#72615=CARTESIAN_POINT('Ctrl Pts',(-1.52844340448471,0.288953078417005,
4.77176228213858));
#72616=CARTESIAN_POINT('Ctrl Pts',(-1.52707593262449,0.296094957746632,
4.77124205807168));
#72617=CARTESIAN_POINT('Ctrl Pts',(-1.52320297555013,0.315581368821034,
4.76982801046675));
#72618=CARTESIAN_POINT('Ctrl Pts',(-1.52059748709042,0.327905800653344,
4.76893958132191));
#72619=CARTESIAN_POINT('Ctrl Pts',(-1.50395760161377,0.402147108094241,
4.7636159120303));
#72620=CARTESIAN_POINT('Ctrl Pts',(-1.48629126669349,0.463196606322958,
4.75935575163557));
#72621=CARTESIAN_POINT('Ctrl Pts',(-1.43308249456964,0.612235503630998,
4.74886735773477));
#72622=CARTESIAN_POINT('Ctrl Pts',(-1.39313960679404,0.698369260059456,
4.74271505038869));
#72623=CARTESIAN_POINT('Ctrl Pts',(-1.33317855207121,0.801766215674174,
4.73470040271835));
#72624=CARTESIAN_POINT('Ctrl Pts',(-1.32023942043558,0.822898474586927,
4.73302743517984));
#72625=CARTESIAN_POINT('Ctrl Pts',(-1.28955429604292,0.870425795424214,
4.72917218819553));
#72626=CARTESIAN_POINT('Ctrl Pts',(-1.27149303922234,0.896602789783632,
4.72698082756456));
#72627=CARTESIAN_POINT('Ctrl Pts',(-1.24379738766127,0.934222100918189,
4.72371720037957));
#72628=CARTESIAN_POINT('Ctrl Pts',(-1.23477927421008,0.946109397475254,
4.72266843820484));
#72629=CARTESIAN_POINT('Ctrl Pts',(-1.21846219984213,0.966987159740279,
4.72079390816695));
#72630=CARTESIAN_POINT('Ctrl Pts',(-1.21123112563465,0.976029429162663,
4.71997087095333));
#72631=CARTESIAN_POINT('Ctrl Pts',(-1.19572019104251,0.994987606549854,
4.71822090312841));
#72632=CARTESIAN_POINT('Ctrl Pts',(-1.18741643820315,1.004882727508,4.71729304286907));
#72633=CARTESIAN_POINT('Ctrl Pts',(-1.16464814530916,1.03133815095531,4.71477206780274));
#72634=CARTESIAN_POINT('Ctrl Pts',(-1.14995464003247,1.04769648180703,4.7131695860798));
#72635=CARTESIAN_POINT('Ctrl Pts',(-1.04893129507252,1.15548008142694,4.70230640276321));
#72636=CARTESIAN_POINT('Ctrl Pts',(-0.952150796382376,1.23644148308719,
4.69257832216735));
#72637=CARTESIAN_POINT('Ctrl Pts',(-0.790028110168338,1.34164144803684,
4.67759851604862));
#72638=CARTESIAN_POINT('Ctrl Pts',(-0.731002016487151,1.37469416185448,
4.67238443315003));
#72639=CARTESIAN_POINT('Ctrl Pts',(-0.655318630388377,1.41081631425189,
4.66612549217126));
#72640=CARTESIAN_POINT('Ctrl Pts',(-0.640519365806971,1.4175966201511,4.66492108803867));
#72641=CARTESIAN_POINT('Ctrl Pts',(-0.618269149151414,1.42737097327888,
4.66314200798544));
#72642=CARTESIAN_POINT('Ctrl Pts',(-0.610897575785989,1.43054143444812,
4.66255771762055));
#72643=CARTESIAN_POINT('Ctrl Pts',(-0.598108061055424,1.43592522165312,
4.66155322531566));
#72644=CARTESIAN_POINT('Ctrl Pts',(-0.592701828646886,1.43816516449059,
4.6611314770918));
#72645=CARTESIAN_POINT('Ctrl Pts',(-0.579865363989483,1.44339896564495,
4.66013680362941));
#72646=CARTESIAN_POINT('Ctrl Pts',(-0.57242448301163,1.44636600940417,4.65956547380703));
#72647=CARTESIAN_POINT('Ctrl Pts',(-0.549862417074104,1.4551612194953,4.65784794487773));
#72648=CARTESIAN_POINT('Ctrl Pts',(-0.534672203317368,1.46081091918562,
4.65671162754101));
#72649=CARTESIAN_POINT('Ctrl Pts',(-0.447708121886464,1.49161713745868,
4.65030435190047));
#72650=CARTESIAN_POINT('Ctrl Pts',(-0.37424517945838,1.51172342252536,4.64526639207819));
#72651=CARTESIAN_POINT('Ctrl Pts',(-0.220104360418011,1.54197826773324,
4.63491506005674));
#72652=CARTESIAN_POINT('Ctrl Pts',(-0.139517540184281,1.55134681465798,
4.62961813671609));
#72653=CARTESIAN_POINT('Ctrl Pts',(-0.0271220723330674,1.55558188772191,
4.62205426207034));
#72654=CARTESIAN_POINT('Ctrl Pts',(0.00435269819245649,1.55581215854594,
4.61991805171286));
#72655=CARTESIAN_POINT('Ctrl Pts',(0.0604927116598626,1.55451933947443,
4.61605794081641));
#72656=CARTESIAN_POINT('Ctrl Pts',(0.0851558335524943,1.55336348381762,
4.61434497984134));
#72657=CARTESIAN_POINT('Ctrl Pts',(0.123216183101447,1.55067064853022,4.61166933840946));
#72658=CARTESIAN_POINT('Ctrl Pts',(0.136639181108704,1.54954554685792,4.61071950996269));
#72659=CARTESIAN_POINT('Ctrl Pts',(0.161503126375638,1.54713590230741,4.60894774831573));
#72660=CARTESIAN_POINT('Ctrl Pts',(0.172947775880819,1.54589838403586,4.60812735120939));
#72661=CARTESIAN_POINT('Ctrl Pts',(0.198382823785304,1.54286209801361,4.60629268879579));
#72662=CARTESIAN_POINT('Ctrl Pts',(0.21236445512609,1.54099984168584,4.60527648483814));
#72663=CARTESIAN_POINT('Ctrl Pts',(0.247946578775081,1.53576711720121,4.60266983205447));
#72664=CARTESIAN_POINT('Ctrl Pts',(0.269504219739021,1.53213104201285,4.60107119621729));
#72665=CARTESIAN_POINT('Ctrl Pts',(0.384624600074086,1.5102092668917,4.59242626857688));
#72666=CARTESIAN_POINT('Ctrl Pts',(0.476418858607355,1.48380843137654,4.58512993525905));
#72667=CARTESIAN_POINT('Ctrl Pts',(0.629771040168057,1.42399843674715,4.57237747368261));
#72668=CARTESIAN_POINT('Ctrl Pts',(0.692583859762,1.39452909629116,4.56698137543402));
#72669=CARTESIAN_POINT('Ctrl Pts',(0.783492461604464,1.34421599173406,4.55906142809076));
#72670=CARTESIAN_POINT('Ctrl Pts',(0.813196589775267,1.32645723849003,4.55645551301168));
#72671=CARTESIAN_POINT('Ctrl Pts',(0.851199896223808,1.30197980126336,4.55311995814195));
#72672=CARTESIAN_POINT('Ctrl Pts',(0.860055029746958,1.29614737924565,4.55234264328249));
#72673=CARTESIAN_POINT('Ctrl Pts',(0.874525238338738,1.2864029963958,4.55107314443031));
#72674=CARTESIAN_POINT('Ctrl Pts',(0.880175222084871,1.2825438183348,4.55057764340932));
#72675=CARTESIAN_POINT('Ctrl Pts',(0.891530391551703,1.2746773757119,4.54958246338089));
#72676=CARTESIAN_POINT('Ctrl Pts',(0.897234444896402,1.27066880312863,4.54908288430815));
#72677=CARTESIAN_POINT('Ctrl Pts',(0.912037844099199,1.26011619911593,4.54778666563331));
#72678=CARTESIAN_POINT('Ctrl Pts',(0.921093954489292,1.25351179118699,4.54699400090288));
#72679=CARTESIAN_POINT('Ctrl Pts',(0.960279530654349,1.22428066806721,4.54356164736946));
#72680=CARTESIAN_POINT('Ctrl Pts',(0.989655198539604,1.20065942562923,4.54098191101041));
#72681=CARTESIAN_POINT('Ctrl Pts',(1.0816614319476,1.12100259481197,4.53277290929936));
#72682=CARTESIAN_POINT('Ctrl Pts',(1.14062080283282,1.06095439050667,4.52730148108551));
#72683=CARTESIAN_POINT('Ctrl Pts',(1.23895514859959,0.943079208231,4.51717441324297));
#72684=CARTESIAN_POINT('Ctrl Pts',(1.27983646298868,0.886806317016336,4.51255384436832));
#72685=CARTESIAN_POINT('Ctrl Pts',(1.33193256132645,0.803954133982975,4.50585710819311));
#72686=CARTESIAN_POINT('Ctrl Pts',(1.34638593216738,0.779507117765701,4.50389383504533));
#72687=CARTESIAN_POINT('Ctrl Pts',(1.36704546296176,0.74227237509779,4.50091362883222));
#72688=CARTESIAN_POINT('Ctrl Pts',(1.37375920408996,0.729772020652281,4.49991479091137));
#72689=CARTESIAN_POINT('Ctrl Pts',(1.38561010704412,0.706963566862782,4.49809427326667));
#72690=CARTESIAN_POINT('Ctrl Pts',(1.39080563561327,0.696686819519434,4.49727472650226));
#72691=CARTESIAN_POINT('Ctrl Pts',(1.40179992371849,0.67432694805489,4.49549259676014));
#72692=CARTESIAN_POINT('Ctrl Pts',(1.40755753466916,0.662224753922708,4.49452865776503));
#72693=CARTESIAN_POINT('Ctrl Pts',(1.42305210973537,0.628540759900732,4.49184663449693));
#72694=CARTESIAN_POINT('Ctrl Pts',(1.43245342776712,0.606809572133582,4.49011729399258));
#72695=CARTESIAN_POINT('Ctrl Pts',(1.48150617338333,0.485924592730933,4.48049739876968));
#72696=CARTESIAN_POINT('Ctrl Pts',(1.51135484391414,0.383121395576644,4.47228752974989));
#72697=CARTESIAN_POINT('Ctrl Pts',(1.54138264068597,0.217868225321859,4.45926116323008));
#72698=CARTESIAN_POINT('Ctrl Pts',(1.54876205009271,0.157047278119586,4.45450889172274));
#72699=CARTESIAN_POINT('Ctrl Pts',(1.55452907558365,0.0637299916082448,
4.44739621538762));
#72700=CARTESIAN_POINT('Ctrl Pts',(1.55551697158987,0.0314558088291498,
4.44496921151467));
#72701=CARTESIAN_POINT('Ctrl Pts',(1.55549426158034,-0.0111900230157694,
4.44182436116208));
#72702=CARTESIAN_POINT('Ctrl Pts',(1.55538520993825,-0.021551769590433,
4.44106510407128));
#72703=CARTESIAN_POINT('Ctrl Pts',(1.55503327193343,-0.0387028079584424,
4.4398172237534));
#72704=CARTESIAN_POINT('Ctrl Pts',(1.55484944367305,-0.0454928359895294,
4.43932549492275));
#72705=CARTESIAN_POINT('Ctrl Pts',(1.5544137180105,-0.0584493484662753,
4.43839185321851));
#72706=CARTESIAN_POINT('Ctrl Pts',(1.55416959387067,-0.0646158659789873,
4.43794949511199));
#72707=CARTESIAN_POINT('Ctrl Pts',(1.55340479991883,-0.0814057703177556,
4.43675010586722));
#72708=CARTESIAN_POINT('Ctrl Pts',(1.55281185106637,-0.092025777352445,
4.43599696481035));
#72709=CARTESIAN_POINT('Ctrl Pts',(1.54999796374082,-0.134577359051323,
4.43299835537197));
#72710=CARTESIAN_POINT('Ctrl Pts',(1.54690045637132,-0.166445423374152,
4.43079557698552));
#72711=CARTESIAN_POINT('Ctrl Pts',(1.53019177512169,-0.296510002970112,
4.4218981528355));
#72712=CARTESIAN_POINT('Ctrl Pts',(1.50819324691509,-0.39339711772293,4.41547621216647));
#72713=CARTESIAN_POINT('Ctrl Pts',(1.45779045323088,-0.546105395332603,
4.4048429632506));
#72714=CARTESIAN_POINT('Ctrl Pts',(1.43499523353654,-0.603466388729109,
4.40072591498259));
#72715=CARTESIAN_POINT('Ctrl Pts',(1.39694279477168,-0.684778199914722,
4.39458096007229));
#72716=CARTESIAN_POINT('Ctrl Pts',(1.38434129430823,-0.709907999815673,
4.39263705199916));
#72717=CARTESIAN_POINT('Ctrl Pts',(1.36439039510398,-0.747140482757923,
4.38968031979611));
#72718=CARTESIAN_POINT('Ctrl Pts',(1.35754490063065,-0.759507650105684,
4.38868515507894));
#72719=CARTESIAN_POINT('Ctrl Pts',(1.34481986832163,-0.781775104078759,
4.38686846884788));
#72720=CARTESIAN_POINT('Ctrl Pts',(1.33899707302187,-0.791706774612295,
4.38604903619909));
#72721=CARTESIAN_POINT('Ctrl Pts',(1.32613625893716,-0.813095100785673,
4.38426383911097));
#72722=CARTESIAN_POINT('Ctrl Pts',(1.31905891396428,-0.824526882871743,
4.38329668194154));
#72723=CARTESIAN_POINT('Ctrl Pts',(1.29900310482698,-0.85600313413033,4.38059652387313));
#72724=CARTESIAN_POINT('Ctrl Pts',(1.28571043326944,-0.875841878720963,
4.37885201729909));
#72725=CARTESIAN_POINT('Ctrl Pts',(1.21411933108679,-0.977545027687594,
4.36967825076646));
#72726=CARTESIAN_POINT('Ctrl Pts',(1.14845354541913,-1.05391075698835,4.36197062707782));
#72727=CARTESIAN_POINT('Ctrl Pts',(1.02854554932362,-1.16874846038424,4.34909950599572));
#72728=CARTESIAN_POINT('Ctrl Pts',(0.978372659379748,-1.21106010396637,
4.34400092813692));
#72729=CARTESIAN_POINT('Ctrl Pts',(0.90736814428987,-1.26363853549167,4.3372720926326));
#72730=CARTESIAN_POINT('Ctrl Pts',(0.888762152577831,-1.27679334611285,
4.33555075944941));
#72731=CARTESIAN_POINT('Ctrl Pts',(0.856107167031115,-1.2988211927873,4.33260934071207));
#72732=CARTESIAN_POINT('Ctrl Pts',(0.842192887064523,-1.307886528707,4.33138011845895));
#72733=CARTESIAN_POINT('Ctrl Pts',(0.821289749962543,-1.32103323057204,
4.32957195685271));
#72734=CARTESIAN_POINT('Ctrl Pts',(0.814410437454078,-1.32528536429933,
4.32898295788945));
#72735=CARTESIAN_POINT('Ctrl Pts',(0.802494214796415,-1.33252300570012,
4.32797354011803));
#72736=CARTESIAN_POINT('Ctrl Pts',(0.7974732780799,-1.33553393802237,4.32755152293823));
#72737=CARTESIAN_POINT('Ctrl Pts',(0.785593818980809,-1.34256687368055,
4.32656077942254));
#72738=CARTESIAN_POINT('Ctrl Pts',(0.778721310588699,-1.34656473536779,
4.32599359626356));
#72739=CARTESIAN_POINT('Ctrl Pts',(0.758016350942587,-1.35839764856804,
4.32430174549617));
#72740=CARTESIAN_POINT('Ctrl Pts',(0.744093639891219,-1.36607381438885,
4.32318653094773));
#72741=CARTESIAN_POINT('Ctrl Pts',(0.628759153273436,-1.4273758440877,4.3141102729709));
#72742=CARTESIAN_POINT('Ctrl Pts',(0.521803467995819,-1.46985329939973,
4.30669296867691));
#72743=CARTESIAN_POINT('Ctrl Pts',(0.345193773878057,-1.51825438254038,
4.29460866749738));
#72744=CARTESIAN_POINT('Ctrl Pts',(0.278138769947949,-1.53195709685333,
4.29005945003893));
#72745=CARTESIAN_POINT('Ctrl Pts',(0.182313848869221,-1.54503905716723,
4.28344145935312));
#72746=CARTESIAN_POINT('Ctrl Pts',(0.154125464502821,-1.54810503427325,
4.28148123655028));
#72747=CARTESIAN_POINT('Ctrl Pts',(0.111736487475051,-1.55154642016391,
4.27850472686826));
#72748=CARTESIAN_POINT('Ctrl Pts',(0.0975878925415331,-1.55250053659826,
4.27750646615948));
#72749=CARTESIAN_POINT('Ctrl Pts',(0.0719302910522939,-1.55387865569258,
4.27568655213387));
#72750=CARTESIAN_POINT('Ctrl Pts',(0.0604257337587508,-1.55436854092594,
4.2748670248509));
#72751=CARTESIAN_POINT('Ctrl Pts',(0.03551516501753,-1.55515231153641,4.27308442068608));
#72752=CARTESIAN_POINT('Ctrl Pts',(0.0221087659811843,-1.555400662389,4.27211998207671));
#72753=CARTESIAN_POINT('Ctrl Pts',(-0.0150056485346113,-1.55560827761934,
4.26943514643759));
#72754=CARTESIAN_POINT('Ctrl Pts',(-0.0387111595504639,-1.55519889861018,
4.26770345465379));
#72755=CARTESIAN_POINT('Ctrl Pts',(-0.168413921750909,-1.54999184722815,
4.258131150699));
#72756=CARTESIAN_POINT('Ctrl Pts',(-0.273698966111196,-1.53490038864118,
4.24997585058189));
#72757=CARTESIAN_POINT('Ctrl Pts',(-0.436441819911803,-1.49428966386498,
4.23696737218199));
#72758=CARTESIAN_POINT('Ctrl Pts',(-0.495336049373005,-1.47581366986062,
4.23217882310577));
#72759=CARTESIAN_POINT('Ctrl Pts',(-0.583279118989948,-1.44236491499426,
4.22502009047497));
#72760=CARTESIAN_POINT('Ctrl Pts',(-0.613213100195878,-1.4298954977857,
4.22258245028437));
#72761=CARTESIAN_POINT('Ctrl Pts',(-0.652187203406116,-1.41221095269598,
4.21942620939261));
#72762=CARTESIAN_POINT('Ctrl Pts',(-0.661593718060217,-1.40782871512499,
4.21866583671004));
#72763=CARTESIAN_POINT('Ctrl Pts',(-0.677086589934567,-1.40042142764064,
4.21741662378376));
#72764=CARTESIAN_POINT('Ctrl Pts',(-0.683198102406986,-1.39745010091746,
4.21692466493895));
#72765=CARTESIAN_POINT('Ctrl Pts',(-0.695592116388903,-1.3913235699585,
4.21592894259169));
#72766=CARTESIAN_POINT('Ctrl Pts',(-0.701873045912329,-1.38816566064146,
4.21542535232761));
#72767=CARTESIAN_POINT('Ctrl Pts',(-0.718351764157794,-1.37974009422637,
4.2141062276919));
#72768=CARTESIAN_POINT('Ctrl Pts',(-0.728513267443662,-1.37440184242834,
4.21329493117076));
#72769=CARTESIAN_POINT('Ctrl Pts',(-0.774146676596818,-1.34978042252123,
4.20965694410608));
#72770=CARTESIAN_POINT('Ctrl Pts',(-0.808921954787956,-1.3292314248599,
4.20689931511098));
#72771=CARTESIAN_POINT('Ctrl Pts',(-0.969469307350372,-1.22572500949163,
4.19404694897266));
#72772=CARTESIAN_POINT('Ctrl Pts',(-1.08354755812998,-1.12614435499403,
4.18446716649846));
#72773=CARTESIAN_POINT('Ctrl Pts',(-1.19992863481184,-0.990227971589131,
4.17222188996328));
#72774=CARTESIAN_POINT('Ctrl Pts',(-1.2177335920345,-0.968248363096394,
4.1702662623625));
#72775=CARTESIAN_POINT('Ctrl Pts',(-1.24354309853171,-0.934548841333982,
4.16729532207042));
#72776=CARTESIAN_POINT('Ctrl Pts',(-1.25200322627368,-0.923184094619307,
4.1662979318824));
#72777=CARTESIAN_POINT('Ctrl Pts',(-1.2670554074814,-0.90237654151281,4.16447892712253));
#72778=CARTESIAN_POINT('Ctrl Pts',(-1.27370015415414,-0.892972974138926,
4.16365942813738));
#72779=CARTESIAN_POINT('Ctrl Pts',(-1.28786133414336,-0.872452575355153,
4.16187610317046));
#72780=CARTESIAN_POINT('Ctrl Pts',(-1.29533947603909,-0.861310590357592,
4.1609109068083));
#72781=CARTESIAN_POINT('Ctrl Pts',(-1.3156542762789,-0.830179722488268,
4.15822180361493));
#72782=CARTESIAN_POINT('Ctrl Pts',(-1.32817810994251,-0.80999218461234,
4.15648654346149));
#72783=CARTESIAN_POINT('Ctrl Pts',(-1.39348787786544,-0.69912782452935,
4.14699739623331));
#72784=CARTESIAN_POINT('Ctrl Pts',(-1.4374497295426,-0.603588467139476,
4.13893673535704));
#72785=CARTESIAN_POINT('Ctrl Pts',(-1.49171395958147,-0.445277598252304,
4.12595855220623));
#72786=CARTESIAN_POINT('Ctrl Pts',(-1.50839238102825,-0.385014066723115,
4.12110617965291));
#72787=CARTESIAN_POINT('Ctrl Pts',(-1.52820213981031,-0.291967360627213,
4.11386659099218));
#72788=CARTESIAN_POINT('Ctrl Pts',(-1.53399545860567,-0.259817285894605,
4.11141040467801));
#72789=CARTESIAN_POINT('Ctrl Pts',(-1.54029408603605,-0.21721553247269,
4.10823431896477));
#72790=CARTESIAN_POINT('Ctrl Pts',(-1.54171231715226,-0.206909656570853,
4.10747201412035));
#72791=CARTESIAN_POINT('Ctrl Pts',(-1.54388657416256,-0.189843995991795,
4.10622049218401));
#72792=CARTESIAN_POINT('Ctrl Pts',(-1.54470182658022,-0.183092244570194,
4.10572813396047));
#72793=CARTESIAN_POINT('Ctrl Pts',(-1.54626892851389,-0.169357525464194,
4.10473250011569));
#72794=CARTESIAN_POINT('Ctrl Pts',(-1.54701781528832,-0.162374428846498,
4.10422938914682));
#72795=CARTESIAN_POINT('Ctrl Pts',(-1.5488627337859,-0.143998189223383,
4.10291299864447));
#72796=CARTESIAN_POINT('Ctrl Pts',(-1.54988038597653,-0.132597346281921,
4.10210392525345));
#72797=CARTESIAN_POINT('Ctrl Pts',(-1.55389503583024,-0.081223310025769,
4.09848818386706));
#72798=CARTESIAN_POINT('Ctrl Pts',(-1.55547235254112,-0.0411509399644201,
4.09574958078276));
#72799=CARTESIAN_POINT('Ctrl Pts',(-1.55549987993421,-0.000705786165981674,
4.09302759314932));
#72800=CARTESIAN_POINT('Ctrl Pts',(-1.55550000000001,-0.000352891711195591,
4.09300384633061));
#72801=CARTESIAN_POINT('Ctrl Pts',(-1.5555,3.27936543916168E-11,4.09298010292487));
#72802=CARTESIAN_POINT('Ctrl Pts',(-1.55549973205925,-0.000912997037756428,
3.95473109533655));
#72803=CARTESIAN_POINT('Ctrl Pts',(-1.55547442119289,-0.0440358596668717,
3.95793925547094));
#72804=CARTESIAN_POINT('Ctrl Pts',(-1.55365590759048,-0.087135391172154,
3.96119733324091));
#72805=CARTESIAN_POINT('Ctrl Pts',(-1.54478301234824,-0.192849268283468,
3.96930457206507));
#72806=CARTESIAN_POINT('Ctrl Pts',(-1.53571114152528,-0.255217351088432,
3.97419014007038));
#72807=CARTESIAN_POINT('Ctrl Pts',(-1.50717787626475,-0.392353145500239,
3.98504927277714));
#72808=CARTESIAN_POINT('Ctrl Pts',(-1.48587679832324,-0.466582170598623,
3.9910076496691));
#72809=CARTESIAN_POINT('Ctrl Pts',(-1.4546499626027,-0.551128654226623,
3.99769308726693));
#72810=CARTESIAN_POINT('Ctrl Pts',(-1.44999215891354,-0.563269097227302,
3.99865040418915));
#72811=CARTESIAN_POINT('Ctrl Pts',(-1.44241760503056,-0.582295095615148,
4.00014489916246));
#72812=CARTESIAN_POINT('Ctrl Pts',(-1.43960263872068,-0.589220140984957,
4.00068764464964));
#72813=CARTESIAN_POINT('Ctrl Pts',(-1.43411876921503,-0.602436974585278,
4.00172080312903));
#72814=CARTESIAN_POINT('Ctrl Pts',(-1.4314581810049,-0.60873182160191,4.00221164564211));
#72815=CARTESIAN_POINT('Ctrl Pts',(-1.4248338683996,-0.624121070490411,
4.00340903529682));
#72816=CARTESIAN_POINT('Ctrl Pts',(-1.42082437689268,-0.633195678206351,
4.00411288801435));
#72817=CARTESIAN_POINT('Ctrl Pts',(-1.4054614535129,-0.667085455942641,
4.00673544167841));
#72818=CARTESIAN_POINT('Ctrl Pts',(-1.39354176396732,-0.691640428234245,
4.00862341613449));
#72819=CARTESIAN_POINT('Ctrl Pts',(-1.35975329036538,-0.756821526832915,
4.01363590687048));
#72820=CARTESIAN_POINT('Ctrl Pts',(-1.33671277383052,-0.796810771144227,
4.01671241455552));
#72821=CARTESIAN_POINT('Ctrl Pts',(-1.24957538040695,-0.933600627281844,
4.02744477658827));
#72822=CARTESIAN_POINT('Ctrl Pts',(-1.17647042366368,-1.02418967787595,
4.03496773987277));
#72823=CARTESIAN_POINT('Ctrl Pts',(-1.07177626557557,-1.1277636087137,4.04501285872777));
#72824=CARTESIAN_POINT('Ctrl Pts',(-1.04892516950108,-1.14904781663746,
4.04716622957676));
#72825=CARTESIAN_POINT('Ctrl Pts',(-1.01422593641133,-1.17946972413543,
4.05039175445449));
#72826=CARTESIAN_POINT('Ctrl Pts',(-1.00286076803103,-1.18914815425578,
4.0514415069433));
#72827=CARTESIAN_POINT('Ctrl Pts',(-0.982230770878005,-1.20621029048426,
4.05333630916446));
#72828=CARTESIAN_POINT('Ctrl Pts',(-0.973017437502269,-1.21365464785958,
4.05417880994716));
#72829=CARTESIAN_POINT('Ctrl Pts',(-0.953119805087376,-1.22935969491474,
4.05599102146509));
#72830=CARTESIAN_POINT('Ctrl Pts',(-0.942411209170514,-1.23758786105403,
4.05696193286735));
#72831=CARTESIAN_POINT('Ctrl Pts',(-0.912540963779694,-1.2599267762182,
4.0596590159752));
#72832=CARTESIAN_POINT('Ctrl Pts',(-0.893161301883402,-1.2737383031633,
4.06139651028508));
#72833=CARTESIAN_POINT('Ctrl Pts',(-0.808751925347577,-1.33102164782062,
4.06891642171485));
#72834=CARTESIAN_POINT('Ctrl Pts',(-0.740819507006789,-1.36999321474931,
4.07485769615849));
#72835=CARTESIAN_POINT('Ctrl Pts',(-0.592947371564184,-1.44060151612279,
4.08749747394751));
#72836=CARTESIAN_POINT('Ctrl Pts',(-0.512722798417722,-1.47106592767015,
4.09419388516707));
#72837=CARTESIAN_POINT('Ctrl Pts',(-0.396722666041979,-1.50446647500579,
4.10340229228826));
#72838=CARTESIAN_POINT('Ctrl Pts',(-0.362726844111519,-1.51302277637698,
4.10604456354845));
#72839=CARTESIAN_POINT('Ctrl Pts',(-0.317585429133268,-1.52277500187325,
4.10945595349642));
#72840=CARTESIAN_POINT('Ctrl Pts',(-0.306677355981792,-1.52500925557806,
4.11027288813249));
#72841=CARTESIAN_POINT('Ctrl Pts',(-0.289489116800832,-1.52833795861851,
4.11154757935786));
#72842=CARTESIAN_POINT('Ctrl Pts',(-0.28322487481074,-1.52951120908663,
4.11200952367222));
#72843=CARTESIAN_POINT('Ctrl Pts',(-0.270120136652234,-1.53188236645063,
4.11297020012463));
#72844=CARTESIAN_POINT('Ctrl Pts',(-0.263278532149541,-1.53307302185879,
4.11346847554919));
#72845=CARTESIAN_POINT('Ctrl Pts',(-0.246061259271781,-1.53595071564451,
4.11471472160873));
#72846=CARTESIAN_POINT('Ctrl Pts',(-0.235675778250731,-1.53757851437402,
4.11545946244713));
#72847=CARTESIAN_POINT('Ctrl Pts',(-0.193421924532214,-1.54376310138674,
4.1184640700009));
#72848=CARTESIAN_POINT('Ctrl Pts',(-0.161429806091551,-1.54743572610124,
4.12068046200815));
#72849=CARTESIAN_POINT('Ctrl Pts',(-0.069073154729982,-1.55514212575297,
4.12697080183731));
#72850=CARTESIAN_POINT('Ctrl Pts',(-0.0085557153238808,-1.55665216966412,
4.13096182223911));
#72851=CARTESIAN_POINT('Ctrl Pts',(0.158779093940321,-1.55106588844895,
4.14198712026154));
#72852=CARTESIAN_POINT('Ctrl Pts',(0.264993374155987,-1.53648674054823,
4.14899373602919));
#72853=CARTESIAN_POINT('Ctrl Pts',(0.392058327885954,-1.50547015195689,
4.15799212555762));
#72854=CARTESIAN_POINT('Ctrl Pts',(0.415114644260933,-1.49927643812977,
4.15964935281536));
#72855=CARTESIAN_POINT('Ctrl Pts',(0.4511213048867,-1.48870960690779,4.16228122017885));
#72856=CARTESIAN_POINT('Ctrl Pts',(0.464172724791209,-1.4846920171426,4.16324436338655));
#72857=CARTESIAN_POINT('Ctrl Pts',(0.488427397740782,-1.47687468681791,
4.1650523315718));
#72858=CARTESIAN_POINT('Ctrl Pts',(0.499643550448358,-1.47311794223613,
4.16589568967408));
#72859=CARTESIAN_POINT('Ctrl Pts',(0.52471110318168,-1.46440258683413,4.16779755271291));
#72860=CARTESIAN_POINT('Ctrl Pts',(0.538537019503519,-1.45937470484351,
4.16885828885042));
#72861=CARTESIAN_POINT('Ctrl Pts',(0.580355041979949,-1.44349215315319,
4.17210369872703));
#72862=CARTESIAN_POINT('Ctrl Pts',(0.608104564417459,-1.43202310729415,
4.17430851122494));
#72863=CARTESIAN_POINT('Ctrl Pts',(0.672733860572164,-1.40309416822269,
4.1795691170087));
#72864=CARTESIAN_POINT('Ctrl Pts',(0.709291584777175,-1.38497257839226,
4.18264462470429));
#72865=CARTESIAN_POINT('Ctrl Pts',(0.80296895081271,-1.33385465506529,4.19078279856107));
#72866=CARTESIAN_POINT('Ctrl Pts',(0.858775778246576,-1.29862640751106,
4.19589598309198));
#72867=CARTESIAN_POINT('Ctrl Pts',(0.971039553426938,-1.21735100782933,
4.20664157984781));
#72868=CARTESIAN_POINT('Ctrl Pts',(1.02685050203534,-1.17065852205525,4.2122611747609));
#72869=CARTESIAN_POINT('Ctrl Pts',(1.09098249133582,-1.10887569058425,4.21890769995172));
#72870=CARTESIAN_POINT('Ctrl Pts',(1.10258950023114,-1.09733520121345,4.22011875144394));
#72871=CARTESIAN_POINT('Ctrl Pts',(1.11971053036842,-1.07976628367956,4.22191460917113));
#72872=CARTESIAN_POINT('Ctrl Pts',(1.12536232322705,-1.07387454977935,4.22250903476636));
#72873=CARTESIAN_POINT('Ctrl Pts',(1.13509510611368,-1.06356734266233,4.22353504796563));
#72874=CARTESIAN_POINT('Ctrl Pts',(1.1391971415892,-1.05917244488544,4.22396819269118));
#72875=CARTESIAN_POINT('Ctrl Pts',(1.14892289373412,-1.04863045886817,4.22499694490678));
#72876=CARTESIAN_POINT('Ctrl Pts',(1.15452284517919,-1.0424618282644,4.22559078463061));
#72877=CARTESIAN_POINT('Ctrl Pts',(1.17155707289206,-1.02339212305458,4.22740291580726));
#72878=CARTESIAN_POINT('Ctrl Pts',(1.1828271290968,-1.01034521796368,4.22860994992658));
#72879=CARTESIAN_POINT('Ctrl Pts',(1.20914514724829,-0.978833725395201,
4.2314559725448));
#72880=CARTESIAN_POINT('Ctrl Pts',(1.22399079902061,-0.960205239184679,
4.23308373034422));
#72881=CARTESIAN_POINT('Ctrl Pts',(1.28111466809978,-0.885046678936661,
4.23947128777618));
#72882=CARTESIAN_POINT('Ctrl Pts',(1.31995416291179,-0.826005317666755,
4.24410058554386));
#72883=CARTESIAN_POINT('Ctrl Pts',(1.40020215534977,-0.683815300086653,
4.25484820172164));
#72884=CARTESIAN_POINT('Ctrl Pts',(1.43844394090004,-0.599204237829116,
4.26096528282764));
#72885=CARTESIAN_POINT('Ctrl Pts',(1.47689132675248,-0.488833807938492,
4.2690022473666));
#72886=CARTESIAN_POINT('Ctrl Pts',(1.48432087280456,-0.46578741930575,4.27068250128885));
#72887=CARTESIAN_POINT('Ctrl Pts',(1.49511524256221,-0.429417194574645,
4.27334276084799));
#72888=CARTESIAN_POINT('Ctrl Pts',(1.4988467587665,-0.41620558349433,4.27431084442048));
#72889=CARTESIAN_POINT('Ctrl Pts',(1.50546540379897,-0.391527700873713,
4.27612325498091));
#72890=CARTESIAN_POINT('Ctrl Pts',(1.50839762775139,-0.380074472994539,
4.27696605090734));
#72891=CARTESIAN_POINT('Ctrl Pts',(1.51466216248913,-0.354390167030362,
4.27886028069304));
#72892=CARTESIAN_POINT('Ctrl Pts',(1.51792497970881,-0.34014347834996,4.27991386570177));
#72893=CARTESIAN_POINT('Ctrl Pts',(1.52716564254308,-0.29701081687955,4.28311343693397));
#72894=CARTESIAN_POINT('Ctrl Pts',(1.53252274268747,-0.268000279806779,
4.28527873165686));
#72895=CARTESIAN_POINT('Ctrl Pts',(1.54804801909595,-0.168094572402591,
4.2927856115967));
#72896=CARTESIAN_POINT('Ctrl Pts',(1.55414335791219,-0.0966666733046356,
4.29824356176868));
#72897=CARTESIAN_POINT('Ctrl Pts',(1.55675352456443,0.0651892654033261,
4.31074068532827));
#72898=CARTESIAN_POINT('Ctrl Pts',(1.55034760134611,0.155416528568425,4.31780165767729));
#72899=CARTESIAN_POINT('Ctrl Pts',(1.53158038601086,0.273288939038589,4.32685879977827));
#72900=CARTESIAN_POINT('Ctrl Pts',(1.52620525445035,0.301866050016731,4.32904014538075));
#72901=CARTESIAN_POINT('Ctrl Pts',(1.51781764021891,0.340468218081552,4.33195288822122));
#72902=CARTESIAN_POINT('Ctrl Pts',(1.51550093803742,0.350636448783077,4.33271690403882));
#72903=CARTESIAN_POINT('Ctrl Pts',(1.51163432371025,0.366852671802875,4.3339293603915));
#72904=CARTESIAN_POINT('Ctrl Pts',(1.51015001318952,0.372915745006729,4.33438133900417));
#72905=CARTESIAN_POINT('Ctrl Pts',(1.506900106992,0.385853194321856,4.33534265808603));
#72906=CARTESIAN_POINT('Ctrl Pts',(1.50512386907097,0.392724794476646,4.33585136537074));
#72907=CARTESIAN_POINT('Ctrl Pts',(1.5004109437553,0.410455585273452,4.33715967514111));
#72908=CARTESIAN_POINT('Ctrl Pts',(1.4974033203625,0.421295743245762,4.33795534936006));
#72909=CARTESIAN_POINT('Ctrl Pts',(1.48323262790042,0.470300194912241,4.34153729535848));
#72910=CARTESIAN_POINT('Ctrl Pts',(1.4707253201229,0.508063929082514,4.34425624880874));
#72911=CARTESIAN_POINT('Ctrl Pts',(1.4248933097274,0.630503034587347,4.35306190865689));
#72912=CARTESIAN_POINT('Ctrl Pts',(1.38559037034461,0.712738548353561,4.35896903796059));
#72913=CARTESIAN_POINT('Ctrl Pts',(1.30120666760964,0.855604378996572,4.3699459590959));
#72914=CARTESIAN_POINT('Ctrl Pts',(1.25848062635195,0.917290599815871,4.37496410860436));
#72915=CARTESIAN_POINT('Ctrl Pts',(1.19888497557155,0.991291197923033,4.381540065551));
#72916=CARTESIAN_POINT('Ctrl Pts',(1.18598966112629,1.00668360627153,4.38294072463355));
#72917=CARTESIAN_POINT('Ctrl Pts',(1.16443389142406,1.03142434404389,4.38524954791367));
#72918=CARTESIAN_POINT('Ctrl Pts',(1.15594986849713,1.04092379602623,4.38615042943682));
#72919=CARTESIAN_POINT('Ctrl Pts',(1.13920890034059,1.05921136294441,4.38791376441057));
#72920=CARTESIAN_POINT('Ctrl Pts',(1.13096451243298,1.06800977829544,4.38877564689549));
#72921=CARTESIAN_POINT('Ctrl Pts',(1.11116567889158,1.08865277302545,4.39083082366904));
#72922=CARTESIAN_POINT('Ctrl Pts',(1.09952309498047,1.10041035549216,4.39202789482905));
#72923=CARTESIAN_POINT('Ctrl Pts',(1.05805487789144,1.14097296796636,4.39625372929405));
#72924=CARTESIAN_POINT('Ctrl Pts',(1.02726956244842,1.16876691246246,4.39932475660458));
#72925=CARTESIAN_POINT('Ctrl Pts',(0.944705135715565,1.23752456501332,4.40740016034365));
#72926=CARTESIAN_POINT('Ctrl Pts',(0.891365997969124,1.27647949066352,4.4124677122007));
#72927=CARTESIAN_POINT('Ctrl Pts',(0.752305845475298,1.36506321244349,4.42523157422567));
#72928=CARTESIAN_POINT('Ctrl Pts',(0.664008124868332,1.41012690672247,4.43295844324156));
#72929=CARTESIAN_POINT('Ctrl Pts',(0.558043028650829,1.45203107233191,4.44144656322845));
#72930=CARTESIAN_POINT('Ctrl Pts',(0.54398282983077,1.45735684784334,4.44255734910481));
#72931=CARTESIAN_POINT('Ctrl Pts',(0.522333352922855,1.46520032167599,4.44424183838768));
#72932=CARTESIAN_POINT('Ctrl Pts',(0.514798661286699,1.4678645918828,4.4448233460133));
#72933=CARTESIAN_POINT('Ctrl Pts',(0.500911398612565,1.47265504719746,4.44588600072083));
#72934=CARTESIAN_POINT('Ctrl Pts',(0.494565390129854,1.47479835744498,4.44636807119652));
#72935=CARTESIAN_POINT('Ctrl Pts',(0.479722101696619,1.47970496524575,4.44748762311549));
#72936=CARTESIAN_POINT('Ctrl Pts',(0.471214587151072,1.48243613761681,4.44812325863881));
#72937=CARTESIAN_POINT('Ctrl Pts',(0.442979032400118,1.49123297648234,4.45021440882616));
#72938=CARTESIAN_POINT('Ctrl Pts',(0.423152862096039,1.49697961719711,4.45165308515535));
#72939=CARTESIAN_POINT('Ctrl Pts',(0.373727058224117,1.51024522437844,4.45518017835617));
#72940=CARTESIAN_POINT('Ctrl Pts',(0.344008552218119,1.51729064633663,4.45724878492633));
#72941=CARTESIAN_POINT('Ctrl Pts',(0.190364084958346,1.54896843078223,4.4677667523882));
#72942=CARTESIAN_POINT('Ctrl Pts',(0.0639816913856013,1.5593107781163,4.47587314684393));
#72943=CARTESIAN_POINT('Ctrl Pts',(-0.102821639041292,1.552628589251,4.48714780763645));
#72944=CARTESIAN_POINT('Ctrl Pts',(-0.143297143133573,1.54941708255568,
4.4899246066898));
#72945=CARTESIAN_POINT('Ctrl Pts',(-0.200299113857424,1.5426416882319,4.49392047399656));
#72946=CARTESIAN_POINT('Ctrl Pts',(-0.216966198733222,1.54038590724449,
4.4950991590511));
#72947=CARTESIAN_POINT('Ctrl Pts',(-0.245440147647349,1.53606086469989,
4.49713222950863));
#72948=CARTESIAN_POINT('Ctrl Pts',(-0.257265916661399,1.53412453199732,
4.49798236659563));
#72949=CARTESIAN_POINT('Ctrl Pts',(-0.281498341991835,1.52986869268484,
4.49973685859751));
#72950=CARTESIAN_POINT('Ctrl Pts',(-0.293901464741539,1.52753443334547,
4.50064162320406));
#72951=CARTESIAN_POINT('Ctrl Pts',(-0.325408081421934,1.52120698484425,
4.50295782937668));
#72952=CARTESIAN_POINT('Ctrl Pts',(-0.344466825296843,1.51700482930801,
4.50437581009712));
#72953=CARTESIAN_POINT('Ctrl Pts',(-0.433359299449749,1.49564396431863,
4.51107197157652));
#72954=CARTESIAN_POINT('Ctrl Pts',(-0.502018098146269,1.47401702174769,
4.51649006189344));
#72955=CARTESIAN_POINT('Ctrl Pts',(-0.594715876326606,1.43758863277048,
4.52413147056179));
#72956=CARTESIAN_POINT('Ctrl Pts',(-0.620229072318338,1.42676692814331,
4.52626971884226));
#72957=CARTESIAN_POINT('Ctrl Pts',(-0.736821710858317,1.37359443451321,
4.53618772662005));
#72958=CARTESIAN_POINT('Ctrl Pts',(-0.823959615080783,1.32316345517248,
4.54403862310551));
#72959=CARTESIAN_POINT('Ctrl Pts',(-0.917680608124188,1.25605023322117,
4.55262197176127));
#72960=CARTESIAN_POINT('Ctrl Pts',(-0.929606601008864,1.24724957277861,
4.55371664852113));
#72961=CARTESIAN_POINT('Ctrl Pts',(-0.9477310997487,1.23347036924187,4.55538187697321));
#72962=CARTESIAN_POINT('Ctrl Pts',(-0.954019894784616,1.22861281004857,
4.555959974721));
#72963=CARTESIAN_POINT('Ctrl Pts',(-0.965545846498206,1.21956812836718,
4.55701963727377));
#72964=CARTESIAN_POINT('Ctrl Pts',(-0.970793345706264,1.21539519668665,
4.55750208251466));
#72965=CARTESIAN_POINT('Ctrl Pts',(-0.983023141665749,1.20554003772583,
4.55862670177602));
#72966=CARTESIAN_POINT('Ctrl Pts',(-0.98998332669063,1.19983094764526,4.55926697142687));
#72967=CARTESIAN_POINT('Ctrl Pts',(-1.01304728036083,1.18057539794609,4.56139093715652));
#72968=CARTESIAN_POINT('Ctrl Pts',(-1.02892647665604,1.16676196356979,4.56285706281999));
#72969=CARTESIAN_POINT('Ctrl Pts',(-1.06777590622846,1.1315563269102,4.56646822650813));
#72970=CARTESIAN_POINT('Ctrl Pts',(-1.09038884359604,1.1097826501421,4.56859220948555));
#72971=CARTESIAN_POINT('Ctrl Pts',(-1.20929138036146,0.988147353447604,
4.57998540407079));
#72972=CARTESIAN_POINT('Ctrl Pts',(-1.29254875000947,0.876436207165882,
4.5888585352482));
#72973=CARTESIAN_POINT('Ctrl Pts',(-1.37524857426569,0.727510853602105,
4.60047252996697));
#72974=CARTESIAN_POINT('Ctrl Pts',(-1.38975613989361,0.699398543073187,
4.60265319254083));
#72975=CARTESIAN_POINT('Ctrl Pts',(-1.40986497311874,0.657332479271937,
4.6059115986384));
#72976=CARTESIAN_POINT('Ctrl Pts',(-1.41613769900417,0.643707402780434,
4.60696624968534));
#72977=CARTESIAN_POINT('Ctrl Pts',(-1.42701210073779,0.619158433751454,
4.60886636366504));
#72978=CARTESIAN_POINT('Ctrl Pts',(-1.43168786070544,0.608268490924934,
4.60970921753692));
#72979=CARTESIAN_POINT('Ctrl Pts',(-1.44140648519587,0.584900592698571,
4.6115183298303));
#72980=CARTESIAN_POINT('Ctrl Pts',(-1.44641272582161,0.572408564205819,
4.61248574655382));
#72981=CARTESIAN_POINT('Ctrl Pts',(-1.45973818233629,0.537866224302745,
4.61516247092041));
#72982=CARTESIAN_POINT('Ctrl Pts',(-1.46771902636209,0.515690200860258,
4.61688281918517));
#72983=CARTESIAN_POINT('Ctrl Pts',(-1.49945329818929,0.420798392316111,
4.6242563644812));
#72984=CARTESIAN_POINT('Ctrl Pts',(-1.51832622078728,0.346574386049884,
4.63006110627107));
#72985=CARTESIAN_POINT('Ctrl Pts',(-1.54756893934855,0.181464405618471,
4.64298626460136));
#72986=CARTESIAN_POINT('Ctrl Pts',(-1.5555449504945,0.0904333168781379,
4.65012314607825));
#72987=CARTESIAN_POINT('Ctrl Pts',(-1.55549980947038,-0.00076989453901936,
4.6570644451624));
#72988=CARTESIAN_POINT('Origin',(0.,0.,-1.2940562256037));
#72989=CARTESIAN_POINT('',(-1.55549996779056,0.00031654948737463,5.4955130075581));
#72990=CARTESIAN_POINT('',(-1.55596473934061,0.00138061827089576,5.3559437743963));
#72991=CARTESIAN_POINT('',(-1.5555,-1.46451138874614E-13,-1.2940562256037));
#72992=CARTESIAN_POINT('Ctrl Pts',(-1.55549996779057,0.000316549412329119,
5.49551300756351));
#72993=CARTESIAN_POINT('Ctrl Pts',(-1.55549621245051,0.0187700076134928,
5.49418400711457));
#72994=CARTESIAN_POINT('Ctrl Pts',(-1.55516407835502,0.0372211631028199,
5.4928448070229));
#72995=CARTESIAN_POINT('Ctrl Pts',(-1.55231211830025,0.116870410297289,
5.48701646529434));
#72996=CARTESIAN_POINT('Ctrl Pts',(-1.54650752544575,0.177888397832393,
5.4824276092901));
#72997=CARTESIAN_POINT('Ctrl Pts',(-1.52706475421104,0.30324956282706,5.47275179185585));
#72998=CARTESIAN_POINT('Ctrl Pts',(-1.51291330701088,0.367395427262038,
5.4676617846248));
#72999=CARTESIAN_POINT('Ctrl Pts',(-1.47445156825068,0.500954823256708,
5.45688328109391));
#73000=CARTESIAN_POINT('Ctrl Pts',(-1.4491836912554,0.569940246680635,5.45120764634296));
#73001=CARTESIAN_POINT('Ctrl Pts',(-1.41249987500531,0.651680267799144,
5.44452157937737));
#73002=CARTESIAN_POINT('Ctrl Pts',(-1.40563093601037,0.666366862158133,
5.44332208834666));
#73003=CARTESIAN_POINT('Ctrl Pts',(-1.39502610307436,0.688147227522723,
5.44154877323677));
#73004=CARTESIAN_POINT('Ctrl Pts',(-1.39146322032869,0.695323341379978,
5.44096542181317));
#73005=CARTESIAN_POINT('Ctrl Pts',(-1.38520221303316,0.707692958404927,
5.4399618773571));
#73006=CARTESIAN_POINT('Ctrl Pts',(-1.3825300678186,0.712899087572182,5.43954014868974));
#73007=CARTESIAN_POINT('Ctrl Pts',(-1.37612476855275,0.725207030025228,
5.43854461740483));
#73008=CARTESIAN_POINT('Ctrl Pts',(-1.37236597171916,0.732295201577709,
5.43797242084335));
#73009=CARTESIAN_POINT('Ctrl Pts',(-1.36081907373747,0.753668631593445,
5.43624949597365));
#73010=CARTESIAN_POINT('Ctrl Pts',(-1.35286124673461,0.767861614852756,
5.43510874071072));
#73011=CARTESIAN_POINT('Ctrl Pts',(-1.31074847083172,0.840282980699899,
5.42929135907679));
#73012=CARTESIAN_POINT('Ctrl Pts',(-1.27304824028396,0.896374579530541,
5.42479564204702));
#73013=CARTESIAN_POINT('Ctrl Pts',(-1.15498083671299,1.04949181271474,5.41202819290048));
#73014=CARTESIAN_POINT('Ctrl Pts',(-1.06634584047179,1.1394371540424,5.40385883240737));
#73015=CARTESIAN_POINT('Ctrl Pts',(-0.950648293228203,1.23139386139362,
5.39366161190992));
#73016=CARTESIAN_POINT('Ctrl Pts',(-0.933160564271279,1.24469847644713,
5.39213265906222));
#73017=CARTESIAN_POINT('Ctrl Pts',(-0.904956305404805,1.26522769368522,
5.38968212424182));
#73018=CARTESIAN_POINT('Ctrl Pts',(-0.894421019026142,1.27269715730894,
5.38877006668614));
#73019=CARTESIAN_POINT('Ctrl Pts',(-0.874266083563081,1.28661304576571,
5.38703067101911));
#73020=CARTESIAN_POINT('Ctrl Pts',(-0.864665026180948,1.29308495217789,
5.38620437966685));
#73021=CARTESIAN_POINT('Ctrl Pts',(-0.842523554910953,1.30765328138751,
5.38430349681577));
#73022=CARTESIAN_POINT('Ctrl Pts',(-0.829937237211112,1.31567746742314,
5.38322629977629));
#73023=CARTESIAN_POINT('Ctrl Pts',(-0.789562264691533,1.34060793889677,
5.37978019578898));
#73024=CARTESIAN_POINT('Ctrl Pts',(-0.761359599075222,1.35682330653378,
5.37738670203064));
#73025=CARTESIAN_POINT('Ctrl Pts',(-0.692140490535513,1.3937836664822,5.37154079301822));
#73026=CARTESIAN_POINT('Ctrl Pts',(-0.650674264042728,1.41361723551713,
5.36806145645192));
#73027=CARTESIAN_POINT('Ctrl Pts',(-0.553023130418471,1.45511696657497,
5.35993379132822));
#73028=CARTESIAN_POINT('Ctrl Pts',(-0.496335421825024,1.47541536721711,
5.35526255576933));
#73029=CARTESIAN_POINT('Ctrl Pts',(-0.36584968592708,1.51376577685326,5.34471810397349));
#73030=CARTESIAN_POINT('Ctrl Pts',(-0.291606432972014,1.5298042704696,5.33886102384214));
#73031=CARTESIAN_POINT('Ctrl Pts',(-0.203851725107997,1.54213728182862,
5.33228991746553));
#73032=CARTESIAN_POINT('Ctrl Pts',(-0.191199653998479,1.54375698936549,
5.33135108336637));
#73033=CARTESIAN_POINT('Ctrl Pts',(-0.171271555272678,1.54605940099818,
5.32988722770739));
#73034=CARTESIAN_POINT('Ctrl Pts',(-0.164008536434367,1.54684673542889,
5.32935681026712));
#73035=CARTESIAN_POINT('Ctrl Pts',(-0.150133032996969,1.54825205401307,
5.32834973849311));
#73036=CARTESIAN_POINT('Ctrl Pts',(-0.143521797418711,1.54887889967481,
5.32787264624057));
#73037=CARTESIAN_POINT('Ctrl Pts',(-0.127388919845725,1.5503043594596,5.32671475310773));
#73038=CARTESIAN_POINT('Ctrl Pts',(-0.117863350193136,1.55105763492817,
5.32603642079458));
#73039=CARTESIAN_POINT('Ctrl Pts',(-0.0827367371431863,1.55350994453142,
5.32355263178784));
#73040=CARTESIAN_POINT('Ctrl Pts',(-0.0571001636006358,1.55466339747332,
5.3217743490185));
#73041=CARTESIAN_POINT('Ctrl Pts',(0.0107791434335332,1.55603588151908,
5.3171290383019));
#73042=CARTESIAN_POINT('Ctrl Pts',(0.0530236251046945,1.55516972000688,
5.31430240506007));
#73043=CARTESIAN_POINT('Ctrl Pts',(0.230439225642614,1.54429302761647,5.30251288258265));
#73044=CARTESIAN_POINT('Ctrl Pts',(0.364019800968434,1.51836453370021,5.29377879978447));
#73045=CARTESIAN_POINT('Ctrl Pts',(0.514328775593441,1.46818709127913,5.282864645061));
#73046=CARTESIAN_POINT('Ctrl Pts',(0.535942891310052,1.46043573888513,5.28126930432832));
#73047=CARTESIAN_POINT('Ctrl Pts',(0.569745076543431,1.44746202452444,5.27872864895791));
#73048=CARTESIAN_POINT('Ctrl Pts',(0.582052037284146,1.44255716390761,5.27779390827196));
#73049=CARTESIAN_POINT('Ctrl Pts',(0.604948257612353,1.43309132911008,5.27603580476125));
#73050=CARTESIAN_POINT('Ctrl Pts',(0.615552436059126,1.42856863232373,5.27521378744696));
#73051=CARTESIAN_POINT('Ctrl Pts',(0.639281239314825,1.41813501582131,5.27335629689604));
#73052=CARTESIAN_POINT('Ctrl Pts',(0.652375894412909,1.41215901813877,5.27231865042575));
#73053=CARTESIAN_POINT('Ctrl Pts',(0.692054750666777,1.39338114832703,5.2691347001366));
#73054=CARTESIAN_POINT('Ctrl Pts',(0.718357864203998,1.38000455159089,5.26696883560596));
#73055=CARTESIAN_POINT('Ctrl Pts',(0.779442782059232,1.34671981587785,5.2618036613646));
#73056=CARTESIAN_POINT('Ctrl Pts',(0.813865891287156,1.32620026695378,5.25878522489259));
#73057=CARTESIAN_POINT('Ctrl Pts',(0.903887237328606,1.26771320455635,5.2506044261875));
#73058=CARTESIAN_POINT('Ctrl Pts',(0.957876222252802,1.22742859499133,5.2453853121892));
#73059=CARTESIAN_POINT('Ctrl Pts',(1.0649128999384,1.13618771307338,5.23447804211464));
#73060=CARTESIAN_POINT('Ctrl Pts',(1.11731116976713,1.08470265375015,5.22880303784704));
#73061=CARTESIAN_POINT('Ctrl Pts',(1.1766153376106,1.01755560735805,5.22211756418395));
#73062=CARTESIAN_POINT('Ctrl Pts',(1.18715702995261,1.00523694118504,5.22091807679578));
#73063=CARTESIAN_POINT('Ctrl Pts',(1.20261788269123,0.986587382388459,5.21914476596098));
#73064=CARTESIAN_POINT('Ctrl Pts',(1.20768345717725,0.980380084307348,5.21856141523433));
#73065=CARTESIAN_POINT('Ctrl Pts',(1.21636573365046,0.969571501423572,5.21755787145548));
#73066=CARTESIAN_POINT('Ctrl Pts',(1.22000465929557,0.964988667697563,5.21713614277651));
#73067=CARTESIAN_POINT('Ctrl Pts',(1.22857121224422,0.954074101744648,5.21614061081295));
#73068=CARTESIAN_POINT('Ctrl Pts',(1.23347582941661,0.94772464407345,5.2155684135923));
#73069=CARTESIAN_POINT('Ctrl Pts',(1.24817724427677,0.928384901951449,5.21384548461502));
#73070=CARTESIAN_POINT('Ctrl Pts',(1.25781993509795,0.915278113448224,5.21270472597334));
#73071=CARTESIAN_POINT('Ctrl Pts',(1.30640099030776,0.847026303321275,5.20688730824865));
#73072=CARTESIAN_POINT('Ctrl Pts',(1.34192965025754,0.789534095063161,5.20239156099648));
#73073=CARTESIAN_POINT('Ctrl Pts',(1.43265852025243,0.61879170371439,5.18962413218974));
#73074=CARTESIAN_POINT('Ctrl Pts',(1.47799723580522,0.500933588962382,5.18145481777101));
#73075=CARTESIAN_POINT('Ctrl Pts',(1.51399746982476,0.357595700974926,5.1712576435497));
#73076=CARTESIAN_POINT('Ctrl Pts',(1.5188973129164,0.336175390965826,5.16972868345068));
#73077=CARTESIAN_POINT('Ctrl Pts',(1.52595406549342,0.30201195694397,5.16727813975036));
#73078=CARTESIAN_POINT('Ctrl Pts',(1.52840881945412,0.289332844118817,5.16636608068866));
#73079=CARTESIAN_POINT('Ctrl Pts',(1.53276445440062,0.265230921318809,5.16462668386954));
#73080=CARTESIAN_POINT('Ctrl Pts',(1.53469621967475,0.253814527282955,5.16380039289171));
#73081=CARTESIAN_POINT('Ctrl Pts',(1.53882611997609,0.227633952170098,5.16189951337155));
#73082=CARTESIAN_POINT('Ctrl Pts',(1.54093951249221,0.212857777948125,5.16082231932134));
#73083=CARTESIAN_POINT('Ctrl Pts',(1.54698126620469,0.165792527845507,5.1573762357485));
#73084=CARTESIAN_POINT('Ctrl Pts',(1.55010943707154,0.133411551167825,5.15498275982972));
#73085=CARTESIAN_POINT('Ctrl Pts',(1.55520234428562,0.0551089108422377,
5.14913690547225));
#73086=CARTESIAN_POINT('Ctrl Pts',(1.55615129434233,0.00915378107127548,
5.14565760640941));
#73087=CARTESIAN_POINT('Ctrl Pts',(1.55364297917172,-0.0969202016699715,
5.13752994080372));
#73088=CARTESIAN_POINT('Ctrl Pts',(1.54873226451111,-0.156932446103068,
5.13285866494629));
#73089=CARTESIAN_POINT('Ctrl Pts',(1.5298019759392,-0.291614089909617,5.12231415018773));
#73090=CARTESIAN_POINT('Ctrl Pts',(1.51376466618073,-0.365857890844107,
5.11645704723095));
#73091=CARTESIAN_POINT('Ctrl Pts',(1.48877506129423,-0.450878851757248,
5.10988591886634));
#73092=CARTESIAN_POINT('Ctrl Pts',(1.48502789896872,-0.463071365392931,
5.10894708400576));
#73093=CARTESIAN_POINT('Ctrl Pts',(1.47889921198597,-0.482172933582224,
5.10748322743332));
#73094=CARTESIAN_POINT('Ctrl Pts',(1.47661835804157,-0.489113328030066,
5.10695280983035));
#73095=CARTESIAN_POINT('Ctrl Pts',(1.47217092464432,-0.5023316822306,5.10594573795506));
#73096=CARTESIAN_POINT('Ctrl Pts',(1.47001293215372,-0.508612162144354,
5.10546864576175));
#73097=CARTESIAN_POINT('Ctrl Pts',(1.46465206160209,-0.523894915229154,
5.10431075305752));
#73098=CARTESIAN_POINT('Ctrl Pts',(1.46140626641931,-0.532882051262191,
5.10363242110919));
#73099=CARTESIAN_POINT('Ctrl Pts',(1.44914058229796,-0.565888757788537,
5.10114863515081));
#73100=CARTESIAN_POINT('Ctrl Pts',(1.43960909547117,-0.589715489355327,
5.09937035497825));
#73101=CARTESIAN_POINT('Ctrl Pts',(1.41284045885494,-0.652108644465265,
5.0947250532553));
#73102=CARTESIAN_POINT('Ctrl Pts',(1.39461416297496,-0.690228723778092,
5.09189842621685));
#73103=CARTESIAN_POINT('Ctrl Pts',(1.31147476961905,-0.847335344281351,
5.08010889340678));
#73104=CARTESIAN_POINT('Ctrl Pts',(1.23271952853975,-0.958302614951366,
5.07137479604307));
#73105=CARTESIAN_POINT('Ctrl Pts',(1.1249724719531,-1.07449725890156,5.06046062751484));
#73106=CARTESIAN_POINT('Ctrl Pts',(1.1089905727636,-1.09098452661708,5.0588652902678));
#73107=CARTESIAN_POINT('Ctrl Pts',(1.08322106388461,-1.1164174358852,5.05632463919935));
#73108=CARTESIAN_POINT('Ctrl Pts',(1.07367356846478,-1.12560242240939,5.05538989926836));
#73109=CARTESIAN_POINT('Ctrl Pts',(1.05560081453365,-1.14254981175479,5.05363179641978));
#73110=CARTESIAN_POINT('Ctrl Pts',(1.04710426202992,-1.15034160285659,5.052809779003));
#73111=CARTESIAN_POINT('Ctrl Pts',(1.02780633183187,-1.16764787959965,5.05095228720443));
#73112=CARTESIAN_POINT('Ctrl Pts',(1.01695804938706,-1.17710820503355,5.04991463957633));
#73113=CARTESIAN_POINT('Ctrl Pts',(0.983476062849216,-1.20549808846037,
5.04673068183193));
#73114=CARTESIAN_POINT('Ctrl Pts',(0.96043490313042,-1.22393438768901,5.04456481086921));
#73115=CARTESIAN_POINT('Ctrl Pts',(0.904903587027513,-1.26583364785535,
5.03939961784058));
#73116=CARTESIAN_POINT('Ctrl Pts',(0.872004593677074,-1.28871751697013,
5.03638116881919));
#73117=CARTESIAN_POINT('Ctrl Pts',(0.781573956407065,-1.34657011074711,
5.02820035338002));
#73118=CARTESIAN_POINT('Ctrl Pts',(0.72259608596092,-1.37911664307269,5.02298123557274));
#73119=CARTESIAN_POINT('Ctrl Pts',(0.595309114351531,-1.4389471892505,5.01207398819018));
#73120=CARTESIAN_POINT('Ctrl Pts',(0.526786462914177,-1.46542146527923,
5.0063990104397));
#73121=CARTESIAN_POINT('Ctrl Pts',(0.441147791099174,-1.49172105070239,
4.99971356173075));
#73122=CARTESIAN_POINT('Ctrl Pts',(0.425576203886753,-1.4962379544405,4.99851407449644));
#73123=CARTESIAN_POINT('Ctrl Pts',(0.402207726986503,-1.50262216781296,
4.99674076384221));
#73124=CARTESIAN_POINT('Ctrl Pts',(0.394462975437901,-1.50467385284933,
4.99615741314501));
#73125=CARTESIAN_POINT('Ctrl Pts',(0.381034339373259,-1.50812046156477,
4.99515386939476));
#73126=CARTESIAN_POINT('Ctrl Pts',(0.375358087371483,-1.50954324341259,
4.9947321407153));
#73127=CARTESIAN_POINT('Ctrl Pts',(0.361880685239677,-1.51284070041495,
4.99373660872308));
#73128=CARTESIAN_POINT('Ctrl Pts',(0.354072888158268,-1.51468710056462,
4.99316441147458));
#73129=CARTESIAN_POINT('Ctrl Pts',(0.330389240424846,-1.52009470401718,
4.99144148232381));
#73130=CARTESIAN_POINT('Ctrl Pts',(0.314470885238262,-1.52346745173387,
4.99030072353941));
#73131=CARTESIAN_POINT('Ctrl Pts',(0.232251836461684,-1.53954415109864,
4.9844833042903));
#73132=CARTESIAN_POINT('Ctrl Pts',(0.165220682807613,-1.54817356979386,
4.97998755576158));
#73133=CARTESIAN_POINT('Ctrl Pts',(-0.0277477083768383,-1.56033447212346,
4.96722012781395));
#73134=CARTESIAN_POINT('Ctrl Pts',(-0.153811437169086,-1.55298175242768,
4.95905081534133));
#73135=CARTESIAN_POINT('Ctrl Pts',(-0.299228323718729,-1.52660585432991,
4.94885364307465));
#73136=CARTESIAN_POINT('Ctrl Pts',(-0.320761192389297,-1.52222705216107,
4.94732468266935));
#73137=CARTESIAN_POINT('Ctrl Pts',(-0.35479124275334,-1.51455280734043,
4.94487413859396));
#73138=CARTESIAN_POINT('Ctrl Pts',(-0.367353063342234,-1.51155507373973,
4.94396207946866));
#73139=CARTESIAN_POINT('Ctrl Pts',(-0.39110379635212,-1.50557368958552,
4.94222268260088));
#73140=CARTESIAN_POINT('Ctrl Pts',(-0.402299613152616,-1.50262081783683,
4.94139639163887));
#73141=CARTESIAN_POINT('Ctrl Pts',(-0.427850472564649,-1.49557581445297,
4.9394955122594));
#73142=CARTESIAN_POINT('Ctrl Pts',(-0.442181459458291,-1.49140154608117,
4.93841831833545));
#73143=CARTESIAN_POINT('Ctrl Pts',(-0.487543935555206,-1.47747727919295,
4.93497223562489));
#73144=CARTESIAN_POINT('Ctrl Pts',(-0.518328833659744,-1.4669605067727,
4.93257876045963));
#73145=CARTESIAN_POINT('Ctrl Pts',(-0.591751697810771,-1.43927803082343,
4.92673290841069));
#73146=CARTESIAN_POINT('Ctrl Pts',(-0.634000856416312,-1.42117330217063,
4.92325361093192));
#73147=CARTESIAN_POINT('Ctrl Pts',(-0.729593954772603,-1.37509795829541,
4.91512486394116));
#73148=CARTESIAN_POINT('Ctrl Pts',(-0.782240100439677,-1.34584603364123,
4.91045247516294));
#73149=CARTESIAN_POINT('Ctrl Pts',(-0.897076039036702,-1.2730206514751,
4.89990987672638));
#73150=CARTESIAN_POINT('Ctrl Pts',(-0.958049270255439,-1.22779118276984,
4.89405579280581));
#73151=CARTESIAN_POINT('Ctrl Pts',(-1.02515790167138,-1.1699549333394,4.88748633894162));
#73152=CARTESIAN_POINT('Ctrl Pts',(-1.03472701062877,-1.16150045675095,
4.88654648085501));
#73153=CARTESIAN_POINT('Ctrl Pts',(-1.04960812759939,-1.1480228386689,4.88508139679141));
#73154=CARTESIAN_POINT('Ctrl Pts',(-1.0549904290706,-1.14307867623974,4.88455076058673));
#73155=CARTESIAN_POINT('Ctrl Pts',(-1.06519577098285,-1.13357059947853,
4.88354355238179));
#73156=CARTESIAN_POINT('Ctrl Pts',(-1.07002468889417,-1.12901350811918,
4.88306653951879));
#73157=CARTESIAN_POINT('Ctrl Pts',(-1.07492232739759,-1.12433191648366,
4.88258214429944));
#73158=CARTESIAN_POINT('Ctrl Pts',(-1.07502026796231,-1.12423827182316,
4.88257245735426));
#73159=CARTESIAN_POINT('Ctrl Pts',(-1.07521532371274,-1.12405172288283,
4.88255316460205));
#73160=CARTESIAN_POINT('Ctrl Pts',(-1.07531243909564,-1.12395881881355,
4.88254355877959));
#73161=CARTESIAN_POINT('Ctrl Pts',(-1.07550595354348,-1.12377364789288,
4.88252441749432));
#73162=CARTESIAN_POINT('Ctrl Pts',(-1.07560235277528,-1.12368138122434,
4.88251488201851));
#73163=CARTESIAN_POINT('Ctrl Pts',(-1.07579453975672,-1.12349738576423,
4.88249587106382));
#73164=CARTESIAN_POINT('Ctrl Pts',(-1.07589032765145,-1.12340565712281,
4.88248639557356));
#73165=CARTESIAN_POINT('Ctrl Pts',(-1.07608139310954,-1.1232226416942,4.88246749458972));
#73166=CARTESIAN_POINT('Ctrl Pts',(-1.0761766707884,-1.12313135503462,4.88245806908718));
#73167=CARTESIAN_POINT('Ctrl Pts',(-1.07636681371685,-1.12294913045878,
4.88243925839793));
#73168=CARTESIAN_POINT('Ctrl Pts',(-1.07646167906463,-1.1228581926381,4.88242987320347));
#73169=CARTESIAN_POINT('Ctrl Pts',(-1.07665109246371,-1.12267657509134,
4.88241113372157));
#73170=CARTESIAN_POINT('Ctrl Pts',(-1.07674564058268,-1.12258589544336,
4.88240177942893));
#73171=CARTESIAN_POINT('Ctrl Pts',(-1.08327110384483,-1.11632584106427,
4.88175615396039));
#73172=CARTESIAN_POINT('Ctrl Pts',(-1.08964909522667,-1.11010113370812,
4.88112399837675));
#73173=CARTESIAN_POINT('Ctrl Pts',(-1.11411280972569,-1.08581135962823,
4.87869317585419));
#73174=CARTESIAN_POINT('Ctrl Pts',(-1.13180680853526,-1.06735523591599,
4.87692193039107));
#73175=CARTESIAN_POINT('Ctrl Pts',(-1.17774155068838,-1.01701444273853,
4.87226003217223));
#73176=CARTESIAN_POINT('Ctrl Pts',(-1.20514236162626,-0.984391153385109,
4.86941088766435));
#73177=CARTESIAN_POINT('Ctrl Pts',(-1.29537292150981,-0.867538975858345,
4.85962107782995));
#73178=CARTESIAN_POINT('Ctrl Pts',(-1.35098488812134,-0.778109473641279,
4.85281550816503));
#73179=CARTESIAN_POINT('Ctrl Pts',(-1.4158416855509,-0.645584115997787,
4.84286751383945));
#73180=CARTESIAN_POINT('Ctrl Pts',(-1.43294988245549,-0.606663533609501,
4.83996403278265));
#73181=CARTESIAN_POINT('Ctrl Pts',(-1.45460039012204,-0.551364926885388,
4.83583219011614));
#73182=CARTESIAN_POINT('Ctrl Pts',(-1.46050179484208,-0.535537156170969,
4.83464892534577));
#73183=CARTESIAN_POINT('Ctrl Pts',(-1.47007419320775,-0.508527807802072,
4.8326269372629));
#73184=CARTESIAN_POINT('Ctrl Pts',(-1.47387826629725,-0.497394719677229,
4.83179269406144));
#73185=CARTESIAN_POINT('Ctrl Pts',(-1.48135396658007,-0.474677088226673,
4.83008820453524));
#73186=CARTESIAN_POINT('Ctrl Pts',(-1.4850168475045,-0.463090552156438,
4.82921773704695));
#73187=CARTESIAN_POINT('Ctrl Pts',(-1.49384990129269,-0.433966577763472,
4.82702626617733));
#73188=CARTESIAN_POINT('Ctrl Pts',(-1.49884719410677,-0.416379098743493,
4.82569974291303));
#73189=CARTESIAN_POINT('Ctrl Pts',(-1.51110387703126,-0.370159020359163,
4.82220395706157));
#73190=CARTESIAN_POINT('Ctrl Pts',(-1.51785942608517,-0.341401780430383,
4.82001923083557));
#73191=CARTESIAN_POINT('Ctrl Pts',(-1.54488019058464,-0.209632836606872,
4.80996148349255));
#73192=CARTESIAN_POINT('Ctrl Pts',(-1.55550000000703,-0.104940599039015,
4.80181512781945));
#73193=CARTESIAN_POINT('Ctrl Pts',(-1.5555,1.042515379579E-10,4.79368285916456));
#73194=CARTESIAN_POINT('Ctrl Pts',(-1.55745457732731,-0.000856696892064714,
4.6559437743963));
#73195=CARTESIAN_POINT('Ctrl Pts',(-1.55778497931963,-0.0507117794212508,
4.65952722214655));
#73196=CARTESIAN_POINT('Ctrl Pts',(-1.53299973239953,-0.615518763747496,
4.70014792479876));
#73197=CARTESIAN_POINT('Ctrl Pts',(-0.843969773291502,-1.63319857630279,
4.77780588235294));
#73198=CARTESIAN_POINT('Ctrl Pts',(0.914045851976043,-1.59503691128215,
4.88891764705882));
#73199=CARTESIAN_POINT('Ctrl Pts',(1.83578508816481,-0.0975483364234787,
5.0000294117647));
#73200=CARTESIAN_POINT('Ctrl Pts',(1.07793273566426,1.48918890180207,5.11114117647059));
#73201=CARTESIAN_POINT('Ctrl Pts',(-0.666138955726334,1.7134414082573,5.22225294117646));
#73202=CARTESIAN_POINT('Ctrl Pts',(-1.49940020022205,0.726840308291178,
5.30385380715171));
#73203=CARTESIAN_POINT('Ctrl Pts',(-1.55693103699923,0.106352731462292,
5.34841741822499));
#73204=CARTESIAN_POINT('Ctrl Pts',(-1.55596473934061,0.00138061827089576,
5.3559437743963));
#73205=CARTESIAN_POINT('Origin',(0.,0.,-1.2940562256037));
#73206=CARTESIAN_POINT('',(-1.5555,8.75720568004264E-11,6.19393713463064));
#73207=CARTESIAN_POINT('',(-1.55549999442795,-0.000131661106665976,6.05447729365266));
#73208=CARTESIAN_POINT('',(-1.5555,-1.46451138874614E-13,-1.2940562256037));
#73209=CARTESIAN_POINT('Ctrl Pts',(-1.5555,8.75698298596905E-11,6.19393713463064));
#73210=CARTESIAN_POINT('Ctrl Pts',(-1.55549999999434,0.100505756995347,
6.18732362246232));
#73211=CARTESIAN_POINT('Ctrl Pts',(-1.54575960958544,0.200767590378707,
6.18070462680335));
#73212=CARTESIAN_POINT('Ctrl Pts',(-1.52327742079485,0.31539202784566,6.17265070533303));
#73213=CARTESIAN_POINT('Ctrl Pts',(-1.51988702902391,0.331345163515344,
6.17151910230652));
#73214=CARTESIAN_POINT('Ctrl Pts',(-1.51360209151602,0.358788638093367,
6.16955213806078));
#73215=CARTESIAN_POINT('Ctrl Pts',(-1.51082589452176,0.370304848823369,
6.16872050526237));
#73216=CARTESIAN_POINT('Ctrl Pts',(-1.5050012643872,0.393309942282735,6.16704602094438));
#73217=CARTESIAN_POINT('Ctrl Pts',(-1.50195213953966,0.404797817175777,
6.16620319790713));
#73218=CARTESIAN_POINT('Ctrl Pts',(-1.49589518743367,0.426606833623501,
6.16458990221574));
#73219=CARTESIAN_POINT('Ctrl Pts',(-1.49291141214447,0.436933984751265,
6.16382025540544));
#73220=CARTESIAN_POINT('Ctrl Pts',(-1.48487232212131,0.463714002399664,
6.16180909012442));
#73221=CARTESIAN_POINT('Ctrl Pts',(-1.47965066269369,0.480114945725162,
6.16056220488934));
#73222=CARTESIAN_POINT('Ctrl Pts',(-1.45985787120231,0.53889056821253,6.15603694656404));
#73223=CARTESIAN_POINT('Ctrl Pts',(-1.44373084518829,0.580713836248065,
6.15270857180386));
#73224=CARTESIAN_POINT('Ctrl Pts',(-1.38489859206161,0.715624052944825,
6.1416075381184));
#73225=CARTESIAN_POINT('Ctrl Pts',(-1.33481246918224,0.805191419101341,
6.13362748948238));
#73226=CARTESIAN_POINT('Ctrl Pts',(-1.25210065049771,0.923913659331325,
6.12243790179828));
#73227=CARTESIAN_POINT('Ctrl Pts',(-1.22649098458838,0.957649628971214,
6.11918284362215));
#73228=CARTESIAN_POINT('Ctrl Pts',(-1.18335880596058,1.00989494618722,6.11406214642334));
#73229=CARTESIAN_POINT('Ctrl Pts',(-1.16670342819835,1.02909142679247,6.11216224374716));
#73230=CARTESIAN_POINT('Ctrl Pts',(-1.14357274068401,1.05446728875482,6.10963482590579));
#73231=CARTESIAN_POINT('Ctrl Pts',(-1.13750463629241,1.06101040936331,6.10898165506301));
#73232=CARTESIAN_POINT('Ctrl Pts',(-1.13129023681397,1.06759667821647,6.1083229860029));
#73233=CARTESIAN_POINT('Ctrl Pts',(-1.1312000912299,1.06769219387,6.10831343356977));
#73234=CARTESIAN_POINT('Ctrl Pts',(-1.13101948973085,1.06788350544808,6.10829430016277));
#73235=CARTESIAN_POINT('Ctrl Pts',(-1.13092903373902,1.06797930130002,6.10828471919453));
#73236=CARTESIAN_POINT('Ctrl Pts',(-1.13074772098684,1.06817126856462,6.10826551918392));
#73237=CARTESIAN_POINT('Ctrl Pts',(-1.13065686412614,1.06826743988027,6.10825590014911));
#73238=CARTESIAN_POINT('Ctrl Pts',(-1.13047465653578,1.06846025598309,6.10823661420777));
#73239=CARTESIAN_POINT('Ctrl Pts',(-1.13038330568018,1.06855690064906,6.1082269473107));
#73240=CARTESIAN_POINT('Ctrl Pts',(-1.13020001392395,1.06875076441187,6.10820755554025));
#73241=CARTESIAN_POINT('Ctrl Pts',(-1.13010807286833,1.06884798336458,6.10819783067807));
#73242=CARTESIAN_POINT('Ctrl Pts',(-1.12992350101001,1.06904310017404,6.10817831251915));
#73243=CARTESIAN_POINT('Ctrl Pts',(-1.1298308700259,1.06914099785809,6.1081685192359));
#73244=CARTESIAN_POINT('Ctrl Pts',(-1.12964481460175,1.06933758061251,6.10814885337328));
#73245=CARTESIAN_POINT('Ctrl Pts',(-1.12955138994786,1.06943626548464,6.10813898080936));
#73246=CARTESIAN_POINT('Ctrl Pts',(-1.12489201240993,1.07435669475281,6.10764672131218));
#73247=CARTESIAN_POINT('Ctrl Pts',(-1.1202950966329,1.07914931813107,6.10716662024116));
#73248=CARTESIAN_POINT('Ctrl Pts',(-1.11057682678282,1.08915229893169,6.10616346098069));
#73249=CARTESIAN_POINT('Ctrl Pts',(-1.10544926680595,1.0943562229969,6.10564088787371));
#73250=CARTESIAN_POINT('Ctrl Pts',(-1.09126925583627,1.10854604979731,6.10421337044226));
#73251=CARTESIAN_POINT('Ctrl Pts',(-1.08214240508445,1.11745728155795,6.10331399368169));
#73252=CARTESIAN_POINT('Ctrl Pts',(-1.01802255185381,1.17853987420884,6.0971197439294));
#73253=CARTESIAN_POINT('Ctrl Pts',(-0.959382040211156,1.22674995535479,
6.09207670739811));
#73254=CARTESIAN_POINT('Ctrl Pts',(-0.848276510567133,1.30523255568569,
6.08310042958823));
#73255=CARTESIAN_POINT('Ctrl Pts',(-0.797126670099014,1.33708415917972,
6.07916043288644));
#73256=CARTESIAN_POINT('Ctrl Pts',(-0.703916199839546,1.38787358345946,
6.07211884124433));
#73257=CARTESIAN_POINT('Ctrl Pts',(-0.662621138862048,1.40805676137398,
6.06904380997088));
#73258=CARTESIAN_POINT('Ctrl Pts',(-0.590670333397883,1.43935634693151,
6.06369956486552));
#73259=CARTESIAN_POINT('Ctrl Pts',(-0.560447348213359,1.45139128213938,
6.06145883067095));
#73260=CARTESIAN_POINT('Ctrl Pts',(-0.515837640255012,1.46755394053074,
6.05814405449518));
#73261=CARTESIAN_POINT('Ctrl Pts',(-0.50173219337852,1.47243601497056,6.05709491713882));
#73262=CARTESIAN_POINT('Ctrl Pts',(-0.476563977497652,1.48074342453098,
6.05521996990831));
#73263=CARTESIAN_POINT('Ctrl Pts',(-0.4655289565391,1.48424967283571,6.05439689518635));
#73264=CARTESIAN_POINT('Ctrl Pts',(-0.442105066125174,1.49140542596913,
6.05264711334185));
#73265=CARTESIAN_POINT('Ctrl Pts',(-0.429707891126956,1.49502446258402,
6.05171947935995));
#73266=CARTESIAN_POINT('Ctrl Pts',(-0.39610023328814,1.50438281264368,6.04919980435372));
#73267=CARTESIAN_POINT('Ctrl Pts',(-0.374811584959257,1.50982754839254,
6.04759841306176));
#73268=CARTESIAN_POINT('Ctrl Pts',(-0.23086252915487,1.5434116603317,6.03672894072802));
#73269=CARTESIAN_POINT('Ctrl Pts',(-0.105314296951799,1.5570207221201,6.02699256671601));
#73270=CARTESIAN_POINT('Ctrl Pts',(0.0879702475561942,1.55447694891604,
6.01200997737115));
#73271=CARTESIAN_POINT('Ctrl Pts',(0.155348183048942,1.54919530245018,6.00680112561446));
#73272=CARTESIAN_POINT('Ctrl Pts',(0.238278572920402,1.53722746586338,6.00054764375608));
#73273=CARTESIAN_POINT('Ctrl Pts',(0.254345077891514,1.53465096909691,5.99934375009415));
#73274=CARTESIAN_POINT('Ctrl Pts',(0.278269692415118,1.53042823861274,5.99756526889735));
#73275=CARTESIAN_POINT('Ctrl Pts',(0.286159697282557,1.52897261274699,5.99698107598373));
#73276=CARTESIAN_POINT('Ctrl Pts',(0.299784681428891,1.52634977614278,5.99597668499117));
#73277=CARTESIAN_POINT('Ctrl Pts',(0.305524696174648,1.52521118456764,5.99555494170796));
#73278=CARTESIAN_POINT('Ctrl Pts',(0.319107981313133,1.52243703680532,5.99456018391639));
#73279=CARTESIAN_POINT('Ctrl Pts',(0.326945216680282,1.52077324660806,5.99398876593171));
#73280=CARTESIAN_POINT('Ctrl Pts',(0.350601178924871,1.51555992270552,5.99227068860269));
#73281=CARTESIAN_POINT('Ctrl Pts',(0.366378190402151,1.51182344928817,5.9911339202866));
#73282=CARTESIAN_POINT('Ctrl Pts',(0.453152783866419,1.4898343159594,5.98491714641951));
#73283=CARTESIAN_POINT('Ctrl Pts',(0.522858350126134,1.4668249869679,5.98005279422658));
#73284=CARTESIAN_POINT('Ctrl Pts',(0.652945980216558,1.41342525492405,5.97078097161365));
#73285=CARTESIAN_POINT('Ctrl Pts',(0.71347804039623,1.38385628121094,5.96637817449022));
#73286=CARTESIAN_POINT('Ctrl Pts',(0.806708636098383,1.33056699957885,5.95922156983969));
#73287=CARTESIAN_POINT('Ctrl Pts',(0.840728887961389,1.30933645186616,5.9565243551852));
#73288=CARTESIAN_POINT('Ctrl Pts',(0.898309517757776,1.27023290224372,5.95176793682155));
#73289=CARTESIAN_POINT('Ctrl Pts',(0.922251110259659,1.25295822473093,5.94972909416547));
#73290=CARTESIAN_POINT('Ctrl Pts',(0.957115568819714,1.22626150835033,5.94665743588395));
#73291=CARTESIAN_POINT('Ctrl Pts',(0.96842320594772,1.21735120997193,5.94564446474324));
#73292=CARTESIAN_POINT('Ctrl Pts',(0.988560351730942,1.2010252233923,5.94380899912389));
#73293=CARTESIAN_POINT('Ctrl Pts',(0.997434270784263,1.19366579016095,5.94298880688795));
#73294=CARTESIAN_POINT('Ctrl Pts',(1.01632691798641,1.17763972109679,5.94121746799815));
#73295=CARTESIAN_POINT('Ctrl Pts',(1.02631831432266,1.16894243418587,5.94026509877406));
#73296=CARTESIAN_POINT('Ctrl Pts',(1.05331511110293,1.14482938447257,5.93764791061511));
#73297=CARTESIAN_POINT('Ctrl Pts',(1.07009169098644,1.12916372215336,5.93597270723586));
#73298=CARTESIAN_POINT('Ctrl Pts',(1.18352889886552,1.01843916648673,5.92429545484538));
#73299=CARTESIAN_POINT('Ctrl Pts',(1.26773120836102,0.911483326915082,5.91374536081626));
#73300=CARTESIAN_POINT('Ctrl Pts',(1.35856837308699,0.758718994893285,5.90000153131931));
#73301=CARTESIAN_POINT('Ctrl Pts',(1.37866050227068,0.721566499344423,5.89675577322499));
#73302=CARTESIAN_POINT('Ctrl Pts',(1.40849053995322,0.660600171865966,5.89162599840744));
#73303=CARTESIAN_POINT('Ctrl Pts',(1.41919304505899,0.637282890891516,5.88970837246558));
#73304=CARTESIAN_POINT('Ctrl Pts',(1.43308407436719,0.604931039847843,5.88711775692739));
#73305=CARTESIAN_POINT('Ctrl Pts',(1.43677266131674,0.596117320092936,5.88641899245111));
#73306=CARTESIAN_POINT('Ctrl Pts',(1.44288699595086,0.581120867482679,5.88524254606759));
#73307=CARTESIAN_POINT('Ctrl Pts',(1.44535474224175,0.574955669600456,5.88476245338597));
#73308=CARTESIAN_POINT('Ctrl Pts',(1.45045438419841,0.561974822980848,5.88375928405301));
#73309=CARTESIAN_POINT('Ctrl Pts',(1.45307785374348,0.555156175417558,5.8832366927621));
#73310=CARTESIAN_POINT('Ctrl Pts',(1.46014977824049,0.536381943934191,5.88180907095295));
#73311=CARTESIAN_POINT('Ctrl Pts',(1.46449948511695,0.524389407318887,5.88090960934952));
#73312=CARTESIAN_POINT('Ctrl Pts',(1.49367994410934,0.44073982453446,5.87471288439105));
#73313=CARTESIAN_POINT('Ctrl Pts',(1.51339226117757,0.367394116034133,5.86966768527994));
#73314=CARTESIAN_POINT('Ctrl Pts',(1.53900290933919,0.233814050823407,5.86069256610842));
#73315=CARTESIAN_POINT('Ctrl Pts',(1.54689314861505,0.17412772902152,5.85675583996998));
#73316=CARTESIAN_POINT('Ctrl Pts',(1.5546787619804,0.0683066064660613,5.8497171105308));
#73317=CARTESIAN_POINT('Ctrl Pts',(1.55601787859658,0.0223544985036325,
5.84664155752925));
#73318=CARTESIAN_POINT('Ctrl Pts',(1.55482789562833,-0.0561124988750462,
5.84129650913789));
#73319=CARTESIAN_POINT('Ctrl Pts',(1.55331452006572,-0.0886123411355607,
5.83905550560502));
#73320=CARTESIAN_POINT('Ctrl Pts',(1.54962210075184,-0.135920582541938,
5.83574040626327));
#73321=CARTESIAN_POINT('Ctrl Pts',(1.54824648071701,-0.15078417498026,5.83469122220941));
#73322=CARTESIAN_POINT('Ctrl Pts',(1.54542434879024,-0.177138075808367,
5.83281622304226));
#73323=CARTESIAN_POINT('Ctrl Pts',(1.54406300689717,-0.188636510822875,
5.83199314364161));
#73324=CARTESIAN_POINT('Ctrl Pts',(1.5409120306448,-0.212925193861889,5.83024338489538));
#73325=CARTESIAN_POINT('Ctrl Pts',(1.53909122751143,-0.225710431933803,
5.82931577903717));
#73326=CARTESIAN_POINT('Ctrl Pts',(1.53374320312031,-0.260182145597517,
5.82679626560476));
#73327=CARTESIAN_POINT('Ctrl Pts',(1.52991547241985,-0.28181823502813,5.82519500983114));
#73328=CARTESIAN_POINT('Ctrl Pts',(1.50108539483435,-0.426805488715601,
5.81432475684774));
#73329=CARTESIAN_POINT('Ctrl Pts',(1.46165321004162,-0.546788576369168,
5.8045873531112));
#73330=CARTESIAN_POINT('Ctrl Pts',(1.37954828209111,-0.72179137571153,5.78960441794395));
#73331=CARTESIAN_POINT('Ctrl Pts',(1.34692905325015,-0.780973861132466,
5.7843962153277));
#73332=CARTESIAN_POINT('Ctrl Pts',(1.30180150011851,-0.85156196904706,5.77814341094369));
#73333=CARTESIAN_POINT('Ctrl Pts',(1.29282334705419,-0.865131655658124,
5.77693958065828));
#73334=CARTESIAN_POINT('Ctrl Pts',(1.27910223437042,-0.885179126897421,
5.77516117381309));
#73335=CARTESIAN_POINT('Ctrl Pts',(1.27451970134879,-0.89176462766739,5.77457699299982));
#73336=CARTESIAN_POINT('Ctrl Pts',(1.26650678670468,-0.903091940787994,
5.77357261458507));
#73337=CARTESIAN_POINT('Ctrl Pts',(1.26310039188334,-0.907850151435346,
5.77315087191335));
#73338=CARTESIAN_POINT('Ctrl Pts',(1.25496668431837,-0.919077286499646,
5.77215610364143));
#73339=CARTESIAN_POINT('Ctrl Pts',(1.25021614416999,-0.925529058269034,
5.77158467470252));
#73340=CARTESIAN_POINT('Ctrl Pts',(1.23570250920406,-0.944924547920943,
5.76986652922714));
#73341=CARTESIAN_POINT('Ctrl Pts',(1.22578634406955,-0.957753092118421,
5.76872970486963));
#73342=CARTESIAN_POINT('Ctrl Pts',(1.16985229575528,-1.02782280620752,5.76250323880995));
#73343=CARTESIAN_POINT('Ctrl Pts',(1.12002016712495,-1.08191109364863,5.75763010560487));
#73344=CARTESIAN_POINT('Ctrl Pts',(1.01787062365482,-1.17813036989517,5.74837773140616));
#73345=CARTESIAN_POINT('Ctrl Pts',(0.966290331923454,-1.220792566977,5.74400270556658));
#73346=CARTESIAN_POINT('Ctrl Pts',(0.879523827842564,-1.283603507024,5.7368651424418));
#73347=CARTESIAN_POINT('Ctrl Pts',(0.846020307262605,-1.30592856110802,
5.73415764346354));
#73348=CARTESIAN_POINT('Ctrl Pts',(0.786437303343166,-1.3423758694586,5.729385059918));
#73349=CARTESIAN_POINT('Ctrl Pts',(0.760749693953393,-1.35709849173012,
5.72734053823085));
#73350=CARTESIAN_POINT('Ctrl Pts',(0.721956173072818,-1.37788505546186,
5.72426201721646));
#73351=CARTESIAN_POINT('Ctrl Pts',(0.709159710732051,-1.38451450761659,
5.72324799699761));
#73352=CARTESIAN_POINT('Ctrl Pts',(0.68596328346975,-1.39612590986945,5.72141140967549));
#73353=CARTESIAN_POINT('Ctrl Pts',(0.675596410996834,-1.40117188767795,
5.72059115736507));
#73354=CARTESIAN_POINT('Ctrl Pts',(0.653210353646895,-1.41176190005422,
5.71882055979193));
#73355=CARTESIAN_POINT('Ctrl Pts',(0.641174658460541,-1.41726866393784,
5.71786900140752));
#73356=CARTESIAN_POINT('Ctrl Pts',(0.608125360827213,-1.4318827725488,5.71525633723756));
#73357=CARTESIAN_POINT('Ctrl Pts',(0.586979336012558,-1.44068035465576,
5.71358490667965));
#73358=CARTESIAN_POINT('Ctrl Pts',(0.439141500713128,-1.49839168348515,
5.70189485446018));
#73359=CARTESIAN_POINT('Ctrl Pts',(0.306732816311562,-1.53098761397395,
5.69132580902141));
#73360=CARTESIAN_POINT('Ctrl Pts',(0.129949078662473,-1.55063465352026,
5.67757159682885));
#73361=CARTESIAN_POINT('Ctrl Pts',(0.0879093842415107,-1.55358520396131,
5.67433328279631));
#73362=CARTESIAN_POINT('Ctrl Pts',(0.0201977969613845,-1.55557973304851,
5.66921369005209));
#73363=CARTESIAN_POINT('Ctrl Pts',(-0.00542038943477336,-1.55570147182633,
5.6672989480957));
#73364=CARTESIAN_POINT('Ctrl Pts',(-0.0405785454446391,-1.5549999390086,
5.66471152350156));
#73365=CARTESIAN_POINT('Ctrl Pts',(-0.0501237690313576,-1.55472153418934,
5.66401314503642));
#73366=CARTESIAN_POINT('Ctrl Pts',(-0.0663008480386664,-1.5541005539251,
5.66283714775373));
#73367=CARTESIAN_POINT('Ctrl Pts',(-0.0729340654963613,-1.55380338636156,
5.66235712254839));
#73368=CARTESIAN_POINT('Ctrl Pts',(-0.0868637001504683,-1.55308993652841,
5.66135387182954));
#73369=CARTESIAN_POINT('Ctrl Pts',(-0.094159368060113,-1.55266470063568,
5.66083113391641));
#73370=CARTESIAN_POINT('Ctrl Pts',(-0.11419068421685,-1.551355441475,5.65940267041467));
#73371=CARTESIAN_POINT('Ctrl Pts',(-0.126919213453564,-1.55036600814602,
5.6585025246396));
#73372=CARTESIAN_POINT('Ctrl Pts',(-0.215431747984915,-1.54238817555035,
5.65228648526826));
#73373=CARTESIAN_POINT('Ctrl Pts',(-0.290636371536021,-1.53000191274858,
5.64722443282021));
#73374=CARTESIAN_POINT('Ctrl Pts',(-0.423572867878734,-1.49794566675011,
5.63820156385544));
#73375=CARTESIAN_POINT('Ctrl Pts',(-0.481623098155619,-1.48030209370686,
5.63423446949909));
#73376=CARTESIAN_POINT('Ctrl Pts',(-0.581199236530258,-1.44355798320697,
5.6271914758283));
#73377=CARTESIAN_POINT('Ctrl Pts',(-0.623188238602572,-1.42593413207612,
5.62414380544839));
#73378=CARTESIAN_POINT('Ctrl Pts',(-0.693560475555203,-1.39269462171343,
5.61884171907256));
#73379=CARTESIAN_POINT('Ctrl Pts',(-0.722339986588968,-1.37798735070021,
5.61661514580918));
#73380=CARTESIAN_POINT('Ctrl Pts',(-0.763680617648392,-1.35520990202905,
5.61331736500265));
#73381=CARTESIAN_POINT('Ctrl Pts',(-0.77661792844527,-1.34783772403101,
5.61227068863502));
#73382=CARTESIAN_POINT('Ctrl Pts',(-0.799420127740366,-1.33440686437997,
5.61039847537237));
#73383=CARTESIAN_POINT('Ctrl Pts',(-0.809327097894377,-1.32842156551155,
5.6095756441021));
#73384=CARTESIAN_POINT('Ctrl Pts',(-0.83016171822836,-1.31551475612854,
5.60782462947459));
#73385=CARTESIAN_POINT('Ctrl Pts',(-0.841071617125858,-1.3085664171523,
5.6068955008717));
#73386=CARTESIAN_POINT('Ctrl Pts',(-0.870358421010073,-1.28939656899751,
5.60436723590744));
#73387=CARTESIAN_POINT('Ctrl Pts',(-0.888563304042817,-1.27691912625267,
5.60275863904885));
#73388=CARTESIAN_POINT('Ctrl Pts',(-1.00820448796809,-1.19112075176179,
5.59193098019633));
#73389=CARTESIAN_POINT('Ctrl Pts',(-1.10072003799945,-1.10618628701079,
5.58224967321679));
#73390=CARTESIAN_POINT('Ctrl Pts',(-1.22620854477788,-0.959483704961743,
5.56728549392952));
#73391=CARTESIAN_POINT('Ctrl Pts',(-1.266946940279,-0.905010297610914,5.5620418073036));
#73392=CARTESIAN_POINT('Ctrl Pts',(-1.31289016560192,-0.8343655282264,5.55575198432674));
#73393=CARTESIAN_POINT('Ctrl Pts',(-1.32156955765091,-0.820548829640439,
5.55454469990656));
#73394=CARTESIAN_POINT('Ctrl Pts',(-1.3341950595696,-0.799730140119969,
5.55276224138154));
#73395=CARTESIAN_POINT('Ctrl Pts',(-1.33830660058748,-0.792830501722975,
5.55217740161241));
#73396=CARTESIAN_POINT('Ctrl Pts',(-1.34532138193611,-0.780848818431469,
5.551172337649));
#73397=CARTESIAN_POINT('Ctrl Pts',(-1.34824957437302,-0.775781919307044,
5.55075056108574));
#73398=CARTESIAN_POINT('Ctrl Pts',(-1.35511454310304,-0.76374660388735,
5.54975636072694));
#73399=CARTESIAN_POINT('Ctrl Pts',(-1.35902622715029,-0.756764178135495,
5.54918552612413));
#73400=CARTESIAN_POINT('Ctrl Pts',(-1.37067696040424,-0.735585702465334,
5.54747107571725));
#73401=CARTESIAN_POINT('Ctrl Pts',(-1.37824902703871,-0.721298363200619,
5.5463372897936));
#73402=CARTESIAN_POINT('Ctrl Pts',(-1.42179095277394,-0.635951047907557,
5.53968277342803));
#73403=CARTESIAN_POINT('Ctrl Pts',(-1.45248739563885,-0.562322750641483,
5.53441881645385));
#73404=CARTESIAN_POINT('Ctrl Pts',(-1.50197208513788,-0.412095804786269,
5.52400209212123));
#73405=CARTESIAN_POINT('Ctrl Pts',(-1.52085201134606,-0.335784731675577,
5.51886206306377));
#73406=CARTESIAN_POINT('Ctrl Pts',(-1.54148635314156,-0.213286078280297,
5.51050282797458));
#73407=CARTESIAN_POINT('Ctrl Pts',(-1.5470891174386,-0.167886129574404,
5.50738338416856));
#73408=CARTESIAN_POINT('Ctrl Pts',(-1.5520094080886,-0.105504418935435,
5.50302932791489));
#73409=CARTESIAN_POINT('Ctrl Pts',(-1.55306153173296,-0.0886804653159927,
5.50184847303187));
#73410=CARTESIAN_POINT('Ctrl Pts',(-1.55438856351805,-0.0599791782285614,
5.49982100710866));
#73411=CARTESIAN_POINT('Ctrl Pts',(-1.55480120029659,-0.048109474691243,
5.49897876276333));
#73412=CARTESIAN_POINT('Ctrl Pts',(-1.55536174447704,-0.0240539016133195,
5.49726363135309));
#73413=CARTESIAN_POINT('Ctrl Pts',(-1.55550244753266,-0.0118687164362759,
5.49639057878115));
#73414=CARTESIAN_POINT('Ctrl Pts',(-1.55549996779057,0.000316549412329119,
5.49551300756351));
#73415=CARTESIAN_POINT('Ctrl Pts',(-1.55549937218933,0.00139754019306266,
5.35621122277575));
#73416=CARTESIAN_POINT('Ctrl Pts',(-1.55559462614257,-0.104622640978542,
5.36319747743842));
#73417=CARTESIAN_POINT('Ctrl Pts',(-1.54485106980132,-0.210368542457165,
5.37012627567963));
#73418=CARTESIAN_POINT('Ctrl Pts',(-1.51948565660077,-0.333355901469767,
5.378727583461));
#73419=CARTESIAN_POINT('Ctrl Pts',(-1.51517400246084,-0.352435106664556,
5.38007698449756));
#73420=CARTESIAN_POINT('Ctrl Pts',(-1.50638888331349,-0.388162038393061,
5.38263597283379));
#73421=CARTESIAN_POINT('Ctrl Pts',(-1.50199619653517,-0.404826654203786,
5.38384292500506));
#73422=CARTESIAN_POINT('Ctrl Pts',(-1.4940289863857,-0.433134959995016,
5.38591787781));
#73423=CARTESIAN_POINT('Ctrl Pts',(-1.49059285227339,-0.444816185850429,
5.38678134560506));
#73424=CARTESIAN_POINT('Ctrl Pts',(-1.48377456560763,-0.46702848731743,
5.38843774130807));
#73425=CARTESIAN_POINT('Ctrl Pts',(-1.48041651470706,-0.477566226628152,
5.38922983404945));
#73426=CARTESIAN_POINT('Ctrl Pts',(-1.47225276490055,-0.502270664768497,
5.39110206806758));
#73427=CARTESIAN_POINT('Ctrl Pts',(-1.46735458199097,-0.516405389317805,
5.39218519503222));
#73428=CARTESIAN_POINT('Ctrl Pts',(-1.44889147902196,-0.567299686470397,
5.39612975787505));
#73429=CARTESIAN_POINT('Ctrl Pts',(-1.43414378380739,-0.603611266726163,
5.39902954514188));
#73430=CARTESIAN_POINT('Ctrl Pts',(-1.3751667166187,-0.734424266385154,
5.40979894090119));
#73431=CARTESIAN_POINT('Ctrl Pts',(-1.32283747958938,-0.824959539373897,
5.41791083537331));
#73432=CARTESIAN_POINT('Ctrl Pts',(-1.23517119294205,-0.946580437038499,
5.42951665995351));
#73433=CARTESIAN_POINT('Ctrl Pts',(-1.20687152197627,-0.98240727084699,
5.43303223237939));
#73434=CARTESIAN_POINT('Ctrl Pts',(-1.15947048249572,-1.03727061677243,
5.43852045687238));
#73435=CARTESIAN_POINT('Ctrl Pts',(-1.14137989423181,-1.05714440225415,
5.44053202404411));
#73436=CARTESIAN_POINT('Ctrl Pts',(-1.11644087966305,-1.08315463597974,
5.44318592154724));
#73437=CARTESIAN_POINT('Ctrl Pts',(-1.11004104675936,-1.08971238800746,
5.44385690565517));
#73438=CARTESIAN_POINT('Ctrl Pts',(-1.10347969926421,-1.09631784851829,
5.44453434613287));
#73439=CARTESIAN_POINT('Ctrl Pts',(-1.10337594716636,-1.09642226850917,
5.4445450556046));
#73440=CARTESIAN_POINT('Ctrl Pts',(-1.10316828171242,-1.0966312114593,5.44456648591301));
#73441=CARTESIAN_POINT('Ctrl Pts',(-1.10306436831849,-1.09673573438144,
5.44457720674692));
#73442=CARTESIAN_POINT('Ctrl Pts',(-1.10285627344347,-1.09694499039339,
5.4445986707756));
#73443=CARTESIAN_POINT('Ctrl Pts',(-1.10275209189547,-1.09704972341412,
5.44460941396514));
#73444=CARTESIAN_POINT('Ctrl Pts',(-1.10254335135056,-1.09725950912321,
5.44463093394031));
#73445=CARTESIAN_POINT('Ctrl Pts',(-1.10243879225428,-1.0973645617121,5.44464171071842));
#73446=CARTESIAN_POINT('Ctrl Pts',(-1.10222918423786,-1.09757509883223,
5.44466330939392));
#73447=CARTESIAN_POINT('Ctrl Pts',(-1.10212413518729,-1.09768058322991,
5.44467413128117));
#73448=CARTESIAN_POINT('Ctrl Pts',(-1.10191343136236,-1.09789209952021,
5.44469583203788));
#73449=CARTESIAN_POINT('Ctrl Pts',(-1.10180777642052,-1.09799813124841,
5.44470671089493));
#73450=CARTESIAN_POINT('Ctrl Pts',(-1.10159574083055,-1.09821086157687,
5.44472853785013));
#73451=CARTESIAN_POINT('Ctrl Pts',(-1.10148935997882,-1.09831755997749,
5.4447394859332));
#73452=CARTESIAN_POINT('Ctrl Pts',(-1.10127574789631,-1.09853174744648,
5.44476146405641));
#73453=CARTESIAN_POINT('Ctrl Pts',(-1.10116851643139,-1.09863923627038,
5.44477249407785));
#73454=CARTESIAN_POINT('Ctrl Pts',(-1.10095307311749,-1.09885513342537,
5.44479464931521));
#73455=CARTESIAN_POINT('Ctrl Pts',(-1.10084486098597,-1.09896354148033,
5.44480577451021));
#73456=CARTESIAN_POINT('Ctrl Pts',(-1.10062732027645,-1.09918141168588,
5.44482813392619));
#73457=CARTESIAN_POINT('Ctrl Pts',(-1.10051799137245,-1.09929087351814,
5.44483936812301));
#73458=CARTESIAN_POINT('Ctrl Pts',(-1.100298074202,-1.09951099238802,5.44486196004768));
#73459=CARTESIAN_POINT('Ctrl Pts',(-1.10018748557034,-1.09962164905443,
5.44487331774715));
#73460=CARTESIAN_POINT('Ctrl Pts',(-1.09996489831589,-1.09984430605457,
5.4448961719414));
#73461=CARTESIAN_POINT('Ctrl Pts',(-1.09985289927611,-1.09995630596934,
5.44490766840417));
#73462=CARTESIAN_POINT('Ctrl Pts',(-1.09962733190117,-1.10018180621022,
5.44493081624437));
#73463=CARTESIAN_POINT('Ctrl Pts',(-1.0995137630907,-1.10029530606754,5.44494246758604));
#73464=CARTESIAN_POINT('Ctrl Pts',(-1.0993475870668,-1.10046132977795,5.44495951144099));
#73465=CARTESIAN_POINT('Ctrl Pts',(-1.0992949937133,-1.10051386739248,5.44496490500675));
#73466=CARTESIAN_POINT('Ctrl Pts',(-1.09918482523972,-1.10062390333105,
5.44497620161535));
#73467=CARTESIAN_POINT('Ctrl Pts',(-1.09912724937277,-1.10068140090909,
5.44498210460103));
#73468=CARTESIAN_POINT('Ctrl Pts',(-1.09900648866035,-1.10080197849289,
5.44499448393808));
#73469=CARTESIAN_POINT('Ctrl Pts',(-1.09894330289011,-1.10086505758171,
5.44500096021925));
#73470=CARTESIAN_POINT('Ctrl Pts',(-1.09881058684144,-1.10099752674318,
5.44501456102142));
#73471=CARTESIAN_POINT('Ctrl Pts',(-1.09874105542098,-1.10106691566946,
5.44502168545441));
#73472=CARTESIAN_POINT('Ctrl Pts',(-1.09859477930165,-1.1012128643647,5.44503667093697));
#73473=CARTESIAN_POINT('Ctrl Pts',(-1.09851803316126,-1.10128942270898,
5.44504453187735));
#73474=CARTESIAN_POINT('Ctrl Pts',(-1.09835629329758,-1.10145073306999,
5.44506109551254));
#73475=CARTESIAN_POINT('Ctrl Pts',(-1.09827129775852,-1.1015354832808,5.44506979806866));
#73476=CARTESIAN_POINT('Ctrl Pts',(-1.09809181694324,-1.10171440462488,
5.44508817109984));
#73477=CARTESIAN_POINT('Ctrl Pts',(-1.09799732935,-1.10180857345365,5.44509784139772));
#73478=CARTESIAN_POINT('Ctrl Pts',(-1.09321282033183,-1.10657571473158,
5.44558739999751));
#73479=CARTESIAN_POINT('Ctrl Pts',(-1.08849301815657,-1.11121871746479,
5.44606494504099));
#73480=CARTESIAN_POINT('Ctrl Pts',(-1.07791713728808,-1.12149046448134,
5.44712303654671));
#73481=CARTESIAN_POINT('Ctrl Pts',(-1.07204645330552,-1.12710364500374,
5.44770241563164));
#73482=CARTESIAN_POINT('Ctrl Pts',(-1.05437109262091,-1.14374066492307,
5.44942417078648));
#73483=CARTESIAN_POINT('Ctrl Pts',(-1.04243798201973,-1.15462730643651,
5.45055685599203));
#73484=CARTESIAN_POINT('Ctrl Pts',(-0.969263986921939,-1.21932492944561,
5.45734134487584));
#73485=CARTESIAN_POINT('Ctrl Pts',(-0.904032371853128,-1.26844584958117,
5.46272408535151));
#73486=CARTESIAN_POINT('Ctrl Pts',(-0.77050932373688,-1.35343405419328,
5.47314789669137));
#73487=CARTESIAN_POINT('Ctrl Pts',(-0.702819439396752,-1.38978858966198,
5.47817721861439));
#73488=CARTESIAN_POINT('Ctrl Pts',(-0.5913365409592,-1.43942837263412,5.48639175438763));
#73489=CARTESIAN_POINT('Ctrl Pts',(-0.549165599718193,-1.45603896530304,
5.48948318920828));
#73490=CARTESIAN_POINT('Ctrl Pts',(-0.490202873436202,-1.47633749702224,
5.49382197940525));
#73491=CARTESIAN_POINT('Ctrl Pts',(-0.473983189648467,-1.48162449963002,
5.49501705984585));
#73492=CARTESIAN_POINT('Ctrl Pts',(-0.446073060886537,-1.49021695527416,
5.49707794238948));
#73493=CARTESIAN_POINT('Ctrl Pts',(-0.434424595378966,-1.49365424552904,
5.49793936765119));
#73494=CARTESIAN_POINT('Ctrl Pts',(-0.410631104486835,-1.50037348542465,
5.49970220788646));
#73495=CARTESIAN_POINT('Ctrl Pts',(-0.398484152931951,-1.50364519166036,
5.5006038828026));
#73496=CARTESIAN_POINT('Ctrl Pts',(-0.367590103931512,-1.51156567899781,
5.50290219303504));
#73497=CARTESIAN_POINT('Ctrl Pts',(-0.348794137251851,-1.51601315096183,
5.50430516668958));
#73498=CARTESIAN_POINT('Ctrl Pts',(-0.269135135186256,-1.53330215573084,
5.5102735262068));
#73499=CARTESIAN_POINT('Ctrl Pts',(-0.207620865705634,-1.54283535705406,
5.51494053166543));
#73500=CARTESIAN_POINT('Ctrl Pts',(-0.0433451858979095,-1.5582914950787,
5.52754013488558));
#73501=CARTESIAN_POINT('Ctrl Pts',(0.0597127087849346,-1.55774954845205,
5.53559818847931));
#73502=CARTESIAN_POINT('Ctrl Pts',(0.190163278075731,-1.54409272431689,
5.54564864748023));
#73503=CARTESIAN_POINT('Ctrl Pts',(0.218282668049377,-1.54036920398571,
5.54780446586955));
#73504=CARTESIAN_POINT('Ctrl Pts',(0.265616686225664,-1.53277894863473,
5.55140012163969));
#73505=CARTESIAN_POINT('Ctrl Pts',(0.284888202360669,-1.52931433458504,
5.55285460324597));
#73506=CARTESIAN_POINT('Ctrl Pts',(0.312675569542116,-1.52377520457266,
5.55493336840922));
#73507=CARTESIAN_POINT('Ctrl Pts',(0.321246522978594,-1.52199131635983,
5.55557200065485));
#73508=CARTESIAN_POINT('Ctrl Pts',(0.336274648206556,-1.51873087644293,
5.55668673109968));
#73509=CARTESIAN_POINT('Ctrl Pts',(0.342738054555045,-1.51728532116043,
5.5571644883669));
#73510=CARTESIAN_POINT('Ctrl Pts',(0.357080720846315,-1.5139812205348,5.55822089230619));
#73511=CARTESIAN_POINT('Ctrl Pts',(0.364954935812276,-1.51210240391644,
5.55879839671195));
#73512=CARTESIAN_POINT('Ctrl Pts',(0.388360694549209,-1.50632421452209,
5.56050863350208));
#73513=CARTESIAN_POINT('Ctrl Pts',(0.403847637240471,-1.50224625362449,
5.56163186640449));
#73514=CARTESIAN_POINT('Ctrl Pts',(0.505375142390776,-1.47382876515868,
5.56895699368908));
#73515=CARTESIAN_POINT('Ctrl Pts',(0.589254314168118,-1.44234493949242,
5.57483218913564));
#73516=CARTESIAN_POINT('Ctrl Pts',(0.73445695181496,-1.37304721856563,5.58542219003687));
#73517=CARTESIAN_POINT('Ctrl Pts',(0.796740934423673,-1.33786720905471,
5.59011948391792));
#73518=CARTESIAN_POINT('Ctrl Pts',(0.892688137963855,-1.27458988108497,
5.59786755097302));
#73519=CARTESIAN_POINT('Ctrl Pts',(0.927969099527476,-1.24913741072054,
5.60083866149626));
#73520=CARTESIAN_POINT('Ctrl Pts',(0.975353457828333,-1.21183698359632,
5.60503643656849));
#73521=CARTESIAN_POINT('Ctrl Pts',(0.988401593924317,-1.20121833692233,
5.60621538346845));
#73522=CARTESIAN_POINT('Ctrl Pts',(1.01053723534928,-1.18259935990777,5.60825722622297));
#73523=CARTESIAN_POINT('Ctrl Pts',(1.01970845382683,-1.17470055939435,5.60911595523393));
#73524=CARTESIAN_POINT('Ctrl Pts',(1.03827316303654,-1.15833029379701,5.61088118354835));
#73525=CARTESIAN_POINT('Ctrl Pts',(1.04765734188957,-1.14984968892041,5.61178802493457));
#73526=CARTESIAN_POINT('Ctrl Pts',(1.0713543156893,-1.12790351044442,5.61411623053505));
#73527=CARTESIAN_POINT('Ctrl Pts',(1.08551686665898,-1.11427979662375,5.61554426965163));
#73528=CARTESIAN_POINT('Ctrl Pts',(1.14677112719925,-1.05307981356902,5.62188773036175));
#73529=CARTESIAN_POINT('Ctrl Pts',(1.19101517158888,-1.00276701712588,5.62692228364672));
#73530=CARTESIAN_POINT('Ctrl Pts',(1.29188112948638,-0.871940913129017,
5.63956985855039));
#73531=CARTESIAN_POINT('Ctrl Pts',(1.34437166160667,-0.788607248880685,
5.64726790177073));
#73532=CARTESIAN_POINT('Ctrl Pts',(1.40119258664077,-0.676028543132031,
5.65692596393689));
#73533=CARTESIAN_POINT('Ctrl Pts',(1.41306765233618,-0.650841956097149,
5.65904122872589));
#73534=CARTESIAN_POINT('Ctrl Pts',(1.43202761020508,-0.607659769720504,
5.66257726609157));
#73535=CARTESIAN_POINT('Ctrl Pts',(1.43946455910997,-0.589826537465558,
5.66401210854213));
#73536=CARTESIAN_POINT('Ctrl Pts',(1.44976955671436,-0.563759107816872,
5.66606827362465));
#73537=CARTESIAN_POINT('Ctrl Pts',(1.45290338031695,-0.555632861058138,
5.66670353323081));
#73538=CARTESIAN_POINT('Ctrl Pts',(1.45809581412612,-0.541824108967194,
5.66777283899854));
#73539=CARTESIAN_POINT('Ctrl Pts',(1.4601897866093,-0.536155350698382,5.66820890626339));
#73540=CARTESIAN_POINT('Ctrl Pts',(1.46493212999062,-0.523083093617968,
5.66920775139164));
#73541=CARTESIAN_POINT('Ctrl Pts',(1.46755747596099,-0.515671533273761,
5.66976918240121));
#73542=CARTESIAN_POINT('Ctrl Pts',(1.47484193114657,-0.49460064621538,5.67135237581244));
#73543=CARTESIAN_POINT('Ctrl Pts',(1.47936745242251,-0.480895519651347,
5.67236679767314));
#73544=CARTESIAN_POINT('Ctrl Pts',(1.51508421425955,-0.367451373582968,
5.68065345741046));
#73545=CARTESIAN_POINT('Ctrl Pts',(1.53634685153535,-0.264850001125193,
5.68746218616178));
#73546=CARTESIAN_POINT('Ctrl Pts',(1.55367329349452,-0.0982229060206245,
5.69849523671166));
#73547=CARTESIAN_POINT('Ctrl Pts',(1.55637601066361,-0.0352325784255422,
5.70265826081442));
#73548=CARTESIAN_POINT('Ctrl Pts',(1.55453394469138,0.0680268280765478,
5.70963963641047));
#73549=CARTESIAN_POINT('Ctrl Pts',(1.55225066405916,0.108262910391544,5.71239847735124));
#73550=CARTESIAN_POINT('Ctrl Pts',(1.54684619303097,0.164667555324142,5.71634630481624));
#73551=CARTESIAN_POINT('Ctrl Pts',(1.5450265039527,0.180946442166766,5.71749508152314));
#73552=CARTESIAN_POINT('Ctrl Pts',(1.54142502752959,0.209126437161502,5.71950161409378));
#73553=CARTESIAN_POINT('Ctrl Pts',(1.53976155660048,0.221041435589435,5.72035559003728));
#73554=CARTESIAN_POINT('Ctrl Pts',(1.53604419563493,0.245585351461588,5.72212684422236));
#73555=CARTESIAN_POINT('Ctrl Pts',(1.53397236411308,0.258210580395583,5.72304462913413));
#73556=CARTESIAN_POINT('Ctrl Pts',(1.52820076146422,0.290855880837561,5.72543578734649));
#73557=CARTESIAN_POINT('Ctrl Pts',(1.52426337095613,0.310830844313258,5.72691656261709));
#73558=CARTESIAN_POINT('Ctrl Pts',(1.50187193334053,0.413737644608457,5.7346407457897));
#73559=CARTESIAN_POINT('Ctrl Pts',(1.47704095767163,0.495119923312487,5.74108392243216));
#73560=CARTESIAN_POINT('Ctrl Pts',(1.41524906417467,0.650735796526316,5.75400031311279));
#73561=CARTESIAN_POINT('Ctrl Pts',(1.37874930691362,0.724870720990935,5.76044575843799));
#73562=CARTESIAN_POINT('Ctrl Pts',(1.31710930035695,0.828399799246312,5.76965378044345));
#73563=CARTESIAN_POINT('Ctrl Pts',(1.29648585262373,0.860318611806963,5.77252248245038));
#73564=CARTESIAN_POINT('Ctrl Pts',(1.26835532361954,0.900543207378694,5.77614788799235));
#73565=CARTESIAN_POINT('Ctrl Pts',(1.26190089368668,0.909565527472956,5.7769617311091));
#73566=CARTESIAN_POINT('Ctrl Pts',(1.2511791377066,0.92421908209416,5.77828363762656));
#73567=CARTESIAN_POINT('Ctrl Pts',(1.24696911625932,0.929891485772563,5.77879537513316));
#73568=CARTESIAN_POINT('Ctrl Pts',(1.23895217507802,0.940540809480468,5.77975585433789));
#73569=CARTESIAN_POINT('Ctrl Pts',(1.23515357567941,0.94552374621654,5.78020517178475));
#73570=CARTESIAN_POINT('Ctrl Pts',(1.22487231516354,0.958842829656581,5.78140631173893));
#73571=CARTESIAN_POINT('Ctrl Pts',(1.21833455901391,0.967136329104839,5.78215438612113));
#73572=CARTESIAN_POINT('Ctrl Pts',(1.19284420130964,0.998803504165049,5.78501420822213));
#73573=CARTESIAN_POINT('Ctrl Pts',(1.17329802236386,1.02169358055151,5.78708872828255));
#73574=CARTESIAN_POINT('Ctrl Pts',(1.09305309766497,1.11032380576659,5.79521855177529));
#73575=CARTESIAN_POINT('Ctrl Pts',(1.02739322846957,1.17134532249325,5.8010455900795));
#73576=CARTESIAN_POINT('Ctrl Pts',(0.900925733994054,1.27001723407601,5.8116223575826));
#73577=CARTESIAN_POINT('Ctrl Pts',(0.842091695323497,1.30976756903908,5.81633119265602));
#73578=CARTESIAN_POINT('Ctrl Pts',(0.755138453555622,1.36022915795142,5.82320093543274));
#73579=CARTESIAN_POINT('Ctrl Pts',(0.729104244124455,1.3743595794835,5.82524645422139));
#73580=CARTESIAN_POINT('Ctrl Pts',(0.689625125179295,1.39434991763002,5.82834173061752));
#73581=CARTESIAN_POINT('Ctrl Pts',(0.676474032564042,1.40077741394932,5.8293717165143));
#73582=CARTESIAN_POINT('Ctrl Pts',(0.652539397502234,1.41205962618346,5.83124541300879));
#73583=CARTESIAN_POINT('Ctrl Pts',(0.641787357941646,1.41697883761974,5.83208681735378));
#73584=CARTESIAN_POINT('Ctrl Pts',(0.618448096165011,1.42733675045644,5.83391315215404));
#73585=CARTESIAN_POINT('Ctrl Pts',(0.605843037113228,1.4327325077978,5.83489946678285));
#73586=CARTESIAN_POINT('Ctrl Pts',(0.570860037997591,1.44716323442029,5.83763754412333));
#73587=CARTESIAN_POINT('Ctrl Pts',(0.548341511132627,1.45584479821499,5.83940092799493));
#73588=CARTESIAN_POINT('Ctrl Pts',(0.432924641821117,1.49728385159557,5.8484485079143));
#73589=CARTESIAN_POINT('Ctrl Pts',(0.33728154179288,1.5216824978213,5.85599758830367));
#73590=CARTESIAN_POINT('Ctrl Pts',(0.174451430080643,1.54710929074434,5.86876889911588));
#73591=CARTESIAN_POINT('Ctrl Pts',(0.108321607269753,1.55314120131835,5.87392807257427));
#73592=CARTESIAN_POINT('Ctrl Pts',(0.0189685137864616,1.55555507088054,
5.88073748017832));
#73593=CARTESIAN_POINT('Ctrl Pts',(-0.00408170450262528,1.55566540117844,
5.88247926609734));
#73594=CARTESIAN_POINT('Ctrl Pts',(-0.0439488770477343,1.55497003356112,
5.88545754294958));
#73595=CARTESIAN_POINT('Ctrl Pts',(-0.0607657296007624,1.55440371073337,
5.88670327397402));
#73596=CARTESIAN_POINT('Ctrl Pts',(-0.0858130022068973,1.55315307657781,
5.88853981094884));
#73597=CARTESIAN_POINT('Ctrl Pts',(-0.0940518914480969,1.55267594835633,
5.88914086000298));
#73598=CARTESIAN_POINT('Ctrl Pts',(-0.108948986900014,1.55169421768988,
5.89022166345651));
#73599=CARTESIAN_POINT('Ctrl Pts',(-0.115608107540542,1.55121229894249,
5.89070258280972));
#73600=CARTESIAN_POINT('Ctrl Pts',(-0.130837720518675,1.5500115162799,5.89179751568691));
#73601=CARTESIAN_POINT('Ctrl Pts',(-0.139405609597813,1.54926443673051,
5.89240997720311));
#73602=CARTESIAN_POINT('Ctrl Pts',(-0.16658455836971,1.54666725855996,5.89434288622661));
#73603=CARTESIAN_POINT('Ctrl Pts',(-0.18516946869602,1.54455248281149,5.8956498005022));
#73604=CARTESIAN_POINT('Ctrl Pts',(-0.35584132537989,1.5220066229701,5.90755289312));
#73605=CARTESIAN_POINT('Ctrl Pts',(-0.504176002461071,1.47950912003686,
5.91724886467921));
#73606=CARTESIAN_POINT('Ctrl Pts',(-0.685890257238166,1.39687595912198,
5.93067715758492));
#73607=CARTESIAN_POINT('Ctrl Pts',(-0.7270052782106,1.37592534870155,5.9338227542899));
#73608=CARTESIAN_POINT('Ctrl Pts',(-0.782056113402773,1.34471671123798,
5.93822487156425));
#73609=CARTESIAN_POINT('Ctrl Pts',(-0.796844605925746,1.33600652357278,
5.93942699358277));
#73610=CARTESIAN_POINT('Ctrl Pts',(-0.821862415753385,1.32070828178135,
5.94149621596701));
#73611=CARTESIAN_POINT('Ctrl Pts',(-0.832164313949627,1.31424150571343,
5.94235884711758));
#73612=CARTESIAN_POINT('Ctrl Pts',(-0.851697782372793,1.30165807719495,
5.94401539628674));
#73613=CARTESIAN_POINT('Ctrl Pts',(-0.860941983413846,1.29556233038056,
5.94480849726516));
#73614=CARTESIAN_POINT('Ctrl Pts',(-0.884966363418037,1.27934966885143,
5.94689423809982));
#73615=CARTESIAN_POINT('Ctrl Pts',(-0.899637875526344,1.26907552284861,
5.94819274983266));
#73616=CARTESIAN_POINT('Ctrl Pts',(-0.953318981497306,1.23008511128515,
5.95303873171313));
#73617=CARTESIAN_POINT('Ctrl Pts',(-0.991154570462774,1.19980755224995,
5.95664514517999));
#73618=CARTESIAN_POINT('Ctrl Pts',(-1.11550428599869,1.09039752656929,5.9691748665564));
#73619=CARTESIAN_POINT('Ctrl Pts',(-1.19445971526106,1.00328340079883,5.97837078010903));
#73620=CARTESIAN_POINT('Ctrl Pts',(-1.28026143751037,0.883967146842678,
5.98964658886706));
#73621=CARTESIAN_POINT('Ctrl Pts',(-1.2969525839575,0.859291264677404,5.99191389710067));
#73622=CARTESIAN_POINT('Ctrl Pts',(-1.32379938764862,0.817035236315087,
5.99567255948169));
#73623=CARTESIAN_POINT('Ctrl Pts',(-1.33433795891441,0.799708515226675,
5.99718018444302));
#73624=CARTESIAN_POINT('Ctrl Pts',(-1.34899755313851,0.77450926251175,5.99931991532146));
#73625=CARTESIAN_POINT('Ctrl Pts',(-1.35339419853894,0.766800593095095,
5.99996751029557));
#73626=CARTESIAN_POINT('Ctrl Pts',(-1.36099080627317,0.75321250048554,6.00109631188464));
#73627=CARTESIAN_POINT('Ctrl Pts',(-1.364219126722,0.747349467227705,6.00157923790042));
#73628=CARTESIAN_POINT('Ctrl Pts',(-1.371239577101,0.734402360311117,6.00263653640742));
#73629=CARTESIAN_POINT('Ctrl Pts',(-1.37501478363253,0.727309533172104,
6.00320986934433));
#73630=CARTESIAN_POINT('Ctrl Pts',(-1.3857895488713,0.706682204405237,6.00486119481532));
#73631=CARTESIAN_POINT('Ctrl Pts',(-1.39264565386833,0.69307325725646,6.0059308312449));
#73632=CARTESIAN_POINT('Ctrl Pts',(-1.44123920171017,0.592984218352183,
6.01367013293471));
#73633=CARTESIAN_POINT('Ctrl Pts',(-1.47509478095636,0.502892925769997,
6.01995637297821));
#73634=CARTESIAN_POINT('Ctrl Pts',(-1.51827150523562,0.344978077444376,
6.03073226641404));
#73635=CARTESIAN_POINT('Ctrl Pts',(-1.53183798483718,0.278621160732913,
6.03519053309801));
#73636=CARTESIAN_POINT('Ctrl Pts',(-1.54676781674349,0.169887914987912,
6.042598042306));
#73637=CARTESIAN_POINT('Ctrl Pts',(-1.55079856868164,0.127968246974907,
6.04547707770907));
#73638=CARTESIAN_POINT('Ctrl Pts',(-1.55404318917488,0.0693305109071148,
6.04956662452576));
#73639=CARTESIAN_POINT('Ctrl Pts',(-1.55469570600136,0.0527084230119468,
6.05073275764942));
#73640=CARTESIAN_POINT('Ctrl Pts',(-1.5553615201138,0.0240109097994755,
6.05275955295973));
#73641=CARTESIAN_POINT('Ctrl Pts',(-1.55550101617352,0.0119396733131739,
6.05361621352016));
#73642=CARTESIAN_POINT('Ctrl Pts',(-1.55549999442795,-0.000131661105043114,
6.05447729365254));
#73643=CARTESIAN_POINT('Origin',(0.,0.,-1.2940562256037));
#73644=CARTESIAN_POINT('',(-1.55549991697348,0.000508228199595362,6.89275239802721));
#73645=CARTESIAN_POINT('',(-1.5555,-1.2376520005909E-10,6.75616363716894));
#73646=CARTESIAN_POINT('',(-1.5555,-1.46451138874614E-13,-1.2940562256037));
#73647=CARTESIAN_POINT('',(-1.55549936109204,-0.00142508202560441,6.19403092979389));
#73648=CARTESIAN_POINT('Ctrl Pts',(-1.55549991697361,0.000508227400676815,
6.8927523980872));
#73649=CARTESIAN_POINT('Ctrl Pts',(-1.55549342449748,0.0203793442693804,
6.89126023457575));
#73650=CARTESIAN_POINT('Ctrl Pts',(-1.55510615917786,0.0402497180585557,
6.88978222333507));
#73651=CARTESIAN_POINT('Ctrl Pts',(-1.55402627507162,0.0681743633031146,
6.88772972553868));
#73652=CARTESIAN_POINT('Ctrl Pts',(-1.55365156229955,0.0762380348004057,
6.88713992681524));
#73653=CARTESIAN_POINT('Ctrl Pts',(-1.55285741420605,0.0908703204861343,
6.88607536342126));
#73654=CARTESIAN_POINT('Ctrl Pts',(-1.55245903086773,0.0974398710232745,
6.88559948895312));
#73655=CARTESIAN_POINT('Ctrl Pts',(-1.55153303461324,0.111257821680616,
6.88460318461379));
#73656=CARTESIAN_POINT('Ctrl Pts',(-1.55099630922104,0.118505337091623,
6.88408325408978));
#73657=CARTESIAN_POINT('Ctrl Pts',(-1.5493921319165,0.138283865563624,6.8826708879077));
#73658=CARTESIAN_POINT('Ctrl Pts',(-1.54822344887407,0.150806448583604,
6.8817838251873));
#73659=CARTESIAN_POINT('Ctrl Pts',(-1.53967876647658,0.231741300147992,
6.87608894454265));
#73660=CARTESIAN_POINT('Ctrl Pts',(-1.52792115720393,0.299623430997248,
6.87148823334955));
#73661=CARTESIAN_POINT('Ctrl Pts',(-1.48388532731362,0.481252482250994,
6.85912751940839));
#73662=CARTESIAN_POINT('Ctrl Pts',(-1.44309657454036,0.592444118163773,
6.85147558106071));
#73663=CARTESIAN_POINT('Ctrl Pts',(-1.37686943514775,0.724350393368029,
6.84138953236598));
#73664=CARTESIAN_POINT('Ctrl Pts',(-1.36286575701312,0.750366356807447,
6.83934918828765));
#73665=CARTESIAN_POINT('Ctrl Pts',(-1.34094704980521,0.788446970763909,
6.83627571548063));
#73666=CARTESIAN_POINT('Ctrl Pts',(-1.3335907151863,0.800826695194638,6.83526246678439));
#73667=CARTESIAN_POINT('Ctrl Pts',(-1.32003736661037,0.822930442925678,
6.83342670452176));
#73668=CARTESIAN_POINT('Ctrl Pts',(-1.31390202523348,0.832691190132706,
6.83260649651835));
#73669=CARTESIAN_POINT('Ctrl Pts',(-1.30048686840046,0.853515990203702,
6.83083535442585));
#73670=CARTESIAN_POINT('Ctrl Pts',(-1.29317315679937,0.864557000311825,
6.82988320027177));
#73671=CARTESIAN_POINT('Ctrl Pts',(-1.27245361975139,0.894984668878109,
6.82722159441595));
#73672=CARTESIAN_POINT('Ctrl Pts',(-1.25874731347701,0.914161287672667,
6.82550090103568));
#73673=CARTESIAN_POINT('Ctrl Pts',(-1.19762732621862,0.995693061502733,
6.81799104430637));
#73674=CARTESIAN_POINT('Ctrl Pts',(-1.14598353095668,1.05471998529052,6.81204165300716));
#73675=CARTESIAN_POINT('Ctrl Pts',(-1.02925092609578,1.16940352904253,6.79941782007523));
#73676=CARTESIAN_POINT('Ctrl Pts',(-0.963561367754265,1.22409633970669,
6.79274633746764));
#73677=CARTESIAN_POINT('Ctrl Pts',(-0.86437221551257,1.29372578440817,6.78349559977576));
#73678=CARTESIAN_POINT('Ctrl Pts',(-0.834320973498121,1.31330678507143,
6.78079071459073));
#73679=CARTESIAN_POINT('Ctrl Pts',(-0.794161120196738,1.33753891088416,
6.77732591922588));
#73680=CARTESIAN_POINT('Ctrl Pts',(-0.784644165101397,1.3431439892473,6.77651550500294));
#73681=CARTESIAN_POINT('Ctrl Pts',(-0.769054216766427,1.35210353574585,
6.77520617713905));
#73682=CARTESIAN_POINT('Ctrl Pts',(-0.763017265955682,1.35551946376564,
6.77470355079349));
#73683=CARTESIAN_POINT('Ctrl Pts',(-0.750952875219959,1.36223979996799,
6.77370809944965));
#73684=CARTESIAN_POINT('Ctrl Pts',(-0.744925996976146,1.36554485714885,
6.77321524525308));
#73685=CARTESIAN_POINT('Ctrl Pts',(-0.72941593334125,1.37391711771678,6.771957696216));
#73686=CARTESIAN_POINT('Ctrl Pts',(-0.719901550179127,1.37892625813991,
6.77119654407822));
#73687=CARTESIAN_POINT('Ctrl Pts',(-0.678195797298543,1.40033419337853,
6.76790119818549));
#73688=CARTESIAN_POINT('Ctrl Pts',(-0.645487916613955,1.41570873658642,
6.76542263308532));
#73689=CARTESIAN_POINT('Ctrl Pts',(-0.543124381169593,1.45953898997125,
6.75789607720686));
#73690=CARTESIAN_POINT('Ctrl Pts',(-0.471916280569133,1.48409389918118,
6.75297575371484));
#73691=CARTESIAN_POINT('Ctrl Pts',(-0.314813232751636,1.52581038777286,
6.74227346169623));
#73692=CARTESIAN_POINT('Ctrl Pts',(-0.228692389286584,1.54107169755881,
6.73649465373794));
#73693=CARTESIAN_POINT('Ctrl Pts',(-0.119857285379126,1.55103122860766,
6.72897915844517));
#73694=CARTESIAN_POINT('Ctrl Pts',(-0.0979235790153293,1.55257029852886,
6.72745459059677));
#73695=CARTESIAN_POINT('Ctrl Pts',(-0.0618410957183949,1.554334553788,6.72492595338788));
#73696=CARTESIAN_POINT('Ctrl Pts',(-0.0477083438185087,1.55483250438405,
6.72393036659501));
#73697=CARTESIAN_POINT('Ctrl Pts',(-0.0220608897234783,1.55538616281825,
6.72211324131705));
#73698=CARTESIAN_POINT('Ctrl Pts',(-0.0105484957400943,1.55550683525241,
6.72129379676679));
#73699=CARTESIAN_POINT('Ctrl Pts',(0.0144039426147126,1.55549137293776,
6.71950895805211));
#73700=CARTESIAN_POINT('Ctrl Pts',(0.0278429078952762,1.55530885558072,
6.71854217542209));
#73701=CARTESIAN_POINT('Ctrl Pts',(0.0658082330556769,1.5543010359791,6.71579460484143));
#73702=CARTESIAN_POINT('Ctrl Pts',(0.0903188070033247,1.55306948328054,
6.71400135543403));
#73703=CARTESIAN_POINT('Ctrl Pts',(0.145922532807744,1.54895496524715,6.7098867729851));
#73704=CARTESIAN_POINT('Ctrl Pts',(0.176977834788359,1.54571455149333,6.7075554733893));
#73705=CARTESIAN_POINT('Ctrl Pts',(0.286963129644274,1.53088047996332,6.69918145406124));
#73706=CARTESIAN_POINT('Ctrl Pts',(0.365068923062777,1.51415493697405,6.69301023202755));
#73707=CARTESIAN_POINT('Ctrl Pts',(0.516215514325651,1.46941042077895,6.68078395274029));
#73708=CARTESIAN_POINT('Ctrl Pts',(0.589133013551162,1.44172467738669,6.67474776217071));
#73709=CARTESIAN_POINT('Ctrl Pts',(0.674310663003219,1.40183684484663,6.66772943405374));
#73710=CARTESIAN_POINT('Ctrl Pts',(0.688838947033825,1.39475530803565,6.66653381552239));
#73711=CARTESIAN_POINT('Ctrl Pts',(0.710392133403156,1.38383065912949,6.66476504616534));
#73712=CARTESIAN_POINT('Ctrl Pts',(0.717501497186652,1.38015792047352,6.66418243640727));
#73713=CARTESIAN_POINT('Ctrl Pts',(0.72976093398955,1.37370429055078,6.66317961170658));
#73714=CARTESIAN_POINT('Ctrl Pts',(0.734923972157448,1.37094903511661,6.66275786978976));
#73715=CARTESIAN_POINT('Ctrl Pts',(0.747137139583626,1.36434265233553,6.66176161238843));
#73716=CARTESIAN_POINT('Ctrl Pts',(0.754173145705648,1.36046596878214,6.66118871136267));
#73717=CARTESIAN_POINT('Ctrl Pts',(0.775413806698982,1.348547406247,6.65946139336219));
#73718=CARTESIAN_POINT('Ctrl Pts',(0.789522739716125,1.34033599417012,6.65831702405038));
#73719=CARTESIAN_POINT('Ctrl Pts',(0.861740535217963,1.29676899974673,6.65246092039309));
#73720=CARTESIAN_POINT('Ctrl Pts',(0.917620610546984,1.2578478482483,6.64793277641949));
#73721=CARTESIAN_POINT('Ctrl Pts',(1.06846628495678,1.13736150270851,6.63518692712743));
#73722=CARTESIAN_POINT('Ctrl Pts',(1.15638051507125,1.0478512119659,6.627066855546));
#73723=CARTESIAN_POINT('Ctrl Pts',(1.24610318389196,0.931286676784698,6.61691915042587));
#73724=CARTESIAN_POINT('Ctrl Pts',(1.259199506514,0.913501252055849,6.6153824971542));
#73725=CARTESIAN_POINT('Ctrl Pts',(1.27936010646699,0.884864598939954,6.61292253251035));
#73726=CARTESIAN_POINT('Ctrl Pts',(1.2866755157358,0.874193193479355,6.6120088760989));
#73727=CARTESIAN_POINT('Ctrl Pts',(1.30028123207379,0.853804967320327,6.61026824971638));
#73728=CARTESIAN_POINT('Ctrl Pts',(1.30659788751557,0.844106718198599,6.60944234820352));
#73729=CARTESIAN_POINT('Ctrl Pts',(1.32078904753555,0.821777387648905,6.60754496338971));
#73730=CARTESIAN_POINT('Ctrl Pts',(1.32859154152943,0.809102138208922,6.60647090898404));
#73731=CARTESIAN_POINT('Ctrl Pts',(1.35273526629831,0.768589261813121,6.60304621392579));
#73732=CARTESIAN_POINT('Ctrl Pts',(1.36839152557638,0.740355659019166,6.6006714190227));
#73733=CARTESIAN_POINT('Ctrl Pts',(1.40395021191578,0.671244795101186,6.59488268006597));
#73734=CARTESIAN_POINT('Ctrl Pts',(1.42296022501471,0.629943892926199,6.5914425288533));
#73735=CARTESIAN_POINT('Ctrl Pts',(1.46307327525252,0.531677562136893,6.58331546255814));
#73736=CARTESIAN_POINT('Ctrl Pts',(1.48270295400637,0.474189566342425,6.5786032278935));
#73737=CARTESIAN_POINT('Ctrl Pts',(1.51927573540323,0.342317698620794,6.56799295098523));
#73738=CARTESIAN_POINT('Ctrl Pts',(1.53421395534008,0.267526301050437,6.56211087485816));
#73739=CARTESIAN_POINT('Ctrl Pts',(1.54518832953776,0.179265839303977,6.55551565943411));
#73740=CARTESIAN_POINT('Ctrl Pts',(1.54660756504172,0.166578158161503,6.55457596191046));
#73741=CARTESIAN_POINT('Ctrl Pts',(1.54859339454342,0.146602016798972,6.55311107045756));
#73742=CARTESIAN_POINT('Ctrl Pts',(1.54926505956831,0.139324922498857,6.55258046855126));
#73743=CARTESIAN_POINT('Ctrl Pts',(1.55044907111383,0.125427329077983,6.55157328176952));
#73744=CARTESIAN_POINT('Ctrl Pts',(1.5509703451918,0.118807942370117,6.5510962564927));
#73745=CARTESIAN_POINT('Ctrl Pts',(1.55213790599631,0.102661339850625,6.54993884845402));
#73746=CARTESIAN_POINT('Ctrl Pts',(1.55273889390393,0.0931309271712147,
6.54926092911641));
#73747=CARTESIAN_POINT('Ctrl Pts',(1.55462859139125,0.058019170562004,6.54678058854424));
#73748=CARTESIAN_POINT('Ctrl Pts',(1.55537326532875,0.0324110880418939,
6.54500524316457));
#73749=CARTESIAN_POINT('Ctrl Pts',(1.55566915878671,-0.0353288835396494,
6.54037009980746));
#73750=CARTESIAN_POINT('Ctrl Pts',(1.55414200454341,-0.077445443790286,
6.53755047812076));
#73751=CARTESIAN_POINT('Ctrl Pts',(1.54047969579514,-0.254832002753672,
6.5257492407853));
#73752=CARTESIAN_POINT('Ctrl Pts',(1.51237382546127,-0.388253205563357,
6.5169986673229));
#73753=CARTESIAN_POINT('Ctrl Pts',(1.45970282601969,-0.537933460574715,
6.50606888377256));
#73754=CARTESIAN_POINT('Ctrl Pts',(1.45162498154463,-0.559365325783071,
6.5044774958865));
#73755=CARTESIAN_POINT('Ctrl Pts',(1.43813695070997,-0.592889148365251,
6.5019417192252));
#73756=CARTESIAN_POINT('Ctrl Pts',(1.43304021444263,-0.605104251887188,
6.50100783491967));
#73757=CARTESIAN_POINT('Ctrl Pts',(1.42321318292333,-0.627835502484376,
6.49925048099795));
#73758=CARTESIAN_POINT('Ctrl Pts',(1.418520598923,-0.6383670413574,6.49842834591411));
#73759=CARTESIAN_POINT('Ctrl Pts',(1.40770007598231,-0.661942923433136,
6.49656943269474));
#73760=CARTESIAN_POINT('Ctrl Pts',(1.40150712732724,-0.674956060674805,
6.49553046691707));
#73761=CARTESIAN_POINT('Ctrl Pts',(1.38204342316198,-0.714431622898365,
6.49233801361806));
#73762=CARTESIAN_POINT('Ctrl Pts',(1.36819802097219,-0.740601459368662,
6.4901648115206));
#73763=CARTESIAN_POINT('Ctrl Pts',(1.33378667858496,-0.80138202287171,6.48497818950137));
#73764=CARTESIAN_POINT('Ctrl Pts',(1.3126078443408,-0.835619659771455,6.48194542037987));
#73765=CARTESIAN_POINT('Ctrl Pts',(1.25276809677292,-0.924458895003148,
6.47378142644174));
#73766=CARTESIAN_POINT('Ctrl Pts',(1.21187362374784,-0.977452507544467,
6.46859517012091));
#73767=CARTESIAN_POINT('Ctrl Pts',(1.11917555562601,-1.08278390434268,6.4577138192272));
#73768=CARTESIAN_POINT('Ctrl Pts',(1.06680247194667,-1.13442033270303,6.45203179458958));
#73769=CARTESIAN_POINT('Ctrl Pts',(0.998650460172741,-1.19270295624394,
6.4453397165859));
#73770=CARTESIAN_POINT('Ctrl Pts',(0.986164747936227,-1.20304705988235,
6.44414019033588));
#73771=CARTESIAN_POINT('Ctrl Pts',(0.967270361846445,-1.21820871920309,
6.44236683388902));
#73772=CARTESIAN_POINT('Ctrl Pts',(0.960982939541029,-1.22317465390252,
6.44178347572466));
#73773=CARTESIAN_POINT('Ctrl Pts',(0.95003710435235,-1.23168339872076,6.44077992471751));
#73774=CARTESIAN_POINT('Ctrl Pts',(0.94539678650017,-1.23524872536742,6.44035819616115));
#73775=CARTESIAN_POINT('Ctrl Pts',(0.934346987829686,-1.24363994784659,
6.43936267143485));
#73776=CARTESIAN_POINT('Ctrl Pts',(0.927920151949377,-1.24844255483235,
6.43879048124495));
#73777=CARTESIAN_POINT('Ctrl Pts',(0.908348774127612,-1.26283310326922,
6.43706759607805));
#73778=CARTESIAN_POINT('Ctrl Pts',(0.895090211005005,-1.27226511038981,
6.43592687347324));
#73779=CARTESIAN_POINT('Ctrl Pts',(0.826076521575695,-1.31974770241644,
6.43010984067056));
#73780=CARTESIAN_POINT('Ctrl Pts',(0.768029270007336,-1.35435210528135,
6.42561441575182));
#73781=CARTESIAN_POINT('Ctrl Pts',(0.595859104949023,-1.44234793327941,
6.41284677000393));
#73782=CARTESIAN_POINT('Ctrl Pts',(0.477284981955651,-1.48580327132771,
6.40467696418149));
#73783=CARTESIAN_POINT('Ctrl Pts',(0.333383973601136,-1.51951245471997,
6.39447929640829));
#73784=CARTESIAN_POINT('Ctrl Pts',(0.311889299054972,-1.52406953769659,
6.39295041365603));
#73785=CARTESIAN_POINT('Ctrl Pts',(0.277618940426029,-1.53057987375258,
6.3904999646751));
#73786=CARTESIAN_POINT('Ctrl Pts',(0.264902497424346,-1.53283191342594,
6.3895879216786));
#73787=CARTESIAN_POINT('Ctrl Pts',(0.240734314445973,-1.53680229869426,
6.38784853715044));
#73788=CARTESIAN_POINT('Ctrl Pts',(0.229288495540479,-1.5385516201553,6.38702224217976));
#73789=CARTESIAN_POINT('Ctrl Pts',(0.203044868390537,-1.54226321940958,
6.38512132713153));
#73790=CARTESIAN_POINT('Ctrl Pts',(0.188236419536967,-1.54414056289323,
6.38404410119657));
#73791=CARTESIAN_POINT('Ctrl Pts',(0.141077800272161,-1.54943067564035,
6.38059779986305));
#73792=CARTESIAN_POINT('Ctrl Pts',(0.108648498473489,-1.55204174449783,
6.37820413364808));
#73793=CARTESIAN_POINT('Ctrl Pts',(0.0302669225208374,-1.55588421969001,
6.37235769627072));
#73794=CARTESIAN_POINT('Ctrl Pts',(-0.015702600348668,-1.55609914166582,
6.36887799714372));
#73795=CARTESIAN_POINT('Ctrl Pts',(-0.121722477203221,-1.55189658106195,
6.3607503367614));
#73796=CARTESIAN_POINT('Ctrl Pts',(-0.181643068539324,-1.54602863598897,
6.35607949086564));
#73797=CARTESIAN_POINT('Ctrl Pts',(-0.315996815293859,-1.52495193879886,
6.3455356476985));
#73798=CARTESIAN_POINT('Ctrl Pts',(-0.389972206914176,-1.50773229667347,
6.33967878809157));
#73799=CARTESIAN_POINT('Ctrl Pts',(-0.474580534252851,-1.4813899675131,
6.33310789414783));
#73800=CARTESIAN_POINT('Ctrl Pts',(-0.486711592315749,-1.47744873796477,
6.33216906740336));
#73801=CARTESIAN_POINT('Ctrl Pts',(-0.505712798017733,-1.47101603753172,
6.33070522056862));
#73802=CARTESIAN_POINT('Ctrl Pts',(-0.51261588740434,-1.4686247221823,6.33017480470086));
#73803=CARTESIAN_POINT('Ctrl Pts',(-0.525761570423404,-1.46396691271776,
6.32916773390703));
#73804=CARTESIAN_POINT('Ctrl Pts',(-0.53200682079032,-1.46170896382921,
6.32869064108331));
#73805=CARTESIAN_POINT('Ctrl Pts',(-0.547202136870961,-1.45610486100228,
6.32753274381423));
#73806=CARTESIAN_POINT('Ctrl Pts',(-0.556136382162363,-1.4527160361182,
6.32685440797989));
#73807=CARTESIAN_POINT('Ctrl Pts',(-0.588943574744586,-1.43992499814422,
6.32437058954716));
#73808=CARTESIAN_POINT('Ctrl Pts',(-0.612615536060612,-1.43001431188423,
6.32259228171073));
#73809=CARTESIAN_POINT('Ctrl Pts',(-0.674574841011769,-1.4022527293616,
6.31794688417625));
#73810=CARTESIAN_POINT('Ctrl Pts',(-0.712400083722901,-1.3834198792131,
6.31512019105145));
#73811=CARTESIAN_POINT('Ctrl Pts',(-0.868154652762827,-1.29778616488796,
6.30333104536437));
#73812=CARTESIAN_POINT('Ctrl Pts',(-0.97784575307332,-1.21727449455587,
6.29459736747511));
#73813=CARTESIAN_POINT('Ctrl Pts',(-1.09230440598828,-1.10769067806239,
6.28368350946017));
#73814=CARTESIAN_POINT('Ctrl Pts',(-1.10853666849747,-1.09144579065017,
6.28208797814043));
#73815=CARTESIAN_POINT('Ctrl Pts',(-1.13355761712477,-1.0652712844266,6.27954708754934));
#73816=CARTESIAN_POINT('Ctrl Pts',(-1.14258952818329,-1.05557800820723,
6.27861230558493));
#73817=CARTESIAN_POINT('Ctrl Pts',(-1.15924677646181,-1.03723674336491,
6.27685416586808));
#73818=CARTESIAN_POINT('Ctrl Pts',(-1.16690196894127,-1.02861699978342,
6.2760321541548));
#73819=CARTESIAN_POINT('Ctrl Pts',(-1.18389752983173,-1.00904610418042,
6.27417473180535));
#73820=CARTESIAN_POINT('Ctrl Pts',(-1.19318301380305,-0.998048932248872,
6.27313714862679));
#73821=CARTESIAN_POINT('Ctrl Pts',(-1.22054427473032,-0.964716267380358,
6.27000931033168));
#73822=CARTESIAN_POINT('Ctrl Pts',(-1.23815423753042,-0.942008325250203,
6.26790082688344));
#73823=CARTESIAN_POINT('Ctrl Pts',(-1.27823778129334,-0.887253923609298,
6.26286527664387));
#73824=CARTESIAN_POINT('Ctrl Pts',(-1.3001498714042,-0.854822329771179,
6.25991974081589));
#73825=CARTESIAN_POINT('Ctrl Pts',(-1.37238293729112,-0.738699749220427,
6.2495078807041));
#73826=CARTESIAN_POINT('Ctrl Pts',(-1.41602951579031,-0.651129947446211,
6.24187405099271));
#73827=CARTESIAN_POINT('Ctrl Pts',(-1.46977048519191,-0.511880553029146,
6.23037358139925));
#73828=CARTESIAN_POINT('Ctrl Pts',(-1.48595504695095,-0.462802043067066,
6.22643684985847));
#73829=CARTESIAN_POINT('Ctrl Pts',(-1.50289908952527,-0.401276164922847,
6.22171066780392));
#73830=CARTESIAN_POINT('Ctrl Pts',(-1.50599145246482,-0.389509953027391,
6.22081613317821));
#73831=CARTESIAN_POINT('Ctrl Pts',(-1.5106886891948,-0.370744475525187,
6.2194054930009));
#73832=CARTESIAN_POINT('Ctrl Pts',(-1.51238361689905,-0.36376858402326,
6.21888459812312));
#73833=CARTESIAN_POINT('Ctrl Pts',(-1.51556714190145,-0.350259028237999,
6.21788290659448));
#73834=CARTESIAN_POINT('Ctrl Pts',(-1.51706190148728,-0.343727126778364,
6.21740180350685));
#73835=CARTESIAN_POINT('Ctrl Pts',(-1.51999579009791,-0.3305143697706,6.21643476606779));
#73836=CARTESIAN_POINT('Ctrl Pts',(-1.52143320471308,-0.323833226670136,
6.21594892682967));
#73837=CARTESIAN_POINT('Ctrl Pts',(-1.52479974894767,-0.307668063178696,
6.21478054706931));
#73838=CARTESIAN_POINT('Ctrl Pts',(-1.52668451867039,-0.298174954858204,
6.21410030742499));
#73839=CARTESIAN_POINT('Ctrl Pts',(-1.53162855524272,-0.271996252420891,
6.21223908357287));
#73840=CARTESIAN_POINT('Ctrl Pts',(-1.53450376919123,-0.255276768131256,
6.2110666868383));
#73841=CARTESIAN_POINT('Ctrl Pts',(-1.54927635669024,-0.16007426657775,
6.20446598056749));
#73842=CARTESIAN_POINT('Ctrl Pts',(-1.55542661858188,-0.0808133767859318,
6.19925484041338));
#73843=CARTESIAN_POINT('Ctrl Pts',(-1.55549934726413,-0.00142501258095274,
6.19403090372774));
#73844=CARTESIAN_POINT('Ctrl Pts',(-1.55549934719923,-0.00142508342168083,
6.19403090838922));
#73845=CARTESIAN_POINT('Ctrl Pts',(-1.55549978240474,-0.00095005026471773,
6.19399965011654));
#73846=CARTESIAN_POINT('Ctrl Pts',(-1.55550000000003,-0.000475022378848535,
6.19396839221188));
#73847=CARTESIAN_POINT('Ctrl Pts',(-1.5555,8.75720568004264E-11,6.19393713463064));
#73848=CARTESIAN_POINT('Ctrl Pts',(-1.55549999442795,-0.000131661105043114,
6.05447729365254));
#73849=CARTESIAN_POINT('Ctrl Pts',(-1.55549891885685,-0.0128389130955966,
6.05538373546313));
#73850=CARTESIAN_POINT('Ctrl Pts',(-1.55534213067335,-0.0255453141076208,
6.05629500695454));
#73851=CARTESIAN_POINT('Ctrl Pts',(-1.55453944217419,-0.0581797939337343,
6.05864874442834));
#73852=CARTESIAN_POINT('Ctrl Pts',(-1.5536660460136,-0.0780993893125099,
6.06009817714194));
#73853=CARTESIAN_POINT('Ctrl Pts',(-1.54739798082632,-0.177395494315716,
6.0673905123979));
#73854=CARTESIAN_POINT('Ctrl Pts',(-1.53630276923752,-0.25628065862964,
6.07340723386863));
#73855=CARTESIAN_POINT('Ctrl Pts',(-1.49532160127272,-0.442709037849519,
6.08810130202347));
#73856=CARTESIAN_POINT('Ctrl Pts',(-1.45980906302283,-0.548576960683833,
6.0968517184342));
#73857=CARTESIAN_POINT('Ctrl Pts',(-1.40476453494278,-0.668306883055246,
6.10674733926469));
#73858=CARTESIAN_POINT('Ctrl Pts',(-1.39586693178538,-0.686697241296948,
6.10826634707701));
#73859=CARTESIAN_POINT('Ctrl Pts',(-1.38261906271256,-0.712756831298517,
6.11041217087565));
#73860=CARTESIAN_POINT('Ctrl Pts',(-1.37856231790894,-0.720571799791614,
6.1110548040551));
#73861=CARTESIAN_POINT('Ctrl Pts',(-1.37130193766944,-0.734272524136705,
6.11217934078617));
#73862=CARTESIAN_POINT('Ctrl Pts',(-1.36812631938116,-0.740172631655696,
6.11266289592588));
#73863=CARTESIAN_POINT('Ctrl Pts',(-1.36108744478608,-0.753050343441263,
6.11371665263352));
#73864=CARTESIAN_POINT('Ctrl Pts',(-1.35720853918558,-0.760018973927848,
6.11428587076964));
#73865=CARTESIAN_POINT('Ctrl Pts',(-1.34567799308509,-0.780364311208439,
6.11594569784607));
#73866=CARTESIAN_POINT('Ctrl Pts',(-1.33788070797264,-0.793657972628437,
6.11702762318056));
#73867=CARTESIAN_POINT('Ctrl Pts',(-1.29968268024331,-0.85661892677765,
6.12215022217867));
#73868=CARTESIAN_POINT('Ctrl Pts',(-1.26670330808152,-0.904674144576514,
6.12605616932858));
#73869=CARTESIAN_POINT('Ctrl Pts',(-1.14977676749239,-1.05607608183673,
6.13873967802301));
#73870=CARTESIAN_POINT('Ctrl Pts',(-1.05528414622087,-1.15050278480546,
6.14732639041046));
#73871=CARTESIAN_POINT('Ctrl Pts',(-0.931288871359076,-1.24612817779305,
6.15810397990325));
#73872=CARTESIAN_POINT('Ctrl Pts',(-0.912324978321146,-1.26007834293831,
6.1597387845353));
#73873=CARTESIAN_POINT('Ctrl Pts',(-0.881930092785917,-1.28139147088921,
6.16234299407571));
#73874=CARTESIAN_POINT('Ctrl Pts',(-0.870706138051312,-1.28904444860889,
6.1633013095483));
#73875=CARTESIAN_POINT('Ctrl Pts',(-0.849612536435622,-1.30302579000318,
6.16509701914697));
#73876=CARTESIAN_POINT('Ctrl Pts',(-0.83976872395198,-1.30939151820358,
6.16593293082245));
#73877=CARTESIAN_POINT('Ctrl Pts',(-0.817375814277437,-1.32351603187859,
6.16783033829811));
#73878=CARTESIAN_POINT('Ctrl Pts',(-0.804786552959673,-1.331208655594,6.16889417812965));
#73879=CARTESIAN_POINT('Ctrl Pts',(-0.766054414817103,-1.35412556682334,
6.17215962239853));
#73880=CARTESIAN_POINT('Ctrl Pts',(-0.739576607306232,-1.36876646073595,
6.17438173397606));
#73881=CARTESIAN_POINT('Ctrl Pts',(-0.676046610608144,-1.40151374436026,
6.1796931399739));
#73882=CARTESIAN_POINT('Ctrl Pts',(-0.638669360039749,-1.41893647949542,
6.18280268555536));
#73883=CARTESIAN_POINT('Ctrl Pts',(-0.540538333491575,-1.4600153274615,
6.19091865722211));
#73884=CARTESIAN_POINT('Ctrl Pts',(-0.478911087475831,-1.48137425091665,
6.19597231066857));
#73885=CARTESIAN_POINT('Ctrl Pts',(-0.34612826006643,-1.51824026452634,
6.20665661292017));
#73886=CARTESIAN_POINT('Ctrl Pts',(-0.274843638463538,-1.53274958321898,
6.21227455061706));
#73887=CARTESIAN_POINT('Ctrl Pts',(-0.186573757483619,-1.54435692800793,
6.2189195114759));
#73888=CARTESIAN_POINT('Ctrl Pts',(-0.170314155907629,-1.54623453351541,
6.22013055025551));
#73889=CARTESIAN_POINT('Ctrl Pts',(-0.145903378087527,-1.54866365067379,
6.22192639304776));
#73890=CARTESIAN_POINT('Ctrl Pts',(-0.137773153591343,-1.54940810144349,
6.22252081619508));
#73891=CARTESIAN_POINT('Ctrl Pts',(-0.123646269454219,-1.55058956283505,
6.22354682706165));
#73892=CARTESIAN_POINT('Ctrl Pts',(-0.117652571583259,-1.55105585580637,
6.22397997187299));
#73893=CARTESIAN_POINT('Ctrl Pts',(-0.103346461462103,-1.55208542435959,
6.22500872667083));
#73894=CARTESIAN_POINT('Ctrl Pts',(-0.0950320274336128,-1.55261668733294,
6.22560256886105));
#73895=CARTESIAN_POINT('Ctrl Pts',(-0.0695016890922142,-1.5540421275825,
6.22741471569362));
#73896=CARTESIAN_POINT('Ctrl Pts',(-0.0522741823592893,-1.5547169816929,
6.22862176272108));
#73897=CARTESIAN_POINT('Ctrl Pts',(-0.0112278487424111,-1.55564179724489,
6.23146782196757));
#73898=CARTESIAN_POINT('Ctrl Pts',(0.0125929534183763,-1.55563138686882,
6.23309560309643));
#73899=CARTESIAN_POINT('Ctrl Pts',(0.106972561377428,-1.55342189114631,
6.23948331706542));
#73900=CARTESIAN_POINT('Ctrl Pts',(0.17735029448606,-1.54696830419104,6.24411274157835));
#73901=CARTESIAN_POINT('Ctrl Pts',(0.338549188883912,-1.52103694495766,
6.25486031440793));
#73902=CARTESIAN_POINT('Ctrl Pts',(0.428539046689323,-1.49817237862083,
6.26097722623209));
#73903=CARTESIAN_POINT('Ctrl Pts',(0.538795062049203,-1.45940616855446,
6.26901400661568));
#73904=CARTESIAN_POINT('Ctrl Pts',(0.561444813765082,-1.45084323598586,
6.27069426177093));
#73905=CARTESIAN_POINT('Ctrl Pts',(0.596608897201168,-1.43660242914495,
6.27335452284987));
#73906=CARTESIAN_POINT('Ctrl Pts',(0.609264154830248,-1.43128120358727,
6.27432260668622));
#73907=CARTESIAN_POINT('Ctrl Pts',(0.632683683067844,-1.42106698637323,
6.27613501748594));
#73908=CARTESIAN_POINT('Ctrl Pts',(0.643465876706036,-1.41621738230264,
6.27697781338439));
#73909=CARTESIAN_POINT('Ctrl Pts',(0.667451370651397,-1.40509875974352,
6.27887204277289));
#73910=CARTESIAN_POINT('Ctrl Pts',(0.680623540577913,-1.39876567935891,
6.2799256274082));
#73911=CARTESIAN_POINT('Ctrl Pts',(0.72010536681641,-1.37909339211758,6.28312519625929));
#73912=CARTESIAN_POINT('Ctrl Pts',(0.746125324150211,-1.36519123418145,
6.28529048893181));
#73913=CARTESIAN_POINT('Ctrl Pts',(0.833910381606084,-1.31502931933881,
6.29279746022178));
#73914=CARTESIAN_POINT('Ctrl Pts',(0.893552150896871,-1.27525321279852,
6.29825550893196));
#73915=CARTESIAN_POINT('Ctrl Pts',(1.02171555102791,-1.17636256027635,6.31075288974442));
#73916=CARTESIAN_POINT('Ctrl Pts',(1.08825879703488,-1.11508974398282,6.31781402111175));
#73917=CARTESIAN_POINT('Ctrl Pts',(1.16870379465346,-1.0269160711064,6.32687110302669));
#73918=CARTESIAN_POINT('Ctrl Pts',(1.1876908866188,-1.00489591618518,6.32905225508688));
#73919=CARTESIAN_POINT('Ctrl Pts',(1.21263661074336,-0.974269695660277,
6.33196478546652));
#73920=CARTESIAN_POINT('Ctrl Pts',(1.21914093808951,-0.966118201150408,
6.33272877653351));
#73921=CARTESIAN_POINT('Ctrl Pts',(1.22940686109999,-0.952983725242446,
6.33394120395661));
#73922=CARTESIAN_POINT('Ctrl Pts',(1.23322114925306,-0.948042621149047,
6.33439317809719));
#73923=CARTESIAN_POINT('Ctrl Pts',(1.24130866152169,-0.937434492690548,
6.33535449875502));
#73924=CARTESIAN_POINT('Ctrl Pts',(1.24557307774413,-0.93176087848597,6.33586321199216));
#73925=CARTESIAN_POINT('Ctrl Pts',(1.25649583159727,-0.91701964095626,6.33717155602481));
#73926=CARTESIAN_POINT('Ctrl Pts',(1.26309505027691,-0.907908426095713,
6.3379672581638));
#73927=CARTESIAN_POINT('Ctrl Pts',(1.29257150196101,-0.866268198171507,
6.3415495616451));
#73928=CARTESIAN_POINT('Ctrl Pts',(1.31429706773243,-0.832937883801895,
6.34426882814623));
#73929=CARTESIAN_POINT('Ctrl Pts',(1.38144977422979,-0.720732906291548,
6.35307639058692));
#73930=CARTESIAN_POINT('Ctrl Pts',(1.4212382337216,-0.638704294957985,6.35898502313633));
#73931=CARTESIAN_POINT('Ctrl Pts',(1.48029636208297,-0.483648818504521,
6.3699618121975));
#73932=CARTESIAN_POINT('Ctrl Pts',(1.50186758119281,-0.411807182706992,
6.37497818575942));
#73933=CARTESIAN_POINT('Ctrl Pts',(1.52254992136098,-0.319100488292828,
6.3815521714696));
#73934=CARTESIAN_POINT('Ctrl Pts',(1.52654176636895,-0.299422036444443,
6.38295276442892));
#73935=CARTESIAN_POINT('Ctrl Pts',(1.53244137061089,-0.267143979001509,
6.38526150707143));
#73936=CARTESIAN_POINT('Ctrl Pts',(1.53457725851367,-0.254588059733397,
6.38616237509039));
#73937=CARTESIAN_POINT('Ctrl Pts',(1.53843459194216,-0.230097020159152,
6.38792570395225));
#73938=CARTESIAN_POINT('Ctrl Pts',(1.54017191326583,-0.218165292539245,
6.38878759405468));
#73939=CARTESIAN_POINT('Ctrl Pts',(1.54396393584145,-0.189814147942544,
6.39084282233865));
#73940=CARTESIAN_POINT('Ctrl Pts',(1.54589564861465,-0.173380074505319,
6.39203993790921));
#73941=CARTESIAN_POINT('Ctrl Pts',(1.55174799834675,-0.115663056454063,
6.39626613263632));
#73942=CARTESIAN_POINT('Ctrl Pts',(1.55427944975152,-0.0742603275400437,
6.39933748552198));
#73943=CARTESIAN_POINT('Ctrl Pts',(1.55654605810355,0.0331765021273517,
6.40741407800293));
#73944=CARTESIAN_POINT('Ctrl Pts',(1.55373695386934,0.0991775117761391,
6.41248251787791));
#73945=CARTESIAN_POINT('Ctrl Pts',(1.53627018918646,0.263119046787456,6.4252457416261));
#73946=CARTESIAN_POINT('Ctrl Pts',(1.51644212052324,0.360227768913582,6.43297100283408));
#73947=CARTESIAN_POINT('Ctrl Pts',(1.48313036904305,0.469180795237614,6.44145780121015));
#73948=CARTESIAN_POINT('Ctrl Pts',(1.47852583983205,0.483495289971375,6.44256872107262));
#73949=CARTESIAN_POINT('Ctrl Pts',(1.47115694426745,0.505313136160052,6.44425337044385));
#73950=CARTESIAN_POINT('Ctrl Pts',(1.4685412448811,0.512865225841132,6.44483490633406));
#73951=CARTESIAN_POINT('Ctrl Pts',(1.46362645685252,0.526709323486124,6.44589758608852));
#73952=CARTESIAN_POINT('Ctrl Pts',(1.46134485434721,0.533006882001296,6.44637965370148));
#73953=CARTESIAN_POINT('Ctrl Pts',(1.45592503669439,0.54766993422602,6.44749916469894));
#73954=CARTESIAN_POINT('Ctrl Pts',(1.45275533334928,0.556023399668781,6.4481347626378));
#73955=CARTESIAN_POINT('Ctrl Pts',(1.44202694052589,0.58357894219157,6.45022564834446));
#73956=CARTESIAN_POINT('Ctrl Pts',(1.43415776785115,0.602658843415823,6.45166410361225));
#73957=CARTESIAN_POINT('Ctrl Pts',(1.4137122332063,0.649561281959369,6.45519052282764));
#73958=CARTESIAN_POINT('Ctrl Pts',(1.40069178859891,0.677181576990041,6.45725868628581));
#73959=CARTESIAN_POINT('Ctrl Pts',(1.32969449510543,0.81696493721394,6.46777030344727));
#73960=CARTESIAN_POINT('Ctrl Pts',(1.2590328286754,0.922148345691461,6.47587116936669));
#73961=CARTESIAN_POINT('Ctrl Pts',(1.14983349281024,1.04838745618907,6.48714364232961));
#73962=CARTESIAN_POINT('Ctrl Pts',(1.12204098814967,1.0780801824028,6.4899249123312));
#73963=CARTESIAN_POINT('Ctrl Pts',(1.08114420445354,1.11847698989951,6.49392631879746));
#73964=CARTESIAN_POINT('Ctrl Pts',(1.06897839805036,1.1301100448707,6.4951059244687));
#73965=CARTESIAN_POINT('Ctrl Pts',(1.04783080289291,1.1496845259716,6.49714007609109));
#73966=CARTESIAN_POINT('Ctrl Pts',(1.03894141183013,1.15772390013262,6.49799036176624));
#73967=CARTESIAN_POINT('Ctrl Pts',(1.02050550359441,1.17401360693342,6.49974470491181));
#73968=CARTESIAN_POINT('Ctrl Pts',(1.01094975540191,1.18225209106726,6.5006491673846));
#73969=CARTESIAN_POINT('Ctrl Pts',(0.986375476327052,1.20292300773872,6.50296362597425));
#73970=CARTESIAN_POINT('Ctrl Pts',(0.971221888887568,1.21519065222927,6.50438014154919));
#73971=CARTESIAN_POINT('Ctrl Pts',(0.899359113021684,1.27116455903029,6.51105167738562));
#73972=CARTESIAN_POINT('Ctrl Pts',(0.839914430006482,1.311200646384,6.5164453010482));
#73973=CARTESIAN_POINT('Ctrl Pts',(0.753405667824963,1.36116213870039,6.5241086207056));
#73974=CARTESIAN_POINT('Ctrl Pts',(0.728497133916217,1.37465425002099,6.526294294851));
#73975=CARTESIAN_POINT('Ctrl Pts',(0.614046406490459,1.43266372666506,6.53622575270472));
#73976=CARTESIAN_POINT('Ctrl Pts',(0.520700832000476,1.46916712238704,6.54404073858959));
#73977=CARTESIAN_POINT('Ctrl Pts',(0.410127217922548,1.50053285047216,6.55260074366641));
#73978=CARTESIAN_POINT('Ctrl Pts',(0.395704787747305,1.50440052333271,6.55370375180703));
#73979=CARTESIAN_POINT('Ctrl Pts',(0.37350169210127,1.51001332784119,6.5553789449783));
#73980=CARTESIAN_POINT('Ctrl Pts',(0.365760039930331,1.51190719455393,6.55595880913418));
#73981=CARTESIAN_POINT('Ctrl Pts',(0.351482620879242,1.51528384260212,6.5570200143663));
#73982=CARTESIAN_POINT('Ctrl Pts',(0.344951591208921,1.51678395264939,6.55750225816576));
#73983=CARTESIAN_POINT('Ctrl Pts',(0.32965882952111,1.52019265431416,6.55862421992107));
#73984=CARTESIAN_POINT('Ctrl Pts',(0.320890006140209,1.52206775946427,6.55926206409218));
#73985=CARTESIAN_POINT('Ctrl Pts',(0.291698005184473,1.52804661109992,6.56136880287382));
#73986=CARTESIAN_POINT('Ctrl Pts',(0.271207647899094,1.53181614173672,6.56282051340074));
#73987=CARTESIAN_POINT('Ctrl Pts',(0.220115559116338,1.54015790641689,6.56638743237477));
#73988=CARTESIAN_POINT('Ctrl Pts',(0.189440707307601,1.54423110309084,6.56848224602219));
#73989=CARTESIAN_POINT('Ctrl Pts',(0.027483329973648,1.5608375705228,6.57939271554638));
#73990=CARTESIAN_POINT('Ctrl Pts',(-0.104872057558046,1.55755356377785,
6.58784179728223));
#73991=CARTESIAN_POINT('Ctrl Pts',(-0.270992468295974,1.53213974314578,
6.599238663491));
#73992=CARTESIAN_POINT('Ctrl Pts',(-0.306550283034025,1.52542312126633,
6.60172194868961));
#73993=CARTESIAN_POINT('Ctrl Pts',(-0.355988635001923,1.51428620108668,
6.60525473743337));
#73994=CARTESIAN_POINT('Ctrl Pts',(-0.370092056801003,1.51090120513725,
6.60627175807881));
#73995=CARTESIAN_POINT('Ctrl Pts',(-0.395823132000781,1.50434355050705,
6.60814535298705));
#73996=CARTESIAN_POINT('Ctrl Pts',(-0.407465301667483,1.50123198836702,
6.60899991344401));
#73997=CARTESIAN_POINT('Ctrl Pts',(-0.431119556579752,1.49461457799594,
6.61075078718267));
#73998=CARTESIAN_POINT('Ctrl Pts',(-0.443127811934734,1.49109843209545,
6.611647379321));
#73999=CARTESIAN_POINT('Ctrl Pts',(-0.473242258886061,1.48188470648877,
6.61391610880233));
#74000=CARTESIAN_POINT('Ctrl Pts',(-0.491288546861568,1.47600000793858,
6.61529425675202));
#74001=CARTESIAN_POINT('Ctrl Pts',(-0.569961919293046,1.44874285369375,
6.6213871515828));
#74002=CARTESIAN_POINT('Ctrl Pts',(-0.629330599190891,1.42395694924085,
6.62621186979829));
#74003=CARTESIAN_POINT('Ctrl Pts',(-0.776810511410972,1.35135803404859,
6.63877269413997));
#74004=CARTESIAN_POINT('Ctrl Pts',(-0.862146972872839,1.2985776765281,6.64661477972965));
#74005=CARTESIAN_POINT('Ctrl Pts',(-0.975603447949265,1.21226248699643,
6.65754609428304));
#74006=CARTESIAN_POINT('Ctrl Pts',(-1.00832655974209,1.18518381912265,6.66076401494641));
#74007=CARTESIAN_POINT('Ctrl Pts',(-1.04868846396093,1.14890047185223,6.66477942967224));
#74008=CARTESIAN_POINT('Ctrl Pts',(-1.05738343732964,1.14090318508391,6.66564732536241));
#74009=CARTESIAN_POINT('Ctrl Pts',(-1.07124397017137,1.12786023849808,6.66703432232451));
#74010=CARTESIAN_POINT('Ctrl Pts',(-1.07646677856929,1.1228765032505,6.66755777736794));
#74011=CARTESIAN_POINT('Ctrl Pts',(-1.08667320815643,1.11300060732359,6.66858199947769));
#74012=CARTESIAN_POINT('Ctrl Pts',(-1.09165890142797,1.10811094194642,6.66908291127039));
#74013=CARTESIAN_POINT('Ctrl Pts',(-1.10310672489565,1.09673135977941,6.67023493997014));
#74014=CARTESIAN_POINT('Ctrl Pts',(-1.10954491903652,1.09021750370645,6.67088423615697));
#74015=CARTESIAN_POINT('Ctrl Pts',(-1.13463418096081,1.06438091115564,6.67342196750682));
#74016=CARTESIAN_POINT('Ctrl Pts',(-1.1528423043679,1.0446321297173,6.67528016670533));
#74017=CARTESIAN_POINT('Ctrl Pts',(-1.20055264881421,0.990116959667581,
6.68022747335239));
#74018=CARTESIAN_POINT('Ctrl Pts',(-1.22905388113729,0.954507940817489,
6.68326932420219));
#74019=CARTESIAN_POINT('Ctrl Pts',(-1.31795762155564,0.832834981930269,
6.69324411218612));
#74020=CARTESIAN_POINT('Ctrl Pts',(-1.37120052306651,0.741912829850248,
6.70006532584687));
#74021=CARTESIAN_POINT('Ctrl Pts',(-1.43090289758623,0.61121708185954,6.70978643701531));
#74022=CARTESIAN_POINT('Ctrl Pts',(-1.44562420875239,0.575534248225999,
6.71243005202752));
#74023=CARTESIAN_POINT('Ctrl Pts',(-1.46417297234898,0.525357116757619,
6.71615584986652));
#74024=CARTESIAN_POINT('Ctrl Pts',(-1.46914163032768,0.511297796009036,
6.71720061972948));
#74025=CARTESIAN_POINT('Ctrl Pts',(-1.47743860611034,0.486700612298808,
6.71903112349834));
#74026=CARTESIAN_POINT('Ctrl Pts',(-1.48085822865961,0.476194514937793,
6.71981380790208));
#74027=CARTESIAN_POINT('Ctrl Pts',(-1.48781391455189,0.454024816074234,
6.72146764272665));
#74028=CARTESIAN_POINT('Ctrl Pts',(-1.49132538049082,0.442354351001214,
6.7223395357087));
#74029=CARTESIAN_POINT('Ctrl Pts',(-1.49948744887246,0.414025072302984,
6.7244597309339));
#74030=CARTESIAN_POINT('Ctrl Pts',(-1.50399794334546,0.397327964505051,
6.72571246942175));
#74031=CARTESIAN_POINT('Ctrl Pts',(-1.51303652285075,0.361506394191948,
6.72840778811516));
#74032=CARTESIAN_POINT('Ctrl Pts',(-1.51748241425307,0.34236449968466,6.72985273621019));
#74033=CARTESIAN_POINT('Ctrl Pts',(-1.54413072324572,0.216887687179912,
6.73935714262994));
#74034=CARTESIAN_POINT('Ctrl Pts',(-1.55550000000864,0.108580928990684,
6.74774433786957));
#74035=CARTESIAN_POINT('Ctrl Pts',(-1.5555,-1.23764089254852E-10,6.75616363716894));
#74036=CARTESIAN_POINT('Origin',(0.,0.,-1.2940562256037));
#74037=CARTESIAN_POINT('',(-1.5555,7.12052432324671E-12,7.59515300361487));
#74038=CARTESIAN_POINT('',(-1.55549969139622,0.000979831791607279,7.45702425421034));
#74039=CARTESIAN_POINT('',(-1.5555,-1.46451138874614E-13,-1.2940562256037));
#74040=CARTESIAN_POINT('',(-1.55549928515668,0.00114196767205917,7.59506639552504));
#74041=CARTESIAN_POINT('Ctrl Pts',(-1.5555,7.12052432324671E-12,7.59515300361487));
#74042=CARTESIAN_POINT('Ctrl Pts',(-1.5555,0.000381318786656916,7.59512425884146));
#74043=CARTESIAN_POINT('Ctrl Pts',(-1.55549985978398,0.000762638266299459,
7.5950955104834));
#74044=CARTESIAN_POINT('Ctrl Pts',(-1.55549957935039,0.00114395836942135,
7.59506675854921));
#74045=CARTESIAN_POINT('Ctrl Pts',(-1.55549958078474,0.00114200635226231,
7.59506690573332));
#74046=CARTESIAN_POINT('Ctrl Pts',(-1.55539690258863,0.140997525261179,
7.58452165790019));
#74047=CARTESIAN_POINT('Ctrl Pts',(-1.5364350984294,0.280184167848922,7.57346929296716));
#74048=CARTESIAN_POINT('Ctrl Pts',(-1.49113558112083,0.443838852949233,
7.56057837485354));
#74049=CARTESIAN_POINT('Ctrl Pts',(-1.48230784617497,0.472484912046339,
7.55832948361562));
#74050=CARTESIAN_POINT('Ctrl Pts',(-1.46940474836623,0.510423321243775,
7.55537642826436));
#74051=CARTESIAN_POINT('Ctrl Pts',(-1.46605908649633,0.519954854628499,
7.55463669503922));
#74052=CARTESIAN_POINT('Ctrl Pts',(-1.46032643477296,0.535791364834251,
7.55341206289291));
#74053=CARTESIAN_POINT('Ctrl Pts',(-1.45799092536346,0.542114518509698,
7.55292428458944));
#74054=CARTESIAN_POINT('Ctrl Pts',(-1.45341894213096,0.554249402754044,
7.55199072282582));
#74055=CARTESIAN_POINT('Ctrl Pts',(-1.45118857518932,0.560063161346824,
7.55154456514949));
#74056=CARTESIAN_POINT('Ctrl Pts',(-1.44494904456049,0.576039808064296,
7.55032112730695));
#74057=CARTESIAN_POINT('Ctrl Pts',(-1.44086753774523,0.586174341370557,
7.54954801244317));
#74058=CARTESIAN_POINT('Ctrl Pts',(-1.42341494134095,0.628225726624473,
7.54634905277599));
#74059=CARTESIAN_POINT('Ctrl Pts',(-1.40908644175102,0.659737437734344,
7.54397342040379));
#74060=CARTESIAN_POINT('Ctrl Pts',(-1.3554204296143,0.768019038473343,7.53579668765277));
#74061=CARTESIAN_POINT('Ctrl Pts',(-1.31076107466121,0.841977017426941,
7.53018074233204));
#74062=CARTESIAN_POINT('Ctrl Pts',(-1.22667573555633,0.958184204824523,
7.52072095353354));
#74063=CARTESIAN_POINT('Ctrl Pts',(-1.19062639134599,1.00262575160022,7.51692680723804));
#74064=CARTESIAN_POINT('Ctrl Pts',(-1.13483589245815,1.06414140246442,7.51129966710616));
#74065=CARTESIAN_POINT('Ctrl Pts',(-1.11698308300774,1.08286568922611,7.50953171157911));
#74066=CARTESIAN_POINT('Ctrl Pts',(-1.08388093255106,1.11589380133523,7.50630195794515));
#74067=CARTESIAN_POINT('Ctrl Pts',(-1.06879416232917,1.13035207720667,7.5048469855179));
#74068=CARTESIAN_POINT('Ctrl Pts',(-1.0527469753002,1.1451222188282,7.50331461323212));
#74069=CARTESIAN_POINT('Ctrl Pts',(-1.05207205393635,1.14574232852659,7.50325019150673));
#74070=CARTESIAN_POINT('Ctrl Pts',(-1.0507426484805,1.14696160529325,7.50312335282905));
#74071=CARTESIAN_POINT('Ctrl Pts',(-1.05008819891914,1.147560809647,7.50306093745084));
#74072=CARTESIAN_POINT('Ctrl Pts',(-1.04879010993488,1.14874728050099,7.5029371882959));
#74073=CARTESIAN_POINT('Ctrl Pts',(-1.04814648905173,1.14933456688584,7.50287585537263));
#74074=CARTESIAN_POINT('Ctrl Pts',(-1.04686031721185,1.15050618449608,7.50275334033047));
#74075=CARTESIAN_POINT('Ctrl Pts',(-1.04621776962111,1.15109051896027,7.50269215837656));
#74076=CARTESIAN_POINT('Ctrl Pts',(-1.04492330720554,1.15226572724585,7.50256895114121));
#74077=CARTESIAN_POINT('Ctrl Pts',(-1.04427137980577,1.15285658667487,7.50250692529661));
#74078=CARTESIAN_POINT('Ctrl Pts',(-1.04294626318161,1.15405552945545,7.50238090068928));
#74079=CARTESIAN_POINT('Ctrl Pts',(-1.04227304269551,1.15466357759097,7.50231690050442));
#74080=CARTESIAN_POINT('Ctrl Pts',(-1.04089090195365,1.15590972397057,7.50218555960168));
#74081=CARTESIAN_POINT('Ctrl Pts',(-1.04018192607556,1.15654775967016,7.50211821633582));
#74082=CARTESIAN_POINT('Ctrl Pts',(-1.03870961004172,1.15787030675017,7.50197842507667));
#74083=CARTESIAN_POINT('Ctrl Pts',(-1.03794617926215,1.15855471609794,7.50190597291));
#74084=CARTESIAN_POINT('Ctrl Pts',(-1.03695162458058,1.1594445540426,7.50181162884939));
#74085=CARTESIAN_POINT('Ctrl Pts',(-1.03672111383359,1.15965067056883,7.50178976543076));
#74086=CARTESIAN_POINT('Ctrl Pts',(-1.03604780494365,1.16025236411008,7.50172591227503));
#74087=CARTESIAN_POINT('Ctrl Pts',(-1.03560484215228,1.16064775597964,7.50168391488717));
#74088=CARTESIAN_POINT('Ctrl Pts',(-1.03417516935702,1.16192242245667,7.50154840244318));
#74089=CARTESIAN_POINT('Ctrl Pts',(-1.03318756730394,1.16280069120689,7.50145484585178));
#74090=CARTESIAN_POINT('Ctrl Pts',(-1.02358436382439,1.17131887077301,7.5005456430759));
#74091=CARTESIAN_POINT('Ctrl Pts',(-1.01488551300116,1.17886395709064,7.4997261085791));
#74092=CARTESIAN_POINT('Ctrl Pts',(-0.995879320688082,1.19498299741572,
7.49794364407895));
#74093=CARTESIAN_POINT('Ctrl Pts',(-0.985543365904937,1.2035215986791,7.4969793540628));
#74094=CARTESIAN_POINT('Ctrl Pts',(-0.956635118103986,1.22678078224174,
7.49429535946929));
#74095=CARTESIAN_POINT('Ctrl Pts',(-0.937835536834242,1.24121159681963,
7.49256437170897));
#74096=CARTESIAN_POINT('Ctrl Pts',(-0.832055279562801,1.31863459756003,
7.48289782519941));
#74097=CARTESIAN_POINT('Ctrl Pts',(-0.739075413016017,1.37290670687798,
7.47463897536454));
#74098=CARTESIAN_POINT('Ctrl Pts',(-0.585928165739531,1.44220595143434,
7.46160162324263));
#74099=CARTESIAN_POINT('Ctrl Pts',(-0.529166296610907,1.46398551124703,
7.45688664199853));
#74100=CARTESIAN_POINT('Ctrl Pts',(-0.440648151115006,1.49212672892797,
7.44982138133246));
#74101=CARTESIAN_POINT('Ctrl Pts',(-0.409725541702313,1.50091249003284,
7.44740538250197));
#74102=CARTESIAN_POINT('Ctrl Pts',(-0.368515263397383,1.51125239279505,
7.44427232374469));
#74103=CARTESIAN_POINT('Ctrl Pts',(-0.358454866863716,1.51367018140817,
7.44351422574362));
#74104=CARTESIAN_POINT('Ctrl Pts',(-0.341754102503843,1.51750798189817,
7.44226772885759));
#74105=CARTESIAN_POINT('Ctrl Pts',(-0.335127362489005,1.51898518725421,
7.44177623787765));
#74106=CARTESIAN_POINT('Ctrl Pts',(-0.321611481665128,1.52190533237724,
7.44078040068717));
#74107=CARTESIAN_POINT('Ctrl Pts',(-0.314721849679658,1.52334498668757,
7.44027623790376));
#74108=CARTESIAN_POINT('Ctrl Pts',(-0.296534226720535,1.52701680444864,
7.43895384844503));
#74109=CARTESIAN_POINT('Ctrl Pts',(-0.285220549470541,1.5291704050455,7.43813989759391));
#74110=CARTESIAN_POINT('Ctrl Pts',(-0.233668787928636,1.53839140560871,
7.43446592244168));
#74111=CARTESIAN_POINT('Ctrl Pts',(-0.19318214248939,1.54399823293092,7.4316766647968));
#74112=CARTESIAN_POINT('Ctrl Pts',(-0.00308236861972627,1.56272790202587,
7.41882979304328));
#74113=CARTESIAN_POINT('Ctrl Pts',(0.147694423946096,1.55573713980212,7.40927731497708));
#74114=CARTESIAN_POINT('Ctrl Pts',(0.322859675577482,1.52188668334205,7.39706756030304));
#74115=CARTESIAN_POINT('Ctrl Pts',(0.350428868147134,1.51577600115621,7.39511517166806));
#74116=CARTESIAN_POINT('Ctrl Pts',(0.391549839146004,1.50547980491476,7.39214815772038));
#74117=CARTESIAN_POINT('Ctrl Pts',(0.405236553384111,1.50185353207271,7.39115138201697));
#74118=CARTESIAN_POINT('Ctrl Pts',(0.42995996560274,1.49494054925149,7.38933301854265));
#74119=CARTESIAN_POINT('Ctrl Pts',(0.441013416173623,1.49171712181223,7.38851353898502));
#74120=CARTESIAN_POINT('Ctrl Pts',(0.464876340434263,1.48446976871056,7.38672970216871));
#74121=CARTESIAN_POINT('Ctrl Pts',(0.477671444152967,1.48040213338803,7.38576396839526));
#74122=CARTESIAN_POINT('Ctrl Pts',(0.512987474518724,1.46866946818924,7.38307183626967));
#74123=CARTESIAN_POINT('Ctrl Pts',(0.535386773774888,1.46065295067844,7.38133404293449));
#74124=CARTESIAN_POINT('Ctrl Pts',(0.654618990339468,1.41486976520334,7.3719145997941));
#74125=CARTESIAN_POINT('Ctrl Pts',(0.747650665361289,1.36798893527285,7.36393265727514));
#74126=CARTESIAN_POINT('Ctrl Pts',(0.888568105608705,1.27828577630645,7.35097903419832));
#74127=CARTESIAN_POINT('Ctrl Pts',(0.939726062804322,1.24116214157326,7.34607275663319));
#74128=CARTESIAN_POINT('Ctrl Pts',(1.0138575576604,1.18014945255675,7.33876504563673));
#74129=CARTESIAN_POINT('Ctrl Pts',(1.03856188656547,1.15846858422583,7.33629335898386));
#74130=CARTESIAN_POINT('Ctrl Pts',(1.07017553479034,1.12889912259303,7.33310070375485));
#74131=CARTESIAN_POINT('Ctrl Pts',(1.07771675836801,1.1217020588801,7.33233679698758));
#74132=CARTESIAN_POINT('Ctrl Pts',(1.09006063688264,1.10968210043244,7.33108335999714));
#74133=CARTESIAN_POINT('Ctrl Pts',(1.09490489789126,1.1049026323606,7.33059066993937));
#74134=CARTESIAN_POINT('Ctrl Pts',(1.10407368262416,1.09573696104061,7.32965690604934));
#74135=CARTESIAN_POINT('Ctrl Pts',(1.10840376139832,1.09135662811307,7.3292153707823));
#74136=CARTESIAN_POINT('Ctrl Pts',(1.12009540483364,1.07938793046968,7.32802127047399));
#74137=CARTESIAN_POINT('Ctrl Pts',(1.12740597889919,1.07174987543459,7.3272725356666));
#74138=CARTESIAN_POINT('Ctrl Pts',(1.15616266336523,1.04108513412876,7.32431599072203));
#74139=CARTESIAN_POINT('Ctrl Pts',(1.17698737872513,1.01748287608994,7.3221493751021));
#74140=CARTESIAN_POINT('Ctrl Pts',(1.25367275794186,0.925061456926306,7.31399604453422));
#74141=CARTESIAN_POINT('Ctrl Pts',(1.30433459807605,0.852143097645051,7.30822547274416));
#74142=CARTESIAN_POINT('Ctrl Pts',(1.38839166482852,0.705939281442061,7.29710678471561));
#74143=CARTESIAN_POINT('Ctrl Pts',(1.42285485436397,0.633611518020097,7.29178865702459));
#74144=CARTESIAN_POINT('Ctrl Pts',(1.46014873392443,0.536760461047925,7.28464599532562));
#74145=CARTESIAN_POINT('Ctrl Pts',(1.46818602598076,0.514369328746782,7.28299394496395));
#74146=CARTESIAN_POINT('Ctrl Pts',(1.47990768124947,0.479197325367883,7.28039274229701));
#74147=CARTESIAN_POINT('Ctrl Pts',(1.48394713744583,0.466537989150183,7.27945529198062));
#74148=CARTESIAN_POINT('Ctrl Pts',(1.49118613864123,0.442805783711019,7.27769479766798));
#74149=CARTESIAN_POINT('Ctrl Pts',(1.49442578275452,0.431746023556222,7.2768731337951));
#74150=CARTESIAN_POINT('Ctrl Pts',(1.50141967928809,0.406847375796675,7.27502004977091));
#74151=CARTESIAN_POINT('Ctrl Pts',(1.50510602078097,0.392990688358007,7.2739865011476));
#74152=CARTESIAN_POINT('Ctrl Pts',(1.51412489847635,0.35709935917171,7.27130270898195));
#74153=CARTESIAN_POINT('Ctrl Pts',(1.51916805067548,0.334996260132577,7.2696434204123));
#74154=CARTESIAN_POINT('Ctrl Pts',(1.55088553042386,0.180488565229036,7.25799410437029));
#74155=CARTESIAN_POINT('Ctrl Pts',(1.56069286359946,0.0452309269969691,
7.24746644241948));
#74156=CARTESIAN_POINT('Ctrl Pts',(1.54949367443541,-0.148966444705023,
7.23243634211637));
#74157=CARTESIAN_POINT('Ctrl Pts',(1.54266051169179,-0.2081388976497,7.22788043423073));
#74158=CARTESIAN_POINT('Ctrl Pts',(1.53034815963467,-0.278864143265942,
7.22256265183272));
#74159=CARTESIAN_POINT('Ctrl Pts',(1.52810153205659,-0.290923414276328,
7.22166053300618));
#74160=CARTESIAN_POINT('Ctrl Pts',(1.52431002742272,-0.310017798245634,
7.22024077293981));
#74161=CARTESIAN_POINT('Ctrl Pts',(1.52285860102057,-0.317070625994361,
7.2197182404839));
#74162=CARTESIAN_POINT('Ctrl Pts',(1.51998051577785,-0.33058009468454,7.21872128282758));
#74163=CARTESIAN_POINT('Ctrl Pts',(1.51856159294465,-0.337038065755799,
7.21824647115214));
#74164=CARTESIAN_POINT('Ctrl Pts',(1.51494480400623,-0.353012578679201,
7.21707595028892));
#74165=CARTESIAN_POINT('Ctrl Pts',(1.51269835405834,-0.362518058353448,
7.21638293980707));
#74166=CARTESIAN_POINT('Ctrl Pts',(1.50432533573781,-0.396513278659992,
7.21391492859844));
#74167=CARTESIAN_POINT('Ctrl Pts',(1.49769200728674,-0.420875670568505,
7.2121657691202));
#74168=CARTESIAN_POINT('Ctrl Pts',(1.46368883568163,-0.534747485918286,
7.20403518910618));
#74169=CARTESIAN_POINT('Ctrl Pts',(1.42886762299845,-0.621836579300651,
7.19794075627715));
#74170=CARTESIAN_POINT('Ctrl Pts',(1.35243316630773,-0.772091167205189,
7.18683277393607));
#74171=CARTESIAN_POINT('Ctrl Pts',(1.31366040007389,-0.836358131879249,
7.18186155662729));
#74172=CARTESIAN_POINT('Ctrl Pts',(1.25386868784669,-0.920985976299065,
7.17477363944725));
#74173=CARTESIAN_POINT('Ctrl Pts',(1.23668584598485,-0.943933152373516,
7.17279235826517));
#74174=CARTESIAN_POINT('Ctrl Pts',(1.21003361731337,-0.977548790318311,
7.16979033704218));
#74175=CARTESIAN_POINT('Ctrl Pts',(1.20103493366668,-0.988583864254332,
7.16878810191941));
#74176=CARTESIAN_POINT('Ctrl Pts',(1.18448526146271,-1.00831918694911,7.16696402008969));
#74177=CARTESIAN_POINT('Ctrl Pts',(1.17698662145754,-1.01706214029753,7.16614434707736));
#74178=CARTESIAN_POINT('Ctrl Pts',(1.16058004152239,-1.0357667618447,7.16436495312093));
#74179=CARTESIAN_POINT('Ctrl Pts',(1.15163949982251,-1.04569845531847,7.1634039093314));
#74180=CARTESIAN_POINT('Ctrl Pts',(1.12663008964768,-1.07277064563147,7.16073816277281));
#74181=CARTESIAN_POINT('Ctrl Pts',(1.11029974307498,-1.08966351953725,7.15902242557114));
#74182=CARTESIAN_POINT('Ctrl Pts',(0.999013892728845,-1.19968323346672,
7.14748590950593));
#74183=CARTESIAN_POINT('Ctrl Pts',(0.892847156125456,-1.28065558278529,
7.1371426245762));
#74184=CARTESIAN_POINT('Ctrl Pts',(0.740241368362435,-1.36875668780563,
7.12351078850172));
#74185=CARTESIAN_POINT('Ctrl Pts',(0.701883031035304,-1.38881706544295,
7.12018217004727));
#74186=CARTESIAN_POINT('Ctrl Pts',(0.639154167554966,-1.41835878297361,
7.11493934295683));
#74187=CARTESIAN_POINT('Ctrl Pts',(0.615295137240123,-1.42887080724425,
7.11298988619982));
#74188=CARTESIAN_POINT('Ctrl Pts',(0.582292250351068,-1.44243140010047,
7.11036409460971));
#74189=CARTESIAN_POINT('Ctrl Pts',(0.573369073462109,-1.4460015653746,7.10966110519878));
#74190=CARTESIAN_POINT('Ctrl Pts',(0.558216219081017,-1.45190189968399,
7.10847973633769));
#74191=CARTESIAN_POINT('Ctrl Pts',(0.552003746040857,-1.45427519580449,
7.10799889807658));
#74192=CARTESIAN_POINT('Ctrl Pts',(0.538956174446572,-1.45916398349868,
7.10699658542337));
#74193=CARTESIAN_POINT('Ctrl Pts',(0.532118362507497,-1.46167142093751,
7.10647557215104));
#74194=CARTESIAN_POINT('Ctrl Pts',(0.513356835232158,-1.46840219673453,
7.10505700212201));
#74195=CARTESIAN_POINT('Ctrl Pts',(0.501398500664107,-1.47252837741128,
7.10416489764243));
#74196=CARTESIAN_POINT('Ctrl Pts',(0.425421146095066,-1.49771117211207,
7.09856491302467));
#74197=CARTESIAN_POINT('Ctrl Pts',(0.360132489538943,-1.5147372350659,7.09405501815836));
#74198=CARTESIAN_POINT('Ctrl Pts',(0.24245472361139,-1.53738237621099,7.08612544050326));
#74199=CARTESIAN_POINT('Ctrl Pts',(0.190503744555038,-1.54468032065917,
7.08269158117875));
#74200=CARTESIAN_POINT('Ctrl Pts',(0.0827450436987772,-1.55429809045216,
7.07555281239651));
#74201=CARTESIAN_POINT('Ctrl Pts',(0.0269844168366512,-1.55626489956129,
7.07184947416365));
#74202=CARTESIAN_POINT('Ctrl Pts',(-0.0658550910428642,-1.5545481585412,
7.06555401922759));
#74203=CARTESIAN_POINT('Ctrl Pts',(-0.102912450346763,-1.55253519602004,
7.06300715402677));
#74204=CARTESIAN_POINT('Ctrl Pts',(-0.155462154540898,-1.54779106329478,
7.05932701600793));
#74205=CARTESIAN_POINT('Ctrl Pts',(-0.171041487461171,-1.5461469642815,
7.05822741662074));
#74206=CARTESIAN_POINT('Ctrl Pts',(-0.198185373520504,-1.54286718691133,
7.05629525478446));
#74207=CARTESIAN_POINT('Ctrl Pts',(-0.209761464858192,-1.54133601561334,
7.05546603863236));
#74208=CARTESIAN_POINT('Ctrl Pts',(-0.233757821912973,-1.53788668422474,
7.0537357638602));
#74209=CARTESIAN_POINT('Ctrl Pts',(-0.246174231068719,-1.53594804716261,
7.05283411376017));
#74210=CARTESIAN_POINT('Ctrl Pts',(-0.278586142805132,-1.53048431190558,
7.05046309366435));
#74211=CARTESIAN_POINT('Ctrl Pts',(-0.298537905712372,-1.52671788956101,
7.04898619758086));
#74212=CARTESIAN_POINT('Ctrl Pts',(-0.404007925354861,-1.50466122474207,
7.04108262632873));
#74213=CARTESIAN_POINT('Ctrl Pts',(-0.487929649173321,-1.47957685529943,
7.03444262145851));
#74214=CARTESIAN_POINT('Ctrl Pts',(-0.630064283695007,-1.42367987377651,
7.02264952354485));
#74215=CARTESIAN_POINT('Ctrl Pts',(-0.689275158980635,-1.39597460793067,
7.01756024766595));
#74216=CARTESIAN_POINT('Ctrl Pts',(-0.791470651501095,-1.34006493623007,
7.00858846773839));
#74217=CARTESIAN_POINT('Ctrl Pts',(-0.835137437374443,-1.31329601618832,
7.00468928163686));
#74218=CARTESIAN_POINT('Ctrl Pts',(-0.88720618553496,-1.27772697177467,
7.00002234678549));
#74219=CARTESIAN_POINT('Ctrl Pts',(-0.896927016511342,-1.27092209832548,
6.99915032755602));
#74220=CARTESIAN_POINT('Ctrl Pts',(-0.912350090150092,-1.25986037662173,
6.99776678085295));
#74221=CARTESIAN_POINT('Ctrl Pts',(-0.918102411110579,-1.25567464884299,
6.99725076179728));
#74222=CARTESIAN_POINT('Ctrl Pts',(-0.92918299377369,-1.24749491002729,
6.99625708247652));
#74223=CARTESIAN_POINT('Ctrl Pts',(-0.934514628689838,-1.24350592987063,
6.99577912705126));
#74224=CARTESIAN_POINT('Ctrl Pts',(-0.947806005168195,-1.2334279284993,
6.9945876136476));
#74225=CARTESIAN_POINT('Ctrl Pts',(-0.955733017712528,-1.2272958450116,
6.99387697928652));
#74226=CARTESIAN_POINT('Ctrl Pts',(-0.984920947884577,-1.20426268244441,
6.99125796376908));
#74227=CARTESIAN_POINT('Ctrl Pts',(-1.00579874122859,-1.18688120606247,
6.98937980686953));
#74228=CARTESIAN_POINT('Ctrl Pts',(-1.12266144652077,-1.08428927317036,
6.97876716189305));
#74229=CARTESIAN_POINT('Ctrl Pts',(-1.20826863693084,-0.988000651735009,
6.97055822786889));
#74230=CARTESIAN_POINT('Ctrl Pts',(-1.31332563932147,-0.835456935168933,
6.95819196247525));
#74231=CARTESIAN_POINT('Ctrl Pts',(-1.34297816820205,-0.786905994096305,
6.95434137180719));
#74232=CARTESIAN_POINT('Ctrl Pts',(-1.37846169548006,-0.720936815949845,
6.94914081286781));
#74233=CARTESIAN_POINT('Ctrl Pts',(-1.38674032973902,-0.704881372190737,
6.94787765719456));
#74234=CARTESIAN_POINT('Ctrl Pts',(-1.4000978672391,-0.677829486043225,
6.94575142942228));
#74235=CARTESIAN_POINT('Ctrl Pts',(-1.40533144353386,-0.666911065132555,
6.94489381962504));
#74236=CARTESIAN_POINT('Ctrl Pts',(-1.41541217431809,-0.645234710930449,
6.94319168423468));
#74237=CARTESIAN_POINT('Ctrl Pts',(-1.42026544215359,-0.634480508001762,
6.94234743964263));
#74238=CARTESIAN_POINT('Ctrl Pts',(-1.43184242481968,-0.608028878363311,
6.94027087483698));
#74239=CARTESIAN_POINT('Ctrl Pts',(-1.43843073710134,-0.592274275761857,
6.93903404908074));
#74240=CARTESIAN_POINT('Ctrl Pts',(-1.46099867244664,-0.535708764438644,
6.9345914556794));
#74241=CARTESIAN_POINT('Ctrl Pts',(-1.4755100302119,-0.494338408018343,
6.93133807683935));
#74242=CARTESIAN_POINT('Ctrl Pts',(-1.52407968646861,-0.334564444665204,
6.91875311365585));
#74243=CARTESIAN_POINT('Ctrl Pts',(-1.54577702329421,-0.212882604652054,
6.90908313443277));
#74244=CARTESIAN_POINT('Ctrl Pts',(-1.55464185047764,-0.0598247080940499,
6.89731533920326));
#74245=CARTESIAN_POINT('Ctrl Pts',(-1.5555097745333,-0.0296621909278112,
6.895017957575));
#74246=CARTESIAN_POINT('Ctrl Pts',(-1.55549991697361,0.000508227400676815,
6.8927523980872));
#74247=CARTESIAN_POINT('',(-1.55549951548814,-0.00134138022456237,6.75626748310733));
#74248=CARTESIAN_POINT('Ctrl Pts',(-1.5555,-1.2376520005909E-10,6.75616363716894));
#74249=CARTESIAN_POINT('Ctrl Pts',(-1.55549999999996,-0.00044681871954324,
6.75619828321149));
#74250=CARTESIAN_POINT('Ctrl Pts',(-1.55549980747644,-0.000893641999218809,
6.75623292926718));
#74251=CARTESIAN_POINT('Ctrl Pts',(-1.55549942241732,-0.00134046984005363,
6.75626757530168));
#74252=CARTESIAN_POINT('Ctrl Pts',(-1.55549942164341,-0.00134136759671164,
6.75626764491173));
#74253=CARTESIAN_POINT('Ctrl Pts',(-1.55543356401629,-0.0777123050950782,
6.76218927703849));
#74254=CARTESIAN_POINT('Ctrl Pts',(-1.54974336159869,-0.153984621809158,
6.7680982895917));
#74255=CARTESIAN_POINT('Ctrl Pts',(-1.53688625173814,-0.240158681815686,
6.7745849384911));
#74256=CARTESIAN_POINT('Ctrl Pts',(-1.53519179243515,-0.250762276864696,
6.77537969145555));
#74257=CARTESIAN_POINT('Ctrl Pts',(-1.53215729839804,-0.268566348617512,
6.77670745552424));
#74258=CARTESIAN_POINT('Ctrl Pts',(-1.53087599817814,-0.275776276012312,
6.77724329745044));
#74259=CARTESIAN_POINT('Ctrl Pts',(-1.52825896087146,-0.289921850295468,
6.77829061423902));
#74260=CARTESIAN_POINT('Ctrl Pts',(-1.5269268031055,-0.296858004127358,
6.77880226826464));
#74261=CARTESIAN_POINT('Ctrl Pts',(-1.52415613878415,-0.310771723097279,
6.77982451108939));
#74262=CARTESIAN_POINT('Ctrl Pts',(-1.52271685195391,-0.317748947320985,
6.78033504522336));
#74263=CARTESIAN_POINT('Ctrl Pts',(-1.51885552814052,-0.335838466091007,
6.78165385608453));
#74264=CARTESIAN_POINT('Ctrl Pts',(-1.5163594155357,-0.346934768629101,
6.78245808447844));
#74265=CARTESIAN_POINT('Ctrl Pts',(-1.50508179484595,-0.394619841508017,
6.78589766059699));
#74266=CARTESIAN_POINT('Ctrl Pts',(-1.49509526501567,-0.430913807499309,
6.78847365200962));
#74267=CARTESIAN_POINT('Ctrl Pts',(-1.45951757092909,-0.544000247662755,
6.7964705677088));
#74268=CARTESIAN_POINT('Ctrl Pts',(-1.42924669940302,-0.619179538743125,
6.8017482615632));
#74269=CARTESIAN_POINT('Ctrl Pts',(-1.36159568743238,-0.755452813043169,
6.81178144621418));
#74270=CARTESIAN_POINT('Ctrl Pts',(-1.32558953404252,-0.816983888008336,
6.81651132814119));
#74271=CARTESIAN_POINT('Ctrl Pts',(-1.26932550607837,-0.899565447977718,
6.82334437503284));
#74272=CARTESIAN_POINT('Ctrl Pts',(-1.25249977591337,-0.922848508511846,
6.82532898033634));
#74273=CARTESIAN_POINT('Ctrl Pts',(-1.2261548057372,-0.957255582282485,
6.82836029018886));
#74274=CARTESIAN_POINT('Ctrl Pts',(-1.21710673640751,-0.968733721844328,
6.82938876507205));
#74275=CARTESIAN_POINT('Ctrl Pts',(-1.20044944490694,-0.989262934131678,
6.83126087195295));
#74276=CARTESIAN_POINT('Ctrl Pts',(-1.19289611899561,-0.998358080950358,
6.83210221628006));
#74277=CARTESIAN_POINT('Ctrl Pts',(-1.17634940328792,-1.01782650612606,
6.83392974762176));
#74278=CARTESIAN_POINT('Ctrl Pts',(-1.1673209501098,-1.02816851352527,6.83491733375478));
#74279=CARTESIAN_POINT('Ctrl Pts',(-1.14199393971563,-1.05641673791046,
6.83766258150053));
#74280=CARTESIAN_POINT('Ctrl Pts',(-1.12541300963202,-1.07406327482656,
6.83943196416016));
#74281=CARTESIAN_POINT('Ctrl Pts',(-1.04339655873115,-1.15736583682646,
6.8480578212119));
#74282=CARTESIAN_POINT('Ctrl Pts',(-0.972602233893648,-1.21746116174307,
6.8551453260723));
#74283=CARTESIAN_POINT('Ctrl Pts',(-0.839226393857363,-1.3115872082482,
6.86778550364487));
#74284=CARTESIAN_POINT('Ctrl Pts',(-0.77885479261496,-1.34831294901422,
6.87328253931281));
#74285=CARTESIAN_POINT('Ctrl Pts',(-0.695055637373284,-1.39177766191555,
6.88048081562188));
#74286=CARTESIAN_POINT('Ctrl Pts',(-0.673664975489797,-1.40225640581979,
6.88228234997592));
#74287=CARTESIAN_POINT('Ctrl Pts',(-0.636390724955477,-1.41946618061489,
6.88535095840511));
#74288=CARTESIAN_POINT('Ctrl Pts',(-0.620620575505404,-1.42643175756307,
6.8866279873954));
#74289=CARTESIAN_POINT('Ctrl Pts',(-0.597061552951793,-1.43637291648053,
6.88850112849282));
#74290=CARTESIAN_POINT('Ctrl Pts',(-0.589359922507101,-1.43955011841694,
6.88910806097096));
#74291=CARTESIAN_POINT('Ctrl Pts',(-0.576057186044204,-1.44491332275271,
6.89014665520168));
#74292=CARTESIAN_POINT('Ctrl Pts',(-0.570468523127038,-1.44712890222484,
6.8905800197178));
#74293=CARTESIAN_POINT('Ctrl Pts',(-0.557260159994005,-1.45227683824166,
6.89159729179705));
#74294=CARTESIAN_POINT('Ctrl Pts',(-0.549630039791709,-1.45518168217065,
6.89217957679007));
#74295=CARTESIAN_POINT('Ctrl Pts',(-0.526636319331132,-1.46372890164956,
6.89391927304625));
#74296=CARTESIAN_POINT('Ctrl Pts',(-0.511205619437367,-1.4691892255961,
6.89506669164575));
#74297=CARTESIAN_POINT('Ctrl Pts',(-0.426789986836612,-1.49756951930608,
6.90125022252184));
#74298=CARTESIAN_POINT('Ctrl Pts',(-0.356341295080016,-1.5158785007227,
6.90607573519465));
#74299=CARTESIAN_POINT('Ctrl Pts',(-0.220773865907341,-1.54113239181254,
6.91517090346062));
#74300=CARTESIAN_POINT('Ctrl Pts',(-0.155999432313185,-1.54903004931677,
6.91943764929614));
#74301=CARTESIAN_POINT('Ctrl Pts',(-0.0498081194877144,-1.55524772942382,
6.92652033607769));
#74302=CARTESIAN_POINT('Ctrl Pts',(-0.00861801806893114,-1.55602111205891,
6.92928828604874));
#74303=CARTESIAN_POINT('Ctrl Pts',(0.0627753667807413,-1.55452672838982,
6.93416440977862));
#74304=CARTESIAN_POINT('Ctrl Pts',(0.092971924686231,-1.55301323629003,
6.93625109168742));
#74305=CARTESIAN_POINT('Ctrl Pts',(0.137806658450898,-1.54945381248803,
6.93939613683114));
#74306=CARTESIAN_POINT('Ctrl Pts',(0.152491895166693,-1.54807751342492,
6.94043374353235));
#74307=CARTESIAN_POINT('Ctrl Pts',(0.178917475238468,-1.54522126620056,
6.94231551098556));
#74308=CARTESIAN_POINT('Ctrl Pts',(0.190664851784905,-1.54381576770796,
6.94315727185257));
#74309=CARTESIAN_POINT('Ctrl Pts',(0.215906888420006,-1.54050322537017,
6.94497783601314));
#74310=CARTESIAN_POINT('Ctrl Pts',(0.229394715047186,-1.53855257129035,
6.94595795018703));
#74311=CARTESIAN_POINT('Ctrl Pts',(0.266306423276641,-1.53271812783106,
6.94866115711974));
#74312=CARTESIAN_POINT('Ctrl Pts',(0.289668850037129,-1.52847499578274,
6.95039539070234));
#74313=CARTESIAN_POINT('Ctrl Pts',(0.419765004339305,-1.50175699558045,
6.96018885265748));
#74314=CARTESIAN_POINT('Ctrl Pts',(0.523983561763028,-1.46864214777638,
6.96858192013735));
#74315=CARTESIAN_POINT('Ctrl Pts',(0.702172139143361,-1.39062658757346,
6.98366602552176));
#74316=CARTESIAN_POINT('Ctrl Pts',(0.777529630383351,-1.34994027656084,
6.99029873168174));
#74317=CARTESIAN_POINT('Ctrl Pts',(0.860275051868481,-1.29602578242185,
6.99762821764474));
#74318=CARTESIAN_POINT('Ctrl Pts',(0.871289707517869,-1.28864668175125,
6.99860469673896));
#74319=CARTESIAN_POINT('Ctrl Pts',(0.888410375825225,-1.27685705722736,
7.00012216088973));
#74320=CARTESIAN_POINT('Ctrl Pts',(0.894580687419041,-1.27254168519657,
7.00066898789664));
#74321=CARTESIAN_POINT('Ctrl Pts',(0.906272785674957,-1.26423743103727,
7.00170466674937));
#74322=CARTESIAN_POINT('Ctrl Pts',(0.911800015807825,-1.26025686954449,
7.00219400449772));
#74323=CARTESIAN_POINT('Ctrl Pts',(0.925205219204615,-1.25046844816577,
7.00338055380765));
#74324=CARTESIAN_POINT('Ctrl Pts',(0.93305502769512,-1.24462217800767,7.00407518895828));
#74325=CARTESIAN_POINT('Ctrl Pts',(0.960369339556774,-1.22387574033662,
7.00649367320614));
#74326=CARTESIAN_POINT('Ctrl Pts',(0.97953747618952,-1.20858909357693,7.00819344585391));
#74327=CARTESIAN_POINT('Ctrl Pts',(1.07988014188439,-1.12460916521844,7.01715466232082));
#74328=CARTESIAN_POINT('Ctrl Pts',(1.15421828521276,-1.04817546634035,7.02403595978699));
#74329=CARTESIAN_POINT('Ctrl Pts',(1.26880833156758,-0.903245640988257,
7.03624721938614));
#74330=CARTESIAN_POINT('Ctrl Pts',(1.31270984608384,-0.838163338072012,
7.04148887553691));
#74331=CARTESIAN_POINT('Ctrl Pts',(1.3613582222812,-0.752781042239624,7.04829226045155));
#74332=CARTESIAN_POINT('Ctrl Pts',(1.37086792099245,-0.73532073792715,7.04967945199191));
#74333=CARTESIAN_POINT('Ctrl Pts',(1.38589756528697,-0.706420106367791,
7.05197185804168));
#74334=CARTESIAN_POINT('Ctrl Pts',(1.39161684050416,-0.695085591967995,
7.052869994566));
#74335=CARTESIAN_POINT('Ctrl Pts',(1.40250517770954,-0.672833823761732,
7.05463213853963));
#74336=CARTESIAN_POINT('Ctrl Pts',(1.40768708989095,-0.661923839792053,
7.05549562128208));
#74337=CARTESIAN_POINT('Ctrl Pts',(1.41971770029561,-0.635814288664593,
7.05756153538044));
#74338=CARTESIAN_POINT('Ctrl Pts',(1.42644999281569,-0.62056307980319,7.05876785163742));
#74339=CARTESIAN_POINT('Ctrl Pts',(1.44838361835991,-0.568631318172157,
7.06287565062986));
#74340=CARTESIAN_POINT('Ctrl Pts',(1.46242415538043,-0.531480718226687,
7.06581505253145));
#74341=CARTESIAN_POINT('Ctrl Pts',(1.51549439644265,-0.372966658578356,
7.07836645208581));
#74342=CARTESIAN_POINT('Ctrl Pts',(1.54094746848227,-0.247588630682528,
7.08836976585726));
#74343=CARTESIAN_POINT('Ctrl Pts',(1.55319512380626,-0.0900143186193632,
7.10050483188289));
#74344=CARTESIAN_POINT('Ctrl Pts',(1.55466611331648,-0.0594237154998162,
7.10283750223579));
#74345=CARTESIAN_POINT('Ctrl Pts',(1.55561619014105,-0.0081324797782678,
7.1066911326726));
#74346=CARTESIAN_POINT('Ctrl Pts',(1.55558685962097,0.0125498159964593,
7.10822934883521));
#74347=CARTESIAN_POINT('Ctrl Pts',(1.55495409226146,0.0421659737962799,
7.11040404994012));
#74348=CARTESIAN_POINT('Ctrl Pts',(1.55468601670212,0.0511037982415989,
7.11105669770986));
#74349=CARTESIAN_POINT('Ctrl Pts',(1.55408231799457,0.0667328398451762,
7.11219098937646));
#74350=CARTESIAN_POINT('Ctrl Pts',(1.55378052270368,0.0734249052651159,
7.11267441179785));
#74351=CARTESIAN_POINT('Ctrl Pts',(1.553024122812,0.0880915109395472,7.1137288624341));
#74352=CARTESIAN_POINT('Ctrl Pts',(1.55255132377454,0.0960647431135248,
7.11429889604774));
#74353=CARTESIAN_POINT('Ctrl Pts',(1.5510131072941,0.119012370088535,7.11593120704107));
#74354=CARTESIAN_POINT('Ctrl Pts',(1.54979227503452,0.133975934444706,7.11698541794224));
#74355=CARTESIAN_POINT('Ctrl Pts',(1.5388645438123,0.247593882349314,7.12492870524367));
#74356=CARTESIAN_POINT('Ctrl Pts',(1.519962033883,0.345149037712844,7.13140663433357));
#74357=CARTESIAN_POINT('Ctrl Pts',(1.4732584614656,0.503415080672014,7.14226980336315));
#74358=CARTESIAN_POINT('Ctrl Pts',(1.45062785691922,0.565327516630805,7.14661400771911));
#74359=CARTESIAN_POINT('Ctrl Pts',(1.40748767260919,0.66353121763253,7.15385763524857));
#74360=CARTESIAN_POINT('Ctrl Pts',(1.38932568602314,0.700763066841547,7.15669109713421));
#74361=CARTESIAN_POINT('Ctrl Pts',(1.36186262717651,0.751787188862223,7.16072696874102));
#74362=CARTESIAN_POINT('Ctrl Pts',(1.35379246896179,0.76622431884272,7.16188660602014));
#74363=CARTESIAN_POINT('Ctrl Pts',(1.33944426324582,0.790958069585852,7.16390580102247));
#74364=CARTESIAN_POINT('Ctrl Pts',(1.33327373699532,0.801315624178988,7.16476144037103));
#74365=CARTESIAN_POINT('Ctrl Pts',(1.32033700789222,0.822467452868074,7.16653027144061));
#74366=CARTESIAN_POINT('Ctrl Pts',(1.31355736765755,0.833252392400646,7.16744390878648));
#74367=CARTESIAN_POINT('Ctrl Pts',(1.2957457897362,0.860829097585475,7.16981125117697));
#74368=CARTESIAN_POINT('Ctrl Pts',(1.28451992295688,0.877492099262659,7.17127208013978));
#74369=CARTESIAN_POINT('Ctrl Pts',(1.22971754596503,0.955531625049105,7.17826313614365));
#74370=CARTESIAN_POINT('Ctrl Pts',(1.18205284603531,1.01390030951067,7.18394693307072));
#74371=CARTESIAN_POINT('Ctrl Pts',(1.06805359454236,1.13448991728216,7.19670231534812));
#74372=CARTESIAN_POINT('Ctrl Pts',(1.00010594861484,1.19481946548832,7.20379889255666));
#74373=CARTESIAN_POINT('Ctrl Pts',(0.895409391353119,1.27255608074704,7.21377645560744));
#74374=CARTESIAN_POINT('Ctrl Pts',(0.86263077526118,1.29500027434961,7.216778947126));
#74375=CARTESIAN_POINT('Ctrl Pts',(0.819511901677323,1.32215994698611,7.2205441951291));
#74376=CARTESIAN_POINT('Ctrl Pts',(0.809932671763496,1.32804961100726,7.22136941638314));
#74377=CARTESIAN_POINT('Ctrl Pts',(0.794205104359225,1.33748602159825,7.22270501663736));
#74378=CARTESIAN_POINT('Ctrl Pts',(0.788095081274072,1.34109535607093,7.22321920871554));
#74379=CARTESIAN_POINT('Ctrl Pts',(0.776563957160568,1.34780103886767,7.22418055378909));
#74380=CARTESIAN_POINT('Ctrl Pts',(0.771148537154053,1.35090679072963,7.22462831860306));
#74381=CARTESIAN_POINT('Ctrl Pts',(0.75663395584758,1.35911520228295,7.22581894755174));
#74382=CARTESIAN_POINT('Ctrl Pts',(0.747501712930587,1.36415918468486,7.22655818298302));
#74383=CARTESIAN_POINT('Ctrl Pts',(0.712706656055614,1.38292307813006,7.22934023908978));
#74384=CARTESIAN_POINT('Ctrl Pts',(0.686709632173666,1.39601474443036,7.23134836728362));
#74385=CARTESIAN_POINT('Ctrl Pts',(0.578642122348085,1.4466855883651,7.23947406719521));
#74386=CARTESIAN_POINT('Ctrl Pts',(0.49373902682435,1.47781951040793,7.245352494799));
#74387=CARTESIAN_POINT('Ctrl Pts',(0.337504171883726,1.52013054002283,7.25602430027631));
#74388=CARTESIAN_POINT('Ctrl Pts',(0.267196509085141,1.53405034870421,7.26077642846143));
#74389=CARTESIAN_POINT('Ctrl Pts',(0.166923065750723,1.54679895917828,7.26768442563731));
#74390=CARTESIAN_POINT('Ctrl Pts',(0.137563338832664,1.54968592506361,7.26972184944561));
#74391=CARTESIAN_POINT('Ctrl Pts',(0.0935608589668794,1.55275246694,7.27280733000339));
#74392=CARTESIAN_POINT('Ctrl Pts',(0.0789677512149749,1.55356297792858,
7.27383580597469));
#74393=CARTESIAN_POINT('Ctrl Pts',(0.0525534007119759,1.55465692763251,
7.27570791373535));
#74394=CARTESIAN_POINT('Ctrl Pts',(0.040736096163147,1.55501144012544,7.27654925783732));
#74395=CARTESIAN_POINT('Ctrl Pts',(0.0151903218739158,1.55548640904937,
7.27837678741731));
#74396=CARTESIAN_POINT('Ctrl Pts',(0.00146209866686334,1.55555988456403,
7.27936437199902));
#74397=CARTESIAN_POINT('Ctrl Pts',(-0.0364762997474025,1.55526073630746,
7.28210961188887));
#74398=CARTESIAN_POINT('Ctrl Pts',(-0.0606786049949006,1.55450457166762,
7.2838789881436));
#74399=CARTESIAN_POINT('Ctrl Pts',(-0.177418451734728,1.5481269419551,7.29250574391708));
#74400=CARTESIAN_POINT('Ctrl Pts',(-0.269332155108154,1.53480593250714,
7.29959422272801));
#74401=CARTESIAN_POINT('Ctrl Pts',(-0.428160277455656,1.49707696217117,
7.31223466896849));
#74402=CARTESIAN_POINT('Ctrl Pts',(-0.495634021809718,1.47611253700752,
7.31773097710641));
#74403=CARTESIAN_POINT('Ctrl Pts',(-0.58366073968408,1.44204280920448,7.32492841959323));
#74404=CARTESIAN_POINT('Ctrl Pts',(-0.605669664631611,1.4329381380798,7.32672982886623));
#74405=CARTESIAN_POINT('Ctrl Pts',(-0.643234382759381,1.41637808930449,
7.32979824853974));
#74406=CARTESIAN_POINT('Ctrl Pts',(-0.658890961819159,1.40916291764155,
7.33107521234063));
#74407=CARTESIAN_POINT('Ctrl Pts',(-0.681932132904314,1.39807661327323,
7.33294827714352));
#74408=CARTESIAN_POINT('Ctrl Pts',(-0.689410162361361,1.39440427673655,
7.33355519730551));
#74409=CARTESIAN_POINT('Ctrl Pts',(-0.702233312337453,1.38797866221476,
7.33459377830803));
#74410=CARTESIAN_POINT('Ctrl Pts',(-0.707592375313756,1.38525428199628,
7.33502714177602));
#74411=CARTESIAN_POINT('Ctrl Pts',(-0.72019194584292,1.37875685464863,7.33604442262311));
#74412=CARTESIAN_POINT('Ctrl Pts',(-0.727418718012756,1.3749577883482,7.33662671730268));
#74413=CARTESIAN_POINT('Ctrl Pts',(-0.749042375059584,1.36337216302356,
7.33836647482544));
#74414=CARTESIAN_POINT('Ctrl Pts',(-0.763347145756502,1.35541481665359,
7.33951394395193));
#74415=CARTESIAN_POINT('Ctrl Pts',(-0.840568254335902,1.3108484308994,7.34570440947457));
#74416=CARTESIAN_POINT('Ctrl Pts',(-0.900988550450904,1.27007906411362,
7.35053620397165));
#74417=CARTESIAN_POINT('Ctrl Pts',(-1.01030080924381,1.18457788069213,7.35968917078256));
#74418=CARTESIAN_POINT('Ctrl Pts',(-1.0596250665221,1.14066951770463,7.36400669224855));
#74419=CARTESIAN_POINT('Ctrl Pts',(-1.13463024463664,1.06482435186035,7.37111202092495));
#74420=CARTESIAN_POINT('Ctrl Pts',(-1.16209981538722,1.03477550427565,7.37384865140367));
#74421=CARTESIAN_POINT('Ctrl Pts',(-1.2076989651629,0.980786371529975,7.37867564156021));
#74422=CARTESIAN_POINT('Ctrl Pts',(-1.2263726401147,0.957334134119339,7.3807451340714));
#74423=CARTESIAN_POINT('Ctrl Pts',(-1.25317844467766,0.921596553591422,
7.38386940465024));
#74424=CARTESIAN_POINT('Ctrl Pts',(-1.26183318270666,0.909710621336774,
7.3849038402507));
#74425=CARTESIAN_POINT('Ctrl Pts',(-1.27714396462003,0.888044730496262,
7.38678223841189));
#74426=CARTESIAN_POINT('Ctrl Pts',(-1.28385947491143,0.878308023578491,
7.38762384003068));
#74427=CARTESIAN_POINT('Ctrl Pts',(-1.29809116923485,0.857161721861683,
7.38944675226847));
#74428=CARTESIAN_POINT('Ctrl Pts',(-1.30556932211668,0.845727866470525,
7.3904294038507));
#74429=CARTESIAN_POINT('Ctrl Pts',(-1.32571399904795,0.814023306143538,
7.39314686269637));
#74430=CARTESIAN_POINT('Ctrl Pts',(-1.33806492298063,0.793557619058135,
7.39489300602276));
#74431=CARTESIAN_POINT('Ctrl Pts',(-1.40277091877301,0.680530614532037,
7.40449883010841));
#74432=CARTESIAN_POINT('Ctrl Pts',(-1.44599136298936,0.583086183931659,
7.41267348448418));
#74433=CARTESIAN_POINT('Ctrl Pts',(-1.49779897912627,0.424128923200931,
7.42563717202522));
#74434=CARTESIAN_POINT('Ctrl Pts',(-1.51325163175455,0.365181236580673,
7.43036297573141));
#74435=CARTESIAN_POINT('Ctrl Pts',(-1.53155567366816,0.27379138177627,7.43745361467981));
#74436=CARTESIAN_POINT('Ctrl Pts',(-1.53691347006018,0.241912887800901,
7.43988352680141));
#74437=CARTESIAN_POINT('Ctrl Pts',(-1.54269475423801,0.199459082121118,
7.44304355194652));
#74438=CARTESIAN_POINT('Ctrl Pts',(-1.54400911742531,0.189015586252565,
7.44381484385131));
#74439=CARTESIAN_POINT('Ctrl Pts',(-1.54601485806347,0.171658285064845,
7.44508582658828));
#74440=CARTESIAN_POINT('Ctrl Pts',(-1.54676608821382,0.164751885556382,
7.44558868083709));
#74441=CARTESIAN_POINT('Ctrl Pts',(-1.5481174348179,0.151503252164928,7.44654754652565));
#74442=CARTESIAN_POINT('Ctrl Pts',(-1.54872490023507,0.145162029150087,
7.44700398581681));
#74443=CARTESIAN_POINT('Ctrl Pts',(-1.5502856627862,0.127742855895553,7.44825138624544));
#74444=CARTESIAN_POINT('Ctrl Pts',(-1.55115919051009,0.116657867414643,
7.44903806432084));
#74445=CARTESIAN_POINT('Ctrl Pts',(-1.55428153014994,0.0707558561728834,
7.45226974807506));
#74446=CARTESIAN_POINT('Ctrl Pts',(-1.55547771071824,0.0358746791423457,
7.45466404925903));
#74447=CARTESIAN_POINT('Ctrl Pts',(-1.55549969139753,0.000979827635642597,
7.4570242544914));
#74448=CARTESIAN_POINT('Origin',(0.,0.,-1.2940562256037));
#74449=CARTESIAN_POINT('',(-1.5555,1.39005191776138E-11,8.29490354205207));
#74450=CARTESIAN_POINT('',(-1.55549980343579,0.000781991825156256,8.1559437743963));
#74451=CARTESIAN_POINT('',(-1.5555,-1.46451138874614E-13,-1.2940562256037));
#74452=CARTESIAN_POINT('Ctrl Pts',(-1.5555,1.39005191776138E-11,8.29490354205207));
#74453=CARTESIAN_POINT('Ctrl Pts',(-1.5555,0.0498749277555234,8.2915600034077));
#74454=CARTESIAN_POINT('Ctrl Pts',(-1.55310128629853,0.0997166037084997,
8.28816961820895));
#74455=CARTESIAN_POINT('Ctrl Pts',(-1.54660273194361,0.167085571741959,
8.28346863249098));
#74456=CARTESIAN_POINT('Ctrl Pts',(-1.54458784708901,0.184786189183087,
8.28222246654726));
#74457=CARTESIAN_POINT('Ctrl Pts',(-1.54085697631155,0.213208387603212,
8.28020173933394));
#74458=CARTESIAN_POINT('Ctrl Pts',(-1.53933191347003,0.223953761646126,
8.27943322035399));
#74459=CARTESIAN_POINT('Ctrl Pts',(-1.53591604314458,0.246335384476098,
8.27782247476751));
#74460=CARTESIAN_POINT('Ctrl Pts',(-1.53400515189999,0.257967813965996,
8.27697965943087));
#74461=CARTESIAN_POINT('Ctrl Pts',(-1.52912633822019,0.285693307821899,
8.27495673027745));
#74462=CARTESIAN_POINT('Ctrl Pts',(-1.52603636462686,0.301763152351375,
8.27377281459713));
#74463=CARTESIAN_POINT('Ctrl Pts',(-1.51412351221886,0.358845358588525,
8.2695249602609));
#74464=CARTESIAN_POINT('Ctrl Pts',(-1.50389663576708,0.399542613280656,
8.26641727889269));
#74465=CARTESIAN_POINT('Ctrl Pts',(-1.47290174394729,0.504700314325537,
8.25817453812039));
#74466=CARTESIAN_POINT('Ctrl Pts',(-1.44954916068012,0.568302267880589,
8.25297168138752));
#74467=CARTESIAN_POINT('Ctrl Pts',(-1.3828667240716,0.718786124973094,8.24022235538064));
#74468=CARTESIAN_POINT('Ctrl Pts',(-1.33540281202833,0.803539806723317,
8.23265443823666));
#74469=CARTESIAN_POINT('Ctrl Pts',(-1.27180170983869,0.895727374432254,
8.22431019134419));
#74470=CARTESIAN_POINT('Ctrl Pts',(-1.26306823834814,0.908000984756745,
8.22319711919407));
#74471=CARTESIAN_POINT('Ctrl Pts',(-1.24949693195612,0.926498644676224,
8.2215185964789));
#74472=CARTESIAN_POINT('Ctrl Pts',(-1.24478809374085,0.932815592964994,
8.22094520036954));
#74473=CARTESIAN_POINT('Ctrl Pts',(-1.23613761242704,0.944238131378665,
8.21990843680867));
#74474=CARTESIAN_POINT('Ctrl Pts',(-1.23221205696043,0.949355199777328,
8.2194440561872));
#74475=CARTESIAN_POINT('Ctrl Pts',(-1.22303971467008,0.961158850615359,
8.21837287510442));
#74476=CARTESIAN_POINT('Ctrl Pts',(-1.2177698098575,0.967827039743228,8.21776769870591));
#74477=CARTESIAN_POINT('Ctrl Pts',(-1.20063394868642,0.989148046121565,
8.2158313258862));
#74478=CARTESIAN_POINT('Ctrl Pts',(-1.1885556300063,1.0036290812869,8.21451404888314));
#74479=CARTESIAN_POINT('Ctrl Pts',(-1.15849097566115,1.03837017806146,8.21133832802212));
#74480=CARTESIAN_POINT('Ctrl Pts',(-1.1402325574487,1.0583873867404,8.20949519734665));
#74481=CARTESIAN_POINT('Ctrl Pts',(-1.05691879731478,1.14506648188989,8.2013992385625));
#74482=CARTESIAN_POINT('Ctrl Pts',(-0.986474622263151,1.20628536746132,
8.19535789655482));
#74483=CARTESIAN_POINT('Ctrl Pts',(-0.851487821977131,1.30381532714595,
8.18433530076217));
#74484=CARTESIAN_POINT('Ctrl Pts',(-0.789042927450533,1.34252565838235,
8.17941689745753));
#74485=CARTESIAN_POINT('Ctrl Pts',(-0.706636999630091,1.38586937611445,
8.17297063429914));
#74486=CARTESIAN_POINT('Ctrl Pts',(-0.688996885039989,1.39472327292096,
8.17159356935438));
#74487=CARTESIAN_POINT('Ctrl Pts',(-0.659962877099033,1.40861074868608,
8.16932882073245));
#74488=CARTESIAN_POINT('Ctrl Pts',(-0.648668207434421,1.41384750976527,
8.16844823629734));
#74489=CARTESIAN_POINT('Ctrl Pts',(-0.626615118402635,1.42375252559121,
8.16672904387845));
#74490=CARTESIAN_POINT('Ctrl Pts',(-0.615864340915131,1.4284358089969,8.16589102246685));
#74491=CARTESIAN_POINT('Ctrl Pts',(-0.590339595825652,1.43921325736795,
8.16390099510722));
#74492=CARTESIAN_POINT('Ctrl Pts',(-0.575522894612236,1.44520206230261,
8.16274551392185));
#74493=CARTESIAN_POINT('Ctrl Pts',(-0.524038484907674,1.46509441762896,
8.15872795045633));
#74494=CARTESIAN_POINT('Ctrl Pts',(-0.486941829054092,1.47783799484669,
8.15582823995077));
#74495=CARTESIAN_POINT('Ctrl Pts',(-0.391265532994785,1.50671156403513,
8.14833293882958));
#74496=CARTESIAN_POINT('Ctrl Pts',(-0.332152878147633,1.52083581366658,
8.14368474066949));
#74497=CARTESIAN_POINT('Ctrl Pts',(-0.178346242655299,1.54819031534426,
8.13161201535519));
#74498=CARTESIAN_POINT('Ctrl Pts',(-0.0829779185374421,1.55621875739644,
8.12413817701859));
#74499=CARTESIAN_POINT('Ctrl Pts',(0.0355490640440596,1.55526413634446,
8.11520254823744));
#74500=CARTESIAN_POINT('Ctrl Pts',(0.0585651203015629,1.5545676376251,8.1134847466427));
#74501=CARTESIAN_POINT('Ctrl Pts',(0.0909620166392629,1.55286664824077,
8.11109866084603));
#74502=CARTESIAN_POINT('Ctrl Pts',(0.10036095300839,1.55228753997022,8.11041020284145));
#74503=CARTESIAN_POINT('Ctrl Pts',(0.116356102426689,1.55115611995029,8.10924567863055));
#74504=CARTESIAN_POINT('Ctrl Pts',(0.122954992250006,1.5506470030533,8.1087673191013));
#74505=CARTESIAN_POINT('Ctrl Pts',(0.136890355597368,1.54948234139476,8.10776171099461));
#74506=CARTESIAN_POINT('Ctrl Pts',(0.144225690901881,1.54881679090983,8.10723500935038));
#74507=CARTESIAN_POINT('Ctrl Pts',(0.164528788754112,1.54682915281767,8.10578378013568));
#74508=CARTESIAN_POINT('Ctrl Pts',(0.177485442587997,1.54539609727671,8.10486513028809));
#74509=CARTESIAN_POINT('Ctrl Pts',(0.206837873151978,1.54177556350944,8.10279779712114));
#74510=CARTESIAN_POINT('Ctrl Pts',(0.223220058960657,1.5394890870877,8.10165378487478));
#74511=CARTESIAN_POINT('Ctrl Pts',(0.277340447103427,1.53105333171405,8.09789760878443));
#74512=CARTESIAN_POINT('Ctrl Pts',(0.314890272061174,1.52377378604029,8.09532885366987));
#74513=CARTESIAN_POINT('Ctrl Pts',(0.467281505637384,1.48835576883424,8.0849200897899));
#74514=CARTESIAN_POINT('Ctrl Pts',(0.57899682786174,1.44855709295447,8.07729663498998));
#74515=CARTESIAN_POINT('Ctrl Pts',(0.719035275405329,1.37985326482531,8.06673537361935));
#74516=CARTESIAN_POINT('Ctrl Pts',(0.752323845071721,1.36198943224894,8.06414621009425));
#74517=CARTESIAN_POINT('Ctrl Pts',(0.797511806891221,1.33557764264314,8.0604995170239));
#74518=CARTESIAN_POINT('Ctrl Pts',(0.80999187436025,1.3280458801925,8.05947793849715));
#74519=CARTESIAN_POINT('Ctrl Pts',(0.831512132198664,1.31464214923158,8.0576899179335));
#74520=CARTESIAN_POINT('Ctrl Pts',(0.840600692844574,1.30884944555208,8.0569264094461));
#74521=CARTESIAN_POINT('Ctrl Pts',(0.859560341062551,1.29648635344244,8.05531547736298));
#74522=CARTESIAN_POINT('Ctrl Pts',(0.86941792035381,1.2898966276277,8.05446736653036));
#74523=CARTESIAN_POINT('Ctrl Pts',(0.893015612861251,1.27372833965384,8.05241089044082));
#74524=CARTESIAN_POINT('Ctrl Pts',(0.906677949446313,1.26403948641139,8.05119839292632));
#74525=CARTESIAN_POINT('Ctrl Pts',(0.956356270985716,1.22758955700567,8.0467064670573));
#74526=CARTESIAN_POINT('Ctrl Pts',(0.99136280374378,1.19949676428923,8.04337629491164));
#74527=CARTESIAN_POINT('Ctrl Pts',(1.08219136073053,1.11991215086681,8.03427374522129));
#74528=CARTESIAN_POINT('Ctrl Pts',(1.13553604611237,1.06578472526734,8.02841306829191));
#74529=CARTESIAN_POINT('Ctrl Pts',(1.23897567812935,0.944209477582968,8.01603310733143));
#74530=CARTESIAN_POINT('Ctrl Pts',(1.28800540508865,0.876148918183707,8.0095275510102));
#74531=CARTESIAN_POINT('Ctrl Pts',(1.33956289015135,0.790825841415402,8.00209143674399));
#74532=CARTESIAN_POINT('Ctrl Pts',(1.34759558838533,0.777058833463272,8.00091267803622));
#74533=CARTESIAN_POINT('Ctrl Pts',(1.35932017644035,0.756235572301677,7.99916372534939));
#74534=CARTESIAN_POINT('Ctrl Pts',(1.36317152234137,0.749270973025572,7.99858436751788));
#74535=CARTESIAN_POINT('Ctrl Pts',(1.36976286526275,0.737132425314385,7.99758468632347));
#74536=CARTESIAN_POINT('Ctrl Pts',(1.37252727191749,0.731972274262188,7.99716287391728));
#74537=CARTESIAN_POINT('Ctrl Pts',(1.37903712627482,0.719654161344171,7.9961633734691));
#74538=CARTESIAN_POINT('Ctrl Pts',(1.38275603240297,0.71248247006364,7.99558733733913));
#74539=CARTESIAN_POINT('Ctrl Pts',(1.39392719605544,0.690522579749311,7.99384034974358));
#74540=CARTESIAN_POINT('Ctrl Pts',(1.40119961792467,0.675643507569316,7.99267978385194));
#74541=CARTESIAN_POINT('Ctrl Pts',(1.41787394338265,0.640100740187546,7.98995506285775));
#74542=CARTESIAN_POINT('Ctrl Pts',(1.42706405491241,0.619341403553678,7.98840107520557));
#74543=CARTESIAN_POINT('Ctrl Pts',(1.46084706203817,0.538280952363602,7.98244848901143));
#74544=CARTESIAN_POINT('Ctrl Pts',(1.4820999386259,0.476656585835822,7.97816433201871));
#74545=CARTESIAN_POINT('Ctrl Pts',(1.52633232424204,0.316408004911839,7.96722464804931));
#74546=CARTESIAN_POINT('Ctrl Pts',(1.54366561223733,0.216558928860968,7.9605797507473));
#74547=CARTESIAN_POINT('Ctrl Pts',(1.552963839516,0.0919408351150383,7.95198354681935));
#74548=CARTESIAN_POINT('Ctrl Pts',(1.55419155567525,0.0681051178718693,
7.95032693204113));
#74549=CARTESIAN_POINT('Ctrl Pts',(1.55525283472131,0.03081495091358,7.94771070236386));
#74550=CARTESIAN_POINT('Ctrl Pts',(1.55546104299214,0.0173742502842062,
7.94676276450098));
#74551=CARTESIAN_POINT('Ctrl Pts',(1.55552413638347,-0.00757966629252008,
7.94499277504774));
#74552=CARTESIAN_POINT('Ctrl Pts',(1.55542543243638,-0.0190919157169097,
7.94417223612611));
#74553=CARTESIAN_POINT('Ctrl Pts',(1.55492081024851,-0.0447371292593568,
7.94233499038163));
#74554=CARTESIAN_POINT('Ctrl Pts',(1.55444997171525,-0.0588676290986065,
7.94131631766446));
#74555=CARTESIAN_POINT('Ctrl Pts',(1.55246684320428,-0.101084193783883,
7.93825291456962));
#74556=CARTESIAN_POINT('Ctrl Pts',(1.55038541710038,-0.129136291236553,
7.93619073924407));
#74557=CARTESIAN_POINT('Ctrl Pts',(1.54126355870704,-0.218984433742546,
7.92949606285495));
#74558=CARTESIAN_POINT('Ctrl Pts',(1.53127847105869,-0.280414159182216,
7.9247790755692));
#74559=CARTESIAN_POINT('Ctrl Pts',(1.49548381989311,-0.439685805323688,
7.91222381179662));
#74560=CARTESIAN_POINT('Ctrl Pts',(1.46376458789457,-0.535899934222685,
7.90429558315751));
#74561=CARTESIAN_POINT('Ctrl Pts',(1.4108043371113,-0.655830265525908,7.89433768279793));
#74562=CARTESIAN_POINT('Ctrl Pts',(1.39787823387293,-0.682948718002875,
7.89208234416779));
#74563=CARTESIAN_POINT('Ctrl Pts',(1.3794301386574,-0.71893035383222,7.88910022975451));
#74564=CARTESIAN_POINT('Ctrl Pts',(1.37459351130218,-0.728135327792465,
7.88833827746536));
#74565=CARTESIAN_POINT('Ctrl Pts',(1.3667608855413,-0.742685980315719,7.88713614044877));
#74566=CARTESIAN_POINT('Ctrl Pts',(1.36382508792764,-0.748063444274921,
7.88669237590003));
#74567=CARTESIAN_POINT('Ctrl Pts',(1.35754348297583,-0.759409478536809,
7.885757366907));
#74568=CARTESIAN_POINT('Ctrl Pts',(1.35418991229818,-0.76537360132106,7.88526665298829));
#74569=CARTESIAN_POINT('Ctrl Pts',(1.34553932117405,-0.780523293425523,
7.88402165775359));
#74570=CARTESIAN_POINT('Ctrl Pts',(1.3401874125863,-0.78967739746249,7.88327078069417));
#74571=CARTESIAN_POINT('Ctrl Pts',(1.31697469208712,-0.828465468905031,
7.88009195651391));
#74572=CARTESIAN_POINT('Ctrl Pts',(1.29821999840131,-0.857556202567658,
7.87771488120675));
#74573=CARTESIAN_POINT('Ctrl Pts',(1.23902691429891,-0.94297258877348,7.87067951656161));
#74574=CARTESIAN_POINT('Ctrl Pts',(1.19577804507411,-0.997246812083528,
7.8661304917929));
#74575=CARTESIAN_POINT('Ctrl Pts',(1.0848135394717,-1.11885757327701,7.85529724406268));
#74576=CARTESIAN_POINT('Ctrl Pts',(1.01425097864081,-1.18319683326125,7.84901539437596));
#74577=CARTESIAN_POINT('Ctrl Pts',(0.920813384843231,-1.25385839582865,
7.84095804251916));
#74578=CARTESIAN_POINT('Ctrl Pts',(0.903101469183544,-1.26667510530303,
7.83944191017711));
#74579=CARTESIAN_POINT('Ctrl Pts',(0.873527168881357,-1.28714004302279,
7.83692430433954));
#74580=CARTESIAN_POINT('Ctrl Pts',(0.861819987823117,-1.29500791133799,
7.83593118248055));
#74581=CARTESIAN_POINT('Ctrl Pts',(0.840367057140992,-1.30900571900514,
7.83411660781216));
#74582=CARTESIAN_POINT('Ctrl Pts',(0.830657062793434,-1.31518880549084,
7.83329721921227));
#74583=CARTESIAN_POINT('Ctrl Pts',(0.809437982938206,-1.32837187644752,
7.83151023493493));
#74584=CARTESIAN_POINT('Ctrl Pts',(0.797904888752767,-1.33533121645665,
7.83054122557862));
#74585=CARTESIAN_POINT('Ctrl Pts',(0.764981532500986,-1.35461913547849,
7.82778050014743));
#74586=CARTESIAN_POINT('Ctrl Pts',(0.743386989515621,-1.36658896586155,
7.82597613123709));
#74587=CARTESIAN_POINT('Ctrl Pts',(0.693637908699188,-1.39263673653997,
7.82183122408097));
#74588=CARTESIAN_POINT('Ctrl Pts',(0.665323241184622,-1.40638379058277,
7.8194805009776));
#74589=CARTESIAN_POINT('Ctrl Pts',(0.562694603887872,-1.4524180780777,7.81099065826851));
#74590=CARTESIAN_POINT('Ctrl Pts',(0.486305826518423,-1.47974581428383,
7.80471902142107));
#74591=CARTESIAN_POINT('Ctrl Pts',(0.334756323017078,-1.52095450401104,
7.79253808429345));
#74592=CARTESIAN_POINT('Ctrl Pts',(0.259995514896561,-1.5355028342328,7.78664787318167));
#74593=CARTESIAN_POINT('Ctrl Pts',(0.168373359356863,-1.54644536481923,
7.7797619623278));
#74594=CARTESIAN_POINT('Ctrl Pts',(0.152252730518989,-1.54811563373617,
7.77856297050395));
#74595=CARTESIAN_POINT('Ctrl Pts',(0.128128495800055,-1.55023466104612,
7.77679023587213));
#74596=CARTESIAN_POINT('Ctrl Pts',(0.120143335079668,-1.55087394792957,
7.77620697476157));
#74597=CARTESIAN_POINT('Ctrl Pts',(0.106316619663395,-1.55187347162566,
7.77520351400373));
#74598=CARTESIAN_POINT('Ctrl Pts',(0.100477612117348,-1.55226246109607,
7.77478177982324));
#74599=CARTESIAN_POINT('Ctrl Pts',(0.0866269028915636,-1.55310669856902,
7.77378614512297));
#74600=CARTESIAN_POINT('Ctrl Pts',(0.0786136956273406,-1.5535329194684,
7.77321385176959));
#74601=CARTESIAN_POINT('Ctrl Pts',(0.0543370607723487,-1.55463586585914,
7.77149032804589));
#74602=CARTESIAN_POINT('Ctrl Pts',(0.038065367958459,-1.5551193761906,7.7703490808232));
#74603=CARTESIAN_POINT('Ctrl Pts',(-0.0457786464836099,-1.5562939142157,
7.76452645096702));
#74604=CARTESIAN_POINT('Ctrl Pts',(-0.113343840037139,-1.55283668762211,
7.76002633918739));
#74605=CARTESIAN_POINT('Ctrl Pts',(-0.305349137925343,-1.53040778528859,
7.74726187364575));
#74606=CARTESIAN_POINT('Ctrl Pts',(-0.427978530902885,-1.50073886531438,
7.7390992386982));
#74607=CARTESIAN_POINT('Ctrl Pts',(-0.56628711455893,-1.44892463721571,
7.72890877973017));
#74608=CARTESIAN_POINT('Ctrl Pts',(-0.586710368673162,-1.44077568006091,
7.72737877538248));
#74609=CARTESIAN_POINT('Ctrl Pts',(-0.618846831649249,-1.42715651326519,
7.72492695359932));
#74610=CARTESIAN_POINT('Ctrl Pts',(-0.630676883834851,-1.42196827127722,
7.7240146783709));
#74611=CARTESIAN_POINT('Ctrl Pts',(-0.652984961366595,-1.41185159949463,
7.72227511731249));
#74612=CARTESIAN_POINT('Ctrl Pts',(-0.663475301074231,-1.40695231272407,
7.72144888121579));
#74613=CARTESIAN_POINT('Ctrl Pts',(-0.687357178937619,-1.39547231376919,
7.71954848394858));
#74614=CARTESIAN_POINT('Ctrl Pts',(-0.700710485243082,-1.38881519898406,
7.71847172199472));
#74615=CARTESIAN_POINT('Ctrl Pts',(-0.742832736594558,-1.36705358617228,
7.71502858482346));
#74616=CARTESIAN_POINT('Ctrl Pts',(-0.771223415446381,-1.35124022105183,
7.71263768290214));
#74617=CARTESIAN_POINT('Ctrl Pts',(-0.83845721471574,-1.31098226403963,
7.70679971505475));
#74618=CARTESIAN_POINT('Ctrl Pts',(-0.876752723347024,-1.28568619076414,
7.70332582762222));
#74619=CARTESIAN_POINT('Ctrl Pts',(-0.962619271141025,-1.22334513110346,
7.6951980668136));
#74620=CARTESIAN_POINT('Ctrl Pts',(-1.00926785940533,-1.1851527083484,7.69052094884011));
#74621=CARTESIAN_POINT('Ctrl Pts',(-1.10941137037855,-1.09295271560774,
7.67996724707086));
#74622=CARTESIAN_POINT('Ctrl Pts',(-1.16141091746499,-1.03752903976306,
7.67410677608936));
#74623=CARTESIAN_POINT('Ctrl Pts',(-1.21718514621918,-0.968608940625206,
7.66753240490009));
#74624=CARTESIAN_POINT('Ctrl Pts',(-1.22508755641713,-0.958594527016345,
7.66659345801247));
#74625=CARTESIAN_POINT('Ctrl Pts',(-1.23732086897498,-0.942693316341622,
7.66512946835919));
#74626=CARTESIAN_POINT('Ctrl Pts',(-1.24173480340049,-0.936871552226248,
7.66459902809574));
#74627=CARTESIAN_POINT('Ctrl Pts',(-1.25008232743238,-0.92569893748762,
7.66359194458746));
#74628=CARTESIAN_POINT('Ctrl Pts',(-1.25402287633284,-0.920353723139987,
7.66311486309041));
#74629=CARTESIAN_POINT('Ctrl Pts',(-1.26354900829962,-0.90725709213594,
7.66195704033614));
#74630=CARTESIAN_POINT('Ctrl Pts',(-1.26909775391023,-0.899478977492918,
7.66127876693306));
#74631=CARTESIAN_POINT('Ctrl Pts',(-1.28927819960503,-0.870631912265411,
7.65879546149752));
#74632=CARTESIAN_POINT('Ctrl Pts',(-1.30346068143328,-0.849251816106625,
7.65701758977415));
#74633=CARTESIAN_POINT('Ctrl Pts',(-1.37438030582783,-0.736374993620883,
7.64789653122593));
#74634=CARTESIAN_POINT('Ctrl Pts',(-1.42203991842964,-0.639512804817598,
7.64093771155881));
#74635=CARTESIAN_POINT('Ctrl Pts',(-1.48577481225728,-0.466792198781864,
7.6287650073626));
#74636=CARTESIAN_POINT('Ctrl Pts',(-1.50691010203791,-0.393244794852944,
7.62365106254135));
#74637=CARTESIAN_POINT('Ctrl Pts',(-1.5266098384456,-0.299057042742007,
7.61698986841265));
#74638=CARTESIAN_POINT('Ctrl Pts',(-1.53029458021167,-0.279591039710081,
7.61560775544697));
#74639=CARTESIAN_POINT('Ctrl Pts',(-1.53569030779542,-0.247771845730677,
7.61333688700059));
#74640=CARTESIAN_POINT('Ctrl Pts',(-1.53762635013508,-0.235458701369292,
7.61245530771335));
#74641=CARTESIAN_POINT('Ctrl Pts',(-1.54099745297788,-0.212200222137321,
7.61078412101403));
#74642=CARTESIAN_POINT('Ctrl Pts',(-1.54246438919643,-0.20126023161635,
7.60999557898374));
#74643=CARTESIAN_POINT('Ctrl Pts',(-1.54521149816861,-0.17897490416236,
7.60838385098927));
#74644=CARTESIAN_POINT('Ctrl Pts',(-1.54648343381458,-0.167629252787794,
7.60756045572661));
#74645=CARTESIAN_POINT('Ctrl Pts',(-1.54980376176165,-0.134746354578356,
7.6051652839023));
#74646=CARTESIAN_POINT('Ctrl Pts',(-1.55152779921143,-0.113179862214762,
7.60358352539287));
#74647=CARTESIAN_POINT('Ctrl Pts',(-1.55460023182954,-0.0610877409083802,
7.59973508029491));
#74648=CARTESIAN_POINT('Ctrl Pts',(-1.5555,-0.0305461090157058,7.59745564652037));
#74649=CARTESIAN_POINT('Ctrl Pts',(-1.5555,7.12052432324671E-12,7.59515300361487));
#74650=CARTESIAN_POINT('Ctrl Pts',(-1.55549969139753,0.000979827635642597,
7.4570242544914));
#74651=CARTESIAN_POINT('Ctrl Pts',(-1.55554501108635,-0.0709662569765335,
7.4618905175078));
#74652=CARTESIAN_POINT('Ctrl Pts',(-1.55059873048183,-0.142833707437426,
7.46660555340356));
#74653=CARTESIAN_POINT('Ctrl Pts',(-1.52818695969918,-0.304108542309095,
7.47732492511803));
#74654=CARTESIAN_POINT('Ctrl Pts',(-1.50781860512254,-0.392833006397477,
7.48332821162779));
#74655=CARTESIAN_POINT('Ctrl Pts',(-1.47236311015355,-0.502308381022113,
7.49124120957554));
#74656=CARTESIAN_POINT('Ctrl Pts',(-1.46436403898692,-0.525171105088764,
7.49292195921004));
#74657=CARTESIAN_POINT('Ctrl Pts',(-1.45099930040647,-0.56068689033579,
7.49558283082459));
#74658=CARTESIAN_POINT('Ctrl Pts',(-1.445993958705,-0.573472064371543,7.49655102155029));
#74659=CARTESIAN_POINT('Ctrl Pts',(-1.4363648897729,-0.597139785805706,
7.49836353105899));
#74660=CARTESIAN_POINT('Ctrl Pts',(-1.43178502306543,-0.608039187825413,
7.49920631741373));
#74661=CARTESIAN_POINT('Ctrl Pts',(-1.42126728914897,-0.632291935734599,
7.50110039234493));
#74662=CARTESIAN_POINT('Ctrl Pts',(-1.41526465435722,-0.645615776032481,
7.50215383040761));
#74663=CARTESIAN_POINT('Ctrl Pts',(-1.39658609541388,-0.685563247233039,
7.50535245857226));
#74664=CARTESIAN_POINT('Ctrl Pts',(-1.38334068868298,-0.711911517572619,
7.50751694021133));
#74665=CARTESIAN_POINT('Ctrl Pts',(-1.33515636046828,-0.801333548544738,
7.51505883579101));
#74666=CARTESIAN_POINT('Ctrl Pts',(-1.29659079138147,-0.862338567550063,
7.52055459377995));
#74667=CARTESIAN_POINT('Ctrl Pts',(-1.20005873142889,-0.993846317926974,
7.53315044886879));
#74668=CARTESIAN_POINT('Ctrl Pts',(-1.1398357096647,-1.06237795471466,7.5402724543805));
#74669=CARTESIAN_POINT('Ctrl Pts',(-1.05362757989018,-1.14465685977957,
7.54930682696506));
#74670=CARTESIAN_POINT('Ctrl Pts',(-1.0327690628747,-1.16351137143775,7.55141433230204));
#74671=CARTESIAN_POINT('Ctrl Pts',(-1.00358394317558,-1.18848879269371,
7.55424582498861));
#74672=CARTESIAN_POINT('Ctrl Pts',(-0.995691850961683,-1.1951084028938,
7.5550002395648));
#74673=CARTESIAN_POINT('Ctrl Pts',(-0.982454434648219,-1.20598932254475,
7.55624622350705));
#74674=CARTESIAN_POINT('Ctrl Pts',(-0.977145831440899,-1.21029458959364,
7.55674080559601));
#74675=CARTESIAN_POINT('Ctrl Pts',(-0.966095798362048,-1.21913604330129,
7.5577595231638));
#74676=CARTESIAN_POINT('Ctrl Pts',(-0.960350459330092,-1.223666941958,7.5582832989696));
#74677=CARTESIAN_POINT('Ctrl Pts',(-0.944888800362732,-1.23568436505123,
7.5596778362951));
#74678=CARTESIAN_POINT('Ctrl Pts',(-0.935115302857628,-1.24309697541163,
7.56054364637968));
#74679=CARTESIAN_POINT('Ctrl Pts',(-0.880895093088227,-1.28321835019784,
7.56526773909854));
#74680=CARTESIAN_POINT('Ctrl Pts',(-0.834814606447781,-1.31366339708889,
7.56899450754268));
#74681=CARTESIAN_POINT('Ctrl Pts',(-0.689990184224478,-1.39864190332242,
7.58017441863464));
#74682=CARTESIAN_POINT('Ctrl Pts',(-0.586862610127516,-1.44494922200853,
7.5874523432492));
#74683=CARTESIAN_POINT('Ctrl Pts',(-0.439414548173491,-1.49274337639757,
7.59790486905357));
#74684=CARTESIAN_POINT('Ctrl Pts',(-0.398682163169277,-1.50413428729183,
7.60079358334716));
#74685=CARTESIAN_POINT('Ctrl Pts',(-0.34089003335134,-1.51778354496018,
7.60492486829894));
#74686=CARTESIAN_POINT('Ctrl Pts',(-0.324177809055433,-1.52144063693451,
7.60612322393444));
#74687=CARTESIAN_POINT('Ctrl Pts',(-0.295613822092171,-1.52719923545792,
7.60817946430359));
#74688=CARTESIAN_POINT('Ctrl Pts',(-0.283791525200369,-1.52944022180075,
7.60903284354371));
#74689=CARTESIAN_POINT('Ctrl Pts',(-0.259598669439202,-1.53373596533948,
7.61078452636559));
#74690=CARTESIAN_POINT('Ctrl Pts',(-0.247226913469297,-1.53577873301453,
7.61168314205691));
#74691=CARTESIAN_POINT('Ctrl Pts',(-0.2159373122994,-1.54055725905988,7.61396367870161));
#74692=CARTESIAN_POINT('Ctrl Pts',(-0.196991721959828,-1.54309422664626,
7.61535174050453));
#74693=CARTESIAN_POINT('Ctrl Pts',(-0.112409963510521,-1.55283741813895,
7.62158360048232));
#74694=CARTESIAN_POINT('Ctrl Pts',(-0.0464097455189875,-1.55620820396565,
7.62654389250547));
#74695=CARTESIAN_POINT('Ctrl Pts',(0.0813748462475464,-1.55459817525299,
7.63631871039768));
#74696=CARTESIAN_POINT('Ctrl Pts',(0.143048662305526,-1.55013990312827,
7.64111312513598));
#74697=CARTESIAN_POINT('Ctrl Pts',(0.280169309291714,-1.53197390890923,
7.65183574469314));
#74698=CARTESIAN_POINT('Ctrl Pts',(0.355211412975751,-1.51633319593973,
7.657748518799));
#74699=CARTESIAN_POINT('Ctrl Pts',(0.441277824915646,-1.49165094091487,
7.66438960607644));
#74700=CARTESIAN_POINT('Ctrl Pts',(0.453707139681548,-1.48791750750077,
7.66534501482946));
#74701=CARTESIAN_POINT('Ctrl Pts',(0.473215165700044,-1.48179062332647,
7.66683722000366));
#74702=CARTESIAN_POINT('Ctrl Pts',(0.480325512241547,-1.4795010824526,7.66737955682743));
#74703=CARTESIAN_POINT('Ctrl Pts',(0.493911285669533,-1.47501817846959,
7.66841247027955));
#74704=CARTESIAN_POINT('Ctrl Pts',(0.500389110822044,-1.47283323045834,
7.66890347074883));
#74705=CARTESIAN_POINT('Ctrl Pts',(0.516244358208881,-1.46736863081503,
7.67010198147855));
#74706=CARTESIAN_POINT('Ctrl Pts',(0.525605376226126,-1.4640416450091,7.67080678506493));
#74707=CARTESIAN_POINT('Ctrl Pts',(0.560656808433647,-1.45120453160755,
7.67343760442499));
#74708=CARTESIAN_POINT('Ctrl Pts',(0.586128065665676,-1.4411053984601,7.6753326425775));
#74709=CARTESIAN_POINT('Ctrl Pts',(0.653991175847012,-1.41210095672429,
7.68037062049658));
#74710=CARTESIAN_POINT('Ctrl Pts',(0.69582693857555,-1.39196230555116,7.68346495140166));
#74711=CARTESIAN_POINT('Ctrl Pts',(0.83987232392017,-1.31450246778687,7.69428600676893));
#74712=CARTESIAN_POINT('Ctrl Pts',(0.936437633789859,-1.24755163216969,
7.70187975334574));
#74713=CARTESIAN_POINT('Ctrl Pts',(1.04732900944869,-1.15047683658335,7.71194323452745));
#74714=CARTESIAN_POINT('Ctrl Pts',(1.06949881943101,-1.12989693132421,7.71403092695091));
#74715=CARTESIAN_POINT('Ctrl Pts',(1.10156804786942,-1.0983377022807,7.71717719237729));
#74716=CARTESIAN_POINT('Ctrl Pts',(1.11193451643538,-1.08784165989357,7.71821498430634));
#74717=CARTESIAN_POINT('Ctrl Pts',(1.13034309840462,-1.06866491873034,7.72009694799972));
#74718=CARTESIAN_POINT('Ctrl Pts',(1.138438509269,-1.06003678007625,7.72093871758969));
#74719=CARTESIAN_POINT('Ctrl Pts',(1.15564391480141,-1.0412747281855,7.72275914335087));
#74720=CARTESIAN_POINT('Ctrl Pts',(1.16472068357953,-1.03111183908427,7.72373910864727));
#74721=CARTESIAN_POINT('Ctrl Pts',(1.18967101869046,-1.00242612722106,7.72648919478016));
#74722=CARTESIAN_POINT('Ctrl Pts',(1.2052434843862,-0.983647951197445,7.72827138705222));
#74723=CARTESIAN_POINT('Ctrl Pts',(1.2717552846064,-0.899492656974708,7.73618506959834));
#74724=CARTESIAN_POINT('Ctrl Pts',(1.31785703449716,-0.830480272124849,
7.74249607873002));
#74725=CARTESIAN_POINT('Ctrl Pts',(1.40457896102814,-0.675113554800244,
7.75624344708667));
#74726=CARTESIAN_POINT('Ctrl Pts',(1.44321167516665,-0.588015219119412,
7.76368241281157));
#74727=CARTESIAN_POINT('Ctrl Pts',(1.48110347531414,-0.475872759306487,
7.77260868062961));
#74728=CARTESIAN_POINT('Ctrl Pts',(1.48806116739201,-0.453647988197631,
7.77434650998924));
#74729=CARTESIAN_POINT('Ctrl Pts',(1.49717988827809,-0.422048374407086,
7.77676598517714));
#74730=CARTESIAN_POINT('Ctrl Pts',(1.49975672308582,-0.412798052793245,
7.77746809908561));
#74731=CARTESIAN_POINT('Ctrl Pts',(1.50400706407234,-0.396974797911779,
7.77865796008569));
#74732=CARTESIAN_POINT('Ctrl Pts',(1.50572351196272,-0.390413821667677,
7.77914806065925));
#74733=CARTESIAN_POINT('Ctrl Pts',(1.50927534931498,-0.376465278684778,
7.78018288636546));
#74734=CARTESIAN_POINT('Ctrl Pts',(1.51109949944088,-0.369075189429433,
7.78072698763484));
#74735=CARTESIAN_POINT('Ctrl Pts',(1.51604196160468,-0.348400921531763,
7.78223832384033));
#74736=CARTESIAN_POINT('Ctrl Pts',(1.51903993116211,-0.335088275633844,
7.7831990776728));
#74737=CARTESIAN_POINT('Ctrl Pts',(1.52547222287481,-0.304662636573098,
7.7853702446455));
#74738=CARTESIAN_POINT('Ctrl Pts',(1.52879454363351,-0.287527608567049,
7.78657538991443));
#74739=CARTESIAN_POINT('Ctrl Pts',(1.53899471157172,-0.229730276543013,
7.79059253443933));
#74740=CARTESIAN_POINT('Ctrl Pts',(1.54454433243337,-0.188849161350949,
7.79335494055843));
#74741=CARTESIAN_POINT('Ctrl Pts',(1.5614980496291,-0.0112211677687543,
7.80519916367641));
#74742=CARTESIAN_POINT('Ctrl Pts',(1.55640850037308,0.126462917313448,7.81403696156534));
#74743=CARTESIAN_POINT('Ctrl Pts',(1.52947174446485,0.284292097957906,7.82507097351137));
#74744=CARTESIAN_POINT('Ctrl Pts',(1.52511593347312,0.306801417298446,7.82666477675015));
#74745=CARTESIAN_POINT('Ctrl Pts',(1.51744418312457,0.342229430904738,7.82920980178042));
#74746=CARTESIAN_POINT('Ctrl Pts',(1.51445670566381,0.355216411740045,7.83015056354671));
#74747=CARTESIAN_POINT('Ctrl Pts',(1.50849274972262,0.379698345419017,7.83193967413344));
#74748=CARTESIAN_POINT('Ctrl Pts',(1.50555077676461,0.391200784379005,7.83278685555756));
#74749=CARTESIAN_POINT('Ctrl Pts',(1.49853864898678,0.417365169759882,7.83472959446937));
#74750=CARTESIAN_POINT('Ctrl Pts',(1.49438450300826,0.43200311809666,7.83582780219911));
#74751=CARTESIAN_POINT('Ctrl Pts',(1.48057771738103,0.478069806601441,7.83932112474375));
#74752=CARTESIAN_POINT('Ctrl Pts',(1.4701436693649,0.509252794487029,7.84174117507829));
#74753=CARTESIAN_POINT('Ctrl Pts',(1.44262990658821,0.583566186402928,7.84764709289507));
#74754=CARTESIAN_POINT('Ctrl Pts',(1.42459442725173,0.626307085626742,7.85116011975138));
#74755=CARTESIAN_POINT('Ctrl Pts',(1.37915667721416,0.721829059536207,7.85926561878956));
#74756=CARTESIAN_POINT('Ctrl Pts',(1.35058263810123,0.773974353633779,7.86387816460538));
#74757=CARTESIAN_POINT('Ctrl Pts',(1.27929767481832,0.888041508362317,7.87430399548356));
#74758=CARTESIAN_POINT('Ctrl Pts',(1.23493296021063,0.948769399816142,7.88010111069342));
#74759=CARTESIAN_POINT('Ctrl Pts',(1.17799083416599,1.01591577035975,7.88663052903239));
#74760=CARTESIAN_POINT('Ctrl Pts',(1.1695095810532,1.02566789301412,7.88758189842874));
#74761=CARTESIAN_POINT('Ctrl Pts',(1.15594341391301,1.0408797708619,7.88906926048383));
#74762=CARTESIAN_POINT('Ctrl Pts',(1.1509393116236,1.04641033096636,7.88961073637658));
#74763=CARTESIAN_POINT('Ctrl Pts',(1.14126898326161,1.05694473028553,7.89064314301965));
#74764=CARTESIAN_POINT('Ctrl Pts',(1.13660926682391,1.06195406288122,7.89113448555217));
#74765=CARTESIAN_POINT('Ctrl Pts',(1.12508241489515,1.07418298424364,7.89233540804815));
#74766=CARTESIAN_POINT('Ctrl Pts',(1.11817851943387,1.08136780814526,7.89304225497267));
#74767=CARTESIAN_POINT('Ctrl Pts',(1.09187769716035,1.10821760281892,7.89569094586617));
#74768=CARTESIAN_POINT('Ctrl Pts',(1.0720259374624,1.12743238591035,7.89760126525488));
#74769=CARTESIAN_POINT('Ctrl Pts',(1.01703404800888,1.17789300289287,7.90269466053605));
#74770=CARTESIAN_POINT('Ctrl Pts',(0.980971021051693,1.20809216230312,7.90582780845656));
#74771=CARTESIAN_POINT('Ctrl Pts',(0.848558641444292,1.30912892404046,7.91684419688309));
#74772=CARTESIAN_POINT('Ctrl Pts',(0.745490409130914,1.37044237654542,7.92459447942765));
#74773=CARTESIAN_POINT('Ctrl Pts',(0.611048232535262,1.43072481308491,7.93467973317257));
#74774=CARTESIAN_POINT('Ctrl Pts',(0.585376855251253,1.44141847111609,7.93660247877976));
#74775=CARTESIAN_POINT('Ctrl Pts',(0.54593030357956,1.45662273534549,7.93956075544931));
#74776=CARTESIAN_POINT('Ctrl Pts',(0.532355076491546,1.46163871628751,7.94057946569314));
#74777=CARTESIAN_POINT('Ctrl Pts',(0.507573323398698,1.47040442411563,7.94244137534904));
#74778=CARTESIAN_POINT('Ctrl Pts',(0.496390171271181,1.47421729499361,7.94328240716746));
#74779=CARTESIAN_POINT('Ctrl Pts',(0.472012608895858,1.48221994759158,7.9451180646437));
#74780=CARTESIAN_POINT('Ctrl Pts',(0.45880363096384,1.48636169259715,7.94611418931359));
#74781=CARTESIAN_POINT('Ctrl Pts',(0.421135317884833,1.49762284769399,7.94895995574469));
#74782=CARTESIAN_POINT('Ctrl Pts',(0.396554983519485,1.50431816887764,7.9508230757082));
#74783=CARTESIAN_POINT('Ctrl Pts',(0.3401556857631,1.51820220207478,7.95511438391351));
#74784=CARTESIAN_POINT('Ctrl Pts',(0.308253577745842,1.52499943520829,7.95755357376472));
#74785=CARTESIAN_POINT('Ctrl Pts',(0.191369183724955,1.54608607556438,7.96653113128168));
#74786=CARTESIAN_POINT('Ctrl Pts',(0.105457668379776,1.55431023266949,7.97321800289549));
#74787=CARTESIAN_POINT('Ctrl Pts',(-0.048717988878883,1.55622500730806,
7.98516739973318));
#74788=CARTESIAN_POINT('Ctrl Pts',(-0.116741969594229,1.55260517797626,
7.9904180726374));
#74789=CARTESIAN_POINT('Ctrl Pts',(-0.200536081905883,1.54260570701948,
7.99671631707399));
#74790=CARTESIAN_POINT('Ctrl Pts',(-0.216725528395855,1.54041461587412,
7.99792504316677));
#74791=CARTESIAN_POINT('Ctrl Pts',(-0.240944147480382,1.53674744759384,
7.99971816136057));
#74792=CARTESIAN_POINT('Ctrl Pts',(-0.249000528164656,1.53546264847509,
8.00031213182518));
#74793=CARTESIAN_POINT('Ctrl Pts',(-0.262976057150327,1.53312099589648,
8.00133770159134));
#74794=CARTESIAN_POINT('Ctrl Pts',(-0.268899547174166,1.53209315360091,
8.00177085266144));
#74795=CARTESIAN_POINT('Ctrl Pts',(-0.283023317204938,1.52955796252907,
8.00280004750523));
#74796=CARTESIAN_POINT('Ctrl Pts',(-0.291217636334798,1.52801899711343,
8.00339431814377));
#74797=CARTESIAN_POINT('Ctrl Pts',(-0.316348447669188,1.52308969889965,
8.00520922405427));
#74798=CARTESIAN_POINT('Ctrl Pts',(-0.333241837158182,1.51948297580786,
8.00641855160604));
#74799=CARTESIAN_POINT('Ctrl Pts',(-0.373338800183416,1.51022137096864,
8.00927108719921));
#74800=CARTESIAN_POINT('Ctrl Pts',(-0.396479564465928,1.5043119800221,8.01090299455057));
#74801=CARTESIAN_POINT('Ctrl Pts',(-0.487791052547428,1.47874035890117,
8.01731842897144));
#74802=CARTESIAN_POINT('Ctrl Pts',(-0.554721623925365,1.45495651178569,
8.02197029547813));
#74803=CARTESIAN_POINT('Ctrl Pts',(-0.704307467571703,1.38997153960911,
8.03270629350585));
#74804=CARTESIAN_POINT('Ctrl Pts',(-0.785377643599008,1.34582655744088,
8.03878926897317));
#74805=CARTESIAN_POINT('Ctrl Pts',(-0.882248482703065,1.28132981264859,
8.04679157504217));
#74806=CARTESIAN_POINT('Ctrl Pts',(-0.902118400686632,1.26741893438338,
8.0484746068063));
#74807=CARTESIAN_POINT('Ctrl Pts',(-0.932720100726244,1.24491050642659,
8.05113828977852));
#74808=CARTESIAN_POINT('Ctrl Pts',(-0.943677459375091,1.23662516002074,
8.05210696701926));
#74809=CARTESIAN_POINT('Ctrl Pts',(-0.963857688656701,1.22094158856382,
8.05391991479804));
#74810=CARTESIAN_POINT('Ctrl Pts',(-0.973108787511704,1.21358117988817,
8.05476264656508));
#74811=CARTESIAN_POINT('Ctrl Pts',(-0.993598597906197,1.1968940436875,8.05665597880033));
#74812=CARTESIAN_POINT('Ctrl Pts',(-1.00479152439945,1.18751315405681,8.05770872099892));
#74813=CARTESIAN_POINT('Ctrl Pts',(-1.03814192957157,1.1587527963208,8.06090292818672));
#74814=CARTESIAN_POINT('Ctrl Pts',(-1.05988183802746,1.1389016557154,8.06306360563173));
#74815=CARTESIAN_POINT('Ctrl Pts',(-1.13420448602974,1.06706448002473,8.07073779300856));
#74816=CARTESIAN_POINT('Ctrl Pts',(-1.18362677185058,1.01196414470508,8.07637732824673));
#74817=CARTESIAN_POINT('Ctrl Pts',(-1.28656600970207,0.879297906224671,
8.08934893362486));
#74818=CARTESIAN_POINT('Ctrl Pts',(-1.33734344073776,0.799956705824113,
8.09670319035794));
#74819=CARTESIAN_POINT('Ctrl Pts',(-1.39195375757237,0.69472831084078,8.10565648818055));
#74820=CARTESIAN_POINT('Ctrl Pts',(-1.40274340943432,0.672676583908957,
8.10749067071032));
#74821=CARTESIAN_POINT('Ctrl Pts',(-1.41710169652014,0.641481818835518,
8.11001833198619));
#74822=CARTESIAN_POINT('Ctrl Pts',(-1.42111211731469,0.632547631045668,
8.11073471144544));
#74823=CARTESIAN_POINT('Ctrl Pts',(-1.42776895139142,0.617334980311334,
8.11194107131618));
#74824=CARTESIAN_POINT('Ctrl Pts',(-1.43045893029285,0.611076028826127,
8.11243357069672));
#74825=CARTESIAN_POINT('Ctrl Pts',(-1.43603484576512,0.597863565778048,
8.11346494516924));
#74826=CARTESIAN_POINT('Ctrl Pts',(-1.4389115467078,0.590906497383016,8.11400328503842));
#74827=CARTESIAN_POINT('Ctrl Pts',(-1.44671119705628,0.571648921121078,
8.11548115601483));
#74828=CARTESIAN_POINT('Ctrl Pts',(-1.4515278193047,0.559305638540478,8.11641466331292));
#74829=CARTESIAN_POINT('Ctrl Pts',(-1.4860272788179,0.46744702058334,8.12327136091529));
#74830=CARTESIAN_POINT('Ctrl Pts',(-1.5093196091122,0.385671174262824,8.1288811744231));
#74831=CARTESIAN_POINT('Ctrl Pts',(-1.54551745552437,0.203022818168026,
8.14114667021932));
#74832=CARTESIAN_POINT('Ctrl Pts',(-1.55545445899327,0.101980137035506,
8.14777563842846));
#74833=CARTESIAN_POINT('Ctrl Pts',(-1.55549984383366,0.000697017553365729,
8.15470102582708));
#74834=CARTESIAN_POINT('Origin',(0.,0.,-1.2940562256037));
#74835=CARTESIAN_POINT('',(-1.55549989237731,-0.000578631300119371,8.99405622560371));
#74836=CARTESIAN_POINT('',(-1.55549943430639,-0.00132660186739827,8.85594377445462));
#74837=CARTESIAN_POINT('',(-1.5555,-1.46451138874614E-13,-1.2940562256037));
#74838=CARTESIAN_POINT('Ctrl Pts',(-1.55549985441797,-0.000672982681023649,
8.99269866830482));
#74839=CARTESIAN_POINT('Ctrl Pts',(-1.55553267497311,0.0751868725337522,
8.98742630842159));
#74840=CARTESIAN_POINT('Ctrl Pts',(-1.55001602977296,0.150960035608289,
8.98240020028567));
#74841=CARTESIAN_POINT('Ctrl Pts',(-1.52948678893842,0.290733889955134,
8.97309402340842));
#74842=CARTESIAN_POINT('Ctrl Pts',(-1.51591498278765,0.354764016580911,
8.96881628542807));
#74843=CARTESIAN_POINT('Ctrl Pts',(-1.48224134326083,0.475542369316228,
8.96046486238954));
#74844=CARTESIAN_POINT('Ctrl Pts',(-1.46279985096064,0.532348806198154,
8.95641083970952));
#74845=CARTESIAN_POINT('Ctrl Pts',(-1.43322416462683,0.604799529158405,
8.95098178540607));
#74846=CARTESIAN_POINT('Ctrl Pts',(-1.42602273462414,0.621589162969467,
8.9497050981529));
#74847=CARTESIAN_POINT('Ctrl Pts',(-1.41356812740971,0.649269967237543,
8.94756694407566));
#74848=CARTESIAN_POINT('Ctrl Pts',(-1.40848053196524,0.660233986733171,
8.94671121123491));
#74849=CARTESIAN_POINT('Ctrl Pts',(-1.39823555126334,0.681654984428218,
8.94502125175909));
#74850=CARTESIAN_POINT('Ctrl Pts',(-1.39308733506298,0.692115480049023,
8.94418739059113));
#74851=CARTESIAN_POINT('Ctrl Pts',(-1.38029969988858,0.717377455103239,
8.94215206023508));
#74852=CARTESIAN_POINT('Ctrl Pts',(-1.37253933582564,0.732115705170182,
8.94094637805252));
#74853=CARTESIAN_POINT('Ctrl Pts',(-1.34470869299248,0.782972565801001,
8.93672029669511));
#74854=CARTESIAN_POINT('Ctrl Pts',(-1.32343883285864,0.818411006594746,
8.93365773422455));
#74855=CARTESIAN_POINT('Ctrl Pts',(-1.24275822895639,0.941451245971655,
8.92259086409341));
#74856=CARTESIAN_POINT('Ctrl Pts',(-1.17585751867034,1.02378331594169,8.91434171520101));
#74857=CARTESIAN_POINT('Ctrl Pts',(-1.05919316212951,1.14070838440239,8.9015520918593));
#74858=CARTESIAN_POINT('Ctrl Pts',(-1.01487802545282,1.18030920119306,8.89698874553265));
#74859=CARTESIAN_POINT('Ctrl Pts',(-0.95639946410656,1.22683152065423,8.8914187863839));
#74860=CARTESIAN_POINT('Ctrl Pts',(-0.944254980961323,1.23620309555228,
8.89028501230685));
#74861=CARTESIAN_POINT('Ctrl Pts',(-0.925727346168003,1.25006799361298,
8.88859198680759));
#74862=CARTESIAN_POINT('Ctrl Pts',(-0.919446176225109,1.25469512002804,
8.88802423971861));
#74863=CARTESIAN_POINT('Ctrl Pts',(-0.907874109613773,1.26308630147697,
8.88698997936066));
#74864=CARTESIAN_POINT('Ctrl Pts',(-0.902594295793504,1.26686461131741,
8.88652254437835));
#74865=CARTESIAN_POINT('Ctrl Pts',(-0.890428722670759,1.2754558040985,8.88545544435651));
#74866=CARTESIAN_POINT('Ctrl Pts',(-0.883527426278372,1.28024611460107,
8.88485728989135));
#74867=CARTESIAN_POINT('Ctrl Pts',(-0.861060874402768,1.29557233831768,
8.88293199360437));
#74868=CARTESIAN_POINT('Ctrl Pts',(-0.845342693180059,1.30588258512195,
8.8816187407413));
#74869=CARTESIAN_POINT('Ctrl Pts',(-0.74503382768297,1.36910917331893,8.87342193271221));
#74870=CARTESIAN_POINT('Ctrl Pts',(-0.655692897678767,1.41407470291416,
8.86692298541292));
#74871=CARTESIAN_POINT('Ctrl Pts',(-0.489882370095687,1.47840715372255,
8.85521038862082));
#74872=CARTESIAN_POINT('Ctrl Pts',(-0.415100300813759,1.50112038314158,
8.85004338496912));
#74873=CARTESIAN_POINT('Ctrl Pts',(-0.310582470666327,1.52445487743302,
8.84272074511322));
#74874=CARTESIAN_POINT('Ctrl Pts',(-0.282060524558848,1.52998883042445,
8.84071333703546));
#74875=CARTESIAN_POINT('Ctrl Pts',(-0.239259822237774,1.53705576889773,
8.83767808685636));
#74876=CARTESIAN_POINT('Ctrl Pts',(-0.225086632746572,1.53919514118514,
8.83666929812719));
#74877=CARTESIAN_POINT('Ctrl Pts',(-0.199439795840611,1.54270460359195,
8.83483618342761));
#74878=CARTESIAN_POINT('Ctrl Pts',(-0.187976474561442,1.54414330875063,
8.83401408410056));
#74879=CARTESIAN_POINT('Ctrl Pts',(-0.163225684585162,1.54696997074087,
8.83223260304774));
#74880=CARTESIAN_POINT('Ctrl Pts',(-0.149934321853342,1.54831469442623,
8.83127192987676));
#74881=CARTESIAN_POINT('Ctrl Pts',(-0.11334180292428,1.55154127656386,8.82861528577729));
#74882=CARTESIAN_POINT('Ctrl Pts',(-0.0900138553004687,1.5530692493693,
8.82690847524604));
#74883=CARTESIAN_POINT('Ctrl Pts',(0.065969882727109,1.55976013093717,8.81540175380699));
#74884=CARTESIAN_POINT('Ctrl Pts',(0.198762797828011,1.54844546091379,8.80508307599745));
#74885=CARTESIAN_POINT('Ctrl Pts',(0.370454402900628,1.51135322317808,8.79150310801523));
#74886=CARTESIAN_POINT('Ctrl Pts',(0.412045831304786,1.50054780924646,8.78820074445084));
#74887=CARTESIAN_POINT('Ctrl Pts',(0.47796263214271,1.48047469666119,8.78299275722727));
#74888=CARTESIAN_POINT('Ctrl Pts',(0.502595081993481,1.47229480319194,8.78105267547694));
#74889=CARTESIAN_POINT('Ctrl Pts',(0.536063150952893,1.46024281321834,8.77843530481333));
#74890=CARTESIAN_POINT('Ctrl Pts',(0.545083143749574,1.45689984363657,8.7777317848158));
#74891=CARTESIAN_POINT('Ctrl Pts',(0.560305072584805,1.45109716241409,8.77654842682252));
#74892=CARTESIAN_POINT('Ctrl Pts',(0.566523157756987,1.44868087170798,8.77606614571825));
#74893=CARTESIAN_POINT('Ctrl Pts',(0.579524720930552,1.44353206496688,8.77506030839839));
#74894=CARTESIAN_POINT('Ctrl Pts',(0.586304758495825,1.44079160907065,8.774537222014));
#74895=CARTESIAN_POINT('Ctrl Pts',(0.604859502310031,1.43313920931707,8.77310898405896));
#74896=CARTESIAN_POINT('Ctrl Pts',(0.616593817598843,1.42812993198109,8.77220938901327));
#74897=CARTESIAN_POINT('Ctrl Pts',(0.697395876080976,1.39245460333515,8.766031141383));
#74898=CARTESIAN_POINT('Ctrl Pts',(0.764220043649146,1.35693099489578,8.76100229023325));
#74899=CARTESIAN_POINT('Ctrl Pts',(0.878753883669385,1.28488837190784,8.75207177040058));
#74900=CARTESIAN_POINT('Ctrl Pts',(0.927430018801354,1.2502079825342,8.74816288035007));
#74901=CARTESIAN_POINT('Ctrl Pts',(1.01007089659661,1.18384048446953,8.74113251847141));
#74902=CARTESIAN_POINT('Ctrl Pts',(1.04483702187327,1.1532721347867,8.73803597924413));
#74903=CARTESIAN_POINT('Ctrl Pts',(1.10174747472538,1.09854501426182,8.73265882609977));
#74904=CARTESIAN_POINT('Ctrl Pts',(1.12458620015126,1.07515313764514,8.73040715993164));
#74905=CARTESIAN_POINT('Ctrl Pts',(1.15677691954164,1.04003420201023,8.72707898062912));
#74906=CARTESIAN_POINT('Ctrl Pts',(1.16672403526809,1.02886295535205,8.72602763622425));
#74907=CARTESIAN_POINT('Ctrl Pts',(1.18408807608228,1.00878636965667,8.72414985587718));
#74908=CARTESIAN_POINT('Ctrl Pts',(1.19156958903233,0.999938204463611,8.72332617607216));
#74909=CARTESIAN_POINT('Ctrl Pts',(1.20717497513209,0.981058328046565,8.72157625664145));
#74910=CARTESIAN_POINT('Ctrl Pts',(1.21527418164574,0.971007470822354,8.72064910173805));
#74911=CARTESIAN_POINT('Ctrl Pts',(1.23678784848405,0.943618874521721,8.7181336773604));
#74912=CARTESIAN_POINT('Ctrl Pts',(1.24996196887213,0.926097050989003,8.71653612252511));
#74913=CARTESIAN_POINT('Ctrl Pts',(1.33662335771646,0.805616828358604,8.70562339865553));
#74914=CARTESIAN_POINT('Ctrl Pts',(1.39767111156665,0.694322197021517,8.69583434962223));
#74915=CARTESIAN_POINT('Ctrl Pts',(1.46951057352821,0.51443447905573,8.68081960147854));
#74916=CARTESIAN_POINT('Ctrl Pts',(1.49038060916645,0.450412683994701,8.67563005265339));
#74917=CARTESIAN_POINT('Ctrl Pts',(1.51106488809414,0.369495699509406,8.66939674120381));
#74918=CARTESIAN_POINT('Ctrl Pts',(1.51484165620203,0.353693341625041,8.66819464299067));
#74919=CARTESIAN_POINT('Ctrl Pts',(1.52011156440548,0.330008116003868,8.66641833243938));
#74920=CARTESIAN_POINT('Ctrl Pts',(1.52179230889233,0.322168746267745,8.66583454144613));
#74921=CARTESIAN_POINT('Ctrl Pts',(1.52459416614423,0.308588854380744,8.66483080181685));
#74922=CARTESIAN_POINT('Ctrl Pts',(1.52574359572114,0.302854644681742,8.66440930901672));
#74923=CARTESIAN_POINT('Ctrl Pts',(1.52838998724825,0.289254900152996,8.66341517173262));
#74924=CARTESIAN_POINT('Ctrl Pts',(1.52985860026244,0.281384116670855,8.66284412299237));
#74925=CARTESIAN_POINT('Ctrl Pts',(1.53411614588725,0.257547238282533,8.66112670408433));
#74926=CARTESIAN_POINT('Ctrl Pts',(1.53671648695876,0.241547970381527,8.65999023362522));
#74927=CARTESIAN_POINT('Ctrl Pts',(1.54973084393972,0.152727320006722,8.65375604609985));
#74928=CARTESIAN_POINT('Ctrl Pts',(1.5552203220981,0.0792701796070533,8.64887582904145));
#74929=CARTESIAN_POINT('Ctrl Pts',(1.55573435553431,-0.0611930989910091,
8.63961565435611));
#74930=CARTESIAN_POINT('Ctrl Pts',(1.55166484794895,-0.128023041368751,
8.63523988570708));
#74931=CARTESIAN_POINT('Ctrl Pts',(1.53828463811049,-0.234255634372873,
8.62810537057456));
#74932=CARTESIAN_POINT('Ctrl Pts',(1.53171951914929,-0.273916567054004,
8.62540191313969));
#74933=CARTESIAN_POINT('Ctrl Pts',(1.51767192973829,-0.34223724329438,8.62063601085943));
#74934=CARTESIAN_POINT('Ctrl Pts',(1.51089316077976,-0.371020323370508,
8.61859407802205));
#74935=CARTESIAN_POINT('Ctrl Pts',(1.49960055046496,-0.413504152618828,
8.61551929210359));
#74936=CARTESIAN_POINT('Ctrl Pts',(1.49570951844169,-0.427364606525818,
8.61450638382327));
#74937=CARTESIAN_POINT('Ctrl Pts',(1.4883900846621,-0.452112202148676,8.61267925056458));
#74938=CARTESIAN_POINT('Ctrl Pts',(1.48503312977889,-0.463019522472326,
8.61186740886039));
#74939=CARTESIAN_POINT('Ctrl Pts',(1.47754035823443,-0.486444781873004,
8.61010917461645));
#74940=CARTESIAN_POINT('Ctrl Pts',(1.47336483575905,-0.49894897221002,8.60916152711336));
#74941=CARTESIAN_POINT('Ctrl Pts',(1.46156938442938,-0.532832319253829,
8.606567923491));
#74942=CARTESIAN_POINT('Ctrl Pts',(1.45363993941149,-0.554099423851205,
8.60491186749038));
#74943=CARTESIAN_POINT('Ctrl Pts',(1.39465243692118,-0.702315527663511,
8.59316467443468));
#74944=CARTESIAN_POINT('Ctrl Pts',(1.32751055839644,-0.822194049727416,
8.58251213240894));
#74945=CARTESIAN_POINT('Ctrl Pts',(1.22056757239217,-0.965162966130685,
8.56870703953378));
#74946=CARTESIAN_POINT('Ctrl Pts',(1.19421112717351,-0.99758958573062,8.56549660346181));
#74947=CARTESIAN_POINT('Ctrl Pts',(1.14973458576417,-1.04801677663082,8.5604155343826));
#74948=CARTESIAN_POINT('Ctrl Pts',(1.13242162142142,-1.06670063448791,8.55851192891728));
#74949=CARTESIAN_POINT('Ctrl Pts',(1.10801453418281,-1.09177594776829,8.55593731808865));
#74950=CARTESIAN_POINT('Ctrl Pts',(1.10130989414631,-1.09853878287706,8.55524088589171));
#74951=CARTESIAN_POINT('Ctrl Pts',(1.08983162989559,-1.10990596059625,8.55406743891075));
#74952=CARTESIAN_POINT('Ctrl Pts',(1.08508997949475,-1.11454204339672,8.55358803584301));
#74953=CARTESIAN_POINT('Ctrl Pts',(1.07505604592461,-1.12422784537089,8.55258493896932));
#74954=CARTESIAN_POINT('Ctrl Pts',(1.0697576000532,-1.12927075281901,8.55206174330038));
#74955=CARTESIAN_POINT('Ctrl Pts',(1.05509410505249,-1.14303121976397,8.55063084708253));
#74956=CARTESIAN_POINT('Ctrl Pts',(1.045656515759,-1.15167114181665,8.54972875609336));
#74957=CARTESIAN_POINT('Ctrl Pts',(0.978826636853056,-1.21135366576549,
8.54346211704602));
#74958=CARTESIAN_POINT('Ctrl Pts',(0.91782136549886,-1.25820766630131,8.538356029285));
#74959=CARTESIAN_POINT('Ctrl Pts',(0.802277215440299,-1.33405394213476,
8.52923804926565));
#74960=CARTESIAN_POINT('Ctrl Pts',(0.749010283104518,-1.36467289970733,
8.52522078665453));
#74961=CARTESIAN_POINT('Ctrl Pts',(0.654100549414535,-1.41199426569515,
8.51817912849731));
#74962=CARTESIAN_POINT('Ctrl Pts',(0.613289978071359,-1.43019239374418,
8.5151862915719));
#74963=CARTESIAN_POINT('Ctrl Pts',(0.542096656064354,-1.45833072463409,
8.50996864507241));
#74964=CARTESIAN_POINT('Ctrl Pts',(0.512086566813048,-1.46913729661563,
8.50777041405878));
#74965=CARTESIAN_POINT('Ctrl Pts',(0.467674750817236,-1.48360380421202,
8.50450640384338));
#74966=CARTESIAN_POINT('Ctrl Pts',(0.453517815577891,-1.48799243429573,
8.50346440581033));
#74967=CARTESIAN_POINT('Ctrl Pts',(0.428200213377002,-1.49544599676828,
8.50159704518089));
#74968=CARTESIAN_POINT('Ctrl Pts',(0.417063834316329,-1.49858996955978,
8.5007743279169));
#74969=CARTESIAN_POINT('Ctrl Pts',(0.393359802187278,-1.504997306523,8.49901981251343));
#74970=CARTESIAN_POINT('Ctrl Pts',(0.380784357193257,-1.50822812629815,
8.49808702927632));
#74971=CARTESIAN_POINT('Ctrl Pts',(0.346514748759987,-1.51657659634958,
8.49553895889787));
#74972=CARTESIAN_POINT('Ctrl Pts',(0.324749422790677,-1.52138580264801,
8.49391396605883));
#74973=CARTESIAN_POINT('Ctrl Pts',(0.181790665866913,-1.54976618777586,
8.48319169304855));
#74974=CARTESIAN_POINT('Ctrl Pts',(0.058282047598181,-1.5592993772551,8.47364714032615));
#74975=CARTESIAN_POINT('Ctrl Pts',(-0.133903731543495,-1.55125842747295,
8.45873638028983));
#74976=CARTESIAN_POINT('Ctrl Pts',(-0.20252225636218,-1.54380034531773,
8.45341325479084));
#74977=CARTESIAN_POINT('Ctrl Pts',(-0.28659488616317,-1.52895821602703,
8.44704025948605));
#74978=CARTESIAN_POINT('Ctrl Pts',(-0.302719159107059,-1.52584764072448,
8.44582507661434));
#74979=CARTESIAN_POINT('Ctrl Pts',(-0.326675858247995,-1.52083135631309,
8.44403311371989));
#74980=CARTESIAN_POINT('Ctrl Pts',(-0.334547031994612,-1.51911929149427,
8.44344653689665));
#74981=CARTESIAN_POINT('Ctrl Pts',(-0.348116805280319,-1.51605713235211,
8.44243948124428));
#74982=CARTESIAN_POINT('Ctrl Pts',(-0.353821454452966,-1.51473592428718,
8.44201743302356));
#74983=CARTESIAN_POINT('Ctrl Pts',(-0.367291044812638,-1.51153609113264,
8.4410239863096));
#74984=CARTESIAN_POINT('Ctrl Pts',(-0.375049148723181,-1.50962982545764,
8.44045416185437));
#74985=CARTESIAN_POINT('Ctrl Pts',(-0.39838587659003,-1.50370468280836,
8.43874630151658));
#74986=CARTESIAN_POINT('Ctrl Pts',(-0.413917746715257,-1.49950366181776,
8.43761798103461));
#74987=CARTESIAN_POINT('Ctrl Pts',(-0.50480489709013,-1.47340083812973,
8.43104935897011));
#74988=CARTESIAN_POINT('Ctrl Pts',(-0.578490200517025,-1.44606025295714,
8.42585845251485));
#74989=CARTESIAN_POINT('Ctrl Pts',(-0.721950174682886,-1.38009909621693,
8.41545721930481));
#74990=CARTESIAN_POINT('Ctrl Pts',(-0.791445947801712,-1.34145369893032,
8.41026058939153));
#74991=CARTESIAN_POINT('Ctrl Pts',(-0.896073288467977,-1.27230116046381,
8.40182306061934));
#74992=CARTESIAN_POINT('Ctrl Pts',(-0.933312709124304,-1.24524066720399,
8.39868453778051));
#74993=CARTESIAN_POINT('Ctrl Pts',(-0.982507086806654,-1.20604536398207,
8.394308201103));
#74994=CARTESIAN_POINT('Ctrl Pts',(-0.99554580391714,-1.19530502748934,
8.39312489348467));
#74995=CARTESIAN_POINT('Ctrl Pts',(-1.01745473833548,-1.17665089351467,
8.39109448953057));
#74996=CARTESIAN_POINT('Ctrl Pts',(-1.02641406734323,-1.16884370977891,
8.39025179109059));
#74997=CARTESIAN_POINT('Ctrl Pts',(-1.04330753791432,-1.15377867791037,
8.38863842982717));
#74998=CARTESIAN_POINT('Ctrl Pts',(-1.05125762724929,-1.14653968386288,
8.38786858979521));
#74999=CARTESIAN_POINT('Ctrl Pts',(-1.06972690309027,-1.12936879927586,
8.38605465524481));
#75000=CARTESIAN_POINT('Ctrl Pts',(-1.08018367993076,-1.11937157515258,
8.38500779707664));
#75001=CARTESIAN_POINT('Ctrl Pts',(-1.11668697388585,-1.08348469641496,
8.38128103196783));
#75002=CARTESIAN_POINT('Ctrl Pts',(-1.14195263354852,-1.05682195936664,
8.37856768622705));
#75003=CARTESIAN_POINT('Ctrl Pts',(-1.23882244495793,-0.947062689311923,
8.36760541269428));
#75004=CARTESIAN_POINT('Ctrl Pts',(-1.30248697525743,-0.857397302255552,
8.35907056362665));
#75005=CARTESIAN_POINT('Ctrl Pts',(-1.37807930922783,-0.722825095911406,
8.34712365320878));
#75006=CARTESIAN_POINT('Ctrl Pts',(-1.39828401373771,-0.682920949841104,
8.3436812071962));
#75007=CARTESIAN_POINT('Ctrl Pts',(-1.42773563792439,-0.617948349643967,
8.33828390243078));
#75008=CARTESIAN_POINT('Ctrl Pts',(-1.43810489739571,-0.593416997797286,
8.33629149515575));
#75009=CARTESIAN_POINT('Ctrl Pts',(-1.45138026564541,-0.559615374337244,
8.33361839725681));
#75010=CARTESIAN_POINT('Ctrl Pts',(-1.45483645805979,-0.550567830455759,
8.33290983986568));
#75011=CARTESIAN_POINT('Ctrl Pts',(-1.46052733847477,-0.535242498883359,
8.33172200045825));
#75012=CARTESIAN_POINT('Ctrl Pts',(-1.46280656492827,-0.528981663066348,
8.33124019557813));
#75013=CARTESIAN_POINT('Ctrl Pts',(-1.46748258722143,-0.51587566298971,
8.33023906264301));
#75014=CARTESIAN_POINT('Ctrl Pts',(-1.46987184416224,-0.509028104259469,
8.32972016380384));
#75015=CARTESIAN_POINT('Ctrl Pts',(-1.47625160774832,-0.490324306391796,
8.3283134912406));
#75016=CARTESIAN_POINT('Ctrl Pts',(-1.48014722981443,-0.478435930045978,
8.32743101996545));
#75017=CARTESIAN_POINT('Ctrl Pts',(-1.50204015428969,-0.408796491783894,
8.32232209697308));
#75018=CARTESIAN_POINT('Ctrl Pts',(-1.51680205742121,-0.350075051712818,
8.31825427213832));
#75019=CARTESIAN_POINT('Ctrl Pts',(-1.54626123119472,-0.195184634162695,
8.30778995457972));
#75020=CARTESIAN_POINT('Ctrl Pts',(-1.55543208973097,-0.0982440506574577,
8.30148832580142));
#75021=CARTESIAN_POINT('Ctrl Pts',(-1.55549987478443,-0.000720777658553386,
8.29495185940666));
#75022=CARTESIAN_POINT('Ctrl Pts',(-1.5555,-0.000360387957164358,8.29492770190879));
#75023=CARTESIAN_POINT('Ctrl Pts',(-1.5555,1.39005191776138E-11,8.29490354205207));
#75024=CARTESIAN_POINT('Ctrl Pts',(-1.55549980343579,0.000781991825156257,
8.1559437743963));
#75025=CARTESIAN_POINT('Ctrl Pts',(-1.55552936418458,-0.0580188005300481,
8.16013588671271));
#75026=CARTESIAN_POINT('Ctrl Pts',(-1.55222041418191,-0.116815327805788,
8.16432799902912));
#75027=CARTESIAN_POINT('Ctrl Pts',(-1.54560073260284,-0.17521023194314,
8.16852011134553));
#75028=CARTESIAN_POINT('Ctrl Pts',(-1.53897825413943,-0.233629808535023,
8.17271399487301));
#75029=CARTESIAN_POINT('Ctrl Pts',(-1.52904232516819,-0.291646928848665,
8.17690787840049));
#75030=CARTESIAN_POINT('Ctrl Pts',(-1.51587230703867,-0.34887160783484,
8.18110176192796));
#75031=CARTESIAN_POINT('Ctrl Pts',(-1.50268199083999,-0.406184483395979,
8.18530210920796));
#75032=CARTESIAN_POINT('Ctrl Pts',(-1.48624775480599,-0.462701993433649,
8.18950245648796));
#75033=CARTESIAN_POINT('Ctrl Pts',(-1.46669934333799,-0.518047571417836,
8.19370280376796));
#75034=CARTESIAN_POINT('Ctrl Pts',(-1.44713327893872,-0.573443128485241,
8.19790694411533));
#75035=CARTESIAN_POINT('Ctrl Pts',(-1.42444763581157,-0.62766418693826,
8.2021110844627));
#75036=CARTESIAN_POINT('Ctrl Pts',(-1.39881978898772,-0.680355383557988,
8.20631522481007));
#75037=CARTESIAN_POINT('Ctrl Pts',(-1.37314037354939,-0.733152605940389,
8.21052782477149));
#75038=CARTESIAN_POINT('Ctrl Pts',(-1.34450718489918,-0.784413388617838,
8.2147404247329));
#75039=CARTESIAN_POINT('Ctrl Pts',(-1.31314231809916,-0.833809032343236,
8.21895302469431));
#75040=CARTESIAN_POINT('Ctrl Pts',(-1.30490869044903,-0.846775940207582,
8.22005887920798));
#75041=CARTESIAN_POINT('Ctrl Pts',(-1.29648703674868,-0.859614489536206,
8.22116473372164));
#75042=CARTESIAN_POINT('Ctrl Pts',(-1.28788183119252,-0.872319115280753,
8.2222705882353));
#75043=CARTESIAN_POINT('Ctrl Pts',(-1.25560500531684,-0.919972246899313,
8.22641848143185));
#75044=CARTESIAN_POINT('Ctrl Pts',(-1.2206119932366,-0.965931613939869,
8.2305663746284));
#75045=CARTESIAN_POINT('Ctrl Pts',(-1.183106798534,-1.00987056262801,8.23471426782495));
#75046=CARTESIAN_POINT('Ctrl Pts',(-1.14566829117055,-1.05373138423014,
8.23885478572423));
#75047=CARTESIAN_POINT('Ctrl Pts',(-1.10572680259751,-1.09557852511303,
8.2429953036235));
#75048=CARTESIAN_POINT('Ctrl Pts',(-1.06352887083094,-1.13511523243636,
8.24713582152278));
#75049=CARTESIAN_POINT('Ctrl Pts',(-1.02137291525576,-1.17461261080864,
8.25127222066162));
#75050=CARTESIAN_POINT('Ctrl Pts',(-0.976965341807128,-1.21180375487596,
8.25540861980046));
#75051=CARTESIAN_POINT('Ctrl Pts',(-0.930590928396772,-1.24642720364474,
8.2595450189393));
#75052=CARTESIAN_POINT('Ctrl Pts',(-0.884244814608526,-1.28102952372542,
8.263678893873));
#75053=CARTESIAN_POINT('Ctrl Pts',(-0.835934656580026,-1.31306694359385,
8.26781276880671));
#75054=CARTESIAN_POINT('Ctrl Pts',(-0.785978149076146,-1.342318367294,8.27194664374041));
#75055=CARTESIAN_POINT('Ctrl Pts',(-0.736032919694587,-1.37156318722717,
8.27607958541538));
#75056=CARTESIAN_POINT('Ctrl Pts',(-0.68444252795948,-1.39802299659105,
8.28021252709034));
#75057=CARTESIAN_POINT('Ctrl Pts',(-0.631551582474378,-1.42152131488561,
8.28434546876531));
#75058=CARTESIAN_POINT('Ctrl Pts',(-0.578612804049106,-1.44504088433465,
8.28848214814528));
#75059=CARTESIAN_POINT('Ctrl Pts',(-0.524371598063827,-1.4655933973829,
8.29261882752526));
#75060=CARTESIAN_POINT('Ctrl Pts',(-0.469193755053609,-1.48305005654519,
8.29675550690523));
#75061=CARTESIAN_POINT('Ctrl Pts',(-0.413993103902056,-1.50051393153774,
8.30089389621011));
#75062=CARTESIAN_POINT('Ctrl Pts',(-0.357855549260668,-1.51487927085603,
8.30503228551499));
#75063=CARTESIAN_POINT('Ctrl Pts',(-0.301160160392097,-1.52606775989555,
8.30917067481987));
#75064=CARTESIAN_POINT('Ctrl Pts',(-0.244354187118708,-1.53727807209257,
8.31331713605666));
#75065=CARTESIAN_POINT('Ctrl Pts',(-0.186988722836364,-1.54529907762868,
8.31746359729344));
#75066=CARTESIAN_POINT('Ctrl Pts',(-0.12945018795521,-1.550104157416,8.32161005853022));
#75067=CARTESIAN_POINT('Ctrl Pts',(-0.0749972835052497,-1.55465155423577,
8.3255341566672));
#75068=CARTESIAN_POINT('Ctrl Pts',(-0.020389782718023,-1.55631914526793,
8.32945825480419));
#75069=CARTESIAN_POINT('Ctrl Pts',(0.0340469216032327,-1.55512734434494,
8.33338235294118));
#75070=CARTESIAN_POINT('Ctrl Pts',(0.0915914686065827,-1.5538675023856,
8.33753048153391));
#75071=CARTESIAN_POINT('Ctrl Pts',(0.149186781034701,-1.54940671355827,
8.34167861012665));
#75072=CARTESIAN_POINT('Ctrl Pts',(0.206447744916351,-1.54173914091164,
8.34582673871939));
#75073=CARTESIAN_POINT('Ctrl Pts',(0.263606876129832,-1.5340852042454,8.3499674902969));
#75074=CARTESIAN_POINT('Ctrl Pts',(0.320432327088291,-1.52323587181396,
8.35410824187442));
#75075=CARTESIAN_POINT('Ctrl Pts',(0.376541027563167,-1.50923725920137,
8.35824899345193));
#75076=CARTESIAN_POINT('Ctrl Pts',(0.432593901171643,-1.49525257488635,
8.36238562507686));
#75077=CARTESIAN_POINT('Ctrl Pts',(0.487930934516398,-1.47812494411918,
8.3665222567018));
#75078=CARTESIAN_POINT('Ctrl Pts',(0.542177958469255,-1.45795175206524,
8.37065888832673));
#75079=CARTESIAN_POINT('Ctrl Pts',(0.596391859938059,-1.43779087748392,
8.37479299418149));
#75080=CARTESIAN_POINT('Ctrl Pts',(0.649516584182981,-1.41458830896911,
8.37892710003626));
#75081=CARTESIAN_POINT('Ctrl Pts',(0.701194011910412,-1.3884909822037,8.38306120589102));
#75082=CARTESIAN_POINT('Ctrl Pts',(0.752859749414292,-1.36239955905224,
8.38719437654789));
#75083=CARTESIAN_POINT('Ctrl Pts',(0.803078375730401,-1.33341491231873,
8.39132754720475));
#75084=CARTESIAN_POINT('Ctrl Pts',(0.851514647952251,-1.30173079180096,
8.39546071786162));
#75085=CARTESIAN_POINT('Ctrl Pts',(0.899994665244785,-1.27001805586694,
8.39959762137889));
#75086=CARTESIAN_POINT('Ctrl Pts',(0.946688674031446,-1.23560125879504,
8.40373452489616));
#75087=CARTESIAN_POINT('Ctrl Pts',(0.991289994255716,-1.19871781386968,
8.40787142841343));
#75088=CARTESIAN_POINT('Ctrl Pts',(1.03590972524781,-1.1618191440017,8.41201003958351));
#75089=CARTESIAN_POINT('Ctrl Pts',(1.07843466168232,-1.12245215003644,8.4161486507536));
#75090=CARTESIAN_POINT('Ctrl Pts',(1.11859332491079,-1.08089278999585,8.42028726192368));
#75091=CARTESIAN_POINT('Ctrl Pts',(1.15883024806078,-1.0392524404005,8.42443393828716));
#75092=CARTESIAN_POINT('Ctrl Pts',(1.19669134031385,-0.995411581656071,
8.42858061465065));
#75093=CARTESIAN_POINT('Ctrl Pts',(1.23194455931703,-0.949680395064139,
8.43272729101412));
#75094=CARTESIAN_POINT('Ctrl Pts',(1.26529002123253,-0.906423989437334,
8.43664956655843));
#75095=CARTESIAN_POINT('Ctrl Pts',(1.29630238303193,-0.861476900372323,
8.44057184210275));
#75096=CARTESIAN_POINT('Ctrl Pts',(1.3248224615,-0.815123116777518,8.44449411764705));
#75097=CARTESIAN_POINT('Ctrl Pts',(1.35498571239949,-0.766098679264947,
8.44864237346172));
#75098=CARTESIAN_POINT('Ctrl Pts',(1.3824873648381,-0.715294892279789,8.45279062927639));
#75099=CARTESIAN_POINT('Ctrl Pts',(1.40711358534507,-0.663032131904138,
8.45693888509106));
#75100=CARTESIAN_POINT('Ctrl Pts',(1.43169603846838,-0.610862256438854,
8.4610797683451));
#75101=CARTESIAN_POINT('Ctrl Pts',(1.45341298298267,-0.557239021481411,
8.46522065159914));
#75102=CARTESIAN_POINT('Ctrl Pts',(1.472095338036,-0.502509269300256,8.46936153485318));
#75103=CARTESIAN_POINT('Ctrl Pts',(1.4907591169349,-0.447833935757737,8.47349830076299));
#75104=CARTESIAN_POINT('Ctrl Pts',(1.50639411724182,-0.392054755200792,
8.4776350666728));
#75105=CARTESIAN_POINT('Ctrl Pts',(1.51887915688401,-0.335538905021935,
8.48177183258261));
#75106=CARTESIAN_POINT('Ctrl Pts',(1.53135658068223,-0.279057529374942,
8.48590607507522));
#75107=CARTESIAN_POINT('Ctrl Pts',(1.54068774061331,-0.22184088232573,8.49004031756784));
#75108=CARTESIAN_POINT('Ctrl Pts',(1.54680178710342,-0.164269538909861,
8.49417456006045));
#75109=CARTESIAN_POINT('Ctrl Pts',(1.55291445365554,-0.106711189324582,
8.49830786945608));
#75110=CARTESIAN_POINT('Ctrl Pts',(1.55581139330419,-0.0487988198840324,
8.50244117885172));
#75111=CARTESIAN_POINT('Ctrl Pts',(1.5554734934391,0.00908081540229456,
8.50657448824735));
#75112=CARTESIAN_POINT('Ctrl Pts',(1.55513528823633,0.0670127526726037,
8.51071153264029));
#75113=CARTESIAN_POINT('Ctrl Pts',(1.55155640385267,0.124911374668306,8.51484857703323));
#75114=CARTESIAN_POINT('Ctrl Pts',(1.54476990279131,0.182390233922014,8.51898562142618));
#75115=CARTESIAN_POINT('Ctrl Pts',(1.53798059816,0.23989283825449,8.52312437487261));
#75116=CARTESIAN_POINT('Ctrl Pts',(1.52798112394513,0.296974819867029,8.52726312831903));
#75117=CARTESIAN_POINT('Ctrl Pts',(1.51485601926137,0.353258391135437,8.53140188176546));
#75118=CARTESIAN_POINT('Ctrl Pts',(1.50170533621045,0.409651648527132,8.53554870086605));
#75119=CARTESIAN_POINT('Ctrl Pts',(1.48541699586244,0.465242884291628,8.53969551996664));
#75120=CARTESIAN_POINT('Ctrl Pts',(1.46612568125884,0.519668872218949,8.54384233906723));
#75121=CARTESIAN_POINT('Ctrl Pts',(1.4478840516408,0.571133416433058,8.54776352016247));
#75122=CARTESIAN_POINT('Ctrl Pts',(1.42695793352342,0.621555884348664,8.5516847012577));
#75123=CARTESIAN_POINT('Ctrl Pts',(1.40349938543629,0.670648734495166,8.55560588235294));
#75124=CARTESIAN_POINT('Ctrl Pts',(1.37868903446763,0.72257056860283,8.55975302218543));
#75125=CARTESIAN_POINT('Ctrl Pts',(1.35094134090304,0.773223041853965,8.56390016201792));
#75126=CARTESIAN_POINT('Ctrl Pts',(1.32040923384716,0.822252823145754,8.56804730185041));
#75127=CARTESIAN_POINT('Ctrl Pts',(1.28993142693501,0.871195406912454,8.57218706615888));
#75128=CARTESIAN_POINT('Ctrl Pts',(1.25667930846831,0.918520588068721,8.57632683046735));
#75129=CARTESIAN_POINT('Ctrl Pts',(1.22085232808823,0.963898253448755,8.58046659477582));
#75130=CARTESIAN_POINT('Ctrl Pts',(1.18506098987666,1.00923077524205,8.58460224067477));
#75131=CARTESIAN_POINT('Ctrl Pts',(1.14670018613223,1.05261921299141,8.58873788657372));
#75132=CARTESIAN_POINT('Ctrl Pts',(1.10601244355904,1.09376264550064,8.59287353247267));
#75133=CARTESIAN_POINT('Ctrl Pts',(1.06534951917612,1.13488098186367,8.59700665576308));
#75134=CARTESIAN_POINT('Ctrl Pts',(1.02236283510628,1.17375665769604,8.6011397790535));
#75135=CARTESIAN_POINT('Ctrl Pts',(0.977333486651823,1.210123756427,8.60527290234391));
#75136=CARTESIAN_POINT('Ctrl Pts',(0.932314274856989,1.24648266847718,8.60940509521748));
#75137=CARTESIAN_POINT('Ctrl Pts',(0.885253716711833,1.28033379728367,8.61353728809105));
#75138=CARTESIAN_POINT('Ctrl Pts',(0.836466171950625,1.31145133084772,8.61766948096463));
#75139=CARTESIAN_POINT('Ctrl Pts',(0.787634374263119,1.34259708968784,8.62180542195932));
#75140=CARTESIAN_POINT('Ctrl Pts',(0.737072899290895,1.37100401637494,8.62594136295401));
#75141=CARTESIAN_POINT('Ctrl Pts',(0.685124159759577,1.39649029202273,8.6300773039487));
#75142=CARTESIAN_POINT('Ctrl Pts',(0.633153887095882,1.42198713191814,8.63421495932118));
#75143=CARTESIAN_POINT('Ctrl Pts',(0.579795683979693,1.44456070275556,8.63835261469365));
#75144=CARTESIAN_POINT('Ctrl Pts',(0.525412614205191,1.46407712735158,8.64249027006613));
#75145=CARTESIAN_POINT('Ctrl Pts',(0.470923225762024,1.48363170647417,8.64663601453715));
#75146=CARTESIAN_POINT('Ctrl Pts',(0.415405467720194,1.50011704573008,8.65078175900817));
#75147=CARTESIAN_POINT('Ctrl Pts',(0.359237374320549,1.51344929181366,8.65492750347918));
#75148=CARTESIAN_POINT('Ctrl Pts',(0.305991619112582,1.52608788195216,8.65885755133906));
#75149=CARTESIAN_POINT('Ctrl Pts',(0.252161912898589,1.53589331464948,8.66278759919894));
#75150=CARTESIAN_POINT('Ctrl Pts',(0.198074609147642,1.54283722382208,8.66671764705882));
#75151=CARTESIAN_POINT('Ctrl Pts',(0.14097417660744,1.55016796855841,8.67086663244245));
#75152=CARTESIAN_POINT('Ctrl Pts',(0.0833465647416978,1.55433986640978,
8.67501561782608));
#75153=CARTESIAN_POINT('Ctrl Pts',(0.0255718487286833,1.55528978989531,
8.67916460320971));
#75154=CARTESIAN_POINT('Ctrl Pts',(-0.0321000232977279,1.55623802243496,
8.68330620304086));
#75155=CARTESIAN_POINT('Ctrl Pts',(-0.0899179635182985,1.55397565623342,
8.68744780287201));
#75156=CARTESIAN_POINT('Ctrl Pts',(-0.147496184456423,1.54849124168359,
8.69158940270316));
#75157=CARTESIAN_POINT('Ctrl Pts',(-0.205017048519614,1.54301229046477,
8.6957268768559));
#75158=CARTESIAN_POINT('Ctrl Pts',(-0.262298150846453,1.53431769938897,
8.69986435100862));
#75159=CARTESIAN_POINT('Ctrl Pts',(-0.318954870054094,1.52244804209168,
8.70400182516135));
#75160=CARTESIAN_POINT('Ctrl Pts',(-0.375576905737759,1.51058565103834,
8.70813676647798));
#75161=CARTESIAN_POINT('Ctrl Pts',(-0.431574807545122,1.49555215326039,
8.7122717077946));
#75162=CARTESIAN_POINT('Ctrl Pts',(-0.486572442200073,1.47743951094163,
8.71640664911123));
#75163=CARTESIAN_POINT('Ctrl Pts',(-0.541557526175869,1.45933100199995,
8.72054064681779));
#75164=CARTESIAN_POINT('Ctrl Pts',(-0.595542301973042,1.43814490626192,
8.72467464452435));
#75165=CARTESIAN_POINT('Ctrl Pts',(-0.648166279563418,1.41402288667366,
8.72880864223091));
#75166=CARTESIAN_POINT('Ctrl Pts',(-0.700837524233219,1.38987920058531,
8.73294635311171));
#75167=CARTESIAN_POINT('Ctrl Pts',(-0.752145053219385,1.36279453703939,
8.7370840639925));
#75168=CARTESIAN_POINT('Ctrl Pts',(-0.801750111840515,1.33295799189762,
8.7412217748733));
#75169=CARTESIAN_POINT('Ctrl Pts',(-0.851375529867434,1.30310920094167,
8.7453611839949));
#75170=CARTESIAN_POINT('Ctrl Pts',(-0.899296652382154,1.27050656899263,
8.74950059311651));
#75171=CARTESIAN_POINT('Ctrl Pts',(-0.945203782165776,1.23538255620658,
8.75364000223811));
#75172=CARTESIAN_POINT('Ctrl Pts',(-0.991200065311743,1.20019033127455,
8.75778745024699));
#75173=CARTESIAN_POINT('Ctrl Pts',(-1.03517414217713,1.16246727941071,8.76193489825587));
#75174=CARTESIAN_POINT('Ctrl Pts',(-1.07685020588591,1.12248558301809,8.76608234626475));
#75175=CARTESIAN_POINT('Ctrl Pts',(-1.11619741000755,1.08473806492036,8.76999803476473));
#75176=CARTESIAN_POINT('Ctrl Pts',(-1.15349632838697,1.04497788410429,8.77391372326472));
#75177=CARTESIAN_POINT('Ctrl Pts',(-1.1885481979314,1.00346072728036,8.7778294117647));
#75178=CARTESIAN_POINT('Ctrl Pts',(-1.22543402886394,0.959771336462947,
8.78194997440151));
#75179=CARTESIAN_POINT('Ctrl Pts',(-1.2599909742097,0.913946641923029,8.78607053703832));
#75180=CARTESIAN_POINT('Ctrl Pts',(-1.29196078906812,0.866266454106636,
8.79019109967512));
#75181=CARTESIAN_POINT('Ctrl Pts',(-1.32388304105718,0.818657202157527,
8.79430553197357));
#75182=CARTESIAN_POINT('Ctrl Pts',(-1.35322549524949,0.769198359162392,
8.79841996427202));
#75183=CARTESIAN_POINT('Ctrl Pts',(-1.37976971947166,0.718203154566374,
8.80253439657047));
#75184=CARTESIAN_POINT('Ctrl Pts',(-1.40628498923961,0.667263575567268,
8.80664434084393));
#75185=CARTESIAN_POINT('Ctrl Pts',(-1.43000783591687,0.614791422342897,
8.81075428511738));
#75186=CARTESIAN_POINT('Ctrl Pts',(-1.45076405764136,0.561127346558663,
8.81486422939084));
#75187=CARTESIAN_POINT('Ctrl Pts',(-1.47150928084373,0.5074917068517,8.81897199584438));
#75188=CARTESIAN_POINT('Ctrl Pts',(-1.48929079903155,0.452665885671134,
8.82307976229793));
#75189=CARTESIAN_POINT('Ctrl Pts',(-1.50398207295083,0.397011554293467,
8.82718752875147));
#75190=CARTESIAN_POINT('Ctrl Pts',(-1.51866896460598,0.341373824061626,
8.83129406989823));
#75191=CARTESIAN_POINT('Ctrl Pts',(-1.53026731166723,0.28490858579035,8.83540061104499));
#75192=CARTESIAN_POINT('Ctrl Pts',(-1.53870081597823,0.227991335159742,
8.83950715219175));
#75193=CARTESIAN_POINT('Ctrl Pts',(-1.54713806779638,0.171048792812259,
8.84361551811878));
#75194=CARTESIAN_POINT('Ctrl Pts',(-1.55240759882802,0.113654360677632,
8.84772388404581));
#75195=CARTESIAN_POINT('Ctrl Pts',(-1.55448476488467,0.0561904417268394,
8.85183224997284));
#75196=CARTESIAN_POINT('Ctrl Pts',(-1.55517768587606,0.0370210760608892,
8.85320275811399));
#75197=CARTESIAN_POINT('Ctrl Pts',(-1.55551578386882,0.0178439958671598,
8.85457326625514));
#75198=CARTESIAN_POINT('Ctrl Pts',(-1.55549943430708,-0.00132660105165622,
8.8559437743963));
#75199=CARTESIAN_POINT('Origin',(0.,0.,0.));
#75200=CARTESIAN_POINT('',(-1.95399958641728,0.00127133045005693,0.22586969212423));
#75201=CARTESIAN_POINT('',(0.861527884061909,1.75382031718868,3.93409125912768E-5));
#75202=CARTESIAN_POINT('Ctrl Pts',(-1.95399958641728,0.00127133045005693,
0.22586969212423));
#75203=CARTESIAN_POINT('Ctrl Pts',(-1.95395605948788,0.0681710118368687,
0.222037453599974));
#75204=CARTESIAN_POINT('Ctrl Pts',(-1.95047708133558,0.134965857971554,
0.218205215075717));
#75205=CARTESIAN_POINT('Ctrl Pts',(-1.9435932731074,0.201398085223423,0.21437297655146));
#75206=CARTESIAN_POINT('Ctrl Pts',(-1.93654157865274,0.269450499380606,
0.210447275216578));
#75207=CARTESIAN_POINT('Ctrl Pts',(-1.9258976952577,0.337264795747382,0.206521573881697));
#75208=CARTESIAN_POINT('Ctrl Pts',(-1.91168774656432,0.404432886442037,
0.202595872546815));
#75209=CARTESIAN_POINT('Ctrl Pts',(-1.89749924293132,0.471499609862856,
0.198676095716234));
#75210=CARTESIAN_POINT('Ctrl Pts',(-1.87975545668369,0.53792158785195,0.194756318885654));
#75211=CARTESIAN_POINT('Ctrl Pts',(-1.8585342111985,0.603296432779744,0.190836542055074));
#75212=CARTESIAN_POINT('Ctrl Pts',(-1.83733826493252,0.668593340126828,
0.186921438243962));
#75213=CARTESIAN_POINT('Ctrl Pts',(-1.81267324464788,0.732845130317064,
0.18300633443285));
#75214=CARTESIAN_POINT('Ctrl Pts',(-1.78466748745849,0.795661962901718,
0.179091230621739));
#75215=CARTESIAN_POINT('Ctrl Pts',(-1.75667960406991,0.858438704602695,
0.175178625503493));
#75216=CARTESIAN_POINT('Ctrl Pts',(-1.72535541282999,0.919781859271184,
0.171266020385248));
#75217=CARTESIAN_POINT('Ctrl Pts',(-1.69087178125732,0.979320488577508,
0.167353415267004));
#75218=CARTESIAN_POINT('Ctrl Pts',(-1.65639845085757,1.03884133212034,0.163441978947404));
#75219=CARTESIAN_POINT('Ctrl Pts',(-1.61876779934057,1.09655829689135,0.159530542627805));
#75220=CARTESIAN_POINT('Ctrl Pts',(-1.57820231359506,1.15212562568637,0.155619106308205));
#75221=CARTESIAN_POINT('Ctrl Pts',(-1.53763517478325,1.2076952188812,0.151707510595382));
#75222=CARTESIAN_POINT('Ctrl Pts',(-1.49413325513439,1.261114608027,0.147795914882558));
#75223=CARTESIAN_POINT('Ctrl Pts',(-1.44796092155806,1.31206904149161,0.143884319169735));
#75224=CARTESIAN_POINT('Ctrl Pts',(-1.40174135600645,1.36307559877922,0.139968722091207));
#75225=CARTESIAN_POINT('Ctrl Pts',(-1.35284625410977,1.41161180422852,0.13605312501268));
#75226=CARTESIAN_POINT('Ctrl Pts',(-1.30157795883662,1.45739864727216,0.132137527934152));
#75227=CARTESIAN_POINT('Ctrl Pts',(-1.2502800764303,1.5032119140815,0.128219671149278));
#75228=CARTESIAN_POINT('Ctrl Pts',(-1.19660665633888,1.54627235318547,0.124301814364404));
#75229=CARTESIAN_POINT('Ctrl Pts',(-1.14089218940229,1.58634202244058,0.12038395757953));
#75230=CARTESIAN_POINT('Ctrl Pts',(-1.08508447629676,1.62647875404688,0.116459543698166));
#75231=CARTESIAN_POINT('Ctrl Pts',(-1.02722931016663,1.66361446039735,0.112535129816801));
#75232=CARTESIAN_POINT('Ctrl Pts',(-0.967688370463982,1.69755565966738,
0.108610715935436));
#75233=CARTESIAN_POINT('Ctrl Pts',(-0.940634266753058,1.71297779995792,
0.106827547905484));
#75234=CARTESIAN_POINT('Ctrl Pts',(-0.913232427096051,1.72774104823343,
0.105044379875532));
#75235=CARTESIAN_POINT('Ctrl Pts',(-0.885518136927234,1.74183053974057,
0.103261211845581));
#75236=CARTESIAN_POINT('Ctrl Pts',(-0.82518277812167,1.77250404861606,0.0993791682412745));
#75237=CARTESIAN_POINT('Ctrl Pts',(-0.763123230766267,1.80010409723702,
0.0954971246369682));
#75238=CARTESIAN_POINT('Ctrl Pts',(-0.699688390744016,1.82443200910805,
0.0916150810326619));
#75239=CARTESIAN_POINT('Ctrl Pts',(-0.636359874122095,1.84871914486438,
0.0877395441378561));
#75240=CARTESIAN_POINT('Ctrl Pts',(-0.57166110601235,1.8697448547059,0.0838640072430504));
#75241=CARTESIAN_POINT('Ctrl Pts',(-0.505964393620445,1.88735689057165,
0.0799884703482445));
#75242=CARTESIAN_POINT('Ctrl Pts',(-0.440329165750188,1.90495244360956,
0.0761165605075702));
#75243=CARTESIAN_POINT('Ctrl Pts',(-0.37369832685301,1.91914052530666,0.0722446506668958));
#75244=CARTESIAN_POINT('Ctrl Pts',(-0.306461522312016,1.9298179539382,0.0683727408262214));
#75245=CARTESIAN_POINT('Ctrl Pts',(-0.239263532761241,1.94048921861993,
0.0645030661920477));
#75246=CARTESIAN_POINT('Ctrl Pts',(-0.171460765852021,1.94765377033001,
0.060633391557874));
#75247=CARTESIAN_POINT('Ctrl Pts',(-0.103453395172505,1.95125943816482,
0.0567637169237003));
#75248=CARTESIAN_POINT('Ctrl Pts',(-0.0354608995727464,1.95486431734104,
0.0528948886936478));
#75249=CARTESIAN_POINT('Ctrl Pts',(0.0327356099712528,1.95491183184047,
0.0490260604635953));
#75250=CARTESIAN_POINT('Ctrl Pts',(0.10073244876722,1.95140179711031,0.0451572322335428));
#75251=CARTESIAN_POINT('Ctrl Pts',(0.168784262098388,1.947888924564,0.0412852761075839));
#75252=CARTESIAN_POINT('Ctrl Pts',(0.236635579734008,1.94081278028754,0.037413319981625));
#75253=CARTESIAN_POINT('Ctrl Pts',(0.303885490047154,1.93022527414258,0.0335413638556661));
#75254=CARTESIAN_POINT('Ctrl Pts',(0.371160973233011,1.91963374192613,0.0296679353553845));
#75255=CARTESIAN_POINT('Ctrl Pts',(0.43783410146098,1.90552829078888,0.0257945068551029));
#75256=CARTESIAN_POINT('Ctrl Pts',(0.503514718071474,1.88801189844911,0.0219210783548213));
#75257=CARTESIAN_POINT('Ctrl Pts',(0.569310398453004,1.87046481970197,0.0180408641190658));
#75258=CARTESIAN_POINT('Ctrl Pts',(0.634109614849086,1.84949501672137,0.0141606498833103));
#75259=CARTESIAN_POINT('Ctrl Pts',(0.697538648848681,1.82525500502323,0.0102804356475549));
#75260=CARTESIAN_POINT('Ctrl Pts',(0.753341645510678,1.8039293563954,0.00686673740256698));
#75261=CARTESIAN_POINT('Ctrl Pts',(0.808084213811854,1.78007341261458,0.00345303915757911));
#75262=CARTESIAN_POINT('Ctrl Pts',(0.861527884061909,1.75382031718868,3.93409125912768E-5));
#75263=CARTESIAN_POINT('',(-0.861525859670558,1.75382131162753,0.));
#75264=CARTESIAN_POINT('Origin',(0.,0.,0.));
#75265=CARTESIAN_POINT('',(-1.95399890574831,0.00206792998054292,0.124130307921897));
#75266=CARTESIAN_POINT('Ctrl Pts',(-0.861525859670557,1.75382131162753,
1.42247325030098E-15));
#75267=CARTESIAN_POINT('Ctrl Pts',(-0.924646993599216,1.72281445316895,
0.00400966066964642));
#75268=CARTESIAN_POINT('Ctrl Pts',(-0.986139593028611,1.68837280142252,
0.00801932133929142));
#75269=CARTESIAN_POINT('Ctrl Pts',(-1.04562298138973,1.65069336364743,0.0120289820089364));
#75270=CARTESIAN_POINT('Ctrl Pts',(-1.10692437825747,1.61186231799848,0.0161611911312997));
#75271=CARTESIAN_POINT('Ctrl Pts',(-1.16609128060864,1.56959254287446,0.020293400253663));
#75272=CARTESIAN_POINT('Ctrl Pts',(-1.22273578558825,1.5241499921733,0.0244256093760263));
#75273=CARTESIAN_POINT('Ctrl Pts',(-1.27766076881784,1.48008691251414,0.0284323796148805));
#75274=CARTESIAN_POINT('Ctrl Pts',(-1.33021395511449,1.43304126902846,0.0324391498537348));
#75275=CARTESIAN_POINT('Ctrl Pts',(-1.38007385230466,1.38329756819889,0.036445920092589));
#75276=CARTESIAN_POINT('Ctrl Pts',(-1.42993485554633,1.33355276389543,0.0404527792143826));
#75277=CARTESIAN_POINT('Ctrl Pts',(-1.47710212591552,1.28111010739876,0.0444596383361762));
#75278=CARTESIAN_POINT('Ctrl Pts',(-1.52129104438919,1.2262909761803,0.0484664974579699));
#75279=CARTESIAN_POINT('Ctrl Pts',(-1.56549289190009,1.1714558056784,0.0524745289286812));
#75280=CARTESIAN_POINT('Ctrl Pts',(-1.6067143674834,1.11424313578918,0.0564825603993924));
#75281=CARTESIAN_POINT('Ctrl Pts',(-1.64471203692479,1.05500631068952,0.0604905918701037));
#75282=CARTESIAN_POINT('Ctrl Pts',(-1.68273110286472,0.995736129316689,
0.064500880264484));
#75283=CARTESIAN_POINT('Ctrl Pts',(-1.71752250663885,0.934439913118181,
0.0685111686588643));
#75284=CARTESIAN_POINT('Ctrl Pts',(-1.74888764786171,0.871497558893162,
0.0725214570532445));
#75285=CARTESIAN_POINT('Ctrl Pts',(-1.78030155646624,0.808457340169785,
0.0765379807539908));
#75286=CARTESIAN_POINT('Ctrl Pts',(-1.80827836601966,0.743766286772777,
0.080554504454737));
#75287=CARTESIAN_POINT('Ctrl Pts',(-1.83266692769222,0.677825886303518,
0.0845710281554833));
#75288=CARTESIAN_POINT('Ctrl Pts',(-1.85707761604864,0.611825660969874,
0.0885911958739181));
#75289=CARTESIAN_POINT('Ctrl Pts',(-1.8778934365429,0.544574268729266,0.0926113635923529));
#75290=CARTESIAN_POINT('Ctrl Pts',(-1.89501335528528,0.476487547886031,
0.0966315313107877));
#75291=CARTESIAN_POINT('Ctrl Pts',(-1.91216481068738,0.408275404265988,
0.100659104593659));
#75292=CARTESIAN_POINT('Ctrl Pts',(-1.92560668578103,0.339225309972099,
0.104686677876531));
#75293=CARTESIAN_POINT('Ctrl Pts',(-1.93528926100571,0.269761888034572,
0.108714251159402));
#75294=CARTESIAN_POINT('Ctrl Pts',(-1.9372828373484,0.2554598422003,0.109543501088153));
#75295=CARTESIAN_POINT('Ctrl Pts',(-1.93911722566992,0.241140282985028,
0.110372751016905));
#75296=CARTESIAN_POINT('Ctrl Pts',(-1.94079226597546,0.226806923020075,
0.111202000945656));
#75297=CARTESIAN_POINT('Ctrl Pts',(-1.94949709445539,0.152319497479718,
0.115511436589025));
#75298=CARTESIAN_POINT('Ctrl Pts',(-1.95391930711152,0.0772811093863,0.119820872232394));
#75299=CARTESIAN_POINT('Ctrl Pts',(-1.95399890574746,0.00206793078572539,
0.124130307875763));
#75300=CARTESIAN_POINT('',(-1.95389762804932,0.000928492481393378,0.824130263460899));
#75301=CARTESIAN_POINT('Ctrl Pts',(-1.95399890574831,0.00206792998054292,
0.124130307921897));
#75302=CARTESIAN_POINT('Ctrl Pts',(-1.95406955740588,-0.0646912266989078,
0.127955359524064));
#75303=CARTESIAN_POINT('Ctrl Pts',(-1.95071478923537,-0.13160956121342,
0.131780411126231));
#75304=CARTESIAN_POINT('Ctrl Pts',(-1.94391228274796,-0.19829532768475,
0.135605462728398));
#75305=CARTESIAN_POINT('Ctrl Pts',(-1.93712039116072,-0.264877035048702,
0.139424545568767));
#75306=CARTESIAN_POINT('Ctrl Pts',(-1.92689148442229,-0.331226385592703,
0.143243628409135));
#75307=CARTESIAN_POINT('Ctrl Pts',(-1.91325525346835,-0.39695130063495,
0.147062711249504));
#75308=CARTESIAN_POINT('Ctrl Pts',(-1.89963070614838,-0.462619902033525,
0.150878521868523));
#75309=CARTESIAN_POINT('Ctrl Pts',(-1.88260471932677,-0.527664624549438,
0.154694332487542));
#75310=CARTESIAN_POINT('Ctrl Pts',(-1.86225862356753,-0.591699939959745,
0.158510143106561));
#75311=CARTESIAN_POINT('Ctrl Pts',(-1.8419222977489,-0.655704506412813,
0.162324121421064));
#75312=CARTESIAN_POINT('Ctrl Pts',(-1.8182691777226,-0.71870013514503,0.166138099735568));
#75313=CARTESIAN_POINT('Ctrl Pts',(-1.79143085391333,-0.780314997707577,
0.169952078050072));
#75314=CARTESIAN_POINT('Ctrl Pts',(-1.76459531424852,-0.841923468489488,
0.173765660711453));
#75315=CARTESIAN_POINT('Ctrl Pts',(-1.73457543415262,-0.902150985105781,
0.177579243372835));
#75316=CARTESIAN_POINT('Ctrl Pts',(-1.70155067162945,-0.96064629904944,
0.181392826034217));
#75317=CARTESIAN_POINT('Ctrl Pts',(-1.66849454045527,-1.01919717490931,
0.185210031036364));
#75318=CARTESIAN_POINT('Ctrl Pts',(-1.63242808464034,-1.07601211415674,
0.189027236038511));
#75319=CARTESIAN_POINT('Ctrl Pts',(-1.59357574474819,-1.13076626486213,
0.192844441040659));
#75320=CARTESIAN_POINT('Ctrl Pts',(-1.55470355505822,-1.18554838965672,
0.196663596266339));
#75321=CARTESIAN_POINT('Ctrl Pts',(-1.5130429731434,-1.23826722921297,0.200482751492019));
#75322=CARTESIAN_POINT('Ctrl Pts',(-1.46885870121783,-1.28863110154018,
0.204301906717699));
#75323=CARTESIAN_POINT('Ctrl Pts',(-1.42459648896941,-1.33908381490286,
0.208127798869854));
#75324=CARTESIAN_POINT('Ctrl Pts',(-1.37780206632569,-1.38717290575991,
0.211953691022008));
#75325=CARTESIAN_POINT('Ctrl Pts',(-1.32877610474772,-1.43264443022387,
0.215779583174163));
#75326=CARTESIAN_POINT('Ctrl Pts',(-1.30048043891891,-1.45888862859442,
0.217987722746546));
#75327=CARTESIAN_POINT('Ctrl Pts',(-1.27144203572435,-1.48426164641819,
0.220195862318929));
#75328=CARTESIAN_POINT('Ctrl Pts',(-1.24172311025443,-1.50872121926486,
0.222404001891312));
#75329=CARTESIAN_POINT('Ctrl Pts',(-1.18891487557722,-1.55218399063252,
0.226327695325534));
#75330=CARTESIAN_POINT('Ctrl Pts',(-1.13371889692835,-1.59295568107147,
0.230251388759756));
#75331=CARTESIAN_POINT('Ctrl Pts',(-1.076440251592,-1.63076435598542,0.234175082193978));
#75332=CARTESIAN_POINT('Ctrl Pts',(-1.01924776964084,-1.66851615589123,
0.238092873276516));
#75333=CARTESIAN_POINT('Ctrl Pts',(-0.959979245251721,-1.70331351914499,
0.242010664359055));
#75334=CARTESIAN_POINT('Ctrl Pts',(-0.89897254650893,-1.73492488616172,
0.245928455441593));
#75335=CARTESIAN_POINT('Ctrl Pts',(-0.838037968455182,-1.76649888296144,
0.24984161500336));
#75336=CARTESIAN_POINT('Ctrl Pts',(-0.775369730677549,-1.79489414000529,
0.253754774565128));
#75337=CARTESIAN_POINT('Ctrl Pts',(-0.711332838444815,-1.8199235129395,
0.257667934126895));
#75338=CARTESIAN_POINT('Ctrl Pts',(-0.647336410006956,-1.84493707024967,
0.261578621031412));
#75339=CARTESIAN_POINT('Ctrl Pts',(-0.581973498435363,-1.86658878482378,
0.26548930793593));
#75340=CARTESIAN_POINT('Ctrl Pts',(-0.515630360478018,-1.8847390618739,
0.269399994840448));
#75341=CARTESIAN_POINT('Ctrl Pts',(-0.44930657342817,-1.90288404486734,
0.273309541079286));
#75342=CARTESIAN_POINT('Ctrl Pts',(-0.38200360027134,-1.91752948866426,
0.277219087318124));
#75343=CARTESIAN_POINT('Ctrl Pts',(-0.31412246064153,-1.92858577193769,
0.281128633556962));
#75344=CARTESIAN_POINT('Ctrl Pts',(-0.246238028086697,-1.93964259155322,
0.285038369448518));
#75345=CARTESIAN_POINT('Ctrl Pts',(-0.177775857649897,-1.94710982862172,
0.288948105340075));
#75346=CARTESIAN_POINT('Ctrl Pts',(-0.109144972932498,-1.9509493522087,
0.292857841231631));
#75347=CARTESIAN_POINT('Ctrl Pts',(-0.0404427080086257,-1.95479286912883,
0.296771643481305));
#75348=CARTESIAN_POINT('Ctrl Pts',(0.0284281309814633,-1.95500111492118,
0.300685445730979));
#75349=CARTESIAN_POINT('Ctrl Pts',(0.0970566172690447,-1.9515880746316,
0.304599247980653));
#75350=CARTESIAN_POINT('Ctrl Pts',(0.165725237059831,-1.94817303841773,
0.308515338997042));
#75351=CARTESIAN_POINT('Ctrl Pts',(0.234150734215375,-1.94113255080181,
0.312431430013431));
#75352=CARTESIAN_POINT('Ctrl Pts',(0.301928186540551,-1.93053240588505,
0.31634752102982));
#75353=CARTESIAN_POINT('Ctrl Pts',(0.369820574104487,-1.91991428551857,
0.320270252851382));
#75354=CARTESIAN_POINT('Ctrl Pts',(0.437062243846608,-1.90572456052515,
0.324192984672943));
#75355=CARTESIAN_POINT('Ctrl Pts',(0.503260179663232,-1.88807976303051,
0.328115716494505));
#75356=CARTESIAN_POINT('Ctrl Pts',(0.53414389705252,-1.8798478305315,0.329945811941993));
#75357=CARTESIAN_POINT('Ctrl Pts',(0.564800681929095,-1.87086458341792,
0.33177590738948));
#75358=CARTESIAN_POINT('Ctrl Pts',(0.595192097517251,-1.86114544489489,
0.333606002836968));
#75359=CARTESIAN_POINT('Ctrl Pts',(0.660365323478706,-1.84030312482348,
0.337530572384713));
#75360=CARTESIAN_POINT('Ctrl Pts',(0.724566803469462,-1.81599359574741,
0.341455141932458));
#75361=CARTESIAN_POINT('Ctrl Pts',(0.787402665257627,-1.78832688363878,
0.345379711480203));
#75362=CARTESIAN_POINT('Ctrl Pts',(0.850146299341622,-1.76070077950889,
0.349298520718008));
#75363=CARTESIAN_POINT('Ctrl Pts',(0.911527848716609,-1.7297274689731,0.353217329955813));
#75364=CARTESIAN_POINT('Ctrl Pts',(0.971169742846146,-1.69556637457227,
0.357136139193618));
#75365=CARTESIAN_POINT('Ctrl Pts',(1.03074429109471,-1.66144385387925,0.361050523426746));
#75366=CARTESIAN_POINT('Ctrl Pts',(1.088582662301,-1.62414094095966,0.364964907659874));
#75367=CARTESIAN_POINT('Ctrl Pts',(1.14433001772578,-1.58386388636515,0.368879291893001));
#75368=CARTESIAN_POINT('Ctrl Pts',(1.20004397769646,-1.5436109597408,0.372791331214195));
#75369=CARTESIAN_POINT('Ctrl Pts',(1.25366901067057,-1.5003877125148,0.376703370535389));
#75370=CARTESIAN_POINT('Ctrl Pts',(1.30487884291397,-1.45444395055826,0.380615409856583));
#75371=CARTESIAN_POINT('Ctrl Pts',(1.35607539351088,-1.40851210445415,0.384526434561618));
#75372=CARTESIAN_POINT('Ctrl Pts',(1.40485762252771,-1.35986147163389,0.388437459266652));
#75373=CARTESIAN_POINT('Ctrl Pts',(1.45093335970032,-1.30878125968732,0.392348483971687));
#75374=CARTESIAN_POINT('Ctrl Pts',(1.49701279774398,-1.25769694490293,0.396259822815984));
#75375=CARTESIAN_POINT('Ctrl Pts',(1.54038498602521,-1.20418302905568,0.40017116166028));
#75376=CARTESIAN_POINT('Ctrl Pts',(1.58079677904237,-1.14856325179298,0.404082500504577));
#75377=CARTESIAN_POINT('Ctrl Pts',(1.62125243037714,-1.09288311121367,0.407998084266718));
#75378=CARTESIAN_POINT('Ctrl Pts',(1.65874098605547,-1.03509294534008,0.41191366802886));
#75379=CARTESIAN_POINT('Ctrl Pts',(1.69305213268919,-0.975546244929774,
0.415829251791001));
#75380=CARTESIAN_POINT('Ctrl Pts',(1.72738425196474,-0.915963146679629,
0.419747228948405));
#75381=CARTESIAN_POINT('Ctrl Pts',(1.75853487473283,-0.854621813839973,
0.42366520610581));
#75382=CARTESIAN_POINT('Ctrl Pts',(1.78634054088466,-0.791898650075812,
0.427583183263214));
#75383=CARTESIAN_POINT('Ctrl Pts',(1.81419434865803,-0.729066889927195,
0.431507943850027));
#75384=CARTESIAN_POINT('Ctrl Pts',(1.83869146635988,-0.664848981323484,
0.435432704436839));
#75385=CARTESIAN_POINT('Ctrl Pts',(1.85971756427337,-0.599638708834834,
0.439357465023652));
#75386=CARTESIAN_POINT('Ctrl Pts',(1.86945094453038,-0.569451634589951,
0.441174311276643));
#75387=CARTESIAN_POINT('Ctrl Pts',(1.87844121977373,-0.539052075038428,
0.442991157529633));
#75388=CARTESIAN_POINT('Ctrl Pts',(1.88668076778593,-0.508479773901289,
0.444808003782624));
#75389=CARTESIAN_POINT('Ctrl Pts',(1.9044236565005,-0.442645951946244,0.448720366551869));
#75390=CARTESIAN_POINT('Ctrl Pts',(1.91875277173103,-0.375748034148455,
0.452632729321114));
#75391=CARTESIAN_POINT('Ctrl Pts',(1.9295452933751,-0.308173588767728,0.456545092090358));
#75392=CARTESIAN_POINT('Ctrl Pts',(1.94032129714163,-0.240702565594617,
0.460451467016235));
#75393=CARTESIAN_POINT('Ctrl Pts',(1.94757137127701,-0.172557552819724,
0.464357841942112));
#75394=CARTESIAN_POINT('Ctrl Pts',(1.95122293739034,-0.104139563095908,
0.46826421686799));
#75395=CARTESIAN_POINT('Ctrl Pts',(1.95487010940956,-0.0358039038233925,
0.47216589107682));
#75396=CARTESIAN_POINT('Ctrl Pts',(1.95492734649464,0.0328035896702445,
0.47606756528565));
#75397=CARTESIAN_POINT('Ctrl Pts',(1.95137369834605,0.101275314876119,0.479969239494481));
#75398=CARTESIAN_POINT('Ctrl Pts',(1.94782233509269,0.169703014699623,0.483868405037166));
#75399=CARTESIAN_POINT('Ctrl Pts',(1.94066471706783,0.237994627663291,0.487767570579851));
#75400=CARTESIAN_POINT('Ctrl Pts',(1.92993197530334,0.30574265437089,0.491666736122537));
#75401=CARTESIAN_POINT('Ctrl Pts',(1.91920242318858,0.373470547129496,0.495564742877225));
#75402=CARTESIAN_POINT('Ctrl Pts',(1.90489993343761,0.440654687062428,0.499462749631914));
#75403=CARTESIAN_POINT('Ctrl Pts',(1.88710726506204,0.506894634169728,0.503360756386602));
#75404=CARTESIAN_POINT('Ctrl Pts',(1.86931373221155,0.573137799612361,0.507258952529921));
#75405=CARTESIAN_POINT('Ctrl Pts',(1.84802981460086,0.63843620516231,0.51115714867324));
#75406=CARTESIAN_POINT('Ctrl Pts',(1.82338849546918,0.702403299102889,0.515055344816559));
#75407=CARTESIAN_POINT('Ctrl Pts',(1.79872096906624,0.766438425236626,0.518957686885801));
#75408=CARTESIAN_POINT('Ctrl Pts',(1.77068909265435,0.829138952520078,0.522860028955043));
#75409=CARTESIAN_POINT('Ctrl Pts',(1.73947412521829,0.890138061031027,0.526762371024285));
#75410=CARTESIAN_POINT('Ctrl Pts',(1.7082406204775,0.951173394441619,0.530667030536409));
#75411=CARTESIAN_POINT('Ctrl Pts',(1.67382051073079,1.01050487141279,0.534571690048533));
#75412=CARTESIAN_POINT('Ctrl Pts',(1.63643976155116,1.06779253922023,0.538476349560657));
#75413=CARTESIAN_POINT('Ctrl Pts',(1.59899385409424,1.12518006499805,0.542387815273642));
#75414=CARTESIAN_POINT('Ctrl Pts',(1.55857729832838,1.18051627299139,0.546299280986626));
#75415=CARTESIAN_POINT('Ctrl Pts',(1.51545734802895,1.23349301834468,0.550210746699611));
#75416=CARTESIAN_POINT('Ctrl Pts',(1.49414703144356,1.25967466297327,0.552143832709167));
#75417=CARTESIAN_POINT('Ctrl Pts',(1.47217701434554,1.28528057601971,0.554076918718724));
#75418=CARTESIAN_POINT('Ctrl Pts',(1.44958276974344,1.31027699119802,0.55601000472828));
#75419=CARTESIAN_POINT('Ctrl Pts',(1.40377828829966,1.36095130473934,0.559928878928912));
#75420=CARTESIAN_POINT('Ctrl Pts',(1.35522274662966,1.40932119078568,0.563847753129544));
#75421=CARTESIAN_POINT('Ctrl Pts',(1.30417707256363,1.45507325018343,0.567766627330176));
#75422=CARTESIAN_POINT('Ctrl Pts',(1.25320829705278,1.50075638567472,0.57167959788139));
#75423=CARTESIAN_POINT('Ctrl Pts',(1.19975719741317,1.54382919586173,0.575592568432604));
#75424=CARTESIAN_POINT('Ctrl Pts',(1.14412310761945,1.58401335682854,0.579505538983818));
#75425=CARTESIAN_POINT('Ctrl Pts',(1.08855453628523,1.62415019421492,0.583413901356782));
#75426=CARTESIAN_POINT('Ctrl Pts',(1.03080847727012,1.66140485211139,0.587322263729745));
#75427=CARTESIAN_POINT('Ctrl Pts',(0.9712176677035,1.69553892374683,0.591230626102709));
#75428=CARTESIAN_POINT('Ctrl Pts',(0.911664288785019,1.72965155482065,0.595136533524349));
#75429=CARTESIAN_POINT('Ctrl Pts',(0.850268883585566,1.76064724411937,0.59904244094599));
#75430=CARTESIAN_POINT('Ctrl Pts',(0.787392215127153,1.78833148480844,0.60294834836763));
#75431=CARTESIAN_POINT('Ctrl Pts',(0.72453349817706,1.81600782155016,0.606853140639068));
#75432=CARTESIAN_POINT('Ctrl Pts',(0.660194807281561,1.84037438850214,0.610757932910506));
#75433=CARTESIAN_POINT('Ctrl Pts',(0.594758853395274,1.86128394027025,0.614662725181944));
#75434=CARTESIAN_POINT('Ctrl Pts',(0.529319162480106,1.88219468617697,0.618567740454967));
#75435=CARTESIAN_POINT('Ctrl Pts',(0.462782553274368,1.89964787770071,0.622472755727991));
#75436=CARTESIAN_POINT('Ctrl Pts',(0.395547203749737,1.9135460301769,0.626377771001015));
#75437=CARTESIAN_POINT('Ctrl Pts',(0.328240393553435,1.92745895421772,0.630286936695153));
#75438=CARTESIAN_POINT('Ctrl Pts',(0.260233843326273,1.93780919873518,0.634196102389291));
#75439=CARTESIAN_POINT('Ctrl Pts',(0.191935248663222,1.94455055483795,0.638105268083429));
#75440=CARTESIAN_POINT('Ctrl Pts',(0.123595941658968,1.95129592941857,0.64201676400542));
#75441=CARTESIAN_POINT('Ctrl Pts',(0.0549647349864728,1.9544281116713,0.64592825992741));
#75442=CARTESIAN_POINT('Ctrl Pts',(-0.0135490597968924,1.95395302476252,
0.6498397558494));
#75443=CARTESIAN_POINT('Ctrl Pts',(-0.0821811566735969,1.95347711752587,
0.6537580057128));
#75444=CARTESIAN_POINT('Ctrl Pts',(-0.15069494646004,1.94938153877401,0.657676255576199));
#75445=CARTESIAN_POINT('Ctrl Pts',(-0.218685496651521,1.94172414455666,
0.661594505439598));
#75446=CARTESIAN_POINT('Ctrl Pts',(-0.251177633442923,1.93806473748206,
0.663467005517711));
#75447=CARTESIAN_POINT('Ctrl Pts',(-0.283550413865308,1.93359263600638,
0.665339505595823));
#75448=CARTESIAN_POINT('Ctrl Pts',(-0.315760658977315,1.92831823261676,
0.667212005673936));
#75449=CARTESIAN_POINT('Ctrl Pts',(-0.383166145740961,1.91728063490121,
0.671130534663431));
#75450=CARTESIAN_POINT('Ctrl Pts',(-0.450125490731316,1.90268265935469,
0.675049063652926));
#75451=CARTESIAN_POINT('Ctrl Pts',(-0.516233959946512,1.88457382413052,
0.678967592642421));
#75452=CARTESIAN_POINT('Ctrl Pts',(-0.582243056814569,1.86649220958597,
0.682880231411985));
#75453=CARTESIAN_POINT('Ctrl Pts',(-0.647403345824134,1.84491033813827,
0.686792870181548));
#75454=CARTESIAN_POINT('Ctrl Pts',(-0.711318768867144,1.81992901209287,
0.690705508951112));
#75455=CARTESIAN_POINT('Ctrl Pts',(-0.775159268726725,1.79497696975372,
0.694613561232184));
#75456=CARTESIAN_POINT('Ctrl Pts',(-0.837757344874346,1.76663356510626,
0.698521613513256));
#75457=CARTESIAN_POINT('Ctrl Pts',(-0.898732394159872,1.73504930295587,
0.702429665794328));
#75458=CARTESIAN_POINT('Ctrl Pts',(-0.959669353667418,1.70348477080239,
0.706335276800723));
#75459=CARTESIAN_POINT('Ctrl Pts',(-1.0189848618327,1.66868362279679,0.710240887807119));
#75460=CARTESIAN_POINT('Ctrl Pts',(-1.07632003494276,1.63084370262169,0.714146498813514));
#75461=CARTESIAN_POINT('Ctrl Pts',(-1.13363904553076,1.59301444934635,0.718051008846098));
#75462=CARTESIAN_POINT('Ctrl Pts',(-1.18897841904067,1.55214839518999,0.721955518878682));
#75463=CARTESIAN_POINT('Ctrl Pts',(-1.24200711024413,1.50848743385652,0.725860028911266));
#75464=CARTESIAN_POINT('Ctrl Pts',(-1.2950390296435,1.46482381460082,0.729764776636372));
#75465=CARTESIAN_POINT('Ctrl Pts',(-1.3457596094451,1.4183652649158,0.733669524361477));
#75466=CARTESIAN_POINT('Ctrl Pts',(-1.39387125524627,1.36939363361971,0.737574272086583));
#75467=CARTESIAN_POINT('Ctrl Pts',(-1.44203433832124,1.32036964561942,0.741483194467836));
#75468=CARTESIAN_POINT('Ctrl Pts',(-1.48758257552104,1.26882756542321,0.745392116849089));
#75469=CARTESIAN_POINT('Ctrl Pts',(-1.53025631837195,1.21508501763569,0.749301039230342));
#75470=CARTESIAN_POINT('Ctrl Pts',(-1.57295564752691,1.16131024691491,0.753212305321565));
#75471=CARTESIAN_POINT('Ctrl Pts',(-1.61277676715721,1.10533278360485,0.757123571412787));
#75472=CARTESIAN_POINT('Ctrl Pts',(-1.64950297744994,1.04749984600657,0.76103483750401));
#75473=CARTESIAN_POINT('Ctrl Pts',(-1.68629282591488,0.989566697076561,
0.764952880930088));
#75474=CARTESIAN_POINT('Ctrl Pts',(-1.71997682037156,0.92977208513841,0.768870924356166));
#75475=CARTESIAN_POINT('Ctrl Pts',(-1.75038428830772,0.868487675931825,
0.772788967782244));
#75476=CARTESIAN_POINT('Ctrl Pts',(-1.76493604024832,0.839159501600691,
0.774663980728026));
#75477=CARTESIAN_POINT('Ctrl Pts',(-1.77873812108614,0.809490427406177,
0.776538993673809));
#75478=CARTESIAN_POINT('Ctrl Pts',(-1.79177582235983,0.77952254772185,0.778414006619591));
#75479=CARTESIAN_POINT('Ctrl Pts',(-1.82180013066274,0.710510009396372,
0.782731943161803));
#75480=CARTESIAN_POINT('Ctrl Pts',(-1.84787001263996,0.639676840066979,
0.787049879704015));
#75481=CARTESIAN_POINT('Ctrl Pts',(-1.86978437594614,0.567470164385505,
0.791367816246227));
#75482=CARTESIAN_POINT('Ctrl Pts',(-1.89163136933685,0.49548546903576,0.795672478434275));
#75483=CARTESIAN_POINT('Ctrl Pts',(-1.9093481871965,0.422135977045125,0.799977140622323));
#75484=CARTESIAN_POINT('Ctrl Pts',(-1.92278189205019,0.347887619216186,
0.80428180281037));
#75485=CARTESIAN_POINT('Ctrl Pts',(-1.93614789390559,0.274013457225047,
0.808564770421985));
#75486=CARTESIAN_POINT('Ctrl Pts',(-1.94527371417388,0.19924976401323,0.812847738033601));
#75487=CARTESIAN_POINT('Ctrl Pts',(-1.95005683809791,0.124073881971984,
0.817130705645216));
#75488=CARTESIAN_POINT('Ctrl Pts',(-1.95266248815594,0.0831211396816443,
0.819463891024273));
#75489=CARTESIAN_POINT('Ctrl Pts',(-1.95398023955751,0.0420463704976374,
0.82179707640333));
#75490=CARTESIAN_POINT('Ctrl Pts',(-1.95399977936455,0.000928570563274659,
0.824130261782387));
#75491=CARTESIAN_POINT('',(-1.9539992614335,-0.00169891651796276,1.52413032658075));
#75492=CARTESIAN_POINT('Ctrl Pts',(-1.95119461725619,0.00092642636832007,
0.824130307875761));
#75493=CARTESIAN_POINT('Ctrl Pts',(-1.94958058750438,-0.38320769809472,
0.845958874438923));
#75494=CARTESIAN_POINT('Ctrl Pts',(-1.65406893488018,-1.42195455262908,
0.904854774650637));
#75495=CARTESIAN_POINT('Ctrl Pts',(0.0349978082279151,-2.30969445268954,
1.0008180085109));
#75496=CARTESIAN_POINT('Ctrl Pts',(1.96019660501107,-1.22214099283921,1.11202000945656));
#75497=CARTESIAN_POINT('Ctrl Pts',(2.08932028008313,0.985264718230409,1.22322201040221));
#75498=CARTESIAN_POINT('Ctrl Pts',(0.304039107037155,2.28987742561639,1.33442401134788));
#75499=CARTESIAN_POINT('Ctrl Pts',(-1.55753832107891,1.5741108521456,1.43472677717238));
#75500=CARTESIAN_POINT('Ctrl Pts',(-1.94902381498454,0.457824381443284,
1.49796220934835));
#75501=CARTESIAN_POINT('Ctrl Pts',(-1.95283689833027,-0.00169757742976787,
1.52413030787576));
#75502=CARTESIAN_POINT('',(-1.95399999997531,9.82336242309353E-6,2.22413030790917));
#75503=CARTESIAN_POINT('Ctrl Pts',(-1.9539992614335,-0.00169891651796276,
1.52413032658075));
#75504=CARTESIAN_POINT('Ctrl Pts',(-1.95392695442445,-0.0848624156019545,
1.52886340490957));
#75505=CARTESIAN_POINT('Ctrl Pts',(-1.94854160179058,-0.167792826350324,
1.53359648323839));
#75506=CARTESIAN_POINT('Ctrl Pts',(-1.93795475085125,-0.249894745149011,
1.53832956156721));
#75507=CARTESIAN_POINT('Ctrl Pts',(-1.92720840960645,-0.333233524670808,
1.54313394345104));
#75508=CARTESIAN_POINT('Ctrl Pts',(-1.91110273860045,-0.415718692889136,
1.54793832533488));
#75509=CARTESIAN_POINT('Ctrl Pts',(-1.88980307899214,-0.496749758562415,
1.55274270721872));
#75510=CARTESIAN_POINT('Ctrl Pts',(-1.88376583842472,-0.519717451281494,
1.55410447589221));
#75511=CARTESIAN_POINT('Ctrl Pts',(-1.87731160600884,-0.542568454780191,
1.55546624456569));
#75512=CARTESIAN_POINT('Ctrl Pts',(-1.8704448365791,-0.565289406688817,
1.55682801323918));
#75513=CARTESIAN_POINT('Ctrl Pts',(-1.85068959414275,-0.630656085726513,
1.56074573183483));
#75514=CARTESIAN_POINT('Ctrl Pts',(-1.82746439869295,-0.695115839472794,
1.56466345043049));
#75515=CARTESIAN_POINT('Ctrl Pts',(-1.80087105238586,-0.758273995781628,
1.56858116902614));
#75516=CARTESIAN_POINT('Ctrl Pts',(-1.77431781679637,-0.821336890706583,
1.57249297853076));
#75517=CARTESIAN_POINT('Ctrl Pts',(-1.74440670199538,-0.883101634631058,
1.57640478803539));
#75518=CARTESIAN_POINT('Ctrl Pts',(-1.71128922679017,-0.943188837016162,
1.58031659754001));
#75519=CARTESIAN_POINT('Ctrl Pts',(-1.67821078334524,-1.00320522152445,
1.58422379664453));
#75520=CARTESIAN_POINT('Ctrl Pts',(-1.64193372088679,-1.06154756222763,
1.58813099574906));
#75521=CARTESIAN_POINT('Ctrl Pts',(-1.60265682155651,-1.11785827022855,
1.59203819485359));
#75522=CARTESIAN_POINT('Ctrl Pts',(-1.56340460731049,-1.17413358759033,
1.59594293832794));
#75523=CARTESIAN_POINT('Ctrl Pts',(-1.52115657694202,-1.22837940247629,
1.5998476818023));
#75524=CARTESIAN_POINT('Ctrl Pts',(-1.47615561562483,-1.28026583116917,
1.60375242527665));
#75525=CARTESIAN_POINT('Ctrl Pts',(-1.43116749310002,-1.33213745664305,
1.60765605472612));
#75526=CARTESIAN_POINT('Ctrl Pts',(-1.383428320985,-1.38165066067867,1.61155968417558));
#75527=CARTESIAN_POINT('Ctrl Pts',(-1.33322102711829,-1.42850890541489,
1.61546331362505));
#75528=CARTESIAN_POINT('Ctrl Pts',(-1.28301082739003,-1.47536986217882,
1.61936716900597));
#75529=CARTESIAN_POINT('Ctrl Pts',(-1.23033258373456,-1.51957522074296,
1.62327102438689));
#75530=CARTESIAN_POINT('Ctrl Pts',(-1.17550447248529,-1.56086682172666,
1.62717487976781));
#75531=CARTESIAN_POINT('Ctrl Pts',(-1.12061789490383,-1.60220245429206,
1.63108289805167));
#75532=CARTESIAN_POINT('Ctrl Pts',(-1.06357726827144,-1.64061783182154,
1.63499091633552));
#75533=CARTESIAN_POINT('Ctrl Pts',(-1.00473128432354,-1.6758970870258,1.63889893461938));
#75534=CARTESIAN_POINT('Ctrl Pts',(-0.94585013040328,-1.71119742727864,
1.64280928857486));
#75535=CARTESIAN_POINT('Ctrl Pts',(-0.885161906579292,-1.74335768452249,
1.64671964253035));
#75536=CARTESIAN_POINT('Ctrl Pts',(-0.823039035615062,-1.77220843747394,
1.65062999648583));
#75537=CARTESIAN_POINT('Ctrl Pts',(-0.760808540287798,-1.80110917272436,
1.65454712490855));
#75538=CARTESIAN_POINT('Ctrl Pts',(-0.697138893503489,-1.82668877696017,
1.65846425333126));
#75539=CARTESIAN_POINT('Ctrl Pts',(-0.632420742890022,-1.84882665600711,
1.66238138175398));
#75540=CARTESIAN_POINT('Ctrl Pts',(-0.601312151342819,-1.8594678475502,
1.66426425923093));
#75541=CARTESIAN_POINT('Ctrl Pts',(-0.569961498234108,-1.86931457355083,
1.66614713670789));
#75542=CARTESIAN_POINT('Ctrl Pts',(-0.538413007585896,-1.87835764253305,
1.66803001418484));
#75543=CARTESIAN_POINT('Ctrl Pts',(-0.472769903991052,-1.89717360176971,
1.67194772684673));
#75544=CARTESIAN_POINT('Ctrl Pts',(-0.40600881106407,-1.91258176029287,
1.67586543950862));
#75545=CARTESIAN_POINT('Ctrl Pts',(-0.338516599480537,-1.9244538217053,
1.67978315217051));
#75546=CARTESIAN_POINT('Ctrl Pts',(-0.271126187234549,-1.93630797634066,
1.68369495569794));
#75547=CARTESIAN_POINT('Ctrl Pts',(-0.203007325537228,-1.94463653440483,
1.68760675922537));
#75548=CARTESIAN_POINT('Ctrl Pts',(-0.134560980986145,-1.94936126523435,
1.69151856275279));
#75549=CARTESIAN_POINT('Ctrl Pts',(-0.0661953069987432,-1.95408042751667,
1.69542575584561));
#75550=CARTESIAN_POINT('Ctrl Pts',(0.00249659480716174,-1.95520416429194,
1.69933294893843));
#75551=CARTESIAN_POINT('Ctrl Pts',(0.0711064711692457,-1.95270578166755,
1.70324014203125));
#75552=CARTESIAN_POINT('Ctrl Pts',(0.139673226624597,-1.95020896926205,
1.70714487947602));
#75553=CARTESIAN_POINT('Ctrl Pts',(0.20815756833239,-1.94409457108146,1.71104961692079));
#75554=CARTESIAN_POINT('Ctrl Pts',(0.276150630565734,-1.93438797278058,
1.71495435436556));
#75555=CARTESIAN_POINT('Ctrl Pts',(0.344124294171014,-1.9246841438018,1.71885797777683));
#75556=CARTESIAN_POINT('Ctrl Pts',(0.411606469711573,-1.91139021870064,
1.7227616011881));
#75557=CARTESIAN_POINT('Ctrl Pts',(0.478194619982706,-1.89458330653988,
1.72666522459936));
#75558=CARTESIAN_POINT('Ctrl Pts',(0.544786624211529,-1.87777542163656,
1.73056907394271));
#75559=CARTESIAN_POINT('Ctrl Pts',(0.610484024023804,-1.85745426888696,
1.73447292328606));
#75560=CARTESIAN_POINT('Ctrl Pts',(0.674897438294774,-1.83374737839844,
1.73837677262941));
#75561=CARTESIAN_POINT('Ctrl Pts',(0.739379541061065,-1.81001520760682,
1.74228478491833));
#75562=CARTESIAN_POINT('Ctrl Pts',(0.802574463128006,-1.78289026391186,
1.74619279720724));
#75563=CARTESIAN_POINT('Ctrl Pts',(0.864111833408501,-1.75254864108344,
1.75010080949616));
#75564=CARTESIAN_POINT('Ctrl Pts',(0.92568598249944,-1.72218888409053,1.7540111574722));
#75565=CARTESIAN_POINT('Ctrl Pts',(0.985600178950291,-1.68860886242822,
1.75792150544823));
#75566=CARTESIAN_POINT('Ctrl Pts',(1.04351022916227,-1.65202978230833,1.76183185342427));
#75567=CARTESIAN_POINT('Ctrl Pts',(1.10152060670916,-1.61538733008622,1.7657489759548));
#75568=CARTESIAN_POINT('Ctrl Pts',(1.15751950676532,-1.57573573348381,1.76966609848533));
#75569=CARTESIAN_POINT('Ctrl Pts',(1.21119389803979,-1.53333797362198,1.77358322101587));
#75570=CARTESIAN_POINT('Ctrl Pts',(1.23699477467599,-1.51295768898583,1.77546615238741));
#75571=CARTESIAN_POINT('Ctrl Pts',(1.2622590616211,-1.49194343294059,1.77734908375895));
#75572=CARTESIAN_POINT('Ctrl Pts',(1.28695506774092,-1.47032739674399,1.77923201513049));
#75573=CARTESIAN_POINT('Ctrl Pts',(1.33833866502721,-1.42535212043969,1.7831497250162));
#75574=CARTESIAN_POINT('Ctrl Pts',(1.3874639142744,-1.37759065900973,1.7870674349019));
#75575=CARTESIAN_POINT('Ctrl Pts',(1.43401335636865,-1.32729864527781,1.79098514478761));
#75576=CARTESIAN_POINT('Ctrl Pts',(1.48049258647854,-1.27708248856851,1.79489694546854));
#75577=CARTESIAN_POINT('Ctrl Pts',(1.52440338854723,-1.2243437128594,1.79880874614948));
#75578=CARTESIAN_POINT('Ctrl Pts',(1.56546274401249,-1.16937692687554,1.80272054683041));
#75579=CARTESIAN_POINT('Ctrl Pts',(1.60647370611654,-1.11447492582312,1.80662773698638));
#75580=CARTESIAN_POINT('Ctrl Pts',(1.64463960306984,-1.05735052198329,1.81053492714236));
#75581=CARTESIAN_POINT('Ctrl Pts',(1.6797167829136,-0.998332374111145,1.81444211729833));
#75582=CARTESIAN_POINT('Ctrl Pts',(1.71477191644938,-0.939351319650439,
1.81834685175182));
#75583=CARTESIAN_POINT('Ctrl Pts',(1.74674193291708,-0.878479304161515,
1.82225158620531));
#75584=CARTESIAN_POINT('Ctrl Pts',(1.77542661964497,-0.81607372109144,1.82615632065881));
#75585=CARTESIAN_POINT('Ctrl Pts',(1.80410312217094,-0.753685943336723,
1.83005994102883));
#75586=CARTESIAN_POINT('Ctrl Pts',(1.82949595035479,-0.689765913428525,
1.83396356139886));
#75587=CARTESIAN_POINT('Ctrl Pts',(1.85145179255203,-0.624693732845057,
1.83786718176888));
#75588=CARTESIAN_POINT('Ctrl Pts',(1.87340890524395,-0.559617786800943,
1.84177102802544));
#75589=CARTESIAN_POINT('Ctrl Pts',(1.89192848221934,-0.493390024716284,
1.84567487428199));
#75590=CARTESIAN_POINT('Ctrl Pts',(1.90690671786495,-0.426406812048687,
1.84957872053854));
#75591=CARTESIAN_POINT('Ctrl Pts',(1.92190092567108,-0.359352171300337,
1.85348672969255));
#75592=CARTESIAN_POINT('Ctrl Pts',(1.93334614807582,-0.291540953333802,
1.85739473884656));
#75593=CARTESIAN_POINT('Ctrl Pts',(1.94118969646704,-0.223379861066723,
1.86130274800057));
#75594=CARTESIAN_POINT('Ctrl Pts',(1.94903793262193,-0.155178031740894,
1.86521309280962));
#75595=CARTESIAN_POINT('Ctrl Pts',(1.95328018036679,-0.0866264030986778,
1.86912343761867));
#75596=CARTESIAN_POINT('Ctrl Pts',(1.95391585121788,-0.0181341214158713,
1.87303378242772));
#75597=CARTESIAN_POINT('Ctrl Pts',(1.95455262334687,0.0504768207916181,
1.87695090177479));
#75598=CARTESIAN_POINT('Ctrl Pts',(1.95157036920284,0.119027719528215,1.88086802112186));
#75599=CARTESIAN_POINT('Ctrl Pts',(1.94502049642343,0.187112983228721,1.88478514046894));
#75600=CARTESIAN_POINT('Ctrl Pts',(1.94187197380637,0.219841556724618,1.88666809900467));
#75601=CARTESIAN_POINT('Ctrl Pts',(1.93789983737931,0.25246266519304,1.88855105754041));
#75602=CARTESIAN_POINT('Ctrl Pts',(1.93311397113303,0.284932228100443,1.89043401607615));
#75603=CARTESIAN_POINT('Ctrl Pts',(1.92315642265863,0.352488910622552,1.89435172917762));
#75604=CARTESIAN_POINT('Ctrl Pts',(1.90963345760212,0.419657244532697,1.89826944227908));
#75605=CARTESIAN_POINT('Ctrl Pts',(1.8925879093297,0.486031897573641,1.90218715538055));
#75606=CARTESIAN_POINT('Ctrl Pts',(1.87556807114542,0.552306436605199,1.90609895932922));
#75607=CARTESIAN_POINT('Ctrl Pts',(1.85503631580055,0.61778919792082,1.91001076327789));
#75608=CARTESIAN_POINT('Ctrl Pts',(1.83108689664052,0.682082676038163,1.91392256722657));
#75609=CARTESIAN_POINT('Ctrl Pts',(1.80716570433876,0.746300377666639,1.91782976071121));
#75610=CARTESIAN_POINT('Ctrl Pts',(1.77983501889488,0.809331120999531,1.92173695419585));
#75611=CARTESIAN_POINT('Ctrl Pts',(1.74923904282111,0.870792036636921,1.9256441476805));
#75612=CARTESIAN_POINT('Ctrl Pts',(1.71866229628285,0.932214324160061,1.92954888549856));
#75613=CARTESIAN_POINT('Ctrl Pts',(1.68482454880486,0.992068301683998,1.93345362331663));
#75614=CARTESIAN_POINT('Ctrl Pts',(1.64791769151329,1.04999203901625,1.93735836113469));
#75615=CARTESIAN_POINT('Ctrl Pts',(1.61102136404073,1.10789925024699,1.9412619849001));
#75616=CARTESIAN_POINT('Ctrl Pts',(1.57105792927715,1.1638768997892,1.94516560866551));
#75617=CARTESIAN_POINT('Ctrl Pts',(1.52826377752397,1.21759017173602,1.94906923243091));
#75618=CARTESIAN_POINT('Ctrl Pts',(1.48546714916836,1.27130655220153,1.95297308210859));
#75619=CARTESIAN_POINT('Ctrl Pts',(1.43983978715841,1.32275791168654,1.95687693178628));
#75620=CARTESIAN_POINT('Ctrl Pts',(1.39165857650034,1.37164222975711,1.96078078146396));
#75621=CARTESIAN_POINT('Ctrl Pts',(1.34342598727786,1.42057867615841,1.96468879405472));
#75622=CARTESIAN_POINT('Ctrl Pts',(1.29263446046224,1.46694226699872,1.96859680664548));
#75623=CARTESIAN_POINT('Ctrl Pts',(1.23959726763818,1.51046834262224,1.97250481923624));
#75624=CARTESIAN_POINT('Ctrl Pts',(1.18652837652109,1.55402043210934,1.97641516749602));
#75625=CARTESIAN_POINT('Ctrl Pts',(1.13121154459855,1.59473133961202,1.98032551575581));
#75626=CARTESIAN_POINT('Ctrl Pts',(1.07399032801683,1.6323788700318,1.98423586401559));
#75627=CARTESIAN_POINT('Ctrl Pts',(1.01666997794584,1.67009162330555,1.98815298679872));
#75628=CARTESIAN_POINT('Ctrl Pts',(0.957439082795922,1.70473015878866,1.99207010958184));
#75629=CARTESIAN_POINT('Ctrl Pts',(0.896666385734625,1.73611790863801,1.99598723236496));
#75630=CARTESIAN_POINT('Ctrl Pts',(0.867453457630535,1.75120573794355,1.99787016058391));
#75631=CARTESIAN_POINT('Ctrl Pts',(0.837884578362065,1.76554313899271,1.99975308880286));
#75632=CARTESIAN_POINT('Ctrl Pts',(0.808002149859811,1.77911453420569,2.0016360170218));
#75633=CARTESIAN_POINT('Ctrl Pts',(0.745827315652347,1.80735183919136,2.00555372905879));
#75634=CARTESIAN_POINT('Ctrl Pts',(0.682046917070363,1.83238209596217,2.00947144109577));
#75635=CARTESIAN_POINT('Ctrl Pts',(0.617024832475356,1.85402167088434,2.01338915313276));
#75636=CARTESIAN_POINT('Ctrl Pts',(0.552100821983804,1.87562860640526,2.01730095600676));
#75637=CARTESIAN_POINT('Ctrl Pts',(0.4859393054637,1.89385485581639,2.02121275888075));
#75638=CARTESIAN_POINT('Ctrl Pts',(0.418925445613308,1.90856424335617,2.02512456175475));
#75639=CARTESIAN_POINT('Ctrl Pts',(0.351990568690836,1.92325629432559,2.02903175415496));
#75640=CARTESIAN_POINT('Ctrl Pts',(0.284205821803741,1.93443961040337,2.03293894655517));
#75641=CARTESIAN_POINT('Ctrl Pts',(0.215971132001531,1.94202792723019,2.03684613895537));
#75642=CARTESIAN_POINT('Ctrl Pts',(0.147779327729397,1.94961147479682,2.04075087568358));
#75643=CARTESIAN_POINT('Ctrl Pts',(0.0791386293835333,1.95360445084957,
2.04465561241179));
#75644=CARTESIAN_POINT('Ctrl Pts',(0.010457205880532,1.95397201792789,2.04856034914));
#75645=CARTESIAN_POINT('Ctrl Pts',(-0.0582046221962698,1.95433948013602,
2.05246397181179));
#75646=CARTESIAN_POINT('Ctrl Pts',(-0.126906660601441,1.95108358408695,
2.05636759448358));
#75647=CARTESIAN_POINT('Ctrl Pts',(-0.195239416744181,1.94422158463211,
2.06027121715538));
#75648=CARTESIAN_POINT('Ctrl Pts',(-0.263576127435452,1.93735918806011,
2.06417506573735));
#75649=CARTESIAN_POINT('Ctrl Pts',(-0.331543024149646,1.92689032545489,
2.06807891431933));
#75650=CARTESIAN_POINT('Ctrl Pts',(-0.39873623534906,1.91288405676341,2.0719827629013));
#75651=CARTESIAN_POINT('Ctrl Pts',(-0.466001098864394,1.89886285231323,
2.07589077440073));
#75652=CARTESIAN_POINT('Ctrl Pts',(-0.532490147758416,1.88129681421564,
2.07979878590016));
#75653=CARTESIAN_POINT('Ctrl Pts',(-0.597811194576149,1.86030582852375,
2.0837067973996));
#75654=CARTESIAN_POINT('Ctrl Pts',(-0.663171281300395,1.83930229731769,
2.08761714456894));
#75655=CARTESIAN_POINT('Ctrl Pts',(-0.727361516769884,1.81486991974442,
2.09152749173828));
#75656=CARTESIAN_POINT('Ctrl Pts',(-0.790008993625948,1.78717704494829,
2.09543783890762));
#75657=CARTESIAN_POINT('Ctrl Pts',(-0.852765004988979,1.75943619323972,
2.0993549606132));
#75658=CARTESIAN_POINT('Ctrl Pts',(-0.913972484550015,1.72842379249747,
2.10327208231878));
#75659=CARTESIAN_POINT('Ctrl Pts',(-0.973283225352221,1.69435408437787,
2.10718920402436));
#75660=CARTESIAN_POINT('Ctrl Pts',(-1.00179355894251,1.67797697071051,2.10907214200539));
#75661=CARTESIAN_POINT('Ctrl Pts',(-1.0298660529186,1.66089405636913,2.11095507998643));
#75662=CARTESIAN_POINT('Ctrl Pts',(-1.05746463830973,1.64313253839259,2.11283801796746));
#75663=CARTESIAN_POINT('Ctrl Pts',(-1.11489578162405,1.60617179312489,2.1167563086881));
#75664=CARTESIAN_POINT('Ctrl Pts',(-1.17050077078353,1.56612305683658,2.12067459940874));
#75665=CARTESIAN_POINT('Ctrl Pts',(-1.22392803543809,1.52319275341916,2.12459289012938));
#75666=CARTESIAN_POINT('Ctrl Pts',(-1.27727472049635,1.48032719796406,2.12850527124026));
#75667=CARTESIAN_POINT('Ctrl Pts',(-1.32844981924711,1.43458900625428,2.13241765235114));
#75668=CARTESIAN_POINT('Ctrl Pts',(-1.37713012110195,1.38622820255314,2.13633003346202));
#75669=CARTESIAN_POINT('Ctrl Pts',(-1.42575303011744,1.33792441501117,2.14023780197495));
#75670=CARTESIAN_POINT('Ctrl Pts',(-1.47188663644957,1.2870045012155,2.14414557048788));
#75671=CARTESIAN_POINT('Ctrl Pts',(-1.51524168221546,1.23375793593268,2.14805333900081));
#75672=CARTESIAN_POINT('Ctrl Pts',(-1.55856945797604,1.18054486234828,2.15195864955605));
#75673=CARTESIAN_POINT('Ctrl Pts',(-1.59912183018387,1.12500842081584,2.15586396011129));
#75674=CARTESIAN_POINT('Ctrl Pts',(-1.63664829953451,1.06747287723427,2.15976927066653));
#75675=CARTESIAN_POINT('Ctrl Pts',(-1.67416403321688,1.00995379356806,2.16367346398054));
#75676=CARTESIAN_POINT('Ctrl Pts',(-1.70865531393348,0.950437154933405,
2.16757765729456));
#75677=CARTESIAN_POINT('Ctrl Pts',(-1.73991470740603,0.889276566064914,
2.17148185060857));
#75678=CARTESIAN_POINT('Ctrl Pts',(-1.77117587693582,0.828112502250339,
2.17538626574618));
#75679=CARTESIAN_POINT('Ctrl Pts',(-1.79920457307696,0.765304741865069,
2.17929068088378));
#75680=CARTESIAN_POINT('Ctrl Pts',(-1.82383994727051,0.701230238039046,
2.18319509602138));
#75681=CARTESIAN_POINT('Ctrl Pts',(-1.84850158070921,0.637087436159569,
2.18710367293844));
#75682=CARTESIAN_POINT('Ctrl Pts',(-1.86976249674088,0.571675656065409,
2.1910122498555));
#75683=CARTESIAN_POINT('Ctrl Pts',(-1.88751089425965,0.505389576516129,
2.19492082677256));
#75684=CARTESIAN_POINT('Ctrl Pts',(-1.9052698733566,0.439063977267521,2.19883173397957));
#75685=CARTESIAN_POINT('Ctrl Pts',(-1.91951206409704,0.371863522385234,
2.20274264118657));
#75686=CARTESIAN_POINT('Ctrl Pts',(-1.93017684355697,0.304192952903994,
2.20665354839357));
#75687=CARTESIAN_POINT('Ctrl Pts',(-1.94086012054759,0.236405012178415,
2.21057123887503));
#75688=CARTESIAN_POINT('Ctrl Pts',(-1.94795355107944,0.168145818399277,
2.21448892935649));
#75689=CARTESIAN_POINT('Ctrl Pts',(-1.95144846778218,0.0998242334835162,
2.21840661983795));
#75690=CARTESIAN_POINT('Ctrl Pts',(-1.9531504750421,0.0665519573676903,
2.22031451585055));
#75691=CARTESIAN_POINT('Ctrl Pts',(-1.953999832782,0.0332648680386802,2.22222241186316));
#75692=CARTESIAN_POINT('Ctrl Pts',(-1.9539999999753,9.82394477163224E-6,
2.22413030787576));
#75693=CARTESIAN_POINT('',(-1.95399926641343,0.00169317918818195,2.92413028879048));
#75694=CARTESIAN_POINT('Ctrl Pts',(-1.95399999997531,9.82336241918865E-6,
2.22413030790917));
#75695=CARTESIAN_POINT('Ctrl Pts',(-1.95400034322258,-0.0682667145672286,
2.22804744403147));
#75696=CARTESIAN_POINT('Ctrl Pts',(-1.95041780549391,-0.136679161354171,
2.23196458015376));
#75697=CARTESIAN_POINT('Ctrl Pts',(-1.9432356042465,-0.204820375911999,
2.23588171627606));
#75698=CARTESIAN_POINT('Ctrl Pts',(-1.93606423675079,-0.272858805129577,
2.23979294372515));
#75699=CARTESIAN_POINT('Ctrl Pts',(-1.92530403292758,-0.340626328588442,
2.24370417117423));
#75700=CARTESIAN_POINT('Ctrl Pts',(-1.91099022196807,-0.407716042782765,
2.24761539862331));
#75701=CARTESIAN_POINT('Ctrl Pts',(-1.89669327592396,-0.474726710079095,
2.25152201775947));
#75702=CARTESIAN_POINT('Ctrl Pts',(-1.87885114017296,-0.541060675100519,
2.25542863689563));
#75703=CARTESIAN_POINT('Ctrl Pts',(-1.85755059422337,-0.606318224944963,
2.25933525603178));
#75704=CARTESIAN_POINT('Ctrl Pts',(-1.83626342508014,-0.671534792853558,
2.26323942179948));
#75705=CARTESIAN_POINT('Ctrl Pts',(-1.81152230636717,-0.735675819692555,
2.26714358756717));
#75706=CARTESIAN_POINT('Ctrl Pts',(-1.78346425066129,-0.798355351089442,
2.27104775333486));
#75707=CARTESIAN_POINT('Ctrl Pts',(-1.75541417838837,-0.861017048113155,
2.27495080823992));
#75708=CARTESIAN_POINT('Ctrl Pts',(-1.72404924363516,-0.92221762619541,
2.27885386314499));
#75709=CARTESIAN_POINT('Ctrl Pts',(-1.68955443659765,-0.981591465821289,
2.28275691805005));
#75710=CARTESIAN_POINT('Ctrl Pts',(-1.65505759687093,-1.04096880419303,
2.28666020295198));
#75711=CARTESIAN_POINT('Ctrl Pts',(-1.61743076815678,-1.09851876612914,
2.29056348785391));
#75712=CARTESIAN_POINT('Ctrl Pts',(-1.57690378390483,-1.15390227329121,
2.29446677275583));
#75713=CARTESIAN_POINT('Ctrl Pts',(-1.53633356553099,-1.20934486349002,
2.29837422167585));
#75714=CARTESIAN_POINT('Ctrl Pts',(-1.49285730840736,-1.26261598859572,
2.30228167059586));
#75715=CARTESIAN_POINT('Ctrl Pts',(-1.44674628823888,-1.31340822955661,
2.30618911951587));
#75716=CARTESIAN_POINT('Ctrl Pts',(-1.40060764199253,-1.36423090121278,
2.31009890947036));
#75717=CARTESIAN_POINT('Ctrl Pts',(-1.35183144081067,-1.41257138658037,
2.31400869942485));
#75718=CARTESIAN_POINT('Ctrl Pts',(-1.30072510863043,-1.45815986495938,
2.31791848937934));
#75719=CARTESIAN_POINT('Ctrl Pts',(-1.24953033896871,-1.50382723239265,
2.32183504507033));
#75720=CARTESIAN_POINT('Ctrl Pts',(-1.19599777456993,-1.54673278059923,
2.32575160076131));
#75721=CARTESIAN_POINT('Ctrl Pts',(-1.14046639934664,-1.58664816262501,
2.3296681564523));
#75722=CARTESIAN_POINT('Ctrl Pts',(-1.11412315929172,-1.6055834129472,2.33152611092112));
#75723=CARTESIAN_POINT('Ctrl Pts',(-1.08733050185621,-1.62384640243154,
2.33338406538995));
#75724=CARTESIAN_POINT('Ctrl Pts',(-1.06012654717021,-1.64141637130406,
2.33524201985877));
#75725=CARTESIAN_POINT('Ctrl Pts',(-1.00276386025002,-1.67846468414182,
2.33915973188768));
#75726=CARTESIAN_POINT('Ctrl Pts',(-0.943342738039523,-1.71257601910822,
2.34307744391659));
#75727=CARTESIAN_POINT('Ctrl Pts',(-0.882196201650275,-1.74351537469385,
2.34699515594549));
#75728=CARTESIAN_POINT('Ctrl Pts',(-0.821141893843108,-1.77440806381127,
2.35090695880853));
#75729=CARTESIAN_POINT('Ctrl Pts',(-0.758367772261743,-1.80213804838734,
2.35481876167158));
#75730=CARTESIAN_POINT('Ctrl Pts',(-0.694234870682419,-1.8265141511438,
2.35873056453462));
#75731=CARTESIAN_POINT('Ctrl Pts',(-0.630177556586263,-1.85086152405628,
2.36263775691964));
#75732=CARTESIAN_POINT('Ctrl Pts',(-0.564765100721728,-1.87186269165573,
2.36654494930467));
#75733=CARTESIAN_POINT('Ctrl Pts',(-0.4983804597485,-1.88937368388069,2.37045214168969));
#75734=CARTESIAN_POINT('Ctrl Pts',(-0.432037541593535,-1.90687367042819,
2.3743568784001));
#75735=CARTESIAN_POINT('Ctrl Pts',(-0.364724125039669,-1.92088770770785,
2.37826161511051));
#75736=CARTESIAN_POINT('Ctrl Pts',(-0.296838859841856,-1.93132148833067,
2.38216635182091));
#75737=CARTESIAN_POINT('Ctrl Pts',(-0.228972962964415,-1.94175229209533,
2.38606997447231));
#75738=CARTESIAN_POINT('Ctrl Pts',(-0.160536027388258,-1.94860479227721,
2.3899735971237));
#75739=CARTESIAN_POINT('Ctrl Pts',(-0.0919356501021985,-1.95183601673918,
2.3938772197751));
#75740=CARTESIAN_POINT('Ctrl Pts',(-0.0233313028251302,-1.95506742819622,
2.39778106833409));
#75741=CARTESIAN_POINT('Ctrl Pts',(0.0454360133624638,-1.95467712726879,
2.40168491689309));
#75742=CARTESIAN_POINT('Ctrl Pts',(0.113956666023218,-1.95067421120721,
2.40558876545209));
#75743=CARTESIAN_POINT('Ctrl Pts',(0.182550386467686,-1.94666702659018,
2.40949677692476));
#75744=CARTESIAN_POINT('Ctrl Pts',(0.250896426330908,-1.93903956738392,
2.41340478839744));
#75745=CARTESIAN_POINT('Ctrl Pts',(0.31858925877276,-1.92785292078899,2.41731279987011));
#75746=CARTESIAN_POINT('Ctrl Pts',(0.38632254860938,-1.9166595883669,2.42122314701049));
#75747=CARTESIAN_POINT('Ctrl Pts',(0.453401373476329,-1.90190294079295,
2.42513349415088));
#75748=CARTESIAN_POINT('Ctrl Pts',(0.519432172520297,-1.88369483148169,
2.42904384129126));
#75749=CARTESIAN_POINT('Ctrl Pts',(0.585577367504033,-1.86545517728826,
2.43296096296478));
#75750=CARTESIAN_POINT('Ctrl Pts',(0.650670446306053,-1.8437522825183,2.4368780846383));
#75751=CARTESIAN_POINT('Ctrl Pts',(0.71433555268926,-1.81874701873684,2.44079520631182));
#75752=CARTESIAN_POINT('Ctrl Pts',(0.74493900811613,-1.80672713030742,2.44267814447602));
#75753=CARTESIAN_POINT('Ctrl Pts',(0.775212841443383,-1.79394487209788,
2.44456108264023));
#75754=CARTESIAN_POINT('Ctrl Pts',(0.805117385821651,-1.78042185873116,
2.44644402080443));
#75755=CARTESIAN_POINT('Ctrl Pts',(0.867337906277968,-1.75228536819742,
2.45036173281107));
#75756=CARTESIAN_POINT('Ctrl Pts',(0.928205375409723,-1.72082739507311,
2.45427944481772));
#75757=CARTESIAN_POINT('Ctrl Pts',(0.987341830831477,-1.68620049492649,
2.45819715682436));
#75758=CARTESIAN_POINT('Ctrl Pts',(1.04638908950262,-1.65162582325645,2.46210895966417));
#75759=CARTESIAN_POINT('Ctrl Pts',(1.10371009503318,-1.61389195719953,2.46602076250398));
#75760=CARTESIAN_POINT('Ctrl Pts',(1.15894853894812,-1.57319874271181,2.4699325653438));
#75761=CARTESIAN_POINT('Ctrl Pts',(1.21412187843032,-1.53255348954338,2.47383975770426));
#75762=CARTESIAN_POINT('Ctrl Pts',(1.26721713674452,-1.4889561053604,2.47774695006472));
#75763=CARTESIAN_POINT('Ctrl Pts',(1.31790580243201,-1.44265044134608,2.48165414242519));
#75764=CARTESIAN_POINT('Ctrl Pts',(1.36856261022785,-1.39637388050121,2.48555887911022));
#75765=CARTESIAN_POINT('Ctrl Pts',(1.41681546334458,-1.34739274741358,2.48946361579526));
#75766=CARTESIAN_POINT('Ctrl Pts',(1.46236908675021,-1.29599099306954,2.49336835248029));
#75767=CARTESIAN_POINT('Ctrl Pts',(1.50790971325896,-1.24460390415165,2.49727197510554));
#75768=CARTESIAN_POINT('Ctrl Pts',(1.55075231267688,-1.1907979330058,2.50117559773079));
#75769=CARTESIAN_POINT('Ctrl Pts',(1.59063990746642,-1.13489236704421,2.50507922035604));
#75770=CARTESIAN_POINT('Ctrl Pts',(1.63052981059415,-1.07898356576715,2.50898306888814));
#75771=CARTESIAN_POINT('Ctrl Pts',(1.66746408590047,-1.02097533043663,2.51288691742025));
#75772=CARTESIAN_POINT('Ctrl Pts',(1.70122841558543,-0.961216873553878,
2.51679076595235));
#75773=CARTESIAN_POINT('Ctrl Pts',(1.73502875024273,-0.90139469256917,2.5206987773972));
#75774=CARTESIAN_POINT('Ctrl Pts',(1.7656521506494,-0.839818994476754,2.52460678884205));
#75775=CARTESIAN_POINT('Ctrl Pts',(1.79293021957056,-0.776863712468706,
2.5285148002869));
#75776=CARTESIAN_POINT('Ctrl Pts',(1.82022459153739,-0.713870804526047,
2.53242514739889));
#75777=CARTESIAN_POINT('Ctrl Pts',(1.84416948134966,-0.649497132924647,
2.53633549451087));
#75778=CARTESIAN_POINT('Ctrl Pts',(1.86464564306295,-0.584134082044838,
2.54024584162286));
#75779=CARTESIAN_POINT('Ctrl Pts',(1.88515727897323,-0.51865779208363,2.54416296326738));
#75780=CARTESIAN_POINT('Ctrl Pts',(1.90218807064011,-0.452189178170086,
2.5480800849119));
#75781=CARTESIAN_POINT('Ctrl Pts',(1.91566956375596,-0.385131305529756,
2.55199720655642));
#75782=CARTESIAN_POINT('Ctrl Pts',(1.92215004186012,-0.352896962373318,
2.55388014495431));
#75783=CARTESIAN_POINT('Ctrl Pts',(1.92781116286614,-0.320526557816258,
2.55576308335219));
#75784=CARTESIAN_POINT('Ctrl Pts',(1.93264959926769,-0.288065142720263,
2.55764602175008));
#75785=CARTESIAN_POINT('Ctrl Pts',(1.94271663104477,-0.220524708129425,
2.56156373381916));
#75786=CARTESIAN_POINT('Ctrl Pts',(1.94925889654111,-0.152321689154477,
2.56548144588824));
#75787=CARTESIAN_POINT('Ctrl Pts',(1.95219981089288,-0.0838564150783238,
2.56939915795732));
#75788=CARTESIAN_POINT('Ctrl Pts',(1.95513628940303,-0.0154944085837447,
2.57331096086068));
#75789=CARTESIAN_POINT('Ctrl Pts',(1.95448217630384,0.0531285803865306,
2.57722276376404));
#75790=CARTESIAN_POINT('Ctrl Pts',(1.95021236620661,0.121604797170189,2.5811345666674));
#75791=CARTESIAN_POINT('Ctrl Pts',(1.94594758853717,0.190000307410026,2.58504175909274));
#75792=CARTESIAN_POINT('Ctrl Pts',(1.93807560765553,0.2582489003026,2.58894895151807));
#75793=CARTESIAN_POINT('Ctrl Pts',(1.92662336528264,0.325942338991097,2.59285614394341));
#75794=CARTESIAN_POINT('Ctrl Pts',(1.91517832065641,0.393593232280572,2.59676088069411));
#75795=CARTESIAN_POINT('Ctrl Pts',(1.90015756004841,0.460689179480282,2.6006656174448));
#75796=CARTESIAN_POINT('Ctrl Pts',(1.88163973730727,0.526828149386717,2.6045703541955));
#75797=CARTESIAN_POINT('Ctrl Pts',(1.86312719787978,0.592948249206345,2.60847397688709));
#75798=CARTESIAN_POINT('Ctrl Pts',(1.84111970956889,0.658111440185297,2.61237759957869));
#75799=CARTESIAN_POINT('Ctrl Pts',(1.8157463772773,0.721928731527132,2.61628122227028));
#75800=CARTESIAN_POINT('Ctrl Pts',(1.79037157659979,0.785749716054033,2.62018507086932));
#75801=CARTESIAN_POINT('Ctrl Pts',(1.76163072937231,0.8482241900587,2.62408891946835));
#75802=CARTESIAN_POINT('Ctrl Pts',(1.72970120722305,0.90898280166961,2.62799276806739));
#75803=CARTESIAN_POINT('Ctrl Pts',(1.69773763666605,0.969806203914456,2.63190077957961));
#75804=CARTESIAN_POINT('Ctrl Pts',(1.66257883451267,1.02890965577615,2.63580879109183));
#75805=CARTESIAN_POINT('Ctrl Pts',(1.62444783189962,1.08594900498901,2.63971680260406));
#75806=CARTESIAN_POINT('Ctrl Pts',(1.5862940398596,1.14302244441704,2.64362714978377));
#75807=CARTESIAN_POINT('Ctrl Pts',(1.54516480673797,1.19802893194669,2.64753749696348));
#75808=CARTESIAN_POINT('Ctrl Pts',(1.50132446399708,1.2506561692983,2.65144784414318));
#75809=CARTESIAN_POINT('Ctrl Pts',(1.45740816947832,1.3033745813988,2.65536496585525));
#75810=CARTESIAN_POINT('Ctrl Pts',(1.41077172517221,1.35370515568967,2.65928208756731));
#75811=CARTESIAN_POINT('Ctrl Pts',(1.36171680191587,1.40137195325867,2.66319920927938));
#75812=CARTESIAN_POINT('Ctrl Pts',(1.33813638335019,1.42428510781584,2.66508214708483));
#75813=CARTESIAN_POINT('Ctrl Pts',(1.31399763238744,1.44658334545152,2.66696508489029));
#75814=CARTESIAN_POINT('Ctrl Pts',(1.28933660976701,1.46823945823374,2.66884802269575));
#75815=CARTESIAN_POINT('Ctrl Pts',(1.23802594780508,1.51329799045605,2.67276573473544));
#75816=CARTESIAN_POINT('Ctrl Pts',(1.18424847215195,1.55575309701275,2.67668344677512));
#75817=CARTESIAN_POINT('Ctrl Pts',(1.12829914852506,1.59532348802292,2.68060115881481));
#75818=CARTESIAN_POINT('Ctrl Pts',(1.07243421441997,1.63483419419405,2.68451296168842));
#75819=CARTESIAN_POINT('Ctrl Pts',(1.01440433211291,1.67146853828116,2.68842476456203));
#75820=CARTESIAN_POINT('Ctrl Pts',(0.954538602825627,1.70498447374623,2.69233656743563));
#75821=CARTESIAN_POINT('Ctrl Pts',(0.89474343170841,1.73846090709376,2.69624375983083));
#75822=CARTESIAN_POINT('Ctrl Pts',(0.833117138063596,1.76882599192038,2.70015095222602));
#75823=CARTESIAN_POINT('Ctrl Pts',(0.770017430669509,1.79588116434945,2.70405814462122));
#75824=CARTESIAN_POINT('Ctrl Pts',(0.706957381513432,1.82291933257181,2.70796288134154));
#75825=CARTESIAN_POINT('Ctrl Pts',(0.642426206728058,1.84665152152243,2.71186761806186));
#75826=CARTESIAN_POINT('Ctrl Pts',(0.576804420210808,1.86692599232676,2.71577235478218));
#75827=CARTESIAN_POINT('Ctrl Pts',(0.511201356225879,1.88719467862789,2.71967597744324));
#75828=CARTESIAN_POINT('Ctrl Pts',(0.44450876806408,1.90400745999413,2.72357960010429));
#75829=CARTESIAN_POINT('Ctrl Pts',(0.377123547021885,1.91726206614579,2.72748322276534));
#75830=CARTESIAN_POINT('Ctrl Pts',(0.309734426316387,1.93051743935736,2.73138707133371));
#75831=CARTESIAN_POINT('Ctrl Pts',(0.241653076395766,1.94021413608686,2.73529091990207));
#75832=CARTESIAN_POINT('Ctrl Pts',(0.173286036508639,1.94630109426859,2.73919476847044));
#75833=CARTESIAN_POINT('Ctrl Pts',(0.104846092653275,1.9523945433472,2.74310277995199));
#75834=CARTESIAN_POINT('Ctrl Pts',(0.0361203418520083,1.95487052808008,
2.74701079143354));
#75835=CARTESIAN_POINT('Ctrl Pts',(-0.0324811150189426,1.95373001644729,
2.7509188029151));
#75836=CARTESIAN_POINT('Ctrl Pts',(-0.101123572329707,1.95258882317477,
2.75482915006409));
#75837=CARTESIAN_POINT('Ctrl Pts',(-0.169641096972235,1.94782686600023,
2.75873949721309));
#75838=CARTESIAN_POINT('Ctrl Pts',(-0.237627981308397,1.9394970849422,2.76264984436209));
#75839=CARTESIAN_POINT('Ctrl Pts',(-0.305732650421314,1.93115287284484,
2.76656696604371));
#75840=CARTESIAN_POINT('Ctrl Pts',(-0.373304360108464,1.9192285855885,2.77048408772534));
#75841=CARTESIAN_POINT('Ctrl Pts',(-0.43994772888382,1.90382824746613,2.77440120940696));
#75842=CARTESIAN_POINT('Ctrl Pts',(-0.471982816614628,1.89642539266002,
2.77628414748511));
#75843=CARTESIAN_POINT('Ctrl Pts',(-0.50380362454953,1.88822007760216,2.77816708556325));
#75844=CARTESIAN_POINT('Ctrl Pts',(-0.535367745366362,1.87922786729586,
2.7800500236414));
#75845=CARTESIAN_POINT('Ctrl Pts',(-0.601041246564359,1.86051833511056,
2.7839677356806));
#75846=CARTESIAN_POINT('Ctrl Pts',(-0.665863320672553,1.83832483006667,
2.7878854477198));
#75847=CARTESIAN_POINT('Ctrl Pts',(-0.729437722121871,1.81274284153756,
2.791803159759));
#75848=CARTESIAN_POINT('Ctrl Pts',(-0.792916232985298,1.78719943885136,
2.79571496263202));
#75849=CARTESIAN_POINT('Ctrl Pts',(-0.855150353294405,1.75827787813295,
2.79962676550505));
#75850=CARTESIAN_POINT('Ctrl Pts',(-0.915758323573785,1.72612360299178,
2.80353856837807));
#75851=CARTESIAN_POINT('Ctrl Pts',(-0.976294860870307,1.69400722510694,
2.80744576077253));
#75852=CARTESIAN_POINT('Ctrl Pts',(-1.03520862193264,1.65866592914393,2.81135295316699));
#75853=CARTESIAN_POINT('Ctrl Pts',(-1.09213889176975,1.62029276400407,2.81526014556146));
#75854=CARTESIAN_POINT('Ctrl Pts',(-1.14903338086615,1.58194371644306,2.81916488228096));
#75855=CARTESIAN_POINT('Ctrl Pts',(-1.20394644456238,1.54056685400413,2.82306961900046));
#75856=CARTESIAN_POINT('Ctrl Pts',(-1.25654436559627,1.49639976519921,2.82697435571997));
#75857=CARTESIAN_POINT('Ctrl Pts',(-1.3091272799316,1.45224527769441,2.8308779783801));
#75858=CARTESIAN_POINT('Ctrl Pts',(-1.35939598624797,1.40530246038736,2.83478160104023));
#75859=CARTESIAN_POINT('Ctrl Pts',(-1.40704946979724,1.35584947156508,2.83868522370036));
#75860=CARTESIAN_POINT('Ctrl Pts',(-1.45470571110967,1.30639362084016,2.84258907226773));
#75861=CARTESIAN_POINT('Ctrl Pts',(-1.49974608962532,1.25442766625078,2.8464929208351));
#75862=CARTESIAN_POINT('Ctrl Pts',(-1.54190740162807,1.20026562260384,2.85039676940246));
#75863=CARTESIAN_POINT('Ctrl Pts',(-1.5841136728226,1.14604582264923,2.85430478088289));
#75864=CARTESIAN_POINT('Ctrl Pts',(-1.62343444760295,1.08962564901291,2.85821279236332));
#75865=CARTESIAN_POINT('Ctrl Pts',(-1.65964832194906,1.03135030297744,2.86212080384375));
#75866=CARTESIAN_POINT('Ctrl Pts',(-1.69588383992779,0.973040128020652,
2.86603115099155));
#75867=CARTESIAN_POINT('Ctrl Pts',(-1.7290085246365,0.912873005093201,2.86994149813935));
#75868=CARTESIAN_POINT('Ctrl Pts',(-1.75884703342753,0.851218604709267,
2.87385184528715));
#75869=CARTESIAN_POINT('Ctrl Pts',(-1.78873723633691,0.789457390345678,
2.87776896696748));
#75870=CARTESIAN_POINT('Ctrl Pts',(-1.8153297098807,0.726204209186377,2.8816860886478));
#75871=CARTESIAN_POINT('Ctrl Pts',(-1.83849764145948,0.661847733506674,
2.88560321032813));
#75872=CARTESIAN_POINT('Ctrl Pts',(-1.84963433424332,0.630911942115114,
2.88748614841444));
#75873=CARTESIAN_POINT('Ctrl Pts',(-1.85998047482828,0.599721424360237,
2.88936908650075));
#75874=CARTESIAN_POINT('Ctrl Pts',(-1.86952616624135,0.568320256315866,
2.89125202458706));
#75875=CARTESIAN_POINT('Ctrl Pts',(-1.89385394953268,0.48829244290548,2.89605080842916));
#75876=CARTESIAN_POINT('Ctrl Pts',(-1.91305798426404,0.406639111708275,
2.90084959227126));
#75877=CARTESIAN_POINT('Ctrl Pts',(-1.92695885244266,0.323953053686572,
2.90564837611336));
#75878=CARTESIAN_POINT('Ctrl Pts',(-1.94065975646689,0.242456435594826,
2.91037812939271));
#75879=CARTESIAN_POINT('Ctrl Pts',(-1.94920892492174,0.159956562486602,
2.91510788267205));
#75880=CARTESIAN_POINT('Ctrl Pts',(-1.95248061093239,0.0770419621574774,
2.9198376359514));
#75881=CARTESIAN_POINT('Ctrl Pts',(-1.9534703885813,0.0519579480110874,
2.9212685202311));
#75882=CARTESIAN_POINT('Ctrl Pts',(-1.9539774795513,0.0268361250322783,
2.92269940451079));
#75883=CARTESIAN_POINT('Ctrl Pts',(-1.95399926641343,0.00169317918818195,
2.92413028879048));
#75884=CARTESIAN_POINT('',(-1.95389457769654,-0.000928448540882686,3.62413035263971));
#75885=CARTESIAN_POINT('Ctrl Pts',(-1.95280791655641,0.00169181170498602,
2.92413030787576));
#75886=CARTESIAN_POINT('Ctrl Pts',(-1.94902086284632,-0.456790150037774,
2.95023821376141));
#75887=CARTESIAN_POINT('Ctrl Pts',(-1.55897155685892,-1.57201467073545,
3.01341345329561));
#75888=CARTESIAN_POINT('Ctrl Pts',(0.300327974436277,-2.29036964049045,
3.11365602647836));
#75889=CARTESIAN_POINT('Ctrl Pts',(2.08771894852419,-0.988645322604532,
3.22485802742402));
#75890=CARTESIAN_POINT('Ctrl Pts',(1.96217801545985,1.21895341072494,3.33606002836968));
#75891=CARTESIAN_POINT('Ctrl Pts',(0.0387356283802723,2.30965138778674,
3.44726202931533));
#75892=CARTESIAN_POINT('Ctrl Pts',(-1.65281353681269,1.42405341209699,3.54328545581736));
#75893=CARTESIAN_POINT('Ctrl Pts',(-1.94956657085447,0.384252923937107,
3.60224154867084));
#75894=CARTESIAN_POINT('Ctrl Pts',(-1.95121488712599,-0.000926387452031019,
3.62413030787576));
#75895=CARTESIAN_POINT('',(-1.95399960711636,-0.0012391081865255,4.32413030787576));
#75896=CARTESIAN_POINT('Ctrl Pts',(-1.95399977938408,-0.000928529456951041,
3.62413035439709));
#75897=CARTESIAN_POINT('Ctrl Pts',(-1.95396384512653,-0.0765486735560237,
3.62842153969855));
#75898=CARTESIAN_POINT('Ctrl Pts',(-1.94953396892489,-0.152021773335561,
3.63271272500001));
#75899=CARTESIAN_POINT('Ctrl Pts',(-1.94078603975606,-0.22686019458684,
3.63700391030146));
#75900=CARTESIAN_POINT('Ctrl Pts',(-1.93200861573635,-0.301950943907116,
3.64130956392658));
#75901=CARTESIAN_POINT('Ctrl Pts',(-1.91888410869524,-0.376402426202599,
3.6456152175517));
#75902=CARTESIAN_POINT('Ctrl Pts',(-1.90153921339991,-0.449738390514354,
3.64992087117681));
#75903=CARTESIAN_POINT('Ctrl Pts',(-1.88411335654505,-0.523416668454385,
3.6542466224979));
#75904=CARTESIAN_POINT('Ctrl Pts',(-1.86242776661361,-0.595968697856712,
3.65857237381899));
#75905=CARTESIAN_POINT('Ctrl Pts',(-1.83665921822363,-0.666932467431417,
3.66289812514008));
#75906=CARTESIAN_POINT('Ctrl Pts',(-1.82322038783094,-0.703941539456255,
3.66515409382894));
#75907=CARTESIAN_POINT('Ctrl Pts',(-1.80867184087001,-0.740519002767186,
3.66741006251779));
#75908=CARTESIAN_POINT('Ctrl Pts',(-1.79304361189968,-0.77660196099787,
3.66966603120665));
#75909=CARTESIAN_POINT('Ctrl Pts',(-1.76590365150813,-0.839263575378505,
3.67358374325044));
#75910=CARTESIAN_POINT('Ctrl Pts',(-1.73542103874449,-0.900625316628146,
3.67750145529423));
#75911=CARTESIAN_POINT('Ctrl Pts',(-1.70174227804019,-0.960306835928284,
3.68141916733802));
#75912=CARTESIAN_POINT('Ctrl Pts',(-1.6681143157071,-1.01989833635871,3.68533097021571));
#75913=CARTESIAN_POINT('Ctrl Pts',(-1.63130001279988,-1.07781421948387,
3.68924277309341));
#75914=CARTESIAN_POINT('Ctrl Pts',(-1.59149350367943,-1.13369503295471,
3.69315457597111));
#75915=CARTESIAN_POINT('Ctrl Pts',(-1.55173391079101,-1.18950998490518,
3.69706176837038));
#75916=CARTESIAN_POINT('Ctrl Pts',(-1.50898939968645,-1.24329423189826,
3.70096896076966));
#75917=CARTESIAN_POINT('Ctrl Pts',(-1.46349854794866,-1.29471541280398,
3.70487615316893));
#75918=CARTESIAN_POINT('Ctrl Pts',(-1.41803628726312,-1.34610427543879,
3.70878088989332));
#75919=CARTESIAN_POINT('Ctrl Pts',(-1.36983143515774,-1.39513265042968,
3.71268562661771));
#75920=CARTESIAN_POINT('Ctrl Pts',(-1.31916319431565,-1.4415007689082,3.7165903633421));
#75921=CARTESIAN_POINT('Ctrl Pts',(-1.26850940961461,-1.48785565811232,
3.72049398600719));
#75922=CARTESIAN_POINT('Ctrl Pts',(-1.21539399417526,-1.53155146551823,
3.72439760867228));
#75923=CARTESIAN_POINT('Ctrl Pts',(-1.16013209377737,-1.57232615095843,
3.72830123133736));
#75924=CARTESIAN_POINT('Ctrl Pts',(-1.10486699530747,-1.61310319607824,
3.73220507990975));
#75925=CARTESIAN_POINT('Ctrl Pts',(-1.04745556267513,-1.6509584935525,3.73610892848213));
#75926=CARTESIAN_POINT('Ctrl Pts',(-0.988243543724006,-1.68567217995903,
3.74001277705452));
#75927=CARTESIAN_POINT('Ctrl Pts',(-0.928968383366187,-1.72042288369802,
3.74392078854002));
#75928=CARTESIAN_POINT('Ctrl Pts',(-0.867889230025287,-1.75202504122151,
3.74782880002552));
#75929=CARTESIAN_POINT('Ctrl Pts',(-0.805377281911555,-1.78030430931927,
3.75173681151102));
#75930=CARTESIAN_POINT('Ctrl Pts',(-0.742827972822654,-1.80860047884251,
3.75564715866393));
#75931=CARTESIAN_POINT('Ctrl Pts',(-0.678844623129316,-1.83356962762598,
3.75955750581684));
#75932=CARTESIAN_POINT('Ctrl Pts',(-0.613816664389189,-1.8550862789957,
3.76346785296976));
#75933=CARTESIAN_POINT('Ctrl Pts',(-0.548676047103823,-1.87664020717203,
3.7673849746552));
#75934=CARTESIAN_POINT('Ctrl Pts',(-0.48248768311705,-1.89472957032568,
3.77130209634063));
#75935=CARTESIAN_POINT('Ctrl Pts',(-0.415653493903269,-1.90927949054244,
3.77521921802607));
#75936=CARTESIAN_POINT('Ctrl Pts',(-0.383526680521459,-1.91627355416501,
3.77710215606815));
#75937=CARTESIAN_POINT('Ctrl Pts',(-0.351250747401493,-1.9224505366792,
3.77898509411023));
#75938=CARTESIAN_POINT('Ctrl Pts',(-0.318870686539781,-1.92780639205955,
3.7808680321523));
#75939=CARTESIAN_POINT('Ctrl Pts',(-0.251499508315918,-1.93894998715381,
3.78478574419611));
#75940=CARTESIAN_POINT('Ctrl Pts',(-0.183409580024177,-1.94657983874897,
3.78870345623992));
#75941=CARTESIAN_POINT('Ctrl Pts',(-0.114999957780594,-1.95061298306724,
3.79262116828373));
#75942=CARTESIAN_POINT('Ctrl Pts',(-0.0466935191847929,-1.95464004411053,
3.79653297116146));
#75943=CARTESIAN_POINT('Ctrl Pts',(0.021931169193035,-1.95508113573335,
3.80044477403918));
#75944=CARTESIAN_POINT('Ctrl Pts',(0.0904668052660995,-1.95190464857916,
3.80435657691691));
#75945=CARTESIAN_POINT('Ctrl Pts',(0.158921664755669,-1.94873190525511,
3.80826376931621));
#75946=CARTESIAN_POINT('Ctrl Pts',(0.22728719125003,-1.94195007354239,3.8121709617155));
#75947=CARTESIAN_POINT('Ctrl Pts',(0.29515476993388,-1.93157957687103,3.8160781541148));
#75948=CARTESIAN_POINT('Ctrl Pts',(0.362979693767063,-1.92121559806867,
3.81998289083921));
#75949=CARTESIAN_POINT('Ctrl Pts',(0.430306805337967,-1.90726750255992,
3.82388762756362));
#75950=CARTESIAN_POINT('Ctrl Pts',(0.49673286944478,-1.88980751835026,3.82779236428803));
#75951=CARTESIAN_POINT('Ctrl Pts',(0.563139981550571,-1.87235251564361,
3.83169598695315));
#75952=CARTESIAN_POINT('Ctrl Pts',(0.628646080911884,-1.85138773830943,
3.83559960961826));
#75953=CARTESIAN_POINT('Ctrl Pts',(0.692860165948776,-1.82703606708829,
3.83950323228338));
#75954=CARTESIAN_POINT('Ctrl Pts',(0.757077967131214,-1.80268298660694,
3.84340708085578));
#75955=CARTESIAN_POINT('Ctrl Pts',(0.820003146414706,-1.77494279994659,
3.84731092942819));
#75956=CARTESIAN_POINT('Ctrl Pts',(0.88126356837749,-1.74398696183503,3.85121477800059));
#75957=CARTESIAN_POINT('Ctrl Pts',(0.942589316084718,-1.71299811361507,
3.85512278948612));
#75958=CARTESIAN_POINT('Ctrl Pts',(1.00224632363735,-1.67878699286616,3.85903080097164));
#75959=CARTESIAN_POINT('Ctrl Pts',(1.05988692335203,-1.64157111015861,3.86293881245716));
#75960=CARTESIAN_POINT('Ctrl Pts',(1.11756197262524,-1.60433298495644,3.8668491596101));
#75961=CARTESIAN_POINT('Ctrl Pts',(1.17321781688942,-1.56408681211669,3.87075950676304));
#75962=CARTESIAN_POINT('Ctrl Pts',(1.22653797929859,-1.5210919056185,3.87466985391597));
#75963=CARTESIAN_POINT('Ctrl Pts',(1.27995051692673,-1.4780225120272,3.87858697560143));
#75964=CARTESIAN_POINT('Ctrl Pts',(1.33101893042946,-1.43219520871446,3.88250409728689));
#75965=CARTESIAN_POINT('Ctrl Pts',(1.3794625018168,-1.38390722452097,3.88642121897235));
#75966=CARTESIAN_POINT('Ctrl Pts',(1.4027490501484,-1.36069546606563,3.88830415701422));
#75967=CARTESIAN_POINT('Ctrl Pts',(1.42542966987338,-1.33691563300483,3.89018709505609));
#75968=CARTESIAN_POINT('Ctrl Pts',(1.44747658103796,-1.31260334730133,3.89207003309796));
#75969=CARTESIAN_POINT('Ctrl Pts',(1.49334821753265,-1.26201828693525,3.89598774514179));
#75970=CARTESIAN_POINT('Ctrl Pts',(1.53665612658425,-1.20892518019095,3.89990545718561));
#75971=CARTESIAN_POINT('Ctrl Pts',(1.57711434691632,-1.15361446625409,3.90382316922944));
#75972=CARTESIAN_POINT('Ctrl Pts',(1.61751154327807,-1.09838717861076,3.90773497210718));
#75973=CARTESIAN_POINT('Ctrl Pts',(1.6550672932089,-1.0409493159769,3.91164677498492));
#75974=CARTESIAN_POINT('Ctrl Pts',(1.68953432902574,-0.981626074961098,
3.91555857786266));
#75975=CARTESIAN_POINT('Ctrl Pts',(1.72396074175136,-0.922372752735072,
3.91946577026197));
#75976=CARTESIAN_POINT('Ctrl Pts',(1.75530542416981,-0.861238888646867,
3.92337296266128));
#75977=CARTESIAN_POINT('Ctrl Pts',(1.78336412918788,-0.798578977137478,
3.9272801550606));
#75978=CARTESIAN_POINT('Ctrl Pts',(1.81140519927783,-0.735958447453981,
3.93118489178502));
#75979=CARTESIAN_POINT('Ctrl Pts',(1.83616418807734,-0.671814220944769,
3.93508962850945));
#75980=CARTESIAN_POINT('Ctrl Pts',(1.85748330359643,-0.606524341523494,
3.93899436523388));
#75981=CARTESIAN_POINT('Ctrl Pts',(1.87879633656486,-0.541253089938719,
3.94289798789901));
#75982=CARTESIAN_POINT('Ctrl Pts',(1.89667129187766,-0.474837301794581,
3.94680161056414));
#75983=CARTESIAN_POINT('Ctrl Pts',(1.91099957848101,-0.40767218576375,3.95070523322927));
#75984=CARTESIAN_POINT('Ctrl Pts',(1.92532869427938,-0.340503182807664,
3.9546090818017));
#75985=CARTESIAN_POINT('Ctrl Pts',(1.93611063372278,-0.27258524757927,3.95851293037412));
#75986=CARTESIAN_POINT('Ctrl Pts',(1.94328785348326,-0.204324052682056,
3.96241677894654));
#75987=CARTESIAN_POINT('Ctrl Pts',(1.95047272675328,-0.135990066686953,
3.96632479043208));
#75988=CARTESIAN_POINT('Ctrl Pts',(1.95404515739319,-0.0673125807662448,
3.97023280191762));
#75989=CARTESIAN_POINT('Ctrl Pts',(1.95399956865673,0.00129834098001337,
3.97414081340316));
#75990=CARTESIAN_POINT('Ctrl Pts',(1.95395395267365,0.0699502688222659,
3.97805116055612));
#75991=CARTESIAN_POINT('Ctrl Pts',(1.95028604012803,0.138535061937052,3.98196150770907));
#75992=CARTESIAN_POINT('Ctrl Pts',(1.94304228980324,0.206646219506102,3.98587185486202));
#75993=CARTESIAN_POINT('Ctrl Pts',(1.93578598994762,0.274875377148873,3.9897889765475));
#75994=CARTESIAN_POINT('Ctrl Pts',(1.92494156558795,0.342628775934079,3.99370609823298));
#75995=CARTESIAN_POINT('Ctrl Pts',(1.91060671806678,0.409509424651126,3.99762321991846));
#75996=CARTESIAN_POINT('Ctrl Pts',(1.9037160386631,0.441658570844584,3.99950615796018));
#75997=CARTESIAN_POINT('Ctrl Pts',(1.89601958163991,0.473606270615025,4.00138909600189));
#75998=CARTESIAN_POINT('Ctrl Pts',(1.88753223325937,0.505309873648744,4.00327203404361));
#75999=CARTESIAN_POINT('Ctrl Pts',(1.86987313549098,0.571273588165984,4.00718974608742));
#76000=CARTESIAN_POINT('Ctrl Pts',(1.84871692100692,0.63644158306265,4.01110745813123));
#76001=CARTESIAN_POINT('Ctrl Pts',(1.82415274352892,0.70041613935997,4.01502517017505));
#76002=CARTESIAN_POINT('Ctrl Pts',(1.79962561670774,0.764294201511163,4.01893697305277));
#76003=CARTESIAN_POINT('Ctrl Pts',(1.7717009034081,0.826981941970619,4.0228487759305));
#76004=CARTESIAN_POINT('Ctrl Pts',(1.740517936403,0.888095328812978,4.02676057880823));
#76005=CARTESIAN_POINT('Ctrl Pts',(1.70937172186249,0.949136686987083,4.03066777120753));
#76006=CARTESIAN_POINT('Ctrl Pts',(1.67497510280882,1.00860694049179,4.03457496360682));
#76007=CARTESIAN_POINT('Ctrl Pts',(1.6375153470833,1.0661423394963,4.03848215600612));
#76008=CARTESIAN_POINT('Ctrl Pts',(1.60007913485701,1.12364157743689,4.04238689273054));
#76009=CARTESIAN_POINT('Ctrl Pts',(1.55958387270889,1.17920796173859,4.04629162945495));
#76010=CARTESIAN_POINT('Ctrl Pts',(1.51626179326266,1.23250402607533,4.05019636617937));
#76011=CARTESIAN_POINT('Ctrl Pts',(1.47295207402633,1.28578488452744,4.05409998884449));
#76012=CARTESIAN_POINT('Ctrl Pts',(1.42681744872955,1.33679632727251,4.0580036115096));
#76013=CARTESIAN_POINT('Ctrl Pts',(1.37813123648841,1.3852329389005,4.06190723417472));
#76014=CARTESIAN_POINT('Ctrl Pts',(1.32944220671819,1.43367235361289,4.06581108274713));
#76015=CARTESIAN_POINT('Ctrl Pts',(1.27820164743175,1.47953629618033,4.06971493131954));
#76016=CARTESIAN_POINT('Ctrl Pts',(1.22471933310697,1.52255658519282,4.07361877989194));
#76017=CARTESIAN_POINT('Ctrl Pts',(1.17117998731088,1.5656227493775,4.07752679137747));
#76018=CARTESIAN_POINT('Ctrl Pts',(1.11539449978614,1.60583889930092,4.081434802863));
#76019=CARTESIAN_POINT('Ctrl Pts',(1.05770449457606,1.64297815023621,4.08534281434852));
#76020=CARTESIAN_POINT('Ctrl Pts',(0.999980010279702,1.68013959786628,4.08925316150146));
#76021=CARTESIAN_POINT('Ctrl Pts',(0.940349170190319,1.71422024250868,4.0931635086544));
#76022=CARTESIAN_POINT('Ctrl Pts',(0.879178799538057,1.74503886445054,4.09707385580733));
#76023=CARTESIAN_POINT('Ctrl Pts',(0.817902453469941,1.77591087852067,4.1009909774928));
#76024=CARTESIAN_POINT('Ctrl Pts',(0.755081703720956,1.80350939274851,4.10490809917826));
#76025=CARTESIAN_POINT('Ctrl Pts',(0.691103149330296,1.8277014080494,4.10882522086373));
#76026=CARTESIAN_POINT('Ctrl Pts',(0.66034902331689,1.83933037175712,4.11070815890558));
#76027=CARTESIAN_POINT('Ctrl Pts',(0.629327587348807,1.85017294903199,4.11259109694742));
#76028=CARTESIAN_POINT('Ctrl Pts',(0.598082753942746,1.86021854077317,4.11447403498927));
#76029=CARTESIAN_POINT('Ctrl Pts',(0.533073572853702,1.88111977856061,4.11839174703309));
#76030=CARTESIAN_POINT('Ctrl Pts',(0.466838218501822,1.89865063147875,4.12230945907691));
#76031=CARTESIAN_POINT('Ctrl Pts',(0.39975926997196,1.91267052208986,4.12622717112072));
#76032=CARTESIAN_POINT('Ctrl Pts',(0.33278149800723,1.92666926621005,4.13013897399845));
#76033=CARTESIAN_POINT('Ctrl Pts',(0.264963134829249,1.93716745808514,4.13405077687618));
#76034=CARTESIAN_POINT('Ctrl Pts',(0.196702446048127,1.94407411065491,4.13796257975391));
#76035=CARTESIAN_POINT('Ctrl Pts',(0.12852220979567,1.95097262299531,4.14186977215321));
#76036=CARTESIAN_POINT('Ctrl Pts',(0.0599011704720178,1.95428795350473,
4.14577696455251));
#76037=CARTESIAN_POINT('Ctrl Pts',(-0.00875347863661003,1.95398039309809,
4.14968415695182));
#76038=CARTESIAN_POINT('Ctrl Pts',(-0.0773649782199373,1.95367302599351,
4.15358889367624));
#76039=CARTESIAN_POINT('Ctrl Pts',(-0.146009554799158,1.94974728694482,
4.15749363040066));
#76040=CARTESIAN_POINT('Ctrl Pts',(-0.214277740888109,1.94221550033973,
4.16139836712508));
#76041=CARTESIAN_POINT('Ctrl Pts',(-0.282526449400711,1.93468586262648,
4.16530198979019));
#76042=CARTESIAN_POINT('Ctrl Pts',(-0.350398491798432,1.92355227367332,
4.16920561245531));
#76043=CARTESIAN_POINT('Ctrl Pts',(-0.417489075214589,1.90887895689498,
4.17310923512043));
#76044=CARTESIAN_POINT('Ctrl Pts',(-0.484583541242724,1.89420479095432,
4.17701308369285));
#76045=CARTESIAN_POINT('Ctrl Pts',(-0.55089597840766,1.87599059810718,4.18091693226526));
#76046=CARTESIAN_POINT('Ctrl Pts',(-0.616033134107817,1.85435141698689,
4.18482078083767));
#76047=CARTESIAN_POINT('Ctrl Pts',(-0.681239749551307,1.83268916068087,
4.1887287923232));
#76048=CARTESIAN_POINT('Ctrl Pts',(-0.745268114533601,1.8075947826105,4.19263680380873));
#76049=CARTESIAN_POINT('Ctrl Pts',(-0.807742426974779,1.77923246701068,
4.19654481529426));
#76050=CARTESIAN_POINT('Ctrl Pts',(-0.870254077897779,1.75085320035106,
4.2004551624472));
#76051=CARTESIAN_POINT('Ctrl Pts',(-0.931209391090382,1.71920233586662,
4.20436550960015));
#76052=CARTESIAN_POINT('Ctrl Pts',(-0.990257288933346,1.68448998266964,
4.20827585675309));
#76053=CARTESIAN_POINT('Ctrl Pts',(-1.04940748508609,1.64971749159833,4.21219297843856));
#76054=CARTESIAN_POINT('Ctrl Pts',(-1.10664326026723,1.61187319710062,4.21611010012403));
#76055=CARTESIAN_POINT('Ctrl Pts',(-1.16164335011394,1.5712099564145,4.22002722180949));
#76056=CARTESIAN_POINT('Ctrl Pts',(-1.18808157945453,1.5516633686546,4.2219101598513));
#76057=CARTESIAN_POINT('Ctrl Pts',(-1.21400372073073,1.53146600340324,4.22379309789311));
#76058=CARTESIAN_POINT('Ctrl Pts',(-1.23937707126458,1.51064902450028,4.22567603593492));
#76059=CARTESIAN_POINT('Ctrl Pts',(-1.29146188795,1.4679172406683,4.22954121261338));
#76060=CARTESIAN_POINT('Ctrl Pts',(-1.34145104924453,1.42239238310119,4.23340638929184));
#76061=CARTESIAN_POINT('Ctrl Pts',(-1.38902358462359,1.37431054764177,4.23727156597029));
#76062=CARTESIAN_POINT('Ctrl Pts',(-1.43651415424535,1.32631155544527,4.24113008308917));
#76063=CARTESIAN_POINT('Ctrl Pts',(-1.48159601034897,1.27576468746548,4.24498860020805));
#76064=CARTESIAN_POINT('Ctrl Pts',(-1.52398108062412,1.22294630540336,4.24884711732693));
#76065=CARTESIAN_POINT('Ctrl Pts',(-1.56632550140521,1.17017857892573,4.25270193392656));
#76066=CARTESIAN_POINT('Ctrl Pts',(-1.6059779459253,1.11514404786349,4.25655675052618));
#76067=CARTESIAN_POINT('Ctrl Pts',(-1.64268815047333,1.05815482812985,4.26041156712581));
#76068=CARTESIAN_POINT('Ctrl Pts',(-1.67937654991031,1.00119945882773,4.26426409404317));
#76069=CARTESIAN_POINT('Ctrl Pts',(-1.71312590054591,0.942292127623766,
4.26811662096054));
#76070=CARTESIAN_POINT('Ctrl Pts',(-1.74372832408474,0.881775216131987,
4.27196914787791));
#76071=CARTESIAN_POINT('Ctrl Pts',(-1.77432373987696,0.821272162600879,
4.27582079259284));
#76072=CARTESIAN_POINT('Ctrl Pts',(-1.80177343135669,0.759160712600748,
4.27967243730778));
#76073=CARTESIAN_POINT('Ctrl Pts',(-1.82591566516403,0.695807432921341,
4.28352408202271));
#76074=CARTESIAN_POINT('Ctrl Pts',(-1.85007491702172,0.632409495017186,
4.28737844179227));
#76075=CARTESIAN_POINT('Ctrl Pts',(-1.87092187371776,0.567768453060736,
4.29123280156184));
#76076=CARTESIAN_POINT('Ctrl Pts',(-1.88834363426166,0.502269169811835,
4.2950871613314));
#76077=CARTESIAN_POINT('Ctrl Pts',(-1.90577213426105,0.436744548738803,
4.29894301212629));
#76078=CARTESIAN_POINT('Ctrl Pts',(-1.91977269465477,0.370361521168322,
4.30279886292118));
#76079=CARTESIAN_POINT('Ctrl Pts',(-1.93028347373097,0.303515586158412,
4.30665471371606));
#76080=CARTESIAN_POINT('Ctrl Pts',(-1.94080991109656,0.236570068331005,
4.31051630871194));
#76081=CARTESIAN_POINT('Ctrl Pts',(-1.94783613896308,0.16916077050416,4.31437790370782));
#76082=CARTESIAN_POINT('Ctrl Pts',(-1.95135225678392,0.101687609590854,
4.31823949870369));
#76083=CARTESIAN_POINT('Ctrl Pts',(-1.95314018630796,0.0673778217440355,
4.32020310176105));
#76084=CARTESIAN_POINT('Ctrl Pts',(-1.9540213521528,0.033051515596815,4.3221667048184));
#76085=CARTESIAN_POINT('Ctrl Pts',(-1.95399960711636,-0.0012391081865255,
4.32413030787576));
#76086=CARTESIAN_POINT('',(-1.95503514488101,0.00166188402949293,5.02413030787576));
#76087=CARTESIAN_POINT('Ctrl Pts',(-1.95619906720822,-0.0012405029508829,
4.32413030787576));
#76088=CARTESIAN_POINT('Ctrl Pts',(-1.95674893362639,-0.0755294225214843,
4.32837955087737));
#76089=CARTESIAN_POINT('Ctrl Pts',(-1.91917105279229,-0.797299711222014,
4.36969612752756));
#76090=CARTESIAN_POINT('Ctrl Pts',(-1.0218363276303,-2.07167577132427,4.44808003782619));
#76091=CARTESIAN_POINT('Ctrl Pts',(1.18748472594414,-1.9813808335618,4.55928203877191));
#76092=CARTESIAN_POINT('Ctrl Pts',(2.30873910126256,-0.0755893131216004,
4.67048403971755));
#76093=CARTESIAN_POINT('Ctrl Pts',(1.31454556387366,1.89946306688404,4.7816860406632));
#76094=CARTESIAN_POINT('Ctrl Pts',(-0.884137760921009,2.13407834946856,
4.89288804160887));
#76095=CARTESIAN_POINT('Ctrl Pts',(-1.89326256884871,0.88351086131374,4.97370279734637));
#76096=CARTESIAN_POINT('Ctrl Pts',(-1.95609296160575,0.118629928772321,
5.01745021943535));
#76097=CARTESIAN_POINT('Ctrl Pts',(-1.95503514488101,0.00166188402949293,
5.02413030787576));
#76098=CARTESIAN_POINT('',(-1.95369680431385,0.000267557090813054,5.72413028758448));
#76099=CARTESIAN_POINT('Ctrl Pts',(-1.95503514488101,0.00166188402949293,
5.02413030787576));
#76100=CARTESIAN_POINT('Ctrl Pts',(-1.95022321215187,-0.530417397378261,
5.0545175530839));
#76101=CARTESIAN_POINT('Ctrl Pts',(-1.4502565862486,-1.71950099814147,5.12197213194059));
#76102=CARTESIAN_POINT('Ctrl Pts',(0.561680408542795,-2.24064836612449,
5.22649404444583));
#76103=CARTESIAN_POINT('Ctrl Pts',(2.18754642622138,-0.742044887511754,
5.33769604539148));
#76104=CARTESIAN_POINT('Ctrl Pts',(1.80901076907705,1.43647833931448,5.44889804633715));
#76105=CARTESIAN_POINT('Ctrl Pts',(-0.22708249317601,2.29878740279546,5.56010004728279));
#76106=CARTESIAN_POINT('Ctrl Pts',(-1.73523991140407,1.27244417468795,5.65184406350195));
#76107=CARTESIAN_POINT('Ctrl Pts',(-1.95119622568095,0.3103015106477,5.70652074607255));
#76108=CARTESIAN_POINT('Ctrl Pts',(-1.95081926741735,0.000270554286225176,
5.72413009499459));
#76109=CARTESIAN_POINT('',(-1.95399918195666,-0.00178799124785366,6.42413030787577));
#76110=CARTESIAN_POINT('Ctrl Pts',(-1.9539999817252,0.000267241306175345,
5.72413030787576));
#76111=CARTESIAN_POINT('Ctrl Pts',(-1.95400974747832,-0.0711374442006378,
5.72817939860468));
#76112=CARTESIAN_POINT('Ctrl Pts',(-1.95010119842815,-0.142484142639079,
5.73222848933361));
#76113=CARTESIAN_POINT('Ctrl Pts',(-1.94231926826411,-0.213335088839061,
5.73627758006253));
#76114=CARTESIAN_POINT('Ctrl Pts',(-1.93451919732893,-0.284351198536104,
5.74033610979009));
#76115=CARTESIAN_POINT('Ctrl Pts',(-1.92282775581061,-0.354868811322742,
5.74439463951765));
#76116=CARTESIAN_POINT('Ctrl Pts',(-1.90734149414534,-0.42445780086063,
5.74845316924521));
#76117=CARTESIAN_POINT('Ctrl Pts',(-1.89183676010772,-0.494129797760376,
5.75251654008123));
#76118=CARTESIAN_POINT('Ctrl Pts',(-1.87252830400951,-0.562870543064802,
5.75657991091725));
#76119=CARTESIAN_POINT('Ctrl Pts',(-1.84956251433186,-0.630265424704857,
5.76064328175326));
#76120=CARTESIAN_POINT('Ctrl Pts',(-1.82653669710265,-0.69783646182618,
5.76471727335198));
#76121=CARTESIAN_POINT('Ctrl Pts',(-1.79983460214371,-0.764054196930572,
5.7687912649507));
#76122=CARTESIAN_POINT('Ctrl Pts',(-1.76965082572354,-0.828523961642621,
5.77286525654942));
#76123=CARTESIAN_POINT('Ctrl Pts',(-1.74584655788662,-0.879367683953132,
5.77607818742431));
#76124=CARTESIAN_POINT('Ctrl Pts',(-1.71987779756399,-0.929124638781733,
5.77929111829921));
#76125=CARTESIAN_POINT('Ctrl Pts',(-1.69185916877391,-0.977613703379642,
5.7825040491741));
#76126=CARTESIAN_POINT('Ctrl Pts',(-1.65769443764956,-1.0367392182958,5.78642176121791));
#76127=CARTESIAN_POINT('Ctrl Pts',(-1.62035868086182,-1.09418914636563,
5.79033947326172));
#76128=CARTESIAN_POINT('Ctrl Pts',(-1.58004116331142,-1.14960250619137,
5.79425718530553));
#76129=CARTESIAN_POINT('Ctrl Pts',(-1.53978445750642,-1.20493228490067,
5.79816898818325));
#76130=CARTESIAN_POINT('Ctrl Pts',(-1.49655520382515,-1.25823119711222,
5.80208079106098));
#76131=CARTESIAN_POINT('Ctrl Pts',(-1.45058757855937,-1.30916449574882,
5.8059925939387));
#76132=CARTESIAN_POINT('Ctrl Pts',(-1.40467413106055,-1.36003776404084,
5.80989978633799));
#76133=CARTESIAN_POINT('Ctrl Pts',(-1.35602904979169,-1.40855059247393,
5.81380697873729));
#76134=CARTESIAN_POINT('Ctrl Pts',(-1.30492754459694,-1.45440025555285,
5.81771417113658));
#76135=CARTESIAN_POINT('Ctrl Pts',(-1.25385815675652,-1.5002211020662,5.821618907861));
#76136=CARTESIAN_POINT('Ctrl Pts',(-1.20033577287194,-1.54338177564893,
5.82552364458541));
#76137=CARTESIAN_POINT('Ctrl Pts',(-1.14467221103605,-1.5836165979434,5.82942838130982));
#76138=CARTESIAN_POINT('Ctrl Pts',(-1.08902453055477,-1.62383994085245,
5.83333200397494));
#76139=CARTESIAN_POINT('Ctrl Pts',(-1.03123728339406,-1.66113880152937,
5.83723562664006));
#76140=CARTESIAN_POINT('Ctrl Pts',(-0.971653654361067,-1.69528911279663,
5.84113924930517));
#76141=CARTESIAN_POINT('Ctrl Pts',(-0.912066577152505,-1.72944140038307,
5.84504309787758));
#76142=CARTESIAN_POINT('Ctrl Pts',(-0.850683339807656,-1.76044453436794,
5.84894694644999));
#76143=CARTESIAN_POINT('Ctrl Pts',(-0.787872676805905,-1.78811986319226,
5.8528507950224));
#76144=CARTESIAN_POINT('Ctrl Pts',(-0.72499503494271,-1.81582470391673,
5.85675880650792));
#76145=CARTESIAN_POINT('Ctrl Pts',(-0.66068738074735,-1.84019445863267,
5.86066681799344));
#76146=CARTESIAN_POINT('Ctrl Pts',(-0.595338496412384,-1.86109862035558,
5.86457482947896));
#76147=CARTESIAN_POINT('Ctrl Pts',(-0.529950555575004,-1.882015275688,5.8684851766319));
#76148=CARTESIAN_POINT('Ctrl Pts',(-0.46352062204288,-1.89946209086813,
5.87239552378484));
#76149=CARTESIAN_POINT('Ctrl Pts',(-0.396449971809546,-1.91335919781211,
5.87630587093778));
#76150=CARTESIAN_POINT('Ctrl Pts',(-0.329263124143222,-1.92728038098239,
5.88022299262325));
#76151=CARTESIAN_POINT('Ctrl Pts',(-0.261433830450867,-1.93763950757668,
5.88414011430871));
#76152=CARTESIAN_POINT('Ctrl Pts',(-0.193369956017992,-1.94440840877363,
5.88805723599417));
#76153=CARTESIAN_POINT('Ctrl Pts',(-0.160652039972154,-1.94766218095351,
5.88994017403604));
#76154=CARTESIAN_POINT('Ctrl Pts',(-0.127879940264592,-1.95008714533632,
5.8918231120779));
#76155=CARTESIAN_POINT('Ctrl Pts',(-0.0950988157093481,-1.95168445586132,
5.89370605011976));
#76156=CARTESIAN_POINT('Ctrl Pts',(-0.026893169201801,-1.95500788050001,
5.89762376216355));
#76157=CARTESIAN_POINT('Ctrl Pts',(0.0416224541382525,-1.95475822391928,
5.90154147420734));
#76158=CARTESIAN_POINT('Ctrl Pts',(0.110042105676551,-1.95089895560438,
5.90545918625112));
#76159=CARTESIAN_POINT('Ctrl Pts',(0.178358558439678,-1.94704550830369,
5.90937098912883));
#76160=CARTESIAN_POINT('Ctrl Pts',(0.246578839436212,-1.93959328196012,
5.91328279200653));
#76161=CARTESIAN_POINT('Ctrl Pts',(0.314294713424914,-1.92855770800698,
5.91719459488423));
#76162=CARTESIAN_POINT('Ctrl Pts',(0.381930777007469,-1.91753514065906,
5.9211017872835));
#76163=CARTESIAN_POINT('Ctrl Pts',(0.449063130968994,-1.90293769205455,
5.92500897968277));
#76164=CARTESIAN_POINT('Ctrl Pts',(0.515288218719501,-1.88483263226444,
5.92891617208205));
#76165=CARTESIAN_POINT('Ctrl Pts',(0.581471683926788,-1.86673895152506,
5.93282090880644));
#76166=CARTESIAN_POINT('Ctrl Pts',(0.646748540525457,-1.84514216210282,
5.93672564553083));
#76167=CARTESIAN_POINT('Ctrl Pts',(0.710726532295221,-1.82016037653049,
5.94063038225522));
#76168=CARTESIAN_POINT('Ctrl Pts',(0.774686270522744,-1.79518571850414,
5.94453400492031));
#76169=CARTESIAN_POINT('Ctrl Pts',(0.837347421484593,-1.76682816038839,
5.9484376275854));
#76170=CARTESIAN_POINT('Ctrl Pts',(0.898335705444953,-1.73525472491007,
5.95234125025049));
#76171=CARTESIAN_POINT('Ctrl Pts',(0.959327518870092,-1.70367946223935,
5.95624509882288));
#76172=CARTESIAN_POINT('Ctrl Pts',(1.01864583733957,-1.66888818118021,5.96014894739527));
#76173=CARTESIAN_POINT('Ctrl Pts',(1.07594070713876,-1.63109398709018,5.96405279596766));
#76174=CARTESIAN_POINT('Ctrl Pts',(1.13329667397083,-1.59325949073353,5.96796080745317));
#76175=CARTESIAN_POINT('Ctrl Pts',(1.18862447442876,-1.55241596212164,5.97186881893867));
#76176=CARTESIAN_POINT('Ctrl Pts',(1.2416037557157,-1.50881944373496,5.97577683042417));
#76177=CARTESIAN_POINT('Ctrl Pts',(1.29461470067135,-1.46519686939429,5.97968717757709));
#76178=CARTESIAN_POINT('Ctrl Pts',(1.34527397005212,-1.41881836300644,5.98359752473));
#76179=CARTESIAN_POINT('Ctrl Pts',(1.3932970015496,-1.36997790692876,5.98750787188292));
#76180=CARTESIAN_POINT('Ctrl Pts',(1.44140323118165,-1.32105283655849,5.99142499356836));
#76181=CARTESIAN_POINT('Ctrl Pts',(1.4868637815959,-1.26965767197482,5.9953421152538));
#76182=CARTESIAN_POINT('Ctrl Pts',(1.52943397159461,-1.21611994742802,5.99925923693924));
#76183=CARTESIAN_POINT('Ctrl Pts',(1.54989721901025,-1.19038466873877,6.0011421749813));
#76184=CARTESIAN_POINT('Ctrl Pts',(1.56969323977391,-1.16415475197086,6.00302511302336));
#76185=CARTESIAN_POINT('Ctrl Pts',(1.58879853394519,-1.13746877694889,6.00490805106542));
#76186=CARTESIAN_POINT('Ctrl Pts',(1.62854973096024,-1.08194492889261,6.00882576310932));
#76187=CARTESIAN_POINT('Ctrl Pts',(1.66546583088142,-1.0242244426078,6.01274347515322));
#76188=CARTESIAN_POINT('Ctrl Pts',(1.69929616333118,-0.964628710586589,
6.01666118719712));
#76189=CARTESIAN_POINT('Ctrl Pts',(1.73307546879098,-0.905122868040263,
6.02057299007493));
#76190=CARTESIAN_POINT('Ctrl Pts',(1.76377800295952,-0.843747817632082,
6.02448479295275));
#76191=CARTESIAN_POINT('Ctrl Pts',(1.79119552880505,-0.780855029815905,
6.02839659583057));
#76192=CARTESIAN_POINT('Ctrl Pts',(1.81858074016145,-0.718036367882554,
6.03230378822995));
#76193=CARTESIAN_POINT('Ctrl Pts',(1.84268843678239,-0.653703969994269,
6.03621098062933));
#76194=CARTESIAN_POINT('Ctrl Pts',(1.86335648554363,-0.588233463671093,
6.04011817302872));
#76195=CARTESIAN_POINT('Ctrl Pts',(1.88401154441264,-0.522804105635826,
6.04402290975322));
#76196=CARTESIAN_POINT('Ctrl Pts',(1.90123109596156,-0.456238526201307,
6.04792764647772));
#76197=CARTESIAN_POINT('Ctrl Pts',(1.91490186176886,-0.388930404820886,
6.05183238320223));
#76198=CARTESIAN_POINT('Ctrl Pts',(1.92856872717395,-0.321641487101036,
6.05573600586743));
#76199=CARTESIAN_POINT('Ctrl Pts',(1.93868871891055,-0.253610929925255,
6.05963962853263));
#76200=CARTESIAN_POINT('Ctrl Pts',(1.94519940677486,-0.185243806597507,
6.06354325119783));
#76201=CARTESIAN_POINT('Ctrl Pts',(1.95171047142043,-0.116872726782948,
6.06744709977033));
#76202=CARTESIAN_POINT('Ctrl Pts',(1.95461177340225,-0.0481655321755956,
6.07135094834282));
#76203=CARTESIAN_POINT('Ctrl Pts',(1.95389279482182,0.0204681787997021,
6.07525479691531));
#76204=CARTESIAN_POINT('Ctrl Pts',(1.95317304955044,0.0891750781096338,
6.07916280840092));
#76205=CARTESIAN_POINT('Ctrl Pts',(1.94882532436429,0.157807844474764,6.08307081988653));
#76206=CARTESIAN_POINT('Ctrl Pts',(1.94089122823017,0.225958492159874,6.08697883137214));
#76207=CARTESIAN_POINT('Ctrl Pts',(1.93295239019346,0.294149870852989,6.09088917852517));
#76208=CARTESIAN_POINT('Ctrl Pts',(1.92142299799078,0.361858072310764,6.09479952567819));
#76209=CARTESIAN_POINT('Ctrl Pts',(1.90639594131311,0.42868463343688,6.09870987283122));
#76210=CARTESIAN_POINT('Ctrl Pts',(1.89134285081281,0.495626969120597,6.10262699451676));
#76211=CARTESIAN_POINT('Ctrl Pts',(1.87278013473514,0.561684142528404,6.10654411620231));
#76212=CARTESIAN_POINT('Ctrl Pts',(1.85085049208168,0.626473028917459,6.11046123788786));
#76213=CARTESIAN_POINT('Ctrl Pts',(1.84030903800031,0.657616676884984,6.11234417592893));
#76214=CARTESIAN_POINT('Ctrl Pts',(1.82899031236449,0.688467566994951,6.11422711397));
#76215=CARTESIAN_POINT('Ctrl Pts',(1.81691400659672,0.718985043399842,6.11611005201107));
#76216=CARTESIAN_POINT('Ctrl Pts',(1.7917875884574,0.782480858051353,6.12002776405482));
#76217=CARTESIAN_POINT('Ctrl Pts',(1.7632787377027,0.844784135642975,6.12394547609856));
#76218=CARTESIAN_POINT('Ctrl Pts',(1.73152174607975,0.905510045694094,6.12786318814231));
#76219=CARTESIAN_POINT('Ctrl Pts',(1.69981265418395,0.966144361599376,6.13177499101997));
#76220=CARTESIAN_POINT('Ctrl Pts',(1.66486537073897,1.02520559928078,6.13568679389763));
#76221=CARTESIAN_POINT('Ctrl Pts',(1.62686246002969,1.08232829407078,6.13959859677529));
#76222=CARTESIAN_POINT('Ctrl Pts',(1.58890433981864,1.13938366365035,6.14350578917452));
#76223=CARTESIAN_POINT('Ctrl Pts',(1.54789801591874,1.19450462023064,6.14741298157376));
#76224=CARTESIAN_POINT('Ctrl Pts',(1.50407133776116,1.24735135824889,6.15132017397299));
#76225=CARTESIAN_POINT('Ctrl Pts',(1.46027220472077,1.30016488203206,6.15522491069735));
#76226=CARTESIAN_POINT('Ctrl Pts',(1.41365654701226,1.35070664473475,6.15912964742171));
#76227=CARTESIAN_POINT('Ctrl Pts',(1.36449385859073,1.39866811998708,6.16303438414607));
#76228=CARTESIAN_POINT('Ctrl Pts',(1.31534519676154,1.44661591136485,6.16693800681113));
#76229=CARTESIAN_POINT('Ctrl Pts',(1.26365129881092,1.49198453330514,6.17084162947618));
#76230=CARTESIAN_POINT('Ctrl Pts',(1.20971878751819,1.53450202187078,6.17474525214124));
#76231=CARTESIAN_POINT('Ctrl Pts',(1.15578315508681,1.57702197097412,6.17864910071359));
#76232=CARTESIAN_POINT('Ctrl Pts',(1.09960904006529,1.61669015652933,6.18255294928594));
#76233=CARTESIAN_POINT('Ctrl Pts',(1.04153499769514,1.653275793259,6.18645679785829));
#76234=CARTESIAN_POINT('Ctrl Pts',(0.983399027412527,1.68990044349655,6.19036480934376));
#76235=CARTESIAN_POINT('Ctrl Pts',(0.92335950353096,1.72343572200999,6.19427282082922));
#76236=CARTESIAN_POINT('Ctrl Pts',(0.861781871380804,1.75369552835132,6.19818083231469));
#76237=CARTESIAN_POINT('Ctrl Pts',(0.800167436659958,1.78397341980932,6.20209117946757));
#76238=CARTESIAN_POINT('Ctrl Pts',(0.737013516630954,1.81097174964362,6.20600152662045));
#76239=CARTESIAN_POINT('Ctrl Pts',(0.672705340160985,1.83455267717198,6.20991187377334));
#76240=CARTESIAN_POINT('Ctrl Pts',(0.608285752142004,1.85817445778945,6.21382899545875));
#76241=CARTESIAN_POINT('Ctrl Pts',(0.542708386512292,1.87836687477056,6.21774611714416));
#76242=CARTESIAN_POINT('Ctrl Pts',(0.476372570451038,1.89504226183003,6.22166323882957));
#76243=CARTESIAN_POINT('Ctrl Pts',(0.444485322194318,1.9030580252368,6.22354617687196));
#76244=CARTESIAN_POINT('Ctrl Pts',(0.412422954664156,1.91026188256864,6.22542911491434));
#76245=CARTESIAN_POINT('Ctrl Pts',(0.380230307819654,1.91664835403247,6.22731205295673));
#76246=CARTESIAN_POINT('Ctrl Pts',(0.313249070295753,1.92993628789278,6.23122976500039));
#76247=CARTESIAN_POINT('Ctrl Pts',(0.245437314789097,1.93973520542814,6.23514747704405));
#76248=CARTESIAN_POINT('Ctrl Pts',(0.177191246535985,1.94594945005029,6.23906518908771));
#76249=CARTESIAN_POINT('Ctrl Pts',(0.109048115238776,1.95215432159878,6.24297699196528));
#76250=CARTESIAN_POINT('Ctrl Pts',(0.0404724573062881,1.9547852065334,6.24688879484285));
#76251=CARTESIAN_POINT('Ctrl Pts',(-0.0281296413821285,1.95379751337638,
6.25080059772042));
#76252=CARTESIAN_POINT('Ctrl Pts',(-0.0966508851536292,1.95281098432147,
6.25470779011956));
#76253=CARTESIAN_POINT('Ctrl Pts',(-0.165198018180031,1.94821435428103,
6.2586149825187));
#76254=CARTESIAN_POINT('Ctrl Pts',(-0.233361982001063,1.94001499616795,
6.26252217491784));
#76255=CARTESIAN_POINT('Ctrl Pts',(-0.301483104693047,1.9318207913608,6.26642691164209));
#76256=CARTESIAN_POINT('Ctrl Pts',(-0.369221048510593,1.92002840874236,
6.27033164836635));
#76257=CARTESIAN_POINT('Ctrl Pts',(-0.436170478628699,1.90469717109382,
6.27423638509061));
#76258=CARTESIAN_POINT('Ctrl Pts',(-0.503100807424284,1.88937030759626,
6.27814000775556));
#76259=CARTESIAN_POINT('Ctrl Pts',(-0.569242589755988,1.87050670317321,
6.28204363042051));
#76260=CARTESIAN_POINT('Ctrl Pts',(-0.634201101710008,1.84821669795233,
6.28594725308546));
#76261=CARTESIAN_POINT('Ctrl Pts',(-0.69916337289066,1.82592540278223,6.28985110165772));
#76262=CARTESIAN_POINT('Ctrl Pts',(-0.762941773203437,1.80020747524087,
6.29375495022997));
#76263=CARTESIAN_POINT('Ctrl Pts',(-0.82515888514281,1.77122240677727,6.29765879880223));
#76264=CARTESIAN_POINT('Ctrl Pts',(-0.887442343003711,1.74220642975785,
6.3015668102876));
#76265=CARTESIAN_POINT('Ctrl Pts',(-0.948160742984259,1.70991656700681,
6.30547482177296));
#76266=CARTESIAN_POINT('Ctrl Pts',(-1.00695965307578,1.67455912319557,6.30938283325833));
#76267=CARTESIAN_POINT('Ctrl Pts',(-1.06579370500315,1.63918054760681,6.31329318041111));
#76268=CARTESIAN_POINT('Ctrl Pts',(-1.12270557615092,1.60073101768641,6.31720352756388));
#76269=CARTESIAN_POINT('Ctrl Pts',(-1.17737067538964,1.55945961561451,6.32111387471666));
#76270=CARTESIAN_POINT('Ctrl Pts',(-1.23213047990089,1.51811671235747,6.32503099640197));
#76271=CARTESIAN_POINT('Ctrl Pts',(-1.2846353673682,1.47394249614177,6.32894811808727));
#76272=CARTESIAN_POINT('Ctrl Pts',(-1.33459527732834,1.42722508586869,6.33286523977257));
#76273=CARTESIAN_POINT('Ctrl Pts',(-1.35861072097803,1.40476829331708,6.33474817781584));
#76274=CARTESIAN_POINT('Ctrl Pts',(-1.38203867359999,1.38172437852258,6.33663111585911));
#76275=CARTESIAN_POINT('Ctrl Pts',(-1.40485023258728,1.35812805876304,6.33851405390238));
#76276=CARTESIAN_POINT('Ctrl Pts',(-1.45168051628269,1.30968672473925,6.34237957325581));
#76277=CARTESIAN_POINT('Ctrl Pts',(-1.49610723096855,1.25871160704438,6.34624509260924));
#76278=CARTESIAN_POINT('Ctrl Pts',(-1.53783880507626,1.20547410158893,6.35011061196267));
#76279=CARTESIAN_POINT('Ctrl Pts',(-1.57951346580268,1.15230920126548,6.35397085953373));
#76280=CARTESIAN_POINT('Ctrl Pts',(-1.61849995954832,1.09688842053841,6.35783110710478));
#76281=CARTESIAN_POINT('Ctrl Pts',(-1.65454370561901,1.03951966128425,6.36169135467584));
#76282=CARTESIAN_POINT('Ctrl Pts',(-1.69055144198506,0.982208216607538,
6.36554774564513));
#76283=CARTESIAN_POINT('Ctrl Pts',(-1.72362199059012,0.922953077188807,
6.36940413661441));
#76284=CARTESIAN_POINT('Ctrl Pts',(-1.753542463168,0.862093283738307,6.3732605275837));
#76285=CARTESIAN_POINT('Ctrl Pts',(-1.7834439502011,0.801272107870848,6.37711447154339));
#76286=CARTESIAN_POINT('Ctrl Pts',(-1.81019910352668,0.738848750838604,
6.38096841550308));
#76287=CARTESIAN_POINT('Ctrl Pts',(-1.83364062917215,0.675187413278106,
6.38482235946277));
#76288=CARTESIAN_POINT('Ctrl Pts',(-1.85708378576909,0.611521646460108,
6.38867657156182));
#76289=CARTESIAN_POINT('Ctrl Pts',(-1.87721266552031,0.546618196918323,
6.39253078366087));
#76290=CARTESIAN_POINT('Ctrl Pts',(-1.89390847856224,0.480860348573328,
6.39638499575992));
#76291=CARTESIAN_POINT('Ctrl Pts',(-1.9106049567987,0.415099880304359,6.40023936141848));
#76292=CARTESIAN_POINT('Ctrl Pts',(-1.92386798326764,0.348485439130104,
6.40409372707703));
#76293=CARTESIAN_POINT('Ctrl Pts',(-1.93362954546735,0.281412119312107,
6.40794809273559));
#76294=CARTESIAN_POINT('Ctrl Pts',(-1.94339988590562,0.214278482754805,
6.41180592449317));
#76295=CARTESIAN_POINT('Ctrl Pts',(-1.94966242192901,0.146685647235719,
6.41566375625076));
#76296=CARTESIAN_POINT('Ctrl Pts',(-1.95240098832497,0.0790340482809151,
6.41952158800834));
#76297=CARTESIAN_POINT('Ctrl Pts',(-1.95349152191573,0.0520942810957384,
6.42105782796415));
#76298=CARTESIAN_POINT('Ctrl Pts',(-1.95402382695803,0.0251452012775251,
6.42259406791996));
#76299=CARTESIAN_POINT('Ctrl Pts',(-1.95399918195666,-0.00178799124785366,
6.42413030787577));
#76300=CARTESIAN_POINT('',(-1.95414064801411,0.000755162503876828,7.12413030787577));
#76301=CARTESIAN_POINT('Ctrl Pts',(-1.954054516794,-0.00178804188155213,
6.42413030787577));
#76302=CARTESIAN_POINT('Ctrl Pts',(-1.95543262626536,-0.151315844023487,
6.43265889019986));
#76303=CARTESIAN_POINT('Ctrl Pts',(-1.87143461050528,-0.949196308976276,
6.47825480617249));
#76304=CARTESIAN_POINT('Ctrl Pts',(-0.776860394673377,-2.17542591450428,
6.56091805579371));
#76305=CARTESIAN_POINT('Ctrl Pts',(1.40742627626055,-1.8317044680295,6.67212005673936));
#76306=CARTESIAN_POINT('Ctrl Pts',(2.30211856357103,0.190368330558137,6.78332205768501));
#76307=CARTESIAN_POINT('Ctrl Pts',(1.08742919413144,2.03801072910203,6.89452405863067));
#76308=CARTESIAN_POINT('Ctrl Pts',(-1.12364812450813,2.01826778932502,7.00572605957632));
#76309=CARTESIAN_POINT('Ctrl Pts',(-1.936824180042,0.731891475031694,7.08226147599136));
#76310=CARTESIAN_POINT('Ctrl Pts',(-1.95706302779737,0.0426910058065101,
7.12172955875784));
#76311=CARTESIAN_POINT('Ctrl Pts',(-1.95685604123946,0.000756211846537467,
7.12413030787577));
#76312=CARTESIAN_POINT('',(-1.95399953930486,0.00134178850078647,7.82413028070635));
#76313=CARTESIAN_POINT('Ctrl Pts',(-1.95399985409717,0.000755108095159142,
7.12413030787577));
#76314=CARTESIAN_POINT('Ctrl Pts',(-1.9540260066976,-0.066920205871119,
7.12801036203239));
#76315=CARTESIAN_POINT('Ctrl Pts',(-1.95053207911632,-0.134738559516202,
7.13189041618902));
#76316=CARTESIAN_POINT('Ctrl Pts',(-1.94349970506361,-0.202299027228677,
7.13577047034564));
#76317=CARTESIAN_POINT('Ctrl Pts',(-1.93647868148827,-0.269750450178347,
7.13964426197035));
#76318=CARTESIAN_POINT('Ctrl Pts',(-1.92593060117903,-0.33694431819104,
7.14351805359506));
#76319=CARTESIAN_POINT('Ctrl Pts',(-1.91188909971567,-0.403479950416863,
7.14739184521977));
#76320=CARTESIAN_POINT('Ctrl Pts',(-1.89786021818198,-0.46995578312616,
7.15126215523833));
#76321=CARTESIAN_POINT('Ctrl Pts',(-1.88034424118874,-0.535774063500215,
7.15513246525689));
#76322=CARTESIAN_POINT('Ctrl Pts',(-1.85942639198367,-0.600541000094582,
7.15900277527546));
#76323=CARTESIAN_POINT('Ctrl Pts',(-1.83851983101935,-0.665272985448707,
7.16287099669538));
#76324=CARTESIAN_POINT('Ctrl Pts',(-1.81421519195131,-0.728954274905217,
7.16673921811531));
#76325=CARTESIAN_POINT('Ctrl Pts',(-1.78664791545218,-0.791204920491756,
7.17060743953524));
#76326=CARTESIAN_POINT('Ctrl Pts',(-1.75908561662076,-0.85344432583018,
7.17447496249223));
#76327=CARTESIAN_POINT('Ctrl Pts',(-1.72826205366677,-0.914253141235299,
7.17834248544923));
#76328=CARTESIAN_POINT('Ctrl Pts',(-1.69436055598944,-0.97327195906754,
7.18221000840622));
#76329=CARTESIAN_POINT('Ctrl Pts',(-1.66042884852077,-1.03234336885866,
7.18608097773194));
#76330=CARTESIAN_POINT('Ctrl Pts',(-1.62341397617838,-1.08962115703652,
7.18995194705767));
#76331=CARTESIAN_POINT('Ctrl Pts',(-1.58354441879559,-1.14477206189762,
7.1938229163834));
#76332=CARTESIAN_POINT('Ctrl Pts',(-1.54365840156346,-1.19994573539838,
7.19769548380993));
#76333=CARTESIAN_POINT('Ctrl Pts',(-1.50091566732535,-1.25299038469823,
7.20156805123646));
#76334=CARTESIAN_POINT('Ctrl Pts',(-1.45558526447401,-1.30360559136808,
7.205440618663));
#76335=CARTESIAN_POINT('Ctrl Pts',(-1.41017027373367,-1.35431524752911,
7.2093204124163));
#76336=CARTESIAN_POINT('Ctrl Pts',(-1.36215832235579,-1.40258604666527,
7.21320020616961));
#76337=CARTESIAN_POINT('Ctrl Pts',(-1.31185514347887,-1.44815471636426,
7.21707999992292));
#76338=CARTESIAN_POINT('Ctrl Pts',(-1.26409889165823,-1.49141617446416,
7.22076335377115));
#76339=CARTESIAN_POINT('Ctrl Pts',(-1.21427813020722,-1.53224230292097,
7.2244467076194));
#76340=CARTESIAN_POINT('Ctrl Pts',(-1.16267879803052,-1.57044389030946,
7.22813006146763));
#76341=CARTESIAN_POINT('Ctrl Pts',(-1.1077963911698,-1.61107610342805,7.23204777349962));
#76342=CARTESIAN_POINT('Ctrl Pts',(-1.05067238186761,-1.64890863561676,
7.23596548553161));
#76343=CARTESIAN_POINT('Ctrl Pts',(-0.99162412135517,-1.68368571946981,
7.23988319756359));
#76344=CARTESIAN_POINT('Ctrl Pts',(-0.932664924562514,-1.71841034832379,
7.24379500042902));
#76345=CARTESIAN_POINT('Ctrl Pts',(-0.871787657231446,-1.7500884275218,
7.24770680329444));
#76346=CARTESIAN_POINT('Ctrl Pts',(-0.809340421898512,-1.77850613760008,
7.25161860615986));
#76347=CARTESIAN_POINT('Ctrl Pts',(-0.746966787327428,-1.80689035436034,
7.25552579854622));
#76348=CARTESIAN_POINT('Ctrl Pts',(-0.683027305285058,-1.83202163077789,
7.25943299093258));
#76349=CARTESIAN_POINT('Ctrl Pts',(-0.617894968048404,-1.85373185991407,
7.26334018331894));
#76350=CARTESIAN_POINT('Ctrl Pts',(-0.552803566566573,-1.87542844414427,
7.26724492003003));
#76351=CARTESIAN_POINT('Ctrl Pts',(-0.486521262762922,-1.89370809099178,
7.27114965674113));
#76352=CARTESIAN_POINT('Ctrl Pts',(-0.419439878198159,-1.90845125391693,
7.27505439345222));
#76353=CARTESIAN_POINT('Ctrl Pts',(-0.35237763261,-1.92319021047318,7.27895801610365));
#76354=CARTESIAN_POINT('Ctrl Pts',(-0.284517239149783,-1.93439458053492,
7.28286163875509));
#76355=CARTESIAN_POINT('Ctrl Pts',(-0.216262723240614,-1.94199547747582,
7.28676526140652));
#76356=CARTESIAN_POINT('Ctrl Pts',(-0.148004257367238,-1.94959681428902,
7.2906691099649));
#76357=CARTESIAN_POINT('Ctrl Pts',(-0.0793521130250479,-1.95359421204594,
7.29457295852329));
#76358=CARTESIAN_POINT('Ctrl Pts',(-0.0107156686257376,-1.95397061760045,
7.29847680708168));
#76359=CARTESIAN_POINT('Ctrl Pts',(0.0579939670161398,-1.95434742453926,
7.30238481855277));
#76360=CARTESIAN_POINT('Ctrl Pts',(0.126687376355374,-1.95109553054233,
7.30629283002387));
#76361=CARTESIAN_POINT('Ctrl Pts',(0.194955961596583,-1.94425002842689,
7.31020084149497));
#76362=CARTESIAN_POINT('Ctrl Pts',(0.263265348328256,-1.93740043501985,
7.31411118863323));
#76363=CARTESIAN_POINT('Ctrl Pts',(0.331148919299421,-1.92695303391652,
7.31802153577148));
#76364=CARTESIAN_POINT('Ctrl Pts',(0.398206779776185,-1.91299434409522,
7.32193188290974));
#76365=CARTESIAN_POINT('Ctrl Pts',(0.465380815524651,-1.89901147135828,
7.32584900458029));
#76366=CARTESIAN_POINT('Ctrl Pts',(0.531725810164595,-1.88150529411959,
7.32976612625084));
#76367=CARTESIAN_POINT('Ctrl Pts',(0.59685641047922,-1.86061237910261,7.33368324792139));
#76368=CARTESIAN_POINT('Ctrl Pts',(0.628164320544014,-1.85056927338604,
7.33556618608536));
#76369=CARTESIAN_POINT('Ctrl Pts',(0.659191914101623,-1.83974432301109,
7.33744912424932));
#76370=CARTESIAN_POINT('Ctrl Pts',(0.689898226227635,-1.82815656808928,
7.33933206241329));
#76371=CARTESIAN_POINT('Ctrl Pts',(0.753786938260937,-1.80404664781379,
7.34324977462961));
#76372=CARTESIAN_POINT('Ctrl Pts',(0.816537243537038,-1.77653569426117,
7.34716748684593));
#76373=CARTESIAN_POINT('Ctrl Pts',(0.877762217461966,-1.74575184078272,
7.35108519906224));
#76374=CARTESIAN_POINT('Ctrl Pts',(0.938894844507095,-1.71501441921978,
7.35499700211314));
#76375=CARTESIAN_POINT('Ctrl Pts',(0.998506270194983,-1.68101411423343,
7.35890880516403));
#76376=CARTESIAN_POINT('Ctrl Pts',(1.05622816292326,-1.64392763461405,7.36282060821492));
#76377=CARTESIAN_POINT('Ctrl Pts',(1.11388202422737,-1.60688486537746,7.36672780078754));
#76378=CARTESIAN_POINT('Ctrl Pts',(1.16965036346901,-1.56676341004483,7.37063499336015));
#76379=CARTESIAN_POINT('Ctrl Pts',(1.22318978220132,-1.52378566626619,7.37454218593276));
#76380=CARTESIAN_POINT('Ctrl Pts',(1.27669555134924,-1.48083493404745,7.37844692283049));
#76381=CARTESIAN_POINT('Ctrl Pts',(1.32797479604209,-1.4350317817024,7.38235165972821));
#76382=CARTESIAN_POINT('Ctrl Pts',(1.37671472845914,-1.38664074527027,7.38625639662593));
#76383=CARTESIAN_POINT('Ctrl Pts',(1.42544075489747,-1.33826351527342,7.39016001946408));
#76384=CARTESIAN_POINT('Ctrl Pts',(1.47162855829193,-1.28730021339475,7.39406364230224));
#76385=CARTESIAN_POINT('Ctrl Pts',(1.51500131607822,-1.23405308325098,7.39796726514039));
#76386=CARTESIAN_POINT('Ctrl Pts',(1.55837658389168,-1.18080287163973,7.4018711138853));
#76387=CARTESIAN_POINT('Ctrl Pts',(1.59893617391789,-1.12526895244265,7.40577496263022));
#76388=CARTESIAN_POINT('Ctrl Pts',(1.6364439274139,-1.06778615482229,7.40967881137514));
#76389=CARTESIAN_POINT('Ctrl Pts',(1.67399167770678,-1.01024205980162,7.4135868230312));
#76390=CARTESIAN_POINT('Ctrl Pts',(1.70848082731213,-0.950745351687654,
7.41749483468727));
#76391=CARTESIAN_POINT('Ctrl Pts',(1.73971946749999,-0.889658459410997,
7.42140284634334));
#76392=CARTESIAN_POINT('Ctrl Pts',(1.77097677780789,-0.828535057875143,
7.42531319366595));
#76393=CARTESIAN_POINT('Ctrl Pts',(1.79897951174431,-0.765820030051449,
7.42922354098856));
#76394=CARTESIAN_POINT('Ctrl Pts',(1.82358369848309,-0.70189635604321,7.43313388831117));
#76395=CARTESIAN_POINT('Ctrl Pts',(1.84823051104832,-0.637861936678382,
7.43705101016318));
#76396=CARTESIAN_POINT('Ctrl Pts',(1.86946687280628,-0.572615159524416,
7.44096813201518));
#76397=CARTESIAN_POINT('Ctrl Pts',(1.88719875594981,-0.506553901911217,
7.44488525386719));
#76398=CARTESIAN_POINT('Ctrl Pts',(1.89572236363867,-0.47479865974266,7.44676819036444));
#76399=CARTESIAN_POINT('Ctrl Pts',(1.90343696461329,-0.442855364101904,
7.44865112686169));
#76400=CARTESIAN_POINT('Ctrl Pts',(1.91033636421216,-0.410768761675791,
7.45053406335894));
#76401=CARTESIAN_POINT('Ctrl Pts',(1.92469152636594,-0.344008114725301,
7.45445177508964));
#76402=CARTESIAN_POINT('Ctrl Pts',(1.93557137089309,-0.276361376031788,
7.45836948682035));
#76403=CARTESIAN_POINT('Ctrl Pts',(1.94287393052167,-0.20822317378063,7.46228719855105));
#76404=CARTESIAN_POINT('Ctrl Pts',(1.95016547554831,-0.140187745791203,
7.46619900111601));
#76405=CARTESIAN_POINT('Ctrl Pts',(1.95389039210975,-0.0716628106656136,
7.47011080368096));
#76406=CARTESIAN_POINT('Ctrl Pts',(1.95399761386033,-0.00305369090163639,
7.47402260624592));
#76407=CARTESIAN_POINT('Ctrl Pts',(1.95410470923865,0.0654745656992405,
7.47792979833446));
#76408=CARTESIAN_POINT('Ctrl Pts',(1.95060257702726,0.134086320225401,7.48183699042299));
#76409=CARTESIAN_POINT('Ctrl Pts',(1.94349206121551,0.202372448698611,7.48574418251153));
#76410=CARTESIAN_POINT('Ctrl Pts',(1.93638601436886,0.270615659283433,7.4896489189266));
#76411=CARTESIAN_POINT('Ctrl Pts',(1.92567613344655,0.338533161531557,7.49355365534167));
#76412=CARTESIAN_POINT('Ctrl Pts',(1.91141526511457,0.405718725580928,7.49745839175673));
#76413=CARTESIAN_POINT('Ctrl Pts',(1.89715846554027,0.472885120967215,7.50136201411437));
#76414=CARTESIAN_POINT('Ctrl Pts',(1.8793527918653,0.539319511655636,7.50526563647201));
#76415=CARTESIAN_POINT('Ctrl Pts',(1.85810227093987,0.604625463182053,7.50916925882965));
#76416=CARTESIAN_POINT('Ctrl Pts',(1.83685052020874,0.669935194080809,7.51307310709691));
#76417=CARTESIAN_POINT('Ctrl Pts',(1.81215368109625,0.734115889098009,7.51697695536416));
#76418=CARTESIAN_POINT('Ctrl Pts',(1.78416520169937,0.796787633591946,7.52088080363141));
#76419=CARTESIAN_POINT('Ctrl Pts',(1.75614687642862,0.859526208904175,7.52478881481732));
#76420=CARTESIAN_POINT('Ctrl Pts',(1.72483010675834,0.920752172299416,7.52869682600323));
#76421=CARTESIAN_POINT('Ctrl Pts',(1.69041551486067,0.980107844636662,7.53260483718913));
#76422=CARTESIAN_POINT('Ctrl Pts',(1.65598035466613,1.03949899160902,7.53651518404517));
#76423=CARTESIAN_POINT('Ctrl Pts',(1.61844395645568,1.09701721080549,7.5404255309012));
#76424=CARTESIAN_POINT('Ctrl Pts',(1.5780501906774,1.15233397750089,7.54433587775724));
#76425=CARTESIAN_POINT('Ctrl Pts',(1.53758644410584,1.20774657856925,7.5482529991531));
#76426=CARTESIAN_POINT('Ctrl Pts',(1.49425576036724,1.2609497336927,7.55217012054896));
#76427=CARTESIAN_POINT('Ctrl Pts',(1.44834159271625,1.31164882144885,7.55608724194482));
#76428=CARTESIAN_POINT('Ctrl Pts',(1.42627088052338,1.33601962095484,7.55797018273142));
#76429=CARTESIAN_POINT('Ctrl Pts',(1.40360374362322,1.35981237217978,7.55985312351801));
#76430=CARTESIAN_POINT('Ctrl Pts',(1.38037443378564,1.38299762203373,7.5617360643046));
#76431=CARTESIAN_POINT('Ctrl Pts',(1.33204272412895,1.43123765895668,7.56565377636901));
#76432=CARTESIAN_POINT('Ctrl Pts',(1.28108314388008,1.47703693965468,7.56957148843341));
#76433=CARTESIAN_POINT('Ctrl Pts',(1.22777211348501,1.52009593031116,7.57348920049781));
#76434=CARTESIAN_POINT('Ctrl Pts',(1.17454149326189,1.56308997416738,7.57740100339297));
#76435=CARTESIAN_POINT('Ctrl Pts',(1.11896684151028,1.60335162427363,7.58131280628814));
#76436=CARTESIAN_POINT('Ctrl Pts',(1.06136114812037,1.64061833259921,7.58522460918331));
#76437=CARTESIAN_POINT('Ctrl Pts',(1.0038233492746,1.67784111807578,7.5891318015954));
#76438=CARTESIAN_POINT('Ctrl Pts',(0.944259674013049,1.71207570611015,7.59303899400749));
#76439=CARTESIAN_POINT('Ctrl Pts',(0.883014435422671,1.7431011177884,7.59694618641958));
#76440=CARTESIAN_POINT('Ctrl Pts',(0.821807689579798,1.77410702993714,7.6008509231539));
#76441=CARTESIAN_POINT('Ctrl Pts',(0.758921914777607,1.80190754488188,7.60475565988822));
#76442=CARTESIAN_POINT('Ctrl Pts',(0.694727169901249,1.82632695851564,7.60866039662254));
#76443=CARTESIAN_POINT('Ctrl Pts',(0.630550740456051,1.85073940503566,7.61256401929469));
#76444=CARTESIAN_POINT('Ctrl Pts',(0.565066541949429,1.87177249038891,7.61646764196684));
#76445=CARTESIAN_POINT('Ctrl Pts',(0.498664133081241,1.88929883353014,7.62037126463899));
#76446=CARTESIAN_POINT('Ctrl Pts',(0.43225788147548,1.9068261909288,7.62427511321556));
#76447=CARTESIAN_POINT('Ctrl Pts',(0.364933790374975,1.92084628012294,7.62817896179212));
#76448=CARTESIAN_POINT('Ctrl Pts',(0.297094313530838,1.93128220849974,7.63208281036869));
#76449=CARTESIAN_POINT('Ctrl Pts',(0.229182495367473,1.94172926533539,7.63599082185407));
#76450=CARTESIAN_POINT('Ctrl Pts',(0.160754681865166,1.94858445876277,7.63989883333945));
#76451=CARTESIAN_POINT('Ctrl Pts',(0.0922202003259246,1.95182259302731,
7.64380684482484));
#76452=CARTESIAN_POINT('Ctrl Pts',(0.0236447584190841,1.9550626625975,7.64771719197518));
#76453=CARTESIAN_POINT('Ctrl Pts',(-0.0450369863285532,1.95468137341821,
7.65162753912552));
#76454=CARTESIAN_POINT('Ctrl Pts',(-0.113416775426539,1.95070567617256,
7.65553788627586));
#76455=CARTESIAN_POINT('Ctrl Pts',(-0.181915029927715,1.94672309118152,
7.65945500795501));
#76456=CARTESIAN_POINT('Ctrl Pts',(-0.250109795935364,1.93913372386523,
7.66337212963417));
#76457=CARTESIAN_POINT('Ctrl Pts',(-0.31759986123396,1.92801616387005,7.66728925131333));
#76458=CARTESIAN_POINT('Ctrl Pts',(-0.350041949471986,1.92267201639057,
7.66917218929231));
#76459=CARTESIAN_POINT('Ctrl Pts',(-0.382321386102698,1.91651337360227,
7.67105512727128));
#76460=CARTESIAN_POINT('Ctrl Pts',(-0.414394857243163,1.90955306349167,
7.67293806525026));
#76461=CARTESIAN_POINT('Ctrl Pts',(-0.481128154164906,1.89507117472934,
7.67685577838726));
#76462=CARTESIAN_POINT('Ctrl Pts',(-0.547234011966056,1.87705809216585,
7.68077349152426));
#76463=CARTESIAN_POINT('Ctrl Pts',(-0.612310900416118,1.855583832984,7.68469120466126));
#76464=CARTESIAN_POINT('Ctrl Pts',(-0.677289632163757,1.83414196383368,
7.6886030086374));
#76465=CARTESIAN_POINT('Ctrl Pts',(-0.741242011283347,1.80924943185615,
7.69251481261354));
#76466=CARTESIAN_POINT('Ctrl Pts',(-0.803777777399279,1.78102703083335,
7.69642661658967));
#76467=CARTESIAN_POINT('Ctrl Pts',(-0.866239838478769,1.75283789290502,
7.70033381008971));
#76468=CARTESIAN_POINT('Ctrl Pts',(-0.927288156122975,1.72132688161915,
7.70424100358976));
#76469=CARTESIAN_POINT('Ctrl Pts',(-0.986550434686132,1.68666364157784,
7.7081481970898));
#76470=CARTESIAN_POINT('Ctrl Pts',(-1.04577546686266,1.65202218740894,7.71205293491579));
#76471=CARTESIAN_POINT('Ctrl Pts',(-1.10321626293826,1.61423268231066,7.71595767274178));
#76472=CARTESIAN_POINT('Ctrl Pts',(-1.15852462868117,1.57351094204621,7.71986241056777));
#76473=CARTESIAN_POINT('Ctrl Pts',(-1.21381721440313,1.53280082009495,7.72376603433364));
#76474=CARTESIAN_POINT('Ctrl Pts',(-1.26697818154531,1.48916041530356,7.7276696580995));
#76475=CARTESIAN_POINT('Ctrl Pts',(-1.31768938370035,1.44284811677577,7.73157328186537));
#76476=CARTESIAN_POINT('Ctrl Pts',(-1.36840352053983,1.39653313813045,7.73547713153604));
#76477=CARTESIAN_POINT('Ctrl Pts',(-1.41666724935367,1.34754629243511,7.73938098120671));
#76478=CARTESIAN_POINT('Ctrl Pts',(-1.46219787034241,1.296184164371,7.74328483087737));
#76479=CARTESIAN_POINT('Ctrl Pts',(-1.50777704327967,1.24476726588329,7.74719284344993));
#76480=CARTESIAN_POINT('Ctrl Pts',(-1.55061696493227,1.19097039895722,7.75110085602249));
#76481=CARTESIAN_POINT('Ctrl Pts',(-1.59047466056467,1.13512393777142,7.75500886859505));
#76482=CARTESIAN_POINT('Ctrl Pts',(-1.63035617754554,1.07924409939229,7.75891921683022));
#76483=CARTESIAN_POINT('Ctrl Pts',(-1.66725165695716,1.0213126439139,7.76282956506539));
#76484=CARTESIAN_POINT('Ctrl Pts',(-1.70096253063604,0.961687303322772,
7.76673991330056));
#76485=CARTESIAN_POINT('Ctrl Pts',(-1.73473180698456,0.901958664338918,
7.77065703604944));
#76486=CARTESIAN_POINT('Ctrl Pts',(-1.76530524686167,0.840530723436104,
7.77457415879833));
#76487=CARTESIAN_POINT('Ctrl Pts',(-1.79253150111232,0.777783271560927,
7.77849128154721));
#76488=CARTESIAN_POINT('Ctrl Pts',(-1.80561893432219,0.747621095084287,
7.78037420976345));
#76489=CARTESIAN_POINT('Ctrl Pts',(-1.81793368352772,0.717154282311143,
7.78225713797968));
#76490=CARTESIAN_POINT('Ctrl Pts',(-1.82946306033964,0.686426187475923,
7.78414006619591));
#76491=CARTESIAN_POINT('Ctrl Pts',(-1.85696340883929,0.613132259236415,
7.78863130479371));
#76492=CARTESIAN_POINT('Ctrl Pts',(-1.88008308402579,0.538109812614524,
7.79312254339151));
#76493=CARTESIAN_POINT('Ctrl Pts',(-1.89863218860916,0.461856917645722,
7.79761378198931));
#76494=CARTESIAN_POINT('Ctrl Pts',(-1.91702938031453,0.386228516257064,
7.80206823838136));
#76495=CARTESIAN_POINT('Ctrl Pts',(-1.93093045748714,0.309389931917262,
7.80652269477342));
#76496=CARTESIAN_POINT('Ctrl Pts',(-1.94019647443928,0.231848313716967,
7.81097715116548));
#76497=CARTESIAN_POINT('Ctrl Pts',(-1.94931671348173,0.155526621518631,
7.8153615276791));
#76498=CARTESIAN_POINT('Ctrl Pts',(-1.95394653914743,0.0785240591470384,
7.81974590419272));
#76499=CARTESIAN_POINT('Ctrl Pts',(-1.95399953930486,0.00134178850078647,
7.82413028070635));
#76500=CARTESIAN_POINT('',(-1.95399946858027,-0.00144110652225904,8.52413033454307));
#76501=CARTESIAN_POINT('Ctrl Pts',(-1.95179084094767,0.00133979406531506,
7.82413030787577));
#76502=CARTESIAN_POINT('Ctrl Pts',(-1.94915888327607,-0.416058890402282,
7.84786756096437));
#76503=CARTESIAN_POINT('Ctrl Pts',(-1.61328277704976,-1.48911958067226,
7.90867214770152));
#76504=CARTESIAN_POINT('Ctrl Pts',(0.153605637297869,-2.30486302861762,
8.00654406808722));
#76505=CARTESIAN_POINT('Ctrl Pts',(2.02039752512168,-1.11981505029072,8.11774606903288));
#76506=CARTESIAN_POINT('Ctrl Pts',(2.03594236675928,1.0912978005846,8.22894806997853));
#76507=CARTESIAN_POINT('Ctrl Pts',(0.185997657197315,2.30247329506165,8.34015007092419));
#76508=CARTESIAN_POINT('Ctrl Pts',(-1.60167333631625,1.50744019525351,8.43854415022327));
#76509=CARTESIAN_POINT('Ctrl Pts',(-1.94908776418844,0.42503214287857,8.4998708958738));
#76510=CARTESIAN_POINT('Ctrl Pts',(-1.95199070173634,-0.00143915622514865,
8.52413030787577));
#76511=CARTESIAN_POINT('',(0.0563173628514251,1.95318825376395,9.046));
#76512=CARTESIAN_POINT('Ctrl Pts',(-1.95399946858027,-0.00144110652225904,
8.52413033454307));
#76513=CARTESIAN_POINT('Ctrl Pts',(-1.95394108830595,-0.0805990474803556,
8.52862855434524));
#76514=CARTESIAN_POINT('Ctrl Pts',(-1.94906859332623,-0.15956158622964,
8.5331267741474));
#76515=CARTESIAN_POINT('Ctrl Pts',(-1.93947676251248,-0.237793792337245,
8.53762499394957));
#76516=CARTESIAN_POINT('Ctrl Pts',(-1.92979252801014,-0.316779654816663,
8.542166547721));
#76517=CARTESIAN_POINT('Ctrl Pts',(-1.91529770080219,-0.395020873365993,
8.54670810149244));
#76518=CARTESIAN_POINT('Ctrl Pts',(-1.89613939174724,-0.471986659837334,
8.55124965526387));
#76519=CARTESIAN_POINT('Ctrl Pts',(-1.88024369201979,-0.535845376570965,
8.55501779444775));
#76520=CARTESIAN_POINT('Ctrl Pts',(-1.86113855148694,-0.598826399085066,
8.55878593363163));
#76521=CARTESIAN_POINT('Ctrl Pts',(-1.83893271500536,-0.660637926312909,
8.56255407281551));
#76522=CARTESIAN_POINT('Ctrl Pts',(-1.81584482408034,-0.724904714899271,
8.56647188904098));
#76523=CARTESIAN_POINT('Ctrl Pts',(-1.78933801786655,-0.78808743988942,
8.57038970526645));
#76524=CARTESIAN_POINT('Ctrl Pts',(-1.75953424924607,-0.849797167405293,
8.57430752149192));
#76525=CARTESIAN_POINT('Ctrl Pts',(-1.72977543886373,-0.911413807343544,
8.57821942778979));
#76526=CARTESIAN_POINT('Ctrl Pts',(-1.69672974863648,-0.971561420181686,
8.58213133408766));
#76527=CARTESIAN_POINT('Ctrl Pts',(-1.66056799715565,-1.02986888817096,
8.58604324038552));
#76528=CARTESIAN_POINT('Ctrl Pts',(-1.6244488798736,-1.08810761247168,8.58995053460063));
#76529=CARTESIAN_POINT('Ctrl Pts',(-1.58522125557365,-1.1445100844651,8.59385782881573));
#76530=CARTESIAN_POINT('Ctrl Pts',(-1.54310202347784,-1.19872938778467,
8.59776512303083));
#76531=CARTESIAN_POINT('Ctrl Pts',(-1.50100927399538,-1.25291460052911,
8.60166996052113));
#76532=CARTESIAN_POINT('Ctrl Pts',(-1.45602882436296,-1.3049189798806,8.60557479801144));
#76533=CARTESIAN_POINT('Ctrl Pts',(-1.40842019527807,-1.35442554373908,
8.60947963550174));
#76534=CARTESIAN_POINT('Ctrl Pts',(-1.36082516356631,-1.40391796816034,
8.61338335774186));
#76535=CARTESIAN_POINT('Ctrl Pts',(-1.31060378335576,-1.45091363883351,
8.61728707998198));
#76536=CARTESIAN_POINT('Ctrl Pts',(-1.25805385227626,-1.49513093231759,
8.6211908022221));
#76537=CARTESIAN_POINT('Ctrl Pts',(-1.20550089809209,-1.53935076954442,
8.62509474903646));
#76538=CARTESIAN_POINT('Ctrl Pts',(-1.15061950517139,-1.58079159745433,
8.62899869585082));
#76539=CARTESIAN_POINT('Ctrl Pts',(-1.09374070200118,-1.61921193078175,
8.63290264266518));
#76540=CARTESIAN_POINT('Ctrl Pts',(-1.03680128579549,-1.65767320683119,
8.63681074973));
#76541=CARTESIAN_POINT('Ctrl Pts',(-0.977860619836667,-1.69310728857217,
8.64071885679481));
#76542=CARTESIAN_POINT('Ctrl Pts',(-0.917278035606657,-1.72531649426811,
8.64462696385963));
#76543=CARTESIAN_POINT('Ctrl Pts',(-0.856659265732519,-1.75754493834534,
8.64853740521529));
#76544=CARTESIAN_POINT('Ctrl Pts',(-0.794397071838185,-1.7865444651238,
8.65244784657095));
#76545=CARTESIAN_POINT('Ctrl Pts',(-0.730872100338047,-1.81216499606064,
8.6563582879266));
#76546=CARTESIAN_POINT('Ctrl Pts',(-0.667237127147759,-1.83782989225477,
8.66027550071636));
#76547=CARTESIAN_POINT('Ctrl Pts',(-0.602335477159023,-1.860103954783,8.66419271350611));
#76548=CARTESIAN_POINT('Ctrl Pts',(-0.536563490459429,-1.87888680359036,
8.66810992629587));
#76549=CARTESIAN_POINT('Ctrl Pts',(-0.504962931939731,-1.88791113967457,
8.66999197545097));
#76550=CARTESIAN_POINT('Ctrl Pts',(-0.473161624289845,-1.89613032872838,
8.67187402460607));
#76551=CARTESIAN_POINT('Ctrl Pts',(-0.441204145161111,-1.90353747068259,
8.67375607376116));
#76552=CARTESIAN_POINT('Ctrl Pts',(-0.374677067461068,-1.91895719469579,
8.67767400576925));
#76553=CARTESIAN_POINT('Ctrl Pts',(-0.307208562193932,-1.93091573611139,
8.68159193777734));
#76554=CARTESIAN_POINT('Ctrl Pts',(-0.239191629429316,-1.93930486628868,
8.68550986978543));
#76555=CARTESIAN_POINT('Ctrl Pts',(-0.171277246094544,-1.94768134813736,
8.68942189471013));
#76556=CARTESIAN_POINT('Ctrl Pts',(-0.102816560589667,-1.95249903956177,
8.69333391963483));
#76557=CARTESIAN_POINT('Ctrl Pts',(-0.0342140732766986,-1.95370043691192,
8.69724594455954));
#76558=CARTESIAN_POINT('Ctrl Pts',(0.034307597884766,-1.95490041897358,
8.70115336098079));
#76559=CARTESIAN_POINT('Ctrl Pts',(0.102970249570712,-1.95249255902204,
8.70506077740205));
#76560=CARTESIAN_POINT('Ctrl Pts',(0.171364756157416,-1.94647119689635,
8.70896819382331));
#76561=CARTESIAN_POINT('Ctrl Pts',(0.239716298321133,-1.94045361730178,
8.71287315566305));
#76562=CARTESIAN_POINT('Ctrl Pts',(0.307799540585961,-1.93082708140255,
8.71677811750279));
#76563=CARTESIAN_POINT('Ctrl Pts',(0.375207424648671,-1.91763797117405,
8.72068307934252));
#76564=CARTESIAN_POINT('Ctrl Pts',(0.442596090587038,-1.90445262118759,
8.72458692786973));
#76565=CARTESIAN_POINT('Ctrl Pts',(0.509309297998933,-1.88770680759631,
8.72849077639694));
#76566=CARTESIAN_POINT('Ctrl Pts',(0.574948968527382,-1.86749824192402,
8.73239462492414));
#76567=CARTESIAN_POINT('Ctrl Pts',(0.640592444226431,-1.8472885047492,8.73629869975976));
#76568=CARTESIAN_POINT('Ctrl Pts',(0.705161790076147,-1.82361576414533,
8.74020277459538));
#76569=CARTESIAN_POINT('Ctrl Pts',(0.768274658390884,-1.79662740969695,
8.744106849431));
#76570=CARTESIAN_POINT('Ctrl Pts',(0.831454808481008,-1.76961028418412,
8.74801508622428));
#76571=CARTESIAN_POINT('Ctrl Pts',(0.893174929122545,-1.73927068450819,
8.75192332301756));
#76572=CARTESIAN_POINT('Ctrl Pts',(0.953074153498006,-1.70580352266434,
8.75583155981085));
#76573=CARTESIAN_POINT('Ctrl Pts',(1.01300917198316,-1.67231636177584,8.75974213205769));
#76574=CARTESIAN_POINT('Ctrl Pts',(1.07112071237652,-1.63569818146923,8.76365270430453));
#76575=CARTESIAN_POINT('Ctrl Pts',(1.12707636833054,-1.59618760174073,8.76756327655137));
#76576=CARTESIAN_POINT('Ctrl Pts',(1.18312892098574,-1.55660860274752,8.77148062061679));
#76577=CARTESIAN_POINT('Ctrl Pts',(1.23701775189246,-1.51412751203579,8.7753979646822));
#76578=CARTESIAN_POINT('Ctrl Pts',(1.2884437217572,-1.46902306852699,8.77931530874762));
#76579=CARTESIAN_POINT('Ctrl Pts',(1.3131360224015,-1.44736606366267,8.78119623073402));
#76580=CARTESIAN_POINT('Ctrl Pts',(1.33726107095573,-1.42510479754797,8.78307715272041));
#76581=CARTESIAN_POINT('Ctrl Pts',(1.36078896807282,-1.40227293504914,8.78495807470681));
#76582=CARTESIAN_POINT('Ctrl Pts',(1.40978407058029,-1.35472727306327,8.78887495538142));
#76583=CARTESIAN_POINT('Ctrl Pts',(1.45638193160015,-1.30451597633669,8.79279183605603));
#76584=CARTESIAN_POINT('Ctrl Pts',(1.50027868844302,-1.25191048282363,8.79670871673064));
#76585=CARTESIAN_POINT('Ctrl Pts',(1.544109203753,-1.19938437259032,8.80061968671392));
#76586=CARTESIAN_POINT('Ctrl Pts',(1.58524639139948,-1.1444716106328,8.8045306566972));
#76587=CARTESIAN_POINT('Ctrl Pts',(1.62342277661471,-1.08748079908042,8.80844162668048));
#76588=CARTESIAN_POINT('Ctrl Pts',(1.66155417433965,-1.03055714615416,8.81234798793187));
#76589=CARTESIAN_POINT('Ctrl Pts',(1.6967314261284,-0.971560713876157,8.81625434918325));
#76590=CARTESIAN_POINT('Ctrl Pts',(1.72872811449635,-0.910832095476386,
8.82016071043464));
#76591=CARTESIAN_POINT('Ctrl Pts',(1.7607047013093,-0.850141629139377,8.82406461755906));
#76592=CARTESIAN_POINT('Ctrl Pts',(1.78950445936108,-0.787721569814372,
8.82796852468349));
#76593=CARTESIAN_POINT('Ctrl Pts',(1.81494582571252,-0.723938982048013,
8.83187243180792));
#76594=CARTESIAN_POINT('Ctrl Pts',(1.84037994989638,-0.66017455070387,8.83577522764181));
#76595=CARTESIAN_POINT('Ctrl Pts',(1.86245739786728,-0.595048817847414,
8.8396780234757));
#76596=CARTESIAN_POINT('Ctrl Pts',(1.88104461086103,-0.528949120379897,
8.8435808193096));
#76597=CARTESIAN_POINT('Ctrl Pts',(1.89963291875866,-0.462845529224006,
8.84748384504274));
#76598=CARTESIAN_POINT('Ctrl Pts',(1.91473045271517,-0.395768334100122,
8.85138687077587));
#76599=CARTESIAN_POINT('Ctrl Pts',(1.92625392995489,-0.32811857206403,8.85528989650902));
#76600=CARTESIAN_POINT('Ctrl Pts',(1.93778973221577,-0.260396454719598,
8.85919709675249));
#76601=CARTESIAN_POINT('Ctrl Pts',(1.94574376603604,-0.192101034489606,
8.86310429699595));
#76602=CARTESIAN_POINT('Ctrl Pts',(1.95008432939565,-0.123641045957689,
8.86701149723942));
#76603=CARTESIAN_POINT('Ctrl Pts',(1.95442749349116,-0.0551400382458394,
8.87092103856055));
#76604=CARTESIAN_POINT('Ctrl Pts',(1.95515287313671,0.0135252417277512,
8.87483057988169));
#76605=CARTESIAN_POINT('Ctrl Pts',(1.95228092335384,0.0819463013728634,
8.87874012120282));
#76606=CARTESIAN_POINT('Ctrl Pts',(1.94940398465482,0.150486216483694,8.8826564538592));
#76607=CARTESIAN_POINT('Ctrl Pts',(1.94291729095136,0.218780574760241,8.88657278651558));
#76608=CARTESIAN_POINT('Ctrl Pts',(1.93289304162917,0.286427110486277,8.89048911917197));
#76609=CARTESIAN_POINT('Ctrl Pts',(1.92805457950627,0.319078453278754,8.8923794379988));
#76610=CARTESIAN_POINT('Ctrl Pts',(1.92239271298801,0.351579039383104,8.89426975682563));
#76611=CARTESIAN_POINT('Ctrl Pts',(1.91591973560057,0.383884835251727,8.89616007565247));
#76612=CARTESIAN_POINT('Ctrl Pts',(1.90250125140227,0.450854760439052,8.9000787071862));
#76613=CARTESIAN_POINT('Ctrl Pts',(1.88554057463531,0.517253144766889,8.90399733871994));
#76614=CARTESIAN_POINT('Ctrl Pts',(1.86510139547736,0.582677255938815,8.90791597025368));
#76615=CARTESIAN_POINT('Ctrl Pts',(1.84469306081434,0.648002636449948,8.9118286882324));
#76616=CARTESIAN_POINT('Ctrl Pts',(1.82081678738595,0.712356196166194,8.91574140621112));
#76617=CARTESIAN_POINT('Ctrl Pts',(1.79358721358966,0.775345669522741,8.91965412418983));
#76618=CARTESIAN_POINT('Ctrl Pts',(1.76638980026698,0.838260746882122,8.92356222091138));
#76619=CARTESIAN_POINT('Ctrl Pts',(1.73584714655751,0.899814488352887,8.92747031763293));
#76620=CARTESIAN_POINT('Ctrl Pts',(1.70212301961931,0.959631817981274,8.93137841435447));
#76621=CARTESIAN_POINT('Ctrl Pts',(1.66842014542599,1.01941145108313,8.93528404821663));
#76622=CARTESIAN_POINT('Ctrl Pts',(1.63154001616097,1.07745641564978,8.93918968207879));
#76623=CARTESIAN_POINT('Ctrl Pts',(1.59169294757376,1.13341499930253,8.94309531594095));
#76624=CARTESIAN_POINT('Ctrl Pts',(1.55185733148111,1.18935749983053,8.94699982728012));
#76625=CARTESIAN_POINT('Ctrl Pts',(1.50905675398589,1.2432144094598,8.95090433861929));
#76626=CARTESIAN_POINT('Ctrl Pts',(1.463544578585,1.29466337960663,8.95480884995846));
#76627=CARTESIAN_POINT('Ctrl Pts',(1.41802988360337,1.34611519799864,8.95871357745366));
#76628=CARTESIAN_POINT('Ctrl Pts',(1.36980362041336,1.39515844560795,8.96261830494887));
#76629=CARTESIAN_POINT('Ctrl Pts',(1.31915791157833,1.44150560329133,8.96652303244408));
#76630=CARTESIAN_POINT('Ctrl Pts',(1.26845847522588,1.48790192837268,8.97043190227078));
#76631=CARTESIAN_POINT('Ctrl Pts',(1.21533483432683,1.53159612280881,8.97434077209748));
#76632=CARTESIAN_POINT('Ctrl Pts',(1.16011353387112,1.57233984511271,8.97824964192418));
#76633=CARTESIAN_POINT('Ctrl Pts',(1.10485938495347,1.61310780387248,8.98216083694714));
#76634=CARTESIAN_POINT('Ctrl Pts',(1.04750550368595,1.65092152669452,8.9860720319701));
#76635=CARTESIAN_POINT('Ctrl Pts',(0.988406507414003,1.68557663014817,8.98998322699307));
#76636=CARTESIAN_POINT('Ctrl Pts',(0.929205523574677,1.7202915381657,8.99390117159371));
#76637=CARTESIAN_POINT('Ctrl Pts',(0.868253850527651,1.7518367215787,8.99781911619435));
#76638=CARTESIAN_POINT('Ctrl Pts',(0.80592892480626,1.78005465313867,9.00173706079499));
#76639=CARTESIAN_POINT('Ctrl Pts',(0.7761021722743,1.79355886917842,9.0036120660627));
#76640=CARTESIAN_POINT('Ctrl Pts',(0.745961172374592,1.8063017746176,9.00548707133041));
#76641=CARTESIAN_POINT('Ctrl Pts',(0.715548514393166,1.81827014592159,9.00736207659812));
#76642=CARTESIAN_POINT('Ctrl Pts',(0.641982771868844,1.84722066127355,9.0118975616202));
#76643=CARTESIAN_POINT('Ctrl Pts',(0.566587126936113,1.87173065517956,9.01643304664227));
#76644=CARTESIAN_POINT('Ctrl Pts',(0.489867649121186,1.89159871176328,9.02096853166434));
#76645=CARTESIAN_POINT('Ctrl Pts',(0.413830713534296,1.91129001026686,9.02546366630681));
#76646=CARTESIAN_POINT('Ctrl Pts',(0.336493559382468,1.92642150295744,9.02995880094929));
#76647=CARTESIAN_POINT('Ctrl Pts',(0.258371108637887,1.93684288733527,9.03445393559177));
#76648=CARTESIAN_POINT('Ctrl Pts',(0.191483468276503,1.94576556965883,9.03830262372784));
#76649=CARTESIAN_POINT('Ctrl Pts',(0.124020571038654,1.95123612952076,9.04215131186392));
#76650=CARTESIAN_POINT('Ctrl Pts',(0.0563173628514251,1.95318825376395,
9.046));
#76651=CARTESIAN_POINT('',(1.57931773120857,1.15059615151895,9.04599749618701));
#76652=CARTESIAN_POINT('Origin',(0.,0.,9.046));
#76653=CARTESIAN_POINT('',(-1.95399928911013,-0.00166678046474256,8.62586971036475));
#76654=CARTESIAN_POINT('Ctrl Pts',(1.57931773120857,1.15059615151895,9.04599749618701));
#76655=CARTESIAN_POINT('Ctrl Pts',(1.62180406402798,1.09227906201092,9.04191010737179));
#76656=CARTESIAN_POINT('Ctrl Pts',(1.66100458682741,1.03167794467588,9.03782271855658));
#76657=CARTESIAN_POINT('Ctrl Pts',(1.69670153662891,0.969185170956047,9.03373532974136));
#76658=CARTESIAN_POINT('Ctrl Pts',(1.73250943747722,0.906498161070356,9.02963523675757));
#76659=CARTESIAN_POINT('Ctrl Pts',(1.76479179770922,0.841908110382457,9.02553514377379));
#76660=CARTESIAN_POINT('Ctrl Pts',(1.79337743867541,0.775830756318696,9.02143505079));
#76661=CARTESIAN_POINT('Ctrl Pts',(1.82201159399195,0.709641258542305,9.01732799930044));
#76662=CARTESIAN_POINT('Ctrl Pts',(1.84693637962684,0.641959817168832,9.01322094781089));
#76663=CARTESIAN_POINT('Ctrl Pts',(1.86803029404575,0.573217952028138,9.00911389632133));
#76664=CARTESIAN_POINT('Ctrl Pts',(1.88918515797369,0.504277461689376,9.00499497777065));
#76665=CARTESIAN_POINT('Ctrl Pts',(1.90648693114897,0.434270830524756,9.00087605921997));
#76666=CARTESIAN_POINT('Ctrl Pts',(1.91986493587304,0.363640795298363,8.99675714066929));
#76667=CARTESIAN_POINT('Ctrl Pts',(1.92479612494991,0.337606265830667,8.99523888988491));
#76668=CARTESIAN_POINT('Ctrl Pts',(1.92919470493638,0.311487076162819,8.99372063910054));
#76669=CARTESIAN_POINT('Ctrl Pts',(1.93305891880402,0.28530547914863,8.99220238831617));
#76670=CARTESIAN_POINT('Ctrl Pts',(1.94304653608131,0.217635370908566,8.98827825050065));
#76671=CARTESIAN_POINT('Ctrl Pts',(1.94949596281419,0.149308463994983,8.98435411268513));
#76672=CARTESIAN_POINT('Ctrl Pts',(1.95233174205724,0.0807265071444236,
8.98042997486961));
#76673=CARTESIAN_POINT('Ctrl Pts',(1.95516326323011,0.0122475296727868,
8.97651172935133));
#76674=CARTESIAN_POINT('Ctrl Pts',(1.95439188677818,-0.0564852517374681,
8.97259348383305));
#76675=CARTESIAN_POINT('Ctrl Pts',(1.94999366271435,-0.125062845697096,
8.96867523831477));
#76676=CARTESIAN_POINT('Ctrl Pts',(1.94560062510422,-0.193559571899607,
8.96476161325207));
#76677=CARTESIAN_POINT('Ctrl Pts',(1.93758926597383,-0.261900987293436,
8.96084798818938));
#76678=CARTESIAN_POINT('Ctrl Pts',(1.92598768409354,-0.32967778317626,8.95693436312668));
#76679=CARTESIAN_POINT('Ctrl Pts',(1.91439341097385,-0.39741188105631,8.95302320356816));
#76680=CARTESIAN_POINT('Ctrl Pts',(1.89921348478838,-0.464581583092648,
8.94911204400965));
#76681=CARTESIAN_POINT('Ctrl Pts',(1.88052769958456,-0.530783921285501,
8.94520088445114));
#76682=CARTESIAN_POINT('Ctrl Pts',(1.86184733350569,-0.596967059924311,
8.94129085918065));
#76683=CARTESIAN_POINT('Ctrl Pts',(1.83966326011543,-0.662182920259353,
8.93738083391015));
#76684=CARTESIAN_POINT('Ctrl Pts',(1.81410569602664,-0.726041681753669,
8.93347080863966));
#76685=CARTESIAN_POINT('Ctrl Pts',(1.78854685562587,-0.789903632272646,
8.92956058810752));
#76686=CARTESIAN_POINT('Ctrl Pts',(1.75961437449215,-0.852407895307245,
8.92565036757539));
#76687=CARTESIAN_POINT('Ctrl Pts',(1.72748670324951,-0.91318436807478,8.92174014704325));
#76688=CARTESIAN_POINT('Ctrl Pts',(1.69532565270611,-0.974023985044349,
8.91782586395624));
#76689=CARTESIAN_POINT('Ctrl Pts',(1.65996301624794,-1.03313179501728,8.91391158086924));
#76690=CARTESIAN_POINT('Ctrl Pts',(1.62162286507377,-1.09016296188687,8.90999729778223));
#76691=CARTESIAN_POINT('Ctrl Pts',(1.58326025666247,-1.14722753400914,8.90608072195561));
#76692=CARTESIAN_POINT('Ctrl Pts',(1.54191695645354,-1.2022126498828,8.90216414612899));
#76693=CARTESIAN_POINT('Ctrl Pts',(1.49785831467467,-1.25480535110428,8.89824757030237));
#76694=CARTESIAN_POINT('Ctrl Pts',(1.45372521165557,-1.30748693654013,8.89432437527276));
#76695=CARTESIAN_POINT('Ctrl Pts',(1.40686794153177,-1.35776767867277,8.89040118024314));
#76696=CARTESIAN_POINT('Ctrl Pts',(1.35758916629552,-1.40537100281635,8.88647798521353));
#76697=CARTESIAN_POINT('Ctrl Pts',(1.33503250184569,-1.42716075315522,8.88468219801245));
#76698=CARTESIAN_POINT('Ctrl Pts',(1.31196894094071,-1.44839007968357,8.88288641081136));
#76699=CARTESIAN_POINT('Ctrl Pts',(1.28842968577039,-1.46903537902448,8.88109062361028));
#76700=CARTESIAN_POINT('Ctrl Pts',(1.23698136643587,-1.51415855499429,8.87716568067094));
#76701=CARTESIAN_POINT('Ctrl Pts',(1.18306183933346,-1.55666164634484,8.87324073773159));
#76702=CARTESIAN_POINT('Ctrl Pts',(1.12696846101711,-1.59626379019031,8.86931579479225));
#76703=CARTESIAN_POINT('Ctrl Pts',(1.07095728038006,-1.63580790215363,8.86539660335533));
#76704=CARTESIAN_POINT('Ctrl Pts',(1.0127789686697,-1.67245922405922,8.8614774119184));
#76705=CARTESIAN_POINT('Ctrl Pts',(0.952764807998448,-1.70597632475943,
8.85755822048148));
#76706=CARTESIAN_POINT('Ctrl Pts',(0.892818261479659,-1.73945566386585,
8.85364344454923));
#76707=CARTESIAN_POINT('Ctrl Pts',(0.831040399816556,-1.76980755730277,
8.84972866861699));
#76708=CARTESIAN_POINT('Ctrl Pts',(0.767790916730049,-1.79683419051031,
8.84581389268475));
#76709=CARTESIAN_POINT('Ctrl Pts',(0.704579218113666,-1.82384467833665,
8.84190145539192));
#76710=CARTESIAN_POINT('Ctrl Pts',(0.639898091779485,-1.84753365493355,
8.83798901809909));
#76711=CARTESIAN_POINT('Ctrl Pts',(0.574129832569124,-1.8677502336646,8.83407658080627));
#76712=CARTESIAN_POINT('Ctrl Pts',(0.508378534791603,-1.88796159860184,
8.83016515251905));
#76713=CARTESIAN_POINT('Ctrl Pts',(0.441541128872701,-1.90470219988416,
8.82625372423183));
#76714=CARTESIAN_POINT('Ctrl Pts',(0.374016098171599,-1.91787068341651,
8.82234229594461));
#76715=CARTESIAN_POINT('Ctrl Pts',(0.306485558790806,-1.93104024123134,
8.81843054856379));
#76716=CARTESIAN_POINT('Ctrl Pts',(0.23826776453298,-1.94063701143983,8.81451880118296));
#76717=CARTESIAN_POINT('Ctrl Pts',(0.169770679301235,-1.94661087956725,
8.81060705380214));
#76718=CARTESIAN_POINT('Ctrl Pts',(0.101199340235007,-1.95259122362886,
8.80669106591617));
#76719=CARTESIAN_POINT('Ctrl Pts',(0.0323485949137836,-1.95494078529888,
8.80277507803019));
#76720=CARTESIAN_POINT('Ctrl Pts',(-0.0363701726601297,-1.95366148821659,
8.79885909014422));
#76721=CARTESIAN_POINT('Ctrl Pts',(-0.105131003167084,-1.9523814080733,
8.79494070527207));
#76722=CARTESIAN_POINT('Ctrl Pts',(-0.173759206487808,-1.94746808317336,
8.79102232039991));
#76723=CARTESIAN_POINT('Ctrl Pts',(-0.241847906718193,-1.93897539695996,
8.78710393552776));
#76724=CARTESIAN_POINT('Ctrl Pts',(-0.310054104760477,-1.93046805527445,
8.78317878886331));
#76725=CARTESIAN_POINT('Ctrl Pts',(-0.377718459628762,-1.91836911046163,
8.77925364219886));
#76726=CARTESIAN_POINT('Ctrl Pts',(-0.444444523564576,-1.90278350462512,
8.77532849553441));
#76727=CARTESIAN_POINT('Ctrl Pts',(-0.474758481769812,-1.89570289210187,
8.77354528332441));
#76728=CARTESIAN_POINT('Ctrl Pts',(-0.504878998460603,-1.88790333932249,
8.77176207111441));
#76729=CARTESIAN_POINT('Ctrl Pts',(-0.534770152701521,-1.87939801100767,
8.76997885890441));
#76730=CARTESIAN_POINT('Ctrl Pts',(-0.600358020416365,-1.86073542127,8.76606609308766));
#76731=CARTESIAN_POINT('Ctrl Pts',(-0.665101228545049,-1.83859735094002,
8.76215332727092));
#76732=CARTESIAN_POINT('Ctrl Pts',(-0.728604197596508,-1.81307802458823,
8.75824056145417));
#76733=CARTESIAN_POINT('Ctrl Pts',(-0.792010130299254,-1.78759769329899,
8.75433377457848));
#76734=CARTESIAN_POINT('Ctrl Pts',(-0.854179130749525,-1.75874654156522,
8.75042698770277));
#76735=CARTESIAN_POINT('Ctrl Pts',(-0.914729957549516,-1.72666878837879,
8.74652020082707));
#76736=CARTESIAN_POINT('Ctrl Pts',(-0.975208078883357,-1.69462955205696,
8.74261810496512));
#76737=CARTESIAN_POINT('Ctrl Pts',(-1.03407145124588,-1.65937163798819,
8.73871600910317));
#76738=CARTESIAN_POINT('Ctrl Pts',(-1.09095975959981,-1.62108692022789,
8.73481391324122));
#76739=CARTESIAN_POINT('Ctrl Pts',(-1.1478115877103,-1.5828267529572,8.73091431964047));
#76740=CARTESIAN_POINT('Ctrl Pts',(-1.20269045553328,-1.54154390667796,
8.72701472603972));
#76741=CARTESIAN_POINT('Ctrl Pts',(-1.25526294505716,-1.49747485413493,
8.72311513243897));
#76742=CARTESIAN_POINT('Ctrl Pts',(-1.3078198900863,-1.45341883181288,8.71921669185975));
#76743=CARTESIAN_POINT('Ctrl Pts',(-1.35807143246626,-1.40657855526525,
8.71531825128053));
#76744=CARTESIAN_POINT('Ctrl Pts',(-1.4057167804035,-1.35723112743998,8.71141981070131));
#76745=CARTESIAN_POINT('Ctrl Pts',(-1.45336450573064,-1.30788123729508,
8.70752117559915));
#76746=CARTESIAN_POINT('Ctrl Pts',(-1.4984054375671,-1.25602430428417,8.70362254049699));
#76747=CARTESIAN_POINT('Ctrl Pts',(-1.54057654137808,-1.2019733441951,8.69972390539483));
#76748=CARTESIAN_POINT('Ctrl Pts',(-1.58279244506785,-1.14786496382907,
8.69582112863252));
#76749=CARTESIAN_POINT('Ctrl Pts',(-1.6221321322931,-1.09155829461757,8.69191835187021));
#76750=CARTESIAN_POINT('Ctrl Pts',(-1.65837433329962,-1.03339758595278,
8.68801557510791));
#76751=CARTESIAN_POINT('Ctrl Pts',(-1.69463809005318,-0.975202285086398,
8.68411047709396));
#76752=CARTESIAN_POINT('Ctrl Pts',(-1.72780045588466,-0.915151182354898,
8.68020537908001));
#76753=CARTESIAN_POINT('Ctrl Pts',(-1.75768620406954,-0.853613031779404,
8.67630028106606));
#76754=CARTESIAN_POINT('Ctrl Pts',(-1.78762387246431,-0.791967971593504,
8.67238839876458));
#76755=CARTESIAN_POINT('Ctrl Pts',(-1.81427337050557,-0.728831161908087,
8.6684765164631));
#76756=CARTESIAN_POINT('Ctrl Pts',(-1.83750799297592,-0.664590381926799,
8.66456463416163));
#76757=CARTESIAN_POINT('Ctrl Pts',(-1.84878817131893,-0.633402121561991,
8.66266545417393));
#76758=CARTESIAN_POINT('Ctrl Pts',(-1.85926421818813,-0.601953867042989,
8.66076627418622));
#76759=CARTESIAN_POINT('Ctrl Pts',(-1.86892596382376,-0.570290927286619,
8.65886709419852));
#76760=CARTESIAN_POINT('Ctrl Pts',(-1.89335341938596,-0.490238617586443,
8.65406546346802));
#76761=CARTESIAN_POINT('Ctrl Pts',(-1.91265188010979,-0.408555106159593,
8.64926383273753));
#76762=CARTESIAN_POINT('Ctrl Pts',(-1.92664168382038,-0.325834040833328,
8.64446220200703));
#76763=CARTESIAN_POINT('Ctrl Pts',(-1.9404305170572,-0.244301304666876,
8.63972954908514));
#76764=CARTESIAN_POINT('Ctrl Pts',(-1.94906207863698,-0.161760582156713,
8.63499689616325));
#76765=CARTESIAN_POINT('Ctrl Pts',(-1.95241040069747,-0.0788011881149867,
8.63026424324136));
#76766=CARTESIAN_POINT('Ctrl Pts',(-1.95344676878525,-0.0531237093620654,
8.62879939894916));
#76767=CARTESIAN_POINT('Ctrl Pts',(-1.95397733306977,-0.0274062753568689,
8.62733455465696));
#76768=CARTESIAN_POINT('Ctrl Pts',(-1.95399928911013,-0.00166678046474256,
8.62586971036475));
#76769=CARTESIAN_POINT('',(-1.95391956053326,0.000983111039680522,7.92586964542572));
#76770=CARTESIAN_POINT('Ctrl Pts',(-1.95285709583883,-0.00166548583676096,
8.62586969212423));
#76771=CARTESIAN_POINT('Ctrl Pts',(-1.94908690947408,0.455599167126523,
8.59983157124703));
#76772=CARTESIAN_POINT('Ctrl Pts',(-1.56067665341042,1.56900554080129,8.53675619546789));
#76773=CARTESIAN_POINT('Ctrl Pts',(0.29402470952025,2.29055514341796,8.43664356478675));
#76774=CARTESIAN_POINT('Ctrl Pts',(2.08370935603324,0.995664930130409,8.32553180008087));
#76775=CARTESIAN_POINT('Ctrl Pts',(1.96685667089089,-1.21015215007575,8.21442003537499));
#76776=CARTESIAN_POINT('Ctrl Pts',(0.0505534074973701,-2.30879278288068,
8.10330827066911));
#76777=CARTESIAN_POINT('Ctrl Pts',(-1.64835232859496,-1.43126968529713,
8.00712482291886));
#76778=CARTESIAN_POINT('Ctrl Pts',(-1.94951883786448,-0.388037689702213,
7.94797863007056));
#76779=CARTESIAN_POINT('Ctrl Pts',(-1.95128693461656,0.000980964721550987,
7.92586969212423));
#76780=CARTESIAN_POINT('',(-1.95399967141271,0.00113318975355872,7.22586969217444));
#76781=CARTESIAN_POINT('Ctrl Pts',(-1.95399975265201,0.000983176418433057,
7.92586964400324));
#76782=CARTESIAN_POINT('Ctrl Pts',(-1.9539615535039,0.0769015208354533,
7.9215609870014));
#76783=CARTESIAN_POINT('Ctrl Pts',(-1.94949473679507,0.152668348582896,
7.91725232999955));
#76784=CARTESIAN_POINT('Ctrl Pts',(-1.94067686563194,0.227792236919909,
7.91294367299771));
#76785=CARTESIAN_POINT('Ctrl Pts',(-1.93182745458122,0.303184829454352,
7.90861960472992));
#76786=CARTESIAN_POINT('Ctrl Pts',(-1.91859594501537,0.377929584192814,
7.90429553646214));
#76787=CARTESIAN_POINT('Ctrl Pts',(-1.901110686543,0.45154640681996,7.89997146819435));
#76788=CARTESIAN_POINT('Ctrl Pts',(-1.88354178211006,0.525515397523577,
7.89562671445346));
#76789=CARTESIAN_POINT('Ctrl Pts',(-1.86167847786223,0.598345356879428,
7.89128196071257));
#76790=CARTESIAN_POINT('Ctrl Pts',(-1.8356992018065,0.66957034020854,7.88693720697168));
#76791=CARTESIAN_POINT('Ctrl Pts',(-1.82403434257111,0.701550808132062,
7.8849863850669));
#76792=CARTESIAN_POINT('Ctrl Pts',(-1.81154030758791,0.733208009754202,
7.88303556316212));
#76793=CARTESIAN_POINT('Ctrl Pts',(-1.79823626484276,0.764501364161226,
7.88108474125734));
#76794=CARTESIAN_POINT('Ctrl Pts',(-1.77151579091149,0.827352429560838,
7.87716661750731));
#76795=CARTESIAN_POINT('Ctrl Pts',(-1.74144327543005,0.888925511096836,
7.87324849375727));
#76796=CARTESIAN_POINT('Ctrl Pts',(-1.70816278471269,0.948839238713599,
7.86933037000724));
#76797=CARTESIAN_POINT('Ctrl Pts',(-1.67493240665714,1.0086627502216,7.86541814603831));
#76798=CARTESIAN_POINT('Ctrl Pts',(-1.63850387705473,1.06683144011301,7.86150592206939));
#76799=CARTESIAN_POINT('Ctrl Pts',(-1.59906902607522,1.12298452787509,7.85759369810046));
#76800=CARTESIAN_POINT('Ctrl Pts',(-1.55968054453133,1.17907158807721,7.85368607431673));
#76801=CARTESIAN_POINT('Ctrl Pts',(-1.51729304348515,1.23314735246802,7.84977845053299));
#76802=CARTESIAN_POINT('Ctrl Pts',(-1.47214297123592,1.28487784331457,7.84587082674926));
#76803=CARTESIAN_POINT('Ctrl Pts',(-1.42702119475532,1.3365759144123,7.84196565189225));
#76804=CARTESIAN_POINT('Ctrl Pts',(-1.37914060416938,1.3859312578222,7.83806047703524));
#76805=CARTESIAN_POINT('Ctrl Pts',(-1.32877848390436,1.43264222355508,7.83415530217822));
#76806=CARTESIAN_POINT('Ctrl Pts',(-1.27843065262459,1.47933993622599,7.83025123531638));
#76807=CARTESIAN_POINT('Ctrl Pts',(-1.22560304983721,1.52339442631165,7.82634716845454));
#76808=CARTESIAN_POINT('Ctrl Pts',(-1.17060914865412,1.56454153702843,7.8224431015927));
#76809=CARTESIAN_POINT('Ctrl Pts',(-1.11561198939385,1.60569108547847,7.81853880343701));
#76810=CARTESIAN_POINT('Ctrl Pts',(-1.0584486723113,1.64393261997036,7.81463450528131));
#76811=CARTESIAN_POINT('Ctrl Pts',(-0.999463548610668,1.67904395862603,
7.81073020712562));
#76812=CARTESIAN_POINT('Ctrl Pts',(-0.940415592690584,1.71419269863304,
7.80682175002775));
#76813=CARTESIAN_POINT('Ctrl Pts',(-0.879542380735666,1.74620433639348,
7.80291329292989));
#76814=CARTESIAN_POINT('Ctrl Pts',(-0.817214011371724,1.77490204225972,
7.79900483583202));
#76815=CARTESIAN_POINT('Ctrl Pts',(-0.754848332138476,1.80361692662215,
7.795094039125));
#76816=CARTESIAN_POINT('Ctrl Pts',(-0.691026219011583,1.82901374922341,
7.79118324241799));
#76817=CARTESIAN_POINT('Ctrl Pts',(-0.626136327081129,1.85096442426897,
7.78727244571097));
#76818=CARTESIAN_POINT('Ctrl Pts',(-0.561134388038692,1.87295300213224,
7.78335489612667));
#76819=CARTESIAN_POINT('Ctrl Pts',(-0.495061463692303,1.89148342333278,
7.77943734654238));
#76820=CARTESIAN_POINT('Ctrl Pts',(-0.4283190278697,1.90647811693834,7.77551979695809));
#76821=CARTESIAN_POINT('Ctrl Pts',(-0.396819038991215,1.91355506395098,
7.77367085682255));
#76822=CARTESIAN_POINT('Ctrl Pts',(-0.365170027134055,1.91984517650397,
7.771821916687));
#76823=CARTESIAN_POINT('Ctrl Pts',(-0.333414556241065,1.92534431561905,
7.76997297655146));
#76824=CARTESIAN_POINT('Ctrl Pts',(-0.266121357066562,1.93699757262809,
7.76605487698298));
#76825=CARTESIAN_POINT('Ctrl Pts',(-0.198083069845987,1.94514171224713,
7.7621367774145));
#76826=CARTESIAN_POINT('Ctrl Pts',(-0.129698212493694,1.94969084053753,
7.75821867784602));
#76827=CARTESIAN_POINT('Ctrl Pts',(-0.0614163370318766,1.95423311822022,
7.75430647860864));
#76828=CARTESIAN_POINT('Ctrl Pts',(0.00721058591247044,1.95519109663471,
7.75039427937127));
#76829=CARTESIAN_POINT('Ctrl Pts',(0.0757754195150875,1.95253017538713,
7.74648208013389));
#76830=CARTESIAN_POINT('Ctrl Pts',(0.144259618546025,1.94987238347327,7.74257448177561));
#76831=CARTESIAN_POINT('Ctrl Pts',(0.212681384064886,1.94360416326027,7.73866688341733));
#76832=CARTESIAN_POINT('Ctrl Pts',(0.28063188646454,1.93374293645752,7.73475928505905));
#76833=CARTESIAN_POINT('Ctrl Pts',(0.348539796439634,1.92388789082406,7.73085413604378));
#76834=CARTESIAN_POINT('Ctrl Pts',(0.415976543572401,1.91044437663898,7.72694898702851));
#76835=CARTESIAN_POINT('Ctrl Pts',(0.482538298520567,1.89348165833759,7.72304383801324));
#76836=CARTESIAN_POINT('Ctrl Pts',(0.549081161686835,1.87652375445215,7.71913979737055));
#76837=CARTESIAN_POINT('Ctrl Pts',(0.61474904924555,1.85604875071694,7.71523575672785));
#76838=CARTESIAN_POINT('Ctrl Pts',(0.679149992795631,1.83217665286012,7.71133171608516));
#76839=CARTESIAN_POINT('Ctrl Pts',(0.743554746171386,1.8083031427797,7.70742744448755));
#76840=CARTESIAN_POINT('Ctrl Pts',(0.806691946412121,1.78103231296019,7.70352317288994));
#76841=CARTESIAN_POINT('Ctrl Pts',(0.868188132147625,1.75053288092455,7.69961890129233));
#76842=CARTESIAN_POINT('Ctrl Pts',(0.929749820141615,1.72000096261912,7.69571047108546));
#76843=CARTESIAN_POINT('Ctrl Pts',(0.989666563819558,1.68623379803899,7.6918020408786));
#76844=CARTESIAN_POINT('Ctrl Pts',(1.04758902961708,1.64944633893496,7.68789361067173));
#76845=CARTESIAN_POINT('Ctrl Pts',(1.10554616473901,1.61263686080367,7.68398284108527));
#76846=CARTESIAN_POINT('Ctrl Pts',(1.16150624557331,1.57280377560179,7.6800720714988));
#76847=CARTESIAN_POINT('Ctrl Pts',(1.21515081690597,1.53020406880022,7.67616130191233));
#76848=CARTESIAN_POINT('Ctrl Pts',(1.26888801742229,1.48753080420954,7.67224377951966));
#76849=CARTESIAN_POINT('Ctrl Pts',(1.32030136025814,1.44208170913874,7.66832625712699));
#76850=CARTESIAN_POINT('Ctrl Pts',(1.36910786927658,1.39415194375826,7.66440873473432));
#76851=CARTESIAN_POINT('Ctrl Pts',(1.39214583381642,1.37152782542968,7.66255956043807));
#76852=CARTESIAN_POINT('Ctrl Pts',(1.41460354007924,1.34835148953263,7.66071038614182));
#76853=CARTESIAN_POINT('Ctrl Pts',(1.43645440818334,1.32465645856224,7.65886121184558));
#76854=CARTESIAN_POINT('Ctrl Pts',(1.48275310772801,1.27445025556959,7.65494308993208));
#76855=CARTESIAN_POINT('Ctrl Pts',(1.52650824377156,1.22171429595432,7.65102496801858));
#76856=CARTESIAN_POINT('Ctrl Pts',(1.56743145063378,1.16673675161285,7.64710684610508));
#76857=CARTESIAN_POINT('Ctrl Pts',(1.60829303453319,1.11184199352957,7.64319462417595));
#76858=CARTESIAN_POINT('Ctrl Pts',(1.64633086118598,1.05471274113225,7.63928240224682));
#76859=CARTESIAN_POINT('Ctrl Pts',(1.6812949773209,0.995672234842132,7.6353701803177));
#76860=CARTESIAN_POINT('Ctrl Pts',(1.71621797829565,0.936701155728806,7.63146255886611));
#76861=CARTESIAN_POINT('Ctrl Pts',(1.74807419765634,0.875823707500208,7.62755493741453));
#76862=CARTESIAN_POINT('Ctrl Pts',(1.7766564641253,0.813392776266045,7.62364731596295));
#76863=CARTESIAN_POINT('Ctrl Pts',(1.80522081661906,0.751000973704732,7.61974214361854));
#76864=CARTESIAN_POINT('Ctrl Pts',(1.8305150823525,0.687058065777789,7.61583697127413));
#76865=CARTESIAN_POINT('Ctrl Pts',(1.85237835253044,0.62194086461384,7.61193179892972));
#76866=CARTESIAN_POINT('Ctrl Pts',(1.87423541855999,0.556842141782514,7.60802773475753));
#76867=CARTESIAN_POINT('Ctrl Pts',(1.89266326534007,0.490570253310812,7.60412367058535));
#76868=CARTESIAN_POINT('Ctrl Pts',(1.90755004342891,0.423519576660118,7.60021960641316));
#76869=CARTESIAN_POINT('Ctrl Pts',(1.92243770281272,0.356464930619655,7.59631531112097));
#76870=CARTESIAN_POINT('Ctrl Pts',(1.93378377320702,0.288631885607086,7.59241101582878));
#76871=CARTESIAN_POINT('Ctrl Pts',(1.94152736539113,0.220425700491966,7.5885067205366));
#76872=CARTESIAN_POINT('Ctrl Pts',(1.94927920573602,0.152146864910871,7.58459826654719));
#76873=CARTESIAN_POINT('Ctrl Pts',(1.95342085438517,0.0834945857094849,
7.58068981255779));
#76874=CARTESIAN_POINT('Ctrl Pts',(1.95394335056589,0.0148789374400819,
7.57678135856838));
#76875=CARTESIAN_POINT('Ctrl Pts',(1.95446615949465,-0.053777781770528,
7.57287056511432));
#76876=CARTESIAN_POINT('Ctrl Pts',(1.95136552682704,-0.122397334968288,
7.56895977166026));
#76877=CARTESIAN_POINT('Ctrl Pts',(1.94468455410621,-0.190572781426713,
7.5650489782062));
#76878=CARTESIAN_POINT('Ctrl Pts',(1.93799204548633,-0.2588659450353,7.561131432065));
#76879=CARTESIAN_POINT('Ctrl Pts',(1.92770693201672,-0.326712985370813,
7.5572138859238));
#76880=CARTESIAN_POINT('Ctrl Pts',(1.91392363193798,-0.393716053913668,
7.5532963397826));
#76881=CARTESIAN_POINT('Ctrl Pts',(1.90741832793335,-0.425339491524659,
7.5514473755683));
#76882=CARTESIAN_POINT('Ctrl Pts',(1.90013450933198,-0.456775136292088,
7.54959841135399));
#76883=CARTESIAN_POINT('Ctrl Pts',(1.89208591038853,-0.487982487092733,
7.54774944713969));
#76884=CARTESIAN_POINT('Ctrl Pts',(1.87503022978535,-0.5541135754308,7.54383133129028));
#76885=CARTESIAN_POINT('Ctrl Pts',(1.85446950223503,-0.619480500000784,
7.53991321544087));
#76886=CARTESIAN_POINT('Ctrl Pts',(1.83048934905426,-0.683684680974283,
7.53599509959146));
#76887=CARTESIAN_POINT('Ctrl Pts',(1.80654530599257,-0.747792181138338,
7.53208288377233));
#76888=CARTESIAN_POINT('Ctrl Pts',(1.77919222713191,-0.810739955536902,
7.5281706679532));
#76889=CARTESIAN_POINT('Ctrl Pts',(1.74856603272248,-0.872142665628258,
7.52425845213407));
#76890=CARTESIAN_POINT('Ctrl Pts',(1.71797585275431,-0.933473170068925,
7.52035083682994));
#76891=CARTESIAN_POINT('Ctrl Pts',(1.68412041986387,-0.993261780504505,
7.51644322152581));
#76892=CARTESIAN_POINT('Ctrl Pts',(1.64718376858347,-1.05114301239895,7.51253560622168));
#76893=CARTESIAN_POINT('Ctrl Pts',(1.61027026762216,-1.10898796680369,7.50863044004431));
#76894=CARTESIAN_POINT('Ctrl Pts',(1.57027964312152,-1.16492750037259,7.50472527386694));
#76895=CARTESIAN_POINT('Ctrl Pts',(1.52744112751909,-1.21862200946938,7.50082010768957));
#76896=CARTESIAN_POINT('Ctrl Pts',(1.48461476834817,-1.27230128149243,7.49691604969451));
#76897=CARTESIAN_POINT('Ctrl Pts',(1.43894242902308,-1.32373640943104,7.49301199169945));
#76898=CARTESIAN_POINT('Ctrl Pts',(1.39069471413912,-1.37261947096255,7.48910793370439));
#76899=CARTESIAN_POINT('Ctrl Pts',(1.34244414300075,-1.42150542636086,7.48520364458994));
#76900=CARTESIAN_POINT('Ctrl Pts',(1.29161824096721,-1.46783866712546,7.48129935547548));
#76901=CARTESIAN_POINT('Ctrl Pts',(1.2385244013895,-1.51134817535959,7.47739506636102));
#76902=CARTESIAN_POINT('Ctrl Pts',(1.18537400774783,-1.55490402869763,7.47348661850765));
#76903=CARTESIAN_POINT('Ctrl Pts',(1.12995123666793,-1.59562983457411,7.46957817065429));
#76904=CARTESIAN_POINT('Ctrl Pts',(1.07259570016622,-1.63329558377684,7.46566972280092));
#76905=CARTESIAN_POINT('Ctrl Pts',(1.01520583236305,-1.67098387856574,7.46175893546806));
#76906=CARTESIAN_POINT('Ctrl Pts',(0.955881321579679,-1.70560822336799,
7.4578481481352));
#76907=CARTESIAN_POINT('Ctrl Pts',(0.89498739328095,-1.73698404306665,7.45393736080234));
#76908=CARTESIAN_POINT('Ctrl Pts',(0.833988319154388,-1.76841403953841,
7.4500198206949));
#76909=CARTESIAN_POINT('Ctrl Pts',(0.771414867231583,-1.79658411394221,
7.44610228058745));
#76910=CARTESIAN_POINT('Ctrl Pts',(0.70765246667827,-1.82135773158492,7.44218474048));
#76911=CARTESIAN_POINT('Ctrl Pts',(0.67755758338143,-1.83305050232956,7.44033572113127));
#76912=CARTESIAN_POINT('Ctrl Pts',(0.647198058887002,-1.84398736789094,
7.43848670178255));
#76913=CARTESIAN_POINT('Ctrl Pts',(0.616615370520906,-1.85415789102152,
7.43663768243382));
#76914=CARTESIAN_POINT('Ctrl Pts',(0.551809973377996,-1.87570945583945,
7.43271956929136));
#76915=CARTESIAN_POINT('Ctrl Pts',(0.485744862813765,-1.89390209508338,
7.42880145614889));
#76916=CARTESIAN_POINT('Ctrl Pts',(0.418801309825052,-1.9085914866437,7.42488334300642));
#76917=CARTESIAN_POINT('Ctrl Pts',(0.351958563940618,-1.92325875814974,
7.42097112996371));
#76918=CARTESIAN_POINT('Ctrl Pts',(0.284240477515498,-1.93443314714333,
7.41705891692099));
#76919=CARTESIAN_POINT('Ctrl Pts',(0.216044487830142,-1.94201976799368,
7.41314670387827));
#76920=CARTESIAN_POINT('Ctrl Pts',(0.147928693872118,-1.94959746728456,
7.40923909143995));
#76921=CARTESIAN_POINT('Ctrl Pts',(0.0793365993349622,-1.95359572344296,
7.40533147900164));
#76922=CARTESIAN_POINT('Ctrl Pts',(0.0106750676280779,-1.95397083983644,
7.40142386656333));
#76923=CARTESIAN_POINT('Ctrl Pts',(-0.0579434289782319,-1.95434572111761,
7.39751870330565));
#76924=CARTESIAN_POINT('Ctrl Pts',(-0.126630785652382,-1.95110196465935,
7.39361354004798));
#76925=CARTESIAN_POINT('Ctrl Pts',(-0.194977357877224,-1.94424788283676,
7.38970837679031));
#76926=CARTESIAN_POINT('Ctrl Pts',(-0.263304534281484,-1.93739574610866,
7.38580432176445));
#76927=CARTESIAN_POINT('Ctrl Pts',(-0.331290629025947,-1.9269353670041,
7.38190026673859));
#76928=CARTESIAN_POINT('Ctrl Pts',(-0.398530164639113,-1.91292700014212,
7.37799621171274));
#76929=CARTESIAN_POINT('Ctrl Pts',(-0.465773680043226,-1.89891780414932,
7.37409192561267));
#76930=CARTESIAN_POINT('Ctrl Pts',(-0.532270067571575,-1.88136030630986,
7.37018763951259));
#76931=CARTESIAN_POINT('Ctrl Pts',(-0.597624891061796,-1.86036568705816,
7.36628335341252));
#76932=CARTESIAN_POINT('Ctrl Pts',(-0.663049327921038,-1.83934870516972,
7.36237490862156));
#76933=CARTESIAN_POINT('Ctrl Pts',(-0.727329304875256,-1.81488744620426,
7.3584664638306));
#76934=CARTESIAN_POINT('Ctrl Pts',(-0.790087354245672,-1.78714240413602,
7.35455801903964));
#76935=CARTESIAN_POINT('Ctrl Pts',(-0.852882968216514,-1.75938075493245,
7.3506472348011));
#76936=CARTESIAN_POINT('Ctrl Pts',(-0.914154402787626,-1.72833163319366,
7.34673645056256));
#76937=CARTESIAN_POINT('Ctrl Pts',(-0.973548459849918,-1.69420169883159,
7.34282566632402));
#76938=CARTESIAN_POINT('Ctrl Pts',(-1.03304507272848,-1.66001283225558,
7.33890812932788));
#76939=CARTESIAN_POINT('Ctrl Pts',(-1.09065742549882,-1.62273280298025,
7.33499059233174));
#76940=CARTESIAN_POINT('Ctrl Pts',(-1.14606171403452,-1.58261130655138,
7.33107305533561));
#76941=CARTESIAN_POINT('Ctrl Pts',(-1.17221209141589,-1.56367428379647,
7.32922400946638));
#76942=CARTESIAN_POINT('Ctrl Pts',(-1.19787105135633,-1.54410482632948,
7.32737496359715));
#76943=CARTESIAN_POINT('Ctrl Pts',(-1.22300732171854,-1.52393211496537,
7.32552591772793));
#76944=CARTESIAN_POINT('Ctrl Pts',(-1.27559540575662,-1.48172839002112,
7.32165749261314));
#76945=CARTESIAN_POINT('Ctrl Pts',(-1.3261134392786,-1.43670517168706,7.31778906749836));
#76946=CARTESIAN_POINT('Ctrl Pts',(-1.3742376675258,-1.38909568898375,7.31392064238358));
#76947=CARTESIAN_POINT('Ctrl Pts',(-1.42227925837674,-1.34156795977201,
7.31005886000553));
#76948=CARTESIAN_POINT('Ctrl Pts',(-1.46793484780101,-1.2914631345989,7.30619707762749));
#76949=CARTESIAN_POINT('Ctrl Pts',(-1.51091317412696,-1.23905503519803,
7.30233529524944));
#76950=CARTESIAN_POINT('Ctrl Pts',(-1.55385038440043,-1.18669707302562,
7.29847720732069));
#76951=CARTESIAN_POINT('Ctrl Pts',(-1.59411508796571,-1.13204059173095,
7.29461911939193));
#76952=CARTESIAN_POINT('Ctrl Pts',(-1.63145346495995,-1.07539555126017,
7.29076103146317));
#76953=CARTESIAN_POINT('Ctrl Pts',(-1.66876970881202,-1.01878408837992,
7.28690523050068));
#76954=CARTESIAN_POINT('Ctrl Pts',(-1.70316278757363,-0.960186824623716,
7.28304942953819));
#76955=CARTESIAN_POINT('Ctrl Pts',(-1.73442094909542,-0.899944426805872,
7.2791936285757));
#76956=CARTESIAN_POINT('Ctrl Pts',(-1.76567195409799,-0.839715821413957,
7.27533871039429));
#76957=CARTESIAN_POINT('Ctrl Pts',(-1.79378923447468,-0.777843278568951,
7.27148379221288));
#76958=CARTESIAN_POINT('Ctrl Pts',(-1.81860692347361,-0.714692142040087,
7.26762887403147));
#76959=CARTESIAN_POINT('Ctrl Pts',(-1.84344269671115,-0.651494988324808,
7.26377114683508));
#76960=CARTESIAN_POINT('Ctrl Pts',(-1.86497388998003,-0.587017851092827,
7.25991341963869));
#76961=CARTESIAN_POINT('Ctrl Pts',(-1.8830832601559,-0.521644932229409,
7.2560556924423));
#76962=CARTESIAN_POINT('Ctrl Pts',(-1.90119957869136,-0.456246930519752,
7.25219648507982));
#76963=CARTESIAN_POINT('Ctrl Pts',(-1.91589134940438,-0.389952956733717,
7.24833727771733));
#76964=CARTESIAN_POINT('Ctrl Pts',(-1.92709227518885,-0.323158417664546,
7.24447807035485));
#76965=CARTESIAN_POINT('Ctrl Pts',(-1.9383106063023,-0.256260085306467,
7.24061286609755));
#76966=CARTESIAN_POINT('Ctrl Pts',(-1.94602720593144,-0.188860137495797,
7.23674766184025));
#76967=CARTESIAN_POINT('Ctrl Pts',(-1.95022767276933,-0.121359072033122,
7.23288245758296));
#76968=CARTESIAN_POINT('Ctrl Pts',(-1.95276802049565,-0.0805359481304121,
7.23054486911345));
#76969=CARTESIAN_POINT('Ctrl Pts',(-1.95402333795018,-0.039675868301506,
7.22820728064394));
#76970=CARTESIAN_POINT('Ctrl Pts',(-1.95399967141271,0.00113318975355588,
7.22586969217444));
#76971=CARTESIAN_POINT('',(-1.9539992470135,-0.00171542142396889,6.52586969212423));
#76972=CARTESIAN_POINT('Ctrl Pts',(-1.9539996714122,0.00113319063008382,
7.22586969212423));
#76973=CARTESIAN_POINT('Ctrl Pts',(-1.95396101146291,0.0677958740412391,
7.22205117909017));
#76974=CARTESIAN_POINT('Ctrl Pts',(-1.95051120810791,0.134358173529546,
7.21823266605611));
#76975=CARTESIAN_POINT('Ctrl Pts',(-1.94367936074665,0.200565556882252,
7.21441415302205));
#76976=CARTESIAN_POINT('Ctrl Pts',(-1.93666931122138,0.268499896117147,
7.21049603775012));
#76977=CARTESIAN_POINT('Ctrl Pts',(-1.92607947596587,0.336200944680773,
7.20657792247819));
#76978=CARTESIAN_POINT('Ctrl Pts',(-1.91193512166022,0.40326181391515,7.20265980720626));
#76979=CARTESIAN_POINT('Ctrl Pts',(-1.89781206650137,0.470221700151785,
7.19874759199245));
#76980=CARTESIAN_POINT('Ctrl Pts',(-1.8801452158854,0.536542842854362,7.19483537677863));
#76981=CARTESIAN_POINT('Ctrl Pts',(-1.85901154704416,0.601823950966119,
7.19092316156481));
#76982=CARTESIAN_POINT('Ctrl Pts',(-1.83790273025389,0.667028292027257,
7.18701554690439));
#76983=CARTESIAN_POINT('Ctrl Pts',(-1.81333534258699,0.7311945616895,7.18310793224396));
#76984=CARTESIAN_POINT('Ctrl Pts',(-1.78543689703329,0.793933930948994,
7.17920031758354));
#76985=CARTESIAN_POINT('Ctrl Pts',(-1.75755593720705,0.856633977461658,
7.17529515207336));
#76986=CARTESIAN_POINT('Ctrl Pts',(-1.72634826040549,0.9179084491972,7.17138998656319));
#76987=CARTESIAN_POINT('Ctrl Pts',(-1.69198992972671,0.977387373411085,
7.16748482105301));
#76988=CARTESIAN_POINT('Ctrl Pts',(-1.65764134922827,1.03684941874213,7.16358076374767));
#76989=CARTESIAN_POINT('Ctrl Pts',(-1.62014413569726,1.09451650234945,7.15967670644233));
#76990=CARTESIAN_POINT('Ctrl Pts',(-1.57971998372168,1.15004381352641,7.15577264913698));
#76991=CARTESIAN_POINT('Ctrl Pts',(-1.53929343886796,1.20557441160199,7.15186836073382));
#76992=CARTESIAN_POINT('Ctrl Pts',(-1.49593990316492,1.25896458962648,7.14796407233065));
#76993=CARTESIAN_POINT('Ctrl Pts',(-1.44992294884486,1.30990054676416,7.14405978392749));
#76994=CARTESIAN_POINT('Ctrl Pts',(-1.40385697888034,1.36089075909542,7.14015133681336));
#76995=CARTESIAN_POINT('Ctrl Pts',(-1.35512225893885,1.40942116781589,7.13624288969924));
#76996=CARTESIAN_POINT('Ctrl Pts',(-1.30402033147456,1.45521372145159,7.13233444258512));
#76997=CARTESIAN_POINT('Ctrl Pts',(-1.25288781614849,1.50103368493992,7.12842365600855));
#76998=CARTESIAN_POINT('Ctrl Pts',(-1.19938565652686,1.54411222333274,7.12451286943198));
#76999=CARTESIAN_POINT('Ctrl Pts',(-1.14384749332535,1.58421239485535,7.12060208285541));
#77000=CARTESIAN_POINT('Ctrl Pts',(-1.08821343236478,1.62438180735327,7.11668454352277));
#77001=CARTESIAN_POINT('Ctrl Pts',(-1.03053676451945,1.66156232251659,7.11276700419013));
#77002=CARTESIAN_POINT('Ctrl Pts',(-0.971178267833906,1.69556149168561,
7.10884946485749));
#77003=CARTESIAN_POINT('Ctrl Pts',(-0.943161861229763,1.7116086391174,7.10700043934372));
#77004=CARTESIAN_POINT('Ctrl Pts',(-0.914771117210568,1.72694775559153,
7.10515141382994));
#77005=CARTESIAN_POINT('Ctrl Pts',(-0.886045494940342,1.74156233907831,
7.10330238831617));
#77006=CARTESIAN_POINT('Ctrl Pts',(-0.825175436213357,1.77253087813178,
7.09938427331234));
#77007=CARTESIAN_POINT('Ctrl Pts',(-0.762559166749165,1.80036572379865,
7.09546615830851));
#77008=CARTESIAN_POINT('Ctrl Pts',(-0.698552192994512,1.82486734686732,
7.09154804330468));
#77009=CARTESIAN_POINT('Ctrl Pts',(-0.634641603700151,1.84933207433575,
7.08763582836733));
#77010=CARTESIAN_POINT('Ctrl Pts',(-0.5693449220044,1.87047336632734,7.08372361342998));
#77011=CARTESIAN_POINT('Ctrl Pts',(-0.503041007328279,1.8881381689236,7.07981139849263));
#77012=CARTESIAN_POINT('Ctrl Pts',(-0.436815062660748,1.90578219861652,
7.07590378411972));
#77013=CARTESIAN_POINT('Ctrl Pts',(-0.369584710408188,1.91995773205846,
7.07199616974681));
#77014=CARTESIAN_POINT('Ctrl Pts',(-0.301745759251162,1.93056092801391,
7.0680885553739));
#77015=CARTESIAN_POINT('Ctrl Pts',(-0.233949327192227,1.94115747825446,
7.06418339015794));
#77016=CARTESIAN_POINT('Ctrl Pts',(-0.165545537791048,1.94818605671898,
7.06027822494199));
#77017=CARTESIAN_POINT('Ctrl Pts',(-0.0969407003716783,1.95159383597393,
7.05637305972603));
#77018=CARTESIAN_POINT('Ctrl Pts',(-0.0283553316912114,1.9550006481664,
7.05246900272117));
#77019=CARTESIAN_POINT('Ctrl Pts',(0.0404304807021455,1.95478867654858,
7.04856494571631));
#77020=CARTESIAN_POINT('Ctrl Pts',(0.109006807350353,1.95095707691156,7.04466088871144));
#77021=CARTESIAN_POINT('Ctrl Pts',(0.177587193221973,1.9471252504715,7.0407566006146));
#77022=CARTESIAN_POINT('Ctrl Pts',(0.245957577760492,1.93967340064045,7.03685231251774));
#77023=CARTESIAN_POINT('Ctrl Pts',(0.313711360341332,1.92865268578684,7.03294802442089));
#77024=CARTESIAN_POINT('Ctrl Pts',(0.381537311761262,1.91762023207281,7.02903957761985));
#77025=CARTESIAN_POINT('Ctrl Pts',(0.44874486405865,1.90301140599275,7.02513113081882));
#77026=CARTESIAN_POINT('Ctrl Pts',(0.514936846692412,1.88492865751425,7.02122268401778));
#77027=CARTESIAN_POINT('Ctrl Pts',(0.581168449507529,1.86683508534162,7.01731189775863));
#77028=CARTESIAN_POINT('Ctrl Pts',(0.646382805798501,1.84526360693987,7.01340111149947));
#77029=CARTESIAN_POINT('Ctrl Pts',(0.710199863729138,1.82036593946358,7.00949032524031));
#77030=CARTESIAN_POINT('Ctrl Pts',(0.774127114542087,1.79542528119719,7.00557278622846));
#77031=CARTESIAN_POINT('Ctrl Pts',(0.836651803667251,1.76714717368171,7.00165524721661));
#77032=CARTESIAN_POINT('Ctrl Pts',(0.897416531653136,1.73573026957407,6.99773770820476));
#77033=CARTESIAN_POINT('Ctrl Pts',(0.926096704373684,1.7209018935405,6.9958886800066));
#77034=CARTESIAN_POINT('Ctrl Pts',(0.954385202896228,1.70537492504266,6.99403965180844));
#77035=CARTESIAN_POINT('Ctrl Pts',(0.982246756649369,1.6891735580016,6.99219062361028));
#77036=CARTESIAN_POINT('Ctrl Pts',(1.04128576129815,1.65484264478231,6.98827250815433));
#77037=CARTESIAN_POINT('Ctrl Pts',(1.09863976305389,1.61734470487865,6.98435439269839));
#77038=CARTESIAN_POINT('Ctrl Pts',(1.15394827459615,1.57687012133421,6.98043627724244));
#77039=CARTESIAN_POINT('Ctrl Pts',(1.20917350031563,1.53645648607599,6.97652406184528));
#77040=CARTESIAN_POINT('Ctrl Pts',(1.26235895514181,1.4930753912049,6.97261184644812));
#77041=CARTESIAN_POINT('Ctrl Pts',(1.31317052241145,1.44696205170337,6.96869963105096));
#77042=CARTESIAN_POINT('Ctrl Pts',(1.36392233800537,1.4009029390139,6.96479201620911));
#77043=CARTESIAN_POINT('Ctrl Pts',(1.41230544761326,1.35211829170706,6.96088440136726));
#77044=CARTESIAN_POINT('Ctrl Pts',(1.4580178789933,1.30088426254447,6.95697678652542));
#77045=CARTESIAN_POINT('Ctrl Pts',(1.50370165947578,1.2496823450171,6.95307162083513));
#77046=CARTESIAN_POINT('Ctrl Pts',(1.54671775544886,1.19603445715405,6.94916645514484));
#77047=CARTESIAN_POINT('Ctrl Pts',(1.58680135072359,1.14025324965193,6.94526128945455));
#77048=CARTESIAN_POINT('Ctrl Pts',(1.62687357109104,1.08448787171946,6.94135723197068));
#77049=CARTESIAN_POINT('Ctrl Pts',(1.66401465588701,1.02659077521422,6.93745317448681));
#77050=CARTESIAN_POINT('Ctrl Pts',(1.69800149227727,0.966905854891855,6.93354911700294));
#77051=CARTESIAN_POINT('Ctrl Pts',(1.73199034047711,0.907217401593002,6.92964482842312));
#77052=CARTESIAN_POINT('Ctrl Pts',(1.76282432841332,0.845741343076677,6.9257405398433));
#77053=CARTESIAN_POINT('Ctrl Pts',(1.79032583296344,0.782846991323184,6.92183625126349));
#77054=CARTESIAN_POINT('Ctrl Pts',(1.81785663112085,0.719885646782544,6.91792780397678));
#77055=CARTESIAN_POINT('Ctrl Pts',(1.8420476644635,0.655503445629625,6.91401935669008));
#77056=CARTESIAN_POINT('Ctrl Pts',(1.86276951251717,0.590089606107866,6.91011090940337));
#77057=CARTESIAN_POINT('Ctrl Pts',(1.88350376394712,0.524636612140858,6.9062001226563));
#77058=CARTESIAN_POINT('Ctrl Pts',(1.90076457378381,0.458151227022748,6.90228933590922));
#77059=CARTESIAN_POINT('Ctrl Pts',(1.91447319502982,0.391035018268564,6.89837854916215));
#77060=CARTESIAN_POINT('Ctrl Pts',(1.92820548693666,0.323802920032551,6.89446100966401));
#77061=CARTESIAN_POINT('Ctrl Pts',(1.93837327580741,0.255938310399714,6.89054347016588));
#77062=CARTESIAN_POINT('Ctrl Pts',(1.94494953168796,0.187849192670067,6.88662593066775));
#77063=CARTESIAN_POINT('Ctrl Pts',(1.94805343260339,0.155712080201971,6.88477690674663));
#77064=CARTESIAN_POINT('Ctrl Pts',(1.95035799978609,0.123524970463383,6.88292788282552));
#77065=CARTESIAN_POINT('Ctrl Pts',(1.95186442108001,0.0913306176592063,
6.8810788589044));
#77066=CARTESIAN_POINT('Ctrl Pts',(1.9550565551626,0.0231101993282924,6.87716074363215));
#77067=CARTESIAN_POINT('Ctrl Pts',(1.95467411130022,-0.0454130105096706,
6.8732426283599));
#77068=CARTESIAN_POINT('Ctrl Pts',(1.95068143748882,-0.113832901379826,
6.86932451308765));
#77069=CARTESIAN_POINT('Ctrl Pts',(1.94669477601163,-0.182149762733948,
6.86541229787626));
#77070=CARTESIAN_POINT('Ctrl Pts',(1.93910870240703,-0.250363126800586,
6.86150008266486));
#77071=CARTESIAN_POINT('Ctrl Pts',(1.92793953197579,-0.318064712039808,
6.85758786745347));
#77072=CARTESIAN_POINT('Ctrl Pts',(1.91678349589624,-0.385686683807701,
6.85368025279955));
#77073=CARTESIAN_POINT('Ctrl Pts',(1.90205281081607,-0.452797588958959,
6.84977263814563));
#77074=CARTESIAN_POINT('Ctrl Pts',(1.88381562063976,-0.518993937761935,
6.8458650234917));
#77075=CARTESIAN_POINT('Ctrl Pts',(1.86558986088048,-0.585148797066506,
6.84195985799057));
#77076=CARTESIAN_POINT('Ctrl Pts',(1.84386208601922,-0.650389763943127,
6.83805469248943));
#77077=CARTESIAN_POINT('Ctrl Pts',(1.81875125798339,-0.714324759184377,
6.83414952698829));
#77078=CARTESIAN_POINT('Ctrl Pts',(1.79364755589508,-0.778241610961009,
6.83024546969451));
#77079=CARTESIAN_POINT('Ctrl Pts',(1.76516288621379,-0.840852769204412,
6.82634141240072));
#77080=CARTESIAN_POINT('Ctrl Pts',(1.7334650825806,-0.901784235542977,6.82243735510694));
#77081=CARTESIAN_POINT('Ctrl Pts',(1.70176540263952,-0.962719308635883,
6.81853306671786));
#77082=CARTESIAN_POINT('Ctrl Pts',(1.66685244041948,-1.02197405724667,6.81462877832878));
#77083=CARTESIAN_POINT('Ctrl Pts',(1.6289400608199,-1.07919890578894,6.81072448993969));
#77084=CARTESIAN_POINT('Ctrl Pts',(1.59098729832058,-1.13648470817653,6.80681604284339));
#77085=CARTESIAN_POINT('Ctrl Pts',(1.55002901465564,-1.19173588462052,6.80290759574709));
#77086=CARTESIAN_POINT('Ctrl Pts',(1.50632194849489,-1.24463255119033,6.79899914865079));
#77087=CARTESIAN_POINT('Ctrl Pts',(1.46258872080689,-1.29756087986208,6.79508836209421));
#77088=CARTESIAN_POINT('Ctrl Pts',(1.4161037690433,-1.34813153165594,6.79117757553764));
#77089=CARTESIAN_POINT('Ctrl Pts',(1.36716169807763,-1.39606048984616,6.78726678898106));
#77090=CARTESIAN_POINT('Ctrl Pts',(1.31813511886586,-1.44407220694123,6.78334924967155));
#77091=CARTESIAN_POINT('Ctrl Pts',(1.26664332158604,-1.48943280161812,6.77943171036206));
#77092=CARTESIAN_POINT('Ctrl Pts',(1.21301437599234,-1.53189820929327,6.77551417105255));
#77093=CARTESIAN_POINT('Ctrl Pts',(1.18770223833766,-1.55194130789861,6.77366514543454));
#77094=CARTESIAN_POINT('Ctrl Pts',(1.16191442903889,-1.57134006731575,6.77181611981653));
#77095=CARTESIAN_POINT('Ctrl Pts',(1.13568750743074,-1.59007228938365,6.76996709419852));
#77096=CARTESIAN_POINT('Ctrl Pts',(1.08011223547602,-1.62976617154388,6.76604897894628));
#77097=CARTESIAN_POINT('Ctrl Pts',(1.02234325355725,-1.6666215811514,6.76213086369404));
#77098=CARTESIAN_POINT('Ctrl Pts',(0.962702363599415,-1.70038823776222,
6.7582127484418));
#77099=CARTESIAN_POINT('Ctrl Pts',(0.903151283387841,-1.73410404712939,
6.75430053325135));
#77100=CARTESIAN_POINT('Ctrl Pts',(0.84173431404722,-1.76474009404042,6.75038831806091));
#77101=CARTESIAN_POINT('Ctrl Pts',(0.778803275672308,-1.79208857420667,
6.74647610287047));
#77102=CARTESIAN_POINT('Ctrl Pts',(0.715946240879911,-1.81940489400243,
6.74256848823879));
#77103=CARTESIAN_POINT('Ctrl Pts',(0.651579122071276,-1.84344112987901,
6.73866087360711));
#77104=CARTESIAN_POINT('Ctrl Pts',(0.586077833243433,-1.86403561483698,
6.73475325897542));
#77105=CARTESIAN_POINT('Ctrl Pts',(0.52061759828876,-1.88461719190583,6.73084809349731));
#77106=CARTESIAN_POINT('Ctrl Pts',(0.454025071610393,-1.90176114998742,
6.7269429280192));
#77107=CARTESIAN_POINT('Ctrl Pts',(0.386694152911894,-1.91535470138138,
6.72303776254109));
#77108=CARTESIAN_POINT('Ctrl Pts',(0.319382341385863,-1.92894439519645,
6.71913370527109));
#77109=CARTESIAN_POINT('Ctrl Pts',(0.251333035740334,-1.93898558515639,
6.71522964800109));
#77110=CARTESIAN_POINT('Ctrl Pts',(0.182951462176241,-1.94541634682337,
6.71132559073109));
#77111=CARTESIAN_POINT('Ctrl Pts',(0.114565840871633,-1.95184748914924,
6.70742130236652));
#77112=CARTESIAN_POINT('Ctrl Pts',(0.0458484025583555,-1.95466773538512,
6.70351701400194));
#77113=CARTESIAN_POINT('Ctrl Pts',(-0.0227911685518328,-1.95386707906041,
6.69961272563736));
#77114=CARTESIAN_POINT('Ctrl Pts',(-0.0915038520423259,-1.95306556990563,
6.6957042785665));
#77115=CARTESIAN_POINT('Ctrl Pts',(-0.160138010013442,-1.94863546685146,
6.69179583149564));
#77116=CARTESIAN_POINT('Ctrl Pts',(-0.22828563931517,-1.94061888759294,
6.68788738442478));
#77117=CARTESIAN_POINT('Ctrl Pts',(-0.296474059404211,-1.93259750989048,
6.68397659789421));
#77118=CARTESIAN_POINT('Ctrl Pts',(-0.364174886377365,-1.92098546674165,
6.68006581136364));
#77119=CARTESIAN_POINT('Ctrl Pts',(-0.430989702599176,-1.90587614399611,
6.67615502483307));
#77120=CARTESIAN_POINT('Ctrl Pts',(-0.497919887916471,-1.89074073199377,
6.67223748555018));
#77121=CARTESIAN_POINT('Ctrl Pts',(-0.563960535973705,-1.87209612159104,
6.6683199462673));
#77122=CARTESIAN_POINT('Ctrl Pts',(-0.628728634016056,-1.85008548580013,
6.66440240698442));
#77123=CARTESIAN_POINT('Ctrl Pts',(-0.659298304830121,-1.83969676186236,
6.66255338115382));
#77124=CARTESIAN_POINT('Ctrl Pts',(-0.689584783439458,-1.82855887907734,
6.66070435532323));
#77125=CARTESIAN_POINT('Ctrl Pts',(-0.719549587778587,-1.81669050493684,
6.65885532949263));
#77126=CARTESIAN_POINT('Ctrl Pts',(-0.783045487526726,-1.79154123027214,
6.65493721417833));
#77127=CARTESIAN_POINT('Ctrl Pts',(-0.845347165958881,-1.76300918659432,
6.65101909886402));
#77128=CARTESIAN_POINT('Ctrl Pts',(-0.906069789364223,-1.73122890941709,
6.64710098354972));
#77129=CARTESIAN_POINT('Ctrl Pts',(-0.966700974122495,-1.6994964883005,
6.64318876829611));
#77130=CARTESIAN_POINT('Ctrl Pts',(-1.02575739066157,-1.66452576748227,
6.63927655304249));
#77131=CARTESIAN_POINT('Ctrl Pts',(-1.08287360038137,-1.62649954368179,
6.63536433778888));
#77132=CARTESIAN_POINT('Ctrl Pts',(-1.13992264447097,-1.58851803670161,
6.6314567230927));
#77133=CARTESIAN_POINT('Ctrl Pts',(-1.19503560549445,-1.54748843401052,
6.62754910839652));
#77134=CARTESIAN_POINT('Ctrl Pts',(-1.24787272958104,-1.50363880329286,
6.62364149370033));
#77135=CARTESIAN_POINT('Ctrl Pts',(-1.30067673725271,-1.45981665595151,
6.61973632815694));
#77136=CARTESIAN_POINT('Ctrl Pts',(-1.35120735987634,-1.41317830014893,
6.61583116261354));
#77137=CARTESIAN_POINT('Ctrl Pts',(-1.399156145627,-1.36399343112575,6.61192599707014));
#77138=CARTESIAN_POINT('Ctrl Pts',(-1.4470913244768,-1.31482251977901,6.60802193973417));
#77139=CARTESIAN_POINT('Ctrl Pts',(-1.49244577773927,-1.26310688183872,
6.60411788239819));
#77140=CARTESIAN_POINT('Ctrl Pts',(-1.53494763511834,-1.20915332255451,
6.60021382506222));
#77141=CARTESIAN_POINT('Ctrl Pts',(-1.57745200833494,-1.15519656956542,
6.59630953663108));
#77142=CARTESIAN_POINT('Ctrl Pts',(-1.61710314806692,-1.09900202020992,
6.59240524819994));
#77143=CARTESIAN_POINT('Ctrl Pts',(-1.65367037796729,-1.04090839223897,
6.5885009597688));
#77144=CARTESIAN_POINT('Ctrl Pts',(-1.69027655795744,-0.982752885038156,
6.58459251263093));
#77145=CARTESIAN_POINT('Ctrl Pts',(-1.72379201000291,-0.922694679357089,
6.58068406549306));
#77146=CARTESIAN_POINT('Ctrl Pts',(-1.75403075561889,-0.861099360319714,
6.5767756183552));
#77147=CARTESIAN_POINT('Ctrl Pts',(-1.78428760109273,-0.799467172473922,
6.57286483175727));
#77148=CARTESIAN_POINT('Ctrl Pts',(-1.81126364354497,-0.73629649260063,
6.56895404515935));
#77149=CARTESIAN_POINT('Ctrl Pts',(-1.83482117177094,-0.671972668805138,
6.56504325856143));
#77150=CARTESIAN_POINT('Ctrl Pts',(-1.8584193767624,-0.607537777113628,
6.56112571921136));
#77151=CARTESIAN_POINT('Ctrl Pts',(-1.87858714210892,-0.541946237426363,
6.55720817986128));
#77152=CARTESIAN_POINT('Ctrl Pts',(-1.8952369370561,-0.475597468893815,
6.55329064051121));
#77153=CARTESIAN_POINT('Ctrl Pts',(-1.90309541360779,-0.44428175339099,
6.55144161526973));
#77154=CARTESIAN_POINT('Ctrl Pts',(-1.91017093194561,-0.412797478057282,
6.54959259002824));
#77155=CARTESIAN_POINT('Ctrl Pts',(-1.91645829519957,-0.381187096792052,
6.54774356478676));
#77156=CARTESIAN_POINT('Ctrl Pts',(-1.93568455106865,-0.284525069519832,
6.54208939292406));
#77157=CARTESIAN_POINT('Ctrl Pts',(-1.94760241356582,-0.186364687119417,
6.53643522106135));
#77158=CARTESIAN_POINT('Ctrl Pts',(-1.95203469361534,-0.0876159512992307,
6.53078104919865));
#77159=CARTESIAN_POINT('Ctrl Pts',(-1.95331802390111,-0.0590240658715734,
6.52914393017384));
#77160=CARTESIAN_POINT('Ctrl Pts',(-1.95397407964231,-0.0303830267533754,
6.52750681114904));
#77161=CARTESIAN_POINT('Ctrl Pts',(-1.9539992470135,-0.00171542142396889,
6.52586969212423));
#77162=CARTESIAN_POINT('',(-1.95079827866809,-3.39314739267183E-5,5.82586969212423));
#77163=CARTESIAN_POINT('Ctrl Pts',(-1.95470819824863,-0.00170936608773048,
6.52586931091837));
#77164=CARTESIAN_POINT('Ctrl Pts',(-1.94992671209745,0.519363870229142,
6.49612347397254));
#77165=CARTESIAN_POINT('Ctrl Pts',(-1.4676232491419,1.69704784902766,6.42934038212473));
#77166=CARTESIAN_POINT('Ctrl Pts',(0.520941041773296,2.24982010296219,6.325520035375));
#77167=CARTESIAN_POINT('Ctrl Pts',(2.17254641826532,0.783014766469865,6.2144082706691));
#77168=CARTESIAN_POINT('Ctrl Pts',(1.83645143012728,-1.40018434850807,6.10329650596323));
#77169=CARTESIAN_POINT('Ctrl Pts',(-0.179844794802092,-2.30233053978416,
5.99218474125735));
#77170=CARTESIAN_POINT('Ctrl Pts',(-1.72101362137731,-1.30002449932279,
5.89970913664434));
#77171=CARTESIAN_POINT('Ctrl Pts',(-1.95084848133978,-0.324013652614182,
5.84427078693331));
#77172=CARTESIAN_POINT('Ctrl Pts',(-1.95079827866809,-3.39314739267183E-5,
5.82586969212423));
#77173=CARTESIAN_POINT('',(-1.95399923079511,0.00173379702722768,5.12586969212423));
#77174=CARTESIAN_POINT('Ctrl Pts',(-1.95079827866809,-3.39314739267183E-5,
5.82586969212423));
#77175=CARTESIAN_POINT('Ctrl Pts',(-1.95074743468102,0.328084477385078,
5.80723353203135));
#77176=CARTESIAN_POINT('Ctrl Pts',(-1.71668384482246,1.30836916436041,5.75156011703652));
#77177=CARTESIAN_POINT('Ctrl Pts',(-0.165267944017257,2.3034227947424,5.65884944713968));
#77178=CARTESIAN_POINT('Ctrl Pts',(1.84527750005803,1.38853196305902,5.54773768243383));
#77179=CARTESIAN_POINT('Ctrl Pts',(2.16754658332468,-0.796750822900473,
5.43662591772792));
#77180=CARTESIAN_POINT('Ctrl Pts',(0.506689737022561,-2.25307247443607,
5.32551415302205));
#77181=CARTESIAN_POINT('Ctrl Pts',(-1.47384180283068,-1.68900403463015,
5.22192884966718));
#77182=CARTESIAN_POINT('Ctrl Pts',(-1.94982277544559,-0.515311787546464,
5.15538080121427));
#77183=CARTESIAN_POINT('Ctrl Pts',(-1.95458374895511,0.0017287873519051,
5.12587000766333));
#77184=CARTESIAN_POINT('',(-1.95399970439072,-0.00107482137716873,4.42586969212423));
#77185=CARTESIAN_POINT('Ctrl Pts',(-1.95399923079511,0.00173379702722768,
5.12586969212423));
#77186=CARTESIAN_POINT('Ctrl Pts',(-1.95391274807805,0.0992003170110558,
5.12030494365936));
#77187=CARTESIAN_POINT('Ctrl Pts',(-1.9465302636818,0.196354128825551,5.1147401951945));
#77188=CARTESIAN_POINT('Ctrl Pts',(-1.93201158427293,0.292313595707092,
5.10917544672964));
#77189=CARTESIAN_POINT('Ctrl Pts',(-1.92689366140619,0.326139891887515,
5.10721383902319));
#77190=CARTESIAN_POINT('Ctrl Pts',(-1.92088939232674,0.359818056639332,
5.10525223131674));
#77191=CARTESIAN_POINT('Ctrl Pts',(-1.914007071507,0.393310221353584,5.10329062361029));
#77192=CARTESIAN_POINT('Ctrl Pts',(-1.90026032370521,0.460207472109741,
5.09937250832143));
#77193=CARTESIAN_POINT('Ctrl Pts',(-1.88297487280552,0.526515765509737,
5.09545439303258));
#77194=CARTESIAN_POINT('Ctrl Pts',(-1.86221641779253,0.591832757883458,
5.09153627774372));
#77195=CARTESIAN_POINT('Ctrl Pts',(-1.84148922172499,0.657051393211835,
5.08762406251592));
#77196=CARTESIAN_POINT('Ctrl Pts',(-1.81729954861703,0.721281225074169,
5.08371184728813));
#77197=CARTESIAN_POINT('Ctrl Pts',(-1.78976399250792,0.784130633964848,
5.07979963206033));
#77198=CARTESIAN_POINT('Ctrl Pts',(-1.76226081675402,0.846906135280302,
5.07589201739038));
#77199=CARTESIAN_POINT('Ctrl Pts',(-1.73141976859218,0.908303989127187,
5.07198440272043));
#77200=CARTESIAN_POINT('Ctrl Pts',(-1.69740648393353,0.96795001332734,5.06807678805048));
#77201=CARTESIAN_POINT('Ctrl Pts',(-1.66341451758442,1.02755865353419,5.06417162253355));
#77202=CARTESIAN_POINT('Ctrl Pts',(-1.6262545018986,1.08541721581697,5.06026645701662));
#77203=CARTESIAN_POINT('Ctrl Pts',(-1.58613850153253,1.14117511975863,5.0563612914997));
#77204=CARTESIAN_POINT('Ctrl Pts',(-1.54603388528254,1.19691720072579,5.0524572341904));
#77205=CARTESIAN_POINT('Ctrl Pts',(-1.50297523674509,1.25055940767055,5.0485531768811));
#77206=CARTESIAN_POINT('Ctrl Pts',(-1.45721751668746,1.30178074538658,5.0446491195718));
#77207=CARTESIAN_POINT('Ctrl Pts',(-1.41145708806801,1.35300511507533,5.0407448311675));
#77208=CARTESIAN_POINT('Ctrl Pts',(-1.36299760034251,1.4018079659198,5.03684054276319));
#77209=CARTESIAN_POINT('Ctrl Pts',(-1.31213259233443,1.44790333245481,5.03293625435889));
#77210=CARTESIAN_POINT('Ctrl Pts',(-1.26121340476127,1.49404779810546,5.02902780724792));
#77211=CARTESIAN_POINT('Ctrl Pts',(-1.20788394858165,1.53747869310908,5.02511936013696));
#77212=CARTESIAN_POINT('Ctrl Pts',(-1.15247198028643,1.57794940814168,5.02121091302599));
#77213=CARTESIAN_POINT('Ctrl Pts',(-1.09702684432159,1.61844434753134,5.01730012645504));
#77214=CARTESIAN_POINT('Ctrl Pts',(-1.03949712746111,1.65597531182826,5.01338933988409));
#77215=CARTESIAN_POINT('Ctrl Pts',(-0.980238426836116,1.69033979618119,
5.00947855331314));
#77216=CARTESIAN_POINT('Ctrl Pts',(-0.920877404256082,1.72476361766412,
5.00556101398987));
#77217=CARTESIAN_POINT('Ctrl Pts',(-0.859781877160007,1.75600982298062,
5.00164347466661));
#77218=CARTESIAN_POINT('Ctrl Pts',(-0.79733000983898,1.78392288381818,4.99772593534334));
#77219=CARTESIAN_POINT('Ctrl Pts',(-0.767853574658789,1.79709747032381,
4.9958769098637));
#77220=CARTESIAN_POINT('Ctrl Pts',(-0.738075242029198,1.80953023862869,
4.99402788438405));
#77221=CARTESIAN_POINT('Ctrl Pts',(-0.708035919494371,1.82120870212773,
4.99217885890441));
#77222=CARTESIAN_POINT('Ctrl Pts',(-0.644382102829161,1.84595555764144,
4.98826074361555));
#77223=CARTESIAN_POINT('Ctrl Pts',(-0.579303134779922,1.8674102658445,4.98434262832669));
#77224=CARTESIAN_POINT('Ctrl Pts',(-0.513172640155052,1.885409727724,4.98042451303783));
#77225=CARTESIAN_POINT('Ctrl Pts',(-0.447141727581096,1.90338208526473,
4.97651229781003));
#77226=CARTESIAN_POINT('Ctrl Pts',(-0.380062901780406,1.91790939455919,
4.97260008258223));
#77227=CARTESIAN_POINT('Ctrl Pts',(-0.312328391621999,1.9288771282243,4.96868786735443));
#77228=CARTESIAN_POINT('Ctrl Pts',(-0.244673533659072,1.93983196441567,
4.96478025268447));
#77229=CARTESIAN_POINT('Ctrl Pts',(-0.176365005912992,1.94723545993428,
4.96087263801452));
#77230=CARTESIAN_POINT('Ctrl Pts',(-0.107806996632855,1.95102374446776,
4.95696502334456));
#77231=CARTESIAN_POINT('Ctrl Pts',(-0.039291957059335,1.95480965464007,
4.95305985782764));
#77232=CARTESIAN_POINT('Ctrl Pts',(0.0294717638388294,1.95498482154557,
4.94915469231071));
#77233=CARTESIAN_POINT('Ctrl Pts',(0.0980746144653294,1.95153718130029,
4.94524952679378));
#77234=CARTESIAN_POINT('Ctrl Pts',(0.166657996979155,1.94809051942614,4.94134546948448));
#77235=CARTESIAN_POINT('Ctrl Pts',(0.235080108818078,1.94102311599331,4.93744141217518));
#77236=CARTESIAN_POINT('Ctrl Pts',(0.302932977910631,1.93037499229922,4.93353735486588));
#77237=CARTESIAN_POINT('Ctrl Pts',(0.370789863455265,1.9197262383049,4.92963306646157));
#77238=CARTESIAN_POINT('Ctrl Pts',(0.438076953822389,1.90549642203426,4.92572877805727));
#77239=CARTESIAN_POINT('Ctrl Pts',(0.504394772752544,1.88777697655732,4.92182448965297));
#77240=CARTESIAN_POINT('Ctrl Pts',(0.570783231022542,1.87003865696856,4.917916042542));
#77241=CARTESIAN_POINT('Ctrl Pts',(0.636199881316839,1.84880341735352,4.91400759543103));
#77242=CARTESIAN_POINT('Ctrl Pts',(0.700259743181115,1.8242127869522,4.91009914832006));
#77243=CARTESIAN_POINT('Ctrl Pts',(0.764357949042219,1.79960743745805,4.90618836174911));
#77244=CARTESIAN_POINT('Ctrl Pts',(0.827097300859291,1.77164290033175,4.90227757517815));
#77245=CARTESIAN_POINT('Ctrl Pts',(0.888114762520646,1.74050802026101,4.8983667886072));
#77246=CARTESIAN_POINT('Ctrl Pts',(0.949237582988419,1.70931937961563,4.89444924928393));
#77247=CARTESIAN_POINT('Ctrl Pts',(1.00863215378542,1.67494971657283,4.89053170996066));
#77248=CARTESIAN_POINT('Ctrl Pts',(1.0659626568427,1.63763231960561,4.8866141706374));
#77249=CARTESIAN_POINT('Ctrl Pts',(1.09302187748232,1.6200190138716,4.88476514515777));
#77250=CARTESIAN_POINT('Ctrl Pts',(1.11962174108735,1.60174963845557,4.88291611967814));
#77251=CARTESIAN_POINT('Ctrl Pts',(1.14572956451243,1.58285178238588,4.88106709419852));
#77252=CARTESIAN_POINT('Ctrl Pts',(1.20105247014453,1.54280691572004,4.87714897890966));
#77253=CARTESIAN_POINT('Ctrl Pts',(1.25438307974971,1.49977875441177,4.8732308636208));
#77254=CARTESIAN_POINT('Ctrl Pts',(1.30538167850735,1.45399266621855,4.86931274833194));
#77255=CARTESIAN_POINT('Ctrl Pts',(1.3563034814526,1.4082755246224,4.86540053310415));
#77256=CARTESIAN_POINT('Ctrl Pts',(1.40489987984092,1.35980902433802,4.86148831787635));
#77257=CARTESIAN_POINT('Ctrl Pts',(1.45086186696259,1.30886051319223,4.85757610264855));
#77258=CARTESIAN_POINT('Ctrl Pts',(1.4967698052224,1.25797191479637,4.8536684879786));
#77259=CARTESIAN_POINT('Ctrl Pts',(1.54004915682881,1.20460746564474,4.84976087330864));
#77260=CARTESIAN_POINT('Ctrl Pts',(1.58042698002786,1.14907204334629,4.84585325863869));
#77261=CARTESIAN_POINT('Ctrl Pts',(1.62077949585239,1.09357142866302,4.84194809312176));
#77262=CARTESIAN_POINT('Ctrl Pts',(1.6582338021363,1.03590293695401,4.83804292760484));
#77263=CARTESIAN_POINT('Ctrl Pts',(1.69255756619582,0.976404058324866,4.83413776208791));
#77264=CARTESIAN_POINT('Ctrl Pts',(1.72687158985972,0.916922064283803,4.83023370477862));
#77265=CARTESIAN_POINT('Ctrl Pts',(1.75805658922141,0.855611140342085,4.82632964746932));
#77266=CARTESIAN_POINT('Ctrl Pts',(1.78592484162299,0.792835708122365,4.82242559016002));
#77267=CARTESIAN_POINT('Ctrl Pts',(1.81379474364533,0.730056560002035,4.81852130175571));
#77268=CARTESIAN_POINT('Ctrl Pts',(1.83834731168824,0.665813182104631,4.81461701335141));
#77269=CARTESIAN_POINT('Ctrl Pts',(1.85944261980839,0.600490752335224,4.8107127249471));
#77270=CARTESIAN_POINT('Ctrl Pts',(1.88056039788703,0.535098743478489,4.80680427783614));
#77271=CARTESIAN_POINT('Ctrl Pts',(1.89821341536483,0.468625857944904,4.80289583072517));
#77272=CARTESIAN_POINT('Ctrl Pts',(1.91231169311282,0.401472275984276,4.7989873836142));
#77273=CARTESIAN_POINT('Ctrl Pts',(1.92641840959765,0.334278498234007,4.79507659704325));
#77274=CARTESIAN_POINT('Ctrl Pts',(1.93696607621066,0.26640369928676,4.7911658104723));
#77275=CARTESIAN_POINT('Ctrl Pts',(1.9439163658891,0.198255296092009,4.78725502390134));
#77276=CARTESIAN_POINT('Ctrl Pts',(1.95087865662763,0.129989221099292,4.78333748457808));
#77277=CARTESIAN_POINT('Ctrl Pts',(1.95423114908046,0.0614490899921429,
4.77941994525481));
#77278=CARTESIAN_POINT('Ctrl Pts',(1.95398761717133,-0.00695643163745314,
4.77550240593155));
#77279=CARTESIAN_POINT('Ctrl Pts',(1.95387267340996,-0.0392429109817258,
4.77365338045191));
#77280=CARTESIAN_POINT('Ctrl Pts',(1.95295739184096,-0.0714994619684756,
4.77180435497227));
#77281=CARTESIAN_POINT('Ctrl Pts',(1.95124721609382,-0.103683661616032,
4.76995532949264));
#77282=CARTESIAN_POINT('Ctrl Pts',(1.94762332566327,-0.171882508028614,
4.76603721420378));
#77283=CARTESIAN_POINT('Ctrl Pts',(1.94041247795351,-0.24002632845082,4.76211909891493));
#77284=CARTESIAN_POINT('Ctrl Pts',(1.92961967910788,-0.307707481221396,
4.75820098362607));
#77285=CARTESIAN_POINT('Ctrl Pts',(1.9188431325079,-0.375286716895494,4.75428876839827));
#77286=CARTESIAN_POINT('Ctrl Pts',(1.9044954164924,-0.442404185793469,4.75037655317047));
#77287=CARTESIAN_POINT('Ctrl Pts',(1.88663346210431,-0.508655266038109,
4.74646433794268));
#77288=CARTESIAN_POINT('Ctrl Pts',(1.86879251242828,-0.574828438522259,
4.74255672327272));
#77289=CARTESIAN_POINT('Ctrl Pts',(1.84744565914114,-0.640136773085806,
4.73864910860277));
#77290=CARTESIAN_POINT('Ctrl Pts',(1.82270092612445,-0.704185582005962,
4.73474149393282));
#77291=CARTESIAN_POINT('Ctrl Pts',(1.79797170222084,-0.768194247424886,
4.73083632841589));
#77292=CARTESIAN_POINT('Ctrl Pts',(1.76984900004189,-0.830944495371427,
4.72693116289897));
#77293=CARTESIAN_POINT('Ctrl Pts',(1.73849027101473,-0.892058057296234,
4.72302599738204));
#77294=CARTESIAN_POINT('Ctrl Pts',(1.70714044096574,-0.95315427641826,4.71912194007274));
#77295=CARTESIAN_POINT('Ctrl Pts',(1.67255663154283,-1.01261429412407,4.71521788276345));
#77296=CARTESIAN_POINT('Ctrl Pts',(1.63494312021436,-1.07008270412325,4.71131382545415));
#77297=CARTESIAN_POINT('Ctrl Pts',(1.59732738240869,-1.12755451588154,4.70740953704984));
#77298=CARTESIAN_POINT('Ctrl Pts',(1.55668185816409,-1.1830340757216,4.70350524864554));
#77299=CARTESIAN_POINT('Ctrl Pts',(1.51325419252364,-1.23619486684326,4.69960096024124));
#77300=CARTESIAN_POINT('Ctrl Pts',(1.46978026930596,-1.28941228291505,4.69569251313027));
#77301=CARTESIAN_POINT('Ctrl Pts',(1.42351860237532,-1.34030561951258,4.69178406601931));
#77302=CARTESIAN_POINT('Ctrl Pts',(1.37475653739245,-1.38858217722133,4.68787561890834));
#77303=CARTESIAN_POINT('Ctrl Pts',(1.32596528513989,-1.43688763159206,4.68396483233739));
#77304=CARTESIAN_POINT('Ctrl Pts',(1.27467102358867,-1.48257286263037,4.68005404576643));
#77305=CARTESIAN_POINT('Ctrl Pts',(1.22119520081885,-1.52538463395204,4.67614325919548));
#77306=CARTESIAN_POINT('Ctrl Pts',(1.16762704138498,-1.56827032832793,4.67222571987222));
#77307=CARTESIAN_POINT('Ctrl Pts',(1.11187020205469,-1.60827237384719,4.66830818054895));
#77308=CARTESIAN_POINT('Ctrl Pts',(1.0542754467429,-1.64518062303051,4.66439064122569));
#77309=CARTESIAN_POINT('Ctrl Pts',(1.02709150261937,-1.66260081655447,4.66254161574605));
#77310=CARTESIAN_POINT('Ctrl Pts',(0.999498482844079,-1.67933246565426,
4.6606925902664));
#77311=CARTESIAN_POINT('Ctrl Pts',(0.971534977350408,-1.69535712691596,
4.65884356478676));
#77312=CARTESIAN_POINT('Ctrl Pts',(0.912279851008944,-1.72931364670408,
4.6549254494979));
#77313=CARTESIAN_POINT('Ctrl Pts',(0.851124875507569,-1.76022716410113,
4.65100733420904));
#77314=CARTESIAN_POINT('Ctrl Pts',(0.788415197746269,-1.78788072196182,
4.64708921892018));
#77315=CARTESIAN_POINT('Ctrl Pts',(0.725799950827496,-1.81549263794424,
4.64317700369238));
#77316=CARTESIAN_POINT('Ctrl Pts',(0.661635094416118,-1.83985414011142,
4.63926478846459));
#77317=CARTESIAN_POINT('Ctrl Pts',(0.596291410110017,-1.86079352810273,
4.63535257323679));
#77318=CARTESIAN_POINT('Ctrl Pts',(0.53102456651486,-1.8817082924831,4.63144495856683));
#77319=CARTESIAN_POINT('Ctrl Pts',(0.464582114316974,-1.89920878546645,
4.62753734389688));
#77320=CARTESIAN_POINT('Ctrl Pts',(0.397354210112301,-1.91317161585312,
4.62362972922693));
#77321=CARTESIAN_POINT('Ctrl Pts',(0.330168441952001,-1.92712569483741,
4.61972456371));
#77322=CARTESIAN_POINT('Ctrl Pts',(0.26219867885986,-1.93754640980326,4.61581939819307));
#77323=CARTESIAN_POINT('Ctrl Pts',(0.193848101334831,-1.94436079820821,
4.61191423267615));
#77324=CARTESIAN_POINT('Ctrl Pts',(0.125516920332409,-1.95117325282646,
4.60801017536685));
#77325=CARTESIAN_POINT('Ctrl Pts',(0.0568056286537933,-1.95438136374034,
4.60410611805755));
#77326=CARTESIAN_POINT('Ctrl Pts',(-0.0118763931020487,-1.95396390736546,
4.60020206074825));
#77327=CARTESIAN_POINT('Ctrl Pts',(-0.0805624803904741,-1.95354642627985,
4.59629777234394));
#77328=CARTESIAN_POINT('Ctrl Pts',(-0.149218802462485,-1.94950295738358,
4.59239348393964));
#77329=CARTESIAN_POINT('Ctrl Pts',(-0.217436718029847,-1.9418643808599,
4.58848919553533));
#77330=CARTESIAN_POINT('Ctrl Pts',(-0.285727296851189,-1.93421766800105,
4.58458074842436));
#77331=CARTESIAN_POINT('Ctrl Pts',(-0.353578047466985,-1.92296826010078,
4.58067230131339));
#77332=CARTESIAN_POINT('Ctrl Pts',(-0.420587196951145,-1.90819873434629,
4.57676385420243));
#77333=CARTESIAN_POINT('Ctrl Pts',(-0.487636455772705,-1.89342036806932,
4.57285306763147));
#77334=CARTESIAN_POINT('Ctrl Pts',(-0.553842636738836,-1.87511782166209,
4.56894228106052));
#77335=CARTESIAN_POINT('Ctrl Pts',(-0.618818615045365,-1.85342372966177,
4.56503149448957));
#77336=CARTESIAN_POINT('Ctrl Pts',(-0.683906787326116,-1.83169217848865,
4.5611139551663));
#77337=CARTESIAN_POINT('Ctrl Pts',(-0.747760059950065,-1.80655757379627,
4.55719641584304));
#77338=CARTESIAN_POINT('Ctrl Pts',(-0.810011598995132,-1.77820055378839,
4.55327887651977));
#77339=CARTESIAN_POINT('Ctrl Pts',(-0.839393481943236,-1.76481642456991,
4.55142985104014));
#77340=CARTESIAN_POINT('Ctrl Pts',(-0.868418907984736,-1.75071509608578,
4.54958082556051));
#77341=CARTESIAN_POINT('Ctrl Pts',(-0.897051447481119,-1.73591897868882,
4.54773180008087));
#77342=CARTESIAN_POINT('Ctrl Pts',(-0.957724267837203,-1.70456576348041,
4.54381368479201));
#77343=CARTESIAN_POINT('Ctrl Pts',(-1.01687162431583,-1.66996566509871,
4.53989556950315));
#77344=CARTESIAN_POINT('Ctrl Pts',(-1.07412401014006,-1.63229090876616,
4.53597745421429));
#77345=CARTESIAN_POINT('Ctrl Pts',(-1.13129018293907,-1.59467288464958,
4.53206523898649));
#77346=CARTESIAN_POINT('Ctrl Pts',(-1.18656664073048,-1.55398965960322,
4.52815302375869));
#77347=CARTESIAN_POINT('Ctrl Pts',(-1.23960798587046,-1.5104595464183,4.52424080853089));
#77348=CARTESIAN_POINT('Ctrl Pts',(-1.29258695719858,-1.46698062234035,
4.52033319386094));
#77349=CARTESIAN_POINT('Ctrl Pts',(-1.3433356574388,-1.42066176945451,4.51642557919098));
#77350=CARTESIAN_POINT('Ctrl Pts',(-1.39153875831127,-1.37176378583105,
4.51251796452103));
#77351=CARTESIAN_POINT('Ctrl Pts',(-1.43971164720521,-1.32289644971376,
4.5086127990041));
#77352=CARTESIAN_POINT('Ctrl Pts',(-1.48534175713883,-1.27145353900056,
4.50470763348718));
#77353=CARTESIAN_POINT('Ctrl Pts',(-1.52814905536641,-1.21773415185037,
4.50080246797025));
#77354=CARTESIAN_POINT('Ctrl Pts',(-1.57094420574158,-1.1640300091845,4.49689841066095));
#77355=CARTESIAN_POINT('Ctrl Pts',(-1.61091782825079,-1.10805105703936,
4.49299435335165));
#77356=CARTESIAN_POINT('Ctrl Pts',(-1.64782998856845,-1.05012967236171,
4.48909029604235));
#77357=CARTESIAN_POINT('Ctrl Pts',(-1.68474433384784,-0.992204859111793,
4.48518600763805));
#77358=CARTESIAN_POINT('Ctrl Pts',(-1.71859659496775,-0.932337801239931,
4.48128171923375));
#77359=CARTESIAN_POINT('Ctrl Pts',(-1.74919100739059,-0.870888523098049,
4.47737743082945));
#77360=CARTESIAN_POINT('Ctrl Pts',(-1.77981800787394,-0.809373791409713,
4.47346898371848));
#77361=CARTESIAN_POINT('Ctrl Pts',(-1.80718001468011,-0.74627391723576,
4.46956053660752));
#77362=CARTESIAN_POINT('Ctrl Pts',(-1.83112841662984,-0.68197120306557,
4.46565208949655));
#77363=CARTESIAN_POINT('Ctrl Pts',(-1.85509115325689,-0.617629999535627,
4.4617413029256));
#77364=CARTESIAN_POINT('Ctrl Pts',(-1.87563607141369,-0.552084992547746,
4.45783051635464));
#77365=CARTESIAN_POINT('Ctrl Pts',(-1.8926645567636,-0.485733337924075,
4.45391972978369));
#77366=CARTESIAN_POINT('Ctrl Pts',(-1.9097224451867,-0.419267113946904,
4.45000219046042));
#77367=CARTESIAN_POINT('Ctrl Pts',(-1.92325168549484,-0.351991944422665,
4.44608465113716));
#77368=CARTESIAN_POINT('Ctrl Pts',(-1.93320499647078,-0.284313984215347,
4.44216711181389));
#77369=CARTESIAN_POINT('Ctrl Pts',(-1.93790282438841,-0.252370904004291,
4.44031808633426));
#77370=CARTESIAN_POINT('Ctrl Pts',(-1.94180479144181,-0.22033814772228,
4.43846906085462));
#77371=CARTESIAN_POINT('Ctrl Pts',(-1.94490995839488,-0.188258475868743,
4.43662003537499));
#77372=CARTESIAN_POINT('Ctrl Pts',(-1.95092783302923,-0.126087440802656,
4.43303658762473));
#77373=CARTESIAN_POINT('Ctrl Pts',(-1.95396529883072,-0.0636233112941925,
4.42945313987448));
#77374=CARTESIAN_POINT('Ctrl Pts',(-1.95399970439072,-0.00107482137716873,
4.42586969212423));
#77375=CARTESIAN_POINT('',(-1.95135083467133,-0.00103713828173369,3.72586969212423));
#77376=CARTESIAN_POINT('Ctrl Pts',(-1.95645520290123,-0.00105911241531774,
4.42586871599238));
#77377=CARTESIAN_POINT('Ctrl Pts',(-1.9525751484303,0.583602094023599,4.39241523421795));
#77378=CARTESIAN_POINT('Ctrl Pts',(-1.36378427143187,1.82232327203781,4.32192449754158));
#77379=CARTESIAN_POINT('Ctrl Pts',(0.742605858221022,2.18668850182256,4.21439650596322));
#77380=CARTESIAN_POINT('Ctrl Pts',(2.23977636166244,0.562558365331892,4.10328474125734));
#77381=CARTESIAN_POINT('Ctrl Pts',(1.68773665970148,-1.57626616793194,3.99217297655146));
#77382=CARTESIAN_POINT('Ctrl Pts',(-0.408442558280547,-2.27293746971917,
3.88106121184558));
#77383=CARTESIAN_POINT('Ctrl Pts',(-1.78454713380843,-1.16814864820909,
3.79229345036984));
#77384=CARTESIAN_POINT('Ctrl Pts',(-1.95259626934014,-0.259551514418081,
3.74056294379605));
#77385=CARTESIAN_POINT('Ctrl Pts',(-1.95135083467133,-0.00103713828173369,
3.72586969212423));
#77386=CARTESIAN_POINT('',(-1.95399929780826,0.00165655208450348,3.02586967148122));
#77387=CARTESIAN_POINT('Ctrl Pts',(-1.95135083467133,-0.00103713828173369,
3.72586969212423));
#77388=CARTESIAN_POINT('Ctrl Pts',(-1.94945690425454,0.392085240919391,
3.70352568889409));
#77389=CARTESIAN_POINT('Ctrl Pts',(-1.64342223932233,1.43955704004953,3.64414443076199));
#77390=CARTESIAN_POINT('Ctrl Pts',(0.0651574691963108,2.30842469421968,
3.54772591772793));
#77391=CARTESIAN_POINT('Ctrl Pts',(1.97449455267556,1.19768164639485,3.43661415302205));
#77392=CARTESIAN_POINT('Ctrl Pts',(2.07733235475046,-1.00884109381311,3.32550238831617));
#77393=CARTESIAN_POINT('Ctrl Pts',(0.279582788264533,-2.29235763554204,
3.21439062361028));
#77394=CARTESIAN_POINT('Ctrl Pts',(-1.56633376284093,-1.56083761130856,
3.11451305821298));
#77395=CARTESIAN_POINT('Ctrl Pts',(-1.94902862841993,-0.451550454744232,
3.05167274771762));
#77396=CARTESIAN_POINT('Ctrl Pts',(-1.95267758926504,0.00165506900100115,
3.02586969212423));
#77397=CARTESIAN_POINT('',(-1.95399999958081,4.04748477694372E-5,2.3258696921786));
#77398=CARTESIAN_POINT('Ctrl Pts',(-1.95399929780826,0.00165655208450348,
3.02586967148122));
#77399=CARTESIAN_POINT('Ctrl Pts',(-1.95392950841898,0.0839771859707575,
3.02118591758554));
#77400=CARTESIAN_POINT('Ctrl Pts',(-1.94865370480582,0.166072172431067,
3.01650216368985));
#77401=CARTESIAN_POINT('Ctrl Pts',(-1.93827999163124,0.247359402574485,
3.01181840979416));
#77402=CARTESIAN_POINT('Ctrl Pts',(-1.92776404327564,0.329761171330941,
3.00707043640715));
#77403=CARTESIAN_POINT('Ctrl Pts',(-1.91200951167843,0.411332865074898,
3.00232246302014));
#77404=CARTESIAN_POINT('Ctrl Pts',(-1.89117786921064,0.491489844257136,
2.99757448963314));
#77405=CARTESIAN_POINT('Ctrl Pts',(-1.88326958784551,0.521919703339655,
2.99577202448826));
#77406=CARTESIAN_POINT('Ctrl Pts',(-1.87463009643616,0.552145899352889,
2.99396955934339));
#77407=CARTESIAN_POINT('Ctrl Pts',(-1.86527001147586,0.582137255541047,
2.99216709419852));
#77408=CARTESIAN_POINT('Ctrl Pts',(-1.84492349210666,0.647331077197404,
2.98824897891026));
#77409=CARTESIAN_POINT('Ctrl Pts',(-1.82111460008519,0.711586141168167,
2.98433086362199));
#77410=CARTESIAN_POINT('Ctrl Pts',(-1.7939488123109,0.774508656380481,2.98041274833373));
#77411=CARTESIAN_POINT('Ctrl Pts',(-1.76682393191034,0.837336420250893,
2.97650053310652));
#77412=CARTESIAN_POINT('Ctrl Pts',(-1.73635238144785,0.898835169809968,
2.97258831787931));
#77413=CARTESIAN_POINT('Ctrl Pts',(-1.70268921043205,0.958626857895342,
2.96867610265209));
#77414=CARTESIAN_POINT('Ctrl Pts',(-1.66906562552191,1.01834823412324,2.96476848798272));
#77415=CARTESIAN_POINT('Ctrl Pts',(-1.63225811409756,1.07636610904359,2.96086087331335));
#77416=CARTESIAN_POINT('Ctrl Pts',(-1.59246878516366,1.13232467441073,2.95695325864398));
#77417=CARTESIAN_POINT('Ctrl Pts',(-1.55270439475709,1.18824816695184,2.95304809312763));
#77418=CARTESIAN_POINT('Ctrl Pts',(-1.5099621785381,1.24211451030917,2.94914292761129));
#77419=CARTESIAN_POINT('Ctrl Pts',(-1.46448809043197,1.29359600841334,2.94523776209494));
#77420=CARTESIAN_POINT('Ctrl Pts',(-1.41902690695965,1.34506289710126,2.94133370478621));
#77421=CARTESIAN_POINT('Ctrl Pts',(-1.37083571608951,1.39414591556065,2.93742964747748));
#77422=CARTESIAN_POINT('Ctrl Pts',(-1.32020020520382,1.44055108141982,2.93352559016876));
#77423=CARTESIAN_POINT('Ctrl Pts',(-1.26956169702248,1.48695899416548,2.92962130176502));
#77424=CARTESIAN_POINT('Ctrl Pts',(-1.21647894593077,1.5306884091681,2.92571701336128));
#77425=CARTESIAN_POINT('Ctrl Pts',(-1.16127253351463,1.57148404475022,2.92181272495754));
#77426=CARTESIAN_POINT('Ctrl Pts',(-1.10600731722641,1.6123231343666,2.91790427784713));
#77427=CARTESIAN_POINT('Ctrl Pts',(-1.04861432161665,1.65022191522982,2.91399583073671));
#77428=CARTESIAN_POINT('Ctrl Pts',(-0.98944425255216,1.68496767657172,2.9100873836263));
#77429=CARTESIAN_POINT('Ctrl Pts',(-0.930238766349994,1.71973423551336,
2.90617659705589));
#77430=CARTESIAN_POINT('Ctrl Pts',(-0.869254526509263,1.75134379249947,
2.90226581048548));
#77431=CARTESIAN_POINT('Ctrl Pts',(-0.806865544602388,1.77963029670027,
2.89835502391507));
#77432=CARTESIAN_POINT('Ctrl Pts',(-0.744368835685812,1.80796564318731,
2.89443748459233));
#77433=CARTESIAN_POINT('Ctrl Pts',(-0.680463001491532,1.83296630582697,
2.8905199452696));
#77434=CARTESIAN_POINT('Ctrl Pts',(-0.615539825796965,1.85451522583608,
2.88660240594686));
#77435=CARTESIAN_POINT('Ctrl Pts',(-0.584896966461044,1.86468602413139,
2.88475338046212));
#77436=CARTESIAN_POINT('Ctrl Pts',(-0.55402765674044,1.87408860595769,2.88290435497738));
#77437=CARTESIAN_POINT('Ctrl Pts',(-0.522973845095926,1.88271462451047,
2.88105532949264));
#77438=CARTESIAN_POINT('Ctrl Pts',(-0.457170309580566,1.90099329911221,
2.87713721420467));
#77439=CARTESIAN_POINT('Ctrl Pts',(-0.390276877561027,1.91585416506222,
2.87321909891671));
#77440=CARTESIAN_POINT('Ctrl Pts',(-0.322681570578035,1.92717217809133,
2.86930098362874));
#77441=CARTESIAN_POINT('Ctrl Pts',(-0.25518805142159,1.93847314798537,2.86538876840185));
#77442=CARTESIAN_POINT('Ctrl Pts',(-0.186995236123241,1.94624177242017,
2.86147655317495));
#77443=CARTESIAN_POINT('Ctrl Pts',(-0.118504816070256,1.95040319128332,
2.85756433794806));
#77444=CARTESIAN_POINT('Ctrl Pts',(-0.0500949371229088,1.95455971653834,
2.85365672327902));
#77445=CARTESIAN_POINT('Ctrl Pts',(0.018611362888003,1.95511743097582,2.84974910860998));
#77446=CARTESIAN_POINT('Ctrl Pts',(0.0872055421906917,1.95205307136134,
2.84584149394094));
#77447=CARTESIAN_POINT('Ctrl Pts',(0.155756729116554,1.94899063237779,2.84193632842493));
#77448=CARTESIAN_POINT('Ctrl Pts',(0.2241954444467,1.94231064457378,2.83803116290892));
#77449=CARTESIAN_POINT('Ctrl Pts',(0.292112973773808,1.932041927742,2.83412599739292));
#77450=CARTESIAN_POINT('Ctrl Pts',(0.360011229468601,1.92177612496605,2.83022194008454));
#77451=CARTESIAN_POINT('Ctrl Pts',(0.427388106646916,1.90792368837881,2.82631788277616));
#77452=CARTESIAN_POINT('Ctrl Pts',(0.493841654345922,1.89056510610793,2.82241382546779));
#77453=CARTESIAN_POINT('Ctrl Pts',(0.560299135666208,1.87320549632097,2.81850953706441));
#77454=CARTESIAN_POINT('Ctrl Pts',(0.625832703735697,1.85233945560431,2.81460524866103));
#77455=CARTESIAN_POINT('Ctrl Pts',(0.690053985753285,1.82809778095867,2.81070096025765));
#77456=CARTESIAN_POINT('Ctrl Pts',(0.754343673955492,1.80383028495881,2.80679251314761));
#77457=CARTESIAN_POINT('Ctrl Pts',(0.817317825459981,1.7761801533597,2.80288406603757));
#77458=CARTESIAN_POINT('Ctrl Pts',(0.878607484600926,1.74532658491276,2.79897561892752));
#77459=CARTESIAN_POINT('Ctrl Pts',(0.939933829592058,1.71445454859692,2.7950648323575));
#77460=CARTESIAN_POINT('Ctrl Pts',(0.99957324842819,1.68037550339476,2.79115404578747));
#77461=CARTESIAN_POINT('Ctrl Pts',(1.05718333684116,1.64331354047406,2.78724325921744));
#77462=CARTESIAN_POINT('Ctrl Pts',(1.11489290055181,1.60618758268899,2.78332571989509));
#77463=CARTESIAN_POINT('Ctrl Pts',(1.1705657414821,1.56606871482815,2.77940818057274));
#77464=CARTESIAN_POINT('Ctrl Pts',(1.22389096795314,1.5232225374392,2.7754906412504));
#77465=CARTESIAN_POINT('Ctrl Pts',(1.24905975243211,1.50299972216366,2.77364161576251));
#77466=CARTESIAN_POINT('Ctrl Pts',(1.2737060714098,1.48216989278257,2.77179259027463));
#77467=CARTESIAN_POINT('Ctrl Pts',(1.29780015455336,1.46076375873762,2.76994356478675));
#77468=CARTESIAN_POINT('Ctrl Pts',(1.34885591135648,1.41540381009871,2.7660254494939));
#77469=CARTESIAN_POINT('Ctrl Pts',(1.39763192331083,1.36727401419716,2.76210733420104));
#77470=CARTESIAN_POINT('Ctrl Pts',(1.4438126318655,1.31663247873718,2.75818921890819));
#77471=CARTESIAN_POINT('Ctrl Pts',(1.48992379958754,1.26606720140861,2.75427700367639));
#77472=CARTESIAN_POINT('Ctrl Pts',(1.53344709136623,1.21299805153902,2.75036478844458));
#77473=CARTESIAN_POINT('Ctrl Pts',(1.57410168834624,1.15772184688099,2.74645257321278));
#77474=CARTESIAN_POINT('Ctrl Pts',(1.614708477674,1.10251064411121,2.74254495853883));
#77475=CARTESIAN_POINT('Ctrl Pts',(1.65245298183955,1.04509793538905,2.73863734386487));
#77476=CARTESIAN_POINT('Ctrl Pts',(1.68709400825014,0.985814286428475,2.73472972919092));
#77477=CARTESIAN_POINT('Ctrl Pts',(1.72171332290509,0.926567794337453,2.73082456367));
#77478=CARTESIAN_POINT('Ctrl Pts',(1.7532327707603,0.865453111888877,2.72691939814908));
#77479=CARTESIAN_POINT('Ctrl Pts',(1.78145481681984,0.802829207010667,2.72301423262816));
#77480=CARTESIAN_POINT('Ctrl Pts',(1.80966885402884,0.740223073540446,2.71911017531488));
#77481=CARTESIAN_POINT('Ctrl Pts',(1.83458714503851,0.676109016099035,2.7152061180016));
#77482=CARTESIAN_POINT('Ctrl Pts',(1.85605922720639,0.610868353331555,2.71130206068832));
#77483=CARTESIAN_POINT('Ctrl Pts',(1.87753258038291,0.545623828738059,2.70739777228006));
#77484=CARTESIAN_POINT('Ctrl Pts',(1.8955591683825,0.479253034445765,2.70349348387179));
#77485=CARTESIAN_POINT('Ctrl Pts',(1.91003815619439,0.412153177691916,2.69958919546352));
#77486=CARTESIAN_POINT('Ctrl Pts',(1.9245325664997,0.344981848600845,2.69568074834865));
#77487=CARTESIAN_POINT('Ctrl Pts',(1.93547173140084,0.277080388989802,2.69177230123377));
#77488=CARTESIAN_POINT('Ctrl Pts',(1.94280600936491,0.208855955087703,2.68786385411889));
#77489=CARTESIAN_POINT('Ctrl Pts',(1.95014467737165,0.140590684421846,2.68395306754406));
#77490=CARTESIAN_POINT('Ctrl Pts',(1.9538741373926,0.0720025459420695,2.68004228096922));
#77491=CARTESIAN_POINT('Ctrl Pts',(1.95399686406196,0.00350074792200107,
2.67613149439438));
#77492=CARTESIAN_POINT('Ctrl Pts',(1.95411980264337,-0.0651193321011138,
2.67221395506731));
#77493=CARTESIAN_POINT('Ctrl Pts',(1.95062360334309,-0.133652283136143,
2.66829641574024));
#77494=CARTESIAN_POINT('Ctrl Pts',(1.94356270676489,-0.20169284784722,2.66437887641317));
#77495=CARTESIAN_POINT('Ctrl Pts',(1.94023005931933,-0.233807071822553,
2.66252985096907));
#77496=CARTESIAN_POINT('Ctrl Pts',(1.93610404326396,-0.265811739818377,
2.66068082552497));
#77497=CARTESIAN_POINT('Ctrl Pts',(1.93119430378674,-0.297665182750104,
2.65883180008087));
#77498=CARTESIAN_POINT('Ctrl Pts',(1.92079048519854,-0.365163151472968,
2.65491368479703));
#77499=CARTESIAN_POINT('Ctrl Pts',(1.90682305849002,-0.432248824807374,
2.6509955695132));
#77500=CARTESIAN_POINT('Ctrl Pts',(1.88933763808645,-0.498517090288694,
2.64707745422936));
#77501=CARTESIAN_POINT('Ctrl Pts',(1.87187854795656,-0.564685566258203,
2.64316523900656));
#77502=CARTESIAN_POINT('Ctrl Pts',(1.85091210235727,-0.63003860547196,2.63925302378377));
#77503=CARTESIAN_POINT('Ctrl Pts',(1.82653528100206,-0.694179276019334,
2.63534080856097));
#77504=CARTESIAN_POINT('Ctrl Pts',(1.80218712549705,-0.758244520536934,
2.63143319389597));
#77505=CARTESIAN_POINT('Ctrl Pts',(1.77443673291253,-0.821099770196362,
2.62752557923097));
#77506=CARTESIAN_POINT('Ctrl Pts',(1.7434309311173,-0.88236307063673,2.62361796456596));
#77507=CARTESIAN_POINT('Ctrl Pts',(1.71244456264873,-0.943587973433383,
2.61971279905396));
#77508=CARTESIAN_POINT('Ctrl Pts',(1.6782070540418,-1.00322246839439,2.61580763354195));
#77509=CARTESIAN_POINT('Ctrl Pts',(1.64091277790259,-1.06090586543576,2.61190246802994));
#77510=CARTESIAN_POINT('Ctrl Pts',(1.60362908513036,-1.11857289308691,2.60799841072552));
#77511=CARTESIAN_POINT('Ctrl Pts',(1.5632906137981,-1.17428950910011,2.6040943534211));
#77512=CARTESIAN_POINT('Ctrl Pts',(1.52013605046243,-1.22772243935039,2.60019029611667));
#77513=CARTESIAN_POINT('Ctrl Pts',(1.47697893265452,-1.28115853248605,2.5962860077172));
#77514=CARTESIAN_POINT('Ctrl Pts',(1.43100570294498,-1.33231029042934,2.59238171931772));
#77515=CARTESIAN_POINT('Ctrl Pts',(1.38249531981184,-1.38087750749238,2.58847743091825));
#77516=CARTESIAN_POINT('Ctrl Pts',(1.3339332651734,-1.42949645659816,2.58456898381201));
#77517=CARTESIAN_POINT('Ctrl Pts',(1.28282901206506,-1.47552502208498,2.58066053670577));
#77518=CARTESIAN_POINT('Ctrl Pts',(1.22949765098527,-1.51870060453721,2.57675208959952));
#77519=CARTESIAN_POINT('Ctrl Pts',(1.1761343676139,-1.56190203038636,2.57284130303324));
#77520=CARTESIAN_POINT('Ctrl Pts',(1.12054172136735,-1.60224678562586,2.56893051646696));
#77521=CARTESIAN_POINT('Ctrl Pts',(1.06306480169621,-1.63951493661833,2.56501972990067));
#77522=CARTESIAN_POINT('Ctrl Pts',(1.0054886366679,-1.67684743850117,2.56110219058195));
#77523=CARTESIAN_POINT('Ctrl Pts',(0.94602213063127,-1.7110924881611,2.55718465126322));
#77524=CARTESIAN_POINT('Ctrl Pts',(0.88503524782068,-1.74207594843479,2.5532671119445));
#77525=CARTESIAN_POINT('Ctrl Pts',(0.856250264768582,-1.7566997222329,2.55141808642133));
#77526=CARTESIAN_POINT('Ctrl Pts',(0.827126876633474,-1.7705976045977,2.54956906089816));
#77527=CARTESIAN_POINT('Ctrl Pts',(0.797705319577693,-1.78375509056525,
2.54772003537499));
#77528=CARTESIAN_POINT('Ctrl Pts',(0.735360559618111,-1.8116360182389,2.54380192009024));
#77529=CARTESIAN_POINT('Ctrl Pts',(0.671428735074593,-1.83629972407899,
2.5398838048055));
#77530=CARTESIAN_POINT('Ctrl Pts',(0.606274899919665,-1.85756473527234,
2.53596568952076));
#77531=CARTESIAN_POINT('Ctrl Pts',(0.541219176122421,-1.87879772472646,
2.53205347429714));
#77532=CARTESIAN_POINT('Ctrl Pts',(0.474945557611846,-1.89664202535494,
2.52814125907352));
#77533=CARTESIAN_POINT('Ctrl Pts',(0.407840094249134,-1.9109637509704,2.52422904384991));
#77534=CARTESIAN_POINT('Ctrl Pts',(0.340813543357728,-1.92526863499495,
2.52032142918422));
#77535=CARTESIAN_POINT('Ctrl Pts',(0.272957569114629,-1.93605906862085,
2.51641381451854));
#77536=CARTESIAN_POINT('Ctrl Pts',(0.204672684488128,-1.94325116550188,
2.51250619985285));
#77537=CARTESIAN_POINT('Ctrl Pts',(0.136430598384416,-1.95043875463389,
2.50860103434024));
#77538=CARTESIAN_POINT('Ctrl Pts',(0.0677606232386084,-1.95403242943041,
2.50469586882763));
#77539=CARTESIAN_POINT('Ctrl Pts',(-0.000928795607166038,-1.95399977925759,
2.50079070331502));
#77540=CARTESIAN_POINT('Ctrl Pts',(-0.0695987217732036,-1.95396713835024,
2.49688664601008));
#77541=CARTESIAN_POINT('Ctrl Pts',(-0.138287589036128,-1.95031021560445,
2.49298258870514));
#77542=CARTESIAN_POINT('Ctrl Pts',(-0.206585940107364,-1.94304869968561,
2.4890785314002));
#77543=CARTESIAN_POINT('Ctrl Pts',(-0.274888333999684,-1.93578675393196,
2.48517424300029));
#77544=CARTESIAN_POINT('Ctrl Pts',(-0.342799676956306,-1.92491984594802,
2.48126995460038));
#77545=CARTESIAN_POINT('Ctrl Pts',(-0.409916440956191,-1.91051943497935,
2.47736566620048));
#77546=CARTESIAN_POINT('Ctrl Pts',(-0.477104695303022,-1.89610368521431,
2.47345721909392));
#77547=CARTESIAN_POINT('Ctrl Pts',(-0.543496199768764,-1.87814702455178,
2.46954877198737));
#77548=CARTESIAN_POINT('Ctrl Pts',(-0.608699413580939,-1.85677166714333,
2.46564032488082));
#77549=CARTESIAN_POINT('Ctrl Pts',(-0.673941655760215,-1.8353835151923,
2.4617295383143));
#77550=CARTESIAN_POINT('Ctrl Pts',(-0.737993732994083,-1.81057277164882,
2.45781875174779));
#77551=CARTESIAN_POINT('Ctrl Pts',(-0.800483669333991,-1.78250999860578,
2.45390796518127));
#77552=CARTESIAN_POINT('Ctrl Pts',(-0.863081507001688,-1.75439876959287,
2.44999042586242));
#77553=CARTESIAN_POINT('Ctrl Pts',(-0.92411138307502,-1.72302452865832,
2.44607288654357));
#77554=CARTESIAN_POINT('Ctrl Pts',(-0.983226296378127,-1.68860357991761,
2.44215534722472));
#77555=CARTESIAN_POINT('Ctrl Pts',(-1.01112773509442,-1.67235735814069,
2.44030632170618));
#77556=CARTESIAN_POINT('Ctrl Pts',(-1.03860300262693,-1.65543304013966,
2.43845729618765));
#77557=CARTESIAN_POINT('Ctrl Pts',(-1.0656180846027,-1.63785655591925,2.43660827066911));
#77558=CARTESIAN_POINT('Ctrl Pts',(-1.12282902060775,-1.60063412162017,
2.43269251425173));
#77559=CARTESIAN_POINT('Ctrl Pts',(-1.17820141177215,-1.56033624286675,
2.42877675783435));
#77560=CARTESIAN_POINT('Ctrl Pts',(-1.23138500423445,-1.51717071265778,
2.42486100141697));
#77561=CARTESIAN_POINT('Ctrl Pts',(-1.28448848720085,-1.47407020191638,
2.42095114323357));
#77562=CARTESIAN_POINT('Ctrl Pts',(-1.33540933515797,-1.42811091996629,
2.41704128505018));
#77563=CARTESIAN_POINT('Ctrl Pts',(-1.383825852666,-1.37954413104229,2.41313142686679));
#77564=CARTESIAN_POINT('Ctrl Pts',(-1.43218550557035,-1.3310343832139,2.40922616076369));
#77565=CARTESIAN_POINT('Ctrl Pts',(-1.47804632320186,-1.27992355751628,
2.40532089466059));
#77566=CARTESIAN_POINT('Ctrl Pts',(-1.5211207485684,-1.22650220883402,2.4014156285575));
#77567=CARTESIAN_POINT('Ctrl Pts',(-1.56416826194705,-1.17311423667798,
2.39751280238188));
#77568=CARTESIAN_POINT('Ctrl Pts',(-1.60443252781338,-1.11741898759487,
2.39360997620626));
#77569=CARTESIAN_POINT('Ctrl Pts',(-1.64166491920676,-1.05974161617153,
2.38970715003064));
#77570=CARTESIAN_POINT('Ctrl Pts',(-1.67888686115016,-1.00208043218031,
2.38580541920198));
#77571=CARTESIAN_POINT('Ctrl Pts',(-1.71307835079115,-0.9424386438043,2.38190368837333));
#77572=CARTESIAN_POINT('Ctrl Pts',(-1.74403397574648,-0.881170523475403,
2.37800195754467));
#77573=CARTESIAN_POINT('Ctrl Pts',(-1.77499156512658,-0.819898515109583,
2.3740999791146));
#77574=CARTESIAN_POINT('Ctrl Pts',(-1.80271266238679,-0.757000410711466,
2.37019800068453));
#77575=CARTESIAN_POINT('Ctrl Pts',(-1.82703856344133,-0.692853583160422,
2.36629602225445));
#77576=CARTESIAN_POINT('Ctrl Pts',(-1.85139041431136,-0.62863832655777,
2.36238988136314));
#77577=CARTESIAN_POINT('Ctrl Pts',(-1.87233966637274,-0.56317214996081,
2.35848374047183));
#77578=CARTESIAN_POINT('Ctrl Pts',(-1.88977676046506,-0.496849872301682,
2.35457759958051));
#77579=CARTESIAN_POINT('Ctrl Pts',(-1.90722439512171,-0.430487503430625,
2.35066909746266));
#77580=CARTESIAN_POINT('Ctrl Pts',(-1.921155546953,-0.363268485977131,2.3467605953448));
#77581=CARTESIAN_POINT('Ctrl Pts',(-1.93151188760856,-0.295597408694372,
2.34285209322695));
#77582=CARTESIAN_POINT('Ctrl Pts',(-1.94188602271753,-0.227810057732313,
2.33893687544947));
#77583=CARTESIAN_POINT('Ctrl Pts',(-1.94867304006574,-0.159569586596278,
2.33502165767198));
#77584=CARTESIAN_POINT('Ctrl Pts',(-1.95186658470269,-0.09128436624665,
2.3311064398945));
#77585=CARTESIAN_POINT('Ctrl Pts',(-1.95329041248901,-0.0608397020313837,
2.32936085732253));
#77586=CARTESIAN_POINT('Ctrl Pts',(-1.95400062983249,-0.0303861200153032,
2.32761527475057));
#77587=CARTESIAN_POINT('Ctrl Pts',(-1.95399999958081,4.04748477704995E-5,
2.3258696921786));
#77588=CARTESIAN_POINT('',(-1.95399927560819,-0.00168253459542325,1.62586971130486));
#77589=CARTESIAN_POINT('Ctrl Pts',(-1.95399999958079,4.04757954714693E-5,
2.32586969212423));
#77590=CARTESIAN_POINT('Ctrl Pts',(-1.95399995466613,0.00220876511265513,
2.32574529673723));
#77591=CARTESIAN_POINT('Ctrl Pts',(-1.95399630063441,0.0043770500002713,
2.32562090135023));
#77592=CARTESIAN_POINT('Ctrl Pts',(-1.95398903752031,0.00654532279172306,
2.32549650596323));
#77593=CARTESIAN_POINT('Ctrl Pts',(-1.95376026924542,0.0748399990821359,
2.32157839071464));
#77594=CARTESIAN_POINT('Ctrl Pts',(-1.94994624385776,0.143258050123744,
2.31766027546604));
#77595=CARTESIAN_POINT('Ctrl Pts',(-1.94253169459442,0.211392089483348,
2.31374216021745));
#77596=CARTESIAN_POINT('Ctrl Pts',(-1.93512831046787,0.279423529771489,
2.30982994502983));
#77597=CARTESIAN_POINT('Ctrl Pts',(-1.92413521564132,0.34717132210442,2.30591772984221));
#77598=CARTESIAN_POINT('Ctrl Pts',(-1.90958915417286,0.414228514548907,
2.30200551465458));
#77599=CARTESIAN_POINT('Ctrl Pts',(-1.89506019810102,0.481206851292453,
2.29809790002448));
#77600=CARTESIAN_POINT('Ctrl Pts',(-1.87698667693864,0.547495722583235,
2.29419028539438));
#77601=CARTESIAN_POINT('Ctrl Pts',(-1.85545685829453,0.612695558175348,
2.29028267076427));
#77602=CARTESIAN_POINT('Ctrl Pts',(-1.83394053376913,0.677854528847234,
2.28637750528697));
#77603=CARTESIAN_POINT('Ctrl Pts',(-1.80897236286763,0.741925351793865,
2.28247233980967));
#77604=CARTESIAN_POINT('Ctrl Pts',(-1.78069079593143,0.804522398249488,
2.27856717433237));
#77605=CARTESIAN_POINT('Ctrl Pts',(-1.75241725473457,0.867101680923494,
2.27466311706242));
#77606=CARTESIAN_POINT('Ctrl Pts',(-1.72083238653793,0.928207569318252,
2.27075905979247));
#77607=CARTESIAN_POINT('Ctrl Pts',(-1.686122546459,0.98747494060488,2.26685500252251));
#77608=CARTESIAN_POINT('Ctrl Pts',(-1.65141065177845,1.04674582014268,2.26295071415722));
#77609=CARTESIAN_POINT('Ctrl Pts',(-1.613573668758,1.10417754335984,2.25904642579192));
#77610=CARTESIAN_POINT('Ctrl Pts',(-1.57284270275735,1.15943168508668,2.25514213742662));
#77611=CARTESIAN_POINT('Ctrl Pts',(-1.5320683515978,1.21474468153647,2.25123369035389));
#77612=CARTESIAN_POINT('Ctrl Pts',(-1.48839415803323,1.26787507083712,2.24732524328116));
#77613=CARTESIAN_POINT('Ctrl Pts',(-1.44209256024326,1.31851622958955,2.24341679620843));
#77614=CARTESIAN_POINT('Ctrl Pts',(-1.39576324792855,1.36918770037685,2.23950600967533));
#77615=CARTESIAN_POINT('Ctrl Pts',(-1.34680375212342,1.4173666302547,2.23559522314223));
#77616=CARTESIAN_POINT('Ctrl Pts',(-1.29552253323629,1.46278411458322,2.23168443660913));
#77617=CARTESIAN_POINT('Ctrl Pts',(-1.24415276709222,1.50828002126094,2.22776689732273));
#77618=CARTESIAN_POINT('Ctrl Pts',(-1.19045366141732,1.55100465976764,2.22384935803633));
#77619=CARTESIAN_POINT('Ctrl Pts',(-1.13476509845124,1.59073070358781,2.21993181874993));
#77620=CARTESIAN_POINT('Ctrl Pts',(-1.10848084604684,1.60948086173847,2.21808279291906));
#77621=CARTESIAN_POINT('Ctrl Pts',(-1.08175379135749,1.62756366470977,2.2162337670882));
#77622=CARTESIAN_POINT('Ctrl Pts',(-1.05462155966551,1.64495877330974,2.21438474125734));
#77623=CARTESIAN_POINT('Ctrl Pts',(-0.997127927251723,1.68181928633346,
2.21046662598212));
#77624=CARTESIAN_POINT('Ctrl Pts',(-0.937585506254232,1.71573501490396,
2.2065485107069));
#77625=CARTESIAN_POINT('Ctrl Pts',(-0.876328230286788,1.74647211051377,
2.20263039543167));
#77626=CARTESIAN_POINT('Ctrl Pts',(-0.815163198082612,1.77716292092193,
2.19871818021799));
#77627=CARTESIAN_POINT('Ctrl Pts',(-0.752288871962661,1.80468437908947,
2.19480596500431));
#77628=CARTESIAN_POINT('Ctrl Pts',(-0.688067038568517,1.82884656284653,
2.19089374979063));
#77629=CARTESIAN_POINT('Ctrl Pts',(-0.623920726658672,1.85298033315157,
2.18698613513542));
#77630=CARTESIAN_POINT('Ctrl Pts',(-0.5584305127052,1.8737625020737,2.18307852048021));
#77631=CARTESIAN_POINT('Ctrl Pts',(-0.491979936173606,1.89105043359573,
2.179170905825));
#77632=CARTESIAN_POINT('Ctrl Pts',(-0.425571008491863,1.90832752965927,
2.1752657403232));
#77633=CARTESIAN_POINT('Ctrl Pts',(-0.358203387217572,1.92211460914435,
2.1713605748214));
#77634=CARTESIAN_POINT('Ctrl Pts',(-0.290276126774211,1.93231875481893,
2.1674554093196));
#77635=CARTESIAN_POINT('Ctrl Pts',(-0.22236814273083,1.94252000476074,2.16355135202579));
#77636=CARTESIAN_POINT('Ctrl Pts',(-0.153901320986516,1.94914026630843,
2.15964729473197));
#77637=CARTESIAN_POINT('Ctrl Pts',(-0.0852834807025519,1.95213798895448,
2.15574323743815));
#77638=CARTESIAN_POINT('Ctrl Pts',(-0.0166615786908634,1.95513588904613,
2.15183894904965));
#77639=CARTESIAN_POINT('Ctrl Pts',(0.0521108680863909,1.95451080561036,
2.14793466066116));
#77640=CARTESIAN_POINT('Ctrl Pts',(0.120624188422045,1.95027326422928,2.14403037227266));
#77641=CARTESIAN_POINT('Ctrl Pts',(0.189210486659719,1.94603120917293,2.14012192517789));
#77642=CARTESIAN_POINT('Ctrl Pts',(0.257536615736428,1.93816904745832,2.13621347808311));
#77643=CARTESIAN_POINT('Ctrl Pts',(0.325197194094168,1.92674927921442,2.13230503098834));
#77644=CARTESIAN_POINT('Ctrl Pts',(0.392898271707902,1.91532267549662,2.12839424443382));
#77645=CARTESIAN_POINT('Ctrl Pts',(0.459932525669257,1.90033433457933,2.1244834578793));
#77646=CARTESIAN_POINT('Ctrl Pts',(0.525906715726977,1.88189748029835,2.12057267132478));
#77647=CARTESIAN_POINT('Ctrl Pts',(0.591994823367634,1.86342879111534,2.11665513201814));
#77648=CARTESIAN_POINT('Ctrl Pts',(0.657018748055493,1.84149986135365,2.1127375927115));
#77649=CARTESIAN_POINT('Ctrl Pts',(0.720603128731074,1.81627286795321,2.10882005340486));
#77650=CARTESIAN_POINT('Ctrl Pts',(0.750614097239236,1.8043660679427,2.10697102778706));
#77651=CARTESIAN_POINT('Ctrl Pts',(0.780304706589721,1.79172523352155,2.10512200216926));
#77652=CARTESIAN_POINT('Ctrl Pts',(0.809637458011172,1.77837093616186,2.10327297655146));
#77653=CARTESIAN_POINT('Ctrl Pts',(0.871794037028583,1.75007296209412,2.09935486108842));
#77654=CARTESIAN_POINT('Ctrl Pts',(0.932588463664215,1.71845627840504,2.09543674562538));
#77655=CARTESIAN_POINT('Ctrl Pts',(0.991643125554879,1.68367452660535,2.09151863016234));
#77656=CARTESIAN_POINT('Ctrl Pts',(1.05060886049195,1.64894515060681,2.0876064147597));
#77657=CARTESIAN_POINT('Ctrl Pts',(1.1078396096568,1.61106041311778,2.08369419935705));
#77658=CARTESIAN_POINT('Ctrl Pts',(1.16297954867285,1.5702211848554,2.07978198395441));
#77659=CARTESIAN_POINT('Ctrl Pts',(1.21805464604646,1.52942998135844,2.07587436910949));
#77660=CARTESIAN_POINT('Ctrl Pts',(1.2710434228508,1.48569147852043,2.07196675426457));
#77661=CARTESIAN_POINT('Ctrl Pts',(1.32161797465028,1.43925047475458,2.06805913941965));
#77662=CARTESIAN_POINT('Ctrl Pts',(1.37216082813179,1.39283857854682,2.06415397372778));
#77663=CARTESIAN_POINT('Ctrl Pts',(1.42029209672764,1.34372787337746,2.06024880803592));
#77664=CARTESIAN_POINT('Ctrl Pts',(1.46571722372466,1.29220316517058,2.05634364234405));
#77665=CARTESIAN_POINT('Ctrl Pts',(1.51112945997923,1.24069307864531,2.05243958486009));
#77666=CARTESIAN_POINT('Ctrl Pts',(1.55383675401182,1.1867707178078,2.04853552737614));
#77667=CARTESIAN_POINT('Ctrl Pts',(1.59358294342151,1.13075611978713,2.04463146989218));
#77668=CARTESIAN_POINT('Ctrl Pts',(1.6333314855435,1.07473820607166,2.04072718131377));
#77669=CARTESIAN_POINT('Ctrl Pts',(1.67011829250234,1.01662821192939,2.03682289273536));
#77670=CARTESIAN_POINT('Ctrl Pts',(1.70372994251718,0.956775983692321,2.03291860415695));
#77671=CARTESIAN_POINT('Ctrl Pts',(1.73737739442587,0.896860003062237,2.02901015687389));
#77672=CARTESIAN_POINT('Ctrl Pts',(1.76784269853303,0.835198514510433,2.02510170959083));
#77673=CARTESIAN_POINT('Ctrl Pts',(1.79495842050219,0.772165959278372,2.02119326230777));
#77674=CARTESIAN_POINT('Ctrl Pts',(1.8220903729889,0.709095674975499,2.01728247556561));
#77675=CARTESIAN_POINT('Ctrl Pts',(1.84586858283634,0.644653152234568,2.01337168882346));
#77676=CARTESIAN_POINT('Ctrl Pts',(1.86617481225867,0.579230152954181,2.00946090208131));
#77677=CARTESIAN_POINT('Ctrl Pts',(1.88651610441448,0.513694187886812,2.00554336259002));
#77678=CARTESIAN_POINT('Ctrl Pts',(1.90337333019351,0.447174843903795,2.00162582309873));
#77679=CARTESIAN_POINT('Ctrl Pts',(1.91667907404262,0.380075422945414,1.99770828360744));
#77680=CARTESIAN_POINT('Ctrl Pts',(1.9229591992879,0.34840543348198,1.99585925968682));
#77681=CARTESIAN_POINT('Ctrl Pts',(1.92844890762637,0.316606311276526,1.9940102357662));
#77682=CARTESIAN_POINT('Ctrl Pts',(1.93314513506615,0.284720717142359,1.99216121184558));
#77683=CARTESIAN_POINT('Ctrl Pts',(1.94309652556393,0.217154569090327,1.98824309686718));
#77684=CARTESIAN_POINT('Ctrl Pts',(1.94952108028574,0.148932131488614,1.98432498188878));
#77685=CARTESIAN_POINT('Ctrl Pts',(1.95234299222131,0.0804539664923356,
1.98040686691037));
#77686=CARTESIAN_POINT('Ctrl Pts',(1.95516065480438,0.012078918768361,1.97649465199266));
#77687=CARTESIAN_POINT('Ctrl Pts',(1.95438642123413,-0.0565506045830932,
1.97258243707494));
#77688=CARTESIAN_POINT('Ctrl Pts',(1.9499959792906,-0.12502672014604,1.96867022215723));
#77689=CARTESIAN_POINT('Ctrl Pts',(1.94561070027235,-0.193422311453924,
1.96476260779533));
#77690=CARTESIAN_POINT('Ctrl Pts',(1.93761768967133,-0.261664364700758,
1.96085499343343));
#77691=CARTESIAN_POINT('Ctrl Pts',(1.92604468353289,-0.329344617436922,
1.95694737907154));
#77692=CARTESIAN_POINT('Ctrl Pts',(1.91447893093686,-0.396982450634276,
1.95304221386124));
#77693=CARTESIAN_POINT('Ctrl Pts',(1.89933771653323,-0.464058698052798,
1.94913704865094));
#77694=CARTESIAN_POINT('Ctrl Pts',(1.88070047635929,-0.530171404568323,
1.94523188344064));
#77695=CARTESIAN_POINT('Ctrl Pts',(1.86206852505165,-0.596265349654448,
1.94132782643608));
#77696=CARTESIAN_POINT('Ctrl Pts',(1.83994265086077,-0.66139582344277,1.93742376943153));
#77697=CARTESIAN_POINT('Ctrl Pts',(1.81445271556354,-0.725174008762105,
1.93351971242698));
#77698=CARTESIAN_POINT('Ctrl Pts',(1.78896127141129,-0.788955969376814,
1.9296154243251));
#77699=CARTESIAN_POINT('Ctrl Pts',(1.7601055557336,-0.851385026801486,1.92571113622322));
#77700=CARTESIAN_POINT('Ctrl Pts',(1.72806365945861,-0.912092094504996,
1.92180684812134));
#77701=CARTESIAN_POINT('Ctrl Pts',(1.69598763326759,-0.97286382527044,1.91789840130725));
#77702=CARTESIAN_POINT('Ctrl Pts',(1.66071888352847,-1.03190946997123,1.91398995449316));
#77703=CARTESIAN_POINT('Ctrl Pts',(1.62248111169852,-1.08888522911349,1.91008150767908));
#77704=CARTESIAN_POINT('Ctrl Pts',(1.58422045204491,-1.14589509199835,1.90617072140228));
#77705=CARTESIAN_POINT('Ctrl Pts',(1.5429875287408,-1.20083221010605,1.90225993512548));
#77706=CARTESIAN_POINT('Ctrl Pts',(1.49904728425969,-1.25338471330779,1.89834914884868));
#77707=CARTESIAN_POINT('Ctrl Pts',(1.45503116810331,-1.30602795898273,1.89443160981231));
#77708=CARTESIAN_POINT('Ctrl Pts',(1.40829873554755,-1.35627801184808,1.89051407077594));
#77709=CARTESIAN_POINT('Ctrl Pts',(1.35915219619628,-1.40385943298281,1.88659653173957));
#77710=CARTESIAN_POINT('Ctrl Pts',(1.33595565971069,-1.42631725373596,1.88474750353961));
#77711=CARTESIAN_POINT('Ctrl Pts',(1.3122218116172,-1.44818115840508,1.88289847533965));
#77712=CARTESIAN_POINT('Ctrl Pts',(1.28798482614457,-1.46942542771702,1.8810494471397));
#77713=CARTESIAN_POINT('Ctrl Pts',(1.23662633221909,-1.51444231637426,1.87713133184096));
#77714=CARTESIAN_POINT('Ctrl Pts',(1.18280308149621,-1.55685262414134,1.87321321654222));
#77715=CARTESIAN_POINT('Ctrl Pts',(1.12681042945077,-1.5963753493715,1.86929510124348));
#77716=CARTESIAN_POINT('Ctrl Pts',(1.07090209351593,-1.63583855960549,1.86538288600896));
#77717=CARTESIAN_POINT('Ctrl Pts',(1.01283123827593,-1.67242253565744,1.86147067077444));
#77718=CARTESIAN_POINT('Ctrl Pts',(0.952927307329273,-1.70588556091731,
1.85755845553992));
#77719=CARTESIAN_POINT('Ctrl Pts',(0.893093820302652,-1.73930923539272,
1.85365084086788));
#77720=CARTESIAN_POINT('Ctrl Pts',(0.831431966017609,-1.76961900915968,
1.84974322619584));
#77721=CARTESIAN_POINT('Ctrl Pts',(0.76829974480643,-1.79661668202496,1.84583561152381));
#77722=CARTESIAN_POINT('Ctrl Pts',(0.705207092658434,-1.82359743369528,
1.84193044600766));
#77723=CARTESIAN_POINT('Ctrl Pts',(0.640646352942322,-1.84727000943735,
1.83802528049152));
#77724=CARTESIAN_POINT('Ctrl Pts',(0.574998277036943,-1.86748306054019,
1.83412011497538));
#77725=CARTESIAN_POINT('Ctrl Pts',(0.509368830786191,-1.88769037556995,
1.8302160576697));
#77726=CARTESIAN_POINT('Ctrl Pts',(0.442653130781479,-1.90443997021895,
1.82631200036403));
#77727=CARTESIAN_POINT('Ctrl Pts',(0.375248250188822,-1.91762998274699,
1.82240794305835));
#77728=CARTESIAN_POINT('Ctrl Pts',(0.307839379710729,-1.93082077602916,
1.81850365466049));
#77729=CARTESIAN_POINT('Ctrl Pts',(0.239741730868927,-1.94045147692993,
1.81459936626262));
#77730=CARTESIAN_POINT('Ctrl Pts',(0.17136196882874,-1.94647144228708,1.81069507786476));
#77731=CARTESIAN_POINT('Ctrl Pts',(0.102909371214237,-1.95249781988699,
1.80678663076439));
#77732=CARTESIAN_POINT('Ctrl Pts',(0.0341745516291942,-1.95490574325592,
1.80287818366402));
#77733=CARTESIAN_POINT('Ctrl Pts',(-0.0344323210079937,-1.95369660266634,
1.79896973656365));
#77734=CARTESIAN_POINT('Ctrl Pts',(-0.103080259282135,-1.95248673832816,
1.79505895000568));
#77735=CARTESIAN_POINT('Ctrl Pts',(-0.171599607462033,-1.9476555357918,
1.79114816344771));
#77736=CARTESIAN_POINT('Ctrl Pts',(-0.239584643263601,-1.93925635198451,
1.78723737688973));
#77737=CARTESIAN_POINT('Ctrl Pts',(-0.307687068716483,-1.93084266532012,
1.78331983758294));
#77738=CARTESIAN_POINT('Ctrl Pts',(-0.375252856385077,-1.91884878728751,
1.77940229827615));
#77739=CARTESIAN_POINT('Ctrl Pts',(-0.441886668296444,-1.90337914572527,
1.77548475896936));
#77740=CARTESIAN_POINT('Ctrl Pts',(-0.473336925339729,-1.89607768435688,
1.77363573345751));
#77741=CARTESIAN_POINT('Ctrl Pts',(-0.504579789940459,-1.88800264381133,
1.77178670794566));
#77742=CARTESIAN_POINT('Ctrl Pts',(-0.535575116404463,-1.87916877759512,
1.76993768243381));
#77743=CARTESIAN_POINT('Ctrl Pts',(-0.601254738444671,-1.86044966537967,
1.76601956603965));
#77744=CARTESIAN_POINT('Ctrl Pts',(-0.66608198802966,-1.83824590595076,
1.7621014496455));
#77745=CARTESIAN_POINT('Ctrl Pts',(-0.729660572885464,-1.81265315170235,
1.75818333325134));
#77746=CARTESIAN_POINT('Ctrl Pts',(-0.793143418573306,-1.78709893604367,
1.75427111691306));
#77747=CARTESIAN_POINT('Ctrl Pts',(-0.855380878611871,-1.75816603597598,
1.75035890057479));
#77748=CARTESIAN_POINT('Ctrl Pts',(-0.915991167107972,-1.72600005265938,
1.74644668423651));
#77749=CARTESIAN_POINT('Ctrl Pts',(-0.976530181170627,-1.69387189480598,
1.74253906845385));
#77750=CARTESIAN_POINT('Ctrl Pts',(-1.03544539143528,-1.65851843388911,
1.73863145267119));
#77751=CARTESIAN_POINT('Ctrl Pts',(-1.09237607387451,-1.62013286900381,
1.73472383688853));
#77752=CARTESIAN_POINT('Ctrl Pts',(-1.1492710742204,-1.58177136280268,1.73081867025815));
#77753=CARTESIAN_POINT('Ctrl Pts',(-1.20418360718472,-1.54038179681547,
1.72691350362778));
#77754=CARTESIAN_POINT('Ctrl Pts',(-1.25677996197875,-1.49620190053638,
1.72300833699741));
#77755=CARTESIAN_POINT('Ctrl Pts',(-1.30936139097415,-1.45203454163252,
1.7191042785756));
#77756=CARTESIAN_POINT('Ctrl Pts',(-1.35962757016161,-1.40507874059613,
1.71520022015379));
#77757=CARTESIAN_POINT('Ctrl Pts',(-1.40727750401264,-1.35561278641799,
1.71129616173197));
#77758=CARTESIAN_POINT('Ctrl Pts',(-1.45493025839965,-1.30614390420844,
1.70739187221777));
#77759=CARTESIAN_POINT('Ctrl Pts',(-1.49996612059321,-1.25416492989935,
1.70348758270357));
#77760=CARTESIAN_POINT('Ctrl Pts',(-1.54212191610968,-1.1999899982309,1.69958329318937));
#77761=CARTESIAN_POINT('Ctrl Pts',(-1.58432261431633,-1.14575736156264,
1.69567484498001));
#77762=CARTESIAN_POINT('Ctrl Pts',(-1.62363682094623,-1.089324488464,1.69176639677066));
#77763=CARTESIAN_POINT('Ctrl Pts',(-1.65984317018685,-1.03103668721539,
1.6878579485613));
#77764=CARTESIAN_POINT('Ctrl Pts',(-1.69607119123201,-0.97271399700772,
1.68394716089692));
#77765=CARTESIAN_POINT('Ctrl Pts',(-1.72918741547169,-0.912534599962121,
1.68003637323254));
#77766=CARTESIAN_POINT('Ctrl Pts',(-1.75901654307767,-0.850868263116606,
1.67612558556816));
#77767=CARTESIAN_POINT('Ctrl Pts',(-1.78889717645636,-0.789095447383394,
1.67220804517057));
#77768=CARTESIAN_POINT('Ctrl Pts',(-1.81547919475816,-0.72583102078802,
1.66829050477299));
#77769=CARTESIAN_POINT('Ctrl Pts',(-1.8386358331236,-0.661463735327861,
1.6643729643754));
#77770=CARTESIAN_POINT('Ctrl Pts',(-1.84956539097328,-0.631083420233703,
1.66252394882624));
#77771=CARTESIAN_POINT('Ctrl Pts',(-1.85973260901456,-0.600457624876922,
1.66067493327709));
#77772=CARTESIAN_POINT('Ctrl Pts',(-1.86912810006625,-0.569628076504945,
1.65882591772793));
#77773=CARTESIAN_POINT('Ctrl Pts',(-1.89347575123831,-0.489735808456053,
1.65403434426414));
#77774=CARTESIAN_POINT('Ctrl Pts',(-1.91271599857493,-0.408219073121368,
1.64924277080036));
#77775=CARTESIAN_POINT('Ctrl Pts',(-1.92666967351934,-0.325668495775797,
1.64445119733657));
#77776=CARTESIAN_POINT('Ctrl Pts',(-1.94042573682919,-0.24428699787267,
1.63972748202973));
#77777=CARTESIAN_POINT('Ctrl Pts',(-1.94904385906538,-0.161900712891478,
1.63500376672289));
#77778=CARTESIAN_POINT('Ctrl Pts',(-1.95239846276358,-0.0790964133094032,
1.63028005141604));
#77779=CARTESIAN_POINT('Ctrl Pts',(-1.95344248159806,-0.0533260821115529,
1.62880993804565));
#77780=CARTESIAN_POINT('Ctrl Pts',(-1.9539770316284,-0.0275154182212127,
1.62733982467525));
#77781=CARTESIAN_POINT('Ctrl Pts',(-1.95399927560819,-0.00168253459542325,
1.62586971130486));
#77782=CARTESIAN_POINT('',(-1.95128228942929,0.000979822369055472,0.92586969212423));
#77783=CARTESIAN_POINT('Ctrl Pts',(-1.95279539392324,-0.00168116113097749,
1.62586969212423));
#77784=CARTESIAN_POINT('Ctrl Pts',(-1.94903666796486,0.455824327828861,
1.59981784575684));
#77785=CARTESIAN_POINT('Ctrl Pts',(-1.56045216071061,1.56950483372459,1.53672874448747));
#77786=CARTESIAN_POINT('Ctrl Pts',(0.294933807152575,2.29043279904662,1.43660238831617));
#77787=CARTESIAN_POINT('Ctrl Pts',(2.08404446099042,0.994902325724279,1.32549062361027));
#77788=CARTESIAN_POINT('Ctrl Pts',(1.96642629593332,-1.21088396446362,1.21437885890441));
#77789=CARTESIAN_POINT('Ctrl Pts',(0.0496914524290246,-2.3088068886435,
1.10326709419851));
#77790=CARTESIAN_POINT('Ctrl Pts',(-1.64863658953277,-1.43079008949268,
1.00709737193847));
#77791=CARTESIAN_POINT('Ctrl Pts',(-1.94952095194778,-0.387800287767629,
0.947964904580365));
#77792=CARTESIAN_POINT('Ctrl Pts',(-1.95128228942929,0.000979822369055472,
0.92586969212423));
#77793=CARTESIAN_POINT('Ctrl Pts',(-1.95128228942929,0.000979822369055472,
0.92586969212423));
#77794=CARTESIAN_POINT('Ctrl Pts',(-1.9524734062589,0.263895099571634,0.910927649678405));
#77795=CARTESIAN_POINT('Ctrl Pts',(-1.78055803458398,1.17701113300587,0.858948352330618));
#77796=CARTESIAN_POINT('Ctrl Pts',(-0.393209187557522,2.27560539746712,
0.769931800080873));
#77797=CARTESIAN_POINT('Ctrl Pts',(1.69826458517494,1.56495710236821,0.65882003537499));
#77798=CARTESIAN_POINT('Ctrl Pts',(2.23594625441704,-0.577613834845561,
0.547708270669108));
#77799=CARTESIAN_POINT('Ctrl Pts',(0.727960807006617,-2.19149445634993,
0.436596505963225));
#77800=CARTESIAN_POINT('Ctrl Pts',(-1.37113217187641,-1.81423802364418,
0.329317307026286));
#77801=CARTESIAN_POINT('Ctrl Pts',(-1.95230380632447,-0.579097070743308,
0.259075362991307));
#77802=CARTESIAN_POINT('Ctrl Pts',(-1.95633563170751,0.00125569164583384,
0.22587067385829));
#77803=CARTESIAN_POINT('Origin',(0.,0.,-1.2940562256037));
#77804=CARTESIAN_POINT('',(-0.840025297123077,1.30917445368953,9.44449999999999));
#77805=CARTESIAN_POINT('Ctrl Pts',(-1.55549943430639,-0.00132660186739831,
8.85594377445462));
#77806=CARTESIAN_POINT('Ctrl Pts',(-1.55543973182031,-0.0713304105477647,
8.86094835465193));
#77807=CARTESIAN_POINT('Ctrl Pts',(-1.55065051292772,-0.141127590573169,
8.86595293484923));
#77808=CARTESIAN_POINT('Ctrl Pts',(-1.54123780639817,-0.210157736305244,
8.87095751504654));
#77809=CARTESIAN_POINT('Ctrl Pts',(-1.53168240264542,-0.280234383389748,
8.87603796499451));
#77810=CARTESIAN_POINT('Ctrl Pts',(-1.51736233716873,-0.349520592233542,
8.88111841494248));
#77811=CARTESIAN_POINT('Ctrl Pts',(-1.49843717350737,-0.417452137437612,
8.88619886489045));
#77812=CARTESIAN_POINT('Ctrl Pts',(-1.49503204889598,-0.429674772898193,
8.8871129687505));
#77813=CARTESIAN_POINT('Ctrl Pts',(-1.49147796610598,-0.441853609476848,
8.88802707261054));
#77814=CARTESIAN_POINT('Ctrl Pts',(-1.48777601674914,-0.453985433671693,
8.88894117647058));
#77815=CARTESIAN_POINT('Ctrl Pts',(-1.47100147783177,-0.508958027156549,
8.8930832295612));
#77816=CARTESIAN_POINT('Ctrl Pts',(-1.45114017341744,-0.563117052848065,
8.89722528265182));
#77817=CARTESIAN_POINT('Ctrl Pts',(-1.42828994739172,-0.616090964208816,
8.90136733574244));
#77818=CARTESIAN_POINT('Ctrl Pts',(-1.40548044525633,-0.668970464960515,
8.90550200682662));
#77819=CARTESIAN_POINT('Ctrl Pts',(-1.37969279869364,-0.720668567521905,
8.9096366779108));
#77820=CARTESIAN_POINT('Ctrl Pts',(-1.35107433676145,-0.770829674146372,
8.91377134899497));
#77821=CARTESIAN_POINT('Ctrl Pts',(-1.32248438637216,-0.820940807066931,
8.91790190085526));
#77822=CARTESIAN_POINT('Ctrl Pts',(-1.29106946520881,-0.869517526065842,
8.92203245271556));
#77823=CARTESIAN_POINT('Ctrl Pts',(-1.25702387485257,-0.916226624831783,
8.92616300457585));
#77824=CARTESIAN_POINT('Ctrl Pts',(-1.22299901527941,-0.962907281846979,
8.93029104129178));
#77825=CARTESIAN_POINT('Ctrl Pts',(-1.1863469685452,-1.00772215129541,8.93441907800771));
#77826=CARTESIAN_POINT('Ctrl Pts',(-1.14730541416721,-1.05036685811321,
8.93854711472363));
#77827=CARTESIAN_POINT('Ctrl Pts',(-1.10827251054623,-1.09300211579399,
8.94267423675665));
#77828=CARTESIAN_POINT('Ctrl Pts',(-1.0668515029429,-1.13346778021883,8.94680135878967));
#77829=CARTESIAN_POINT('Ctrl Pts',(-1.02331895594617,-1.17149415892749,
8.95092848082269));
#77830=CARTESIAN_POINT('Ctrl Pts',(-0.979746190478903,-1.20955566911588,
8.95505941578528));
#77831=CARTESIAN_POINT('Ctrl Pts',(-0.934058380981908,-1.24517304472543,
8.95919035074787));
#77832=CARTESIAN_POINT('Ctrl Pts',(-0.886566399666688,-1.27811590592639,
8.96332128571047));
#77833=CARTESIAN_POINT('Ctrl Pts',(-0.839054400608773,-1.31107265245496,
8.96745396185106));
#77834=CARTESIAN_POINT('Ctrl Pts',(-0.789737159647339,-1.3413523627722,
8.97158663799166));
#77835=CARTESIAN_POINT('Ctrl Pts',(-0.738953100619293,-1.36876899624631,
8.97571931413225));
#77836=CARTESIAN_POINT('Ctrl Pts',(-0.688068277551448,-1.39624002889212,
8.97986019019131));
#77837=CARTESIAN_POINT('Ctrl Pts',(-0.635711294687051,-1.420836408742,8.98400106625037));
#77838=CARTESIAN_POINT('Ctrl Pts',(-0.582242820401354,-1.44241933850426,
8.98814194230942));
#77839=CARTESIAN_POINT('Ctrl Pts',(-0.53097645972821,-1.4631133694516,8.9921122752651));
#77840=CARTESIAN_POINT('Ctrl Pts',(-0.478688799021197,-1.48103727978222,
8.99608260822078));
#77841=CARTESIAN_POINT('Ctrl Pts',(-0.425708788396775,-1.49611238798486,
9.00005294117646));
#77842=CARTESIAN_POINT('Ctrl Pts',(-0.370250558459497,-1.51189265694248,
9.00420899240009));
#77843=CARTESIAN_POINT('Ctrl Pts',(-0.313799216031233,-1.52461775351157,
9.00836504362372));
#77844=CARTESIAN_POINT('Ctrl Pts',(-0.256722338787837,-1.53416879474434,
9.01252109484735));
#77845=CARTESIAN_POINT('Ctrl Pts',(-0.199747628091171,-1.54370273979127,
9.01666970681673));
#77846=CARTESIAN_POINT('Ctrl Pts',(-0.142150112715516,-1.55007382314112,
9.02081831878611));
#77847=CARTESIAN_POINT('Ctrl Pts',(-0.0843106401441304,-1.55321343219742,
9.02496693075549));
#77848=CARTESIAN_POINT('Ctrl Pts',(-0.0265292103499676,-1.556349890609,
9.02911137953062));
#77849=CARTESIAN_POINT('Ctrl Pts',(0.0314931802133244,-1.5562612727405,
9.03325582830573));
#77850=CARTESIAN_POINT('Ctrl Pts',(0.0893691334599006,-1.55293058698212,
9.03740027708085));
#77851=CARTESIAN_POINT('Ctrl Pts',(0.147209030981919,-1.54960197618375,
9.04154214393559));
#77852=CARTESIAN_POINT('Ctrl Pts',(0.204902155333508,-1.54303533153495,
9.04568401079032));
#77853=CARTESIAN_POINT('Ctrl Pts',(0.262061867499625,-1.53326573939504,
9.04982587764506));
#77854=CARTESIAN_POINT('Ctrl Pts',(0.319207719778275,-1.52349851615172,
9.05396674019437));
#77855=CARTESIAN_POINT('Ctrl Pts',(0.375819905685316,-1.51052997465528,
9.0581076027437));
#77856=CARTESIAN_POINT('Ctrl Pts',(0.4315198464109,-1.4944466775879,9.06224846529302));
#77857=CARTESIAN_POINT('Ctrl Pts',(0.487267719514499,-1.47834954009871,
9.06639289124629));
#77858=CARTESIAN_POINT('Ctrl Pts',(0.542101278672587,-1.45913243303908,
9.07053731719956));
#77859=CARTESIAN_POINT('Ctrl Pts',(0.595656362187317,-1.4369320610891,9.07468174315283));
#77860=CARTESIAN_POINT('Ctrl Pts',(0.649232471956938,-1.41472297305377,
9.07882779624868));
#77861=CARTESIAN_POINT('Ctrl Pts',(0.701528636045423,-1.38952850838614,
9.08297384934453));
#77862=CARTESIAN_POINT('Ctrl Pts',(0.752202910871132,-1.36153260367756,
9.08711990244037));
#77863=CARTESIAN_POINT('Ctrl Pts',(0.802972913637875,-1.33348381236479,
9.09127378777709));
#77864=CARTESIAN_POINT('Ctrl Pts',(0.852114462357514,-1.30262328027436,
9.09542767311381));
#77865=CARTESIAN_POINT('Ctrl Pts',(0.899313161807077,-1.2691792966325,9.09958155845052));
#77866=CARTESIAN_POINT('Ctrl Pts',(0.943184497516362,-1.23809301139754,
9.10344260759446));
#77867=CARTESIAN_POINT('Ctrl Pts',(0.985377319286091,-1.20477534810784,
9.10730365673841));
#77868=CARTESIAN_POINT('Ctrl Pts',(1.02566651802248,-1.16943937158266,9.11116470588235));
#77869=CARTESIAN_POINT('Ctrl Pts',(1.06901228936252,-1.13142260265758,9.11531867663816));
#77870=CARTESIAN_POINT('Ctrl Pts',(1.11032977131098,-1.09091527354039,9.11947264739397));
#77871=CARTESIAN_POINT('Ctrl Pts',(1.14932007750667,-1.04816201488132,9.12362661814979));
#77872=CARTESIAN_POINT('Ctrl Pts',(1.18824256998146,-1.00548311464189,9.12777336412998));
#77873=CARTESIAN_POINT('Ctrl Pts',(1.22484557426173,-0.96056641928244,9.13192011011017));
#77874=CARTESIAN_POINT('Ctrl Pts',(1.25886528700759,-0.913694937693807,
9.13606685609037));
#77875=CARTESIAN_POINT('Ctrl Pts',(1.2928519207076,-0.866869031560226,9.14020956998477));
#77876=CARTESIAN_POINT('Ctrl Pts',(1.32425993691622,-0.818092523598639,
9.14435228387917));
#77877=CARTESIAN_POINT('Ctrl Pts',(1.35286540666698,-0.767681862130256,
9.14849499777358));
#77878=CARTESIAN_POINT('Ctrl Pts',(1.38145396231313,-0.717301007940313,
9.1526352621261));
#77879=CARTESIAN_POINT('Ctrl Pts',(1.40724300119445,-0.665288366385306,
9.15677552647862));
#77880=CARTESIAN_POINT('Ctrl Pts',(1.43005280857806,-0.61198792036934,9.16091579083114));
#77881=CARTESIAN_POINT('Ctrl Pts',(1.45285782014583,-0.558698680897996,
9.1650551846833));
#77882=CARTESIAN_POINT('Ctrl Pts',(1.47268463995099,-0.504122651506405,
9.16919457853547));
#77883=CARTESIAN_POINT('Ctrl Pts',(1.48940121121041,-0.44862487898575,9.17333397238763));
#77884=CARTESIAN_POINT('Ctrl Pts',(1.50613305510685,-0.393076402446755,
9.17747714808351));
#77885=CARTESIAN_POINT('Ctrl Pts',(1.51974882106387,-0.336604997763444,
9.18162032377938));
#77886=CARTESIAN_POINT('Ctrl Pts',(1.53016642110373,-0.279590725394439,
9.18576349947525));
#77887=CARTESIAN_POINT('Ctrl Pts',(1.54058840773718,-0.222552445726188,
9.18990841975988));
#77888=CARTESIAN_POINT('Ctrl Pts',(1.54780947771502,-0.164971358526727,
9.19405334004451));
#77889=CARTESIAN_POINT('Ctrl Pts',(1.55179929110059,-0.107234370141864,
9.19819826032914));
#77890=CARTESIAN_POINT('Ctrl Pts',(1.5557968462222,-0.0493853503206549,
9.20235122331545));
#77891=CARTESIAN_POINT('Ctrl Pts',(1.55655060718025,0.00861965443070754,
9.20650418630176));
#77892=CARTESIAN_POINT('Ctrl Pts',(1.55408244028937,0.0663929121535176,
9.21065714928806));
#77893=CARTESIAN_POINT('Ctrl Pts',(1.5517805958615,0.120273001000367,9.21453025638812));
#77894=CARTESIAN_POINT('Ctrl Pts',(1.54667699860277,0.173951210085379,9.21840336348818));
#77895=CARTESIAN_POINT('Ctrl Pts',(1.53882965619224,0.2271200986775,9.22227647058824));
#77896=CARTESIAN_POINT('Ctrl Pts',(1.53051710541967,0.283440960291726,9.2263791843138));
#77897=CARTESIAN_POINT('Ctrl Pts',(1.51908864750968,0.339437969704746,9.23048189803935));
#77898=CARTESIAN_POINT('Ctrl Pts',(1.50458123384946,0.394734797994868,9.23458461176491));
#77899=CARTESIAN_POINT('Ctrl Pts',(1.49002394797367,0.450221720495112,9.23870142941196));
#77900=CARTESIAN_POINT('Ctrl Pts',(1.47236650807424,0.505003095242158,9.24281824705901));
#77901=CARTESIAN_POINT('Ctrl Pts',(1.45169879005861,0.558704638375561,9.24693506470606));
#77902=CARTESIAN_POINT('Ctrl Pts',(1.43115897989575,0.612073834751231,9.25102640429573));
#77903=CARTESIAN_POINT('Ctrl Pts',(1.40764621358612,0.664376016200432,9.25511774388541));
#77904=CARTESIAN_POINT('Ctrl Pts',(1.38129899902813,0.715257523752038,9.25920908347508));
#77905=CARTESIAN_POINT('Ctrl Pts',(1.35496716769441,0.766109323357077,9.26329803427354));
#77906=CARTESIAN_POINT('Ctrl Pts',(1.32580441021765,0.815541619358912,9.26738698507201));
#77907=CARTESIAN_POINT('Ctrl Pts',(1.29399652331559,0.863222594495276,9.27147593587048));
#77908=CARTESIAN_POINT('Ctrl Pts',(1.26219434468097,0.910895012767786,9.27556415286274));
#77909=CARTESIAN_POINT('Ctrl Pts',(1.22774827427068,0.956816290476871,9.279652369855));
#77910=CARTESIAN_POINT('Ctrl Pts',(1.19088777442527,1.00068304608624,9.28374058684726));
#77911=CARTESIAN_POINT('Ctrl Pts',(1.15358469214915,1.04507650793688,9.2878778908845));
#77912=CARTESIAN_POINT('Ctrl Pts',(1.11380914503604,1.08736533131285,9.29201519492173));
#77913=CARTESIAN_POINT('Ctrl Pts',(1.07183952108797,1.12727117014226,9.29615249895897));
#77914=CARTESIAN_POINT('Ctrl Pts',(1.03030294825522,1.16676525241093,9.30024711345174));
#77915=CARTESIAN_POINT('Ctrl Pts',(0.986617827983286,1.20392500632945,9.30434172794452));
#77916=CARTESIAN_POINT('Ctrl Pts',(0.941087448215,1.23852116042165,9.30843634243729));
#77917=CARTESIAN_POINT('Ctrl Pts',(0.894845033952962,1.27365835228226,9.31259499124676));
#77918=CARTESIAN_POINT('Ctrl Pts',(0.846699616070225,1.30615074376982,9.31675364005623));
#77919=CARTESIAN_POINT('Ctrl Pts',(0.796996945149251,1.33580541974599,9.3209122888657));
#77920=CARTESIAN_POINT('Ctrl Pts',(0.747294274228271,1.36546009572216,9.32507093767517));
#77921=CARTESIAN_POINT('Ctrl Pts',(0.696034890907428,1.39227686998508,9.32922958648464));
#77922=CARTESIAN_POINT('Ctrl Pts',(0.643584947354596,1.41611393098811,9.33338823529411));
#77923=CARTESIAN_POINT('Ctrl Pts',(0.589802482825656,1.44055658623288,9.33765253696792));
#77924=CARTESIAN_POINT('Ctrl Pts',(0.534533878903967,1.46197317255622,9.34191683864173));
#77925=CARTESIAN_POINT('Ctrl Pts',(0.478142784720276,1.48018908502257,9.34618114031555));
#77926=CARTESIAN_POINT('Ctrl Pts',(0.42187304527927,1.49836579648737,9.35043626512837));
#77927=CARTESIAN_POINT('Ctrl Pts',(0.364486077933698,1.5133553832069,9.35469138994119));
#77928=CARTESIAN_POINT('Ctrl Pts',(0.306365181237462,1.52503135237455,9.35894651475401));
#77929=CARTESIAN_POINT('Ctrl Pts',(0.248318301789434,1.53669245213795,9.36319622064443));
#77930=CARTESIAN_POINT('Ctrl Pts',(0.189539821845199,1.5450482175854,9.36744592653485));
#77931=CARTESIAN_POINT('Ctrl Pts',(0.130426816967745,1.55002228868351,9.37169563242526));
#77932=CARTESIAN_POINT('Ctrl Pts',(0.0713711454148003,1.55499153546194,
9.37594121655317));
#77933=CARTESIAN_POINT('Ctrl Pts',(0.0119820753840637,1.55658556146196,
9.38018680068109));
#77934=CARTESIAN_POINT('Ctrl Pts',(-0.0473362918699389,1.55477957456097,
9.384432384809));
#77935=CARTESIAN_POINT('Ctrl Pts',(-0.106615111848175,1.55297479170294,
9.38867513842599));
#77936=CARTESIAN_POINT('Ctrl Pts',(-0.165822838377672,1.54777451490192,
9.39291789204299));
#77937=CARTESIAN_POINT('Ctrl Pts',(-0.224555229378385,1.539206028756,9.39716064565998));
#77938=CARTESIAN_POINT('Ctrl Pts',(-0.283283918780829,1.53063808263737,
9.4014031318782));
#77939=CARTESIAN_POINT('Ctrl Pts',(-0.341536850008862,1.51870240632424,
9.40564561809641));
#77940=CARTESIAN_POINT('Ctrl Pts',(-0.398916173355118,1.50347801335294,
9.40988810431463));
#77941=CARTESIAN_POINT('Ctrl Pts',(-0.45628943741574,1.48825522808526,9.41413014252415));
#77942=CARTESIAN_POINT('Ctrl Pts',(-0.512788809163372,1.46974454738153,
9.41837218073367));
#77943=CARTESIAN_POINT('Ctrl Pts',(-0.568030026120002,1.4480753224284,9.42261421894319));
#77944=CARTESIAN_POINT('Ctrl Pts',(-0.62331200894357,1.42639010643109,9.42685938761172));
#77945=CARTESIAN_POINT('Ctrl Pts',(-0.677333531145685,1.40154187177771,
9.43110455628025));
#77946=CARTESIAN_POINT('Ctrl Pts',(-0.729729856627479,1.37370833379813,
9.43534972494878));
#77947=CARTESIAN_POINT('Ctrl Pts',(-0.767375851189521,1.35371034329428,
9.43839981663252));
#77948=CARTESIAN_POINT('Ctrl Pts',(-0.804183296364171,1.33217229576637,
9.44144990831626));
#77949=CARTESIAN_POINT('Ctrl Pts',(-0.840025297123083,1.30917445368953,
9.44449999999999));
#77950=CARTESIAN_POINT('',(0.964986447796937,1.21999237930745,9.44449999999999));
#77951=CARTESIAN_POINT('Origin',(0.,0.,9.4445));
#77952=CARTESIAN_POINT('Ctrl Pts',(-1.55549989237731,-0.000578631300119371,
8.99405622560371));
#77953=CARTESIAN_POINT('Ctrl Pts',(-1.5554901928385,-0.0266533209394235,
8.99593481580826));
#77954=CARTESIAN_POINT('Ctrl Pts',(-1.55482490216014,-0.0527164090981486,
8.99781340601282));
#77955=CARTESIAN_POINT('Ctrl Pts',(-1.55350552651592,-0.0787453432559613,
8.99969199621737));
#77956=CARTESIAN_POINT('Ctrl Pts',(-1.55058691562536,-0.136324343623012,
9.00384765412568));
#77957=CARTESIAN_POINT('Ctrl Pts',(-1.5444568005893,-0.193860047852549,
9.00800331203398));
#77958=CARTESIAN_POINT('Ctrl Pts',(-1.53512090481116,-0.250966247953344,
9.01215896994229));
#77959=CARTESIAN_POINT('Ctrl Pts',(-1.52580175101302,-0.307970040006427,
9.01630717554572));
#77960=CARTESIAN_POINT('Ctrl Pts',(-1.51328831174432,-0.364545349116219,
9.02045538114915));
#77961=CARTESIAN_POINT('Ctrl Pts',(-1.49763817662938,-0.420309578646767,
9.02460358675258));
#77962=CARTESIAN_POINT('Ctrl Pts',(-1.48200377836541,-0.476017734963701,
9.02874762116561));
#77963=CARTESIAN_POINT('Ctrl Pts',(-1.46323907375425,-0.530915930872425,
9.03289165557864));
#77964=CARTESIAN_POINT('Ctrl Pts',(-1.44145263545854,-0.584631978025173,
9.03703568999167));
#77965=CARTESIAN_POINT('Ctrl Pts',(-1.41967980895633,-0.638314464311682,
9.04117713528298));
#77966=CARTESIAN_POINT('Ctrl Pts',(-1.39488918624381,-0.690815786388868,
9.04531858057428));
#77967=CARTESIAN_POINT('Ctrl Pts',(-1.36723840323526,-0.741781233733169,
9.04946002586559));
#77968=CARTESIAN_POINT('Ctrl Pts',(-1.33959436840948,-0.792734242943131,
9.05360046043579));
#77969=CARTESIAN_POINT('Ctrl Pts',(-1.30909180633639,-0.842151665824471,
9.057740895006));
#77970=CARTESIAN_POINT('Ctrl Pts',(-1.27593449635465,-0.889702990335659,
9.06188132957621));
#77971=CARTESIAN_POINT('Ctrl Pts',(-1.24274862502127,-0.937295275048407,
9.0660253306724));
#77972=CARTESIAN_POINT('Ctrl Pts',(-1.20690373175877,-0.983017821460801,
9.0701693317686));
#77973=CARTESIAN_POINT('Ctrl Pts',(-1.16864643086464,-1.02656990489072,
9.07431333286479));
#77974=CARTESIAN_POINT('Ctrl Pts',(-1.13037415153796,-1.07013903975733,
9.07845895641316));
#77975=CARTESIAN_POINT('Ctrl Pts',(-1.0896879441992,-1.11153564492548,9.08260457996152));
#77976=CARTESIAN_POINT('Ctrl Pts',(-1.04687198965965,-1.15049523565552,
9.08675020350989));
#77977=CARTESIAN_POINT('Ctrl Pts',(-1.00397488784166,-1.18952866485981,
9.09090368408426));
#77978=CARTESIAN_POINT('Ctrl Pts',(-0.958940375162835,-1.22611551941561,
9.09505716465863));
#77979=CARTESIAN_POINT('Ctrl Pts',(-0.912085762463041,-1.2600316709957,
9.099210645233));
#77980=CARTESIAN_POINT('Ctrl Pts',(-0.868153216420064,-1.29183265717479,
9.10310509587635));
#77981=CARTESIAN_POINT('Ctrl Pts',(-0.822621105439473,-1.32128589012233,
9.10699954651969));
#77982=CARTESIAN_POINT('Ctrl Pts',(-0.775770919578585,-1.34824320147969,
9.11089399716303));
#77983=CARTESIAN_POINT('Ctrl Pts',(-0.725804427847385,-1.3769936162386,
9.11504749265707));
#77984=CARTESIAN_POINT('Ctrl Pts',(-0.674135562699792,-1.40302129179383,
9.11920098815111));
#77985=CARTESIAN_POINT('Ctrl Pts',(-0.621092211084585,-1.42612226521083,
9.12335448364515));
#77986=CARTESIAN_POINT('Ctrl Pts',(-0.568141288735605,-1.44918298464769,
9.12750074157729));
#77987=CARTESIAN_POINT('Ctrl Pts',(-0.513821106347082,-1.46932691961064,
9.13164699950943));
#77988=CARTESIAN_POINT('Ctrl Pts',(-0.458484563219447,-1.48639569270416,
9.13579325744156));
#77989=CARTESIAN_POINT('Ctrl Pts',(-0.403201937413972,-1.50344783478884,
9.13993547545519));
#77990=CARTESIAN_POINT('Ctrl Pts',(-0.346905406819296,-1.51743060000223,
9.14407769346883));
#77991=CARTESIAN_POINT('Ctrl Pts',(-0.289966662188531,-1.52823413939725,
9.14821991148246));
#77992=CARTESIAN_POINT('Ctrl Pts',(-0.233061683793884,-1.5390312719973,
9.15235967304728));
#77993=CARTESIAN_POINT('Ctrl Pts',(-0.175515755424508,-1.54665281998605,
9.1564994346121));
#77994=CARTESIAN_POINT('Ctrl Pts',(-0.117712368437924,-1.55103966690628,
9.16063919617692));
#77995=CARTESIAN_POINT('Ctrl Pts',(-0.0599212198648014,-1.555425585022,
9.16477808125134));
#77996=CARTESIAN_POINT('Ctrl Pts',(-0.00187323828847601,-1.55657812269653,
9.16891696632577));
#77997=CARTESIAN_POINT('Ctrl Pts',(0.0560435218902042,-1.55449006868945,
9.17305585140019));
#77998=CARTESIAN_POINT('Ctrl Pts',(0.114013266983416,-1.55240010443459,
9.17719852291694));
#77999=CARTESIAN_POINT('Ctrl Pts',(0.171851030721492,-1.54706364185241,
9.18134119443368));
#78000=CARTESIAN_POINT('Ctrl Pts',(0.229170667221835,-1.53852561086421,
9.18548386595042));
#78001=CARTESIAN_POINT('Ctrl Pts',(0.286514385640701,-1.52998399276034,
9.18962827794363));
#78002=CARTESIAN_POINT('Ctrl Pts',(0.343339033121586,-1.51823822868701,
9.19377268993684));
#78003=CARTESIAN_POINT('Ctrl Pts',(0.399268682012365,-1.50338443838032,
9.19791710193004));
#78004=CARTESIAN_POINT('Ctrl Pts',(0.455307235367057,-1.48850172523749,
9.20206958379272));
#78005=CARTESIAN_POINT('Ctrl Pts',(0.510446811804607,-1.47049905229525,
9.20622206565539));
#78006=CARTESIAN_POINT('Ctrl Pts',(0.564327542277097,-1.44952222301953,
9.21037454751807));
#78007=CARTESIAN_POINT('Ctrl Pts',(0.615024959781817,-1.42978472016108,
9.21428169771494));
#78008=CARTESIAN_POINT('Ctrl Pts',(0.664607737056635,-1.40741471629783,
9.21818884791181));
#78009=CARTESIAN_POINT('Ctrl Pts',(0.712796415253884,-1.38257062040288,
9.22209599810868));
#78010=CARTESIAN_POINT('Ctrl Pts',(0.763391522821897,-1.35648586872969,
9.2261982622066));
#78011=CARTESIAN_POINT('Ctrl Pts',(0.812672697808314,-1.32755818907571,
9.23030052630453));
#78012=CARTESIAN_POINT('Ctrl Pts',(0.860295839293345,-1.29594418047019,
9.23440279040245));
#78013=CARTESIAN_POINT('Ctrl Pts',(0.908132233227251,-1.26418860697535,
9.23852342409628));
#78014=CARTESIAN_POINT('Ctrl Pts',(0.954295192671738,-1.22972276755281,
9.24264405779011));
#78015=CARTESIAN_POINT('Ctrl Pts',(0.998458660824575,-1.19275334945009,
9.24676469148394));
#78016=CARTESIAN_POINT('Ctrl Pts',(1.04230309037482,-1.15605099985406,9.25085555756054));
#78017=CARTESIAN_POINT('Ctrl Pts',(1.08417639440084,-1.11688145289402,9.25494642363714));
#78018=CARTESIAN_POINT('Ctrl Pts',(1.12378878969793,-1.07549012368745,9.25903728971374));
#78019=CARTESIAN_POINT('Ctrl Pts',(1.16337799901314,-1.03412302171083,9.26312576131896));
#78020=CARTESIAN_POINT('Ctrl Pts',(1.20070855244863,-0.990537097348186,
9.26721423292418));
#78021=CARTESIAN_POINT('Ctrl Pts',(1.23552663022966,-0.945015447489269,
9.2713027045294));
#78022=CARTESIAN_POINT('Ctrl Pts',(1.27033841526179,-0.89950202485972,9.27539043721603));
#78023=CARTESIAN_POINT('Ctrl Pts',(1.30263830177598,-0.852053994283024,
9.27947816990265));
#78024=CARTESIAN_POINT('Ctrl Pts',(1.33221350220979,-0.80298657182417,9.28356590258928));
#78025=CARTESIAN_POINT('Ctrl Pts',(1.3621982727763,-0.753239642534148,9.28771024396137));
#78026=CARTESIAN_POINT('Ctrl Pts',(1.38938199043749,-0.701828586715616,
9.29185458533345));
#78027=CARTESIAN_POINT('Ctrl Pts',(1.41359048438248,-0.649108767821922,
9.29599892670554));
#78028=CARTESIAN_POINT('Ctrl Pts',(1.43750571082689,-0.597027609455958,
9.30009306253248));
#78029=CARTESIAN_POINT('Ctrl Pts',(1.45851728171959,-0.543669757738866,
9.30418719835942));
#78030=CARTESIAN_POINT('Ctrl Pts',(1.47650651044374,-0.489396336947121,
9.30828133418636));
#78031=CARTESIAN_POINT('Ctrl Pts',(1.49482663648289,-0.434124600469282,
9.31245077833102));
#78032=CARTESIAN_POINT('Ctrl Pts',(1.51001195109945,-0.37790382886161,9.31662022247569));
#78033=CARTESIAN_POINT('Ctrl Pts',(1.52199141655154,-0.321126731904137,
9.32078966662035));
#78034=CARTESIAN_POINT('Ctrl Pts',(1.53397088200363,-0.264349634946657,
9.32495911076502));
#78035=CARTESIAN_POINT('Ctrl Pts',(1.54274449746717,-0.207016792366188,
9.32912855490969));
#78036=CARTESIAN_POINT('Ctrl Pts',(1.54829678086355,-0.149523671596055,
9.33329799905435));
#78037=CARTESIAN_POINT('Ctrl Pts',(1.5539750612308,-0.0907258697522934,
9.33756205964687));
#78038=CARTESIAN_POINT('Ctrl Pts',(1.55630942801978,-0.0315034819748185,
9.34182612023938));
#78039=CARTESIAN_POINT('Ctrl Pts',(1.55525257737604,0.0277429372124185,
9.3460901808319));
#78040=CARTESIAN_POINT('Ctrl Pts',(1.55419800600909,0.0868615814976223,
9.35034504525809));
#78041=CARTESIAN_POINT('Ctrl Pts',(1.54976676979609,0.146003672121871,9.35459990968429));
#78042=CARTESIAN_POINT('Ctrl Pts',(1.54196344786062,0.204765659869519,9.35885477411049));
#78043=CARTESIAN_POINT('Ctrl Pts',(1.5341700838921,0.263452660331324,9.36310420882358));
#78044=CARTESIAN_POINT('Ctrl Pts',(1.52301324130298,0.321760042456003,9.36735364353668));
#78045=CARTESIAN_POINT('Ctrl Pts',(1.50854939055218,0.379287471800296,9.37160307824977));
#78046=CARTESIAN_POINT('Ctrl Pts',(1.49409960192587,0.436758971510931,9.37584838155408));
#78047=CARTESIAN_POINT('Ctrl Pts',(1.47634930865275,0.493451555208341,9.3800936848584));
#78048=CARTESIAN_POINT('Ctrl Pts',(1.45540604204976,0.548974956409712,9.38433898816271));
#78049=CARTESIAN_POINT('Ctrl Pts',(1.43447678114563,0.604461226629996,9.38858145244288));
#78050=CARTESIAN_POINT('Ctrl Pts',(1.41035896085714,0.658779414523991,9.39282391672304));
#78051=CARTESIAN_POINT('Ctrl Pts',(1.38320942293468,0.711556000821227,9.39706638100321));
#78052=CARTESIAN_POINT('Ctrl Pts',(1.35606162195232,0.764329210642272,9.40130857386416));
#78053=CARTESIAN_POINT('Ctrl Pts',(1.32588269933253,0.815560577204835,9.40555076672511));
#78054=CARTESIAN_POINT('Ctrl Pts',(1.29287636066414,0.864899396482526,9.40979295958606));
#78055=CARTESIAN_POINT('Ctrl Pts',(1.2598735525539,0.914232938180896,9.41403469867633));
#78056=CARTESIAN_POINT('Ctrl Pts',(1.22404420512749,0.961673934813684,9.41827643776661));
#78057=CARTESIAN_POINT('Ctrl Pts',(1.18563523847262,1.00690085474787,9.42251817685689));
#78058=CARTESIAN_POINT('Ctrl Pts',(1.14719782176396,1.05216127488829,9.42676305786208));
#78059=CARTESIAN_POINT('Ctrl Pts',(1.10617728710028,1.09520397430549,9.43100793886727));
#78060=CARTESIAN_POINT('Ctrl Pts',(1.06285997935682,1.13574157020056,9.43525281987246));
#78061=CARTESIAN_POINT('Ctrl Pts',(1.03140539151689,1.16517768794019,9.4383352132483));
#78062=CARTESIAN_POINT('Ctrl Pts',(0.99874058480781,1.19329361845858,9.44141760662415));
#78063=CARTESIAN_POINT('Ctrl Pts',(0.964986447796939,1.21999237930745,9.44449999999999));
#78064=CARTESIAN_POINT('Origin',(0.,0.,9.5));
#78065=CARTESIAN_POINT('',(-1.84236513795726,-0.000200609048493022,9.15763482856377));
#78066=CARTESIAN_POINT('Ctrl Pts',(0.964986447796979,1.21999237930743,9.44449999999999));
#78067=CARTESIAN_POINT('Ctrl Pts',(1.08560030229,1.13318400160663,9.43775928913704));
#78068=CARTESIAN_POINT('Ctrl Pts',(1.19286327134867,1.02899315757803,9.43165929429191));
#78069=CARTESIAN_POINT('Ctrl Pts',(1.38336247774274,0.78338519890483,9.41850392344787));
#78070=CARTESIAN_POINT('Ctrl Pts',(1.46275942778644,0.640439473146718,9.41142100787987));
#78071=CARTESIAN_POINT('Ctrl Pts',(1.59405703872584,0.289070474707947,9.39396691671519));
#78072=CARTESIAN_POINT('Ctrl Pts',(1.62885716287837,0.0760950411825039,
9.38329941785984));
#78073=CARTESIAN_POINT('Ctrl Pts',(1.61182773281384,-0.347980912653401,
9.3646306987772));
#78074=CARTESIAN_POINT('Ctrl Pts',(1.56058342560136,-0.555567132615176,
9.35695125924503));
#78075=CARTESIAN_POINT('Ctrl Pts',(1.39250704246998,-0.922566442698323,
9.34073391190102));
#78076=CARTESIAN_POINT('Ctrl Pts',(1.28243138363951,-1.08322129741915,9.33237183821666));
#78077=CARTESIAN_POINT('Ctrl Pts',(1.03840088300862,-1.33466736093396,9.3163239698559));
#78078=CARTESIAN_POINT('Ctrl Pts',(0.866309261774041,-1.48184220392284,
9.3056566762329));
#78079=CARTESIAN_POINT('Ctrl Pts',(0.412140887062194,-1.67767483685419,
9.28642581763546));
#78080=CARTESIAN_POINT('Ctrl Pts',(0.194750287412152,-1.72435577821932,
9.27861688942565));
#78081=CARTESIAN_POINT('Ctrl Pts',(-0.257099384488897,-1.736029196837,9.26045970387453));
#78082=CARTESIAN_POINT('Ctrl Pts',(-0.489372106073173,-1.69608434724234,
9.25004792636098));
#78083=CARTESIAN_POINT('Ctrl Pts',(-0.884973762473043,-1.5427681115351,
9.23180320826604));
#78084=CARTESIAN_POINT('Ctrl Pts',(-1.04951278218718,-1.44452702535207,
9.22468464517327));
#78085=CARTESIAN_POINT('Ctrl Pts',(-1.37115962638764,-1.17394870584797,
9.20956351272862));
#78086=CARTESIAN_POINT('Ctrl Pts',(-1.51720372489576,-0.99309098074786,
9.20123624930322));
#78087=CARTESIAN_POINT('Ctrl Pts',(-1.69399973984075,-0.664427569501659,
9.18603024705193));
#78088=CARTESIAN_POINT('Ctrl Pts',(-1.74712287279637,-0.530140739618914,
9.17986752410044));
#78089=CARTESIAN_POINT('Ctrl Pts',(-1.81744855644709,-0.263866966136998,
9.16821855214639));
#78090=CARTESIAN_POINT('Ctrl Pts',(-1.83715573107123,-0.133049066016314,
9.16279996303978));
#78091=CARTESIAN_POINT('Ctrl Pts',(-1.84209656264027,-0.000614842640808093,
9.15790333475071));
#78092=CARTESIAN_POINT('Ctrl Pts',(1.57783641624473,1.14957158812871,9.04780057559153));
#78093=CARTESIAN_POINT('Ctrl Pts',(1.52810092067142,1.20153114569838,9.0574016669285));
#78094=CARTESIAN_POINT('Ctrl Pts',(1.4757016834809,1.25063809809762,9.06692903469903));
#78095=CARTESIAN_POINT('Ctrl Pts',(1.42089948536213,1.29662118218321,9.07641432798314));
#78096=CARTESIAN_POINT('Ctrl Pts',(1.36749733311227,1.34142952457733,9.08565729803691));
#78097=CARTESIAN_POINT('Ctrl Pts',(1.31181359643843,1.38327130064711,9.09486045306681));
#78098=CARTESIAN_POINT('Ctrl Pts',(1.25409138389606,1.42188378312268,9.10408368015105));
#78099=CARTESIAN_POINT('Ctrl Pts',(1.21543754680529,1.44774073734434,9.11026003932826));
#78100=CARTESIAN_POINT('Ctrl Pts',(1.17586965463972,1.47214936941216,9.11644603315947));
#78101=CARTESIAN_POINT('Ctrl Pts',(1.13546015350029,1.49502814066238,9.12266707759137));
#78102=CARTESIAN_POINT('Ctrl Pts',(1.10079817205115,1.51465282105421,9.12800329112069));
#78103=CARTESIAN_POINT('Ctrl Pts',(1.06551698574574,1.53315187233987,9.13336540041012));
#78104=CARTESIAN_POINT('Ctrl Pts',(1.02966136659078,1.55047227609227,9.13877276809619));
#78105=CARTESIAN_POINT('Ctrl Pts',(1.01944191431497,1.555408881392,9.14031395849557));
#78106=CARTESIAN_POINT('Ctrl Pts',(1.00917785748784,1.56024865575544,9.14185853052058));
#78107=CARTESIAN_POINT('Ctrl Pts',(0.998880077105522,1.5649861731208,9.14340550186703));
#78108=CARTESIAN_POINT('Ctrl Pts',(0.938429655183682,1.59279652767935,9.15248659188081));
#78109=CARTESIAN_POINT('Ctrl Pts',(0.876724909237559,1.61713151747312,9.16166360683785));
#78110=CARTESIAN_POINT('Ctrl Pts',(0.813962174626755,1.63784581666518,9.17104583411974));
#78111=CARTESIAN_POINT('Ctrl Pts',(0.793731103129688,1.64452290730766,9.17407012093769));
#78112=CARTESIAN_POINT('Ctrl Pts',(0.773389798665458,1.65082359212481,9.17711583460595));
#78113=CARTESIAN_POINT('Ctrl Pts',(0.752943954195354,1.656742326203,9.18018689597204));
#78114=CARTESIAN_POINT('Ctrl Pts',(0.685138060299321,1.67637101189959,9.19037165803664));
#78115=CARTESIAN_POINT('Ctrl Pts',(0.616177319257057,1.69180559672274,9.20083482083306));
#78116=CARTESIAN_POINT('Ctrl Pts',(0.546368309836355,1.70301140123728,9.21149051924861));
#78117=CARTESIAN_POINT('Ctrl Pts',(0.485285426593238,1.71281648018751,9.22081425536221));
#78118=CARTESIAN_POINT('Ctrl Pts',(0.423553097709839,1.71938155637349,9.23028512190475));
#78119=CARTESIAN_POINT('Ctrl Pts',(0.361421529909612,1.72264105607437,9.23985292365802));
#78120=CARTESIAN_POINT('Ctrl Pts',(0.34963016087468,1.72325964603118,9.24166870724952));
#78121=CARTESIAN_POINT('Ctrl Pts',(0.337823543788487,1.72375903562151,9.24348816903752));
#78122=CARTESIAN_POINT('Ctrl Pts',(0.326020291990775,1.72413841101507,9.24530843418927));
#78123=CARTESIAN_POINT('Ctrl Pts',(0.260499809734028,1.72624434412302,9.25541282343905));
#78124=CARTESIAN_POINT('Ctrl Pts',(0.19495931580534,1.72466195618245,9.26555860148615));
#78125=CARTESIAN_POINT('Ctrl Pts',(0.129717803358982,1.71940174492272,9.27571201101684));
#78126=CARTESIAN_POINT('Ctrl Pts',(0.0648998775900165,1.71417568608109,
9.28579949857782));
#78127=CARTESIAN_POINT('Ctrl Pts',(0.000376941694672228,1.7053181900444,
9.29589425669667));
#78128=CARTESIAN_POINT('Ctrl Pts',(-0.0634948351275549,1.69282106251119,
9.30598856445142));
#78129=CARTESIAN_POINT('Ctrl Pts',(-0.126013627091431,1.68058865948019,
9.31586904622187));
#78130=CARTESIAN_POINT('Ctrl Pts',(-0.187908231055998,1.66486839910538,
9.32574896303347));
#78131=CARTESIAN_POINT('Ctrl Pts',(-0.24880479275547,1.64564964474991,9.3356483009401));
#78132=CARTESIAN_POINT('Ctrl Pts',(-0.265085021026627,1.64051165831418,
9.33829481293282));
#78133=CARTESIAN_POINT('Ctrl Pts',(-0.281293709851209,1.63512364377799,
9.34094287203815));
#78134=CARTESIAN_POINT('Ctrl Pts',(-0.297423275648299,1.62948545004139,
9.34359321518114));
#78135=CARTESIAN_POINT('Ctrl Pts',(-0.30743974502818,1.625984128578,9.34523907975505));
#78136=CARTESIAN_POINT('Ctrl Pts',(-0.317424735746893,1.62238658086478,
9.34688567512058));
#78137=CARTESIAN_POINT('Ctrl Pts',(-0.327364914290974,1.61869735262368,
9.34853128806519));
#78138=CARTESIAN_POINT('Ctrl Pts',(-0.385432578540992,1.59714594226462,
9.35814448560777));
#78139=CARTESIAN_POINT('Ctrl Pts',(-0.442079483362686,1.57243010146291,
9.36773988234226));
#78140=CARTESIAN_POINT('Ctrl Pts',(-0.497012128252419,1.54462866539572,
9.37737904315513));
#78141=CARTESIAN_POINT('Ctrl Pts',(-0.551000823362909,1.51730496273262,
9.38685256687298));
#78142=CARTESIAN_POINT('Ctrl Pts',(-0.603333782033549,1.48700109740394,
9.39636859881508));
#78143=CARTESIAN_POINT('Ctrl Pts',(-0.653723422148521,1.45377417399759,
9.40600700702671));
#78144=CARTESIAN_POINT('Ctrl Pts',(-0.699035964422128,1.4238950883753,9.41467428027064));
#78145=CARTESIAN_POINT('Ctrl Pts',(-0.742776628534788,1.39165290498635,
9.42344082135282));
#78146=CARTESIAN_POINT('Ctrl Pts',(-0.784729150829576,1.3570706466195,9.43237741146729));
#78147=CARTESIAN_POINT('Ctrl Pts',(-0.788069690410533,1.35431697660029,
9.43308900236489));
#78148=CARTESIAN_POINT('Ctrl Pts',(-0.791398865710535,1.35154847642802,
9.43380167144245));
#78149=CARTESIAN_POINT('Ctrl Pts',(-0.7947165535573,1.34876516188143,9.43451545443494));
#78150=CARTESIAN_POINT('Ctrl Pts',(-0.810068690312162,1.33588576287689,
9.43781838545804));
#78151=CARTESIAN_POINT('Ctrl Pts',(-0.825175397375869,1.32268873629791,
9.44114528312219));
#78152=CARTESIAN_POINT('Ctrl Pts',(-0.840025297123097,1.30917445368955,
9.44449999999998));
#78153=CARTESIAN_POINT('Ctrl Pts',(-1.84249520620809,-1.04387282595019E-15,
9.15750479379191));
#78154=CARTESIAN_POINT('Ctrl Pts',(-1.84342557490868,0.0255843048651023,
9.15657442509132));
#78155=CARTESIAN_POINT('Ctrl Pts',(-1.84380342678949,0.0512172914604668,
9.15566374529628));
#78156=CARTESIAN_POINT('Ctrl Pts',(-1.8436302880131,0.0768851883582362,
9.15476723119598));
#78157=CARTESIAN_POINT('Ctrl Pts',(-1.84315348435067,0.147571533166139,
9.15229833765667));
#78158=CARTESIAN_POINT('Ctrl Pts',(-1.8385033733487,0.218128048887438,9.1499488369688));
#78159=CARTESIAN_POINT('Ctrl Pts',(-1.829823624367,0.288237312311215,9.14761363519918));
#78160=CARTESIAN_POINT('Ctrl Pts',(-1.82117196456348,0.358119689958019,
9.14528599054886));
#78161=CARTESIAN_POINT('Ctrl Pts',(-1.80851533144921,0.427557438695703,
9.14297219045531));
#78162=CARTESIAN_POINT('Ctrl Pts',(-1.79197172346283,0.49620682453524,9.14059582919536));
#78163=CARTESIAN_POINT('Ctrl Pts',(-1.77951701963477,0.547888886230224,
9.13880680737464));
#78164=CARTESIAN_POINT('Ctrl Pts',(-1.76485880483925,0.5991234665025,9.1369828833152));
#78165=CARTESIAN_POINT('Ctrl Pts',(-1.74804397062882,0.649754936470355,
9.1351034343108));
#78166=CARTESIAN_POINT('Ctrl Pts',(-1.73847181500994,0.678577837944145,
9.13403352317622));
#78167=CARTESIAN_POINT('Ctrl Pts',(-1.72820074137517,0.707205162873137,
9.13294581355773));
#78168=CARTESIAN_POINT('Ctrl Pts',(-1.71723927293521,0.735607328247734,
9.1318381060832));
#78169=CARTESIAN_POINT('Ctrl Pts',(-1.71240747914154,0.748126947050236,
9.13134983080056));
#78170=CARTESIAN_POINT('Ctrl Pts',(-1.70744153904584,0.760602809394986,
9.13085768542315));
#78171=CARTESIAN_POINT('Ctrl Pts',(-1.70234218031443,0.773032349297603,
9.1303615558247));
#78172=CARTESIAN_POINT('Ctrl Pts',(-1.69796348408131,0.783705295136006,
9.12993554131614));
#78173=CARTESIAN_POINT('Ctrl Pts',(-1.69348687217055,0.794342776028454,
9.12950663900286));
#78174=CARTESIAN_POINT('Ctrl Pts',(-1.6889179804492,0.804931912536332,9.12907527449553));
#78175=CARTESIAN_POINT('Ctrl Pts',(-1.66040388987596,0.871017872960098,
9.1263831628452));
#78176=CARTESIAN_POINT('Ctrl Pts',(-1.62824798634224,0.935339672795842,
9.12358735490002));
#78177=CARTESIAN_POINT('Ctrl Pts',(-1.59268341757425,0.99755604372753,9.12070265019255));
#78178=CARTESIAN_POINT('Ctrl Pts',(-1.55704284135595,1.05990538148225,9.11781178038713));
#78179=CARTESIAN_POINT('Ctrl Pts',(-1.51797988143916,1.12014042703985,9.11483190560086));
#78180=CARTESIAN_POINT('Ctrl Pts',(-1.47570599844027,1.17793996136523,9.11181284126448));
#78181=CARTESIAN_POINT('Ctrl Pts',(-1.43416890647619,1.23473210825217,9.10884639616671));
#78182=CARTESIAN_POINT('Ctrl Pts',(-1.38953274198914,1.2891736439028,9.10584254470439));
#78183=CARTESIAN_POINT('Ctrl Pts',(-1.34196257272456,1.34097455280792,9.10287683639888));
#78184=CARTESIAN_POINT('Ctrl Pts',(-1.32667583540764,1.35762084394903,9.10192380208083));
#78185=CARTESIAN_POINT('Ctrl Pts',(-1.3110857787495,1.3739945103908,9.10097490118564));
#78186=CARTESIAN_POINT('Ctrl Pts',(-1.29519684402696,1.39008601519461,9.1000331596533));
#78187=CARTESIAN_POINT('Ctrl Pts',(-1.28692690184776,1.39846139193493,9.09954299790513));
#78188=CARTESIAN_POINT('Ctrl Pts',(-1.27858264381706,1.4067535669247,9.09905517532569));
#78189=CARTESIAN_POINT('Ctrl Pts',(-1.2701663787571,1.41496029262394,9.09857020654789));
#78190=CARTESIAN_POINT('Ctrl Pts',(-1.22072939905454,1.46316644213651,9.09572150923928));
#78191=CARTESIAN_POINT('Ctrl Pts',(-1.16879887319286,1.50843891952808,9.09296975259348));
#78192=CARTESIAN_POINT('Ctrl Pts',(-1.11453995621698,1.550592707069,9.09040919115646));
#78193=CARTESIAN_POINT('Ctrl Pts',(-1.06201853480217,1.5913966331896,9.08793062479745));
#78194=CARTESIAN_POINT('Ctrl Pts',(-1.0073091984942,1.62928311296455,9.0856308892326));
#78195=CARTESIAN_POINT('Ctrl Pts',(-0.950637932866433,1.66420382554962,
9.08341792443461));
#78196=CARTESIAN_POINT('Ctrl Pts',(-0.947477902479955,1.66615102951029,
9.08329452793149));
#78197=CARTESIAN_POINT('Ctrl Pts',(-0.944311758662973,1.66808901067078,
9.08317140122102));
#78198=CARTESIAN_POINT('Ctrl Pts',(-0.941139535971432,1.67001775994204,
9.08304852834237));
#78199=CARTESIAN_POINT('Ctrl Pts',(-0.879859752551074,1.70727659991257,
9.0806749171163));
#78200=CARTESIAN_POINT('Ctrl Pts',(-0.816315831409928,1.74108997628849,
9.07839543674175));
#78201=CARTESIAN_POINT('Ctrl Pts',(-0.750802631996302,1.77133860261608,
9.07611199979561));
#78202=CARTESIAN_POINT('Ctrl Pts',(-0.735354339772224,1.77847135789392,
9.0755735556113));
#78203=CARTESIAN_POINT('Ctrl Pts',(-0.719796650695635,1.78540568824835,
9.07503498604674));
#78204=CARTESIAN_POINT('Ctrl Pts',(-0.704133638622343,1.79213966692767,
9.07449519169253));
#78205=CARTESIAN_POINT('Ctrl Pts',(-0.689232335423251,1.79854616508826,
9.07398164810976));
#78206=CARTESIAN_POINT('Ctrl Pts',(-0.674231156838674,1.80477300329879,
9.07346684130825));
#78207=CARTESIAN_POINT('Ctrl Pts',(-0.659161822527577,1.81080758331309,
9.07295085375021));
#78208=CARTESIAN_POINT('Ctrl Pts',(-0.59180873473216,1.83777941824091,9.07064462345622));
#78209=CARTESIAN_POINT('Ctrl Pts',(-0.522999968241605,1.86095469047836,
9.06830887730024));
#78210=CARTESIAN_POINT('Ctrl Pts',(-0.453122176480387,1.88028588298503,
9.06588658332271));
#78211=CARTESIAN_POINT('Ctrl Pts',(-0.382259594422812,1.89988951070062,
9.06343015186683));
#78212=CARTESIAN_POINT('Ctrl Pts',(-0.3102979315688,1.91553942838373,9.06088454492288));
#78213=CARTESIAN_POINT('Ctrl Pts',(-0.237641237294552,1.92717683998401,
9.05822660172882));
#78214=CARTESIAN_POINT('Ctrl Pts',(-0.165233254770242,1.93877441546137,
9.05557775696277));
#78215=CARTESIAN_POINT('Ctrl Pts',(-0.0921354293764491,1.94638696167918,
9.05281738641335));
#78216=CARTESIAN_POINT('Ctrl Pts',(-0.0187427861903081,1.94995074918594,
9.04995917573888));
#78217=CARTESIAN_POINT('Ctrl Pts',(0.00621919604093061,1.95116284888092,
9.0489870537254));
#78218=CARTESIAN_POINT('Ctrl Pts',(0.031215354135369,1.95190653702187,9.04800392274799));
#78219=CARTESIAN_POINT('Ctrl Pts',(0.0562304113113475,1.95217907313218,
9.0470112666143));
#78220=CARTESIAN_POINT('',(-1.,-1.22464679914735E-16,10.));
#78221=CARTESIAN_POINT('',(-1.5,1.83697019872103E-16,9.5));
#78222=CARTESIAN_POINT('Origin',(0.,0.,10.));
#78223=CARTESIAN_POINT('Ctrl Pts',(1.13606309729039,-1.59291788311565,-0.231572901724461));
#78224=CARTESIAN_POINT('Ctrl Pts',(1.66580374373072,-1.21512888180952,-0.194523781698427));
#78225=CARTESIAN_POINT('Ctrl Pts',(2.30944801597464,0.103719845647892,-0.120437406770433));
#78226=CARTESIAN_POINT('Ctrl Pts',(1.16339425275335,2.00013089295272,-0.00931377694047787));
#78227=CARTESIAN_POINT('Ctrl Pts',(-1.04791896608993,2.06049732145338,0.101797987765405));
#78228=CARTESIAN_POINT('Ctrl Pts',(-2.29996171030973,0.238632901556859,
0.212909752471286));
#78229=CARTESIAN_POINT('Ctrl Pts',(-1.44799824011824,-1.80309610357979,
0.324021517177169));
#78230=CARTESIAN_POINT('Ctrl Pts',(0.728904987242802,-2.1943368700259,0.435133281883051));
#78231=CARTESIAN_POINT('Ctrl Pts',(2.23884632299531,-0.578363011946529,
0.546245046588933));
#78232=CARTESIAN_POINT('Ctrl Pts',(1.70046726949765,1.56698688412613,0.657356811294816));
#78233=CARTESIAN_POINT('Ctrl Pts',(-0.393719188013592,2.27855690477491,
0.768468576000697));
#78234=CARTESIAN_POINT('Ctrl Pts',(-2.12767440764199,0.905496867856805,
0.879580340706581));
#78235=CARTESIAN_POINT('Ctrl Pts',(-1.91498907715104,-1.29605005156759,
0.990692105412462));
#78236=CARTESIAN_POINT('Ctrl Pts',(0.0497559032715141,-2.31180145897258,
1.10180387011835));
#78237=CARTESIAN_POINT('Ctrl Pts',(1.9689767915461,-1.21245450603212,1.21291563482423));
#78238=CARTESIAN_POINT('Ctrl Pts',(2.08674750979809,0.996192734636249,1.32402739953011));
#78239=CARTESIAN_POINT('Ctrl Pts',(0.295316342405819,2.29340353780112,1.435139164236));
#78240=CARTESIAN_POINT('Ctrl Pts',(-1.76630463899123,1.49234098525026,1.54625092894187));
#78241=CARTESIAN_POINT('Ctrl Pts',(-2.21190301684171,-0.67409086830421,
1.65736269364776));
#78242=CARTESIAN_POINT('Ctrl Pts',(-0.633792933399775,-2.22378495174526,
1.76847445835364));
#78243=CARTESIAN_POINT('Ctrl Pts',(1.52418525493671,-1.73889983355718,1.87958622305952));
#78244=CARTESIAN_POINT('Ctrl Pts',(2.28765995870177,0.336934972534499,1.9906979877654));
#78245=CARTESIAN_POINT('Ctrl Pts',(0.958114915389017,2.10450208243153,2.10180975247129));
#78246=CARTESIAN_POINT('Ctrl Pts',(-1.24802606205186,1.9466237960034,2.21292151717718));
#78247=CARTESIAN_POINT('Ctrl Pts',(-2.31232637129592,0.00774565228208377,
2.32403328188306));
#78248=CARTESIAN_POINT('Ctrl Pts',(-1.26103921283396,-1.93821911551469,
2.43514504658893));
#78249=CARTESIAN_POINT('Ctrl Pts',(0.943994572770135,-2.11087363186064,
2.54625681129481));
#78250=CARTESIAN_POINT('Ctrl Pts',(2.28535136603151,-0.352253281953543,
2.65736857600071));
#78251=CARTESIAN_POINT('Ctrl Pts',(1.53580059245491,1.72864969858349,2.76848034070657));
#78252=CARTESIAN_POINT('Ctrl Pts',(-0.618880756285069,2.22798111542639,
2.87959210541247));
#78253=CARTESIAN_POINT('Ctrl Pts',(-2.20733737683441,0.68889400174652,2.99070387011834));
#78254=CARTESIAN_POINT('Ctrl Pts',(-1.7762627812942,-1.48047417152237,3.10181563482422));
#78255=CARTESIAN_POINT('Ctrl Pts',(0.279945412928593,-2.29533087084941,
3.21292739953011));
#78256=CARTESIAN_POINT('Ctrl Pts',(2.08002669781736,-1.01014958159571,3.32403916423598));
#78257=CARTESIAN_POINT('Ctrl Pts',(1.97705551298443,1.19923506428337,3.43515092894188));
#78258=CARTESIAN_POINT('Ctrl Pts',(0.0652419797826839,2.31141876883474,
3.54626269364775));
#78259=CARTESIAN_POINT('Ctrl Pts',(-1.90626257127342,1.30884538819506,3.65737445835364));
#78260=CARTESIAN_POINT('Ctrl Pts',(-2.1336944630698,-0.891213318517691,
3.76848622305952));
#78261=CARTESIAN_POINT('Ctrl Pts',(-0.408972316733737,-2.27588551666947,
3.8795979877654));
#78262=CARTESIAN_POINT('Ctrl Pts',(1.68992568908689,-1.57831061778191,3.99070975247128));
#78263=CARTESIAN_POINT('Ctrl Pts',(2.24268139796916,0.563288015177147,4.10182151717717));
#78264=CARTESIAN_POINT('Ctrl Pts',(0.743569033391774,2.18952468207605,4.21293328188306));
#78265=CARTESIAN_POINT('Ctrl Pts',(-1.43584752482253,1.81252727601552,4.32404504658893));
#78266=CARTESIAN_POINT('Ctrl Pts',(-2.30158230139483,-0.222782743374198,
4.43515681129481));
#78267=CARTESIAN_POINT('Ctrl Pts',(-1.06155954729496,-2.05426497034491,
4.54626857600071));
#78268=CARTESIAN_POINT('Ctrl Pts',(1.14970243193213,-2.00626457847626,4.65738034070657));
#78269=CARTESIAN_POINT('Ctrl Pts',(2.30908173348749,-0.122697958066977,
4.76849210541246));
#78270=CARTESIAN_POINT('Ctrl Pts',(1.35584214399455,1.87312715035776,4.87960387011834));
#78271=CARTESIAN_POINT('Ctrl Pts',(-0.837880917841919,2.15519577030842,
4.99071563482423));
#78272=CARTESIAN_POINT('Ctrl Pts',(-2.2650122086686,0.465438433546961,5.1018273995301));
#78273=CARTESIAN_POINT('Ctrl Pts',(-1.61984458036479,-1.65015659144846,
5.21293916423598));
#78274=CARTESIAN_POINT('Ctrl Pts',(0.507346924100459,-2.25599475607619,
5.32405092894189));
#78275=CARTESIAN_POINT('Ctrl Pts',(2.17035793611363,-0.79778422521133,5.43516269364775));
#78276=CARTESIAN_POINT('Ctrl Pts',(1.8476708631746,1.39033291775907,5.54627445835364));
#78277=CARTESIAN_POINT('Ctrl Pts',(-0.165482299961806,2.30641038179036,
5.6573862230595));
#78278=CARTESIAN_POINT('Ctrl Pts',(-2.02723283931421,1.11231302073658,5.76849798776541));
#78279=CARTESIAN_POINT('Ctrl Pts',(-2.03423292489276,-1.09945879779015,
5.87960975247127));
#78280=CARTESIAN_POINT('Ctrl Pts',(-0.180078057223998,-2.30531671015481,
5.99072151717718));
#78281=CARTESIAN_POINT('Ctrl Pts',(1.83883334564853,-1.40200041659325,6.10183328188304));
#78282=CARTESIAN_POINT('Ctrl Pts',(2.17536425594361,0.784030352831153,6.21294504658893));
#78283=CARTESIAN_POINT('Ctrl Pts',(0.521616713088515,2.25273816620926,6.32405681129482));
#78284=CARTESIAN_POINT('Ctrl Pts',(-1.60936700050969,1.66037679481931,6.43516857600069));
#78285=CARTESIAN_POINT('Ctrl Pts',(-2.2679129552827,-0.451092078529837,
6.54628034070658));
#78286=CARTESIAN_POINT('Ctrl Pts',(-0.851506051454237,-2.14984899164026,
6.65739210541246));
#78287=CARTESIAN_POINT('Ctrl Pts',(1.34395850160194,-1.88167181004001,6.76850387011834));
#78288=CARTESIAN_POINT('Ctrl Pts',(2.30981211862901,0.108079520188228,6.87961563482422));
#78289=CARTESIAN_POINT('Ctrl Pts',(1.16237862931446,1.99894701892701,6.9907273995301));
#78290=CARTESIAN_POINT('Ctrl Pts',(-1.048535261215,2.06094326183436,7.10183916423599));
#78291=CARTESIAN_POINT('Ctrl Pts',(-2.30012597472422,0.237346780966457,
7.21295092894187));
#78292=CARTESIAN_POINT('Ctrl Pts',(-1.4472917606237,-1.80340234398078,7.32406269364775));
#78293=CARTESIAN_POINT('Ctrl Pts',(0.729695116197456,-2.19418748774512,
7.43517445835364));
#78294=CARTESIAN_POINT('Ctrl Pts',(2.23907061743849,-0.577472336492666,
7.54628622305951));
#78295=CARTESIAN_POINT('Ctrl Pts',(1.6998828851918,1.56758199492804,7.6573979877654));
#78296=CARTESIAN_POINT('Ctrl Pts',(-0.394559581775687,2.27842890415167,
7.76850975247128));
#78297=CARTESIAN_POINT('Ctrl Pts',(-2.12800802962129,0.904700757977686,
7.87962151717716));
#78298=CARTESIAN_POINT('Ctrl Pts',(-1.91451385442197,-1.29675194351212,
7.99073328188305));
#78299=CARTESIAN_POINT('Ctrl Pts',(0.0506189763134289,-2.31178733491431,
8.10184504658893));
#78300=CARTESIAN_POINT('Ctrl Pts',(1.96940772470891,-1.21172174246582,8.21295681129481));
#78301=CARTESIAN_POINT('Ctrl Pts',(2.08641197020285,0.996956328156063,8.3240685760007));
#78302=CARTESIAN_POINT('Ctrl Pts',(0.294406065655051,2.29352604085566,8.43518034070657));
#78303=CARTESIAN_POINT('Ctrl Pts',(-1.76673675864417,1.49166283229086,8.54629210541247));
#78304=CARTESIAN_POINT('Ctrl Pts',(-2.21188103147225,-0.674860552072349,
8.65740387011833));
#78305=CARTESIAN_POINT('Ctrl Pts',(-0.632537782229339,-2.22411004328669,
8.76851563482423));
#78306=CARTESIAN_POINT('Ctrl Pts',(1.52400006892491,-1.73816200658177,8.8796273995301));
#78307=CARTESIAN_POINT('Ctrl Pts',(2.28913633277906,0.33743832952732,8.99073916423599));
#78308=CARTESIAN_POINT('Ctrl Pts',(0.953931268377545,2.1057836989737,9.10186283730748));
#78309=CARTESIAN_POINT('Ctrl Pts',(-0.50962975476275,1.9979286932635,9.17594925547701));
#78310=CARTESIAN_POINT('Ctrl Pts',(-1.05712610504189,1.64636300407581,9.21299841874458));
#78311=CARTESIAN_POINT('Ctrl Pts',(1.05790529558725,-1.4833298150454,-0.153859353408328));
#78312=CARTESIAN_POINT('Ctrl Pts',(1.55120134269385,-1.13153158654066,-0.116810233382295));
#78313=CARTESIAN_POINT('Ctrl Pts',(2.15056478096174,0.0965842251456926,
-0.0427238584543007));
#78314=CARTESIAN_POINT('Ctrl Pts',(1.08335614789265,1.8625277667843,0.068399771375655));
#78315=CARTESIAN_POINT('Ctrl Pts',(-0.975825221518905,1.91874116244765,
0.179511536081537));
#78316=CARTESIAN_POINT('Ctrl Pts',(-2.14173110524213,0.222215659377068,
0.29062330078742));
#78317=CARTESIAN_POINT('Ctrl Pts',(-1.34838021750347,-1.6790483917481,0.401735065493302));
#78318=CARTESIAN_POINT('Ctrl Pts',(0.678758466693704,-2.04337294349185,
0.512846830199185));
#78319=CARTESIAN_POINT('Ctrl Pts',(2.08482027692988,-0.538573336788539,
0.623958594905066));
#78320=CARTESIAN_POINT('Ctrl Pts',(1.58348011977939,1.45918279256373,0.73507035961095));
#78321=CARTESIAN_POINT('Ctrl Pts',(-0.366632465192586,2.12179888740995,
0.84618212431683));
#78322=CARTESIAN_POINT('Ctrl Pts',(-1.98129666256959,0.843201345002855,
0.957293889022715));
#78323=CARTESIAN_POINT('Ctrl Pts',(-1.78324345764042,-1.20688561768239,
1.06840565372859));
#78324=CARTESIAN_POINT('Ctrl Pts',(0.0463328433809853,-2.15275631399923,
1.17951741843448));
#78325=CARTESIAN_POINT('Ctrl Pts',(1.83351697597882,-1.12904119995556,1.29062918314035));
#78326=CARTESIAN_POINT('Ctrl Pts',(1.94318541499513,0.927657602743041,1.40174094784624));
#78327=CARTESIAN_POINT('Ctrl Pts',(0.274999446113248,2.13562411572477,1.51285271255212));
#78328=CARTESIAN_POINT('Ctrl Pts',(-1.6447880717769,1.38967231211328,1.62396447725801));
#78329=CARTESIAN_POINT('Ctrl Pts',(-2.05973059104138,-0.627715398015217,
1.73507624196389));
#78330=CARTESIAN_POINT('Ctrl Pts',(-0.590189842578783,-2.07079508374983,
1.84618800666977));
#78331=CARTESIAN_POINT('Ctrl Pts',(1.41932578964969,-1.61926863640188,1.95729977137565));
#78332=CARTESIAN_POINT('Ctrl Pts',(2.13027567798452,0.313754836824603,2.06841153608153));
#78333=CARTESIAN_POINT('Ctrl Pts',(0.892199425532491,1.95971852521992,2.17952330078742));
#78334=CARTESIAN_POINT('Ctrl Pts',(-1.16216553748166,1.81270180082412,2.2906350654933));
#78335=CARTESIAN_POINT('Ctrl Pts',(-2.15324511389767,0.00721277417295179,
2.40174683019918));
#78336=CARTESIAN_POINT('Ctrl Pts',(-1.17428342174132,-1.804875337648,2.51285859490507));
#78337=CARTESIAN_POINT('Ctrl Pts',(0.879050520979899,-1.96565173077709,
2.62397035961094));
#78338=CARTESIAN_POINT('Ctrl Pts',(2.12812590970401,-0.328019291582862,
2.73508212431683));
#78339=CARTESIAN_POINT('Ctrl Pts',(1.43014202608922,1.60972368058472,2.84619388902271));
#78340=CARTESIAN_POINT('Ctrl Pts',(-0.576303579416129,2.07470256370406,
2.95730565372859));
#78341=CARTESIAN_POINT('Ctrl Pts',(-2.05547905364616,0.641500119389611,
3.06841741843448));
#78342=CARTESIAN_POINT('Ctrl Pts',(-1.65406112316078,-1.37862190028811,
3.17952918314036));
#78343=CARTESIAN_POINT('Ctrl Pts',(0.260685991402141,-2.13741885392462,
3.29064094784625));
#78344=CARTESIAN_POINT('Ctrl Pts',(1.93692697512326,-0.940654259656997,
3.40175271255211));
#78345=CARTESIAN_POINT('Ctrl Pts',(1.8410399051291,1.11673121694138,3.51286447725801));
#78346=CARTESIAN_POINT('Ctrl Pts',(0.060753523348571,2.15239995181797,3.62397624196388));
#78347=CARTESIAN_POINT('Ctrl Pts',(-1.77511730971615,1.218800672761,3.73508800666977));
#78348=CARTESIAN_POINT('Ctrl Pts',(-1.98690255587955,-0.829900461872639,
3.84619977137565));
#78349=CARTESIAN_POINT('Ctrl Pts',(-0.380836223492431,-2.11931128295378,
3.95731153608153));
#78350=CARTESIAN_POINT('Ctrl Pts',(1.57366376911455,-1.46972748662942,4.06842330078742));
#78351=CARTESIAN_POINT('Ctrl Pts',(2.0883915100185,0.524535455484849,4.1795350654933));
#78352=CARTESIAN_POINT('Ctrl Pts',(0.692413669571699,2.03889181992781,4.29064683019919));
#78353=CARTESIAN_POINT('Ctrl Pts',(-1.33706543570381,1.68783072724259,4.40175859490506));
#78354=CARTESIAN_POINT('Ctrl Pts',(-2.14324020442421,-0.207455945486791,
4.51287035961095));
#78355=CARTESIAN_POINT('Ctrl Pts',(-0.988527370832692,-1.91293757877584,
4.62398212431683));
#78356=CARTESIAN_POINT('Ctrl Pts',(1.07060628409766,-1.86823947277342,4.73509388902271));
#78357=CARTESIAN_POINT('Ctrl Pts',(2.15022369763304,-0.114256699215363,
4.84620565372859));
#78358=CARTESIAN_POINT('Ctrl Pts',(1.26256418990569,1.74426150835986,4.95731741843447));
#78359=CARTESIAN_POINT('Ctrl Pts',(-0.780237173595914,2.00692463638197,
5.06842918314036));
#78360=CARTESIAN_POINT('Ctrl Pts',(-2.10918602658192,0.433417637447724,
5.17954094784624));
#78361=CARTESIAN_POINT('Ctrl Pts',(-1.50840403467324,-1.53663066849473,
5.29065271255212));
#78362=CARTESIAN_POINT('Ctrl Pts',(0.472442947038698,-2.10078894822159,
5.40176447725801));
#78363=CARTESIAN_POINT('Ctrl Pts',(2.02104368974809,-0.74289901555643,5.51287624196389));
#78364=CARTESIAN_POINT('Ctrl Pts',(1.72055653890764,1.29468209981882,5.62398800666977));
#78365=CARTESIAN_POINT('Ctrl Pts',(-0.154097604149901,2.14773612708039,
5.73509977137565));
#78366=CARTESIAN_POINT('Ctrl Pts',(-1.88776517890069,1.03578915448837,5.84621153608153));
#78367=CARTESIAN_POINT('Ctrl Pts',(-1.89428367916776,-1.02381926429645,
5.95732330078742));
#78368=CARTESIAN_POINT('Ctrl Pts',(-0.167689216215796,-2.14671769683858,
6.06843506549329));
#78369=CARTESIAN_POINT('Ctrl Pts',(1.71232701661002,-1.30554690902911,6.17954683019919));
#78370=CARTESIAN_POINT('Ctrl Pts',(2.02570558948953,0.730091369167335,6.29065859490506));
#78371=CARTESIAN_POINT('Ctrl Pts',(0.485731016489559,2.09775640216495,6.40177035961095));
#78372=CARTESIAN_POINT('Ctrl Pts',(-1.49864728151395,1.54614775191534,6.51288212431683));
#78373=CARTESIAN_POINT('Ctrl Pts',(-2.11188721035553,-0.420058269485543,
6.62399388902271));
#78374=CARTESIAN_POINT('Ctrl Pts',(-0.792924938065964,-2.00194570036965,
6.73510565372859));
#78375=CARTESIAN_POINT('Ctrl Pts',(1.25149810717844,-1.75221832057249,6.84621741843447));
#78376=CARTESIAN_POINT('Ctrl Pts',(2.15090383442374,0.100643966892662,6.95732918314036));
#78377=CARTESIAN_POINT('Ctrl Pts',(1.08241039636101,1.86142533981164,7.06844094784623));
#78378=CARTESIAN_POINT('Ctrl Pts',(-0.976399117350945,1.91915642344125,
7.17955271255213));
#78379=CARTESIAN_POINT('Ctrl Pts',(-2.14188406874776,0.221018020102809,
7.290664477258));
#78380=CARTESIAN_POINT('Ctrl Pts',(-1.34772234172149,-1.67933356370967,
7.40177624196389));
#78381=CARTESIAN_POINT('Ctrl Pts',(0.679494237098812,-2.04323383827288,
7.51288800666976));
#78382=CARTESIAN_POINT('Ctrl Pts',(2.08502914057466,-0.537743937187812,
7.62399977137566));
#78383=CARTESIAN_POINT('Ctrl Pts',(1.58293593939601,1.45973696149177,7.73511153608152));
#78384=CARTESIAN_POINT('Ctrl Pts',(-0.367415042334137,2.12167969285334,
7.84622330078743));
#78385=CARTESIAN_POINT('Ctrl Pts',(-1.98160733233737,0.842460005143296,
7.95733506549329));
#78386=CARTESIAN_POINT('Ctrl Pts',(-1.78280092883823,-1.2075392215243,8.0684468301992));
#78387=CARTESIAN_POINT('Ctrl Pts',(0.0471365395345726,-2.15274316163464,
8.17955859490505));
#78388=CARTESIAN_POINT('Ctrl Pts',(1.83391826220672,-1.12835884836871,8.29067035961095));
#78389=CARTESIAN_POINT('Ctrl Pts',(1.94287295953775,0.928368663273228,8.40178212431683));
#78390=CARTESIAN_POINT('Ctrl Pts',(0.274151793727225,2.13573819092923,8.51289388902271));
#78391=CARTESIAN_POINT('Ctrl Pts',(-1.6451904628679,1.38904081408411,8.6240056537286));
#78392=CARTESIAN_POINT('Ctrl Pts',(-2.05971011820072,-0.628432129802549,
8.73511741843447));
#78393=CARTESIAN_POINT('Ctrl Pts',(-0.58902104211943,-2.07109780994878,
8.84622918314036));
#78394=CARTESIAN_POINT('Ctrl Pts',(1.41915334389115,-1.61858156975358,8.95734094784623));
#78395=CARTESIAN_POINT('Ctrl Pts',(2.13165048186501,0.314223564335907,9.06845271255213));
#78396=CARTESIAN_POINT('Ctrl Pts',(0.888303601137828,1.96091197031123,9.17957638562361));
#78397=CARTESIAN_POINT('Ctrl Pts',(-0.474568725661671,1.86047707196044,
9.25366280379315));
#78398=CARTESIAN_POINT('Ctrl Pts',(-0.984398936374817,1.53309806878228,
9.29071196706072));
#78399=CARTESIAN_POINT('Ctrl Pts',(0.97974749388411,-1.37374174697515,-0.0761458050921956));
#78400=CARTESIAN_POINT('Ctrl Pts',(1.43659894165698,-1.0479342912718,-0.039096685066162));
#78401=CARTESIAN_POINT('Ctrl Pts',(1.99168154594883,0.0894486046434957,
0.034989689861832));
#78402=CARTESIAN_POINT('Ctrl Pts',(1.00331804303196,1.72492464061588,0.146113319691788));
#78403=CARTESIAN_POINT('Ctrl Pts',(-0.903731476947885,1.77698500344193,
0.257225084397669));
#78404=CARTESIAN_POINT('Ctrl Pts',(-1.98350050017455,0.205798417197274,
0.368336849103552));
#78405=CARTESIAN_POINT('Ctrl Pts',(-1.2487621948887,-1.5550006799164,0.479448613809434));
#78406=CARTESIAN_POINT('Ctrl Pts',(0.628611946144605,-1.89240901695779,
0.590560378515317));
#78407=CARTESIAN_POINT('Ctrl Pts',(1.93079423086444,-0.498783661630547,
0.701672143221198));
#78408=CARTESIAN_POINT('Ctrl Pts',(1.46649297006114,1.35137870100134,0.812783907927082));
#78409=CARTESIAN_POINT('Ctrl Pts',(-0.339545742371582,1.96504087004499,
0.923895672632963));
#78410=CARTESIAN_POINT('Ctrl Pts',(-1.83491891749717,0.780905822148899,
1.03500743733885));
#78411=CARTESIAN_POINT('Ctrl Pts',(-1.6514978381298,-1.11772118379719,1.14611920204473));
#78412=CARTESIAN_POINT('Ctrl Pts',(0.0429097834904605,-1.99371116902587,
1.25723096675061));
#78413=CARTESIAN_POINT('Ctrl Pts',(1.69805716041152,-1.04562789387901,1.36834273145649));
#78414=CARTESIAN_POINT('Ctrl Pts',(1.79962332019217,0.859122470849831,1.47945449616237));
#78415=CARTESIAN_POINT('Ctrl Pts',(0.254682549820674,1.9778446936484,1.59056626086826));
#78416=CARTESIAN_POINT('Ctrl Pts',(-1.52327150456256,1.28700363897632,1.70167802557414));
#78417=CARTESIAN_POINT('Ctrl Pts',(-1.90755816524105,-0.581339927726226,
1.81278979028002));
#78418=CARTESIAN_POINT('Ctrl Pts',(-0.546586751757789,-1.91780521575438,
1.9239015549859));
#78419=CARTESIAN_POINT('Ctrl Pts',(1.31446632436265,-1.49963743924658,2.03501331969179));
#78420=CARTESIAN_POINT('Ctrl Pts',(1.97289139726728,0.29057470111471,2.14612508439767));
#78421=CARTESIAN_POINT('Ctrl Pts',(0.826283935675965,1.81493496800831,2.25723684910355));
#78422=CARTESIAN_POINT('Ctrl Pts',(-1.07630501291146,1.67877980564486,2.36834861380944));
#78423=CARTESIAN_POINT('Ctrl Pts',(-1.99416385649942,0.00667989606382068,
2.47946037851531));
#78424=CARTESIAN_POINT('Ctrl Pts',(-1.08752763064868,-1.6715315597813,2.5905721432212));
#78425=CARTESIAN_POINT('Ctrl Pts',(0.814106469189659,-1.82042982969354,
2.70168390792707));
#78426=CARTESIAN_POINT('Ctrl Pts',(1.97090045337651,-0.303785301212181,
2.81279567263297));
#78427=CARTESIAN_POINT('Ctrl Pts',(1.32448345972351,1.49079766258596,2.92390743733884));
#78428=CARTESIAN_POINT('Ctrl Pts',(-0.533726402547186,1.92142401198172,
3.03501920204473));
#78429=CARTESIAN_POINT('Ctrl Pts',(-1.9036207304579,0.594106237032703,3.14613096675061));
#78430=CARTESIAN_POINT('Ctrl Pts',(-1.53185946502735,-1.27676962905383,
3.25724273145649));
#78431=CARTESIAN_POINT('Ctrl Pts',(0.241426569875686,-1.97950683699981,
3.36835449616238));
#78432=CARTESIAN_POINT('Ctrl Pts',(1.79382725242915,-0.871158937718284,
3.47946626086825));
#78433=CARTESIAN_POINT('Ctrl Pts',(1.70502429727377,1.03422736959939,3.59057802557414));
#78434=CARTESIAN_POINT('Ctrl Pts',(0.0562650669144604,1.9933811348012,3.70168979028002));
#78435=CARTESIAN_POINT('Ctrl Pts',(-1.64397204815888,1.12875595732695,3.81280155498591));
#78436=CARTESIAN_POINT('Ctrl Pts',(-1.84011064868929,-0.768587605227587,
3.92391331969179));
#78437=CARTESIAN_POINT('Ctrl Pts',(-0.35270013025113,-1.96273704923809,
4.03502508439767));
#78438=CARTESIAN_POINT('Ctrl Pts',(1.45740184914221,-1.36114435547694,4.14613684910356));
#78439=CARTESIAN_POINT('Ctrl Pts',(1.93410162206783,0.48578289579255,4.25724861380943));
#78440=CARTESIAN_POINT('Ctrl Pts',(0.641258305751626,1.88825895777957,4.36836037851532));
#78441=CARTESIAN_POINT('Ctrl Pts',(-1.23828334658509,1.56313417846968,4.4794721432212));
#78442=CARTESIAN_POINT('Ctrl Pts',(-1.9848981074536,-0.192129147599384,
4.59058390792708));
#78443=CARTESIAN_POINT('Ctrl Pts',(-0.915495194370431,-1.77161018720676,
4.70169567263296));
#78444=CARTESIAN_POINT('Ctrl Pts',(0.991510136263189,-1.73021436707057,
4.81280743733884));
#78445=CARTESIAN_POINT('Ctrl Pts',(1.99136566177859,-0.105815440363751,
4.92391920204473));
#78446=CARTESIAN_POINT('Ctrl Pts',(1.16928623581682,1.61539586636197,5.03503096675061));
#78447=CARTESIAN_POINT('Ctrl Pts',(-0.722593429349912,1.85865350245553,
5.1461427314565));
#78448=CARTESIAN_POINT('Ctrl Pts',(-1.95335984449524,0.40139684134849,5.25725449616237));
#78449=CARTESIAN_POINT('Ctrl Pts',(-1.39696348898167,-1.42310474554101,
5.36836626086826));
#78450=CARTESIAN_POINT('Ctrl Pts',(0.437538969976939,-1.945583140367,5.47947802557413));
#78451=CARTESIAN_POINT('Ctrl Pts',(1.87172944338254,-0.688013805901528,
5.59058979028003));
#78452=CARTESIAN_POINT('Ctrl Pts',(1.59344221464069,1.19903128187857,5.7017015549859));
#78453=CARTESIAN_POINT('Ctrl Pts',(-0.142712908337992,1.98906187237041,
5.81281331969179));
#78454=CARTESIAN_POINT('Ctrl Pts',(-1.74829751848718,0.959265288240166,
5.92392508439767));
#78455=CARTESIAN_POINT('Ctrl Pts',(-1.75433443344276,-0.94817973080275,
6.03503684910355));
#78456=CARTESIAN_POINT('Ctrl Pts',(-0.155300375207596,-1.98811868352235,
6.14614861380944));
#78457=CARTESIAN_POINT('Ctrl Pts',(1.58582068757151,-1.20909340146497,6.25726037851532));
#78458=CARTESIAN_POINT('Ctrl Pts',(1.87604692303546,0.676152385503515,6.3683721432212));
#78459=CARTESIAN_POINT('Ctrl Pts',(0.449845319890602,1.94277463812065,6.47948390792708));
#78460=CARTESIAN_POINT('Ctrl Pts',(-1.38792756251823,1.43191870901136,6.59059567263297));
#78461=CARTESIAN_POINT('Ctrl Pts',(-1.95586146542837,-0.389024460441244,
6.70170743733884));
#78462=CARTESIAN_POINT('Ctrl Pts',(-0.734343824677687,-1.85404240909904,
6.81281920204473));
#78463=CARTESIAN_POINT('Ctrl Pts',(1.15903771275493,-1.62276483110497,6.9239309667506));
#78464=CARTESIAN_POINT('Ctrl Pts',(1.99199555021847,0.093208413597094,7.0350427314565));
#78465=CARTESIAN_POINT('Ctrl Pts',(1.00244216340755,1.72390366069626,7.14615449616237));
#78466=CARTESIAN_POINT('Ctrl Pts',(-0.904262973486885,1.77736958504813,
7.25726626086827));
#78467=CARTESIAN_POINT('Ctrl Pts',(-1.98364216277129,0.20468925923916,7.36837802557414));
#78468=CARTESIAN_POINT('Ctrl Pts',(-1.24815292281929,-1.55526478343856,
7.47948979028002));
#78469=CARTESIAN_POINT('Ctrl Pts',(0.629293358000169,-1.89228018880065,
7.59060155498591));
#78470=CARTESIAN_POINT('Ctrl Pts',(1.93098766371084,-0.498015537882957,
7.70171331969178));
#78471=CARTESIAN_POINT('Ctrl Pts',(1.46598899360024,1.35189192805549,7.81282508439768));
#78472=CARTESIAN_POINT('Ctrl Pts',(-0.340270502892587,1.964930481555,7.92393684910355));
#78473=CARTESIAN_POINT('Ctrl Pts',(-1.83520663505345,0.780219252308907,
8.03504861380944));
#78474=CARTESIAN_POINT('Ctrl Pts',(-1.65108800325447,-1.11832649953649,
8.14616037851531));
#78475=CARTESIAN_POINT('Ctrl Pts',(0.0436541027557139,-1.99369898835498,
8.25727214322121));
#78476=CARTESIAN_POINT('Ctrl Pts',(1.69842879970453,-1.0449959542716,8.36838390792707));
#78477=CARTESIAN_POINT('Ctrl Pts',(1.79933394887264,0.859780998390392,8.47949567263297));
#78478=CARTESIAN_POINT('Ctrl Pts',(0.253897521799402,1.97795034100281,8.59060743733884));
#78479=CARTESIAN_POINT('Ctrl Pts',(-1.52364416709162,1.28641879587735,8.70171920204473));
#78480=CARTESIAN_POINT('Ctrl Pts',(-1.90753920492918,-0.582003707532747,
8.8128309667506));
#78481=CARTESIAN_POINT('Ctrl Pts',(-0.545504302009522,-1.91808557661087,
8.9239427314565));
#78482=CARTESIAN_POINT('Ctrl Pts',(1.31430661885738,-1.49900113292539,9.03505449616237));
#78483=CARTESIAN_POINT('Ctrl Pts',(1.97416463095097,0.291008799144495,9.14616626086825));
#78484=CARTESIAN_POINT('Ctrl Pts',(0.822675933898107,1.81604024164875,9.25728993393975));
#78485=CARTESIAN_POINT('Ctrl Pts',(-0.439507696560592,1.7230254506574,9.33137635210928));
#78486=CARTESIAN_POINT('Ctrl Pts',(-0.911671767707743,1.41983313348876,
9.36842551537684));
#78487=CARTESIAN_POINT('Ctrl Pts',(0.901589692180969,-1.2641536789049,0.00156774322393706));
#78488=CARTESIAN_POINT('Ctrl Pts',(1.32199654062011,-0.964336996002927,
0.0386168632499707));
#78489=CARTESIAN_POINT('Ctrl Pts',(1.83279831093593,0.082312984141298,0.112703238177965));
#78490=CARTESIAN_POINT('Ctrl Pts',(0.923279938171269,1.58732151444747,0.223826868007921));
#78491=CARTESIAN_POINT('Ctrl Pts',(-0.831637732376869,1.63522884443621,
0.334938632713803));
#78492=CARTESIAN_POINT('Ctrl Pts',(-1.82526989510695,0.189381175017482,
0.446050397419685));
#78493=CARTESIAN_POINT('Ctrl Pts',(-1.14914417227393,-1.4309529680847,0.557162162125568));
#78494=CARTESIAN_POINT('Ctrl Pts',(0.578465425595506,-1.74144509042373,
0.668273926831449));
#78495=CARTESIAN_POINT('Ctrl Pts',(1.77676818479901,-0.458993986472553,
0.779385691537333));
#78496=CARTESIAN_POINT('Ctrl Pts',(1.34950582034287,1.24357460943893,0.890497456243214));
#78497=CARTESIAN_POINT('Ctrl Pts',(-0.312459019550576,1.80828285268003,
1.0016092209491));
#78498=CARTESIAN_POINT('Ctrl Pts',(-1.68854117242476,0.718610299294945,
1.11272098565498));
#78499=CARTESIAN_POINT('Ctrl Pts',(-1.51975221861918,-1.02855674991199,
1.22383275036086));
#78500=CARTESIAN_POINT('Ctrl Pts',(0.0394867235999322,-1.83466602405251,
1.33494451506675));
#78501=CARTESIAN_POINT('Ctrl Pts',(1.56259734484424,-0.962214587802463,
1.44605627977263));
#78502=CARTESIAN_POINT('Ctrl Pts',(1.65606122538921,0.79058733895662,1.55716804447851));
#78503=CARTESIAN_POINT('Ctrl Pts',(0.234365653528104,1.82006527157203,1.66827980918439));
#78504=CARTESIAN_POINT('Ctrl Pts',(-1.40175493734822,1.18433496583934,1.77939157389028));
#78505=CARTESIAN_POINT('Ctrl Pts',(-1.75538573944072,-0.534964457437233,
1.89050333859615));
#78506=CARTESIAN_POINT('Ctrl Pts',(-0.502983660936798,-1.76481534775894,
2.00161510330204));
#78507=CARTESIAN_POINT('Ctrl Pts',(1.20960685907562,-1.38000624209127,2.11272686800792));
#78508=CARTESIAN_POINT('Ctrl Pts',(1.81550711655005,0.267394565404816,2.2238386327138));
#78509=CARTESIAN_POINT('Ctrl Pts',(0.76036844581944,1.6701514107967,2.33495039741969));
#78510=CARTESIAN_POINT('Ctrl Pts',(-0.990444488341258,1.54485781046558,
2.44606216212557));
#78511=CARTESIAN_POINT('Ctrl Pts',(-1.83508259910117,0.00614701795468853,
2.55717392683145));
#78512=CARTESIAN_POINT('Ctrl Pts',(-1.00077183955604,-1.5381877819146,2.66828569153734));
#78513=CARTESIAN_POINT('Ctrl Pts',(0.749162417399423,-1.67520792861,2.77939745624321));
#78514=CARTESIAN_POINT('Ctrl Pts',(1.81367499704902,-0.2795513108415,2.8905092209491));
#78515=CARTESIAN_POINT('Ctrl Pts',(1.21882489335781,1.3718716445872,3.00162098565498));
#78516=CARTESIAN_POINT('Ctrl Pts',(-0.491149225678246,1.76814546025939,
3.11273275036087));
#78517=CARTESIAN_POINT('Ctrl Pts',(-1.75176240726965,0.546712354675795,
3.22384451506675));
#78518=CARTESIAN_POINT('Ctrl Pts',(-1.40965780689392,-1.17491735781956,
3.33495627977263));
#78519=CARTESIAN_POINT('Ctrl Pts',(0.22216714834923,-1.821594820075,3.44606804447851));
#78520=CARTESIAN_POINT('Ctrl Pts',(1.65072752973505,-0.801663615779567,
3.55717980918439));
#78521=CARTESIAN_POINT('Ctrl Pts',(1.56900868941844,0.951723522257404,3.66829157389028));
#78522=CARTESIAN_POINT('Ctrl Pts',(0.0517766104803488,1.83436231778444,
3.77940333859616));
#78523=CARTESIAN_POINT('Ctrl Pts',(-1.5128267866016,1.03871124189289,3.89051510330204));
#78524=CARTESIAN_POINT('Ctrl Pts',(-1.69331874149904,-0.707274748582536,
4.00162686800792));
#78525=CARTESIAN_POINT('Ctrl Pts',(-0.324564037009825,-1.80616281552239,
4.11273863271381));
#78526=CARTESIAN_POINT('Ctrl Pts',(1.34113992916987,-1.25256122432444,4.22385039741969));
#78527=CARTESIAN_POINT('Ctrl Pts',(1.77981173411717,0.447030336100252,4.33496216212557));
#78528=CARTESIAN_POINT('Ctrl Pts',(0.590102941931552,1.73762609563133,4.44607392683145));
#78529=CARTESIAN_POINT('Ctrl Pts',(-1.13950125746637,1.43843762969677,4.55718569153734));
#78530=CARTESIAN_POINT('Ctrl Pts',(-1.82655601048297,-0.176802349711979,
4.66829745624321));
#78531=CARTESIAN_POINT('Ctrl Pts',(-0.842463017908167,-1.63028279563768,
4.7794092209491));
#78532=CARTESIAN_POINT('Ctrl Pts',(0.912413988428717,-1.59218926136772,
4.89052098565498));
#78533=CARTESIAN_POINT('Ctrl Pts',(1.83250762592413,-0.0973741815121382,
5.00163275036086));
#78534=CARTESIAN_POINT('Ctrl Pts',(1.07600828172795,1.48653022436408,5.11274451506675));
#78535=CARTESIAN_POINT('Ctrl Pts',(-0.664949685103911,1.71038236852908,
5.22385627977262));
#78536=CARTESIAN_POINT('Ctrl Pts',(-1.79753366240856,0.369376045249255,
5.33496804447852));
#78537=CARTESIAN_POINT('Ctrl Pts',(-1.28552294329012,-1.30957882258728,
5.44607980918439));
#78538=CARTESIAN_POINT('Ctrl Pts',(0.402634992915184,-1.7903773325124,5.55719157389028));
#78539=CARTESIAN_POINT('Ctrl Pts',(1.722415197017,-0.633128596246625,5.66830333859616));
#78540=CARTESIAN_POINT('Ctrl Pts',(1.46632789037372,1.10338046393831,5.77941510330204));
#78541=CARTESIAN_POINT('Ctrl Pts',(-0.131328212526088,1.83038761766044,
5.89052686800793));
#78542=CARTESIAN_POINT('Ctrl Pts',(-1.60882985807365,0.88274142199196,6.0016386327138));
#78543=CARTESIAN_POINT('Ctrl Pts',(-1.61438518771777,-0.872540197309049,
6.11275039741969));
#78544=CARTESIAN_POINT('Ctrl Pts',(-0.142911534199397,-1.82951967020612,
6.22386216212556));
#78545=CARTESIAN_POINT('Ctrl Pts',(1.459314358533,-1.11263989390083,6.33497392683146));
#78546=CARTESIAN_POINT('Ctrl Pts',(1.72638825658138,0.622213401839696,6.44608569153733));
#78547=CARTESIAN_POINT('Ctrl Pts',(0.413959623291646,1.78779287407635,6.55719745624322));
#78548=CARTESIAN_POINT('Ctrl Pts',(-1.27720784352249,1.31768966610738,6.66830922094909));
#78549=CARTESIAN_POINT('Ctrl Pts',(-1.79983572050121,-0.357990651396945,
6.77942098565499));
#78550=CARTESIAN_POINT('Ctrl Pts',(-0.67576271128941,-1.70613911782843,
6.89053275036086));
#78551=CARTESIAN_POINT('Ctrl Pts',(1.06657731833143,-1.49331134163745,7.00164451506675));
#78552=CARTESIAN_POINT('Ctrl Pts',(1.8330872660132,0.085772860301527,7.11275627977262));
#78553=CARTESIAN_POINT('Ctrl Pts',(0.922473930454079,1.58638198158088,7.22386804447851));
#78554=CARTESIAN_POINT('Ctrl Pts',(-0.832126829622823,1.635582746655,7.33497980918439));
#78555=CARTESIAN_POINT('Ctrl Pts',(-1.82540025679483,0.188360498375512,
7.44609157389027));
#78556=CARTESIAN_POINT('Ctrl Pts',(-1.14858350391709,-1.43119600316746,
7.55720333859616));
#78557=CARTESIAN_POINT('Ctrl Pts',(0.579092478901528,-1.7413265393284,7.66831510330204));
#78558=CARTESIAN_POINT('Ctrl Pts',(1.77694618684701,-0.458287138578105,
7.77942686800792));
#78559=CARTESIAN_POINT('Ctrl Pts',(1.34904204780445,1.24404689461921,7.8905386327138));
#78560=CARTESIAN_POINT('Ctrl Pts',(-0.313125963451037,1.80818127025666,
8.00165039741968));
#78561=CARTESIAN_POINT('Ctrl Pts',(-1.68880593776952,0.71797849947452,8.11276216212556));
#78562=CARTESIAN_POINT('Ctrl Pts',(-1.51937507767073,-1.02911377754868,
8.22387392683146));
#78563=CARTESIAN_POINT('Ctrl Pts',(0.0401716659768548,-1.83465481507531,
8.33498569153734));
#78564=CARTESIAN_POINT('Ctrl Pts',(1.56293933720236,-0.961633060174499,
8.4460974562432));
#78565=CARTESIAN_POINT('Ctrl Pts',(1.65579493820754,0.791193333507556,8.5572092209491));
#78566=CARTESIAN_POINT('Ctrl Pts',(0.233643249871581,1.82016249107638,8.66832098565497));
#78567=CARTESIAN_POINT('Ctrl Pts',(-1.40209787131535,1.1837967776706,8.77943275036085));
#78568=CARTESIAN_POINT('Ctrl Pts',(-1.75536829165764,-0.535575285262948,
8.89054451506673));
#78569=CARTESIAN_POINT('Ctrl Pts',(-0.501987561899616,-1.76507334327297,
9.00165627977261));
#78570=CARTESIAN_POINT('Ctrl Pts',(1.20945989382363,-1.37942069609719,9.11276804447851));
#78571=CARTESIAN_POINT('Ctrl Pts',(1.81667878003692,0.267794033953083,9.22387980918439));
#78572=CARTESIAN_POINT('Ctrl Pts',(0.75704826665839,1.67116851298627,9.33500348225587));
#78573=CARTESIAN_POINT('Ctrl Pts',(-0.404446667459514,1.58557382935436,
9.40908990042542));
#78574=CARTESIAN_POINT('Ctrl Pts',(-0.838944599040669,1.30656819819523,
9.44613906369298));
#78575=CARTESIAN_POINT('Ctrl Pts',(0.863568020353677,1.75641452067799,3.4477629085039E-17));
#78576=CARTESIAN_POINT('Ctrl Pts',(0.902604744553564,1.73244180767701,-5.99597736019976E-15));
#78577=CARTESIAN_POINT('Ctrl Pts',(0.940679665251258,1.70703474391515,-4.40943913592352E-15));
#78578=CARTESIAN_POINT('Ctrl Pts',(0.977702286264216,1.68018861076749,-4.36976843598558E-15));
#78579=CARTESIAN_POINT('Ctrl Pts',(1.03605877752412,1.63787269440259,-4.43296922755967E-15));
#78580=CARTESIAN_POINT('Ctrl Pts',(1.09180306576185,1.59198254673329,-2.65889931022495E-15));
#78581=CARTESIAN_POINT('Ctrl Pts',(1.14477205735549,1.54286237604396,-3.09821612809458E-15));
#78582=CARTESIAN_POINT('Ctrl Pts',(1.16982237017091,1.5196322634008,-3.30597963994575E-15));
#78583=CARTESIAN_POINT('Ctrl Pts',(1.19425134178148,1.49567928312504,-2.72106579808279E-15));
#78584=CARTESIAN_POINT('Ctrl Pts',(1.21803815377256,1.47103794919798,-4.64212002171394E-15));
#78585=CARTESIAN_POINT('Ctrl Pts',(1.23019217561359,1.45844730397601,-5.76026679289046E-15));
#78586=CARTESIAN_POINT('Ctrl Pts',(1.24217850624866,1.44567693083781,-3.72464628310254E-15));
#78587=CARTESIAN_POINT('Ctrl Pts',(1.25399412029808,1.43273135759888,-2.41820452551167E-15));
#78588=CARTESIAN_POINT('Ctrl Pts',(1.26387705342325,1.42190329279817,-1.3484661602068E-15));
#78589=CARTESIAN_POINT('Ctrl Pts',(1.2736338482894,1.41095997328553,-6.32726586808925E-15));
#78590=CARTESIAN_POINT('Ctrl Pts',(1.28326192166555,1.39990597410979,-5.98132654516803E-15));
#78591=CARTESIAN_POINT('Ctrl Pts',(1.33009865628678,1.34613267952935,-3.80188911589394E-15));
#78592=CARTESIAN_POINT('Ctrl Pts',(1.37390394515539,1.28973012991194,-4.25185171829959E-15));
#78593=CARTESIAN_POINT('Ctrl Pts',(1.41451494832603,1.23103154357669,-3.94129173741931E-15));
#78594=CARTESIAN_POINT('Ctrl Pts',(1.45486584844222,1.17270890662475,-3.63272081352632E-15));
#78595=CARTESIAN_POINT('Ctrl Pts',(1.49206356397675,1.11211847710431,-7.13207777158734E-16));
#78596=CARTESIAN_POINT('Ctrl Pts',(1.52589939946977,1.04957342610525,-2.692290834716E-15));
#78597=CARTESIAN_POINT('Ctrl Pts',(1.53053080128998,1.04101234703564,-2.96318495456163E-15));
#78598=CARTESIAN_POINT('Ctrl Pts',(1.53509913603607,1.03241463996483,-2.92290991889344E-15));
#78599=CARTESIAN_POINT('Ctrl Pts',(1.53960379146143,1.02378110502453,-2.83800760669806E-15));
#78600=CARTESIAN_POINT('Ctrl Pts',(1.54537176342799,1.01272632218197,-2.70321459129075E-15));
#78601=CARTESIAN_POINT('Ctrl Pts',(1.55103093390346,1.00162120437101,-4.3669508804682E-15));
#78602=CARTESIAN_POINT('Ctrl Pts',(1.5565797653852,0.990469147617545,-4.08006961549745E-15));
#78603=CARTESIAN_POINT('Ctrl Pts',(1.58754040005414,0.928244379017568,-2.50540767500275E-15));
#78604=CARTESIAN_POINT('Ctrl Pts',(1.61507828167858,0.864543360735049,-2.82488097698718E-15));
#78605=CARTESIAN_POINT('Ctrl Pts',(1.63904016583111,0.799672791855858,-2.70616862252382E-15));
#78606=CARTESIAN_POINT('Ctrl Pts',(1.66267588766689,0.735685222614781,-2.58907214669142E-15));
#78607=CARTESIAN_POINT('Ctrl Pts',(1.68283248873858,0.670558732897526,7.68102358593484E-16));
#78608=CARTESIAN_POINT('Ctrl Pts',(1.69931294953593,0.604582527528084,-9.85322934354826E-16));
#78609=CARTESIAN_POINT('Ctrl Pts',(1.71527503781385,0.540681522131514,-2.68359640249016E-15));
#78610=CARTESIAN_POINT('Ctrl Pts',(1.72778860472168,0.47598262367475,1.07798551632638E-15));
#78611=CARTESIAN_POINT('Ctrl Pts',(1.73662635850792,0.410756644998871,3.05311331771918E-16));
#78612=CARTESIAN_POINT('Ctrl Pts',(1.73865577550429,0.395778776987271,1.27881844515988E-16));
#78613=CARTESIAN_POINT('Ctrl Pts',(1.74049115966569,0.380773177713919,-4.3644896247511E-16));
#78614=CARTESIAN_POINT('Ctrl Pts',(1.74212938372161,0.365743253928758,-1.38777878078145E-17));
#78615=CARTESIAN_POINT('Ctrl Pts',(1.74338441815136,0.3542289120664,3.87855657381648E-16));
#78616=CARTESIAN_POINT('Ctrl Pts',(1.74452367514155,0.342699905808244,-1.50379722807899E-15));
#78617=CARTESIAN_POINT('Ctrl Pts',(1.74554463432397,0.331172964306999,-1.51267887105178E-15));
#78618=CARTESIAN_POINT('Ctrl Pts',(1.75129363197339,0.266265022112653,-1.3177032770474E-15));
#78619=CARTESIAN_POINT('Ctrl Pts',(1.75330947147495,0.201304509751003,1.38313017624184E-15));
#78620=CARTESIAN_POINT('Ctrl Pts',(1.75142501653378,0.136551819838442,1.4432899320127E-15));
#78621=CARTESIAN_POINT('Ctrl Pts',(1.75088238549665,0.117906205917835,1.35711357567772E-15));
#78622=CARTESIAN_POINT('Ctrl Pts',(1.75001603328345,0.0992778655205721,
3.28733412684628E-15));
#78623=CARTESIAN_POINT('Ctrl Pts',(1.74882116957219,0.0806731627252346,
2.63677968348475E-15));
#78624=CARTESIAN_POINT('Ctrl Pts',(1.74456363386159,0.0143809272263788,
6.91801324858725E-16));
#78625=CARTESIAN_POINT('Ctrl Pts',(1.73613879272151,-0.0516130402840126,
4.04016429869329E-16));
#78626=CARTESIAN_POINT('Ctrl Pts',(1.72372214259613,-0.11700388521066,9.71445146547012E-16));
#78627=CARTESIAN_POINT('Ctrl Pts',(1.71175302959027,-0.180037827906305,
1.51842185637614E-15));
#78628=CARTESIAN_POINT('Ctrl Pts',(1.69607381160222,-0.242511988113435,
2.89105311828119E-15));
#78629=CARTESIAN_POINT('Ctrl Pts',(1.67680526621061,-0.304125446889571,
1.19348975147204E-15));
#78630=CARTESIAN_POINT('Ctrl Pts',(1.67349606673433,-0.314707004623689,
9.48250798678759E-16));
#78631=CARTESIAN_POINT('Ctrl Pts',(1.67008251071857,-0.325257870756689,
2.04358541335377E-15));
#78632=CARTESIAN_POINT('Ctrl Pts',(1.66656792507904,-0.335769504324591,
1.99840144432528E-15));
#78633=CARTESIAN_POINT('Ctrl Pts',(1.64602352982566,-0.397214914090365,
1.51477858788014E-15));
#78634=CARTESIAN_POINT('Ctrl Pts',(1.62200717575525,-0.457397724739045,
1.74320425236897E-15));
#78635=CARTESIAN_POINT('Ctrl Pts',(1.59470526868992,-0.516044303385602,
2.16493489801906E-15));
#78636=CARTESIAN_POINT('Ctrl Pts',(1.56766219269019,-0.574134893162653,
2.58266739833275E-15));
#78637=CARTESIAN_POINT('Ctrl Pts',(1.53739478791158,-0.630719029504753,
8.07801581179909E-18));
#78638=CARTESIAN_POINT('Ctrl Pts',(1.50404540903,-0.685498994844113,7.21644966006352E-16));
#78639=CARTESIAN_POINT('Ctrl Pts',(1.47097211704488,-0.739825457565848,
1.4293045652605E-15));
#78640=CARTESIAN_POINT('Ctrl Pts',(1.43486696802975,-0.792378215342184,
-2.4045611359052E-16));
#78641=CARTESIAN_POINT('Ctrl Pts',(1.39584139349689,-0.842824299455657,
2.22044604925031E-15));
#78642=CARTESIAN_POINT('Ctrl Pts',(1.38890909242928,-0.851785280733763,
2.64967646930877E-15));
#78643=CARTESIAN_POINT('Ctrl Pts',(1.38188458496569,-0.860679662653789,
2.3719929389117E-16));
#78644=CARTESIAN_POINT('Ctrl Pts',(1.37476842993966,-0.869505410466458,
-2.22044604925031E-16));
#78645=CARTESIAN_POINT('Ctrl Pts',(1.36798353599758,-0.877920314673784,
-4.05596237883174E-16));
#78646=CARTESIAN_POINT('Ctrl Pts',(1.36111848029899,-0.886268835999708,
1.31266055721992E-15));
#78647=CARTESIAN_POINT('Ctrl Pts',(1.35417907408573,-0.894543489490856,
1.4432899320127E-15));
#78648=CARTESIAN_POINT('Ctrl Pts',(1.31426263110496,-0.942140463081207,
2.31521532630317E-15));
#78649=CARTESIAN_POINT('Ctrl Pts',(1.27183845241668,-0.987359134401659,
5.67715419627107E-16));
#78650=CARTESIAN_POINT('Ctrl Pts',(1.22704572742311,-1.02993139787447,3.05311331771918E-16));
#78651=CARTESIAN_POINT('Ctrl Pts',(1.18365605299434,-1.07117016269724,5.11265742594509E-17));
#78652=CARTESIAN_POINT('Ctrl Pts',(1.13804315862614,-1.10992612710962,-1.65473560180465E-15));
#78653=CARTESIAN_POINT('Ctrl Pts',(1.09031115841745,-1.14591358180653,-8.88178419700125E-16));
#78654=CARTESIAN_POINT('Ctrl Pts',(1.04296628811536,-1.18160916061483,-1.278383918949E-16));
#78655=CARTESIAN_POINT('Ctrl Pts',(0.993535978873267,-1.21458145867935,
2.50738491799621E-16));
#78656=CARTESIAN_POINT('Ctrl Pts',(0.942108816666581,-1.24450267784172,
-4.44089209850063E-16));
#78657=CARTESIAN_POINT('Ctrl Pts',(0.929396434173388,-1.25189896350738,
-6.16937577112259E-16));
#78658=CARTESIAN_POINT('Ctrl Pts',(0.916561996392962,-1.25910856034592,
8.48047714131713E-16));
#78659=CARTESIAN_POINT('Ctrl Pts',(0.903606778650234,-1.26612599672282,
1.38777878078145E-16));
#78660=CARTESIAN_POINT('Ctrl Pts',(-0.68439852523474,1.39375347375506,-0.231693356019416));
#78661=CARTESIAN_POINT('Ctrl Pts',(-1.14819351642417,1.16601490671122,-0.194620613066161));
#78662=CARTESIAN_POINT('Ctrl Pts',(-1.82243947067649,0.215139425440093,
-0.120480536464354));
#78663=CARTESIAN_POINT('Ctrl Pts',(-1.16700196451825,-1.41845288290798,
-0.00927312621399557));
#78664=CARTESIAN_POINT('Ctrl Pts',(0.559230889619531,-1.74776969680176,
0.10192887473166));
#78665=CARTESIAN_POINT('Ctrl Pts',(1.77226725459718,-0.47789618903822,0.213130875677316));
#78666=CARTESIAN_POINT('Ctrl Pts',(1.36182366705032,1.23103394611838,0.324332876622972));
#78667=CARTESIAN_POINT('Ctrl Pts',(-0.296644861836514,1.8113809601377,0.435534877568628));
#78668=CARTESIAN_POINT('Ctrl Pts',(-1.68319109737169,0.732320442306668,
0.546736878514283));
#78669=CARTESIAN_POINT('Ctrl Pts',(-1.52752491192947,-1.01791849072323,
0.65793887945994));
#78670=CARTESIAN_POINT('Ctrl Pts',(0.0278106025051759,-1.8353719156861,
0.769140880405594));
#78671=CARTESIAN_POINT('Ctrl Pts',(1.55764750349177,-0.97116016910973,0.880342881351252));
#78672=CARTESIAN_POINT('Ctrl Pts',(1.6602541346855,0.782929184096576,0.991544882296906));
#78673=CARTESIAN_POINT('Ctrl Pts',(0.241601151042511,1.81962454490285,1.10274688324257));
#78674=CARTESIAN_POINT('Ctrl Pts',(-1.39842339561947,1.18904387044759,1.21394888418822));
#78675=CARTESIAN_POINT('Ctrl Pts',(-1.75710394763706,-0.531035633958278,
1.32515088513388));
#78676=CARTESIAN_POINT('Ctrl Pts',(-0.505787344160485,-1.76453676504907,
1.43635288607953));
#78677=CARTESIAN_POINT('Ctrl Pts',(1.20897096626336,-1.38123183937464,1.54755488702519));
#78678=CARTESIAN_POINT('Ctrl Pts',(1.81597539920978,0.267666584309658,1.65875688797085));
#78679=CARTESIAN_POINT('Ctrl Pts',(0.759040591941426,1.67130761262598,1.7699588889165));
#78680=CARTESIAN_POINT('Ctrl Pts',(-0.993386711824161,1.5435656135746,1.88116088986216));
#78681=CARTESIAN_POINT('Ctrl Pts',(-1.83559519323598,0.00148761400844592,
1.99236289080781));
#78682=CARTESIAN_POINT('Ctrl Pts',(-0.995887320575892,-1.54195341526314,
2.10356489175347));
#78683=CARTESIAN_POINT('Ctrl Pts',(0.756330647254053,-1.67253576128902,
2.21476689269912));
#78684=CARTESIAN_POINT('Ctrl Pts',(1.81553913667872,-0.270609601690128,
2.32596889364478));
#78685=CARTESIAN_POINT('Ctrl Pts',(1.21120821638892,1.37927030188772,2.43717089459044));
#78686=CARTESIAN_POINT('Ctrl Pts',(-0.502926704453015,1.76535453762567,
2.54837289553609));
#78687=CARTESIAN_POINT('Ctrl Pts',(-1.75624071862036,0.533882431307681,
2.65957489648175));
#78688=CARTESIAN_POINT('Ctrl Pts',(-1.40034918806097,-1.1867746472047,2.7707768974274));
#78689=CARTESIAN_POINT('Ctrl Pts',(0.23865214255216,-1.82001567774525,2.88197889837307));
#78690=CARTESIAN_POINT('Ctrl Pts',(1.65898165512988,-0.785615542163932,
2.99318089931871));
#78691=CARTESIAN_POINT('Ctrl Pts',(1.55922200833015,0.968627193943045,3.10438290026438));
#78692=CARTESIAN_POINT('Ctrl Pts',(0.0307808179488378,1.8353376946604,3.21558490121002));
#78693=CARTESIAN_POINT('Ctrl Pts',(-1.5258641729711,1.02036779535577,3.32678690215569));
#78694=CARTESIAN_POINT('Ctrl Pts',(-1.68439268635781,-0.729543138065348,
3.43798890310133));
#78695=CARTESIAN_POINT('Ctrl Pts',(-0.299548459802115,-1.81098940703584,
3.549190904047));
#78696=CARTESIAN_POINT('Ctrl Pts',(1.35976556877685,-1.23306508754754,3.66039290499265));
#78697=CARTESIAN_POINT('Ctrl Pts',(1.77315569340789,0.474690213818483,3.77159490593831));
#78698=CARTESIAN_POINT('Ctrl Pts',(0.561841446517521,1.74749709617399,3.88279690688396));
#78699=CARTESIAN_POINT('Ctrl Pts',(-1.16427601683786,1.41911002701576,3.99399890782962));
#78700=CARTESIAN_POINT('Ctrl Pts',(-1.82359244222051,-0.209576995008506,
4.10520090877527));
#78701=CARTESIAN_POINT('Ctrl Pts',(-0.811990389454478,-1.64623313039021,
4.21640290972094));
#78702=CARTESIAN_POINT('Ctrl Pts',(0.943620968464573,-1.57448130507625,
4.32760491066658));
#78703=CARTESIAN_POINT('Ctrl Pts',(1.83461275675203,-0.0600661712062762,
4.43880691161225));
#78704=CARTESIAN_POINT('Ctrl Pts',(1.04458839004179,1.50938630163076,4.5500089125579));
#78705=CARTESIAN_POINT('Ctrl Pts',(-0.702569820048048,1.69582061554822,
4.66121091350355));
#78706=CARTESIAN_POINT('Ctrl Pts',(-1.80597843602436,0.328411024138448,
4.77241291444921));
#78707=CARTESIAN_POINT('Ctrl Pts',(-1.2546079083578,-1.33991451535041,4.88361491539487));
#78708=CARTESIAN_POINT('Ctrl Pts',(0.446332823906676,-1.78050524359359,
4.99481691634052));
#78709=CARTESIAN_POINT('Ctrl Pts',(1.73830840277212,-0.589657365774751,
5.10601891728618));
#78710=CARTESIAN_POINT('Ctrl Pts',(1.43750943198197,1.14148085622289,5.21722091823183));
#78711=CARTESIAN_POINT('Ctrl Pts',(-0.180448470157521,1.8267047549561,5.32842291917749));
#78712=CARTESIAN_POINT('Ctrl Pts',(-1.63306532560299,0.838158430413411,
5.43962492012315));
#78713=CARTESIAN_POINT('Ctrl Pts',(-1.58933959627052,-0.918374411602515,
5.55082692106879));
#78714=CARTESIAN_POINT('Ctrl Pts',(-0.0893362261792351,-1.83342056028012,
5.66202892201447));
#78715=CARTESIAN_POINT('Ctrl Pts',(1.49252400382976,-1.06854293790466,5.77323092296011));
#78716=CARTESIAN_POINT('Ctrl Pts',(1.7068166352141,0.675417564113012,5.88443292390577));
#78717=CARTESIAN_POINT('Ctrl Pts',(0.357189945282142,1.8005074993413,5.99563492485143));
#78718=CARTESIAN_POINT('Ctrl Pts',(-1.31972219832623,1.27583119234171,6.10683692579707));
#78719=CARTESIAN_POINT('Ctrl Pts',(-1.78740131588285,-0.417861757196418,
6.21803892674275));
#78720=CARTESIAN_POINT('Ctrl Pts',(-0.617323104851327,-1.72867697867472,
6.32924092768838));
#78721=CARTESIAN_POINT('Ctrl Pts',(1.11839497117872,-1.45554271671877,6.44044292863406));
#78722=CARTESIAN_POINT('Ctrl Pts',(1.82935182324127,0.15127398653771,6.5516449295797));
#78723=CARTESIAN_POINT('Ctrl Pts',(0.864113000263691,1.61948159493796,6.66284693052535));
#78724=CARTESIAN_POINT('Ctrl Pts',(-0.892893953325356,1.60379309676545,
6.77404893147102));
#78725=CARTESIAN_POINT('Ctrl Pts',(-1.83176140908467,0.118583529746572,
6.88525093241666));
#78726=CARTESIAN_POINT('Ctrl Pts',(-1.09222533755543,-1.47528157745168,
6.99645293336233));
#78727=CARTESIAN_POINT('Ctrl Pts',(0.648093284931744,-1.71737793864714,
7.10765493430798));
#78728=CARTESIAN_POINT('Ctrl Pts',(1.79457799181862,-0.385877905180821,
7.21885693525364));
#78729=CARTESIAN_POINT('Ctrl Pts',(1.29672953139232,1.29919378271827,7.3300589361993));
#78730=CARTESIAN_POINT('Ctrl Pts',(-0.389284259787326,1.79384211159125,
7.44126093714495));
#78731=CARTESIAN_POINT('Ctrl Pts',(-1.71860528684267,0.644831698141129,
7.55246293809061));
#78732=CARTESIAN_POINT('Ctrl Pts',(-1.4732052694108,-1.09502439495669,7.66366493903626));
#78733=CARTESIAN_POINT('Ctrl Pts',(0.122060938605742,-1.83153268056824,
7.77486693998192));
#78734=CARTESIAN_POINT('Ctrl Pts',(1.60548546662183,-0.889848045343311,
7.88606894092758));
#78735=CARTESIAN_POINT('Ctrl Pts',(1.61783799478507,0.86718714352479,7.99727094187323));
#78736=CARTESIAN_POINT('Ctrl Pts',(0.147800881629908,1.82963370650723,8.10847294281889));
#78737=CARTESIAN_POINT('Ctrl Pts',(-1.45766388768593,1.11563340286439,8.21967494376454));
#78738=CARTESIAN_POINT('Ctrl Pts',(-1.72750093382561,-0.620611265472203,
8.3308769447102));
#78739=CARTESIAN_POINT('Ctrl Pts',(-0.414469315409945,-1.78817747583527,
8.44207894565586));
#78740=CARTESIAN_POINT('Ctrl Pts',(1.27833776903631,-1.31732416609453,8.5532809466015));
#78741=CARTESIAN_POINT('Ctrl Pts',(1.79981975869741,0.360658199260608,8.66448294754718));
#78742=CARTESIAN_POINT('Ctrl Pts',(0.672188007145546,1.70799954328245,8.77568494849281));
#78743=CARTESIAN_POINT('Ctrl Pts',(-1.07139767954464,1.49067611804192,8.88688694943849));
#78744=CARTESIAN_POINT('Ctrl Pts',(-1.83320374739229,-0.0931665699783311,
8.99808895038412));
#78745=CARTESIAN_POINT('Ctrl Pts',(-0.915438807724953,-1.59041186183777,
9.1092909513298));
#78746=CARTESIAN_POINT('Ctrl Pts',(0.841415087544887,-1.63276538935367,
9.22049295227544));
#78747=CARTESIAN_POINT('Ctrl Pts',(1.82685908457424,-0.174175557263367,
9.3317068594123));
#78748=CARTESIAN_POINT('Ctrl Pts',(1.36830267541603,0.897665970907806,9.40585343290059));
#78749=CARTESIAN_POINT('Ctrl Pts',(0.962873456568253,1.21812346587503,9.44293267274032));
#78750=CARTESIAN_POINT('Ctrl Pts',(-0.743729541425814,1.51457899699737,
-0.153978113886642));
#78751=CARTESIAN_POINT('Ctrl Pts',(-1.24773126468288,1.267097604523,-0.116905370933388));
#78752=CARTESIAN_POINT('Ctrl Pts',(-1.98042810121144,0.233790021932478,
-0.0427652943315806));
#78753=CARTESIAN_POINT('Ctrl Pts',(-1.26817023110404,-1.54141961626444,
0.068442115918778));
#78754=CARTESIAN_POINT('Ctrl Pts',(0.607711030565455,-1.89928514921112,
0.179644116864434));
#78755=CARTESIAN_POINT('Ctrl Pts',(1.9259064184767,-0.519325364414904,0.29084611781009));
#78756=CARTESIAN_POINT('Ctrl Pts',(1.47988117164744,1.33775319272089,0.402048118755746));
#78757=CARTESIAN_POINT('Ctrl Pts',(-0.322361225112689,1.96841092018517,
0.513250119701402));
#78758=CARTESIAN_POINT('Ctrl Pts',(-1.82910818305885,0.795805845061834,
0.624452120647057));
#78759=CARTESIAN_POINT('Ctrl Pts',(-1.65994718044751,-1.10616260029898,
0.735654121592714));
#78760=CARTESIAN_POINT('Ctrl Pts',(0.0302215242805287,-1.99448166947888,
0.846856122538369));
#78761=CARTESIAN_POINT('Ctrl Pts',(1.69268112183274,-1.05535076507549,0.958058123484026));
#78762=CARTESIAN_POINT('Ctrl Pts',(1.80418279805099,0.850801896245051,1.06926012442968));
#78763=CARTESIAN_POINT('Ctrl Pts',(0.262545734170277,1.97736914743293,1.18046212537534));
#78764=CARTESIAN_POINT('Ctrl Pts',(-1.51965375785472,1.29212296622041,1.291664126321));
#78765=CARTESIAN_POINT('Ctrl Pts',(-1.90942859318027,-0.5770715072612,1.40286612726665));
#78766=CARTESIAN_POINT('Ctrl Pts',(-0.54963442447871,-1.91750576705121,
1.51406812821231));
#78767=CARTESIAN_POINT('Ctrl Pts',(1.31377755676458,-1.50097185283753,1.62527012915796));
#78768=CARTESIAN_POINT('Ctrl Pts',(1.97340365459093,0.290870799196052,1.73647213010362));
#78769=CARTESIAN_POINT('Ctrl Pts',(0.824842384303165,1.81619451019926,1.84767413104928));
#78770=CARTESIAN_POINT('Ctrl Pts',(-1.07950414327688,1.67737846242548,1.95887613199493));
#78771=CARTESIAN_POINT('Ctrl Pts',(-1.9947243031253,0.0016165763711305,
2.07007813294059));
#78772=CARTESIAN_POINT('Ctrl Pts',(-1.08222153165756,-1.67562650144563,
2.18128013388624));
#78773=CARTESIAN_POINT('Ctrl Pts',(0.821897512499189,-1.81752912798159,
2.2924821348319));
#78774=CARTESIAN_POINT('Ctrl Pts',(1.97292957213719,-0.294068948937909,
2.40368413577756));
#78775=CARTESIAN_POINT('Ctrl Pts',(1.31620875576429,1.49884026820977,2.51488613672321));
#78776=CARTESIAN_POINT('Ctrl Pts',(-0.546525793791478,1.91839443293952,
2.62608813766886));
#78777=CARTESIAN_POINT('Ctrl Pts',(-1.90849053019933,0.580165095586069,
2.73729013861453));
#78778=CARTESIAN_POINT('Ctrl Pts',(-1.52174649867255,-1.2896570223301,2.84849213956018));
#78779=CARTESIAN_POINT('Ctrl Pts',(0.259341073944776,-1.97779418787179,
2.95969414050583));
#78780=CARTESIAN_POINT('Ctrl Pts',(1.8028000062981,-0.853721136687417,3.07089614145149));
#78781=CARTESIAN_POINT('Ctrl Pts',(1.69439212166436,1.05259820441132,3.18209814239715));
#78782=CARTESIAN_POINT('Ctrl Pts',(0.0334492299058641,1.99444448180705,
3.2933001433428));
#78783=CARTESIAN_POINT('Ctrl Pts',(-1.65814247079603,1.10882423696829,3.40450214428846));
#78784=CARTESIAN_POINT('Ctrl Pts',(-1.83041393868615,-0.792787774254176,
3.51570414523411));
#78785=CARTESIAN_POINT('Ctrl Pts',(-0.325516538141336,-1.96798542305425,
3.62690614617977));
#78786=CARTESIAN_POINT('Ctrl Pts',(1.47764465530687,-1.3399604153083,3.73810814712542));
#78787=CARTESIAN_POINT('Ctrl Pts',(1.92687187670742,0.5158414608235,3.84931014807109));
#78788=CARTESIAN_POINT('Ctrl Pts',(0.610547898578811,1.89898891663257,3.96051214901674));
#78789=CARTESIAN_POINT('Ctrl Pts',(-1.2652079689957,1.54213372868275,4.0717141499624));
#78790=CARTESIAN_POINT('Ctrl Pts',(-1.9816810247145,-0.227745380277678,
4.18291615090805));
#78791=CARTESIAN_POINT('Ctrl Pts',(-0.882382439067989,-1.78894630248535,
4.2941181518537));
#78792=CARTESIAN_POINT('Ctrl Pts',(1.02542417068364,-1.71097425817256,4.40532015279937));
#78793=CARTESIAN_POINT('Ctrl Pts',(1.99365669849328,-0.0652733521761122,
4.51652215374502));
#78794=CARTESIAN_POINT('Ctrl Pts',(1.13514453298693,1.64023612055744,4.62772415469067));
#78795=CARTESIAN_POINT('Ctrl Pts',(-0.763476119275289,1.84283256354119,
4.73892615563633));
#78796=CARTESIAN_POINT('Ctrl Pts',(-1.96254004724607,0.356881219605069,
4.85012815658198));
#78797=CARTESIAN_POINT('Ctrl Pts',(-1.36337079924614,-1.4560726993232,4.96133015752764));
#78798=CARTESIAN_POINT('Ctrl Pts',(0.485025747730156,-1.93485856485438,
5.0725321584733));
#78799=CARTESIAN_POINT('Ctrl Pts',(1.88900364857879,-0.640775200524594,
5.18373415941895));
#78800=CARTESIAN_POINT('Ctrl Pts',(1.56212819172362,1.24043667898587,5.29493616036461));
#78801=CARTESIAN_POINT('Ctrl Pts',(-0.196091681984855,1.98506314615144,
5.40613816131026));
#78802=CARTESIAN_POINT('Ctrl Pts',(-1.77463697092647,0.910819006922554,
5.51734016225592));
#78803=CARTESIAN_POINT('Ctrl Pts',(-1.72712062565998,-0.997988971066346,
5.62854216320158));
#78804=CARTESIAN_POINT('Ctrl Pts',(-0.0970808499422429,-1.99236114962424,
5.73974416414723));
#78805=CARTESIAN_POINT('Ctrl Pts',(1.62191201764294,-1.16117571838582,5.85094616509288));
#78806=CARTESIAN_POINT('Ctrl Pts',(1.8547818363144,0.73397001411775,5.96214816603855));
#78807=CARTESIAN_POINT('Ctrl Pts',(0.3881550067857,1.9565948310008,6.07335016698419));
#78808=CARTESIAN_POINT('Ctrl Pts',(-1.43412989534715,1.38643394547295,6.18455216792986));
#78809=CARTESIAN_POINT('Ctrl Pts',(-1.94235246276944,-0.45408650311232,
6.29575416887551));
#78810=CARTESIAN_POINT('Ctrl Pts',(-0.670839303058379,-1.87853726917684,
6.40695616982117));
#78811=CARTESIAN_POINT('Ctrl Pts',(1.21534946143024,-1.58172479530061,6.51815817076683));
#78812=CARTESIAN_POINT('Ctrl Pts',(1.9879396907512,0.164388040723421,6.62936017171248));
#78813=CARTESIAN_POINT('Ctrl Pts',(0.93902359769959,1.7598756565667,6.74056217265814));
#78814=CARTESIAN_POINT('Ctrl Pts',(-0.970299592946644,1.74282711084183,
6.85176417360379));
#78815=CARTESIAN_POINT('Ctrl Pts',(-1.99055816538004,0.128863623966512,
6.96296617454945));
#78816=CARTESIAN_POINT('Ctrl Pts',(-1.18691116284208,-1.60317483252287,
7.07416817549511));
#78817=CARTESIAN_POINT('Ctrl Pts',(0.704276972891066,-1.86625870698184,
7.18537017644076));
#78818=CARTESIAN_POINT('Ctrl Pts',(1.95015129006943,-0.419329947223466,
7.29657217738642));
#78819=CARTESIAN_POINT('Ctrl Pts',(1.40914397704898,1.41182185615162,7.40777417833207));
#78820=CARTESIAN_POINT('Ctrl Pts',(-0.423031601239362,1.9493516158389,7.51897617927772));
#78821=CARTESIAN_POINT('Ctrl Pts',(-1.86759245490351,0.700732636720482,
7.63017818022339));
#78822=CARTESIAN_POINT('Ctrl Pts',(-1.60091852779667,-1.18995287260722,
7.74138018116903));
#78823=CARTESIAN_POINT('Ctrl Pts',(0.13264249198098,-1.99030960821872,7.85258218211471));
#78824=CARTESIAN_POINT('Ctrl Pts',(1.74466619349733,-0.966989632940643,
7.96378418306033));
#78825=CARTESIAN_POINT('Ctrl Pts',(1.75808957149651,0.942364240721947,8.07498618400602));
#78826=CARTESIAN_POINT('Ctrl Pts',(0.16061384977306,1.98824601068674,8.18618818495165));
#78827=CARTESIAN_POINT('Ctrl Pts',(-1.58402985215346,1.21234849070882,8.29739018589733));
#78828=CARTESIAN_POINT('Ctrl Pts',(-1.87725927212678,-0.674412516764297,
8.40859218684298));
#78829=CARTESIAN_POINT('Ctrl Pts',(-0.45039996802915,-1.94319590860429,
8.51979418778862));
#78830=CARTESIAN_POINT('Ctrl Pts',(1.38915781916185,-1.43152397592121,8.63099618873429));
#78831=CARTESIAN_POINT('Ctrl Pts',(1.95584746960999,0.391923926276063,8.74219818967994));
#78832=CARTESIAN_POINT('Ctrl Pts',(0.730460484459456,1.85606729156128,8.8534001906256));
#78833=CARTESIAN_POINT('Ctrl Pts',(-1.16427793969766,1.61990393726448,8.96460219157125));
#78834=CARTESIAN_POINT('Ctrl Pts',(-1.99212554106622,-0.101243249088571,
9.07580419251692));
#78835=CARTESIAN_POINT('Ctrl Pts',(-0.994798877509525,-1.72828584672519,
9.18700619346256));
#78836=CARTESIAN_POINT('Ctrl Pts',(0.914357986078193,-1.77431103298107,
9.29820819440823));
#78837=CARTESIAN_POINT('Ctrl Pts',(1.98523085471874,-0.189274965615466,
9.40942210154506));
#78838=CARTESIAN_POINT('Ctrl Pts',(1.48692185005784,0.975485300275654,9.48356867503336));
#78839=CARTESIAN_POINT('Ctrl Pts',(1.04634567127244,1.32372349336162,9.5206479148731));
#78840=CARTESIAN_POINT('Ctrl Pts',(-0.80306055761689,1.63540452023967,-0.0762628717538682));
#78841=CARTESIAN_POINT('Ctrl Pts',(-1.34726901294161,1.36818030233479,-0.0391901288006135));
#78842=CARTESIAN_POINT('Ctrl Pts',(-2.1384167317464,0.252440618424864,0.0349499478011931));
#78843=CARTESIAN_POINT('Ctrl Pts',(-1.36933849768983,-1.66438634962091,
0.146157358051552));
#78844=CARTESIAN_POINT('Ctrl Pts',(0.656191171511376,-2.05080060162047,
0.257359358997207));
#78845=CARTESIAN_POINT('Ctrl Pts',(2.0795455823562,-0.56075453979159,0.368561359942864));
#78846=CARTESIAN_POINT('Ctrl Pts',(1.59793867624458,1.4444724393234,0.479763360888519));
#78847=CARTESIAN_POINT('Ctrl Pts',(-0.348077588388865,2.12544088023263,
0.590965361834176));
#78848=CARTESIAN_POINT('Ctrl Pts',(-1.97502526874602,0.859291247817001,
0.702167362779829));
#78849=CARTESIAN_POINT('Ctrl Pts',(-1.79236944896554,-1.19440670987473,
0.813369363725489));
#78850=CARTESIAN_POINT('Ctrl Pts',(0.0326324460558829,-2.15359142327166,
0.924571364671141));
#78851=CARTESIAN_POINT('Ctrl Pts',(1.8277147401737,-1.13954136104124,1.03577336561681));
#78852=CARTESIAN_POINT('Ctrl Pts',(1.94811146141648,0.918674608393528,1.14697536656246));
#78853=CARTESIAN_POINT('Ctrl Pts',(0.283490317298041,2.13511374996301,1.25817736750812));
#78854=CARTESIAN_POINT('Ctrl Pts',(-1.64088412008999,1.39520206199323,1.36937936845377));
#78855=CARTESIAN_POINT('Ctrl Pts',(-2.06175323872349,-0.62310738056412,
1.48058136939943));
#78856=CARTESIAN_POINT('Ctrl Pts',(-0.593481504796934,-2.07047476905335,
1.59178337034508));
#78857=CARTESIAN_POINT('Ctrl Pts',(1.4185841472658,-1.62071186630041,1.70298537129074));
#78858=CARTESIAN_POINT('Ctrl Pts',(2.13083190997207,0.314075014082447,1.81418737223639));
#78859=CARTESIAN_POINT('Ctrl Pts',(0.890644176664907,1.96108140777255,1.92538937318205));
#78860=CARTESIAN_POINT('Ctrl Pts',(-1.16562157472959,1.81119131127637,2.03659137412771));
#78861=CARTESIAN_POINT('Ctrl Pts',(-2.15385341301462,0.0017455387338156,
2.14779337507336));
#78862=CARTESIAN_POINT('Ctrl Pts',(-1.16855574273922,-1.80929958762813,
2.25899537601902));
#78863=CARTESIAN_POINT('Ctrl Pts',(0.887464377744325,-1.96252249467416,
2.37019737696467));
#78864=CARTESIAN_POINT('Ctrl Pts',(2.13032000759568,-0.31752829618569,2.48139937791033));
#78865=CARTESIAN_POINT('Ctrl Pts',(1.42120929513966,1.61841023453182,2.59260137885599));
#78866=CARTESIAN_POINT('Ctrl Pts',(-0.590124883129942,2.07143432825337,
2.70380337980164));
#78867=CARTESIAN_POINT('Ctrl Pts',(-2.06074034177829,0.626447759864455,
2.8150053807473));
#78868=CARTESIAN_POINT('Ctrl Pts',(-1.64314380928414,-1.39253939745549,
2.92620738169295));
#78869=CARTESIAN_POINT('Ctrl Pts',(0.280030005337393,-2.13557269799833,
3.03740938263861));
#78870=CARTESIAN_POINT('Ctrl Pts',(1.94661835746632,-0.921826731210898,
3.14861138358427));
#78871=CARTESIAN_POINT('Ctrl Pts',(1.82956223499856,1.13656921487958,3.25981338452992));
#78872=CARTESIAN_POINT('Ctrl Pts',(0.0361176418628893,2.1535512689537,3.37101538547558));
#78873=CARTESIAN_POINT('Ctrl Pts',(-1.79042076862095,1.19728067858081,3.48221738642123));
#78874=CARTESIAN_POINT('Ctrl Pts',(-1.97643519101449,-0.856032410443005,
3.59341938736689));
#78875=CARTESIAN_POINT('Ctrl Pts',(-0.351484616480558,-2.12498143907265,
3.70462138831255));
#78876=CARTESIAN_POINT('Ctrl Pts',(1.59552374183691,-1.44685574306907,3.8158233892582));
#78877=CARTESIAN_POINT('Ctrl Pts',(2.08058806000694,0.556992707828519,3.92702539020386));
#78878=CARTESIAN_POINT('Ctrl Pts',(0.659254350640102,2.05048073709114,4.03822739114951));
#78879=CARTESIAN_POINT('Ctrl Pts',(-1.36613992115355,1.66515743034975,4.14942939209517));
#78880=CARTESIAN_POINT('Ctrl Pts',(-2.13976960720848,-0.245913765546851,
4.26063139304082));
#78881=CARTESIAN_POINT('Ctrl Pts',(-0.952774488681501,-1.93165947458048,
4.37183339398649));
#78882=CARTESIAN_POINT('Ctrl Pts',(1.10722737290271,-1.84746721126887,4.48303539493214));
#78883=CARTESIAN_POINT('Ctrl Pts',(2.15270064023453,-0.0704805331459489,
4.59423739587779));
#78884=CARTESIAN_POINT('Ctrl Pts',(1.22570067593207,1.77108593948412,4.70543939682345));
#78885=CARTESIAN_POINT('Ctrl Pts',(-0.824382418502531,1.98984451153416,
4.8166413977691));
#78886=CARTESIAN_POINT('Ctrl Pts',(-2.11910165846778,0.385351415071689,
4.92784339871477));
#78887=CARTESIAN_POINT('Ctrl Pts',(-1.47213369013448,-1.57223088329599,
5.0390453996604));
#78888=CARTESIAN_POINT('Ctrl Pts',(0.523718671553637,-2.08921188611517,
5.15024740060608));
#78889=CARTESIAN_POINT('Ctrl Pts',(2.03969889438546,-0.691893035274437,
5.26144940155171));
#78890=CARTESIAN_POINT('Ctrl Pts',(1.68674695146527,1.33939250174884,5.37265140249739));
#78891=CARTESIAN_POINT('Ctrl Pts',(-0.21173489381219,2.14342153734678,5.48385340344304));
#78892=CARTESIAN_POINT('Ctrl Pts',(-1.91620861624996,0.983479583431696,
5.5950554043887));
#78893=CARTESIAN_POINT('Ctrl Pts',(-1.86490165504943,-1.07760353053018,
5.70625740533434));
#78894=CARTESIAN_POINT('Ctrl Pts',(-0.104825473705251,-2.15130173896834,
5.81745940628001));
#78895=CARTESIAN_POINT('Ctrl Pts',(1.75130003145614,-1.25380849886698,5.92866140722567));
#78896=CARTESIAN_POINT('Ctrl Pts',(2.0027470374147,0.792522464122489,6.03986340817132));
#78897=CARTESIAN_POINT('Ctrl Pts',(0.419120068289257,2.11268216266031,6.15106540911698));
#78898=CARTESIAN_POINT('Ctrl Pts',(-1.54853759236808,1.4970366986042,6.26226741006263));
#78899=CARTESIAN_POINT('Ctrl Pts',(-2.09730360965604,-0.490311249028223,
6.37346941100829));
#78900=CARTESIAN_POINT('Ctrl Pts',(-0.724355501265427,-2.02839755967897,
6.48467141195395));
#78901=CARTESIAN_POINT('Ctrl Pts',(1.31230395168176,-1.70790687388245,6.59587341289959));
#78902=CARTESIAN_POINT('Ctrl Pts',(2.14652755826115,0.177502094909133,6.70707541384526));
#78903=CARTESIAN_POINT('Ctrl Pts',(1.01393419513548,1.90026971819544,6.81827741479091));
#78904=CARTESIAN_POINT('Ctrl Pts',(-1.04770523256793,1.88186112491823,6.92947941573657));
#78905=CARTESIAN_POINT('Ctrl Pts',(-2.14935492167541,0.139143718186449,
7.04068141668223));
#78906=CARTESIAN_POINT('Ctrl Pts',(-1.28159698812875,-1.73106808759405,
7.15188341762787));
#78907=CARTESIAN_POINT('Ctrl Pts',(0.76046066085039,-2.01513947531656,7.26308541857355));
#78908=CARTESIAN_POINT('Ctrl Pts',(2.10572458832024,-0.452781989266107,
7.37428741951918));
#78909=CARTESIAN_POINT('Ctrl Pts',(1.52155842270565,1.52444992958496,7.48548942046485));
#78910=CARTESIAN_POINT('Ctrl Pts',(-0.456778942691401,2.10486112008655,
7.59669142141051));
#78911=CARTESIAN_POINT('Ctrl Pts',(-2.01657962296436,0.756633575299834,
7.70789342235615));
#78912=CARTESIAN_POINT('Ctrl Pts',(-1.72863178618255,-1.28488135025776,
7.81909542330182));
#78913=CARTESIAN_POINT('Ctrl Pts',(0.14322404535622,-2.14908653586922,7.93029742424747));
#78914=CARTESIAN_POINT('Ctrl Pts',(1.88384692037282,-1.04413122053797,8.04149942519313));
#78915=CARTESIAN_POINT('Ctrl Pts',(1.89834114820795,1.0175413379191,8.15270142613878));
#78916=CARTESIAN_POINT('Ctrl Pts',(0.173426817916207,2.14685831486625,8.26390342708444));
#78917=CARTESIAN_POINT('Ctrl Pts',(-1.710395816621,1.30906357855325,8.3751054280301));
#78918=CARTESIAN_POINT('Ctrl Pts',(-2.02701761042795,-0.728213768056391,
8.48630742897575));
#78919=CARTESIAN_POINT('Ctrl Pts',(-0.486330620648357,-2.0982143413733,
8.59750942992142));
#78920=CARTESIAN_POINT('Ctrl Pts',(1.4999778692874,-1.54572378574789,8.70871143086706));
#78921=CARTESIAN_POINT('Ctrl Pts',(2.11187518052256,0.423189653291518,8.81991343181272));
#78922=CARTESIAN_POINT('Ctrl Pts',(0.788732961773369,2.00413503984011,8.93111543275837));
#78923=CARTESIAN_POINT('Ctrl Pts',(-1.25715819985068,1.74913175648703,9.04231743370403));
#78924=CARTESIAN_POINT('Ctrl Pts',(-2.15104733474015,-0.109319928198811,
9.15351943464968));
#78925=CARTESIAN_POINT('Ctrl Pts',(-1.0741589472941,-1.86615983161261,9.26472143559535));
#78926=CARTESIAN_POINT('Ctrl Pts',(0.987300884611498,-1.91585667660846,
9.37592343654099));
#78927=CARTESIAN_POINT('Ctrl Pts',(2.14360262486323,-0.204374373967568,
9.48713734367785));
#78928=CARTESIAN_POINT('Ctrl Pts',(1.60554102469966,1.0533046296435,9.56128391716614));
#78929=CARTESIAN_POINT('Ctrl Pts',(1.12981788597663,1.42932352084821,9.59836315700588));
#78930=CARTESIAN_POINT('Ctrl Pts',(-0.862391573807965,1.75623004348198,
0.00145237037890559));
#78931=CARTESIAN_POINT('Ctrl Pts',(-1.44680676120033,1.46926300014658,0.0385251133321603));
#78932=CARTESIAN_POINT('Ctrl Pts',(-2.29640536228136,0.271091214917251,
0.112665189933967));
#78933=CARTESIAN_POINT('Ctrl Pts',(-1.47050676427563,-1.78735308297738,
0.223872600184326));
#78934=CARTESIAN_POINT('Ctrl Pts',(0.704671312457304,-2.20231605402983,
0.335074601129981));
#78935=CARTESIAN_POINT('Ctrl Pts',(2.23318474623571,-0.602183715168276,
0.446276602075638));
#78936=CARTESIAN_POINT('Ctrl Pts',(1.71599618084173,1.55119168592591,0.557478603021293));
#78937=CARTESIAN_POINT('Ctrl Pts',(-0.373793951665039,2.2824708402801,0.66868060396695));
#78938=CARTESIAN_POINT('Ctrl Pts',(-2.12094235443319,0.922776650572171,
0.779882604912605));
#78939=CARTESIAN_POINT('Ctrl Pts',(-1.92479171748357,-1.28265081945048,
0.891084605858262));
#78940=CARTESIAN_POINT('Ctrl Pts',(0.0350433678312346,-2.31270117706443,
1.00228660680391));
#78941=CARTESIAN_POINT('Ctrl Pts',(1.96274835851467,-1.22373195700699,1.11348860774957));
#78942=CARTESIAN_POINT('Ctrl Pts',(2.09204012478197,0.986547320542003,1.22469060869523));
#78943=CARTESIAN_POINT('Ctrl Pts',(0.304434900425805,2.29285835249309,1.33589260964088));
#78944=CARTESIAN_POINT('Ctrl Pts',(-1.76211448232525,1.49828115776604,1.44709461058654));
#78945=CARTESIAN_POINT('Ctrl Pts',(-2.2140778842667,-0.669143253867042,
1.55829661153219));
#78946=CARTESIAN_POINT('Ctrl Pts',(-0.637328585115159,-2.22344377105548,
1.66949861247785));
#78947=CARTESIAN_POINT('Ctrl Pts',(1.52339073776703,-1.7404518797633,1.7807006134235));
#78948=CARTESIAN_POINT('Ctrl Pts',(2.28826016535321,0.337279228968842,1.89190261436916));
#78949=CARTESIAN_POINT('Ctrl Pts',(0.956445969026647,2.10596830534583,2.00310461531481));
#78950=CARTESIAN_POINT('Ctrl Pts',(-1.2517390061823,1.94500416012725,2.11430661626047));
#78951=CARTESIAN_POINT('Ctrl Pts',(-2.31298252290394,0.00187450109649862,
2.22550861720613));
#78952=CARTESIAN_POINT('Ctrl Pts',(-1.25488995382088,-1.94297267381061,
2.33671061815178));
#78953=CARTESIAN_POINT('Ctrl Pts',(0.95303124298946,-2.10751586136672,2.44791261909744));
#78954=CARTESIAN_POINT('Ctrl Pts',(2.28771044305415,-0.340987643433472,
2.55911462004309));
#78955=CARTESIAN_POINT('Ctrl Pts',(1.52620983451504,1.73798020085387,2.67031662098875));
#78956=CARTESIAN_POINT('Ctrl Pts',(-0.633723972468404,2.22447422356722,
2.78151862193441));
#78957=CARTESIAN_POINT('Ctrl Pts',(-2.21299015335724,0.672730424142846,
2.89272062288006));
#78958=CARTESIAN_POINT('Ctrl Pts',(-1.76454111989571,-1.49542177258089,
3.00392262382573));
#78959=CARTESIAN_POINT('Ctrl Pts',(0.300718936730009,-2.29335120812486,
3.11512462477137));
#78960=CARTESIAN_POINT('Ctrl Pts',(2.09043670863454,-0.989932325734382,
3.22632662571703));
#78961=CARTESIAN_POINT('Ctrl Pts',(1.96473234833276,1.22054022534784,3.33752862666269));
#78962=CARTESIAN_POINT('Ctrl Pts',(0.0387860538199159,2.31265805610036,
3.44873062760834));
#78963=CARTESIAN_POINT('Ctrl Pts',(-1.92269906644588,1.28573712019333,3.559932628554));
#78964=CARTESIAN_POINT('Ctrl Pts',(-2.12245644334284,-0.919277046631835,
3.67113462949965));
#78965=CARTESIAN_POINT('Ctrl Pts',(-0.377452694819782,-2.28197745509106,
3.78233663044531));
#78966=CARTESIAN_POINT('Ctrl Pts',(1.71340282836695,-1.55375107082984,3.89353863139097));
#78967=CARTESIAN_POINT('Ctrl Pts',(2.23430424330645,0.598143954833538,4.00474063233662));
#78968=CARTESIAN_POINT('Ctrl Pts',(0.707960802701394,2.20197255754971,4.11594263328228));
#78969=CARTESIAN_POINT('Ctrl Pts',(-1.46707187331139,1.78818113201674,4.22714463422794));
#78970=CARTESIAN_POINT('Ctrl Pts',(-2.29785818970246,-0.264082150816026,
4.33834663517359));
#78971=CARTESIAN_POINT('Ctrl Pts',(-1.02316653829502,-2.07437264667561,
4.44954863611926));
#78972=CARTESIAN_POINT('Ctrl Pts',(1.18903057512178,-1.98396016436518,4.5607506370649));
#78973=CARTESIAN_POINT('Ctrl Pts',(2.31174458197577,-0.0756877141157843,
4.67195263801057));
#78974=CARTESIAN_POINT('Ctrl Pts',(1.3162568188772,1.90193575841081,4.78315463895623));
#78975=CARTESIAN_POINT('Ctrl Pts',(-0.885288717729772,2.13685645952712,
4.89435663990187));
#78976=CARTESIAN_POINT('Ctrl Pts',(-2.2756632696895,0.413821610538309,5.00555864084753));
#78977=CARTESIAN_POINT('Ctrl Pts',(-1.58089658102282,-1.68838906726877,
5.1167606417932));
#78978=CARTESIAN_POINT('Ctrl Pts',(0.562411595377116,-2.24356520737596,
5.22796264273883));
#78979=CARTESIAN_POINT('Ctrl Pts',(2.19039414019213,-0.743010870024276,
5.3391646436845));
#78980=CARTESIAN_POINT('Ctrl Pts',(1.81136571120691,1.43834832451181,5.45036664463017));
#78981=CARTESIAN_POINT('Ctrl Pts',(-0.227378105639523,2.30177992854213,
5.56156864557579));
#78982=CARTESIAN_POINT('Ctrl Pts',(-2.05778026157344,1.05614015994084,5.67277064652148));
#78983=CARTESIAN_POINT('Ctrl Pts',(-2.00268268443888,-1.15721808999401,
5.78397264746711));
#78984=CARTESIAN_POINT('Ctrl Pts',(-0.11257009746826,-2.31024232831246,
5.89517464841279));
#78985=CARTESIAN_POINT('Ctrl Pts',(1.88068804526933,-1.34644127934815,6.00637664935843));
#78986=CARTESIAN_POINT('Ctrl Pts',(2.15071223851501,0.851074914127227,6.11757865030409));
#78987=CARTESIAN_POINT('Ctrl Pts',(0.450085129792815,2.26876949431981,6.22878065124975));
#78988=CARTESIAN_POINT('Ctrl Pts',(-1.662945289389,1.60763945173544,6.33998265219541));
#78989=CARTESIAN_POINT('Ctrl Pts',(-2.25225475654263,-0.526535994944125,
6.45118465314106));
#78990=CARTESIAN_POINT('Ctrl Pts',(-0.777871699472479,-2.1782578501811,
6.56238665408672));
#78991=CARTESIAN_POINT('Ctrl Pts',(1.40925844193328,-1.83408895246428,6.67358865503238));
#78992=CARTESIAN_POINT('Ctrl Pts',(2.30511542577108,0.190616149094843,6.78479065597802));
#78993=CARTESIAN_POINT('Ctrl Pts',(1.08884479257138,2.04066377982418,6.89599265692368));
#78994=CARTESIAN_POINT('Ctrl Pts',(-1.12511087218922,2.02089513899462,7.00719465786934));
#78995=CARTESIAN_POINT('Ctrl Pts',(-2.30815167797076,0.149423812406389,
7.118396658815));
#78996=CARTESIAN_POINT('Ctrl Pts',(-1.37628281341541,-1.85896134266524,
7.22959865976065));
#78997=CARTESIAN_POINT('Ctrl Pts',(0.816644348809715,-2.16402024365127,
7.34080066070631));
#78998=CARTESIAN_POINT('Ctrl Pts',(2.26129788657104,-0.486234031308752,
7.45200266165195));
#78999=CARTESIAN_POINT('Ctrl Pts',(1.63397286836232,1.63707800301831,7.56320466259762));
#79000=CARTESIAN_POINT('Ctrl Pts',(-0.490526284143436,2.2603706243342,7.67440666354327));
#79001=CARTESIAN_POINT('Ctrl Pts',(-2.16556679102521,0.812534513879188,
7.78560866448893));
#79002=CARTESIAN_POINT('Ctrl Pts',(-1.85634504456841,-1.37980982790828,
7.8968106654346));
#79003=CARTESIAN_POINT('Ctrl Pts',(0.153805598731459,-2.3078634635197,8.00801266638024));
#79004=CARTESIAN_POINT('Ctrl Pts',(2.02302764724831,-1.1212728081353,8.11921466732591));
#79005=CARTESIAN_POINT('Ctrl Pts',(2.03859272491938,1.09271843511626,8.23041666827155));
#79006=CARTESIAN_POINT('Ctrl Pts',(0.186239786059356,2.30547061904575,8.34161866921722));
#79007=CARTESIAN_POINT('Ctrl Pts',(-1.83676178108854,1.40577866639767,8.45282067016287));
#79008=CARTESIAN_POINT('Ctrl Pts',(-2.17677594872913,-0.782015019348484,
8.56402267110853));
#79009=CARTESIAN_POINT('Ctrl Pts',(-0.522261273267561,-2.25323277414232,
8.67522467205418));
#79010=CARTESIAN_POINT('Ctrl Pts',(1.61079791941295,-1.65992359557459,8.78642667299984));
#79011=CARTESIAN_POINT('Ctrl Pts',(2.26790289143513,0.454455380306972,8.8976286739455));
#79012=CARTESIAN_POINT('Ctrl Pts',(0.847005439087281,2.15220278811892,9.00883067489114));
#79013=CARTESIAN_POINT('Ctrl Pts',(-1.3500384600037,1.87835957570958,9.12003267583681));
#79014=CARTESIAN_POINT('Ctrl Pts',(-2.30996912841407,-0.117396607309049,
9.23123467678246));
#79015=CARTESIAN_POINT('Ctrl Pts',(-1.15351901707866,-2.00403381650003,
9.34243667772811));
#79016=CARTESIAN_POINT('Ctrl Pts',(1.0602437831448,-2.05740232023586,9.45363867867378));
#79017=CARTESIAN_POINT('Ctrl Pts',(2.30197439500773,-0.219473782319668,
9.56485258581061));
#79018=CARTESIAN_POINT('Ctrl Pts',(1.72416019934148,1.13112395901135,9.63899915929891));
#79019=CARTESIAN_POINT('Ctrl Pts',(1.21329010068083,1.53492354833479,9.67607839913864));
#79020=CARTESIAN_POINT('',(-0.904509582502828,-1.26706033424728,-0.000727943534944579));
#79021=CARTESIAN_POINT('Ctrl Pts',(-0.905550660636154,-1.26792405592273,
3.33717428691038E-16));
#79022=CARTESIAN_POINT('Ctrl Pts',(-0.937331646933895,-1.25093119319315,
-1.91748806585551E-15));
#79023=CARTESIAN_POINT('Ctrl Pts',(-0.968423391396879,-1.23278887404085,
-3.93171517975868E-15));
#79024=CARTESIAN_POINT('Ctrl Pts',(-0.998756220109606,-1.21351103938414,
-3.10862446895044E-15));
#79025=CARTESIAN_POINT('Ctrl Pts',(-1.0491021278163,-1.18151402078745,-1.75196333938182E-15));
#79026=CARTESIAN_POINT('Ctrl Pts',(-1.09735862263973,-1.14639180321778,
-1.66246197192591E-15));
#79027=CARTESIAN_POINT('Ctrl Pts',(-1.14344573691603,-1.10847083762139,
-1.88390969491081E-15));
#79028=CARTESIAN_POINT('Ctrl Pts',(-1.16929613914609,-1.08720085296273,
-2.0081203946255E-15));
#79029=CARTESIAN_POINT('Ctrl Pts',(-1.19446376238245,-1.06504939091104,
-9.9374122142534E-16));
#79030=CARTESIAN_POINT('Ctrl Pts',(-1.21893184621839,-1.04206746474762,
-1.99493199737333E-15));
#79031=CARTESIAN_POINT('Ctrl Pts',(-1.23255995383574,-1.02926710959479,
-2.49718249979953E-15));
#79032=CARTESIAN_POINT('Ctrl Pts',(-1.24597488110422,-1.01620487704946,
4.81999660303363E-16));
#79033=CARTESIAN_POINT('Ctrl Pts',(-1.25915060380592,-1.0029128321029,5.62050406216485E-16));
#79034=CARTESIAN_POINT('Ctrl Pts',(-1.30279148681256,-0.958886664311984,
4.90052638460193E-16));
#79035=CARTESIAN_POINT('Ctrl Pts',(-1.34385262686326,-0.912305708298536,
-1.22866962404621E-15));
#79036=CARTESIAN_POINT('Ctrl Pts',(-1.3822468326494,-0.863513449211606,
6.59194920871187E-16));
#79037=CARTESIAN_POINT('Ctrl Pts',(-1.40779034735979,-0.831052150371822,
1.91518380739542E-15));
#79038=CARTESIAN_POINT('Ctrl Pts',(-1.4321530736785,-0.797610973924513,
1.23008985062119E-15));
#79039=CARTESIAN_POINT('Ctrl Pts',(-1.45530339706809,-0.763280061968941,
7.14706072102445E-16));
#79040=CARTESIAN_POINT('Ctrl Pts',(-1.46804523103353,-0.74438448229783,
4.31041156332024E-16));
#79041=CARTESIAN_POINT('Ctrl Pts',(-1.48041969259617,-0.725219227959009,
1.33627721405136E-16));
#79042=CARTESIAN_POINT('Ctrl Pts',(-1.49242075014977,-0.705798385792698,
6.73072708679001E-16));
#79043=CARTESIAN_POINT('Ctrl Pts',(-1.50150857656975,-0.691091911654995,
1.08156857544523E-15));
#79044=CARTESIAN_POINT('Ctrl Pts',(-1.51038448432321,-0.676234681791649,
1.10657574010046E-15));
#79045=CARTESIAN_POINT('Ctrl Pts',(-1.51903027706774,-0.661260208511432,
1.11022302462516E-15));
#79046=CARTESIAN_POINT('Ctrl Pts',(-1.55206526232624,-0.60404376593845,
1.12415905039712E-15));
#79047=CARTESIAN_POINT('Ctrl Pts',(-1.58178299126492,-0.545059351017348,
2.78962851734901E-16));
#79048=CARTESIAN_POINT('Ctrl Pts',(-1.60808638764007,-0.484680550384653,
1.16573417585641E-15));
#79049=CARTESIAN_POINT('Ctrl Pts',(-1.63436099254972,-0.424367839854187,
2.05153484791377E-15));
#79050=CARTESIAN_POINT('Ctrl Pts',(-1.65722893541898,-0.362663618825764,
1.62943944703187E-15));
#79051=CARTESIAN_POINT('Ctrl Pts',(-1.67655774217872,-0.29990105864075,
2.37310171513627E-15));
#79052=CARTESIAN_POINT('Ctrl Pts',(-1.68825939151139,-0.261904638083861,
2.82331445674351E-15));
#79053=CARTESIAN_POINT('Ctrl Pts',(-1.6986632113407,-0.22351958384957,1.0977060151425E-15));
#79054=CARTESIAN_POINT('Ctrl Pts',(-1.70773212765127,-0.184814675751519,
1.67921232474555E-15));
#79055=CARTESIAN_POINT('Ctrl Pts',(-1.71421027330989,-0.157166826353006,
2.09459630735212E-15));
#79056=CARTESIAN_POINT('Ctrl Pts',(-1.72000709785751,-0.129355980394314,
2.03148131458715E-15));
#79057=CARTESIAN_POINT('Ctrl Pts',(-1.72510714810462,-0.10140553099961,
1.41553435639707E-15));
#79058=CARTESIAN_POINT('Ctrl Pts',(-1.72714678432153,-0.0902274550783656,
1.16920193558766E-15));
#79059=CARTESIAN_POINT('Ctrl Pts',(-1.72907514617003,-0.0790258298363134,
8.63363090934406E-16));
#79060=CARTESIAN_POINT('Ctrl Pts',(-1.73089043201219,-0.0678066984905213,
9.99200722162641E-16));
#79061=CARTESIAN_POINT('Ctrl Pts',(-1.74172160283504,-0.000866095931864194,
1.93493306363864E-15));
#79062=CARTESIAN_POINT('Ctrl Pts',(-1.748486900033,0.0664195158076903,2.98350052951504E-15));
#79063=CARTESIAN_POINT('Ctrl Pts',(-1.75106690168969,0.1336922072272,1.33226762955019E-15));
#79064=CARTESIAN_POINT('Ctrl Pts',(-1.75197579459359,0.157391289628444,
9.56040573665211E-16));
#79065=CARTESIAN_POINT('Ctrl Pts',(-1.7523649021625,0.181089059905602,2.7599826661696E-15));
#79066=CARTESIAN_POINT('Ctrl Pts',(-1.75222770108741,0.204770690960272,
2.17881268582687E-15));
#79067=CARTESIAN_POINT('Ctrl Pts',(-1.75184793058349,0.270321088092813,
4.77379898077456E-16));
#79068=CARTESIAN_POINT('Ctrl Pts',(-1.74743979276228,0.335747132875219,
1.54789476185541E-15));
#79069=CARTESIAN_POINT('Ctrl Pts',(-1.73922727433975,0.400805521086702,
1.60982338570648E-15));
#79070=CARTESIAN_POINT('Ctrl Pts',(-1.73101475591721,0.465863909298186,
1.67175200955754E-15));
#79071=CARTESIAN_POINT('Ctrl Pts',(-1.71899757684948,0.530555453607267,
3.18517571214417E-15));
#79072=CARTESIAN_POINT('Ctrl Pts',(-1.70334767938921,0.594640505552196,
9.15933995315754E-16));
#79073=CARTESIAN_POINT('Ctrl Pts',(-1.70064831213801,0.605694193983742,
3.51217563452488E-16));
#79074=CARTESIAN_POINT('Ctrl Pts',(-1.69784071539616,0.616729589129694,
2.72828645400985E-15));
#79075=CARTESIAN_POINT('Ctrl Pts',(-1.69492950185833,0.627731892802464,
2.38697950294409E-15));
#79076=CARTESIAN_POINT('Ctrl Pts',(-1.67764017062698,0.693073191211115,
2.64844180626529E-16));
#79077=CARTESIAN_POINT('Ctrl Pts',(-1.65667167698021,0.757368056664447,
3.89680800276467E-16));
#79078=CARTESIAN_POINT('Ctrl Pts',(-1.632278840768,0.820363247272086,-1.11022302462516E-16));
#79079=CARTESIAN_POINT('Ctrl Pts',(-1.60714941139895,0.885260710576183,
-6.26845191842105E-16));
#79080=CARTESIAN_POINT('Ctrl Pts',(-1.578385616419,0.948779708185034,2.13504031261271E-15));
#79081=CARTESIAN_POINT('Ctrl Pts',(-1.54620991004292,1.01064658923624,1.85962356624714E-15));
#79082=CARTESIAN_POINT('Ctrl Pts',(-1.51403420366684,1.07251347028744,1.58420681988156E-15));
#79083=CARTESIAN_POINT('Ctrl Pts',(-1.47844619815798,1.13272920500638,2.35794009978941E-15));
#79084=CARTESIAN_POINT('Ctrl Pts',(-1.43961707028964,1.19100921034501,2.41473507855972E-15));
#79085=CARTESIAN_POINT('Ctrl Pts',(-1.42987064738873,1.20563795968555,2.47976585367877E-15));
#79086=CARTESIAN_POINT('Ctrl Pts',(-1.41991978147756,1.22014465371079,1.22964269444539E-15));
#79087=CARTESIAN_POINT('Ctrl Pts',(-1.40976671738967,1.23452457045435,1.22124532708767E-15));
#79088=CARTESIAN_POINT('Ctrl Pts',(-1.40016197586479,1.24812789081909,1.2626273074017E-15));
#79089=CARTESIAN_POINT('Ctrl Pts',(-1.39037610631028,1.2616175763207,1.15601544640403E-15));
#79090=CARTESIAN_POINT('Ctrl Pts',(-1.38042895433654,1.27496651867268,7.49400541621981E-16));
#79091=CARTESIAN_POINT('Ctrl Pts',(-1.33728364574509,1.33286693465769,-1.01427267771033E-15));
#79092=CARTESIAN_POINT('Ctrl Pts',(-1.29103059232721,1.38823206717148,-5.46656303023409E-16));
#79093=CARTESIAN_POINT('Ctrl Pts',(-1.24190881939456,1.44078043502317,-4.44089209850063E-16));
#79094=CARTESIAN_POINT('Ctrl Pts',(-1.19270542345375,1.49341611967151,-3.41351686454363E-16));
#79095=CARTESIAN_POINT('Ctrl Pts',(-1.14062332922914,1.54322667971843,1.00148334219595E-15));
#79096=CARTESIAN_POINT('Ctrl Pts',(-1.08585348598407,1.58991235213884,8.32667268468867E-17));
#79097=CARTESIAN_POINT('Ctrl Pts',(-1.03227982431091,1.63557840248782,-8.14895900226442E-16));
#79098=CARTESIAN_POINT('Ctrl Pts',(-0.97613396306252,1.67825542174933,-1.71497774819462E-15));
#79099=CARTESIAN_POINT('Ctrl Pts',(-0.917555232362004,1.7176331456658,-1.99840144432528E-15));
#79100=CARTESIAN_POINT('Ctrl Pts',(-0.899118809741871,1.73002645551156,
-2.08760308765107E-15));
#79101=CARTESIAN_POINT('Ctrl Pts',(-0.880441136441611,1.74209268004149,
-1.43728562686843E-15));
#79102=CARTESIAN_POINT('Ctrl Pts',(-0.861525859670561,1.75382131162753,
1.94289029309402E-16));
#79103=CARTESIAN_POINT('Ctrl Pts',(-0.903762994389396,-1.26601449437687,
-0.000727943534944708));
#79104=CARTESIAN_POINT('Ctrl Pts',(-0.898466996491729,-1.26979512006444,
-0.000485295689962951));
#79105=CARTESIAN_POINT('Ctrl Pts',(-0.893147275587681,-1.27354251394864,
-0.000242647844981202));
#79106=CARTESIAN_POINT('Ctrl Pts',(-0.887804250576279,-1.27725638094264,
5.55111512312578E-16));
#79107=CARTESIAN_POINT('Origin',(-0.866025403784439,-1.5,-4.));
#79108=CARTESIAN_POINT('',(-0.866025403784439,-1.5,-4.));
#79109=CARTESIAN_POINT('',(0.866025403784439,-1.5,-4.));
#79110=CARTESIAN_POINT('',(-0.43301270189222,-1.5,-4.));
#79111=CARTESIAN_POINT('',(-0.866025403784439,-1.5,-2.));
#79112=CARTESIAN_POINT('',(-0.866025403784439,-1.5,-4.));
#79113=CARTESIAN_POINT('',(0.866025403784439,-1.5,-2.));
#79114=CARTESIAN_POINT('',(-0.866025403784439,-1.5,-2.));
#79115=CARTESIAN_POINT('',(0.866025403784439,-1.5,-4.));
#79116=CARTESIAN_POINT('Origin',(-1.73205080756888,2.12115047744981E-16,
-4.));
#79117=CARTESIAN_POINT('',(-1.73205080756888,2.12115047744981E-16,-4.));
#79118=CARTESIAN_POINT('',(-1.51554445662277,-0.375,-4.));
#79119=CARTESIAN_POINT('',(-1.73205080756888,2.77555756156289E-16,-2.));
#79120=CARTESIAN_POINT('',(-1.73205080756888,2.12115047744981E-16,-4.));
#79121=CARTESIAN_POINT('',(-1.73205080756888,2.12115047744981E-16,-2.));
#79122=CARTESIAN_POINT('Origin',(-0.866025403784438,1.5,-4.));
#79123=CARTESIAN_POINT('',(-0.866025403784438,1.5,-4.));
#79124=CARTESIAN_POINT('',(-1.08253175473055,1.125,-4.));
#79125=CARTESIAN_POINT('',(-0.866025403784438,1.5,-2.));
#79126=CARTESIAN_POINT('',(-0.866025403784438,1.5,-4.));
#79127=CARTESIAN_POINT('',(-0.866025403784438,1.5,-2.));
#79128=CARTESIAN_POINT('Origin',(0.866025403784439,1.5,-4.));
#79129=CARTESIAN_POINT('',(0.866025403784439,1.5,-4.));
#79130=CARTESIAN_POINT('',(0.43301270189222,1.5,-4.));
#79131=CARTESIAN_POINT('',(0.866025403784439,1.5,-2.));
#79132=CARTESIAN_POINT('',(0.866025403784439,1.5,-4.));
#79133=CARTESIAN_POINT('',(0.866025403784439,1.5,-2.));
#79134=CARTESIAN_POINT('Origin',(1.73205080756888,0.,-4.));
#79135=CARTESIAN_POINT('',(1.73205080756888,0.,-4.));
#79136=CARTESIAN_POINT('',(1.51554445662277,0.375,-4.));
#79137=CARTESIAN_POINT('',(1.73205080756888,0.,-2.));
#79138=CARTESIAN_POINT('',(1.73205080756888,0.,-4.));
#79139=CARTESIAN_POINT('',(1.73205080756888,0.,-2.));
#79140=CARTESIAN_POINT('Origin',(0.866025403784439,-1.5,-4.));
#79141=CARTESIAN_POINT('',(1.08253175473055,-1.125,-4.));
#79142=CARTESIAN_POINT('',(0.866025403784439,-1.5,-2.));
#79143=CARTESIAN_POINT('Origin',(0.,2.77555756156289E-16,-2.));
#79144=CARTESIAN_POINT('Origin',(0.,0.,0.));
#79145=CARTESIAN_POINT('',(-3.5,-4.28626379701574E-16,0.));
#79146=CARTESIAN_POINT('Origin',(0.,0.,0.));
#79147=CARTESIAN_POINT('Origin',(0.,0.,-4.));
#79148=CARTESIAN_POINT('',(-3.5,-4.28626379701574E-16,-4.));
#79149=CARTESIAN_POINT('',(-3.5,-4.28626379701574E-16,-4.));
#79150=CARTESIAN_POINT('Origin',(0.,0.,-4.));
#79151=CARTESIAN_POINT('Origin',(0.,0.,-4.));
#79152=CARTESIAN_POINT('Origin',(0.,0.,10.));
#79153=CARTESIAN_POINT('',(0.,0.,0.));
#79154=CARTESIAN_POINT('Origin',(0.,0.,2.15141010809499));
#79155=CARTESIAN_POINT('',(4.2909266281567,8.33003803918541,4.52288275511062));
#79156=CARTESIAN_POINT('',(4.29092662815669,8.33003803918541,4.32570756359748));
#79157=CARTESIAN_POINT('',(4.29092662815669,8.33003803918541,2.15141010809499));
#79158=CARTESIAN_POINT('',(-5.44048627969075,-7.62906901941493,4.00000000616494));
#79159=CARTESIAN_POINT('Ctrl Pts',(-5.44048627969075,-7.62906901941493,
4.00000000616494));
#79160=CARTESIAN_POINT('Ctrl Pts',(-5.25102146993863,-7.76418127168548,
4.00395293893828));
#79161=CARTESIAN_POINT('Ctrl Pts',(-5.05649608080199,-7.89224980204389,
4.00790587171162));
#79162=CARTESIAN_POINT('Ctrl Pts',(-4.85745790948893,-8.01290756966805,
4.01185880448497));
#79163=CARTESIAN_POINT('Ctrl Pts',(-4.65844439494387,-8.13355039025684,
4.0158112475706));
#79164=CARTESIAN_POINT('Ctrl Pts',(-4.45491946109027,-8.24678413124755,
4.01976369065623));
#79165=CARTESIAN_POINT('Ctrl Pts',(-4.24745820141938,-8.3522861474985,4.02371613374186));
#79166=CARTESIAN_POINT('Ctrl Pts',(-4.03998379596611,-8.45779484888453,
4.02766882727405));
#79167=CARTESIAN_POINT('Ctrl Pts',(-3.82857282246667,-8.55557071332864,
4.03162152080623));
#79168=CARTESIAN_POINT('Ctrl Pts',(-3.61382422694981,-8.645337443918,4.03557421433841));
#79169=CARTESIAN_POINT('Ctrl Pts',(-3.39907558674732,-8.73510419318633,
4.03952690869308));
#79170=CARTESIAN_POINT('Ctrl Pts',(-3.18098959057493,-8.81686169639834,
4.04347960304776));
#79171=CARTESIAN_POINT('Ctrl Pts',(-2.96018499421697,-8.89038187382931,
4.04743229740243));
#79172=CARTESIAN_POINT('Ctrl Pts',(-2.73933409392948,-8.96391746884293,
4.05138582065869));
#79173=CARTESIAN_POINT('Ctrl Pts',(-2.51576372857753,-9.02921219607435,
4.05533934391495));
#79174=CARTESIAN_POINT('Ctrl Pts',(-2.29010878757626,-9.08608754104681,
4.05929286717121));
#79175=CARTESIAN_POINT('Ctrl Pts',(-2.20846628460654,-9.10666517830223,
4.06072326143937));
#79176=CARTESIAN_POINT('Ctrl Pts',(-2.12655103750013,-9.12614118745565,
4.06215365570753));
#79177=CARTESIAN_POINT('Ctrl Pts',(-2.04439351365759,-9.14450874699209,
4.06358404997569));
#79178=CARTESIAN_POINT('Ctrl Pts',(-1.8164772133919,-9.19546288994408,4.06755216092004));
#79179=CARTESIAN_POINT('Ctrl Pts',(-1.58661959870168,-9.23789988448231,
4.07152027186439));
#79180=CARTESIAN_POINT('Ctrl Pts',(-1.35547239192246,-9.27169238366093,
4.07548838280874));
#79181=CARTESIAN_POINT('Ctrl Pts',(-1.12436567230507,-9.3054789638306,4.07945579870879));
#79182=CARTESIAN_POINT('Ctrl Pts',(-0.891970092874594,-9.33062402994177,
4.08342321460883));
#79183=CARTESIAN_POINT('Ctrl Pts',(-0.65894540976201,-9.34705172818968,
4.08739063050888));
#79184=CARTESIAN_POINT('Ctrl Pts',(-0.425946105705265,-9.36347763727317,
4.09135761431191));
#79185=CARTESIAN_POINT('Ctrl Pts',(-0.192318118472125,-9.37118805412488,
4.09532459811494));
#79186=CARTESIAN_POINT('Ctrl Pts',(0.0412748677381543,-9.37015909404922,
4.09929158191797));
#79187=CARTESIAN_POINT('Ctrl Pts',(0.274886125731263,-9.36913005348768,
4.10325887602084));
#79188=CARTESIAN_POINT('Ctrl Pts',(0.508462092689314,-9.35936026837331,
4.10722617012371));
#79189=CARTESIAN_POINT('Ctrl Pts',(0.741339046271913,-9.34087798234046,
4.11119346422658));
#79190=CARTESIAN_POINT('Ctrl Pts',(0.974213587877025,-9.32239588773426,
4.11516071723898));
#79191=CARTESIAN_POINT('Ctrl Pts',(1.20638884712689,-9.2952014974446,4.11912797025138));
#79192=CARTESIAN_POINT('Ctrl Pts',(1.43720550210129,-9.25937500089665,4.12309522326378));
#79193=CARTESIAN_POINT('Ctrl Pts',(1.66807196794911,-9.22354077289151,4.12706333242037));
#79194=CARTESIAN_POINT('Ctrl Pts',(1.89757896236427,-9.17907075958204,4.13103144157696));
#79195=CARTESIAN_POINT('Ctrl Pts',(2.12507535254614,-9.12609663593921,4.13499955073354));
#79196=CARTESIAN_POINT('Ctrl Pts',(2.26498852057068,-9.09351687739329,4.13743998823992));
#79197=CARTESIAN_POINT('Ctrl Pts',(2.40414138272164,-9.05772152559798,4.1398804257463));
#79198=CARTESIAN_POINT('Ctrl Pts',(2.54238478313434,-9.01875072706786,4.14232086325268));
#79199=CARTESIAN_POINT('Ctrl Pts',(2.7671614585895,-8.95538620834737,4.14628888941307));
#79200=CARTESIAN_POINT('Ctrl Pts',(2.98960313356232,-8.88360437568409,4.15025691557347));
#79201=CARTESIAN_POINT('Ctrl Pts',(3.20907578261301,-8.80360254009384,4.15422494173386));
#79202=CARTESIAN_POINT('Ctrl Pts',(3.42850982836864,-8.72361477611788,4.1581922699536));
#79203=CARTESIAN_POINT('Ctrl Pts',(3.64497562342645,-8.63540999266812,4.16215959817334));
#79204=CARTESIAN_POINT('Ctrl Pts',(3.85785651725796,-8.53923463518542,4.16612692639308));
#79205=CARTESIAN_POINT('Ctrl Pts',(4.07071408462154,-8.4430698161374,4.17009381989201));
#79206=CARTESIAN_POINT('Ctrl Pts',(4.27998727585202,-8.33893628395689,4.17406071339094));
#79207=CARTESIAN_POINT('Ctrl Pts',(4.48508065509893,-8.22712808820657,4.17802760688987));
#79208=CARTESIAN_POINT('Ctrl Pts',(4.69018990518877,-8.11531124034704,4.18199480736089));
#79209=CARTESIAN_POINT('Ctrl Pts',(4.89111844574226,-7.99581867584552,4.18596200783191));
#79210=CARTESIAN_POINT('Ctrl Pts',(5.0872955554571,-7.86899034145591,4.18992920830294));
#79211=CARTESIAN_POINT('Ctrl Pts',(5.28347054755643,-7.74216337610293,4.19389636595038));
#79212=CARTESIAN_POINT('Ctrl Pts',(5.47489397364357,-7.60800095560125,4.19786352359783));
#79213=CARTESIAN_POINT('Ctrl Pts',(5.66102364641474,-7.46688665624658,4.20183068124527));
#79214=CARTESIAN_POINT('Ctrl Pts',(5.84719339031636,-7.32574197694542,4.2057986929666));
#79215=CARTESIAN_POINT('Ctrl Pts',(6.02806687655178,-7.17764259984669,4.20976670468793));
#79216=CARTESIAN_POINT('Ctrl Pts',(6.20313356829267,-7.02301352671491,4.21373471640925));
#79217=CARTESIAN_POINT('Ctrl Pts',(6.31082868044312,-6.92789094681666,4.21617570311605));
#79218=CARTESIAN_POINT('Ctrl Pts',(6.41632697248547,-6.83029813531336,4.21861668982285));
#79219=CARTESIAN_POINT('Ctrl Pts',(6.51951615140972,-6.73034131482259,4.22105767652964));
#79220=CARTESIAN_POINT('Ctrl Pts',(6.68727388033173,-6.56783852750894,4.2250260614953));
#79221=CARTESIAN_POINT('Ctrl Pts',(6.84897881607757,-6.39903529653706,4.22899444646095));
#79222=CARTESIAN_POINT('Ctrl Pts',(7.00416659244396,-6.22440643015797,4.2329628314266));
#79223=CARTESIAN_POINT('Ctrl Pts',(7.15932727382635,-6.04980805307677,4.23693052353274));
#79224=CARTESIAN_POINT('Ctrl Pts',(7.30797287830809,-5.86938628342057,4.24089821563888));
#79225=CARTESIAN_POINT('Ctrl Pts',(7.44967766344872,-5.68365091936629,4.24486590774502));
#79226=CARTESIAN_POINT('Ctrl Pts',(7.5913670642109,-5.49793571993192,4.24883316909311));
#79227=CARTESIAN_POINT('Ctrl Pts',(7.72611697770568,-5.3069083039586,4.25280043044121));
#79228=CARTESIAN_POINT('Ctrl Pts',(7.85354293705376,-5.11111029017698,4.2567676917893));
#79229=CARTESIAN_POINT('Ctrl Pts',(7.9809788630519,-4.9152969620097,4.26073526343762));
#79230=CARTESIAN_POINT('Ctrl Pts',(8.10108953265346,-4.71471252726251,4.26470283508595));
#79231=CARTESIAN_POINT('Ctrl Pts',(8.21353402334295,-4.50992726215045,4.26867040673428));
#79232=CARTESIAN_POINT('Ctrl Pts',(8.32597733634152,-4.30514414186331,4.27263793682812));
#79233=CARTESIAN_POINT('Ctrl Pts',(8.43075449607761,-4.09616052962373,4.27660546692196));
#79234=CARTESIAN_POINT('Ctrl Pts',(8.52757040875384,-3.8835715502931,4.28057299701581));
#79235=CARTESIAN_POINT('Ctrl Pts',(8.62440715027032,-3.67093683486632,4.28454138067853));
#79236=CARTESIAN_POINT('Ctrl Pts',(8.71327910398296,-3.45469546121587,4.28850976434126));
#79237=CARTESIAN_POINT('Ctrl Pts',(8.7939387006584,-3.2354639839693,4.29247814800399));
#79238=CARTESIAN_POINT('Ctrl Pts',(8.84350826760687,-3.10073470392698,4.29491692860486));
#79239=CARTESIAN_POINT('Ctrl Pts',(8.88997717625413,-2.96487653354668,4.29735570920574));
#79240=CARTESIAN_POINT('Ctrl Pts',(8.93329716455643,-2.82803586119909,4.29979448980662));
#79241=CARTESIAN_POINT('Ctrl Pts',(9.00378208945738,-2.60538565071178,4.3037625718454));
#79242=CARTESIAN_POINT('Ctrl Pts',(9.06594996777659,-2.38006435863928,4.30773065388419));
#79243=CARTESIAN_POINT('Ctrl Pts',(9.11961752138882,-2.15271022807948,4.31169873592298));
#79244=CARTESIAN_POINT('Ctrl Pts',(9.17327565227445,-1.92539601541551,4.31566612126236));
#79245=CARTESIAN_POINT('Ctrl Pts',(9.21843637224543,-1.69604995349702,4.31963350660175));
#79246=CARTESIAN_POINT('Ctrl Pts',(9.25496700757332,-1.46532274643825,4.32360089194114));
#79247=CARTESIAN_POINT('Ctrl Pts',(9.29149364991311,-1.23462075906115,4.32756784362472));
#79248=CARTESIAN_POINT('Ctrl Pts',(9.31939204656531,-1.00253820888336,4.33153479530829));
#79249=CARTESIAN_POINT('Ctrl Pts',(9.33858095781304,-0.769734211836592,
4.33550174699186));
#79250=CARTESIAN_POINT('Ctrl Pts',(9.35777135971476,-0.536912129855148,
4.33946900684052));
#79251=CARTESIAN_POINT('Ctrl Pts',(9.36825089799271,-0.303368772356388,
4.34343626668917));
#79252=CARTESIAN_POINT('Ctrl Pts',(9.36999026231452,-0.069767805119505,
4.34740352653782));
#79253=CARTESIAN_POINT('Ctrl Pts',(9.37172960811471,0.163830674618765,4.35137074414113));
#79254=CARTESIAN_POINT('Ctrl Pts',(9.36472896622191,0.397486478320609,4.35533796174443));
#79255=CARTESIAN_POINT('Ctrl Pts',(9.34901115800388,0.630535827704491,4.35930517934774));
#79256=CARTESIAN_POINT('Ctrl Pts',(9.33328996401887,0.863635378158366,4.36327325152785));
#79257=CARTESIAN_POINT('Ctrl Pts',(9.30884787032399,1.09612792925555,4.36724132370797));
#79258=CARTESIAN_POINT('Ctrl Pts',(9.27575969940313,1.3273534048733,4.37120939588808));
#79259=CARTESIAN_POINT('Ctrl Pts',(9.25540821168189,1.46957288382631,4.37365003161992));
#79260=CARTESIAN_POINT('Ctrl Pts',(9.23178685324645,1.6113131150379,4.37609066735175));
#79261=CARTESIAN_POINT('Ctrl Pts',(9.2049227175773,1.75242198854309,4.37853130308359));
#79262=CARTESIAN_POINT('Ctrl Pts',(9.16124396846532,1.98185274928728,4.38249956460213));
#79263=CARTESIAN_POINT('Ctrl Pts',(9.10897640766371,2.20968525647264,4.38646782612066));
#79264=CARTESIAN_POINT('Ctrl Pts',(9.04826179870715,2.43527072099938,4.3904360876392));
#79265=CARTESIAN_POINT('Ctrl Pts',(8.98755781666017,2.66081670118501,4.39440365459086));
#79266=CARTESIAN_POINT('Ctrl Pts',(8.91840981162146,2.8841161492307,4.39837122154252));
#79267=CARTESIAN_POINT('Ctrl Pts',(8.84100999989763,3.10453333759039,4.40233878849418));
#79268=CARTESIAN_POINT('Ctrl Pts',(8.76361861725768,3.32492652182233,4.40630592336528));
#79269=CARTESIAN_POINT('Ctrl Pts',(8.67797731640622,3.54243780477886,4.41027305823637));
#79270=CARTESIAN_POINT('Ctrl Pts',(8.58432757403525,3.75644847750612,4.41424019310746));
#79271=CARTESIAN_POINT('Ctrl Pts',(8.49067053215933,3.97047583123993,4.41820763719586));
#79272=CARTESIAN_POINT('Ctrl Pts',(8.38900391283925,4.18100176773534,4.42217508128425));
#79273=CARTESIAN_POINT('Ctrl Pts',(8.2796170556023,4.3874282301913,4.42614252537265));
#79274=CARTESIAN_POINT('Ctrl Pts',(8.17023135513512,4.59385250968034,4.43010992750518));
#79275=CARTESIAN_POINT('Ctrl Pts',(8.05312571522298,4.79617715151202,4.43407732963772));
#79276=CARTESIAN_POINT('Ctrl Pts',(7.92863540959037,4.99382875199879,4.43804473177026));
#79277=CARTESIAN_POINT('Ctrl Pts',(7.80411831327078,5.19152288770252,4.44201298769963));
#79278=CARTESIAN_POINT('Ctrl Pts',(7.67221352701147,5.38454173157018,4.445981243629));
#79279=CARTESIAN_POINT('Ctrl Pts',(7.53330033274568,5.57233982803937,4.44994949955837));
#79280=CARTESIAN_POINT('Ctrl Pts',(7.44790157019147,5.68779124453922,4.45238903849243));
#79281=CARTESIAN_POINT('Ctrl Pts',(7.35985494056502,5.80127013253363,4.4548285774265));
#79282=CARTESIAN_POINT('Ctrl Pts',(7.26925637269257,5.9126556512762,4.45726811636056));
#79283=CARTESIAN_POINT('Ctrl Pts',(7.1218891046023,6.09383489050017,4.4612362606321));
#79284=CARTESIAN_POINT('Ctrl Pts',(6.96772199556515,6.26953005321884,4.46520440490365));
#79285=CARTESIAN_POINT('Ctrl Pts',(6.80718780779681,6.43923747130687,4.46917254917519));
#79286=CARTESIAN_POINT('Ctrl Pts',(6.64668232113569,6.60891454825156,4.47313998400199));
#79287=CARTESIAN_POINT('Ctrl Pts',(6.47981222351787,6.77260581099257,4.4771074188288));
#79288=CARTESIAN_POINT('Ctrl Pts',(6.30704847372739,6.92984304386131,4.48107485365561));
#79289=CARTESIAN_POINT('Ctrl Pts',(6.13429054707556,7.08707497692492,4.48504215475689));
#79290=CARTESIAN_POINT('Ctrl Pts',(5.95563957335986,7.23785312094247,4.48900945585817));
#79291=CARTESIAN_POINT('Ctrl Pts',(5.77160190009354,7.38174752814919,4.49297675695945));
#79292=CARTESIAN_POINT('Ctrl Pts',(5.58757698307014,7.52563196157184,4.49694378307434));
#79293=CARTESIAN_POINT('Ctrl Pts',(5.39816633708207,7.66263343692668,4.50091080918922));
#79294=CARTESIAN_POINT('Ctrl Pts',(5.2039083970397,7.79236308559347,4.50487783530411));
#79295=CARTESIAN_POINT('Ctrl Pts',(5.00962904136831,7.92210703607993,4.5088452987569));
#79296=CARTESIAN_POINT('Ctrl Pts',(4.8105015600904,8.04457739943509,4.51281276220968));
#79297=CARTESIAN_POINT('Ctrl Pts',(4.60709330808357,8.15942867565564,4.51678022566247));
#79298=CARTESIAN_POINT('Ctrl Pts',(4.50280292518609,8.2183146031199,4.51881440214518));
#79299=CARTESIAN_POINT('Ctrl Pts',(4.39738767139772,8.27519837060822,4.5208485786279));
#79300=CARTESIAN_POINT('Ctrl Pts',(4.2909266281567,8.33003803918541,4.52288275511062));
#79301=CARTESIAN_POINT('',(5.44031476324452,-7.62919132931687,4.));
#79302=CARTESIAN_POINT('Origin',(0.,0.,4.));
#79303=CARTESIAN_POINT('Ctrl Pts',(5.4403147632445,-7.62919132931689,4.));
#79304=CARTESIAN_POINT('Ctrl Pts',(5.63163361488636,-7.49276340030762,4.00399116231736));
#79305=CARTESIAN_POINT('Ctrl Pts',(5.81783001121082,-7.34912682304943,4.00798232463471));
#79306=CARTESIAN_POINT('Ctrl Pts',(5.99837034461235,-7.19869003856779,4.01197348695207));
#79307=CARTESIAN_POINT('Ctrl Pts',(6.17889790555384,-7.04826389684825,4.01596436691168));
#79308=CARTESIAN_POINT('Ctrl Pts',(6.35376998977345,-6.89103868632153,4.01995524687129));
#79309=CARTESIAN_POINT('Ctrl Pts',(6.52248626448773,-6.72746296846508,4.0239461268309));
#79310=CARTESIAN_POINT('Ctrl Pts',(6.69119837955165,-6.56389128352005,4.02793690839654));
#79311=CARTESIAN_POINT('Ctrl Pts',(6.85375478956946,-6.39396959740036,4.03192768996218));
#79312=CARTESIAN_POINT('Ctrl Pts',(7.00969145999219,-6.21818387459012,4.03591847152781));
#79313=CARTESIAN_POINT('Ctrl Pts',(7.16565269850069,-6.04237045644239,4.03990988184782));
#79314=CARTESIAN_POINT('Ctrl Pts',(7.31499192758445,-5.86069136148633,4.04390129216783));
#79315=CARTESIAN_POINT('Ctrl Pts',(7.45728404103732,-5.67366722621182,4.04789270248784));
#79316=CARTESIAN_POINT('Ctrl Pts',(7.59957951299597,-5.48663867662633,4.05188420701669));
#79317=CARTESIAN_POINT('Ctrl Pts',(7.73482737157571,-5.29426505732967,4.05587571154554));
#79318=CARTESIAN_POINT('Ctrl Pts',(7.86264424336983,-5.0970982494654,4.05986721607439));
#79319=CARTESIAN_POINT('Ctrl Pts',(7.99048979912466,-4.89988719450848,4.06385961635477));
#79320=CARTESIAN_POINT('Ctrl Pts',(8.11090088481625,-4.69788103431545,4.06785201663515));
#79321=CARTESIAN_POINT('Ctrl Pts',(8.22353799921463,-4.4916598087982,4.07184441691554));
#79322=CARTESIAN_POINT('Ctrl Pts',(8.28835611888543,-4.372987804942,4.07414188236935));
#79323=CARTESIAN_POINT('Ctrl Pts',(8.35060068502593,-4.25292046048218,4.07643934782316));
#79324=CARTESIAN_POINT('Ctrl Pts',(8.41021389672587,-4.13157201000043,4.07873681327698));
#79325=CARTESIAN_POINT('Ctrl Pts',(8.51286305170545,-3.92261974011218,4.0826928639695));
#79326=CARTESIAN_POINT('Ctrl Pts',(8.60774154426674,-3.7097985754997,4.08664891466201));
#79327=CARTESIAN_POINT('Ctrl Pts',(8.69457254615899,-3.49370767267074,4.09060496535453));
#79328=CARTESIAN_POINT('Ctrl Pts',(8.78138469611393,-3.27766368548326,4.09456015714622));
#79329=CARTESIAN_POINT('Ctrl Pts',(8.860152735148,-3.05835164405682,4.09851534893791));
#79330=CARTESIAN_POINT('Ctrl Pts',(8.9306479334078,-2.83639076151701,4.1024705407296));
#79331=CARTESIAN_POINT('Ctrl Pts',(9.00113315883176,-2.61446127940588,4.10642517298702));
#79332=CARTESIAN_POINT('Ctrl Pts',(9.06334779259856,-2.38988397867899,4.11037980524445));
#79333=CARTESIAN_POINT('Ctrl Pts',(9.11711265558626,-2.16329422128587,4.11433443750188));
#79334=CARTESIAN_POINT('Ctrl Pts',(9.17088030342069,-1.93669272727321,4.11828927459653));
#79335=CARTESIAN_POINT('Ctrl Pts',(9.21619723620421,-1.70807884785548,4.12224411169117));
#79336=CARTESIAN_POINT('Ctrl Pts',(9.25293491462444,-1.47810031060957,4.12619894878581));
#79337=CARTESIAN_POINT('Ctrl Pts',(9.28967183907163,-1.24812649324858,4.13015370471472));
#79338=CARTESIAN_POINT('Ctrl Pts',(9.31782981766358,-1.01678835886159,4.13410846064363));
#79339=CARTESIAN_POINT('Ctrl Pts',(9.33733182685642,-0.784741624787566,
4.13806321657254));
#79340=CARTESIAN_POINT('Ctrl Pts',(9.35683815486933,-0.552643502772676,
4.14201884830246));
#79341=CARTESIAN_POINT('Ctrl Pts',(9.367684658499,-0.319836754653946,4.14597448003238));
#79342=CARTESIAN_POINT('Ctrl Pts',(9.36984628052905,-0.0869812724440373,
4.1499301117623));
#79343=CARTESIAN_POINT('Ctrl Pts',(9.371220374384,0.0610396501543117,4.15244461669285));
#79344=CARTESIAN_POINT('Ctrl Pts',(9.36908608027918,0.209080203978885,4.1549591216234));
#79345=CARTESIAN_POINT('Ctrl Pts',(9.36344791379007,0.356970906714329,4.15747362655395));
#79346=CARTESIAN_POINT('Ctrl Pts',(9.35453505750838,0.59075764951879,4.16144857498955));
#79347=CARTESIAN_POINT('Ctrl Pts',(9.3368608834607,0.824241622865925,4.16542352342516));
#79348=CARTESIAN_POINT('Ctrl Pts',(9.31046978563811,1.05675798233078,4.16939847186076));
#79349=CARTESIAN_POINT('Ctrl Pts',(9.28408274894252,1.28923856160682,4.17337280862153));
#79350=CARTESIAN_POINT('Ctrl Pts',(9.24898149814363,1.5207515437012,4.1773471453823));
#79351=CARTESIAN_POINT('Ctrl Pts',(9.20526225747678,1.75063755060077,4.18132148214307));
#79352=CARTESIAN_POINT('Ctrl Pts',(9.16154709179196,1.98050213029045,4.18529544846395));
#79353=CARTESIAN_POINT('Ctrl Pts',(9.10921559300724,2.20873976020429,4.18926941478483));
#79354=CARTESIAN_POINT('Ctrl Pts',(9.04841522339024,2.43470059917432,4.1932433811057));
#79355=CARTESIAN_POINT('Ctrl Pts',(8.98760946972035,2.66068144764617,4.19721769933307));
#79356=CARTESIAN_POINT('Ctrl Pts',(8.91833341744046,2.8843848288063,4.20119201756044));
#79357=CARTESIAN_POINT('Ctrl Pts',(8.84078492762598,3.10517421829458,4.20516633578781));
#79358=CARTESIAN_POINT('Ctrl Pts',(8.76323701558619,3.32596196279246,4.20914062440454));
#79359=CARTESIAN_POINT('Ctrl Pts',(8.67741688511913,3.5438354933019,4.21311491302127));
#79360=CARTESIAN_POINT('Ctrl Pts',(8.58357148754597,3.75817583152888,4.217089201638));
#79361=CARTESIAN_POINT('Ctrl Pts',(8.48970657263908,3.97256074681582,4.22106431680051));
#79362=CARTESIAN_POINT('Ctrl Pts',(8.38781316853626,4.18341074254101,4.22503943196302));
#79363=CARTESIAN_POINT('Ctrl Pts',(8.27818590624073,4.39012792116783,4.22901454712552));
#79364=CARTESIAN_POINT('Ctrl Pts',(8.21203553618309,4.51486348034444,4.23141317802732));
#79365=CARTESIAN_POINT('Ctrl Pts',(8.14307013498791,4.63809468964582,4.23381180892912));
#79366=CARTESIAN_POINT('Ctrl Pts',(8.07136251134545,4.75969455668611,4.23621043983092));
#79367=CARTESIAN_POINT('Ctrl Pts',(7.95282183904832,4.96071265292186,4.24017564332322));
#79368=CARTESIAN_POINT('Ctrl Pts',(7.82674836240878,5.15733320729825,4.24414084681553));
#79369=CARTESIAN_POINT('Ctrl Pts',(7.69349381338828,5.34899411159297,4.24810605030783));
#79370=CARTESIAN_POINT('Ctrl Pts',(7.56026374539025,5.54061980467023,4.25207052532793));
#79371=CARTESIAN_POINT('Ctrl Pts',(7.41985540119335,5.72728743222036,4.25603500034802));
#79372=CARTESIAN_POINT('Ctrl Pts',(7.27266360645564,5.90846419383546,4.25999947536812));
#79373=CARTESIAN_POINT('Ctrl Pts',(7.1254887635541,6.08962008962181,4.26396349380616));
#79374=CARTESIAN_POINT('Ctrl Pts',(6.97153220975379,6.26528616061904,4.26792751224421));
#79375=CARTESIAN_POINT('Ctrl Pts',(6.81122940235113,6.43496224472588,4.27189153068225));
#79376=CARTESIAN_POINT('Ctrl Pts',(6.6509146792536,6.60465094126588,4.27585584377537));
#79377=CARTESIAN_POINT('Ctrl Pts',(6.48425295375723,6.76834855171432,4.27982015686848));
#79378=CARTESIAN_POINT('Ctrl Pts',(6.3117177675682,6.92559050804074,4.28378446996159));
#79379=CARTESIAN_POINT('Ctrl Pts',(6.13918454255197,7.08283067702943,4.28774873799315));
#79380=CARTESIAN_POINT('Ctrl Pts',(5.96077820279671,7.23361514805867,4.29171300602471));
#79381=CARTESIAN_POINT('Ctrl Pts',(5.77700720297046,7.37751806770593,4.29567727405627));
#79382=CARTESIAN_POINT('Ctrl Pts',(5.5931958823245,7.52145256079887,4.29964241187978));
#79383=CARTESIAN_POINT('Ctrl Pts',(5.40401777414671,7.65850230917455,4.30360754970329));
#79384=CARTESIAN_POINT('Ctrl Pts',(5.21001331738214,7.78828262810235,4.30757268752681));
#79385=CARTESIAN_POINT('Ctrl Pts',(5.08974018917379,7.86873998046237,4.31003087605384));
#79386=CARTESIAN_POINT('Ctrl Pts',(4.96761272167605,7.9464042405453,4.31248906458086));
#79387=CARTESIAN_POINT('Ctrl Pts',(4.84376519430004,8.0211921685612,4.31494725310789));
#79388=CARTESIAN_POINT('Ctrl Pts',(4.66305789252323,8.13031606439967,4.31853402327109));
#79389=CARTESIAN_POINT('Ctrl Pts',(4.47863653723643,8.23334587002001,4.32212079343428));
#79390=CARTESIAN_POINT('Ctrl Pts',(4.29092662815669,8.33003803918541,4.32570756359748));
#79391=CARTESIAN_POINT('Origin',(0.,0.,2.15141010809499));
#79392=CARTESIAN_POINT('',(4.29092662824368,8.3300380391406,5.52332385470008));
#79393=CARTESIAN_POINT('',(4.29107337327626,8.33032226950541,5.32570196571484));
#79394=CARTESIAN_POINT('',(4.29092662815669,8.33003803918541,2.15141010809499));
#79395=CARTESIAN_POINT('',(-9.37024999988096,-4.72315641780741E-5,4.84858989189159));
#79396=CARTESIAN_POINT('Ctrl Pts',(4.29092662824368,8.3300380391406,5.52332385470008));
#79397=CARTESIAN_POINT('Ctrl Pts',(4.30909507620923,8.32067920106532,5.52297898293736));
#79398=CARTESIAN_POINT('Ctrl Pts',(4.32723302628988,8.31126086070106,5.52263369329497));
#79399=CARTESIAN_POINT('Ctrl Pts',(4.41533040593975,8.26514870907859,5.52095168178576));
#79400=CARTESIAN_POINT('Ctrl Pts',(4.48485443823517,8.22763066811243,5.5196091375804));
#79401=CARTESIAN_POINT('Ctrl Pts',(4.64323615607706,8.1395572955024,5.51651478898844));
#79402=CARTESIAN_POINT('Ctrl Pts',(4.73175753796161,8.08841798492619,5.51475888294013));
#79403=CARTESIAN_POINT('Ctrl Pts',(4.87244379785407,8.00404264613812,5.51192560151866));
#79404=CARTESIAN_POINT('Ctrl Pts',(4.92514727114748,7.9717207419738,5.51085441560341));
#79405=CARTESIAN_POINT('Ctrl Pts',(5.12344530755721,7.84739163462611,5.5067876207667));
#79406=CARTESIAN_POINT('Ctrl Pts',(5.26681327141406,7.75189815671566,5.50377156838725));
#79407=CARTESIAN_POINT('Ctrl Pts',(5.65818993135744,7.47534090837869,5.49535394952008));
#79408=CARTESIAN_POINT('Ctrl Pts',(5.90005409796334,7.28595889095345,5.48993302101319));
#79409=CARTESIAN_POINT('Ctrl Pts',(6.17316694856976,7.04957676464134,5.48369654948811));
#79410=CARTESIAN_POINT('Ctrl Pts',(6.21384049665758,7.01375142378264,5.48276480463732));
#79411=CARTESIAN_POINT('Ctrl Pts',(6.2858505287979,6.94920676426068,5.48111158818323));
#79412=CARTESIAN_POINT('Ctrl Pts',(6.31730671024373,6.92062334409074,5.48038824199516));
#79413=CARTESIAN_POINT('Ctrl Pts',(6.38816371649126,6.85535175472566,5.47875664165225));
#79414=CARTESIAN_POINT('Ctrl Pts',(6.42744493442588,6.81853613192231,5.47785027718395));
#79415=CARTESIAN_POINT('Ctrl Pts',(6.57501729705512,6.67781811277222,5.47443355503534));
#79416=CARTESIAN_POINT('Ctrl Pts',(6.68112443144793,6.57165761287772,5.47195241033107));
#79417=CARTESIAN_POINT('Ctrl Pts',(7.07939359856972,6.153567907938,5.46245236199959));
#79418=CARTESIAN_POINT('Ctrl Pts',(7.35263722660913,5.82434015209542,5.45550655010311));
#79419=CARTESIAN_POINT('Ctrl Pts',(7.65760418600059,5.40107242808615,5.44677835320756));
#79420=CARTESIAN_POINT('Ctrl Pts',(7.71159425174281,5.32370165250565,5.44519179283013));
#79421=CARTESIAN_POINT('Ctrl Pts',(7.80861322335863,5.1800946378015,5.44226050116453));
#79422=CARTESIAN_POINT('Ctrl Pts',(7.85199075973317,5.11410422302103,5.44091862361481));
#79423=CARTESIAN_POINT('Ctrl Pts',(7.94928526458551,4.96193322788634,5.43783496256));
#79424=CARTESIAN_POINT('Ctrl Pts',(8.00264433563143,4.87540779251708,5.43608918833203));
#79425=CARTESIAN_POINT('Ctrl Pts',(8.11407277047682,4.68795919410896,5.43232353170647));
#79426=CARTESIAN_POINT('Ctrl Pts',(8.17169029613192,4.58678710487238,5.43030097009842));
#79427=CARTESIAN_POINT('Ctrl Pts',(8.34969542963781,4.26021812142622,5.42380980846068));
#79428=CARTESIAN_POINT('Ctrl Pts',(8.46275541558365,4.03096049876388,5.41930591136478));
#79429=CARTESIAN_POINT('Ctrl Pts',(8.6391151273044,3.63311915163546,5.4116660329636));
#79430=CARTESIAN_POINT('Ctrl Pts',(8.70718734253554,3.46680744204485,5.40852335375439));
#79431=CARTESIAN_POINT('Ctrl Pts',(8.78992777798511,3.24681696834646,5.40447128498013));
#79432=CARTESIAN_POINT('Ctrl Pts',(8.80895975538209,3.19482062330553,5.40352115035421));
#79433=CARTESIAN_POINT('Ctrl Pts',(8.84168901153034,3.10288620665194,5.40185641789314));
#79434=CARTESIAN_POINT('Ctrl Pts',(8.85557923190739,3.06301874961054,5.40113965774569));
#79435=CARTESIAN_POINT('Ctrl Pts',(8.88907683694042,2.96474180971866,5.39938497313259));
#79436=CARTESIAN_POINT('Ctrl Pts',(8.90837843762463,2.90623031578625,5.39835056772016));
#79437=CARTESIAN_POINT('Ctrl Pts',(8.99669241159858,2.62936331626399,5.39349579251123));
#79438=CARTESIAN_POINT('Ctrl Pts',(9.05826232367745,2.40871545968441,5.38974134843689));
#79439=CARTESIAN_POINT('Ctrl Pts',(9.18390717722119,1.88501051595979,5.38091335775758));
#79440=CARTESIAN_POINT('Ctrl Pts',(9.24116543460513,1.5805937405746,5.37584209895201));
#79441=CARTESIAN_POINT('Ctrl Pts',(9.29694865280996,1.17408758278307,5.36899291985751));
#79442=CARTESIAN_POINT('Ctrl Pts',(9.30903521166844,1.07405738584783,5.36730211041737));
#79443=CARTESIAN_POINT('Ctrl Pts',(9.32771828769406,0.895265271872616,5.36426686005305));
#79444=CARTESIAN_POINT('Ctrl Pts',(9.33493592288354,0.816578008257973,5.36292653471785));
#79445=CARTESIAN_POINT('Ctrl Pts',(9.34853632443067,0.644387788687521,5.35998263484578));
#79446=CARTESIAN_POINT('Ctrl Pts',(9.35451328451033,0.550861312777691,5.35837661627558));
#79447=CARTESIAN_POINT('Ctrl Pts',(9.3702005036311,0.229779900858516,5.35283875658311));
#79448=CARTESIAN_POINT('Ctrl Pts',(9.37301721710175,0.00196992043196061,
5.34886587277333));
#79449=CARTESIAN_POINT('Ctrl Pts',(9.3595110523351,-0.55855710398833,5.33902828124393));
#79450=CARTESIAN_POINT('Ctrl Pts',(9.33375725204855,-0.890734980494798,
5.33313941316707));
#79451=CARTESIAN_POINT('Ctrl Pts',(9.28229772351839,-1.2823343645511,5.32631522602013));
#79452=CARTESIAN_POINT('Ctrl Pts',(9.27360581838168,-1.3437513167376,5.32524874161302));
#79453=CARTESIAN_POINT('Ctrl Pts',(9.25797073376504,-1.44684042484873,5.3234674583097));
#79454=CARTESIAN_POINT('Ctrl Pts',(9.25135441618257,-1.48855997641121,5.32274913503323));
#79455=CARTESIAN_POINT('Ctrl Pts',(9.2353013604433,-1.58553979211666,5.32108547221462));
#79456=CARTESIAN_POINT('Ctrl Pts',(9.22565038432783,-1.64076282757804,5.32014249847219));
#79457=CARTESIAN_POINT('Ctrl Pts',(9.18256055017881,-1.8749131269906,5.31615694757912));
#79458=CARTESIAN_POINT('Ctrl Pts',(9.14440727346621,-2.05293290461334,5.31315778020996));
#79459=CARTESIAN_POINT('Ctrl Pts',(9.00832253669811,-2.60839058020552,5.30376874740674));
#79460=CARTESIAN_POINT('Ctrl Pts',(8.89201073994553,-2.98089268469196,5.29741166381981));
#79461=CARTESIAN_POINT('Ctrl Pts',(8.7191428358556,-3.43322601229582,5.28931012887362));
#79462=CARTESIAN_POINT('Ctrl Pts',(8.68412033788075,-3.52087298069941,5.2877229279646));
#79463=CARTESIAN_POINT('Ctrl Pts',(8.61737472662243,-3.68085225698182,5.28479104534174));
#79464=CARTESIAN_POINT('Ctrl Pts',(8.58604966783635,-3.75334138927913,5.28344922535036));
#79465=CARTESIAN_POINT('Ctrl Pts',(8.51233498054549,-3.91817051417761,5.28036652751484));
#79466=CARTESIAN_POINT('Ctrl Pts',(8.46935224894049,-4.01023433390722,5.2786216689724));
#79467=CARTESIAN_POINT('Ctrl Pts',(8.3739607644635,-4.20617388656357,5.27485849874081));
#79468=CARTESIAN_POINT('Ctrl Pts',(8.32109727711225,-4.3098094696729,5.27283751600699));
#79469=CARTESIAN_POINT('Ctrl Pts',(8.14622343496993,-4.6374206915481,5.26635639966138));
#79470=CARTESIAN_POINT('Ctrl Pts',(8.01699369787421,-4.85741068153063,5.26186109976634));
#79471=CARTESIAN_POINT('Ctrl Pts',(7.7815146890906,-5.22321928561321,5.25422330514409));
#79472=CARTESIAN_POINT('Ctrl Pts',(7.67973553178773,-5.37174580836739,5.25107432771301));
#79473=CARTESIAN_POINT('Ctrl Pts',(7.5410520259919,-5.56212204368915,5.24701342822879));
#79474=CARTESIAN_POINT('Ctrl Pts',(7.50796466713723,-5.60670436742131,5.24606068472085));
#79475=CARTESIAN_POINT('Ctrl Pts',(7.44902844620289,-5.68465845638359,5.24439350454844));
#79476=CARTESIAN_POINT('Ctrl Pts',(7.42334678089738,-5.71815434680769,5.24367687489309));
#79477=CARTESIAN_POINT('Ctrl Pts',(7.35974181281689,-5.79996185612797,5.24192556279333));
#79478=CARTESIAN_POINT('Ctrl Pts',(7.32156822988528,-5.8480762446981,5.24089435937829));
#79479=CARTESIAN_POINT('Ctrl Pts',(7.13622975671459,-6.077019449251,5.23597328820953));
#79480=CARTESIAN_POINT('Ctrl Pts',(6.9828227890841,-6.25268959347655,5.23215205934308));
#79481=CARTESIAN_POINT('Ctrl Pts',(6.6146762197271,-6.64379744760478,5.22334805705528));
#79482=CARTESIAN_POINT('Ctrl Pts',(6.3956817480936,-6.8548698365087,5.21836708433383));
#79483=CARTESIAN_POINT('Ctrl Pts',(6.09042649808538,-7.12169814943474,5.21160070412585));
#79484=CARTESIAN_POINT('Ctrl Pts',(6.0129562276732,-7.18722733731433,5.20989828161544));
#79485=CARTESIAN_POINT('Ctrl Pts',(5.87325348178848,-7.30155662718354,5.20685067965745));
#79486=CARTESIAN_POINT('Ctrl Pts',(5.81143859198803,-7.35085145402365,5.20550975404875));
#79487=CARTESIAN_POINT('Ctrl Pts',(5.675410858047,-7.45653960185108,5.20257418559018));
#79488=CARTESIAN_POINT('Ctrl Pts',(5.60096544796234,-7.51261986511956,5.2009772018096));
#79489=CARTESIAN_POINT('Ctrl Pts',(5.34736987280335,-7.69779029270513,5.1955688007151));
#79490=CARTESIAN_POINT('Ctrl Pts',(5.16449760945591,-7.82165607741675,5.19171922486761));
#79491=CARTESIAN_POINT('Ctrl Pts',(4.77465652949561,-8.06607183300903,5.18364917760876));
#79492=CARTESIAN_POINT('Ctrl Pts',(4.56709572181718,-8.1853830936207,5.17942735316141));
#79493=CARTESIAN_POINT('Ctrl Pts',(4.24421777957966,-8.35487345114201,5.17305040822101));
#79494=CARTESIAN_POINT('Ctrl Pts',(4.13208193362544,-8.41089733506212,5.17086980193708));
#79495=CARTESIAN_POINT('Ctrl Pts',(3.97184818325022,-8.48697324727121,5.16781689051998));
#79496=CARTESIAN_POINT('Ctrl Pts',(3.92465535052403,-8.50889965192357,5.16692535859639));
#79497=CARTESIAN_POINT('Ctrl Pts',(3.83824324230581,-8.54817599114268,5.16530838173322));
#79498=CARTESIAN_POINT('Ctrl Pts',(3.79908294871078,-8.56565191386198,5.1645814989491));
#79499=CARTESIAN_POINT('Ctrl Pts',(3.69689646509036,-8.61041568987403,5.16269892566188));
#79500=CARTESIAN_POINT('Ctrl Pts',(3.63368772189618,-8.63728055575679,5.16154821345073));
#79501=CARTESIAN_POINT('Ctrl Pts',(3.48757958020344,-8.69749142219622,5.15891419232269));
#79502=CARTESIAN_POINT('Ctrl Pts',(3.404487059831,-8.73035144054452,5.15743513315476));
#79503=CARTESIAN_POINT('Ctrl Pts',(3.08448492985425,-8.85163708170513,5.15179204931195));
#79504=CARTESIAN_POINT('Ctrl Pts',(2.84450167840352,-8.93164804660555,5.14766751778081));
#79505=CARTESIAN_POINT('Ctrl Pts',(2.40543244206359,-9.05854103613891,5.14015352979828));
#79506=CARTESIAN_POINT('Ctrl Pts',(2.20748849201208,-9.10880152014438,5.13677812701546));
#79507=CARTESIAN_POINT('Ctrl Pts',(1.91621330759283,-9.1727070053693,5.13178848039399));
#79508=CARTESIAN_POINT('Ctrl Pts',(1.82406706618621,-9.19147466572156,5.13020694851042));
#79509=CARTESIAN_POINT('Ctrl Pts',(1.65402536571385,-9.22344970516967,5.12728027256988));
#79510=CARTESIAN_POINT('Ctrl Pts',(1.57621524195944,-9.237065002016,5.12593791945143));
#79511=CARTESIAN_POINT('Ctrl Pts',(1.39749140633512,-9.26601424108131,5.12284655789034));
#79512=CARTESIAN_POINT('Ctrl Pts',(1.29648070178976,-9.28068638980815,5.12109347874753));
#79513=CARTESIAN_POINT('Ctrl Pts',(1.13407825325526,-9.30157274539724,5.11826564271921));
#79514=CARTESIAN_POINT('Ctrl Pts',(1.07282970459229,-9.30883587961009,5.11719706510379));
#79515=CARTESIAN_POINT('Ctrl Pts',(0.840940592752878,-9.33401533690024,
5.11314435610554));
#79516=CARTESIAN_POINT('Ctrl Pts',(0.669891012023075,-9.34784837302521,
5.11013991607962));
#79517=CARTESIAN_POINT('Ctrl Pts',(0.189337248990873,-9.37345324890715,
5.1016873489309));
#79518=CARTESIAN_POINT('Ctrl Pts',(-0.120510981533038,-9.37459075531224,
5.09621887966962));
#79519=CARTESIAN_POINT('Ctrl Pts',(-0.483389314709819,-9.35792673690669,
5.08994832228886));
#79520=CARTESIAN_POINT('Ctrl Pts',(-0.536911076156703,-9.35500852782843,
5.08902709174467));
#79521=CARTESIAN_POINT('Ctrl Pts',(-0.632744057619878,-9.34895821832732,
5.08738577131017));
#79522=CARTESIAN_POINT('Ctrl Pts',(-0.675064556748423,-9.34599768205513,
5.0866639081461));
#79523=CARTESIAN_POINT('Ctrl Pts',(-0.771557788055997,-9.33858864907045,
5.08502515085003));
#79524=CARTESIAN_POINT('Ctrl Pts',(-0.825714729355456,-9.33395599843451,
5.08411025858169));
#79525=CARTESIAN_POINT('Ctrl Pts',(-1.03542689403885,-9.31417749798637,
5.08058151734085));
#79526=CARTESIAN_POINT('Ctrl Pts',(-1.1906343964783,-9.29561193914324,5.07799942852732));
#79527=CARTESIAN_POINT('Ctrl Pts',(-1.6677299979759,-9.22639732005442,5.07007179193347));
#79528=CARTESIAN_POINT('Ctrl Pts',(-1.98749561648295,-9.1628375654723,5.06476480547068));
#79529=CARTESIAN_POINT('Ctrl Pts',(-2.43560509423968,-9.0492012474576,5.05710358327929));
#79530=CARTESIAN_POINT('Ctrl Pts',(-2.56716098837107,-9.01276315605733,
5.05482762174399));
#79531=CARTESIAN_POINT('Ctrl Pts',(-2.77765854105335,-8.9494770304733,5.05113242463971));
#79532=CARTESIAN_POINT('Ctrl Pts',(-2.85711987703535,-8.9244267075862,5.04972512089733));
#79533=CARTESIAN_POINT('Ctrl Pts',(-3.01478295436201,-8.87240159829483,
5.04690646764129));
#79534=CARTESIAN_POINT('Ctrl Pts',(-3.09298270675076,-8.84544426924775,
5.04549534488736));
#79535=CARTESIAN_POINT('Ctrl Pts',(-3.29543773716293,-8.77264010189487,
5.04180709418841));
#79536=CARTESIAN_POINT('Ctrl Pts',(-3.41909588813482,-8.72518810101619,
5.03951958685846));
#79537=CARTESIAN_POINT('Ctrl Pts',(-3.70411089490155,-8.60882796228113,
5.03416912915469));
#79538=CARTESIAN_POINT('Ctrl Pts',(-3.86462120026677,-8.53797746290866,
5.03109618261708));
#79539=CARTESIAN_POINT('Ctrl Pts',(-4.29836974891504,-8.33177866316471,
5.02265890395396));
#79540=CARTESIAN_POINT('Ctrl Pts',(-4.56714084589703,-8.18753583542816,
5.01727751785577));
#79541=CARTESIAN_POINT('Ctrl Pts',(-4.87352912645226,-8.00331628677599,
5.01110860639607));
#79542=CARTESIAN_POINT('Ctrl Pts',(-4.91842681612778,-7.97580311960925,
5.01020391518273));
#79543=CARTESIAN_POINT('Ctrl Pts',(-4.99898258372196,-7.92549990805732,
5.00858103466217));
#79544=CARTESIAN_POINT('Ctrl Pts',(-5.03472264660238,-7.90284401676706,
5.00786123290643));
#79545=CARTESIAN_POINT('Ctrl Pts',(-5.11675589977332,-7.85006017285951,
5.00620988021578));
#79546=CARTESIAN_POINT('Ctrl Pts',(-5.16293852386699,-7.81976351771826,
5.00528051957097));
#79547=CARTESIAN_POINT('Ctrl Pts',(-5.34872575716939,-7.69552029511861,
5.00153775658285));
#79548=CARTESIAN_POINT('Ctrl Pts',(-5.48605626666353,-7.5982291888244,4.99876131523456));
#79549=CARTESIAN_POINT('Ctrl Pts',(-5.93190998958374,-7.26397430503297,
4.98960562722068));
#79550=CARTESIAN_POINT('Ctrl Pts',(-6.22829694162656,-7.01150455702873,
4.98327068926761));
#79551=CARTESIAN_POINT('Ctrl Pts',(-6.58021918381101,-6.67175686134455,
4.9751016317372));
#79552=CARTESIAN_POINT('Ctrl Pts',(-6.65118275884932,-6.60101446507654,
4.97341936824743));
#79553=CARTESIAN_POINT('Ctrl Pts',(-6.775979279902,-6.47255096499091,4.97039400392658));
#79554=CARTESIAN_POINT('Ctrl Pts',(-6.83024335164318,-6.41526203048747,
4.9690549279602));
#79555=CARTESIAN_POINT('Ctrl Pts',(-6.94106091539931,-6.29526705291492,
4.96626984407561));
#79556=CARTESIAN_POINT('Ctrl Pts',(-6.9975034646115,-6.23246814039217,4.96482303795468));
#79557=CARTESIAN_POINT('Ctrl Pts',(-7.07247150911673,-6.14675512301173,
4.96286256331029));
#79558=CARTESIAN_POINT('Ctrl Pts',(-7.09174896482245,-6.1245039315732,4.96235489540127));
#79559=CARTESIAN_POINT('Ctrl Pts',(-7.14436707674367,-6.06318742893959,
4.96095945445767));
#79560=CARTESIAN_POINT('Ctrl Pts',(-7.17749190410883,-6.0239383034768,4.96007009994488));
#79561=CARTESIAN_POINT('Ctrl Pts',(-7.31276281609086,-5.86095793001278,
4.9563934710575));
#79562=CARTESIAN_POINT('Ctrl Pts',(-7.41204515851131,-5.73488572178633,
4.95358743790647));
#79563=CARTESIAN_POINT('Ctrl Pts',(-7.70580535318572,-5.34147954251365,
4.94497010133452));
#79564=CARTESIAN_POINT('Ctrl Pts',(-7.88941712361181,-5.06635346696581,
4.93912543085288));
#79565=CARTESIAN_POINT('Ctrl Pts',(-8.08791570527353,-4.73187238007334,
4.93241108558769));
#79566=CARTESIAN_POINT('Ctrl Pts',(-8.11725446204665,-4.68136483270345,
4.93140752800033));
#79567=CARTESIAN_POINT('Ctrl Pts',(-8.1595668887964,-4.60692888611154,4.92994536341637));
#79568=CARTESIAN_POINT('Ctrl Pts',(-8.17291157676088,-4.58321305838657,
4.92948199469067));
#79569=CARTESIAN_POINT('Ctrl Pts',(-8.20501409254679,-4.52557524869298,
4.92836212830084));
#79570=CARTESIAN_POINT('Ctrl Pts',(-8.22366509940608,-4.49159436396222,
4.9277070783752));
#79571=CARTESIAN_POINT('Ctrl Pts',(-8.26571891481978,-4.41383506998117,
4.92621882304978));
#79572=CARTESIAN_POINT('Ctrl Pts',(-8.28898578134038,-4.3699844316459,4.92538722935787));
#79573=CARTESIAN_POINT('Ctrl Pts',(-8.33188936037925,-4.28754928659676,
4.92383647634219));
#79574=CARTESIAN_POINT('Ctrl Pts',(-8.35160924465963,-4.24900955865545,
4.92311655950612));
#79575=CARTESIAN_POINT('Ctrl Pts',(-8.4890706996906,-3.97570626977537,4.91804294957473));
#79576=CARTESIAN_POINT('Ctrl Pts',(-8.59716371885337,-3.73621979453179,
4.91375796074802));
#79577=CARTESIAN_POINT('Ctrl Pts',(-8.7836339157327,-3.27197810478023,4.90554848595926));
#79578=CARTESIAN_POINT('Ctrl Pts',(-8.86379163783522,-3.04815728187916,
4.90163179999078));
#79579=CARTESIAN_POINT('Ctrl Pts',(-8.96469883642099,-2.7285999022936,4.89603082504856));
#79580=CARTESIAN_POINT('Ctrl Pts',(-8.99259261697984,-2.63521547886795,
4.89439336229877));
#79581=CARTESIAN_POINT('Ctrl Pts',(-9.04041372930677,-2.46550682924856,
4.89141331303917));
#79582=CARTESIAN_POINT('Ctrl Pts',(-9.06084372199404,-2.38933365902394,
4.89007420702657));
#79583=CARTESIAN_POINT('Ctrl Pts',(-9.09895901610244,-2.23969601352763,
4.88743978025226));
#79584=CARTESIAN_POINT('Ctrl Pts',(-9.11672210829258,-2.16625745950231,
4.88614507862456));
#79585=CARTESIAN_POINT('Ctrl Pts',(-9.1742065975365,-1.91535571926908,4.88171552388456));
#79586=CARTESIAN_POINT('Ctrl Pts',(-9.2096493356327,-1.73695509247306,4.87855461468278));
#79587=CARTESIAN_POINT('Ctrl Pts',(-9.28017682298766,-1.31858710597104,
4.87113282955306));
#79588=CARTESIAN_POINT('Ctrl Pts',(-9.31118319396439,-1.07806358201149,
4.86685789418943));
#79589=CARTESIAN_POINT('Ctrl Pts',(-9.34726139722848,-0.675591935739253,
4.85977058185828));
#79590=CARTESIAN_POINT('Ctrl Pts',(-9.35752588391314,-0.51422725676902,
4.8569473045786));
#79591=CARTESIAN_POINT('Ctrl Pts',(-9.36564690581209,-0.298613729662839,
4.85322873812419));
#79592=CARTESIAN_POINT('Ctrl Pts',(-9.36721494029457,-0.244533032443576,
4.85230060338259));
#79593=CARTESIAN_POINT('Ctrl Pts',(-9.36895425008626,-0.158971942375714,
4.85084096482924));
#79594=CARTESIAN_POINT('Ctrl Pts',(-9.36943540354766,-0.127499186728518,
4.85030597995095));
#79595=CARTESIAN_POINT('Ctrl Pts',(-9.37008580015194,-0.0640355894891263,
4.84923110042245));
#79596=CARTESIAN_POINT('Ctrl Pts',(-9.37024981349469,-0.0320452041784548,
4.84869121345059));
#79597=CARTESIAN_POINT('Ctrl Pts',(-9.37024999984103,-5.45819878978748E-5,
4.8481529963742));
#79598=CARTESIAN_POINT('Ctrl Pts',(4.2909266281567,8.33003803918541,4.52288275511062));
#79599=CARTESIAN_POINT('Ctrl Pts',(4.08324923132093,8.4370157586096,4.52685089654315));
#79600=CARTESIAN_POINT('Ctrl Pts',(3.87159094101272,8.5362119836809,4.53081903797568));
#79601=CARTESIAN_POINT('Ctrl Pts',(3.6565558870526,8.62735093220167,4.53478717940821));
#79602=CARTESIAN_POINT('Ctrl Pts',(3.63455910839878,8.63667389253038,4.53519309615132));
#79603=CARTESIAN_POINT('Ctrl Pts',(3.61252701312059,8.64591258237561,4.53559901289443));
#79604=CARTESIAN_POINT('Ctrl Pts',(3.59046025986583,8.65506673485677,4.53600492963755));
#79605=CARTESIAN_POINT('Ctrl Pts',(3.37473763072933,8.74455692029336,4.53997313583552));
#79606=CARTESIAN_POINT('Ctrl Pts',(3.15563410300656,8.82599184272615,4.54394134203349));
#79607=CARTESIAN_POINT('Ctrl Pts',(2.93376971124411,8.89913368502163,4.54790954823147));
#79608=CARTESIAN_POINT('Ctrl Pts',(2.71194418949467,8.97226271307352,4.55187705921096));
#79609=CARTESIAN_POINT('Ctrl Pts',(2.48735903927923,9.0371014721892,4.55584457019044));
#79610=CARTESIAN_POINT('Ctrl Pts',(2.26065108681041,9.09346148208717,4.55981208116993));
#79611=CARTESIAN_POINT('Ctrl Pts',(2.03396785131846,9.14981534729967,4.56377915958904));
#79612=CARTESIAN_POINT('Ctrl Pts',(1.80516255165042,9.19769224036156,4.56774623800816));
#79613=CARTESIAN_POINT('Ctrl Pts',(1.57488484377305,9.2369541945034,4.57171331642727));
#79614=CARTESIAN_POINT('Ctrl Pts',(1.34458920502211,9.27621920582842,4.57568070374811));
#79615=CARTESIAN_POINT('Ctrl Pts',(1.11282120893339,9.30686788712794,4.57964809106895));
#79616=CARTESIAN_POINT('Ctrl Pts',(0.880239536965458,9.32881361267674,4.58361547838978));
#79617=CARTESIAN_POINT('Ctrl Pts',(0.647660329530003,9.35075910567947,4.58758282367053));
#79618=CARTESIAN_POINT('Ctrl Pts',(0.4142677469141,9.36400180288017,4.59155016895128));
#79619=CARTESIAN_POINT('Ctrl Pts',(0.18072509314386,9.3685070050253,4.59551751423203));
#79620=CARTESIAN_POINT('Ctrl Pts',(-0.0528678350307668,9.37301317699907,
4.59948571355771));
#79621=CARTESIAN_POINT('Ctrl Pts',(-0.286610614390155,9.36877808960251,
4.60345391288339));
#79622=CARTESIAN_POINT('Ctrl Pts',(-0.519839129798677,9.35581916999416,
4.60742211220908));
#79623=CARTESIAN_POINT('Ctrl Pts',(-0.663241419070258,9.34785128178346,
4.60986198911089));
#79624=CARTESIAN_POINT('Ctrl Pts',(-0.806449300964467,9.33658637512197,
4.6123018660127));
#79625=CARTESIAN_POINT('Ctrl Pts',(-0.949309040297671,9.32203826469883,
4.61474174291451));
#79626=CARTESIAN_POINT('Ctrl Pts',(-1.1816554027776,9.29837729098048,4.61870994645234));
#79627=CARTESIAN_POINT('Ctrl Pts',(-1.4131527990255,9.26602167570447,4.62267814999016));
#79628=CARTESIAN_POINT('Ctrl Pts',(-1.64314262419167,9.22505649733727,4.62664635352799));
#79629=CARTESIAN_POINT('Ctrl Pts',(-1.87309215598527,9.18409849591884,4.63061386185113));
#79630=CARTESIAN_POINT('Ctrl Pts',(-2.1015343639731,9.13453399216639,4.63458137017427));
#79631=CARTESIAN_POINT('Ctrl Pts',(-2.32781928923107,9.07649945844673,4.63854887849741));
#79632=CARTESIAN_POINT('Ctrl Pts',(-2.55407954429396,9.01847125180903,4.64251595427205));
#79633=CARTESIAN_POINT('Ctrl Pts',(-2.77818271075123,8.95197492958084,4.6464830300467));
#79634=CARTESIAN_POINT('Ctrl Pts',(-2.99949152115984,8.87719751255937,4.65045010582134));
#79635=CARTESIAN_POINT('Ctrl Pts',(-3.22081756616842,8.80241427218696,4.65441749053517));
#79636=CARTESIAN_POINT('Ctrl Pts',(-3.43934854982918,8.71934873670342,4.658384875249));
#79637=CARTESIAN_POINT('Ctrl Pts',(-3.65446363721919,8.6282373974493,4.66235225996283));
#79638=CARTESIAN_POINT('Ctrl Pts',(-3.86957644654803,8.53712702306105,4.6663196026622));
#79639=CARTESIAN_POINT('Ctrl Pts',(-4.08127317085655,8.43797112833676,4.67028694536157));
#79640=CARTESIAN_POINT('Ctrl Pts',(-4.28895356073467,8.33105409995406,4.67425428806094));
#79641=CARTESIAN_POINT('Ctrl Pts',(-4.49667866070997,8.22411405413226,4.6782224848625));
#79642=CARTESIAN_POINT('Ctrl Pts',(-4.70038544530948,8.1094096658853,4.68219068166407));
#79643=CARTESIAN_POINT('Ctrl Pts',(-4.89949770003467,7.98727158357941,4.68615887846563));
#79644=CARTESIAN_POINT('Ctrl Pts',(-5.02192421672368,7.91217354407187,4.68859877104092));
#79645=CARTESIAN_POINT('Ctrl Pts',(-5.14261424304615,7.83426605531338,4.6910386636162));
#79646=CARTESIAN_POINT('Ctrl Pts',(-5.26143903274313,7.75363426834327,4.69347855619149));
#79647=CARTESIAN_POINT('Ctrl Pts',(-5.45469360010939,7.62249613507483,4.69744675495926));
#79648=CARTESIAN_POINT('Ctrl Pts',(-5.64307293369046,7.48410891559784,4.70141495372704));
#79649=CARTESIAN_POINT('Ctrl Pts',(-5.82603778824631,7.33886018073829,4.70538315249482));
#79650=CARTESIAN_POINT('Ctrl Pts',(-6.00897058460416,7.19363689564456,4.70935065597441));
#79651=CARTESIAN_POINT('Ctrl Pts',(-6.18649057295735,7.04155467179857,4.713318159454));
#79652=CARTESIAN_POINT('Ctrl Pts',(-6.35809051827845,6.88304220703881,4.71728566293359));
#79653=CARTESIAN_POINT('Ctrl Pts',(-6.52967175275135,6.72454702609963,4.72125273380607));
#79654=CARTESIAN_POINT('Ctrl Pts',(-6.69533402412701,6.5596231971171,4.72521980467856));
#79655=CARTESIAN_POINT('Ctrl Pts',(-6.85460526669439,6.38873788007503,4.72918687555104));
#79656=CARTESIAN_POINT('Ctrl Pts',(-7.01388891051791,6.21783925747601,4.73315425530956));
#79657=CARTESIAN_POINT('Ctrl Pts',(-7.16678033507799,6.04097842544005,4.73712163506808));
#79658=CARTESIAN_POINT('Ctrl Pts',(-7.31284542473205,5.85865828125139,4.7410890148266));
#79659=CARTESIAN_POINT('Ctrl Pts',(-7.45890896675378,5.67634006883543,4.74505635254875));
#79660=CARTESIAN_POINT('Ctrl Pts',(-7.5981461423945,5.48856288339455,4.74902369027091));
#79661=CARTESIAN_POINT('Ctrl Pts',(-7.73016369326455,5.29586200139643,4.75299102799306));
#79662=CARTESIAN_POINT('Ctrl Pts',(-7.86220966529799,5.10311963413203,4.75695921981645));
#79663=CARTESIAN_POINT('Ctrl Pts',(-7.98703274566321,4.90545168679088,4.76092741163984));
#79664=CARTESIAN_POINT('Ctrl Pts',(-8.10428279342827,4.70342273952092,4.76489560346324));
#79665=CARTESIAN_POINT('Ctrl Pts',(-8.17637632720368,4.579201206044,4.76733552546498));
#79666=CARTESIAN_POINT('Ctrl Pts',(-8.24560762261028,4.45333148453508,4.76977544746672));
#79667=CARTESIAN_POINT('Ctrl Pts',(-8.3119037953007,4.32594964836229,4.77221536946846));
#79668=CARTESIAN_POINT('Ctrl Pts',(-8.41958533930194,4.11904972880207,4.77617841224646));
#79669=CARTESIAN_POINT('Ctrl Pts',(-8.51955540201662,3.90809337079972,4.78014145502446));
#79670=CARTESIAN_POINT('Ctrl Pts',(-8.61152381266068,3.69367603973035,4.78410449780246));
#79671=CARTESIAN_POINT('Ctrl Pts',(-8.70347571661736,3.47929719274295,4.78806682928506));
#79672=CARTESIAN_POINT('Ctrl Pts',(-8.78742872247465,3.2614588753116,4.79202916076765));
#79673=CARTESIAN_POINT('Ctrl Pts',(-8.86314034588119,3.04077757682359,4.79599149225024));
#79674=CARTESIAN_POINT('Ctrl Pts',(-8.93884369382226,2.82012039934083,4.79995339064032));
#79675=CARTESIAN_POINT('Ctrl Pts',(-9.0063073650719,2.59662113164217,4.8039152890304));
#79676=CARTESIAN_POINT('Ctrl Pts',(-9.06533808393958,2.37091342869679,4.80787718742048));
#79677=CARTESIAN_POINT('Ctrl Pts',(-9.12437314964507,2.14518910534093,4.81183937755238));
#79678=CARTESIAN_POINT('Ctrl Pts',(-9.17497394725667,1.91725629782274,4.81580156768429));
#79679=CARTESIAN_POINT('Ctrl Pts',(-9.21699757135214,1.68776207807521,4.8197637578162));
#79680=CARTESIAN_POINT('Ctrl Pts',(-9.25902113879243,1.45826816772595,4.82372594260638));
#79681=CARTESIAN_POINT('Ctrl Pts',(-9.29246750688886,1.22721313113998,4.82768812739656));
#79682=CARTESIAN_POINT('Ctrl Pts',(-9.31724510133541,0.995253125662686,
4.83165031218674));
#79683=CARTESIAN_POINT('Ctrl Pts',(-9.34202778586263,0.763245468459468,
4.83561331093165));
#79684=CARTESIAN_POINT('Ctrl Pts',(-9.35813810845432,0.530332755368636,
4.83957630967657));
#79685=CARTESIAN_POINT('Ctrl Pts',(-9.36553635714658,0.297176387799428,
4.84353930842148));
#79686=CARTESIAN_POINT('Ctrl Pts',(-9.36867921898414,0.198128859080778,
4.84522283624485));
#79687=CARTESIAN_POINT('Ctrl Pts',(-9.37025049932568,0.0990373939094512,
4.84690636406822));
#79688=CARTESIAN_POINT('Ctrl Pts',(-9.37024999988096,-4.72315641784071E-5,
4.84858989189159));
#79689=CARTESIAN_POINT('',(-9.37024999716748,0.000230397442772534,4.65141010809498));
#79690=CARTESIAN_POINT('Ctrl Pts',(4.29092662815669,8.33003803918541,4.32570756359748));
#79691=CARTESIAN_POINT('Ctrl Pts',(4.08323685626887,8.43702213318318,4.32967610996065));
#79692=CARTESIAN_POINT('Ctrl Pts',(3.87152104582792,8.53624681226013,4.33364465632381));
#79693=CARTESIAN_POINT('Ctrl Pts',(3.65637888263525,8.62742595037008,4.33761320268698));
#79694=CARTESIAN_POINT('Ctrl Pts',(3.44126117347791,8.7185947246451,4.34158129796714));
#79695=CARTESIAN_POINT('Ctrl Pts',(3.22271815071608,8.80171967295272,4.3455493932473));
#79696=CARTESIAN_POINT('Ctrl Pts',(3.00137009412446,8.87656254529845,4.34951748852746));
#79697=CARTESIAN_POINT('Ctrl Pts',(2.78000532367065,8.95141106898567,4.35348588343617));
#79698=CARTESIAN_POINT('Ctrl Pts',(2.55583536440449,9.01797617310764,4.35745427834489));
#79699=CARTESIAN_POINT('Ctrl Pts',(2.32949747142113,9.07606889535016,4.3614226732536));
#79700=CARTESIAN_POINT('Ctrl Pts',(2.10316342368601,9.13416063065701,4.36539100074337));
#79701=CARTESIAN_POINT('Ctrl Pts',(1.87466179169094,9.18378020323483,4.36935932823313));
#79702=CARTESIAN_POINT('Ctrl Pts',(1.64464254583845,9.2247892094572,4.37332765572289));
#79703=CARTESIAN_POINT('Ctrl Pts',(1.41457270427431,9.26580723614152,4.37729685609767));
#79704=CARTESIAN_POINT('Ctrl Pts',(1.18298486156662,9.29821086110538,4.38126605647245));
#79705=CARTESIAN_POINT('Ctrl Pts',(0.950537996967608,9.32191303214211,4.38523525684723));
#79706=CARTESIAN_POINT('Ctrl Pts',(0.785609791352374,9.33873045209318,4.38805152669311));
#79707=CARTESIAN_POINT('Ctrl Pts',(0.620249312325084,9.35116833922283,4.39086779653899));
#79708=CARTESIAN_POINT('Ctrl Pts',(0.454693388915478,9.35921145100251,4.39368406638487));
#79709=CARTESIAN_POINT('Ctrl Pts',(0.221425913977992,9.37054415560678,4.3976521766292));
#79710=CARTESIAN_POINT('Ctrl Pts',(-0.0123016923509516,9.37315340084888,
4.40162028687353));
#79711=CARTESIAN_POINT('Ctrl Pts',(-0.245825537082703,9.36702486747089,
4.40558839711786));
#79712=CARTESIAN_POINT('Ctrl Pts',(-0.479308478010276,9.3608974075607,4.40955581231195));
#79713=CARTESIAN_POINT('Ctrl Pts',(-0.712587444304115,9.34603523157118,
4.41352322750604));
#79714=CARTESIAN_POINT('Ctrl Pts',(-0.944999409875851,9.32247612911046,
4.41749064270013));
#79715=CARTESIAN_POINT('Ctrl Pts',(-1.17738606289793,9.2989195925286,4.42145762579343));
#79716=CARTESIAN_POINT('Ctrl Pts',(-1.40890562077441,9.26666804936217,4.42542460888673));
#79717=CARTESIAN_POINT('Ctrl Pts',(-1.63890005106618,9.22581116678178,4.42939159198003));
#79718=CARTESIAN_POINT('Ctrl Pts',(-1.86891247163174,9.18495108835658,4.43335888537263));
#79719=CARTESIAN_POINT('Ctrl Pts',(-2.09739924558008,9.13548437240156,4.43732617876524));
#79720=CARTESIAN_POINT('Ctrl Pts',(-2.32371119420569,9.07755205704838,4.44129347215784));
#79721=CARTESIAN_POINT('Ctrl Pts',(-2.55002079889967,9.01962034170499,4.44526072446086));
#79722=CARTESIAN_POINT('Ctrl Pts',(-2.7741553482376,8.95322327506606,4.44922797676388));
#79723=CARTESIAN_POINT('Ctrl Pts',(-2.99547885963476,8.87855232929227,4.4531952290669));
#79724=CARTESIAN_POINT('Ctrl Pts',(-3.21685013360765,8.80386526920383,4.4571633375202));
#79725=CARTESIAN_POINT('Ctrl Pts',(-3.43540888766111,8.72090085272899,4.46113144597351));
#79726=CARTESIAN_POINT('Ctrl Pts',(-3.65053599001042,8.62989988633348,4.46509955442682));
#79727=CARTESIAN_POINT('Ctrl Pts',(-3.78284214223221,8.57393302962054,4.46753999617183));
#79728=CARTESIAN_POINT('Ctrl Pts',(-3.91385065471667,8.51492737183186,4.46998043791684));
#79729=CARTESIAN_POINT('Ctrl Pts',(-4.04342140416922,8.45294791246263,4.47242087966185));
#79730=CARTESIAN_POINT('Ctrl Pts',(-4.25409642109582,8.35217267031204,4.47638890568709));
#79731=CARTESIAN_POINT('Ctrl Pts',(-4.4610349470167,8.2435017315231,4.48035693171233));
#79732=CARTESIAN_POINT('Ctrl Pts',(-4.66364590191146,8.12723765889029,4.48432495773758));
#79733=CARTESIAN_POINT('Ctrl Pts',(-4.86622121919317,8.01099403615879,4.48829228581943));
#79734=CARTESIAN_POINT('Ctrl Pts',(-5.06447023819458,7.88716008710131,4.49225961390129));
#79735=CARTESIAN_POINT('Ctrl Pts',(-5.25782737985817,7.75608382536662,4.49622694198314));
#79736=CARTESIAN_POINT('Ctrl Pts',(-5.45116333425983,7.62502192641713,4.50019383534188));
#79737=CARTESIAN_POINT('Ctrl Pts',(-5.63960824613416,7.48671945886708,4.50416072870062));
#79738=CARTESIAN_POINT('Ctrl Pts',(-5.82262555986898,7.3415677244074,4.50812762205936));
#79739=CARTESIAN_POINT('Ctrl Pts',(-6.0056570360086,7.19640475769008,4.51209482238769));
#79740=CARTESIAN_POINT('Ctrl Pts',(-6.18325984999699,7.04439163952304,4.51606202271602));
#79741=CARTESIAN_POINT('Ctrl Pts',(-6.35492962710765,6.88596068076266,4.52002922304435));
#79742=CARTESIAN_POINT('Ctrl Pts',(-6.52659755109422,6.72753143221728,4.52399638054793));
#79743=CARTESIAN_POINT('Ctrl Pts',(-6.69233235869759,6.56268467626563,4.52796353805151));
#79744=CARTESIAN_POINT('Ctrl Pts',(-6.85166523277426,6.39189084704147,4.53193069555509));
#79745=CARTESIAN_POINT('Ctrl Pts',(-7.01103240896822,6.22106024831824,4.53589870713165));
#79746=CARTESIAN_POINT('Ctrl Pts',(-7.16399470317032,6.04428022584574,4.53986671870821));
#79747=CARTESIAN_POINT('Ctrl Pts',(-7.31012155068943,5.86205663369487,4.54383473028477));
#79748=CARTESIAN_POINT('Ctrl Pts',(-7.40001388311578,5.74995879541495,4.54627571783612));
#79749=CARTESIAN_POINT('Ctrl Pts',(-7.48732024782275,5.63580162497169,4.54871670538747));
#79750=CARTESIAN_POINT('Ctrl Pts',(-7.57194811517745,5.51970894192444,4.55115769293881));
#79751=CARTESIAN_POINT('Ctrl Pts',(-7.70953013057689,5.33097364933076,4.55512607826361));
#79752=CARTESIAN_POINT('Ctrl Pts',(-7.84007340603901,5.13706263804828,4.55909446358841));
#79753=CARTESIAN_POINT('Ctrl Pts',(-7.96320136618022,4.93852296381878,4.5630628489132));
#79754=CARTESIAN_POINT('Ctrl Pts',(-8.08630782896132,4.7400179533559,4.56703054138312));
#79755=CARTESIAN_POINT('Ctrl Pts',(-8.20200141091816,4.53688613470146,4.57099823385303));
#79756=CARTESIAN_POINT('Ctrl Pts',(-8.30994956254122,4.32970245288531,4.57496592632294));
#79757=CARTESIAN_POINT('Ctrl Pts',(-8.41788599471889,4.1225412640698,4.57893318803833));
#79758=CARTESIAN_POINT('Ctrl Pts',(-8.51807854411905,3.91132934254721,4.58290044975372));
#79759=CARTESIAN_POINT('Ctrl Pts',(-8.61024075945783,3.69666594740059,4.5868677114691));
#79760=CARTESIAN_POINT('Ctrl Pts',(-8.70241018334596,3.48198576216627,4.59083528348738));
#79761=CARTESIAN_POINT('Ctrl Pts',(-8.78654790321575,3.26385382410653,4.59480285550565));
#79762=CARTESIAN_POINT('Ctrl Pts',(-8.86241526205238,3.0428902026595,4.59877042752393));
#79763=CARTESIAN_POINT('Ctrl Pts',(-8.93828182630696,2.82192889543202,4.60273795798861));
#79764=CARTESIAN_POINT('Ctrl Pts',(-9.00587811252011,2.59813623389435,4.60670548845329));
#79765=CARTESIAN_POINT('Ctrl Pts',(-9.06501485916737,2.37214895518278,4.61067301891797));
#79766=CARTESIAN_POINT('Ctrl Pts',(-9.12416432839442,2.14611305794979,4.61464140295046));
#79767=CARTESIAN_POINT('Ctrl Pts',(-9.17485054897775,1.91788187526179,4.61860978698294));
#79768=CARTESIAN_POINT('Ctrl Pts',(-9.21693474273365,1.68810515391944,4.62257817101543));
#79769=CARTESIAN_POINT('Ctrl Pts',(-9.24279766877059,1.54689540701168,4.62501694941555));
#79770=CARTESIAN_POINT('Ctrl Pts',(-9.26541282832956,1.40510218022082,4.62745572781567));
#79771=CARTESIAN_POINT('Ctrl Pts',(-9.28475763552364,1.26287794821412,4.62989450621579));
#79772=CARTESIAN_POINT('Ctrl Pts',(-9.31766281178971,1.02095703494084,4.63404282531376));
#79773=CARTESIAN_POINT('Ctrl Pts',(-9.3411101003066,0.777738127303933,4.63819114441173));
#79774=CARTESIAN_POINT('Ctrl Pts',(-9.35502482080844,0.5339435031519,4.6423394635097));
#79775=CARTESIAN_POINT('Ctrl Pts',(-9.36516671854218,0.356251098488865,
4.6453630117048));
#79776=CARTESIAN_POINT('Ctrl Pts',(-9.37024561991429,0.17825301840621,4.64838655989989));
#79777=CARTESIAN_POINT('Ctrl Pts',(-9.37024999716748,0.000230397442772201,
4.65141010809498));
#79778=CARTESIAN_POINT('Ctrl Pts',(-9.37005177233215,0.000230392568781948,
4.65141010809498));
#79779=CARTESIAN_POINT('Ctrl Pts',(-9.36899086722885,-1.12278293672488,
4.67048384522757));
#79780=CARTESIAN_POINT('Ctrl Pts',(-8.88872140496492,-3.79195700889602,
4.71580318678582));
#79781=CARTESIAN_POINT('Ctrl Pts',(-6.41096662595373,-7.36066080332452,
4.78736813276973));
#79782=CARTESIAN_POINT('Ctrl Pts',(-2.14758775427819,-9.52195991129607,
4.86610494604671));
#79783=CARTESIAN_POINT('Ctrl Pts',(2.63077110884112,-9.39994022549094,4.94484175932368));
#79784=CARTESIAN_POINT('Ctrl Pts',(6.77828505812936,-7.0238660749718,5.02357857260066));
#79785=CARTESIAN_POINT('Ctrl Pts',(9.30040197326703,-2.96350510038334,5.10231538587762));
#79786=CARTESIAN_POINT('Ctrl Pts',(9.59233161819711,1.80748833353102,5.18105219915461));
#79787=CARTESIAN_POINT('Ctrl Pts',(7.69309920158116,5.90956937174799,5.25551439243367));
#79788=CARTESIAN_POINT('Ctrl Pts',(5.44029904606853,7.73691003764319,5.30373098128708));
#79789=CARTESIAN_POINT('Ctrl Pts',(4.29107337327626,8.33032226950541,5.32570196571484));
#79790=CARTESIAN_POINT('Origin',(0.,0.,2.15141010809499));
#79791=CARTESIAN_POINT('',(4.29092662818983,8.33003803916834,6.5228999581952));
#79792=CARTESIAN_POINT('',(4.2909266281297,8.33003803919931,6.32526713834515));
#79793=CARTESIAN_POINT('',(4.29092662815669,8.33003803918541,2.15141010809499));
#79794=CARTESIAN_POINT('Ctrl Pts',(4.29092662818983,8.33003803916834,6.5228999581952));
#79795=CARTESIAN_POINT('Ctrl Pts',(4.29797836970654,8.32640558211273,6.52276053773968));
#79796=CARTESIAN_POINT('Ctrl Pts',(4.30502553725844,8.32276415076952,6.52262110685617));
#79797=CARTESIAN_POINT('Ctrl Pts',(4.47939483293704,8.23238285509755,6.51916868615752));
#79798=CARTESIAN_POINT('Ctrl Pts',(4.64406688057744,8.14062334548274,6.51585119351331));
#79799=CARTESIAN_POINT('Ctrl Pts',(4.85195946814674,8.01641803857893,6.51162498623148));
#79800=CARTESIAN_POINT('Ctrl Pts',(4.89782183385779,7.98847983939348,6.51069028967824));
#79801=CARTESIAN_POINT('Ctrl Pts',(5.00742201422516,7.92041552435395,6.50845285726873));
#79802=CARTESIAN_POINT('Ctrl Pts',(5.07092125250739,7.8799121187666,6.50715347214246));
#79803=CARTESIAN_POINT('Ctrl Pts',(5.17058929057112,7.8146344968257,6.50511305185087));
#79804=CARTESIAN_POINT('Ctrl Pts',(5.20708436143209,7.79036445920005,6.50436575312504));
#79805=CARTESIAN_POINT('Ctrl Pts',(5.28436655602216,7.73818438394952,6.50278388491557));
#79806=CARTESIAN_POINT('Ctrl Pts',(5.32510580567832,7.71020593959584,6.50195019760504));
#79807=CARTESIAN_POINT('Ctrl Pts',(5.45625696894976,7.61860009271787,6.49926387070566));
#79808=CARTESIAN_POINT('Ctrl Pts',(5.54576482713954,7.55369446553352,6.49742661690263));
#79809=CARTESIAN_POINT('Ctrl Pts',(5.82822047147332,7.34114771683431,6.49158496139705));
#79810=CARTESIAN_POINT('Ctrl Pts',(6.01658374320558,7.1875812426981,6.48761995136545));
#79811=CARTESIAN_POINT('Ctrl Pts',(6.37565826412705,6.87082293595608,6.47975956464935));
#79812=CARTESIAN_POINT('Ctrl Pts',(6.54659443707317,6.70815376287564,6.47586829353886));
#79813=CARTESIAN_POINT('Ctrl Pts',(6.77698558293327,6.47170263741448,6.47034476269931));
#79814=CARTESIAN_POINT('Ctrl Pts',(6.84173918542697,6.40320806179622,6.46875964211212));
#79815=CARTESIAN_POINT('Ctrl Pts',(6.9588298524724,6.27554849879587,6.46582967635094));
#79816=CARTESIAN_POINT('Ctrl Pts',(7.01147339696298,6.21667617351406,6.46448766695632));
#79817=CARTESIAN_POINT('Ctrl Pts',(7.12910111627834,6.0817357737788,6.46143133272535));
#79818=CARTESIAN_POINT('Ctrl Pts',(7.19362390436604,6.00527832861569,6.45971334397219));
#79819=CARTESIAN_POINT('Ctrl Pts',(7.45659510795616,5.68334480834854,6.45253620193066));
#79820=CARTESIAN_POINT('Ctrl Pts',(7.64379975319975,5.42895409634451,6.44699132615086));
#79821=CARTESIAN_POINT('Ctrl Pts',(7.90556553848391,5.03278848210838,6.43864347000669));
#79822=CARTESIAN_POINT('Ctrl Pts',(7.98992439449997,4.89775812708453,6.43584667517733));
#79823=CARTESIAN_POINT('Ctrl Pts',(8.10723019040145,4.69888759006388,6.43182325388195));
#79824=CARTESIAN_POINT('Ctrl Pts',(8.1429480494839,4.6367146814176,6.43057866774914));
#79825=CARTESIAN_POINT('Ctrl Pts',(8.2066495018906,4.52282497540583,6.42832650363028));
#79826=CARTESIAN_POINT('Ctrl Pts',(8.2348666078045,4.47124297917986,6.42731664269658));
#79827=CARTESIAN_POINT('Ctrl Pts',(8.28052529076429,4.3858785913627,6.42566410413058));
#79828=CARTESIAN_POINT('Ctrl Pts',(8.29824998887332,4.35224967583713,6.42501791034206));
#79829=CARTESIAN_POINT('Ctrl Pts',(8.34098544902496,4.26995788076397,6.42344839470047));
#79830=CARTESIAN_POINT('Ctrl Pts',(8.36577553788806,4.22118208945593,6.42252783638855));
#79831=CARTESIAN_POINT('Ctrl Pts',(8.4637719890552,4.024114535551,6.41884232653913));
#79832=CARTESIAN_POINT('Ctrl Pts',(8.53347413533364,3.87411326280363,6.41611299551519));
#79833=CARTESIAN_POINT('Ctrl Pts',(8.70502288045284,3.47781025192313,6.40901655426777));
#79834=CARTESIAN_POINT('Ctrl Pts',(8.80039658885993,3.22887092662536,6.40466878052362));
#79835=CARTESIAN_POINT('Ctrl Pts',(8.92263273869552,2.8639526516323,6.39831646930224));
#79836=CARTESIAN_POINT('Ctrl Pts',(8.95810338300139,2.75099681531146,6.39635365658527));
#79837=CARTESIAN_POINT('Ctrl Pts',(9.02035773920073,2.53875921789903,6.39266260587086));
#79838=CARTESIAN_POINT('Ctrl Pts',(9.04766606901024,2.43964971760152,6.39093779054136));
#79839=CARTESIAN_POINT('Ctrl Pts',(9.09307541141424,2.26358358695376,6.38786788633506));
#79840=CARTESIAN_POINT('Ctrl Pts',(9.11184368551238,2.18680948184148,6.38652733855971));
#79841=CARTESIAN_POINT('Ctrl Pts',(9.15069325699719,2.01869813387108,6.38358673408461));
#79842=CARTESIAN_POINT('Ctrl Pts',(9.17038300423659,1.92727910274634,6.3819842738755));
#79843=CARTESIAN_POINT('Ctrl Pts',(9.26833835446695,1.43692618078032,6.37337066577344));
#79844=CARTESIAN_POINT('Ctrl Pts',(9.32194726066565,1.03351261863197,6.36619798043127));
#79845=CARTESIAN_POINT('Ctrl Pts',(9.36056632967618,0.458489235388605,6.35608538475653));
#79846=CARTESIAN_POINT('Ctrl Pts',(9.3673373467023,0.288800448365255,6.35311809429535));
#79847=CARTESIAN_POINT('Ctrl Pts',(9.37019690329816,0.0636928941325103,
6.34923783549445));
#79848=CARTESIAN_POINT('Ctrl Pts',(9.37040964598114,0.00835923589021939,
6.34828858091579));
#79849=CARTESIAN_POINT('Ctrl Pts',(9.36992018507858,-0.0892777163247355,
6.34662348338829));
#79850=CARTESIAN_POINT('Ctrl Pts',(9.36942161718815,-0.131580195257945,
6.34590549206801));
#79851=CARTESIAN_POINT('Ctrl Pts',(9.36766138818819,-0.22642220979244,6.3443029237654));
#79852=CARTESIAN_POINT('Ctrl Pts',(9.3662441640581,-0.278957300985878,6.34341999739258));
#79853=CARTESIAN_POINT('Ctrl Pts',(9.35365790987852,-0.634524243101665,
6.3374689104538));
#79854=CARTESIAN_POINT('Ctrl Pts',(9.32822644121875,-0.936872642381898,
6.33252414150284));
#79855=CARTESIAN_POINT('Ctrl Pts',(9.26487977208946,-1.41234446645252,6.32465700099598));
#79856=CARTESIAN_POINT('Ctrl Pts',(9.23664464906192,-1.586540119386,6.32175652438732));
#79857=CARTESIAN_POINT('Ctrl Pts',(9.17854881997311,-1.89036728723269,6.31662717101886));
#79858=CARTESIAN_POINT('Ctrl Pts',(9.1508150188378,-2.02035424545892,6.31440994942017));
#79859=CARTESIAN_POINT('Ctrl Pts',(9.10133451121557,-2.23027976250025,6.3107829131888));
#79860=CARTESIAN_POINT('Ctrl Pts',(9.08127624989633,-2.31059718232633,6.30938415407222));
#79861=CARTESIAN_POINT('Ctrl Pts',(9.03891947307997,-2.47112294977449,6.30656478489693));
#79862=CARTESIAN_POINT('Ctrl Pts',(9.01661103990227,-2.5513210674882,6.30514422179718));
#79863=CARTESIAN_POINT('Ctrl Pts',(8.9550483655426,-2.76173660934026,6.30138462669632));
#79864=CARTESIAN_POINT('Ctrl Pts',(8.91402267510996,-2.89141486447328,6.29903438682642));
#79865=CARTESIAN_POINT('Ctrl Pts',(8.76511594765119,-3.3287537872509,6.2910003379743));
#79866=CARTESIAN_POINT('Ctrl Pts',(8.64400983001463,-3.63165970240849,6.28524440192507));
#79867=CARTESIAN_POINT('Ctrl Pts',(8.44161305504887,-4.07005668263084,6.276778427748));
#79868=CARTESIAN_POINT('Ctrl Pts',(8.37229436885112,-4.21080510197038,6.27404042195399));
#79869=CARTESIAN_POINT('Ctrl Pts',(8.27422225465868,-4.3979302471218,6.27040042071508));
#79870=CARTESIAN_POINT('Ctrl Pts',(8.24855035923976,-4.44589264010016,6.26946750886459));
#79871=CARTESIAN_POINT('Ctrl Pts',(8.20212052503937,-4.53085015952079,6.26781689374751));
#79872=CARTESIAN_POINT('Ctrl Pts',(8.18152636757493,-4.56793285560849,6.26709723844419));
#79873=CARTESIAN_POINT('Ctrl Pts',(8.13436536245574,-4.65151079431682,6.26547645212584));
#79874=CARTESIAN_POINT('Ctrl Pts',(8.10765032454756,-4.69792068375847,6.26457714179801));
#79875=CARTESIAN_POINT('Ctrl Pts',(7.92364234787666,-5.01133817118041,6.25850057302204));
#79876=CARTESIAN_POINT('Ctrl Pts',(7.7535845761446,-5.27063053081631,6.25345045743045));
#79877=CARTESIAN_POINT('Ctrl Pts',(7.42230898386911,-5.72490979123455,6.24422680341853));
#79878=CARTESIAN_POINT('Ctrl Pts',(7.26545059468403,-5.92270967411836,6.24006968033552));
#79879=CARTESIAN_POINT('Ctrl Pts',(7.03871309445834,-6.18604539636911,6.23425738695618));
#79880=CARTESIAN_POINT('Ctrl Pts',(6.97553083379545,-6.25720458376089,6.2326575134944));
#79881=CARTESIAN_POINT('Ctrl Pts',(6.85798355628047,-6.38559903867024,6.2297138089068));
#79882=CARTESIAN_POINT('Ctrl Pts',(6.80395806979736,-6.44313340632123,6.22837299684091));
#79883=CARTESIAN_POINT('Ctrl Pts',(6.67942499876343,-6.5724415504481,6.22530858688787));
#79884=CARTESIAN_POINT('Ctrl Pts',(6.60847534566374,-6.64377601865944,6.223581199562));
#79885=CARTESIAN_POINT('Ctrl Pts',(6.29810138241555,-6.94594156012155,6.21610323311482));
#79886=CARTESIAN_POINT('Ctrl Pts',(6.04763116742202,-7.165077850579,6.21025558557988));
#79887=CARTESIAN_POINT('Ctrl Pts',(5.62686625070864,-7.49539284920534,6.20085307228581));
#79888=CARTESIAN_POINT('Ctrl Pts',(5.46368154606181,-7.61516395416045,6.19730176973065));
#79889=CARTESIAN_POINT('Ctrl Pts',(5.24316996232073,-7.76627144920301,6.19267881502676));
#79890=CARTESIAN_POINT('Ctrl Pts',(5.18921263392935,-7.80242755461016,6.19156114438331));
#79891=CARTESIAN_POINT('Ctrl Pts',(5.09936073018297,-7.86129179410294,6.18972490364699));
#79892=CARTESIAN_POINT('Ctrl Pts',(5.06367996591732,-7.88432202222585,6.18900221662726));
#79893=CARTESIAN_POINT('Ctrl Pts',(4.98222752880574,-7.9361146713629,6.18736758330726));
#79894=CARTESIAN_POINT('Ctrl Pts',(4.9363611414305,-7.96472510040765,6.18645757473401));
#79895=CARTESIAN_POINT('Ctrl Pts',(4.77906301488812,-8.06096345532177,6.18336800656867));
#79896=CARTESIAN_POINT('Ctrl Pts',(4.66646870967089,-8.12666260381104,6.18120937408592));
#79897=CARTESIAN_POINT('Ctrl Pts',(4.34465584543885,-8.30554753097073,6.17514298835352));
#79898=CARTESIAN_POINT('Ctrl Pts',(4.13244691829045,-8.41314667080247,6.17126130703369));
#79899=CARTESIAN_POINT('Ctrl Pts',(3.78197144090259,-8.57439005388915,6.16492046631412));
#79900=CARTESIAN_POINT('Ctrl Pts',(3.64612306664921,-8.63303302623325,6.16247964835117));
#79901=CARTESIAN_POINT('Ctrl Pts',(3.39853799328566,-8.73302365249722,6.15804064072109));
#79902=CARTESIAN_POINT('Ctrl Pts',(3.28729281796078,-8.77550388492159,6.15604953240927));
#79903=CARTESIAN_POINT('Ctrl Pts',(3.0992567467844,-8.8432301798998,6.15268339896144));
#79904=CARTESIAN_POINT('Ctrl Pts',(3.02289414871753,-8.86962362939408,6.15131627246433));
#79905=CARTESIAN_POINT('Ctrl Pts',(2.86437967720139,-8.9221266022952,6.14847682098003));
#79906=CARTESIAN_POINT('Ctrl Pts',(2.78218956367326,-8.94809673789507,6.14700370183043));
#79907=CARTESIAN_POINT('Ctrl Pts',(2.54985574724562,-9.01799817913463,6.14283650197007));
#79908=CARTESIAN_POINT('Ctrl Pts',(2.39895380235328,-9.05930879884373,6.14012602362838));
#79909=CARTESIAN_POINT('Ctrl Pts',(1.94294509942392,-9.17195166287925,6.13193426643136));
#79910=CARTESIAN_POINT('Ctrl Pts',(1.63522489843687,-9.23178052515135,6.12639920138766));
#79911=CARTESIAN_POINT('Ctrl Pts',(1.25640516750639,-9.28589494026231,6.11969931301949));
#79912=CARTESIAN_POINT('Ctrl Pts',(1.18761448160606,-9.29494328376726,6.11848757379081));
#79913=CARTESIAN_POINT('Ctrl Pts',(1.03015114826317,-9.31387853026773,6.1157289574021));
#79914=CARTESIAN_POINT('Ctrl Pts',(0.941424887848997,-9.32326465939015,
6.11418542965282));
#79915=CARTESIAN_POINT('Ctrl Pts',(0.806637048814814,-9.33557978508224,
6.11186328709341));
#79916=CARTESIAN_POINT('Ctrl Pts',(0.760665659336862,-9.33943793913225,
6.11107528946117));
#79917=CARTESIAN_POINT('Ctrl Pts',(0.668656956501475,-9.34647592960889,
6.10950741242211));
#79918=CARTESIAN_POINT('Ctrl Pts',(0.62262087780027,-9.34965548471017,6.10872755630882));
#79919=CARTESIAN_POINT('Ctrl Pts',(0.487440543333029,-9.35798908965392,
6.10644885548497));
#79920=CARTESIAN_POINT('Ctrl Pts',(0.39824377356692,-9.36220914353442,6.10495962525912));
#79921=CARTESIAN_POINT('Ctrl Pts',(-0.0331035061062979,-9.37644130616774,
6.0978015585962));
#79922=CARTESIAN_POINT('Ctrl Pts',(-0.375569396244216,-9.36897520793617,
6.09224150176936));
#79923=CARTESIAN_POINT('Ctrl Pts',(-0.845687809321002,-9.33290372724416,
6.08447323246501));
#79924=CARTESIAN_POINT('Ctrl Pts',(-0.974299004435995,-9.32035520804936,
6.0823352537515));
#79925=CARTESIAN_POINT('Ctrl Pts',(-1.2108281733077,-9.2923278010977,6.07836669457467));
#79926=CARTESIAN_POINT('Ctrl Pts',(-1.31881490934292,-9.27761758119378,
6.07654075023429));
#79927=CARTESIAN_POINT('Ctrl Pts',(-1.50514886545598,-9.24891567160424,
6.07336097741795));
#79928=CARTESIAN_POINT('Ctrl Pts',(-1.58361990668614,-9.23580327662374,
6.07201293080726));
#79929=CARTESIAN_POINT('Ctrl Pts',(-1.75042590141695,-9.20574184790195,
6.06912712952669));
#79930=CARTESIAN_POINT('Ctrl Pts',(-1.83870307526634,-9.18851700538763,
6.06758771273284));
#79931=CARTESIAN_POINT('Ctrl Pts',(-2.10897489767909,-9.13173005448163,
6.06283659647974));
#79932=CARTESIAN_POINT('Ctrl Pts',(-2.29004861689295,-9.08801110613602,
6.05959949585475));
#79933=CARTESIAN_POINT('Ctrl Pts',(-2.73735902819464,-8.96579283545478,
6.05148702746107));
#79934=CARTESIAN_POINT('Ctrl Pts',(-3.00163855594821,-8.88080746592874,
6.04658743583834));
#79935=CARTESIAN_POINT('Ctrl Pts',(-3.38593459776506,-8.73811068617633,
6.03941460946368));
#79936=CARTESIAN_POINT('Ctrl Pts',(-3.50912161481898,-8.68937265396421,
6.03710864202932));
#79937=CARTESIAN_POINT('Ctrl Pts',(-3.67928076784952,-8.61784163956654,
6.03393157693828));
#79938=CARTESIAN_POINT('Ctrl Pts',(-3.72715816494055,-8.59724336768051,
6.03303859831938));
#79939=CARTESIAN_POINT('Ctrl Pts',(-3.81409027490409,-8.55897993295781,
6.03142053305565));
#79940=CARTESIAN_POINT('Ctrl Pts',(-3.85320026453933,-8.54144424774349,
6.03069399017489));
#79941=CARTESIAN_POINT('Ctrl Pts',(-3.95450570122614,-8.49518468852865,
6.02881462164188));
#79942=CARTESIAN_POINT('Ctrl Pts',(-4.01650896232153,-8.46604594965714,
6.02766673834312));
#79943=CARTESIAN_POINT('Ctrl Pts',(-4.24400346178812,-8.356072043054,6.0234548202241));
#79944=CARTESIAN_POINT('Ctrl Pts',(-4.40742086466586,-8.27104268183566,
6.02042803844561));
#79945=CARTESIAN_POINT('Ctrl Pts',(-4.65862540963312,-8.1307757476858,6.01570927403594));
#79946=CARTESIAN_POINT('Ctrl Pts',(-4.74818167273247,-8.07880410522671,
6.01401360517946));
#79947=CARTESIAN_POINT('Ctrl Pts',(-5.05541858156953,-7.89363340305294,
6.00812922588155));
#79948=CARTESIAN_POINT('Ctrl Pts',(-5.26850614530403,-7.75303474666433,
6.00392624755133));
#79949=CARTESIAN_POINT('Ctrl Pts',(-5.55291261219695,-7.54823330863531,
5.99806447957599));
#79950=CARTESIAN_POINT('Ctrl Pts',(-5.62938311193821,-7.49137572701669,
5.99646247084077));
#79951=CARTESIAN_POINT('Ctrl Pts',(-5.76757545985104,-7.38531555798363,
5.99351675087762));
#79952=CARTESIAN_POINT('Ctrl Pts',(-5.82956837730591,-7.33648042842947,
5.99217608511301));
#79953=CARTESIAN_POINT('Ctrl Pts',(-5.96904774795024,-7.22372085032136,
5.98911461852156));
#79954=CARTESIAN_POINT('Ctrl Pts',(-6.04613801525816,-7.15932182358294,
5.98739005921991));
#79955=CARTESIAN_POINT('Ctrl Pts',(-6.37509514466811,-6.87541706319275,
5.97988897899086));
#79956=CARTESIAN_POINT('Ctrl Pts',(-6.61615684437095,-6.64376885822131,
5.97401424475727));
#79957=CARTESIAN_POINT('Ctrl Pts',(-6.94578318227007,-6.29124361292791,
5.96553126290414));
#79958=CARTESIAN_POINT('Ctrl Pts',(-7.04464193042249,-6.18034549131344,
5.96292373882137));
#79959=CARTESIAN_POINT('Ctrl Pts',(-7.20284675540514,-5.99414378659714,
5.95866883074758));
#79960=CARTESIAN_POINT('Ctrl Pts',(-7.26374801988948,-5.92019644062888,
5.95700966611933));
#79961=CARTESIAN_POINT('Ctrl Pts',(-7.35295932851441,-5.80842522315705,
5.95455446022486));
#79962=CARTESIAN_POINT('Ctrl Pts',(-7.3821345084353,-5.77130007640062,5.95374742496283));
#79963=CARTESIAN_POINT('Ctrl Pts',(-7.43525214507516,-5.70264655188049,
5.95227171676185));
#79964=CARTESIAN_POINT('Ctrl Pts',(-7.45927777044506,-5.67118394184633,
5.95160182563131));
#79965=CARTESIAN_POINT('Ctrl Pts',(-7.52861826158614,-5.57917656238893,
5.94965995209038));
#79966=CARTESIAN_POINT('Ctrl Pts',(-7.57340051885043,-5.51823419822869,
5.94839505712186));
#79967=CARTESIAN_POINT('Ctrl Pts',(-7.82736911044628,-5.1637029629282,5.94113963924782));
#79968=CARTESIAN_POINT('Ctrl Pts',(-8.02021247361393,-4.85877858788658,
5.93528986976471));
#79969=CARTESIAN_POINT('Ctrl Pts',(-8.2586217050041,-4.42876550521456,5.9271915306902));
#79970=CARTESIAN_POINT('Ctrl Pts',(-8.31981803805225,-4.31270496076447,
5.92502147048924));
#79971=CARTESIAN_POINT('Ctrl Pts',(-8.42784465491668,-4.09696686404027,
5.92100249862582));
#79972=CARTESIAN_POINT('Ctrl Pts',(-8.47539365344757,-3.99767499291938,
5.91915846108813));
#79973=CARTESIAN_POINT('Ctrl Pts',(-8.55432243203215,-3.82511446594908,
5.91595859966093));
#79974=CARTESIAN_POINT('Ctrl Pts',(-8.58653729177827,-3.7522406974054,5.91460878320093));
#79975=CARTESIAN_POINT('Ctrl Pts',(-8.65292864388995,-3.59672178566555,
5.91173017171816));
#79976=CARTESIAN_POINT('Ctrl Pts',(-8.68685929488228,-3.5139802592186,5.91019982629159));
#79977=CARTESIAN_POINT('Ctrl Pts',(-8.7861365804028,-3.26165810067457,5.90553606838316));
#79978=CARTESIAN_POINT('Ctrl Pts',(-8.84773900544608,-3.09065101830168,
5.9023787313846));
#79979=CARTESIAN_POINT('Ctrl Pts',(-8.92143575200027,-2.86576110103158,
5.89824015406613));
#79980=CARTESIAN_POINT('Ctrl Pts',(-8.93808253384746,-2.813411306161,5.89727780029478));
#79981=CARTESIAN_POINT('Ctrl Pts',(-9.02492128230767,-2.53177404848862,
5.8921080068485));
#79982=CARTESIAN_POINT('Ctrl Pts',(-9.08675259832259,-2.30000242308958,
5.88787790850983));
#79983=CARTESIAN_POINT('Ctrl Pts',(-9.15313115094227,-2.00637157004691,
5.88261507124184));
#79984=CARTESIAN_POINT('Ctrl Pts',(-9.16605072242308,-1.94649708756365,
5.88154704021331));
#79985=CARTESIAN_POINT('Ctrl Pts',(-9.18634564342182,-1.84775628457683,
5.8797960962851));
#79986=CARTESIAN_POINT('Ctrl Pts',(-9.19406357114437,-1.80896230547793,
5.87911080001503));
#79987=CARTESIAN_POINT('Ctrl Pts',(-9.21305141692628,-1.71025866895324,
5.87737475558814));
#79988=CARTESIAN_POINT('Ctrl Pts',(-9.22398277836167,-1.65028568873828,
5.87632697283346));
#79989=CARTESIAN_POINT('Ctrl Pts',(-9.2414876487661,-1.54863515568507,5.87456528383404));
#79990=CARTESIAN_POINT('Ctrl Pts',(-9.24836627933908,-1.50701227075214,
5.87384806991923));
#79991=CARTESIAN_POINT('Ctrl Pts',(-9.26370188605477,-1.41015414784513,
5.87218878995313));
#79992=CARTESIAN_POINT('Ctrl Pts',(-9.27194631986713,-1.35488701197608,
5.87124905520164));
#79993=CARTESIAN_POINT('Ctrl Pts',(-9.30470506315215,-1.12096655920038,
5.86729561230279));
#79994=CARTESIAN_POINT('Ctrl Pts',(-9.3245539718842,-0.941698441403416,
5.86432427290705));
#79995=CARTESIAN_POINT('Ctrl Pts',(-9.35989205572344,-0.50857055636118,
5.85718944343998));
#79996=CARTESIAN_POINT('Ctrl Pts',(-9.37024469947905,-0.254435793981661,
5.85303770209661));
#79997=CARTESIAN_POINT('Ctrl Pts',(-9.37025337653925,0.161920866284036,
5.84616237230288));
#79998=CARTESIAN_POINT('Ctrl Pts',(-9.36604956202626,0.32400939424748,5.84346835364772));
#79999=CARTESIAN_POINT('Ctrl Pts',(-9.35313306729956,0.572756601392295,
5.83928903134108));
#80000=CARTESIAN_POINT('Ctrl Pts',(-9.34741440879344,0.659539328381405,
5.83782263723035));
#80001=CARTESIAN_POINT('Ctrl Pts',(-9.33408152616977,0.826425788163054,
5.83498477956949));
#80002=CARTESIAN_POINT('Ctrl Pts',(-9.3266419559059,0.906535885206288,5.83361455810884));
#80003=CARTESIAN_POINT('Ctrl Pts',(-9.30590426327884,1.10240970446815,5.83024393264564));
#80004=CARTESIAN_POINT('Ctrl Pts',(-9.29147670765068,1.21804014813801,5.8282366022995));
#80005=CARTESIAN_POINT('Ctrl Pts',(-9.25453854669684,1.47498107085413,5.82373830076327));
#80006=CARTESIAN_POINT('Ctrl Pts',(-9.23094006979387,1.61610586103673,5.82124181962598));
#80007=CARTESIAN_POINT('Ctrl Pts',(-9.15982028755866,1.98874737800959,5.81459446969821));
#80008=CARTESIAN_POINT('Ctrl Pts',(-9.10675651189692,2.21910106209131,5.81042655133858));
#80009=CARTESIAN_POINT('Ctrl Pts',(-9.00820080604955,2.58337036682101,5.80381665043818));
#80010=CARTESIAN_POINT('Ctrl Pts',(-8.96828910552953,2.71868992655045,5.80135750874224));
#80011=CARTESIAN_POINT('Ctrl Pts',(-8.90874957789901,2.90494992414661,5.79798828779435));
#80012=CARTESIAN_POINT('Ctrl Pts',(-8.89170929156123,2.95669731222532,5.79705397262397));
#80013=CARTESIAN_POINT('Ctrl Pts',(-8.86060430044073,3.04845448913544,5.79540213715716));
#80014=CARTESIAN_POINT('Ctrl Pts',(-8.84671749096731,3.08852278247073,5.79468264775012));
#80015=CARTESIAN_POINT('Ctrl Pts',(-8.81109853745735,3.18908438125109,5.79288080152028));
#80016=CARTESIAN_POINT('Ctrl Pts',(-8.78901504353268,3.2494509105338,5.79180251080762));
#80017=CARTESIAN_POINT('Ctrl Pts',(-8.75124199561557,3.34950281330605,5.79001754411294));
#80018=CARTESIAN_POINT('Ctrl Pts',(-8.73589935815571,3.38931674125589,5.78930783492399));
#80019=CARTESIAN_POINT('Ctrl Pts',(-8.62482910979277,3.67177732170096,5.78427297957588));
#80020=CARTESIAN_POINT('Ctrl Pts',(-8.519277803058,3.91043888348666,5.7800164718201));
#80021=CARTESIAN_POINT('Ctrl Pts',(-8.29622964708334,4.36273173068542,5.77174222042305));
#80022=CARTESIAN_POINT('Ctrl Pts',(-8.18008400091835,4.57679798033519,5.7677308151304));
#80023=CARTESIAN_POINT('Ctrl Pts',(-8.00632577414337,4.86925968558907,5.76204374878382));
#80024=CARTESIAN_POINT('Ctrl Pts',(-7.95563229643581,4.95165194586734,5.76041810259866));
#80025=CARTESIAN_POINT('Ctrl Pts',(-7.86130708763694,5.09977023372098,5.75744966370739));
#80026=CARTESIAN_POINT('Ctrl Pts',(-7.81810368657875,5.16575844142914,5.75611020708584));
#80027=CARTESIAN_POINT('Ctrl Pts',(-7.71892638309235,5.31314575875241,5.7530789228856));
#80028=CARTESIAN_POINT('Ctrl Pts',(-7.66248799979673,5.39422097711547,5.7513836579507));
#80029=CARTESIAN_POINT('Ctrl Pts',(-7.5396056171217,5.56492374772573,5.74775451231939));
#80030=CARTESIAN_POINT('Ctrl Pts',(-7.47282137830764,5.65428773124383,5.74581838759129));
#80031=CARTESIAN_POINT('Ctrl Pts',(-7.26299883473211,5.92483870400857,5.73984878710464));
#80032=CARTESIAN_POINT('Ctrl Pts',(-7.1148486581083,6.10195001087115,5.73578644039121));
#80033=CARTESIAN_POINT('Ctrl Pts',(-6.94012615383007,6.29580359824902,5.73119970603883));
#80034=CARTESIAN_POINT('Ctrl Pts',(-6.91983385748313,6.31810045536646,5.73066999538527));
#80035=CARTESIAN_POINT('Ctrl Pts',(-6.77448107054488,6.47627154568714,5.72689771971454));
#80036=CARTESIAN_POINT('Ctrl Pts',(-6.6455352368933,6.60852091175285,5.72366571988583));
#80037=CARTESIAN_POINT('Ctrl Pts',(-6.4723246343232,6.77596951443039,5.71951081612198));
#80038=CARTESIAN_POINT('Ctrl Pts',(-6.43153220993575,6.81470046919124,5.71854526454732));
#80039=CARTESIAN_POINT('Ctrl Pts',(-6.35955184330272,6.88182125059916,5.71686589235061));
#80040=CARTESIAN_POINT('Ctrl Pts',(-6.32851653348345,6.91037204968196,5.71614972884859));
#80041=CARTESIAN_POINT('Ctrl Pts',(-6.25248567924997,6.9793745180606,5.71441409449984));
#80042=CARTESIAN_POINT('Ctrl Pts',(-6.20728911051949,7.01960168064195,5.71339791475549));
#80043=CARTESIAN_POINT('Ctrl Pts',(-6.13222377202788,7.085121599341,5.71173277944348));
#80044=CARTESIAN_POINT('Ctrl Pts',(-6.10258055835842,7.11066994041068,5.71108091403971));
#80045=CARTESIAN_POINT('Ctrl Pts',(-6.02684683139344,7.17511950169752,5.70942877853367));
#80046=CARTESIAN_POINT('Ctrl Pts',(-5.98053915367905,7.21376282102248,5.70843091286447));
#80047=CARTESIAN_POINT('Ctrl Pts',(-5.75377046770128,7.39931468068321,5.70359646046525));
#80048=CARTESIAN_POINT('Ctrl Pts',(-5.56825253617325,7.53991354848985,5.69979769622794));
#80049=CARTESIAN_POINT('Ctrl Pts',(-5.32336961606374,7.71153172122506,5.69488759623671));
#80050=CARTESIAN_POINT('Ctrl Pts',(-5.26864300773012,7.74902486802278,5.69379687088433));
#80051=CARTESIAN_POINT('Ctrl Pts',(-5.06542434549197,7.88510169512479,5.68976623371663));
#80052=CARTESIAN_POINT('Ctrl Pts',(-4.91452683398795,7.98002370086844,5.68681070606336));
#80053=CARTESIAN_POINT('Ctrl Pts',(-4.68363054104729,8.11623448779535,5.68231818233365));
#80054=CARTESIAN_POINT('Ctrl Pts',(-4.6055941483689,8.16076955922156,5.68080496026396));
#80055=CARTESIAN_POINT('Ctrl Pts',(-4.45725626679338,8.24261997046261,5.67793589359257));
#80056=CARTESIAN_POINT('Ctrl Pts',(-4.38709623516137,8.28017536011301,5.67658195657102));
#80057=CARTESIAN_POINT('Ctrl Pts',(-4.21957067892398,8.36712173638765,5.67335540794998));
#80058=CARTESIAN_POINT('Ctrl Pts',(-4.12180364422911,8.4157137248719,5.67147734535286));
#80059=CARTESIAN_POINT('Ctrl Pts',(-3.78534652021014,8.57566928264624,5.66503193458509));
#80060=CARTESIAN_POINT('Ctrl Pts',(-3.54282168133793,8.67867303179076,5.66041269444136));
#80061=CARTESIAN_POINT('Ctrl Pts',(-3.05760085682517,8.86102004005712,5.65129975405944));
#80062=CARTESIAN_POINT('Ctrl Pts',(-2.81535784850433,8.94093729681579,5.64681101242222));
#80063=CARTESIAN_POINT('Ctrl Pts',(-2.50988256764019,9.02806752346637,5.64132137755137));
#80064=CARTESIAN_POINT('Ctrl Pts',(-2.44943644833561,9.04465448888287,5.64024347965621));
#80065=CARTESIAN_POINT('Ctrl Pts',(-2.34794387842794,9.07141291855236,5.63845009821669));
#80066=CARTESIAN_POINT('Ctrl Pts',(-2.30698692145097,9.08191522506695,5.63773095817806));
#80067=CARTESIAN_POINT('Ctrl Pts',(-2.21203624626077,9.10557900923839,5.63607457769256));
#80068=CARTESIAN_POINT('Ctrl Pts',(-2.15799384139358,9.11853804334601,5.6351396001533));
#80069=CARTESIAN_POINT('Ctrl Pts',(-1.93469469456448,9.16998747010512,5.63130281407443));
#80070=CARTESIAN_POINT('Ctrl Pts',(-1.76449932718783,9.20425207409953,5.62844039362714));
#80071=CARTESIAN_POINT('Ctrl Pts',(-1.19802870119357,9.30200660162239,5.61899845871164));
#80072=CARTESIAN_POINT('Ctrl Pts',(-0.798633312236216,9.34477310776482,
5.61246080334827));
#80073=CARTESIAN_POINT('Ctrl Pts',(-0.304015341916333,9.36578655495732,
5.60417653922342));
#80074=CARTESIAN_POINT('Ctrl Pts',(-0.210247573615239,9.36836053027925,
5.6025988438428));
#80075=CARTESIAN_POINT('Ctrl Pts',(-0.0374557112724693,9.37050822109672,
5.59967566187743));
#80076=CARTESIAN_POINT('Ctrl Pts',(0.0415548547491671,9.3704909376299,5.59833291818088));
#80077=CARTESIAN_POINT('Ctrl Pts',(0.22293590423829,9.36815713473454,5.5952355165982));
#80078=CARTESIAN_POINT('Ctrl Pts',(0.325287513047653,9.36516185023385,5.59347672545005));
#80079=CARTESIAN_POINT('Ctrl Pts',(0.489479198022377,9.35766188821574,5.59063788466171));
#80080=CARTESIAN_POINT('Ctrl Pts',(0.551359490608713,9.35421982837435,5.58956403485926));
#80081=CARTESIAN_POINT('Ctrl Pts',(0.785724603006797,9.33884973187025,5.58548282153041));
#80082=CARTESIAN_POINT('Ctrl Pts',(0.957901646960043,9.32276255626564,5.5824548761334));
#80083=CARTESIAN_POINT('Ctrl Pts',(1.19745369199001,9.29367369569156,5.57821609179894));
#80084=CARTESIAN_POINT('Ctrl Pts',(1.26528055767802,9.28468261244795,5.57701309724961));
#80085=CARTESIAN_POINT('Ctrl Pts',(1.39967898785248,9.26536676720865,5.57462589253961));
#80086=CARTESIAN_POINT('Ctrl Pts',(1.46624987638042,9.25506531061842,5.57344174909946));
#80087=CARTESIAN_POINT('Ctrl Pts',(1.69493854922914,9.21714771648842,5.56937225193449));
#80088=CARTESIAN_POINT('Ctrl Pts',(1.85643733937426,9.1859822199621,5.56649507576767));
#80089=CARTESIAN_POINT('Ctrl Pts',(2.07811015190131,9.13711962346229,5.5625724296476));
#80090=CARTESIAN_POINT('Ctrl Pts',(2.13905173157476,9.12304524446193,5.56149689495644));
#80091=CARTESIAN_POINT('Ctrl Pts',(2.24093903202218,9.09843746414717,5.55970602659849));
#80092=CARTESIAN_POINT('Ctrl Pts',(2.28196248477532,9.08823521196743,5.55898706378743));
#80093=CARTESIAN_POINT('Ctrl Pts',(2.37684966566549,9.06395443914295,5.55732921714552));
#80094=CARTESIAN_POINT('Ctrl Pts',(2.43065964684377,9.04967281776047,5.55639261714228));
#80095=CARTESIAN_POINT('Ctrl Pts',(2.65326570889496,8.98846259871728,5.55252721304878));
#80096=CARTESIAN_POINT('Ctrl Pts',(2.82085680085678,8.93728404406734,5.54963855329337));
#80097=CARTESIAN_POINT('Ctrl Pts',(3.36514064422939,8.75423603011843,5.54020740940771));
#80098=CARTESIAN_POINT('Ctrl Pts',(3.73485381572756,8.60300453240689,5.53370493249914));
#80099=CARTESIAN_POINT('Ctrl Pts',(4.15989264231646,8.39656342359426,5.52579822219299));
#80100=CARTESIAN_POINT('Ctrl Pts',(4.22560673919744,8.36368528660159,5.52456375066252));
#80101=CARTESIAN_POINT('Ctrl Pts',(4.29092662824368,8.3300380391406,5.52332385470008));
#80102=CARTESIAN_POINT('',(-9.37096239705712,-4.07005226067136E-5,5.65143860498297));
#80103=CARTESIAN_POINT('Ctrl Pts',(4.29107337327626,8.33032226950541,5.32570196571484));
#80104=CARTESIAN_POINT('Ctrl Pts',(4.06748288923697,8.44577507507538,5.32997658571274));
#80105=CARTESIAN_POINT('Ctrl Pts',(2.43791876811844,9.20543064297083,5.3604968101363));
#80106=CARTESIAN_POINT('Ctrl Pts',(-0.970645488733943,9.71275900755431,
5.41726263898552));
#80107=CARTESIAN_POINT('Ctrl Pts',(-5.46572508632491,8.08737839383646,5.4959994522625));
#80108=CARTESIAN_POINT('Ctrl Pts',(-8.62234106295286,4.55381982533101,5.57404860769815));
#80109=CARTESIAN_POINT('Ctrl Pts',(-9.37063486116336,1.50430010234368,5.62585215870815));
#80110=CARTESIAN_POINT('Ctrl Pts',(-9.3710117781914,-4.11794517302605E-5,
5.65141010529249));
#80111=CARTESIAN_POINT('Ctrl Pts',(-9.37024999993907,-3.37912498182759E-5,
5.65184975587397));
#80112=CARTESIAN_POINT('Ctrl Pts',(-9.37024989579904,-0.0289116261349408,
5.65234466512349));
#80113=CARTESIAN_POINT('Ctrl Pts',(-9.37011629532077,-0.0577893348672783,
5.65283817878753));
#80114=CARTESIAN_POINT('Ctrl Pts',(-9.36958296607992,-0.115449952971927,
5.65382049981617));
#80115=CARTESIAN_POINT('Ctrl Pts',(-9.36918409739989,-0.144232451791148,
5.65430925987687));
#80116=CARTESIAN_POINT('Ctrl Pts',(-9.36765285470081,-0.22714934709786,
5.65571291340118));
#80117=CARTESIAN_POINT('Ctrl Pts',(-9.36618387985989,-0.28127633830779,
5.65662395395215));
#80118=CARTESIAN_POINT('Ctrl Pts',(-9.35846354684279,-0.496833177514481,
5.66023613480282));
#80119=CARTESIAN_POINT('Ctrl Pts',(-9.34850706241727,-0.658102699117982,
5.662903321492));
#80120=CARTESIAN_POINT('Ctrl Pts',(-9.31375530258424,-1.05416221238166,
5.66943839173724));
#80121=CARTESIAN_POINT('Ctrl Pts',(-9.28424756929226,-1.28842654786451,
5.67329194823512));
#80122=CARTESIAN_POINT('Ctrl Pts',(-9.21560675066315,-1.70559407591073,
5.68025348527256));
#80123=CARTESIAN_POINT('Ctrl Pts',(-9.17978558185586,-1.88891378916537,
5.68334704105314));
#80124=CARTESIAN_POINT('Ctrl Pts',(-9.12177378990983,-2.14489213035734,
5.68774328943355));
#80125=CARTESIAN_POINT('Ctrl Pts',(-9.1041422414575,-2.21853856044011,5.68901699097461));
#80126=CARTESIAN_POINT('Ctrl Pts',(-9.06632832593687,-2.36843751355314,
5.69162916419587));
#80127=CARTESIAN_POINT('Ctrl Pts',(-9.04607193855923,-2.44466521596368,
5.69296802678948));
#80128=CARTESIAN_POINT('Ctrl Pts',(-8.99883070541919,-2.6138077123164,5.69596331360591));
#80129=CARTESIAN_POINT('Ctrl Pts',(-8.97136427215402,-2.70657862575678,
5.69762278063558));
#80130=CARTESIAN_POINT('Ctrl Pts',(-8.86969277872221,-3.0314174889467,5.70349221376078));
#80131=CARTESIAN_POINT('Ctrl Pts',(-8.78787913977127,-3.2610000671582,5.70774945973942));
#80132=CARTESIAN_POINT('Ctrl Pts',(-8.60017657053575,-3.72914669000218,
5.71660729636332));
#80133=CARTESIAN_POINT('Ctrl Pts',(-8.49308173452594,-3.967005779683,5.72120741426368));
#80134=CARTESIAN_POINT('Ctrl Pts',(-8.35709812718722,-4.23819694879667,
5.7264833822988));
#80135=CARTESIAN_POINT('Ctrl Pts',(-8.3377293872886,-4.27617482744637,5.72722287248126));
#80136=CARTESIAN_POINT('Ctrl Pts',(-8.2954431205099,-4.35770934711342,5.72881092762362));
#80137=CARTESIAN_POINT('Ctrl Pts',(-8.27244021015677,-4.40122031953226,
5.72965867337914));
#80138=CARTESIAN_POINT('Ctrl Pts',(-8.23075656345284,-4.47858530181541,
5.73116524002601));
#80139=CARTESIAN_POINT('Ctrl Pts',(-8.21220706887636,-4.51250872325204,
5.73182557814925));
#80140=CARTESIAN_POINT('Ctrl Pts',(-8.1792144487369,-4.57196857993514,5.73298187667849));
#80141=CARTESIAN_POINT('Ctrl Pts',(-8.16486038344219,-4.59755376402362,
5.73347902203042));
#80142=CARTESIAN_POINT('Ctrl Pts',(-8.12032239722587,-4.6760733860798,5.73500407578025));
#80143=CARTESIAN_POINT('Ctrl Pts',(-8.08974204413658,-4.7287812203867,5.73602689665022));
#80144=CARTESIAN_POINT('Ctrl Pts',(-7.92605554652935,-5.00467340397007,
5.74138510962711));
#80145=CARTESIAN_POINT('Ctrl Pts',(-7.78422154660125,-5.22254806498498,
5.74563493653989));
#80146=CARTESIAN_POINT('Ctrl Pts',(-7.51975885549578,-5.59404027625978,
5.75310958534515));
#80147=CARTESIAN_POINT('Ctrl Pts',(-7.40101298807343,-5.75022316452486,
5.75632766516728));
#80148=CARTESIAN_POINT('Ctrl Pts',(-7.22990259146722,-5.9611904641756,5.76082578575394));
#80149=CARTESIAN_POINT('Ctrl Pts',(-7.18164520809691,-6.01924042669869,
5.76207992244942));
#80150=CARTESIAN_POINT('Ctrl Pts',(-7.11119041329583,-6.10193864436893,
5.7638922317589));
#80151=CARTESIAN_POINT('Ctrl Pts',(-7.08955530454295,-6.12706209332143,
5.76444627605989));
#80152=CARTESIAN_POINT('Ctrl Pts',(-7.01196733192476,-6.21619880240184,
5.76642472547702));
#80153=CARTESIAN_POINT('Ctrl Pts',(-6.95527721952354,-6.27956464848709,
5.76785480225397));
#80154=CARTESIAN_POINT('Ctrl Pts',(-6.84433833877763,-6.40022195420276,
5.77062600334781));
#80155=CARTESIAN_POINT('Ctrl Pts',(-6.79021280718335,-6.45761708049246,
5.7719659884356));
#80156=CARTESIAN_POINT('Ctrl Pts',(-6.66612540844515,-6.58591507542862,
5.77501210351289));
#80157=CARTESIAN_POINT('Ctrl Pts',(-6.5957447901225,-6.65639962288557,5.77672182945038));
#80158=CARTESIAN_POINT('Ctrl Pts',(-6.24064946601922,-7.00085675724952,
5.78525986158919));
#80159=CARTESIAN_POINT('Ctrl Pts',(-5.93992882897042,-7.25775057819928,
5.79223458689192));
#80160=CARTESIAN_POINT('Ctrl Pts',(-5.49241591368908,-7.59354808339555,
5.80204878857817));
#80161=CARTESIAN_POINT('Ctrl Pts',(-5.35836315436023,-7.68872873936398,
5.80491999001603));
#80162=CARTESIAN_POINT('Ctrl Pts',(-5.17623845460289,-7.81096418633117,
5.80869999228001));
#80163=CARTESIAN_POINT('Ctrl Pts',(-5.13033222445535,-7.8411923420122,5.80964278023133));
#80164=CARTESIAN_POINT('Ctrl Pts',(-5.04859240513639,-7.89399093801382,
5.81130208134062));
#80165=CARTESIAN_POINT('Ctrl Pts',(-5.01286699732228,-7.91672550188332,
5.81202066478612));
#80166=CARTESIAN_POINT('Ctrl Pts',(-4.92314657136959,-7.9729700304823,5.81380943499928));
#80167=CARTESIAN_POINT('Ctrl Pts',(-4.86896255644299,-8.00617429995087,
5.81487570446277));
#80168=CARTESIAN_POINT('Ctrl Pts',(-4.65897621502866,-8.13193492871861,
5.81896194121221));
#80169=CARTESIAN_POINT('Ctrl Pts',(-4.50083869776133,-8.22051558191104,
5.8219433426094));
#80170=CARTESIAN_POINT('Ctrl Pts',(-4.12461908357614,-8.41714262003123,
5.8289083865292));
#80171=CARTESIAN_POINT('Ctrl Pts',(-3.90469932876008,-8.52139047096103,
5.8328842860495));
#80172=CARTESIAN_POINT('Ctrl Pts',(-3.57605834438582,-8.6617785360276,5.83878805626679));
#80173=CARTESIAN_POINT('Ctrl Pts',(-3.47033427033911,-8.70467579328038,
5.84068128097275));
#80174=CARTESIAN_POINT('Ctrl Pts',(-3.27025966716364,-8.78163097126256,
5.84426111042753));
#80175=CARTESIAN_POINT('Ctrl Pts',(-3.17609418153422,-8.81612536729526,
5.84594473506969));
#80176=CARTESIAN_POINT('Ctrl Pts',(-3.00757029402036,-8.87480797823594,
5.84895903747043));
#80177=CARTESIAN_POINT('Ctrl Pts',(-2.93342854093253,-8.89958946730819,
5.85028555830016));
#80178=CARTESIAN_POINT('Ctrl Pts',(-2.76846507914372,-8.95244219328348,
5.85323889290671));
#80179=CARTESIAN_POINT('Ctrl Pts',(-2.6775087629876,-8.98006497108694,5.8548685395246));
#80180=CARTESIAN_POINT('Ctrl Pts',(-2.22586671497069,-9.10975344980545,
5.86296697387117));
#80181=CARTESIAN_POINT('Ctrl Pts',(-1.85970338242008,-9.1914955855669,5.8695683725386));
#80182=CARTESIAN_POINT('Ctrl Pts',(-1.29841769536839,-9.28187524300104,
5.87955474604179));
#80183=CARTESIAN_POINT('Ctrl Pts',(-1.10629282416263,-9.30672945098972,
5.88294659698164));
#80184=CARTESIAN_POINT('Ctrl Pts',(-0.85718651856507,-9.33113187370542,
5.88726292983199));
#80185=CARTESIAN_POINT('Ctrl Pts',(-0.800788287175399,-9.33614100746879,
5.88823470407168));
#80186=CARTESIAN_POINT('Ctrl Pts',(-0.702278390065371,-9.34399118261003,
5.88992062896209));
#80187=CARTESIAN_POINT('Ctrl Pts',(-0.660186722569009,-9.34705941217063,
5.89063719723311));
#80188=CARTESIAN_POINT('Ctrl Pts',(-0.556893519628924,-9.35388765530491,
5.89238676057105));
#80189=CARTESIAN_POINT('Ctrl Pts',(-0.49567316430912,-9.3573314999089,5.89341629746416));
#80190=CARTESIAN_POINT('Ctrl Pts',(-0.148751782971023,-9.3734327754173,
5.89921859690431));
#80191=CARTESIAN_POINT('Ctrl Pts',(0.137378082591571,-9.37360643657555,
5.90388657303226));
#80192=CARTESIAN_POINT('Ctrl Pts',(0.673437879476852,-9.34937857496442,
5.91268538258595));
#80193=CARTESIAN_POINT('Ctrl Pts',(0.923252734535412,-9.32802241842335,
5.91680711075412));
#80194=CARTESIAN_POINT('Ctrl Pts',(1.27393290959422,-9.28381678721565,5.92270552928298));
#80195=CARTESIAN_POINT('Ctrl Pts',(1.37573731508842,-9.26927753213982,5.92443090862054));
#80196=CARTESIAN_POINT('Ctrl Pts',(1.55532738118887,-9.24060540239003,5.92750141527083));
#80197=CARTESIAN_POINT('Ctrl Pts',(1.63321228097212,-9.22715823408952,5.92884199466574));
#80198=CARTESIAN_POINT('Ctrl Pts',(1.80283291570744,-9.19565758063653,5.93178222275854));
#80199=CARTESIAN_POINT('Ctrl Pts',(1.89448744222888,-9.17721320110186,5.93338427021411));
#80200=CARTESIAN_POINT('Ctrl Pts',(2.38356005989273,-9.07115416345611,5.94200468403278));
#80201=CARTESIAN_POINT('Ctrl Pts',(2.77522746517241,-8.95909065037087,5.9491849994521));
#80202=CARTESIAN_POINT('Ctrl Pts',(3.31793600891249,-8.76479395183734,5.95929956410146));
#80203=CARTESIAN_POINT('Ctrl Pts',(3.47593008452458,-8.70334548886938,5.96226151706799));
#80204=CARTESIAN_POINT('Ctrl Pts',(3.68315929617666,-8.61620462959695,5.96613622428821));
#80205=CARTESIAN_POINT('Ctrl Pts',(3.73395717965211,-8.59431256236282,5.9670851352119));
#80206=CARTESIAN_POINT('Ctrl Pts',(3.8232613194498,-8.55488444411153,5.96874992511386));
#80207=CARTESIAN_POINT('Ctrl Pts',(3.86184798868055,-8.5375350707468,5.969467948299));
#80208=CARTESIAN_POINT('Ctrl Pts',(3.95763751639169,-8.49368381194098,5.97124775036518));
#80209=CARTESIAN_POINT('Ctrl Pts',(4.01469281919533,-8.46686488627385,5.97230571577114));
#80210=CARTESIAN_POINT('Ctrl Pts',(4.2943905263886,-8.33192970363889,5.97749098320125));
#80211=CARTESIAN_POINT('Ctrl Pts',(4.51296022332444,-8.21559696187818,5.98154205998362));
#80212=CARTESIAN_POINT('Ctrl Pts',(4.90127265389691,-7.9887422866103,5.98891320350184));
#80213=CARTESIAN_POINT('Ctrl Pts',(5.07252944799921,-7.88111171000584,5.99222895008845));
#80214=CARTESIAN_POINT('Ctrl Pts',(5.29669247002343,-7.7298953858856,5.99670493233763));
#80215=CARTESIAN_POINT('Ctrl Pts',(5.35279778207977,-7.69115008866333,5.99783688370306));
#80216=CARTESIAN_POINT('Ctrl Pts',(5.49750932464677,-7.58886445666173,6.0007894917787));
#80217=CARTESIAN_POINT('Ctrl Pts',(5.58543813831908,-7.5243839109072,6.00261631358706));
#80218=CARTESIAN_POINT('Ctrl Pts',(5.73554978053464,-7.41022157855666,6.00579706183785));
#80219=CARTESIAN_POINT('Ctrl Pts',(5.79826198238004,-7.36125485754256,6.00714519553937));
#80220=CARTESIAN_POINT('Ctrl Pts',(5.93050039040628,-7.25526253176817,6.01003064519876));
#80221=CARTESIAN_POINT('Ctrl Pts',(5.9998447730445,-7.19802277959892,6.01156961779686));
#80222=CARTESIAN_POINT('Ctrl Pts',(6.21008701616427,-7.01933072453739,6.01631635684503));
#80223=CARTESIAN_POINT('Ctrl Pts',(6.3482006653884,-6.89467421333244,6.01954944924155));
#80224=CARTESIAN_POINT('Ctrl Pts',(6.68304780143827,-6.57385633702655,6.02766218432736));
#80225=CARTESIAN_POINT('Ctrl Pts',(6.87494211602099,-6.37290244745842,6.03256623544286));
#80226=CARTESIAN_POINT('Ctrl Pts',(7.11868235019254,-6.09381340562548,6.03904980089865));
#80227=CARTESIAN_POINT('Ctrl Pts',(7.17869567645664,-6.02299997189171,6.04066808171214));
#80228=CARTESIAN_POINT('Ctrl Pts',(7.28243353406133,-5.8968397757551,6.04349723011847));
#80229=CARTESIAN_POINT('Ctrl Pts',(7.32660380893084,-5.84186906573156,6.04471245642751));
#80230=CARTESIAN_POINT('Ctrl Pts',(7.39677938674177,-5.7524863658962,6.04665711473027));
#80231=CARTESIAN_POINT('Ctrl Pts',(7.42317490797182,-5.71838429931365,6.04739180323136));
#80232=CARTESIAN_POINT('Ctrl Pts',(7.48039739906122,-5.64339100616804,6.04899089194547));
#80233=CARTESIAN_POINT('Ctrl Pts',(7.51112641869461,-5.60242690575665,6.04985398855079));
#80234=CARTESIAN_POINT('Ctrl Pts',(7.60611145105714,-5.47361843266442,6.05253897098111));
#80235=CARTESIAN_POINT('Ctrl Pts',(7.66917390194261,-5.38490500557184,6.05434665620785));
#80236=CARTESIAN_POINT('Ctrl Pts',(7.8676380456355,-5.09515441374848,6.06014851421637));
#80237=CARTESIAN_POINT('Ctrl Pts',(7.99678989160347,-4.88995692451142,6.06410411972999));
#80238=CARTESIAN_POINT('Ctrl Pts',(8.23452758477266,-4.47758008298047,6.07191898043548));
#80239=CARTESIAN_POINT('Ctrl Pts',(8.34360334940062,-4.27088405500965,6.07577381401048));
#80240=CARTESIAN_POINT('Ctrl Pts',(8.48561924244266,-3.97551351444562,6.08125750714715));
#80241=CARTESIAN_POINT('Ctrl Pts',(8.52511868798272,-3.89008906491107,6.08284028780693));
#80242=CARTESIAN_POINT('Ctrl Pts',(8.59539006149435,-3.73190209083887,6.08576811064334));
#80243=CARTESIAN_POINT('Ctrl Pts',(8.6265415508776,-3.65931747216172,6.08711034630741));
#80244=CARTESIAN_POINT('Ctrl Pts',(8.69513139988357,-3.49375442873971,6.09017015153204));
#80245=CARTESIAN_POINT('Ctrl Pts',(8.73200308364739,-3.40055174197167,6.09189142017786));
#80246=CARTESIAN_POINT('Ctrl Pts',(8.87818120420275,-3.01298447179128,6.09904358072649));
#80247=CARTESIAN_POINT('Ctrl Pts',(8.97415229833049,-2.7138102195224,6.10455903332022));
#80248=CARTESIAN_POINT('Ctrl Pts',(9.11316904644161,-2.19157598664342,6.11406000186328));
#80249=CARTESIAN_POINT('Ctrl Pts',(9.1634651163244,-1.97072647352548,6.11803795897781));
#80250=CARTESIAN_POINT('Ctrl Pts',(9.21716623175992,-1.68795757367764,6.12300989367577));
#80251=CARTESIAN_POINT('Ctrl Pts',(9.22802765733316,-1.62753177992911,6.12406526133904));
#80252=CARTESIAN_POINT('Ctrl Pts',(9.24535277854114,-1.52539124957618,6.12583486318534));
#80253=CARTESIAN_POINT('Ctrl Pts',(9.2521298298479,-1.48373181188135,6.12655249295961));
#80254=CARTESIAN_POINT('Ctrl Pts',(9.26717202857151,-1.3871524800995,6.12820651012829));
#80255=CARTESIAN_POINT('Ctrl Pts',(9.27523082090141,-1.33220217993527,6.12914063691566));
#80256=CARTESIAN_POINT('Ctrl Pts',(9.30734094334531,-1.09881998767124,6.13308421471276));
#80257=CARTESIAN_POINT('Ctrl Pts',(9.32673551689654,-0.919785730008978,
6.13605122836288));
#80258=CARTESIAN_POINT('Ctrl Pts',(9.36110517231301,-0.486118346054322,
6.14319396722927));
#80259=CARTESIAN_POINT('Ctrl Pts',(9.37086654878271,-0.23121682214252,6.14735761199216));
#80260=CARTESIAN_POINT('Ctrl Pts',(9.36992485280812,0.140084800764607,6.15348879838844));
#80261=CARTESIAN_POINT('Ctrl Pts',(9.36746390813516,0.256389058886919,6.15541820411153));
#80262=CARTESIAN_POINT('Ctrl Pts',(9.35879843840504,0.474128364609442,6.15905592536975));
#80263=CARTESIAN_POINT('Ctrl Pts',(9.35310795757786,0.575567010995413,6.1607610334505));
#80264=CARTESIAN_POINT('Ctrl Pts',(9.34006485145293,0.755651429500956,6.1638101563054));
#80265=CARTESIAN_POINT('Ctrl Pts',(9.33336521440224,0.834334617044215,6.1651498692248));
#80266=CARTESIAN_POINT('Ctrl Pts',(9.31647616355166,1.00685918106568,6.16810487434907));
#80267=CARTESIAN_POINT('Ctrl Pts',(9.30586172229825,1.10065029206905,6.16972274481083));
#80268=CARTESIAN_POINT('Ctrl Pts',(9.24415484696524,1.58085645258049,6.17806514221114));
#80269=CARTESIAN_POINT('Ctrl Pts',(9.17040470885361,1.96397053843015,6.18493543586881));
#80270=CARTESIAN_POINT('Ctrl Pts',(9.02751260845457,2.51768919120335,6.19497591976177));
#80271=CARTESIAN_POINT('Ctrl Pts',(8.97688258804136,2.69264221034147,6.19816170903787));
#80272=CARTESIAN_POINT('Ctrl Pts',(8.90403957850057,2.91938474008857,6.20226775289852));
#80273=CARTESIAN_POINT('Ctrl Pts',(8.88641342281548,2.97260568770848,6.20322978455498));
#80274=CARTESIAN_POINT('Ctrl Pts',(8.85467119449909,3.06564305738611,6.20490658662642));
#80275=CARTESIAN_POINT('Ctrl Pts',(8.84076158880002,3.10552795067008,6.20562365861683));
#80276=CARTESIAN_POINT('Ctrl Pts',(8.80576343239858,3.20374191747348,6.20738551631121));
#80277=CARTESIAN_POINT('Ctrl Pts',(8.78436457079818,3.26195815636694,6.2084266982899));
#80278=CARTESIAN_POINT('Ctrl Pts',(8.64991813925135,3.61680362908467,6.21476486532073));
#80279=CARTESIAN_POINT('Ctrl Pts',(8.52243474113213,3.90774360523559,6.21993373757005));
#80280=CARTESIAN_POINT('Ctrl Pts',(8.30689683913583,4.33867169560046,6.22784173171171));
#80281=CARTESIAN_POINT('Ctrl Pts',(8.22950596118469,4.48373044069475,6.23054789652886));
#80282=CARTESIAN_POINT('Ctrl Pts',(8.08549781613653,4.73735243139542,6.23538890072163));
#80283=CARTESIAN_POINT('Ctrl Pts',(8.02040793978089,4.84673491668542,6.23751414641699));
#80284=CARTESIAN_POINT('Ctrl Pts',(7.9097753326328,5.02431643515025,6.2410346559183));
#80285=CARTESIAN_POINT('Ctrl Pts',(7.86552966502222,5.09330388890879,6.24242018847512));
#80286=CARTESIAN_POINT('Ctrl Pts',(7.77953288199946,5.22359578512762,6.24507261741535));
#80287=CARTESIAN_POINT('Ctrl Pts',(7.73794769652738,5.28500238471348,6.24633816674097));
#80288=CARTESIAN_POINT('Ctrl Pts',(7.62146209408408,5.4526878180565,6.24983747911631));
#80289=CARTESIAN_POINT('Ctrl Pts',(7.54507200662133,5.55791122351216,6.25208235871162));
#80290=CARTESIAN_POINT('Ctrl Pts',(7.25428179429235,5.94141136517929,6.26044358964722));
#80291=CARTESIAN_POINT('Ctrl Pts',(7.02647520775919,6.20915597284784,6.26665132712106));
#80292=CARTESIAN_POINT('Ctrl Pts',(6.68409099636591,6.56852845116939,6.27534631296114));
#80293=CARTESIAN_POINT('Ctrl Pts',(6.58157750046899,6.67124248291188,6.27787581403516));
#80294=CARTESIAN_POINT('Ctrl Pts',(6.43813779063008,6.80843721004593,6.28129415108693));
#80295=CARTESIAN_POINT('Ctrl Pts',(6.39924073447242,6.8450093859593,6.2822093666758));
#80296=CARTESIAN_POINT('Ctrl Pts',(6.32876291553775,6.91014892476682,6.28384501022444));
#80297=CARTESIAN_POINT('Ctrl Pts',(6.29729606227471,6.93883711491506,6.28456717303119));
#80298=CARTESIAN_POINT('Ctrl Pts',(6.22492724507355,7.00391769543092,6.28621039219053));
#80299=CARTESIAN_POINT('Ctrl Pts',(6.18389968847303,7.04016810531864,6.28712942377716));
#80300=CARTESIAN_POINT('Ctrl Pts',(5.87847339219256,7.30530141027337,6.29388843375093));
#80301=CARTESIAN_POINT('Ctrl Pts',(5.60176269398799,7.51958344087067,6.29956979912413));
#80302=CARTESIAN_POINT('Ctrl Pts',(5.13520482715964,7.84080554308283,6.30887825699849));
#80303=CARTESIAN_POINT('Ctrl Pts',(4.95247676866788,7.95748286948099,6.31245969834133));
#80304=CARTESIAN_POINT('Ctrl Pts',(4.68590103401696,8.11495797011017,6.31764236401883));
#80305=CARTESIAN_POINT('Ctrl Pts',(4.60523607126288,8.16100557731572,6.31920503690089));
#80306=CARTESIAN_POINT('Ctrl Pts',(4.45463507415977,8.24403221831331,6.3221147965681));
#80307=CARTESIAN_POINT('Ctrl Pts',(4.38488951279526,8.28133955270473,6.3234593300468));
#80308=CARTESIAN_POINT('Ctrl Pts',(4.30676807497231,8.32186356866996,6.32496243791178));
#80309=CARTESIAN_POINT('Ctrl Pts',(4.29885024370113,8.32595646683595,6.3251147489697));
#80310=CARTESIAN_POINT('Ctrl Pts',(4.2909266281297,8.33003803919931,6.32526713834515));
#80311=CARTESIAN_POINT('Origin',(0.,0.,2.15141010809499));
#80312=CARTESIAN_POINT('',(4.29124165107371,8.33064876708861,7.52288355898759));
#80313=CARTESIAN_POINT('',(4.2909265843892,8.3300380617307,7.32568828984052));
#80314=CARTESIAN_POINT('',(4.29092662815669,8.33003803918541,2.15141010809499));
#80315=CARTESIAN_POINT('',(-9.36967603564898,0.000162953396886864,6.84858989190502));
#80316=CARTESIAN_POINT('Ctrl Pts',(-9.36967603564898,0.000162953396886864,
6.84858989190502));
#80317=CARTESIAN_POINT('Ctrl Pts',(-9.36906102305612,-0.971808257735063,
6.8650963705856));
#80318=CARTESIAN_POINT('Ctrl Pts',(-8.97915541211587,-3.48971372166328,
6.90784845369182));
#80319=CARTESIAN_POINT('Ctrl Pts',(-6.75951736416114,-7.04192909134281,
6.97684614122372));
#80320=CARTESIAN_POINT('Ctrl Pts',(-2.6056775367071,-9.40692749512803,7.05558295450069));
#80321=CARTESIAN_POINT('Ctrl Pts',(2.17299000962536,-9.51619434133018,7.13431976777767));
#80322=CARTESIAN_POINT('Ctrl Pts',(6.43058602207351,-7.34352801700983,7.21305658105463));
#80323=CARTESIAN_POINT('Ctrl Pts',(9.14616145115302,-3.40992243802385,7.29179339433162));
#80324=CARTESIAN_POINT('Ctrl Pts',(9.6685356435055,1.34136454186004,7.37053020760858));
#80325=CARTESIAN_POINT('Ctrl Pts',(7.91137941483978,5.67497928827927,7.44756026249395));
#80326=CARTESIAN_POINT('Ctrl Pts',(5.57491667009454,7.66849856053472,7.49834471295364));
#80327=CARTESIAN_POINT('Ctrl Pts',(4.2912416510688,8.33064876709114,7.52288355898769));
#80328=CARTESIAN_POINT('Ctrl Pts',(-9.37024999848114,0.000168713661654052,
6.84892119005222));
#80329=CARTESIAN_POINT('Ctrl Pts',(-9.37024174247316,0.458702171958208,
6.84096250684365));
#80330=CARTESIAN_POINT('Ctrl Pts',(-9.33657615779602,0.916613734320751,
6.83280799835693));
#80331=CARTESIAN_POINT('Ctrl Pts',(-9.26117378581003,1.42671188575608,6.82386213762273));
#80332=CARTESIAN_POINT('Ctrl Pts',(-9.25230611491123,1.48313123801808,6.82287514079911));
#80333=CARTESIAN_POINT('Ctrl Pts',(-9.23619781542005,1.57984514384641,6.82118932015834));
#80334=CARTESIAN_POINT('Ctrl Pts',(-9.22920788916571,1.62017977724394,6.82048807311815));
#80335=CARTESIAN_POINT('Ctrl Pts',(-9.21446289039731,1.702070997951,6.81906891847766));
#80336=CARTESIAN_POINT('Ctrl Pts',(-9.20669049302843,1.74362329928961,6.81835139424002));
#80337=CARTESIAN_POINT('Ctrl Pts',(-9.18672196617001,1.84652005018696,6.81658040300009));
#80338=CARTESIAN_POINT('Ctrl Pts',(-9.17419234626702,1.90779757813584,6.8155306468891));
#80339=CARTESIAN_POINT('Ctrl Pts',(-9.12649736516666,2.12971138493879,6.81174003623811));
#80340=CARTESIAN_POINT('Ctrl Pts',(-9.08771855457536,2.28954067268794,6.80903053365417));
#80341=CARTESIAN_POINT('Ctrl Pts',(-9.03624107412047,2.47971648816626,6.80579543716441));
#80342=CARTESIAN_POINT('Ctrl Pts',(-9.02756419917994,2.51112151073629,6.80526085579008));
#80343=CARTESIAN_POINT('Ctrl Pts',(-9.00680286197389,2.58476642305526,6.80400596324978));
#80344=CARTESIAN_POINT('Ctrl Pts',(-8.99458477067406,2.62696784526347,6.80328585368802));
#80345=CARTESIAN_POINT('Ctrl Pts',(-8.92317946438855,2.86726302420927,6.79917710657475));
#80346=CARTESIAN_POINT('Ctrl Pts',(-8.85774573983435,3.06344075383916,6.79578848590553));
#80347=CARTESIAN_POINT('Ctrl Pts',(-8.74896410420198,3.35685681789658,6.79060979358623));
#80348=CARTESIAN_POINT('Ctrl Pts',(-8.71036184534189,3.45578602512267,6.7888445318475));
#80349=CARTESIAN_POINT('Ctrl Pts',(-8.63494860686427,3.63975687279058,6.78551937821395));
#80350=CARTESIAN_POINT('Ctrl Pts',(-8.59854136401997,3.72495018706322,6.78396221380906));
#80351=CARTESIAN_POINT('Ctrl Pts',(-8.52987155896806,3.87926438556947,6.78110724981502));
#80352=CARTESIAN_POINT('Ctrl Pts',(-8.49801683060932,3.94855807883894,6.77981238981641));
#80353=CARTESIAN_POINT('Ctrl Pts',(-8.42374798529678,4.10505255456956,6.77685776503906));
#80354=CARTESIAN_POINT('Ctrl Pts',(-8.38081906958307,4.19199931505509,6.77519450020538));
#80355=CARTESIAN_POINT('Ctrl Pts',(-8.22110539957664,4.50321451100649,6.76916211847607));
#80356=CARTESIAN_POINT('Ctrl Pts',(-8.09660496314985,4.72339942635138,6.76474130708951));
#80357=CARTESIAN_POINT('Ctrl Pts',(-7.85266114107542,5.11677757496733,6.75660984586563));
#80358=CARTESIAN_POINT('Ctrl Pts',(-7.73599886821021,5.29150463687477,6.7529087933557));
#80359=CARTESIAN_POINT('Ctrl Pts',(-7.56559312488128,5.52902865643566,6.74780295833642));
#80360=CARTESIAN_POINT('Ctrl Pts',(-7.51674348616794,5.59525911980468,6.74637103658131));
#80361=CARTESIAN_POINT('Ctrl Pts',(-7.43186477738892,5.70721987863468,6.74394137435124));
#80362=CARTESIAN_POINT('Ctrl Pts',(-7.39627038011127,5.75327361569894,6.74293929555495));
#80363=CARTESIAN_POINT('Ctrl Pts',(-7.35966877889239,5.79972942532535,6.74192694366899));
#80364=CARTESIAN_POINT('Ctrl Pts',(-7.35908828302135,5.8004659799611,6.74191089248809));
#80365=CARTESIAN_POINT('Ctrl Pts',(-7.35755458642954,5.80241139011471,6.74186849661121));
#80366=CARTESIAN_POINT('Ctrl Pts',(-7.35660119833329,5.80362009793067,6.74184215448131));
#80367=CARTESIAN_POINT('Ctrl Pts',(-7.35415656162453,5.80671784417866,6.74177464074576));
#80368=CARTESIAN_POINT('Ctrl Pts',(-7.35266488295041,5.80860654320961,6.74173347507072));
#80369=CARTESIAN_POINT('Ctrl Pts',(-7.34897529552922,5.81327444070427,6.74163172866638));
#80370=CARTESIAN_POINT('Ctrl Pts',(-7.3467765376102,5.81605296774968,6.74157115977476));
#80371=CARTESIAN_POINT('Ctrl Pts',(-7.34322220186211,5.82053928005766,6.7414733550675));
#80372=CARTESIAN_POINT('Ctrl Pts',(-7.34186760316945,5.8222478403231,6.74143610541152));
#80373=CARTESIAN_POINT('Ctrl Pts',(-7.31428791394129,5.85700927284497,6.74067820771852));
#80374=CARTESIAN_POINT('Ctrl Pts',(-7.28784050782147,5.8898850630803,6.73996086584397));
#80375=CARTESIAN_POINT('Ctrl Pts',(-7.22592419142597,5.96579537834134,6.73830331550946));
#80376=CARTESIAN_POINT('Ctrl Pts',(-7.19029143554791,6.00869403511289,6.73736541525924));
#80377=CARTESIAN_POINT('Ctrl Pts',(-7.04432670067132,6.1812647352471,6.73358219127143));
#80378=CARTESIAN_POINT('Ctrl Pts',(-6.9308527311781,6.30823692848806,6.7307742557749));
#80379=CARTESIAN_POINT('Ctrl Pts',(-6.63460323537928,6.62207772888062,6.72368494586477));
#80380=CARTESIAN_POINT('Ctrl Pts',(-6.44735336632636,6.80452115523511,6.71941962861559));
#80381=CARTESIAN_POINT('Ctrl Pts',(-6.16522885965651,7.05728974505148,6.71316611543111));
#80382=CARTESIAN_POINT('Ctrl Pts',(-6.0762679787279,7.13402781096093,6.71121801563212));
#80383=CARTESIAN_POINT('Ctrl Pts',(-5.90720839705525,7.27440255069153,6.70755043766786));
#80384=CARTESIAN_POINT('Ctrl Pts',(-5.82746473998336,7.33843976279926,6.70583428676418));
#80385=CARTESIAN_POINT('Ctrl Pts',(-5.68428987080573,7.4496090376287,6.70277355194577));
#80386=CARTESIAN_POINT('Ctrl Pts',(-5.62128058872318,7.4972682130247,6.70143340391258));
#80387=CARTESIAN_POINT('Ctrl Pts',(-5.48208747517783,7.59981029453659,6.6984866560835));
#80388=CARTESIAN_POINT('Ctrl Pts',(-5.40566616993475,7.6543564590344,6.69687757748631));
#80389=CARTESIAN_POINT('Ctrl Pts',(-4.99972262731092,7.93498913695198,6.68837552092417));
#80390=CARTESIAN_POINT('Ctrl Pts',(-4.65680760682547,8.14097159027103,6.68132764224587));
#80391=CARTESIAN_POINT('Ctrl Pts',(-4.14652522274127,8.40466899107092,6.67124621532479));
#80392=CARTESIAN_POINT('Ctrl Pts',(-3.98903967474142,8.48054803865381,6.66819039764238));
#80393=CARTESIAN_POINT('Ctrl Pts',(-3.77873692086913,8.57472033849949,6.66421830000596));
#80394=CARTESIAN_POINT('Ctrl Pts',(-3.7277481343934,8.59700968165085,6.66326355323828));
#80395=CARTESIAN_POINT('Ctrl Pts',(-3.63767886321769,8.63543077804461,6.66159346396252));
#80396=CARTESIAN_POINT('Ctrl Pts',(-3.59868232226685,8.65175460709144,6.66087590706295));
#80397=CARTESIAN_POINT('Ctrl Pts',(-3.51125278832007,8.68765894326536,6.65927898621263));
#80398=CARTESIAN_POINT('Ctrl Pts',(-3.46276394665995,8.70709939779863,6.65840121836173));
#80399=CARTESIAN_POINT('Ctrl Pts',(-3.12886272983523,8.83773883551723,6.65240319934048));
#80400=CARTESIAN_POINT('Ctrl Pts',(-2.83830833995859,8.93529054394326,6.64740935290815));
#80401=CARTESIAN_POINT('Ctrl Pts',(-2.29485172730786,9.08856333244864,6.63814782826857));
#80402=CARTESIAN_POINT('Ctrl Pts',(-2.04341195090278,9.14837662853422,6.63389389336607));
#80403=CARTESIAN_POINT('Ctrl Pts',(-1.69615718729479,9.2159503814685,6.62797725810729));
#80404=CARTESIAN_POINT('Ctrl Pts',(-1.60221820176393,9.23274538885601,6.62637301511406));
#80405=CARTESIAN_POINT('Ctrl Pts',(-1.43796624952718,9.25952908725064,6.62355893382753));
#80406=CARTESIAN_POINT('Ctrl Pts',(-1.36776573092296,9.27015872211614,6.62235335481336));
#80407=CARTESIAN_POINT('Ctrl Pts',(-1.20248569920118,9.29326680749097,6.61950748597603));
#80408=CARTESIAN_POINT('Ctrl Pts',(-1.10732207204248,9.30508557626445,6.6178631056096));
#80409=CARTESIAN_POINT('Ctrl Pts',(-0.777732754721942,9.34089090067309,
6.61214780552308));
#80410=CARTESIAN_POINT('Ctrl Pts',(-0.542595719124867,9.35749433550255,
6.60803304030991));
#80411=CARTESIAN_POINT('Ctrl Pts',(-0.0414449364577233,9.3739270047127,
6.59923027845724));
#80412=CARTESIAN_POINT('Ctrl Pts',(0.224444660868916,9.37133127361447,6.59453960626259));
#80413=CARTESIAN_POINT('Ctrl Pts',(0.581562626996471,9.35263608624222,6.58831647710312));
#80414=CARTESIAN_POINT('Ctrl Pts',(0.673186514475996,9.34648794124671,6.5867270922813));
#80415=CARTESIAN_POINT('Ctrl Pts',(0.81111981367436,9.33519354144149,6.58435203501646));
#80416=CARTESIAN_POINT('Ctrl Pts',(0.857505359061592,9.33104701412207,6.58355635303037));
#80417=CARTESIAN_POINT('Ctrl Pts',(0.943616297067151,9.32270180285456,6.5820860467029));
#80418=CARTESIAN_POINT('Ctrl Pts',(0.983349462781458,9.31859455392666,6.58141034315896));
#80419=CARTESIAN_POINT('Ctrl Pts',(1.10065906486532,9.30570952181116,6.5794219238715));
#80420=CARTESIAN_POINT('Ctrl Pts',(1.17815354946662,9.29621613030456,6.57811683437324));
#80421=CARTESIAN_POINT('Ctrl Pts',(1.60934123220643,9.23791554706517,6.57088242241443));
#80422=CARTESIAN_POINT('Ctrl Pts',(1.96013945505633,9.16989193264125,6.56508747683734));
#80423=CARTESIAN_POINT('Ctrl Pts',(2.43300685114192,9.04981655363189,6.55705140180732));
#80424=CARTESIAN_POINT('Ctrl Pts',(2.55912557962672,9.0149641240943,6.55488716664965));
#80425=CARTESIAN_POINT('Ctrl Pts',(2.78974850008086,8.946002587799,6.5508773383682));
#80426=CARTESIAN_POINT('Ctrl Pts',(2.89446202384925,8.91267347685104,6.54903657578847));
#80427=CARTESIAN_POINT('Ctrl Pts',(3.07402830222481,8.85202120897565,6.54584035820915));
#80428=CARTESIAN_POINT('Ctrl Pts',(3.14916347179829,8.82557073964811,6.54449086971189));
#80429=CARTESIAN_POINT('Ctrl Pts',(3.30800163769169,8.76736694218404,6.54161100474566));
#80430=CARTESIAN_POINT('Ctrl Pts',(3.39160532867814,8.73536554356725,6.54007905802973));
#80431=CARTESIAN_POINT('Ctrl Pts',(3.64423474391702,8.63449176354428,6.53540009955608));
#80432=CARTESIAN_POINT('Ctrl Pts',(3.81171791914635,8.56187485510295,6.53222890978592));
#80433=CARTESIAN_POINT('Ctrl Pts',(4.0825764503003,8.43491298136176,6.52699730798063));
#80434=CARTESIAN_POINT('Ctrl Pts',(4.18724592612468,8.38344551260659,6.52494983632478));
#80435=CARTESIAN_POINT('Ctrl Pts',(4.29092662818984,8.33003803916834,6.5228999581952));
#80436=CARTESIAN_POINT('Ctrl Pts',(4.2909266281297,8.33003803919931,6.32526713834515));
#80437=CARTESIAN_POINT('Ctrl Pts',(4.20824026393393,8.37263101659524,6.32685738755457));
#80438=CARTESIAN_POINT('Ctrl Pts',(4.12492400055656,8.41399063344705,6.32845622925807));
#80439=CARTESIAN_POINT('Ctrl Pts',(3.72134241221821,8.60689996893795,6.33618347881133));
#80440=CARTESIAN_POINT('Ctrl Pts',(3.3932713294365,8.74144289771762,6.34242481601055));
#80441=CARTESIAN_POINT('Ctrl Pts',(2.87651681075672,8.91987955999178,6.35202744607353));
#80442=CARTESIAN_POINT('Ctrl Pts',(2.69276846007288,8.97705957941376,6.35539642645059));
#80443=CARTESIAN_POINT('Ctrl Pts',(2.45288962748264,9.04367828578183,6.35968954079036));
#80444=CARTESIAN_POINT('Ctrl Pts',(2.3982530822198,9.05832029876584,6.36066033871355));
#80445=CARTESIAN_POINT('Ctrl Pts',(2.30262220965142,9.08302248135346,6.36234534204425));
#80446=CARTESIAN_POINT('Ctrl Pts',(2.26168648128923,9.09330196918904,6.36306195347132));
#80447=CARTESIAN_POINT('Ctrl Pts',(2.16104659776772,9.11785230962641,6.36481271171676));
#80448=CARTESIAN_POINT('Ctrl Pts',(2.10126909235884,9.13181369521687,6.36584338614031));
#80449=CARTESIAN_POINT('Ctrl Pts',(1.7288101627805,9.21495275809605,6.37221909341532));
#80450=CARTESIAN_POINT('Ctrl Pts',(1.4128894275344,9.26865061007484,6.37743276842286));
#80451=CARTESIAN_POINT('Ctrl Pts',(0.932333361058202,9.32518704685286,6.38537475168573));
#80452=CARTESIAN_POINT('Ctrl Pts',(0.76935417498574,9.34004566161037,6.38806870842036));
#80453=CARTESIAN_POINT('Ctrl Pts',(0.479428746746019,9.35883745518134,6.39289142743024));
#80454=CARTESIAN_POINT('Ctrl Pts',(0.35263413409879,9.36447219458713,6.39501071926421));
#80455=CARTESIAN_POINT('Ctrl Pts',(0.143887695419758,9.36950314043737,6.39852434619891));
#80456=CARTESIAN_POINT('Ctrl Pts',(0.0619886648817329,9.37040288012853,
6.39990903381663));
#80457=CARTESIAN_POINT('Ctrl Pts',(-0.0941224008508102,9.37007114797953,
6.40256151633704));
#80458=CARTESIAN_POINT('Ctrl Pts',(-0.168328701385573,9.36903184778882,
6.40382798079593));
#80459=CARTESIAN_POINT('Ctrl Pts',(-0.372867328048197,9.3637363381592,6.40733483900856));
#80460=CARTESIAN_POINT('Ctrl Pts',(-0.50313497886277,9.35764090503565,6.4095864368847));
#80461=CARTESIAN_POINT('Ctrl Pts',(-0.960429953277878,9.32666653321074,
6.41754968359261));
#80462=CARTESIAN_POINT('Ctrl Pts',(-1.28623767891919,9.28734222648609,6.42333788372226));
#80463=CARTESIAN_POINT('Ctrl Pts',(-1.77075907769906,9.20287213044927,6.4319649872657));
#80464=CARTESIAN_POINT('Ctrl Pts',(-1.93144257299956,9.17049469789188,6.4348274384152));
#80465=CARTESIAN_POINT('Ctrl Pts',(-2.14473741065076,9.12166123210943,6.43859828039155));
#80466=CARTESIAN_POINT('Ctrl Pts',(-2.19817172710813,9.10893205984011,6.43954045247104));
#80467=CARTESIAN_POINT('Ctrl Pts',(-2.29259999103672,9.08555798128995,6.4411992058699));
#80468=CARTESIAN_POINT('Ctrl Pts',(-2.33363923979937,9.07510366062315,6.44191785002316));
#80469=CARTESIAN_POINT('Ctrl Pts',(-2.43612903831635,9.04825426077827,6.44370754459808));
#80470=CARTESIAN_POINT('Ctrl Pts',(-2.49748609012978,9.03151112028137,6.44477466704706));
#80471=CARTESIAN_POINT('Ctrl Pts',(-2.73366320524356,8.9644721657767,6.44887322371298));
#80472=CARTESIAN_POINT('Ctrl Pts',(-2.90717534258993,8.90971422774936,6.45186578918107));
#80473=CARTESIAN_POINT('Ctrl Pts',(-3.18788479722213,8.81205257097316,6.45674217652053));
#80474=CARTESIAN_POINT('Ctrl Pts',(-3.29607728271606,8.77215791843709,6.45863016648515));
#80475=CARTESIAN_POINT('Ctrl Pts',(-3.56501848524114,8.66731095973559,6.46336515421568));
#80476=CARTESIAN_POINT('Ctrl Pts',(-3.72475240996275,8.59987531305519,6.46621594881002));
#80477=CARTESIAN_POINT('Ctrl Pts',(-3.93902149984893,8.50232605457052,6.47012079239418));
#80478=CARTESIAN_POINT('Ctrl Pts',(-3.99526265433698,8.47604359499193,6.47115336904407));
#80479=CARTESIAN_POINT('Ctrl Pts',(-4.14366428661825,8.40488773471997,6.47390008629846));
#80480=CARTESIAN_POINT('Ctrl Pts',(-4.23535657858824,8.3590577302389,6.47562007556154));
#80481=CARTESIAN_POINT('Ctrl Pts',(-4.39636673767234,8.27525152679643,6.47868487060906));
#80482=CARTESIAN_POINT('Ctrl Pts',(-4.46599078959337,8.23788532072609,6.48002519394716));
#80483=CARTESIAN_POINT('Ctrl Pts',(-4.61714414592048,8.15428403568982,6.48296920031215));
#80484=CARTESIAN_POINT('Ctrl Pts',(-4.69846921875761,8.10769727751822,6.48457532857659));
#80485=CARTESIAN_POINT('Ctrl Pts',(-5.12550919225414,7.85448579046357,6.49312796643928));
#80486=CARTESIAN_POINT('Ctrl Pts',(-5.45833183394866,7.62695231257382,6.50023235948535));
#80487=CARTESIAN_POINT('Ctrl Pts',(-5.91131825881639,7.27239020338144,6.5103276591376));
#80488=CARTESIAN_POINT('Ctrl Pts',(-6.04419722406677,7.16233362996991,6.51334310653496));
#80489=CARTESIAN_POINT('Ctrl Pts',(-6.21571679698328,7.01209888397556,6.51727338736357));
#80490=CARTESIAN_POINT('Ctrl Pts',(-6.25714541854583,6.97515571792162,6.5182256857719));
#80491=CARTESIAN_POINT('Ctrl Pts',(-6.32955403462572,6.90942248458571,6.51989354515226));
#80492=CARTESIAN_POINT('Ctrl Pts',(-6.3606717625331,6.88078687945077,6.52061129108964));
#80493=CARTESIAN_POINT('Ctrl Pts',(-6.43749596167262,6.80912410331586,6.52238629887018));
#80494=CARTESIAN_POINT('Ctrl Pts',(-6.48296585722228,6.7658465125396,6.5234398030005));
#80495=CARTESIAN_POINT('Ctrl Pts',(-6.71016004486372,6.54521311962335,6.52872824975175));
#80496=CARTESIAN_POINT('Ctrl Pts',(-6.88505713637971,6.36097883502184,6.53288252106733));
#80497=CARTESIAN_POINT('Ctrl Pts',(-7.22621487569311,5.97103024232393,6.54137494910345));
#80498=CARTESIAN_POINT('Ctrl Pts',(-7.39168681102954,5.7649240447985,6.5457105629208));
#80499=CARTESIAN_POINT('Ctrl Pts',(-7.61292421675052,5.46414603557416,6.55193142581384));
#80500=CARTESIAN_POINT('Ctrl Pts',(-7.67607818208552,5.37506564516312,6.55376083588463));
#80501=CARTESIAN_POINT('Ctrl Pts',(-7.78254362240083,5.21918887593585,6.55694445207441));
#80502=CARTESIAN_POINT('Ctrl Pts',(-7.8265874254669,5.15290665493554,6.55829283325664));
#80503=CARTESIAN_POINT('Ctrl Pts',(-7.91854415724771,5.01062014153191,6.56117721864386));
#80504=CARTESIAN_POINT('Ctrl Pts',(-7.96621910439647,4.93447149192677,6.56271486322442));
#80505=CARTESIAN_POINT('Ctrl Pts',(-8.1051545293239,4.70529467012887,6.56732522604309));
#80506=CARTESIAN_POINT('Ctrl Pts',(-8.19315310824621,4.55033731634271,6.57042050558338));
#80507=CARTESIAN_POINT('Ctrl Pts',(-8.30265755532397,4.3440226589768,6.57450460622988));
#80508=CARTESIAN_POINT('Ctrl Pts',(-8.32820029713551,4.29484983992455,6.57547524030563));
#80509=CARTESIAN_POINT('Ctrl Pts',(-8.4624976702542,4.03060786958886,6.58067430231056));
#80510=CARTESIAN_POINT('Ctrl Pts',(-8.56336057146384,3.81162987168666,6.58492594136708));
#80511=CARTESIAN_POINT('Ctrl Pts',(-8.68919922298438,3.50814271958098,6.59066975704457));
#80512=CARTESIAN_POINT('Ctrl Pts',(-8.72159448101979,3.4268116714448,6.59219457370145));
#80513=CARTESIAN_POINT('Ctrl Pts',(-8.77701592261415,3.28179232405076,6.59488159768706));
#80514=CARTESIAN_POINT('Ctrl Pts',(-8.80050030155519,3.2182858540113,6.5960475993619));
#80515=CARTESIAN_POINT('Ctrl Pts',(-8.83769088598625,3.11426292908294,6.59793708464703));
#80516=CARTESIAN_POINT('Ctrl Pts',(-8.85181160523465,3.07389738191817,6.59866524703378));
#80517=CARTESIAN_POINT('Ctrl Pts',(-8.88265658544073,2.98374847660182,6.60027964150398));
#80518=CARTESIAN_POINT('Ctrl Pts',(-8.89923961049517,2.93391843071666,6.60116427426703));
#80519=CARTESIAN_POINT('Ctrl Pts',(-8.95186257493057,2.77124061841614,6.60403089765138));
#80520=CARTESIAN_POINT('Ctrl Pts',(-8.98618170022141,2.6578481346027,6.60599580352137));
#80521=CARTESIAN_POINT('Ctrl Pts',(-9.0461723918034,2.44517062483138,6.60964168680928));
#80522=CARTESIAN_POINT('Ctrl Pts',(-9.07238208013147,2.34605578698333,6.61132501026122));
#80523=CARTESIAN_POINT('Ctrl Pts',(-9.1529821868891,2.0196788000834,6.61683843514445));
#80524=CARTESIAN_POINT('Ctrl Pts',(-9.20049903656893,1.79081063880487,6.62065987325839));
#80525=CARTESIAN_POINT('Ctrl Pts',(-9.25172869110868,1.4874718417392,6.62574405826794));
#80526=CARTESIAN_POINT('Ctrl Pts',(-9.26318228279751,1.41439394421316,6.62697014179774));
#80527=CARTESIAN_POINT('Ctrl Pts',(-9.29022982107847,1.22737124525593,6.63011435924624));
#80528=CARTESIAN_POINT('Ctrl Pts',(-9.30459347820935,1.1132611619497,6.63203890163003));
#80529=CARTESIAN_POINT('Ctrl Pts',(-9.32540890492238,0.919116408501615,
6.63532923704868));
#80530=CARTESIAN_POINT('Ctrl Pts',(-9.33293908699647,0.839210450188303,
6.63668800124707));
#80531=CARTESIAN_POINT('Ctrl Pts',(-9.34652946062281,0.672029815884449,
6.63954153538251));
#80532=CARTESIAN_POINT('Ctrl Pts',(-9.35239583542012,0.584747059711993,
6.6410374130638));
#80533=CARTESIAN_POINT('Ctrl Pts',(-9.36584853270982,0.331673772450509,
6.64539283026322));
#80534=CARTESIAN_POINT('Ctrl Pts',(-9.37025365261961,0.165748127334882,
6.64827145372313));
#80535=CARTESIAN_POINT('Ctrl Pts',(-9.37024411107238,-0.267496655689389,
6.65583566090191));
#80536=CARTESIAN_POINT('Ctrl Pts',(-9.35880136501872,-0.534664099895355,
6.66055035175185));
#80537=CARTESIAN_POINT('Ctrl Pts',(-9.32190719239578,-0.964692744892784,
6.66812158653535));
#80538=CARTESIAN_POINT('Ctrl Pts',(-9.30355699977813,-1.12801294492445,
6.67099194262106));
#80539=CARTESIAN_POINT('Ctrl Pts',(-9.27339214416323,-1.34490555949817,
6.67476612574503));
#80540=CARTESIAN_POINT('Ctrl Pts',(-9.26538899607317,-1.3989780531286,6.6757038546749));
#80541=CARTESIAN_POINT('Ctrl Pts',(-9.25101802354444,-1.49053545540155,
6.67728451737122));
#80542=CARTESIAN_POINT('Ctrl Pts',(-9.24489437543979,-1.52805706938749,
6.67793014740305));
#80543=CARTESIAN_POINT('Ctrl Pts',(-9.22870856086925,-1.62357253562602,
6.67956846566657));
#80544=CARTESIAN_POINT('Ctrl Pts',(-9.21832801407941,-1.68151066811122,
6.68055755853936));
#80545=CARTESIAN_POINT('Ctrl Pts',(-9.19407233098427,-1.80991046540066,
6.68274262716521));
#80546=CARTESIAN_POINT('Ctrl Pts',(-9.17993165798706,-1.88031824547836,
6.68393616856785));
#80547=CARTESIAN_POINT('Ctrl Pts',(-9.13174724951051,-2.10671992351238,
6.6877677277722));
#80548=CARTESIAN_POINT('Ctrl Pts',(-9.09452550754735,-2.26200853588946,
6.69038639023632));
#80549=CARTESIAN_POINT('Ctrl Pts',(-8.9722266583208,-2.72024154516597,6.69816078213647));
#80550=CARTESIAN_POINT('Ctrl Pts',(-8.87584161743937,-3.01993382881891,
6.70331344426076));
#80551=CARTESIAN_POINT('Ctrl Pts',(-8.72914153835272,-3.40788848839428,
6.71023805630158));
#80552=CARTESIAN_POINT('Ctrl Pts',(-8.6922178724756,-3.50099476428026,6.71191909911516));
#80553=CARTESIAN_POINT('Ctrl Pts',(-8.62351997479047,-3.66643234666547,
6.71494403657693));
#80554=CARTESIAN_POINT('Ctrl Pts',(-8.59231017433845,-3.73898766280242,
6.71628393186724));
#80555=CARTESIAN_POINT('Ctrl Pts',(-8.52188798483405,-3.89716268693931,
6.71923526735081));
#80556=CARTESIAN_POINT('Ctrl Pts',(-8.48229462132644,-3.98260338665169,
6.7208492417781));
#80557=CARTESIAN_POINT('Ctrl Pts',(-8.33964061557356,-4.27866297031005,
6.72651149998721));
#80558=CARTESIAN_POINT('Ctrl Pts',(-8.22996871619734,-4.48599784199792,
6.73060372285002));
#80559=CARTESIAN_POINT('Ctrl Pts',(-7.99124605928136,-4.89902198805559,
6.73897662866561));
#80560=CARTESIAN_POINT('Ctrl Pts',(-7.86174600062069,-5.10425115443418,
6.74325582356164));
#80561=CARTESIAN_POINT('Ctrl Pts',(-7.66329096277337,-5.39325703853608,
6.74937581354169));
#80562=CARTESIAN_POINT('Ctrl Pts',(-7.6006183271226,-5.4812271443114,6.75125145799657));
#80563=CARTESIAN_POINT('Ctrl Pts',(-7.50609528106919,-5.60916448234785,
6.75398799496152));
#80564=CARTESIAN_POINT('Ctrl Pts',(-7.47541641059412,-5.64998602318732,
6.75486247957521));
#80565=CARTESIAN_POINT('Ctrl Pts',(-7.41818798621652,-5.7248524647942,6.75646720631707));
#80566=CARTESIAN_POINT('Ctrl Pts',(-7.39173394995275,-5.75896847993369,
6.75719866677571));
#80567=CARTESIAN_POINT('Ctrl Pts',(-7.32123968676158,-5.84859429466323,
6.75912210074726));
#80568=CARTESIAN_POINT('Ctrl Pts',(-7.27680389508847,-5.9037895357871,6.76030863794319));
#80569=CARTESIAN_POINT('Ctrl Pts',(-7.17230964560699,-6.03061323333406,
6.7630459445076));
#80570=CARTESIAN_POINT('Ctrl Pts',(-7.11179686280728,-6.10185767273908,
6.76459198180125));
#80571=CARTESIAN_POINT('Ctrl Pts',(-6.86398704101554,-6.38492045084358,
6.77079127370103));
#80572=CARTESIAN_POINT('Ctrl Pts',(-6.66821250212998,-6.58911751679026,
6.77539837018513));
#80573=CARTESIAN_POINT('Ctrl Pts',(-6.33207159013447,-6.90937115017145,
6.78304898417604));
#80574=CARTESIAN_POINT('Ctrl Pts',(-6.19702705033104,-7.03074645840779,
6.78605910316685));
#80575=CARTESIAN_POINT('Ctrl Pts',(-5.99034192139613,-7.20592682846436,
6.79060033235791));
#80576=CARTESIAN_POINT('Ctrl Pts',(-5.9213176254947,-7.26275259962494,6.79210632935388));
#80577=CARTESIAN_POINT('Ctrl Pts',(-5.78925777866192,-7.36833958383894,
6.79497002433603));
#80578=CARTESIAN_POINT('Ctrl Pts',(-5.72639267547684,-7.41730144608719,
6.79632591308752));
#80579=CARTESIAN_POINT('Ctrl Pts',(-5.57516702464599,-7.5320134527295,6.79957115904164));
#80580=CARTESIAN_POINT('Ctrl Pts',(-5.48625677808336,-7.59701918400953,
6.80146615713298));
#80581=CARTESIAN_POINT('Ctrl Pts',(-5.28889509188134,-7.73604605996295,
6.80564378570293));
#80582=CARTESIAN_POINT('Ctrl Pts',(-5.17999185345099,-7.80938564894754,
6.80793057915229));
#80583=CARTESIAN_POINT('Ctrl Pts',(-4.76568183430128,-8.07591730049529,
6.81654959844975));
#80584=CARTESIAN_POINT('Ctrl Pts',(-4.45072574246145,-8.25367816709756,
6.82295252042373));
#80585=CARTESIAN_POINT('Ctrl Pts',(-4.05894037752644,-8.44584014711669,
6.83051973501605));
#80586=CARTESIAN_POINT('Ctrl Pts',(-3.99119314048399,-8.47806523539099,
6.83181392379026));
#80587=CARTESIAN_POINT('Ctrl Pts',(-3.88719491010502,-8.52601085077349,
6.83377506317719));
#80588=CARTESIAN_POINT('Ctrl Pts',(-3.85121938346786,-8.54232138067351,
6.83444884426768));
#80589=CARTESIAN_POINT('Ctrl Pts',(-3.77185744820174,-8.57769912527549,
6.83592422271375));
#80590=CARTESIAN_POINT('Ctrl Pts',(-3.72842735553502,-8.59666565364904,
6.83672452647371));
#80591=CARTESIAN_POINT('Ctrl Pts',(-3.59577947189541,-8.65340054786662,
6.83914995720847));
#80592=CARTESIAN_POINT('Ctrl Pts',(-3.50611803014959,-8.6901155050585,6.84076354239898));
#80593=CARTESIAN_POINT('Ctrl Pts',(-3.17405114999465,-8.82011573141159,
6.84666964571213));
#80594=CARTESIAN_POINT('Ctrl Pts',(-2.92836656533185,-8.90470168302863,
6.8509066761065));
#80595=CARTESIAN_POINT('Ctrl Pts',(-2.55894849871085,-9.01494263754395,
6.85723461668853));
#80596=CARTESIAN_POINT('Ctrl Pts',(-2.43769923618985,-9.04848222343519,
6.85930423678493));
#80597=CARTESIAN_POINT('Ctrl Pts',(-2.17296332295374,-9.11600507887425,
6.86382446354094));
#80598=CARTESIAN_POINT('Ctrl Pts',(-2.02927535180065,-9.14906331664298,
6.86627886565215));
#80599=CARTESIAN_POINT('Ctrl Pts',(-1.80168774660806,-9.1957988772824,6.87018116784542));
#80600=CARTESIAN_POINT('Ctrl Pts',(-1.71827961100136,-9.21174852377251,
6.87161432072911));
#80601=CARTESIAN_POINT('Ctrl Pts',(-1.55442491328724,-9.24077859510195,
6.87443732298519));
#80602=CARTESIAN_POINT('Ctrl Pts',(-1.47400156303259,-9.25394754739045,
6.8758264642474));
#80603=CARTESIAN_POINT('Ctrl Pts',(-1.27072721898639,-9.28451563240686,
6.87934730439972));
#80604=CARTESIAN_POINT('Ctrl Pts',(-1.14768358519643,-9.30052689150229,
6.88148751923919));
#80605=CARTESIAN_POINT('Ctrl Pts',(-0.941650831733427,-9.32318626282142,
6.8850846845736));
#80606=CARTESIAN_POINT('Ctrl Pts',(-0.858825653195946,-9.33118035664859,
6.88653430504898));
#80607=CARTESIAN_POINT('Ctrl Pts',(-0.479909591704592,-9.36266468880521,
6.89317829524937));
#80608=CARTESIAN_POINT('Ctrl Pts',(-0.182912844519505,-9.37317158931048,
6.89842552408248));
#80609=CARTESIAN_POINT('Ctrl Pts',(0.24299964819959,-9.36798585782343,6.90587752519452));
#80610=CARTESIAN_POINT('Ctrl Pts',(0.371873723630866,-9.36375554708974,
6.90812183222999));
#80611=CARTESIAN_POINT('Ctrl Pts',(0.553381355308638,-9.35404436110688,
6.91125145093967));
#80612=CARTESIAN_POINT('Ctrl Pts',(0.606118372661325,-9.35077522824464,
6.91215700200157));
#80613=CARTESIAN_POINT('Ctrl Pts',(0.697093125253195,-9.34436289766654,
6.91371106324044));
#80614=CARTESIAN_POINT('Ctrl Pts',(0.735344259706685,-9.34143059753206,
6.9143618910544));
#80615=CARTESIAN_POINT('Ctrl Pts',(0.836137512132898,-9.33308094233698,
6.91607065001953));
#80616=CARTESIAN_POINT('Ctrl Pts',(0.898645087838587,-9.32726984962665,
6.91712422029971));
#80617=CARTESIAN_POINT('Ctrl Pts',(1.03929038806274,-9.31276762991967,6.91948527949529));
#80618=CARTESIAN_POINT('Ctrl Pts',(1.11738669302317,-9.30372035554436,6.92078967664173));
#80619=CARTESIAN_POINT('Ctrl Pts',(1.38466822944068,-9.26934244925843,6.92524301788084));
#80620=CARTESIAN_POINT('Ctrl Pts',(1.57318859254317,-9.23921497825125,6.92836612083579));
#80621=CARTESIAN_POINT('Ctrl Pts',(1.90277358341188,-9.17616335895287,6.93386709901732));
#80622=CARTESIAN_POINT('Ctrl Pts',(2.04424103698314,-9.14568749830089,6.93624151186545));
#80623=CARTESIAN_POINT('Ctrl Pts',(2.34674941250458,-9.07314928903009,6.94137589001569));
#80624=CARTESIAN_POINT('Ctrl Pts',(2.50749050614896,-9.03004772700305,6.94413953779842));
#80625=CARTESIAN_POINT('Ctrl Pts',(2.75091014398372,-8.95777541339391,6.94839897024734));
#80626=CARTESIAN_POINT('Ctrl Pts',(2.83446874477871,-8.93168706726343,6.94987455007341));
#80627=CARTESIAN_POINT('Ctrl Pts',(2.99389692452198,-8.87944841323074,6.95271776789886));
#80628=CARTESIAN_POINT('Ctrl Pts',(3.06982027395367,-8.85348667859727,6.954084027142));
#80629=CARTESIAN_POINT('Ctrl Pts',(3.25357576202563,-8.7880041922735,6.95742149962108));
#80630=CARTESIAN_POINT('Ctrl Pts',(3.36103278337511,-8.74747000299489,6.95939929650354));
#80631=CARTESIAN_POINT('Ctrl Pts',(3.53628416320187,-8.67765676063081,6.96266717501181));
#80632=CARTESIAN_POINT('Ctrl Pts',(3.60452576168345,-8.64953331398509,6.96395033874386));
#80633=CARTESIAN_POINT('Ctrl Pts',(3.8865367723986,-8.52939500478843,6.9692954103017));
#80634=CARTESIAN_POINT('Ctrl Pts',(4.09717290202295,-8.43023849353389,6.97339175267438));
#80635=CARTESIAN_POINT('Ctrl Pts',(4.42356175811659,-8.26146685409431,6.97984933135097));
#80636=CARTESIAN_POINT('Ctrl Pts',(4.54187739601849,-8.19701671408261,6.98221346224923));
#80637=CARTESIAN_POINT('Ctrl Pts',(4.74597502743253,-8.0800624820426,6.98631299854088));
#80638=CARTESIAN_POINT('Ctrl Pts',(4.83237813562274,-8.02868671168288,6.98805532770705));
#80639=CARTESIAN_POINT('Ctrl Pts',(4.95875878869117,-7.95076073072815,6.99060546671732));
#80640=CARTESIAN_POINT('Ctrl Pts',(4.99938575423751,-7.92527772480189,6.99142549233828));
#80641=CARTESIAN_POINT('Ctrl Pts',(5.07746044682174,-7.87546661841097,6.99300050630066));
#80642=CARTESIAN_POINT('Ctrl Pts',(5.11493337697594,-7.85118052249396,6.99375596452528));
#80643=CARTESIAN_POINT('Ctrl Pts',(5.21942339510289,-7.78239524545958,6.99586302392873));
#80644=CARTESIAN_POINT('Ctrl Pts',(5.28604325525921,-7.73729946991745,6.99720709272916));
#80645=CARTESIAN_POINT('Ctrl Pts',(5.68943589982201,-7.45659621182798,7.00537358316229));
#80646=CARTESIAN_POINT('Ctrl Pts',(6.01098747014009,-7.19989863398696,7.01202482010297));
#80647=CARTESIAN_POINT('Ctrl Pts',(6.42387333014739,-6.82329049339524,7.02127026093402));
#80648=CARTESIAN_POINT('Ctrl Pts',(6.53072688329048,-6.72108978648761,7.02373148963341));
#80649=CARTESIAN_POINT('Ctrl Pts',(6.69511957194784,-6.55623214210041,7.02764170698326));
#80650=CARTESIAN_POINT('Ctrl Pts',(6.75430037471817,-6.49524690761594,7.02907583600945));
#80651=CARTESIAN_POINT('Ctrl Pts',(6.86856800093705,-6.37424453053456,7.03189915001919));
#80652=CARTESIAN_POINT('Ctrl Pts',(6.92371796196137,-6.31429721067544,7.03328761009658));
#80653=CARTESIAN_POINT('Ctrl Pts',(7.06070612409384,-6.16143991978158,7.03680318679329));
#80654=CARTESIAN_POINT('Ctrl Pts',(7.14149743609768,-6.06761296595567,7.03893876246352));
#80655=CARTESIAN_POINT('Ctrl Pts',(7.27326137161348,-5.90831036327752,7.04252636774702));
#80656=CARTESIAN_POINT('Ctrl Pts',(7.32526637198046,-5.84370900020765,7.04397107732937));
#80657=CARTESIAN_POINT('Ctrl Pts',(7.55819068929469,-5.54637118333083,7.05057077721524));
#80658=CARTESIAN_POINT('Ctrl Pts',(7.72892242561306,-5.30586820443467,7.05577791298135));
#80659=CARTESIAN_POINT('Ctrl Pts',(7.95834876750401,-4.94805422640624,7.06321600005997));
#80660=CARTESIAN_POINT('Ctrl Pts',(8.02637016214393,-4.83693476344721,7.06548437821871));
#80661=CARTESIAN_POINT('Ctrl Pts',(8.11902851726629,-4.67822867553789,7.06864948910207));
#80662=CARTESIAN_POINT('Ctrl Pts',(8.14560814460253,-4.63179399118876,7.06956669535995));
#80663=CARTESIAN_POINT('Ctrl Pts',(8.19241668858898,-4.54837014446286,7.07119709045023));
#80664=CARTESIAN_POINT('Ctrl Pts',(8.21279634348789,-4.51146743210387,7.07191210741618));
#80665=CARTESIAN_POINT('Ctrl Pts',(8.26418950128087,-4.41690427309674,7.07372942580617));
#80666=CARTESIAN_POINT('Ctrl Pts',(8.29484899126454,-4.35905399279979,7.0748273572166));
#80667=CARTESIAN_POINT('Ctrl Pts',(8.41997977847145,-4.11684785274186,7.07937580197943));
#80668=CARTESIAN_POINT('Ctrl Pts',(8.50893112498655,-3.92970575533234,7.08277578363099));
#80669=CARTESIAN_POINT('Ctrl Pts',(8.72248789516042,-3.43908837073114,7.09154828466975));
#80670=CARTESIAN_POINT('Ctrl Pts',(8.83749408574656,-3.13174419156877,7.09691498034088));
#80671=CARTESIAN_POINT('Ctrl Pts',(8.96628318117,-2.72348724385437,7.1040642157495));
#80672=CARTESIAN_POINT('Ctrl Pts',(8.99488210780268,-2.62749170408588,7.10574588558639));
#80673=CARTESIAN_POINT('Ctrl Pts',(9.043249995996,-2.45508462859423,7.10877064023812));
#80674=CARTESIAN_POINT('Ctrl Pts',(9.0636029571511,-2.37884686879552,7.11010970740197));
#80675=CARTESIAN_POINT('Ctrl Pts',(9.1064612874211,-2.20976749098957,7.11308388486321));
#80676=CARTESIAN_POINT('Ctrl Pts',(9.12851471293581,-2.11682040351344,7.11472179836349));
#80677=CARTESIAN_POINT('Ctrl Pts',(9.20545767216222,-1.76893611265383,7.12086327856555));
#80678=CARTESIAN_POINT('Ctrl Pts',(9.251118673416,-1.51208077544671,7.12542316841205));
#80679=CARTESIAN_POINT('Ctrl Pts',(9.3265428172602,-0.953404045537311,7.13532760134473));
#80680=CARTESIAN_POINT('Ctrl Pts',(9.35249213363519,-0.65136124541213,7.14067520388304));
#80681=CARTESIAN_POINT('Ctrl Pts',(9.36571616415753,-0.296142938690236,
7.14680846368754));
#80682=CARTESIAN_POINT('Ctrl Pts',(9.36722805303101,-0.243677093503678,
7.14771018482407));
#80683=CARTESIAN_POINT('Ctrl Pts',(9.36916215981244,-0.148911549578908,
7.14932979358075));
#80684=CARTESIAN_POINT('Ctrl Pts',(9.36973890572044,-0.106616515382582,
7.15004926455041));
#80685=CARTESIAN_POINT('Ctrl Pts',(9.37040951820078,-0.00892101066067758,
7.15170307109131));
#80686=CARTESIAN_POINT('Ctrl Pts',(9.37029849203117,0.0464791618998744,
7.15263518081541));
#80687=CARTESIAN_POINT('Ctrl Pts',(9.36783909579904,0.272675564747029,7.15642301810922));
#80688=CARTESIAN_POINT('Ctrl Pts',(9.36131206417663,0.443393806085254,7.15924063211639));
#80689=CARTESIAN_POINT('Ctrl Pts',(9.32358430163558,1.01807143864961,7.1687017247207));
#80690=CARTESIAN_POINT('Ctrl Pts',(9.27086014771178,1.42015699321713,7.17530005573792));
#80691=CARTESIAN_POINT('Ctrl Pts',(9.17412768401483,1.90937825200955,7.18364564360164));
#80692=CARTESIAN_POINT('Ctrl Pts',(9.15459945514986,2.00091300018584,7.18521993623567));
#80693=CARTESIAN_POINT('Ctrl Pts',(9.11605900845249,2.16916993297434,7.18814004570542));
#80694=CARTESIAN_POINT('Ctrl Pts',(9.09744094893623,2.24597377333545,7.18948316243218));
#80695=CARTESIAN_POINT('Ctrl Pts',(9.05240222169807,2.42201218012098,7.19258606800701));
#80696=CARTESIAN_POINT('Ctrl Pts',(9.02531737331991,2.52106628692512,7.19435004691618));
#80697=CARTESIAN_POINT('Ctrl Pts',(8.9635674239314,2.73313245972967,7.19816522765187));
#80698=CARTESIAN_POINT('Ctrl Pts',(8.92838080980068,2.84597435489088,7.20021927321259));
#80699=CARTESIAN_POINT('Ctrl Pts',(8.80729820765775,3.20990608009049,7.20691534830602));
#80700=CARTESIAN_POINT('Ctrl Pts',(8.71286968855318,3.45801967668251,7.21159540621311));
#80701=CARTESIAN_POINT('Ctrl Pts',(8.54214442014896,3.85501949070504,7.21917725123089));
#80702=CARTESIAN_POINT('Ctrl Pts',(8.47216981388657,4.00646296343008,7.22209155546404));
#80703=CARTESIAN_POINT('Ctrl Pts',(8.37389306850937,4.20505659358886,7.22591073862778));
#80704=CARTESIAN_POINT('Ctrl Pts',(8.34916584597256,4.2539412046895,7.2268505885105));
#80705=CARTESIAN_POINT('Ctrl Pts',(8.30655843588268,4.33637137507222,7.22843322686966));
#80706=CARTESIAN_POINT('Ctrl Pts',(8.28890031029224,4.37002990860614,7.22907873592303));
#80707=CARTESIAN_POINT('Ctrl Pts',(8.24344661195211,4.45540345403634,7.23071445338078));
#80708=CARTESIAN_POINT('Ctrl Pts',(8.21536893371334,4.50696630644274,7.23170109548439));
#80709=CARTESIAN_POINT('Ctrl Pts',(8.15199867269176,4.62078165902737,7.23387954894929));
#80710=CARTESIAN_POINT('Ctrl Pts',(8.1164737920253,4.6829006729324,7.23506894932531));
#80711=CARTESIAN_POINT('Ctrl Pts',(7.99994097880888,4.88136036543957,7.23887877248502));
#80712=CARTESIAN_POINT('Ctrl Pts',(7.91618221466055,5.01605362639661,7.24148005582004));
#80713=CARTESIAN_POINT('Ctrl Pts',(7.65488875594652,5.41338410937503,7.24927550520336));
#80714=CARTESIAN_POINT('Ctrl Pts',(7.46740711201449,5.66920451927245,7.25446603737995));
#80715=CARTESIAN_POINT('Ctrl Pts',(7.20426399547315,5.99250736618144,7.26142608067284));
#80716=CARTESIAN_POINT('Ctrl Pts',(7.13996925883983,6.0689705197547,7.26310289678615));
#80717=CARTESIAN_POINT('Ctrl Pts',(7.02268353417167,6.20400972765649,7.26612339065504));
#80718=CARTESIAN_POINT('Ctrl Pts',(6.9701512277802,6.26297154314259,7.26746311932829));
#80719=CARTESIAN_POINT('Ctrl Pts',(6.85322076775757,6.39091971759516,7.27041779050818));
#80720=CARTESIAN_POINT('Ctrl Pts',(6.78851303041146,6.45961148272738,7.2720353072796));
#80721=CARTESIAN_POINT('Ctrl Pts',(6.5572011618538,6.69785014332778,7.27775692048023));
#80722=CARTESIAN_POINT('Ctrl Pts',(6.38519499485934,6.86202359131373,7.28190638246082));
#80723=CARTESIAN_POINT('Ctrl Pts',(5.9681271086905,7.23082537403374,7.291679412853));
#80724=CARTESIAN_POINT('Ctrl Pts',(5.71848225455219,7.42982756564254,7.29731836284638));
#80725=CARTESIAN_POINT('Ctrl Pts',(5.40800898609829,7.6523843975673,7.30392053059611));
#80726=CARTESIAN_POINT('Ctrl Pts',(5.35647515706879,7.68854486102214,7.30500323169772));
#80727=CARTESIAN_POINT('Ctrl Pts',(5.26971096723597,7.74813014467398,7.30680173562611));
#80728=CARTESIAN_POINT('Ctrl Pts',(5.23467942270256,7.77184056545524,7.30752125051269));
#80729=CARTESIAN_POINT('Ctrl Pts',(5.15341940515213,7.82604114853768,7.30917472462255));
#80730=CARTESIAN_POINT('Ctrl Pts',(5.10707889812488,7.85636027504752,7.31010646280213));
#80731=CARTESIAN_POINT('Ctrl Pts',(4.9170074215257,7.97832564293945,7.31388810734709));
#80732=CARTESIAN_POINT('Ctrl Pts',(4.77105673647798,8.06645275232094,7.31670005968695));
#80733=CARTESIAN_POINT('Ctrl Pts',(4.51335545110058,8.21261432760951,7.32156719322873));
#80734=CARTESIAN_POINT('Ctrl Pts',(4.40271363731969,8.27245488700144,7.32362653531074));
#80735=CARTESIAN_POINT('Ctrl Pts',(4.29092658438921,8.33003806173069,7.32568828984052));
#80736=CARTESIAN_POINT('Origin',(0.,0.,2.15141010809499));
#80737=CARTESIAN_POINT('',(4.2909266557441,8.33003802497472,8.52320208943219));
#80738=CARTESIAN_POINT('',(4.29124604933685,8.33065733261336,8.3257038672742));
#80739=CARTESIAN_POINT('',(4.29092662815669,8.33003803918541,2.15141010809499));
#80740=CARTESIAN_POINT('',(-9.37091712982845,0.000108538499879093,7.84858856853279));
#80741=CARTESIAN_POINT('Ctrl Pts',(4.2909266557441,8.33003802497472,8.52320208943219));
#80742=CARTESIAN_POINT('Ctrl Pts',(4.36344197094789,8.29268430605715,8.52184882563512));
#80743=CARTESIAN_POINT('Ctrl Pts',(4.43547931258882,8.25437864654634,8.52049018201438));
#80744=CARTESIAN_POINT('Ctrl Pts',(4.58991690527409,8.16965043141316,8.5175432457802));
#80745=CARTESIAN_POINT('Ctrl Pts',(4.67212074926457,8.12291899616669,8.51595321555757));
#80746=CARTESIAN_POINT('Ctrl Pts',(4.82164273272179,8.03489764252445,8.51301871480337));
#80747=CARTESIAN_POINT('Ctrl Pts',(4.88917329138468,7.99398544287827,8.51167714122255));
#80748=CARTESIAN_POINT('Ctrl Pts',(5.04220741846923,7.89860779762343,8.50859865202764));
#80749=CARTESIAN_POINT('Ctrl Pts',(5.12736031653314,7.84359846669364,8.50685779957073));
#80750=CARTESIAN_POINT('Ctrl Pts',(5.3079575713716,7.72273357330122,8.50310550189753));
#80751=CARTESIAN_POINT('Ctrl Pts',(5.40310608046931,7.65646602675577,8.50109142123788));
#80752=CARTESIAN_POINT('Ctrl Pts',(5.70184795087703,7.44006029150815,8.4946539704502));
#80753=CARTESIAN_POINT('Ctrl Pts',(5.90060290481796,7.28343683428866,8.49019599922936));
#80754=CARTESIAN_POINT('Ctrl Pts',(6.2258919485955,7.00503773270286,8.4826782468142));
#80755=CARTESIAN_POINT('Ctrl Pts',(6.35578617798489,6.8873991117217,8.47961215822225));
#80756=CARTESIAN_POINT('Ctrl Pts',(6.52118828560187,6.72893661015646,8.47565778645712));
#80757=CARTESIAN_POINT('Ctrl Pts',(6.55974902551487,6.69135093226922,8.47473223207736));
#80758=CARTESIAN_POINT('Ctrl Pts',(6.62812929513128,6.62354055920766,8.47308603464598));
#80759=CARTESIAN_POINT('Ctrl Pts',(6.65807138177038,6.59344166474343,8.47236357658209));
#80760=CARTESIAN_POINT('Ctrl Pts',(6.72572691118265,6.52450100814893,8.47072783629683));
#80761=CARTESIAN_POINT('Ctrl Pts',(6.76331028640827,6.4855338929692,8.46981650914498));
#80762=CARTESIAN_POINT('Ctrl Pts',(6.9062406769936,6.33474749016277,8.46633567537435));
#80763=CARTESIAN_POINT('Ctrl Pts',(7.00916981038996,6.22066916677316,8.46379682500955));
#80764=CARTESIAN_POINT('Ctrl Pts',(7.37902952436973,5.78990634753019,8.45445844636285));
#80765=CARTESIAN_POINT('Ctrl Pts',(7.6276837256657,5.45816211997136,8.44772407548045));
#80766=CARTESIAN_POINT('Ctrl Pts',(7.90667951235207,5.0294614370168,8.4391748526069));
#80767=CARTESIAN_POINT('Ctrl Pts',(7.95850792929903,4.94704100826315,8.43753901755185));
#80768=CARTESIAN_POINT('Ctrl Pts',(8.04997800265542,4.7964214357382,8.43456057440645));
#80769=CARTESIAN_POINT('Ctrl Pts',(8.09006084931744,4.72850080397772,8.4332214269191));
#80770=CARTESIAN_POINT('Ctrl Pts',(8.17807955769171,4.57495655410679,8.43020191499276));
#80771=CARTESIAN_POINT('Ctrl Pts',(8.22553745318002,4.48906964382114,8.42851824058472));
#80772=CARTESIAN_POINT('Ctrl Pts',(8.32352900955655,4.30495624848496,8.42492024954387));
#80773=CARTESIAN_POINT('Ctrl Pts',(8.37369245513698,4.20654942477857,8.42300378453386));
#80774=CARTESIAN_POINT('Ctrl Pts',(8.52100077415318,3.90448909675622,8.41714562724172));
#80775=CARTESIAN_POINT('Ctrl Pts',(8.61254039109112,3.69819374111411,8.41317634492159));
#80776=CARTESIAN_POINT('Ctrl Pts',(8.75561028093878,3.34156255193806,8.40642185749983));
#80777=CARTESIAN_POINT('Ctrl Pts',(8.81092770248506,3.19285214677145,8.40363659706919));
#80778=CARTESIAN_POINT('Ctrl Pts',(8.89232045407592,2.95578876156814,8.39927466166068));
#80779=CARTESIAN_POINT('Ctrl Pts',(8.92091457168261,2.8683328841694,8.39768208076638));
#80780=CARTESIAN_POINT('Ctrl Pts',(8.96204389721282,2.73596889592536,8.39530334269566));
#80781=CARTESIAN_POINT('Ctrl Pts',(8.97553952944504,2.69136522655317,8.39450713169773));
#80782=CARTESIAN_POINT('Ctrl Pts',(9.00161047138237,2.60282204866018,8.39293844633724));
#80783=CARTESIAN_POINT('Ctrl Pts',(9.01419815601723,2.55888751369075,8.3921658634987));
#80784=CARTESIAN_POINT('Ctrl Pts',(9.04972695784281,2.43136585640224,8.38993794903868));
#80785=CARTESIAN_POINT('Ctrl Pts',(9.07183037012952,2.34755015603192,8.38849160001895));
#80786=CARTESIAN_POINT('Ctrl Pts',(9.15516214312644,2.01278689871448,8.3827668432091));
#80787=CARTESIAN_POINT('Ctrl Pts',(9.20716567911062,1.75966070518796,8.37855084839455));
#80788=CARTESIAN_POINT('Ctrl Pts',(9.28851398988429,1.25965616908904,8.37024058491939));
#80789=CARTESIAN_POINT('Ctrl Pts',(9.31862770210545,1.01311551308332,8.36615123785798));
#80790=CARTESIAN_POINT('Ctrl Pts',(9.34683353284748,0.669088163298444,8.36038095390027));
#80791=CARTESIAN_POINT('Ctrl Pts',(9.35325332384938,0.572388209463317,8.35875245665025));
#80792=CARTESIAN_POINT('Ctrl Pts',(9.36217511024265,0.396840452050202,8.35578123035131));
#80793=CARTESIAN_POINT('Ctrl Pts',(9.36518359141979,0.318027364628808,8.3544418722678));
#80794=CARTESIAN_POINT('Ctrl Pts',(9.36971341789963,0.140626475176787,8.35141395236109));
#80795=CARTESIAN_POINT('Ctrl Pts',(9.37067438553663,0.0420337402154264,
8.34972198944694));
#80796=CARTESIAN_POINT('Ctrl Pts',(9.36840230577147,-0.334402311027361,
8.34322705920681));
#80797=CARTESIAN_POINT('Ctrl Pts',(9.35436783476926,-0.612035926906702,
8.33835992751789));
#80798=CARTESIAN_POINT('Ctrl Pts',(9.30239725441764,-1.15757302214544,8.32872695647232));
#80799=CARTESIAN_POINT('Ctrl Pts',(9.26515783328865,-1.42527917465293,8.32396711170294));
#80800=CARTESIAN_POINT('Ctrl Pts',(9.20535084655738,-1.75124300259456,8.31824260680378));
#80801=CARTESIAN_POINT('Ctrl Pts',(9.19370751294297,-1.8113747412928,8.31718978853459));
#80802=CARTESIAN_POINT('Ctrl Pts',(9.17304752706486,-1.9127375505105,8.31542285344433));
#80803=CARTESIAN_POINT('Ctrl Pts',(9.16434036909686,-1.95402955044761,8.31470537056174));
#80804=CARTESIAN_POINT('Ctrl Pts',(9.14328656651823,-2.05063594667606,8.31303228415601));
#80805=CARTESIAN_POINT('Ctrl Pts',(9.13071645508904,-2.10589982197977,8.31207917613357));
#80806=CARTESIAN_POINT('Ctrl Pts',(9.07267616193807,-2.35077695590852,8.30786735201178));
#80807=CARTESIAN_POINT('Ctrl Pts',(9.02179517913297,-2.53905834164524,8.30465860065171));
#80808=CARTESIAN_POINT('Ctrl Pts',(8.85652030319598,-3.0826794403061,8.29533564212096));
#80809=CARTESIAN_POINT('Ctrl Pts',(8.72672904118709,-3.43293814656882,8.28924287155239));
#80810=CARTESIAN_POINT('Ctrl Pts',(8.5380804245009,-3.86158197994939,8.28140962055638));
#80811=CARTESIAN_POINT('Ctrl Pts',(8.49844117525268,-3.94805398369551,8.27981034378085));
#80812=CARTESIAN_POINT('Ctrl Pts',(8.42384128408788,-4.10446015662358,8.27687997532733));
#80813=CARTESIAN_POINT('Ctrl Pts',(8.38930876311664,-4.17458903380878,8.27555201410437));
#80814=CARTESIAN_POINT('Ctrl Pts',(8.30851876247877,-4.33360592558777,8.27250767373788));
#80815=CARTESIAN_POINT('Ctrl Pts',(8.26170486233959,-4.4222004754789,8.27078746473928));
#80816=CARTESIAN_POINT('Ctrl Pts',(8.07599428318759,-4.76040908811691,8.26412730852763));
#80817=CARTESIAN_POINT('Ctrl Pts',(7.9271326481714,-5.00437260267519,8.25911956003787));
#80818=CARTESIAN_POINT('Ctrl Pts',(7.62473444566546,-5.45252510732725,8.24961490153297));
#80819=CARTESIAN_POINT('Ctrl Pts',(7.47353908490545,-5.657987218979,8.24512594071311));
#80820=CARTESIAN_POINT('Ctrl Pts',(7.27497461600892,-5.90595105868186,8.23963611495651));
#80821=CARTESIAN_POINT('Ctrl Pts',(7.23530686270483,-5.95448135438398,8.23855823669244));
#80822=CARTESIAN_POINT('Ctrl Pts',(7.16806947125792,-6.03507687142065,8.23676487614228));
#80823=CARTESIAN_POINT('Ctrl Pts',(7.14076439062226,-6.06735994665542,8.23604573758916));
#80824=CARTESIAN_POINT('Ctrl Pts',(7.07706629952926,-6.14164522997826,8.23438934499278));
#80825=CARTESIAN_POINT('Ctrl Pts',(7.0405163356843,-6.18351059552723,8.23345435403023));
#80826=CARTESIAN_POINT('Ctrl Pts',(6.88827333928311,-6.35479415544751,8.22961733414545));
#80827=CARTESIAN_POINT('Ctrl Pts',(6.7693670927049,-6.48131066029187,8.22675469946));
#80828=CARTESIAN_POINT('Ctrl Pts',(6.36420265300372,-6.88908626361945,8.21731285399485));
#80829=CARTESIAN_POINT('Ctrl Pts',(6.0634004440858,-7.15526100348339,8.21077548697879));
#80830=CARTESIAN_POINT('Ctrl Pts',(5.67237492260607,-7.45885688571624,8.20249151435682));
#80831=CARTESIAN_POINT('Ctrl Pts',(5.5974259745648,-7.51526484628704,8.20091380304));
#80832=CARTESIAN_POINT('Ctrl Pts',(5.45781014933223,-7.61709495893508,8.19799060660632));
#80833=CARTESIAN_POINT('Ctrl Pts',(5.39339120674733,-7.66284271643219,8.19664786457746));
#80834=CARTESIAN_POINT('Ctrl Pts',(5.24417981113299,-7.76599294025426,8.19355048836432));
#80835=CARTESIAN_POINT('Ctrl Pts',(5.15900963674238,-7.82283118418899,8.1917917211806));
#80836=CARTESIAN_POINT('Ctrl Pts',(5.02081980004225,-7.91181358980023,8.18895292658103));
#80837=CARTESIAN_POINT('Ctrl Pts',(4.9683827972286,-7.9448472679103,8.1878790989168));
#80838=CARTESIAN_POINT('Ctrl Pts',(4.76843333232829,-8.06805547216641,8.18379800555763));
#80839=CARTESIAN_POINT('Ctrl Pts',(4.61876299063875,-8.15466147443709,8.1807701591455));
#80840=CARTESIAN_POINT('Ctrl Pts',(4.40725426485434,-8.26935793309367,8.17654377344696));
#80841=CARTESIAN_POINT('Ctrl Pts',(4.34737749094334,-8.30099269539958,8.17535310312928));
#80842=CARTESIAN_POINT('Ctrl Pts',(4.22203950750026,-8.3654845279821,8.17287486611625));
#80843=CARTESIAN_POINT('Ctrl Pts',(4.15652528157499,-8.39822877633345,8.17158739559903));
#80844=CARTESIAN_POINT('Ctrl Pts',(3.93729722771659,-8.50460603218191,8.16731058557016));
#80845=CARTESIAN_POINT('Ctrl Pts',(3.78195867013653,-8.5748132403217,8.16433048423798));
#80846=CARTESIAN_POINT('Ctrl Pts',(3.57694454729628,-8.66081664725144,8.16049542308772));
#80847=CARTESIAN_POINT('Ctrl Pts',(3.52893143876956,-8.68049078148484,8.15960421196886));
#80848=CARTESIAN_POINT('Ctrl Pts',(3.44153601469506,-8.71545750289904,8.15799608526108));
#80849=CARTESIAN_POINT('Ctrl Pts',(3.40220906028954,-8.73088444262237,8.15727768980722));
#80850=CARTESIAN_POINT('Ctrl Pts',(3.31049794657761,-8.76614657546564,8.15561473079433));
#80851=CARTESIAN_POINT('Ctrl Pts',(3.2580376927825,-8.78577901206424,8.15467252319907));
#80852=CARTESIAN_POINT('Ctrl Pts',(3.03517493625877,-8.86691134095931,8.15070214284174));
#80853=CARTESIAN_POINT('Ctrl Pts',(2.86318342954323,-8.92393325100653,8.14771695942125));
#80854=CARTESIAN_POINT('Ctrl Pts',(2.31509453134558,-9.08816860317451,8.13832288761082));
#80855=CARTESIAN_POINT('Ctrl Pts',(1.93388536658853,-9.1768490510491,8.1319476455794));
#80856=CARTESIAN_POINT('Ctrl Pts',(1.45522563313312,-9.25704058909419,8.12382771717759));
#80857=CARTESIAN_POINT('Ctrl Pts',(1.3619680911812,-9.27122025278297,8.1222414279016));
#80858=CARTESIAN_POINT('Ctrl Pts',(1.19027088630096,-9.29468000106789,8.11931038611918));
#80859=CARTESIAN_POINT('Ctrl Pts',(1.11189733835005,-9.30438097781153,8.11796848397056));
#80860=CARTESIAN_POINT('Ctrl Pts',(0.932359803220728,-9.32430304440704,
8.1148844139126));
#80861=CARTESIAN_POINT('Ctrl Pts',(0.831133342483466,-9.33387054569329,
8.11313825102579));
#80862=CARTESIAN_POINT('Ctrl Pts',(0.442755711045977,-9.36421022784628,
8.10641114208985));
#80863=CARTESIAN_POINT('Ctrl Pts',(0.154860154632144,-9.37339228622713,
8.10136181471848));
#80864=CARTESIAN_POINT('Ctrl Pts',(-0.381054647071033,-9.36578488169506,
8.09193879344202));
#80865=CARTESIAN_POINT('Ctrl Pts',(-0.628873094677841,-9.35241402688368,
8.08757324481115));
#80866=CARTESIAN_POINT('Ctrl Pts',(-0.938642045194109,-9.32333156281816,
8.08219577092791));
#80867=CARTESIAN_POINT('Ctrl Pts',(-1.00135466709883,-9.31680466557163,
8.08111137969538));
#80868=CARTESIAN_POINT('Ctrl Pts',(-1.10603066796173,-9.30484127513795,
8.07931107214876));
#80869=CARTESIAN_POINT('Ctrl Pts',(-1.14803156983099,-9.29975260558561,
8.07859142419867));
#80870=CARTESIAN_POINT('Ctrl Pts',(-1.24485672754942,-9.28735569145919,
8.07693896429046));
#80871=CARTESIAN_POINT('Ctrl Pts',(-1.299653499173,-9.2798461632101,8.07600835875151));
#80872=CARTESIAN_POINT('Ctrl Pts',(-1.52201076864112,-9.24736544799571,
8.07224537313422));
#80873=CARTESIAN_POINT('Ctrl Pts',(-1.68894655055455,-9.21833739850408,
8.0694504687491));
#80874=CARTESIAN_POINT('Ctrl Pts',(-2.25401499833203,-9.10421361344375,
8.05997930775724));
#80875=CARTESIAN_POINT('Ctrl Pts',(-2.64734984596758,-8.99771237805869,
8.05334992761102));
#80876=CARTESIAN_POINT('Ctrl Pts',(-3.12095994443126,-8.83571913568714,
8.04497297683809));
#80877=CARTESIAN_POINT('Ctrl Pts',(-3.20895155063616,-8.80414411013471,
8.04340046948753));
#80878=CARTESIAN_POINT('Ctrl Pts',(-3.37043804657536,-8.74345348753124,
8.04048197126432));
#80879=CARTESIAN_POINT('Ctrl Pts',(-3.44406542247971,-8.71471427221091,
8.03913865808122));
#80880=CARTESIAN_POINT('Ctrl Pts',(-3.61263947844372,-8.64644418200136,
8.03603284573427));
#80881=CARTESIAN_POINT('Ctrl Pts',(-3.70731651126421,-8.60627475780529,
8.03426612644284));
#80882=CARTESIAN_POINT('Ctrl Pts',(-4.03045477290982,-8.46285228669809,
8.02815917910937));
#80883=CARTESIAN_POINT('Ctrl Pts',(-4.2554219813586,-8.3519948198441,8.02377066006185));
#80884=CARTESIAN_POINT('Ctrl Pts',(-4.72690093961701,-8.09566332968275,
8.01433991910639));
#80885=CARTESIAN_POINT('Ctrl Pts',(-4.97174627405936,-7.94764723766363,
8.00929659191953));
#80886=CARTESIAN_POINT('Ctrl Pts',(-5.26037647699285,-7.7545973298444,8.00329849319699));
#80887=CARTESIAN_POINT('Ctrl Pts',(-5.31097866911419,-7.72002888780753,
8.00224507953479));
#80888=CARTESIAN_POINT('Ctrl Pts',(-5.39584930750706,-7.66082086038846,
8.00047752265552));
#80889=CARTESIAN_POINT('Ctrl Pts',(-5.43029686549057,-7.63644170872416,
7.99976000647542));
#80890=CARTESIAN_POINT('Ctrl Pts',(-5.51059499199026,-7.57879520286504,
7.99808734753222));
#80891=CARTESIAN_POINT('Ctrl Pts',(-5.55631081479998,-7.54534320241335,
7.99713469446265));
#80892=CARTESIAN_POINT('Ctrl Pts',(-5.75750040289201,-7.39530512082562,
7.99293430486887));
#80893=CARTESIAN_POINT('Ctrl Pts',(-5.90962912229764,-7.27431322069525,
7.98973618890659));
#80894=CARTESIAN_POINT('Ctrl Pts',(-6.34323369383115,-6.90687090415995,
7.98041028633625));
#80895=CARTESIAN_POINT('Ctrl Pts',(-6.6138467242539,-6.64819603811661,7.97430444251095));
#80896=CARTESIAN_POINT('Ctrl Pts',(-6.93295524357736,-6.30434437472377,
7.96645789512514));
#80897=CARTESIAN_POINT('Ctrl Pts',(-6.99657200333878,-6.23366718320731,
7.96485916110048));
#80898=CARTESIAN_POINT('Ctrl Pts',(-7.11050704185395,-6.1031455026004,7.96192930296934));
#80899=CARTESIAN_POINT('Ctrl Pts',(-7.1611731543421,-6.04361600691027,7.96060130260048));
#80900=CARTESIAN_POINT('Ctrl Pts',(-7.26947812978644,-5.91309005670211,
7.95770636707091));
#80901=CARTESIAN_POINT('Ctrl Pts',(-7.32683457061386,-5.84186968545867,
7.95613728428783));
#80902=CARTESIAN_POINT('Ctrl Pts',(-7.4500513148117,-5.68419991882513,7.95268636796294));
#80903=CARTESIAN_POINT('Ctrl Pts',(-7.51546870559611,-5.59742113574193,
7.95080153032853));
#80904=CARTESIAN_POINT('Ctrl Pts',(-7.70725783249856,-5.3335799961464,7.94511784689496));
#80905=CARTESIAN_POINT('Ctrl Pts',(-7.82898836062203,-5.15323585511615,
7.94129335474755));
#80906=CARTESIAN_POINT('Ctrl Pts',(-8.0615447779394,-4.78141608851392,7.93358325209606));
#80907=CARTESIAN_POINT('Ctrl Pts',(-8.17208970304495,-4.58992312252395,
7.92970012495918));
#80908=CARTESIAN_POINT('Ctrl Pts',(-8.30562602027414,-4.33845787224488,
7.92477811090807));
#80909=CARTESIAN_POINT('Ctrl Pts',(-8.33491858038175,-4.28191225779835,
7.92368266465286));
#80910=CARTESIAN_POINT('Ctrl Pts',(-8.38132928579615,-4.19004114871298,
7.92192362156729));
#80911=CARTESIAN_POINT('Ctrl Pts',(-8.39880581361861,-4.15489907766306,
7.92125567970066));
#80912=CARTESIAN_POINT('Ctrl Pts',(-8.43796284742283,-4.07490486873738,
7.91974675409031));
#80913=CARTESIAN_POINT('Ctrl Pts',(-8.45950745328853,-4.02998763840995,
7.91890742129331));
#80914=CARTESIAN_POINT('Ctrl Pts',(-8.50614349197759,-3.93073650210613,
7.91706806703292));
#80915=CARTESIAN_POINT('Ctrl Pts',(-8.53107466250537,-3.87632966567911,
7.9160697544822));
#80916=CARTESIAN_POINT('Ctrl Pts',(-8.58000542909778,-3.76679001329679,
7.91407652877246));
#80917=CARTESIAN_POINT('Ctrl Pts',(-8.60399898131218,-3.71165754226315,
7.913081699358));
#80918=CARTESIAN_POINT('Ctrl Pts',(-8.7177206039368,-3.44331814532167,7.90827286668289));
#80919=CARTESIAN_POINT('Ctrl Pts',(-8.80006357837955,-3.22706889901276,
7.90449637741208));
#80920=CARTESIAN_POINT('Ctrl Pts',(-8.89542184456499,-2.94573867605372,
7.89961916779074));
#80921=CARTESIAN_POINT('Ctrl Pts',(-8.91586805364957,-2.88326255864508,
7.89853845417325));
#80922=CARTESIAN_POINT('Ctrl Pts',(-8.99045642810158,-2.64696477003479,
7.89445543032018));
#80923=CARTESIAN_POINT('Ctrl Pts',(-9.04018623481913,-2.47179324152747,
7.89143686062912));
#80924=CARTESIAN_POINT('Ctrl Pts',(-9.10669552311684,-2.2085482092304,7.88688602457657));
#80925=CARTESIAN_POINT('Ctrl Pts',(-9.12736635162331,-2.12150229303535,
7.88537904888074));
#80926=CARTESIAN_POINT('Ctrl Pts',(-9.16345501551127,-1.95922740405079,
7.88256353634716));
#80927=CARTESIAN_POINT('Ctrl Pts',(-9.1792007313458,-1.88407901763928,7.88125727615615));
#80928=CARTESIAN_POINT('Ctrl Pts',(-9.20907837175296,-1.73220821967822,
7.87861186992756));
#80929=CARTESIAN_POINT('Ctrl Pts',(-9.22317930783414,-1.65548578893449,
7.87727263446506));
#80930=CARTESIAN_POINT('Ctrl Pts',(-9.25443140584141,-1.47263068696262,
7.87407416891602));
#80931=CARTESIAN_POINT('Ctrl Pts',(-9.27071724724699,-1.36636138497699,
7.87220999662095));
#80932=CARTESIAN_POINT('Ctrl Pts',(-9.34183065442542,-0.842245272326605,
7.86299607335696));
#80933=CARTESIAN_POINT('Ctrl Pts',(-9.3702545781991,-0.421311037842885,
7.85551027891911));
#80934=CARTESIAN_POINT('Ctrl Pts',(-9.37024999944691,0.000101810025349425,
7.84820354462752));
#80935=CARTESIAN_POINT('Ctrl Pts',(4.2912416510688,8.33064876709114,7.52288355898769));
#80936=CARTESIAN_POINT('Ctrl Pts',(4.20195778222728,8.37670351717924,7.5245903173793));
#80937=CARTESIAN_POINT('Ctrl Pts',(2.72745792095632,9.10710664797032,7.55254268019657));
#80938=CARTESIAN_POINT('Ctrl Pts',(-0.499675883778941,9.74834161973542,
7.60674064743951));
#80939=CARTESIAN_POINT('Ctrl Pts',(-5.06811753411523,8.34230333806495,7.68547746071647));
#80940=CARTESIAN_POINT('Ctrl Pts',(-8.42125135251966,4.93582475191143,7.76421427399345));
#80941=CARTESIAN_POINT('Ctrl Pts',(-9.34226565951642,1.76620876927797,7.81858508438964));
#80942=CARTESIAN_POINT('Ctrl Pts',(-9.37098492218543,0.110745121527537,
7.84671029036016));
#80943=CARTESIAN_POINT('Ctrl Pts',(-9.37091942283365,0.000108561626433589,
7.84858989190502));
#80944=CARTESIAN_POINT('',(-9.36966470910927,0.000159076414697548,7.65141010809498));
#80945=CARTESIAN_POINT('Ctrl Pts',(4.2909265843892,8.33003806173069,7.32568828984052));
#80946=CARTESIAN_POINT('Ctrl Pts',(4.04231038249422,8.45810396756635,7.33027366504272));
#80947=CARTESIAN_POINT('Ctrl Pts',(3.78802961208239,8.57500427684227,7.33487502092718));
#80948=CARTESIAN_POINT('Ctrl Pts',(3.44216616747705,8.71560847533341,7.34112308215479));
#80949=CARTESIAN_POINT('Ctrl Pts',(3.35496931930943,8.74954397857682,7.34269693401101));
#80950=CARTESIAN_POINT('Ctrl Pts',(3.1932113224947,8.80972371093231,7.34561664634709));
#80951=CARTESIAN_POINT('Ctrl Pts',(3.11879807584541,8.83634137759264,7.34695981226159));
#80952=CARTESIAN_POINT('Ctrl Pts',(2.94690660549949,8.89538522789968,7.35006343717151));
#80953=CARTESIAN_POINT('Ctrl Pts',(2.84921408072378,8.9271560950038,7.35182809365274));
#80954=CARTESIAN_POINT('Ctrl Pts',(2.41202984221905,9.06142649974026,7.35972785094122));
#80955=CARTESIAN_POINT('Ctrl Pts',(2.0674046928293,9.14621089955978,7.36597449147862));
#80956=CARTESIAN_POINT('Ctrl Pts',(1.54373572909195,9.24392679224437,7.37533158121962));
#80957=CARTESIAN_POINT('Ctrl Pts',(1.36776737729832,9.27159723060213,7.37845092257349));
#80958=CARTESIAN_POINT('Ctrl Pts',(1.1283029973751,9.30228616297731,7.38262395395606));
#80959=CARTESIAN_POINT('Ctrl Pts',(1.06540851654924,9.30969925569383,7.38371322311891));
#80960=CARTESIAN_POINT('Ctrl Pts',(0.960358146850123,9.32100257412341,7.38551875525336));
#80961=CARTESIAN_POINT('Ctrl Pts',(0.918242476432774,9.32524570873777,7.38623880628932));
#80962=CARTESIAN_POINT('Ctrl Pts',(0.82122710244084,9.3343563580369,7.38788843042142));
#80963=CARTESIAN_POINT('Ctrl Pts',(0.766310433441146,9.33902515849433,7.3888158385484));
#80964=CARTESIAN_POINT('Ctrl Pts',(0.545313274224173,9.3558510248116,7.39252754668975));
#80965=CARTESIAN_POINT('Ctrl Pts',(0.378962827235572,9.364064419969,7.3952756680047));
#80966=CARTESIAN_POINT('Ctrl Pts',(-0.115911456643848,9.37528917672946,
7.403409727051));
#80967=CARTESIAN_POINT('Ctrl Pts',(-0.444468673421632,9.36546476760892,
7.40876317643165));
#80968=CARTESIAN_POINT('Ctrl Pts',(-0.899869561346608,9.32782535748185,
7.4163462339333));
#80969=CARTESIAN_POINT('Ctrl Pts',(-1.02767742426524,9.31461057237031,7.41849117757631));
#80970=CARTESIAN_POINT('Ctrl Pts',(-1.22856400102596,9.28965472692301,7.42189694485045));
#80971=CARTESIAN_POINT('Ctrl Pts',(-1.30184455291793,9.27966891558475,7.42314651584613));
#80972=CARTESIAN_POINT('Ctrl Pts',(-1.45628643463555,9.2567579597057,7.42579638976125));
#80973=CARTESIAN_POINT('Ctrl Pts',(-1.53741148303551,9.24363045551501,7.42719789851145));
#80974=CARTESIAN_POINT('Ctrl Pts',(-1.74521668542947,9.2071924583808,7.43081332670424));
#80975=CARTESIAN_POINT('Ctrl Pts',(-1.87160770360422,9.18233405583594,7.43303680161501));
#80976=CARTESIAN_POINT('Ctrl Pts',(-2.0836941816202,9.13606022976917,7.43680724505908));
#80977=CARTESIAN_POINT('Ctrl Pts',(-2.16967223638292,9.11602437016743,7.43834672457213));
#80978=CARTESIAN_POINT('Ctrl Pts',(-2.58880252693475,9.01208698865118,7.44589965795934));
#80979=CARTESIAN_POINT('Ctrl Pts',(-2.91745012382002,8.91112195831109,7.45198223345832));
#80980=CARTESIAN_POINT('Ctrl Pts',(-3.32265275109734,8.76181252309734,7.45949218176258));
#80981=CARTESIAN_POINT('Ctrl Pts',(-3.40506103552275,8.73011680338023,7.46101940279675));
#80982=CARTESIAN_POINT('Ctrl Pts',(-3.52968224276099,8.68015218954677,7.46332269446726));
#80983=CARTESIAN_POINT('Ctrl Pts',(-3.57222886162526,8.66272934715109,7.46410792884781));
#80984=CARTESIAN_POINT('Ctrl Pts',(-3.65736738427479,8.6271312214192,7.46567572799275));
#80985=CARTESIAN_POINT('Ctrl Pts',(-3.69995624188434,8.60895191735874,7.46645822350026));
#80986=CARTESIAN_POINT('Ctrl Pts',(-3.82514246705008,8.55441489141405,7.46875540663353));
#80987=CARTESIAN_POINT('Ctrl Pts',(-3.90735146798894,8.51717873477945,7.47026024603327));
#80988=CARTESIAN_POINT('Ctrl Pts',(-4.22743914431247,8.36658681106154,7.47612619328647));
#80989=CARTESIAN_POINT('Ctrl Pts',(-4.46103118718842,8.24440525488119,7.48042496285821));
#80990=CARTESIAN_POINT('Ctrl Pts',(-4.89511597159933,7.99349814615369,7.48865284328449));
#80991=CARTESIAN_POINT('Ctrl Pts',(-5.09646033428096,7.86665523414928,7.49257390672609));
#80992=CARTESIAN_POINT('Ctrl Pts',(-5.3725946549927,7.67764103538125,7.49816806471463));
#80993=CARTESIAN_POINT('Ctrl Pts',(-5.45157920589582,7.62176024934758,7.49979395664641));
#80994=CARTESIAN_POINT('Ctrl Pts',(-5.59335651221209,7.5181226706588,7.50276263987606));
#80995=CARTESIAN_POINT('Ctrl Pts',(-5.6564386459398,7.47077689232608,7.50410209212282));
#80996=CARTESIAN_POINT('Ctrl Pts',(-5.79715090731655,7.36236243650978,7.50713310109671));
#80997=CARTESIAN_POINT('Ctrl Pts',(-5.87442832954561,7.30085139044931,7.50882809213423));
#80998=CARTESIAN_POINT('Ctrl Pts',(-6.03686868546358,7.16730352242169,7.51245649857238));
#80999=CARTESIAN_POINT('Ctrl Pts',(-6.12174706937035,7.09494440054348,7.51439215570155));
#81000=CARTESIAN_POINT('Ctrl Pts',(-6.37817604354789,6.86830968935955,7.52035906903658));
#81001=CARTESIAN_POINT('Ctrl Pts',(-6.54533726029579,6.70920020582771,7.52441916490341));
#81002=CARTESIAN_POINT('Ctrl Pts',(-6.72675217328434,6.5232840568858,7.52898462028908));
#81003=CARTESIAN_POINT('Ctrl Pts',(-6.74695219512636,6.50238923509666,7.52949526148573));
#81004=CARTESIAN_POINT('Ctrl Pts',(-6.89592684480622,6.34684884561467,7.53327754072286));
#81005=CARTESIAN_POINT('Ctrl Pts',(-7.02075765590993,6.2084828725395,7.53653863198782));
#81006=CARTESIAN_POINT('Ctrl Pts',(-7.17769709367798,6.02373605563979,7.5407189900927));
#81007=CARTESIAN_POINT('Ctrl Pts',(-7.21362912281673,5.98065937289526,7.54168182995705));
#81008=CARTESIAN_POINT('Ctrl Pts',(-7.27589665129806,5.90463308437941,7.54335860006113));
#81009=CARTESIAN_POINT('Ctrl Pts',(-7.30240036867556,5.87182363525381,7.54407484151696));
#81010=CARTESIAN_POINT('Ctrl Pts',(-7.33053103196896,5.8365151125376,7.54483794075264));
#81011=CARTESIAN_POINT('Ctrl Pts',(-7.33237915578109,5.8341931563336,7.54488808880286));
#81012=CARTESIAN_POINT('Ctrl Pts',(-7.33639729808852,5.82913989505332,7.54499715047581));
#81013=CARTESIAN_POINT('Ctrl Pts',(-7.33856689512836,5.82640825528336,7.54505605811935));
#81014=CARTESIAN_POINT('Ctrl Pts',(-7.34219185163393,5.82183900251341,7.54515451446979));
#81015=CARTESIAN_POINT('Ctrl Pts',(-7.34364804774374,5.8200020539736,7.5451940748616));
#81016=CARTESIAN_POINT('Ctrl Pts',(-7.34601991394989,5.81700770709245,7.54525852619065));
#81017=CARTESIAN_POINT('Ctrl Pts',(-7.34693600013598,5.81585063859342,7.54528342288178));
#81018=CARTESIAN_POINT('Ctrl Pts',(-7.34839882210075,5.81400211479826,7.54532318420669));
#81019=CARTESIAN_POINT('Ctrl Pts',(-7.34894573370705,5.81331079872384,7.54533805125667));
#81020=CARTESIAN_POINT('Ctrl Pts',(-7.38547755100022,5.76711986478796,7.5463312070787));
#81021=CARTESIAN_POINT('Ctrl Pts',(-7.42103931452482,5.72128706704285,7.54730369962533));
#81022=CARTESIAN_POINT('Ctrl Pts',(-7.5059559935398,5.60972066953171,7.54964344589641));
#81023=CARTESIAN_POINT('Ctrl Pts',(-7.5548760579241,5.54366207093679,7.55100614761297));
#81024=CARTESIAN_POINT('Ctrl Pts',(-7.72537946250415,5.30697567989573,7.55582296682178));
#81025=CARTESIAN_POINT('Ctrl Pts',(-7.84210267372028,5.1329235927607,7.55924721209016));
#81026=CARTESIAN_POINT('Ctrl Pts',(-8.08698111497736,4.73989620406924,7.56684259534743));
#81027=CARTESIAN_POINT('Ctrl Pts',(-8.21227767944174,4.5193333985128,7.57101747848766));
#81028=CARTESIAN_POINT('Ctrl Pts',(-8.37290870071318,4.20777699009645,7.57687702529179));
#81029=CARTESIAN_POINT('Ctrl Pts',(-8.41600291666158,4.12090792871133,7.5785064710362));
#81030=CARTESIAN_POINT('Ctrl Pts',(-8.49057025217792,3.96454520034833,7.58143469815022));
#81031=CARTESIAN_POINT('Ctrl Pts',(-8.52255770216196,3.89530641101939,7.58272969404166));
#81032=CARTESIAN_POINT('Ctrl Pts',(-8.59152353711384,3.74110845307417,7.58561096833774));
#81033=CARTESIAN_POINT('Ctrl Pts',(-8.62809425907516,3.65597573154188,7.58719992463265));
#81034=CARTESIAN_POINT('Ctrl Pts',(-8.70385797463682,3.47213449309127,7.5906274480045));
#81035=CARTESIAN_POINT('Ctrl Pts',(-8.74264757763201,3.37327360933953,7.59246833312108));
#81036=CARTESIAN_POINT('Ctrl Pts',(-8.85198807294151,3.08003963825092,7.59791848456092));
#81037=CARTESIAN_POINT('Ctrl Pts',(-8.9177953093454,2.88396663022594,7.60155090967412));
#81038=CARTESIAN_POINT('Ctrl Pts',(-8.98972656973892,2.64354938814965,7.60596299562891));
#81039=CARTESIAN_POINT('Ctrl Pts',(-9.00209148657416,2.60113168335239,7.60673981165297));
#81040=CARTESIAN_POINT('Ctrl Pts',(-9.03704354801635,2.47799408069812,7.60898924156054));
#81041=CARTESIAN_POINT('Ctrl Pts',(-9.05884820454744,2.39705652330416,7.61046080176516));
#81042=CARTESIAN_POINT('Ctrl Pts',(-9.1109329989659,2.19285080281186,7.61414954394344));
#81043=CARTESIAN_POINT('Ctrl Pts',(-9.13979996608033,2.06923934640825,7.61636072737865));
#81044=CARTESIAN_POINT('Ctrl Pts',(-9.17768809670054,1.89069231410202,7.61950774854431));
#81045=CARTESIAN_POINT('Ctrl Pts',(-9.1887449292979,1.83620338479388,7.62046190085535));
#81046=CARTESIAN_POINT('Ctrl Pts',(-9.2073404579694,1.74018615122084,7.62213041069662));
#81047=CARTESIAN_POINT('Ctrl Pts',(-9.21508470499457,1.6986995128911,7.62284697773679));
#81048=CARTESIAN_POINT('Ctrl Pts',(-9.23010239968762,1.61512202475682,7.62428213940653));
#81049=CARTESIAN_POINT('Ctrl Pts',(-9.23736881828136,1.57303108274252,7.62500075387933));
#81050=CARTESIAN_POINT('Ctrl Pts',(-9.25454643839661,1.46930338917469,7.62676296202449));
#81051=CARTESIAN_POINT('Ctrl Pts',(-9.26412995946588,1.40761441638011,7.62780342632758));
#81052=CARTESIAN_POINT('Ctrl Pts',(-9.33777378647577,0.900192111112405,
7.63631450621329));
#81053=CARTESIAN_POINT('Ctrl Pts',(-9.37024262317214,0.450467170292491,
7.64359007600784));
#81054=CARTESIAN_POINT('Ctrl Pts',(-9.37024999874316,0.0001534728895565,
7.65107226318331));
#81055=CARTESIAN_POINT('Ctrl Pts',(-9.36966470910927,0.000159076414697548,
7.65141010809498));
#81056=CARTESIAN_POINT('Ctrl Pts',(-9.36906894256188,-0.965940399241459,
7.66781681340257));
#81057=CARTESIAN_POINT('Ctrl Pts',(-8.98250254660737,-3.47796327412567,
7.71046912313581));
#81058=CARTESIAN_POINT('Ctrl Pts',(-6.77274903485361,-7.02920412114798,
7.77936703729473));
#81059=CARTESIAN_POINT('Ctrl Pts',(-2.62336437052269,-9.40201039381186,
7.8581038505717));
#81060=CARTESIAN_POINT('Ctrl Pts',(2.15508922207328,-9.52026420383269,7.93684066384868));
#81061=CARTESIAN_POINT('Ctrl Pts',(6.41676379514821,-7.35560891178627,8.01557747712564));
#81062=CARTESIAN_POINT('Ctrl Pts',(9.13973228190865,-3.42711743027742,8.09431429040262));
#81063=CARTESIAN_POINT('Ctrl Pts',(9.67104121278963,1.32317872050558,8.17305110367959));
#81064=CARTESIAN_POINT('Ctrl Pts',(7.91977215059093,5.66570957463458,8.25018096263681));
#81065=CARTESIAN_POINT('Ctrl Pts',(5.58015555167917,7.66584979211291,8.30106521716837));
#81066=CARTESIAN_POINT('Ctrl Pts',(4.29124604933307,8.33065733261531,8.32570386727427));
#81067=CARTESIAN_POINT('Origin',(0.,0.,2.15141010809499));
#81068=CARTESIAN_POINT('',(4.29092667702531,8.33003801401246,9.52315240206829));
#81069=CARTESIAN_POINT('',(4.29092661458801,8.33003804617484,9.32538978630507));
#81070=CARTESIAN_POINT('',(4.29092662815669,8.33003803918541,2.15141010809499));
#81071=CARTESIAN_POINT('Ctrl Pts',(4.29092667702531,8.33003801401246,9.52315240206829));
#81072=CARTESIAN_POINT('Ctrl Pts',(4.53655035743086,8.20351359707842,9.51833436278683));
#81073=CARTESIAN_POINT('Ctrl Pts',(4.77651276604139,8.0661588380477,9.51346043102322));
#81074=CARTESIAN_POINT('Ctrl Pts',(5.15459381020808,7.82693962096863,9.50560935836044));
#81075=CARTESIAN_POINT('Ctrl Pts',(5.29655681628916,7.73157858064885,9.50262087595));
#81076=CARTESIAN_POINT('Ctrl Pts',(5.48096469357036,7.60024219273754,9.49871858682182));
#81077=CARTESIAN_POINT('Ctrl Pts',(5.52581229919439,7.56769805248282,9.49776797732741));
#81078=CARTESIAN_POINT('Ctrl Pts',(5.60438058801465,7.50961332908845,9.4961016538837));
#81079=CARTESIAN_POINT('Ctrl Pts',(5.63822172271278,7.48423876800121,9.49538377525311));
#81080=CARTESIAN_POINT('Ctrl Pts',(5.7219620913717,7.42055873632359,9.49360640368073));
#81081=CARTESIAN_POINT('Ctrl Pts',(5.77164950557834,7.38197833547766,9.49255069601179));
#81082=CARTESIAN_POINT('Ctrl Pts',(6.06694834477417,7.14788579571534,9.48625836594702));
#81083=CARTESIAN_POINT('Ctrl Pts',(6.30299734301444,6.94063107224696,9.48114574855487));
#81084=CARTESIAN_POINT('Ctrl Pts',(6.64674984012617,6.60678530211221,9.4732815543103));
#81085=CARTESIAN_POINT('Ctrl Pts',(6.76223432132835,6.48853468046768,9.47056128196258));
#81086=CARTESIAN_POINT('Ctrl Pts',(6.96129923039886,6.27361163007989,9.46569917405322));
#81087=CARTESIAN_POINT('Ctrl Pts',(7.04614340965096,6.17816742966272,9.46356707552349));
#81088=CARTESIAN_POINT('Ctrl Pts',(7.18223538320132,6.01862163160117,9.46003864499625));
#81089=CARTESIAN_POINT('Ctrl Pts',(7.23463882411581,5.95552789360259,9.45865214098032));
#81090=CARTESIAN_POINT('Ctrl Pts',(7.33280058411274,5.8341333372522,9.45599976231085));
#81091=CARTESIAN_POINT('Ctrl Pts',(7.37870879379131,5.77596162658633,9.45473525371776));
#81092=CARTESIAN_POINT('Ctrl Pts',(7.50298628873414,5.61458575766365,9.45124450731841));
#81093=CARTESIAN_POINT('Ctrl Pts',(7.57991212246916,5.51029114991421,9.44900725204018));
#81094=CARTESIAN_POINT('Ctrl Pts',(7.84393413441098,5.13633973768745,9.44105517721986));
#81095=CARTESIAN_POINT('Ctrl Pts',(8.01900261473456,4.8584858071132,9.43526318669941));
#81096=CARTESIAN_POINT('Ctrl Pts',(8.25963368823789,4.42800826986699,9.42661203351528));
#81097=CARTESIAN_POINT('Ctrl Pts',(8.33631847964263,4.28189214804586,9.42373001321036));
#81098=CARTESIAN_POINT('Ctrl Pts',(8.43337251481296,4.08446310033048,9.41993869383379));
#81099=CARTESIAN_POINT('Ctrl Pts',(8.45720441038539,4.03488591799286,9.41899515228053));
#81100=CARTESIAN_POINT('Ctrl Pts',(8.49860547716727,3.94678131045373,9.4173351826119));
#81101=CARTESIAN_POINT('Ctrl Pts',(8.51635252066377,3.90833948311989,9.41661667506771));
#81102=CARTESIAN_POINT('Ctrl Pts',(8.56005614033439,3.81196196892723,9.41482904241899));
#81103=CARTESIAN_POINT('Ctrl Pts',(8.58568559739771,3.75388039605313,9.41376382152321));
#81104=CARTESIAN_POINT('Ctrl Pts',(8.68184900646131,3.52981683746638,9.40969315287613));
#81105=CARTESIAN_POINT('Ctrl Pts',(8.74817605744322,3.36207154880467,9.40672588775671));
#81106=CARTESIAN_POINT('Ctrl Pts',(8.89273712931841,2.96316108957192,9.39976399701432));
#81107=CARTESIAN_POINT('Ctrl Pts',(8.96686474473988,2.73064715455162,9.39577739382965));
#81108=CARTESIAN_POINT('Ctrl Pts',(9.06225290468573,2.38541461162855,9.38986060591404));
#81109=CARTESIAN_POINT('Ctrl Pts',(9.09065591924087,2.27477591423973,9.38796526118295));
#81110=CARTESIAN_POINT('Ctrl Pts',(9.14020187420241,2.06600241434345,9.38438203727956));
#81111=CARTESIAN_POINT('Ctrl Pts',(9.16180435576896,1.96799318074359,9.38269715138645));
#81112=CARTESIAN_POINT('Ctrl Pts',(9.19742641111772,1.79305426802685,9.37968154163352));
#81113=CARTESIAN_POINT('Ctrl Pts',(9.21206526222652,1.71626040210631,9.37835498994969));
#81114=CARTESIAN_POINT('Ctrl Pts',(9.24235958490316,1.54576758662341,9.37540272357384));
#81115=CARTESIAN_POINT('Ctrl Pts',(9.25755458509737,1.45199558362127,9.37377418846392));
#81116=CARTESIAN_POINT('Ctrl Pts',(9.29560300523196,1.19223357970133,9.36924960925944));
#81117=CARTESIAN_POINT('Ctrl Pts',(9.31543417348264,1.02583723526141,9.36633589613563));
#81118=CARTESIAN_POINT('Ctrl Pts',(9.35639340952671,0.580921644502694,9.35852038266875));
#81119=CARTESIAN_POINT('Ctrl Pts',(9.36954963341063,0.301839177342059,9.35358915406841));
#81120=CARTESIAN_POINT('Ctrl Pts',(9.37044699854996,-0.0704308501302653,
9.34707510341973));
#81121=CARTESIAN_POINT('Ctrl Pts',(9.36928612722907,-0.163447161744229,
9.34545327309791));
#81122=CARTESIAN_POINT('Ctrl Pts',(9.36480789685254,-0.327025070621559,
9.34261875581561));
#81123=CARTESIAN_POINT('Ctrl Pts',(9.36207724474583,-0.397595322602507,
9.34140168813984));
#81124=CARTESIAN_POINT('Ctrl Pts',(9.35639398578417,-0.511211793718479,
9.33945495319131));
#81125=CARTESIAN_POINT('Ctrl Pts',(9.35394138236341,-0.554280212197695,
9.33872000764582));
#81126=CARTESIAN_POINT('Ctrl Pts',(9.34792994862151,-0.648389055888332,
9.33712141256178));
#81127=CARTESIAN_POINT('Ctrl Pts',(9.34425031656819,-0.699420280653494,
9.33625905632767));
#81128=CARTESIAN_POINT('Ctrl Pts',(9.33145772012152,-0.858644430268895,
9.33357914529558));
#81129=CARTESIAN_POINT('Ctrl Pts',(9.3208821198359,-0.9667109456824,9.3317757186527));
#81130=CARTESIAN_POINT('Ctrl Pts',(9.30401212629843,-1.11284684644981,9.32934543124297));
#81131=CARTESIAN_POINT('Ctrl Pts',(9.29935729966201,-1.15109667967718,9.32871012117066));
#81132=CARTESIAN_POINT('Ctrl Pts',(9.26443491950193,-1.42401380191301,9.32418010830899));
#81133=CARTESIAN_POINT('Ctrl Pts',(9.22552433555031,-1.65748924902257,9.32031827007886));
#81134=CARTESIAN_POINT('Ctrl Pts',(9.13595634008771,-2.09260510684001,9.31301364505869));
#81135=CARTESIAN_POINT('Ctrl Pts',(9.08734657670621,-2.29452090664058,9.30957984551121));
#81136=CARTESIAN_POINT('Ctrl Pts',(9.00755067226226,-2.58342753083447,9.30456132642562));
#81137=CARTESIAN_POINT('Ctrl Pts',(8.98172415534935,-2.67183421391164,9.30301139706521));
#81138=CARTESIAN_POINT('Ctrl Pts',(8.93127584265924,-2.83551887206895,9.30011268701998));
#81139=CARTESIAN_POINT('Ctrl Pts',(8.90699476095773,-2.91089328999987,9.29876629690617));
#81140=CARTESIAN_POINT('Ctrl Pts',(8.84890288132995,-3.08368857217402,9.29565205285586));
#81141=CARTESIAN_POINT('Ctrl Pts',(8.81443349841996,-3.18087714990394,9.29387995360391));
#81142=CARTESIAN_POINT('Ctrl Pts',(8.67896695350965,-3.54370963719546,9.28718743234917));
#81143=CARTESIAN_POINT('Ctrl Pts',(8.5675069263532,-3.80528176575947,9.2822017180191));
#81144=CARTESIAN_POINT('Ctrl Pts',(8.36861799256515,-4.2188071011161,9.27413412590122));
#81145=CARTESIAN_POINT('Ctrl Pts',(8.28851544384235,-4.37408416826252,9.27106175304408));
#81146=CARTESIAN_POINT('Ctrl Pts',(8.16777757532142,-4.59289155616682,9.26670327874903));
#81147=CARTESIAN_POINT('Ctrl Pts',(8.13064405627935,-4.6583119935548,9.26539643963388));
#81148=CARTESIAN_POINT('Ctrl Pts',(8.06205954814954,-4.77582268297343,9.26304652122073));
#81149=CARTESIAN_POINT('Ctrl Pts',(8.03088121694346,-4.82806724897704,9.26200084765485));
#81150=CARTESIAN_POINT('Ctrl Pts',(7.97722788383948,-4.91601461416808,9.26024134918533));
#81151=CARTESIAN_POINT('Ctrl Pts',(7.95501663813909,-4.95187587661961,9.25952424108078));
#81152=CARTESIAN_POINT('Ctrl Pts',(7.902769861629,-5.03497236498125,9.25786344988203));
#81153=CARTESIAN_POINT('Ctrl Pts',(7.87255178934908,-5.08209076517123,9.25692211816725));
#81154=CARTESIAN_POINT('Ctrl Pts',(7.74318500037833,-5.27988680221872,9.25296645397048));
#81155=CARTESIAN_POINT('Ctrl Pts',(7.64011840087408,-5.42795631934355,9.24999445273794));
#81156=CARTESIAN_POINT('Ctrl Pts',(7.51077716053704,-5.60278394269041,9.24642399614157));
#81157=CARTESIAN_POINT('Ctrl Pts',(7.4885350553743,-5.63247762437499,9.24581540170336));
#81158=CARTESIAN_POINT('Ctrl Pts',(7.32742010786547,-5.8449281566664,9.24144326797074));
#81159=CARTESIAN_POINT('Ctrl Pts',(7.18204980015554,-6.0226598065445,9.23768824680844));
#81160=CARTESIAN_POINT('Ctrl Pts',(6.95673023654192,-6.27836546937115,9.23205466590245));
#81161=CARTESIAN_POINT('Ctrl Pts',(6.88167852858946,-6.36054000133931,9.2302068695419));
#81162=CARTESIAN_POINT('Ctrl Pts',(6.73738896231142,-6.51297938112824,9.22669991103106));
#81163=CARTESIAN_POINT('Ctrl Pts',(6.66847044716011,-6.58352582454055,9.22504345183941));
#81164=CARTESIAN_POINT('Ctrl Pts',(6.54245442012927,-6.70850917518572,9.22204441711765));
#81165=CARTESIAN_POINT('Ctrl Pts',(6.4857586256957,-6.76333794872587,9.22070555330623));
#81166=CARTESIAN_POINT('Ctrl Pts',(6.35788910450053,-6.88391004436583,9.21770787794153));
#81167=CARTESIAN_POINT('Ctrl Pts',(6.28637424503067,-6.94927839092255,9.21604599682086));
#81168=CARTESIAN_POINT('Ctrl Pts',(6.02948753800526,-7.17687542740149,9.21012753209563));
#81169=CARTESIAN_POINT('Ctrl Pts',(5.8387475392438,-7.33289078417603,9.20582242655031));
#81170=CARTESIAN_POINT('Ctrl Pts',(5.50115396283354,-7.58749283641007,9.19839581687746));
#81171=CARTESIAN_POINT('Ctrl Pts',(5.35724960377537,-7.68977367399845,9.19528693947165));
#81172=CARTESIAN_POINT('Ctrl Pts',(5.08796162469178,-7.8699417889886,9.18961019070575));
#81173=CARTESIAN_POINT('Ctrl Pts',(4.96346131076589,-7.94904958337707,9.18703839956719));
#81174=CARTESIAN_POINT('Ctrl Pts',(4.79123360275638,-8.05285907872073,9.18357484853085));
#81175=CARTESIAN_POINT('Ctrl Pts',(4.74508494056717,-8.08013785168453,9.18265581543761));
#81176=CARTESIAN_POINT('Ctrl Pts',(4.66189838538814,-8.12835151058474,9.18101701259624));
#81177=CARTESIAN_POINT('Ctrl Pts',(4.62494733022896,-8.14943292677324,9.18029546081728));
#81178=CARTESIAN_POINT('Ctrl Pts',(4.54035388409291,-8.19693475373523,9.17865734960211));
#81179=CARTESIAN_POINT('Ctrl Pts',(4.49262208188251,-8.22319278604103,9.17774276906602));
#81180=CARTESIAN_POINT('Ctrl Pts',(4.19453131861664,-8.38380715774307,9.17208350968724));
#81181=CARTESIAN_POINT('Ctrl Pts',(3.93839708150444,-8.50713495504286,9.16744448817043));
#81182=CARTESIAN_POINT('Ctrl Pts',(3.44263854538389,-8.71864544135651,9.15860726727459));
#81183=CARTESIAN_POINT('Ctrl Pts',(3.20423974175878,-8.8090513500388,9.15441704631916));
#81184=CARTESIAN_POINT('Ctrl Pts',(2.86494923647387,-8.92211935581875,9.14844879939828));
#81185=CARTESIAN_POINT('Ctrl Pts',(2.76691725996314,-8.95300601669009,9.14672431696656));
#81186=CARTESIAN_POINT('Ctrl Pts',(2.59263891609513,-9.00477952789019,9.14365476592094));
#81187=CARTESIAN_POINT('Ctrl Pts',(2.51659902380786,-9.02632595327815,9.14231423436405));
#81188=CARTESIAN_POINT('Ctrl Pts',(2.34999857392712,-9.07126444299362,9.13937339891728));
#81189=CARTESIAN_POINT('Ctrl Pts',(2.25934193176152,-9.0942677480084,9.13777068866701));
#81190=CARTESIAN_POINT('Ctrl Pts',(1.77310745676169,-9.20992593034401,9.12916118171145));
#81191=CARTESIAN_POINT('Ctrl Pts',(1.37216367968342,-9.2781360682612,9.12199309533682));
#81192=CARTESIAN_POINT('Ctrl Pts',(0.799001641982031,-9.33766953932976,
9.11188168263922));
#81193=CARTESIAN_POINT('Ctrl Pts',(0.629490727653586,-9.35062659657888,
9.10891117063052));
#81194=CARTESIAN_POINT('Ctrl Pts',(0.404443021924749,-9.36168114953993,
9.10502756096534));
#81195=CARTESIAN_POINT('Ctrl Pts',(0.349141860416359,-9.36390666783527,
9.10407809876825));
#81196=CARTESIAN_POINT('Ctrl Pts',(0.251541049242236,-9.36696865500938,
9.10241281362844));
#81197=CARTESIAN_POINT('Ctrl Pts',(0.209249627321041,-9.36800882151119,
9.10169483981409));
#81198=CARTESIAN_POINT('Ctrl Pts',(0.114419571983502,-9.36969870369127,
9.10009248913521));
#81199=CARTESIAN_POINT('Ctrl Pts',(0.0618797252813041,-9.3701929836948,
9.09920976079177));
#81200=CARTESIAN_POINT('Ctrl Pts',(-0.294255055835618,-9.37054790958427,
9.09325286770774));
#81201=CARTESIAN_POINT('Ctrl Pts',(-0.597685142130283,-9.35609577851258,
9.08830240290459));
#81202=CARTESIAN_POINT('Ctrl Pts',(-1.07531902166894,-9.3100128939096,9.08043226456062));
#81203=CARTESIAN_POINT('Ctrl Pts',(-1.25024713984585,-9.28813937303063,
9.07753466725273));
#81204=CARTESIAN_POINT('Ctrl Pts',(-1.555726937633,-9.24115463964584,9.07240955003862));
#81205=CARTESIAN_POINT('Ctrl Pts',(-1.68655571299866,-9.21817525708584,
9.07019365337112));
#81206=CARTESIAN_POINT('Ctrl Pts',(-1.89804940717955,-9.17637423860968,
9.06656815380644));
#81207=CARTESIAN_POINT('Ctrl Pts',(-1.97903099948778,-9.1592506234975,9.06516958693894));
#81208=CARTESIAN_POINT('Ctrl Pts',(-2.14099090091565,-9.12275583160073,
9.06235018572201));
#81209=CARTESIAN_POINT('Ctrl Pts',(-2.22195920245591,-9.10337372977637,
9.06092939412982));
#81210=CARTESIAN_POINT('Ctrl Pts',(-2.43456898125982,-9.04947388979151,
9.05716807084339));
#81211=CARTESIAN_POINT('Ctrl Pts',(-2.56573514857004,-9.01316297400307,
9.05481631093867));
#81212=CARTESIAN_POINT('Ctrl Pts',(-3.00824289621076,-8.88022026009241,
9.04678124313245));
#81213=CARTESIAN_POINT('Ctrl Pts',(-3.31531523609645,-8.77020643205332,
9.04102587809431));
#81214=CARTESIAN_POINT('Ctrl Pts',(-3.76064999033695,-8.58391940228398,
9.0325623314531));
#81215=CARTESIAN_POINT('Ctrl Pts',(-3.90373212527148,-8.51980260235047,
9.02982611835058));
#81216=CARTESIAN_POINT('Ctrl Pts',(-4.09420059841487,-8.42864550009434,
9.02618800970519));
#81217=CARTESIAN_POINT('Ctrl Pts',(-4.14305743641789,-8.40473786640785,
9.02525523816701));
#81218=CARTESIAN_POINT('Ctrl Pts',(-4.2296407228366,-8.36143072241235,9.02360474481637));
#81219=CARTESIAN_POINT('Ctrl Pts',(-4.26744865942165,-8.34219793043387,
9.02288507267542));
#81220=CARTESIAN_POINT('Ctrl Pts',(-4.35269498263181,-8.29810218482182,
9.0212641201556));
#81221=CARTESIAN_POINT('Ctrl Pts',(-4.40005339633608,-8.27308791246818,
9.02036466200209));
#81222=CARTESIAN_POINT('Ctrl Pts',(-4.71992563628664,-8.10061079552707,
9.01428864104597));
#81223=CARTESIAN_POINT('Ctrl Pts',(-4.98519543132521,-7.94011469892821,
9.00923917339297));
#81224=CARTESIAN_POINT('Ctrl Pts',(-5.38420151980779,-7.67081357029556,
9.00134200093529));
#81225=CARTESIAN_POINT('Ctrl Pts',(-5.52371483394541,-7.57096962837416,
8.99852062308063));
#81226=CARTESIAN_POINT('Ctrl Pts',(-5.70955103074617,-7.43010193071963,
8.99465231770901));
#81227=CARTESIAN_POINT('Ctrl Pts',(-5.75832447725486,-7.39236679793993,
8.993626458969));
#81228=CARTESIAN_POINT('Ctrl Pts',(-5.88681654913273,-7.29091150882686,
8.99089378213007));
#81229=CARTESIAN_POINT('Ctrl Pts',(-5.96587261084626,-7.22636586649598,
8.98918113876672));
#81230=CARTESIAN_POINT('Ctrl Pts',(-6.10421984257092,-7.10959382680616,
8.98612410231501));
#81231=CARTESIAN_POINT('Ctrl Pts',(-6.16393453174081,-7.05788462099976,
8.98478410253716));
#81232=CARTESIAN_POINT('Ctrl Pts',(-6.29329596295239,-6.9429716117047,8.98183478794692));
#81233=CARTESIAN_POINT('Ctrl Pts',(-6.36265939710194,-6.8794617681,8.98022296319369));
#81234=CARTESIAN_POINT('Ctrl Pts',(-6.71952225635856,-6.54269991373574,
8.97176921967462));
#81235=CARTESIAN_POINT('Ctrl Pts',(-6.99041353231866,-6.25244086853392,
8.96477520895331));
#81236=CARTESIAN_POINT('Ctrl Pts',(-7.35438901821969,-5.80911913994624,
8.95470662886602));
#81237=CARTESIAN_POINT('Ctrl Pts',(-7.46278760415433,-5.66918905010321,
8.95161188861302));
#81238=CARTESIAN_POINT('Ctrl Pts',(-7.60005385784144,-5.48122955615698,
8.94759956921163));
#81239=CARTESIAN_POINT('Ctrl Pts',(-7.63254631137156,-5.43589301895453,
8.94664254552966));
#81240=CARTESIAN_POINT('Ctrl Pts',(-7.68894429827777,-5.35569853915122,
8.94497036964128));
#81241=CARTESIAN_POINT('Ctrl Pts',(-7.71302224522151,-5.32096411497662,
8.9442529757433));
#81242=CARTESIAN_POINT('Ctrl Pts',(-7.76626302693181,-5.24303913760968,
8.94265833093854));
#81243=CARTESIAN_POINT('Ctrl Pts',(-7.79530213182425,-5.19976590731973,
8.94178265397177));
#81244=CARTESIAN_POINT('Ctrl Pts',(-7.99202140965166,-4.90126861409037,
8.93580201065583));
#81245=CARTESIAN_POINT('Ctrl Pts',(-8.14749938200692,-4.63822117625748,
8.930822900853));
#81246=CARTESIAN_POINT('Ctrl Pts',(-8.40268299762345,-4.15392395794922,
8.92184448933034));
#81247=CARTESIAN_POINT('Ctrl Pts',(-8.50717124373083,-3.93550540418218,
8.91786084378229));
#81248=CARTESIAN_POINT('Ctrl Pts',(-8.64340597654639,-3.61987161047319,
8.91212218162982));
#81249=CARTESIAN_POINT('Ctrl Pts',(-8.68220217287086,-3.52580525756368,
8.9104145444596));
#81250=CARTESIAN_POINT('Ctrl Pts',(-8.74837621495052,-3.35763835336013,
8.90736277249834));
#81251=CARTESIAN_POINT('Ctrl Pts',(-8.7763635092829,-3.28378824371271,8.90602297027732));
#81252=CARTESIAN_POINT('Ctrl Pts',(-8.83570347310056,-3.12102797649012,
8.9030699097792));
#81253=CARTESIAN_POINT('Ctrl Pts',(-8.86665467245573,-3.03198059981565,
8.90145409643289));
#81254=CARTESIAN_POINT('Ctrl Pts',(-9.01940183949125,-2.57016698236896,
8.89307300459722));
#81255=CARTESIAN_POINT('Ctrl Pts',(-9.11905242678053,-2.19049023604211,
8.88615978438924));
#81256=CARTESIAN_POINT('Ctrl Pts',(-9.22936587530118,-1.62877216532722,
8.87610977621629));
#81257=CARTESIAN_POINT('Ctrl Pts',(-9.25899705466085,-1.45088492859274,
8.87295584223503));
#81258=CARTESIAN_POINT('Ctrl Pts',(-9.29107632182573,-1.21680646084682,
8.86888253320462));
#81259=CARTESIAN_POINT('Ctrl Pts',(-9.29817817201224,-1.1612923327927,8.86792220440896));
#81260=CARTESIAN_POINT('Ctrl Pts',(-9.30976764725163,-1.0637651521011,8.86624698229964));
#81261=CARTESIAN_POINT('Ctrl Pts',(-9.31446921792621,-1.02177939750383,
8.865529807736));
#81262=CARTESIAN_POINT('Ctrl Pts',(-9.32538519108151,-0.917953563784677,
8.86376572573016));
#81263=CARTESIAN_POINT('Ctrl Pts',(-9.33126858183865,-0.856080829411509,
8.86272244821995));
#81264=CARTESIAN_POINT('Ctrl Pts',(-9.35899521502701,-0.530110439331893,
8.85725832551379));
#81265=CARTESIAN_POINT('Ctrl Pts',(-9.37024340926094,-0.265231948612504,
8.85292626627514));
#81266=CARTESIAN_POINT('Ctrl Pts',(-9.37025268437787,0.107863849306275,
8.84681041898646));
#81267=CARTESIAN_POINT('Ctrl Pts',(-9.36838483711979,0.215952541891298,
8.84503746952965));
#81268=CARTESIAN_POINT('Ctrl Pts',(-9.35805287421797,0.514593863841188,
8.84011970950323));
#81269=CARTESIAN_POINT('Ctrl Pts',(-9.34564047711994,0.70495687852041,8.83696255375387));
#81270=CARTESIAN_POINT('Ctrl Pts',(-9.31858177038158,0.987015371593162,
8.83221905460276));
#81271=CARTESIAN_POINT('Ctrl Pts',(-9.30836922471958,1.07908659499721,8.83066041181346));
#81272=CARTESIAN_POINT('Ctrl Pts',(-9.28699981374936,1.24874373085893,8.82776693649957));
#81273=CARTESIAN_POINT('Ctrl Pts',(-9.27623135574785,1.32637032822497,8.82643472508075));
#81274=CARTESIAN_POINT('Ctrl Pts',(-9.24896706100079,1.50629648236639,8.82332666186428));
#81275=CARTESIAN_POINT('Ctrl Pts',(-9.23174559910193,1.60847564732476,8.82154632488248));
#81276=CARTESIAN_POINT('Ctrl Pts',(-9.16591337043864,1.96308263203714,8.815314961699));
#81277=CARTESIAN_POINT('Ctrl Pts',(-9.10861374643787,2.21377869414352,8.81081285321358));
#81278=CARTESIAN_POINT('Ctrl Pts',(-8.96757869368305,2.73173674989091,8.80137773342682));
#81279=CARTESIAN_POINT('Ctrl Pts',(-8.88202516743433,2.99824659482927,8.79644607764688));
#81280=CARTESIAN_POINT('Ctrl Pts',(-8.76571321950822,3.31161995711214,8.79067409615914));
#81281=CARTESIAN_POINT('Ctrl Pts',(-8.7463047242291,3.36254496998548,8.78973715264741));
#81282=CARTESIAN_POINT('Ctrl Pts',(-8.71095547586105,3.45291902218372,8.78807800945795));
#81283=CARTESIAN_POINT('Ctrl Pts',(-8.69518822609136,3.49243422396195,8.78735388533094));
#81284=CARTESIAN_POINT('Ctrl Pts',(-8.65895304607231,3.58147862292254,8.78572560255436));
#81285=CARTESIAN_POINT('Ctrl Pts',(-8.63832826958899,3.63094226129281,8.78482328010475));
#81286=CARTESIAN_POINT('Ctrl Pts',(-8.55942728271194,3.81568957318128,8.78145678281294));
#81287=CARTESIAN_POINT('Ctrl Pts',(-8.49838794363135,3.94977023643038,8.77902071717173));
#81288=CARTESIAN_POINT('Ctrl Pts',(-8.3490870545859,4.25822824305022,8.77338125894572));
#81289=CARTESIAN_POINT('Ctrl Pts',(-8.25848078896065,4.43139454157599,8.77018785547254));
#81290=CARTESIAN_POINT('Ctrl Pts',(-8.14459213335217,4.63341535357859,8.76638071203237));
#81291=CARTESIAN_POINT('Ctrl Pts',(-8.12647125538625,4.66512419894607,8.76578074295402));
#81292=CARTESIAN_POINT('Ctrl Pts',(-8.00653210231113,4.87218044198863,8.76184577427303));
#81293=CARTESIAN_POINT('Ctrl Pts',(-7.89923074998114,5.0442890245467,8.75849231976839));
#81294=CARTESIAN_POINT('Ctrl Pts',(-7.73467287586928,5.29009230476958,8.75354114846756));
#81295=CARTESIAN_POINT('Ctrl Pts',(-7.68176637577617,5.36662895915337,8.75197586510107));
#81296=CARTESIAN_POINT('Ctrl Pts',(-7.58180019025184,5.50673624388029,8.74906380736425));
#81297=CARTESIAN_POINT('Ctrl Pts',(-7.53505846102861,5.57052350677772,8.74771961945226));
#81298=CARTESIAN_POINT('Ctrl Pts',(-7.4252933693707,5.71640740366725,8.74460161172465));
#81299=CARTESIAN_POINT('Ctrl Pts',(-7.36170611254615,5.79806676962057,8.74282344627031));
#81300=CARTESIAN_POINT('Ctrl Pts',(-7.25726145635692,5.92770688216262,8.73994721918224));
#81301=CARTESIAN_POINT('Ctrl Pts',(-7.21724995715422,5.97635806893226,8.73885542658812));
#81302=CARTESIAN_POINT('Ctrl Pts',(-7.06266816843614,6.16050218218445,8.73467621288963));
#81303=CARTESIAN_POINT('Ctrl Pts',(-6.9447484415149,6.29313416713875,8.73156725799665));
#81304=CARTESIAN_POINT('Ctrl Pts',(-6.61916881284147,6.63903214181431,8.72322126585896));
#81305=CARTESIAN_POINT('Ctrl Pts',(-6.40499584022498,6.84588724794792,8.71796969001007));
#81306=CARTESIAN_POINT('Ctrl Pts',(-6.14067002705748,7.07790121621837,8.71189733168689));
#81307=CARTESIAN_POINT('Ctrl Pts',(-6.09968780999389,7.11324979494781,8.71096699855222));
#81308=CARTESIAN_POINT('Ctrl Pts',(-6.02598635861062,7.17571452818762,8.70931538650168));
#81309=CARTESIAN_POINT('Ctrl Pts',(-5.99338460022587,7.20296686352822,8.70859224656729));
#81310=CARTESIAN_POINT('Ctrl Pts',(-5.91900693847331,7.2642857543988,8.70695972052593));
#81311=CARTESIAN_POINT('Ctrl Pts',(-5.87712026633571,7.29821540186579,8.70605223885133));
#81312=CARTESIAN_POINT('Ctrl Pts',(-5.71690315241531,7.42572298086308,8.70262132886636));
#81313=CARTESIAN_POINT('Ctrl Pts',(-5.59661140932683,7.51680014530366,8.70012742959838));
#81314=CARTESIAN_POINT('Ctrl Pts',(-5.12897549253816,7.85341320761312,8.69064833319487));
#81315=CARTESIAN_POINT('Ctrl Pts',(-4.76726099745434,8.07810075660881,8.6837346824621));
#81316=CARTESIAN_POINT('Ctrl Pts',(-4.30789064341698,8.32181646966828,8.67503548251408));
#81317=CARTESIAN_POINT('Ctrl Pts',(-4.22357670241305,8.36492384509776,8.67344322681352));
#81318=CARTESIAN_POINT('Ctrl Pts',(-4.06779610322451,8.44161432035405,8.67050665793764));
#81319=CARTESIAN_POINT('Ctrl Pts',(-3.99653042713863,8.47558623236571,8.66916526938074));
#81320=CARTESIAN_POINT('Ctrl Pts',(-3.83295609984953,8.55103926757147,8.66609003884345));
#81321=CARTESIAN_POINT('Ctrl Pts',(-3.74038771363289,8.59193369979667,8.66435229403882));
#81322=CARTESIAN_POINT('Ctrl Pts',(-3.54065440162147,8.67633125956585,8.66060842470857));
#81323=CARTESIAN_POINT('Ctrl Pts',(-3.43330958231042,8.71936597133163,8.65859969221885));
#81324=CARTESIAN_POINT('Ctrl Pts',(-3.09020852552795,8.84959722763654,8.65219580415127));
#81325=CARTESIAN_POINT('Ctrl Pts',(-2.85172765751044,8.92930057492297,8.64776647826332));
#81326=CARTESIAN_POINT('Ctrl Pts',(-2.43413672260732,9.05042652684473,8.64013135673377));
#81327=CARTESIAN_POINT('Ctrl Pts',(-2.25647770286536,9.09634820085321,8.63692072725445));
#81328=CARTESIAN_POINT('Ctrl Pts',(-2.02262624886551,9.14952155925395,8.6327845502938));
#81329=CARTESIAN_POINT('Ctrl Pts',(-1.96755564824971,9.16152206222707,8.63181702790354));
#81330=CARTESIAN_POINT('Ctrl Pts',(-1.87110188287424,9.18163061503288,8.63013575518547));
#81331=CARTESIAN_POINT('Ctrl Pts',(-1.82976623019635,9.18995748394981,8.62941963901196));
#81332=CARTESIAN_POINT('Ctrl Pts',(-1.72911548642306,9.20952708937885,8.62768629425005));
#81333=CARTESIAN_POINT('Ctrl Pts',(-1.6697453413667,9.22047613163792,8.62667232903793));
#81334=CARTESIAN_POINT('Ctrl Pts',(-1.57184460688778,9.23755440094811,8.62501143381089));
#81335=CARTESIAN_POINT('Ctrl Pts',(-1.53337423738643,9.24401807829263,8.62436159870206));
#81336=CARTESIAN_POINT('Ctrl Pts',(-1.43559707673912,9.25981913804211,8.62271600745567));
#81337=CARTESIAN_POINT('Ctrl Pts',(-1.37623881255984,9.26882712000772,8.62172263441406));
#81338=CARTESIAN_POINT('Ctrl Pts',(-1.08842890310867,9.30967833675424,8.61692603914));
#81339=CARTESIAN_POINT('Ctrl Pts',(-0.858940535065887,9.33364932121365,
8.61316018367611));
#81340=CARTESIAN_POINT('Ctrl Pts',(-0.563496147272652,9.35352026102381,
8.60829858381005));
#81341=CARTESIAN_POINT('Ctrl Pts',(-0.498146311825352,9.35722819136987,
8.60722256040794));
#81342=CARTESIAN_POINT('Ctrl Pts',(-0.250080797523833,9.36869728378259,
8.60313095678301));
#81343=CARTESIAN_POINT('Ctrl Pts',(-0.0671909225601672,9.37179354697312,
8.60009902462655));
#81344=CARTESIAN_POINT('Ctrl Pts',(0.205221869031554,9.36843047139318,8.59553300048761));
#81345=CARTESIAN_POINT('Ctrl Pts',(0.294751411040575,9.36604116322681,8.59402448099187));
#81346=CARTESIAN_POINT('Ctrl Pts',(0.463807694672769,9.35910307217614,8.5911589339721));
#81347=CARTESIAN_POINT('Ctrl Pts',(0.543337609215069,9.35482293263922,8.58980375019918));
#81348=CARTESIAN_POINT('Ctrl Pts',(0.732349121603673,9.34223224885276,8.58656517048775));
#81349=CARTESIAN_POINT('Ctrl Pts',(0.841758138276836,9.33301032771867,8.58467620134214));
#81350=CARTESIAN_POINT('Ctrl Pts',(1.01952946797695,9.31487480947402,8.58158415975769));
#81351=CARTESIAN_POINT('Ctrl Pts',(1.08800004555837,9.30712570747342,8.58038773265554));
#81352=CARTESIAN_POINT('Ctrl Pts',(1.36071115732413,9.27321128911757,8.57560209269231));
#81353=CARTESIAN_POINT('Ctrl Pts',(1.56415000423328,9.24107228193029,8.57198501153264));
#81354=CARTESIAN_POINT('Ctrl Pts',(1.79910806723469,9.19597231952212,8.56777863886149));
#81355=CARTESIAN_POINT('Ctrl Pts',(1.83181834033569,9.18951240856489,8.56719242032351));
#81356=CARTESIAN_POINT('Ctrl Pts',(2.06511807065275,9.14214318361481,8.56300790403777));
#81357=CARTESIAN_POINT('Ctrl Pts',(2.26435430636634,9.09484439319207,8.55941494560655));
#81358=CARTESIAN_POINT('Ctrl Pts',(2.52425635911401,9.02407302886399,8.55475701333782));
#81359=CARTESIAN_POINT('Ctrl Pts',(2.58645412892499,9.00644320828199,8.55364465287884));
#81360=CARTESIAN_POINT('Ctrl Pts',(2.68917311007708,8.97617591837421,8.55181419076773));
#81361=CARTESIAN_POINT('Ctrl Pts',(2.72979969582687,8.96390427061243,8.55109203371547));
#81362=CARTESIAN_POINT('Ctrl Pts',(2.82216184314708,8.93531925161914,8.54945479215524));
#81363=CARTESIAN_POINT('Ctrl Pts',(2.87384181467495,8.91883180912912,8.54854168608087));
#81364=CARTESIAN_POINT('Ctrl Pts',(3.07257372937519,8.85352375627285,8.54503715444029));
#81365=CARTESIAN_POINT('Ctrl Pts',(3.21854968678172,8.80150728031443,8.54247692843226));
#81366=CARTESIAN_POINT('Ctrl Pts',(3.67977565580826,8.62414626538968,8.5343500946697));
#81367=CARTESIAN_POINT('Ctrl Pts',(3.98948105651241,8.48531714292376,8.52882759647274));
#81368=CARTESIAN_POINT('Ctrl Pts',(4.2909266557441,8.33003802497472,8.52320208943219));
#81369=CARTESIAN_POINT('',(-9.37090856232268,0.000113764305748557,8.65141010809498));
#81370=CARTESIAN_POINT('Ctrl Pts',(4.29124604933307,8.33065733261531,8.32570386727427));
#81371=CARTESIAN_POINT('Ctrl Pts',(4.20718224374021,8.37401666214134,8.32731082159403));
#81372=CARTESIAN_POINT('Ctrl Pts',(2.73864022413988,9.10315303786724,8.35516338033944));
#81373=CARTESIAN_POINT('Ctrl Pts',(-0.481341462362255,9.74926409850946,
8.40926154351051));
#81374=CARTESIAN_POINT('Ctrl Pts',(-5.05241933911021,8.35182009430635,8.48799835678748));
#81375=CARTESIAN_POINT('Ctrl Pts',(-8.41195372822347,4.95165371770902,8.56673517006447));
#81376=CARTESIAN_POINT('Ctrl Pts',(-9.34062849382632,1.77796225280113,8.62120575383362));
#81377=CARTESIAN_POINT('Ctrl Pts',(-9.37098027739613,0.11662354713027,8.64943073317713));
#81378=CARTESIAN_POINT('Ctrl Pts',(-9.37090856232268,0.000113764305748557,
8.65141010809498));
#81379=CARTESIAN_POINT('Ctrl Pts',(-9.37024999923123,0.000120029827953283,
8.65179019859247));
#81380=CARTESIAN_POINT('Ctrl Pts',(-9.37025649351159,-0.506862539567674,
8.66022018103747));
#81381=CARTESIAN_POINT('Ctrl Pts',(-9.32911740577704,-1.01301141890215,
8.66838655607132));
#81382=CARTESIAN_POINT('Ctrl Pts',(-9.23415704073925,-1.59326290303693,
8.67820000093685));
#81383=CARTESIAN_POINT('Ctrl Pts',(-9.22004279010089,-1.67300742574552,
8.67955740785975));
#81384=CARTESIAN_POINT('Ctrl Pts',(-9.19091374104503,-1.82600079619343,
8.68218056154493));
#81385=CARTESIAN_POINT('Ctrl Pts',(-9.17605240004904,-1.8992726571765,8.6834452427055));
#81386=CARTESIAN_POINT('Ctrl Pts',(-9.1425183203875,-2.05501651736957,8.68615242586457));
#81387=CARTESIAN_POINT('Ctrl Pts',(-9.1236028633992,-2.13742950176123,8.68759640972734));
#81388=CARTESIAN_POINT('Ctrl Pts',(-9.06924779594286,-2.36036650616878,
8.69153441147084));
#81389=CARTESIAN_POINT('Ctrl Pts',(-9.03165952283508,-2.50034231722196,
8.69404180889817));
#81390=CARTESIAN_POINT('Ctrl Pts',(-8.89818534630605,-2.95500993066266,
8.70229312028935));
#81391=CARTESIAN_POINT('Ctrl Pts',(-8.78897519415825,-3.26553212579828,
8.70810559910809));
#81392=CARTESIAN_POINT('Ctrl Pts',(-8.62602421719554,-3.66101807210239,
8.71559638661592));
#81393=CARTESIAN_POINT('Ctrl Pts',(-8.58694185550096,-3.75176981543268,
8.71732073550425));
#81394=CARTESIAN_POINT('Ctrl Pts',(-8.52387012760105,-3.89207541651779,
8.71998739585848));
#81395=CARTESIAN_POINT('Ctrl Pts',(-8.50086699364746,-3.9420646078181,8.72093763028548));
#81396=CARTESIAN_POINT('Ctrl Pts',(-8.46489474930453,-4.01845829131022,
8.72238849431909));
#81397=CARTESIAN_POINT('Ctrl Pts',(-8.45223942401119,-4.04500913199401,
8.72289250407785));
#81398=CARTESIAN_POINT('Ctrl Pts',(-8.42210804684026,-4.10746585137936,
8.72407716398779));
#81399=CARTESIAN_POINT('Ctrl Pts',(-8.40452708144422,-4.14332043467043,
8.72475641937645));
#81400=CARTESIAN_POINT('Ctrl Pts',(-8.36243547271856,-4.22779165106396,
8.7263544926167));
#81401=CARTESIAN_POINT('Ctrl Pts',(-8.33772928665667,-4.27630911427389,
8.72727088393162));
#81402=CARTESIAN_POINT('Ctrl Pts',(-8.24302551963114,-4.45834517063397,
8.73070826573865));
#81403=CARTESIAN_POINT('Ctrl Pts',(-8.17023191687614,-4.59038364940285,
8.73320003919488));
#81404=CARTESIAN_POINT('Ctrl Pts',(-7.97092248808497,-4.93213348267305,
8.73970804781442));
#81405=CARTESIAN_POINT('Ctrl Pts',(-7.83931645284388,-5.13874145147038,
8.74370413828197));
#81406=CARTESIAN_POINT('Ctrl Pts',(-7.62300846940553,-5.45063939024056,
8.74995271346713));
#81407=CARTESIAN_POINT('Ctrl Pts',(-7.54387025056358,-5.5596537142795,8.75217942520501));
#81408=CARTESIAN_POINT('Ctrl Pts',(-7.39887450017957,-5.75058934533885,
8.75617124492425));
#81409=CARTESIAN_POINT('Ctrl Pts',(-7.33393688583391,-5.83318021079825,
8.75792975967393));
#81410=CARTESIAN_POINT('Ctrl Pts',(-7.2603462110113,-5.92360455365559,8.7598935915555));
#81411=CARTESIAN_POINT('Ctrl Pts',(-7.25305154821531,-5.93253413396541,
8.76008794645715));
#81412=CARTESIAN_POINT('Ctrl Pts',(-7.19716777405375,-6.00068573098142,
8.76157453942852));
#81413=CARTESIAN_POINT('Ctrl Pts',(-7.14787062688023,-6.05932328570263,
8.76287244827627));
#81414=CARTESIAN_POINT('Ctrl Pts',(-7.0397092725749,-6.18482112374989,8.76569250652734));
#81415=CARTESIAN_POINT('Ctrl Pts',(-6.98059944490879,-6.25145985486362,
8.76721663869678));
#81416=CARTESIAN_POINT('Ctrl Pts',(-6.80004969288245,-6.44925228181714,
8.77182222273557));
#81417=CARTESIAN_POINT('Ctrl Pts',(-6.67579884112476,-6.57778384554991,
8.7749266421142));
#81418=CARTESIAN_POINT('Ctrl Pts',(-6.50794149452138,-6.74176613693223,
8.77902915899157));
#81419=CARTESIAN_POINT('Ctrl Pts',(-6.46758536447351,-6.78049059347675,
8.78000878000278));
#81420=CARTESIAN_POINT('Ctrl Pts',(-6.25058012645332,-6.98502177091228,
8.78523884335845));
#81421=CARTESIAN_POINT('Ctrl Pts',(-6.06789709761703,-7.1442918334176,8.78951308171902));
#81422=CARTESIAN_POINT('Ctrl Pts',(-5.81092756514548,-7.35135389984565,
8.79528279649356));
#81423=CARTESIAN_POINT('Ctrl Pts',(-5.74183756484015,-7.40544291400544,
8.79681113376359));
#81424=CARTESIAN_POINT('Ctrl Pts',(-5.61801874114108,-7.49960327764675,
8.79950353717946));
#81425=CARTESIAN_POINT('Ctrl Pts',(-5.56359528717286,-7.54006574310596,
8.80067141840661));
#81426=CARTESIAN_POINT('Ctrl Pts',(-5.47413396201793,-7.60508200134966,
8.80256299492667));
#81427=CARTESIAN_POINT('Ctrl Pts',(-5.43935876060615,-7.6299928686922,8.80329139093743));
#81428=CARTESIAN_POINT('Ctrl Pts',(-5.36155757113156,-7.68492275115254,
8.80490511187983));
#81429=CARTESIAN_POINT('Ctrl Pts',(-5.31844768359039,-7.71482025281318,
8.80578884960698));
#81430=CARTESIAN_POINT('Ctrl Pts',(-5.17589242883806,-7.81192217115338,
8.80868080996282));
#81431=CARTESIAN_POINT('Ctrl Pts',(-5.07540661178859,-7.8775782003973,8.81067136628687));
#81432=CARTESIAN_POINT('Ctrl Pts',(-4.71574411320661,-8.10283753209318,
8.81767229039129));
#81433=CARTESIAN_POINT('Ctrl Pts',(-4.45008302409401,-8.25172589465102,
8.82262681961192));
#81434=CARTESIAN_POINT('Ctrl Pts',(-4.10237482544841,-8.4249141011128,8.82903181691401));
#81435=CARTESIAN_POINT('Ctrl Pts',(-4.02660029643606,-8.46139154308939,
8.83042250700612));
#81436=CARTESIAN_POINT('Ctrl Pts',(-3.83707872366889,-8.5495037431181,8.8338931352177));
#81437=CARTESIAN_POINT('Ctrl Pts',(-3.72277093542957,-8.59989324540736,
8.83597976144523));
#81438=CARTESIAN_POINT('Ctrl Pts',(-3.53216935808484,-8.67940234897603,
8.83945566758665));
#81439=CARTESIAN_POINT('Ctrl Pts',(-3.45644133667225,-8.70983689623617,
8.84083575548635));
#81440=CARTESIAN_POINT('Ctrl Pts',(-3.31083666003457,-8.76615633024836,
8.84348883802847));
#81441=CARTESIAN_POINT('Ctrl Pts',(-3.24102979006502,-8.79220461928763,
8.84476059539537));
#81442=CARTESIAN_POINT('Ctrl Pts',(-3.04614320967676,-8.86228973316891,
8.84831103785598));
#81443=CARTESIAN_POINT('Ctrl Pts',(-2.92042849819513,-8.90450812838076,
8.85060143761581));
#81444=CARTESIAN_POINT('Ctrl Pts',(-2.48150036838146,-9.04161657027524,
8.85859371404788));
#81445=CARTESIAN_POINT('Ctrl Pts',(-2.16424369987789,-9.12275847598576,
8.86437043201816));
#81446=CARTESIAN_POINT('Ctrl Pts',(-1.68553094623397,-9.21881202350778,
8.87293328401931));
#81447=CARTESIAN_POINT('Ctrl Pts',(-1.5268755165505,-9.24641341817009,8.87574477115394));
#81448=CARTESIAN_POINT('Ctrl Pts',(-1.31345513209849,-9.27789926544446,
8.87946215863326));
#81449=CARTESIAN_POINT('Ctrl Pts',(-1.25925367298145,-9.28541110394687,
8.8804006527585));
#81450=CARTESIAN_POINT('Ctrl Pts',(-1.16296617978838,-9.29789709440801,
8.88205615227625));
#81451=CARTESIAN_POINT('Ctrl Pts',(-1.12090661431731,-9.30306127451821,
8.88277517591812));
#81452=CARTESIAN_POINT('Ctrl Pts',(-1.01532586045348,-9.31529834487063,
8.88457047768975));
#81453=CARTESIAN_POINT('Ctrl Pts',(-0.951764730674192,-9.32200696104571,
8.88564276325307));
#81454=CARTESIAN_POINT('Ctrl Pts',(-0.674168104554508,-9.34843737650498,
8.89029750645207));
#81455=CARTESIAN_POINT('Ctrl Pts',(-0.459558030535231,-9.3614417157428,
8.89382407419309));
#81456=CARTESIAN_POINT('Ctrl Pts',(-0.0237327382236607,-9.37282654862851,
8.90097120743279));
#81457=CARTESIAN_POINT('Ctrl Pts',(0.197360061906829,-9.37077849600656,
8.90458961010421));
#81458=CARTESIAN_POINT('Ctrl Pts',(0.527511108743546,-9.35602991781153,
8.91005457984867));
#81459=CARTESIAN_POINT('Ctrl Pts',(0.636755304105967,-9.34923025744096,
8.91187267288838));
#81460=CARTESIAN_POINT('Ctrl Pts',(0.843070483548437,-9.33275566558614,
8.91533188743398));
#81461=CARTESIAN_POINT('Ctrl Pts',(0.940158572698511,-9.32347563692473,
8.91697048231726));
#81462=CARTESIAN_POINT('Ctrl Pts',(1.11546184711251,-9.30395341845594,8.91995165965995));
#81463=CARTESIAN_POINT('Ctrl Pts',(1.1937263356886,-9.29423594208151,8.92129074788899));
#81464=CARTESIAN_POINT('Ctrl Pts',(1.36890081031289,-9.27023675847889,8.92430720448221));
#81465=CARTESIAN_POINT('Ctrl Pts',(1.46572830498296,-9.25542108495653,8.92598784943448));
#81466=CARTESIAN_POINT('Ctrl Pts',(1.96930571665265,-9.17026748581176,8.93479795188238));
#81467=CARTESIAN_POINT('Ctrl Pts',(2.37131248951925,-9.07462639303872,8.94209108834571));
#81468=CARTESIAN_POINT('Ctrl Pts',(2.91222676684544,-8.90752718030262,8.95201464584753));
#81469=CARTESIAN_POINT('Ctrl Pts',(3.05762405374741,-8.85867036180168,8.95469053969041));
#81470=CARTESIAN_POINT('Ctrl Pts',(3.25261505000611,-8.78777610492714,8.95826483745553));
#81471=CARTESIAN_POINT('Ctrl Pts',(3.30331221492835,-8.76884496170915,8.9591927718682));
#81472=CARTESIAN_POINT('Ctrl Pts',(3.39348834589402,-8.7342787132902,8.96083909884673));
#81473=CARTESIAN_POINT('Ctrl Pts',(3.43303024272975,-8.71881248499707,8.96155938269754));
#81474=CARTESIAN_POINT('Ctrl Pts',(3.52250252080767,-8.68311368722409,8.96318618392866));
#81475=CARTESIAN_POINT('Ctrl Pts',(3.57236626219022,-8.66271820041673,8.96409082525554));
#81476=CARTESIAN_POINT('Ctrl Pts',(3.9065566415305,-8.52264997470714,8.97014846811936));
#81477=CARTESIAN_POINT('Ctrl Pts',(4.18500092408065,-8.38942884047758,8.97517599875433));
#81478=CARTESIAN_POINT('Ctrl Pts',(4.60754088934357,-8.16098557584915,8.98305592539259));
#81479=CARTESIAN_POINT('Ctrl Pts',(4.75643757903536,-8.07511114579943,8.98588255202885));
#81480=CARTESIAN_POINT('Ctrl Pts',(4.95550129770197,-7.95288649967249,8.98975738093278));
#81481=CARTESIAN_POINT('Ctrl Pts',(5.00779391868184,-7.92006293177221,8.99078444265306));
#81482=CARTESIAN_POINT('Ctrl Pts',(5.1457210626929,-7.83157525036053,8.99351963598093));
#81483=CARTESIAN_POINT('Ctrl Pts',(5.23077626667062,-7.77502384161036,8.99523359707421));
#81484=CARTESIAN_POINT('Ctrl Pts',(5.37994666454844,-7.67228772205651,8.99829202600943));
#81485=CARTESIAN_POINT('Ctrl Pts',(5.44443420080633,-7.62666120939076,8.99963208458573));
#81486=CARTESIAN_POINT('Ctrl Pts',(5.58436646907857,-7.52497635037023,9.00258044368349));
#81487=CARTESIAN_POINT('Ctrl Pts',(5.65956027510835,-7.46858724064621,9.00419124247521));
#81488=CARTESIAN_POINT('Ctrl Pts',(6.06783623525312,-7.15270727278511,9.01308473621582));
#81489=CARTESIAN_POINT('Ctrl Pts',(6.38393357032377,-6.87206271680478,9.02054351403957));
#81490=CARTESIAN_POINT('Ctrl Pts',(6.78887792386997,-6.46040376722805,9.03066664266109));
#81491=CARTESIAN_POINT('Ctrl Pts',(6.89496706837064,-6.34705519562832,9.03337556447927));
#81492=CARTESIAN_POINT('Ctrl Pts',(7.03427944987019,-6.19059308379712,9.03698483476996));
#81493=CARTESIAN_POINT('Ctrl Pts',(7.070014591424,-6.14974989760854,9.03791544704441));
#81494=CARTESIAN_POINT('Ctrl Pts',(7.13305754462955,-6.07641966428299,9.0395640752394));
#81495=CARTESIAN_POINT('Ctrl Pts',(7.16050315276846,-6.04405331477298,9.04028401514766));
#81496=CARTESIAN_POINT('Ctrl Pts',(7.2221776112587,-5.97031146692123,9.04190755788627));
#81497=CARTESIAN_POINT('Ctrl Pts',(7.25627255293997,-5.9288259474065,9.04280931461069));
#81498=CARTESIAN_POINT('Ctrl Pts',(7.4842753167746,-5.6464871995492,9.04887656295522));
#81499=CARTESIAN_POINT('Ctrl Pts',(7.66651586119667,-5.39645540114406,9.05391571170361));
#81500=CARTESIAN_POINT('Ctrl Pts',(7.93020307887804,-4.99429096450534,9.06180493938049));
#81501=CARTESIAN_POINT('Ctrl Pts',(8.02038047081523,-4.84815016867082,9.06462896093072));
#81502=CARTESIAN_POINT('Ctrl Pts',(8.13743829024166,-4.64623399533749,9.06850055257106));
#81503=CARTESIAN_POINT('Ctrl Pts',(8.16785693122783,-4.59254890066005,9.06952701774821));
#81504=CARTESIAN_POINT('Ctrl Pts',(8.24719269307496,-4.44924945286953,9.07226096398601));
#81505=CARTESIAN_POINT('Ctrl Pts',(8.29517917683794,-4.35912954238198,9.07397427244909));
#81506=CARTESIAN_POINT('Ctrl Pts',(8.37766459330117,-4.19792336978694,9.07703201357378));
#81507=CARTESIAN_POINT('Ctrl Pts',(8.41275514733286,-4.12715100932985,9.07837204489025));
#81508=CARTESIAN_POINT('Ctrl Pts',(8.4876402074263,-3.97119467049436,9.08132088348316));
#81509=CARTESIAN_POINT('Ctrl Pts',(8.52705598745204,-3.88583833073623,9.08293219483968));
#81510=CARTESIAN_POINT('Ctrl Pts',(8.64790506360248,-3.61343821167718,9.08806641989808));
#81511=CARTESIAN_POINT('Ctrl Pts',(8.72451814475009,-3.42432188459326,9.09162026154793));
#81512=CARTESIAN_POINT('Ctrl Pts',(8.88220447016806,-2.99534058677072,9.0996306532592));
#81513=CARTESIAN_POINT('Ctrl Pts',(8.95985390916496,-2.75438546126452,9.10409650664386));
#81514=CARTESIAN_POINT('Ctrl Pts',(9.05160193300469,-2.42447433270116,9.11008498225815));
#81515=CARTESIAN_POINT('Ctrl Pts',(9.07431567654206,-2.33802660233176,9.11164231616266));
#81516=CARTESIAN_POINT('Ctrl Pts',(9.11229333738226,-2.18458554615929,9.11437894841737));
#81517=CARTESIAN_POINT('Ctrl Pts',(9.12806371592651,-2.11772441690329,9.11556223420342));
#81518=CARTESIAN_POINT('Ctrl Pts',(9.15248277653463,-2.00885120021582,9.117470999953));
#81519=CARTESIAN_POINT('Ctrl Pts',(9.1615807070791,-1.96694257393415,9.1182013607875));
#81520=CARTESIAN_POINT('Ctrl Pts',(9.18107941320792,-1.87405255775308,9.1198098440302));
#81521=CARTESIAN_POINT('Ctrl Pts',(9.19134388215054,-1.82304411277993,9.12068647592737));
#81522=CARTESIAN_POINT('Ctrl Pts',(9.22481840108056,-1.64922166023898,9.12365502975451));
#81523=CARTESIAN_POINT('Ctrl Pts',(9.24599590988204,-1.5260296210376,9.1257272832381));
#81524=CARTESIAN_POINT('Ctrl Pts',(9.30053058112563,-1.16576916000017,9.13173605406027));
#81525=CARTESIAN_POINT('Ctrl Pts',(9.32727567616135,-0.927801470194707,
9.13564266026207));
#81526=CARTESIAN_POINT('Ctrl Pts',(9.3611353018873,-0.468612158267803,9.14320709225622));
#81527=CARTESIAN_POINT('Ctrl Pts',(9.36958493038416,-0.247647516424963,
9.14685849954795));
#81528=CARTESIAN_POINT('Ctrl Pts',(9.37047681472042,0.0666270813668387,
9.15211856129269));
#81529=CARTESIAN_POINT('Ctrl Pts',(9.36935027356958,0.159844617067774,9.15368680849294));
#81530=CARTESIAN_POINT('Ctrl Pts',(9.36469816193931,0.332059817509742,9.15660150176988));
#81531=CARTESIAN_POINT('Ctrl Pts',(9.3615631865161,0.411059676493539,9.15794532393824));
#81532=CARTESIAN_POINT('Ctrl Pts',(9.35212443510981,0.591305782787501,9.16102777307061));
#81533=CARTESIAN_POINT('Ctrl Pts',(9.34517555676523,0.692508283373146,9.16277032763103));
#81534=CARTESIAN_POINT('Ctrl Pts',(9.31082330089939,1.09666872352164,9.16977631634854));
#81535=CARTESIAN_POINT('Ctrl Pts',(9.27031824432144,1.39832438656474,9.1751175447742));
#81536=CARTESIAN_POINT('Ctrl Pts',(9.17326469454376,1.92520712561603,9.18453673277341));
#81537=CARTESIAN_POINT('Ctrl Pts',(9.12288771495009,2.15130838613727,9.18860673414977));
#81538=CARTESIAN_POINT('Ctrl Pts',(9.04844451971082,2.4353836196773,9.19368081484227));
#81539=CARTESIAN_POINT('Ctrl Pts',(9.03210538794984,2.49529835645666,9.19474859042465));
#81540=CARTESIAN_POINT('Ctrl Pts',(9.00473109297531,2.59188524460918,9.19646367090862));
#81541=CARTESIAN_POINT('Ctrl Pts',(8.99406463776188,2.6286598264887,9.19711512974104));
#81542=CARTESIAN_POINT('Ctrl Pts',(8.96802301510867,2.71642871540583,9.19866594246824));
#81543=CARTESIAN_POINT('Ctrl Pts',(8.95243791102571,2.76735925239995,9.19956283808722));
#81544=CARTESIAN_POINT('Ctrl Pts',(8.8952639406108,2.9486589758543,9.20274900353141));
#81545=CARTESIAN_POINT('Ctrl Pts',(8.85125451149005,3.07824691894899,9.20501443844159));
#81546=CARTESIAN_POINT('Ctrl Pts',(8.72323401710809,3.42973060140032,9.21117552840955));
#81547=CARTESIAN_POINT('Ctrl Pts',(8.63360938319676,3.6494729682151,9.21504734074808));
#81548=CARTESIAN_POINT('Ctrl Pts',(8.47548134842539,3.99864210870136,9.22134864994204));
#81549=CARTESIAN_POINT('Ctrl Pts',(8.41211698584192,4.13027971127311,9.2237592546705));
#81550=CARTESIAN_POINT('Ctrl Pts',(8.29200584046233,4.36556654079858,9.22815188300912));
#81551=CARTESIAN_POINT('Ctrl Pts',(8.23632670163978,4.46972643959692,9.23012708931915));
#81552=CARTESIAN_POINT('Ctrl Pts',(8.13933018087235,4.64320960663476,9.2334750543598));
#81553=CARTESIAN_POINT('Ctrl Pts',(8.09905921990877,4.71310205292105,9.23484012451003));
#81554=CARTESIAN_POINT('Ctrl Pts',(8.01375454898479,4.85683036681564,9.23768249641162));
#81555=CARTESIAN_POINT('Ctrl Pts',(7.96859089034378,4.9305803270714,9.23916066369751));
#81556=CARTESIAN_POINT('Ctrl Pts',(7.83777723630174,5.13769924641422,9.24336877141393));
#81557=CARTESIAN_POINT('Ctrl Pts',(7.74975542007111,5.26953472718861,9.24611567679825));
#81558=CARTESIAN_POINT('Ctrl Pts',(7.56971670678642,5.5249145167292,9.25156635365711));
#81559=CARTESIAN_POINT('Ctrl Pts',(7.47791291009582,5.64854935561786,9.25426825172031));
#81560=CARTESIAN_POINT('Ctrl Pts',(7.2643258184405,5.92185482634075,9.26036499693299));
#81561=CARTESIAN_POINT('Ctrl Pts',(7.14088190719151,6.07014002019938,9.26376124258444));
#81562=CARTESIAN_POINT('Ctrl Pts',(6.96054091037085,6.27365122676355,9.2685074930826));
#81563=CARTESIAN_POINT('Ctrl Pts',(6.90738629903688,6.33212792291947,9.26988153380585));
#81564=CARTESIAN_POINT('Ctrl Pts',(6.81053289056493,6.43600780235583,9.27233623655947));
#81565=CARTESIAN_POINT('Ctrl Pts',(6.76710368660461,6.48165583833664,9.2734198448776));
#81566=CARTESIAN_POINT('Ctrl Pts',(6.69647746403019,6.55440678838525,9.27515241146473));
#81567=CARTESIAN_POINT('Ctrl Pts',(6.66956855385851,6.58178654270764,9.2758056986922));
#81568=CARTESIAN_POINT('Ctrl Pts',(6.60532326079376,6.64635740498306,9.27734895453715));
#81569=CARTESIAN_POINT('Ctrl Pts',(6.56783995378636,6.68340036901566,9.27823658371734));
#81570=CARTESIAN_POINT('Ctrl Pts',(6.43789364531425,6.80967113921202,9.28127420167015));
#81571=CARTESIAN_POINT('Ctrl Pts',(6.34390877490551,6.8973123193857,9.28340344119814));
#81572=CARTESIAN_POINT('Ctrl Pts',(6.07034234467736,7.14209050971353,9.28945438486384));
#81573=CARTESIAN_POINT('Ctrl Pts',(5.88652160832528,7.29433867066382,9.29334826993278));
#81574=CARTESIAN_POINT('Ctrl Pts',(5.52441899195938,7.57163659008751,9.30084280293973));
#81575=CARTESIAN_POINT('Ctrl Pts',(5.34719633922741,7.697816361735,9.30443639328988));
#81576=CARTESIAN_POINT('Ctrl Pts',(5.08820500229021,7.86895116726165,9.30963251603522));
#81577=CARTESIAN_POINT('Ctrl Pts',(5.00990745746512,7.91903086453169,9.31119617815515));
#81578=CARTESIAN_POINT('Ctrl Pts',(4.86362667830771,8.0095552550443,9.31410680898949));
#81579=CARTESIAN_POINT('Ctrl Pts',(4.79585122892441,8.05031991946148,9.31545121184316));
#81580=CARTESIAN_POINT('Ctrl Pts',(4.63964198338355,8.14160169837309,9.31854126168806));
#81581=CARTESIAN_POINT('Ctrl Pts',(4.55088441073539,8.19154484569427,9.32029091250437));
#81582=CARTESIAN_POINT('Ctrl Pts',(4.40483248759764,8.27062050622593,9.32315990405494));
#81583=CARTESIAN_POINT('Ctrl Pts',(4.34802808787325,8.30062422716301,9.32427328759775));
#81584=CARTESIAN_POINT('Ctrl Pts',(4.29092661458802,8.33003804617484,9.32538978630507));
#81585=CARTESIAN_POINT('Origin',(0.,0.,2.15141010809499));
#81586=CARTESIAN_POINT('',(4.29126860009405,8.33070247396426,10.522886232912));
#81587=CARTESIAN_POINT('',(4.29092662690317,8.33003803983112,10.3254369059772));
#81588=CARTESIAN_POINT('',(4.29092662815669,8.33003803918541,2.15141010809499));
#81589=CARTESIAN_POINT('',(-9.36953457099031,3.84033400625157E-5,9.84861910993532));
#81590=CARTESIAN_POINT('Ctrl Pts',(-9.36948395328014,3.79045209737E-5,9.84858989190502));
#81591=CARTESIAN_POINT('Ctrl Pts',(-9.36936718066919,-0.814935059669627,
9.86242933876059));
#81592=CARTESIAN_POINT('Ctrl Pts',(-9.06438402558837,-3.17553663979636,
9.90251439004182));
#81593=CARTESIAN_POINT('Ctrl Pts',(-7.1048427973132,-6.69335858514711,9.9688450457487));
#81594=CARTESIAN_POINT('Ctrl Pts',(-3.07509487664221,-9.26410448038798,
10.0475818590257));
#81595=CARTESIAN_POINT('Ctrl Pts',(1.69204456314026,-9.61336702306967,10.1263186723027));
#81596=CARTESIAN_POINT('Ctrl Pts',(6.05344064836948,-7.65739489908703,10.2050554855796));
#81597=CARTESIAN_POINT('Ctrl Pts',(8.96325362003102,-3.8652198989057,10.2837922988566));
#81598=CARTESIAN_POINT('Ctrl Pts',(9.72372568736471,0.853814429943271,10.3625291121336));
#81599=CARTESIAN_POINT('Ctrl Pts',(8.15249966287939,5.36810856546769,10.4412659254106));
#81600=CARTESIAN_POINT('Ctrl Pts',(5.75868655187378,7.55886885973291,10.4947182990034));
#81601=CARTESIAN_POINT('Ctrl Pts',(4.34157152446891,8.30481265751835,10.5219250681705));
#81602=CARTESIAN_POINT('Ctrl Pts',(4.29126860009441,8.33070247396408,10.522886232912));
#81603=CARTESIAN_POINT('Ctrl Pts',(-9.37024999988976,4.54536311663567E-5,
9.84903207652725));
#81604=CARTESIAN_POINT('Ctrl Pts',(-9.37024974762411,0.0520499281900485,
9.84814461163007));
#81605=CARTESIAN_POINT('Ctrl Pts',(-9.36981656158823,0.104053458913103,
9.84725444355175));
#81606=CARTESIAN_POINT('Ctrl Pts',(-9.36789957813314,0.219145087514164,
9.84527828613022));
#81607=CARTESIAN_POINT('Ctrl Pts',(-9.36621133906909,0.282227233061156,
9.84419109651768));
#81608=CARTESIAN_POINT('Ctrl Pts',(-9.35520247250146,0.580777832043862,
9.8390270125095));
#81609=CARTESIAN_POINT('Ctrl Pts',(-9.33763858581784,0.815856103645878,
9.83490326508495));
#81610=CARTESIAN_POINT('Ctrl Pts',(-9.27856332103884,1.33971565203357,9.82564089655357));
#81611=CARTESIAN_POINT('Ctrl Pts',(-9.23239279194585,1.62772817421331,9.82049684806399));
#81612=CARTESIAN_POINT('Ctrl Pts',(-9.16301326767674,1.96038365300944,9.81462428506578));
#81613=CARTESIAN_POINT('Ctrl Pts',(-9.15279038805863,2.00757175076584,9.81379302783404));
#81614=CARTESIAN_POINT('Ctrl Pts',(-9.13376995447467,2.09220233701906,9.81230661095988));
#81615=CARTESIAN_POINT('Ctrl Pts',(-9.12510571381771,2.1296736648983,9.81165004482906));
#81616=CARTESIAN_POINT('Ctrl Pts',(-9.10699847921789,2.20584462395371,9.81031931725714));
#81617=CARTESIAN_POINT('Ctrl Pts',(-9.0975389093729,2.24453950786064,9.80964541056631));
#81618=CARTESIAN_POINT('Ctrl Pts',(-9.06899220921226,2.35816543529988,9.80767123382159));
#81619=CARTESIAN_POINT('Ctrl Pts',(-9.04922396630676,2.43292202167366,9.80637842426282));
#81620=CARTESIAN_POINT('Ctrl Pts',(-8.94337370986254,2.81405897278214,9.79980037592466));
#81621=CARTESIAN_POINT('Ctrl Pts',(-8.84264863934384,3.11615590514634,9.79462300969131));
#81622=CARTESIAN_POINT('Ctrl Pts',(-8.68837498155519,3.51067337539497,9.78766159179826));
#81623=CARTESIAN_POINT('Ctrl Pts',(-8.64834885809028,3.60815040641361,9.78592553120387));
#81624=CARTESIAN_POINT('Ctrl Pts',(-8.57980787977317,3.76737353073208,9.78305586700497));
#81625=CARTESIAN_POINT('Ctrl Pts',(-8.55224968151939,3.82952111136531,9.78192716972226));
#81626=CARTESIAN_POINT('Ctrl Pts',(-8.48179379436362,3.98385448775289,9.77910031506187));
#81627=CARTESIAN_POINT('Ctrl Pts',(-8.43806740645392,4.07565220900377,9.77739730208818));
#81628=CARTESIAN_POINT('Ctrl Pts',(-8.35935956885488,4.23419022927559,9.77441444012392));
#81629=CARTESIAN_POINT('Ctrl Pts',(-8.32505094184776,4.30125401316118,9.7731394182075));
#81630=CARTESIAN_POINT('Ctrl Pts',(-8.25079477081679,4.44218660673623,9.77043078646325));
#81631=CARTESIAN_POINT('Ctrl Pts',(-8.21065528678723,4.51594684649965,9.7689958818351));
#81632=CARTESIAN_POINT('Ctrl Pts',(-8.0985975445243,4.71542988388175,9.76506721782281));
#81633=CARTESIAN_POINT('Ctrl Pts',(-8.02474732280894,4.84004043338668,9.76256006691141));
#81634=CARTESIAN_POINT('Ctrl Pts',(-7.77585480204574,5.2386404171029,9.75437404140671));
#81635=CARTESIAN_POINT('Ctrl Pts',(-7.58943709331942,5.50524430743699,9.74862968388853));
#81636=CARTESIAN_POINT('Ctrl Pts',(-7.32903756728009,5.83921879721361,9.74121366945544));
#81637=CARTESIAN_POINT('Ctrl Pts',(-7.26731361530268,5.91586178832416,9.73949644827523));
#81638=CARTESIAN_POINT('Ctrl Pts',(-7.16929080085027,6.03372756372094,9.7368391180679));
#81639=CARTESIAN_POINT('Ctrl Pts',(-7.1338173722374,6.07562742567897,9.73589114609851));
#81640=CARTESIAN_POINT('Ctrl Pts',(-7.07171151984965,6.14769062591785,9.73425661573435));
#81641=CARTESIAN_POINT('Ctrl Pts',(-7.04524924007102,6.17799862454553,9.73356788713856));
#81642=CARTESIAN_POINT('Ctrl Pts',(-6.99038002590721,6.2400308838965,9.73215642384123));
#81643=CARTESIAN_POINT('Ctrl Pts',(-6.96195046996255,6.2717337309615,9.73143423670698));
#81644=CARTESIAN_POINT('Ctrl Pts',(-6.89647052485058,6.34375896771048,9.72979080349397));
#81645=CARTESIAN_POINT('Ctrl Pts',(-6.85928079487896,6.38395257931692,9.72887158413273));
#81646=CARTESIAN_POINT('Ctrl Pts',(-6.59946348466353,6.65986425235365,9.72253812629533));
#81647=CARTESIAN_POINT('Ctrl Pts',(-6.36508351529453,6.8842155563636,9.71726072590991));
#81648=CARTESIAN_POINT('Ctrl Pts',(-5.93965687468235,7.25110258736728,9.70803923335513));
#81649=CARTESIAN_POINT('Ctrl Pts',(-5.75393369285374,7.39934180084282,9.70412111269622));
#81650=CARTESIAN_POINT('Ctrl Pts',(-5.48685033527731,7.59637817479089,9.69856826591055));
#81651=CARTESIAN_POINT('Ctrl Pts',(-5.4100798096171,7.6512433221824,9.69698146893474));
#81652=CARTESIAN_POINT('Ctrl Pts',(-5.26756155546809,7.74987845294711,9.69404995902405));
#81653=CARTESIAN_POINT('Ctrl Pts',(-5.2020638203045,7.79399465946988,9.69270810277671));
#81654=CARTESIAN_POINT('Ctrl Pts',(-5.05245420713939,7.89203857983942,9.68965421081878));
#81655=CARTESIAN_POINT('Ctrl Pts',(-4.96802172762202,7.94545949007751,9.6879385360291));
#81656=CARTESIAN_POINT('Ctrl Pts',(-4.6123131296426,8.16263139348787,9.68074305000772));
#81657=CARTESIAN_POINT('Ctrl Pts',(-4.33367501773777,8.31391862634465,9.67517666434931));
#81658=CARTESIAN_POINT('Ctrl Pts',(-3.90484276208053,8.5193282001683,9.66681736999822));
#81659=CARTESIAN_POINT('Ctrl Pts',(-3.76005679862803,8.58421359019149,9.6640304442582));
#81660=CARTESIAN_POINT('Ctrl Pts',(-3.54766125799607,8.67299295073623,9.6600191147831));
#81661=CARTESIAN_POINT('Ctrl Pts',(-3.48131487885573,8.69983642768055,9.65877685003699));
#81662=CARTESIAN_POINT('Ctrl Pts',(-3.35998793109808,8.74731466579623,9.65652834389364));
#81663=CARTESIAN_POINT('Ctrl Pts',(-3.3051084299359,8.7681977080831,9.65551983087911));
#81664=CARTESIAN_POINT('Ctrl Pts',(-3.21438645160945,8.8017469577506,9.65386871577831));
#81665=CARTESIAN_POINT('Ctrl Pts',(-3.17865687575951,8.81471328201536,9.65322261236271));
#81666=CARTESIAN_POINT('Ctrl Pts',(-3.09124649999818,8.84583407691863,9.65165214028041));
#81667=CARTESIAN_POINT('Ctrl Pts',(-3.03948358654614,8.86375343664419,9.65073054789263));
#81668=CARTESIAN_POINT('Ctrl Pts',(-2.82958851631258,8.93436035992963,9.64702229241396));
#81669=CARTESIAN_POINT('Ctrl Pts',(-2.67022025543596,8.9832783726295,9.64427184140417));
#81670=CARTESIAN_POINT('Ctrl Pts',(-2.25388039479043,9.09901486867829,9.63717124727921));
#81671=CARTESIAN_POINT('Ctrl Pts',(-1.99522349845942,9.15921021058904,9.6328397228581));
#81672=CARTESIAN_POINT('Ctrl Pts',(-1.61819653155814,9.23022198285666,9.62650685270609));
#81673=CARTESIAN_POINT('Ctrl Pts',(-1.50162896872437,9.24990098466322,9.62454690799501));
#81674=CARTESIAN_POINT('Ctrl Pts',(-1.28315502308573,9.2825451309883,9.62086043098271));
#81675=CARTESIAN_POINT('Ctrl Pts',(-1.18134708126341,9.29605023260777,9.61913730267377));
#81676=CARTESIAN_POINT('Ctrl Pts',(-1.00083840925674,9.31698194567585,9.61606918747457));
#81677=CARTESIAN_POINT('Ctrl Pts',(-0.922226994541179,9.32509128289532,
9.61472872119132));
#81678=CARTESIAN_POINT('Ctrl Pts',(-0.750320111469826,9.34062966048367,
9.61178694211199));
#81679=CARTESIAN_POINT('Ctrl Pts',(-0.656996884485406,9.34765734088302,
9.61018321132451));
#81680=CARTESIAN_POINT('Ctrl Pts',(-0.159085799734555,9.37765907867496,
9.60159053004482));
#81681=CARTESIAN_POINT('Ctrl Pts',(0.246566480881064,9.37576660647323,9.59444130340288));
#81682=CARTESIAN_POINT('Ctrl Pts',(0.821122688949824,9.33576390710877,9.58433471452698));
#81683=CARTESIAN_POINT('Ctrl Pts',(0.991074477874135,9.31925436161385,9.58135095911158));
#81684=CARTESIAN_POINT('Ctrl Pts',(1.21544711270105,9.2912508188199,9.57745358147534));
#81685=CARTESIAN_POINT('Ctrl Pts',(1.27035196925926,9.28390323922144,9.57650327199206));
#81686=CARTESIAN_POINT('Ctrl Pts',(1.36706241237875,9.27008708871701,9.57483722031274));
#81687=CARTESIAN_POINT('Ctrl Pts',(1.40889514008422,9.26382149866546,9.57411931704548));
#81688=CARTESIAN_POINT('Ctrl Pts',(1.51285476689746,9.2475302438798,9.57234152044998));
#81689=CARTESIAN_POINT('Ctrl Pts',(1.57492569933575,9.23716158921034,9.5712854173374));
#81690=CARTESIAN_POINT('Ctrl Pts',(1.88481357589713,9.18218192864615,9.56603012210176));
#81691=CARTESIAN_POINT('Ctrl Pts',(2.130866718515,9.12821971109235,9.56191004885437));
#81692=CARTESIAN_POINT('Ctrl Pts',(2.64710362672033,8.99299004396167,9.55316307358536));
#81693=CARTESIAN_POINT('Ctrl Pts',(2.91639769053659,8.90930140530272,9.54853743418999));
#81694=CARTESIAN_POINT('Ctrl Pts',(3.27807339161354,8.77874477158698,9.54212035097174));
#81695=CARTESIAN_POINT('Ctrl Pts',(3.3740588222899,8.74230243818654,9.54039770043964));
#81696=CARTESIAN_POINT('Ctrl Pts',(3.54283326637152,8.67503096623534,9.53733009158272));
#81697=CARTESIAN_POINT('Ctrl Pts',(3.61586749603739,8.64484424589884,9.53598964806143));
#81698=CARTESIAN_POINT('Ctrl Pts',(3.77455683394854,8.57689146887311,9.53304753445643));
#81699=CARTESIAN_POINT('Ctrl Pts',(3.86004554597474,8.53875839272353,9.53144344226448));
#81700=CARTESIAN_POINT('Ctrl Pts',(4.06144905723485,8.44527755315026,9.52761849528154));
#81701=CARTESIAN_POINT('Ctrl Pts',(4.17679897906308,8.38882689144013,9.52539107763482));
#81702=CARTESIAN_POINT('Ctrl Pts',(4.29092667702531,8.33003801401246,9.52315240206829));
#81703=CARTESIAN_POINT('Ctrl Pts',(4.29092661458801,8.33003804617484,9.32538978630507));
#81704=CARTESIAN_POINT('Ctrl Pts',(4.03195386670708,8.46343876417583,9.33045345141923));
#81705=CARTESIAN_POINT('Ctrl Pts',(3.76687068924532,8.58470572170595,9.33558688684702));
#81706=CARTESIAN_POINT('Ctrl Pts',(3.31896268203108,8.76485628035645,9.34406654540643));
#81707=CARTESIAN_POINT('Ctrl Pts',(3.13924074862046,8.83082027695114,9.34741784325804));
#81708=CARTESIAN_POINT('Ctrl Pts',(2.9039949514902,8.90907362156652,9.3516929856681));
#81709=CARTESIAN_POINT('Ctrl Pts',(2.85020474931201,8.92642775021501,9.35266301114549));
#81710=CARTESIAN_POINT('Ctrl Pts',(2.75597499661287,8.95589015575653,9.3543472864938));
#81711=CARTESIAN_POINT('Ctrl Pts',(2.7156047370626,8.96821373414142,9.35506393320161));
#81712=CARTESIAN_POINT('Ctrl Pts',(2.61626987464547,8.99780483390906,9.35681564259426));
#81713=CARTESIAN_POINT('Ctrl Pts',(2.55721617472214,9.01476596183512,9.35784722157616));
#81714=CARTESIAN_POINT('Ctrl Pts',(2.19185847909412,9.11582329857587,9.36418022467171));
#81715=CARTESIAN_POINT('Ctrl Pts',(1.88160822869861,9.18488052119056,9.36935248666992));
#81716=CARTESIAN_POINT('Ctrl Pts',(1.40585615884353,9.26565445627061,9.37727224953256));
#81717=CARTESIAN_POINT('Ctrl Pts',(1.24256161270218,9.28896251107406,9.37998707829357));
#81718=CARTESIAN_POINT('Ctrl Pts',(0.952056619930774,9.32263036054288,9.38484104708303));
#81719=CARTESIAN_POINT('Ctrl Pts',(0.825089541315198,9.33472419379216,9.38697050552061));
#81720=CARTESIAN_POINT('Ctrl Pts',(0.616152079787817,9.35032963192814,9.39049588610954));
#81721=CARTESIAN_POINT('Ctrl Pts',(0.534312166825084,9.35536306523416,9.39188201760079));
#81722=CARTESIAN_POINT('Ctrl Pts',(0.378378712063795,9.36290067605776,9.3945344184598));
#81723=CARTESIAN_POINT('Ctrl Pts',(0.304300799970728,9.36560091583814,9.39579932908));
#81724=CARTESIAN_POINT('Ctrl Pts',(0.100489631490954,9.37060945262223,9.39929337241661));
#81725=CARTESIAN_POINT('Ctrl Pts',(-0.0292713981281078,9.37110253526522,
9.40153356066672));
#81726=CARTESIAN_POINT('Ctrl Pts',(-0.487088472794289,9.36333288012718,
9.40948794086229));
#81727=CARTESIAN_POINT('Ctrl Pts',(-0.814657004363527,9.34053480480239,
9.41527917770297));
#81728=CARTESIAN_POINT('Ctrl Pts',(-1.30388664945109,9.28055012118306,9.42392540199743));
#81729=CARTESIAN_POINT('Ctrl Pts',(-1.46686521689535,9.25618915325333,9.4268033891527));
#81730=CARTESIAN_POINT('Ctrl Pts',(-1.68327001953415,9.21798302666872,9.43059049158773));
#81731=CARTESIAN_POINT('Ctrl Pts',(-1.73733809467374,9.20794577536662,9.43153375404264));
#81732=CARTESIAN_POINT('Ctrl Pts',(-1.83287618305926,9.18933854177397,9.43319347771691));
#81733=CARTESIAN_POINT('Ctrl Pts',(-1.87438208356734,9.18096235396794,9.43391201496386));
#81734=CARTESIAN_POINT('Ctrl Pts',(-1.9779955273892,9.15932049385449,9.43570007594577));
#81735=CARTESIAN_POINT('Ctrl Pts',(-2.04002755989652,9.14570422643407,9.43676569056657));
#81736=CARTESIAN_POINT('Ctrl Pts',(-2.27798699308665,9.09092975027342,9.44084224748833));
#81737=CARTESIAN_POINT('Ctrl Pts',(-2.45284902290051,9.0453170476123,9.44381486217189));
#81738=CARTESIAN_POINT('Ctrl Pts',(-2.73830229590598,8.96196985483505,9.44869410655845));
#81739=CARTESIAN_POINT('Ctrl Pts',(-2.84970069272937,8.92717251490891,9.45060485667693));
#81740=CARTESIAN_POINT('Ctrl Pts',(-3.1249073818841,8.83553026856915,9.45536293490086));
#81741=CARTESIAN_POINT('Ctrl Pts',(-3.28784270638461,8.77620256449062,9.45821397125729));
#81742=CARTESIAN_POINT('Ctrl Pts',(-3.50676049499352,8.68953796035684,9.46211911492545));
#81743=CARTESIAN_POINT('Ctrl Pts',(-3.56425453046974,8.66611382123478,9.46315174656721));
#81744=CARTESIAN_POINT('Ctrl Pts',(-3.71605103224567,8.60250295156872,9.46589857868443));
#81745=CARTESIAN_POINT('Ctrl Pts',(-3.80993395611077,8.56133724881142,9.46761862800888));
#81746=CARTESIAN_POINT('Ctrl Pts',(-3.974955731117,8.48572656250711,9.47068348660121));
#81747=CARTESIAN_POINT('Ctrl Pts',(-4.0463697734286,8.451906292723,9.47202381269341));
#81748=CARTESIAN_POINT('Ctrl Pts',(-4.20153121473128,8.37600759084149,9.47496777637325));
#81749=CARTESIAN_POINT('Ctrl Pts',(-4.28509235027471,8.33356773563355,9.47657385867571));
#81750=CARTESIAN_POINT('Ctrl Pts',(-4.72435785518277,8.10211534927251,9.48512727306745));
#81751=CARTESIAN_POINT('Ctrl Pts',(-5.06823393754072,7.89156711337965,9.49223253473872));
#81752=CARTESIAN_POINT('Ctrl Pts',(-5.5384719377203,7.56020234115585,9.50232805073771));
#81753=CARTESIAN_POINT('Ctrl Pts',(-5.67668490589927,7.45698193683747,9.50534288132208));
#81754=CARTESIAN_POINT('Ctrl Pts',(-5.85550806685538,7.31557865764241,9.50927252240919));
#81755=CARTESIAN_POINT('Ctrl Pts',(-5.89873904376682,7.28076531209686,9.51022478267901));
#81756=CARTESIAN_POINT('Ctrl Pts',(-5.974357769707,7.21875492068353,9.5118926073746));
#81757=CARTESIAN_POINT('Ctrl Pts',(-6.00687529009995,7.19171903079481,9.51261035630734));
#81758=CARTESIAN_POINT('Ctrl Pts',(-6.08720596864857,7.12400513653154,9.51438541742146));
#81759=CARTESIAN_POINT('Ctrl Pts',(-6.13479539615825,7.08306509666565,9.51543897126861));
#81760=CARTESIAN_POINT('Ctrl Pts',(-6.37276443549706,6.87414851277008,9.5207268618826));
#81761=CARTESIAN_POINT('Ctrl Pts',(-6.55667311383526,6.69896133036394,9.52488055410098));
#81762=CARTESIAN_POINT('Ctrl Pts',(-6.92633141750336,6.31700938178691,9.53359293971307));
#81763=CARTESIAN_POINT('Ctrl Pts',(-7.11045903993934,6.10901351860957,9.53814999706784));
#81764=CARTESIAN_POINT('Ctrl Pts',(-7.35024905648573,5.81258648169658,9.5445112572555));
#81765=CARTESIAN_POINT('Ctrl Pts',(-7.41407880064955,5.73094741444385,9.54624960282394));
#81766=CARTESIAN_POINT('Ctrl Pts',(-7.52421327207485,5.58516376609647,9.54933392043113));
#81767=CARTESIAN_POINT('Ctrl Pts',(-7.57108442372572,5.52145997656743,9.55067518687867));
#81768=CARTESIAN_POINT('Ctrl Pts',(-7.6712769460494,5.38161079920131,9.55360674545033));
#81769=CARTESIAN_POINT('Ctrl Pts',(-7.72428305133752,5.30524985893696,9.55519932796924));
#81770=CARTESIAN_POINT('Ctrl Pts',(-7.88924684219942,5.05988748740033,9.56029135120862));
#81771=CARTESIAN_POINT('Ctrl Pts',(-7.99686035958828,4.88803652246012,9.56382154466096));
#81772=CARTESIAN_POINT('Ctrl Pts',(-8.22788491704698,4.49102992423959,9.57187006718879));
#81773=CARTESIAN_POINT('Ctrl Pts',(-8.34778847267389,4.26402010317994,9.57639931994303));
#81774=CARTESIAN_POINT('Ctrl Pts',(-8.48548882411757,3.9751828837433,9.58199567596121));
#81775=CARTESIAN_POINT('Ctrl Pts',(-8.51217425262138,3.91771477420357,9.5831009738114));
#81776=CARTESIAN_POINT('Ctrl Pts',(-8.57292277155079,3.78333907937482,9.58566345317276));
#81777=CARTESIAN_POINT('Ctrl Pts',(-8.60653733217042,3.70623456373532,9.5871172331749));
#81778=CARTESIAN_POINT('Ctrl Pts',(-8.65663929268137,3.5869527921276,9.58933559207532));
#81779=CARTESIAN_POINT('Ctrl Pts',(-8.67386665471468,3.54509117666246,9.59010836817494));
#81780=CARTESIAN_POINT('Ctrl Pts',(-8.70840352038536,3.45940932067852,9.59167719122824));
#81781=CARTESIAN_POINT('Ctrl Pts',(-8.72568722142075,3.41558007495524,9.59247294514734));
#81782=CARTESIAN_POINT('Ctrl Pts',(-8.77687615482799,3.28284682051177,9.59486499276071));
#81783=CARTESIAN_POINT('Ctrl Pts',(-8.80975856340142,3.19355482422796,9.596450197656));
#81784=CARTESIAN_POINT('Ctrl Pts',(-8.97175681844046,2.73209415675855,9.60455267378654));
#81785=CARTESIAN_POINT('Ctrl Pts',(-9.07867054082573,2.35255224189992,9.61093634227378));
#81786=CARTESIAN_POINT('Ctrl Pts',(-9.17571145966846,1.90067441587618,9.61858676474256));
#81787=CARTESIAN_POINT('Ctrl Pts',(-9.18931321881071,1.83378476824568,9.6197199360753));
#81788=CARTESIAN_POINT('Ctrl Pts',(-9.22275520653687,1.65960118615181,9.62267504954877));
#81789=CARTESIAN_POINT('Ctrl Pts',(-9.24145435870355,1.55209888607979,9.62450316030754));
#81790=CARTESIAN_POINT('Ctrl Pts',(-9.27053645623702,1.36567574796332,9.62768533650688));
#81791=CARTESIAN_POINT('Ctrl Pts',(-9.28179912522165,1.28690380360389,9.62903359317636));
#81792=CARTESIAN_POINT('Ctrl Pts',(-9.30364364642972,1.11887329046776,9.63191851110152));
#81793=CARTESIAN_POINT('Ctrl Pts',(-9.31394728413052,1.02958655737983,9.63345682088396));
#81794=CARTESIAN_POINT('Ctrl Pts',(-9.34159453834653,0.755428062834336,
9.63819708275899));
#81795=CARTESIAN_POINT('Ctrl Pts',(-9.35472909901267,0.570178209122063,
9.64142424983722));
#81796=CARTESIAN_POINT('Ctrl Pts',(-9.36496457604756,0.321054768496945,
9.6457860800192));
#81797=CARTESIAN_POINT('Ctrl Pts',(-9.36692964016035,0.257423353421096,
9.64690199720882));
#81798=CARTESIAN_POINT('Ctrl Pts',(-9.36958360770654,0.12911589718899,9.64915451793947));
#81799=CARTESIAN_POINT('Ctrl Pts',(-9.37025159845246,0.064442796714051,
9.65029110781168));
#81800=CARTESIAN_POINT('Ctrl Pts',(-9.37024358895048,-0.259047479483722,
9.65597809842893));
#81801=CARTESIAN_POINT('Ctrl Pts',(-9.35951408025761,-0.517751976556725,
9.66053531542523));
#81802=CARTESIAN_POINT('Ctrl Pts',(-9.33293198962286,-0.837762740394519,
9.66608396316692));
#81803=CARTESIAN_POINT('Ctrl Pts',(-9.32715600163992,-0.899792686609805,
9.66715516455485));
#81804=CARTESIAN_POINT('Ctrl Pts',(-9.31642463142568,-1.00379419831254,
9.66894143775335));
#81805=CARTESIAN_POINT('Ctrl Pts',(-9.31180311198124,-1.04579803244511,
9.66966008853402));
#81806=CARTESIAN_POINT('Ctrl Pts',(-9.30041346314148,-1.14324726840369,
9.67132068835133));
#81807=CARTESIAN_POINT('Ctrl Pts',(-9.29343340020085,-1.19866615767885,
9.67226031462418));
#81808=CARTESIAN_POINT('Ctrl Pts',(-9.2620913657378,-1.43075253853213,9.6761810893079));
#81809=CARTESIAN_POINT('Ctrl Pts',(-9.23318381867372,-1.60676888386266,
9.67912060677995));
#81810=CARTESIAN_POINT('Ctrl Pts',(-9.12516184268949,-2.16445983477208,
9.68844857363957));
#81811=CARTESIAN_POINT('Ctrl Pts',(-9.02725585264652,-2.54206937849595,
9.69480125181812));
#81812=CARTESIAN_POINT('Ctrl Pts',(-8.87634208554641,-3.00355062240493,
9.70292052773782));
#81813=CARTESIAN_POINT('Ctrl Pts',(-8.84516634645638,-3.09415536256451,
9.70453113878462));
#81814=CARTESIAN_POINT('Ctrl Pts',(-8.78847859361354,-3.25104140297041,
9.70735159396909));
#81815=CARTESIAN_POINT('Ctrl Pts',(-8.76359239414913,-3.31754043214808,
9.70855710340201));
#81816=CARTESIAN_POINT('Ctrl Pts',(-8.70346618504043,-3.47280602909746,
9.71139612319075));
#81817=CARTESIAN_POINT('Ctrl Pts',(-8.66762011776722,-3.56132935650102,
9.71303364994337));
#81818=CARTESIAN_POINT('Ctrl Pts',(-8.52908317945916,-3.88896384342072,
9.7191652373926));
#81819=CARTESIAN_POINT('Ctrl Pts',(-8.41779952544404,-4.12431204797088,
9.72371534481235));
#81820=CARTESIAN_POINT('Ctrl Pts',(-8.15585355459549,-4.62338652996406,
9.73361778681148));
#81821=CARTESIAN_POINT('Ctrl Pts',(-8.00187477903875,-4.88504356293677,
9.73897343965614));
#81822=CARTESIAN_POINT('Ctrl Pts',(-7.80665175202878,-5.18271507167016,
9.74511573233332));
#81823=CARTESIAN_POINT('Ctrl Pts',(-7.77746063282999,-5.2264187750404,9.7460186516215));
#81824=CARTESIAN_POINT('Ctrl Pts',(-7.72411063671725,-5.30485529244543,
9.74763957931448));
#81825=CARTESIAN_POINT('Ctrl Pts',(-7.70008131063667,-5.33967439344528,
9.74835918281124));
#81826=CARTESIAN_POINT('Ctrl Pts',(-7.64408135382787,-5.41965560677047,
9.75001199453729));
#81827=CARTESIAN_POINT('Ctrl Pts',(-7.61194491914114,-5.4646995532118,9.75094299131173));
#81828=CARTESIAN_POINT('Ctrl Pts',(-7.47959141150761,-5.6467795316409,9.75471237306425));
#81829=CARTESIAN_POINT('Ctrl Pts',(-7.37605755223019,-5.78136507104649,
9.75751311880526));
#81830=CARTESIAN_POINT('Ctrl Pts',(-7.01236547097728,-6.22845145238243,
9.76698166705506));
#81831=CARTESIAN_POINT('Ctrl Pts',(-6.73555294790581,-6.52680653794717,
9.77360304184834));
#81832=CARTESIAN_POINT('Ctrl Pts',(-6.37231870554139,-6.87050822425527,
9.78197190944461));
#81833=CARTESIAN_POINT('Ctrl Pts',(-6.3034389444158,-6.93375701660995,9.78354488189183));
#81834=CARTESIAN_POINT('Ctrl Pts',(-6.17461756645689,-7.04854091761982,
9.78646380293057));
#81835=CARTESIAN_POINT('Ctrl Pts',(-6.11494821616971,-7.10036896499729,
9.78780706802258));
#81836=CARTESIAN_POINT('Ctrl Pts',(-5.97617340185612,-7.21786008568665,
9.79091213425945));
#81837=CARTESIAN_POINT('Ctrl Pts',(-5.8966287278457,-7.28298855686858,9.79267814776122));
#81838=CARTESIAN_POINT('Ctrl Pts',(-5.76714118453818,-7.38549628720978,
9.79553091301787));
#81839=CARTESIAN_POINT('Ctrl Pts',(-5.71786863286161,-7.42370871828058,
9.79661143902064));
#81840=CARTESIAN_POINT('Ctrl Pts',(-5.52920715715587,-7.5670290944832,9.80072893218102));
#81841=CARTESIAN_POINT('Ctrl Pts',(-5.38727216035137,-7.66872607079314,
9.80378683133338));
#81842=CARTESIAN_POINT('Ctrl Pts',(-4.98682264548113,-7.93904293532666,
9.81227435301447));
#81843=CARTESIAN_POINT('Ctrl Pts',(-4.72269351334376,-8.09894864659562,
9.81772228609287));
#81844=CARTESIAN_POINT('Ctrl Pts',(-4.40558604622563,-8.27013171682081,
9.82393826689908));
#81845=CARTESIAN_POINT('Ctrl Pts',(-4.3598112718619,-8.29435426740229,9.82482774298874));
#81846=CARTESIAN_POINT('Ctrl Pts',(-4.2763438906194,-8.33764066683544,9.8264339927257));
#81847=CARTESIAN_POINT('Ctrl Pts',(-4.23871879245749,-8.35683145536787,
9.82715222903956));
#81848=CARTESIAN_POINT('Ctrl Pts',(-4.15080318801228,-8.4009265653471,9.82881678798085));
#81849=CARTESIAN_POINT('Ctrl Pts',(-4.10041625598607,-8.42563474221881,
9.8297607323785));
#81850=CARTESIAN_POINT('Ctrl Pts',(-3.88466274348786,-8.52903974838739,
9.83376579403471));
#81851=CARTESIAN_POINT('Ctrl Pts',(-3.71722965249949,-8.60333236482007,
9.83678295736674));
#81852=CARTESIAN_POINT('Ctrl Pts',(-3.18824879321056,-8.81972240889044,
9.8461656271432));
#81853=CARTESIAN_POINT('Ctrl Pts',(-2.81997669327092,-8.94428113492334,
9.852499443628));
#81854=CARTESIAN_POINT('Ctrl Pts',(-2.35386133549086,-9.07027247794415,
9.86057740704464));
#81855=CARTESIAN_POINT('Ctrl Pts',(-2.26231545268818,-9.09353807649935,
9.86216576435602));
#81856=CARTESIAN_POINT('Ctrl Pts',(-2.09362052017528,-9.13370532419569,
9.86509872029589));
#81857=CARTESIAN_POINT('Ctrl Pts',(-2.01657938627992,-9.15102329670546,
9.86644044284018));
#81858=CARTESIAN_POINT('Ctrl Pts',(-1.84002220860776,-9.18837343863706,
9.86952143020735));
#81859=CARTESIAN_POINT('Ctrl Pts',(-1.74038111291792,-9.20776637889404,
9.87126465783764));
#81860=CARTESIAN_POINT('Ctrl Pts',(-1.52606764319236,-9.24587466851182,
9.87502339841439));
#81861=CARTESIAN_POINT('Ctrl Pts',(-1.41132234542842,-9.26408387193702,
9.87704156786157));
#81862=CARTESIAN_POINT('Ctrl Pts',(-1.04453288943186,-9.31531767021668,
9.88350482828411));
#81863=CARTESIAN_POINT('Ctrl Pts',(-0.791471129584119,-9.3402229772792,
9.88798485372612));
#81864=CARTESIAN_POINT('Ctrl Pts',(-0.35766752165376,-9.3651578686177,9.89561376672246));
#81865=CARTESIAN_POINT('Ctrl Pts',(-0.177361926881824,-9.37030687927314,
9.89876879652595));
#81866=CARTESIAN_POINT('Ctrl Pts',(0.0588891785469922,-9.37023174565514,
9.90284269214161));
#81867=CARTESIAN_POINT('Ctrl Pts',(0.114797201998923,-9.36971357750192,
9.90380229020137));
#81868=CARTESIAN_POINT('Ctrl Pts',(0.212875920683018,-9.36792658652917,
9.90547596270072));
#81869=CARTESIAN_POINT('Ctrl Pts',(0.255048706833781,-9.36687326974289,
9.90619231046621));
#81870=CARTESIAN_POINT('Ctrl Pts',(0.358103001206895,-9.36360286478244,
9.90793506744506));
#81871=CARTESIAN_POINT('Ctrl Pts',(0.418972653271255,-9.36107677080669,
9.90895809982717));
#81872=CARTESIAN_POINT('Ctrl Pts',(0.555077681256161,-9.35409821581126,
9.9112353263616));
#81873=CARTESIAN_POINT('Ctrl Pts',(0.630292761214921,-9.34933129862128,
9.91248675054797));
#81874=CARTESIAN_POINT('Ctrl Pts',(0.88027935557292,-9.33045741555708,9.91663281677526));
#81875=CARTESIAN_POINT('Ctrl Pts',(1.05471181424678,-9.31235257618543,9.91950489440887));
#81876=CARTESIAN_POINT('Ctrl Pts',(1.50919004826045,-9.25224709061706,9.92701884197792));
#81877=CARTESIAN_POINT('Ctrl Pts',(1.78801986441566,-9.20242985800251,9.9316630122928));
#81878=CARTESIAN_POINT('Ctrl Pts',(2.16479118799068,-9.11734096523421,9.93810639296833));
#81879=CARTESIAN_POINT('Ctrl Pts',(2.26503523445243,-9.09295565157567,9.93983661510628));
#81880=CARTESIAN_POINT('Ctrl Pts',(2.4414824316134,-9.04693426771318,9.94291412478002));
#81881=CARTESIAN_POINT('Ctrl Pts',(2.51785231068971,-9.02597783156358,9.94425682685667));
#81882=CARTESIAN_POINT('Ctrl Pts',(2.68241691613286,-8.97856898476106,9.94717443915054));
#81883=CARTESIAN_POINT('Ctrl Pts',(2.77050598193635,-8.95177960393573,9.94875145966676));
#81884=CARTESIAN_POINT('Ctrl Pts',(3.05560844493263,-8.86046365535634,9.95390573533058));
#81885=CARTESIAN_POINT('Ctrl Pts',(3.25087767545638,-8.79069695728085,9.95751585593953));
#81886=CARTESIAN_POINT('Ctrl Pts',(3.66366784875799,-8.62757666542081,9.96529382930089));
#81887=CARTESIAN_POINT('Ctrl Pts',(3.88029324998445,-8.53234231505328,9.96946621869982));
#81888=CARTESIAN_POINT('Ctrl Pts',(4.21864521747847,-8.36804047238172,9.97605365122695));
#81889=CARTESIAN_POINT('Ctrl Pts',(4.34283050140176,-8.30426951834388,9.97848655990627));
#81890=CARTESIAN_POINT('Ctrl Pts',(4.51325602011697,-8.21188470577031,9.98182637580691));
#81891=CARTESIAN_POINT('Ctrl Pts',(4.56074158649539,-8.18560727883163,9.98275702292428));
#81892=CARTESIAN_POINT('Ctrl Pts',(4.64494607027385,-8.13805024875633,9.98440568117488));
#81893=CARTESIAN_POINT('Ctrl Pts',(4.68175361218616,-8.1169310064189,9.98512561672085));
#81894=CARTESIAN_POINT('Ctrl Pts',(4.77423451743203,-8.06302944789251,9.98693340132294));
#81895=CARTESIAN_POINT('Ctrl Pts',(4.82971465980063,-8.02992001443279,9.98801711641608));
#81896=CARTESIAN_POINT('Ctrl Pts',(5.10596503801475,-7.86116054582482,9.99341959155332));
#81897=CARTESIAN_POINT('Ctrl Pts',(5.32138474383488,-7.71696763199003,9.99765609796726));
#81898=CARTESIAN_POINT('Ctrl Pts',(5.61283675979855,-7.5038682782924,10.0035744018121));
#81899=CARTESIAN_POINT('Ctrl Pts',(5.69413472440661,-7.4423655750336,10.0052461634472));
#81900=CARTESIAN_POINT('Ctrl Pts',(5.93011288971839,-7.25771534454979,10.0101753126293));
#81901=CARTESIAN_POINT('Ctrl Pts',(6.0819175931054,-7.13098513228169,10.0134465010815));
#81902=CARTESIAN_POINT('Ctrl Pts',(6.29880186446494,-6.93795809258288,10.0183069684175));
#81903=CARTESIAN_POINT('Ctrl Pts',(6.36708711737817,-6.87534501025839,10.0198657758053));
#81904=CARTESIAN_POINT('Ctrl Pts',(6.49140104026012,-6.75791675334553,10.0227593995406));
#81905=CARTESIAN_POINT('Ctrl Pts',(6.5476921027984,-6.70339126148892,10.0240915927329));
#81906=CARTESIAN_POINT('Ctrl Pts',(6.67679546625164,-6.57515931750424,10.0271993824212));
#81907=CARTESIAN_POINT('Ctrl Pts',(6.74908248183686,-6.50093864979676,10.0289794612467));
#81908=CARTESIAN_POINT('Ctrl Pts',(6.99631005643468,-6.23852894797105,10.0352084125642));
#81909=CARTESIAN_POINT('Ctrl Pts',(7.16472974978712,-6.04435642627596,10.0397083122808));
#81910=CARTESIAN_POINT('Ctrl Pts',(7.4995418505116,-5.62466276451453,10.0491445588355));
#81911=CARTESIAN_POINT('Ctrl Pts',(7.66423248166289,-5.39810152453402,10.0540796025458));
#81912=CARTESIAN_POINT('Ctrl Pts',(7.84856231051454,-5.11904516081682,10.0598546207685));
#81913=CARTESIAN_POINT('Ctrl Pts',(7.87819533098797,-5.07332159876972,10.0607913574135));
#81914=CARTESIAN_POINT('Ctrl Pts',(7.93025297572879,-4.99144094248541,10.0624502660807));
#81915=CARTESIAN_POINT('Ctrl Pts',(7.95283328991462,-4.95538470997463,10.0631743605529));
#81916=CARTESIAN_POINT('Ctrl Pts',(8.00330636277727,-4.87355571612625,10.0648027808887));
#81917=CARTESIAN_POINT('Ctrl Pts',(8.03105343390526,-4.82769497937798,10.0657052683927));
#81918=CARTESIAN_POINT('Ctrl Pts',(8.13362829384361,-4.65482605398787,10.0690737660567));
#81919=CARTESIAN_POINT('Ctrl Pts',(8.20584928938428,-4.52629566972687,10.071511623549));
#81920=CARTESIAN_POINT('Ctrl Pts',(8.35771802366737,-4.24042620322682,10.0768386037089));
#81921=CARTESIAN_POINT('Ctrl Pts',(8.43601774708716,-4.08243427465195,10.079721745573));
#81922=CARTESIAN_POINT('Ctrl Pts',(8.61304511349541,-3.69835878634989,10.0866598002569));
#81923=CARTESIAN_POINT('Ctrl Pts',(8.70739405120004,-3.47040230679455,10.0907222646891));
#81924=CARTESIAN_POINT('Ctrl Pts',(8.82613240427037,-3.14807237852955,10.0964645423729));
#81925=CARTESIAN_POINT('Ctrl Pts',(8.85821219937101,-3.05664022915963,10.0980927746213));
#81926=CARTESIAN_POINT('Ctrl Pts',(8.9138218446291,-2.88991095673984,10.1010637458748));
#81927=CARTESIAN_POINT('Ctrl Pts',(8.93782988886079,-2.81478277312453,10.1024031171963));
#81928=CARTESIAN_POINT('Ctrl Pts',(8.98971475246432,-2.64505908544872,10.1054313643346));
#81929=CARTESIAN_POINT('Ctrl Pts',(9.01705245589767,-2.5503085773541,10.1071236446912));
#81930=CARTESIAN_POINT('Ctrl Pts',(9.15334005028203,-2.04832847139825,10.1160981001334));
#81931=CARTESIAN_POINT('Ctrl Pts',(9.23621199523202,-1.63452368460492,10.1235516805611));
#81932=CARTESIAN_POINT('Ctrl Pts',(9.30957423374593,-1.07424875450005,10.1334496880995));
#81933=CARTESIAN_POINT('Ctrl Pts',(9.32493571689913,-0.931534684471982,
10.1359516481559));
#81934=CARTESIAN_POINT('Ctrl Pts',(9.34154150826324,-0.734903384540886,
10.1393506899484));
#81935=CARTESIAN_POINT('Ctrl Pts',(9.34560786727666,-0.68124470198844,10.1402733026146));
#81936=CARTESIAN_POINT('Ctrl Pts',(9.35205860019965,-0.585142569214773,
10.1419151087129));
#81937=CARTESIAN_POINT('Ctrl Pts',(9.35461677888467,-0.542712454683558,
10.1426361282046));
#81938=CARTESIAN_POINT('Ctrl Pts',(9.36037542913204,-0.435003751700202,
10.1444574765857));
#81939=CARTESIAN_POINT('Ctrl Pts',(9.36318181358036,-0.369706360836267,
10.1455535170896));
#81940=CARTESIAN_POINT('Ctrl Pts',(9.36672434902895,-0.260709731672432,
10.1473730654771));
#81941=CARTESIAN_POINT('Ctrl Pts',(9.36783831417369,-0.217025162038524,
10.1480996381313));
#81942=CARTESIAN_POINT('Ctrl Pts',(9.371149455807,-0.0380594066177049,10.1510677295456));
#81943=CARTESIAN_POINT('Ctrl Pts',(9.37072208491539,0.0972541268768818,
10.1532921637666));
#81944=CARTESIAN_POINT('Ctrl Pts',(9.35817740144804,0.60265224564294,10.1615866244958));
#81945=CARTESIAN_POINT('Ctrl Pts',(9.32705958226323,0.971922420416597,10.1676325813907));
#81946=CARTESIAN_POINT('Ctrl Pts',(9.26057223576685,1.43263976702856,10.175418197495));
#81947=CARTESIAN_POINT('Ctrl Pts',(9.24553328644854,1.52668563535637,10.1770193723744));
#81948=CARTESIAN_POINT('Ctrl Pts',(9.21554614774134,1.69746973842361,10.179951533437));
#81949=CARTESIAN_POINT('Ctrl Pts',(9.20106621668669,1.77428147638907,10.1812793657297));
#81950=CARTESIAN_POINT('Ctrl Pts',(9.16586305781981,1.94898706400914,10.1843211279145));
#81951=CARTESIAN_POINT('Ctrl Pts',(9.14452940958802,2.0467481478695,10.1860388606589));
#81952=CARTESIAN_POINT('Ctrl Pts',(9.05795775111327,2.41504118320277,10.1925691210189));
#81953=CARTESIAN_POINT('Ctrl Pts',(8.98224569737743,2.68296173546328,10.1974453808365));
#81954=CARTESIAN_POINT('Ctrl Pts',(8.81287232303262,3.19414980005386,10.2069120801483));
#81955=CARTESIAN_POINT('Ctrl Pts',(8.72076503834788,3.43766913277399,10.2114956504665));
#81956=CARTESIAN_POINT('Ctrl Pts',(8.59356862578152,3.73580588414019,10.2170993937782));
#81957=CARTESIAN_POINT('Ctrl Pts',(8.56789565763895,3.79431566388508,10.218198551966));
#81958=CARTESIAN_POINT('Ctrl Pts',(8.52420453726292,3.89118459735888,10.2200147205667));
#81959=CARTESIAN_POINT('Ctrl Pts',(8.50652101932823,3.92969219266625,10.2207356334923));
#81960=CARTESIAN_POINT('Ctrl Pts',(8.46539933715897,4.01766034645509,10.2223797446501));
#81961=CARTESIAN_POINT('Ctrl Pts',(8.44178785323156,4.06703804463813,10.2233008597347));
#81962=CARTESIAN_POINT('Ctrl Pts',(8.34693818774827,4.26100799774475,10.2269173926668));
#81963=CARTESIAN_POINT('Ctrl Pts',(8.2724065346243,4.40395920592978,10.2295789707237));
#81964=CARTESIAN_POINT('Ctrl Pts',(8.03547639432324,4.83113066091047,10.237608762058));
#81965=CARTESIAN_POINT('Ctrl Pts',(7.8618418958453,5.10883024933997,10.2429413159281));
#81966=CARTESIAN_POINT('Ctrl Pts',(7.59802477075159,5.48535784760032,10.250565521944));
#81967=CARTESIAN_POINT('Ctrl Pts',(7.51972351230309,5.59221685002455,10.2527756127599));
#81968=CARTESIAN_POINT('Ctrl Pts',(7.39389292400272,5.75651638269419,10.2562559910987));
#81969=CARTESIAN_POINT('Ctrl Pts',(7.34789898012279,5.81511083178934,10.2575140718019));
#81970=CARTESIAN_POINT('Ctrl Pts',(7.25004745267303,5.93675502850652,10.2601627510037));
#81971=CARTESIAN_POINT('Ctrl Pts',(7.19805467209914,5.99968809478711,10.2615543830147));
#81972=CARTESIAN_POINT('Ctrl Pts',(7.06436046471031,6.15727445154968,10.2650944106049));
#81973=CARTESIAN_POINT('Ctrl Pts',(6.98157465898671,6.25098653039777,10.2672515303675));
#81974=CARTESIAN_POINT('Ctrl Pts',(6.83992665839876,6.40500441705825,10.2708836146243));
#81975=CARTESIAN_POINT('Ctrl Pts',(6.78208158589228,6.46622359704468,10.2723512136757));
#81976=CARTESIAN_POINT('Ctrl Pts',(6.51067300889796,6.74581455875415,10.2791614672836));
#81977=CARTESIAN_POINT('Ctrl Pts',(6.28733887298216,6.9544407703665,10.2845597209468));
#81978=CARTESIAN_POINT('Ctrl Pts',(5.96381700735658,7.2283123901585,10.2919687211966));
#81979=CARTESIAN_POINT('Ctrl Pts',(5.87197468072702,7.30311760674897,10.2940284546498));
#81980=CARTESIAN_POINT('Ctrl Pts',(5.73739892780726,7.40854888094058,10.2969715259456));
#81981=CARTESIAN_POINT('Ctrl Pts',(5.69578739033028,7.440587947122,10.2978714487297));
#81982=CARTESIAN_POINT('Ctrl Pts',(5.61980684758141,7.49807874036028,10.2994948408777));
#81983=CARTESIAN_POINT('Ctrl Pts',(5.58552886306757,7.52364812568489,10.3002198542422));
#81984=CARTESIAN_POINT('Ctrl Pts',(5.49652949781402,7.58909301991513,10.3020843812633));
#81985=CARTESIAN_POINT('Ctrl Pts',(5.44154875263911,7.62861170789344,10.3032191192111));
#81986=CARTESIAN_POINT('Ctrl Pts',(5.31451082038049,7.71785094881704,10.3058075571702));
#81987=CARTESIAN_POINT('Ctrl Pts',(5.24217542081502,7.76716456835253,10.3072572125868));
#81988=CARTESIAN_POINT('Ctrl Pts',(4.96814617483051,7.94840807426826,10.3126766369177));
#81989=CARTESIAN_POINT('Ctrl Pts',(4.76207819457341,8.07355429152338,10.3166095639365));
#81990=CARTESIAN_POINT('Ctrl Pts',(4.50298005476758,8.21753162763616,10.3214790341816));
#81991=CARTESIAN_POINT('Ctrl Pts',(4.45430718417808,8.24401618924771,10.3223904804223));
#81992=CARTESIAN_POINT('Ctrl Pts',(4.36738060196495,8.29032132115237,10.3240136632783));
#81993=CARTESIAN_POINT('Ctrl Pts',(4.32922113029058,8.31031197093883,10.3247246573602));
#81994=CARTESIAN_POINT('Ctrl Pts',(4.29092662690317,8.33003803983111,10.3254369059772));
#81995=CARTESIAN_POINT('Origin',(0.,0.,2.15141010809499));
#81996=CARTESIAN_POINT('',(4.29092665208775,8.33003802685816,11.5229686882669));
#81997=CARTESIAN_POINT('',(4.29126566285743,8.33069681713359,11.3257065478457));
#81998=CARTESIAN_POINT('',(4.29092662815669,8.33003803918541,2.15141010809499));
#81999=CARTESIAN_POINT('',(-9.3705222398215,0.000212818811248933,10.848589891905));
#82000=CARTESIAN_POINT('Ctrl Pts',(4.29092665208775,8.33003802685817,11.5229686882669));
#82001=CARTESIAN_POINT('Ctrl Pts',(4.41956745097948,8.26377323542136,11.520593532693));
#82002=CARTESIAN_POINT('Ctrl Pts',(4.54667758961367,8.19452631572227,11.5182115257494));
#82003=CARTESIAN_POINT('Ctrl Pts',(4.79074666401042,8.05413244729533,11.5135455764697));
#82004=CARTESIAN_POINT('Ctrl Pts',(4.90783147706481,7.98332594377128,11.5112643737165));
#82005=CARTESIAN_POINT('Ctrl Pts',(5.09369302732341,7.8652924519121,11.5075630917925));
#82006=CARTESIAN_POINT('Ctrl Pts',(5.16346283178717,7.8196665885812,11.5061550238087));
#82007=CARTESIAN_POINT('Ctrl Pts',(5.3011925865166,7.72695129776469,11.5033363700435));
#82008=CARTESIAN_POINT('Ctrl Pts',(5.36915669174465,7.67988122162119,11.5019260264738));
#82009=CARTESIAN_POINT('Ctrl Pts',(5.54411586436051,7.5552515284045,11.4982436699576));
#82010=CARTESIAN_POINT('Ctrl Pts',(5.65010874439515,7.47631710174249,11.4959613451287));
#82011=CARTESIAN_POINT('Ctrl Pts',(5.89233053951926,7.28783723043592,11.490627464591));
#82012=CARTESIAN_POINT('Ctrl Pts',(6.0272343899226,7.17666886986867,11.487566013402));
#82013=CARTESIAN_POINT('Ctrl Pts',(6.22268468063554,7.00620670604878,11.4830100673927));
#82014=CARTESIAN_POINT('Ctrl Pts',(6.2856640753546,6.94976000813127,11.4815226882742));
#82015=CARTESIAN_POINT('Ctrl Pts',(6.44779136540077,6.80044295749968,11.477648220966));
#82016=CARTESIAN_POINT('Ctrl Pts',(6.54569916649103,6.70625531905782,11.4752626692437));
#82017=CARTESIAN_POINT('Ctrl Pts',(6.71814143510164,6.53298990960608,11.4709973305568));
#82018=CARTESIAN_POINT('Ctrl Pts',(6.79341414591935,6.45468092517459,11.4691124029034));
#82019=CARTESIAN_POINT('Ctrl Pts',(6.90074705988993,6.3390607087022,11.4664009833136));
#82020=CARTESIAN_POINT('Ctrl Pts',(6.93390164910408,6.30277784693286,11.4655600580448));
#82021=CARTESIAN_POINT('Ctrl Pts',(6.99616820966099,6.23355019936897,11.4639756940377));
#82022=CARTESIAN_POINT('Ctrl Pts',(7.02533672241702,6.20065816188936,11.4632314877448));
#82023=CARTESIAN_POINT('Ctrl Pts',(7.10440876173399,6.11021793265991,11.4612068228262));
#82024=CARTESIAN_POINT('Ctrl Pts',(7.15384384563408,6.05226447818558,11.4599329441222));
#82025=CARTESIAN_POINT('Ctrl Pts',(7.23749526199406,5.95174168749394,11.4577575676415));
#82026=CARTESIAN_POINT('Ctrl Pts',(7.27205609996119,5.90946417809317,11.4568528002402));
#82027=CARTESIAN_POINT('Ctrl Pts',(7.42771419027369,5.7156175570998,11.45274501019));
#82028=CARTESIAN_POINT('Ctrl Pts',(7.54445596275977,5.56061207042768,11.4495712522038));
#82029=CARTESIAN_POINT('Ctrl Pts',(7.7448806877038,5.27655332609422,11.4438717521632));
#82030=CARTESIAN_POINT('Ctrl Pts',(7.83035820075265,5.14885251612277,11.4413496440123));
#82031=CARTESIAN_POINT('Ctrl Pts',(7.99712577256745,4.88594233667946,11.4362056494782));
#82032=CARTESIAN_POINT('Ctrl Pts',(8.07821927640738,4.7506658748682,11.4335836670146));
#82033=CARTESIAN_POINT('Ctrl Pts',(8.1983822181979,4.53823459202642,11.4294874255465));
#82034=CARTESIAN_POINT('Ctrl Pts',(8.23986295004745,4.46247719652791,11.4280307771367));
#82035=CARTESIAN_POINT('Ctrl Pts',(8.31807038809955,4.31483536528738,11.4251980787988));
#82036=CARTESIAN_POINT('Ctrl Pts',(8.3549272510876,4.24302837651527,11.4238231214834));
#82037=CARTESIAN_POINT('Ctrl Pts',(8.44358182885378,4.06467037068358,11.4204138706668));
#82038=CARTESIAN_POINT('Ctrl Pts',(8.49429522482729,3.95759622105893,11.4183722483068));
#82039=CARTESIAN_POINT('Ctrl Pts',(8.60448467211024,3.71306507309902,11.4137225784626));
#82040=CARTESIAN_POINT('Ctrl Pts',(8.66272303336974,3.57508576030736,11.411107819149));
#82041=CARTESIAN_POINT('Ctrl Pts',(8.80487176216494,3.21440975469719,11.4043110814434));
#82042=CARTESIAN_POINT('Ctrl Pts',(8.88365088034356,2.98980664153678,11.400113946015));
#82043=CARTESIAN_POINT('Ctrl Pts',(8.99224547400813,2.63782414370871,11.3936676029783));
#82044=CARTESIAN_POINT('Ctrl Pts',(9.02808914705693,2.51240947766224,11.3913964020703));
#82045=CARTESIAN_POINT('Ctrl Pts',(9.07499655340303,2.33429084753194,11.3882237482713));
#82046=CARTESIAN_POINT('Ctrl Pts',(9.08824200729681,2.28217734621896,11.3873018729595));
#82047=CARTESIAN_POINT('Ctrl Pts',(9.11115567449772,2.18866049084321,11.3856606905596));
#82048=CARTESIAN_POINT('Ctrl Pts',(9.12099199704146,2.14730003942896,11.3849395664472));
#82049=CARTESIAN_POINT('Ctrl Pts',(9.14525037058485,2.04212175727382,11.3831169446179));
#82050=CARTESIAN_POINT('Ctrl Pts',(9.15928613498678,1.97821716170038,11.3820197497822));
#82051=CARTESIAN_POINT('Ctrl Pts',(9.21488352024748,1.71179607794913,11.3774789058821));
#82052=CARTESIAN_POINT('Ctrl Pts',(9.25040667040158,1.50807859038459,11.3740855975635));
#82053=CARTESIAN_POINT('Ctrl Pts',(9.32482095701645,0.978289381433982,11.3653145179413));
#82054=CARTESIAN_POINT('Ctrl Pts',(9.35336664289584,0.651051407220187,11.3599427391217));
#82055=CARTESIAN_POINT('Ctrl Pts',(9.36813634946008,0.222826483443642,11.3527871234167));
#82056=CARTESIAN_POINT('Ctrl Pts',(9.36998381588262,0.122611295240142,11.3511043556485));
#82057=CARTESIAN_POINT('Ctrl Pts',(9.37041177136695,-0.0565206334172836,
11.3480784729755));
#82058=CARTESIAN_POINT('Ctrl Pts',(9.36960356803008,-0.135426331802459,
11.3467393890732));
#82059=CARTESIAN_POINT('Ctrl Pts',(9.36561540221525,-0.30975294512381,11.3437661793526));
#82060=CARTESIAN_POINT('Ctrl Pts',(9.3619735382191,-0.405154489659079,11.3421292614089));
#82061=CARTESIAN_POINT('Ctrl Pts',(9.34302093234984,-0.759486130723608,
11.3360129447384));
#82062=CARTESIAN_POINT('Ctrl Pts',(9.31841938269814,-1.01780086647856,11.331477924072));
#82063=CARTESIAN_POINT('Ctrl Pts',(9.24218551477918,-1.57295549186521,11.3216332951951));
#82064=CARTESIAN_POINT('Ctrl Pts',(9.18689308391084,-1.86900451967697,11.3163205799458));
#82065=CARTESIAN_POINT('Ctrl Pts',(9.10500382251618,-2.21436219384678,11.3101929599984));
#82066=CARTESIAN_POINT('Ctrl Pts',(9.09210607575656,-2.26673810961586,11.3092657843955));
#82067=CARTESIAN_POINT('Ctrl Pts',(9.06824678374012,-2.36014592674293,11.3076177528998));
#82068=CARTESIAN_POINT('Ctrl Pts',(9.05745717183549,-2.40122013266702,11.306895066372));
#82069=CARTESIAN_POINT('Ctrl Pts',(9.03229942467694,-2.49440861672463,11.3052604307046));
#82070=CARTESIAN_POINT('Ctrl Pts',(9.01775882031005,-2.5464746456243,11.304350419329));
#82071=CARTESIAN_POINT('Ctrl Pts',(8.96043308002719,-2.74509225004799,11.3008868630333));
#82072=CARTESIAN_POINT('Ctrl Pts',(8.91451913581543,-2.89071639504993,11.2983635816078));
#82073=CARTESIAN_POINT('Ctrl Pts',(8.7325342431694,-3.4222572814741,11.2891220299348));
#82074=CARTESIAN_POINT('Ctrl Pts',(8.5747884665114,-3.80026347487041,11.2824686121042));
#82075=CARTESIAN_POINT('Ctrl Pts',(8.34856989435705,-4.25592271021784,11.2739712717521));
#82076=CARTESIAN_POINT('Ctrl Pts',(8.30287903862549,-4.34438683858014,11.2722993850308));
#82077=CARTESIAN_POINT('Ctrl Pts',(8.21847405207963,-4.50160997968997,11.2692846791357));
#82078=CARTESIAN_POINT('Ctrl Pts',(8.18028472012145,-4.57064000093292,11.2679457589937));
#82079=CARTESIAN_POINT('Ctrl Pts',(8.09368341799795,-4.72261536244842,11.2649628543155));
#82080=CARTESIAN_POINT('Ctrl Pts',(8.0448587383063,-4.80531528140412,11.2633159665235));
#82081=CARTESIAN_POINT('Ctrl Pts',(7.85070507319806,-5.1229201154839,11.2568984069792));
#82082=CARTESIAN_POINT('Ctrl Pts',(7.69628890173883,-5.35210394959635,11.252063319376));
#82083=CARTESIAN_POINT('Ctrl Pts',(7.36461346989674,-5.80027634665401,11.2422639406318));
#82084=CARTESIAN_POINT('Ctrl Pts',(7.1871509706775,-6.01877052242378,11.2373040598758));
#82085=CARTESIAN_POINT('Ctrl Pts',(6.96395562108168,-6.26959871158336,11.2315064998035));
#82086=CARTESIAN_POINT('Ctrl Pts',(6.92743032477523,-6.3099330431662,11.2305710187155));
#82087=CARTESIAN_POINT('Ctrl Pts',(6.86173280590428,-6.38122378245983,11.2289135456529));
#82088=CARTESIAN_POINT('Ctrl Pts',(6.8326972498147,-6.41230398323212,11.2281896432418));
#82089=CARTESIAN_POINT('Ctrl Pts',(6.76655410739108,-6.48214546462628,11.2265604414798));
#82090=CARTESIAN_POINT('Ctrl Pts',(6.72932323347633,-6.52078777064284,11.2256569932477));
#82091=CARTESIAN_POINT('Ctrl Pts',(6.58811985198719,-6.66484691055137,11.2222766763406));
#82092=CARTESIAN_POINT('Ctrl Pts',(6.48198528521763,-6.76811454724948,11.2198282182329));
#82093=CARTESIAN_POINT('Ctrl Pts',(6.24282807631506,-6.99002386893736,11.2144596525456));
#82094=CARTESIAN_POINT('Ctrl Pts',(6.10877730509157,-7.10747325032063,11.2115457586906));
#82095=CARTESIAN_POINT('Ctrl Pts',(5.78325070996419,-7.37666879835267,11.2046152544383));
#82096=CARTESIAN_POINT('Ctrl Pts',(5.58902957218264,-7.5248906488868,11.2005913816635));
#82097=CARTESIAN_POINT('Ctrl Pts',(5.31006543084032,-7.72102050088655,11.1948906137783));
#82098=CARTESIAN_POINT('Ctrl Pts',(5.23003243792723,-7.77545581266769,11.1932641087567));
#82099=CARTESIAN_POINT('Ctrl Pts',(5.08327708936292,-7.87198192700135,11.1902948312084));
#82100=CARTESIAN_POINT('Ctrl Pts',(5.01683903818444,-7.91448870475178,11.188955405277));
#82101=CARTESIAN_POINT('Ctrl Pts',(4.86604866299914,-8.00830203948611,11.1859251403872));
#82102=CARTESIAN_POINT('Ctrl Pts',(4.78140616886971,-8.05912440221307,11.184230875049));
#82103=CARTESIAN_POINT('Ctrl Pts',(4.59952608815703,-8.16445758318166,11.1806044186245));
#82104=CARTESIAN_POINT('Ctrl Pts',(4.50208681872962,-8.21859002871254,11.1786699918157));
#82105=CARTESIAN_POINT('Ctrl Pts',(4.20036041618973,-8.37923792720377,11.1727101113469));
#82106=CARTESIAN_POINT('Ctrl Pts',(3.99309236801689,-8.47996868092159,11.1686558996977));
#82107=CARTESIAN_POINT('Ctrl Pts',(3.75691725811887,-8.58416733975753,11.1641189104818));
#82108=CARTESIAN_POINT('Ctrl Pts',(3.73146099534917,-8.59526352370031,11.1636309757074));
#82109=CARTESIAN_POINT('Ctrl Pts',(3.53274050550957,-8.68083501623256,11.1598311223301));
#82110=CARTESIAN_POINT('Ctrl Pts',(3.3573124198528,-8.75017746713286,11.1565297031563));
#82111=CARTESIAN_POINT('Ctrl Pts',(3.12733545232831,-8.83314677988633,11.1523138361618));
#82112=CARTESIAN_POINT('Ctrl Pts',(3.07459083549419,-8.85164393093529,11.1513545256751));
#82113=CARTESIAN_POINT('Ctrl Pts',(2.98175121337683,-8.88327217007262,11.1496811296333));
#82114=CARTESIAN_POINT('Ctrl Pts',(2.94172734329044,-8.89660637489602,11.148964774093));
#82115=CARTESIAN_POINT('Ctrl Pts',(2.84366959299135,-8.92854086865132,11.1472216771474));
#82116=CARTESIAN_POINT('Ctrl Pts',(2.78554178894041,-8.94684613501642,11.1461983166975));
#82117=CARTESIAN_POINT('Ctrl Pts',(2.50732838193869,-9.03148527318126,11.1413391922819));
#82118=CARTESIAN_POINT('Ctrl Pts',(2.28502919967817,-9.09027304966173,11.13757045591));
#82119=CARTESIAN_POINT('Ctrl Pts',(1.75800011902292,-9.20909139405502,11.1287147046982));
#82120=CARTESIAN_POINT('Ctrl Pts',(1.45200243512864,-9.26226846554898,11.1236300890653));
#82121=CARTESIAN_POINT('Ctrl Pts',(1.04403483791344,-9.31244902217868,11.1167685895778));
#82122=CARTESIAN_POINT('Ctrl Pts',(0.943946140021,-9.32312614703433,11.1150794346931));
#82123=CARTESIAN_POINT('Ctrl Pts',(0.765017581838083,-9.3393027303344,11.1120459368315));
#82124=CARTESIAN_POINT('Ctrl Pts',(0.68624340031113,-9.34542119709954,11.1107056897563));
#82125=CARTESIAN_POINT('Ctrl Pts',(0.513811422372697,-9.35662219639776,
11.107760560202));
#82126=CARTESIAN_POINT('Ctrl Pts',(0.4201356265172,-9.36129622988581,11.1061532186484));
#82127=CARTESIAN_POINT('Ctrl Pts',(0.0977176434978746,-9.37253423872393,
11.1005954177021));
#82128=CARTESIAN_POINT('Ctrl Pts',(-0.131184775563268,-9.37212551621604,
11.0966034596699));
#82129=CARTESIAN_POINT('Ctrl Pts',(-0.600847890812155,-9.35407594509233,
11.0883564337875));
#82130=CARTESIAN_POINT('Ctrl Pts',(-0.841406803379838,-9.33551228055605,
11.0841017271851));
#82131=CARTESIAN_POINT('Ctrl Pts',(-1.19395801001081,-9.29456751719272,
11.0779013244183));
#82132=CARTESIAN_POINT('Ctrl Pts',(-1.3066871768029,-9.27939059390266,11.0759245243684));
#82133=CARTESIAN_POINT('Ctrl Pts',(-1.47050124401979,-9.25429165176958,
11.0730722028225));
#82134=CARTESIAN_POINT('Ctrl Pts',(-1.52182389823631,-9.24599047823566,
11.0721815138153));
#82135=CARTESIAN_POINT('Ctrl Pts',(-1.61536118648213,-9.23006139141782,
11.070565168352));
#82136=CARTESIAN_POINT('Ctrl Pts',(-1.65759747059468,-9.22256990624319,
11.0698380847778));
#82137=CARTESIAN_POINT('Ctrl Pts',(-1.76741941471712,-9.20231190062029,
11.0679536289174));
#82138=CARTESIAN_POINT('Ctrl Pts',(-1.83491865618041,-9.18909077451248,
11.0668012560411));
#82139=CARTESIAN_POINT('Ctrl Pts',(-1.98994013058943,-9.15695039037478,
11.0641624796589));
#82140=CARTESIAN_POINT('Ctrl Pts',(-2.07734904930345,-9.13751734068116,
11.0626803475791));
#82141=CARTESIAN_POINT('Ctrl Pts',(-2.41173922755492,-9.05812835902748,
11.0570132250866));
#82142=CARTESIAN_POINT('Ctrl Pts',(-2.65652176010058,-8.98938640445197,
11.0528680142331));
#82143=CARTESIAN_POINT('Ctrl Pts',(-3.09066409352482,-8.8481827887134,11.0453617406064));
#82144=CARTESIAN_POINT('Ctrl Pts',(-3.28104253042078,-8.77936801606186,
11.0420155841091));
#82145=CARTESIAN_POINT('Ctrl Pts',(-3.55643267666661,-8.66961485324422,
11.0370552617146));
#82146=CARTESIAN_POINT('Ctrl Pts',(-3.64329313475421,-8.63347265979584,
11.0354730491027));
#82147=CARTESIAN_POINT('Ctrl Pts',(-3.80205441782347,-8.56459024628363,
11.0325457510767));
#82148=CARTESIAN_POINT('Ctrl Pts',(-3.8741138293466,-8.53223686299977,11.0312034651188));
#82149=CARTESIAN_POINT('Ctrl Pts',(-4.03827770859339,-8.45602174037447,
11.028113161768));
#82150=CARTESIAN_POINT('Ctrl Pts',(-4.1300921798462,-8.41155925146307,11.0263610846436));
#82151=CARTESIAN_POINT('Ctrl Pts',(-4.27617910585212,-8.33784593483541,
11.0235351781345));
#82152=CARTESIAN_POINT('Ctrl Pts',(-4.33092075136979,-8.3095431890033,11.0224675244031));
#82153=CARTESIAN_POINT('Ctrl Pts',(-4.5368013356058,-8.20051084294139,11.0184197966665));
#82154=CARTESIAN_POINT('Ctrl Pts',(-4.68599511580999,-8.11618099861006,
11.015419461597));
#82155=CARTESIAN_POINT('Ctrl Pts',(-5.09890024896231,-7.86760944597705,
11.0069544059769));
#82156=CARTESIAN_POINT('Ctrl Pts',(-5.35687832412414,-7.69427820438116,
11.0014689889127));
#82157=CARTESIAN_POINT('Ctrl Pts',(-5.64855046442738,-7.47651742973718,
10.995186281113));
#82158=CARTESIAN_POINT('Ctrl Pts',(-5.69105616193072,-7.44421352491204,
10.9942687869764));
#82159=CARTESIAN_POINT('Ctrl Pts',(-5.7668182963076,-7.38560690305223,10.9926316623988));
#82160=CARTESIAN_POINT('Ctrl Pts',(-5.80017661920584,-7.35943841559748,
10.9919102948555));
#82161=CARTESIAN_POINT('Ctrl Pts',(-5.8350227041693,-7.33171873697793,10.9911563566436));
#82162=CARTESIAN_POINT('Ctrl Pts',(-5.83668859953585,-7.33039260806499,
10.9911203115629));
#82163=CARTESIAN_POINT('Ctrl Pts',(-5.83932710802561,-7.32829076495229,
10.9910632196975));
#82164=CARTESIAN_POINT('Ctrl Pts',(-5.84030001886517,-7.32751542474334,
10.991042167425));
#82165=CARTESIAN_POINT('Ctrl Pts',(-5.84278858338152,-7.32553140669771,
10.9909883174671));
#82166=CARTESIAN_POINT('Ctrl Pts',(-5.84430401647933,-7.3243224521844,10.9909555238261));
#82167=CARTESIAN_POINT('Ctrl Pts',(-5.84722781351326,-7.32198847366916,
10.9908922509943));
#82168=CARTESIAN_POINT('Ctrl Pts',(-5.84863622818902,-7.32086351341033,
10.9908617708811));
#82169=CARTESIAN_POINT('Ctrl Pts',(-5.85136808453669,-7.31868017291583,
10.9908026473251));
#82170=CARTESIAN_POINT('Ctrl Pts',(-5.85269156388538,-7.31762183992801,
10.9907740032027));
#82171=CARTESIAN_POINT('Ctrl Pts',(-5.85527085484812,-7.31555813774285,
10.990718177404));
#82172=CARTESIAN_POINT('Ctrl Pts',(-5.8565266947959,-7.31455280406621,10.9906909952205));
#82173=CARTESIAN_POINT('Ctrl Pts',(-5.85898460764888,-7.31258413987955,
10.9906377926643));
#82174=CARTESIAN_POINT('Ctrl Pts',(-5.8601867020153,-7.31162083624473,10.9906117719101));
#82175=CARTESIAN_POINT('Ctrl Pts',(-5.86254855687697,-7.30972719677886,
10.9905606449096));
#82176=CARTESIAN_POINT('Ctrl Pts',(-5.86370833358325,-7.30879688127502,
10.9905355383772));
#82177=CARTESIAN_POINT('Ctrl Pts',(-5.86599517222388,-7.30696159776288,
10.9904860317233));
#82178=CARTESIAN_POINT('Ctrl Pts',(-5.86712224628781,-7.30605664492484,
10.990461631389));
#82179=CARTESIAN_POINT('Ctrl Pts',(-5.86935195390955,-7.30426551439291,
10.9904133580948));
#82180=CARTESIAN_POINT('Ctrl Pts',(-5.8704545962716,-7.30337934772153,10.9903894849814));
#82181=CARTESIAN_POINT('Ctrl Pts',(-5.87264271588078,-7.30161999386635,
10.9903421086721));
#82182=CARTESIAN_POINT('Ctrl Pts',(-5.87372819915641,-7.3007468142411,10.9903186053719));
#82183=CARTESIAN_POINT('Ctrl Pts',(-5.87588853919116,-7.29900820946103,
10.9902718271435));
#82184=CARTESIAN_POINT('Ctrl Pts',(-5.876963399581,-7.29814278887192,10.9902485521529));
#82185=CARTESIAN_POINT('Ctrl Pts',(-5.87910849967673,-7.29641488683421,
10.9902021004964));
#82186=CARTESIAN_POINT('Ctrl Pts',(-5.88017874085686,-7.29555240727954,
10.9901789238053));
#82187=CARTESIAN_POINT('Ctrl Pts',(-5.88232023900376,-7.2938258522208,10.9901325466618));
#82188=CARTESIAN_POINT('Ctrl Pts',(-5.8833914954546,-7.29296177611884,10.9901093462182));
#82189=CARTESIAN_POINT('Ctrl Pts',(-5.88554042640442,-7.29122766548963,
10.9900628045193));
#82190=CARTESIAN_POINT('Ctrl Pts',(-5.8866180984459,-7.29035762798312,10.9900394633056));
#82191=CARTESIAN_POINT('Ctrl Pts',(-5.88878514402303,-7.2886073122139,10.9899925255518));
#82192=CARTESIAN_POINT('Ctrl Pts',(-5.88987451318281,-7.28772702857922,
10.9899689290853));
#82193=CARTESIAN_POINT('Ctrl Pts',(-5.8920702199633,-7.28595193575882,10.9899213666281));
#82194=CARTESIAN_POINT('Ctrl Pts',(-5.8931765512165,-7.28505711874372,10.9898974007439));
#82195=CARTESIAN_POINT('Ctrl Pts',(-5.89541152672902,-7.28324859535273,
10.98984898353));
#82196=CARTESIAN_POINT('Ctrl Pts',(-5.89654016249166,-7.28233487854823,
10.9898245323415));
#82197=CARTESIAN_POINT('Ctrl Pts',(-5.89882525879532,-7.28048403914862,
10.9897750249269));
#82198=CARTESIAN_POINT('Ctrl Pts',(-5.89998170854144,-7.2795469032747,10.9897499688789));
#82199=CARTESIAN_POINT('Ctrl Pts',(-5.90232820048541,-7.27764448322589,
10.9896991265545));
#82200=CARTESIAN_POINT('Ctrl Pts',(-5.90351822930849,-7.27667918261458,
10.9896733404973));
#82201=CARTESIAN_POINT('Ctrl Pts',(-5.90593799330101,-7.27471538900458,
10.9896209053994));
#82202=CARTESIAN_POINT('Ctrl Pts',(-5.90716771216731,-7.27371687599022,
10.9895942566238));
#82203=CARTESIAN_POINT('Ctrl Pts',(-5.90967341098587,-7.27168123213273,
10.9895399537077));
#82204=CARTESIAN_POINT('Ctrl Pts',(-5.91094937126689,-7.2706440771492,10.9895122998847));
#82205=CARTESIAN_POINT('Ctrl Pts',(-5.91355464990306,-7.26852525634999,
10.9894558326538));
#82206=CARTESIAN_POINT('Ctrl Pts',(-5.91488394465064,-7.26744356159045,
10.9894270196241));
#82207=CARTESIAN_POINT('Ctrl Pts',(-5.91760364206364,-7.2652292058871,10.9893680655056));
#82208=CARTESIAN_POINT('Ctrl Pts',(-5.91899401646741,-7.26409651034892,
10.989337924866));
#82209=CARTESIAN_POINT('Ctrl Pts',(-5.92184439811943,-7.26177302981517,
10.9892761301267));
#82210=CARTESIAN_POINT('Ctrl Pts',(-5.92330437158937,-7.26058220348756,
10.9892444765593));
#82211=CARTESIAN_POINT('Ctrl Pts',(-5.92630338806166,-7.25813455120618,
10.9891794506432));
#82212=CARTESIAN_POINT('Ctrl Pts',(-5.92784239064463,-7.25687767586319,
10.9891460789259));
#82213=CARTESIAN_POINT('Ctrl Pts',(-5.93100996751195,-7.25428909359632,
10.9890773880983));
#82214=CARTESIAN_POINT('Ctrl Pts',(-5.93263849335326,-7.25295732755823,
10.9890420697376));
#82215=CARTESIAN_POINT('Ctrl Pts',(-5.9359968582298,-7.25020905632485,10.9889692299022));
#82216=CARTESIAN_POINT('Ctrl Pts',(-5.93772663907653,-7.24879248019496,
10.9889317093189));
#82217=CARTESIAN_POINT('Ctrl Pts',(-5.98494343423164,-7.21009680594858,
10.9879074417202));
#82218=CARTESIAN_POINT('Ctrl Pts',(-6.03007904898525,-7.1723908526717,10.9869260154301));
#82219=CARTESIAN_POINT('Ctrl Pts',(-6.15938598691588,-7.06228540998663,
10.9841033016293));
#82220=CARTESIAN_POINT('Ctrl Pts',(-6.24262948299761,-6.9888116417459,10.9822722821226));
#82221=CARTESIAN_POINT('Ctrl Pts',(-6.62404769718664,-6.63990493115117,
10.9737743527757));
#82222=CARTESIAN_POINT('Ctrl Pts',(-6.90542848173967,-6.34676320576499,
10.9671691391112));
#82223=CARTESIAN_POINT('Ctrl Pts',(-7.22965082951393,-5.96181335335713,
10.9587569783418));
#82224=CARTESIAN_POINT('Ctrl Pts',(-7.29122314183169,-5.88635155368662,
10.957120612771));
#82225=CARTESIAN_POINT('Ctrl Pts',(-7.39653820379273,-5.75309122269123,
10.9542498059002));
#82226=CARTESIAN_POINT('Ctrl Pts',(-7.44080749616265,-5.69571942741086,
10.9530197989552));
#82227=CARTESIAN_POINT('Ctrl Pts',(-7.53862946217726,-5.56585774482449,
10.9502480853874));
#82228=CARTESIAN_POINT('Ctrl Pts',(-7.59181075722689,-5.49309712100544,
10.9487035799898));
#82229=CARTESIAN_POINT('Ctrl Pts',(-7.76784447735452,-5.24481405172247,
10.9434612820827));
#82230=CARTESIAN_POINT('Ctrl Pts',(-7.88572431280793,-5.0658497587383,10.9397275930791));
#82231=CARTESIAN_POINT('Ctrl Pts',(-8.18079569777134,-4.58258287090693,
10.9297996673474));
#82232=CARTESIAN_POINT('Ctrl Pts',(-8.34715161977635,-4.27206551216097,
10.9235675773498));
#82233=CARTESIAN_POINT('Ctrl Pts',(-8.5185670040455,-3.90365907013084,10.9165515102537));
#82234=CARTESIAN_POINT('Ctrl Pts',(-8.54106201876819,-3.8541922042012,10.9156173113304));
#82235=CARTESIAN_POINT('Ctrl Pts',(-8.58013100758253,-3.76625691576903,
10.9139722220597));
#82236=CARTESIAN_POINT('Ctrl Pts',(-8.59687971231175,-3.72786782140688,
10.9132593310904));
#82237=CARTESIAN_POINT('Ctrl Pts',(-8.62288713202287,-3.66714967919227,
10.9121404383629));
#82238=CARTESIAN_POINT('Ctrl Pts',(-8.63231772131513,-3.64489506312267,
10.9117321071465));
#82239=CARTESIAN_POINT('Ctrl Pts',(-8.64642644225138,-3.61123894377407,
10.9111170769088));
#82240=CARTESIAN_POINT('Ctrl Pts',(-8.65116835627592,-3.59986430325827,
10.9109096466553));
#82241=CARTESIAN_POINT('Ctrl Pts',(-8.6609540451265,-3.57625993122506,10.9104800518261));
#82242=CARTESIAN_POINT('Ctrl Pts',(-8.66599438844497,-3.56402880560234,
10.9102579249601));
#82243=CARTESIAN_POINT('Ctrl Pts',(-8.67837828280957,-3.53379589583153,
10.9097100049437));
#82244=CARTESIAN_POINT('Ctrl Pts',(-8.68569174295965,-3.51578184760399,
10.9093845213264));
#82245=CARTESIAN_POINT('Ctrl Pts',(-8.72055402322892,-3.42913859213306,
10.9078235073762));
#82246=CARTESIAN_POINT('Ctrl Pts',(-8.74734584718554,-3.36020752593731,
10.9065950763379));
#82247=CARTESIAN_POINT('Ctrl Pts',(-8.83265925331908,-3.13277229428126,
10.9025764115461));
#82248=CARTESIAN_POINT('Ctrl Pts',(-8.88771016492782,-2.9730018386727,10.8998074235589));
#82249=CARTESIAN_POINT('Ctrl Pts',(-9.02968001927931,-2.52169973952233,
10.8920529674702));
#82250=CARTESIAN_POINT('Ctrl Pts',(-9.10676862325481,-2.22729780275952,
10.8870663932108));
#82251=CARTESIAN_POINT('Ctrl Pts',(-9.18996168082823,-1.83198121796618,
10.8803192193218));
#82252=CARTESIAN_POINT('Ctrl Pts',(-9.20895754288809,-1.73396995010261,
10.8786429454963));
#82253=CARTESIAN_POINT('Ctrl Pts',(-9.24015543529145,-1.55799129262525,
10.8756237450521));
#82254=CARTESIAN_POINT('Ctrl Pts',(-9.25294555037285,-1.48013781267209,
10.874284770683));
#82255=CARTESIAN_POINT('Ctrl Pts',(-9.27598441316437,-1.32790585972024,
10.8716593122357));
#82256=CARTESIAN_POINT('Ctrl Pts',(-9.28632542938372,-1.25354728533169,
10.8703735259577));
#82257=CARTESIAN_POINT('Ctrl Pts',(-9.30795068350567,-1.0830544509598,10.8674175790309));
#82258=CARTESIAN_POINT('Ctrl Pts',(-9.31864115091131,-0.986853542837705,
10.8657439699172));
#82259=CARTESIAN_POINT('Ctrl Pts',(-9.3561038556868,-0.594439909765311,
10.8588966555578));
#82260=CARTESIAN_POINT('Ctrl Pts',(-9.37025666368476,-0.29719841436659,
10.8536567989704));
#82261=CARTESIAN_POINT('Ctrl Pts',(-9.37024999764631,0.000210022444156327,
10.8484327663521));
#82262=CARTESIAN_POINT('Ctrl Pts',(4.29126860009441,8.33070247396408,10.522886232912));
#82263=CARTESIAN_POINT('Ctrl Pts',(2.96799777839083,9.01176106266219,10.5481706725962));
#82264=CARTESIAN_POINT('Ctrl Pts',(-0.0657392449123033,9.74679514529692,
10.599700716706));
#82265=CARTESIAN_POINT('Ctrl Pts',(-4.64250383747633,8.58644271179361,10.6774763652415));
#82266=CARTESIAN_POINT('Ctrl Pts',(-8.16258095402662,5.35276680725565,10.7562131785184));
#82267=CARTESIAN_POINT('Ctrl Pts',(-9.29464270735565,2.08042600373183,10.8132510207396));
#82268=CARTESIAN_POINT('Ctrl Pts',(-9.37078403118896,0.267868275173487,
10.8440432585352));
#82269=CARTESIAN_POINT('Ctrl Pts',(-9.3705222398215,0.000212818811248933,
10.848589891905));
#82270=CARTESIAN_POINT('',(-9.36953762859325,3.21162273520589E-5,10.6513777224354));
#82271=CARTESIAN_POINT('Ctrl Pts',(4.29092662690317,8.33003803983112,10.3254369059772));
#82272=CARTESIAN_POINT('Ctrl Pts',(4.17084852669809,8.39189205718544,10.3276702672494));
#82273=CARTESIAN_POINT('Ctrl Pts',(4.04944275948985,8.45114463703808,10.3299162156179));
#82274=CARTESIAN_POINT('Ctrl Pts',(3.84522640799292,8.54540166368771,10.3336854708738));
#82275=CARTESIAN_POINT('Ctrl Pts',(3.76312163318825,8.58187457660759,10.3351985495077));
#82276=CARTESIAN_POINT('Ctrl Pts',(3.60732266131618,8.64841840941565,10.3380675133813));
#82277=CARTESIAN_POINT('Ctrl Pts',(3.53374498682596,8.67874208054923,10.3394214930332));
#82278=CARTESIAN_POINT('Ctrl Pts',(3.3583172671846,8.7484405633889,10.342648426147));
#82279=CARTESIAN_POINT('Ctrl Pts',(3.25614771850194,8.78697952131914,10.3445268344419));
#82280=CARTESIAN_POINT('Ctrl Pts',(2.90463136731083,8.91260067885413,10.3509851546152));
#82281=CARTESIAN_POINT('Ctrl Pts',(2.65228898312657,8.99092300707285,10.3556173114874));
#82282=CARTESIAN_POINT('Ctrl Pts',(2.15139289303251,9.12346580228876,10.3647264880036));
#82283=CARTESIAN_POINT('Ctrl Pts',(1.90326719737982,9.17843635979939,10.3691984159237));
#82284=CARTESIAN_POINT('Ctrl Pts',(1.59143747703267,9.23433001889079,10.3746733536811));
#82285=CARTESIAN_POINT('Ctrl Pts',(1.52955015718988,9.24478233837405,10.3757527078762));
#82286=CARTESIAN_POINT('Ctrl Pts',(1.42579690258112,9.26123514859852,10.3775476421041));
#82287=CARTESIAN_POINT('Ctrl Pts',(1.38398706489976,9.26757536280537,10.3782668954658));
#82288=CARTESIAN_POINT('Ctrl Pts',(1.28719448313514,9.28158376399305,10.3799223917948));
#82289=CARTESIAN_POINT('Ctrl Pts',(1.23218377333498,9.28904677420117,10.3808563845891));
#82290=CARTESIAN_POINT('Ctrl Pts',(1.00586567563936,9.31770433558347,10.3846761142934));
#82291=CARTESIAN_POINT('Ctrl Pts',(0.83405440267793,9.33465229385922,10.3875229099805));
#82292=CARTESIAN_POINT('Ctrl Pts',(0.260280078110764,9.37528265384661,10.3969714201718));
#82293=CARTESIAN_POINT('Ctrl Pts',(-0.142726959625376,9.3778088918647,10.4035301470733));
#82294=CARTESIAN_POINT('Ctrl Pts',(-0.638212744594506,9.34896005978609,
10.4118357138485));
#82295=CARTESIAN_POINT('Ctrl Pts',(-0.731693548918824,9.34210865938655,
10.4134122411993));
#82296=CARTESIAN_POINT('Ctrl Pts',(-0.903762422886792,9.32689882553345,
10.4163343693944));
#82297=CARTESIAN_POINT('Ctrl Pts',(-0.982377914809031,9.3189463898799,10.4176772420524));
#82298=CARTESIAN_POINT('Ctrl Pts',(-1.16271416244987,9.29839690535284,10.4207765320311));
#82299=CARTESIAN_POINT('Ctrl Pts',(-1.26434759413489,9.2851232798917,10.4225371020645));
#82300=CARTESIAN_POINT('Ctrl Pts',(-1.4271471743319,9.26113861058198,10.4253793702454));
#82301=CARTESIAN_POINT('Ctrl Pts',(-1.48846027190029,9.25148222862207,10.4264548621507));
#82302=CARTESIAN_POINT('Ctrl Pts',(-1.72059244062901,9.21255565636578,10.430544977191));
#82303=CARTESIAN_POINT('Ctrl Pts',(-1.89068364028855,9.17915765302955,10.4335802678523));
#82304=CARTESIAN_POINT('Ctrl Pts',(-2.16696870775239,9.1169024986307,10.4385551699373));
#82305=CARTESIAN_POINT('Ctrl Pts',(-2.27375384451124,9.09085848527484,10.4404888377625));
#82306=CARTESIAN_POINT('Ctrl Pts',(-2.41009923006539,9.05505226965471,10.4429656944004));
#82307=CARTESIAN_POINT('Ctrl Pts',(-2.44010302073046,9.047013162023,10.4435112309203));
#82308=CARTESIAN_POINT('Ctrl Pts',(-2.63568170282498,8.99356680053742,10.4470696416051));
#82309=CARTESIAN_POINT('Ctrl Pts',(-2.80002239407253,8.9437652419079,10.4500713420335));
#82310=CARTESIAN_POINT('Ctrl Pts',(-3.01597626837983,8.87178685542622,10.4539966889123));
#82311=CARTESIAN_POINT('Ctrl Pts',(-3.06889102393441,8.85362201373918,10.4549569064722));
#82312=CARTESIAN_POINT('Ctrl Pts',(-3.16141412992714,8.82093108677411,10.4566311695366));
#82313=CARTESIAN_POINT('Ctrl Pts',(-3.2010927628784,8.80660943088274,10.4573474956131));
#82314=CARTESIAN_POINT('Ctrl Pts',(-3.29779346753757,8.77096626741891,10.4590894986237));
#82315=CARTESIAN_POINT('Ctrl Pts',(-3.35470696247938,8.749356104244,10.4601118077736));
#82316=CARTESIAN_POINT('Ctrl Pts',(-3.48152592292905,8.69978335403628,10.4623870595677));
#82317=CARTESIAN_POINT('Ctrl Pts',(-3.55131316488792,8.6715297379965,10.4636372396361));
#82318=CARTESIAN_POINT('Ctrl Pts',(-3.78214520791813,8.57482257479602,10.4677763243759));
#82319=CARTESIAN_POINT('Ctrl Pts',(-3.94161256469758,8.50269928546953,10.4706427375352));
#82320=CARTESIAN_POINT('Ctrl Pts',(-4.35406821020759,8.30205707136569,10.4781604999754));
#82321=CARTESIAN_POINT('Ctrl Pts',(-4.60340213844989,8.16644046362437,10.4828140784136));
#82322=CARTESIAN_POINT('Ctrl Pts',(-4.93446891518701,7.96638177345371,10.4892668222479));
#82323=CARTESIAN_POINT('Ctrl Pts',(-5.02185289938023,7.91158741487993,10.4909966376514));
#82324=CARTESIAN_POINT('Ctrl Pts',(-5.17469994002073,7.8121915178682,10.4940737066543));
#82325=CARTESIAN_POINT('Ctrl Pts',(-5.24053549278105,7.76818147935085,10.4954163796566));
#82326=CARTESIAN_POINT('Ctrl Pts',(-5.38170407843096,7.67120105499485,10.4983342362967));
#82327=CARTESIAN_POINT('Ctrl Pts',(-5.45683010777319,7.61794391789181,10.4999115334583));
#82328=CARTESIAN_POINT('Ctrl Pts',(-5.69863114852838,7.44111779788576,10.5050690923258));
#82329=CARTESIAN_POINT('Ctrl Pts',(-5.86198911404908,7.31311931897104,10.5086822848689));
#82330=CARTESIAN_POINT('Ctrl Pts',(-6.2022406729732,7.02778536731364,10.5164639555822));
#82331=CARTESIAN_POINT('Ctrl Pts',(-6.37769598684529,6.8689555463784,10.5206369271679));
#82332=CARTESIAN_POINT('Ctrl Pts',(-6.5639400543861,6.68706511831051,10.5251961126254));
#82333=CARTESIAN_POINT('Ctrl Pts',(-6.58086525938917,6.67040938567406,10.5256116405552));
#82334=CARTESIAN_POINT('Ctrl Pts',(-6.68306185774739,6.56907233736003,10.5281275915564));
#82335=CARTESIAN_POINT('Ctrl Pts',(-6.76676120586251,6.4828211511382,10.530217744517));
#82336=CARTESIAN_POINT('Ctrl Pts',(-6.88457529125023,6.35664685625078,10.5331894753512));
#82337=CARTESIAN_POINT('Ctrl Pts',(-6.92004961411017,6.31800993595218,10.5340882664836));
#82338=CARTESIAN_POINT('Ctrl Pts',(-6.98294720420412,6.24833963827138,10.5356874646636));
#82339=CARTESIAN_POINT('Ctrl Pts',(-7.01049257980542,6.21741857037591,10.5363896326605));
#82340=CARTESIAN_POINT('Ctrl Pts',(-7.0670898907368,6.15303091527123,10.5378368926243));
#82341=CARTESIAN_POINT('Ctrl Pts',(-7.09611120003982,6.11953877462381,10.5385815942532));
#82342=CARTESIAN_POINT('Ctrl Pts',(-7.16845388233287,6.0348448351629,10.5404462052842));
#82343=CARTESIAN_POINT('Ctrl Pts',(-7.2114651944997,5.98338140362511,10.5415624072961));
#82344=CARTESIAN_POINT('Ctrl Pts',(-7.34286258718182,5.82268806260461,10.545002969708));
#82345=CARTESIAN_POINT('Ctrl Pts',(-7.42934716756123,5.71192857428453,10.547311731627));
#82346=CARTESIAN_POINT('Ctrl Pts',(-7.72600151146538,5.31386648615137,10.5554545385955));
#82347=CARTESIAN_POINT('Ctrl Pts',(-7.92225948381115,5.01658057194837,10.5612707111013));
#82348=CARTESIAN_POINT('Ctrl Pts',(-8.14911128210152,4.62630381098445,10.5688161945727));
#82349=CARTESIAN_POINT('Ctrl Pts',(-8.19582882814969,4.54302667869393,10.5704204362597));
#82350=CARTESIAN_POINT('Ctrl Pts',(-8.27590875014456,4.39502209205269,10.5732642101574));
#82351=CARTESIAN_POINT('Ctrl Pts',(-8.30980468164635,4.33059244871261,10.5744997392411));
#82352=CARTESIAN_POINT('Ctrl Pts',(-8.37697956259821,4.19921268808174,10.5770149800967));
#82353=CARTESIAN_POINT('Ctrl Pts',(-8.41021496778702,4.13224611552453,10.5782948973097));
#82354=CARTESIAN_POINT('Ctrl Pts',(-8.51804068768397,3.90829552380059,10.582568379875));
#82355=CARTESIAN_POINT('Ctrl Pts',(-8.58906441221237,3.74963508513248,10.5855855671387));
#82356=CARTESIAN_POINT('Ctrl Pts',(-8.76948400339504,3.31452612854787,10.5938164149497));
#82357=CARTESIAN_POINT('Ctrl Pts',(-8.8702047099001,3.03469949200296,10.5990675614163));
#82358=CARTESIAN_POINT('Ctrl Pts',(-8.99525444303348,2.62746346553764,10.6065204232535));
#82359=CARTESIAN_POINT('Ctrl Pts',(-9.03051240725097,2.5035999221864,10.6087618874665));
#82360=CARTESIAN_POINT('Ctrl Pts',(-9.07660802574035,2.32799441099751,10.611887772485));
#82361=CARTESIAN_POINT('Ctrl Pts',(-9.08957798530984,2.27682746302171,10.6127923944102));
#82362=CARTESIAN_POINT('Ctrl Pts',(-9.11199007597492,2.18516603287298,10.6144002930796));
#82363=CARTESIAN_POINT('Ctrl Pts',(-9.12159627948588,2.14471327901367,10.6151053631754));
#82364=CARTESIAN_POINT('Ctrl Pts',(-9.14085835014687,2.06112766235579,10.6165535738545));
#82365=CARTESIAN_POINT('Ctrl Pts',(-9.15047890386238,2.01798772476627,10.6172963705571));
#82366=CARTESIAN_POINT('Ctrl Pts',(-9.1738576626009,1.90954806495943,10.6191535449164));
#82367=CARTESIAN_POINT('Ctrl Pts',(-9.18722420856145,1.84416636789655,10.6202642578069));
#82368=CARTESIAN_POINT('Ctrl Pts',(-9.24935707109379,1.52278981144875,10.6256902528088));
#82369=CARTESIAN_POINT('Ctrl Pts',(-9.28812803990355,1.26497952136606,10.6299420395103));
#82370=CARTESIAN_POINT('Ctrl Pts',(-9.33998953135348,0.784661013487193,
10.6378700542443));
#82371=CARTESIAN_POINT('Ctrl Pts',(-9.35598837409497,0.562653100174978,
10.6415365143556));
#82372=CARTESIAN_POINT('Ctrl Pts',(-9.36631987521606,0.278349433131978,
10.646284592698));
#82373=CARTESIAN_POINT('Ctrl Pts',(-9.36795609253744,0.216390954739834,
10.6473223976902));
#82374=CARTESIAN_POINT('Ctrl Pts',(-9.36982567910073,0.102959950969734,
10.6492288829697));
#82375=CARTESIAN_POINT('Ctrl Pts',(-9.37024986173454,0.0514929715521591,
10.6500963627277));
#82376=CARTESIAN_POINT('Ctrl Pts',(-9.37024999996621,2.5166514242315E-5,
10.6509665184497));
#82377=CARTESIAN_POINT('Ctrl Pts',(-9.36948152355139,3.26635738060604E-5,
10.651410108095));
#82378=CARTESIAN_POINT('Ctrl Pts',(-9.36938165429842,-0.809065474210415,
10.6651497815776));
#82379=CARTESIAN_POINT('Ctrl Pts',(-9.067402610047,-3.16378076784896,10.7051350594858));
#82380=CARTESIAN_POINT('Ctrl Pts',(-7.11741830632754,-6.67998478431112,
10.7713659418197));
#82381=CARTESIAN_POINT('Ctrl Pts',(-3.09251227489688,-9.25830480679301,
10.8501027550967));
#82382=CARTESIAN_POINT('Ctrl Pts',(1.67396187580663,-9.61653220782942,10.9288395683737));
#82383=CARTESIAN_POINT('Ctrl Pts',(6.03902880492754,-7.66876594760393,11.0075763816506));
#82384=CARTESIAN_POINT('Ctrl Pts',(8.95596850446328,-3.88207009376908,11.0863131949276));
#82385=CARTESIAN_POINT('Ctrl Pts',(9.72531423192883,0.835525676515664,11.1650500082046));
#82386=CARTESIAN_POINT('Ctrl Pts',(8.16258094297421,5.35276680000807,11.2437868214815));
#82387=CARTESIAN_POINT('Ctrl Pts',(5.76843016600557,7.55212420695635,11.2973390013619));
#82388=CARTESIAN_POINT('Ctrl Pts',(4.3467929946426,8.30212031658,11.3246455768166));
#82389=CARTESIAN_POINT('Ctrl Pts',(4.29126566285802,8.33069681713329,11.3257065478457));
#82390=CARTESIAN_POINT('Origin',(0.,0.,2.15141010809499));
#82391=CARTESIAN_POINT('',(4.290926628303,8.33003803911004,12.5233065119449));
#82392=CARTESIAN_POINT('',(4.29092662693973,8.33003803981228,12.3256242449617));
#82393=CARTESIAN_POINT('',(4.29092662815669,8.33003803918541,2.15141010809499));
#82394=CARTESIAN_POINT('Ctrl Pts',(4.290926628303,8.33003803911004,12.5233065119449));
#82395=CARTESIAN_POINT('Ctrl Pts',(4.31768745450385,8.31625313906499,12.522789592722));
#82396=CARTESIAN_POINT('Ctrl Pts',(4.34438201512415,8.30233919913577,12.522271794311));
#82397=CARTESIAN_POINT('Ctrl Pts',(4.72117556798361,8.10362911267626,12.5149325355195));
#82398=CARTESIAN_POINT('Ctrl Pts',(5.05928586639326,7.89695680217288,12.5079521348845));
#82399=CARTESIAN_POINT('Ctrl Pts',(5.52861123889295,7.56753317679459,12.4978867421488));
#82400=CARTESIAN_POINT('Ctrl Pts',(5.67098855288102,7.46143349127118,12.4947820990599));
#82401=CARTESIAN_POINT('Ctrl Pts',(5.85405036834622,7.31674750020578,12.4907595613347));
#82402=CARTESIAN_POINT('Ctrl Pts',(5.89752482581023,7.28175120731637,12.4898019715551));
#82403=CARTESIAN_POINT('Ctrl Pts',(5.97336591183359,7.2195755217487,12.4881292753579));
#82404=CARTESIAN_POINT('Ctrl Pts',(6.00586595612234,7.19256179340198,12.4874119204674));
#82405=CARTESIAN_POINT('Ctrl Pts',(6.0858671959053,7.12514520003728,12.4856441854311));
#82406=CARTESIAN_POINT('Ctrl Pts',(6.13314984898458,7.08448633307427,12.4845974780775));
#82407=CARTESIAN_POINT('Ctrl Pts',(6.37412201409765,6.87305118113548,12.4792434036888));
#82408=CARTESIAN_POINT('Ctrl Pts',(6.56109867829342,6.69479268331256,12.4750199897462));
#82409=CARTESIAN_POINT('Ctrl Pts',(6.93719980386168,6.30531893845217,12.4661453635287));
#82410=CARTESIAN_POINT('Ctrl Pts',(7.12458827741994,6.09278502444773,12.4614955802605));
#82411=CARTESIAN_POINT('Ctrl Pts',(7.36482366196115,5.7940475851451,12.4550934906634));
#82412=CARTESIAN_POINT('Ctrl Pts',(7.4263294058878,5.71500187943143,12.4534119729375));
#82413=CARTESIAN_POINT('Ctrl Pts',(7.53356231017847,5.57253387423459,12.4503998626127));
#82414=CARTESIAN_POINT('Ctrl Pts',(7.57978514818136,5.50949652287706,12.4490734015712));
#82415=CARTESIAN_POINT('Ctrl Pts',(7.68051825700837,5.36845222556593,12.4461183062698));
#82416=CARTESIAN_POINT('Ctrl Pts',(7.73463983131766,5.29017831611879,12.4444868184951));
#82417=CARTESIAN_POINT('Ctrl Pts',(7.99457690859153,4.90172330316235,12.4364310473885));
#82418=CARTESIAN_POINT('Ctrl Pts',(8.18297423164529,4.58029270845286,12.429876357283));
#82419=CARTESIAN_POINT('Ctrl Pts',(8.44050656628248,4.07403415704362,12.4198983845134));
#82420=CARTESIAN_POINT('Ctrl Pts',(8.52377396044781,3.89681706447842,12.4164695681118));
#82421=CARTESIAN_POINT('Ctrl Pts',(8.62392438883952,3.66506872529488,12.4121157715288));
#82422=CARTESIAN_POINT('Ctrl Pts',(8.64594635112469,3.61281224799119,12.4111424747668));
#82423=CARTESIAN_POINT('Ctrl Pts',(8.68352633023267,3.52132591469574,12.4094551121683));
#82424=CARTESIAN_POINT('Ctrl Pts',(8.69929610620092,3.48218508807503,12.4087386106085));
#82425=CARTESIAN_POINT('Ctrl Pts',(8.7372908901871,3.3860123137855,12.4069909060387));
#82426=CARTESIAN_POINT('Ctrl Pts',(8.7592224676561,3.32886666533055,12.4059631390923));
#82427=CARTESIAN_POINT('Ctrl Pts',(8.84033349413811,3.1111681580762,12.4020816273175));
#82428=CARTESIAN_POINT('Ctrl Pts',(8.8956713634313,2.94921937233149,12.3992629356841));
#82429=CARTESIAN_POINT('Ctrl Pts',(9.02186337899823,2.54396280847758,12.392294634973));
#82430=CARTESIAN_POINT('Ctrl Pts',(9.08734236000264,2.29912470790987,12.3881573625467));
#82431=CARTESIAN_POINT('Ctrl Pts',(9.16822482178275,1.93873619910536,12.3820580012193));
#82432=CARTESIAN_POINT('Ctrl Pts',(9.19152561894286,1.82507565604921,12.380133548302));
#82433=CARTESIAN_POINT('Ctrl Pts',(9.23122779132561,1.61130474348554,12.3765037452252));
#82434=CARTESIAN_POINT('Ctrl Pts',(9.24812579897358,1.51130362661827,12.3748015710626));
#82435=CARTESIAN_POINT('Ctrl Pts',(9.27528704512642,1.33299261894002,12.3717555245437));
#82436=CARTESIAN_POINT('Ctrl Pts',(9.28618979629196,1.25479007218304,12.3704159184955));
#82437=CARTESIAN_POINT('Ctrl Pts',(9.30797014856434,1.08268686936887,12.3674586564388));
#82438=CARTESIAN_POINT('Ctrl Pts',(9.3184178527194,0.988740516517039,12.3658383951677));
#82439=CARTESIAN_POINT('Ctrl Pts',(9.36438511037658,0.509496321658585,12.3575423377637));
#82440=CARTESIAN_POINT('Ctrl Pts',(9.37743592327813,0.122423116124578,12.3507233469904));
#82441=CARTESIAN_POINT('Ctrl Pts',(9.36132260650613,-0.44852429036887,12.3406939307722));
#82442=CARTESIAN_POINT('Ctrl Pts',(9.35069315540362,-0.63251309503906,12.337469699865));
#82443=CARTESIAN_POINT('Ctrl Pts',(9.32975361413182,-0.872031116921657,
12.3333242380941));
#82444=CARTESIAN_POINT('Ctrl Pts',(9.32435803271197,-0.927948310420261,
12.3323602261645));
#82445=CARTESIAN_POINT('Ctrl Pts',(9.31402587797725,-1.02581213604907,12.3306815858558));
#82446=CARTESIAN_POINT('Ctrl Pts',(9.3093079511679,-1.06777997220159,12.3299646322375));
#82447=CARTESIAN_POINT('Ctrl Pts',(9.29697857528566,-1.17115455288273,12.3282053529332));
#82448=CARTESIAN_POINT('Ctrl Pts',(9.28904231010952,-1.23252042674737,12.3271666006287));
#82449=CARTESIAN_POINT('Ctrl Pts',(9.24422172927056,-1.55402011319282,12.3217443681254));
#82450=CARTESIAN_POINT('Ctrl Pts',(9.19701619811235,-1.81259701714246,12.3174484145618));
#82451=CARTESIAN_POINT('Ctrl Pts',(9.07721437690192,-2.34181399057279,12.3085541546786));
#82452=CARTESIAN_POINT('Ctrl Pts',(9.00322327822113,-2.6118735916883,12.3039578885883));
#82453=CARTESIAN_POINT('Ctrl Pts',(8.88651362181195,-2.97346227375342,12.2976123397843));
#82454=CARTESIAN_POINT('Ctrl Pts',(8.85424671387549,-3.06821076687526,12.2959318633118));
#82455=CARTESIAN_POINT('Ctrl Pts',(8.79408861608191,-3.23600059891934,12.2929208330468));
#82456=CARTESIAN_POINT('Ctrl Pts',(8.7667894685895,-3.30924415002731,12.2915943982546));
#82457=CARTESIAN_POINT('Ctrl Pts',(8.70421178981572,-3.47092884835966,12.2886384179297));
#82458=CARTESIAN_POINT('Ctrl Pts',(8.66849515900038,-3.55919114023889,12.2870060085619));
#82459=CARTESIAN_POINT('Ctrl Pts',(8.48708053475402,-3.98856187417292,12.2789721476223));
#82460=CARTESIAN_POINT('Ctrl Pts',(8.32256218853322,-4.32135600933472,12.272441410467));
#82461=CARTESIAN_POINT('Ctrl Pts',(8.07187973856076,-4.76073033741008,12.2635547296593));
#82462=CARTESIAN_POINT('Ctrl Pts',(8.00248088373386,-4.87648394459782,12.2611888336418));
#82463=CARTESIAN_POINT('Ctrl Pts',(7.88251095357354,-5.06712545621422,12.2572701126206));
#82464=CARTESIAN_POINT('Ctrl Pts',(7.83331329552449,-5.14285350772862,12.2557075220137));
#82465=CARTESIAN_POINT('Ctrl Pts',(7.75723779701233,-5.25632875071231,12.253363359492));
#82466=CARTESIAN_POINT('Ctrl Pts',(7.7311620076357,-5.29460708634321,12.2525721461766));
#82467=CARTESIAN_POINT('Ctrl Pts',(7.6786440189412,-5.3704863776482,12.2510040493329));
#82468=CARTESIAN_POINT('Ctrl Pts',(7.65220678702168,-5.40808923754237,12.2502271370004));
#82469=CARTESIAN_POINT('Ctrl Pts',(7.57421709398963,-5.51730057842604,12.2479689852066));
#82470=CARTESIAN_POINT('Ctrl Pts',(7.52192851287517,-5.58837738256038,12.246497102835));
#82471=CARTESIAN_POINT('Ctrl Pts',(7.26113367411501,-5.93258753177329,12.2393330610985));
#82472=CARTESIAN_POINT('Ctrl Pts',(7.03871492603658,-6.19484872235001,12.2337518715515));
#82473=CARTESIAN_POINT('Ctrl Pts',(6.74167830782909,-6.50839094719336,12.2266361713548));
#82474=CARTESIAN_POINT('Ctrl Pts',(6.68005915448358,-6.5716199517705,12.225177412303));
#82475=CARTESIAN_POINT('Ctrl Pts',(6.52636420886475,-6.72493464546262,12.2215750783265));
#82476=CARTESIAN_POINT('Ctrl Pts',(6.43330688563364,-6.81401043168187,12.2194247562383));
#82477=CARTESIAN_POINT('Ctrl Pts',(6.27791974906918,-6.95672781128971,12.2158752408831));
#82478=CARTESIAN_POINT('Ctrl Pts',(6.21666784493071,-7.01151760209755,12.2144861342732));
#82479=CARTESIAN_POINT('Ctrl Pts',(6.09893920477838,-7.11407020396582,12.2118337656106));
#82480=CARTESIAN_POINT('Ctrl Pts',(6.04260210313655,-7.16198394902114,12.2105719194326));
#82481=CARTESIAN_POINT('Ctrl Pts',(5.88686302153342,-7.29129159602268,12.2071031705798));
#82482=CARTESIAN_POINT('Ctrl Pts',(5.78634521117979,-7.37131591609927,12.2048855036173));
#82483=CARTESIAN_POINT('Ctrl Pts',(5.42307591316495,-7.64851174347065,12.1969491060007));
#82484=CARTESIAN_POINT('Ctrl Pts',(5.15164083068724,-7.833905772279,12.1911523702776));
#82485=CARTESIAN_POINT('Ctrl Pts',(4.72877138774327,-8.0912322490523,12.1824680911832));
#82486=CARTESIAN_POINT('Ctrl Pts',(4.58422578394628,-8.17399488450496,12.1795586532532));
#82487=CARTESIAN_POINT('Ctrl Pts',(4.38900943065454,-8.27896242601902,12.1757386842921));
#82488=CARTESIAN_POINT('Ctrl Pts',(4.34023813127251,-8.30463458656947,12.1747932596799));
#82489=CARTESIAN_POINT('Ctrl Pts',(4.25361451141622,-8.34925986753677,12.1731316073053));
#82490=CARTESIAN_POINT('Ctrl Pts',(4.21585515532868,-8.36838945432873,12.1724132773586));
#82491=CARTESIAN_POINT('Ctrl Pts',(4.12128384976489,-8.4154984859769,12.1706284298743));
#82492=CARTESIAN_POINT('Ctrl Pts',(4.06431553200544,-8.44315904273697,12.1695657843411));
#82493=CARTESIAN_POINT('Ctrl Pts',(3.84812099432839,-8.54543558814328,12.1655727269206));
#82494=CARTESIAN_POINT('Ctrl Pts',(3.68708524587108,-8.61614225157389,12.162678453186));
#82495=CARTESIAN_POINT('Ctrl Pts',(3.41142548659548,-8.72803316537669,12.1577961270468));
#82496=CARTESIAN_POINT('Ctrl Pts',(3.29781525396879,-8.77159058246325,12.1558042439823));
#82497=CARTESIAN_POINT('Ctrl Pts',(3.02021248754538,-8.87186578024343,12.1509626313201));
#82498=CARTESIAN_POINT('Ctrl Pts',(2.85543050044,-8.92626475029556,12.1481095210349));
#82499=CARTESIAN_POINT('Ctrl Pts',(2.56321265425257,-9.01381344288971,12.1430499940944));
#82500=CARTESIAN_POINT('Ctrl Pts',(2.43641070713661,-9.04891123995747,12.1408547127254));
#82501=CARTESIAN_POINT('Ctrl Pts',(2.22887617803558,-9.10167654244627,12.1372531168472));
#82502=CARTESIAN_POINT('Ctrl Pts',(2.14857482402044,-9.12096656544736,12.1358575367338));
#82503=CARTESIAN_POINT('Ctrl Pts',(1.99622560421177,-9.1554403571349,12.1332046202023));
#82504=CARTESIAN_POINT('Ctrl Pts',(1.92423321744663,-9.17084136235773,12.1319488185789));
#82505=CARTESIAN_POINT('Ctrl Pts',(1.72862142527257,-9.21028291423305,12.1285302440255));
#82506=CARTESIAN_POINT('Ctrl Pts',(1.60468698926372,-9.23268232591389,12.1263572770347));
#82507=CARTESIAN_POINT('Ctrl Pts',(1.1269363856613,-9.30911864044745,12.1179578338046));
#82508=CARTESIAN_POINT('Ctrl Pts',(0.770584967044567,-9.3453663649633,12.1116328240685));
#82509=CARTESIAN_POINT('Ctrl Pts',(0.26714107833705,-9.36757962838908,12.102804531421));
#82510=CARTESIAN_POINT('Ctrl Pts',(0.12111309110198,-9.37060533107966,12.1002583678878));
#82511=CARTESIAN_POINT('Ctrl Pts',(-0.0784015928789827,-9.37007459436128,
12.0968222014112));
#82512=CARTESIAN_POINT('Ctrl Pts',(-0.131874998409679,-9.36947456989195,
12.0959054683887));
#82513=CARTESIAN_POINT('Ctrl Pts',(-0.227896953071996,-9.36757491615893,
12.0942685755694));
#82514=CARTESIAN_POINT('Ctrl Pts',(-0.270447174767061,-9.36644303653121,
12.0935466621319));
#82515=CARTESIAN_POINT('Ctrl Pts',(-0.367596158602747,-9.36319622116999,
12.0919054979266));
#82516=CARTESIAN_POINT('Ctrl Pts',(-0.422187097348309,-9.36089357295241,
12.0909882535312));
#82517=CARTESIAN_POINT('Ctrl Pts',(-0.76127936111548,-9.34361830948762,
12.085313904801));
#82518=CARTESIAN_POINT('Ctrl Pts',(-1.04499589300671,-9.31615447717814,
12.0806628034758));
#82519=CARTESIAN_POINT('Ctrl Pts',(-1.34703121687503,-9.27294454852215,
12.0756601624593));
#82520=CARTESIAN_POINT('Ctrl Pts',(-1.36703291916714,-9.27001697393318,
12.0753286546273));
#82521=CARTESIAN_POINT('Ctrl Pts',(-1.55780039781454,-9.24146420012366,
12.0721644163741));
#82522=CARTESIAN_POINT('Ctrl Pts',(-1.72783637447812,-9.21118797701864,
12.0693244979953));
#82523=CARTESIAN_POINT('Ctrl Pts',(-2.02540021078924,-9.14967468117147,
12.0642844711312));
#82524=CARTESIAN_POINT('Ctrl Pts',(-2.15329014571789,-9.12042401441933,
12.062095355139));
#82525=CARTESIAN_POINT('Ctrl Pts',(-2.36056867514636,-9.06841282913668,
12.0585009056206));
#82526=CARTESIAN_POINT('Ctrl Pts',(-2.44034488269627,-9.04727099878149,
12.0571062168502));
#82527=CARTESIAN_POINT('Ctrl Pts',(-2.60027428526652,-9.0026181875827,12.0542860011298));
#82528=CARTESIAN_POINT('Ctrl Pts',(-2.68041328563258,-8.97908375996134,
12.0528604305153));
#82529=CARTESIAN_POINT('Ctrl Pts',(-2.89199885550701,-8.91386231903143,
12.0490629272598));
#82530=CARTESIAN_POINT('Ctrl Pts',(-3.02285790261838,-8.87033983337841,
12.0466793375126));
#82531=CARTESIAN_POINT('Ctrl Pts',(-3.2595648777168,-8.78576677266696,12.0423068772961));
#82532=CARTESIAN_POINT('Ctrl Pts',(-3.36571883771927,-8.74565021119915,
12.0403232838729));
#82533=CARTESIAN_POINT('Ctrl Pts',(-3.70120976738887,-8.61185196119105,
12.0339907080032));
#82534=CARTESIAN_POINT('Ctrl Pts',(-3.92757215616201,-8.51100022322967,
12.0296197323768));
#82535=CARTESIAN_POINT('Ctrl Pts',(-4.22908925915903,-8.36207121424635,
12.0237393932926));
#82536=CARTESIAN_POINT('Ctrl Pts',(-4.30794670470571,-8.32172014609047,
12.0221962295652));
#82537=CARTESIAN_POINT('Ctrl Pts',(-4.44654438578843,-8.24830214068262,
12.0194811946656));
#82538=CARTESIAN_POINT('Ctrl Pts',(-4.50651761873477,-8.21568890375367,
12.0183054206292));
#82539=CARTESIAN_POINT('Ctrl Pts',(-4.60353057891062,-8.16155167566449,
12.0164050495242));
#82540=CARTESIAN_POINT('Ctrl Pts',(-4.64078846161003,-8.1404239460805,12.0156756594924));
#82541=CARTESIAN_POINT('Ctrl Pts',(-4.72316218725313,-8.09296316096412,
12.0140646914092));
#82542=CARTESIAN_POINT('Ctrl Pts',(-4.7682052379348,-8.06650683983694,12.0131846504033));
#82543=CARTESIAN_POINT('Ctrl Pts',(-4.91212813504827,-7.98034608720673,
12.010371898226));
#82544=CARTESIAN_POINT('Ctrl Pts',(-5.01012627566328,-7.91918943520432,
12.0084553236772));
#82545=CARTESIAN_POINT('Ctrl Pts',(-5.36535934533826,-7.68826917166705,
12.0014624309415));
#82546=CARTESIAN_POINT('Ctrl Pts',(-5.61530603107275,-7.50765626233686,
11.996446696073));
#82547=CARTESIAN_POINT('Ctrl Pts',(-5.92189770962247,-7.26222142632168,
11.9899717510559));
#82548=CARTESIAN_POINT('Ctrl Pts',(-5.98717935567564,-7.20849608891725,
11.9885737668783));
#82549=CARTESIAN_POINT('Ctrl Pts',(-6.14741223177839,-7.07294960324019,
11.9850889353469));
#82550=CARTESIAN_POINT('Ctrl Pts',(-6.24146564526041,-6.99009296935818,
11.9829953919736));
#82551=CARTESIAN_POINT('Ctrl Pts',(-6.39401662379642,-6.85016838043453,
11.9795115075811));
#82552=CARTESIAN_POINT('Ctrl Pts',(-6.45348030475094,-6.7941774590525,11.9781304544785));
#82553=CARTESIAN_POINT('Ctrl Pts',(-6.56572897680617,-6.68568093125183,
11.975477552825));
#82554=CARTESIAN_POINT('Ctrl Pts',(-6.61863514620357,-6.63330952727339,
11.9742069615877));
#82555=CARTESIAN_POINT('Ctrl Pts',(-6.76369071321681,-6.48625682465321,
11.9706660948966));
#82556=CARTESIAN_POINT('Ctrl Pts',(-6.85447002140418,-6.39024884019002,
11.9683842175856));
#82557=CARTESIAN_POINT('Ctrl Pts',(-7.16305048776074,-6.04975107257849,
11.9603981760712));
#82558=CARTESIAN_POINT('Ctrl Pts',(-7.37004563413656,-5.79579212824392,
11.9546187912052));
#82559=CARTESIAN_POINT('Ctrl Pts',(-7.65873605046277,-5.40106202987235,
11.9460419306215));
#82560=CARTESIAN_POINT('Ctrl Pts',(-7.75075888256456,-5.26815393992269,
11.9432194906204));
#82561=CARTESIAN_POINT('Ctrl Pts',(-7.86929729639372,-5.08711551261701,
11.939490601839));
#82562=CARTESIAN_POINT('Ctrl Pts',(-7.89889439409746,-5.04103675320063,
11.9385513057282));
#82563=CARTESIAN_POINT('Ctrl Pts',(-7.95067030425345,-4.9588528842676,11.9368951020214));
#82564=CARTESIAN_POINT('Ctrl Pts',(-7.97301122279005,-4.92285204510769,
11.9361761664174));
#82565=CARTESIAN_POINT('Ctrl Pts',(-8.02840211687665,-4.83222727265073,
11.9343821126553));
#82566=CARTESIAN_POINT('Ctrl Pts',(-8.06113938964473,-4.77741485878555,
11.9333109727464));
#82567=CARTESIAN_POINT('Ctrl Pts',(-8.20259025926706,-4.53498784909508,
11.9286256711248));
#82568=CARTESIAN_POINT('Ctrl Pts',(-8.30533315051947,-4.34396634320174,
11.9250685175744));
#82569=CARTESIAN_POINT('Ctrl Pts',(-8.49875368586371,-3.95235907577431,
11.9179085175732));
#82570=CARTESIAN_POINT('Ctrl Pts',(-8.58917751727127,-3.75179769084914,
11.9143077709331));
#82571=CARTESIAN_POINT('Ctrl Pts',(-8.69955341164976,-3.48202162076621,
11.9094874259298));
#82572=CARTESIAN_POINT('Ctrl Pts',(-8.72588707195513,-3.41549394942228,
11.9083007041134));
#82573=CARTESIAN_POINT('Ctrl Pts',(-8.7916714721266,-3.24357223855757,11.9052361840654));
#82574=CARTESIAN_POINT('Ctrl Pts',(-8.82999014524001,-3.13775749349727,
11.9033520720758));
#82575=CARTESIAN_POINT('Ctrl Pts',(-8.89225845062993,-2.9556246716787,11.9001073741583));
#82576=CARTESIAN_POINT('Ctrl Pts',(-8.91715389490071,-2.87964302172243,
11.8987533002724));
#82577=CARTESIAN_POINT('Ctrl Pts',(-8.96751835157484,-2.71900950293269,
11.8958884625798));
#82578=CARTESIAN_POINT('Ctrl Pts',(-8.99276805780504,-2.63429699815862,
11.894376378849));
#82579=CARTESIAN_POINT('Ctrl Pts',(-9.0639176832807,-2.38263649627961,11.8898800803435));
#82580=CARTESIAN_POINT('Ctrl Pts',(-9.10639327740534,-2.21475994489731,
11.886874639974));
#82581=CARTESIAN_POINT('Ctrl Pts',(-9.1739359796859,-1.91286219049046,11.8814692094131));
#82582=CARTESIAN_POINT('Ctrl Pts',(-9.20077589344695,-1.77928806024528,
11.879077549587));
#82583=CARTESIAN_POINT('Ctrl Pts',(-9.25801055837496,-1.45836671059114,
11.8733473993307));
#82584=CARTESIAN_POINT('Ctrl Pts',(-9.28564481324938,-1.270587842022,11.8700069862619));
#82585=CARTESIAN_POINT('Ctrl Pts',(-9.31661131678583,-1.00423294841858,
11.8653271500902));
#82586=CARTESIAN_POINT('Ctrl Pts',(-9.32468663864451,-0.92625556382907,
11.8639642606496));
#82587=CARTESIAN_POINT('Ctrl Pts',(-9.33745343762587,-0.785794629060744,
11.8615268929345));
#82588=CARTESIAN_POINT('Ctrl Pts',(-9.34249847499613,-0.723347889784348,
11.8604495279132));
#82589=CARTESIAN_POINT('Ctrl Pts',(-9.34962152018528,-0.622601895133839,
11.8587238749866));
#82590=CARTESIAN_POINT('Ctrl Pts',(-9.35209128426676,-0.584332367268015,
11.8580713271808));
#82591=CARTESIAN_POINT('Ctrl Pts',(-9.35740965877822,-0.49322360764179,
11.8565251923766));
#82592=CARTESIAN_POINT('Ctrl Pts',(-9.360045745514,-0.440373373567076,11.8556339907632));
#82593=CARTESIAN_POINT('Ctrl Pts',(-9.36757495534957,-0.258464796838727,
11.8525820450118));
#82594=CARTESIAN_POINT('Ctrl Pts',(-9.3702475293314,-0.129329034047358,
11.8504422176639));
#82595=CARTESIAN_POINT('Ctrl Pts',(-9.37025521179012,0.272536502316905,
11.8438187299654));
#82596=CARTESIAN_POINT('Ctrl Pts',(-9.3583545938649,0.545122483164087,11.8393735828791));
#82597=CARTESIAN_POINT('Ctrl Pts',(-9.31843072554074,1.00138145124772,11.8318325973368));
#82598=CARTESIAN_POINT('Ctrl Pts',(-9.29680819974264,1.18544211185105,11.8287637389125));
#82599=CARTESIAN_POINT('Ctrl Pts',(-9.25630800454349,1.45972824430486,11.8241211423927));
#82600=CARTESIAN_POINT('Ctrl Pts',(-9.24153407112169,1.55051358705666,11.8225732072624));
#82601=CARTESIAN_POINT('Ctrl Pts',(-9.21294407325015,1.71123522865247,11.8198104337153));
#82602=CARTESIAN_POINT('Ctrl Pts',(-9.19966197425767,1.78125911624256,11.818599157384));
#82603=CARTESIAN_POINT('Ctrl Pts',(-9.16580725045099,1.94925178333843,11.8156742323284));
#82604=CARTESIAN_POINT('Ctrl Pts',(-9.14446106787503,2.04705563640768,11.8139557171911));
#82605=CARTESIAN_POINT('Ctrl Pts',(-9.05660865640911,2.42073290306697,11.807329844894));
#82606=CARTESIAN_POINT('Ctrl Pts',(-8.97915094847459,2.69387364756707,11.8023557080151));
#82607=CARTESIAN_POINT('Ctrl Pts',(-8.80793681155371,3.20752703268637,11.792837111582));
#82608=CARTESIAN_POINT('Ctrl Pts',(-8.71640624928135,3.44851316553865,11.7883002807386));
#82609=CARTESIAN_POINT('Ctrl Pts',(-8.59051156057177,3.74280535145512,11.7827691006842));
#82610=CARTESIAN_POINT('Ctrl Pts',(-8.56539002994553,3.79994400378733,11.7816958151419));
#82611=CARTESIAN_POINT('Ctrl Pts',(-8.52230334638117,3.89534555620233,11.7799073347184));
#82612=CARTESIAN_POINT('Ctrl Pts',(-8.50464684481857,3.93374546589195,11.7791885367245));
#82613=CARTESIAN_POINT('Ctrl Pts',(-8.46309178607405,4.02253308057806,11.7775292748518));
#82614=CARTESIAN_POINT('Ctrl Pts',(-8.43900205156082,4.07282940435385,11.7765911148939));
#82615=CARTESIAN_POINT('Ctrl Pts',(-8.33667464099605,4.28166997018778,11.7726974978685));
#82616=CARTESIAN_POINT('Ctrl Pts',(-8.25440663762145,4.43819932377759,11.7697829387557));
#82617=CARTESIAN_POINT('Ctrl Pts',(-7.97325843676583,4.93824223131119,11.7603621423175));
#82618=CARTESIAN_POINT('Ctrl Pts',(-7.7569770859817,5.27146970706157,11.7538941366296));
#82619=CARTESIAN_POINT('Ctrl Pts',(-7.46412620310846,5.66544319775799,11.7456803092022));
#82620=CARTESIAN_POINT('Ctrl Pts',(-7.40689871715314,5.74005905394645,11.744098833228));
#82621=CARTESIAN_POINT('Ctrl Pts',(-7.29954870910749,5.87574787192606,11.7411722087659));
#82622=CARTESIAN_POINT('Ctrl Pts',(-7.24975812758066,5.9370726346314,11.7398298505216));
#82623=CARTESIAN_POINT('Ctrl Pts',(-7.13386549974865,6.07618022443728,11.7367384035546));
#82624=CARTESIAN_POINT('Ctrl Pts',(-7.06725595756548,6.15352713880212,11.734985243239));
#82625=CARTESIAN_POINT('Ctrl Pts',(-6.95838822267886,6.27584439643485,11.7321572507454));
#82626=CARTESIAN_POINT('Ctrl Pts',(-6.91692632224145,6.3215124602114,11.7310885981292));
#82627=CARTESIAN_POINT('Ctrl Pts',(-6.75842377658053,6.49266800867973,11.727035484177));
#82628=CARTESIAN_POINT('Ctrl Pts',(-6.63839483318035,6.6153415358973,11.7240307103267));
#82629=CARTESIAN_POINT('Ctrl Pts',(-6.29255806242352,6.94990225579621,11.7155791120917));
#82630=CARTESIAN_POINT('Ctrl Pts',(-6.05951949966166,7.15399553328796,11.7101119736628));
#82631=CARTESIAN_POINT('Ctrl Pts',(-5.77477243179699,7.37946225318874,11.7038423802237));
#82632=CARTESIAN_POINT('Ctrl Pts',(-5.73245273624548,7.41238459799262,11.7029208649586));
#82633=CARTESIAN_POINT('Ctrl Pts',(-5.65614444124179,7.47070378512315,11.7012792237194));
#82634=CARTESIAN_POINT('Ctrl Pts',(-5.62226155175163,7.49623639216644,11.7005573217241));
#82635=CARTESIAN_POINT('Ctrl Pts',(-5.54458789699379,7.55394485498502,11.6989187645929));
#82636=CARTESIAN_POINT('Ctrl Pts',(-5.50068839392389,7.58597159437817,11.6980041082215));
#82637=CARTESIAN_POINT('Ctrl Pts',(-5.3296024309688,7.70852081376689,11.6944785937235));
#82638=CARTESIAN_POINT('Ctrl Pts',(-5.20043979304515,7.79624149439363,11.6918994206645));
#82639=CARTESIAN_POINT('Ctrl Pts',(-4.79518944701295,8.05691307577214,11.683975655643));
#82640=CARTESIAN_POINT('Ctrl Pts',(-4.5122308978803,8.21872634248886,11.6786697306729));
#82641=CARTESIAN_POINT('Ctrl Pts',(-4.09942670878109,8.42703734176916,11.6710071682898));
#82642=CARTESIAN_POINT('Ctrl Pts',(-3.97609987545458,8.48592289238806,11.6687286762741));
#82643=CARTESIAN_POINT('Ctrl Pts',(-3.77555926556937,8.57634433478516,11.6650305411088));
#82644=CARTESIAN_POINT('Ctrl Pts',(-3.6991353764765,8.60958345939405,11.6636228680681));
#82645=CARTESIAN_POINT('Ctrl Pts',(-3.54601561508339,8.67376482080338,11.660804214718));
#82646=CARTESIAN_POINT('Ctrl Pts',(-3.46933314955876,8.70472000513018,11.6593934686362));
#82647=CARTESIAN_POINT('Ctrl Pts',(-3.26893155683732,8.78254934622352,11.6557080694746));
#82648=CARTESIAN_POINT('Ctrl Pts',(-3.14461184481551,8.82782548204847,11.6534230696947));
#82649=CARTESIAN_POINT('Ctrl Pts',(-2.85360994322664,8.92687836152949,11.6480806377425));
#82650=CARTESIAN_POINT('Ctrl Pts',(-2.68629561574012,8.9786448102217,11.6450132582269));
#82651=CARTESIAN_POINT('Ctrl Pts',(-2.22216486717069,9.10810959351065,11.6365483081471));
#82652=CARTESIAN_POINT('Ctrl Pts',(-1.92283108406904,9.17596850813177,11.6311331181685));
#82653=CARTESIAN_POINT('Ctrl Pts',(-1.56936955167219,9.23803990805093,11.6249420034389));
#82654=CARTESIAN_POINT('Ctrl Pts',(-1.51795523852665,9.24662717112057,11.6240466083681));
#82655=CARTESIAN_POINT('Ctrl Pts',(-1.42472817250501,9.26139951555455,11.6224339312574));
#82656=CARTESIAN_POINT('Ctrl Pts',(-1.3829402198343,9.26773153021587,11.6217151280375));
#82657=CARTESIAN_POINT('Ctrl Pts',(-1.28592130504233,9.28176174121341,11.6200559118559));
#82658=CARTESIAN_POINT('Ctrl Pts',(-1.23066173236495,9.28925004202506,11.6191178021681));
#82659=CARTESIAN_POINT('Ctrl Pts',(-0.999990891364524,9.31841411197458,
11.6152251054627));
#82660=CARTESIAN_POINT('Ctrl Pts',(-0.824050520857134,9.33561805437676,
11.6123113916896));
#82661=CARTESIAN_POINT('Ctrl Pts',(-0.251742936183824,9.37527429773653,
11.6028902622184));
#82662=CARTESIAN_POINT('Ctrl Pts',(0.145585102336383,9.37752353199337,11.5964211353018));
#82663=CARTESIAN_POINT('Ctrl Pts',(0.63572453665119,9.34913259230495,11.5882061735526));
#82664=CARTESIAN_POINT('Ctrl Pts',(0.729505680538814,9.3422827683105,11.5866247573239));
#82665=CARTESIAN_POINT('Ctrl Pts',(0.901852109414604,9.32708353275679,11.583698187452));
#82666=CARTESIAN_POINT('Ctrl Pts',(0.980445530950322,9.3191496919704,11.582355823305));
#82667=CARTESIAN_POINT('Ctrl Pts',(1.16034896044711,9.29868777838511,11.5792642833489));
#82668=CARTESIAN_POINT('Ctrl Pts',(1.26157334566924,9.28549604128712,11.5775110349829));
#82669=CARTESIAN_POINT('Ctrl Pts',(1.42359122582153,9.26168333156963,11.5746828729114));
#82670=CARTESIAN_POINT('Ctrl Pts',(1.4845305379115,9.25211106616551,11.5736141390854));
#82671=CARTESIAN_POINT('Ctrl Pts',(1.71463578571621,9.21363451018178,11.5695605870278));
#82672=CARTESIAN_POINT('Ctrl Pts',(1.88309090595818,9.18068653139277,11.5665554520948));
#82673=CARTESIAN_POINT('Ctrl Pts',(2.35254963772108,9.07540022118774,11.5581048889017));
#82674=CARTESIAN_POINT('Ctrl Pts',(2.65101256716353,8.99274772605419,11.5526391767798));
#82675=CARTESIAN_POINT('Ctrl Pts',(2.99575315419421,8.87862177831205,11.5463706182945));
#82676=CARTESIAN_POINT('Ctrl Pts',(3.04652381915877,8.86132914855666,11.5454487995259));
#82677=CARTESIAN_POINT('Ctrl Pts',(3.13718633835103,8.82957796548903,11.5438068165941));
#82678=CARTESIAN_POINT('Ctrl Pts',(3.17713368817045,8.81528256586302,11.5430848734763));
#82679=CARTESIAN_POINT('Ctrl Pts',(3.26800483273021,8.78206584837673,11.5414465312668));
#82680=CARTESIAN_POINT('Ctrl Pts',(3.31886382690908,8.7629720454028,11.5405321276272));
#82681=CARTESIAN_POINT('Ctrl Pts',(3.51504188231941,8.68736876222667,11.5370100553647));
#82682=CARTESIAN_POINT('Ctrl Pts',(3.65910814093394,8.6276777483283,11.5344339918744));
#82683=CARTESIAN_POINT('Ctrl Pts',(3.96697679396072,8.49101944946439,11.5288947975458));
#82684=CARTESIAN_POINT('Ctrl Pts',(4.13014723284788,8.41285790029682,11.525937234304));
#82685=CARTESIAN_POINT('Ctrl Pts',(4.29092665208774,8.33003802685817,11.5229686882669));
#82686=CARTESIAN_POINT('',(-9.37050454109232,0.000215087252814772,11.651410108095));
#82687=CARTESIAN_POINT('Ctrl Pts',(4.29126566285802,8.33069681713329,11.3257065478457));
#82688=CARTESIAN_POINT('Ctrl Pts',(2.97319433370317,9.00902701698846,11.3508911812423));
#82689=CARTESIAN_POINT('Ctrl Pts',(-0.0532844634904993,9.74542354540215,
11.4023214190646));
#82690=CARTESIAN_POINT('Ctrl Pts',(-4.62634724705184,8.5951585916474,11.4799972613125));
#82691=CARTESIAN_POINT('Ctrl Pts',(-8.15249965184079,5.36810855819908,11.5587340745894));
#82692=CARTESIAN_POINT('Ctrl Pts',(-9.29270465558192,2.09218219148154,11.6158716901836));
#82693=CARTESIAN_POINT('Ctrl Pts',(-9.37077357298385,0.273745585815924,
11.6467637013521));
#82694=CARTESIAN_POINT('Ctrl Pts',(-9.37050454109232,0.000215087252814772,
11.651410108095));
#82695=CARTESIAN_POINT('Ctrl Pts',(-9.37024999747657,0.000217463326891779,
11.6515570258181));
#82696=CARTESIAN_POINT('Ctrl Pts',(-9.37025827752224,-0.356560385193558,
11.6574103826834));
#82697=CARTESIAN_POINT('Ctrl Pts',(-9.34988983196303,-0.713046871971945,
11.6632368410448));
#82698=CARTESIAN_POINT('Ctrl Pts',(-9.30017325739077,-1.14660450984069,
11.6705259364666));
#82699=CARTESIAN_POINT('Ctrl Pts',(-9.29009465983067,-1.22558789929131,
11.6718615117638));
#82700=CARTESIAN_POINT('Ctrl Pts',(-9.26850688948526,-1.3791512725268,11.6744751217685));
#82701=CARTESIAN_POINT('Ctrl Pts',(-9.25710100482538,-1.45373971200085,
11.6757524102328));
#82702=CARTESIAN_POINT('Ctrl Pts',(-9.2307098134581,-1.61339421914325,11.6785042685968));
#82703=CARTESIAN_POINT('Ctrl Pts',(-9.21544665626782,-1.69840732695462,
11.6799805256023));
#82704=CARTESIAN_POINT('Ctrl Pts',(-9.16899758383324,-1.93802497468943,
11.6841730948638));
#82705=CARTESIAN_POINT('Ctrl Pts',(-9.13508075466979,-2.09206999482552,
11.6869061554968));
#82706=CARTESIAN_POINT('Ctrl Pts',(-9.06029448911578,-2.39509736007106,
11.6923503286997));
#82707=CARTESIAN_POINT('Ctrl Pts',(-9.01959673036752,-2.54407198973181,
11.69505984241));
#82708=CARTESIAN_POINT('Ctrl Pts',(-8.91965966099798,-2.87726960487477,
11.7011740319431));
#82709=CARTESIAN_POINT('Ctrl Pts',(-8.85835789972438,-3.06080124531979,
11.7045801598438));
#82710=CARTESIAN_POINT('Ctrl Pts',(-8.76403786258211,-3.31654749783302,
11.7093381471368));
#82711=CARTESIAN_POINT('Ctrl Pts',(-8.73571703466561,-3.39044169524443,
11.7107141432158));
#82712=CARTESIAN_POINT('Ctrl Pts',(-8.69839420879118,-3.48425023785669,
11.7124591174993));
#82713=CARTESIAN_POINT('Ctrl Pts',(-8.69025398025114,-3.50450385807561,
11.7128357511666));
#82714=CARTESIAN_POINT('Ctrl Pts',(-8.67671405437051,-3.53785513815779,
11.7134556598215));
#82715=CARTESIAN_POINT('Ctrl Pts',(-8.67135529482384,-3.55096931993642,
11.7136993428759));
#82716=CARTESIAN_POINT('Ctrl Pts',(-8.66142895547395,-3.5751050119766,11.7141476564716));
#82717=CARTESIAN_POINT('Ctrl Pts',(-8.65687002775453,-3.58613004785622,
11.7143523789189));
#82718=CARTESIAN_POINT('Ctrl Pts',(-8.64256086462344,-3.62054817205658,
11.7149912504345));
#82719=CARTESIAN_POINT('Ctrl Pts',(-8.63273676439685,-3.64391044394445,
11.715424564271));
#82720=CARTESIAN_POINT('Ctrl Pts',(-8.60651997705432,-3.7055543621546,11.7165667439014));
#82721=CARTESIAN_POINT('Ctrl Pts',(-8.58996674643086,-3.74376689228073,
11.7172734238478));
#82722=CARTESIAN_POINT('Ctrl Pts',(-8.54766339280212,-3.83966484214877,
11.7190441258113));
#82723=CARTESIAN_POINT('Ctrl Pts',(-8.52158367695186,-3.89720248897324,
11.7201041999243));
#82724=CARTESIAN_POINT('Ctrl Pts',(-8.35623533372941,-4.25240075359274,
11.726645896193));
#82725=CARTESIAN_POINT('Ctrl Pts',(-8.2019689250405,-4.54282827246313,11.7319921452607));
#82726=CARTESIAN_POINT('Ctrl Pts',(-7.91543234453419,-5.01990496137961,
11.7411308290787));
#82727=CARTESIAN_POINT('Ctrl Pts',(-7.79101374945527,-5.21091348249928,
11.7448920640079));
#82728=CARTESIAN_POINT('Ctrl Pts',(-7.60687702618811,-5.47224224650487,
11.7502406899701));
#82729=CARTESIAN_POINT('Ctrl Pts',(-7.55289781558291,-5.54650771505646,
11.7517844227582));
#82730=CARTESIAN_POINT('Ctrl Pts',(-7.45466177793009,-5.67756855555524,
11.7545539473547));
#82731=CARTESIAN_POINT('Ctrl Pts',(-7.41082517599283,-5.73466974739523,
11.7557763210703));
#82732=CARTESIAN_POINT('Ctrl Pts',(-7.30682033736164,-5.86696124805619,
11.7586461930245));
#82733=CARTESIAN_POINT('Ctrl Pts',(-7.24614235792571,-5.94174036772694,
11.7602977143204));
#82734=CARTESIAN_POINT('Ctrl Pts',(-6.91921007521248,-6.33219159654407,
11.7690779390418));
#82735=CARTESIAN_POINT('Ctrl Pts',(-6.63345731220092,-6.63093951384705,
11.7763718719545));
#82736=CARTESIAN_POINT('Ctrl Pts',(-6.24864500311747,-6.98339999644782,
11.7855212771274));
#82737=CARTESIAN_POINT('Ctrl Pts',(-6.16707842948267,-7.05553567062235,
11.7874243282979));
#82738=CARTESIAN_POINT('Ctrl Pts',(-6.04003874193091,-7.16400028434122,
11.7903234887166));
#82739=CARTESIAN_POINT('Ctrl Pts',(-5.99545352098128,-7.20135439857369,
11.79132906257));
#82740=CARTESIAN_POINT('Ctrl Pts',(-5.94885312234674,-7.23966409899496,
11.7923666577955));
#82741=CARTESIAN_POINT('Ctrl Pts',(-5.94718241385495,-7.24103660216315,
11.792403839693));
#82742=CARTESIAN_POINT('Ctrl Pts',(-5.94393575601392,-7.24370188134245,
11.7924760599835));
#82743=CARTESIAN_POINT('Ctrl Pts',(-5.94235985959501,-7.24499472163091,
11.7925110991815));
#82744=CARTESIAN_POINT('Ctrl Pts',(-5.93929179923145,-7.24751003497578,
11.7925792849198));
#82745=CARTESIAN_POINT('Ctrl Pts',(-5.93779967941335,-7.24873256167256,
11.7926124321375));
#82746=CARTESIAN_POINT('Ctrl Pts',(-5.93488928784949,-7.25111560808192,
11.7926770582424));
#82747=CARTESIAN_POINT('Ctrl Pts',(-5.93347105295981,-7.252276172657,11.7927085377008));
#82748=CARTESIAN_POINT('Ctrl Pts',(-5.93069952696751,-7.25454280007351,
11.7927700299057));
#82749=CARTESIAN_POINT('Ctrl Pts',(-5.92934626668653,-7.25564890047763,
11.792800043134));
#82750=CARTESIAN_POINT('Ctrl Pts',(-5.92669662205911,-7.25781337686115,
11.7928587851456));
#82751=CARTESIAN_POINT('Ctrl Pts',(-5.92540026348583,-7.25887178428949,
11.7928875143352));
#82752=CARTESIAN_POINT('Ctrl Pts',(-5.92285706276996,-7.26094703637782,
11.7929438541598));
#82753=CARTESIAN_POINT('Ctrl Pts',(-5.92161024215835,-7.26196390730866,
11.7929714651365));
#82754=CARTESIAN_POINT('Ctrl Pts',(-5.91915935108872,-7.26396173248286,
11.7930257207095));
#82755=CARTESIAN_POINT('Ctrl Pts',(-5.91795529852006,-7.26494270860241,
11.7930523655923));
#82756=CARTESIAN_POINT('Ctrl Pts',(-5.91558366571431,-7.26687396496663,
11.7931048298424));
#82757=CARTESIAN_POINT('Ctrl Pts',(-5.91441610025334,-7.26782426327441,
11.7931306494476));
#82758=CARTESIAN_POINT('Ctrl Pts',(-5.91211155551752,-7.26969904225769,
11.793181594908));
#82759=CARTESIAN_POINT('Ctrl Pts',(-5.9109745882872,-7.2706235376692,11.7932067209585));
#82760=CARTESIAN_POINT('Ctrl Pts',(-5.90872565431023,-7.27245132379723,
11.7932564040477));
#82761=CARTESIAN_POINT('Ctrl Pts',(-5.90761369720132,-7.27335462627414,
11.7932809612428));
#82762=CARTESIAN_POINT('Ctrl Pts',(-5.90540941011123,-7.27514444808972,
11.793329626319));
#82763=CARTESIAN_POINT('Ctrl Pts',(-5.90431708754685,-7.27603097652172,
11.793353734322));
#82764=CARTESIAN_POINT('Ctrl Pts',(-5.9021468208591,-7.27779155331112,11.7934016176372));
#82765=CARTESIAN_POINT('Ctrl Pts',(-5.90106888212153,-7.27866560826097,
11.7934253930383));
#82766=CARTESIAN_POINT('Ctrl Pts',(-5.89892216894355,-7.28040549689321,
11.7934727267066));
#82767=CARTESIAN_POINT('Ctrl Pts',(-5.89785339795813,-7.28127133477668,
11.7934962850305));
#82768=CARTESIAN_POINT('Ctrl Pts',(-5.89571974466799,-7.28299908222527,
11.7935433011611));
#82769=CARTESIAN_POINT('Ctrl Pts',(-5.89465486390261,-7.28386099365109,
11.7935667589929));
#82770=CARTESIAN_POINT('Ctrl Pts',(-5.89252354773943,-7.28558530132259,
11.7936136941554));
#82771=CARTESIAN_POINT('Ctrl Pts',(-5.89145711194916,-7.28644769703149,
11.7936371714784));
#82772=CARTESIAN_POINT('Ctrl Pts',(-5.88931695290851,-7.28817760459654,
11.793684271709));
#82773=CARTESIAN_POINT('Ctrl Pts',(-5.88824322722204,-7.28904511338984,
11.7937078945741));
#82774=CARTESIAN_POINT('Ctrl Pts',(-5.88608232136698,-7.29079021236492,
11.7937554212038));
#82775=CARTESIAN_POINT('Ctrl Pts',(-5.88499513654329,-7.29166779670379,
11.7937793248869));
#82776=CARTESIAN_POINT('Ctrl Pts',(-5.85056202449961,-7.31944976461304,
11.794536153742));
#82777=CARTESIAN_POINT('Ctrl Pts',(-5.81703210747886,-7.3461253965394,11.7952658228471));
#82778=CARTESIAN_POINT('Ctrl Pts',(-5.74226706309223,-7.40477389789333,
11.7968760680792));
#82779=CARTESIAN_POINT('Ctrl Pts',(-5.70094554022213,-7.43663414903239,
11.7977551206528));
#82780=CARTESIAN_POINT('Ctrl Pts',(-5.56128925478417,-7.54246563961377,
11.800693446891));
#82781=CARTESIAN_POINT('Ctrl Pts',(-5.46176384850315,-7.61484483813702,
11.802733836577));
#82782=CARTESIAN_POINT('Ctrl Pts',(-5.2752615515039,-7.74493952598008,11.8064843216716));
#82783=CARTESIAN_POINT('Ctrl Pts',(-5.18869012234299,-7.80320239063289,
11.8081971854807));
#82784=CARTESIAN_POINT('Ctrl Pts',(-4.9081546311232,-7.98527060121895,11.8136812670319));
#82785=CARTESIAN_POINT('Ctrl Pts',(-4.71059719536616,-8.1033821584547,11.8174453030595));
#82786=CARTESIAN_POINT('Ctrl Pts',(-4.4112387782878,-8.2677062937956,11.8230899708851));
#82787=CARTESIAN_POINT('Ctrl Pts',(-4.31263626913686,-8.31956508827047,
11.824939685282));
#82788=CARTESIAN_POINT('Ctrl Pts',(-4.12498324431703,-8.41402624101412,
11.828449725641));
#82789=CARTESIAN_POINT('Ctrl Pts',(-4.03613839187225,-8.45700367568024,
11.8301073371404));
#82790=CARTESIAN_POINT('Ctrl Pts',(-3.8750992870705,-8.53178825929391,11.8331075391023));
#82791=CARTESIAN_POINT('Ctrl Pts',(-3.80315071724062,-8.56410240331542,
11.8344464038826));
#82792=CARTESIAN_POINT('Ctrl Pts',(-3.64199001933242,-8.6340527835849,11.8374429479094));
#82793=CARTESIAN_POINT('Ctrl Pts',(-3.55258519599724,-8.6712223552983,11.8391036840123));
#82794=CARTESIAN_POINT('Ctrl Pts',(-3.12233623126596,-8.84232479916431,
11.847088160262));
#82795=CARTESIAN_POINT('Ctrl Pts',(-2.77441251175253,-8.95758472270911,
11.8535362898012));
#82796=CARTESIAN_POINT('Ctrl Pts',(-2.29028575988383,-9.08704483258368,
11.8623400492072));
#82797=CARTESIAN_POINT('Ctrl Pts',(-2.15919256488033,-9.11908329911449,
11.8647057340253));
#82798=CARTESIAN_POINT('Ctrl Pts',(-1.98486550951542,-9.15771787966835,
11.8678121401052));
#82799=CARTESIAN_POINT('Ctrl Pts',(-1.94221241042051,-9.16685872117275,
11.8685690679227));
#82800=CARTESIAN_POINT('Ctrl Pts',(-1.83557692591325,-9.18893374027633,
11.8704524922185));
#82801=CARTESIAN_POINT('Ctrl Pts',(-1.77152020411468,-9.20149781989316,
11.8715758751053));
#82802=CARTESIAN_POINT('Ctrl Pts',(-1.66555002747531,-9.22113519650408,
11.8734183512872));
#82803=CARTESIAN_POINT('Ctrl Pts',(-1.62371049846678,-9.22859444566639,
11.8741416277109));
#82804=CARTESIAN_POINT('Ctrl Pts',(-1.5287348974826,-9.24486103343541,11.8757735556247));
#82805=CARTESIAN_POINT('Ctrl Pts',(-1.4755708388355,-9.25349537372788,11.8766803122785));
#82806=CARTESIAN_POINT('Ctrl Pts',(-1.2934246070044,-9.28146797229241,11.8797681129884));
#82807=CARTESIAN_POINT('Ctrl Pts',(-1.16411436464797,-9.29857154877264,
11.8819281225086));
#82808=CARTESIAN_POINT('Ctrl Pts',(-0.742275708960373,-9.34542958307081,
11.8889214358734));
#82809=CARTESIAN_POINT('Ctrl Pts',(-0.448696487790422,-9.36411763976509,
11.8937104597581));
#82810=CARTESIAN_POINT('Ctrl Pts',(-0.0719032005515667,-9.37034024772009,
11.8999256695569));
#82811=CARTESIAN_POINT('Ctrl Pts',(0.0109332770555784,-9.37060973820518,
11.9012958804959));
#82812=CARTESIAN_POINT('Ctrl Pts',(0.217470262225723,-9.36854294601706,
11.9047265089184));
#82813=CARTESIAN_POINT('Ctrl Pts',(0.341141269917283,-9.36485519204564,
11.9067935901955));
#82814=CARTESIAN_POINT('Ctrl Pts',(0.546042859255265,-9.35468090271269,
11.9102469638122));
#82815=CARTESIAN_POINT('Ctrl Pts',(0.627326774636237,-9.34958173808023,
11.9116243333842));
#82816=CARTESIAN_POINT('Ctrl Pts',(0.783015607445258,-9.33777548820628,
11.9142780418331));
#82817=CARTESIAN_POINT('Ctrl Pts',(0.857427151325094,-9.33123695773185,
11.9155532009062));
#82818=CARTESIAN_POINT('Ctrl Pts',(1.06510286449693,-9.31048338520604,11.9191316300244));
#82819=CARTESIAN_POINT('Ctrl Pts',(1.19815171700217,-9.29429810635462,11.9214469468847));
#82820=CARTESIAN_POINT('Ctrl Pts',(1.67231561757276,-9.22626546439931,11.9297744272908));
#82821=CARTESIAN_POINT('Ctrl Pts',(2.01085680972513,-9.15844240941028,11.9358713800179));
#82822=CARTESIAN_POINT('Ctrl Pts',(2.48447884280982,-9.03602450417845,11.9444400285374));
#82823=CARTESIAN_POINT('Ctrl Pts',(2.62322371920065,-8.99672559744819,11.9469533426583));
#82824=CARTESIAN_POINT('Ctrl Pts',(2.81194389204922,-8.93853443819587,11.9503543376118));
#82825=CARTESIAN_POINT('Ctrl Pts',(2.86274628214175,-8.92239374249897,11.9512680596098));
#82826=CARTESIAN_POINT('Ctrl Pts',(2.95389400960604,-8.89257610321638,11.9529024767391));
#82827=CARTESIAN_POINT('Ctrl Pts',(2.99428889907819,-8.87905589350197,11.9536248882178));
#82828=CARTESIAN_POINT('Ctrl Pts',(3.08648844251275,-8.8474958697544,11.9552701430638));
#82829=CARTESIAN_POINT('Ctrl Pts',(3.13822969621515,-8.82927564766102,11.9561909434569));
#82830=CARTESIAN_POINT('Ctrl Pts',(3.49314319483674,-8.70078205373212,11.9624985801331));
#82831=CARTESIAN_POINT('Ctrl Pts',(3.79060579018193,-8.57536980418779,11.9677500916013));
#82832=CARTESIAN_POINT('Ctrl Pts',(4.25137374587279,-8.35243828596401,11.9761518310564));
#82833=CARTESIAN_POINT('Ctrl Pts',(4.41920331139903,-8.26486817217375,11.9792696752741));
#82834=CARTESIAN_POINT('Ctrl Pts',(4.68363508910786,-8.11653429246689,11.9843156648112));
#82835=CARTESIAN_POINT('Ctrl Pts',(4.78197973690698,-8.05898481659339,11.9862227861367));
#82836=CARTESIAN_POINT('Ctrl Pts',(4.94765415409519,-7.95793460858439,11.98949341468));
#82837=CARTESIAN_POINT('Ctrl Pts',(5.01552001053204,-7.91533725447361,11.9908501167608));
#82838=CARTESIAN_POINT('Ctrl Pts',(5.15663836149598,-7.82421782497642,11.993708238018));
#82839=CARTESIAN_POINT('Ctrl Pts',(5.22977160146937,-7.77552523719921,11.9952108541188));
#82840=CARTESIAN_POINT('Ctrl Pts',(5.44146337477904,-7.63024159168775,11.9996240581793));
#82841=CARTESIAN_POINT('Ctrl Pts',(5.57810783188802,-7.53092445428313,12.002554594613));
#82842=CARTESIAN_POINT('Ctrl Pts',(5.94788856088106,-7.24656880777628,12.01070155656));
#82843=CARTESIAN_POINT('Ctrl Pts',(6.17500838431288,-7.05403492187524,12.0159580231464));
#82844=CARTESIAN_POINT('Ctrl Pts',(6.49226981816965,-6.75800325425452,12.0235534315158));
#82845=CARTESIAN_POINT('Ctrl Pts',(6.589917005805,-6.66281992903234,12.0259280685498));
#82846=CARTESIAN_POINT('Ctrl Pts',(6.72225980316967,-6.52806002571574,12.0291796694575));
#82847=CARTESIAN_POINT('Ctrl Pts',(6.75875136620614,-6.49027153107556,12.0300798561044));
#82848=CARTESIAN_POINT('Ctrl Pts',(6.82436717948298,-6.42117015036403,12.0317034536345));
#82849=CARTESIAN_POINT('Ctrl Pts',(6.85359841793103,-6.38996105031942,12.0324284118396));
#82850=CARTESIAN_POINT('Ctrl Pts',(6.92854065598597,-6.3088421883687,12.0342923907706));
#82851=CARTESIAN_POINT('Ctrl Pts',(6.97392643238248,-6.25863527671691,12.0354266419463));
#82852=CARTESIAN_POINT('Ctrl Pts',(7.14205487513995,-6.06854746489289,12.039657781273));
#82853=CARTESIAN_POINT('Ctrl Pts',(7.26116580383477,-5.92551159874945,12.0427160681941));
#82854=CARTESIAN_POINT('Ctrl Pts',(7.52068723082718,-5.59427674264096,12.0496174400519));
#82855=CARTESIAN_POINT('Ctrl Pts',(7.65844368588057,-5.40415663244292,12.0534554557688));
#82856=CARTESIAN_POINT('Ctrl Pts',(7.83013353655825,-5.1474353838737,12.0585593638696));
#82857=CARTESIAN_POINT('Ctrl Pts',(7.87061773326577,-5.08531795545669,12.0597882999757));
#82858=CARTESIAN_POINT('Ctrl Pts',(7.97209948606517,-4.9254929656291,12.062938268785));
#82859=CARTESIAN_POINT('Ctrl Pts',(8.03204040018019,-4.82712938370015,12.0648657164095));
#82860=CARTESIAN_POINT('Ctrl Pts',(8.13065694977619,-4.65837390049898,12.0681593441981));
#82861=CARTESIAN_POINT('Ctrl Pts',(8.17026877206463,-4.58854421237305,12.0695184580675));
#82862=CARTESIAN_POINT('Ctrl Pts',(8.25112824350716,-4.44163359396412,12.0723712670849));
#82863=CARTESIAN_POINT('Ctrl Pts',(8.29220441069198,-4.36446700522779,12.0738660554183));
#82864=CARTESIAN_POINT('Ctrl Pts',(8.40790182903271,-4.13958420977134,12.0782122273806));
#82865=CARTESIAN_POINT('Ctrl Pts',(8.47969712123332,-3.99045198665932,12.081082558403));
#82866=CARTESIAN_POINT('Ctrl Pts',(8.6072584635711,-3.70647438194532,12.086517603255));
#82867=CARTESIAN_POINT('Ctrl Pts',(8.6638981718463,-3.57207488314956,12.0890772590472));
#82868=CARTESIAN_POINT('Ctrl Pts',(8.78743743275953,-3.25868419831798,12.0949984299578));
#82869=CARTESIAN_POINT('Ctrl Pts',(8.85204542551602,-3.07885875328019,12.0983615603606));
#82870=CARTESIAN_POINT('Ctrl Pts',(8.93542891699001,-2.82238919875888,12.1030684412296));
#82871=CARTESIAN_POINT('Ctrl Pts',(8.95880374598082,-2.74729070118157,12.1044358897558));
#82872=CARTESIAN_POINT('Ctrl Pts',(8.99913608122187,-2.61171935539102,12.1068803476539));
#82873=CARTESIAN_POINT('Ctrl Pts',(9.01643633490976,-2.55135337505736,12.1079602680587));
#82874=CARTESIAN_POINT('Ctrl Pts',(9.04332681009985,-2.45383315457247,12.1096887491837));
#82875=CARTESIAN_POINT('Ctrl Pts',(9.05329786412195,-2.41678603573668,12.1103415980538));
#82876=CARTESIAN_POINT('Ctrl Pts',(9.07645680296243,-2.3285848730109,12.1118865447318));
#82877=CARTESIAN_POINT('Ctrl Pts',(9.08944016255843,-2.27737857085425,12.1127762760613));
#82878=CARTESIAN_POINT('Ctrl Pts',(9.13261111436083,-2.10086012345344,12.115822590472));
#82879=CARTESIAN_POINT('Ctrl Pts',(9.16064577368532,-1.97503625220237,12.1179583196231));
#82880=CARTESIAN_POINT('Ctrl Pts',(9.23312794103505,-1.61487177038786,12.1240137606862));
#82881=CARTESIAN_POINT('Ctrl Pts',(9.2712368780749,-1.37935833436649,12.1279059235321));
#82882=CARTESIAN_POINT('Ctrl Pts',(9.32678024421574,-0.927275916618748,
12.1353907912067));
#82883=CARTESIAN_POINT('Ctrl Pts',(9.3457518377083,-0.711050291764133,12.1389763471467));
#82884=CARTESIAN_POINT('Ctrl Pts',(9.36210116757148,-0.401592965387163,
12.1441635712763));
#82885=CARTESIAN_POINT('Ctrl Pts',(9.36562249229279,-0.308756313786629,
12.1457265801955));
#82886=CARTESIAN_POINT('Ctrl Pts',(9.36958498997166,-0.136812392930031,
12.1486366355776));
#82887=CARTESIAN_POINT('Ctrl Pts',(9.37040600137804,-0.0577221845912397,
12.1499811244683));
#82888=CARTESIAN_POINT('Ctrl Pts',(9.36999326106826,0.123264445837158,12.153072276048));
#82889=CARTESIAN_POINT('Ctrl Pts',(9.36809882276587,0.22514931227928,12.1548229535946));
#82890=CARTESIAN_POINT('Ctrl Pts',(9.3521635163753,0.681524574679411,12.1627114301312));
#82891=CARTESIAN_POINT('Ctrl Pts',(9.31965950871019,1.03507615203196,12.1689609089425));
#82892=CARTESIAN_POINT('Ctrl Pts',(9.23878266715062,1.57586931631202,12.1785654032703));
#82893=CARTESIAN_POINT('Ctrl Pts',(9.20454378320442,1.76489188325154,12.1819283182393));
#82894=CARTESIAN_POINT('Ctrl Pts',(9.15273601766901,2.00803539605582,12.1862152699104));
#82895=CARTESIAN_POINT('Ctrl Pts',(9.14045113240248,2.06323432434942,12.1871858046079));
#82896=CARTESIAN_POINT('Ctrl Pts',(9.11812559441515,2.15943329564272,12.1888705597519));
#82897=CARTESIAN_POINT('Ctrl Pts',(9.10830621776878,2.20048275670053,12.1895871830892));
#82898=CARTESIAN_POINT('Ctrl Pts',(9.08352143422814,2.30108534985934,12.1913382648875));
#82899=CARTESIAN_POINT('Ctrl Pts',(9.06824737958857,2.3605602980635,12.1923692471056));
#82900=CARTESIAN_POINT('Ctrl Pts',(8.96970950176652,2.72917483732367,12.1987437884873));
#82901=CARTESIAN_POINT('Ctrl Pts',(8.87123168093822,3.03402934284792,12.2039560889006));
#82902=CARTESIAN_POINT('Ctrl Pts',(8.69912827900111,3.48619190754937,12.2118970419112));
#82903=CARTESIAN_POINT('Ctrl Pts',(8.63691643007624,3.63758728599481,12.2145913868715));
#82904=CARTESIAN_POINT('Ctrl Pts',(8.51947382736378,3.90336509756044,12.2194146876727));
#82905=CARTESIAN_POINT('Ctrl Pts',(8.46582257005918,4.01840036236476,12.2215341691647));
#82906=CARTESIAN_POINT('Ctrl Pts',(8.37373213570585,4.20581777581546,12.2250480153088));
#82907=CARTESIAN_POINT('Ctrl Pts',(8.33665082353039,4.27884868316025,12.2264327298131));
#82908=CARTESIAN_POINT('Ctrl Pts',(8.25946693929844,4.42604771072856,12.2292567500072));
#82909=CARTESIAN_POINT('Ctrl Pts',(8.21931116987626,4.50017958651058,12.2306963387084));
#82910=CARTESIAN_POINT('Ctrl Pts',(8.10824983003253,4.69876403269093,12.234600582531));
#82911=CARTESIAN_POINT('Ctrl Pts',(8.03548238136048,4.82214904975152,12.2370781948386));
#82912=CARTESIAN_POINT('Ctrl Pts',(7.78509626690922,5.22528942198437,12.2453399415565));
#82913=CARTESIAN_POINT('Ctrl Pts',(7.59547031766549,5.49729050660566,12.251195002146));
#82914=CARTESIAN_POINT('Ctrl Pts',(7.30450904084259,5.87076863777904,12.2594863465227));
#82915=CARTESIAN_POINT('Ctrl Pts',(7.21464150038117,5.98086322676164,12.2619627342723));
#82916=CARTESIAN_POINT('Ctrl Pts',(7.08779656307944,6.12923691234635,12.2653240936072));
#82917=CARTESIAN_POINT('Ctrl Pts',(7.05294561096457,6.16930818432155,12.2662343416934));
#82918=CARTESIAN_POINT('Ctrl Pts',(6.98950372935933,6.24101277806357,12.2678659305045));
#82919=CARTESIAN_POINT('Ctrl Pts',(6.96103405399495,6.27275121275399,12.2685889444367));
#82920=CARTESIAN_POINT('Ctrl Pts',(6.89527172062327,6.34506500475445,12.2702390267609));
#82921=CARTESIAN_POINT('Ctrl Pts',(6.85783573197619,6.38550789732074,12.2711640091832));
#82922=CARTESIAN_POINT('Ctrl Pts',(6.63309201289867,6.62404716998508,12.2766402117316));
#82923=CARTESIAN_POINT('Ctrl Pts',(6.43756735176066,6.81422323365515,12.2810950206056));
#82924=CARTESIAN_POINT('Ctrl Pts',(6.05015218479438,7.15946255742574,12.2896018127144));
#82925=CARTESIAN_POINT('Ctrl Pts',(5.85988667665508,7.31600801767173,12.2936474633893));
#82926=CARTESIAN_POINT('Ctrl Pts',(5.57564918258047,7.53166186261353,12.2995900297831));
#82927=CARTESIAN_POINT('Ctrl Pts',(5.48644825185093,7.59688618555996,12.3014408343938));
#82928=CARTESIAN_POINT('Ctrl Pts',(5.33094146338329,7.70642610698145,12.3046482390422));
#82929=CARTESIAN_POINT('Ctrl Pts',(5.26518495138276,7.75150099152724,12.3059987469718));
#82930=CARTESIAN_POINT('Ctrl Pts',(5.12461637582803,7.84524415887816,12.3088748448073));
#82931=CARTESIAN_POINT('Ctrl Pts',(5.04966796620778,7.89369383081742,12.3104019446758));
#82932=CARTESIAN_POINT('Ctrl Pts',(4.82136350883556,8.03669671835688,12.3150351412617));
#82933=CARTESIAN_POINT('Ctrl Pts',(4.66596225545873,8.12790478021591,12.318164657097));
#82934=CARTESIAN_POINT('Ctrl Pts',(4.45941974016268,8.24125203543735,12.32228413474));
#82935=CARTESIAN_POINT('Ctrl Pts',(4.41057468704577,8.26749602083678,12.3232554227997));
#82936=CARTESIAN_POINT('Ctrl Pts',(4.33802651072136,8.30564954902547,12.3246931548461));
#82937=CARTESIAN_POINT('Ctrl Pts',(4.31450196866873,8.31789403025546,12.3251585999007));
#82938=CARTESIAN_POINT('Ctrl Pts',(4.29092662693973,8.33003803981228,12.3256242449617));
#82939=CARTESIAN_POINT('Origin',(0.,0.,2.15141010809499));
#82940=CARTESIAN_POINT('',(4.29092664483271,8.33003803059534,13.5226410022223));
#82941=CARTESIAN_POINT('',(4.29092662791762,8.33003803930856,13.3252837277684));
#82942=CARTESIAN_POINT('',(4.29092662815669,8.33003803918541,2.15141010809499));
#82943=CARTESIAN_POINT('',(-9.37024987213592,-9.34868092301034E-5,12.8489977063995));
#82944=CARTESIAN_POINT('Ctrl Pts',(4.2909266448327,8.33003803059535,13.5226410022224));
#82945=CARTESIAN_POINT('Ctrl Pts',(4.40796820389162,8.26974818048013,13.5203344890077));
#82946=CARTESIAN_POINT('Ctrl Pts',(4.52374228459837,8.20698994738235,13.5180376176366));
#82947=CARTESIAN_POINT('Ctrl Pts',(4.68510179281196,8.11506768681626,13.5148314800693));
#82948=CARTESIAN_POINT('Ctrl Pts',(4.73180090659712,8.08792696355659,13.51390303251));
#82949=CARTESIAN_POINT('Ctrl Pts',(4.8148018533311,8.03872331042009,13.5122535599883));
#82950=CARTESIAN_POINT('Ctrl Pts',(4.85119319956073,8.01681444888224,13.5115306921446));
#82951=CARTESIAN_POINT('Ctrl Pts',(4.93350281422246,7.9664954971173,13.509896912888));
#82952=CARTESIAN_POINT('Ctrl Pts',(4.97932691627481,7.93793449218484,13.508987925753));
#82953=CARTESIAN_POINT('Ctrl Pts',(5.15313839658482,7.82750486555867,13.5055376762997));
#82954=CARTESIAN_POINT('Ctrl Pts',(5.27937501874081,7.74292369971175,13.5030263768984));
#82955=CARTESIAN_POINT('Ctrl Pts',(5.733786246584,7.42217762197547,13.4938767684595));
#82956=CARTESIAN_POINT('Ctrl Pts',(6.04863860605967,7.16791440375308,13.4873027375562));
#82957=CARTESIAN_POINT('Ctrl Pts',(6.42014281635164,6.82594193639402,13.4788738896804));
#82958=CARTESIAN_POINT('Ctrl Pts',(6.49309802369832,6.75658161286644,13.4771846073928));
#82959=CARTESIAN_POINT('Ctrl Pts',(6.62129752846268,6.63070482702753,13.4741509746564));
#82960=CARTESIAN_POINT('Ctrl Pts',(6.67697115520701,6.57463942908205,13.4728107216251));
#82961=CARTESIAN_POINT('Ctrl Pts',(6.79716265176064,6.45050074814443,13.4698656871598));
#82962=CARTESIAN_POINT('Ctrl Pts',(6.86138102899827,6.38214935078093,13.4682584478128));
#82963=CARTESIAN_POINT('Ctrl Pts',(7.0786694477314,6.14380561256954,13.4627021973097));
#82964=CARTESIAN_POINT('Ctrl Pts',(7.22653440708546,5.9691798735086,13.4587117230776));
#82965=CARTESIAN_POINT('Ctrl Pts',(7.51686139568803,5.59969106398734,13.4504665526502));
#82966=CARTESIAN_POINT('Ctrl Pts',(7.65848604660077,5.40438125065069,13.4462122005262));
#82967=CARTESIAN_POINT('Ctrl Pts',(7.85563123530068,5.10916813071561,13.4400105444198));
#82968=CARTESIAN_POINT('Ctrl Pts',(7.91711453012031,5.01336600708722,13.4380321912112));
#82969=CARTESIAN_POINT('Ctrl Pts',(8.00412189833516,4.87219887262912,13.4351781170507));
#82970=CARTESIAN_POINT('Ctrl Pts',(8.03103757062529,4.82770388210212,13.4342872034832));
#82971=CARTESIAN_POINT('Ctrl Pts',(8.07947530161691,4.74610404549726,13.4326706901483));
#82972=CARTESIAN_POINT('Ctrl Pts',(8.10111556349292,4.70907118071052,13.4319436604033));
#82973=CARTESIAN_POINT('Ctrl Pts',(8.15678005902085,4.61229347094315,13.4300597077864));
#82974=CARTESIAN_POINT('Ctrl Pts',(8.19040239141105,4.55232036364884,13.4289077786814));
#82975=CARTESIAN_POINT('Ctrl Pts',(8.26626105152168,4.41344778591673,13.4262702732956));
#82976=CARTESIAN_POINT('Ctrl Pts',(8.30803324173971,4.33430234683507,13.424788962643));
#82977=CARTESIAN_POINT('Ctrl Pts',(8.46390505203484,4.02843797199665,13.4191282788039));
#82978=CARTESIAN_POINT('Ctrl Pts',(8.5699096572916,3.79771642036605,13.4149886084481));
#82979=CARTESIAN_POINT('Ctrl Pts',(8.74311171727017,3.3764278537845,13.4074993697508));
#82980=CARTESIAN_POINT('Ctrl Pts',(8.81376294545501,3.1874519517316,13.4041647016374));
#82981=CARTESIAN_POINT('Ctrl Pts',(8.90845995259179,2.90686178372168,13.3992102782388));
#82982=CARTESIAN_POINT('Ctrl Pts',(8.93730494022251,2.81692820416644,13.3976220813808));
#82983=CARTESIAN_POINT('Ctrl Pts',(8.98776167940976,2.65102996634805,13.3946892785676));
#82984=CARTESIAN_POINT('Ctrl Pts',(9.00978204245337,2.57519851702767,13.3933475467423));
#82985=CARTESIAN_POINT('Ctrl Pts',(9.05791628867108,2.40125865897946,13.3902663388288));
#82986=CARTESIAN_POINT('Ctrl Pts',(9.08339946490536,2.30298604670164,13.3885228975579));
#82987=CARTESIAN_POINT('Ctrl Pts',(9.13461457037467,2.09138765711117,13.3847635747976));
#82988=CARTESIAN_POINT('Ctrl Pts',(9.15984541991545,1.97795790561759,13.3827450348816));
#82989=CARTESIAN_POINT('Ctrl Pts',(9.23354833862487,1.61487913396577,13.3762794186493));
#82990=CARTESIAN_POINT('Ctrl Pts',(9.27397074063018,1.3637139732343,13.3717973772946));
#82991=CARTESIAN_POINT('Ctrl Pts',(9.32551032435178,0.932177414901172,13.3641670438992));
#82992=CARTESIAN_POINT('Ctrl Pts',(9.34172122356433,0.752557259324356,13.3610125667854));
#82993=CARTESIAN_POINT('Ctrl Pts',(9.35615234546906,0.516834318716708,13.3569402614641));
#82994=CARTESIAN_POINT('Ctrl Pts',(9.3590667275941,0.461057949065512,13.3559816784151));
#82995=CARTESIAN_POINT('Ctrl Pts',(9.36330690478786,0.363109810734202,13.3543089746373));
#82996=CARTESIAN_POINT('Ctrl Pts',(9.36484685291686,0.320949147487481,13.3535925924372));
#82997=CARTESIAN_POINT('Ctrl Pts',(9.36791664019424,0.21781401273862,13.3518486041548));
#82998=CARTESIAN_POINT('Ctrl Pts',(9.36913596651226,0.156832353626897,13.3508243897097));
#82999=CARTESIAN_POINT('Ctrl Pts',(9.37053194993767,0.0203589357649303,
13.348543933461));
#83000=CARTESIAN_POINT('Ctrl Pts',(9.37039188189736,-0.0551318765680639,
13.3472904737359));
#83001=CARTESIAN_POINT('Ctrl Pts',(9.36688762051223,-0.306505458640138,
13.3431329580897));
#83002=CARTESIAN_POINT('Ctrl Pts',(9.35948297504986,-0.482294432059399,
13.3402515862976));
#83003=CARTESIAN_POINT('Ctrl Pts',(9.32732807791046,-0.939225902899539,
13.3327437566695));
#83004=CARTESIAN_POINT('Ctrl Pts',(9.29481931695558,-1.21964246199828,13.328114885758));
#83005=CARTESIAN_POINT('Ctrl Pts',(9.23320783818254,-1.60003373388339,13.3216867735744));
#83006=CARTESIAN_POINT('Ctrl Pts',(9.21502623143167,-1.70162464059846,13.3199559355863));
#83007=CARTESIAN_POINT('Ctrl Pts',(9.17993312386435,-1.88060745799853,13.3168777623345));
#83008=CARTESIAN_POINT('Ctrl Pts',(9.16371137205373,-1.9581242109515,13.3155350199275));
#83009=CARTESIAN_POINT('Ctrl Pts',(9.12651509793152,-2.12527156590577,13.3126177900176));
#83010=CARTESIAN_POINT('Ctrl Pts',(9.10519851538116,-2.21481760072378,13.311041197156));
#83011=CARTESIAN_POINT('Ctrl Pts',(9.03165830748466,-2.50471503646468,13.3058919526134));
#83012=CARTESIAN_POINT('Ctrl Pts',(8.9741135292501,-2.70365217101305,13.3022865354116));
#83013=CARTESIAN_POINT('Ctrl Pts',(8.83681892454648,-3.12540380615162,13.2945142281144));
#83014=CARTESIAN_POINT('Ctrl Pts',(8.75512353169543,-3.34743625235401,13.2903427351711));
#83015=CARTESIAN_POINT('Ctrl Pts',(8.6119601426669,-3.6952990829628,13.2837544929934));
#83016=CARTESIAN_POINT('Ctrl Pts',(8.55592301990391,-3.82325440791566,13.2813199846486));
#83017=CARTESIAN_POINT('Ctrl Pts',(8.47411685331421,-3.99923586314651,13.2779763550341));
#83018=CARTESIAN_POINT('Ctrl Pts',(8.45075800260977,-4.0483617837587,13.2770435148628));
#83019=CARTESIAN_POINT('Ctrl Pts',(8.40842491531257,-4.13542921196689,13.2753929619564));
#83020=CARTESIAN_POINT('Ctrl Pts',(8.38961837023935,-4.17345036231935,13.2746732980573));
#83021=CARTESIAN_POINT('Ctrl Pts',(8.34160660844577,-4.26887956262941,13.272869088469));
#83022=CARTESIAN_POINT('Ctrl Pts',(8.31206643884393,-4.32611662748276,13.2717886359332));
#83023=CARTESIAN_POINT('Ctrl Pts',(8.26192182652364,-4.42086688117238,13.2699994655871));
#83024=CARTESIAN_POINT('Ctrl Pts',(8.24164632175286,-4.45855157669259,13.2692877106335));
#83025=CARTESIAN_POINT('Ctrl Pts',(8.09578006991762,-4.72526807249007,13.2642450766829));
#83026=CARTESIAN_POINT('Ctrl Pts',(7.96091869776515,-4.94909966143834,13.25998285017));
#83027=CARTESIAN_POINT('Ctrl Pts',(7.68297386424863,-5.36958741986179,13.2517125645945));
#83028=CARTESIAN_POINT('Ctrl Pts',(7.54124098901064,-5.56688784775669,13.2477110441061));
#83029=CARTESIAN_POINT('Ctrl Pts',(7.33258708968269,-5.83473218891323,13.242034929786));
#83030=CARTESIAN_POINT('Ctrl Pts',(7.27199246496761,-5.91008110564837,13.2404100563124));
#83031=CARTESIAN_POINT('Ctrl Pts',(7.15987037501171,-6.04516847618693,13.2374423712309));
#83032=CARTESIAN_POINT('Ctrl Pts',(7.10873384052372,-6.10521980304239,13.2361028862485));
#83033=CARTESIAN_POINT('Ctrl Pts',(6.99182560121766,-6.23904858616611,13.2330706805898));
#83034=CARTESIAN_POINT('Ctrl Pts',(6.92563248994424,-6.31244540951852,13.2313745126429));
#83035=CARTESIAN_POINT('Ctrl Pts',(6.81827461710172,-6.42776518121584,13.2286559160603));
#83036=CARTESIAN_POINT('Ctrl Pts',(6.77785520908137,-6.47037191601856,13.2276394580657));
#83037=CARTESIAN_POINT('Ctrl Pts',(6.67880844333969,-6.57283210868215,13.2251660589487));
#83038=CARTESIAN_POINT('Ctrl Pts',(6.61977372892985,-6.63228466667112,13.2237062771434));
#83039=CARTESIAN_POINT('Ctrl Pts',(6.3444963603943,-6.90217296165201,13.2169691272194));
#83040=CARTESIAN_POINT('Ctrl Pts',(6.11896635179262,-7.10287800087862,13.2116373767196));
#83041=CARTESIAN_POINT('Ctrl Pts',(5.78715224157288,-7.37061649434051,13.2041818518444));
#83042=CARTESIAN_POINT('Ctrl Pts',(5.68860472919086,-7.44693862932104,13.2020136427525));
#83043=CARTESIAN_POINT('Ctrl Pts',(5.54678927775254,-7.55231238636502,13.1989727352766));
#83044=CARTESIAN_POINT('Ctrl Pts',(5.50475662497567,-7.58300390274411,13.1980810716903));
#83045=CARTESIAN_POINT('Ctrl Pts',(5.42763000836478,-7.63834119975101,13.1964639964031));
#83046=CARTESIAN_POINT('Ctrl Pts',(5.39261849500465,-7.66309921355812,13.1957371451792));
#83047=CARTESIAN_POINT('Ctrl Pts',(5.30110525512929,-7.72687405946329,13.1938548665736));
#83048=CARTESIAN_POINT('Ctrl Pts',(5.24434236902495,-7.76551175430718,13.1927044141857));
#83049=CARTESIAN_POINT('Ctrl Pts',(5.11277454421888,-7.85296756324806,13.1900711366269));
#83050=CARTESIAN_POINT('Ctrl Pts',(5.03768591250549,-7.90134696016396,13.1885925578243));
#83051=CARTESIAN_POINT('Ctrl Pts',(4.74758360898969,-8.0824424134982,13.182953220033));
#83052=CARTESIAN_POINT('Ctrl Pts',(4.52792604785014,-8.20751555069617,13.1788319096193));
#83053=CARTESIAN_POINT('Ctrl Pts',(4.12193316203394,-8.4174237759249,13.1713178799442));
#83054=CARTESIAN_POINT('Ctrl Pts',(3.93736170677208,-8.50532412339891,13.1679390964062));
#83055=CARTESIAN_POINT('Ctrl Pts',(3.66387530964422,-8.62475785530703,13.1629457176721));
#83056=CARTESIAN_POINT('Ctrl Pts',(3.57712459516057,-8.66109750112375,13.1613639165582));
#83057=CARTESIAN_POINT('Ctrl Pts',(3.41653627533654,-8.72554319548189,13.1584369949076));
#83058=CARTESIAN_POINT('Ctrl Pts',(3.34286192067799,-8.75403326029941,13.1570946686814));
#83059=CARTESIAN_POINT('Ctrl Pts',(3.17320524220403,-8.81718583374221,13.1540037271484));
#83060=CARTESIAN_POINT('Ctrl Pts',(3.07699929109938,-8.85121871992185,13.1522510454903));
#83061=CARTESIAN_POINT('Ctrl Pts',(2.9218029982917,-8.90328331038958,13.1494239748187));
#83062=CARTESIAN_POINT('Ctrl Pts',(2.86315704662275,-8.92231574079415,13.1483557636404));
#83063=CARTESIAN_POINT('Ctrl Pts',(2.64070284205451,-8.99208988836369,13.1443050305917));
#83064=CARTESIAN_POINT('Ctrl Pts',(2.47570039370991,-9.03891029960496,13.141302218957));
#83065=CARTESIAN_POINT('Ctrl Pts',(2.0090424774951,-9.15758980948017,13.1328448263403));
#83066=CARTESIAN_POINT('Ctrl Pts',(1.70497090449188,-9.21904427436467,13.127369764697));
#83067=CARTESIAN_POINT('Ctrl Pts',(1.34549468835034,-9.2733000237612,13.1210944567717));
#83068=CARTESIAN_POINT('Ctrl Pts',(1.29250805154037,-9.28083359619497,13.1201746583157));
#83069=CARTESIAN_POINT('Ctrl Pts',(1.19741911663357,-9.29352308917012,13.1185349478401));
#83070=CARTESIAN_POINT('Ctrl Pts',(1.15534091009123,-9.2988478506439,13.117813276403));
#83071=CARTESIAN_POINT('Ctrl Pts',(1.05918668209728,-9.31035288735936,13.1161734934029));
#83072=CARTESIAN_POINT('Ctrl Pts',(1.00509017404632,-9.31634805462525,13.1152573994326));
#83073=CARTESIAN_POINT('Ctrl Pts',(0.794547377858548,-9.33782598410069,
13.111712140444));
#83074=CARTESIAN_POINT('Ctrl Pts',(0.6377730940271,-9.34984199877075,13.1091151211794));
#83075=CARTESIAN_POINT('Ctrl Pts',(0.15508990447036,-9.37464026168652,13.1011678181589));
#83076=CARTESIAN_POINT('Ctrl Pts',(-0.171241853759035,-9.37435914366116,
13.09585555272));
#83077=CARTESIAN_POINT('Ctrl Pts',(-0.632409571113196,-9.34986949561738,
13.0882012423772));
#83078=CARTESIAN_POINT('Ctrl Pts',(-0.767752975622561,-9.33973001090355,
13.085938121223));
#83079=CARTESIAN_POINT('Ctrl Pts',(-0.985637489753486,-9.31863860542893,
13.0822578279393));
#83080=CARTESIAN_POINT('Ctrl Pts',(-1.06833635235231,-9.30952007996978,
13.0808523939818));
#83081=CARTESIAN_POINT('Ctrl Pts',(-1.23309690467648,-9.28912893962376,
13.0780336943179));
#83082=CARTESIAN_POINT('Ctrl Pts',(-1.31515251543884,-9.27786711780006,
13.0766206171028));
#83083=CARTESIAN_POINT('Ctrl Pts',(-1.52873209547759,-9.24566375107585,
13.0729176005749));
#83084=CARTESIAN_POINT('Ctrl Pts',(-1.65997771398991,-9.22300351609862,
13.0706171122036));
#83085=CARTESIAN_POINT('Ctrl Pts',(-1.96447316743057,-9.16372051266204,
13.0652249817773));
#83086=CARTESIAN_POINT('Ctrl Pts',(-2.13725681400388,-9.12496912538269,
13.0621230880308));
#83087=CARTESIAN_POINT('Ctrl Pts',(-2.60195739059717,-9.00682381242067,
13.0536988860746));
#83088=CARTESIAN_POINT('Ctrl Pts',(-2.89129678421748,-8.91815343809958,
13.0483609096829));
#83089=CARTESIAN_POINT('Ctrl Pts',(-3.22516296886264,-8.79787800074208,
13.0422380548354));
#83090=CARTESIAN_POINT('Ctrl Pts',(-3.27433557615743,-8.77969589689867,
13.0413374050691));
#83091=CARTESIAN_POINT('Ctrl Pts',(-3.36289610044361,-8.74610219057587,
13.0397189759948));
#83092=CARTESIAN_POINT('Ctrl Pts',(-3.4023371009814,-8.73083478126839,13.038999623827));
#83093=CARTESIAN_POINT('Ctrl Pts',(-3.49325666819293,-8.69493063056182,
13.0373449283989));
#83094=CARTESIAN_POINT('Ctrl Pts',(-3.54465796816425,-8.67410287741465,
13.0364118238669));
#83095=CARTESIAN_POINT('Ctrl Pts',(-3.75447803791881,-8.58690749041558,
13.0326072193572));
#83096=CARTESIAN_POINT('Ctrl Pts',(-3.91124293509302,-8.51664632560923,
13.029774266869));
#83097=CARTESIAN_POINT('Ctrl Pts',(-4.41159463152439,-8.27566123374181,
13.0206513555163));
#83098=CARTESIAN_POINT('Ctrl Pts',(-4.74665250849149,-8.08814107561432,
13.0144016021705));
#83099=CARTESIAN_POINT('Ctrl Pts',(-5.15395694547843,-7.82613901459014,
13.0063149420751));
#83100=CARTESIAN_POINT('Ctrl Pts',(-5.2377582367167,-7.77030325407255,13.0046245402432));
#83101=CARTESIAN_POINT('Ctrl Pts',(-5.38560970812548,-7.66831286297231,
13.001590759307));
#83102=CARTESIAN_POINT('Ctrl Pts',(-5.45000732781649,-7.62267893760626,
13.000251503766));
#83103=CARTESIAN_POINT('Ctrl Pts',(-5.59070029913252,-7.52028565004488,
12.9972847648431));
#83104=CARTESIAN_POINT('Ctrl Pts',(-5.6667237002757,-7.46316746026565,12.9956545645022));
#83105=CARTESIAN_POINT('Ctrl Pts',(-5.94010496518926,-7.25118381433151,
12.9896923591598));
#83106=CARTESIAN_POINT('Ctrl Pts',(-6.13209185138352,-7.08956715082722,
12.9853089005774));
#83107=CARTESIAN_POINT('Ctrl Pts',(-6.5491797400863,-6.70882635959014,12.9753902718138));
#83108=CARTESIAN_POINT('Ctrl Pts',(-6.7702188440969,-6.48569529935909,12.9698463124284));
#83109=CARTESIAN_POINT('Ctrl Pts',(-7.01474859725542,-6.21270115495295,
12.9635223486083));
#83110=CARTESIAN_POINT('Ctrl Pts',(-7.04952377421502,-6.17321375751872,
12.9626183578704));
#83111=CARTESIAN_POINT('Ctrl Pts',(-7.11166009930628,-6.10144785663763,
12.9609962510237));
#83112=CARTESIAN_POINT('Ctrl Pts',(-7.13913864378171,-6.06927300067393,
12.9602765293121));
#83113=CARTESIAN_POINT('Ctrl Pts',(-7.19269167513335,-6.00570038276606,
12.9588693898657));
#83114=CARTESIAN_POINT('Ctrl Pts',(-7.21878072655044,-5.97431631660935,
12.9581815993275));
#83115=CARTESIAN_POINT('Ctrl Pts',(-7.28064058040269,-5.89890461516016,
12.9565439995588));
#83116=CARTESIAN_POINT('Ctrl Pts',(-7.3162182622989,-5.85472059752223,12.9555966355733));
#83117=CARTESIAN_POINT('Ctrl Pts',(-7.41600621310316,-5.72846360879097,
12.9529197627028));
#83118=CARTESIAN_POINT('Ctrl Pts',(-7.47925174568263,-5.64563874710119,
12.9511993836763));
#83119=CARTESIAN_POINT('Ctrl Pts',(-7.77145333516526,-5.24944836914489,
12.9430999503543));
#83120=CARTESIAN_POINT('Ctrl Pts',(-7.98217777109818,-4.92311219068823,
12.9367885478748));
#83121=CARTESIAN_POINT('Ctrl Pts',(-8.22462584507596,-4.49095284698223,
12.9285329196642));
#83122=CARTESIAN_POINT('Ctrl Pts',(-8.27557684785323,-4.39635707418454,
12.9267330607153));
#83123=CARTESIAN_POINT('Ctrl Pts',(-8.36077921373284,-4.23143827232256,
12.9236031074117));
#83124=CARTESIAN_POINT('Ctrl Pts',(-8.39579763103608,-4.16152388187751,
12.9222786570999));
#83125=CARTESIAN_POINT('Ctrl Pts',(-8.46505390344619,-4.01882029167887,
12.9195791303703));
#83126=CARTESIAN_POINT('Ctrl Pts',(-8.4992377913579,-3.94601204453747,12.918203800745));
#83127=CARTESIAN_POINT('Ctrl Pts',(-8.57016498219457,-3.78974549753141,
12.9152558493934));
#83128=CARTESIAN_POINT('Ctrl Pts',(-8.60663598511223,-3.70617265250556,
12.9136815698809));
#83129=CARTESIAN_POINT('Ctrl Pts',(-8.67261252243909,-3.54875999022363,
12.9107214972547));
#83130=CARTESIAN_POINT('Ctrl Pts',(-8.70240922746164,-3.4750509412293,12.9093375195691));
#83131=CARTESIAN_POINT('Ctrl Pts',(-8.82893292208684,-3.15022853642411,
12.9032509199261));
#83132=CARTESIAN_POINT('Ctrl Pts',(-8.9157549222299,-2.89539463019322,12.8985039438546));
#83133=CARTESIAN_POINT('Ctrl Pts',(-9.03709174969183,-2.48169550405554,
12.8909421878323));
#83134=CARTESIAN_POINT('Ctrl Pts',(-9.07865412938785,-2.32505469080471,
12.8881123461397));
#83135=CARTESIAN_POINT('Ctrl Pts',(-9.12874984060905,-2.11435242857279,
12.8843797880283));
#83136=CARTESIAN_POINT('Ctrl Pts',(-9.140902234698,-2.0611807777376,12.8834441404231));
#83137=CARTESIAN_POINT('Ctrl Pts',(-9.16073828440998,-1.97076258804941,
12.8818654108044));
#83138=CARTESIAN_POINT('Ctrl Pts',(-9.16866064140778,-1.93357005070896,
12.88121965639));
#83139=CARTESIAN_POINT('Ctrl Pts',(-9.18485258293491,-1.85521711875724,
12.8798666610249));
#83140=CARTESIAN_POINT('Ctrl Pts',(-9.19307236590699,-1.81404741159164,
12.8791599214581));
#83141=CARTESIAN_POINT('Ctrl Pts',(-9.21241883691012,-1.71363857649148,
12.8774450081386));
#83142=CARTESIAN_POINT('Ctrl Pts',(-9.22325115943001,-1.65434460348244,
12.8764397023883));
#83143=CARTESIAN_POINT('Ctrl Pts',(-9.2532452330598,-1.48070244117914,12.8735125096194));
#83144=CARTESIAN_POINT('Ctrl Pts',(-9.27085773806322,-1.36609807419211,
12.8716017353241));
#83145=CARTESIAN_POINT('Ctrl Pts',(-9.33095789351405,-0.920036641902406,
12.8642063249432));
#83146=CARTESIAN_POINT('Ctrl Pts',(-9.3578305814888,-0.586727814351847,
12.8587604154233));
#83147=CARTESIAN_POINT('Ctrl Pts',(-9.3691130617853,-0.168514986455563,
12.8518128918622));
#83148=CARTESIAN_POINT('Ctrl Pts',(-9.3702491589803,-0.0843061205128449,
12.8504087881159));
#83149=CARTESIAN_POINT('Ctrl Pts',(-9.37024999953324,-9.35274742388515E-5,
12.8489979277639));
#83150=CARTESIAN_POINT('Ctrl Pts',(-9.37024999953368,-9.34831142609071E-5,
12.8489979270207));
#83151=CARTESIAN_POINT('Ctrl Pts',(-9.37025068795026,0.0689097317925185,
12.8478418778276));
#83152=CARTESIAN_POINT('Ctrl Pts',(-9.36948915928981,0.13791078196804,12.8466813796634));
#83153=CARTESIAN_POINT('Ctrl Pts',(-9.36645008943694,0.275514971673631,
12.8443569913286));
#83154=CARTESIAN_POINT('Ctrl Pts',(-9.36418075739126,0.344114077532216,
12.8431932232752));
#83155=CARTESIAN_POINT('Ctrl Pts',(-9.35719707657167,0.502529865745441,
12.8404934081459));
#83156=CARTESIAN_POINT('Ctrl Pts',(-9.35194285634548,0.592315927649199,
12.8389540316959));
#83157=CARTESIAN_POINT('Ctrl Pts',(-9.33251077801821,0.858587506071259,
12.8343610783562));
#83158=CARTESIAN_POINT('Ctrl Pts',(-9.31462281536421,1.03476152411561,12.8312853539796));
#83159=CARTESIAN_POINT('Ctrl Pts',(-9.24801550851545,1.54611188847006,12.8222692063276));
#83160=CARTESIAN_POINT('Ctrl Pts',(-9.18610627931292,1.87928272811455,12.8162752902034));
#83161=CARTESIAN_POINT('Ctrl Pts',(-9.08511188705283,2.2957371633505,12.8088138303866));
#83162=CARTESIAN_POINT('Ctrl Pts',(-9.06266800784841,2.38279578757585,12.8072564536651));
#83163=CARTESIAN_POINT('Ctrl Pts',(-9.02834732016025,2.50841699045259,12.805018757162));
#83164=CARTESIAN_POINT('Ctrl Pts',(-9.01746883241015,2.54724694437324,12.8043284122212));
#83165=CARTESIAN_POINT('Ctrl Pts',(-8.99460288295917,2.62688270505295,12.802916184013));
#83166=CARTESIAN_POINT('Ctrl Pts',(-8.98258761326947,2.66767942945808,12.8021948252546));
#83167=CARTESIAN_POINT('Ctrl Pts',(-8.95457446358068,2.76045998732238,12.8005583708945));
#83168=CARTESIAN_POINT('Ctrl Pts',(-8.93840088449609,2.81238916414691,12.7996452392358));
#83169=CARTESIAN_POINT('Ctrl Pts',(-8.83539783251091,3.13323907016311,12.7940130163272));
#83170=CARTESIAN_POINT('Ctrl Pts',(-8.73689171841284,3.39825930246818,12.7893985545897));
#83171=CARTESIAN_POINT('Ctrl Pts',(-8.51914741384282,3.91170031804821,12.7802548303991));
#83172=CARTESIAN_POINT('Ctrl Pts',(-8.40063319704573,4.16012419588458,12.7757308071256));
#83173=CARTESIAN_POINT('Ctrl Pts',(-8.23478779205425,4.47167902837219,12.7698290285569));
#83174=CARTESIAN_POINT('Ctrl Pts',(-8.19735952861368,4.53992731674847,12.7685219947654));
#83175=CARTESIAN_POINT('Ctrl Pts',(-8.13014546214521,4.65894660077353,12.7662159730845));
#83176=CARTESIAN_POINT('Ctrl Pts',(-8.10072343900325,4.70991809009699,12.7652196566524));
#83177=CARTESIAN_POINT('Ctrl Pts',(-8.02810698053066,4.83302725600549,12.7627913962187));
#83178=CARTESIAN_POINT('Ctrl Pts',(-7.98441805263359,4.90486722229292,12.7613558627459));
#83179=CARTESIAN_POINT('Ctrl Pts',(-7.8676074262543,5.09124763279602,12.7575820106739));
#83180=CARTESIAN_POINT('Ctrl Pts',(-7.79295076391193,5.20480233121666,12.7552326984802));
#83181=CARTESIAN_POINT('Ctrl Pts',(-7.52382022283719,5.59537805712278,12.7469812473793));
#83182=CARTESIAN_POINT('Ctrl Pts',(-7.31683180453062,5.86345438910015,12.7410005236719));
#83183=CARTESIAN_POINT('Ctrl Pts',(-7.03063885861127,6.19529303366789,12.7333255214571));
#83184=CARTESIAN_POINT('Ctrl Pts',(-6.96427807975564,6.26979819611523,12.7315840841177));
#83185=CARTESIAN_POINT('Ctrl Pts',(-6.88863653807405,6.35204022389922,12.7296468582307));
#83186=CARTESIAN_POINT('Ctrl Pts',(-6.88051605684362,6.36083541300986,12.7294394919915));
#83187=CARTESIAN_POINT('Ctrl Pts',(-6.86773833749641,6.37462169782446,12.7291141596582));
#83188=CARTESIAN_POINT('Ctrl Pts',(-6.86309246289031,6.37962330459454,12.7289960703085));
#83189=CARTESIAN_POINT('Ctrl Pts',(-6.85336239926296,6.39007546467776,12.7287491697594));
#83190=CARTESIAN_POINT('Ctrl Pts',(-6.84827716374798,6.39552503774588,12.7286203704845));
#83191=CARTESIAN_POINT('Ctrl Pts',(-6.83908434605188,6.40535294984171,12.7283879687194));
#83192=CARTESIAN_POINT('Ctrl Pts',(-6.83497904844297,6.409733419716,12.7282843395184));
#83193=CARTESIAN_POINT('Ctrl Pts',(-6.82755388256784,6.41764103899447,12.728097191415));
#83194=CARTESIAN_POINT('Ctrl Pts',(-6.82423548397376,6.42116956512113,12.7280136547766));
#83195=CARTESIAN_POINT('Ctrl Pts',(-6.81822653213817,6.42754909636868,12.727862572655));
#83196=CARTESIAN_POINT('Ctrl Pts',(-6.81553692308385,6.43040098904178,12.7277950154882));
#83197=CARTESIAN_POINT('Ctrl Pts',(-6.8106589097118,6.43556682985437,12.7276726127832));
#83198=CARTESIAN_POINT('Ctrl Pts',(-6.80847111389313,6.43788135159733,12.7276177595633));
#83199=CARTESIAN_POINT('Ctrl Pts',(-6.80449613629775,6.44208228340539,12.727518178698));
#83200=CARTESIAN_POINT('Ctrl Pts',(-6.80270934908332,6.44396906626288,12.7274734459909));
#83201=CARTESIAN_POINT('Ctrl Pts',(-6.79945695108753,6.44740062095882,12.7273920756374));
#83202=CARTESIAN_POINT('Ctrl Pts',(-6.7979915981891,6.44894563690718,12.7273554346395));
#83203=CARTESIAN_POINT('Ctrl Pts',(-6.79531943581326,6.45176114702816,12.7272886541176));
#83204=CARTESIAN_POINT('Ctrl Pts',(-6.79411279639709,6.45303180240709,12.7272585123605));
#83205=CARTESIAN_POINT('Ctrl Pts',(-6.79190861199632,6.4553516220754,12.7272034768958));
#83206=CARTESIAN_POINT('Ctrl Pts',(-6.79091118017791,6.45640089378566,12.7271785816891));
#83207=CARTESIAN_POINT('Ctrl Pts',(-6.78908624261721,6.45831978875433,12.7271330495524));
#83208=CARTESIAN_POINT('Ctrl Pts',(-6.78825881287262,6.45918948421297,12.7271124116087));
#83209=CARTESIAN_POINT('Ctrl Pts',(-6.78674271439468,6.46078241302412,12.7270746084777));
#83210=CARTESIAN_POINT('Ctrl Pts',(-6.7860540971278,6.46150569532258,12.7270574425997));
#83211=CARTESIAN_POINT('Ctrl Pts',(-6.78479069749854,6.46283226983135,12.727025956674));
#83212=CARTESIAN_POINT('Ctrl Pts',(-6.78421595026531,6.46343559548651,12.7270116361522));
#83213=CARTESIAN_POINT('Ctrl Pts',(-6.783160244788,6.46454349834128,12.7269853376597));
#83214=CARTESIAN_POINT('Ctrl Pts',(-6.78267931071224,6.46504809854151,12.7269733593619));
#83215=CARTESIAN_POINT('Ctrl Pts',(-6.78048266630905,6.46735232198527,12.7269186589345));
#83216=CARTESIAN_POINT('Ctrl Pts',(-6.77876629592429,6.46915131605748,12.7268759457779));
#83217=CARTESIAN_POINT('Ctrl Pts',(-6.77544051880157,6.47263441460103,12.7267932349078));
#83218=CARTESIAN_POINT('Ctrl Pts',(-6.77383119971992,6.47431860249386,12.7267532359936));
#83219=CARTESIAN_POINT('Ctrl Pts',(-6.77070781143242,6.4775848578038,12.7266756527707));
#83220=CARTESIAN_POINT('Ctrl Pts',(-6.76919381534365,6.47916699492733,12.7266380674492));
#83221=CARTESIAN_POINT('Ctrl Pts',(-6.76625039196162,6.48224073634446,12.7265650381346));
#83222=CARTESIAN_POINT('Ctrl Pts',(-6.76482102572094,6.48373239890491,12.7265295932876));
#83223=CARTESIAN_POINT('Ctrl Pts',(-6.74383561979175,6.50561792176144,12.7260094878117));
#83224=CARTESIAN_POINT('Ctrl Pts',(-6.72418791086855,6.5259237164346,12.7255261302429));
#83225=CARTESIAN_POINT('Ctrl Pts',(-6.67491057299716,6.57639275062133,12.7243231318315));
#83226=CARTESIAN_POINT('Ctrl Pts',(-6.64516820719732,6.60644475262474,12.7236054847017));
#83227=CARTESIAN_POINT('Ctrl Pts',(-6.57817743453521,6.67322281916118,12.7220073445606));
#83228=CARTESIAN_POINT('Ctrl Pts',(-6.54082293949006,6.70984026964447,12.7211284594741));
#83229=CARTESIAN_POINT('Ctrl Pts',(-6.27623946923494,6.96489410060998,12.7149808490458));
#83230=CARTESIAN_POINT('Ctrl Pts',(-6.03842135734806,7.17205695632022,12.7098457561277));
#83231=CARTESIAN_POINT('Ctrl Pts',(-5.65671499568797,7.47209260172947,12.7018802957643));
#83232=CARTESIAN_POINT('Ctrl Pts',(-5.51996942592922,7.57367346626392,12.6990784672235));
#83233=CARTESIAN_POINT('Ctrl Pts',(-5.33027186584697,7.70672145381521,12.6952344702456));
#83234=CARTESIAN_POINT('Ctrl Pts',(-5.27966683229501,7.74147736919135,12.6942131041715));
#83235=CARTESIAN_POINT('Ctrl Pts',(-5.14428730960835,7.83251214534628,12.6914898236771));
#83236=CARTESIAN_POINT('Ctrl Pts',(-5.05893157485354,7.88791161746215,12.6897820997537));
#83237=CARTESIAN_POINT('Ctrl Pts',(-4.90575605715464,7.98381984146777,12.6867302367064));
#83238=CARTESIAN_POINT('Ctrl Pts',(-4.83829437248597,8.02488188603704,12.685390431205));
#83239=CARTESIAN_POINT('Ctrl Pts',(-4.68918771397459,8.11307520800644,12.6824374364602));
#83240=CARTESIAN_POINT('Ctrl Pts',(-4.60733425417488,8.15983711612044,12.6808216929367));
#83241=CARTESIAN_POINT('Ctrl Pts',(-4.18131940413554,8.39476019069,12.6724393018009));
#83242=CARTESIAN_POINT('Ctrl Pts',(-3.82629694868124,8.56241082020753,12.6655246390163));
#83243=CARTESIAN_POINT('Ctrl Pts',(-3.29433056417342,8.77390778054548,12.6554743066057));
#83244=CARTESIAN_POINT('Ctrl Pts',(-3.12495517088969,8.83565091517452,12.652321438248));
#83245=CARTESIAN_POINT('Ctrl Pts',(-2.90079579789922,8.91011226362078,12.6482492252726));
#83246=CARTESIAN_POINT('Ctrl Pts',(-2.84753014880143,8.92727779799855,12.6472889543156));
#83247=CARTESIAN_POINT('Ctrl Pts',(-2.75378773997722,8.95656312711505,12.6456137856883));
#83248=CARTESIAN_POINT('Ctrl Pts',(-2.71337704906949,8.96888816747332,12.6448966074594));
#83249=CARTESIAN_POINT('Ctrl Pts',(-2.61331199889471,8.99866927085689,12.6431324490398));
#83250=CARTESIAN_POINT('Ctrl Pts',(-2.55356478393201,9.01580585248389,12.6420890996788));
#83251=CARTESIAN_POINT('Ctrl Pts',(-2.2428860759334,9.1015780689023,12.6367059270095));
#83252=CARTESIAN_POINT('Ctrl Pts',(-1.98934548662513,9.16033660958113,12.6324515687093));
#83253=CARTESIAN_POINT('Ctrl Pts',(-1.44765654606138,9.26232097921423,12.6234165312014));
#83254=CARTESIAN_POINT('Ctrl Pts',(-1.15927120322874,9.30281618959144,12.6186366857865));
#83255=CARTESIAN_POINT('Ctrl Pts',(-0.773104579368081,9.33880406983154,
12.6121530474745));
#83256=CARTESIAN_POINT('Ctrl Pts',(-0.67660526437447,9.34629110413154,12.6105265685955));
#83257=CARTESIAN_POINT('Ctrl Pts',(-0.501289393057884,9.35716379971669,
12.6075573165885));
#83258=CARTESIAN_POINT('Ctrl Pts',(-0.422512941165264,9.36105166160757,
12.6062178897357));
#83259=CARTESIAN_POINT('Ctrl Pts',(-0.245039371129517,9.36756570265129,
12.6031875938936));
#83260=CARTESIAN_POINT('Ctrl Pts',(-0.146330940901112,9.36962745675422,
12.6014932981909));
#83261=CARTESIAN_POINT('Ctrl Pts',(0.356140373736641,9.37218045634467,12.5928234976521));
#83262=CARTESIAN_POINT('Ctrl Pts',(0.759598769324292,9.34813397349099,12.5856932237886));
#83263=CARTESIAN_POINT('Ctrl Pts',(1.31811063074986,9.27844168522384,12.5758234835243));
#83264=CARTESIAN_POINT('Ctrl Pts',(1.4754527460543,9.25472501895612,12.5730460091534));
#83265=CARTESIAN_POINT('Ctrl Pts',(1.68585375626433,9.21750836184417,12.5693643964998));
#83266=CARTESIAN_POINT('Ctrl Pts',(1.73950867985349,9.20753348401263,12.5684284459436));
#83267=CARTESIAN_POINT('Ctrl Pts',(1.83468370863912,9.18897807017679,12.5667751820613));
#83268=CARTESIAN_POINT('Ctrl Pts',(1.87623821958174,9.18058344714477,12.5660558813679));
#83269=CARTESIAN_POINT('Ctrl Pts',(1.96996115498921,9.160987117938,12.564438651363));
#83270=CARTESIAN_POINT('Ctrl Pts',(2.02209362602352,9.14962126599199,12.5635425113279));
#83271=CARTESIAN_POINT('Ctrl Pts',(2.37715871531596,9.06902758353891,12.5574545000721));
#83272=CARTESIAN_POINT('Ctrl Pts',(2.67658333092039,8.98521275253325,12.5523907831215));
#83273=CARTESIAN_POINT('Ctrl Pts',(3.13376318343708,8.83235313510846,12.5444824385657));
#83274=CARTESIAN_POINT('Ctrl Pts',(3.2947156829486,8.773584330605,12.5416645053969));
#83275=CARTESIAN_POINT('Ctrl Pts',(3.51124418559039,8.68772386550307,12.5378004817293));
#83276=CARTESIAN_POINT('Ctrl Pts',(3.56829672573757,8.66444690434702,12.536775412961));
#83277=CARTESIAN_POINT('Ctrl Pts',(3.71917235501035,8.60114794219391,12.5340443878932));
#83278=CARTESIAN_POINT('Ctrl Pts',(3.81257846468535,8.56015387204622,12.5323326090934));
#83279=CARTESIAN_POINT('Ctrl Pts',(3.97709530717437,8.48472372760624,12.529276483005));
#83280=CARTESIAN_POINT('Ctrl Pts',(4.04847489125391,8.45089787166887,12.5279365185356));
#83281=CARTESIAN_POINT('Ctrl Pts',(4.17688098086435,8.38804765013894,12.5254996843973));
#83282=CARTESIAN_POINT('Ctrl Pts',(4.23405345369067,8.35933425819504,12.5244050892833));
#83283=CARTESIAN_POINT('Ctrl Pts',(4.290926628303,8.33003803911004,12.5233065119449));
#83284=CARTESIAN_POINT('Ctrl Pts',(4.29092662693973,8.33003803981228,12.3256242449617));
#83285=CARTESIAN_POINT('Ctrl Pts',(4.10018693584926,8.42829089476957,12.3293916132614));
#83286=CARTESIAN_POINT('Ctrl Pts',(3.90612200113809,8.51996701307972,12.3331737430698));
#83287=CARTESIAN_POINT('Ctrl Pts',(3.65267042137266,8.62921527930986,12.3379988945992));
#83288=CARTESIAN_POINT('Ctrl Pts',(3.59602888310997,8.65297254301987,12.3390699215654));
#83289=CARTESIAN_POINT('Ctrl Pts',(3.50246379508337,8.69113933399208,12.3408251808568));
#83290=CARTESIAN_POINT('Ctrl Pts',(3.465675147465,8.70587453023978,12.341511809104));
#83291=CARTESIAN_POINT('Ctrl Pts',(3.37198635540229,8.74271234330628,12.3432506201701));
#83292=CARTESIAN_POINT('Ctrl Pts',(3.31496160327234,8.76449317941675,12.3442998345609));
#83293=CARTESIAN_POINT('Ctrl Pts',(3.21816935841031,8.80038357627886,12.3460630149162));
#83294=CARTESIAN_POINT('Ctrl Pts',(3.1785121382877,8.81478449590424,12.3467803051359));
#83295=CARTESIAN_POINT('Ctrl Pts',(3.08617057416272,8.84761274560848,12.3484385798004));
#83296=CARTESIAN_POINT('Ctrl Pts',(3.03341627330563,8.86583813529258,12.3493772464112));
#83297=CARTESIAN_POINT('Ctrl Pts',(2.81872121646125,8.93786971398334,12.3531676549845));
#83298=CARTESIAN_POINT('Ctrl Pts',(2.65548716333115,8.98771898657934,12.3559818463684));
#83299=CARTESIAN_POINT('Ctrl Pts',(2.41796575284859,9.05321841104248,12.3600290138679));
#83300=CARTESIAN_POINT('Ctrl Pts',(2.34470724966143,9.07246768528441,12.3612707179495));
#83301=CARTESIAN_POINT('Ctrl Pts',(2.06588739233299,9.14212715791704,12.3659813008466));
#83302=CARTESIAN_POINT('Ctrl Pts',(1.85887235999473,9.18645595886654,12.3694487713326));
#83303=CARTESIAN_POINT('Ctrl Pts',(1.58162114140453,9.23606846910573,12.3741086040337));
#83304=CARTESIAN_POINT('Ctrl Pts',(1.51257168796278,9.24762742935078,12.3752702779839));
#83305=CARTESIAN_POINT('Ctrl Pts',(1.33378496775185,9.27550052830089,12.3782837637686));
#83306=CARTESIAN_POINT('Ctrl Pts',(1.22387605106547,9.2906415127309,12.3801418237822));
#83307=CARTESIAN_POINT('Ctrl Pts',(1.0345210397253,9.31330845353266,12.3833573270572));
#83308=CARTESIAN_POINT('Ctrl Pts',(0.955199923120752,9.32177779206421,12.3847085871674));
#83309=CARTESIAN_POINT('Ctrl Pts',(0.787122701057217,9.33755601762871,12.3875820708725));
#83310=CARTESIAN_POINT('Ctrl Pts',(0.698350956302175,9.34461451440436,12.389105761754));
#83311=CARTESIAN_POINT('Ctrl Pts',(0.431346196273203,9.36201881970316,12.3937072643365));
#83312=CARTESIAN_POINT('Ctrl Pts',(0.252905212216841,9.36853748148371,12.3968079771902));
#83313=CARTESIAN_POINT('Ctrl Pts',(0.00740264328893203,9.37048651556237,
12.4011000631563));
#83314=CARTESIAN_POINT('Ctrl Pts',(-0.0595861065972801,9.37029998575161,
12.4022737802285));
#83315=CARTESIAN_POINT('Ctrl Pts',(-0.360700199179532,9.36623236775615,
12.4075579214997));
#83316=CARTESIAN_POINT('Ctrl Pts',(-0.594632414339054,9.35429450392961,
12.4116878511372));
#83317=CARTESIAN_POINT('Ctrl Pts',(-0.888142150973626,9.3282608105357,12.4168383796325));
#83318=CARTESIAN_POINT('Ctrl Pts',(-0.948359976785155,9.32233123195316,
12.4178932766622));
#83319=CARTESIAN_POINT('Ctrl Pts',(-1.04750943995519,9.31159746387329,12.4196252838786));
#83320=CARTESIAN_POINT('Ctrl Pts',(-1.08647583805339,9.30713133110853,12.4203047226472));
#83321=CARTESIAN_POINT('Ctrl Pts',(-1.18557402264217,9.29514236646072,12.4220285930561));
#83322=CARTESIAN_POINT('Ctrl Pts',(-1.24566305324711,9.28728060078173,12.4230700726671));
#83323=CARTESIAN_POINT('Ctrl Pts',(-1.34743361270927,9.27295995436028,12.4248252300336));
#83324=CARTESIAN_POINT('Ctrl Pts',(-1.38915533010638,9.26680155918781,12.4255421422928));
#83325=CARTESIAN_POINT('Ctrl Pts',(-1.48634614085464,9.25178444133653,12.4272060081606));
#83326=CARTESIAN_POINT('Ctrl Pts',(-1.54177985667985,9.24270821201918,12.4281505698583));
#83327=CARTESIAN_POINT('Ctrl Pts',(-1.77991433949845,9.20151619537182,12.4321950481225));
#83328=CARTESIAN_POINT('Ctrl Pts',(-1.96172140641083,9.16447733875931,12.4352500879022));
#83329=CARTESIAN_POINT('Ctrl Pts',(-2.38595017380165,9.06484758045496,12.4424028587785));
#83330=CARTESIAN_POINT('Ctrl Pts',(-2.62720089302723,8.99789060438845,12.4464908829958));
#83331=CARTESIAN_POINT('Ctrl Pts',(-2.97538731318275,8.88605542407084,12.4525307071389));
#83332=CARTESIAN_POINT('Ctrl Pts',(-3.0846318429092,8.8487262913478,12.4544458015077));
#83333=CARTESIAN_POINT('Ctrl Pts',(-3.28818196763926,8.77494502546297,12.4580606397742));
#83334=CARTESIAN_POINT('Ctrl Pts',(-3.38264167823421,8.73896653290437,12.4597572668517));
#83335=CARTESIAN_POINT('Ctrl Pts',(-3.54980692525323,8.67217893350925,12.4627975253513));
#83336=CARTESIAN_POINT('Ctrl Pts',(-3.62274003534073,8.64196570602424,12.4641369577684));
#83337=CARTESIAN_POINT('Ctrl Pts',(-3.78238397439797,8.57345556815873,12.4670986264043));
#83338=CARTESIAN_POINT('Ctrl Pts',(-3.86891307157105,8.53475720195737,12.4687235199776));
#83339=CARTESIAN_POINT('Ctrl Pts',(-4.34430541480735,8.31343226183535,12.4777603550593));
#83340=CARTESIAN_POINT('Ctrl Pts',(-4.720839110414,8.10554250504209,12.4853549651812));
#83341=CARTESIAN_POINT('Ctrl Pts',(-5.20538432107292,7.79276621272657,12.4954593706856));
#83342=CARTESIAN_POINT('Ctrl Pts',(-5.32709854324198,7.71007473970601,12.4980247854707));
#83343=CARTESIAN_POINT('Ctrl Pts',(-5.49040896891864,7.59340929124898,12.5014815291635));
#83344=CARTESIAN_POINT('Ctrl Pts',(-5.53373476161795,7.56189360649492,12.5023999956596));
#83345=CARTESIAN_POINT('Ctrl Pts',(-5.61097929889184,7.50468564582699,12.5040383296582));
#83346=CARTESIAN_POINT('Ctrl Pts',(-5.64499770620132,7.47913071367678,12.5047599721763));
#83347=CARTESIAN_POINT('Ctrl Pts',(-5.72220490318684,7.42030512635671,12.5063988411738));
#83348=CARTESIAN_POINT('Ctrl Pts',(-5.76527975067285,7.38688747281286,12.5073140819593));
#83349=CARTESIAN_POINT('Ctrl Pts',(-6.0410691708539,7.1690470277892,12.5131878210227));
#83350=CARTESIAN_POINT('Ctrl Pts',(-6.26519866683398,6.97402603365502,12.5180309843374));
#83351=CARTESIAN_POINT('Ctrl Pts',(-6.60774895259073,6.64610159922737,12.5258082207553));
#83352=CARTESIAN_POINT('Ctrl Pts',(-6.7323027751634,6.51990121634516,12.5287223046292));
#83353=CARTESIAN_POINT('Ctrl Pts',(-6.94409460980743,6.29276558707732,12.5338716642795));
#83354=CARTESIAN_POINT('Ctrl Pts',(-7.03289761939615,6.19335931646279,12.536095133488));
#83355=CARTESIAN_POINT('Ctrl Pts',(-7.17340675698332,6.02915272654743,12.5397294195011));
#83356=CARTESIAN_POINT('Ctrl Pts',(-7.22642664434636,5.96550123768505,12.5411290887672));
#83357=CARTESIAN_POINT('Ctrl Pts',(-7.33098032339454,5.83654276931601,12.5439483263265));
#83358=CARTESIAN_POINT('Ctrl Pts',(-7.38250239972979,5.77123576703363,12.5453678279671));
#83359=CARTESIAN_POINT('Ctrl Pts',(-7.51570779995777,5.59768768567244,12.5491193757425));
#83360=CARTESIAN_POINT('Ctrl Pts',(-7.59592281972188,5.48834469772859,12.5514625351314));
#83361=CARTESIAN_POINT('Ctrl Pts',(-7.86090650556243,5.11019673058696,12.5594918122024));
#83362=CARTESIAN_POINT('Ctrl Pts',(-8.03400283670296,4.83350379233838,12.565250382179));
#83363=CARTESIAN_POINT('Ctrl Pts',(-8.26869221245894,4.41079021604326,12.5737276883858));
#83364=CARTESIAN_POINT('Ctrl Pts',(-8.34158933103926,4.27132636338498,12.5764740932088));
#83365=CARTESIAN_POINT('Ctrl Pts',(-8.43493433332424,4.08122913472762,12.5801229601713));
#83366=CARTESIAN_POINT('Ctrl Pts',(-8.45850214303701,4.03215698752978,12.5810565283575));
#83367=CARTESIAN_POINT('Ctrl Pts',(-8.49966855575182,3.94449214631311,12.5827077165169));
#83368=CARTESIAN_POINT('Ctrl Pts',(-8.51743519037644,3.90598023921442,12.5834272964882));
#83369=CARTESIAN_POINT('Ctrl Pts',(-8.55702361428688,3.81861165148472,12.5850473179145));
#83370=CARTESIAN_POINT('Ctrl Pts',(-8.57868960430758,3.76968603065122,12.5859459458041));
#83371=CARTESIAN_POINT('Ctrl Pts',(-8.72305585277571,3.43599040955934,12.5920250303003));
#83372=CARTESIAN_POINT('Ctrl Pts',(-8.83197472711547,3.14546619399227,12.5970781241561));
#83373=CARTESIAN_POINT('Ctrl Pts',(-8.97844502858045,2.68672899232054,12.6049781222875));
#83374=CARTESIAN_POINT('Ctrl Pts',(-9.02610672054987,2.52198039704787,12.6077986057257));
#83375=CARTESIAN_POINT('Ctrl Pts',(-9.08472261532293,2.29634516751517,12.6116658000495));
#83376=CARTESIAN_POINT('Ctrl Pts',(-9.09963501140484,2.23652157870451,12.6126914543787));
#83377=CARTESIAN_POINT('Ctrl Pts',(-9.13765780546985,2.07730757723042,12.615423705342));
#83378=CARTESIAN_POINT('Ctrl Pts',(-9.15973691788171,1.97767956659277,12.6171361265439));
#83379=CARTESIAN_POINT('Ctrl Pts',(-9.19601293007418,1.8003250758322,12.620192933027));
#83380=CARTESIAN_POINT('Ctrl Pts',(-9.21086225564588,1.7227421927309,12.6215329277304));
#83381=CARTESIAN_POINT('Ctrl Pts',(-9.24124005282667,1.55238949577581,12.6244824208304));
#83382=CARTESIAN_POINT('Ctrl Pts',(-9.25635621775802,1.45955485492888,12.6260944312275));
#83383=CARTESIAN_POINT('Ctrl Pts',(-9.30000516016737,1.16345070975723,12.6312511241511));
#83384=CARTESIAN_POINT('Ctrl Pts',(-9.32325802937735,0.959464835855618,
12.6348272221993));
#83385=CARTESIAN_POINT('Ctrl Pts',(-9.36009399285118,0.503710460934793,
12.6428416194209));
#83386=CARTESIAN_POINT('Ctrl Pts',(-9.37025445438468,0.251823575469268,
12.6472885537035));
#83387=CARTESIAN_POINT('Ctrl Pts',(-9.37024777945855,-0.125660008993952,
12.6538898603629));
#83388=CARTESIAN_POINT('Ctrl Pts',(-9.36772447063175,-0.251141934044318,
12.6560732124325));
#83389=CARTESIAN_POINT('Ctrl Pts',(-9.36058956714581,-0.428553724362328,
12.6591292337324));
#83390=CARTESIAN_POINT('Ctrl Pts',(-9.35806408724459,-0.48055373735057,
12.6600211776118));
#83391=CARTESIAN_POINT('Ctrl Pts',(-9.35266863418075,-0.575337177688494,
12.6616384666671));
#83392=CARTESIAN_POINT('Ctrl Pts',(-9.34993810082631,-0.618126975254532,
12.6623652549006));
#83393=CARTESIAN_POINT('Ctrl Pts',(-9.34207338985221,-0.729355841125541,
12.6642469254591));
#83394=CARTESIAN_POINT('Ctrl Pts',(-9.3364808253961,-0.797759985463153,
12.6653968396457));
#83395=CARTESIAN_POINT('Ctrl Pts',(-9.32188707556834,-0.954973034984231,
12.668028575662));
#83396=CARTESIAN_POINT('Ctrl Pts',(-9.31236735529,-1.0437271845457,12.6695061581443));
#83397=CARTESIAN_POINT('Ctrl Pts',(-9.27109792347475,-1.38273642558648,
12.6751377293242));
#83398=CARTESIAN_POINT('Ctrl Pts',(-9.23051565711507,-1.63180812299914,
12.6792523619423));
#83399=CARTESIAN_POINT('Ctrl Pts',(-9.13885095435991,-2.07965453734036,
12.6867675659307));
#83400=CARTESIAN_POINT('Ctrl Pts',(-9.09119689265554,-2.27896872641043,
12.6901544577921));
#83401=CARTESIAN_POINT('Ctrl Pts',(-9.01218731680539,-2.56727726220549,
12.6951563606688));
#83402=CARTESIAN_POINT('Ctrl Pts',(-8.98596209643664,-2.65761508153139,
12.6967383725954));
#83403=CARTESIAN_POINT('Ctrl Pts',(-8.93522059776889,-2.823058082827,12.6996654918217));
#83404=CARTESIAN_POINT('Ctrl Pts',(-8.91110604765518,-2.89827759945263,
12.7010078022192));
#83405=CARTESIAN_POINT('Ctrl Pts',(-8.85367091620872,-3.06993573480985,
12.704098435573));
#83406=CARTESIAN_POINT('Ctrl Pts',(-8.81972047407431,-3.16615299646679,
12.7058508216072));
#83407=CARTESIAN_POINT('Ctrl Pts',(-8.76274867611298,-3.31958132814912,
12.7086773215939));
#83408=CARTESIAN_POINT('Ctrl Pts',(-8.74072205927097,-3.37715300566313,
12.7097452587643));
#83409=CARTESIAN_POINT('Ctrl Pts',(-8.65529935627304,-3.5939896555623,12.7137945115269));
#83410=CARTESIAN_POINT('Ctrl Pts',(-8.58810526253273,-3.75172178793961,
12.7167961027377));
#83411=CARTESIAN_POINT('Ctrl Pts',(-8.38721848115428,-4.18956375899621,
12.7252572305336));
#83412=CARTESIAN_POINT('Ctrl Pts',(-8.24388370220131,-4.46500393824816,
12.7307373534822));
#83413=CARTESIAN_POINT('Ctrl Pts',(-8.06014858242053,-4.77895880835748,
12.7370162877287));
#83414=CARTESIAN_POINT('Ctrl Pts',(-8.03275481892451,-4.82486191493164,
12.7379349684493));
#83415=CARTESIAN_POINT('Ctrl Pts',(-7.982927898071,-4.90675508555095,12.7395734257385));
#83416=CARTESIAN_POINT('Ctrl Pts',(-7.96064039456578,-4.94283196374476,
12.740294950886));
#83417=CARTESIAN_POINT('Ctrl Pts',(-7.9091591695063,-5.02491341500588,12.7419355499385));
#83418=CARTESIAN_POINT('Ctrl Pts',(-7.87980761818948,-5.07081704614308,
12.7428525938493));
#83419=CARTESIAN_POINT('Ctrl Pts',(-7.76381515635722,-5.2487813217405,12.7464110358226));
#83420=CARTESIAN_POINT('Ctrl Pts',(-7.67424096165355,-5.37889924499028,
12.7490199785164));
#83421=CARTESIAN_POINT('Ctrl Pts',(-7.38963317210013,-5.77073734565759,
12.7569828281751));
#83422=CARTESIAN_POINT('Ctrl Pts',(-7.18418257138099,-6.02458371304721,
12.762299151219));
#83423=CARTESIAN_POINT('Ctrl Pts',(-6.87555506321372,-6.36761939360104,
12.7699479345883));
#83424=CARTESIAN_POINT('Ctrl Pts',(-6.78304107448008,-6.46607978686093,
12.7722009630794));
#83425=CARTESIAN_POINT('Ctrl Pts',(-6.63022776282626,-6.6218253791488,12.7758695459237));
#83426=CARTESIAN_POINT('Ctrl Pts',(-6.57123807541899,-6.68036837730453,
12.7772735135125));
#83427=CARTESIAN_POINT('Ctrl Pts',(-6.45185741836016,-6.79573358313071,
12.7800922993934));
#83428=CARTESIAN_POINT('Ctrl Pts',(-6.39147534676179,-6.85255440930589,
12.7815069596919));
#83429=CARTESIAN_POINT('Ctrl Pts',(-6.2317213458274,-6.9989376462568,12.7852219176209));
#83430=CARTESIAN_POINT('Ctrl Pts',(-6.13117178901886,-7.08718642700513,
12.7875329021493));
#83431=CARTESIAN_POINT('Ctrl Pts',(-5.89222525986094,-7.28800930340297,
12.7929588891941));
#83432=CARTESIAN_POINT('Ctrl Pts',(-5.75243434474582,-7.39884430122177,
12.7960843535902));
#83433=CARTESIAN_POINT('Ctrl Pts',(-5.37563497706413,-7.68045733034773,
12.8043496006305));
#83434=CARTESIAN_POINT('Ctrl Pts',(-5.1336580771413,-7.84426104338588,12.8095024459661));
#83435=CARTESIAN_POINT('Ctrl Pts',(-4.83179624496502,-8.0286445717061,12.8156132743452));
#83436=CARTESIAN_POINT('Ctrl Pts',(-4.77884886991007,-8.06027245911707,
12.8166735515385));
#83437=CARTESIAN_POINT('Ctrl Pts',(-4.68913456765904,-8.11266815987354,
12.8184483005386));
#83438=CARTESIAN_POINT('Ctrl Pts',(-4.65253263985235,-8.13371426319955,
12.8191662248213));
#83439=CARTESIAN_POINT('Ctrl Pts',(-4.56676460752064,-8.18226249848533,
12.8208340779508));
#83440=CARTESIAN_POINT('Ctrl Pts',(-4.51749035206061,-8.20956999565315,
12.8217815829397));
#83441=CARTESIAN_POINT('Ctrl Pts',(-4.30322510176282,-8.32580131530933,
12.8258617395966));
#83442=CARTESIAN_POINT('Ctrl Pts',(-4.13583254852035,-8.41020828416124,
12.8289483060192));
#83443=CARTESIAN_POINT('Ctrl Pts',(-3.63894454658943,-8.64233731345837,
12.837950020607));
#83444=CARTESIAN_POINT('Ctrl Pts',(-3.30331186751,-8.77610632138951,12.8438402315696));
#83445=CARTESIAN_POINT('Ctrl Pts',(-2.864535648327,-8.92223712349573,12.8515584681707));
#83446=CARTESIAN_POINT('Ctrl Pts',(-2.76775693789938,-8.95273149575373,
12.8532609156138));
#83447=CARTESIAN_POINT('Ctrl Pts',(-2.59472014175691,-9.00418031141225,
12.8563085481742));
#83448=CARTESIAN_POINT('Ctrl Pts',(-2.51865598712167,-9.02575247163691,
12.8576494791912));
#83449=CARTESIAN_POINT('Ctrl Pts',(-2.35235038248011,-9.07065151074197,
12.8605850445473));
#83450=CARTESIAN_POINT('Ctrl Pts',(-2.2620154449943,-9.09359979454418,12.8621820196724));
#83451=CARTESIAN_POINT('Ctrl Pts',(-1.95656691257297,-9.16636143959714,
12.8675902620821));
#83452=CARTESIAN_POINT('Ctrl Pts',(-1.74003986548826,-9.20991839245714,
12.8714396843452));
#83453=CARTESIAN_POINT('Ctrl Pts',(-1.28603651421049,-9.28466311576228,
12.8795095500928));
#83454=CARTESIAN_POINT('Ctrl Pts',(-1.04849290017805,-9.31447914050837,
12.8837313486381));
#83455=CARTESIAN_POINT('Ctrl Pts',(-0.685190450612173,-9.34600509403241,
12.890108429688));
#83456=CARTESIAN_POINT('Ctrl Pts',(-0.560106606395548,-9.35433471193091,
12.8922891930124));
#83457=CARTESIAN_POINT('Ctrl Pts',(-0.382911040754098,-9.36256760574047,
12.8953422833438));
#83458=CARTESIAN_POINT('Ctrl Pts',(-0.330909614492647,-9.36454974253682,
12.8962338398777));
#83459=CARTESIAN_POINT('Ctrl Pts',(-0.236031105329159,-9.36737493981823,
12.8978508380989));
#83460=CARTESIAN_POINT('Ctrl Pts',(-0.193159726206334,-9.36835702052225,
12.8985777179172));
#83461=CARTESIAN_POINT('Ctrl Pts',(-0.0816155101726701,-9.37014623242085,
12.9004602497299));
#83462=CARTESIAN_POINT('Ctrl Pts',(-0.0129377950548491,-9.37049273811119,
12.9016109239267));
#83463=CARTESIAN_POINT('Ctrl Pts',(0.145080983855336,-9.36955276896177,
12.9042448350719));
#83464=CARTESIAN_POINT('Ctrl Pts',(0.23441232761244,-9.36774351118985,12.9057238227766));
#83465=CARTESIAN_POINT('Ctrl Pts',(0.57638925116337,-9.35592253657426,12.9113663418915));
#83466=CARTESIAN_POINT('Ctrl Pts',(0.82861742339648,-9.33696441907064,12.91549038688));
#83467=CARTESIAN_POINT('Ctrl Pts',(1.2826110092072,-9.28429816204319,12.9230043641579));
#83468=CARTESIAN_POINT('Ctrl Pts',(1.48462839762076,-9.25414293830244,12.926380260416));
#83469=CARTESIAN_POINT('Ctrl Pts',(1.77800053430736,-9.20049683013941,12.9313704623495));
#83470=CARTESIAN_POINT('Ctrl Pts',(1.8702426285614,-9.18219038561656,12.9329520442414));
#83471=CARTESIAN_POINT('Ctrl Pts',(2.03943142549801,-9.14595778687076,12.935878770292));
#83472=CARTESIAN_POINT('Ctrl Pts',(2.11645710575987,-9.12844092187949,12.9372211229269));
#83473=CARTESIAN_POINT('Ctrl Pts',(2.29247750111284,-9.08606341337091,12.9403124241253));
#83474=CARTESIAN_POINT('Ctrl Pts',(2.39130591134677,-9.06055502784747,12.9420654426933));
#83475=CARTESIAN_POINT('Ctrl Pts',(2.54915388756929,-9.01705068641718,12.9448931608116));
#83476=CARTESIAN_POINT('Ctrl Pts',(2.60844678982134,-9.00007744159723,12.9459616812974));
#83477=CARTESIAN_POINT('Ctrl Pts',(2.83203035385175,-8.93367911495131,12.9500140796322));
#83478=CARTESIAN_POINT('Ctrl Pts',(2.99512025600217,-8.88033067454188,12.9530182631492));
#83479=CARTESIAN_POINT('Ctrl Pts',(3.44826668350166,-8.7181974509313,12.961471577699));
#83480=CARTESIAN_POINT('Ctrl Pts',(3.73452808140036,-8.59946569538645,12.9669410724945));
#83481=CARTESIAN_POINT('Ctrl Pts',(4.06280398248845,-8.44381907086855,12.9732123726924));
#83482=CARTESIAN_POINT('Ctrl Pts',(4.11102701454227,-8.42044616418483,12.9741333839756));
#83483=CARTESIAN_POINT('Ctrl Pts',(4.19706122418084,-8.3778315672746,12.9757744599883));
#83484=CARTESIAN_POINT('Ctrl Pts',(4.23494718523305,-8.35874434623318,12.9764962958481));
#83485=CARTESIAN_POINT('Ctrl Pts',(4.32108674439266,-8.3146106335009,12.9781352196089));
#83486=CARTESIAN_POINT('Ctrl Pts',(4.36925449945335,-8.28940020607268,12.9790503031754));
#83487=CARTESIAN_POINT('Ctrl Pts',(4.55516101788885,-8.19002835626909,12.9825816351926));
#83488=CARTESIAN_POINT('Ctrl Pts',(4.69125394763809,-8.11284124380121,12.985166063275));
#83489=CARTESIAN_POINT('Ctrl Pts',(5.1046727407326,-7.86448213000443,12.9930967927187));
#83490=CARTESIAN_POINT('Ctrl Pts',(5.37505129806971,-7.68222537600135,12.9984046178871));
#83491=CARTESIAN_POINT('Ctrl Pts',(5.74433574557468,-7.40424124303973,13.0060647548957));
#83492=CARTESIAN_POINT('Ctrl Pts',(5.85148253379142,-7.31985884805236,13.0083386899635));
#83493=CARTESIAN_POINT('Ctrl Pts',(6.02104684056877,-7.18021712838541,13.0120315384967));
#83494=CARTESIAN_POINT('Ctrl Pts',(6.08463542393567,-7.12641107332891,13.0134385508191));
#83495=CARTESIAN_POINT('Ctrl Pts',(6.20993449032956,-7.01748836042729,13.0162572184229));
#83496=CARTESIAN_POINT('Ctrl Pts',(6.27164926696716,-6.96238785879778,13.0176686529798));
#83497=CARTESIAN_POINT('Ctrl Pts',(6.43032537021254,-6.81689596977543,13.0213592351785));
#83498=CARTESIAN_POINT('Ctrl Pts',(6.52611247782977,-6.72525172832812,13.0236487888546));
#83499=CARTESIAN_POINT('Ctrl Pts',(6.74425156272492,-6.50749696273514,13.0290057971199));
#83500=CARTESIAN_POINT('Ctrl Pts',(6.86506517188461,-6.37991581599831,13.0320832877704));
#83501=CARTESIAN_POINT('Ctrl Pts',(7.18269361790264,-6.02501955053656,13.0404505777085));
#83502=CARTESIAN_POINT('Ctrl Pts',(7.37227181144334,-5.79150730705789,13.0457564438124));
#83503=CARTESIAN_POINT('Ctrl Pts',(7.58240183465557,-5.50560679575271,13.0518826554628));
#83504=CARTESIAN_POINT('Ctrl Pts',(7.6141266033911,-5.46164808974323,13.0528145677359));
#83505=CARTESIAN_POINT('Ctrl Pts',(7.67004182562688,-5.38273629649582,13.0544679764983));
#83506=CARTESIAN_POINT('Ctrl Pts',(7.69437924526506,-5.34788927463507,13.0551913491622));
#83507=CARTESIAN_POINT('Ctrl Pts',(7.74899907637573,-5.26853830235075,13.0568228488166));
#83508=CARTESIAN_POINT('Ctrl Pts',(7.77913672583986,-5.22393667145605,13.0577290878064));
#83509=CARTESIAN_POINT('Ctrl Pts',(7.89178738878311,-5.05408472171865,13.0611442062727));
#83510=CARTESIAN_POINT('Ctrl Pts',(7.97167359667654,-4.9271189225842,13.0636239084289));
#83511=CARTESIAN_POINT('Ctrl Pts',(8.26741873616163,-4.43104675282184,13.0731259570789));
#83512=CARTESIAN_POINT('Ctrl Pts',(8.46096716752743,-4.04924970220302,13.0800750421999));
#83513=CARTESIAN_POINT('Ctrl Pts',(8.66455974168202,-3.56873699642781,13.0888062508559));
#83514=CARTESIAN_POINT('Ctrl Pts',(8.70003898389042,-3.48135044073475,13.0903922939249));
#83515=CARTESIAN_POINT('Ctrl Pts',(8.7627920051014,-3.31983396945678,13.0933231135957));
#83516=CARTESIAN_POINT('Ctrl Pts',(8.7904592948343,-3.24586608804979,13.0946650429543));
#83517=CARTESIAN_POINT('Ctrl Pts',(8.8516080132118,-3.07586766535325,13.0977495036896));
#83518=CARTESIAN_POINT('Ctrl Pts',(8.8844677068294,-2.97962410561035,13.0994960340303));
#83519=CARTESIAN_POINT('Ctrl Pts',(8.99008920548138,-2.65297150767494,13.1054243968104));
#83520=CARTESIAN_POINT('Ctrl Pts',(9.05550432857714,-2.42028973016568,13.1096506692804));
#83521=CARTESIAN_POINT('Ctrl Pts',(9.18324912565045,-1.88765355191921,13.119273402367));
#83522=CARTESIAN_POINT('Ctrl Pts',(9.24001388046839,-1.58664561440863,13.1246774811176));
#83523=CARTESIAN_POINT('Ctrl Pts',(9.28907055922692,-1.23185273654909,13.1308562623385));
#83524=CARTESIAN_POINT('Ctrl Pts',(9.29576844986479,-1.18024656775215,13.1317501245812));
#83525=CARTESIAN_POINT('Ctrl Pts',(9.30712570265132,-1.08663787399349,13.1333611335782));
#83526=CARTESIAN_POINT('Ctrl Pts',(9.31193145695597,-1.0446546177922,13.1340797863737));
#83527=CARTESIAN_POINT('Ctrl Pts',(9.32242962766803,-0.947106437277983,
13.1357403679375));
#83528=CARTESIAN_POINT('Ctrl Pts',(9.32790952965615,-0.89152038246043,13.1366799741992));
#83529=CARTESIAN_POINT('Ctrl Pts',(9.34879909981048,-0.658283431274132,
13.1406003733128));
#83530=CARTESIAN_POINT('Ctrl Pts',(9.35963314326727,-0.48025981470389,13.1435395454143));
#83531=CARTESIAN_POINT('Ctrl Pts',(9.37794377329943,0.0875082831141098,
13.1528676378549));
#83532=CARTESIAN_POINT('Ctrl Pts',(9.3661904525347,0.477455175517611,13.1592207647935));
#83533=CARTESIAN_POINT('Ctrl Pts',(9.32133925177111,0.96093675570428,13.1673404949271));
#83534=CARTESIAN_POINT('Ctrl Pts',(9.31102639980315,1.05619705567807,13.168951083296));
#83535=CARTESIAN_POINT('Ctrl Pts',(9.29053091358485,1.22174528592883,13.1717715166063));
#83536=CARTESIAN_POINT('Ctrl Pts',(9.2810067474086,1.29210677964924,13.172977027119));
#83537=CARTESIAN_POINT('Ctrl Pts',(9.25679874402869,1.4568399459976,13.1758160722478));
#83538=CARTESIAN_POINT('Ctrl Pts',(9.24146996357503,1.55110878714696,13.1774536235183));
#83539=CARTESIAN_POINT('Ctrl Pts',(9.17901015662336,1.90133906214024,13.1835858347068));
#83540=CARTESIAN_POINT('Ctrl Pts',(9.12266314410927,2.15553564234341,13.1881365587494));
#83541=CARTESIAN_POINT('Ctrl Pts',(8.97787556137494,2.70025458588588,13.1980388728562));
#83542=CARTESIAN_POINT('Ctrl Pts',(8.88574909795208,2.98949624088858,13.2033937619685));
#83543=CARTESIAN_POINT('Ctrl Pts',(8.76139256352825,3.32300279817431,13.2095353509837));
#83544=CARTESIAN_POINT('Ctrl Pts',(8.7426164696698,3.37209201074434,13.2104382964981));
#83545=CARTESIAN_POINT('Ctrl Pts',(8.70798289222226,3.46040586687653,13.2120592530836));
#83546=CARTESIAN_POINT('Ctrl Pts',(8.69227088699294,3.49968593709256,13.2127788595037));
#83547=CARTESIAN_POINT('Ctrl Pts',(8.65539685000357,3.59009078517071,13.2144316495641));
#83548=CARTESIAN_POINT('Ctrl Pts',(8.63404696896634,3.64113710720642,13.2153626220637));
#83549=CARTESIAN_POINT('Ctrl Pts',(8.54536381959219,3.84800679678382,13.2191316044131));
#83550=CARTESIAN_POINT('Ctrl Pts',(8.47425412391052,4.00217647000133,13.2219319852535));
#83551=CARTESIAN_POINT('Ctrl Pts',(8.21873165430379,4.51877778819516,13.2314006962793));
#83552=CARTESIAN_POINT('Ctrl Pts',(8.0149380815139,4.87110566085093,13.2380225707983));
#83553=CARTESIAN_POINT('Ctrl Pts',(7.73692410563497,5.28680754316323,13.2463919431851));
#83554=CARTESIAN_POINT('Ctrl Pts',(7.68378153509765,5.36375147471542,13.2479648868423));
#83555=CARTESIAN_POINT('Ctrl Pts',(7.58361418222493,5.50423719684747,13.2508837819991));
#83556=CARTESIAN_POINT('Ctrl Pts',(7.53691978885827,5.56800424267922,13.2522270503616));
#83557=CARTESIAN_POINT('Ctrl Pts',(7.42764431889087,5.71333992846203,13.2553321639237));
#83558=CARTESIAN_POINT('Ctrl Pts',(7.36451637838112,5.79448459369722,13.2570982219685));
#83559=CARTESIAN_POINT('Ctrl Pts',(7.14308511982483,6.0696471600657,13.2631991908054));
#83560=CARTESIAN_POINT('Ctrl Pts',(6.97834851778531,6.25834905152918,13.2675822606507));
#83561=CARTESIAN_POINT('Ctrl Pts',(6.60964995333837,6.64800245765126,13.2770091556841));
#83562=CARTESIAN_POINT('Ctrl Pts',(6.40363534762744,6.84666808760753,13.2820541836698));
#83563=CARTESIAN_POINT('Ctrl Pts',(6.14273390542827,7.07616976783365,13.2880566769176));
#83564=CARTESIAN_POINT('Ctrl Pts',(6.09621340191157,7.11628699528127,13.289112657993));
#83565=CARTESIAN_POINT('Ctrl Pts',(6.01706772419022,7.1831930651257,13.290882901814));
#83566=CARTESIAN_POINT('Ctrl Pts',(5.98465001734411,7.2102240459162,13.29160056726));
#83567=CARTESIAN_POINT('Ctrl Pts',(5.9083911308696,7.27294265078089,13.2932714101589));
#83568=CARTESIAN_POINT('Ctrl Pts',(5.86440754171859,7.30845433464309,13.294222122728));
#83569=CARTESIAN_POINT('Ctrl Pts',(5.66993537020783,7.46258225059225,13.2983753006177));
#83570=CARTESIAN_POINT('Ctrl Pts',(5.51614962886845,7.57696474061692,13.3015295518007));
#83571=CARTESIAN_POINT('Ctrl Pts',(5.06747275471185,7.88977648066575,13.3105053524285));
#83572=CARTESIAN_POINT('Ctrl Pts',(4.76465719249937,8.07625498798875,13.3163052553085));
#83573=CARTESIAN_POINT('Ctrl Pts',(4.39857396922947,8.27392388623823,13.3232478694169));
#83574=CARTESIAN_POINT('Ctrl Pts',(4.34488551263815,8.30224301434379,13.3242640118924));
#83575=CARTESIAN_POINT('Ctrl Pts',(4.29092662791762,8.33003803930856,13.3252837277684));
#83576=CARTESIAN_POINT('Origin',(0.,0.,2.15141010809499));
#83577=CARTESIAN_POINT('',(4.29092664592493,8.33003803003272,14.5226929117958));
#83578=CARTESIAN_POINT('',(4.29092662550047,8.33003804055367,14.3259466798393));
#83579=CARTESIAN_POINT('',(4.29092662815669,8.33003803918541,2.15141010809499));
#83580=CARTESIAN_POINT('Ctrl Pts',(4.29092664592493,8.33003803003272,14.5226929117958));
#83581=CARTESIAN_POINT('Ctrl Pts',(4.41553143336263,8.26585224832338,14.5203910368916));
#83582=CARTESIAN_POINT('Ctrl Pts',(4.53869923662709,8.1988689706793,14.5180966839689));
#83583=CARTESIAN_POINT('Ctrl Pts',(4.80974732334025,8.04348037186033,14.5129714010413));
#83584=CARTESIAN_POINT('Ctrl Pts',(4.95676878350567,7.95372169977639,14.5101388142208));
#83585=CARTESIAN_POINT('Ctrl Pts',(5.1530909291932,7.82630570587419,14.5062565808397));
#83586=CARTESIAN_POINT('Ctrl Pts',(5.20461481983927,7.79213652924653,14.5052281564504));
#83587=CARTESIAN_POINT('Ctrl Pts',(5.34042591853822,7.70012245118076,14.5024901163469));
#83588=CARTESIAN_POINT('Ctrl Pts',(5.4241109934168,7.64140396903468,14.5007746664135));
#83589=CARTESIAN_POINT('Ctrl Pts',(5.57073460871978,7.53490157113011,14.4977146713401));
#83590=CARTESIAN_POINT('Ctrl Pts',(5.6340610406389,7.48766865747195,14.4963745535729));
#83591=CARTESIAN_POINT('Ctrl Pts',(5.77134902899967,7.38254263772988,14.4934272965316));
#83592=CARTESIAN_POINT('Ctrl Pts',(5.8450527417186,7.32432684983428,14.4918176722641));
#83593=CARTESIAN_POINT('Ctrl Pts',(6.22724754380438,7.01300205932098,14.483325113055));
#83594=CARTESIAN_POINT('Ctrl Pts',(6.52021169938399,6.74148691573541,14.4762878326506));
#83595=CARTESIAN_POINT('Ctrl Pts',(6.91561422797623,6.3250740976944,14.466208962389));
#83596=CARTESIAN_POINT('Ctrl Pts',(7.03267048619861,6.19466129951294,14.4631455211113));
#83597=CARTESIAN_POINT('Ctrl Pts',(7.18201270378426,6.01858604658367,14.4591655379477));
#83598=CARTESIAN_POINT('Ctrl Pts',(7.21764473847748,5.9758086420046,14.4582103386609));
#83599=CARTESIAN_POINT('Ctrl Pts',(7.27965813316047,5.89999572049102,14.4565398354746));
#83600=CARTESIAN_POINT('Ctrl Pts',(7.30620094821504,5.86709465966543,14.4558223117547));
#83601=CARTESIAN_POINT('Ctrl Pts',(7.36502958496784,5.79315549761531,14.4542258462433));
#83602=CARTESIAN_POINT('Ctrl Pts',(7.3971967733645,5.75202497548105,14.4533484961273));
#83603=CARTESIAN_POINT('Ctrl Pts',(7.61575329263613,5.46770238935765,14.4473492554394));
#83604=CARTESIAN_POINT('Ctrl Pts',(7.79046114654486,5.21576306877197,14.4423538894095));
#83605=CARTESIAN_POINT('Ctrl Pts',(8.0891311184044,4.73648301312642,14.4330912607407));
#83606=CARTESIAN_POINT('Ctrl Pts',(8.21662561139473,4.51169331703398,14.4288377725612));
#83607=CARTESIAN_POINT('Ctrl Pts',(8.37827401906551,4.19704835303852,14.4229216178048));
#83608=CARTESIAN_POINT('Ctrl Pts',(8.42057988858439,4.11151124284804,14.4213173937684));
#83609=CARTESIAN_POINT('Ctrl Pts',(8.49547003210463,3.95408656582391,14.4183695760692));
#83610=CARTESIAN_POINT('Ctrl Pts',(8.52846670560356,3.88240482873441,14.4170290552328));
#83611=CARTESIAN_POINT('Ctrl Pts',(8.60133125536355,3.71870158749817,14.4139706021536));
#83612=CARTESIAN_POINT('Ctrl Pts',(8.64063516318555,3.62643968251163,14.4122489431954));
#83613=CARTESIAN_POINT('Ctrl Pts',(8.80228287424431,3.22943220904156,14.4048495947702));
#83614=CARTESIAN_POINT('Ctrl Pts',(8.91004183844394,2.91900134520566,14.3990775107848));
#83615=CARTESIAN_POINT('Ctrl Pts',(9.05866365599653,2.40517105667305,14.389674935079));
#83616=CARTESIAN_POINT('Ctrl Pts',(9.10947144826249,2.20494111084259,14.38604955173));
#83617=CARTESIAN_POINT('Ctrl Pts',(9.16760365959272,1.93930547025714,14.3813463270801));
#83618=CARTESIAN_POINT('Ctrl Pts',(9.18091632633381,1.87527011502343,14.3802207141548));
#83619=CARTESIAN_POINT('Ctrl Pts',(9.20170405316214,1.7697468946918,14.3783820031541));
#83620=CARTESIAN_POINT('Ctrl Pts',(9.20957147844763,1.72833872712739,14.3776646376361));
#83621=CARTESIAN_POINT('Ctrl Pts',(9.22679819527974,1.63421139341723,14.3760438498222));
#83622=CARTESIAN_POINT('Ctrl Pts',(9.23598552473437,1.58146236728408,14.3751423213675));
#83623=CARTESIAN_POINT('Ctrl Pts',(9.26724655979226,1.39240542106139,14.3719310383201));
#83624=CARTESIAN_POINT('Ctrl Pts',(9.28675885884841,1.25569174178744,14.3696455056696));
#83625=CARTESIAN_POINT('Ctrl Pts',(9.33774124030956,0.831676988831244,14.3626126174047));
#83626=CARTESIAN_POINT('Ctrl Pts',(9.35894797618795,0.543314996162689,14.3579040089817));
#83627=CARTESIAN_POINT('Ctrl Pts',(9.36902687240109,0.172269232477673,14.3517813640476));
#83628=CARTESIAN_POINT('Ctrl Pts',(9.37017754171549,0.0900779407209574,
14.3504215121783));
#83629=CARTESIAN_POINT('Ctrl Pts',(9.37035024095918,-0.115223120611711,
14.3470111847114));
#83630=CARTESIAN_POINT('Ctrl Pts',(9.36802776886569,-0.238318309557992,
14.3449540587861));
#83631=CARTESIAN_POINT('Ctrl Pts',(9.36014352363104,-0.442624763483723,
14.3415121533339));
#83632=CARTESIAN_POINT('Ctrl Pts',(9.35594784627133,-0.523873387064799,
14.3401361603886));
#83633=CARTESIAN_POINT('Ctrl Pts',(9.34519705755782,-0.690018646916564,
14.337306252971));
#83634=CARTESIAN_POINT('Ctrl Pts',(9.33854173039163,-0.774901339090052,
14.3358518202348));
#83635=CARTESIAN_POINT('Ctrl Pts',(9.31706256520254,-1.00802991795948,14.3318328033841));
#83636=CARTESIAN_POINT('Ctrl Pts',(9.2998586721235,-1.15603098362047,14.3292538033239));
#83637=CARTESIAN_POINT('Ctrl Pts',(9.23416013762911,-1.62369352665651,14.3210257166661));
#83638=CARTESIAN_POINT('Ctrl Pts',(9.1726495594576,-1.94128647176708,14.3153135305538));
#83639=CARTESIAN_POINT('Ctrl Pts',(9.06096294510859,-2.39172768718551,14.3071869788792));
#83640=CARTESIAN_POINT('Ctrl Pts',(9.02400055794059,-2.52761249779053,14.3047334804076));
#83641=CARTESIAN_POINT('Ctrl Pts',(8.96893557800252,-2.71340865089643,14.301396743458));
#83642=CARTESIAN_POINT('Ctrl Pts',(8.95345052841331,-2.76407589645491,14.3004886972824));
#83643=CARTESIAN_POINT('Ctrl Pts',(8.92472210135113,-2.85530041607536,14.298858886342));
#83644=CARTESIAN_POINT('Ctrl Pts',(8.91162989479709,-2.89590360158452,14.2981354757689));
#83645=CARTESIAN_POINT('Ctrl Pts',(8.87732055692088,-2.99987164762169,14.2962873148611));
#83646=CARTESIAN_POINT('Ctrl Pts',(8.85570206141893,-3.06310156585481,14.2951671561396));
#83647=CARTESIAN_POINT('Ctrl Pts',(8.72566871974879,-3.43053688915144,14.2886669335851));
#83648=CARTESIAN_POINT('Ctrl Pts',(8.60226124141433,-3.7292065038023,14.2834122025149));
#83649=CARTESIAN_POINT('Ctrl Pts',(8.36584030670943,-4.2268530833878,14.2743642038139));
#83650=CARTESIAN_POINT('Ctrl Pts',(8.26051643301879,-4.42915780090858,14.2706003591972));
#83651=CARTESIAN_POINT('Ctrl Pts',(8.10163124318907,-4.70892148459844,14.2652164407184));
#83652=CARTESIAN_POINT('Ctrl Pts',(8.05412333252604,-4.78972521546493,14.2636398575589));
#83653=CARTESIAN_POINT('Ctrl Pts',(7.96434743445288,-4.93730676312348,14.2607176836783));
#83654=CARTESIAN_POINT('Ctrl Pts',(7.92243150690984,-5.00428887199618,14.2593748218893));
#83655=CARTESIAN_POINT('Ctrl Pts',(7.82516460160302,-5.15543694010044,14.2563056384726));
#83656=CARTESIAN_POINT('Ctrl Pts',(7.76929352468109,-5.23925654506466,14.2545755227633));
#83657=CARTESIAN_POINT('Ctrl Pts',(7.53614208166534,-5.57710497999386,14.2474867627891));
#83658=CARTESIAN_POINT('Ctrl Pts',(7.34766892289693,-5.82316901339678,14.2420465038897));
#83659=CARTESIAN_POINT('Ctrl Pts',(6.99525451965885,-6.23885589991609,14.2324653663628));
#83660=CARTESIAN_POINT('Ctrl Pts',(6.83645003253995,-6.41247691052005,14.2283323215129));
#83661=CARTESIAN_POINT('Ctrl Pts',(6.63007250681849,-6.6217193702175,14.2232602747088));
#83662=CARTESIAN_POINT('Ctrl Pts',(6.5884720756188,-6.66311223036442,14.2222523428036));
#83663=CARTESIAN_POINT('Ctrl Pts',(6.51929243672265,-6.73066532733789,14.2206018408587));
#83664=CARTESIAN_POINT('Ctrl Pts',(6.49193811252706,-6.75705329093956,14.2199557758819));
#83665=CARTESIAN_POINT('Ctrl Pts',(6.42475116195198,-6.82108209363545,14.2183848887671));
#83666=CARTESIAN_POINT('Ctrl Pts',(6.38474747299337,-6.8585412549335,14.217462848424));
#83667=CARTESIAN_POINT('Ctrl Pts',(6.2213330296312,-7.00889253964606,14.21374449792));
#83668=CARTESIAN_POINT('Ctrl Pts',(6.09523824214875,-7.1188222615964,14.2109846643167));
#83669=CARTESIAN_POINT('Ctrl Pts',(5.76192869360673,-7.3940508719286,14.2038821902126));
#83670=CARTESIAN_POINT('Ctrl Pts',(5.55052295966463,-7.55403901986238,14.1995578552151));
#83671=CARTESIAN_POINT('Ctrl Pts',(5.23548843609199,-7.77207823608147,14.1932335911115));
#83672=CARTESIAN_POINT('Ctrl Pts',(5.13709326449169,-7.83746208810513,14.191274920228));
#83673=CARTESIAN_POINT('Ctrl Pts',(4.9509365725732,-7.95615161802202,14.1875904749214));
#83674=CARTESIAN_POINT('Ctrl Pts',(4.86348396457868,-8.00990918627904,14.1858680962079));
#83675=CARTESIAN_POINT('Ctrl Pts',(4.70717430941078,-8.10248972113392,14.1828007753582));
#83676=CARTESIAN_POINT('Ctrl Pts',(4.63867604494597,-8.14189868375936,14.1814603447239));
#83677=CARTESIAN_POINT('Ctrl Pts',(4.48796000798931,-8.22609042712171,14.1785180404294));
#83678=CARTESIAN_POINT('Ctrl Pts',(4.4055529838738,-8.27051700920359,14.1769137423157));
#83679=CARTESIAN_POINT('Ctrl Pts',(3.96347272233249,-8.50036522412387,14.1683304761735));
#83680=CARTESIAN_POINT('Ctrl Pts',(3.59273783926825,-8.66357640937482,14.1611917970008));
#83681=CARTESIAN_POINT('Ctrl Pts',(3.05185516295581,-8.86098489521453,14.1510878866383));
#83682=CARTESIAN_POINT('Ctrl Pts',(2.88951236659296,-8.91524491032447,14.1480967020569));
#83683=CARTESIAN_POINT('Ctrl Pts',(2.67275125768042,-8.98115010212507,14.1441916059361));
#83684=CARTESIAN_POINT('Ctrl Pts',(2.61958582631218,-8.99680090698764,14.1432408255099));
#83685=CARTESIAN_POINT('Ctrl Pts',(2.52560543177585,-9.02356311271159,14.1415743471479));
#83686=CARTESIAN_POINT('Ctrl Pts',(2.48484846218899,-9.03487145283563,14.1408564824741));
#83687=CARTESIAN_POINT('Ctrl Pts',(2.38330148272883,-9.06230734732912,14.1390793526512));
#83688=CARTESIAN_POINT('Ctrl Pts',(2.3224231313323,-9.07809953902534,14.1380238699629));
#83689=CARTESIAN_POINT('Ctrl Pts',(1.9566946973666,-9.16905186367538,14.1317308710709));
#83690=CARTESIAN_POINT('Ctrl Pts',(1.64838192905665,-9.22946395273604,14.1266174208279));
#83691=CARTESIAN_POINT('Ctrl Pts',(1.13902322594581,-9.30292812518079,14.1181715317708));
#83692=CARTESIAN_POINT('Ctrl Pts',(0.939559463208026,-9.3251848961384,14.1148662869053));
#83693=CARTESIAN_POINT('Ctrl Pts',(0.629275673813051,-9.34975030003893,
14.1096822416045));
#83694=CARTESIAN_POINT('Ctrl Pts',(0.518869910488682,-9.35652673159926,
14.1078296364565));
#83695=CARTESIAN_POINT('Ctrl Pts',(0.328714744639834,-9.36482187551713,
14.1046202270309));
#83696=CARTESIAN_POINT('Ctrl Pts',(0.249018208894852,-9.36727986347498,
14.1032695374666));
#83697=CARTESIAN_POINT('Ctrl Pts',(0.0801230676384112,-9.37033193130456,
14.1003941092843));
#83698=CARTESIAN_POINT('Ctrl Pts',(-0.00907231179823951,-9.3706700856364,
14.0988678714167));
#83699=CARTESIAN_POINT('Ctrl Pts',(-0.277989500013457,-9.36784999826492,
14.0942426997848));
#83700=CARTESIAN_POINT('Ctrl Pts',(-0.457628244701591,-9.36079418651735,
14.0911204785561));
#83701=CARTESIAN_POINT('Ctrl Pts',(-0.692409234804157,-9.344797711926,14.0870059677661));
#83702=CARTESIAN_POINT('Ctrl Pts',(-0.747831548845888,-9.34052583068818,
14.0860322951669));
#83703=CARTESIAN_POINT('Ctrl Pts',(-1.04376177960404,-9.31506514575889,
14.0808226317056));
#83704=CARTESIAN_POINT('Ctrl Pts',(-1.28342109327622,-9.2850798357019,14.076563229374));
#83705=CARTESIAN_POINT('Ctrl Pts',(-1.60810050393344,-9.23164520673233,
14.0708105156161));
#83706=CARTESIAN_POINT('Ctrl Pts',(-1.69434327439867,-9.21620645209041,
14.0692844882224));
#83707=CARTESIAN_POINT('Ctrl Pts',(-1.84686722416187,-9.18668905603141,
14.0665956147054));
#83708=CARTESIAN_POINT('Ctrl Pts',(-1.91323609195933,-9.17309664421673,
14.0654289671049));
#83709=CARTESIAN_POINT('Ctrl Pts',(-2.02125451952012,-9.14975105238991,
14.0635387651339));
#83710=CARTESIAN_POINT('Ctrl Pts',(-2.06299492529017,-9.14043030240214,
14.0628105244323));
#83711=CARTESIAN_POINT('Ctrl Pts',(-2.15582573560471,-9.11903264506006,
14.0611963698826));
#83712=CARTESIAN_POINT('Ctrl Pts',(-2.20688130723002,-9.10681151097122,
14.0603120511362));
#83713=CARTESIAN_POINT('Ctrl Pts',(-2.37210703373872,-9.06579048459115,
14.0574577347068));
#83714=CARTESIAN_POINT('Ctrl Pts',(-2.48583789377713,-9.03526751037888,
14.055504573038));
#83715=CARTESIAN_POINT('Ctrl Pts',(-2.8929529565998,-8.91773745403488,14.0485127964624));
#83716=CARTESIAN_POINT('Ctrl Pts',(-3.1826087914494,-8.81851574618484,14.0435320856308));
#83717=CARTESIAN_POINT('Ctrl Pts',(-3.54519577559341,-8.6741153008183,14.0370971522446));
#83718=CARTESIAN_POINT('Ctrl Pts',(-3.62307690161824,-8.64187497462917,
14.0357033242861));
#83719=CARTESIAN_POINT('Ctrl Pts',(-3.81543564102982,-8.55918709783806,
14.032226584086));
#83720=CARTESIAN_POINT('Ctrl Pts',(-3.92935789753884,-8.5074896005878,14.0301369802971));
#83721=CARTESIAN_POINT('Ctrl Pts',(-4.11586141311511,-8.41830948493116,
14.0266576421233));
#83722=CARTESIAN_POINT('Ctrl Pts',(-4.1890486065118,-8.38213108294013,14.0252771410141));
#83723=CARTESIAN_POINT('Ctrl Pts',(-4.328082189294,-8.31112727242924,14.0226241444642));
#83724=CARTESIAN_POINT('Ctrl Pts',(-4.39400449189261,-8.27646400782297,
14.0213528949536));
#83725=CARTESIAN_POINT('Ctrl Pts',(-4.57594156285564,-8.17801142773907,
14.0178066109427));
#83726=CARTESIAN_POINT('Ctrl Pts',(-4.691027999729,-8.11254388328858,14.0155199107824));
#83727=CARTESIAN_POINT('Ctrl Pts',(-5.08569937248299,-7.87682566338534,
14.0075303317785));
#83728=CARTESIAN_POINT('Ctrl Pts',(-5.35772294839735,-7.69438263699696,
14.0017524467386));
#83729=CARTESIAN_POINT('Ctrl Pts',(-5.74869479152734,-7.40135825181959,
13.9931835222997));
#83730=CARTESIAN_POINT('Ctrl Pts',(-5.87523154447009,-7.30131839634986,
13.9903672980119));
#83731=CARTESIAN_POINT('Ctrl Pts',(-6.04117228970698,-7.16301742965472,
13.9866449361048));
#83732=CARTESIAN_POINT('Ctrl Pts',(-6.08291338559152,-7.12760451297037,
13.9857060951486));
#83733=CARTESIAN_POINT('Ctrl Pts',(-6.15641123895333,-7.06413343204732,
13.9840502928625));
#83734=CARTESIAN_POINT('Ctrl Pts',(-6.18829226972866,-7.03622194613415,
13.9833313090473));
#83735=CARTESIAN_POINT('Ctrl Pts',(-6.26776091341443,-6.96569013772745,
13.9815365549696));
#83736=CARTESIAN_POINT('Ctrl Pts',(-6.31510397482343,-6.92279768425885,
13.9804647710152));
#83737=CARTESIAN_POINT('Ctrl Pts',(-6.52040655012673,-6.73293645606438,
13.9757968909284));
#83738=CARTESIAN_POINT('Ctrl Pts',(-6.67370215175149,-6.5810208221157,13.9722571648482));
#83739=CARTESIAN_POINT('Ctrl Pts',(-6.97282701830862,-6.26337892853039,
13.9651044947037));
#83740=CARTESIAN_POINT('Ctrl Pts',(-7.11832015696917,-6.09752000679087,
13.9614936836005));
#83741=CARTESIAN_POINT('Ctrl Pts',(-7.32698429942988,-5.84198956299416,
13.9560381194012));
#83742=CARTESIAN_POINT('Ctrl Pts',(-7.39465595401591,-5.75609279209739,
13.954221715597));
#83743=CARTESIAN_POINT('Ctrl Pts',(-7.51977380125169,-5.59142968937894,
13.9507652199054));
#83744=CARTESIAN_POINT('Ctrl Pts',(-7.57752447288718,-5.51291273253487,
13.9491276447415));
#83745=CARTESIAN_POINT('Ctrl Pts',(-7.67976947159933,-5.3692592791391,13.9461474813707));
#83746=CARTESIAN_POINT('Ctrl Pts',(-7.72468626654299,-5.30443459696192,
13.9448083749976));
#83747=CARTESIAN_POINT('Ctrl Pts',(-7.82357904406067,-5.15779044241598,
13.9417908055288));
#83748=CARTESIAN_POINT('Ctrl Pts',(-7.87710032031722,-5.0756755005845,13.9401090536203));
#83749=CARTESIAN_POINT('Ctrl Pts',(-8.1155793114134,-4.6969298635971,13.9323882307437));
#83750=CARTESIAN_POINT('Ctrl Pts',(-8.28513585671026,-4.39093376793133,
13.9262383423604));
#83751=CARTESIAN_POINT('Ctrl Pts',(-8.49942070118269,-3.94739055133575,
13.9175816780624));
#83752=CARTESIAN_POINT('Ctrl Pts',(-8.55868626075188,-3.81718928196004,
13.9150720414695));
#83753=CARTESIAN_POINT('Ctrl Pts',(-8.65177061248846,-3.59961305642349,
13.9109524808511));
#83754=CARTESIAN_POINT('Ctrl Pts',(-8.68730131349187,-3.5129965623906,13.9093316048868));
#83755=CARTESIAN_POINT('Ctrl Pts',(-8.73866235313251,-3.38224210000726,
13.9069203213655));
#83756=CARTESIAN_POINT('Ctrl Pts',(-8.7554690546953,-3.33849412008678,13.9061194645881));
#83757=CARTESIAN_POINT('Ctrl Pts',(-8.78593169694011,-3.25738718520531,
13.9046468129294));
#83758=CARTESIAN_POINT('Ctrl Pts',(-8.79967930924727,-3.22006383724469,
13.9039738752412));
#83759=CARTESIAN_POINT('Ctrl Pts',(-8.83931408695079,-3.11030991042829,
13.9020074291811));
#83760=CARTESIAN_POINT('Ctrl Pts',(-8.86454759273273,-3.03764666924492,
13.9007212916723));
#83761=CARTESIAN_POINT('Ctrl Pts',(-9.0023590937942,-2.62445198028432,13.8934771973611));
#83762=CARTESIAN_POINT('Ctrl Pts',(-9.09620752522032,-2.27798771930265,
13.8876565836677));
#83763=CARTESIAN_POINT('Ctrl Pts',(-9.19690587418681,-1.7987964615335,13.8795913462017));
#83764=CARTESIAN_POINT('Ctrl Pts',(-9.22115485537858,-1.67004473007707,
13.8774243699864));
#83765=CARTESIAN_POINT('Ctrl Pts',(-9.26078058992441,-1.43234862053761,
13.8734102385142));
#83766=CARTESIAN_POINT('Ctrl Pts',(-9.27695358451175,-1.32356027968628,
13.8715679342886));
#83767=CARTESIAN_POINT('Ctrl Pts',(-9.30153318469591,-1.13552257876829,
13.8683700018249));
#83768=CARTESIAN_POINT('Ctrl Pts',(-9.31085073514806,-1.05640412072303,
13.8670203593496));
#83769=CARTESIAN_POINT('Ctrl Pts',(-9.32848884955114,-0.888192580895698,
13.8641410870145));
#83770=CARTESIAN_POINT('Ctrl Pts',(-9.33654443321036,-0.799079642526897,
13.8626098962689));
#83771=CARTESIAN_POINT('Ctrl Pts',(-9.35712095283545,-0.528249251967711,
13.8579381253025));
#83772=CARTESIAN_POINT('Ctrl Pts',(-9.36562098330871,-0.346270188238063,
13.8547734871127));
#83773=CARTESIAN_POINT('Ctrl Pts',(-9.36977196277894,-0.109368393421076,
13.8506298389285));
#83774=CARTESIAN_POINT('Ctrl Pts',(-9.37025134270526,-0.0545696691307214,
13.8496697702825));
#83775=CARTESIAN_POINT('Ctrl Pts',(-9.37024410499375,0.240202499639741,
13.8444989748901));
#83776=CARTESIAN_POINT('Ctrl Pts',(-9.36101966834846,0.480085975229739,
13.8402656326414));
#83777=CARTESIAN_POINT('Ctrl Pts',(-9.33338372985667,0.839009173947528,
13.8339726392789));
#83778=CARTESIAN_POINT('Ctrl Pts',(-9.32187231826443,0.958480490726684,
13.8318853256884));
#83779=CARTESIAN_POINT('Ctrl Pts',(-9.30203540768689,1.12981175493476,13.828916184414));
#83780=CARTESIAN_POINT('Ctrl Pts',(-9.29556404183573,1.18187414226275,13.8280172043398));
#83781=CARTESIAN_POINT('Ctrl Pts',(-9.28302299728749,1.2762832362994,13.8263945473307));
#83782=CARTESIAN_POINT('Ctrl Pts',(-9.27709991355352,1.3186478149317,13.82566933824));
#83783=CARTESIAN_POINT('Ctrl Pts',(-9.26103750239161,1.42806444618472,13.8238028578907));
#83784=CARTESIAN_POINT('Ctrl Pts',(-9.25045999356793,1.49504970572261,13.8226663843218));
#83785=CARTESIAN_POINT('Ctrl Pts',(-9.2245315301432,1.64842375461007,13.8200730063592));
#83786=CARTESIAN_POINT('Ctrl Pts',(-9.20869245601344,1.73472364442692,13.8186201685728));
#83787=CARTESIAN_POINT('Ctrl Pts',(-9.14456988660279,2.05842506823737,13.8131770683576));
#83788=CARTESIAN_POINT('Ctrl Pts',(-9.08829808655264,2.29414697965855,13.809223927235));
#83789=CARTESIAN_POINT('Ctrl Pts',(-9.00787157824631,2.58127136314302,13.8043251368891));
#83790=CARTESIAN_POINT('Ctrl Pts',(-8.99230635888001,2.63498359823216,13.8034051992696));
#83791=CARTESIAN_POINT('Ctrl Pts',(-8.92497186402435,2.85979298909571,13.7995370126706));
#83792=CARTESIAN_POINT('Ctrl Pts',(-8.86879299126211,3.02952955320144,13.7965721042473));
#83793=CARTESIAN_POINT('Ctrl Pts',(-8.77739722496202,3.2812828844081,13.7920823504153));
#83794=CARTESIAN_POINT('Ctrl Pts',(-8.74580849991994,3.3645732342173,13.7905816794239));
#83795=CARTESIAN_POINT('Ctrl Pts',(-8.6836921765146,3.52156742356715,13.7877218401226));
#83796=CARTESIAN_POINT('Ctrl Pts',(-8.65340150464513,3.59535663040606,13.7863644077925));
#83797=CARTESIAN_POINT('Ctrl Pts',(-8.5787619580089,3.7707719751039,13.7831047109074));
#83798=CARTESIAN_POINT('Ctrl Pts',(-8.533544168338,3.87201521926783,13.7811966584083));
#83799=CARTESIAN_POINT('Ctrl Pts',(-8.39944085077717,4.15850803882637,13.7757217426879));
#83800=CARTESIAN_POINT('Ctrl Pts',(-8.30624515895175,4.34166864832538,13.7721287101676));
#83801=CARTESIAN_POINT('Ctrl Pts',(-8.05845255641957,4.79143249282006,13.7631112123862));
#83802=CARTESIAN_POINT('Ctrl Pts',(-7.89658530055598,5.05375343474557,13.7576700050687));
#83803=CARTESIAN_POINT('Ctrl Pts',(-7.68632861431998,5.35965707542605,13.7512542474664));
#83804=CARTESIAN_POINT('Ctrl Pts',(-7.6500397832216,5.41132727481883,13.750168299531));
#83805=CARTESIAN_POINT('Ctrl Pts',(-7.58856337718146,5.49700658673556,13.748366327086));
#83806=CARTESIAN_POINT('Ctrl Pts',(-7.56366272111175,5.53121883511605,13.7476465529267));
#83807=CARTESIAN_POINT('Ctrl Pts',(-7.50571931583751,5.6097071804396,13.7459950099833));
#83808=CARTESIAN_POINT('Ctrl Pts',(-7.47251510179593,5.65386196955163,13.745065434287));
#83809=CARTESIAN_POINT('Ctrl Pts',(-7.33648406212632,5.83146357684849,13.7413191909838));
#83810=CARTESIAN_POINT('Ctrl Pts',(-7.23045730687502,5.96242008795891,13.7385395727592));
#83811=CARTESIAN_POINT('Ctrl Pts',(-6.86833710671536,6.38581143121096,13.7293857777355));
#83812=CARTESIAN_POINT('Ctrl Pts',(-6.597585176304,6.66517158078645,13.7230556719449));
#83813=CARTESIAN_POINT('Ctrl Pts',(-6.23617953434901,6.99440452879525,13.7148912824687));
#83814=CARTESIAN_POINT('Ctrl Pts',(-6.16101153239794,7.06070582382147,13.7132085478911));
#83815=CARTESIAN_POINT('Ctrl Pts',(-6.02478838954073,7.17702836814655,13.710182699458));
#83816=CARTESIAN_POINT('Ctrl Pts',(-5.96413747681894,7.22750824696467,13.7088436162022));
#83817=CARTESIAN_POINT('Ctrl Pts',(-5.82871354320694,7.33735630198543,13.7058703777662));
#83818=CARTESIAN_POINT('Ctrl Pts',(-5.75365614288103,7.39635991566899,13.7042334301289));
#83819=CARTESIAN_POINT('Ctrl Pts',(-5.47134176914888,7.61139277225039,13.6981163713023));
#83820=CARTESIAN_POINT('Ctrl Pts',(-5.25853540764957,7.75994105164088,13.6935806175734));
#83821=CARTESIAN_POINT('Ctrl Pts',(-4.78490249907385,8.06211771660023,13.6837104485165));
#83822=CARTESIAN_POINT('Ctrl Pts',(-4.52223913675435,8.21233143266858,13.6783726615362));
#83823=CARTESIAN_POINT('Ctrl Pts',(-4.20524620297512,8.37378852487856,13.6722325124629));
#83824=CARTESIAN_POINT('Ctrl Pts',(-4.15751321550853,8.39758975934428,13.6713158948368));
#83825=CARTESIAN_POINT('Ctrl Pts',(-4.07148282404111,8.43957402324355,13.6696797521683));
#83826=CARTESIAN_POINT('Ctrl Pts',(-4.03326036959856,8.4579071222804,13.668958498521));
#83827=CARTESIAN_POINT('Ctrl Pts',(-3.94553406769704,8.49925444428757,13.6673163981042));
#83828=CARTESIAN_POINT('Ctrl Pts',(-3.89595097587032,8.52209664343502,13.6663976042258));
#83829=CARTESIAN_POINT('Ctrl Pts',(-3.70089060088279,8.60989993093465,13.6628144775688));
#83830=CARTESIAN_POINT('Ctrl Pts',(-3.55396547309669,8.67157988848993,13.6601831845256));
#83831=CARTESIAN_POINT('Ctrl Pts',(-3.02974909658397,8.87608674710629,13.6509321499499));
#83832=CARTESIAN_POINT('Ctrl Pts',(-2.64488564121107,8.99827071226635,13.6443685991963));
#83833=CARTESIAN_POINT('Ctrl Pts',(-2.1574835876537,9.11902428057033,13.6359792982354));
#83834=CARTESIAN_POINT('Ctrl Pts',(-2.06124918664057,9.14125762625234,13.6343204519353));
#83835=CARTESIAN_POINT('Ctrl Pts',(-1.88756472396255,9.17850232539342,13.631319006617));
#83836=CARTESIAN_POINT('Ctrl Pts',(-1.8102423634587,9.19406482881105,13.6299801483228));
#83837=CARTESIAN_POINT('Ctrl Pts',(-1.63765413609716,9.22653965598941,13.6269848413324));
#83838=CARTESIAN_POINT('Ctrl Pts',(-1.54230420375037,9.24295638718684,13.6253253495142));
#83839=CARTESIAN_POINT('Ctrl Pts',(-1.39055284394043,9.26667034765137,13.6226768121504));
#83840=CARTESIAN_POINT('Ctrl Pts',(-1.33430969910463,9.27493580352531,13.6216935997887));
#83841=CARTESIAN_POINT('Ctrl Pts',(-1.19900741971246,9.29356355473358,13.6193248381689));
#83842=CARTESIAN_POINT('Ctrl Pts',(-1.11988446667426,9.30342953395587,13.617936755534));
#83843=CARTESIAN_POINT('Ctrl Pts',(-0.771594301594879,9.34235086819596,
13.6118172990465));
#83844=CARTESIAN_POINT('Ctrl Pts',(-0.501366810691159,9.36074293800375,
13.6070410959149));
#83845=CARTESIAN_POINT('Ctrl Pts',(-0.0707876889876929,9.37134831852746,
13.5994875825991));
#83846=CARTESIAN_POINT('Ctrl Pts',(0.0892237044766844,9.3711909369757,13.5966940444714));
#83847=CARTESIAN_POINT('Ctrl Pts',(0.303562747941404,9.3654896971273,13.5929988984837));
#83848=CARTESIAN_POINT('Ctrl Pts',(0.357959227598983,9.36356838061255,13.5920652172544));
#83849=CARTESIAN_POINT('Ctrl Pts',(0.450334831579198,9.3594994694455,13.5904883042248));
#83850=CARTESIAN_POINT('Ctrl Pts',(0.488323042781744,9.35759436977103,13.5898424226135));
#83851=CARTESIAN_POINT('Ctrl Pts',(0.585353674315503,9.35213583389683,13.5881990380156));
#83852=CARTESIAN_POINT('Ctrl Pts',(0.64437588747053,9.34825455996213,13.587205186828));
#83853=CARTESIAN_POINT('Ctrl Pts',(0.741139622399783,9.34097065095967,13.5855827060884));
#83854=CARTESIAN_POINT('Ctrl Pts',(0.778904206077944,9.33789745523028,13.5849512155016));
#83855=CARTESIAN_POINT('Ctrl Pts',(0.925824708121688,9.325043925158,13.5824996066932));
#83856=CARTESIAN_POINT('Ctrl Pts',(1.03482449804371,9.3135779338721,13.5806917763604));
#83857=CARTESIAN_POINT('Ctrl Pts',(1.46760170511265,9.26036154279829,13.5735225127501));
#83858=CARTESIAN_POINT('Ctrl Pts',(1.78930156091811,9.20361618019595,13.5682045452544));
#83859=CARTESIAN_POINT('Ctrl Pts',(2.23876338725272,9.09987384593492,13.5605580647563));
#83860=CARTESIAN_POINT('Ctrl Pts',(2.369473878563,9.06671709686617,13.5583091919493));
#83861=CARTESIAN_POINT('Ctrl Pts',(2.57948071776047,9.00859392337947,13.5546454349429));
#83862=CARTESIAN_POINT('Ctrl Pts',(2.65924012028335,8.9853729579693,13.5532420754153));
#83863=CARTESIAN_POINT('Ctrl Pts',(2.81800442582266,8.93685158160099,13.5504232560687));
#83864=CARTESIAN_POINT('Ctrl Pts',(2.89700323087115,8.91155639475026,13.5490079416203));
#83865=CARTESIAN_POINT('Ctrl Pts',(3.10273509008446,8.84265686678181,13.5452880202451));
#83866=CARTESIAN_POINT('Ctrl Pts',(3.22888655714876,8.79737670857217,13.5429726688563));
#83867=CARTESIAN_POINT('Ctrl Pts',(3.5210834338707,8.68536510333768,13.53753254773));
#83868=CARTESIAN_POINT('Ctrl Pts',(3.68627499020414,8.61655220993656,13.5343972276331));
#83869=CARTESIAN_POINT('Ctrl Pts',(3.99842497119523,8.47590125834029,13.5283814288471));
#83870=CARTESIAN_POINT('Ctrl Pts',(4.14565216786008,8.40487107718726,13.5255038955705));
#83871=CARTESIAN_POINT('Ctrl Pts',(4.29092664483271,8.33003803059534,13.5226410022223));
#83872=CARTESIAN_POINT('',(-9.37024987374761,-0.000112039410554904,13.6510063850557));
#83873=CARTESIAN_POINT('Ctrl Pts',(4.29092662791762,8.33003803930856,13.3252837277684));
#83874=CARTESIAN_POINT('Ctrl Pts',(4.25433914434803,8.34888479688114,13.3259751586246));
#83875=CARTESIAN_POINT('Ctrl Pts',(4.21762732641183,8.36749058838333,13.3266682295477));
#83876=CARTESIAN_POINT('Ctrl Pts',(4.11001364099518,8.42114172422255,13.3286980998132));
#83877=CARTESIAN_POINT('Ctrl Pts',(4.03878991457186,8.45553168409844,13.3300394013147));
#83878=CARTESIAN_POINT('Ctrl Pts',(3.88295348583062,8.52835812967984,13.3329705620834));
#83879=CARTESIAN_POINT('Ctrl Pts',(3.79818706397135,8.56644588695825,13.3345627067117));
#83880=CARTESIAN_POINT('Ctrl Pts',(3.51333351220943,8.6893786974053,13.3399059043401));
#83881=CARTESIAN_POINT('Ctrl Pts',(3.3108640048278,8.76852287938427,13.3436937119541));
#83882=CARTESIAN_POINT('Ctrl Pts',(2.8807517340493,8.91962812301239,13.3516877117272));
#83883=CARTESIAN_POINT('Ctrl Pts',(2.65273902985008,8.9900763044122,13.3558960421617));
#83884=CARTESIAN_POINT('Ctrl Pts',(2.29803065092168,9.08499782782943,13.3623198403822));
#83885=CARTESIAN_POINT('Ctrl Pts',(2.17310234121991,9.11568739968306,13.3645587888549));
#83886=CARTESIAN_POINT('Ctrl Pts',(1.99611700393168,9.1553199506668,13.3676814064442));
#83887=CARTESIAN_POINT('Ctrl Pts',(1.94455584931509,9.16640982381599,13.3685852419767));
#83888=CARTESIAN_POINT('Ctrl Pts',(1.85531382107322,9.18481729852027,13.3701378910811));
#83889=CARTESIAN_POINT('Ctrl Pts',(1.81767668326768,9.19233972702623,13.3707890017838));
#83890=CARTESIAN_POINT('Ctrl Pts',(1.71820388056441,9.21158626296818,13.372500725644));
#83891=CARTESIAN_POINT('Ctrl Pts',(1.65629445430179,9.22291899359172,13.3735569462511));
#83892=CARTESIAN_POINT('Ctrl Pts',(1.51652562678216,9.24705144006855,13.3759253234861));
#83893=CARTESIAN_POINT('Ctrl Pts',(1.43860920456866,9.25949317755083,13.3772343595031));
#83894=CARTESIAN_POINT('Ctrl Pts',(1.17029444650478,9.29886932455034,13.3817155947945));
#83895=CARTESIAN_POINT('Ctrl Pts',(0.979229412805784,9.32092644435171,13.3848616491889));
#83896=CARTESIAN_POINT('Ctrl Pts',(0.635871400396342,9.34989007814254,13.390510587555));
#83897=CARTESIAN_POINT('Ctrl Pts',(0.483832263893323,9.35898943108613,13.3930100647453));
#83898=CARTESIAN_POINT('Ctrl Pts',(0.171616570313395,9.37004654132625,13.3981701871388));
#83899=CARTESIAN_POINT('Ctrl Pts',(0.0114753247046249,9.37161098934903,
13.4008317258371));
#83900=CARTESIAN_POINT('Ctrl Pts',(-0.235314128884163,9.36769602938699,
13.4049736159322));
#83901=CARTESIAN_POINT('Ctrl Pts',(-0.321978008241194,9.36511781864869,
13.406435648632));
#83902=CARTESIAN_POINT('Ctrl Pts',(-0.489080552862117,9.357824308307,13.4092711335111));
#83903=CARTESIAN_POINT('Ctrl Pts',(-0.56951884636652,9.35327342806366,13.4106434099543));
#83904=CARTESIAN_POINT('Ctrl Pts',(-0.766973779805546,9.33954557521882,
13.4140308856371));
#83905=CARTESIAN_POINT('Ctrl Pts',(-0.883895705368397,9.32920621531617,
13.4160531862818));
#83906=CARTESIAN_POINT('Ctrl Pts',(-1.14444585285477,9.30122364509327,13.4205950135276));
#83907=CARTESIAN_POINT('Ctrl Pts',(-1.28792203176478,9.28244441389174,13.4231202465825));
#83908=CARTESIAN_POINT('Ctrl Pts',(-1.77496948206278,9.2071860483114,13.4317572321618));
#83909=CARTESIAN_POINT('Ctrl Pts',(-2.11580271625539,9.13488753207197,13.4379213658748));
#83910=CARTESIAN_POINT('Ctrl Pts',(-2.51590364716088,9.02641802794577,13.445093518079));
#83911=CARTESIAN_POINT('Ctrl Pts',(-2.57980068845243,9.0083640032538,13.4462365482159));
#83912=CARTESIAN_POINT('Ctrl Pts',(-2.68438407198202,8.97761010597331,13.448100592264));
#83913=CARTESIAN_POINT('Ctrl Pts',(-2.72518514955378,8.96530908456337,13.4488260173978));
#83914=CARTESIAN_POINT('Ctrl Pts',(-2.81674254388668,8.93702288651081,13.4504492977752));
#83915=CARTESIAN_POINT('Ctrl Pts',(-2.86744935859713,8.92088285012275,13.4513453995999));
#83916=CARTESIAN_POINT('Ctrl Pts',(-3.05411120213506,8.85971223272662,13.4546376995935));
#83917=CARTESIAN_POINT('Ctrl Pts',(-3.18916641099927,8.81199829225072,13.4570073764402));
#83918=CARTESIAN_POINT('Ctrl Pts',(-3.63963761670756,8.6411371821161,13.4649387472786));
#83919=CARTESIAN_POINT('Ctrl Pts',(-3.94945969166991,8.50399802181716,13.4704483143879));
#83920=CARTESIAN_POINT('Ctrl Pts',(-4.37440080033387,8.28766080376121,13.4783483641807));
#83921=CARTESIAN_POINT('Ctrl Pts',(-4.4962185495701,8.22220910492731,13.4806533717839));
#83922=CARTESIAN_POINT('Ctrl Pts',(-4.68927174158877,8.1129095002676,13.4843822928311));
#83923=CARTESIAN_POINT('Ctrl Pts',(-4.76144623391158,8.07076203021758,13.4857938321148));
#83924=CARTESIAN_POINT('Ctrl Pts',(-4.90370752894744,7.98511366048696,13.4886126039226));
#83925=CARTESIAN_POINT('Ctrl Pts',(-4.97380307506328,7.94164155779215,13.4900195251673));
#83926=CARTESIAN_POINT('Ctrl Pts',(-5.15359399022164,7.82682408025446,13.4936759768804));
#83927=CARTESIAN_POINT('Ctrl Pts',(-5.26238501085859,7.75409634032873,13.4959355242761));
#83928=CARTESIAN_POINT('Ctrl Pts',(-5.51054458422183,7.58057087901413,13.5011969569443));
#83929=CARTESIAN_POINT('Ctrl Pts',(-5.64873244267406,7.47816675660149,13.504208304193));
#83930=CARTESIAN_POINT('Ctrl Pts',(-6.02629836797052,7.18193170602994,13.5126377322141));
#83931=CARTESIAN_POINT('Ctrl Pts',(-6.2590553988498,6.98001725548903,13.5180755394343));
#83932=CARTESIAN_POINT('Ctrl Pts',(-6.52045378298172,6.72964967995398,13.5243245926291));
#83933=CARTESIAN_POINT('Ctrl Pts',(-6.55913643633165,6.69195274769418,13.5252530369555));
#83934=CARTESIAN_POINT('Ctrl Pts',(-6.62765443832374,6.62401585158094,13.5269025077077));
#83935=CARTESIAN_POINT('Ctrl Pts',(-6.65761412518977,6.59390351270326,13.5276253769656));
#83936=CARTESIAN_POINT('Ctrl Pts',(-6.70652647631659,6.5440687451038,13.5288079280013));
#83937=CARTESIAN_POINT('Ctrl Pts',(-6.72559924420123,6.52446533648689,13.5292697246983));
#83938=CARTESIAN_POINT('Ctrl Pts',(-6.74588871697685,6.50342786556879,13.529761878767));
#83939=CARTESIAN_POINT('Ctrl Pts',(-6.74719110455674,6.50207665158473,13.5297934742631));
#83940=CARTESIAN_POINT('Ctrl Pts',(-6.74986273210688,6.4993031978665,13.5298582953334));
#83941=CARTESIAN_POINT('Ctrl Pts',(-6.7512319287222,6.49788091647469,13.5298915202851));
#83942=CARTESIAN_POINT('Ctrl Pts',(-6.75404628966078,6.49495559086128,13.529959822912));
#83943=CARTESIAN_POINT('Ctrl Pts',(-6.75549140199688,6.49345249676073,13.5299948998474));
#83944=CARTESIAN_POINT('Ctrl Pts',(-6.75846753347835,6.49035488613068,13.5300671494523));
#83945=CARTESIAN_POINT('Ctrl Pts',(-6.75999849034144,6.4887603099193,13.5301043212438));
#83946=CARTESIAN_POINT('Ctrl Pts',(-6.76315719485408,6.48546801333634,13.5301810269608));
#83947=CARTESIAN_POINT('Ctrl Pts',(-6.76478486786365,6.48377022154854,13.5302205598446));
#83948=CARTESIAN_POINT('Ctrl Pts',(-6.76814896026576,6.48025856115504,13.5303022807183));
#83949=CARTESIAN_POINT('Ctrl Pts',(-6.7698852901399,6.47844460701169,13.5303444674724));
#83950=CARTESIAN_POINT('Ctrl Pts',(-6.77211693355532,6.47611131897801,13.5303986986174));
#83951=CARTESIAN_POINT('Ctrl Pts',(-6.77261291676864,6.47559262594246,13.5304107521363));
#83952=CARTESIAN_POINT('Ctrl Pts',(-6.77370170220674,6.47445372584381,13.5304372134979));
#83953=CARTESIAN_POINT('Ctrl Pts',(-6.77429447885283,6.47383349433359,13.530451620993));
#83954=CARTESIAN_POINT('Ctrl Pts',(-6.77559762132539,6.47246962094165,13.5304832960176));
#83955=CARTESIAN_POINT('Ctrl Pts',(-6.77630794992216,6.47172594351342,13.5305005630431));
#83956=CARTESIAN_POINT('Ctrl Pts',(-6.77787205860917,6.47008786250413,13.5305385871085));
#83957=CARTESIAN_POINT('Ctrl Pts',(-6.7787257841355,6.46919340682398,13.5305593434135));
#83958=CARTESIAN_POINT('Ctrl Pts',(-6.78060907252633,6.46721948702191,13.5306051353573));
#83959=CARTESIAN_POINT('Ctrl Pts',(-6.78163855472392,6.46613994596658,13.5306301699158));
#83960=CARTESIAN_POINT('Ctrl Pts',(-6.78391412917726,6.46375257985646,13.5306855127569));
#83961=CARTESIAN_POINT('Ctrl Pts',(-6.78516010114829,6.4624446401836,13.5307158194399));
#83962=CARTESIAN_POINT('Ctrl Pts',(-6.78792022660939,6.45954556327803,13.5307829653193));
#83963=CARTESIAN_POINT('Ctrl Pts',(-6.78943419904825,6.45795425376123,13.5308198021282));
#83964=CARTESIAN_POINT('Ctrl Pts',(-6.79279577912509,6.45441846801403,13.5309016075294));
#83965=CARTESIAN_POINT('Ctrl Pts',(-6.79464311168072,6.45247373044106,13.5309465725318));
#83966=CARTESIAN_POINT('Ctrl Pts',(-6.79875460407693,6.44814172622635,13.5310466696401));
#83967=CARTESIAN_POINT('Ctrl Pts',(-6.80101834215558,6.44575405966016,13.5311017963118));
#83968=CARTESIAN_POINT('Ctrl Pts',(-6.8060682203297,6.4404221037233,13.5312248040075));
#83969=CARTESIAN_POINT('Ctrl Pts',(-6.80885370850797,6.43747719763367,13.5312926767637));
#83970=CARTESIAN_POINT('Ctrl Pts',(-6.81508028691074,6.43088569982227,13.5314444481101));
#83971=CARTESIAN_POINT('Ctrl Pts',(-6.81852036315749,6.427238151682,13.5315283340916));
#83972=CARTESIAN_POINT('Ctrl Pts',(-6.82622218909576,6.41905868397918,13.5317162230106));
#83973=CARTESIAN_POINT('Ctrl Pts',(-6.83048235678544,6.41452527759748,13.5318202067563));
#83974=CARTESIAN_POINT('Ctrl Pts',(-6.83581736602381,6.4088367501763,13.5319504973718));
#83975=CARTESIAN_POINT('Ctrl Pts',(-6.83689643411496,6.40768559631603,13.5319768538595));
#83976=CARTESIAN_POINT('Ctrl Pts',(-6.83991637373446,6.40446228216286,13.5320506269842));
#83977=CARTESIAN_POINT('Ctrl Pts',(-6.84185659370975,6.40238951286484,13.5320980360213));
#83978=CARTESIAN_POINT('Ctrl Pts',(-6.84727134802902,6.39659956842215,13.5322303789693));
#83979=CARTESIAN_POINT('Ctrl Pts',(-6.85074379732056,6.3928804443511,13.5323152889368));
#83980=CARTESIAN_POINT('Ctrl Pts',(-6.8603721072006,6.38255130806522,13.5325508365931));
#83981=CARTESIAN_POINT('Ctrl Pts',(-6.86652144271549,6.37593521972591,13.5327014013063));
#83982=CARTESIAN_POINT('Ctrl Pts',(-6.93615342164577,6.30080039642089,13.5344078235381));
#83983=CARTESIAN_POINT('Ctrl Pts',(-6.99861778938336,6.23134488018772,13.5359528434712));
#83984=CARTESIAN_POINT('Ctrl Pts',(-7.24561567658521,5.94830273481953,13.5421431376852));
#83985=CARTESIAN_POINT('Ctrl Pts',(-7.42149442495577,5.72736176771968,13.5467423619323));
#83986=CARTESIAN_POINT('Ctrl Pts',(-7.69108316605216,5.355390062222,13.5543121666704));
#83987=CARTESIAN_POINT('Ctrl Pts',(-7.79094626176988,5.20904204871112,13.5572487189054));
#83988=CARTESIAN_POINT('Ctrl Pts',(-7.93564574326462,4.98350886893447,13.5617375451873));
#83989=CARTESIAN_POINT('Ctrl Pts',(-7.98357661967185,4.9063569293355,13.56326670701));
#83990=CARTESIAN_POINT('Ctrl Pts',(-8.0607747123919,4.77796773001299,13.5658029458229));
#83991=CARTESIAN_POINT('Ctrl Pts',(-8.09069311721066,4.72712909301443,13.5668050708216));
#83992=CARTESIAN_POINT('Ctrl Pts',(-8.15750155968644,4.61111286571039,13.5690875019796));
#83993=CARTESIAN_POINT('Ctrl Pts',(-8.19409423277976,4.54576871744796,13.5703698976355));
#83994=CARTESIAN_POINT('Ctrl Pts',(-8.2753842187533,4.39643624774469,13.5732936553552));
#83995=CARTESIAN_POINT('Ctrl Pts',(-8.31959361320003,4.31219175204795,13.5749381984306));
#83996=CARTESIAN_POINT('Ctrl Pts',(-8.43663871818134,4.08065064213426,13.5794432985791));
#83997=CARTESIAN_POINT('Ctrl Pts',(-8.50689503605345,3.93208839828071,13.5823181862141));
#83998=CARTESIAN_POINT('Ctrl Pts',(-8.70144067558025,3.4910551139186,13.5907809104323));
#83999=CARTESIAN_POINT('Ctrl Pts',(-8.81480414028925,3.19402000867285,13.5963957164846));
#84000=CARTESIAN_POINT('Ctrl Pts',(-8.93197983695458,2.83287127004801,13.6029556739764));
#84001=CARTESIAN_POINT('Ctrl Pts',(-8.95051508756268,2.77375253638042,13.6040208854829));
#84002=CARTESIAN_POINT('Ctrl Pts',(-8.98069810694544,2.67402888723112,13.6058008279254));
#84003=CARTESIAN_POINT('Ctrl Pts',(-8.99266003679972,2.63352130335847,13.6065190684839));
#84004=CARTESIAN_POINT('Ctrl Pts',(-9.01571346782891,2.55346484677153,13.6079290138334));
#84005=CARTESIAN_POINT('Ctrl Pts',(-9.02681957508127,2.51392132425797,13.6086210345943));
#84006=CARTESIAN_POINT('Ctrl Pts',(-9.06586012559356,2.37132156994564,13.61110265384));
#84007=CARTESIAN_POINT('Ctrl Pts',(-9.09229265372062,2.26786247488045,13.612877129768));
#84008=CARTESIAN_POINT('Ctrl Pts',(-9.1726701409767,1.92922735115369,13.6186296391887));
#84009=CARTESIAN_POINT('Ctrl Pts',(-9.21930174663869,1.69241584346927,13.6225678326773));
#84010=CARTESIAN_POINT('Ctrl Pts',(-9.29374705406242,1.21848989243408,13.6304422903755));
#84011=CARTESIAN_POINT('Ctrl Pts',(-9.32174570217052,0.981584683065158,
13.6343752900242));
#84012=CARTESIAN_POINT('Ctrl Pts',(-9.34803975904847,0.651413976895667,
13.6399165415983));
#84013=CARTESIAN_POINT('Ctrl Pts',(-9.35402963813424,0.558853275222426,
13.6414761429096));
#84014=CARTESIAN_POINT('Ctrl Pts',(-9.36253092642073,0.388202739958158,
13.6443654091715));
#84015=CARTESIAN_POINT('Ctrl Pts',(-9.36544175453,0.310140976588955,13.6456923957318));
#84016=CARTESIAN_POINT('Ctrl Pts',(-9.36929292215148,0.154678726856719,
13.6483465531186));
#84017=CARTESIAN_POINT('Ctrl Pts',(-9.37025092521758,0.0772847412573868,
13.649673507729));
#84018=CARTESIAN_POINT('Ctrl Pts',(-9.37024999932951,-0.000112095055203477,
13.6510061684742));
#84019=CARTESIAN_POINT('Ctrl Pts',(-9.37024999933013,-0.000112043156642308,
13.6510061675806));
#84020=CARTESIAN_POINT('Ctrl Pts',(-9.3702488395512,-0.0971051916695123,
13.6526762482647));
#84021=CARTESIAN_POINT('Ctrl Pts',(-9.36874168983789,-0.194092347865134,
13.6543551374663));
#84022=CARTESIAN_POINT('Ctrl Pts',(-9.35727739558263,-0.563017704195856,
13.6607723877306));
#84023=CARTESIAN_POINT('Ctrl Pts',(-9.33698236069871,-0.834499158935258,
13.6655627546302));
#84024=CARTESIAN_POINT('Ctrl Pts',(-9.28821281498095,-1.24528170400177,
13.6728319962421));
#84025=CARTESIAN_POINT('Ctrl Pts',(-9.26834038644242,-1.38545674867222,
13.6753153670229));
#84026=CARTESIAN_POINT('Ctrl Pts',(-9.23433930152131,-1.59157077577059,
13.6789514452263));
#84027=CARTESIAN_POINT('Ctrl Pts',(-9.22266274298759,-1.65789379164598,
13.680119019226));
#84028=CARTESIAN_POINT('Ctrl Pts',(-9.20210088476301,-1.76773772935149,
13.6820458455685));
#84029=CARTESIAN_POINT('Ctrl Pts',(-9.19361926202526,-1.81133162275184,
13.6828087302879));
#84030=CARTESIAN_POINT('Ctrl Pts',(-9.17665669737404,-1.89532606738809,
13.6842740739909));
#84031=CARTESIAN_POINT('Ctrl Pts',(-9.16821806360247,-1.93573412450207,
13.6849769243828));
#84032=CARTESIAN_POINT('Ctrl Pts',(-9.1485064433321,-2.02710104929343,13.6865608217591));
#84033=CARTESIAN_POINT('Ctrl Pts',(-9.13707419514622,-2.07802405580281,
13.6874400801842));
#84034=CARTESIAN_POINT('Ctrl Pts',(-9.09652690156851,-2.25182823997268,
13.690432805628));
#84035=CARTESIAN_POINT('Ctrl Pts',(-9.06535349208769,-2.37421530471821,
13.6925261731818));
#84036=CARTESIAN_POINT('Ctrl Pts',(-8.9680224060908,-2.72641465877341,13.6985511172254));
#84037=CARTESIAN_POINT('Ctrl Pts',(-8.89552976691311,-2.95437188039995,
13.702453500911));
#84038=CARTESIAN_POINT('Ctrl Pts',(-8.73978894374367,-3.38615207178213,
13.7099950089209));
#84039=CARTESIAN_POINT('Ctrl Pts',(-8.65792305638591,-3.5903070277325,13.7136275092206));
#84040=CARTESIAN_POINT('Ctrl Pts',(-8.53260618597959,-3.87353655356323,
13.7188113975454));
#84041=CARTESIAN_POINT('Ctrl Pts',(-8.49508156019532,-3.95515397870763,
13.7203223247542));
#84042=CARTESIAN_POINT('Ctrl Pts',(-8.42516410698837,-4.10163988209509,
13.7230674668507));
#84043=CARTESIAN_POINT('Ctrl Pts',(-8.39318082495865,-4.16669600109397,
13.7242987057597));
#84044=CARTESIAN_POINT('Ctrl Pts',(-8.31763183327126,-4.3159674212755,13.7271526156484));
#84045=CARTESIAN_POINT('Ctrl Pts',(-8.27353638210375,-4.39990565492697,
13.7287789468099));
#84046=CARTESIAN_POINT('Ctrl Pts',(-8.05299790657777,-4.80467128592429,
13.7367269244048));
#84047=CARTESIAN_POINT('Ctrl Pts',(-7.85912786791901,-5.11563760000234,
13.7431734173052));
#84048=CARTESIAN_POINT('Ctrl Pts',(-7.56927819585957,-5.52503098289925,
13.7519857710494));
#84049=CARTESIAN_POINT('Ctrl Pts',(-7.48860440561291,-5.63389243082866,
13.7543611222191));
#84050=CARTESIAN_POINT('Ctrl Pts',(-7.36531764093396,-5.79292702966547,
13.7578620449607));
#84051=CARTESIAN_POINT('Ctrl Pts',(-7.32449091579521,-5.84446236802974,
13.7590014404581));
#84052=CARTESIAN_POINT('Ctrl Pts',(-7.25553149641298,-5.92965185922325,
13.7608904811255));
#84053=CARTESIAN_POINT('Ctrl Pts',(-7.22769881137141,-5.96354578823632,
13.7616435645954));
#84054=CARTESIAN_POINT('Ctrl Pts',(-7.19084388313023,-6.00778975364928,
13.7626279164477));
#84055=CARTESIAN_POINT('Ctrl Pts',(-7.18203542694448,-6.01831709051949,
13.7628622290497));
#84056=CARTESIAN_POINT('Ctrl Pts',(-7.14583761409164,-6.06138589571277,
13.7638211676936));
#84057=CARTESIAN_POINT('Ctrl Pts',(-7.11825003917088,-6.09375996931984,
13.7645426017951));
#84058=CARTESIAN_POINT('Ctrl Pts',(-7.05486366659474,-6.16712619217975,
13.7661796906556));
#84059=CARTESIAN_POINT('Ctrl Pts',(-7.01892625268463,-6.20799654486537,
13.7670933757751));
#84060=CARTESIAN_POINT('Ctrl Pts',(-6.7951602908998,-6.45805065350713,13.772701764963));
#84061=CARTESIAN_POINT('Ctrl Pts',(-6.59835168244718,-6.65900727849565,
13.7772929655006));
#84062=CARTESIAN_POINT('Ctrl Pts',(-6.19073253694149,-7.03937538634662,
13.7864335172351));
#84063=CARTESIAN_POINT('Ctrl Pts',(-5.98041546821213,-7.21890610815664,
13.7909780570726));
#84064=CARTESIAN_POINT('Ctrl Pts',(-5.68674279324379,-7.44793692484547,
13.7972054426393));
#84065=CARTESIAN_POINT('Ctrl Pts',(-5.61011036175369,-7.50582904846296,
13.7988197056933));
#84066=CARTESIAN_POINT('Ctrl Pts',(-5.46893391151629,-7.60911098911496,
13.8017771181343));
#84067=CARTESIAN_POINT('Ctrl Pts',(-5.40468054243189,-7.65488317179611,
13.8031170710849));
#84068=CARTESIAN_POINT('Ctrl Pts',(-5.25804851565517,-7.75657284362428,
13.8061623786707));
#84069=CARTESIAN_POINT('Ctrl Pts',(-5.17534124270567,-7.81199970732012,
13.8078713206606));
#84070=CARTESIAN_POINT('Ctrl Pts',(-4.7596988949833,-8.08104718565987,13.8164162478065));
#84071=CARTESIAN_POINT('Ctrl Pts',(-4.41435408850214,-8.27475268583837,
13.8233990795122));
#84072=CARTESIAN_POINT('Ctrl Pts',(-3.90989542643503,-8.51711398219828,
13.8332160880435));
#84073=CARTESIAN_POINT('Ctrl Pts',(-3.76014205512594,-8.58427893381587,
13.8360823078156));
#84074=CARTESIAN_POINT('Ctrl Pts',(-3.55799656371564,-8.66863681984948,
13.8398570956303));
#84075=CARTESIAN_POINT('Ctrl Pts',(-3.50710581689088,-8.68935053209578,
13.8407995335197));
#84076=CARTESIAN_POINT('Ctrl Pts',(-3.41667362048382,-8.72523465420003,
13.8424585232164));
#84077=CARTESIAN_POINT('Ctrl Pts',(-3.37720621963715,-8.74058673958096,
13.8431771410749));
#84078=CARTESIAN_POINT('Ctrl Pts',(-3.27822944408186,-8.77831639459607,
13.8449664362186));
#84079=CARTESIAN_POINT('Ctrl Pts',(-3.21859394449918,-8.80035681431302,
13.8460331901405));
#84080=CARTESIAN_POINT('Ctrl Pts',(-2.98775606263299,-8.88301086273159,
13.850126468475));
#84081=CARTESIAN_POINT('Ctrl Pts',(-2.81502917382757,-8.93924937499039,
13.853114253816));
#84082=CARTESIAN_POINT('Ctrl Pts',(-2.40764319637441,-9.05891163475776,
13.8600807134449));
#84083=CARTESIAN_POINT('Ctrl Pts',(-2.17193396774468,-9.11829636181049,
13.8640517689999));
#84084=CARTESIAN_POINT('Ctrl Pts',(-1.82261311485674,-9.19198936923752,
13.8699496450467));
#84085=CARTESIAN_POINT('Ctrl Pts',(-1.71062202561537,-9.21348790309958,
13.8718419071577));
#84086=CARTESIAN_POINT('Ctrl Pts',(-1.49949240640433,-9.25003547556912,
13.8754201945896));
#84087=CARTESIAN_POINT('Ctrl Pts',(-1.40045027589751,-9.26554762206088,
13.8771032457719));
#84088=CARTESIAN_POINT('Ctrl Pts',(-1.22376658372984,-9.29032242952756,
13.8801169522891));
#84089=CARTESIAN_POINT('Ctrl Pts',(-1.14622196893779,-9.30020809774215,
13.8814434576106));
#84090=CARTESIAN_POINT('Ctrl Pts',(-0.974101705526609,-9.31996520418596,
13.8843972734573));
#84091=CARTESIAN_POINT('Ctrl Pts',(-0.87948115784808,-9.32936966655224,
13.8860274224552));
#84092=CARTESIAN_POINT('Ctrl Pts',(-0.411906267705348,-9.36866589391062,
13.8941143850369));
#84093=CARTESIAN_POINT('Ctrl Pts',(-0.0375377533519839,-9.37764125779603,
13.9007032140654));
#84094=CARTESIAN_POINT('Ctrl Pts',(0.530470229929351,-9.35723858627385,
13.910687297424));
#84095=CARTESIAN_POINT('Ctrl Pts',(0.724317669826966,-9.34423227924921,
13.9140890615151));
#84096=CARTESIAN_POINT('Ctrl Pts',(0.973991234309995,-9.31966386376122,
13.9184154491261));
#84097=CARTESIAN_POINT('Ctrl Pts',(1.03031031349024,-9.31360586110844,13.9193876386048));
#84098=CARTESIAN_POINT('Ctrl Pts',(1.1284880250913,-9.30214388292615,13.9210739559138));
#84099=CARTESIAN_POINT('Ctrl Pts',(1.1703712791237,-9.2969670923339,13.9217905062967));
#84100=CARTESIAN_POINT('Ctrl Pts',(1.27298962079049,-9.28357897025028,13.9235395637917));
#84101=CARTESIAN_POINT('Ctrl Pts',(1.33368174977877,-9.27505439803486,13.9245686187555));
#84102=CARTESIAN_POINT('Ctrl Pts',(1.66110742052958,-9.22578521844333,13.9301006027028));
#84103=CARTESIAN_POINT('Ctrl Pts',(1.92607114230827,-9.17412893969969,13.9345104140168));
#84104=CARTESIAN_POINT('Ctrl Pts',(2.45141032152367,-9.04794549424095,13.9433670959542));
#84105=CARTESIAN_POINT('Ctrl Pts',(2.71152595300367,-8.97342502698393,13.9478102729578));
#84106=CARTESIAN_POINT('Ctrl Pts',(3.06426236312623,-8.8556292745728,13.9540186405165));
#84107=CARTESIAN_POINT('Ctrl Pts',(3.15994399790798,-8.82194012349555,13.9557211508394));
#84108=CARTESIAN_POINT('Ctrl Pts',(3.3290995586658,-8.75927596397847,13.9587675531186));
#84109=CARTESIAN_POINT('Ctrl Pts',(3.40278973355542,-8.73091296945605,13.9601071747271));
#84110=CARTESIAN_POINT('Ctrl Pts',(3.56387414860746,-8.66656317947355,13.9630641893285));
#84111=CARTESIAN_POINT('Ctrl Pts',(3.6511002022442,-8.63017865095102,13.9646841845423));
#84112=CARTESIAN_POINT('Ctrl Pts',(4.0928654372712,-8.43800915099113,13.972985525147));
#84113=CARTESIAN_POINT('Ctrl Pts',(4.43805154466072,-8.26167303368647,13.9798103564765));
#84114=CARTESIAN_POINT('Ctrl Pts',(4.92969813772146,-7.97079169099115,13.9898410155151));
#84115=CARTESIAN_POINT('Ctrl Pts',(5.08527017036665,-7.87245016012284,13.993060849823));
#84116=CARTESIAN_POINT('Ctrl Pts',(5.28441488240712,-7.7381973806287,13.9972018092981));
#84117=CARTESIAN_POINT('Ctrl Pts',(5.33070084992959,-7.70638487354804,13.9981656001143));
#84118=CARTESIAN_POINT('Ctrl Pts',(5.41128651810698,-7.64992463386581,13.9998440371506));
#84119=CARTESIAN_POINT('Ctrl Pts',(5.44571059389155,-7.62545767918514,14.0005610059473));
#84120=CARTESIAN_POINT('Ctrl Pts',(5.53017262909851,-7.56456253831623,14.0023205816138));
#84121=CARTESIAN_POINT('Ctrl Pts',(5.58001722997495,-7.52786978116809,14.0033596116509));
#84122=CARTESIAN_POINT('Ctrl Pts',(5.83940258885416,-7.33293322436741,14.0087794992078));
#84123=CARTESIAN_POINT('Ctrl Pts',(6.04258754219039,-7.16642651979467,14.0130729547129));
#84124=CARTESIAN_POINT('Ctrl Pts',(6.44999944221824,-6.80289865363994,14.0220231254108));
#84125=CARTESIAN_POINT('Ctrl Pts',(6.65281593973745,-6.60469245245984,14.0266781392838));
#84126=CARTESIAN_POINT('Ctrl Pts',(6.91380466829742,-6.32539763868048,14.0330644744242));
#84127=CARTESIAN_POINT('Ctrl Pts',(6.98012755157119,-6.25213320242099,14.034724232765));
#84128=CARTESIAN_POINT('Ctrl Pts',(7.09727898347821,-6.11853223684106,14.0377266047631));
#84129=CARTESIAN_POINT('Ctrl Pts',(7.14852801491084,-6.05857680392513,14.0390654666562));
#84130=CARTESIAN_POINT('Ctrl Pts',(7.26091022182691,-5.9236912495488,14.0420598927709));
#84131=CARTESIAN_POINT('Ctrl Pts',(7.3216527215268,-5.84844736953184,14.0437184901695));
#84132=CARTESIAN_POINT('Ctrl Pts',(7.53089780984262,-5.58087809637662,14.0495756486846));
#84133=CARTESIAN_POINT('Ctrl Pts',(7.67307420248443,-5.38373046035281,14.0538211947711));
#84134=CARTESIAN_POINT('Ctrl Pts',(7.95181649890856,-4.96370691945652,14.0626739870144));
#84135=CARTESIAN_POINT('Ctrl Pts',(8.08704835178767,-4.7401920944263,14.0672809942824));
#84136=CARTESIAN_POINT('Ctrl Pts',(8.23335724525742,-4.47383977677964,14.0725662094236));
#84137=CARTESIAN_POINT('Ctrl Pts',(8.25368952862727,-4.43621720024175,14.0733080496746));
#84138=CARTESIAN_POINT('Ctrl Pts',(8.30398373691876,-4.34161074761176,14.0751606629056));
#84139=CARTESIAN_POINT('Ctrl Pts',(8.33361731162677,-4.28445472821126,14.0762683510741));
#84140=CARTESIAN_POINT('Ctrl Pts',(8.38179337469239,-4.1891435795849,14.0780937440536));
#84141=CARTESIAN_POINT('Ctrl Pts',(8.40066995091835,-4.1511598981866,14.0788154501327));
#84142=CARTESIAN_POINT('Ctrl Pts',(8.44317316453484,-4.0641570969368,14.0804550654945));
#84143=CARTESIAN_POINT('Ctrl Pts',(8.46663195944546,-4.01505781731479,14.0813709598252));
#84144=CARTESIAN_POINT('Ctrl Pts',(8.55359693070508,-3.82888826466691,14.0848131214733));
#84145=CARTESIAN_POINT('Ctrl Pts',(8.61421307191322,-3.69049308303046,14.0873100183094));
#84146=CARTESIAN_POINT('Ctrl Pts',(8.77682263964054,-3.29337005745303,14.0943690361267));
#84147=CARTESIAN_POINT('Ctrl Pts',(8.87068213815949,-3.03148488040831,14.0989026590275));
#84148=CARTESIAN_POINT('Ctrl Pts',(9.00261858105593,-2.60441539438768,14.106277952206));
#84149=CARTESIAN_POINT('Ctrl Pts',(9.04810650261124,-2.44169804349248,14.1090828817782));
#84150=CARTESIAN_POINT('Ctrl Pts',(9.11052904981039,-2.19261599338061,14.113389709835));
#84151=CARTESIAN_POINT('Ctrl Pts',(9.13068745996118,-2.10709537645805,14.1148706167864));
#84152=CARTESIAN_POINT('Ctrl Pts',(9.16692374633916,-1.94306810944073,14.1177171346256));
#84153=CARTESIAN_POINT('Ctrl Pts',(9.18320314125478,-1.86461381532694,14.119081289081));
#84154=CARTESIAN_POINT('Ctrl Pts',(9.21667915248794,-1.69219778039077,14.1220858188662));
#84155=CARTESIAN_POINT('Ctrl Pts',(9.23344924686129,-1.59816234354427,14.123728760266));
#84156=CARTESIAN_POINT('Ctrl Pts',(9.27289931150107,-1.35554778126336,14.1279780411825));
#84157=CARTESIAN_POINT('Ctrl Pts',(9.29344754055521,-1.20664993231808,14.1305961902874));
#84158=CARTESIAN_POINT('Ctrl Pts',(9.3132197589559,-1.03254285440637,14.1336636038634));
#84159=CARTESIAN_POINT('Ctrl Pts',(9.31593491146598,-1.00775182936722,14.1341005010924));
#84160=CARTESIAN_POINT('Ctrl Pts',(9.3448111886594,-0.733999359204234,14.1389259176537));
#84161=CARTESIAN_POINT('Ctrl Pts',(9.3610844354928,-0.484096357613643,14.1433433977092));
#84162=CARTESIAN_POINT('Ctrl Pts',(9.36955204471279,-0.144898352261821,
14.149276784836));
#84163=CARTESIAN_POINT('Ctrl Pts',(9.37050549716812,-0.0559269650014783,
14.1508269401777));
#84164=CARTESIAN_POINT('Ctrl Pts',(9.3699502470512,0.101520915351514,14.1535526357441));
#84165=CARTESIAN_POINT('Ctrl Pts',(9.36895814132929,0.169992668069073,14.1547321204751));
#84166=CARTESIAN_POINT('Ctrl Pts',(9.36612498950733,0.281290733248407,14.1566366368255));
#84167=CARTESIAN_POINT('Ctrl Pts',(9.36474047270412,0.32412605040461,14.1573665048075));
#84168=CARTESIAN_POINT('Ctrl Pts',(9.36102048436284,0.419044783592841,14.1589762348358));
#84169=CARTESIAN_POINT('Ctrl Pts',(9.35854411329062,0.471121147066671,14.1598545829335));
#84170=CARTESIAN_POINT('Ctrl Pts',(9.34873889424838,0.64646242697372,14.1627994941332));
#84171=CARTESIAN_POINT('Ctrl Pts',(9.33940814390406,0.769602657850774,14.1648469957626));
#84172=CARTESIAN_POINT('Ctrl Pts',(9.2988415187647,1.19355954943503,14.1718712139198));
#84173=CARTESIAN_POINT('Ctrl Pts',(9.25548015963627,1.49302562623371,14.1767946298674));
#84174=CARTESIAN_POINT('Ctrl Pts',(9.18169541596998,1.87218780738994,14.18316402135));
#84175=CARTESIAN_POINT('Ctrl Pts',(9.16457205598315,1.95428680130627,14.1845509462329));
#84176=CARTESIAN_POINT('Ctrl Pts',(9.13357936896066,2.09350574812983,14.186919457915));
#84177=CARTESIAN_POINT('Ctrl Pts',(9.1202704541596,2.15074527503112,14.187898074138));
#84178=CARTESIAN_POINT('Ctrl Pts',(9.0831273777399,2.30394396110407,14.1905316590833));
#84179=CARTESIAN_POINT('Ctrl Pts',(9.05831142265086,2.39965723480705,14.1921922824883));
#84180=CARTESIAN_POINT('Ctrl Pts',(9.01098471015623,2.57098432400586,14.1951955301113));
#84181=CARTESIAN_POINT('Ctrl Pts',(8.98902495323411,2.6467406744008,14.1965343920573));
#84182=CARTESIAN_POINT('Ctrl Pts',(8.93803365229024,2.8146900901836,14.1995279718484));
#84183=CARTESIAN_POINT('Ctrl Pts',(8.90852680445793,2.90672943133771,14.2011857133898));
#84184=CARTESIAN_POINT('Ctrl Pts',(8.75897239000766,3.3495424961027,14.2092450097335));
#84185=CARTESIAN_POINT('Ctrl Pts',(8.61960232405398,3.69343815297207,14.2157747011192));
#84186=CARTESIAN_POINT('Ctrl Pts',(8.37720385009096,4.20253959151443,14.2256791512094));
#84187=CARTESIAN_POINT('Ctrl Pts',(8.28880911021248,4.37430305825597,14.2290611951622));
#84188=CARTESIAN_POINT('Ctrl Pts',(8.16772926763208,4.59271016896832,14.233367575451));
#84189=CARTESIAN_POINT('Ctrl Pts',(8.13984085144974,4.64195853262973,14.2343389341716));
#84190=CARTESIAN_POINT('Ctrl Pts',(8.09037949166492,4.72748621960444,14.2360244666473));
#84191=CARTESIAN_POINT('Ctrl Pts',(8.06900452681866,4.76387785604273,14.2367410530863));
#84192=CARTESIAN_POINT('Ctrl Pts',(8.01595898686053,4.85280844276493,14.2384911239669));
#84193=CARTESIAN_POINT('Ctrl Pts',(7.98401698954685,4.90518307472376,14.2395211441924));
#84194=CARTESIAN_POINT('Ctrl Pts',(7.7966041232852,5.20579896216548,14.2454395942777));
#84195=CARTESIAN_POINT('Ctrl Pts',(7.63007535076783,5.44695604864743,14.2502180831965));
#84196=CARTESIAN_POINT('Ctrl Pts',(7.34446345513417,5.8217026768721,14.257945259275));
#84197=CARTESIAN_POINT('Ctrl Pts',(7.23237792301404,5.96037540087566,14.2608753367251));
#84198=CARTESIAN_POINT('Ctrl Pts',(7.07530787708384,6.14374433227486,14.2648784138511));
#84199=CARTESIAN_POINT('Ctrl Pts',(7.03372646838804,6.19130583399345,14.2659288374536));
#84200=CARTESIAN_POINT('Ctrl Pts',(6.92263394212747,6.31581157447978,14.2687127816063));
#84201=CARTESIAN_POINT('Ctrl Pts',(6.85232123332965,6.39202864401884,14.2704522117669));
#84202=CARTESIAN_POINT('Ctrl Pts',(6.72617230220585,6.52429663206588,14.2735376890089));
#84203=CARTESIAN_POINT('Ctrl Pts',(6.67086401812933,6.58083684648114,14.2748790172971));
#84204=CARTESIAN_POINT('Ctrl Pts',(6.54904381618991,6.70225646738273,14.277809876534));
#84205=CARTESIAN_POINT('Ctrl Pts',(6.48226928993804,6.76686053200486,14.2794016890251));
#84206=CARTESIAN_POINT('Ctrl Pts',(6.25875292759917,6.97676669420283,14.2846824856896));
#84207=CARTESIAN_POINT('Ctrl Pts',(6.09800125886097,7.11769919408694,14.28840670949));
#84208=CARTESIAN_POINT('Ctrl Pts',(5.74040957320299,7.41018991821878,14.2965061155114));
#84209=CARTESIAN_POINT('Ctrl Pts',(5.5420765222233,7.55966959651852,14.3008867212513));
#84210=CARTESIAN_POINT('Ctrl Pts',(5.26517628984571,7.75160397355025,14.306778053449));
#84211=CARTESIAN_POINT('Ctrl Pts',(5.19159691751922,7.80107473482848,14.3083226731288));
#84212=CARTESIAN_POINT('Ctrl Pts',(5.06010362839054,7.88679925441331,14.3110399292378));
#84213=CARTESIAN_POINT('Ctrl Pts',(5.00247442135708,7.92347782893592,14.3122164771855));
#84214=CARTESIAN_POINT('Ctrl Pts',(4.90806201162543,7.98212674103074,14.3141177138571));
#84215=CARTESIAN_POINT('Ctrl Pts',(4.87152017484449,8.00448069694584,14.314847204581));
#84216=CARTESIAN_POINT('Ctrl Pts',(4.79009800143786,8.05352548169367,14.3164579180339));
#84217=CARTESIAN_POINT('Ctrl Pts',(4.74514534138318,8.08009327007958,14.3173376085199));
#84218=CARTESIAN_POINT('Ctrl Pts',(4.59384622702819,8.16781555331623,14.3202702504623));
#84219=CARTESIAN_POINT('Ctrl Pts',(4.48652115299682,8.22725726828478,14.3223044718701));
#84220=CARTESIAN_POINT('Ctrl Pts',(4.34909343642689,8.299882210852,14.3248682218991));
#84221=CARTESIAN_POINT('Ctrl Pts',(4.32004864042978,8.31503685704886,14.3254077642749));
#84222=CARTESIAN_POINT('Ctrl Pts',(4.29092662550047,8.33003804055367,14.3259466798393));
#84223=CARTESIAN_POINT('Origin',(0.,0.,2.15141010809499));
#84224=CARTESIAN_POINT('',(4.29092662820214,8.330038039162,15.5233208859591));
#84225=CARTESIAN_POINT('',(4.29092660882816,8.33003804914182,15.3259008099036));
#84226=CARTESIAN_POINT('',(4.29092662815669,8.33003803918541,2.15141010809499));
#84227=CARTESIAN_POINT('',(-9.37025014160435,-4.63021129950685E-5,14.8481494226183));
#84228=CARTESIAN_POINT('Ctrl Pts',(4.29092662820214,8.330038039162,15.5233208859591));
#84229=CARTESIAN_POINT('Ctrl Pts',(4.33935081577568,8.30509401910726,15.5224026034553));
#84230=CARTESIAN_POINT('Ctrl Pts',(4.38755686544741,8.27972807481678,15.5214813896534));
#84231=CARTESIAN_POINT('Ctrl Pts',(4.50754295733572,8.2152494349333,15.5191702036362));
#84232=CARTESIAN_POINT('Ctrl Pts',(4.5790371221348,8.17561531550437,15.517776531901));
#84233=CARTESIAN_POINT('Ctrl Pts',(4.75923231172826,8.07261556020889,15.5142208310236));
#84234=CARTESIAN_POINT('Ctrl Pts',(4.86719237865973,8.00798678832569,15.5120499065674));
#84235=CARTESIAN_POINT('Ctrl Pts',(5.0459017858884,7.89605563927071,15.5083892081614));
#84236=CARTESIAN_POINT('Ctrl Pts',(5.11736736903765,7.8499280678712,15.5069068274078));
#84237=CARTESIAN_POINT('Ctrl Pts',(5.44855282337396,7.62971901269379,15.4999546733999));
#84238=CARTESIAN_POINT('Ctrl Pts',(5.70008238239256,7.44368190771533,15.4944268838185));
#84239=CARTESIAN_POINT('Ctrl Pts',(6.02999976377421,7.17312254237613,15.4869753909228));
#84240=CARTESIAN_POINT('Ctrl Pts',(6.11683257009331,7.09922133635338,15.4849947019738));
#84241=CARTESIAN_POINT('Ctrl Pts',(6.24021474873496,6.99026924087005,15.4821636193275));
#84242=CARTESIAN_POINT('Ctrl Pts',(6.27786250450247,6.95647802841728,15.4812974748673));
#84243=CARTESIAN_POINT('Ctrl Pts',(6.34725010961787,6.89317627459973,15.4796983208853));
#84244=CARTESIAN_POINT('Ctrl Pts',(6.37906234436655,6.86374727904147,15.4789642024782));
#84245=CARTESIAN_POINT('Ctrl Pts',(6.46320769282369,6.7848154358819,15.4770184824566));
#84246=CARTESIAN_POINT('Ctrl Pts',(6.51517613150117,6.73492792778792,15.4758125673697));
#84247=CARTESIAN_POINT('Ctrl Pts',(6.6348602640968,6.61735445414581,15.4730187587819));
#84248=CARTESIAN_POINT('Ctrl Pts',(6.70212417354252,6.54921997759249,15.4714358714828));
#84249=CARTESIAN_POINT('Ctrl Pts',(6.97662312607475,6.26250994682324,15.4648975382805));
#84250=CARTESIAN_POINT('Ctrl Pts',(7.17430341899172,6.03503702676669,15.4599923135375));
#84251=CARTESIAN_POINT('Ctrl Pts',(7.46337372856823,5.66808391348065,15.4522819256152));
#84252=CARTESIAN_POINT('Ctrl Pts',(7.56258128798143,5.53502363960272,15.4495255390682));
#84253=CARTESIAN_POINT('Ctrl Pts',(7.70860770660702,5.32790803044528,15.4452744539986));
#84254=CARTESIAN_POINT('Ctrl Pts',(7.75800899646399,5.25571433029615,15.4437998234166));
#84255=CARTESIAN_POINT('Ctrl Pts',(7.85078361579663,5.11597721535241,15.4409571854984));
#84256=CARTESIAN_POINT('Ctrl Pts',(7.89431416618906,5.04854732176828,15.4395905430191));
#84257=CARTESIAN_POINT('Ctrl Pts',(7.99810124856001,4.88315343516171,15.4362498024808));
#84258=CARTESIAN_POINT('Ctrl Pts',(8.0574307707709,4.78462332153161,15.4342690870405));
#84259=CARTESIAN_POINT('Ctrl Pts',(8.15191612657592,4.62096528971853,15.4309953821624));
#84260=CARTESIAN_POINT('Ctrl Pts',(8.18814084867399,4.55646860669659,15.4297093190472));
#84261=CARTESIAN_POINT('Ctrl Pts',(8.33561394386875,4.2864594783281,15.4243444427109));
#84262=CARTESIAN_POINT('Ctrl Pts',(8.43991826323459,4.07725078992402,15.4202309488007));
#84263=CARTESIAN_POINT('Ctrl Pts',(8.57547336090902,3.77781256878966,15.4144545626041));
#84264=CARTESIAN_POINT('Ctrl Pts',(8.61333593996565,3.69067137232837,15.4127867276333));
#84265=CARTESIAN_POINT('Ctrl Pts',(8.69855566968307,3.48607921000245,15.4089104043076));
#84266=CARTESIAN_POINT('Ctrl Pts',(8.74487023235722,3.36821373453112,15.4067070338864));
#84267=CARTESIAN_POINT('Ctrl Pts',(8.80690215932029,3.20043586511774,15.40362797199));
#84268=CARTESIAN_POINT('Ctrl Pts',(8.82461216202641,3.15127523024656,15.4027326645201));
#84269=CARTESIAN_POINT('Ctrl Pts',(8.85608776180026,3.06155659512679,15.4011128316326));
#84270=CARTESIAN_POINT('Ctrl Pts',(8.86998820694999,3.02104757272192,15.4003868204502));
#84271=CARTESIAN_POINT('Ctrl Pts',(8.90531397794677,2.91575442730613,15.3985125285794));
#84272=CARTESIAN_POINT('Ctrl Pts',(8.92631027422995,2.85082897538292,15.3973691332845));
#84273=CARTESIAN_POINT('Ctrl Pts',(8.97291138126556,2.70116308632557,15.3947560261009));
#84274=CARTESIAN_POINT('Ctrl Pts',(8.99802827712394,2.61627747889864,15.3932904692535));
#84275=CARTESIAN_POINT('Ctrl Pts',(9.08874712726964,2.29290957289445,15.3877514901989));
#84276=CARTESIAN_POINT('Ctrl Pts',(9.14610071108229,2.0522184935753,15.3837163239251));
#84277=CARTESIAN_POINT('Ctrl Pts',(9.20263711253572,1.76496990078625,15.3789049621883));
#84278=CARTESIAN_POINT('Ctrl Pts',(9.21108532995398,1.72033590238561,15.378157568222));
#84279=CARTESIAN_POINT('Ctrl Pts',(9.25165391299683,1.4971317965843,15.3744191913772));
#84280=CARTESIAN_POINT('Ctrl Pts',(9.27890753717816,1.3177171056856,15.3714107107534));
#84281=CARTESIAN_POINT('Ctrl Pts',(9.31178783815821,1.04889604943718,15.3668713480873));
#84282=CARTESIAN_POINT('Ctrl Pts',(9.3213702803212,0.960016518343662,15.3653655449496));
#84283=CARTESIAN_POINT('Ctrl Pts',(9.33708638277133,0.791676790400857,15.3625019975769));
#84284=CARTESIAN_POINT('Ctrl Pts',(9.34348092839117,0.712248808982456,15.3611460599758));
#84285=CARTESIAN_POINT('Ctrl Pts',(9.35630024015266,0.522843592754961,15.3579003228717));
#84286=CARTESIAN_POINT('Ctrl Pts',(9.36180018442812,0.412815728414672,15.3560048774186));
#84287=CARTESIAN_POINT('Ctrl Pts',(9.36960160727936,0.171457652376472,15.3518259888494));
#84288=CARTESIAN_POINT('Ctrl Pts',(9.37108435235863,0.0401241521074494,
15.3495383777897));
#84289=CARTESIAN_POINT('Ctrl Pts',(9.36628490606437,-0.452983999286923,
15.3409106620924));
#84290=CARTESIAN_POINT('Ctrl Pts',(9.34181261882488,-0.814262715226743,
15.3344996789749));
#84291=CARTESIAN_POINT('Ctrl Pts',(9.28715851549517,-1.24733834440628,15.3269306623763));
#84292=CARTESIAN_POINT('Ctrl Pts',(9.27691856474018,-1.3213433396882,15.3256419266638));
#84293=CARTESIAN_POINT('Ctrl Pts',(9.25991983117765,-1.43423377531867,15.3236869620909));
#84294=CARTESIAN_POINT('Ctrl Pts',(9.25379857205968,-1.47321207019614,15.3230139685745));
#84295=CARTESIAN_POINT('Ctrl Pts',(9.23976889032109,-1.55900942102823,15.3215378638506));
#84296=CARTESIAN_POINT('Ctrl Pts',(9.23175041975164,-1.6058093665504,15.3207360657735));
#84297=CARTESIAN_POINT('Ctrl Pts',(9.20618895917069,-1.74847584563897,15.3182995616863));
#84298=CARTESIAN_POINT('Ctrl Pts',(9.18750575039273,-1.84413153076017,15.3166765496582));
#84299=CARTESIAN_POINT('Ctrl Pts',(9.11373699811146,-2.19281432008148,15.3107744611561));
#84300=CARTESIAN_POINT('Ctrl Pts',(9.04966192038923,-2.44382004581928,15.3065500884788));
#84301=CARTESIAN_POINT('Ctrl Pts',(8.90794165483375,-2.91634949553053,15.2984525425213));
#84302=CARTESIAN_POINT('Ctrl Pts',(8.83221064078816,-3.13824371771744,15.2945872632762));
#84303=CARTESIAN_POINT('Ctrl Pts',(8.71394455913219,-3.44643566001338,15.2890669377829));
#84304=CARTESIAN_POINT('Ctrl Pts',(8.67828149669257,-3.53527633230051,15.2874577450569));
#84305=CARTESIAN_POINT('Ctrl Pts',(8.61380597216685,-3.68903418287639,15.2846386608485));
#84306=CARTESIAN_POINT('Ctrl Pts',(8.58560507004405,-3.75419926020087,15.2834330868386));
#84307=CARTESIAN_POINT('Ctrl Pts',(8.5177079037643,-3.90632486886088,15.2805924913161));
#84308=CARTESIAN_POINT('Ctrl Pts',(8.47741621957076,-3.99301090612813,15.2789534373301));
#84309=CARTESIAN_POINT('Ctrl Pts',(8.32156185013121,-4.31532915353274,15.272782004556));
#84310=CARTESIAN_POINT('Ctrl Pts',(8.19744350193355,-4.54668850934292,15.2681924599812));
#84311=CARTESIAN_POINT('Ctrl Pts',(7.91048751387181,-5.03153593599281,15.2582935960347));
#84312=CARTESIAN_POINT('Ctrl Pts',(7.74480648804397,-5.28300477363558,15.2529821099818));
#84313=CARTESIAN_POINT('Ctrl Pts',(7.5363222263582,-5.56850011965685,15.2468823245477));
#84314=CARTESIAN_POINT('Ctrl Pts',(7.50497621543816,-5.61067538747026,15.2459795401482));
#84315=CARTESIAN_POINT('Ctrl Pts',(7.44775700661573,-5.68632484975614,15.2443587630593));
#84316=CARTESIAN_POINT('Ctrl Pts',(7.42200876565529,-5.71989166203922,15.2436391765799));
#84317=CARTESIAN_POINT('Ctrl Pts',(7.36205630105453,-5.79696251956892,15.2419862623234));
#84318=CARTESIAN_POINT('Ctrl Pts',(7.32769231179728,-5.84034013014577,15.2410551475539));
#84319=CARTESIAN_POINT('Ctrl Pts',(7.18628106290558,-6.01563038867596,15.2372837973001));
#84320=CARTESIAN_POINT('Ctrl Pts',(7.07603979912934,-6.14492518965123,15.2344812515384));
#84321=CARTESIAN_POINT('Ctrl Pts',(6.69035300379286,-6.57312154815875,15.2250135059318));
#84322=CARTESIAN_POINT('Ctrl Pts',(6.39900494690285,-6.85707561528014,15.2183945960659));
#84323=CARTESIAN_POINT('Ctrl Pts',(6.01907309668896,-7.18199760461406,15.2100282214637));
#84324=CARTESIAN_POINT('Ctrl Pts',(5.94709592123443,-7.24171116424869,15.2084551101879));
#84325=CARTESIAN_POINT('Ctrl Pts',(5.81266409366925,-7.34988211675825,15.2055360691962));
#84326=CARTESIAN_POINT('Ctrl Pts',(5.75046682254399,-7.39864597646568,15.2041928247729));
#84327=CARTESIAN_POINT('Ctrl Pts',(5.60597515164211,-7.50900743532391,15.2010880060906));
#84328=CARTESIAN_POINT('Ctrl Pts',(5.52326920004079,-7.57004936155757,15.1993222219529));
#84329=CARTESIAN_POINT('Ctrl Pts',(5.24105648381663,-7.77125174732075,15.193335314287));
#84330=CARTESIAN_POINT('Ctrl Pts',(5.03708944676859,-7.90498298287792,15.1890691484747));
#84331=CARTESIAN_POINT('Ctrl Pts',(4.57742676264317,-8.18134018628447,15.1796454357825));
#84332=CARTESIAN_POINT('Ctrl Pts',(4.31979155718149,-8.32025025313945,15.1744838599681));
#84333=CARTESIAN_POINT('Ctrl Pts',(4.00064797383993,-8.47349881940574,15.1683680291139));
#84334=CARTESIAN_POINT('Ctrl Pts',(3.94495386638531,-8.49957089916678,15.1673109028652));
#84335=CARTESIAN_POINT('Ctrl Pts',(3.85060289873225,-8.54261225784336,15.1655394618291));
#84336=CARTESIAN_POINT('Ctrl Pts',(3.81208082364247,-8.55987188454036,15.1648217310514));
#84337=CARTESIAN_POINT('Ctrl Pts',(3.72174907090171,-8.59961385488393,15.1631517020717));
#84338=CARTESIAN_POINT('Ctrl Pts',(3.66985026084444,-8.62188921773207,15.1622018576813));
#84339=CARTESIAN_POINT('Ctrl Pts',(3.44207158677377,-8.71722426960827,15.1580689763533));
#84340=CARTESIAN_POINT('Ctrl Pts',(3.26418849650919,-8.7853815902678,15.1549335562591));
#84341=CARTESIAN_POINT('Ctrl Pts',(2.74733699008249,-8.96555102199639,15.1459507960855));
#84342=CARTESIAN_POINT('Ctrl Pts',(2.40388622295269,-9.06368007285904,15.1401259874661));
#84343=CARTESIAN_POINT('Ctrl Pts',(1.95640495745719,-9.16430127891586,15.13247203829));
#84344=CARTESIAN_POINT('Ctrl Pts',(1.85677610714491,-9.18500521010514,15.1307648799918));
#84345=CARTESIAN_POINT('Ctrl Pts',(1.67915162220254,-9.21890929897867,15.1277122160855));
#84346=CARTESIAN_POINT('Ctrl Pts',(1.60128874887153,-9.23275219759082,15.1263710207339));
#84347=CARTESIAN_POINT('Ctrl Pts',(1.43149948503482,-9.2607258274759,15.1234387035838));
#84348=CARTESIAN_POINT('Ctrl Pts',(1.33951905329488,-9.27447692751331,15.1218452817024));
#84349=CARTESIAN_POINT('Ctrl Pts',(1.03106221792878,-9.31590681595326,15.1164850990747));
#84350=CARTESIAN_POINT('Ctrl Pts',(0.813826998264375,-9.33739225592145,
15.1126812210327));
#84351=CARTESIAN_POINT('Ctrl Pts',(0.357768902005902,-9.36646094808392,
15.1046674866449));
#84352=CARTESIAN_POINT('Ctrl Pts',(0.119003646567082,-9.37253580038925,
15.1004556988116));
#84353=CARTESIAN_POINT('Ctrl Pts',(-0.247577994081873,-9.36785126926592,
15.0940426829013));
#84354=CARTESIAN_POINT('Ctrl Pts',(-0.375377232773101,-9.36360103526062,
15.0918174741581));
#84355=CARTESIAN_POINT('Ctrl Pts',(-0.555496136424005,-9.35391723791089,
15.0887121957051));
#84356=CARTESIAN_POINT('Ctrl Pts',(-0.607918110990462,-9.35065662069869,
15.0878121606238));
#84357=CARTESIAN_POINT('Ctrl Pts',(-0.702965723866272,-9.34394204004306,
15.0861886842621));
#84358=CARTESIAN_POINT('Ctrl Pts',(-0.745600266551923,-9.3406366965886,
15.0854636975381));
#84359=CARTESIAN_POINT('Ctrl Pts',(-0.855665183063269,-9.33134527720796,
15.083599418309));
#84360=CARTESIAN_POINT('Ctrl Pts',(-0.923056049086309,-9.32492011494468,
15.0824648987653));
#84361=CARTESIAN_POINT('Ctrl Pts',(-1.07739796879355,-9.30851534093726,
15.0798770807735));
#84362=CARTESIAN_POINT('Ctrl Pts',(-1.16429075373411,-9.29804664016778,
15.0784278241706));
#84363=CARTESIAN_POINT('Ctrl Pts',(-1.48971480386679,-9.25420672114131,
15.0730113504534));
#84364=CARTESIAN_POINT('Ctrl Pts',(-1.72707711171348,-9.21286042357409,
15.0690809404721));
#84365=CARTESIAN_POINT('Ctrl Pts',(-2.01670252623431,-9.15082287834424,
15.0642151143947));
#84366=CARTESIAN_POINT('Ctrl Pts',(-2.07071879989919,-9.13875112237347,
15.0633047191856));
#84367=CARTESIAN_POINT('Ctrl Pts',(-2.29832845694405,-9.08576246673031,
15.059453337675));
#84368=CARTESIAN_POINT('Ctrl Pts',(-2.47084160092836,-9.0403724926916,15.0564959515221));
#84369=CARTESIAN_POINT('Ctrl Pts',(-2.72816795555704,-8.96475094425637,
15.0520012975801));
#84370=CARTESIAN_POINT('Ctrl Pts',(-2.8140131811171,-8.93817596912533,15.0504878415896));
#84371=CARTESIAN_POINT('Ctrl Pts',(-2.97513025740711,-8.88574796245285,
15.0476185979804));
#84372=CARTESIAN_POINT('Ctrl Pts',(-3.05048094698526,-8.86016268802724,
15.0462647211034));
#84373=CARTESIAN_POINT('Ctrl Pts',(-3.22838460551438,-8.79721712208813,
15.0430387594063));
#84374=CARTESIAN_POINT('Ctrl Pts',(-3.33062864280929,-8.75901872430125,
15.0411612295487));
#84375=CARTESIAN_POINT('Ctrl Pts',(-3.49572151098055,-8.69403123188319,
15.0380916394055));
#84376=CARTESIAN_POINT('Ctrl Pts',(-3.558985784548,-8.66832556556886,15.0369061873254));
#84377=CARTESIAN_POINT('Ctrl Pts',(-3.80894683168125,-8.56356312493695,
15.0321872949181));
#84378=CARTESIAN_POINT('Ctrl Pts',(-3.99333727966357,-8.47914774197705,
15.0286267220198));
#84379=CARTESIAN_POINT('Ctrl Pts',(-4.39568130863915,-8.27891412341059,
15.020725365523));
#84380=CARTESIAN_POINT('Ctrl Pts',(-4.61209346458263,-8.16033256116785,
15.0163849802468));
#84381=CARTESIAN_POINT('Ctrl Pts',(-4.87760027625507,-8.00091068312191,
15.0110324338467));
#84382=CARTESIAN_POINT('Ctrl Pts',(-4.93129787019399,-7.96792680413757,
15.0099486129987));
#84383=CARTESIAN_POINT('Ctrl Pts',(-5.02048133033249,-7.91189876113124,
15.0081489150559));
#84384=CARTESIAN_POINT('Ctrl Pts',(-5.05615109013546,-7.88915147304997,
15.0074293129255));
#84385=CARTESIAN_POINT('Ctrl Pts',(-5.13811500259475,-7.83609729257674,
15.0057765148429));
#84386=CARTESIAN_POINT('Ctrl Pts',(-5.18429710298221,-7.80562041900588,
15.0048455302148));
#84387=CARTESIAN_POINT('Ctrl Pts',(-5.3710606590213,-7.67998117484013,15.001076323176));
#84388=CARTESIAN_POINT('Ctrl Pts',(-5.50931414247387,-7.58141553172918,
14.9982757355824));
#84389=CARTESIAN_POINT('Ctrl Pts',(-5.96933379448044,-7.23422021752676,
14.9888071174083));
#84390=CARTESIAN_POINT('Ctrl Pts',(-6.27756778527526,-6.96843102223886,
14.9821855266378));
#84391=CARTESIAN_POINT('Ctrl Pts',(-6.63425889966502,-6.61792547708285,
14.9738164439272));
#84392=CARTESIAN_POINT('Ctrl Pts',(-6.69996976496323,-6.55139175010933,
14.9722434870024));
#84393=CARTESIAN_POINT('Ctrl Pts',(-6.81936111007782,-6.4268301034296,14.9693245847937));
#84394=CARTESIAN_POINT('Ctrl Pts',(-6.87332441821854,-6.36908490570559,
14.9679813228595));
#84395=CARTESIAN_POINT('Ctrl Pts',(-6.98842678446998,-6.24274917189362,
14.9650628025681));
#84396=CARTESIAN_POINT('Ctrl Pts',(-7.04930057660508,-6.17392804251074,
14.9634854599055));
#84397=CARTESIAN_POINT('Ctrl Pts',(-7.13641989890285,-6.07246639257281,
14.9611780634694));
#84398=CARTESIAN_POINT('Ctrl Pts',(-7.16347434761205,-6.04052748764616,
14.9604542740297));
#84399=CARTESIAN_POINT('Ctrl Pts',(-7.28159928472947,-5.89916636229705,
14.9572621998112));
#84400=CARTESIAN_POINT('Ctrl Pts',(-7.37038310319124,-5.78785838473884,
14.9547782515122));
#84401=CARTESIAN_POINT('Ctrl Pts',(-7.60020054385354,-5.48586977190057,
14.9481292821605));
#84402=CARTESIAN_POINT('Ctrl Pts',(-7.73658983258874,-5.29178543343197,
14.9439467207313));
#84403=CARTESIAN_POINT('Ctrl Pts',(-7.94339503146362,-4.97238547519062,
14.9372815294534));
#84404=CARTESIAN_POINT('Ctrl Pts',(-8.01854800132615,-4.85026082620992,
14.9347820783155));
#84405=CARTESIAN_POINT('Ctrl Pts',(-8.11753144594043,-4.68081854793995,
14.931401903969));
#84406=CARTESIAN_POINT('Ctrl Pts',(-8.14380709840801,-4.63495253645753,
14.9304955583149));
#84407=CARTESIAN_POINT('Ctrl Pts',(-8.18320258068852,-4.56481560820111,
14.9291240582881));
#84408=CARTESIAN_POINT('Ctrl Pts',(-8.19660558461286,-4.54070511126053,
14.9286551968177));
#84409=CARTESIAN_POINT('Ctrl Pts',(-8.22917363783605,-4.48150475451051,
14.9275103599715));
#84410=CARTESIAN_POINT('Ctrl Pts',(-8.24822091913862,-4.44635078496461,
14.9268359224103));
#84411=CARTESIAN_POINT('Ctrl Pts',(-8.31466112898951,-4.32183149433479,
14.9244641431966));
#84412=CARTESIAN_POINT('Ctrl Pts',(-8.36083148895304,-4.2318216004866,14.9227806193413));
#84413=CARTESIAN_POINT('Ctrl Pts',(-8.44303455798622,-4.06496644788605,
14.9197022744777));
#84414=CARTESIAN_POINT('Ctrl Pts',(-8.47949802155801,-3.98834528359802,
14.9183048100877));
#84415=CARTESIAN_POINT('Ctrl Pts',(-8.65205766662259,-3.61267642319097,
14.9115117630621));
#84416=CARTESIAN_POINT('Ctrl Pts',(-8.77340144976112,-3.30710748288676,
14.9061569370261));
#84417=CARTESIAN_POINT('Ctrl Pts',(-8.91942322996013,-2.87435253332653,
14.8985772359048));
#84418=CARTESIAN_POINT('Ctrl Pts',(-8.9579055098469,-2.75207957634599,14.8964372536469));
#84419=CARTESIAN_POINT('Ctrl Pts',(-9.0146059836085,-2.55811012854314,14.8930371648305));
#84420=CARTESIAN_POINT('Ctrl Pts',(-9.03450441893329,-2.48692145966704,
14.891788239452));
#84421=CARTESIAN_POINT('Ctrl Pts',(-9.0727718210926,-2.34349133834688,14.8892687212566));
#84422=CARTESIAN_POINT('Ctrl Pts',(-9.09112524341568,-2.27125118617137,
14.8879981241305));
#84423=CARTESIAN_POINT('Ctrl Pts',(-9.12776300880281,-2.11947780354789,
14.8853247988519));
#84424=CARTESIAN_POINT('Ctrl Pts',(-9.14587417724437,-2.03990911636392,
14.8839210752183));
#84425=CARTESIAN_POINT('Ctrl Pts',(-9.22487873389747,-1.67058659117372,
14.8773960535077));
#84426=CARTESIAN_POINT('Ctrl Pts',(-9.27305614763012,-1.37828720650158,
14.8721987555121));
#84427=CARTESIAN_POINT('Ctrl Pts',(-9.33415293420309,-0.853801898862271,
14.8629150560277));
#84428=CARTESIAN_POINT('Ctrl Pts',(-9.35242749034445,-0.622486220083037,
14.8588367076895));
#84429=CARTESIAN_POINT('Ctrl Pts',(-9.3647488749212,-0.327260078623795,
14.8537270545419));
#84430=CARTESIAN_POINT('Ctrl Pts',(-9.36675234064347,-0.263763654014486,
14.8526338499193));
#84431=CARTESIAN_POINT('Ctrl Pts',(-9.36884081189437,-0.166061462144396,
14.8509629765942));
#84432=CARTESIAN_POINT('Ctrl Pts',(-9.36938448135584,-0.131867431932818,
14.8503803333988));
#84433=CARTESIAN_POINT('Ctrl Pts',(-9.37008015239402,-0.0651306203950395,
14.8492477688838));
#84434=CARTESIAN_POINT('Ctrl Pts',(-9.37024983919293,-0.032588570022699,
14.8486975781768));
#84435=CARTESIAN_POINT('Ctrl Pts',(-9.37024999988576,-4.62699946108937E-5,
14.8481491766056));
#84436=CARTESIAN_POINT('Ctrl Pts',(-9.37024999988558,-4.63062477912489E-5,
14.8481491772165));
#84437=CARTESIAN_POINT('Ctrl Pts',(-9.37025016016673,0.032387210047458,
14.8476026088632));
#84438=CARTESIAN_POINT('Ctrl Pts',(-9.37008192584371,0.0648205413103381,
14.8470578249882));
#84439=CARTESIAN_POINT('Ctrl Pts',(-9.36929780245289,0.140366629717473,
14.8457924112172));
#84440=CARTESIAN_POINT('Ctrl Pts',(-9.36855272598917,0.183477326384378,
14.8450729797667));
#84441=CARTESIAN_POINT('Ctrl Pts',(-9.36256155825491,0.431169014311936,
14.8409515014231));
#84442=CARTESIAN_POINT('Ctrl Pts',(-9.35091197546653,0.63554016256853,14.8375966945186));
#84443=CARTESIAN_POINT('Ctrl Pts',(-9.31000650999248,1.09035195682257,14.8301116941649));
#84444=CARTESIAN_POINT('Ctrl Pts',(-9.2773173533605,1.34032498169207,14.825983467721));
#84445=CARTESIAN_POINT('Ctrl Pts',(-9.21854480882273,1.68195584608197,14.8202287393192));
#84446=CARTESIAN_POINT('Ctrl Pts',(-9.20108483103443,1.77498781506405,14.8186503810149));
#84447=CARTESIAN_POINT('Ctrl Pts',(-9.1673099459977,1.94103261517819,14.8158093206971));
#84448=CARTESIAN_POINT('Ctrl Pts',(-9.15152444755324,2.01414486010617,14.814549980076));
#84449=CARTESIAN_POINT('Ctrl Pts',(-9.11727783589863,2.16403904591509,14.8119494245596));
#84450=CARTESIAN_POINT('Ctrl Pts',(-9.09871801239683,2.24079241037001,14.8106076588955));
#84451=CARTESIAN_POINT('Ctrl Pts',(-9.05450247207541,2.4140289254047,14.8075552341209));
#84452=CARTESIAN_POINT('Ctrl Pts',(-9.02827049074515,2.51035506438266,14.8058409508684));
#84453=CARTESIAN_POINT('Ctrl Pts',(-8.91216590888784,2.91131522585685,14.798634094877));
#84454=CARTESIAN_POINT('Ctrl Pts',(-8.80837422098841,3.2116972951539,14.7930544204129));
#84455=CARTESIAN_POINT('Ctrl Pts',(-8.63030217313856,3.653015846571,14.7846881166589));
#84456=CARTESIAN_POINT('Ctrl Pts',(-8.56736252369659,3.79828117371726,14.7819073399662));
#84457=CARTESIAN_POINT('Ctrl Pts',(-8.47070038269466,4.00673563098657,14.7779035477802));
#84458=CARTESIAN_POINT('Ctrl Pts',(-8.4398861570895,4.07124269412026,14.7766627327093));
#84459=CARTESIAN_POINT('Ctrl Pts',(-8.38455397178697,4.18374757192508,14.7744990100095));
#84460=CARTESIAN_POINT('Ctrl Pts',(-8.36035443240386,4.23189825408347,14.7735730814653));
#84461=CARTESIAN_POINT('Ctrl Pts',(-8.3304346079049,4.29017240575354,14.7724537844061));
#84462=CARTESIAN_POINT('Ctrl Pts',(-8.32510914963593,4.30049737524762,14.7722555185418));
#84463=CARTESIAN_POINT('Ctrl Pts',(-8.30052497412412,4.34794424393631,14.7713446947745));
#84464=CARTESIAN_POINT('Ctrl Pts',(-8.28103712268044,4.38494676906722,14.7706353079543));
#84465=CARTESIAN_POINT('Ctrl Pts',(-8.23173478286286,4.47705855580376,14.7688709866335));
#84466=CARTESIAN_POINT('Ctrl Pts',(-8.2016140212376,4.53200157987228,14.7678198419312));
#84467=CARTESIAN_POINT('Ctrl Pts',(-8.0635371416166,4.77798096631243,14.7631110000088));
#84468=CARTESIAN_POINT('Ctrl Pts',(-7.94944151650463,4.96549227394637,14.7595120048732));
#84469=CARTESIAN_POINT('Ctrl Pts',(-7.70888392173955,5.33126381070386,14.7523355753741));
#84470=CARTESIAN_POINT('Ctrl Pts',(-7.58255894241874,5.50945232116996,14.7487601897487));
#84471=CARTESIAN_POINT('Ctrl Pts',(-7.38410509968045,5.76961229989866,14.7433485562269));
#84472=CARTESIAN_POINT('Ctrl Pts',(-7.3165821598779,5.85500295849619,14.7415400788273));
#84473=CARTESIAN_POINT('Ctrl Pts',(-7.19789848197688,5.99983233225335,14.7384101950405));
#84474=CARTESIAN_POINT('Ctrl Pts',(-7.1474511249961,6.05984100096852,14.7370942558684));
#84475=CARTESIAN_POINT('Ctrl Pts',(-7.04636934006488,6.17706240065272,14.734483773726));
#84476=CARTESIAN_POINT('Ctrl Pts',(-6.99577636210066,6.23430299546772,14.7331896416136));
#84477=CARTESIAN_POINT('Ctrl Pts',(-6.88501087086556,6.35657604047414,14.7303817997884));
#84478=CARTESIAN_POINT('Ctrl Pts',(-6.82460449781062,6.42138669226045,14.7288661594031));
#84479=CARTESIAN_POINT('Ctrl Pts',(-6.64233222177486,6.61147104829941,14.7243380358121));
#84480=CARTESIAN_POINT('Ctrl Pts',(-6.5178713035553,6.73420226328853,14.7213038271286));
#84481=CARTESIAN_POINT('Ctrl Pts',(-6.29190752288132,6.94488955315872,14.7159047195832));
#84482=CARTESIAN_POINT('Ctrl Pts',(-6.19180926871345,7.03427957149033,14.7135487994992));
#84483=CARTESIAN_POINT('Ctrl Pts',(-5.94579009655439,7.24465888683698,14.7078587022797));
#84484=CARTESIAN_POINT('Ctrl Pts',(-5.7980504584273,7.36343080644468,14.7045225426141));
#84485=CARTESIAN_POINT('Ctrl Pts',(-5.58429191104298,7.52485259018563,14.6998477731187));
#84486=CARTESIAN_POINT('Ctrl Pts',(-5.52118313442434,7.57127858974637,14.6984857403366));
#84487=CARTESIAN_POINT('Ctrl Pts',(-5.40659596619699,7.65338007166294,14.6960497051497));
#84488=CARTESIAN_POINT('Ctrl Pts',(-5.35532798436316,7.68934123764587,14.6949728205539));
#84489=CARTESIAN_POINT('Ctrl Pts',(-5.27209128272421,7.74649010615319,14.6932476986284));
#84490=CARTESIAN_POINT('Ctrl Pts',(-5.24034631436417,7.76800012730232,14.6925952067104));
#84491=CARTESIAN_POINT('Ctrl Pts',(-5.16446878294425,7.81873704859955,14.6910488448522));
#84492=CARTESIAN_POINT('Ctrl Pts',(-5.12021891757649,7.84778599976995,14.6901573638823));
#84493=CARTESIAN_POINT('Ctrl Pts',(-4.96712621598174,7.9464415680789,14.6871043888964));
#84494=CARTESIAN_POINT('Ctrl Pts',(-4.85709114600769,8.01417133611161,14.6849638226828));
#84495=CARTESIAN_POINT('Ctrl Pts',(-4.66310339031397,8.12811328731931,14.6812558365575));
#84496=CARTESIAN_POINT('Ctrl Pts',(-4.57977716083409,8.17535320487262,14.679683637225));
#84497=CARTESIAN_POINT('Ctrl Pts',(-4.29359779329665,8.3318475864602,14.6743350245929));
#84498=CARTESIAN_POINT('Ctrl Pts',(-4.08744615058297,8.43489478694661,14.670566181726));
#84499=CARTESIAN_POINT('Ctrl Pts',(-3.77623673975164,8.57636548957207,14.6649156068853));
#84500=CARTESIAN_POINT('Ctrl Pts',(-3.67395178675623,8.62067788066451,14.6630648746156));
#84501=CARTESIAN_POINT('Ctrl Pts',(-3.47962571686501,8.7007779294017,14.6595532010026));
#84502=CARTESIAN_POINT('Ctrl Pts',(-3.38776186047385,8.73695606154295,14.6578949802547));
#84503=CARTESIAN_POINT('Ctrl Pts',(-3.2215125181812,8.79941262404106,14.6548941671624));
#84504=CARTESIAN_POINT('Ctrl Pts',(-3.14733425013258,8.8262162061279,14.6535553079421));
#84505=CARTESIAN_POINT('Ctrl Pts',(-2.98139592767012,8.88381845089406,14.6505593833357));
#84506=CARTESIAN_POINT('Ctrl Pts',(-2.88947922730363,8.9141383027309,14.6488992679234));
#84507=CARTESIAN_POINT('Ctrl Pts',(-2.55683799549484,9.01817844156007,14.6428891652543));
#84508=CARTESIAN_POINT('Ctrl Pts',(-2.31363638457182,9.08361430133465,14.6384879564239));
#84509=CARTESIAN_POINT('Ctrl Pts',(-2.02586832571781,9.14873308876972,14.6333050892782));
#84510=CARTESIAN_POINT('Ctrl Pts',(-1.98357433715222,9.15799609361822,14.6325440689058));
#84511=CARTESIAN_POINT('Ctrl Pts',(-1.76436540003371,9.20441628115723,14.6286047910578));
#84512=CARTESIAN_POINT('Ctrl Pts',(-1.58646624535125,9.23674127075432,14.6254241521223));
#84513=CARTESIAN_POINT('Ctrl Pts',(-1.33208108117045,9.27539767696573,14.6209353588839));
#84514=CARTESIAN_POINT('Ctrl Pts',(-1.25628044552962,9.2859679920136,14.6196053665935));
#84515=CARTESIAN_POINT('Ctrl Pts',(-1.11925918377197,9.30336698687795,14.6172192598907));
#84516=CARTESIAN_POINT('Ctrl Pts',(-1.05808450070686,9.31052284392828,14.6161604317797));
#84517=CARTESIAN_POINT('Ctrl Pts',(-0.954866776683514,9.32156621647971,
14.6143872062694));
#84518=CARTESIAN_POINT('Ctrl Pts',(-0.912860102034708,9.32577362677442,
14.6136693731625));
#84519=CARTESIAN_POINT('Ctrl Pts',(-0.815681048787701,9.33484423928135,
14.6120176879915));
#84520=CARTESIAN_POINT('Ctrl Pts',(-0.760491246312097,9.33950242936874,
14.6110860649273));
#84521=CARTESIAN_POINT('Ctrl Pts',(-0.526056044526549,9.35719767436545,
14.6071502532815));
#84522=CARTESIAN_POINT('Ctrl Pts',(-0.346496114815447,9.36556587242737,
14.6041884291376));
#84523=CARTESIAN_POINT('Ctrl Pts',(0.0886052375417247,9.37331264770265,
14.5970431134733));
#84524=CARTESIAN_POINT('Ctrl Pts',(0.344095864972601,9.36741367288125,14.5928719316847));
#84525=CARTESIAN_POINT('Ctrl Pts',(0.715194620127776,9.34364127931472,14.586731659203));
#84526=CARTESIAN_POINT('Ctrl Pts',(0.831214765062937,9.33403544221045,14.5848008479602));
#84527=CARTESIAN_POINT('Ctrl Pts',(1.0481475003125,9.31199780124703,14.5811608818815));
#84528=CARTESIAN_POINT('Ctrl Pts',(1.14909538516653,9.30008042771529,14.5794549434649));
#84529=CARTESIAN_POINT('Ctrl Pts',(1.32809077750361,9.27599028476565,14.5764049540663));
#84530=CARTESIAN_POINT('Ctrl Pts',(1.40621595242587,9.26446855129081,14.5750652150476));
#84531=CARTESIAN_POINT('Ctrl Pts',(1.57734076495685,9.23701695855951,14.572110860953));
#84532=CARTESIAN_POINT('Ctrl Pts',(1.6702643192013,9.22066717917013,14.5704936753074));
#84533=CARTESIAN_POINT('Ctrl Pts',(2.18261586985526,9.12252032692422,14.5615050151998));
#84534=CARTESIAN_POINT('Ctrl Pts',(2.59631456429605,9.01350850611793,14.553952755));
#84535=CARTESIAN_POINT('Ctrl Pts',(3.1432999897111,8.82857721398656,14.5438341908778));
#84536=CARTESIAN_POINT('Ctrl Pts',(3.2843034278182,8.77709870381412,14.5412163785394));
#84537=CARTESIAN_POINT('Ctrl Pts',(3.47412330407415,8.70258299118752,14.5377037727648));
#84538=CARTESIAN_POINT('Ctrl Pts',(3.52406654396406,8.68247882011976,14.5367807183511));
#84539=CARTESIAN_POINT('Ctrl Pts',(3.61312345621974,8.64573481026152,14.5351385426375));
#84540=CARTESIAN_POINT('Ctrl Pts',(3.65230225720898,8.62925719524365,14.5344175898242));
#84541=CARTESIAN_POINT('Ctrl Pts',(3.74118399425694,8.59116202478304,14.532784688199));
#84542=CARTESIAN_POINT('Ctrl Pts',(3.79081419107952,8.56937864729061,14.5318746711408));
#84543=CARTESIAN_POINT('Ctrl Pts',(3.99240531836963,8.47880349360051,14.5281805499157));
#84544=CARTESIAN_POINT('Ctrl Pts',(4.14268294627997,8.40640056746697,14.5254314779371));
#84545=CARTESIAN_POINT('Ctrl Pts',(4.29092664592494,8.33003803003272,14.5226929117958));
#84546=CARTESIAN_POINT('Ctrl Pts',(4.29092662550047,8.33003804055367,14.3259466798393));
#84547=CARTESIAN_POINT('Ctrl Pts',(4.05084536093733,8.45370747464059,14.3303894881587));
#84548=CARTESIAN_POINT('Ctrl Pts',(3.80551611770131,8.56694707685406,14.3347937749374));
#84549=CARTESIAN_POINT('Ctrl Pts',(3.47798520775956,8.70127839277931,14.3406310429407));
#84550=CARTESIAN_POINT('Ctrl Pts',(3.39992225332927,8.73207623756258,14.342018827415));
#84551=CARTESIAN_POINT('Ctrl Pts',(3.26648413190112,8.78266034162208,14.3443885984858));
#84552=CARTESIAN_POINT('Ctrl Pts',(3.2113171583457,8.80298150385962,14.3453676102072));
#84553=CARTESIAN_POINT('Ctrl Pts',(3.06284214511523,8.85609191613734,14.3480020271751));
#84554=CARTESIAN_POINT('Ctrl Pts',(2.96920028501613,8.88792527187953,14.3496630885747));
#84555=CARTESIAN_POINT('Ctrl Pts',(2.80000432352773,8.94247067099421,14.3526667798033));
#84556=CARTESIAN_POINT('Ctrl Pts',(2.72463396102764,8.96572226082316,14.3540056420404));
#84557=CARTESIAN_POINT('Ctrl Pts',(2.55629726413946,9.01533501480509,14.3569987948649));
#84558=CARTESIAN_POINT('Ctrl Pts',(2.46319858758205,9.04121528277558,14.3586561043616));
#84559=CARTESIAN_POINT('Ctrl Pts',(2.01042058168902,9.15956922139413,14.3667257668998));
#84560=CARTESIAN_POINT('Ctrl Pts',(1.64586025526886,9.23204422622544,14.3732667824454));
#84561=CARTESIAN_POINT('Ctrl Pts',(1.08714467519491,9.30896366021473,14.3831732090329));
#84562=CARTESIAN_POINT('Ctrl Pts',(0.895558215445643,9.32934423204637,14.3865462398719));
#84563=CARTESIAN_POINT('Ctrl Pts',(0.647066226770523,9.3480527859424,14.390843468458));
#84564=CARTESIAN_POINT('Ctrl Pts',(0.590615274597854,9.35178909129636,14.391814441156));
#84565=CARTESIAN_POINT('Ctrl Pts',(0.491996767333084,9.35741981357484,14.3934996093404));
#84566=CARTESIAN_POINT('Ctrl Pts',(0.449844045780326,9.35954094634964,14.3942162129236));
#84567=CARTESIAN_POINT('Ctrl Pts',(0.346364072686315,9.36404739122861,14.3959667566645));
#84568=CARTESIAN_POINT('Ctrl Pts',(0.285025072492648,9.36611511507469,14.3969972269791));
#84569=CARTESIAN_POINT('Ctrl Pts',(-0.0965361060028026,9.3752256673999,
14.4033737098141));
#84570=CARTESIAN_POINT('Ctrl Pts',(-0.416925000390062,9.36644814392845,
14.4085882986319));
#84571=CARTESIAN_POINT('Ctrl Pts',(-0.899340459825774,9.32842647220958,
14.4165309663505));
#84572=CARTESIAN_POINT('Ctrl Pts',(-1.06208100147298,9.31130160122788,14.4192246645185));
#84573=CARTESIAN_POINT('Ctrl Pts',(-1.35010068027961,9.27334441438653,14.4240469960312));
#84574=CARTESIAN_POINT('Ctrl Pts',(-1.47556199507631,9.25421013125627,14.4261661615369));
#84575=CARTESIAN_POINT('Ctrl Pts',(-1.68129145381729,9.21854389970623,14.4296796424607));
#84576=CARTESIAN_POINT('Ctrl Pts',(-1.76180021195588,9.20349675718852,14.4310643121705));
#84577=CARTESIAN_POINT('Ctrl Pts',(-1.9148651920481,9.17280675706991,14.4337167960061));
#84578=CARTESIAN_POINT('Ctrl Pts',(-1.98745315663559,9.15735346202679,14.4349832800418));
#84579=CARTESIAN_POINT('Ctrl Pts',(-2.18706434551763,9.11237290345313,14.4384902996344));
#84580=CARTESIAN_POINT('Ctrl Pts',(-2.31366631626269,9.0810538165816,14.4407420411893));
#84581=CARTESIAN_POINT('Ctrl Pts',(-2.75620799057858,8.96172138813919,14.4487053985504));
#84582=CARTESIAN_POINT('Ctrl Pts',(-3.06814178782416,8.85977637288835,14.4544935594099));
#84583=CARTESIAN_POINT('Ctrl Pts',(-3.47976170918821,8.70090079202678,14.4622328724799));
#84584=CARTESIAN_POINT('Ctrl Pts',(-3.58468944130418,8.65819945654388,14.46421390005));
#84585=CARTESIAN_POINT('Ctrl Pts',(-3.76298356364481,8.58184416268024,14.4675817042819));
#84586=CARTESIAN_POINT('Ctrl Pts',(-3.83673670643166,8.54912545397693,14.4689752828404));
#84587=CARTESIAN_POINT('Ctrl Pts',(-3.95067431189847,8.49680852002755,14.4711240803083));
#84588=CARTESIAN_POINT('Ctrl Pts',(-3.99115657033654,8.47786835217413,14.4718867275096));
#84589=CARTESIAN_POINT('Ctrl Pts',(-4.07473980431761,8.43803145218863,14.4734585209734));
#84590=CARTESIAN_POINT('Ctrl Pts',(-4.11781914576937,8.41709241703564,14.4742671666284));
#84591=CARTESIAN_POINT('Ctrl Pts',(-4.25045517172635,8.3513617033913,14.4767550251326));
#84592=CARTESIAN_POINT('Ctrl Pts',(-4.3394559970726,8.30546405714749,14.4784218257828));
#84593=CARTESIAN_POINT('Ctrl Pts',(-4.76830583917766,8.07553113557125,14.486476355208));
#84594=CARTESIAN_POINT('Ctrl Pts',(-5.09728372106305,7.87201651796003,14.4927425875687));
#84595=CARTESIAN_POINT('Ctrl Pts',(-5.46846809484981,7.60934296379044,14.5002696190677));
#84596=CARTESIAN_POINT('Ctrl Pts',(-5.52374997446446,7.56930841279338,14.5014027449445));
#84597=CARTESIAN_POINT('Ctrl Pts',(-5.66625192062478,7.46371745369295,14.504357765077));
#84598=CARTESIAN_POINT('Ctrl Pts',(-5.75277301358116,7.39723540453827,14.5061858278198));
#84599=CARTESIAN_POINT('Ctrl Pts',(-5.90035128572482,7.27968207350246,14.5093679508152));
#84600=CARTESIAN_POINT('Ctrl Pts',(-5.96195525657858,7.22931572629689,14.510716202894));
#84601=CARTESIAN_POINT('Ctrl Pts',(-6.09176068910101,7.12040128765922,14.5136011405656));
#84602=CARTESIAN_POINT('Ctrl Pts',(-6.15977636972704,7.06164412982918,14.515139474987));
#84603=CARTESIAN_POINT('Ctrl Pts',(-6.3656906445377,6.87852072121091,14.5198799773297));
#84604=CARTESIAN_POINT('Ctrl Pts',(-6.50074610111098,6.75102691832861,14.5231073643514));
#84605=CARTESIAN_POINT('Ctrl Pts',(-6.82837374691557,6.42278958076299,14.531220486772));
#84606=CARTESIAN_POINT('Ctrl Pts',(-7.01596464021389,6.2173269044752,14.5361308942662));
#84607=CARTESIAN_POINT('Ctrl Pts',(-7.25364136442272,5.93252862694117,14.5426215921704));
#84608=CARTESIAN_POINT('Ctrl Pts',(-7.31207985259046,5.86034958288285,14.5442407057133));
#84609=CARTESIAN_POINT('Ctrl Pts',(-7.41300339468307,5.7318358025775,14.5470711140271));
#84610=CARTESIAN_POINT('Ctrl Pts',(-7.45594317718138,5.67586754348695,14.5482867726703));
#84611=CARTESIAN_POINT('Ctrl Pts',(-7.52411042032971,5.58490889441025,14.5502319188713));
#84612=CARTESIAN_POINT('Ctrl Pts',(-7.54973536840059,5.55021989351209,14.5509666680425));
#84613=CARTESIAN_POINT('Ctrl Pts',(-7.60525486849176,5.47396607638004,14.5525656420107));
#84614=CARTESIAN_POINT('Ctrl Pts',(-7.63505003540046,5.43233073298915,14.553428565614));
#84615=CARTESIAN_POINT('Ctrl Pts',(-7.72707723534672,5.30148038065266,14.5561123583616));
#84616=CARTESIAN_POINT('Ctrl Pts',(-7.78809810351027,5.21142445617067,14.5579190439355));
#84617=CARTESIAN_POINT('Ctrl Pts',(-7.9184003742091,5.01172001446904,14.5618583395755));
#84618=CARTESIAN_POINT('Ctrl Pts',(-7.98700127024777,4.90165408575369,14.5639864987368));
#84619=CARTESIAN_POINT('Ctrl Pts',(-8.06904069476718,4.76372920379202,14.5666175706578));
#84620=CARTESIAN_POINT('Ctrl Pts',(-8.08465512460191,4.73718114254341,14.567122384326));
#84621=CARTESIAN_POINT('Ctrl Pts',(-8.23598463194248,4.47695924952901,14.5720562953741));
#84622=CARTESIAN_POINT('Ctrl Pts',(-8.36166217790112,4.23759509557695,14.5764872566878));
#84623=CARTESIAN_POINT('Ctrl Pts',(-8.52439840272248,3.89213086903517,14.5828459701593));
#84624=CARTESIAN_POINT('Ctrl Pts',(-8.57016901720414,3.79028412666944,14.5847156788946));
#84625=CARTESIAN_POINT('Ctrl Pts',(-8.6455334452908,3.61423747804889,14.5879442155574));
#84626=CARTESIAN_POINT('Ctrl Pts',(-8.67601865115214,3.54043237918989,14.589296713674));
#84627=CARTESIAN_POINT('Ctrl Pts',(-8.73838622968068,3.38379480239614,14.5921661954579));
#84628=CARTESIAN_POINT('Ctrl Pts',(-8.77004261627735,3.30088073475064,14.5936845794317));
#84629=CARTESIAN_POINT('Ctrl Pts',(-8.86096118134483,3.05220227377164,14.5982374753096));
#84630=CARTESIAN_POINT('Ctrl Pts',(-8.91673504347879,2.88520495304862,14.6012941059062));
#84631=CARTESIAN_POINT('Ctrl Pts',(-8.98426472226402,2.66229383709832,14.6053650068161));
#84632=CARTESIAN_POINT('Ctrl Pts',(-9.00026166360764,2.60770225575625,14.6063611900446));
#84633=CARTESIAN_POINT('Ctrl Pts',(-9.0823796197847,2.31770422175702,14.6116466204395));
#84634=CARTESIAN_POINT('Ctrl Pts',(-9.13976442393024,2.07992274142518,14.6159607080618));
#84635=CARTESIAN_POINT('Ctrl Pts',(-9.20508217569917,1.75379776084045,14.6217760392419));
#84636=CARTESIAN_POINT('Ctrl Pts',(-9.22116237515398,1.6671859356969,14.6233105317947));
#84637=CARTESIAN_POINT('Ctrl Pts',(-9.24748800528196,1.51333238846675,14.6260123354634));
#84638=CARTESIAN_POINT('Ctrl Pts',(-9.25822705038691,1.44618160734907,14.6271834980128));
#84639=CARTESIAN_POINT('Ctrl Pts',(-9.27453246328535,1.33658684568228,14.6290787286666));
#84640=CARTESIAN_POINT('Ctrl Pts',(-9.28054062028352,1.29421119818023,14.6298075358139));
#84641=CARTESIAN_POINT('Ctrl Pts',(-9.29325418805039,1.19989750487372,14.6314200992881));
#84642=CARTESIAN_POINT('Ctrl Pts',(-9.29981492965487,1.14794151269805,14.6323022893931));
#84643=CARTESIAN_POINT('Ctrl Pts',(-9.32081629198952,0.969611833663032,
14.6353130541187));
#84644=CARTESIAN_POINT('Ctrl Pts',(-9.33311920349649,0.843000325885971,
14.6374212494292));
#84645=CARTESIAN_POINT('Ctrl Pts',(-9.36110118395367,0.477963431696432,
14.6434571253253));
#84646=CARTESIAN_POINT('Ctrl Pts',(-9.37024427109779,0.2391380051819,14.6473561618306));
#84647=CARTESIAN_POINT('Ctrl Pts',(-9.37025135436427,-0.05639555157854,
14.6522120430209));
#84648=CARTESIAN_POINT('Ctrl Pts',(-9.36973951704211,-0.113014508858485,
14.6531436177697));
#84649=CARTESIAN_POINT('Ctrl Pts',(-9.36581304919372,-0.329880466951533,
14.6567195284928));
#84650=CARTESIAN_POINT('Ctrl Pts',(-9.35880020392255,-0.490034425258301,
14.6593769645584));
#84651=CARTESIAN_POINT('Ctrl Pts',(-9.34118377445768,-0.743404788223204,
14.6636271706575));
#84652=CARTESIAN_POINT('Ctrl Pts',(-9.33328283111655,-0.836777466382237,
14.6652032868241));
#84653=CARTESIAN_POINT('Ctrl Pts',(-9.31614035832275,-1.00864134985332,
14.6681250429189));
#84654=CARTESIAN_POINT('Ctrl Pts',(-9.30730368775735,-1.08716446716224,
14.6694679598235));
#84655=CARTESIAN_POINT('Ctrl Pts',(-9.28472180551968,-1.26729534730405,
14.672567911156));
#84656=CARTESIAN_POINT('Ctrl Pts',(-9.27029994115426,-1.36880803354643,
14.674329105132));
#84657=CARTESIAN_POINT('Ctrl Pts',(-9.24447254778108,-1.53139439240809,
14.6771725761396));
#84658=CARTESIAN_POINT('Ctrl Pts',(-9.23412046928646,-1.59262695455721,
14.6782486446894));
#84659=CARTESIAN_POINT('Ctrl Pts',(-9.19254818345805,-1.82448025464363,
14.6823418897166));
#84660=CARTESIAN_POINT('Ctrl Pts',(-9.15720136853533,-1.99432524401874,
14.6853797638788));
#84661=CARTESIAN_POINT('Ctrl Pts',(-9.08915235353315,-2.28114346069903,
14.6905579095618));
#84662=CARTESIAN_POINT('Ctrl Pts',(-9.05885351970946,-2.39864105233331,
14.6926929153118));
#84663=CARTESIAN_POINT('Ctrl Pts',(-8.97895674897119,-2.68532992761396,
14.6979202285522));
#84664=CARTESIAN_POINT('Ctrl Pts',(-8.92684915818135,-2.85377390227389,
14.7010074689203));
#84665=CARTESIAN_POINT('Ctrl Pts',(-8.84961105654361,-3.08058074754514,
14.7051489325922));
#84666=CARTESIAN_POINT('Ctrl Pts',(-8.82859417818543,-3.14030547207364,
14.7062379365153));
#84667=CARTESIAN_POINT('Ctrl Pts',(-8.79251940762764,-3.23959551889592,
14.7080431842528));
#84668=CARTESIAN_POINT('Ctrl Pts',(-8.77779583854697,-3.27927993516069,
14.7087632130622));
#84669=CARTESIAN_POINT('Ctrl Pts',(-8.74327932431064,-3.37041397817867,
14.7104129896911));
#84670=CARTESIAN_POINT('Ctrl Pts',(-8.72330028836909,-3.42179131814794,
14.7113405703043));
#84671=CARTESIAN_POINT('Ctrl Pts',(-8.6410924679992,-3.6277936418695,14.715054989824));
#84672=CARTESIAN_POINT('Ctrl Pts',(-8.5751962791023,-3.78092248589737,14.7178055821021));
#84673=CARTESIAN_POINT('Ctrl Pts',(-8.36739408396648,-4.23039204866728,
14.7259425156153));
#84674=CARTESIAN_POINT('Ctrl Pts',(-8.21395248892635,-4.52111548752836,
14.7312964588699));
#84675=CARTESIAN_POINT('Ctrl Pts',(-7.97975984102508,-4.91339966486704,
14.7388783260067));
#84676=CARTESIAN_POINT('Ctrl Pts',(-7.91170073927985,-5.02225593489993,
14.7410215039779));
#84677=CARTESIAN_POINT('Ctrl Pts',(-7.80094838019064,-5.19155628873473,
14.7444252512929));
#84678=CARTESIAN_POINT('Ctrl Pts',(-7.75973896565726,-5.25295188319357,
14.7456745934583));
#84679=CARTESIAN_POINT('Ctrl Pts',(-7.67119566417211,-5.38155162198325,
14.7483245262173));
#84680=CARTESIAN_POINT('Ctrl Pts',(-7.62369540382396,-5.44863369385304,
14.7497263275338));
#84681=CARTESIAN_POINT('Ctrl Pts',(-7.49944580980689,-5.61929847813231,
14.753343977036));
#84682=CARTESIAN_POINT('Ctrl Pts',(-7.42143044993666,-5.72193785193335,
14.7555694055062));
#84683=CARTESIAN_POINT('Ctrl Pts',(-7.28638913881069,-5.89219252091804,
14.7593439547139));
#84684=CARTESIAN_POINT('Ctrl Pts',(-7.23047849674247,-5.96066943053437,
14.7608855831825));
#84685=CARTESIAN_POINT('Ctrl Pts',(-6.95176818780392,-6.2923290105902,14.768463030344));
#84686=CARTESIAN_POINT('Ctrl Pts',(-6.71552700823923,-6.54386595828249,
14.7745684557952));
#84687=CARTESIAN_POINT('Ctrl Pts',(-6.4027891990157,-6.84203872762999,14.7820815678534));
#84688=CARTESIAN_POINT('Ctrl Pts',(-6.33877828813087,-6.90138343751596,
14.7835911190928));
#84689=CARTESIAN_POINT('Ctrl Pts',(-6.23992586951538,-6.99049413546934,
14.7858739778964));
#84690=CARTESIAN_POINT('Ctrl Pts',(-6.20567974074907,-7.02091319451156,
14.786656213681));
#84691=CARTESIAN_POINT('Ctrl Pts',(-6.13623055794022,-7.08169617023907,
14.7882240397799));
#84692=CARTESIAN_POINT('Ctrl Pts',(-6.10102181769235,-7.11205166601367,
14.7890095096051));
#84693=CARTESIAN_POINT('Ctrl Pts',(-5.99597819946792,-7.20126176582358,
14.7913276799931));
#84694=CARTESIAN_POINT('Ctrl Pts',(-5.92550707995577,-7.25935889061715,
14.7928502637643));
#84695=CARTESIAN_POINT('Ctrl Pts',(-5.74690385742039,-7.40226745508306,
14.7966425463728));
#84696=CARTESIAN_POINT('Ctrl Pts',(-5.63773418436791,-7.48574784570016,
14.7989012243898));
#84697=CARTESIAN_POINT('Ctrl Pts',(-5.23094710274699,-7.78286402140929,
14.8071649672548));
#84698=CARTESIAN_POINT('Ctrl Pts',(-4.92271110412059,-7.98139680474615,
14.8131484634814));
#84699=CARTESIAN_POINT('Ctrl Pts',(-4.52056863147075,-8.20823624073675,
14.8208704554806));
#84700=CARTESIAN_POINT('Ctrl Pts',(-4.4367808478872,-8.25382690557972,14.8224740389974));
#84701=CARTESIAN_POINT('Ctrl Pts',(-4.28309913330269,-8.33443189851926,
14.8254084763126));
#84702=CARTESIAN_POINT('Ctrl Pts',(-4.21343511912902,-8.36986605155365,
14.8267361464593));
#84703=CARTESIAN_POINT('Ctrl Pts',(-4.05375281063335,-8.4485885708916,14.8297746572075));
#84704=CARTESIAN_POINT('Ctrl Pts',(-3.9634693143098,-8.49131742534833,14.8314892666445));
#84705=CARTESIAN_POINT('Ctrl Pts',(-3.62763479183893,-8.6437360045026,14.8378547593405));
#84706=CARTESIAN_POINT('Ctrl Pts',(-3.37807916548652,-8.74428307273401,
14.8425643928425));
#84707=CARTESIAN_POINT('Ctrl Pts',(-2.86323900478452,-8.92638063170287,
14.8521629574976));
#84708=CARTESIAN_POINT('Ctrl Pts',(-2.59795908274709,-9.00716480402229,
14.857048185045));
#84709=CARTESIAN_POINT('Ctrl Pts',(-2.27651965451766,-9.0896663267212,14.8627790601197));
#84710=CARTESIAN_POINT('Ctrl Pts',(-2.2234320178086,-9.10279768797023,14.8637193224976));
#84711=CARTESIAN_POINT('Ctrl Pts',(-2.12881805343246,-9.12532361765254,
14.8653822659638));
#84712=CARTESIAN_POINT('Ctrl Pts',(-2.08733696132503,-9.13490130550559,
14.8661069032441));
#84713=CARTESIAN_POINT('Ctrl Pts',(-1.99364354946407,-9.15586293153534,
14.8677331491781));
#84714=CARTESIAN_POINT('Ctrl Pts',(-1.94139632872598,-9.16708355670175,
14.8686329550725));
#84715=CARTESIAN_POINT('Ctrl Pts',(-1.74642443891925,-9.20721414667796,
14.8719689919735));
#84716=CARTESIAN_POINT('Ctrl Pts',(-1.60312755750746,-9.23324281741756,
14.8743777718265));
#84717=CARTESIAN_POINT('Ctrl Pts',(-1.10868226379325,-9.31119671788151,
14.8826162851932));
#84718=CARTESIAN_POINT('Ctrl Pts',(-0.755225319006357,-9.34650714695677,
14.8883906199345));
#84719=CARTESIAN_POINT('Ctrl Pts',(-0.272997798198905,-9.36714333229914,
14.8964014782491));
#84720=CARTESIAN_POINT('Ctrl Pts',(-0.145278763930164,-9.36999444847109,
14.8985343542295));
#84721=CARTESIAN_POINT('Ctrl Pts',(0.0563156259553912,-9.3703718460242,
14.9019263187443));
#84722=CARTESIAN_POINT('Ctrl Pts',(0.130171878215257,-9.36963687863521,
14.903174328213));
#84723=CARTESIAN_POINT('Ctrl Pts',(0.286281796148723,-9.36623720540823,
14.9058246348694));
#84724=CARTESIAN_POINT('Ctrl Pts',(0.368524675021764,-9.36336190588312,
14.9072281715753));
#84725=CARTESIAN_POINT('Ctrl Pts',(0.580136466425123,-9.35317136042498,
14.9108589869445));
#84726=CARTESIAN_POINT('Ctrl Pts',(0.709410561265598,-9.34425541896425,
14.9130959933781));
#84727=CARTESIAN_POINT('Ctrl Pts',(1.00699831646342,-9.31751976764447,14.9182863726715));
#84728=CARTESIAN_POINT('Ctrl Pts',(1.17509734816618,-9.29781513267433,14.9212487925555));
#84729=CARTESIAN_POINT('Ctrl Pts',(1.64518656150708,-9.22975852311878,14.9295905060204));
#84730=CARTESIAN_POINT('Ctrl Pts',(1.9454773503055,-9.17116128743463,14.9349906750936));
#84731=CARTESIAN_POINT('Ctrl Pts',(2.30373964137129,-9.08286102712808,14.9413683756027));
#84732=CARTESIAN_POINT('Ctrl Pts',(2.36496006767125,-9.06711335973801,14.942455604498));
#84733=CARTESIAN_POINT('Ctrl Pts',(2.46689317939797,-9.03979059796486,14.9442589502369));
#84734=CARTESIAN_POINT('Ctrl Pts',(2.50769509508009,-9.02855699103623,14.9449788315351));
#84735=CARTESIAN_POINT('Ctrl Pts',(2.60153369943944,-9.00203609771469,14.9466296350848));
#84736=CARTESIAN_POINT('Ctrl Pts',(2.65451409950806,-8.98655587020102,14.9475583751003));
#84737=CARTESIAN_POINT('Ctrl Pts',(2.86791102105804,-8.92215208268953,14.9512911744615));
#84738=CARTESIAN_POINT('Ctrl Pts',(3.02713800522539,-8.86939384821649,14.954058524797));
#84739=CARTESIAN_POINT('Ctrl Pts',(3.49397727825909,-8.70067466763205,14.9622148063664));
#84740=CARTESIAN_POINT('Ctrl Pts',(3.7969985637573,-8.57277194888512,14.9675719519537));
#84741=CARTESIAN_POINT('Ctrl Pts',(4.20749628118755,-8.37346123146881,14.975145721397));
#84742=CARTESIAN_POINT('Ctrl Pts',(4.32116943254741,-8.31536965892312,14.9772770574238));
#84743=CARTESIAN_POINT('Ctrl Pts',(4.4986757871922,-8.22003371662507,14.9806672610655));
#84744=CARTESIAN_POINT('Ctrl Pts',(4.56331609471864,-8.18432552708443,14.9819150716935));
#84745=CARTESIAN_POINT('Ctrl Pts',(4.69909484115661,-8.10721078688609,14.9845654388003));
#84746=CARTESIAN_POINT('Ctrl Pts',(4.77012345888892,-8.06562342401307,14.985969239139));
#84747=CARTESIAN_POINT('Ctrl Pts',(4.95162020213482,-7.9561206670151,14.9896020532128));
#84748=CARTESIAN_POINT('Ctrl Pts',(5.06124288631309,-7.88683834003664,14.9918408171678));
#84749=CARTESIAN_POINT('Ctrl Pts',(5.31070775317086,-7.72183109226504,14.9970367141201));
#84750=CARTESIAN_POINT('Ctrl Pts',(5.449461815304,-7.62454313184033,15.0000029260064));
#84751=CARTESIAN_POINT('Ctrl Pts',(5.838435773624,-7.33576782638403,15.0085108856225));
#84752=CARTESIAN_POINT('Ctrl Pts',(6.0817399418717,-7.13535293226558,15.014075560044));
#84753=CARTESIAN_POINT('Ctrl Pts',(6.35368277420726,-6.8873154888373,15.0204277575143));
#84754=CARTESIAN_POINT('Ctrl Pts',(6.39257420994285,-6.85123305869351,15.0213393608049));
#84755=CARTESIAN_POINT('Ctrl Pts',(6.46196353379338,-6.78575025795265,15.0229699066767));
#84756=CARTESIAN_POINT('Ctrl Pts',(6.4925723971653,-6.75646971134094,15.0236905291332));
#84757=CARTESIAN_POINT('Ctrl Pts',(6.56236296419189,-6.68879559419791,15.0253364167723));
#84758=CARTESIAN_POINT('Ctrl Pts',(6.60140808083821,-6.65026356948071,15.0262595722346));
#84759=CARTESIAN_POINT('Ctrl Pts',(6.75503020580465,-6.49597406578625,15.0299062021755));
#84760=CARTESIAN_POINT('Ctrl Pts',(6.86691937385006,-6.37758032174672,15.0325951067752));
#84761=CARTESIAN_POINT('Ctrl Pts',(7.19447386980348,-6.01236451097467,15.0406585865365));
#84762=CARTESIAN_POINT('Ctrl Pts',(7.40033223573199,-5.75708817217689,15.0459985038913));
#84763=CARTESIAN_POINT('Ctrl Pts',(7.66926069909016,-5.38527884090373,15.0536098250143));
#84764=CARTESIAN_POINT('Ctrl Pts',(7.74388835269695,-5.2774028570135,15.0557986345105));
#84765=CARTESIAN_POINT('Ctrl Pts',(7.85721281820569,-5.10600765984033,15.0592546247565));
#84766=CARTESIAN_POINT('Ctrl Pts',(7.89745994506394,-5.04353386837535,15.0605099136011));
#84767=CARTESIAN_POINT('Ctrl Pts',(7.98043747169921,-4.91130263900006,15.0631587853762));
#84768=CARTESIAN_POINT('Ctrl Pts',(8.02300615893516,-4.84145102089897,15.0645534564323));
#84769=CARTESIAN_POINT('Ctrl Pts',(8.12890958111824,-4.66243920237817,15.0681167863805));
#84770=CARTESIAN_POINT('Ctrl Pts',(8.1909635842154,-4.55254057947949,15.0702944241105));
#84771=CARTESIAN_POINT('Ctrl Pts',(8.29128752695059,-4.36616995769018,15.0739690672849));
#84772=CARTESIAN_POINT('Ctrl Pts',(8.33076473325884,-4.29036687031483,15.0754586663927));
#84773=CARTESIAN_POINT('Ctrl Pts',(8.51144201287931,-3.93153634955085,15.0824819419));
#84774=CARTESIAN_POINT('Ctrl Pts',(8.63928969651244,-3.64201814470987,15.0880748743119));
#84775=CARTESIAN_POINT('Ctrl Pts',(8.79080935000653,-3.24575277713097,15.0954807079435));
#84776=CARTESIAN_POINT('Ctrl Pts',(8.82762133949223,-3.14425534954562,15.0973555561701));
#84777=CARTESIAN_POINT('Ctrl Pts',(8.87924706107478,-2.99385426826711,15.1000911703786));
#84778=CARTESIAN_POINT('Ctrl Pts',(8.89542788383968,-2.94542943050717,15.1009655164933));
#84779=CARTESIAN_POINT('Ctrl Pts',(8.92455936139365,-2.85581672614698,15.102570148329));
#84780=CARTESIAN_POINT('Ctrl Pts',(8.93762263297203,-2.81466705601372,15.1033016505745));
#84781=CARTESIAN_POINT('Ctrl Pts',(8.97137908065879,-2.70572833975215,15.105225441598));
#84782=CARTESIAN_POINT('Ctrl Pts',(8.99158834455321,-2.63779217062365,15.1064122900545));
#84783=CARTESIAN_POINT('Ctrl Pts',(9.03666732100547,-2.47971210454445,15.1091505006019));
#84784=CARTESIAN_POINT('Ctrl Pts',(9.06096232529297,-2.38941210034794,15.1106971262895));
#84785=CARTESIAN_POINT('Ctrl Pts',(9.15333455809474,-2.02438965171595,15.1169016304677));
#84786=CARTESIAN_POINT('Ctrl Pts',(9.21030078596373,-1.74701081497711,15.1215132882247));
#84787=CARTESIAN_POINT('Ctrl Pts',(9.2830167155094,-1.28842956847979,15.1291646404631));
#84788=CARTESIAN_POINT('Ctrl Pts',(9.30620598902747,-1.10859365665703,15.1321707160256));
#84789=CARTESIAN_POINT('Ctrl Pts',(9.33301699705726,-0.839265364406819,
15.1367073458948));
#84790=CARTESIAN_POINT('Ctrl Pts',(9.3405972919208,-0.750209838905443,15.138212871676));
#84791=CARTESIAN_POINT('Ctrl Pts',(9.35252421224344,-0.581571865928536,
15.14107622203));
#84792=CARTESIAN_POINT('Ctrl Pts',(9.35713178070997,-0.502015716461471,
15.1424322438239));
#84793=CARTESIAN_POINT('Ctrl Pts',(9.36569166262584,-0.31232660322585,15.1456787454651));
#84794=CARTESIAN_POINT('Ctrl Pts',(9.36871698526925,-0.202163767082633,
15.1475748789663));
#84795=CARTESIAN_POINT('Ctrl Pts',(9.37108834110714,0.0394182011394155,
15.1517556994895));
#84796=CARTESIAN_POINT('Ctrl Pts',(9.36961419443536,0.17082218711811,15.1540445620345));
#84797=CARTESIAN_POINT('Ctrl Pts',(9.35368840482981,0.664452319270811,15.1626855823257));
#84798=CARTESIAN_POINT('Ctrl Pts',(9.32098606602358,1.02576885517853,15.1691088980123));
#84799=CARTESIAN_POINT('Ctrl Pts',(9.25646844379374,1.45769945460381,15.1766807073362));
#84800=CARTESIAN_POINT('Ctrl Pts',(9.24462963869411,1.53098616402235,15.1779611413842));
#84801=CARTESIAN_POINT('Ctrl Pts',(9.22517811390165,1.64293192510444,15.179906716406));
#84802=CARTESIAN_POINT('Ctrl Pts',(9.21819036109052,1.68169647223961,15.1805785220759));
#84803=CARTESIAN_POINT('Ctrl Pts',(9.20221454731507,1.76722960168414,15.1820558052592));
#84804=CARTESIAN_POINT('Ctrl Pts',(9.1931139443524,1.81397603595547,15.1828599392524));
#84805=CARTESIAN_POINT('Ctrl Pts',(9.16412567605563,1.95705408039645,15.1853138312532));
#84806=CARTESIAN_POINT('Ctrl Pts',(9.14307721210707,2.05314374972946,15.1869516544349));
#84807=CARTESIAN_POINT('Ctrl Pts',(9.08491392674533,2.30000645015942,15.1911510365151));
#84808=CARTESIAN_POINT('Ctrl Pts',(9.04555749451854,2.4502204985434,15.1936985187694));
#84809=CARTESIAN_POINT('Ctrl Pts',(8.91263752020387,2.91056371866555,15.2015535554786));
#84810=CARTESIAN_POINT('Ctrl Pts',(8.8067145978278,3.21687211462933,15.2068555368832));
#84811=CARTESIAN_POINT('Ctrl Pts',(8.64749778597169,3.61004532016563,15.213939327009));
#84812=CARTESIAN_POINT('Ctrl Pts',(8.60836043250434,3.70240135207181,15.2156233076951));
#84813=CARTESIAN_POINT('Ctrl Pts',(8.53579668638417,3.86626262981798,15.2186504463519));
#84814=CARTESIAN_POINT('Ctrl Pts',(8.50293526566627,3.93800757088068,15.219989558651));
#84815=CARTESIAN_POINT('Ctrl Pts',(8.42834993689971,4.09555911756303,15.2229617375705));
#84816=CARTESIAN_POINT('Ctrl Pts',(8.38621375928479,4.18116082799509,15.2245975843047));
#84817=CARTESIAN_POINT('Ctrl Pts',(8.22535744100787,4.49573087222814,15.2306874684807));
#84818=CARTESIAN_POINT('Ctrl Pts',(8.09850717779906,4.72041117744608,15.2351963973872));
#84819=CARTESIAN_POINT('Ctrl Pts',(7.80041307499569,5.20093660647382,15.2451304074111));
#84820=CARTESIAN_POINT('Ctrl Pts',(7.62550443927557,5.45416062726863,15.2505603927787));
#84821=CARTESIAN_POINT('Ctrl Pts',(7.40687826366323,5.73955020121121,15.2567619833702));
#84822=CARTESIAN_POINT('Ctrl Pts',(7.37495389243577,5.78051357793326,15.2576540100204));
#84823=CARTESIAN_POINT('Ctrl Pts',(7.31644424456274,5.85431580783031,15.2592630236567));
#84824=CARTESIAN_POINT('Ctrl Pts',(7.28997432245437,5.88724420715825,15.2599814985525));
#84825=CARTESIAN_POINT('Ctrl Pts',(7.22792538535899,5.96337250412848,15.2616437270448));
#84826=CARTESIAN_POINT('Ctrl Pts',(7.19218032034089,6.0064348209689,15.2625851349745));
#84827=CARTESIAN_POINT('Ctrl Pts',(7.03967501287623,6.18684553104261,15.2665398802811));
#84828=CARTESIAN_POINT('Ctrl Pts',(6.91934942525058,6.32113010747913,15.2695106592199));
#84829=CARTESIAN_POINT('Ctrl Pts',(6.52518241178908,6.73627449098843,15.2789100080205));
#84830=CARTESIAN_POINT('Ctrl Pts',(6.2375507427531,7.00345344388833,15.2853040262032));
#84831=CARTESIAN_POINT('Ctrl Pts',(5.86107149062879,7.31151913900467,15.2934429722194));
#84832=CARTESIAN_POINT('Ctrl Pts',(5.78722061869043,7.37011184409929,15.2950283112351));
#84833=CARTESIAN_POINT('Ctrl Pts',(5.64989843130722,7.47572534876947,15.2979584827));
#84834=CARTESIAN_POINT('Ctrl Pts',(5.58669241970508,7.52307713294167,15.2993004766885));
#84835=CARTESIAN_POINT('Ctrl Pts',(5.44069856637601,7.62959613208488,15.3023860041862));
#84836=CARTESIAN_POINT('Ctrl Pts',(5.3575304237325,7.68822513442907,15.3041335477523));
#84837=CARTESIAN_POINT('Ctrl Pts',(5.07333675975128,7.88171503962326,15.3100707132721));
#84838=CARTESIAN_POINT('Ctrl Pts',(4.86804651796867,8.01013734082422,15.3143049608386));
#84839=CARTESIAN_POINT('Ctrl Pts',(4.53713320989625,8.19972048212067,15.3210050454066));
#84840=CARTESIAN_POINT('Ctrl Pts',(4.4147394240174,8.26626022482994,15.3234567955017));
#84841=CARTESIAN_POINT('Ctrl Pts',(4.29092660882816,8.33003804914182,15.3259008099036));
#84842=CARTESIAN_POINT('Origin',(0.,0.,2.15141010809499));
#84843=CARTESIAN_POINT('',(4.29092663733565,8.33003803445719,16.522914704178));
#84844=CARTESIAN_POINT('',(4.29092662815671,8.3300380391854,16.3257048922231));
#84845=CARTESIAN_POINT('',(4.29092662815669,8.33003803918541,2.15141010809499));
#84846=CARTESIAN_POINT('Ctrl Pts',(4.29092663733565,8.33003803445719,16.522914704178));
#84847=CARTESIAN_POINT('Ctrl Pts',(4.34419074622071,8.30260089879425,16.5218617865547));
#84848=CARTESIAN_POINT('Ctrl Pts',(4.3971956545877,8.27465085053372,16.5208081053267));
#84849=CARTESIAN_POINT('Ctrl Pts',(4.59003078621386,8.17059025536445,16.5169558422932));
#84850=CARTESIAN_POINT('Ctrl Pts',(4.72817847057187,8.09143103549738,16.5141589721163));
#84851=CARTESIAN_POINT('Ctrl Pts',(4.92552548441208,7.97156978210543,16.5101354584452));
#84852=CARTESIAN_POINT('Ctrl Pts',(4.98637943026975,7.93364646900825,16.5088908545452));
#84853=CARTESIAN_POINT('Ctrl Pts',(5.09633041068881,7.86336176326533,16.5066386623559));
#84854=CARTESIAN_POINT('Ctrl Pts',(5.14556957709859,7.83122950910619,16.505628791034));
#84855=CARTESIAN_POINT('Ctrl Pts',(5.22614112555678,7.77756253902676,16.5039762412962));
#84856=CARTESIAN_POINT('Ctrl Pts',(5.25765053963257,7.75629685644575,16.5033300466127));
#84857=CARTESIAN_POINT('Ctrl Pts',(5.33419320423295,7.70395751391395,16.5017605373996));
#84858=CARTESIAN_POINT('Ctrl Pts',(5.37908530880289,7.67268009076504,16.5008399863193));
#84859=CARTESIAN_POINT('Ctrl Pts',(5.5585497033799,7.54529365225603,16.4971546337167));
#84860=CARTESIAN_POINT('Ctrl Pts',(5.6908414002494,7.44602280243445,16.4944254486344));
#84861=CARTESIAN_POINT('Ctrl Pts',(6.02926471379512,7.17778226458798,16.4873290361088));
#84862=CARTESIAN_POINT('Ctrl Pts',(6.23093677260032,7.00342903492275,16.4829811501577));
#84863=CARTESIAN_POINT('Ctrl Pts',(6.5110773636398,6.73954535803286,16.4766287048069));
#84864=CARTESIAN_POINT('Ctrl Pts',(6.59570502211195,6.65674659631357,16.4746658724048));
#84865=CARTESIAN_POINT('Ctrl Pts',(6.75084345273616,6.49909723971123,16.4709747903405));
#84866=CARTESIAN_POINT('Ctrl Pts',(6.8217352395538,6.42464633324573,16.4692499634749));
#84867=CARTESIAN_POINT('Ctrl Pts',(6.9449375509302,6.2909199257943,16.4661800470896));
#84868=CARTESIAN_POINT('Ctrl Pts',(6.99774996248071,6.23212054825388,16.4648394988121));
#84869=CARTESIAN_POINT('Ctrl Pts',(7.11141179672457,6.10230705578462,16.4618989025599));
#84870=CARTESIAN_POINT('Ctrl Pts',(7.17195477191904,6.03103588450162,16.4602964511755));
#84871=CARTESIAN_POINT('Ctrl Pts',(7.48995401030316,5.64512613113075,16.451682696129));
#84872=CARTESIAN_POINT('Ctrl Pts',(7.72779409538944,5.31488992298295,16.4445098461343));
#84873=CARTESIAN_POINT('Ctrl Pts',(8.03349204271351,4.82632549789793,16.434397206636));
#84874=CARTESIAN_POINT('Ctrl Pts',(8.11962294895016,4.67997175777033,16.4314300300769));
#84875=CARTESIAN_POINT('Ctrl Pts',(8.22848817208142,4.48292640430834,16.4275498898206));
#84876=CARTESIAN_POINT('Ctrl Pts',(8.25481691869994,4.43425804416627,16.4266006426443));
#84877=CARTESIAN_POINT('Ctrl Pts',(8.30051226322842,4.34797320098906,16.4249355519017));
#84878=CARTESIAN_POINT('Ctrl Pts',(8.32005794672287,4.31045363676942,16.4242175600519));
#84879=CARTESIAN_POINT('Ctrl Pts',(8.3633132423917,4.22603106398965,16.4226149843629));
#84880=CARTESIAN_POINT('Ctrl Pts',(8.38688364109877,4.17905847656221,16.4217320512057));
#84881=CARTESIAN_POINT('Ctrl Pts',(8.54377464018161,3.85972220707158,16.4157808671813));
#84882=CARTESIAN_POINT('Ctrl Pts',(8.66420144452708,3.58122262967216,16.4108360116664));
#84883=CARTESIAN_POINT('Ctrl Pts',(8.86254100790409,3.0536455925217,16.4015919269044));
#84884=CARTESIAN_POINT('Ctrl Pts',(8.94397019457801,2.80620404010665,16.3973051509225));
#84885=CARTESIAN_POINT('Ctrl Pts',(9.04103727051634,2.46380836098728,16.3913532155405));
#84886=CARTESIAN_POINT('Ctrl Pts',(9.0656798728991,2.37153008674136,16.3897476093256));
#84887=CARTESIAN_POINT('Ctrl Pts',(9.10809759128846,2.20235540923167,16.3867984793622));
#84888=CARTESIAN_POINT('Ctrl Pts',(9.12632017262488,2.12558019234843,16.3854580454985));
#84889=CARTESIAN_POINT('Ctrl Pts',(9.16547215295705,1.95083076080501,16.3824014523416));
#84890=CARTESIAN_POINT('Ctrl Pts',(9.18580437482541,1.85273267483054,16.3806815859644));
#84891=CARTESIAN_POINT('Ctrl Pts',(9.2655241613127,1.43446101329832,16.3733317109346));
#84892=CARTESIAN_POINT('Ctrl Pts',(9.30977347201924,1.11163507932695,16.3676091066765));
#84893=CARTESIAN_POINT('Ctrl Pts',(9.35537412618965,0.570732537952196,16.358066770792));
#84894=CARTESIAN_POINT('Ctrl Pts',(9.3660896407541,0.35373137883533,16.3542532180947));
#84895=CARTESIAN_POINT('Ctrl Pts',(9.37015353226316,0.0748995286265283,
16.3494356565903));
#84896=CARTESIAN_POINT('Ctrl Pts',(9.37044353016443,0.0132374696732548,
16.3483755858442));
#84897=CARTESIAN_POINT('Ctrl Pts',(9.36990669744964,-0.0906426147310336,
16.3466010558192));
#84898=CARTESIAN_POINT('Ctrl Pts',(9.36940317148674,-0.13286017860814,16.3458831464376));
#84899=CARTESIAN_POINT('Ctrl Pts',(9.36758052959633,-0.230394450235545,
16.344232283201));
#84900=CARTESIAN_POINT('Ctrl Pts',(9.36605674187886,-0.285705631614874,
16.3433015471269));
#84901=CARTESIAN_POINT('Ctrl Pts',(9.35759441368305,-0.518085611577563,
16.3394086400234));
#84902=CARTESIAN_POINT('Ctrl Pts',(9.34612360690806,-0.694953100015896,
16.3364875781861));
#84903=CARTESIAN_POINT('Ctrl Pts',(9.32574054154149,-0.913187127621161,
16.3328882216055));
#84904=CARTESIAN_POINT('Ctrl Pts',(9.32155575686584,-0.95495845525837,16.3321995426532));
#84905=CARTESIAN_POINT('Ctrl Pts',(9.29268786405095,-1.2248136761063,16.3277493466816));
#84906=CARTESIAN_POINT('Ctrl Pts',(9.25991608958468,-1.45195391693056,16.3239962271645));
#84907=CARTESIAN_POINT('Ctrl Pts',(9.19892194793587,-1.78712002499303,16.318364985256));
#84908=CARTESIAN_POINT('Ctrl Pts',(9.17705466648271,-1.89621479923809,16.3165175938012));
#84909=CARTESIAN_POINT('Ctrl Pts',(9.13215258815439,-2.10121313163741,16.3130112856188));
#84910=CARTESIAN_POINT('Ctrl Pts',(9.10953623704109,-2.1971929825401,16.3113550694203));
#84911=CARTESIAN_POINT('Ctrl Pts',(9.06611131269506,-2.36926799417323,16.3083562797361));
#84912=CARTESIAN_POINT('Ctrl Pts',(9.04584861607053,-2.4454913502132,16.3070174150153));
#84913=CARTESIAN_POINT('Ctrl Pts',(8.99855204910986,-2.61477247145234,16.3040194966337));
#84914=CARTESIAN_POINT('Ctrl Pts',(8.97103204148134,-2.70768500896524,16.3023573706975));
#84915=CARTESIAN_POINT('Ctrl Pts',(8.86763496968194,-3.03787560972726,16.2963907004436));
#84916=CARTESIAN_POINT('Ctrl Pts',(8.78374417735473,-3.27253351165463,16.2920362852277));
#84917=CARTESIAN_POINT('Ctrl Pts',(8.57638338538348,-3.78689208258241,16.2822948866805));
#84918=CARTESIAN_POINT('Ctrl Pts',(8.44837630966893,-4.06446080939157,16.2769011145216));
#84919=CARTESIAN_POINT('Ctrl Pts',(8.27909160684131,-4.38883544321028,16.2705827134957));
#84920=CARTESIAN_POINT('Ctrl Pts',(8.25062494498381,-4.44211913651728,16.2695445616066));
#84921=CARTESIAN_POINT('Ctrl Pts',(8.20141655799285,-4.53212197000876,16.2677928406647));
#84922=CARTESIAN_POINT('Ctrl Pts',(8.18093866352746,-4.56898300552095,16.2670760757343));
#84923=CARTESIAN_POINT('Ctrl Pts',(8.13252582853682,-4.65475902563531,16.2654097281733));
#84924=CARTESIAN_POINT('Ctrl Pts',(8.10439730127077,-4.70356272855464,16.2644625700254));
#84925=CARTESIAN_POINT('Ctrl Pts',(7.98427441283909,-4.90770196235974,16.2604988675927));
#84926=CARTESIAN_POINT('Ctrl Pts',(7.88824070472727,-5.06061611109365,16.257524516251));
#84927=CARTESIAN_POINT('Ctrl Pts',(7.64694809538953,-5.42125185958143,16.2504008340038));
#84928=CARTESIAN_POINT('Ctrl Pts',(7.49756290821882,-5.62604099934838,16.2462628871382));
#84929=CARTESIAN_POINT('Ctrl Pts',(7.26794283967614,-5.9154081121667,16.2401627114989));
#84930=CARTESIAN_POINT('Ctrl Pts',(7.19414196812091,-6.00494525522994,16.2382381314519));
#84931=CARTESIAN_POINT('Ctrl Pts',(7.05275037422716,-6.17013635214738,16.234608125144));
#84932=CARTESIAN_POINT('Ctrl Pts',(6.98555675143945,-6.24610816840465,16.2329058756864));
#84933=CARTESIAN_POINT('Ctrl Pts',(6.86388115370386,-6.37925972460924,16.229859750427));
#84934=CARTESIAN_POINT('Ctrl Pts',(6.80988454728909,-6.43686970080591,16.2285201418467));
#84935=CARTESIAN_POINT('Ctrl Pts',(6.68966418889043,-6.5619289479247,16.2255629386361));
#84936=CARTESIAN_POINT('Ctrl Pts',(6.62313490120561,-6.62907252195861,16.2239427394424));
#84937=CARTESIAN_POINT('Ctrl Pts',(6.25090007311462,-6.99354615576505,16.2149657535695));
#84938=CARTESIAN_POINT('Ctrl Pts',(5.92618796862801,-7.27074490740096,16.2074292034106));
#84939=CARTESIAN_POINT('Ctrl Pts',(5.46297211156788,-7.61446869719605,16.1973207054333));
#84940=CARTESIAN_POINT('Ctrl Pts',(5.34007191773079,-7.70115770261324,16.1946977411072));
#84941=CARTESIAN_POINT('Ctrl Pts',(5.17038991504525,-7.8148291275132,16.1911796533957));
#84942=CARTESIAN_POINT('Ctrl Pts',(5.12538346545211,-7.84442034286915,16.1902561574537));
#84943=CARTESIAN_POINT('Ctrl Pts',(5.04441390457464,-7.89666255626724,16.1886136088818));
#84944=CARTESIAN_POINT('Ctrl Pts',(5.00854723078353,-7.91945994406787,16.1878927193168));
#84945=CARTESIAN_POINT('Ctrl Pts',(4.92661405052329,-7.97075864390634,16.1862603800322));
#84946=CARTESIAN_POINT('Ctrl Pts',(4.88045300067559,-7.99910606801568,16.1853508569566));
#84947=CARTESIAN_POINT('Ctrl Pts',(4.57086839635086,-8.18554401717489,16.1793101140676));
#84948=CARTESIAN_POINT('Ctrl Pts',(4.30005163390314,-8.33099791695939,16.1743028689377));
#84949=CARTESIAN_POINT('Ctrl Pts',(3.86709982593019,-8.53678859425633,16.1664389556998));
#84950=CARTESIAN_POINT('Ctrl Pts',(3.70961335697883,-8.6063923424553,16.1636075506105));
#84951=CARTESIAN_POINT('Ctrl Pts',(3.49310126985347,-8.69503585929266,16.1597267852866));
#84952=CARTESIAN_POINT('Ctrl Pts',(3.43567295285092,-8.71788715365546,16.1586986310291));
#84953=CARTESIAN_POINT('Ctrl Pts',(3.28268972839102,-8.77701425376229,16.1559611555106));
#84954=CARTESIAN_POINT('Ctrl Pts',(3.18676035955294,-8.81229762359147,16.1542460009714));
#84955=CARTESIAN_POINT('Ctrl Pts',(3.01569577931341,-8.87205751639885,16.1511863175207));
#84956=CARTESIAN_POINT('Ctrl Pts',(2.94079200790026,-8.89716628709695,16.1498462123963));
#84957=CARTESIAN_POINT('Ctrl Pts',(2.77615015947903,-8.9500501764275,16.1468987401513));
#84958=CARTESIAN_POINT('Ctrl Pts',(2.68629379737132,-8.97742911121932,16.1452888854231));
#84959=CARTESIAN_POINT('Ctrl Pts',(2.39755486011037,-9.06068363760305,16.1401117634759));
#84960=CARTESIAN_POINT('Ctrl Pts',(2.19723094552465,-9.11133541096132,16.1365125147237));
#84961=CARTESIAN_POINT('Ctrl Pts',(1.74989549431628,-9.2088319102773,16.1284872782335));
#84962=CARTESIAN_POINT('Ctrl Pts',(1.50234069437424,-9.25244247241578,16.1240532110747));
#84963=CARTESIAN_POINT('Ctrl Pts',(1.16502267084434,-9.29797010508297,16.1181009250778));
#84964=CARTESIAN_POINT('Ctrl Pts',(1.07654636089967,-9.30862900100692,16.1165482987409));
#84965=CARTESIAN_POINT('Ctrl Pts',(0.919762059057807,-9.32525185256086,
16.1138188382958));
#84966=CARTESIAN_POINT('Ctrl Pts',(0.851515331387109,-9.33173113801424,
16.1126380449183));
#84967=CARTESIAN_POINT('Ctrl Pts',(0.740487244954019,-9.3410439043735,16.1107320679288));
#84968=CARTESIAN_POINT('Ctrl Pts',(0.69774679075457,-9.34433368525447,16.1100020326202));
#84969=CARTESIAN_POINT('Ctrl Pts',(0.603014675231229,-9.35097174350932,
16.1083927425419));
#84970=CARTESIAN_POINT('Ctrl Pts',(0.551014728230223,-9.35417992300858,
16.1075149935758));
#84971=CARTESIAN_POINT('Ctrl Pts',(0.373433854733403,-9.36365001289734,
16.1045328374649));
#84972=CARTESIAN_POINT('Ctrl Pts',(0.247754654171279,-9.36781789927196,
16.1024483570671));
#84973=CARTESIAN_POINT('Ctrl Pts',(-0.178748909620081,-9.37337275888033,
16.0954148305606));
#84974=CARTESIAN_POINT('Ctrl Pts',(-0.479541597051895,-9.36280451559987,
16.0905171298384));
#84975=CARTESIAN_POINT('Ctrl Pts',(-0.862682952782038,-9.33082866763476,
16.0841771922614));
#84976=CARTESIAN_POINT('Ctrl Pts',(-0.945964686502081,-9.32275368585295,
16.0827934093149));
#84977=CARTESIAN_POINT('Ctrl Pts',(-1.08744835825269,-9.30712007235797,
16.0804295026583));
#84978=CARTESIAN_POINT('Ctrl Pts',(-1.14570784493946,-9.30012803652572,
16.0794523338354));
#84979=CARTESIAN_POINT('Ctrl Pts',(-1.3018530011159,-9.27989871202747,16.0768217956801));
#84980=CARTESIAN_POINT('Ctrl Pts',(-1.39960128038713,-9.26566012414879,
16.0751627770707));
#84981=CARTESIAN_POINT('Ctrl Pts',(-1.57496288897138,-9.23727759940475,
16.0721611575476));
#84982=CARTESIAN_POINT('Ctrl Pts',(-1.65265746572546,-9.22369388138638,
16.0708222994514));
#84983=CARTESIAN_POINT('Ctrl Pts',(-1.82524531056657,-9.19126883326174,
16.0678271622371));
#84984=CARTESIAN_POINT('Ctrl Pts',(-1.92003696256901,-9.17193552151032,
16.0661678418955));
#84985=CARTESIAN_POINT('Ctrl Pts',(-2.25233651167558,-9.09878380443507,
16.0603005317881));
#84986=CARTESIAN_POINT('Ctrl Pts',(-2.48802880309683,-9.03717867421254,
16.0560453134387));
#84987=CARTESIAN_POINT('Ctrl Pts',(-2.89213241007543,-8.91454536325154,
16.0486288738686));
#84988=CARTESIAN_POINT('Ctrl Pts',(-3.06169156952756,-8.85774201750675,
16.0454798163883));
#84989=CARTESIAN_POINT('Ctrl Pts',(-3.36870308004292,-8.74502186423979,
16.0397492884474));
#84990=CARTESIAN_POINT('Ctrl Pts',(-3.50665246994715,-8.69062463295451,
16.037163689291));
#84991=CARTESIAN_POINT('Ctrl Pts',(-3.69270650274365,-8.61210688181122,
16.033685403748));
#84992=CARTESIAN_POINT('Ctrl Pts',(-3.74197970608444,-8.59081219419687,
16.032765149478));
#84993=CARTESIAN_POINT('Ctrl Pts',(-3.82996034720434,-8.55188853669681,
16.0311253268392));
#84994=CARTESIAN_POINT('Ctrl Pts',(-3.86873572972371,-8.53441724190768,
16.0304039613926));
#84995=CARTESIAN_POINT('Ctrl Pts',(-3.9568277213642,-8.49400128814837,16.0287674492606));
#84996=CARTESIAN_POINT('Ctrl Pts',(-4.00606618446022,-8.47088999116988,
16.0278542670405));
#84997=CARTESIAN_POINT('Ctrl Pts',(-4.31011536622006,-8.32493299142422,
16.0222172156383));
#84998=CARTESIAN_POINT('Ctrl Pts',(-4.55945676453774,-8.19102918162043,
16.0175981848308));
#84999=CARTESIAN_POINT('Ctrl Pts',(-4.81644832639015,-8.03764143406757,
16.0126912699411));
#85000=CARTESIAN_POINT('Ctrl Pts',(-4.83051592478062,-8.02919486647417,
16.0124222065597));
#85001=CARTESIAN_POINT('Ctrl Pts',(-4.99534124367152,-7.92963931384419,
16.0092640065528));
#85002=CARTESIAN_POINT('Ctrl Pts',(-5.14352296018176,-7.8343337423779,16.006368115123));
#85003=CARTESIAN_POINT('Ctrl Pts',(-5.39852713277017,-7.65996849923668,
16.0012455081852));
#85004=CARTESIAN_POINT('Ctrl Pts',(-5.50651907508048,-7.58270796968518,
15.9990303970227));
#85005=CARTESIAN_POINT('Ctrl Pts',(-5.67910349282999,-7.45360436703456,
15.9954058084714));
#85006=CARTESIAN_POINT('Ctrl Pts',(-5.74471459781343,-7.40315396936248,
15.994007355565));
#85007=CARTESIAN_POINT('Ctrl Pts',(-5.87497382561442,-7.30021916203003,
15.991187934991));
#85008=CARTESIAN_POINT('Ctrl Pts',(-5.93960795857675,-7.2477289218264,15.9897670075863));
#85009=CARTESIAN_POINT('Ctrl Pts',(-6.10805686349279,-7.10716252253127,
15.9860046570422));
#85010=CARTESIAN_POINT('Ctrl Pts',(-6.21066640580657,-7.01767343262509,
15.9836519935949));
#85011=CARTESIAN_POINT('Ctrl Pts',(-6.55220899096653,-6.70644326921703,
15.9756163210451));
#85012=CARTESIAN_POINT('Ctrl Pts',(-6.78150918809198,-6.4744849912915,15.9698612963954));
#85013=CARTESIAN_POINT('Ctrl Pts',(-7.10246121855436,-6.11401557726361,
15.9613991920208));
#85014=CARTESIAN_POINT('Ctrl Pts',(-7.20371591262726,-5.99438229713728,
15.9586640429115));
#85015=CARTESIAN_POINT('Ctrl Pts',(-7.33600669269451,-5.82988411490018,
15.9550270576576));
#85016=CARTESIAN_POINT('Ctrl Pts',(-7.36972092689752,-5.78720627472664,
15.9540943694905));
#85017=CARTESIAN_POINT('Ctrl Pts',(-7.42906577083377,-5.71072378941442,
15.9524439484673));
#85018=CARTESIAN_POINT('Ctrl Pts',(-7.45484186933651,-5.67703418440411,
15.9517242662979));
#85019=CARTESIAN_POINT('Ctrl Pts',(-7.51918623003714,-5.59174156425845,
15.94991981167));
#85020=CARTESIAN_POINT('Ctrl Pts',(-7.55745273731492,-5.53991366672258,
15.9488391351669));
#85021=CARTESIAN_POINT('Ctrl Pts',(-7.70643218282382,-5.33372036898968,
15.9445935478327));
#85022=CARTESIAN_POINT('Ctrl Pts',(-7.81297495879755,-5.17639765267232,
15.9414709713661));
#85023=CARTESIAN_POINT('Ctrl Pts',(-8.04118813872398,-4.81629996874281,
15.934478420199));
#85024=CARTESIAN_POINT('Ctrl Pts',(-8.1601147017571,-4.61193885824473,15.9306136914542));
#85025=CARTESIAN_POINT('Ctrl Pts',(-8.30616009651294,-4.33760629751067,
15.9254780298822));
#85026=CARTESIAN_POINT('Ctrl Pts',(-8.34034956838809,-4.27149774643698,
15.9242445278765));
#85027=CARTESIAN_POINT('Ctrl Pts',(-8.42556261749079,-4.10180584325191,
15.9210853616981));
#85028=CARTESIAN_POINT('Ctrl Pts',(-8.47546570838047,-3.99767401489658,
15.9191532724041));
#85029=CARTESIAN_POINT('Ctrl Pts',(-8.55679664914613,-3.81958986170785,
15.9158543845303));
#85030=CARTESIAN_POINT('Ctrl Pts',(-8.58922099584045,-3.74610708015055,
15.9144947122147));
#85031=CARTESIAN_POINT('Ctrl Pts',(-8.65491605529649,-3.59188492248353,
15.9116430500496));
#85032=CARTESIAN_POINT('Ctrl Pts',(-8.68801092646013,-3.51107893916356,
15.9101499901404));
#85033=CARTESIAN_POINT('Ctrl Pts',(-8.78027370323774,-3.27651029281188,
15.9058184116452));
#85034=CARTESIAN_POINT('Ctrl Pts',(-8.83652197419855,-3.12163500985146,
15.9029611601497));
#85035=CARTESIAN_POINT('Ctrl Pts',(-8.93509828852161,-2.82615259307612,
15.8975234305245));
#85036=CARTESIAN_POINT('Ctrl Pts',(-8.97826216947224,-2.68587568938342,
15.8949476755025));
#85037=CARTESIAN_POINT('Ctrl Pts',(-9.07003165260838,-2.36064832172299,
15.8890077995921));
#85038=CARTESIAN_POINT('Ctrl Pts',(-9.11630640308529,-2.17510743230606,
15.8856420940714));
#85039=CARTESIAN_POINT('Ctrl Pts',(-9.17356775207786,-1.91139477540088,
15.8809321505888));
#85040=CARTESIAN_POINT('Ctrl Pts',(-9.18929349213915,-1.83430107689474,
15.8795641882862));
#85041=CARTESIAN_POINT('Ctrl Pts',(-9.21582413948716,-1.69532170627578,
15.8771189323152));
#85042=CARTESIAN_POINT('Ctrl Pts',(-9.22698118336977,-1.63350804274296,
15.8760387248672));
#85043=CARTESIAN_POINT('Ctrl Pts',(-9.24454578964052,-1.53026631886198,
15.8742493150969));
#85044=CARTESIAN_POINT('Ctrl Pts',(-9.25129834930941,-1.48889916765478,
15.8735363683235));
#85045=CARTESIAN_POINT('Ctrl Pts',(-9.26615189226422,-1.39389959494387,
15.8719086043672));
#85046=CARTESIAN_POINT('Ctrl Pts',(-9.27406519000285,-1.34023947143676,
15.8709958434625));
#85047=CARTESIAN_POINT('Ctrl Pts',(-9.30307803061953,-1.13092723939612,
15.8674565590222));
#85048=CARTESIAN_POINT('Ctrl Pts',(-9.32072841432442,-0.974822735321517,
15.8648620125391));
#85049=CARTESIAN_POINT('Ctrl Pts',(-9.35829827594381,-0.546284030860297,
15.8577888096516));
#85050=CARTESIAN_POINT('Ctrl Pts',(-9.37024418740387,-0.27330729227416,
15.8533345246508));
#85051=CARTESIAN_POINT('Ctrl Pts',(-9.37025356323642,0.167381950165816,
15.8460620169799));
#85052=CARTESIAN_POINT('Ctrl Pts',(-9.36576149366356,0.334932770290093,
15.8432789744368));
#85053=CARTESIAN_POINT('Ctrl Pts',(-9.35207842141409,0.589833238234219,
15.8389972685167));
#85054=CARTESIAN_POINT('Ctrl Pts',(-9.34614929998464,0.67732360578869,15.8375191778604));
#85055=CARTESIAN_POINT('Ctrl Pts',(-9.33244939828673,0.844631469072172,
15.8346744278891));
#85056=CARTESIAN_POINT('Ctrl Pts',(-9.32488025672346,0.924457815456634,
15.8333091841404));
#85057=CARTESIAN_POINT('Ctrl Pts',(-9.304027518363,1.11791982015351,15.8299803229));
#85058=CARTESIAN_POINT('Ctrl Pts',(-9.28968552131401,1.23142827823779,15.828010210307));
#85059=CARTESIAN_POINT('Ctrl Pts',(-9.26273907565275,1.41726287271645,15.8247576515957));
#85060=CARTESIAN_POINT('Ctrl Pts',(-9.25135676604782,1.48975407358555,15.8234821009583));
#85061=CARTESIAN_POINT('Ctrl Pts',(-9.2007427136253,1.78911283046138,15.8181886459976));
#85062=CARTESIAN_POINT('Ctrl Pts',(-9.15400777384044,2.01462961897199,15.8141369440333));
#85063=CARTESIAN_POINT('Ctrl Pts',(-9.09234931818992,2.26529194695014,15.8096000269021));
#85064=CARTESIAN_POINT('Ctrl Pts',(-9.08556296639746,2.29235889705144,15.80910971416));
#85065=CARTESIAN_POINT('Ctrl Pts',(-9.03194861919503,2.50221800996891,15.8053056703467));
#85066=CARTESIAN_POINT('Ctrl Pts',(-8.97972952517669,2.68358879427491,15.8020024326592));
#85067=CARTESIAN_POINT('Ctrl Pts',(-8.90499334285409,2.91647076131029,15.797784950666));
#85068=CARTESIAN_POINT('Ctrl Pts',(-8.88744105032833,2.96952853735195,15.7968257856545));
#85069=CARTESIAN_POINT('Ctrl Pts',(-8.85580758261927,3.06235805249446,15.7951525281267));
#85070=CARTESIAN_POINT('Ctrl Pts',(-8.84193055550554,3.10219742113524,15.7944361673277));
#85071=CARTESIAN_POINT('Ctrl Pts',(-8.80734745982603,3.19936412141319,15.7926928924964));
#85072=CARTESIAN_POINT('Ctrl Pts',(-8.78635021194856,3.25658564094406,15.7916693615523));
#85073=CARTESIAN_POINT('Ctrl Pts',(-8.68355102012543,3.52849969874744,15.7868120236144));
#85074=CARTESIAN_POINT('Ctrl Pts',(-8.59442944174783,3.74034112336728,15.7830451638138));
#85075=CARTESIAN_POINT('Ctrl Pts',(-8.36675180305747,4.23030483455728,15.7741890389838));
#85076=CARTESIAN_POINT('Ctrl Pts',(-8.22197364695728,4.50523734701086,15.7691021879588));
#85077=CARTESIAN_POINT('Ctrl Pts',(-8.01255894856545,4.85907514277056,15.7622386246166));
#85078=CARTESIAN_POINT('Ctrl Pts',(-7.95991245021477,4.94484639474211,15.7605497449081));
#85079=CARTESIAN_POINT('Ctrl Pts',(-7.86348522324334,5.09641318705451,15.7575165383232));
#85080=CARTESIAN_POINT('Ctrl Pts',(-7.8202343906044,5.16253438455124,15.756176304074));
#85081=CARTESIAN_POINT('Ctrl Pts',(-7.72381733034893,5.30594282880879,15.7532309689126));
#85082=CARTESIAN_POINT('Ctrl Pts',(-7.67031626384744,5.38299468810639,15.7516234064154));
#85083=CARTESIAN_POINT('Ctrl Pts',(-7.4822445113779,5.64535620915769,15.7460622480555));
#85084=CARTESIAN_POINT('Ctrl Pts',(-7.34204351717437,5.82652778161682,15.7420670764762));
#85085=CARTESIAN_POINT('Ctrl Pts',(-7.04082143476646,6.18761743948393,15.733816031374));
#85086=CARTESIAN_POINT('Ctrl Pts',(-6.87920049817855,6.36681839973998,15.7295605562487));
#85087=CARTESIAN_POINT('Ctrl Pts',(-6.631600299452,6.620902905275,15.7233628608246));
#85088=CARTESIAN_POINT('Ctrl Pts',(-6.55088357298351,6.70077624879833,15.7213894181907));
#85089=CARTESIAN_POINT('Ctrl Pts',(-6.43114263043601,6.81503407580786,15.7185408880979));
#85090=CARTESIAN_POINT('Ctrl Pts',(-6.39325238808896,6.85059186536449,15.7176506872935));
#85091=CARTESIAN_POINT('Ctrl Pts',(-6.32354089130607,6.91492995526093,15.7160347061809));
#85092=CARTESIAN_POINT('Ctrl Pts',(-6.29181407858179,6.94381028604951,15.7153075049748));
#85093=CARTESIAN_POINT('Ctrl Pts',(-6.20866679389262,7.01845997636821,15.7134219517893));
#85094=CARTESIAN_POINT('Ctrl Pts',(-6.15693826418206,7.06388243403045,15.7122686115244));
#85095=CARTESIAN_POINT('Ctrl Pts',(-6.03670209454123,7.16713678806433,15.7096270636883));
#85096=CARTESIAN_POINT('Ctrl Pts',(-5.9678555492318,7.22456380063715,15.7081431401988));
#85097=CARTESIAN_POINT('Ctrl Pts',(-5.70013244705699,7.44144121742001,15.7024619433389));
#85098=CARTESIAN_POINT('Ctrl Pts',(-5.49560484848972,7.59373985443148,15.6983046173089));
#85099=CARTESIAN_POINT('Ctrl Pts',(-5.11764353183826,7.85190714034292,15.6907783993391));
#85100=CARTESIAN_POINT('Ctrl Pts',(-4.94649463491711,7.96083610739333,15.6874246305098));
#85101=CARTESIAN_POINT('Ctrl Pts',(-4.69137527066045,8.1118030086513,15.6824637778958));
#85102=CARTESIAN_POINT('Ctrl Pts',(-4.6100941510685,8.15827076323484,15.6808889699364));
#85103=CARTESIAN_POINT('Ctrl Pts',(-4.45894775038666,8.24169973553113,15.6779684005877));
#85104=CARTESIAN_POINT('Ctrl Pts',(-4.38928480825566,8.27901011048647,15.6766253458315));
#85105=CARTESIAN_POINT('Ctrl Pts',(-4.22807452093195,8.36274508994909,15.6735232980258));
#85106=CARTESIAN_POINT('Ctrl Pts',(-4.13621966528828,8.40855554793786,15.6717601236956));
#85107=CARTESIAN_POINT('Ctrl Pts',(-3.8189423435365,8.56033308520592,15.665685025036));
#85108=CARTESIAN_POINT('Ctrl Pts',(-3.59005814216845,8.65881659981613,15.6613255098028));
#85109=CARTESIAN_POINT('Ctrl Pts',(-3.08997590857638,8.85074912450476,15.651912879018));
#85110=CARTESIAN_POINT('Ctrl Pts',(-2.81785793593207,8.94110665445982,15.6468581113258));
#85111=CARTESIAN_POINT('Ctrl Pts',(-2.48235116529867,9.03567163966352,15.6408354451146));
#85112=CARTESIAN_POINT('Ctrl Pts',(-2.42250893029571,9.05189923693731,15.6397694073616));
#85113=CARTESIAN_POINT('Ctrl Pts',(-2.32163553941544,9.07818140482797,15.6379885954601));
#85114=CARTESIAN_POINT('Ctrl Pts',(-2.28068961480581,9.08855456564394,15.6372703021023));
#85115=CARTESIAN_POINT('Ctrl Pts',(-2.18522188514386,9.11205438695823,15.6356063438053));
#85116=CARTESIAN_POINT('Ctrl Pts',(-2.13064971155267,9.1249691322488,15.6346630487893));
#85117=CARTESIAN_POINT('Ctrl Pts',(-1.89810781504891,9.17780135525472,15.6306710703351));
#85118=CARTESIAN_POINT('Ctrl Pts',(-1.71910832552624,9.21300808442412,15.6276659755268));
#85119=CARTESIAN_POINT('Ctrl Pts',(-1.15510815692486,9.30692881872542,15.6182790533383));
#85120=CARTESIAN_POINT('Ctrl Pts',(-0.767408870734917,9.34688623888578,
15.6119296456137));
#85121=CARTESIAN_POINT('Ctrl Pts',(-0.284024001470532,9.36642020355662,
15.6038358871157));
#85122=CARTESIAN_POINT('Ctrl Pts',(-0.189645543171991,9.36880630477435,
15.6022483038232));
#85123=CARTESIAN_POINT('Ctrl Pts',(-0.016288041175524,9.37056855125156,
15.5993160680699));
#85124=CARTESIAN_POINT('Ctrl Pts',(0.0626781072318076,9.37037308196079,
15.5979742820961));
#85125=CARTESIAN_POINT('Ctrl Pts',(0.243186585160061,9.36764436726062,15.5948921573239));
#85126=CARTESIAN_POINT('Ctrl Pts',(0.344709074986845,9.36445814185987,15.5931478437941));
#85127=CARTESIAN_POINT('Ctrl Pts',(0.761531885481913,9.34458880828794,15.5859419970708));
#85128=CARTESIAN_POINT('Ctrl Pts',(1.07594183185033,9.31362541768284,15.5803951409329));
#85129=CARTESIAN_POINT('Ctrl Pts',(1.60482165262962,9.23439855919564,15.5709935129916));
#85130=CARTESIAN_POINT('Ctrl Pts',(1.82025330259932,9.19435955158589,15.5671457668868));
#85131=CARTESIAN_POINT('Ctrl Pts',(2.0963290126656,9.13296533618817,15.5622565085354));
#85132=CARTESIAN_POINT('Ctrl Pts',(2.15843161451212,9.11848804101339,15.561159569068));
#85133=CARTESIAN_POINT('Ctrl Pts',(2.26153797896965,9.09333963077009,15.5593457944175));
#85134=CARTESIAN_POINT('Ctrl Pts',(2.30262571044512,9.08302232331562,15.5586250823846));
#85135=CARTESIAN_POINT('Ctrl Pts',(2.39671545272811,9.05871651133231,15.5569797715574));
#85136=CARTESIAN_POINT('Ctrl Pts',(2.44966739368923,9.04454086578479,15.5560572739475));
#85137=CARTESIAN_POINT('Ctrl Pts',(2.65892101363595,8.98654958981423,15.5524204011845));
#85138=CARTESIAN_POINT('Ctrl Pts',(2.81419763513012,8.93914014082858,15.5497403583112));
#85139=CARTESIAN_POINT('Ctrl Pts',(3.27887686829661,8.7839547558277,15.5416877245926));
#85140=CARTESIAN_POINT('Ctrl Pts',(3.58393364941571,8.66396643681611,15.5363501164303));
#85141=CARTESIAN_POINT('Ctrl Pts',(4.00183291132801,8.47373771938385,15.5287346085468));
#85142=CARTESIAN_POINT('Ctrl Pts',(4.12042486130357,8.41670935804079,15.5265389735733));
#85143=CARTESIAN_POINT('Ctrl Pts',(4.25552198162736,8.34820421466785,15.5239913328453));
#85144=CARTESIAN_POINT('Ctrl Pts',(4.27323885690915,8.33914927352573,15.5236563045117));
#85145=CARTESIAN_POINT('Ctrl Pts',(4.29092662820214,8.330038039162,15.5233208859591));
#85146=CARTESIAN_POINT('',(-9.37024999994221,-3.29085560364655E-5,15.651410108095));
#85147=CARTESIAN_POINT('Ctrl Pts',(4.29092660882816,8.33003804914182,15.3259008099036));
#85148=CARTESIAN_POINT('Ctrl Pts',(4.14338165943684,8.40604064908272,15.3288132869415));
#85149=CARTESIAN_POINT('Ctrl Pts',(3.99382155619009,8.47812106179566,15.3317149276861));
#85150=CARTESIAN_POINT('Ctrl Pts',(3.79486872530126,8.56757098912454,15.3354781348473));
#85151=CARTESIAN_POINT('Ctrl Pts',(3.74715706517178,8.58854558352599,15.3363733892997));
#85152=CARTESIAN_POINT('Ctrl Pts',(3.66044193914147,8.6258064036087,15.337985915101));
#85153=CARTESIAN_POINT('Ctrl Pts',(3.62149862581783,8.64222882253731,15.3387047062237));
#85154=CARTESIAN_POINT('Ctrl Pts',(3.53091024838905,8.67971015704992,15.3403640552681));
#85155=CARTESIAN_POINT('Ctrl Pts',(3.47918572957726,8.7005725254746,15.3413023080991));
#85156=CARTESIAN_POINT('Ctrl Pts',(3.26264434492313,8.78567170098749,15.3451975990018));
#85157=CARTESIAN_POINT('Ctrl Pts',(3.09621109067015,8.84569684167798,15.3481136942107));
#85158=CARTESIAN_POINT('Ctrl Pts',(2.55131166892319,9.02495391183104,15.3575338867737));
#85159=CARTESIAN_POINT('Ctrl Pts',(2.16695257128601,9.12487264814757,15.3639998561766));
#85160=CARTESIAN_POINT('Ctrl Pts',(1.68509077809691,9.2179659879519,15.372211626545));
#85161=CARTESIAN_POINT('Ctrl Pts',(1.59249864456165,9.23441259087598,15.373793214));
#85162=CARTESIAN_POINT('Ctrl Pts',(1.4217037147495,9.26210467021329,15.3767199451349));
#85163=CARTESIAN_POINT('Ctrl Pts',(1.34357599216646,9.2737601809637,15.3780622972214));
#85164=CARTESIAN_POINT('Ctrl Pts',(1.16418493369478,9.29820814942461,15.3811535897687));
#85165=CARTESIAN_POINT('Ctrl Pts',(1.06284128407922,9.31033671164013,15.3829066001443));
#85166=CARTESIAN_POINT('Ctrl Pts',(0.899972766852598,9.32713447904183,15.385734302485));
#85167=CARTESIAN_POINT('Ctrl Pts',(0.838564682809169,9.33285582392137,15.3868028154152));
#85168=CARTESIAN_POINT('Ctrl Pts',(0.60613591919492,9.35219851453027,15.3908551729958));
#85169=CARTESIAN_POINT('Ctrl Pts',(0.434809019184202,9.36172840385953,15.3938593229248));
#85170=CARTESIAN_POINT('Ctrl Pts',(-0.0462849266090543,9.37525318514394,
15.4023127357885));
#85171=CARTESIAN_POINT('Ctrl Pts',(-0.356128831416666,9.36860113135022,
15.4077823653244));
#85172=CARTESIAN_POINT('Ctrl Pts',(-0.718523987558737,9.34281434062199,
15.4140537628747));
#85173=CARTESIAN_POINT('Ctrl Pts',(-0.771941332846491,9.33855251734523,
15.4149747451152));
#85174=CARTESIAN_POINT('Ctrl Pts',(-0.867576173558023,9.33009626181011,
15.4166157884542));
#85175=CARTESIAN_POINT('Ctrl Pts',(-0.909807239364471,9.32607288610909,
15.4173376204022));
#85176=CARTESIAN_POINT('Ctrl Pts',(-1.00609510332455,9.31623923279315,15.4189765648432));
#85177=CARTESIAN_POINT('Ctrl Pts',(-1.06013145991945,9.3102450078071,15.4198916726837));
#85178=CARTESIAN_POINT('Ctrl Pts',(-1.26945444804055,9.28517891965654,15.4234233371553));
#85179=CARTESIAN_POINT('Ctrl Pts',(-1.42430646756362,9.26268932466101,15.4260080656733));
#85180=CARTESIAN_POINT('Ctrl Pts',(-1.89972177579867,9.18143911745269,15.4339391924436));
#85181=CARTESIAN_POINT('Ctrl Pts',(-2.21783816644118,9.10982772513381,15.4392471254171));
#85182=CARTESIAN_POINT('Ctrl Pts',(-2.66285879524998,8.98495187757467,15.4469071235945));
#85183=CARTESIAN_POINT('Ctrl Pts',(-2.7933210807633,8.94525205912265,15.4491807988518));
#85184=CARTESIAN_POINT('Ctrl Pts',(-3.00200667067457,8.87673806215471,15.452873345799));
#85185=CARTESIAN_POINT('Ctrl Pts',(-3.08079304782268,8.84970264091211,15.4542803202716));
#85186=CARTESIAN_POINT('Ctrl Pts',(-3.23709628302548,8.7937271551059,15.4570989883812));
#85187=CARTESIAN_POINT('Ctrl Pts',(-3.31461123286781,8.7648035893701,15.4585104620641));
#85188=CARTESIAN_POINT('Ctrl Pts',(-3.5153101038635,8.68687249918063,15.4622013399725));
#85189=CARTESIAN_POINT('Ctrl Pts',(-3.63785482021707,8.63627067103908,15.4644911536243));
#85190=CARTESIAN_POINT('Ctrl Pts',(-3.92022880447052,8.51259439739314,15.4698489950298));
#85191=CARTESIAN_POINT('Ctrl Pts',(-4.07915837899617,8.43758993700404,15.47292706393));
#85192=CARTESIAN_POINT('Ctrl Pts',(-4.50612693615062,8.22120389245774,15.4813364207233));
#85193=CARTESIAN_POINT('Ctrl Pts',(-4.76956812564212,8.07122008554411,15.4866842231501));
#85194=CARTESIAN_POINT('Ctrl Pts',(-5.07018872589917,7.88020319686578,15.4928315089698));
#85195=CARTESIAN_POINT('Ctrl Pts',(-5.11485377660323,7.85128569091352,15.4937458660693));
#85196=CARTESIAN_POINT('Ctrl Pts',(-5.19464443469504,7.79865693552052,15.4953794827591));
#85197=CARTESIAN_POINT('Ctrl Pts',(-5.22986001849909,7.77508488734085,15.4961004489973));
#85198=CARTESIAN_POINT('Ctrl Pts',(-5.31017132640637,7.72053486786514,15.4977442422347));
#85199=CARTESIAN_POINT('Ctrl Pts',(-5.35515797613774,7.68939927632527,15.4986649908635));
#85200=CARTESIAN_POINT('Ctrl Pts',(-5.53135626676057,7.56515486078743,15.5022761904285));
#85201=CARTESIAN_POINT('Ctrl Pts',(-5.66043376802533,7.46906688071462,15.5049329300348));
#85202=CARTESIAN_POINT('Ctrl Pts',(-6.04432512846104,7.16762066575808,15.5129566813675));
#85203=CARTESIAN_POINT('Ctrl Pts',(-6.29091476325641,6.95219705395721,15.5182878564457));
#85204=CARTESIAN_POINT('Ctrl Pts',(-6.62095580651084,6.63190301697132,15.5259143344115));
#85205=CARTESIAN_POINT('Ctrl Pts',(-6.7142079554203,6.53747694566034,15.5281282640163));
#85206=CARTESIAN_POINT('Ctrl Pts',(-6.85664729006891,6.38698098219872,15.5316130428055));
#85207=CARTESIAN_POINT('Ctrl Pts',(-6.9072240032617,6.33225036368195,15.5328716280295));
#85208=CARTESIAN_POINT('Ctrl Pts',(-7.00726979730507,6.22136276646034,15.5354054517924));
#85209=CARTESIAN_POINT('Ctrl Pts',(-7.05672975127081,6.16520477137091,15.5366806469937));
#85210=CARTESIAN_POINT('Ctrl Pts',(-7.1581946305707,6.04717832442305,15.5393446860341));
#85211=CARTESIAN_POINT('Ctrl Pts',(-7.21008251642192,5.98521729999843,15.5407343566862));
#85212=CARTESIAN_POINT('Ctrl Pts',(-7.33508712685367,5.83196030945969,15.5441498466552));
#85213=CARTESIAN_POINT('Ctrl Pts',(-7.40730842900602,5.73995173823779,15.5461819925114));
#85214=CARTESIAN_POINT('Ctrl Pts',(-7.63353648519067,5.44035891165868,15.552734583431));
#85215=CARTESIAN_POINT('Ctrl Pts',(-7.7806841981848,5.22774686800166,15.5572911315491));
#85216=CARTESIAN_POINT('Ctrl Pts',(-8.01155606378281,4.86277943992659,15.5648713679657));
#85217=CARTESIAN_POINT('Ctrl Pts',(-8.10017274757297,4.71368817210393,15.5679036604525));
#85218=CARTESIAN_POINT('Ctrl Pts',(-8.2117572333541,4.51350629059428,15.5718560814117));
#85219=CARTESIAN_POINT('Ctrl Pts',(-8.23847763144406,4.46454725925851,15.5728135061304));
#85220=CARTESIAN_POINT('Ctrl Pts',(-8.28339881190472,4.38046275075152,15.5744403123562));
#85221=CARTESIAN_POINT('Ctrl Pts',(-8.30181710245382,4.3454553953276,15.5751123616867));
#85222=CARTESIAN_POINT('Ctrl Pts',(-8.33637823538616,4.27874381368598,15.5763832283343));
#85223=CARTESIAN_POINT('Ctrl Pts',(-8.3525631985838,4.24706236419942,15.5769826868324));
#85224=CARTESIAN_POINT('Ctrl Pts',(-8.41750174756852,4.11814058462066,15.5794070040464));
#85225=CARTESIAN_POINT('Ctrl Pts',(-8.4647408767115,4.02014670667257,15.581215203477));
#85226=CARTESIAN_POINT('Ctrl Pts',(-8.5877689860493,3.75314658120452,15.586074671246));
#85227=CARTESIAN_POINT('Ctrl Pts',(-8.66027093213542,3.58267958439453,15.5891062476071));
#85228=CARTESIAN_POINT('Ctrl Pts',(-8.76065627671584,3.32576308295427,15.5936276220563));
#85229=CARTESIAN_POINT('Ctrl Pts',(-8.79241269015809,3.24087604777668,15.5951137916613));
#85230=CARTESIAN_POINT('Ctrl Pts',(-8.89243744406557,2.96120563484695,15.5999964691581));
#85231=CARTESIAN_POINT('Ctrl Pts',(-8.95550230967423,2.76462665102001,15.6034081676231));
#85232=CARTESIAN_POINT('Ctrl Pts',(-9.03775390475236,2.47576583469663,15.6084337563054));
#85233=CARTESIAN_POINT('Ctrl Pts',(-9.06212307647707,2.3850235646686,15.6100139733665));
#85234=CARTESIAN_POINT('Ctrl Pts',(-9.10446240417055,2.21733842881238,15.6129394536193));
#85235=CARTESIAN_POINT('Ctrl Pts',(-9.12283196555392,2.14050514396401,15.6142819423674));
#85236=CARTESIAN_POINT('Ctrl Pts',(-9.15708425758601,1.98878161322273,15.6169377682931));
#85237=CARTESIAN_POINT('Ctrl Pts',(-9.17302514074449,1.91391069353834,15.6182506169118));
#85238=CARTESIAN_POINT('Ctrl Pts',(-9.20810113699684,1.73864932055023,15.6213291301637));
#85239=CARTESIAN_POINT('Ctrl Pts',(-9.22651484183486,1.63812448195104,15.6230989791019));
#85240=CARTESIAN_POINT('Ctrl Pts',(-9.28250340262572,1.30148774251282,15.6290362989418));
#85241=CARTESIAN_POINT('Ctrl Pts',(-9.31268635841509,1.06424248018041,15.6332399503902));
#85242=CARTESIAN_POINT('Ctrl Pts',(-9.35140417596125,0.626787906599619,
15.6409604976902));
#85243=CARTESIAN_POINT('Ctrl Pts',(-9.36265617330869,0.426957596360454,
15.6444750097962));
#85244=CARTESIAN_POINT('Ctrl Pts',(-9.36854682124597,0.183785776007762,
15.6486908625793));
#85245=CARTESIAN_POINT('Ctrl Pts',(-9.36929377931046,0.140644366409776,
15.6494364201494));
#85246=CARTESIAN_POINT('Ctrl Pts',(-9.37008099742837,0.0649922206876054,
15.6507388237825));
#85247=CARTESIAN_POINT('Ctrl Pts',(-9.37025008779887,0.0324835742681818,
15.651296864785));
#85248=CARTESIAN_POINT('Ctrl Pts',(-9.3702499999658,-2.53166982348E-5,15.65185308165));
#85249=CARTESIAN_POINT('Ctrl Pts',(-9.37024999994221,-3.29085560364655E-5,
15.651410108095));
#85250=CARTESIAN_POINT('Ctrl Pts',(-9.37024988706599,-0.0321728302279683,
15.6519561937273));
#85251=CARTESIAN_POINT('Ctrl Pts',(-9.37008441347547,-0.0643126166714824,
15.6525022793597));
#85252=CARTESIAN_POINT('Ctrl Pts',(-9.36975358934515,-0.0964506996016772,
15.653048364992));
#85253=CARTESIAN_POINT('Ctrl Pts',(-9.36734961314108,-0.32998622355172,
15.6570165666596));
#85254=CARTESIAN_POINT('Ctrl Pts',(-9.35620981951031,-0.563468090583012,
15.6609847683271));
#85255=CARTESIAN_POINT('Ctrl Pts',(-9.33635895696654,-0.796232685319189,
15.6649529699946));
#85256=CARTESIAN_POINT('Ctrl Pts',(-9.31651157239417,-1.02895649852255,
15.6689204764132));
#85257=CARTESIAN_POINT('Ctrl Pts',(-9.28795618961534,-1.26096300696166,
15.6728879828317));
#85258=CARTESIAN_POINT('Ctrl Pts',(-9.25076952484415,-1.49159252502647,
15.6768554892503));
#85259=CARTESIAN_POINT('Ctrl Pts',(-9.21358691453216,-1.7221968975726,15.6808225630919));
#85260=CARTESIAN_POINT('Ctrl Pts',(-9.16777494645078,-1.95142429874742,
15.6847896369335));
#85261=CARTESIAN_POINT('Ctrl Pts',(-9.11346183096947,-2.17862307845176,
15.6887567107752));
#85262=CARTESIAN_POINT('Ctrl Pts',(-9.05914448620663,-2.40583954978719,
15.6927240935269));
#85263=CARTESIAN_POINT('Ctrl Pts',(-8.99632473461012,-2.63102680662034,
15.6966914762787));
#85264=CARTESIAN_POINT('Ctrl Pts',(-8.92518154797546,-2.85354505802489,
15.7006588590305));
#85265=CARTESIAN_POINT('Ctrl Pts',(-8.85403911498194,-3.07606095222681,
15.7046261997546));
#85266=CARTESIAN_POINT('Ctrl Pts',(-8.77457351207394,-3.2959076272409,15.7085935404787));
#85267=CARTESIAN_POINT('Ctrl Pts',(-8.68701328200696,-3.5124614304978,15.7125608812028));
#85268=CARTESIAN_POINT('Ctrl Pts',(-8.59943420184895,-3.72906185376586,
15.7165290760216));
#85269=CARTESIAN_POINT('Ctrl Pts',(-8.50375711873428,-3.94236772478265,
15.7204972708405));
#85270=CARTESIAN_POINT('Ctrl Pts',(-8.4002588336377,-4.1517751131765,15.7244654656593));
#85271=CARTESIAN_POINT('Ctrl Pts',(-8.33662135806883,-4.28053239210552,
15.7269053698626));
#85272=CARTESIAN_POINT('Ctrl Pts',(-8.27002794412772,-4.40781622564588,
15.7293452740658));
#85273=CARTESIAN_POINT('Ctrl Pts',(-8.20055166581281,-4.5334906461616,15.7317851782691));
#85274=CARTESIAN_POINT('Ctrl Pts',(-8.08755711336536,-4.73788450899779,
15.7357533799366));
#85275=CARTESIAN_POINT('Ctrl Pts',(-7.96689962036225,-4.93808352651896,
15.7397215816041));
#85276=CARTESIAN_POINT('Ctrl Pts',(-7.83891604164744,-5.13351539926613,
15.7436897832716));
#85277=CARTESIAN_POINT('Ctrl Pts',(-7.71095488630218,-5.32891303136188,
15.7476572896901));
#85278=CARTESIAN_POINT('Ctrl Pts',(-7.57567036319796,-5.51954494802817,
15.7516247961087));
#85279=CARTESIAN_POINT('Ctrl Pts',(-7.43344319830096,-5.70486698180888,
15.7555923025272));
#85280=CARTESIAN_POINT('Ctrl Pts',(-7.2912315404208,-5.89016880994251,15.7595593763688));
#85281=CARTESIAN_POINT('Ctrl Pts',(-7.14207892523925,-6.07016168550439,
15.7635264502104));
#85282=CARTESIAN_POINT('Ctrl Pts',(-6.98640758373676,-6.24433296168658,
15.767493524052));
#85283=CARTESIAN_POINT('Ctrl Pts',(-6.83072412033846,-6.41851780032698,
15.7714609068038));
#85284=CARTESIAN_POINT('Ctrl Pts',(-6.66852110374997,-6.5868799197005,15.7754282895555));
#85285=CARTESIAN_POINT('Ctrl Pts',(-6.50025980967756,-6.74894121097455,
15.7793956723073));
#85286=CARTESIAN_POINT('Ctrl Pts',(-6.33200029804755,-6.9110007854847,15.7833630130314));
#85287=CARTESIAN_POINT('Ctrl Pts',(-6.15768284375902,-7.06675946964164,
15.7873303537554));
#85288=CARTESIAN_POINT('Ctrl Pts',(-5.97780468782581,-7.21577689349579,
15.7912976944795));
#85289=CARTESIAN_POINT('Ctrl Pts',(-5.79788780746694,-7.36482639803323,
15.7952658892984));
#85290=CARTESIAN_POINT('Ctrl Pts',(-5.61240805228575,-7.50713156048764,
15.7992340841172));
#85291=CARTESIAN_POINT('Ctrl Pts',(-5.42189577170874,-7.64229228067253,
15.803202278936));
#85292=CARTESIAN_POINT('Ctrl Pts',(-5.30475643370081,-7.72539788016028,
15.8056421831394));
#85293=CARTESIAN_POINT('Ctrl Pts',(-5.18571513404556,-7.80580326579222,
15.8080820873427));
#85294=CARTESIAN_POINT('Ctrl Pts',(-5.06490074054801,-7.88342346641966,
15.810521991546));
#85295=CARTESIAN_POINT('Ctrl Pts',(-4.86841110907637,-8.00966309875578,
15.8144901932135));
#85296=CARTESIAN_POINT('Ctrl Pts',(-4.66716894661539,-8.12857259914405,
15.8184583948811));
#85297=CARTESIAN_POINT('Ctrl Pts',(-4.46174243832586,-8.23980821843215,
15.8224265965486));
#85298=CARTESIAN_POINT('Ctrl Pts',(-4.25635192179843,-8.35102434867778,
15.8263941029671));
#85299=CARTESIAN_POINT('Ctrl Pts',(-4.04677877289066,-8.45456914623218,
15.8303616093857));
#85300=CARTESIAN_POINT('Ctrl Pts',(-3.83361643124384,-8.55014445027669,
15.8343291158042));
#85301=CARTESIAN_POINT('Ctrl Pts',(-3.62047733067052,-8.64570933375325,
15.8382961896458));
#85302=CARTESIAN_POINT('Ctrl Pts',(-3.4037500781858,-8.73330634226022,15.8422632634875));
#85303=CARTESIAN_POINT('Ctrl Pts',(-3.18404967662088,-8.81268476227934,
15.8462303373291));
#85304=CARTESIAN_POINT('Ctrl Pts',(-2.96433216731255,-8.89206936337792,
15.8501977200809));
#85305=CARTESIAN_POINT('Ctrl Pts',(-2.74164131289812,-8.96323399778914,
15.8541651028326));
#85306=CARTESIAN_POINT('Ctrl Pts',(-2.51661008151512,-9.02597688674841,
15.8581324855844));
#85307=CARTESIAN_POINT('Ctrl Pts',(-2.29158123395598,-9.08871911105329,
15.8620998263085));
#85308=CARTESIAN_POINT('Ctrl Pts',(-2.06421233366606,-9.14303969408616,
15.8660671670326));
#85309=CARTESIAN_POINT('Ctrl Pts',(-1.83515008414716,-9.18878714690653,
15.8700345077567));
#85310=CARTESIAN_POINT('Ctrl Pts',(-1.6060385217808,-9.23454444830373,15.8740027025755));
#85311=CARTESIAN_POINT('Ctrl Pts',(-1.37523316074441,-9.27172487541669,
15.8779708973944));
#85312=CARTESIAN_POINT('Ctrl Pts',(-1.14339072392327,-9.3002281001568,15.8819390922132));
#85313=CARTESIAN_POINT('Ctrl Pts',(-1.00083891839998,-9.317753736126,15.8843789964165));
#85314=CARTESIAN_POINT('Ctrl Pts',(-0.85789520831772,-9.33199988680165,
15.8868189006197));
#85315=CARTESIAN_POINT('Ctrl Pts',(-0.714713353468726,-9.34295295315531,
15.889258804823));
#85316=CARTESIAN_POINT('Ctrl Pts',(-0.481845819402004,-9.36076675752972,
15.8932270064905));
#85317=CARTESIAN_POINT('Ctrl Pts',(-0.248275795756671,-9.36987287027141,
15.8971952081581));
#85318=CARTESIAN_POINT('Ctrl Pts',(-0.0146665502080458,-9.37023852176694,
15.9011634098256));
#85319=CARTESIAN_POINT('Ctrl Pts',(0.218901765820847,-9.37060410919847,
15.9051309162442));
#85320=CARTESIAN_POINT('Ctrl Pts',(0.452509005685188,-9.36223229176214,
15.9090984226627));
#85321=CARTESIAN_POINT('Ctrl Pts',(0.685491319762012,-9.34514241266718,
15.9130659290813));
#85322=CARTESIAN_POINT('Ctrl Pts',(0.918448231795425,-9.32805439688039,
15.917033002923));
#85323=CARTESIAN_POINT('Ctrl Pts',(1.15078007046233,-9.30225023808432,15.9210000767646));
#85324=CARTESIAN_POINT('Ctrl Pts',(1.38182653551341,-9.26780127582864,15.9249671506063));
#85325=CARTESIAN_POINT('Ctrl Pts',(1.61289099180863,-9.23334963108358,15.928934533358));
#85326=CARTESIAN_POINT('Ctrl Pts',(1.84266959266458,-9.19025187685204,15.9329019161098));
#85327=CARTESIAN_POINT('Ctrl Pts',(2.0705094599306,-9.13863094992012,15.9368692988616));
#85328=CARTESIAN_POINT('Ctrl Pts',(2.29834691362034,-9.08701056982421,15.9408366395857));
#85329=CARTESIAN_POINT('Ctrl Pts',(2.52424539782052,-9.02686726265966,15.9448039803098));
#85330=CARTESIAN_POINT('Ctrl Pts',(2.74756382262737,-8.95837474674336,15.9487713210339));
#85331=CARTESIAN_POINT('Ctrl Pts',(2.97093032374271,-8.88986748566072,15.9527395158528));
#85332=CARTESIAN_POINT('Ctrl Pts',(3.19171538339562,-8.81300750727174,15.9567077106716));
#85333=CARTESIAN_POINT('Ctrl Pts',(3.40929338392328,-8.72801831373176,15.9606759054905));
#85334=CARTESIAN_POINT('Ctrl Pts',(3.54307448647365,-8.67576143119276,15.9631158096937));
#85335=CARTESIAN_POINT('Ctrl Pts',(3.6756434598503,-8.62043219518479,15.9655557138968));
#85336=CARTESIAN_POINT('Ctrl Pts',(3.80685852306037,-8.56209163977486,15.9679956181));
#85337=CARTESIAN_POINT('Ctrl Pts',(4.02026355427017,-8.46720795993301,15.9719638197674));
#85338=CARTESIAN_POINT('Ctrl Pts',(4.23015258035528,-8.36432708726278,15.9759320214349));
#85339=CARTESIAN_POINT('Ctrl Pts',(4.43592629921327,-8.2537350896699,15.9799002231023));
#85340=CARTESIAN_POINT('Ctrl Pts',(4.64166396547619,-8.14316246835367,15.9838677295208));
#85341=CARTESIAN_POINT('Ctrl Pts',(4.84328751329962,-8.02488155355912,15.9878352359392));
#85342=CARTESIAN_POINT('Ctrl Pts',(5.0402218707143,-7.89922455412386,15.9918027423577));
#85343=CARTESIAN_POINT('Ctrl Pts',(5.23713475639108,-7.77358125506161,15.9957698161992));
#85344=CARTESIAN_POINT('Ctrl Pts',(5.42935923271748,-7.64056363003513,15.9997368900408));
#85345=CARTESIAN_POINT('Ctrl Pts',(5.61634803854036,-7.50054796481456,16.0037039638823));
#85346=CARTESIAN_POINT('Ctrl Pts',(5.80335140490346,-7.36052139678237,16.007671346634));
#85347=CARTESIAN_POINT('Ctrl Pts',(5.98511805662897,-7.21349586788017,16.0116387293857));
#85348=CARTESIAN_POINT('Ctrl Pts',(6.16113176228737,-7.05988955085232,16.0156061121374));
#85349=CARTESIAN_POINT('Ctrl Pts',(6.33714360337977,-6.90628486102227,16.0195734528614));
#85350=CARTESIAN_POINT('Ctrl Pts',(6.50740240741105,-6.74609971124894,16.0235407935854));
#85351=CARTESIAN_POINT('Ctrl Pts',(6.67142642805035,-6.5797913703712,16.0275081343094));
#85352=CARTESIAN_POINT('Ctrl Pts',(6.83548576001426,-6.41344722639715,16.0314763291281));
#85353=CARTESIAN_POINT('Ctrl Pts',(6.99330742641979,-6.24097745961411,16.0354445239469));
#85354=CARTESIAN_POINT('Ctrl Pts',(7.14444693463981,-6.06287580778428,16.0394127187657));
#85355=CARTESIAN_POINT('Ctrl Pts',(7.23737733203747,-5.9533673313002,16.0418526229694));
#85356=CARTESIAN_POINT('Ctrl Pts',(7.32778222870503,-5.84173036731443,16.0442925271732));
#85357=CARTESIAN_POINT('Ctrl Pts',(7.41556582078254,-5.72808594734242,16.0467324313769));
#85358=CARTESIAN_POINT('Ctrl Pts',(7.55833494915475,-5.54325738884095,16.0507006330447));
#85359=CARTESIAN_POINT('Ctrl Pts',(7.69421269716705,-5.35305982094031,16.0546688347124));
#85360=CARTESIAN_POINT('Ctrl Pts',(7.82280743777052,-5.15802955149176,16.0586370363801));
#85361=CARTESIAN_POINT('Ctrl Pts',(7.95137964792578,-4.9630334523317,16.0626045427989));
#85362=CARTESIAN_POINT('Ctrl Pts',(8.0726712412503,-4.76320657916864,16.0665720492176));
#85363=CARTESIAN_POINT('Ctrl Pts',(8.18633382265112,-4.55911434454307,16.0705395556364));
#85364=CARTESIAN_POINT('Ctrl Pts',(8.29998401142945,-4.35504436207808,16.0745066294782));
#85365=CARTESIAN_POINT('Ctrl Pts',(8.40600671068612,-4.14671019513277,16.07847370332));
#85366=CARTESIAN_POINT('Ctrl Pts',(8.50409892869981,-3.93470284435645,16.0824407771619));
#85367=CARTESIAN_POINT('Ctrl Pts',(8.60219878500862,-3.72267898488307,16.0864081599139));
#85368=CARTESIAN_POINT('Ctrl Pts',(8.69236680400761,-3.50698162702699,16.0903755426658));
#85369=CARTESIAN_POINT('Ctrl Pts',(8.77434719056013,-3.28822390387419,16.0943429254178));
#85370=CARTESIAN_POINT('Ctrl Pts',(8.85632670866975,-3.06946849808776,16.0983102661421));
#85371=CARTESIAN_POINT('Ctrl Pts',(8.93011867006442,-2.84765305904123,16.1022776068664));
#85372=CARTESIAN_POINT('Ctrl Pts',(8.99551619221329,-2.62340875544175,16.1062449475907));
#85373=CARTESIAN_POINT('Ctrl Pts',(9.06092779323377,-2.39911617620958,16.1102131424097));
#85374=CARTESIAN_POINT('Ctrl Pts',(9.11794126387308,-2.1723939606798,16.1141813372288));
#85375=CARTESIAN_POINT('Ctrl Pts',(9.16639982352533,-1.94388768651246,16.1181495320479));
#85376=CARTESIAN_POINT('Ctrl Pts',(9.19619529696115,-1.80338717079906,16.1205894362499));
#85377=CARTESIAN_POINT('Ctrl Pts',(9.22275749985951,-1.66221243362113,16.1230293404519));
#85378=CARTESIAN_POINT('Ctrl Pts',(9.24605957875349,-1.52051548122368,16.1254692446539));
#85379=CARTESIAN_POINT('Ctrl Pts',(9.28395752090944,-1.29006295679158,16.129437446321));
#85380=CARTESIAN_POINT('Ctrl Pts',(9.31324122410686,-1.0581570665037,16.1334056479881));
#85381=CARTESIAN_POINT('Ctrl Pts',(9.33382064644945,-0.825455754364823,
16.1373738496552));
#85382=CARTESIAN_POINT('Ctrl Pts',(9.35439646317327,-0.592795212671557,
16.1413413560733));
#85383=CARTESIAN_POINT('Ctrl Pts',(9.36627101816281,-0.359339810557692,
16.1453088624915));
#85384=CARTESIAN_POINT('Ctrl Pts',(9.36940613650569,-0.125752581323693,
16.1492763689096));
#85385=CARTESIAN_POINT('Ctrl Pts',(9.37254091302685,0.107809179912775,16.1532434427508));
#85386=CARTESIAN_POINT('Ctrl Pts',(9.36693815158309,0.341502455215567,16.157210516592));
#85387=CARTESIAN_POINT('Ctrl Pts',(9.35261178570038,0.574663247892473,16.1611775904332));
#85388=CARTESIAN_POINT('Ctrl Pts',(9.33828430424486,0.807842196453683,16.1651449731845));
#85389=CARTESIAN_POINT('Ctrl Pts',(9.31523187552841,1.04048829538867,16.1691123559359));
#85390=CARTESIAN_POINT('Ctrl Pts',(9.28352047903083,1.27194047734756,16.1730797386872));
#85391=CARTESIAN_POINT('Ctrl Pts',(9.25180941846159,1.50339020746409,16.1770470794109));
#85392=CARTESIAN_POINT('Ctrl Pts',(9.2114396144082,1.73364576433429,16.1810144201346));
#85393=CARTESIAN_POINT('Ctrl Pts',(9.16252865747875,1.96205343030729,16.1849817608583));
#85394=CARTESIAN_POINT('Ctrl Pts',(9.1136071709288,2.19051026820809,16.1889499556767));
#85395=CARTESIAN_POINT('Ctrl Pts',(9.05614091651315,2.41711814193612,16.1929181504951));
#85396=CARTESIAN_POINT('Ctrl Pts',(8.99029842080894,2.64123444004886,16.1968863453136));
#85397=CARTESIAN_POINT('Ctrl Pts',(8.94981417304946,2.77903571326451,16.1993262495193));
#85398=CARTESIAN_POINT('Ctrl Pts',(8.90616420613945,2.91589526715953,16.2017661537251));
#85399=CARTESIAN_POINT('Ctrl Pts',(8.85939705632466,3.05166657105358,16.2042060579309));
#85400=CARTESIAN_POINT('Ctrl Pts',(8.78333608578722,3.27248176261888,16.2081742595991));
#85401=CARTESIAN_POINT('Ctrl Pts',(8.69900366671695,3.4904861670358,16.2121424612672));
#85402=CARTESIAN_POINT('Ctrl Pts',(8.60663293394173,3.70505797564485,16.2161106629354));
#85403=CARTESIAN_POINT('Ctrl Pts',(8.51427838498551,3.91959219018913,16.2200781693545));
#85404=CARTESIAN_POINT('Ctrl Pts',(8.41388844601816,4.13069474823769,16.2240456757737));
#85405=CARTESIAN_POINT('Ctrl Pts',(8.30574431645046,4.33776398761515,16.2280131821929));
#85406=CARTESIAN_POINT('Ctrl Pts',(8.19761197782881,4.54481065024951,16.2319802560351));
#85407=CARTESIAN_POINT('Ctrl Pts',(8.08172726827439,4.747824620156,16.2359473298774));
#85408=CARTESIAN_POINT('Ctrl Pts',(7.95841770537457,4.94622812750085,16.2399144037196));
#85409=CARTESIAN_POINT('Ctrl Pts',(7.83509854054274,5.14464708423132,16.243881786472));
#85410=CARTESIAN_POINT('Ctrl Pts',(7.70435351479008,5.33845461785254,16.2478491692244));
#85411=CARTESIAN_POINT('Ctrl Pts',(7.56655456068198,5.52710024721125,16.2518165519768));
#85412=CARTESIAN_POINT('Ctrl Pts',(7.42875706631973,5.71574387818997,16.2557838927015));
#85413=CARTESIAN_POINT('Ctrl Pts',(7.28390596267929,5.89922548585459,16.2597512334262));
#85414=CARTESIAN_POINT('Ctrl Pts',(7.13241511590066,6.077025561652,16.2637185741509));
#85415=CARTESIAN_POINT('Ctrl Pts',(6.98089165595732,6.25486391450231,16.2676867689704));
#85416=CARTESIAN_POINT('Ctrl Pts',(6.82272578088743,6.42701807455547,16.2716549637898));
#85417=CARTESIAN_POINT('Ctrl Pts',(6.65837091266764,6.59300249141781,16.2756231586093));
#85418=CARTESIAN_POINT('Ctrl Pts',(6.55731485281472,6.69506050373457,16.2780630628088));
#85419=CARTESIAN_POINT('Ctrl Pts',(6.45391974796182,6.79478667527731,16.2805029670084));
#85420=CARTESIAN_POINT('Ctrl Pts',(6.34829788533103,6.89207508821557,16.2829428712079));
#85421=CARTESIAN_POINT('Ctrl Pts',(6.1765156888821,7.05030385683692,16.286911103656));
#85422=CARTESIAN_POINT('Ctrl Pts',(5.99878819175189,7.20213159787593,16.2908793361041));
#85423=CARTESIAN_POINT('Ctrl Pts',(5.81561581276912,7.34712173444607,16.2948475685522));
#85424=CARTESIAN_POINT('Ctrl Pts',(5.63247800506067,7.49208450611647,16.2988150520508));
#85425=CARTESIAN_POINT('Ctrl Pts',(5.44389759010635,7.63021207327026,16.3027825355495));
#85426=CARTESIAN_POINT('Ctrl Pts',(5.25040770241951,7.76110842733651,16.3067500190481));
#85427=CARTESIAN_POINT('Ctrl Pts',(5.05692965561876,7.8919967710161,16.310717259751));
#85428=CARTESIAN_POINT('Ctrl Pts',(4.85854297054156,8.01565462433856,16.3146845004539));
#85429=CARTESIAN_POINT('Ctrl Pts',(4.65581028347088,8.13172894695997,16.3186517411569));
#85430=CARTESIAN_POINT('Ctrl Pts',(4.53566764739617,8.20051644887604,16.3210027915123));
#85431=CARTESIAN_POINT('Ctrl Pts',(4.41399926836326,8.26664148966478,16.3233538418677));
#85432=CARTESIAN_POINT('Ctrl Pts',(4.29092662815671,8.3300380391854,16.3257048922231));
#85433=CARTESIAN_POINT('Origin',(0.,0.,2.15141010809499));
#85434=CARTESIAN_POINT('',(4.29125029737385,8.33066558789108,17.5228836507406));
#85435=CARTESIAN_POINT('',(4.29092662815677,8.33003803918537,17.3256735943175));
#85436=CARTESIAN_POINT('',(4.29092662815669,8.33003803918541,2.15141010809499));
#85437=CARTESIAN_POINT('',(-9.36966006811048,0.00015743873267679,16.848589891905));
#85438=CARTESIAN_POINT('Ctrl Pts',(-9.36966006811048,0.00015743873267679,
16.848589891905));
#85439=CARTESIAN_POINT('Ctrl Pts',(-9.36907237380321,-0.963482148612044,
16.8649547993108));
#85440=CARTESIAN_POINT('Ctrl Pts',(-8.98390107505351,-3.47304054260515,
16.9075653111423));
#85441=CARTESIAN_POINT('Ctrl Pts',(-6.7782850671257,-7.0238660837389,16.9764214273993));
#85442=CARTESIAN_POINT('Ctrl Pts',(-2.630771112749,-9.39994023956942,17.0551582406763));
#85443=CARTESIAN_POINT('Ctrl Pts',(2.14758775784479,-9.52195992174593,17.1338950539533));
#85444=CARTESIAN_POINT('Ctrl Pts',(6.41096663338061,-7.36066081768614,17.2126318672303));
#85445=CARTESIAN_POINT('Ctrl Pts',(9.13702913819428,-3.43432004152829,17.2913686805072));
#85446=CARTESIAN_POINT('Ctrl Pts',(9.67208108851768,1.31556407398382,17.3701054937842));
#85447=CARTESIAN_POINT('Ctrl Pts',(7.92328567786768,5.66181210550089,17.4472771505287));
#85448=CARTESIAN_POINT('Ctrl Pts',(5.58235227426782,7.66474807205545,17.4982032028475));
#85449=CARTESIAN_POINT('Ctrl Pts',(4.29125029737042,8.33066558789285,17.5228836507406));
#85450=CARTESIAN_POINT('Ctrl Pts',(-9.3702499985761,0.0001633542619707,
16.8489304074991));
#85451=CARTESIAN_POINT('Ctrl Pts',(-9.37024181960975,0.469321358043213,
16.8407937247888));
#85452=CARTESIAN_POINT('Ctrl Pts',(-9.33499852673591,0.937813119156036,
16.8324468196874));
#85453=CARTESIAN_POINT('Ctrl Pts',(-9.25639715191407,1.45734889239428,16.8233336223895));
#85454=CARTESIAN_POINT('Ctrl Pts',(-9.24747481473559,1.5129321186541,16.8223610407942));
#85455=CARTESIAN_POINT('Ctrl Pts',(-9.23124416801755,1.60853052280593,16.8206942247754));
#85456=CARTESIAN_POINT('Ctrl Pts',(-9.22417518117763,1.64858471639062,16.819997660776));
#85457=CARTESIAN_POINT('Ctrl Pts',(-9.20921162645301,1.73026033840815,16.8185818235094));
#85458=CARTESIAN_POINT('Ctrl Pts',(-9.20129518058143,1.77187658187216,16.8178629924835));
#85459=CARTESIAN_POINT('Ctrl Pts',(-9.18075773030714,1.87598975018297,16.8160704694915));
#85460=CARTESIAN_POINT('Ctrl Pts',(-9.16778057927006,1.93841412578864,16.815000738157));
#85461=CARTESIAN_POINT('Ctrl Pts',(-9.11491148928658,2.18031555355801,16.8108672694784));
#85462=CARTESIAN_POINT('Ctrl Pts',(-9.07037770777503,2.3587360981436,16.8078432520672));
#85463=CARTESIAN_POINT('Ctrl Pts',(-8.95533634872791,2.76798486425719,16.8008689808035));
#85464=CARTESIAN_POINT('Ctrl Pts',(-8.88110353182279,2.99763061625038,16.7969256611321));
#85465=CARTESIAN_POINT('Ctrl Pts',(-8.75897437016394,3.33089735251735,16.7910615635904));
#85466=CARTESIAN_POINT('Ctrl Pts',(-8.7179181160513,3.43691909083854,16.789174844691));
#85467=CARTESIAN_POINT('Ctrl Pts',(-8.63795502644643,3.6327526524998,16.7856421045001));
#85468=CARTESIAN_POINT('Ctrl Pts',(-8.59955054522782,3.72275291062085,16.7839994136168));
#85469=CARTESIAN_POINT('Ctrl Pts',(-8.53210853098703,3.87418677894387,16.7811998233642));
#85470=CARTESIAN_POINT('Ctrl Pts',(-8.50379950769038,3.93593611410202,16.7800480700436));
#85471=CARTESIAN_POINT('Ctrl Pts',(-8.43654087258266,4.07853102900152,16.7773638869738));
#85472=CARTESIAN_POINT('Ctrl Pts',(-8.39709634887749,4.15913574051146,16.7758280646212));
#85473=CARTESIAN_POINT('Ctrl Pts',(-8.27955578858586,4.39083905292596,16.7713587749051));
#85474=CARTESIAN_POINT('Ctrl Pts',(-8.19849619758667,4.54039331501592,16.7684054560219));
#85475=CARTESIAN_POINT('Ctrl Pts',(-7.96784682624004,4.93960188790244,16.7603485331533));
#85476=CARTESIAN_POINT('Ctrl Pts',(-7.81062614248576,5.18462810757901,16.7552092857057));
#85477=CARTESIAN_POINT('Ctrl Pts',(-7.58757638156798,5.49901818483393,16.7484626723151));
#85478=CARTESIAN_POINT('Ctrl Pts',(-7.53172932983633,5.57526409224734,16.7468144912902));
#85479=CARTESIAN_POINT('Ctrl Pts',(-7.44238859463641,5.69344489683138,16.7442477448354));
#85480=CARTESIAN_POINT('Ctrl Pts',(-7.40967183700969,5.7359590366,16.7433218916292));
#85481=CARTESIAN_POINT('Ctrl Pts',(-7.35000236941168,5.81213467445593,16.741660079054));
#85482=CARTESIAN_POINT('Ctrl Pts',(-7.32317894333512,5.84589552402361,16.7409225255032));
#85483=CARTESIAN_POINT('Ctrl Pts',(-7.2691603902236,5.91292980191826,16.7394569802778));
#85484=CARTESIAN_POINT('Ctrl Pts',(-7.24196755441882,5.94620362577631,16.7387291305881));
#85485=CARTESIAN_POINT('Ctrl Pts',(-7.16830705656106,6.0350815989535,16.7367824920474));
#85486=CARTESIAN_POINT('Ctrl Pts',(-7.12142160299381,6.0903358161585,16.735569547554));
#85487=CARTESIAN_POINT('Ctrl Pts',(-6.83447510730782,6.42065596860322,16.7282841803512));
#85488=CARTESIAN_POINT('Ctrl Pts',(-6.57914634471105,6.68204374545883,16.7223612608149));
#85489=CARTESIAN_POINT('Ctrl Pts',(-6.21187474633604,7.01651851507457,16.7141799772493));
#85490=CARTESIAN_POINT('Ctrl Pts',(-6.11267336090889,7.10310806739002,16.712002314275));
#85491=CARTESIAN_POINT('Ctrl Pts',(-5.92704092455368,7.25837077997098,16.707971414249));
#85492=CARTESIAN_POINT('Ctrl Pts',(-5.8411576163619,7.32766252761595,16.7061231084371));
#85493=CARTESIAN_POINT('Ctrl Pts',(-5.69116614514037,7.44436467587544,16.7029184915326));
#85494=CARTESIAN_POINT('Ctrl Pts',(-5.62763971293949,7.49250350322979,16.7015682412572));
#85495=CARTESIAN_POINT('Ctrl Pts',(-5.49164506799169,7.59285159623958,16.6986912276238));
#85496=CARTESIAN_POINT('Ctrl Pts',(-5.41902888138777,7.64484707824218,16.6971629394608));
#85497=CARTESIAN_POINT('Ctrl Pts',(-5.20275508520661,7.79507592725685,16.6926338884447));
#85498=CARTESIAN_POINT('Ctrl Pts',(-5.05709197096571,7.89035421744078,16.689611842163));
#85499=CARTESIAN_POINT('Ctrl Pts',(-4.66266365935591,8.13293877463738,16.6815185091125));
#85500=CARTESIAN_POINT('Ctrl Pts',(-4.40959309941721,8.27288424482264,16.6764136668451));
#85501=CARTESIAN_POINT('Ctrl Pts',(-4.0296580003687,8.46059079840007,16.6689970363393));
#85502=CARTESIAN_POINT('Ctrl Pts',(-3.90758202608788,8.51766066103064,16.6666507852358));
#85503=CARTESIAN_POINT('Ctrl Pts',(-3.73641490031448,8.59322585855475,16.6634299495345));
#85504=CARTESIAN_POINT('Ctrl Pts',(-3.6883356067873,8.61397164098076,16.662532701195));
#85505=CARTESIAN_POINT('Ctrl Pts',(-3.60064640445006,8.65093997035938,16.6609113803635));
#85506=CARTESIAN_POINT('Ctrl Pts',(-3.56109454869803,8.66729614783114,16.6601857975763));
#85507=CARTESIAN_POINT('Ctrl Pts',(-3.45840695827095,8.7089397624329,16.6583156574734));
#85508=CARTESIAN_POINT('Ctrl Pts',(-3.39510543856361,8.73381185783161,16.6571759389361));
#85509=CARTESIAN_POINT('Ctrl Pts',(-3.1479506207643,8.82782950165556,16.65276749471));
#85510=CARTESIAN_POINT('Ctrl Pts',(-2.96221150961838,8.89187664179254,16.6495421735003));
#85511=CARTESIAN_POINT('Ctrl Pts',(-2.74130839687928,8.96035869497896,16.6457500761035));
#85512=CARTESIAN_POINT('Ctrl Pts',(-2.70796277882292,8.97049258726913,16.6451788475486));
#85513=CARTESIAN_POINT('Ctrl Pts',(-2.47711860808384,9.03924277036251,16.6412309906005));
#85514=CARTESIAN_POINT('Ctrl Pts',(-2.27779045042254,9.09151785806547,16.637854163583));
#85515=CARTESIAN_POINT('Ctrl Pts',(-2.00968994884745,9.15245771518472,16.6333040229718));
#85516=CARTESIAN_POINT('Ctrl Pts',(-1.9423114697882,9.16699307603529,16.6321599504571));
#85517=CARTESIAN_POINT('Ctrl Pts',(-1.76718873247439,9.2027543367994,16.6291824767245));
#85518=CARTESIAN_POINT('Ctrl Pts',(-1.65922095241976,9.22283194841569,16.6273428758723));
#85519=CARTESIAN_POINT('Ctrl Pts',(-1.47237979820681,9.2541896451788,16.6241479508398));
#85520=CARTESIAN_POINT('Ctrl Pts',(-1.39366937541875,9.26637004963315,16.6227985786645));
#85521=CARTESIAN_POINT('Ctrl Pts',(-1.22615237168245,9.29011055235098,16.6199182666768));
#85522=CARTESIAN_POINT('Ctrl Pts',(-1.13731597222442,9.30140398241826,16.6183857495498));
#85523=CARTESIAN_POINT('Ctrl Pts',(-0.866688774887697,9.33187269145,16.6137013502423));
#85524=CARTESIAN_POINT('Ctrl Pts',(-0.684487092087161,9.34700349990969,
16.6105251989289));
#85525=CARTESIAN_POINT('Ctrl Pts',(-0.377921660298956,9.36344969135507,
16.605155853724));
#85526=CARTESIAN_POINT('Ctrl Pts',(-0.253763164707002,9.36763679412889,
16.6029745812385));
#85527=CARTESIAN_POINT('Ctrl Pts',(0.058856776555768,9.37195966630942,16.597478690213));
#85528=CARTESIAN_POINT('Ctrl Pts',(0.247307739141228,9.36888099461859,16.5941618313608));
#85529=CARTESIAN_POINT('Ctrl Pts',(0.489174449052452,9.35762665287357,16.5899363554316));
#85530=CARTESIAN_POINT('Ctrl Pts',(0.542789030154573,9.35466986567322,16.5890017629769));
#85531=CARTESIAN_POINT('Ctrl Pts',(0.671531270746277,9.34645934096579,16.5867645333661));
#85532=CARTESIAN_POINT('Ctrl Pts',(0.746626902874601,9.34076039567737,16.5854652468591));
#85533=CARTESIAN_POINT('Ctrl Pts',(0.865303772421255,9.33031377999916,16.5834249399983));
#85534=CARTESIAN_POINT('Ctrl Pts',(0.908934374176971,9.32616449451436,16.5826776572712));
#85535=CARTESIAN_POINT('Ctrl Pts',(1.00170076526,9.3166852050695,16.5810957754857));
#85536=CARTESIAN_POINT('Ctrl Pts',(1.05082667328386,9.31127225197728,16.5802620590381));
#85537=CARTESIAN_POINT('Ctrl Pts',(1.20971099260783,9.29249211075097,16.5775754900517));
#85538=CARTESIAN_POINT('Ctrl Pts',(1.31927641995736,9.2775708110679,16.5757380271228));
#85539=CARTESIAN_POINT('Ctrl Pts',(1.66864671608303,9.22367715549834,16.5698962231511));
#85540=CARTESIAN_POINT('Ctrl Pts',(1.90721034479679,9.17731721296951,16.5659312652029));
#85541=CARTESIAN_POINT('Ctrl Pts',(2.3733181609767,9.06777708273342,16.5580711277267));
#85542=CARTESIAN_POINT('Ctrl Pts',(2.60081384248497,9.00516447289314,16.5541800554601));
#85543=CARTESIAN_POINT('Ctrl Pts',(2.91556770618963,8.90561246782929,16.54865674158));
#85544=CARTESIAN_POINT('Ctrl Pts',(3.00499773611537,8.87583556788492,16.5470716332787));
#85545=CARTESIAN_POINT('Ctrl Pts',(3.16850746490285,8.81863834914141,16.5441416784427));
#85546=CARTESIAN_POINT('Ctrl Pts',(3.2427190138618,8.79162074088098,16.5427996675298));
#85547=CARTESIAN_POINT('Ctrl Pts',(3.41014346238886,8.72825953560375,16.5397433138038));
#85548=CARTESIAN_POINT('Ctrl Pts',(3.50313365119126,8.6913547568976,16.5380253068828));
#85549=CARTESIAN_POINT('Ctrl Pts',(3.83165148774084,8.5548477509526,16.5318830065843));
#85550=CARTESIAN_POINT('Ctrl Pts',(4.0636487589826,8.44711225407878,16.527407502209));
#85551=CARTESIAN_POINT('Ctrl Pts',(4.29092663733566,8.33003803445718,16.522914704178));
#85552=CARTESIAN_POINT('',(-9.37024999773577,-0.000205992430197824,16.651410108095));
#85553=CARTESIAN_POINT('Ctrl Pts',(4.29092662815671,8.3300380391854,16.3257048922231));
#85554=CARTESIAN_POINT('Ctrl Pts',(4.08324528991728,8.43701778888531,16.3296722182125));
#85555=CARTESIAN_POINT('Ctrl Pts',(3.87156411057383,8.53622542790688,16.333639544202));
#85556=CARTESIAN_POINT('Ctrl Pts',(3.65648539798877,8.62738080745222,16.3376068701914));
#85557=CARTESIAN_POINT('Ctrl Pts',(3.43897743753376,8.71956575895721,16.341619005907));
#85558=CARTESIAN_POINT('Ctrl Pts',(3.21799499775753,8.8035153233757,16.3456311416225));
#85559=CARTESIAN_POINT('Ctrl Pts',(2.99418171318639,8.87898985982754,16.3496432773381));
#85560=CARTESIAN_POINT('Ctrl Pts',(2.77036842861529,8.95446439627936,16.3536554130537));
#85561=CARTESIAN_POINT('Ctrl Pts',(2.54372458648862,9.02146381586769,16.3576675487692));
#85562=CARTESIAN_POINT('Ctrl Pts',(2.31491039177459,9.07980037999482,16.3616796844848));
#85563=CARTESIAN_POINT('Ctrl Pts',(2.08860177878142,9.13749814184432,16.365647886152));
#85564=CARTESIAN_POINT('Ctrl Pts',(1.86009982710217,9.18673974318476,16.3696160878191));
#85565=CARTESIAN_POINT('Ctrl Pts',(1.63005222104112,9.22737854534965,16.3735842894863));
#85566=CARTESIAN_POINT('Ctrl Pts',(1.40004492048336,9.268010227391,16.3775517959044));
#85567=CARTESIAN_POINT('Ctrl Pts',(1.1684927861248,9.30004206946954,16.3815193023226));
#85568=CARTESIAN_POINT('Ctrl Pts',(0.936053060732539,9.32337866494723,16.3854868087407));
#85569=CARTESIAN_POINT('Ctrl Pts',(0.703638678226125,9.34671271603767,16.389453882582));
#85570=CARTESIAN_POINT('Ctrl Pts',(0.470337180866043,9.3613533849971,16.3934209564232));
#85571=CARTESIAN_POINT('Ctrl Pts',(0.236811280348955,9.36725709479565,16.3973880302644));
#85572=CARTESIAN_POINT('Ctrl Pts',(0.00326719551702451,9.37316126430731,
16.4013554130158));
#85573=CARTESIAN_POINT('Ctrl Pts',(-0.230501043047988,9.37032710511516,
16.4053227957672));
#85574=CARTESIAN_POINT('Ctrl Pts',(-0.463829138258932,9.35876314440119,
16.4092901785186));
#85575=CARTESIAN_POINT('Ctrl Pts',(-0.697154761755315,9.34719930618771,
16.4132575192423));
#85576=CARTESIAN_POINT('Ctrl Pts',(-0.930039967179378,9.32690586773196,
16.417224859966));
#85577=CARTESIAN_POINT('Ctrl Pts',(-1.16182331345612,9.29794340974443,16.4211922006897));
#85578=CARTESIAN_POINT('Ctrl Pts',(-1.39365655838131,9.26897471667775,16.4251603955081));
#85579=CARTESIAN_POINT('Ctrl Pts',(-1.6243871877291,9.23133330977507,16.4291285903266));
#85580=CARTESIAN_POINT('Ctrl Pts',(-1.85336041727917,9.18513147571458,16.4330967851451));
#85581=CARTESIAN_POINT('Ctrl Pts',(-1.99414804775193,9.15672358386778,16.4355366893506));
#85582=CARTESIAN_POINT('Ctrl Pts',(-2.13427143373024,9.12508035706661,16.4379765935562));
#85583=CARTESIAN_POINT('Ctrl Pts',(-2.27358039414982,9.09023746960648,16.4404164977618));
#85584=CARTESIAN_POINT('Ctrl Pts',(-2.50014914560209,9.03356983326021,16.4443846994328));
#85585=CARTESIAN_POINT('Ctrl Pts',(-2.72463341497766,8.96841854676107,16.4483529011038));
#85586=CARTESIAN_POINT('Ctrl Pts',(-2.94639355199476,8.89496206283443,16.4523211027748));
#85587=CARTESIAN_POINT('Ctrl Pts',(-3.1681148355162,8.82151844885465,16.4562886091968));
#85588=CARTESIAN_POINT('Ctrl Pts',(-3.38711266946891,8.73977263145653,16.4602561156189));
#85589=CARTESIAN_POINT('Ctrl Pts',(-3.6027633152631,8.64995269100904,16.4642236220409));
#85590=CARTESIAN_POINT('Ctrl Pts',(-3.81839044868502,8.5601425436223,16.468190695886));
#85591=CARTESIAN_POINT('Ctrl Pts',(-4.03067086008051,8.46226014019331,16.4721577697311));
#85592=CARTESIAN_POINT('Ctrl Pts',(-4.2390006054817,8.35658177302333,16.4761248435763));
#85593=CARTESIAN_POINT('Ctrl Pts',(-4.44734657320953,8.25089517683648,16.4800922263315));
#85594=CARTESIAN_POINT('Ctrl Pts',(-4.65174100518809,8.13741152999273,16.4840596090868));
#85595=CARTESIAN_POINT('Ctrl Pts',(-4.85160330036171,8.01645373456489,16.488026991842));
#85596=CARTESIAN_POINT('Ctrl Pts',(-5.0514634783335,7.89549722047962,16.4919943325696));
#85597=CARTESIAN_POINT('Ctrl Pts',(-5.24679137328432,7.76706686538866,16.4959616732972));
#85598=CARTESIAN_POINT('Ctrl Pts',(-5.43703361189728,7.6315300278253,16.4999290140247));
#85599=CARTESIAN_POINT('Ctrl Pts',(-5.62731680612774,7.49596401170036,16.503897208847));
#85600=CARTESIAN_POINT('Ctrl Pts',(-5.81251192428975,7.35328862087679,16.5078654036693));
#85601=CARTESIAN_POINT('Ctrl Pts',(-5.99209600092064,7.20391355988194,16.5118335984915));
#85602=CARTESIAN_POINT('Ctrl Pts',(-6.10251596750279,7.11206806025471,16.514273502674));
#85603=CARTESIAN_POINT('Ctrl Pts',(-6.21081524723272,7.01769050615019,16.5167134068564));
#85604=CARTESIAN_POINT('Ctrl Pts',(-6.3168786029285,6.92088359809382,16.5191533110388));
#85605=CARTESIAN_POINT('Ctrl Pts',(-6.48937750139262,6.76343916411478,16.5231215126959));
#85606=CARTESIAN_POINT('Ctrl Pts',(-6.65601394485932,6.59951792492163,16.5270897143529));
#85607=CARTESIAN_POINT('Ctrl Pts',(-6.81630970183415,6.42958063260596,16.53105791601));
#85608=CARTESIAN_POINT('Ctrl Pts',(-6.97657737418056,6.25967311416452,16.535025422418));
#85609=CARTESIAN_POINT('Ctrl Pts',(-7.13050638246639,6.0837518534588,16.538992928826));
#85610=CARTESIAN_POINT('Ctrl Pts',(-7.27765606150406,5.9023137253922,16.542960435234));
#85611=CARTESIAN_POINT('Ctrl Pts',(-7.42478969682335,5.720895379511,16.5469275090651));
#85612=CARTESIAN_POINT('Ctrl Pts',(-7.56514529956278,5.53396158811509,16.5508945828962));
#85613=CARTESIAN_POINT('Ctrl Pts',(-7.6983225160623,5.34204225939745,16.5548616567274));
#85614=CARTESIAN_POINT('Ctrl Pts',(-7.83151010287551,5.15010798620438,16.5588290394686));
#85615=CARTESIAN_POINT('Ctrl Pts',(-7.95751802192521,4.95318763203713,16.5627964222099));
#85616=CARTESIAN_POINT('Ctrl Pts',(-8.0759885932591,4.75184104364287,16.5667638049512));
#85617=CARTESIAN_POINT('Ctrl Pts',(-8.19445790960027,4.55049658817071,16.5707311456649));
#85618=CARTESIAN_POINT('Ctrl Pts',(-8.3053898955734,4.34472623859289,16.5746984863786));
#85619=CARTESIAN_POINT('Ctrl Pts',(-8.40847194162357,4.1351160406244,16.5786658270923));
#85620=CARTESIAN_POINT('Ctrl Pts',(-8.51157617932724,3.92546071746618,16.5826340219009));
#85621=CARTESIAN_POINT('Ctrl Pts',(-8.6068269743147,3.71196414930906,16.5866022167094));
#85622=CARTESIAN_POINT('Ctrl Pts',(-8.6939585842418,3.49523521354261,16.590570411518));
#85623=CARTESIAN_POINT('Ctrl Pts',(-8.74753276520119,3.36197616744439,16.5930103157839));
#85624=CARTESIAN_POINT('Ctrl Pts',(-8.79803834624232,3.22749552049675,16.5954502200498));
#85625=CARTESIAN_POINT('Ctrl Pts',(-8.84542266732393,3.0919383724279,16.5978901243158));
#85626=CARTESIAN_POINT('Ctrl Pts',(-8.922438993179,2.87160993362477,16.6018558340212));
#85627=CARTESIAN_POINT('Ctrl Pts',(-8.99123166558292,2.64836642609172,16.6058215437266));
#85628=CARTESIAN_POINT('Ctrl Pts',(-9.05159840689145,2.42283952065755,16.6097872534321));
#85629=CARTESIAN_POINT('Ctrl Pts',(-9.1119560688391,2.1973465352283,16.6137523666814));
#85630=CARTESIAN_POINT('Ctrl Pts',(-9.16389025429189,1.96957111243754,16.6177174799308));
#85631=CARTESIAN_POINT('Ctrl Pts',(-9.20724887214798,1.74015897803329,16.6216825931802));
#85632=CARTESIAN_POINT('Ctrl Pts',(-9.2506016704499,1.51077763511656,16.6256471742356));
#85633=CARTESIAN_POINT('Ctrl Pts',(-9.28538114690515,1.27976029945655,16.6296117552911));
#85634=CARTESIAN_POINT('Ctrl Pts',(-9.31148637694957,1.04776262310823,16.6335763363466));
#85635=CARTESIAN_POINT('Ctrl Pts',(-9.33759198184268,0.815761615472395,
16.63754097433));
#85636=CARTESIAN_POINT('Ctrl Pts',(-9.35502305804944,0.582780522227092,
16.6415056123135));
#85637=CARTESIAN_POINT('Ctrl Pts',(-9.36373045858973,0.349480988580246,
16.645470250297));
#85638=CARTESIAN_POINT('Ctrl Pts',(-9.36807896163217,0.232970472362477,
16.6474502028963));
#85639=CARTESIAN_POINT('Ctrl Pts',(-9.37025256073633,0.116380602494191,
16.6494301554957));
#85640=CARTESIAN_POINT('Ctrl Pts',(-9.37024999773577,-0.000205992430197824,
16.651410108095));
#85641=CARTESIAN_POINT('Ctrl Pts',(4.29092662815677,8.33003803918537,17.3256735943175));
#85642=CARTESIAN_POINT('Ctrl Pts',(4.29097821771431,8.33001146463611,17.3256726426547));
#85643=CARTESIAN_POINT('Ctrl Pts',(4.29102980690335,8.32998488935409,17.3256716911546));
#85644=CARTESIAN_POINT('Ctrl Pts',(4.55103047200112,8.19604856257909,17.3208754687787));
#85645=CARTESIAN_POINT('Ctrl Pts',(4.80456773014874,8.05004459447934,17.3161045805035));
#85646=CARTESIAN_POINT('Ctrl Pts',(5.09711683934695,7.86282397573055,17.310300584825));
#85647=CARTESIAN_POINT('Ctrl Pts',(5.14311149972626,7.83281590687947,17.3093787568522));
#85648=CARTESIAN_POINT('Ctrl Pts',(5.22431663423013,7.77881199345624,17.3077323279032));
#85649=CARTESIAN_POINT('Ctrl Pts',(5.25963223861385,7.75497704956278,17.3070097806095));
#85650=CARTESIAN_POINT('Ctrl Pts',(5.33872017865953,7.70081085156908,17.3053761130227));
#85651=CARTESIAN_POINT('Ctrl Pts',(5.38239884798838,7.67034572503948,17.3044632873311));
#85652=CARTESIAN_POINT('Ctrl Pts',(5.54292574620206,7.55633457580999,17.301072589534));
#85653=CARTESIAN_POINT('Ctrl Pts',(5.6581078311972,7.47047746970393,17.2985688759324));
#85654=CARTESIAN_POINT('Ctrl Pts',(6.04020614479632,7.17175211095036,17.2900737525178));
#85655=CARTESIAN_POINT('Ctrl Pts',(6.29745265428763,6.94695689234439,17.2840411098817));
#85656=CARTESIAN_POINT('Ctrl Pts',(6.63951357058691,6.61339924804405,17.2757321501428));
#85657=CARTESIAN_POINT('Ctrl Pts',(6.73507844538356,6.51605007359311,17.2733748032426));
#85658=CARTESIAN_POINT('Ctrl Pts',(6.88552669058092,6.35594572163212,17.269607123924));
#85659=CARTESIAN_POINT('Ctrl Pts',(6.94175720427595,6.29448415514974,17.268185488443));
#85660=CARTESIAN_POINT('Ctrl Pts',(7.05218246569183,6.17050654252348,17.2653659519672));
#85661=CARTESIAN_POINT('Ctrl Pts',(7.10638371389131,6.10800614519696,17.2639680783824));
#85662=CARTESIAN_POINT('Ctrl Pts',(7.24524107305612,5.94353674131959,17.2603481490724));
#85663=CARTESIAN_POINT('Ctrl Pts',(7.3285741974771,5.84047494373094,17.2581370587214));
#85664=CARTESIAN_POINT('Ctrl Pts',(7.51718633223192,5.59681454889321,17.2530272833262));
#85665=CARTESIAN_POINT('Ctrl Pts',(7.62075432577292,5.45495436401649,17.2501401062778));
#85666=CARTESIAN_POINT('Ctrl Pts',(7.89369928815981,5.05813630903082,17.2422406223595));
#85667=CARTESIAN_POINT('Ctrl Pts',(8.05466766021304,4.79766178725524,17.2372513318832));
#85668=CARTESIAN_POINT('Ctrl Pts',(8.22776116285262,4.48422122416561,17.2312609920759));
#85669=CARTESIAN_POINT('Ctrl Pts',(8.25254077159945,4.4384529442126,17.2303864332977));
#85670=CARTESIAN_POINT('Ctrl Pts',(8.29674693255514,4.35515339897856,17.2287929971384));
#85671=CARTESIAN_POINT('Ctrl Pts',(8.31630327395232,4.31769274533853,17.2280756817685));
#85672=CARTESIAN_POINT('Ctrl Pts',(8.36111570018489,4.23041940344972,17.2264023488769));
#85673=CARTESIAN_POINT('Ctrl Pts',(8.38618106739974,4.18051087384237,17.2254440747611));
#85674=CARTESIAN_POINT('Ctrl Pts',(8.48935096073708,3.97042344232227,17.221409115352));
#85675=CARTESIAN_POINT('Ctrl Pts',(8.56332389732108,3.80825755096658,17.2182924292607));
#85676=CARTESIAN_POINT('Ctrl Pts',(8.78425592282335,3.28488183961869,17.2083197981168));
#85677=CARTESIAN_POINT('Ctrl Pts',(8.91331857529786,2.91656577402384,17.2014450133711));
#85678=CARTESIAN_POINT('Ctrl Pts',(9.04504406615057,2.44906947532125,17.1930721413029));
#85679=CARTESIAN_POINT('Ctrl Pts',(9.06961110394666,2.35646301386921,17.1914292588907));
#85680=CARTESIAN_POINT('Ctrl Pts',(9.10990494028154,2.194597504292,17.1885848480121));
#85681=CARTESIAN_POINT('Ctrl Pts',(9.12627248775778,2.12550622923451,17.1873792455703));
#85682=CARTESIAN_POINT('Ctrl Pts',(9.16281199939242,1.96305458056824,17.1845637172916));
#85683=CARTESIAN_POINT('Ctrl Pts',(9.18234491090999,1.8695585082897,17.1829580670465));
#85684=CARTESIAN_POINT('Ctrl Pts',(9.24980199262434,1.52005848018524,17.1770051044867));
#85685=CARTESIAN_POINT('Ctrl Pts',(9.28847604180394,1.26238982578057,17.1727173771272));
#85686=CARTESIAN_POINT('Ctrl Pts',(9.34883473311864,0.701996810682248,17.1634732001829));
#85687=CARTESIAN_POINT('Ctrl Pts',(9.36665291698789,0.399151532677687,17.1585291761472));
#85688=CARTESIAN_POINT('Ctrl Pts',(9.37029669010384,0.043432259178177,17.152578941747));
#85689=CARTESIAN_POINT('Ctrl Pts',(9.37039290977881,-0.00911714825853897,
17.1516960927985));
#85690=CARTESIAN_POINT('Ctrl Pts',(9.36976869162356,-0.103968379140538,
17.150093607563));
#85691=CARTESIAN_POINT('Ctrl Pts',(9.36920380497295,-0.146269669516118,
17.1493756210499));
#85692=CARTESIAN_POINT('Ctrl Pts',(9.3672388513215,-0.243892738731495,17.1477104414955));
#85693=CARTESIAN_POINT('Ctrl Pts',(9.36563513975845,-0.299208582180905,
17.1467610990478));
#85694=CARTESIAN_POINT('Ctrl Pts',(9.35711484212669,-0.524254037369697,
17.1428794367222));
#85695=CARTESIAN_POINT('Ctrl Pts',(9.3460734591053,-0.693794700578072,17.1399107978014));
#85696=CARTESIAN_POINT('Ctrl Pts',(9.29300097226347,-1.26763373188855,17.129798698072));
#85697=CARTESIAN_POINT('Ctrl Pts',(9.22928214763292,-1.66946608927697,17.1226279385625));
#85698=CARTESIAN_POINT('Ctrl Pts',(9.11905861058671,-2.1571046249412,17.1140160470477));
#85699=CARTESIAN_POINT('Ctrl Pts',(9.0970764569506,-2.24800584913341,17.1124134811086));
#85700=CARTESIAN_POINT('Ctrl Pts',(9.05401323509711,-2.41509323408203,17.1094727773957));
#85701=CARTESIAN_POINT('Ctrl Pts',(9.03332172287519,-2.49137104329371,17.1081322349168));
#85702=CARTESIAN_POINT('Ctrl Pts',(8.98350471923446,-2.66623203914725,17.1050624741105));
#85703=CARTESIAN_POINT('Ctrl Pts',(8.95371701658031,-2.76461606426321,17.103337795225));
#85704=CARTESIAN_POINT('Ctrl Pts',(8.84740733806106,-3.09598090465691,17.0975303391178));
#85705=CARTESIAN_POINT('Ctrl Pts',(8.76336132044562,-3.32644152001317,17.0934961308356));
#85706=CARTESIAN_POINT('Ctrl Pts',(8.55898765480028,-3.82512611068331,17.0846580178484));
#85707=CARTESIAN_POINT('Ctrl Pts',(8.4348854419078,-4.09152363095245,17.0798659581457));
#85708=CARTESIAN_POINT('Ctrl Pts',(8.27317273202257,-4.3999053278032,17.0740462335787));
#85709=CARTESIAN_POINT('Ctrl Pts',(8.24744774601936,-4.44793880431639,17.0731314747842));
#85710=CARTESIAN_POINT('Ctrl Pts',(8.20089362376026,-4.53307166772422,17.0714931584655));
#85711=CARTESIAN_POINT('Ctrl Pts',(8.18022800721909,-4.57025871508599,17.0707715816735));
#85712=CARTESIAN_POINT('Ctrl Pts',(8.13295565134325,-4.65397574624297,17.0691329026291));
#85713=CARTESIAN_POINT('Ctrl Pts',(8.10620156262185,-4.70042062819725,17.0682140202201));
#85714=CARTESIAN_POINT('Ctrl Pts',(8.00438795634122,-4.87371340453068,17.0647522984064));
#85715=CARTESIAN_POINT('Ctrl Pts',(7.9267375773768,-4.99901391063899,17.0621822223329));
#85716=CARTESIAN_POINT('Ctrl Pts',(7.73945763839032,-5.28587563644333,17.0561799381729));
#85717=CARTESIAN_POINT('Ctrl Pts',(7.62766990621187,-5.44594689668563,17.0527404654126));
#85718=CARTESIAN_POINT('Ctrl Pts',(7.48937676635854,-5.63135191587965,17.0486805955986));
#85719=CARTESIAN_POINT('Ctrl Pts',(7.46762176250229,-5.66016907543471,17.0480472924013));
#85720=CARTESIAN_POINT('Ctrl Pts',(7.32256166434807,-5.85002681877477,17.0438604933698));
#85721=CARTESIAN_POINT('Ctrl Pts',(7.19422191126563,-6.00715362435688,17.0403280457051));
#85722=CARTESIAN_POINT('Ctrl Pts',(6.99963023851738,-6.23020412000172,17.0352297521916));
#85723=CARTESIAN_POINT('Ctrl Pts',(6.9373324142933,-6.29949885950972,17.0336331785939));
#85724=CARTESIAN_POINT('Ctrl Pts',(6.82028156666327,-6.42585366950758,17.0306979786604));
#85725=CARTESIAN_POINT('Ctrl Pts',(6.76581973634784,-6.48317201371972,17.0293570161597));
#85726=CARTESIAN_POINT('Ctrl Pts',(6.63855381292601,-6.61376261403732,17.026278612557));
#85727=CARTESIAN_POINT('Ctrl Pts',(6.56525050549346,-6.68653411803638,17.02454580959));
#85728=CARTESIAN_POINT('Ctrl Pts',(6.30733281678178,-6.93424971425095,17.0185787986013));
#85729=CARTESIAN_POINT('Ctrl Pts',(6.11680993016669,-7.10287991658575,17.0143976462547));
#85730=CARTESIAN_POINT('Ctrl Pts',(5.6998908030982,-7.44266153172543,17.0055794290911));
#85731=CARTESIAN_POINT('Ctrl Pts',(5.47210311943554,-7.61170493555478,17.0009502407934));
#85732=CARTESIAN_POINT('Ctrl Pts',(5.19187925310141,-7.80057280477059,16.9953021767148));
#85733=CARTESIAN_POINT('Ctrl Pts',(5.14649072274355,-7.83059253727644,16.994388579299));
#85734=CARTESIAN_POINT('Ctrl Pts',(5.06516458721259,-7.88336868523873,16.9927515899709));
#85735=CARTESIAN_POINT('Ctrl Pts',(5.02932867364814,-7.90627897403325,16.9920301667832));
#85736=CARTESIAN_POINT('Ctrl Pts',(4.94793455871087,-7.9575377917346,16.9903906365047));
#85737=CARTESIAN_POINT('Ctrl Pts',(4.90228648256506,-7.98574049975846,16.9894707367409));
#85738=CARTESIAN_POINT('Ctrl Pts',(4.72979449247776,-8.0902746872298,16.9859967598212));
#85739=CARTESIAN_POINT('Ctrl Pts',(4.6013900103263,-8.16398862205698,16.9834152011726));
#85740=CARTESIAN_POINT('Ctrl Pts',(4.3147640646925,-8.31962267731639,16.9777004811355));
#85741=CARTESIAN_POINT('Ctrl Pts',(4.15584300709399,-8.40013567278593,16.9745632525693));
#85742=CARTESIAN_POINT('Ctrl Pts',(3.77372685231633,-8.58022486177475,16.9671443789502));
#85743=CARTESIAN_POINT('Ctrl Pts',(3.54874009158387,-8.67569695014541,16.9628750328181));
#85744=CARTESIAN_POINT('Ctrl Pts',(3.22976906664956,-8.79656439964517,16.956993016288));
#85745=CARTESIAN_POINT('Ctrl Pts',(3.13873266361254,-8.8294569928234,16.9553327575967));
#85746=CARTESIAN_POINT('Ctrl Pts',(2.97262061413491,-8.88658157534683,16.9523366876462));
#85747=CARTESIAN_POINT('Ctrl Pts',(2.89771739835293,-8.91128718669281,16.9509978248047));
#85748=CARTESIAN_POINT('Ctrl Pts',(2.72837950968133,-8.96477971128716,16.9479971442045));
#85749=CARTESIAN_POINT('Ctrl Pts',(2.63378374427351,-8.99302581285969,16.9463390579085));
#85750=CARTESIAN_POINT('Ctrl Pts',(2.21933037904024,-9.10968034689929,16.9391455563678));
#85751=CARTESIAN_POINT('Ctrl Pts',(1.89535036876822,-9.18255688027763,16.9337147862008));
#85752=CARTESIAN_POINT('Ctrl Pts',(1.43833131696962,-9.26013698830243,16.926114906563));
#85753=CARTESIAN_POINT('Ctrl Pts',(1.30802335832507,-9.27944011414782,16.9239534697342));
#85754=CARTESIAN_POINT('Ctrl Pts',(1.0700269771862,-9.30958273908951,16.9199899821528));
#85755=CARTESIAN_POINT('Ctrl Pts',(0.962474731967153,-9.3213159368621,16.9181929602705));
#85756=CARTESIAN_POINT('Ctrl Pts',(0.803861869723648,-9.3358449991477,16.9155206818583));
#85757=CARTESIAN_POINT('Ctrl Pts',(0.752942768047164,-9.34008955665099,
16.9146594449482));
#85758=CARTESIAN_POINT('Ctrl Pts',(0.658952691285274,-9.34715086080005,
16.9130615829383));
#85759=CARTESIAN_POINT('Ctrl Pts',(0.615892158792157,-9.35008688138868,
16.9123262354685));
#85760=CARTESIAN_POINT('Ctrl Pts',(0.502162628556854,-9.35705231095244,
16.9103762954763));
#85761=CARTESIAN_POINT('Ctrl Pts',(0.431465648488899,-9.36057864739199,
16.9091563911607));
#85762=CARTESIAN_POINT('Ctrl Pts',(0.267477455635561,-9.36689654443972,
16.9063135991086));
#85763=CARTESIAN_POINT('Ctrl Pts',(0.174170907549871,-9.3690959813016,16.9046862966759));
#85764=CARTESIAN_POINT('Ctrl Pts',(-0.200775427095719,-9.37233116890465,
16.8981248857096));
#85765=CARTESIAN_POINT('Ctrl Pts',(-0.482364603050553,-9.36206318588132,
16.893151395504));
#85766=CARTESIAN_POINT('Ctrl Pts',(-0.944970258845761,-9.32426551511288,
16.885033961657));
#85767=CARTESIAN_POINT('Ctrl Pts',(-1.12640475273726,-9.30409097512259,
16.881862691635));
#85768=CARTESIAN_POINT('Ctrl Pts',(-1.39577434323878,-9.26614331836725,
16.8771836418002));
#85769=CARTESIAN_POINT('Ctrl Pts',(-1.48423081080008,-9.25238655497331,
16.8756516825369));
#85770=CARTESIAN_POINT('Ctrl Pts',(-1.65099896652092,-9.22399760919633,
16.8727718018418));
#85771=CARTESIAN_POINT('Ctrl Pts',(-1.72934770077451,-9.20963007107948,
16.8714223100646));
#85772=CARTESIAN_POINT('Ctrl Pts',(-1.91532078282375,-9.1730695582339,16.8682260960225));
#85773=CARTESIAN_POINT('Ctrl Pts',(-2.02275672949112,-9.1499789134594,16.8663853401387));
#85774=CARTESIAN_POINT('Ctrl Pts',(-2.25716806895841,-9.09526766875971,
16.8623755330154));
#85775=CARTESIAN_POINT('Ctrl Pts',(-2.38393767917349,-9.062866152648,16.8602113121964));
#85776=CARTESIAN_POINT('Ctrl Pts',(-2.85397349386821,-8.93218301487741,
16.8521754033214));
#85777=CARTESIAN_POINT('Ctrl Pts',(-3.19221074927094,-8.81696357961916,
16.8463806051515));
#85778=CARTESIAN_POINT('Ctrl Pts',(-3.59539403557866,-8.65337060819131,
16.8391462493862));
#85779=CARTESIAN_POINT('Ctrl Pts',(-3.66737286305208,-8.62311181598989,
16.8378410518825));
#85780=CARTESIAN_POINT('Ctrl Pts',(-3.77559264859349,-8.57601777422294,
16.8358525056425));
#85781=CARTESIAN_POINT('Ctrl Pts',(-3.81211802075441,-8.55984444381708,
16.8351767846005));
#85782=CARTESIAN_POINT('Ctrl Pts',(-3.89099827972331,-8.52431147259437,
16.8337064842666));
#85783=CARTESIAN_POINT('Ctrl Pts',(-3.93331450613576,-8.50486864555631,
16.8329108260949));
#85784=CARTESIAN_POINT('Ctrl Pts',(-4.05862720630252,-8.44615655348398,
16.8305359431349));
#85785=CARTESIAN_POINT('Ctrl Pts',(-4.14119324005963,-8.40598202507336,
16.8289467109252));
#85786=CARTESIAN_POINT('Ctrl Pts',(-4.46040163015587,-8.24481873040064,
16.822723960162));
#85787=CARTESIAN_POINT('Ctrl Pts',(-4.69244432369842,-8.11499752280547,
16.8180335125414));
#85788=CARTESIAN_POINT('Ctrl Pts',(-5.11923355461663,-7.8517875083662,16.8092306299026));
#85789=CARTESIAN_POINT('Ctrl Pts',(-5.31507562599017,-7.72056287171288,
16.805115527491));
#85790=CARTESIAN_POINT('Ctrl Pts',(-5.58335485243704,-7.52575104827351,
16.7993998525602));
#85791=CARTESIAN_POINT('Ctrl Pts',(-5.66007773063634,-7.46821935879904,
16.7977554267389));
#85792=CARTESIAN_POINT('Ctrl Pts',(-5.79204618653272,-7.36605911080785,
16.7949095095351));
#85793=CARTESIAN_POINT('Ctrl Pts',(-5.84769251055562,-7.32196136136638,
16.7937039271404));
#85794=CARTESIAN_POINT('Ctrl Pts',(-5.91590658827746,-7.26663042287683,
16.7922187216342));
#85795=CARTESIAN_POINT('Ctrl Pts',(-5.92895222260626,-7.2559902154205,16.7919343449152));
#85796=CARTESIAN_POINT('Ctrl Pts',(-5.95218554088438,-7.23693629417004,
16.7914272749044));
#85797=CARTESIAN_POINT('Ctrl Pts',(-5.96238423530891,-7.22853608067931,
16.7912044740943));
#85798=CARTESIAN_POINT('Ctrl Pts',(-5.98343058941076,-7.21112628423795,
16.790744246759));
#85799=CARTESIAN_POINT('Ctrl Pts',(-5.99427574802073,-7.2021137287882,16.7905068447255));
#85800=CARTESIAN_POINT('Ctrl Pts',(-6.01541970319076,-7.18446181415948,
16.790043507225));
#85801=CARTESIAN_POINT('Ctrl Pts',(-6.02572033476423,-7.17582470605425,
16.7898175546311));
#85802=CARTESIAN_POINT('Ctrl Pts',(-6.04688035580724,-7.15800428075745,
16.7893529095406));
#85803=CARTESIAN_POINT('Ctrl Pts',(-6.05773749657959,-7.14881834595813,
16.7891142383724));
#85804=CARTESIAN_POINT('Ctrl Pts',(-6.14037392405159,-7.07857845767196,
16.7872955984859));
#85805=CARTESIAN_POINT('Ctrl Pts',(-6.21124954062057,-7.0164694897886,16.7857240069436));
#85806=CARTESIAN_POINT('Ctrl Pts',(-6.40076432343102,-6.84527373599244,
16.7814837297196));
#85807=CARTESIAN_POINT('Ctrl Pts',(-6.51754560203392,-6.73417819148485,
16.7788296313941));
#85808=CARTESIAN_POINT('Ctrl Pts',(-6.80295871702365,-6.44827886962707,
16.7721977297799));
#85809=CARTESIAN_POINT('Ctrl Pts',(-6.96776867662509,-6.26982830417255,
16.7682346350307));
#85810=CARTESIAN_POINT('Ctrl Pts',(-7.19756409823333,-6.00074857568759,
16.7623874816041));
#85811=CARTESIAN_POINT('Ctrl Pts',(-7.26816125172843,-5.9150438985552,16.7605424983826));
#85812=CARTESIAN_POINT('Ctrl Pts',(-7.36799788332486,-5.78935584816625,
16.7578472238621));
#85813=CARTESIAN_POINT('Ctrl Pts',(-7.39846979736714,-5.7503633440447,16.7570124599158));
#85814=CARTESIAN_POINT('Ctrl Pts',(-7.44107685636038,-5.69494312784722,
16.7558266185048));
#85815=CARTESIAN_POINT('Ctrl Pts',(-7.45346938164514,-5.67871430752099,
16.7554794203767));
#85816=CARTESIAN_POINT('Ctrl Pts',(-7.49562042445197,-5.62313908894502,
16.7542907047262));
#85817=CARTESIAN_POINT('Ctrl Pts',(-7.52512117603729,-5.58359830514575,
16.7534454519072));
#85818=CARTESIAN_POINT('Ctrl Pts',(-7.58976103262434,-5.4955166515773,16.7515653023237));
#85819=CARTESIAN_POINT('Ctrl Pts',(-7.62474953930849,-5.44686792969848,
16.750528693163));
#85820=CARTESIAN_POINT('Ctrl Pts',(-7.72537132473201,-5.3040918188752,16.7474953048833));
#85821=CARTESIAN_POINT('Ctrl Pts',(-7.78974512303527,-5.20909041676758,
16.7454881327025));
#85822=CARTESIAN_POINT('Ctrl Pts',(-8.06892284822416,-4.78033371981941,
16.7365123809888));
#85823=CARTESIAN_POINT('Ctrl Pts',(-8.26413935400905,-4.43431058576743,
16.729507295104));
#85824=CARTESIAN_POINT('Ctrl Pts',(-8.47955789367914,-3.98852462923679,
16.7209659679655));
#85825=CARTESIAN_POINT('Ctrl Pts',(-8.52089692251835,-3.89942899530525,
16.7192806679644));
#85826=CARTESIAN_POINT('Ctrl Pts',(-8.5917745123903,-3.74015901009377,16.7163063871222));
#85827=CARTESIAN_POINT('Ctrl Pts',(-8.62187280820106,-3.67024358891125,
16.7150136412525));
#85828=CARTESIAN_POINT('Ctrl Pts',(-8.68604885631471,-3.51602159070716,
16.7121893293927));
#85829=CARTESIAN_POINT('Ctrl Pts',(-8.71975805295934,-3.43156991874006,
16.7106604031516));
#85830=CARTESIAN_POINT('Ctrl Pts',(-8.78934440374716,-3.24958566665368,
16.7074005401155));
#85831=CARTESIAN_POINT('Ctrl Pts',(-8.82483905176287,-3.15191970458903,
16.7056721783171));
#85832=CARTESIAN_POINT('Ctrl Pts',(-8.92300631952262,-2.86713754845002,
16.7006844083225));
#85833=CARTESIAN_POINT('Ctrl Pts',(-8.98140220320273,-2.67860675160458,
16.6974475151484));
#85834=CARTESIAN_POINT('Ctrl Pts',(-9.10203752618945,-2.24065166865257,
16.6900015982356));
#85835=CARTESIAN_POINT('Ctrl Pts',(-9.16005424429774,-1.99022921663034,
16.6857987266927));
#85836=CARTESIAN_POINT('Ctrl Pts',(-9.21929447170523,-1.67633513054968,
16.680464029308));
#85837=CARTESIAN_POINT('Ctrl Pts',(-9.230268799106,-1.61481512757205,16.6794151657529));
#85838=CARTESIAN_POINT('Ctrl Pts',(-9.24763336297542,-1.51150552066212,
16.6776451265327));
#85839=CARTESIAN_POINT('Ctrl Pts',(-9.25435764363617,-1.46977425305238,
16.6769276505856));
#85840=CARTESIAN_POINT('Ctrl Pts',(-9.26703970870357,-1.38752904068702,
16.6755083229828));
#85841=CARTESIAN_POINT('Ctrl Pts',(-9.2730147117165,-1.34701891219052,16.6748068519934));
#85842=CARTESIAN_POINT('Ctrl Pts',(-9.28669218998233,-1.24987971195934,
16.6731201305645));
#85843=CARTESIAN_POINT('Ctrl Pts',(-9.29414249731049,-1.19321680688366,
16.6721324524756));
#85844=CARTESIAN_POINT('Ctrl Pts',(-9.3471401732769,-0.759481734484727,
16.6645515043299));
#85845=CARTESIAN_POINT('Ctrl Pts',(-9.37024148570975,-0.380022225320088,
16.6578162803345));
#85846=CARTESIAN_POINT('Ctrl Pts',(-9.3702499976469,-0.000209995816083108,
16.6511809802189));
#85847=CARTESIAN_POINT('Origin',(0.,0.,0.));
#85848=CARTESIAN_POINT('',(-9.94199999699462,0.000244456475345012,4.321310091674));
#85849=CARTESIAN_POINT('',(-9.94181728593973,0.000151535147386895,4.17868990831418));
#85850=CARTESIAN_POINT('',(-9.942,-1.2175438477123E-15,0.));
#85851=CARTESIAN_POINT('',(4.30700280829072,8.96064120525846,4.00000358309546));
#85852=CARTESIAN_POINT('Ctrl Pts',(-9.94199999699462,0.000244456475334202,
4.321310091674));
#85853=CARTESIAN_POINT('Ctrl Pts',(-9.94199371857738,0.255586533386308,
4.31722274465953));
#85854=CARTESIAN_POINT('Ctrl Pts',(-9.9321461097209,0.510880897282077,4.31313539764506));
#85855=CARTESIAN_POINT('Ctrl Pts',(-9.9124941605588,0.765391087541386,4.30904805063059));
#85856=CARTESIAN_POINT('Ctrl Pts',(-9.89766379861191,0.957457442363556,
4.30596353035593));
#85857=CARTESIAN_POINT('Ctrl Pts',(-9.87725095393373,1.14907722439271,4.30287901008128));
#85858=CARTESIAN_POINT('Ctrl Pts',(-9.85129109814319,1.3399357072803,4.29979448980662));
#85859=CARTESIAN_POINT('Ctrl Pts',(-9.8183833284707,1.58187568743978,4.29588442637762));
#85860=CARTESIAN_POINT('Ctrl Pts',(-9.77655344436225,1.82263975150708,4.29197436294863));
#85861=CARTESIAN_POINT('Ctrl Pts',(-9.72590990526167,2.06156263905151,4.28806429951963));
#85862=CARTESIAN_POINT('Ctrl Pts',(-9.67527512730493,2.30044419382526,4.28415491251706));
#85863=CARTESIAN_POINT('Ctrl Pts',(-9.61582979615066,2.53748493387791,4.28024552551449));
#85864=CARTESIAN_POINT('Ctrl Pts',(-9.54773345703507,2.77202991207041,4.27633613851192));
#85865=CARTESIAN_POINT('Ctrl Pts',(-9.47964453321882,3.00654934966495,4.27242717721909));
#85866=CARTESIAN_POINT('Ctrl Pts',(-9.40290656051405,3.23857329900516,4.26851821592626));
#85867=CARTESIAN_POINT('Ctrl Pts',(-9.31772921026913,3.46746108328521,4.26460925463343));
#85868=CARTESIAN_POINT('Ctrl Pts',(-9.23254528386269,3.69636653896539,4.26069999154721));
#85869=CARTESIAN_POINT('Ctrl Pts',(-9.13892077283841,3.92213508202157,4.256790728461));
#85870=CARTESIAN_POINT('Ctrl Pts',(-9.03711430361115,4.14414394820773,4.25288146537478));
#85871=CARTESIAN_POINT('Ctrl Pts',(-8.935309270365,4.36614968295696,4.24897225742876));
#85872=CARTESIAN_POINT('Ctrl Pts',(-8.8253226284171,4.58439559298429,4.24506304948273));
#85873=CARTESIAN_POINT('Ctrl Pts',(-8.7074602835775,4.79828088068221,4.2411538415367));
#85874=CARTESIAN_POINT('Ctrl Pts',(-8.58957211277988,5.01221303485363,4.23724377700633));
#85875=CARTESIAN_POINT('Ctrl Pts',(-8.46380492523922,5.22178241140812,4.23333371247595));
#85876=CARTESIAN_POINT('Ctrl Pts',(-8.33051021589283,5.42641350644283,4.22942364794557));
#85877=CARTESIAN_POINT('Ctrl Pts',(-8.23544445933727,5.57235635713554,4.22663499080693));
#85878=CARTESIAN_POINT('Ctrl Pts',(-8.13655075276863,5.71578786046067,4.22384633366829));
#85879=CARTESIAN_POINT('Ctrl Pts',(-8.03397008202494,5.8565082362384,4.22105767652965));
#85880=CARTESIAN_POINT('Ctrl Pts',(-7.89015201606858,6.05379815585272,4.21714798015716));
#85881=CARTESIAN_POINT('Ctrl Pts',(-7.73904114242797,6.24581814187268,4.21323828378467));
#85882=CARTESIAN_POINT('Ctrl Pts',(-7.58104868104173,6.43203427351529,4.20932858741217));
#85883=CARTESIAN_POINT('Ctrl Pts',(-7.4230835710149,6.61821816776949,4.20541956787901));
#85884=CARTESIAN_POINT('Ctrl Pts',(-7.258239432691,6.79859999967778,4.20151054834584));
#85885=CARTESIAN_POINT('Ctrl Pts',(-7.08696755126958,6.97267917856917,4.19760152881267));
#85886=CARTESIAN_POINT('Ctrl Pts',(-6.91571429346933,7.1467394285818,4.19369293433525));
#85887=CARTESIAN_POINT('Ctrl Pts',(-6.73803488467048,7.31449819419016,4.18978433985784));
#85888=CARTESIAN_POINT('Ctrl Pts',(-6.55441795136341,7.47549124264386,4.18587574538043));
#85889=CARTESIAN_POINT('Ctrl Pts',(-6.37078667023574,7.63649687108861,4.18196684548558));
#85890=CARTESIAN_POINT('Ctrl Pts',(-6.18121714631811,7.79073553883579,4.17805794559074));
#85891=CARTESIAN_POINT('Ctrl Pts',(-5.98623258749013,7.93778202072035,4.17414904569589));
#85892=CARTESIAN_POINT('Ctrl Pts',(-5.7912506492937,8.08482652627072,4.17024019833744));
#85893=CARTESIAN_POINT('Ctrl Pts',(-5.59085404685443,8.22467887212325,4.16633135097899));
#85894=CARTESIAN_POINT('Ctrl Pts',(-5.38559716822796,8.35695561443131,4.16242250362055));
#85895=CARTESIAN_POINT('Ctrl Pts',(-5.18029496458159,8.48926156621589,4.15851279310669));
#85896=CARTESIAN_POINT('Ctrl Pts',(-4.97013057542729,8.61398841903633,4.15460308259284));
#85897=CARTESIAN_POINT('Ctrl Pts',(-4.75568650205221,8.7307966357142,4.15069337207899));
#85898=CARTESIAN_POINT('Ctrl Pts',(-4.602611665205,8.81417687760648,4.14790253580355));
#85899=CARTESIAN_POINT('Ctrl Pts',(-4.44735674001143,8.89352316422356,4.14511169952811));
#85900=CARTESIAN_POINT('Ctrl Pts',(-4.29014120223573,8.96872635689591,4.14232086325267));
#85901=CARTESIAN_POINT('Ctrl Pts',(-4.0698917999291,9.07408145393005,4.13841107144521));
#85902=CARTESIAN_POINT('Ctrl Pts',(-3.84572585590248,9.17133563349291,4.13450127963775));
#85903=CARTESIAN_POINT('Ctrl Pts',(-3.61825880447004,9.26021421047456,4.13059148783029));
#85904=CARTESIAN_POINT('Ctrl Pts',(-3.3908312192436,9.34907736676031,4.12668237438327));
#85905=CARTESIAN_POINT('Ctrl Pts',(-3.16010393093553,9.42956771938564,4.12277326093625));
#85906=CARTESIAN_POINT('Ctrl Pts',(-2.92671181169661,9.50145893909328,4.11886414748923));
#85907=CARTESIAN_POINT('Ctrl Pts',(-2.69334517628228,9.573342309079,4.11495546087393));
#85908=CARTESIAN_POINT('Ctrl Pts',(-2.45731455872118,9.63662833838923,4.11104677425864));
#85909=CARTESIAN_POINT('Ctrl Pts',(-2.2192704343439,9.69114042511236,4.10713808764335));
#85910=CARTESIAN_POINT('Ctrl Pts',(-1.98120791360177,9.74565672460167,4.10322909895958));
#85911=CARTESIAN_POINT('Ctrl Pts',(-1.74113184770521,9.79139766103141,4.09932011027581));
#85912=CARTESIAN_POINT('Ctrl Pts',(-1.49970462775759,9.82823738162049,4.09541112159205));
#85913=CARTESIAN_POINT('Ctrl Pts',(-1.25828077687107,9.86507658811979,4.09150218745731));
#85914=CARTESIAN_POINT('Ctrl Pts',(-1.01550608710088,9.89301478694713,4.08759325332258));
#85915=CARTESIAN_POINT('Ctrl Pts',(-0.77205055605658,9.91197770068581,4.08368431918785));
#85916=CARTESIAN_POINT('Ctrl Pts',(-0.528541500513394,9.93094478348341,
4.0797745256611));
#85917=CARTESIAN_POINT('Ctrl Pts',(-0.284351584124645,9.94093261553057,
4.07586473213434));
#85918=CARTESIAN_POINT('Ctrl Pts',(-0.0401547022073373,9.94191890933992,
4.07195493860759));
#85919=CARTESIAN_POINT('Ctrl Pts',(0.134120903294355,9.94262279609505,4.06916464239696));
#85920=CARTESIAN_POINT('Ctrl Pts',(0.308399974733068,9.93874308293179,4.06637434618633));
#85921=CARTESIAN_POINT('Ctrl Pts',(0.482437680168755,9.93028790543121,4.0635840499757));
#85922=CARTESIAN_POINT('Ctrl Pts',(0.725404420706052,9.91848398677555,4.05968863447517));
#85923=CARTESIAN_POINT('Ctrl Pts',(0.967980146918817,9.8977565807835,4.05579321897465));
#85924=CARTESIAN_POINT('Ctrl Pts',(1.20949750393456,9.86815483198232,4.05189780347412));
#85925=CARTESIAN_POINT('Ctrl Pts',(1.45096980006146,9.83855860610145,4.04800311475732));
#85926=CARTESIAN_POINT('Ctrl Pts',(1.69138383892895,9.80009137703121,4.04410842604052));
#85927=CARTESIAN_POINT('Ctrl Pts',(1.93007805039346,9.75285408069809,4.04021373732372));
#85928=CARTESIAN_POINT('Ctrl Pts',(2.16876458339275,9.70561830392397,4.03631917389371));
#85929=CARTESIAN_POINT('Ctrl Pts',(2.40573111986605,9.64961307557972,4.0324246104637));
#85930=CARTESIAN_POINT('Ctrl Pts',(2.64032578724286,9.58499054445128,4.02853004703369));
#85931=CARTESIAN_POINT('Ctrl Pts',(2.87490700908714,9.52037171709135,4.02463570681626));
#85932=CARTESIAN_POINT('Ctrl Pts',(3.1071163594724,9.44713665029117,4.02074136659882));
#85933=CARTESIAN_POINT('Ctrl Pts',(3.33631586752145,9.36548773060563,4.01684702638139));
#85934=CARTESIAN_POINT('Ctrl Pts',(3.56554539613377,9.28382811654042,4.01295217608307));
#85935=CARTESIAN_POINT('Ctrl Pts',(3.79176402657543,9.19375254278092,4.00905732578475));
#85936=CARTESIAN_POINT('Ctrl Pts',(4.01435139560835,9.09551245794195,4.00516247548644));
#85937=CARTESIAN_POINT('Ctrl Pts',(4.11262682739479,9.05213808859552,4.00344284468944));
#85938=CARTESIAN_POINT('Ctrl Pts',(4.21019465842555,9.0071728053732,4.00172321389245));
#85939=CARTESIAN_POINT('Ctrl Pts',(4.30700280829072,8.96064120525846,4.00000358309546));
#85940=CARTESIAN_POINT('',(-4.3070027565882,8.96064123010969,4.));
#85941=CARTESIAN_POINT('Origin',(0.,0.,4.));
#85942=CARTESIAN_POINT('Ctrl Pts',(-4.30700275658821,8.96064123010968,4.));
#85943=CARTESIAN_POINT('Ctrl Pts',(-5.78466622438202,8.25039065030607,4.02624560442566));
#85944=CARTESIAN_POINT('Ctrl Pts',(-8.38051839602705,6.0857098575996,4.07873681327696));
#85945=CARTESIAN_POINT('Ctrl Pts',(-9.80601533347217,2.52304867962029,4.13830011604837));
#85946=CARTESIAN_POINT('Ctrl Pts',(-9.94223863637244,0.441937600389724,
4.1716178143941));
#85947=CARTESIAN_POINT('Ctrl Pts',(-9.94181728593973,0.000151535147386895,
4.17868990831418));
#85948=CARTESIAN_POINT('Origin',(0.,0.,0.));
#85949=CARTESIAN_POINT('',(-9.94207409670986,-4.38639028224127E-5,5.32131009168581));
#85950=CARTESIAN_POINT('',(-9.94280319079831,-5.01184069386897E-5,5.17868990831418));
#85951=CARTESIAN_POINT('',(-9.942,-1.2175438477123E-15,0.));
#85952=CARTESIAN_POINT('Ctrl Pts',(-9.94199999990324,-4.38635759112934E-5,
5.32131009168581));
#85953=CARTESIAN_POINT('Ctrl Pts',(-9.94200107587134,0.243832168292933,
5.31740472848196));
#85954=CARTESIAN_POINT('Ctrl Pts',(-9.93302443488287,0.487747049262697,
5.3134993652781));
#85955=CARTESIAN_POINT('Ctrl Pts',(-9.91508755863515,0.731028525160635,
5.30959400207425));
#85956=CARTESIAN_POINT('Ctrl Pts',(-9.89715382840315,0.974267331011731,
5.30568932384664));
#85957=CARTESIAN_POINT('Ctrl Pts',(-9.8702630207256,1.21687267283672,5.30178464561903));
#85958=CARTESIAN_POINT('Ctrl Pts',(-9.83448462780497,1.45817560858349,5.29787996739142));
#85959=CARTESIAN_POINT('Ctrl Pts',(-9.79871008838425,1.69945255487779,5.29397570971588));
#85960=CARTESIAN_POINT('Ctrl Pts',(-9.75404991628052,1.93942709670595,5.29007145204033));
#85961=CARTESIAN_POINT('Ctrl Pts',(-9.70062519645207,2.17743766798482,5.28616719436479));
#85962=CARTESIAN_POINT('Ctrl Pts',(-9.64719641649626,2.4154663273929,5.28226263997673));
#85963=CARTESIAN_POINT('Ctrl Pts',(-9.58500181681745,2.65153044260325,5.27835808558866));
#85964=CARTESIAN_POINT('Ctrl Pts',(-9.51421339977782,2.88497961578381,5.27445353120059));
#85965=CARTESIAN_POINT('Ctrl Pts',(-9.44342531074129,3.11842770726125,5.27054899490455));
#85966=CARTESIAN_POINT('Ctrl Pts',(-9.3640435680187,3.349260612132,5.26664445860852));
#85967=CARTESIAN_POINT('Ctrl Pts',(-9.27628997551958,3.57684334156179,5.26273992231248));
#85968=CARTESIAN_POINT('Ctrl Pts',(-9.18851772000748,3.80447447219447,5.25883455561839));
#85969=CARTESIAN_POINT('Ctrl Pts',(-9.09237015821423,4.02885378329661,5.25492918892431));
#85970=CARTESIAN_POINT('Ctrl Pts',(-8.98811764605377,4.24936526797789,5.25102382223022));
#85971=CARTESIAN_POINT('Ctrl Pts',(-8.9312795738624,4.36958728877725,5.24889463119691));
#85972=CARTESIAN_POINT('Ctrl Pts',(-8.87203322919054,4.48866000202154,5.24676544016361));
#85973=CARTESIAN_POINT('Ctrl Pts',(-8.81042829879265,4.60648642588184,5.2446362491303));
#85974=CARTESIAN_POINT('Ctrl Pts',(-8.69730190640501,4.82285349541935,5.24072637213268));
#85975=CARTESIAN_POINT('Ctrl Pts',(-8.57618401983683,5.03508441183726,5.23681649513506));
#85976=CARTESIAN_POINT('Ctrl Pts',(-8.44740258010487,5.24259035684055,5.23290661813745));
#85977=CARTESIAN_POINT('Ctrl Pts',(-8.31864343361715,5.45006038066823,5.22899741797528));
#85978=CARTESIAN_POINT('Ctrl Pts',(-8.182223529961,5.65280682781202,5.2250882178131));
#85979=CARTESIAN_POINT('Ctrl Pts',(-8.03851535595362,5.85026793165047,5.22117901765093));
#85980=CARTESIAN_POINT('Ctrl Pts',(-7.89482282669338,6.04770753894523,5.21727024306266));
#85981=CARTESIAN_POINT('Ctrl Pts',(-7.74384377619892,6.23986272524124,5.21336146847438));
#85982=CARTESIAN_POINT('Ctrl Pts',(-7.58599299013171,6.42620217186423,5.20945269388611));
#85983=CARTESIAN_POINT('Ctrl Pts',(-7.42812995405602,6.61255607935789,5.20554361595743));
#85984=CARTESIAN_POINT('Ctrl Pts',(-7.26339429566316,6.7930931294541,5.20163453802875));
#85985=CARTESIAN_POINT('Ctrl Pts',(-7.0922407608604,6.96731547943613,5.19772546010007));
#85986=CARTESIAN_POINT('Ctrl Pts',(-6.92108958951511,7.14153542358344,5.19381643615181));
#85987=CARTESIAN_POINT('Ctrl Pts',(-6.74352091693189,7.3094406434833,5.18990741220355));
#85988=CARTESIAN_POINT('Ctrl Pts',(-6.56002649548621,7.47057001697454,5.18599838825529));
#85989=CARTESIAN_POINT('Ctrl Pts',(-6.37649171998725,7.63173482600257,5.18208850463533));
#85990=CARTESIAN_POINT('Ctrl Pts',(-6.18702880168393,7.7861206252772,5.17817862101537));
#85991=CARTESIAN_POINT('Ctrl Pts',(-5.99216377963559,7.93330556817418,5.17426873739541));
#85992=CARTESIAN_POINT('Ctrl Pts',(-5.8531243360058,8.03832448001357,5.17147897021472));
#85993=CARTESIAN_POINT('Ctrl Pts',(-5.71133536582068,8.13967821350184,5.16868920303402));
#85994=CARTESIAN_POINT('Ctrl Pts',(-5.56699758600683,8.23722658893114,5.16589943585332));
#85995=CARTESIAN_POINT('Ctrl Pts',(-5.3647072438242,8.37394127492951,5.16198955890828));
#85996=CARTESIAN_POINT('Ctrl Pts',(-5.157347343778,8.5032214925011,5.15807968196324));
#85997=CARTESIAN_POINT('Ctrl Pts',(-4.94548606880177,8.62470472209267,5.15416980501819));
#85998=CARTESIAN_POINT('Ctrl Pts',(-4.73366146894007,8.74616692183177,5.15026060490842));
#85999=CARTESIAN_POINT('Ctrl Pts',(-4.51733729271575,8.85983468858871,5.14635140479866));
#86000=CARTESIAN_POINT('Ctrl Pts',(-4.29710808425141,8.96539046066936,5.14244220468889));
#86001=CARTESIAN_POINT('Ctrl Pts',(-4.07690285095632,9.07093474146091,5.13853343015271));
#86002=CARTESIAN_POINT('Ctrl Pts',(-3.85279368692719,9.16836866975112,5.13462465561653));
#86003=CARTESIAN_POINT('Ctrl Pts',(-3.625397907429,9.25742156395664,5.13071588108035));
#86004=CARTESIAN_POINT('Ctrl Pts',(-3.39798448083671,9.3464813691295,5.12680680320296));
#86005=CARTESIAN_POINT('Ctrl Pts',(-3.16728418902501,9.4271587354904,5.12289772532556));
#86006=CARTESIAN_POINT('Ctrl Pts',(-2.93393362254536,9.49923141619878,5.11898864744816));
#86007=CARTESIAN_POINT('Ctrl Pts',(-2.70058627836868,9.57130310166632,5.11507962355064));
#86008=CARTESIAN_POINT('Ctrl Pts',(-2.46458900117124,9.6347702583646,5.11117059965312));
#86009=CARTESIAN_POINT('Ctrl Pts',(-2.22659351668162,9.68946052737052,5.10726157575559));
#86010=CARTESIAN_POINT('Ctrl Pts',(-1.98854569220281,9.7441628238655,5.10335169218516));
#86011=CARTESIAN_POINT('Ctrl Pts',(-1.74849905541982,9.79008431199061,5.09944180861474));
#86012=CARTESIAN_POINT('Ctrl Pts',(-1.50711686048621,9.82710347807726,5.09553192504431));
#86013=CARTESIAN_POINT('Ctrl Pts',(-1.33488661684927,9.85351727382592,5.09274215755499));
#86014=CARTESIAN_POINT('Ctrl Pts',(-1.16197667358011,9.87539990567294,5.08995239006567));
#86015=CARTESIAN_POINT('Ctrl Pts',(-0.988630237267956,9.89272329816009,
5.08716262257635));
#86016=CARTESIAN_POINT('Ctrl Pts',(-0.74568410805907,9.91700214253127,5.08325274575776));
#86017=CARTESIAN_POINT('Ctrl Pts',(-0.50180601029982,9.93233094993677,5.07934286893916));
#86018=CARTESIAN_POINT('Ctrl Pts',(-0.257668121537375,9.93866042981364,
5.07543299212057));
#86019=CARTESIAN_POINT('Ctrl Pts',(-0.0135724953327912,9.94498881399818,
5.07152379213831));
#86020=CARTESIAN_POINT('Ctrl Pts',(0.230782552021626,9.94232097324931,5.06761459215605));
#86021=CARTESIAN_POINT('Ctrl Pts',(0.474722987673566,9.93065970039122,5.0637053921738));
#86022=CARTESIAN_POINT('Ctrl Pts',(0.718636866802504,9.91899969703509,5.05979661776576));
#86023=CARTESIAN_POINT('Ctrl Pts',(0.962135944468283,9.89834822983191,5.05588784335772));
#86024=CARTESIAN_POINT('Ctrl Pts',(1.20454840477681,9.86876016227721,5.05197906894968));
#86025=CARTESIAN_POINT('Ctrl Pts',(1.44697967754732,9.83916979853527,5.04806999120051));
#86026=CARTESIAN_POINT('Ctrl Pts',(1.68832388582526,9.80064147956073,5.04416091345133));
#86027=CARTESIAN_POINT('Ctrl Pts',(1.92791524550065,9.75328184798154,5.04025183570216));
#86028=CARTESIAN_POINT('Ctrl Pts',(2.16750329670333,9.70592287038273,5.03634281193272));
#86029=CARTESIAN_POINT('Ctrl Pts',(2.40533827310429,9.64973288046047,5.03243378816328));
#86030=CARTESIAN_POINT('Ctrl Pts',(2.64076475604249,9.58486961326255,5.02852476439384));
#86031=CARTESIAN_POINT('Ctrl Pts',(2.8762430140654,9.51999208130941,5.02461488095035));
#86032=CARTESIAN_POINT('Ctrl Pts',(3.10931144962395,9.44643753422734,5.02070499750686));
#86033=CARTESIAN_POINT('Ctrl Pts',(3.33932863834611,9.36441392961255,5.01679511406338));
#86034=CARTESIAN_POINT('Ctrl Pts',(3.50344980983362,9.30588869437342,5.01400534580871));
#86035=CARTESIAN_POINT('Ctrl Pts',(3.66601786421949,9.24305285729568,5.01121557755405));
#86036=CARTESIAN_POINT('Ctrl Pts',(3.82680542478557,9.17599717964384,5.00842580929938));
#86037=CARTESIAN_POINT('Ctrl Pts',(4.05215018450145,9.08201823304599,5.00451593185117));
#86038=CARTESIAN_POINT('Ctrl Pts',(4.27406584119732,8.97971984947631,5.00060605440295));
#86039=CARTESIAN_POINT('Ctrl Pts',(4.49193740712761,8.86937778710816,4.99669617695474));
#86040=CARTESIAN_POINT('Ctrl Pts',(4.70977125761973,8.75905482589814,4.99278697633987));
#86041=CARTESIAN_POINT('Ctrl Pts',(4.92356216489259,8.64069109208017,4.988877775725));
#86042=CARTESIAN_POINT('Ctrl Pts',(5.13271823667751,8.51460906342024,4.98496857511014));
#86043=CARTESIAN_POINT('Ctrl Pts',(5.34185153879447,8.38854076061537,4.98105980006838));
#86044=CARTESIAN_POINT('Ctrl Pts',(5.54635077291072,8.25475598533229,4.97715102502662));
#86045=CARTESIAN_POINT('Ctrl Pts',(5.7456507202051,8.1136219902955,4.97324224998487));
#86046=CARTESIAN_POINT('Ctrl Pts',(5.94496613406024,7.97247704263408,4.96933317160481));
#86047=CARTESIAN_POINT('Ctrl Pts',(6.13908122430094,7.82398189508741,4.96542409322476));
#86048=CARTESIAN_POINT('Ctrl Pts',(6.32746066457328,7.6685465075383,4.9615150148447));
#86049=CARTESIAN_POINT('Ctrl Pts',(6.51583750342458,7.51311326647018,4.95760599044696));
#86050=CARTESIAN_POINT('Ctrl Pts',(6.69847863580534,7.35074015708262,4.95369696604923));
#86051=CARTESIAN_POINT('Ctrl Pts',(6.8748821158566,7.18187718448841,4.94978794165149));
#86052=CARTESIAN_POINT('Ctrl Pts',(7.05132439024468,7.01297707585224,4.94587805758812));
#86053=CARTESIAN_POINT('Ctrl Pts',(7.22152606800094,6.83758444533033,4.94196817352475));
#86054=CARTESIAN_POINT('Ctrl Pts',(7.38502136451266,6.6561868547759,4.93805828946138));
#86055=CARTESIAN_POINT('Ctrl Pts',(7.50167785954103,6.52675678814917,4.93526852498172));
#86056=CARTESIAN_POINT('Ctrl Pts',(7.61492085874833,6.39427035216825,4.93247876050206));
#86057=CARTESIAN_POINT('Ctrl Pts',(7.72459333987783,6.25891537996122,4.9296889960224));
#86058=CARTESIAN_POINT('Ctrl Pts',(7.87830014207589,6.06921437451954,4.9257791202483));
#86059=CARTESIAN_POINT('Ctrl Pts',(8.02503905688031,5.8738194963267,4.92186924447419));
#86060=CARTESIAN_POINT('Ctrl Pts',(8.16439975760317,5.67326542637037,4.91795936870009));
#86061=CARTESIAN_POINT('Ctrl Pts',(8.30373633355847,5.47274607438184,4.91405016976561));
#86062=CARTESIAN_POINT('Ctrl Pts',(8.4356970852241,5.26706954355613,4.91014097083112));
#86063=CARTESIAN_POINT('Ctrl Pts',(8.55991419398573,5.05680066757645,4.90623177189664));
#86064=CARTESIAN_POINT('Ctrl Pts',(8.68411777986816,4.8465546824903,4.90232299853659));
#86065=CARTESIAN_POINT('Ctrl Pts',(8.80057926354646,4.63171759173032,4.89841422517654));
#86066=CARTESIAN_POINT('Ctrl Pts',(8.90897556018459,4.4128809714328,4.89450545181648));
#86067=CARTESIAN_POINT('Ctrl Pts',(9.01738026913759,4.19402736787466,4.89059637510813));
#86068=CARTESIAN_POINT('Ctrl Pts',(9.11771841317532,3.97117386439473,4.88668729839978));
#86069=CARTESIAN_POINT('Ctrl Pts',(9.20971349255164,3.74493543136758,4.88277822169143));
#86070=CARTESIAN_POINT('Ctrl Pts',(9.30170730171872,3.51870012209607,4.87886919895711));
#86071=CARTESIAN_POINT('Ctrl Pts',(9.38535817293,3.28908023720895,4.87496017622279));
#86072=CARTESIAN_POINT('Ctrl Pts',(9.46043799751566,3.05671014248356,4.87105115348847));
#86073=CARTESIAN_POINT('Ctrl Pts',(9.53553433399791,2.8242889438698,4.86714127106408));
#86074=CARTESIAN_POINT('Ctrl Pts',(9.60205577016382,2.5891165933797,4.8632313886397));
#86075=CARTESIAN_POINT('Ctrl Pts',(9.65982385427233,2.35184334181326,4.85932150621531));
#86076=CARTESIAN_POINT('Ctrl Pts',(9.70104246646758,2.1825444237073,4.85653173172535));
#86077=CARTESIAN_POINT('Ctrl Pts',(9.73780570645368,2.01217625026479,4.85374195723539));
#86078=CARTESIAN_POINT('Ctrl Pts',(9.77006455811022,1.84097868818695,4.85095218274543));
#86079=CARTESIAN_POINT('Ctrl Pts',(9.81527545634597,1.6010446806247,4.84704230362422));
#86080=CARTESIAN_POINT('Ctrl Pts',(9.85165052663618,1.35940771688456,4.84313242450301));
#86081=CARTESIAN_POINT('Ctrl Pts',(9.87908249715191,1.11673318857586,4.83922254538179));
#86082=CARTESIAN_POINT('Ctrl Pts',(9.90650971898777,0.874100669048388,4.83531334308998));
#86083=CARTESIAN_POINT('Ctrl Pts',(9.92499689997156,0.630431221893893,4.83140414079818));
#86084=CARTESIAN_POINT('Ctrl Pts',(9.93448849574636,0.386396594036773,4.82749493850637));
#86085=CARTESIAN_POINT('Ctrl Pts',(9.94397905822149,0.14238853293462,4.82358616178867));
#86086=CARTESIAN_POINT('Ctrl Pts',(9.94447597994659,-0.101984349500512,
4.81967738507097));
#86087=CARTESIAN_POINT('Ctrl Pts',(9.93597578375624,-0.346048009110941,
4.81576860835327));
#86088=CARTESIAN_POINT('Ctrl Pts',(9.92747492794263,-0.590130608291953,
4.8118595283108));
#86089=CARTESIAN_POINT('Ctrl Pts',(9.90997556579693,-0.833903656436583,
4.80795044826834));
#86090=CARTESIAN_POINT('Ctrl Pts',(9.8835263270113,-1.07669463789624,4.80404136822587));
#86091=CARTESIAN_POINT('Ctrl Pts',(9.85707745354458,-1.31948226590828,4.80013234217592));
#86092=CARTESIAN_POINT('Ctrl Pts',(9.82167898307732,-1.56128757590726,4.79622331612596));
#86093=CARTESIAN_POINT('Ctrl Pts',(9.77743134303264,-1.80144395757484,4.79231429007601));
#86094=CARTESIAN_POINT('Ctrl Pts',(9.73317397244035,-2.04165315229877,4.7884044043878));
#86095=CARTESIAN_POINT('Ctrl Pts',(9.68006359359426,-2.28021241815636,4.78449451869959));
#86096=CARTESIAN_POINT('Ctrl Pts',(9.61825187905802,-2.51646474066237,4.78058463301138));
#86097=CARTESIAN_POINT('Ctrl Pts',(9.57414841327525,-2.68503385899083,4.77779487849707));
#86098=CARTESIAN_POINT('Ctrl Pts',(9.52561616142817,-2.85242871088613,4.77500512398277));
#86099=CARTESIAN_POINT('Ctrl Pts',(9.4727258673293,-3.01841492217858,4.77221536946846));
#86100=CARTESIAN_POINT('Ctrl Pts',(9.39859949374544,-3.25104656315668,4.7683054954763));
#86101=CARTESIAN_POINT('Ctrl Pts',(9.31588817074526,-3.48098188411319,4.76439562148414));
#86102=CARTESIAN_POINT('Ctrl Pts',(9.22481340416182,-3.70758434272189,4.76048574749199));
#86103=CARTESIAN_POINT('Ctrl Pts',(9.13375440358504,-3.93414757404505,4.75657655034043));
#86104=CARTESIAN_POINT('Ctrl Pts',(9.03433495404485,-4.15737883478786,4.75266735318887));
#86105=CARTESIAN_POINT('Ctrl Pts',(8.92682510426777,-4.37666054861634,4.74875815603731));
#86106=CARTESIAN_POINT('Ctrl Pts',(8.8193269584278,-4.59591839059128,4.74484938445603));
#86107=CARTESIAN_POINT('Ctrl Pts',(8.70374029427993,-4.81122729255618,4.74094061287476));
#86108=CARTESIAN_POINT('Ctrl Pts',(8.58038207571801,-5.02199237700508,4.73703184129349));
#86109=CARTESIAN_POINT('Ctrl Pts',(8.45701428308233,-5.23277381934636,4.73312276634477));
#86110=CARTESIAN_POINT('Ctrl Pts',(8.32587386974536,-5.43901049601501,4.72921369139605));
#86111=CARTESIAN_POINT('Ctrl Pts',(8.18732293327937,-5.64013361421498,4.72530461644733));
#86112=CARTESIAN_POINT('Ctrl Pts',(8.04877390936083,-5.84125395612547,4.72139559545921));
#86113=CARTESIAN_POINT('Ctrl Pts',(7.90281472763088,-6.03726065105612,4.7174865744711));
#86114=CARTESIAN_POINT('Ctrl Pts',(7.74985026922005,-6.2276146962276,4.71357755348298));
#86115=CARTESIAN_POINT('Ctrl Pts',(7.59685216885469,-6.41801060656304,4.70966767277158));
#86116=CARTESIAN_POINT('Ctrl Pts',(7.43684588811653,-6.60275116378262,4.70575779206017));
#86117=CARTESIAN_POINT('Ctrl Pts',(7.27027685317035,-6.7813301407803,4.70184791134877));
#86118=CARTESIAN_POINT('Ctrl Pts',(7.15142621853708,-6.90875013066734,4.69905812629634));
#86119=CARTESIAN_POINT('Ctrl Pts',(7.02923524624691,-7.03303386317473,4.69626834124391));
#86120=CARTESIAN_POINT('Ctrl Pts',(6.90387748118228,-7.15400864724276,4.69347855619148));
#86121=CARTESIAN_POINT('Ctrl Pts',(6.72818879098361,-7.3235545971807,4.68956867728175));
#86122=CARTESIAN_POINT('Ctrl Pts',(6.5462246180508,-7.48665149996543,4.68565879837202));
#86123=CARTESIAN_POINT('Ctrl Pts',(6.35848213136219,-7.6428442994181,4.68174891946229));
#86124=CARTESIAN_POINT('Ctrl Pts',(6.17077214485523,-7.79901006026889,4.67783971739336));
#86125=CARTESIAN_POINT('Ctrl Pts',(5.97728605677042,-7.94827392443534,4.67393051532443));
#86126=CARTESIAN_POINT('Ctrl Pts',(5.77855475406128,-8.09022057513364,4.67002131325549));
#86127=CARTESIAN_POINT('Ctrl Pts',(5.57984508671291,-8.23215177246876,4.66611253677124));
#86128=CARTESIAN_POINT('Ctrl Pts',(5.37589157292128,-8.36676718403924,4.66220376028698));
#86129=CARTESIAN_POINT('Ctrl Pts',(5.16725561277052,-8.49369374490814,4.65829498380273));
#86130=CARTESIAN_POINT('Ctrl Pts',(4.958603463037,-8.62063015493275,4.65438590400805));
#86131=CARTESIAN_POINT('Ctrl Pts',(4.74526837880589,-8.73987637374855,4.65047682421338));
#86132=CARTESIAN_POINT('Ctrl Pts',(4.52783909783716,-8.8511037223669,4.64656774441871));
#86133=CARTESIAN_POINT('Ctrl Pts',(4.31041282044257,-8.96232953448755,4.64265871862417));
#86134=CARTESIAN_POINT('Ctrl Pts',(4.08889270993251,-9.06553657212145,4.63874969282963));
#86135=CARTESIAN_POINT('Ctrl Pts',(3.86389101420379,-9.16044268746632,4.63484066703509));
#86136=CARTESIAN_POINT('Ctrl Pts',(3.63883983869041,-9.25536967347235,4.63093078161257));
#86137=CARTESIAN_POINT('Ctrl Pts',(3.41030580608748,-9.34199197973344,4.62702089619005));
#86138=CARTESIAN_POINT('Ctrl Pts',(3.17892128675169,-9.42007555450788,4.62311101076753));
#86139=CARTESIAN_POINT('Ctrl Pts',(3.01382531333293,-9.4757892376117,4.62032125481652));
#86140=CARTESIAN_POINT('Ctrl Pts',(2.84727857387036,-9.52715684556414,4.61753149886552));
#86141=CARTESIAN_POINT('Ctrl Pts',(2.67951578883477,-9.57410879076404,4.61474174291451));
#86142=CARTESIAN_POINT('Ctrl Pts',(2.4443939330779,-9.63991258917172,4.61083186149373));
#86143=CARTESIAN_POINT('Ctrl Pts',(2.20681090843899,-9.6970610561153,4.60692198007295));
#86144=CARTESIAN_POINT('Ctrl Pts',(1.96742032879298,-9.74538974335312,4.60301209865217));
#86145=CARTESIAN_POINT('Ctrl Pts',(1.72807118751074,-9.79371006492456,4.59910289402949));
#86146=CARTESIAN_POINT('Ctrl Pts',(1.48691539044466,-9.8332135989825,4.59519368940681));
#86147=CARTESIAN_POINT('Ctrl Pts',(1.24461735909541,-9.86378688077953,4.59128448478413));
#86148=CARTESIAN_POINT('Ctrl Pts',(1.00234570392804,-9.89435683441728,4.5873757057113));
#86149=CARTESIAN_POINT('Ctrl Pts',(0.758932340745822,-9.9159984417523,4.58346692663847));
#86150=CARTESIAN_POINT('Ctrl Pts',(0.515048485219441,-9.9286499111346,4.57955814756564));
#86151=CARTESIAN_POINT('Ctrl Pts',(0.27114570285142,-9.94130236234638,4.57564906514825));
#86152=CARTESIAN_POINT('Ctrl Pts',(0.0267726349693093,-9.94496326390372,
4.57173998273085));
#86153=CARTESIAN_POINT('Ctrl Pts',(-0.217396516537479,-9.93962286782539,
4.56783090031346));
#86154=CARTESIAN_POINT('Ctrl Pts',(-0.461562296017011,-9.93428254549904,
4.56392187188131));
#86155=CARTESIAN_POINT('Ctrl Pts',(-0.705523884537556,-9.91994118234583,
4.56001284344917));
#86156=CARTESIAN_POINT('Ctrl Pts',(-0.948608481140175,-9.89664114482833,
4.55610381501702));
#86157=CARTESIAN_POINT('Ctrl Pts',(-1.19174653440938,-9.873335983406,4.55219392695151));
#86158=CARTESIAN_POINT('Ctrl Pts',(-1.43400693115669,-9.84106823678216,
4.548284038886));
#86159=CARTESIAN_POINT('Ctrl Pts',(-1.6747219958265,-9.79993215469857,4.54437415082049));
#86160=CARTESIAN_POINT('Ctrl Pts',(-1.84647436524944,-9.77058118916459,
4.54158441042617));
#86161=CARTESIAN_POINT('Ctrl Pts',(-2.01744012065032,-9.73671648235652,
4.53879467003186));
#86162=CARTESIAN_POINT('Ctrl Pts',(-2.18737964906489,-9.6983882305699,4.53600492963754));
#86163=CARTESIAN_POINT('Ctrl Pts',(-2.42555191910766,-9.64467072988035,
4.53209507529851));
#86164=CARTESIAN_POINT('Ctrl Pts',(-2.66178090260783,-9.58216724556021,
4.52818522095948));
#86165=CARTESIAN_POINT('Ctrl Pts',(-2.89541328308477,-9.51104336653641,
4.52427536662045));
#86166=CARTESIAN_POINT('Ctrl Pts',(-3.12900521299153,-9.43993180173658,
4.52036618922456));
#86167=CARTESIAN_POINT('Ctrl Pts',(-3.36000116928354,-9.36020290322677,
4.51645701182867));
#86168=CARTESIAN_POINT('Ctrl Pts',(-3.587762529562,-9.27207226198496,4.51254783443278));
#86169=CARTESIAN_POINT('Ctrl Pts',(-3.81549909215251,-9.18395121603244,
4.5086390826515));
#86170=CARTESIAN_POINT('Ctrl Pts',(-4.04000150056862,-9.08743035491912,
4.50473033087022));
#86171=CARTESIAN_POINT('Ctrl Pts',(-4.26064968623793,-8.98277397306425,
4.50082157908893));
#86172=CARTESIAN_POINT('Ctrl Pts',(-4.48131500117173,-8.87810946657044,
4.49691252386512));
#86173=CARTESIAN_POINT('Ctrl Pts',(-4.69812524087963,-8.76530829469485,
4.49300346864131));
#86174=CARTESIAN_POINT('Ctrl Pts',(-4.91048241798382,-8.64468197348357,
4.48909441341749));
#86175=CARTESIAN_POINT('Ctrl Pts',(-5.12283666769756,-8.52405731513269,
4.48518541208087));
#86176=CARTESIAN_POINT('Ctrl Pts',(-5.3307377348432,-8.39560786344257,4.48127641074424));
#86177=CARTESIAN_POINT('Ctrl Pts',(-5.53361360808909,-8.25969033538009,
4.47736740940762));
#86178=CARTESIAN_POINT('Ctrl Pts',(-5.73653411367527,-8.12374290569714,
4.47345754809748));
#86179=CARTESIAN_POINT('Ctrl Pts',(-5.93442698278003,-7.98032427197115,
4.46954768678734));
#86180=CARTESIAN_POINT('Ctrl Pts',(-6.12674934828163,-7.82983438032571,
4.4656378254772));
#86181=CARTESIAN_POINT('Ctrl Pts',(-6.26398202980047,-7.72245149057122,
4.46284792243832));
#86182=CARTESIAN_POINT('Ctrl Pts',(-6.3983790349284,-7.61146909301393,4.46005801939944));
#86183=CARTESIAN_POINT('Ctrl Pts',(-6.52975327862434,-7.49704515928074,
4.45726811636056));
#86184=CARTESIAN_POINT('Ctrl Pts',(-6.71386901944704,-7.33668459898784,
4.45335817899099));
#86185=CARTESIAN_POINT('Ctrl Pts',(-6.89210275204051,-7.16951384949421,
4.44944824162141));
#86186=CARTESIAN_POINT('Ctrl Pts',(-7.06395809425259,-6.99598885381068,
4.44553830425183));
#86187=CARTESIAN_POINT('Ctrl Pts',(-7.23578369717028,-6.82249388635242,
4.44162904349071));
#86188=CARTESIAN_POINT('Ctrl Pts',(-7.40123291594315,-6.64264706679494,
4.4377197827296));
#86189=CARTESIAN_POINT('Ctrl Pts',(-7.55984604129784,-6.45694136816135,
4.43381052196848));
#86190=CARTESIAN_POINT('Ctrl Pts',(-7.71844190155171,-6.27125588366579,
4.42990168673193));
#86191=CARTESIAN_POINT('Ctrl Pts',(-7.8702029721684,-6.07971300651,4.42599285149538));
#86192=CARTESIAN_POINT('Ctrl Pts',(-8.0147089969722,-5.88283976442099,4.42208401625883));
#86193=CARTESIAN_POINT('Ctrl Pts',(-8.15922622264439,-5.68595126240579,
4.41817487804287));
#86194=CARTESIAN_POINT('Ctrl Pts',(-8.29648711048636,-5.48373179403123,
4.41426573982692));
#86195=CARTESIAN_POINT('Ctrl Pts',(-8.42611325824664,-5.27673946288807,
4.41035660161097));
#86196=CARTESIAN_POINT('Ctrl Pts',(-8.55573760615249,-5.06975000582602,
4.40644751767326));
#86197=CARTESIAN_POINT('Ctrl Pts',(-8.67772727895973,-4.85798805720064,
4.40253843373555));
#86198=CARTESIAN_POINT('Ctrl Pts',(-8.79174819658104,-4.64203916914905,
4.39862934979784));
#86199=CARTESIAN_POINT('Ctrl Pts',(-8.90579416360266,-4.42604283901178,
4.39471940706851));
#86200=CARTESIAN_POINT('Ctrl Pts',(-9.01186774549705,-4.2058579789586,4.39080946433918));
#86201=CARTESIAN_POINT('Ctrl Pts',(-9.10968103650867,-3.98209435009699,
4.38689952160985));
#86202=CARTESIAN_POINT('Ctrl Pts',(-9.17946236500216,-3.82245834226004,
4.38411011543443));
#86203=CARTESIAN_POINT('Ctrl Pts',(-9.24504051037593,-3.6610013945544,4.38132070925901));
#86204=CARTESIAN_POINT('Ctrl Pts',(-9.30632586764886,-3.49795123538475,
4.37853130308359));
#86205=CARTESIAN_POINT('Ctrl Pts',(-9.39202256166296,-3.26995452913916,
4.374630813666));
#86206=CARTESIAN_POINT('Ctrl Pts',(-9.46935111084644,-3.03876848928669,
4.37073032424842));
#86207=CARTESIAN_POINT('Ctrl Pts',(-9.53809144555643,-2.80502684054953,
4.36682983483083));
#86208=CARTESIAN_POINT('Ctrl Pts',(-9.60682298126833,-2.57131511154334,
4.36292984468924));
#86209=CARTESIAN_POINT('Ctrl Pts',(-9.66696841488264,-2.33504869741452,
4.35902985454765));
#86210=CARTESIAN_POINT('Ctrl Pts',(-9.7183574872742,-2.09687666531474,4.35512986440605));
#86211=CARTESIAN_POINT('Ctrl Pts',(-9.76973981138758,-1.85873590934144,
4.35123038640094));
#86212=CARTESIAN_POINT('Ctrl Pts',(-9.81236801113123,-1.61869031178751,
4.34733090839582));
#86213=CARTESIAN_POINT('Ctrl Pts',(-9.84612272724908,-1.37740017422287,
4.3434314303907));
#86214=CARTESIAN_POINT('Ctrl Pts',(-9.8798799731463,-1.13609195293888,4.33953166013549));
#86215=CARTESIAN_POINT('Ctrl Pts',(-9.90476236463304,-0.893539285235661,
4.33563188988028));
#86216=CARTESIAN_POINT('Ctrl Pts',(-9.9207021378468,-0.650409941592197,
4.33173211962506));
#86217=CARTESIAN_POINT('Ctrl Pts',(-9.93490167191397,-0.433824463775272,
4.32825811031198));
#86218=CARTESIAN_POINT('Ctrl Pts',(-9.94200533327122,-0.216781588312717,
4.32478410099889));
#86219=CARTESIAN_POINT('Ctrl Pts',(-9.94199999699464,0.000244455737705986,
4.32131009168581));
#86220=CARTESIAN_POINT('Ctrl Pts',(-9.94181728593973,0.000151535147386895,
4.17868990831418));
#86221=CARTESIAN_POINT('Ctrl Pts',(-9.94067494153095,-1.19759694767415,
4.19786341881976));
#86222=CARTESIAN_POINT('Ctrl Pts',(-9.42716810349573,-4.0356543903417,4.24328253375099));
#86223=CARTESIAN_POINT('Ctrl Pts',(-6.78745657491302,-7.82265052093215,
4.3149472531079));
#86224=CARTESIAN_POINT('Ctrl Pts',(-2.25961972835393,-10.1071926315035,
4.39368406638486));
#86225=CARTESIAN_POINT('Ctrl Pts',(2.81004432863975,-9.9682562140793,4.47242087966184));
#86226=CARTESIAN_POINT('Ctrl Pts',(7.2058836988398,-7.4388954948298,4.55115769293881));
#86227=CARTESIAN_POINT('Ctrl Pts',(9.87378550027097,-3.1257728072169,4.62989450621579));
#86228=CARTESIAN_POINT('Ctrl Pts',(10.1740080784303,1.9369173557757,4.70863131949275));
#86229=CARTESIAN_POINT('Ctrl Pts',(8.03455597735996,6.5351327702113,4.78736813276973));
#86230=CARTESIAN_POINT('Ctrl Pts',(3.96846040700314,9.5662641254359,4.86610494604671));
#86231=CARTESIAN_POINT('Ctrl Pts',(-1.04925135204577,10.3034526025732,4.94484175932367));
#86232=CARTESIAN_POINT('Ctrl Pts',(-5.81535800483383,8.56992920228316,5.02357857260066));
#86233=CARTESIAN_POINT('Ctrl Pts',(-9.15325378605286,4.81926962775394,5.10152795559748));
#86234=CARTESIAN_POINT('Ctrl Pts',(-9.94235238109963,1.58985384631345,5.15323173416867));
#86235=CARTESIAN_POINT('Ctrl Pts',(-9.94280319079831,-5.01184069386897E-5,
5.17868990831418));
#86236=CARTESIAN_POINT('Origin',(0.,0.,0.));
#86237=CARTESIAN_POINT('',(-9.94155665446311,-0.000214602085816251,6.32131009168581));
#86238=CARTESIAN_POINT('',(-9.94154134406803,-0.000211681655451256,6.17868990831418));
#86239=CARTESIAN_POINT('',(-9.942,-1.2175438477123E-15,0.));
#86240=CARTESIAN_POINT('Ctrl Pts',(-9.94155665446311,-0.000214602085816251,
6.32131009168581));
#86241=CARTESIAN_POINT('Ctrl Pts',(-9.94066724770169,1.10548046214137,6.30361166836752));
#86242=CARTESIAN_POINT('Ctrl Pts',(-9.48359125834515,3.85156620137575,6.25966764062359));
#86243=CARTESIAN_POINT('Ctrl Pts',(-7.00230141619256,7.63084835322035,6.18947800845398));
#86244=CARTESIAN_POINT('Ctrl Pts',(-2.53974329043462,10.0405067467589,6.110741195177));
#86245=CARTESIAN_POINT('Ctrl Pts',(2.53183186998833,10.0425046226134,6.03200438190005));
#86246=CARTESIAN_POINT('Ctrl Pts',(6.99628711260754,7.63636290068329,5.95326756862306));
#86247=CARTESIAN_POINT('Ctrl Pts',(9.7830696364778,3.39906166477283,5.87453075534608));
#86248=CARTESIAN_POINT('Ctrl Pts',(10.2239237027893,-1.65331661598174,5.79579394206911));
#86249=CARTESIAN_POINT('Ctrl Pts',(8.21313483354066,-6.30923829939991,5.71705712879214));
#86250=CARTESIAN_POINT('Ctrl Pts',(4.23287958537107,-9.45223794295327,5.63832031551517));
#86251=CARTESIAN_POINT('Ctrl Pts',(-0.762397843559365,-10.3286408224073,
5.55958350223819));
#86252=CARTESIAN_POINT('Ctrl Pts',(-5.57485629398454,-8.72829015437749,
5.48084668896123));
#86253=CARTESIAN_POINT('Ctrl Pts',(-9.05049363283098,-5.03494157965019,
5.40210987568424));
#86254=CARTESIAN_POINT('Ctrl Pts',(-9.93214544881101,-1.72500676017719,
5.34893100992577));
#86255=CARTESIAN_POINT('Ctrl Pts',(-9.9428190193766,-0.0429890845476765,
5.32199774859297));
#86256=CARTESIAN_POINT('Ctrl Pts',(-9.9428082600987,-4.38671419117354E-5,
5.32131009168581));
#86257=CARTESIAN_POINT('Ctrl Pts',(-9.94280319079831,-5.01184069386897E-5,
5.17868990831418));
#86258=CARTESIAN_POINT('Ctrl Pts',(-9.94281713450084,-0.0492264072162153,
5.17947733859432));
#86259=CARTESIAN_POINT('Ctrl Pts',(-9.93054952213869,-1.73747597041708,
5.20651037330044));
#86260=CARTESIAN_POINT('Ctrl Pts',(-9.04100851487771,-5.05195381719555,
5.25978901243127));
#86261=CARTESIAN_POINT('Ctrl Pts',(-5.55843129702091,-8.73875925129238,
5.3385258257087));
#86262=CARTESIAN_POINT('Ctrl Pts',(-0.742971601277903,-10.3300564063074,
5.41726263898546));
#86263=CARTESIAN_POINT('Ctrl Pts',(4.25064876577104,-9.44426053244652,5.49599945226253));
#86264=CARTESIAN_POINT('Ctrl Pts',(8.2249859947697,-6.29378085182736,5.57473626553945));
#86265=CARTESIAN_POINT('Ctrl Pts',(10.2270149997805,-1.63408573721985,5.65347307881644));
#86266=CARTESIAN_POINT('Ctrl Pts',(9.77665979209908,3.41745450715161,5.7322098920934));
#86267=CARTESIAN_POINT('Ctrl Pts',(6.9819131739284,7.64950720241167,5.81094670537039));
#86268=CARTESIAN_POINT('Ctrl Pts',(2.51294063151338,10.0472484483636,5.88968351864737));
#86269=CARTESIAN_POINT('Ctrl Pts',(-2.55862180937833,10.035712552753,5.96842033192432));
#86270=CARTESIAN_POINT('Ctrl Pts',(-7.01664024644669,7.61766576156723,6.04715714520133));
#86271=CARTESIAN_POINT('Ctrl Pts',(-9.48730107152748,3.83910257889644,6.11724700399791));
#86272=CARTESIAN_POINT('Ctrl Pts',(-9.94067098893944,1.09925498394695,6.16109125836888));
#86273=CARTESIAN_POINT('Ctrl Pts',(-9.94154134406803,-0.000211681655451256,
6.17868990831418));
#86274=CARTESIAN_POINT('Origin',(0.,0.,0.));
#86275=CARTESIAN_POINT('',(-9.94199999856713,0.00016879341615152,7.32131009168581));
#86276=CARTESIAN_POINT('',(-9.94199999849644,0.000172907010996282,7.17868990831418));
#86277=CARTESIAN_POINT('',(-9.942,-1.2175438477123E-15,0.));
#86278=CARTESIAN_POINT('Ctrl Pts',(-9.94137899628422,0.000169123441638015,
7.32131008623474));
#86279=CARTESIAN_POINT('Ctrl Pts',(-9.94175804919024,0.614877989386383,
7.3114711889337));
#86280=CARTESIAN_POINT('Ctrl Pts',(-9.73589259794127,2.86909352714112,7.27538668720702));
#86281=CARTESIAN_POINT('Ctrl Pts',(-8.05196685992069,6.5136703477983,7.21305658105461));
#86282=CARTESIAN_POINT('Ctrl Pts',(-3.99397426891797,9.55563923828576,7.13431976777767));
#86283=CARTESIAN_POINT('Ctrl Pts',(1.02175226903423,10.3062162801764,7.05558295450068));
#86284=CARTESIAN_POINT('Ctrl Pts',(5.7924680063296,8.58541706084741,6.97684614122372));
#86285=CARTESIAN_POINT('Ctrl Pts',(9.17418049203979,4.8058801496214,6.89810932794675));
#86286=CARTESIAN_POINT('Ctrl Pts',(10.3559729229203,-0.126081452991023,
6.81937251466976));
#86287=CARTESIAN_POINT('Ctrl Pts',(9.05445771229864,-5.02780938871426,6.74063570139281));
#86288=CARTESIAN_POINT('Ctrl Pts',(5.58173133745689,-8.72389517300014,6.66189888811582));
#86289=CARTESIAN_POINT('Ctrl Pts',(0.770535251822135,-10.3280369450708,
6.58316207483886));
#86290=CARTESIAN_POINT('Ctrl Pts',(-4.22543111982425,-9.45556997566333,
6.50442526156187));
#86291=CARTESIAN_POINT('Ctrl Pts',(-8.20816141345054,-6.31570723860668,
6.42568844828491));
#86292=CARTESIAN_POINT('Ctrl Pts',(-9.7698093539024,-2.70757066804228,6.36465005832621));
#86293=CARTESIAN_POINT('Ctrl Pts',(-9.94198617976778,-0.534193013242581,
6.32985727279318));
#86294=CARTESIAN_POINT('Ctrl Pts',(-9.94155665446311,-0.000214602085816251,
6.32131009168581));
#86295=CARTESIAN_POINT('Ctrl Pts',(-9.94154134406803,-0.000211681655451256,
6.17868990831418));
#86296=CARTESIAN_POINT('Ctrl Pts',(-9.94196898602932,-0.540425745784602,
6.18733686279454));
#86297=CARTESIAN_POINT('Ctrl Pts',(-9.76726376589108,-2.72004674445215,
6.22222942170057));
#86298=CARTESIAN_POINT('Ctrl Pts',(-8.1962690674157,-6.33113302482017,6.28336758503222));
#86299=CARTESIAN_POINT('Ctrl Pts',(-4.20764072636975,-9.46349996150261,
6.36210439830921));
#86300=CARTESIAN_POINT('Ctrl Pts',(0.789957650256369,-10.3265695617805,
6.44084121158617));
#86301=CARTESIAN_POINT('Ctrl Pts',(5.5981283522494,-8.71338229135328,6.51957802486315));
#86302=CARTESIAN_POINT('Ctrl Pts',(9.06389742585678,-5.0107719422322,6.59831483814014));
#86303=CARTESIAN_POINT('Ctrl Pts',(10.3561917417607,-0.106604931408537,
6.67705165141709));
#86304=CARTESIAN_POINT('Ctrl Pts',(9.1651259445603,4.82312537923973,6.75578846469407));
#86305=CARTESIAN_POINT('Ctrl Pts',(5.77631132522008,8.59629568347027,6.83452527797105));
#86306=CARTESIAN_POINT('Ctrl Pts',(1.00236774113876,10.3081196595228,6.91326209124801));
#86307=CARTESIAN_POINT('Ctrl Pts',(-4.0119383361334,9.54811095403596,6.99199890452499));
#86308=CARTESIAN_POINT('Ctrl Pts',(-8.06420277796297,6.49851564277618,7.07073571780195));
#86309=CARTESIAN_POINT('Ctrl Pts',(-9.73858672170967,2.85661735838654,7.13296605057013));
#86310=CARTESIAN_POINT('Ctrl Pts',(-9.94177600318943,0.608646416867156,
7.16895077891262));
#86311=CARTESIAN_POINT('Ctrl Pts',(-9.9413910139488,0.000173239089263606,
7.17868990282947));
#86312=CARTESIAN_POINT('Origin',(0.,0.,0.));
#86313=CARTESIAN_POINT('',(-9.94201937032046,0.000120688446031495,8.32131009183368));
#86314=CARTESIAN_POINT('',(-9.94202513961595,0.000115166331718865,8.17868990849874));
#86315=CARTESIAN_POINT('',(-9.942,-1.2175438477123E-15,0.));
#86316=CARTESIAN_POINT('Ctrl Pts',(-9.94199999926736,0.000120697445917958,
8.32131009168581));
#86317=CARTESIAN_POINT('Ctrl Pts',(-9.94199849861958,0.123730936968088,
8.31933071676796));
#86318=CARTESIAN_POINT('Ctrl Pts',(-9.93969150660321,0.247335251271708,
8.31735134185011));
#86319=CARTESIAN_POINT('Ctrl Pts',(-9.93508086580521,0.370853326682161,
8.31537196693226));
#86320=CARTESIAN_POINT('Ctrl Pts',(-9.92597342585771,0.614839684222309,
8.31146208997856));
#86321=CARTESIAN_POINT('Ctrl Pts',(-9.90787250252231,0.858527721681658,
8.30755221302486));
#86322=CARTESIAN_POINT('Ctrl Pts',(-9.88082101026864,1.10124482429378,8.30364233607117));
#86323=CARTESIAN_POINT('Ctrl Pts',(-9.8537742008759,1.34391991035369,8.29973313595296));
#86324=CARTESIAN_POINT('Ctrl Pts',(-9.81777994660197,1.58562411863887,8.29582393583475));
#86325=CARTESIAN_POINT('Ctrl Pts',(-9.7729330111231,1.82569010516582,8.29191473571654));
#86326=CARTESIAN_POINT('Ctrl Pts',(-9.72809095789121,2.0657299569876,8.28800596117213));
#86327=CARTESIAN_POINT('Ctrl Pts',(-9.67439819919527,2.30413166770891,8.28409718662772));
#86328=CARTESIAN_POINT('Ctrl Pts',(-9.61200077950874,2.54023719654748,8.2801884120833));
#86329=CARTESIAN_POINT('Ctrl Pts',(-9.54959851746434,2.77636104837876,8.27627933419805));
#86330=CARTESIAN_POINT('Ctrl Pts',(-9.47849031325711,3.0101880904526,8.27237025631281));
#86331=CARTESIAN_POINT('Ctrl Pts',(-9.39887268267154,3.2410733245224,8.26846117842756));
#86332=CARTESIAN_POINT('Ctrl Pts',(-9.31925615151854,3.47195537031916,8.26455215452241));
#86333=CARTESIAN_POINT('Ctrl Pts',(-9.23113052233324,3.69989542501469,8.26064313061727));
#86334=CARTESIAN_POINT('Ctrl Pts',(-9.13474151043455,3.9242657322796,8.25673410671212));
#86335=CARTESIAN_POINT('Ctrl Pts',(-9.03833130066592,4.14868538305886,8.2528242231345));
#86336=CARTESIAN_POINT('Ctrl Pts',(-8.93365418670862,4.36953345967599,8.24891433955687));
#86337=CARTESIAN_POINT('Ctrl Pts',(-8.82100372639414,4.58620292387293,8.24500445597925));
#86338=CARTESIAN_POINT('Ctrl Pts',(-8.74062573554202,4.74080021679601,8.24221468853793));
#86339=CARTESIAN_POINT('Ctrl Pts',(-8.65618946552648,4.89327058548648,8.23942492109661));
#86340=CARTESIAN_POINT('Ctrl Pts',(-8.56781586218719,5.04340116901815,8.23663515365529));
#86341=CARTESIAN_POINT('Ctrl Pts',(-8.44395969055699,5.2538101443029,8.2327252767015));
#86342=CARTESIAN_POINT('Ctrl Pts',(-8.31232996790346,5.45968661003823,8.2288153997477));
#86343=CARTESIAN_POINT('Ctrl Pts',(-8.17328380973805,5.66045897127379,8.2249055227939));
#86344=CARTESIAN_POINT('Ctrl Pts',(-8.03426172173523,5.86119657697606,8.22099632267559));
#86345=CARTESIAN_POINT('Ctrl Pts',(-7.88782592059668,6.05683161164939,8.21708712255727));
#86346=CARTESIAN_POINT('Ctrl Pts',(-7.73437665197683,6.24682173631965,8.21317792243896));
#86347=CARTESIAN_POINT('Ctrl Pts',(-7.58094408856136,6.4367911777772,8.20926914789444));
#86348=CARTESIAN_POINT('Ctrl Pts',(-7.42049975822438,6.62111671826791,8.20536037334992));
#86349=CARTESIAN_POINT('Ctrl Pts',(-7.25348462197907,6.79928855386453,8.2014515988054));
#86350=CARTESIAN_POINT('Ctrl Pts',(-7.08645652450817,6.97747421650344,8.19754252092005));
#86351=CARTESIAN_POINT('Ctrl Pts',(-6.91285679167045,7.14950501337471,8.19363344303471));
#86352=CARTESIAN_POINT('Ctrl Pts',(-6.7331646120328,7.31490658226537,8.18972436514936));
#86353=CARTESIAN_POINT('Ctrl Pts',(-6.55347491374794,7.48030586714096,8.18581534124412));
#86354=CARTESIAN_POINT('Ctrl Pts',(-6.36769314457287,7.63907591878491,8.18190631733887));
#86355=CARTESIAN_POINT('Ctrl Pts',(-6.17633360753728,7.79078090876682,8.17799729343363));
#86356=CARTESIAN_POINT('Ctrl Pts',(-5.98493198671523,7.9425192617078,8.1740874098559));
#86357=CARTESIAN_POINT('Ctrl Pts',(-5.78795036607489,8.08718927333725,8.17017752627818));
#86358=CARTESIAN_POINT('Ctrl Pts',(-5.58593531836972,8.22439606408822,8.16626764270046));
#86359=CARTESIAN_POINT('Ctrl Pts',(-5.44179419717811,8.32229540811536,8.16347787525975));
#86360=CARTESIAN_POINT('Ctrl Pts',(-5.2950912022544,8.41639603664618,8.16068810781903));
#86361=CARTESIAN_POINT('Ctrl Pts',(-5.14603384120051,8.50656803330339,8.15789834037832));
#86362=CARTESIAN_POINT('Ctrl Pts',(-4.93712899405506,8.63294466472426,8.15398846342456));
#86363=CARTESIAN_POINT('Ctrl Pts',(-4.72353458475305,8.75164146899183,8.1500785864708));
#86364=CARTESIAN_POINT('Ctrl Pts',(-4.50583629543312,8.86232493642371,8.14616870951704));
#86365=CARTESIAN_POINT('Ctrl Pts',(-4.28817569167947,8.9729892435344,8.14225950939876));
#86366=CARTESIAN_POINT('Ctrl Pts',(-4.06641287581174,9.07564285596032,8.13835030928048));
#86367=CARTESIAN_POINT('Ctrl Pts',(-3.84115759866731,9.16999848975998,8.1344411091622));
#86368=CARTESIAN_POINT('Ctrl Pts',(-3.61592684386395,9.26434385156485,8.1305323346177));
#86369=CARTESIAN_POINT('Ctrl Pts',(-3.38720464537729,9.35039293019651,8.12662356007319));
#86370=CARTESIAN_POINT('Ctrl Pts',(-3.15562114063695,9.42790640687343,8.12271478552869));
#86371=CARTESIAN_POINT('Ctrl Pts',(-2.92401966383752,9.50542589899081,8.11880570764338));
#86372=CARTESIAN_POINT('Ctrl Pts',(-2.6895567019394,9.57440837365246,8.11489662975807));
#86373=CARTESIAN_POINT('Ctrl Pts',(-2.45287920940295,9.63466385423377,8.11098755187276));
#86374=CARTESIAN_POINT('Ctrl Pts',(-2.21620498512436,9.69491850275266,8.10707852796755));
#86375=CARTESIAN_POINT('Ctrl Pts',(-1.97731656353971,9.7464463310455,8.10316950406234));
#86376=CARTESIAN_POINT('Ctrl Pts',(-1.73687350823773,9.78910794793795,8.09926048015713));
#86377=CARTESIAN_POINT('Ctrl Pts',(-1.49637757470285,9.83177894697251,8.09535059657944));
#86378=CARTESIAN_POINT('Ctrl Pts',(-1.25432660022208,9.86557978848185,8.09144071300176));
#86379=CARTESIAN_POINT('Ctrl Pts',(-1.01138910720974,9.89042244162591,8.08753082942407));
#86380=CARTESIAN_POINT('Ctrl Pts',(-0.838049135644045,9.90814809087096,
8.08474106198316));
#86381=CARTESIAN_POINT('Ctrl Pts',(-0.664258019573462,9.92131414527844,
8.08195129454226));
#86382=CARTESIAN_POINT('Ctrl Pts',(-0.490260069134713,9.92990478628129,
8.07916152710135));
#86383=CARTESIAN_POINT('Ctrl Pts',(-0.246400826084693,9.94194462472183,
8.07525165014757));
#86384=CARTESIAN_POINT('Ctrl Pts',(-0.00206054199540842,9.94499890041737,
8.07134177319379));
#86385=CARTESIAN_POINT('Ctrl Pts',(0.242086977852535,9.93905216281483,8.06743189624002));
#86386=CARTESIAN_POINT('Ctrl Pts',(0.486192233530556,9.933106454647,8.06352269612172));
#86387=CARTESIAN_POINT('Ctrl Pts',(0.730104511490238,9.91816285043824,8.05961349600342));
#86388=CARTESIAN_POINT('Ctrl Pts',(0.973150770743396,9.8942580104524,8.05570429588512));
#86389=CARTESIAN_POINT('Ctrl Pts',(1.21617057084558,9.87035577285909,8.05179552134061));
#86390=CARTESIAN_POINT('Ctrl Pts',(1.45832426162768,9.83749427479797,8.0478867467961));
#86391=CARTESIAN_POINT('Ctrl Pts',(1.69894363287301,9.79576207001376,8.04397797225158));
#86392=CARTESIAN_POINT('Ctrl Pts',(1.93958167740699,9.75402662659793,8.04006889436626));
#86393=CARTESIAN_POINT('Ctrl Pts',(2.17868488774968,9.70341914576017,8.03615981648093));
#86394=CARTESIAN_POINT('Ctrl Pts',(2.41559367981177,9.644079591856,8.03225073859561));
#86395=CARTESIAN_POINT('Ctrl Pts',(2.65249920042207,9.58474085736629,8.02834171469038));
#86396=CARTESIAN_POINT('Ctrl Pts',(2.88721009192831,9.51667036108042,8.02443269078515));
#86397=CARTESIAN_POINT('Ctrl Pts',(3.11907969004966,9.44005857434792,8.02052366687993));
#86398=CARTESIAN_POINT('Ctrl Pts',(3.35100028092948,9.36342993915245,8.01661378330222));
#86399=CARTESIAN_POINT('Ctrl Pts',(3.58007806327249,9.27825634717009,8.01270389972452));
#86400=CARTESIAN_POINT('Ctrl Pts',(3.80568287314964,9.18477772561838,8.00879401614681));
#86401=CARTESIAN_POINT('Ctrl Pts',(3.96665568489176,9.11807916295409,8.006004248706));
#86402=CARTESIAN_POINT('Ctrl Pts',(4.12586072984047,9.04715349288538,8.00321448126518));
#86403=CARTESIAN_POINT('Ctrl Pts',(4.28307547960545,8.97210278786431,8.00042471382436));
#86404=CARTESIAN_POINT('Ctrl Pts',(4.50341295931977,8.86691874362008,7.99651483687059));
#86405=CARTESIAN_POINT('Ctrl Pts',(4.71990760785408,8.75359809155395,7.99260495991682));
#86406=CARTESIAN_POINT('Ctrl Pts',(4.93195907173531,8.63244714520325,7.98869508296305));
#86407=CARTESIAN_POINT('Ctrl Pts',(5.14397382756745,8.51131717119014,7.98478588284476));
#86408=CARTESIAN_POINT('Ctrl Pts',(5.35154669088702,8.38235974775407,7.98087668272647));
#86409=CARTESIAN_POINT('Ctrl Pts',(5.55410272223126,8.24592668842643,7.97696748260818));
#86410=CARTESIAN_POINT('Ctrl Pts',(5.75663670237951,8.1095084818391,7.97305870806369));
#86411=CARTESIAN_POINT('Ctrl Pts',(5.95415470864741,7.96561642085696,7.96914993351919));
#86412=CARTESIAN_POINT('Ctrl Pts',(6.14611069131394,7.81464569703045,7.9652411589747));
#86413=CARTESIAN_POINT('Ctrl Pts',(6.33808157074289,7.66366325710645,7.96133208108938));
#86414=CARTESIAN_POINT('Ctrl Pts',(6.5244893418278,7.50560122753595,7.95742300320406));
#86415=CARTESIAN_POINT('Ctrl Pts',(6.70481995563336,7.34089595094091,7.95351392531874));
#86416=CARTESIAN_POINT('Ctrl Pts',(6.88514807926968,7.17619294874623,7.94960490141353));
#86417=CARTESIAN_POINT('Ctrl Pts',(7.05939900786635,7.00484707357231,7.94569587750831));
#86418=CARTESIAN_POINT('Ctrl Pts',(7.22709404313149,6.82733298526836,7.9417868536031));
#86419=CARTESIAN_POINT('Ctrl Pts',(7.39482595788652,6.6497798580685,7.9378769700254));
#86420=CARTESIAN_POINT('Ctrl Pts',(7.55599890510306,6.46605601035192,7.9339670864477));
#86421=CARTESIAN_POINT('Ctrl Pts',(7.71017218932104,6.27667179411354,7.93005720287));
#86422=CARTESIAN_POINT('Ctrl Pts',(7.82017741070812,6.14154298278805,7.92726743542914));
#86423=CARTESIAN_POINT('Ctrl Pts',(7.92661985514905,6.00353318953312,7.92447766798827));
#86424=CARTESIAN_POINT('Ctrl Pts',(8.02935213713326,5.86283790138475,7.92168790054741));
#86425=CARTESIAN_POINT('Ctrl Pts',(8.17333208895804,5.66565255303739,7.91777802359364));
#86426=CARTESIAN_POINT('Ctrl Pts',(8.3100668280156,5.46313066739671,7.91386814663987));
#86427=CARTESIAN_POINT('Ctrl Pts',(8.43917341423422,5.25582686972111,7.9099582696861));
#86428=CARTESIAN_POINT('Ctrl Pts',(8.56825765092119,5.04855895823009,7.90604906956781));
#86429=CARTESIAN_POINT('Ctrl Pts',(8.68971622267877,4.83651102498741,7.90213986944953));
#86430=CARTESIAN_POINT('Ctrl Pts',(8.80321015901788,4.62026567376427,7.89823066933124));
#86431=CARTESIAN_POINT('Ctrl Pts',(8.91669173987671,4.40404386402059,7.89432189478675));
#86432=CARTESIAN_POINT('Ctrl Pts',(9.02221028635395,4.18362579678715,7.89041312024226));
#86433=CARTESIAN_POINT('Ctrl Pts',(9.11947284906492,3.95961853657239,7.88650434569776));
#86434=CARTESIAN_POINT('Ctrl Pts',(9.21674295984642,3.73559389225267,7.88259526781245));
#86435=CARTESIAN_POINT('Ctrl Pts',(9.30575569214643,3.50797975428848,7.87868618992713));
#86436=CARTESIAN_POINT('Ctrl Pts',(9.38626579840481,3.27740421091083,7.87477711204181));
#86437=CARTESIAN_POINT('Ctrl Pts',(9.46677479290646,3.0468318515299,7.87086808813659));
#86438=CARTESIAN_POINT('Ctrl Pts',(9.53878130572403,2.8132984338617,7.86695906423138));
#86439=CARTESIAN_POINT('Ctrl Pts',(9.60208939387815,2.57744898532885,7.86305004032616));
#86440=CARTESIAN_POINT('Ctrl Pts',(9.66541140474609,2.34154766878874,7.85914015674846));
#86441=CARTESIAN_POINT('Ctrl Pts',(9.72003109486716,2.10332957420899,7.85523027317077));
#86442=CARTESIAN_POINT('Ctrl Pts',(9.76580291369538,1.86345309864746,7.85132038959307));
#86443=CARTESIAN_POINT('Ctrl Pts',(9.79846187331387,1.69229721432065,7.84853062215219));
#86444=CARTESIAN_POINT('Ctrl Pts',(9.82661738093856,1.52029731779854,7.84574085471131));
#86445=CARTESIAN_POINT('Ctrl Pts',(9.85023253620607,1.34769543394173,7.84295108727042));
#86446=CARTESIAN_POINT('Ctrl Pts',(9.88332932771172,1.10579278715493,7.83904121031665));
#86447=CARTESIAN_POINT('Ctrl Pts',(9.90751588863965,0.862633347076693,7.83513133336288));
#86448=CARTESIAN_POINT('Ctrl Pts',(9.92271851932728,0.618887054477162,7.83122145640911));
#86449=CARTESIAN_POINT('Ctrl Pts',(9.93791851830041,0.375182956591622,7.82731225629082));
#86450=CARTESIAN_POINT('Ctrl Pts',(9.94413767412424,0.130892488609745,7.82340305617253));
#86451=CARTESIAN_POINT('Ctrl Pts',(9.94135426861737,-0.113310660766393,
7.81949385605424));
#86452=CARTESIAN_POINT('Ctrl Pts',(9.93857116612502,-0.357487225046637,
7.81558508150975));
#86453=CARTESIAN_POINT('Ctrl Pts',(9.92678746236054,-0.601576209516069,
7.81167630696525));
#86454=CARTESIAN_POINT('Ctrl Pts',(9.90603355599169,-0.844904247572915,
7.80776753242075));
#86455=CARTESIAN_POINT('Ctrl Pts',(9.88527803901394,-1.0882511691254,7.80385845453544));
#86456=CARTESIAN_POINT('Ctrl Pts',(9.85555094918939,-1.330836746692,7.79994937665012));
#86457=CARTESIAN_POINT('Ctrl Pts',(9.81693464940344,-1.57199175867503,7.7960402987648));
#86458=CARTESIAN_POINT('Ctrl Pts',(9.77831888286646,-1.81314344057035,7.79213127485958));
#86459=CARTESIAN_POINT('Ctrl Pts',(9.73081419822735,-2.05286431991402,7.78822225095437));
#86460=CARTESIAN_POINT('Ctrl Pts',(9.67455439391132,-2.29049367588109,7.78431322704915));
#86461=CARTESIAN_POINT('Ctrl Pts',(9.61828221693993,-2.52817529129268,7.78040334347145));
#86462=CARTESIAN_POINT('Ctrl Pts',(9.55325113659201,-2.76376419112236,7.77649345989376));
#86463=CARTESIAN_POINT('Ctrl Pts',(9.47964564948824,-2.99661181338835,7.77258357631606));
#86464=CARTESIAN_POINT('Ctrl Pts',(9.42712690121589,-3.16275249312277,7.76979380887519));
#86465=CARTESIAN_POINT('Ctrl Pts',(9.37024392991821,-3.32749782564914,7.76700404143432));
#86466=CARTESIAN_POINT('Ctrl Pts',(9.30907916889137,-3.49061728456626,7.76421427399346));
#86467=CARTESIAN_POINT('Ctrl Pts',(9.22335636418052,-3.71923025200932,7.76030439703968));
#86468=CARTESIAN_POINT('Ctrl Pts',(9.12919493734011,-3.94471889634479,7.7563945200859));
#86469=CARTESIAN_POINT('Ctrl Pts',(9.02684810190676,-4.16645860955107,7.75248464313212));
#86470=CARTESIAN_POINT('Ctrl Pts',(8.92451898364732,-4.38815993758361,7.74857544301383));
#86471=CARTESIAN_POINT('Ctrl Pts',(8.81400740279927,-4.60611337560326,7.74466624289554));
#86472=CARTESIAN_POINT('Ctrl Pts',(8.69561410139413,-4.81971569697172,7.74075704277724));
#86473=CARTESIAN_POINT('Ctrl Pts',(8.57723368883694,-5.03329476459347,7.73684826823274));
#86474=CARTESIAN_POINT('Ctrl Pts',(8.45097340479124,-5.24252341628014,7.73293949368823));
#86475=CARTESIAN_POINT('Ctrl Pts',(8.31717970653713,-5.44682345309328,7.72903071914373));
#86476=CARTESIAN_POINT('Ctrl Pts',(8.18337562521034,-5.65113934463021,7.7251216412584));
#86477=CARTESIAN_POINT('Ctrl Pts',(8.04203711248242,-5.85052562081983,7.72121256337308));
#86478=CARTESIAN_POINT('Ctrl Pts',(7.89355439149914,-6.04443240250436,7.71730348548776));
#86479=CARTESIAN_POINT('Ctrl Pts',(7.74507372090031,-6.2383365065477,7.71339446158253));
#86480=CARTESIAN_POINT('Ctrl Pts',(7.58944921142076,-6.42676104609965,7.70948543767731));
#86481=CARTESIAN_POINT('Ctrl Pts',(7.42711231873426,-6.60918804429907,7.70557641377209));
#86482=CARTESIAN_POINT('Ctrl Pts',(7.2647397249207,-6.79165516184126,7.70166653019439));
#86483=CARTESIAN_POINT('Ctrl Pts',(7.09565198389555,-6.96812189232981,7.69775664661669));
#86484=CARTESIAN_POINT('Ctrl Pts',(6.92031939813044,-7.13810503059878,7.69384676303898));
#86485=CARTESIAN_POINT('Ctrl Pts',(6.79521666057704,-7.25939084773635,7.69105699559815));
#86486=CARTESIAN_POINT('Ctrl Pts',(6.66693544661113,-7.37737655515755,7.68826722815731));
#86487=CARTESIAN_POINT('Ctrl Pts',(6.53565775611913,-7.49189840393474,7.68547746071647));
#86488=CARTESIAN_POINT('Ctrl Pts',(6.35167123126217,-7.65240150920526,7.6815675837627));
#86489=CARTESIAN_POINT('Ctrl Pts',(6.16174122976612,-7.80614837115822,7.67765770680893));
#86490=CARTESIAN_POINT('Ctrl Pts',(5.96638715909732,-7.95270949222708,7.67374782985516));
#86491=CARTESIAN_POINT('Ctrl Pts',(5.77106690600597,-8.09924524222459,7.66983862973687));
#86492=CARTESIAN_POINT('Ctrl Pts',(5.57032468222324,-8.23859756634138,7.66592942961858));
#86493=CARTESIAN_POINT('Ctrl Pts',(5.36471157364193,-8.3703783505665,7.66202022950029));
#86494=CARTESIAN_POINT('Ctrl Pts',(5.15912084906475,-8.50214478851945,7.6581114549558));
#86495=CARTESIAN_POINT('Ctrl Pts',(4.9486605343707,-8.62634118119008,7.65420268041131));
#86496=CARTESIAN_POINT('Ctrl Pts',(4.7339100668253,-8.7426231463566,7.65029390586682));
#86497=CARTESIAN_POINT('Ctrl Pts',(4.51914293354909,-8.85891413559627,7.6463848279815));
#86498=CARTESIAN_POINT('Ctrl Pts',(4.30008522719591,-8.9672893338659,7.64247575009619));
#86499=CARTESIAN_POINT('Ctrl Pts',(4.07734145772143,-9.06745006256699,7.63856667221087));
#86500=CARTESIAN_POINT('Ctrl Pts',(3.85460076409528,-9.16760940815774,7.63465764830566));
#86501=CARTESIAN_POINT('Ctrl Pts',(3.62817436566375,-9.25955439795779,7.63074862440044));
#86502=CARTESIAN_POINT('Ctrl Pts',(3.39868791455605,-9.34303400718689,7.62683960049522));
#86503=CARTESIAN_POINT('Ctrl Pts',(3.16915099479163,-9.42653197525033,7.62292971691752));
#86504=CARTESIAN_POINT('Ctrl Pts',(2.93655294083511,-9.50156074593007,7.61901983333983));
#86505=CARTESIAN_POINT('Ctrl Pts',(2.70153708495892,-9.56791834092409,7.61510994976214));
#86506=CARTESIAN_POINT('Ctrl Pts',(2.53384933421514,-9.61526559674149,7.61232018232126));
#86507=CARTESIAN_POINT('Ctrl Pts',(2.36493103553724,-9.65819932922395,7.60953041488038));
#86508=CARTESIAN_POINT('Ctrl Pts',(2.19502011278985,-9.69666183304585,7.6067406474395));
#86509=CARTESIAN_POINT('Ctrl Pts',(1.95688886524932,-9.75056727873787,7.60283077048573));
#86510=CARTESIAN_POINT('Ctrl Pts',(1.71673450088473,-9.79570467238615,7.59892089353196));
#86511=CARTESIAN_POINT('Ctrl Pts',(1.47521806992349,-9.83194261812849,7.59501101657819));
#86512=CARTESIAN_POINT('Ctrl Pts',(1.23374344766685,-9.86817429075075,7.5911018164599));
#86513=CARTESIAN_POINT('Ctrl Pts',(0.99090750656723,-9.89550954923192,7.58719261634161));
#86514=CARTESIAN_POINT('Ctrl Pts',(0.747379528890581,-9.91386845987959,
7.58328341622332));
#86515=CARTESIAN_POINT('Ctrl Pts',(0.503878062807174,-9.93222537189048,
7.57937464167882));
#86516=CARTESIAN_POINT('Ctrl Pts',(0.259684989983711,-9.94160786617092,
7.57546586713432));
#86517=CARTESIAN_POINT('Ctrl Pts',(0.0154737816735091,-9.94198795825466,
7.57155709258982));
#86518=CARTESIAN_POINT('Ctrl Pts',(-0.228756378670423,-9.94236807983549,
7.5676480147045));
#86519=CARTESIAN_POINT('Ctrl Pts',(-0.473004396991685,-9.93374439971354,
7.56373893681918));
#86520=CARTESIAN_POINT('Ctrl Pts',(-0.71659643482113,-9.91614106140093,
7.55982985893386));
#86521=CARTESIAN_POINT('Ctrl Pts',(-0.960185108910316,-9.89853796617122,
7.55592083502865));
#86522=CARTESIAN_POINT('Ctrl Pts',(-1.20311754117273,-9.87195548300951,
7.55201181112343));
#86523=CARTESIAN_POINT('Ctrl Pts',(-1.4447239111017,-9.83646973363366,7.54810278721821));
#86524=CARTESIAN_POINT('Ctrl Pts',(-1.6863834151002,-9.8009761802323,7.54419290364051));
#86525=CARTESIAN_POINT('Ctrl Pts',(-1.92671599645066,-9.75657548794391,
7.54028302006281));
#86526=CARTESIAN_POINT('Ctrl Pts',(-2.16505956076288,-9.70339533866106,
7.53637313648511));
#86527=CARTESIAN_POINT('Ctrl Pts',(-2.33512168722852,-9.66545041114058,
7.53358336904425));
#86528=CARTESIAN_POINT('Ctrl Pts',(-2.50417135425084,-9.62303688626508,
7.53079360160339));
#86529=CARTESIAN_POINT('Ctrl Pts',(-2.67197176687381,-9.57621693974344,
7.52800383416253));
#86530=CARTESIAN_POINT('Ctrl Pts',(-2.90714512094575,-9.51059848452723,
7.52409395720876));
#86531=CARTESIAN_POINT('Ctrl Pts',(-3.13993609929161,-9.43630270113784,
7.52018408025499));
#86532=CARTESIAN_POINT('Ctrl Pts',(-3.36970052527798,-9.35352780345156,
7.51627420330122));
#86533=CARTESIAN_POINT('Ctrl Pts',(-3.59942517693922,-9.27076723485769,
7.51236500318294));
#86534=CARTESIAN_POINT('Ctrl Pts',(-3.82612405852241,-9.17953057701249,
7.50845580306465));
#86535=CARTESIAN_POINT('Ctrl Pts',(-4.04917018174292,-9.08006524421956,
7.50454660294637));
#86536=CARTESIAN_POINT('Ctrl Pts',(-4.27219202312049,-8.98061073968741,
7.50063782840187));
#86537=CARTESIAN_POINT('Ctrl Pts',(-4.49156164421575,-8.8729294629758,7.49672905385738));
#86538=CARTESIAN_POINT('Ctrl Pts',(-4.70667303463914,-8.75731653790137,
7.49282027931288));
#86539=CARTESIAN_POINT('Ctrl Pts',(-4.92180111880257,-8.64169464067482,
7.48891120142756));
#86540=CARTESIAN_POINT('Ctrl Pts',(-5.13267006359499,-8.5181399951333,7.48500212354224));
#86541=CARTESIAN_POINT('Ctrl Pts',(-5.33869828494172,-8.38699377741276,
7.48109304565692));
#86542=CARTESIAN_POINT('Ctrl Pts',(-5.54472366126301,-8.25584937067871,
7.47718402175172));
#86543=CARTESIAN_POINT('Ctrl Pts',(-5.74590821245139,-8.11711375369856,
7.47327499784651));
#86544=CARTESIAN_POINT('Ctrl Pts',(-5.9416985690445,-7.97117194110217,7.4693659739413));
#86545=CARTESIAN_POINT('Ctrl Pts',(-6.1375319838504,-7.82519803298416,7.4654560903636));
#86546=CARTESIAN_POINT('Ctrl Pts',(-6.32796860821478,-7.67201492936341,
7.4615462067859));
#86547=CARTESIAN_POINT('Ctrl Pts',(-6.5124863523695,-7.5120493548832,7.4576363232082));
#86548=CARTESIAN_POINT('Ctrl Pts',(-6.64414285432868,-7.3979112373464,7.45484655576732));
#86549=CARTESIAN_POINT('Ctrl Pts',(-6.77278667189716,-7.28032099449203,
7.45205678832644));
#86550=CARTESIAN_POINT('Ctrl Pts',(-6.89823892120803,-7.15944577365669,
7.44926702088556));
#86551=CARTESIAN_POINT('Ctrl Pts',(-7.07406105290008,-6.99003837671675,
7.44535714393178));
#86552=CARTESIAN_POINT('Ctrl Pts',(-7.24366659743927,-6.81412515296562,
7.441447266978));
#86553=CARTESIAN_POINT('Ctrl Pts',(-7.40658272194256,-6.63218639537686,
7.43753739002422));
#86554=CARTESIAN_POINT('Ctrl Pts',(-7.56947064417336,-6.45027913305252,
7.43362818990593));
#86555=CARTESIAN_POINT('Ctrl Pts',(-7.72567127109786,-6.26234862782684,
7.42971898978765));
#86556=CARTESIAN_POINT('Ctrl Pts',(-7.87475025689373,-6.06891031335545,
7.42580978966936));
#86557=CARTESIAN_POINT('Ctrl Pts',(-8.02381301325494,-5.87549305748242,
7.42190101512485));
#86558=CARTESIAN_POINT('Ctrl Pts',(-8.1657555054564,-5.67656941152338,7.41799224058034));
#86559=CARTESIAN_POINT('Ctrl Pts',(-8.30018450206481,-5.47268683844445,
7.41408346603584));
#86560=CARTESIAN_POINT('Ctrl Pts',(-8.43462393104828,-5.26878844303907,
7.41017438815051));
#86561=CARTESIAN_POINT('Ctrl Pts',(-8.5615485424511,-5.05993058387834,7.40626531026519));
#86562=CARTESIAN_POINT('Ctrl Pts',(-8.68060846738418,-4.84668965748562,
7.40235623237986));
#86563=CARTESIAN_POINT('Ctrl Pts',(-8.7996667482294,-4.6334516757178,7.39844720847464));
#86564=CARTESIAN_POINT('Ctrl Pts',(-8.91086042494945,-4.4158309935355,7.39453818456942));
#86565=CARTESIAN_POINT('Ctrl Pts',(-9.01388527420231,-4.19442919400469,
7.3906291606642));
#86566=CARTESIAN_POINT('Ctrl Pts',(-9.11693278067868,-3.97297870379297,
7.3867192770865));
#86567=CARTESIAN_POINT('Ctrl Pts',(-9.21180775078023,-3.74774568848959,
7.38280939350879));
#86568=CARTESIAN_POINT('Ctrl Pts',(-9.29825329373128,-3.51935358917165,
7.37889950993109));
#86569=CARTESIAN_POINT('Ctrl Pts',(-9.35993363697869,-3.35639199971292,
7.37610974249025));
#86570=CARTESIAN_POINT('Ctrl Pts',(-9.41732349670219,-3.19182255840282,
7.37331997504941));
#86571=CARTESIAN_POINT('Ctrl Pts',(-9.47034479553102,-3.02587730315665,
7.37053020760858));
#86572=CARTESIAN_POINT('Ctrl Pts',(-9.54829975444413,-2.78189505752545,
7.36642853128168));
#86573=CARTESIAN_POINT('Ctrl Pts',(-9.61683348021652,-2.53486048040967,
7.36232685495478));
#86574=CARTESIAN_POINT('Ctrl Pts',(-9.67573071718072,-2.28551943518437,
7.35822517862788));
#86575=CARTESIAN_POINT('Ctrl Pts',(-9.73198857835279,-2.04735216911533,
7.35430731169108));
#86576=CARTESIAN_POINT('Ctrl Pts',(-9.77945461065712,-1.80708091427208,
7.35038944475427));
#86577=CARTESIAN_POINT('Ctrl Pts',(-9.81799288608731,-1.56536886666977,
7.34647157781746));
#86578=CARTESIAN_POINT('Ctrl Pts',(-9.85652590123158,-1.32368981157854,
7.34255424565031));
#86579=CARTESIAN_POINT('Ctrl Pts',(-9.88613354943089,-1.08057063060592,
7.33863691348316));
#86580=CARTESIAN_POINT('Ctrl Pts',(-9.90673132562275,-0.836682999662867,
7.33471958131601));
#86581=CARTESIAN_POINT('Ctrl Pts',(-9.92732820978895,-0.592805930735089,
7.33080241879634));
#86582=CARTESIAN_POINT('Ctrl Pts',(-9.93891597733403,-0.348160754885544,
7.32688525627666));
#86583=CARTESIAN_POINT('Ctrl Pts',(-9.94146204244371,-0.103423685154355,
7.32296809375699));
#86584=CARTESIAN_POINT('Ctrl Pts',(-9.94182126345331,-0.0688940508019636,
7.32241542639993));
#86585=CARTESIAN_POINT('Ctrl Pts',(-9.94200058483451,-0.0343625907378737,
7.32186275904287));
#86586=CARTESIAN_POINT('Ctrl Pts',(-9.94199999856713,0.00016879341615152,
7.32131009168581));
#86587=CARTESIAN_POINT('Ctrl Pts',(-9.94199999849644,0.000172907010996282,
7.17868990831418));
#86588=CARTESIAN_POINT('Ctrl Pts',(-9.94200425406554,-0.244518547686264,
7.18260616056646));
#86589=CARTESIAN_POINT('Ctrl Pts',(-9.93297068691858,-0.489214384721641,
7.18652241281874));
#86590=CARTESIAN_POINT('Ctrl Pts',(-9.9149243805595,-0.733238384010886,
7.19043866507102));
#86591=CARTESIAN_POINT('Ctrl Pts',(-9.89687582244228,-0.977292831803824,
7.19435540598024));
#86592=CARTESIAN_POINT('Ctrl Pts',(-9.86981229670883,-1.22067499698101,
7.19827214688947));
#86593=CARTESIAN_POINT('Ctrl Pts',(-9.83381087633608,-1.46271242848835,
7.20218888779869));
#86594=CARTESIAN_POINT('Ctrl Pts',(-9.79780826943771,-1.70475783700344,
7.20610575779485));
#86595=CARTESIAN_POINT('Ctrl Pts',(-9.75286722345113,-1.94545814884843,
7.21002262779102));
#86596=CARTESIAN_POINT('Ctrl Pts',(-9.69911630576427,-2.1841490075674,7.21393949778719));
#86597=CARTESIAN_POINT('Ctrl Pts',(-9.64535454834625,-2.42288800211082,
7.21785715768276));
#86598=CARTESIAN_POINT('Ctrl Pts',(-9.58277943156352,-2.659616462913,7.22177481757832));
#86599=CARTESIAN_POINT('Ctrl Pts',(-9.51157027869964,-2.89368188185186,
7.22569247747389));
#86600=CARTESIAN_POINT('Ctrl Pts',(-9.49632104290438,-2.94380631981191,
7.22653143310123));
#86601=CARTESIAN_POINT('Ctrl Pts',(-9.48067604143394,-2.99380868649339,
7.22737038872857));
#86602=CARTESIAN_POINT('Ctrl Pts',(-9.46463733237618,-3.043682665225,7.22820934435591));
#86603=CARTESIAN_POINT('Ctrl Pts',(-9.38989037691179,-3.27611584009324,
7.23211922130968));
#86604=CARTESIAN_POINT('Ctrl Pts',(-9.30656568547276,-3.5058297900949,7.23602909826345));
#86605=CARTESIAN_POINT('Ctrl Pts',(-9.21488646225066,-3.73218856541701,
7.23993897521723));
#86606=CARTESIAN_POINT('Ctrl Pts',(-9.12322310954142,-3.9585081559628,7.24384817533551));
#86607=CARTESIAN_POINT('Ctrl Pts',(-9.02320821725852,-4.18147347157786,
7.24775737545379));
#86608=CARTESIAN_POINT('Ctrl Pts',(-8.91511348169684,-4.40046765792766,
7.25166657557206));
#86609=CARTESIAN_POINT('Ctrl Pts',(-8.80703051383299,-4.61943800354738,
7.25557535011656));
#86610=CARTESIAN_POINT('Ctrl Pts',(-8.69086958300834,-4.83443783183468,
7.25948412466105));
#86611=CARTESIAN_POINT('Ctrl Pts',(-8.56694923994193,-5.04487311240415,
7.26339289920555));
#86612=CARTESIAN_POINT('Ctrl Pts',(-8.44301928002533,-5.2553247238239,7.26730197709087));
#86613=CARTESIAN_POINT('Ctrl Pts',(-8.31132884421814,-5.46121083658938,
7.27121105497619));
#86614=CARTESIAN_POINT('Ctrl Pts',(-8.17224154714534,-5.66196362537871,
7.27512013286151));
#86615=CARTESIAN_POINT('Ctrl Pts',(-8.03315617071619,-5.86271364199129,
7.27902915676673));
#86616=CARTESIAN_POINT('Ctrl Pts',(-7.88667429864726,-6.05833024714368,
7.28293818067196));
#86617=CARTESIAN_POINT('Ctrl Pts',(-7.73320224947866,-6.24827551958604,
7.28684720457718));
#86618=CARTESIAN_POINT('Ctrl Pts',(-7.57969644873958,-6.43826256478954,
7.29075708815488));
#86619=CARTESIAN_POINT('Ctrl Pts',(-7.41919757461236,-6.62257556633314,
7.29466697173257));
#86620=CARTESIAN_POINT('Ctrl Pts',(-7.25215240306761,-6.80070948671392,
7.29857685531027));
#86621=CARTESIAN_POINT('Ctrl Pts',(-7.13296287441027,-6.92781102345233,
7.30136662275114));
#86622=CARTESIAN_POINT('Ctrl Pts',(-7.01044143160069,-7.05176743944137,
7.30415639019201));
#86623=CARTESIAN_POINT('Ctrl Pts',(-6.88476207621815,-7.17240651063981,
7.30694615763288));
#86624=CARTESIAN_POINT('Ctrl Pts',(-6.70862165391008,-7.34148294235024,
7.31085603458667));
#86625=CARTESIAN_POINT('Ctrl Pts',(-6.52622298655171,-7.50409360981993,
7.31476591154045));
#86626=CARTESIAN_POINT('Ctrl Pts',(-6.33806445520069,-7.6597847856008,7.31867578849423));
#86627=CARTESIAN_POINT('Ctrl Pts',(-6.14993849581341,-7.81544900981432,
7.32258498861253));
#86628=CARTESIAN_POINT('Ctrl Pts',(-5.95605487869896,-7.96419595486187,
7.32649418873084));
#86629=CARTESIAN_POINT('Ctrl Pts',(-5.75694559672558,-8.10561172252545,
7.33040338884914));
#86630=CARTESIAN_POINT('Ctrl Pts',(-5.55785799071956,-8.24701209500738,
7.33431216339364));
#86631=CARTESIAN_POINT('Ctrl Pts',(-5.35354608419188,-8.38108272141303,
7.33822093793813));
#86632=CARTESIAN_POINT('Ctrl Pts',(-5.14457227027934,-8.5074520366484,7.34212971248263));
#86633=CARTESIAN_POINT('Ctrl Pts',(-4.93558223893361,-8.63383115878678,
7.34603879036796));
#86634=CARTESIAN_POINT('Ctrl Pts',(-4.7219298155718,-8.75250762783033,7.34994786825329));
#86635=CARTESIAN_POINT('Ctrl Pts',(-4.50420461246222,-8.8631543374283,7.35385694613861));
#86636=CARTESIAN_POINT('Ctrl Pts',(-4.28648241590029,-8.97379951911586,
7.35776597004384));
#86637=CARTESIAN_POINT('Ctrl Pts',(-4.06468780291484,-9.07641503795604,
7.36167499394906));
#86638=CARTESIAN_POINT('Ctrl Pts',(-3.83943377164353,-9.17072038136389,
7.36558401785429));
#86639=CARTESIAN_POINT('Ctrl Pts',(-3.61413020250931,-9.26504646440134,
7.36949390143199));
#86640=CARTESIAN_POINT('Ctrl Pts',(-3.38536595317228,-9.35105861098243,
7.37340378500969));
#86641=CARTESIAN_POINT('Ctrl Pts',(-3.15377401580192,-9.42852445811393,
7.37731366858738));
#86642=CARTESIAN_POINT('Ctrl Pts',(-2.98852928828145,-9.48379763794366,
7.38010343602821));
#86643=CARTESIAN_POINT('Ctrl Pts',(-2.82184538566752,-9.53472085093501,
7.38289320346904));
#86644=CARTESIAN_POINT('Ctrl Pts',(-2.65395721633737,-9.58122513532851,
7.38568297090986));
#86645=CARTESIAN_POINT('Ctrl Pts',(-2.4186608706746,-9.64640118804926,7.38959284786364));
#86646=CARTESIAN_POINT('Ctrl Pts',(-2.18092646501398,-9.70291539328967,
7.39350272481741));
#86647=CARTESIAN_POINT('Ctrl Pts',(-1.94140804813236,-9.75060504741356,
7.39741260177118));
#86648=CARTESIAN_POINT('Ctrl Pts',(-1.70193109408101,-9.79828644602183,
7.40132180188947));
#86649=CARTESIAN_POINT('Ctrl Pts',(-1.46067102007947,-9.83714628825918,
7.40523100200776));
#86650=CARTESIAN_POINT('Ctrl Pts',(-1.21829254648774,-9.86707288263203,
7.40914020212605));
#86651=CARTESIAN_POINT('Ctrl Pts',(-0.975940459349413,-9.89699621905596,
7.41304897667054));
#86652=CARTESIAN_POINT('Ctrl Pts',(-0.732470493816496,-9.91798821507781,
7.41695775121503));
#86653=CARTESIAN_POINT('Ctrl Pts',(-0.488554026537994,-9.92998887024319,
7.42086652575952));
#86654=CARTESIAN_POINT('Ctrl Pts',(-0.244618630098674,-9.94199045672056,
7.42477560364484));
#86655=CARTESIAN_POINT('Ctrl Pts',(-0.00023694251214787,-9.94499929121525,
7.42868468153016));
#86656=CARTESIAN_POINT('Ctrl Pts',(0.243916812219465,-9.93900742472389,
7.43259375941547));
#86657=CARTESIAN_POINT('Ctrl Pts',(0.488067195453498,-9.93301564097369,
7.43650278332068));
#86658=CARTESIAN_POINT('Ctrl Pts',(0.731989371933233,-9.91802341375415,
7.44041180722589));
#86659=CARTESIAN_POINT('Ctrl Pts',(0.975010657641103,-9.89407490458235,
7.44432083113109));
#86660=CARTESIAN_POINT('Ctrl Pts',(1.21808538858709,-9.87012112865472,7.44823071470879));
#86661=CARTESIAN_POINT('Ctrl Pts',(1.4602585537056,-9.83720716155028,7.45214059828648));
#86662=CARTESIAN_POINT('Ctrl Pts',(1.70086273280917,-9.79542903420472,7.45605048186417));
#86663=CARTESIAN_POINT('Ctrl Pts',(1.87253784580596,-9.76561964037139,7.45884024930506));
#86664=CARTESIAN_POINT('Ctrl Pts',(2.04341428824696,-9.73129853269632,7.46163001674595));
#86665=CARTESIAN_POINT('Ctrl Pts',(2.21325257474585,-9.69251654836766,7.46441978418684));
#86666=CARTESIAN_POINT('Ctrl Pts',(2.4512820221177,-9.63816334869736,7.46832966114061));
#86667=CARTESIAN_POINT('Ctrl Pts',(2.68734471051714,-9.57502928361013,7.47223953809439));
#86668=CARTESIAN_POINT('Ctrl Pts',(2.92078776089226,-9.50328168875478,7.47614941504817));
#86669=CARTESIAN_POINT('Ctrl Pts',(3.15419040013818,-9.43154651406496,7.48005861516645));
#86670=CARTESIAN_POINT('Ctrl Pts',(3.38497403880572,-9.3512008684512,7.48396781528473));
#86671=CARTESIAN_POINT('Ctrl Pts',(3.61250062547665,-9.26246205017493,7.48787701540301));
#86672=CARTESIAN_POINT('Ctrl Pts',(3.84000244254066,-9.17373289242089,7.4917857899475));
#86673=CARTESIAN_POINT('Ctrl Pts',(4.06424765453406,-9.07661248822206,7.495694564492));
#86674=CARTESIAN_POINT('Ctrl Pts',(4.28461689387206,-8.97136678955588,7.49960333903649));
#86675=CARTESIAN_POINT('Ctrl Pts',(4.50500323498623,-8.86611292328706,7.50351241692182));
#86676=CARTESIAN_POINT('Ctrl Pts',(4.72151274811741,-8.75273262060361,7.50742149480714));
#86677=CARTESIAN_POINT('Ctrl Pts',(4.93354827288646,-8.63153899597859,7.51133057269246));
#86678=CARTESIAN_POINT('Ctrl Pts',(5.14558086967583,-8.51034704490553,7.51523959659768));
#86679=CARTESIAN_POINT('Ctrl Pts',(5.35313935930815,-8.38134212857493,7.51914862050289));
#86680=CARTESIAN_POINT('Ctrl Pts',(5.5556526779625,-8.24488249290723,7.52305764440811));
#86681=CARTESIAN_POINT('Ctrl Pts',(5.75821053334288,-8.10839284703848,7.5269675279858));
#86682=CARTESIAN_POINT('Ctrl Pts',(5.95572076759188,-7.96444536181908,7.53087741156349));
#86683=CARTESIAN_POINT('Ctrl Pts',(6.14764157634194,-7.81344143440213,7.53478729514119));
#86684=CARTESIAN_POINT('Ctrl Pts',(6.28458028892445,-7.70569760219314,7.53757706258206));
#86685=CARTESIAN_POINT('Ctrl Pts',(6.41867400228529,-7.59436219430282,7.54036683002293));
#86686=CARTESIAN_POINT('Ctrl Pts',(6.54973608136051,-7.47959365637762,7.54315659746381));
#86687=CARTESIAN_POINT('Ctrl Pts',(6.7334204254323,-7.31874481468657,7.54706647441758));
#86688=CARTESIAN_POINT('Ctrl Pts',(6.91120480998118,-7.151101694818,7.55097635137135));
#86689=CARTESIAN_POINT('Ctrl Pts',(7.08259408263057,-6.97712154550043,7.55488622832512));
#86690=CARTESIAN_POINT('Ctrl Pts',(7.25395368622877,-6.80317151373853,7.55879542844342));
#86691=CARTESIAN_POINT('Ctrl Pts',(7.41892019123391,-6.6228868419756,7.56270462856172));
#86692=CARTESIAN_POINT('Ctrl Pts',(7.57703521653159,-6.43676171125202,7.56661382868002));
#86693=CARTESIAN_POINT('Ctrl Pts',(7.73513302868866,-6.25065684298004,7.57052260322452));
#86694=CARTESIAN_POINT('Ctrl Pts',(7.88638066901538,-6.05871299882367,7.57443137776902));
#86695=CARTESIAN_POINT('Ctrl Pts',(8.03035930006862,-5.86145830931189,7.57834015231353));
#86696=CARTESIAN_POINT('Ctrl Pts',(8.17434910459688,-5.66418831183164,7.58224923019884));
#86697=CARTESIAN_POINT('Ctrl Pts',(8.31106860489795,-5.46160687006061,7.58615830808415));
#86698=CARTESIAN_POINT('Ctrl Pts',(8.44014090012236,-5.25427307875045,7.59006738596947));
#86699=CARTESIAN_POINT('Ctrl Pts',(8.56921141299867,-5.04694215049458,7.59397640987466));
#86700=CARTESIAN_POINT('Ctrl Pts',(8.69063478559434,-4.83485924302001,7.59788543377986));
#86701=CARTESIAN_POINT('Ctrl Pts',(8.8040785123749,-4.61861078116988,7.60179445768506));
#86702=CARTESIAN_POINT('Ctrl Pts',(8.91754718769865,-4.4023147619603,7.60570434126275));
#86703=CARTESIAN_POINT('Ctrl Pts',(9.02303257948988,-4.18185160573529,7.60961422484044));
#86704=CARTESIAN_POINT('Ctrl Pts',(9.12024842102828,-3.95783182294689,7.61352410841814));
#86705=CARTESIAN_POINT('Ctrl Pts',(9.18961355277002,-3.797989954585,7.61631387585902));
#86706=CARTESIAN_POINT('Ctrl Pts',(9.2547695724198,-3.63633788959191,7.61910364329989));
#86707=CARTESIAN_POINT('Ctrl Pts',(9.31562744933925,-3.47310368764268,7.62189341074077));
#86708=CARTESIAN_POINT('Ctrl Pts',(9.40092015400574,-3.24432990710551,7.62580328769455));
#86709=CARTESIAN_POINT('Ctrl Pts',(9.47779447774866,-3.01237766767267,7.62971316464833));
#86710=CARTESIAN_POINT('Ctrl Pts',(9.54603172979293,-2.77788448532092,7.6336230416021));
#86711=CARTESIAN_POINT('Ctrl Pts',(9.61425716934443,-2.54343189588486,7.6375322417204));
#86712=CARTESIAN_POINT('Ctrl Pts',(9.67384844358402,-2.30643951060475,7.6414414418387));
#86713=CARTESIAN_POINT('Ctrl Pts',(9.7246367590727,-2.06755989129506,7.64535064195699));
#86714=CARTESIAN_POINT('Ctrl Pts',(9.77541954550824,-1.82870627753594,7.64925941650152));
#86715=CARTESIAN_POINT('Ctrl Pts',(9.81740122839898,-1.58796611404812,7.65316819104604));
#86716=CARTESIAN_POINT('Ctrl Pts',(9.85046393545143,-1.34600306699901,7.65707696559056));
#86717=CARTESIAN_POINT('Ctrl Pts',(9.88352920833822,-1.10402124238596,7.66098604347588));
#86718=CARTESIAN_POINT('Ctrl Pts',(9.90767408132998,-0.860816621909657,
7.6648951213612));
#86719=CARTESIAN_POINT('Ctrl Pts',(9.92283229194109,-0.617060212630194,
7.66880419924652));
#86720=CARTESIAN_POINT('Ctrl Pts',(9.93799029323388,-0.373307169360157,
7.67271322315175));
#86721=CARTESIAN_POINT('Ctrl Pts',(9.94416186499507,-0.129002632442874,
7.67662224705698));
#86722=CARTESIAN_POINT('Ctrl Pts',(9.94133279304864,0.11517941593772,7.68053127096221));
#86723=CARTESIAN_POINT('Ctrl Pts',(9.93850309893275,0.359415164830415,7.68444115453991));
#86724=CARTESIAN_POINT('Ctrl Pts',(9.9266688081334,0.603528090943824,7.68835103811762));
#86725=CARTESIAN_POINT('Ctrl Pts',(9.90586783682596,0.846844967710685,7.69226092169532));
#86726=CARTESIAN_POINT('Ctrl Pts',(9.89102599528838,1.02045563593478,7.69505068913613));
#86727=CARTESIAN_POINT('Ctrl Pts',(9.87162025165008,1.19366104614316,7.69784045657694));
#86728=CARTESIAN_POINT('Ctrl Pts',(9.84768052877536,1.36621821213837,7.70063022401775));
#86729=CARTESIAN_POINT('Ctrl Pts',(9.81412885368649,1.60805818656187,7.70454010097152));
#86730=CARTESIAN_POINT('Ctrl Pts',(9.77165905958133,1.84869862293395,7.70844997792529));
#86731=CARTESIAN_POINT('Ctrl Pts',(9.72038135817977,2.0874746109956,7.71235985487907));
#86732=CARTESIAN_POINT('Ctrl Pts',(9.66911253341755,2.3262092647487,7.71626905499736));
#86733=CARTESIAN_POINT('Ctrl Pts',(9.60903890388976,2.56307984055212,7.72017825511565));
#86734=CARTESIAN_POINT('Ctrl Pts',(9.54032173960847,2.79743187669584,7.72408745523394));
#86735=CARTESIAN_POINT('Ctrl Pts',(9.47161205619935,3.03175840017991,7.72799622977841));
#86736=CARTESIAN_POINT('Ctrl Pts',(9.39426079570349,3.26356666257054,7.73190500432288));
#86737=CARTESIAN_POINT('Ctrl Pts',(9.3084793161308,3.49221660570547,7.73581377886735));
#86738=CARTESIAN_POINT('Ctrl Pts',(9.22269117947747,3.72088429324302,7.73972285675267));
#86739=CARTESIAN_POINT('Ctrl Pts',(9.12847161206856,3.94639290822294,7.743631934638));
#86740=CARTESIAN_POINT('Ctrl Pts',(9.02608087917656,4.16812043522776,7.74754101252332));
#86741=CARTESIAN_POINT('Ctrl Pts',(8.92369156018958,4.38984490041583,7.75145003642852));
#86742=CARTESIAN_POINT('Ctrl Pts',(8.81313142078586,4.60778812841426,7.75535906033371));
#86743=CARTESIAN_POINT('Ctrl Pts',(8.69470794663225,4.82135019706825,7.75926808423891));
#86744=CARTESIAN_POINT('Ctrl Pts',(8.57625842878933,5.03495923229034,7.76317796781661));
#86745=CARTESIAN_POINT('Ctrl Pts',(8.44994225586479,5.24418493719256,7.7670878513943));
#86746=CARTESIAN_POINT('Ctrl Pts',(8.31611243483096,5.44845280526958,7.770997734972));
#86747=CARTESIAN_POINT('Ctrl Pts',(8.2206226152689,5.59420135155263,7.77378750241291));
#86748=CARTESIAN_POINT('Ctrl Pts',(8.12130850322945,5.73742636390593,7.77657726985382));
#86749=CARTESIAN_POINT('Ctrl Pts',(8.01831179973468,5.87792819641713,7.77936703729473));
#86750=CARTESIAN_POINT('Ctrl Pts',(7.87396125947004,6.07484241544546,7.78327691424849));
#86751=CARTESIAN_POINT('Ctrl Pts',(7.72233137996099,6.2664667423681,7.78718679120226));
#86752=CARTESIAN_POINT('Ctrl Pts',(7.56383484723372,6.45226831461408,7.79109666815602));
#86753=CARTESIAN_POINT('Ctrl Pts',(7.4053657517068,6.63803772290749,7.7950058682743));
#86754=CARTESIAN_POINT('Ctrl Pts',(7.24003255766605,6.8179861755101,7.79891506839259));
#86755=CARTESIAN_POINT('Ctrl Pts',(7.06828792687707,6.99161424727965,7.80282426851087));
#86756=CARTESIAN_POINT('Ctrl Pts',(6.89656199300847,7.16522341708867,7.80673304305542));
#86757=CARTESIAN_POINT('Ctrl Pts',(6.71842621308035,7.33251338069906,7.81064181759997));
#86758=CARTESIAN_POINT('Ctrl Pts',(6.53437049287093,7.49302117052246,7.81455059214452));
#86759=CARTESIAN_POINT('Ctrl Pts',(6.35030048900216,7.65354141656613,7.81845967002984));
#86760=CARTESIAN_POINT('Ctrl Pts',(6.16030983610599,7.80727825055503,7.82236874791516));
#86761=CARTESIAN_POINT('Ctrl Pts',(5.96492291697458,7.95380780472796,7.82627782580048));
#86762=CARTESIAN_POINT('Ctrl Pts',(5.7695386959235,8.10033533548751,7.8301868497057));
#86763=CARTESIAN_POINT('Ctrl Pts',(5.56875858317553,8.23965561893869,7.83409587361092));
#86764=CARTESIAN_POINT('Ctrl Pts',(5.36313803080051,8.37138665112186,7.83800489751614));
#86765=CARTESIAN_POINT('Ctrl Pts',(5.15747225835721,8.50314665359132,7.84191478109382));
#86766=CARTESIAN_POINT('Ctrl Pts',(4.94696415479746,8.62731391767307,7.84582466467151));
#86767=CARTESIAN_POINT('Ctrl Pts',(4.73219716868203,8.74355042055101,7.8497345482492));
#86768=CARTESIAN_POINT('Ctrl Pts',(4.5789573257747,8.82648711283918,7.85252431569003));
#86769=CARTESIAN_POINT('Ctrl Pts',(4.42354984516279,8.90538712539935,7.85531408313087));
#86770=CARTESIAN_POINT('Ctrl Pts',(4.26619422686902,8.98014202664019,7.8581038505717));
#86771=CARTESIAN_POINT('Ctrl Pts',(4.04565931900907,9.08491149998974,7.86201372752548));
#86772=CARTESIAN_POINT('Ctrl Pts',(3.82122939880236,9.18156921538278,7.86592360447926));
#86773=CARTESIAN_POINT('Ctrl Pts',(3.59352066665073,9.26984213556812,7.86983348143305));
#86774=CARTESIAN_POINT('Ctrl Pts',(3.36585135296539,9.35809977490281,7.87374268155133));
#86775=CARTESIAN_POINT('Ctrl Pts',(3.13490462160849,9.43797541525348,7.87765188166961));
#86776=CARTESIAN_POINT('Ctrl Pts',(2.90131598019713,9.50924442755852,7.8815610817879));
#86777=CARTESIAN_POINT('Ctrl Pts',(2.66775276833403,9.5805056811867,7.88546985633244));
#86778=CARTESIAN_POINT('Ctrl Pts',(2.43154848868883,9.64316209580086,7.88937863087698));
#86779=CARTESIAN_POINT('Ctrl Pts',(2.1933541179885,9.69703881157041,7.89328740542152));
#86780=CARTESIAN_POINT('Ctrl Pts',(1.95514126219346,9.75091970844714,7.89719648330684));
#86781=CARTESIAN_POINT('Ctrl Pts',(1.71493827948303,9.79601948017549,7.90110556119217));
#86782=CARTESIAN_POINT('Ctrl Pts',(1.47340792594346,9.83221404790228,7.90501463907749));
#86783=CARTESIAN_POINT('Ctrl Pts',(1.23188090767481,9.86840811582155,7.90892366298271));
#86784=CARTESIAN_POINT('Ctrl Pts',(0.989026832775131,9.89569718617389,7.91283268688793));
#86785=CARTESIAN_POINT('Ctrl Pts',(0.745515925243001,9.91400877572786,7.91674171079315));
#86786=CARTESIAN_POINT('Ctrl Pts',(0.501951464795785,9.93232439236633,7.92065159437085));
#86787=CARTESIAN_POINT('Ctrl Pts',(0.257730162638098,9.94165856113522,7.92456147794855));
#86788=CARTESIAN_POINT('Ctrl Pts',(0.0135260010340399,9.94199079899474,
7.92847136152625));
#86789=CARTESIAN_POINT('Ctrl Pts',(-0.160717759787675,9.94222785627398,
7.93126112896706));
#86790=CARTESIAN_POINT('Ctrl Pts',(-0.334952715461978,9.9378830625175,7.93405089640787));
#86791=CARTESIAN_POINT('Ctrl Pts',(-0.50893420191229,9.92896520177828,7.93684066384868));
#86792=CARTESIAN_POINT('Ctrl Pts',(-0.752770370584818,9.91646676277897,
7.94075054080245));
#86793=CARTESIAN_POINT('Ctrl Pts',(-0.996183221306001,9.89497985671139,
7.94466041775621));
#86794=CARTESIAN_POINT('Ctrl Pts',(-1.23850080090203,9.86455674453571,7.94857029470998));
#86795=CARTESIAN_POINT('Ctrl Pts',(-1.48077643310591,9.83413889887937,7.95247949482824));
#86796=CARTESIAN_POINT('Ctrl Pts',(-1.72195689468176,9.79478797005676,7.9563886949465));
#86797=CARTESIAN_POINT('Ctrl Pts',(-1.96137622353292,9.74660798995013,7.96029789506476));
#86798=CARTESIAN_POINT('Ctrl Pts',(-2.20076948807947,9.69843325494082,7.96420666960927));
#86799=CARTESIAN_POINT('Ctrl Pts',(-2.43840172801783,9.64143144307598,7.96811544415377));
#86800=CARTESIAN_POINT('Ctrl Pts',(-2.67361699645525,9.57575773274709,7.97202421869828));
#86801=CARTESIAN_POINT('Ctrl Pts',(-2.90885051879443,9.51007892580408,7.97593329658358));
#86802=CARTESIAN_POINT('Ctrl Pts',(-3.14166642400791,9.43572694807743,7.97984237446888));
#86803=CARTESIAN_POINT('Ctrl Pts',(-3.37142250812632,9.35290726307597,7.98375145235419));
#86804=CARTESIAN_POINT('Ctrl Pts',(-3.60117541956527,9.27008872172351,7.98766047625941));
#86805=CARTESIAN_POINT('Ctrl Pts',(-3.82786833139425,9.17880280395587,7.99156950016463));
#86806=CARTESIAN_POINT('Ctrl Pts',(-4.05087696386306,9.07930392836607,7.99547852406986));
#86807=CARTESIAN_POINT('Ctrl Pts',(-4.27393464038622,8.97978317098538,7.99938840764754));
#86808=CARTESIAN_POINT('Ctrl Pts',(-4.49330616203895,8.87204596004266,8.00329829122523));
#86809=CARTESIAN_POINT('Ctrl Pts',(-4.70838863024301,8.75639426399921,8.00720817480292));
#86810=CARTESIAN_POINT('Ctrl Pts',(-4.86185357491026,8.67387484118349,8.00999794224383));
#86811=CARTESIAN_POINT('Ctrl Pts',(-5.01313538300588,8.58732709971643,8.01278770968474));
#86812=CARTESIAN_POINT('Ctrl Pts',(-5.16202289555346,8.49687493292575,8.01557747712564));
#86813=CARTESIAN_POINT('Ctrl Pts',(-5.3706896989147,8.37010564127491,8.01948735407942));
#86814=CARTESIAN_POINT('Ctrl Pts',(-5.57471636343669,8.23562656040008,8.0233972310332));
#86815=CARTESIAN_POINT('Ctrl Pts',(-5.77353631399771,8.09380271757039,8.02730710798698));
#86816=CARTESIAN_POINT('Ctrl Pts',(-5.97232184700733,7.95200342574468,8.03121630810531));
#86817=CARTESIAN_POINT('Ctrl Pts',(-6.16590223722477,7.80286207275889,8.03512550822363));
#86818=CARTESIAN_POINT('Ctrl Pts',(-6.35374076226922,7.64678640514292,8.03903470834196));
#86819=CARTESIAN_POINT('Ctrl Pts',(-6.54155883833198,7.49072772865519,8.04294348288645));
#86820=CARTESIAN_POINT('Ctrl Pts',(-6.72363608180163,7.32773642390535,8.04685225743094));
#86821=CARTESIAN_POINT('Ctrl Pts',(-6.89946886822186,7.15826049654784,8.05076103197544));
#86822=CARTESIAN_POINT('Ctrl Pts',(-7.07531530016244,6.98877141699464,8.05467010986075));
#86823=CARTESIAN_POINT('Ctrl Pts',(-7.24491610276115,6.81279690159378,8.05857918774607));
#86824=CARTESIAN_POINT('Ctrl Pts',(-7.40780362128749,6.63082268715127,8.06248826563139));
#86825=CARTESIAN_POINT('Ctrl Pts',(-7.57068889051531,6.44885098557368,8.06639728953661));
#86826=CARTESIAN_POINT('Ctrl Pts',(-7.72686087564606,6.26087996090083,8.07030631344184));
#86827=CARTESIAN_POINT('Ctrl Pts',(-7.87589094016651,6.06742992531459,8.07421533734707));
#86828=CARTESIAN_POINT('Ctrl Pts',(-8.02495377937637,5.87393734619963,8.07812522092477));
#86829=CARTESIAN_POINT('Ctrl Pts',(-8.1668713876149,5.67496357002263,8.08203510450247));
#86830=CARTESIAN_POINT('Ctrl Pts',(-8.30125652188631,5.47106060630295,8.08594498808017));
#86831=CARTESIAN_POINT('Ctrl Pts',(-8.39714256674417,5.32557242539756,8.08873475552099));
#86832=CARTESIAN_POINT('Ctrl Pts',(-8.48919464823231,5.17757542777426,8.09152452296181));
#86833=CARTESIAN_POINT('Ctrl Pts',(-8.57728574728243,5.02727890706948,8.09431429040262));
#86834=CARTESIAN_POINT('Ctrl Pts',(-8.70074598736116,4.81663736973718,8.09822416735638));
#86835=CARTESIAN_POINT('Ctrl Pts',(-8.81646194851285,4.60141348778399,8.10213404431014));
#86836=CARTESIAN_POINT('Ctrl Pts',(-8.92410829539135,4.3821975231757,8.1060439212639));
#86837=CARTESIAN_POINT('Ctrl Pts',(-9.03173600770174,4.16301950685775,8.10995312138216));
#86838=CARTESIAN_POINT('Ctrl Pts',(-9.13129677082162,3.93985103889644,8.11386232150042));
#86839=CARTESIAN_POINT('Ctrl Pts',(-9.2225118052798,3.71330580500376,8.11777152161869));
#86840=CARTESIAN_POINT('Ctrl Pts',(-9.31371690964388,3.48678523388193,8.12168029616319));
#86841=CARTESIAN_POINT('Ctrl Pts',(-9.3965779947819,3.25688889075372,8.1255890707077));
#86842=CARTESIAN_POINT('Ctrl Pts',(-9.47086452516024,3.02425017914547,8.1294978452522));
#86843=CARTESIAN_POINT('Ctrl Pts',(-9.54515682055158,2.79159341358864,8.13340692313752));
#86844=CARTESIAN_POINT('Ctrl Pts',(-9.61087314333275,2.5561941204022,8.13731600102283));
#86845=CARTESIAN_POINT('Ctrl Pts',(-9.66783252914784,2.31870183256729,8.14122507890814));
#86846=CARTESIAN_POINT('Ctrl Pts',(-9.7247911284166,2.08121282423906,8.1451341028134));
#86847=CARTESIAN_POINT('Ctrl Pts',(-9.77299296919053,1.84163115214548,8.14904312671865));
#86848=CARTESIAN_POINT('Ctrl Pts',(-9.8123078429667,1.60061825394256,8.15295215062391));
#86849=CARTESIAN_POINT('Ctrl Pts',(-9.85163136286887,1.3595523521895,8.1568620342016));
#86850=CARTESIAN_POINT('Ctrl Pts',(-9.88206396436873,1.11705487199665,8.16077191777929));
#86851=CARTESIAN_POINT('Ctrl Pts',(-9.90352691887924,0.873795494972577,
8.16468180135698));
#86852=CARTESIAN_POINT('Ctrl Pts',(-9.91884109652381,0.700225853773725,
8.16747156879785));
#86853=CARTESIAN_POINT('Ctrl Pts',(-9.92958984817822,0.526268498795954,
8.17026133623872));
#86854=CARTESIAN_POINT('Ctrl Pts',(-9.93576075318437,0.352167936475189,
8.1730511036796));
#86855=CARTESIAN_POINT('Ctrl Pts',(-9.93991839099059,0.234867948990494,
8.17493070522446));
#86856=CARTESIAN_POINT('Ctrl Pts',(-9.94199863950366,0.117494126326893,
8.17681030676932));
#86857=CARTESIAN_POINT('Ctrl Pts',(-9.94199999933284,0.000115177566633559,
8.17868990831418));
#86858=CARTESIAN_POINT('Origin',(0.,0.,0.));
#86859=CARTESIAN_POINT('',(-9.94203306522525,-0.000246459597145754,9.32131009168581));
#86860=CARTESIAN_POINT('',(-9.94201384449759,-0.000246996700943528,9.17868990831418));
#86861=CARTESIAN_POINT('',(-9.942,-1.2175438477123E-15,0.));
#86862=CARTESIAN_POINT('Ctrl Pts',(-9.94203306522525,-0.000246459597145754,
9.32131009168581));
#86863=CARTESIAN_POINT('Ctrl Pts',(-9.94075486143226,1.27189406067909,9.30094463654252));
#86864=CARTESIAN_POINT('Ctrl Pts',(-9.37944397540424,4.184577855052,9.25433357697359));
#86865=CARTESIAN_POINT('Ctrl Pts',(-6.60999555386334,7.97308161822977,9.18147691297896));
#86866=CARTESIAN_POINT('Ctrl Pts',(-2.03198716815049,10.1554468075767,9.102740099702));
#86867=CARTESIAN_POINT('Ctrl Pts',(3.03328101436287,9.90258945937622,9.02400328642504));
#86868=CARTESIAN_POINT('Ctrl Pts',(7.37118442122004,7.27514343098548,8.94526647314806));
#86869=CARTESIAN_POINT('Ctrl Pts',(9.94151671366969,2.90315641067999,8.86652965987108));
#86870=CARTESIAN_POINT('Ctrl Pts',(10.127925775832,-2.16499219219985,8.7877928465941));
#86871=CARTESIAN_POINT('Ctrl Pts',(7.88571169858605,-6.71398709559572,8.70905603331714));
#86872=CARTESIAN_POINT('Ctrl Pts',(3.75254558182297,-9.65300333416441,8.63031922004016));
#86873=CARTESIAN_POINT('Ctrl Pts',(-1.28046115713836,-10.2772803278934,
8.55158240676318));
#86874=CARTESIAN_POINT('Ctrl Pts',(-6.00642006970657,-8.43711974901828,
8.47284559348621));
#86875=CARTESIAN_POINT('Ctrl Pts',(-9.20947267408825,-4.67090341485341,
8.39608815690507));
#86876=CARTESIAN_POINT('Ctrl Pts',(-9.9417658544231,-1.51539093007022,8.34557632474959));
#86877=CARTESIAN_POINT('Ctrl Pts',(-9.94269874599832,0.000120372804752957,
8.32131009701976));
#86878=CARTESIAN_POINT('Ctrl Pts',(-9.94271026920365,0.000114860154877621,
8.17868991352832));
#86879=CARTESIAN_POINT('Ctrl Pts',(-9.94180931568194,-1.52162252819528,
8.20305591467107));
#86880=CARTESIAN_POINT('Ctrl Pts',(-9.20484461096283,-4.68332756624991,
8.25366752023947));
#86881=CARTESIAN_POINT('Ctrl Pts',(-5.99054191069908,-8.44840100963923,
8.33052473023354));
#86882=CARTESIAN_POINT('Ctrl Pts',(-1.26113059141423,-10.2796703076955,
8.40926154351052));
#86883=CARTESIAN_POINT('Ctrl Pts',(3.7706931866413,-9.64592892860662,8.48799835678748));
#86884=CARTESIAN_POINT('Ctrl Pts',(7.89832464265885,-6.69914470978837,8.56673517006446));
#86885=CARTESIAN_POINT('Ctrl Pts',(10.1319795417494,-2.14594095191081,8.64547198334144));
#86886=CARTESIAN_POINT('Ctrl Pts',(9.93603922976301,2.9218481185934,8.72420879661841));
#86887=CARTESIAN_POINT('Ctrl Pts',(7.35748915921657,7.28899343363155,8.80294560989537));
#86888=CARTESIAN_POINT('Ctrl Pts',(3.01465202579901,9.90827659923074,8.88168242317236));
#86889=CARTESIAN_POINT('Ctrl Pts',(-2.05108275015378,10.1516073385222,8.96041923644931));
#86890=CARTESIAN_POINT('Ctrl Pts',(-6.6249787095393,7.96063622467871,9.03915604972631));
#86891=CARTESIAN_POINT('Ctrl Pts',(-9.38351441362882,4.17212598300604,9.11191294034793));
#86892=CARTESIAN_POINT('Ctrl Pts',(-9.94074419905553,1.26566817442551,9.15842422654388));
#86893=CARTESIAN_POINT('Ctrl Pts',(-9.94201384449759,-0.000246996700943528,
9.17868990831418));
#86894=CARTESIAN_POINT('Origin',(0.,0.,0.));
#86895=CARTESIAN_POINT('',(-9.94192231880967,3.46674950698458E-5,10.321310091553));
#86896=CARTESIAN_POINT('',(-9.94192360013012,4.02297458262757E-5,10.1786899081637));
#86897=CARTESIAN_POINT('',(-9.942,-1.2175438477123E-15,0.));
#86898=CARTESIAN_POINT('Ctrl Pts',(-9.94118463298723,3.47437145860917E-5,
10.321310090292));
#86899=CARTESIAN_POINT('Ctrl Pts',(-9.94128107438378,0.7814167037778,10.3088041598135));
#86900=CARTESIAN_POINT('Ctrl Pts',(-9.65921574289398,3.20257951356252,10.2700526249096));
#86901=CARTESIAN_POINT('Ctrl Pts',(-7.71447438862192,6.91006198382807,10.2050554855795));
#86902=CARTESIAN_POINT('Ctrl Pts',(-3.50874605737789,9.74426871642388,10.1263186723027));
#86903=CARTESIAN_POINT('Ctrl Pts',(1.53836105703164,10.2418512472725,10.0475818590256));
#86904=CARTESIAN_POINT('Ctrl Pts',(6.21657731041338,8.28349191203197,9.96884504574875));
#86905=CARTESIAN_POINT('Ctrl Pts',(9.40409113980849,4.338794941827,9.8901082324717));
#86906=CARTESIAN_POINT('Ctrl Pts',(10.3365535546535,-0.646322152507229,
9.81137141919478));
#86907=CARTESIAN_POINT('Ctrl Pts',(8.79036498999971,-5.47645460637042,9.73263460591779));
#86908=CARTESIAN_POINT('Ctrl Pts',(5.13629330188293,-8.99336215383757,9.65389779264081));
#86909=CARTESIAN_POINT('Ctrl Pts',(0.250565592598979,-10.3537089295021,
9.57516097936385));
#86910=CARTESIAN_POINT('Ctrl Pts',(-4.69524642314623,-9.23129095733535,
9.49642416608685));
#86911=CARTESIAN_POINT('Ctrl Pts',(-8.51516313111776,-5.89525814222708,
9.41768735280992));
#86912=CARTESIAN_POINT('Ctrl Pts',(-9.8332983350383,-2.37409022605825,9.35931599467621));
#86913=CARTESIAN_POINT('Ctrl Pts',(-9.94240212297835,-0.36755355461397,
9.32719024096818));
#86914=CARTESIAN_POINT('Ctrl Pts',(-9.94203306522525,-0.000246459597145754,
9.32131009168581));
#86915=CARTESIAN_POINT('Ctrl Pts',(-9.94201384449759,-0.000246996700943528,
9.17868990831418));
#86916=CARTESIAN_POINT('Ctrl Pts',(-9.94238848679333,-0.373788577851782,
9.18466983096953));
#86917=CARTESIAN_POINT('Ctrl Pts',(-9.83108043390191,-2.386564907723,9.21689535805057));
#86918=CARTESIAN_POINT('Ctrl Pts',(-8.50406097389976,-5.91126204424316,
9.2753664895572));
#86919=CARTESIAN_POINT('Ctrl Pts',(-4.67787699712806,-9.24010491300058,
9.35410330283421));
#86920=CARTESIAN_POINT('Ctrl Pts',(0.270037190743816,-10.353219398773,9.43284011611116));
#86921=CARTESIAN_POINT('Ctrl Pts',(5.15319788570366,-8.98368652359915,9.51157692938814));
#86922=CARTESIAN_POINT('Ctrl Pts',(8.80064892952824,-5.45991304167992,9.59031374266511));
#86923=CARTESIAN_POINT('Ctrl Pts',(10.3377508154774,-0.626881233260456,
9.66905055594209));
#86924=CARTESIAN_POINT('Ctrl Pts',(9.39591462510088,4.35647338581691,9.74778736921906));
#86925=CARTESIAN_POINT('Ctrl Pts',(6.20098770524082,8.29516868321373,9.82652418249605));
#86926=CARTESIAN_POINT('Ctrl Pts',(1.51909666642319,10.2447263175536,9.905260995773));
#86927=CARTESIAN_POINT('Ctrl Pts',(-3.52706573424475,9.73765265912863,9.98399780904999));
#86928=CARTESIAN_POINT('Ctrl Pts',(-7.72745638993747,6.89554129457067,10.062734622327));
#86929=CARTESIAN_POINT('Ctrl Pts',(-9.66224715534303,3.19010468602984,10.1276319882147));
#86930=CARTESIAN_POINT('Ctrl Pts',(-9.94129826951133,0.775187770297893,
10.1662837496767));
#86931=CARTESIAN_POINT('Ctrl Pts',(-9.94118721097574,4.03173988009065E-5,
10.1786899067132));
#86932=CARTESIAN_POINT('Origin',(0.,0.,0.));
#86933=CARTESIAN_POINT('',(-9.94199999738095,0.000228204292448325,11.3213100916997));
#86934=CARTESIAN_POINT('',(-9.94199999743591,0.000225797020978443,11.1786899083289));
#86935=CARTESIAN_POINT('',(-9.942,-1.2175438477123E-15,0.));
#86936=CARTESIAN_POINT('Ctrl Pts',(-9.94199999738093,0.000228205157929791,
11.3213100916858));
#86937=CARTESIAN_POINT('Ctrl Pts',(-9.94199401568914,0.260826958870159,
11.3171378156917));
#86938=CARTESIAN_POINT('Ctrl Pts',(-9.93173751176087,0.52137996381255,11.3129655396974));
#86939=CARTESIAN_POINT('Ctrl Pts',(-9.91126722981454,0.781118364400918,
11.3087932637032));
#86940=CARTESIAN_POINT('Ctrl Pts',(-9.90894101982313,0.810634619437711,
11.3083191329546));
#86941=CARTESIAN_POINT('Ctrl Pts',(-9.90648296757901,0.840140358466671,
11.3078450022059));
#86942=CARTESIAN_POINT('Ctrl Pts',(-9.90389316948274,0.869634456236144,
11.3073708714572));
#86943=CARTESIAN_POINT('Ctrl Pts',(-9.88253663034234,1.11285490432175,11.3034609945034));
#86944=CARTESIAN_POINT('Ctrl Pts',(-9.85221296102367,1.35532547595535,11.2995511175496));
#86945=CARTESIAN_POINT('Ctrl Pts',(-9.81299882147288,1.59637656264802,11.2956412405958));
#86946=CARTESIAN_POINT('Ctrl Pts',(-9.77379147024857,1.83738592119121,11.2917320404775));
#86947=CARTESIAN_POINT('Ctrl Pts',(-9.72569676601436,2.07697600878047,11.2878228403592));
#86948=CARTESIAN_POINT('Ctrl Pts',(-9.66884288755413,2.31448508653521,11.2839136402409));
#86949=CARTESIAN_POINT('Ctrl Pts',(-9.61199519847276,2.55196830794197,11.2800048656963));
#86950=CARTESIAN_POINT('Ctrl Pts',(-9.54639030435697,2.78737069935341,11.2760960911518));
#86951=CARTESIAN_POINT('Ctrl Pts',(-9.47220713250327,3.02004239025783,11.2721873166073));
#86952=CARTESIAN_POINT('Ctrl Pts',(-9.3980182036574,3.25273213767116,11.268278238722));
#86953=CARTESIAN_POINT('Ctrl Pts',(-9.31524974907149,3.4826904931156,11.2643691608367));
#86954=CARTESIAN_POINT('Ctrl Pts',(-9.22413044818521,3.7092831483809,11.2604600829514));
#86955=CARTESIAN_POINT('Ctrl Pts',(-9.13301240555704,3.93587267464892,11.2565510590461));
#86956=CARTESIAN_POINT('Ctrl Pts',(-9.03354385376056,4.15909633437172,11.2526420351409));
#86957=CARTESIAN_POINT('Ctrl Pts',(-8.92600174318481,4.37833951180831,11.2487330112357));
#86958=CARTESIAN_POINT('Ctrl Pts',(-8.81843598194971,4.59763090520117,11.244823127658));
#86959=CARTESIAN_POINT('Ctrl Pts',(-8.70279323670446,4.81293981492584,11.2409132440803));
#86960=CARTESIAN_POINT('Ctrl Pts',(-8.57939719879916,5.02367472128095,11.2370033605026));
#86961=CARTESIAN_POINT('Ctrl Pts',(-8.49135205831714,5.17403760771933,11.2342135930618));
#86962=CARTESIAN_POINT('Ctrl Pts',(-8.39936064633872,5.32207232369151,11.2314238256211));
#86963=CARTESIAN_POINT('Ctrl Pts',(-8.30355445241722,5.46757235487032,11.2286340581803));
#86964=CARTESIAN_POINT('Ctrl Pts',(-8.16928145741151,5.67149158138516,11.2247241812266));
#86965=CARTESIAN_POINT('Ctrl Pts',(-8.02747249641354,5.87049339446522,11.2208143042728));
#86966=CARTESIAN_POINT('Ctrl Pts',(-7.87851295708677,6.0640248667874,11.216904427319));
#86967=CARTESIAN_POINT('Ctrl Pts',(-7.72957920401926,6.25752283704086,11.2129952272008));
#86968=CARTESIAN_POINT('Ctrl Pts',(-7.57349751450093,6.44555213487252,11.2090860270825));
#86969=CARTESIAN_POINT('Ctrl Pts',(-7.41069488170033,6.62759121931495,11.2051768269642));
#86970=CARTESIAN_POINT('Ctrl Pts',(-7.24790997235539,6.80961048613165,11.2012680524197));
#86971=CARTESIAN_POINT('Ctrl Pts',(-7.07840576743427,6.98564063277572,11.1973592778752));
#86972=CARTESIAN_POINT('Ctrl Pts',(-6.90264828910006,7.15519465821749,11.1934505033307));
#86973=CARTESIAN_POINT('Ctrl Pts',(-6.72687717108975,7.32476184191579,11.1895414254454));
#86974=CARTESIAN_POINT('Ctrl Pts',(-6.54485200959105,7.48785170332357,11.1856323475601));
#86975=CARTESIAN_POINT('Ctrl Pts',(-6.35707522503604,7.64401455932896,11.1817232696748));
#86976=CARTESIAN_POINT('Ctrl Pts',(-6.16930103347395,7.80017525889535,11.1778142457695));
#86977=CARTESIAN_POINT('Ctrl Pts',(-5.97577559455427,7.9494089667049,11.1739052218643));
#86978=CARTESIAN_POINT('Ctrl Pts',(-5.77703446244014,8.09130624928873,11.1699961979591));
#86979=CARTESIAN_POINT('Ctrl Pts',(-5.57824962317884,8.2332347379211,11.1660863143814));
#86980=CARTESIAN_POINT('Ctrl Pts',(-5.37424702639142,8.36782341366317,11.1621764308037));
#86981=CARTESIAN_POINT('Ctrl Pts',(-5.16559239746636,8.49470536176728,11.158266547226));
#86982=CARTESIAN_POINT('Ctrl Pts',(-5.01671382382033,8.5852377575856,11.1554767797851));
#86983=CARTESIAN_POINT('Ctrl Pts',(-4.86546750306949,8.67184749995319,11.1526870123442));
#86984=CARTESIAN_POINT('Ctrl Pts',(-4.71206720910581,8.75441526413214,11.1498972449033));
#86985=CARTESIAN_POINT('Ctrl Pts',(-4.49707571365825,8.87013451497527,11.1459873679495));
#86986=CARTESIAN_POINT('Ctrl Pts',(-4.27778650126964,8.97794798518521,11.1420774909958));
#86987=CARTESIAN_POINT('Ctrl Pts',(-4.05480127339336,9.07755201765804,11.138167614042));
#86988=CARTESIAN_POINT('Ctrl Pts',(-3.83185464630065,9.17713880776134,11.1342584139237));
#86989=CARTESIAN_POINT('Ctrl Pts',(-3.60521353674567,9.26851888275453,11.1303492138054));
#86990=CARTESIAN_POINT('Ctrl Pts',(-3.37550136157379,9.35143596235431,11.1264400136871));
#86991=CARTESIAN_POINT('Ctrl Pts',(-3.14581419394281,9.43434401521331,11.1225312391426));
#86992=CARTESIAN_POINT('Ctrl Pts',(-2.91305689180422,9.50879081712528,11.1186224645981));
#86993=CARTESIAN_POINT('Ctrl Pts',(-2.67787082253296,9.57456901681881,11.1147136900536));
#86994=CARTESIAN_POINT('Ctrl Pts',(-2.44266650162415,9.64035232123585,11.1108046121683));
#86995=CARTESIAN_POINT('Ctrl Pts',(-2.2050333060942,9.69746560073451,11.106895534283));
#86996=CARTESIAN_POINT('Ctrl Pts',(-1.9656269196001,9.74575162893778,11.1029864563977));
#86997=CARTESIAN_POINT('Ctrl Pts',(-1.72622383904753,9.79403699036358,11.0990774324924));
#86998=CARTESIAN_POINT('Ctrl Pts',(-1.48504789170557,9.83349529087901,11.0951684085872));
#86999=CARTESIAN_POINT('Ctrl Pts',(-1.24276481245015,9.86402045927196,11.091259384682));
#87000=CARTESIAN_POINT('Ctrl Pts',(-1.00042845030313,9.89455234075953,11.0873495011043));
#87001=CARTESIAN_POINT('Ctrl Pts',(-0.756984747826042,9.91614712852152,
11.0834396175266));
#87002=CARTESIAN_POINT('Ctrl Pts',(-0.513105806483867,9.92875049698362,
11.0795297339489));
#87003=CARTESIAN_POINT('Ctrl Pts',(-0.339094095764794,9.93774321154456,
11.0767399665081));
#87004=CARTESIAN_POINT('Ctrl Pts',(-0.164860935590121,9.94215942126182,
11.0739501990672));
#87005=CARTESIAN_POINT('Ctrl Pts',(0.00934887766037717,9.94199560442905,
11.0711604316263));
#87006=CARTESIAN_POINT('Ctrl Pts',(0.25350504780319,9.94176601408768,11.0672505546726));
#87007=CARTESIAN_POINT('Ctrl Pts',(0.497690115999459,9.93253804037882,11.0633406777188));
#87008=CARTESIAN_POINT('Ctrl Pts',(0.741230351838202,9.91433011178838,11.059430800765));
#87009=CARTESIAN_POINT('Ctrl Pts',(0.984728428633159,9.89612533515702,11.0555216006467));
#87010=CARTESIAN_POINT('Ctrl Pts',(1.22758161650919,9.86894372769043,11.0516124005284));
#87011=CARTESIAN_POINT('Ctrl Pts',(1.46911956701285,9.83285572444852,11.0477032004101));
#87012=CARTESIAN_POINT('Ctrl Pts',(1.71063122256676,9.79677164991524,11.0437944258656));
#87013=CARTESIAN_POINT('Ctrl Pts',(1.95082764951087,9.75178315697382,11.0398856513211));
#87014=CARTESIAN_POINT('Ctrl Pts',(2.18904593176937,9.69801226585139,11.0359768767766));
#87015=CARTESIAN_POINT('Ctrl Pts',(2.42728270098026,9.64423720183386,11.0320677988913));
#87016=CARTESIAN_POINT('Ctrl Pts',(2.66354074463202,9.58167843647964,11.028158721006));
#87017=CARTESIAN_POINT('Ctrl Pts',(2.89716834532257,9.51050890220186,11.0242496431207));
#87018=CARTESIAN_POINT('Ctrl Pts',(3.13079271987071,9.43934035069775,11.0203406192154));
#87019=CARTESIAN_POINT('Ctrl Pts',(3.36178645654225,9.35956135174123,11.0164315953102));
#87020=CARTESIAN_POINT('Ctrl Pts',(3.58951327945751,9.27139463169367,11.012522571405));
#87021=CARTESIAN_POINT('Ctrl Pts',(3.81729018405234,9.18320852202232,11.0086126878273));
#87022=CARTESIAN_POINT('Ctrl Pts',(4.04179847741524,9.08663110568986,11.0047028042496));
#87023=CARTESIAN_POINT('Ctrl Pts',(4.26242084838829,8.98193367328132,11.0007929206719));
#87024=CARTESIAN_POINT('Ctrl Pts',(4.41983860649652,8.90723030110401,10.998003153231));
#87025=CARTESIAN_POINT('Ctrl Pts',(4.57527841400071,8.82839399439376,10.9952133857902));
#87026=CARTESIAN_POINT('Ctrl Pts',(4.72852315291297,8.74553787896239,10.9924236183493));
#87027=CARTESIAN_POINT('Ctrl Pts',(4.94329663696212,8.6294145019885,10.9885137413956));
#87028=CARTESIAN_POINT('Ctrl Pts',(5.15382327057646,8.50535790374517,10.9846038644418));
#87029=CARTESIAN_POINT('Ctrl Pts',(5.35951885138358,8.37370417925449,10.980693987488));
#87030=CARTESIAN_POINT('Ctrl Pts',(5.56517882440315,8.2420732452284,10.9767847873697));
#87031=CARTESIAN_POINT('Ctrl Pts',(5.76600917808123,8.1028479612908,10.9728755872514));
#87032=CARTESIAN_POINT('Ctrl Pts',(5.96145337837691,7.95640858788929,10.9689663871331));
#87033=CARTESIAN_POINT('Ctrl Pts',(6.15687630170379,7.80998515656217,10.9650576125886));
#87034=CARTESIAN_POINT('Ctrl Pts',(6.34691401818147,7.65634937189688,10.9611488380441));
#87035=CARTESIAN_POINT('Ctrl Pts',(6.53104102680897,7.49592336581278,10.9572400634996));
#87036=CARTESIAN_POINT('Ctrl Pts',(6.71518232463051,7.33548490985321,10.9533309856143));
#87037=CARTESIAN_POINT('Ctrl Pts',(6.89341178465676,7.16825536135321,10.949421907729));
#87038=CARTESIAN_POINT('Ctrl Pts',(7.06523793413341,6.99469634323623,10.9455128298437));
#87039=CARTESIAN_POINT('Ctrl Pts',(7.23706171087819,6.82113972178014,10.9416038059385));
#87040=CARTESIAN_POINT('Ctrl Pts',(7.40248215815702,6.64125400617729,10.9376947820333));
#87041=CARTESIAN_POINT('Ctrl Pts',(7.56104503468376,6.45553731175678,10.933785758128));
#87042=CARTESIAN_POINT('Ctrl Pts',(7.71964278235607,6.26977977452347,10.9298758745504));
#87043=CARTESIAN_POINT('Ctrl Pts',(7.87137976295408,6.07818890873618,10.9259659909727));
#87044=CARTESIAN_POINT('Ctrl Pts',(8.01584148358403,5.88129656708904,10.922056107395));
#87045=CARTESIAN_POINT('Ctrl Pts',(8.11891734163886,5.74081058248908,10.9192663399541));
#87046=CARTESIAN_POINT('Ctrl Pts',(8.21829015114393,5.59762628955164,10.9164765725132));
#87047=CARTESIAN_POINT('Ctrl Pts',(8.31382253625065,5.45194633463416,10.9136868050724));
#87048=CARTESIAN_POINT('Ctrl Pts',(8.44771178644265,5.24777494385274,10.9097769281186));
#87049=CARTESIAN_POINT('Ctrl Pts',(8.57409681002822,5.03863783848373,10.9058670511648));
#87050=CARTESIAN_POINT('Ctrl Pts',(8.69262302131867,4.82510818627321,10.901957174211));
#87051=CARTESIAN_POINT('Ctrl Pts',(8.8111287146372,4.61161549799969,10.8980479740928));
#87052=CARTESIAN_POINT('Ctrl Pts',(8.92177817541596,4.39373202575933,10.8941387739745));
#87053=CARTESIAN_POINT('Ctrl Pts',(9.02426213795181,4.17205667093934,10.8902295738562));
#87054=CARTESIAN_POINT('Ctrl Pts',(9.12673494360457,3.95040544873441,10.8863207993117));
#87055=CARTESIAN_POINT('Ctrl Pts',(9.22104390834463,3.72496342252037,10.8824120247672));
#87056=CARTESIAN_POINT('Ctrl Pts',(9.30692695861191,3.49635161090283,10.8785032502227));
#87057=CARTESIAN_POINT('Ctrl Pts',(9.39281667384156,3.26772205784369,10.8745941723374));
#87058=CARTESIAN_POINT('Ctrl Pts',(9.47027906653661,3.03592248918386,10.870685094452));
#87059=CARTESIAN_POINT('Ctrl Pts',(9.53910076116268,2.8015925236168,10.8667760165667));
#87060=CARTESIAN_POINT('Ctrl Pts',(9.60792150543619,2.56726579389107,10.8628669926615));
#87061=CARTESIAN_POINT('Ctrl Pts',(9.66810171325942,2.33040900669161,10.8589579687563));
#87062=CARTESIAN_POINT('Ctrl Pts',(9.71947810260246,2.09167622088871,10.8550489448511));
#87063=CARTESIAN_POINT('Ctrl Pts',(9.77086579064031,1.85289093297496,10.8511390612734));
#87064=CARTESIAN_POINT('Ctrl Pts',(9.81344573149039,1.6122290960096,10.8472291776957));
#87065=CARTESIAN_POINT('Ctrl Pts',(9.84710564373104,1.37035558932723,10.843319294118));
#87066=CARTESIAN_POINT('Ctrl Pts',(9.87112255506979,1.19777478983935,10.8405295266771));
#87067=CARTESIAN_POINT('Ctrl Pts',(9.89059929140837,1.02457734830544,10.8377397592363));
#87068=CARTESIAN_POINT('Ctrl Pts',(9.90551116104081,0.851006838101755,10.8349499917954));
#87069=CARTESIAN_POINT('Ctrl Pts',(9.92641024193192,0.607746655276199,10.8310401148417));
#87070=CARTESIAN_POINT('Ctrl Pts',(9.93834719397318,0.363679016690832,10.8271302378879));
#87071=CARTESIAN_POINT('Ctrl Pts',(9.94128207593601,0.119476720215765,10.8232203609341));
#87072=CARTESIAN_POINT('Ctrl Pts',(9.9442164498439,-0.12468330260688,10.8193111608158));
#87073=CARTESIAN_POINT('Ctrl Pts',(9.9381518611066,-0.368977656633764,10.8154019606975));
#87074=CARTESIAN_POINT('Ctrl Pts',(9.92310047264189,-0.612732412929361,
10.8114927605793));
#87075=CARTESIAN_POINT('Ctrl Pts',(9.90805072274167,-0.856460632943218,
10.8075839860348));
#87076=CARTESIAN_POINT('Ctrl Pts',(9.88401614382216,-1.099649092846,10.8036752114903));
#87077=CARTESIAN_POINT('Ctrl Pts',(9.85106093362055,-1.34162680432937,10.7997664369458));
#87078=CARTESIAN_POINT('Ctrl Pts',(9.8181031659267,-1.58362329451614,10.7958573590604));
#87079=CARTESIAN_POINT('Ctrl Pts',(9.77622341841801,-1.82440857035617,10.7919482811751));
#87080=CARTESIAN_POINT('Ctrl Pts',(9.72553757910684,-2.06331839457237,10.7880392032898));
#87081=CARTESIAN_POINT('Ctrl Pts',(9.67485243971184,-2.30222491970443,10.7841301793846));
#87082=CARTESIAN_POINT('Ctrl Pts',(9.61536151191283,-2.53925577121022,10.7802211554794));
#87083=CARTESIAN_POINT('Ctrl Pts',(9.54723162710495,-2.77375778654283,10.7763121315741));
#87084=CARTESIAN_POINT('Ctrl Pts',(9.47908675917379,-3.00831137355526,10.7724022479964));
#87085=CARTESIAN_POINT('Ctrl Pts',(9.40229921522416,-3.24033474355998,10.7684923644187));
#87086=CARTESIAN_POINT('Ctrl Pts',(9.31708584979874,-3.46918942513668,10.764582480841));
#87087=CARTESIAN_POINT('Ctrl Pts',(9.25628468585954,-3.63248107478965,10.7617927134002));
#87088=CARTESIAN_POINT('Ctrl Pts',(9.19119493046871,-3.79415983268962,10.7590029459593));
#87089=CARTESIAN_POINT('Ctrl Pts',(9.12191049700365,-3.95399960605141,10.7562131785184));
#87090=CARTESIAN_POINT('Ctrl Pts',(9.02480791931507,-4.1780160731618,10.7523033015647));
#87091=CARTESIAN_POINT('Ctrl Pts',(8.91943438172357,-4.39848811357532,10.7483934246109));
#87092=CARTESIAN_POINT('Ctrl Pts',(8.80607416515645,-4.6148046326756,10.7444835476571));
#87093=CARTESIAN_POINT('Ctrl Pts',(8.69273357228029,-4.83108370540671,10.7405743475388));
#87094=CARTESIAN_POINT('Ctrl Pts',(8.57140919039356,-5.04320844466578,10.7366651474205));
#87095=CARTESIAN_POINT('Ctrl Pts',(8.4424316944315,-5.25059149857028,10.7327559473023));
#87096=CARTESIAN_POINT('Ctrl Pts',(8.31346823956229,-5.45795197578654,10.7288471727578));
#87097=CARTESIAN_POINT('Ctrl Pts',(8.17685348213841,-5.66057156039699,10.7249383982133));
#87098=CARTESIAN_POINT('Ctrl Pts',(8.03296249691575,-5.85789019384498,10.7210296236688));
#87099=CARTESIAN_POINT('Ctrl Pts',(7.88906034501943,-6.05522414022437,10.7171205457834));
#87100=CARTESIAN_POINT('Ctrl Pts',(7.73788099969172,-6.24725608511637,10.7132114678981));
#87101=CARTESIAN_POINT('Ctrl Pts',(7.5798418231581,-6.43345645325305,10.7093023900128));
#87102=CARTESIAN_POINT('Ctrl Pts',(7.42180482897308,-6.6196542501658,10.7053933661076));
#87103=CARTESIAN_POINT('Ctrl Pts',(7.25690837600702,-6.80002041898686,10.7014843422024));
#87104=CARTESIAN_POINT('Ctrl Pts',(7.0856094037922,-6.97405931842363,10.6975753182972));
#87105=CARTESIAN_POINT('Ctrl Pts',(6.91427275951001,-7.14813649249254,10.6936654347195));
#87106=CARTESIAN_POINT('Ctrl Pts',(6.73653097846631,-7.31588341617678,10.6897555511418));
#87107=CARTESIAN_POINT('Ctrl Pts',(6.55287805059349,-7.47684112804666,10.6858456675641));
#87108=CARTESIAN_POINT('Ctrl Pts',(6.42183860954114,-7.59168715223366,10.6830559001232));
#87109=CARTESIAN_POINT('Ctrl Pts',(6.28779054217795,-7.7030775137971,10.6802661326823));
#87110=CARTESIAN_POINT('Ctrl Pts',(6.15092384703256,-7.81085781639931,10.6774763652415));
#87111=CARTESIAN_POINT('Ctrl Pts',(5.9591042963248,-7.961912601483,10.6735664882877));
#87112=CARTESIAN_POINT('Ctrl Pts',(5.76168828718638,-8.10592101222527,10.6696566113339));
#87113=CARTESIAN_POINT('Ctrl Pts',(5.55921615363473,-8.24248019452681,10.6657467343802));
#87114=CARTESIAN_POINT('Ctrl Pts',(5.35677906986235,-8.37901573718415,10.6618375342619));
#87115=CARTESIAN_POINT('Ctrl Pts',(5.14928784117524,-8.50810446893057,10.6579283341436));
#87116=CARTESIAN_POINT('Ctrl Pts',(4.93731236042211,-8.62938645881751,10.6540191340253));
#87117=CARTESIAN_POINT('Ctrl Pts',(4.72535995631054,-8.7506552453802,10.6501103594808));
#87118=CARTESIAN_POINT('Ctrl Pts',(4.50892451807305,-8.86411884786377,10.6462015849363));
#87119=CARTESIAN_POINT('Ctrl Pts',(4.28860205653772,-8.96946243654883,10.6422928103918));
#87120=CARTESIAN_POINT('Ctrl Pts',(4.06826249685655,-9.07481420043323,10.6383837325065));
#87121=CARTESIAN_POINT('Ctrl Pts',(3.84403556269861,-9.17204456765895,10.6344746546212));
#87122=CARTESIAN_POINT('Ctrl Pts',(3.61654000924394,-9.26088561432101,10.6305655767359));
#87123=CARTESIAN_POINT('Ctrl Pts',(3.38904759725478,-9.3497254341851,10.6266565528307));
#87124=CARTESIAN_POINT('Ctrl Pts',(3.15828691811466,-9.43017606512544,10.6227475289255));
#87125=CARTESIAN_POINT('Ctrl Pts',(2.92489544780518,-9.50201823926941,10.6188385050203));
#87126=CARTESIAN_POINT('Ctrl Pts',(2.69145265004704,-9.57387621294324,10.6149286214426));
#87127=CARTESIAN_POINT('Ctrl Pts',(2.45537817276939,-9.6371218634826,10.6110187378649));
#87128=CARTESIAN_POINT('Ctrl Pts',(2.2173246851161,-9.69158579597657,10.6071088542872));
#87129=CARTESIAN_POINT('Ctrl Pts',(2.04746953320531,-9.73044672432767,10.6043190868463));
#87130=CARTESIAN_POINT('Ctrl Pts',(1.87660717283238,-9.76483786884059,10.6015293194054));
#87131=CARTESIAN_POINT('Ctrl Pts',(1.70497812703294,-9.79471355305193,10.5987395519645));
#87132=CARTESIAN_POINT('Ctrl Pts',(1.46443891901959,-9.83658451600917,10.5948296750108));
#87133=CARTESIAN_POINT('Ctrl Pts',(1.22231975523784,-9.86959684035226,10.590919798057));
#87134=CARTESIAN_POINT('Ctrl Pts',(0.979287453550111,-9.89365251478539,
10.5870099211032));
#87135=CARTESIAN_POINT('Ctrl Pts',(0.736297222977956,-9.91770402496113,
10.5831007209849));
#87136=CARTESIAN_POINT('Ctrl Pts',(0.492394448858487,-9.93280195273444,
10.5791915208666));
#87137=CARTESIAN_POINT('Ctrl Pts',(0.248251584657012,-9.9389000976323,10.5752823207483));
#87138=CARTESIAN_POINT('Ctrl Pts',(0.00413529898891532,-9.9449975786576,
10.5713735462038));
#87139=CARTESIAN_POINT('Ctrl Pts',(-0.240220744457244,-9.9420972260719,
10.5674647716593));
#87140=CARTESIAN_POINT('Ctrl Pts',(-0.484142519031698,-9.93020493349788,
10.5635559971148));
#87141=CARTESIAN_POINT('Ctrl Pts',(-0.72808322317909,-9.91831171802134,
10.5596469192295));
#87142=CARTESIAN_POINT('Ctrl Pts',(-0.971589310969119,-9.89742517876364,
10.5557378413442));
#87143=CARTESIAN_POINT('Ctrl Pts',(-1.21398900849319,-9.8676032899209,10.5518287634588));
#87144=CARTESIAN_POINT('Ctrl Pts',(-1.45638535874182,-9.83778181288591,
10.5479197395536));
#87145=CARTESIAN_POINT('Ctrl Pts',(-1.69767507130053,-9.79902526931551,
10.5440107156484));
#87146=CARTESIAN_POINT('Ctrl Pts',(-1.93719299711377,-9.75144334403546,
10.5401016917431));
#87147=CARTESIAN_POINT('Ctrl Pts',(-2.17676359770571,-9.70385095453909,
10.5361918081654));
#87148=CARTESIAN_POINT('Ctrl Pts',(-2.41456135771808,-9.64742935878473,
10.5322819245877));
#87149=CARTESIAN_POINT('Ctrl Pts',(-2.64993143541098,-9.58233934838569,
10.52837204101));
#87150=CARTESIAN_POINT('Ctrl Pts',(-2.81787192935261,-9.53589653541546,
10.5255822735692));
#87151=CARTESIAN_POINT('Ctrl Pts',(-2.98457669063517,-9.48504164796262,
10.5227925061284));
#87152=CARTESIAN_POINT('Ctrl Pts',(-3.14981234787036,-9.42984868241285,
10.5200027386875));
#87153=CARTESIAN_POINT('Ctrl Pts',(-3.38139118082571,-9.35249538734794,
10.5160928617338));
#87154=CARTESIAN_POINT('Ctrl Pts',(-3.61015460183394,-9.26659544417436,
10.51218298478));
#87155=CARTESIAN_POINT('Ctrl Pts',(-3.83546920859118,-9.17237918699118,
10.5082731078262));
#87156=CARTESIAN_POINT('Ctrl Pts',(-4.06074481132836,-9.07817923950419,
10.5043639077079));
#87157=CARTESIAN_POINT('Ctrl Pts',(-4.28257253311977,-8.97566595992073,
10.5004547075896));
#87158=CARTESIAN_POINT('Ctrl Pts',(-4.50033861067485,-8.86511795687283,
10.4965455074713));
#87159=CARTESIAN_POINT('Ctrl Pts',(-4.71808098119718,-8.7545819885971,10.4926367329268));
#87160=CARTESIAN_POINT('Ctrl Pts',(-4.93176234050012,-8.63601317018212,
10.4887279583823));
#87161=CARTESIAN_POINT('Ctrl Pts',(-5.14079227414487,-8.50973670533304,
10.4848191838378));
#87162=CARTESIAN_POINT('Ctrl Pts',(-5.34983842957712,-8.38345044078712,
10.4809101059525));
#87163=CARTESIAN_POINT('Ctrl Pts',(-5.5542321965262,-8.24945547690787,10.4770010280672));
#87164=CARTESIAN_POINT('Ctrl Pts',(-5.7534098701922,-8.10812178408631,10.4730919501819));
#87165=CARTESIAN_POINT('Ctrl Pts',(-5.95258479343194,-7.96679004292877,
10.4691829262767));
#87166=CARTESIAN_POINT('Ctrl Pts',(-6.14654354001739,-7.81811993941443,
10.4652739023714));
#87167=CARTESIAN_POINT('Ctrl Pts',(-6.33475278705149,-7.66252380922522,
10.4613648784662));
#87168=CARTESIAN_POINT('Ctrl Pts',(-6.52300342506034,-7.50689346033742,
10.4574549948885));
#87169=CARTESIAN_POINT('Ctrl Pts',(-6.70550182020335,-7.34433421912267,
10.4535451113108));
#87170=CARTESIAN_POINT('Ctrl Pts',(-6.88174798573715,-7.17529850673843,
10.4496352277331));
#87171=CARTESIAN_POINT('Ctrl Pts',(-7.00750257776358,-7.05468869384181,
10.4468454602923));
#87172=CARTESIAN_POINT('Ctrl Pts',(-7.13007481817835,-6.93078250798911,
10.4440556928514));
#87173=CARTESIAN_POINT('Ctrl Pts',(-7.24929444846751,-6.80375587447243,
10.4412659254105));
#87174=CARTESIAN_POINT('Ctrl Pts',(-7.41638152464334,-6.62572723322198,
10.4373560484568));
#87175=CARTESIAN_POINT('Ctrl Pts',(-7.57693294207992,-6.44151337547009,
10.433446171503));
#87176=CARTESIAN_POINT('Ctrl Pts',(-7.73050060056086,-6.25161774780961,
10.4295362945492));
#87177=CARTESIAN_POINT('Ctrl Pts',(-7.88404167507496,-6.06175499281985,
10.4256270944309));
#87178=CARTESIAN_POINT('Ctrl Pts',(-8.0306012278009,-5.86621264919321,10.4217178943126));
#87179=CARTESIAN_POINT('Ctrl Pts',(-8.16977136282007,-5.66552732578752,
10.4178086941943));
#87180=CARTESIAN_POINT('Ctrl Pts',(-8.30892634712724,-5.46486384992503,
10.4138999196498));
#87181=CARTESIAN_POINT('Ctrl Pts',(-8.44069336027146,-5.25905874245601,
10.4099911451054));
#87182=CARTESIAN_POINT('Ctrl Pts',(-8.56470717829073,-5.0486785350362,10.4060823705609));
#87183=CARTESIAN_POINT('Ctrl Pts',(-8.68873062041477,-4.83828200103931,
10.4021732926755));
#87184=CARTESIAN_POINT('Ctrl Pts',(-8.80499952012981,-4.62330989756555,
10.3982642147902));
#87185=CARTESIAN_POINT('Ctrl Pts',(-8.91319341518002,-4.40435547425404,
10.3943551369049));
#87186=CARTESIAN_POINT('Ctrl Pts',(-9.02138581619064,-4.1854040744641,10.3904461129997));
#87187=CARTESIAN_POINT('Ctrl Pts',(-9.12150331320995,-3.96247071705256,
10.3865370890944));
#87188=CARTESIAN_POINT('Ctrl Pts',(-9.21327229751492,-3.73617151263753,
10.3826280651892));
#87189=CARTESIAN_POINT('Ctrl Pts',(-9.30506146365344,-3.50982254050509,
10.3787181816115));
#87190=CARTESIAN_POINT('Ctrl Pts',(-9.38849834211504,-3.2801065017816,10.3748082980338));
#87191=CARTESIAN_POINT('Ctrl Pts',(-9.46335769533473,-3.04765895896324,
10.3708984144561));
#87192=CARTESIAN_POINT('Ctrl Pts',(-9.51677109808855,-2.88180374261834,
10.3681086470153));
#87193=CARTESIAN_POINT('Ctrl Pts',(-9.56581864139616,-2.71455830767852,
10.3653188795744));
#87194=CARTESIAN_POINT('Ctrl Pts',(-9.61043400671089,-2.54615832238587,
10.3625291121336));
#87195=CARTESIAN_POINT('Ctrl Pts',(-9.67358840539533,-2.30778305111777,
10.3585801119639));
#87196=CARTESIAN_POINT('Ctrl Pts',(-9.72787744028907,-2.06702769942914,
10.3546311117943));
#87197=CARTESIAN_POINT('Ctrl Pts',(-9.77314381814786,-1.82456129242024,
10.3506821116246));
#87198=CARTESIAN_POINT('Ctrl Pts',(-9.8184012216236,-1.58214295611016,10.3467338943725));
#87199=CARTESIAN_POINT('Ctrl Pts',(-9.85463949074573,-1.33801450552071,
10.3427856771203));
#87200=CARTESIAN_POINT('Ctrl Pts',(-9.88175247637308,-1.09285497468534,
10.3388374598682));
#87201=CARTESIAN_POINT('Ctrl Pts',(-9.90886135115302,-0.847732614725825,
10.3348898412414));
#87202=CARTESIAN_POINT('Ctrl Pts',(-9.92684767526548,-0.60157975325512,
10.3309422226145));
#87203=CARTESIAN_POINT('Ctrl Pts',(-9.93565705376861,-0.35508155386905,
10.3269946039877));
#87204=CARTESIAN_POINT('Ctrl Pts',(-9.93988551191906,-0.236763636220732,
10.3250997665537));
#87205=CARTESIAN_POINT('Ctrl Pts',(-9.9420004127048,-0.118366224562907,
10.3232049291198));
#87206=CARTESIAN_POINT('Ctrl Pts',(-9.94199999993959,3.46594688641578E-5,
10.3213100916858));
#87207=CARTESIAN_POINT('Ctrl Pts',(-9.94199999991864,4.02206518999385E-5,
10.1786899083142));
#87208=CARTESIAN_POINT('Ctrl Pts',(-9.94200099753697,-0.246557507493905,
10.1826363574975));
#87209=CARTESIAN_POINT('Ctrl Pts',(-9.9328228723075,-0.493140709085339,
10.1865828066807));
#87210=CARTESIAN_POINT('Ctrl Pts',(-9.91449490077624,-0.739022910661104,
10.190529255864));
#87211=CARTESIAN_POINT('Ctrl Pts',(-9.89616588732431,-0.984919090311048,
10.1944759293976));
#87212=CARTESIAN_POINT('Ctrl Pts',(-9.8686860119547,-1.23011392251438,10.1984226029312));
#87213=CARTESIAN_POINT('Ctrl Pts',(-9.83213649965829,-1.47392532106863,
10.2023692764648));
#87214=CARTESIAN_POINT('Ctrl Pts',(-9.79557838003627,-1.71779413664332,
10.2063168794309));
#87215=CARTESIAN_POINT('Ctrl Pts',(-9.74994639552095,-1.96027860167608,
10.210264482397));
#87216=CARTESIAN_POINT('Ctrl Pts',(-9.69537327931219,-2.20070465415039,
10.2142120853631));
#87217=CARTESIAN_POINT('Ctrl Pts',(-9.66774222224862,-2.32243539699589,
10.2162108065357));
#87218=CARTESIAN_POINT('Ctrl Pts',(-9.63781989743059,-2.44363862069704,
10.2182095277083));
#87219=CARTESIAN_POINT('Ctrl Pts',(-9.6056284949816,-2.56422799618083,10.2202082488808));
#87220=CARTESIAN_POINT('Ctrl Pts',(-9.54265601824438,-2.80012364112642,
10.2241181258346));
#87221=CARTESIAN_POINT('Ctrl Pts',(-9.47097999825955,-3.03373453810706,
10.2280280027884));
#87222=CARTESIAN_POINT('Ctrl Pts',(-9.39079139998841,-3.26441432448513,
10.2319378797422));
#87223=CARTESIAN_POINT('Ctrl Pts',(-9.31061668309735,-3.49505417808148,
10.2358470798605));
#87224=CARTESIAN_POINT('Ctrl Pts',(-9.22193242156242,-3.72276366932522,
10.2397562799788));
#87225=CARTESIAN_POINT('Ctrl Pts',(-9.12497897075438,-3.94691307014613,
10.2436654800971));
#87226=CARTESIAN_POINT('Ctrl Pts',(-9.02803607475191,-4.17103806901615,
10.2475742546416));
#87227=CARTESIAN_POINT('Ctrl Pts',(-8.92282589816911,-4.39160349413485,
10.2514830291861));
#87228=CARTESIAN_POINT('Ctrl Pts',(-8.80963673853617,-4.60800005805489,
10.2553918037306));
#87229=CARTESIAN_POINT('Ctrl Pts',(-8.69643879484802,-4.82441341545029,
10.259300881616));
#87230=CARTESIAN_POINT('Ctrl Pts',(-8.5752607580191,-5.03665701536165,10.2632099595013));
#87231=CARTESIAN_POINT('Ctrl Pts',(-8.44643724938797,-5.24414547778295,
10.2671190373867));
#87232=CARTESIAN_POINT('Ctrl Pts',(-8.31761551966884,-5.45163107501514,
10.2710280612919));
#87233=CARTESIAN_POINT('Ctrl Pts',(-8.18114867891522,-5.65436142901064,
10.2749370851971));
#87234=CARTESIAN_POINT('Ctrl Pts',(-8.03741550114447,-5.85177888013231,
10.2788461091024));
#87235=CARTESIAN_POINT('Ctrl Pts',(-7.89365071357565,-6.04923974729657,
10.2827559926801));
#87236=CARTESIAN_POINT('Ctrl Pts',(-7.7426165601319,-6.24138514960407,10.2866658762578));
#87237=CARTESIAN_POINT('Ctrl Pts',(-7.58473387359504,-6.42768823658553,
10.2905757598355));
#87238=CARTESIAN_POINT('Ctrl Pts',(-7.47208193150732,-6.56061861055974,
10.2933655272763));
#87239=CARTESIAN_POINT('Ctrl Pts',(-7.35594423870371,-6.69057526995616,
10.2961552947171));
#87240=CARTESIAN_POINT('Ctrl Pts',(-7.23648592246827,-6.81737746453272,
10.2989450621579));
#87241=CARTESIAN_POINT('Ctrl Pts',(-7.06906432640432,-6.99509155317414,
10.3028549391117));
#87242=CARTESIAN_POINT('Ctrl Pts',(-6.89506747952576,-7.16666253062903,
10.3067648160654));
#87243=CARTESIAN_POINT('Ctrl Pts',(-6.71497033289561,-7.33161219844121,
10.3106746930192));
#87244=CARTESIAN_POINT('Ctrl Pts',(-6.53490436273011,-7.49653331195598,
10.3145838931375));
#87245=CARTESIAN_POINT('Ctrl Pts',(-6.34874040747306,-7.65483521468815,
10.3184930932557));
#87246=CARTESIAN_POINT('Ctrl Pts',(-6.15698898899959,-7.80607779805824,
10.322402293374));
#87247=CARTESIAN_POINT('Ctrl Pts',(-5.96525844548086,-7.95730391645452,
10.3263110679185));
#87248=CARTESIAN_POINT('Ctrl Pts',(-5.76794187328411,-8.10147207642846,
10.330219842463));
#87249=CARTESIAN_POINT('Ctrl Pts',(-5.56558228343562,-8.23818292139156,
10.3341286170075));
#87250=CARTESIAN_POINT('Ctrl Pts',(-5.36320698945194,-8.37490437581277,
10.3380376948928));
#87251=CARTESIAN_POINT('Ctrl Pts',(-5.15578812636428,-8.50416719934732,
10.3419467727781));
#87252=CARTESIAN_POINT('Ctrl Pts',(-4.94389812404694,-8.62561507018747,
10.3458558506635));
#87253=CARTESIAN_POINT('Ctrl Pts',(-4.73201104769909,-8.74706126396518,
10.3497648745687));
#87254=CARTESIAN_POINT('Ctrl Pts',(-4.51565319984096,-8.86069258326714,
10.3536738984739));
#87255=CARTESIAN_POINT('Ctrl Pts',(-4.29542270806301,-8.96619806601754,
10.3575829223791));
#87256=CARTESIAN_POINT('Ctrl Pts',(-4.07514378319907,-9.07172675153191,
10.3614928059568));
#87257=CARTESIAN_POINT('Ctrl Pts',(-3.85099076509672,-9.16912590763516,
10.3654026895345));
#87258=CARTESIAN_POINT('Ctrl Pts',(-3.62358416969242,-9.2581316562876,10.3693125731122));
#87259=CARTESIAN_POINT('Ctrl Pts',(-3.46132575378416,-9.32163874919929,
10.3721023405531));
#87260=CARTESIAN_POINT('Ctrl Pts',(-3.29741138999951,-9.38087369123851,
10.374892107994));
#87261=CARTESIAN_POINT('Ctrl Pts',(-3.13207222452432,-9.43575580334523,
10.3776818754349));
#87262=CARTESIAN_POINT('Ctrl Pts',(-2.90034832411135,-9.51267343531538,
10.3815917523886));
#87263=CARTESIAN_POINT('Ctrl Pts',(-2.66575417575368,-9.58106267851264,
10.3855016293424));
#87264=CARTESIAN_POINT('Ctrl Pts',(-2.42893482585825,-9.64072816812781,
10.3894115062962));
#87265=CARTESIAN_POINT('Ctrl Pts',(-2.19215647155972,-9.70038332910065,
10.3933207064145));
#87266=CARTESIAN_POINT('Ctrl Pts',(-1.95315395635775,-9.75131768266605,
10.3972299065328));
#87267=CARTESIAN_POINT('Ctrl Pts',(-1.71258554818099,-9.79338627544945,
10.401139106651));
#87268=CARTESIAN_POINT('Ctrl Pts',(-1.47204332940521,-9.83545028844927,
10.4050478811955));
#87269=CARTESIAN_POINT('Ctrl Pts',(-1.22993583404403,-9.86865041952894,
10.40895665574));
#87270=CARTESIAN_POINT('Ctrl Pts',(-0.986930575442055,-9.8928930065607,
10.4128654302845));
#87271=CARTESIAN_POINT('Ctrl Pts',(-0.743906458393762,-9.91713747494075,
10.4167745081699));
#87272=CARTESIAN_POINT('Ctrl Pts',(-0.499984717526206,-9.93242297934668,
10.4206835860552));
#87273=CARTESIAN_POINT('Ctrl Pts',(-0.25583832558724,-9.93870770025765,
10.4245926639405));
#87274=CARTESIAN_POINT('Ctrl Pts',(-0.0116953050438629,-9.94499233438348,
10.4285016878457));
#87275=CARTESIAN_POINT('Ctrl Pts',(0.232672080077057,-9.94227642844191,
10.4324107117509));
#87276=CARTESIAN_POINT('Ctrl Pts',(0.476589776450805,-9.93057028498276,
10.4363197356562));
#87277=CARTESIAN_POINT('Ctrl Pts',(0.720561115200695,-9.91886156710872,
10.4402296192339));
#87278=CARTESIAN_POINT('Ctrl Pts',(0.964082287443854,-9.89815867350911,
10.4441395028116));
#87279=CARTESIAN_POINT('Ctrl Pts',(1.20648189053527,-9.8685239751348,10.4480493863892));
#87280=CARTESIAN_POINT('Ctrl Pts',(1.37943806862752,-9.84737912132989,10.4508391538301));
#87281=CARTESIAN_POINT('Ctrl Pts',(1.55182330419681,-9.82168811958619,10.453628921271));
#87282=CARTESIAN_POINT('Ctrl Pts',(1.72339585979075,-9.79148970843845,10.4564186887118));
#87283=CARTESIAN_POINT('Ctrl Pts',(1.96385589641953,-9.74916644161072,10.4603285656656));
#87284=CARTESIAN_POINT('Ctrl Pts',(2.2027929078169,-9.69797457103325,10.4642384426194));
#87285=CARTESIAN_POINT('Ctrl Pts',(2.43954643095548,-9.6380484129938,10.4681483195732));
#87286=CARTESIAN_POINT('Ctrl Pts',(2.67625896989115,-9.57813262872109,10.4720575196914));
#87287=CARTESIAN_POINT('Ctrl Pts',(2.91078850349805,-9.50948564399854,10.4759667198097));
#87288=CARTESIAN_POINT('Ctrl Pts',(3.14248686696847,-9.43229241971063,10.479875919928));
#87289=CARTESIAN_POINT('Ctrl Pts',(3.37416000667388,-9.35510759903732,10.4837846944725));
#87290=CARTESIAN_POINT('Ctrl Pts',(3.60300232580942,-9.26937848504128,10.4876934690169));
#87291=CARTESIAN_POINT('Ctrl Pts',(3.82838187488862,-9.17533956973933,10.4916022435614));
#87292=CARTESIAN_POINT('Ctrl Pts',(4.05377891456901,-9.08129335653847,10.4955113214468));
#87293=CARTESIAN_POINT('Ctrl Pts',(4.27571238733031,-8.97893615854595,10.4994203993321));
#87294=CARTESIAN_POINT('Ctrl Pts',(4.49357015286368,-8.86855068662815,10.5033294772174));
#87295=CARTESIAN_POINT('Ctrl Pts',(4.71142491001955,-8.75816673901301,10.5072385011226));
#87296=CARTESIAN_POINT('Ctrl Pts',(4.92520382337884,-8.63975486773634,10.5111475250278));
#87297=CARTESIAN_POINT('Ctrl Pts',(5.13431854831178,-8.51364416947652,10.5150565489331));
#87298=CARTESIAN_POINT('Ctrl Pts',(5.34347926175107,-8.38750573695433,10.5189664325108));
#87299=CARTESIAN_POINT('Ctrl Pts',(5.54797349649055,-8.25366523825415,10.5228763160884));
#87300=CARTESIAN_POINT('Ctrl Pts',(5.74723996198683,-8.11249633709265,10.5267861996661));
#87301=CARTESIAN_POINT('Ctrl Pts',(5.88941992373083,-8.01176996089786,10.529575967107));
#87302=CARTESIAN_POINT('Ctrl Pts',(6.02893896155573,-7.90731358197614,10.5323657345479));
#87303=CARTESIAN_POINT('Ctrl Pts',(6.16560271410765,-7.79927606716087,10.5351555019887));
#87304=CARTESIAN_POINT('Ctrl Pts',(6.35713783946976,-7.64786079751144,10.5390653789425));
#87305=CARTESIAN_POINT('Ctrl Pts',(6.5431218798354,-7.48936335350043,10.5429752558963));
#87306=CARTESIAN_POINT('Ctrl Pts',(6.72303733110427,-7.32421552417584,10.5468851328501));
#87307=CARTESIAN_POINT('Ctrl Pts',(6.90292163736157,-7.15909628345229,10.5507943329684));
#87308=CARTESIAN_POINT('Ctrl Pts',(7.0767392452124,-6.98732914501542,10.5547035330866));
#87309=CARTESIAN_POINT('Ctrl Pts',(7.2440075194695,-6.80938463136496,10.5586127332049));
#87310=CARTESIAN_POINT('Ctrl Pts',(7.41125758412091,-6.63145948958549,10.5625215077494));
#87311=CARTESIAN_POINT('Ctrl Pts',(7.57195954687699,-6.44735851951732,10.5664302822939));
#87312=CARTESIAN_POINT('Ctrl Pts',(7.72566856026041,-6.25758813737401,10.5703390568384));
#87313=CARTESIAN_POINT('Ctrl Pts',(7.87938950224671,-6.06780302808179,10.5742481347237));
#87314=CARTESIAN_POINT('Ctrl Pts',(8.02611623163984,-5.87234784346272,10.5781572126091));
#87315=CARTESIAN_POINT('Ctrl Pts',(8.1654442285848,-5.67176203219698,10.5820662904944));
#87316=CARTESIAN_POINT('Ctrl Pts',(8.30477030156209,-5.4711789908025,10.5859753143996));
#87317=CARTESIAN_POINT('Ctrl Pts',(8.43669768819625,-5.26546569586995,10.5898843383048));
#87318=CARTESIAN_POINT('Ctrl Pts',(8.560864834489,-5.05519112256002,10.5937933622101));
#87319=CARTESIAN_POINT('Ctrl Pts',(8.68505928761892,-4.84487030566871,10.5977032457878));
#87320=CARTESIAN_POINT('Ctrl Pts',(8.80148994681545,-4.62998644696003,10.6016131293655));
#87321=CARTESIAN_POINT('Ctrl Pts',(8.90984022814631,-4.41113490032959,10.6055230129432));
#87322=CARTESIAN_POINT('Ctrl Pts',(8.98714996923117,-4.25498065505952,10.6083127803841));
#87323=CARTESIAN_POINT('Ctrl Pts',(9.06034688051059,-4.09680698723904,10.6111025478249));
#87324=CARTESIAN_POINT('Ctrl Pts',(9.12933058355592,-3.93683719451928,10.6138923152658));
#87325=CARTESIAN_POINT('Ctrl Pts',(9.22601168563367,-3.71263850444416,10.6178021922195));
#87326=CARTESIAN_POINT('Ctrl Pts',(9.31444476382986,-3.48484233742335,10.6217120691733));
#87327=CARTESIAN_POINT('Ctrl Pts',(9.39437936772289,-3.25407441453056,10.6256219461271));
#87328=CARTESIAN_POINT('Ctrl Pts',(9.47430013420437,-3.02334643967738,10.6295311462454));
#87329=CARTESIAN_POINT('Ctrl Pts',(9.54572527145567,-2.7896480006273,10.6334403463637));
#87330=CARTESIAN_POINT('Ctrl Pts',(9.60845340728022,-2.55362235268355,10.6373495464819));
#87331=CARTESIAN_POINT('Ctrl Pts',(9.67117471422747,-2.31762239959221,10.6412583210265));
#87332=CARTESIAN_POINT('Ctrl Pts',(9.72520083822318,-2.07929601426984,10.645167095571));
#87333=CARTESIAN_POINT('Ctrl Pts',(9.77038070587608,-1.83930010119187,10.6490758701155));
#87334=CARTESIAN_POINT('Ctrl Pts',(9.81556407971648,-1.59928556321053,10.6529849480009));
#87335=CARTESIAN_POINT('Ctrl Pts',(9.85189977054961,-1.35760151350027,10.6568940258862));
#87336=CARTESIAN_POINT('Ctrl Pts',(9.87928788070018,-1.11491478160916,10.6608031037715));
#87337=CARTESIAN_POINT('Ctrl Pts',(9.90667561265078,-0.872231400957463,
10.6647121276767));
#87338=CARTESIAN_POINT('Ctrl Pts',(9.92511598164183,-0.628545644608861,
10.6686211515819));
#87339=CARTESIAN_POINT('Ctrl Pts',(9.93456092304684,-0.384529928966166,
10.6725301754871));
#87340=CARTESIAN_POINT('Ctrl Pts',(9.94400794158324,-0.140460549390556,
10.6764400590648));
#87341=CARTESIAN_POINT('Ctrl Pts',(9.94445556775577,0.103938654300622,10.6803499426425));
#87342=CARTESIAN_POINT('Ctrl Pts',(9.93590783939905,0.347993400754234,10.6842598262202));
#87343=CARTESIAN_POINT('Ctrl Pts',(9.92980889200356,0.52213055136565,10.6870495936611));
#87344=CARTESIAN_POINT('Ctrl Pts',(9.91913144379351,0.696092297483225,10.6898393611019));
#87345=CARTESIAN_POINT('Ctrl Pts',(9.90389316948275,0.869634456236079,10.6926291285428));
#87346=CARTESIAN_POINT('Ctrl Pts',(9.88253663034249,1.11285490432005,10.6965390054965));
#87347=CARTESIAN_POINT('Ctrl Pts',(9.85221296102409,1.35532547595203,10.7004488824503));
#87348=CARTESIAN_POINT('Ctrl Pts',(9.81299882147368,1.59637656264312,10.7043587594041));
#87349=CARTESIAN_POINT('Ctrl Pts',(9.7737914702497,1.83738592118506,10.7082679595223));
#87350=CARTESIAN_POINT('Ctrl Pts',(9.7256967660159,2.07697600877312,10.7121771596406));
#87351=CARTESIAN_POINT('Ctrl Pts',(9.66884288755617,2.31448508652667,10.7160863597589));
#87352=CARTESIAN_POINT('Ctrl Pts',(9.61199519847483,2.55196830793424,10.7199951343034));
#87353=CARTESIAN_POINT('Ctrl Pts',(9.54639030435901,2.78737069934648,10.723903908848));
#87354=CARTESIAN_POINT('Ctrl Pts',(9.47220713250522,3.0200423902517,10.7278126833925));
#87355=CARTESIAN_POINT('Ctrl Pts',(9.39801820365983,3.25273213766403,10.7317217612778));
#87356=CARTESIAN_POINT('Ctrl Pts',(9.31524974907448,3.48269049310751,10.7356308391631));
#87357=CARTESIAN_POINT('Ctrl Pts',(9.22413044818883,3.70928314837189,10.7395399170484));
#87358=CARTESIAN_POINT('Ctrl Pts',(9.13301240556115,3.93587267463934,10.7434489409537));
#87359=CARTESIAN_POINT('Ctrl Pts',(9.03354385376521,4.15909633436158,10.7473579648589));
#87360=CARTESIAN_POINT('Ctrl Pts',(8.92600174319003,4.37833951179765,10.7512669887641));
#87361=CARTESIAN_POINT('Ctrl Pts',(8.81843598195587,4.59763090518929,10.7551768723418));
#87362=CARTESIAN_POINT('Ctrl Pts',(8.70279323671164,4.81293981491277,10.7590867559195));
#87363=CARTESIAN_POINT('Ctrl Pts',(8.57939719880746,5.02367472126676,10.7629966394972));
#87364=CARTESIAN_POINT('Ctrl Pts',(8.49135205832294,5.17403760770999,10.765786406938));
#87365=CARTESIAN_POINT('Ctrl Pts',(8.39936064634176,5.32207232368689,10.7685761743789));
#87366=CARTESIAN_POINT('Ctrl Pts',(8.30355445241727,5.46757235487024,10.7713659418197));
#87367=CARTESIAN_POINT('Ctrl Pts',(8.1692814574114,5.67149158138533,10.7752758187735));
#87368=CARTESIAN_POINT('Ctrl Pts',(8.02747249641325,5.87049339446562,10.7791856957273));
#87369=CARTESIAN_POINT('Ctrl Pts',(7.87851295708629,6.06402486678801,10.783095572681));
#87370=CARTESIAN_POINT('Ctrl Pts',(7.72957920401992,6.25752283703997,10.7870047727993));
#87371=CARTESIAN_POINT('Ctrl Pts',(7.57349751450284,6.4455521348702,10.7909139729175));
#87372=CARTESIAN_POINT('Ctrl Pts',(7.4106948817036,6.62759121931129,10.7948231730358));
#87373=CARTESIAN_POINT('Ctrl Pts',(7.24790997235995,6.80961048612674,10.7987319475803));
#87374=CARTESIAN_POINT('Ctrl Pts',(7.07840576744021,6.98564063276964,10.8026407221247));
#87375=CARTESIAN_POINT('Ctrl Pts',(6.90264828910748,7.15519465821033,10.8065494966692));
#87376=CARTESIAN_POINT('Ctrl Pts',(6.72687717109729,7.32476184190886,10.8104585745545));
#87377=CARTESIAN_POINT('Ctrl Pts',(6.54485200959871,7.48785170331687,10.8143676524398));
#87378=CARTESIAN_POINT('Ctrl Pts',(6.35707522504381,7.64401455932249,10.8182767303251));
#87379=CARTESIAN_POINT('Ctrl Pts',(6.16930103348131,7.80017525888955,10.8221857542303));
#87380=CARTESIAN_POINT('Ctrl Pts',(5.97577559456118,7.94940896669972,10.8260947781355));
#87381=CARTESIAN_POINT('Ctrl Pts',(5.77703446244656,8.09130624928415,10.8300038020407));
#87382=CARTESIAN_POINT('Ctrl Pts',(5.57824962318541,8.23323473791665,10.8339136856184));
#87383=CARTESIAN_POINT('Ctrl Pts',(5.37424702639811,8.36782341365887,10.8378235691961));
#87384=CARTESIAN_POINT('Ctrl Pts',(5.16559239747318,8.49470536176313,10.8417334527738));
#87385=CARTESIAN_POINT('Ctrl Pts',(5.01671382382499,8.58523775758293,10.8445232202148));
#87386=CARTESIAN_POINT('Ctrl Pts',(4.86546750307192,8.67184749995188,10.8473129876557));
#87387=CARTESIAN_POINT('Ctrl Pts',(4.71206720910593,8.75441526413207,10.8501027550966));
#87388=CARTESIAN_POINT('Ctrl Pts',(4.49707571365821,8.8701345149753,10.8540126320504));
#87389=CARTESIAN_POINT('Ctrl Pts',(4.27778650126944,8.97794798518531,10.8579225090042));
#87390=CARTESIAN_POINT('Ctrl Pts',(4.05480127339299,9.07755201765821,10.861832385958));
#87391=CARTESIAN_POINT('Ctrl Pts',(3.83185464629978,9.17713880776172,10.8657415860763));
#87392=CARTESIAN_POINT('Ctrl Pts',(3.60521353674429,9.26851888275508,10.8696507861946));
#87393=CARTESIAN_POINT('Ctrl Pts',(3.3755013615719,9.35143596235499,10.8735599863129));
#87394=CARTESIAN_POINT('Ctrl Pts',(3.14581419394019,9.4343440152142,10.8774687608574));
#87395=CARTESIAN_POINT('Ctrl Pts',(2.91305689180085,9.50879081712634,10.8813775354019));
#87396=CARTESIAN_POINT('Ctrl Pts',(2.67787082252882,9.57456901681996,10.8852863099464));
#87397=CARTESIAN_POINT('Ctrl Pts',(2.44266650161963,9.640352321237,10.8891953878318));
#87398=CARTESIAN_POINT('Ctrl Pts',(2.2050333060893,9.69746560073563,10.8931044657171));
#87399=CARTESIAN_POINT('Ctrl Pts',(1.96562691959482,9.74575162893885,10.8970135436024));
#87400=CARTESIAN_POINT('Ctrl Pts',(1.72622383904111,9.79403699036474,10.9009225675077));
#87401=CARTESIAN_POINT('Ctrl Pts',(1.485047891698,9.83349529088018,10.9048315914129));
#87402=CARTESIAN_POINT('Ctrl Pts',(1.24276481244143,9.86402045927306,10.9087406153181));
#87403=CARTESIAN_POINT('Ctrl Pts',(1.00042845029488,9.89455234076035,10.9126504988958));
#87404=CARTESIAN_POINT('Ctrl Pts',(0.75698474781826,9.9161471285221,10.9165603824735));
#87405=CARTESIAN_POINT('Ctrl Pts',(0.513105806476577,9.928750496984,10.9204702660512));
#87406=CARTESIAN_POINT('Ctrl Pts',(0.339094095759849,9.93774321154469,10.923260033492));
#87407=CARTESIAN_POINT('Ctrl Pts',(0.164860935587527,9.94215942126182,10.9260498009328));
#87408=CARTESIAN_POINT('Ctrl Pts',(-0.00934887766062076,9.94199560442905,
10.9288395683737));
#87409=CARTESIAN_POINT('Ctrl Pts',(-0.253505047802842,9.94176601408767,
10.9327494453274));
#87410=CARTESIAN_POINT('Ctrl Pts',(-0.497690115998496,9.93253804037886,
10.9366593222812));
#87411=CARTESIAN_POINT('Ctrl Pts',(-0.741230351836662,9.9143301117885,10.940569199235));
#87412=CARTESIAN_POINT('Ctrl Pts',(-0.984728428630572,9.89612533515725,
10.9444783993532));
#87413=CARTESIAN_POINT('Ctrl Pts',(-1.22758161650558,9.86894372769085,10.9483875994715));
#87414=CARTESIAN_POINT('Ctrl Pts',(-1.46911956700822,9.83285572444921,10.9522967995898));
#87415=CARTESIAN_POINT('Ctrl Pts',(-1.71063122256193,9.79677164991608,10.9562055741343));
#87416=CARTESIAN_POINT('Ctrl Pts',(-1.95082764950584,9.75178315697482,10.9601143486788));
#87417=CARTESIAN_POINT('Ctrl Pts',(-2.18904593176416,9.69801226585256,10.9640231232233));
#87418=CARTESIAN_POINT('Ctrl Pts',(-2.42728270097545,9.64423720183507,10.9679322011086));
#87419=CARTESIAN_POINT('Ctrl Pts',(-2.66354074462762,9.58167843648087,10.971841278994));
#87420=CARTESIAN_POINT('Ctrl Pts',(-2.89716834531858,9.51050890220308,10.9757503568793));
#87421=CARTESIAN_POINT('Ctrl Pts',(-3.13079271986601,9.43934035069929,10.9796593807845));
#87422=CARTESIAN_POINT('Ctrl Pts',(-3.36178645653683,9.35956135174315,10.9835684046897));
#87423=CARTESIAN_POINT('Ctrl Pts',(-3.58951327945143,9.27139463169602,10.9874774285949));
#87424=CARTESIAN_POINT('Ctrl Pts',(-3.81729018404561,9.1832085220251,10.9913873121726));
#87425=CARTESIAN_POINT('Ctrl Pts',(-4.04179847740791,9.0866311056931,10.9952971957503));
#87426=CARTESIAN_POINT('Ctrl Pts',(-4.26242084838038,8.98193367328508,10.999207079328));
#87427=CARTESIAN_POINT('Ctrl Pts',(-4.41983860649131,8.90723030110665,11.0019968467689));
#87428=CARTESIAN_POINT('Ctrl Pts',(-4.57527841399815,8.82839399439515,11.0047866142098));
#87429=CARTESIAN_POINT('Ctrl Pts',(-4.72852315291297,8.74553787896239,11.0075763816507));
#87430=CARTESIAN_POINT('Ctrl Pts',(-4.94329663696178,8.62941450198869,11.0114862586044));
#87431=CARTESIAN_POINT('Ctrl Pts',(-5.15382327057579,8.50535790374556,11.0153961355582));
#87432=CARTESIAN_POINT('Ctrl Pts',(-5.3595188513826,8.37370417925511,11.019306012512));
#87433=CARTESIAN_POINT('Ctrl Pts',(-5.56517882440243,8.24207324522889,11.0232152126303));
#87434=CARTESIAN_POINT('Ctrl Pts',(-5.76600917808077,8.10284796129113,11.0271244127486));
#87435=CARTESIAN_POINT('Ctrl Pts',(-5.96145337837669,7.95640858788946,11.0310336128668));
#87436=CARTESIAN_POINT('Ctrl Pts',(-6.15687630170377,7.8099851565622,11.0349423874114));
#87437=CARTESIAN_POINT('Ctrl Pts',(-6.34691401818163,7.65634937189676,11.0388511619559));
#87438=CARTESIAN_POINT('Ctrl Pts',(-6.53104102680931,7.49592336581249,11.0427599365004));
#87439=CARTESIAN_POINT('Ctrl Pts',(-6.71518232463094,7.33548490985282,11.0466690143857));
#87440=CARTESIAN_POINT('Ctrl Pts',(-6.89341178465727,7.16825536135272,11.050578092271));
#87441=CARTESIAN_POINT('Ctrl Pts',(-7.065237934134,6.99469634323564,11.0544871701563));
#87442=CARTESIAN_POINT('Ctrl Pts',(-7.23706171087906,6.82113972177923,11.0583961940615));
#87443=CARTESIAN_POINT('Ctrl Pts',(-7.40248215815815,6.64125400617605,11.0623052179668));
#87444=CARTESIAN_POINT('Ctrl Pts',(-7.56104503468513,6.45553731175519,11.066214241872));
#87445=CARTESIAN_POINT('Ctrl Pts',(-7.71964278235733,6.26977977452191,11.0701241254497));
#87446=CARTESIAN_POINT('Ctrl Pts',(-7.87137976295526,6.07818890873466,11.0740340090274));
#87447=CARTESIAN_POINT('Ctrl Pts',(-8.01584148358511,5.88129656708757,11.0779438926051));
#87448=CARTESIAN_POINT('Ctrl Pts',(-8.11891734163962,5.74081058248799,11.0807336600459));
#87449=CARTESIAN_POINT('Ctrl Pts',(-8.21829015114439,5.59762628955095,11.0835234274868));
#87450=CARTESIAN_POINT('Ctrl Pts',(-8.31382253625083,5.45194633463389,11.0863131949276));
#87451=CARTESIAN_POINT('Ctrl Pts',(-8.44771178644246,5.247774943853,11.0902230718814));
#87452=CARTESIAN_POINT('Ctrl Pts',(-8.57409681002773,5.03863783848452,11.0941329488352));
#87453=CARTESIAN_POINT('Ctrl Pts',(-8.69262302131791,4.82510818627457,11.0980428257889));
#87454=CARTESIAN_POINT('Ctrl Pts',(-8.81112871463591,4.6116154980021,11.1019520259072));
#87455=CARTESIAN_POINT('Ctrl Pts',(-8.9217781754142,4.39373202576283,11.1058612260255));
#87456=CARTESIAN_POINT('Ctrl Pts',(-9.02426213794967,4.17205667094396,11.1097704261438));
#87457=CARTESIAN_POINT('Ctrl Pts',(-9.12673494360241,3.95040544873938,11.1136792006882));
#87458=CARTESIAN_POINT('Ctrl Pts',(-9.22104390834246,3.72496342252571,11.1175879752327));
#87459=CARTESIAN_POINT('Ctrl Pts',(-9.30692695860978,3.49635161090852,11.1214967497772));
#87460=CARTESIAN_POINT('Ctrl Pts',(-9.39281667383949,3.26772205784961,11.1254058276625));
#87461=CARTESIAN_POINT('Ctrl Pts',(-9.47027906653463,3.03592248919001,11.1293149055479));
#87462=CARTESIAN_POINT('Ctrl Pts',(-9.5391007611608,2.80159252362319,11.1332239834332));
#87463=CARTESIAN_POINT('Ctrl Pts',(-9.60792150543459,2.56726579389709,11.1371330073384));
#87464=CARTESIAN_POINT('Ctrl Pts',(-9.66810171325807,2.33040900669727,11.1410420312436));
#87465=CARTESIAN_POINT('Ctrl Pts',(-9.71947810260133,2.09167622089398,11.1449510551489));
#87466=CARTESIAN_POINT('Ctrl Pts',(-9.77086579063905,1.85289093298144,11.1488609387265));
#87467=CARTESIAN_POINT('Ctrl Pts',(-9.81344573148909,1.6122290960173,11.1527708223042));
#87468=CARTESIAN_POINT('Ctrl Pts',(-9.84710564372979,1.37035558933617,11.1566807058819));
#87469=CARTESIAN_POINT('Ctrl Pts',(-9.87112255506911,1.19777478984533,11.1594704733228));
#87470=CARTESIAN_POINT('Ctrl Pts',(-9.89059929140811,1.02457734830841,11.1622602407637));
#87471=CARTESIAN_POINT('Ctrl Pts',(-9.90551116104081,0.85100683810172,11.1650500082046));
#87472=CARTESIAN_POINT('Ctrl Pts',(-9.92783320511444,0.59118371235366,11.1692260983465));
#87473=CARTESIAN_POINT('Ctrl Pts',(-9.93992857739201,0.330476623162821,
11.1734021884884));
#87474=CARTESIAN_POINT('Ctrl Pts',(-9.9417559862999,0.0696556449266178,
11.1775782786304));
#87475=CARTESIAN_POINT('Ctrl Pts',(-9.94191813174516,0.046513077619066,
11.1779488218583));
#87476=CARTESIAN_POINT('Ctrl Pts',(-9.94199947180459,0.0233696156365881,
11.1783193650862));
#87477=CARTESIAN_POINT('Ctrl Pts',(-9.94199999743589,0.000225797940864191,
11.1786899083142));
#87478=CARTESIAN_POINT('Origin',(0.,0.,0.));
#87479=CARTESIAN_POINT('',(-9.94199999835375,-0.000180925794382757,12.3213100916858));
#87480=CARTESIAN_POINT('',(-9.94199999827757,-0.000185064137654065,12.1786899083142));
#87481=CARTESIAN_POINT('',(-9.942,-1.2175438477123E-15,0.));
#87482=CARTESIAN_POINT('Ctrl Pts',(-9.94199999835374,-0.000180925794382757,
12.3213100916858));
#87483=CARTESIAN_POINT('Ctrl Pts',(-9.94200442539233,0.243087966494525,
12.317414885382));
#87484=CARTESIAN_POINT('Ctrl Pts',(-9.93307575954664,0.486394731463211,
12.3135196790782));
#87485=CARTESIAN_POINT('Ctrl Pts',(-9.9152317361037,0.72907038025286,12.3096244727743));
#87486=CARTESIAN_POINT('Ctrl Pts',(-9.8973905132846,0.971707941040203,12.3057298778241));
#87487=CARTESIAN_POINT('Ctrl Pts',(-9.87063674690965,1.21371429979925,12.3018352828739));
#87488=CARTESIAN_POINT('Ctrl Pts',(-9.83504017978952,1.45442382472429,12.2979406879236));
#87489=CARTESIAN_POINT('Ctrl Pts',(-9.79944208775857,1.69514366133356,12.294045926134));
#87490=CARTESIAN_POINT('Ctrl Pts',(-9.75500047577314,1.93456627110119,12.2901511643444));
#87491=CARTESIAN_POINT('Ctrl Pts',(-9.70183671624221,2.17203322520045,12.2862564025547));
#87492=CARTESIAN_POINT('Ctrl Pts',(-9.64867488166776,2.40949158108244,12.2823617817868));
#87493=CARTESIAN_POINT('Ctrl Pts',(-9.58679159441755,2.64499414551934,12.278467161019));
#87494=CARTESIAN_POINT('Ctrl Pts',(-9.51635906541771,2.87789404565945,12.2745725402511));
#87495=CARTESIAN_POINT('Ctrl Pts',(-9.4459094703647,3.11085037827668,12.2706769758027));
#87496=CARTESIAN_POINT('Ctrl Pts',(-9.36690657469958,3.34120251339907,12.2667814113543));
#87497=CARTESIAN_POINT('Ctrl Pts',(-9.27957248525616,3.56831872047282,12.2628858469059));
#87498=CARTESIAN_POINT('Ctrl Pts',(-9.19981206165476,3.77573927066567,12.2593281081976));
#87499=CARTESIAN_POINT('Ctrl Pts',(-9.11310339949484,3.98046083360219,12.2557703694892));
#87500=CARTESIAN_POINT('Ctrl Pts',(-9.01965091992122,4.18201641349771,12.2522126307809));
#87501=CARTESIAN_POINT('Ctrl Pts',(-8.91694869074934,4.40352158330965,12.2483027538271));
#87502=CARTESIAN_POINT('Ctrl Pts',(-8.8060671984233,4.62127556763162,12.2443928768734));
#87503=CARTESIAN_POINT('Ctrl Pts',(-8.68730599303533,4.83467460987526,12.2404829999196));
#87504=CARTESIAN_POINT('Ctrl Pts',(-8.56856534629907,5.04803671079138,12.2365737998013));
#87505=CARTESIAN_POINT('Ctrl Pts',(-8.44194784569837,5.25704512973018,12.232664599683));
#87506=CARTESIAN_POINT('Ctrl Pts',(-8.30779882393879,5.4611210113823,12.2287553995648));
#87507=CARTESIAN_POINT('Ctrl Pts',(-8.17366440626839,5.66517467638062,12.2248466250203));
#87508=CARTESIAN_POINT('Ctrl Pts',(-8.03200025846291,5.8642966421205,12.2209378504758));
#87509=CARTESIAN_POINT('Ctrl Pts',(-7.88319541304502,6.05793645392108,12.2170290759313));
#87510=CARTESIAN_POINT('Ctrl Pts',(-7.73437901961274,6.25159129315795,12.213119998046));
#87511=CARTESIAN_POINT('Ctrl Pts',(-7.57842098963884,6.4397629041926,12.2092109201607));
#87512=CARTESIAN_POINT('Ctrl Pts',(-7.41575186360424,6.62193236883693,12.2053018422754));
#87513=CARTESIAN_POINT('Ctrl Pts',(-7.25308498385263,6.80409931791989,12.2013928183701));
#87514=CARTESIAN_POINT('Ctrl Pts',(-7.08370738163779,6.98026407865271,12.1974837944649));
#87515=CARTESIAN_POINT('Ctrl Pts',(-6.90808830936432,7.14994265082064,12.1935747705597));
#87516=CARTESIAN_POINT('Ctrl Pts',(-6.73243061494724,7.31965853869747,12.189664886982));
#87517=CARTESIAN_POINT('Ctrl Pts',(-6.55052890870874,7.48288519216336,12.1857550034043));
#87518=CARTESIAN_POINT('Ctrl Pts',(-6.36288855985471,7.63917621048697,12.1818451198266));
#87519=CARTESIAN_POINT('Ctrl Pts',(-6.22900402712456,7.75069247064087,12.1790553523857));
#87520=CARTESIAN_POINT('Ctrl Pts',(-6.09219867152078,7.85867854238801,12.1762655849448));
#87521=CARTESIAN_POINT('Ctrl Pts',(-5.9526663120779,7.9629848534989,12.173475817504));
#87522=CARTESIAN_POINT('Ctrl Pts',(-5.75711081576817,8.10917081723498,12.1695659405502));
#87523=CARTESIAN_POINT('Ctrl Pts',(-5.5561377292358,8.24817197377081,12.1656560635964));
#87524=CARTESIAN_POINT('Ctrl Pts',(-5.35029734095619,8.37959917677195,12.1617461866427));
#87525=CARTESIAN_POINT('Ctrl Pts',(-5.14449258553204,8.51100362852117,12.1578369865244));
#87526=CARTESIAN_POINT('Ctrl Pts',(-4.93382244647279,8.63483659325366,12.1539277864061));
#87527=CARTESIAN_POINT('Ctrl Pts',(-4.71886568293697,8.75075257714443,12.1500185862878));
#87528=CARTESIAN_POINT('Ctrl Pts',(-4.50393232059929,8.86665594187931,12.1461098117434));
#87529=CARTESIAN_POINT('Ctrl Pts',(-4.28471351218789,8.9746439136719,12.1422010371989));
#87530=CARTESIAN_POINT('Ctrl Pts',(-4.06181299303673,9.07441674211616,12.1382922626544));
#87531=CARTESIAN_POINT('Ctrl Pts',(-3.83889517566848,9.17419731344074,12.1343831847691));
#87532=CARTESIAN_POINT('Ctrl Pts',(-3.61229533124862,9.26576135016725,12.1304741068838));
#87533=CARTESIAN_POINT('Ctrl Pts',(-3.38263875336924,9.34885656453262,12.1265650289985));
#87534=CARTESIAN_POINT('Ctrl Pts',(-3.15298534679653,9.43195063144378,12.1226560050932));
#87535=CARTESIAN_POINT('Ctrl Pts',(-2.92027555549027,9.50657601644278,12.118746981188));
#87536=CARTESIAN_POINT('Ctrl Pts',(-2.68515216503208,9.57252954294859,12.1148379572828));
#87537=CARTESIAN_POINT('Ctrl Pts',(-2.4499770662418,9.63849757395284,12.1109280737051));
#87538=CARTESIAN_POINT('Ctrl Pts',(-2.21238757740481,9.69578985901981,12.1070181901274));
#87539=CARTESIAN_POINT('Ctrl Pts',(-1.97304041898176,9.74425346063331,12.1031083065497));
#87540=CARTESIAN_POINT('Ctrl Pts',(-1.80226221130059,9.77883305236884,12.1003185391088));
#87541=CARTESIAN_POINT('Ctrl Pts',(-1.63058945480415,9.80891895754833,12.0975287716679));
#87542=CARTESIAN_POINT('Ctrl Pts',(-1.45826374455853,9.8344715593318,12.094739004227));
#87543=CARTESIAN_POINT('Ctrl Pts',(-1.21674815686027,9.87028369455039,12.0908291272733));
#87544=CARTESIAN_POINT('Ctrl Pts',(-0.973875761408798,9.8972002796991,12.0869192503195));
#87545=CARTESIAN_POINT('Ctrl Pts',(-0.730315628791058,9.9151400939343,12.0830093733658));
#87546=CARTESIAN_POINT('Ctrl Pts',(-0.486797658661161,9.93307680262349,
12.0791001732475));
#87547=CARTESIAN_POINT('Ctrl Pts',(-0.24259246843857,9.942039821876,12.0751909731292));
#87548=CARTESIAN_POINT('Ctrl Pts',(0.00162653965630068,9.94199986694673,
12.0712817730109));
#87549=CARTESIAN_POINT('Ctrl Pts',(0.245818960931708,9.94195991636714,12.0673729984664));
#87550=CARTESIAN_POINT('Ctrl Pts',(0.490024916872339,9.93291894860618,12.0634642239218));
#87551=CARTESIAN_POINT('Ctrl Pts',(0.733570741879149,9.91489979609773,12.0595554493773));
#87552=CARTESIAN_POINT('Ctrl Pts',(0.977135467280196,9.89687924521144,12.055646371492));
#87553=CARTESIAN_POINT('Ctrl Pts',(1.22003967959193,9.86987913495575,12.0517372936067));
#87554=CARTESIAN_POINT('Ctrl Pts',(1.46161327421379,9.83397430526652,12.0478282157213));
#87555=CARTESIAN_POINT('Ctrl Pts',(1.70318353296792,9.79806997138381,12.0439191918161));
#87556=CARTESIAN_POINT('Ctrl Pts',(1.94342293380041,9.7532612072464,12.0400101679109));
#87557=CARTESIAN_POINT('Ctrl Pts',(2.18166929454196,9.6996743805786,12.0361011440057));
#87558=CARTESIAN_POINT('Ctrl Pts',(2.4199680504199,9.64607576909661,12.032191260428));
#87559=CARTESIAN_POINT('Ctrl Pts',(2.65627261658128,9.58369529823059,12.0282813768503));
#87560=CARTESIAN_POINT('Ctrl Pts',(2.88993239941065,9.51271016728864,12.0243714932726));
#87561=CARTESIAN_POINT('Ctrl Pts',(3.05665256931344,9.46206108704081,12.0215817258317));
#87562=CARTESIAN_POINT('Ctrl Pts',(3.22202650588926,9.40703238440347,12.0187919583909));
#87563=CARTESIAN_POINT('Ctrl Pts',(3.38582277126201,9.34770389783522,12.01600219095));
#87564=CARTESIAN_POINT('Ctrl Pts',(3.61538428729282,9.26455464355015,12.0120923139963));
#87565=CARTESIAN_POINT('Ctrl Pts',(3.8419164732703,9.1729322022759,12.0081824370425));
#87566=CARTESIAN_POINT('Ctrl Pts',(4.0647919160909,9.07308275498918,12.0042725600887));
#87567=CARTESIAN_POINT('Ctrl Pts',(4.28762877713359,8.97325059255516,12.0003633599704));
#87568=CARTESIAN_POINT('Ctrl Pts',(4.50680990297581,8.8651943816225,11.9964541598521));
#87569=CARTESIAN_POINT('Ctrl Pts',(4.72172872663316,8.74920806885327,11.9925449597338));
#87570=CARTESIAN_POINT('Ctrl Pts',(4.93662415322192,8.63323438289666,11.9886361851893));
#87571=CARTESIAN_POINT('Ctrl Pts',(5.14725795752613,8.50933245192701,11.9847274106448));
#87572=CARTESIAN_POINT('Ctrl Pts',(5.35304808513623,8.377842216121,11.9808186361003));
#87573=CARTESIAN_POINT('Ctrl Pts',(5.55885418310928,8.24634177600242,11.976909558215));
#87574=CARTESIAN_POINT('Ctrl Pts',(5.75981561540428,8.10725200268,11.9730004803296));
#87575=CARTESIAN_POINT('Ctrl Pts',(5.95537815395821,7.96095691756697,11.9690914024443));
#87576=CARTESIAN_POINT('Ctrl Pts',(6.15093799200599,7.81466385263008,11.9651823785391));
#87577=CARTESIAN_POINT('Ctrl Pts',(6.34109886218146,7.66116584446778,11.9612733546339));
#87578=CARTESIAN_POINT('Ctrl Pts',(6.52533797351644,7.50088850279647,11.9573643307287));
#87579=CARTESIAN_POINT('Ctrl Pts',(6.70961760271482,7.3405759129339,11.953454447151));
#87580=CARTESIAN_POINT('Ctrl Pts',(6.8879726586008,7.17348119376462,11.9495445635733));
#87581=CARTESIAN_POINT('Ctrl Pts',(7.05991468331884,7.00006918996227,11.9456346799956));
#87582=CARTESIAN_POINT('Ctrl Pts',(7.18259819875828,6.87633681981741,11.9428449125547));
#87583=CARTESIAN_POINT('Ctrl Pts',(7.30201751837408,6.74938910177999,11.9400551451139));
#87584=CARTESIAN_POINT('Ctrl Pts',(7.41800685906114,6.61940618476626,11.937265377673));
#87585=CARTESIAN_POINT('Ctrl Pts',(7.58056666365085,6.43723429324081,11.9333555007193));
#87586=CARTESIAN_POINT('Ctrl Pts',(7.73643741773675,6.2490434033201,11.9294456237655));
#87587=CARTESIAN_POINT('Ctrl Pts',(7.88518381604907,6.05534806490245,11.9255357468117));
#87588=CARTESIAN_POINT('Ctrl Pts',(8.03390446499868,5.86168625692037,11.9216265466935));
#87589=CARTESIAN_POINT('Ctrl Pts',(8.17550304945856,5.66252212479608,11.9177173465752));
#87590=CARTESIAN_POINT('Ctrl Pts',(8.30958528924128,5.45840235974089,11.9138081464569));
#87591=CARTESIAN_POINT('Ctrl Pts',(8.44365293220342,5.25430481611929,11.9098993719124));
#87592=CARTESIAN_POINT('Ctrl Pts',(8.57020571045967,5.0452529509567,11.905990597368));
#87593=CARTESIAN_POINT('Ctrl Pts',(8.68889275436497,4.83182229631264,11.9020818228235));
#87594=CARTESIAN_POINT('Ctrl Pts',(8.80758900899101,4.6183750783598,11.8981727449382));
#87595=CARTESIAN_POINT('Ctrl Pts',(8.91841817060669,4.4005486354097,11.8942636670529));
#87596=CARTESIAN_POINT('Ctrl Pts',(9.02107478865042,4.17894408404513,11.8903545891676));
#87597=CARTESIAN_POINT('Ctrl Pts',(9.1237299891183,3.95734259279755,11.8864455652624));
#87598=CARTESIAN_POINT('Ctrl Pts',(9.21821275575972,3.73196335270697,11.8825365413571));
#87599=CARTESIAN_POINT('Ctrl Pts',(9.30426505132221,3.50342915651852,11.8786275174519));
#87600=CARTESIAN_POINT('Ctrl Pts',(9.39033627150416,3.27484470109331,11.8747176338742));
#87601=CARTESIAN_POINT('Ctrl Pts',(9.46797321618458,3.04310416524609,11.8708077502965));
#87602=CARTESIAN_POINT('Ctrl Pts',(9.53696669288317,2.80884857171706,11.8668978667188));
#87603=CARTESIAN_POINT('Ctrl Pts',(9.58619469446056,2.64170328089288,11.8641080992779));
#87604=CARTESIAN_POINT('Ctrl Pts',(9.6310232746454,2.47327794012498,11.861318331837));
#87605=CARTESIAN_POINT('Ctrl Pts',(9.67139205901706,2.30380981002811,11.8585285643961));
#87606=CARTESIAN_POINT('Ctrl Pts',(9.7279691691198,2.06629913923054,11.8546186874423));
#87607=CARTESIAN_POINT('Ctrl Pts',(9.77580150726998,1.82666698267465,11.8507088104885));
#87608=CARTESIAN_POINT('Ctrl Pts',(9.81475025993748,1.58557287283091,11.8467989335348));
#87609=CARTESIAN_POINT('Ctrl Pts',(9.85369227021962,1.34452049858287,11.8428897334165));
#87610=CARTESIAN_POINT('Ctrl Pts',(9.88375372019248,1.10200695283348,11.8389805332982));
#87611=CARTESIAN_POINT('Ctrl Pts',(9.90484716277328,0.85870057767661,11.8350713331799));
#87612=CARTESIAN_POINT('Ctrl Pts',(9.92593830902312,0.615420689991385,11.8311625586354));
#87613=CARTESIAN_POINT('Ctrl Pts',(9.9380633730338,0.371348424390499,11.8272537840909));
#87614=CARTESIAN_POINT('Ctrl Pts',(9.94118680661349,0.127156895266496,11.8233450095465));
#87615=CARTESIAN_POINT('Ctrl Pts',(9.94431048258757,-0.117053584366446,
11.8194359316612));
#87616=CARTESIAN_POINT('Ctrl Pts',(9.9384311255953,-0.361383065752061,11.8155268537758));
#87617=CARTESIAN_POINT('Ctrl Pts',(9.92356530800884,-0.605157481721497,
11.8116177758905));
#87618=CARTESIAN_POINT('Ctrl Pts',(9.9086996957031,-0.84892853143216,11.8077087519853));
#87619=CARTESIAN_POINT('Ctrl Pts',(9.88484789010907,-1.09214425137222,11.8037997280801));
#87620=CARTESIAN_POINT('Ctrl Pts',(9.85207848366101,-1.33413400818049,11.7998907041749));
#87621=CARTESIAN_POINT('Ctrl Pts',(9.81930187056549,-1.57617698337315,11.7959808205972));
#87622=CARTESIAN_POINT('Ctrl Pts',(9.77760377452297,-1.8169931786777,11.7920709370195));
#87623=CARTESIAN_POINT('Ctrl Pts',(9.72710443168097,-2.05591910715679,11.7881610534418));
#87624=CARTESIAN_POINT('Ctrl Pts',(9.69107230447155,-2.22639676021308,11.7853712860009));
#87625=CARTESIAN_POINT('Ctrl Pts',(9.65056048832801,-2.39591221604449,11.78258151856));
#87626=CARTESIAN_POINT('Ctrl Pts',(9.60562849498159,-2.56422799618084,11.7797917511191));
#87627=CARTESIAN_POINT('Ctrl Pts',(9.54265601824462,-2.80012364112552,11.7758818741654));
#87628=CARTESIAN_POINT('Ctrl Pts',(9.4709799982601,-3.03373453810527,11.7719719972116));
#87629=CARTESIAN_POINT('Ctrl Pts',(9.39079139998933,-3.26441432448249,11.7680621202578));
#87630=CARTESIAN_POINT('Ctrl Pts',(9.310616683099,-3.49505417807695,11.7641529201396));
#87631=CARTESIAN_POINT('Ctrl Pts',(9.22193242156492,-3.72276366931889,11.7602437200213));
#87632=CARTESIAN_POINT('Ctrl Pts',(9.12497897075788,-3.94691307013804,11.756334519903));
#87633=CARTESIAN_POINT('Ctrl Pts',(9.02803607475598,-4.17103806900728,11.7524257453585));
#87634=CARTESIAN_POINT('Ctrl Pts',(8.92282589817382,-4.39160349412523,11.748516970814));
#87635=CARTESIAN_POINT('Ctrl Pts',(8.80963673854157,-4.60800005804456,11.7446081962695));
#87636=CARTESIAN_POINT('Ctrl Pts',(8.69643879485385,-4.82441341543975,11.7406991183842));
#87637=CARTESIAN_POINT('Ctrl Pts',(8.57526075802538,-5.03665701535093,11.7367900404989));
#87638=CARTESIAN_POINT('Ctrl Pts',(8.44643724939473,-5.24414547777206,11.7328809626135));
#87639=CARTESIAN_POINT('Ctrl Pts',(8.31761551967681,-5.4516310750029,11.7289719387083));
#87640=CARTESIAN_POINT('Ctrl Pts',(8.18114867892451,-5.65436142899711,11.7250629148031));
#87641=CARTESIAN_POINT('Ctrl Pts',(8.03741550115518,-5.8517788801176,11.7211538908979));
#87642=CARTESIAN_POINT('Ctrl Pts',(7.89365071358688,-6.0492397472819,11.7172440073202));
#87643=CARTESIAN_POINT('Ctrl Pts',(7.74261656014366,-6.24138514958947,11.7133341237425));
#87644=CARTESIAN_POINT('Ctrl Pts',(7.58473387360734,-6.42768823657102,11.7094242401648));
#87645=CARTESIAN_POINT('Ctrl Pts',(7.47208193151584,-6.5606186105502,11.7066344727239));
#87646=CARTESIAN_POINT('Ctrl Pts',(7.3559442387082,-6.69057526995139,11.703844705283));
#87647=CARTESIAN_POINT('Ctrl Pts',(7.23648592246849,-6.81737746453248,11.7010549378421));
#87648=CARTESIAN_POINT('Ctrl Pts',(7.06906432640483,-6.9950915531736,11.6971450608884));
#87649=CARTESIAN_POINT('Ctrl Pts',(6.89506747952659,-7.16666253062821,11.6932351839346));
#87650=CARTESIAN_POINT('Ctrl Pts',(6.71497033289678,-7.33161219844013,11.6893253069808));
#87651=CARTESIAN_POINT('Ctrl Pts',(6.53490436273144,-7.49653331195481,11.6854161068626));
#87652=CARTESIAN_POINT('Ctrl Pts',(6.34874040747457,-7.6548352146869,11.6815069067443));
#87653=CARTESIAN_POINT('Ctrl Pts',(6.15698898900126,-7.80607779805693,11.677597706626));
#87654=CARTESIAN_POINT('Ctrl Pts',(5.96525844548466,-7.95730391645159,11.6736889320816));
#87655=CARTESIAN_POINT('Ctrl Pts',(5.76794187329016,-8.10147207642406,11.6697801575371));
#87656=CARTESIAN_POINT('Ctrl Pts',(5.56558228344404,-8.23818292138587,11.6658713829927));
#87657=CARTESIAN_POINT('Ctrl Pts',(5.36320698946049,-8.3749043758073,11.6619623051073));
#87658=CARTESIAN_POINT('Ctrl Pts',(5.15578812637295,-8.50416719934206,11.658053227222));
#87659=CARTESIAN_POINT('Ctrl Pts',(4.94389812405574,-8.62561507018243,11.6541441493367));
#87660=CARTESIAN_POINT('Ctrl Pts',(4.73201104770847,-8.74706126396009,11.6502351254315));
#87661=CARTESIAN_POINT('Ctrl Pts',(4.51565319985091,-8.86069258326205,11.6463261015263));
#87662=CARTESIAN_POINT('Ctrl Pts',(4.29542270807355,-8.96619806601249,11.6424170776211));
#87663=CARTESIAN_POINT('Ctrl Pts',(4.07514378320925,-9.07172675152735,11.6385071940434));
#87664=CARTESIAN_POINT('Ctrl Pts',(3.85099076510653,-9.16912590763106,11.6345973104657));
#87665=CARTESIAN_POINT('Ctrl Pts',(3.62358416970183,-9.25813165628391,11.630687426888));
#87666=CARTESIAN_POINT('Ctrl Pts',(3.46132575379055,-9.32163874919698,11.627897659447));
#87667=CARTESIAN_POINT('Ctrl Pts',(3.29741139000283,-9.3808736912374,11.6251078920061));
#87668=CARTESIAN_POINT('Ctrl Pts',(3.13207222452451,-9.43575580334517,11.6223181245651));
#87669=CARTESIAN_POINT('Ctrl Pts',(2.90034832411118,-9.51267343531544,11.6184082476114));
#87670=CARTESIAN_POINT('Ctrl Pts',(2.66575417575317,-9.58106267851279,11.6144983706576));
#87671=CARTESIAN_POINT('Ctrl Pts',(2.42893482585738,-9.64072816812803,11.6105884937038));
#87672=CARTESIAN_POINT('Ctrl Pts',(2.19215647155919,-9.70038332910076,11.6066792935855));
#87673=CARTESIAN_POINT('Ctrl Pts',(1.95315395635757,-9.75131768266608,11.6027700934672));
#87674=CARTESIAN_POINT('Ctrl Pts',(1.71258554818117,-9.79338627544942,11.5988608933489));
#87675=CARTESIAN_POINT('Ctrl Pts',(1.47204332940585,-9.83545028844916,11.5949521188044));
#87676=CARTESIAN_POINT('Ctrl Pts',(1.22993583404512,-9.86865041952879,11.59104334426));
#87677=CARTESIAN_POINT('Ctrl Pts',(0.986930575443621,-9.89289300656054,
11.5871345697155));
#87678=CARTESIAN_POINT('Ctrl Pts',(0.743906458394857,-9.91713747494068,
11.5832254918301));
#87679=CARTESIAN_POINT('Ctrl Pts',(0.499984717526834,-9.93242297934666,
11.5793164139448));
#87680=CARTESIAN_POINT('Ctrl Pts',(0.255838325587391,-9.93870770025765,
11.5754073360595));
#87681=CARTESIAN_POINT('Ctrl Pts',(0.0116953050447619,-9.94499233438346,
11.5714983121543));
#87682=CARTESIAN_POINT('Ctrl Pts',(-0.23267208007543,-9.94227642844193,
11.5675892882491));
#87683=CARTESIAN_POINT('Ctrl Pts',(-0.47658977644844,-9.93057028498287,
11.5636802643439));
#87684=CARTESIAN_POINT('Ctrl Pts',(-0.720561115199568,-9.91886156710883,
11.5597703807662));
#87685=CARTESIAN_POINT('Ctrl Pts',(-0.964082287443942,-9.89815867350913,
11.5558604971884));
#87686=CARTESIAN_POINT('Ctrl Pts',(-1.20648189053658,-9.86852397513464,
11.5519506136107));
#87687=CARTESIAN_POINT('Ctrl Pts',(-1.37943806862841,-9.84737912132976,
11.5491608461699));
#87688=CARTESIAN_POINT('Ctrl Pts',(-1.55182330419729,-9.82168811958611,
11.546371078729));
#87689=CARTESIAN_POINT('Ctrl Pts',(-1.72339585979082,-9.79148970843844,
11.5435813112882));
#87690=CARTESIAN_POINT('Ctrl Pts',(-1.96385589641977,-9.74916644161068,
11.5396714343344));
#87691=CARTESIAN_POINT('Ctrl Pts',(-2.20279290781731,-9.69797457103316,
11.5357615573806));
#87692=CARTESIAN_POINT('Ctrl Pts',(-2.43954643095606,-9.63804841299366,
11.5318516804268));
#87693=CARTESIAN_POINT('Ctrl Pts',(-2.67625896989279,-9.57813262872066,
11.5279424803086));
#87694=CARTESIAN_POINT('Ctrl Pts',(-2.91078850350073,-9.50948564399775,
11.5240332801903));
#87695=CARTESIAN_POINT('Ctrl Pts',(-3.14248686697217,-9.4322924197094,11.520124080072));
#87696=CARTESIAN_POINT('Ctrl Pts',(-3.37416000667744,-9.35510759903604,
11.5162153055275));
#87697=CARTESIAN_POINT('Ctrl Pts',(-3.60300232581281,-9.26937848503996,
11.512306530983));
#87698=CARTESIAN_POINT('Ctrl Pts',(-3.82838187489187,-9.17533956973797,
11.5083977564385));
#87699=CARTESIAN_POINT('Ctrl Pts',(-4.05377891457193,-9.08129335653716,
11.5044886785532));
#87700=CARTESIAN_POINT('Ctrl Pts',(-4.27571238733293,-8.97893615854469,
11.5005796006679));
#87701=CARTESIAN_POINT('Ctrl Pts',(-4.493570152866,-8.86855068662698,11.4966705227826));
#87702=CARTESIAN_POINT('Ctrl Pts',(-4.71142491002214,-8.75816673901163,
11.4927614988773));
#87703=CARTESIAN_POINT('Ctrl Pts',(-4.92520382338169,-8.63975486773473,
11.4888524749721));
#87704=CARTESIAN_POINT('Ctrl Pts',(-5.13431854831489,-8.51364416947465,
11.4849434510669));
#87705=CARTESIAN_POINT('Ctrl Pts',(-5.34347926175485,-8.38750573695195,
11.4810335674892));
#87706=CARTESIAN_POINT('Ctrl Pts',(-5.54797349649497,-8.25366523825121,
11.4771236839115));
#87707=CARTESIAN_POINT('Ctrl Pts',(-5.74723996199185,-8.11249633708909,
11.4732138003338));
#87708=CARTESIAN_POINT('Ctrl Pts',(-5.88941992373415,-8.01176996089537,
11.4704240328929));
#87709=CARTESIAN_POINT('Ctrl Pts',(-6.02893896155739,-7.90731358197483,
11.4676342654521));
#87710=CARTESIAN_POINT('Ctrl Pts',(-6.16560271410774,-7.7992760671608,11.4648444980112));
#87711=CARTESIAN_POINT('Ctrl Pts',(-6.35713783946964,-7.64786079751152,
11.4609346210575));
#87712=CARTESIAN_POINT('Ctrl Pts',(-6.5431218798351,-7.48936335350068,11.4570247441037));
#87713=CARTESIAN_POINT('Ctrl Pts',(-6.72303733110379,-7.32421552417628,
11.4531148671499));
#87714=CARTESIAN_POINT('Ctrl Pts',(-6.90292163736225,-7.15909628345168,
11.4492056670316));
#87715=CARTESIAN_POINT('Ctrl Pts',(-7.07673924521416,-6.98732914501369,
11.4452964669133));
#87716=CARTESIAN_POINT('Ctrl Pts',(-7.24400751947226,-6.80938463136203,
11.441387266795));
#87717=CARTESIAN_POINT('Ctrl Pts',(-7.41125758412094,-6.63145948958531,
11.4374784922506));
#87718=CARTESIAN_POINT('Ctrl Pts',(-7.57195954687448,-6.44735851952012,
11.4335697177061));
#87719=CARTESIAN_POINT('Ctrl Pts',(-7.7256685602556,-6.25758813737994,11.4296609431617));
#87720=CARTESIAN_POINT('Ctrl Pts',(-7.87938950224148,-6.06780302808854,
11.4257518652764));
#87721=CARTESIAN_POINT('Ctrl Pts',(-8.02611623163426,-5.87234784347031,
11.4218427873911));
#87722=CARTESIAN_POINT('Ctrl Pts',(-8.16544422857891,-5.67176203220546,
11.4179337095058));
#87723=CARTESIAN_POINT('Ctrl Pts',(-8.30477030155618,-5.47117899081146,
11.4140246856006));
#87724=CARTESIAN_POINT('Ctrl Pts',(-8.43669768819032,-5.26546569587943,
11.4101156616953));
#87725=CARTESIAN_POINT('Ctrl Pts',(-8.56086483448311,-5.05519112256999,
11.4062066377901));
#87726=CARTESIAN_POINT('Ctrl Pts',(-8.68505928761271,-4.84487030567978,
11.4022967542124));
#87727=CARTESIAN_POINT('Ctrl Pts',(-8.80148994680901,-4.62998644697222,
11.3983868706347));
#87728=CARTESIAN_POINT('Ctrl Pts',(-8.9098402281397,-4.41113490034294,11.394476987057));
#87729=CARTESIAN_POINT('Ctrl Pts',(-8.98714996922696,-4.2549806550686,11.3916872196161));
#87730=CARTESIAN_POINT('Ctrl Pts',(-9.06034688050858,-4.09680698724369,
11.3888974521752));
#87731=CARTESIAN_POINT('Ctrl Pts',(-9.12933058355585,-3.93683719451945,
11.3861076847342));
#87732=CARTESIAN_POINT('Ctrl Pts',(-9.22562982053677,-3.71352403070184,
11.382213250773));
#87733=CARTESIAN_POINT('Ctrl Pts',(-9.31374835312292,-3.48663634832032,
11.3783188168118));
#87734=CARTESIAN_POINT('Ctrl Pts',(-9.39343666062907,-3.25679469766667,
11.3744243828506));
#87735=CARTESIAN_POINT('Ctrl Pts',(-9.47311002949082,-3.02699613391994,
11.3705306789534));
#87736=CARTESIAN_POINT('Ctrl Pts',(-9.5443562345871,-2.79424497617588,11.3666369750562));
#87737=CARTESIAN_POINT('Ctrl Pts',(-9.60697480470969,-2.55917938051893,
11.362743271159));
#87738=CARTESIAN_POINT('Ctrl Pts',(-9.6695917581785,-2.32411985366366,11.3588496677875));
#87739=CARTESIAN_POINT('Ctrl Pts',(-9.72358144507331,-2.0867462825211,11.3549560644159));
#87740=CARTESIAN_POINT('Ctrl Pts',(-9.76879364488237,-1.84771067099419,
11.3510624610443));
#87741=CARTESIAN_POINT('Ctrl Pts',(-9.81400323699699,-1.60868884627345,
11.3471690822433));
#87742=CARTESIAN_POINT('Ctrl Pts',(-9.85043630164515,-1.36800545269013,
11.3432757034422));
#87743=CARTESIAN_POINT('Ctrl Pts',(-9.87799384897245,-1.12632212073742,
11.3393823246412));
#87744=CARTESIAN_POINT('Ctrl Pts',(-9.90555545351527,-0.884603206468445,
11.3354883726296));
#87745=CARTESIAN_POINT('Ctrl Pts',(-9.92423889681383,-0.641884342588685,
11.331594420618));
#87746=CARTESIAN_POINT('Ctrl Pts',(-9.93399699326778,-0.398832969733717,
11.3277004686064));
#87747=CARTESIAN_POINT('Ctrl Pts',(-9.93933500753949,-0.265875511977494,
11.3255703429709));
#87748=CARTESIAN_POINT('Ctrl Pts',(-9.94200305127928,-0.132818623544602,
11.3234402173353));
#87749=CARTESIAN_POINT('Ctrl Pts',(-9.94199999738095,0.000228204292474588,
11.3213100916997));
#87750=CARTESIAN_POINT('Ctrl Pts',(-9.94199999743591,0.000225797020946319,
11.1786899083289));
#87751=CARTESIAN_POINT('Ctrl Pts',(-9.94200552108102,-0.242984141546804,
11.1825838119575));
#87752=CARTESIAN_POINT('Ctrl Pts',(-9.93308227899852,-0.486228017217286,
11.1864777155862));
#87753=CARTESIAN_POINT('Ctrl Pts',(-9.91524887911624,-0.728837200741169,
11.1903716192148));
#87754=CARTESIAN_POINT('Ctrl Pts',(-9.89741786708007,-0.971413899522894,
11.1942650014598));
#87755=CARTESIAN_POINT('Ctrl Pts',(-9.87067909983736,-1.21335579191454,
11.1981583837048));
#87756=CARTESIAN_POINT('Ctrl Pts',(-9.83510318760652,-1.45399769227194,
11.2020517659498));
#87757=CARTESIAN_POINT('Ctrl Pts',(-9.7995252600358,-1.69465322475247,11.205945368751));
#87758=CARTESIAN_POINT('Ctrl Pts',(-9.75510922572029,-1.93400833586019,
11.2098389715522));
#87759=CARTESIAN_POINT('Ctrl Pts',(-9.7019773071014,-2.17140515162176,11.2137325743534));
#87760=CARTESIAN_POINT('Ctrl Pts',(-9.6488460243958,-2.408799126082,11.2176261305538));
#87761=CARTESIAN_POINT('Ctrl Pts',(-9.58699913029883,-2.64423457461387,
11.2215196867541));
#87762=CARTESIAN_POINT('Ctrl Pts',(-9.51660966073042,-2.87706526955722,
11.2254132429544));
#87763=CARTESIAN_POINT('Ctrl Pts',(-9.44620464128667,-3.10994739958461,
11.2293076592879));
#87764=CARTESIAN_POINT('Ctrl Pts',(-9.36725335772919,-3.34022335347587,
11.2332020756213));
#87765=CARTESIAN_POINT('Ctrl Pts',(-9.27997867577238,-3.56726222434095,
11.2370964919548));
#87766=CARTESIAN_POINT('Ctrl Pts',(-9.23000144926437,-3.69727442055797,
11.239326601797));
#87767=CARTESIAN_POINT('Ctrl Pts',(-9.17729572185186,-3.82622542439781,
11.2415567116393));
#87768=CARTESIAN_POINT('Ctrl Pts',(-9.12191049700363,-3.95399960605144,
11.2437868214816));
#87769=CARTESIAN_POINT('Ctrl Pts',(-9.0248079193148,-4.17801607316244,11.2476966984354));
#87770=CARTESIAN_POINT('Ctrl Pts',(-8.91943438172299,-4.39848811357653,
11.2516065753892));
#87771=CARTESIAN_POINT('Ctrl Pts',(-8.80607416515553,-4.61480463267736,
11.2555164523429));
#87772=CARTESIAN_POINT('Ctrl Pts',(-8.69273357227901,-4.83108370540904,
11.2594256524612));
#87773=CARTESIAN_POINT('Ctrl Pts',(-8.57140919039189,-5.04320844466865,
11.2633348525795));
#87774=CARTESIAN_POINT('Ctrl Pts',(-8.44243169442939,-5.25059149857366,
11.2672440526978));
#87775=CARTESIAN_POINT('Ctrl Pts',(-8.31346823956048,-5.45795197578927,
11.2711528272423));
#87776=CARTESIAN_POINT('Ctrl Pts',(-8.17685348213692,-5.6605715603991,11.2750616017868));
#87777=CARTESIAN_POINT('Ctrl Pts',(-8.03296249691464,-5.8578901938465,11.2789703763313));
#87778=CARTESIAN_POINT('Ctrl Pts',(-7.88906034501808,-6.05522414022614,
11.2828794542166));
#87779=CARTESIAN_POINT('Ctrl Pts',(-7.7378809996901,-6.24725608511839,11.2867885321019));
#87780=CARTESIAN_POINT('Ctrl Pts',(-7.57984182315619,-6.43345645325529,
11.2906976099872));
#87781=CARTESIAN_POINT('Ctrl Pts',(-7.42180482897088,-6.61965425016828,
11.2946066338925));
#87782=CARTESIAN_POINT('Ctrl Pts',(-7.25690837600449,-6.80002041898957,
11.2985156577977));
#87783=CARTESIAN_POINT('Ctrl Pts',(-7.08560940378933,-6.97405931842655,
11.3024246817029));
#87784=CARTESIAN_POINT('Ctrl Pts',(-6.91427275950652,-7.14813649249594,
11.3063345652806));
#87785=CARTESIAN_POINT('Ctrl Pts',(-6.73653097846217,-7.31588341618062,
11.3102444488583));
#87786=CARTESIAN_POINT('Ctrl Pts',(-6.55287805058865,-7.4768411280509,11.314154332436));
#87787=CARTESIAN_POINT('Ctrl Pts',(-6.42183860953779,-7.59168715223645,
11.3169440998769));
#87788=CARTESIAN_POINT('Ctrl Pts',(-6.28779054217615,-7.70307751379853,
11.3197338673177));
#87789=CARTESIAN_POINT('Ctrl Pts',(-6.15092384703237,-7.81085781639946,
11.3225236347586));
#87790=CARTESIAN_POINT('Ctrl Pts',(-5.95910429632489,-7.96191260148291,
11.3264335117123));
#87791=CARTESIAN_POINT('Ctrl Pts',(-5.76168828718676,-8.10592101222499,
11.3303433886661));
#87792=CARTESIAN_POINT('Ctrl Pts',(-5.55921615363541,-8.24248019452635,
11.3342532656199));
#87793=CARTESIAN_POINT('Ctrl Pts',(-5.35677906986329,-8.37901573718354,
11.3381624657381));
#87794=CARTESIAN_POINT('Ctrl Pts',(-5.14928784117645,-8.50810446892983,
11.3420716658564));
#87795=CARTESIAN_POINT('Ctrl Pts',(-4.93731236042359,-8.62938645881667,
11.3459808659747));
#87796=CARTESIAN_POINT('Ctrl Pts',(-4.72535995631246,-8.75065524537915,
11.3498896405192));
#87797=CARTESIAN_POINT('Ctrl Pts',(-4.50892451807544,-8.86411884786254,
11.3537984150637));
#87798=CARTESIAN_POINT('Ctrl Pts',(-4.28860205654056,-8.96946243654747,
11.3577071896082));
#87799=CARTESIAN_POINT('Ctrl Pts',(-4.06826249685949,-9.07481420043191,
11.3616162674935));
#87800=CARTESIAN_POINT('Ctrl Pts',(-3.84403556270164,-9.17204456765768,
11.3655253453788));
#87801=CARTESIAN_POINT('Ctrl Pts',(-3.61654000924706,-9.26088561431979,
11.3694344232641));
#87802=CARTESIAN_POINT('Ctrl Pts',(-3.38904759725678,-9.34972543418441,
11.3733434471694));
#87803=CARTESIAN_POINT('Ctrl Pts',(-3.15828691811552,-9.43017606512519,
11.3772524710746));
#87804=CARTESIAN_POINT('Ctrl Pts',(-2.92489544780486,-9.50201823926951,
11.3811614949798));
#87805=CARTESIAN_POINT('Ctrl Pts',(-2.69145265004682,-9.5738762129433,11.3850713785575));
#87806=CARTESIAN_POINT('Ctrl Pts',(-2.45537817276924,-9.63712186348263,
11.3889812621352));
#87807=CARTESIAN_POINT('Ctrl Pts',(-2.21732468511605,-9.69158579597658,
11.3928911457129));
#87808=CARTESIAN_POINT('Ctrl Pts',(-2.04746953320517,-9.7304467243277,11.3956809131538));
#87809=CARTESIAN_POINT('Ctrl Pts',(-1.87660717283218,-9.76483786884063,
11.3984706805947));
#87810=CARTESIAN_POINT('Ctrl Pts',(-1.70497812703265,-9.79471355305198,
11.4012604480355));
#87811=CARTESIAN_POINT('Ctrl Pts',(-1.46443891901957,-9.83658451600917,
11.4051703249893));
#87812=CARTESIAN_POINT('Ctrl Pts',(-1.22231975523809,-9.86959684035222,
11.4090802019431));
#87813=CARTESIAN_POINT('Ctrl Pts',(-0.979287453550639,-9.89365251478534,
11.4129900788969));
#87814=CARTESIAN_POINT('Ctrl Pts',(-0.736297222978803,-9.91770402496106,
11.4168992790151));
#87815=CARTESIAN_POINT('Ctrl Pts',(-0.49239444885965,-9.93280195273437,
11.4208084791334));
#87816=CARTESIAN_POINT('Ctrl Pts',(-0.248251584658489,-9.93890009763226,
11.4247176792517));
#87817=CARTESIAN_POINT('Ctrl Pts',(-0.00413529899127343,-9.94499757865758,
11.4286264537962));
#87818=CARTESIAN_POINT('Ctrl Pts',(0.240220744454,-9.94209722607196,11.4325352283407));
#87819=CARTESIAN_POINT('Ctrl Pts',(0.484142519027582,-9.93020493349808,
11.4364440028852));
#87820=CARTESIAN_POINT('Ctrl Pts',(0.728083223174456,-9.91831171802167,
11.4403530807705));
#87821=CARTESIAN_POINT('Ctrl Pts',(0.971589310963972,-9.89742517876413,
11.4442621586558));
#87822=CARTESIAN_POINT('Ctrl Pts',(1.21398900848753,-9.86760328992159,11.4481712365411));
#87823=CARTESIAN_POINT('Ctrl Pts',(1.45638535873538,-9.83778181288685,11.4520802604463));
#87824=CARTESIAN_POINT('Ctrl Pts',(1.69767507129333,-9.79902526931674,11.4559892843515));
#87825=CARTESIAN_POINT('Ctrl Pts',(1.93719299710581,-9.75144334403704,11.4598983082567));
#87826=CARTESIAN_POINT('Ctrl Pts',(2.17676359769762,-9.7038509545409,11.4638081918344));
#87827=CARTESIAN_POINT('Ctrl Pts',(2.41456135770987,-9.64742935878678,11.4677180754121));
#87828=CARTESIAN_POINT('Ctrl Pts',(2.64993143540265,-9.582339348388,11.4716279589898));
#87829=CARTESIAN_POINT('Ctrl Pts',(2.81787192934708,-9.53589653541714,11.4744177264307));
#87830=CARTESIAN_POINT('Ctrl Pts',(2.9845766906324,-9.48504164796354,11.4772074938716));
#87831=CARTESIAN_POINT('Ctrl Pts',(3.14981234787031,-9.42984868241287,11.4799972613124));
#87832=CARTESIAN_POINT('Ctrl Pts',(3.3813911808257,-9.35249538734794,11.4839071382662));
#87833=CARTESIAN_POINT('Ctrl Pts',(3.61015460183397,-9.26659544417435,11.48781701522));
#87834=CARTESIAN_POINT('Ctrl Pts',(3.83546920859124,-9.17237918699115,11.4917268921738));
#87835=CARTESIAN_POINT('Ctrl Pts',(4.06074481132754,-9.07817923950453,11.495636092292));
#87836=CARTESIAN_POINT('Ctrl Pts',(4.28257253311811,-8.9756659599215,11.4995452924103));
#87837=CARTESIAN_POINT('Ctrl Pts',(4.50033861067237,-8.86511795687409,11.5034544925286));
#87838=CARTESIAN_POINT('Ctrl Pts',(4.71808098119441,-8.75458198859858,11.5073632670731));
#87839=CARTESIAN_POINT('Ctrl Pts',(4.93176234049709,-8.63601317018384,11.5112720416176));
#87840=CARTESIAN_POINT('Ctrl Pts',(5.14079227414159,-8.50973670533502,11.5151808161621));
#87841=CARTESIAN_POINT('Ctrl Pts',(5.34983842957387,-8.3834504407892,11.5190898940474));
#87842=CARTESIAN_POINT('Ctrl Pts',(5.55423219652298,-8.24945547691004,11.5229989719327));
#87843=CARTESIAN_POINT('Ctrl Pts',(5.75340987018901,-8.10812178408858,11.526908049818));
#87844=CARTESIAN_POINT('Ctrl Pts',(5.95258479342843,-7.96679004293138,11.5308170737233));
#87845=CARTESIAN_POINT('Ctrl Pts',(6.14654354001359,-7.8181199394174,11.5347260976285));
#87846=CARTESIAN_POINT('Ctrl Pts',(6.33475278704742,-7.66252380922858,11.5386351215337));
#87847=CARTESIAN_POINT('Ctrl Pts',(6.52300342505649,-7.50689346034078,11.5425450051114));
#87848=CARTESIAN_POINT('Ctrl Pts',(6.7055018201997,-7.34433421912601,11.5464548886891));
#87849=CARTESIAN_POINT('Ctrl Pts',(6.88174798573371,-7.17529850674173,11.5503647722668));
#87850=CARTESIAN_POINT('Ctrl Pts',(7.00750257776134,-7.05468869384408,11.5531545397077));
#87851=CARTESIAN_POINT('Ctrl Pts',(7.13007481817725,-6.93078250799029,11.5559443071486));
#87852=CARTESIAN_POINT('Ctrl Pts',(7.24929444846749,-6.80375587447245,11.5587340745895));
#87853=CARTESIAN_POINT('Ctrl Pts',(7.41638152464323,-6.6257272332221,11.5626439515432));
#87854=CARTESIAN_POINT('Ctrl Pts',(7.57693294207971,-6.44151337547033,11.566553828497));
#87855=CARTESIAN_POINT('Ctrl Pts',(7.73050060056057,-6.25161774780998,11.5704637054508));
#87856=CARTESIAN_POINT('Ctrl Pts',(7.88404167507424,-6.06175499282076,11.5743729055691));
#87857=CARTESIAN_POINT('Ctrl Pts',(8.03060122779979,-5.86621264919469,11.5782821056874));
#87858=CARTESIAN_POINT('Ctrl Pts',(8.16977136281862,-5.66552732578961,11.5821913058056));
#87859=CARTESIAN_POINT('Ctrl Pts',(8.30892634712674,-5.46486384992587,11.5861000803502));
#87860=CARTESIAN_POINT('Ctrl Pts',(8.44069336027182,-5.25905874245552,11.5900088548947));
#87861=CARTESIAN_POINT('Ctrl Pts',(8.56470717829184,-5.04867853503431,11.5939176294392));
#87862=CARTESIAN_POINT('Ctrl Pts',(8.6887306204162,-4.83828200103678,11.5978267073245));
#87863=CARTESIAN_POINT('Ctrl Pts',(8.80499952013151,-4.62330989756236,11.6017357852098));
#87864=CARTESIAN_POINT('Ctrl Pts',(8.91319341518193,-4.40435547425017,11.6056448630952));
#87865=CARTESIAN_POINT('Ctrl Pts',(9.02138581619239,-4.18540407446033,11.6095538870004));
#87866=CARTESIAN_POINT('Ctrl Pts',(9.12150331321155,-3.96247071704888,11.6134629109056));
#87867=CARTESIAN_POINT('Ctrl Pts',(9.21327229751636,-3.73617151263396,11.6173719348108));
#87868=CARTESIAN_POINT('Ctrl Pts',(9.30506146365513,-3.50982254050067,11.6212818183885));
#87869=CARTESIAN_POINT('Ctrl Pts',(9.3884983421169,-3.28010650177633,11.6251917019663));
#87870=CARTESIAN_POINT('Ctrl Pts',(9.46335769533672,-3.04765895895708,11.629101585544));
#87871=CARTESIAN_POINT('Ctrl Pts',(9.51677109808978,-2.88180374261414,11.6318913529848));
#87872=CARTESIAN_POINT('Ctrl Pts',(9.56581864139675,-2.71455830767632,11.6346811204256));
#87873=CARTESIAN_POINT('Ctrl Pts',(9.61043400671094,-2.5461583223857,11.6374708878664));
#87874=CARTESIAN_POINT('Ctrl Pts',(9.6729627272319,-2.31014466337345,11.6413807648202));
#87875=CARTESIAN_POINT('Ctrl Pts',(9.72680275868779,-2.07179040173455,11.645290641774));
#87876=CARTESIAN_POINT('Ctrl Pts',(9.77179875501628,-1.83175137272019,11.6492005187277));
#87877=CARTESIAN_POINT('Ctrl Pts',(9.81678696212597,-1.59175389665878,11.653109718846));
#87878=CARTESIAN_POINT('Ctrl Pts',(9.85293413867704,-1.35007251079478,11.6570189189643));
#87879=CARTESIAN_POINT('Ctrl Pts',(9.88013606741105,-1.1073731482402,11.6609281190826));
#87880=CARTESIAN_POINT('Ctrl Pts',(9.90733503481589,-0.864700207073136,
11.664836893627));
#87881=CARTESIAN_POINT('Ctrl Pts',(9.92559066760065,-0.621009788950606,
11.6687456681715));
#87882=CARTESIAN_POINT('Ctrl Pts',(9.93485051105835,-0.376973902178435,
11.672654442716));
#87883=CARTESIAN_POINT('Ctrl Pts',(9.94411107312712,-0.132919076977237,
11.6765635206013));
#87884=CARTESIAN_POINT('Ctrl Pts',(9.94437443719738,0.111480990436544,11.6804725984866));
#87885=CARTESIAN_POINT('Ctrl Pts',(9.93564022871477,0.355552029307629,11.6843816763719));
#87886=CARTESIAN_POINT('Ctrl Pts',(9.92690614084202,0.599619697824516,11.6882907002771));
#87887=CARTESIAN_POINT('Ctrl Pts',(9.90917474099365,0.843358066809444,11.6921997241823));
#87888=CARTESIAN_POINT('Ctrl Pts',(9.88249774454809,1.08609499078209,11.6961087480876));
#87889=CARTESIAN_POINT('Ctrl Pts',(9.85581488129786,1.32888529745553,11.7000186316653));
#87890=CARTESIAN_POINT('Ctrl Pts',(9.82018252005589,1.5706734401891,11.703928515243));
#87891=CARTESIAN_POINT('Ctrl Pts',(9.77570418321469,1.81079311967955,11.7078383988207));
#87892=CARTESIAN_POINT('Ctrl Pts',(9.7439681446654,1.98212253408547,11.7106281662616));
#87893=CARTESIAN_POINT('Ctrl Pts',(9.70772964888463,2.15260264564454,11.7134179337025));
#87894=CARTESIAN_POINT('Ctrl Pts',(9.66704222013039,2.32199455516511,11.7162077011434));
#87895=CARTESIAN_POINT('Ctrl Pts',(9.61001852788217,2.55939840233825,11.7201175780971));
#87896=CARTESIAN_POINT('Ctrl Pts',(9.54423661801645,2.79473697410858,11.7240274550509));
#87897=CARTESIAN_POINT('Ctrl Pts',(9.46987114979066,3.02735931239793,11.7279373320047));
#87898=CARTESIAN_POINT('Ctrl Pts',(9.39551855490818,3.25994138163106,11.7318465321229));
#87899=CARTESIAN_POINT('Ctrl Pts',(9.312585453156,3.48980788915068,11.7357557322412));
#87900=CARTESIAN_POINT('Ctrl Pts',(9.22129629668423,3.71632326483553,11.7396649323595));
#87901=CARTESIAN_POINT('Ctrl Pts',(9.13001707837692,3.94281398099733,11.7435737069039));
#87902=CARTESIAN_POINT('Ctrl Pts',(9.03038372642572,4.16595403386053,11.7474824814484));
#87903=CARTESIAN_POINT('Ctrl Pts',(8.92266913374048,4.38512708251367,11.7513912559929));
#87904=CARTESIAN_POINT('Ctrl Pts',(8.81494618185332,4.60431714011355,11.7553003338782));
#87905=CARTESIAN_POINT('Ctrl Pts',(8.6991408569652,4.81953932540157,11.7592094117635));
#87906=CARTESIAN_POINT('Ctrl Pts',(8.57557296203935,5.0302000330742,11.7631184896488));
#87907=CARTESIAN_POINT('Ctrl Pts',(8.45200677345155,5.24085783175187,11.767027513554));
#87908=CARTESIAN_POINT('Ctrl Pts',(8.32067837282204,5.44695403803358,11.7709365374592));
#87909=CARTESIAN_POINT('Ctrl Pts',(8.18195239855599,5.64792164851496,11.7748455613645));
#87910=CARTESIAN_POINT('Ctrl Pts',(8.04319591567539,5.84893345579076,11.7787554449422));
#87911=CARTESIAN_POINT('Ctrl Pts',(7.8970387668655,6.04481418221851,11.7826653285198));
#87912=CARTESIAN_POINT('Ctrl Pts',(7.74388841035309,6.23502656674365,11.7865752120975));
#87913=CARTESIAN_POINT('Ctrl Pts',(7.6346130650195,6.37074629002112,11.7893649795385));
#87914=CARTESIAN_POINT('Ctrl Pts',(7.52177833014649,6.50358084734934,11.7921547469794));
#87915=CARTESIAN_POINT('Ctrl Pts',(7.40554473796219,6.63334539535222,11.7949445144204));
#87916=CARTESIAN_POINT('Ctrl Pts',(7.24264261333854,6.81521124130301,11.7988543913741));
#87917=CARTESIAN_POINT('Ctrl Pts',(7.07301291689818,6.99110117596129,11.8027642683279));
#87918=CARTESIAN_POINT('Ctrl Pts',(6.89711843085032,7.16052521473284,11.8066741452817));
#87919=CARTESIAN_POINT('Ctrl Pts',(6.72125439374738,7.32991992465311,11.8105833454));
#87920=CARTESIAN_POINT('Ctrl Pts',(6.53912793371752,7.49285077870811,11.8144925455183));
#87921=CARTESIAN_POINT('Ctrl Pts',(6.35123834987866,7.64886497612755,11.8184017456366));
#87922=CARTESIAN_POINT('Ctrl Pts',(6.16336922057874,7.80486218911169,11.822310520181));
#87923=CARTESIAN_POINT('Ctrl Pts',(5.96973843576041,7.95394406991516,11.8262192947255));
#87924=CARTESIAN_POINT('Ctrl Pts',(5.77087879767107,8.09569774031803,11.83012806927));
#87925=CARTESIAN_POINT('Ctrl Pts',(5.57200372705975,8.23746241152859,11.8340371471553));
#87926=CARTESIAN_POINT('Ctrl Pts',(5.36789921882674,8.37189757073825,11.8379462250406));
#87927=CARTESIAN_POINT('Ctrl Pts',(5.15912856639042,8.49863262151355,11.841855302926));
#87928=CARTESIAN_POINT('Ctrl Pts',(4.95036079684898,8.62536592221611,11.8457643268312));
#87929=CARTESIAN_POINT('Ctrl Pts',(4.73692725267336,8.74439918343619,11.8496733507364));
#87930=CARTESIAN_POINT('Ctrl Pts',(4.51941805693071,8.85540650826876,11.8535823746416));
#87931=CARTESIAN_POINT('Ctrl Pts',(4.30186102656903,8.96643824583052,11.8574922582193));
#87932=CARTESIAN_POINT('Ctrl Pts',(4.08022680296493,9.06944039173825,11.861402141797));
#87933=CARTESIAN_POINT('Ctrl Pts',(3.85512907384744,9.16413355555102,11.8653120253747));
#87934=CARTESIAN_POINT('Ctrl Pts',(3.69451807271944,9.23169871446921,11.8681017928156));
#87935=CARTESIAN_POINT('Ctrl Pts',(3.53214427256707,9.29503469190088,11.8708915602565));
#87936=CARTESIAN_POINT('Ctrl Pts',(3.36823671880771,9.35405502475132,11.8736813276974));
#87937=CARTESIAN_POINT('Ctrl Pts',(3.13851923139242,9.43677239962426,11.8775912046511));
#87938=CARTESIAN_POINT('Ctrl Pts',(2.90571805417042,9.51103621929828,11.8815010816049));
#87939=CARTESIAN_POINT('Ctrl Pts',(2.67047311957186,9.57663496838238,11.8854109585587));
#87940=CARTESIAN_POINT('Ctrl Pts',(2.43526890802444,9.64222236172265,11.8893201586769));
#87941=CARTESIAN_POINT('Ctrl Pts',(2.1976220534538,9.69914760356212,11.8932293587952));
#87942=CARTESIAN_POINT('Ctrl Pts',(1.95818697265278,9.74724924171599,11.8971385589135));
#87943=CARTESIAN_POINT('Ctrl Pts',(1.71877795787394,9.79534564330067,11.901047333458));
#87944=CARTESIAN_POINT('Ctrl Pts',(1.47758138028183,9.83462030397606,11.9049561080025));
#87945=CARTESIAN_POINT('Ctrl Pts',(1.235262188295,9.86496281423142,11.908864882547));
#87946=CARTESIAN_POINT('Ctrl Pts',(0.992924191103593,9.89530767922025,11.9127739604323));
#87947=CARTESIAN_POINT('Ctrl Pts',(0.749463683207167,9.91671897080718,11.9166830383176));
#87948=CARTESIAN_POINT('Ctrl Pts',(0.505552373690955,9.92913796849734,11.9205921162029));
#87949=CARTESIAN_POINT('Ctrl Pts',(0.26164443232356,9.9415567946947,11.9245011401081));
#87950=CARTESIAN_POINT('Ctrl Pts',(0.0172859818579282,9.9449835631453,11.9284101640133));
#87951=CARTESIAN_POINT('Ctrl Pts',(-0.226848878373291,9.93941163180099,
11.9323191879186));
#87952=CARTESIAN_POINT('Ctrl Pts',(-0.471037428739418,9.93383847507761,
11.9362290714963));
#87953=CARTESIAN_POINT('Ctrl Pts',(-0.715002010243568,9.91926266958761,
11.940138955074));
#87954=CARTESIAN_POINT('Ctrl Pts',(-0.95806986473244,9.89572969185656,11.9440488386517));
#87955=CARTESIAN_POINT('Ctrl Pts',(-1.13150285139464,9.87893851796179,11.9468386060925));
#87956=CARTESIAN_POINT('Ctrl Pts',(-1.30447933666542,9.85758828243919,11.9496283735334));
#87957=CARTESIAN_POINT('Ctrl Pts',(-1.4767566858202,9.83171163586917,11.9524181409743));
#87958=CARTESIAN_POINT('Ctrl Pts',(-1.71820449514073,9.79544534980461,11.9563280179281));
#87959=CARTESIAN_POINT('Ctrl Pts',(-1.95835265971994,9.75027498254813,11.9602378948819));
#87960=CARTESIAN_POINT('Ctrl Pts',(-2.1965375493256,9.69631820818617,11.9641477718357));
#87961=CARTESIAN_POINT('Ctrl Pts',(-2.43468120694782,9.64237077423548,11.968056971954));
#87962=CARTESIAN_POINT('Ctrl Pts',(-2.67086199478642,9.57964003135387,11.9719661720723));
#87963=CARTESIAN_POINT('Ctrl Pts',(-2.90442730406609,9.50829459132369,11.9758753721906));
#87964=CARTESIAN_POINT('Ctrl Pts',(-3.13796718633633,9.43695691829103,11.9797841467351));
#87965=CARTESIAN_POINT('Ctrl Pts',(-3.36889189058786,9.35700650252349,11.9836929212796));
#87966=CARTESIAN_POINT('Ctrl Pts',(-3.59656377335176,9.26866187883741,11.9876016958242));
#87967=CARTESIAN_POINT('Ctrl Pts',(-3.82425332461187,9.18031039915914,11.9915107737095));
#87968=CARTESIAN_POINT('Ctrl Pts',(-4.04868928751855,9.08356350842259,11.9954198515948));
#87969=CARTESIAN_POINT('Ctrl Pts',(-4.26925260961267,8.97868844293616,11.9993289294802));
#87970=CARTESIAN_POINT('Ctrl Pts',(-4.48981288596899,8.87381482565947,12.0032379533854));
#87971=CARTESIAN_POINT('Ctrl Pts',(-4.70650037618384,8.76081338035352,12.0071469772906));
#87972=CARTESIAN_POINT('Ctrl Pts',(-4.91871865012074,8.63999831255507,12.0110560011959));
#87973=CARTESIAN_POINT('Ctrl Pts',(-5.13098359509581,8.51915667510954,12.0149658847736));
#87974=CARTESIAN_POINT('Ctrl Pts',(-5.33877711565538,8.39049811943732,12.0188757683513));
#87975=CARTESIAN_POINT('Ctrl Pts',(-5.54152870707573,8.25438208399972,12.022785651929));
#87976=CARTESIAN_POINT('Ctrl Pts',(-5.68619536455216,8.15726101216125,12.0255754193697));
#87977=CARTESIAN_POINT('Ctrl Pts',(-5.82829568684554,8.05634423746679,12.0283651868105));
#87978=CARTESIAN_POINT('Ctrl Pts',(-5.96763163245033,7.951775694735,12.0311549542513));
#87979=CARTESIAN_POINT('Ctrl Pts',(-6.162911853515,7.80522221169484,12.035064831205));
#87980=CARTESIAN_POINT('Ctrl Pts',(-6.352820743239,7.65144927313826,12.0389747081588));
#87981=CARTESIAN_POINT('Ctrl Pts',(-6.53683010861459,7.49087552500439,12.0428845851126));
#87982=CARTESIAN_POINT('Ctrl Pts',(-6.72080762028672,7.33032957365437,12.0467937852309));
#87983=CARTESIAN_POINT('Ctrl Pts',(-6.89888743518115,7.1629853470611,12.0507029853492));
#87984=CARTESIAN_POINT('Ctrl Pts',(-7.07057524467959,6.98930108875875,12.0546121854675));
#87985=CARTESIAN_POINT('Ctrl Pts',(-7.24224436343932,6.81563573853785,12.058520960012));
#87986=CARTESIAN_POINT('Ctrl Pts',(-7.4075226692328,6.63563193400119,12.0624297345565));
#87987=CARTESIAN_POINT('Ctrl Pts',(-7.56595272707869,6.44978475079677,12.066338509101));
#87988=CARTESIAN_POINT('Ctrl Pts',(-7.7243950799046,6.26392314490366,12.0702475869863));
#87989=CARTESIAN_POINT('Ctrl Pts',(-7.87598793863131,6.07221746555143,12.0741566648717));
#87990=CARTESIAN_POINT('Ctrl Pts',(-8.02031335293776,5.87519682399563,12.078065742757));
#87991=CARTESIAN_POINT('Ctrl Pts',(-8.16463677426606,5.67817890308216,12.0819747666622));
#87992=CARTESIAN_POINT('Ctrl Pts',(-8.30169278788719,5.47584639411476,12.0858837905673));
#87993=CARTESIAN_POINT('Ctrl Pts',(-8.43110565365917,5.26875900538603,12.0897928144725));
#87994=CARTESIAN_POINT('Ctrl Pts',(-8.56054697990804,5.06162607399965,12.0937026980502));
#87995=CARTESIAN_POINT('Ctrl Pts',(-8.6823416501597,4.8497364106546,12.0976125816279));
#87996=CARTESIAN_POINT('Ctrl Pts',(-8.79615821714132,4.63367722430223,12.1015224652056));
#87997=CARTESIAN_POINT('Ctrl Pts',(-8.8773682446238,4.47951537487349,12.1043122326465));
#87998=CARTESIAN_POINT('Ctrl Pts',(-8.9545174967614,4.32323137086869,12.1071020000874));
#87999=CARTESIAN_POINT('Ctrl Pts',(-9.02750001457516,4.16504591653506,12.1098917675283));
#88000=CARTESIAN_POINT('Ctrl Pts',(-9.12940431381605,3.9441741467353,12.1137870743034));
#88001=CARTESIAN_POINT('Ctrl Pts',(-9.22321658138155,3.71952196105995,12.1176823810786));
#88002=CARTESIAN_POINT('Ctrl Pts',(-9.30867171303844,3.49170373011198,12.1215776878538));
#88003=CARTESIAN_POINT('Ctrl Pts',(-9.39411098950818,3.26392776813745,12.1254722719009));
#88004=CARTESIAN_POINT('Ctrl Pts',(-9.47119612523989,3.03298719968502,12.129366855948));
#88005=CARTESIAN_POINT('Ctrl Pts',(-9.53971060835845,2.79951522745873,12.1332614399952));
#88006=CARTESIAN_POINT('Ctrl Pts',(-9.60822488072106,2.56604397341062,12.1371560120623));
#88007=CARTESIAN_POINT('Ctrl Pts',(-9.66816846912883,2.3300416029902,12.1410505841294));
#88008=CARTESIAN_POINT('Ctrl Pts',(-9.71937473864423,2.09215646876718,12.1449451561965));
#88009=CARTESIAN_POINT('Ctrl Pts',(-9.77057792428616,1.85428566106437,12.1488394937148));
#88010=CARTESIAN_POINT('Ctrl Pts',(-9.81304478356313,1.61453259450658,12.1527338312331));
#88011=CARTESIAN_POINT('Ctrl Pts',(-9.84665965976869,1.37355653130258,12.1566281687514));
#88012=CARTESIAN_POINT('Ctrl Pts',(-9.88028121308345,1.13253260168737,12.1605232798236));
#88013=CARTESIAN_POINT('Ctrl Pts',(-9.90504722845266,0.890285471654712,
12.1644183908958));
#88014=CARTESIAN_POINT('Ctrl Pts',(-9.92089368692205,0.647481623515401,
12.1683135019679));
#88015=CARTESIAN_POINT('Ctrl Pts',(-9.93496511211645,0.431875329364309,
12.1717723040834));
#88016=CARTESIAN_POINT('Ctrl Pts',(-9.94200401926865,0.215830279218862,
12.1752311061988));
#88017=CARTESIAN_POINT('Ctrl Pts',(-9.94199999827757,-0.000185064137654065,
12.1786899083142));
#88018=CARTESIAN_POINT('Origin',(0.,0.,0.));
#88019=CARTESIAN_POINT('',(-9.94195875194945,-0.000111575420876506,13.3213100922243));
#88020=CARTESIAN_POINT('',(-9.94195498619804,-0.000106503573575908,13.1786899087943));
#88021=CARTESIAN_POINT('',(-9.942,-1.2175438477123E-15,0.));
#88022=CARTESIAN_POINT('Ctrl Pts',(-9.94125749983017,-0.000111533904790795,
13.3213100916858));
#88023=CARTESIAN_POINT('Ctrl Pts',(-9.94087740012148,0.947889144334461,
13.3061371289177));
#88024=CARTESIAN_POINT('Ctrl Pts',(-9.57342153214947,3.5359933036782,13.2647185617242));
#88025=CARTESIAN_POINT('Ctrl Pts',(-7.35748914925443,7.28899342376248,13.1970543901046));
#88026=CARTESIAN_POINT('Ctrl Pts',(-3.01465202171707,9.90827658581459,13.1183175768277));
#88027=CARTESIAN_POINT('Ctrl Pts',(2.05108274737684,10.1516073247769,13.0395807635506));
#88028=CARTESIAN_POINT('Ctrl Pts',(6.62497870056853,7.96063621389991,12.9608439502738));
#88029=CARTESIAN_POINT('Ctrl Pts',(9.61023973221781,3.86074656023302,12.8821071369967));
#88030=CARTESIAN_POINT('Ctrl Pts',(10.2910160050407,-1.16492973910139,12.8033703237197));
#88031=CARTESIAN_POINT('Ctrl Pts',(8.50406096238505,-5.91126203623941,12.7246335104427));
#88032=CARTESIAN_POINT('Ctrl Pts',(4.67787699079448,-9.24010490048894,12.6458966971659));
#88033=CARTESIAN_POINT('Ctrl Pts',(-0.270037190378026,-10.3532193847547,
12.5671598838888));
#88034=CARTESIAN_POINT('Ctrl Pts',(-5.15319787872579,-8.98368651143514,
12.4884230706118));
#88035=CARTESIAN_POINT('Ctrl Pts',(-8.80064891761229,-5.45991303428693,
12.4096862573348));
#88036=CARTESIAN_POINT('Ctrl Pts',(-9.88811005993012,-2.04066390104026,
12.3539819310262));
#88037=CARTESIAN_POINT('Ctrl Pts',(-9.94269391643093,-0.200861641353821,
12.3245232091432));
#88038=CARTESIAN_POINT('Ctrl Pts',(-9.94252421102867,-0.000180935334070931,
12.3213100916858));
#88039=CARTESIAN_POINT('Ctrl Pts',(-9.94250794012056,-0.000185073592678929,
12.1786899083142));
#88040=CARTESIAN_POINT('Ctrl Pts',(-9.94268579522292,-0.207098276547491,
12.1820027991445));
#88041=CARTESIAN_POINT('Ctrl Pts',(-9.8862140376245,-2.05313606585478,12.2115612944009));
#88042=CARTESIAN_POINT('Ctrl Pts',(-8.79036500190181,-5.47645461378649,
12.2673653940818));
#88043=CARTESIAN_POINT('Ctrl Pts',(-5.13629330883765,-8.99336216601434,
12.3461022073594));
#88044=CARTESIAN_POINT('Ctrl Pts',(-0.250565592938094,-10.3537089435215,
12.4248390206361));
#88045=CARTESIAN_POINT('Ctrl Pts',(4.6952464295034,-9.2312909698346,12.5035758339132));
#88046=CARTESIAN_POINT('Ctrl Pts',(8.51516314264787,-5.89525815020917,12.5823126471901));
#88047=CARTESIAN_POINT('Ctrl Pts',(10.2931886826346,-1.14557354508644,12.661049460467));
#88048=CARTESIAN_POINT('Ctrl Pts',(9.60296191052419,3.87881354908099,12.7397862737441));
#88049=CARTESIAN_POINT('Ctrl Pts',(6.60999556281344,7.97308162902553,12.8185230870211));
#88050=CARTESIAN_POINT('Ctrl Pts',(2.03198717090202,10.1554468213272,12.8972599002979));
#88051=CARTESIAN_POINT('Ctrl Pts',(-3.0332810184704,9.90258947278456,12.975996713575));
#88052=CARTESIAN_POINT('Ctrl Pts',(-7.37118443120105,7.27514344083582,13.054733526852));
#88053=CARTESIAN_POINT('Ctrl Pts',(-9.57679763346346,3.52352256269792,13.1222979250984));
#88054=CARTESIAN_POINT('Ctrl Pts',(-9.94088989120619,0.941662455610846,
13.1636167189191));
#88055=CARTESIAN_POINT('Ctrl Pts',(-9.94124998359704,-0.000106466024951112,
13.1786899083142));
#88056=CARTESIAN_POINT('Origin',(0.,0.,0.));
#88057=CARTESIAN_POINT('',(-9.94199999708082,0.000240925445847458,14.3213100916727));
#88058=CARTESIAN_POINT('',(-9.9419999970495,0.000242214229021048,14.178689908302));
#88059=CARTESIAN_POINT('',(-9.942,-1.2175438477123E-15,0.));
#88060=CARTESIAN_POINT('Ctrl Pts',(-9.94199999708082,0.00024092544577925,
14.3213100916727));
#88061=CARTESIAN_POINT('Ctrl Pts',(-9.94199381537137,0.255334591941568,
14.3172267605938));
#88062=CARTESIAN_POINT('Ctrl Pts',(-9.93216543361595,0.510380829635011,
14.3131434295148));
#88063=CARTESIAN_POINT('Ctrl Pts',(-9.91255176743128,0.764644661261096,
14.3090600984358));
#88064=CARTESIAN_POINT('Ctrl Pts',(-9.89703643234913,0.965779345098612,
14.3058299909513));
#88065=CARTESIAN_POINT('Ctrl Pts',(-9.87539892454686,1.16642442817123,14.3025998834667));
#88066=CARTESIAN_POINT('Ctrl Pts',(-9.84768052877541,1.36621821213805,14.2993697759822));
#88067=CARTESIAN_POINT('Ctrl Pts',(-9.81412885368643,1.60805818656242,14.2954598990284));
#88068=CARTESIAN_POINT('Ctrl Pts',(-9.77165905958109,1.84869862293535,14.2915500220746));
#88069=CARTESIAN_POINT('Ctrl Pts',(-9.72038135817929,2.08747461099783,14.2876401451208));
#88070=CARTESIAN_POINT('Ctrl Pts',(-9.66911253341697,2.32620926475113,14.2837309450025));
#88071=CARTESIAN_POINT('Ctrl Pts',(-9.60903890388906,2.56307984055476,14.2798217448842));
#88072=CARTESIAN_POINT('Ctrl Pts',(-9.54032173960764,2.79743187669866,14.2759125447659));
#88073=CARTESIAN_POINT('Ctrl Pts',(-9.47161205619742,3.03175840018625,14.2720037702214));
#88074=CARTESIAN_POINT('Ctrl Pts',(-9.39426079570019,3.26356666258029,14.2680949956769));
#88075=CARTESIAN_POINT('Ctrl Pts',(-9.3084793161259,3.49221660571855,14.2641862211323));
#88076=CARTESIAN_POINT('Ctrl Pts',(-9.22269117947215,3.72088429325624,14.260277143247));
#88077=CARTESIAN_POINT('Ctrl Pts',(-9.12847161206279,3.9463929082363,14.2563680653617));
#88078=CARTESIAN_POINT('Ctrl Pts',(-9.02608087917035,4.16812043524122,14.2524589874764));
#88079=CARTESIAN_POINT('Ctrl Pts',(-8.92369156018213,4.38984490043109,14.2485499635712));
#88080=CARTESIAN_POINT('Ctrl Pts',(-8.81313142077705,4.60778812843122,14.2446409396659));
#88081=CARTESIAN_POINT('Ctrl Pts',(-8.69470794662194,4.82135019708683,14.2407319157607));
#88082=CARTESIAN_POINT('Ctrl Pts',(-8.57625842877817,5.03495923230939,14.236822032183));
#88083=CARTESIAN_POINT('Ctrl Pts',(-8.44994225585272,5.24418493721204,14.2329121486053));
#88084=CARTESIAN_POINT('Ctrl Pts',(-8.31611243481795,5.44845280528943,14.2290022650276));
#88085=CARTESIAN_POINT('Ctrl Pts',(-8.22062261525989,5.59420135156561,14.2262124975868));
#88086=CARTESIAN_POINT('Ctrl Pts',(-8.1213085032248,5.73742636391226,14.2234227301461));
#88087=CARTESIAN_POINT('Ctrl Pts',(-8.01831179973473,5.87792819641707,14.2206329627053));
#88088=CARTESIAN_POINT('Ctrl Pts',(-7.87396125947005,6.07484241544545,14.2167230857515));
#88089=CARTESIAN_POINT('Ctrl Pts',(-7.72233137996095,6.26646674236815,14.2128132087978));
#88090=CARTESIAN_POINT('Ctrl Pts',(-7.56383484723363,6.45226831461419,14.208903331844));
#88091=CARTESIAN_POINT('Ctrl Pts',(-7.40536575170677,6.63803772290751,14.2049941317257));
#88092=CARTESIAN_POINT('Ctrl Pts',(-7.24003255766611,6.81798617551003,14.2010849316075));
#88093=CARTESIAN_POINT('Ctrl Pts',(-7.06828792687721,6.99161424727952,14.1971757314892));
#88094=CARTESIAN_POINT('Ctrl Pts',(-6.89656199301152,7.1652234170856,14.1932669569447));
#88095=CARTESIAN_POINT('Ctrl Pts',(-6.71842621308652,7.33251338069326,14.1893581824002));
#88096=CARTESIAN_POINT('Ctrl Pts',(-6.53437049288043,7.49302117051417,14.1854494078557));
#88097=CARTESIAN_POINT('Ctrl Pts',(-6.35030048901242,7.65354141655759,14.1815403299704));
#88098=CARTESIAN_POINT('Ctrl Pts',(-6.16030983611704,7.80727825054629,14.1776312520851));
#88099=CARTESIAN_POINT('Ctrl Pts',(-5.96492291698645,7.95380780471907,14.1737221741998));
#88100=CARTESIAN_POINT('Ctrl Pts',(-5.76953869593587,8.10033533547869,14.1698131502946));
#88101=CARTESIAN_POINT('Ctrl Pts',(-5.5687585831884,8.23965561892998,14.1659041263894));
#88102=CARTESIAN_POINT('Ctrl Pts',(-5.3631380308139,8.37138665111328,14.1619951024842));
#88103=CARTESIAN_POINT('Ctrl Pts',(-5.15747225837047,8.50314665358329,14.1580852189065));
#88104=CARTESIAN_POINT('Ctrl Pts',(-4.94696415481059,8.62731391766556,14.1541753353288));
#88105=CARTESIAN_POINT('Ctrl Pts',(-4.73219716869498,8.743550420544,14.1502654517511));
#88106=CARTESIAN_POINT('Ctrl Pts',(-4.57895732578351,8.82648711283471,14.1474756843102));
#88107=CARTESIAN_POINT('Ctrl Pts',(-4.42354984516734,8.90538712539718,14.1446859168692));
#88108=CARTESIAN_POINT('Ctrl Pts',(-4.26619422686921,8.9801420266401,14.1418961494283));
#88109=CARTESIAN_POINT('Ctrl Pts',(-4.04565931900939,9.08491149998959,14.1379862724745));
#88110=CARTESIAN_POINT('Ctrl Pts',(-3.82122939880282,9.18156921538258,14.1340763955208));
#88111=CARTESIAN_POINT('Ctrl Pts',(-3.59352066665134,9.26984213556788,14.130166518567));
#88112=CARTESIAN_POINT('Ctrl Pts',(-3.36585135296519,9.3580997749029,14.1262573184487));
#88113=CARTESIAN_POINT('Ctrl Pts',(-3.13490462160746,9.43797541525384,14.1223481183304));
#88114=CARTESIAN_POINT('Ctrl Pts',(-2.90131598019526,9.50924442755909,14.1184389182121));
#88115=CARTESIAN_POINT('Ctrl Pts',(-2.6677527683341,9.58050568118663,14.1145301436676));
#88116=CARTESIAN_POINT('Ctrl Pts',(-2.43154848869088,9.64316209580029,14.1106213691231));
#88117=CARTESIAN_POINT('Ctrl Pts',(-2.19335411799256,9.69703881156949,14.1067125945786));
#88118=CARTESIAN_POINT('Ctrl Pts',(-1.95514126219735,9.75091970844636,14.1028035166932));
#88119=CARTESIAN_POINT('Ctrl Pts',(-1.71493827948673,9.79601948017485,14.0988944388079));
#88120=CARTESIAN_POINT('Ctrl Pts',(-1.47340792594698,9.83221404790176,14.0949853609226));
#88121=CARTESIAN_POINT('Ctrl Pts',(-1.23188090767788,9.86840811582118,14.0910763370174));
#88122=CARTESIAN_POINT('Ctrl Pts',(-0.989026832777744,9.89569718617364,
14.0871673131121));
#88123=CARTESIAN_POINT('Ctrl Pts',(-0.745515925245146,9.9140087757277,14.0832582892069));
#88124=CARTESIAN_POINT('Ctrl Pts',(-0.501951464797451,9.93232439236626,
14.0793484056292));
#88125=CARTESIAN_POINT('Ctrl Pts',(-0.257730162639278,9.9416585611352,14.0754385220515));
#88126=CARTESIAN_POINT('Ctrl Pts',(-0.0135260010347294,9.94199079899474,
14.0715286384738));
#88127=CARTESIAN_POINT('Ctrl Pts',(0.160717759787237,9.94222785627399,14.068738871033));
#88128=CARTESIAN_POINT('Ctrl Pts',(0.334952715461797,9.93788306251751,14.0659491035921));
#88129=CARTESIAN_POINT('Ctrl Pts',(0.508934201912364,9.92896520177827,14.0631593361513));
#88130=CARTESIAN_POINT('Ctrl Pts',(0.752770370585048,9.91646676277895,14.0592494591976));
#88131=CARTESIAN_POINT('Ctrl Pts',(0.996183221306394,9.89497985671135,14.0553395822438));
#88132=CARTESIAN_POINT('Ctrl Pts',(1.23850080090258,9.86455674453564,14.05142970529));
#88133=CARTESIAN_POINT('Ctrl Pts',(1.48077643310792,9.8341388988791,14.0475205051717));
#88134=CARTESIAN_POINT('Ctrl Pts',(1.72195689468522,9.79478797005619,14.0436113050534));
#88135=CARTESIAN_POINT('Ctrl Pts',(1.9613762235378,9.74660798994915,14.0397021049352));
#88136=CARTESIAN_POINT('Ctrl Pts',(2.20076948808366,9.69843325493985,14.0357933303907));
#88137=CARTESIAN_POINT('Ctrl Pts',(2.43840172802136,9.64143144307507,14.0318845558462));
#88138=CARTESIAN_POINT('Ctrl Pts',(2.6736169964581,9.57575773274629,14.0279757813017));
#88139=CARTESIAN_POINT('Ctrl Pts',(2.90885051879817,9.51007892580296,14.0240667034164));
#88140=CARTESIAN_POINT('Ctrl Pts',(3.14166642401248,9.43572694807593,14.020157625531));
#88141=CARTESIAN_POINT('Ctrl Pts',(3.37142250813172,9.35290726307402,14.0162485476457));
#88142=CARTESIAN_POINT('Ctrl Pts',(3.60117541957035,9.27008872172152,14.0123395237405));
#88143=CARTESIAN_POINT('Ctrl Pts',(3.82786833139906,9.17880280395386,14.0084304998353));
#88144=CARTESIAN_POINT('Ctrl Pts',(4.05087696386757,9.07930392836406,14.00452147593));
#88145=CARTESIAN_POINT('Ctrl Pts',(4.27393464039106,8.97978317098309,14.0006115923523));
#88146=CARTESIAN_POINT('Ctrl Pts',(4.4933061620441,8.87204596004006,13.9967017087747));
#88147=CARTESIAN_POINT('Ctrl Pts',(4.70838863024847,8.75639426399628,13.992791825197));
#88148=CARTESIAN_POINT('Ctrl Pts',(4.86185357491384,8.67387484118144,13.9900020577561));
#88149=CARTESIAN_POINT('Ctrl Pts',(5.01313538300763,8.58732709971537,13.9872122903152));
#88150=CARTESIAN_POINT('Ctrl Pts',(5.16202289555344,8.49687493292576,13.9844225228743));
#88151=CARTESIAN_POINT('Ctrl Pts',(5.37068969891424,8.3701056412752,13.9805126459206));
#88152=CARTESIAN_POINT('Ctrl Pts',(5.57471636343581,8.23562656040066,13.9766027689668));
#88153=CARTESIAN_POINT('Ctrl Pts',(5.77353631399643,8.0938027175713,13.972692892013));
#88154=CARTESIAN_POINT('Ctrl Pts',(5.97232184700406,7.95200342574706,13.9687836918947));
#88155=CARTESIAN_POINT('Ctrl Pts',(6.16590223721962,7.80286207276289,13.9648744917764));
#88156=CARTESIAN_POINT('Ctrl Pts',(6.3537407622623,7.64678640514866,13.9609652916581));
#88157=CARTESIAN_POINT('Ctrl Pts',(6.54155883832555,7.49072772866082,13.9570565171137));
#88158=CARTESIAN_POINT('Ctrl Pts',(6.72363608179566,7.32773642391084,13.9531477425692));
#88159=CARTESIAN_POINT('Ctrl Pts',(6.89946886821635,7.15826049655315,13.9492389680247));
#88160=CARTESIAN_POINT('Ctrl Pts',(7.07531530015708,6.98877141700007,13.9453298901393));
#88161=CARTESIAN_POINT('Ctrl Pts',(7.24491610275595,6.81279690159931,13.941420812254));
#88162=CARTESIAN_POINT('Ctrl Pts',(7.40780362128244,6.63082268715691,13.9375117343687));
#88163=CARTESIAN_POINT('Ctrl Pts',(7.57068889050987,6.44885098558002,13.9336027104635));
#88164=CARTESIAN_POINT('Ctrl Pts',(7.72686087564029,6.26087996090791,13.9296936865583));
#88165=CARTESIAN_POINT('Ctrl Pts',(7.87589094016046,6.06742992532245,13.9257846626531));
#88166=CARTESIAN_POINT('Ctrl Pts',(8.02495377937031,5.8739373462079,13.9218747790754));
#88167=CARTESIAN_POINT('Ctrl Pts',(8.16687138760884,5.67496357003133,13.9179648954977));
#88168=CARTESIAN_POINT('Ctrl Pts',(8.30125652188029,5.47106060631209,13.91405501192));
#88169=CARTESIAN_POINT('Ctrl Pts',(8.39714256674027,5.32557242540382,13.9112652444791));
#88170=CARTESIAN_POINT('Ctrl Pts',(8.48919464823038,5.17757542777753,13.9084754770382));
#88171=CARTESIAN_POINT('Ctrl Pts',(8.57728574728231,5.02727890706968,13.9056857095974));
#88172=CARTESIAN_POINT('Ctrl Pts',(8.70074598736159,4.81663736973645,13.9017758326436));
#88173=CARTESIAN_POINT('Ctrl Pts',(8.81646194851377,4.60141348778228,13.8978659556898));
#88174=CARTESIAN_POINT('Ctrl Pts',(8.92410829539268,4.38219752317299,13.893956078736));
#88175=CARTESIAN_POINT('Ctrl Pts',(9.03173600770384,4.1630195068533,13.8900468786177));
#88176=CARTESIAN_POINT('Ctrl Pts',(9.13129677082437,3.93985103889019,13.8861376784995));
#88177=CARTESIAN_POINT('Ctrl Pts',(9.22251180528306,3.71330580499569,13.8822284783812));
#88178=CARTESIAN_POINT('Ctrl Pts',(9.31371690964677,3.48678523387418,13.8783197038367));
#88179=CARTESIAN_POINT('Ctrl Pts',(9.39657799478445,3.25688889074633,13.8744109292922));
#88180=CARTESIAN_POINT('Ctrl Pts',(9.47086452516248,3.02425017913844,13.8705021547477));
#88181=CARTESIAN_POINT('Ctrl Pts',(9.54515682055384,2.79159341358098,13.8665930768624));
#88182=CARTESIAN_POINT('Ctrl Pts',(9.61087314333497,2.55619412039391,13.8626839989771));
#88183=CARTESIAN_POINT('Ctrl Pts',(9.66783252914998,2.31870183255837,13.8587749210917));
#88184=CARTESIAN_POINT('Ctrl Pts',(9.72479112841801,2.08121282423224,13.8548658971865));
#88185=CARTESIAN_POINT('Ctrl Pts',(9.77299296919136,1.84163115214076,13.8509568732813));
#88186=CARTESIAN_POINT('Ctrl Pts',(9.81230784296712,1.60061825394001,13.8470478493761));
#88187=CARTESIAN_POINT('Ctrl Pts',(9.85163136286934,1.35955235218624,13.8431379657984));
#88188=CARTESIAN_POINT('Ctrl Pts',(9.88206396436919,1.11705487199269,13.8392280822207));
#88189=CARTESIAN_POINT('Ctrl Pts',(9.90352691887965,0.87379549496791,13.835318198643));
#88190=CARTESIAN_POINT('Ctrl Pts',(9.918841096524,0.700225853770615,13.8325284312021));
#88191=CARTESIAN_POINT('Ctrl Pts',(9.92958984817828,0.526268498794397,13.8297386637613));
#88192=CARTESIAN_POINT('Ctrl Pts',(9.93576075318437,0.352167936475196,13.8269488963204));
#88193=CARTESIAN_POINT('Ctrl Pts',(9.94440931611256,0.108164882212393,13.8230390193667));
#88194=CARTESIAN_POINT('Ctrl Pts',(9.94406649723332,-0.136194250016732,
13.8191291424129));
#88195=CARTESIAN_POINT('Ctrl Pts',(9.9347262146747,-0.380235505253301,13.8152192654591));
#88196=CARTESIAN_POINT('Ctrl Pts',(9.92538754900448,-0.624234514715135,
13.8113100653409));
#88197=CARTESIAN_POINT('Ctrl Pts',(9.90705453957857,-0.867915477063908,
13.8074008652226));
#88198=CARTESIAN_POINT('Ctrl Pts',(9.87977319968096,-1.11060592599979,13.8034916651043));
#88199=CARTESIAN_POINT('Ctrl Pts',(9.85249482975749,-1.35326995451939,13.7995828905598));
#88200=CARTESIAN_POINT('Ctrl Pts',(9.81627010574047,-1.59494340648189,13.7956741160153));
#88201=CARTESIAN_POINT('Ctrl Pts',(9.77119686222301,-1.83495936731123,13.7917653414708));
#88202=CARTESIAN_POINT('Ctrl Pts',(9.72612012079218,-2.07499395460216,13.7878562635855));
#88203=CARTESIAN_POINT('Ctrl Pts',(9.6721935364453,-2.31337051765586,13.7839471857002));
#88204=CARTESIAN_POINT('Ctrl Pts',(9.60956622949839,-2.54943148189631,13.7800381078149));
#88205=CARTESIAN_POINT('Ctrl Pts',(9.54693978736628,-2.78548918639237,13.7761290839096));
#88206=CARTESIAN_POINT('Ctrl Pts',(9.47561293680516,-3.01923108559936,13.7722200600044));
#88207=CARTESIAN_POINT('Ctrl Pts',(9.39578512063412,-3.25001322564547,13.7683110360992));
#88208=CARTESIAN_POINT('Ctrl Pts',(9.31593974873091,-3.48084611929645,13.7644011525215));
#88209=CARTESIAN_POINT('Ctrl Pts',(9.2275897662953,-3.70871768781189,13.7604912689438));
#88210=CARTESIAN_POINT('Ctrl Pts',(9.13098383784858,-3.93300116360878,13.7565813853661));
#88211=CARTESIAN_POINT('Ctrl Pts',(9.06205388931622,-4.09303118135107,13.7537916179252));
#88212=CARTESIAN_POINT('Ctrl Pts',(8.98892181722655,-4.2512348382156,13.7510018504843));
#88213=CARTESIAN_POINT('Ctrl Pts',(8.91169277773993,-4.40739104631959,13.7482120830434));
#88214=CARTESIAN_POINT('Ctrl Pts',(8.80345578377937,-4.62624497310424,13.7443022060896));
#88215=CARTESIAN_POINT('Ctrl Pts',(8.68713639102615,-4.84114332558387,13.7403923291359));
#88216=CARTESIAN_POINT('Ctrl Pts',(8.56304922948336,-5.0514900666481,13.7364824521821));
#88217=CARTESIAN_POINT('Ctrl Pts',(8.43898354856387,-5.26180039476637,13.7325732520638));
#88218=CARTESIAN_POINT('Ctrl Pts',(8.30715292547827,-5.46756044303394,13.7286640519455));
#88219=CARTESIAN_POINT('Ctrl Pts',(8.16791713252317,-5.66820021843217,13.7247548518272));
#88220=CARTESIAN_POINT('Ctrl Pts',(8.02869649742703,-5.86881815124701,13.7208460772827));
#88221=CARTESIAN_POINT('Ctrl Pts',(7.88207246185683,-6.06431669397078,13.7169373027382));
#88222=CARTESIAN_POINT('Ctrl Pts',(7.72844777031341,-6.25415534357259,13.7130285281937));
#88223=CARTESIAN_POINT('Ctrl Pts',(7.57481115671128,-6.44400872562077,13.7091194503083));
#88224=CARTESIAN_POINT('Ctrl Pts',(7.41417297550338,-6.62820111702483,13.705210372423));
#88225=CARTESIAN_POINT('Ctrl Pts',(7.24697667341301,-6.80622458452612,13.7013012945377));
#88226=CARTESIAN_POINT('Ctrl Pts',(7.07978268012128,-6.98424559371742,13.6973922706325));
#88227=CARTESIAN_POINT('Ctrl Pts',(6.90603094048115,-7.15609764644923,13.6934832467273));
#88228=CARTESIAN_POINT('Ctrl Pts',(6.72620272329846,-7.32130868937326,13.689574222822));
#88229=CARTESIAN_POINT('Ctrl Pts',(6.54633495829673,-7.48655606550757,13.6856643392443));
#88230=CARTESIAN_POINT('Ctrl Pts',(6.36038825134543,-7.64515932306672,13.6817544556666));
#88231=CARTESIAN_POINT('Ctrl Pts',(6.16887903163457,-7.79668490405117,13.6778445720889));
#88232=CARTESIAN_POINT('Ctrl Pts',(6.03223399473014,-7.90480094481853,13.6750548046481));
#88233=CARTESIAN_POINT('Ctrl Pts',(5.89275778374903,-8.0093145017494,13.6722650372073));
#88234=CARTESIAN_POINT('Ctrl Pts',(5.75064791577785,-8.11008092122143,13.6694752697664));
#88235=CARTESIAN_POINT('Ctrl Pts',(5.55148002473702,-8.25130570413412,13.6655653928127));
#88236=CARTESIAN_POINT('Ctrl Pts',(5.34707683448481,-8.38521178630878,13.6616555158589));
#88237=CARTESIAN_POINT('Ctrl Pts',(5.13799824028541,-8.51142397503638,13.6577456389051));
#88238=CARTESIAN_POINT('Ctrl Pts',(4.928955839504,-8.6376143152791,13.6538364387868));
#88239=CARTESIAN_POINT('Ctrl Pts',(4.71523989028925,-8.75611327602244,13.6499272386685));
#88240=CARTESIAN_POINT('Ctrl Pts',(4.49743765245278,-8.86659001884603,13.6460180385503));
#88241=CARTESIAN_POINT('Ctrl Pts',(4.27965912558583,-8.97705473465507,13.6421092640058));
#88242=CARTESIAN_POINT('Ctrl Pts',(4.0577954482182,-9.07949884955958,13.6382004894613));
#88243=CARTESIAN_POINT('Ctrl Pts',(3.83245769875314,-9.17363788184752,13.6342917149168));
#88244=CARTESIAN_POINT('Ctrl Pts',(3.6071024619304,-9.26778421980409,13.6303826370314));
#88245=CARTESIAN_POINT('Ctrl Pts',(3.37827287176535,-9.35362407638387,13.6264735591461));
#88246=CARTESIAN_POINT('Ctrl Pts',(3.14660036520514,-9.43092095935974,13.6225644812608));
#88247=CARTESIAN_POINT('Ctrl Pts',(2.91493105778971,-9.50821677494992,13.6186554573556));
#88248=CARTESIAN_POINT('Ctrl Pts',(2.68041917906492,-9.57696976610555,13.6147464334504));
#88249=CARTESIAN_POINT('Ctrl Pts',(2.44371241810416,-9.63699297590299,13.6108374095452));
#88250=CARTESIAN_POINT('Ctrl Pts',(2.20695360059577,-9.6970293860039,13.6069275259675));
#88251=CARTESIAN_POINT('Ctrl Pts',(1.96799920791167,-9.74833210865252,13.6030176423898));
#88252=CARTESIAN_POINT('Ctrl Pts',(1.72750959691687,-9.79076476035249,13.5991077588121));
#88253=CARTESIAN_POINT('Ctrl Pts',(1.55591623018638,-9.82104116827872,13.5963179913712));
#88254=CARTESIAN_POINT('Ctrl Pts',(1.38354153945845,-9.84680282601728,13.5935282239303));
#88255=CARTESIAN_POINT('Ctrl Pts',(1.21062803919123,-9.86801620138131,13.5907384564895));
#88256=CARTESIAN_POINT('Ctrl Pts',(0.96828866000674,-9.89774688295436,13.5868285795357));
#88257=CARTESIAN_POINT('Ctrl Pts',(0.724816478307781,-9.91855072316058,
13.5829187025819));
#88258=CARTESIAN_POINT('Ctrl Pts',(0.48088239469076,-9.93036334292338,13.5790088256282));
#88259=CARTESIAN_POINT('Ctrl Pts',(0.236990538295991,-9.9421739178136,13.5750996255099));
#88260=CARTESIAN_POINT('Ctrl Pts',(-0.00736278055499909,-9.94499636575971,
13.5711904253916));
#88261=CARTESIAN_POINT('Ctrl Pts',(-0.251503636338526,-9.93881833624644,
13.5672812252733));
#88262=CARTESIAN_POINT('Ctrl Pts',(-0.49561791380746,-9.93264097930234,
13.5633724507288));
#88263=CARTESIAN_POINT('Ctrl Pts',(-0.739519494277679,-9.91746510839929,
13.5594636761843));
#88264=CARTESIAN_POINT('Ctrl Pts',(-0.982535498819007,-9.89333048035698,
13.5555549016399));
#88265=CARTESIAN_POINT('Ctrl Pts',(-1.22557036264081,-9.86919397934454,
13.5516458237545));
#88266=CARTESIAN_POINT('Ctrl Pts',(-1.46771923394983,-9.83609735660985,
13.5477367458692));
#88267=CARTESIAN_POINT('Ctrl Pts',(-1.70831410082192,-9.79413227054511,
13.5438276679839));
#88268=CARTESIAN_POINT('Ctrl Pts',(-1.94890564534161,-9.75216776397237,
13.5399186440787));
#88269=CARTESIAN_POINT('Ctrl Pts',(-2.18794295253656,-9.70133508919492,
13.5360096201735));
#88270=CARTESIAN_POINT('Ctrl Pts',(-2.42476722548671,-9.64177721699716,
13.5321005962683));
#88271=CARTESIAN_POINT('Ctrl Pts',(-2.66164358082723,-9.58220624683308,
13.5281907126906));
#88272=CARTESIAN_POINT('Ctrl Pts',(-2.89630565723214,-9.51390631248867,
13.5242808291129));
#88273=CARTESIAN_POINT('Ctrl Pts',(-3.12810752025186,-9.43707090901323,
13.5203709455352));
#88274=CARTESIAN_POINT('Ctrl Pts',(-3.29350203324386,-9.3822475612937,13.5175811780943));
#88275=CARTESIAN_POINT('Ctrl Pts',(-3.45744066278369,-9.32307981029869,
13.5147914106534));
#88276=CARTESIAN_POINT('Ctrl Pts',(-3.61969405072859,-9.25965328611823,
13.5120016432125));
#88277=CARTESIAN_POINT('Ctrl Pts',(-3.84709321415005,-9.17076060584786,
13.5080917662588));
#88278=CARTESIAN_POINT('Ctrl Pts',(-4.07125104332576,-9.07347355302008,
13.504181889305));
#88279=CARTESIAN_POINT('Ctrl Pts',(-4.29154651074866,-8.96805399995345,
13.5002720123512));
#88280=CARTESIAN_POINT('Ctrl Pts',(-4.51180384301016,-8.86265269597618,
13.4963628122329));
#88281=CARTESIAN_POINT('Ctrl Pts',(-4.72819989548968,-8.74912182300618,
13.4924536121146));
#88282=CARTESIAN_POINT('Ctrl Pts',(-4.94013568073457,-8.62777048002166,
13.4885444119964));
#88283=CARTESIAN_POINT('Ctrl Pts',(-5.15204839365958,-8.50643234791137,
13.4846356374519));
#88284=CARTESIAN_POINT('Ctrl Pts',(-5.359501565704,-8.37727558493515,13.4807268629074));
#88285=CARTESIAN_POINT('Ctrl Pts',(-5.5619218702263,-8.24065465296892,13.4768180883629));
#88286=CARTESIAN_POINT('Ctrl Pts',(-5.76435788359565,-8.10402311852223,
13.4729090104775));
#88287=CARTESIAN_POINT('Ctrl Pts',(-5.96176001492486,-7.9599264118996,13.4689999325922));
#88288=CARTESIAN_POINT('Ctrl Pts',(-6.15358386304595,-7.80876236291389,
13.4650908547069));
#88289=CARTESIAN_POINT('Ctrl Pts',(-6.34540506228902,-7.65760040133873,
13.4611818308017));
#88290=CARTESIAN_POINT('Ctrl Pts',(-6.53164791347946,-7.49937146771238,
13.4572728068964));
#88291=CARTESIAN_POINT('Ctrl Pts',(-6.71180048787439,-7.33451417688786,
13.4533637829912));
#88292=CARTESIAN_POINT('Ctrl Pts',(-6.89199268142085,-7.16962063065036,
13.4494538994135));
#88293=CARTESIAN_POINT('Ctrl Pts',(-7.06609171432072,-6.99809600303789,
13.4455440158358));
#88294=CARTESIAN_POINT('Ctrl Pts',(-7.23362096621123,-6.82041726855397,
13.4416341322581));
#88295=CARTESIAN_POINT('Ctrl Pts',(-7.35315589430491,-6.69364051458034,
13.4388443648172));
#88296=CARTESIAN_POINT('Ctrl Pts',(-7.46934684466363,-6.56373146921644,
13.4360545973764));
#88297=CARTESIAN_POINT('Ctrl Pts',(-7.58203261433193,-6.43087439118561,
13.4332648299355));
#88298=CARTESIAN_POINT('Ctrl Pts',(-7.73996244295911,-6.24467434456856,
13.4293549529818));
#88299=CARTESIAN_POINT('Ctrl Pts',(-7.89105405542264,-6.05262532043193,
13.425445076028));
#88300=CARTESIAN_POINT('Ctrl Pts',(-8.03488521642281,-5.85525264688982,
13.4215351990742));
#88301=CARTESIAN_POINT('Ctrl Pts',(-8.17869147893296,-5.65791414036345,
13.4176259989559));
#88302=CARTESIAN_POINT('Ctrl Pts',(-8.3152396339323,-5.45525405052717,13.4137167988376));
#88303=CARTESIAN_POINT('Ctrl Pts',(-8.44414926606862,-5.24782880554929,
13.4098075987193));
#88304=CARTESIAN_POINT('Ctrl Pts',(-8.57304486449993,-5.04042614185295,
13.4058988241748));
#88305=CARTESIAN_POINT('Ctrl Pts',(-8.69430345253167,-4.82825959679366,
13.4019900496303));
#88306=CARTESIAN_POINT('Ctrl Pts',(-8.80758873651319,-4.61191333921682,
13.3980812750858));
#88307=CARTESIAN_POINT('Ctrl Pts',(-8.92088281200999,-4.39555029206798,
13.3941721972005));
#88308=CARTESIAN_POINT('Ctrl Pts',(-9.02620221428049,-4.17500713117138,
13.3902631193152));
#88309=CARTESIAN_POINT('Ctrl Pts',(-9.12325669743927,-3.95089246027141,
13.3863540414298));
#88310=CARTESIAN_POINT('Ctrl Pts',(-9.22030984038136,-3.72678088415093,
13.3824450175246));
#88311=CARTESIAN_POINT('Ctrl Pts',(-9.3090981829599,-3.49909815472667,13.3785359936194));
#88312=CARTESIAN_POINT('Ctrl Pts',(-9.38937942241948,-3.26847335339386,
13.3746269697142));
#88313=CARTESIAN_POINT('Ctrl Pts',(-9.46967831732807,-3.03779783305806,
13.3707170861365));
#88314=CARTESIAN_POINT('Ctrl Pts',(-9.54146627763864,-2.80417921246332,
13.3668072025588));
#88315=CARTESIAN_POINT('Ctrl Pts',(-9.60455028812226,-2.56826356959923,
13.3628973189811));
#88316=CARTESIAN_POINT('Ctrl Pts',(-9.6495617865438,-2.39993380576549,13.3601075515403));
#88317=CARTESIAN_POINT('Ctrl Pts',(-9.69014308115675,-2.23043496936777,
13.3573177840994));
#88318=CARTESIAN_POINT('Ctrl Pts',(-9.72623977981077,-2.06000576349351,
13.3545280166586));
#88319=CARTESIAN_POINT('Ctrl Pts',(-9.77790824323873,-1.81605505555838,
13.350534770673));
#88320=CARTESIAN_POINT('Ctrl Pts',(-9.82039913593903,-1.57013722047607,
13.3465415246875));
#88321=CARTESIAN_POINT('Ctrl Pts',(-9.85358736138807,-1.3229437295264,13.342548278702));
#88322=CARTESIAN_POINT('Ctrl Pts',(-9.88676782727094,-1.07580803359969,
13.3385559663566));
#88323=CARTESIAN_POINT('Ctrl Pts',(-9.91064993630569,-0.827397529053514,
13.3345636540111));
#88324=CARTESIAN_POINT('Ctrl Pts',(-9.92516018494209,-0.57841101583585,
13.3305713416656));
#88325=CARTESIAN_POINT('Ctrl Pts',(-9.93638033506975,-0.385880472213324,
13.3274842585291));
#88326=CARTESIAN_POINT('Ctrl Pts',(-9.94199783454639,-0.19300570929332,
13.3243971753925));
#88327=CARTESIAN_POINT('Ctrl Pts',(-9.94199999937389,-0.000111577862839334,
13.321310092256));
#88328=CARTESIAN_POINT('Ctrl Pts',(-9.94199999942951,-0.000106505970992509,
13.1786899088249));
#88329=CARTESIAN_POINT('Ctrl Pts',(-9.94199732858428,-0.249421572746613,
13.1826799425284));
#88330=CARTESIAN_POINT('Ctrl Pts',(-9.93261222415611,-0.498704725276454,
13.1866699762318));
#88331=CARTESIAN_POINT('Ctrl Pts',(-9.91387787977736,-0.747254564965084,
13.1906600099353));
#88332=CARTESIAN_POINT('Ctrl Pts',(-9.89513752219156,-0.995884182286508,
13.1946513243293));
#88333=CARTESIAN_POINT('Ctrl Pts',(-9.86704194641944,-1.24377976230886,
13.1986426387234));
#88334=CARTESIAN_POINT('Ctrl Pts',(-9.82967631540366,-1.49024411905982,
13.2026339531174));
#88335=CARTESIAN_POINT('Ctrl Pts',(-9.79980239131882,-1.6872930456546,13.2058250198802));
#88336=CARTESIAN_POINT('Ctrl Pts',(-9.76400401434294,-1.8834271732374,13.209016086643));
#88337=CARTESIAN_POINT('Ctrl Pts',(-9.72234836197068,-2.07829409095199,
13.2122071534058));
#88338=CARTESIAN_POINT('Ctrl Pts',(-9.6713094814617,-2.31705614992799,13.2161170303596));
#88339=CARTESIAN_POINT('Ctrl Pts',(-9.61146324235827,-2.55397371089278,
13.2200269073133));
#88340=CARTESIAN_POINT('Ctrl Pts',(-9.54296788786523,-2.7883916315993,13.2239367842671));
#88341=CARTESIAN_POINT('Ctrl Pts',(-9.47448439054498,-3.0227689724182,13.2278459843854));
#88342=CARTESIAN_POINT('Ctrl Pts',(-9.39735484524539,-3.25464726783933,
13.2317551845036));
#88343=CARTESIAN_POINT('Ctrl Pts',(-9.31178765908832,-3.48338550724012,
13.2356643846219));
#88344=CARTESIAN_POINT('Ctrl Pts',(-9.22622978817491,-3.71209884512747,
13.2395731591664));
#88345=CARTESIAN_POINT('Ctrl Pts',(-9.13223620864876,-3.93767254709915,
13.2434819337109));
#88346=CARTESIAN_POINT('Ctrl Pts',(-9.03006423638719,-4.15948360818035,
13.2473907082554));
#88347=CARTESIAN_POINT('Ctrl Pts',(-8.92788433505995,-4.38131188293015,
13.2512997861407));
#88348=CARTESIAN_POINT('Ctrl Pts',(-8.81752488726968,-4.59937667741979,
13.255208864026));
#88349=CARTESIAN_POINT('Ctrl Pts',(-8.69929067555455,-4.81307653608476,
13.2591179419113));
#88350=CARTESIAN_POINT('Ctrl Pts',(-8.58105809652494,-5.02677344378773,
13.2630269658165));
#88351=CARTESIAN_POINT('Ctrl Pts',(-8.45495110856853,-5.23610529192399,
13.2669359897218));
#88352=CARTESIAN_POINT('Ctrl Pts',(-8.32131998410183,-5.44049609155154,
13.270845013627));
#88353=CARTESIAN_POINT('Ctrl Pts',(-8.18765947148013,-5.64493184080084,
13.2747548972047));
#88354=CARTESIAN_POINT('Ctrl Pts',(-8.04647166857423,-5.84442413499898,
13.2786647807824));
#88355=CARTESIAN_POINT('Ctrl Pts',(-7.89815040162596,-6.03842564194473,
13.2825746643601));
#88356=CARTESIAN_POINT('Ctrl Pts',(-7.79232069260521,-6.17684896755466,
13.285364431801));
#88357=CARTESIAN_POINT('Ctrl Pts',(-7.68286020402429,-6.31247749867597,
13.2881541992419));
#88358=CARTESIAN_POINT('Ctrl Pts',(-7.56992477163206,-6.44512241558152,
13.2909439666829));
#88359=CARTESIAN_POINT('Ctrl Pts',(-7.41164503910113,-6.6310251170161,13.2948538436367));
#88360=CARTESIAN_POINT('Ctrl Pts',(-7.24648966419361,-6.81112288259956,
13.2987637205905));
#88361=CARTESIAN_POINT('Ctrl Pts',(-7.07490896788178,-6.98491425116916,
13.3026735975443));
#88362=CARTESIAN_POINT('Ctrl Pts',(-6.90335797375851,-7.15867553486259,
13.3065827976626));
#88363=CARTESIAN_POINT('Ctrl Pts',(-6.72538407543683,-7.32613240143615,
13.3104919977809));
#88364=CARTESIAN_POINT('Ctrl Pts',(-6.54147503382302,-7.48681964400573,
13.3144011978992));
#88365=CARTESIAN_POINT('Ctrl Pts',(-6.35758601340758,-7.64748939341059,
13.3183099724437));
#88366=CARTESIAN_POINT('Ctrl Pts',(-6.167763350815,-7.80139080594464,13.3222187469882));
#88367=CARTESIAN_POINT('Ctrl Pts',(-5.97252930289241,-7.94809774261059,
13.3261275215327));
#88368=CARTESIAN_POINT('Ctrl Pts',(-5.77728010381255,-8.09481606448262,
13.330036599418));
#88369=CARTESIAN_POINT('Ctrl Pts',(-5.5766189025228,-8.23433862398428,13.3339456773033));
#88370=CARTESIAN_POINT('Ctrl Pts',(-5.37109950009994,-8.36628078419714,
13.3378547551886));
#88371=CARTESIAN_POINT('Ctrl Pts',(-5.16558293567578,-8.49822112243272,
13.3417637790938));
#88372=CARTESIAN_POINT('Ctrl Pts',(-4.95520854130392,-8.62258112102101,
13.3456728029991));
#88373=CARTESIAN_POINT('Ctrl Pts',(-4.74055806269171,-8.73902015412762,
13.3495818269043));
#88374=CARTESIAN_POINT('Ctrl Pts',(-4.52586037814926,-8.85548479450474,
13.353491710482));
#88375=CARTESIAN_POINT('Ctrl Pts',(-4.30688497630831,-8.96402485403609,
13.3574015940597));
#88376=CARTESIAN_POINT('Ctrl Pts',(-4.08423832896597,-9.06434560639682,
13.3613114776374));
#88377=CARTESIAN_POINT('Ctrl Pts',(-3.92537621575494,-9.1359261440298,13.3641012450782));
#88378=CARTESIAN_POINT('Ctrl Pts',(-3.76464556609823,-9.20332314153561,
13.366891012519));
#88379=CARTESIAN_POINT('Ctrl Pts',(-3.60227317993511,-9.26644440641178,
13.3696807799599));
#88380=CARTESIAN_POINT('Ctrl Pts',(-3.37470723974289,-9.3549092638121,13.3735906569136));
#88381=CARTESIAN_POINT('Ctrl Pts',(-3.14384611613994,-9.4350007404964,13.3775005338674));
#88382=CARTESIAN_POINT('Ctrl Pts',(-2.91032422327388,-9.50649130412611,
13.3814104108212));
#88383=CARTESIAN_POINT('Ctrl Pts',(-2.67684275518445,-9.57796949208503,
13.3853196109395));
#88384=CARTESIAN_POINT('Ctrl Pts',(-2.44070170520027,-9.64084965714869,
13.3892288110578));
#88385=CARTESIAN_POINT('Ctrl Pts',(-2.20255122552143,-9.69495395032664,
13.393138011176));
#88386=CARTESIAN_POINT('Ctrl Pts',(-1.96442667201731,-9.74905235345825,
13.3970467857205));
#88387=CARTESIAN_POINT('Ctrl Pts',(-1.72429339884424,-9.79437673021801,
13.400955560265));
#88388=CARTESIAN_POINT('Ctrl Pts',(-1.48281336938402,-9.83079999346828,
13.4048643348095));
#88389=CARTESIAN_POINT('Ctrl Pts',(-1.24131459984261,-9.86722608334945,
13.4087734126948));
#88390=CARTESIAN_POINT('Ctrl Pts',(-0.998469141906446,-9.89474963458269,
13.4126824905802));
#88391=CARTESIAN_POINT('Ctrl Pts',(-0.754947016616046,-9.91329506279837,
13.4165915684655));
#88392=CARTESIAN_POINT('Ctrl Pts',(-0.511428254100723,-9.9318402349219,
13.4205005923707));
#88393=CARTESIAN_POINT('Ctrl Pts',(-0.267233122595606,-9.94140751275124,
13.4244096162759));
#88394=CARTESIAN_POINT('Ctrl Pts',(-0.0230353415490897,-9.94197331383663,
13.4283186401811));
#88395=CARTESIAN_POINT('Ctrl Pts',(0.221216143469949,-9.94253923935299,
13.4322285237588));
#88396=CARTESIAN_POINT('Ctrl Pts',(0.465469998774068,-9.93409973088492,
13.4361384073365));
#88397=CARTESIAN_POINT('Ctrl Pts',(0.709052535746479,-9.9166833418009,13.4400482909142));
#88398=CARTESIAN_POINT('Ctrl Pts',(0.882852756982974,-9.90425645638634,
13.4428380583551));
#88399=CARTESIAN_POINT('Ctrl Pts',(1.05631120637462,-9.88726047604474,13.445627825796));
#88400=CARTESIAN_POINT('Ctrl Pts',(1.22918450521996,-9.86572194277374,13.4484175932369));
#88401=CARTESIAN_POINT('Ctrl Pts',(1.47146754185372,-9.83553555030947,13.4523274701906));
#88402=CARTESIAN_POINT('Ctrl Pts',(1.71267513534455,-9.79641522475994,13.4562373471444));
#88403=CARTESIAN_POINT('Ctrl Pts',(1.95214090753327,-9.74846192366443,13.4601472240982));
#88404=CARTESIAN_POINT('Ctrl Pts',(2.1915652260052,-9.70051692372421,13.4640564242164));
#88405=CARTESIAN_POINT('Ctrl Pts',(2.42924805036886,-9.64374205561775,13.4679656243347));
#88406=CARTESIAN_POINT('Ctrl Pts',(2.66453274019601,-9.57828947549736,13.471874824453));
#88407=CARTESIAN_POINT('Ctrl Pts',(2.89979181583238,-9.51284402085069,13.4757835989975));
#88408=CARTESIAN_POINT('Ctrl Pts',(3.13265300825618,-9.43872281554012,13.479692373542));
#88409=CARTESIAN_POINT('Ctrl Pts',(3.36247338287568,-9.35612829911244,13.4836011480865));
#88410=CARTESIAN_POINT('Ctrl Pts',(3.59231159272715,-9.27352737292947,13.4875102259718));
#88411=CARTESIAN_POINT('Ctrl Pts',(3.81910824838988,-9.18245191359552,13.4914193038571));
#88412=CARTESIAN_POINT('Ctrl Pts',(4.04223777636832,-9.08315351402259,13.4953283817424));
#88413=CARTESIAN_POINT('Ctrl Pts',(4.26536422317144,-8.98385648565221,13.4992374056476));
#88414=CARTESIAN_POINT('Ctrl Pts',(4.48482338829301,-8.87633686000137,13.5031464295529));
#88415=CARTESIAN_POINT('Ctrl Pts',(4.700011132911,-8.76089375295196,13.5070554534581));
#88416=CARTESIAN_POINT('Ctrl Pts',(4.91524620161468,-8.64542525765611,13.5109653370358));
#88417=CARTESIAN_POINT('Ctrl Pts',(5.12620772520819,-8.52202993077017,13.5148752206135));
#88418=CARTESIAN_POINT('Ctrl Pts',(5.33231634522919,-8.3910527584089,13.5187851041911));
#88419=CARTESIAN_POINT('Ctrl Pts',(5.479378298863,-8.29759835147086,13.521574871632));
#88420=CARTESIAN_POINT('Ctrl Pts',(5.62397012744568,-8.20028493965103,13.5243646390729));
#88421=CARTESIAN_POINT('Ctrl Pts',(5.76589023444149,-8.0992514348162,13.5271544065137));
#88422=CARTESIAN_POINT('Ctrl Pts',(5.96479217425593,-7.95765233005725,13.5310642834675));
#88423=CARTESIAN_POINT('Ctrl Pts',(6.1585059299626,-7.80870104983866,13.5349741604213));
#88424=CARTESIAN_POINT('Ctrl Pts',(6.34649295335573,-7.65280283249256,13.5388840373751));
#88425=CARTESIAN_POINT('Ctrl Pts',(6.53444743447464,-7.49693160255467,13.5427932374934));
#88426=CARTESIAN_POINT('Ctrl Pts',(6.71667694657671,-7.33411601495616,13.5467024376116));
#88427=CARTESIAN_POINT('Ctrl Pts',(6.89267581991407,-7.16480174474995,13.5506116377299));
#88428=CARTESIAN_POINT('Ctrl Pts',(7.06865553319191,-6.99550590688613,13.5545204122744));
#88429=CARTESIAN_POINT('Ctrl Pts',(7.23840576011248,-6.81971299327947,13.558429186819));
#88430=CARTESIAN_POINT('Ctrl Pts',(7.40145676719534,-6.63790642622645,13.5623379613635));
#88431=CARTESIAN_POINT('Ctrl Pts',(7.564520427867,-6.45608575005762,13.5662470392488));
#88432=CARTESIAN_POINT('Ctrl Pts',(7.72088364040559,-6.26825069455036,13.5701561171341));
#88433=CARTESIAN_POINT('Ctrl Pts',(7.87011528808262,-6.07491969924609,13.5740651950194));
#88434=CARTESIAN_POINT('Ctrl Pts',(8.01934487503333,-5.88159137363204,13.5779742189247));
#88435=CARTESIAN_POINT('Ctrl Pts',(8.16144292442014,-5.68276748317503,13.5818832428299));
#88436=CARTESIAN_POINT('Ctrl Pts',(8.29601974734786,-5.47899811567903,13.5857922667351));
#88437=CARTESIAN_POINT('Ctrl Pts',(8.43062616640853,-5.27518393522667,13.5897021503128));
#88438=CARTESIAN_POINT('Ctrl Pts',(8.55770789852269,-5.06642233795103,13.5936120338905));
#88439=CARTESIAN_POINT('Ctrl Pts',(8.67691884248351,-4.85329201686387,13.5975219174682));
#88440=CARTESIAN_POINT('Ctrl Pts',(8.76197784832004,-4.70121996187494,13.6003116849091));
#88441=CARTESIAN_POINT('Ctrl Pts',(8.84303069884756,-4.54692436104982,13.6031014523499));
#88442=CARTESIAN_POINT('Ctrl Pts',(8.91996592148114,-4.39062318579209,13.6058912197908));
#88443=CARTESIAN_POINT('Ctrl Pts',(9.02779112923973,-4.17156608660955,13.6098010967445));
#88444=CARTESIAN_POINT('Ctrl Pts',(9.1275595110882,-3.94850158245876,13.6137109736983));
#88445=CARTESIAN_POINT('Ctrl Pts',(9.21898948979115,-3.72204201845175,13.6176208506521));
#88446=CARTESIAN_POINT('Ctrl Pts',(9.310403641128,-3.49562165666787,13.6215300507704));
#88447=CARTESIAN_POINT('Ctrl Pts',(9.39348216588967,-3.26580766803928,13.6254392508887));
#88448=CARTESIAN_POINT('Ctrl Pts',(9.46799162194494,-3.03323237599435,13.629348451007));
#88449=CARTESIAN_POINT('Ctrl Pts',(9.54249296655266,-2.80068240318251,13.6332572255515));
#88450=CARTESIAN_POINT('Ctrl Pts',(9.60842701960371,-2.56537199401636,13.637166000096));
#88451=CARTESIAN_POINT('Ctrl Pts',(9.66560988833804,-2.32794963142717,13.6410747746405));
#88452=CARTESIAN_POINT('Ctrl Pts',(9.72279719475438,-2.09050884365275,13.6449838525258));
#88453=CARTESIAN_POINT('Ctrl Pts',(9.77123189118644,-1.8509560467701,13.6488929304111));
#88454=CARTESIAN_POINT('Ctrl Pts',(9.81078069718854,-1.60995220788467,13.6528020082964));
#88455=CARTESIAN_POINT('Ctrl Pts',(9.85032895706476,-1.36895169699941,13.6567110322016));
#88456=CARTESIAN_POINT('Ctrl Pts',(9.88099152855776,-1.12650046114897,13.6606200561068));
#88457=CARTESIAN_POINT('Ctrl Pts',(9.90268661803924,-0.883267651907685,
13.6645290800121));
#88458=CARTESIAN_POINT('Ctrl Pts',(9.92438647870449,-0.639981350910512,
13.6684389635898));
#88459=CARTESIAN_POINT('Ctrl Pts',(9.93711489079659,-0.395913412295458,
13.6723488471675));
#88460=CARTESIAN_POINT('Ctrl Pts',(9.94084200360668,-0.151737468441802,
13.6762587307452));
#88461=CARTESIAN_POINT('Ctrl Pts',(9.94350136104263,0.0224861585459037,
13.679048498186));
#88462=CARTESIAN_POINT('Ctrl Pts',(9.94157918780769,0.196764677770003,13.6818382656269));
#88463=CARTESIAN_POINT('Ctrl Pts',(9.93508086580521,0.370853326682132,13.6846280330678));
#88464=CARTESIAN_POINT('Ctrl Pts',(9.92597342585754,0.614839684226999,13.6885379100215));
#88465=CARTESIAN_POINT('Ctrl Pts',(9.90787250252161,0.858527721690995,13.6924477869753));
#88466=CARTESIAN_POINT('Ctrl Pts',(9.88082101026709,1.10124482430766,13.6963576639291));
#88467=CARTESIAN_POINT('Ctrl Pts',(9.85377420087345,1.34391991037255,13.7002668640474));
#88468=CARTESIAN_POINT('Ctrl Pts',(9.81777994659825,1.58562411866262,13.7041760641657));
#88469=CARTESIAN_POINT('Ctrl Pts',(9.77293301111777,1.82569010519433,13.7080852642839));
#88470=CARTESIAN_POINT('Ctrl Pts',(9.72809095788426,2.06572995702092,13.7119940388284));
#88471=CARTESIAN_POINT('Ctrl Pts',(9.67439819918634,2.3041316677469,13.7159028133729));
#88472=CARTESIAN_POINT('Ctrl Pts',(9.6120007794975,2.54023719659,13.7198115879174));
#88473=CARTESIAN_POINT('Ctrl Pts',(9.54959851745092,2.7763610484253,13.7237206658027));
#88474=CARTESIAN_POINT('Ctrl Pts',(9.47849031324122,3.010188090503,13.7276297436881));
#88475=CARTESIAN_POINT('Ctrl Pts',(9.39887268265288,3.2410733245765,13.7315388215734));
#88476=CARTESIAN_POINT('Ctrl Pts',(9.31925615149717,3.4719553703768,13.7354478454786));
#88477=CARTESIAN_POINT('Ctrl Pts',(9.23113052230889,3.69989542507572,13.7393568693838));
#88478=CARTESIAN_POINT('Ctrl Pts',(9.13474151040695,3.92426573234384,13.743265893289));
#88479=CARTESIAN_POINT('Ctrl Pts',(9.03833130063493,4.14868538312664,13.7471757768667));
#88480=CARTESIAN_POINT('Ctrl Pts',(8.93365418667395,4.36953345974712,13.7510856604444));
#88481=CARTESIAN_POINT('Ctrl Pts',(8.82100372635553,4.58620292394721,13.7549955440221));
#88482=CARTESIAN_POINT('Ctrl Pts',(8.74062573551506,4.74080021684468,13.757785311463));
#88483=CARTESIAN_POINT('Ctrl Pts',(8.6561894655125,4.8932705855102,13.7605750789039));
#88484=CARTESIAN_POINT('Ctrl Pts',(8.56781586218746,5.04340116901768,13.7633648463447));
#88485=CARTESIAN_POINT('Ctrl Pts',(8.44395969055799,5.25381014430122,13.7672747232985));
#88486=CARTESIAN_POINT('Ctrl Pts',(8.31232996790528,5.4596866100354,13.7711846002523));
#88487=CARTESIAN_POINT('Ctrl Pts',(8.17328380974075,5.66045897126989,13.7750944772061));
#88488=CARTESIAN_POINT('Ctrl Pts',(8.0342617217387,5.86119657697125,13.7790036773243));
#88489=CARTESIAN_POINT('Ctrl Pts',(7.88782592060099,6.05683161164373,13.7829128774426));
#88490=CARTESIAN_POINT('Ctrl Pts',(7.73437665198203,6.24682173631321,13.7868220775609));
#88491=CARTESIAN_POINT('Ctrl Pts',(7.58094408856781,6.43679117776955,13.7907308521054));
#88492=CARTESIAN_POINT('Ctrl Pts',(7.42049975823215,6.62111671825914,13.7946396266499));
#88493=CARTESIAN_POINT('Ctrl Pts',(7.25348462198825,6.79928855385473,13.7985484011944));
#88494=CARTESIAN_POINT('Ctrl Pts',(7.08645652451837,6.97747421649305,13.8024574790797));
#88495=CARTESIAN_POINT('Ctrl Pts',(6.91285679168171,7.14950501336379,13.806366556965));
#88496=CARTESIAN_POINT('Ctrl Pts',(6.73316461204516,7.31490658225399,13.8102756348504));
#88497=CARTESIAN_POINT('Ctrl Pts',(6.55347491376161,7.48030586712894,13.8141846587556));
#88498=CARTESIAN_POINT('Ctrl Pts',(6.36769314458791,7.63907591877233,13.8180936826608));
#88499=CARTESIAN_POINT('Ctrl Pts',(6.17633360755374,7.79078090875377,13.822002706566));
#88500=CARTESIAN_POINT('Ctrl Pts',(5.984931986733,7.94251926169437,13.8259125901437));
#88501=CARTESIAN_POINT('Ctrl Pts',(5.78795036609402,8.08718927332352,13.8298224737214));
#88502=CARTESIAN_POINT('Ctrl Pts',(5.58593531839025,8.22439606407428,13.8337323572991));
#88503=CARTESIAN_POINT('Ctrl Pts',(5.44179419719196,8.32229540810648,13.83652212474));
#88504=CARTESIAN_POINT('Ctrl Pts',(5.29509120226131,8.416396036642,13.8393118921808));
#88505=CARTESIAN_POINT('Ctrl Pts',(5.14603384120027,8.50656803330354,13.8421016596217));
#88506=CARTESIAN_POINT('Ctrl Pts',(4.93712899405436,8.63294466472467,13.8460115365754));
#88507=CARTESIAN_POINT('Ctrl Pts',(4.72353458475188,8.75164146899247,13.8499214135292));
#88508=CARTESIAN_POINT('Ctrl Pts',(4.50583629543146,8.86232493642455,13.853831290483));
#88509=CARTESIAN_POINT('Ctrl Pts',(4.28817569167732,8.97298924353544,13.8577404906013));
#88510=CARTESIAN_POINT('Ctrl Pts',(4.06641287580908,9.07564285596153,13.8616496907195));
#88511=CARTESIAN_POINT('Ctrl Pts',(3.84115759866413,9.16999848976132,13.8655588908378));
#88512=CARTESIAN_POINT('Ctrl Pts',(3.61592684386145,9.2643438515658,13.8694676653823));
#88513=CARTESIAN_POINT('Ctrl Pts',(3.38720464537551,9.35039293019713,13.8733764399268));
#88514=CARTESIAN_POINT('Ctrl Pts',(3.15562114063591,9.42790640687378,13.8772852144713));
#88515=CARTESIAN_POINT('Ctrl Pts',(2.92401966383604,9.50542589899128,13.8811942923566));
#88516=CARTESIAN_POINT('Ctrl Pts',(2.68955670193747,9.57440837365301,13.885103370242));
#88517=CARTESIAN_POINT('Ctrl Pts',(2.45287920940057,9.63466385423438,13.8890124481273));
#88518=CARTESIAN_POINT('Ctrl Pts',(2.21620498512208,9.69491850275318,13.8929214720325));
#88519=CARTESIAN_POINT('Ctrl Pts',(1.97731656353752,9.74644633104595,13.8968304959377));
#88520=CARTESIAN_POINT('Ctrl Pts',(1.73687350823564,9.78910794793832,13.9007395198429));
#88521=CARTESIAN_POINT('Ctrl Pts',(1.49637757470016,9.83177894697293,13.9046494034206));
#88522=CARTESIAN_POINT('Ctrl Pts',(1.2543266002188,9.86557978848229,13.9085592869983));
#88523=CARTESIAN_POINT('Ctrl Pts',(1.01138910720584,9.89042244162631,13.912469170576));
#88524=CARTESIAN_POINT('Ctrl Pts',(0.83804913564136,9.90814809087116,13.9152589380169));
#88525=CARTESIAN_POINT('Ctrl Pts',(0.664258019571988,9.92131414527852,13.9180487054578));
#88526=CARTESIAN_POINT('Ctrl Pts',(0.490260069134454,9.9299047862813,13.9208384728987));
#88527=CARTESIAN_POINT('Ctrl Pts',(0.24640082608494,9.94194462472182,13.9247483498524));
#88528=CARTESIAN_POINT('Ctrl Pts',(0.00206054199615485,9.94499890041736,
13.9286582268062));
#88529=CARTESIAN_POINT('Ctrl Pts',(-0.242086977851291,9.93905216281486,
13.93256810376));
#88530=CARTESIAN_POINT('Ctrl Pts',(-0.486192233529097,9.93310645464706,
13.9364773038783));
#88531=CARTESIAN_POINT('Ctrl Pts',(-0.730104511488564,9.91816285043836,
13.9403865039966));
#88532=CARTESIAN_POINT('Ctrl Pts',(-0.973150770741514,9.89425801045259,
13.9442957041149));
#88533=CARTESIAN_POINT('Ctrl Pts',(-1.21617057084281,9.87035577285941,13.9482044786594));
#88534=CARTESIAN_POINT('Ctrl Pts',(-1.45832426162404,9.83749427479848,13.9521132532039));
#88535=CARTESIAN_POINT('Ctrl Pts',(-1.69894363286851,9.79576207001454,13.9560220277484));
#88536=CARTESIAN_POINT('Ctrl Pts',(-1.93958167740217,9.75402662659888,13.9599311056337));
#88537=CARTESIAN_POINT('Ctrl Pts',(-2.17868488774455,9.70341914576131,13.963840183519));
#88538=CARTESIAN_POINT('Ctrl Pts',(-2.41559367980634,9.64407959185736,13.9677492614043));
#88539=CARTESIAN_POINT('Ctrl Pts',(-2.65249920041627,9.58474085736789,13.9716582853095));
#88540=CARTESIAN_POINT('Ctrl Pts',(-2.88721009192215,9.51667036108228,13.9755673092148));
#88541=CARTESIAN_POINT('Ctrl Pts',(-3.11907969004316,9.44005857435007,13.97947633312));
#88542=CARTESIAN_POINT('Ctrl Pts',(-3.35100028092263,9.36342993915489,13.9833862166977));
#88543=CARTESIAN_POINT('Ctrl Pts',(-3.58007806326531,9.27825634717285,13.9872961002754));
#88544=CARTESIAN_POINT('Ctrl Pts',(-3.80568287314214,9.18477772562149,13.9912059838531));
#88545=CARTESIAN_POINT('Ctrl Pts',(-3.9666556848868,9.1180791629563,13.9939957512939));
#88546=CARTESIAN_POINT('Ctrl Pts',(-4.12586072983799,9.04715349288656,13.9967855187348));
#88547=CARTESIAN_POINT('Ctrl Pts',(-4.2830754796054,8.97210278786434,13.9995752861756));
#88548=CARTESIAN_POINT('Ctrl Pts',(-4.50341295931952,8.86691874362021,14.0034851631294));
#88549=CARTESIAN_POINT('Ctrl Pts',(-4.71990760785364,8.75359809155419,14.0073950400832));
#88550=CARTESIAN_POINT('Ctrl Pts',(-4.93195907173468,8.63244714520361,14.0113049170369));
#88551=CARTESIAN_POINT('Ctrl Pts',(-5.14397382756636,8.51131717119078,14.0152141171552));
#88552=CARTESIAN_POINT('Ctrl Pts',(-5.3515466908855,8.38235974775502,14.0191233172735));
#88553=CARTESIAN_POINT('Ctrl Pts',(-5.55410272222934,8.24592668842773,14.0230325173918));
#88554=CARTESIAN_POINT('Ctrl Pts',(-5.75663670237712,8.10950848184078,14.0269412919362));
#88555=CARTESIAN_POINT('Ctrl Pts',(-5.95415470864457,7.96561642085906,14.0308500664807));
#88556=CARTESIAN_POINT('Ctrl Pts',(-6.14611069131068,7.81464569703301,14.0347588410252));
#88557=CARTESIAN_POINT('Ctrl Pts',(-6.33808157073958,7.66366325710919,14.0386679189105));
#88558=CARTESIAN_POINT('Ctrl Pts',(-6.52448934182446,7.50560122753885,14.0425769967958));
#88559=CARTESIAN_POINT('Ctrl Pts',(-6.70481995562998,7.34089595094399,14.0464860746812));
#88560=CARTESIAN_POINT('Ctrl Pts',(-6.88514807926637,7.17619294874941,14.0503950985864));
#88561=CARTESIAN_POINT('Ctrl Pts',(-7.05939900786311,7.00484707357558,14.0543041224916));
#88562=CARTESIAN_POINT('Ctrl Pts',(-7.22709404312832,6.82733298527172,14.0582131463968));
#88563=CARTESIAN_POINT('Ctrl Pts',(-7.39482595788342,6.64977985807195,14.0621230299745));
#88564=CARTESIAN_POINT('Ctrl Pts',(-7.55599890510002,6.46605601035547,14.0660329135522));
#88565=CARTESIAN_POINT('Ctrl Pts',(-7.71017218931807,6.27667179411718,14.0699427971299));
#88566=CARTESIAN_POINT('Ctrl Pts',(-7.82017741070618,6.14154298279056,14.0727325645708));
#88567=CARTESIAN_POINT('Ctrl Pts',(-7.92661985514808,6.00353318953445,14.0755223320117));
#88568=CARTESIAN_POINT('Ctrl Pts',(-8.02935213713319,5.86283790138485,14.0783120994526));
#88569=CARTESIAN_POINT('Ctrl Pts',(-8.17333208895841,5.66565255303689,14.0822219764063));
#88570=CARTESIAN_POINT('Ctrl Pts',(-8.31006682801636,5.46313066739559,14.0861318533601));
#88571=CARTESIAN_POINT('Ctrl Pts',(-8.43917341423532,5.25582686971933,14.0900417303139));
#88572=CARTESIAN_POINT('Ctrl Pts',(-8.56825765092245,5.04855895822799,14.0939509304322));
#88573=CARTESIAN_POINT('Ctrl Pts',(-8.68971622268014,4.83651102498496,14.0978601305505));
#88574=CARTESIAN_POINT('Ctrl Pts',(-8.80321015901934,4.62026567376148,14.1017693306688));
#88575=CARTESIAN_POINT('Ctrl Pts',(-8.91669173987867,4.40404386401669,14.1056781052133));
#88576=CARTESIAN_POINT('Ctrl Pts',(-9.02221028635632,4.18362579678211,14.1095868797578));
#88577=CARTESIAN_POINT('Ctrl Pts',(-9.11947284906762,3.95961853656617,14.1134956543023));
#88578=CARTESIAN_POINT('Ctrl Pts',(-9.21674295984921,3.73559389224583,14.1174047321876));
#88579=CARTESIAN_POINT('Ctrl Pts',(-9.30575569214927,3.507979754281,14.121313810073));
#88580=CARTESIAN_POINT('Ctrl Pts',(-9.38626579840765,3.2774042109027,14.1252228879583));
#88581=CARTESIAN_POINT('Ctrl Pts',(-9.46677479290924,3.04683185152128,14.1291319118635));
#88582=CARTESIAN_POINT('Ctrl Pts',(-9.53878130572673,2.81329843385258,14.1330409357688));
#88583=CARTESIAN_POINT('Ctrl Pts',(-9.60208939388073,2.57744898531923,14.136949959674));
#88584=CARTESIAN_POINT('Ctrl Pts',(-9.66541140474864,2.34154766877827,14.1408598432517));
#88585=CARTESIAN_POINT('Ctrl Pts',(-9.72003109486963,2.10332957419767,14.1447697268294));
#88586=CARTESIAN_POINT('Ctrl Pts',(-9.7658029136977,1.86345309863528,14.1486796104071));
#88587=CARTESIAN_POINT('Ctrl Pts',(-9.79846187331522,1.69229721431242,14.1514693778479));
#88588=CARTESIAN_POINT('Ctrl Pts',(-9.82661738093914,1.5202973177943,14.1542591452887));
#88589=CARTESIAN_POINT('Ctrl Pts',(-9.8502325362061,1.34769543394151,14.1570489127296));
#88590=CARTESIAN_POINT('Ctrl Pts',(-9.88482225034695,1.09488109691296,14.1611351555345));
#88591=CARTESIAN_POINT('Ctrl Pts',(-9.90967623294466,0.840722795474834,
14.1652213983395));
#88592=CARTESIAN_POINT('Ctrl Pts',(-9.92471777929082,0.585953071012211,
14.1693076411444));
#88593=CARTESIAN_POINT('Ctrl Pts',(-9.93622988735837,0.390964036450559,
14.1724350635303));
#88594=CARTESIAN_POINT('Ctrl Pts',(-9.94199523718629,0.195617028572116,
14.1755624859161));
#88595=CARTESIAN_POINT('Ctrl Pts',(-9.9419999970495,0.000242214229054161,
14.178689908302));
#88596=CARTESIAN_POINT('Origin',(0.,0.,0.));
#88597=CARTESIAN_POINT('',(-9.94207718462978,-3.49168275919068E-5,15.3213100916858));
#88598=CARTESIAN_POINT('',(-9.9420751122847,-4.12289121522736E-5,15.1786899083142));
#88599=CARTESIAN_POINT('',(-9.942,-1.2175438477123E-15,0.));
#88600=CARTESIAN_POINT('Ctrl Pts',(-9.94199999993869,-3.49165565174472E-5,
15.3213100916858));
#88601=CARTESIAN_POINT('Ctrl Pts',(-9.94200085662577,0.243894721467326,
15.3174038606442));
#88602=CARTESIAN_POINT('Ctrl Pts',(-9.93302005102662,0.487862969434573,
15.3134976296025));
#88603=CARTESIAN_POINT('Ctrl Pts',(-9.91507511453682,0.731197287394158,
15.3095913985609));
#88604=CARTESIAN_POINT('Ctrl Pts',(-9.89713332233784,0.974488968598745,
15.3056858519645));
#88605=CARTESIAN_POINT('Ctrl Pts',(-9.87023055529752,1.21714666105488,15.3017803053682));
#88606=CARTESIAN_POINT('Ctrl Pts',(-9.8344363552134,1.45850113995739,15.2978747587718));
#88607=CARTESIAN_POINT('Ctrl Pts',(-9.79864602746684,1.69982950831646,15.2939696346906));
#88608=CARTESIAN_POINT('Ctrl Pts',(-9.75396622853532,1.93985466640253,15.2900645106095));
#88609=CARTESIAN_POINT('Ctrl Pts',(-9.70051809299003,2.17791476591096,15.2861593865283));
#88610=CARTESIAN_POINT('Ctrl Pts',(-9.64706588965377,2.41599298352052,15.2822539652389));
#88611=CARTESIAN_POINT('Ctrl Pts',(-9.58484407510101,2.65210556853956,15.2783485439495));
#88612=CARTESIAN_POINT('Ctrl Pts',(-9.51402470257343,2.88560183650179,15.27444312266));
#88613=CARTESIAN_POINT('Ctrl Pts',(-9.44320579862831,3.11909655951593,15.2705377272112));
#88614=CARTESIAN_POINT('Ctrl Pts',(-9.36378953438648,3.34997473150565,15.2666323317623));
#88615=CARTESIAN_POINT('Ctrl Pts',(-9.27599776630388,3.57760107327877,15.2627269363134));
#88616=CARTESIAN_POINT('Ctrl Pts',(-9.18818719966375,3.80527615591877,15.2588207046153));
#88617=CARTESIAN_POINT('Ctrl Pts',(-9.09199764660268,4.02969775428937,15.2549144729171));
#88618=CARTESIAN_POINT('Ctrl Pts',(-8.98769952200388,4.25024955763438,15.251008241219));
#88619=CARTESIAN_POINT('Ctrl Pts',(-8.92720783120775,4.37816702061652,15.2487426725813));
#88620=CARTESIAN_POINT('Ctrl Pts',(-8.86398942047525,4.50478311840303,15.2464771039436));
#88621=CARTESIAN_POINT('Ctrl Pts',(-8.798104277811,4.62998111408283,15.2442115353059));
#88622=CARTESIAN_POINT('Ctrl Pts',(-8.68440090259071,4.84604552715019,15.2403016583521));
#88623=CARTESIAN_POINT('Ctrl Pts',(-8.56271709935375,5.05795247620724,15.2363917813984));
#88624=CARTESIAN_POINT('Ctrl Pts',(-8.43338237923258,5.26511402019458,15.2324819044446));
#88625=CARTESIAN_POINT('Ctrl Pts',(-8.3040700481352,5.47223970262259,15.2285727043263));
#88626=CARTESIAN_POINT('Ctrl Pts',(-8.16710959241722,5.67462138216799,15.224663504208));
#88627=CARTESIAN_POINT('Ctrl Pts',(-8.02287499666421,5.87169828822125,15.2207543040897));
#88628=CARTESIAN_POINT('Ctrl Pts',(-7.87865610296278,6.06875373956228,15.2168455295452));
#88629=CARTESIAN_POINT('Ctrl Pts',(-7.7271648158754,6.26050534438171,15.2129367550007));
#88630=CARTESIAN_POINT('Ctrl Pts',(-7.5688173374294,6.44642289278543,15.2090279804562));
#88631=CARTESIAN_POINT('Ctrl Pts',(-7.41045757041219,6.63235486933829,15.2051189025708));
#88632=CARTESIAN_POINT('Ctrl Pts',(-7.24524072827637,6.81245166938742,15.2012098246855));
#88633=CARTESIAN_POINT('Ctrl Pts',(-7.07362288382047,6.98621666551299,15.1973007468002));
#88634=CARTESIAN_POINT('Ctrl Pts',(-6.90200740922004,7.15997926213325,15.1933917228949));
#88635=CARTESIAN_POINT('Ctrl Pts',(-6.72399130753356,7.32741003169691,15.1894826989897));
#88636=CARTESIAN_POINT('Ctrl Pts',(-6.54006755990517,7.48804916596279,15.1855736750845));
#88637=CARTESIAN_POINT('Ctrl Pts',(-6.35610336376876,7.64872362798484,15.1816637915068));
#88638=CARTESIAN_POINT('Ctrl Pts',(-6.16622913619626,7.80260328498453,15.177753907929));
#88639=CARTESIAN_POINT('Ctrl Pts',(-5.97097204008465,7.94926769561369,15.1738440243513));
#88640=CARTESIAN_POINT('Ctrl Pts',(-5.83165283057599,8.05391520988496,15.1710542569105));
#88641=CARTESIAN_POINT('Ctrl Pts',(-5.6895938845075,8.15489022091912,15.1682644894697));
#88642=CARTESIAN_POINT('Ctrl Pts',(-5.54499629222769,8.25205308509229,15.1654747220289));
#88643=CARTESIAN_POINT('Ctrl Pts',(-5.34234183961776,8.38822746215193,15.1615648450752));
#88644=CARTESIAN_POINT('Ctrl Pts',(-5.13463768644058,8.51695386885005,15.1576549681214));
#88645=CARTESIAN_POINT('Ctrl Pts',(-4.92245298101037,8.63787130314767,15.1537450911676));
#88646=CARTESIAN_POINT('Ctrl Pts',(-4.71030500669503,8.75876780553054,15.1498358910494));
#88647=CARTESIAN_POINT('Ctrl Pts',(-4.49367827187,8.87185789530211,15.1459266909311));
#88648=CARTESIAN_POINT('Ctrl Pts',(-4.27316816597247,8.97682559846851,15.1420174908128));
#88649=CARTESIAN_POINT('Ctrl Pts',(-4.05268206583625,9.08178187435987,15.1381087162683));
#88650=CARTESIAN_POINT('Ctrl Pts',(-3.82831369174776,9.17861740875552,15.1341999417239));
#88651=CARTESIAN_POINT('Ctrl Pts',(-3.60068107910359,9.26706316837138,15.1302911671794));
#88652=CARTESIAN_POINT('Ctrl Pts',(-3.37303080100701,9.35551579182955,15.1263820892941));
#88653=CARTESIAN_POINT('Ctrl Pts',(-3.14211603835447,9.43557723512077,15.1224730114088));
#88654=CARTESIAN_POINT('Ctrl Pts',(-2.90857397250981,9.50702695096835,15.1185639335235));
#88655=CARTESIAN_POINT('Ctrl Pts',(-2.67503513162568,9.57847568017349,15.1146549096182));
#88656=CARTESIAN_POINT('Ctrl Pts',(-2.43886932877706,9.64131283973038,15.110745885713));
#88657=CARTESIAN_POINT('Ctrl Pts',(-2.20072874732272,9.69536781049112,15.1068368618078));
#88658=CARTESIAN_POINT('Ctrl Pts',(-1.96253579399613,9.74943466902002,15.1029269782301));
#88659=CARTESIAN_POINT('Ctrl Pts',(-1.72236746751696,9.79471541647667,15.0990170946524));
#88660=CARTESIAN_POINT('Ctrl Pts',(-1.48088734394482,9.83109030955082,15.0951072110747));
#88661=CARTESIAN_POINT('Ctrl Pts',(-1.30858722989211,9.85704440520316,15.0923174436338));
#88662=CARTESIAN_POINT('Ctrl Pts',(-1.1356195102959,9.87846553942996,15.0895276761929));
#88663=CARTESIAN_POINT('Ctrl Pts',(-0.962227465787131,9.89532628588289,
15.086737908752));
#88664=CARTESIAN_POINT('Ctrl Pts',(-0.719217403783887,9.91895673013168,
15.0828280317982));
#88665=CARTESIAN_POINT('Ctrl Pts',(-0.475299260203229,9.93363468164528,
15.0789181548444));
#88666=CARTESIAN_POINT('Ctrl Pts',(-0.231145341779765,9.93931264378848,
15.0750082778907));
#88667=CARTESIAN_POINT('Ctrl Pts',(0.0129663113656991,9.94498962302446,
15.0710990777724));
#88668=CARTESIAN_POINT('Ctrl Pts',(0.257313377781516,9.94166971645738,15.0671898776541));
#88669=CARTESIAN_POINT('Ctrl Pts',(0.5012218344231,9.9293575156048,15.0632806775358));
#88670=CARTESIAN_POINT('Ctrl Pts',(0.745103738049442,9.91704665511598,15.0593719029914));
#88671=CARTESIAN_POINT('Ctrl Pts',(0.988546847393906,9.8957454691014,15.0554631284469));
#88672=CARTESIAN_POINT('Ctrl Pts',(1.23087949531634,9.86551061364843,15.0515543539024));
#88673=CARTESIAN_POINT('Ctrl Pts',(1.4732309494886,9.83527341181642,15.0476452760171));
#88674=CARTESIAN_POINT('Ctrl Pts',(1.71447149148974,9.79610118686422,15.0437361981318));
#88675=CARTESIAN_POINT('Ctrl Pts',(1.95393562411819,9.74810235773106,15.0398271202465));
#88676=CARTESIAN_POINT('Ctrl Pts',(2.1933964500083,9.70010419140935,15.0359180963413));
#88677=CARTESIAN_POINT('Ctrl Pts',(2.43108064112902,9.6432797217921,15.0320090724361));
#88678=CARTESIAN_POINT('Ctrl Pts',(2.66633320203375,9.57778843239568,15.0281000485309));
#88679=CARTESIAN_POINT('Ctrl Pts',(2.90163749967821,9.51228274015585,15.0241901649532));
#88680=CARTESIAN_POINT('Ctrl Pts',(3.13450882813705,9.43810649385022,15.0202802813755));
#88681=CARTESIAN_POINT('Ctrl Pts',(3.36430632022437,9.35546936202019,15.0163703977978));
#88682=CARTESIAN_POINT('Ctrl Pts',(3.52827068097552,9.29650638391392,15.0135806303569));
#88683=CARTESIAN_POINT('Ctrl Pts',(3.69067042796834,9.23323696641594,15.010790862916));
#88684=CARTESIAN_POINT('Ctrl Pts',(3.85127842770058,9.1657524771471,15.008001095475));
#88685=CARTESIAN_POINT('Ctrl Pts',(4.07637156899041,9.07117253279072,15.0040912185213));
#88686=CARTESIAN_POINT('Ctrl Pts',(4.29801341969897,8.96828233382643,15.0001813415675));
#88687=CARTESIAN_POINT('Ctrl Pts',(4.51558973027739,8.85735927846519,14.9962714646138));
#88688=CARTESIAN_POINT('Ctrl Pts',(4.73312837640567,8.74645542489976,14.9923622644955));
#88689=CARTESIAN_POINT('Ctrl Pts',(4.9466026377054,8.62752161806375,14.9884530643772));
#88690=CARTESIAN_POINT('Ctrl Pts',(5.15542148469268,8.50088191396452,14.9845438642589));
#88691=CARTESIAN_POINT('Ctrl Pts',(5.36421759868521,8.37425599645481,14.9806350897144));
#88692=CARTESIAN_POINT('Ctrl Pts',(5.56835907071416,8.23992600199358,14.9767263151699));
#88693=CARTESIAN_POINT('Ctrl Pts',(5.76728166413054,8.09826069020896,14.9728175406254));
#88694=CARTESIAN_POINT('Ctrl Pts',(5.96621969495306,7.9565843844748,14.96890846274));
#88695=CARTESIAN_POINT('Ctrl Pts',(6.1599378077519,7.80757178404671,14.9649993848547));
#88696=CARTESIAN_POINT('Ctrl Pts',(6.34790177220379,7.6516342757905,14.9610903069694));
#88697=CARTESIAN_POINT('Ctrl Pts',(6.53586314107918,7.4956989208605,14.9571812830642));
#88698=CARTESIAN_POINT('Ctrl Pts',(6.71807030609076,7.33283902992702,14.9532722591589));
#88699=CARTESIAN_POINT('Ctrl Pts',(6.8940225241547,7.16350594586531,14.9493632352537));
#88700=CARTESIAN_POINT('Ctrl Pts',(7.07001343762662,6.99413562207542,14.945453351676));
#88701=CARTESIAN_POINT('Ctrl Pts',(7.23974645274272,6.81828945432251,14.9415434680983));
#88702=CARTESIAN_POINT('Ctrl Pts',(7.40275708775905,6.6364562455902,14.9376335845206));
#88703=CARTESIAN_POINT('Ctrl Pts',(7.51906790700664,6.50671520463325,14.9348438170798));
#88704=CARTESIAN_POINT('Ctrl Pts',(7.63195707931439,6.37392690775254,14.9320540496389));
#88705=CARTESIAN_POINT('Ctrl Pts',(7.74126808372366,6.23827960706488,14.929264282198));
#88706=CARTESIAN_POINT('Ctrl Pts',(7.8944681572043,6.04816904550609,14.9253544052442));
#88707=CARTESIAN_POINT('Ctrl Pts',(8.04068516920822,5.85238322265478,14.9214445282905));
#88708=CARTESIAN_POINT('Ctrl Pts',(8.17951022117169,5.65145791294139,14.9175346513367));
#88709=CARTESIAN_POINT('Ctrl Pts',(8.31831124124791,5.45056738523832,14.9136254512184));
#88710=CARTESIAN_POINT('Ctrl Pts',(8.44972269642412,5.24453937720431,14.9097162511001));
#88711=CARTESIAN_POINT('Ctrl Pts',(8.57337827652759,5.03393970241648,14.9058070509818));
#88712=CARTESIAN_POINT('Ctrl Pts',(8.69702039490751,4.82336295449209,14.9018982764373));
#88713=CARTESIAN_POINT('Ctrl Pts',(8.81290818221483,4.60821577517653,14.8979895018928));
#88714=CARTESIAN_POINT('Ctrl Pts',(8.92072013326175,4.38909060102641,14.8940807273483));
#88715=CARTESIAN_POINT('Ctrl Pts',(9.02854045106496,4.1699484216472,14.8901716494629));
#88716=CARTESIAN_POINT('Ctrl Pts',(9.12828355377994,3.94682788074227,14.8862625715776));
#88717=CARTESIAN_POINT('Ctrl Pts',(9.21967458357322,3.72034468470515,14.8823534936923));
#88718=CARTESIAN_POINT('Ctrl Pts',(9.3110643513558,3.4938646161546,14.8784444697871));
#88719=CARTESIAN_POINT('Ctrl Pts',(9.39410217389248,3.26402224607422,14.8745354458819));
#88720=CARTESIAN_POINT('Ctrl Pts',(9.46856163601043,3.03145254705917,14.8706264219767));
#88721=CARTESIAN_POINT('Ctrl Pts',(9.5430374732524,2.79883170131868,14.866716538399));
#88722=CARTESIAN_POINT('Ctrl Pts',(9.60893109396079,2.56348259491659,14.8628066548213));
#88723=CARTESIAN_POINT('Ctrl Pts',(9.66606578210403,2.32605595290345,14.8588967712436));
#88724=CARTESIAN_POINT('Ctrl Pts',(9.70683233935735,2.15664806586246,14.8561070038027));
#88725=CARTESIAN_POINT('Ctrl Pts',(9.74314070936392,1.9861828222507,14.8533172363619));
#88726=CARTESIAN_POINT('Ctrl Pts',(9.77494251660834,1.81490021681704,14.8505274689211));
#88727=CARTESIAN_POINT('Ctrl Pts',(9.81951295334562,1.57484654719376,14.8466175919673));
#88728=CARTESIAN_POINT('Ctrl Pts',(9.85524305899185,1.33311350729371,14.8427077150135));
#88729=CARTESIAN_POINT('Ctrl Pts',(9.88202733768561,1.09036677188656,14.8387978380597));
#88730=CARTESIAN_POINT('Ctrl Pts',(9.90880697977562,0.847662058160643,14.8348886379414));
#88731=CARTESIAN_POINT('Ctrl Pts',(9.92664385555036,0.603944277707854,14.8309794378232));
#88732=CARTESIAN_POINT('Ctrl Pts',(9.93548421339401,0.359885322566067,14.8270702377049));
#88733=CARTESIAN_POINT('Ctrl Pts',(9.94432360883498,0.115852936822927,14.8231614631604));
#88734=CARTESIAN_POINT('Ctrl Pts',(9.94416843175336,-0.128520269429035,
14.8192526886159));
#88735=CARTESIAN_POINT('Ctrl Pts',(9.93501700366949,-0.372560245863747,
14.8153439140714));
#88736=CARTESIAN_POINT('Ctrl Pts',(9.9258648653882,-0.616619161043476,14.8114348361861));
#88737=CARTESIAN_POINT('Ctrl Pts',(9.9077150884957,-0.860344514487166,14.8075257583008));
#88738=CARTESIAN_POINT('Ctrl Pts',(9.88061809710591,-1.10306392341661,14.8036166804155));
#88739=CARTESIAN_POINT('Ctrl Pts',(9.85352147989596,-1.34577998065622,14.7997076565102));
#88740=CARTESIAN_POINT('Ctrl Pts',(9.817477928441,-1.58748984279357,14.795798632605));
#88741=CARTESIAN_POINT('Ctrl Pts',(9.77258964864251,-1.82752717059015,14.7918896086998));
#88742=CARTESIAN_POINT('Ctrl Pts',(9.72769149701424,-2.06761728739204,14.7879797251221));
#88743=CARTESIAN_POINT('Ctrl Pts',(9.67394478089711,-2.30603385904891,14.7840698415444));
#88744=CARTESIAN_POINT('Ctrl Pts',(9.61150292554344,-2.54212027887545,14.7801599579667));
#88745=CARTESIAN_POINT('Ctrl Pts',(9.56694961556588,-2.71057189493409,14.7773701905259));
#88746=CARTESIAN_POINT('Ctrl Pts',(9.51797062780309,-2.87783741968628,14.774580423085));
#88747=CARTESIAN_POINT('Ctrl Pts',(9.46463733237617,-3.04368266522501,14.7717906556441));
#88748=CARTESIAN_POINT('Ctrl Pts',(9.3898903769119,-3.27611584009292,14.7678807786904));
#88749=CARTESIAN_POINT('Ctrl Pts',(9.30656568547299,-3.50582979009426,14.7639709017366));
#88750=CARTESIAN_POINT('Ctrl Pts',(9.21488646225104,-3.73218856541607,14.7600610247828));
#88751=CARTESIAN_POINT('Ctrl Pts',(9.12322310954175,-3.95850815596207,14.7561518246646));
#88752=CARTESIAN_POINT('Ctrl Pts',(9.02320821725878,-4.18147347157733,14.7522426245463));
#88753=CARTESIAN_POINT('Ctrl Pts',(8.91511348169699,-4.40046765792734,14.748333424428));
#88754=CARTESIAN_POINT('Ctrl Pts',(8.8070305138338,-4.61943800354575,14.7444246498835));
#88755=CARTESIAN_POINT('Ctrl Pts',(8.69086958300992,-4.83443783183178,14.740515875339));
#88756=CARTESIAN_POINT('Ctrl Pts',(8.56694923994434,-5.04487311240005,14.7366071007946));
#88757=CARTESIAN_POINT('Ctrl Pts',(8.44301928002809,-5.25532472381943,14.7326980229092));
#88758=CARTESIAN_POINT('Ctrl Pts',(8.31132884422128,-5.46121083658457,14.7287889450239));
#88759=CARTESIAN_POINT('Ctrl Pts',(8.17224154714889,-5.66196362537357,14.7248798671386));
#88760=CARTESIAN_POINT('Ctrl Pts',(8.03315617072061,-5.86271364198518,14.7209708432334));
#88761=CARTESIAN_POINT('Ctrl Pts',(7.8866742986526,-6.05833024713667,14.7170618193282));
#88762=CARTESIAN_POINT('Ctrl Pts',(7.73320224948501,-6.24827551957818,14.713152795423));
#88763=CARTESIAN_POINT('Ctrl Pts',(7.57969644874574,-6.43826256478231,14.7092429118453));
#88764=CARTESIAN_POINT('Ctrl Pts',(7.4191975746183,-6.62257556632651,14.7053330282676));
#88765=CARTESIAN_POINT('Ctrl Pts',(7.25215240307327,-6.80070948670788,14.7014231446899));
#88766=CARTESIAN_POINT('Ctrl Pts',(7.13296287441414,-6.92781102344842,14.698633377249));
#88767=CARTESIAN_POINT('Ctrl Pts',(7.01044143160265,-7.05176743943949,14.695843609808));
#88768=CARTESIAN_POINT('Ctrl Pts',(6.88476207621809,-7.17240651063987,14.6930538423671));
#88769=CARTESIAN_POINT('Ctrl Pts',(6.70862165391074,-7.34148294234961,14.6891439654134));
#88770=CARTESIAN_POINT('Ctrl Pts',(6.52622298655312,-7.50409360981867,14.6852340884596));
#88771=CARTESIAN_POINT('Ctrl Pts',(6.33806445520289,-7.65978478559899,14.6813242115058));
#88772=CARTESIAN_POINT('Ctrl Pts',(6.1499384958169,-7.81544900981153,14.6774150113875));
#88773=CARTESIAN_POINT('Ctrl Pts',(5.9560548787038,-7.9641959548582,14.6735058112693));
#88774=CARTESIAN_POINT('Ctrl Pts',(5.75694559673185,-8.105611722521,14.669596611151));
#88775=CARTESIAN_POINT('Ctrl Pts',(5.55785799072428,-8.24701209500426,14.6656878366065));
#88776=CARTESIAN_POINT('Ctrl Pts',(5.35354608419496,-8.38108272141112,14.6617790620619));
#88777=CARTESIAN_POINT('Ctrl Pts',(5.1445722702807,-8.50745203664757,14.6578702875174));
#88778=CARTESIAN_POINT('Ctrl Pts',(4.93558223893498,-8.633831158786,14.6539612096321));
#88779=CARTESIAN_POINT('Ctrl Pts',(4.72192981557315,-8.7525076278296,14.6500521317467));
#88780=CARTESIAN_POINT('Ctrl Pts',(4.50420461246357,-8.86315433742761,14.6461430538614));
#88781=CARTESIAN_POINT('Ctrl Pts',(4.28648241590132,-8.97379951911538,14.6422340299562));
#88782=CARTESIAN_POINT('Ctrl Pts',(4.06468780291554,-9.07641503795574,14.638325006051));
#88783=CARTESIAN_POINT('Ctrl Pts',(3.83943377164389,-9.17072038136375,14.6344159821457));
#88784=CARTESIAN_POINT('Ctrl Pts',(3.61413020250926,-9.26504646440137,14.630506098568));
#88785=CARTESIAN_POINT('Ctrl Pts',(3.38536595317184,-9.3510586109826,14.6265962149903));
#88786=CARTESIAN_POINT('Ctrl Pts',(3.15377401580106,-9.42852445811422,14.6226863314126));
#88787=CARTESIAN_POINT('Ctrl Pts',(2.98852928828094,-9.48379763794382,14.6198965639718));
#88788=CARTESIAN_POINT('Ctrl Pts',(2.82184538566737,-9.53472085093505,14.617106796531));
#88789=CARTESIAN_POINT('Ctrl Pts',(2.65395721633758,-9.58122513532845,14.6143170290901));
#88790=CARTESIAN_POINT('Ctrl Pts',(2.41866087067466,-9.64640118804924,14.6104071521364));
#88791=CARTESIAN_POINT('Ctrl Pts',(2.18092646501388,-9.70291539328969,14.6064972751826));
#88792=CARTESIAN_POINT('Ctrl Pts',(1.94140804813212,-9.75060504741361,14.6025873982288));
#88793=CARTESIAN_POINT('Ctrl Pts',(1.70193109407979,-9.79828644602207,14.5986781981105));
#88794=CARTESIAN_POINT('Ctrl Pts',(1.46067102007726,-9.83714628825954,14.5947689979922));
#88795=CARTESIAN_POINT('Ctrl Pts',(1.21829254648454,-9.86707288263243,14.5908597978739));
#88796=CARTESIAN_POINT('Ctrl Pts',(0.975940459346045,-9.89699621905629,
14.5869510233294));
#88797=CARTESIAN_POINT('Ctrl Pts',(0.732470493812973,-9.91798821507807,
14.5830422487849));
#88798=CARTESIAN_POINT('Ctrl Pts',(0.488554026534318,-9.92998887024337,
14.5791334742404));
#88799=CARTESIAN_POINT('Ctrl Pts',(0.244618630095396,-9.94199045672063,
14.5752243963551));
#88800=CARTESIAN_POINT('Ctrl Pts',(0.000236942509269006,-9.94499929121524,
14.5713153184698));
#88801=CARTESIAN_POINT('Ctrl Pts',(-0.243916812221935,-9.93900742472383,
14.5674062405845));
#88802=CARTESIAN_POINT('Ctrl Pts',(-0.48806719545689,-9.93301564097355,
14.5634972166792));
#88803=CARTESIAN_POINT('Ctrl Pts',(-0.731989371937555,-9.91802341375385,
14.559588192774));
#88804=CARTESIAN_POINT('Ctrl Pts',(-0.975010657646331,-9.89407490458184,
14.5556791688688));
#88805=CARTESIAN_POINT('Ctrl Pts',(-1.21808538859319,-9.87012112865399,
14.5517692852911));
#88806=CARTESIAN_POINT('Ctrl Pts',(-1.46025855371254,-9.83720716154928,
14.5478594017134));
#88807=CARTESIAN_POINT('Ctrl Pts',(-1.70086273281695,-9.79542903420338,
14.5439495181357));
#88808=CARTESIAN_POINT('Ctrl Pts',(-1.8725378458111,-9.76561964037036,14.5411597506948));
#88809=CARTESIAN_POINT('Ctrl Pts',(-2.04341428824949,-9.73129853269574,
14.538369983254));
#88810=CARTESIAN_POINT('Ctrl Pts',(-2.21325257474579,-9.69251654836767,
14.5355802158131));
#88811=CARTESIAN_POINT('Ctrl Pts',(-2.45128202211772,-9.63816334869736,
14.5316703388594));
#88812=CARTESIAN_POINT('Ctrl Pts',(-2.68734471051723,-9.57502928361011,
14.5277604619056));
#88813=CARTESIAN_POINT('Ctrl Pts',(-2.92078776089241,-9.50328168875474,
14.5238505849518));
#88814=CARTESIAN_POINT('Ctrl Pts',(-3.15419040013839,-9.43154651406489,
14.5199413848335));
#88815=CARTESIAN_POINT('Ctrl Pts',(-3.38497403880597,-9.35120086845111,
14.5160321847152));
#88816=CARTESIAN_POINT('Ctrl Pts',(-3.61250062547696,-9.26246205017481,
14.5121229845969));
#88817=CARTESIAN_POINT('Ctrl Pts',(-3.84000244254035,-9.173732892421,14.5082142100525));
#88818=CARTESIAN_POINT('Ctrl Pts',(-4.06424765453314,-9.07661248822245,
14.504305435508));
#88819=CARTESIAN_POINT('Ctrl Pts',(-4.28461689387056,-8.97136678955659,
14.5003966609635));
#88820=CARTESIAN_POINT('Ctrl Pts',(-4.5050032349847,-8.86611292328784,14.4964875830782));
#88821=CARTESIAN_POINT('Ctrl Pts',(-4.72151274811587,-8.75273262060444,
14.4925785051928));
#88822=CARTESIAN_POINT('Ctrl Pts',(-4.93354827288488,-8.63153899597949,
14.4886694273075));
#88823=CARTESIAN_POINT('Ctrl Pts',(-5.1455808696755,-8.51034704490577,14.4847604034023));
#88824=CARTESIAN_POINT('Ctrl Pts',(-5.35313935930901,-8.38134212857442,
14.480851379497));
#88825=CARTESIAN_POINT('Ctrl Pts',(-5.5556526779645,-8.24488249290588,14.4769423555918));
#88826=CARTESIAN_POINT('Ctrl Pts',(-5.75821053334468,-8.1083928470372,14.4730324720141));
#88827=CARTESIAN_POINT('Ctrl Pts',(-5.9557207675935,-7.96444536181786,14.4691225884364));
#88828=CARTESIAN_POINT('Ctrl Pts',(-6.14764157634337,-7.81344143440101,
14.4652127048587));
#88829=CARTESIAN_POINT('Ctrl Pts',(-6.2845802889253,-7.70569760219243,14.4624229374179));
#88830=CARTESIAN_POINT('Ctrl Pts',(-6.41867400228556,-7.59436219430257,
14.459633169977));
#88831=CARTESIAN_POINT('Ctrl Pts',(-6.54973608136025,-7.47959365637784,
14.4568434025362));
#88832=CARTESIAN_POINT('Ctrl Pts',(-6.73342042543229,-7.31874481468659,
14.4529335255824));
#88833=CARTESIAN_POINT('Ctrl Pts',(-6.91120480998141,-7.15110169481779,
14.4490236486286));
#88834=CARTESIAN_POINT('Ctrl Pts',(-7.08259408263102,-6.97712154549998,
14.4451137716748));
#88835=CARTESIAN_POINT('Ctrl Pts',(-7.25395368622958,-6.80317151373768,
14.4412045715565));
#88836=CARTESIAN_POINT('Ctrl Pts',(-7.41892019123506,-6.62288684197434,
14.4372953714382));
#88837=CARTESIAN_POINT('Ctrl Pts',(-7.57703521653304,-6.43676171125032,
14.4333861713199));
#88838=CARTESIAN_POINT('Ctrl Pts',(-7.73513302868985,-6.25065684297856,
14.4294773967754));
#88839=CARTESIAN_POINT('Ctrl Pts',(-7.88638066901632,-6.05871299882243,
14.4255686222309));
#88840=CARTESIAN_POINT('Ctrl Pts',(-8.03035930006934,-5.8614583093109,14.4216598476864));
#88841=CARTESIAN_POINT('Ctrl Pts',(-8.17434910459761,-5.66418831183059,
14.4177507698011));
#88842=CARTESIAN_POINT('Ctrl Pts',(-8.31106860489869,-5.46160687005948,
14.4138416919158));
#88843=CARTESIAN_POINT('Ctrl Pts',(-8.44014090012312,-5.25427307874923,
14.4099326140305));
#88844=CARTESIAN_POINT('Ctrl Pts',(-8.5692114129995,-5.04694215049318,14.4060235901253));
#88845=CARTESIAN_POINT('Ctrl Pts',(-8.69063478559525,-4.83485924301839,
14.4021145662201));
#88846=CARTESIAN_POINT('Ctrl Pts',(-8.80407851237586,-4.61861078116804,
14.3982055423149));
#88847=CARTESIAN_POINT('Ctrl Pts',(-8.91754718770018,-4.40231476195727,
14.3942956587372));
#88848=CARTESIAN_POINT('Ctrl Pts',(-9.02303257949188,-4.18185160573104,
14.3903857751595));
#88849=CARTESIAN_POINT('Ctrl Pts',(-9.12024842103068,-3.95783182294138,
14.3864758915818));
#88850=CARTESIAN_POINT('Ctrl Pts',(-9.18961355277154,-3.79798995458123,
14.3836861241409));
#88851=CARTESIAN_POINT('Ctrl Pts',(-9.25476957242055,-3.63633788958992,
14.3808963567001));
#88852=CARTESIAN_POINT('Ctrl Pts',(-9.31562744933931,-3.47310368764251,
14.3781065892592));
#88853=CARTESIAN_POINT('Ctrl Pts',(-9.40073229793138,-3.24483377838614,
14.3742053237587));
#88854=CARTESIAN_POINT('Ctrl Pts',(-9.47745710973565,-3.01339584872495,
14.3703040582581));
#88855=CARTESIAN_POINT('Ctrl Pts',(-9.54558346248208,-2.77942446574622,
14.3664027927576));
#88856=CARTESIAN_POINT('Ctrl Pts',(-9.61370093894827,-2.54548356723466,
14.3625020355585));
#88857=CARTESIAN_POINT('Ctrl Pts',(-9.67322211152418,-2.30901014511221,
14.3586012783594));
#88858=CARTESIAN_POINT('Ctrl Pts',(-9.72397841135791,-2.07065396806064,
14.3547005211603));
#88859=CARTESIAN_POINT('Ctrl Pts',(-9.77472803701372,-1.83232913355255,
14.3508002768896));
#88860=CARTESIAN_POINT('Ctrl Pts',(-9.8167150329033,-1.59212231511132,14.3469000326189));
#88861=CARTESIAN_POINT('Ctrl Pts',(-9.8498217594818,-1.35069437936156,14.3429997883482));
#88862=CARTESIAN_POINT('Ctrl Pts',(-9.88293073090551,-1.1092500732725,14.3390992796164));
#88863=CARTESIAN_POINT('Ctrl Pts',(-9.90715818883622,-0.866584764294565,
14.3351987708845));
#88864=CARTESIAN_POINT('Ctrl Pts',(-9.9224381093107,-0.623366639225106,
14.3312982621526));
#88865=CARTESIAN_POINT('Ctrl Pts',(-9.93548071998098,-0.415760891633932,
14.327968871997));
#88866=CARTESIAN_POINT('Ctrl Pts',(-9.94200503739041,-0.207752580076446,
14.3246394818414));
#88867=CARTESIAN_POINT('Ctrl Pts',(-9.94199999708083,0.000240924627958939,
14.3213100916858));
#88868=CARTESIAN_POINT('Ctrl Pts',(-9.94199999704952,0.000242213467125498,
14.1786899083142));
#88869=CARTESIAN_POINT('Ctrl Pts',(-9.94200593246289,-0.243385362018565,
14.1825897269062));
#88870=CARTESIAN_POINT('Ctrl Pts',(-9.93305242611158,-0.487033811773988,
14.1864895454982));
#88871=CARTESIAN_POINT('Ctrl Pts',(-9.91516094928765,-0.730032430595599,
14.1903893640902));
#88872=CARTESIAN_POINT('Ctrl Pts',(-9.89726842140917,-0.973045324639196,
14.1942894117814));
#88873=CARTESIAN_POINT('Ctrl Pts',(-9.87043689098207,-1.21540802900749,
14.1981894594725));
#88874=CARTESIAN_POINT('Ctrl Pts',(-9.83473984509367,-1.45645328772565,
14.2020895071637));
#88875=CARTESIAN_POINT('Ctrl Pts',(-9.7990438019972,-1.69749177506449,14.2059894452957));
#88876=CARTESIAN_POINT('Ctrl Pts',(-9.75448278445375,-1.93721261106689,
14.2098893834278));
#88877=CARTESIAN_POINT('Ctrl Pts',(-9.70118182189137,-2.17495638085099,
14.2137893215598));
#88878=CARTESIAN_POINT('Ctrl Pts',(-9.6478680282462,-2.41275738243441,14.2176901985198));
#88879=CARTESIAN_POINT('Ctrl Pts',(-9.58581014560736,-2.64858009013482,
14.2215910754797));
#88880=CARTESIAN_POINT('Ctrl Pts',(-9.51518406546778,-2.88177657015045,
14.2254919524396));
#88881=CARTESIAN_POINT('Ctrl Pts',(-9.45306052381708,-3.08689897267394,
14.2289232102953));
#88882=CARTESIAN_POINT('Ctrl Pts',(-9.38430840258609,-3.28998947716511,
14.2323544681509));
#88883=CARTESIAN_POINT('Ctrl Pts',(-9.30907916889128,-3.4906172845665,14.2357857260066));
#88884=CARTESIAN_POINT('Ctrl Pts',(-9.22335636418048,-3.7192302520094,14.2396956029604));
#88885=CARTESIAN_POINT('Ctrl Pts',(-9.12919493734013,-3.94471889634473,
14.2436054799141));
#88886=CARTESIAN_POINT('Ctrl Pts',(-9.02684810190686,-4.16645860955087,
14.2475153568679));
#88887=CARTESIAN_POINT('Ctrl Pts',(-8.92451898364727,-4.38815993758374,
14.2514245569862));
#88888=CARTESIAN_POINT('Ctrl Pts',(-8.81400740279905,-4.6061133756037,14.2553337571045));
#88889=CARTESIAN_POINT('Ctrl Pts',(-8.69561410139372,-4.81971569697246,
14.2592429572228));
#88890=CARTESIAN_POINT('Ctrl Pts',(-8.57723368883644,-5.03329476459433,
14.2631517317673));
#88891=CARTESIAN_POINT('Ctrl Pts',(-8.45097340479063,-5.24252341628112,
14.2670605063118));
#88892=CARTESIAN_POINT('Ctrl Pts',(-8.31717970653641,-5.44682345309437,
14.2709692808563));
#88893=CARTESIAN_POINT('Ctrl Pts',(-8.1833756252098,-5.65113934463098,14.2748783587416));
#88894=CARTESIAN_POINT('Ctrl Pts',(-8.04203711248208,-5.85052562082029,
14.278787436627));
#88895=CARTESIAN_POINT('Ctrl Pts',(-7.89355439149902,-6.04443240250452,
14.2826965145123));
#88896=CARTESIAN_POINT('Ctrl Pts',(-7.74507372090081,-6.23833650654704,
14.2866055384175));
#88897=CARTESIAN_POINT('Ctrl Pts',(-7.58944921142196,-6.4267610460982,14.2905145623227));
#88898=CARTESIAN_POINT('Ctrl Pts',(-7.4271123187362,-6.60918804429689,14.2944235862279));
#88899=CARTESIAN_POINT('Ctrl Pts',(-7.26473972492272,-6.7916551618391,14.2983334698056));
#88900=CARTESIAN_POINT('Ctrl Pts',(-7.09565198389764,-6.96812189232768,
14.3022433533833));
#88901=CARTESIAN_POINT('Ctrl Pts',(-6.92031939813261,-7.13810503059667,
14.306153236961));
#88902=CARTESIAN_POINT('Ctrl Pts',(-6.79521666057857,-7.25939084773495,
14.3089430044018));
#88903=CARTESIAN_POINT('Ctrl Pts',(-6.66693544661198,-7.37737655515681,
14.3117327718427));
#88904=CARTESIAN_POINT('Ctrl Pts',(-6.53565775611927,-7.49189840393462,
14.3145225392835));
#88905=CARTESIAN_POINT('Ctrl Pts',(-6.35167123126275,-7.65240150920476,
14.3184324162373));
#88906=CARTESIAN_POINT('Ctrl Pts',(-6.16174122976717,-7.80614837115737,
14.3223422931911));
#88907=CARTESIAN_POINT('Ctrl Pts',(-5.96638715909887,-7.95270949222591,
14.3262521701448));
#88908=CARTESIAN_POINT('Ctrl Pts',(-5.77106690600795,-8.09924524222316,
14.3301613702631));
#88909=CARTESIAN_POINT('Ctrl Pts',(-5.57032468222568,-8.23859756633971,
14.3340705703814));
#88910=CARTESIAN_POINT('Ctrl Pts',(-5.36471157364484,-8.37037835056463,
14.3379797704996));
#88911=CARTESIAN_POINT('Ctrl Pts',(-5.15912084906745,-8.50214478851782,
14.3418885450441));
#88912=CARTESIAN_POINT('Ctrl Pts',(-4.94866053437317,-8.62634118118867,
14.3457973195886));
#88913=CARTESIAN_POINT('Ctrl Pts',(-4.73391006682754,-8.74262314635538,
14.3497060941331));
#88914=CARTESIAN_POINT('Ctrl Pts',(-4.51914293355178,-8.85891413559488,
14.3536151720184));
#88915=CARTESIAN_POINT('Ctrl Pts',(-4.30008522719908,-8.96728933386437,
14.3575242499037));
#88916=CARTESIAN_POINT('Ctrl Pts',(-4.07734145772508,-9.06745006256535,
14.361433327789));
#88917=CARTESIAN_POINT('Ctrl Pts',(-3.85460076409937,-9.16760940815601,
14.3653423516942));
#88918=CARTESIAN_POINT('Ctrl Pts',(-3.62817436566829,-9.259554397956,14.3692513755994));
#88919=CARTESIAN_POINT('Ctrl Pts',(-3.39868791456105,-9.34303400718507,
14.3731603995047));
#88920=CARTESIAN_POINT('Ctrl Pts',(-3.16915099479696,-9.42653197524853,
14.3770702830823));
#88921=CARTESIAN_POINT('Ctrl Pts',(-2.93655294084078,-9.50156074592832,
14.38098016666));
#88922=CARTESIAN_POINT('Ctrl Pts',(-2.70153708496493,-9.5679183409224,14.3848900502377));
#88923=CARTESIAN_POINT('Ctrl Pts',(-2.53384933421917,-9.61526559674046,
14.3876798176786));
#88924=CARTESIAN_POINT('Ctrl Pts',(-2.36493103553926,-9.65819932922349,
14.3904695851195));
#88925=CARTESIAN_POINT('Ctrl Pts',(-2.19502011278984,-9.69666183304585,
14.3932593525605));
#88926=CARTESIAN_POINT('Ctrl Pts',(-1.95688886524821,-9.75056727873812,
14.3971692295142));
#88927=CARTESIAN_POINT('Ctrl Pts',(-1.71673450088251,-9.79570467238657,
14.401079106468));
#88928=CARTESIAN_POINT('Ctrl Pts',(-1.47521806992016,-9.83194261812899,
14.4049889834218));
#88929=CARTESIAN_POINT('Ctrl Pts',(-1.23374344766249,-9.86817429075132,
14.4088981835401));
#88930=CARTESIAN_POINT('Ctrl Pts',(-0.990907506561842,-9.89550954923249,
14.4128073836584));
#88931=CARTESIAN_POINT('Ctrl Pts',(-0.747379528884163,-9.91386845988007,
14.4167165837767));
#88932=CARTESIAN_POINT('Ctrl Pts',(-0.503878062801711,-9.93222537189074,
14.4206253583212));
#88933=CARTESIAN_POINT('Ctrl Pts',(-0.259684989979209,-9.94160786617101,
14.4245341328657));
#88934=CARTESIAN_POINT('Ctrl Pts',(-0.0154737816699827,-9.94198795825467,
14.4284429074102));
#88935=CARTESIAN_POINT('Ctrl Pts',(0.228756378674564,-9.94236807983541,
14.4323519852955));
#88936=CARTESIAN_POINT('Ctrl Pts',(0.473004396996434,-9.93374439971333,
14.4362610631809));
#88937=CARTESIAN_POINT('Ctrl Pts',(0.716596434826483,-9.91614106140055,
14.4401701410662));
#88938=CARTESIAN_POINT('Ctrl Pts',(0.960185108916133,-9.89853796617067,
14.4440791649714));
#88939=CARTESIAN_POINT('Ctrl Pts',(1.203117541179,-9.87195548300876,14.4479881888767));
#88940=CARTESIAN_POINT('Ctrl Pts',(1.44472391110842,-9.83646973363267,14.4518972127819));
#88941=CARTESIAN_POINT('Ctrl Pts',(1.68638341510737,-9.80097618023107,14.4558070963596));
#88942=CARTESIAN_POINT('Ctrl Pts',(1.92671599645829,-9.75657548794242,14.4597169799373));
#88943=CARTESIAN_POINT('Ctrl Pts',(2.16505956077095,-9.70339533865926,14.463626863515));
#88944=CARTESIAN_POINT('Ctrl Pts',(2.33512168723394,-9.66545041113922,14.4664166309558));
#88945=CARTESIAN_POINT('Ctrl Pts',(2.50417135425363,-9.6230368862643,14.4692063983967));
#88946=CARTESIAN_POINT('Ctrl Pts',(2.67197176687402,-9.57621693974338,14.4719961658375));
#88947=CARTESIAN_POINT('Ctrl Pts',(2.90714512094574,-9.51059848452723,14.4759060427912));
#88948=CARTESIAN_POINT('Ctrl Pts',(3.1399360992914,-9.4363027011379,14.479815919745));
#88949=CARTESIAN_POINT('Ctrl Pts',(3.36970052527757,-9.35352780345171,14.4837257966988));
#88950=CARTESIAN_POINT('Ctrl Pts',(3.59942517693956,-9.27076723485758,14.4876349968171));
#88951=CARTESIAN_POINT('Ctrl Pts',(3.82612405852349,-9.17953057701206,14.4915441969354));
#88952=CARTESIAN_POINT('Ctrl Pts',(4.04917018174472,-9.08006524421876,14.4954533970537));
#88953=CARTESIAN_POINT('Ctrl Pts',(4.27219202312241,-8.9806107396865,14.4993621715982));
#88954=CARTESIAN_POINT('Ctrl Pts',(4.49156164421777,-8.87292946297478,14.5032709461427));
#88955=CARTESIAN_POINT('Ctrl Pts',(4.70667303464128,-8.75731653790022,14.5071797206872));
#88956=CARTESIAN_POINT('Ctrl Pts',(4.92180111880482,-8.64169464067354,14.5110887985725));
#88957=CARTESIAN_POINT('Ctrl Pts',(5.13267006359735,-8.51813999513188,14.5149978764578));
#88958=CARTESIAN_POINT('Ctrl Pts',(5.33869828494419,-8.38699377741119,14.5189069543431));
#88959=CARTESIAN_POINT('Ctrl Pts',(5.54472366126592,-8.25584937067677,14.5228159782484));
#88960=CARTESIAN_POINT('Ctrl Pts',(5.74590821245473,-8.11711375369622,14.5267250021536));
#88961=CARTESIAN_POINT('Ctrl Pts',(5.94169856904823,-7.97117194109939,14.5306340260588));
#88962=CARTESIAN_POINT('Ctrl Pts',(6.13753198385399,-7.82519803298134,14.5345439096365));
#88963=CARTESIAN_POINT('Ctrl Pts',(6.32796860821824,-7.67201492936055,14.5384537932142));
#88964=CARTESIAN_POINT('Ctrl Pts',(6.51248635237282,-7.51204935488031,14.5423636767919));
#88965=CARTESIAN_POINT('Ctrl Pts',(6.64414285433088,-7.39791123734439,14.5451534442327));
#88966=CARTESIAN_POINT('Ctrl Pts',(6.77278667189828,-7.28032099449095,14.5479432116736));
#88967=CARTESIAN_POINT('Ctrl Pts',(6.89823892120813,-7.1594457736566,14.5507329791145));
#88968=CARTESIAN_POINT('Ctrl Pts',(7.07406105289956,-6.99003837671724,14.5546428560682));
#88969=CARTESIAN_POINT('Ctrl Pts',(7.2436665974382,-6.81412515296673,14.558552733022));
#88970=CARTESIAN_POINT('Ctrl Pts',(7.40658272194097,-6.63218639537863,14.5624626099758));
#88971=CARTESIAN_POINT('Ctrl Pts',(7.56947064417157,-6.45027913305461,14.5663718100941));
#88972=CARTESIAN_POINT('Ctrl Pts',(7.72567127109587,-6.26234862782928,14.5702810102123));
#88973=CARTESIAN_POINT('Ctrl Pts',(7.87475025689159,-6.06891031335823,14.5741902103306));
#88974=CARTESIAN_POINT('Ctrl Pts',(8.02381301325228,-5.87549305748602,14.5780989848751));
#88975=CARTESIAN_POINT('Ctrl Pts',(8.16575550545327,-5.67656941152785,14.5820077594196));
#88976=CARTESIAN_POINT('Ctrl Pts',(8.30018450206128,-5.4726868384498,14.5859165339641));
#88977=CARTESIAN_POINT('Ctrl Pts',(8.43462393104462,-5.26878844304489,14.5898256118494));
#88978=CARTESIAN_POINT('Ctrl Pts',(8.56154854244736,-5.05993058388463,14.5937346897347));
#88979=CARTESIAN_POINT('Ctrl Pts',(8.68060846738039,-4.8466896574924,14.5976437676201));
#88980=CARTESIAN_POINT('Ctrl Pts',(8.79966674822597,-4.63345167572433,14.6015527915253));
#88981=CARTESIAN_POINT('Ctrl Pts',(8.91086042494637,-4.41583099354175,14.6054618154305));
#88982=CARTESIAN_POINT('Ctrl Pts',(9.01388527419954,-4.19442919401064,14.6093708393357));
#88983=CARTESIAN_POINT('Ctrl Pts',(9.11693278067592,-3.9729787037993,14.6132807229134));
#88984=CARTESIAN_POINT('Ctrl Pts',(9.21180775077748,-3.74774568849631,14.6171906064911));
#88985=CARTESIAN_POINT('Ctrl Pts',(9.29825329372859,-3.51935358917877,14.6211004900688));
#88986=CARTESIAN_POINT('Ctrl Pts',(9.35993363697699,-3.35639199971779,14.6238902575097));
#88987=CARTESIAN_POINT('Ctrl Pts',(9.41732349670136,-3.1918225584054,14.6266800249506));
#88988=CARTESIAN_POINT('Ctrl Pts',(9.47034479553094,-3.0258773031569,14.6294697923914));
#88989=CARTESIAN_POINT('Ctrl Pts',(9.5446544857636,-2.79330396404026,14.6333796693452));
#88990=CARTESIAN_POINT('Ctrl Pts',(9.61040408220088,-2.55795636240189,14.637289546299));
#88991=CARTESIAN_POINT('Ctrl Pts',(9.66740547853949,-2.32048169859289,14.6411994232527));
#88992=CARTESIAN_POINT('Ctrl Pts',(9.72439700741507,-2.08304814382013,14.645108623371));
#88993=CARTESIAN_POINT('Ctrl Pts',(9.77264329387064,-1.84348853434929,14.6490178234893));
#88994=CARTESIAN_POINT('Ctrl Pts',(9.81200678838167,-1.60246272491815,14.6529270236077));
#88995=CARTESIAN_POINT('Ctrl Pts',(9.85136599759855,-1.36146315468411,14.6568357981521));
#88996=CARTESIAN_POINT('Ctrl Pts',(9.88184430053851,-1.11899797973397,14.6607445726966));
#88997=CARTESIAN_POINT('Ctrl Pts',(9.90335553954652,-0.875735723453872,
14.6646533472411));
#88998=CARTESIAN_POINT('Ctrl Pts',(9.92486844793628,-0.632454588783239,
14.6685624251264));
#88999=CARTESIAN_POINT('Ctrl Pts',(9.93741287412366,-0.38837652814623,14.6724715030118));
#89000=CARTESIAN_POINT('Ctrl Pts',(9.94095456111795,-0.144174941609904,
14.6763805808971));
#89001=CARTESIAN_POINT('Ctrl Pts',(9.9444961992054,0.100023272768773,14.6802896048023));
#89002=CARTESIAN_POINT('Ctrl Pts',(9.93903534473031,0.344344729305567,14.6841986287075));
#89003=CARTESIAN_POINT('Ctrl Pts',(9.92458987162252,0.588115532942081,14.6881076526127));
#89004=CARTESIAN_POINT('Ctrl Pts',(9.91014122166646,0.831939946650653,14.6920175361904));
#89005=CARTESIAN_POINT('Ctrl Pts',(9.88670402048512,1.07521318548938,14.6959274197681));
#89006=CARTESIAN_POINT('Ctrl Pts',(9.85434817734733,1.3172645898267,14.6998373033458));
#89007=CARTESIAN_POINT('Ctrl Pts',(9.83126174116239,1.48997232227285,14.7026270707866));
#89008=CARTESIAN_POINT('Ctrl Pts',(9.80363585762131,1.66205807871755,14.7054168382275));
#89009=CARTESIAN_POINT('Ctrl Pts',(9.77151197839084,1.83328057213408,14.7082066056684));
#89010=CARTESIAN_POINT('Ctrl Pts',(9.7264901557007,2.07324999437786,14.7121164826221));
#89011=CARTESIAN_POINT('Ctrl Pts',(9.67261739787909,2.31159686134554,14.7160263595759));
#89012=CARTESIAN_POINT('Ctrl Pts',(9.6100354321011,2.54766226053638,14.7199362365297));
#89013=CARTESIAN_POINT('Ctrl Pts',(9.54746429983418,2.78368679464603,14.7238454366479));
#89014=CARTESIAN_POINT('Ctrl Pts',(9.4761870410031,3.01743037855659,14.7277546367662));
#89015=CARTESIAN_POINT('Ctrl Pts',(9.39639588603101,3.24824696613103,14.7316638368845));
#89016=CARTESIAN_POINT('Ctrl Pts',(9.31661341749703,3.47903842593282,14.735572611429));
#89017=CARTESIAN_POINT('Ctrl Pts',(9.22831899501513,3.70690326080634,14.7394813859735));
#89018=CARTESIAN_POINT('Ctrl Pts',(9.13175419485938,3.9312121953245,14.743390160518));
#89019=CARTESIAN_POINT('Ctrl Pts',(9.03518190078283,4.15553853735955,14.7472992384033));
#89020=CARTESIAN_POINT('Ctrl Pts',(8.93033805457291,4.37630816893196,14.7512083162886));
#89021=CARTESIAN_POINT('Ctrl Pts',(8.81751222578281,4.59291216421245,14.7551173941739));
#89022=CARTESIAN_POINT('Ctrl Pts',(8.70468795499463,4.80951316842747,14.7590264180791));
#89023=CARTESIAN_POINT('Ctrl Pts',(8.58388205340214,5.02194840372532,14.7629354419844));
#89024=CARTESIAN_POINT('Ctrl Pts',(8.45543020613305,5.22963325953291,14.7668444658896));
#89025=CARTESIAN_POINT('Ctrl Pts',(8.32695010973508,5.43736378939177,14.7707543494673));
#89026=CARTESIAN_POINT('Ctrl Pts',(8.19082085439789,5.6403416132436,14.774664233045));
#89027=CARTESIAN_POINT('Ctrl Pts',(8.04742238556117,5.83800967354191,14.7785741166227));
#89028=CARTESIAN_POINT('Ctrl Pts',(7.94510517547423,5.97904914639744,14.7813638840636));
#89029=CARTESIAN_POINT('Ctrl Pts',(7.83908808971278,6.11738596196061,14.7841536515045));
#89030=CARTESIAN_POINT('Ctrl Pts',(7.7295221690902,6.25282744344853,14.7869434189454));
#89031=CARTESIAN_POINT('Ctrl Pts',(7.57596482890402,6.44264954807725,14.7908532958992));
#89032=CARTESIAN_POINT('Ctrl Pts',(7.41538811977392,6.62684135982234,14.7947631728529));
#89033=CARTESIAN_POINT('Ctrl Pts',(7.24822961692489,6.80489025777293,14.7986730498067));
#89034=CARTESIAN_POINT('Ctrl Pts',(7.08110005074217,6.98290833383016,14.802582249925));
#89035=CARTESIAN_POINT('Ctrl Pts',(6.90739115704458,7.15478541460849,14.8064914500433));
#89036=CARTESIAN_POINT('Ctrl Pts',(6.72757885036217,7.32004418102511,14.8104006501616));
#89037=CARTESIAN_POINT('Ctrl Pts',(6.54778611888903,7.48528495659898,14.8143094247061));
#89038=CARTESIAN_POINT('Ctrl Pts',(6.36189150742211,7.64390866680942,14.8182181992506));
#89039=CARTESIAN_POINT('Ctrl Pts',(6.17040639744928,7.79547618111408,14.8221269737951));
#89040=CARTESIAN_POINT('Ctrl Pts',(5.97890642725549,7.94705545783072,14.8260360516804));
#89041=CARTESIAN_POINT('Ctrl Pts',(5.78181530953639,8.09157726805006,14.8299451295657));
#89042=CARTESIAN_POINT('Ctrl Pts',(5.57967700313877,8.22864317738012,14.8338542074511));
#89043=CARTESIAN_POINT('Ctrl Pts',(5.3775414880496,8.36570719398021,14.8377632313563));
#89044=CARTESIAN_POINT('Ctrl Pts',(5.17035915684901,8.49531535998442,14.8416722552615));
#89045=CARTESIAN_POINT('Ctrl Pts',(4.95870301034087,8.61711253583452,14.8455812791668));
#89046=CARTESIAN_POINT('Ctrl Pts',(4.74700031641688,8.73893649731729,14.8494911627445));
#89047=CARTESIAN_POINT('Ctrl Pts',(4.53082208377621,8.85294589546851,14.8534010463222));
#89048=CARTESIAN_POINT('Ctrl Pts',(4.31076718511858,8.95883085428589,14.8573109298999));
#89049=CARTESIAN_POINT('Ctrl Pts',(4.15375432801763,9.03438154645112,14.8601006973407));
#89050=CARTESIAN_POINT('Ctrl Pts',(3.9947683775805,9.10579698298566,14.8628904647815));
#89051=CARTESIAN_POINT('Ctrl Pts',(3.83403374497742,9.17297930022599,14.8656802322223));
#89052=CARTESIAN_POINT('Ctrl Pts',(3.6087631268991,9.26713574855057,14.8695901091761));
#89053=CARTESIAN_POINT('Ctrl Pts',(3.37998791368454,9.35300428089725,14.8734999861299));
#89054=CARTESIAN_POINT('Ctrl Pts',(3.14833660037946,9.43034149173354,14.8774098630837));
#89055=CARTESIAN_POINT('Ctrl Pts',(2.91672538803731,9.50766531479066,14.8813190632019));
#89056=CARTESIAN_POINT('Ctrl Pts',(2.68223933523787,9.57646067574101,14.8852282633202));
#89057=CARTESIAN_POINT('Ctrl Pts',(2.445523918826,9.63653344115247,14.8891374634385));
#89058=CARTESIAN_POINT('Ctrl Pts',(2.20883427235932,9.69659966676228,14.893046237983));
#89059=CARTESIAN_POINT('Ctrl Pts',(1.96991601846588,9.74794512391848,14.8969550125275));
#89060=CARTESIAN_POINT('Ctrl Pts',(1.72942771726594,9.7904261281495,14.900863787072));
#89061=CARTESIAN_POINT('Ctrl Pts',(1.48892075294888,9.83291042912282,14.9047728649573));
#89062=CARTESIAN_POINT('Ctrl Pts',(1.24684377337754,9.86652885077642,14.9086819428426));
#89063=CARTESIAN_POINT('Ctrl Pts',(1.00386468823217,9.89118899261967,14.912591020728));
#89064=CARTESIAN_POINT('Ctrl Pts',(0.760888958364166,9.91584879393313,14.9165000446331));
#89065=CARTESIAN_POINT('Ctrl Pts',(0.51701142694094,9.93155053658849,14.9204090685384));
#89066=CARTESIAN_POINT('Ctrl Pts',(0.272905007874495,9.93825371263367,14.9243180924436));
#89067=CARTESIAN_POINT('Ctrl Pts',(0.0287449049263693,9.94495836284129,
14.9282279760213));
#89068=CARTESIAN_POINT('Ctrl Pts',(-0.215643905956332,9.94266048342952,
14.932137859599));
#89069=CARTESIAN_POINT('Ctrl Pts',(-0.459587231326087,9.93137168656989,
14.9360477431767));
#89070=CARTESIAN_POINT('Ctrl Pts',(-0.6336448811275,9.92331694087232,14.9388375106175));
#89071=CARTESIAN_POINT('Ctrl Pts',(-0.807475704560176,9.91068595367717,
14.9416272780584));
#89072=CARTESIAN_POINT('Ctrl Pts',(-0.980835732711074,9.89349914163018,
14.9444170454993));
#89073=CARTESIAN_POINT('Ctrl Pts',(-1.22380092358777,9.86941171436048,14.948326922453));
#89074=CARTESIAN_POINT('Ctrl Pts',(-1.46591555237888,9.83636614652125,14.9522367994068));
#89075=CARTESIAN_POINT('Ctrl Pts',(-1.70651091401231,9.79444661532018,14.9561466763606));
#89076=CARTESIAN_POINT('Ctrl Pts',(-1.9470646263869,9.75253434077357,14.9600558764788));
#89077=CARTESIAN_POINT('Ctrl Pts',(-2.18609932059487,9.70175121748677,14.9639650765971));
#89078=CARTESIAN_POINT('Ctrl Pts',(-2.42295473941667,9.64223284985061,14.9678742767154));
#89079=CARTESIAN_POINT('Ctrl Pts',(-2.65978437305416,9.58272096166123,14.97178305126));
#89080=CARTESIAN_POINT('Ctrl Pts',(-2.89443493325438,9.51447579616935,14.9756918258045));
#89081=CARTESIAN_POINT('Ctrl Pts',(-3.12625860050512,9.43768356975205,14.9796006003491));
#89082=CARTESIAN_POINT('Ctrl Pts',(-3.35810025845128,9.36088538386748,14.9835096782344));
#89083=CARTESIAN_POINT('Ctrl Pts',(-3.58711431801025,9.27553889690189,14.9874187561197));
#89084=CARTESIAN_POINT('Ctrl Pts',(-3.81266907988396,9.18187989941585,14.991327834005));
#89085=CARTESIAN_POINT('Ctrl Pts',(-4.0382207270906,9.08822219525917,14.9952368579102));
#89086=CARTESIAN_POINT('Ctrl Pts',(-4.26031291404368,8.98625231956187,14.9991458818154));
#89087=CARTESIAN_POINT('Ctrl Pts',(-4.47833417492712,8.87625410957121,15.0030549057206));
#89088=CARTESIAN_POINT('Ctrl Pts',(-4.69640338304489,8.7662317087749,15.0069647892984));
#89089=CARTESIAN_POINT('Ctrl Pts',(-4.91039962535968,8.64817757115304,15.0108746728761));
#89090=CARTESIAN_POINT('Ctrl Pts',(-5.11973505570604,8.5224220125135,15.0147845564538));
#89091=CARTESIAN_POINT('Ctrl Pts',(-5.26909939256813,8.43269331445298,15.0175743238946));
#89092=CARTESIAN_POINT('Ctrl Pts',(-5.41609137512249,8.33904474758301,15.0203640913354));
#89093=CARTESIAN_POINT('Ctrl Pts',(-5.56050597917073,8.24161011305476,15.0231538587763));
#89094=CARTESIAN_POINT('Ctrl Pts',(-5.76290397259949,8.10505484810113,15.02706373573));
#89095=CARTESIAN_POINT('Ctrl Pts',(-5.96030020701914,7.96101933280805,15.0309736126838));
#89096=CARTESIAN_POINT('Ctrl Pts',(-6.15214611927763,7.80989514187337,15.0348834896376));
#89097=CARTESIAN_POINT('Ctrl Pts',(-6.3439588212522,7.65879711191979,15.0387926897559));
#89098=CARTESIAN_POINT('Ctrl Pts',(-6.53022289897422,7.5006130292946,15.0427018898742));
#89099=CARTESIAN_POINT('Ctrl Pts',(-6.71042164104554,7.33577571899439,15.0466110899924));
#89100=CARTESIAN_POINT('Ctrl Pts',(-6.89060076584068,7.1709563536532,15.0505198645369));
#89101=CARTESIAN_POINT('Ctrl Pts',(-7.06471566664228,6.9994853959583,15.0544286390814));
#89102=CARTESIAN_POINT('Ctrl Pts',(-7.23228460824575,6.82183430943112,15.058337413626));
#89103=CARTESIAN_POINT('Ctrl Pts',(-7.39986655405268,6.64416943627468,15.0622464915113));
#89104=CARTESIAN_POINT('Ctrl Pts',(-7.56090133099839,6.4603236777518,15.0661555693966));
#89105=CARTESIAN_POINT('Ctrl Pts',(-7.71494492832411,6.27080447414254,15.0700646472819));
#89106=CARTESIAN_POINT('Ctrl Pts',(-7.86898639847684,6.08128788758545,15.0739736711872));
#89107=CARTESIAN_POINT('Ctrl Pts',(-8.01603670687459,5.88609823146361,15.0778826950924));
#89108=CARTESIAN_POINT('Ctrl Pts',(-8.15569246207227,5.68577562554992,15.0817917189977));
#89109=CARTESIAN_POINT('Ctrl Pts',(-8.29537893036041,5.48540896469336,15.0857016025753));
#89110=CARTESIAN_POINT('Ctrl Pts',(-8.42766743480796,5.27990732789923,15.089611486153));
#89111=CARTESIAN_POINT('Ctrl Pts',(-8.55219743893893,5.06984052662472,15.0935213697307));
#89112=CARTESIAN_POINT('Ctrl Pts',(-8.64105168332479,4.91995434435036,15.0963111371716));
#89113=CARTESIAN_POINT('Ctrl Pts',(-8.72595692350404,4.76774462980351,15.0991009046124));
#89114=CARTESIAN_POINT('Ctrl Pts',(-8.80679624371355,4.61342648383097,15.1018906720533));
#89115=CARTESIAN_POINT('Ctrl Pts',(-8.91997001929561,4.39738350901037,15.1057963025491));
#89116=CARTESIAN_POINT('Ctrl Pts',(-9.02520827542342,4.1771395377998,15.109701933045));
#89117=CARTESIAN_POINT('Ctrl Pts',(-9.12221448249565,3.95329823506229,15.1136075635409));
#89118=CARTESIAN_POINT('Ctrl Pts',(-9.21920355188142,3.72949647744441,15.1175125040451));
#89119=CARTESIAN_POINT('Ctrl Pts',(-9.30796336338345,3.50209891511801,15.1214174445494));
#89120=CARTESIAN_POINT('Ctrl Pts',(-9.38824499467587,3.27173041675862,15.1253223850536));
#89121=CARTESIAN_POINT('Ctrl Pts',(-9.46851786192404,3.04138706686318,15.1292268992702));
#89122=CARTESIAN_POINT('Ctrl Pts',(-9.54031430430537,2.80807369426392,15.1331314134867));
#89123=CARTESIAN_POINT('Ctrl Pts',(-9.60343452253734,2.57243257857965,15.1370359277033));
#89124=CARTESIAN_POINT('Ctrl Pts',(-9.66655941457757,2.33677401458134,15.140940731034));
#89125=CARTESIAN_POINT('Ctrl Pts',(-9.72100672317706,2.09878763433068,15.1448455343648));
#89126=CARTESIAN_POINT('Ctrl Pts',(-9.76662693389493,1.85912945598688,15.1487503376955));
#89127=CARTESIAN_POINT('Ctrl Pts',(-9.81224685516775,1.61947279819445,15.1526551162516));
#89128=CARTESIAN_POINT('Ctrl Pts',(-9.84903974021967,1.37814464055025,15.1565598948077));
#89129=CARTESIAN_POINT('Ctrl Pts',(-9.87690733898645,1.13581046705674,15.1604646733637));
#89130=CARTESIAN_POINT('Ctrl Pts',(-9.90478082891521,0.893425064539732,
15.1643702773832));
#89131=CARTESIAN_POINT('Ctrl Pts',(-9.92372523004582,0.650033500982153,
15.1682758814027));
#89132=CARTESIAN_POINT('Ctrl Pts',(-9.93369410819283,0.40630698351737,15.1721814854221));
#89133=CARTESIAN_POINT('Ctrl Pts',(-9.93923159351023,0.270922440540864,
15.1743509597195));
#89134=CARTESIAN_POINT('Ctrl Pts',(-9.94200056172094,0.1354346160241,15.1765204340168));
#89135=CARTESIAN_POINT('Ctrl Pts',(-9.94199999991451,-4.12286006677384E-5,
15.1786899083142));
#89136=CARTESIAN_POINT('Origin',(0.,0.,0.));
#89137=CARTESIAN_POINT('',(-9.94157881028341,-0.000218552330966126,16.3213100916858));
#89138=CARTESIAN_POINT('',(-9.94156315955438,-0.000215792232726663,16.1786899083142));
#89139=CARTESIAN_POINT('',(-9.942,-1.2175438477123E-15,0.));
#89140=CARTESIAN_POINT('Ctrl Pts',(-9.94157881028341,-0.000218552330966126,
16.3213100916858));
#89141=CARTESIAN_POINT('Ctrl Pts',(-9.94066271461031,1.11431393761154,16.3034700970927));
#89142=CARTESIAN_POINT('Ctrl Pts',(-9.47830442710447,3.86925058390486,16.2593844980741));
#89143=CARTESIAN_POINT('Ctrl Pts',(-6.98191316447499,7.64950719205534,16.1890532946296));
#89144=CARTESIAN_POINT('Ctrl Pts',(-2.51294062811132,10.0472484347585,16.1103164813527));
#89145=CARTESIAN_POINT('Ctrl Pts',(2.55862180591419,10.0357125391651,16.0315796680756));
#89146=CARTESIAN_POINT('Ctrl Pts',(7.01664023694587,7.61766575125248,15.9528428547988));
#89147=CARTESIAN_POINT('Ctrl Pts',(9.79210537743402,3.37294292723244,15.8741060415217));
#89148=CARTESIAN_POINT('Ctrl Pts',(10.2194753373836,-1.68059380627902,15.7953692282448));
#89149=CARTESIAN_POINT('Ctrl Pts',(8.19626905631817,-6.33113301624731,15.7166324149677));
#89150=CARTESIAN_POINT('Ctrl Pts',(4.20764072067247,-9.46349994868898,15.6378956016907));
#89151=CARTESIAN_POINT('Ctrl Pts',(-0.789957649186856,-10.3265695477982,
15.5591587884139));
#89152=CARTESIAN_POINT('Ctrl Pts',(-5.59812834466891,-8.71338227955533,
15.4804219751368));
#89153=CARTESIAN_POINT('Ctrl Pts',(-9.06389741358393,-5.01077193544794,
15.4016851618598));
#89154=CARTESIAN_POINT('Ctrl Pts',(-9.93438976965992,-1.70731401312795,
15.3486478673762));
#89155=CARTESIAN_POINT('Ctrl Pts',(-9.9428212718197,-0.0341387347268834,
15.3218561773182));
#89156=CARTESIAN_POINT('Ctrl Pts',(-9.9428143739607,-3.4919416618262E-5,
15.3213100916858));
#89157=CARTESIAN_POINT('Ctrl Pts',(-9.94281021402477,-4.12319605559286E-5,
15.1786899083142));
#89158=CARTESIAN_POINT('Ctrl Pts',(-9.94281975151917,-0.040376084069569,
15.1793357673195));
#89159=CARTESIAN_POINT('Ctrl Pts',(-9.94257935794541,-0.0807108220809731,
15.1799816263249));
#89160=CARTESIAN_POINT('Ctrl Pts',(-9.92213453281451,-1.7599907672817,15.2068730897559));
#89161=CARTESIAN_POINT('Ctrl Pts',(-9.0544577245587,-5.02780939552147,15.2593642986071));
#89162=CARTESIAN_POINT('Ctrl Pts',(-5.58173134501452,-8.72389518481278,
15.3381011118842));
#89163=CARTESIAN_POINT('Ctrl Pts',(-0.770535252865366,-10.3280369590551,
15.4168379251612));
#89164=CARTESIAN_POINT('Ctrl Pts',(4.22543112554584,-9.45556998846635,15.4955747384382));
#89165=CARTESIAN_POINT('Ctrl Pts',(8.20816142456435,-6.31570724715832,15.5743115517152));
#89166=CARTESIAN_POINT('Ctrl Pts',(10.2226179418717,-1.66137124630252,15.653048364992));
#89167=CARTESIAN_POINT('Ctrl Pts',(9.78574463819948,3.39135280964152,15.7317851782691));
#89168=CARTESIAN_POINT('Ctrl Pts',(7.00230142567361,7.63084836355288,15.8105219915461));
#89169=CARTESIAN_POINT('Ctrl Pts',(2.53974329387374,10.0405067603537,15.8892588048229));
#89170=CARTESIAN_POINT('Ctrl Pts',(-2.53183187341625,10.0425046362111,15.9679956181));
#89171=CARTESIAN_POINT('Ctrl Pts',(-6.99628712208093,7.63636291102297,16.046732431377));
#89172=CARTESIAN_POINT('Ctrl Pts',(-9.48203316727476,3.8567874690065,16.1169638614483));
#89173=CARTESIAN_POINT('Ctrl Pts',(-9.9406658297407,1.10808848775586,16.1609496870941));
#89174=CARTESIAN_POINT('Ctrl Pts',(-9.94156315955438,-0.000215792232726663,
16.1786899083142));
#89175=CARTESIAN_POINT('Origin',(0.,0.,0.));
#89176=CARTESIAN_POINT('',(-9.94136243353558,0.000162173653817377,17.3213100916858));
#89177=CARTESIAN_POINT('',(-9.94137407189289,0.000167045264107003,17.1786899083142));
#89178=CARTESIAN_POINT('',(-9.942,-1.2175438477123E-15,0.));
#89179=CARTESIAN_POINT('Ctrl Pts',(-9.94136243353558,0.000162173653817377,
17.3213100916858));
#89180=CARTESIAN_POINT('Ctrl Pts',(-9.94173254800261,0.623719662799634,
17.311329621293));
#89181=CARTESIAN_POINT('Ctrl Pts',(-9.73204865908736,2.88679819383414,17.2751035464743));
#89182=CARTESIAN_POINT('Ctrl Pts',(-8.03455596699662,6.53513275653972,17.2126318672303));
#89183=CARTESIAN_POINT('Ctrl Pts',(-3.96846040138357,9.56626411515653,17.1338950539532));
#89184=CARTESIAN_POINT('Ctrl Pts',(1.0492513505079,10.3034525871473,17.0551582406764));
#89185=CARTESIAN_POINT('Ctrl Pts',(5.81535799701473,8.56992919148952,16.9764214273993));
#89186=CARTESIAN_POINT('Ctrl Pts',(9.18697258070385,4.78138115006309,16.8976846141223));
#89187=CARTESIAN_POINT('Ctrl Pts',(10.3555995890163,-0.153716407029685,
16.8189478008455));
#89188=CARTESIAN_POINT('Ctrl Pts',(9.041008502631,-5.05195381048614,16.7402109875684));
#89189=CARTESIAN_POINT('Ctrl Pts',(5.55843128949705,-8.73875923938874,16.6614741742914));
#89190=CARTESIAN_POINT('Ctrl Pts',(0.742971600270773,-10.3300563923589,
16.5827373610144));
#89191=CARTESIAN_POINT('Ctrl Pts',(-4.25064876001462,-9.4442605196381,16.5040005477376));
#89192=CARTESIAN_POINT('Ctrl Pts',(-8.22498598363295,-6.29378084331697,
16.4252637344605));
#89193=CARTESIAN_POINT('Ctrl Pts',(-9.77340015076588,-2.68986805686518,
16.3643669157766));
#89194=CARTESIAN_POINT('Ctrl Pts',(-9.94201044397911,-0.525349050959409,
16.3297157015184));
#89195=CARTESIAN_POINT('Ctrl Pts',(-9.94157881028341,-0.000218552330966126,
16.3213100916858));
#89196=CARTESIAN_POINT('Ctrl Pts',(-9.94156315955438,-0.000215792232726663,
16.1786899083142));
#89197=CARTESIAN_POINT('Ctrl Pts',(-9.94199337594416,-0.531581917419294,
16.1871952915198));
#89198=CARTESIAN_POINT('Ctrl Pts',(-9.77087211432573,-2.70234409750878,
16.2219462791508));
#89199=CARTESIAN_POINT('Ctrl Pts',(-8.2131348446615,-6.30923830794241,16.282942871208));
#89200=CARTESIAN_POINT('Ctrl Pts',(-4.23287959110267,-9.45223795575133,
16.3616796844848));
#89201=CARTESIAN_POINT('Ctrl Pts',(0.762397844591911,-10.3286408363935,
16.4404164977619));
#89202=CARTESIAN_POINT('Ctrl Pts',(5.57485630153356,-8.72829016619386,16.5191533110387));
#89203=CARTESIAN_POINT('Ctrl Pts',(9.05049364508474,-5.03494158647097,16.5978901243158));
#89204=CARTESIAN_POINT('Ctrl Pts',(10.3558703866554,-0.134240594147907,
16.6766269375928));
#89205=CARTESIAN_POINT('Ctrl Pts',(9.1779640746773,4.79865058833391,16.7553637508696));
#89206=CARTESIAN_POINT('Ctrl Pts',(5.79923042414636,8.580850681741,16.8341005641467));
#89207=CARTESIAN_POINT('Ctrl Pts',(1.02987193105673,10.3054080930073,16.9128373774237));
#89208=CARTESIAN_POINT('Ctrl Pts',(-3.98644441696093,9.5587830107304,16.9915741907007));
#89209=CARTESIAN_POINT('Ctrl Pts',(-8.04683243255047,6.52001228063464,17.0703110039775));
#89210=CARTESIAN_POINT('Ctrl Pts',(-9.73476031103565,2.87432000866741,17.1326829098488));
#89211=CARTESIAN_POINT('Ctrl Pts',(-9.94175055725434,0.617488319087645,
17.1688092112943));
#89212=CARTESIAN_POINT('Ctrl Pts',(-9.94137407189289,0.000167045264107003,
17.1786899083142));
#89213=CARTESIAN_POINT('Origin',(0.,0.,0.));
#89214=CARTESIAN_POINT('',(-4.30729783501544,8.96073829072084,18.));
#89215=CARTESIAN_POINT('Ctrl Pts',(-9.94137407189289,0.000167045264107003,
17.1786899083142));
#89216=CARTESIAN_POINT('Ctrl Pts',(-9.94075051789995,-1.02227149985294,
17.19505481572));
#89217=CARTESIAN_POINT('Ctrl Pts',(-9.53207699775168,-3.68495707954238,
17.2376653275512));
#89218=CARTESIAN_POINT('Ctrl Pts',(-7.19187963366665,-7.45244541015752,
17.3065214438087));
#89219=CARTESIAN_POINT('Ctrl Pts',(-2.79129440548034,-9.9735018662042,17.3852582570854));
#89220=CARTESIAN_POINT('Ctrl Pts',(2.27862837048033,-10.1029668943729,17.4639950703625));
#89221=CARTESIAN_POINT('Ctrl Pts',(6.8021483171817,-7.80979054448228,17.5427318836394));
#89222=CARTESIAN_POINT('Ctrl Pts',(9.69454856507843,-3.64387394710659,17.6214686969163));
#89223=CARTESIAN_POINT('Ctrl Pts',(10.2622480917845,1.39583661306226,17.7002055101934));
#89224=CARTESIAN_POINT('Ctrl Pts',(8.36911304595686,6.10080919945852,17.7789423234704));
#89225=CARTESIAN_POINT('Ctrl Pts',(4.46911207265963,9.34288597599586,17.8576791367474));
#89226=CARTESIAN_POINT('Ctrl Pts',(-0.183634414914874,10.2802458074126,
17.9313650289238));
#89227=CARTESIAN_POINT('Ctrl Pts',(-3.11352491188595,9.53306574361534,17.9788053166748));
#89228=CARTESIAN_POINT('Ctrl Pts',(-4.30729783501544,8.96073829072084,18.));
#89229=CARTESIAN_POINT('',(4.30700275658802,8.96064123010977,18.));
#89230=CARTESIAN_POINT('Origin',(0.,0.,18.));
#89231=CARTESIAN_POINT('Ctrl Pts',(4.30700275658802,8.96064123010977,18.));
#89232=CARTESIAN_POINT('Ctrl Pts',(5.78466622438187,8.25039065030617,17.9737543955743));
#89233=CARTESIAN_POINT('Ctrl Pts',(8.38051870287619,6.0857105851668,17.9212631867231));
#89234=CARTESIAN_POINT('Ctrl Pts',(10.2648846152864,1.37622265143462,17.842526373446));
#89235=CARTESIAN_POINT('Ctrl Pts',(9.68766298633001,-3.66194177412479,17.7637895601691));
#89236=CARTESIAN_POINT('Ctrl Pts',(6.78745652630585,-7.82265065129397,17.6850527468922));
#89237=CARTESIAN_POINT('Ctrl Pts',(2.25961974458035,-10.1071925353341,17.6063159336151));
#89238=CARTESIAN_POINT('Ctrl Pts',(-2.81004433424633,-9.96825624824068,
17.5275791203381));
#89239=CARTESIAN_POINT('Ctrl Pts',(-7.20588368450361,-7.43889545753228,
17.4488423070613));
#89240=CARTESIAN_POINT('Ctrl Pts',(-9.53560930616682,-3.67249284691441,
17.3800859641771));
#89241=CARTESIAN_POINT('Ctrl Pts',(-9.94075925941884,-1.01604705686179,
17.3375752257186));
#89242=CARTESIAN_POINT('Ctrl Pts',(-9.94136243353558,0.000162173653817377,
17.3213100916858));
#89243=CARTESIAN_POINT('Origin',(0.,0.,2.15141010809499));
#89244=CARTESIAN_POINT('',(5.43505795426094,-7.63293718671423,18.));
#89245=CARTESIAN_POINT('Ctrl Pts',(5.43505795426094,-7.63293718671423,18.));
#89246=CARTESIAN_POINT('Ctrl Pts',(5.17173340930988,-7.82043829245888,17.9943178253384));
#89247=CARTESIAN_POINT('Ctrl Pts',(4.8988798102261,-7.99418927223705,17.9886342308681));
#89248=CARTESIAN_POINT('Ctrl Pts',(4.54641891280022,-8.19379950750167,17.9816362724925));
#89249=CARTESIAN_POINT('Ctrl Pts',(4.47472144112314,-8.23317334688816,17.9802292444045));
#89250=CARTESIAN_POINT('Ctrl Pts',(4.33644627871265,-8.30676957699183,17.9775472605171));
#89251=CARTESIAN_POINT('Ctrl Pts',(4.26995593257482,-8.34114281713787,17.9762713286267));
#89252=CARTESIAN_POINT('Ctrl Pts',(4.1276715741662,-8.41255178530606,17.9735694011271));
#89253=CARTESIAN_POINT('Ctrl Pts',(4.0517747605446,-8.44936811214072,17.9721450558189));
#89254=CARTESIAN_POINT('Ctrl Pts',(3.84668008784851,-8.54545728989826,17.968338909957));
#89255=CARTESIAN_POINT('Ctrl Pts',(3.71661343720383,-8.60282353122374,17.9659703690349));
#89256=CARTESIAN_POINT('Ctrl Pts',(3.27981056713658,-8.78372084504184,17.9581405576608));
#89257=CARTESIAN_POINT('Ctrl Pts',(2.96784776287721,-8.89397484187954,17.9527567734968));
#89258=CARTESIAN_POINT('Ctrl Pts',(2.55580612313983,-9.01549947057141,17.9456816874559));
#89259=CARTESIAN_POINT('Ctrl Pts',(2.46046313216061,-9.041985222169,17.9440462316115));
#89260=CARTESIAN_POINT('Ctrl Pts',(2.33702254301936,-9.07417929918066,17.9419223979961));
#89261=CARTESIAN_POINT('Ctrl Pts',(2.3092933810926,-9.08127570324028,17.9414448897797));
#89262=CARTESIAN_POINT('Ctrl Pts',(2.27360711410161,-9.09023445889745,17.9408295961921));
#89263=CARTESIAN_POINT('Ctrl Pts',(2.26567947211113,-9.09221361147132,17.9406928615992));
#89264=CARTESIAN_POINT('Ctrl Pts',(2.24168151600013,-9.09817141670899,17.9402787908133));
#89265=CARTESIAN_POINT('Ctrl Pts',(2.22560324193713,-9.10211785003997,17.9400011550254));
#89266=CARTESIAN_POINT('Ctrl Pts',(2.19659036470876,-9.10915762858463,17.9394997187239));
#89267=CARTESIAN_POINT('Ctrl Pts',(2.18365947172891,-9.11226608720395,17.9392760705546));
#89268=CARTESIAN_POINT('Ctrl Pts',(2.14432794399045,-9.12163246819743,17.9385952632139));
#89269=CARTESIAN_POINT('Ctrl Pts',(2.11790672340901,-9.1278032584424,17.9381371833745));
#89270=CARTESIAN_POINT('Ctrl Pts',(2.05069967107279,-9.14319224111505,17.9369696900891));
#89271=CARTESIAN_POINT('Ctrl Pts',(2.00987843827555,-9.15225229909239,17.9362582711727));
#89272=CARTESIAN_POINT('Ctrl Pts',(1.90661786928515,-9.17444627171035,17.9344532117096));
#89273=CARTESIAN_POINT('Ctrl Pts',(1.84410260853059,-9.18721620698452,17.9333556057256));
#89274=CARTESIAN_POINT('Ctrl Pts',(1.60055448070495,-9.23437952569823,17.9290670197665));
#89275=CARTESIAN_POINT('Ctrl Pts',(1.41865333028027,-9.26406834607901,17.9258379397813));
#89276=CARTESIAN_POINT('Ctrl Pts',(1.06960173865389,-9.31051633678268,17.9196515202567));
#89277=CARTESIAN_POINT('Ctrl Pts',(0.902642524715984,-9.3281830427163,17.9166966088536));
#89278=CARTESIAN_POINT('Ctrl Pts',(0.590802233253205,-9.35272936024783,
17.9112144478403));
#89279=CARTESIAN_POINT('Ctrl Pts',(0.446060717354184,-9.3607491020278,17.9086845123872));
#89280=CARTESIAN_POINT('Ctrl Pts',(0.189989278514941,-9.36898435356703,
17.9042438448726));
#89281=CARTESIAN_POINT('Ctrl Pts',(0.078732203131157,-9.37057976180315,
17.9023261134129));
#89282=CARTESIAN_POINT('Ctrl Pts',(-0.095456492859394,-9.36997509513793,
17.8993427759256));
#89283=CARTESIAN_POINT('Ctrl Pts',(-0.158382204390103,-9.36912270812688,
17.8982689273276));
#89284=CARTESIAN_POINT('Ctrl Pts',(-0.264010037201853,-9.36662742871493,
17.8964726770231));
#89285=CARTESIAN_POINT('Ctrl Pts',(-0.30671808787091,-9.36532619335901,
17.8957481403264));
#89286=CARTESIAN_POINT('Ctrl Pts',(-0.44330767803551,-9.36022923493316,
17.8934362089332));
#89287=CARTESIAN_POINT('Ctrl Pts',(-0.537141697500538,-9.35531356388984,
17.8918560202705));
#89288=CARTESIAN_POINT('Ctrl Pts',(-1.04408865822473,-9.32110389608918,
17.8833548000159));
#89289=CARTESIAN_POINT('Ctrl Pts',(-1.45498681725177,-9.26585732928013,
17.876616120775));
#89290=CARTESIAN_POINT('Ctrl Pts',(-1.97151996293981,-9.16119194995781,
17.8679552600374));
#89291=CARTESIAN_POINT('Ctrl Pts',(-2.08174572454483,-9.13677533736938,
17.8660942221446));
#89292=CARTESIAN_POINT('Ctrl Pts',(-2.24918875884167,-9.09649686264499,
17.8632327463826));
#89293=CARTESIAN_POINT('Ctrl Pts',(-2.30674121291386,-9.08207301241379,
17.8622429414518));
#89294=CARTESIAN_POINT('Ctrl Pts',(-2.36633916169708,-9.06653346874789,
17.8612098175093));
#89295=CARTESIAN_POINT('Ctrl Pts',(-2.36852541298319,-9.06596258188607,
17.8611719076688));
#89296=CARTESIAN_POINT('Ctrl Pts',(-2.37276464952788,-9.0648539692787,17.8610983765297));
#89297=CARTESIAN_POINT('Ctrl Pts',(-2.37481765904612,-9.06431633675032,
17.861062756166));
#89298=CARTESIAN_POINT('Ctrl Pts',(-2.37880579743203,-9.06327049379004,
17.860993540846));
#89299=CARTESIAN_POINT('Ctrl Pts',(-2.38074094654839,-9.06276236094318,
17.8609599466752));
#89300=CARTESIAN_POINT('Ctrl Pts',(-2.38450706501532,-9.06177216135061,
17.8608945490873));
#89301=CARTESIAN_POINT('Ctrl Pts',(-2.3863380513045,-9.06129015936651,17.8608627463318));
#89302=CARTESIAN_POINT('Ctrl Pts',(-2.38990809638021,-9.06034919792419,
17.8608007214468));
#89303=CARTESIAN_POINT('Ctrl Pts',(-2.39164716937723,-9.05989029264033,
17.8607704998755));
#89304=CARTESIAN_POINT('Ctrl Pts',(-2.39504439832398,-9.05899278807569,
17.8607114482788));
#89305=CARTESIAN_POINT('Ctrl Pts',(-2.39670256619049,-9.05855423417919,
17.8606826187249));
#89306=CARTESIAN_POINT('Ctrl Pts',(-2.39994793551505,-9.0576949421774,17.8606261800599));
#89307=CARTESIAN_POINT('Ctrl Pts',(-2.40153514698501,-9.05727424209537,
17.8605985713466));
#89308=CARTESIAN_POINT('Ctrl Pts',(-2.40464765545685,-9.05644837705684,
17.8605444185095));
#89309=CARTESIAN_POINT('Ctrl Pts',(-2.4061729608505,-9.05604324391514,17.8605178747209));
#89310=CARTESIAN_POINT('Ctrl Pts',(-2.40916995419383,-9.05524640822137,
17.8604657086887));
#89311=CARTESIAN_POINT('Ctrl Pts',(-2.41064164915234,-9.05485473219576,
17.8604400867266));
#89312=CARTESIAN_POINT('Ctrl Pts',(-2.41353909346036,-9.05408285162861,
17.8603896319029));
#89313=CARTESIAN_POINT('Ctrl Pts',(-2.41496484861779,-9.0537026690607,17.8603647992761));
#89314=CARTESIAN_POINT('Ctrl Pts',(-2.41777757870084,-9.05295193312329,
17.8603157992498));
#89315=CARTESIAN_POINT('Ctrl Pts',(-2.4191645583989,-9.05258139775035,17.8602916320438));
#89316=CARTESIAN_POINT('Ctrl Pts',(-2.42190650722443,-9.05184820355637,
17.8602438456585));
#89317=CARTESIAN_POINT('Ctrl Pts',(-2.42326148018509,-9.05148555921146,
17.8602202266361));
#89318=CARTESIAN_POINT('Ctrl Pts',(-2.42594589511924,-9.05076645765053,
17.8601734242729));
#89319=CARTESIAN_POINT('Ctrl Pts',(-2.42727534008299,-9.05041001172889,
17.8601502410554));
#89320=CARTESIAN_POINT('Ctrl Pts',(-2.42991499213949,-9.04970165441712,
17.860104201023));
#89321=CARTESIAN_POINT('Ctrl Pts',(-2.43122520144201,-9.04934975138309,
17.8600813442998));
#89322=CARTESIAN_POINT('Ctrl Pts',(-2.43383259373152,-9.0486488368531,17.860035849225));
#89323=CARTESIAN_POINT('Ctrl Pts',(-2.43512977817829,-9.04829983093077,
17.8600132109349));
#89324=CARTESIAN_POINT('Ctrl Pts',(-2.43771736071058,-9.04760304820377,
17.8599680440296));
#89325=CARTESIAN_POINT('Ctrl Pts',(-2.4390077595318,-9.04725527425414,17.8599455154464));
#89326=CARTESIAN_POINT('Ctrl Pts',(-2.44158815874383,-9.04655924155516,
17.8599004565054));
#89327=CARTESIAN_POINT('Ctrl Pts',(-2.44287815913675,-9.04621098291973,
17.8598779261494));
#89328=CARTESIAN_POINT('Ctrl Pts',(-2.44546443228321,-9.04551217876263,
17.8598327470999));
#89329=CARTESIAN_POINT('Ctrl Pts',(-2.44676070426629,-9.04516163049414,
17.8598100983761));
#89330=CARTESIAN_POINT('Ctrl Pts',(-2.44936663183124,-9.04445631347901,
17.8597645581481));
#89331=CARTESIAN_POINT('Ctrl Pts',(-2.45067628580571,-9.04410153888975,
17.8597416665786));
#89332=CARTESIAN_POINT('Ctrl Pts',(-2.45331671935038,-9.04338565131626,
17.8596955049889));
#89333=CARTESIAN_POINT('Ctrl Pts',(-2.45464749636279,-9.04302452902106,
17.859672234864));
#89334=CARTESIAN_POINT('Ctrl Pts',(-2.45733878565391,-9.0422935775603,17.8596251650918));
#89335=CARTESIAN_POINT('Ctrl Pts',(-2.45869929426579,-9.04192373506014,
17.8596013652938));
#89336=CARTESIAN_POINT('Ctrl Pts',(-2.46145982746429,-9.04117263886177,
17.8595530643505));
#89337=CARTESIAN_POINT('Ctrl Pts',(-2.46285984706647,-9.04079136700049,
17.8595285629984));
#89338=CARTESIAN_POINT('Ctrl Pts',(-2.46571075296803,-9.04001425922299,
17.8594786593226));
#89339=CARTESIAN_POINT('Ctrl Pts',(-2.4671616326451,-9.03961839917265,17.8594532567222));
#89340=CARTESIAN_POINT('Ctrl Pts',(-2.47012771793563,-9.03880836100521,
17.859401313607));
#89341=CARTESIAN_POINT('Ctrl Pts',(-2.47164291482507,-9.03839415114688,
17.8593747727259));
#89342=CARTESIAN_POINT('Ctrl Pts',(-2.47475394849737,-9.03754284607514,
17.8593202655879));
#89343=CARTESIAN_POINT('Ctrl Pts',(-2.47634977378964,-9.03710570913601,
17.8592922988465));
#89344=CARTESIAN_POINT('Ctrl Pts',(-2.47964229611515,-9.0362028663305,17.859234583188));
#89345=CARTESIAN_POINT('Ctrl Pts',(-2.48133897791757,-9.03573710522994,
17.8592048336251));
#89346=CARTESIAN_POINT('Ctrl Pts',(-2.4848589247123,-9.0347697681043,17.8591430985237));
#89347=CARTESIAN_POINT('Ctrl Pts',(-2.4866821692442,-9.03426811797922,17.8591111121125));
#89348=CARTESIAN_POINT('Ctrl Pts',(-2.48940337214991,-9.0335185161175,17.8590633584406));
#89349=CARTESIAN_POINT('Ctrl Pts',(-2.49030144569378,-9.03327098231225,
17.8590475961459));
#89350=CARTESIAN_POINT('Ctrl Pts',(-2.49269679964682,-9.03261037242341,
17.8590055487498));
#89351=CARTESIAN_POINT('Ctrl Pts',(-2.4941940142548,-9.03219705798294,17.8589792608062));
#89352=CARTESIAN_POINT('Ctrl Pts',(-2.49840305712354,-9.03103400186164,
17.8589053412177));
#89353=CARTESIAN_POINT('Ctrl Pts',(-2.50111465039944,-9.03028341106633,
17.8588576993873));
#89354=CARTESIAN_POINT('Ctrl Pts',(-2.50571645285452,-9.02900736345855,
17.8587768119355));
#89355=CARTESIAN_POINT('Ctrl Pts',(-2.50760683593739,-9.0284825340615,17.8587435739284));
#89356=CARTESIAN_POINT('Ctrl Pts',(-2.51922633715825,-9.02525266669247,
17.8585392094608));
#89357=CARTESIAN_POINT('Ctrl Pts',(-2.52895123905259,-9.02253249735524,
17.858367898119));
#89358=CARTESIAN_POINT('Ctrl Pts',(-2.57692837139369,-9.00902906769203,
17.8575213750912));
#89359=CARTESIAN_POINT('Ctrl Pts',(-2.61511606462939,-8.99801825578328,
17.8568432510961));
#89360=CARTESIAN_POINT('Ctrl Pts',(-2.7269507693098,-8.96500042612023,17.8548457722729));
#89361=CARTESIAN_POINT('Ctrl Pts',(-2.80039834061533,-8.94232979869343,
17.8535191871347));
#89362=CARTESIAN_POINT('Ctrl Pts',(-3.21514719986506,-8.80870075620339,
17.8459594578482));
#89363=CARTESIAN_POINT('Ctrl Pts',(-3.55013107320787,-8.6791100095911,17.8396009484144));
#89364=CARTESIAN_POINT('Ctrl Pts',(-3.99617198722411,-8.47640085071411,
17.8310292850766));
#89365=CARTESIAN_POINT('Ctrl Pts',(-4.11433821616512,-8.41967832491412,
17.8287464056948));
#89366=CARTESIAN_POINT('Ctrl Pts',(-4.32944669356626,-8.31081117938263,
17.8245744894209));
#89367=CARTESIAN_POINT('Ctrl Pts',(-4.42673494212108,-8.25940124774662,
17.8226813163502));
#89368=CARTESIAN_POINT('Ctrl Pts',(-4.59289171300171,-8.16781991949712,
17.8194376033794));
#89369=CARTESIAN_POINT('Ctrl Pts',(-4.66219448547851,-8.12846105600316,
17.8180814487509));
#89370=CARTESIAN_POINT('Ctrl Pts',(-4.80825529160954,-8.04302674492959,
17.815215577553));
#89371=CARTESIAN_POINT('Ctrl Pts',(-4.88487225454889,-7.99672565947357,
17.8137076877283));
#89372=CARTESIAN_POINT('Ctrl Pts',(-5.11556459424748,-7.85276116603642,
17.8091499442718));
#89373=CARTESIAN_POINT('Ctrl Pts',(-5.26746235997193,-7.75169011417247,
17.8061254821021));
#89374=CARTESIAN_POINT('Ctrl Pts',(-5.47110055238523,-7.60744054226601,
17.8020133765405));
#89375=CARTESIAN_POINT('Ctrl Pts',(-5.52546911852387,-7.56804359707743,
17.8009095887904));
#89376=CARTESIAN_POINT('Ctrl Pts',(-5.73553736469515,-7.41235197194009,
17.7966166110124));
#89377=CARTESIAN_POINT('Ctrl Pts',(-5.88802745512071,-7.29180932295328,
17.7934401692021));
#89378=CARTESIAN_POINT('Ctrl Pts',(-6.15059826452214,-7.07063783835505,
17.7877910600257));
#89379=CARTESIAN_POINT('Ctrl Pts',(-6.26223254759748,-6.97195967658334,
17.7853276886563));
#89380=CARTESIAN_POINT('Ctrl Pts',(-6.41088827117743,-6.83410471048899,
17.7819303760864));
#89381=CARTESIAN_POINT('Ctrl Pts',(-6.44999480582586,-6.79720844219528,
17.7810251689012));
#89382=CARTESIAN_POINT('Ctrl Pts',(-6.51948245708224,-6.73050849004815,
17.7793938098659));
#89383=CARTESIAN_POINT('Ctrl Pts',(-6.54998208221477,-6.70083060120725,
17.7786695235695));
#89384=CARTESIAN_POINT('Ctrl Pts',(-6.61901516356093,-6.63273577637062,
17.7770117166984));
#89385=CARTESIAN_POINT('Ctrl Pts',(-6.65741825669758,-6.59418893821198,
17.7760762915812));
#89386=CARTESIAN_POINT('Ctrl Pts',(-6.90114577647515,-6.34524974414563,
17.7700606523033));
#89387=CARTESIAN_POINT('Ctrl Pts',(-7.09680853719885,-6.12562776781217,
17.7648739067136));
#89388=CARTESIAN_POINT('Ctrl Pts',(-7.39447503280842,-5.75806949730283,
17.7565634306888));
#89389=CARTESIAN_POINT('Ctrl Pts',(-7.50311871094122,-5.61576666118042,
17.7534266386592));
#89390=CARTESIAN_POINT('Ctrl Pts',(-7.68587913412623,-5.36160575399376,
17.7479844753182));
#89391=CARTESIAN_POINT('Ctrl Pts',(-7.76179416352488,-5.25110520178583,
17.7456685424781));
#89392=CARTESIAN_POINT('Ctrl Pts',(-7.88080730734507,-5.06964914838692,
17.7419479200684));
#89393=CARTESIAN_POINT('Ctrl Pts',(-7.92537907135638,-4.99968328172741,
17.7405324801543));
#89394=CARTESIAN_POINT('Ctrl Pts',(-8.01271269076847,-4.85848953299843,
17.7377135355649));
#89395=CARTESIAN_POINT('Ctrl Pts',(-8.05546810646493,-4.7872663213259,17.7363101750378));
#89396=CARTESIAN_POINT('Ctrl Pts',(-8.16511258240989,-4.59898850408819,
17.7326468294348));
#89397=CARTESIAN_POINT('Ctrl Pts',(-8.23043242904693,-4.48104239159288,
17.7303983629533));
#89398=CARTESIAN_POINT('Ctrl Pts',(-8.44519726647871,-4.07269859987177,
17.7227502607937));
#89399=CARTESIAN_POINT('Ctrl Pts',(-8.58199585935785,-3.77592076526816,
17.7174303767798));
#89400=CARTESIAN_POINT('Ctrl Pts',(-8.76170886081674,-3.32552559871771,
17.7094574446755));
#89401=CARTESIAN_POINT('Ctrl Pts',(-8.81665846743111,-3.1769790456373,17.706841786847));
#89402=CARTESIAN_POINT('Ctrl Pts',(-8.88542812814894,-2.9755207694532,17.7032759598392));
#89403=CARTESIAN_POINT('Ctrl Pts',(-8.90258869274198,-2.92377691001589,
17.7023584285052));
#89404=CARTESIAN_POINT('Ctrl Pts',(-8.93228939684027,-2.83153461312139,
17.7007175813594));
#89405=CARTESIAN_POINT('Ctrl Pts',(-8.94500803018642,-2.7910953864332,17.6999963039132));
#89406=CARTESIAN_POINT('Ctrl Pts',(-8.97312511096158,-2.69952989921963,
17.6983591543055));
#89407=CARTESIAN_POINT('Ctrl Pts',(-8.98836184050942,-2.64835559195336,
17.6974415425835));
#89408=CARTESIAN_POINT('Ctrl Pts',(-9.08923736807116,-2.29865220910489,
17.6911593580062));
#89409=CARTESIAN_POINT('Ctrl Pts',(-9.16042570936088,-1.99615590881768,
17.6856746100559));
#89410=CARTESIAN_POINT('Ctrl Pts',(-9.24738045489873,-1.5221379244134,17.6772099419781));
#89411=CARTESIAN_POINT('Ctrl Pts',(-9.27366979599149,-1.35277413855341,
17.6742093367514));
#89412=CARTESIAN_POINT('Ctrl Pts',(-9.30307904527794,-1.12165193445107,
17.6701613101347));
#89413=CARTESIAN_POINT('Ctrl Pts',(-9.31025464449662,-1.06044389441446,
17.669093620974));
#89414=CARTESIAN_POINT('Ctrl Pts',(-9.327702919294,-0.897746231131952,17.6662677079331));
#89415=CARTESIAN_POINT('Ctrl Pts',(-9.33692305467132,-0.796151987863134,
17.6645156600135));
#89416=CARTESIAN_POINT('Ctrl Pts',(-9.35033546607144,-0.615669393400805,
17.661425569898));
#89417=CARTESIAN_POINT('Ctrl Pts',(-9.35519237750183,-0.536840519826683,
17.6600834659791));
#89418=CARTESIAN_POINT('Ctrl Pts',(-9.36364869020217,-0.364023800022639,
17.6571567877683));
#89419=CARTESIAN_POINT('Ctrl Pts',(-9.3668306914568,-0.270024021379157,
17.6555750100059));
#89420=CARTESIAN_POINT('Ctrl Pts',(-9.37244921469699,0.0290670400761349,
17.6505696804282));
#89421=CARTESIAN_POINT('Ctrl Pts',(-9.36956780917658,0.234197798430648,
17.6471792276701));
#89422=CARTESIAN_POINT('Ctrl Pts',(-9.34814447079211,0.690895122437159,
17.6396630215888));
#89423=CARTESIAN_POINT('Ctrl Pts',(-9.32617337359789,0.942141712008976,
17.6355508486332));
#89424=CARTESIAN_POINT('Ctrl Pts',(-9.28274444142092,1.28070425840881,17.6299221748402));
#89425=CARTESIAN_POINT('Ctrl Pts',(-9.27012730391731,1.369046194616,17.6284450033721));
#89426=CARTESIAN_POINT('Ctrl Pts',(-9.2455797347387,1.52497492148424,17.6258139309914));
#89427=CARTESIAN_POINT('Ctrl Pts',(-9.23416498448879,1.59263622613457,17.6246642674182));
#89428=CARTESIAN_POINT('Ctrl Pts',(-9.21441227425665,1.70235999137002,17.6227829179499));
#89429=CARTESIAN_POINT('Ctrl Pts',(-9.2065269247092,1.74450138629159,17.622056197817));
#89430=CARTESIAN_POINT('Ctrl Pts',(-9.18842549147059,1.83769771091373,17.6204388904723));
#89431=CARTESIAN_POINT('Ctrl Pts',(-9.17807255192514,1.88872446491027,17.6195468587525));
#89432=CARTESIAN_POINT('Ctrl Pts',(-9.14364260010235,2.05144842909699,17.6166841016798));
#89433=CARTESIAN_POINT('Ctrl Pts',(-9.11794764537212,2.16279247266174,17.6146980598199));
#89434=CARTESIAN_POINT('Ctrl Pts',(-9.03172707097941,2.50751054212063,17.60848999762));
#89435=CARTESIAN_POINT('Ctrl Pts',(-8.96422744525356,2.73903803209347,17.6042371945682));
#89436=CARTESIAN_POINT('Ctrl Pts',(-8.8155583916291,3.18428183696196,17.5960009448771));
#89437=CARTESIAN_POINT('Ctrl Pts',(-8.73534978439387,3.39814440108498,17.5920177556867));
#89438=CARTESIAN_POINT('Ctrl Pts',(-8.61129849737214,3.69539094008042,17.5864689864665));
#89439=CARTESIAN_POINT('Ctrl Pts',(-8.5738909715581,3.78137140125063,17.5848621231655));
#89440=CARTESIAN_POINT('Ctrl Pts',(-8.50258983866926,3.93875558063206,17.581917248113));
#89441=CARTESIAN_POINT('Ctrl Pts',(-8.4690710749203,4.01031976907668,17.5805767848049));
#89442=CARTESIAN_POINT('Ctrl Pts',(-8.39078039496613,4.17211381894889,17.5775419233537));
#89443=CARTESIAN_POINT('Ctrl Pts',(-8.34545074462236,4.26206303199321,17.5758516325593));
#89444=CARTESIAN_POINT('Ctrl Pts',(-8.15480909024632,4.6256525542636,17.5689986414954));
#89445=CARTESIAN_POINT('Ctrl Pts',(-7.99741806875747,4.89273723055219,17.5639232311556));
#89446=CARTESIAN_POINT('Ctrl Pts',(-7.69792564336745,5.34777710476087,17.5549937080992));
#89447=CARTESIAN_POINT('Ctrl Pts',(-7.56143022874022,5.53909300302034,17.5511420183421));
#89448=CARTESIAN_POINT('Ctrl Pts',(-7.38197849851632,5.77160577303791,17.5462304507517));
#89449=CARTESIAN_POINT('Ctrl Pts',(-7.34562996101493,5.81779685152484,17.5452427180747));
#89450=CARTESIAN_POINT('Ctrl Pts',(-7.28506001311455,5.89329541735242,17.543605792899));
#89451=CARTESIAN_POINT('Ctrl Pts',(-7.26109060063673,5.92280284624779,17.5429601787401));
#89452=CARTESIAN_POINT('Ctrl Pts',(-7.20217142363888,5.9944397671214,17.5413781864001));
#89453=CARTESIAN_POINT('Ctrl Pts',(-7.16703090961068,6.03641029581767,17.5404390969865));
#89454=CARTESIAN_POINT('Ctrl Pts',(-7.02390939662403,6.20433770297883,17.53663612949));
#89455=CARTESIAN_POINT('Ctrl Pts',(-6.91295983407911,6.32772436311716,17.5337376670905));
#89456=CARTESIAN_POINT('Ctrl Pts',(-6.61571769808706,6.64113264382029,17.5261598168459));
#89457=CARTESIAN_POINT('Ctrl Pts',(-6.42450354344367,6.82628142864941,17.5214674537071));
#89458=CARTESIAN_POINT('Ctrl Pts',(-6.13725192150899,7.08164673447656,17.5147571853769));
#89459=CARTESIAN_POINT('Ctrl Pts',(-6.04735193846027,7.15856942725955,17.5127010557886));
#89460=CARTESIAN_POINT('Ctrl Pts',(-5.87669772026817,7.29907982997101,17.5088826400314));
#89461=CARTESIAN_POINT('Ctrl Pts',(-5.79630704782713,7.36308136169744,17.5071174985878));
#89462=CARTESIAN_POINT('Ctrl Pts',(-5.65225519607771,7.47394413925783,17.5040134495763));
#89463=CARTESIAN_POINT('Ctrl Pts',(-5.58902317741581,7.52134627273996,17.5026703381065));
#89464=CARTESIAN_POINT('Ctrl Pts',(-5.44965948607934,7.62309282923207,17.4997512290324));
#89465=CARTESIAN_POINT('Ctrl Pts',(-5.37329833790121,7.6771086889815,17.4981779204531));
#89466=CARTESIAN_POINT('Ctrl Pts',(-4.96105298026001,7.95955596448136,17.489814956217));
#89467=CARTESIAN_POINT('Ctrl Pts',(-4.61139195497046,8.16710731926021,17.4831994402264));
#89468=CARTESIAN_POINT('Ctrl Pts',(-4.09779590051228,8.42843855321351,17.4737323081364));
#89469=CARTESIAN_POINT('Ctrl Pts',(-3.94415149332015,8.50142201912503,17.4709267787813));
#89470=CARTESIAN_POINT('Ctrl Pts',(-3.73798435551296,8.59256198411049,17.4671522037786));
#89471=CARTESIAN_POINT('Ctrl Pts',(-3.68716471958991,8.61449155809334,17.4662209372371));
#89472=CARTESIAN_POINT('Ctrl Pts',(-3.59716792531311,8.65238448829839,17.4645679384425));
#89473=CARTESIAN_POINT('Ctrl Pts',(-3.55807147983913,8.66853515562089,17.4638484218738));
#89474=CARTESIAN_POINT('Ctrl Pts',(-3.46049619639913,8.70807198395108,17.4620494472781));
#89475=CARTESIAN_POINT('Ctrl Pts',(-3.40188852154157,8.731134294211,17.4609662711997));
#89476=CARTESIAN_POINT('Ctrl Pts',(-3.05004679173551,8.86550472347874,17.4544569331904));
#89477=CARTESIAN_POINT('Ctrl Pts',(-2.7516073127372,8.9626232997902,17.4489151936215));
#89478=CARTESIAN_POINT('Ctrl Pts',(-2.289278927606,9.08780064158446,17.4405056123968));
#89479=CARTESIAN_POINT('Ctrl Pts',(-2.12858066178144,9.12677725577002,17.437612546485));
#89480=CARTESIAN_POINT('Ctrl Pts',(-1.84205614088508,9.18829297884701,17.4325233808913));
#89481=CARTESIAN_POINT('Ctrl Pts',(-1.71664166978723,9.21254797552443,17.4303188085686));
#89482=CARTESIAN_POINT('Ctrl Pts',(-1.50993939243815,9.24815633737036,17.4267248355999));
#89483=CARTESIAN_POINT('Ctrl Pts',(-1.42892894402909,9.26101909726844,17.4253261191149));
#89484=CARTESIAN_POINT('Ctrl Pts',(-1.27442953798112,9.28347485399893,17.4226766578634));
#89485=CARTESIAN_POINT('Ctrl Pts',(-1.20097517839325,9.29326286405183,17.4214247553364));
#89486=CARTESIAN_POINT('Ctrl Pts',(-0.998794625944924,9.31776689324801,
17.417998685079));
#89487=CARTESIAN_POINT('Ctrl Pts',(-0.869867223823576,9.33068602629054,
17.4158360257985));
#89488=CARTESIAN_POINT('Ctrl Pts',(-0.389845385362464,9.36875061026307,
17.4078466738288));
#89489=CARTESIAN_POINT('Ctrl Pts',(-0.0376895342458689,9.3767823092476,
17.4021202534462));
#89490=CARTESIAN_POINT('Ctrl Pts',(0.459198076892439,9.36011777438784,17.3939371295269));
#89491=CARTESIAN_POINT('Ctrl Pts',(0.604181764716027,9.35187851683964,17.3915352355229));
#89492=CARTESIAN_POINT('Ctrl Pts',(0.802143936256767,9.33600566197487,17.3882068704053));
#89493=CARTESIAN_POINT('Ctrl Pts',(0.8553355003856,9.331282751013,17.3873076833968));
#89494=CARTESIAN_POINT('Ctrl Pts',(0.950864154843593,9.32197702039714,17.3856819018984));
#89495=CARTESIAN_POINT('Ctrl Pts',(0.993215774129613,9.31755979942169,17.384957101502));
#89496=CARTESIAN_POINT('Ctrl Pts',(1.08994031614121,9.30680458690925,17.3832930709139));
#89497=CARTESIAN_POINT('Ctrl Pts',(1.14429071831867,9.30027850368848,17.3823518758648));
#89498=CARTESIAN_POINT('Ctrl Pts',(1.54549695993146,9.24853377581089,17.3753658993395));
#89499=CARTESIAN_POINT('Ctrl Pts',(1.88963550895892,9.18440066605291,17.3691734691346));
#89500=CARTESIAN_POINT('Ctrl Pts',(2.43983833349401,9.04962562656187,17.359240707693));
#89501=CARTESIAN_POINT('Ctrl Pts',(2.64844483369874,8.99078837493938,17.3554642978226));
#89502=CARTESIAN_POINT('Ctrl Pts',(2.9432811953222,8.8964771745061,17.3501331714831));
#89503=CARTESIAN_POINT('Ctrl Pts',(3.03131267439286,8.86686832175376,17.3485419562679));
#89504=CARTESIAN_POINT('Ctrl Pts',(3.19347262899132,8.80962957948602,17.3456116555802));
#89505=CARTESIAN_POINT('Ctrl Pts',(3.26771946954745,8.78236017605666,17.344270295258));
#89506=CARTESIAN_POINT('Ctrl Pts',(3.43684076487632,8.71780364758471,17.3412144874972));
#89507=CARTESIAN_POINT('Ctrl Pts',(3.5314699299078,8.67990178988407,17.3395043855483));
#89508=CARTESIAN_POINT('Ctrl Pts',(3.85125396758341,8.54572323888136,17.3337174454855));
#89509=CARTESIAN_POINT('Ctrl Pts',(4.0732459106679,8.44216861802731,17.329689109298));
#89510=CARTESIAN_POINT('Ctrl Pts',(4.29092662815677,8.33003803918537,17.3256735943175));
#89511=CARTESIAN_POINT('',(-5.44031476324441,-7.62919132931695,18.));
#89512=CARTESIAN_POINT('Origin',(0.,0.,18.));
#89513=CARTESIAN_POINT('',(-9.37025622235751,0.0001620501840075,17.8485898927132));
#89514=CARTESIAN_POINT('Ctrl Pts',(-9.37024999859875,0.000162049617987492,
17.848589892721));
#89515=CARTESIAN_POINT('Ctrl Pts',(-9.37025401433264,-0.232041092363098,
17.8525347710883));
#89516=CARTESIAN_POINT('Ctrl Pts',(-9.36162238595604,-0.464285151285067,
17.8564796494555));
#89517=CARTESIAN_POINT('Ctrl Pts',(-9.34437206291106,-0.695913652968009,
17.8604245278228));
#89518=CARTESIAN_POINT('Ctrl Pts',(-9.32712467813233,-0.927502701116926,
17.8643687342546));
#89519=CARTESIAN_POINT('Ctrl Pts',(-9.30126155031182,-1.15847611112298,
17.8683129406865));
#89520=CARTESIAN_POINT('Ctrl Pts',(-9.26685163678969,-1.38818075344252,
17.8722571471183));
#89521=CARTESIAN_POINT('Ctrl Pts',(-9.23122356614152,-1.62601724842557,
17.8763409837521));
#89522=CARTESIAN_POINT('Ctrl Pts',(-9.18643257651936,-1.86249318006461,
17.8804248203858));
#89523=CARTESIAN_POINT('Ctrl Pts',(-9.13261349805945,-2.09689192796442,
17.8845086570195));
#89524=CARTESIAN_POINT('Ctrl Pts',(-9.0806330980643,-2.32328266193568,17.8884529731953));
#89525=CARTESIAN_POINT('Ctrl Pts',(-9.02023131849495,-2.54773548938585,
17.8923972893711));
#89526=CARTESIAN_POINT('Ctrl Pts',(-8.95158132950295,-2.76961671785001,
17.8963416055469));
#89527=CARTESIAN_POINT('Ctrl Pts',(-8.8829280686371,-2.99150852122316,17.9002861097097));
#89528=CARTESIAN_POINT('Ctrl Pts',(-8.80602590278989,-3.21082820383465,
17.9042306138725));
#89529=CARTESIAN_POINT('Ctrl Pts',(-8.72109763885253,-3.42695798575075,
17.9081751180353));
#89530=CARTESIAN_POINT('Ctrl Pts',(-8.63614852834321,-3.64314081908745,
17.9121205904198));
#89531=CARTESIAN_POINT('Ctrl Pts',(-8.5431694923091,-3.85613191730517,17.9160660628043));
#89532=CARTESIAN_POINT('Ctrl Pts',(-8.44243160884847,-4.06533314654732,
17.9200115351888));
#89533=CARTESIAN_POINT('Ctrl Pts',(-8.43177899963791,-4.08745530024887,
17.9204287523668));
#89534=CARTESIAN_POINT('Ctrl Pts',(-8.42103967296831,-4.10953509567068,
17.9208459695449));
#89535=CARTESIAN_POINT('Ctrl Pts',(-8.41021397995651,-4.13157184057642,
17.921263186723));
#89536=CARTESIAN_POINT('Ctrl Pts',(-8.30662153564395,-4.34244427774887,
17.9252555913884));
#89537=CARTESIAN_POINT('Ctrl Pts',(-8.19508047047344,-4.54944676716263,
17.9292479960538));
#89538=CARTESIAN_POINT('Ctrl Pts',(-8.0759039439886,-4.75198490632803,17.9332404007192));
#89539=CARTESIAN_POINT('Ctrl Pts',(-7.95674906674446,-4.95448625303896,
17.9372320801367));
#89540=CARTESIAN_POINT('Ctrl Pts',(-7.82996163792674,-5.15252462967349,
17.9412237595541));
#89541=CARTESIAN_POINT('Ctrl Pts',(-7.69589996486297,-5.34553166610415,
17.9452154389716));
#89542=CARTESIAN_POINT('Ctrl Pts',(-7.56185645952786,-5.53851254666648,
17.9492065774459));
#89543=CARTESIAN_POINT('Ctrl Pts',(-7.42054083642917,-5.72646322075847,
17.9531977159202));
#89544=CARTESIAN_POINT('Ctrl Pts',(-7.27235438521001,-5.90884479051674,
17.9571888543944));
#89545=CARTESIAN_POINT('Ctrl Pts',(-7.12416940821138,-6.09122454586719,
17.9611799531632));
#89546=CARTESIAN_POINT('Ctrl Pts',(-6.96911391244025,-6.26803509066209,
17.965171051932));
#89547=CARTESIAN_POINT('Ctrl Pts',(-6.80762984841542,-6.43877013951139,
17.9691621507008));
#89548=CARTESIAN_POINT('Ctrl Pts',(-6.64615731476965,-6.60949299743743,
17.9731529644948));
#89549=CARTESIAN_POINT('Ctrl Pts',(-6.47825732118779,-6.77414102530206,
17.9771437782888));
#89550=CARTESIAN_POINT('Ctrl Pts',(-6.30440966688583,-6.93224377922304,
17.9811345920828));
#89551=CARTESIAN_POINT('Ctrl Pts',(-6.13054820256237,-7.09035909243013,
17.9851257228971));
#89552=CARTESIAN_POINT('Ctrl Pts',(-5.95073833798997,-7.24192790543682,
17.9891168537113));
#89553=CARTESIAN_POINT('Ctrl Pts',(-5.76549496927381,-7.38651831526724,
17.9931079845256));
#89554=CARTESIAN_POINT('Ctrl Pts',(-5.65886686284328,-7.46974613451433,
17.9954053230171));
#89555=CARTESIAN_POINT('Ctrl Pts',(-5.5504391147669,-7.55066254303808,17.9977026615085));
#89556=CARTESIAN_POINT('Ctrl Pts',(-5.44031476324441,-7.62919132931695,
18.));
#89557=CARTESIAN_POINT('Ctrl Pts',(4.29125029737042,8.33066558789285,17.5228836507406));
#89558=CARTESIAN_POINT('Ctrl Pts',(4.20937266281399,8.37289598640675,17.5244488072731));
#89559=CARTESIAN_POINT('Ctrl Pts',(2.7433241481266,9.10149525341159,17.5522595682313));
#89560=CARTESIAN_POINT('Ctrl Pts',(-0.473662841069232,9.74960156866327,
17.6063159336151));
#89561=CARTESIAN_POINT('Ctrl Pts',(-5.04583236791708,8.35587341299396,17.6850527468921));
#89562=CARTESIAN_POINT('Ctrl Pts',(-8.40806015501699,4.95813329461504,17.7637895601691));
#89563=CARTESIAN_POINT('Ctrl Pts',(-9.33992788001211,1.78304083363767,17.81830194184));
#89564=CARTESIAN_POINT('Ctrl Pts',(-9.37097584595092,0.119140517507502,
17.8465687190854));
#89565=CARTESIAN_POINT('Ctrl Pts',(-9.37090218672064,0.000162108931356462,
17.848589891905));
#89566=CARTESIAN_POINT('Ctrl Pts',(-4.05890219815148,8.44447251167999,3.66935213444816));
#89567=CARTESIAN_POINT('Ctrl Pts',(-5.45144634927424,7.77513520159967,3.69559773887382));
#89568=CARTESIAN_POINT('Ctrl Pts',(-7.89776706951283,5.73514866702576,3.74808894772514));
#89569=CARTESIAN_POINT('Ctrl Pts',(-9.67358643625363,1.29694711723465,3.82682576100211));
#89570=CARTESIAN_POINT('Ctrl Pts',(-9.12961484805542,-3.45099953375481,
3.90556257427908));
#89571=CARTESIAN_POINT('Ctrl Pts',(-6.39647197105479,-7.37203461182231,
3.98429938755606));
#89572=CARTESIAN_POINT('Ctrl Pts',(-2.12945660839726,-9.52497797369592,
4.06303620083303));
#89573=CARTESIAN_POINT('Ctrl Pts',(2.64817455363187,-9.39404484874638,4.14177301411));
#89574=CARTESIAN_POINT('Ctrl Pts',(6.79079602168952,-7.01038540771718,4.22050982738697));
#89575=CARTESIAN_POINT('Ctrl Pts',(9.30501602531431,-2.94571581100747,4.29924664066395));
#89576=CARTESIAN_POINT('Ctrl Pts',(9.58794458405767,1.82534318116471,4.37798345394092));
#89577=CARTESIAN_POINT('Ctrl Pts',(7.57173346773308,6.15868302513809,4.4567202672179));
#89578=CARTESIAN_POINT('Ctrl Pts',(3.73986123984316,9.01520910973077,4.53545708049487));
#89579=CARTESIAN_POINT('Ctrl Pts',(-0.988810284069998,9.70993258668408,
4.61419389377184));
#89580=CARTESIAN_POINT('Ctrl Pts',(-5.48037016060699,8.07626705693223,4.69293070704882));
#89581=CARTESIAN_POINT('Ctrl Pts',(-8.65776628439157,4.50595450829045,4.77166752032579));
#89582=CARTESIAN_POINT('Ctrl Pts',(-9.75907571166627,-0.144861728555519,
4.85040433360277));
#89583=CARTESIAN_POINT('Ctrl Pts',(-8.52021031990554,-4.76094110276756,
4.92914114687973));
#89584=CARTESIAN_POINT('Ctrl Pts',(-5.23824345717932,-8.23537182090993,
5.00787796015672));
#89585=CARTESIAN_POINT('Ctrl Pts',(-0.70017347004904,-9.73500390508311,
5.08661477343368));
#89586=CARTESIAN_POINT('Ctrl Pts',(4.00579442225045,-8.90023341090876,5.16535158671067));
#89587=CARTESIAN_POINT('Ctrl Pts',(7.75119395567349,-5.93123394107183,5.24408839998763));
#89588=CARTESIAN_POINT('Ctrl Pts',(9.63789809505959,-1.53995587317032,5.3228252132646));
#89589=CARTESIAN_POINT('Ctrl Pts',(9.21348514579648,3.22059548021945,5.40156202654158));
#89590=CARTESIAN_POINT('Ctrl Pts',(6.57972709342064,7.20886503988206,5.48029883981855));
#89591=CARTESIAN_POINT('Ctrl Pts',(2.36818521591906,9.46848681488684,5.55903565309553));
#89592=CARTESIAN_POINT('Ctrl Pts',(-2.41123497551512,9.45761543293126,5.63777246637249));
#89593=CARTESIAN_POINT('Ctrl Pts',(-6.61245374788223,7.17885779318626,5.71650927964948));
#89594=CARTESIAN_POINT('Ctrl Pts',(-9.22804101623034,3.17864794936077,5.79524609292644));
#89595=CARTESIAN_POINT('Ctrl Pts',(-9.63079276036606,-1.5837848938706,5.87398290620342));
#89596=CARTESIAN_POINT('Ctrl Pts',(-7.72413123801395,-5.96643447973725,
5.95271971948039));
#89597=CARTESIAN_POINT('Ctrl Pts',(-3.96526381766737,-8.9183645720204,6.03145653275737));
#89598=CARTESIAN_POINT('Ctrl Pts',(0.744452934971506,-9.73171791672532,
6.11019334603434));
#89599=CARTESIAN_POINT('Ctrl Pts',(5.27565380349995,-8.21145667520394,6.18893015931131));
#89600=CARTESIAN_POINT('Ctrl Pts',(8.54178073820683,-4.72213146825887,6.26766697258829));
#89601=CARTESIAN_POINT('Ctrl Pts',(9.75963374084516,-0.100464061641155,
6.34640378586526));
#89602=CARTESIAN_POINT('Ctrl Pts',(8.63717808998542,4.54529409664561,6.42514059914223));
#89603=CARTESIAN_POINT('Ctrl Pts',(5.44357272566864,8.10111472351062,6.50387741241921));
#89604=CARTESIAN_POINT('Ctrl Pts',(0.944627356376894,9.71433080251592,6.58261422569617));
#89605=CARTESIAN_POINT('Ctrl Pts',(-3.7808346666298,8.99810163349664,6.66135103897316));
#89606=CARTESIAN_POINT('Ctrl Pts',(-7.59967249422965,6.12417519047048,6.74008785225012));
#89607=CARTESIAN_POINT('Ctrl Pts',(-9.59614897362004,1.78170386406272,6.81882466552711));
#89608=CARTESIAN_POINT('Ctrl Pts',(-9.29151958371627,-2.98801064398065,
6.89756147880407));
#89609=CARTESIAN_POINT('Ctrl Pts',(-6.75883284418958,-7.04121597221882,
6.97629829208105));
#89610=CARTESIAN_POINT('Ctrl Pts',(-2.60541366604633,-9.40597487833683,
7.05503510535802));
#89611=CARTESIAN_POINT('Ctrl Pts',(2.17276995618375,-9.5152306593498,7.133771918635));
#89612=CARTESIAN_POINT('Ctrl Pts',(6.42993481218324,-7.34278435569223,7.21250873191196));
#89613=CARTESIAN_POINT('Ctrl Pts',(9.14523524150828,-3.40957712342747,7.29124554518895));
#89614=CARTESIAN_POINT('Ctrl Pts',(9.66755653428997,1.34122870511777,7.36998235846591));
#89615=CARTESIAN_POINT('Ctrl Pts',(7.87164880166345,5.77041497003424,7.44871917174289));
#89616=CARTESIAN_POINT('Ctrl Pts',(4.18816123796882,8.81588618505821,7.52745598501985));
#89617=CARTESIAN_POINT('Ctrl Pts',(-0.499625282810953,9.74735442876174,
7.60619279829684));
#89618=CARTESIAN_POINT('Ctrl Pts',(-5.0676042981128,8.34145853318671,7.6849296115738));
#89619=CARTESIAN_POINT('Ctrl Pts',(-8.42039855276698,4.93532491287903,7.76366642485078));
#89620=CARTESIAN_POINT('Ctrl Pts',(-9.75402568268881,0.34572643024801,7.84240323812776));
#89621=CARTESIAN_POINT('Ctrl Pts',(-8.74868894185552,-4.32677542539241,
7.92114005140473));
#89622=CARTESIAN_POINT('Ctrl Pts',(-5.64546277391199,-7.96173937349739,
7.9998768646817));
#89623=CARTESIAN_POINT('Ctrl Pts',(-1.18848443312888,-9.68752024696387,
8.07861367795868));
#89624=CARTESIAN_POINT('Ctrl Pts',(3.5534862011415,-9.0902849021041,8.15735049123564));
#89625=CARTESIAN_POINT('Ctrl Pts',(7.44334960193927,-6.31324722202728,8.23608730451263));
#89626=CARTESIAN_POINT('Ctrl Pts',(9.54833705892713,-2.02232618344405,8.31482411778959));
#89627=CARTESIAN_POINT('Ctrl Pts',(9.36368369138254,2.75353799880477,8.39356093106657));
#89628=CARTESIAN_POINT('Ctrl Pts',(6.93366840212465,6.86911830386571,8.47229774434354));
#89629=CARTESIAN_POINT('Ctrl Pts',(2.84099603035075,9.33752029923663,8.55103455762052));
#89630=CARTESIAN_POINT('Ctrl Pts',(-1.93293219291658,9.56683421622385,8.62977137089749));
#89631=CARTESIAN_POINT('Ctrl Pts',(-6.24335347956852,7.50207178799861,8.70850818417446));
#89632=CARTESIAN_POINT('Ctrl Pts',(-9.05665155821197,3.63835214571946,8.78724499745144));
#89633=CARTESIAN_POINT('Ctrl Pts',(-9.69821239996552,-1.09782513556562,
8.86598181072841));
#89634=CARTESIAN_POINT('Ctrl Pts',(-8.01419310154301,-5.57074974436163,
8.94471862400538));
#89635=CARTESIAN_POINT('Ctrl Pts',(-4.40841260138079,-8.70783797042137,
9.02345543728235));
#89636=CARTESIAN_POINT('Ctrl Pts',(0.254481970185954,-9.7568326166833,9.10219225055933));
#89637=CARTESIAN_POINT('Ctrl Pts',(4.85635310861981,-8.46619030423503,9.1809290638363));
#89638=CARTESIAN_POINT('Ctrl Pts',(8.2936964065283,-5.14540024677036,9.25966587711328));
#89639=CARTESIAN_POINT('Ctrl Pts',(9.74225508555788,-0.590770370826471,
9.33840269039025));
#89640=CARTESIAN_POINT('Ctrl Pts',(8.85467242089165,4.10552312157971,9.41713950366722));
#89641=CARTESIAN_POINT('Ctrl Pts',(5.84378605029053,7.81733384099428,9.4958763169442));
#89642=CARTESIAN_POINT('Ctrl Pts',(1.43159063205072,9.65458917020032,9.57461313022116));
#89643=CARTESIAN_POINT('Ctrl Pts',(-3.32389266290867,9.17672497945682,9.65334994349815));
#89644=CARTESIAN_POINT('Ctrl Pts',(-7.28232404292288,6.49833057923279,9.73208675677511));
#89645=CARTESIAN_POINT('Ctrl Pts',(-9.49449255818395,2.26167080843221,9.81082357005209));
#89646=CARTESIAN_POINT('Ctrl Pts',(-9.42993187596523,-2.51732568369289,
9.88956038332907));
#89647=CARTESIAN_POINT('Ctrl Pts',(-7.10412330707039,-6.69268076491505,
9.96829719660603));
#89648=CARTESIAN_POINT('Ctrl Pts',(-3.07478346922299,-9.26316632693798,
10.047034009883));
#89649=CARTESIAN_POINT('Ctrl Pts',(1.69187321388056,-9.61239350064688,10.12577082316));
#89650=CARTESIAN_POINT('Ctrl Pts',(6.05282763107886,-7.65661945322955,10.2045076364369));
#89651=CARTESIAN_POINT('Ctrl Pts',(8.96234593301987,-3.86482847743687,10.2832444497139));
#89652=CARTESIAN_POINT('Ctrl Pts',(9.72274098918695,0.853727966221407,10.3619812629909));
#89653=CARTESIAN_POINT('Ctrl Pts',(8.15167407896019,5.36756495009922,10.4407180762679));
#89654=CARTESIAN_POINT('Ctrl Pts',(4.6258787543211,8.59428819236621,10.5194548895448));
#89655=CARTESIAN_POINT('Ctrl Pts',(-0.00917787727279524,9.76014649222507,
10.5981917028218));
#89656=CARTESIAN_POINT('Ctrl Pts',(-4.64203370234336,8.5855731835116,10.6769285160988));
#89657=CARTESIAN_POINT('Ctrl Pts',(-8.16175434919945,5.35222474550992,10.7556653293757));
#89658=CARTESIAN_POINT('Ctrl Pts',(-9.72432938604995,0.83544106598262,10.8344021426527));
#89659=CARTESIAN_POINT('Ctrl Pts',(-8.9550615673234,-3.88167697117781,10.9131389559297));
#89660=CARTESIAN_POINT('Ctrl Pts',(-6.03841725526543,-7.6679893606106,10.9918757692066));
#89661=CARTESIAN_POINT('Ctrl Pts',(-1.67379236000308,-9.61555837789571,
11.0706125824837));
#89662=CARTESIAN_POINT('Ctrl Pts',(3.09219910784695,-9.25736725319652,11.1493493957606));
#89663=CARTESIAN_POINT('Ctrl Pts',(7.11669755222962,-6.67930832745529,11.2280862090376));
#89664=CARTESIAN_POINT('Ctrl Pts',(9.43464949004539,-2.49958652242944,11.3068230223146));
#89665=CARTESIAN_POINT('Ctrl Pts',(9.49022228223122,2.27952293626696,11.3855598355915));
#89666=CARTESIAN_POINT('Ctrl Pts',(7.27008986656942,6.51201482761895,11.4642966488685));
#89667=CARTESIAN_POINT('Ctrl Pts',(3.30662827706433,9.18295993786554,11.5430334621455));
#89668=CARTESIAN_POINT('Ctrl Pts',(-1.44974531879287,9.65187972851728,11.6217702754224));
#89669=CARTESIAN_POINT('Ctrl Pts',(-5.85847763988178,7.80632970903293,11.7005070886994));
#89670=CARTESIAN_POINT('Ctrl Pts',(-8.86237794769954,4.08886303209752,11.7792439019764));
#89671=CARTESIAN_POINT('Ctrl Pts',(-9.74112680492853,-0.609091416314159,
11.8579807152534));
#89672=CARTESIAN_POINT('Ctrl Pts',(-8.28400487420087,-5.16098895826575,
11.9367175285304));
#89673=CARTESIAN_POINT('Ctrl Pts',(-4.84042230288836,-8.47530859100871,
12.0154543418073));
#89674=CARTESIAN_POINT('Ctrl Pts',(-0.236132014171883,-9.75729396169901,
12.0941911550843));
#89675=CARTESIAN_POINT('Ctrl Pts',(4.42478148508795,-8.6995317455796,12.1729279683613));
#89676=CARTESIAN_POINT('Ctrl Pts',(8.02465574103572,-5.555667738534,12.2516647816382));
#89677=CARTESIAN_POINT('Ctrl Pts',(9.7002599095219,-1.07958393413709,12.3304015949152));
#89678=CARTESIAN_POINT('Ctrl Pts',(9.04979295584846,3.65537839893496,12.4091384081922));
#89679=CARTESIAN_POINT('Ctrl Pts',(6.22923342192782,7.51380028735541,12.4878752214692));
#89680=CARTESIAN_POINT('Ctrl Pts',(1.91493659528631,9.57045252948668,12.5666120347461));
#89681=CARTESIAN_POINT('Ctrl Pts',(-2.85855191865109,9.33216077398482,12.6453488480231));
#89682=CARTESIAN_POINT('Ctrl Pts',(-6.94657477175178,6.85606612596367,12.7240856613001));
#89683=CARTESIAN_POINT('Ctrl Pts',(-9.36884566302788,2.73592301161571,12.802822474577));
#89684=CARTESIAN_POINT('Ctrl Pts',(-9.54451681903836,-2.04027999897532,
12.881559287854));
#89685=CARTESIAN_POINT('Ctrl Pts',(-7.43146322387599,-6.32723463570806,
12.960296101131));
#89686=CARTESIAN_POINT('Ctrl Pts',(-3.53638397561942,-9.09695180596813,
13.039032914408));
#89687=CARTESIAN_POINT('Ctrl Pts',(1.20670148270599,-9.68526795265676,13.1177697276849));
#89688=CARTESIAN_POINT('Ctrl Pts',(5.66042629521671,-7.95110796930491,13.1965065409619));
#89689=CARTESIAN_POINT('Ctrl Pts',(8.75681076146596,-4.3103142659206,13.2752433542389));
#89690=CARTESIAN_POINT('Ctrl Pts',(9.7533582311345,0.364070045850259,13.3539801675159));
#89691=CARTESIAN_POINT('Ctrl Pts',(8.41110188140746,4.9511522824196,13.4327169807928));
#89692=CARTESIAN_POINT('Ctrl Pts',(5.05190769966626,8.35097433699671,13.5114537940698));
#89693=CARTESIAN_POINT('Ctrl Pts',(0.481292718728248,9.74827682731795,13.5901906073468));
#89694=CARTESIAN_POINT('Ctrl Pts',(-4.20473371559156,8.80799399205588,13.6689274206238));
#89695=CARTESIAN_POINT('Ctrl Pts',(-7.88248720017234,5.75560069169532,13.7476642339007));
#89696=CARTESIAN_POINT('Ctrl Pts',(-9.67006186293461,1.32304472718883,13.8264010471777));
#89697=CARTESIAN_POINT('Ctrl Pts',(-9.13880673570443,-3.42677037902575,
13.9051378604547));
#89698=CARTESIAN_POINT('Ctrl Pts',(-6.4161139936889,-7.35486403702436,13.9838746737316));
#89699=CARTESIAN_POINT('Ctrl Pts',(-2.15487098431875,-9.51930012259652,
14.0626114870086));
#89700=CARTESIAN_POINT('Ctrl Pts',(2.62309871231088,-9.4010582876928,14.1413483002856));
#89701=CARTESIAN_POINT('Ctrl Pts',(6.77206318411236,-7.02849230016758,14.2200851135626));
#89702=CARTESIAN_POINT('Ctrl Pts',(9.29712265162198,-2.97053095991647,14.2988219268396));
#89703=CARTESIAN_POINT('Ctrl Pts',(9.59278118340142,1.79974802417014,14.3775587401165));
#89704=CARTESIAN_POINT('Ctrl Pts',(7.58814142420382,6.13845693227594,14.4562955533935));
#89705=CARTESIAN_POINT('Ctrl Pts',(3.76390540652066,9.00519627070335,14.5350323666704));
#89706=CARTESIAN_POINT('Ctrl Pts',(-0.962895259358665,9.71253707857168,
14.6137691799475));
#89707=CARTESIAN_POINT('Ctrl Pts',(-5.4587987248176,8.09086276394888,14.6925059932244));
#89708=CARTESIAN_POINT('Ctrl Pts',(-8.64571107107811,4.52904226725275,14.7712428065014));
#89709=CARTESIAN_POINT('Ctrl Pts',(-9.7594275400581,-0.118818657963835,
14.8499796197784));
#89710=CARTESIAN_POINT('Ctrl Pts',(-8.53288480140027,-4.73818749620118,
14.9287164330553));
#89711=CARTESIAN_POINT('Ctrl Pts',(-5.26020132936178,-8.22136398401781,
15.0074532463323));
#89712=CARTESIAN_POINT('Ctrl Pts',(-0.726149345231843,-9.73310078605705,
15.0861900596093));
#89713=CARTESIAN_POINT('Ctrl Pts',(3.98202941880643,-8.91089139709851,15.1649268728862));
#89714=CARTESIAN_POINT('Ctrl Pts',(7.73533854789984,-5.95189728847034,15.2436636861632));
#89715=CARTESIAN_POINT('Ctrl Pts',(9.63375432524542,-1.56566962796746,15.3224004994402));
#89716=CARTESIAN_POINT('Ctrl Pts',(9.22204666848199,3.19599734472079,15.4011373127172));
#89717=CARTESIAN_POINT('Ctrl Pts',(6.59894090044666,7.19128102465388,15.4798741259942));
#89718=CARTESIAN_POINT('Ctrl Pts',(2.39344393789276,9.46213347502903,15.5586109392711));
#89719=CARTESIAN_POINT('Ctrl Pts',(-2.3859882468475,9.46401626525843,15.6373477525481));
#89720=CARTESIAN_POINT('Ctrl Pts',(-6.59327304475852,7.19647791216796,15.7160845658251));
#89721=CARTESIAN_POINT('Ctrl Pts',(-9.21952577002525,3.20326214334899,15.7948213791021));
#89722=CARTESIAN_POINT('Ctrl Pts',(-9.63498488216568,-1.55807897862842,
15.873558192379));
#89723=CARTESIAN_POINT('Ctrl Pts',(-7.74002547913806,-5.94580098598721,
15.952295005656));
#89724=CARTESIAN_POINT('Ctrl Pts',(-3.98904882300254,-8.90775130277384,
16.031031818933));
#89725=CARTESIAN_POINT('Ctrl Pts',(0.718480684171045,-9.73366987764925,
16.1097686322099));
#89726=CARTESIAN_POINT('Ctrl Pts',(5.25372231584012,-8.22550579692042,16.1885054454869));
#89727=CARTESIAN_POINT('Ctrl Pts',(8.52914906873457,-4.74490884446967,16.2672422587639));
#89728=CARTESIAN_POINT('Ctrl Pts',(9.75933089707706,-0.126507799846194,
16.3459790720408));
#89729=CARTESIAN_POINT('Ctrl Pts',(8.64927669253978,4.52222915143409,16.4247158853178));
#89730=CARTESIAN_POINT('Ctrl Pts',(5.46517159297118,8.08655941555927,16.5034526985948));
#89731=CARTESIAN_POINT('Ctrl Pts',(0.970547195120261,9.71177543306001,16.5821895118718));
#89732=CARTESIAN_POINT('Ctrl Pts',(-3.75680929901023,9.0081589371075,16.6609263251487));
#89733=CARTESIAN_POINT('Ctrl Pts',(-7.58330275007955,6.14443353614328,16.7396631384257));
#89734=CARTESIAN_POINT('Ctrl Pts',(-9.5913602389158,1.80730529622961,16.8183999517027));
#89735=CARTESIAN_POINT('Ctrl Pts',(-9.29946015674463,-2.96320499781051,
16.8971367649797));
#89736=CARTESIAN_POINT('Ctrl Pts',(-6.77759864659425,-7.02315479381199,
16.9758735782566));
#89737=CARTESIAN_POINT('Ctrl Pts',(-2.63050470092249,-9.39898833036069,
17.0546103915336));
#89738=CARTESIAN_POINT('Ctrl Pts',(2.14737027682777,-9.52099565589916,17.1333472048106));
#89739=CARTESIAN_POINT('Ctrl Pts',(6.41031741029837,-7.35991542137126,17.2120840180876));
#89740=CARTESIAN_POINT('Ctrl Pts',(9.13610385335678,-3.43397225624563,17.2908208313645));
#89741=CARTESIAN_POINT('Ctrl Pts',(9.67110162026351,1.31543084999252,17.3695576446415));
#89742=CARTESIAN_POINT('Ctrl Pts',(7.88701871315299,5.74937822649567,17.4482944579185));
#89743=CARTESIAN_POINT('Ctrl Pts',(4.21167337024702,8.80469843374058,17.5270312711955));
#89744=CARTESIAN_POINT('Ctrl Pts',(-0.473614874379152,9.74861425009761,
17.6057680844724));
#89745=CARTESIAN_POINT('Ctrl Pts',(-5.04532138867952,8.35502723390706,17.6845048977494));
#89746=CARTESIAN_POINT('Ctrl Pts',(-8.40720869110497,4.95763119645048,17.7632417110264));
#89747=CARTESIAN_POINT('Ctrl Pts',(-9.75304724334012,0.372042784836709,
17.8419785243033));
#89748=CARTESIAN_POINT('Ctrl Pts',(-8.76018319001389,-4.30436209043516,
17.9207211504403));
#89749=CARTESIAN_POINT('Ctrl Pts',(-6.69727900373269,-6.7319066656312,17.9732181721515));
#89750=CARTESIAN_POINT('Ctrl Pts',(-5.43892795783426,-7.62901472696143,
17.9994695894372));
#89751=CARTESIAN_POINT('Ctrl Pts',(-4.14169175030982,8.61671467552761,3.77968718924866));
#89752=CARTESIAN_POINT('Ctrl Pts',(-5.5626396670332,7.9337248718815,3.80593279367432));
#89753=CARTESIAN_POINT('Ctrl Pts',(-8.05885806575159,5.85212866962865,3.85842400252563));
#89754=CARTESIAN_POINT('Ctrl Pts',(-9.8708988743772,1.32340098721405,3.93716081580261));
#89755=CARTESIAN_POINT('Ctrl Pts',(-9.31583188107312,-3.52138967669254,
4.01589762907957));
#89756=CARTESIAN_POINT('Ctrl Pts',(-6.52694100529715,-7.52240222705742,
4.09463444235655));
#89757=CARTESIAN_POINT('Ctrl Pts',(-2.17289119990582,-9.71925924046788,
4.17337125563352));
#89758=CARTESIAN_POINT('Ctrl Pts',(2.70218945091914,-9.585655468568,4.2521080689105));
#89759=CARTESIAN_POINT('Ctrl Pts',(6.92930809564152,-7.15337645308571,4.33084488218747));
#89760=CARTESIAN_POINT('Ctrl Pts',(9.49481072150404,-3.00579966641305,4.40958169546445));
#89761=CARTESIAN_POINT('Ctrl Pts',(9.78351018270518,1.86257476180559,4.48831850874142));
#89762=CARTESIAN_POINT('Ctrl Pts',(7.72617434663415,6.28430187098475,4.56705532201839));
#89763=CARTESIAN_POINT('Ctrl Pts',(3.81614330382639,9.19909260540809,4.64579213529537));
#89764=CARTESIAN_POINT('Ctrl Pts',(-1.00897907764797,9.90798637834857,4.72452894857234));
#89765=CARTESIAN_POINT('Ctrl Pts',(-5.59215343822949,8.24099892286858,4.80326576184931));
#89766=CARTESIAN_POINT('Ctrl Pts',(-8.8343590078385,4.59786260007872,4.88200257512628));
#89767=CARTESIAN_POINT('Ctrl Pts',(-9.95813187715264,-0.147816477659208,
4.96073938840327));
#89768=CARTESIAN_POINT('Ctrl Pts',(-8.69399731014175,-4.85805016391465,
5.03947620168022));
#89769=CARTESIAN_POINT('Ctrl Pts',(-5.34508806903368,-8.40334895157867,
5.11821301495721));
#89770=CARTESIAN_POINT('Ctrl Pts',(-0.714454929711948,-9.93356907719506,
5.19694982823418));
#89771=CARTESIAN_POINT('Ctrl Pts',(4.08750073348098,-9.08177174374406,5.27568664151115));
#89772=CARTESIAN_POINT('Ctrl Pts',(7.90929529563061,-6.05221350100097,5.35442345478813));
#89773=CARTESIAN_POINT('Ctrl Pts',(9.83448259699735,-1.57136640016983,5.43316026806509));
#89774=CARTESIAN_POINT('Ctrl Pts',(9.4014128838399,3.28628606463705,5.51189708134208));
#89775=CARTESIAN_POINT('Ctrl Pts',(6.71393398799339,7.35590448037256,5.59063389461904));
#89776=CARTESIAN_POINT('Ctrl Pts',(2.41648916212977,9.66161582976643,5.66937070789602));
#89777=CARTESIAN_POINT('Ctrl Pts',(-2.46041700898769,9.65052270390096,5.74810752117299));
#89778=CARTESIAN_POINT('Ctrl Pts',(-6.74732816902602,7.325285174949,5.82684433444997));
#89779=CARTESIAN_POINT('Ctrl Pts',(-9.41626565080774,3.24348292870976,5.90558114772694));
#89780=CARTESIAN_POINT('Ctrl Pts',(-9.82723233457501,-1.61608940274454,
5.98431796100391));
#89781=CARTESIAN_POINT('Ctrl Pts',(-7.88168057889206,-6.08813202612909,
6.06305477428089));
#89782=CARTESIAN_POINT('Ctrl Pts',(-4.04614342491783,-9.10027272670288,
6.14179158755786));
#89783=CARTESIAN_POINT('Ctrl Pts',(0.759637564233405,-9.93021606443235,
6.22052840083484));
#89784=CARTESIAN_POINT('Ctrl Pts',(5.38326147533128,-8.37894600791499,6.29926521411181));
#89785=CARTESIAN_POINT('Ctrl Pts',(8.71600770092424,-4.81844892810506,6.37800202738878));
#89786=CARTESIAN_POINT('Ctrl Pts',(9.95870128846972,-0.102513230176209,
6.45673884066575));
#89787=CARTESIAN_POINT('Ctrl Pts',(8.813350875402,4.63800459921958,6.53547565394273));
#89788=CARTESIAN_POINT('Ctrl Pts',(5.55460544488635,8.2663534080614,6.6142124672197));
#89789=CARTESIAN_POINT('Ctrl Pts',(0.963894949428697,9.91247430472313,6.69294928049667));
#89790=CARTESIAN_POINT('Ctrl Pts',(-3.85795246685114,9.18163618745848,6.77168609377365));
#89791=CARTESIAN_POINT('Ctrl Pts',(-7.75468324630784,6.24909017895906,6.85042290705061));
#89792=CARTESIAN_POINT('Ctrl Pts',(-9.79188191745213,1.81804533221925,6.92915972032761));
#89793=CARTESIAN_POINT('Ctrl Pts',(-9.48103899257435,-3.0489571883867,7.00789653360456));
#89794=CARTESIAN_POINT('Ctrl Pts',(-6.89669296423347,-7.18483586955351,
7.08663334688156));
#89795=CARTESIAN_POINT('Ctrl Pts',(-2.65855636820297,-9.59782883533654,
7.1653701601585));
#89796=CARTESIAN_POINT('Ctrl Pts',(2.21708801137054,-9.70931310985319,7.2441069734355));
#89797=CARTESIAN_POINT('Ctrl Pts',(6.56108638901859,-7.49255535255931,7.32284378671246));
#89798=CARTESIAN_POINT('Ctrl Pts',(9.33177088416849,-3.47912237219609,7.40158059998944));
#89799=CARTESIAN_POINT('Ctrl Pts',(9.86474598031898,1.36858578799824,7.48031741326641));
#89800=CARTESIAN_POINT('Ctrl Pts',(8.03220706279482,5.88811430049716,7.55905422654339));
#89801=CARTESIAN_POINT('Ctrl Pts',(4.27358729071193,8.99570408495051,7.63779103982036));
#89802=CARTESIAN_POINT('Ctrl Pts',(-0.509816154970842,9.94617151488255,
7.71652785309733));
#89803=CARTESIAN_POINT('Ctrl Pts',(-5.17096837782566,8.51159951776734,7.7952646663743));
#89804=CARTESIAN_POINT('Ctrl Pts',(-8.59214967933906,5.03599088592941,7.87400147965128));
#89805=CARTESIAN_POINT('Ctrl Pts',(-9.9529788425798,0.352778222809711,7.95273829292826));
#89806=CARTESIAN_POINT('Ctrl Pts',(-8.92713621752499,-4.41502879595184,
8.03147510620521));
#89807=CARTESIAN_POINT('Ctrl Pts',(-5.76061345061262,-8.12413521477522,
8.11021191948221));
#89808=CARTESIAN_POINT('Ctrl Pts',(-1.21272598642642,-9.88511689345029,
8.18894873275916));
#89809=CARTESIAN_POINT('Ctrl Pts',(3.62596676776546,-9.27569972101245,8.26768554603615));
#89810=CARTESIAN_POINT('Ctrl Pts',(7.59517183120687,-6.44201871852076,8.34642235931312));
#89811=CARTESIAN_POINT('Ctrl Pts',(9.7430947816743,-2.06357563240139,8.42515917259009));
#89812=CARTESIAN_POINT('Ctrl Pts',(9.5546750337497,2.80970199750268,8.50389598586707));
#89813=CARTESIAN_POINT('Ctrl Pts',(7.07509464838597,7.00922791980045,8.58263279914403));
#89814=CARTESIAN_POINT('Ctrl Pts',(2.89894391319049,9.52797798609473,8.66136961242102));
#89815=CARTESIAN_POINT('Ctrl Pts',(-1.97235826991761,9.76196922605361,8.74010642569798));
#89816=CARTESIAN_POINT('Ctrl Pts',(-6.37069935126138,7.65509177548957,8.81884323897496));
#89817=CARTESIAN_POINT('Ctrl Pts',(-9.24138035677726,3.71256372560816,8.89758005225193));
#89818=CARTESIAN_POINT('Ctrl Pts',(-9.89602713462341,-1.12021750840057,
8.97631686552891));
#89819=CARTESIAN_POINT('Ctrl Pts',(-8.17765884311456,-5.68437649711558,
9.05505367880587));
#89820=CARTESIAN_POINT('Ctrl Pts',(-4.49833112791335,-8.88545200757823,
9.13379049208287));
#89821=CARTESIAN_POINT('Ctrl Pts',(0.259672646707696,-9.95584302969276,
9.21252730535982));
#89822=CARTESIAN_POINT('Ctrl Pts',(4.95540829136565,-8.638875446561,9.2912641186368));
#89823=CARTESIAN_POINT('Ctrl Pts',(8.46286318555204,-5.25035113282513,9.37000093191377));
#89824=CARTESIAN_POINT('Ctrl Pts',(9.94096816021956,-0.602820332131643,
9.44873774519074));
#89825=CARTESIAN_POINT('Ctrl Pts',(9.03528144482141,4.18926360213774,9.52747455846772));
#89826=CARTESIAN_POINT('Ctrl Pts',(5.96298193291937,7.97678423821325,9.60621137174469));
#89827=CARTESIAN_POINT('Ctrl Pts',(1.46079082991595,9.85151412050775,9.68494818502168));
#89828=CARTESIAN_POINT('Ctrl Pts',(-3.39169020311791,9.36390291926418,9.76368499829864));
#89829=CARTESIAN_POINT('Ctrl Pts',(-7.43086182894297,6.63087722661854,9.84242181157562));
#89830=CARTESIAN_POINT('Ctrl Pts',(-9.6881520130042,2.30780217701878,9.92115862485258));
#89831=CARTESIAN_POINT('Ctrl Pts',(-9.62227448457758,-2.56867165258183,
9.99989543812957));
#89832=CARTESIAN_POINT('Ctrl Pts',(-7.24902632723626,-6.82919157897666,
10.0786322514066));
#89833=CARTESIAN_POINT('Ctrl Pts',(-3.13749992159695,-9.45210741355117,
10.1573690646836));
#89834=CARTESIAN_POINT('Ctrl Pts',(1.72638240352046,-9.80845778459312,10.2361058779605));
#89835=CARTESIAN_POINT('Ctrl Pts',(6.17628734121842,-7.81279175417053,10.3148426912375));
#89836=CARTESIAN_POINT('Ctrl Pts',(9.14515117686653,-3.94365950198376,10.3935795045144));
#89837=CARTESIAN_POINT('Ctrl Pts',(9.92105603422868,0.871141481634682,10.4723163177914));
#89838=CARTESIAN_POINT('Ctrl Pts',(8.31794402422896,5.47704733639615,10.5510531310684));
#89839=CARTESIAN_POINT('Ctrl Pts',(4.72023294462003,8.76958615123051,10.6297899443454));
#89840=CARTESIAN_POINT('Ctrl Pts',(-0.00936507871595034,9.95922449845521,
10.7085267576224));
#89841=CARTESIAN_POINT('Ctrl Pts',(-4.73671740561069,8.76069338207398,10.7872635708993));
#89842=CARTESIAN_POINT('Ctrl Pts',(-8.32822990204828,5.46139423718515,10.8660003841763));
#89843=CARTESIAN_POINT('Ctrl Pts',(-9.92267682967102,0.852481582932977,
10.9447371974533));
#89844=CARTESIAN_POINT('Ctrl Pts',(-9.13771823174039,-3.9608516549663,11.0234740107302));
#89845=CARTESIAN_POINT('Ctrl Pts',(-6.16158303652923,-7.82439357389984,
11.1022108240072));
#89846=CARTESIAN_POINT('Ctrl Pts',(-1.707932753914,-9.81168721593988,11.1809476372842));
#89847=CARTESIAN_POINT('Ctrl Pts',(3.15527078753404,-9.44619005592542,11.2596844505612));
#89848=CARTESIAN_POINT('Ctrl Pts',(7.2618570496582,-6.81554638350144,11.3384212638381));
#89849=CARTESIAN_POINT('Ctrl Pts',(9.62708832397628,-2.5505706651041,11.4171580771151));
#89850=CARTESIAN_POINT('Ctrl Pts',(9.6837946361024,2.32601843525042,11.4958948903921));
#89851=CARTESIAN_POINT('Ctrl Pts',(7.41837811172063,6.64484059303715,11.5746317036691));
#89852=CARTESIAN_POINT('Ctrl Pts',(3.37407367506801,9.37026505231005,11.653368516946));
#89853=CARTESIAN_POINT('Ctrl Pts',(-1.47931581835828,9.84874941425992,11.732105330223));
#89854=CARTESIAN_POINT('Ctrl Pts',(-5.97797318731239,7.96555565463604,11.8108421435));
#89855=CARTESIAN_POINT('Ctrl Pts',(-9.04314414149503,4.17226369630137,11.8895789567769));
#89856=CARTESIAN_POINT('Ctrl Pts',(-9.93981686601572,-0.621515072543928,
11.9683157700539));
#89857=CARTESIAN_POINT('Ctrl Pts',(-8.45297397474363,-5.26625780774518,
12.0470525833309));
#89858=CARTESIAN_POINT('Ctrl Pts',(-4.93915254450293,-8.64817971930859,
12.1257893966079));
#89859=CARTESIAN_POINT('Ctrl Pts',(-0.240948406080153,-9.95631378477686,
12.2045262098849));
#89860=CARTESIAN_POINT('Ctrl Pts',(4.51503388824163,-8.87697636041459,12.2832630231618));
#89861=CARTESIAN_POINT('Ctrl Pts',(8.18833488938468,-5.66898686315428,12.3619998364388));
#89862=CARTESIAN_POINT('Ctrl Pts',(9.89811640729478,-1.10160424062915,12.4407366497158));
#89863=CARTESIAN_POINT('Ctrl Pts',(9.23438185929177,3.72993726383072,12.5194734629927));
#89864=CARTESIAN_POINT('Ctrl Pts',(6.35629128637356,7.66705950140611,12.5982102762697));
#89865=CARTESIAN_POINT('Ctrl Pts',(1.95399561553263,9.76566134216263,12.6769470895467));
#89866=CARTESIAN_POINT('Ctrl Pts',(-2.91685788948089,9.52250914244261,12.7556839028237));
#89867=CARTESIAN_POINT('Ctrl Pts',(-7.08826426962872,6.99590951622696,12.8344207161006));
#89868=CARTESIAN_POINT('Ctrl Pts',(-9.55994229428842,2.79172771688173,12.9131575293776));
#89869=CARTESIAN_POINT('Ctrl Pts',(-9.73919662023581,-2.08189565245661,
12.9918943426546));
#89870=CARTESIAN_POINT('Ctrl Pts',(-7.58304300632705,-6.45629143390576,
13.0706311559316));
#89871=CARTESIAN_POINT('Ctrl Pts',(-3.60851570762686,-9.28250260991829,
13.1493679692085));
#89872=CARTESIAN_POINT('Ctrl Pts',(1.23131460972035,-9.88281865902736,13.2281047824855));
#89873=CARTESIAN_POINT('Ctrl Pts',(5.77588218331859,-8.1132869615066,13.3068415957625));
#89874=CARTESIAN_POINT('Ctrl Pts',(8.93542369813816,-4.39823187770733,13.3855784090395));
#89875=CARTESIAN_POINT('Ctrl Pts',(9.95229777699576,0.371495993699875,13.4643152223164));
#89876=CARTESIAN_POINT('Ctrl Pts',(8.58266338348975,5.05214108681008,13.5430520355934));
#89877=CARTESIAN_POINT('Ctrl Pts',(5.15495161538101,8.5213094157184,13.6217888488704));
#89878=CARTESIAN_POINT('Ctrl Pts',(0.491109661018408,9.94711272763029,13.7005256621473));
#89879=CARTESIAN_POINT('Ctrl Pts',(-4.2904977976671,8.98765091464637,13.7792624754243));
#89880=CARTESIAN_POINT('Ctrl Pts',(-8.04326653244926,5.87299785487033,13.8579992887013));
#89881=CARTESIAN_POINT('Ctrl Pts',(-9.86730241022852,1.35003091091588,13.9367361019783));
#89882=CARTESIAN_POINT('Ctrl Pts',(-9.32521125593535,-3.49666631915414,
14.0154729152552));
#89883=CARTESIAN_POINT('Ctrl Pts',(-6.54698366686712,-7.50488142352065,
14.0942097285322));
#89884=CARTESIAN_POINT('Ctrl Pts',(-2.19882395362953,-9.71346557806612,
14.1729465418092));
#89885=CARTESIAN_POINT('Ctrl Pts',(2.67660213689652,-9.59281196084291,14.2516833550862));
#89886=CARTESIAN_POINT('Ctrl Pts',(6.9101931638039,-7.17185267237469,14.3304201683631));
#89887=CARTESIAN_POINT('Ctrl Pts',(9.48675634642733,-3.0311209706726,14.4091569816401));
#89888=CARTESIAN_POINT('Ctrl Pts',(9.78844543431353,1.83645753961172,14.4878937949171));
#89889=CARTESIAN_POINT('Ctrl Pts',(7.74291697669439,6.26366322588849,14.566630608194));
#89890=CARTESIAN_POINT('Ctrl Pts',(3.84067790010628,9.18887553419707,14.645367421471));
#89891=CARTESIAN_POINT('Ctrl Pts',(-0.98253546338574,9.91064399413679,14.724104234748));
#89892=CARTESIAN_POINT('Ctrl Pts',(-5.57014200920517,8.25589233896724,14.802841048025));
#89893=CARTESIAN_POINT('Ctrl Pts',(-8.82205790397076,4.62142128076604,14.8815778613019));
#89894=CARTESIAN_POINT('Ctrl Pts',(-9.95849088179891,-0.121242205760894,
14.9603146745789));
#89895=CARTESIAN_POINT('Ctrl Pts',(-8.70693031342283,-4.83483245133989,
15.0390514878559));
#89896=CARTESIAN_POINT('Ctrl Pts',(-5.36749381660599,-8.38905539640943,
15.1177883011329));
#89897=CARTESIAN_POINT('Ctrl Pts',(-0.740960635614568,-9.93162714019209,
15.1965251144098));
#89898=CARTESIAN_POINT('Ctrl Pts',(4.06325099453557,-9.09264712120377,15.2752619276868));
#89899=CARTESIAN_POINT('Ctrl Pts',(7.89311648462012,-6.07329831932775,15.3539987409638));
#89900=CARTESIAN_POINT('Ctrl Pts',(9.83025430658368,-1.59760463920927,15.4327355542408));
#89901=CARTESIAN_POINT('Ctrl Pts',(9.41014903616523,3.26118620021702,15.5114723675177));
#89902=CARTESIAN_POINT('Ctrl Pts',(6.73353969962842,7.33796180344845,15.5902091807947));
#89903=CARTESIAN_POINT('Ctrl Pts',(2.44226308702735,9.65513290064143,15.6689459940717));
#89904=CARTESIAN_POINT('Ctrl Pts',(-2.43465532202399,9.65705409420066,15.7476828073487));
#89905=CARTESIAN_POINT('Ctrl Pts',(-6.72775623651459,7.34326469203596,15.8264196206256));
#89906=CARTESIAN_POINT('Ctrl Pts',(-9.40757671886562,3.26859917916485,15.9051564339026));
#89907=CARTESIAN_POINT('Ctrl Pts',(-9.83150996321104,-1.5898591631637,15.9838932471796));
#89908=CARTESIAN_POINT('Ctrl Pts',(-7.89789901533805,-6.06707767037656,
16.0626300604565));
#89909=CARTESIAN_POINT('Ctrl Pts',(-4.07041357373357,-9.0894429782792,16.1413668737335));
#89910=CARTESIAN_POINT('Ctrl Pts',(0.733135556639757,-9.93220783956288,
16.2201036870105));
#89911=CARTESIAN_POINT('Ctrl Pts',(5.36088265044753,-8.39328168999638,16.2988405002875));
#89912=CARTESIAN_POINT('Ctrl Pts',(8.70311838290376,-4.84169089515441,16.3775773135644));
#89913=CARTESIAN_POINT('Ctrl Pts',(9.95839226758806,-0.129088183305203,
16.4563141268414));
#89914=CARTESIAN_POINT('Ctrl Pts',(8.82569625352232,4.61446919761579,16.5350509401184));
#89915=CARTESIAN_POINT('Ctrl Pts',(5.57664486494524,8.25150121504901,16.6137877533954));
#89916=CARTESIAN_POINT('Ctrl Pts',(0.990343475914901,9.90986681331834,16.6925245666723));
#89917=CARTESIAN_POINT('Ctrl Pts',(-3.83343705307411,9.1918986301984,16.7712613799493));
#89918=CARTESIAN_POINT('Ctrl Pts',(-7.73797960798613,6.26976173472755,16.8499981932263));
#89919=CARTESIAN_POINT('Ctrl Pts',(-9.7869955067798,1.84416895758031,16.9287350065032));
#89920=CARTESIAN_POINT('Ctrl Pts',(-9.4891415297134,-3.02364558069367,17.0074718197802));
#89921=CARTESIAN_POINT('Ctrl Pts',(-6.9158415332832,-7.16640629673887,17.0862086330572));
#89922=CARTESIAN_POINT('Ctrl Pts',(-2.68415918568418,-9.59069978252784,
17.1649454463342));
#89923=CARTESIAN_POINT('Ctrl Pts',(2.19117025397864,-9.71519569521335,17.2436822596111));
#89924=CARTESIAN_POINT('Ctrl Pts',(6.54106885038804,-7.51003584110843,17.3224190728881));
#89925=CARTESIAN_POINT('Ctrl Pts',(9.32245324281387,-3.50401509328376,17.4011558861651));
#89926=CARTESIAN_POINT('Ctrl Pts',(9.86836337551943,1.34226173323373,17.479892699442));
#89927=CARTESIAN_POINT('Ctrl Pts',(8.04789047483866,5.86664846985783,17.5586295127191));
#89928=CARTESIAN_POINT('Ctrl Pts',(4.29757900067065,8.98428813672743,17.637366325996));
#89929=CARTESIAN_POINT('Ctrl Pts',(-0.483275211443491,9.94745703283269,
17.716103139273));
#89930=CARTESIAN_POINT('Ctrl Pts',(-5.14823096320779,8.52544497969089,17.7948399525499));
#89931=CARTESIAN_POINT('Ctrl Pts',(-8.57869078366569,5.05875215144844,17.873576765827));
#89932=CARTESIAN_POINT('Ctrl Pts',(-9.95198044597383,0.379631352887077,
17.9523135791039));
#89933=CARTESIAN_POINT('Ctrl Pts',(-8.93886491421426,-4.39215829551661,
18.0310562052408));
#89934=CARTESIAN_POINT('Ctrl Pts',(-6.83388360821196,-6.86921757158827,
18.0835532269521));
#89935=CARTESIAN_POINT('Ctrl Pts',(-5.54986593758053,-7.78462397345723,
18.1098046442377));
#89936=CARTESIAN_POINT('Ctrl Pts',(-4.22448130246814,8.78895683937523,3.89002224404915));
#89937=CARTESIAN_POINT('Ctrl Pts',(-5.67383298479217,8.09231454216333,3.91626784847481));
#89938=CARTESIAN_POINT('Ctrl Pts',(-8.21994906199031,5.96910867223154,3.96875905732613));
#89939=CARTESIAN_POINT('Ctrl Pts',(-10.0682113125008,1.34985485719344,4.0474958706031));
#89940=CARTESIAN_POINT('Ctrl Pts',(-9.50204891409078,-3.59177981963027,
4.12623268388007));
#89941=CARTESIAN_POINT('Ctrl Pts',(-6.65741003953953,-7.67276984229252,
4.20496949715705));
#89942=CARTESIAN_POINT('Ctrl Pts',(-2.21632579141437,-9.91354050723984,
4.28370631043402));
#89943=CARTESIAN_POINT('Ctrl Pts',(2.75620434820641,-9.77726608838962,4.362443123711));
#89944=CARTESIAN_POINT('Ctrl Pts',(7.06782016959352,-7.29636749845425,4.44117993698797));
#89945=CARTESIAN_POINT('Ctrl Pts',(9.68460541769376,-3.06588352181864,4.51991675026494));
#89946=CARTESIAN_POINT('Ctrl Pts',(9.97907578135268,1.89980634244646,4.59865356354192));
#89947=CARTESIAN_POINT('Ctrl Pts',(7.88061522553522,6.40992071683142,4.67739037681889));
#89948=CARTESIAN_POINT('Ctrl Pts',(3.89242536780961,9.3829761010854,4.75612719009586));
#89949=CARTESIAN_POINT('Ctrl Pts',(-1.02914787122592,10.1060401700131,4.83486400337284));
#89950=CARTESIAN_POINT('Ctrl Pts',(-5.703936715852,8.40573078880492,4.9136008166498));
#89951=CARTESIAN_POINT('Ctrl Pts',(-9.01095173128544,4.68977069186698,4.99233762992679));
#89952=CARTESIAN_POINT('Ctrl Pts',(-10.157188042639,-0.150771226762893,
5.07107444320375));
#89953=CARTESIAN_POINT('Ctrl Pts',(-8.86778430037797,-4.95515922506173,
5.14981125648073));
#89954=CARTESIAN_POINT('Ctrl Pts',(-5.45193268088805,-8.57132608224742,
5.2285480697577));
#89955=CARTESIAN_POINT('Ctrl Pts',(-0.728736389374847,-10.1321342493071,
5.30728488303467));
#89956=CARTESIAN_POINT('Ctrl Pts',(4.16920704471151,-9.26331007657935,5.38602169631165));
#89957=CARTESIAN_POINT('Ctrl Pts',(8.06739663558773,-6.1731930609301,5.46475850958863));
#89958=CARTESIAN_POINT('Ctrl Pts',(10.0310670989351,-1.60277692716936,5.54349532286559));
#89959=CARTESIAN_POINT('Ctrl Pts',(9.58934062188332,3.35197664905467,5.62223213614258));
#89960=CARTESIAN_POINT('Ctrl Pts',(6.84814088256617,7.50294392086303,5.70096894941953));
#89961=CARTESIAN_POINT('Ctrl Pts',(2.46479310834046,9.85474484464604,5.77970576269653));
#89962=CARTESIAN_POINT('Ctrl Pts',(-2.50959904246025,9.84342997487063,5.85844257597348));
#89963=CARTESIAN_POINT('Ctrl Pts',(-6.8822025901698,7.47171255671175,5.93717938925047));
#89964=CARTESIAN_POINT('Ctrl Pts',(-9.60449028538516,3.30831790805872,6.01591620252743));
#89965=CARTESIAN_POINT('Ctrl Pts',(-10.0236719087839,-1.64839391161847,
6.09465301580442));
#89966=CARTESIAN_POINT('Ctrl Pts',(-8.03922991977018,-6.20982957252095,
6.17338982908138));
#89967=CARTESIAN_POINT('Ctrl Pts',(-4.12702303216825,-9.28218088138534,
6.25212664235836));
#89968=CARTESIAN_POINT('Ctrl Pts',(0.774822193495284,-10.1287142121394,
6.33086345563533));
#89969=CARTESIAN_POINT('Ctrl Pts',(5.49086914716262,-8.54643534062606,6.40960026891231));
#89970=CARTESIAN_POINT('Ctrl Pts',(8.89023466364162,-4.91476638795123,6.48833708218927));
#89971=CARTESIAN_POINT('Ctrl Pts',(10.1577688360944,-0.104562398711278,
6.56707389546626));
#89972=CARTESIAN_POINT('Ctrl Pts',(8.98952366081856,4.73071510179355,6.64581070874322));
#89973=CARTESIAN_POINT('Ctrl Pts',(5.66563816410407,8.43159209261217,6.7245475220202));
#89974=CARTESIAN_POINT('Ctrl Pts',(0.983162542480492,10.1106178069303,6.80328433529717));
#89975=CARTESIAN_POINT('Ctrl Pts',(-3.93507026707246,9.36517074142033,6.88202114857415));
#89976=CARTESIAN_POINT('Ctrl Pts',(-7.90969399838605,6.37400516744763,6.96075796185111));
#89977=CARTESIAN_POINT('Ctrl Pts',(-9.98761486128421,1.85438680037579,7.0394947751281));
#89978=CARTESIAN_POINT('Ctrl Pts',(-9.67055840143241,-3.10990373279276,
7.11823158840506));
#89979=CARTESIAN_POINT('Ctrl Pts',(-7.03455308427736,-7.32845576688822,
7.19696840168204));
#89980=CARTESIAN_POINT('Ctrl Pts',(-2.71169907035961,-9.78968279233623,
7.275705214959));
#89981=CARTESIAN_POINT('Ctrl Pts',(2.26140606655735,-9.90339556035661,7.35444202823599));
#89982=CARTESIAN_POINT('Ctrl Pts',(6.6922379658539,-7.64232634942638,7.43317884151296));
#89983=CARTESIAN_POINT('Ctrl Pts',(9.51830652682872,-3.54866762096472,7.51191565478993));
#89984=CARTESIAN_POINT('Ctrl Pts',(10.061935426348,1.39594287087871,7.59065246806691));
#89985=CARTESIAN_POINT('Ctrl Pts',(8.1927653239262,6.00581363096009,7.66938928134388));
#89986=CARTESIAN_POINT('Ctrl Pts',(4.35901334345506,9.17552198484281,7.74812609462085));
#89987=CARTESIAN_POINT('Ctrl Pts',(-0.520007027130731,10.1449886010034,
7.82686290789783));
#89988=CARTESIAN_POINT('Ctrl Pts',(-5.2743324575385,8.68174050234795,7.9055997211748));
#89989=CARTESIAN_POINT('Ctrl Pts',(-8.7639008059111,5.13665685897979,7.98433653445178));
#89990=CARTESIAN_POINT('Ctrl Pts',(-10.1519320024708,0.359830015371412,
8.06307334772874));
#89991=CARTESIAN_POINT('Ctrl Pts',(-9.10558349319444,-4.50328216651126,
8.14181016100572));
#89992=CARTESIAN_POINT('Ctrl Pts',(-5.87576412731326,-8.28653105605306,
8.2205469742827));
#89993=CARTESIAN_POINT('Ctrl Pts',(-1.23696753972395,-10.0827135399367,
8.29928378755967));
#89994=CARTESIAN_POINT('Ctrl Pts',(3.69844733438944,-9.46111453992081,8.37802060083665));
#89995=CARTESIAN_POINT('Ctrl Pts',(7.74699406047446,-6.57079021501422,8.45675741411361));
#89996=CARTESIAN_POINT('Ctrl Pts',(9.93785250442149,-2.10482508135873,8.53549422739059));
#89997=CARTESIAN_POINT('Ctrl Pts',(9.74566637611686,2.86586599620061,8.61423104066756));
#89998=CARTESIAN_POINT('Ctrl Pts',(7.21652089464729,7.1493375357352,8.69296785394453));
#89999=CARTESIAN_POINT('Ctrl Pts',(2.95689179603023,9.71843567295284,8.77170466722151));
#90000=CARTESIAN_POINT('Ctrl Pts',(-2.01178434691864,9.95710423588336,8.85044148049848));
#90001=CARTESIAN_POINT('Ctrl Pts',(-6.49804522295423,7.80811176298054,8.92917829377545));
#90002=CARTESIAN_POINT('Ctrl Pts',(-9.42610915534255,3.78677530549685,9.00791510705244));
#90003=CARTESIAN_POINT('Ctrl Pts',(-10.0938418692813,-1.14260988123551,
9.08665192032941));
#90004=CARTESIAN_POINT('Ctrl Pts',(-8.34112458468613,-5.79800324986954,
9.16538873360637));
#90005=CARTESIAN_POINT('Ctrl Pts',(-4.58824965444592,-9.06306604473511,
9.24412554688336));
#90006=CARTESIAN_POINT('Ctrl Pts',(0.264863323229445,-10.1548534427022,
9.32286236016032));
#90007=CARTESIAN_POINT('Ctrl Pts',(5.05446347411148,-8.81156058888697,9.4015991734373));
#90008=CARTESIAN_POINT('Ctrl Pts',(8.6320299645758,-5.35530201887989,9.48033598671427));
#90009=CARTESIAN_POINT('Ctrl Pts',(10.1396812348812,-0.614870293436814,
9.55907279999125));
#90010=CARTESIAN_POINT('Ctrl Pts',(9.21589046875117,4.27300408269577,9.63780961326821));
#90011=CARTESIAN_POINT('Ctrl Pts',(6.0821778155482,8.13623463543219,9.71654642654519));
#90012=CARTESIAN_POINT('Ctrl Pts',(1.48999102778118,10.0484390708152,9.79528323982216));
#90013=CARTESIAN_POINT('Ctrl Pts',(-3.45948774332716,9.55108085907153,9.87402005309914));
#90014=CARTESIAN_POINT('Ctrl Pts',(-7.57939961496306,6.76342387400428,9.95275686637611));
#90015=CARTESIAN_POINT('Ctrl Pts',(-9.88181146782447,2.35393354560535,10.0314936796531));
#90016=CARTESIAN_POINT('Ctrl Pts',(-9.81461709318993,-2.62001762147078,
10.11023049293));
#90017=CARTESIAN_POINT('Ctrl Pts',(-7.39392934740214,-6.96570239303823,
10.188967306207));
#90018=CARTESIAN_POINT('Ctrl Pts',(-3.2002163739709,-9.64104850016438,10.267704119484));
#90019=CARTESIAN_POINT('Ctrl Pts',(1.76089159316035,-10.0045220685393,10.346440932761));
#90020=CARTESIAN_POINT('Ctrl Pts',(6.299747051358,-7.96896405511154,10.4251777460379));
#90021=CARTESIAN_POINT('Ctrl Pts',(9.32795642071318,-4.02249052653063,10.5039145593149));
#90022=CARTESIAN_POINT('Ctrl Pts',(10.1193710792704,0.888554997047943,10.5826513725919));
#90023=CARTESIAN_POINT('Ctrl Pts',(8.48421396949771,5.58652972269309,10.6613881858689));
#90024=CARTESIAN_POINT('Ctrl Pts',(4.81458713491896,8.94488411009478,10.7401249991458));
#90025=CARTESIAN_POINT('Ctrl Pts',(-0.00955228015910545,10.1583025046853,
10.8188618124228));
#90026=CARTESIAN_POINT('Ctrl Pts',(-4.83140110887802,8.93581358063637,10.8975986256998));
#90027=CARTESIAN_POINT('Ctrl Pts',(-8.49470545489712,5.57056372886038,10.9763354389768));
#90028=CARTESIAN_POINT('Ctrl Pts',(-10.1210242732921,0.869522099883329,
11.0550722522537));
#90029=CARTESIAN_POINT('Ctrl Pts',(-9.32037489615738,-4.04002633875481,
11.1338090655307));
#90030=CARTESIAN_POINT('Ctrl Pts',(-6.28474881779303,-7.98079778718909,
11.2125458788077));
#90031=CARTESIAN_POINT('Ctrl Pts',(-1.74207314782492,-10.007816053984,11.2912826920847));
#90032=CARTESIAN_POINT('Ctrl Pts',(3.21834246722113,-9.63501285865432,11.3700195053616));
#90033=CARTESIAN_POINT('Ctrl Pts',(7.40701654708679,-6.95178443954758,11.4487563186386));
#90034=CARTESIAN_POINT('Ctrl Pts',(9.81952715790716,-2.60155480777876,11.5274931319156));
#90035=CARTESIAN_POINT('Ctrl Pts',(9.87736698997358,2.37251393423389,11.6062299451925));
#90036=CARTESIAN_POINT('Ctrl Pts',(7.56666635687184,6.77766635845533,11.6849667584695));
#90037=CARTESIAN_POINT('Ctrl Pts',(3.44151907307169,9.55757016675457,11.7637035717465));
#90038=CARTESIAN_POINT('Ctrl Pts',(-1.50888631792369,10.0456191000026,11.8424403850235));
#90039=CARTESIAN_POINT('Ctrl Pts',(-6.09746873474301,8.12478160023917,11.9211771983004));
#90040=CARTESIAN_POINT('Ctrl Pts',(-9.22391033529052,4.25566436050519,11.9999140115774));
#90041=CARTESIAN_POINT('Ctrl Pts',(-10.138506927103,-0.633938728773694,
12.0786508248544));
#90042=CARTESIAN_POINT('Ctrl Pts',(-8.62194307528639,-5.37152665722461,
12.1573876381314));
#90043=CARTESIAN_POINT('Ctrl Pts',(-5.03788278611751,-8.82105084760849,
12.2361244514083));
#90044=CARTESIAN_POINT('Ctrl Pts',(-0.245764797988416,-10.1553336078547,
12.3148612646853));
#90045=CARTESIAN_POINT('Ctrl Pts',(4.60528629139531,-9.05442097524958,12.3935980779623));
#90046=CARTESIAN_POINT('Ctrl Pts',(8.35201403773365,-5.78230598777455,12.4723348912392));
#90047=CARTESIAN_POINT('Ctrl Pts',(10.0959729050677,-1.12362454712121,12.5510717045162));
#90048=CARTESIAN_POINT('Ctrl Pts',(9.41897076273508,3.80449612872647,12.6298085177932));
#90049=CARTESIAN_POINT('Ctrl Pts',(6.48334915081932,7.82031871545681,12.7085453310702));
#90050=CARTESIAN_POINT('Ctrl Pts',(1.99305463577895,9.96087015483855,12.7872821443471));
#90051=CARTESIAN_POINT('Ctrl Pts',(-2.97516386031069,9.7128575109004,12.8660189576241));
#90052=CARTESIAN_POINT('Ctrl Pts',(-7.22995376750567,7.13575290649022,12.9447557709011));
#90053=CARTESIAN_POINT('Ctrl Pts',(-9.75103892554896,2.84753242214774,13.0234925841781));
#90054=CARTESIAN_POINT('Ctrl Pts',(-9.93387642143324,-2.12351130593791,
13.102229397455));
#90055=CARTESIAN_POINT('Ctrl Pts',(-7.73462278877812,-6.58534823210344,
13.180966210732));
#90056=CARTESIAN_POINT('Ctrl Pts',(-3.68064743963431,-9.46805341386847,
13.259703024009));
#90057=CARTESIAN_POINT('Ctrl Pts',(1.25592773673471,-10.0803693653979,13.338439837286));
#90058=CARTESIAN_POINT('Ctrl Pts',(5.89133807142048,-8.2754659537083,13.4171766505629));
#90059=CARTESIAN_POINT('Ctrl Pts',(9.11403663481036,-4.48614948949405,13.4959134638399));
#90060=CARTESIAN_POINT('Ctrl Pts',(10.1512373228571,0.378921941549486,13.5746502771169));
#90061=CARTESIAN_POINT('Ctrl Pts',(8.75422488557203,5.15312989120056,13.6533870903938));
#90062=CARTESIAN_POINT('Ctrl Pts',(5.25799553109575,8.69164449444008,13.7321239036708));
#90063=CARTESIAN_POINT('Ctrl Pts',(0.500926603308566,10.1459486279426,13.8108607169478));
#90064=CARTESIAN_POINT('Ctrl Pts',(-4.37626187974265,9.16730783723688,13.8895975302248));
#90065=CARTESIAN_POINT('Ctrl Pts',(-8.20404586472617,5.99039501804534,13.9683343435018));
#90066=CARTESIAN_POINT('Ctrl Pts',(-10.0645429575225,1.37701709464294,14.0470711567787));
#90067=CARTESIAN_POINT('Ctrl Pts',(-9.51161577616627,-3.56656225928252,
14.1258079700557));
#90068=CARTESIAN_POINT('Ctrl Pts',(-6.67785334004534,-7.65489881001693,
14.2045447833327));
#90069=CARTESIAN_POINT('Ctrl Pts',(-2.24277692294032,-9.90763103353571,
14.2832815966096));
#90070=CARTESIAN_POINT('Ctrl Pts',(2.73010556148216,-9.78456563399303,14.3620184098866));
#90071=CARTESIAN_POINT('Ctrl Pts',(7.04832314349544,-7.3152130445818,14.4407552231636));
#90072=CARTESIAN_POINT('Ctrl Pts',(9.67639004123265,-3.09171098142872,14.5194920364405));
#90073=CARTESIAN_POINT('Ctrl Pts',(9.98410968522563,1.87316705505327,14.5982288497175));
#90074=CARTESIAN_POINT('Ctrl Pts',(7.89769252918495,6.38886951950104,14.6769656629945));
#90075=CARTESIAN_POINT('Ctrl Pts',(3.91745039369191,9.37255479769078,14.7557024762715));
#90076=CARTESIAN_POINT('Ctrl Pts',(-1.00217566741281,10.1087509097019,14.8344392895485));
#90077=CARTESIAN_POINT('Ctrl Pts',(-5.68148529359275,8.4209219139856,14.9131761028254));
#90078=CARTESIAN_POINT('Ctrl Pts',(-8.99840473686339,4.71380029427931,14.9919129161024));
#90079=CARTESIAN_POINT('Ctrl Pts',(-10.1575542235398,-0.123665753557948,
15.0706497293794));
#90080=CARTESIAN_POINT('Ctrl Pts',(-8.88097582544536,-4.93147740647859,
15.1493865426563));
#90081=CARTESIAN_POINT('Ctrl Pts',(-5.47478630385019,-8.55674680880107,
15.2281233559333));
#90082=CARTESIAN_POINT('Ctrl Pts',(-0.755771925997289,-10.1301534943271,
15.3068601692103));
#90083=CARTESIAN_POINT('Ctrl Pts',(4.1444725702647,-9.27440284530902,15.3855969824873));
#90084=CARTESIAN_POINT('Ctrl Pts',(8.05089442134039,-6.19469935018516,15.4643337957642));
#90085=CARTESIAN_POINT('Ctrl Pts',(10.0267542879219,-1.62953965045109,15.5430706090412));
#90086=CARTESIAN_POINT('Ctrl Pts',(9.59825140384847,3.32637505571324,15.6218074223182));
#90087=CARTESIAN_POINT('Ctrl Pts',(6.86813849881018,7.48464258224303,15.7005442355952));
#90088=CARTESIAN_POINT('Ctrl Pts',(2.49108223616196,9.84813232625381,15.7792810488721));
#90089=CARTESIAN_POINT('Ctrl Pts',(-2.4833223972005,9.8500919231429,15.8580178621491));
#90090=CARTESIAN_POINT('Ctrl Pts',(-6.86223942827068,7.49005147190398,15.9367546754261));
#90091=CARTESIAN_POINT('Ctrl Pts',(-9.59562766770601,3.33393621498071,16.0154914887031));
#90092=CARTESIAN_POINT('Ctrl Pts',(-10.0280350442564,-1.62163934769899,
16.09422830198));
#90093=CARTESIAN_POINT('Ctrl Pts',(-8.05577255153804,-6.18835435476593,
16.172965115257));
#90094=CARTESIAN_POINT('Ctrl Pts',(-4.15177832446459,-9.27113465378456,
16.251701928534));
#90095=CARTESIAN_POINT('Ctrl Pts',(0.747790429108468,-10.1307458014765,
16.3304387418109));
#90096=CARTESIAN_POINT('Ctrl Pts',(5.46804298505493,-8.56105758307237,16.4091755550879));
#90097=CARTESIAN_POINT('Ctrl Pts',(8.87708769707297,-4.93847294583914,16.4879123683649));
#90098=CARTESIAN_POINT('Ctrl Pts',(10.1574536380991,-0.131668566764218,
16.5666491816419));
#90099=CARTESIAN_POINT('Ctrl Pts',(9.00211581450489,4.70670924379752,16.6453859949188));
#90100=CARTESIAN_POINT('Ctrl Pts',(5.68811813691929,8.41644301453876,16.7241228081958));
#90101=CARTESIAN_POINT('Ctrl Pts',(1.01013975670955,10.1079581935767,16.8028596214728));
#90102=CARTESIAN_POINT('Ctrl Pts',(-3.91006480713798,9.37563832328931,16.8815964347498));
#90103=CARTESIAN_POINT('Ctrl Pts',(-7.8926564658927,6.39508993331182,16.9603332480267));
#90104=CARTESIAN_POINT('Ctrl Pts',(-9.98263077464382,1.88103261893102,17.0390700613037));
#90105=CARTESIAN_POINT('Ctrl Pts',(-9.67882290268214,-3.08408616357684,
17.1178068745807));
#90106=CARTESIAN_POINT('Ctrl Pts',(-7.05408441997216,-7.30965779966574,
17.1965436878577));
#90107=CARTESIAN_POINT('Ctrl Pts',(-2.73781367044585,-9.78241123469498,
17.2752805011346));
#90108=CARTESIAN_POINT('Ctrl Pts',(2.2349702311295,-9.90939573452754,17.3540173144116));
#90109=CARTESIAN_POINT('Ctrl Pts',(6.6718202904777,-7.66015626084561,17.4327541276886));
#90110=CARTESIAN_POINT('Ctrl Pts',(9.50880263227094,-3.57405793032188,17.5114909409656));
#90111=CARTESIAN_POINT('Ctrl Pts',(10.0656251307754,1.36909261647494,17.5902277542425));
#90112=CARTESIAN_POINT('Ctrl Pts',(8.20876223652433,5.98391871322,17.6689645675195));
#90113=CARTESIAN_POINT('Ctrl Pts',(4.38348463109427,9.16387783971426,17.7477013807964));
#90114=CARTESIAN_POINT('Ctrl Pts',(-0.492935548507827,10.1462998155679,
17.8264381940735));
#90115=CARTESIAN_POINT('Ctrl Pts',(-5.25114053773606,8.6958627254747,17.9051750073504));
#90116=CARTESIAN_POINT('Ctrl Pts',(-8.7501728762264,5.15987310644641,17.9839118206274));
#90117=CARTESIAN_POINT('Ctrl Pts',(-10.1509136486076,0.387219920937437,
18.0626486339044));
#90118=CARTESIAN_POINT('Ctrl Pts',(-9.11754663841461,-4.47995450059806,
18.1413912600413));
#90119=CARTESIAN_POINT('Ctrl Pts',(-6.97048821269124,-7.00652847754534,
18.1938882817526));
#90120=CARTESIAN_POINT('Ctrl Pts',(-5.66080391732681,-7.94023321995303,
18.2201396990381));
#90121=CARTESIAN_POINT('Ctrl Pts',(-4.30727085462648,8.96119900322285,4.00035729884965));
#90122=CARTESIAN_POINT('Ctrl Pts',(-5.78502630255113,8.25090421244517,4.02660290327531));
#90123=CARTESIAN_POINT('Ctrl Pts',(-8.38104005822907,6.08608867483443,4.07909411212662));
#90124=CARTESIAN_POINT('Ctrl Pts',(-10.2655237506244,1.37630872717284,4.1578309254036));
#90125=CARTESIAN_POINT('Ctrl Pts',(-9.68826594710846,-3.662169962568,4.23656773868056));
#90126=CARTESIAN_POINT('Ctrl Pts',(-6.7878790737819,-7.82313745752762,4.31530455195755));
#90127=CARTESIAN_POINT('Ctrl Pts',(-2.25976038292293,-10.1078217740118,
4.39404136523451));
#90128=CARTESIAN_POINT('Ctrl Pts',(2.8102192454937,-9.96887670821123,4.47277817851149));
#90129=CARTESIAN_POINT('Ctrl Pts',(7.20633224354552,-7.43935854382279,4.55151499178846));
#90130=CARTESIAN_POINT('Ctrl Pts',(9.87440011388349,-3.12596737722422,4.63025180506544));
#90131=CARTESIAN_POINT('Ctrl Pts',(10.1746413800002,1.93703792308732,4.70898861834241));
#90132=CARTESIAN_POINT('Ctrl Pts',(8.03505610443629,6.5355395626781,4.78772543161938));
#90133=CARTESIAN_POINT('Ctrl Pts',(3.96870743179283,9.56685959676272,4.86646224489636));
#90134=CARTESIAN_POINT('Ctrl Pts',(-1.04931666480389,10.3040939616776,4.94519905817333));
#90135=CARTESIAN_POINT('Ctrl Pts',(-5.8157199934745,8.57046265474128,5.0239358714503));
#90136=CARTESIAN_POINT('Ctrl Pts',(-9.18754445473239,4.78167878365525,5.10267268472728));
#90137=CARTESIAN_POINT('Ctrl Pts',(-10.3562442081254,-0.15372597586658,
5.18140949800426));
#90138=CARTESIAN_POINT('Ctrl Pts',(-9.04157129061419,-5.0522682862088,5.26014631128122));
#90139=CARTESIAN_POINT('Ctrl Pts',(-5.5587772927424,-8.73930321291617,5.3388831245582));
#90140=CARTESIAN_POINT('Ctrl Pts',(-0.74301784903776,-10.330699421419,5.41761993783518));
#90141=CARTESIAN_POINT('Ctrl Pts',(4.25091335594205,-9.44484840941464,5.49635675111214));
#90142=CARTESIAN_POINT('Ctrl Pts',(8.22549797554484,-6.29417262085923,5.57509356438912));
#90143=CARTESIAN_POINT('Ctrl Pts',(10.2276516008729,-1.63418745416888,5.65383037766609));
#90144=CARTESIAN_POINT('Ctrl Pts',(9.77726835992674,3.41766723347228,5.73256719094306));
#90145=CARTESIAN_POINT('Ctrl Pts',(6.98234777713893,7.64998336135349,5.81130400422005));
#90146=CARTESIAN_POINT('Ctrl Pts',(2.51309705455117,10.0478738595257,5.89004081749701));
#90147=CARTESIAN_POINT('Ctrl Pts',(-2.55878107593283,10.0363372458403,5.96877763077398));
#90148=CARTESIAN_POINT('Ctrl Pts',(-7.01707701131357,7.6181399384745,6.04751444405097));
#90149=CARTESIAN_POINT('Ctrl Pts',(-9.79271491996257,3.3731528874077,6.12625125732793));
#90150=CARTESIAN_POINT('Ctrl Pts',(-10.2201114829928,-1.68069842049241,
6.20498807060491));
#90151=CARTESIAN_POINT('Ctrl Pts',(-8.19677926064828,-6.33152711891279,
6.28372488388187));
#90152=CARTESIAN_POINT('Ctrl Pts',(-4.2079026394187,-9.46408903606783,6.36246169715886));
#90153=CARTESIAN_POINT('Ctrl Pts',(0.790006822757178,-10.3272123598464,
6.44119851043582));
#90154=CARTESIAN_POINT('Ctrl Pts',(5.59847681899395,-8.7139246733371,6.51993532371281));
#90155=CARTESIAN_POINT('Ctrl Pts',(9.06446162635903,-5.01108384779742,6.59867213698977));
#90156=CARTESIAN_POINT('Ctrl Pts',(10.3568363837189,-0.106611567246333,
6.67740895026675));
#90157=CARTESIAN_POINT('Ctrl Pts',(9.16569644623514,4.82342560436751,6.75614576354371));
#90158=CARTESIAN_POINT('Ctrl Pts',(5.77667088332179,8.59683077716295,6.8348825768207));
#90159=CARTESIAN_POINT('Ctrl Pts',(1.00243013553229,10.3087613091375,6.91361939009766));
#90160=CARTESIAN_POINT('Ctrl Pts',(-4.0121880672938,9.54870529538218,6.99235620337465));
#90161=CARTESIAN_POINT('Ctrl Pts',(-8.06470475046425,6.4989201559362,7.0710930166516));
#90162=CARTESIAN_POINT('Ctrl Pts',(-10.1833478051164,1.89072826853232,7.14982982992859));
#90163=CARTESIAN_POINT('Ctrl Pts',(-9.86007781029048,-3.1708502771988,7.22856664320556));
#90164=CARTESIAN_POINT('Ctrl Pts',(-7.17241320432127,-7.47207566422293,
7.30730345648254));
#90165=CARTESIAN_POINT('Ctrl Pts',(-2.76484177251623,-9.98153674933592,
7.38604026975951));
#90166=CARTESIAN_POINT('Ctrl Pts',(2.30572412174414,-10.09747801086,7.46477708303648));
#90167=CARTESIAN_POINT('Ctrl Pts',(6.82338954268924,-7.79209734629346,7.54351389631346));
#90168=CARTESIAN_POINT('Ctrl Pts',(9.70484216948892,-3.61821286973333,7.62225070959043));
#90169=CARTESIAN_POINT('Ctrl Pts',(10.2591248723769,1.42329995375918,7.7009875228674));
#90170=CARTESIAN_POINT('Ctrl Pts',(8.35332358505756,6.12351296142299,7.77972433614438));
#90171=CARTESIAN_POINT('Ctrl Pts',(4.44443939619817,9.35533988473514,7.85846114942134));
#90172=CARTESIAN_POINT('Ctrl Pts',(-0.530197899290624,10.3438056871242,
7.93719796269834));
#90173=CARTESIAN_POINT('Ctrl Pts',(-5.37769653725135,8.85188148692859,8.0159347759753));
#90174=CARTESIAN_POINT('Ctrl Pts',(-8.93565193248317,5.23732283203015,8.09467158925227));
#90175=CARTESIAN_POINT('Ctrl Pts',(-10.3508851623618,0.366881807933114,
8.17340840252925));
#90176=CARTESIAN_POINT('Ctrl Pts',(-9.28403076886391,-4.59153553707068,
8.25214521580621));
#90177=CARTESIAN_POINT('Ctrl Pts',(-5.99091480401388,-8.44892689733091,
8.33088202908319));
#90178=CARTESIAN_POINT('Ctrl Pts',(-1.26120909302149,-10.2803101864231,
8.40961884236016));
#90179=CARTESIAN_POINT('Ctrl Pts',(3.77092790101342,-9.64652935882917,8.48835565563714));
#90180=CARTESIAN_POINT('Ctrl Pts',(7.89881628974206,-6.69956171150768,8.56709246891411));
#90181=CARTESIAN_POINT('Ctrl Pts',(10.1326102271687,-2.14607453031608,8.64582928219108));
#90182=CARTESIAN_POINT('Ctrl Pts',(9.93665771848401,2.92202999489853,8.72456609546806));
#90183=CARTESIAN_POINT('Ctrl Pts',(7.35794714090862,7.28944715166994,8.80330290874504));
#90184=CARTESIAN_POINT('Ctrl Pts',(3.01483967886997,9.90889335981096,8.88203972202201));
#90185=CARTESIAN_POINT('Ctrl Pts',(-2.05121042391966,10.1522392457131,8.96077653529897));
#90186=CARTESIAN_POINT('Ctrl Pts',(-6.62539109464709,7.96113175047151,9.03951334857597));
#90187=CARTESIAN_POINT('Ctrl Pts',(-9.61083795390783,3.86098688538555,9.11825016185292));
#90188=CARTESIAN_POINT('Ctrl Pts',(-10.2916566039392,-1.16500225407046,
9.1969869751299));
#90189=CARTESIAN_POINT('Ctrl Pts',(-8.50459032625769,-5.91163000262351,
9.27572378840688));
#90190=CARTESIAN_POINT('Ctrl Pts',(-4.67816818097848,-9.24068008189199,
9.35446060168385));
#90191=CARTESIAN_POINT('Ctrl Pts',(0.270053999751182,-10.3538638557117,
9.43319741496082));
#90192=CARTESIAN_POINT('Ctrl Pts',(5.15351865685732,-8.98424573121294,9.51193422823778));
#90193=CARTESIAN_POINT('Ctrl Pts',(8.80119674359953,-5.46025290493465,9.59067104151478));
#90194=CARTESIAN_POINT('Ctrl Pts',(10.3383943095429,-0.626920254741986,
9.66940785479173));
#90195=CARTESIAN_POINT('Ctrl Pts',(9.39649949268091,4.3567445632538,9.74814466806871));
#90196=CARTESIAN_POINT('Ctrl Pts',(6.20137369817706,8.29568503265116,9.8268814813457));
#90197=CARTESIAN_POINT('Ctrl Pts',(1.51919122564639,10.2453640211226,9.90561829462266));
#90198=CARTESIAN_POINT('Ctrl Pts',(-3.52728528353637,9.7382587988789,9.98435510789964));
#90199=CARTESIAN_POINT('Ctrl Pts',(-7.72793740098316,6.89597052139002,10.0630919211766));
#90200=CARTESIAN_POINT('Ctrl Pts',(-10.0754709226447,2.40006491419192,10.1418287344536));
#90201=CARTESIAN_POINT('Ctrl Pts',(-10.0069597018023,-2.67136359035973,
10.2205655477306));
#90202=CARTESIAN_POINT('Ctrl Pts',(-7.538832367568,-7.10221320709983,10.2993023610076));
#90203=CARTESIAN_POINT('Ctrl Pts',(-3.26293282634487,-9.82998958677756,
10.3780391742845));
#90204=CARTESIAN_POINT('Ctrl Pts',(1.79540078280026,-10.2005863524856,10.4567759875615));
#90205=CARTESIAN_POINT('Ctrl Pts',(6.42320676149755,-8.12513635605253,10.5355128008385));
#90206=CARTESIAN_POINT('Ctrl Pts',(9.51076166455986,-4.10132155107751,10.6142496141155));
#90207=CARTESIAN_POINT('Ctrl Pts',(10.3176861243121,0.905968512461215,10.6929864273924));
#90208=CARTESIAN_POINT('Ctrl Pts',(8.65048391476648,5.69601210899002,10.7717232406694));
#90209=CARTESIAN_POINT('Ctrl Pts',(4.90894132521788,9.12018206895907,10.8504600539464));
#90210=CARTESIAN_POINT('Ctrl Pts',(-0.00973948160225924,10.3573805109155,
10.9291968672234));
#90211=CARTESIAN_POINT('Ctrl Pts',(-4.92608481214535,9.11093377919877,11.0079336805003));
#90212=CARTESIAN_POINT('Ctrl Pts',(-8.66118100774594,5.67973322053559,11.0866704937773));
#90213=CARTESIAN_POINT('Ctrl Pts',(-10.3193717169132,0.886562616833696,
11.1654073070543));
#90214=CARTESIAN_POINT('Ctrl Pts',(-9.50303156057435,-4.11920102254332,
11.2441441203313));
#90215=CARTESIAN_POINT('Ctrl Pts',(-6.40791459905685,-8.13720200047834,
11.3228809336082));
#90216=CARTESIAN_POINT('Ctrl Pts',(-1.77621354173583,-10.2039448920282,
11.4016177468852));
#90217=CARTESIAN_POINT('Ctrl Pts',(3.28141414690822,-9.82383566138324,11.4803545601622));
#90218=CARTESIAN_POINT('Ctrl Pts',(7.55217604451536,-7.08802249559372,11.5590913734392));
#90219=CARTESIAN_POINT('Ctrl Pts',(10.011965991838,-2.65253895045342,11.6378281867161));
#90220=CARTESIAN_POINT('Ctrl Pts',(10.0709393438447,2.41900943321736,11.7165649999931));
#90221=CARTESIAN_POINT('Ctrl Pts',(7.71495460202305,6.91049212387352,11.7953018132701));
#90222=CARTESIAN_POINT('Ctrl Pts',(3.50896447107535,9.74487528119909,11.874038626547));
#90223=CARTESIAN_POINT('Ctrl Pts',(-1.53845681748908,10.2424887857452,11.952775439824));
#90224=CARTESIAN_POINT('Ctrl Pts',(-6.21696428217363,8.28400754584229,12.031512253101));
#90225=CARTESIAN_POINT('Ctrl Pts',(-9.404676529086,4.33906502470902,12.110249066378));
#90226=CARTESIAN_POINT('Ctrl Pts',(-10.3371969881901,-0.646362385003455,
12.188985879655));
#90227=CARTESIAN_POINT('Ctrl Pts',(-8.79091217582913,-5.47679550670405,
12.2677226929319));
#90228=CARTESIAN_POINT('Ctrl Pts',(-5.13661302773209,-8.99392197590836,
12.3464595062089));
#90229=CARTESIAN_POINT('Ctrl Pts',(-0.250581189896677,-10.3543534309325,
12.4251963194859));
#90230=CARTESIAN_POINT('Ctrl Pts',(4.69553869454898,-9.23186559008456,12.5039331327628));
#90231=CARTESIAN_POINT('Ctrl Pts',(8.51569318608262,-5.89562511239483,12.5826699460398));
#90232=CARTESIAN_POINT('Ctrl Pts',(10.2938294028405,-1.14564485361329,12.6614067593168));
#90233=CARTESIAN_POINT('Ctrl Pts',(9.6035596661784,3.87905499362223,12.7401435725938));
#90234=CARTESIAN_POINT('Ctrl Pts',(6.61040701526504,7.97357792950751,12.8188803858707));
#90235=CARTESIAN_POINT('Ctrl Pts',(2.03211365602528,10.1560789675144,12.8976171991477));
#90236=CARTESIAN_POINT('Ctrl Pts',(-3.0334698311405,9.9032058793582,12.9763540124247));
#90237=CARTESIAN_POINT('Ctrl Pts',(-7.37164326538263,7.2755962967535,13.0550908257017));
#90238=CARTESIAN_POINT('Ctrl Pts',(-9.94213555680948,2.90333712741376,13.1338276389786));
#90239=CARTESIAN_POINT('Ctrl Pts',(-10.1285562226306,-2.1651269594192,13.2125644522556));
#90240=CARTESIAN_POINT('Ctrl Pts',(-7.88620257122917,-6.71440503030112,
13.2913012655326));
#90241=CARTESIAN_POINT('Ctrl Pts',(-3.75277917164178,-9.65360421781864,
13.3700380788095));
#90242=CARTESIAN_POINT('Ctrl Pts',(1.28054086374907,-10.2779200717686,13.4487748920865));
#90243=CARTESIAN_POINT('Ctrl Pts',(6.00679395952235,-8.43764494590998,13.5275117053635));
#90244=CARTESIAN_POINT('Ctrl Pts',(9.29264957148258,-4.57406710128077,13.6062485186405));
#90245=CARTESIAN_POINT('Ctrl Pts',(10.3501768687183,0.386347889399096,13.6849853319174));
#90246=CARTESIAN_POINT('Ctrl Pts',(8.92578638765432,5.25411869559104,13.7637221451944));
#90247=CARTESIAN_POINT('Ctrl Pts',(5.3610394468105,8.86197957316176,13.8424589584714));
#90248=CARTESIAN_POINT('Ctrl Pts',(0.51074354559872,10.344784528255,13.9211957717484));
#90249=CARTESIAN_POINT('Ctrl Pts',(-4.46202596181818,9.34696475982737,13.9999325850253));
#90250=CARTESIAN_POINT('Ctrl Pts',(-8.36482519700309,6.10779218122034,14.0786693983023));
#90251=CARTESIAN_POINT('Ctrl Pts',(-10.2617835048164,1.40400327837,14.1574062115793));
#90252=CARTESIAN_POINT('Ctrl Pts',(-9.69802029639719,-3.6364581994109,14.2361430248563));
#90253=CARTESIAN_POINT('Ctrl Pts',(-6.80872301322356,-7.80491619651322,
14.3148798381332));
#90254=CARTESIAN_POINT('Ctrl Pts',(-2.28672989225111,-10.1017964890053,
14.3936166514102));
#90255=CARTESIAN_POINT('Ctrl Pts',(2.78360898606781,-9.97631930714313,14.4723534646872));
#90256=CARTESIAN_POINT('Ctrl Pts',(7.18645312318698,-7.45857341678894,14.5510902779641));
#90257=CARTESIAN_POINT('Ctrl Pts',(9.86602373603799,-3.15230099218483,14.6298270912411));
#90258=CARTESIAN_POINT('Ctrl Pts',(10.1797739361378,1.90987657049483,14.7085639045181));
#90259=CARTESIAN_POINT('Ctrl Pts',(8.05246808167551,6.51407581311359,14.787300717795));
#90260=CARTESIAN_POINT('Ctrl Pts',(3.99422288727754,9.55623406118449,14.8660375310721));
#90261=CARTESIAN_POINT('Ctrl Pts',(-1.02181587143989,10.306857825267,14.944774344349));
#90262=CARTESIAN_POINT('Ctrl Pts',(-5.79282857798032,8.58595148900395,15.023511157626));
#90263=CARTESIAN_POINT('Ctrl Pts',(-9.17475156975602,4.80617930779259,15.102247970903));
#90264=CARTESIAN_POINT('Ctrl Pts',(-10.3566175652806,-0.126089301355015,
15.1809847841799));
#90265=CARTESIAN_POINT('Ctrl Pts',(-9.0550213374679,-5.02812236161728,15.2597215974569));
#90266=CARTESIAN_POINT('Ctrl Pts',(-5.58207879109441,-8.72443822119271,
15.3384584107339));
#90267=CARTESIAN_POINT('Ctrl Pts',(-0.770583216380001,-10.3286798484622,
15.4171952240108));
#90268=CARTESIAN_POINT('Ctrl Pts',(4.22569414599381,-9.45615856941429,15.4959320372878));
#90269=CARTESIAN_POINT('Ctrl Pts',(8.2086723580607,-6.31610038104256,15.5746688505648));
#90270=CARTESIAN_POINT('Ctrl Pts',(10.2232542692602,-1.66147466169291,15.6534056638418));
#90271=CARTESIAN_POINT('Ctrl Pts',(9.78635377153171,3.39156391120948,15.7321424771188));
#90272=CARTESIAN_POINT('Ctrl Pts',(7.00273729799194,7.63132336103759,15.8108792903957));
#90273=CARTESIAN_POINT('Ctrl Pts',(2.53990138529655,10.0411317518662,15.8896161036727));
#90274=CARTESIAN_POINT('Ctrl Pts',(-2.531989472377,10.0431297520852,15.9683529169496));
#90275=CARTESIAN_POINT('Ctrl Pts',(-6.99672262002677,7.63683825177198,16.0470897302267));
#90276=CARTESIAN_POINT('Ctrl Pts',(-9.78367861654637,3.39927325079658,16.1258265435036));
#90277=CARTESIAN_POINT('Ctrl Pts',(-10.2245601253017,-1.65341953223427,
16.2045633567806));
#90278=CARTESIAN_POINT('Ctrl Pts',(-8.21364608773801,-6.30963103915528,
16.2833001700575));
#90279=CARTESIAN_POINT('Ctrl Pts',(-4.23314307519562,-9.45282632928991,
16.3620369833346));
#90280=CARTESIAN_POINT('Ctrl Pts',(0.762445301577178,-10.3292837633901,
16.4407737966115));
#90281=CARTESIAN_POINT('Ctrl Pts',(5.57520331966233,-8.72883347614835,16.5195106098885));
#90282=CARTESIAN_POINT('Ctrl Pts',(9.05105701124216,-5.03525499652388,16.5982474231654));
#90283=CARTESIAN_POINT('Ctrl Pts',(10.3565150086101,-0.134248950223226,
16.6769842364424));
#90284=CARTESIAN_POINT('Ctrl Pts',(9.17853537548744,4.79894928997922,16.7557210497194));
#90285=CARTESIAN_POINT('Ctrl Pts',(5.79959140889334,8.58138481402851,16.8344578629964));
#90286=CARTESIAN_POINT('Ctrl Pts',(1.02993603750419,10.306049573835,16.9131946762733));
#90287=CARTESIAN_POINT('Ctrl Pts',(-3.98669256120186,9.55937801638022,16.9919314895503));
#90288=CARTESIAN_POINT('Ctrl Pts',(-8.0473333237993,6.52041813189609,17.0706683028273));
#90289=CARTESIAN_POINT('Ctrl Pts',(-10.1782660425078,1.91789628028175,17.1494051161043));
#90290=CARTESIAN_POINT('Ctrl Pts',(-9.86850427565091,-3.14452674646001,
17.2281419293812));
#90291=CARTESIAN_POINT('Ctrl Pts',(-7.1923273066611,-7.4529093025926,17.3068787426582));
#90292=CARTESIAN_POINT('Ctrl Pts',(-2.79146815520754,-9.97412268686214,
17.3856155559352));
#90293=CARTESIAN_POINT('Ctrl Pts',(2.27877020828039,-10.1035957738417,17.4643523692122));
#90294=CARTESIAN_POINT('Ctrl Pts',(6.80257173056734,-7.8102766805828,17.5430891824891));
#90295=CARTESIAN_POINT('Ctrl Pts',(9.69515202172803,-3.64410076735999,17.6218259957661));
#90296=CARTESIAN_POINT('Ctrl Pts',(10.2628868860313,1.39592349971614,17.7005628090431));
#90297=CARTESIAN_POINT('Ctrl Pts',(8.36963399820998,6.10118895658217,17.77929962232));
#90298=CARTESIAN_POINT('Ctrl Pts',(4.4693902615179,9.3434675427011,17.858036435597));
#90299=CARTESIAN_POINT('Ctrl Pts',(-0.502595885572172,10.3451425983029,
17.936773248874));
#90300=CARTESIAN_POINT('Ctrl Pts',(-5.35405011226431,8.86628047125853,18.015510062151));
#90301=CARTESIAN_POINT('Ctrl Pts',(-8.92165496878712,5.26099406144437,18.094246875428));
#90302=CARTESIAN_POINT('Ctrl Pts',(-10.3498468512413,0.394808488987801,
18.1729836887049));
#90303=CARTESIAN_POINT('Ctrl Pts',(-9.29622836261498,-4.56775070567949,
18.2517263148418));
#90304=CARTESIAN_POINT('Ctrl Pts',(-7.10709281717051,-7.14383938350242,
18.304223336553));
#90305=CARTESIAN_POINT('Ctrl Pts',(-5.77174189707308,-8.09584246644884,
18.3304747538387));
#90306=CARTESIAN_POINT('Ctrl Pts',(-4.3073013591307,8.9607364793544,18.));
#90307=CARTESIAN_POINT('Ctrl Pts',(-4.52760625432587,8.84750150850078,18.));
#90308=CARTESIAN_POINT('Ctrl Pts',(-4.74323706131295,8.72624255457085,18.));
#90309=CARTESIAN_POINT('Ctrl Pts',(-4.95372227598611,8.59714960774005,18.));
#90310=CARTESIAN_POINT('Ctrl Pts',(-5.01160312760282,8.56165063118779,18.));
#90311=CARTESIAN_POINT('Ctrl Pts',(-5.06909476851584,8.52555897874492,18.));
#90312=CARTESIAN_POINT('Ctrl Pts',(-5.1261871168107,8.48887796796154,18.));
#90313=CARTESIAN_POINT('Ctrl Pts',(-5.33322421369055,8.35585961769175,18.));
#90314=CARTESIAN_POINT('Ctrl Pts',(-5.53501269654285,8.21509436198934,18.));
#90315=CARTESIAN_POINT('Ctrl Pts',(-5.7312285379337,8.06700108805411,18.));
#90316=CARTESIAN_POINT('Ctrl Pts',(-5.92834760164166,7.9182261099859,18.));
#90317=CARTESIAN_POINT('Ctrl Pts',(-6.11984306788491,7.76205502130544,18.));
#90318=CARTESIAN_POINT('Ctrl Pts',(-6.30535299141809,7.59887183662814,18.));
#90319=CARTESIAN_POINT('Ctrl Pts',(-6.49030070142005,7.43618320120592,18.));
#90320=CARTESIAN_POINT('Ctrl Pts',(-6.66929951885765,7.26652439975838,18.));
#90321=CARTESIAN_POINT('Ctrl Pts',(-6.84195102169195,7.09024304306413,18.));
#90322=CARTESIAN_POINT('Ctrl Pts',(-6.99683870006296,6.93209898042791,18.));
#90323=CARTESIAN_POINT('Ctrl Pts',(-7.14661770651649,6.76862435341091,18.));
#90324=CARTESIAN_POINT('Ctrl Pts',(-7.29096872875563,6.60005246861241,18.));
#90325=CARTESIAN_POINT('Ctrl Pts',(-7.31275740699813,6.57460783717417,18.));
#90326=CARTESIAN_POINT('Ctrl Pts',(-7.33441899362598,6.54905088798603,18.));
#90327=CARTESIAN_POINT('Ctrl Pts',(-7.3559421054481,6.523395076923,18.));
#90328=CARTESIAN_POINT('Ctrl Pts',(-7.51382905139519,6.33519191708182,18.));
#90329=CARTESIAN_POINT('Ctrl Pts',(-7.66443332067489,6.14147855738646,18.));
#90330=CARTESIAN_POINT('Ctrl Pts',(-7.80743627194425,5.94265874500182,18.));
#90331=CARTESIAN_POINT('Ctrl Pts',(-7.95018354749679,5.74419440358892,18.));
#90332=CARTESIAN_POINT('Ctrl Pts',(-8.08535707059586,5.54064133904095,18.));
#90333=CARTESIAN_POINT('Ctrl Pts',(-8.2126006506496,5.33236758982748,18.));
#90334=CARTESIAN_POINT('Ctrl Pts',(-8.28587672164632,5.21242847755421,18.));
#90335=CARTESIAN_POINT('Ctrl Pts',(-8.35652223535198,5.09092327046725,18.));
#90336=CARTESIAN_POINT('Ctrl Pts',(-8.42446243614109,4.96791819110294,18.));
#90337=CARTESIAN_POINT('Ctrl Pts',(-8.54281535446282,4.75364137204628,18.));
#90338=CARTESIAN_POINT('Ctrl Pts',(-8.65296146393977,4.53481380518235,18.));
#90339=CARTESIAN_POINT('Ctrl Pts',(-8.75476116990247,4.31194123524967,18.));
#90340=CARTESIAN_POINT('Ctrl Pts',(-8.8562212171741,4.08981228834281,18.));
#90341=CARTESIAN_POINT('Ctrl Pts',(-8.94939060020028,3.86366463572551,18.));
#90342=CARTESIAN_POINT('Ctrl Pts',(-9.03408085695094,3.6339875819897,18.));
#90343=CARTESIAN_POINT('Ctrl Pts',(-9.05818284480564,3.56862382266211,18.));
#90344=CARTESIAN_POINT('Ctrl Pts',(-9.08159777671273,3.50297417480271,18.));
#90345=CARTESIAN_POINT('Ctrl Pts',(-9.10432053672134,3.43704986001775,18.));
#90346=CARTESIAN_POINT('Ctrl Pts',(-9.11838840419275,3.39623551690155,18.));
#90347=CARTESIAN_POINT('Ctrl Pts',(-9.13219095806272,3.35531589487388,18.));
#90348=CARTESIAN_POINT('Ctrl Pts',(-9.14572691705035,3.31429365769524,18.));
#90349=CARTESIAN_POINT('Ctrl Pts',(-9.15617345111333,3.28263426818186,18.));
#90350=CARTESIAN_POINT('Ctrl Pts',(-9.16646082010693,3.25091466828912,18.));
#90351=CARTESIAN_POINT('Ctrl Pts',(-9.17658220167961,3.21915638737006,18.));
#90352=CARTESIAN_POINT('Ctrl Pts',(-9.25054140040622,2.98709152618069,18.));
#90353=CARTESIAN_POINT('Ctrl Pts',(-9.31573488780019,2.75268296772533,18.));
#90354=CARTESIAN_POINT('Ctrl Pts',(-9.37209036933886,2.51644592272189,18.));
#90355=CARTESIAN_POINT('Ctrl Pts',(-9.42853307221032,2.27984325383666,18.));
#90356=CARTESIAN_POINT('Ctrl Pts',(-9.47611053782495,2.04140578250418,18.));
#90357=CARTESIAN_POINT('Ctrl Pts',(-9.51470041111593,1.80163458795178,18.));
#90358=CARTESIAN_POINT('Ctrl Pts',(-9.5529252224677,1.56413163969781,18.));
#90359=CARTESIAN_POINT('Ctrl Pts',(-9.58233174292863,1.32531944671551,18.));
#90360=CARTESIAN_POINT('Ctrl Pts',(-9.60275090844265,1.0856784282915,18.));
#90361=CARTESIAN_POINT('Ctrl Pts',(-9.62309540351779,0.846913748325436,
18.));
#90362=CARTESIAN_POINT('Ctrl Pts',(-9.63451826958938,0.607325689922282,
18.));
#90363=CARTESIAN_POINT('Ctrl Pts',(-9.63680089853934,0.367392081352794,
18.));
#90364=CARTESIAN_POINT('Ctrl Pts',(-9.63858576602893,0.179779592864777,
18.));
#90365=CARTESIAN_POINT('Ctrl Pts',(-9.63478088238045,-0.00804422448828743,
18.));
#90366=CARTESIAN_POINT('Ctrl Pts',(-9.62541795260051,-0.195838307668789,
18.));
#90367=CARTESIAN_POINT('Ctrl Pts',(-9.62262270781222,-0.251903069940943,
18.));
#90368=CARTESIAN_POINT('Ctrl Pts',(-9.61933196404203,-0.307965141664495,
18.));
#90369=CARTESIAN_POINT('Ctrl Pts',(-9.61554626324484,-0.364017993970899,
18.));
#90370=CARTESIAN_POINT('Ctrl Pts',(-9.61250490227994,-0.409049803431933,
18.));
#90371=CARTESIAN_POINT('Ctrl Pts',(-9.60914339172037,-0.454082657053631,
18.));
#90372=CARTESIAN_POINT('Ctrl Pts',(-9.60546607932598,-0.499066988202734,
18.));
#90373=CARTESIAN_POINT('Ctrl Pts',(-9.58595145068401,-0.737788212546353,
18.));
#90374=CARTESIAN_POINT('Ctrl Pts',(-9.55753446716396,-0.975378206055743,
18.));
#90375=CARTESIAN_POINT('Ctrl Pts',(-9.52041083245154,-1.21135394166142,
18.));
#90376=CARTESIAN_POINT('Ctrl Pts',(-9.48257537067788,-1.45185439354827,
18.));
#90377=CARTESIAN_POINT('Ctrl Pts',(-9.43569613673507,-1.69067876605208,
18.));
#90378=CARTESIAN_POINT('Ctrl Pts',(-9.37992571664595,-1.92731195007808,
18.));
#90379=CARTESIAN_POINT('Ctrl Pts',(-9.32477727545944,-2.1613060855209,18.));
#90380=CARTESIAN_POINT('Ctrl Pts',(-9.26093458221553,-2.39315826150895,
18.));
#90381=CARTESIAN_POINT('Ctrl Pts',(-9.18849501396502,-2.62235702764131,
18.));
#90382=CARTESIAN_POINT('Ctrl Pts',(-9.11482995641156,-2.85543324145767,
18.));
#90383=CARTESIAN_POINT('Ctrl Pts',(-9.03227465025842,-3.08576625698368,
18.));
#90384=CARTESIAN_POINT('Ctrl Pts',(-8.94088139600402,-3.31279382281833,
18.));
#90385=CARTESIAN_POINT('Ctrl Pts',(-8.84948814174963,-3.53982138865298,
18.));
#90386=CARTESIAN_POINT('Ctrl Pts',(-8.74925676736514,-3.76354421054282,
18.));
#90387=CARTESIAN_POINT('Ctrl Pts',(-8.64019169798513,-3.98336495971754,
18.));
#90388=CARTESIAN_POINT('Ctrl Pts',(-8.62858600317367,-4.00675624844683,
18.));
#90389=CARTESIAN_POINT('Ctrl Pts',(-8.61688134356907,-4.03010103399861,
18.));
#90390=CARTESIAN_POINT('Ctrl Pts',(-8.60508170405194,-4.0533909536201,18.));
#90391=CARTESIAN_POINT('Ctrl Pts',(-8.58155518124463,-4.0998271879101,18.));
#90392=CARTESIAN_POINT('Ctrl Pts',(-8.5576466944477,-4.14605418913442,18.));
#90393=CARTESIAN_POINT('Ctrl Pts',(-8.53335745420521,-4.19206686624084,
18.));
#90394=CARTESIAN_POINT('Ctrl Pts',(-8.42201512723478,-4.40298982999017,
18.));
#90395=CARTESIAN_POINT('Ctrl Pts',(-8.30267566618238,-4.60941115010306,
18.));
#90396=CARTESIAN_POINT('Ctrl Pts',(-8.17572619796266,-4.81098138527243,
18.));
#90397=CARTESIAN_POINT('Ctrl Pts',(-8.04812742875072,-5.01358257988993,
18.));
#90398=CARTESIAN_POINT('Ctrl Pts',(-7.91284017586144,-5.21128344591977,
18.));
#90399=CARTESIAN_POINT('Ctrl Pts',(-7.77021399871967,-5.40369944292422,
18.));
#90400=CARTESIAN_POINT('Ctrl Pts',(-7.68992477437975,-5.51201708460596,
18.));
#90401=CARTESIAN_POINT('Ctrl Pts',(-7.60730913056893,-5.61865939762238,
18.));
#90402=CARTESIAN_POINT('Ctrl Pts',(-7.52242418953522,-5.72355274841017,
18.));
#90403=CARTESIAN_POINT('Ctrl Pts',(-7.47738280262866,-5.7792109362963,18.));
#90404=CARTESIAN_POINT('Ctrl Pts',(-7.43170242560918,-5.83437663101952,
18.));
#90405=CARTESIAN_POINT('Ctrl Pts',(-7.38539120988832,-5.88903836524094,
18.));
#90406=CARTESIAN_POINT('Ctrl Pts',(-7.35170722773477,-5.92879601036723,
18.));
#90407=CARTESIAN_POINT('Ctrl Pts',(-7.31768946871676,-5.96828709416038,
18.));
#90408=CARTESIAN_POINT('Ctrl Pts',(-7.28334090389888,-6.00750717725608,
18.));
#90409=CARTESIAN_POINT('Ctrl Pts',(-7.25650547538877,-6.03814856625314,
18.));
#90410=CARTESIAN_POINT('Ctrl Pts',(-7.22947175915789,-6.06862028964852,
18.));
#90411=CARTESIAN_POINT('Ctrl Pts',(-7.20225223828727,-6.0989084687769,18.));
#90412=CARTESIAN_POINT('Ctrl Pts',(-7.04281668321099,-6.27631837523831,
18.));
#90413=CARTESIAN_POINT('Ctrl Pts',(-6.8769088257654,-6.44754939973975,18.));
#90414=CARTESIAN_POINT('Ctrl Pts',(-6.70488545274962,-6.61223355200001,
18.));
#90415=CARTESIAN_POINT('Ctrl Pts',(-6.53342044592134,-6.77638316025832,
18.));
#90416=CARTESIAN_POINT('Ctrl Pts',(-6.35587907752285,-6.93402877733524,
18.));
#90417=CARTESIAN_POINT('Ctrl Pts',(-6.17257983213519,-7.08476792573877,
18.));
#90418=CARTESIAN_POINT('Ctrl Pts',(-5.99170876215547,-7.23351022416951,
18.));
#90419=CARTESIAN_POINT('Ctrl Pts',(-5.80523086450408,-7.37552817919547,
18.));
#90420=CARTESIAN_POINT('Ctrl Pts',(-5.6134254389644,-7.51039211345532,18.));
#90421=CARTESIAN_POINT('Ctrl Pts',(-5.5561940083516,-7.55063318522919,18.));
#90422=CARTESIAN_POINT('Ctrl Pts',(-5.49848810023155,-7.5902370047748,18.));
#90423=CARTESIAN_POINT('Ctrl Pts',(-5.44031476324441,-7.62919132931695,
18.));
#90424=CARTESIAN_POINT('Ctrl Pts',(-5.4406043999737,-7.62923403168952,4.));
#90425=CARTESIAN_POINT('Ctrl Pts',(-5.63890667642695,-7.49673345057434,
4.));
#90426=CARTESIAN_POINT('Ctrl Pts',(-5.83187819659435,-7.35682734686391,
4.));
#90427=CARTESIAN_POINT('Ctrl Pts',(-6.01906043119416,-7.20976889497537,
4.));
#90428=CARTESIAN_POINT('Ctrl Pts',(-6.06595632464851,-7.17292545464531,
4.));
#90429=CARTESIAN_POINT('Ctrl Pts',(-6.11248873150584,-7.13563283968316,
4.));
#90430=CARTESIAN_POINT('Ctrl Pts',(-6.15865021542981,-7.09789457099519,
4.));
#90431=CARTESIAN_POINT('Ctrl Pts',(-6.34204542282573,-6.94796400064803,
4.));
#90432=CARTESIAN_POINT('Ctrl Pts',(-6.51958844489126,-6.79100259370661,
4.));
#90433=CARTESIAN_POINT('Ctrl Pts',(-6.69101403836337,-6.62745756012925,
4.));
#90434=CARTESIAN_POINT('Ctrl Pts',(-6.81071898340218,-6.51325553895363,
4.));
#90435=CARTESIAN_POINT('Ctrl Pts',(-6.92744041708859,-6.39584230707921,
4.));
#90436=CARTESIAN_POINT('Ctrl Pts',(-7.04107814220401,-6.27535881881818,
4.));
#90437=CARTESIAN_POINT('Ctrl Pts',(-7.09297519101191,-6.22033538831146,
4.));
#90438=CARTESIAN_POINT('Ctrl Pts',(-7.14422896803321,-6.16467149349175,
4.));
#90439=CARTESIAN_POINT('Ctrl Pts',(-7.19482929716662,-6.10837999905884,
4.));
#90440=CARTESIAN_POINT('Ctrl Pts',(-7.22002600107554,-6.08034934901944,
4.));
#90441=CARTESIAN_POINT('Ctrl Pts',(-7.24506190537271,-6.05216166512634,
4.));
#90442=CARTESIAN_POINT('Ctrl Pts',(-7.26993182670183,-6.02382294123104,
4.));
#90443=CARTESIAN_POINT('Ctrl Pts',(-7.32949916007229,-5.9559472856861,4.));
#90444=CARTESIAN_POINT('Ctrl Pts',(-7.38807638127959,-5.8872485811258,4.));
#90445=CARTESIAN_POINT('Ctrl Pts',(-7.44564690314271,-5.81775662713007,
4.));
#90446=CARTESIAN_POINT('Ctrl Pts',(-7.59853619808971,-5.63320773809693,
4.));
#90447=CARTESIAN_POINT('Ctrl Pts',(-7.74433637265751,-5.44305767811413,
4.));
#90448=CARTESIAN_POINT('Ctrl Pts',(-7.88277765536633,-5.24776290323712,
4.));
#90449=CARTESIAN_POINT('Ctrl Pts',(-8.02123619232692,-5.05244378832838,
4.));
#90450=CARTESIAN_POINT('Ctrl Pts',(-8.15233441656134,-4.85197814519116,
4.));
#90451=CARTESIAN_POINT('Ctrl Pts',(-8.27576400153287,-4.64678738411282,
4.));
#90452=CARTESIAN_POINT('Ctrl Pts',(-8.34639728459589,-4.52936580230562,
4.));
#90453=CARTESIAN_POINT('Ctrl Pts',(-8.41451852921977,-4.41039625175062,
4.));
#90454=CARTESIAN_POINT('Ctrl Pts',(-8.48006348530507,-4.28995353694912,
4.));
#90455=CARTESIAN_POINT('Ctrl Pts',(-8.52315852127724,-4.21076387176417,
4.));
#90456=CARTESIAN_POINT('Ctrl Pts',(-8.56513975274644,-4.13093731242842,
4.));
#90457=CARTESIAN_POINT('Ctrl Pts',(-8.60598770490748,-4.05049453408062,
4.));
#90458=CARTESIAN_POINT('Ctrl Pts',(-8.62649497932659,-4.01010910364066,
4.));
#90459=CARTESIAN_POINT('Ctrl Pts',(-8.64671849536238,-3.96956421778801,
4.));
#90460=CARTESIAN_POINT('Ctrl Pts',(-8.6666390866119,-3.9288971669964,4.));
#90461=CARTESIAN_POINT('Ctrl Pts',(-8.75648890768642,-3.74547252906847,
4.));
#90462=CARTESIAN_POINT('Ctrl Pts',(-8.84025123269583,-3.55942237588939,
4.));
#90463=CARTESIAN_POINT('Ctrl Pts',(-8.91776910989646,-3.37102286161559,
4.));
#90464=CARTESIAN_POINT('Ctrl Pts',(-9.00791436630044,-3.1519337542521,4.));
#90465=CARTESIAN_POINT('Ctrl Pts',(-9.08961652951227,-2.92966789467907,
4.));
#90466=CARTESIAN_POINT('Ctrl Pts',(-9.16289515281366,-2.70474471828656,
4.));
#90467=CARTESIAN_POINT('Ctrl Pts',(-9.23731564864513,-2.47631665076847,
4.));
#90468=CARTESIAN_POINT('Ctrl Pts',(-9.30304826291371,-2.24514723374452,
4.));
#90469=CARTESIAN_POINT('Ctrl Pts',(-9.36006571799165,-2.01175648923436,
4.));
#90470=CARTESIAN_POINT('Ctrl Pts',(-9.41722423408095,-1.77778833672838,
4.));
#90471=CARTESIAN_POINT('Ctrl Pts',(-9.46562455384306,-1.54158720587045,
4.));
#90472=CARTESIAN_POINT('Ctrl Pts',(-9.50518897333799,-1.30366226406109,
4.));
#90473=CARTESIAN_POINT('Ctrl Pts',(-9.54451505536745,-1.06717059053488,
4.));
#90474=CARTESIAN_POINT('Ctrl Pts',(-9.57511144928619,-0.828975161295982,
4.));
#90475=CARTESIAN_POINT('Ctrl Pts',(-9.59685078292151,-0.589571184533304,
4.));
#90476=CARTESIAN_POINT('Ctrl Pts',(-9.60170018041594,-0.536167291638293,
4.));
#90477=CARTESIAN_POINT('Ctrl Pts',(-9.60610864276964,-0.482703263990903,
4.));
#90478=CARTESIAN_POINT('Ctrl Pts',(-9.61007440021997,-0.429184616207386,
4.));
#90479=CARTESIAN_POINT('Ctrl Pts',(-9.62255729760149,-0.260725552170613,
4.));
#90480=CARTESIAN_POINT('Ctrl Pts',(-9.63062282883421,-0.0921565796354109,
4.));
#90481=CARTESIAN_POINT('Ctrl Pts',(-9.63427539043941,0.0763415761908876,
4.));
#90482=CARTESIAN_POINT('Ctrl Pts',(-9.6395510673353,0.31971647955428,4.));
#90483=CARTESIAN_POINT('Ctrl Pts',(-9.63562264690952,0.562944862804888,
4.));
#90484=CARTESIAN_POINT('Ctrl Pts',(-9.62246124849151,0.805502024763583,
4.));
#90485=CARTESIAN_POINT('Ctrl Pts',(-9.61376654195987,0.965740570349518,
4.));
#90486=CARTESIAN_POINT('Ctrl Pts',(-9.60104133774746,1.12568650575829,4.));
#90487=CARTESIAN_POINT('Ctrl Pts',(-9.58426497005538,1.28519040638768,4.));
#90488=CARTESIAN_POINT('Ctrl Pts',(-9.55895733896447,1.52580660822461,4.00000000000001));
#90489=CARTESIAN_POINT('Ctrl Pts',(-9.52443315490438,1.76541730862835,4.));
#90490=CARTESIAN_POINT('Ctrl Pts',(-9.48091210802519,2.00354972609759,4.));
#90491=CARTESIAN_POINT('Ctrl Pts',(-9.43726373818328,2.24237881166393,4.));
#90492=CARTESIAN_POINT('Ctrl Pts',(-9.38456561231773,2.47972158484106,4.00000000000001));
#90493=CARTESIAN_POINT('Ctrl Pts',(-9.3229878038817,2.71509158677534,4.));
#90494=CARTESIAN_POINT('Ctrl Pts',(-9.28748541748832,2.8507930182864,4.));
#90495=CARTESIAN_POINT('Ctrl Pts',(-9.24903044791309,2.98583846655917,4.));
#90496=CARTESIAN_POINT('Ctrl Pts',(-9.20764807916007,3.12013200861045,4.));
#90497=CARTESIAN_POINT('Ctrl Pts',(-9.19463326690819,3.16236751346685,4.));
#90498=CARTESIAN_POINT('Ctrl Pts',(-9.18132886310879,3.20452862831681,4.));
#90499=CARTESIAN_POINT('Ctrl Pts',(-9.16773554415993,3.24661231613881,4.));
#90500=CARTESIAN_POINT('Ctrl Pts',(-9.15670129834845,3.28077334464322,4.));
#90501=CARTESIAN_POINT('Ctrl Pts',(-9.14547611387815,3.31488477940298,4.00000000000001));
#90502=CARTESIAN_POINT('Ctrl Pts',(-9.13406922931753,3.34891920626068,4.00000000000001));
#90503=CARTESIAN_POINT('Ctrl Pts',(-9.05631917672066,3.58090003014193,4.00000000000001));
#90504=CARTESIAN_POINT('Ctrl Pts',(-8.9700425839685,3.80958444813462,4.));
#90505=CARTESIAN_POINT('Ctrl Pts',(-8.87551055116939,4.03450558990744,4.));
#90506=CARTESIAN_POINT('Ctrl Pts',(-8.78048518937392,4.26060051497725,4.));
#90507=CARTESIAN_POINT('Ctrl Pts',(-8.67711781422885,4.48289341815704,4.));
#90508=CARTESIAN_POINT('Ctrl Pts',(-8.5656314199461,4.7009025036125,4.));
#90509=CARTESIAN_POINT('Ctrl Pts',(-8.45449720704987,4.91822290644901,4.));
#90510=CARTESIAN_POINT('Ctrl Pts',(-8.33529494633942,5.13128713343155,4.));
#90511=CARTESIAN_POINT('Ctrl Pts',(-8.20819692963572,5.33960104088448,4.));
#90512=CARTESIAN_POINT('Ctrl Pts',(-8.12092504012807,5.4826398449952,4.));
#90513=CARTESIAN_POINT('Ctrl Pts',(-8.02992938519569,5.6234385784565,4.));
#90514=CARTESIAN_POINT('Ctrl Pts',(-7.9352532849449,5.76183032119093,4.));
#90515=CARTESIAN_POINT('Ctrl Pts',(-7.82259240106539,5.92651112254192,4.));
#90516=CARTESIAN_POINT('Ctrl Pts',(-7.70472028337977,6.08778406995721,4.));
#90517=CARTESIAN_POINT('Ctrl Pts',(-7.58184069322956,6.24546702512108,4.));
#90518=CARTESIAN_POINT('Ctrl Pts',(-7.52808087253885,6.31445331800527,4.));
#90519=CARTESIAN_POINT('Ctrl Pts',(-7.47336236631123,6.38275226745228,4.));
#90520=CARTESIAN_POINT('Ctrl Pts',(-7.4177012476084,6.45034764911358,4.));
#90521=CARTESIAN_POINT('Ctrl Pts',(-7.38744554517405,6.48709045632159,4.));
#90522=CARTESIAN_POINT('Ctrl Pts',(-7.35691132086333,6.52362537091555,4.));
#90523=CARTESIAN_POINT('Ctrl Pts',(-7.32610108765794,6.55994970757211,4.));
#90524=CARTESIAN_POINT('Ctrl Pts',(-7.30425531243344,6.58570521836257,4.));
#90525=CARTESIAN_POINT('Ctrl Pts',(-7.28227098144389,6.61135450032982,4.));
#90526=CARTESIAN_POINT('Ctrl Pts',(-7.26016370234522,6.63687994473654,4.));
#90527=CARTESIAN_POINT('Ctrl Pts',(-7.10051291614676,6.82121548641077,4.));
#90528=CARTESIAN_POINT('Ctrl Pts',(-6.93426438810104,6.99931954457605,4.));
#90529=CARTESIAN_POINT('Ctrl Pts',(-6.76187972113722,7.17093268814279,4.));
#90530=CARTESIAN_POINT('Ctrl Pts',(-6.58682736884097,7.34520157757143,4.));
#90531=CARTESIAN_POINT('Ctrl Pts',(-6.40544712427759,7.51277759797145,4.));
#90532=CARTESIAN_POINT('Ctrl Pts',(-6.21817619061028,7.67336148139723,4.));
#90533=CARTESIAN_POINT('Ctrl Pts',(-6.03066159759768,7.8341543014857,4.));
#90534=CARTESIAN_POINT('Ctrl Pts',(-5.83724049632752,7.98793722962644,4.));
#90535=CARTESIAN_POINT('Ctrl Pts',(-5.63831244115613,8.13437529745182,4.));
#90536=CARTESIAN_POINT('Ctrl Pts',(-5.44040076795292,8.28006517009946,4.));
#90537=CARTESIAN_POINT('Ctrl Pts',(-5.2370377676165,8.4184854581206,4.));
#90538=CARTESIAN_POINT('Ctrl Pts',(-5.02858537665499,8.54926573852366,4.));
#90539=CARTESIAN_POINT('Ctrl Pts',(-4.82013298569347,8.68004601892672,4.));
#90540=CARTESIAN_POINT('Ctrl Pts',(-4.60659073270969,8.80318675135613,4.));
#90541=CARTESIAN_POINT('Ctrl Pts',(-4.38829619315135,8.91827026601966,4.));
#90542=CARTESIAN_POINT('Ctrl Pts',(-4.36127103682207,8.93251775925059,4.));
#90543=CARTESIAN_POINT('Ctrl Pts',(-4.33417301792296,8.94664169673992,4.));
#90544=CARTESIAN_POINT('Ctrl Pts',(-4.30700275658822,8.96064123010968,4.));
#90545=CARTESIAN_POINT('Ctrl Pts',(5.77174310293177,-8.09584396947078,3.66952413717531));
#90546=CARTESIAN_POINT('Ctrl Pts',(7.10709424093549,-7.14384070838492,3.69577555387736));
#90547=CARTESIAN_POINT('Ctrl Pts',(9.2962305957292,-4.5677522174272,3.74827257500505));
#90548=CARTESIAN_POINT('Ctrl Pts',(10.3498486095772,0.394808939182714,3.82701520055842));
#90549=CARTESIAN_POINT('Ctrl Pts',(8.92165680290257,5.2609948509435,3.90575201383539));
#90550=CARTESIAN_POINT('Ctrl Pts',(5.35405107811436,8.86628230701266,3.98448882711236));
#90551=CARTESIAN_POINT('Ctrl Pts',(0.502596015216245,10.3451445080436,4.06322564038934));
#90552=CARTESIAN_POINT('Ctrl Pts',(-4.46939113767733,9.34346938332682,4.14196245366631));
#90553=CARTESIAN_POINT('Ctrl Pts',(-8.36963559720786,6.10119010282693,4.2206992669433));
#90554=CARTESIAN_POINT('Ctrl Pts',(-10.2628888627734,1.39592378273276,4.29943608022025));
#90555=CARTESIAN_POINT('Ctrl Pts',(-9.69515388203774,-3.64410147588179,
4.37817289349724));
#90556=CARTESIAN_POINT('Ctrl Pts',(-6.80257303895417,-7.81027817659755,
4.4569097067742));
#90557=CARTESIAN_POINT('Ctrl Pts',(-2.27877064542789,-10.1035977177542,
4.53564652005118));
#90558=CARTESIAN_POINT('Ctrl Pts',(2.79146869119749,-9.97412460187197,4.61438333332815));
#90559=CARTESIAN_POINT('Ctrl Pts',(7.19232868879842,-7.45291073539475,4.69312014660512));
#90560=CARTESIAN_POINT('Ctrl Pts',(9.8685061716992,-3.14452735022185,4.7718569598821));
#90561=CARTESIAN_POINT('Ctrl Pts',(10.1782679982284,1.91789664855303,4.85059377315908));
#90562=CARTESIAN_POINT('Ctrl Pts',(8.04733486999838,6.5204193848677,4.92933058643604));
#90563=CARTESIAN_POINT('Ctrl Pts',(3.98669332722565,9.5593798530638,5.00806739971302));
#90564=CARTESIAN_POINT('Ctrl Pts',(-1.02993623540529,10.3060515540929,5.08680421298999));
#90565=CARTESIAN_POINT('Ctrl Pts',(-5.79959252323165,8.58138646284841,5.16554102626697));
#90566=CARTESIAN_POINT('Ctrl Pts',(-9.17853713906726,4.79895021206766,5.24427783954394));
#90567=CARTESIAN_POINT('Ctrl Pts',(-10.3565169985255,-0.134248976023967,
5.32301465282091));
#90568=CARTESIAN_POINT('Ctrl Pts',(-9.05105875032658,-5.03525596400226,
5.40175146609789));
#90569=CARTESIAN_POINT('Ctrl Pts',(-5.57520439089005,-8.72883515332142,
5.48048827937486));
#90570=CARTESIAN_POINT('Ctrl Pts',(-0.762445448074686,-10.3292857480735,
5.55922509265183));
#90571=CARTESIAN_POINT('Ctrl Pts',(4.2331438885583,-9.4528281455708,5.63796190592881));
#90572=CARTESIAN_POINT('Ctrl Pts',(8.21364766592046,-6.30963225149706,5.71669871920578));
#90573=CARTESIAN_POINT('Ctrl Pts',(10.2245620898643,-1.65341984992491,5.79543553248275));
#90574=CARTESIAN_POINT('Ctrl Pts',(9.78368049639725,3.39927390393817,5.87417234575973));
#90575=CARTESIAN_POINT('Ctrl Pts',(6.99672396438769,7.63683971912566,5.95290915903669));
#90576=CARTESIAN_POINT('Ctrl Pts',(2.53198995887729,10.0431316817874,6.03164597231369));
#90577=CARTESIAN_POINT('Ctrl Pts',(-2.53990187331711,10.0411336811845,6.11038278559064));
#90578=CARTESIAN_POINT('Ctrl Pts',(-7.00273864350857,7.63132482733166,6.18911959886763));
#90579=CARTESIAN_POINT('Ctrl Pts',(-9.78635565189662,3.39156456286966,6.26785641214459));
#90580=CARTESIAN_POINT('Ctrl Pts',(-10.2232562335718,-1.66147498093125,
6.34659322542156));
#90581=CARTESIAN_POINT('Ctrl Pts',(-8.20867393528745,-6.3161015946277,6.42533003869855));
#90582=CARTESIAN_POINT('Ctrl Pts',(-4.22569495792512,-9.45616038633497,
6.50406685197551));
#90583=CARTESIAN_POINT('Ctrl Pts',(0.770583364441047,-10.3286818330304,
6.5828036652525));
#90584=CARTESIAN_POINT('Ctrl Pts',(5.58207986364352,-8.72443989751954,6.66154047852946));
#90585=CARTESIAN_POINT('Ctrl Pts',(9.05502307731348,-5.02812332772831,6.74027729180644));
#90586=CARTESIAN_POINT('Ctrl Pts',(10.3566195552168,-0.126089325581968,
6.8190141050834));
#90587=CARTESIAN_POINT('Ctrl Pts',(9.17475333260671,4.80618023125926,6.89775091836039));
#90588=CARTESIAN_POINT('Ctrl Pts',(5.79282969102316,8.58595313872173,6.97648773163736));
#90589=CARTESIAN_POINT('Ctrl Pts',(1.02181606777311,10.3068598056424,7.05522454491433));
#90590=CARTESIAN_POINT('Ctrl Pts',(-3.99422365473359,9.55623589733384,7.13396135819131));
#90591=CARTESIAN_POINT('Ctrl Pts',(-8.05246962888899,6.514077064738,7.21269817146827));
#90592=CARTESIAN_POINT('Ctrl Pts',(-10.1797758920949,1.9098769374614,7.29143498474526));
#90593=CARTESIAN_POINT('Ctrl Pts',(-9.86602563171077,-3.15230159787276,
7.37017179802222));
#90594=CARTESIAN_POINT('Ctrl Pts',(-7.186454504003,-7.45857484989058,7.44890861129921));
#90595=CARTESIAN_POINT('Ctrl Pts',(-2.78360952091465,-9.9763212240083,7.52764542457617));
#90596=CARTESIAN_POINT('Ctrl Pts',(2.28673033162688,-10.1017984299799,7.60638223785315));
#90597=CARTESIAN_POINT('Ctrl Pts',(6.80872432146195,-7.80491769616169,7.68511905113011));
#90598=CARTESIAN_POINT('Ctrl Pts',(9.69802215978954,-3.63645889812552,7.7638558644071));
#90599=CARTESIAN_POINT('Ctrl Pts',(10.261785476531,1.40400354813729,7.84259267768406));
#90600=CARTESIAN_POINT('Ctrl Pts',(8.36482680423332,6.10779335478084,7.92132949096105));
#90601=CARTESIAN_POINT('Ctrl Pts',(4.46202681915855,9.34696655576745,8.000066304238));
#90602=CARTESIAN_POINT('Ctrl Pts',(-0.510743643733886,10.3447865159176,
8.07880311751499));
#90603=CARTESIAN_POINT('Ctrl Pts',(-5.36104047688882,8.86198127591595,8.15753993079196));
#90604=CARTESIAN_POINT('Ctrl Pts',(-8.92578810266849,5.25411970512538,8.23627674406893));
#90605=CARTESIAN_POINT('Ctrl Pts',(-10.3501788574171,0.38634796363252,8.31501355734591));
#90606=CARTESIAN_POINT('Ctrl Pts',(-9.29265135698636,-4.57406798014904,
8.39375037062287));
#90607=CARTESIAN_POINT('Ctrl Pts',(-6.00679511367681,-8.43764656713195,
8.47248718389986));
#90608=CARTESIAN_POINT('Ctrl Pts',(-1.28054110979408,-10.2779220465838,
8.55122399717681));
#90609=CARTESIAN_POINT('Ctrl Pts',(3.75277989270658,-9.65360607267681,8.62996081045381));
#90610=CARTESIAN_POINT('Ctrl Pts',(7.88620408649619,-6.71440632041701,8.70869762373077));
#90611=CARTESIAN_POINT('Ctrl Pts',(10.1285581687469,-2.16512737542992,8.78743443700775));
#90612=CARTESIAN_POINT('Ctrl Pts',(9.9421374671065,2.90333768526539,8.86617125028472));
#90613=CARTESIAN_POINT('Ctrl Pts',(7.37164468178136,7.27559769469767,8.9449080635617));
#90614=CARTESIAN_POINT('Ctrl Pts',(3.03347041399593,9.90320778217525,9.02364487683867));
#90615=CARTESIAN_POINT('Ctrl Pts',(-2.03211404647875,10.156080918919,9.10238169011564));
#90616=CARTESIAN_POINT('Ctrl Pts',(-6.61040828539873,7.97357946156285,9.18111850339261));
#90617=CARTESIAN_POINT('Ctrl Pts',(-9.603561511421,3.8790557389497,9.25985531666959));
#90618=CARTESIAN_POINT('Ctrl Pts',(-10.2938313807125,-1.14564507373933,
9.33859212994656));
#90619=CARTESIAN_POINT('Ctrl Pts',(-8.51569482230081,-5.89562624518926,
9.41732894322354));
#90620=CARTESIAN_POINT('Ctrl Pts',(-4.69553959675684,-9.23186736390931,
9.4960657565005));
#90621=CARTESIAN_POINT('Ctrl Pts',(0.250581238043845,-10.3543554204337,
9.57480256977749));
#90622=CARTESIAN_POINT('Ctrl Pts',(5.13661401468883,-8.99392370401415,9.65353938305445));
#90623=CARTESIAN_POINT('Ctrl Pts',(8.7909138649284,-5.47679655902376,9.73227619633144));
#90624=CARTESIAN_POINT('Ctrl Pts',(10.3371989743949,-0.646362509196422,
9.8110130096084));
#90625=CARTESIAN_POINT('Ctrl Pts',(9.40467833611481,4.33906585842369,9.88974982288538));
#90626=CARTESIAN_POINT('Ctrl Pts',(6.21696547671049,8.28400913754416,9.96848663616235));
#90627=CARTESIAN_POINT('Ctrl Pts',(1.53845711309042,10.2424907537526,10.0472234494393));
#90628=CARTESIAN_POINT('Ctrl Pts',(-3.50896514529322,9.74487715359423,10.1259602627163));
#90629=CARTESIAN_POINT('Ctrl Pts',(-7.71495608438624,6.91049345166589,10.2046970759932));
#90630=CARTESIAN_POINT('Ctrl Pts',(-10.0709412788904,2.41900989800939,10.2834338892702));
#90631=CARTESIAN_POINT('Ctrl Pts',(-10.0119679155524,-2.65253946011637,
10.3621707025472));
#90632=CARTESIAN_POINT('Ctrl Pts',(-7.5521774956019,-7.0880238574972,10.4409075158241));
#90633=CARTESIAN_POINT('Ctrl Pts',(-3.28141477740401,-9.82383754895001,
10.5196443291011));
#90634=CARTESIAN_POINT('Ctrl Pts',(1.77621388302032,-10.2039468526297,10.5983811423781));
#90635=CARTESIAN_POINT('Ctrl Pts',(6.40791583028337,-8.13720356397264,10.6771179556551));
#90636=CARTESIAN_POINT('Ctrl Pts',(9.50303338650133,-4.11920181401277,10.755854768932));
#90637=CARTESIAN_POINT('Ctrl Pts',(10.3193736996929,0.886562787179303,10.834591582209));
#90638=CARTESIAN_POINT('Ctrl Pts',(8.66118267191835,5.67973431184827,10.913328395486));
#90639=CARTESIAN_POINT('Ctrl Pts',(4.9260857586507,9.11093552978749,10.992065208763));
#90640=CARTESIAN_POINT('Ctrl Pts',(0.0097394834735438,10.3573825009983,
11.0708020220399));
#90641=CARTESIAN_POINT('Ctrl Pts',(-4.90894226842936,9.1201838213247,11.1495388353169));
#90642=CARTESIAN_POINT('Ctrl Pts',(-8.65048557688362,5.69601320343043,11.2282756485939));
#90643=CARTESIAN_POINT('Ctrl Pts',(-10.3176881067681,0.905968686535361,
11.3070124618708));
#90644=CARTESIAN_POINT('Ctrl Pts',(-9.51076349197205,-4.10132233911171,
11.3857492751478));
#90645=CARTESIAN_POINT('Ctrl Pts',(-6.42320799566222,-8.12513791722861,
11.4644860884248));
#90646=CARTESIAN_POINT('Ctrl Pts',(-1.79540112777125,-10.2005883124418,
11.5432229017018));
#90647=CARTESIAN_POINT('Ctrl Pts',(3.26293345328981,-9.8299914755267,11.6219597149788));
#90648=CARTESIAN_POINT('Ctrl Pts',(7.5388338160908,-7.10221457172981,11.7006965282557));
#90649=CARTESIAN_POINT('Ctrl Pts',(10.0069616245548,-2.67136410363949,11.7794333415327));
#90650=CARTESIAN_POINT('Ctrl Pts',(10.075472858561,2.40006537534412,11.8581701548097));
#90651=CARTESIAN_POINT('Ctrl Pts',(7.72793888584071,6.89597184639239,11.9369069680867));
#90652=CARTESIAN_POINT('Ctrl Pts',(3.52728596127422,9.7382606700028,12.0156437813636));
#90653=CARTESIAN_POINT('Ctrl Pts',(-1.51919151754623,10.2453659896824,12.0943805946406));
#90654=CARTESIAN_POINT('Ctrl Pts',(-6.2013748897185,8.29568662659662,12.1731174079176));
#90655=CARTESIAN_POINT('Ctrl Pts',(-9.39650129813868,4.35674540036522,12.2518542211946));
#90656=CARTESIAN_POINT('Ctrl Pts',(-10.3383962959777,-0.626920375199499,
12.3305910344715));
#90657=CARTESIAN_POINT('Ctrl Pts',(-8.80119843467484,-5.46025395407599,
12.4093278477485));
#90658=CARTESIAN_POINT('Ctrl Pts',(-5.15351964706217,-8.98424745745961,
12.4880646610255));
#90659=CARTESIAN_POINT('Ctrl Pts',(-0.270054051639655,-10.3538658451188,
12.5668014743024));
#90660=CARTESIAN_POINT('Ctrl Pts',(4.67816907984897,-9.24068185741022,12.6455382875794));
#90661=CARTESIAN_POINT('Ctrl Pts',(8.50459196034266,-5.91163113849298,12.7242751008564));
#90662=CARTESIAN_POINT('Ctrl Pts',(10.2916585813938,-1.16500247791564,12.8030119141334));
#90663=CARTESIAN_POINT('Ctrl Pts',(9.61083980054881,3.86098762724155,12.8817487274103));
#90664=CARTESIAN_POINT('Ctrl Pts',(6.62539236765973,7.96113328013551,12.9604855406873));
#90665=CARTESIAN_POINT('Ctrl Pts',(2.05121081804228,10.1522411963798,13.0392223539643));
#90666=CARTESIAN_POINT('Ctrl Pts',(-3.01484025814591,9.90889526372077,13.1179591672413));
#90667=CARTESIAN_POINT('Ctrl Pts',(-7.35794855467586,7.28944855227533,13.1966959805182));
#90668=CARTESIAN_POINT('Ctrl Pts',(-9.93665962772858,2.92203055634167,13.2754327937952));
#90669=CARTESIAN_POINT('Ctrl Pts',(-10.1326121740638,-2.14607494266621,
13.3541696070722));
#90670=CARTESIAN_POINT('Ctrl Pts',(-7.89881780743255,-6.69956299877176,
13.4329064203492));
#90671=CARTESIAN_POINT('Ctrl Pts',(-3.77092862556512,-9.64653121232802,
13.5116432336261));
#90672=CARTESIAN_POINT('Ctrl Pts',(1.26120933535224,-10.2803121616975,13.5903800469031));
#90673=CARTESIAN_POINT('Ctrl Pts',(5.99091595511748,-8.4489285207205,13.6691168601801));
#90674=CARTESIAN_POINT('Ctrl Pts',(9.28403255271173,-4.59153641929518,13.747853673457));
#90675=CARTESIAN_POINT('Ctrl Pts',(10.3508871511966,0.36688187842646,13.826590486734));
#90676=CARTESIAN_POINT('Ctrl Pts',(8.93565364939284,5.23732383833744,13.905327300011));
#90677=CARTESIAN_POINT('Ctrl Pts',(5.37769757053005,8.85188318774262,13.984064113288));
#90678=CARTESIAN_POINT('Ctrl Pts',(0.530198001163546,10.3438076745988,14.0628009265649));
#90679=CARTESIAN_POINT('Ctrl Pts',(-4.44444025015958,9.35534168228432,14.1415377398419));
#90680=CARTESIAN_POINT('Ctrl Pts',(-8.3533251900779,6.12351413800404,14.2202745531189));
#90681=CARTESIAN_POINT('Ctrl Pts',(-10.2591268435809,1.42330022723409,14.2990113663959));
#90682=CARTESIAN_POINT('Ctrl Pts',(-9.70484403419201,-3.6182135649424,14.3777481796728));
#90683=CARTESIAN_POINT('Ctrl Pts',(-6.82339085374557,-7.79209884347897,
14.4564849929498));
#90684=CARTESIAN_POINT('Ctrl Pts',(-2.30572456476937,-10.0974799510048,
14.5352218062268));
#90685=CARTESIAN_POINT('Ctrl Pts',(2.76484230375725,-9.98153866720356,14.6139586195037));
#90686=CARTESIAN_POINT('Ctrl Pts',(7.1724145824397,-7.47207709991883,14.6926954327807));
#90687=CARTESIAN_POINT('Ctrl Pts',(9.86007970482085,-3.17085088645072,14.7714322460577));
#90688=CARTESIAN_POINT('Ctrl Pts',(10.1833497617602,1.8907286318198,14.8501690593347));
#90689=CARTESIAN_POINT('Ctrl Pts',(8.06470630002883,6.49892140464869,14.9289058726116));
#90690=CARTESIAN_POINT('Ctrl Pts',(4.01218883820157,9.54870713008499,15.0076426858886));
#90691=CARTESIAN_POINT('Ctrl Pts',(-1.00243032814087,10.3087632898786,15.0863794991656));
#90692=CARTESIAN_POINT('Ctrl Pts',(-5.77667199326021,8.596832428971,15.1651163124426));
#90693=CARTESIAN_POINT('Ctrl Pts',(-9.16569820734604,4.82342653114775,15.2438531257195));
#90694=CARTESIAN_POINT('Ctrl Pts',(-10.3568383736971,-0.106611587730943,
15.3225899389965));
#90695=CARTESIAN_POINT('Ctrl Pts',(-9.06446336801841,-5.01108481063476,
15.4013267522735));
#90696=CARTESIAN_POINT('Ctrl Pts',(-5.59847789469375,-8.71392634764388,
15.4800635655504));
#90697=CARTESIAN_POINT('Ctrl Pts',(-0.790006974550176,-10.3272143441326,
15.5588003788274));
#90698=CARTESIAN_POINT('Ctrl Pts',(4.20790344793164,-9.46409085451224,15.6375371921044));
#90699=CARTESIAN_POINT('Ctrl Pts',(8.19678083559,-6.33152833546188,15.7162740053814));
#90700=CARTESIAN_POINT('Ctrl Pts',(10.2201134467006,-1.68069874342431,15.7950108186583));
#90701=CARTESIAN_POINT('Ctrl Pts',(9.79271680154967,3.3731535355307,15.8737476319353));
#90702=CARTESIAN_POINT('Ctrl Pts',(7.01707835958532,7.6181414022353,15.9524844452123));
#90703=CARTESIAN_POINT('Ctrl Pts',(2.55878156758079,10.0363391742379,16.0312212584893));
#90704=CARTESIAN_POINT('Ctrl Pts',(-2.51309753742156,10.0478757901385,16.1099580717662));
#90705=CARTESIAN_POINT('Ctrl Pts',(-6.98234911873795,7.64998483123455,16.1886948850432));
#90706=CARTESIAN_POINT('Ctrl Pts',(-9.77727023854604,3.41766789014466,16.2674316983202));
#90707=CARTESIAN_POINT('Ctrl Pts',(-10.2276535660293,-1.63418776815829,
16.3461685115972));
#90708=CARTESIAN_POINT('Ctrl Pts',(-8.22549955600462,-6.29417383024248,
16.4249053248741));
#90709=CARTESIAN_POINT('Ctrl Pts',(-4.25091417271837,-9.44485022414144,
16.5036421381511));
#90710=CARTESIAN_POINT('Ctrl Pts',(0.743017991801421,-10.3307014064138,
16.5823789514281));
#90711=CARTESIAN_POINT('Ctrl Pts',(5.55877836081692,-8.73930489202781,16.6611157647051));
#90712=CARTESIAN_POINT('Ctrl Pts',(9.04157302787004,-5.05226925709063,16.739852577982));
#90713=CARTESIAN_POINT('Ctrl Pts',(10.3562461980019,-0.1537260051618,16.818589391259));
#90714=CARTESIAN_POINT('Ctrl Pts',(9.18754622001517,4.78167970197118,16.897326204536));
#90715=CARTESIAN_POINT('Ctrl Pts',(5.81572111097091,8.57046430229322,16.976063017813));
#90716=CARTESIAN_POINT('Ctrl Pts',(1.04931686630384,10.3040959400471,17.0547998310899));
#90717=CARTESIAN_POINT('Ctrl Pts',(-3.96870819410001,9.56686143762709,17.1335366443669));
#90718=CARTESIAN_POINT('Ctrl Pts',(-8.03505764881968,6.5355408136042,17.2122734576439));
#90719=CARTESIAN_POINT('Ctrl Pts',(-10.1746433338992,1.93703830392091,17.2910102709208));
#90720=CARTESIAN_POINT('Ctrl Pts',(-9.87440201338592,-3.12596799325867,
17.3697470841978));
#90721=CARTESIAN_POINT('Ctrl Pts',(-7.2063336236016,-7.43935994600553,17.4484838974748));
#90722=CARTESIAN_POINT('Ctrl Pts',(-2.8102197948658,-9.96887867130796,17.5272207107518));
#90723=CARTESIAN_POINT('Ctrl Pts',(2.25976083640424,-10.1078236336547,17.6059575240287));
#90724=CARTESIAN_POINT('Ctrl Pts',(6.787880338596,-7.82313910163977,17.6846943373057));
#90725=CARTESIAN_POINT('Ctrl Pts',(9.68826788900902,-3.66217042766011,17.7634311505827));
#90726=CARTESIAN_POINT('Ctrl Pts',(10.265525559982,1.37630858348745,17.8421679638596));
#90727=CARTESIAN_POINT('Ctrl Pts',(8.38104198679141,6.0860905800779,17.9209047771366));
#90728=CARTESIAN_POINT('Ctrl Pts',(5.7850274219278,8.25090580895841,17.9733959859879));
#90729=CARTESIAN_POINT('Ctrl Pts',(4.30727168806404,8.96120073717495,17.9996415904136));
#90730=CARTESIAN_POINT('Ctrl Pts',(5.66080476763815,-7.94023422788095,3.77985954388849));
#90731=CARTESIAN_POINT('Ctrl Pts',(6.97048919982341,-7.00652936557954,3.80611096059054));
#90732=CARTESIAN_POINT('Ctrl Pts',(9.11754829327675,-4.47995572025153,3.85860798171824));
#90733=CARTESIAN_POINT('Ctrl Pts',(10.1509147771437,0.3872203397439,3.93735060727159));
#90734=CARTESIAN_POINT('Ctrl Pts',(8.75017416132892,5.15987357781277,4.01608742054857));
#90735=CARTESIAN_POINT('Ctrl Pts',(5.25114117670495,8.69586401537322,4.09482423382554));
#90736=CARTESIAN_POINT('Ctrl Pts',(0.492935646717676,10.1463010928695,4.17356104710252));
#90737=CARTESIAN_POINT('Ctrl Pts',(-4.38348523304028,9.16387910691155,4.25229786037949));
#90738=CARTESIAN_POINT('Ctrl Pts',(-8.20876332281697,5.98391948609178,4.33103467365646));
#90739=CARTESIAN_POINT('Ctrl Pts',(-10.0656264785274,1.36909281366648,4.40977148693343));
#90740=CARTESIAN_POINT('Ctrl Pts',(-9.5088038985219,-3.57405841537725,4.48850830021041));
#90741=CARTESIAN_POINT('Ctrl Pts',(-6.6718211819854,-7.66015727834556,4.56724511348738));
#90742=CARTESIAN_POINT('Ctrl Pts',(-2.23497052865009,-9.90939705925389,
4.64598192676436));
#90743=CARTESIAN_POINT('Ctrl Pts',(2.73781403538504,-9.78241253852996,4.72471874004133));
#90744=CARTESIAN_POINT('Ctrl Pts',(7.05408536136851,-7.30965877574727,4.8034555533183));
#90745=CARTESIAN_POINT('Ctrl Pts',(9.67882419400217,-3.08408657465411,4.88219236659527));
#90746=CARTESIAN_POINT('Ctrl Pts',(9.9826321066513,1.88103286968048,4.96092917987225));
#90747=CARTESIAN_POINT('Ctrl Pts',(7.89265751896129,6.39509078671749,5.03966599314922));
#90748=CARTESIAN_POINT('Ctrl Pts',(3.91006532886167,9.37563957418694,5.1184028064262));
#90749=CARTESIAN_POINT('Ctrl Pts',(-1.01013989149727,10.1079595422914,5.19713961970317));
#90750=CARTESIAN_POINT('Ctrl Pts',(-5.68811889586561,8.41644413750198,5.27587643298014));
#90751=CARTESIAN_POINT('Ctrl Pts',(-9.00211701563495,4.70670987181179,5.35461324625711));
#90752=CARTESIAN_POINT('Ctrl Pts',(-10.1574549933796,-0.131668584338251,
5.43335005953409));
#90753=CARTESIAN_POINT('Ctrl Pts',(-8.87708888151934,-4.93847360476317,
5.51208687281107));
#90754=CARTESIAN_POINT('Ctrl Pts',(-5.46804371464078,-8.56105872535287,
5.59082368608803));
#90755=CARTESIAN_POINT('Ctrl Pts',(-0.747790528884207,-10.1307471531937,
5.66956049936502));
#90756=CARTESIAN_POINT('Ctrl Pts',(4.15177887842533,-9.27113589080745,5.74829731264197));
#90757=CARTESIAN_POINT('Ctrl Pts',(8.05577362639801,-6.18835518046099,5.82703412591897));
#90758=CARTESIAN_POINT('Ctrl Pts',(10.02803638227,-1.62163956407002,5.90577093919592));
#90759=CARTESIAN_POINT('Ctrl Pts',(9.59562894802464,3.33393665981891,5.98450775247291));
#90760=CARTESIAN_POINT('Ctrl Pts',(6.86224034388074,7.49005247128131,6.06324456574988));
#90761=CARTESIAN_POINT('Ctrl Pts',(2.48332272854344,9.85009323741409,6.14198137902686));
#90762=CARTESIAN_POINT('Ctrl Pts',(-2.49108256854038,9.84813364026348,6.22071819230382));
#90763=CARTESIAN_POINT('Ctrl Pts',(-6.86813941520742,7.48464358089862,6.29945500558081));
#90764=CARTESIAN_POINT('Ctrl Pts',(-9.59825268451726,3.3263754995424,6.37819181885778));
#90765=CARTESIAN_POINT('Ctrl Pts',(-10.0267556257647,-1.62953986787626,
6.45692863213474));
#90766=CARTESIAN_POINT('Ctrl Pts',(-8.05089549554946,-6.1947001767272,6.53566544541173));
#90767=CARTESIAN_POINT('Ctrl Pts',(-4.14447312325044,-9.27440408276756,
6.6144022586887));
#90768=CARTESIAN_POINT('Ctrl Pts',(0.755772026837927,-10.1301548459661,
6.69313907196567));
#90769=CARTESIAN_POINT('Ctrl Pts',(5.47478703433619,-8.55674795050467,6.77187588524263));
#90770=CARTESIAN_POINT('Ctrl Pts',(8.88097701040999,-4.93147806447222,6.85061269851962));
#90771=CARTESIAN_POINT('Ctrl Pts',(10.1575555788348,-0.123665770058277,
6.92934951179658));
#90772=CARTESIAN_POINT('Ctrl Pts',(8.99840593749619,4.71380092322904,7.00808632507357));
#90773=CARTESIAN_POINT('Ctrl Pts',(5.68148605165791,8.42092303756649,7.08682313835054));
#90774=CARTESIAN_POINT('Ctrl Pts',(1.00217580113035,10.1087522584852,7.16555995162751));
#90775=CARTESIAN_POINT('Ctrl Pts',(-3.91745091638676,9.37255604824544,7.2442967649045));
#90776=CARTESIAN_POINT('Ctrl Pts',(-7.89769358295277,6.38887037195061,7.32303357818146));
#90777=CARTESIAN_POINT('Ctrl Pts',(-9.98411101737842,1.87316730498484,7.40177039145844));
#90778=CARTESIAN_POINT('Ctrl Pts',(-9.67639133232721,-3.09171139394741,
7.4805072047354));
#90779=CARTESIAN_POINT('Ctrl Pts',(-7.04832408393412,-7.31521402063096,
7.55924401801238));
#90780=CARTESIAN_POINT('Ctrl Pts',(-2.73010592575272,-9.7845669395212,7.63798083128934));
#90781=CARTESIAN_POINT('Ctrl Pts',(2.24277722218803,-9.90763235548413,7.71671764456634));
#90782=CARTESIAN_POINT('Ctrl Pts',(6.6778542310533,-7.6548998313894,7.7954544578433));
#90783=CARTESIAN_POINT('Ctrl Pts',(9.51161704527546,-3.56656273515928,7.87419127112028));
#90784=CARTESIAN_POINT('Ctrl Pts',(10.0645443004072,1.37701727837461,7.95292808439723));
#90785=CARTESIAN_POINT('Ctrl Pts',(8.20404695936982,5.99039581732761,8.03166489767423));
#90786=CARTESIAN_POINT('Ctrl Pts',(4.37626246365533,9.16730906040605,8.11040171095119));
#90787=CARTESIAN_POINT('Ctrl Pts',(-0.500926670145997,10.1459499816891,
8.18913852422817));
#90788=CARTESIAN_POINT('Ctrl Pts',(-5.25799623265597,8.69164565414265,8.26787533750514));
#90789=CARTESIAN_POINT('Ctrl Pts',(-8.75422605362463,5.15313057876873,8.34661215078212));
#90790=CARTESIAN_POINT('Ctrl Pts',(-10.1512386773093,0.378921992107938,
8.42534896405908));
#90791=CARTESIAN_POINT('Ctrl Pts',(-9.11403785087162,-4.48615008806894,
8.50408577733605));
#90792=CARTESIAN_POINT('Ctrl Pts',(-5.89133885748571,-8.27546705788142,
8.58282259061303));
#90793=CARTESIAN_POINT('Ctrl Pts',(-1.25592790430966,-10.0803707103944,
8.66155940389002));
#90794=CARTESIAN_POINT('Ctrl Pts',(3.68064793073329,-9.46805467716523,8.74029621716696));
#90795=CARTESIAN_POINT('Ctrl Pts',(7.73462382078804,-6.58534911076854,8.81903303044396));
#90796=CARTESIAN_POINT('Ctrl Pts',(9.93387774688354,-2.12351158927219,8.89776984372092));
#90797=CARTESIAN_POINT('Ctrl Pts',(9.75104022660372,2.84753280208635,8.97650665699791));
#90798=CARTESIAN_POINT('Ctrl Pts',(7.22995473217883,7.13575385859452,9.05524347027487));
#90799=CARTESIAN_POINT('Ctrl Pts',(2.97516425727868,9.71285880686077,9.13398028355186));
#90800=CARTESIAN_POINT('Ctrl Pts',(-1.99305490170695,9.96087148389051,9.21271709682881));
#90801=CARTESIAN_POINT('Ctrl Pts',(-6.48335001587512,7.82031975890077,9.2914539101058));
#90802=CARTESIAN_POINT('Ctrl Pts',(-9.41897201948297,3.80449663635003,9.37019072338278));
#90803=CARTESIAN_POINT('Ctrl Pts',(-10.095974252146,-1.12362469704354,9.44892753665973));
#90804=CARTESIAN_POINT('Ctrl Pts',(-8.35201515212025,-5.7823067592921,9.52766434993672));
#90805=CARTESIAN_POINT('Ctrl Pts',(-4.6052869058661,-9.05442218335658,9.60640116321369));
#90806=CARTESIAN_POINT('Ctrl Pts',(0.245764830780288,-10.1553349628534,
9.68513797649068));
#90807=CARTESIAN_POINT('Ctrl Pts',(5.03788345830874,-8.82105202457739,9.76387478976763));
#90808=CARTESIAN_POINT('Ctrl Pts',(8.621944225689,-5.3715273739328,9.84261160304463));
#90809=CARTESIAN_POINT('Ctrl Pts',(10.1385082798565,-0.633938813358303,
9.92134841632157));
#90810=CARTESIAN_POINT('Ctrl Pts',(9.2239115660119,4.25566492832712,10.0000852295986));
#90811=CARTESIAN_POINT('Ctrl Pts',(6.09746954831168,8.12478268430691,10.0788220428756));
#90812=CARTESIAN_POINT('Ctrl Pts',(1.50888651925018,10.0456204403623,10.1575588561525));
#90813=CARTESIAN_POINT('Ctrl Pts',(-3.44151953226439,9.55757144199531,10.2362956694295));
#90814=CARTESIAN_POINT('Ctrl Pts',(-7.5666673664718,6.77766726278093,10.3150324827065));
#90815=CARTESIAN_POINT('Ctrl Pts',(-9.87736830788399,2.37251425079188,10.3937692959835));
#90816=CARTESIAN_POINT('Ctrl Pts',(-9.81952846810011,-2.60155515489731,
10.4725061092604));
#90817=CARTESIAN_POINT('Ctrl Pts',(-7.40701753538492,-6.95178536710547,
10.5512429225374));
#90818=CARTESIAN_POINT('Ctrl Pts',(-3.21834289663573,-9.63501414422814,
10.6299797358144));
#90819=CARTESIAN_POINT('Ctrl Pts',(1.74207338026517,-10.0078173892998,10.7087165490914));
#90820=CARTESIAN_POINT('Ctrl Pts',(6.2847496563502,-7.98079885204531,10.7874533623683));
#90821=CARTESIAN_POINT('Ctrl Pts',(9.32037613974987,-4.0400268778045,10.8661901756453));
#90822=CARTESIAN_POINT('Ctrl Pts',(10.121025623713,0.869522215901469,10.9449269889223));
#90823=CARTESIAN_POINT('Ctrl Pts',(8.49470658832261,5.57056447212576,11.0236638021992));
#90824=CARTESIAN_POINT('Ctrl Pts',(4.83140175351872,8.93581477291791,11.1024006154762));
#90825=CARTESIAN_POINT('Ctrl Pts',(0.00955228143353725,10.1583038600802,
11.1811374287532));
#90826=CARTESIAN_POINT('Ctrl Pts',(-4.81458777731637,8.94488530358647,11.2598742420302));
#90827=CARTESIAN_POINT('Ctrl Pts',(-8.48421510152349,5.58653046808861,11.3386110553071));
#90828=CARTESIAN_POINT('Ctrl Pts',(-10.1193724294707,0.888555115605388,
11.4173478685841));
#90829=CARTESIAN_POINT('Ctrl Pts',(-9.32795766531719,-4.02249106324075,
11.4960846818611));
#90830=CARTESIAN_POINT('Ctrl Pts',(-6.29974789191615,-7.96896511838893,
11.5748214951381));
#90831=CARTESIAN_POINT('Ctrl Pts',(-1.7608918281113,-10.0045234034157,11.653558308415));
#90832=CARTESIAN_POINT('Ctrl Pts',(3.20021680096722,-9.64104978654342,11.732295121692));
#90833=CARTESIAN_POINT('Ctrl Pts',(7.39393033395425,-6.965703322453,11.811031934969));
#90834=CARTESIAN_POINT('Ctrl Pts',(9.81461840272779,-2.62001797105254,11.8897687482459));
#90835=CARTESIAN_POINT('Ctrl Pts',(9.88181278632787,2.35393385968446,11.9685055615229));
#90836=CARTESIAN_POINT('Ctrl Pts',(7.57940062626177,6.76342477642978,12.0472423747999));
#90837=CARTESIAN_POINT('Ctrl Pts',(3.4594882049171,9.55108213344652,12.1259791880769));
#90838=CARTESIAN_POINT('Ctrl Pts',(-1.48999122658679,10.0484404115512,12.2047160013539));
#90839=CARTESIAN_POINT('Ctrl Pts',(-6.08217862707687,8.13623572102791,12.2834528146308));
#90840=CARTESIAN_POINT('Ctrl Pts',(-9.21589169840261,4.27300465283104,12.3621896279078));
#90841=CARTESIAN_POINT('Ctrl Pts',(-10.1396825877914,-0.614870375477425,
12.4409264411848));
#90842=CARTESIAN_POINT('Ctrl Pts',(-8.63203111632417,-5.35530273342346,
12.5196632544618));
#90843=CARTESIAN_POINT('Ctrl Pts',(-5.05446414851482,-8.81156176458976,
12.5984000677387));
#90844=CARTESIAN_POINT('Ctrl Pts',(-0.264863358569285,-10.1548547976369,
12.6771368810157));
#90845=CARTESIAN_POINT('Ctrl Pts',(4.58825026664382,-9.06306725399544,12.7558736942927));
#90846=CARTESIAN_POINT('Ctrl Pts',(8.34112569761994,-5.79800402348134,12.8346105075696));
#90847=CARTESIAN_POINT('Ctrl Pts',(10.0938432160754,-1.14261003369072,12.9133473208466));
#90848=CARTESIAN_POINT('Ctrl Pts',(9.42611041304279,3.78677581075619,12.9920841341236));
#90849=CARTESIAN_POINT('Ctrl Pts',(6.49804608997074,7.80811280479587,13.0708209474006));
#90850=CARTESIAN_POINT('Ctrl Pts',(2.0117846153455,9.95710556443289,13.1495577606775));
#90851=CARTESIAN_POINT('Ctrl Pts',(-2.95689219056041,9.71843696965745,13.2282945739545));
#90852=CARTESIAN_POINT('Ctrl Pts',(-7.2165218575283,7.14933848965189,13.3070313872315));
#90853=CARTESIAN_POINT('Ctrl Pts',(-9.74566767645484,2.8658663785852,13.3857682005084));
#90854=CARTESIAN_POINT('Ctrl Pts',(-9.93785383040227,-2.1048253622,13.4645050137854));
#90855=CARTESIAN_POINT('Ctrl Pts',(-7.74699509413485,-6.57079109173712,
13.5432418270624));
#90856=CARTESIAN_POINT('Ctrl Pts',(-3.69844782786315,-9.46111580229183,
13.6219786403394));
#90857=CARTESIAN_POINT('Ctrl Pts',(1.23696770476934,-10.0827148852459,13.7007154536163));
#90858=CARTESIAN_POINT('Ctrl Pts',(5.8757649113007,-8.28653216170243,13.7794522668933));
#90859=CARTESIAN_POINT('Ctrl Pts',(9.10558470812793,-4.5032827673719,13.8581890801703));
#90860=CARTESIAN_POINT('Ctrl Pts',(10.1519333570157,0.359830063382712,13.9369258934473));
#90861=CARTESIAN_POINT('Ctrl Pts',(8.76390197525464,5.13665754435015,14.0156627067242));
#90862=CARTESIAN_POINT('Ctrl Pts',(5.27433316127832,8.68174166072924,14.0943995200012));
#90863=CARTESIAN_POINT('Ctrl Pts',(0.520007096513734,10.1449899546218,14.1731363332782));
#90864=CARTESIAN_POINT('Ctrl Pts',(-4.35901392506651,9.1755232091079,14.2518731465552));
#90865=CARTESIAN_POINT('Ctrl Pts',(-8.19276641706479,6.00581443229949,14.3306099598321));
#90866=CARTESIAN_POINT('Ctrl Pts',(-10.0619367688849,1.39594305713547,14.4093467731091));
#90867=CARTESIAN_POINT('Ctrl Pts',(-9.51830779683059,-3.54866809445402,
14.4880835863861));
#90868=CARTESIAN_POINT('Ctrl Pts',(-6.69223885878102,-7.64232736912144,
14.566820399663));
#90869=CARTESIAN_POINT('Ctrl Pts',(-2.26140636829051,-9.90339688173995,
14.64555721294));
#90870=CARTESIAN_POINT('Ctrl Pts',(2.71169943217442,-9.78968409854713,14.724294026217));
#90871=CARTESIAN_POINT('Ctrl Pts',(7.03455402287886,-7.32845674470418,14.803030839494));
#90872=CARTESIAN_POINT('Ctrl Pts',(9.67055969174893,-3.1099041477387,14.881767652771));
#90873=CARTESIAN_POINT('Ctrl Pts',(9.98761619390468,1.8543870478017,14.9605044660479));
#90874=CARTESIAN_POINT('Ctrl Pts',(7.90969505375507,6.37400601791403,15.0392412793249));
#90875=CARTESIAN_POINT('Ctrl Pts',(3.93507079211811,9.36517199098984,15.1179780926019));
#90876=CARTESIAN_POINT('Ctrl Pts',(-0.983162673661375,10.1106191559627,
15.1967149058789));
#90877=CARTESIAN_POINT('Ctrl Pts',(-5.66563892005498,8.43159321761664,15.2754517191558));
#90878=CARTESIAN_POINT('Ctrl Pts',(-8.9895248602665,4.73071573299997,15.3541885324328));
#90879=CARTESIAN_POINT('Ctrl Pts',(-10.157770191418,-0.104562412662874,
15.4329253457097));
#90880=CARTESIAN_POINT('Ctrl Pts',(-8.89023584984156,-4.91476704371533,
15.5116621589867));
#90881=CARTESIAN_POINT('Ctrl Pts',(-5.49086987979438,-8.54643648095388,
15.5903989722637));
#90882=CARTESIAN_POINT('Ctrl Pts',(-0.774822296877582,-10.1287155635864,
15.6691357855407));
#90883=CARTESIAN_POINT('Ctrl Pts',(4.12702358282595,-9.28218211988161,15.7478725988177));
#90884=CARTESIAN_POINT('Ctrl Pts',(8.039230992423,-6.20983040108157,15.8266094120946));
#90885=CARTESIAN_POINT('Ctrl Pts',(10.0236732462154,-1.64839413155914,15.9053462253716));
#90886=CARTESIAN_POINT('Ctrl Pts',(9.60449156688632,3.30831834947895,15.9840830386486));
#90887=CARTESIAN_POINT('Ctrl Pts',(6.88220350844336,7.47171355364201,16.0628198519255));
#90888=CARTESIAN_POINT('Ctrl Pts',(2.50959937730913,9.84343128825342,16.1415566652025));
#90889=CARTESIAN_POINT('Ctrl Pts',(-2.46479343721129,9.85474615953707,16.2202934784795));
#90890=CARTESIAN_POINT('Ctrl Pts',(-6.84814179629524,7.50294492196215,16.2990302917565));
#90891=CARTESIAN_POINT('Ctrl Pts',(-9.58934190136322,3.35197709629649,16.3777671050334));
#90892=CARTESIAN_POINT('Ctrl Pts',(-10.0310684373532,-1.60277714101786,
16.4565039183104));
#90893=CARTESIAN_POINT('Ctrl Pts',(-8.06739771199873,-6.17319388461373,
16.5352407315874));
#90894=CARTESIAN_POINT('Ctrl Pts',(-4.16920760099691,-9.26331131253746,
16.6139775448644));
#90895=CARTESIAN_POINT('Ctrl Pts',(0.728736486607317,-10.1321356012481,
16.6927143581413));
#90896=CARTESIAN_POINT('Ctrl Pts',(5.45193340832726,-8.5713272258263,16.7714511714183));
#90897=CARTESIAN_POINT('Ctrl Pts',(8.8677854835772,-4.95515988634399,16.8501879846953));
#90898=CARTESIAN_POINT('Ctrl Pts',(10.1571893978969,-0.150771246642594,
16.9289247979723));
#90899=CARTESIAN_POINT('Ctrl Pts',(9.01095293356691,4.68977131717587,17.0076616112492));
#90900=CARTESIAN_POINT('Ctrl Pts',(5.7039374769669,8.40573191115353,17.0863984245262));
#90901=CARTESIAN_POINT('Ctrl Pts',(1.02914800842723,10.1060415169882,17.1651352378032));
#90902=CARTESIAN_POINT('Ctrl Pts',(-3.89242588692388,9.38297735565258,17.2438720510802));
#90903=CARTESIAN_POINT('Ctrl Pts',(-7.88061627753002,6.40992156736009,17.3226088643571));
#90904=CARTESIAN_POINT('Ctrl Pts',(-9.9790771117823,1.89980660441441,17.4013456776341));
#90905=CARTESIAN_POINT('Ctrl Pts',(-9.684606712062,-3.06588394600143,17.4800824909111));
#90906=CARTESIAN_POINT('Ctrl Pts',(-7.06782110814213,-7.29636844528527,
17.5588193041881));
#90907=CARTESIAN_POINT('Ctrl Pts',(-2.75620472519069,-9.77726743968932,
17.637556117465));
#90908=CARTESIAN_POINT('Ctrl Pts',(2.21632610604956,-9.91354174907297,17.716292930742));
#90909=CARTESIAN_POINT('Ctrl Pts',(6.65741088915815,-7.67277100430263,17.795029744019));
#90910=CARTESIAN_POINT('Ctrl Pts',(9.50205026076092,-3.59178006489433,17.8737665572959));
#90911=CARTESIAN_POINT('Ctrl Pts',(10.0682124959338,1.34985463701419,17.9525033705729));
#90912=CARTESIAN_POINT('Ctrl Pts',(8.21995047085605,5.96911019038295,18.0312401838499));
#90913=CARTESIAN_POINT('Ctrl Pts',(5.67383374951871,8.09231563285626,18.0837313927012));
#90914=CARTESIAN_POINT('Ctrl Pts',(4.22448187184914,8.7889580239625,18.1099769971269));
#90915=CARTESIAN_POINT('Ctrl Pts',(5.54986643234452,-7.78462448629111,3.89019495060166));
#90916=CARTESIAN_POINT('Ctrl Pts',(6.83388415871134,-6.86921802277418,3.91644636730371));
#90917=CARTESIAN_POINT('Ctrl Pts',(8.93886599082429,-4.39215922307585,3.96894338843142));
#90918=CARTESIAN_POINT('Ctrl Pts',(9.95198094471023,0.379631740305084,4.04768601398477));
#90919=CARTESIAN_POINT('Ctrl Pts',(8.57869151975529,5.05875230468204,4.12642282726174));
#90920=CARTESIAN_POINT('Ctrl Pts',(5.14823127529553,8.52544572373377,4.20515964053872));
#90921=CARTESIAN_POINT('Ctrl Pts',(0.48327527821911,9.94745767769539,4.28389645381569));
#90922=CARTESIAN_POINT('Ctrl Pts',(-4.29757932840324,8.9842888304963,4.36263326709267));
#90923=CARTESIAN_POINT('Ctrl Pts',(-8.04789104842608,5.86664886935661,4.44137008036965));
#90924=CARTESIAN_POINT('Ctrl Pts',(-9.86836409428141,1.34226184460021,4.52010689364661));
#90925=CARTESIAN_POINT('Ctrl Pts',(-9.32245391500608,-3.50401535487271,
4.59884370692359));
#90926=CARTESIAN_POINT('Ctrl Pts',(-6.54106932501662,-7.51003638009355,
4.67758052020056));
#90927=CARTESIAN_POINT('Ctrl Pts',(-2.1911704118723,-9.71519640075353,4.75631733347753));
#90928=CARTESIAN_POINT('Ctrl Pts',(2.6841593795726,-9.59070047518796,4.83505414675451));
#90929=CARTESIAN_POINT('Ctrl Pts',(6.9158420339386,-7.16640681609978,4.91379096003148));
#90930=CARTESIAN_POINT('Ctrl Pts',(9.48914221630516,-3.02364579908635,4.99252777330845));
#90931=CARTESIAN_POINT('Ctrl Pts',(9.7869962150742,1.84416909080794,5.07126458658543));
#90932=CARTESIAN_POINT('Ctrl Pts',(7.73798016792419,6.26976218856729,5.15000139986241));
#90933=CARTESIAN_POINT('Ctrl Pts',(3.83343733049769,9.19189929531005,5.22873821313939));
#90934=CARTESIAN_POINT('Ctrl Pts',(-0.990343547589242,9.90986753048978,
5.30747502641634));
#90935=CARTESIAN_POINT('Ctrl Pts',(-5.5766452684996,8.25150181215553,5.38621183969333));
#90936=CARTESIAN_POINT('Ctrl Pts',(-8.82569689220261,4.61446953155593,5.46494865297029));
#90937=CARTESIAN_POINT('Ctrl Pts',(-9.95839298823366,-0.12908819265254,
5.54368546624728));
#90938=CARTESIAN_POINT('Ctrl Pts',(-8.70311901271208,-4.84169124552408,
5.62242227952423));
#90939=CARTESIAN_POINT('Ctrl Pts',(-5.36088303839152,-8.39328229738432,
5.70115909280123));
#90940=CARTESIAN_POINT('Ctrl Pts',(-0.73313560969372,-9.93220855831381,
5.77989590607818));
#90941=CARTESIAN_POINT('Ctrl Pts',(4.07041386829234,-9.08944363604411,5.85863271935516));
#90942=CARTESIAN_POINT('Ctrl Pts',(7.89789958687557,-6.06707810942492,5.93736953263214));
#90943=CARTESIAN_POINT('Ctrl Pts',(9.83151067467579,-1.58985927821512,6.0161063459091));
#90944=CARTESIAN_POINT('Ctrl Pts',(9.40757739965206,3.26859941569965,6.0948431591861));
#90945=CARTESIAN_POINT('Ctrl Pts',(6.72775672337378,7.34326522343693,6.17357997246305));
#90946=CARTESIAN_POINT('Ctrl Pts',(2.4346554982096,9.6570547930408,6.25231678574004));
#90947=CARTESIAN_POINT('Ctrl Pts',(-2.44226326376367,9.65513359934245,6.331053599017));
#90948=CARTESIAN_POINT('Ctrl Pts',(-6.73354018690624,7.33796233446559,6.40979041229398));
#90949=CARTESIAN_POINT('Ctrl Pts',(-9.41014971713789,3.26118643621514,6.48852722557094));
#90950=CARTESIAN_POINT('Ctrl Pts',(-9.83025501795751,-1.59760475482128,
6.56726403884793));
#90951=CARTESIAN_POINT('Ctrl Pts',(-7.89311705581146,-6.07329875882669,
6.64600085212489));
#90952=CARTESIAN_POINT('Ctrl Pts',(-4.06325128857577,-9.09264777920014,
6.72473766540188));
#90953=CARTESIAN_POINT('Ctrl Pts',(0.740960689234815,-9.93162785890187,
6.80347447867885));
#90954=CARTESIAN_POINT('Ctrl Pts',(5.36749420502885,-8.3890560034898,6.88221129195582));
#90955=CARTESIAN_POINT('Ctrl Pts',(8.70693094350651,-4.83483280121613,6.9609481052328));
#90956=CARTESIAN_POINT('Ctrl Pts',(9.95849160245273,-0.121242214534584,
7.03968491850977));
#90957=CARTESIAN_POINT('Ctrl Pts',(8.82205854238565,4.62142161519883,7.11842173178673));
#90958=CARTESIAN_POINT('Ctrl Pts',(5.57014241229265,8.25589293641125,7.19715854506373));
#90959=CARTESIAN_POINT('Ctrl Pts',(0.982535534487584,9.91064471132812,7.27589535834069));
#90960=CARTESIAN_POINT('Ctrl Pts',(-3.84067817803991,9.18887619915703,7.35463217161766));
#90961=CARTESIAN_POINT('Ctrl Pts',(-7.74291753701654,6.26366367916321,7.43336898489463));
#90962=CARTESIAN_POINT('Ctrl Pts',(-9.78844614266187,1.83645767250828,7.51210579817161));
#90963=CARTESIAN_POINT('Ctrl Pts',(-9.48675703294365,-3.03112119002206,
7.59084261144859));
#90964=CARTESIAN_POINT('Ctrl Pts',(-6.91019366386524,-7.17185319137134,
7.66957942472556));
#90965=CARTESIAN_POINT('Ctrl Pts',(-2.67660233059081,-9.5928126550341,7.74831623800253));
#90966=CARTESIAN_POINT('Ctrl Pts',(2.19882411274918,-9.71346628098845,7.8270530512795));
#90967=CARTESIAN_POINT('Ctrl Pts',(6.54698414064464,-7.50488196661709,7.90578986455649));
#90968=CARTESIAN_POINT('Ctrl Pts',(9.32521193076139,-3.49666657219303,7.98452667783345));
#90969=CARTESIAN_POINT('Ctrl Pts',(9.86730312428339,1.35003100861192,8.06326349111042));
#90970=CARTESIAN_POINT('Ctrl Pts',(8.04326711450635,5.87299827987438,8.14200030438739));
#90971=CARTESIAN_POINT('Ctrl Pts',(4.29049810815211,8.98765156504466,8.22073711766438));
#90972=CARTESIAN_POINT('Ctrl Pts',(-0.491109696558105,9.94711344746069,
8.29947393094134));
#90973=CARTESIAN_POINT('Ctrl Pts',(-5.15495198842312,8.52131003236937,8.37821074421831));
#90974=CARTESIAN_POINT('Ctrl Pts',(-8.58266400458077,5.05214145241206,8.4569475574953));
#90975=CARTESIAN_POINT('Ctrl Pts',(-9.95229849720142,0.371496020583359,
8.53568437077227));
#90976=CARTESIAN_POINT('Ctrl Pts',(-8.93542434475686,-4.39823219598886,
8.61442118404923));
#90977=CARTESIAN_POINT('Ctrl Pts',(-5.7758826012946,-8.11328754863087,8.69315799732622));
#90978=CARTESIAN_POINT('Ctrl Pts',(-1.23131469882525,-9.88281937420509,
8.77189481060318));
#90979=CARTESIAN_POINT('Ctrl Pts',(3.60851596876001,-9.28250328165365,8.85063162388015));
#90980=CARTESIAN_POINT('Ctrl Pts',(7.58304355507985,-6.45629190112006,8.92936843715714));
#90981=CARTESIAN_POINT('Ctrl Pts',(9.73919732502021,-2.08189580311446,9.0081052504341));
#90982=CARTESIAN_POINT('Ctrl Pts',(9.55994298610092,2.79172791890731,9.08684206371107));
#90983=CARTESIAN_POINT('Ctrl Pts',(7.08826478257631,6.99591002249136,9.16557887698806));
#90984=CARTESIAN_POINT('Ctrl Pts',(2.91685810056142,9.52250983154629,9.24431569026502));
#90985=CARTESIAN_POINT('Ctrl Pts',(-1.95399575693514,9.76566204886213,9.32305250354201));
#90986=CARTESIAN_POINT('Ctrl Pts',(-6.35629174635151,7.66706005623865,9.40178931681896));
#90987=CARTESIAN_POINT('Ctrl Pts',(-9.23438252754493,3.72993753375037,9.48052613009595));
#90988=CARTESIAN_POINT('Ctrl Pts',(-9.8981171235795,-1.10160432034774,9.55926294337291));
#90989=CARTESIAN_POINT('Ctrl Pts',(-8.1883354819397,-5.66898727339496,9.6379997566499));
#90990=CARTESIAN_POINT('Ctrl Pts',(-4.51503421497537,-8.87697700280384,
9.71673656992686));
#90991=CARTESIAN_POINT('Ctrl Pts',(0.240948423516744,-9.95631450527311,
9.79547338320386));
#90992=CARTESIAN_POINT('Ctrl Pts',(4.93915290192862,-8.64818034514063,9.87421019648081));
#90993=CARTESIAN_POINT('Ctrl Pts',(8.45297458644962,-5.26625818884181,9.9529470097578));
#90994=CARTESIAN_POINT('Ctrl Pts',(9.93981758531818,-0.621515117520195,
10.0316838230348));
#90995=CARTESIAN_POINT('Ctrl Pts',(9.04314479590899,4.17226399823058,10.1104206363118));
#90996=CARTESIAN_POINT('Ctrl Pts',(5.97797361991285,7.96555623106965,10.1891574495887));
#90997=CARTESIAN_POINT('Ctrl Pts',(1.47931592540995,9.84875012697221,10.2678942628657));
#90998=CARTESIAN_POINT('Ctrl Pts',(-3.37407391923556,9.37026573039639,10.3466310761427));
#90999=CARTESIAN_POINT('Ctrl Pts',(-7.41837864855737,6.64484107389598,10.4253678894196));
#91000=CARTESIAN_POINT('Ctrl Pts',(-9.68379533687761,2.32601860357435,10.5041047026966));
#91001=CARTESIAN_POINT('Ctrl Pts',(-9.62708902064784,-2.55057084967824,
10.5828415159736));
#91002=CARTESIAN_POINT('Ctrl Pts',(-7.26185757516794,-6.81554687671376,
10.6615783292506));
#91003=CARTESIAN_POINT('Ctrl Pts',(-3.15527101586746,-9.44619073950626,
10.7403151425275));
#91004=CARTESIAN_POINT('Ctrl Pts',(1.70793287751002,-9.81168792597006,10.8190519558045));
#91005=CARTESIAN_POINT('Ctrl Pts',(6.16158348241702,-7.82439414011797,10.8977887690815));
#91006=CARTESIAN_POINT('Ctrl Pts',(9.1377188929984,-3.96085194159623,10.9765255823584));
#91007=CARTESIAN_POINT('Ctrl Pts',(9.92267754773311,0.852481644623632,11.0552623956354));
#91008=CARTESIAN_POINT('Ctrl Pts',(8.32823050472688,5.46139463240326,11.1339992089124));
#91009=CARTESIAN_POINT('Ctrl Pts',(4.73671774838673,8.76069401604832,11.2127360221894));
#91010=CARTESIAN_POINT('Ctrl Pts',(0.00936507939353068,9.9592252191621,
11.2914728354663));
#91011=CARTESIAN_POINT('Ctrl Pts',(-4.72023328620338,8.76958678584825,11.3702096487433));
#91012=CARTESIAN_POINT('Ctrl Pts',(-8.31794462616336,5.4770477327468,11.4489464620203));
#91013=CARTESIAN_POINT('Ctrl Pts',(-9.92105675217349,0.87114154467542,11.5276832752972));
#91014=CARTESIAN_POINT('Ctrl Pts',(-9.14515183866235,-3.94365978736978,
11.6064200885743));
#91015=CARTESIAN_POINT('Ctrl Pts',(-6.17628778817008,-7.81279231954925,
11.6851569018512));
#91016=CARTESIAN_POINT('Ctrl Pts',(-1.72638252845134,-9.80845849438966,
11.7638937151282));
#91017=CARTESIAN_POINT('Ctrl Pts',(3.13750014864465,-9.45210809756012,11.8426305284052));
#91018=CARTESIAN_POINT('Ctrl Pts',(7.24902685181769,-6.8291920731762,11.9213673416821));
#91019=CARTESIAN_POINT('Ctrl Pts',(9.62227518090085,-2.56867183846557,12.0001041549591));
#91020=CARTESIAN_POINT('Ctrl Pts',(9.68815271409469,2.30780234402479,12.0788409682361));
#91021=CARTESIAN_POINT('Ctrl Pts',(7.43086236668286,6.63087770646717,12.1575777815131));
#91022=CARTESIAN_POINT('Ctrl Pts',(3.39169044855997,9.36390359689024,12.23631459479));
#91023=CARTESIAN_POINT('Ctrl Pts',(-1.46079093562736,9.85151483342006,12.315051408067));
#91024=CARTESIAN_POINT('Ctrl Pts',(-5.96298236443524,7.97678481545922,12.393788221344));
#91025=CARTESIAN_POINT('Ctrl Pts',(-9.03528209866653,4.18926390529685,12.472525034621));
#91026=CARTESIAN_POINT('Ctrl Pts',(-9.94096887960528,-0.602820375755343,
12.5512618478979));
#91027=CARTESIAN_POINT('Ctrl Pts',(-8.46286379797352,-5.25035151277091,
12.6299986611749));
#91028=CARTESIAN_POINT('Ctrl Pts',(-4.95540864996746,-8.63887607171988,
12.7087354744519));
#91029=CARTESIAN_POINT('Ctrl Pts',(-0.259672665498926,-9.95584375015496,
12.7874722877288));
#91030=CARTESIAN_POINT('Ctrl Pts',(4.49833145343869,-8.88545265058065,12.8662091010058));
#91031=CARTESIAN_POINT('Ctrl Pts',(8.17765943489719,-5.6843769084697,12.9449459142828));
#91032=CARTESIAN_POINT('Ctrl Pts',(9.89602785075699,-1.12021758946579,13.0236827275598));
#91033=CARTESIAN_POINT('Ctrl Pts',(9.24138102553675,3.71256399427083,13.1024195408367));
#91034=CARTESIAN_POINT('Ctrl Pts',(6.37069981228177,7.65509232945621,13.1811563541137));
#91035=CARTESIAN_POINT('Ctrl Pts',(1.9723584126487,9.761969932486,13.2598931673907));
#91036=CARTESIAN_POINT('Ctrl Pts',(-2.89894412297489,9.5279786755941,13.3386299806676));
#91037=CARTESIAN_POINT('Ctrl Pts',(-7.07509516038074,7.00922842702848,13.4173667939446));
#91038=CARTESIAN_POINT('Ctrl Pts',(-9.55467572518108,2.80970220082872,13.4961036072216));
#91039=CARTESIAN_POINT('Ctrl Pts',(-9.74309548674077,-2.06357578173378,
13.5748404204986));
#91040=CARTESIAN_POINT('Ctrl Pts',(-7.59517238083715,-6.44201918470249,
13.6535772337755));
#91041=CARTESIAN_POINT('Ctrl Pts',(-3.62596703016116,-9.27570039225563,
13.7323140470525));
#91042=CARTESIAN_POINT('Ctrl Pts',(1.21272607418644,-9.88511760879428,13.8110508603295));
#91043=CARTESIAN_POINT('Ctrl Pts',(5.76061386748395,-8.12413580268438,13.8897876736065));
#91044=CARTESIAN_POINT('Ctrl Pts',(8.9271368635441,-4.41502911544861,13.9685244868834));
#91045=CARTESIAN_POINT('Ctrl Pts',(9.95297956283469,0.352778248338951,14.0472613001604));
#91046=CARTESIAN_POINT('Ctrl Pts',(8.59215030111643,5.03599125036287,14.1259981134374));
#91047=CARTESIAN_POINT('Ctrl Pts',(5.17096875202658,8.51160013371584,14.2047349267144));
#91048=CARTESIAN_POINT('Ctrl Pts',(0.509816191863926,9.94617223464483,14.2834717399913));
#91049=CARTESIAN_POINT('Ctrl Pts',(-4.27358759997346,8.99570473593146,14.3622085532683));
#91050=CARTESIAN_POINT('Ctrl Pts',(-8.0322076440517,5.88811472659494,14.4409453665453));
#91051=CARTESIAN_POINT('Ctrl Pts',(-9.86474669418887,1.36858588703684,14.5196821798223));
#91052=CARTESIAN_POINT('Ctrl Pts',(-9.33177155946915,-3.47912262396562,
14.5984189930992));
#91053=CARTESIAN_POINT('Ctrl Pts',(-6.56108686381646,-7.49255589476393,
14.6771558063762));
#91054=CARTESIAN_POINT('Ctrl Pts',(-2.21708817181164,-9.70931381247509,
14.7558926196532));
#91055=CARTESIAN_POINT('Ctrl Pts',(2.65855656059159,-9.59782952989072,14.8346294329302));
#91056=CARTESIAN_POINT('Ctrl Pts',(6.89669346331803,-7.18483638948953,14.9133662462071));
#91057=CARTESIAN_POINT('Ctrl Pts',(9.48103967867699,-3.04895740902669,14.9921030594841));
#91058=CARTESIAN_POINT('Ctrl Pts',(9.79188262604912,1.81804546378362,15.0708398727611));
#91059=CARTESIAN_POINT('Ctrl Pts',(7.75468380748131,6.24909063117937,15.1495766860381));
#91060=CARTESIAN_POINT('Ctrl Pts',(3.85795274603463,9.18163685189467,15.228313499315));
#91061=CARTESIAN_POINT('Ctrl Pts',(-0.963895019181878,9.91247502204688,
15.307050312592));
#91062=CARTESIAN_POINT('Ctrl Pts',(-5.55460584684975,8.26635400626227,15.385787125869));
#91063=CARTESIAN_POINT('Ctrl Pts',(-8.81335151318695,4.63800493485218,15.464523939146));
#91064=CARTESIAN_POINT('Ctrl Pts',(-9.95870200913874,-0.102513237594813,
15.5432607524229));
#91065=CARTESIAN_POINT('Ctrl Pts',(-8.71600833166472,-4.81844927679591,
15.6219975656999));
#91066=CARTESIAN_POINT('Ctrl Pts',(-5.38326186489501,-8.37894661426389,
15.7007343789769));
#91067=CARTESIAN_POINT('Ctrl Pts',(-0.759637619204987,-9.93021678304004,
15.7794711922538));
#91068=CARTESIAN_POINT('Ctrl Pts',(4.04614371772026,-9.10027338525098,15.8582080055308));
#91069=CARTESIAN_POINT('Ctrl Pts',(7.881681149256,-6.08813246670124,15.9369448188078));
#91070=CARTESIAN_POINT('Ctrl Pts',(9.82723304573019,-1.61608951969397,16.0156816320848));
#91071=CARTESIAN_POINT('Ctrl Pts',(9.41626633222295,3.24348316342719,16.0944184453617));
#91072=CARTESIAN_POINT('Ctrl Pts',(6.74732865730142,7.32528570504871,16.1731552586387));
#91073=CARTESIAN_POINT('Ctrl Pts',(2.46041718703747,9.65052340226892,16.2518920719157));
#91074=CARTESIAN_POINT('Ctrl Pts',(-2.41648933700102,9.66161652893571,16.3306288851926));
#91075=CARTESIAN_POINT('Ctrl Pts',(-6.71393447385249,7.35590501268973,16.4093656984696));
#91076=CARTESIAN_POINT('Ctrl Pts',(-9.40141356418044,3.28628630244833,16.4881025117466));
#91077=CARTESIAN_POINT('Ctrl Pts',(-9.83448330867708,-1.57136651387741,
16.5668393250236));
#91078=CARTESIAN_POINT('Ctrl Pts',(-7.90929586799285,-6.05221393898498,
16.6455761383005));
#91079=CARTESIAN_POINT('Ctrl Pts',(-4.08750102927544,-9.0817724009335,16.7243129515775));
#91080=CARTESIAN_POINT('Ctrl Pts',(0.714454981413205,-9.93356979608242,
16.8030497648545));
#91081=CARTESIAN_POINT('Ctrl Pts',(5.3450884558376,-8.40334955962479,16.8817865781315));
#91082=CARTESIAN_POINT('Ctrl Pts',(8.69399793928435,-4.85805051559736,16.9605233914084));
#91083=CARTESIAN_POINT('Ctrl Pts',(9.95813259779199,-0.147816488123383,
17.0392602046854));
#91084=CARTESIAN_POINT('Ctrl Pts',(8.83435964711863,4.59786293238055,17.1179970179624));
#91085=CARTESIAN_POINT('Ctrl Pts',(5.5921538429629,8.24099952001386,17.1967338312394));
#91086=CARTESIAN_POINT('Ctrl Pts',(1.00897915055061,9.90798709392943,17.2754706445163));
#91087=CARTESIAN_POINT('Ctrl Pts',(-3.81614357974774,9.19909327367808,17.3542074577933));
#91088=CARTESIAN_POINT('Ctrl Pts',(-7.72617490624037,6.28430232111598,17.4329442710703));
#91089=CARTESIAN_POINT('Ctrl Pts',(-9.78351088966547,1.8625749049079,17.5116810843473));
#91090=CARTESIAN_POINT('Ctrl Pts',(-9.49481141073808,-3.00579989874418,
17.5904178976242));
#91091=CARTESIAN_POINT('Ctrl Pts',(-6.92930859268264,-7.15337694456503,
17.6691547109012));
#91092=CARTESIAN_POINT('Ctrl Pts',(-2.70218965551557,-9.58565620807068,
17.7478915241782));
#91093=CARTESIAN_POINT('Ctrl Pts',(2.17289137569487,-9.71925986449121,17.8266283374551));
#91094=CARTESIAN_POINT('Ctrl Pts',(6.52694143972031,-7.52240290696552,17.9053651507321));
#91095=CARTESIAN_POINT('Ctrl Pts',(9.31583263251279,-3.52138970212855,17.9841019640091));
#91096=CARTESIAN_POINT('Ctrl Pts',(9.87089943188555,1.32340069054093,18.0628387772861));
#91097=CARTESIAN_POINT('Ctrl Pts',(8.05885895492069,5.85212980068802,18.141575590563));
#91098=CARTESIAN_POINT('Ctrl Pts',(5.56264007710963,7.93372545675409,18.1940667994144));
#91099=CARTESIAN_POINT('Ctrl Pts',(4.14169205563424,8.61671531075004,18.22031240384));
#91100=CARTESIAN_POINT('Ctrl Pts',(5.43892809705089,-7.62901474470127,4.00053035731484));
#91101=CARTESIAN_POINT('Ctrl Pts',(6.69727911759927,-6.7319066799688,4.02678177401689));
#91102=CARTESIAN_POINT('Ctrl Pts',(8.76018368837185,-4.30436272590017,4.07927879514459));
#91103=CARTESIAN_POINT('Ctrl Pts',(9.75304711227676,0.372043140866268,4.15802142069795));
#91104=CARTESIAN_POINT('Ctrl Pts',(8.40720887818163,4.9576310315513,4.23675823397493));
#91105=CARTESIAN_POINT('Ctrl Pts',(5.04532137388612,8.35502743209433,4.3154950472519));
#91106=CARTESIAN_POINT('Ctrl Pts',(0.473614909720539,9.7486142625213,4.39423186052886));
#91107=CARTESIAN_POINT('Ctrl Pts',(-4.21167342376619,8.80469855408104,4.47296867380585));
#91108=CARTESIAN_POINT('Ctrl Pts',(-7.8870187740352,5.74937825262146,4.55170548708282));
#91109=CARTESIAN_POINT('Ctrl Pts',(-9.67110171003543,1.31543087553393,4.6304423003598));
#91110=CARTESIAN_POINT('Ctrl Pts',(-9.13610393149024,-3.43397229436816,
4.70917911363676));
#91111=CARTESIAN_POINT('Ctrl Pts',(-6.41031746804786,-7.35991548184156,
4.78791592691374));
#91112=CARTESIAN_POINT('Ctrl Pts',(-2.14737029509449,-9.52099574225318,
4.86665274019072));
#91113=CARTESIAN_POINT('Ctrl Pts',(2.63050472376014,-9.39898841184597,4.94538955346768));
#91114=CARTESIAN_POINT('Ctrl Pts',(6.7775987065087,-7.02315485645229,5.02412636674467));
#91115=CARTESIAN_POINT('Ctrl Pts',(9.29946023860813,-2.96320502351861,5.10286318002163));
#91116=CARTESIAN_POINT('Ctrl Pts',(9.59136032349711,1.80730531193538,5.18159999329862));
#91117=CARTESIAN_POINT('Ctrl Pts',(7.5833028168871,6.14443359041709,5.26033680657558));
#91118=CARTESIAN_POINT('Ctrl Pts',(3.75680933213372,9.00815901643317,5.33907361985255));
#91119=CARTESIAN_POINT('Ctrl Pts',(-0.970547203681225,9.71177551868821,
5.41781043312952));
#91120=CARTESIAN_POINT('Ctrl Pts',(-5.46517164113355,8.08655948680911,5.4965472464065));
#91121=CARTESIAN_POINT('Ctrl Pts',(-8.64927676877029,4.52222919130004,5.57528405968347));
#91122=CARTESIAN_POINT('Ctrl Pts',(-9.75933098308775,-0.126507800966816,
5.65402087296046));
#91123=CARTESIAN_POINT('Ctrl Pts',(-8.52914914390484,-4.74490888628499,
5.73275768623743));
#91124=CARTESIAN_POINT('Ctrl Pts',(-5.25372236214226,-8.22550586941576,
5.81149449951439));
#91125=CARTESIAN_POINT('Ctrl Pts',(-0.718480690503233,-9.73366996343397,
5.89023131279138));
#91126=CARTESIAN_POINT('Ctrl Pts',(3.98904885815936,-8.90775138128075,5.96896812606833));
#91127=CARTESIAN_POINT('Ctrl Pts',(7.74002554735313,-5.94580103838886,6.04770493934533));
#91128=CARTESIAN_POINT('Ctrl Pts',(9.63498496708154,-1.55807899236021,6.12644175262228));
#91129=CARTESIAN_POINT('Ctrl Pts',(9.21952585127947,3.20326217158038,6.20517856589926));
#91130=CARTESIAN_POINT('Ctrl Pts',(6.5932731028668,7.19647797559256,6.28391537917623));
#91131=CARTESIAN_POINT('Ctrl Pts',(2.38598826787577,9.4640163486675,6.36265219245321));
#91132=CARTESIAN_POINT('Ctrl Pts',(-2.39344395898697,9.46213355842142,6.44138900573019));
#91133=CARTESIAN_POINT('Ctrl Pts',(-6.59894095860507,7.19128108803257,6.52012581900716));
#91134=CARTESIAN_POINT('Ctrl Pts',(-9.22204674975853,3.19599737288787,6.59886263228413));
#91135=CARTESIAN_POINT('Ctrl Pts',(-9.63375441015036,-1.5656696417663,6.67759944556111));
#91136=CARTESIAN_POINT('Ctrl Pts',(-7.73533861607347,-5.95189734092617,
6.75633625883808));
#91137=CARTESIAN_POINT('Ctrl Pts',(-3.98202945390109,-8.91089147563272,
6.83507307211505));
#91138=CARTESIAN_POINT('Ctrl Pts',(0.726149351631704,-9.7331008718376,6.91380988539203));
#91139=CARTESIAN_POINT('Ctrl Pts',(5.2602013757215,-8.22136405647494,6.99254669866899));
#91140=CARTESIAN_POINT('Ctrl Pts',(8.53288487660304,-4.73818753796005,7.07128351194597));
#91141=CARTESIAN_POINT('Ctrl Pts',(9.75942762607066,-0.118818659010883,
7.15002032522295));
#91142=CARTESIAN_POINT('Ctrl Pts',(8.64571114727513,4.5290423071686,7.22875713849992));
#91143=CARTESIAN_POINT('Ctrl Pts',(5.45879877292739,8.09086283525602,7.30749395177689));
#91144=CARTESIAN_POINT('Ctrl Pts',(0.962895267844818,9.71253716417098,7.38623076505386));
#91145=CARTESIAN_POINT('Ctrl Pts',(-3.76390543969308,9.00519635006864,7.46496757833085));
#91146=CARTESIAN_POINT('Ctrl Pts',(-7.58814149108033,6.13845698637581,7.54370439160781));
#91147=CARTESIAN_POINT('Ctrl Pts',(-9.5927812679453,1.79974804003172,7.62244120488479));
#91148=CARTESIAN_POINT('Ctrl Pts',(-9.2971227335601,-2.9705309860967,7.70117801816176));
#91149=CARTESIAN_POINT('Ctrl Pts',(-6.77206324379635,-7.02849236211172,
7.77991483143874));
#91150=CARTESIAN_POINT('Ctrl Pts',(-2.62309873542888,-9.40105837054699,
7.85865164471571));
#91151=CARTESIAN_POINT('Ctrl Pts',(2.15487100331034,-9.51930020649275,7.93738845799269));
#91152=CARTESIAN_POINT('Ctrl Pts',(6.41611405023598,-7.35486410184478,8.01612527126965));
#91153=CARTESIAN_POINT('Ctrl Pts',(9.13880681624731,-3.42677040922677,8.09486208454663));
#91154=CARTESIAN_POINT('Ctrl Pts',(9.67006194815957,1.32304473884924,8.1735988978236));
#91155=CARTESIAN_POINT('Ctrl Pts',(7.88248726964285,5.75560074242115,8.25233571110058));
#91156=CARTESIAN_POINT('Ctrl Pts',(4.20473375264889,8.80799406968328,8.33107252437755));
#91157=CARTESIAN_POINT('Ctrl Pts',(-0.481292722970219,9.74827691323223,
8.40980933765452));
#91158=CARTESIAN_POINT('Ctrl Pts',(-5.05190774419027,8.35097441059609,8.48854615093149));
#91159=CARTESIAN_POINT('Ctrl Pts',(-8.4111019555369,4.95115232605539,8.56728296420848));
#91160=CARTESIAN_POINT('Ctrl Pts',(-9.75335831709361,0.364070049058778,
8.64601977748544));
#91161=CARTESIAN_POINT('Ctrl Pts',(-8.75681083864211,-4.31031430390876,
8.72475659076242));
#91162=CARTESIAN_POINT('Ctrl Pts',(-5.6604263451035,-7.95110803938034,8.80349340403939));
#91163=CARTESIAN_POINT('Ctrl Pts',(-1.20670149334083,-9.68526803801576,
8.88223021731637));
#91164=CARTESIAN_POINT('Ctrl Pts',(3.53638400678673,-9.09695188614206,8.96096703059333));
#91165=CARTESIAN_POINT('Ctrl Pts',(7.43146328937169,-6.3272346914716,9.03970384387032));
#91166=CARTESIAN_POINT('Ctrl Pts',(9.54451690315688,-2.04028001695672,9.11844065714729));
#91167=CARTESIAN_POINT('Ctrl Pts',(9.36884574559812,2.73592303572826,9.19717747042426));
#91168=CARTESIAN_POINT('Ctrl Pts',(6.94657483297379,6.8560661863882,9.27591428370123));
#91169=CARTESIAN_POINT('Ctrl Pts',(2.85855194384417,9.33216085623181,9.35465109697821));
#91170=CARTESIAN_POINT('Ctrl Pts',(-1.91493661216333,9.57045261383372,9.43338791025518));
#91171=CARTESIAN_POINT('Ctrl Pts',(-6.2292334768279,7.51380035357655,9.51212472353215));
#91172=CARTESIAN_POINT('Ctrl Pts',(-9.04979303560688,3.65537843115071,9.59086153680913));
#91173=CARTESIAN_POINT('Ctrl Pts',(-9.70025999501298,-1.07958394365195,
9.6695983500861));
#91174=CARTESIAN_POINT('Ctrl Pts',(-8.02465581175916,-5.55566778749779,
9.74833516336308));
#91175=CARTESIAN_POINT('Ctrl Pts',(-4.42478152408464,-8.69953182225111,
9.82707197664002));
#91176=CARTESIAN_POINT('Ctrl Pts',(0.236132016253185,-9.75729404769278,
9.90580878991702));
#91177=CARTESIAN_POINT('Ctrl Pts',(4.84042234554853,-8.47530866570387,9.98454560319398));
#91178=CARTESIAN_POINT('Ctrl Pts',(8.28400494721021,-5.16098900375083,10.063282416471));
#91179=CARTESIAN_POINT('Ctrl Pts',(9.74112689077983,-0.609091421682083,
10.1420192297479));
#91180=CARTESIAN_POINT('Ctrl Pts',(8.86237802580607,4.08886306813402,10.2207560430249));
#91181=CARTESIAN_POINT('Ctrl Pts',(5.85847769151402,7.80632977783241,10.2994928563019));
#91182=CARTESIAN_POINT('Ctrl Pts',(1.44974533156971,9.65187981358203,10.3782296695789));
#91183=CARTESIAN_POINT('Ctrl Pts',(-3.30662830620673,9.18296001879747,10.4569664828558));
#91184=CARTESIAN_POINT('Ctrl Pts',(-7.27008993064292,6.51201488501103,10.5357032961328));
#91185=CARTESIAN_POINT('Ctrl Pts',(-9.49022236587123,2.27952295635682,10.6144401094098));
#91186=CARTESIAN_POINT('Ctrl Pts',(-9.43464957319556,-2.49958654445917,
10.6931769226868));
#91187=CARTESIAN_POINT('Ctrl Pts',(-7.11669761495095,-6.67930838632205,
10.7719137359637));
#91188=CARTESIAN_POINT('Ctrl Pts',(-3.09219913509919,-9.25736733478436,
10.8506505492407));
#91189=CARTESIAN_POINT('Ctrl Pts',(1.67379237475489,-9.61555846264028,10.9293873625177));
#91190=CARTESIAN_POINT('Ctrl Pts',(6.03841730848384,-7.66798942819062,11.0081241757946));
#91191=CARTESIAN_POINT('Ctrl Pts',(8.95506164624695,-3.88167700538795,11.0868609890716));
#91192=CARTESIAN_POINT('Ctrl Pts',(9.72432947175317,0.835441073345797,11.1655978023486));
#91193=CARTESIAN_POINT('Ctrl Pts',(8.16175442113116,5.35222479268075,11.2443346156255));
#91194=CARTESIAN_POINT('Ctrl Pts',(4.64203374325474,8.58557325917873,11.3230714289025));
#91195=CARTESIAN_POINT('Ctrl Pts',(0.00917787735352807,9.76014657824398,
11.4018082421795));
#91196=CARTESIAN_POINT('Ctrl Pts',(-4.62587879509039,8.59428826811001,11.4805450554565));
#91197=CARTESIAN_POINT('Ctrl Pts',(-8.15167415080322,5.36756499740499,11.5592818687334));
#91198=CARTESIAN_POINT('Ctrl Pts',(-9.72274107487621,0.853727973745442,
11.6380186820104));
#91199=CARTESIAN_POINT('Ctrl Pts',(-8.96234601200748,-3.8648285114988,11.7167554952874));
#91200=CARTESIAN_POINT('Ctrl Pts',(-6.05282768442402,-7.65661952070957,
11.7954923085644));
#91201=CARTESIAN_POINT('Ctrl Pts',(-1.69187322879139,-9.61239358536361,
11.8742291218413));
#91202=CARTESIAN_POINT('Ctrl Pts',(3.07478349632207,-9.26316640857683,11.9529659351183));
#91203=CARTESIAN_POINT('Ctrl Pts',(7.10412336968115,-6.6926808238994,12.0317027483953));
#91204=CARTESIAN_POINT('Ctrl Pts',(9.4299319590739,-2.51732570587861,12.1104395616723));
#91205=CARTESIAN_POINT('Ctrl Pts',(9.49449264186152,2.26167082836512,12.1891763749493));
#91206=CARTESIAN_POINT('Ctrl Pts',(7.28232410710392,6.49833063650456,12.2679131882262));
#91207=CARTESIAN_POINT('Ctrl Pts',(3.32389269220285,9.17672506033395,12.3466500015032));
#91208=CARTESIAN_POINT('Ctrl Pts',(-1.43159064466794,9.65458925528889,12.4253868147802));
#91209=CARTESIAN_POINT('Ctrl Pts',(-5.84378610179361,7.81733390989052,12.5041236280571));
#91210=CARTESIAN_POINT('Ctrl Pts',(-8.85467249893046,4.10552315776266,12.5828604413341));
#91211=CARTESIAN_POINT('Ctrl Pts',(-9.74225517141907,-0.590770376033278,
12.6615972546111));
#91212=CARTESIAN_POINT('Ctrl Pts',(-8.29369647962288,-5.14540029211835,
12.7403340678881));
#91213=CARTESIAN_POINT('Ctrl Pts',(-4.85635315142008,-8.46619037885003,
12.819070881165));
#91214=CARTESIAN_POINT('Ctrl Pts',(-0.254481972428574,-9.75683270267301,
12.897807694442));
#91215=CARTESIAN_POINT('Ctrl Pts',(4.40841264023357,-8.70783804716588,12.976544507719));
#91216=CARTESIAN_POINT('Ctrl Pts',(8.01419317217444,-5.57074979345805,13.0552813209959));
#91217=CARTESIAN_POINT('Ctrl Pts',(9.6982124854386,-1.09782514524086,13.1340181342729));
#91218=CARTESIAN_POINT('Ctrl Pts',(9.05665163803072,3.63835217778546,13.2127549475499));
#91219=CARTESIAN_POINT('Ctrl Pts',(6.24335353459279,7.50207185411658,13.2914917608269));
#91220=CARTESIAN_POINT('Ctrl Pts',(1.93293220995191,9.56683430053906,13.3702285741039));
#91221=CARTESIAN_POINT('Ctrl Pts',(-2.84099605538939,9.33752038153078,13.4489653873808));
#91222=CARTESIAN_POINT('Ctrl Pts',(-6.93366846323316,6.86911836440503,13.5277022006578));
#91223=CARTESIAN_POINT('Ctrl Pts',(-9.36368377390736,2.75353802307226,13.6064390139348));
#91224=CARTESIAN_POINT('Ctrl Pts',(-9.54833714307926,-2.02232620126758,
13.6851758272117));
#91225=CARTESIAN_POINT('Ctrl Pts',(-7.44334966753948,-6.31324727766785,
13.7639126404887));
#91226=CARTESIAN_POINT('Ctrl Pts',(-3.55348623245917,-9.0902849822194,13.8426494537657));
#91227=CARTESIAN_POINT('Ctrl Pts',(1.18848444360352,-9.68752033234268,13.9213862670427));
#91228=CARTESIAN_POINT('Ctrl Pts',(5.6454628236672,-7.96173944366632,14.0001230803196));
#91229=CARTESIAN_POINT('Ctrl Pts',(8.74868901896026,-4.32677546352531,14.0788598935966));
#91230=CARTESIAN_POINT('Ctrl Pts',(9.75402576865375,0.345726433295193,14.1575967068736));
#91231=CARTESIAN_POINT('Ctrl Pts',(8.42039862697821,4.93532495637561,14.2363335201505));
#91232=CARTESIAN_POINT('Ctrl Pts',(5.06760434277485,8.34145860670244,14.3150703334275));
#91233=CARTESIAN_POINT('Ctrl Pts',(0.499625287214116,9.7473545146679,14.3938071467045));
#91234=CARTESIAN_POINT('Ctrl Pts',(-4.1881612748804,8.81588626275501,14.4725439599815));
#91235=CARTESIAN_POINT('Ctrl Pts',(-7.87164887103858,5.77041502089042,14.5512807732584));
#91236=CARTESIAN_POINT('Ctrl Pts',(-9.6675566194929,1.34122871693821,14.6300175865354));
#91237=CARTESIAN_POINT('Ctrl Pts',(-9.14523532210772,-3.40957715347724,
14.7087543998124));
#91238=CARTESIAN_POINT('Ctrl Pts',(-6.4299348688519,-7.3427844204064,14.7874912130894));
#91239=CARTESIAN_POINT('Ctrl Pts',(-2.17276997533279,-9.51523074321021,
14.8662280263663));
#91240=CARTESIAN_POINT('Ctrl Pts',(2.60541368900876,-9.4059749612343,14.9449648396433));
#91241=CARTESIAN_POINT('Ctrl Pts',(6.75883290375718,-7.04121603427487,15.0237016529203));
#91242=CARTESIAN_POINT('Ctrl Pts',(9.29151966560509,-2.98801067031467,15.1024384661973));
#91243=CARTESIAN_POINT('Ctrl Pts',(9.59614905819356,1.78170387976553,15.1811752794742));
#91244=CARTESIAN_POINT('Ctrl Pts',(7.59967256120758,6.12417524444471,15.2599120927512));
#91245=CARTESIAN_POINT('Ctrl Pts',(3.78083469995116,8.99810171279953,15.3386489060282));
#91246=CARTESIAN_POINT('Ctrl Pts',(-0.944627364702379,9.71433088813101,
15.4173857193052));
#91247=CARTESIAN_POINT('Ctrl Pts',(-5.44357277364452,8.10111479490791,15.4961225325821));
#91248=CARTESIAN_POINT('Ctrl Pts',(-8.63717816610739,4.54529413670439,15.5748593458591));
#91249=CARTESIAN_POINT('Ctrl Pts',(-9.75963382685953,-0.100464062526747,
15.6535961591361));
#91250=CARTESIAN_POINT('Ctrl Pts',(-8.54178081348788,-4.7221315098765,15.7323329724131));
#91251=CARTESIAN_POINT('Ctrl Pts',(-5.27565384999563,-8.21145674757389,
15.81106978569));
#91252=CARTESIAN_POINT('Ctrl Pts',(-0.744452941532393,-9.7317180024937,
15.889806598967));
#91253=CARTESIAN_POINT('Ctrl Pts',(3.96526385261457,-8.91836465062037,15.968543412244));
#91254=CARTESIAN_POINT('Ctrl Pts',(7.72413130608901,-5.96643453232091,16.0472802255209));
#91255=CARTESIAN_POINT('Ctrl Pts',(9.63079284524497,-1.5837849078288,16.1260170387979));
#91256=CARTESIAN_POINT('Ctrl Pts',(9.22804109755958,3.17864797737543,16.2047538520749));
#91257=CARTESIAN_POINT('Ctrl Pts',(6.61245380615948,7.17885785645543,16.2834906653519));
#91258=CARTESIAN_POINT('Ctrl Pts',(2.41123499676581,9.45761551628439,16.3622274786288));
#91259=CARTESIAN_POINT('Ctrl Pts',(-2.36818523679073,9.46848689833435,16.4409642919058));
#91260=CARTESIAN_POINT('Ctrl Pts',(-6.57972715140979,7.2088651034173,16.5197011051828));
#91261=CARTESIAN_POINT('Ctrl Pts',(-9.21348522699762,3.22059550860017,16.5984379184598));
#91262=CARTESIAN_POINT('Ctrl Pts',(-9.63789818000097,-1.53995588673697,
16.6771747317367));
#91263=CARTESIAN_POINT('Ctrl Pts',(-7.75119402398696,-5.93123399335623,
16.7559115450137));
#91264=CARTESIAN_POINT('Ctrl Pts',(-4.00579445755397,-8.90023348932953,
16.8346483582907));
#91265=CARTESIAN_POINT('Ctrl Pts',(0.700173476219099,-9.73500399091671,
16.9133851715676));
#91266=CARTESIAN_POINT('Ctrl Pts',(5.23824350334795,-8.23537189342328,16.9921219848446));
#91267=CARTESIAN_POINT('Ctrl Pts',(8.52021039499149,-4.76094114485073,17.0708587981216));
#91268=CARTESIAN_POINT('Ctrl Pts',(9.75907579768703,-0.144861729604177,
17.1495956113986));
#91269=CARTESIAN_POINT('Ctrl Pts',(8.65776636067038,4.50595454758523,17.2283324246755));
#91270=CARTESIAN_POINT('Ctrl Pts',(5.48037020895889,8.07626712887417,17.3070692379525));
#91271=CARTESIAN_POINT('Ctrl Pts',(0.988810292674002,9.70993267087064,17.3858060512295));
#91272=CARTESIAN_POINT('Ctrl Pts',(-3.7398612725716,9.01520919170358,17.4645428645065));
#91273=CARTESIAN_POINT('Ctrl Pts',(-7.5717335349507,6.15868307487187,17.5432796777834));
#91274=CARTESIAN_POINT('Ctrl Pts',(-9.58794466754864,1.8253432054014,17.6220164910604));
#91275=CARTESIAN_POINT('Ctrl Pts',(-9.30501610941416,-2.94571585148694,
17.7007533043374));
#91276=CARTESIAN_POINT('Ctrl Pts',(-6.79079607722315,-7.01038544384477,
17.7794901176143));
#91277=CARTESIAN_POINT('Ctrl Pts',(-2.64817458584047,-9.39404497645205,
17.8582269308913));
#91278=CARTESIAN_POINT('Ctrl Pts',(2.12945664534019,-9.52497797990943,17.9369637441683));
#91279=CARTESIAN_POINT('Ctrl Pts',(6.39647199028245,-7.37203480962839,18.0157005574453));
#91280=CARTESIAN_POINT('Ctrl Pts',(9.12961500426467,-3.45099933936275,18.0944373707222));
#91281=CARTESIAN_POINT('Ctrl Pts',(9.6735863678373,1.29694674406767,18.1731741839992));
#91282=CARTESIAN_POINT('Ctrl Pts',(7.89776743898533,5.73514941099307,18.2519109972762));
#91283=CARTESIAN_POINT('Ctrl Pts',(5.45144640470055,7.77513528065193,18.3044022061275));
#91284=CARTESIAN_POINT('Ctrl Pts',(4.05890223941934,8.44447259753758,18.3306478105532));
#91285=CARTESIAN_POINT('',(5.44054447803332,-7.62915214953083,18.0000585632373));
#91286=CARTESIAN_POINT('Ctrl Pts',(5.44060438077288,-7.62923406419748,18.));
#91287=CARTESIAN_POINT('Ctrl Pts',(5.63908049858948,-7.49661732771331,18.));
#91288=CARTESIAN_POINT('Ctrl Pts',(5.83209798667451,-7.356661156938,18.));
#91289=CARTESIAN_POINT('Ctrl Pts',(6.01921567302457,-7.20964694412941,18.));
#91290=CARTESIAN_POINT('Ctrl Pts',(6.06606615359304,-7.17283756146319,18.));
#91291=CARTESIAN_POINT('Ctrl Pts',(6.11254669610509,-7.1355854670293,18.));
#91292=CARTESIAN_POINT('Ctrl Pts',(6.15865019795423,-7.09789459962803,18.));
#91293=CARTESIAN_POINT('Ctrl Pts',(6.34251836556963,-6.94757736889825,18.));
#91294=CARTESIAN_POINT('Ctrl Pts',(6.52039177856815,-6.79028495952252,18.));
#91295=CARTESIAN_POINT('Ctrl Pts',(6.69202469675709,-6.62649321917725,18.));
#91296=CARTESIAN_POINT('Ctrl Pts',(6.86398651234873,-6.46238760735236,18.));
#91297=CARTESIAN_POINT('Ctrl Pts',(7.0296843088185,-6.29175722463819,18.));
#91298=CARTESIAN_POINT('Ctrl Pts',(7.1888389091338,-6.11503780430435,18.));
#91299=CARTESIAN_POINT('Ctrl Pts',(7.34753690632627,-5.93882537930102,18.));
#91300=CARTESIAN_POINT('Ctrl Pts',(7.49972959262976,-5.75655827630888,18.));
#91301=CARTESIAN_POINT('Ctrl Pts',(7.64510234867658,-5.56863371957282,18.));
#91302=CARTESIAN_POINT('Ctrl Pts',(7.71778872669999,-5.47467144120479,18.));
#91303=CARTESIAN_POINT('Ctrl Pts',(7.7887694932955,-5.37929430472954,18.));
#91304=CARTESIAN_POINT('Ctrl Pts',(7.85800127979533,-5.28254931711788,18.));
#91305=CARTESIAN_POINT('Ctrl Pts',(7.89298282651811,-5.23366585656554,18.));
#91306=CARTESIAN_POINT('Ctrl Pts',(7.92751779717385,-5.18443314532346,18.));
#91307=CARTESIAN_POINT('Ctrl Pts',(7.96160031305259,-5.13485710286307,18.));
#91308=CARTESIAN_POINT('Ctrl Pts',(7.97841946488067,-5.11039215467253,18.));
#91309=CARTESIAN_POINT('Ctrl Pts',(7.99512842932023,-5.08584359508419,18.));
#91310=CARTESIAN_POINT('Ctrl Pts',(8.01172648209115,-5.06121212757392,18.));
#91311=CARTESIAN_POINT('Ctrl Pts',(8.02805976181813,-5.03697358257809,18.));
#91312=CARTESIAN_POINT('Ctrl Pts',(8.04428165797018,-5.01266061493114,18.));
#91313=CARTESIAN_POINT('Ctrl Pts',(8.06038683280492,-4.9882814087714,18.));
#91314=CARTESIAN_POINT('Ctrl Pts',(8.19275521184893,-4.78790879345619,18.));
#91315=CARTESIAN_POINT('Ctrl Pts',(8.31734444140616,-4.58291260001262,18.));
#91316=CARTESIAN_POINT('Ctrl Pts',(8.43390799998684,-4.37375983102443,18.));
#91317=CARTESIAN_POINT('Ctrl Pts',(8.55097522304311,-4.16370332487345,18.));
#91318=CARTESIAN_POINT('Ctrl Pts',(8.65994769799928,-3.94945372966206,18.));
#91319=CARTESIAN_POINT('Ctrl Pts',(8.76053783217777,-3.73144799113718,18.));
#91320=CARTESIAN_POINT('Ctrl Pts',(8.8154658148089,-3.61240435413465,18.));
#91321=CARTESIAN_POINT('Ctrl Pts',(8.8678936654753,-3.49224013192352,18.));
#91322=CARTESIAN_POINT('Ctrl Pts',(8.91776911684323,-3.3710227923076,18.));
#91323=CARTESIAN_POINT('Ctrl Pts',(9.00877320867449,-3.14984636977119,18.));
#91324=CARTESIAN_POINT('Ctrl Pts',(9.09128260143624,-2.92516487707576,18.));
#91325=CARTESIAN_POINT('Ctrl Pts',(9.16525623050192,-2.69748761681311,18.));
#91326=CARTESIAN_POINT('Ctrl Pts',(9.23941857399464,-2.4692295281625,18.));
#91327=CARTESIAN_POINT('Ctrl Pts',(9.3050016942559,-2.23795972868455,18.));
#91328=CARTESIAN_POINT('Ctrl Pts',(9.36191409108156,-2.00417709010597,18.));
#91329=CARTESIAN_POINT('Ctrl Pts',(9.38858160860227,-1.89463324802476,18.));
#91330=CARTESIAN_POINT('Ctrl Pts',(9.41334466163771,-1.78453754436346,18.));
#91331=CARTESIAN_POINT('Ctrl Pts',(9.43618992040111,-1.67394083647048,18.));
#91332=CARTESIAN_POINT('Ctrl Pts',(9.4414550134228,-1.64845187348782,18.));
#91333=CARTESIAN_POINT('Ctrl Pts',(9.44661801742425,-1.62293716459345,18.));
#91334=CARTESIAN_POINT('Ctrl Pts',(9.4516763764568,-1.59740995483373,18.));
#91335=CARTESIAN_POINT('Ctrl Pts',(9.49875085486108,-1.35984672991766,18.));
#91336=CARTESIAN_POINT('Ctrl Pts',(9.53682634772605,-1.12091537343081,18.));
#91337=CARTESIAN_POINT('Ctrl Pts',(9.56592491913746,-0.881154213382847,
18.));
#91338=CARTESIAN_POINT('Ctrl Pts',(9.59514317894571,-0.640406866471459,
18.));
#91339=CARTESIAN_POINT('Ctrl Pts',(9.61531064791162,-0.39882222764125,18.));
#91340=CARTESIAN_POINT('Ctrl Pts',(9.62640020763537,-0.156925741005529,
18.));
#91341=CARTESIAN_POINT('Ctrl Pts',(9.637454051899,0.0841916845548948,18.));
#91342=CARTESIAN_POINT('Ctrl Pts',(9.63948844587604,0.325619611769683,18.));
#91343=CARTESIAN_POINT('Ctrl Pts',(9.63242601287159,0.566847217814661,18.));
#91344=CARTESIAN_POINT('Ctrl Pts',(9.62540501294608,0.806659617168582,18.));
#91345=CARTESIAN_POINT('Ctrl Pts',(9.60939367539977,1.04627467889501,18.));
#91346=CARTESIAN_POINT('Ctrl Pts',(9.58426491595667,1.28519029797862,18.));
#91347=CARTESIAN_POINT('Ctrl Pts',(9.55893834752381,1.5259866170369,18.));
#91348=CARTESIAN_POINT('Ctrl Pts',(9.52435004681638,1.76607306295997,18.));
#91349=CARTESIAN_POINT('Ctrl Pts',(9.48065298058511,2.00496676972802,18.));
#91350=CARTESIAN_POINT('Ctrl Pts',(9.47776845394166,2.02073659872469,18.));
#91351=CARTESIAN_POINT('Ctrl Pts',(9.47484421719539,2.03650122469258,18.));
#91352=CARTESIAN_POINT('Ctrl Pts',(9.47188030676458,2.05226050618878,18.));
#91353=CARTESIAN_POINT('Ctrl Pts',(9.46699294616702,2.07824688237274,18.));
#91354=CARTESIAN_POINT('Ctrl Pts',(9.46199776850117,2.10421821966082,18.));
#91355=CARTESIAN_POINT('Ctrl Pts',(9.45689766603046,2.13016061400735,18.));
#91356=CARTESIAN_POINT('Ctrl Pts',(9.41044452583058,2.36645109809496,18.));
#91357=CARTESIAN_POINT('Ctrl Pts',(9.35523815544362,2.6006253577108,18.));
#91358=CARTESIAN_POINT('Ctrl Pts',(9.29156327949617,2.83223149451236,18.));
#91359=CARTESIAN_POINT('Ctrl Pts',(9.22550315875267,3.07251353879421,18.));
#91360=CARTESIAN_POINT('Ctrl Pts',(9.15032830215148,3.31003211717532,18.));
#91361=CARTESIAN_POINT('Ctrl Pts',(9.06629873032425,3.5442816002362,18.));
#91362=CARTESIAN_POINT('Ctrl Pts',(8.98378308036435,3.77431071888128,18.));
#91363=CARTESIAN_POINT('Ctrl Pts',(8.89272851982826,4.00118809602247,18.));
#91364=CARTESIAN_POINT('Ctrl Pts',(8.79332932928383,4.22442436011723,18.));
#91365=CARTESIAN_POINT('Ctrl Pts',(8.69119461023845,4.45380422718833,18.));
#91366=CARTESIAN_POINT('Ctrl Pts',(8.58024964935816,4.67934061636778,18.));
#91367=CARTESIAN_POINT('Ctrl Pts',(8.46065218408456,4.90048044154929,18.));
#91368=CARTESIAN_POINT('Ctrl Pts',(8.34105471881097,5.12162026673081,18.));
#91369=CARTESIAN_POINT('Ctrl Pts',(8.21280451965211,5.33836427804101,18.));
#91370=CARTESIAN_POINT('Ctrl Pts',(8.07600905803291,5.55012586177464,18.));
#91371=CARTESIAN_POINT('Ctrl Pts',(8.06012001225815,5.57472236123051,18.));
#91372=CARTESIAN_POINT('Ctrl Pts',(8.04411564478489,5.59925148901493,18.));
#91373=CARTESIAN_POINT('Ctrl Pts',(8.02800402746578,5.62370047380093,18.));
#91374=CARTESIAN_POINT('Ctrl Pts',(7.99747825883122,5.67002258027512,18.));
#91375=CARTESIAN_POINT('Ctrl Pts',(7.96656056320155,5.71606781954641,18.));
#91376=CARTESIAN_POINT('Ctrl Pts',(7.93525343239553,5.76183067239227,18.));
#91377=CARTESIAN_POINT('Ctrl Pts',(7.79770776576771,5.96288653217314,18.));
#91378=CARTESIAN_POINT('Ctrl Pts',(7.65264895522489,6.15849356205626,18.));
#91379=CARTESIAN_POINT('Ctrl Pts',(7.50052757437793,6.34837497204547,18.));
#91380=CARTESIAN_POINT('Ctrl Pts',(7.34701857641731,6.53998843766418,18.));
#91381=CARTESIAN_POINT('Ctrl Pts',(7.18631717033013,6.72577182484101,18.));
#91382=CARTESIAN_POINT('Ctrl Pts',(7.01884082387205,6.90541294124557,18.));
#91383=CARTESIAN_POINT('Ctrl Pts',(6.92175824280081,7.00954718835513,18.));
#91384=CARTESIAN_POINT('Ctrl Pts',(6.82239827758366,7.11161690764809,18.));
#91385=CARTESIAN_POINT('Ctrl Pts',(6.72083616319641,7.21155611066385,18.));
#91386=CARTESIAN_POINT('Ctrl Pts',(6.66929208915534,7.26227653639473,18.));
#91387=CARTESIAN_POINT('Ctrl Pts',(6.617180742554,7.31244814185575,18.));
#91388=CARTESIAN_POINT('Ctrl Pts',(6.56451156701509,7.36206188025258,18.));
#91389=CARTESIAN_POINT('Ctrl Pts',(6.52219163648823,7.40192675264994,18.));
#91390=CARTESIAN_POINT('Ctrl Pts',(6.47951155539951,7.44143144973857,18.));
#91391=CARTESIAN_POINT('Ctrl Pts',(6.43647610849305,7.48057113719609,18.));
#91392=CARTESIAN_POINT('Ctrl Pts',(6.40510030277937,7.50910666587389,18.));
#91393=CARTESIAN_POINT('Ctrl Pts',(6.37353721864763,7.53744658432229,18.));
#91394=CARTESIAN_POINT('Ctrl Pts',(6.34180463558981,7.56557530387894,18.));
#91395=CARTESIAN_POINT('Ctrl Pts',(6.28236444622681,7.61826488209385,18.));
#91396=CARTESIAN_POINT('Ctrl Pts',(6.22231565827699,7.67022618764865,18.));
#91397=CARTESIAN_POINT('Ctrl Pts',(6.16167255213736,7.72144997951763,18.));
#91398=CARTESIAN_POINT('Ctrl Pts',(5.97233596776844,7.88137809679721,18.));
#91399=CARTESIAN_POINT('Ctrl Pts',(5.77721063648874,8.03411825327571,18.));
#91400=CARTESIAN_POINT('Ctrl Pts',(5.57671927434662,8.17935389220667,18.));
#91401=CARTESIAN_POINT('Ctrl Pts',(5.37540325211635,8.32518691365587,18.));
#91402=CARTESIAN_POINT('Ctrl Pts',(5.16867649244539,8.46345403723429,18.));
#91403=CARTESIAN_POINT('Ctrl Pts',(4.95693127547179,8.59379583228999,18.));
#91404=CARTESIAN_POINT('Ctrl Pts',(4.7451860584982,8.7241376273457,18.));
#91405=CARTESIAN_POINT('Ctrl Pts',(4.52842188794294,8.84655456454867,18.));
#91406=CARTESIAN_POINT('Ctrl Pts',(4.30700275658802,8.96064123010977,18.));
#91407=CARTESIAN_POINT('Ctrl Pts',(5.43505795426094,-7.63293718671423,18.));
#91408=CARTESIAN_POINT('Ctrl Pts',(5.43686761498028,-7.63164861186465,18.0000195210791));
#91409=CARTESIAN_POINT('Ctrl Pts',(5.43867681744549,-7.63035939344787,18.0000390421582));
#91410=CARTESIAN_POINT('Ctrl Pts',(5.44048556119893,-7.62906953178997,18.0000585632373));
#91411=CARTESIAN_POINT('Ctrl Pts',(4.30729780905827,8.96073832123217,4.));
#91412=CARTESIAN_POINT('Ctrl Pts',(4.52735866241683,8.84762889800062,3.99999999999999));
#91413=CARTESIAN_POINT('Ctrl Pts',(4.74289519135029,8.72644163152856,3.99999999999999));
#91414=CARTESIAN_POINT('Ctrl Pts',(4.95341780643153,8.59733634854351,3.99999999999999));
#91415=CARTESIAN_POINT('Ctrl Pts',(5.01139145305849,8.5617833793266,3.99999999999999));
#91416=CARTESIAN_POINT('Ctrl Pts',(5.06898473711946,8.52562968458252,4.));
#91417=CARTESIAN_POINT('Ctrl Pts',(5.12618709348549,8.48887799458869,4.));
#91418=CARTESIAN_POINT('Ctrl Pts',(5.33414451424221,8.35526834727518,3.99999999999999));
#91419=CARTESIAN_POINT('Ctrl Pts',(5.53693773709606,8.21375835063172,4.));
#91420=CARTESIAN_POINT('Ctrl Pts',(5.73421561007242,8.06474571286238,3.99999999999999));
#91421=CARTESIAN_POINT('Ctrl Pts',(5.93164891033915,7.91561567403752,3.99999999999999));
#91422=CARTESIAN_POINT('Ctrl Pts',(6.12355862014355,7.75897067554847,4.));
#91423=CARTESIAN_POINT('Ctrl Pts',(6.30955580572295,7.5951727274196,4.));
#91424=CARTESIAN_POINT('Ctrl Pts',(6.34223834170209,7.56639093528467,4.));
#91425=CARTESIAN_POINT('Ctrl Pts',(6.37473822150666,7.53738820927742,4.));
#91426=CARTESIAN_POINT('Ctrl Pts',(6.40705320087122,7.50816641433773,4.));
#91427=CARTESIAN_POINT('Ctrl Pts',(6.43174166095423,7.48584112952835,4.));
#91428=CARTESIAN_POINT('Ctrl Pts',(6.45631548500609,7.46339403274824,4.));
#91429=CARTESIAN_POINT('Ctrl Pts',(6.48077183163878,7.44082803617405,4.));
#91430=CARTESIAN_POINT('Ctrl Pts',(6.63832117297785,7.2954564502082,4.));
#91431=CARTESIAN_POINT('Ctrl Pts',(6.79102402996194,7.14512773488293,4.));
#91432=CARTESIAN_POINT('Ctrl Pts',(6.93866063600344,6.99010918328356,4.));
#91433=CARTESIAN_POINT('Ctrl Pts',(7.10847998508006,6.81179873417987,4.));
#91434=CARTESIAN_POINT('Ctrl Pts',(7.27159731884034,6.62728364575909,4.));
#91435=CARTESIAN_POINT('Ctrl Pts',(7.42764239363171,6.43693772257308,4.00000000000001));
#91436=CARTESIAN_POINT('Ctrl Pts',(7.58218650243463,6.24842269829321,4.00000000000001));
#91437=CARTESIAN_POINT('Ctrl Pts',(7.72979410893354,6.05418794787021,4.00000000000001));
#91438=CARTESIAN_POINT('Ctrl Pts',(7.87006275526019,5.85456913669398,4.00000000000001));
#91439=CARTESIAN_POINT('Ctrl Pts',(7.92865109023734,5.77119103272556,4.00000000000001));
#91440=CARTESIAN_POINT('Ctrl Pts',(7.98595850701148,5.6868733272343,4.00000000000001));
#91441=CARTESIAN_POINT('Ctrl Pts',(8.04195320620857,5.60163937017,4.00000000000001));
#91442=CARTESIAN_POINT('Ctrl Pts',(8.05864268878731,5.5762349897208,4.));
#91443=CARTESIAN_POINT('Ctrl Pts',(8.07521588798848,5.55074859303754,4.00000000000001));
#91444=CARTESIAN_POINT('Ctrl Pts',(8.09166333406113,5.525194394489,4.00000000000001));
#91445=CARTESIAN_POINT('Ctrl Pts',(8.20895789598644,5.34295524861398,4.00000000000001));
#91446=CARTESIAN_POINT('Ctrl Pts',(8.31996633523362,5.15710734281305,4.));
#91447=CARTESIAN_POINT('Ctrl Pts',(8.42446245528993,4.96791812226087,4.00000000000001));
#91448=CARTESIAN_POINT('Ctrl Pts',(8.5415709437287,4.75589433002977,4.00000000000001));
#91449=CARTESIAN_POINT('Ctrl Pts',(8.65050135921717,4.53967410763202,4.));
#91450=CARTESIAN_POINT('Ctrl Pts',(8.75117985411016,4.31977266478955,4.));
#91451=CARTESIAN_POINT('Ctrl Pts',(8.85287322430194,4.09765453661874,4.));
#91452=CARTESIAN_POINT('Ctrl Pts',(8.94614769538898,3.87177998411824,4.));
#91453=CARTESIAN_POINT('Ctrl Pts',(9.03087895681104,3.64265834953363,4.));
#91454=CARTESIAN_POINT('Ctrl Pts',(9.11548314304982,3.41388033869804,4.));
#91455=CARTESIAN_POINT('Ctrl Pts',(9.19156986905553,3.18186432688568,4.));
#91456=CARTESIAN_POINT('Ctrl Pts',(9.25896493253069,2.94710551021159,4.));
#91457=CARTESIAN_POINT('Ctrl Pts',(9.32561355021895,2.71494680578028,4.));
#91458=CARTESIAN_POINT('Ctrl Pts',(9.38376203708655,2.48010509232614,4.00000000000001));
#91459=CARTESIAN_POINT('Ctrl Pts',(9.43319110917098,2.24305718438921,4.));
#91460=CARTESIAN_POINT('Ctrl Pts',(9.44421566232366,2.19018653255259,4.));
#91461=CARTESIAN_POINT('Ctrl Pts',(9.45480625606057,2.13720614422637,4.));
#91462=CARTESIAN_POINT('Ctrl Pts',(9.46496010189184,2.08412134345432,4.));
#91463=CARTESIAN_POINT('Ctrl Pts',(9.47020198198243,2.05671653891976,4.));
#91464=CARTESIAN_POINT('Ctrl Pts',(9.47532601316739,2.0292913927946,4.));
#91465=CARTESIAN_POINT('Ctrl Pts',(9.48033096475668,2.00185258817826,4.));
#91466=CARTESIAN_POINT('Ctrl Pts',(9.52392327882317,1.76286506410242,4.));
#91467=CARTESIAN_POINT('Ctrl Pts',(9.55851334216252,1.52270096690633,4.00000000000001));
#91468=CARTESIAN_POINT('Ctrl Pts',(9.58400922469124,1.28186074651651,4.));
#91469=CARTESIAN_POINT('Ctrl Pts',(9.60946255717459,1.04142246405902,4.));
#91470=CARTESIAN_POINT('Ctrl Pts',(9.62585215468648,0.800309667757621,4.00000000000001));
#91471=CARTESIAN_POINT('Ctrl Pts',(9.63303576261776,0.559010656769312,4.00000000000001));
#91472=CARTESIAN_POINT('Ctrl Pts',(9.63493699332233,0.495147888497155,4.00000000000001));
#91473=CARTESIAN_POINT('Ctrl Pts',(9.63619309821743,0.431272053532241,4.));
#91474=CARTESIAN_POINT('Ctrl Pts',(9.63680082693735,0.367392178681336,4.));
#91475=CARTESIAN_POINT('Ctrl Pts',(9.63910369572888,0.125331921562864,4.00000000000001));
#91476=CARTESIAN_POINT('Ctrl Pts',(9.63210067711924,-0.116786870509174,
4.00000000000001));
#91477=CARTESIAN_POINT('Ctrl Pts',(9.61592042259555,-0.358453301654759,
4.00000000000001));
#91478=CARTESIAN_POINT('Ctrl Pts',(9.59976867571333,-0.599693945927636,
4.00000000000001));
#91479=CARTESIAN_POINT('Ctrl Pts',(9.57447182128881,-0.840484470113809,
4.));
#91480=CARTESIAN_POINT('Ctrl Pts',(9.54010755134981,-1.08030443174907,4.00000000000001));
#91481=CARTESIAN_POINT('Ctrl Pts',(9.52066457166946,-1.21599230317178,4.));
#91482=CARTESIAN_POINT('Ctrl Pts',(9.49831804338267,-1.35136920346387,4.00000000000001));
#91483=CARTESIAN_POINT('Ctrl Pts',(9.47307521435284,-1.4863379289703,4.00000000000001));
#91484=CARTESIAN_POINT('Ctrl Pts',(9.4649303911865,-1.52988678797252,4.00000000000001));
#91485=CARTESIAN_POINT('Ctrl Pts',(9.45648402016263,-1.57339303349641,4.00000000000001));
#91486=CARTESIAN_POINT('Ctrl Pts',(9.44773617789971,-1.61685363980245,4.00000000000001));
#91487=CARTESIAN_POINT('Ctrl Pts',(9.44045759216671,-1.653014756967,4.00000000000001));
#91488=CARTESIAN_POINT('Ctrl Pts',(9.4329703892861,-1.68914330368502,4.00000000000001));
#91489=CARTESIAN_POINT('Ctrl Pts',(9.42528051679276,-1.72521129584486,4.00000000000001));
#91490=CARTESIAN_POINT('Ctrl Pts',(9.37504487203195,-1.96083273728565,4.));
#91491=CARTESIAN_POINT('Ctrl Pts',(9.31610795885698,-2.19415568001356,4.));
#91492=CARTESIAN_POINT('Ctrl Pts',(9.24864539615387,-2.42469127009468,4.));
#91493=CARTESIAN_POINT('Ctrl Pts',(9.18110633204538,-2.65548828363685,4.));
#91494=CARTESIAN_POINT('Ctrl Pts',(9.10502208698088,-2.88349226619126,4.));
#91495=CARTESIAN_POINT('Ctrl Pts',(9.02051769106837,-3.10820223924067,4.));
#91496=CARTESIAN_POINT('Ctrl Pts',(8.93678495719486,-3.33086024618686,4.));
#91497=CARTESIAN_POINT('Ctrl Pts',(8.84478490227422,-3.55028471986832,4.));
#91498=CARTESIAN_POINT('Ctrl Pts',(8.7445922820912,-3.7659688277657,4.));
#91499=CARTESIAN_POINT('Ctrl Pts',(8.67781695430482,-3.90971571228528,4.));
#91500=CARTESIAN_POINT('Ctrl Pts',(8.60740168442632,-4.05180078366608,4.));
#91501=CARTESIAN_POINT('Ctrl Pts',(8.53335765314134,-4.19206717736045,4.));
#91502=CARTESIAN_POINT('Ctrl Pts',(8.44331101733595,-4.36264833899545,4.));
#91503=CARTESIAN_POINT('Ctrl Pts',(8.34789785964412,-4.53054022772032,4.));
#91504=CARTESIAN_POINT('Ctrl Pts',(8.24728117878015,-4.69552960580368,4.));
#91505=CARTESIAN_POINT('Ctrl Pts',(8.20326138090216,-4.76771245871515,4.));
#91506=CARTESIAN_POINT('Ctrl Pts',(8.15824539656185,-4.83933955682702,4.));
#91507=CARTESIAN_POINT('Ctrl Pts',(8.11224599398009,-4.91039207263641,4.));
#91508=CARTESIAN_POINT('Ctrl Pts',(8.08753260385713,-4.94856536280674,4.));
#91509=CARTESIAN_POINT('Ctrl Pts',(8.06253567255053,-4.9865723101471,4.));
#91510=CARTESIAN_POINT('Ctrl Pts',(8.03725606161742,-5.02441150090253,4.));
#91511=CARTESIAN_POINT('Ctrl Pts',(8.01764312895937,-5.05376865762798,4.));
#91512=CARTESIAN_POINT('Ctrl Pts',(7.9978615337744,-5.08302244104312,4.));
#91513=CARTESIAN_POINT('Ctrl Pts',(7.97792532987057,-5.11215275381745,4.));
#91514=CARTESIAN_POINT('Ctrl Pts',(7.8440295483756,-5.30779812406573,4.));
#91515=CARTESIAN_POINT('Ctrl Pts',(7.70302251457516,-5.49808894505449,4.));
#91516=CARTESIAN_POINT('Ctrl Pts',(7.55529935414448,-5.68269963489007,4.));
#91517=CARTESIAN_POINT('Ctrl Pts',(7.40624743847603,-5.86897087964711,4.));
#91518=CARTESIAN_POINT('Ctrl Pts',(7.25035761889544,-6.04945986263983,4.));
#91519=CARTESIAN_POINT('Ctrl Pts',(7.08799183256734,-6.22380270966777,4.));
#91520=CARTESIAN_POINT('Ctrl Pts',(6.92609832025987,-6.39763844495009,4.));
#91521=CARTESIAN_POINT('Ctrl Pts',(6.75776597786644,-6.56536420217669,4.));
#91522=CARTESIAN_POINT('Ctrl Pts',(6.58331694003355,-6.72658296228736,4.));
#91523=CARTESIAN_POINT('Ctrl Pts',(6.40972058594001,-6.88701370649991,4.));
#91524=CARTESIAN_POINT('Ctrl Pts',(6.23006671722395,-7.0410013431429,4.));
#91525=CARTESIAN_POINT('Ctrl Pts',(6.04464352038724,-7.18811202239736,4.));
#91526=CARTESIAN_POINT('Ctrl Pts',(5.85922032355054,-7.33522270165183,4.));
#91527=CARTESIAN_POINT('Ctrl Pts',(5.66802736285917,-7.47545689991215,4.));
#91528=CARTESIAN_POINT('Ctrl Pts',(5.47133023013366,-7.60833117514228,4.));
#91529=CARTESIAN_POINT('Ctrl Pts',(5.46100689439012,-7.61530486985696,4.));
#91530=CARTESIAN_POINT('Ctrl Pts',(5.45066839308308,-7.62225827926665,4.));
#91531=CARTESIAN_POINT('Ctrl Pts',(5.44031476324456,-7.62919132931685,4.));
#91532=CARTESIAN_POINT('Origin',(0.,0.,4.));
#91533=CARTESIAN_POINT('',(-14.,-1.71450551880629E-15,4.));
#91534=CARTESIAN_POINT('Origin',(0.,0.,4.));
#91535=CARTESIAN_POINT('Origin',(0.,0.,0.));
#91536=CARTESIAN_POINT('',(-14.,-1.71450551880629E-15,0.));
#91537=CARTESIAN_POINT('',(-14.,-1.71450551880629E-15,0.));
#91538=CARTESIAN_POINT('Origin',(0.,0.,0.));
#91539=CARTESIAN_POINT('Origin',(0.,0.,0.));
#91540=CARTESIAN_POINT('',(-5.,-6.12323399573677E-16,0.));
#91541=CARTESIAN_POINT('Origin',(0.,0.,0.));
#91542=CARTESIAN_POINT('',(-5.,-6.12323399573677E-16,18.));
#91543=CARTESIAN_POINT('',(-5.,-6.12323399573677E-16,0.));
#91544=CARTESIAN_POINT('Origin',(0.,0.,18.));
#91545=CARTESIAN_POINT('Origin',(0.,0.,18.));
#91546=CARTESIAN_POINT('Origin',(0.,0.,0.));
#91547=CARTESIAN_POINT('',(0.,0.,0.));
#91548=CARTESIAN_POINT('Origin',(0.,0.,-2.20842344717745));
#91549=CARTESIAN_POINT('',(6.1363657837075,-7.99235873417456,3.56263847785126));
#91550=CARTESIAN_POINT('',(6.13575050161833,-7.99155833647621,3.64579035276345));
#91551=CARTESIAN_POINT('',(6.13615379320824,-7.992083121821,-2.20842344717745));
#91552=CARTESIAN_POINT('',(2.60234962446753,9.73414364143214,4.));
#91553=CARTESIAN_POINT('Ctrl Pts',(6.13575050161833,-7.99155833647621,3.64579035276345));
#91554=CARTESIAN_POINT('Ctrl Pts',(6.89661927295215,-7.40686050907605,3.66094475600081));
#91555=CARTESIAN_POINT('Ctrl Pts',(8.72642379835497,-5.53871638815614,3.70182802903188));
#91556=CARTESIAN_POINT('Ctrl Pts',(10.3690110414678,-1.51793686145572,3.76844017185666));
#91557=CARTESIAN_POINT('Ctrl Pts',(9.88113494348103,3.49068484817476,3.84562678123777));
#91558=CARTESIAN_POINT('Ctrl Pts',(7.11402078469617,7.69533055119267,3.92281339061889));
#91559=CARTESIAN_POINT('Ctrl Pts',(4.1759640497451,9.31344973557609,3.97427113020629));
#91560=CARTESIAN_POINT('Ctrl Pts',(2.6023496244676,9.73414364143212,4.));
#91561=CARTESIAN_POINT('',(-2.60241879177085,9.73440315357327,3.99999685169366));
#91562=CARTESIAN_POINT('Origin',(0.,0.,4.));
#91563=CARTESIAN_POINT('Ctrl Pts',(6.1363657837075,-7.99235873417456,3.56263847785126));
#91564=CARTESIAN_POINT('Ctrl Pts',(7.2256962454093,-7.15441785607105,3.58434919887163));
#91565=CARTESIAN_POINT('Ctrl Pts',(9.23098036694038,-4.83331139710073,3.6317887896857));
#91566=CARTESIAN_POINT('Ctrl Pts',(10.4771042016857,-0.228210237258418,
3.70495725029349));
#91567=CARTESIAN_POINT('Ctrl Pts',(9.37532803384437,4.68240093714628,3.7821438596746));
#91568=CARTESIAN_POINT('Ctrl Pts',(6.11133502294712,8.51314763294832,3.85933046905572));
#91569=CARTESIAN_POINT('Ctrl Pts',(1.71450917131053,10.2699119982464,3.93194813306207));
#91570=CARTESIAN_POINT('Ctrl Pts',(-1.30803602033293,10.0791359541843,3.97883692727472));
#91571=CARTESIAN_POINT('Ctrl Pts',(-2.60241879177086,9.73440315357327,3.99999685169366));
#91572=CARTESIAN_POINT('Origin',(0.,0.,-2.20842344717745));
#91573=CARTESIAN_POINT('',(6.1362409016225,-7.9921963794308,2.56263886265602));
#91574=CARTESIAN_POINT('',(6.13615379320825,-7.992083121821,2.64578903198487));
#91575=CARTESIAN_POINT('',(6.13615379320824,-7.992083121821,-2.20842344717745));
#91576=CARTESIAN_POINT('',(-10.0759999978312,-0.000209059053492667,3.29157655282254));
#91577=CARTESIAN_POINT('Ctrl Pts',(6.13615379320825,-7.99208312182099,2.64578903198487));
#91578=CARTESIAN_POINT('Ctrl Pts',(6.33194935528241,-7.84175539592005,2.64968751815102));
#91579=CARTESIAN_POINT('Ctrl Pts',(6.52222043055739,-7.68422727429467,2.65358600431717));
#91580=CARTESIAN_POINT('Ctrl Pts',(6.70644559174884,-7.51993108511724,2.65748449048332));
#91581=CARTESIAN_POINT('Ctrl Pts',(6.89066877557437,-7.35563665939972,2.66138293480539));
#91582=CARTESIAN_POINT('Ctrl Pts',(7.06884596855911,-7.18457449847276,2.66528137912746));
#91583=CARTESIAN_POINT('Ctrl Pts',(7.24049064021804,-7.00721565879879,2.66917982344952));
#91584=CARTESIAN_POINT('Ctrl Pts',(7.41216962074527,-6.82982136809093,2.67307904700471));
#91585=CARTESIAN_POINT('Ctrl Pts',(7.577313276671,-6.64612808368434,2.67697827055989));
#91586=CARTESIAN_POINT('Ctrl Pts',(7.73547266915676,-6.45664298104897,2.68087749411508));
#91587=CARTESIAN_POINT('Ctrl Pts',(7.82944273932568,-6.34406080612556,2.68319420958373));
#91588=CARTESIAN_POINT('Ctrl Pts',(7.92094801835551,-6.22943471971775,2.68551092505239));
#91589=CARTESIAN_POINT('Ctrl Pts',(8.00990108241083,-6.11287662643324,2.68782764052105));
#91590=CARTESIAN_POINT('Ctrl Pts',(8.15961682553693,-5.91669921828237,2.69172687414144));
#91591=CARTESIAN_POINT('Ctrl Pts',(8.30214348409879,-5.71499078402337,2.69562610776184));
#91592=CARTESIAN_POINT('Ctrl Pts',(8.43708493598507,-5.50830044414553,2.69952534138223));
#91593=CARTESIAN_POINT('Ctrl Pts',(8.5720042784268,-5.30164396938878,2.70342393613378));
#91594=CARTESIAN_POINT('Ctrl Pts',(8.69934074296439,-5.09000745174317,2.70732253088533));
#91595=CARTESIAN_POINT('Ctrl Pts',(8.81874158981831,-4.87396889321309,2.71122112563688));
#91596=CARTESIAN_POINT('Ctrl Pts',(8.93813026163517,-4.65795236365119,2.71511932285745));
#91597=CARTESIAN_POINT('Ctrl Pts',(9.0495847967984,-4.43753493328373,2.71901752007802));
#91598=CARTESIAN_POINT('Ctrl Pts',(9.15279795110948,-4.21332002892803,2.72291571729859));
#91599=CARTESIAN_POINT('Ctrl Pts',(9.25601879101199,-3.98908842879206,2.72681420479177));
#91600=CARTESIAN_POINT('Ctrl Pts',(9.35099690476323,-3.76105904159036,2.73071269228494));
#91601=CARTESIAN_POINT('Ctrl Pts',(9.43747229274958,-3.52985732340331,2.73461117977812));
#91602=CARTESIAN_POINT('Ctrl Pts',(9.52394672476821,-3.29865816110396,2.73850962417431));
#91603=CARTESIAN_POINT('Ctrl Pts',(9.60191852337963,-3.06428699969025,2.74240806857051));
#91604=CARTESIAN_POINT('Ctrl Pts',(9.67117660924036,-2.82738730860881,2.7463065129667));
#91605=CARTESIAN_POINT('Ctrl Pts',(9.74044856055598,-2.59044019025672,2.75020573783068));
#91606=CARTESIAN_POINT('Ctrl Pts',(9.80100323464222,-2.35096379811987,2.75410496269466));
#91607=CARTESIAN_POINT('Ctrl Pts',(9.85267964124371,-2.10961605203928,2.75800418755864));
#91608=CARTESIAN_POINT('Ctrl Pts',(9.88364774769249,-1.96498365239441,2.76034087500648));
#91609=CARTESIAN_POINT('Ctrl Pts',(9.91142842287093,-1.81967945557351,2.76267756245433));
#91610=CARTESIAN_POINT('Ctrl Pts',(9.93599580785843,-1.67384685865215,2.76501424990217));
#91611=CARTESIAN_POINT('Ctrl Pts',(9.97699142497022,-1.43049587486422,2.76891348231826));
#91612=CARTESIAN_POINT('Ctrl Pts',(10.0090484682785,-1.18560314388318,2.77281271473435));
#91613=CARTESIAN_POINT('Ctrl Pts',(10.0320724880943,-0.939839131778517,
2.77671194715044));
#91614=CARTESIAN_POINT('Ctrl Pts',(10.0550927355203,-0.694115387083012,
2.78061054069355));
#91615=CARTESIAN_POINT('Ctrl Pts',(10.0690828880855,-0.447520923549086,
2.78450913423665));
#91616=CARTESIAN_POINT('Ctrl Pts',(10.0740003400475,-0.200731533953737,
2.78840772777976));
#91617=CARTESIAN_POINT('Ctrl Pts',(10.078917290587,0.0460326910366703,2.79230592379132));
#91618=CARTESIAN_POINT('Ctrl Pts',(10.0747633822627,0.292991523916393,2.79620411980289));
#91619=CARTESIAN_POINT('Ctrl Pts',(10.0615481113648,0.539467888470903,2.80010231581446));
#91620=CARTESIAN_POINT('Ctrl Pts',(10.0483318563879,0.785962606958579,2.80400080210631));
#91621=CARTESIAN_POINT('Ctrl Pts',(10.0260529026826,1.0319745069307,2.80789928839816));
#91622=CARTESIAN_POINT('Ctrl Pts',(9.99477281292278,1.27682904809517,2.81179777469001));
#91623=CARTESIAN_POINT('Ctrl Pts',(9.96349306890727,1.52168088283989,2.81569621789121));
#91624=CARTESIAN_POINT('Ctrl Pts',(9.92321242523012,1.76537510822755,2.81959466109241));
#91625=CARTESIAN_POINT('Ctrl Pts',(9.87404412123745,2.00724405388487,2.82349310429362));
#91626=CARTESIAN_POINT('Ctrl Pts',(9.8248659735366,2.24916142275643,2.82739232798009));
#91627=CARTESIAN_POINT('Ctrl Pts',(9.76679666510075,2.4892525084711,2.83129155166657));
#91628=CARTESIAN_POINT('Ctrl Pts',(9.70000048496686,2.72686020757258,2.83519077535305));
#91629=CARTESIAN_POINT('Ctrl Pts',(9.65997142049938,2.86925179173558,2.83752746999646));
#91630=CARTESIAN_POINT('Ctrl Pts',(9.61680927882901,3.01075175524593,2.83986416463987));
#91631=CARTESIAN_POINT('Ctrl Pts',(9.57055803349138,3.15122118036384,2.84220085928328));
#91632=CARTESIAN_POINT('Ctrl Pts',(9.49337873111043,3.38562205232547,2.8461000940204));
#91633=CARTESIAN_POINT('Ctrl Pts',(9.40757284882014,3.61721981916801,2.84999932875753));
#91634=CARTESIAN_POINT('Ctrl Pts',(9.31336939248879,3.84537729736016,2.85389856349465));
#91635=CARTESIAN_POINT('Ctrl Pts',(9.21918137083707,4.07349739329779,2.8577971593652));
#91636=CARTESIAN_POINT('Ctrl Pts',(9.11659862816643,4.29817806842485,2.86169575523576));
#91637=CARTESIAN_POINT('Ctrl Pts',(9.00589851916906,4.51880159582477,2.86559435110631));
#91638=CARTESIAN_POINT('Ctrl Pts',(8.89520969803949,4.73940262668668,2.86949254944487));
#91639=CARTESIAN_POINT('Ctrl Pts',(8.77640528827373,4.95594708693956,2.87339074778343));
#91640=CARTESIAN_POINT('Ctrl Pts',(8.64980933678775,5.16784040361344,2.87728894612199));
#91641=CARTESIAN_POINT('Ctrl Pts',(8.52320395885865,5.3797494980454,2.88118743472375));
#91642=CARTESIAN_POINT('Ctrl Pts',(8.38880602045493,5.58700651623069,2.8850859233255));
#91643=CARTESIAN_POINT('Ctrl Pts',(8.24698444863633,5.7890434014568,2.88898441192725));
#91644=CARTESIAN_POINT('Ctrl Pts',(8.1051644448861,5.99107805283623,2.89288285742487));
#91645=CARTESIAN_POINT('Ctrl Pts',(7.95592113370849,6.18789245983946,2.89678130292248));
#91646=CARTESIAN_POINT('Ctrl Pts',(7.79966595708087,6.37894873454504,2.9006797484201));
#91647=CARTESIAN_POINT('Ctrl Pts',(7.64337949893426,6.57004325777854,2.90457897436735));
#91648=CARTESIAN_POINT('Ctrl Pts',(7.48007854648031,6.75537712924579,2.90847820031461));
#91649=CARTESIAN_POINT('Ctrl Pts',(7.31021477843386,6.93444560820598,2.91237742626187));
#91650=CARTESIAN_POINT('Ctrl Pts',(7.20842088115244,7.04175559292638,2.91471410706271));
#91651=CARTESIAN_POINT('Ctrl Pts',(7.10427088804325,7.14681619519958,2.91705078786355));
#91652=CARTESIAN_POINT('Ctrl Pts',(6.99786846178245,7.24952501834365,2.91938746866439));
#91653=CARTESIAN_POINT('Ctrl Pts',(6.82031418339718,7.42091576212657,2.92328669998824));
#91654=CARTESIAN_POINT('Ctrl Pts',(6.63643488235327,7.58580503799604,2.92718593131208));
#91655=CARTESIAN_POINT('Ctrl Pts',(6.44673020355477,7.74373589958843,2.93108516263593));
#91656=CARTESIAN_POINT('Ctrl Pts',(6.2570566070791,7.90164088486583,2.93498375508694));
#91657=CARTESIAN_POINT('Ctrl Pts',(6.06155975231665,8.05258955369743,2.93888234753795));
#91658=CARTESIAN_POINT('Ctrl Pts',(5.86077298722548,8.19616471236445,2.94278093998896));
#91659=CARTESIAN_POINT('Ctrl Pts',(5.66000669578056,8.3397252310874,2.94667913491177));
#91660=CARTESIAN_POINT('Ctrl Pts',(5.45395179764753,8.4759135789366,2.95057732983457));
#91661=CARTESIAN_POINT('Ctrl Pts',(5.24317215460739,8.60435481353191,2.95447552475737));
#91662=CARTESIAN_POINT('Ctrl Pts',(5.03237681511165,8.73280561296046,2.95837400997312));
#91663=CARTESIAN_POINT('Ctrl Pts',(4.81685626416003,8.85350799896822,2.96227249518887));
#91664=CARTESIAN_POINT('Ctrl Pts',(4.5972017067638,8.96613141033122,2.96617098040462));
#91665=CARTESIAN_POINT('Ctrl Pts',(4.37754957674429,9.07875357710612,2.97006942253867));
#91666=CARTESIAN_POINT('Ctrl Pts',(4.1537637805712,9.18329682254549,2.97396786467271));
#91667=CARTESIAN_POINT('Ctrl Pts',(3.92645907121909,9.2794770952916,2.97786630680676));
#91668=CARTESIAN_POINT('Ctrl Pts',(3.69910885325884,9.37567662426146,2.98176552944674));
#91669=CARTESIAN_POINT('Ctrl Pts',(3.46823857085602,9.46350972581889,2.98566475208673));
#91670=CARTESIAN_POINT('Ctrl Pts',(3.23448312098629,9.54274043134648,2.98956397472671));
#91671=CARTESIAN_POINT('Ctrl Pts',(3.09439965596286,9.59022129980426,2.99190067583298));
#91672=CARTESIAN_POINT('Ctrl Pts',(2.95328040588612,9.6346137339204,2.99423737693925));
#91673=CARTESIAN_POINT('Ctrl Pts',(2.81126481955898,9.67587547017375,2.99657407804552));
#91674=CARTESIAN_POINT('Ctrl Pts',(2.57428456164226,9.74472859504756,3.00047331224339));
#91675=CARTESIAN_POINT('Ctrl Pts',(2.33473955692088,9.80488130013986,3.00437254644126));
#91676=CARTESIAN_POINT('Ctrl Pts',(2.09328485806413,9.85616226038307,3.00827178063913));
#91677=CARTESIAN_POINT('Ctrl Pts',(1.85186972071869,9.90743481841957,3.01217037596107));
#91678=CARTESIAN_POINT('Ctrl Pts',(1.60854578631715,9.94983847561576,3.016068971283));
#91679=CARTESIAN_POINT('Ctrl Pts',(1.36397939188466,9.98325278746932,3.01996756660493));
#91680=CARTESIAN_POINT('Ctrl Pts',(1.11943793588059,10.0166636920664,3.02386576438721));
#91681=CARTESIAN_POINT('Ctrl Pts',(0.873654548801523,10.0410870439685,3.02776396216948));
#91682=CARTESIAN_POINT('Ctrl Pts',(0.627302865707757,10.0564540030109,3.03166215995176));
#91683=CARTESIAN_POINT('Ctrl Pts',(0.380932839531959,10.0718221062607,3.03556064798966));
#91684=CARTESIAN_POINT('Ctrl Pts',(0.133994710725798,10.078132449085,3.03945913602756));
#91685=CARTESIAN_POINT('Ctrl Pts',(-0.112834385489892,10.0753682017806,
3.04335762406546));
#91686=CARTESIAN_POINT('Ctrl Pts',(-0.359660752396465,10.0726039850418,
3.04725606899589));
#91687=CARTESIAN_POINT('Ctrl Pts',(-0.606377810516523,10.060765384096,3.05115451392631));
#91688=CARTESIAN_POINT('Ctrl Pts',(-0.852309274447887,10.0398876936294,
3.05505295885674));
#91689=CARTESIAN_POINT('Ctrl Pts',(-1.09828997256641,10.0190058235588,3.05895218423536));
#91690=CARTESIAN_POINT('Ctrl Pts',(-1.3434844844748,9.98908127118697,3.06285140961398));
#91691=CARTESIAN_POINT('Ctrl Pts',(-1.587221119285,9.9502012602005,3.06675063499261));
#91692=CARTESIAN_POINT('Ctrl Pts',(-1.73328488188769,9.92690168236256,3.06908731913728));
#91693=CARTESIAN_POINT('Ctrl Pts',(-1.87882520253984,9.90038698736819,3.07142400328195));
#91694=CARTESIAN_POINT('Ctrl Pts',(-2.02369901335421,9.87068479404287,3.07376068742663));
#91695=CARTESIAN_POINT('Ctrl Pts',(-2.2654507249401,9.82112058341097,3.07765992489568));
#91696=CARTESIAN_POINT('Ctrl Pts',(-2.50541538755697,9.76266356830015,3.08155916236472));
#91697=CARTESIAN_POINT('Ctrl Pts',(-2.74293361492496,9.69546755881916,3.08545839983376));
#91698=CARTESIAN_POINT('Ctrl Pts',(-2.98041292794163,9.6282825585527,3.08935699846217));
#91699=CARTESIAN_POINT('Ctrl Pts',(-3.21544633787951,9.55236149802127,3.09325559709058));
#91700=CARTESIAN_POINT('Ctrl Pts',(-3.44738819534,9.46790846125111,3.09715419571898));
#91701=CARTESIAN_POINT('Ctrl Pts',(-3.6793064032186,9.38346403560027,3.10105239683299));
#91702=CARTESIAN_POINT('Ctrl Pts',(-3.90813342633422,9.29048946612366,3.10495059794699));
#91703=CARTESIAN_POINT('Ctrl Pts',(-4.13324121621327,9.18923789269795,3.108848799061));
#91704=CARTESIAN_POINT('Ctrl Pts',(-4.35836576819106,9.08797877982249,3.11274729044498));
#91705=CARTESIAN_POINT('Ctrl Pts',(-4.57977027827707,8.97844154322405,3.11664578182896));
#91706=CARTESIAN_POINT('Ctrl Pts',(-4.79684784816732,8.86092696739639,3.12054427321294));
#91707=CARTESIAN_POINT('Ctrl Pts',(-5.01392301786911,8.7434136909067,3.12444272149198));
#91708=CARTESIAN_POINT('Ctrl Pts',(-5.22667109902227,8.61792338611242,3.12834116977103));
#91709=CARTESIAN_POINT('Ctrl Pts',(-5.43451024495873,8.48480255500613,3.13223961805008));
#91710=CARTESIAN_POINT('Ctrl Pts',(-5.64239099821483,8.35165507444002,3.13613884675951));
#91711=CARTESIAN_POINT('Ctrl Pts',(-5.84536061763127,8.21087416514267,3.14003807546894));
#91712=CARTESIAN_POINT('Ctrl Pts',(-6.04286552996029,8.06285012801415,3.14393730417836));
#91713=CARTESIAN_POINT('Ctrl Pts',(-6.16122295248895,7.97414477228288,3.14627396838816));
#91714=CARTESIAN_POINT('Ctrl Pts',(-6.27761847520027,7.88283911723174,3.14861063259795));
#91715=CARTESIAN_POINT('Ctrl Pts',(-6.39193840660977,7.78902429102047,3.15094729680774));
#91716=CARTESIAN_POINT('Ctrl Pts',(-6.58270521411611,7.63247455667032,3.15484651163424));
#91717=CARTESIAN_POINT('Ctrl Pts',(-6.76774539581126,7.4688906653599,3.15874572646074));
#91718=CARTESIAN_POINT('Ctrl Pts',(-6.94654731124955,7.29871608247448,3.16264494128724));
#91719=CARTESIAN_POINT('Ctrl Pts',(-7.12531992698819,7.12856938555525,3.16654351716185));
#91720=CARTESIAN_POINT('Ctrl Pts',(-7.29785611545559,6.95183434509883,3.17044209303645));
#91721=CARTESIAN_POINT('Ctrl Pts',(-7.46367982602414,6.76899249922766,3.17434066891105));
#91722=CARTESIAN_POINT('Ctrl Pts',(-7.62948662668822,6.58616929868853,3.17823884722764));
#91723=CARTESIAN_POINT('Ctrl Pts',(-7.78858212915114,6.3972407425548,3.18213702554422));
#91724=CARTESIAN_POINT('Ctrl Pts',(-7.94052872327196,6.2027235626693,3.18603520386081));
#91725=CARTESIAN_POINT('Ctrl Pts',(-8.09248663550991,6.00819189369153,3.18993367254283));
#91726=CARTESIAN_POINT('Ctrl Pts',(-8.23729440162687,5.80807098703512,3.19383214122485));
#91727=CARTESIAN_POINT('Ctrl Pts',(-8.37455533405834,5.60290986513214,3.19773060990687));
#91728=CARTESIAN_POINT('Ctrl Pts',(-8.51181475203737,5.39775100685039,3.20162903557559));
#91729=CARTESIAN_POINT('Ctrl Pts',(-8.6415273496758,5.18755227732144,3.20552746124431));
#91730=CARTESIAN_POINT('Ctrl Pts',(-8.76333991521675,4.9728914657741,3.20942588691303));
#91731=CARTESIAN_POINT('Ctrl Pts',(-8.88517687554087,4.75818766519742,3.21332509329964));
#91732=CARTESIAN_POINT('Ctrl Pts',(-8.99911050445519,4.53902023920256,3.21722429968625));
#91733=CARTESIAN_POINT('Ctrl Pts',(-9.10483302185017,4.31599254450547,3.22112350607286));
#91734=CARTESIAN_POINT('Ctrl Pts',(-9.16819267974994,4.18233172383667,3.22346030611153));
#91735=CARTESIAN_POINT('Ctrl Pts',(-9.22860410251766,4.04728490777612,3.22579710615019));
#91736=CARTESIAN_POINT('Ctrl Pts',(-9.28600918186325,3.91098574202865,3.22813390618886));
#91737=CARTESIAN_POINT('Ctrl Pts',(-9.38143382290358,3.68441521701905,3.23201837612452));
#91738=CARTESIAN_POINT('Ctrl Pts',(-9.46857807619525,3.45431307415355,3.23590284606019));
#91739=CARTESIAN_POINT('Ctrl Pts',(-9.54719691433382,3.22130518252072,3.23978731599585));
#91740=CARTESIAN_POINT('Ctrl Pts',(-9.62580180803594,2.98833861894379,3.24367109695232));
#91741=CARTESIAN_POINT('Ctrl Pts',(-9.69588421470461,2.75246760335617,3.24755487790879));
#91742=CARTESIAN_POINT('Ctrl Pts',(-9.75724831562987,2.51433516205339,3.25143865886526));
#91743=CARTESIAN_POINT('Ctrl Pts',(-9.8186109875981,2.27620826602907,3.25532234938194));
#91744=CARTESIAN_POINT('Ctrl Pts',(-9.87125568580342,2.03582032264973,3.25920603989862));
#91745=CARTESIAN_POINT('Ctrl Pts',(-9.91503696250514,1.79382775989134,3.2630897304153));
#91746=CARTESIAN_POINT('Ctrl Pts',(-9.95881591686286,1.5518480334415,3.26697321492462));
#91747=CARTESIAN_POINT('Ctrl Pts',(-9.99373233985306,1.30826413626401,3.27085669943393));
#91748=CARTESIAN_POINT('Ctrl Pts',(-10.0196920909372,1.06374169929095,3.27474018394325));
#91749=CARTESIAN_POINT('Ctrl Pts',(-10.0456553125043,0.819186572830302,
3.27862418762423));
#91750=CARTESIAN_POINT('Ctrl Pts',(-10.0626594394833,0.573692937217471,
3.2825081913052));
#91751=CARTESIAN_POINT('Ctrl Pts',(-10.0706621796009,0.327931798330226,
3.28639219498617));
#91752=CARTESIAN_POINT('Ctrl Pts',(-10.0742228583788,0.218584692361075,
3.28812031426496));
#91753=CARTESIAN_POINT('Ctrl Pts',(-10.0760022675563,0.109184672134251,
3.28984843354375));
#91754=CARTESIAN_POINT('Ctrl Pts',(-10.0759999978312,-0.000209059053492667,
3.29157655282254));
#91755=CARTESIAN_POINT('Ctrl Pts',(-10.0762484745384,-0.000209064208945703,
3.29157655282254));
#91756=CARTESIAN_POINT('Ctrl Pts',(-10.0765172050036,-0.290223858717575,
3.29615787373835));
#91757=CARTESIAN_POINT('Ctrl Pts',(-9.99523566685694,-2.20882270727419,
3.32646806444787));
#91758=CARTESIAN_POINT('Ctrl Pts',(-8.81522447115248,-5.66688708944764,
3.38250712495108));
#91759=CARTESIAN_POINT('Ctrl Pts',(-5.15686684570512,-9.12295875983689,
3.4596937343322));
#91760=CARTESIAN_POINT('Ctrl Pts',(-0.309172458345963,-10.4750423473345,
3.53688034371331));
#91761=CARTESIAN_POINT('Ctrl Pts',(3.64403776703417,-9.62007385115271,3.59891254985707));
#91762=CARTESIAN_POINT('Ctrl Pts',(5.60483013146509,-8.39954983073467,3.63521588620711));
#91763=CARTESIAN_POINT('Ctrl Pts',(6.13575050161833,-7.99155833647621,3.64579035276345));
#91764=CARTESIAN_POINT('',(-10.0752881866894,-8.86040407210159E-5,3.20842344717745));
#91765=CARTESIAN_POINT('Ctrl Pts',(-10.0752881866894,-8.86040407210159E-5,
3.20842344717745));
#91766=CARTESIAN_POINT('Ctrl Pts',(-10.0755181733502,-0.705362299928891,
3.21956149612057));
#91767=CARTESIAN_POINT('Ctrl Pts',(-9.83358734487156,-3.03966120371691,
3.25642841485739));
#91768=CARTESIAN_POINT('Ctrl Pts',(-8.04938962653146,-6.71037259617267,
3.31902420338792));
#91769=CARTESIAN_POINT('Ctrl Pts',(-3.99287690887074,-9.6891020991096,3.39621081276903));
#91770=CARTESIAN_POINT('Ctrl Pts',(0.984510208053555,-10.4332411960233,
3.47339742215015));
#91771=CARTESIAN_POINT('Ctrl Pts',(4.39868813687642,-9.23866752856937,3.52887331051089));
#91772=CARTESIAN_POINT('Ctrl Pts',(5.93475608800304,-8.14744207333764,3.55862032907792));
#91773=CARTESIAN_POINT('Ctrl Pts',(6.1363657837075,-7.99235873417456,3.56263847785126));
#91774=CARTESIAN_POINT('Ctrl Pts',(6.1362409016225,-7.9921963794308,2.56263886265602));
#91775=CARTESIAN_POINT('Ctrl Pts',(7.16828197515765,-7.19822956485664,2.58320748142331));
#91776=CARTESIAN_POINT('Ctrl Pts',(9.14580362631273,-4.9594312981428,2.6295049699843));
#91777=CARTESIAN_POINT('Ctrl Pts',(10.4697637918774,-0.453671087720179,
2.701531328339));
#91778=CARTESIAN_POINT('Ctrl Pts',(9.47394258585729,4.47952935166234,2.77871793772012));
#91779=CARTESIAN_POINT('Ctrl Pts',(6.29315192521423,8.37961873334699,2.85590454710123));
#91780=CARTESIAN_POINT('Ctrl Pts',(1.6609755745572,10.347121897175,2.93309115648235));
#91781=CARTESIAN_POINT('Ctrl Pts',(-3.35427053915678,9.92827478991659,3.01027776586346));
#91782=CARTESIAN_POINT('Ctrl Pts',(-7.59592332616536,7.21967591544794,3.08746437524457));
#91783=CARTESIAN_POINT('Ctrl Pts',(-9.72645285448307,3.47712916071539,3.15351293568257));
#91784=CARTESIAN_POINT('Ctrl Pts',(-10.0749869046441,0.923818464413679,
3.19383262632687));
#91785=CARTESIAN_POINT('Ctrl Pts',(-10.0752881866894,-8.86040407210159E-5,
3.20842344717745));
#91786=CARTESIAN_POINT('Origin',(0.,0.,-2.20842344717745));
#91787=CARTESIAN_POINT('',(6.13611323687281,-7.99203043615932,1.56263897033545));
#91788=CARTESIAN_POINT('',(6.13568652661064,-7.99147452837712,1.64578849738327));
#91789=CARTESIAN_POINT('',(6.13615379320824,-7.992083121821,-2.20842344717745));
#91790=CARTESIAN_POINT('',(-10.0759999984503,-0.000176720804854386,2.29157655282254));
#91791=CARTESIAN_POINT('Ctrl Pts',(6.13568652661064,-7.99147452837712,1.64578849738327));
#91792=CARTESIAN_POINT('Ctrl Pts',(6.78214643002692,-7.49513482539196,1.65865957111104));
#91793=CARTESIAN_POINT('Ctrl Pts',(8.54213696741524,-5.77384824740789,1.69725951463251));
#91794=CARTESIAN_POINT('Ctrl Pts',(10.2941112079739,-1.9629174193269,1.76158832794768));
#91795=CARTESIAN_POINT('Ctrl Pts',(10.022138899288,3.06243403856305,1.8387749373288));
#91796=CARTESIAN_POINT('Ctrl Pts',(7.43876696437783,7.38149824946882,1.91596154670991));
#91797=CARTESIAN_POINT('Ctrl Pts',(3.13979685689322,9.99817213565975,1.99314815609103));
#91798=CARTESIAN_POINT('Ctrl Pts',(-1.88330263600878,10.3089738354113,2.07033476547214));
#91799=CARTESIAN_POINT('Ctrl Pts',(-6.47205721978153,8.24222334685567,2.14752137485326));
#91800=CARTESIAN_POINT('Ctrl Pts',(-9.43020620361965,4.45136803055563,2.22126863579156));
#91801=CARTESIAN_POINT('Ctrl Pts',(-10.0752698966321,1.41075423147899,2.26928702693616));
#91802=CARTESIAN_POINT('Ctrl Pts',(-10.0764446330389,-0.000176441506157512,
2.29157654828705));
#91803=CARTESIAN_POINT('Ctrl Pts',(-10.0759999984503,-0.000176720804854386,
2.29157655282254));
#91804=CARTESIAN_POINT('Ctrl Pts',(-10.0759961802274,-0.217878384328413,
2.29501589975352));
#91805=CARTESIAN_POINT('Ctrl Pts',(-10.068934916524,-0.435554421608969,
2.2984552466845));
#91806=CARTESIAN_POINT('Ctrl Pts',(-10.0548329534,-0.652771230387034,2.30189459361548));
#91807=CARTESIAN_POINT('Ctrl Pts',(-10.0388453706317,-0.899032809606319,
2.30579382688141));
#91808=CARTESIAN_POINT('Ctrl Pts',(-10.0138040511016,-1.14474211387924,
2.30969306014734));
#91809=CARTESIAN_POINT('Ctrl Pts',(-9.97977104745379,-1.3892249063428,2.31359229341327));
#91810=CARTESIAN_POINT('Ctrl Pts',(-9.94574361994677,-1.63366764149921,
2.31749088780894));
#91811=CARTESIAN_POINT('Ctrl Pts',(-9.90272748779683,-1.87688399017187,
2.32138948220462));
#91812=CARTESIAN_POINT('Ctrl Pts',(-9.85083638520011,-2.1182064375357,2.32528807660029));
#91813=CARTESIAN_POINT('Ctrl Pts',(-9.79895057382811,-2.35950427776585,
2.32918627346463));
#91814=CARTESIAN_POINT('Ctrl Pts',(-9.73819165759179,-2.59890832998929,
2.33308447032897));
#91815=CARTESIAN_POINT('Ctrl Pts',(-9.66872437485874,-2.83576179588704,
2.33698266719331));
#91816=CARTESIAN_POINT('Ctrl Pts',(-9.59925191932735,-3.07263289879557,
2.34088115433223));
#91817=CARTESIAN_POINT('Ctrl Pts',(-9.52106987730694,-3.30695276769737,
2.34477964147116));
#91818=CARTESIAN_POINT('Ctrl Pts',(-9.43439307949502,-3.53807902986585,
2.34867812861008));
#91819=CARTESIAN_POINT('Ctrl Pts',(-9.3477172398397,-3.76920273708122,2.35257657265371));
#91820=CARTESIAN_POINT('Ctrl Pts',(-9.25254693202794,-3.99713264800795,
2.35647501669735));
#91821=CARTESIAN_POINT('Ctrl Pts',(-9.14914570445701,-4.22124494416231,
2.36037346074099));
#91822=CARTESIAN_POINT('Ctrl Pts',(-9.0457237758488,-4.44540210784007,2.36427268525732));
#91823=CARTESIAN_POINT('Ctrl Pts',(-8.93406775112007,-4.66573987626492,
2.36817190977366));
#91824=CARTESIAN_POINT('Ctrl Pts',(-8.81448843710067,-4.88165643938803,
2.37207113429));
#91825=CARTESIAN_POINT('Ctrl Pts',(-8.74282810193653,-5.01104882976736,
2.37440782385887));
#91826=CARTESIAN_POINT('Ctrl Pts',(-8.66832321219159,-5.13885390250795,
2.37674451342773));
#91827=CARTESIAN_POINT('Ctrl Pts',(-8.59104846906926,-5.26494655263496,
2.3790812029966));
#91828=CARTESIAN_POINT('Ctrl Pts',(-8.46210012681553,-5.47535732266519,
2.38298043622717));
#91829=CARTESIAN_POINT('Ctrl Pts',(-8.32539954109015,-5.68105875354989,
2.38687966945774));
#91830=CARTESIAN_POINT('Ctrl Pts',(-8.18131593054936,-5.88148328608857,
2.39077890268831));
#91831=CARTESIAN_POINT('Ctrl Pts',(-8.03725592740549,-6.08187498004505,
2.39467749704854));
#91832=CARTESIAN_POINT('Ctrl Pts',(-7.88581547691877,-6.27699127552694,
2.39857609140876));
#91833=CARTESIAN_POINT('Ctrl Pts',(-7.72740638591762,-6.46629465357709,
2.40247468576899));
#91834=CARTESIAN_POINT('Ctrl Pts',(-7.56901344755157,-6.65557872876796,
2.40637288259791));
#91835=CARTESIAN_POINT('Ctrl Pts',(-7.40365346630422,-6.83905085647716,
2.41027107942683));
#91836=CARTESIAN_POINT('Ctrl Pts',(-7.2317783757314,-7.01620677605099,2.41416927625576));
#91837=CARTESIAN_POINT('Ctrl Pts',(-7.05989048667257,-7.19337588734183,
2.41806776335954));
#91838=CARTESIAN_POINT('Ctrl Pts',(-6.88148671091967,-7.3642276487559,2.42196625046332));
#91839=CARTESIAN_POINT('Ctrl Pts',(-6.69705657292911,-7.52829391422698,
2.4258647375671));
#91840=CARTESIAN_POINT('Ctrl Pts',(-6.5126284736855,-7.69235836605957,2.42976318157582));
#91841=CARTESIAN_POINT('Ctrl Pts',(-6.32217435503862,-7.84963728834382,
2.43366162558454));
#91842=CARTESIAN_POINT('Ctrl Pts',(-6.12621819150001,-7.99970166132052,
2.43756006959325));
#91843=CARTESIAN_POINT('Ctrl Pts',(-5.93022279729805,-8.14979607736804,
2.44145929407522));
#91844=CARTESIAN_POINT('Ctrl Pts',(-5.72872337816251,-8.29267288815728,
2.44535851855719));
#91845=CARTESIAN_POINT('Ctrl Pts',(-5.52227545736255,-8.4279445758151,2.44925774303916));
#91846=CARTESIAN_POINT('Ctrl Pts',(-5.39855733116427,-8.50900889295551,
2.45159443281868));
#91847=CARTESIAN_POINT('Ctrl Pts',(-5.27306265851896,-8.58734283382268,
2.4539311225982));
#91848=CARTESIAN_POINT('Ctrl Pts',(-5.14591584904406,-8.66287054471883,
2.45626781237772));
#91849=CARTESIAN_POINT('Ctrl Pts',(-4.93374602039322,-8.78890360481217,
2.46016704565127));
#91850=CARTESIAN_POINT('Ctrl Pts',(-4.71691333637528,-8.90715637330441,
2.46406627892482));
#91851=CARTESIAN_POINT('Ctrl Pts',(-4.49600902900801,-9.01729886446481,
2.46796551219837));
#91852=CARTESIAN_POINT('Ctrl Pts',(-4.27514091573067,-9.12742330931694,
2.47186410660163));
#91853=CARTESIAN_POINT('Ctrl Pts',(-4.05020276013291,-9.22944000533982,
2.47576270100488));
#91854=CARTESIAN_POINT('Ctrl Pts',(-3.82180946694097,-9.32306539708912,
2.47966129540814));
#91855=CARTESIAN_POINT('Ctrl Pts',(-3.59343946252863,-9.41668124205582,
2.48355949228));
#91856=CARTESIAN_POINT('Ctrl Pts',(-3.36161528174511,-9.50190738564849,
2.48745768915185));
#91857=CARTESIAN_POINT('Ctrl Pts',(-3.12697182419795,-9.57850840218205,
2.49135588602371));
#91858=CARTESIAN_POINT('Ctrl Pts',(-2.89231089421434,-9.65511512271608,
2.49525437317));
#91859=CARTESIAN_POINT('Ctrl Pts',(-2.65483053200803,-9.72309534371056,
2.49915286031629));
#91860=CARTESIAN_POINT('Ctrl Pts',(-2.41518205709183,-9.78226311397836,
2.50305134746258));
#91861=CARTESIAN_POINT('Ctrl Pts',(-2.17553623134171,-9.84143023018295,
2.5069497915135));
#91862=CARTESIAN_POINT('Ctrl Pts',(-1.93372261184902,-9.89178502575761,
2.51084823556442));
#91863=CARTESIAN_POINT('Ctrl Pts',(-1.69040475534258,-9.93319222421046,
2.51474667961534));
#91864=CARTESIAN_POINT('Ctrl Pts',(-1.44703818635148,-9.97460771242696,
2.51864590413877));
#91865=CARTESIAN_POINT('Ctrl Pts',(-1.20216705328294,-10.0070719768972,
2.52254512866219));
#91866=CARTESIAN_POINT('Ctrl Pts',(-0.956463475878432,-10.0305011649125,
2.52644435318561));
#91867=CARTESIAN_POINT('Ctrl Pts',(-0.809220614642379,-10.0445415818907,
2.52878104271002));
#91868=CARTESIAN_POINT('Ctrl Pts',(-0.661678939472876,-10.0553382699226,
2.53111773223442));
#91869=CARTESIAN_POINT('Ctrl Pts',(-0.513983875818206,-10.0628821207147,
2.53345442175883));
#91870=CARTESIAN_POINT('Ctrl Pts',(-0.267525157741719,-10.0754705427618,
2.5373536550201));
#91871=CARTESIAN_POINT('Ctrl Pts',(-0.0205683639859459,-10.0790020847021,
2.54125288828137));
#91872=CARTESIAN_POINT('Ctrl Pts',(0.226209615553745,-10.0734604386889,
2.54515212154265));
#91873=CARTESIAN_POINT('Ctrl Pts',(0.472947161739886,-10.0679197006471,
2.5490507159338));
#91874=CARTESIAN_POINT('Ctrl Pts',(0.719505673756191,-10.0533087486379,
2.55294931032495));
#91875=CARTESIAN_POINT('Ctrl Pts',(0.965208964084447,-10.0296633869563,
2.55684790471611));
#91876=CARTESIAN_POINT('Ctrl Pts',(1.21088720058246,-10.0060204363407,2.56074610157607));
#91877=CARTESIAN_POINT('Ctrl Pts',(1.45571011226613,-9.9733449422247,2.56464429843603));
#91878=CARTESIAN_POINT('Ctrl Pts',(1.6990062599891,-9.93172460998179,2.56854249529599));
#91879=CARTESIAN_POINT('Ctrl Pts',(1.94232052448544,-9.89010117852775,2.57244098243079));
#91880=CARTESIAN_POINT('Ctrl Pts',(2.18410752271826,-9.83953162225846,2.57633946956558));
#91881=CARTESIAN_POINT('Ctrl Pts',(2.42370435354384,-9.78015507068332,2.58023795670038));
#91882=CARTESIAN_POINT('Ctrl Pts',(2.66329853578938,-9.72077917547558,2.58413640074005));
#91883=CARTESIAN_POINT('Ctrl Pts',(2.90070232909134,-9.65259654875453,2.58803484477972));
#91884=CARTESIAN_POINT('Ctrl Pts',(3.13526563019086,-9.57579685603992,2.59193328881939));
#91885=CARTESIAN_POINT('Ctrl Pts',(3.36987589113122,-9.49898178793909,2.59583251333202));
#91886=CARTESIAN_POINT('Ctrl Pts',(3.60164425852563,-9.41354629294794,2.59973173784464));
#91887=CARTESIAN_POINT('Ctrl Pts',(3.82993702673016,-9.3197295224315,2.60363096235726));
#91888=CARTESIAN_POINT('Ctrl Pts',(3.96674611124785,-9.26350791459125,2.60596765195149));
#91889=CARTESIAN_POINT('Ctrl Pts',(4.10230736223007,-9.20427732353835,2.60830434154571));
#91890=CARTESIAN_POINT('Ctrl Pts',(4.2364878777232,-9.14209748700507,2.61064103113994));
#91891=CARTESIAN_POINT('Ctrl Pts',(4.46039355290455,-9.03833861985149,2.61454024153842));
#91892=CARTESIAN_POINT('Ctrl Pts',(4.68051769765676,-8.92633516334218,2.6184394519369));
#91893=CARTESIAN_POINT('Ctrl Pts',(4.89625388547097,-8.80638824314545,2.62233866233539));
#91894=CARTESIAN_POINT('Ctrl Pts',(5.11249823727535,-8.68615878942389,2.62624705727697));
#91895=CARTESIAN_POINT('Ctrl Pts',(5.32433367772899,-8.55794851900752,2.63015545221855));
#91896=CARTESIAN_POINT('Ctrl Pts',(5.53117432236376,-8.42210701758318,2.63406384716013));
#91897=CARTESIAN_POINT('Ctrl Pts',(5.73801496699853,-8.28626551615884,2.63797224210171));
#91898=CARTESIAN_POINT('Ctrl Pts',(5.93986057789858,-8.14279293543828,2.64188063704329));
#91899=CARTESIAN_POINT('Ctrl Pts',(6.13615379320825,-7.99208312182099,2.64578903198487));
#91900=CARTESIAN_POINT('',(-10.0753832650889,-0.000140516250313333,2.20842344717745));
#91901=CARTESIAN_POINT('Ctrl Pts',(-10.0753832650889,-0.000140516250313333,
2.20842344717745));
#91902=CARTESIAN_POINT('Ctrl Pts',(-10.0757149532685,-0.63308601055591,
2.21841952213574));
#91903=CARTESIAN_POINT('Ctrl Pts',(-9.86563371722133,-2.89495068052824,
2.25414446688773));
#91904=CARTESIAN_POINT('Ctrl Pts',(-8.19195912274756,-6.53556248896653,
2.31559828143343));
#91905=CARTESIAN_POINT('Ctrl Pts',(-4.20050058358688,-9.60091486080197,
2.39278489081454));
#91906=CARTESIAN_POINT('Ctrl Pts',(0.759716778100874,-10.4520142428044,
2.46997150019566));
#91907=CARTESIAN_POINT('Ctrl Pts',(4.26961744480485,-9.30813086285984,2.52658949080948));
#91908=CARTESIAN_POINT('Ctrl Pts',(5.87732264030094,-8.1913866175406,2.5574786116296));
#91909=CARTESIAN_POINT('Ctrl Pts',(6.1362409016225,-7.9921963794308,2.56263886265602));
#91910=CARTESIAN_POINT('Ctrl Pts',(6.13611323687281,-7.99203043615932,1.56263897033545));
#91911=CARTESIAN_POINT('Ctrl Pts',(7.1109225332917,-7.24211522249615,1.58206557922476));
#91912=CARTESIAN_POINT('Ctrl Pts',(9.05946263688066,-5.08416455109786,1.62722105790779));
#91913=CARTESIAN_POINT('Ctrl Pts',(10.4575734376389,-0.678917602467889,
1.69810540638452));
#91914=CARTESIAN_POINT('Ctrl Pts',(9.56816533664898,4.27457406171102,1.77529201576563));
#91915=CARTESIAN_POINT('Ctrl Pts',(6.47205724804309,8.24222338284801,1.85247862514674));
#91916=CARTESIAN_POINT('Ctrl Pts',(1.8833026442324,10.3089738804262,1.92966523452786));
#91917=CARTESIAN_POINT('Ctrl Pts',(-3.1397968706035,9.99817217931868,2.00685184390897));
#91918=CARTESIAN_POINT('Ctrl Pts',(-7.43876699686031,7.38149828170111,2.08403845329009));
#91919=CARTESIAN_POINT('Ctrl Pts',(-9.6875785856742,3.62177575817932,2.15122898771292));
#91920=CARTESIAN_POINT('Ctrl Pts',(-10.074861221977,0.996050653330273,2.19269065234204));
#91921=CARTESIAN_POINT('Ctrl Pts',(-10.0753832650889,-0.000140516250313333,
2.20842344717745));
#91922=CARTESIAN_POINT('Origin',(0.,0.,-2.20842344717745));
#91923=CARTESIAN_POINT('',(6.13615379320823,-7.99208312182101,0.562637467686473));
#91924=CARTESIAN_POINT('',(6.13570130489945,-7.99149349283587,0.645787560180936));
#91925=CARTESIAN_POINT('',(6.13615379320824,-7.992083121821,-2.20842344717745));
#91926=CARTESIAN_POINT('',(-10.0759532185556,-0.00022630263218971,0.208423447557889));
#91927=CARTESIAN_POINT('Ctrl Pts',(-10.0759999974585,-0.000226308042700162,
0.208423447626752));
#91928=CARTESIAN_POINT('Ctrl Pts',(-10.0759942294301,-0.25703845579838,
0.212479650651435));
#91929=CARTESIAN_POINT('Ctrl Pts',(-10.0661658676225,-0.513807198917835,
0.216535853676117));
#91930=CARTESIAN_POINT('Ctrl Pts',(-10.0465508416353,-0.769800095114306,
0.220592056700798));
#91931=CARTESIAN_POINT('Ctrl Pts',(-10.0288714897423,-1.00053078580477,
0.224247980514977));
#91932=CARTESIAN_POINT('Ctrl Pts',(-10.0032424030593,-1.23063110424319,
0.227903904329156));
#91933=CARTESIAN_POINT('Ctrl Pts',(-9.96972602448593,-1.45956808566372,
0.231559828143335));
#91934=CARTESIAN_POINT('Ctrl Pts',(-9.93400236370396,-1.70358212932921,
0.235456519484748));
#91935=CARTESIAN_POINT('Ctrl Pts',(-9.88931045279285,-1.94632091839481,
0.239353210826162));
#91936=CARTESIAN_POINT('Ctrl Pts',(-9.83576585870345,-2.18711818902491,
0.243249902167575));
#91937=CARTESIAN_POINT('Ctrl Pts',(-9.78223042362828,-2.42787427033115,
0.24714592696455));
#91938=CARTESIAN_POINT('Ctrl Pts',(-9.71984538890546,-2.66668922356591,
0.251041951761524));
#91939=CARTESIAN_POINT('Ctrl Pts',(-9.64877730110775,-2.90290761024662,
0.254937976558499));
#91940=CARTESIAN_POINT('Ctrl Pts',(-9.57771682973085,-3.13910068122392,
0.258833583815545));
#91941=CARTESIAN_POINT('Ctrl Pts',(-9.49797524383153,-3.37269747383736,
0.262729191072592));
#91942=CARTESIAN_POINT('Ctrl Pts',(-9.40976907379589,-3.6030573098182,0.266624798329638));
#91943=CARTESIAN_POINT('Ctrl Pts',(-9.32155660289302,-3.83343360118696,
0.270520683863183));
#91944=CARTESIAN_POINT('Ctrl Pts',(-9.22487843689419,-4.06057221193792,
0.274416569396729));
#91945=CARTESIAN_POINT('Ctrl Pts',(-9.11999988210158,-4.28385085530149,
0.278312454930274));
#91946=CARTESIAN_POINT('Ctrl Pts',(-9.01512255625489,-4.50712688233057,
0.282208294812612));
#91947=CARTESIAN_POINT('Ctrl Pts',(-8.90204515448193,-4.72654278042739,
0.286104134694949));
#91948=CARTESIAN_POINT('Ctrl Pts',(-8.78108005545656,-4.94149866535073,
0.289999974577287));
#91949=CARTESIAN_POINT('Ctrl Pts',(-8.66009032665029,-5.15649831757879,
0.293896607694066));
#91950=CARTESIAN_POINT('Ctrl Pts',(-8.53120982810265,-5.36703589826419,
0.297793240810845));
#91951=CARTESIAN_POINT('Ctrl Pts',(-8.39479627757849,-5.57253725496333,
0.301689873927624));
#91952=CARTESIAN_POINT('Ctrl Pts',(-8.31245075295972,-5.69658737287492,
0.304042061793237));
#91953=CARTESIAN_POINT('Ctrl Pts',(-8.22736113194365,-5.81880286809109,
0.30639424965885));
#91954=CARTESIAN_POINT('Ctrl Pts',(-8.13961371352563,-5.93906260234605,
0.308746437524462));
#91955=CARTESIAN_POINT('Ctrl Pts',(-7.99412393307036,-6.1384594923037,0.312646487261849));
#91956=CARTESIAN_POINT('Ctrl Pts',(-7.84128311980634,-6.33253588031595,
0.316546536999235));
#91957=CARTESIAN_POINT('Ctrl Pts',(-7.6815052180949,-6.520755599191,0.320446586736622));
#91958=CARTESIAN_POINT('Ctrl Pts',(-7.52175316747803,-6.70894486525812,
0.324346005469636));
#91959=CARTESIAN_POINT('Ctrl Pts',(-7.35506644915583,-6.89127914173186,
0.328245424202651));
#91960=CARTESIAN_POINT('Ctrl Pts',(-7.18189903465007,-7.06725563822991,
0.332144842935665));
#91961=CARTESIAN_POINT('Ctrl Pts',(-7.0087490348349,-7.24321443754025,0.336043869521167));
#91962=CARTESIAN_POINT('Ctrl Pts',(-6.82911983543161,-7.41281653523007,
0.339942896106669));
#91963=CARTESIAN_POINT('Ctrl Pts',(-6.64350272377713,-7.57559552505054,
0.343841922692171));
#91964=CARTESIAN_POINT('Ctrl Pts',(-6.45787168682691,-7.73838672681394,
0.34774124178895));
#91965=CARTESIAN_POINT('Ctrl Pts',(-6.26625204748849,-7.89435361222738,
0.351640560885729));
#91966=CARTESIAN_POINT('Ctrl Pts',(-6.06916965264334,-8.04306880036675,
0.355539879982508));
#91967=CARTESIAN_POINT('Ctrl Pts',(-5.87208944175096,-8.19178234053068,
0.359439155869295));
#91968=CARTESIAN_POINT('Ctrl Pts',(-5.66954681992957,-8.33324417813178,
0.363338431756081));
#91969=CARTESIAN_POINT('Ctrl Pts',(-5.46209882225758,-8.46706870504146,
0.367237707642868));
#91970=CARTESIAN_POINT('Ctrl Pts',(-5.25460959742125,-8.60091982755979,
0.371137758451995));
#91971=CARTESIAN_POINT('Ctrl Pts',(-5.04221328251075,-8.72713045517242,
0.375037809261121));
#91972=CARTESIAN_POINT('Ctrl Pts',(-4.82549501839948,-8.84535888629748,
0.378937860070248));
#91973=CARTESIAN_POINT('Ctrl Pts',(-4.69592536044032,-8.91604428720148,
0.381269589015356));
#91974=CARTESIAN_POINT('Ctrl Pts',(-4.56481133630743,-8.98387730628482,
0.383601317960464));
#91975=CARTESIAN_POINT('Ctrl Pts',(-4.43228219470303,-9.04879276735402,
0.385933046905572));
#91976=CARTESIAN_POINT('Ctrl Pts',(-4.21066501416261,-9.15734535647877,
0.38983219835516));
#91977=CARTESIAN_POINT('Ctrl Pts',(-3.98502618871533,-9.25776808083673,
0.393731349804748));
#91978=CARTESIAN_POINT('Ctrl Pts',(-3.75598155591525,-9.34977959909347,
0.397630501254335));
#91979=CARTESIAN_POINT('Ctrl Pts',(-3.52697444811622,-9.44177604285457,
0.401529013895406));
#91980=CARTESIAN_POINT('Ctrl Pts',(-3.29456290534006,-9.52536392768369,
0.405427526536476));
#91981=CARTESIAN_POINT('Ctrl Pts',(-3.05938262588567,-9.60031009647235,
0.409326039177547));
#91982=CARTESIAN_POINT('Ctrl Pts',(-2.8242263093315,-9.67524862887428,0.413224154592839));
#91983=CARTESIAN_POINT('Ctrl Pts',(-2.58630208482971,-9.74154711887444,
0.417122270008131));
#91984=CARTESIAN_POINT('Ctrl Pts',(-2.34626170857426,-9.79902199175398,
0.421020385423424));
#91985=CARTESIAN_POINT('Ctrl Pts',(-2.10620339325966,-9.85650115993235,
0.424918792158552));
#91986=CARTESIAN_POINT('Ctrl Pts',(-1.8640288805491,-9.9051553257431,0.42881719889368));
#91987=CARTESIAN_POINT('Ctrl Pts',(-1.62040231297615,-9.94485154962615,
0.432715605628809));
#91988=CARTESIAN_POINT('Ctrl Pts',(-1.37677839311814,-9.98454734209366,
0.43661396999635));
#91989=CARTESIAN_POINT('Ctrl Pts',(-1.13170272534691,-10.0152853446242,
0.440512334363892));
#91990=CARTESIAN_POINT('Ctrl Pts',(-0.885847572329198,-10.0369841127003,
0.444410698731434));
#91991=CARTESIAN_POINT('Ctrl Pts',(-0.639943094035444,-10.0586872341435,
0.448309845217618));
#91992=CARTESIAN_POINT('Ctrl Pts',(-0.393259095630425,-10.0713474723984,
0.452208991703801));
#91993=CARTESIAN_POINT('Ctrl Pts',(-0.146472237457178,-10.0749353290061,
0.456108138189985));
#91994=CARTESIAN_POINT('Ctrl Pts',(0.00145334302901629,-10.0770859126121,
0.458445310888883));
#91995=CARTESIAN_POINT('Ctrl Pts',(0.149415822465978,-10.0759779000816,
0.460782483587781));
#91996=CARTESIAN_POINT('Ctrl Pts',(0.297269420956911,-10.0716139169134,
0.46311965628668));
#91997=CARTESIAN_POINT('Ctrl Pts',(0.543933112644408,-10.0643334975681,
0.467018754123361));
#91998=CARTESIAN_POINT('Ctrl Pts',(0.790364757584853,-10.0479861342427,
0.470917851960043));
#91999=CARTESIAN_POINT('Ctrl Pts',(1.03588839359109,-10.0226100011935,0.474816949796724));
#92000=CARTESIAN_POINT('Ctrl Pts',(1.28137167075645,-9.99723803943839,0.478715406705014));
#92001=CARTESIAN_POINT('Ctrl Pts',(1.52594695987715,-9.96284029941278,0.482613863613304));
#92002=CARTESIAN_POINT('Ctrl Pts',(1.76894318917324,-9.91950684225167,0.486512320521594));
#92003=CARTESIAN_POINT('Ctrl Pts',(2.01191453732034,-9.87617782213967,0.490410378254607));
#92004=CARTESIAN_POINT('Ctrl Pts',(2.25330687424229,-9.82391496077854,0.49430843598762));
#92005=CARTESIAN_POINT('Ctrl Pts',(2.49245803488221,-9.76285967042193,0.498206493720633));
#92006=CARTESIAN_POINT('Ctrl Pts',(2.73162691207991,-9.7017998570282,0.502104840225671));
#92007=CARTESIAN_POINT('Ctrl Pts',(2.96855401051834,-9.6319463793504,0.506003186730709));
#92008=CARTESIAN_POINT('Ctrl Pts',(3.20258981139837,-9.55349122048727,0.509901533235747));
#92009=CARTESIAN_POINT('Ctrl Pts',(3.43662298778403,-9.47503694142596,0.513799836024446));
#92010=CARTESIAN_POINT('Ctrl Pts',(3.6677646678912,-9.38798126467973,0.517698138813145));
#92011=CARTESIAN_POINT('Ctrl Pts',(3.89538215396801,-9.2925655162903,0.521596441601844));
#92012=CARTESIAN_POINT('Ctrl Pts',(4.12304520773466,-9.19713066622593,0.525495524807968));
#92013=CARTESIAN_POINT('Ctrl Pts',(4.34718240042929,-9.09333250760053,0.529394608014092));
#92014=CARTESIAN_POINT('Ctrl Pts',(4.56718135925702,-8.98146037299365,0.533293691220216));
#92015=CARTESIAN_POINT('Ctrl Pts',(4.69907211370827,-8.91439232724472,0.535631216036079));
#92016=CARTESIAN_POINT('Ctrl Pts',(4.82947597035662,-8.8444233435605,0.537968740851943));
#92017=CARTESIAN_POINT('Ctrl Pts',(4.95826512212948,-8.77162373672483,0.540306265667806));
#92018=CARTESIAN_POINT('Ctrl Pts',(5.17310996842347,-8.65018012035209,0.544205702482626));
#92019=CARTESIAN_POINT('Ctrl Pts',(5.38352161164181,-8.52082199850081,0.548105139297447));
#92020=CARTESIAN_POINT('Ctrl Pts',(5.58891975052209,-8.38389837857211,0.552004576112267));
#92021=CARTESIAN_POINT('Ctrl Pts',(5.77561133736504,-8.25944502169106,0.55554887330367));
#92022=CARTESIAN_POINT('Ctrl Pts',(5.9581612082682,-8.12874209528196,0.559093170495071));
#92023=CARTESIAN_POINT('Ctrl Pts',(6.13615379320823,-7.99208312182101,0.562637467686473));
#92024=CARTESIAN_POINT('',(-2.60234962446759,9.73414364143212,0.));
#92025=CARTESIAN_POINT('Ctrl Pts',(-2.60234962446759,9.73414364143212,0.));
#92026=CARTESIAN_POINT('Ctrl Pts',(-4.17596404974509,9.31344973557609,0.0257288697937048));
#92027=CARTESIAN_POINT('Ctrl Pts',(-7.11402029978251,7.69532831508128,0.0771866093811144));
#92028=CARTESIAN_POINT('Ctrl Pts',(-9.60465795441405,3.91079428092824,0.146661091773599));
#92029=CARTESIAN_POINT('Ctrl Pts',(-10.0747624470573,1.14044107610686,0.190406704372379));
#92030=CARTESIAN_POINT('Ctrl Pts',(-10.0756947894608,-0.000226272741935124,
0.208423447177455));
#92031=CARTESIAN_POINT('',(2.60261129514636,9.73435190842889,-4.86806775445991E-16));
#92032=CARTESIAN_POINT('Origin',(0.,0.,0.));
#92033=CARTESIAN_POINT('',(-10.0767271183091,-6.71673636424164E-5,0.291576552822545));
#92034=CARTESIAN_POINT('Ctrl Pts',(2.60261129514636,9.73435190842889,-4.86806775445991E-16));
#92035=CARTESIAN_POINT('Ctrl Pts',(1.30817124105572,10.0791274528727,0.0211609738543883));
#92036=CARTESIAN_POINT('Ctrl Pts',(-1.71444551568512,10.2699371933317,0.0680508175024821));
#92037=CARTESIAN_POINT('Ctrl Pts',(-6.11133505897136,8.51314768957044,0.14066953094428));
#92038=CARTESIAN_POINT('Ctrl Pts',(-9.32646956261626,4.73974294579722,0.216700741364073));
#92039=CARTESIAN_POINT('Ctrl Pts',(-10.0761339447278,1.55531013884913,0.267003081990161));
#92040=CARTESIAN_POINT('Ctrl Pts',(-10.0767271183091,-6.71673636424164E-5,
0.291576552822545));
#92041=CARTESIAN_POINT('Ctrl Pts',(-10.0767271183091,-6.71673636424164E-5,
0.291576552822545));
#92042=CARTESIAN_POINT('Ctrl Pts',(-10.0767550082293,-0.0731981196951006,
0.292731951783866));
#92043=CARTESIAN_POINT('Ctrl Pts',(-10.0585961450043,-1.7748235789123,0.319616220538893));
#92044=CARTESIAN_POINT('Ctrl Pts',(-9.16254767717503,-5.08620698909665,
0.372229359087624));
#92045=CARTESIAN_POINT('Ctrl Pts',(-5.73484093405497,-8.77116607832706,
0.449415968468739));
#92046=CARTESIAN_POINT('Ctrl Pts',(-0.984510201175506,-10.4332411554452,
0.526602577849852));
#92047=CARTESIAN_POINT('Ctrl Pts',(3.2365044433575,-9.80218273326553,0.592059775087324));
#92048=CARTESIAN_POINT('Ctrl Pts',(5.43245140071271,-8.53118528820037,0.631788102531087));
#92049=CARTESIAN_POINT('Ctrl Pts',(6.13570130491008,-7.99149349282772,0.645787560181147));
#92050=CARTESIAN_POINT('Origin',(0.,0.,0.));
#92051=CARTESIAN_POINT('',(-9.51749999795141,-0.000197471173248046,3.61402667816495));
#92052=CARTESIAN_POINT('',(-9.51745740801614,-0.000133057486098593,3.88597332183505));
#92053=CARTESIAN_POINT('',(-9.5175,-1.16555759108849E-15,0.));
#92054=CARTESIAN_POINT('',(-7.17753992463813,-6.25025814508694,4.));
#92055=CARTESIAN_POINT('Ctrl Pts',(-9.5174999990699,-0.000133058081536771,
3.88597332183505));
#92056=CARTESIAN_POINT('Ctrl Pts',(-9.51749665273006,-0.239493111281163,
3.8899746778871));
#92057=CARTESIAN_POINT('Ctrl Pts',(-9.50845929853709,-0.478827423920704,
3.89397603393915));
#92058=CARTESIAN_POINT('Ctrl Pts',(-9.49041975691978,-0.717453195314301,
3.8979773899912));
#92059=CARTESIAN_POINT('Ctrl Pts',(-9.47175816398719,-0.964307417192166,
3.90211672342915));
#92060=CARTESIAN_POINT('Ctrl Pts',(-9.44346254832326,-1.21040305961421,
3.9062560568671));
#92061=CARTESIAN_POINT('Ctrl Pts',(-9.40562656251792,-1.45498976506963,
3.91039539030505));
#92062=CARTESIAN_POINT('Ctrl Pts',(-9.36779057671258,-1.69957647052505,
3.91453472374299));
#92063=CARTESIAN_POINT('Ctrl Pts',(-9.32041427950108,-1.94265392739488,
3.91867405718094));
#92064=CARTESIAN_POINT('Ctrl Pts',(-9.26365005209081,-2.1834820728364,3.92281339061889));
#92065=CARTESIAN_POINT('Ctrl Pts',(-9.20909822162236,-2.41492389388337,
3.92679139272094));
#92066=CARTESIAN_POINT('Ctrl Pts',(-9.14586184258494,-2.64434941741664,
3.93076939482299));
#92067=CARTESIAN_POINT('Ctrl Pts',(-9.07411450088742,-2.87110645479834,
3.93474739692504));
#92068=CARTESIAN_POINT('Ctrl Pts',(-9.00237951233866,-3.09782445012847,
3.93872471411179));
#92069=CARTESIAN_POINT('Ctrl Pts',(-8.92213657000647,-3.32187461370113,
3.94270203129855));
#92070=CARTESIAN_POINT('Ctrl Pts',(-8.83360907565096,-3.54262006833601,
3.9466793484853));
#92071=CARTESIAN_POINT('Ctrl Pts',(-8.74509286899693,-3.76333737681344,
3.95065615854408));
#92072=CARTESIAN_POINT('Ctrl Pts',(-8.64829432222514,-3.98075056177624,
3.95463296860285));
#92073=CARTESIAN_POINT('Ctrl Pts',(-8.54348531568343,-4.19424187556007,
3.95860977866163));
#92074=CARTESIAN_POINT('Ctrl Pts',(-8.43867709176879,-4.40773159516714,
3.96258655902487));
#92075=CARTESIAN_POINT('Ctrl Pts',(-8.32585864693373,-4.6172992533984,3.96656333938812));
#92076=CARTESIAN_POINT('Ctrl Pts',(-8.205348783061,-4.82234980049347,3.97054011975136));
#92077=CARTESIAN_POINT('Ctrl Pts',(-8.08484685271647,-5.02738684849189,
3.97451663831115));
#92078=CARTESIAN_POINT('Ctrl Pts',(-7.95665465562245,-5.22790714217913,
3.97849315687094));
#92079=CARTESIAN_POINT('Ctrl Pts',(-7.82113590955983,-5.42334208161294,
3.98246967543072));
#92080=CARTESIAN_POINT('Ctrl Pts',(-7.68560746080289,-5.61879101354249,
3.98644647869609));
#92081=CARTESIAN_POINT('Ctrl Pts',(-7.54275157160334,-5.80915363661822,
3.99042328196147));
#92082=CARTESIAN_POINT('Ctrl Pts',(-7.3929747953963,-5.99389105044754,3.99440008522684));
#92083=CARTESIAN_POINT('Ctrl Pts',(-7.32267233336095,-6.08060339231482,
3.99626672348456));
#92084=CARTESIAN_POINT('Ctrl Pts',(-7.25084566524277,-6.16607684126215,
3.99813336174228));
#92085=CARTESIAN_POINT('Ctrl Pts',(-7.17753992463813,-6.25025814508694,
4.));
#92086=CARTESIAN_POINT('',(7.17753995915506,-6.25025810544912,3.99999685725335));
#92087=CARTESIAN_POINT('Origin',(0.,0.,4.));
#92088=CARTESIAN_POINT('Ctrl Pts',(7.17753995915506,-6.25025810544912,3.99999685725336));
#92089=CARTESIAN_POINT('Ctrl Pts',(7.02281523419272,-6.42793763121434,3.99605653063733));
#92090=CARTESIAN_POINT('Ctrl Pts',(6.86146956740091,-6.59989196979162,3.9921162040213));
#92091=CARTESIAN_POINT('Ctrl Pts',(6.69395260357331,-6.76563410118476,3.98817587740527));
#92092=CARTESIAN_POINT('Ctrl Pts',(6.52645659093536,-6.93135550336488,3.9842360436022));
#92093=CARTESIAN_POINT('Ctrl Pts',(6.35279102598433,-7.09086604782969,3.98029620979912));
#92094=CARTESIAN_POINT('Ctrl Pts',(6.17344244262228,-7.24371552848605,3.97635637599605));
#92095=CARTESIAN_POINT('Ctrl Pts',(5.99408383571268,-7.39657355169127,3.97241632200104));
#92096=CARTESIAN_POINT('Ctrl Pts',(5.80904179231516,-7.54276957913585,3.96847626800604));
#92097=CARTESIAN_POINT('Ctrl Pts',(5.61883685492493,-7.68189290785399,3.96453621401103));
#92098=CARTESIAN_POINT('Ctrl Pts',(5.4286329598901,-7.82101547415262,3.96059618160819));
#92099=CARTESIAN_POINT('Ctrl Pts',(5.23326646037713,-7.95306525185556,3.95665614920535));
#92100=CARTESIAN_POINT('Ctrl Pts',(5.03328843794528,-8.07767378336402,3.95271611680251));
#92101=CARTESIAN_POINT('Ctrl Pts',(4.83327086321585,-8.20230696034932,3.94877530512736));
#92102=CARTESIAN_POINT('Ctrl Pts',(4.62864018694421,-8.31949579925618,3.94483449345222));
#92103=CARTESIAN_POINT('Ctrl Pts',(4.41997478684035,-8.42891624906166,3.94089368177707));
#92104=CARTESIAN_POINT('Ctrl Pts',(4.34272795189276,-8.46942312476701,3.93943481399699));
#92105=CARTESIAN_POINT('Ctrl Pts',(4.26492842864018,-8.50886583895404,3.93797594621691));
#92106=CARTESIAN_POINT('Ctrl Pts',(4.1866063912307,-8.54722956137872,3.93651707843683));
#92107=CARTESIAN_POINT('Ctrl Pts',(3.97426764245315,-8.65123738711385,3.9325619443609));
#92108=CARTESIAN_POINT('Ctrl Pts',(3.7580202469193,-8.74734377138224,3.92860681028497));
#92109=CARTESIAN_POINT('Ctrl Pts',(3.53847147788908,-8.83527169079511,3.92465167620904));
#92110=CARTESIAN_POINT('Ctrl Pts',(3.31895909650136,-8.923185037183,3.92069719765036));
#92111=CARTESIAN_POINT('Ctrl Pts',(3.09614669616946,-9.00292251954423,3.91674271909167));
#92112=CARTESIAN_POINT('Ctrl Pts',(2.87066135613154,-9.07425532087416,3.91278824053299));
#92113=CARTESIAN_POINT('Ctrl Pts',(2.6451990166122,-9.14558084593762,3.9088341653489));
#92114=CARTESIAN_POINT('Ctrl Pts',(2.41706455120558,-9.20850331658646,3.90488009016482));
#92115=CARTESIAN_POINT('Ctrl Pts',(2.18690098528352,-9.26284353374092,3.90092601498073));
#92116=CARTESIAN_POINT('Ctrl Pts',(1.95672016055529,-9.31718782559449,3.89697164330046));
#92117=CARTESIAN_POINT('Ctrl Pts',(1.72451020578604,-9.36294851051478,3.8930172716202));
#92118=CARTESIAN_POINT('Ctrl Pts',(1.49092635594465,-9.39999706655006,3.88906289993994));
#92119=CARTESIAN_POINT('Ctrl Pts',(1.2573443349623,-9.4370453325114,3.88510855922067));
#92120=CARTESIAN_POINT('Ctrl Pts',(1.02238871995914,-9.46538156400081,3.8811542185014));
#92121=CARTESIAN_POINT('Ctrl Pts',(0.786722634961963,-9.48492876861174,
3.87719987778213));
#92122=CARTESIAN_POINT('Ctrl Pts',(0.55101021466734,-9.50447981648055,3.87324475958334));
#92123=CARTESIAN_POINT('Ctrl Pts',(0.314587327016663,-9.51523836115445,
3.86928964138456));
#92124=CARTESIAN_POINT('Ctrl Pts',(0.0781211806985837,-9.5171793789508,
3.86533452318578));
#92125=CARTESIAN_POINT('Ctrl Pts',(-0.0415343703337308,-9.51816156417098,
3.86333317180909));
#92126=CARTESIAN_POINT('Ctrl Pts',(-0.161200965586209,-9.51688683390705,
3.8613318204324));
#92127=CARTESIAN_POINT('Ctrl Pts',(-0.280792149199087,-9.51335703203386,
3.85933046905572));
#92128=CARTESIAN_POINT('Ctrl Pts',(-0.517128894444723,-9.50638141844039,
3.85537538761769));
#92129=CARTESIAN_POINT('Ctrl Pts',(-0.753240109108659,-9.49059360653506,
3.85142030617966));
#92130=CARTESIAN_POINT('Ctrl Pts',(-0.988459419836826,-9.4660315985811,
3.84746522474164));
#92131=CARTESIAN_POINT('Ctrl Pts',(-1.22363961627426,-9.44147367500915,
3.84351080098858));
#92132=CARTESIAN_POINT('Ctrl Pts',(-1.45792792382192,-9.4081444973385,3.83955637723552));
#92133=CARTESIAN_POINT('Ctrl Pts',(-1.69066291833379,-9.36613394878437,
3.83560195348247));
#92134=CARTESIAN_POINT('Ctrl Pts',(-1.92337405506483,-9.32412770675262,
3.83164793509937));
#92135=CARTESIAN_POINT('Ctrl Pts',(-2.15453191862022,-9.27344192099779,
3.82769391671627));
#92136=CARTESIAN_POINT('Ctrl Pts',(-2.38348410703422,-9.21421780519189,
3.82373989833317));
#92137=CARTESIAN_POINT('Ctrl Pts',(-2.61245331344558,-9.15498928726233,
3.81978558604821));
#92138=CARTESIAN_POINT('Ctrl Pts',(-2.83921624277278,-9.08722123935626,
3.81583127376325));
#92139=CARTESIAN_POINT('Ctrl Pts',(-3.06313331524021,-9.01110540073001,
3.81187696147829));
#92140=CARTESIAN_POINT('Ctrl Pts',(-3.28704855605815,-8.93499018473399,
3.80792268153975));
#92141=CARTESIAN_POINT('Ctrl Pts',(-3.50811771966648,-8.85052740772846,
3.8039684016012));
#92142=CARTESIAN_POINT('Ctrl Pts',(-3.72571826786526,-8.75795807471668,
3.80001412166265));
#92143=CARTESIAN_POINT('Ctrl Pts',(-3.94336150501496,-8.66537058142108,
3.7960590659721));
#92144=CARTESIAN_POINT('Ctrl Pts',(-4.1575345068657,-8.56467346500325,3.79210401028154));
#92145=CARTESIAN_POINT('Ctrl Pts',(-4.36763534766171,-8.45615561114245,
3.78814895459099));
#92146=CARTESIAN_POINT('Ctrl Pts',(-4.47396975352136,-8.40123350101794,
3.78614725628553));
#92147=CARTESIAN_POINT('Ctrl Pts',(-4.57926143832089,-8.34430886723251,
3.78414555798007));
#92148=CARTESIAN_POINT('Ctrl Pts',(-4.68343473375798,-8.28542366717776,
3.78214385967461));
#92149=CARTESIAN_POINT('Ctrl Pts',(-4.88928158859004,-8.16906627273643,
3.77818849569411));
#92150=CARTESIAN_POINT('Ctrl Pts',(-5.09081992575374,-8.04501697995684,
3.77423313171361));
#92151=CARTESIAN_POINT('Ctrl Pts',(-5.2874778747596,-7.91362015603022,3.77027776773312));
#92152=CARTESIAN_POINT('Ctrl Pts',(-5.48410332337008,-7.78224504721225,
3.7663230574302));
#92153=CARTESIAN_POINT('Ctrl Pts',(-5.67584975902805,-7.64352498817002,
3.76236834712729));
#92154=CARTESIAN_POINT('Ctrl Pts',(-5.86217387975088,-7.49784793481213,
3.75841363682438));
#92155=CARTESIAN_POINT('Ctrl Pts',(-6.04847904865881,-7.35218569888389,
3.75445932877179));
#92156=CARTESIAN_POINT('Ctrl Pts',(-6.22936278134758,-7.19956805559108,
3.7505050207192));
#92157=CARTESIAN_POINT('Ctrl Pts',(-6.40431369012583,-7.04042416395965,
3.74655071266661));
#92158=CARTESIAN_POINT('Ctrl Pts',(-6.57927771753765,-6.88126833897837,
3.7425961081016));
#92159=CARTESIAN_POINT('Ctrl Pts',(-6.74830782127441,-6.71558547602045,
3.73864150353658));
#92160=CARTESIAN_POINT('Ctrl Pts',(-6.91092751357785,-6.54384345412332,
3.73468689897157));
#92161=CARTESIAN_POINT('Ctrl Pts',(-7.07354591645346,-6.37210279398589,
3.73073232576301));
#92162=CARTESIAN_POINT('Ctrl Pts',(-7.22975381691432,-6.19430327777564,
3.72677775255445));
#92163=CARTESIAN_POINT('Ctrl Pts',(-7.37911277218885,-6.01094842311256,
3.72282317934589));
#92164=CARTESIAN_POINT('Ctrl Pts',(-7.52850101353397,-5.82755761651606,
3.7188678307308));
#92165=CARTESIAN_POINT('Ctrl Pts',(-7.67103744775897,-5.63860951403788,
3.7149124821157));
#92166=CARTESIAN_POINT('Ctrl Pts',(-7.80632418994686,-5.44464038219702,
3.71095713350061));
#92167=CARTESIAN_POINT('Ctrl Pts',(-7.87472984615139,-5.34656288005296,
3.70895717243157));
#92168=CARTESIAN_POINT('Ctrl Pts',(-7.94128266403896,-5.24720216376444,
3.70695721136252));
#92169=CARTESIAN_POINT('Ctrl Pts',(-8.00593538759606,-5.14663043355915,
3.70495725029348));
#92170=CARTESIAN_POINT('Ctrl Pts',(-8.13379265773527,-4.9477397114093,3.70100212592124));
#92171=CARTESIAN_POINT('Ctrl Pts',(-8.25425339444311,-4.74405309913378,
3.697047001549));
#92172=CARTESIAN_POINT('Ctrl Pts',(-8.36697222093433,-4.53614176411114,
3.69309187717676));
#92173=CARTESIAN_POINT('Ctrl Pts',(-8.47967233150307,-4.32826495084983,
3.68913740951648));
#92174=CARTESIAN_POINT('Ctrl Pts',(-8.58463296330333,-4.11616506353748,
3.6851829418562));
#92175=CARTESIAN_POINT('Ctrl Pts',(-8.68155433255552,-3.90043851648587,
3.68122847419592));
#92176=CARTESIAN_POINT('Ctrl Pts',(-8.77846578695878,-3.68473403779898,
3.67727441106922));
#92177=CARTESIAN_POINT('Ctrl Pts',(-8.867339505136,-3.4654038979101,3.67332034794253));
#92178=CARTESIAN_POINT('Ctrl Pts',(-8.94792314470012,-3.24306608729145,
3.66936628481584));
#92179=CARTESIAN_POINT('Ctrl Pts',(-9.02851279306713,-3.02071169782274,
3.66541192685032));
#92180=CARTESIAN_POINT('Ctrl Pts',(-9.10081102881558,-2.79534945434882,
3.6614575688848));
#92181=CARTESIAN_POINT('Ctrl Pts',(-9.16461443518121,-2.56761533420958,
3.65750321091927));
#92182=CARTESIAN_POINT('Ctrl Pts',(-9.22841732703322,-2.33988305052884,
3.65354888484188));
#92183=CARTESIAN_POINT('Ctrl Pts',(-9.28372545245174,-2.10977920124336,
3.64959455876448));
#92184=CARTESIAN_POINT('Ctrl Pts',(-9.33038566644054,-1.87795355786051,
3.64564023268709));
#92185=CARTESIAN_POINT('Ctrl Pts',(-9.37705503894105,-1.64608241151724,
3.64168513045076));
#92186=CARTESIAN_POINT('Ctrl Pts',(-9.41507305247464,-1.41248907295379,
3.63773002821444));
#92187=CARTESIAN_POINT('Ctrl Pts',(-9.44433770997892,-1.17783337950249,
3.63377492597812));
#92188=CARTESIAN_POINT('Ctrl Pts',(-9.45914671157632,-1.05908889945336,
3.63177349762287));
#92189=CARTESIAN_POINT('Ctrl Pts',(-9.47171502900033,-0.940072506192662,
3.62977206926762));
#92190=CARTESIAN_POINT('Ctrl Pts',(-9.48203449694926,-0.820870299538334,
3.62777064091237));
#92191=CARTESIAN_POINT('Ctrl Pts',(-9.50373124089866,-0.570246937095671,
3.62356262565696));
#92192=CARTESIAN_POINT('Ctrl Pts',(-9.51548761186254,-0.318757908470078,
3.61935461040155));
#92193=CARTESIAN_POINT('Ctrl Pts',(-9.51726304323121,-0.0671596303259994,
3.61514659514614));
#92194=CARTESIAN_POINT('Ctrl Pts',(-9.5174205470755,-0.0448395920950911,
3.61477328948574));
#92195=CARTESIAN_POINT('Ctrl Pts',(-9.51749953482576,-0.0225186960109495,
3.61439998382535));
#92196=CARTESIAN_POINT('Ctrl Pts',(-9.51749999795141,-0.000197471173248046,
3.61402667816495));
#92197=CARTESIAN_POINT('Origin',(0.,0.,0.));
#92198=CARTESIAN_POINT('',(-9.51791998781483,-0.000166932759165794,2.61402667816495));
#92199=CARTESIAN_POINT('',(-9.51744795729939,-8.37115215137324E-5,2.88597332205635));
#92200=CARTESIAN_POINT('',(-9.5175,-1.16555759108849E-15,0.));
#92201=CARTESIAN_POINT('Ctrl Pts',(-9.51682764166119,-8.38638332260327E-5,
2.88597332469409));
#92202=CARTESIAN_POINT('Ctrl Pts',(-9.51704486858051,-0.666265069291475,
2.8971113726842));
#92203=CARTESIAN_POINT('Ctrl Pts',(-9.28852394762602,-2.87117666120216,
2.93397829046798));
#92204=CARTESIAN_POINT('Ctrl Pts',(-7.60322208917357,-6.33842508774048,
2.99657407804553));
#92205=CARTESIAN_POINT('Ctrl Pts',(-3.77155676659138,-9.15204736286997,
3.07376068742662));
#92206=CARTESIAN_POINT('Ctrl Pts',(0.929940046163851,-9.85493976609273,
3.15094729680775));
#92207=CARTESIAN_POINT('Ctrl Pts',(5.41696593703601,-8.28499142533159,3.22813390618885));
#92208=CARTESIAN_POINT('Ctrl Pts',(8.65467923647761,-4.80428494172239,3.30532051556997));
#92209=CARTESIAN_POINT('Ctrl Pts',(9.89637150055028,-0.21556083099493,3.38250712495109));
#92210=CARTESIAN_POINT('Ctrl Pts',(8.85566539917763,4.42286134570138,3.45969373433219));
#92211=CARTESIAN_POINT('Ctrl Pts',(5.77259141334861,8.04127457290448,3.53688034371332));
#92212=CARTESIAN_POINT('Ctrl Pts',(1.35817110792663,9.80506885261808,3.61406695309443));
#92213=CARTESIAN_POINT('Ctrl Pts',(-3.36944939868327,9.30765437281576,3.69125356247554));
#92214=CARTESIAN_POINT('Ctrl Pts',(-7.32004314469702,6.66336788144076,3.76844017185665));
#92215=CARTESIAN_POINT('Ctrl Pts',(-9.22237333027156,3.14792279530392,3.83334675830983));
#92216=CARTESIAN_POINT('Ctrl Pts',(-9.51671069117059,0.804315052831599,
3.87252447496929));
#92217=CARTESIAN_POINT('Ctrl Pts',(-9.51680985342271,-0.000133048433053571,
3.88597332183505));
#92218=CARTESIAN_POINT('Ctrl Pts',(-9.51773470173007,-0.000197284648878047,
3.61402667496411));
#92219=CARTESIAN_POINT('Ctrl Pts',(-9.51656296408864,1.26431828378534,3.59287912715316));
#92220=CARTESIAN_POINT('Ctrl Pts',(-8.95387422534848,4.06829986255365,3.54600270954852));
#92221=CARTESIAN_POINT('Ctrl Pts',(-6.27947569657596,7.65198082141816,3.47339742215013));
#92222=CARTESIAN_POINT('Ctrl Pts',(-1.98809297574734,9.69701483877292,3.39621081276903));
#92223=CARTESIAN_POINT('Ctrl Pts',(2.76180201423585,9.50563346318468,3.31902420338792));
#92224=CARTESIAN_POINT('Ctrl Pts',(6.87474452053818,7.12197324301039,3.2418375940068));
#92225=CARTESIAN_POINT('Ctrl Pts',(9.40216890275978,3.09577706353974,3.16465098462569));
#92226=CARTESIAN_POINT('Ctrl Pts',(9.76117699939271,-1.64439638338132,3.08746437524458));
#92227=CARTESIAN_POINT('Ctrl Pts',(7.86897092521903,-6.00532365023846,3.01027776586345));
#92228=CARTESIAN_POINT('Ctrl Pts',(4.16194902035729,-8.98124691528834,2.93309115648234));
#92229=CARTESIAN_POINT('Ctrl Pts',(-0.504940590312465,-9.88583080328021,
2.85590454710123));
#92230=CARTESIAN_POINT('Ctrl Pts',(-5.05537606528319,-8.51045172514667,
2.77871793772012));
#92231=CARTESIAN_POINT('Ctrl Pts',(-8.43989332168798,-5.17231248367099,
2.701531328339));
#92232=CARTESIAN_POINT('Ctrl Pts',(-9.46265691397307,-1.9497308459096,2.64663424182061));
#92233=CARTESIAN_POINT('Ctrl Pts',(-9.51809120030368,-0.205810744375301,
2.61746602509593));
#92234=CARTESIAN_POINT('Ctrl Pts',(-9.51791998781483,-0.000166932759165794,
2.61402667816495));
#92235=CARTESIAN_POINT('Origin',(0.,0.,0.));
#92236=CARTESIAN_POINT('',(-9.5175,4.49712710671297E-14,1.6143576464275));
#92237=CARTESIAN_POINT('',(-9.51749999907439,-0.000132736732560753,1.88597332185171));
#92238=CARTESIAN_POINT('',(-9.5175,-1.16555759108849E-15,0.));
#92239=CARTESIAN_POINT('Ctrl Pts',(-9.51749999907439,-0.000132736732560753,
1.88597332185171));
#92240=CARTESIAN_POINT('Ctrl Pts',(-9.51749661865394,-0.242515918735408,
1.8900256477718));
#92241=CARTESIAN_POINT('Ctrl Pts',(-9.50822970172581,-0.484864835621161,
1.89407797369188));
#92242=CARTESIAN_POINT('Ctrl Pts',(-9.48973308058393,-0.726479393562538,
1.89813029961196));
#92243=CARTESIAN_POINT('Ctrl Pts',(-9.47123110468,-0.968163898790906,1.90218379867825));
#92244=CARTESIAN_POINT('Ctrl Pts',(-9.44349410461844,-1.20911336980557,
1.90623729774455));
#92245=CARTESIAN_POINT('Ctrl Pts',(-9.40660785953286,-1.44863205368883,
1.91029079681084));
#92246=CARTESIAN_POINT('Ctrl Pts',(-9.38940686296382,-1.5603257229723,1.9121810467772));
#92247=CARTESIAN_POINT('Ctrl Pts',(-9.37021701025927,-1.67170834747593,
1.91407129674355));
#92248=CARTESIAN_POINT('Ctrl Pts',(-9.34905082871763,-1.78270997418374,
1.9159615467099));
#92249=CARTESIAN_POINT('Ctrl Pts',(-9.3047620390922,-2.01497329875517,1.91991676569613));
#92250=CARTESIAN_POINT('Ctrl Pts',(-9.25180717594818,-2.24561919650383,
1.92387198468235));
#92251=CARTESIAN_POINT('Ctrl Pts',(-9.19032924885024,-2.4739956644521,1.92782720366858));
#92252=CARTESIAN_POINT('Ctrl Pts',(-9.12886151153041,-2.70233427970032,
1.93178176708937));
#92253=CARTESIAN_POINT('Ctrl Pts',(-9.05887360372417,-2.92840394323743,
1.93573633051016));
#92254=CARTESIAN_POINT('Ctrl Pts',(-8.98055897850418,-3.1515657511161,1.93969089393095));
#92255=CARTESIAN_POINT('Ctrl Pts',(-8.90225234766956,-3.37470477855642,
1.94364505366848));
#92256=CARTESIAN_POINT('Ctrl Pts',(-8.81562079020307,-3.59493627644656,
1.947599213406));
#92257=CARTESIAN_POINT('Ctrl Pts',(-8.7209070145311,-3.81163837396759,1.95155337314352));
#92258=CARTESIAN_POINT('Ctrl Pts',(-8.62618616259571,-4.0283566617536,1.95550782830456));
#92259=CARTESIAN_POINT('Ctrl Pts',(-8.52338199664531,-4.24154476222042,
1.95946228346559));
#92260=CARTESIAN_POINT('Ctrl Pts',(-8.41278508446992,-4.45060146188361,
1.96341673862662));
#92261=CARTESIAN_POINT('Ctrl Pts',(-8.30218905947044,-4.65965648455541,
1.96737116206617));
#92262=CARTESIAN_POINT('Ctrl Pts',(-8.18380054746117,-4.86457992394017,
1.97132558550573));
#92263=CARTESIAN_POINT('Ctrl Pts',(-8.05795606390058,-5.06479519055291,
1.97528000894529));
#92264=CARTESIAN_POINT('Ctrl Pts',(-7.93208689157643,-5.26504973633976,
1.97923520818226));
#92265=CARTESIAN_POINT('Ctrl Pts',(-7.79875897531133,-5.46059402434427,
1.98319040741923));
#92266=CARTESIAN_POINT('Ctrl Pts',(-7.65835284563321,-5.65087939543765,
1.9871456066562));
#92267=CARTESIAN_POINT('Ctrl Pts',(-7.58732441917897,-5.74714065210079,
1.98914645646781));
#92268=CARTESIAN_POINT('Ctrl Pts',(-7.51448526741096,-5.8420565548024,1.99114730627942));
#92269=CARTESIAN_POINT('Ctrl Pts',(-7.43988872314389,-5.93555911749149,
1.99314815609103));
#92270=CARTESIAN_POINT('Ctrl Pts',(-7.29242854574708,-6.12039213645585,
1.99710337507688));
#92271=CARTESIAN_POINT('Ctrl Pts',(-7.13805564648719,-6.2997542161798,2.00105859406273));
#92272=CARTESIAN_POINT('Ctrl Pts',(-6.97720050024153,-6.4731352086473,2.00501381304859));
#92273=CARTESIAN_POINT('Ctrl Pts',(-6.8163720152435,-6.64648746374655,2.00896837646901));
#92274=CARTESIAN_POINT('Ctrl Pts',(-6.64906362018808,-6.81386040344975,
2.01292293988944));
#92275=CARTESIAN_POINT('Ctrl Pts',(-6.47574430996344,-6.97477898445364,
2.01687750330986));
#92276=CARTESIAN_POINT('Ctrl Pts',(-6.30244269223591,-7.13568113883128,
2.02083166304704));
#92277=CARTESIAN_POINT('Ctrl Pts',(-6.12313159158954,-7.29013005785499,
2.02478582278421));
#92278=CARTESIAN_POINT('Ctrl Pts',(-5.93831563774861,-7.43768872946901,
2.02873998252139));
#92279=CARTESIAN_POINT('Ctrl Pts',(-5.7534858759237,-7.58525842549803,2.03269443768206));
#92280=CARTESIAN_POINT('Ctrl Pts',(-5.56315065832492,-7.72593666706023,
2.03664889284273));
#92281=CARTESIAN_POINT('Ctrl Pts',(-5.36784732493689,-7.85932702883446,
2.04060334800339));
#92282=CARTESIAN_POINT('Ctrl Pts',(-5.17254555821376,-7.99271632059112,
2.04455777144261));
#92283=CARTESIAN_POINT('Ctrl Pts',(-4.97227599009689,-8.11881769196253,
2.04851219488182));
#92284=CARTESIAN_POINT('Ctrl Pts',(-4.76760513036824,-8.2372779224017,2.05246661832103));
#92285=CARTESIAN_POINT('Ctrl Pts',(-4.56289411734637,-8.3557613929268,2.05642181755766));
#92286=CARTESIAN_POINT('Ctrl Pts',(-4.35378033202857,-8.46660058548498,
2.06037701679428));
#92287=CARTESIAN_POINT('Ctrl Pts',(-4.14085620286599,-8.56948750843283,
2.06433221603091));
#92288=CARTESIAN_POINT('Ctrl Pts',(-4.03314248765502,-8.62153577915219,
2.06633306584466));
#92289=CARTESIAN_POINT('Ctrl Pts',(-3.92445403915644,-8.67154969530967,
2.0683339156584));
#92290=CARTESIAN_POINT('Ctrl Pts',(-3.81486973445662,-8.71949397379956,
2.07033476547215));
#92291=CARTESIAN_POINT('Ctrl Pts',(-3.59824681779616,-8.81426876360283,
2.07428998445757));
#92292=CARTESIAN_POINT('Ctrl Pts',(-3.37805880764698,-8.90098086104498,
2.07824520344299));
#92293=CARTESIAN_POINT('Ctrl Pts',(-3.15492436404717,-8.97937962818933,
2.08220042242841));
#92294=CARTESIAN_POINT('Ctrl Pts',(-2.93182690429828,-9.05776540097804,
2.08615498584839));
#92295=CARTESIAN_POINT('Ctrl Pts',(-2.70578425252372,-9.12784050045745,
2.09010954926838));
#92296=CARTESIAN_POINT('Ctrl Pts',(-2.47743278142928,-9.18940330290817,
2.09406411268836));
#92297=CARTESIAN_POINT('Ctrl Pts',(-2.2491046205356,-9.25095982100576,2.09801827242508));
#92298=CARTESIAN_POINT('Ctrl Pts',(-2.01846838372202,-9.30400570358082,
2.1019724321618));
#92299=CARTESIAN_POINT('Ctrl Pts',(-1.78617423957292,-9.34838958515776,
2.10592659189852));
#92300=CARTESIAN_POINT('Ctrl Pts',(-1.55386274024469,-9.3927767827469,2.10988104705874));
#92301=CARTESIAN_POINT('Ctrl Pts',(-1.31989336320424,-9.42850063055647,
2.11383550221897));
#92302=CARTESIAN_POINT('Ctrl Pts',(-1.08492629424608,-9.45546091875237,
2.11778995737919));
#92303=CARTESIAN_POINT('Ctrl Pts',(-0.849961110124046,-9.48242099068084,
2.12174438081795));
#92304=CARTESIAN_POINT('Ctrl Pts',(-0.613998531151393,-9.5006176136475,
2.12569880425671));
#92305=CARTESIAN_POINT('Ctrl Pts',(-0.377704407636725,-9.51000239907708,
2.12965322769547));
#92306=CARTESIAN_POINT('Ctrl Pts',(-0.141363926827158,-9.5193890256581,
2.13360842693166));
#92307=CARTESIAN_POINT('Ctrl Pts',(0.095307946013853,-9.51996034913527,
2.13756362616785));
#92308=CARTESIAN_POINT('Ctrl Pts',(0.331643515915196,-9.51172007727054,
2.14151882540404));
#92309=CARTESIAN_POINT('Ctrl Pts',(0.451200573198273,-9.50755150181755,
2.14351967522044));
#92310=CARTESIAN_POINT('Ctrl Pts',(0.570671569610272,-9.50112875311945,
2.14552052503685));
#92311=CARTESIAN_POINT('Ctrl Pts',(0.689970275166106,-9.49245738833666,
2.14752137485325));
#92312=CARTESIAN_POINT('Ctrl Pts',(0.925796323506403,-9.47531609848851,
2.15147659384181));
#92313=CARTESIAN_POINT('Ctrl Pts',(1.16101762167841,-9.44937985683982,2.15543181283037));
#92314=CARTESIAN_POINT('Ctrl Pts',(1.39497000565972,-9.41471534000417,2.15938703181893));
#92315=CARTESIAN_POINT('Ctrl Pts',(1.6288836127502,-9.38005656870596,2.16334159524207));
#92316=CARTESIAN_POINT('Ctrl Pts',(1.86152844603758,-9.33667245155772,2.1672961586652));
#92317=CARTESIAN_POINT('Ctrl Pts',(2.09224752123643,-9.28468128477656,2.17125072208833));
#92318=CARTESIAN_POINT('Ctrl Pts',(2.32294304454896,-9.23269542527243,2.1752048818282));
#92319=CARTESIAN_POINT('Ctrl Pts',(2.5517129266733,-9.17210433261013,2.17915904156808));
#92320=CARTESIAN_POINT('Ctrl Pts',(2.77791140813789,-9.10307719721949,2.18311320130795));
#92321=CARTESIAN_POINT('Ctrl Pts',(3.0041267893614,-9.03404490466802,2.18706765647132));
#92322=CARTESIAN_POINT('Ctrl Pts',(3.22777011493119,-8.95657538995117,2.19102211163469));
#92323=CARTESIAN_POINT('Ctrl Pts',(3.44821061147869,-8.87088777005356,2.19497656679806));
#92324=CARTESIAN_POINT('Ctrl Pts',(3.66864933971731,-8.78520083751685,2.19893099023995));
#92325=CARTESIAN_POINT('Ctrl Pts',(3.8858850277074,-8.69129603618083,2.20288541368184));
#92326=CARTESIAN_POINT('Ctrl Pts',(4.09930604925287,-8.58944096926912,2.20683983712373));
#92327=CARTESIAN_POINT('Ctrl Pts',(4.31276894073802,-8.48756591995138,2.21079503636301));
#92328=CARTESIAN_POINT('Ctrl Pts',(4.52241541524672,-8.37773761022079,2.21475023560229));
#92329=CARTESIAN_POINT('Ctrl Pts',(4.72765650136042,-8.26027059212618,2.21870543484157));
#92330=CARTESIAN_POINT('Ctrl Pts',(4.83148353023195,-8.2008465668976,2.22070628463917));
#92331=CARTESIAN_POINT('Ctrl Pts',(4.93418355225682,-8.13946842834864,2.22270713443677));
#92332=CARTESIAN_POINT('Ctrl Pts',(5.03568287172116,-8.07618129226023,2.22470798423436));
#92333=CARTESIAN_POINT('Ctrl Pts',(5.23632363706051,-7.95107720793802,2.22866320321354));
#92334=CARTESIAN_POINT('Ctrl Pts',(5.43232928174857,-7.81847428665558,2.23261842219272));
#92335=CARTESIAN_POINT('Ctrl Pts',(5.62314331351494,-7.67874114198885,2.2365736411719));
#92336=CARTESIAN_POINT('Ctrl Pts',(5.81392571843859,-7.53903115766389,2.24052820458562));
#92337=CARTESIAN_POINT('Ctrl Pts',(5.99951800026322,-7.39219347604901,2.24448276799933));
#92338=CARTESIAN_POINT('Ctrl Pts',(6.17939408300175,-7.23863903071309,2.24843733141305));
#92339=CARTESIAN_POINT('Ctrl Pts',(6.35925180392463,-7.08510026027056,2.25239149114351));
#92340=CARTESIAN_POINT('Ctrl Pts',(6.53339427600142,-6.92484627861794,2.25634565087396));
#92341=CARTESIAN_POINT('Ctrl Pts',(6.70132907997949,-6.75832781180532,2.26029981060441));
#92342=CARTESIAN_POINT('Ctrl Pts',(6.86927643071827,-6.59179690404951,2.26425426575841));
#92343=CARTESIAN_POINT('Ctrl Pts',(7.03101498405441,-6.41900077305369,2.26820872091242));
#92344=CARTESIAN_POINT('Ctrl Pts',(7.18608885391577,-6.24042732780597,2.27216317606642));
#92345=CARTESIAN_POINT('Ctrl Pts',(7.34116147982196,-6.06185531501984,2.27611759949899));
#92346=CARTESIAN_POINT('Ctrl Pts',(7.48956934558283,-5.87750629557614,2.28007202293156));
#92347=CARTESIAN_POINT('Ctrl Pts',(7.63089610808493,-5.68790214733115,2.28402644636413));
#92348=CARTESIAN_POINT('Ctrl Pts',(7.77225059674074,-5.49826080164624,2.28798164559423));
#92349=CARTESIAN_POINT('Ctrl Pts',(7.90652103730829,-5.3033624937494,2.29193684482432));
#92350=CARTESIAN_POINT('Ctrl Pts',(8.03333301603455,-5.10376007503186,2.29589204405441));
#92351=CARTESIAN_POINT('Ctrl Pts',(8.09748445678891,-5.00278552304238,2.2978928939081));
#92352=CARTESIAN_POINT('Ctrl Pts',(8.1597278654975,-4.90060759347963,2.29989374376179));
#92353=CARTESIAN_POINT('Ctrl Pts',(8.2200190771079,-4.79730055572737,2.30189459361549));
#92354=CARTESIAN_POINT('Ctrl Pts',(8.33920090638921,-4.59308635256111,2.30584981261525));
#92355=CARTESIAN_POINT('Ctrl Pts',(8.45078623942393,-4.38439887927302,2.30980503161502));
#92356=CARTESIAN_POINT('Ctrl Pts',(8.55445459915314,-4.17182367329058,2.31376025061478));
#92357=CARTESIAN_POINT('Ctrl Pts',(8.65810577617019,-3.95928370099551,2.31771481404915));
#92358=CARTESIAN_POINT('Ctrl Pts',(8.75384247554235,-3.74285753626607,2.32166937748351));
#92359=CARTESIAN_POINT('Ctrl Pts',(8.84139085815206,-3.52315397667845,2.32562394091788));
#92360=CARTESIAN_POINT('Ctrl Pts',(8.92893030379139,-3.30347284450921,2.32957810066899));
#92361=CARTESIAN_POINT('Ctrl Pts',(9.00828299709468,-3.08051524797425,2.3335322604201));
#92362=CARTESIAN_POINT('Ctrl Pts',(9.07922342536782,-2.85490949808435,2.33748642017121));
#92363=CARTESIAN_POINT('Ctrl Pts',(9.15016915374615,-2.62928689272523,2.34144087534572));
#92364=CARTESIAN_POINT('Ctrl Pts',(9.21270127393181,-2.40101600751153,2.34539533052023));
#92365=CARTESIAN_POINT('Ctrl Pts',(9.2666439278642,-2.17074101729745,2.34934978569474));
#92366=CARTESIAN_POINT('Ctrl Pts',(9.32058614908351,-1.94046787428577,2.3533042091477));
#92367=CARTESIAN_POINT('Ctrl Pts',(9.36593897961776,-1.70819093414095,2.35725863260066));
#92368=CARTESIAN_POINT('Ctrl Pts',(9.40257738038337,-1.47456598899577,2.36121305605362));
#92369=CARTESIAN_POINT('Ctrl Pts',(9.43922296904109,-1.24089521022067,2.3651682553038));
#92370=CARTESIAN_POINT('Ctrl Pts',(9.46715066796878,-1.00587617730016,2.36912345455397));
#92371=CARTESIAN_POINT('Ctrl Pts',(9.48628697188397,-0.770172537204796,
2.37307865380415));
#92372=CARTESIAN_POINT('Ctrl Pts',(9.49596761402503,-0.650935165075816,
2.37507950353496));
#92373=CARTESIAN_POINT('Ctrl Pts',(9.50339924749681,-0.531522685471028,
2.37708035326578));
#92374=CARTESIAN_POINT('Ctrl Pts',(9.50857742367356,-0.41202139265514,2.3790812029966));
#92375=CARTESIAN_POINT('Ctrl Pts',(9.51881348503294,-0.175794867323725,
2.38303642196104));
#92376=CARTESIAN_POINT('Ctrl Pts',(9.5202436499388,0.0608476937335277,2.38699164092549));
#92377=CARTESIAN_POINT('Ctrl Pts',(9.51285736796984,0.297238871384691,2.39094685988993));
#92378=CARTESIAN_POINT('Ctrl Pts',(9.50547231025459,0.53359086791902,2.3949014232889));
#92379=CARTESIAN_POINT('Ctrl Pts',(9.48927373159097,0.769691281850639,2.39885598668786));
#92380=CARTESIAN_POINT('Ctrl Pts',(9.46430318507777,1.00487385821641,2.40281055008682));
#92381=CARTESIAN_POINT('Ctrl Pts',(9.43933518756685,1.2400324270611,2.40676470980255));
#92382=CARTESIAN_POINT('Ctrl Pts',(9.40559704001639,1.47427306446482,2.41071886951827));
#92383=CARTESIAN_POINT('Ctrl Pts',(9.3631821461448,1.70693478144754,2.414673029234));
#92384=CARTESIAN_POINT('Ctrl Pts',(9.32076408336619,1.93961388108241,2.41862748437341));
#92385=CARTESIAN_POINT('Ctrl Pts',(9.26966802701636,2.17071354604124,2.42258193951283));
#92386=CARTESIAN_POINT('Ctrl Pts',(9.21003870508313,2.39958190126337,2.42653639465224));
#92387=CARTESIAN_POINT('Ctrl Pts',(9.1504098614765,2.62844842057961,2.43049081807033));
#92388=CARTESIAN_POINT('Ctrl Pts',(9.08224796266383,2.8550833930223,2.43444524148842));
#92389=CARTESIAN_POINT('Ctrl Pts',(9.00574811127941,3.07884835712761,2.43839966490651));
#92390=CARTESIAN_POINT('Ctrl Pts',(8.92923325178689,3.30265722051782,2.44235486412237));
#92391=CARTESIAN_POINT('Ctrl Pts',(8.84437726259469,3.52359468298996,2.44631006333823));
#92392=CARTESIAN_POINT('Ctrl Pts',(8.75142449937058,3.74103935849604,2.45026526255409));
#92393=CARTESIAN_POINT('Ctrl Pts',(8.70440170211514,3.851039927989,2.4522661124953));
#92394=CARTESIAN_POINT('Ctrl Pts',(8.65530760636025,3.96014694989684,2.45426696243651));
#92395=CARTESIAN_POINT('Ctrl Pts',(8.6041785058948,4.06828200702679,2.45626781237772));
#92396=CARTESIAN_POINT('Ctrl Pts',(8.50310806286357,4.2820400827965,2.46022303138521));
#92397=CARTESIAN_POINT('Ctrl Pts',(8.39405322125943,4.4920610098125,2.4641782503927));
#92398=CARTESIAN_POINT('Ctrl Pts',(8.27731579054074,4.69774941367299,2.4681334694002));
#92399=CARTESIAN_POINT('Ctrl Pts',(8.16059770869367,4.9034037253105,2.47208803284226));
#92400=CARTESIAN_POINT('Ctrl Pts',(8.03619971911926,5.10472670159992,2.47604259628431));
#92401=CARTESIAN_POINT('Ctrl Pts',(7.90446918377241,5.30114828813459,2.47999715972637));
#92402=CARTESIAN_POINT('Ctrl Pts',(7.77275209552822,5.49754982387976,2.4839513194851));
#92403=CARTESIAN_POINT('Ctrl Pts',(7.63370411346527,5.68905073426294,2.48790547924383));
#92404=CARTESIAN_POINT('Ctrl Pts',(7.4877160160783,5.87510979578804,2.49185963900257));
#92405=CARTESIAN_POINT('Ctrl Pts',(7.34171701162601,6.06118275816104,2.49581409418455));
#92406=CARTESIAN_POINT('Ctrl Pts',(7.18877702816723,6.24181283526938,2.49976854936654));
#92407=CARTESIAN_POINT('Ctrl Pts',(7.02932800121784,6.41649079336165,2.50372300454853));
#92408=CARTESIAN_POINT('Ctrl Pts',(6.86988025332853,6.59116735023118,2.50767742800887));
#92409=CARTESIAN_POINT('Ctrl Pts',(6.70392375861793,6.75989167636968,2.5116318514692));
#92410=CARTESIAN_POINT('Ctrl Pts',(6.53192876504471,6.92218988892832,2.51558627492954));
#92411=CARTESIAN_POINT('Ctrl Pts',(6.35990002870103,7.08451994189825,2.5195414741869));
#92412=CARTESIAN_POINT('Ctrl Pts',(6.18183063194394,7.24042116815391,2.52349667344426));
#92413=CARTESIAN_POINT('Ctrl Pts',(5.99822643580178,7.38945775242329,2.52745187270162));
#92414=CARTESIAN_POINT('Ctrl Pts',(5.90534504747037,7.46485213419654,2.52945272238735));
#92415=CARTESIAN_POINT('Ctrl Pts',(5.81104777392244,7.53849039205081,2.53145357207309));
#92416=CARTESIAN_POINT('Ctrl Pts',(5.71540328092111,7.61032007122146,2.53345442175882));
#92417=CARTESIAN_POINT('Ctrl Pts',(5.52633614700454,7.75231080319966,2.53740964075376));
#92418=CARTESIAN_POINT('Ctrl Pts',(5.33194754946568,7.88727309826655,2.54136485974869));
#92419=CARTESIAN_POINT('Ctrl Pts',(5.13278205151137,8.01482093759323,2.54532007874363));
#92420=CARTESIAN_POINT('Ctrl Pts',(4.93364956461967,8.14234763626174,2.5492746421733));
#92421=CARTESIAN_POINT('Ctrl Pts',(4.72974199575358,8.26246218005756,2.55322920560298));
#92422=CARTESIAN_POINT('Ctrl Pts',(4.52163240384909,8.37482218643846,2.55718376903265));
#92423=CARTESIAN_POINT('Ctrl Pts',(4.31354405583911,8.48717072307354,2.56113792877921));
#92424=CARTESIAN_POINT('Ctrl Pts',(4.10125478989817,8.59176616866206,2.56509208852577));
#92425=CARTESIAN_POINT('Ctrl Pts',(3.88536263429271,8.68831188724496,2.56904624827233));
#92426=CARTESIAN_POINT('Ctrl Pts',(3.66945434892627,8.78486481896332,2.57300070344255));
#92427=CARTESIAN_POINT('Ctrl Pts',(3.44994289296842,8.87336670414171,2.57695515861277));
#92428=CARTESIAN_POINT('Ctrl Pts',(3.22744779244037,8.9535683946163,2.580909613783));
#92429=CARTESIAN_POINT('Ctrl Pts',(3.00495447669792,9.03376944173819,2.58486403723183));
#92430=CARTESIAN_POINT('Ctrl Pts',(2.77947783092414,9.1056703336265,2.58881846068065));
#92431=CARTESIAN_POINT('Ctrl Pts',(2.55165479540441,9.16907105736943,2.59277288412948));
#92432=CARTESIAN_POINT('Ctrl Pts',(2.32378706448556,9.23248421936578,2.59672808337578));
#92433=CARTESIAN_POINT('Ctrl Pts',(2.09357229636057,9.28739380525412,2.60068328262208));
#92434=CARTESIAN_POINT('Ctrl Pts',(1.86166119100045,9.33365008235914,2.60463848186838));
#92435=CARTESIAN_POINT('Ctrl Pts',(1.74434237848203,9.35705013253379,2.60663933162557));
#92436=CARTESIAN_POINT('Ctrl Pts',(1.6265896381928,9.37823649583386,2.60864018138276));
#92437=CARTESIAN_POINT('Ctrl Pts',(1.50848817155244,9.3971947775007,2.61064103113995));
#92438=CARTESIAN_POINT('Ctrl Pts',(1.27502878868999,9.43467093138751,2.61459625001065));
#92439=CARTESIAN_POINT('Ctrl Pts',(1.0401381629618,9.4634483247574,2.61855146888136));
#92440=CARTESIAN_POINT('Ctrl Pts',(0.804478019009862,9.4834393216243,2.62250668775207));
#92441=CARTESIAN_POINT('Ctrl Pts',(0.568856935043161,9.50342700504146,2.62646125105672));
#92442=CARTESIAN_POINT('Ctrl Pts',(0.332466868962747,9.51463117523941,2.63041581436137));
#92443=CARTESIAN_POINT('Ctrl Pts',(0.0959744124212834,9.51701608500061,
2.63437037766602));
#92444=CARTESIAN_POINT('Ctrl Pts',(-0.140493902868283,9.5194007513092,2.63832453728715));
#92445=CARTESIAN_POINT('Ctrl Pts',(-0.377064305227066,9.51296795195225,
2.64227869690828));
#92446=CARTESIAN_POINT('Ctrl Pts',(-0.613069439541559,9.49773405146197,
2.6462328565294));
#92447=CARTESIAN_POINT('Ctrl Pts',(-0.849092206317806,9.48249901281354,
2.65018731157447));
#92448=CARTESIAN_POINT('Ctrl Pts',(-1.08454933842956,9.45846157469296,2.65414176661955));
#92449=CARTESIAN_POINT('Ctrl Pts',(-1.31877660028806,9.42569013539766,2.65809622166462));
#92450=CARTESIAN_POINT('Ctrl Pts',(-1.55300198327195,9.39291895898134,2.66205064498868));
#92451=CARTESIAN_POINT('Ctrl Pts',(-1.78599723613496,9.3514139629418,2.66600506831275));
#92452=CARTESIAN_POINT('Ctrl Pts',(-2.01710562344348,9.30129513314531,2.66995949163681));
#92453=CARTESIAN_POINT('Ctrl Pts',(-2.24825935076771,9.25116647078258,2.6739146907597));
#92454=CARTESIAN_POINT('Ctrl Pts',(-2.47752519658103,9.19242065784401,2.67786988988259));
#92455=CARTESIAN_POINT('Ctrl Pts',(-2.70425769253583,9.12522857699251,2.68182508900548));
#92456=CARTESIAN_POINT('Ctrl Pts',(-2.81895680501513,9.09123754272612,2.68382593951067));
#92457=CARTESIAN_POINT('Ctrl Pts',(-2.93300781075947,9.05508579835512,2.68582679001586));
#92458=CARTESIAN_POINT('Ctrl Pts',(-3.04632862255624,9.01680032901886,2.68782764052105));
#92459=CARTESIAN_POINT('Ctrl Pts',(-3.27033769614246,8.94111879813458,2.69178285987525));
#92460=CARTESIAN_POINT('Ctrl Pts',(-3.49155770459215,8.85707437037551,2.69573807922945));
#92461=CARTESIAN_POINT('Ctrl Pts',(-3.70936237479386,8.7648980041107,2.69969329858366));
#92462=CARTESIAN_POINT('Ctrl Pts',(-3.9271309446225,8.67273691576076,2.70364786237389));
#92463=CARTESIAN_POINT('Ctrl Pts',(-4.14148504606553,8.57244668962403,2.70760242616412));
#92464=CARTESIAN_POINT('Ctrl Pts',(-4.35181829019908,8.46430645824505,2.71155698995435));
#92465=CARTESIAN_POINT('Ctrl Pts',(-4.56213006345908,8.35617726584966,2.71551115006166));
#92466=CARTESIAN_POINT('Ctrl Pts',(-4.76842154770438,8.24019979745532,2.71946531016896));
#92467=CARTESIAN_POINT('Ctrl Pts',(-4.97010997249879,8.11669964402208,2.72341947027627));
#92468=CARTESIAN_POINT('Ctrl Pts',(-5.17181346574513,7.99319026370272,2.72737392580495));
#92469=CARTESIAN_POINT('Ctrl Pts',(-5.36891296993222,7.86215722064698,2.73132838133363));
#92470=CARTESIAN_POINT('Ctrl Pts',(-5.56085273197587,7.72397068503478,2.73528283686231));
#92471=CARTESIAN_POINT('Ctrl Pts',(-5.75279095424601,7.58578525797852,2.73923726066768));
#92472=CARTESIAN_POINT('Ctrl Pts',(-5.93956928911505,7.44044662013735,2.74319168447304));
#92473=CARTESIAN_POINT('Ctrl Pts',(-6.12066266831653,7.28836708396856,2.74714610827841));
#92474=CARTESIAN_POINT('Ctrl Pts',(-6.30179157503234,7.13625771231974,2.75110130787607));
#92475=CARTESIAN_POINT('Ctrl Pts',(-6.47723308103396,6.97740498165161,2.75505650747373));
#92476=CARTESIAN_POINT('Ctrl Pts',(-6.64649581339093,6.81226097948228,2.75901170707139));
#92477=CARTESIAN_POINT('Ctrl Pts',(-6.7321220694572,6.72871829751884,2.76101255468165));
#92478=CARTESIAN_POINT('Ctrl Pts',(-6.81616766093029,6.64356621178076,2.76301340229191));
#92479=CARTESIAN_POINT('Ctrl Pts',(-6.8985725468889,6.55686686347305,2.76501424990217));
#92480=CARTESIAN_POINT('Ctrl Pts',(-7.06146816113144,6.38548207927338,2.76896946805079));
#92481=CARTESIAN_POINT('Ctrl Pts',(-7.21799764663385,6.20799899698917,2.77292468619942));
#92482=CARTESIAN_POINT('Ctrl Pts',(-7.3677146191458,6.02491390318777,2.77687990434805));
#92483=CARTESIAN_POINT('Ctrl Pts',(-7.51740677642026,5.84185915531179,2.78083446692853));
#92484=CARTESIAN_POINT('Ctrl Pts',(-7.66028849593555,5.65320446816517,2.78478902950901));
#92485=CARTESIAN_POINT('Ctrl Pts',(-7.79595344294093,5.45947947752324,2.7887435920895));
#92486=CARTESIAN_POINT('Ctrl Pts',(-7.93160454121154,5.26577426240972,2.79269775098657));
#92487=CARTESIAN_POINT('Ctrl Pts',(-8.06004017588902,5.06700000870574,2.79665190988365));
#92488=CARTESIAN_POINT('Ctrl Pts',(-8.18089656553735,4.86371644259606,2.80060606878072));
#92489=CARTESIAN_POINT('Ctrl Pts',(-8.3017619847953,4.66041768844997,2.80456052310703));
#92490=CARTESIAN_POINT('Ctrl Pts',(-8.41504688079174,4.452609190299,2.80851497743335));
#92491=CARTESIAN_POINT('Ctrl Pts',(-8.52043215627187,4.24087751772772,2.81246943175966));
#92492=CARTESIAN_POINT('Ctrl Pts',(-8.62581658650851,4.02914754335209,2.81642385436924));
#92493=CARTESIAN_POINT('Ctrl Pts',(-8.72330139905377,3.81349471154006,2.82037827697882));
#92494=CARTESIAN_POINT('Ctrl Pts',(-8.81261428931502,3.59452856961254,2.8243326995884));
#92495=CARTESIAN_POINT('Ctrl Pts',(-8.90194470168324,3.37551946918093,2.82828789800778));
#92496=CARTESIAN_POINT('Ctrl Pts',(-8.98309988145253,3.15319602152038,2.83224309642717));
#92497=CARTESIAN_POINT('Ctrl Pts',(-9.05585587648387,2.92818725397687,2.83619829484655));
#92498=CARTESIAN_POINT('Ctrl Pts',(-9.09266166151467,2.81435987350209,2.83819914965879));
#92499=CARTESIAN_POINT('Ctrl Pts',(-9.12731875453222,2.69984556005899,2.84020000447104));
#92500=CARTESIAN_POINT('Ctrl Pts',(-9.1598030074911,2.58472728038319,2.84220085928328));
#92501=CARTESIAN_POINT('Ctrl Pts',(-9.22440370066167,2.35579418245803,2.84617991362596));
#92502=CARTESIAN_POINT('Ctrl Pts',(-9.28042584834167,2.12440861146206,2.85015896796863));
#92503=CARTESIAN_POINT('Ctrl Pts',(-9.32770455370037,1.89122553093949,2.85413802231131));
#92504=CARTESIAN_POINT('Ctrl Pts',(-9.37497426678215,1.65808680118366,2.85811631984903));
#92505=CARTESIAN_POINT('Ctrl Pts',(-9.4135038034141,1.42315151436673,2.86209461738675));
#92506=CARTESIAN_POINT('Ctrl Pts',(-9.4431792573843,1.18708540674502,2.86607291492447));
#92507=CARTESIAN_POINT('Ctrl Pts',(-9.4728517539696,0.95104282490803,2.87005081599455));
#92508=CARTESIAN_POINT('Ctrl Pts',(-9.49367189415953,0.713869920319275,
2.87402871706464));
#92509=CARTESIAN_POINT('Ctrl Pts',(-9.50557743464729,0.476239313711379,
2.87800661813472));
#92510=CARTESIAN_POINT('Ctrl Pts',(-9.51352533747236,0.317601831312081,
2.88066218603483));
#92511=CARTESIAN_POINT('Ctrl Pts',(-9.51750139653877,0.158760508638162,
2.88331775393494));
#92512=CARTESIAN_POINT('Ctrl Pts',(-9.51749999963197,-8.36987430888474E-5,
2.88597332183505));
#92513=CARTESIAN_POINT('Ctrl Pts',(-9.51749999860915,-0.000162710879915706,
2.61426907583));
#92514=CARTESIAN_POINT('Ctrl Pts',(-9.51750793601857,0.464122739643576,
2.6062757959423));
#92515=CARTESIAN_POINT('Ctrl Pts',(-9.48354236659388,0.927792039220556,
2.59820482324316));
#92516=CARTESIAN_POINT('Ctrl Pts',(-9.39663191626681,1.51774366931572,2.58812418496722));
#92517=CARTESIAN_POINT('Ctrl Pts',(-9.37467393353151,1.64794599472725,2.58590862243221));
#92518=CARTESIAN_POINT('Ctrl Pts',(-9.27630610838416,2.16533738281314,2.57713658796837));
#92519=CARTESIAN_POINT('Ctrl Pts',(-9.17855681534807,2.54806539167245,2.57073690299094));
#92520=CARTESIAN_POINT('Ctrl Pts',(-8.96282147259733,3.2164104855471,2.55938495258945));
#92521=CARTESIAN_POINT('Ctrl Pts',(-8.85416999457468,3.50444530344994,2.55442589450221));
#92522=CARTESIAN_POINT('Ctrl Pts',(-8.66174893614724,3.94814841316177,2.54639430837918));
#92523=CARTESIAN_POINT('Ctrl Pts',(-8.58727452692463,4.10761310330301,2.54341345597166));
#92524=CARTESIAN_POINT('Ctrl Pts',(-8.35047470048624,4.58002364993561,2.53436724317746));
#92525=CARTESIAN_POINT('Ctrl Pts',(-8.17514366886643,4.88611002607679,2.52823269237713));
#92526=CARTESIAN_POINT('Ctrl Pts',(-7.81529420596976,5.44050887824939,2.51687964908705));
#92527=CARTESIAN_POINT('Ctrl Pts',(-7.63486811434855,5.69093587142652,2.51164737487751));
#92528=CARTESIAN_POINT('Ctrl Pts',(-7.19841536251561,6.23851776600686,2.49998452723066));
#92529=CARTESIAN_POINT('Ctrl Pts',(-6.9355483207026,6.52950676514747,2.493629926593));
#92530=CARTESIAN_POINT('Ctrl Pts',(-6.43405315804867,7.02009481943592,2.48228989373565));
#92531=CARTESIAN_POINT('Ctrl Pts',(-6.20216587270621,7.22578077337415,2.47729788544506));
#92532=CARTESIAN_POINT('Ctrl Pts',(-5.82379944253089,7.52974017304037,2.46923870460397));
#92533=CARTESIAN_POINT('Ctrl Pts',(-5.68392075607238,7.63588046970078,2.4662652152463));
#92534=CARTESIAN_POINT('Ctrl Pts',(-5.25440320159795,7.94345475118456,2.45722245839205));
#92535=CARTESIAN_POINT('Ctrl Pts',(-4.95642331173384,8.13271757623477,2.45108329603022));
#92536=CARTESIAN_POINT('Ctrl Pts',(-4.37919983454863,8.45581156141909,2.43972032158993));
#92537=CARTESIAN_POINT('Ctrl Pts',(-4.10259279258243,8.59342042334503,2.43448279099346));
#92538=CARTESIAN_POINT('Ctrl Pts',(-3.45764823998831,8.87602382574983,2.42275448484561));
#92539=CARTESIAN_POINT('Ctrl Pts',(-3.08597433999832,9.01198613702497,2.41634306592113));
#92540=CARTESIAN_POINT('Ctrl Pts',(-2.41248762401099,9.21178765133125,2.40498796256226));
#92541=CARTESIAN_POINT('Ctrl Pts',(-2.11399843359201,9.28483370433371,2.40003744111097));
#92542=CARTESIAN_POINT('Ctrl Pts',(-1.63965098128222,9.37685198671634,2.39201296595234));
#92543=CARTESIAN_POINT('Ctrl Pts',(-1.46590359117822,9.40557993230006,2.38903016770001));
#92544=CARTESIAN_POINT('Ctrl Pts',(-0.942314241685625,9.47729077363448,
2.37998303650244));
#92545=CARTESIAN_POINT('Ctrl Pts',(-0.59078066399349,9.50568122664751,2.37384969792749));
#92546=CARTESIAN_POINT('Ctrl Pts',(0.0698136978474623,9.52223919566713,
2.36249926076456));
#92547=CARTESIAN_POINT('Ctrl Pts',(0.378305648054733,9.51497766278343,2.35726836399894));
#92548=CARTESIAN_POINT('Ctrl Pts',(1.07565873047447,9.46459025914108,2.34562344848382));
#92549=CARTESIAN_POINT('Ctrl Pts',(1.46331197777882,9.41245079619403,2.33928447787069));
#92550=CARTESIAN_POINT('Ctrl Pts',(2.15127981040714,9.27637988604303,2.32794850121074));
#92551=CARTESIAN_POINT('Ctrl Pts',(2.45276557221386,9.20125902427386,2.32294501131215));
#92552=CARTESIAN_POINT('Ctrl Pts',(2.91797376977633,9.06085024926193,2.31487616134734));
#92553=CARTESIAN_POINT('Ctrl Pts',(3.08447512671743,9.00553108062806,2.31190518397676));
#92554=CARTESIAN_POINT('Ctrl Pts',(3.58097263053224,8.82518690538203,2.30286359892522));
#92555=CARTESIAN_POINT('Ctrl Pts',(3.90563995603974,8.68638395756977,2.29672285411906));
#92556=CARTESIAN_POINT('Ctrl Pts',(4.49866219156555,8.39286845153751,2.28535646575933));
#92557=CARTESIAN_POINT('Ctrl Pts',(4.76864204310226,8.24246669790521,2.28011712558757));
#92558=CARTESIAN_POINT('Ctrl Pts',(5.36746836191316,7.86958414295812,2.26836720291976));
#92559=CARTESIAN_POINT('Ctrl Pts',(5.69067463900333,7.63912919155653,2.26193709783562));
#92560=CARTESIAN_POINT('Ctrl Pts',(6.23632658057496,7.19616738790312,2.25057693152237));
#92561=CARTESIAN_POINT('Ctrl Pts',(6.46463531907069,6.9917867905503,2.24563997288196));
#92562=CARTESIAN_POINT('Ctrl Pts',(6.80818548770489,6.65300533300363,2.23762676249105));
#92563=CARTESIAN_POINT('Ctrl Pts',(6.93021629669238,6.525792699333,2.23464083968749));
#92564=CARTESIAN_POINT('Ctrl Pts',(7.28536913966018,6.1343554266646,2.2255922292939));
#92565=CARTESIAN_POINT('Ctrl Pts',(7.50742580846015,5.8605015631703,2.21946083160097));
#92566=CARTESIAN_POINT('Ctrl Pts',(7.89436179833537,5.32511875410795,2.20811456333893));
#92567=CARTESIAN_POINT('Ctrl Pts',(8.06269030460154,5.06664236285625,2.20288586837272));
#92568=CARTESIAN_POINT('Ctrl Pts',(8.41445230070014,4.46444022242666,2.19127043535467));
#92569=CARTESIAN_POINT('Ctrl Pts',(8.58993370844498,4.11670673748643,2.18495722699093));
#92570=CARTESIAN_POINT('Ctrl Pts',(8.86676559282271,3.47281665013247,2.17362784763163));
#92571=CARTESIAN_POINT('Ctrl Pts',(8.97575005238465,3.18054971855134,2.16860536408051));
#92572=CARTESIAN_POINT('Ctrl Pts',(9.12327202495145,2.71650624104769,2.16052045931768));
#92573=CARTESIAN_POINT('Ctrl Pts',(9.17172841210101,2.54811601545726,2.15755357796201));
#92574=CARTESIAN_POINT('Ctrl Pts',(9.3037177426002,2.03671977214956,2.14851389567492));
#92575=CARTESIAN_POINT('Ctrl Pts',(9.37284594708001,1.69031090114701,2.14237056044812));
#92576=CARTESIAN_POINT('Ctrl Pts',(9.46611043193154,1.03491904538352,2.13099857671449));
#92577=CARTESIAN_POINT('Ctrl Pts',(9.49472104373032,0.727033896911485,2.12575626767931));
#92578=CARTESIAN_POINT('Ctrl Pts',(9.52581608644059,0.0202217071744701,
2.11397171439774));
#92579=CARTESIAN_POINT('Ctrl Pts',(9.51831238536809,-0.378565470332814,
2.10751174711588));
#92580=CARTESIAN_POINT('Ctrl Pts',(9.46098874159688,-1.07955511888953,2.09614338615257));
#92581=CARTESIAN_POINT('Ctrl Pts',(9.42155678110355,-1.38203223701904,2.09122802465508));
#92582=CARTESIAN_POINT('Ctrl Pts',(9.33647784150751,-1.85584217956872,2.08323266696666));
#92583=CARTESIAN_POINT('Ctrl Pts',(9.30045110827429,-2.02868837834661,2.08024168338257));
#92584=CARTESIAN_POINT('Ctrl Pts',(9.17822857542973,-2.54301334937323,2.07119066573233));
#92585=CARTESIAN_POINT('Ctrl Pts',(9.07786909989473,-2.88081414296955,2.06506239715364));
#92586=CARTESIAN_POINT('Ctrl Pts',(8.85504339872357,-3.50227402478332,2.05372284037786));
#92587=CARTESIAN_POINT('Ctrl Pts',(8.73704430828451,-3.78705367301889,2.04849768585152));
#92588=CARTESIAN_POINT('Ctrl Pts',(8.44040208699418,-4.414939216129,2.03693218157599));
#92589=CARTESIAN_POINT('Ctrl Pts',(8.25424467058249,-4.75389546033557,2.03066279434049));
#92590=CARTESIAN_POINT('Ctrl Pts',(7.88047528540663,-5.34597074275425,2.01934437453605));
#92591=CARTESIAN_POINT('Ctrl Pts',(7.69992694305407,-5.60289361808539,2.01428937614376));
#92592=CARTESIAN_POINT('Ctrl Pts',(7.39956056908833,-5.98831105896093,2.00617681981901));
#92593=CARTESIAN_POINT('Ctrl Pts',(7.28832527603495,-6.12320825437251,2.00321678278712));
#92594=CARTESIAN_POINT('Ctrl Pts',(6.94130724951403,-6.52118219734963,1.99418025738971));
#92595=CARTESIAN_POINT('Ctrl Pts',(6.69453549425969,-6.77427183689836,1.98803256501737));
#92596=CARTESIAN_POINT('Ctrl Pts',(6.20635388392835,-7.22216363663306,1.97665115039945));
#92597=CARTESIAN_POINT('Ctrl Pts',(5.96838048269892,-7.42003452760417,1.97140382900469));
#92598=CARTESIAN_POINT('Ctrl Pts',(5.40029111145813,-7.84735032630688,1.95956278169603));
#92599=CARTESIAN_POINT('Ctrl Pts',(5.06443308118453,-8.06818258618791,1.95305428034658));
#92600=CARTESIAN_POINT('Ctrl Pts',(4.4527672262796,-8.41708086538624,1.94167234367945));
#92601=CARTESIAN_POINT('Ctrl Pts',(4.18290177044801,-8.55439753223893,1.93679189471401));
#92602=CARTESIAN_POINT('Ctrl Pts',(3.74556064042098,-8.7512804354366,1.92882516881779));
#92603=CARTESIAN_POINT('Ctrl Pts',(3.58217186807243,-8.81942045403042,1.92582577578345));
#92604=CARTESIAN_POINT('Ctrl Pts',(3.08860280501219,-9.00928000311882,1.91677072755454));
#92605=CARTESIAN_POINT('Ctrl Pts',(2.75347385538079,-9.11728995033518,1.91064761992418));
#92606=CARTESIAN_POINT('Ctrl Pts',(2.11543854411611,-9.28452681479049,1.89931910672918));
#92607=CARTESIAN_POINT('Ctrl Pts',(1.81413097599623,-9.34807194207792,1.89409976658499));
#92608=CARTESIAN_POINT('Ctrl Pts',(1.13389278176502,-9.45740004270625,1.88262577824753));
#92609=CARTESIAN_POINT('Ctrl Pts',(0.754217159231396,-9.49522439648685,
1.87643739650504));
#92610=CARTESIAN_POINT('Ctrl Pts',(0.0612225515307943,-9.52242609115569,
1.86522595191986));
#92611=CARTESIAN_POINT('Ctrl Pts',(-0.251264301273633,-9.51930728206631,
1.86019677271956));
#92612=CARTESIAN_POINT('Ctrl Pts',(-0.73302922742814,-9.49075739552366,
1.85219390454869));
#92613=CARTESIAN_POINT('Ctrl Pts',(-0.902726115623141,-9.47612221062986,
1.84931584692176));
#92614=CARTESIAN_POINT('Ctrl Pts',(-1.43621072314985,-9.41565212364951,
1.84013877049304));
#92615=CARTESIAN_POINT('Ctrl Pts',(-1.79779422730175,-9.35334929421928,
1.83375416030769));
#92616=CARTESIAN_POINT('Ctrl Pts',(-2.45498103473692,-9.20058696143206,
1.82216536762711));
#92617=CARTESIAN_POINT('Ctrl Pts',(-2.75151767060223,-9.11629774929942,
1.8169397630396));
#92618=CARTESIAN_POINT('Ctrl Pts',(-3.40985861879621,-8.89411167640492,
1.80536771529789));
#92619=CARTESIAN_POINT('Ctrl Pts',(-3.76839537704575,-8.74823159571515,
1.79909257082554));
#92620=CARTESIAN_POINT('Ctrl Pts',(-4.39975954854341,-8.44530858302767,
1.7877727304967));
#92621=CARTESIAN_POINT('Ctrl Pts',(-4.67558008643426,-8.29578627527581,
1.78272201927272));
#92622=CARTESIAN_POINT('Ctrl Pts',(-5.09293896594558,-8.04209897228491,
1.77461312084655));
#92623=CARTESIAN_POINT('Ctrl Pts',(-5.23982984286413,-7.9471734037367,1.77165219332543));
#92624=CARTESIAN_POINT('Ctrl Pts',(-5.67525620547695,-7.64846442593763,
1.76261525881214));
#92625=CARTESIAN_POINT('Ctrl Pts',(-5.95514508304704,-7.43261656040967,
1.75646813538162));
#92626=CARTESIAN_POINT('Ctrl Pts',(-6.45640735853107,-6.99951838564554,
1.74508795367418));
#92627=CARTESIAN_POINT('Ctrl Pts',(-6.68043184272131,-6.78603609293816,
1.73984128818269));
#92628=CARTESIAN_POINT('Ctrl Pts',(-7.17025078878727,-6.27146207578129,
1.72800750827385));
#92629=CARTESIAN_POINT('Ctrl Pts',(-7.42818869754932,-5.96370246256312,
1.72150523835751));
#92630=CARTESIAN_POINT('Ctrl Pts',(-7.84545710683259,-5.39660659396451,
1.71012506182612));
#92631=CARTESIAN_POINT('Ctrl Pts',(-8.01322645576272,-5.1441967112806,1.70524014268924));
#92632=CARTESIAN_POINT('Ctrl Pts',(-8.25947253865058,-4.73235941888736,
1.69726976680273));
#92633=CARTESIAN_POINT('Ctrl Pts',(-8.34601916679679,-4.57799901935649,
1.694271466573));
#92634=CARTESIAN_POINT('Ctrl Pts',(-8.59167244494509,-4.10971828127492,
1.68521694419208));
#92635=CARTESIAN_POINT('Ctrl Pts',(-8.73772708440675,-3.78929360163275,
1.67909316854293));
#92636=CARTESIAN_POINT('Ctrl Pts',(-8.97764848396376,-3.17480262877663,
1.66776322766917));
#92637=CARTESIAN_POINT('Ctrl Pts',(-9.07561965533232,-2.88282391581456,
1.66254313663657));
#92638=CARTESIAN_POINT('Ctrl Pts',(-9.2630694192839,-2.21905841259104,1.65105645539985));
#92639=CARTESIAN_POINT('Ctrl Pts',(-9.34464928971266,-1.84559107399456,
1.64485678250202));
#92640=CARTESIAN_POINT('Ctrl Pts',(-9.45249982852046,-1.15484249598211,
1.63355507572099));
#92641=CARTESIAN_POINT('Ctrl Pts',(-9.48573401283639,-0.839203371475859,
1.62844777237369));
#92642=CARTESIAN_POINT('Ctrl Pts',(-9.51271184691391,-0.34853247812069,
1.6202903080208));
#92643=CARTESIAN_POINT('Ctrl Pts',(-9.51749788160196,-0.174339772736851,
1.61734085559278));
#92644=CARTESIAN_POINT('Ctrl Pts',(-9.51749999976682,-7.71235715145945E-5,
1.61435896612853));
#92645=CARTESIAN_POINT('Ctrl Pts',(-9.5175,-3.85617845035904E-5,1.61435830627905));
#92646=CARTESIAN_POINT('Ctrl Pts',(-9.5175,4.49712710671297E-14,1.6143576464275));
#92647=CARTESIAN_POINT('Origin',(0.,0.,0.));
#92648=CARTESIAN_POINT('',(-9.51749999978858,-6.34387934023151E-5,0.614026678148392));
#92649=CARTESIAN_POINT('',(-9.5175,1.29540191486526E-8,0.886232496861817));
#92650=CARTESIAN_POINT('',(-9.5175,-1.16555759108849E-15,0.));
#92651=CARTESIAN_POINT('',(7.17753992463814,-6.25025814508694,0.));
#92652=CARTESIAN_POINT('Ctrl Pts',(-9.51749999978858,-6.34387934024261E-5,
0.614026678148392));
#92653=CARTESIAN_POINT('Ctrl Pts',(-9.51750157309347,0.235973984443455,
0.610078395618323));
#92654=CARTESIAN_POINT('Ctrl Pts',(-9.50871808344016,0.472047698466928,
0.606130113088254));
#92655=CARTESIAN_POINT('Ctrl Pts',(-9.49116749065726,0.707492695574145,
0.602181830558185));
#92656=CARTESIAN_POINT('Ctrl Pts',(-9.47361983589632,0.942898278481555,
0.598234208982472));
#92657=CARTESIAN_POINT('Ctrl Pts',(-9.44730802880415,1.17767507083165,0.594286587406759));
#92658=CARTESIAN_POINT('Ctrl Pts',(-9.41230203424797,1.41116145996537,0.590338965831046));
#92659=CARTESIAN_POINT('Ctrl Pts',(-9.37729948274158,1.64462488431054,0.586391732527623));
#92660=CARTESIAN_POINT('Ctrl Pts',(-9.33360449344291,1.87679787746023,0.582444499224199));
#92661=CARTESIAN_POINT('Ctrl Pts',(-9.28133860497358,2.10702632869812,0.578497265920775));
#92662=CARTESIAN_POINT('Ctrl Pts',(-9.22906886065934,2.33727176472719,0.574549741415577));
#92663=CARTESIAN_POINT('Ctrl Pts',(-9.16822701462845,2.56557209412563,0.570602216910379));
#92664=CARTESIAN_POINT('Ctrl Pts',(-9.09898547666434,2.79128456905625,0.566654692405182));
#92665=CARTESIAN_POINT('Ctrl Pts',(-9.0297433768793,3.01699887540188,0.56270713587005));
#92666=CARTESIAN_POINT('Ctrl Pts',(-8.95210153512587,3.24012501402205,0.558759579334919));
#92667=CARTESIAN_POINT('Ctrl Pts',(-8.86628209425272,3.46003584882203,0.554812022799787));
#92668=CARTESIAN_POINT('Ctrl Pts',(-8.7804466407393,3.67998771573614,0.550863729708904));
#92669=CARTESIAN_POINT('Ctrl Pts',(-8.686430644007,3.89672281538416,0.546915436618021));
#92670=CARTESIAN_POINT('Ctrl Pts',(-8.58450466405445,4.10963330758687,0.542967143527137));
#92671=CARTESIAN_POINT('Ctrl Pts',(-8.5616076317501,4.1574623146778,0.542080184240691));
#92672=CARTESIAN_POINT('Ctrl Pts',(-8.53831161263153,4.20509840113271,0.541193224954246));
#92673=CARTESIAN_POINT('Ctrl Pts',(-8.51461999986089,4.2525348332458,0.5403062656678));
#92674=CARTESIAN_POINT('Ctrl Pts',(-8.40897578712231,4.46406051426343,0.53635119023858));
#92675=CARTESIAN_POINT('Ctrl Pts',(-8.29543000322107,4.67167836467458,0.53239611480936));
#92676=CARTESIAN_POINT('Ctrl Pts',(-8.17429717557496,4.87479968156511,0.52844103938014));
#92677=CARTESIAN_POINT('Ctrl Pts',(-8.05318442491694,5.0778873324021,0.524486619479267));
#92678=CARTESIAN_POINT('Ctrl Pts',(-7.92448728551114,5.27647969478293,0.520532199578394));
#92679=CARTESIAN_POINT('Ctrl Pts',(-7.7885652819688,5.47001435999123,0.516577779677521));
#92680=CARTESIAN_POINT('Ctrl Pts',(-7.65265713781373,5.66352929129476,0.512623762991988));
#92681=CARTESIAN_POINT('Ctrl Pts',(-7.50952576290969,5.85198732392743,0.508669746306455));
#92682=CARTESIAN_POINT('Ctrl Pts',(-7.35957346783313,6.03485580785214,0.504715729620922));
#92683=CARTESIAN_POINT('Ctrl Pts',(-7.20960990419972,6.21773803390667,0.500761415800478));
#92684=CARTESIAN_POINT('Ctrl Pts',(-7.05282457337414,6.39502965166002,0.496807101980035));
#92685=CARTESIAN_POINT('Ctrl Pts',(-6.88966024492865,6.56623087923732,0.492852788159591));
#92686=CARTESIAN_POINT('Ctrl Pts',(-6.72649717499597,6.73743078631191,0.488898504839409));
#92687=CARTESIAN_POINT('Ctrl Pts',(-6.5569554025413,6.90254019411832,0.484944221519226));
#92688=CARTESIAN_POINT('Ctrl Pts',(-6.3815152392756,7.06109548872506,0.480989938199044));
#92689=CARTESIAN_POINT('Ctrl Pts',(-6.20604053498182,7.21968200003144,0.47703487635125));
#92690=CARTESIAN_POINT('Ctrl Pts',(-6.02466532918881,7.37171163013427,0.473079814503457));
#92691=CARTESIAN_POINT('Ctrl Pts',(-5.83790471857849,7.51675959086088,0.469124752655664));
#92692=CARTESIAN_POINT('Ctrl Pts',(-5.74338319082455,7.59016990367079,0.467123053866004));
#92693=CARTESIAN_POINT('Ctrl Pts',(-5.64748273071767,7.66179251461856,0.465121355076345));
#92694=CARTESIAN_POINT('Ctrl Pts',(-5.55027320997788,7.73157639453959,0.463119656286685));
#92695=CARTESIAN_POINT('Ctrl Pts',(-5.35819783036131,7.86946170788075,0.459164518436237));
#92696=CARTESIAN_POINT('Ctrl Pts',(-5.16095366513679,8.00020602784342,0.455209380585788));
#92697=CARTESIAN_POINT('Ctrl Pts',(-4.959093428077,8.12343514909817,0.45125424273534));
#92698=CARTESIAN_POINT('Ctrl Pts',(-4.75726671610235,8.24664380437684,0.447299761756869));
#92699=CARTESIAN_POINT('Ctrl Pts',(-4.55082570383888,8.3623396052951,0.443345280778399));
#92700=CARTESIAN_POINT('Ctrl Pts',(-4.34035065611748,8.4701925852923,0.439390799799929));
#92701=CARTESIAN_POINT('Ctrl Pts',(-4.12989714982282,8.57803452689282,0.43543672354954));
#92702=CARTESIAN_POINT('Ctrl Pts',(-3.91541068393433,8.67803512147413,0.431482647299151));
#92703=CARTESIAN_POINT('Ctrl Pts',(-3.69749550318223,8.76991067536878,0.427528571048762));
#92704=CARTESIAN_POINT('Ctrl Pts',(-3.47956409399778,8.86179307135769,0.423574200333074));
#92705=CARTESIAN_POINT('Ctrl Pts',(-3.2582037191723,8.94554910533614,0.419619829617386));
#92706=CARTESIAN_POINT('Ctrl Pts',(-3.03403909481477,9.02094302282946,0.415665458901698));
#92707=CARTESIAN_POINT('Ctrl Pts',(-2.80987629130963,9.09633632791039,0.411711120306713));
#92708=CARTESIAN_POINT('Ctrl Pts',(-2.58290955247713,9.16336756440958,0.407756781711728));
#92709=CARTESIAN_POINT('Ctrl Pts',(-2.35377994774284,9.22185047632002,0.403802443116743));
#92710=CARTESIAN_POINT('Ctrl Pts',(-2.12460539387736,9.28034486102151,0.399847328785753));
#92711=CARTESIAN_POINT('Ctrl Pts',(-1.89326740023424,9.33028750035805,0.395892214454763));
#92712=CARTESIAN_POINT('Ctrl Pts',(-1.66041971099122,9.37154270295728,0.391937100123772));
#92713=CARTESIAN_POINT('Ctrl Pts',(-1.54259505823751,9.39241849492387,0.389935749051038));
#92714=CARTESIAN_POINT('Ctrl Pts',(-1.42438401416757,9.41107066063499,0.387934397978304));
#92715=CARTESIAN_POINT('Ctrl Pts',(-1.30587213655077,9.42748663287201,0.38593304690557));
#92716=CARTESIAN_POINT('Ctrl Pts',(-1.07161009624955,9.45993603142265,0.381976982795493));
#92717=CARTESIAN_POINT('Ctrl Pts',(-0.836104249548172,9.48365409010825,
0.378020918685415));
#92718=CARTESIAN_POINT('Ctrl Pts',(-0.600018338006404,9.49856748378702,
0.374064854575338));
#92719=CARTESIAN_POINT('Ctrl Pts',(-0.363971284152349,9.51347842285089,
0.370109441599006));
#92720=CARTESIAN_POINT('Ctrl Pts',(-0.127344637748537,9.51958757203093,
0.366154028622673));
#92721=CARTESIAN_POINT('Ctrl Pts',(0.109194117260377,9.51687358825133,0.362198615646341));
#92722=CARTESIAN_POINT('Ctrl Pts',(0.3457088405748,9.5141598802051,0.358243604529215));
#92723=CARTESIAN_POINT('Ctrl Pts',(0.582135408055343,9.50262483234878,0.354288593412089));
#92724=CARTESIAN_POINT('Ctrl Pts',(0.817806698357784,9.4822992177067,0.350333582294962));
#92725=CARTESIAN_POINT('Ctrl Pts',(1.05349539243161,9.46197210206572,0.346378279109552));
#92726=CARTESIAN_POINT('Ctrl Pts',(1.28842841629673,9.43285314413454,0.342422975924142));
#92727=CARTESIAN_POINT('Ctrl Pts',(1.52194289042441,9.39502507118989,0.338467672738731));
#92728=CARTESIAN_POINT('Ctrl Pts',(1.7554552913616,9.3571973340908,0.334512404669332));
#92729=CARTESIAN_POINT('Ctrl Pts',(1.98754888935041,9.31066068399785,0.330557136599934));
#92730=CARTESIAN_POINT('Ctrl Pts',(2.21756941301968,9.25554926238522,0.326601868530535));
#92731=CARTESIAN_POINT('Ctrl Pts',(2.44763444350595,9.20042717722867,0.322645835153809));
#92732=CARTESIAN_POINT('Ctrl Pts',(2.67562532348104,9.13672707109781,0.318689801777082));
#92733=CARTESIAN_POINT('Ctrl Pts',(2.90090014069909,9.06463372804947,0.314733768400356));
#92734=CARTESIAN_POINT('Ctrl Pts',(3.01454890114918,9.02826339968642,0.312737991441723));
#92735=CARTESIAN_POINT('Ctrl Pts',(3.12750662476514,8.98975770540854,0.31074221448309));
#92736=CARTESIAN_POINT('Ctrl Pts',(3.23969245632158,8.94914515685454,0.308746437524456));
#92737=CARTESIAN_POINT('Ctrl Pts',(3.46187307311825,8.86871324346383,0.304793862145678));
#92738=CARTESIAN_POINT('Ctrl Pts',(3.68109027492723,8.77999103353609,0.3008412867669));
#92739=CARTESIAN_POINT('Ctrl Pts',(3.8967236268419,8.68322239874185,0.296888711388122));
#92740=CARTESIAN_POINT('Ctrl Pts',(4.11232065731574,8.58647006372782,0.292936801784056));
#92741=CARTESIAN_POINT('Ctrl Pts',(4.32433478448108,8.48167412535776,0.288984892179989));
#92742=CARTESIAN_POINT('Ctrl Pts',(4.53216647343998,8.36912619734143,0.285032982575923));
#92743=CARTESIAN_POINT('Ctrl Pts',(4.73997681778519,8.25658982815936,0.281081478838663));
#92744=CARTESIAN_POINT('Ctrl Pts',(4.94360533247279,8.13630319390262,0.277129975101402));
#92745=CARTESIAN_POINT('Ctrl Pts',(5.14247708649228,8.0086038524141,0.273178471364142));
#92746=CARTESIAN_POINT('Ctrl Pts',(5.34136449032563,7.88089446188198,0.26922665667122));
#92747=CARTESIAN_POINT('Ctrl Pts',(5.53549414558515,7.74577134940408,0.265274841978297));
#92748=CARTESIAN_POINT('Ctrl Pts',(5.72431908569665,7.60361606442153,0.261323027285375));
#92749=CARTESIAN_POINT('Ctrl Pts',(5.91314314972675,7.46146143898956,0.257371230927485));
#92750=CARTESIAN_POINT('Ctrl Pts',(6.09666232288001,7.312274878722,0.253419434569594));
#92751=CARTESIAN_POINT('Ctrl Pts',(6.27436122760346,7.15647940230016,0.249467638211704));
#92752=CARTESIAN_POINT('Ctrl Pts',(6.45209667352698,7.00065188880031,0.245515029224261));
#92753=CARTESIAN_POINT('Ctrl Pts',(6.62400924636439,6.83821293048068,0.241562420236818));
#92754=CARTESIAN_POINT('Ctrl Pts',(6.78961811626248,6.66962458353694,0.237609811249375));
#92755=CARTESIAN_POINT('Ctrl Pts',(6.87411343469442,6.58360910581711,0.235593150214031));
#92756=CARTESIAN_POINT('Ctrl Pts',(6.95696838808337,6.49599345866659,0.233576489178686));
#92757=CARTESIAN_POINT('Ctrl Pts',(7.0381228724021,6.40684264540424,0.231559828143342));
#92758=CARTESIAN_POINT('Ctrl Pts',(7.19753392928209,6.23172446822446,0.227598518183558));
#92759=CARTESIAN_POINT('Ctrl Pts',(7.35042765725365,6.05063002888739,0.223637208223773));
#92760=CARTESIAN_POINT('Ctrl Pts',(7.49636750072117,5.8640668945819,0.219675898263989));
#92761=CARTESIAN_POINT('Ctrl Pts',(7.64228387241871,5.67753376556402,0.215715225408878));
#92762=CARTESIAN_POINT('Ctrl Pts',(7.78124841937268,5.48553391856034,0.211754552553766));
#92763=CARTESIAN_POINT('Ctrl Pts',(7.91286536696382,5.28860737191792,0.207793879698655));
#92764=CARTESIAN_POINT('Ctrl Pts',(8.04446888443175,5.0917009195554,0.203833610988492));
#92765=CARTESIAN_POINT('Ctrl Pts',(8.16872614363592,4.88986900480745,0.199873342278328));
#92766=CARTESIAN_POINT('Ctrl Pts',(8.28528457174957,4.68368079774109,0.195913073568165));
#92767=CARTESIAN_POINT('Ctrl Pts',(8.40185037767259,4.47747953956113,0.191952554184515));
#92768=CARTESIAN_POINT('Ctrl Pts',(8.51071623831146,4.26692168130982,0.187992034800864));
#92769=CARTESIAN_POINT('Ctrl Pts',(8.6115748389386,4.05260225575614,0.184031515417214));
#92770=CARTESIAN_POINT('Ctrl Pts',(8.71243170439413,3.83828651735436,0.180071064170348));
#92771=CARTESIAN_POINT('Ctrl Pts',(8.80528146745874,3.62020959599289,0.176110612923482));
#92772=CARTESIAN_POINT('Ctrl Pts',(8.88986408205819,3.39898850432475,0.172150161676617));
#92773=CARTESIAN_POINT('Ctrl Pts',(8.97446126969002,3.17772929770653,0.168189028069853));
#92774=CARTESIAN_POINT('Ctrl Pts',(9.05078836227741,2.95332510066818,0.164227894463089));
#92775=CARTESIAN_POINT('Ctrl Pts',(9.11863406808458,2.72641137438343,0.160266760856326));
#92776=CARTESIAN_POINT('Ctrl Pts',(9.15228197150256,2.61387409504633,0.158302246824959));
#92777=CARTESIAN_POINT('Ctrl Pts',(9.18384452523986,2.50071981772256,0.156337732793593));
#92778=CARTESIAN_POINT('Ctrl Pts',(9.2133005174545,2.38702740350266,0.154373218762227));
#92779=CARTESIAN_POINT('Ctrl Pts',(9.27243444618333,2.15878592820287,0.150429388526563));
#92780=CARTESIAN_POINT('Ctrl Pts',(9.3230923220925,1.92830928422966,0.146485558290898));
#92781=CARTESIAN_POINT('Ctrl Pts',(9.36512475076436,1.6962442785816,0.142541728055234));
#92782=CARTESIAN_POINT('Ctrl Pts',(9.40715003705868,1.46421870667399,0.138598567976525));
#92783=CARTESIAN_POINT('Ctrl Pts',(9.44055275076671,1.23060559304961,0.134655407897817));
#92784=CARTESIAN_POINT('Ctrl Pts',(9.46523468695665,0.996061529641996,0.130712247819109));
#92785=CARTESIAN_POINT('Ctrl Pts',(9.48991421482022,0.761540351742488,0.126769472492079));
#92786=CARTESIAN_POINT('Ctrl Pts',(9.5058746342629,0.526088689685904,0.122826697165049));
#92787=CARTESIAN_POINT('Ctrl Pts',(9.51306954646726,0.29036882421709,0.118883921838019));
#92788=CARTESIAN_POINT('Ctrl Pts',(9.5202651941705,0.0546248623183552,0.114940743461338));
#92789=CARTESIAN_POINT('Ctrl Pts',(9.51869353268557,-0.181387072038218,
0.110997565084658));
#92790=CARTESIAN_POINT('Ctrl Pts',(9.50836026040628,-0.417002887671913,
0.107054386707978));
#92791=CARTESIAN_POINT('Ctrl Pts',(9.49802686177878,-0.652621584254886,
0.103111160116805));
#92792=CARTESIAN_POINT('Ctrl Pts',(9.47893165385032,-0.887843866900617,
0.0991679335256324));
#92793=CARTESIAN_POINT('Ctrl Pts',(9.45113239905309,-1.12200830013374,0.0952247069344598));
#92794=CARTESIAN_POINT('Ctrl Pts',(9.42332632570476,-1.35623016879688,0.0912805131557782));
#92795=CARTESIAN_POINT('Ctrl Pts',(9.38681197351291,-1.5893933855905,0.0873363193770966));
#92796=CARTESIAN_POINT('Ctrl Pts',(9.34169883327627,-1.82084298015092,0.0833921255984151));
#92797=CARTESIAN_POINT('Ctrl Pts',(9.31803955594689,-1.94222513436924,0.0813236201926478));
#92798=CARTESIAN_POINT('Ctrl Pts',(9.29201611827713,-2.06313611452594,0.0792551147868806));
#92799=CARTESIAN_POINT('Ctrl Pts',(9.26364992592769,-2.18348260809652,0.0771866093811133));
#92800=CARTESIAN_POINT('Ctrl Pts',(9.20909789291053,-2.41492522858947,0.0732085930932201));
#92801=CARTESIAN_POINT('Ctrl Pts',(9.14586125259741,-2.64435153131898,0.069230576805327));
#92802=CARTESIAN_POINT('Ctrl Pts',(9.07411359320576,-2.87110932351913,0.0652525605174338));
#92803=CARTESIAN_POINT('Ctrl Pts',(9.00237828592216,-3.09782807699977,0.0612752290865439));
#92804=CARTESIAN_POINT('Ctrl Pts',(8.92213496819583,-3.32187897427633,0.0572978976556541));
#92805=CARTESIAN_POINT('Ctrl Pts',(8.83360704406796,-3.5426251341333,0.0533205662247642));
#92806=CARTESIAN_POINT('Ctrl Pts',(8.74509040743746,-3.76334314838846,0.0493437419120355));
#92807=CARTESIAN_POINT('Ctrl Pts',(8.64829137627522,-3.98075701063916,0.0453669175993068));
#92808=CARTESIAN_POINT('Ctrl Pts',(8.54348183318892,-4.19424896924001,0.0413900932865782));
#92809=CARTESIAN_POINT('Ctrl Pts',(8.43867307522417,-4.40773932858633,0.0374132987639847));
#92810=CARTESIAN_POINT('Ctrl Pts',(8.32585404456452,-4.61730759427663,0.0334365042413912));
#92811=CARTESIAN_POINT('Ctrl Pts',(8.20534354533062,-4.82235871261162,0.0294597097187977));
#92812=CARTESIAN_POINT('Ctrl Pts',(8.08484098218856,-5.02739632752143,0.025483177083814));
#92813=CARTESIAN_POINT('Ctrl Pts',(7.95664810308623,-5.22791715209812,0.0215066444488302));
#92814=CARTESIAN_POINT('Ctrl Pts',(7.82112862805113,-5.42335258244188,0.0175301118138464));
#92815=CARTESIAN_POINT('Ctrl Pts',(7.68559945771733,-5.61880199457589,0.013553294690809));
#92816=CARTESIAN_POINT('Ctrl Pts',(7.5427428007723,-5.80916505843287,0.00957647756777154));
#92817=CARTESIAN_POINT('Ctrl Pts',(7.39296521290532,-5.99390286964777,0.0055996604447341));
#92818=CARTESIAN_POINT('Ctrl Pts',(7.32266580776647,-6.08061115771684,0.00373310696315578));
#92819=CARTESIAN_POINT('Ctrl Pts',(7.250842335954,-6.16608066448073,0.00186655348157747));
#92820=CARTESIAN_POINT('Ctrl Pts',(7.17753992463814,-6.25025814508694,-8.42340928558192E-16));
#92821=CARTESIAN_POINT('',(-7.17208764054957,-6.25651381571847,0.));
#92822=CARTESIAN_POINT('Origin',(0.,0.,0.));
#92823=CARTESIAN_POINT('Ctrl Pts',(-7.17208764054957,-6.25651381571847,
-1.39027244577816E-13));
#92824=CARTESIAN_POINT('Ctrl Pts',(-6.93903462647267,-6.52367164371758,
0.0061230893854338));
#92825=CARTESIAN_POINT('Ctrl Pts',(-6.69123339070042,-6.7776024280055,0.0122580412302597));
#92826=CARTESIAN_POINT('Ctrl Pts',(-6.30452767684011,-7.1319440507319,0.0211629916357882));
#92827=CARTESIAN_POINT('Ctrl Pts',(-6.17615941472648,-7.24339356681062,
0.0240227154141973));
#92828=CARTESIAN_POINT('Ctrl Pts',(-5.7288020833808,-7.61124719676084,0.0336737688681814));
#92829=CARTESIAN_POINT('Ctrl Pts',(-5.39629636960243,-7.85049324062235,
0.040304840357762));
#92830=CARTESIAN_POINT('Ctrl Pts',(-4.79736821589071,-8.22535628963563,
0.0517290676460848));
#92831=CARTESIAN_POINT('Ctrl Pts',(-4.53805647802596,-8.37121672575455,
0.0565290406610172));
#92832=CARTESIAN_POINT('Ctrl Pts',(-4.11474818325647,-8.58386614549834,
0.0644019772056237));
#92833=CARTESIAN_POINT('Ctrl Pts',(-3.95498339006568,-8.65863821250177,
0.0673918993382834));
#92834=CARTESIAN_POINT('Ctrl Pts',(-3.47181792969002,-8.86860217795716,
0.0764142496008092));
#92835=CARTESIAN_POINT('Ctrl Pts',(-3.1429312215907,-8.99041759378516,0.0825128523844614));
#92836=CARTESIAN_POINT('Ctrl Pts',(-2.51460321804215,-9.18443879372131,
0.0938065623632663));
#92837=CARTESIAN_POINT('Ctrl Pts',(-2.21691375716944,-9.26080128867718,
0.0990152614899264));
#92838=CARTESIAN_POINT('Ctrl Pts',(-1.53378042111751,-9.40120358700342,
0.110629246100296));
#92839=CARTESIAN_POINT('Ctrl Pts',(-1.14703762926181,-9.45618408232794,
0.116959106760903));
#92840=CARTESIAN_POINT('Ctrl Pts',(-0.44811666409676,-9.51202640574503,
0.128290902657562));
#92841=CARTESIAN_POINT('Ctrl Pts',(-0.137195121195117,-9.52158759614352,
0.133299261341023));
#92842=CARTESIAN_POINT('Ctrl Pts',(0.348202834178003,-9.51273071377279,
0.141359313310886));
#92843=CARTESIAN_POINT('Ctrl Pts',(0.522649299077872,-9.50474235636138,
0.14431573135038));
#92844=CARTESIAN_POINT('Ctrl Pts',(1.04948183162352,-9.46606920895727,0.153356122087019));
#92845=CARTESIAN_POINT('Ctrl Pts',(1.40047109956027,-9.42053925790094,0.159511759865588));
#92846=CARTESIAN_POINT('Ctrl Pts',(2.0521469596991,-9.29877219378344,0.170900693840379));
#92847=CARTESIAN_POINT('Ctrl Pts',(2.35323402853859,-9.22717524016697,0.176147835831803));
#92848=CARTESIAN_POINT('Ctrl Pts',(3.03168093204356,-9.03047034069168,0.18791434374575));
#92849=CARTESIAN_POINT('Ctrl Pts',(3.40576693954906,-8.89613606310804,0.194353012662929));
#92850=CARTESIAN_POINT('Ctrl Pts',(4.05117081013989,-8.61767658636625,0.205715393491159));
#92851=CARTESIAN_POINT('Ctrl Pts',(4.3259700327581,-8.48306053270267,0.210646029435909));
#92852=CARTESIAN_POINT('Ctrl Pts',(4.74852512589343,-8.25018320678865,0.218659539627829));
#92853=CARTESIAN_POINT('Ctrl Pts',(4.90083559481307,-8.16062638286779,0.221652710352832));
#92854=CARTESIAN_POINT('Ctrl Pts',(5.3488746056791,-7.88011538115239,0.230703101108145));
#92855=CARTESIAN_POINT('Ctrl Pts',(5.63659598376065,-7.67694369687641,0.236828327815319));
#92856=CARTESIAN_POINT('Ctrl Pts',(6.15383059494878,-7.26691760843837,0.248165056450992));
#92857=CARTESIAN_POINT('Ctrl Pts',(6.38582419056159,-7.0639205655047,0.253390331038366));
#92858=CARTESIAN_POINT('Ctrl Pts',(6.88594454724076,-6.58150257688345,0.264963075984794));
#92859=CARTESIAN_POINT('Ctrl Pts',(7.14769691895456,-6.29625592632983,0.271239177315086));
#92860=CARTESIAN_POINT('Ctrl Pts',(7.58889963078379,-5.75236682723046,0.282559928318293));
#92861=CARTESIAN_POINT('Ctrl Pts',(7.77427785843031,-5.49924753245593,0.287610598788987));
#92862=CARTESIAN_POINT('Ctrl Pts',(8.04300668964976,-5.09150268042808,0.295718146938713));
#92863=CARTESIAN_POINT('Ctrl Pts',(8.13515071825344,-4.9429422055558,0.298677714877409));
#92864=CARTESIAN_POINT('Ctrl Pts',(8.40099810587543,-4.48673708245598,0.307714144528223));
#92865=CARTESIAN_POINT('Ctrl Pts',(8.56171720086413,-4.17187945843736,0.313862251834349));
#92866=CARTESIAN_POINT('Ctrl Pts',(8.82963434257283,-3.56595280291705,0.325243688844295));
#92867=CARTESIAN_POINT('Ctrl Pts',(8.9408444187103,-3.27715805945244,0.330490642303489));
#92868=CARTESIAN_POINT('Ctrl Pts',(9.16382244088416,-2.60169089969545,0.342339346020211));
#92869=CARTESIAN_POINT('Ctrl Pts',(9.26553193865112,-2.21231928162504,0.348855359099864));
#92870=CARTESIAN_POINT('Ctrl Pts',(9.40003846699103,-1.52099879019535,0.36023896822764));
#92871=CARTESIAN_POINT('Ctrl Pts',(9.44359705905848,-1.22173368101764,0.365113575888356));
#92872=CARTESIAN_POINT('Ctrl Pts',(9.48997557148242,-0.744664192243146,
0.37307549570592));
#92873=CARTESIAN_POINT('Ctrl Pts',(9.50218701820347,-0.567980319390919,
0.376076271696077));
#92874=CARTESIAN_POINT('Ctrl Pts',(9.52391782942472,-0.0395498460445606,
0.385132330140256));
#92875=CARTESIAN_POINT('Ctrl Pts',(9.51887201789631,0.312492190247613,0.391254949842456));
#92876=CARTESIAN_POINT('Ctrl Pts',(9.484396062492,0.805866170593425,0.399749285239025));
#92877=CARTESIAN_POINT('Ctrl Pts',(9.47124065166592,0.948045161219863,0.402188627261551));
#92878=CARTESIAN_POINT('Ctrl Pts',(9.42341516528679,1.3629413531227,0.409272371137488));
#92879=CARTESIAN_POINT('Ctrl Pts',(9.38012353863364,1.63451710866645,0.413861802731057));
#92880=CARTESIAN_POINT('Ctrl Pts',(9.23734497894092,2.33385669724583,0.425606340552339));
#92881=CARTESIAN_POINT('Ctrl Pts',(9.1199126850069,2.75728499585502,0.432627478567698));
#92882=CARTESIAN_POINT('Ctrl Pts',(8.90643697025229,3.36138657875957,0.443044725695659));
#92883=CARTESIAN_POINT('Ctrl Pts',(8.83315617802637,3.54949167379445,0.446353177511085));
#92884=CARTESIAN_POINT('Ctrl Pts',(8.62923560964239,4.02741703509139,0.455072861877973));
#92885=CARTESIAN_POINT('Ctrl Pts',(8.4899596294393,4.31327946293116,0.460572111123676));
#92886=CARTESIAN_POINT('Ctrl Pts',(8.14767411006479,4.93473826048226,0.47283405036059));
#92887=CARTESIAN_POINT('Ctrl Pts',(7.9376999305089,5.26584831376671,0.479573883988482));
#92888=CARTESIAN_POINT('Ctrl Pts',(7.53246248753103,5.82531367544405,0.491181991726077));
#92889=CARTESIAN_POINT('Ctrl Pts',(7.34568158336914,6.05914466004674,0.496114180341433));
#92890=CARTESIAN_POINT('Ctrl Pts',(6.92143901901578,6.54174662953664,0.506581109895527));
#92891=CARTESIAN_POINT('Ctrl Pts',(6.68088222440156,6.78723647116784,0.512087080439486));
#92892=CARTESIAN_POINT('Ctrl Pts',(6.28566320240162,7.14914509421464,0.520811728326618));
#92893=CARTESIAN_POINT('Ctrl Pts',(6.13983283273638,7.27477081400398,0.523972939784433));
#92894=CARTESIAN_POINT('Ctrl Pts',(5.70965804937142,7.62319053641709,0.53327316987596));
#92895=CARTESIAN_POINT('Ctrl Pts',(5.41631201448006,7.83433420932491,0.539546928319713));
#92896=CARTESIAN_POINT('Ctrl Pts',(4.79156620939356,8.23211480678324,0.552337823888925));
#92897=CARTESIAN_POINT('Ctrl Pts',(4.45954718942792,8.41660639181572,0.558836830020347));
#92898=CARTESIAN_POINT('Ctrl Pts',(3.6171240691741,8.82083450440868,0.57447283004648));
#92899=CARTESIAN_POINT('Ctrl Pts',(3.09681563521564,9.01667563362379,0.583371743534608));
#92900=CARTESIAN_POINT('Ctrl Pts',(2.40311850818849,9.2106018729805,0.595051578877104));
#92901=CARTESIAN_POINT('Ctrl Pts',(2.24268654987239,9.25097411902166,0.597746499402488));
#92902=CARTESIAN_POINT('Ctrl Pts',(1.92204906354856,9.32283020852283,0.603179909631795));
#92903=CARTESIAN_POINT('Ctrl Pts',(1.76192419563051,9.35441382094635,0.605925368279426));
#92904=CARTESIAN_POINT('Ctrl Pts',(1.19689896788042,9.45083850133323,0.615694606522176));
#92905=CARTESIAN_POINT('Ctrl Pts',(0.788695762157428,9.49362292415194,0.62284887419601));
#92906=CARTESIAN_POINT('Ctrl Pts',(0.240331629698746,9.51547731476212,0.632261001700232));
#92907=CARTESIAN_POINT('Ctrl Pts',(0.101551135275765,9.5179701267666,0.634628281815932));
#92908=CARTESIAN_POINT('Ctrl Pts',(-0.313076632471723,9.5163480064041,0.641649272785042));
#92909=CARTESIAN_POINT('Ctrl Pts',(-0.588742290031258,9.50327733658267,
0.646245392585186));
#92910=CARTESIAN_POINT('Ctrl Pts',(-1.29686298829185,9.43876883670776,0.657925204241282));
#92911=CARTESIAN_POINT('Ctrl Pts',(-1.72705398894358,9.36960477193262,0.664882384171149));
#92912=CARTESIAN_POINT('Ctrl Pts',(-2.33948415145625,9.22751643348909,0.675116364779935));
#92913=CARTESIAN_POINT('Ctrl Pts',(-2.52659310716908,9.17804843189477,0.678294144464204));
#92914=CARTESIAN_POINT('Ctrl Pts',(-3.06181965502673,9.01893600376006,0.687673717547856));
#92915=CARTESIAN_POINT('Ctrl Pts',(-3.40530615496613,8.89493314214931,0.694014113124501));
#92916=CARTESIAN_POINT('Ctrl Pts',(-4.08749631636078,8.60333201070961,0.706825838192722));
#92917=CARTESIAN_POINT('Ctrl Pts',(-4.42506069933576,8.43467776045108,0.713280882380909));
#92918=CARTESIAN_POINT('Ctrl Pts',(-5.24141516659108,7.96428153648384,0.729046276778006));
#92919=CARTESIAN_POINT('Ctrl Pts',(-5.70499077821504,7.63906352539674,0.738098833647876));
#92920=CARTESIAN_POINT('Ctrl Pts',(-6.30478761351065,7.13306853728811,0.750832383610307));
#92921=CARTESIAN_POINT('Ctrl Pts',(-6.46765868318376,6.98572861633838,0.754419700370793));
#92922=CARTESIAN_POINT('Ctrl Pts',(-6.87325735196992,6.5924531042719,0.76388476937299));
#92923=CARTESIAN_POINT('Ctrl Pts',(-7.10795440520615,6.33869763974769,0.769872491752266));
#92924=CARTESIAN_POINT('Ctrl Pts',(-7.58547631657443,5.76244433440629,0.782804768294171));
#92925=CARTESIAN_POINT('Ctrl Pts',(-7.822648572792,5.43611892772742,0.789722275950427));
#92926=CARTESIAN_POINT('Ctrl Pts',(-8.34470945056656,4.61257954687358,0.806049318590966));
#92927=CARTESIAN_POINT('Ctrl Pts',(-8.60681087485979,4.10278811277121,0.815211938072408));
#92928=CARTESIAN_POINT('Ctrl Pts',(-8.90373927600287,3.36959661091949,0.828048651279066));
#92929=CARTESIAN_POINT('Ctrl Pts',(-8.97890475680381,3.1638620915177,0.831626665530576));
#92930=CARTESIAN_POINT('Ctrl Pts',(-9.15392422270132,2.62816006554718,0.841068894646166));
#92931=CARTESIAN_POINT('Ctrl Pts',(-9.24307231355284,2.29503099039305,0.847042466013865));
#92932=CARTESIAN_POINT('Ctrl Pts',(-9.39664789694852,1.5644182744876,0.859943462994976));
#92933=CARTESIAN_POINT('Ctrl Pts',(-9.454332849096,1.16618635295279,0.866844176838761));
#92934=CARTESIAN_POINT('Ctrl Pts',(-9.50721563147286,0.510823228395225,
0.877855553603315));
#92935=CARTESIAN_POINT('Ctrl Pts',(-9.51749999965232,0.255449492998535,
0.882066736325325));
#92936=CARTESIAN_POINT('Ctrl Pts',(-9.5175,1.29540203563927E-8,0.886232496861817));
#92937=CARTESIAN_POINT('Origin',(0.,0.,0.));
#92938=CARTESIAN_POINT('Ctrl Pts',(-9.5175,1.29540191486526E-8,0.886232496861817));
#92939=CARTESIAN_POINT('Ctrl Pts',(-9.51750000009661,-0.0709834321008029,
0.887390064432916));
#92940=CARTESIAN_POINT('Ctrl Pts',(-9.51670588696209,-0.141972721806853,
0.888544370346134));
#92941=CARTESIAN_POINT('Ctrl Pts',(-9.50834368299895,-0.515608100225471,
0.894608759845094));
#92942=CARTESIAN_POINT('Ctrl Pts',(-9.48713394327634,-0.817765315791146,
0.899469037072768));
#92943=CARTESIAN_POINT('Ctrl Pts',(-9.4300283608135,-1.30036435445735,0.907393967643415));
#92944=CARTESIAN_POINT('Ctrl Pts',(-9.40324558456404,-1.48167305946214,
0.910411653856429));
#92945=CARTESIAN_POINT('Ctrl Pts',(-9.32253051541496,-1.93676161781098,
0.918187617085166));
#92946=CARTESIAN_POINT('Ctrl Pts',(-9.26176363468904,-2.20915240447229,
0.923003836304866));
#92947=CARTESIAN_POINT('Ctrl Pts',(-9.1108138684556,-2.76880843345181,0.933021129377397));
#92948=CARTESIAN_POINT('Ctrl Pts',(-9.01879084958096,-3.05526468133464,
0.938215956004931));
#92949=CARTESIAN_POINT('Ctrl Pts',(-8.81658594895157,-3.59538706373471,
0.948028533439706));
#92950=CARTESIAN_POINT('Ctrl Pts',(-8.7086102079461,-3.84955912891823,0.952654765272702));
#92951=CARTESIAN_POINT('Ctrl Pts',(-8.53013525825724,-4.22359508010476,
0.959495498211941));
#92952=CARTESIAN_POINT('Ctrl Pts',(-8.46781261296457,-4.34719594757657,
0.9617625407189));
#92953=CARTESIAN_POINT('Ctrl Pts',(-8.21187337611752,-4.82838211024614,
0.970641832374481));
#92954=CARTESIAN_POINT('Ctrl Pts',(-7.99812237261707,-5.1747631784986,0.977134414953339));
#92955=CARTESIAN_POINT('Ctrl Pts',(-7.66765777885033,-5.64064867599083,
0.986500687327036));
#92956=CARTESIAN_POINT('Ctrl Pts',(-7.56897356942488,-5.7723939968927,0.989233766450829));
#92957=CARTESIAN_POINT('Ctrl Pts',(-7.20619398893471,-6.2314026107354,0.999125624719866));
#92958=CARTESIAN_POINT('Ctrl Pts',(-6.9238916009016,-6.54364856002412,1.00646724688607));
#92959=CARTESIAN_POINT('Ctrl Pts',(-6.39344966556373,-7.05745974374448,
1.01916838056406));
#92960=CARTESIAN_POINT('Ctrl Pts',(-6.15408358454014,-7.26713106377084,
1.02457215942581));
#92961=CARTESIAN_POINT('Ctrl Pts',(-5.59026126480687,-7.713137863628,1.03655932876923));
#92962=CARTESIAN_POINT('Ctrl Pts',(-5.26045213186174,-7.94173543092669,
1.04306374587039));
#92963=CARTESIAN_POINT('Ctrl Pts',(-4.62927364203687,-8.32260350261557,
1.05497990239583));
#92964=CARTESIAN_POINT('Ctrl Pts',(-4.33233022242226,-8.48096783617631,
1.06039584712114));
#92965=CARTESIAN_POINT('Ctrl Pts',(-3.83450372799791,-8.71348509654136,
1.06956772537983));
#92966=CARTESIAN_POINT('Ctrl Pts',(-3.63840107148738,-8.7971744169989,1.07321030995441));
#92967=CARTESIAN_POINT('Ctrl Pts',(-2.89479862660065,-9.08539580088091,
1.0869385278474));
#92968=CARTESIAN_POINT('Ctrl Pts',(-2.33163893413568,-9.24595860678656,
1.09708550198641));
#92969=CARTESIAN_POINT('Ctrl Pts',(-1.36198023479308,-9.42812950366615,
1.11354527106545));
#92970=CARTESIAN_POINT('Ctrl Pts',(-0.962329782394407,-9.4772643269652,
1.1200743946241));
#92971=CARTESIAN_POINT('Ctrl Pts',(-0.220705783416766,-9.52103682263299,
1.13208344913632));
#92972=CARTESIAN_POINT('Ctrl Pts',(0.120189287118578,-9.52283595927135,
1.13756765893452));
#92973=CARTESIAN_POINT('Ctrl Pts',(0.676338012850338,-9.49589876290568,
1.14686460760526));
#92974=CARTESIAN_POINT('Ctrl Pts',(0.891813199580838,-9.47809022878366,
1.150560149241));
#92975=CARTESIAN_POINT('Ctrl Pts',(1.68050463678258,-9.38577189627498,1.16423315658238));
#92976=CARTESIAN_POINT('Ctrl Pts',(2.24721370120664,-9.26643699723771,1.1742650943042));
#92977=CARTESIAN_POINT('Ctrl Pts',(3.18164403407643,-8.97884963655408,1.19057989921377));
#92978=CARTESIAN_POINT('Ctrl Pts',(3.55591300970609,-8.83731202866592,1.19707125070835));
#92979=CARTESIAN_POINT('Ctrl Pts',(4.23647968674317,-8.52968570655022,1.2091447559891));
#92980=CARTESIAN_POINT('Ctrl Pts',(4.54472595273265,-8.36951379449738,1.21473009194926));
#92981=CARTESIAN_POINT('Ctrl Pts',(5.03363069834457,-8.08047876267821,1.22421674216097));
#92982=CARTESIAN_POINT('Ctrl Pts',(5.2197612553087,-7.96151155746337,1.22799519729326));
#92983=CARTESIAN_POINT('Ctrl Pts',(5.86946345419365,-7.51366309695892,1.24158810181947));
#92984=CARTESIAN_POINT('Ctrl Pts',(6.30752619709711,-7.14988537595363,1.25144708784685));
#92985=CARTESIAN_POINT('Ctrl Pts',(6.99884823637462,-6.46252678755998,1.26772109283909));
#92986=CARTESIAN_POINT('Ctrl Pts',(7.26851519100125,-6.15766333443829,1.27432224142334));
#92987=CARTESIAN_POINT('Ctrl Pts',(7.72771518166854,-5.5661775759193,1.28642676817886));
#92988=CARTESIAN_POINT('Ctrl Pts',(7.92283889302851,-5.28474554875495,1.2919353148367));
#92989=CARTESIAN_POINT('Ctrl Pts',(8.2163607199155,-4.80847373089049,1.30127742306168));
#92990=CARTESIAN_POINT('Ctrl Pts',(8.32397498198234,-4.61967989770632,1.30499241947281));
#92991=CARTESIAN_POINT('Ctrl Pts',(8.69280250666164,-3.91782220788186,1.31864595980406));
#92992=CARTESIAN_POINT('Ctrl Pts',(8.91379728922954,-3.38502260911586,1.32863655767747));
#92993=CARTESIAN_POINT('Ctrl Pts',(9.20512044025394,-2.45159674083597,1.34495527392816));
#92994=CARTESIAN_POINT('Ctrl Pts',(9.30048909355446,-2.06045460944007,1.3514856796273));
#92995=CARTESIAN_POINT('Ctrl Pts',(9.43113728749645,-1.32490888918622,1.36356210594341));
#92996=CARTESIAN_POINT('Ctrl Pts',(9.47294779987285,-0.98233950570191,1.3691120887308));
#92997=CARTESIAN_POINT('Ctrl Pts',(9.51077182367394,-0.419592301126781,
1.37853180592365));
#92998=CARTESIAN_POINT('Ctrl Pts',(9.51791174868415,-0.200482182594715,
1.38228065357111));
#92999=CARTESIAN_POINT('Ctrl Pts',(9.5163598494172,0.590341328961604,1.39590131545597));
#93000=CARTESIAN_POINT('Ctrl Pts',(9.46373474772706,1.16075227234511,1.40582110477999));
#93001=CARTESIAN_POINT('Ctrl Pts',(9.2873062968508,2.11921343781519,1.42208777159612));
#93002=CARTESIAN_POINT('Ctrl Pts',(9.18928490171559,2.5104120253562,1.42862995167621));
#93003=CARTESIAN_POINT('Ctrl Pts',(8.9616333863762,3.22357935857759,1.44073171797963));
#93004=CARTESIAN_POINT('Ctrl Pts',(8.83863055512849,3.54696257932293,1.44629535229075));
#93005=CARTESIAN_POINT('Ctrl Pts',(8.60909437881218,4.06381768465117,1.45574083722301));
#93006=CARTESIAN_POINT('Ctrl Pts',(8.51294908304052,4.26155099639194,1.45950103847777));
#93007=CARTESIAN_POINT('Ctrl Pts',(8.14302371815457,4.9597657913796,1.47311094827104));
#93008=CARTESIAN_POINT('Ctrl Pts',(7.83123379026358,5.43874091396667,1.48300729939254));
#93009=CARTESIAN_POINT('Ctrl Pts',(7.22026958258221,6.21487967318774,1.4994950345681));
#93010=CARTESIAN_POINT('Ctrl Pts',(6.94080315408772,6.52550959230831,1.50626438682662));
#93011=CARTESIAN_POINT('Ctrl Pts',(6.40811169889246,7.0445304849691,1.51828584179066));
#93012=CARTESIAN_POINT('Ctrl Pts',(6.16281611713813,7.26009642940727,1.52354553115818));
#93013=CARTESIAN_POINT('Ctrl Pts',(5.74478265732109,7.5909845103392,1.53243986894394));
#93014=CARTESIAN_POINT('Ctrl Pts',(5.57849042110374,7.71401431749304,1.53597000730131));
#93015=CARTESIAN_POINT('Ctrl Pts',(4.91565986945029,8.17175417268464,1.54982722161673));
#93016=CARTESIAN_POINT('Ctrl Pts',(4.39197993134727,8.46473901976796,1.5602317445063));
#93017=CARTESIAN_POINT('Ctrl Pts',(3.48825078254916,8.86376671524525,1.57670306897099));
#93018=CARTESIAN_POINT('Ctrl Pts',(3.12294022559557,8.99897215398034,1.58302319371211));
#93019=CARTESIAN_POINT('Ctrl Pts',(2.43487386643304,9.20667201160169,1.59464239024727));
#93020=CARTESIAN_POINT('Ctrl Pts',(2.11463642651796,9.28545801484259,1.59994642489134));
#93021=CARTESIAN_POINT('Ctrl Pts',(1.61089233735988,9.3819745939804,1.60847675699062));
#93022=CARTESIAN_POINT('Ctrl Pts',(1.42986599896998,9.41126469890302,1.61158999878252));
#93023=CARTESIAN_POINT('Ctrl Pts',(0.947551587933962,9.47506556934312,1.61993150954111));
#93024=CARTESIAN_POINT('Ctrl Pts',(0.645266352138142,9.50043963158541,1.62519878088986));
#93025=CARTESIAN_POINT('Ctrl Pts',(0.0163566163675249,9.5230723323936,1.63603187654348));
#93026=CARTESIAN_POINT('Ctrl Pts',(-0.309962191910088,9.51804075318925,
1.64158125982926));
#93027=CARTESIAN_POINT('Ctrl Pts',(-1.03510627631471,9.46952261383766,1.65370907829757));
#93028=CARTESIAN_POINT('Ctrl Pts',(-1.43274608035249,9.41756570862793,1.66021429049689));
#93029=CARTESIAN_POINT('Ctrl Pts',(-2.16556940359027,9.27431292046044,1.6722849408458));
#93030=CARTESIAN_POINT('Ctrl Pts',(-2.50133510045622,9.18944451473523,1.67785386858916));
#93031=CARTESIAN_POINT('Ctrl Pts',(-3.04181774660979,9.02100743667884,1.68730937198493));
#93032=CARTESIAN_POINT('Ctrl Pts',(-3.24957184120873,8.94826866024951,1.69107400291466));
#93033=CARTESIAN_POINT('Ctrl Pts',(-3.98559894776873,8.6615548823838,1.70467975429173));
#93034=CARTESIAN_POINT('Ctrl Pts',(-4.49694169379472,8.407440795952,1.71456700217436));
#93035=CARTESIAN_POINT('Ctrl Pts',(-5.3351203097085,7.89243978082905,1.73098817343587));
#93036=CARTESIAN_POINT('Ctrl Pts',(-5.67325707085544,7.65299093832427,1.73770301967802));
#93037=CARTESIAN_POINT('Ctrl Pts',(-6.25216992893393,7.18352527932954,1.74975070899744));
#93038=CARTESIAN_POINT('Ctrl Pts',(-6.49852477355208,6.96145367325152,1.75509057393998));
#93039=CARTESIAN_POINT('Ctrl Pts',(-6.88120304579825,6.57844523581017,1.76412584499518));
#93040=CARTESIAN_POINT('Ctrl Pts',(-7.02465856119573,6.42503446352992,1.76771220481145));
#93041=CARTESIAN_POINT('Ctrl Pts',(-7.55234717807932,5.82190884061152,1.78150281214749));
#93042=CARTESIAN_POINT('Ctrl Pts',(-7.89944596455147,5.34147351644425,1.7917761810398));
#93043=CARTESIAN_POINT('Ctrl Pts',(-8.40286584019894,4.48718015892417,1.80831405038249));
#93044=CARTESIAN_POINT('Ctrl Pts',(-8.58408122184459,4.12995051875902,1.81480864133918));
#93045=CARTESIAN_POINT('Ctrl Pts',(-8.87670376182314,3.45001158098685,1.82677429801291));
#93046=CARTESIAN_POINT('Ctrl Pts',(-8.99429601809596,3.1306685694704,1.83224922210518));
#93047=CARTESIAN_POINT('Ctrl Pts',(-9.15814142220127,2.59957548864125,1.84152901497371));
#93048=CARTESIAN_POINT('Ctrl Pts',(-9.21471084429669,2.39132804659979,1.845217208863));
#93049=CARTESIAN_POINT('Ctrl Pts',(-9.37556316853414,1.70818806618257,1.85730125071232));
#93050=CARTESIAN_POINT('Ctrl Pts',(-9.45056093730129,1.2271902920474,1.86574950853255));
#93051=CARTESIAN_POINT('Ctrl Pts',(-9.50782497638863,0.495479466538355,
1.87812526961015));
#93052=CARTESIAN_POINT('Ctrl Pts',(-9.51750331214565,0.247723883817967,
1.88224283254318));
#93053=CARTESIAN_POINT('Ctrl Pts',(-9.51749999914974,-0.000127219278908824,
1.88630958681444));
#93054=CARTESIAN_POINT('Ctrl Pts',(-9.5175,4.28129753871076E-14,1.6143576464275));
#93055=CARTESIAN_POINT('Ctrl Pts',(-9.5175,0.264761493468821,1.60982716935015));
#93056=CARTESIAN_POINT('Ctrl Pts',(-9.50645215077221,0.52940754234781,1.60523476644285));
#93057=CARTESIAN_POINT('Ctrl Pts',(-9.45622299125277,1.1299673470939,1.59483331464208));
#93058=CARTESIAN_POINT('Ctrl Pts',(-9.41014897222432,1.46494985718653,1.58905042110134));
#93059=CARTESIAN_POINT('Ctrl Pts',(-9.28756606562341,2.10259528478863,1.57815890498963));
#93060=CARTESIAN_POINT('Ctrl Pts',(-9.21379885947898,2.40534870654743,1.57303816255892));
#93061=CARTESIAN_POINT('Ctrl Pts',(-9.02445704727179,3.04434376581629,1.56220410346681));
#93062=CARTESIAN_POINT('Ctrl Pts',(-8.90462410263793,3.37883442441522,1.55651873363559));
#93063=CARTESIAN_POINT('Ctrl Pts',(-8.69937575696479,3.86436089007564,1.54789936944457));
#93064=CARTESIAN_POINT('Ctrl Pts',(-8.62807894391787,4.02102942210529,1.54505365113255));
#93065=CARTESIAN_POINT('Ctrl Pts',(-8.35010441820943,4.59037334156988,1.53436890401086));
#93066=CARTESIAN_POINT('Ctrl Pts',(-8.11774221915953,4.98979305431516,1.52629305526653));
#93067=CARTESIAN_POINT('Ctrl Pts',(-7.68513605518206,5.62268586176387,1.51313169187247));
#93068=CARTESIAN_POINT('Ctrl Pts',(-7.50093240933939,5.86616802154874,1.50795966199409));
#93069=CARTESIAN_POINT('Ctrl Pts',(-7.06613244881998,6.38685125320868,1.4966666137911));
#93070=CARTESIAN_POINT('Ctrl Pts',(-6.81027080041151,6.65900215906905,1.49060605364395));
#93071=CARTESIAN_POINT('Ctrl Pts',(-6.29712230193908,7.14422527189098,1.47918850938335));
#93072=CARTESIAN_POINT('Ctrl Pts',(-6.04331432663649,7.36016666724828,1.47383042745737));
#93073=CARTESIAN_POINT('Ctrl Pts',(-5.6322595852246,7.67427073357231,1.46522512280138));
#93074=CARTESIAN_POINT('Ctrl Pts',(-5.48258691858798,7.7819032765208,1.46209448304978));
#93075=CARTESIAN_POINT('Ctrl Pts',(-5.07523783550537,8.05724767519826,1.45366293975163));
#93076=CARTESIAN_POINT('Ctrl Pts',(-4.8124017716518,8.21693791717208,1.44832219459679));
#93077=CARTESIAN_POINT('Ctrl Pts',(-4.2586334686578,8.51769034242477,1.43747821489138));
#93078=CARTESIAN_POINT('Ctrl Pts',(-3.96731105771364,8.65721969523227,1.43198855888441));
#93079=CARTESIAN_POINT('Ctrl Pts',(-3.2986213280283,8.93663461916127,1.4198985575001));
#93080=CARTESIAN_POINT('Ctrl Pts',(-2.91833753917993,9.06794621845669,1.41337503165388));
#93081=CARTESIAN_POINT('Ctrl Pts',(-2.20248782327214,9.26541472798439,1.40137128161269));
#93082=CARTESIAN_POINT('Ctrl Pts',(-1.86945804271425,9.33830746283857,1.39588685475002));
#93083=CARTESIAN_POINT('Ctrl Pts',(-1.31991486168347,9.42800889821091,1.38658964569432));
#93084=CARTESIAN_POINT('Ctrl Pts',(-1.10546520227142,9.45555246712023,1.38289407822976));
#93085=CARTESIAN_POINT('Ctrl Pts',(-0.314877301443695,9.52982963798949,
1.3692211811255));
#93086=CARTESIAN_POINT('Ctrl Pts',(0.264249849316982,9.53136856804752,1.35918938483596));
#93087=CARTESIAN_POINT('Ctrl Pts',(1.23865909769983,9.44503907041455,1.34286553088786));
#93088=CARTESIAN_POINT('Ctrl Pts',(1.63476269772059,9.38459333124713,1.3363655596436));
#93089=CARTESIAN_POINT('Ctrl Pts',(2.36432459889632,9.22565740458415,1.32429520373077));
#93090=CARTESIAN_POINT('Ctrl Pts',(2.69848705746629,9.13350697884167,1.31872143531038));
#93091=CARTESIAN_POINT('Ctrl Pts',(3.23571916524843,8.95329268710885,1.30925687709717));
#93092=CARTESIAN_POINT('Ctrl Pts',(3.44206362159594,8.87600840896958,1.30548830653284));
#93093=CARTESIAN_POINT('Ctrl Pts',(4.1715046915936,8.5735384260078,1.29188631534715));
#93094=CARTESIAN_POINT('Ctrl Pts',(4.67684682199093,8.30867797420584,1.2820072251757));
#93095=CARTESIAN_POINT('Ctrl Pts',(5.50126233918816,7.77741213732115,1.26563560574402));
#93096=CARTESIAN_POINT('Ctrl Pts',(5.83223738557223,7.53239906320663,1.25896018315535));
#93097=CARTESIAN_POINT('Ctrl Pts',(6.40222011234015,7.05029898061277,1.24689317110066));
#93098=CARTESIAN_POINT('Ctrl Pts',(6.64650562897295,6.82049104681496,1.24149509720949));
#93099=CARTESIAN_POINT('Ctrl Pts',(7.02495406145976,6.42479064197713,1.23235569169641));
#93100=CARTESIAN_POINT('Ctrl Pts',(7.16657105544514,6.26643218831147,1.22872670363757));
#93101=CARTESIAN_POINT('Ctrl Pts',(7.67858620869205,5.65380873401212,1.21498385977178));
#93102=CARTESIAN_POINT('Ctrl Pts',(8.01207445502674,5.17038849466746,1.20480683163048));
#93103=CARTESIAN_POINT('Ctrl Pts',(8.49231149569004,4.31502135256395,1.18844265166231));
#93104=CARTESIAN_POINT('Ctrl Pts',(8.66402535120185,3.95896832027939,1.182029016208));
#93105=CARTESIAN_POINT('Ctrl Pts',(8.93698042392705,3.28949984757043,1.17034139351991));
#93106=CARTESIAN_POINT('Ctrl Pts',(9.04504697864608,2.9795219455272,1.165061024439));
#93107=CARTESIAN_POINT('Ctrl Pts',(9.18810202132165,2.48898493300804,1.15656353112484));
#93108=CARTESIAN_POINT('Ctrl Pts',(9.23423912596728,2.31194531108307,1.15345793506077));
#93109=CARTESIAN_POINT('Ctrl Pts',(9.34280345625023,1.84001094025654,1.14515576011107));
#93110=CARTESIAN_POINT('Ctrl Pts',(9.39637539755217,1.5432907537012,1.13992055245723));
#93111=CARTESIAN_POINT('Ctrl Pts',(9.47862265951926,0.91970829998119,1.12909159986179));
#93112=CARTESIAN_POINT('Ctrl Pts',(9.50466385171467,0.592889640484698,1.12351550500536));
#93113=CARTESIAN_POINT('Ctrl Pts',(9.52501408299184,-0.136663810044939,
1.11133484460832));
#93114=CARTESIAN_POINT('Ctrl Pts',(9.51073273060235,-0.539012884039947,
1.10480407896102));
#93115=CARTESIAN_POINT('Ctrl Pts',(9.43694723227837,-1.28303735839833,1.09271763727561));
#93116=CARTESIAN_POINT('Ctrl Pts',(9.38416061643455,-1.62471051488265,1.08715805100552));
#93117=CARTESIAN_POINT('Ctrl Pts',(9.26762675434479,-2.17764310362065,1.07772026221169));
#93118=CARTESIAN_POINT('Ctrl Pts',(9.21491349662537,-2.3909000773591,1.07396348437403));
#93119=CARTESIAN_POINT('Ctrl Pts',(9.00038329897622,-3.14566184874142,1.06044851978369));
#93120=CARTESIAN_POINT('Ctrl Pts',(8.79779626617351,-3.67435460839335,1.05064288044717));
#93121=CARTESIAN_POINT('Ctrl Pts',(8.38391734895862,-4.52048277085164,1.03491019560779));
#93122=CARTESIAN_POINT('Ctrl Pts',(8.19836247541849,-4.84888534068094,1.02877269366243));
#93123=CARTESIAN_POINT('Ctrl Pts',(7.79566940206617,-5.47207912857135,1.01677089600701));
#93124=CARTESIAN_POINT('Ctrl Pts',(7.5800333126896,-5.76707923219049,1.01091158062097));
#93125=CARTESIAN_POINT('Ctrl Pts',(7.2249739602744,-6.19838841220579,1.00160584477148));
#93126=CARTESIAN_POINT('Ctrl Pts',(7.09743288508585,-6.34402968623607,0.998310764385156));
#93127=CARTESIAN_POINT('Ctrl Pts',(6.66895602783513,-6.80420866893346,0.987512098119311));
#93128=CARTESIAN_POINT('Ctrl Pts',(6.35086776959386,-7.10202171304785,0.979931314721207));
#93129=CARTESIAN_POINT('Ctrl Pts',(5.7997222059246,-7.55129863768712,0.967835529235672));
#93130=CARTESIAN_POINT('Ctrl Pts',(5.57844989191139,-7.71620288040075,0.963213636922584));
#93131=CARTESIAN_POINT('Ctrl Pts',(5.23552847678581,-7.9492965527016,0.956370800280709));
#93132=CARTESIAN_POINT('Ctrl Pts',(5.11903587400575,-8.02480815752726,0.954097640522328));
#93133=CARTESIAN_POINT('Ctrl Pts',(4.65190413314435,-8.31329522290424,0.945154462255196));
#93134=CARTESIAN_POINT('Ctrl Pts',(4.28930622862586,-8.50605306174694,0.938605970301876));
#93135=CARTESIAN_POINT('Ctrl Pts',(3.76674501507339,-8.74191289695796,0.929197005362934));
#93136=CARTESIAN_POINT('Ctrl Pts',(3.61638438658702,-8.80517876324774,0.926485078033962));
#93137=CARTESIAN_POINT('Ctrl Pts',(3.05140223158275,-9.0259868013857,0.916221382627433));
#93138=CARTESIAN_POINT('Ctrl Pts',(2.62755500426413,-9.15835410790396,0.908468029780455));
#93139=CARTESIAN_POINT('Ctrl Pts',(1.89931565720075,-9.33104462015247,0.895619263562257));
#93140=CARTESIAN_POINT('Ctrl Pts',(1.59939445150892,-9.387104603334,0.890450771772977));
#93141=CARTESIAN_POINT('Ctrl Pts',(0.927005229180607,-9.47961924549221,
0.879151891938266));
#93142=CARTESIAN_POINT('Ctrl Pts',(0.554031379839827,-9.50871023728457,
0.873082597931436));
#93143=CARTESIAN_POINT('Ctrl Pts',(-0.151533636219758,-9.5220799272509,
0.861673920852244));
#93144=CARTESIAN_POINT('Ctrl Pts',(-0.483481035362257,-9.51100478918671,
0.856333179038857));
#93145=CARTESIAN_POINT('Ctrl Pts',(-0.997464084631463,-9.46687471710456,
0.847752516089616));
#93146=CARTESIAN_POINT('Ctrl Pts',(-1.18026368524024,-9.44582594283233,
0.844628058884999));
#93147=CARTESIAN_POINT('Ctrl Pts',(-1.66507118868918,-9.37570848981499,
0.836228332183765));
#93148=CARTESIAN_POINT('Ctrl Pts',(-1.96551933731419,-9.31735508734775,
0.830913511219793));
#93149=CARTESIAN_POINT('Ctrl Pts',(-2.57730521635309,-9.16761980296353,
0.820073723258781));
#93150=CARTESIAN_POINT('Ctrl Pts',(-2.88783927625287,-9.07458767418222,
0.814563355697036));
#93151=CARTESIAN_POINT('Ctrl Pts',(-3.56973830841872,-8.83174310080167,
0.802486489628474));
#93152=CARTESIAN_POINT('Ctrl Pts',(-3.93762183158052,-8.67397565987705,
0.795993969897333));
#93153=CARTESIAN_POINT('Ctrl Pts',(-4.60216739881697,-8.33796906248207,
0.783956301026481));
#93154=CARTESIAN_POINT('Ctrl Pts',(-4.90116241004204,-8.16579920828296,
0.77840771084053));
#93155=CARTESIAN_POINT('Ctrl Pts',(-5.37386692839181,-7.85826929007571,
0.768989382474449));
#93156=CARTESIAN_POINT('Ctrl Pts',(-5.5533964324459,-7.7324400316803,0.765240411931296));
#93157=CARTESIAN_POINT('Ctrl Pts',(-6.18494761952274,-7.25644792347482,
0.751619593183426));
#93158=CARTESIAN_POINT('Ctrl Pts',(-6.6095536186583,-6.87193044407949,0.741699786648745));
#93159=CARTESIAN_POINT('Ctrl Pts',(-7.28716879695542,-6.13702774236959,
0.725014942153507));
#93160=CARTESIAN_POINT('Ctrl Pts',(-7.55570764647677,-5.80320800478434,
0.718081456810211));
#93161=CARTESIAN_POINT('Ctrl Pts',(-7.9734895773645,-5.20548378812184,0.706294202698439));
#93162=CARTESIAN_POINT('Ctrl Pts',(-8.13428214553769,-4.95045942633501,
0.701431470414448));
#93163=CARTESIAN_POINT('Ctrl Pts',(-8.37356853475163,-4.52771261325523,
0.693350862669414));
#93164=CARTESIAN_POINT('Ctrl Pts',(-8.45974468860711,-4.36457900772039,
0.690217683334457));
#93165=CARTESIAN_POINT('Ctrl Pts',(-8.67700828290358,-3.92265114541777,
0.68177272119757));
#93166=CARTESIAN_POINT('Ctrl Pts',(-8.79939504543731,-3.63982306623629,
0.67642097272025));
#93167=CARTESIAN_POINT('Ctrl Pts',(-9.02134429858824,-3.04992120864695,
0.665575716783025));
#93168=CARTESIAN_POINT('Ctrl Pts',(-9.1194412350741,-2.74271142732486,0.660095335448847));
#93169=CARTESIAN_POINT('Ctrl Pts',(-9.2659594934796,-2.18814063947224,0.650526801736613));
#93170=CARTESIAN_POINT('Ctrl Pts',(-9.32050527252575,-1.94271640788156,
0.646399466767897));
#93171=CARTESIAN_POINT('Ctrl Pts',(-9.44720738662408,-1.24283118030191,
0.634827590642327));
#93172=CARTESIAN_POINT('Ctrl Pts',(-9.49622449932472,-0.784901646146257,
0.62751102293297));
#93173=CARTESIAN_POINT('Ctrl Pts',(-9.5156462769228,-0.216878343335995,
0.618080772081449));
#93174=CARTESIAN_POINT('Ctrl Pts',(-9.51749935373479,-0.10847143398478,
0.616260847688148));
#93175=CARTESIAN_POINT('Ctrl Pts',(-9.51749999983099,-5.67194278485892E-5,
0.614423068612269));
#93176=CARTESIAN_POINT('Origin',(0.,0.,-2.20842344717745));
#93177=CARTESIAN_POINT('',(-10.0766107346517,-0.000128399830713298,1.29157655282254));
#93178=CARTESIAN_POINT('Ctrl Pts',(6.13570130491008,-7.99149349282772,0.645787560181147));
#93179=CARTESIAN_POINT('Ctrl Pts',(6.72491755688915,-7.53931401154324,0.65751697232479));
#93180=CARTESIAN_POINT('Ctrl Pts',(8.44842283158552,-5.88942327299567,0.694975254262141));
#93181=CARTESIAN_POINT('Ctrl Pts',(10.2494764494997,-2.18403346540847,0.758162405993196));
#93182=CARTESIAN_POINT('Ctrl Pts',(10.0857330432995,2.846007611683,0.835349015374309));
#93183=CARTESIAN_POINT('Ctrl Pts',(7.5959232928945,7.21967588414949,0.912535624755426));
#93184=CARTESIAN_POINT('Ctrl Pts',(3.35427052456325,9.92827474644192,0.989722234136537));
#93185=CARTESIAN_POINT('Ctrl Pts',(-1.6609755673321,10.3471218520573,1.06690884351765));
#93186=CARTESIAN_POINT('Ctrl Pts',(-6.29315189771966,8.37961869672186,1.14409545289877));
#93187=CARTESIAN_POINT('Ctrl Pts',(-9.3792698747427,4.59561112228605,1.21898468933373));
#93188=CARTESIAN_POINT('Ctrl Pts',(-10.075640881915,1.48301858797571,1.26814505597499));
#93189=CARTESIAN_POINT('Ctrl Pts',(-10.0766107346517,-0.000128399830713298,
1.29157655282254));
#93190=CARTESIAN_POINT('Ctrl Pts',(-10.0766107346517,-0.000128399830713298,
1.29157655282254));
#93191=CARTESIAN_POINT('Ctrl Pts',(-10.076705825181,-0.145545561487931,
1.2938739257687));
#93192=CARTESIAN_POINT('Ctrl Pts',(-10.0390551969694,-1.91947760598252,
1.32190016850855));
#93193=CARTESIAN_POINT('Ctrl Pts',(-9.05094988379608,-5.28224162230782,
1.37565528104211));
#93194=CARTESIAN_POINT('Ctrl Pts',(-5.54472111010466,-8.89257207845922,
1.45284189042322));
#93195=CARTESIAN_POINT('Ctrl Pts',(-0.759716774784057,-10.4520141971627,
1.53002849980434));
#93196=CARTESIAN_POINT('Ctrl Pts',(3.37337104626303,-9.74283791843435,1.59434403545769));
#93197=CARTESIAN_POINT('Ctrl Pts',(5.48989350430804,-8.4873022126398,1.63293070131733));
#93198=CARTESIAN_POINT('Ctrl Pts',(6.13568652661064,-7.99147452837712,1.64578849738327));
#93199=CARTESIAN_POINT('',(-10.075999998343,-0.000182733646683074,1.20842344717745));
#93200=CARTESIAN_POINT('Ctrl Pts',(-10.07551961303,-0.000183021653669313,
1.2084234518637));
#93201=CARTESIAN_POINT('Ctrl Pts',(-10.0759095234531,-0.560797522139529,
1.21727755127508));
#93202=CARTESIAN_POINT('Ctrl Pts',(-9.89602121837179,-2.75023774228373,
1.25186052048016));
#93203=CARTESIAN_POINT('Ctrl Pts',(-8.33073300645692,-6.35772433572561,
1.31217235947894));
#93204=CARTESIAN_POINT('Ctrl Pts',(-4.40617793665544,-9.50827888762232,
1.38935896886006));
#93205=CARTESIAN_POINT('Ctrl Pts',(0.534571201485628,-10.4659450075294,
1.46654557824117));
#93206=CARTESIAN_POINT('Ctrl Pts',(4.13955618575929,-9.37633040870524,1.52430557873297));
#93207=CARTESIAN_POINT('Ctrl Pts',(5.81987160391175,-8.2353133147925,1.55633670943106));
#93208=CARTESIAN_POINT('Ctrl Pts',(6.13611323687281,-7.99203043615932,1.56263897033545));
#93209=CARTESIAN_POINT('Ctrl Pts',(6.13615379320823,-7.99208312182101,0.562637467686473));
#93210=CARTESIAN_POINT('Ctrl Pts',(6.33192762783051,-7.8417720778019,0.566535835994544));
#93211=CARTESIAN_POINT('Ctrl Pts',(6.52218751259431,-7.68425508730315,0.570434204302615));
#93212=CARTESIAN_POINT('Ctrl Pts',(6.70641049035147,-7.51996238919476,0.574332572610686));
#93213=CARTESIAN_POINT('Ctrl Pts',(6.89064675943679,-7.35565783768898,0.578231222178418));
#93214=CARTESIAN_POINT('Ctrl Pts',(7.06884504128707,-7.18457678496899,0.582129871746151));
#93215=CARTESIAN_POINT('Ctrl Pts',(7.24051686463347,-7.00718856125324,0.586028521313884));
#93216=CARTESIAN_POINT('Ctrl Pts',(7.41218583111252,-6.82980328953401,0.589927106002451));
#93217=CARTESIAN_POINT('Ctrl Pts',(7.57732836392031,-6.6461112582751,0.593825690691018));
#93218=CARTESIAN_POINT('Ctrl Pts',(7.73549362466678,-6.45661787492024,0.597724275379586));
#93219=CARTESIAN_POINT('Ctrl Pts',(7.89369145557608,-6.26708547016258,0.601623662883749));
#93220=CARTESIAN_POINT('Ctrl Pts',(8.04490896415257,-6.07174953956683,0.605523050387913));
#93221=CARTESIAN_POINT('Ctrl Pts',(8.1887354273855,-5.87114878880459,0.609422437892076));
#93222=CARTESIAN_POINT('Ctrl Pts',(8.28795976554738,-5.73275647711348,0.612112583611023));
#93223=CARTESIAN_POINT('Ctrl Pts',(8.38366719749756,-5.59185907723408,0.61480272932997));
#93224=CARTESIAN_POINT('Ctrl Pts',(8.47573470011338,-5.44864178427009,0.617492875048916));
#93225=CARTESIAN_POINT('Ctrl Pts',(8.60917882552726,-5.24106032652736,0.6213920157066));
#93226=CARTESIAN_POINT('Ctrl Pts',(8.73501259619979,-5.02854433367632,0.625291156364284));
#93227=CARTESIAN_POINT('Ctrl Pts',(8.85288535627763,-4.81167298022268,0.629190297021968));
#93228=CARTESIAN_POINT('Ctrl Pts',(8.97073876951656,-4.5948372225686,0.633088797701033));
#93229=CARTESIAN_POINT('Ctrl Pts',(9.08063364767773,-4.37364777613102,0.636987298380097));
#93230=CARTESIAN_POINT('Ctrl Pts',(9.1822648995648,-4.14870911419688,0.640885799059162));
#93231=CARTESIAN_POINT('Ctrl Pts',(9.2838857665332,-3.92379343702054,0.644783901380323));
#93232=CARTESIAN_POINT('Ctrl Pts',(9.37724457861858,-3.69512956318479,0.648682003701484));
#93233=CARTESIAN_POINT('Ctrl Pts',(9.46208363779331,-3.46334364904843,0.652580106022644));
#93234=CARTESIAN_POINT('Ctrl Pts',(9.5469290019391,-3.23154050931465,0.656478498038464));
#93235=CARTESIAN_POINT('Ctrl Pts',(9.62325324959217,-2.99661512640118,0.660376890054283));
#93236=CARTESIAN_POINT('Ctrl Pts',(9.69084754622438,-2.75921181423914,0.664275282070102));
#93237=CARTESIAN_POINT('Ctrl Pts',(9.75844109264562,-2.52181113695281,0.668173630818714));
#93238=CARTESIAN_POINT('Ctrl Pts',(9.81730480755064,-2.28193285402501,0.672071979567326));
#93239=CARTESIAN_POINT('Ctrl Pts',(9.86728006718831,-2.04023529909375,0.675970328315938));
#93240=CARTESIAN_POINT('Ctrl Pts',(9.91726533662121,-1.79848933334785,0.679869457884359));
#93241=CARTESIAN_POINT('Ctrl Pts',(9.9583585364723,-1.55492364035389,0.683768587452779));
#93242=CARTESIAN_POINT('Ctrl Pts',(9.99045213222051,-1.31020692785933,0.6876677170212));
#93243=CARTESIAN_POINT('Ctrl Pts',(10.0096900009765,-1.16351635338152,0.690004972824143));
#93244=CARTESIAN_POINT('Ctrl Pts',(10.0256951503675,-1.01641237119571,0.692342228627085));
#93245=CARTESIAN_POINT('Ctrl Pts',(10.0384533319705,-0.869040103707079,
0.694679484430028));
#93246=CARTESIAN_POINT('Ctrl Pts',(10.0597380023151,-0.623176686093138,
0.698578764188304));
#93247=CARTESIAN_POINT('Ctrl Pts',(10.0719888081203,-0.376495669821744,
0.702478043946578));
#93248=CARTESIAN_POINT('Ctrl Pts',(10.0751655531142,-0.129672963032486,
0.706377323704853));
#93249=CARTESIAN_POINT('Ctrl Pts',(10.0783417780477,0.117109336767591,0.710275965117666));
#93250=CARTESIAN_POINT('Ctrl Pts',(10.0724469041336,0.364033002303638,0.714174606530479));
#93251=CARTESIAN_POINT('Ctrl Pts',(10.0574928395634,0.61042098762322,0.718073247943291));
#93252=CARTESIAN_POINT('Ctrl Pts',(10.0425402983381,0.856783873821194,0.721971492208187));
#93253=CARTESIAN_POINT('Ctrl Pts',(10.0185304260666,1.10261091075286,0.725869736473084));
#93254=CARTESIAN_POINT('Ctrl Pts',(9.98552716731234,1.34722796544131,0.72976798073798));
#93255=CARTESIAN_POINT('Ctrl Pts',(9.95252144897754,1.59186325031002,0.733666515521032));
#93256=CARTESIAN_POINT('Ctrl Pts',(9.9105210393986,1.83528809624206,0.737565050304084));
#93257=CARTESIAN_POINT('Ctrl Pts',(9.85964157667784,2.076835087205,0.741463585087136));
#93258=CARTESIAN_POINT('Ctrl Pts',(9.8087626756148,2.31837941173388,0.745362076834313));
#93259=CARTESIAN_POINT('Ctrl Pts',(9.7490049769451,2.55804565053755,0.749260568581491));
#93260=CARTESIAN_POINT('Ctrl Pts',(9.68053507517198,2.7951773930048,0.753159060328668));
#93261=CARTESIAN_POINT('Ctrl Pts',(9.61205146960001,3.03235659582491,0.757058332333234));
#93262=CARTESIAN_POINT('Ctrl Pts',(9.53485225355829,3.26700002080037,0.7609576043378));
#93263=CARTESIAN_POINT('Ctrl Pts',(9.4491540555673,3.49846589724069,0.764856876342365));
#93264=CARTESIAN_POINT('Ctrl Pts',(9.39780452966456,3.6371579969173,0.767193282165289));
#93265=CARTESIAN_POINT('Ctrl Pts',(9.34340457618121,3.77470957192005,0.769529687988214));
#93266=CARTESIAN_POINT('Ctrl Pts',(9.28600918091763,3.91098574427386,0.771866093811138));
#93267=CARTESIAN_POINT('Ctrl Pts',(9.19022230922501,4.13841632779142,0.775765309135897));
#93268=CARTESIAN_POINT('Ctrl Pts',(9.08606241920951,4.36235890696156,0.779664524460656));
#93269=CARTESIAN_POINT('Ctrl Pts',(8.97380903247485,4.58219679287925,0.783563739785414));
#93270=CARTESIAN_POINT('Ctrl Pts',(8.86157404334637,4.80199864878514,0.787462316053927));
#93271=CARTESIAN_POINT('Ctrl Pts',(8.74124833222895,5.01769690638174,0.791360892322439));
#93272=CARTESIAN_POINT('Ctrl Pts',(8.61315804758224,5.22869815990264,0.795259468590952));
#93273=CARTESIAN_POINT('Ctrl Pts',(8.48508082841011,5.43967789085827,0.799157647196603));
#93274=CARTESIAN_POINT('Ctrl Pts',(8.34924076172232,5.64596133630848,0.803055825802255));
#93275=CARTESIAN_POINT('Ctrl Pts',(8.20600867413201,5.84698192575197,0.806954004407906));
#93276=CARTESIAN_POINT('Ctrl Pts',(8.0627659234321,6.04801748044951,0.810852473218821));
#93277=CARTESIAN_POINT('Ctrl Pts',(7.91213021163992,6.24378916769073,0.814750942029737));
#93278=CARTESIAN_POINT('Ctrl Pts',(7.75451496679167,6.43376045791293,0.818649410840652));
#93279=CARTESIAN_POINT('Ctrl Pts',(7.59690146465065,6.62372964767624,0.822547836547299));
#93280=CARTESIAN_POINT('Ctrl Pts',(7.43230876335148,6.80789835558618,0.826446262253945));
#93281=CARTESIAN_POINT('Ctrl Pts',(7.26119024091035,6.98576354347242,0.830344687960591));
#93282=CARTESIAN_POINT('Ctrl Pts',(7.09003745561853,7.16366434508584,0.834243894244209));
#93283=CARTESIAN_POINT('Ctrl Pts',(6.91235643113467,7.33525890347479,0.838143100527827));
#93284=CARTESIAN_POINT('Ctrl Pts',(6.72863798502884,7.50008045733024,0.842042306811444));
#93285=CARTESIAN_POINT('Ctrl Pts',(6.61853530976719,7.59885820341359,0.844379105605051));
#93286=CARTESIAN_POINT('Ctrl Pts',(6.5062649230313,7.69520406090904,0.846715904398658));
#93287=CARTESIAN_POINT('Ctrl Pts',(6.39193840722856,7.78902429051267,0.849052703192264));
#93288=CARTESIAN_POINT('Ctrl Pts',(6.20117049557353,7.94557493099018,0.852951940588631));
#93289=CARTESIAN_POINT('Ctrl Pts',(6.00462111121729,8.09513628796777,0.856851177984997));
#93290=CARTESIAN_POINT('Ctrl Pts',(5.80282504410468,8.23729309345682,0.860750415381363));
#93291=CARTESIAN_POINT('Ctrl Pts',(5.60106203859183,8.37942660844536,0.86464901393958));
#93292=CARTESIAN_POINT('Ctrl Pts',(5.39405429405047,8.51415783336777,0.868547612497796));
#93293=CARTESIAN_POINT('Ctrl Pts',(5.18236699596795,8.64111383555975,0.872446211056012));
#93294=CARTESIAN_POINT('Ctrl Pts',(4.97070128209821,8.76805689297238,0.876344412102514));
#93295=CARTESIAN_POINT('Ctrl Pts',(4.75435720631203,8.88722616742383,0.880242613149017));
#93296=CARTESIAN_POINT('Ctrl Pts',(4.53392696973158,8.99829329557226,0.884140814195519));
#93297=CARTESIAN_POINT('Ctrl Pts',(4.31348031909844,9.10936869419084,0.888039305516524));
#93298=CARTESIAN_POINT('Ctrl Pts',(4.08894714727352,9.21234061309443,0.891937796837528));
#93299=CARTESIAN_POINT('Ctrl Pts',(3.86094333935531,9.30692712608667,0.895836288158533));
#93300=CARTESIAN_POINT('Ctrl Pts',(3.63294205227916,9.40151259331717,0.899734736377271));
#93301=CARTESIAN_POINT('Ctrl Pts',(3.40147046404377,9.48771273523951,0.903633184596009));
#93302=CARTESIAN_POINT('Ctrl Pts',(3.16716418952138,9.56529387926024,0.907531632814748));
#93303=CARTESIAN_POINT('Ctrl Pts',(2.93281100895227,9.64289055434079,0.911430861468388));
#93304=CARTESIAN_POINT('Ctrl Pts',(2.69562227260788,9.71186469568564,0.915330090122028));
#93305=CARTESIAN_POINT('Ctrl Pts',(2.45624980566499,9.77203217822018,0.919229318775668));
#93306=CARTESIAN_POINT('Ctrl Pts',(2.31280267311102,9.80808834187509,0.921565983374903));
#93307=CARTESIAN_POINT('Ctrl Pts',(2.16857161230189,9.84098284917659,0.923902647974138));
#93308=CARTESIAN_POINT('Ctrl Pts',(2.02369901330553,9.87068479405285,0.926239312573372));
#93309=CARTESIAN_POINT('Ctrl Pts',(1.78194750865926,9.92024896225652,0.930138546704824));
#93310=CARTESIAN_POINT('Ctrl Pts',(1.53833954659131,9.96093457202526,0.934037780836275));
#93311=CARTESIAN_POINT('Ctrl Pts',(1.29354184001541,9.9926235548093,0.937937014967726));
#93312=CARTESIAN_POINT('Ctrl Pts',(1.04878424115534,10.0243073456627,0.941835610247708));
#93313=CARTESIAN_POINT('Ctrl Pts',(0.802837563134465,10.0469974163812,0.94573420552769));
#93314=CARTESIAN_POINT('Ctrl Pts',(0.556375673130158,10.0606273219094,0.949632800807672));
#93315=CARTESIAN_POINT('Ctrl Pts',(0.309938913293379,10.0742558376819,0.953530998572434));
#93316=CARTESIAN_POINT('Ctrl Pts',(0.0629873244840109,10.0788260175434,
0.957429196337196));
#93317=CARTESIAN_POINT('Ctrl Pts',(-0.18380210348543,10.0743234406462,0.961327394101958));
#93318=CARTESIAN_POINT('Ctrl Pts',(-0.430609909472234,10.0698205284493,
0.965225882159325));
#93319=CARTESIAN_POINT('Ctrl Pts',(-0.677255251833692,10.0562435117472,
0.969124370216694));
#93320=CARTESIAN_POINT('Ctrl Pts',(-0.923061836352939,10.0336300931552,
0.973022858274062));
#93321=CARTESIAN_POINT('Ctrl Pts',(-1.16886570418859,10.0110169244893,0.976921303244876));
#93322=CARTESIAN_POINT('Ctrl Pts',(-1.41383055543933,9.97936758131172,0.980819748215689));
#93323=CARTESIAN_POINT('Ctrl Pts',(-1.65728513653646,9.93877165328872,0.984718193186504));
#93324=CARTESIAN_POINT('Ctrl Pts',(-1.90078845796559,9.89816759784005,0.988617418637608));
#93325=CARTESIAN_POINT('Ctrl Pts',(-2.14278063006369,9.84861342389478,0.992516644088713));
#93326=CARTESIAN_POINT('Ctrl Pts',(-2.38259915674125,9.79025011214197,0.996415869539818));
#93327=CARTESIAN_POINT('Ctrl Pts',(-2.52631491628535,9.75527480062511,0.99875255367804));
#93328=CARTESIAN_POINT('Ctrl Pts',(-2.66925026464293,9.71713690675989,1.00108923781626));
#93329=CARTESIAN_POINT('Ctrl Pts',(-2.81126481973547,9.67587547012247,1.00342592195448));
#93330=CARTESIAN_POINT('Ctrl Pts',(-3.0482449078802,9.60702239457016,1.00732515335849));
#93331=CARTESIAN_POINT('Ctrl Pts',(-3.28272829929941,9.52944914124046,1.01122438476249));
#93332=CARTESIAN_POINT('Ctrl Pts',(-3.51407012138599,9.44336206983415,1.01512361616649));
#93333=CARTESIAN_POINT('Ctrl Pts',(-3.74537403774056,9.35728910393383,1.01902220867512));
#93334=CARTESIAN_POINT('Ctrl Pts',(-3.97353715134841,9.26270520197138,1.02292080118374));
#93335=CARTESIAN_POINT('Ctrl Pts',(-4.19793232657444,9.1598657294472,1.02681939369237));
#93336=CARTESIAN_POINT('Ctrl Pts',(-4.42230461957367,9.05703674376228,1.03071758865021));
#93337=CARTESIAN_POINT('Ctrl Pts',(-4.64290948820314,8.94595398455712,1.03461578360805));
#93338=CARTESIAN_POINT('Ctrl Pts',(-4.85914128733917,8.82692029813773,1.03851397856589));
#93339=CARTESIAN_POINT('Ctrl Pts',(-5.07538918704402,8.70787774849809,1.04241246378241));
#93340=CARTESIAN_POINT('Ctrl Pts',(-5.28726312115754,8.58088322060709,1.04631094899893));
#93341=CARTESIAN_POINT('Ctrl Pts',(-5.49418235928347,8.4462853493674,1.05020943421545));
#93342=CARTESIAN_POINT('Ctrl Pts',(-5.70109930973822,8.31168896622361,1.05410787633084));
#93343=CARTESIAN_POINT('Ctrl Pts',(-5.90306144133676,8.16948956156915,1.05800631844623));
#93344=CARTESIAN_POINT('Ctrl Pts',(-6.09951667220483,8.02007932413984,1.06190476056162));
#93345=CARTESIAN_POINT('Ctrl Pts',(-6.29601123380888,7.87063917447772,1.06580398315304));
#93346=CARTESIAN_POINT('Ctrl Pts',(-6.48699646955251,7.71398547575149,1.06970320574446));
#93347=CARTESIAN_POINT('Ctrl Pts',(-6.67195200307348,7.55055179895376,1.07360242833587));
#93348=CARTESIAN_POINT('Ctrl Pts',(-6.78279096391377,7.4526103177895,1.07593912933578));
#93349=CARTESIAN_POINT('Ctrl Pts',(-6.89146511561747,7.35223472945497,1.0782758303357));
#93350=CARTESIAN_POINT('Ctrl Pts',(-6.99786846164796,7.24952501847347,1.08061253133561));
#93351=CARTESIAN_POINT('Ctrl Pts',(-7.17542289291094,7.07813412712613,1.08451176601712));
#93352=CARTESIAN_POINT('Ctrl Pts',(-7.34670327209188,6.90019254495825,1.08841100069863));
#93353=CARTESIAN_POINT('Ctrl Pts',(-7.51123529203221,6.71618346888542,1.09231023538014));
#93354=CARTESIAN_POINT('Ctrl Pts',(-7.67574035495956,6.53220454095674,1.09620883120898));
#93355=CARTESIAN_POINT('Ctrl Pts',(-7.83349908025185,6.34216031129303,1.10010742703783));
#93356=CARTESIAN_POINT('Ctrl Pts',(-7.98407569837239,6.14656906270966,1.10400602286667));
#93357=CARTESIAN_POINT('Ctrl Pts',(-8.13463696303662,5.95099775747292,1.10790422117748));
#93358=CARTESIAN_POINT('Ctrl Pts',(-8.27801741291023,5.74988078341287,1.1118024194883));
#93359=CARTESIAN_POINT('Ctrl Pts',(-8.41382242583546,5.54376841025202,1.11570061779911));
#93360=CARTESIAN_POINT('Ctrl Pts',(-8.54963755165739,5.33764068866558,1.11959910639432));
#93361=CARTESIAN_POINT('Ctrl Pts',(-8.67787595768428,5.12651705582506,1.12349759498954));
#93362=CARTESIAN_POINT('Ctrl Pts',(-8.79818640959344,4.91097667496449,1.12739608358475));
#93363=CARTESIAN_POINT('Ctrl Pts',(-8.91849553164639,4.69543867658783,1.13129452908787));
#93364=CARTESIAN_POINT('Ctrl Pts',(-9.03087674088284,4.47548427217523,1.13519297459099));
#93365=CARTESIAN_POINT('Ctrl Pts',(-9.13502445222196,4.25171780076087,1.13909142009411));
#93366=CARTESIAN_POINT('Ctrl Pts',(-9.23919301391776,4.02790653133145,1.14299064606545));
#93367=CARTESIAN_POINT('Ctrl Pts',(-9.33512466596635,3.80028192242132,1.14688987203679));
#93368=CARTESIAN_POINT('Ctrl Pts',(-9.42256116463429,3.56947014257379,1.15078909800813));
#93369=CARTESIAN_POINT('Ctrl Pts',(-9.47495905030496,3.43115205532025,1.153125778911));
#93370=CARTESIAN_POINT('Ctrl Pts',(-9.52430706016383,3.29168977936706,1.15546245981386));
#93371=CARTESIAN_POINT('Ctrl Pts',(-9.57055803352992,3.15122118024678,1.15779914071672));
#93372=CARTESIAN_POINT('Ctrl Pts',(-9.64777480921259,2.91670649829887,1.16170026867116));
#93373=CARTESIAN_POINT('Ctrl Pts',(-9.71637906497317,2.67931785308615,1.16560139662559));
#93374=CARTESIAN_POINT('Ctrl Pts',(-9.77617606632402,2.43970439197731,1.16950252458003));
#93375=CARTESIAN_POINT('Ctrl Pts',(-9.83596427335629,2.20012617071438,1.1734030787973));
#93376=CARTESIAN_POINT('Ctrl Pts',(-9.88694774353637,1.95832405617931,1.17730363301457));
#93377=CARTESIAN_POINT('Ctrl Pts',(-9.92898217526058,1.71496033871275,1.18120418723184));
#93378=CARTESIAN_POINT('Ctrl Pts',(-9.97101121735301,1.4716278252085,1.18510424132219));
#93379=CARTESIAN_POINT('Ctrl Pts',(-10.0040934654087,1.22673438257842,1.18900429541253));
#93380=CARTESIAN_POINT('Ctrl Pts',(-10.0281359350344,0.980951409841928,
1.19290434950288));
#93381=CARTESIAN_POINT('Ctrl Pts',(-10.0521781282351,0.735171262962186,
1.19680435875288));
#93382=CARTESIAN_POINT('Ctrl Pts',(-10.067180722547,0.488501882977814,1.20070436800288));
#93383=CARTESIAN_POINT('Ctrl Pts',(-10.0731025921405,0.241619883725561,
1.20460437725288));
#93384=CARTESIAN_POINT('Ctrl Pts',(-10.0750355819202,0.161033782700128,
1.20587740056107));
#93385=CARTESIAN_POINT('Ctrl Pts',(-10.0760014602083,0.0804250515856432,
1.20715042386926));
#93386=CARTESIAN_POINT('Ctrl Pts',(-10.075999998343,-0.000182733646683074,
1.20842344717745));
#93387=CARTESIAN_POINT('Origin',(-12.,0.,2.));
#93388=CARTESIAN_POINT('',(-13.,1.22464679914735E-16,4.));
#93389=CARTESIAN_POINT('Origin',(-12.,0.,4.));
#93390=CARTESIAN_POINT('',(-13.,1.22464679914735E-16,2.77555756156289E-16));
#93391=CARTESIAN_POINT('',(-13.,1.22464679914735E-16,2.));
#93392=CARTESIAN_POINT('Origin',(-12.,0.,0.));
#93393=CARTESIAN_POINT('Origin',(12.,0.,2.));
#93394=CARTESIAN_POINT('',(11.,1.22464679914735E-16,4.));
#93395=CARTESIAN_POINT('Origin',(12.,0.,4.));
#93396=CARTESIAN_POINT('',(11.,1.22464679914735E-16,2.77555756156289E-16));
#93397=CARTESIAN_POINT('',(11.,1.22464679914735E-16,2.));
#93398=CARTESIAN_POINT('Origin',(12.,0.,0.));
#93399=CARTESIAN_POINT('Ctrl Pts',(7.17621738932614,-6.25041224556232,0.000500910460653174));
#93400=CARTESIAN_POINT('Ctrl Pts',(8.18687236526029,-5.09006444337945,0.0262352698176417));
#93401=CARTESIAN_POINT('Ctrl Pts',(9.63395471253335,-2.27150058536375,0.0776984989683351));
#93402=CARTESIAN_POINT('Ctrl Pts',(9.58138228729352,2.48258398187168,0.154890597912733));
#93403=CARTESIAN_POINT('Ctrl Pts',(7.31935428374419,6.66274001420286,0.232077207293848));
#93404=CARTESIAN_POINT('Ctrl Pts',(3.36913192154157,9.30677822701765,0.309263816674962));
#93405=CARTESIAN_POINT('Ctrl Pts',(-1.35804311095471,9.80414545245253,0.386450426056077));
#93406=CARTESIAN_POINT('Ctrl Pts',(-5.77204792492632,8.04051749446169,0.463637035437191));
#93407=CARTESIAN_POINT('Ctrl Pts',(-8.85483151763869,4.42244483853405,0.540823644818305));
#93408=CARTESIAN_POINT('Ctrl Pts',(-9.89543967406733,-0.215540505644021,
0.61801025419942));
#93409=CARTESIAN_POINT('Ctrl Pts',(-8.65386430243906,-4.80383258549442,
0.695196863580534));
#93410=CARTESIAN_POINT('Ctrl Pts',(-5.41645587973474,-8.28421130130496,
0.772383472961649));
#93411=CARTESIAN_POINT('Ctrl Pts',(-0.929852480502083,-9.85401182891119,
0.849570082342763));
#93412=CARTESIAN_POINT('Ctrl Pts',(3.77120163523642,-9.15118560282794,0.926756691723877));
#93413=CARTESIAN_POINT('Ctrl Pts',(7.60250616986962,-6.33782826253284,1.00394330110499));
#93414=CARTESIAN_POINT('Ctrl Pts',(9.68044931280096,-2.06278099798744,1.0811299104861));
#93415=CARTESIAN_POINT('Ctrl Pts',(9.52579656035691,2.68800387653829,1.15831651986722));
#93416=CARTESIAN_POINT('Ctrl Pts',(7.17421526680798,6.81885624067874,1.23550312924833));
#93417=CARTESIAN_POINT('Ctrl Pts',(3.16804921250801,9.37707998257651,1.31268973862945));
#93418=CARTESIAN_POINT('Ctrl Pts',(-1.5687620600508,9.77267366930781,1.38987634801056));
#93419=CARTESIAN_POINT('Ctrl Pts',(-5.9437707149038,7.91440172128742,1.46706295739167));
#93420=CARTESIAN_POINT('Ctrl Pts',(-8.94797124967819,4.23083626353518,1.54424956677279));
#93421=CARTESIAN_POINT('Ctrl Pts',(-9.88850677017832,-0.42848432033699,
1.6214361761539));
#93422=CARTESIAN_POINT('Ctrl Pts',(-8.54846215945662,-4.98898383099503,
1.69862278553501));
#93423=CARTESIAN_POINT('Ctrl Pts',(-5.23689106701696,-8.39887712217299,
1.77580939491613));
#93424=CARTESIAN_POINT('Ctrl Pts',(-0.717539063250466,-9.87174263493707,
1.85299600429724));
#93425=CARTESIAN_POINT('Ctrl Pts',(3.96729852598773,-9.06789431817403,1.93018261367836));
#93426=CARTESIAN_POINT('Ctrl Pts',(7.73716053739322,-6.17272320596467,2.00736922305947));
#93427=CARTESIAN_POINT('Ctrl Pts',(9.7226060531113,-1.85394080142852,2.08455583244059));
#93428=CARTESIAN_POINT('Ctrl Pts',(9.46573301557702,2.89241481066607,2.1617424418217));
#93429=CARTESIAN_POINT('Ctrl Pts',(7.02578389278733,6.9716946039717,2.23892905120282));
#93430=CARTESIAN_POINT('Ctrl Pts',(2.96548262493255,9.4430968310228,2.31611566058393));
#93431=CARTESIAN_POINT('Ctrl Pts',(-1.77874604604193,9.7366435419793,2.39330226996505));
#93432=CARTESIAN_POINT('Ctrl Pts',(-6.11274362884173,7.78463424226082,2.47048887934616));
#93433=CARTESIAN_POINT('Ctrl Pts',(-9.03696297170373,4.03725961627666,2.54767548872727));
#93434=CARTESIAN_POINT('Ctrl Pts',(-9.87699319615832,-0.641225670598249,
2.62486209810839));
#93435=CARTESIAN_POINT('Ctrl Pts',(-8.4390986575348,-5.17182548091403,2.7020487074895));
#93436=CARTESIAN_POINT('Ctrl Pts',(-5.05490007275752,-8.50965041751702,
2.77923531687063));
#93437=CARTESIAN_POINT('Ctrl Pts',(-0.504893047272655,-9.88489999585637,
2.85642192625173));
#93438=CARTESIAN_POINT('Ctrl Pts',(4.16155714909012,-8.98040127960293,2.93360853563285));
#93439=CARTESIAN_POINT('Ctrl Pts',(7.86823001667005,-6.00475821472291,3.01079514501396));
#93440=CARTESIAN_POINT('Ctrl Pts',(9.76025792883615,-1.6442415540714,3.08798175439507));
#93441=CARTESIAN_POINT('Ctrl Pts',(9.40128363486594,3.09548557845033,3.16516836377619));
#93442=CARTESIAN_POINT('Ctrl Pts',(6.87409722408249,7.12130266855917,3.2423549731573));
#93443=CARTESIAN_POINT('Ctrl Pts',(2.76154197480476,9.50473845351135,3.31954158253842));
#93444=CARTESIAN_POINT('Ctrl Pts',(-1.98790578544033,9.69610180945044,3.39672819191953));
#93445=CARTESIAN_POINT('Ctrl Pts',(-6.27888444807983,7.6512603437263,3.47391480130065));
#93446=CARTESIAN_POINT('Ctrl Pts',(-9.12176718588067,3.84181136814036,3.55110141068176));
#93447=CARTESIAN_POINT('Ctrl Pts',(-9.86090390749274,-0.853667969225371,
3.62828802006288));
#93448=CARTESIAN_POINT('Ctrl Pts',(-8.32582367444923,-5.35227467481443,
3.70547462944399));
#93449=CARTESIAN_POINT('Ctrl Pts',(-4.870569570912,-8.61647326987962,3.78266123882511));
#93450=CARTESIAN_POINT('Ctrl Pts',(-0.292007921251256,-9.89349231567484,
3.85984784820622));
#93451=CARTESIAN_POINT('Ctrl Pts',(4.35387734572572,-8.88871763543166,3.93703445758733));
#93452=CARTESIAN_POINT('Ctrl Pts',(7.99567403095283,-5.83406956269694,4.01422106696845));
#93453=CARTESIAN_POINT('Ctrl Pts',(9.79334762174143,-1.43366453103774,4.09140767634956));
#93454=CARTESIAN_POINT('Ctrl Pts',(9.33255727203353,3.29689012957999,4.16859428573068));
#93455=CARTESIAN_POINT('Ctrl Pts',(6.71906686705208,7.26810366491508,4.24578089511179));
#93456=CARTESIAN_POINT('Ctrl Pts',(3.944124220863,8.79638862890064,4.2972386346992));
#93457=CARTESIAN_POINT('Ctrl Pts',(2.45787321508261,9.19372658581085,4.3229675044929));
#93458=CARTESIAN_POINT('Ctrl Pts',(7.31697141119783,-6.37300756482166,-0.107266287678314));
#93459=CARTESIAN_POINT('Ctrl Pts',(8.3474493307344,-5.18990075032541,-0.0815319283213253));
#93460=CARTESIAN_POINT('Ctrl Pts',(9.82291468946153,-2.31605370098554,-0.0300686991706319));
#93461=CARTESIAN_POINT('Ctrl Pts',(9.76931111091479,2.53127727823173,0.0471233997737662));
#93462=CARTESIAN_POINT('Ctrl Pts',(7.46291578655946,6.79342271273417,0.124310009154881));
#93463=CARTESIAN_POINT('Ctrl Pts',(3.43521393138684,9.48932097831013,0.201496618535995));
#93464=CARTESIAN_POINT('Ctrl Pts',(-1.38467971062437,9.99644354329634,0.278683227917109));
#93465=CARTESIAN_POINT('Ctrl Pts',(-5.88526062679874,8.1982238617407,0.355869837298224));
#93466=CARTESIAN_POINT('Ctrl Pts',(-9.02850980544496,4.50918648301867,0.433056446679338));
#93467=CARTESIAN_POINT('Ctrl Pts',(-10.089528405881,-0.219768107930814,
0.510243056060454));
#93468=CARTESIAN_POINT('Ctrl Pts',(-8.82360082785589,-4.89805475298508,
0.587429665441566));
#93469=CARTESIAN_POINT('Ctrl Pts',(-5.52269401439564,-8.44669746852,0.664616274822683));
#93470=CARTESIAN_POINT('Ctrl Pts',(-0.948090567404625,-10.0472879967365,
0.741802884203794));
#93471=CARTESIAN_POINT('Ctrl Pts',(3.84516982330136,-9.33067656702422,0.818989493584912));
#93472=CARTESIAN_POINT('Ctrl Pts',(7.75162140170541,-6.4621381558215,0.896176102966023));
#93473=CARTESIAN_POINT('Ctrl Pts',(9.8703212328362,-2.10324029652249,0.973362712347141));
#93474=CARTESIAN_POINT('Ctrl Pts',(9.71263512790029,2.74072626995299,1.05054932172825));
#93475=CARTESIAN_POINT('Ctrl Pts',(7.31493001913396,6.95260099621914,1.12773593110937));
#93476=CARTESIAN_POINT('Ctrl Pts',(3.2301871946727,9.56100162950478,1.20492254049048));
#93477=CARTESIAN_POINT('Ctrl Pts',(-1.59953169220272,9.96435447393901,1.2821091498716));
#93478=CARTESIAN_POINT('Ctrl Pts',(-6.06035158025637,8.06963445916912,1.35929575925271));
#93479=CARTESIAN_POINT('Ctrl Pts',(-9.12347637621708,4.31381970560019,1.43648236863382));
#93480=CARTESIAN_POINT('Ctrl Pts',(-10.0824595203107,-0.436888593524985,
1.51366897801494));
#93481=CARTESIAN_POINT('Ctrl Pts',(-8.71613133173546,-5.08683754711988,
1.59085558739605));
#93482=CARTESIAN_POINT('Ctrl Pts',(-5.33960722509808,-8.56361233990904,
1.66804219677717));
#93483=CARTESIAN_POINT('Ctrl Pts',(-0.73161284384033,-10.0653665740357,
1.74522880615828));
#93484=CARTESIAN_POINT('Ctrl Pts',(4.04511295010607,-9.24575161066474,1.82241541553939));
#93485=CARTESIAN_POINT('Ctrl Pts',(7.88891687425179,-6.2937947357141,1.89960202492051));
#93486=CARTESIAN_POINT('Ctrl Pts',(9.91330483365338,-1.89030391725346,1.97678863430162));
#93487=CARTESIAN_POINT('Ctrl Pts',(9.65139349931427,2.94914651142642,2.05397524368274));
#93488=CARTESIAN_POINT('Ctrl Pts',(7.16358731847254,7.10843712465253,2.13116185306385));
#93489=CARTESIAN_POINT('Ctrl Pts',(3.02364747468623,9.62831332960143,2.20834846244497));
#93490=CARTESIAN_POINT('Ctrl Pts',(-1.81363429514113,9.92761765322946,2.28553507182608));
#93491=CARTESIAN_POINT('Ctrl Pts',(-6.23263872172306,7.93732172634232,2.36272168120719));
#93492=CARTESIAN_POINT('Ctrl Pts',(-9.21421357808373,4.1164462542367,2.43990829058831));
#93493=CARTESIAN_POINT('Ctrl Pts',(-10.0707201195409,-0.653802643558734,
2.51709489996942));
#93494=CARTESIAN_POINT('Ctrl Pts',(-8.60462277875034,-5.2732654453638,2.59428150935053));
#93495=CARTESIAN_POINT('Ctrl Pts',(-5.15404666723755,-8.67655833794445,
2.67146811873166));
#93496=CARTESIAN_POINT('Ctrl Pts',(-0.514795997972617,-10.078782002871,
2.74865472811276));
#93497=CARTESIAN_POINT('Ctrl Pts',(4.24318175355855,-9.15654248736592,2.82584133749388));
#93498=CARTESIAN_POINT('Ctrl Pts',(8.0225571447062,-6.12253528629633,2.90302794687499));
#93499=CARTESIAN_POINT('Ctrl Pts',(9.95169521166317,-1.67649163780051,2.98021455625611));
#93500=CARTESIAN_POINT('Ctrl Pts',(9.58568001119813,3.15620030059083,3.05740116563722));
#93501=CARTESIAN_POINT('Ctrl Pts',(7.00892547391585,7.26097959543934,3.13458777501834));
#93502=CARTESIAN_POINT('Ctrl Pts',(2.81570674134309,9.691163988245,3.21177438439945));
#93503=CARTESIAN_POINT('Ctrl Pts',(-2.02689648474925,9.88628073688752,3.28896099378057));
#93504=CARTESIAN_POINT('Ctrl Pts',(-6.40203821990527,7.80133183784919,3.36614760316168));
#93505=CARTESIAN_POINT('Ctrl Pts',(-9.30068113850137,3.91716449249559,3.4433342125428));
#93506=CARTESIAN_POINT('Ctrl Pts',(-10.0543152562534,-0.870411776372325,
3.52052082192391));
#93507=CARTESIAN_POINT('Ctrl Pts',(-8.48912602497671,-5.45725396205879,
3.59770743130503));
#93508=CARTESIAN_POINT('Ctrl Pts',(-4.9661007147889,-8.78547640917823,3.67489404068614));
#93509=CARTESIAN_POINT('Ctrl Pts',(-0.297735352167109,-10.0875428520841,
3.75208065006725));
#93510=CARTESIAN_POINT('Ctrl Pts',(4.4392741103302,-9.06306056410737,3.82926725944837));
#93511=CARTESIAN_POINT('Ctrl Pts',(8.15250084045075,-5.94849875432791,3.90645386882949));
#93512=CARTESIAN_POINT('Ctrl Pts',(9.98543392439411,-1.46178436601633,3.98364047821059));
#93513=CARTESIAN_POINT('Ctrl Pts',(9.51560565241569,3.3615551919982,4.06082708759171));
#93514=CARTESIAN_POINT('Ctrl Pts',(6.85085435807332,7.41065994027801,4.13801369697282));
#93515=CARTESIAN_POINT('Ctrl Pts',(4.02148410514878,8.96892062037927,4.18947143656024));
#93516=CARTESIAN_POINT('Ctrl Pts',(2.50608183551656,9.37405194703336,4.21520030635394));
#93517=CARTESIAN_POINT('Ctrl Pts',(7.4577254330695,-6.49560288408101,-0.215033485817281));
#93518=CARTESIAN_POINT('Ctrl Pts',(8.50802629620849,-5.28973705727136,-0.189299126460293));
#93519=CARTESIAN_POINT('Ctrl Pts',(10.0118746663897,-2.36060681660734,-0.137835897309599));
#93520=CARTESIAN_POINT('Ctrl Pts',(9.95723993453606,2.57997057459178,-0.0606437983652013));
#93521=CARTESIAN_POINT('Ctrl Pts',(7.60647728937472,6.92410541126547,0.0165428110159138));
#93522=CARTESIAN_POINT('Ctrl Pts',(3.50129594123211,9.67186372960258,0.0937294203970275));
#93523=CARTESIAN_POINT('Ctrl Pts',(-1.41131631029405,10.1887416341402,0.170916029778142));
#93524=CARTESIAN_POINT('Ctrl Pts',(-5.99847332867116,8.3559302290197,0.248102639159256));
#93525=CARTESIAN_POINT('Ctrl Pts',(-9.20218809325122,4.5959281275033,0.325289248540371));
#93526=CARTESIAN_POINT('Ctrl Pts',(-10.2836171376947,-0.223995710217611,
0.402475857921486));
#93527=CARTESIAN_POINT('Ctrl Pts',(-8.99333735327271,-4.99227692047576,
0.479662467302599));
#93528=CARTESIAN_POINT('Ctrl Pts',(-5.62893214905654,-8.60918363573503,
0.556849076683716));
#93529=CARTESIAN_POINT('Ctrl Pts',(-0.966328654307157,-10.2405641645618,
0.634035686064827));
#93530=CARTESIAN_POINT('Ctrl Pts',(3.9191380113663,-9.51016753122048,0.711222295445945));
#93531=CARTESIAN_POINT('Ctrl Pts',(7.9007366335412,-6.58644804911019,0.788408904827056));
#93532=CARTESIAN_POINT('Ctrl Pts',(10.0601931528714,-2.14369959505755,0.865595514208172));
#93533=CARTESIAN_POINT('Ctrl Pts',(9.89947369544367,2.79344866336769,0.942782123589285));
#93534=CARTESIAN_POINT('Ctrl Pts',(7.45564477145993,7.08634575175956,1.0199687329704));
#93535=CARTESIAN_POINT('Ctrl Pts',(3.29232517683739,9.74492327643303,1.09715534235151));
#93536=CARTESIAN_POINT('Ctrl Pts',(-1.63030132435465,10.1560352785702,1.17434195173263));
#93537=CARTESIAN_POINT('Ctrl Pts',(-6.17693244560895,8.22486719705081,1.25152856111374));
#93538=CARTESIAN_POINT('Ctrl Pts',(-9.29898150275598,4.39680314766522,1.32871517049486));
#93539=CARTESIAN_POINT('Ctrl Pts',(-10.2764122704431,-0.445292866712986,
1.40590177987597));
#93540=CARTESIAN_POINT('Ctrl Pts',(-8.8838005040143,-5.18469126324474,1.48308838925709));
#93541=CARTESIAN_POINT('Ctrl Pts',(-5.4423233831792,-8.72834755764508,1.5602749986382));
#93542=CARTESIAN_POINT('Ctrl Pts',(-0.745686624430195,-10.2589905131343,
1.63746160801931));
#93543=CARTESIAN_POINT('Ctrl Pts',(4.12292737422438,-9.42360890315545,1.71464821740043));
#93544=CARTESIAN_POINT('Ctrl Pts',(8.04067321111036,-6.41486626546352,1.79183482678154));
#93545=CARTESIAN_POINT('Ctrl Pts',(10.1040036141955,-1.92666703307842,1.86902143616266));
#93546=CARTESIAN_POINT('Ctrl Pts',(9.83705398305152,3.00587821218677,1.94620804554377));
#93547=CARTESIAN_POINT('Ctrl Pts',(7.30139074415778,7.24517964533336,2.02339465492489));
#93548=CARTESIAN_POINT('Ctrl Pts',(3.0818123244399,9.81352982818008,2.100581264306));
#93549=CARTESIAN_POINT('Ctrl Pts',(-1.84852254424032,10.1185917644796,2.17776787368711));
#93550=CARTESIAN_POINT('Ctrl Pts',(-6.35253381460441,8.09000921042384,2.25495448306823));
#93551=CARTESIAN_POINT('Ctrl Pts',(-9.39146418446372,4.19563289219672,2.33214109244934));
#93552=CARTESIAN_POINT('Ctrl Pts',(-10.2644470429234,-0.666379616519211,
2.40932770183046));
#93553=CARTESIAN_POINT('Ctrl Pts',(-8.77014689996588,-5.37470540981357,
2.48651431121157));
#93554=CARTESIAN_POINT('Ctrl Pts',(-5.25319326171758,-8.84346625837187,
2.56370092059269));
#93555=CARTESIAN_POINT('Ctrl Pts',(-0.524698948672571,-10.2726640098856,
2.6408875299738));
#93556=CARTESIAN_POINT('Ctrl Pts',(4.32480635802698,-9.33268369512891,2.71807413935492));
#93557=CARTESIAN_POINT('Ctrl Pts',(8.17688427274236,-6.24031235786978,2.79526074873603));
#93558=CARTESIAN_POINT('Ctrl Pts',(10.1431324944901,-1.70874172152963,2.87244735811714));
#93559=CARTESIAN_POINT('Ctrl Pts',(9.77007638753031,3.21691502273131,2.94963396749826));
#93560=CARTESIAN_POINT('Ctrl Pts',(7.14375372374919,7.40065652231953,3.02682057687937));
#93561=CARTESIAN_POINT('Ctrl Pts',(2.86987150788144,9.87758952297865,3.10400718626049));
#93562=CARTESIAN_POINT('Ctrl Pts',(-2.06588718405818,10.0764596643246,3.1811937956416));
#93563=CARTESIAN_POINT('Ctrl Pts',(-6.52519199173069,7.95140333197205,3.25838040502272));
#93564=CARTESIAN_POINT('Ctrl Pts',(-9.47959509112208,3.99251761685082,3.33556701440383));
#93565=CARTESIAN_POINT('Ctrl Pts',(-10.2477266050142,-0.88715558351928,
3.41275362378494));
#93566=CARTESIAN_POINT('Ctrl Pts',(-8.65242837550419,-5.56223324930316,
3.48994023316606));
#93567=CARTESIAN_POINT('Ctrl Pts',(-5.06163185866582,-8.95447954847683,
3.56712684254717));
#93568=CARTESIAN_POINT('Ctrl Pts',(-0.303462783082962,-10.2815933884932,
3.64431345192829));
#93569=CARTESIAN_POINT('Ctrl Pts',(4.52467087493469,-9.23740349278308,3.7215000613094));
#93570=CARTESIAN_POINT('Ctrl Pts',(8.30932764994867,-6.06292794595889,3.79868667069052));
#93571=CARTESIAN_POINT('Ctrl Pts',(10.1775202270467,-1.48990420099491,3.87587328007163));
#93572=CARTESIAN_POINT('Ctrl Pts',(9.69865403279785,3.42622025441641,3.95305988945275));
#93573=CARTESIAN_POINT('Ctrl Pts',(6.98264184909456,7.55321621564095,4.03024649883386));
#93574=CARTESIAN_POINT('Ctrl Pts',(4.09884398943458,9.14145261185791,4.08170423842127));
#93575=CARTESIAN_POINT('Ctrl Pts',(2.55429045595051,9.55437730825585,4.10743310821497));
#93576=CARTESIAN_POINT('Ctrl Pts',(7.59847945494118,-6.61819820334034,-0.322800683956248));
#93577=CARTESIAN_POINT('Ctrl Pts',(8.6686032616826,-5.38957336421732,-0.297066324599259));
#93578=CARTESIAN_POINT('Ctrl Pts',(10.2008346433178,-2.40515993222915,-0.245603095448566));
#93579=CARTESIAN_POINT('Ctrl Pts',(10.1451687581573,2.62866387095184,-0.168410996504169));
#93580=CARTESIAN_POINT('Ctrl Pts',(7.75003879218998,7.05478810979676,-0.0912243871230533));
#93581=CARTESIAN_POINT('Ctrl Pts',(3.56737795107737,9.85440648089508,-0.0140377777419394));
#93582=CARTESIAN_POINT('Ctrl Pts',(-1.43795290996372,10.381039724984,0.0631488316391753));
#93583=CARTESIAN_POINT('Ctrl Pts',(-6.11168603054357,8.51363659629871,0.140335441020289));
#93584=CARTESIAN_POINT('Ctrl Pts',(-9.37586638105749,4.68266977198792,0.217522050401404));
#93585=CARTESIAN_POINT('Ctrl Pts',(-10.4777058695083,-0.228223312504405,
0.294708659782519));
#93586=CARTESIAN_POINT('Ctrl Pts',(-9.16307387868954,-5.08649908796642,
0.371895269163633));
#93587=CARTESIAN_POINT('Ctrl Pts',(-5.73517028371745,-8.77166980295006,
0.449081878544748));
#93588=CARTESIAN_POINT('Ctrl Pts',(-0.984566741209693,-10.4338403323871,
0.526268487925861));
#93589=CARTESIAN_POINT('Ctrl Pts',(3.99310619943123,-9.68965849541676,0.603455097306976));
#93590=CARTESIAN_POINT('Ctrl Pts',(8.04985186537699,-6.71075794239885,0.68064170668809));
#93591=CARTESIAN_POINT('Ctrl Pts',(10.2500650729067,-2.18415889359261,0.757828316069205));
#93592=CARTESIAN_POINT('Ctrl Pts',(10.086312262987,2.84617105678237,0.835014925450318));
#93593=CARTESIAN_POINT('Ctrl Pts',(7.59635952378591,7.22009050729999,0.912201534831435));
#93594=CARTESIAN_POINT('Ctrl Pts',(3.35446315900208,9.92884492336128,0.989388144212546));
#93595=CARTESIAN_POINT('Ctrl Pts',(-1.66107095650658,10.3477160832014,1.06657475359366));
#93596=CARTESIAN_POINT('Ctrl Pts',(-6.29351331096151,8.38009993493251,1.14376136297478));
#93597=CARTESIAN_POINT('Ctrl Pts',(-9.47448662929488,4.47978658973023,1.22094797235589));
#93598=CARTESIAN_POINT('Ctrl Pts',(-10.4703650205756,-0.453697139900987,
1.29813458173701));
#93599=CARTESIAN_POINT('Ctrl Pts',(-9.05146967629314,-5.28254497936959,
1.37532119111812));
#93600=CARTESIAN_POINT('Ctrl Pts',(-5.54503954126032,-8.89308277538113,
1.45250780049923));
#93601=CARTESIAN_POINT('Ctrl Pts',(-0.759760405020054,-10.452614452233,
1.52969440988035));
#93602=CARTESIAN_POINT('Ctrl Pts',(4.20074179834271,-9.60146619564616,1.60688101926146));
#93603=CARTESIAN_POINT('Ctrl Pts',(8.19242954796893,-6.53593779521296,1.68406762864258));
#93604=CARTESIAN_POINT('Ctrl Pts',(10.2947023947376,-1.96303014890336,1.76125423802369));
#93605=CARTESIAN_POINT('Ctrl Pts',(10.0227144667888,3.06260991294711,1.83844084740481));
#93606=CARTESIAN_POINT('Ctrl Pts',(7.43919416984301,7.3819221660142,1.91562745678592));
#93607=CARTESIAN_POINT('Ctrl Pts',(3.13997717419355,9.99874632675871,1.99281406616704));
#93608=CARTESIAN_POINT('Ctrl Pts',(-1.8834107933395,10.3095658757298,2.07000067554815));
#93609=CARTESIAN_POINT('Ctrl Pts',(-6.47242890748576,8.24269669450534,2.14718728492927));
#93610=CARTESIAN_POINT('Ctrl Pts',(-9.5687147908437,4.27481953015676,2.22437389431038));
#93611=CARTESIAN_POINT('Ctrl Pts',(-10.458173966306,-0.678956589479688,
2.30156050369149));
#93612=CARTESIAN_POINT('Ctrl Pts',(-8.93567102118141,-5.47614537426334,
2.37874711307261));
#93613=CARTESIAN_POINT('Ctrl Pts',(-5.35233985619761,-9.01037417879928,
2.45593372245372));
#93614=CARTESIAN_POINT('Ctrl Pts',(-0.534601899372525,-10.4665460169004,
2.53312033183484));
#93615=CARTESIAN_POINT('Ctrl Pts',(4.40643096249542,-9.5088249028919,2.61030694121595));
#93616=CARTESIAN_POINT('Ctrl Pts',(8.33121140077849,-6.35808942944322,2.68749355059706));
#93617=CARTESIAN_POINT('Ctrl Pts',(10.3345697773172,-1.74099180525873,2.76468015997818));
#93618=CARTESIAN_POINT('Ctrl Pts',(9.9544727638625,3.27762974487179,2.84186676935929));
#93619=CARTESIAN_POINT('Ctrl Pts',(7.27858197358255,7.54033344919971,2.9190533787404));
#93620=CARTESIAN_POINT('Ctrl Pts',(2.92403627441977,10.0640150577123,2.99623998812152));
#93621=CARTESIAN_POINT('Ctrl Pts',(-2.10487788336711,10.2666385917617,3.07342659750264));
#93622=CARTESIAN_POINT('Ctrl Pts',(-6.64834576355613,8.10147482609493,3.15061320688375));
#93623=CARTESIAN_POINT('Ctrl Pts',(-9.65850904374278,4.06787074120605,3.22779981626486));
#93624=CARTESIAN_POINT('Ctrl Pts',(-10.4411379537749,-0.903899390666233,
3.30498642564598));
#93625=CARTESIAN_POINT('Ctrl Pts',(-8.81573072603167,-5.66721253654752,
3.38217303502709));
#93626=CARTESIAN_POINT('Ctrl Pts',(-5.15716300254271,-9.12348268777542,
3.45935964440821));
#93627=CARTESIAN_POINT('Ctrl Pts',(-0.309190213998818,-10.4756439249024,
3.53654625378932));
#93628=CARTESIAN_POINT('Ctrl Pts',(4.61006763953917,-9.41174642145879,3.61373286317044));
#93629=CARTESIAN_POINT('Ctrl Pts',(8.46615445944659,-6.17735713758986,3.69091947255155));
#93630=CARTESIAN_POINT('Ctrl Pts',(10.3696065296995,-1.5180240359735,3.76810608193267));
#93631=CARTESIAN_POINT('Ctrl Pts',(9.88170241318002,3.49088531683462,3.84529269131378));
#93632=CARTESIAN_POINT('Ctrl Pts',(7.1144293401158,7.69577249100388,3.9224793006949));
#93633=CARTESIAN_POINT('Ctrl Pts',(4.17620387372036,9.31398460333654,3.9739370402823));
#93634=CARTESIAN_POINT('Ctrl Pts',(2.60249907638446,9.73470266947836,3.99966591007601));
#93635=CARTESIAN_POINT('Ctrl Pts',(2.6023496244676,9.73414364143212,4.));
#93636=CARTESIAN_POINT('Ctrl Pts',(2.83853694256798,9.66402616844161,4.));
#93637=CARTESIAN_POINT('Ctrl Pts',(3.07166134324788,9.58522029115185,4.));
#93638=CARTESIAN_POINT('Ctrl Pts',(3.30132667682908,9.49806665648961,4.));
#93639=CARTESIAN_POINT('Ctrl Pts',(3.5400502322276,9.40747559858787,4.));
#93640=CARTESIAN_POINT('Ctrl Pts',(3.77503717013813,9.30786527649238,4.));
#93641=CARTESIAN_POINT('Ctrl Pts',(4.00582730120758,9.19956194039239,4.));
#93642=CARTESIAN_POINT('Ctrl Pts',(4.23171368243693,9.09355979656879,4.));
#93643=CARTESIAN_POINT('Ctrl Pts',(4.45358020203394,8.9792295867419,4.));
#93644=CARTESIAN_POINT('Ctrl Pts',(4.67097238674394,8.85682947856375,4.));
#93645=CARTESIAN_POINT('Ctrl Pts',(4.89544359643902,8.73044360877633,4.));
#93646=CARTESIAN_POINT('Ctrl Pts',(5.11514514178304,8.59545357942288,4.));
#93647=CARTESIAN_POINT('Ctrl Pts',(5.32954166532511,8.45209673940295,4.));
#93648=CARTESIAN_POINT('Ctrl Pts',(5.54393818886718,8.30873989938302,4.));
#93649=CARTESIAN_POINT('Ctrl Pts',(5.75303036100492,8.15701585598298,4.));
#93650=CARTESIAN_POINT('Ctrl Pts',(5.95623735557635,7.99712024365205,4.));
#93651=CARTESIAN_POINT('Ctrl Pts',(5.97890496335302,7.97928399233023,4.));
#93652=CARTESIAN_POINT('Ctrl Pts',(6.00149928764221,7.96134602092925,4.));
#93653=CARTESIAN_POINT('Ctrl Pts',(6.02401948143154,7.94330657213126,4.));
#93654=CARTESIAN_POINT('Ctrl Pts',(6.0505106021892,7.92208627442959,4.00000000000001));
#93655=CARTESIAN_POINT('Ctrl Pts',(6.07689301758066,7.9007304096383,4.00000000000001));
#93656=CARTESIAN_POINT('Ctrl Pts',(6.10315549849619,7.87924789105142,4.00000000000001));
#93657=CARTESIAN_POINT('Ctrl Pts',(6.29514744453683,7.72219987404892,4.00000000000001));
#93658=CARTESIAN_POINT('Ctrl Pts',(6.48089722280961,7.55825453484683,4.));
#93659=CARTESIAN_POINT('Ctrl Pts',(6.65998212635876,7.38768689939716,4.));
#93660=CARTESIAN_POINT('Ctrl Pts',(6.69015407484989,7.35894992710609,4.));
#93661=CARTESIAN_POINT('Ctrl Pts',(6.72013677327834,7.33002488212823,4.));
#93662=CARTESIAN_POINT('Ctrl Pts',(6.74992811418605,7.30091296200115,4.));
#93663=CARTESIAN_POINT('Ctrl Pts',(6.9262582868153,7.12860417209207,4.));
#93664=CARTESIAN_POINT('Ctrl Pts',(7.09588772648024,6.94975169953822,4.));
#93665=CARTESIAN_POINT('Ctrl Pts',(7.25857969279764,6.76483090696196,4.));
#93666=CARTESIAN_POINT('Ctrl Pts',(7.42201105991826,6.5790696882377,4.));
#93667=CARTESIAN_POINT('Ctrl Pts',(7.57844211565621,6.38718430988767,4.00000000000001));
#93668=CARTESIAN_POINT('Ctrl Pts',(7.72759196996615,6.18962354908701,4.00000000000001));
#93669=CARTESIAN_POINT('Ctrl Pts',(7.8762793761675,5.99267533732698,4.));
#93670=CARTESIAN_POINT('Ctrl Pts',(8.0177309789071,5.7900863001285,4.));
#93671=CARTESIAN_POINT('Ctrl Pts',(8.15162291233038,5.58227682514063,4.));
#93672=CARTESIAN_POINT('Ctrl Pts',(8.26759771712329,5.40227596415038,4.00000000000001));
#93673=CARTESIAN_POINT('Ctrl Pts',(8.37790014202984,5.21835776304691,4.));
#93674=CARTESIAN_POINT('Ctrl Pts',(8.48228911756457,5.03078568934111,4.));
#93675=CARTESIAN_POINT('Ctrl Pts',(8.50112007146166,4.99694915579681,4.));
#93676=CARTESIAN_POINT('Ctrl Pts',(8.51975857415101,4.96299335747099,4.));
#93677=CARTESIAN_POINT('Ctrl Pts',(8.53818915232497,4.92894630654343,4.));
#93678=CARTESIAN_POINT('Ctrl Pts',(8.65535538855079,4.71250356806194,4.));
#93679=CARTESIAN_POINT('Ctrl Pts',(8.76426876468842,4.49211446879426,4.));
#93680=CARTESIAN_POINT('Ctrl Pts',(8.86469547420092,4.2682386905176,4.));
#93681=CARTESIAN_POINT('Ctrl Pts',(8.96498207431523,4.04467525046966,4.));
#93682=CARTESIAN_POINT('Ctrl Pts',(9.0568059746215,3.8176342698159,4.));
#93683=CARTESIAN_POINT('Ctrl Pts',(9.13988914425725,3.58754843136135,4.));
#93684=CARTESIAN_POINT('Ctrl Pts',(9.1781696365212,3.48153659770576,4.));
#93685=CARTESIAN_POINT('Ctrl Pts',(9.21459390332125,3.37487807624388,4.));
#93686=CARTESIAN_POINT('Ctrl Pts',(9.24913123944987,3.26761391216937,3.99999999999999));
#93687=CARTESIAN_POINT('Ctrl Pts',(9.32430819331323,3.03413345253597,3.99999999999999));
#93688=CARTESIAN_POINT('Ctrl Pts',(9.39054833689072,2.797783920754,3.99999999999999));
#93689=CARTESIAN_POINT('Ctrl Pts',(9.44781367990102,2.55908882180367,3.99999999999999));
#93690=CARTESIAN_POINT('Ctrl Pts',(9.50492475352923,2.32103675306121,3.99999999999999));
#93691=CARTESIAN_POINT('Ctrl Pts',(9.55310933215745,2.08065107338521,3.99999999999999));
#93692=CARTESIAN_POINT('Ctrl Pts',(9.59227815520829,1.83844879803419,3.99999999999999));
#93693=CARTESIAN_POINT('Ctrl Pts',(9.6139614565568,1.7043690755744,3.99999999999999));
#93694=CARTESIAN_POINT('Ctrl Pts',(9.63288089979977,1.56973266133125,3.99999999999998));
#93695=CARTESIAN_POINT('Ctrl Pts',(9.64901448005129,1.43462810174663,3.99999999999999));
#93696=CARTESIAN_POINT('Ctrl Pts',(9.65375203401828,1.39495524970519,3.99999999999999));
#93697=CARTESIAN_POINT('Ctrl Pts',(9.6582496986183,1.35523779998252,3.99999999999999));
#93698=CARTESIAN_POINT('Ctrl Pts',(9.66250334791277,1.31551317054319,3.99999999999999));
#93699=CARTESIAN_POINT('Ctrl Pts',(9.68848620150609,1.07286053058192,3.99999999999999));
#93700=CARTESIAN_POINT('Ctrl Pts',(9.70540234538228,0.829675292048995,3.99999999999999));
#93701=CARTESIAN_POINT('Ctrl Pts',(9.71327562900262,0.586475884702219,3.99999999999999));
#93702=CARTESIAN_POINT('Ctrl Pts',(9.72116108183257,0.342900580244727,3.99999999999999));
#93703=CARTESIAN_POINT('Ctrl Pts',(9.71997572067835,0.099310397190577,3.99999999999998));
#93704=CARTESIAN_POINT('Ctrl Pts',(9.70969154440537,-0.143780047697638,
3.99999999999999));
#93705=CARTESIAN_POINT('Ctrl Pts',(9.69949615601932,-0.38477178420512,3.99999999999999));
#93706=CARTESIAN_POINT('Ctrl Pts',(9.68035832847905,-0.625273010146937,
3.99999999999998));
#93707=CARTESIAN_POINT('Ctrl Pts',(9.65220012606401,-0.864778721030272,
3.99999999999999));
#93708=CARTESIAN_POINT('Ctrl Pts',(9.63108912131042,-1.04434296048145,3.99999999999999));
#93709=CARTESIAN_POINT('Ctrl Pts',(9.60490679924936,-1.22334761187656,3.99999999999999));
#93710=CARTESIAN_POINT('Ctrl Pts',(9.57360159863658,-1.4015752955962,3.99999999999999));
#93711=CARTESIAN_POINT('Ctrl Pts',(9.54008127908224,-1.59241415926013,3.99999999999999));
#93712=CARTESIAN_POINT('Ctrl Pts',(9.50068747829056,-1.7823624612145,3.99999999999999));
#93713=CARTESIAN_POINT('Ctrl Pts',(9.4555050228853,-1.9711691265491,3.99999999999999));
#93714=CARTESIAN_POINT('Ctrl Pts',(9.43573769864551,-2.05377204263296,3.99999999999999));
#93715=CARTESIAN_POINT('Ctrl Pts',(9.41486214872224,-2.13615632006512,3.99999999999999));
#93716=CARTESIAN_POINT('Ctrl Pts',(9.39288438044855,-2.21830029733162,3.99999999999999));
#93717=CARTESIAN_POINT('Ctrl Pts',(9.38127565021983,-2.26168901906741,3.99999999999999));
#93718=CARTESIAN_POINT('Ctrl Pts',(9.36935939152565,-2.30501069026336,4.));
#93719=CARTESIAN_POINT('Ctrl Pts',(9.35713641742303,-2.34826206837094,4.));
#93720=CARTESIAN_POINT('Ctrl Pts',(9.34817713074373,-2.37996478593278,4.));
#93721=CARTESIAN_POINT('Ctrl Pts',(9.33905529757631,-2.41162171069674,4.));
#93722=CARTESIAN_POINT('Ctrl Pts',(9.32977347375216,-2.44322504264465,4.));
#93723=CARTESIAN_POINT('Ctrl Pts',(9.30913094759651,-2.51351000158156,4.));
#93724=CARTESIAN_POINT('Ctrl Pts',(9.28769420834347,-2.58354024740004,4.));
#93725=CARTESIAN_POINT('Ctrl Pts',(9.26547043733762,-2.65330301792625,4.));
#93726=CARTESIAN_POINT('Ctrl Pts',(9.19195458649819,-2.8840770585155,4.));
#93727=CARTESIAN_POINT('Ctrl Pts',(9.1098301701063,-3.11192550815888,4.));
#93728=CARTESIAN_POINT('Ctrl Pts',(9.01932452687049,-3.33637596952591,4.));
#93729=CARTESIAN_POINT('Ctrl Pts',(8.93690618262992,-3.54077024515911,4.));
#93730=CARTESIAN_POINT('Ctrl Pts',(8.84753676833139,-3.74234683886697,4.));
#93731=CARTESIAN_POINT('Ctrl Pts',(8.75135417901126,-3.94073274238285,4.));
#93732=CARTESIAN_POINT('Ctrl Pts',(8.67921723702116,-4.08952217001975,4.));
#93733=CARTESIAN_POINT('Ctrl Pts',(8.60324720993827,-4.23651654842593,4.));
#93734=CARTESIAN_POINT('Ctrl Pts',(8.5234913277534,-4.38155078557716,4.00000000000001));
#93735=CARTESIAN_POINT('Ctrl Pts',(8.49892468404568,-4.42622466206011,4.00000000000001));
#93736=CARTESIAN_POINT('Ctrl Pts',(8.47399670555403,-4.47071589760201,4.00000000000001));
#93737=CARTESIAN_POINT('Ctrl Pts',(8.44872637787968,-4.51498912509729,4.00000000000001));
#93738=CARTESIAN_POINT('Ctrl Pts',(8.32958796863387,-4.72371779549438,4.00000000000001));
#93739=CARTESIAN_POINT('Ctrl Pts',(8.2027667345669,-4.92774605616295,4.));
#93740=CARTESIAN_POINT('Ctrl Pts',(8.06846284138562,-5.12660291060759,4.00000000000001));
#93741=CARTESIAN_POINT('Ctrl Pts',(7.95380309505733,-5.29637368899813,4.00000000000001));
#93742=CARTESIAN_POINT('Ctrl Pts',(7.83368866631315,-5.46237506898967,4.));
#93743=CARTESIAN_POINT('Ctrl Pts',(7.70821968708721,-5.62429639443576,4.));
#93744=CARTESIAN_POINT('Ctrl Pts',(7.5607552682559,-5.81460346715293,4.));
#93745=CARTESIAN_POINT('Ctrl Pts',(7.40589473957772,-5.99927573772719,4.00000000000001));
#93746=CARTESIAN_POINT('Ctrl Pts',(7.24403667673219,-6.17797150278237,4.00000000000001));
#93747=CARTESIAN_POINT('Ctrl Pts',(7.22210427859886,-6.20218547516675,4.00000000000001));
#93748=CARTESIAN_POINT('Ctrl Pts',(7.20004334827914,-6.22628964950583,4.));
#93749=CARTESIAN_POINT('Ctrl Pts',(7.17785483368835,-6.25028311638451,4.));
#93750=CARTESIAN_POINT('Ctrl Pts',(7.17753992463812,-6.25025814508695,-2.77555756156289E-16));
#93751=CARTESIAN_POINT('Ctrl Pts',(7.33800998986773,-6.07641108632488,-1.70645015963758E-15));
#93752=CARTESIAN_POINT('Ctrl Pts',(7.49158121534325,-5.89679618497648,-2.48618949564423E-15));
#93753=CARTESIAN_POINT('Ctrl Pts',(7.63811298721216,-5.71192498565071,-2.14932238673526E-15));
#93754=CARTESIAN_POINT('Ctrl Pts',(7.78666634752559,-5.52450325768861,-1.2836841867506E-15));
#93755=CARTESIAN_POINT('Ctrl Pts',(7.92798505737963,-5.33167874732615,-3.99093992625071E-16));
#93756=CARTESIAN_POINT('Ctrl Pts',(8.06188982433472,-5.13394157588505,9.92261828258734E-16));
#93757=CARTESIAN_POINT('Ctrl Pts',(8.19685995208136,-4.93463118614655,2.15043722649999E-15));
#93758=CARTESIAN_POINT('Ctrl Pts',(8.32429807361849,-4.7303291359084,1.79060540631703E-15));
#93759=CARTESIAN_POINT('Ctrl Pts',(8.44398181039031,-4.52150145755031,7.63278329429795E-16));
#93760=CARTESIAN_POINT('Ctrl Pts',(8.56345030282558,-4.31304934379516,-7.43045306890748E-16));
#93761=CARTESIAN_POINT('Ctrl Pts',(8.67519260394167,-4.1000872941033,-3.85651484159796E-16));
#93762=CARTESIAN_POINT('Ctrl Pts',(8.77894385085711,-3.88305148407251,1.12410081243297E-15));
#93763=CARTESIAN_POINT('Ctrl Pts',(8.84287719073254,-3.74931020750599,1.05649064180309E-15));
#93764=CARTESIAN_POINT('Ctrl Pts',(8.90377525885169,-3.61402152351891,1.62340193009639E-15));
#93765=CARTESIAN_POINT('Ctrl Pts',(8.96156696082794,-3.47728373804748,1.06165076729781E-15));
#93766=CARTESIAN_POINT('Ctrl Pts',(9.00491073731013,-3.37473039894392,5.29634336720259E-16));
#93767=CARTESIAN_POINT('Ctrl Pts',(9.04650704156076,-3.27136187970652,-1.10473652131748E-15));
#93768=CARTESIAN_POINT('Ctrl Pts',(9.08632311880722,-3.16721890424697,2.22044604925031E-16));
#93769=CARTESIAN_POINT('Ctrl Pts',(9.09814351372692,-3.13630146628783,3.53555780382128E-16));
#93770=CARTESIAN_POINT('Ctrl Pts',(9.10980868158756,-3.10531118606065,-8.44808349090084E-16));
#93771=CARTESIAN_POINT('Ctrl Pts',(9.12131183370369,-3.07426508737355,-1.02695629777827E-15));
#93772=CARTESIAN_POINT('Ctrl Pts',(9.20591217134567,-2.84593546042613,-2.36656980581918E-15));
#93773=CARTESIAN_POINT('Ctrl Pts',(9.2816705280804,-2.61481991374847,-1.78377060807565E-16));
#93774=CARTESIAN_POINT('Ctrl Pts',(9.3483940664643,-2.38140358669778,-1.66533453693773E-15));
#93775=CARTESIAN_POINT('Ctrl Pts',(9.36427745395793,-2.32583935764635,-2.01930140308367E-15));
#93776=CARTESIAN_POINT('Ctrl Pts',(9.37964867883204,-2.27014461564336,-2.72027826337243E-15));
#93777=CARTESIAN_POINT('Ctrl Pts',(9.39450477735965,-2.21432566613214,-2.52575738102223E-15));
#93778=CARTESIAN_POINT('Ctrl Pts',(9.45650188159823,-1.98138340172106,-1.63274350975922E-15));
#93779=CARTESIAN_POINT('Ctrl Pts',(9.50953176974578,-1.74627967148825,-4.98055778690125E-16));
#93780=CARTESIAN_POINT('Ctrl Pts',(9.55366962715838,-1.50954126955344,-7.21644966006352E-16));
#93781=CARTESIAN_POINT('Ctrl Pts',(9.59810773930183,-1.27119241733133,-9.4675515400523E-16));
#93782=CARTESIAN_POINT('Ctrl Pts',(9.63353251352791,-1.03118594416952,-4.86217381181644E-15));
#93783=CARTESIAN_POINT('Ctrl Pts',(9.65996981531948,-0.790043545297951,
-3.81639164714898E-15));
#93784=CARTESIAN_POINT('Ctrl Pts',(9.68639436464155,-0.549017465448327,
-2.77111393279442E-15));
#93785=CARTESIAN_POINT('Ctrl Pts',(9.703840143681,-0.306855896272764,-4.36666804480211E-15));
#93786=CARTESIAN_POINT('Ctrl Pts',(9.71228155096646,-0.064073667508046,
-4.3159920082303E-15));
#93787=CARTESIAN_POINT('Ctrl Pts',(9.71962495034288,0.147128897067642,-4.27190760822724E-15));
#93788=CARTESIAN_POINT('Ctrl Pts',(9.72015333295581,0.358801518323463,-3.13158552209261E-15));
#93789=CARTESIAN_POINT('Ctrl Pts',(9.71381780952735,0.570603154075694,-1.52655665885959E-16));
#93790=CARTESIAN_POINT('Ctrl Pts',(9.71299313018453,0.598172846738271,3.49337317364136E-16));
#93791=CARTESIAN_POINT('Ctrl Pts',(9.71205204699908,0.625745335211232,-3.50308968122191E-15));
#93792=CARTESIAN_POINT('Ctrl Pts',(9.71099513918219,0.653304042026428,-3.38618022510673E-15));
#93793=CARTESIAN_POINT('Ctrl Pts',(9.70161065125207,0.898003104086462,-2.15789795742488E-15));
#93794=CARTESIAN_POINT('Ctrl Pts',(9.68309081241473,1.14191242342517,1.50994968166066E-15));
#93795=CARTESIAN_POINT('Ctrl Pts',(9.65550811589912,1.3845043278793,1.80411241501588E-15));
#93796=CARTESIAN_POINT('Ctrl Pts',(9.62779434503325,1.62824904116905,1.60411412740023E-15));
#93797=CARTESIAN_POINT('Ctrl Pts',(9.59093142972806,1.87066445397657,1.89804298519407E-15));
#93798=CARTESIAN_POINT('Ctrl Pts',(9.54494106673758,2.11122282572072,2.16493489801906E-15));
#93799=CARTESIAN_POINT('Ctrl Pts',(9.52299473622331,2.22601586476162,2.79879565106048E-15));
#93800=CARTESIAN_POINT('Ctrl Pts',(9.49896919359987,2.34038607617966,1.28207721328556E-15));
#93801=CARTESIAN_POINT('Ctrl Pts',(9.47286261042038,2.45427603255219,2.1094237467878E-15));
#93802=CARTESIAN_POINT('Ctrl Pts',(9.41829613481954,2.69232225571569,3.98098628479859E-15));
#93803=CARTESIAN_POINT('Ctrl Pts',(9.35464154134197,2.9282712247136,3.88869133735323E-15));
#93804=CARTESIAN_POINT('Ctrl Pts',(9.28216391978015,3.16167853502839,2.77555756156289E-15));
#93805=CARTESIAN_POINT('Ctrl Pts',(9.20955144462212,3.39552012856739,1.37319592695381E-15));
#93806=CARTESIAN_POINT('Ctrl Pts',(9.12808282575743,3.62681119853611,2.89145976353516E-15));
#93807=CARTESIAN_POINT('Ctrl Pts',(9.03797511128659,3.8550881756909,3.05311331771918E-15));
#93808=CARTESIAN_POINT('Ctrl Pts',(8.98726023624883,3.98356816698121,4.01994859505052E-15));
#93809=CARTESIAN_POINT('Ctrl Pts',(8.93380786638176,4.11109302736784,6.30449953712883E-15));
#93810=CARTESIAN_POINT('Ctrl Pts',(8.87765027447099,4.23757668725412,4.02455846426619E-15));
#93811=CARTESIAN_POINT('Ctrl Pts',(8.86122693757481,4.27456694427003,2.69626927025734E-15));
#93812=CARTESIAN_POINT('Ctrl Pts',(8.84457022494813,4.31147221868278,1.27775149067983E-16));
#93813=CARTESIAN_POINT('Ctrl Pts',(8.82769617356933,4.34825761285522,3.88578058618805E-16));
#93814=CARTESIAN_POINT('Ctrl Pts',(8.72485940884878,4.57244152937544,1.97800829358891E-15));
#93815=CARTESIAN_POINT('Ctrl Pts',(8.61384827011246,4.79241862612696,3.30332224731784E-15));
#93816=CARTESIAN_POINT('Ctrl Pts',(8.49498716931974,5.0077596047636,2.4980018054066E-15));
#93817=CARTESIAN_POINT('Ctrl Pts',(8.37548437725773,5.22426313721297,1.68833370818081E-15));
#93818=CARTESIAN_POINT('Ctrl Pts',(8.2480463831814,5.43608096212101,-1.79289508799685E-15));
#93819=CARTESIAN_POINT('Ctrl Pts',(8.11295156724744,5.64276359635317,-3.13638004456607E-15));
#93820=CARTESIAN_POINT('Ctrl Pts',(7.97823586637413,5.84886621943632,-4.47609479443058E-15));
#93821=CARTESIAN_POINT('Ctrl Pts',(7.83590594907037,6.04986301653102,-4.53666372321089E-15));
#93822=CARTESIAN_POINT('Ctrl Pts',(7.68619128271507,6.24528632274246,-4.71844785465692E-15));
#93823=CARTESIAN_POINT('Ctrl Pts',(7.57338197961842,6.39253687286717,-4.85542135018466E-15));
#93824=CARTESIAN_POINT('Ctrl Pts',(7.45637896929152,6.53662265622548,-5.76567150700508E-15));
#93825=CARTESIAN_POINT('Ctrl Pts',(7.33526444267627,6.6773322800225,-7.105427357601E-15));
#93826=CARTESIAN_POINT('Ctrl Pts',(7.20393068439424,6.82991450311471,-8.37772598309406E-15));
#93827=CARTESIAN_POINT('Ctrl Pts',(7.06776233301774,6.97852710790817,-7.71770923598613E-15));
#93828=CARTESIAN_POINT('Ctrl Pts',(6.92698202333213,7.12300579317397,-7.66053886991358E-15));
#93829=CARTESIAN_POINT('Ctrl Pts',(6.86539063784465,7.18621521797778,-6.99661795502185E-15));
#93830=CARTESIAN_POINT('Ctrl Pts',(6.80291629536247,7.24863316335114,-9.1940653235129E-15));
#93831=CARTESIAN_POINT('Ctrl Pts',(6.73957677015636,7.31024478793457,-8.65973959207622E-15));
#93832=CARTESIAN_POINT('Ctrl Pts',(6.71407214296748,7.33505364954804,-8.43710487480707E-15));
#93833=CARTESIAN_POINT('Ctrl Pts',(6.68842723008856,7.3597317670364,-8.81881235844313E-15));
#93834=CARTESIAN_POINT('Ctrl Pts',(6.66264317018596,7.38427813926213,-9.52016243616072E-15));
#93835=CARTESIAN_POINT('Ctrl Pts',(6.64018129830422,7.40566179529529,-1.01311459526996E-14));
#93836=CARTESIAN_POINT('Ctrl Pts',(6.6176136785009,7.42694554332174,-1.02041435804245E-14));
#93837=CARTESIAN_POINT('Ctrl Pts',(6.59495234791835,7.44811834977477,-9.38138455808257E-15));
#93838=CARTESIAN_POINT('Ctrl Pts',(6.41390316478046,7.61727520043247,-2.80807905990282E-15));
#93839=CARTESIAN_POINT('Ctrl Pts',(6.22670570529577,7.77951654972426,-8.71920794202464E-15));
#93840=CARTESIAN_POINT('Ctrl Pts',(6.03383377828811,7.93459536759427,-9.27036225562006E-15));
#93841=CARTESIAN_POINT('Ctrl Pts',(5.83693737649259,8.09291006744219,-9.83301698129566E-15));
#93842=CARTESIAN_POINT('Ctrl Pts',(5.63412705071208,8.2437605256776,-1.02724545597727E-14));
#93843=CARTESIAN_POINT('Ctrl Pts',(5.42586725408438,8.38684523466999,-1.12132525487141E-14));
#93844=CARTESIAN_POINT('Ctrl Pts',(5.2696724066136,8.49415876641429,-1.19188510404201E-14));
#93845=CARTESIAN_POINT('Ctrl Pts',(5.11041134210566,8.59710331969617,-1.08867618319524E-14));
#93846=CARTESIAN_POINT('Ctrl Pts',(4.9482678399785,8.6955353474984,-1.12687636999453E-14));
#93847=CARTESIAN_POINT('Ctrl Pts',(4.8988306515854,8.72554705094956,-1.13852352086196E-14));
#93848=CARTESIAN_POINT('Ctrl Pts',(4.84912544012257,8.75513915261243,-1.12031239875748E-14));
#93849=CARTESIAN_POINT('Ctrl Pts',(4.79915725517255,8.78430729888448,-1.0769163338864E-14));
#93850=CARTESIAN_POINT('Ctrl Pts',(4.75991955858719,8.80721169043932,-1.04283941818269E-14));
#93851=CARTESIAN_POINT('Ctrl Pts',(4.72052094035713,8.82985381860244,-1.24133512762974E-14));
#93852=CARTESIAN_POINT('Ctrl Pts',(4.6809837830536,8.85222064328245,-1.21014309684142E-14));
#93853=CARTESIAN_POINT('Ctrl Pts',(4.46299776725799,8.97553894258666,-1.03816749262894E-14));
#93854=CARTESIAN_POINT('Ctrl Pts',(4.24064629173592,9.09058407405512,-1.0004645565113E-14));
#93855=CARTESIAN_POINT('Ctrl Pts',(4.01438138172824,9.19707375790166,-8.43769498715119E-15));
#93856=CARTESIAN_POINT('Ctrl Pts',(3.81972423991358,9.28868751051407,-7.08963743434491E-15));
#93857=CARTESIAN_POINT('Ctrl Pts',(3.6221698828145,9.37396868113959,-6.94744677900428E-15));
#93858=CARTESIAN_POINT('Ctrl Pts',(3.42198926643324,9.45271166426703,-6.21724893790088E-15));
#93859=CARTESIAN_POINT('Ctrl Pts',(3.18987041866164,9.54401785986204,-5.32066284343393E-15));
#93860=CARTESIAN_POINT('Ctrl Pts',(2.95422040193964,9.62653437420915,-2.00867961754982E-15));
#93861=CARTESIAN_POINT('Ctrl Pts',(2.71555643549459,9.70021149728078,-1.4432899320127E-15));
#93862=CARTESIAN_POINT('Ctrl Pts',(2.67798368606114,9.71181045009038,-1.35428091526265E-15));
#93863=CARTESIAN_POINT('Ctrl Pts',(2.64033620760127,9.72319022676346,-2.52363653881751E-15));
#93864=CARTESIAN_POINT('Ctrl Pts',(2.60261598667549,9.73435052034593,9.99200722162641E-16));
#93865=CARTESIAN_POINT('Ctrl Pts',(-2.60250042474766,9.73470771305938,0.000337104101208169));
#93866=CARTESIAN_POINT('Ctrl Pts',(-4.17620603742513,9.31398942894217,0.026065973894913));
#93867=CARTESIAN_POINT('Ctrl Pts',(-7.11443254118295,7.6957742419676,0.0775237134823225));
#93868=CARTESIAN_POINT('Ctrl Pts',(-9.88170779441914,3.49088825292512,0.154710322863437));
#93869=CARTESIAN_POINT('Ctrl Pts',(-10.3696118635881,-1.51802545263044,
0.231896932244551));
#93870=CARTESIAN_POINT('Ctrl Pts',(-8.46615891068372,-6.1773600095809,0.309083541625665));
#93871=CARTESIAN_POINT('Ctrl Pts',(-4.61007004150353,-9.41175154011344,
0.38627015100678));
#93872=CARTESIAN_POINT('Ctrl Pts',(0.309190375968473,-10.4756492852767,
0.463456760387894));
#93873=CARTESIAN_POINT('Ctrl Pts',(5.15716569486616,-9.1234875171854,0.540643369769009));
#93874=CARTESIAN_POINT('Ctrl Pts',(8.81573533404148,-5.66721546296529,0.617829979150123));
#93875=CARTESIAN_POINT('Ctrl Pts',(10.4411434074219,-0.90389988182744,0.695016588531238));
#93876=CARTESIAN_POINT('Ctrl Pts',(9.65851409104835,4.06787287683326,0.772203197912351));
#93877=CARTESIAN_POINT('Ctrl Pts',(6.64834923647149,8.1014790533001,0.849389807293467));
#93878=CARTESIAN_POINT('Ctrl Pts',(2.10487898349287,10.2666439587759,0.92657641667458));
#93879=CARTESIAN_POINT('Ctrl Pts',(-2.92403780237063,10.064020314243,1.0037630260557));
#93880=CARTESIAN_POINT('Ctrl Pts',(-7.27858577628976,7.54033738966125,1.08094963543681));
#93881=CARTESIAN_POINT('Ctrl Pts',(-9.95447796485031,3.27763145687328,1.15813624481793));
#93882=CARTESIAN_POINT('Ctrl Pts',(-10.3345751767764,-1.74099271462887,
1.23532285419904));
#93883=CARTESIAN_POINT('Ctrl Pts',(-8.33121575360925,-6.35809275148398,
1.31250946358015));
#93884=CARTESIAN_POINT('Ctrl Pts',(-4.40643326471,-9.5088298708975,1.38969607296127));
#93885=CARTESIAN_POINT('Ctrl Pts',(0.534602178678755,-10.4665514853921,
1.46688268234238));
#93886=CARTESIAN_POINT('Ctrl Pts',(5.35234265263788,-9.01037888642927,1.5440692917235));
#93887=CARTESIAN_POINT('Ctrl Pts',(8.9356756897984,-5.47614823539465,1.62125590110461));
#93888=CARTESIAN_POINT('Ctrl Pts',(10.4581794303881,-0.678956944208766,
1.69844251048573));
#93889=CARTESIAN_POINT('Ctrl Pts',(9.56871979020855,4.27482176361841,1.77562911986684));
#93890=CARTESIAN_POINT('Ctrl Pts',(6.47243228913536,8.24270100106766,1.85281572924795));
#93891=CARTESIAN_POINT('Ctrl Pts',(1.88341177736483,10.3095712621668,1.93000233862907));
#93892=CARTESIAN_POINT('Ctrl Pts',(-3.13997881473699,9.99875155080307,2.00718894801018));
#93893=CARTESIAN_POINT('Ctrl Pts',(-7.439198056598,7.38192602284617,2.0843755573913));
#93894=CARTESIAN_POINT('Ctrl Pts',(-10.0227197033554,3.06261151306865,2.16156216677241));
#93895=CARTESIAN_POINT('Ctrl Pts',(-10.2947077734096,-1.96303117452732,
2.23874877615352));
#93896=CARTESIAN_POINT('Ctrl Pts',(-8.19243382826692,-6.53594121004401,
2.31593538553464));
#93897=CARTESIAN_POINT('Ctrl Pts',(-4.20074399310361,-9.60147121212246,
2.39312199491575));
#93898=CARTESIAN_POINT('Ctrl Pts',(0.759760801971393,-10.4526199134108,
2.47030860429687));
#93899=CARTESIAN_POINT('Ctrl Pts',(5.54504243837757,-8.89308742174652,2.54749521367798));
#93900=CARTESIAN_POINT('Ctrl Pts',(9.0514744054115,-5.28254773934542,2.6246818230591));
#93901=CARTESIAN_POINT('Ctrl Pts',(10.4703704910301,-0.453697376934528,
2.70186843244021));
#93902=CARTESIAN_POINT('Ctrl Pts',(9.47449157942137,4.47978893026564,2.77905504182133));
#93903=CARTESIAN_POINT('Ctrl Pts',(6.29351659914733,8.38010431331672,2.85624165120244));
#93904=CARTESIAN_POINT('Ctrl Pts',(1.66107182433835,10.347721489507,2.93342826058356));
#93905=CARTESIAN_POINT('Ctrl Pts',(-3.3544649115547,9.92885011100522,3.01061486996467));
#93906=CARTESIAN_POINT('Ctrl Pts',(-7.5963634927572,7.22009427935256,3.08780147934578));
#93907=CARTESIAN_POINT('Ctrl Pts',(-10.0863175325862,2.84617254424586,3.1649880887269));
#93908=CARTESIAN_POINT('Ctrl Pts',(-10.2500704286301,-2.18416003554074,
3.24217469810801));
#93909=CARTESIAN_POINT('Ctrl Pts',(-8.04985607047069,-6.71076144710083,
3.31936130748913));
#93910=CARTESIAN_POINT('Ctrl Pts',(-3.99310828706469,-9.68966356068127,
3.39654791687024));
#93911=CARTESIAN_POINT('Ctrl Pts',(0.984567258195362,-10.4338457787741,
3.47373452625136));
#93912=CARTESIAN_POINT('Ctrl Pts',(5.7351732752715,-8.77167439498682,3.55092113563247));
#93913=CARTESIAN_POINT('Ctrl Pts',(9.16307867541303,-5.08650172897933,3.62810774501358));
#93914=CARTESIAN_POINT('Ctrl Pts',(10.4777113261985,-0.228223461525968,
3.7052943543947));
#93915=CARTESIAN_POINT('Ctrl Pts',(9.37587131291801,4.68267227169952,3.78248096377581));
#93916=CARTESIAN_POINT('Ctrl Pts',(6.11168916100159,8.51364095061604,3.85966757315693));
#93917=CARTESIAN_POINT('Ctrl Pts',(1.43795377928683,10.3810453119631,3.93685418253804));
#93918=CARTESIAN_POINT('Ctrl Pts',(-3.56738003678192,9.85441135035922,4.01404079191916));
#93919=CARTESIAN_POINT('Ctrl Pts',(-7.75004242324465,7.05479226584377,4.09122740130027));
#93920=CARTESIAN_POINT('Ctrl Pts',(-10.1451748614197,2.62866444414504,4.16841401068139));
#93921=CARTESIAN_POINT('Ctrl Pts',(-10.2008382774016,-2.40515970586688,
4.24560611132689));
#93922=CARTESIAN_POINT('Ctrl Pts',(-8.66860765197138,-5.38957635420927,
4.29706934217869));
#93923=CARTESIAN_POINT('Ctrl Pts',(-7.59848317952396,-6.61820187589613,
4.32280370323678));
#93924=CARTESIAN_POINT('Ctrl Pts',(-2.5542913309526,9.55438058121967,-0.107431152205371));
#93925=CARTESIAN_POINT('Ctrl Pts',(-4.09884539354156,9.14145574336953,-0.0817022824116669));
#93926=CARTESIAN_POINT('Ctrl Pts',(-6.98264376512165,7.55321660826708,-0.0302445428242573));
#93927=CARTESIAN_POINT('Ctrl Pts',(-9.69865761183838,3.42622253467468,0.0469420665568571));
#93928=CARTESIAN_POINT('Ctrl Pts',(-10.1775236755531,-1.48990532986955,
0.124128675937972));
#93929=CARTESIAN_POINT('Ctrl Pts',(-8.30933056009907,-6.06292970045364,
0.201315285319086));
#93930=CARTESIAN_POINT('Ctrl Pts',(-4.52467243813745,-9.23740689507186,
0.278501894700201));
#93931=CARTESIAN_POINT('Ctrl Pts',(0.303462888781973,-10.2815968447254,
0.355688504081315));
#93932=CARTESIAN_POINT('Ctrl Pts',(5.0616336125901,-8.95448271654383,0.432875113462429));
#93933=CARTESIAN_POINT('Ctrl Pts',(8.65243137929479,-5.56223514510909,0.510061722843545));
#93934=CARTESIAN_POINT('Ctrl Pts',(10.2477301587364,-0.887155909849574,
0.587248332224658));
#93935=CARTESIAN_POINT('Ctrl Pts',(9.47959838086883,3.99251901206505,0.664434941605773));
#93936=CARTESIAN_POINT('Ctrl Pts',(6.52519425487164,7.95140608507103,0.741621550986887));
#93937=CARTESIAN_POINT('Ctrl Pts',(2.06588790115624,10.0764631630832,0.818808160368001));
#93938=CARTESIAN_POINT('Ctrl Pts',(-2.86987250374691,9.87759294821029,0.895994769749116));
#93939=CARTESIAN_POINT('Ctrl Pts',(-7.14375620198966,7.40065909066546,0.97318137913023));
#93940=CARTESIAN_POINT('Ctrl Pts',(-9.77007977712095,3.21691613831752,1.05036798851134));
#93941=CARTESIAN_POINT('Ctrl Pts',(-10.1431360133889,-1.70874231409945,
1.12755459789246));
#93942=CARTESIAN_POINT('Ctrl Pts',(-8.17688710955856,-6.24031452293913,
1.20474120727357));
#93943=CARTESIAN_POINT('Ctrl Pts',(-4.32480785841224,-9.33268693283367,
1.28192781665468));
#93944=CARTESIAN_POINT('Ctrl Pts',(0.524699130698473,-10.2726675738001,
1.3591144260358));
#93945=CARTESIAN_POINT('Ctrl Pts',(5.25319508420306,-8.84346932640218,1.43630103541691));
#93946=CARTESIAN_POINT('Ctrl Pts',(8.77014994257647,-5.37470727446133,1.51348764479803));
#93947=CARTESIAN_POINT('Ctrl Pts',(10.2644506039523,-0.666379847699995,
1.59067425417914));
#93948=CARTESIAN_POINT('Ctrl Pts',(9.39146744262841,4.19563434777797,1.66786086356025));
#93949=CARTESIAN_POINT('Ctrl Pts',(6.3525360184789,8.09001201707886,1.74504747294137));
#93950=CARTESIAN_POINT('Ctrl Pts',(1.84852318554509,10.1185952749053,1.82223408232248));
#93951=CARTESIAN_POINT('Ctrl Pts',(-3.08181339360786,9.81353323277227,1.8994206917036));
#93952=CARTESIAN_POINT('Ctrl Pts',(-7.30139327721728,7.24518215889154,1.97660730108471));
#93953=CARTESIAN_POINT('Ctrl Pts',(-9.83705739580452,3.00587925501121,2.05379391046583));
#93954=CARTESIAN_POINT('Ctrl Pts',(-10.1040071195608,-1.92666770149365,
2.13098051984694));
#93955=CARTESIAN_POINT('Ctrl Pts',(-8.04067600064811,-6.41486849096287,
2.20816712922805));
#93956=CARTESIAN_POINT('Ctrl Pts',(-4.12292880458458,-9.42361217247189,
2.28535373860917));
#93957=CARTESIAN_POINT('Ctrl Pts',(0.745686883129435,-10.2589940722704,
2.36254034799028));
#93958=CARTESIAN_POINT('Ctrl Pts',(5.44232527127653,-8.72835058575378,2.4397269573714));
#93959=CARTESIAN_POINT('Ctrl Pts',(8.88380358605459,-5.18469306196619,2.51691356675251));
#93960=CARTESIAN_POINT('Ctrl Pts',(10.2764158356259,-0.445293021188328,
2.59410017613363));
#93961=CARTESIAN_POINT('Ctrl Pts',(9.29898472882896,4.39680467302303,2.67128678551474));
#93962=CARTESIAN_POINT('Ctrl Pts',(6.17693458857629,8.22487005052414,2.74847339489586));
#93963=CARTESIAN_POINT('Ctrl Pts',(1.63030188992512,10.1560388019235,2.82566000427697));
#93964=CARTESIAN_POINT('Ctrl Pts',(-3.29232631898595,9.74492665734239,2.90284661365808));
#93965=CARTESIAN_POINT('Ctrl Pts',(-7.45564735813477,7.08634820999072,2.9800332230392));
#93966=CARTESIAN_POINT('Ctrl Pts',(-9.89947712966015,2.79344963291115,3.05721983242031));
#93967=CARTESIAN_POINT('Ctrl Pts',(-10.0601966434038,-2.14370033954394,
3.13440644180143));
#93968=CARTESIAN_POINT('Ctrl Pts',(-7.90073937383241,-6.58645033269596,
3.21159305118254));
#93969=CARTESIAN_POINT('Ctrl Pts',(-3.91913937235699,-9.51017083322676,
3.28877966056366));
#93970=CARTESIAN_POINT('Ctrl Pts',(0.96632899208538,-10.2405677124156,3.36596626994477));
#93971=CARTESIAN_POINT('Ctrl Pts',(5.62893409708374,-8.60918663143969,3.44315287932589));
#93972=CARTESIAN_POINT('Ctrl Pts',(8.99334048243757,-4.99227863621464,3.520339488707));
#93973=CARTESIAN_POINT('Ctrl Pts',(10.2836206881034,-0.223995817158145,
3.59752609808812));
#93974=CARTESIAN_POINT('Ctrl Pts',(9.20219131838785,4.59592977413402,3.67471270746923));
#93975=CARTESIAN_POINT('Ctrl Pts',(5.99847534815945,8.35593303586498,3.75189931685034));
#93976=CARTESIAN_POINT('Ctrl Pts',(1.41131691576919,10.1887453290789,3.82908592623146));
#93977=CARTESIAN_POINT('Ctrl Pts',(-3.50129737367821,9.67186681105117,3.90627253561257));
#93978=CARTESIAN_POINT('Ctrl Pts',(-7.6064795179152,6.92410827485778,3.98345914499369));
#93979=CARTESIAN_POINT('Ctrl Pts',(-9.95724417683243,2.57997068427531,4.0606457543748));
#93980=CARTESIAN_POINT('Ctrl Pts',(-10.0118764756561,-2.36060618005391,
4.13783785502032));
#93981=CARTESIAN_POINT('Ctrl Pts',(-8.50802911165971,-5.28973906330818,
4.18930108587212));
#93982=CARTESIAN_POINT('Ctrl Pts',(-7.45772777951767,-6.49560534835832,
4.21503544693021));
#93983=CARTESIAN_POINT('Ctrl Pts',(-2.50608223715753,9.37405344937994,-0.215199408511951));
#93984=CARTESIAN_POINT('Ctrl Pts',(-4.02148474965799,8.96892205779688,-0.189470538718247));
#93985=CARTESIAN_POINT('Ctrl Pts',(-6.85085498906034,7.41065897456655,-0.138012799130837));
#93986=CARTESIAN_POINT('Ctrl Pts',(-9.51560742925762,3.36155681642425,-0.0608261897497226));
#93987=CARTESIAN_POINT('Ctrl Pts',(-9.9854354875181,-1.46178520710867,0.0163604196313919));
#93988=CARTESIAN_POINT('Ctrl Pts',(-8.15250220951439,-5.94849939132635,
0.093547029012506));
#93989=CARTESIAN_POINT('Ctrl Pts',(-4.43927483477137,-9.06306225003029,
0.170733638393621));
#93990=CARTESIAN_POINT('Ctrl Pts',(0.297735401595483,-10.0875444041741,
0.247920247774735));
#93991=CARTESIAN_POINT('Ctrl Pts',(4.96610153031403,-8.78547791590226,0.32510685715585));
#93992=CARTESIAN_POINT('Ctrl Pts',(8.4891274245481,-5.45725482725287,0.402293466536964));
#93993=CARTESIAN_POINT('Ctrl Pts',(10.0543169100508,-0.870411937871706,
0.479480075918078));
#93994=CARTESIAN_POINT('Ctrl Pts',(9.30068267068929,3.91716514729685,0.556666685299193));
#93995=CARTESIAN_POINT('Ctrl Pts',(6.40203927327179,7.80133311684196,0.633853294680306));
#93996=CARTESIAN_POINT('Ctrl Pts',(2.0268968188196,9.88628236739044,0.711039904061421));
#93997=CARTESIAN_POINT('Ctrl Pts',(-2.81570720512321,9.69116558217758,0.788226513442536));
#93998=CARTESIAN_POINT('Ctrl Pts',(-7.00892662768955,7.26098079166965,0.86541312282365));
#93999=CARTESIAN_POINT('Ctrl Pts',(-9.58568158939161,3.15620081976177,0.942599732204765));
#94000=CARTESIAN_POINT('Ctrl Pts',(-9.95169685000138,-1.67649191357006,
1.01978634158588));
#94001=CARTESIAN_POINT('Ctrl Pts',(-8.02255846550788,-6.12253629439428,
1.09697295096699));
#94002=CARTESIAN_POINT('Ctrl Pts',(-4.24318245211449,-9.15654399476985,
1.17415956034811));
#94003=CARTESIAN_POINT('Ctrl Pts',(0.514796082718195,-10.078783662208,1.25134616972922));
#94004=CARTESIAN_POINT('Ctrl Pts',(5.15404751576823,-8.6765597663751,1.32853277911034));
#94005=CARTESIAN_POINT('Ctrl Pts',(8.60462419535454,-5.27326631352799,1.40571938849145));
#94006=CARTESIAN_POINT('Ctrl Pts',(10.0707217775164,-0.653802751191223,
1.48290599787256));
#94007=CARTESIAN_POINT('Ctrl Pts',(9.21421509504826,4.11644693193751,1.56009260725368));
#94008=CARTESIAN_POINT('Ctrl Pts',(6.23263974782243,7.93732303309007,1.63727921663479));
#94009=CARTESIAN_POINT('Ctrl Pts',(1.81363459372535,9.92761928764379,1.71446582601591));
#94010=CARTESIAN_POINT('Ctrl Pts',(-3.02364797247873,9.62831491474147,1.79165243539702));
#94011=CARTESIAN_POINT('Ctrl Pts',(-7.16358849783658,7.10843829493689,1.86883904477814));
#94012=CARTESIAN_POINT('Ctrl Pts',(-9.65139508825367,2.94914699695377,1.94602565415925));
#94013=CARTESIAN_POINT('Ctrl Pts',(-9.91330646571203,-1.89030422845998,
2.02321226354037));
#94014=CARTESIAN_POINT('Ctrl Pts',(-7.88891817302927,-6.29379577188174,
2.10039887292148));
#94015=CARTESIAN_POINT('Ctrl Pts',(-4.04511361606556,-9.24575313282132,
2.17758548230259));
#94016=CARTESIAN_POINT('Ctrl Pts',(0.731612964287487,-10.0653682311302,
2.25477209168371));
#94017=CARTESIAN_POINT('Ctrl Pts',(5.33960810417548,-8.56361374976105,2.33195870106482));
#94018=CARTESIAN_POINT('Ctrl Pts',(8.71613276669772,-5.08683838458696,2.40914531044594));
#94019=CARTESIAN_POINT('Ctrl Pts',(10.0824611802217,-0.436888665442129,
2.48633191982705));
#94020=CARTESIAN_POINT('Ctrl Pts',(9.12347787823656,4.31382041578043,2.56351852920817));
#94021=CARTESIAN_POINT('Ctrl Pts',(6.06035257800524,8.06963578773155,2.64070513858928));
#94022=CARTESIAN_POINT('Ctrl Pts',(1.5995319555119,9.96435611433997,2.7178917479704));
#94023=CARTESIAN_POINT('Ctrl Pts',(-3.2301877264172,9.56100320367956,2.79507835735151));
#94024=CARTESIAN_POINT('Ctrl Pts',(-7.31493122351235,6.95260214062888,2.87226496673263));
#94025=CARTESIAN_POINT('Ctrl Pts',(-9.71263672673402,2.74072672157646,2.94945157611374));
#94026=CARTESIAN_POINT('Ctrl Pts',(-9.87032285817758,-2.10324064354715,
3.02663818549485));
#94027=CARTESIAN_POINT('Ctrl Pts',(-7.75162267719414,-6.46213921829106,
3.10382479487597));
#94028=CARTESIAN_POINT('Ctrl Pts',(-3.84517045764928,-9.33067810577225,
3.18101140425708));
#94029=CARTESIAN_POINT('Ctrl Pts',(0.948090725975405,-10.0472896460573,
3.2581980136382));
#94030=CARTESIAN_POINT('Ctrl Pts',(5.52269491889597,-8.44669886789258,3.33538462301931));
#94031=CARTESIAN_POINT('Ctrl Pts',(8.82360228946212,-4.89805554344996,3.41257123240042));
#94032=CARTESIAN_POINT('Ctrl Pts',(10.0895300500082,-0.219768172790326,
3.48975784178154));
#94033=CARTESIAN_POINT('Ctrl Pts',(9.02851132385769,4.50918727656851,3.56694445116265));
#94034=CARTESIAN_POINT('Ctrl Pts',(5.88526153531729,8.19822512111389,3.64413106054377));
#94035=CARTESIAN_POINT('Ctrl Pts',(1.38468005225154,9.99644534619459,3.72131766992488));
#94036=CARTESIAN_POINT('Ctrl Pts',(-3.43521471057451,9.48932227174309,3.798504279306));
#94037=CARTESIAN_POINT('Ctrl Pts',(-7.46291661258574,6.79342428387181,3.87569088868711));
#94038=CARTESIAN_POINT('Ctrl Pts',(-9.76931349224516,2.53127692440558,3.95287749806823));
#94039=CARTESIAN_POINT('Ctrl Pts',(-9.82291467391069,-2.31605265424095,
4.03006959871373));
#94040=CARTESIAN_POINT('Ctrl Pts',(-8.34745057134804,-5.1899017724071,4.08153282956553));
#94041=CARTESIAN_POINT('Ctrl Pts',(-7.3169723795114,-6.37300882082051,4.10726719062362));
#94042=CARTESIAN_POINT('Ctrl Pts',(-2.45787314336247,9.19372631754022,-0.322967664818532));
#94043=CARTESIAN_POINT('Ctrl Pts',(-3.94412410577443,8.79638837222423,-0.297238795024827));
#94044=CARTESIAN_POINT('Ctrl Pts',(-6.71906621299902,7.26810134086602,-0.245781055437418));
#94045=CARTESIAN_POINT('Ctrl Pts',(-9.33255724667688,3.29689109817383,-0.168594446056303));
#94046=CARTESIAN_POINT('Ctrl Pts',(-9.79334729948307,-1.43366508434778,
-0.0914078366751879));
#94047=CARTESIAN_POINT('Ctrl Pts',(-7.99567385892974,-5.83406908219907,
-0.0142212272940741));
#94048=CARTESIAN_POINT('Ctrl Pts',(-4.3538772314053,-8.88871760498874,0.062965382087041));
#94049=CARTESIAN_POINT('Ctrl Pts',(0.292007914408984,-9.89349196362283,
0.140151991468154));
#94050=CARTESIAN_POINT('Ctrl Pts',(4.87056944803797,-8.6164731152607,0.21733860084927));
#94051=CARTESIAN_POINT('Ctrl Pts',(8.32582346980139,-5.35227450939667,0.294525210230383));
#94052=CARTESIAN_POINT('Ctrl Pts',(9.86090366136514,-0.85366796589384,0.371711819611499));
#94053=CARTESIAN_POINT('Ctrl Pts',(9.12176696050975,3.84181128252864,0.448898428992612));
#94054=CARTESIAN_POINT('Ctrl Pts',(6.27888429167194,7.6512601486129,0.526085038373727));
#94055=CARTESIAN_POINT('Ctrl Pts',(1.98790573648296,9.69610157169772,0.603271647754841));
#94056=CARTESIAN_POINT('Ctrl Pts',(-2.76154190649949,9.50473821614484,0.680458257135956));
#94057=CARTESIAN_POINT('Ctrl Pts',(-6.87409705338946,7.12130249267385,0.75764486651707));
#94058=CARTESIAN_POINT('Ctrl Pts',(-9.40128340166224,3.09548550120601,0.834831475898185));
#94059=CARTESIAN_POINT('Ctrl Pts',(-9.76025768661387,-1.64424151304064,
0.912018085279298));
#94060=CARTESIAN_POINT('Ctrl Pts',(-7.86822982145718,-6.00475806584942,
0.989204694660414));
#94061=CARTESIAN_POINT('Ctrl Pts',(-4.16155704581674,-8.98040105670602,
1.06639130404152));
#94062=CARTESIAN_POINT('Ctrl Pts',(0.504893034737917,-9.88489975061589,
1.14357791342264));
#94063=CARTESIAN_POINT('Ctrl Pts',(5.0548999473334,-8.50965020634803,1.22076452280375));
#94064=CARTESIAN_POINT('Ctrl Pts',(8.43909844813259,-5.17182535259465,1.29795113218487));
#94065=CARTESIAN_POINT('Ctrl Pts',(9.87699295108057,-0.641225654682458,
1.37513774156598));
#94066=CARTESIAN_POINT('Ctrl Pts',(9.03696274746812,4.03725951609706,1.45232435094709));
#94067=CARTESIAN_POINT('Ctrl Pts',(6.11274347716597,7.78463404910127,1.52951096032821));
#94068=CARTESIAN_POINT('Ctrl Pts',(1.77874600190563,9.73664330038228,1.60669756970932));
#94069=CARTESIAN_POINT('Ctrl Pts',(-2.96548255134962,9.44309659671067,1.68388417909044));
#94070=CARTESIAN_POINT('Ctrl Pts',(-7.02578371845584,6.97169443098224,1.76107078847155));
#94071=CARTESIAN_POINT('Ctrl Pts',(-9.46573278070284,2.89241473889634,1.83825739785267));
#94072=CARTESIAN_POINT('Ctrl Pts',(-9.72260581186326,-1.85394075542631,
1.91544400723378));
#94073=CARTESIAN_POINT('Ctrl Pts',(-7.73716034541045,-6.17272305280058,
1.9926306166149));
#94074=CARTESIAN_POINT('Ctrl Pts',(-3.96729842754654,-9.06789409317076,
2.06981722599601));
#94075=CARTESIAN_POINT('Ctrl Pts',(0.717539045445532,-9.87174238998988,
2.14700383537712));
#94076=CARTESIAN_POINT('Ctrl Pts',(5.23689093707443,-8.39887691376832,2.22419044475824));
#94077=CARTESIAN_POINT('Ctrl Pts',(8.54846194734082,-4.98898370720772,2.30137705413935));
#94078=CARTESIAN_POINT('Ctrl Pts',(9.88850652481755,-0.428484309695933,
2.37856366352047));
#94079=CARTESIAN_POINT('Ctrl Pts',(8.94797102764415,4.23083615853781,2.45575027290158));
#94080=CARTESIAN_POINT('Ctrl Pts',(5.94377056743419,7.91440152493896,2.5329368822827));
#94081=CARTESIAN_POINT('Ctrl Pts',(1.56876202109868,9.77267342675648,2.61012349166382));
#94082=CARTESIAN_POINT('Ctrl Pts',(-3.16804913384846,9.37707975001673,2.68731010104494));
#94083=CARTESIAN_POINT('Ctrl Pts',(-7.17421508888992,6.81885607126705,2.76449671042605));
#94084=CARTESIAN_POINT('Ctrl Pts',(-9.52579632380792,2.68800381024176,2.84168331980716));
#94085=CARTESIAN_POINT('Ctrl Pts',(-9.6804490729513,-2.06278094755036,2.91886992918827));
#94086=CARTESIAN_POINT('Ctrl Pts',(-7.60250598055586,-6.33782810388617,
2.99605653856938));
#94087=CARTESIAN_POINT('Ctrl Pts',(-3.77120154294156,-9.15118537831773,
3.0732431479505));
#94088=CARTESIAN_POINT('Ctrl Pts',(0.929852459865417,-9.85401157969884,
3.15042975733161));
#94089=CARTESIAN_POINT('Ctrl Pts',(5.41645574070821,-8.28421110434545,3.22761636671273));
#94090=CARTESIAN_POINT('Ctrl Pts',(8.65386409648666,-4.80383245068529,3.30480297609384));
#94091=CARTESIAN_POINT('Ctrl Pts',(9.89543941191297,-0.215540528422498,
3.38198958547497));
#94092=CARTESIAN_POINT('Ctrl Pts',(8.85483132932753,4.422444779003,3.45917619485608));
#94093=CARTESIAN_POINT('Ctrl Pts',(5.77204772247514,8.04051720636283,3.53636280423719));
#94094=CARTESIAN_POINT('Ctrl Pts',(1.3580431887339,9.80414536331033,3.61354941361831));
#94095=CARTESIAN_POINT('Ctrl Pts',(-3.3691320474708,9.30677773243504,3.69073602299942));
#94096=CARTESIAN_POINT('Ctrl Pts',(-7.31935370725628,6.66274029288581,3.76792263238054));
#94097=CARTESIAN_POINT('Ctrl Pts',(-9.58138280765788,2.48258316453586,3.84510924176164));
#94098=CARTESIAN_POINT('Ctrl Pts',(-9.63395287216528,-2.27149912842799,
3.92230134240716));
#94099=CARTESIAN_POINT('Ctrl Pts',(-8.18687203103637,-5.09006448150602,
3.97376457325895));
#94100=CARTESIAN_POINT('Ctrl Pts',(-7.1762169795051,-6.2504122932827,3.99949893431705));
#94101=CARTESIAN_POINT('Ctrl Pts',(-7.17753992463813,-6.25025814508694,
4.));
#94102=CARTESIAN_POINT('Ctrl Pts',(-7.33747899506258,-6.07698634554822,
4.));
#94103=CARTESIAN_POINT('Ctrl Pts',(-7.49056477224393,-5.89798477017908,
4.));
#94104=CARTESIAN_POINT('Ctrl Pts',(-7.63665808758676,-5.71375997989628,
4.));
#94105=CARTESIAN_POINT('Ctrl Pts',(-7.78906164494726,-5.5215779260685,3.99999999999999));
#94106=CARTESIAN_POINT('Ctrl Pts',(-7.93385621938739,-5.32371142534202,
4.));
#94107=CARTESIAN_POINT('Ctrl Pts',(-8.07084803407231,-5.12068881632814,
4.));
#94108=CARTESIAN_POINT('Ctrl Pts',(-8.20560462808296,-4.920978816422,4.));
#94109=CARTESIAN_POINT('Ctrl Pts',(-8.33281124379099,-4.71627890600225,
4.));
#94110=CARTESIAN_POINT('Ctrl Pts',(-8.45224397122025,-4.50705565782589,
4.));
#94111=CARTESIAN_POINT('Ctrl Pts',(-8.57464826197255,-4.29262680023249,
4.));
#94112=CARTESIAN_POINT('Ctrl Pts',(-8.68888758368522,-4.07344621776482,
4.));
#94113=CARTESIAN_POINT('Ctrl Pts',(-8.7946726372693,-3.84998637008127,4.));
#94114=CARTESIAN_POINT('Ctrl Pts',(-8.90045769085338,-3.62652652239772,
4.));
#94115=CARTESIAN_POINT('Ctrl Pts',(-8.99778888243601,-3.39878676423124,
4.));
#94116=CARTESIAN_POINT('Ctrl Pts',(-9.08632214621229,-3.16721896610309,
3.99999999999999));
#94117=CARTESIAN_POINT('Ctrl Pts',(-9.09637755523444,-3.14091801629939,
3.99999999999999));
#94118=CARTESIAN_POINT('Ctrl Pts',(-9.10632000329729,-3.1145660732672,4.));
#94119=CARTESIAN_POINT('Ctrl Pts',(-9.11614707610044,-3.08816879512771,
4.));
#94120=CARTESIAN_POINT('Ctrl Pts',(-9.2011017289242,-2.8599653774107,4.));
#94121=CARTESIAN_POINT('Ctrl Pts',(-9.27721888532258,-2.6289661896699,3.99999999999999));
#94122=CARTESIAN_POINT('Ctrl Pts',(-9.34430660102968,-2.39565692690494,
3.99999999999999));
#94123=CARTESIAN_POINT('Ctrl Pts',(-9.36164354845565,-2.33536466057994,
3.99999999999999));
#94124=CARTESIAN_POINT('Ctrl Pts',(-9.37837727232265,-2.27491796400755,
3.99999999999999));
#94125=CARTESIAN_POINT('Ctrl Pts',(-9.39450398955669,-2.21432490746539,
3.99999999999999));
#94126=CARTESIAN_POINT('Ctrl Pts',(-9.45637742813918,-1.98184729233293,
3.99999999999999));
#94127=CARTESIAN_POINT('Ctrl Pts',(-9.50931939125301,-1.74721683731709,
4.));
#94128=CARTESIAN_POINT('Ctrl Pts',(-9.5534046592155,-1.51095720471577,3.99999999999999));
#94129=CARTESIAN_POINT('Ctrl Pts',(-9.59786987686295,-1.2726613641674,3.99999999999999));
#94130=CARTESIAN_POINT('Ctrl Pts',(-9.63332517643522,-1.03270751657381,
3.99999999999999));
#94131=CARTESIAN_POINT('Ctrl Pts',(-9.6597965096359,-0.791617070439592,
4.));
#94132=CARTESIAN_POINT('Ctrl Pts',(-9.68630729112195,-0.550167344904968,
4.));
#94133=CARTESIAN_POINT('Ctrl Pts',(-9.70380736090579,-0.307576969625407,
3.99999999999999));
#94134=CARTESIAN_POINT('Ctrl Pts',(-9.71227104245719,-0.0643635234899073,
3.99999999999999));
#94135=CARTESIAN_POINT('Ctrl Pts',(-9.71962412171651,0.14693551174726,4.));
#94136=CARTESIAN_POINT('Ctrl Pts',(-9.72015594631123,0.358705188501749,
4.));
#94137=CARTESIAN_POINT('Ctrl Pts',(-9.71381756308937,0.570603998902445,
4.));
#94138=CARTESIAN_POINT('Ctrl Pts',(-9.71288073663889,0.601923091399803,
4.));
#94139=CARTESIAN_POINT('Ctrl Pts',(-9.71179372592443,0.633244541288576,
4.));
#94140=CARTESIAN_POINT('Ctrl Pts',(-9.71055727203426,0.664548046919412,
4.));
#94141=CARTESIAN_POINT('Ctrl Pts',(-9.70089181440524,0.909250020620887,
4.));
#94142=CARTESIAN_POINT('Ctrl Pts',(-9.68209046391963,1.15315389789666,4.));
#94143=CARTESIAN_POINT('Ctrl Pts',(-9.6542249499493,1.3957320236345,4.));
#94144=CARTESIAN_POINT('Ctrl Pts',(-9.62623041699829,1.63943330046702,4.));
#94145=CARTESIAN_POINT('Ctrl Pts',(-9.58908764235844,1.88179718600469,4.));
#94146=CARTESIAN_POINT('Ctrl Pts',(-9.54281751783194,2.1222959970689,4.));
#94147=CARTESIAN_POINT('Ctrl Pts',(-9.52144752059438,2.23337110180816,4.));
#94148=CARTESIAN_POINT('Ctrl Pts',(-9.49812985694202,2.3440484113249,4.));
#94149=CARTESIAN_POINT('Ctrl Pts',(-9.47286282919077,2.45427585926503,4.));
#94150=CARTESIAN_POINT('Ctrl Pts',(-9.4182963957366,2.69232201024344,4.));
#94151=CARTESIAN_POINT('Ctrl Pts',(-9.35464183349599,2.92827092193509,4.00000000000001));
#94152=CARTESIAN_POINT('Ctrl Pts',(-9.28216423542203,3.16167818670979,4.00000000000001));
#94153=CARTESIAN_POINT('Ctrl Pts',(-9.20955177323737,3.39551976862565,4.00000000000001));
#94154=CARTESIAN_POINT('Ctrl Pts',(-9.12808315699099,3.62681083804243,4.));
#94155=CARTESIAN_POINT('Ctrl Pts',(-9.03797543804018,3.8550878224443,4.00000000000001));
#94156=CARTESIAN_POINT('Ctrl Pts',(-8.9872605556436,3.98356783006835,4.00000000000001));
#94157=CARTESIAN_POINT('Ctrl Pts',(-8.93380817564648,4.11109270907783,4.00000000000001));
#94158=CARTESIAN_POINT('Ctrl Pts',(-8.87765057142394,4.23757638926947,4.));
#94159=CARTESIAN_POINT('Ctrl Pts',(-8.86122721555927,4.27456668683681,4.00000000000001));
#94160=CARTESIAN_POINT('Ctrl Pts',(-8.84457048332952,4.31147200181025,4.00000000000001));
#94161=CARTESIAN_POINT('Ctrl Pts',(-8.82769641176815,4.34825743645122,4.00000000000001));
#94162=CARTESIAN_POINT('Ctrl Pts',(-8.72485965105928,4.5724413227164,4.00000000000001));
#94163=CARTESIAN_POINT('Ctrl Pts',(-8.61384851499838,4.79241839623982,4.00000000000001));
#94164=CARTESIAN_POINT('Ctrl Pts',(-8.49498741868439,5.00775935556626,4.00000000000001));
#94165=CARTESIAN_POINT('Ctrl Pts',(-8.37548461346274,5.22426290060047,4.00000000000001));
#94166=CARTESIAN_POINT('Ctrl Pts',(-8.24804660570247,5.43608074067127,4.00000000000001));
#94167=CARTESIAN_POINT('Ctrl Pts',(-8.11295177885207,5.64276338936583,4.00000000000001));
#94168=CARTESIAN_POINT('Ctrl Pts',(-7.97823605130347,5.84886605102726,4.00000000000001));
#94169=CARTESIAN_POINT('Ctrl Pts',(-7.83590610828956,6.04986288481014,4.00000000000001));
#94170=CARTESIAN_POINT('Ctrl Pts',(-7.68619142052777,6.2452862224332,4.00000000000001));
#94171=CARTESIAN_POINT('Ctrl Pts',(-7.57338204776326,6.39253686611006,4.));
#94172=CARTESIAN_POINT('Ctrl Pts',(-7.45637896623167,6.53662273702222,4.00000000000001));
#94173=CARTESIAN_POINT('Ctrl Pts',(-7.33526436842416,6.67733244061277,4.00000000000001));
#94174=CARTESIAN_POINT('Ctrl Pts',(-7.20393059754577,6.82991467517624,4.00000000000001));
#94175=CARTESIAN_POINT('Ctrl Pts',(-7.06776223834323,6.97852728621961,4.));
#94176=CARTESIAN_POINT('Ctrl Pts',(-6.92698192470154,7.12300597353219,4.));
#94177=CARTESIAN_POINT('Ctrl Pts',(-6.86539053748327,7.18621539923147,4.));
#94178=CARTESIAN_POINT('Ctrl Pts',(-6.80291619401115,7.24863334469569,4.));
#94179=CARTESIAN_POINT('Ctrl Pts',(-6.73957666848095,7.3102449686502,4.));
#94180=CARTESIAN_POINT('Ctrl Pts',(-6.71407204307116,7.33505382815293,4.));
#94181=CARTESIAN_POINT('Ctrl Pts',(-6.68842713210028,7.35973194343344,4.));
#94182=CARTESIAN_POINT('Ctrl Pts',(-6.66264307422955,7.38427831335995,4.));
#94183=CARTESIAN_POINT('Ctrl Pts',(-6.64018120243431,7.4056619689929,4.));
#94184=CARTESIAN_POINT('Ctrl Pts',(-6.61761358279404,7.42694571653633,4.));
#94185=CARTESIAN_POINT('Ctrl Pts',(-6.59495225244961,7.44811852242564,4.));
#94186=CARTESIAN_POINT('Ctrl Pts',(-6.41390307437516,7.61727536562624,3.99999999999999));
#94187=CARTESIAN_POINT('Ctrl Pts',(-6.22670562493156,7.77951670257842,4.));
#94188=CARTESIAN_POINT('Ctrl Pts',(-6.03383371121318,7.93459550516718,4.));
#94189=CARTESIAN_POINT('Ctrl Pts',(-5.8369373182061,8.09291019325686,4.));
#94190=CARTESIAN_POINT('Ctrl Pts',(-5.63412700431251,8.24376063630574,4.));
#94191=CARTESIAN_POINT('Ctrl Pts',(-5.42586722089454,8.38684532869713,4.));
#94192=CARTESIAN_POINT('Ctrl Pts',(-5.26967238333106,8.49415884799068,3.99999999999999));
#94193=CARTESIAN_POINT('Ctrl Pts',(-5.11041132947551,8.5971033880251,4.));
#94194=CARTESIAN_POINT('Ctrl Pts',(-4.94826783799957,8.69553540262911,4.));
#94195=CARTESIAN_POINT('Ctrl Pts',(-4.8988306475216,8.72554710529329,4.));
#94196=CARTESIAN_POINT('Ctrl Pts',(-4.84912543391596,8.75513920608326,3.99999999999999));
#94197=CARTESIAN_POINT('Ctrl Pts',(-4.79915724674574,8.78430735141901,3.99999999999999));
#94198=CARTESIAN_POINT('Ctrl Pts',(-4.75991954981983,8.80721174141972,3.99999999999999));
#94199=CARTESIAN_POINT('Ctrl Pts',(-4.72052093121596,8.8298538680067,3.99999999999999));
#94200=CARTESIAN_POINT('Ctrl Pts',(-4.68098377349437,8.85222069110153,3.99999999999999));
#94201=CARTESIAN_POINT('Ctrl Pts',(-4.46299777204146,8.97553897224803,3.99999999999999));
#94202=CARTESIAN_POINT('Ctrl Pts',(-4.24064631017737,9.09058408654495,3.99999999999999));
#94203=CARTESIAN_POINT('Ctrl Pts',(-4.01438141143131,9.19707375614046,3.99999999999999));
#94204=CARTESIAN_POINT('Ctrl Pts',(-3.81972428610794,9.28868749329092,3.99999999999999));
#94205=CARTESIAN_POINT('Ctrl Pts',(-3.62216994392975,9.3739686510575,3.99999999999999));
#94206=CARTESIAN_POINT('Ctrl Pts',(-3.42198933978191,9.45271162518228,3.99999999999999));
#94207=CARTESIAN_POINT('Ctrl Pts',(-3.18987047803637,9.54401782141498,3.99999999999999));
#94208=CARTESIAN_POINT('Ctrl Pts',(-2.95422044287104,9.62653433945234,3.99999999999999));
#94209=CARTESIAN_POINT('Ctrl Pts',(-2.715556454544,9.7002114681284,3.99999999999999));
#94210=CARTESIAN_POINT('Ctrl Pts',(-2.67798216851998,9.71181089511238,3.99999999999999));
#94211=CARTESIAN_POINT('Ctrl Pts',(-2.64033314728563,9.72319112812026,3.99999999999999));
#94212=CARTESIAN_POINT('Ctrl Pts',(-2.60261137764844,9.73435186015536,4.));
#94213=CARTESIAN_POINT('',(-7.17774563074874,-6.25019011963611,-8.27625731986589E-5));
#94214=CARTESIAN_POINT('Ctrl Pts',(-7.17208764054957,-6.25651381571847,
0.));
#94215=CARTESIAN_POINT('Ctrl Pts',(-7.17394681951216,-6.25438256581607,
-2.7587524399553E-5));
#94216=CARTESIAN_POINT('Ctrl Pts',(-7.17580504849477,-6.25225048720616,
-5.51750487991059E-5));
#94217=CARTESIAN_POINT('Ctrl Pts',(-7.177662326759,-6.25011758073595,-8.27625731986589E-5));
#94218=CARTESIAN_POINT('Ctrl Pts',(-2.60234962446759,9.73414364143212,-1.0842021724855E-19));
#94219=CARTESIAN_POINT('Ctrl Pts',(-2.83921919055991,9.66382362790923,1.12529727208794E-15));
#94220=CARTESIAN_POINT('Ctrl Pts',(-3.07300811801843,9.58476494231999,1.21052675641511E-15));
#94221=CARTESIAN_POINT('Ctrl Pts',(-3.30331680122151,9.49731112534334,1.74339709335669E-15));
#94222=CARTESIAN_POINT('Ctrl Pts',(-3.53610216223959,9.40891685347229,1.54456933875653E-15));
#94223=CARTESIAN_POINT('Ctrl Pts',(-3.76533259408592,9.31194565425811,1.1980971909858E-15));
#94224=CARTESIAN_POINT('Ctrl Pts',(-3.99058148198477,9.20670059788145,9.54097911787244E-16));
#94225=CARTESIAN_POINT('Ctrl Pts',(-4.21670322288308,9.10104771057611,5.48408101539471E-16));
#94226=CARTESIAN_POINT('Ctrl Pts',(-4.43881307462945,8.98705639487405,2.2267367935286E-15));
#94227=CARTESIAN_POINT('Ctrl Pts',(-4.65645683809879,8.86498601204875,2.69922972861991E-15));
#94228=CARTESIAN_POINT('Ctrl Pts',(-4.87235333431775,8.74389562322261,3.71048904750986E-15));
#94229=CARTESIAN_POINT('Ctrl Pts',(-5.08385566981937,8.61485497615695,2.80017349659852E-15));
#94230=CARTESIAN_POINT('Ctrl Pts',(-5.29049031594336,8.47807629762164,3.2612801348364E-15));
#94231=CARTESIAN_POINT('Ctrl Pts',(-5.42081859913753,8.39180746185063,3.14924689181288E-15));
#94232=CARTESIAN_POINT('Ctrl Pts',(-5.54920986020766,8.30245959621931,1.78699762241744E-15));
#94233=CARTESIAN_POINT('Ctrl Pts',(-5.67553765180558,8.21007850173578,1.83880688453542E-15));
#94234=CARTESIAN_POINT('Ctrl Pts',(-5.77028349550405,8.1407926808731,2.64557878001586E-15));
#94235=CARTESIAN_POINT('Ctrl Pts',(-5.8638685187314,8.06980054949169,2.65661309570741E-15));
#94236=CARTESIAN_POINT('Ctrl Pts',(-5.9562368606778,7.9971194985086,2.49106291150269E-15));
#94237=CARTESIAN_POINT('Ctrl Pts',(-5.98417863604779,7.97513320366526,1.4537999406096E-15));
#94238=CARTESIAN_POINT('Ctrl Pts',(-6.0120107941499,7.95299094799323,1.58948515428829E-15));
#94239=CARTESIAN_POINT('Ctrl Pts',(-6.03972595387582,7.93069785471182,-1.17961196366423E-16));
#94240=CARTESIAN_POINT('Ctrl Pts',(-6.06885454317143,7.90726784872431,-1.91248462629996E-15));
#94241=CARTESIAN_POINT('Ctrl Pts',(-6.09784513215552,7.88367828862461,-6.97452302353175E-16));
#94242=CARTESIAN_POINT('Ctrl Pts',(-6.12669201119307,7.85993367550021,-6.80011602582908E-16));
#94243=CARTESIAN_POINT('Ctrl Pts',(-6.31817074079434,7.70232257483264,-5.64244381074444E-16));
#94244=CARTESIAN_POINT('Ctrl Pts',(-6.50339066876894,7.53782638481512,2.86787635648006E-15));
#94245=CARTESIAN_POINT('Ctrl Pts',(-6.68192791724629,7.36671835802232,1.77635683940025E-15));
#94246=CARTESIAN_POINT('Ctrl Pts',(-6.70470366833599,7.34489034251901,1.63711319672862E-15));
#94247=CARTESIAN_POINT('Ctrl Pts',(-6.72737062736575,7.32295467056579,1.21696534810119E-15));
#94248=CARTESIAN_POINT('Ctrl Pts',(-6.7499278780749,7.30091186031464,1.40165656858926E-15));
#94249=CARTESIAN_POINT('Ctrl Pts',(-6.92625813246103,7.12860299213362,2.35832437895416E-15));
#94250=CARTESIAN_POINT('Ctrl Pts',(-7.09588765341928,6.94975046126885,2.35575650814671E-15));
#94251=CARTESIAN_POINT('Ctrl Pts',(-7.25857969872179,6.76482962390105,1.85962356624714E-15));
#94252=CARTESIAN_POINT('Ctrl Pts',(-7.42201108691358,6.57906842641648,1.77113455101788E-15));
#94253=CARTESIAN_POINT('Ctrl Pts',(-7.5784421663849,6.38718308731999,7.63037625231977E-16));
#94254=CARTESIAN_POINT('Ctrl Pts',(-7.72759204547317,6.18962237682373,-3.46944695195361E-16));
#94255=CARTESIAN_POINT('Ctrl Pts',(-7.87627943705517,5.99267426729565,-1.38191786245987E-15));
#94256=CARTESIAN_POINT('Ctrl Pts',(-8.0177310300406,5.79008534630041,1.33121440589865E-15));
#94257=CARTESIAN_POINT('Ctrl Pts',(-8.15162295721404,5.58227599425002,-5.41233724504764E-16));
#94258=CARTESIAN_POINT('Ctrl Pts',(-8.26759776180428,5.4022752316585,-1.92647886301059E-15));
#94259=CARTESIAN_POINT('Ctrl Pts',(-8.37790018862867,5.21835713365747,-1.85568084733084E-15));
#94260=CARTESIAN_POINT('Ctrl Pts',(-8.48228916729079,5.03078516303735,-2.66453525910038E-15));
#94261=CARTESIAN_POINT('Ctrl Pts',(-8.5011201218663,4.99694864788359,-2.58432894335183E-15));
#94262=CARTESIAN_POINT('Ctrl Pts',(-8.51975862523132,4.96299286801841,-1.66636520228865E-15));
#94263=CARTESIAN_POINT('Ctrl Pts',(-8.53818920411381,4.92894583550654,-1.99840144432528E-15));
#94264=CARTESIAN_POINT('Ctrl Pts',(-8.6553554767611,4.71250315513553,-4.10921137120173E-15));
#94265=CARTESIAN_POINT('Ctrl Pts',(-8.76426888616404,4.49211411010674,-1.84066867355076E-16));
#94266=CARTESIAN_POINT('Ctrl Pts',(-8.86469562417359,4.26823837544914,-2.72004641033163E-15));
#94267=CARTESIAN_POINT('Ctrl Pts',(-8.96498221895465,4.04467505428677,-5.25248705154183E-15));
#94268=CARTESIAN_POINT('Ctrl Pts',(-9.05680611487477,3.81763418427641,-6.54395179005909E-15));
#94269=CARTESIAN_POINT('Ctrl Pts',(-9.13988927972611,3.5875484410629,-6.49480469405717E-15));
#94270=CARTESIAN_POINT('Ctrl Pts',(-9.17816975363287,3.48153669602212,-6.47216022535571E-15));
#94271=CARTESIAN_POINT('Ctrl Pts',(-9.21459400355786,3.37487826045069,-7.00076967452139E-15));
#94272=CARTESIAN_POINT('Ctrl Pts',(-9.24913132420256,3.26761417878569,-6.68909372336657E-15));
#94273=CARTESIAN_POINT('Ctrl Pts',(-9.32430828445378,3.03413377401809,-6.05927787474007E-15));
#94274=CARTESIAN_POINT('Ctrl Pts',(-9.39054843147571,2.79778427755245,-6.09227021689154E-15));
#94275=CARTESIAN_POINT('Ctrl Pts',(-9.44781377586706,2.55908919896884,-6.49480469405717E-15));
#94276=CARTESIAN_POINT('Ctrl Pts',(-9.50492485430018,2.32103713625129,-7.09737120362222E-15));
#94277=CARTESIAN_POINT('Ctrl Pts',(-9.55310943460919,2.08065144744669,-6.42576610657209E-15));
#94278=CARTESIAN_POINT('Ctrl Pts',(-9.5922782570777,1.83844915244229,-6.74460487459783E-15));
#94279=CARTESIAN_POINT('Ctrl Pts',(-9.61396155849863,1.70436941666152,-5.65810346699789E-15));
#94280=CARTESIAN_POINT('Ctrl Pts',(-9.63288100101979,1.56973298585168,-4.9195398534525E-15));
#94281=CARTESIAN_POINT('Ctrl Pts',(-9.64901457990071,1.43462840724832,-6.43929354282591E-15));
#94282=CARTESIAN_POINT('Ctrl Pts',(-9.65375213453723,1.39495554064496,-7.49285349155712E-15));
#94283=CARTESIAN_POINT('Ctrl Pts',(-9.65824979964318,1.35523807611954,-5.32935632051397E-15));
#94284=CARTESIAN_POINT('Ctrl Pts',(-9.66250344928149,1.31551343168508,-5.19029264012261E-15));
#94285=CARTESIAN_POINT('Ctrl Pts',(-9.68848629612735,1.07286078275713,-4.34084084773944E-15));
#94286=CARTESIAN_POINT('Ctrl Pts',(-9.70540243338582,0.829675528430131,
-3.52635615547212E-15));
#94287=CARTESIAN_POINT('Ctrl Pts',(-9.71327571138526,0.586476102990858,
-3.96904731303493E-15));
#94288=CARTESIAN_POINT('Ctrl Pts',(-9.72116115923157,0.342900760459978,
-4.41242274512731E-15));
#94289=CARTESIAN_POINT('Ctrl Pts',(-9.71997579260738,0.0993105370203054,
-4.56754410064086E-15));
#94290=CARTESIAN_POINT('Ctrl Pts',(-9.70969161124852,-0.143779945942933,
-3.63598040564739E-15));
#94291=CARTESIAN_POINT('Ctrl Pts',(-9.69949621789526,-0.384771718429206,
-2.71245932286486E-15));
#94292=CARTESIAN_POINT('Ctrl Pts',(-9.68035838589556,-0.625272978090111,
2.79940693609296E-15));
#94293=CARTESIAN_POINT('Ctrl Pts',(-9.65220018038254,-0.864778715928871,
3.77475828372553E-15));
#94294=CARTESIAN_POINT('Ctrl Pts',(-9.63108916824546,-1.04434301863547,
4.50600708891906E-15));
#94295=CARTESIAN_POINT('Ctrl Pts',(-9.60490683713541,-1.22334772921605,
2.71191758976982E-15));
#94296=CARTESIAN_POINT('Ctrl Pts',(-9.5736016261349,-1.40157546597075,5.27355936696949E-15));
#94297=CARTESIAN_POINT('Ctrl Pts',(-9.54008130266794,-1.59241434537346,
7.34930365900901E-15));
#94298=CARTESIAN_POINT('Ctrl Pts',(-9.50068749895529,-1.78236265639502,
9.6353898453109E-15));
#94299=CARTESIAN_POINT('Ctrl Pts',(-9.45550504145372,-1.97116932539336,
8.24340595784179E-15));
#94300=CARTESIAN_POINT('Ctrl Pts',(-9.43573771629679,-2.05377224308013,
7.6084078733068E-15));
#94301=CARTESIAN_POINT('Ctrl Pts',(-9.41486216561421,-2.13615652108099,
6.2416746576837E-15));
#94302=CARTESIAN_POINT('Ctrl Pts',(-9.39288439672517,-2.21830049798781,
5.68989300120393E-15));
#94303=CARTESIAN_POINT('Ctrl Pts',(-9.38127566596173,-2.2616892203174,5.67346700880721E-15));
#94304=CARTESIAN_POINT('Ctrl Pts',(-9.36935940676183,-2.30501089184594,
1.02851375672538E-14));
#94305=CARTESIAN_POINT('Ctrl Pts',(-9.35713643218052,-2.34826227004022,
8.90953977261688E-15));
#94306=CARTESIAN_POINT('Ctrl Pts',(-9.34817714544189,-2.37996498663392,
7.90124387891348E-15));
#94307=CARTESIAN_POINT('Ctrl Pts',(-9.33905531224074,-2.41162191029918,
8.29834598157197E-15));
#94308=CARTESIAN_POINT('Ctrl Pts',(-9.32977348840701,-2.44322524102662,
8.27116153345742E-15));
#94309=CARTESIAN_POINT('Ctrl Pts',(-9.3091309585129,-2.51351020990564,8.21070404224538E-15));
#94310=CARTESIAN_POINT('Ctrl Pts',(-9.28769421535577,-2.58354046496828,
8.78374978742755E-15));
#94311=CARTESIAN_POINT('Ctrl Pts',(-9.26547044027429,-2.65330324410549,
8.99280649946377E-15));
#94312=CARTESIAN_POINT('Ctrl Pts',(-9.19195459005424,-2.88407726891374,
9.68436236129214E-15));
#94313=CARTESIAN_POINT('Ctrl Pts',(-9.10983017570767,-3.11192569697261,
9.50023376670274E-15));
#94314=CARTESIAN_POINT('Ctrl Pts',(-9.01932453558736,-3.33637613353048,
9.82547376793264E-15));
#94315=CARTESIAN_POINT('Ctrl Pts',(-8.93690619259326,-3.54077039051611,
1.0121651353563E-14));
#94316=CARTESIAN_POINT('Ctrl Pts',(-8.84753678016074,-3.74234696279182,
9.54369029972911E-15));
#94317=CARTESIAN_POINT('Ctrl Pts',(-8.75135419307074,-3.94073284400927,
9.76996261670138E-15));
#94318=CARTESIAN_POINT('Ctrl Pts',(-8.67921725275325,-4.08952225492236,
9.93966685443058E-15));
#94319=CARTESIAN_POINT('Ctrl Pts',(-8.60324722754804,-4.23651661611678,
6.6596841948106E-15));
#94320=CARTESIAN_POINT('Ctrl Pts',(-8.52349134733745,-4.38155083638406,
6.77236045021345E-15));
#94321=CARTESIAN_POINT('Ctrl Pts',(-8.49892470414398,-4.42622470783708,
6.80706732518681E-15));
#94322=CARTESIAN_POINT('Ctrl Pts',(-8.47399672617423,-4.47071593837625,
1.1327567305792E-14));
#94323=CARTESIAN_POINT('Ctrl Pts',(-8.44872639902523,-4.51498916092465,
1.04360964314765E-14));
#94324=CARTESIAN_POINT('Ctrl Pts',(-8.32958798602576,-4.72371781891507,
6.23320564280544E-15));
#94325=CARTESIAN_POINT('Ctrl Pts',(-8.20276674746981,-4.92774606792883,
6.92432169967517E-15));
#94326=CARTESIAN_POINT('Ctrl Pts',(-8.06846284876383,-5.12660291388634,
6.55031584528842E-15));
#94327=CARTESIAN_POINT('Ctrl Pts',(-7.95380311179895,-5.29637366418355,
6.23101451970896E-15));
#94328=CARTESIAN_POINT('Ctrl Pts',(-7.83368869300271,-5.46237501931451,
5.51132532032376E-15));
#94329=CARTESIAN_POINT('Ctrl Pts',(-7.70821972408079,-5.62429632476034,
4.49640324973188E-15));
#94330=CARTESIAN_POINT('Ctrl Pts',(-7.5607553014238,-5.81460339453705,3.00534834520389E-15));
#94331=CARTESIAN_POINT('Ctrl Pts',(-7.40589476781386,-5.99927566766814,
4.03884969480374E-15));
#94332=CARTESIAN_POINT('Ctrl Pts',(-7.24403669908448,-6.17797143930764,
1.72084568816899E-15));
#94333=CARTESIAN_POINT('Ctrl Pts',(-7.22210430648793,-6.20218540559124,
1.40674720476935E-15));
#94334=CARTESIAN_POINT('Ctrl Pts',(-7.20004338176182,-6.22628957396681,
7.04844233411283E-16));
#94335=CARTESIAN_POINT('Ctrl Pts',(-7.17785487282089,-6.25028303501658,
1.77635683940025E-15));
#94336=CARTESIAN_POINT('Origin',(0.,0.,4.));
#94337=CARTESIAN_POINT('',(-14.,-1.71450551880629E-15,4.));
#94338=CARTESIAN_POINT('Origin',(0.,0.,4.));
#94339=CARTESIAN_POINT('Origin',(0.,0.,0.));
#94340=CARTESIAN_POINT('',(-14.,-1.71450551880629E-15,0.));
#94341=CARTESIAN_POINT('',(-14.,-1.71450551880629E-15,0.));
#94342=CARTESIAN_POINT('Origin',(0.,0.,0.));
#94343=CARTESIAN_POINT('Origin',(0.,0.,0.));
#94344=CARTESIAN_POINT('',(0.,0.,0.));
#94345=CARTESIAN_POINT('Origin',(0.,0.,0.));
#94346=CARTESIAN_POINT('',(-3.,-3.67394039744206E-16,0.));
#94347=CARTESIAN_POINT('Origin',(0.,0.,0.));
#94348=CARTESIAN_POINT('',(-3.,-3.67394039744206E-16,18.));
#94349=CARTESIAN_POINT('',(-3.,-3.67394039744206E-16,0.));
#94350=CARTESIAN_POINT('Origin',(0.,0.,18.));
#94351=CARTESIAN_POINT('Origin',(0.,0.,0.));
#94352=CARTESIAN_POINT('',(-5.,-6.12323399573677E-16,18.));
#94353=CARTESIAN_POINT('Origin',(0.,0.,18.));
#94354=CARTESIAN_POINT('',(-5.,-6.12323399573677E-16,0.));
#94355=CARTESIAN_POINT('',(-5.,-6.12323399573677E-16,0.));
#94356=CARTESIAN_POINT('Origin',(0.,0.,0.));
#94357=CARTESIAN_POINT('Origin',(0.,0.,18.));
#94358=CARTESIAN_POINT('Origin',(0.,0.,0.));
#94359=CARTESIAN_POINT('',(0.,0.,0.));
#94360=CARTESIAN_POINT('',(0.,0.,120.));
#94361=CARTESIAN_POINT('',(0.,0.,117.));
#94362=CARTESIAN_POINT('',(-130.,-90.,123.));
#94363=CARTESIAN_POINT('',(0.,0.,20.));
#94364=CARTESIAN_POINT('',(-100.,-55.,23.));
#94365=CARTESIAN_POINT('',(-60.,-114.,63.));
#94366=CARTESIAN_POINT('',(-60.,-107.,63.));
#94367=CARTESIAN_POINT('',(-60.,-114.,63.));
#94368=CARTESIAN_POINT('',(-130.,90.,123.));
#94369=CARTESIAN_POINT('',(130.,-90.,123.));
#94370=CARTESIAN_POINT('',(130.,90.,123.));
#94371=CARTESIAN_POINT('',(-100.,55.,23.));
#94372=CARTESIAN_POINT('',(100.,-55.,23.));
#94373=CARTESIAN_POINT('',(100.,55.,23.));
#94374=CARTESIAN_POINT('',(60.,-114.,63.));
#94375=CARTESIAN_POINT('',(60.,-107.,63.));
#94376=CARTESIAN_POINT('',(60.,-114.,63.));
#94377=UNCERTAINTY_MEASURE_WITH_UNIT(LENGTH_MEASURE(0.01),#94413,
'DISTANCE_ACCURACY_VALUE',
'Maximum model space distance between geometric entities at asserted c
onnectivities');
#94378=UNCERTAINTY_MEASURE_WITH_UNIT(LENGTH_MEASURE(0.01),#94413,
'DISTANCE_ACCURACY_VALUE',
'Maximum model space distance between geometric entities at asserted c
onnectivities');
#94379=UNCERTAINTY_MEASURE_WITH_UNIT(LENGTH_MEASURE(0.01),#94413,
'DISTANCE_ACCURACY_VALUE',
'Maximum model space distance between geometric entities at asserted c
onnectivities');
#94380=UNCERTAINTY_MEASURE_WITH_UNIT(LENGTH_MEASURE(0.01),#94413,
'DISTANCE_ACCURACY_VALUE',
'Maximum model space distance between geometric entities at asserted c
onnectivities');
#94381=UNCERTAINTY_MEASURE_WITH_UNIT(LENGTH_MEASURE(0.01),#94413,
'DISTANCE_ACCURACY_VALUE',
'Maximum model space distance between geometric entities at asserted c
onnectivities');
#94382=UNCERTAINTY_MEASURE_WITH_UNIT(LENGTH_MEASURE(0.01),#94413,
'DISTANCE_ACCURACY_VALUE',
'Maximum model space distance between geometric entities at asserted c
onnectivities');
#94383=UNCERTAINTY_MEASURE_WITH_UNIT(LENGTH_MEASURE(0.01),#94413,
'DISTANCE_ACCURACY_VALUE',
'Maximum model space distance between geometric entities at asserted c
onnectivities');
#94384=UNCERTAINTY_MEASURE_WITH_UNIT(LENGTH_MEASURE(0.01),#94413,
'DISTANCE_ACCURACY_VALUE',
'Maximum model space distance between geometric entities at asserted c
onnectivities');
#94385=UNCERTAINTY_MEASURE_WITH_UNIT(LENGTH_MEASURE(0.01),#94413,
'DISTANCE_ACCURACY_VALUE',
'Maximum model space distance between geometric entities at asserted c
onnectivities');
#94386=UNCERTAINTY_MEASURE_WITH_UNIT(LENGTH_MEASURE(0.01),#94413,
'DISTANCE_ACCURACY_VALUE',
'Maximum model space distance between geometric entities at asserted c
onnectivities');
#94387=UNCERTAINTY_MEASURE_WITH_UNIT(LENGTH_MEASURE(0.01),#94413,
'DISTANCE_ACCURACY_VALUE',
'Maximum model space distance between geometric entities at asserted c
onnectivities');
#94388=UNCERTAINTY_MEASURE_WITH_UNIT(LENGTH_MEASURE(0.01),#94413,
'DISTANCE_ACCURACY_VALUE',
'Maximum model space distance between geometric entities at asserted c
onnectivities');
#94389=UNCERTAINTY_MEASURE_WITH_UNIT(LENGTH_MEASURE(0.01),#94413,
'DISTANCE_ACCURACY_VALUE',
'Maximum model space distance between geometric entities at asserted c
onnectivities');
#94390=UNCERTAINTY_MEASURE_WITH_UNIT(LENGTH_MEASURE(0.01),#94413,
'DISTANCE_ACCURACY_VALUE',
'Maximum model space distance between geometric entities at asserted c
onnectivities');
#94391=UNCERTAINTY_MEASURE_WITH_UNIT(LENGTH_MEASURE(0.01),#94413,
'DISTANCE_ACCURACY_VALUE',
'Maximum model space distance between geometric entities at asserted c
onnectivities');
#94392=UNCERTAINTY_MEASURE_WITH_UNIT(LENGTH_MEASURE(0.01),#94413,
'DISTANCE_ACCURACY_VALUE',
'Maximum model space distance between geometric entities at asserted c
onnectivities');
#94393=UNCERTAINTY_MEASURE_WITH_UNIT(LENGTH_MEASURE(0.01),#94413,
'DISTANCE_ACCURACY_VALUE',
'Maximum model space distance between geometric entities at asserted c
onnectivities');
#94394=UNCERTAINTY_MEASURE_WITH_UNIT(LENGTH_MEASURE(0.01),#94413,
'DISTANCE_ACCURACY_VALUE',
'Maximum model space distance between geometric entities at asserted c
onnectivities');
#94395=(
GEOMETRIC_REPRESENTATION_CONTEXT(3)
GLOBAL_UNCERTAINTY_ASSIGNED_CONTEXT((#94377))
GLOBAL_UNIT_ASSIGNED_CONTEXT((#94413,#94415,#94416))
REPRESENTATION_CONTEXT('','3D')
);
#94396=(
GEOMETRIC_REPRESENTATION_CONTEXT(3)
GLOBAL_UNCERTAINTY_ASSIGNED_CONTEXT((#94378))
GLOBAL_UNIT_ASSIGNED_CONTEXT((#94413,#94415,#94416))
REPRESENTATION_CONTEXT('','3D')
);
#94397=(
GEOMETRIC_REPRESENTATION_CONTEXT(3)
GLOBAL_UNCERTAINTY_ASSIGNED_CONTEXT((#94379))
GLOBAL_UNIT_ASSIGNED_CONTEXT((#94413,#94415,#94416))
REPRESENTATION_CONTEXT('','3D')
);
#94398=(
GEOMETRIC_REPRESENTATION_CONTEXT(3)
GLOBAL_UNCERTAINTY_ASSIGNED_CONTEXT((#94380))
GLOBAL_UNIT_ASSIGNED_CONTEXT((#94413,#94415,#94416))
REPRESENTATION_CONTEXT('','3D')
);
#94399=(
GEOMETRIC_REPRESENTATION_CONTEXT(3)
GLOBAL_UNCERTAINTY_ASSIGNED_CONTEXT((#94381))
GLOBAL_UNIT_ASSIGNED_CONTEXT((#94413,#94415,#94416))
REPRESENTATION_CONTEXT('','3D')
);
#94400=(
GEOMETRIC_REPRESENTATION_CONTEXT(3)
GLOBAL_UNCERTAINTY_ASSIGNED_CONTEXT((#94382))
GLOBAL_UNIT_ASSIGNED_CONTEXT((#94413,#94415,#94416))
REPRESENTATION_CONTEXT('','3D')
);
#94401=(
GEOMETRIC_REPRESENTATION_CONTEXT(3)
GLOBAL_UNCERTAINTY_ASSIGNED_CONTEXT((#94383))
GLOBAL_UNIT_ASSIGNED_CONTEXT((#94413,#94415,#94416))
REPRESENTATION_CONTEXT('','3D')
);
#94402=(
GEOMETRIC_REPRESENTATION_CONTEXT(3)
GLOBAL_UNCERTAINTY_ASSIGNED_CONTEXT((#94384))
GLOBAL_UNIT_ASSIGNED_CONTEXT((#94413,#94415,#94416))
REPRESENTATION_CONTEXT('','3D')
);
#94403=(
GEOMETRIC_REPRESENTATION_CONTEXT(3)
GLOBAL_UNCERTAINTY_ASSIGNED_CONTEXT((#94385))
GLOBAL_UNIT_ASSIGNED_CONTEXT((#94413,#94415,#94416))
REPRESENTATION_CONTEXT('','3D')
);
#94404=(
GEOMETRIC_REPRESENTATION_CONTEXT(3)
GLOBAL_UNCERTAINTY_ASSIGNED_CONTEXT((#94386))
GLOBAL_UNIT_ASSIGNED_CONTEXT((#94413,#94415,#94416))
REPRESENTATION_CONTEXT('','3D')
);
#94405=(
GEOMETRIC_REPRESENTATION_CONTEXT(3)
GLOBAL_UNCERTAINTY_ASSIGNED_CONTEXT((#94387))
GLOBAL_UNIT_ASSIGNED_CONTEXT((#94413,#94415,#94416))
REPRESENTATION_CONTEXT('','3D')
);
#94406=(
GEOMETRIC_REPRESENTATION_CONTEXT(3)
GLOBAL_UNCERTAINTY_ASSIGNED_CONTEXT((#94388))
GLOBAL_UNIT_ASSIGNED_CONTEXT((#94413,#94415,#94416))
REPRESENTATION_CONTEXT('','3D')
);
#94407=(
GEOMETRIC_REPRESENTATION_CONTEXT(3)
GLOBAL_UNCERTAINTY_ASSIGNED_CONTEXT((#94389))
GLOBAL_UNIT_ASSIGNED_CONTEXT((#94413,#94415,#94416))
REPRESENTATION_CONTEXT('','3D')
);
#94408=(
GEOMETRIC_REPRESENTATION_CONTEXT(3)
GLOBAL_UNCERTAINTY_ASSIGNED_CONTEXT((#94390))
GLOBAL_UNIT_ASSIGNED_CONTEXT((#94413,#94415,#94416))
REPRESENTATION_CONTEXT('','3D')
);
#94409=(
GEOMETRIC_REPRESENTATION_CONTEXT(3)
GLOBAL_UNCERTAINTY_ASSIGNED_CONTEXT((#94391))
GLOBAL_UNIT_ASSIGNED_CONTEXT((#94413,#94415,#94416))
REPRESENTATION_CONTEXT('','3D')
);
#94410=(
GEOMETRIC_REPRESENTATION_CONTEXT(3)
GLOBAL_UNCERTAINTY_ASSIGNED_CONTEXT((#94392))
GLOBAL_UNIT_ASSIGNED_CONTEXT((#94413,#94415,#94416))
REPRESENTATION_CONTEXT('','3D')
);
#94411=(
GEOMETRIC_REPRESENTATION_CONTEXT(3)
GLOBAL_UNCERTAINTY_ASSIGNED_CONTEXT((#94393))
GLOBAL_UNIT_ASSIGNED_CONTEXT((#94413,#94415,#94416))
REPRESENTATION_CONTEXT('','3D')
);
#94412=(
GEOMETRIC_REPRESENTATION_CONTEXT(3)
GLOBAL_UNCERTAINTY_ASSIGNED_CONTEXT((#94394))
GLOBAL_UNIT_ASSIGNED_CONTEXT((#94413,#94415,#94416))
REPRESENTATION_CONTEXT('','3D')
);
#94413=(
LENGTH_UNIT()
NAMED_UNIT(*)
SI_UNIT(.MILLI.,.METRE.)
);
#94414=(
LENGTH_UNIT()
NAMED_UNIT(*)
SI_UNIT($,.METRE.)
);
#94415=(
NAMED_UNIT(*)
PLANE_ANGLE_UNIT()
SI_UNIT($,.RADIAN.)
);
#94416=(
NAMED_UNIT(*)
SI_UNIT($,.STERADIAN.)
SOLID_ANGLE_UNIT()
);
#94417=SHAPE_DEFINITION_REPRESENTATION(#94434,#94486);
#94418=SHAPE_DEFINITION_REPRESENTATION(#94435,#94487);
#94419=SHAPE_DEFINITION_REPRESENTATION(#94436,#94488);
#94420=SHAPE_DEFINITION_REPRESENTATION(#94437,#94489);
#94421=SHAPE_DEFINITION_REPRESENTATION(#94438,#94490);
#94422=SHAPE_DEFINITION_REPRESENTATION(#94439,#94491);
#94423=SHAPE_DEFINITION_REPRESENTATION(#94440,#94492);
#94424=SHAPE_DEFINITION_REPRESENTATION(#94441,#94493);
#94425=SHAPE_DEFINITION_REPRESENTATION(#94442,#94494);
#94426=SHAPE_DEFINITION_REPRESENTATION(#94460,#94495);
#94427=SHAPE_DEFINITION_REPRESENTATION(#94461,#94496);
#94428=SHAPE_DEFINITION_REPRESENTATION(#94462,#94497);
#94429=SHAPE_DEFINITION_REPRESENTATION(#94463,#94498);
#94430=SHAPE_DEFINITION_REPRESENTATION(#94464,#94499);
#94431=SHAPE_DEFINITION_REPRESENTATION(#94465,#94500);
#94432=SHAPE_DEFINITION_REPRESENTATION(#94466,#94501);
#94433=SHAPE_DEFINITION_REPRESENTATION(#94467,#94502);
#94434=PRODUCT_DEFINITION_SHAPE('',$,#94504);
#94435=PRODUCT_DEFINITION_SHAPE('',$,#94505);
#94436=PRODUCT_DEFINITION_SHAPE('',$,#94506);
#94437=PRODUCT_DEFINITION_SHAPE('',$,#94507);
#94438=PRODUCT_DEFINITION_SHAPE('',$,#94508);
#94439=PRODUCT_DEFINITION_SHAPE('',$,#94509);
#94440=PRODUCT_DEFINITION_SHAPE('',$,#94510);
#94441=PRODUCT_DEFINITION_SHAPE('',$,#94511);
#94442=PRODUCT_DEFINITION_SHAPE('',$,#94512);
#94443=PRODUCT_DEFINITION_SHAPE($,$,#116);
#94444=PRODUCT_DEFINITION_SHAPE($,$,#117);
#94445=PRODUCT_DEFINITION_SHAPE($,$,#118);
#94446=PRODUCT_DEFINITION_SHAPE($,$,#119);
#94447=PRODUCT_DEFINITION_SHAPE($,$,#120);
#94448=PRODUCT_DEFINITION_SHAPE($,$,#121);
#94449=PRODUCT_DEFINITION_SHAPE($,$,#122);
#94450=PRODUCT_DEFINITION_SHAPE($,$,#123);
#94451=PRODUCT_DEFINITION_SHAPE($,$,#124);
#94452=PRODUCT_DEFINITION_SHAPE($,$,#125);
#94453=PRODUCT_DEFINITION_SHAPE($,$,#126);
#94454=PRODUCT_DEFINITION_SHAPE($,$,#127);
#94455=PRODUCT_DEFINITION_SHAPE($,$,#128);
#94456=PRODUCT_DEFINITION_SHAPE($,$,#129);
#94457=PRODUCT_DEFINITION_SHAPE($,$,#130);
#94458=PRODUCT_DEFINITION_SHAPE($,$,#131);
#94459=PRODUCT_DEFINITION_SHAPE($,$,#132);
#94460=PRODUCT_DEFINITION_SHAPE('',$,#94513);
#94461=PRODUCT_DEFINITION_SHAPE('',$,#94514);
#94462=PRODUCT_DEFINITION_SHAPE('',$,#94515);
#94463=PRODUCT_DEFINITION_SHAPE('',$,#94516);
#94464=PRODUCT_DEFINITION_SHAPE('',$,#94517);
#94465=PRODUCT_DEFINITION_SHAPE('',$,#94518);
#94466=PRODUCT_DEFINITION_SHAPE('',$,#94519);
#94467=PRODUCT_DEFINITION_SHAPE('',$,#94520);
#94468=PRODUCT_DEFINITION_SHAPE($,$,#133);
#94469=PRODUCT_DEFINITION_SHAPE($,$,#134);
#94470=PRODUCT_DEFINITION_SHAPE($,$,#135);
#94471=PRODUCT_DEFINITION_SHAPE($,$,#136);
#94472=PRODUCT_DEFINITION_SHAPE($,$,#137);
#94473=PRODUCT_DEFINITION_SHAPE($,$,#138);
#94474=PRODUCT_DEFINITION_SHAPE($,$,#139);
#94475=PRODUCT_DEFINITION_SHAPE($,$,#140);
#94476=PRODUCT_DEFINITION_SHAPE($,$,#141);
#94477=PRODUCT_DEFINITION_SHAPE($,$,#142);
#94478=PRODUCT_DEFINITION_SHAPE($,$,#143);
#94479=PRODUCT_DEFINITION_SHAPE($,$,#144);
#94480=PRODUCT_DEFINITION_SHAPE($,$,#145);
#94481=PRODUCT_DEFINITION_SHAPE($,$,#146);
#94482=PRODUCT_DEFINITION_SHAPE($,$,#147);
#94483=PRODUCT_DEFINITION_SHAPE($,$,#148);
#94484=PRODUCT_DEFINITION_SHAPE($,$,#149);
#94485=PRODUCT_DEFINITION_SHAPE($,$,#150);
#94486=SHAPE_REPRESENTATION('',(#8432,#8924,#8925,#8926,#8927,#8928,#8929,
#8930,#8931,#8932,#8933,#8934,#8935,#8936,#8937,#8938,#8939,#8940,#8941),
#94395);
#94487=SHAPE_REPRESENTATION('',(#8433,#8693,#8694,#8695,#8696,#8697,#8698,
#8699,#8700,#8701,#8702,#8703,#8704,#8705,#8706,#8707,#8708,#8709),#94396);
#94488=SHAPE_REPRESENTATION('',(#8434),#94397);
#94489=SHAPE_REPRESENTATION('',(#8453),#94398);
#94490=SHAPE_REPRESENTATION('',(#8466),#94399);
#94491=SHAPE_REPRESENTATION('',(#8473),#94400);
#94492=SHAPE_REPRESENTATION('',(#8512),#94401);
#94493=SHAPE_REPRESENTATION('',(#8614),#94402);
#94494=SHAPE_REPRESENTATION('',(#8647),#94403);
#94495=SHAPE_REPRESENTATION('',(#8710),#94404);
#94496=SHAPE_REPRESENTATION('',(#8731),#94405);
#94497=SHAPE_REPRESENTATION('',(#8754),#94406);
#94498=SHAPE_REPRESENTATION('',(#8773),#94407);
#94499=SHAPE_REPRESENTATION('',(#8810),#94408);
#94500=SHAPE_REPRESENTATION('',(#8845),#94409);
#94501=SHAPE_REPRESENTATION('',(#8889),#94410);
#94502=SHAPE_REPRESENTATION('',(#8915),#94411);
#94503=PRODUCT_DEFINITION_CONTEXT('part definition',#94556,'design');
#94504=PRODUCT_DEFINITION('MAS-640','TAS-012',#94521,#94503);
#94505=PRODUCT_DEFINITION('Enclosure shell','Enclosure shell',#94522,#94503);
#94506=PRODUCT_DEFINITION('Base panel','Base panel',#94523,#94503);
#94507=PRODUCT_DEFINITION('Entry panel','Entry panel',#94524,#94503);
#94508=PRODUCT_DEFINITION('Rear panel','Rear panel',#94525,#94503);
#94509=PRODUCT_DEFINITION('Side panel','Side panel',#94526,#94503);
#94510=PRODUCT_DEFINITION('Corner pillar','Corner pillar',#94527,#94503);
#94511=PRODUCT_DEFINITION('Socket head cap screw M6x12',
'Socket head cap screw M6x12',#94528,#94503);
#94512=PRODUCT_DEFINITION('Tray pillar','Tray pillar',#94529,#94503);
#94513=PRODUCT_DEFINITION('Lid','Lid',#94530,#94503);
#94514=PRODUCT_DEFINITION('Lid gasket','Lid gasket',#94531,#94503);
#94515=PRODUCT_DEFINITION('Mounting tray','Mounting tray',#94532,#94503);
#94516=PRODUCT_DEFINITION('Socket head cap screw M6x16',
'Socket head cap screw M6x16',#94533,#94503);
#94517=PRODUCT_DEFINITION('Socket head cap screw M4x10',
'Socket head cap screw M4x10',#94534,#94503);
#94518=PRODUCT_DEFINITION('Cable entry body','Cable entry body',#94535,
#94503);
#94519=PRODUCT_DEFINITION('Entry locknut','Entry locknut',#94536,#94503);
#94520=PRODUCT_DEFINITION('Cable entry seal','Cable entry seal',#94537,
#94503);
#94521=PRODUCT_DEFINITION_FORMATION('',$,#94558);
#94522=PRODUCT_DEFINITION_FORMATION('',$,#94559);
#94523=PRODUCT_DEFINITION_FORMATION('',$,#94560);
#94524=PRODUCT_DEFINITION_FORMATION('',$,#94561);
#94525=PRODUCT_DEFINITION_FORMATION('',$,#94562);
#94526=PRODUCT_DEFINITION_FORMATION('',$,#94563);
#94527=PRODUCT_DEFINITION_FORMATION('',$,#94564);
#94528=PRODUCT_DEFINITION_FORMATION('',$,#94565);
#94529=PRODUCT_DEFINITION_FORMATION('',$,#94566);
#94530=PRODUCT_DEFINITION_FORMATION('',$,#94567);
#94531=PRODUCT_DEFINITION_FORMATION('',$,#94568);
#94532=PRODUCT_DEFINITION_FORMATION('',$,#94569);
#94533=PRODUCT_DEFINITION_FORMATION('',$,#94570);
#94534=PRODUCT_DEFINITION_FORMATION('',$,#94571);
#94535=PRODUCT_DEFINITION_FORMATION('',$,#94572);
#94536=PRODUCT_DEFINITION_FORMATION('',$,#94573);
#94537=PRODUCT_DEFINITION_FORMATION('',$,#94574);
#94538=PRODUCT_RELATED_PRODUCT_CATEGORY('TAS-012','TAS-012',(#94558));
#94539=PRODUCT_RELATED_PRODUCT_CATEGORY('Enclosure shell',
'Enclosure shell',(#94559));
#94540=PRODUCT_RELATED_PRODUCT_CATEGORY('Base panel','Base panel',(#94560));
#94541=PRODUCT_RELATED_PRODUCT_CATEGORY('Entry panel','Entry panel',(#94561));
#94542=PRODUCT_RELATED_PRODUCT_CATEGORY('Rear panel','Rear panel',(#94562));
#94543=PRODUCT_RELATED_PRODUCT_CATEGORY('Side panel','Side panel',(#94563));
#94544=PRODUCT_RELATED_PRODUCT_CATEGORY('Corner pillar','Corner pillar',
(#94564));
#94545=PRODUCT_RELATED_PRODUCT_CATEGORY('Socket head cap screw M6x12',
'Socket head cap screw M6x12',(#94565));
#94546=PRODUCT_RELATED_PRODUCT_CATEGORY('Tray pillar','Tray pillar',(#94566));
#94547=PRODUCT_RELATED_PRODUCT_CATEGORY('Lid','Lid',(#94567));
#94548=PRODUCT_RELATED_PRODUCT_CATEGORY('Lid gasket','Lid gasket',(#94568));
#94549=PRODUCT_RELATED_PRODUCT_CATEGORY('Mounting tray','Mounting tray',
(#94569));
#94550=PRODUCT_RELATED_PRODUCT_CATEGORY('Socket head cap screw M6x16',
'Socket head cap screw M6x16',(#94570));
#94551=PRODUCT_RELATED_PRODUCT_CATEGORY('Socket head cap screw M4x10',
'Socket head cap screw M4x10',(#94571));
#94552=PRODUCT_RELATED_PRODUCT_CATEGORY('Cable entry body',
'Cable entry body',(#94572));
#94553=PRODUCT_RELATED_PRODUCT_CATEGORY('Entry locknut','Entry locknut',
(#94573));
#94554=PRODUCT_RELATED_PRODUCT_CATEGORY('Cable entry seal',
'Cable entry seal',(#94574));
#94555=APPLICATION_PROTOCOL_DEFINITION('international standard',
'automotive_design',2009,#94556);
#94556=APPLICATION_CONTEXT(
'Core Data for Automotive Mechanical Design Process');
#94557=PRODUCT_CONTEXT('part definition',#94556,'mechanical');
#94558=PRODUCT('MAS-640','TAS-012',
'Independent welded steel electronics enclosure with removable sealed 
lid, internal mounting tray and two threaded cable entries. 300 x 220 
mm body. No ingress or electrical safety rating assigned.',(#94557));
#94559=PRODUCT('Enclosure shell','Enclosure shell',$,(#94557));
#94560=PRODUCT('Base panel','Base panel',
'3 mm steel sheet; weld adjoining shell-panel edges continuously. Fabr
ication weld specification remains to be selected.',(#94557));
#94561=PRODUCT('Entry panel','Entry panel',
'3 mm steel sheet; weld adjoining shell-panel edges continuously. Fabr
ication weld specification remains to be selected.',(#94557));
#94562=PRODUCT('Rear panel','Rear panel',
'3 mm steel sheet; weld adjoining shell-panel edges continuously. Fabr
ication weld specification remains to be selected.',(#94557));
#94563=PRODUCT('Side panel','Side panel',
'3 mm steel sheet; weld adjoining shell-panel edges continuously. Fabr
ication weld specification remains to be selected.',(#94557));
#94564=PRODUCT('Corner pillar','Corner pillar',$,(#94557));
#94565=PRODUCT('Socket head cap screw M6x12',
'Socket head cap screw M6x12',$,(#94557));
#94566=PRODUCT('Tray pillar','Tray pillar',
'Steel tray boss welded to the base panel.',(#94557));
#94567=PRODUCT('Lid','Lid',$,(#94557));
#94568=PRODUCT('Lid gasket','Lid gasket',
'Closed-cell elastomer gasket, nominal 3 mm thickness. Seal compressio
n and environmental rating require validation.',(#94557));
#94569=PRODUCT('Mounting tray','Mounting tray',$,(#94557));
#94570=PRODUCT('Socket head cap screw M6x16',
'Socket head cap screw M6x16',$,(#94557));
#94571=PRODUCT('Socket head cap screw M4x10',
'Socket head cap screw M4x10',$,(#94557));
#94572=PRODUCT('Cable entry body','Cable entry body',$,(#94557));
#94573=PRODUCT('Entry locknut','Entry locknut',$,(#94557));
#94574=PRODUCT('Cable entry seal','Cable entry seal',$,(#94557));
#94575=PRESENTATION_STYLE_ASSIGNMENT((#94582));
#94576=PRESENTATION_STYLE_ASSIGNMENT((#94583));
#94577=PRESENTATION_STYLE_ASSIGNMENT((#94584));
#94578=PRESENTATION_STYLE_ASSIGNMENT((#94585));
#94579=PRESENTATION_STYLE_ASSIGNMENT((#94586));
#94580=PRESENTATION_STYLE_ASSIGNMENT((#94587));
#94581=PRESENTATION_STYLE_ASSIGNMENT((#94588));
#94582=SURFACE_STYLE_USAGE(.BOTH.,#94589);
#94583=SURFACE_STYLE_USAGE(.BOTH.,#94590);
#94584=SURFACE_STYLE_USAGE(.BOTH.,#94591);
#94585=SURFACE_STYLE_USAGE(.BOTH.,#94592);
#94586=SURFACE_STYLE_USAGE(.BOTH.,#94593);
#94587=SURFACE_STYLE_USAGE(.BOTH.,#94594);
#94588=SURFACE_STYLE_USAGE(.BOTH.,#94595);
#94589=SURFACE_SIDE_STYLE('',(#94596));
#94590=SURFACE_SIDE_STYLE('',(#94597));
#94591=SURFACE_SIDE_STYLE('',(#94598));
#94592=SURFACE_SIDE_STYLE('',(#94599));
#94593=SURFACE_SIDE_STYLE('',(#94600));
#94594=SURFACE_SIDE_STYLE('',(#94601));
#94595=SURFACE_SIDE_STYLE('',(#94602));
#94596=SURFACE_STYLE_FILL_AREA(#94603);
#94597=SURFACE_STYLE_FILL_AREA(#94604);
#94598=SURFACE_STYLE_FILL_AREA(#94605);
#94599=SURFACE_STYLE_FILL_AREA(#94606);
#94600=SURFACE_STYLE_FILL_AREA(#94607);
#94601=SURFACE_STYLE_FILL_AREA(#94608);
#94602=SURFACE_STYLE_FILL_AREA(#94609);
#94603=FILL_AREA_STYLE('Steel - Satin',(#94610));
#94604=FILL_AREA_STYLE('Opaque(23,69,131)',(#94611));
#94605=FILL_AREA_STYLE('Opaque(104,114,127)',(#94612));
#94606=FILL_AREA_STYLE('Opaque(64,72,82)',(#94613));
#94607=FILL_AREA_STYLE('Opaque(169,212,242)',(#94614));
#94608=FILL_AREA_STYLE('Opaque(81,175,227)',(#94615));
#94609=FILL_AREA_STYLE('Opaque(185,192,202)',(#94616));
#94610=FILL_AREA_STYLE_COLOUR('Steel - Satin',#94617);
#94611=FILL_AREA_STYLE_COLOUR('Opaque(23,69,131)',#94618);
#94612=FILL_AREA_STYLE_COLOUR('Opaque(104,114,127)',#94619);
#94613=FILL_AREA_STYLE_COLOUR('Opaque(64,72,82)',#94620);
#94614=FILL_AREA_STYLE_COLOUR('Opaque(169,212,242)',#94621);
#94615=FILL_AREA_STYLE_COLOUR('Opaque(81,175,227)',#94622);
#94616=FILL_AREA_STYLE_COLOUR('Opaque(185,192,202)',#94623);
#94617=COLOUR_RGB('Steel - Satin',0.627450980392157,0.627450980392157,0.627450980392157);
#94618=COLOUR_RGB('Opaque(23,69,131)',0.0901960784313725,0.270588235294118,
0.513725490196078);
#94619=COLOUR_RGB('Opaque(104,114,127)',0.407843137254902,0.447058823529412,
0.498039215686275);
#94620=COLOUR_RGB('Opaque(64,72,82)',0.250980392156863,0.282352941176471,
0.32156862745098);
#94621=COLOUR_RGB('Opaque(169,212,242)',0.662745098039216,0.831372549019608,
0.949019607843137);
#94622=COLOUR_RGB('Opaque(81,175,227)',0.317647058823529,0.686274509803922,
0.890196078431372);
#94623=COLOUR_RGB('Opaque(185,192,202)',0.725490196078431,0.752941176470588,
0.792156862745098);
ENDSEC;
END-ISO-10303-21;
